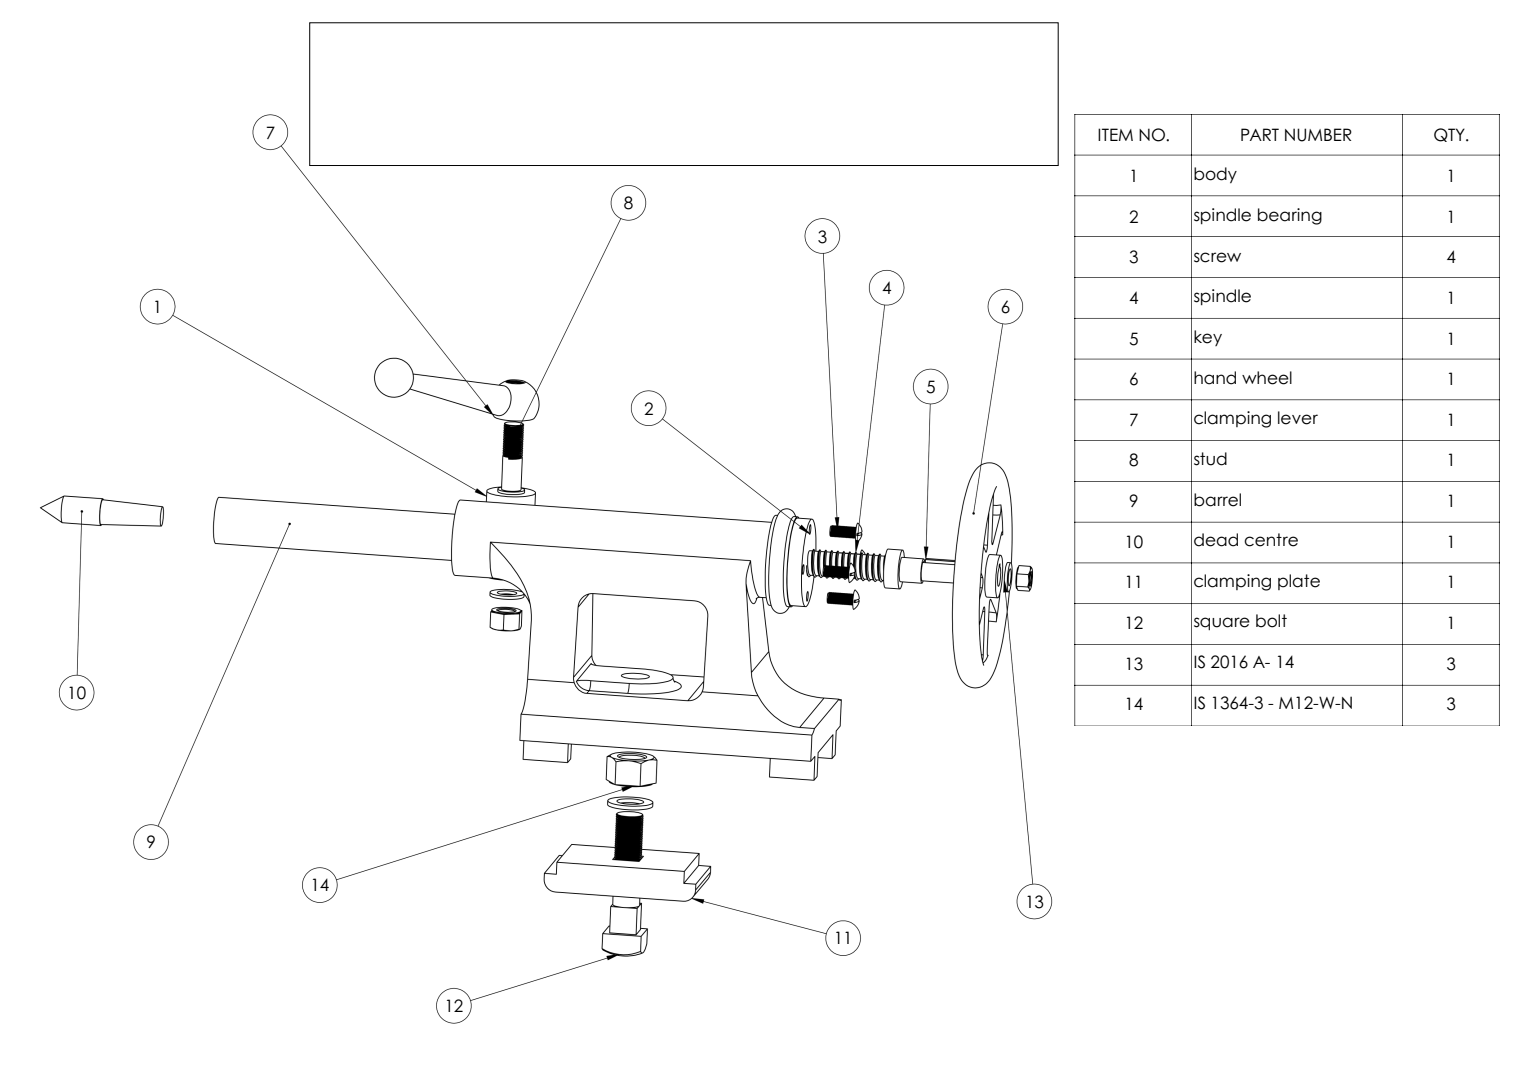
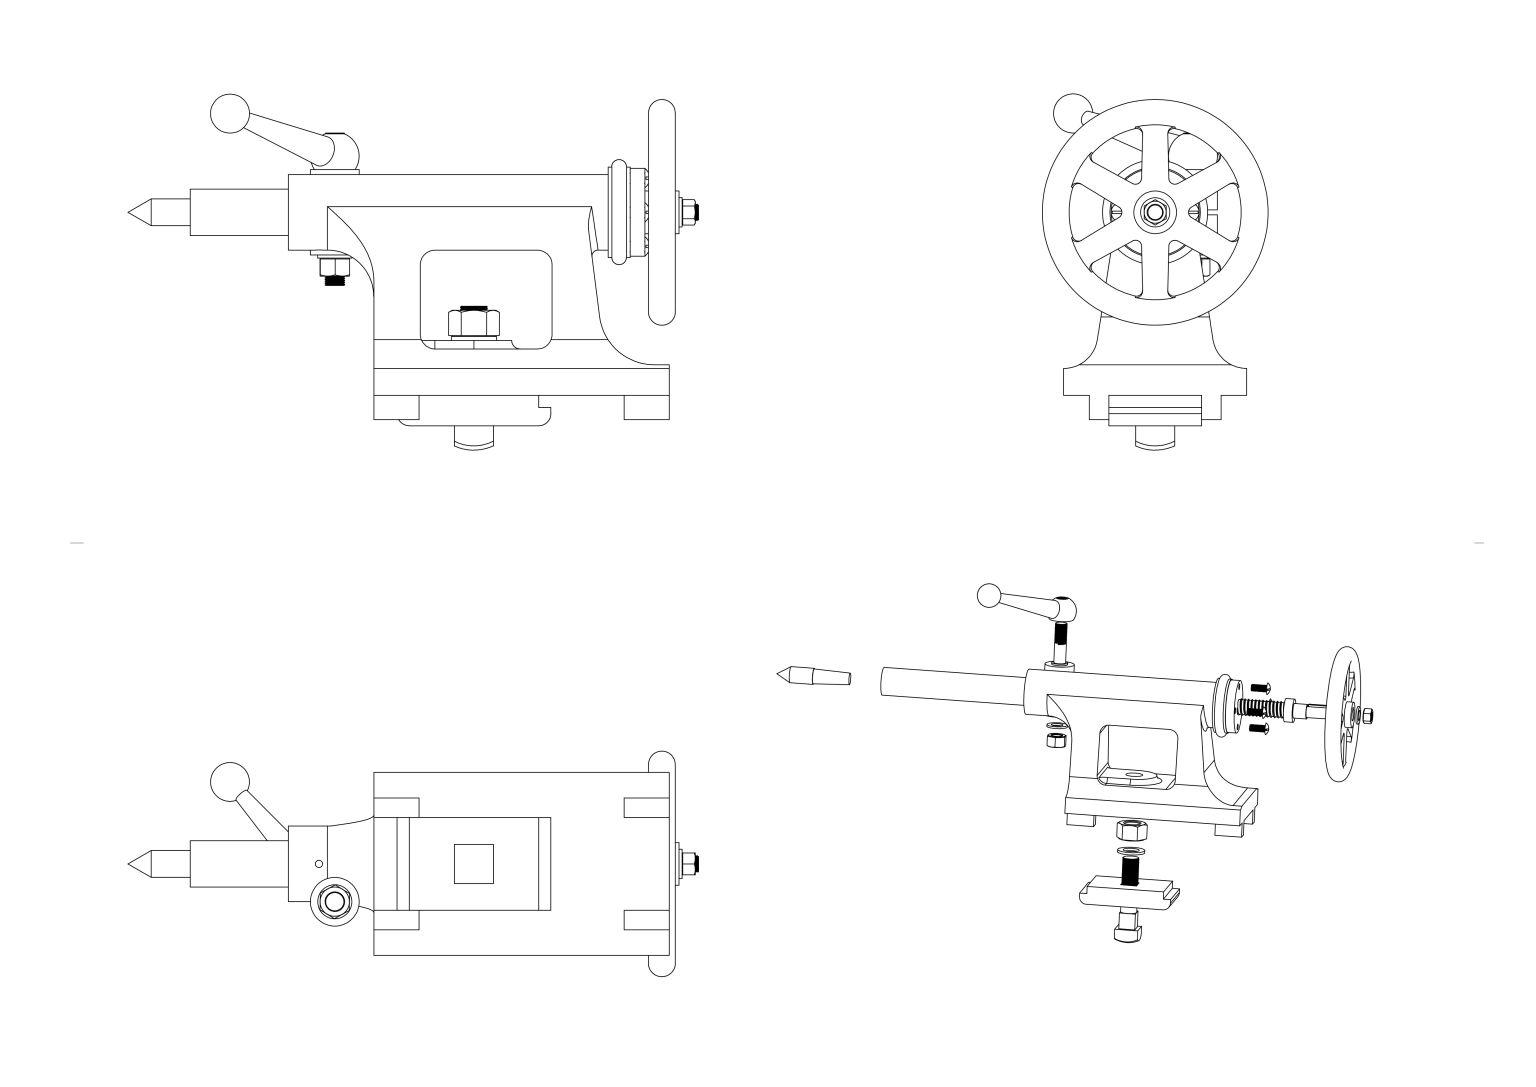
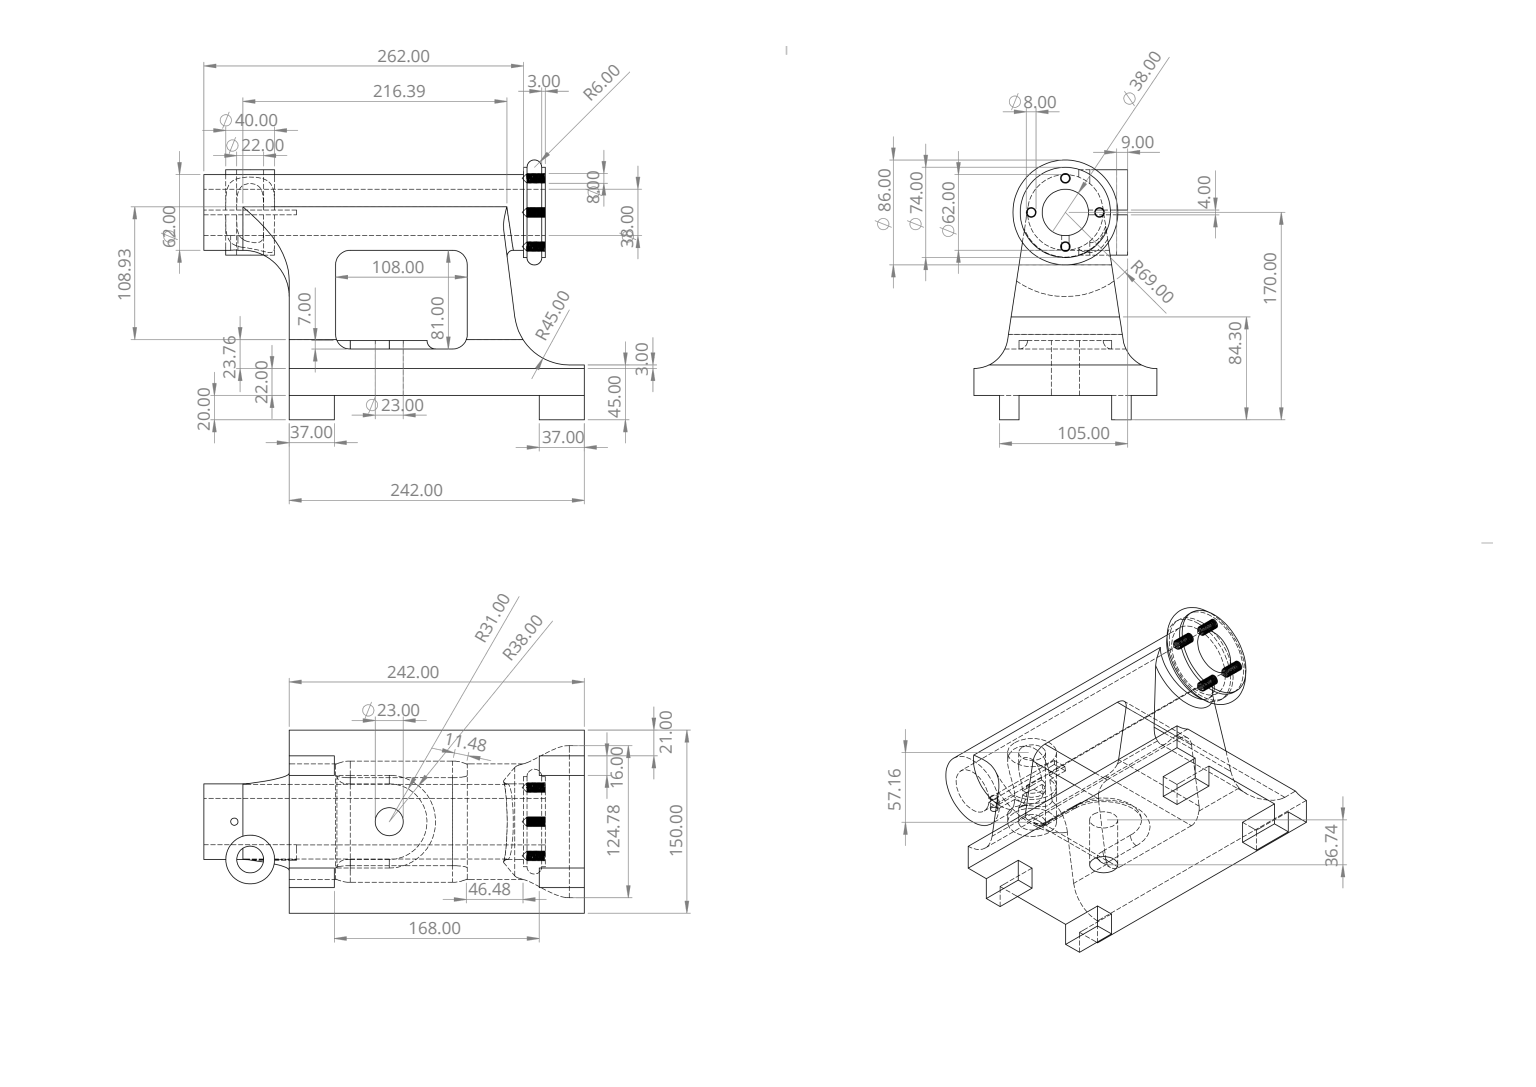
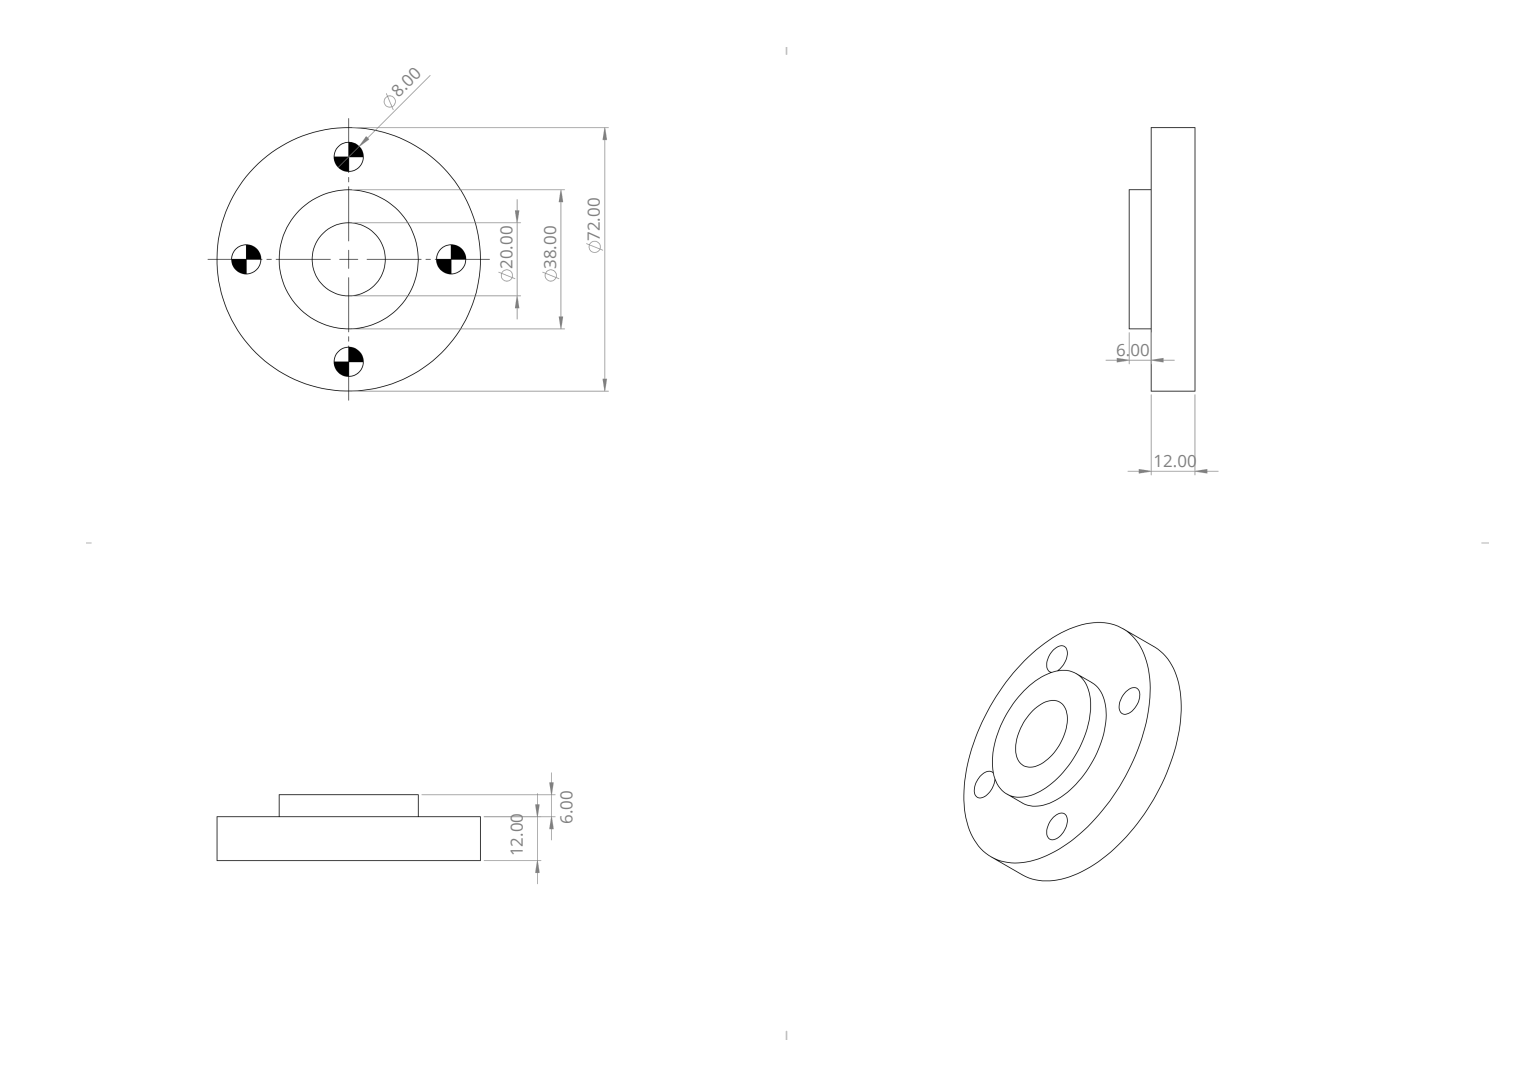
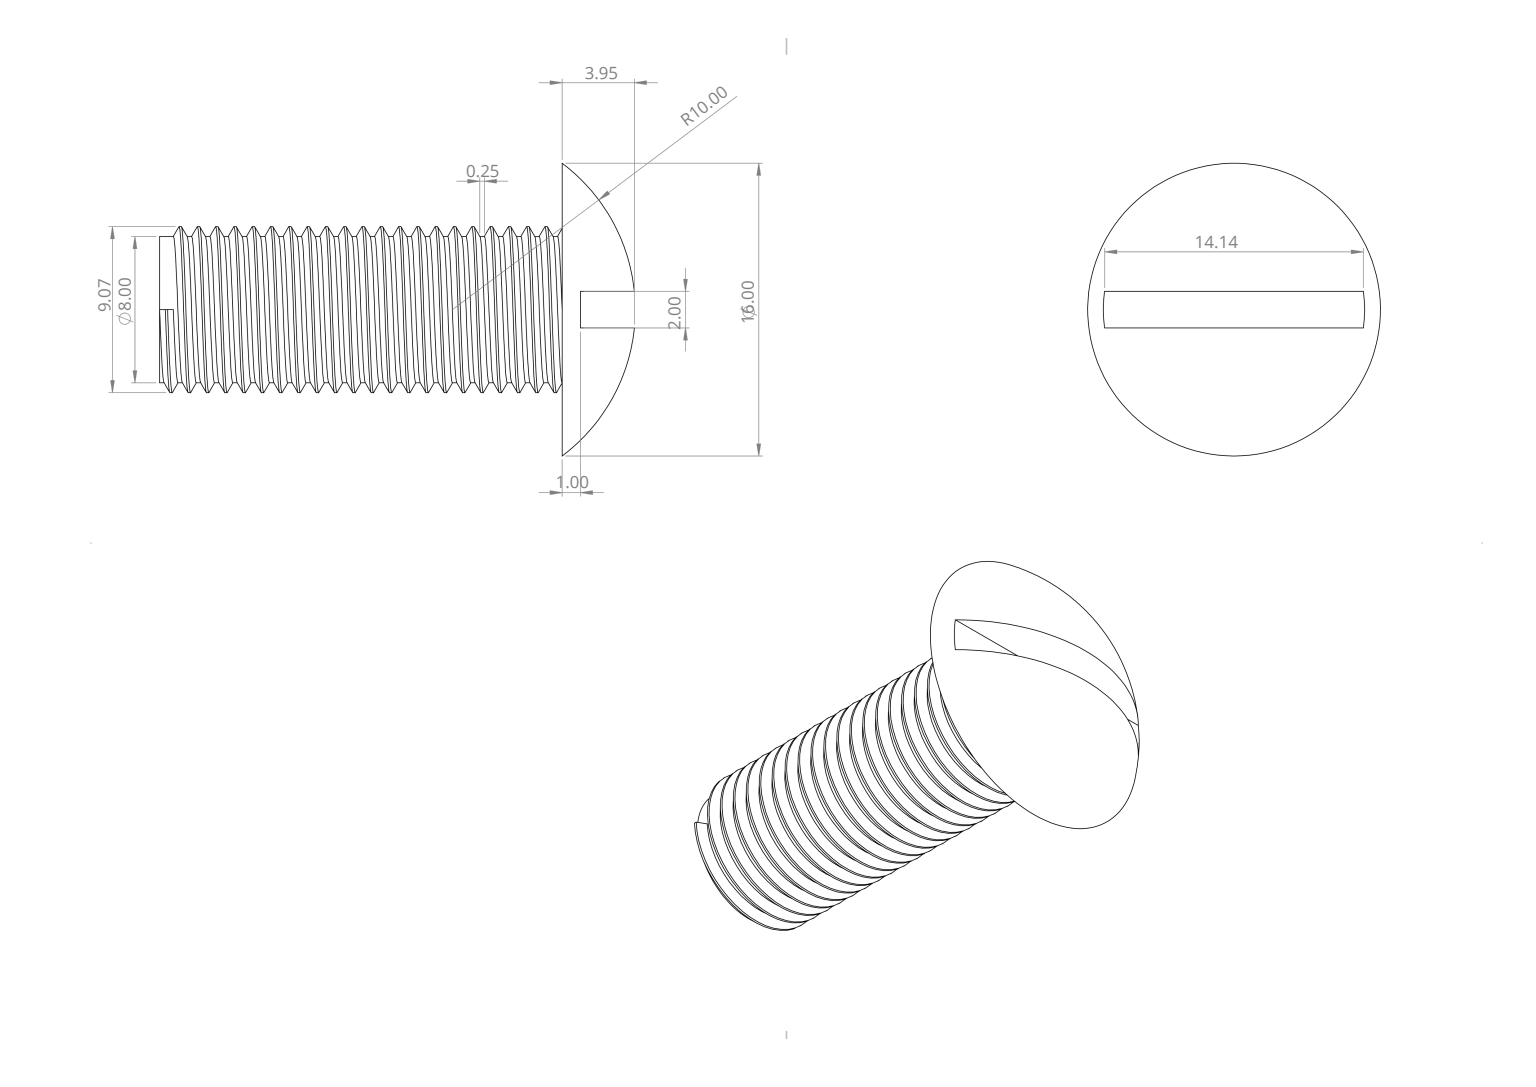
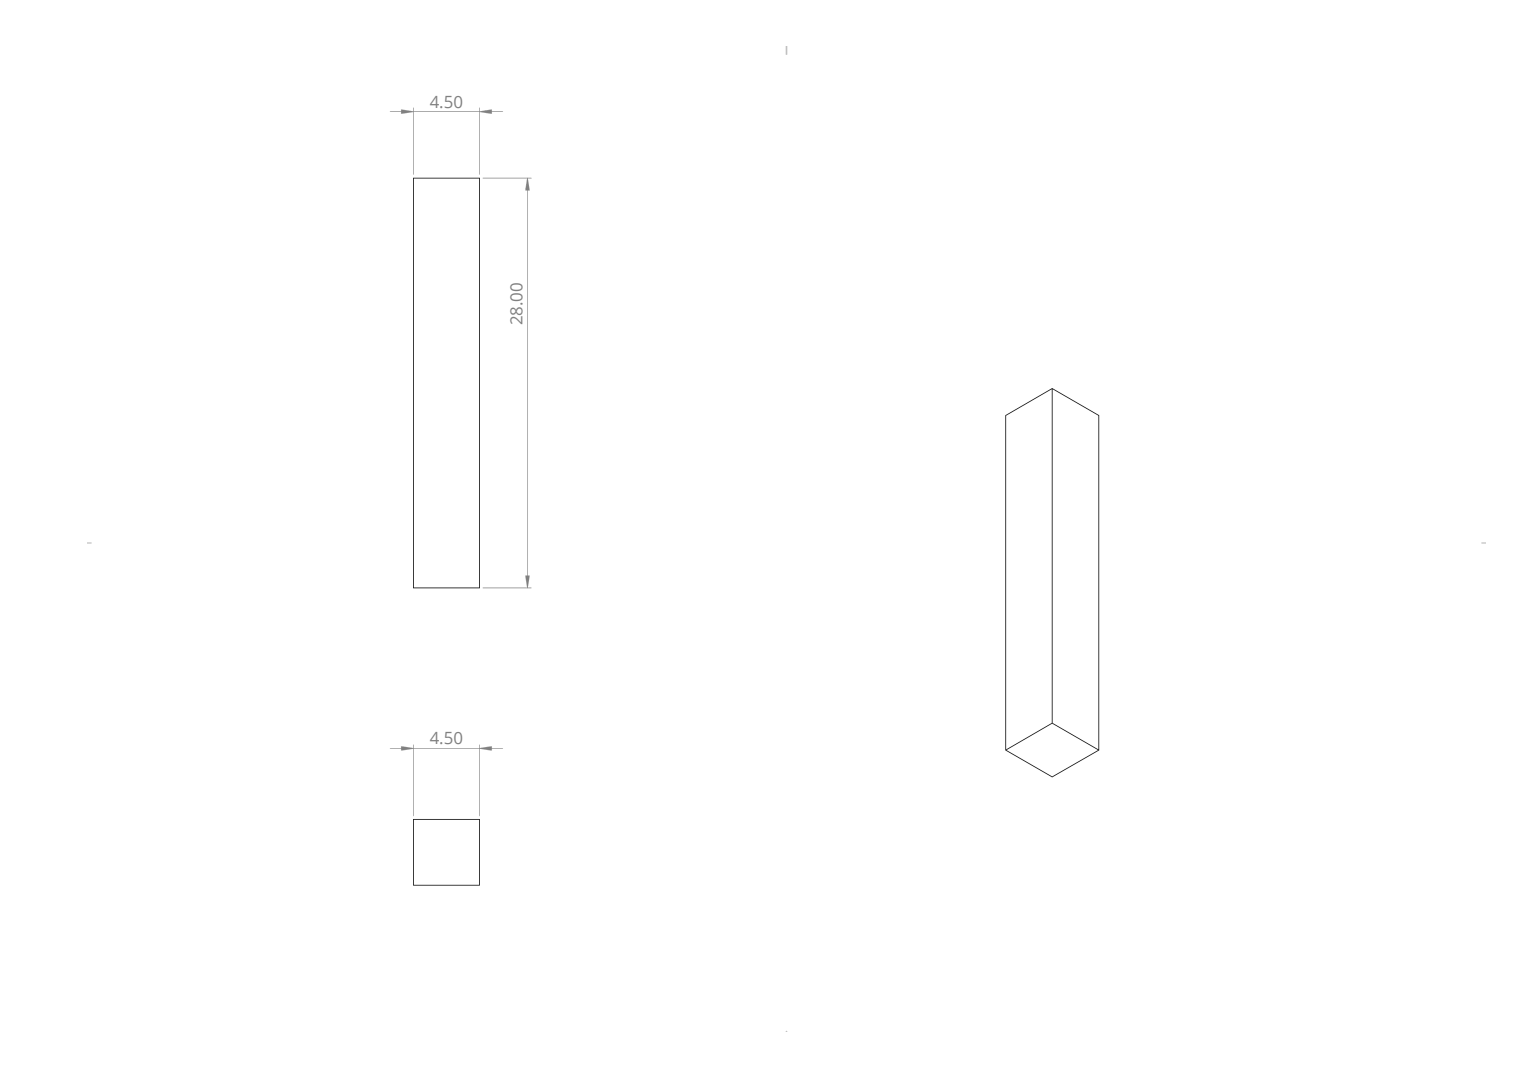
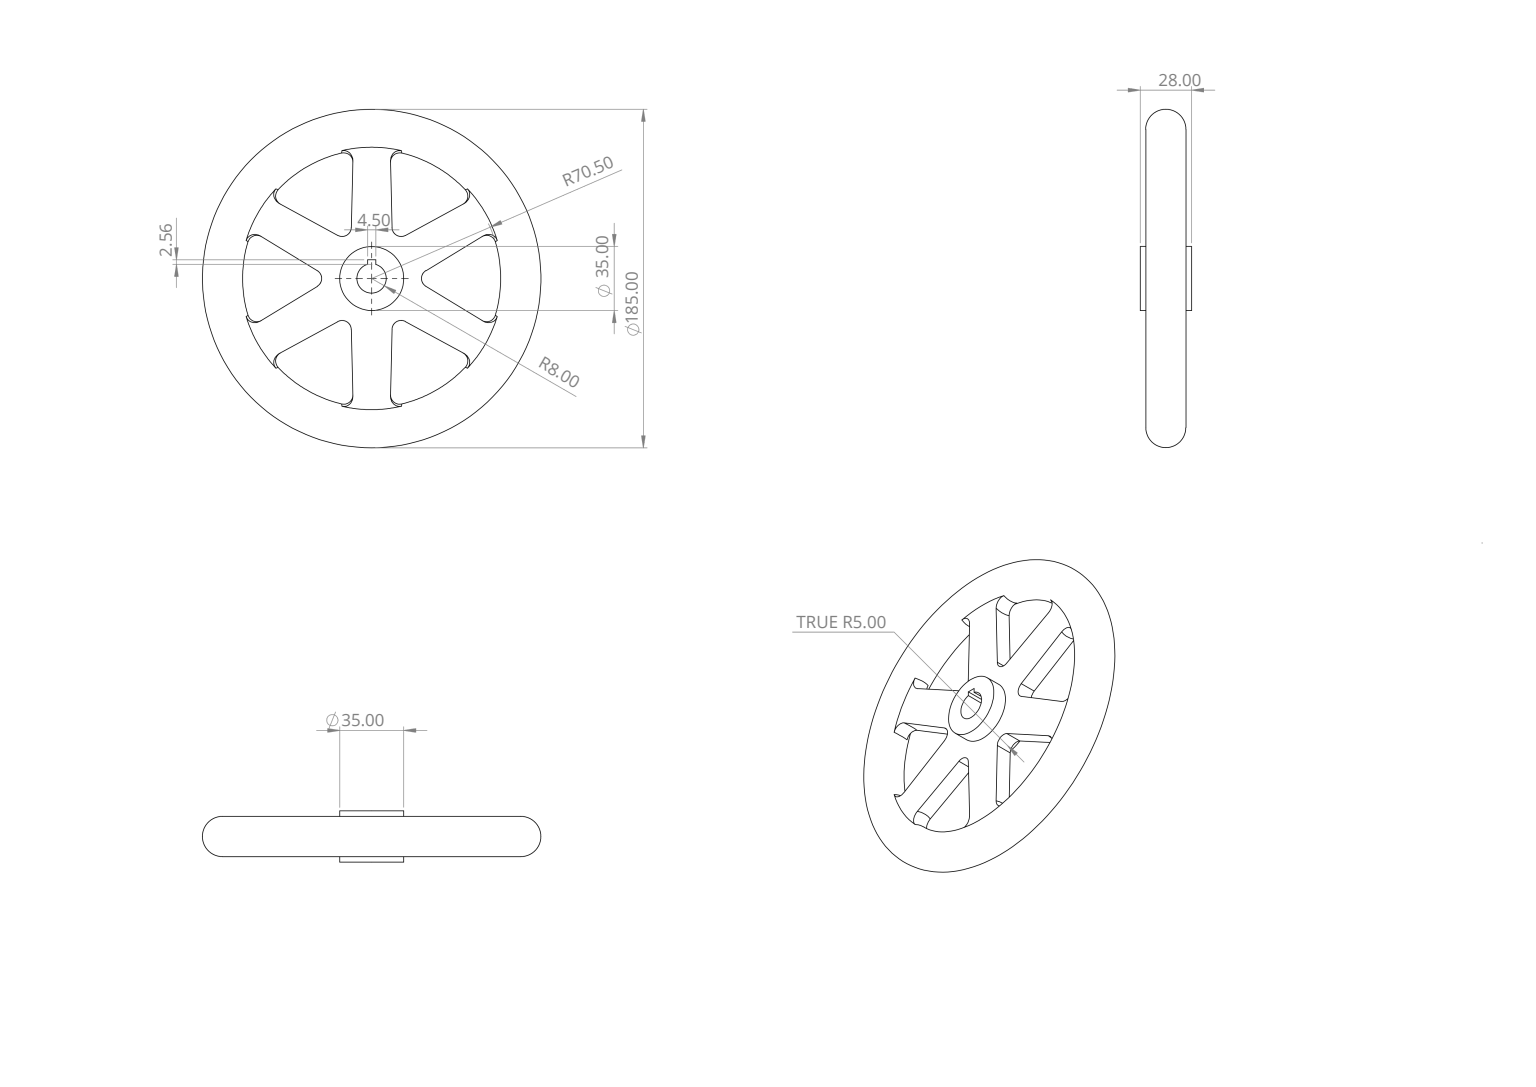
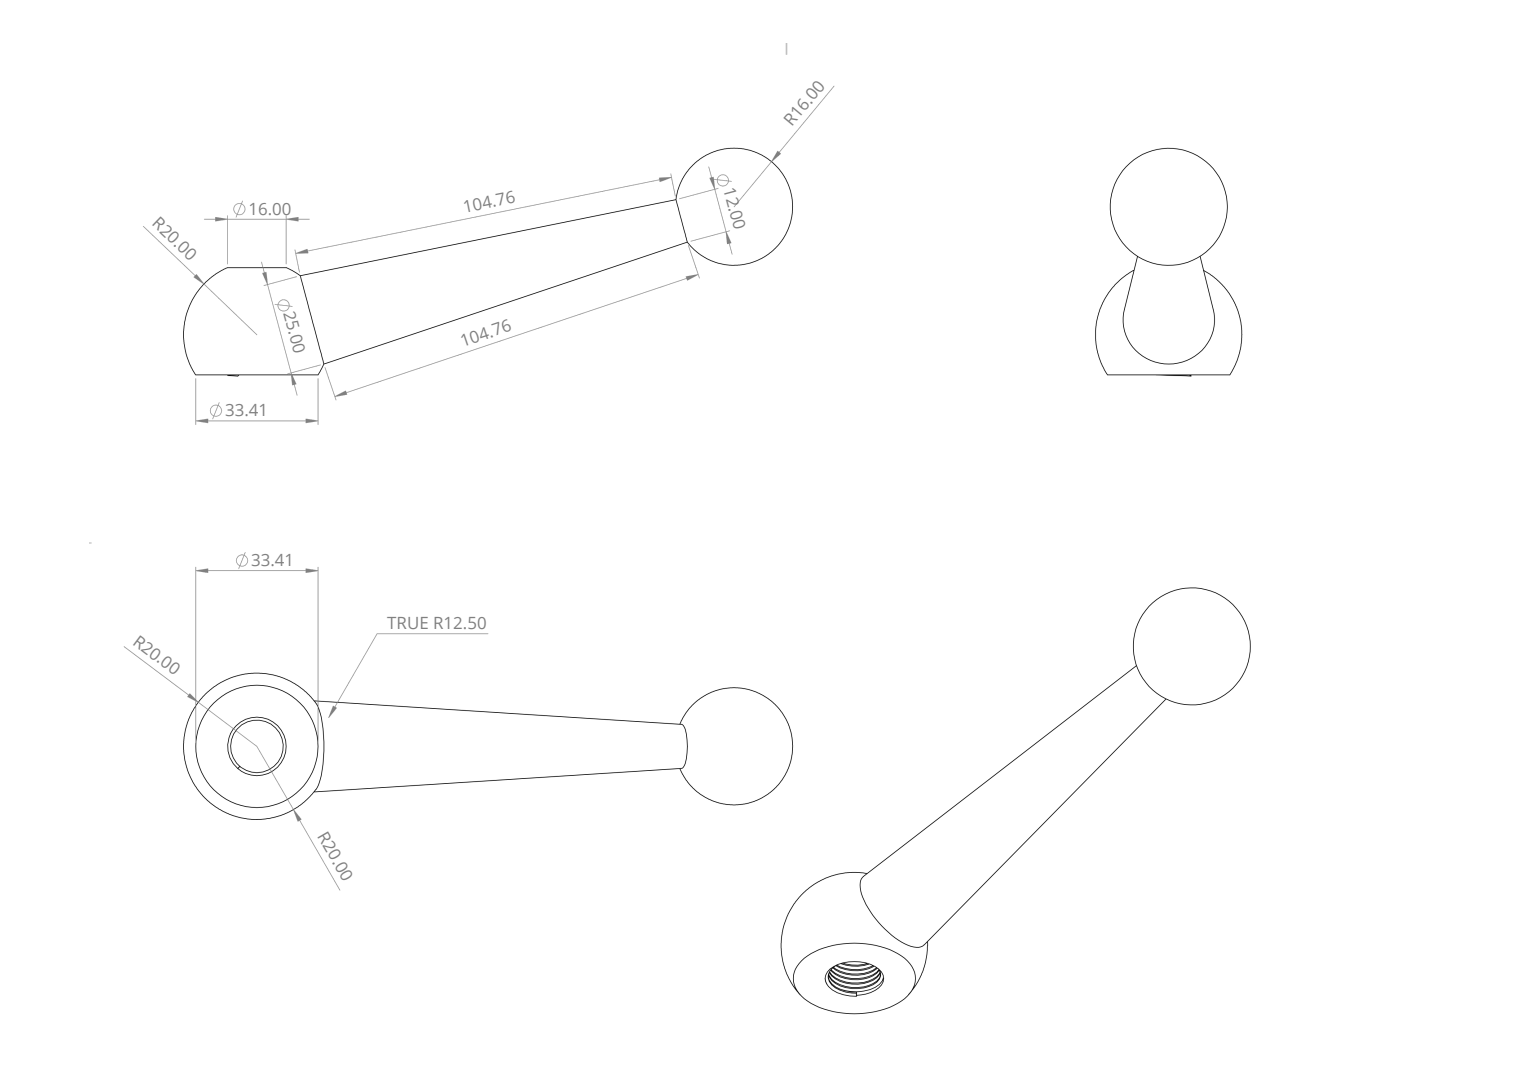
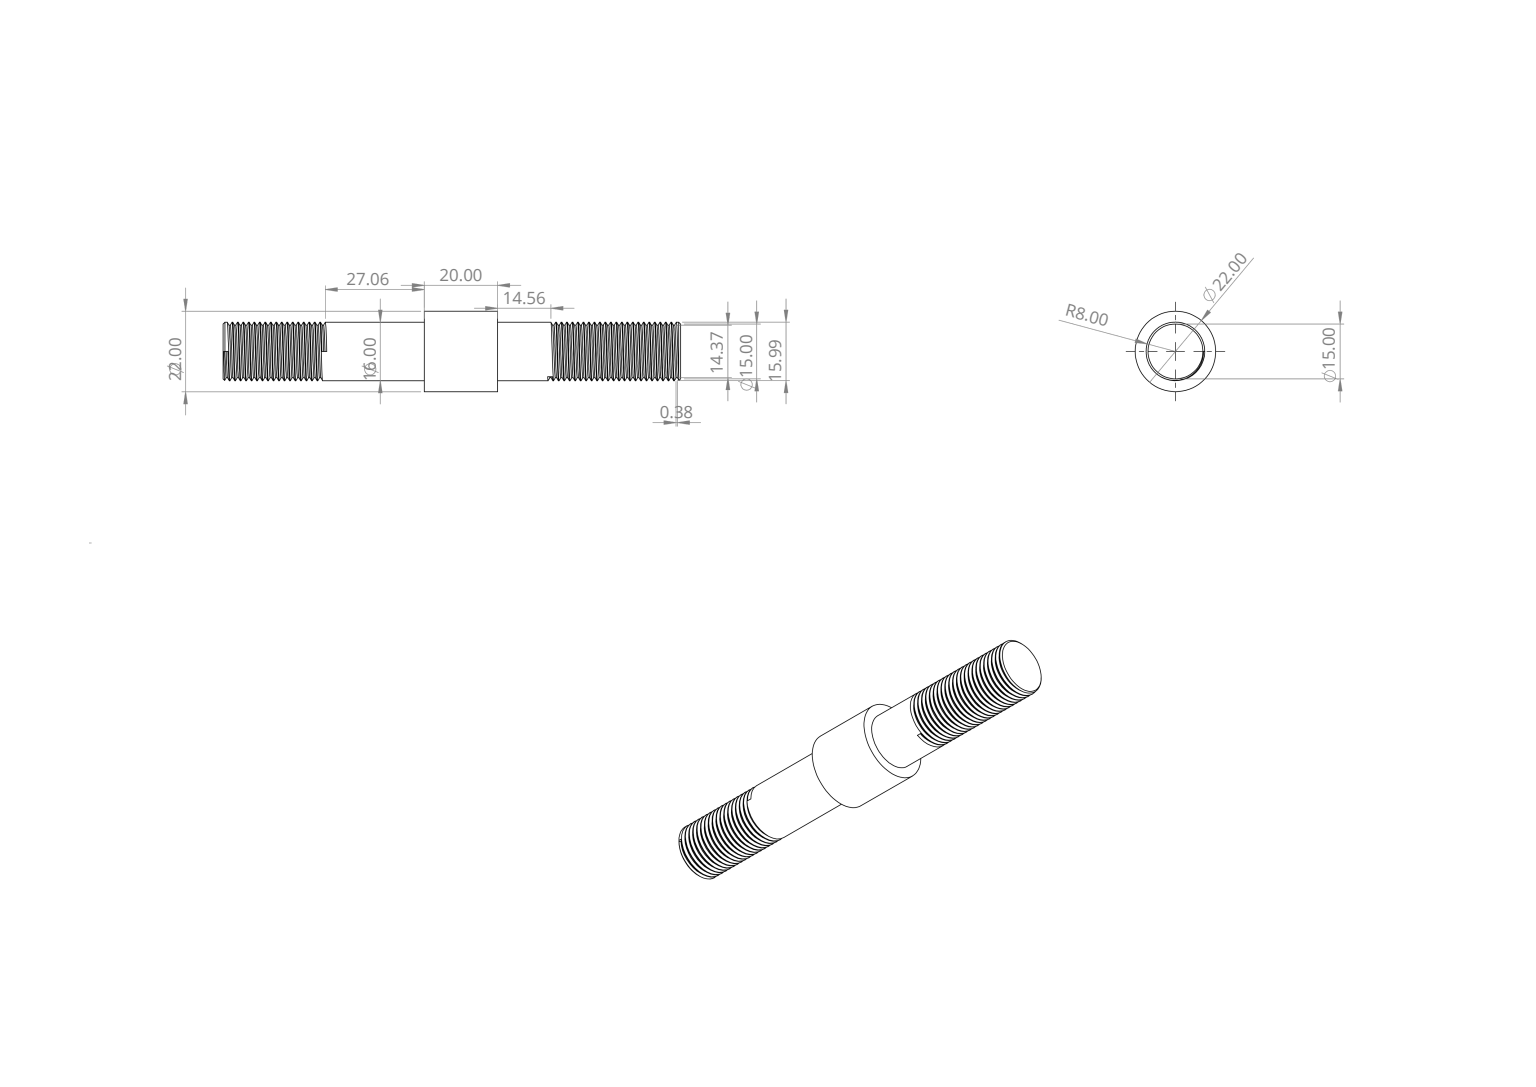
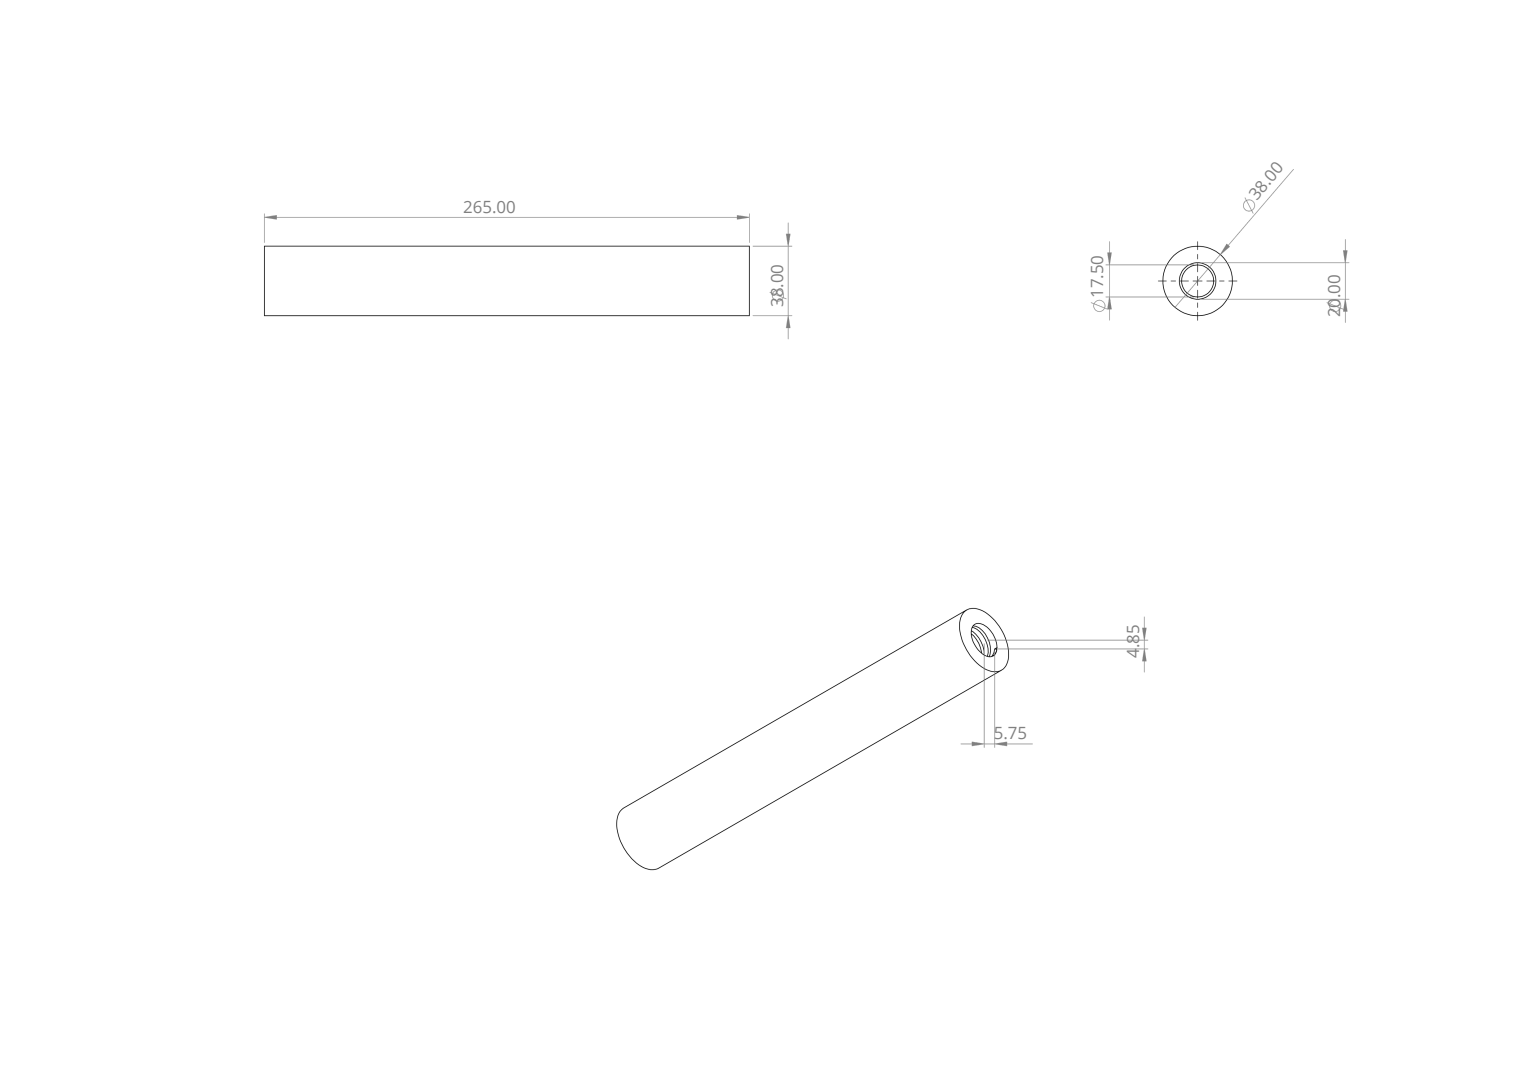
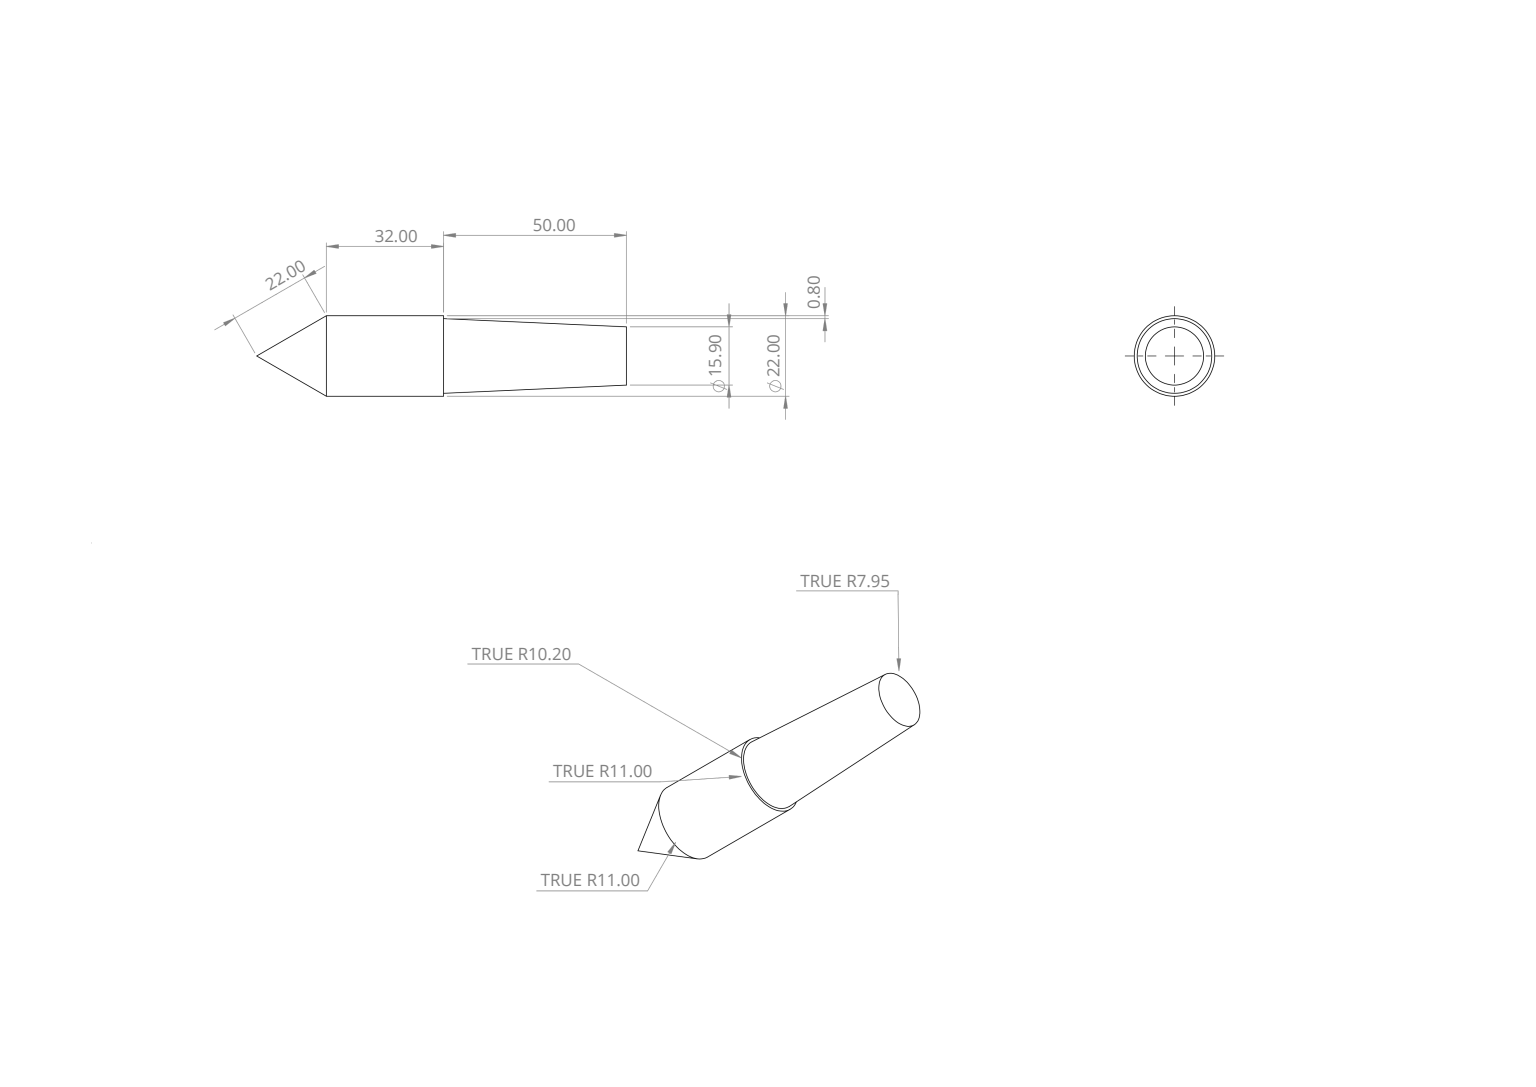
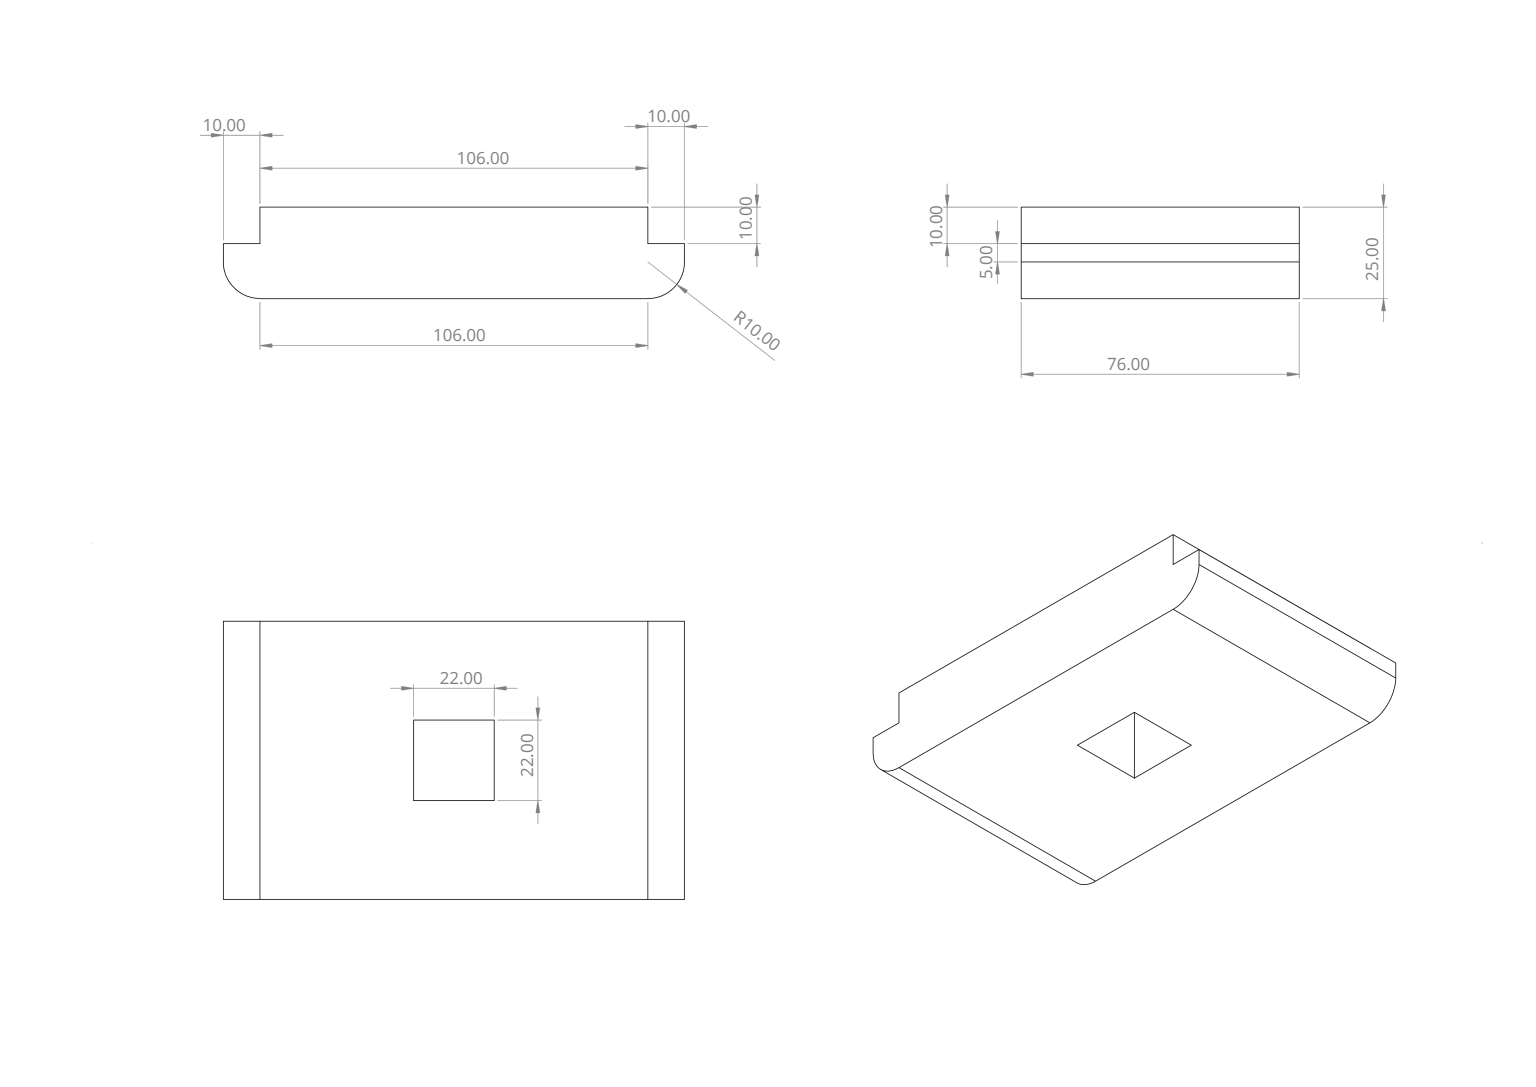
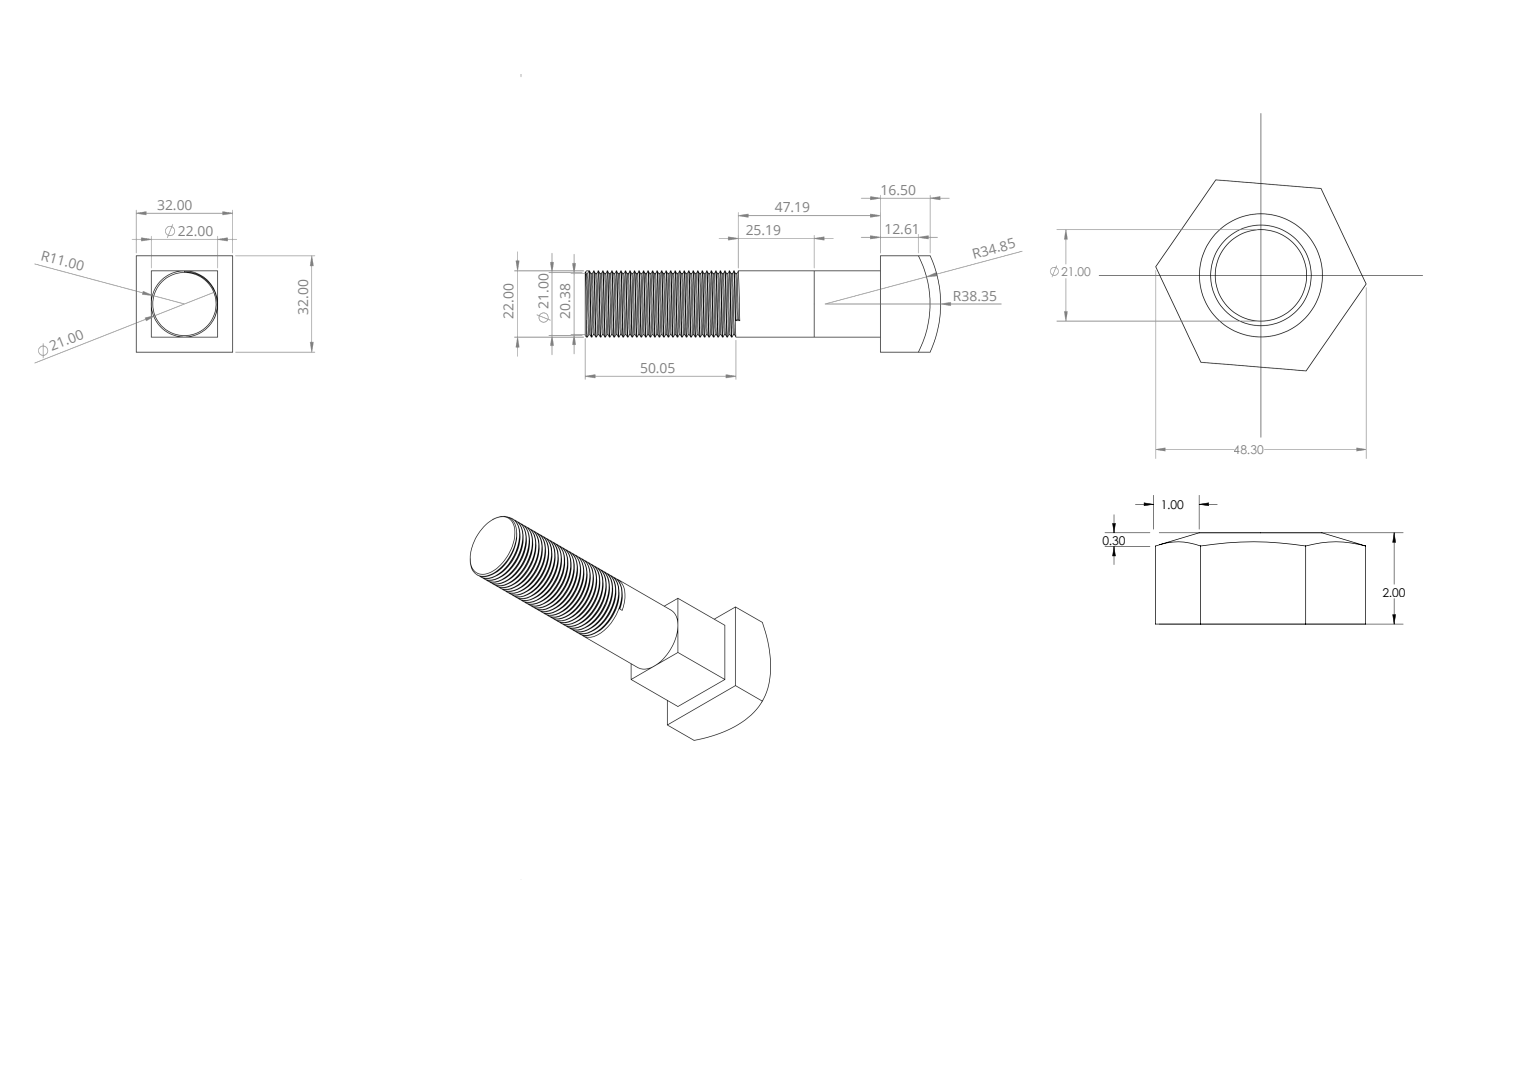
ISO-10303-21;
HEADER;
FILE_DESCRIPTION (('STEP AP214'),
    '1' );
FILE_NAME ('MAT-050',
    '2026-10-26T19:46:16',
    ( '' ),
    ( '' ),
    'SwSTEP 2.0',
    'SolidWorks 2025',
    '' );
FILE_SCHEMA (( 'AUTOMOTIVE_DESIGN' ));
ENDSEC;

DATA;
#1 = CARTESIAN_POINT ( 'NONE',  ( 7.204075437095966983, 7.204075437095967871, 116.9687500020483810 ) ) ;
#2 = CARTESIAN_POINT ( 'NONE',  ( 3.042071309553167069, 186.8229166632527267, -11.35316468749999785 ) ) ;
#3 = VERTEX_POINT ( 'NONE', #4394 ) ;
#4 = FACE_OUTER_BOUND ( 'NONE', #11968, .T. ) ;
#5 = CARTESIAN_POINT ( 'NONE',  ( -6.238412754330611322E-16, 10.18810118749999916, 71.78125000204838102 ) ) ;
#6 = CARTESIAN_POINT ( 'NONE',  ( 4.000000000000015987, 196.5000000000000000, 198.0000000000000284 ) ) ;
#8 = CARTESIAN_POINT ( 'NONE',  ( -9.832129032723418760, 182.8645833299193555, -5.676582343750004256 ) ) ;
#7 = LINE ( 'NONE', #69019, #15785 ) ;
#9 = CARTESIAN_POINT ( 'NONE',  ( -7.999999999999991118, 0.000000000000000000, 5.386552784329824206 ) ) ;
#10 = CARTESIAN_POINT ( 'NONE',  ( 3.313708498984756279, 7.999999999999991118, 4.861552779823363757 ) ) ;
#11 = CARTESIAN_POINT ( 'NONE',  ( -2.679491924311222295, 249.1666666734946887, 10.00000000000000178 ) ) ;
#12 = LINE ( 'NONE', #6025, #67368 ) ;
#13 = ORIENTED_EDGE ( 'NONE', *, *, #39325, .T. ) ;
#14 =( REPRESENTATION_RELATIONSHIP ('NONE','NONE', #46008, #61424 ) REPRESENTATION_RELATIONSHIP_WITH_TRANSFORMATION ( #30454 )SHAPE_REPRESENTATION_RELATIONSHIP( ) );
#15 = CIRCLE ( 'NONE', #38546, 16.70329308849007077 ) ;
#16 = CARTESIAN_POINT ( 'NONE',  ( 2.977408999572646486, 7.188101187499992051, 28.01780278187175455 ) ) ;
#17 = CARTESIAN_POINT ( 'NONE',  ( -8.311093377946836114, 122.9687499965860127, -8.311093377946837890 ) ) ;
#18 = CARTESIAN_POINT ( 'NONE',  ( -0.4500000000000013989, 255.9999999999997726, 5.815332135061025198 ) ) ;
#19 = VERTEX_POINT ( 'NONE', #73420 ) ;
#20 = CARTESIAN_POINT ( 'NONE',  ( -8.342170076843785083E-16, 9.187499998634407916, 4.541265875000002339 ) ) ;
#21 = AXIS2_PLACEMENT_3D ( 'NONE', #49195, #67684, #9968 ) ;
#22 = CARTESIAN_POINT ( 'NONE',  ( 7.188101187500001821, 14.06249999795161365, -2.977408999572650483 ) ) ;
#23 = CARTESIAN_POINT ( 'NONE',  ( 5.656854249492381470, 104.7500000040967905, 5.656854249492379694 ) ) ;
#24 = CARTESIAN_POINT ( 'NONE',  ( -25.55430564589119058, 197.5625000013656063, 167.5543056458915316 ) ) ;
#25 = CARTESIAN_POINT ( 'NONE',  ( -2.828427124746190735, 8.375000000000000000, -2.828427124746191623 ) ) ;
#26 = CARTESIAN_POINT ( 'NONE',  ( -4.000000000000001776, 21.24999999726881583, -4.898587196589415787E-16 ) ) ;
#27 = CARTESIAN_POINT ( 'NONE',  ( -4.541265875000003227, 9.874999998634404363, 1.881053915767121110 ) ) ;
#28 = CARTESIAN_POINT ( 'NONE',  ( 1.469576158976822172E-15, -7.999999999999991118, 20.89280278392014623 ) ) ;
#29 = CARTESIAN_POINT ( 'NONE',  ( -2.751064625579944321E-14, 198.7500000000000000, 146.0000000000000284 ) ) ;
#30 = ORIENTED_EDGE ( 'NONE', *, *, #66787, .T. ) ;
#31 = LINE ( 'NONE', #63370, #20979 ) ;
#32 = CARTESIAN_POINT ( 'NONE',  ( -4.401442555609581635E-16, 107.2812500020483810, -7.188101187500000044 ) ) ;
#34 = CARTESIAN_POINT ( 'NONE',  ( 6.000000000000003553, 293.5625000000001137, -2.485281374238571761 ) ) ;
#33 = DIRECTION ( 'NONE',  ( 0.000000000000000000, 0.000000000000000000, 1.000000000000000000 ) ) ;
#35 =( NAMED_UNIT ( * ) PLANE_ANGLE_UNIT ( ) SI_UNIT ( $, .RADIAN. ) );
#36 = EDGE_CURVE ( 'NONE', #35937, #61038, #73180, .T. ) ;
#37 = EDGE_CURVE ( 'NONE', #72225, #25230, #72296, .T. ) ;
#38 = CARTESIAN_POINT ( 'NONE',  ( 1.881053915767122664, 22.12499999863441502, 4.541265875000001451 ) ) ;
#39 = CARTESIAN_POINT ( 'NONE',  ( 9.797174393178825657E-16, 125.0000000000000000, -8.000000000000000000 ) ) ;
#40 = ORIENTED_EDGE ( 'NONE', *, *, #24458, .F. ) ;
#41 = ORIENTED_EDGE ( 'NONE', *, *, #6114, .F. ) ;
#42 = CARTESIAN_POINT ( 'NONE',  ( -7.204075437095967871, 7.204075437095967871, 89.96875000204838102 ) ) ;
#43 = CARTESIAN_POINT ( 'NONE',  ( -10.99999999999989342, 4.556349186104152515, 92.40625000000000000 ) ) ;
#44 = CARTESIAN_POINT ( 'NONE',  ( -29.43265458321766914, 197.7500000013656063, 166.5412658750003629 ) ) ;
#45 = CARTESIAN_POINT ( 'NONE',  ( 11.00000000000000000, 4.556349186104045934, 99.34375000000000000 ) ) ;
#46 = CARTESIAN_POINT ( 'NONE',  ( -1.432654583217608080, 202.8750000013656347, 201.4587341250000350 ) ) ;
#48 = CARTESIAN_POINT ( 'NONE',  ( -4.088227598258586603E-16, 298.3593750017070079, -6.676582343750001591 ) ) ;
#47 = CARTESIAN_POINT ( 'NONE',  ( 0.000000000000000000, 210.0000000000000284, 207.0000000000000568 ) ) ;
#49 = CARTESIAN_POINT ( 'NONE',  ( -10.00000000000000355, 117.7083333333333286, 2.679491924311223183 ) ) ;
#50 = ADVANCED_FACE ( 'NONE', ( #38735 ), #56452, .F. ) ;
#51 = CARTESIAN_POINT ( 'NONE',  ( -5.656854249492380582, 97.81250000000000000, -5.656854249492380582 ) ) ;
#52 = CARTESIAN_POINT ( 'NONE',  ( -4.088227598258586603E-16, 288.3593750017070079, -6.676582343750001591 ) ) ;
#53 = CARTESIAN_POINT ( 'NONE',  ( 7.188101187499991163, 2.977408999572648707, 4.205302781871751883 ) ) ;
#54 = FACE_OUTER_BOUND ( 'NONE', #64584, .T. ) ;
#55 = AXIS2_PLACEMENT_3D ( 'NONE', #16883, #63657, #58395 ) ;
#56 = CARTESIAN_POINT ( 'NONE',  ( 25.55430564589115150, 201.3125000013656063, 172.4456943541086957 ) ) ;
#57 = CARTESIAN_POINT ( 'NONE',  ( 7.188101187500000044, 0.8437499979516100979, 0.000000000000000000 ) ) ;
#58 = CARTESIAN_POINT ( 'NONE',  ( 12.00000000000000178, -4.647306338817273286, -0.4736860157878156619 ) ) ;
#59 = CARTESIAN_POINT ( 'NONE',  ( -5.082755093536325930, 121.3437500020483952, -5.082755093536325930 ) ) ;
#61 = CARTESIAN_POINT ( 'NONE',  ( 2.823223908292128659, 194.8377262638588832, 195.3889393478124532 ) ) ;
#60 = PRESENTATION_STYLE_ASSIGNMENT (( #57392 ) ) ;
#62 = CARTESIAN_POINT ( 'NONE',  ( 3.042071309553163960, 237.7604166700806161, -11.35316468749999785 ) ) ;
#63 = CARTESIAN_POINT ( 'NONE',  ( 10.00000000000000178, 52.08333332650536818, -2.679491924311226736 ) ) ;
#64 = CARTESIAN_POINT ( 'NONE',  ( 27.99999999999996447, 197.0000000000000000, 173.9999999999999147 ) ) ;
#65 = CARTESIAN_POINT ( 'NONE',  ( -3.042071309553173730, 19.32291666325268409, 11.35316468749999785 ) ) ;
#66 =( BOUNDED_CURVE ( )  B_SPLINE_CURVE ( 2, ( #62124, #31597, #54994, #3301, #26287, #72324, #20638, #17588, #51930, #27790, #56850, #34966, #23250 ),
 .UNSPECIFIED., .F., .F. ) 
 B_SPLINE_CURVE_WITH_KNOTS ( ( 3, 2, 2, 2, 2, 2, 3 ),
 ( 0.4866946232415507168, 0.4919272298211807559, 0.4971598364008106841, 0.5023924429804407232, 0.5076250495600707069, 0.5128576561397006905, 0.5180902627193306742 ),
 .UNSPECIFIED. ) 
 CURVE ( )  GEOMETRIC_REPRESENTATION_ITEM ( )  RATIONAL_B_SPLINE_CURVE ( ( 0.9999999999999911182, 0.9659258262890771940, 1.000000000000000000, 0.9659258262890683122, 1.000000000000000000, 0.9659258262890683122, 1.000000000000000000, 0.9659258262890683122, 1.000000000000000000, 0.9659258262890683122, 1.000000000000000000, 0.9659258262893768432, 0.9999999999996914690 ) ) 
 REPRESENTATION_ITEM ( '' )  );
#67 = CARTESIAN_POINT ( 'NONE',  ( 2.977408999572650927, -7.188101187499990274, 0.8303027818717529929 ) ) ;
#69 = CARTESIAN_POINT ( 'NONE',  ( 3.042071309553167069, 217.1354166632526983, -11.35316468749999785 ) ) ;
#68 =( BOUNDED_CURVE ( )  B_SPLINE_CURVE ( 2, ( #33279, #10252, #21187, #32531, #61186, #72505, #55916, #72881, #38182 ),
 .UNSPECIFIED., .F., .F. ) 
 B_SPLINE_CURVE_WITH_KNOTS ( ( 3, 2, 2, 2, 3 ),
 ( 0.7708333333333317050, 0.7812499999999983347, 0.7916666666666649643, 0.8020833333333317050, 0.8124999999999983347 ),
 .UNSPECIFIED. ) 
 CURVE ( )  GEOMETRIC_REPRESENTATION_ITEM ( )  RATIONAL_B_SPLINE_CURVE ( ( 1.000000000000012212, 0.9238795325112745260, 1.000000000000000000, 0.9238795325112867385, 1.000000000000000000, 0.9238795325112867385, 1.000000000000000000, 0.9238795325112989509, 0.9999999999999877875 ) ) 
 REPRESENTATION_ITEM ( '' )  );
#70 = CARTESIAN_POINT ( 'NONE',  ( -30.82842712474615610, 198.3750000000000284, 172.8284271247465824 ) ) ;
#71 = CARTESIAN_POINT ( 'NONE',  ( -7.320508075688770155, 240.6249999999999716, 7.320508075688774596 ) ) ;
#73 = CARTESIAN_POINT ( 'NONE',  ( 2.449293598294707893E-16, 11.99999999726881406, -4.000000000000001776 ) ) ;
#72 = CARTESIAN_POINT ( 'NONE',  ( 4.000000000000016875, 208.4375000000000853, 199.6568542494924259 ) ) ;
#74 = AXIS2_PLACEMENT_3D ( 'NONE', #50594, #44950, #67957 ) ;
#75 = EDGE_LOOP ( 'NONE', ( #23247, #62636, #23741 ) ) ;
#76 = VECTOR ( 'NONE', #5091, 999.9999999999998863 ) ;
#77 = CARTESIAN_POINT ( 'NONE',  ( 3.458734124999960358, 199.6250000013656063, 143.4326545832176976 ) ) ;
#78 = CARTESIAN_POINT ( 'NONE',  ( 11.35316468749999785, 25.57291666325268409, 3.042071309553174174 ) ) ;
#79 = CARTESIAN_POINT ( 'NONE',  ( 7.778174593052023411, -7.778174593052021635, 93.25000000409677625 ) ) ;
#80 = CARTESIAN_POINT ( 'NONE',  ( 2.679491924311234730, 226.4583333333333144, 9.999999999999998224 ) ) ;
#81 = EDGE_CURVE ( 'NONE', #73625, #45401, #67113, .T. ) ;
#82 = CARTESIAN_POINT ( 'NONE',  ( -30.44569435410875968, 197.8125000013656063, 172.4456943541092642 ) ) ;
#83 = CARTESIAN_POINT ( 'NONE',  ( 5.656854249492378806, 7.124999995903221084, 5.656854249492381470 ) ) ;
#85 = CARTESIAN_POINT ( 'NONE',  ( 11.35316468750000141, 25.78124999658601624, 0.000000000000000000 ) ) ;
#84 = CARTESIAN_POINT ( 'NONE',  ( 2.977408999572654480, 112.6250000020483810, 7.188101187499999156 ) ) ;
#86 = CARTESIAN_POINT ( 'NONE',  ( -3.313708498984757167, 7.999999999999991118, 23.04905277982336642 ) ) ;
#87 = CARTESIAN_POINT ( 'NONE',  ( 5.676582343749993598, 129.9479166632526983, 9.832129032723422313 ) ) ;
#88 = CARTESIAN_POINT ( 'NONE',  ( 7.320508075688771044, 101.2499999931720112, 7.320508075688775484 ) ) ;
#89 = CARTESIAN_POINT ( 'NONE',  ( -7.188101187500000044, 114.0312500020483952, 0.000000000000000000 ) ) ;
#90 = DIRECTION ( 'NONE',  ( 0.000000000000000000, 0.000000000000000000, 1.000000000000000000 ) ) ;
#91 = CARTESIAN_POINT ( 'NONE',  ( -31.45873412499999944, 208.9375000013656063, 170.0000000000003979 ) ) ;
#92 = CARTESIAN_POINT ( 'NONE',  ( -5.000000000000000888, 53.34243969459547685, -47.33397984627131905 ) ) ;
#93 = ORIENTED_EDGE ( 'NONE', *, *, #56073, .F. ) ;
#94 = CARTESIAN_POINT ( 'NONE',  ( 5.676582343750001591, 11.92708332991935016, -9.832129032723420536 ) ) ;
#95 = CARTESIAN_POINT ( 'NONE',  ( -5.000000000000005329, 155.2083333265053682, 8.660254037844387298 ) ) ;
#96 = CARTESIAN_POINT ( 'NONE',  ( 1.226468279477575784E-15, 298.7031250017070079, 6.676582343750001591 ) ) ;
#97 = CARTESIAN_POINT ( 'NONE',  ( 11.35316468750000141, 140.7812499965860411, 0.000000000000000000 ) ) ;
#98 = CARTESIAN_POINT ( 'NONE',  ( -7.999999999999991118, 0.000000000000000000, 21.88655278432982243 ) ) ;
#99 = CARTESIAN_POINT ( 'NONE',  ( 13.99999999999999822, 2.249999999994893862, 7.677076266393539683 ) ) ;
#100 = CARTESIAN_POINT ( 'NONE',  ( 8.311093377946834337, 262.0312500034139589, -8.311093377946836114 ) ) ;
#101 = CARTESIAN_POINT ( 'NONE',  ( -4.220049686691937474, -10.18810118749999738, 95.31250000204838102 ) ) ;
#102 = EDGE_LOOP ( 'NONE', ( #72383, #48157, #74168, #29001 ) ) ;
#103 = VECTOR ( 'NONE', #43518, 1000.000000000000000 ) ;
#104 = CARTESIAN_POINT ( 'NONE',  ( 5.000000000000000000, 10.43216530810821219, 65.93415491242824089 ) ) ;
#105 = CARTESIAN_POINT ( 'NONE',  ( 5.000000000000000888, 66.79063484153816432, -23.29724706625311370 ) ) ;
#106 = CARTESIAN_POINT ( 'NONE',  ( 2.445694354108840063, 203.0625000013656063, 200.4456943541088663 ) ) ;
#107 = CARTESIAN_POINT ( 'NONE',  ( -2.085542519210945728E-15, 79.84374999658601268, 11.35316468750000141 ) ) ;
#108 = ORIENTED_EDGE ( 'NONE', *, *, #11114, .F. ) ;
#109 = CARTESIAN_POINT ( 'NONE',  ( 10.18810118749999916, 1.247682550866122264E-15, 105.9062500020483810 ) ) ;
#110 = CARTESIAN_POINT ( 'NONE',  ( 4.541265875000001451, 14.37499999863440969, 1.881053915767124440 ) ) ;
#111 = VERTEX_POINT ( 'NONE', #39096 ) ;
#112 = VERTEX_POINT ( 'NONE', #66264 ) ;
#113 = CARTESIAN_POINT ( 'NONE',  ( -5.656854249492381470, 0.9375000000000001110, 5.656854249492379694 ) ) ;
#114 = CARTESIAN_POINT ( 'NONE',  ( -8.660254037844390851, 109.7916666598387110, 4.999999999999998224 ) ) ;
#115 = CARTESIAN_POINT ( 'NONE',  ( -4.999999999999999112, -67.53158052529141742, -22.66975313813551907 ) ) ;
#116 = CARTESIAN_POINT ( 'NONE',  ( -1.320432766682874540E-15, 25.96874999795161543, 7.188101187500000044 ) ) ;
#117 = CARTESIAN_POINT ( 'NONE',  ( -38.00000000000000000, 272.0000000000000000, 20.00000000000003553 ) ) ;
#118 = CARTESIAN_POINT ( 'NONE',  ( 7.204075437095968759, -7.204075437095966983, 106.0937500020483810 ) ) ;
#119 = AXIS2_PLACEMENT_3D ( 'NONE', #48713, #60410, #49084 ) ;
#120 = CARTESIAN_POINT ( 'NONE',  ( 2.449293598294707893E-16, 10.99999999726881406, -4.000000000000001776 ) ) ;
#121 = CARTESIAN_POINT ( 'NONE',  ( 4.541265875000002339, 0.3749999986344066949, -1.881053915767121776 ) ) ;
#122 = EDGE_LOOP ( 'NONE', ( #35073, #51251, #40742, #51400, #60040, #5045 ) ) ;
#123 = EDGE_CURVE ( 'NONE', #13669, #16043, #62099, .T. ) ;
#124 = EDGE_CURVE ( 'NONE', #54105, #45186, #50774, .T. ) ;
#125 = DIRECTION ( 'NONE',  ( 0.000000000000000000, 0.000000000000000000, -1.000000000000000000 ) ) ;
#126 = CARTESIAN_POINT ( 'NONE',  ( 1.432654583217664479, 201.7500000013655779, 201.4587341250000065 ) ) ;
#127 = CONICAL_SURFACE ( 'NONE', #43492, 10.99999999999998934, 0.5235987755982931535 ) ;
#128 = CARTESIAN_POINT ( 'NONE',  ( -26.56734541678243033, 206.3750000013656063, 166.5412658750003345 ) ) ;
#129 = CARTESIAN_POINT ( 'NONE',  ( 30.82842712474616675, 199.5000000027312126, 167.1715728752537018 ) ) ;
#130 = CARTESIAN_POINT ( 'NONE',  ( -3.211159895383562723, 11.93749999863440614, 3.211159895383561391 ) ) ;
#131 = CARTESIAN_POINT ( 'NONE',  ( -4.000000000000001776, 10.18749999726881406, -1.656854249492381470 ) ) ;
#132 = CARTESIAN_POINT ( 'NONE',  ( -5.082755093536319713, 5.082755093536319713, 16.29905278187175455 ) ) ;
#133 = EDGE_LOOP ( 'NONE', ( #61900, #64409, #43973, #55022 ) ) ;
#134 = EDGE_LOOP ( 'NONE', ( #71997, #44977, #22170 ) ) ;
#135 = CARTESIAN_POINT ( 'NONE',  ( -6.238412754330611322E-16, 10.18810118749999916, 112.2812500020483810 ) ) ;
#136 = CARTESIAN_POINT ( 'NONE',  ( -8.660254037844385522, 220.4166666666666856, 5.000000000000004441 ) ) ;
#137 = CARTESIAN_POINT ( 'NONE',  ( -27.99999999999995737, 205.5000000000000284, 174.0000000000003695 ) ) ;
#138 = CARTESIAN_POINT ( 'NONE',  ( 2.754378923186476579E-14, 201.1875000013656063, 194.5412658750000219 ) ) ;
#139 = FACE_OUTER_BOUND ( 'NONE', #14459, .T. ) ;
#140 = CARTESIAN_POINT ( 'NONE',  ( 6.123233995736767268E-16, 81.25000000000000000, -10.00000000000000178 ) ) ;
#141 = EDGE_CURVE ( 'NONE', #28745, #3534, #4029, .T. ) ;
#142 = CARTESIAN_POINT ( 'NONE',  ( 8.000000000000000000, 121.2500000000000000, -9.797174393178825657E-16 ) ) ;
#143 = CARTESIAN_POINT ( 'NONE',  ( -2.085542519210945728E-15, 54.84374999658601979, 11.35316468750000141 ) ) ;
#144 = CARTESIAN_POINT ( 'NONE',  ( -6.000000000000003553, 289.9375000000000000, -2.485281374238571317 ) ) ;
#145 = EDGE_LOOP ( 'NONE', ( #69571, #68618, #12629, #39333 ) ) ;
#146 = ADVANCED_FACE ( 'NONE', ( #37606 ), #60606, .T. ) ;
#147 = CARTESIAN_POINT ( 'NONE',  ( 5.000000000000004441, 251.6666666666667140, 8.660254037844385522 ) ) ;
#148 = CARTESIAN_POINT ( 'NONE',  ( 0.3752463838878496993, -10.12385607954436928, 70.07152133708838448 ) ) ;
#149 = CARTESIAN_POINT ( 'NONE',  ( 1.656854249492348607, 196.3125000027312126, 138.0000000000000568 ) ) ;
#150 = CARTESIAN_POINT ( 'NONE',  ( -11.00000000000000000, 0.000000000000000000, 77.49999999999998579 ) ) ;
#151 = CARTESIAN_POINT ( 'NONE',  ( 8.000000000000000000, 5.812499995903220196, 0.000000000000000000 ) ) ;
#152 = CARTESIAN_POINT ( 'NONE',  ( -7.320508075688771932, 234.3750000000000000, -7.320508075688771932 ) ) ;
#153 = DIRECTION ( 'NONE',  ( -0.000000000000000000, -1.000000000000000000, -0.000000000000000000 ) ) ;
#154 = CARTESIAN_POINT ( 'NONE',  ( -10.18810118749999916, 4.220049686691934809, 67.93750000204838102 ) ) ;
#155 = CARTESIAN_POINT ( 'NONE',  ( 8.660254037844385522, 199.5833333333333428, 5.000000000000005329 ) ) ;
#156 = CARTESIAN_POINT ( 'NONE',  ( -7.188101187499992051, 2.977408999572646930, 18.26780278187175455 ) ) ;
#157 = CARTESIAN_POINT ( 'NONE',  ( 11.35316468749999785, 170.8854166632526983, 3.042071309553174174 ) ) ;
#158 = CARTESIAN_POINT ( 'NONE',  ( 4.000000000000001776, 1.749999997268813168, 0.000000000000000000 ) ) ;
#159 = CARTESIAN_POINT ( 'NONE',  ( -30.64284399271078740, 271.9999999999999432, 174.6921329945331536 ) ) ;
#160 = ORIENTED_EDGE ( 'NONE', *, *, #64767, .F. ) ;
#161 = CARTESIAN_POINT ( 'NONE',  ( -1.432654583217664479, 195.7500000013656063, 138.5412658750000787 ) ) ;
#162 = CARTESIAN_POINT ( 'NONE',  ( 11.35316468749999785, 40.88541666325268409, 3.042071309553174174 ) ) ;
#163 = CARTESIAN_POINT ( 'NONE',  ( -7.778174593052023411, 7.778174593052023411, 109.0000000040967763 ) ) ;
#164 = ADVANCED_FACE ( 'NONE', ( #60981 ), #9302, .F. ) ;
#165 = CARTESIAN_POINT ( 'NONE',  ( -3.426202465283580523, 194.4587341250000350, 198.4732635780662235 ) ) ;
#166 = CARTESIAN_POINT ( 'NONE',  ( 23.99999999999999289, 207.8750000027312126, 169.9999999999999432 ) ) ;
#168 = CARTESIAN_POINT ( 'NONE',  ( 3.000000000000001332, -45.00000000000001421, 151.2383369607063344 ) ) ;
#167 = DIRECTION ( 'NONE',  ( 0.000000000000000000, 0.000000000000000000, 1.000000000000000000 ) ) ;
#169 = CARTESIAN_POINT ( 'NONE',  ( -24.96426921882697059, -51.06966541334224985, 188.3850155782641025 ) ) ;
#170 = CARTESIAN_POINT ( 'NONE',  ( -3.458734125000015425, 197.9375000013655779, 142.0000000000000568 ) ) ;
#171 =( BOUNDED_CURVE ( )  B_SPLINE_CURVE ( 2, ( #47416, #64413, #24036, #1427, #24411, #35019, #22928, #63283, #6340 ),
 .UNSPECIFIED., .F., .F. ) 
 B_SPLINE_CURVE_WITH_KNOTS ( ( 3, 2, 2, 2, 3 ),
 ( 0.4558823529411764608, 0.4595588235294117418, 0.4632352941176470784, 0.4669117647058824150, 0.4705882352941176960 ),
 .UNSPECIFIED. ) 
 CURVE ( )  GEOMETRIC_REPRESENTATION_ITEM ( )  RATIONAL_B_SPLINE_CURVE ( ( 1.000000000000000000, 0.9238795325112867385, 1.000000000000000000, 0.9238795325112867385, 1.000000000000000000, 0.9238795325112867385, 1.000000000000000000, 0.9238795325112856283, 1.000000000000001110 ) ) 
 REPRESENTATION_ITEM ( '' )  );
#172 = CARTESIAN_POINT ( 'NONE',  ( 2.679491924311228956, 57.91666665983870388, -10.00000000000000000 ) ) ;
#173 = CARTESIAN_POINT ( 'NONE',  ( -7.188101187500000044, 98.65625000204838102, 0.000000000000000000 ) ) ;
#174 = CARTESIAN_POINT ( 'NONE',  ( 3.211159895383560947, 12.31249999863440792, 3.211159895383562723 ) ) ;
#175 = CARTESIAN_POINT ( 'NONE',  ( -30.82842712474624847, 206.2500000027312126, 167.1715728752542418 ) ) ;
#176 = CARTESIAN_POINT ( 'NONE',  ( -5.656854249492373476, -5.656854249492376141, 5.517802779823364645 ) ) ;
#177 = CARTESIAN_POINT ( 'NONE',  ( 8.660254037844385522, 101.4583333265053824, 5.000000000000005329 ) ) ;
#178 = ORIENTED_EDGE ( 'NONE', *, *, #23200, .T. ) ;
#179 = EDGE_LOOP ( 'NONE', ( #4857, #25944, #64866, #27879 ) ) ;
#180 = CARTESIAN_POINT ( 'NONE',  ( 2.751064625579944321E-14, 204.8750000027312126, 194.0000000000000568 ) ) ;
#181 = CARTESIAN_POINT ( 'NONE',  ( 1.226468279477575784E-15, 298.8593750017070079, 6.676582343750001591 ) ) ;
#182 = CARTESIAN_POINT ( 'NONE',  ( -4.556349186104045934, 11.00000000000000000, 104.2187500000000000 ) ) ;
#183 = CARTESIAN_POINT ( 'NONE',  ( -0.4368895104449371236, 51.14729664189285785, -48.52014062454940557 ) ) ;
#184 = CARTESIAN_POINT ( 'NONE',  ( 8.311093377946834337, 155.1562499965860127, 8.311093377946839666 ) ) ;
#185 = CARTESIAN_POINT ( 'NONE',  ( 2.828427124746190291, 6.875000000000000000, 2.828427124746192067 ) ) ;
#186 = CARTESIAN_POINT ( 'NONE',  ( 7.204075437095968759, -7.204075437095966983, 81.71875000204836681 ) ) ;
#187 = DIRECTION ( 'NONE',  ( -1.000000000000000000, -0.000000000000000000, -0.000000000000000000 ) ) ;
#188 = CARTESIAN_POINT ( 'NONE',  ( 2.751064625579944321E-14, 205.7500000000000284, 194.0000000000000568 ) ) ;
#189 = CARTESIAN_POINT ( 'NONE',  ( 7.458676001334752392, -2.916525548322098427, -0.000000000000000000 ) ) ;
#190 = CARTESIAN_POINT ( 'NONE',  ( 1.871523826299183495E-15, -10.18810118749999916, 116.4062500020483810 ) ) ;
#191 = EDGE_LOOP ( 'NONE', ( #73079, #34833, #18935, #37812 ) ) ;
#192 =( BOUNDED_CURVE ( )  B_SPLINE_CURVE ( 2, ( #22202, #22962, #68610, #56933, #28993, #11272, #73520, #10154, #349 ),
 .UNSPECIFIED., .F., .F. ) 
 B_SPLINE_CURVE_WITH_KNOTS ( ( 3, 2, 2, 2, 3 ),
 ( 0.7159090909090909394, 0.7215909090909090606, 0.7272727272727272929, 0.7329545454545454142, 0.7386363636363636465 ),
 .UNSPECIFIED. ) 
 CURVE ( )  GEOMETRIC_REPRESENTATION_ITEM ( )  RATIONAL_B_SPLINE_CURVE ( ( 1.000000000000000000, 0.9238795325112867385, 1.000000000000000000, 0.9238795325112867385, 1.000000000000000000, 0.9238795325112867385, 1.000000000000000000, 0.9238795325112867385, 1.000000000000000000 ) ) 
 REPRESENTATION_ITEM ( '' )  );
#193 = CARTESIAN_POINT ( 'NONE',  ( 31.43535510153570911, -32.23507837658848985, 169.5164923427215342 ) ) ;
#194 = CARTESIAN_POINT ( 'NONE',  ( 19.81901786545334332, 177.9744831197517954, 139.1998822286107895 ) ) ;
#195 = CARTESIAN_POINT ( 'NONE',  ( -3.042071309553163960, 132.5520833299193555, -11.35316468749999963 ) ) ;
#196 = CARTESIAN_POINT ( 'NONE',  ( 2.445694354108838731, 198.0625000013656063, 195.5543056458912190 ) ) ;
#197 = CARTESIAN_POINT ( 'NONE',  ( 5.082755093536324154, 26.15624999795161543, 5.082755093536326818 ) ) ;
#198 = CARTESIAN_POINT ( 'NONE',  ( -7.204075437095967871, 7.204075437095967871, 75.34375000204838102 ) ) ;
#199 = CARTESIAN_POINT ( 'NONE',  ( 3.042071309553159519, 30.05208332991934839, 11.35316468750000141 ) ) ;
#200 = ORIENTED_EDGE ( 'NONE', *, *, #53117, .T. ) ;
#201 = CARTESIAN_POINT ( 'NONE',  ( 4.999999999999993783, 36.04166665983870388, 8.660254037844390851 ) ) ;
#202 = CARTESIAN_POINT ( 'NONE',  ( 4.541265875000002339, 2.499999998634407028, -1.881053915767121776 ) ) ;
#203 = CARTESIAN_POINT ( 'NONE',  ( -4.903558642999205574E-16, 8.008118988124991233, 12.63811528394063011 ) ) ;
#204 = CARTESIAN_POINT ( 'NONE',  ( -3.458734125000016757, 208.1250000013656063, 140.5673454167824161 ) ) ;
#205 = CONICAL_SURFACE ( 'NONE', #29092, 10.49999999999998224, 0.7853981633974378429 ) ;
#206 = CARTESIAN_POINT ( 'NONE',  ( 5.082755093536324154, 9.281249997951610098, 5.082755093536326818 ) ) ;
#207 = CARTESIAN_POINT ( 'NONE',  ( 2.485281374238575314, 296.3750000034140157, 6.000000000000000888 ) ) ;
#208 = CARTESIAN_POINT ( 'NONE',  ( -33.01026376120496053, -12.09627671384102676, 145.3380100151787815 ) ) ;
#209 = CARTESIAN_POINT ( 'NONE',  ( 5.082755093536325930, 5.531249997951610098, -5.082755093536325930 ) ) ;
#210 = CARTESIAN_POINT ( 'NONE',  ( 5.082755093536320601, -5.082755093536318824, 14.04905278187175455 ) ) ;
#211 = CARTESIAN_POINT ( 'NONE',  ( 5.676582343749993598, 150.2604166632526699, 9.832129032723422313 ) ) ;
#212 = CARTESIAN_POINT ( 'NONE',  ( -6.238412754330611322E-16, 10.18810118749999916, 71.78125000204838102 ) ) ;
#213 = CARTESIAN_POINT ( 'NONE',  ( -26.56734541678232731, 207.2500000013655779, 173.4587341250003760 ) ) ;
#214 = DIRECTION ( 'NONE',  ( 0.000000000000000000, 0.000000000000000000, 1.000000000000000000 ) ) ;
#215 = CARTESIAN_POINT ( 'NONE',  ( -1.881053915767124440, 20.12499999863441147, 4.541265875000001451 ) ) ;
#216 = ORIENTED_EDGE ( 'NONE', *, *, #37600, .T. ) ;
#217 = ADVANCED_FACE ( 'NONE', ( #26642 ), #49664, .T. ) ;
#218 = CARTESIAN_POINT ( 'NONE',  ( -3.999999999999960032, 199.0625000027312126, 196.3431457505076594 ) ) ;
#219 = CARTESIAN_POINT ( 'NONE',  ( 1.656854249492347719, 206.8125000000000000, 146.0000000000000284 ) ) ;
#220 = CARTESIAN_POINT ( 'NONE',  ( -23.99999999999995737, 200.8125000027311842, 171.6568542494926817 ) ) ;
#221 = DIRECTION ( 'NONE',  ( 0.000000000000000000, -1.000000000000000000, -0.000000000000000000 ) ) ;
#222 = CARTESIAN_POINT ( 'NONE',  ( 7.999999999999992895, -3.313708498984756279, 9.174052783920144449 ) ) ;
#223 = ORIENTED_EDGE ( 'NONE', *, *, #26791, .F. ) ;
#224 = CARTESIAN_POINT ( 'NONE',  ( -2.977408999572654480, 16.49999999795161543, 7.188101187499999156 ) ) ;
#225 = PLANE ( 'NONE',  #9909 ) ;
#226 = CARTESIAN_POINT ( 'NONE',  ( 3.373128826976368178, -10.27267468567300668, -63.92035228378879452 ) ) ;
#227 = CARTESIAN_POINT ( 'NONE',  ( -1.836970198721029983E-15, 43.75000000000000711, 10.00000000000000178 ) ) ;
#228 = CARTESIAN_POINT ( 'NONE',  ( 1.320432766682874540E-15, 108.4062500020483810, 7.188101187500000044 ) ) ;
#229 = CARTESIAN_POINT ( 'NONE',  ( -28.00000000000002487, 207.6875000013656063, 166.5412658750003629 ) ) ;
#230 = CARTESIAN_POINT ( 'NONE',  ( -25.17157287525381903, 196.8750000000000284, 167.1715728752541565 ) ) ;
#232 = CARTESIAN_POINT ( 'NONE',  ( 28.00000000000002132, 201.1250000027312126, 173.9999999999999147 ) ) ;
#231 = CARTESIAN_POINT ( 'NONE',  ( -9.000000000000000000, 0.000000000000000000, -10.20000000000000462 ) ) ;
#233 = ORIENTED_EDGE ( 'NONE', *, *, #22637, .F. ) ;
#234 = ADVANCED_FACE ( 'NONE', ( #9685 ), #32705, .T. ) ;
#235 = CARTESIAN_POINT ( 'NONE',  ( 9.832129032723420536, 250.9895833367473017, 5.676582343749996262 ) ) ;
#236 = CARTESIAN_POINT ( 'NONE',  ( -7.188101187499992051, 0.000000000000000000, 15.36155278187175455 ) ) ;
#237 = AXIS2_PLACEMENT_3D ( 'NONE', #10666, #63087, #11411 ) ;
#238 = CARTESIAN_POINT ( 'NONE',  ( -4.999999999999998224, 8.541666659838698550, -8.660254037844389075 ) ) ;
#239 = CARTESIAN_POINT ( 'NONE',  ( -9.950350709847000985, 219.9999999999999432, 3.187220239308521386 ) ) ;
#240 = CARTESIAN_POINT ( 'NONE',  ( 2.828427124746208943, 198.7500000027312126, 195.1715728752538439 ) ) ;
#241 = CARTESIAN_POINT ( 'NONE',  ( 0.000000000000000000, 125.0000000000000000, 0.000000000000000000 ) ) ;
#242 = CARTESIAN_POINT ( 'NONE',  ( -2.679491924311235618, 158.5416666666666003, 10.00000000000000000 ) ) ;
#243 = CARTESIAN_POINT ( 'NONE',  ( 0.000000000000000000, 19.05255888325788050, 10.99999999999998934 ) ) ;
#244 = DIRECTION ( 'NONE',  ( -0.000000000000000000, 1.000000000000000000, -1.563033456626094573E-30 ) ) ;
#245 = CARTESIAN_POINT ( 'NONE',  ( 11.35316468750000141, 131.0937499965860127, 0.000000000000000000 ) ) ;
#246 = CARTESIAN_POINT ( 'NONE',  ( -6.000000000000003553, 294.0000000034140157, -2.485281374238571317 ) ) ;
#247 = CARTESIAN_POINT ( 'NONE',  ( -8.000000000000000000, 5.156250000000000888, -3.313708498984762496 ) ) ;
#250 = CARTESIAN_POINT ( 'NONE',  ( -4.556349186104045934, 11.00000000000000000, 84.90625000409676204 ) ) ;
#249 = CARTESIAN_POINT ( 'NONE',  ( 24.54126587499998990, 196.1875000013655779, 169.9999999999999432 ) ) ;
#248 = CARTESIAN_POINT ( 'NONE',  ( 25.17157287525378706, 209.8750000000000284, 172.8284271247460424 ) ) ;
#251 = ORIENTED_EDGE ( 'NONE', *, *, #53078, .F. ) ;
#252 = CARTESIAN_POINT ( 'NONE',  ( -2.828427124746152987, 206.1250000000000284, 200.8284271247462129 ) ) ;
#253 = DIRECTION ( 'NONE',  ( 1.000000000000000000, -0.000000000000000000, 0.000000000000000000 ) ) ;
#254 = CARTESIAN_POINT ( 'NONE',  ( -3.190679070438028606E-13, 193.7500000000000000, 10.00000000000000533 ) ) ;
#255 = EDGE_CURVE ( 'NONE', #7966, #8230, #16802, .T. ) ;
#256 = CARTESIAN_POINT ( 'NONE',  ( -10.00000000000000355, 19.58333332650536818, 2.679491924311223183 ) ) ;
#257 = CARTESIAN_POINT ( 'NONE',  ( -2.977408999572651815, 119.9375000020483952, 7.188101187500000933 ) ) ;
#258 = CARTESIAN_POINT ( 'NONE',  ( 4.541265875000002339, 21.37499999863441147, -1.881053915767121554 ) ) ;
#259 = CARTESIAN_POINT ( 'NONE',  ( -3.511653767260603853, -51.69076377080480711, 48.72852442694462383 ) ) ;
#260 = CARTESIAN_POINT ( 'NONE',  ( -5.656854249492373476, -5.656854249492376141, 22.01780277982336997 ) ) ;
#262 = CARTESIAN_POINT ( 'NONE',  ( -32.00000000000001421, 207.1875000000000284, 168.3431457505080289 ) ) ;
#261 = PLANE ( 'NONE',  #994 ) ;
#263 = CARTESIAN_POINT ( 'NONE',  ( 9.832129032723416984, 105.3645833299193555, 5.676582343750006032 ) ) ;
#264 = ORIENTED_EDGE ( 'NONE', *, *, #10411, .T. ) ;
#265 = CARTESIAN_POINT ( 'NONE',  ( -2.828427124746209831, 205.5000000027312126, 139.1715728752538723 ) ) ;
#266 = CARTESIAN_POINT ( 'NONE',  ( -5.082755093536326818, 23.90624999795161543, 5.082755093536325042 ) ) ;
#267 = DIRECTION ( 'NONE',  ( -0.000000000000000000, 0.000000000000000000, 1.000000000000000000 ) ) ;
#268 = CARTESIAN_POINT ( 'NONE',  ( -11.35316468749999785, 244.0104166700806729, -3.042071309553164848 ) ) ;
#269 = AXIS2_PLACEMENT_3D ( 'NONE', #63986, #56848, #58346 ) ;
#270 = CARTESIAN_POINT ( 'NONE',  ( -11.35316468749999785, 108.0729166632526699, -3.042071309553167513 ) ) ;
#271 = VERTEX_POINT ( 'NONE', #62834 ) ;
#272 = CARTESIAN_POINT ( 'NONE',  ( 3.313708498984802020, 25.78125000000000355, -7.999999999999958256 ) ) ;
#273 = CARTESIAN_POINT ( 'NONE',  ( -6.238412754330611322E-16, 10.18810118749999916, 103.2812500020483810 ) ) ;
#274 = CARTESIAN_POINT ( 'NONE',  ( 10.00000000000000000, 226.6666666598386541, 2.679491924311236062 ) ) ;
#275 = CARTESIAN_POINT ( 'NONE',  ( 3.458734125000015869, 202.1875000013656063, 198.0000000000000284 ) ) ;
#276 = CARTESIAN_POINT ( 'NONE',  ( 4.556349186104052151, -10.99999999999999822, 68.96875000000000000 ) ) ;
#278 = CARTESIAN_POINT ( 'NONE',  ( -2.085542519210945728E-15, 99.53124999658602690, 11.35316468750000141 ) ) ;
#277 = CARTESIAN_POINT ( 'NONE',  ( -2.828427124746153876, 206.0000000027312126, 195.1715728752538439 ) ) ;
#279 = CARTESIAN_POINT ( 'NONE',  ( 5.656854249492376141, -5.656854249492374365, 13.58030278392014623 ) ) ;
#280 = CARTESIAN_POINT ( 'NONE',  ( -24.54126587499999346, 198.4375000013655779, 170.0000000000003411 ) ) ;
#281 = CARTESIAN_POINT ( 'NONE',  ( -5.656854249492381470, 27.74999999590322020, 5.656854249492379694 ) ) ;
#282 = VERTEX_POINT ( 'NONE', #23223 ) ;
#283 = CARTESIAN_POINT ( 'NONE',  ( -2.679491924311235618, 190.4166666598387394, 10.00000000000000000 ) ) ;
#284 = CARTESIAN_POINT ( 'NONE',  ( 3.313708498984652362, 115.5312500000000000, -8.000000000000108358 ) ) ;
#285 = EDGE_CURVE ( 'NONE', #59945, #25965, #51151, .T. ) ;
#286 = CARTESIAN_POINT ( 'NONE',  ( 2.775557561562891351E-14, 271.9999999999999432, 170.0000000000000284 ) ) ;
#287 = CARTESIAN_POINT ( 'NONE',  ( -8.311093377946841443, 89.21874999658602690, 8.311093377946834337 ) ) ;
#288 = CARTESIAN_POINT ( 'NONE',  ( -2.765530957081996810, 290.2656250017068942, -6.676582343750003368 ) ) ;
#289 = CARTESIAN_POINT ( 'NONE',  ( -2.977408999572650039, 5.812499997951610986, -7.188101187500000933 ) ) ;
#290 =( BOUNDED_CURVE ( )  B_SPLINE_CURVE ( 2, ( #68375, #16672, #62703, #11041, #5381, #30972, #35180, #7969, #58556 ),
 .UNSPECIFIED., .F., .F. ) 
 B_SPLINE_CURVE_WITH_KNOTS ( ( 3, 2, 2, 2, 3 ),
 ( 0.4895833333333333148, 0.4947916666666666852, 0.5000000000000000000, 0.5052083333333333703, 0.5104166666666666297 ),
 .UNSPECIFIED. ) 
 CURVE ( )  GEOMETRIC_REPRESENTATION_ITEM ( )  RATIONAL_B_SPLINE_CURVE ( ( 1.000000000000000000, 0.9238795325112867385, 1.000000000000000000, 0.9238795325112867385, 1.000000000000000000, 0.9238795325112867385, 1.000000000000000000, 0.9238795325112867385, 1.000000000000000000 ) ) 
 REPRESENTATION_ITEM ( '' )  );
#291 = CARTESIAN_POINT ( 'NONE',  ( 10.18810118750000093, -4.220049686691933033, 95.68750000204838102 ) ) ;
#292 = CARTESIAN_POINT ( 'NONE',  ( 11.35316468750000141, 215.7812499965860411, 0.000000000000000000 ) ) ;
#293 = ORIENTED_EDGE ( 'NONE', *, *, #58065, .F. ) ;
#294 = CARTESIAN_POINT ( 'NONE',  ( -7.347880794884122694E-16, 20.49999999726881583, 4.000000000000001776 ) ) ;
#295 = CARTESIAN_POINT ( 'NONE',  ( 1.656854249492521136, 196.8125000027311557, 194.0000000000001990 ) ) ;
#296 = CARTESIAN_POINT ( 'NONE',  ( 11.35316468750000141, 220.7812499965860127, 0.000000000000000000 ) ) ;
#297 = CARTESIAN_POINT ( 'NONE',  ( -7.320508075688770155, 218.7500000068280031, 7.320508075688774596 ) ) ;
#298 = CARTESIAN_POINT ( 'NONE',  ( -0.8721677472748831095, -16.44158143986581422, -68.58266913489941885 ) ) ;
#299 = CARTESIAN_POINT ( 'NONE',  ( 4.721056650415999201, 295.0781250017069510, -4.721056650415999201 ) ) ;
#300 = VERTEX_POINT ( 'NONE', #243 ) ;
#301 = CARTESIAN_POINT ( 'NONE',  ( -1.736494649845399918, -51.27805538754612513, -48.57014059985662868 ) ) ;
#302 = CARTESIAN_POINT ( 'NONE',  ( -11.35316468750000141, 203.5937499965860127, -1.390361679473963753E-15 ) ) ;
#303 = CARTESIAN_POINT ( 'NONE',  ( -6.238412754330611322E-16, 10.18810118749999916, 86.78125000204836681 ) ) ;
#304 = AXIS2_PLACEMENT_3D ( 'NONE', #33197, #73902, #51638 ) ;
#305 = CARTESIAN_POINT ( 'NONE',  ( -25.55430564589119413, 204.3125000013656063, 167.5543056458915316 ) ) ;
#306 = CARTESIAN_POINT ( 'NONE',  ( -3.313708498984760720, 18.46875000000000000, -8.000000000000000000 ) ) ;
#307 = EDGE_LOOP ( 'NONE', ( #31448, #30350, #12542, #61216 ) ) ;
#308 = ADVANCED_FACE ( 'NONE', ( #40955 ), #58321, .T. ) ;
#309 = CARTESIAN_POINT ( 'NONE',  ( 1.320432766682874540E-15, 121.5312500020483810, 7.188101187500000044 ) ) ;
#310 = CARTESIAN_POINT ( 'NONE',  ( -3.313708498984759387, -7.999999999999989342, 19.11155277982337353 ) ) ;
#311 = EDGE_CURVE ( 'NONE', #38095, #9013, #57196, .T. ) ;
#312 = CARTESIAN_POINT ( 'NONE',  ( -2.679491924311235618, 28.54166666666667140, 10.00000000000000000 ) ) ;
#313 = VECTOR ( 'NONE', #22146, 1000.000000000000000 ) ;
#314 = CARTESIAN_POINT ( 'NONE',  ( -5.000000000000000000, -50.64189880742115690, 41.08656465431877791 ) ) ;
#315 = CARTESIAN_POINT ( 'NONE',  ( 1.871523826299183495E-15, -10.18810118749999916, 77.40625000204836681 ) ) ;
#316 = ORIENTED_EDGE ( 'NONE', *, *, #39996, .F. ) ;
#317 = ADVANCED_FACE ( 'NONE', ( #63964 ), #68502, .F. ) ;
#318 = CARTESIAN_POINT ( 'NONE',  ( -1.737867177246331662, 21.99999999999999645, 4.195582608135537406 ) ) ;
#319 = DIRECTION ( 'NONE',  ( -1.000000000000000000, 0.000000000000000000, -0.000000000000000000 ) ) ;
#320 = PRESENTATION_STYLE_ASSIGNMENT (( #23298 ) ) ;
#321 = CARTESIAN_POINT ( 'NONE',  ( -5.000000000000000000, -10.28295106684163684, 65.17663434001590872 ) ) ;
#322 = CARTESIAN_POINT ( 'NONE',  ( 27.99999999999996803, 199.0000000000000000, 173.9999999999999147 ) ) ;
#323 = CARTESIAN_POINT ( 'NONE',  ( 4.721056650416000089, 294.8281250017069510, 4.721056650415999201 ) ) ;
#325 = CARTESIAN_POINT ( 'NONE',  ( -47.32259252271279593, 145.2267040872997939, 65.76194439203463560 ) ) ;
#324 = CARTESIAN_POINT ( 'NONE',  ( -5.676582343749992710, 239.7395833367473301, 9.832129032723422313 ) ) ;
#326 = CONTEXT_DEPENDENT_SHAPE_REPRESENTATION ( #26968, #29511 ) ;
#327 = VERTEX_POINT ( 'NONE', #22463 ) ;
#328 = CARTESIAN_POINT ( 'NONE',  ( -9.832129032723418760, 243.8020833367473301, -5.676582343749998927 ) ) ;
#329 = CARTESIAN_POINT ( 'NONE',  ( -2.977408999572648707, -7.188101187499990274, 4.767802781871753659 ) ) ;
#330 = EDGE_LOOP ( 'NONE', ( #38792, #67335, #71147 ) ) ;
#331 = CARTESIAN_POINT ( 'NONE',  ( 1.871523826299183495E-15, -10.18810118749999916, 69.53125000204838102 ) ) ;
#332 = CARTESIAN_POINT ( 'NONE',  ( -5.676582343750006032, 89.42708332991934128, 9.832129032723418760 ) ) ;
#333 = CARTESIAN_POINT ( 'NONE',  ( 1.656854249492381914, 20.81250000000000000, 4.000000000000000888 ) ) ;
#334 = CARTESIAN_POINT ( 'NONE',  ( -7.778174593052023411, 7.778174593052023411, 84.81249999999998579 ) ) ;
#337 = DIRECTION ( 'NONE',  ( 0.000000000000000000, 0.000000000000000000, -1.000000000000000000 ) ) ;
#336 = CARTESIAN_POINT ( 'NONE',  ( 26.56734541678238060, 207.3750000013656063, 173.4587341249998929 ) ) ;
#335 = CARTESIAN_POINT ( 'NONE',  ( 24.54126587499999701, 206.4375000013656063, 169.9999999999998863 ) ) ;
#338 = VERTEX_POINT ( 'NONE', #45122 ) ;
#339 = FACE_OUTER_BOUND ( 'NONE', #9097, .T. ) ;
#340 = CARTESIAN_POINT ( 'NONE',  ( 2.751064625579944321E-14, 202.8750000027312126, 194.0000000000000568 ) ) ;
#341 = CARTESIAN_POINT ( 'NONE',  ( 5.676582343750001591, 201.6145833299193555, -9.832129032723420536 ) ) ;
#342 = CARTESIAN_POINT ( 'NONE',  ( 2.445694354108783664, 205.3125000013656063, 144.4456943541088663 ) ) ;
#343 = CARTESIAN_POINT ( 'NONE',  ( 24.54126587500000056, 204.3750000013656063, 168.5673454167822172 ) ) ;
#344 = ADVANCED_FACE ( 'NONE', ( #11537 ), #51902, .T. ) ;
#345 = CARTESIAN_POINT ( 'NONE',  ( -7.188101187500000044, 22.59374999795161187, -8.802885111219163269E-16 ) ) ;
#346 = CARTESIAN_POINT ( 'NONE',  ( 11.35316468750000141, 186.0937499965860411, 0.000000000000000000 ) ) ;
#347 = CYLINDRICAL_SURFACE ( 'NONE', #9469, 10.50000000000000000 ) ;
#348 = CARTESIAN_POINT ( 'NONE',  ( -2.977408999572652260, 96.31250000204838102, 7.188101187500000044 ) ) ;
#350 = CARTESIAN_POINT ( 'NONE',  ( -10.00000000000000000, 107.7083333333333428, 2.679491924311222295 ) ) ;
#349 = CARTESIAN_POINT ( 'NONE',  ( 2.449293598294707893E-16, 16.99999999726881583, -4.000000000000001776 ) ) ;
#351 = CARTESIAN_POINT ( 'NONE',  ( -4.541265875000003227, 10.87499999863440792, 1.881053915767121110 ) ) ;
#352 = CARTESIAN_POINT ( 'NONE',  ( 24.54126587499998280, 203.5000000013655779, 171.4326545832175555 ) ) ;
#353 = CARTESIAN_POINT ( 'NONE',  ( -4.401442555609577197E-16, 7.188101187499992051, 8.986552781871752771 ) ) ;
#354 = CARTESIAN_POINT ( 'NONE',  ( 5.676582343749993598, 69.94791666325268409, 9.832129032723422313 ) ) ;
#355 = CARTESIAN_POINT ( 'NONE',  ( -5.000000000000000000, -53.20585484986825975, 47.69738026034712419 ) ) ;
#356 = CARTESIAN_POINT ( 'NONE',  ( 7.999999999999991118, 3.313708498984757611, 1.730302784329821320 ) ) ;
#357 = ORIENTED_EDGE ( 'NONE', *, *, #65945, .F. ) ;
#358 = LINE ( 'NONE', #74275, #65132 ) ;
#359 = CARTESIAN_POINT ( 'NONE',  ( -4.556349186104048599, -10.99999999999999822, 116.7812499999999858 ) ) ;
#360 = CARTESIAN_POINT ( 'NONE',  ( -9.832129032723418760, 67.86458332991935549, -5.676582343750004256 ) ) ;
#361 = CARTESIAN_POINT ( 'NONE',  ( 4.556349186104045934, 11.00000000000000000, 71.21875000409677625 ) ) ;
#362 = CARTESIAN_POINT ( 'NONE',  ( -2.445694354108840063, 196.0625000013656063, 139.5543056458912190 ) ) ;
#363 = CARTESIAN_POINT ( 'NONE',  ( -30.93541659651594955, -37.37294455265293180, 167.9999999999997442 ) ) ;
#365 = CARTESIAN_POINT ( 'NONE',  ( -3.042071309553173730, 59.32291666325267698, 11.35316468749999785 ) ) ;
#364 = CARTESIAN_POINT ( 'NONE',  ( 1.320432766682874540E-15, 91.53125000204836681, 7.188101187500000044 ) ) ;
#366 = CARTESIAN_POINT ( 'NONE',  ( 5.656854249492374365, 5.656854249492375253, 1.767802779823364423 ) ) ;
#367 = CARTESIAN_POINT ( 'NONE',  ( -0.4888677760596382704, 194.9085675716885078, 145.8857357277319693 ) ) ;
#368 = CARTESIAN_POINT ( 'NONE',  ( 6.123233995736767268E-16, 153.1249999931720538, -10.00000000000000178 ) ) ;
#369 = VECTOR ( 'NONE', #48280, 1000.000000000000000 ) ;
#370 = CARTESIAN_POINT ( 'NONE',  ( 5.082755093536326818, 95.09375000204838102, 5.082755093536325042 ) ) ;
#371 = CARTESIAN_POINT ( 'NONE',  ( -4.556349186104045934, 11.00000000000000000, 108.7187499999999858 ) ) ;
#372 = CARTESIAN_POINT ( 'NONE',  ( -9.832129032723418760, 43.17708332991934839, -5.676582343750004256 ) ) ;
#373 = CARTESIAN_POINT ( 'NONE',  ( 1.871523826299183495E-15, -10.18810118749999916, 110.4062500020483668 ) ) ;
#374 = CARTESIAN_POINT ( 'NONE',  ( -5.676582343750006032, 179.1145833299193555, 9.832129032723418760 ) ) ;
#375 = ORIENTED_EDGE ( 'NONE', *, *, #72099, .F. ) ;
#376 = CARTESIAN_POINT ( 'NONE',  ( -2.266287154879899290, 60.33498852648347821, 22.96738997677451977 ) ) ;
#377 = CARTESIAN_POINT ( 'NONE',  ( -10.18810118749999738, -4.220049686691941915, 73.75000000204836681 ) ) ;
#378 = CARTESIAN_POINT ( 'NONE',  ( 27.99999999999996447, 203.6250000027312126, 165.9999999999998863 ) ) ;
#380 = CARTESIAN_POINT ( 'NONE',  ( 11.35316468749999785, 185.5729166632526983, 3.042071309553174174 ) ) ;
#379 = CARTESIAN_POINT ( 'NONE',  ( 2.449293598294707893E-16, 18.99999999726881228, -4.000000000000001776 ) ) ;
#381 = CARTESIAN_POINT ( 'NONE',  ( 3.313708498984762496, -7.999999999999989342, 7.355302784329823318 ) ) ;
#382 = CONICAL_SURFACE ( 'NONE', #64214, 18.00000000000000355, 1.047197551196596965 ) ;
#383 = DIRECTION ( 'NONE',  ( 0.000000000000000000, -0.5207998305029613029, -0.8536788251726096233 ) ) ;
#384 = CARTESIAN_POINT ( 'NONE',  ( -10.00000000000000000, 253.1250000068279746, 0.000000000000000000 ) ) ;
#385 = CARTESIAN_POINT ( 'NONE',  ( 5.000000000000000000, 16.14408868864073554, 27.96238185062412640 ) ) ;
#386 = ORIENTED_EDGE ( 'NONE', *, *, #24022, .T. ) ;
#387 = CARTESIAN_POINT ( 'NONE',  ( 8.311093377946837890, 166.7187499965860127, -8.311093377946837890 ) ) ;
#388 = CARTESIAN_POINT ( 'NONE',  ( 1.320432766682872962E-15, -7.188101187499992051, 24.36155278187175810 ) ) ;
#389 = CARTESIAN_POINT ( 'NONE',  ( 11.35316468749999963, 126.3020833299193555, -3.042071309553165293 ) ) ;
#390 = CARTESIAN_POINT ( 'NONE',  ( 30.82842712474616675, 195.1250000000000284, 172.8284271247460993 ) ) ;
#391 = ORIENTED_EDGE ( 'NONE', *, *, #6730, .T. ) ;
#392 = CARTESIAN_POINT ( 'NONE',  ( -3.211159895383562723, 13.06249999863440792, 3.211159895383561391 ) ) ;
#393 = CARTESIAN_POINT ( 'NONE',  ( 5.082755093536324154, 12.28124999795161187, 5.082755093536326818 ) ) ;
#394 = CARTESIAN_POINT ( 'NONE',  ( -5.656854249492378806, 104.3750000040967763, 5.656854249492381470 ) ) ;
#395 = EDGE_CURVE ( 'NONE', #73730, #54851, #613, .T. ) ;
#396 =( BOUNDED_CURVE ( )  B_SPLINE_CURVE ( 2, ( #48168, #19867, #36494, #24780, #47795, #35759, #30090, #2902, #53479, #70818, #36125, #65892, #2158 ),
 .UNSPECIFIED., .F., .F. ) 
 B_SPLINE_CURVE_WITH_KNOTS ( ( 3, 2, 2, 2, 2, 2, 3 ),
 ( 1.522886666904841757, 1.528120630700553040, 1.533354594496264545, 1.538588558291975827, 1.543822522087687332, 1.549056485883398615, 1.554290449679109676 ),
 .UNSPECIFIED. ) 
 CURVE ( )  GEOMETRIC_REPRESENTATION_ITEM ( )  RATIONAL_B_SPLINE_CURVE ( ( 0.9999999999999790168, 0.9659258262890890734, 0.9999999999999998890, 0.9659258262890682012, 0.9999999999999998890, 0.9659258262890682012, 0.9999999999999998890, 0.9659258262890682012, 0.9999999999999998890, 0.9659258262890682012, 0.9999999999999998890, 0.9659258262890682012, 0.9999999999999998890 ) ) 
 REPRESENTATION_ITEM ( '' )  );
#397 = CARTESIAN_POINT ( 'NONE',  ( -27.99999999999996447, 198.1875000013655779, 173.4587341250003760 ) ) ;
#398 = ADVANCED_FACE ( 'NONE', ( #69251 ), #45859, .F. ) ;
#399 = CARTESIAN_POINT ( 'NONE',  ( 1.656854249492381914, 11.81249999999999822, 4.000000000000000888 ) ) ;
#400 = CARTESIAN_POINT ( 'NONE',  ( 4.000000000000001776, 21.81249999726881583, -1.656854249492381248 ) ) ;
#401 = CARTESIAN_POINT ( 'NONE',  ( 3.211159895383560947, 13.18749999863440792, 3.211159895383562723 ) ) ;
#402 = CARTESIAN_POINT ( 'NONE',  ( 5.656854249492374365, 5.656854249492375253, 19.95530278392014623 ) ) ;
#403 = CARTESIAN_POINT ( 'NONE',  ( -8.660254037844389075, 187.0833333333333428, -5.000000000000006217 ) ) ;
#404 = ORIENTED_EDGE ( 'NONE', *, *, #58829, .T. ) ;
#405 = CARTESIAN_POINT ( 'NONE',  ( 2.828427124746152987, 205.1250000000000284, 139.1715728752538723 ) ) ;
#406 = CARTESIAN_POINT ( 'NONE',  ( -7.188101187500000044, 103.1562500020483810, 0.000000000000000000 ) ) ;
#408 = CARTESIAN_POINT ( 'NONE',  ( -8.000000000000001776, 15.65624999590322197, 3.313708498984759387 ) ) ;
#407 = DIRECTION ( 'NONE',  ( -1.000000000000000000, -0.000000000000000000, -0.000000000000000000 ) ) ;
#409 = ORIENTED_EDGE ( 'NONE', *, *, #69841, .T. ) ;
#410 = CARTESIAN_POINT ( 'NONE',  ( -4.330454160168800470, 16.29811171461321706, -69.49285720719208825 ) ) ;
#411 = CARTESIAN_POINT ( 'NONE',  ( 7.188101187499993827, -2.977408999572645598, 24.64280278187176165 ) ) ;
#412 = ORIENTED_EDGE ( 'NONE', *, *, #14077, .T. ) ;
#413 = VERTEX_POINT ( 'NONE', #63581 ) ;
#414 = CARTESIAN_POINT ( 'NONE',  ( -10.18810118749999738, -4.220049686691941915, 84.25000000204838102 ) ) ;
#415 = CARTESIAN_POINT ( 'NONE',  ( -4.000000000000001776, 9.187499997268814056, -1.656854249492381470 ) ) ;
#416 = CARTESIAN_POINT ( 'NONE',  ( -25.55430564589114795, 196.3125000013656063, 172.4456943541091789 ) ) ;
#417 = CARTESIAN_POINT ( 'NONE',  ( -10.99999999999999822, -4.556349186104052151, 100.0937500000000142 ) ) ;
#420 = CARTESIAN_POINT ( 'NONE',  ( -4.721056650415999201, 297.4843750017070079, -4.721056650415999201 ) ) ;
#419 = CARTESIAN_POINT ( 'NONE',  ( 29.65685424949235482, 206.5625000027312126, 165.9999999999998863 ) ) ;
#418 = CARTESIAN_POINT ( 'NONE',  ( -6.000000000000001776, 290.0625000034140157, 0.000000000000000000 ) ) ;
#421 = CARTESIAN_POINT ( 'NONE',  ( -8.660254037844390851, 137.9166666666666856, 4.999999999999998224 ) ) ;
#422 = AXIS2_PLACEMENT_3D ( 'NONE', #37971, #67004, #72668 ) ;
#423 = CARTESIAN_POINT ( 'NONE',  ( 5.656854249492379694, 100.4375000000000000, -5.656854249492380582 ) ) ;
#424 = CARTESIAN_POINT ( 'NONE',  ( 6.123233995736767268E-16, 138.1249999931720538, -10.00000000000000178 ) ) ;
#425 = CARTESIAN_POINT ( 'NONE',  ( 2.977408999572650927, -7.188101187499990274, 0.8303027818717529929 ) ) ;
#426 = CARTESIAN_POINT ( 'NONE',  ( 8.000000000000000000, 1.593750000000000222, -3.313708498984761164 ) ) ;
#427 = CARTESIAN_POINT ( 'NONE',  ( 31.45873412500001010, 202.7500000013655779, 168.5673454167822740 ) ) ;
#428 = CARTESIAN_POINT ( 'NONE',  ( -7.188101187500002709, 6.187499997951610986, 2.977408999572649151 ) ) ;
#429 = CARTESIAN_POINT ( 'NONE',  ( -3.317071493978880348, -8.008118988124989457, 5.794365283940630995 ) ) ;
#430 = CARTESIAN_POINT ( 'NONE',  ( -2.754378923186476579E-14, 196.1875000013655779, 145.4587341250000350 ) ) ;
#431 = CARTESIAN_POINT ( 'NONE',  ( -2.977408999572652260, 114.3125000020483668, 7.188101187500000044 ) ) ;
#433 = CARTESIAN_POINT ( 'NONE',  ( -5.656854249492373476, -5.656854249492376141, 7.017802779823365533 ) ) ;
#432 = LINE ( 'NONE', #45678, #46783 ) ;
#434 = CARTESIAN_POINT ( 'NONE',  ( 11.35316468749999963, 236.7187500034139873, -1.390361679473963556E-15 ) ) ;
#435 = CARTESIAN_POINT ( 'NONE',  ( -8.000000000000000000, 3.656250000000000444, -3.313708498984762496 ) ) ;
#436 = CARTESIAN_POINT ( 'NONE',  ( 5.082755093536318824, 5.082755093536319713, 25.29905278187175810 ) ) ;
#437 = CARTESIAN_POINT ( 'NONE',  ( 25.17157287525378351, 199.8750000000000284, 172.8284271247460424 ) ) ;
#438 = AXIS2_PLACEMENT_3D ( 'NONE', #32326, #55339, #3643 ) ;
#439 = CARTESIAN_POINT ( 'NONE',  ( -8.311093377946836114, 32.65624999658601268, -8.311093377946837890 ) ) ;
#440 = CARTESIAN_POINT ( 'NONE',  ( 10.00000000000033040, 25.00000000000018829, 0.000000000000000000 ) ) ;
#441 = CARTESIAN_POINT ( 'NONE',  ( 11.35316468749999963, 226.3020833299193555, -3.042071309553165293 ) ) ;
#442 = CARTESIAN_POINT ( 'NONE',  ( -7.320508075688773708, 218.7499999931720538, -7.320508075688774596 ) ) ;
#444 = CARTESIAN_POINT ( 'NONE',  ( -3.458734124999959914, 194.4587341250000065, 198.0000000000000284 ) ) ;
#443 = CARTESIAN_POINT ( 'NONE',  ( -4.556349186104045934, 11.00000000000000000, 99.71875000000000000 ) ) ;
#445 = VERTEX_POINT ( 'NONE', #68875 ) ;
#446 = CARTESIAN_POINT ( 'NONE',  ( -3.458734125000015425, 198.2500000013656347, 143.4326545832176976 ) ) ;
#447 = CARTESIAN_POINT ( 'NONE',  ( -11.35316468750000141, 18.28124999658601624, -1.390361679473963753E-15 ) ) ;
#448 = CARTESIAN_POINT ( 'NONE',  ( 7.778174593052021635, 7.778174593052023411, 92.12500000409677625 ) ) ;
#449 = CARTESIAN_POINT ( 'NONE',  ( -2.839093476692135984E-14, 208.9375000013656063, 138.5412658750000503 ) ) ;
#450 = CARTESIAN_POINT ( 'NONE',  ( -31.45873412499999233, 194.6875000013655779, 170.0000000000004547 ) ) ;
#451 = CARTESIAN_POINT ( 'NONE',  ( 0.000000000000000000, 0.000000000000000000, 0.000000000000000000 ) ) ;
#453 = CARTESIAN_POINT ( 'NONE',  ( -8.311093377946836114, 22.65624999658601979, -8.311093377946837890 ) ) ;
#452 = CARTESIAN_POINT ( 'NONE',  ( -7.188101187499999156, 109.2500000020483952, 2.977408999572654924 ) ) ;
#454 = CARTESIAN_POINT ( 'NONE',  ( 7.999999999999991118, 9.797174393178815797E-16, 22.58030277982336997 ) ) ;
#455 = CARTESIAN_POINT ( 'NONE',  ( 8.311093377946834337, 140.1562499965860127, 8.311093377946839666 ) ) ;
#456 = CARTESIAN_POINT ( 'NONE',  ( 10.00000000000000000, 111.6666666598387110, 2.679491924311236062 ) ) ;
#457 = CARTESIAN_POINT ( 'NONE',  ( 7.188101187500001821, 116.3750000020483810, -2.977408999572651371 ) ) ;
#458 = DIRECTION ( 'NONE',  ( 0.000000000000000000, 0.000000000000000000, -1.000000000000000000 ) ) ;
#459 = CARTESIAN_POINT ( 'NONE',  ( -28.00000000000002487, 209.6875000013656063, 166.5412658750003629 ) ) ;
#460 = AXIS2_PLACEMENT_3D ( 'NONE', #38862, #22233, #61866 ) ;
#461 = CARTESIAN_POINT ( 'NONE',  ( -4.999999999999998224, 53.32026166094924235, -44.27875806161890182 ) ) ;
#462 = ORIENTED_EDGE ( 'NONE', *, *, #68450, .F. ) ;
#463 = CARTESIAN_POINT ( 'NONE',  ( -2.085542519210945728E-15, 4.843749996586016238, 11.35316468750000141 ) ) ;
#464 = CARTESIAN_POINT ( 'NONE',  ( 11.00000000000000000, 1.347111479062088405E-15, 100.7499999999999858 ) ) ;
#465 = CARTESIAN_POINT ( 'NONE',  ( -4.721056650415999201, 297.3281250017069510, -4.721056650415999201 ) ) ;
#466 = CARTESIAN_POINT ( 'NONE',  ( 3.042071309553159519, 134.7395833299193555, 11.35316468750000141 ) ) ;
#467 = CARTESIAN_POINT ( 'NONE',  ( 7.999999999999992895, -3.313708498984756279, 24.04280278432983309 ) ) ;
#468 = CARTESIAN_POINT ( 'NONE',  ( -26.34314575050754570, 198.9375000000000568, 166.0000000000004263 ) ) ;
#469 = CARTESIAN_POINT ( 'NONE',  ( 3.042071309553163960, 252.4479166700806729, -11.35316468749999785 ) ) ;
#470 = CARTESIAN_POINT ( 'NONE',  ( -7.204075437095965206, -7.204075437095968759, 99.71875000204838102 ) ) ;
#471 = VERTEX_POINT ( 'NONE', #17185 ) ;
#472 = EDGE_CURVE ( 'NONE', #10738, #68741, #23593, .T. ) ;
#473 = EDGE_CURVE ( 'NONE', #34245, #9171, #2555, .T. ) ;
#474 = DIRECTION ( 'NONE',  ( -1.000000000000000000, 0.000000000000000000, 0.000000000000000000 ) ) ;
#475 = CARTESIAN_POINT ( 'NONE',  ( 5.000000000000000888, 62.69792629052230382, -24.03557775816830500 ) ) ;
#476 = CARTESIAN_POINT ( 'NONE',  ( -3.042071309553173730, 84.63541666325265567, 11.35316468749999785 ) ) ;
#477 = ORIENTED_EDGE ( 'NONE', *, *, #61037, .F. ) ;
#478 = CARTESIAN_POINT ( 'NONE',  ( -10.18810118749999916, 4.220049686691934809, 109.5625000020483810 ) ) ;
#479 = CARTESIAN_POINT ( 'NONE',  ( -1.881053915767121776, 14.74999999863440969, -4.541265875000002339 ) ) ;
#480 = ORIENTED_EDGE ( 'NONE', *, *, #52569, .F. ) ;
#481 = ORIENTED_EDGE ( 'NONE', *, *, #22346, .T. ) ;
#482 = AXIS2_PLACEMENT_3D ( 'NONE', #15243, #60904, #55265 ) ;
#483 = CARTESIAN_POINT ( 'NONE',  ( -8.000000000000000000, 3.750000000000000888, -9.797174393178825657E-16 ) ) ;
#484 = LINE ( 'NONE', #23464, #58928 ) ;
#485 = CARTESIAN_POINT ( 'NONE',  ( 11.00000000000010836, -4.556349186103939353, 76.84375000409676204 ) ) ;
#486 = CARTESIAN_POINT ( 'NONE',  ( 5.082755093536325930, 26.53124999795161543, -5.082755093536325930 ) ) ;
#487 = CARTESIAN_POINT ( 'NONE',  ( -7.999999999999998224, 120.7812500040967905, 3.313708498984766493 ) ) ;
#488 = CARTESIAN_POINT ( 'NONE',  ( -10.18810118749999916, 0.000000000000000000, 102.5312500020483810 ) ) ;
#489 =( BOUNDED_CURVE ( )  B_SPLINE_CURVE ( 2, ( #5942, #35723, #28941, #1035, #12332, #51960, #24015, #40634, #63634 ),
 .UNSPECIFIED., .F., .F. ) 
 B_SPLINE_CURVE_WITH_KNOTS ( ( 3, 2, 2, 2, 3 ),
 ( 0.5824082574719842142, 0.5890265270166560319, 0.5956448026011128549, 0.6022630781855697890, 0.6088813560782819767 ),
 .UNSPECIFIED. ) 
 CURVE ( )  GEOMETRIC_REPRESENTATION_ITEM ( )  RATIONAL_B_SPLINE_CURVE ( ( 1.000000000000000000, 0.9238795325112867385, 1.000000000000000000, 0.9238795325112867385, 1.000000000000000000, 0.9238795325112867385, 1.000000000000000000, 0.9238795325112867385, 1.000000000000000000 ) ) 
 REPRESENTATION_ITEM ( '' )  );
#490 = CARTESIAN_POINT ( 'NONE',  ( 4.000000000000016875, 204.4375000000000568, 199.6568542494924259 ) ) ;
#491 = CARTESIAN_POINT ( 'NONE',  ( 2.449293598294707893E-16, 11.99999999726881406, -4.000000000000001776 ) ) ;
#492 = CARTESIAN_POINT ( 'NONE',  ( -3.211159895383561391, 1.687499998634406584, -3.211159895383561835 ) ) ;
#493 = VERTEX_POINT ( 'NONE', #52645 ) ;
#494 = CARTESIAN_POINT ( 'NONE',  ( -7.320508075688771932, 262.5000000068279746, -7.320508075688771932 ) ) ;
#495 = CARTESIAN_POINT ( 'NONE',  ( 3.458734125000015425, 199.0000000013656063, 196.5673454167823877 ) ) ;
#496 = CARTESIAN_POINT ( 'NONE',  ( -27.99999999999991829, 203.9375000013656063, 173.4587341250003760 ) ) ;
#497 = CARTESIAN_POINT ( 'NONE',  ( 1.881053915767122664, 12.12499999863440969, 4.541265875000001451 ) ) ;
#498 = AXIS2_PLACEMENT_3D ( 'NONE', #69594, #73760, #22068 ) ;
#499 = CARTESIAN_POINT ( 'NONE',  ( 7.188101187499993827, -2.977408999572645598, 11.14280278187175810 ) ) ;
#500 = ORIENTED_EDGE ( 'NONE', *, *, #41762, .F. ) ;
#501 =( BOUNDED_SURFACE ( )  B_SPLINE_SURFACE ( 3, 2, ( 
 ( #20909, #43929, #9609 ),
 ( #55637, #25068, #36784 ),
 ( #59794, #25441, #71462 ),
 ( #14117, #71837, #20153 ),
 ( #60529, #31864, #51074 ),
 ( #74087, #61658, #15989 ),
 ( #9976, #57120, #62023 ),
 ( #11464, #4321, #45050 ),
 ( #21280, #34498, #27310 ),
 ( #39020, #22386, #50326 ),
 ( #73713, #34119, #16726 ),
 ( #33745, #39752, #3953 ),
 ( #63136, #10347, #68060 ),
 ( #21651, #45407, #17106 ),
 ( #28063, #22764, #33372 ),
 ( #33007, #62387, #56373 ),
 ( #68423, #4693, #56008 ),
 ( #39388, #73347, #26941 ) ),
 .UNSPECIFIED., .F., .F., .T. ) 
 B_SPLINE_SURFACE_WITH_KNOTS ( ( 4, 2, 2, 2, 2, 2, 2, 2, 4 ),
 ( 3, 3 ),
 ( 0.04202945594034800114, 0.04396162471218434398, 0.04589379348402068681, 0.04782596225585702965, 0.04975813102769336554, 0.05169029979952970144, 0.05265638418544787286, 0.05362246857136604428, 0.05748680611503872995 ),
 ( 0.000000000000000000, 1.000000000000000000 ),
 .UNSPECIFIED. ) 
 GEOMETRIC_REPRESENTATION_ITEM ( )  RATIONAL_B_SPLINE_SURFACE ( (
 ( 1.000000000000000000, 0.6241276099607504513, 1.000000000000000000),
 ( 1.000000000000000000, 0.6218761496800027100, 1.000000000000000000),
 ( 1.000000000000000000, 0.6198047272363174098, 1.000000000000000000),
 ( 1.000000000000000000, 0.6161935119824322182, 1.000000000000000000),
 ( 1.000000000000000000, 0.6146642324080623387, 1.000000000000000000),
 ( 1.000000000000000000, 0.6121850116870836134, 1.000000000000000000),
 ( 1.000000000000000000, 0.6112350889398197040, 1.000000000000000000),
 ( 1.000000000000000000, 0.6099522725974151349, 1.000000000000000000),
 ( 1.000000000000000000, 0.6096208180308361202, 1.000000000000000000),
 ( 1.000000000000000000, 0.6096183796348998429, 1.000000000000000000),
 ( 1.000000000000000000, 0.6099422200100823588, 1.000000000000000000),
 ( 1.000000000000000000, 0.6109087447823940975, 1.000000000000000000),
 ( 1.000000000000000000, 0.6113123981688524111, 1.000000000000000000),
 ( 1.000000000000000000, 0.6122677719809250796, 1.000000000000000000),
 ( 1.000000000000000000, 0.6128199619021360567, 1.000000000000000000),
 ( 1.000000000000000000, 0.6159350830264649357, 1.000000000000000000),
 ( 1.000000000000000000, 0.6195556778516543295, 1.000000000000000000),
 ( 1.000000000000000000, 0.6241278272307883013, 1.000000000000000000) ) ) 
 REPRESENTATION_ITEM ( '' )  SURFACE ( )  );
#502 = VERTEX_POINT ( 'NONE', #16429 ) ;
#503 = CARTESIAN_POINT ( 'NONE',  ( -10.18810118749999738, -4.220049686691941915, 111.2500000020483952 ) ) ;
#504 = CARTESIAN_POINT ( 'NONE',  ( -18.00000000000000000, -10.39230484541329247, -1.607695154586745501 ) ) ;
#505 = CARTESIAN_POINT ( 'NONE',  ( -26.34314575050764518, 203.9375000000000000, 166.0000000000003695 ) ) ;
#506 = CARTESIAN_POINT ( 'NONE',  ( -1.432654583217607192, 201.2500000013656063, 194.5412658750000219 ) ) ;
#507 = CARTESIAN_POINT ( 'NONE',  ( 25.55430564589118703, 197.3125000013656063, 172.4456943541087526 ) ) ;
#508 = CARTESIAN_POINT ( 'NONE',  ( 4.999999999999993783, 94.16666666666667140, 8.660254037844390851 ) ) ;
#509 = CARTESIAN_POINT ( 'NONE',  ( -5.656854249492380582, 117.3125000000000000, -5.656854249492380582 ) ) ;
#510 = CARTESIAN_POINT ( 'NONE',  ( 11.35316468750000141, 61.09374999658602690, 0.000000000000000000 ) ) ;
#511 = CARTESIAN_POINT ( 'NONE',  ( 2.765530957081996366, 299.2968750017070079, -6.676582343750003368 ) ) ;
#512 = VERTEX_POINT ( 'NONE', #39465 ) ;
#513 = FACE_OUTER_BOUND ( 'NONE', #13877, .T. ) ;
#514 = CARTESIAN_POINT ( 'NONE',  ( -0.3794862803136856422, -10.12385276104027376, 70.07165850195889334 ) ) ;
#515 = CARTESIAN_POINT ( 'NONE',  ( 3.458734124999959914, 207.3750000013656063, 143.4326545832176976 ) ) ;
#516 = CARTESIAN_POINT ( 'NONE',  ( -8.660254037844390851, 104.7916666598386968, 4.999999999999998224 ) ) ;
#517 = CARTESIAN_POINT ( 'NONE',  ( 27.99999999999996092, 194.4587341250000350, 173.4587341249998929 ) ) ;
#518 = CARTESIAN_POINT ( 'NONE',  ( 7.320508075688771044, 233.1250000000000284, -7.320508075688771932 ) ) ;
#519 = FACE_OUTER_BOUND ( 'NONE', #6926, .T. ) ;
#520 = CARTESIAN_POINT ( 'NONE',  ( 4.556349186104045934, 11.00000000000000000, 117.5312500000000142 ) ) ;
#521 = CARTESIAN_POINT ( 'NONE',  ( -10.00000000000000178, 202.5000000000000000, -1.224646799147353454E-15 ) ) ;
#522 = CARTESIAN_POINT ( 'NONE',  ( 2.977408999572650927, -7.188101187499990274, 12.83030278187175277 ) ) ;
#523 = CARTESIAN_POINT ( 'NONE',  ( -8.311093377946836114, 182.9687499965859843, -8.311093377946837890 ) ) ;
#524 = DIRECTION ( 'NONE',  ( 0.000000000000000000, 0.000000000000000000, -1.000000000000000000 ) ) ;
#526 = CARTESIAN_POINT ( 'NONE',  ( -7.999999999999991118, 0.000000000000000000, 24.83030277982336642 ) ) ;
#525 = CARTESIAN_POINT ( 'NONE',  ( 1.836970198721029589E-15, 229.3750000068279746, 10.00000000000000000 ) ) ;
#527 = ORIENTED_EDGE ( 'NONE', *, *, #13294, .T. ) ;
#528 = VECTOR ( 'NONE', #35232, 1000.000000000000000 ) ;
#529 = CARTESIAN_POINT ( 'NONE',  ( 2.445694354108784108, 209.5625000013656063, 144.4456943541088663 ) ) ;
#530 = CARTESIAN_POINT ( 'NONE',  ( 6.951808397369818766E-16, 37.34374999658601979, -11.35316468750000141 ) ) ;
#531 = CARTESIAN_POINT ( 'NONE',  ( -4.556349186104047710, -10.99999999999999822, 107.9687500040967905 ) ) ;
#532 = CARTESIAN_POINT ( 'NONE',  ( -29.43265458321755546, 204.8750000013656063, 173.4587341250004044 ) ) ;
#533 = CARTESIAN_POINT ( 'NONE',  ( -2.679491924311226292, 123.3333333265053540, -10.00000000000000178 ) ) ;
#535 = CARTESIAN_POINT ( 'NONE',  ( -7.778174593052020747, -7.778174593052023411, 107.8750000040967763 ) ) ;
#534 = FACE_OUTER_BOUND ( 'NONE', #63677, .T. ) ;
#536 = CARTESIAN_POINT ( 'NONE',  ( 2.445694354108782775, 200.5625000013656063, 139.5543056458912190 ) ) ;
#537 = EDGE_CURVE ( 'NONE', #26622, #55859, #33424, .T. ) ;
#538 = CARTESIAN_POINT ( 'NONE',  ( 4.999999999999993783, 81.04166665983871098, 8.660254037844390851 ) ) ;
#539 = CARTESIAN_POINT ( 'NONE',  ( -4.401442555609581635E-16, 96.78125000204838102, -7.188101187500000044 ) ) ;
#540 = CARTESIAN_POINT ( 'NONE',  ( -1.881053915767121554, 13.74999999863440969, -4.541265875000002339 ) ) ;
#541 = CARTESIAN_POINT ( 'NONE',  ( 2.679491924311583784, 216.0416666666667709, -10.00000000000005151 ) ) ;
#542 = CARTESIAN_POINT ( 'NONE',  ( 7.999999999999991118, 9.797174393178815797E-16, 1.580302779823364201 ) ) ;
#543 = CARTESIAN_POINT ( 'NONE',  ( -4.000000000000001776, 4.249999997268813168, -4.898587196589415787E-16 ) ) ;
#544 = ORIENTED_EDGE ( 'NONE', *, *, #25083, .T. ) ;
#545 = VERTEX_POINT ( 'NONE', #46971 ) ;
#546 = CARTESIAN_POINT ( 'NONE',  ( -7.999999999999948486, 3.313708498984799355, 11.23655277982336642 ) ) ;
#547 = CARTESIAN_POINT ( 'NONE',  ( -2.765530957081998586, 297.7968750017069510, 6.676582343750001591 ) ) ;
#548 = CARTESIAN_POINT ( 'NONE',  ( -15.99999999999999645, 15.99999999999999645, 20.00000000000000000 ) ) ;
#549 = CARTESIAN_POINT ( 'NONE',  ( 10.00000000000000178, 42.08333332650537528, -2.679491924311226736 ) ) ;
#550 = CARTESIAN_POINT ( 'NONE',  ( -8.311093377946841443, 158.9062499965860411, 8.311093377946830785 ) ) ;
#551 = CARTESIAN_POINT ( 'NONE',  ( -8.000000000000000000, 6.468749995903221084, -3.313708498984762496 ) ) ;
#552 = CARTESIAN_POINT ( 'NONE',  ( 7.204075437095968759, -7.204075437095966983, 83.21875000204836681 ) ) ;
#553 = CARTESIAN_POINT ( 'NONE',  ( -31.06932850344458785, 194.5499615265469799, 168.2019267050766018 ) ) ;
#554 = CARTESIAN_POINT ( 'NONE',  ( -1.656854249492348607, 202.1875000000000568, 202.0000000000000284 ) ) ;
#555 = DIRECTION ( 'NONE',  ( 0.000000000000000000, 0.000000000000000000, 1.000000000000000000 ) ) ;
#556 = CARTESIAN_POINT ( 'NONE',  ( 4.220049686691941027, -10.18810118749999738, 113.5000000020483810 ) ) ;
#557 = ORIENTED_EDGE ( 'NONE', *, *, #10968, .F. ) ;
#558 = CARTESIAN_POINT ( 'NONE',  ( -1.469576158976823947E-15, 17.43749999590322375, 8.000000000000000000 ) ) ;
#559 = CARTESIAN_POINT ( 'NONE',  ( 23.97073152254042938, 177.5684002068729512, 142.3808650461618868 ) ) ;
#560 = CARTESIAN_POINT ( 'NONE',  ( -3.042071309553163960, 122.5520833299193271, -11.35316468749999963 ) ) ;
#561 = CARTESIAN_POINT ( 'NONE',  ( 3.458734125000015425, 200.0000000013656063, 196.5673454167823877 ) ) ;
#562 = CARTESIAN_POINT ( 'NONE',  ( -1.320432766682874540E-15, 24.46874999795161543, 7.188101187500000044 ) ) ;
#563 = CARTESIAN_POINT ( 'NONE',  ( 1.871523826299183495E-15, -10.18810118749999916, 78.90625000204836681 ) ) ;
#564 = CARTESIAN_POINT ( 'NONE',  ( 11.35316468750000141, 51.09374999658601268, 0.000000000000000000 ) ) ;
#565 = ORIENTED_EDGE ( 'NONE', *, *, #46470, .T. ) ;
#566 = CARTESIAN_POINT ( 'NONE',  ( 10.00000000000000178, 36.87499999317203958, 0.000000000000000000 ) ) ;
#567 = CARTESIAN_POINT ( 'NONE',  ( 1.881053915767122664, 1.249999998634407028, 4.541265875000001451 ) ) ;
#568 = CARTESIAN_POINT ( 'NONE',  ( -3.317071493978878571, 8.008118988124991233, 17.23186528394063188 ) ) ;
#569 = CARTESIAN_POINT ( 'NONE',  ( 3.458734124999959469, 205.7500000013656063, 140.5673454167824161 ) ) ;
#570 = EDGE_CURVE ( 'NONE', #31223, #17827, #41112, .T. ) ;
#571 = ADVANCED_FACE ( 'NONE', ( #36403 ), #25054, .F. ) ;
#572 = CARTESIAN_POINT ( 'NONE',  ( -2.977408999572650039, 17.43749999795161187, -7.188101187500001821 ) ) ;
#573 = CARTESIAN_POINT ( 'NONE',  ( -2.485281374238571761, 295.8750000034140157, -6.000000000000003553 ) ) ;
#574 = CARTESIAN_POINT ( 'NONE',  ( 0.000000000000000000, 0.000000000000000000, 0.000000000000000000 ) ) ;
#575 = CARTESIAN_POINT ( 'NONE',  ( -2.977408999572654480, 4.874999997951610098, 7.188101187499999156 ) ) ;
#576 = CARTESIAN_POINT ( 'NONE',  ( 5.082755093536320601, -5.082755093536318824, 11.04905278187175455 ) ) ;
#577 = CARTESIAN_POINT ( 'NONE',  ( 1.871523826299183495E-15, -10.18810118749999916, 71.03125000204838102 ) ) ;
#578 = CARTESIAN_POINT ( 'NONE',  ( -30.44569435410883429, 205.8125000013656063, 167.5543056458915885 ) ) ;
#579 = CARTESIAN_POINT ( 'NONE',  ( -7.347880794884122694E-16, 15.75000000000000000, 4.000000000000001776 ) ) ;
#580 = CARTESIAN_POINT ( 'NONE',  ( 2.780723358947928197E-16, 18.68749999863440436, -4.541265875000002339 ) ) ;
#581 = UNCERTAINTY_MEASURE_WITH_UNIT (LENGTH_MEASURE( 1.000000000000000082E-05 ), #26051, 'distance_accuracy_value', 'NONE');
#582 = ORIENTED_EDGE ( 'NONE', *, *, #25162, .F. ) ;
#583 = AXIS2_PLACEMENT_3D ( 'NONE', #68483, #27005, #16786 ) ;
#584 = CARTESIAN_POINT ( 'NONE',  ( 1.656854249492405451, 194.4375000027312126, 202.0000000000000284 ) ) ;
#585 = EDGE_CURVE ( 'NONE', #64535, #11426, #41555, .T. ) ;
#586 = CARTESIAN_POINT ( 'NONE',  ( -2.751064625579944321E-14, 207.7500000000000284, 146.0000000000000284 ) ) ;
#587 = CARTESIAN_POINT ( 'NONE',  ( -29.65685424949245785, 201.1875000027312694, 166.0000000000004263 ) ) ;
#588 = CARTESIAN_POINT ( 'NONE',  ( -5.082755093536325930, 116.4687500020483810, -5.082755093536325930 ) ) ;
#589 = CARTESIAN_POINT ( 'NONE',  ( 3.313708498984762496, -7.999999999999989342, 8.986552783920146226 ) ) ;
#590 = ORIENTED_EDGE ( 'NONE', *, *, #3458, .F. ) ;
#591 = CARTESIAN_POINT ( 'NONE',  ( 4.401442555609581635E-16, 15.84374999795161365, -7.188101187500000044 ) ) ;
#592 = ORIENTED_EDGE ( 'NONE', *, *, #73366, .T. ) ;
#593 = CARTESIAN_POINT ( 'NONE',  ( 0.000000000000000000, 0.000000000000000000, 0.000000000000000000 ) ) ;
#594 = CARTESIAN_POINT ( 'NONE',  ( 5.000000000000000000, -10.26105934116143281, -64.40045319026697257 ) ) ;
#595 = CARTESIAN_POINT ( 'NONE',  ( -10.00000000000000000, 47.29166666666667140, -2.679491924311229845 ) ) ;
#596 = CARTESIAN_POINT ( 'NONE',  ( 2.977408999572650039, 98.56250000204838102, -7.188101187500001821 ) ) ;
#597 = CARTESIAN_POINT ( 'NONE',  ( -31.45873412499999944, 208.9375000013656063, 170.0000000000003979 ) ) ;
#598 = CARTESIAN_POINT ( 'NONE',  ( -2.485281374238571761, 299.8125000000000000, -6.000000000000003553 ) ) ;
#599 = VECTOR ( 'NONE', #15894, 1000.000000000000000 ) ;
#601 = CARTESIAN_POINT ( 'NONE',  ( -1.836970198721029983E-15, 195.6249999931720254, 10.00000000000000178 ) ) ;
#600 = CARTESIAN_POINT ( 'NONE',  ( -2.485281374238288432, 288.2500000034140726, 6.000000000000285105 ) ) ;
#602 =( BOUNDED_CURVE ( )  B_SPLINE_CURVE ( 2, ( #25679, #36654, #49451, #55504, #3816, #48698, #59664, #30983, #20021 ),
 .UNSPECIFIED., .F., .F. ) 
 B_SPLINE_CURVE_WITH_KNOTS ( ( 3, 2, 2, 2, 3 ),
 ( 0.1333333333333334425, 0.1416666666666667740, 0.1500000000000001332, 0.1583333333333334925, 0.1666666666666668239 ),
 .UNSPECIFIED. ) 
 CURVE ( )  GEOMETRIC_REPRESENTATION_ITEM ( )  RATIONAL_B_SPLINE_CURVE ( ( 0.9999999999999990008, 0.9238795325112877377, 1.000000000000000000, 0.9238795325112867385, 1.000000000000000000, 0.9238795325112867385, 1.000000000000000000, 0.9238795325112851842, 1.000000000000001554 ) ) 
 REPRESENTATION_ITEM ( '' )  );
#603 = ORIENTED_EDGE ( 'NONE', *, *, #5179, .F. ) ;
#604 = CARTESIAN_POINT ( 'NONE',  ( -9.832129032723415207, 244.3229166700806445, 5.676582343750005144 ) ) ;
#605 = PRODUCT_DEFINITION_SHAPE ( 'NONE', 'NONE',  #74669 ) ;
#606 = CARTESIAN_POINT ( 'NONE',  ( -7.188101187499990274, -2.977408999572651371, 19.95530278187175810 ) ) ;
#607 = AXIS2_PLACEMENT_3D ( 'NONE', #26720, #11985, #40282 ) ;
#608 = CARTESIAN_POINT ( 'NONE',  ( 4.999999999999993783, 90.83333333333332860, -8.660254037844374864 ) ) ;
#609 = CARTESIAN_POINT ( 'NONE',  ( 30.82842712474617031, 206.1250000000000284, 172.8284271247460993 ) ) ;
#610 = CARTESIAN_POINT ( 'NONE',  ( 2.849036369511732440E-14, 198.3750000027312126, 202.0000000000000000 ) ) ;
#611 = LINE ( 'NONE', #23591, #74060 ) ;
#612 = CARTESIAN_POINT ( 'NONE',  ( -2.679491924311225848, 161.4583333333333144, -10.00000000000000178 ) ) ;
#613 = LINE ( 'NONE', #28883, #48986 ) ;
#614 = CARTESIAN_POINT ( 'NONE',  ( -10.99999999999999822, 218.7023502760175973, 0.000000000000000000 ) ) ;
#615 = CARTESIAN_POINT ( 'NONE',  ( 2.775557561562891351E-14, 210.0000000000000284, 198.0000000000000284 ) ) ;
#616 = CARTESIAN_POINT ( 'NONE',  ( 3.042071309553167069, 142.1354166632526415, -11.35316468749999785 ) ) ;
#617 = DIRECTION ( 'NONE',  ( 1.000000000000000000, -0.000000000000000000, -0.000000000000000000 ) ) ;
#618 = DIRECTION ( 'NONE',  ( -0.000000000000000000, -1.000000000000000000, -0.000000000000000000 ) ) ;
#621 = CARTESIAN_POINT ( 'NONE',  ( 2.775557561562891351E-14, 195.0000000000000000, 198.0000000000000284 ) ) ;
#620 = CARTESIAN_POINT ( 'NONE',  ( 1.469576158976823947E-15, 110.3750000000000000, 8.000000000000000000 ) ) ;
#619 = CARTESIAN_POINT ( 'NONE',  ( 29.65685424949240101, 204.4375000000000853, 165.9999999999998863 ) ) ;
#622 = ORIENTED_EDGE ( 'NONE', *, *, #15879, .T. ) ;
#623 = CARTESIAN_POINT ( 'NONE',  ( 5.656854249492378806, 10.31250000000000178, 5.656854249492381470 ) ) ;
#624 = LINE ( 'NONE', #36416, #49421 ) ;
#625 = CARTESIAN_POINT ( 'NONE',  ( 2.445694354108783664, 209.3125000013656063, 144.4456943541088663 ) ) ;
#626 =( BOUNDED_SURFACE ( )  B_SPLINE_SURFACE ( 1, 2, ( 
 ( #14631, #37671, #32007, #26708, #55026, #72743, #65580, #11596, #16491, #33150, #68566, #27829, #33513, #10111, #27083, #33887, #73111, #44442, #56517, #56144, #67454, #4454, #5575, #16117, #45548, #62898, #67824, #21418, #39893, #39155, #40269, #11230, #4832, #74223, #5203, #15749, #34258, #50461, #73476, #63270, #62158, #28575, #61793, #27446, #21784, #38790, #57262, #74599, #16867, #44813, #50839, #57638, #28201, #10481, #73850, #22156, #50095, #34631, #51214, #45184, #22527, #68195, #39529, #62525, #10853, #51581, #56889, #22912, #45924, #68937, #17247, #51968, #23284, #35373, #63645, #46294, #58021, #59115, #69689, #24397, #41752, #46667, #305, #18744, #18002, #19101, #64760, #58384, #53079, #58747, #69315, #13061, #29329, #52338, #42106, #41019, #7425, #40642, #11974, #676, #17624, #36099, #53451, #47404, #35005, #29694, #36464, #7057, #6327, #23662, #64027, #5949, #65117, #12340, #24755, #18374, #30432, #6690, #1771, #1043, #24023, #30065, #52710, #47032, #47765, #28948, #13427, #1413, #70427, #70066, #70786, #41388, #64400, #12699, #35730, #48878, #71512, #14169, #37578, #2869, #31915, #54937, #66237, #20955, #37203, #48506, #49251, #36835, #14914, #8526, #19466, #13790, #71888, #7792, #59480, #60578, #31541, #60955, #43220, #54562, #14540, #59842, #60202, #72268, #54191, #8902, #8156, #66608, #53817, #65860, #32294, #25492, #31164, #25856, #42479, #25118, #20200, #3245, #26233, #2498, #20581, #66988, #43594, #37954, #65495, #9273, #55310, #19835, #3617, #26614, #30796, #72653, #42842, #2126, #49637, #43976, #15288, #48136, #71144, #74502, #62433, #62070, #26991, #4365, #73021, #57163, #10025, #33058, #10396, #10759, #45830, #62802, #27357, #5115, #28482, #5480, #51491, #39434, #50745, #68106, #16398, #22066, #56795, #38324, #55687, #68843, #28106, #45092, #33797, #61329, #39797, #9657, #32677, #73392, #22434, #51120, #56419, #22813, #74132, #50004, #4002 ),
 ( #21332, #44353, #11142, #68471, #45454, #16771, #73759, #56057, #33420, #34164, #61704, #67364, #38703, #15662, #21697, #50374, #44723, #67740, #16035, #39067, #4741, #27734, #58290, #40921, #12240, #29599, #46205, #23930, #40177, #63180, #69593, #11507, #28851, #51873, #24298, #23192, #40546, #34540, #52613, #213, #11876, #35278, #52245, #46571, #6592, #47310, #18277, #69219, #17529, #63551, #18649, #34912, #35635, #69968, #63931, #949, #57921, #6229, #12967, #64303, #29232, #17905, #578, #59021, #46939, #41292, #12607, #58650, #6957, #17156, #57547, #25673, #29967, #52982, #1314, #5855, #41656, #23560, #70335, #64666, #36004, #8334, #31347, #54376, #2685, #48691, #71697, #56239, #37769, #54749, #72839, #66803, #44539, #9468, #15477, #33239, #4553, #67552, #27175, #38515, #26807, #32486, #43405, #15106, #55497, #20391, #3809, #72072, #14356, #55123, #3058, #27547, #49820, #10210, #61517, #38138, #43789, #61138, #20769, #21144, #44168, #26042, #67181, #20016, #43026, #49444, #66049, #8713, #31727, #4187, #49062, #66419, #37386, #9840, #14730, #60767, #32866, #32105, #26418, #55871, #50192, #73212, #9090, #3427, #72462, #21518, #15848, #38883, #61887, #60388, #28299, #50936, #33608, #63362, #11323, #4931, #62623, #56616, #34727, #33988, #45644, #45279, #56983, #74319, #73575, #6037, #68289, #21885, #27927, #10578, #52061, #73948, #51678, #29042, #62999, #5297, #16214, #22251, #62251, #11688, #16586, #39623, #51307, #34356, #397, #40362, #10954, #5668, #57731, #50561, #44914, #28664, #39995, #67921, #24, #22625, #68660, #16970, #39252, #23011, #57356, #46017, #69037, #17340, #14978, #72330, #39126, #15724, #43660, #72714, #20645, #10453, #67051, #27056, #32358, #15351, #32737, #14605, #56486, #55372, #66298, #66672, #26293, #50810, #61013, #56116, #4804, #67426, #38386, #31976, #9338, #3307, #62130, #38014, #3678, #61390, #38767, #73821, #67800, #26677, #10084 ) ),
 .UNSPECIFIED., .F., .F., .F. ) 
 B_SPLINE_SURFACE_WITH_KNOTS ( ( 2, 2 ),
 ( 3, 2, 2, 2, 2, 2, 2, 2, 2, 2, 2, 2, 2, 2, 2, 2, 2, 2, 2, 2, 2, 2, 2, 2, 2, 2, 2, 2, 2, 2, 2, 2, 2, 2, 2, 2, 2, 2, 2, 2, 2, 2, 2, 2, 2, 2, 2, 2, 2, 2, 2, 2, 2, 2, 2, 2, 2, 2, 2, 2, 2, 2, 2, 2, 2, 2, 2, 2, 2, 2, 2, 2, 2, 2, 2, 2, 2, 2, 2, 2, 2, 2, 2, 2, 2, 2, 2, 2, 2, 2, 2, 2, 2, 2, 2, 2, 2, 2, 2, 2, 2, 2, 2, 2, 2, 2, 2, 2, 2, 2, 2, 2, 2, 2, 2, 2, 2, 2, 2, 2, 3 ),
 ( 0.000000000000000000, 1.000000000000000000 ),
 ( 0.000000000000000000, 0.008333333333333333218, 0.01666666666666666644, 0.02500000000000000139, 0.03333333333333333287, 0.04166666666666666435, 0.05000000000000000278, 0.05833333333333333426, 0.06666666666666666574, 0.07499999999999999722, 0.08333333333333332871, 0.09166666666666666019, 0.1000000000000000056, 0.1083333333333333370, 0.1166666666666666685, 0.1250000000000000000, 0.1333333333333333315, 0.1416666666666666630, 0.1499999999999999944, 0.1583333333333333259, 0.1666666666666666574, 0.1749999999999999889, 0.1833333333333333204, 0.1916666666666666796, 0.2000000000000000111, 0.2083333333333333426, 0.2166666666666666741, 0.2250000000000000056, 0.2333333333333333370, 0.2416666666666666685, 0.2500000000000000000, 0.2583333333333333592, 0.2666666666666666630, 0.2750000000000000222, 0.2833333333333333259, 0.2916666666666666852, 0.2999999999999999889, 0.3083333333333333481, 0.3166666666666666519, 0.3250000000000000111, 0.3333333333333333148, 0.3416666666666666741, 0.3499999999999999778, 0.3583333333333333370, 0.3666666666666666408, 0.3750000000000000000, 0.3833333333333333592, 0.3916666666666666630, 0.4000000000000000222, 0.4083333333333333259, 0.4166666666666666852, 0.4249999999999999889, 0.4333333333333333481, 0.4416666666666666519, 0.4500000000000000111, 0.4583333333333333148, 0.4666666666666666741, 0.4749999999999999778, 0.4833333333333333370, 0.4916666666666666408, 0.5000000000000000000, 0.5083333333333333037, 0.5166666666666667185, 0.5250000000000000222, 0.5333333333333333259, 0.5416666666666666297, 0.5500000000000000444, 0.5583333333333333481, 0.5666666666666666519, 0.5749999999999999556, 0.5833333333333333703, 0.5916666666666666741, 0.5999999999999999778, 0.6083333333333332815, 0.6166666666666666963, 0.6250000000000000000, 0.6333333333333333037, 0.6416666666666667185, 0.6500000000000000222, 0.6583333333333333259, 0.6666666666666666297, 0.6750000000000000444, 0.6833333333333333481, 0.6916666666666666519, 0.6999999999999999556, 0.7083333333333333703, 0.7166666666666666741, 0.7249999999999999778, 0.7333333333333332815, 0.7416666666666666963, 0.7500000000000000000, 0.7583333333333333037, 0.7666666666666667185, 0.7750000000000000222, 0.7833333333333333259, 0.7916666666666666297, 0.8000000000000000444, 0.8083333333333333481, 0.8166666666666666519, 0.8249999999999999556, 0.8333333333333333703, 0.8416666666666666741, 0.8499999999999999778, 0.8583333333333332815, 0.8666666666666666963, 0.8750000000000000000, 0.8833333333333333037, 0.8916666666666667185, 0.9000000000000000222, 0.9083333333333333259, 0.9166666666666666297, 0.9250000000000000444, 0.9333333333333333481, 0.9416666666666666519, 0.9499999999999999556, 0.9583333333333333703, 0.9666666666666666741, 0.9749999999999999778, 0.9833333333333332815, 0.9916666666666666963, 1.000000000000000000 ),
 .UNSPECIFIED. ) 
 GEOMETRIC_REPRESENTATION_ITEM ( )  RATIONAL_B_SPLINE_SURFACE ( (
 ( 1.000000000000000000, 0.9238795325112867385, 1.000000000000000000, 0.9238795325112867385, 1.000000000000000000, 0.9238795325112867385, 1.000000000000000000, 0.9238795325112867385, 1.000000000000000000, 0.9238795325112867385, 1.000000000000000000, 0.9238795325112867385, 1.000000000000000000, 0.9238795325112867385, 1.000000000000000000, 0.9238795325112867385, 1.000000000000000000, 0.9238795325112867385, 1.000000000000000000, 0.9238795325112867385, 1.000000000000000000, 0.9238795325112867385, 1.000000000000000000, 0.9238795325112867385, 1.000000000000000000, 0.9238795325112867385, 1.000000000000000000, 0.9238795325112867385, 1.000000000000000000, 0.9238795325112867385, 1.000000000000000000, 0.9238795325112867385, 1.000000000000000000, 0.9238795325112867385, 1.000000000000000000, 0.9238795325112867385, 1.000000000000000000, 0.9238795325112867385, 1.000000000000000000, 0.9238795325112867385, 1.000000000000000000, 0.9238795325112867385, 1.000000000000000000, 0.9238795325112867385, 1.000000000000000000, 0.9238795325112867385, 1.000000000000000000, 0.9238795325112867385, 1.000000000000000000, 0.9238795325112867385, 1.000000000000000000, 0.9238795325112867385, 1.000000000000000000, 0.9238795325112867385, 1.000000000000000000, 0.9238795325112867385, 1.000000000000000000, 0.9238795325112867385, 1.000000000000000000, 0.9238795325112867385, 1.000000000000000000, 0.9238795325112867385, 1.000000000000000000, 0.9238795325112867385, 1.000000000000000000, 0.9238795325112867385, 1.000000000000000000, 0.9238795325112867385, 1.000000000000000000, 0.9238795325112867385, 1.000000000000000000, 0.9238795325112867385, 1.000000000000000000, 0.9238795325112867385, 1.000000000000000000, 0.9238795325112867385, 1.000000000000000000, 0.9238795325112867385, 1.000000000000000000, 0.9238795325112867385, 1.000000000000000000, 0.9238795325112867385, 1.000000000000000000, 0.9238795325112867385, 1.000000000000000000, 0.9238795325112867385, 1.000000000000000000, 0.9238795325112867385, 1.000000000000000000, 0.9238795325112867385, 1.000000000000000000, 0.9238795325112867385, 1.000000000000000000, 0.9238795325112867385, 1.000000000000000000, 0.9238795325112867385, 1.000000000000000000, 0.9238795325112867385, 1.000000000000000000, 0.9238795325112867385, 1.000000000000000000, 0.9238795325112867385, 1.000000000000000000, 0.9238795325112867385, 1.000000000000000000, 0.9238795325112867385, 1.000000000000000000, 0.9238795325112867385, 1.000000000000000000, 0.9238795325112867385, 1.000000000000000000, 0.9238795325112867385, 1.000000000000000000, 0.9238795325112867385, 1.000000000000000000, 0.9238795325112867385, 1.000000000000000000, 0.9238795325112867385, 1.000000000000000000, 0.9238795325112867385, 1.000000000000000000, 0.9238795325112867385, 1.000000000000000000, 0.9238795325112867385, 1.000000000000000000, 0.9238795325112867385, 1.000000000000000000, 0.9238795325112867385, 1.000000000000000000, 0.9238795325112867385, 1.000000000000000000, 0.9238795325112867385, 1.000000000000000000, 0.9238795325112867385, 1.000000000000000000, 0.9238795325112867385, 1.000000000000000000, 0.9238795325112867385, 1.000000000000000000, 0.9238795325112867385, 1.000000000000000000, 0.9238795325112867385, 1.000000000000000000, 0.9238795325112867385, 1.000000000000000000, 0.9238795325112867385, 1.000000000000000000, 0.9238795325112867385, 1.000000000000000000, 0.9238795325112867385, 1.000000000000000000, 0.9238795325112867385, 1.000000000000000000, 0.9238795325112867385, 1.000000000000000000, 0.9238795325112867385, 1.000000000000000000, 0.9238795325112867385, 1.000000000000000000, 0.9238795325112867385, 1.000000000000000000, 0.9238795325112867385, 1.000000000000000000, 0.9238795325112867385, 1.000000000000000000, 0.9238795325112867385, 1.000000000000000000, 0.9238795325112867385, 1.000000000000000000, 0.9238795325112867385, 1.000000000000000000, 0.9238795325112867385, 1.000000000000000000, 0.9238795325112867385, 1.000000000000000000, 0.9238795325112867385, 1.000000000000000000, 0.9238795325112867385, 1.000000000000000000, 0.9238795325112867385, 1.000000000000000000, 0.9238795325112867385, 1.000000000000000000, 0.9238795325112867385, 1.000000000000000000, 0.9238795325112867385, 1.000000000000000000, 0.9238795325112867385, 1.000000000000000000, 0.9238795325112867385, 1.000000000000000000, 0.9238795325112867385, 1.000000000000000000, 0.9238795325112867385, 1.000000000000000000, 0.9238795325112867385, 1.000000000000000000, 0.9238795325112867385, 1.000000000000000000, 0.9238795325112867385, 1.000000000000000000, 0.9238795325112867385, 1.000000000000000000, 0.9238795325112867385, 1.000000000000000000, 0.9238795325112867385, 1.000000000000000000, 0.9238795325112867385, 1.000000000000000000, 0.9238795325112867385, 1.000000000000000000, 0.9238795325112867385, 1.000000000000000000, 0.9238795325112867385, 1.000000000000000000, 0.9238795325112867385, 1.000000000000000000, 0.9238795325112867385, 1.000000000000000000, 0.9238795325112867385, 1.000000000000000000, 0.9238795325112867385, 1.000000000000000000, 0.9238795325112867385, 1.000000000000000000, 0.9238795325112867385, 1.000000000000000000, 0.9238795325112867385, 1.000000000000000000, 0.9238795325112867385, 1.000000000000000000, 0.9238795325112867385, 1.000000000000000000, 0.9238795325112867385, 1.000000000000000000, 0.9238795325112867385, 1.000000000000000000, 0.9238795325112867385, 1.000000000000000000, 0.9238795325112867385, 1.000000000000000000),
 ( 1.000000000000000000, 0.9238795325112867385, 1.000000000000000000, 0.9238795325112867385, 1.000000000000000000, 0.9238795325112867385, 1.000000000000000000, 0.9238795325112867385, 1.000000000000000000, 0.9238795325112867385, 1.000000000000000000, 0.9238795325112867385, 1.000000000000000000, 0.9238795325112867385, 1.000000000000000000, 0.9238795325112867385, 1.000000000000000000, 0.9238795325112867385, 1.000000000000000000, 0.9238795325112867385, 1.000000000000000000, 0.9238795325112867385, 1.000000000000000000, 0.9238795325112867385, 1.000000000000000000, 0.9238795325112867385, 1.000000000000000000, 0.9238795325112867385, 1.000000000000000000, 0.9238795325112867385, 1.000000000000000000, 0.9238795325112867385, 1.000000000000000000, 0.9238795325112867385, 1.000000000000000000, 0.9238795325112867385, 1.000000000000000000, 0.9238795325112867385, 1.000000000000000000, 0.9238795325112867385, 1.000000000000000000, 0.9238795325112867385, 1.000000000000000000, 0.9238795325112867385, 1.000000000000000000, 0.9238795325112867385, 1.000000000000000000, 0.9238795325112867385, 1.000000000000000000, 0.9238795325112867385, 1.000000000000000000, 0.9238795325112867385, 1.000000000000000000, 0.9238795325112867385, 1.000000000000000000, 0.9238795325112867385, 1.000000000000000000, 0.9238795325112867385, 1.000000000000000000, 0.9238795325112867385, 1.000000000000000000, 0.9238795325112867385, 1.000000000000000000, 0.9238795325112867385, 1.000000000000000000, 0.9238795325112867385, 1.000000000000000000, 0.9238795325112867385, 1.000000000000000000, 0.9238795325112867385, 1.000000000000000000, 0.9238795325112867385, 1.000000000000000000, 0.9238795325112867385, 1.000000000000000000, 0.9238795325112867385, 1.000000000000000000, 0.9238795325112867385, 1.000000000000000000, 0.9238795325112867385, 1.000000000000000000, 0.9238795325112867385, 1.000000000000000000, 0.9238795325112867385, 1.000000000000000000, 0.9238795325112867385, 1.000000000000000000, 0.9238795325112867385, 1.000000000000000000, 0.9238795325112867385, 1.000000000000000000, 0.9238795325112867385, 1.000000000000000000, 0.9238795325112867385, 1.000000000000000000, 0.9238795325112867385, 1.000000000000000000, 0.9238795325112867385, 1.000000000000000000, 0.9238795325112867385, 1.000000000000000000, 0.9238795325112867385, 1.000000000000000000, 0.9238795325112867385, 1.000000000000000000, 0.9238795325112867385, 1.000000000000000000, 0.9238795325112867385, 1.000000000000000000, 0.9238795325112867385, 1.000000000000000000, 0.9238795325112867385, 1.000000000000000000, 0.9238795325112867385, 1.000000000000000000, 0.9238795325112867385, 1.000000000000000000, 0.9238795325112867385, 1.000000000000000000, 0.9238795325112867385, 1.000000000000000000, 0.9238795325112867385, 1.000000000000000000, 0.9238795325112867385, 1.000000000000000000, 0.9238795325112867385, 1.000000000000000000, 0.9238795325112867385, 1.000000000000000000, 0.9238795325112867385, 1.000000000000000000, 0.9238795325112867385, 1.000000000000000000, 0.9238795325112867385, 1.000000000000000000, 0.9238795325112867385, 1.000000000000000000, 0.9238795325112867385, 1.000000000000000000, 0.9238795325112867385, 1.000000000000000000, 0.9238795325112867385, 1.000000000000000000, 0.9238795325112867385, 1.000000000000000000, 0.9238795325112867385, 1.000000000000000000, 0.9238795325112867385, 1.000000000000000000, 0.9238795325112867385, 1.000000000000000000, 0.9238795325112867385, 1.000000000000000000, 0.9238795325112867385, 1.000000000000000000, 0.9238795325112867385, 1.000000000000000000, 0.9238795325112867385, 1.000000000000000000, 0.9238795325112867385, 1.000000000000000000, 0.9238795325112867385, 1.000000000000000000, 0.9238795325112867385, 1.000000000000000000, 0.9238795325112867385, 1.000000000000000000, 0.9238795325112867385, 1.000000000000000000, 0.9238795325112867385, 1.000000000000000000, 0.9238795325112867385, 1.000000000000000000, 0.9238795325112867385, 1.000000000000000000, 0.9238795325112867385, 1.000000000000000000, 0.9238795325112867385, 1.000000000000000000, 0.9238795325112867385, 1.000000000000000000, 0.9238795325112867385, 1.000000000000000000, 0.9238795325112867385, 1.000000000000000000, 0.9238795325112867385, 1.000000000000000000, 0.9238795325112867385, 1.000000000000000000, 0.9238795325112867385, 1.000000000000000000, 0.9238795325112867385, 1.000000000000000000, 0.9238795325112867385, 1.000000000000000000, 0.9238795325112867385, 1.000000000000000000, 0.9238795325112867385, 1.000000000000000000, 0.9238795325112867385, 1.000000000000000000, 0.9238795325112867385, 1.000000000000000000, 0.9238795325112867385, 1.000000000000000000, 0.9238795325112867385, 1.000000000000000000, 0.9238795325112867385, 1.000000000000000000, 0.9238795325112867385, 1.000000000000000000, 0.9238795325112867385, 1.000000000000000000, 0.9238795325112867385, 1.000000000000000000, 0.9238795325112867385, 1.000000000000000000, 0.9238795325112867385, 1.000000000000000000, 0.9238795325112867385, 1.000000000000000000, 0.9238795325112867385, 1.000000000000000000, 0.9238795325112867385, 1.000000000000000000, 0.9238795325112867385, 1.000000000000000000, 0.9238795325112867385, 1.000000000000000000, 0.9238795325112867385, 1.000000000000000000, 0.9238795325112867385, 1.000000000000000000, 0.9238795325112867385, 1.000000000000000000, 0.9238795325112867385, 1.000000000000000000, 0.9238795325112867385, 1.000000000000000000, 0.9238795325112867385, 1.000000000000000000) ) ) 
 REPRESENTATION_ITEM ( '' )  SURFACE ( )  );
#627 = CARTESIAN_POINT ( 'NONE',  ( 29.43265458321766204, 195.1250000013656063, 166.5412658749999650 ) ) ;
#628 = CARTESIAN_POINT ( 'NONE',  ( 6.123233995736767268E-16, 18.12499999317203248, -10.00000000000000178 ) ) ;
#629 = CARTESIAN_POINT ( 'NONE',  ( -7.188101187500001821, 118.0625000020483952, -2.977408999572650483 ) ) ;
#630 = CARTESIAN_POINT ( 'NONE',  ( 4.541265875000001451, 1.374999998634407250, 1.881053915767124440 ) ) ;
#631 = CARTESIAN_POINT ( 'NONE',  ( -4.336811714532579742, -52.00708776949259260, 48.85034107299725292 ) ) ;
#632 = CARTESIAN_POINT ( 'NONE',  ( -4.898587196589407898E-16, 7.999999999999991118, 19.95530277982336642 ) ) ;
#634 = CARTESIAN_POINT ( 'NONE',  ( 0.000000000000000000, 0.000000000000000000, 0.000000000000000000 ) ) ;
#633 = CARTESIAN_POINT ( 'NONE',  ( -2.250000000000000888, -2.250000000000000000, 28.00000000000000000 ) ) ;
#635 = CARTESIAN_POINT ( 'NONE',  ( -8.311093377946841443, 108.9062499965860127, 8.311093377946830785 ) ) ;
#636 = ORIENTED_EDGE ( 'NONE', *, *, #73110, .F. ) ;
#637 = FACE_OUTER_BOUND ( 'NONE', #19104, .T. ) ;
#638 = CARTESIAN_POINT ( 'NONE',  ( -5.000000000000000000, 16.24494643555759410, 69.83755725260752456 ) ) ;
#639 = DIRECTION ( 'NONE',  ( -1.000000000000000000, -0.000000000000000000, -0.000000000000000000 ) ) ;
#640 = CARTESIAN_POINT ( 'NONE',  ( -5.676582343749992710, 245.0520833367473301, 9.832129032723422313 ) ) ;
#641 = CARTESIAN_POINT ( 'NONE',  ( -5.676582343750006032, 109.1145833299193555, 9.832129032723418760 ) ) ;
#642 = ORIENTED_EDGE ( 'NONE', *, *, #30933, .T. ) ;
#643 = EDGE_CURVE ( 'NONE', #25993, #13507, #1348, .T. ) ;
#644 = CARTESIAN_POINT ( 'NONE',  ( 10.18810118749999916, 1.247682550866122264E-15, 101.4062500020483810 ) ) ;
#645 = CARTESIAN_POINT ( 'NONE',  ( -2.679491924311225848, 223.3333333265053398, -10.00000000000000178 ) ) ;
#646 = CARTESIAN_POINT ( 'NONE',  ( 2.445694354108839175, 200.3125000013656063, 195.5543056458912190 ) ) ;
#647 = LINE ( 'NONE', #58717, #5863 ) ;
#649 = CARTESIAN_POINT ( 'NONE',  ( 9.832129032723416984, 105.3645833299193555, 5.676582343750006032 ) ) ;
#648 = CARTESIAN_POINT ( 'NONE',  ( -2.679491924310645423, 183.5416666666667425, 10.00000000000033573 ) ) ;
#650 = CARTESIAN_POINT ( 'NONE',  ( -3.313708498984757167, 7.999999999999991118, 5.236552783920145338 ) ) ;
#651 = CARTESIAN_POINT ( 'NONE',  ( -26.56734541678237704, 195.6250000013656063, 166.5412658750003629 ) ) ;
#652 = CARTESIAN_POINT ( 'NONE',  ( -3.166186134455097228E-13, 171.2500000000000284, -9.999999999999998224 ) ) ;
#653 = VERTEX_POINT ( 'NONE', #71083 ) ;
#654 = CARTESIAN_POINT ( 'NONE',  ( -4.999999999999998224, 198.5416666598387110, -8.660254037844389075 ) ) ;
#655 = CARTESIAN_POINT ( 'NONE',  ( 28.00000000000002132, 201.1250000027312126, 173.9999999999999147 ) ) ;
#656 = CARTESIAN_POINT ( 'NONE',  ( 10.99999999999989342, 4.556349186104152515, 99.53125000409680467 ) ) ;
#657 = CARTESIAN_POINT ( 'NONE',  ( -5.676582343750006032, 94.42708332991935549, 9.832129032723418760 ) ) ;
#658 = CARTESIAN_POINT ( 'NONE',  ( 4.898587196589415787E-16, 0.000000000000000000, 4.000000000000001776 ) ) ;
#659 = CARTESIAN_POINT ( 'NONE',  ( 5.082755093536325930, 8.531249997951611874, -5.082755093536325930 ) ) ;
#661 = CARTESIAN_POINT ( 'NONE',  ( -4.220049686691935698, 10.18810118749999916, 93.25000000204838102 ) ) ;
#660 = B_SPLINE_CURVE_WITH_KNOTS ( 'NONE', 3,
 ( #33434, #4754, #74144, #61716, #22080, #21344, #10036, #57179, #33072, #68119, #44364, #4014, #26626, #62818, #16413, #27370, #67377, #56068, #50389, #72664, #62445, #73405 ),
 .UNSPECIFIED., .F., .F.,
 ( 4, 2, 2, 2, 2, 2, 2, 2, 2, 2, 4 ),
 ( 0.000000000000000000, 0.001156727053362476953, 0.001735090580043700901, 0.002313454106724924849, 0.003470181160087385322, 0.004048544686768620546, 0.004626908213449854902, 0.005783635266812324482, 0.006940362320174794063, 0.008097089373537263643, 0.009253816426899734091 ),
 .UNSPECIFIED. ) ;
#662 = CARTESIAN_POINT ( 'NONE',  ( 6.951808397369818766E-16, 222.0312499965860127, -11.35316468750000141 ) ) ;
#663 = VERTEX_POINT ( 'NONE', #70001 ) ;
#664 = DIRECTION ( 'NONE',  ( -1.000000000000000000, 0.000000000000000000, 0.000000000000000000 ) ) ;
#665 = DIRECTION ( 'NONE',  ( 1.000000000000000000, -0.000000000000000000, 0.000000000000000000 ) ) ;
#666 = CARTESIAN_POINT ( 'NONE',  ( 3.042071309553159519, 214.7395833299193555, 11.35316468750000141 ) ) ;
#667 = CARTESIAN_POINT ( 'NONE',  ( -4.220049686691937474, -10.18810118749999738, 77.31250000204836681 ) ) ;
#668 = EDGE_CURVE ( 'NONE', #30116, #59754, #15135, .T. ) ;
#669 = CARTESIAN_POINT ( 'NONE',  ( 7.320508075688774596, 47.49999999317203958, -7.320508075688774596 ) ) ;
#670 = CARTESIAN_POINT ( 'NONE',  ( 1.836970198721029589E-15, 241.2500000000000284, 10.00000000000000000 ) ) ;
#671 = CARTESIAN_POINT ( 'NONE',  ( -6.676582343750001591, 296.4531250017069510, 0.000000000000000000 ) ) ;
#672 = EDGE_LOOP ( 'NONE', ( #69972, #67314, #71784, #73672 ) ) ;
#673 = CARTESIAN_POINT ( 'NONE',  ( -2.160335347077957380, -51.35526406371566566, -48.59969451235782856 ) ) ;
#674 = CARTESIAN_POINT ( 'NONE',  ( -11.35316468749999785, 203.3854166632526983, -3.042071309553167957 ) ) ;
#675 = CARTESIAN_POINT ( 'NONE',  ( 7.204075437095966983, 7.204075437095967871, 89.59375000204838102 ) ) ;
#676 = CARTESIAN_POINT ( 'NONE',  ( -24.54126587500000056, 203.2500000013656063, 168.5673454167827003 ) ) ;
#677 = CARTESIAN_POINT ( 'NONE',  ( -3.313708498984765161, 16.03125000000000355, 7.999999999999998224 ) ) ;
#678 = ORIENTED_EDGE ( 'NONE', *, *, #60948, .F. ) ;
#679 = CARTESIAN_POINT ( 'NONE',  ( -2.977408999572651815, 121.4375000020483668, 7.188101187500000933 ) ) ;
#680 = LINE ( 'NONE', #62903, #65729 ) ;
#681 = ADVANCED_FACE ( 'NONE', ( #981 ), #70368, .T. ) ;
#682 = CARTESIAN_POINT ( 'NONE',  ( -7.320508075688778149, 33.12500000000000000, 7.320508075688769267 ) ) ;
#683 = EDGE_CURVE ( 'NONE', #64551, #25226, #40143, .T. ) ;
#684 = FACE_OUTER_BOUND ( 'NONE', #68235, .T. ) ;
#685 = CARTESIAN_POINT ( 'NONE',  ( -7.204075437095965206, -7.204075437095968759, 75.71875000204836681 ) ) ;
#686 = ORIENTED_EDGE ( 'NONE', *, *, #62121, .F. ) ;
#687 = CARTESIAN_POINT ( 'NONE',  ( -1.320432766682874540E-15, 1.593749997951610098, 7.188101187500000044 ) ) ;
#688 = ADVANCED_FACE ( 'NONE', ( #24331 ), #48445, .F. ) ;
#689 = CARTESIAN_POINT ( 'NONE',  ( -4.556349186104048599, -10.99999999999999822, 112.2812500000000000 ) ) ;
#690 = ADVANCED_FACE ( 'NONE', ( #59416 ), #70723, .F. ) ;
#691 = CARTESIAN_POINT ( 'NONE',  ( 2.977408999572650039, 124.0625000020483810, -7.188101187500001821 ) ) ;
#692 = CARTESIAN_POINT ( 'NONE',  ( 1.469576158976823947E-15, 101.5625000040967763, 8.000000000000000000 ) ) ;
#693 = CARTESIAN_POINT ( 'NONE',  ( -6.676582343750001591, 297.4531250017069510, 0.000000000000000000 ) ) ;
#695 = CARTESIAN_POINT ( 'NONE',  ( -27.99999999999999645, 195.0000000000000000, 170.0000000000003695 ) ) ;
#694 = CARTESIAN_POINT ( 'NONE',  ( -6.951808397369817780E-16, 232.6562500034139873, -11.35316468749999963 ) ) ;
#696 = ORIENTED_EDGE ( 'NONE', *, *, #25087, .F. ) ;
#697 = CARTESIAN_POINT ( 'NONE',  ( -9.832129032723418760, 238.8020833367473301, -5.676582343749998927 ) ) ;
#698 = ADVANCED_FACE ( 'NONE', ( #64702 ), #56549, .F. ) ;
#699 = CARTESIAN_POINT ( 'NONE',  ( -2.977408999572647819, 7.188101187499991163, 5.705302781871753659 ) ) ;
#700 = EDGE_LOOP ( 'NONE', ( #13343, #47684, #31600, #1250 ) ) ;
#701 = CARTESIAN_POINT ( 'NONE',  ( 7.204075437095968759, -7.204075437095966983, 68.21875000204836681 ) ) ;
#702 = CARTESIAN_POINT ( 'NONE',  ( -9.832129032723418760, 88.17708332991934128, -5.676582343750004256 ) ) ;
#703 = DIRECTION ( 'NONE',  ( 1.000000000000000000, 0.000000000000000000, 0.000000000000000000 ) ) ;
#704 = CARTESIAN_POINT ( 'NONE',  ( -6.735557395310442023E-16, 11.00000000000000000, 84.62499999999997158 ) ) ;
#707 = CARTESIAN_POINT ( 'NONE',  ( -6.676582343750001591, 287.6093750017069510, 0.000000000000000000 ) ) ;
#706 = CARTESIAN_POINT ( 'NONE',  ( 24.54126587499999701, 209.1875000013656063, 169.9999999999999432 ) ) ;
#705 = CARTESIAN_POINT ( 'NONE',  ( 25.55430564589119768, 207.3125000013656063, 167.5543056458910485 ) ) ;
#708 = ORIENTED_EDGE ( 'NONE', *, *, #37558, .F. ) ;
#709 = CARTESIAN_POINT ( 'NONE',  ( -25.17157287525373732, 195.7500000027312126, 172.8284271247464972 ) ) ;
#710 = CARTESIAN_POINT ( 'NONE',  ( -37.94562015984925551, 146.0000000000000000, 127.0000000000000000 ) ) ;
#711 = CONICAL_SURFACE ( 'NONE', #72949, 8.999999999999998224, 1.047197551196595855 ) ;
#712 = CARTESIAN_POINT ( 'NONE',  ( 11.35316468749999963, 200.9895833299193839, -3.042071309553165293 ) ) ;
#713 = CARTESIAN_POINT ( 'NONE',  ( 3.458734124999959025, 205.5000000013655779, 140.5673454167824161 ) ) ;
#714 = CARTESIAN_POINT ( 'NONE',  ( 24.54126587499998280, 205.5000000013655779, 171.4326545832175555 ) ) ;
#715 = CARTESIAN_POINT ( 'NONE',  ( -7.188101187500002709, 21.18749999795161187, 2.977408999572649151 ) ) ;
#716 = CARTESIAN_POINT ( 'NONE',  ( -11.35316468749999785, 183.3854166632526699, -3.042071309553167513 ) ) ;
#717 = CARTESIAN_POINT ( 'NONE',  ( 7.188101187500002709, 99.68750000204838102, 2.977408999572649151 ) ) ;
#719 = CARTESIAN_POINT ( 'NONE',  ( 1.656854249492381914, 9.812500000000000000, 4.000000000000000888 ) ) ;
#718 = DIRECTION ( 'NONE',  ( 1.000000000000000000, 0.000000000000000000, 0.000000000000000000 ) ) ;
#720 = CARTESIAN_POINT ( 'NONE',  ( -1.881053915767121554, 10.62499999863440792, -4.541265875000002339 ) ) ;
#721 = CARTESIAN_POINT ( 'NONE',  ( 24.54126587500000412, 203.3750000013656063, 168.5673454167822172 ) ) ;
#722 = AXIS2_PLACEMENT_3D ( 'NONE', #11419, #28762, #52161 ) ;
#723 = CARTESIAN_POINT ( 'NONE',  ( 7.188101187499993827, -2.977408999572645598, 10.01780278187175632 ) ) ;
#724 = CARTESIAN_POINT ( 'NONE',  ( -11.35316468749999785, 68.07291666325266988, -3.042071309553167513 ) ) ;
#725 =( BOUNDED_CURVE ( )  B_SPLINE_CURVE ( 2, ( #40249, #284, #10464, #63251, #46275, #74203, #63623, #11953, #68176 ),
 .UNSPECIFIED., .F., .F. ) 
 B_SPLINE_CURVE_WITH_KNOTS ( ( 3, 2, 2, 2, 3 ),
 ( 0.2604166666666664631, 0.2656249999999997780, 0.2708333333333330928, 0.2760416666666664631, 0.2812499999999997780 ),
 .UNSPECIFIED. ) 
 CURVE ( )  GEOMETRIC_REPRESENTATION_ITEM ( )  RATIONAL_B_SPLINE_CURVE ( ( 1.000000000000003331, 0.9238795325112835188, 1.000000000000000000, 0.9238795325112867385, 1.000000000000000000, 0.9238795325112867385, 1.000000000000000000, 0.9238795325112899581, 0.9999999999999967804 ) ) 
 REPRESENTATION_ITEM ( '' )  );
#726 = CARTESIAN_POINT ( 'NONE',  ( 26.34314575050762031, 205.6875000027312126, 165.9999999999998579 ) ) ;
#727 = CARTESIAN_POINT ( 'NONE',  ( -5.656854249492373476, -5.656854249492376141, 1.074052784329823984 ) ) ;
#728 = VERTEX_POINT ( 'NONE', #11183 ) ;
#729 = CARTESIAN_POINT ( 'NONE',  ( 6.000000000000023093, 10.39230484541324984, 0.000000000000000000 ) ) ;
#730 = CARTESIAN_POINT ( 'NONE',  ( 7.778174593052023411, -7.778174593052021635, 117.0625000000000000 ) ) ;
#731 = CARTESIAN_POINT ( 'NONE',  ( 9.832129032723416984, 75.36458332991935549, 5.676582343750006032 ) ) ;
#732 = CARTESIAN_POINT ( 'NONE',  ( 4.556349186104045934, 11.00000000000000000, 68.21875000409676204 ) ) ;
#733 = CARTESIAN_POINT ( 'NONE',  ( -1.432654583217664701, 198.0000000013656063, 138.5412658750000787 ) ) ;
#734 = CARTESIAN_POINT ( 'NONE',  ( 4.898587196589412829E-16, 25.68749999590322375, -8.000000000000000000 ) ) ;
#736 = CARTESIAN_POINT ( 'NONE',  ( 5.676582343750001591, 56.61458332991934839, -9.832129032723420536 ) ) ;
#735 = CARTESIAN_POINT ( 'NONE',  ( -5.082755093536324154, 89.84375000204839523, 5.082755093536326818 ) ) ;
#737 = CARTESIAN_POINT ( 'NONE',  ( 3.313708498984762496, -7.999999999999989342, 22.48655278392014623 ) ) ;
#738 = DIRECTION ( 'NONE',  ( 0.000000000000000000, 0.2588190451025140781, -0.9659258262890700886 ) ) ;
#739 = CARTESIAN_POINT ( 'NONE',  ( -1.836970198721029983E-15, 150.6249999931720538, 10.00000000000000178 ) ) ;
#740 = CARTESIAN_POINT ( 'NONE',  ( -7.188101187500001821, 98.93750000204838102, -2.977408999572650483 ) ) ;
#741 = LINE ( 'NONE', #18067, #38801 ) ;
#742 = CARTESIAN_POINT ( 'NONE',  ( -5.676582343750006032, 54.42708332991935549, 9.832129032723418760 ) ) ;
#743 = EDGE_CURVE ( 'NONE', #22266, #8905, #71825, .T. ) ;
#744 = CARTESIAN_POINT ( 'NONE',  ( -4.220049686691937474, -10.18810118749999738, 111.8125000020483952 ) ) ;
#745 = CARTESIAN_POINT ( 'NONE',  ( -5.676582343749998039, 177.4479166632526983, -9.832129032723420536 ) ) ;
#746 = VERTEX_POINT ( 'NONE', #28151 ) ;
#747 = CARTESIAN_POINT ( 'NONE',  ( 3.223881452106005518, 60.47365957010377002, 23.05198836891398528 ) ) ;
#748 = CARTESIAN_POINT ( 'NONE',  ( 1.871523826299183495E-15, -10.18810118749999916, 68.03125000204838102 ) ) ;
#749 = DIRECTION ( 'NONE',  ( -0.000000000000000000, 1.000000000000000000, 4.476705744456276341E-16 ) ) ;
#751 = CARTESIAN_POINT ( 'NONE',  ( -3.042071309553173730, 179.3229166632526699, 11.35316468749999785 ) ) ;
#750 = CARTESIAN_POINT ( 'NONE',  ( -14.00000000000000178, 0.000000000000000000, 0.000000000000000000 ) ) ;
#752 = CARTESIAN_POINT ( 'NONE',  ( -5.656854249492381470, 11.24999999590322197, 5.656854249492379694 ) ) ;
#753 = CARTESIAN_POINT ( 'NONE',  ( 10.00000000000000178, 250.4166666734946887, 2.679491924311222739 ) ) ;
#754 = FACE_OUTER_BOUND ( 'NONE', #36560, .T. ) ;
#755 = ORIENTED_EDGE ( 'NONE', *, *, #38449, .F. ) ;
#756 = CARTESIAN_POINT ( 'NONE',  ( 11.35316468749999785, 170.8854166632526983, 3.042071309553174174 ) ) ;
#757 = EDGE_CURVE ( 'NONE', #39246, #4559, #64250, .T. ) ;
#758 = CARTESIAN_POINT ( 'NONE',  ( -7.188101187499990274, -2.977408999572651815, 25.58030278187175455 ) ) ;
#759 = CARTESIAN_POINT ( 'NONE',  ( 11.35316468750000141, 126.0937499965860127, 0.000000000000000000 ) ) ;
#760 = DIRECTION ( 'NONE',  ( 1.000000000000000000, 0.000000000000000000, 0.000000000000000000 ) ) ;
#761 = EDGE_LOOP ( 'NONE', ( #29482, #20834, #25330, #23440, #49814, #57819 ) ) ;
#762 = VECTOR ( 'NONE', #41647, 1000.000000000000000 ) ;
#763 = CARTESIAN_POINT ( 'NONE',  ( -5.656854249492378806, 105.8750000040967763, 5.656854249492381470 ) ) ;
#764 = EDGE_CURVE ( 'NONE', #68433, #34625, #61728, .T. ) ;
#765 = EDGE_CURVE ( 'NONE', #10294, #72478, #11549, .T. ) ;
#766 = CARTESIAN_POINT ( 'NONE',  ( -4.000000000000002665, 12.56250000000000000, 1.656854249492380804 ) ) ;
#767 = LINE ( 'NONE', #12059, #60085 ) ;
#768 = CARTESIAN_POINT ( 'NONE',  ( 3.211159895383560947, 12.18749999863440614, 3.211159895383562723 ) ) ;
#769 = CARTESIAN_POINT ( 'NONE',  ( -7.999999999999991118, 3.313708498984756723, 18.92405278392014978 ) ) ;
#770 = DIRECTION ( 'NONE',  ( -0.000000000000000000, -0.000000000000000000, 1.000000000000000000 ) ) ;
#771 = ORIENTED_EDGE ( 'NONE', *, *, #45418, .F. ) ;
#772 = DIRECTION ( 'NONE',  ( 0.000000000000000000, 0.000000000000000000, 1.000000000000000000 ) ) ;
#773 = CARTESIAN_POINT ( 'NONE',  ( 5.082755093536325042, 107.0937500020483810, -5.082755093536325930 ) ) ;
#775 = CARTESIAN_POINT ( 'NONE',  ( -1.656854249492418107, 209.3125000000000000, 138.0000000000000568 ) ) ;
#774 = CARTESIAN_POINT ( 'NONE',  ( -29.43265458321755546, 194.8750000013656063, 173.4587341250004044 ) ) ;
#776 = CARTESIAN_POINT ( 'NONE',  ( 1393.688200795887042, 596.9677537767821605, 1032.842160456058991 ) ) ;
#777 = ORIENTED_EDGE ( 'NONE', *, *, #6709, .F. ) ;
#779 = AXIS2_PLACEMENT_3D ( 'NONE', #50257, #71768, #60455 ) ;
#778 = CARTESIAN_POINT ( 'NONE',  ( 4.336811714531698669, 16.30209246799961065, -69.46462972172668060 ) ) ;
#780 = CARTESIAN_POINT ( 'NONE',  ( 7.188101187499992051, 8.802885111219154394E-16, 21.73655278187175455 ) ) ;
#781 = ORIENTED_EDGE ( 'NONE', *, *, #3044, .F. ) ;
#782 = EDGE_CURVE ( 'NONE', #49563, #64433, #74386, .T. ) ;
#783 = VERTEX_POINT ( 'NONE', #47718 ) ;
#784 = CARTESIAN_POINT ( 'NONE',  ( 4.220049686691934809, 10.18810118749999916, 86.68750000204838102 ) ) ;
#785 = CARTESIAN_POINT ( 'NONE',  ( -1.469576158976823947E-15, 2.625000000000000444, 8.000000000000000000 ) ) ;
#786 = CARTESIAN_POINT ( 'NONE',  ( -31.45873412499999944, 195.8750000013655779, 168.5673454167827572 ) ) ;
#787 = CARTESIAN_POINT ( 'NONE',  ( -7.778174593052023411, 7.778174593052023411, 102.8124999999999858 ) ) ;
#790 = CARTESIAN_POINT ( 'NONE',  ( -4.721056650415999201, 298.4843750017070079, -4.721056650415999201 ) ) ;
#789 = CARTESIAN_POINT ( 'NONE',  ( 28.00000000000002132, 205.1250000027312126, 173.9999999999999147 ) ) ;
#788 = DIRECTION ( 'NONE',  ( -0.000000000000000000, 1.000000000000000000, -0.000000000000000000 ) ) ;
#791 = CARTESIAN_POINT ( 'NONE',  ( 10.00000000000000178, 135.0000000000000000, 0.000000000000000000 ) ) ;
#792 = CARTESIAN_POINT ( 'NONE',  ( 8.000000000000001776, 98.65625000000001421, 3.313708498984759387 ) ) ;
#793 = CARTESIAN_POINT ( 'NONE',  ( -4.088227598258586603E-16, 289.3593750017070079, -6.676582343750001591 ) ) ;
#794 = CARTESIAN_POINT ( 'NONE',  ( -4.556349186104045934, 11.00000000000000000, 78.71874999999998579 ) ) ;
#795 = DIRECTION ( 'NONE',  ( 0.000000000000000000, 0.000000000000000000, 1.000000000000000000 ) ) ;
#796 = CARTESIAN_POINT ( 'NONE',  ( 26.56734541678238060, 202.0000000013656063, 166.5412658749999650 ) ) ;
#797 = CARTESIAN_POINT ( 'NONE',  ( 4.401442555609581635E-16, 4.218749997951610098, -7.188101187500000044 ) ) ;
#798 = CARTESIAN_POINT ( 'NONE',  ( -8.008118988124989457, -3.317071493978883900, 2.606865283940627886 ) ) ;
#799 = CARTESIAN_POINT ( 'NONE',  ( -1.432654583217664479, 195.7500000013656063, 138.5412658750000787 ) ) ;
#800 = CARTESIAN_POINT ( 'NONE',  ( 7.188101187500000933, 113.3750000020483810, -2.977408999572651371 ) ) ;
#802 = CARTESIAN_POINT ( 'NONE',  ( 2.845451689122903360, 194.6919015541251099, 200.3652389120658484 ) ) ;
#801 = LINE ( 'NONE', #7551, #68493 ) ;
#803 = CARTESIAN_POINT ( 'NONE',  ( -3.042071309553159075, 230.2604166700806445, 11.35316468749999963 ) ) ;
#804 = CARTESIAN_POINT ( 'NONE',  ( -5.082755093536319713, 5.082755093536319713, 27.17405278187175455 ) ) ;
#805 = CARTESIAN_POINT ( 'NONE',  ( 31.99999999999999289, 197.2500000000000000, 169.9999999999999432 ) ) ;
#806 = CARTESIAN_POINT ( 'NONE',  ( -2.085542519210945728E-15, 29.53124999658601624, 11.35316468750000141 ) ) ;
#807 = CARTESIAN_POINT ( 'NONE',  ( -3.999999999999960032, 202.9375000000000284, 196.3431457505076594 ) ) ;
#808 = CARTESIAN_POINT ( 'NONE',  ( -9.832129032723418760, 218.1770833299193555, -5.676582343750004256 ) ) ;
#809 = CARTESIAN_POINT ( 'NONE',  ( 0.000000000000000000, 300.0000000000000000, 0.000000000000000000 ) ) ;
#811 = FACE_OUTER_BOUND ( 'NONE', #21335, .T. ) ;
#810 = LINE ( 'NONE', #23798, #70809 ) ;
#812 = EDGE_LOOP ( 'NONE', ( #5205, #42655, #24587, #50982, #58213 ) ) ;
#813 = CARTESIAN_POINT ( 'NONE',  ( 2.445694354108784108, 195.5625000013656063, 144.4456943541088663 ) ) ;
#814 = CARTESIAN_POINT ( 'NONE',  ( -3.042071309553164404, 17.23958332991935194, -11.35316468749999963 ) ) ;
#815 = CARTESIAN_POINT ( 'NONE',  ( 11.00000000000000355, -4.556349186104045046, 84.34375000409677625 ) ) ;
#816 = AXIS2_PLACEMENT_3D ( 'NONE', #7526, #69789, #63751 ) ;
#817 = CARTESIAN_POINT ( 'NONE',  ( -1.432654583217662481, 207.3750000013656063, 145.4587341250000350 ) ) ;
#818 = CARTESIAN_POINT ( 'NONE',  ( -24.54126587499995793, 195.1250000013656063, 171.4326545832179534 ) ) ;
#819 = DIRECTION ( 'NONE',  ( -0.000000000000000000, 1.000000000000000000, -1.563033456626094573E-30 ) ) ;
#821 = CARTESIAN_POINT ( 'NONE',  ( -5.676582343749998039, 22.44791666325268409, -9.832129032723420536 ) ) ;
#820 = CARTESIAN_POINT ( 'NONE',  ( 5.082755093536326818, 114.2187500020483810, 5.082755093536325042 ) ) ;
#823 = EDGE_CURVE ( 'NONE', #12576, #61133, #52080, .T. ) ;
#822 = CARTESIAN_POINT ( 'NONE',  ( -4.898587196589407898E-16, 7.999999999999991118, 21.45530277982336642 ) ) ;
#824 = CARTESIAN_POINT ( 'NONE',  ( -11.35316468749999785, 143.0729166632526983, -3.042071309553167513 ) ) ;
#825 = CARTESIAN_POINT ( 'NONE',  ( -10.00000000000000000, 109.1666666598386968, -2.679491924311229845 ) ) ;
#826 = CARTESIAN_POINT ( 'NONE',  ( 7.188101187500000044, 116.2812500020483810, -8.802885111219163269E-16 ) ) ;
#827 = CYLINDRICAL_SURFACE ( 'NONE', #62611, 10.00000000000000000 ) ;
#828 = CARTESIAN_POINT ( 'NONE',  ( -31.45873412499999944, 204.9375000013656063, 170.0000000000003979 ) ) ;
#829 = EDGE_LOOP ( 'NONE', ( #61003, #27181, #44033, #34713 ) ) ;
#830 = CARTESIAN_POINT ( 'NONE',  ( -2.085542519210945728E-15, 14.84374999658601624, 11.35316468750000141 ) ) ;
#831 = EDGE_CURVE ( 'NONE', #72883, #74244, #48089, .T. ) ;
#832 = VERTEX_POINT ( 'NONE', #13014 ) ;
#833 = CARTESIAN_POINT ( 'NONE',  ( -0.8761883848948450737, 16.44150283900180654, -68.58316157021027948 ) ) ;
#834 = CARTESIAN_POINT ( 'NONE',  ( -2.765530957081998586, 296.6406250017069510, 6.676582343750001591 ) ) ;
#835 = CARTESIAN_POINT ( 'NONE',  ( 5.676582343749993598, 144.9479166632526983, 9.832129032723422313 ) ) ;
#836 =( NAMED_UNIT ( * ) SI_UNIT ( $, .STERADIAN. ) SOLID_ANGLE_UNIT ( ) );
#837 = CARTESIAN_POINT ( 'NONE',  ( 7.999999999999991118, 3.313708498984757611, 22.73030278432982598 ) ) ;
#838 = CARTESIAN_POINT ( 'NONE',  ( 48.00617930786962972, 193.9745438402055413, 62.51665008897824549 ) ) ;
#839 = CARTESIAN_POINT ( 'NONE',  ( -6.951808397369817780E-16, 247.6562500034140157, -11.35316468749999963 ) ) ;
#840 = CARTESIAN_POINT ( 'NONE',  ( 7.204075437095968759, -7.204075437095966983, 94.09375000204838102 ) ) ;
#841 = ORIENTED_EDGE ( 'NONE', *, *, #24658, .F. ) ;
#842 =( BOUNDED_CURVE ( )  B_SPLINE_CURVE ( 2, ( #34612, #69667, #17981, #12322, #41000, #6670, #31141, #14148, #65098 ),
 .UNSPECIFIED., .F., .F. ) 
 B_SPLINE_CURVE_WITH_KNOTS ( ( 3, 2, 2, 2, 3 ),
 ( 0.5000000000000004441, 0.5083333333333337478, 0.5166666666666671626, 0.5250000000000004663, 0.5333333333333337700 ),
 .UNSPECIFIED. ) 
 CURVE ( )  GEOMETRIC_REPRESENTATION_ITEM ( )  RATIONAL_B_SPLINE_CURVE ( ( 0.9999999999999958922, 0.9238795325112908463, 1.000000000000000000, 0.9238795325112867385, 1.000000000000000000, 0.9238795325112867385, 1.000000000000000000, 0.9238795325112826307, 1.000000000000003997 ) ) 
 REPRESENTATION_ITEM ( '' )  );
#843 = CARTESIAN_POINT ( 'NONE',  ( -10.00000000000000000, 204.1666666598387110, -2.679491924311229845 ) ) ;
#844 = CARTESIAN_POINT ( 'NONE',  ( 5.000000000000000888, 63.85408791058100064, -24.15552328276435290 ) ) ;
#845 = UNCERTAINTY_MEASURE_WITH_UNIT (LENGTH_MEASURE( 1.000000000000000082E-05 ), #3126, 'distance_accuracy_value', 'NONE');
#846 = CARTESIAN_POINT ( 'NONE',  ( 5.676582343750001591, 91.92708332991935549, -9.832129032723420536 ) ) ;
#848 = ADVANCED_FACE ( 'NONE', ( #30384 ), #19058, .F. ) ;
#847 = ORIENTED_EDGE ( 'NONE', *, *, #10496, .T. ) ;
#849 = CARTESIAN_POINT ( 'NONE',  ( -10.18810118749999738, -4.220049686691941915, 108.2500000020483810 ) ) ;
#850 = CARTESIAN_POINT ( 'NONE',  ( 4.541265875000002339, 17.49999999863440436, -1.881053915767121776 ) ) ;
#851 = VERTEX_POINT ( 'NONE', #13380 ) ;
#852 = VERTEX_POINT ( 'NONE', #71097 ) ;
#853 = CARTESIAN_POINT ( 'NONE',  ( -3.313708498984760720, 7.968750000000000888, -8.000000000000000000 ) ) ;
#854 = CARTESIAN_POINT ( 'NONE',  ( -3.211159895383561391, 1.812499998634406584, -3.211159895383561835 ) ) ;
#855 = CARTESIAN_POINT ( 'NONE',  ( -1.320432766682874540E-15, 21.46874999795161543, 7.188101187500000044 ) ) ;
#856 = CARTESIAN_POINT ( 'NONE',  ( 8.000000000000001776, 121.3437500040967763, 3.313708498984759387 ) ) ;
#857 = CARTESIAN_POINT ( 'NONE',  ( 7.204075437095968759, -7.204075437095966983, 104.5937500020483810 ) ) ;
#858 = CARTESIAN_POINT ( 'NONE',  ( -3.313708498984765161, 7.031250000000000888, 7.999999999999998224 ) ) ;
#859 = CARTESIAN_POINT ( 'NONE',  ( 4.000000000000000888, 14.68749999726881406, 1.656854249492384135 ) ) ;
#860 = CARTESIAN_POINT ( 'NONE',  ( -4.898587196589407898E-16, 7.999999999999991118, 12.64280278392014623 ) ) ;
#861 = EDGE_LOOP ( 'NONE', ( #74104, #6053, #73709, #24682 ) ) ;
#862 = CARTESIAN_POINT ( 'NONE',  ( -6.123233995736766282E-16, 261.8750000068280315, -10.00000000000000178 ) ) ;
#863 = CARTESIAN_POINT ( 'NONE',  ( 3.458734125000016313, 196.8750000013656063, 199.4326545832176691 ) ) ;
#864 = AXIS2_PLACEMENT_3D ( 'NONE', #54667, #60688, #2976 ) ;
#865 = CARTESIAN_POINT ( 'NONE',  ( -28.00000000000007105, 203.4375000013656063, 166.5412658750003629 ) ) ;
#866 = B_SPLINE_CURVE_WITH_KNOTS ( 'NONE', 3,
 ( #46307, #1054, #11983, #45563, #68576, #58029 ),
 .UNSPECIFIED., .F., .F.,
 ( 4, 2, 4 ),
 ( 0.009270618776430220032, 0.01189894710419331543, 0.01452727543195641083 ),
 .UNSPECIFIED. ) ;
#867 = CARTESIAN_POINT ( 'NONE',  ( 4.541265875000002339, 13.31249999863440792, 0.000000000000000000 ) ) ;
#868 = CARTESIAN_POINT ( 'NONE',  ( -2.828427124746152987, 200.2500000027312126, 200.8284271247462129 ) ) ;
#869 = CARTESIAN_POINT ( 'NONE',  ( -7.188101187499992051, 0.000000000000000000, 11.98655278187175277 ) ) ;
#870 = VERTEX_POINT ( 'NONE', #53404 ) ;
#871 = EDGE_LOOP ( 'NONE', ( #7452, #65352, #2298, #33672 ) ) ;
#872 = CARTESIAN_POINT ( 'NONE',  ( 4.220049686691941027, -10.18810118749999738, 105.6250000020483668 ) ) ;
#873 = CARTESIAN_POINT ( 'NONE',  ( -7.778174593052020747, -7.778174593052023411, 103.1874999999999858 ) ) ;
#874 = CARTESIAN_POINT ( 'NONE',  ( -25.17157287525382259, 203.8750000000000284, 167.1715728752541565 ) ) ;
#875 = CARTESIAN_POINT ( 'NONE',  ( -3.458734124999959914, 201.4375000013656063, 198.0000000000000284 ) ) ;
#876 = PLANE ( 'NONE',  #50648 ) ;
#877 = CARTESIAN_POINT ( 'NONE',  ( -7.320508075688773708, 91.87500000000001421, -7.320508075688774596 ) ) ;
#878 = CARTESIAN_POINT ( 'NONE',  ( -3.313708498984762496, 116.2812500000000000, 7.999999999999998224 ) ) ;
#879 = CARTESIAN_POINT ( 'NONE',  ( 5.676582343750001591, 66.92708332991935549, -9.832129032723420536 ) ) ;
#880 = CARTESIAN_POINT ( 'NONE',  ( 2.765530957081996366, 298.2968750017069510, -6.676582343750003368 ) ) ;
#881 = ORIENTED_EDGE ( 'NONE', *, *, #18697, .T. ) ;
#882 = EDGE_CURVE ( 'NONE', #48510, #70312, #66666, .T. ) ;
#883 = VECTOR ( 'NONE', #74149, 1000.000000000000000 ) ;
#884 = CARTESIAN_POINT ( 'NONE',  ( 2.828427124746209831, 203.3750000000000284, 200.8284271247462129 ) ) ;
#885 = CARTESIAN_POINT ( 'NONE',  ( 5.656854249492380582, 14.99999999590322020, -5.656854249492380582 ) ) ;
#886 = CARTESIAN_POINT ( 'NONE',  ( 1.432654583217607192, 208.2500000013656063, 145.4587341250000634 ) ) ;
#887 = CARTESIAN_POINT ( 'NONE',  ( 7.320508075688781702, 85.62500000000000000, -7.320508075688781702 ) ) ;
#888 = CARTESIAN_POINT ( 'NONE',  ( -1.469576158976823947E-15, 12.93749999590322197, 8.000000000000000000 ) ) ;
#889 = CARTESIAN_POINT ( 'NONE',  ( 2.679491924311225848, 223.5416666666666856, -10.00000000000000000 ) ) ;
#890 = CARTESIAN_POINT ( 'NONE',  ( -29.65685424949240456, 202.1875000027311842, 166.0000000000003695 ) ) ;
#891 = CARTESIAN_POINT ( 'NONE',  ( 4.220049686691934809, 10.18810118749999916, 70.56250000204836681 ) ) ;
#892 = CARTESIAN_POINT ( 'NONE',  ( 10.00000000000000178, 220.2083333333333428, -2.679491924311226736 ) ) ;
#893 = CARTESIAN_POINT ( 'NONE',  ( -2.977408999572647819, 7.188101187499992051, 10.58030278187175455 ) ) ;
#894 = CARTESIAN_POINT ( 'NONE',  ( 11.35316468749999785, 185.8854166632526983, 3.042071309553174174 ) ) ;
#895 = CARTESIAN_POINT ( 'NONE',  ( -1.881053915767121554, 3.624999998634406584, -4.541265875000002339 ) ) ;
#897 = CARTESIAN_POINT ( 'NONE',  ( 8.660254037844385522, 86.45833332650538239, 5.000000000000005329 ) ) ;
#896 = CARTESIAN_POINT ( 'NONE',  ( -6.123233995736766282E-16, 226.8750000068279746, -10.00000000000000000 ) ) ;
#898 = ORIENTED_EDGE ( 'NONE', *, *, #73539, .T. ) ;
#899 = CARTESIAN_POINT ( 'NONE',  ( 3.458734124999960358, 209.6875000013656063, 142.0000000000000568 ) ) ;
#900 = CARTESIAN_POINT ( 'NONE',  ( -11.35316468750000141, 38.59374999658601979, -1.390361679473963753E-15 ) ) ;
#901 = CARTESIAN_POINT ( 'NONE',  ( -11.00000000000000000, 4.556349186104045934, 106.0937500040968047 ) ) ;
#902 = CARTESIAN_POINT ( 'NONE',  ( -31.45873412499996391, 203.7500000013656063, 171.4326545832181239 ) ) ;
#903 = CARTESIAN_POINT ( 'NONE',  ( -11.00000000000000000, 0.000000000000000000, 71.49999999999998579 ) ) ;
#905 = DIRECTION ( 'NONE',  ( 1.000000000000000000, 0.000000000000000000, 0.000000000000000000 ) ) ;
#904 = LINE ( 'NONE', #74455, #27987 ) ;
#907 = ADVANCED_FACE ( 'NONE', ( #34825 ), #6872, .F. ) ;
#906 = CARTESIAN_POINT ( 'NONE',  ( -2.839093476692135984E-14, 199.6875000013656063, 138.5412658750000503 ) ) ;
#908 = CARTESIAN_POINT ( 'NONE',  ( 10.00000000000000178, 72.08333332650536818, -2.679491924311226736 ) ) ;
#909 = CARTESIAN_POINT ( 'NONE',  ( 1.320432766682874540E-15, 96.03125000204838102, 7.188101187500000044 ) ) ;
#910 = CARTESIAN_POINT ( 'NONE',  ( -1.881053915767121554, 11.74999999863440792, -4.541265875000002339 ) ) ;
#911 = CARTESIAN_POINT ( 'NONE',  ( 7.320508075688808347, 64.37500000000002842, 7.320508075688812788 ) ) ;
#912 = CARTESIAN_POINT ( 'NONE',  ( -4.999999999999998224, 48.54166665983870388, -8.660254037844389075 ) ) ;
#913 = CARTESIAN_POINT ( 'NONE',  ( 8.660254037844389075, 102.2916666598386968, -5.000000000000000000 ) ) ;
#914 = EDGE_LOOP ( 'NONE', ( #12849, #200, #42003, #17496 ) ) ;
#915 = ORIENTED_EDGE ( 'NONE', *, *, #33524, .F. ) ;
#916 = EDGE_CURVE ( 'NONE', #51725, #18289, #18190, .T. ) ;
#917 = CARTESIAN_POINT ( 'NONE',  ( -3.673940397442060854E-16, 288.7500000000000000, -6.000000000000001776 ) ) ;
#918 = CARTESIAN_POINT ( 'NONE',  ( -2.765530957081996810, 296.4218750017070079, -6.676582343750003368 ) ) ;
#919 = DIRECTION ( 'NONE',  ( 1.000000000000000000, 0.000000000000000000, 0.000000000000000000 ) ) ;
#920 = AXIS2_PLACEMENT_3D ( 'NONE', #37998, #55729, #39750 ) ;
#921 = CARTESIAN_POINT ( 'NONE',  ( -1.739508062057944393, 51.27839935804234983, -48.57027215863329417 ) ) ;
#922 = CARTESIAN_POINT ( 'NONE',  ( -9.832129032723420536, 153.6979166632526983, 5.676582343749997150 ) ) ;
#923 = CARTESIAN_POINT ( 'NONE',  ( -7.204075437095965206, -7.204075437095968759, 84.34375000204836681 ) ) ;
#924 = CARTESIAN_POINT ( 'NONE',  ( -1.836970198721029983E-15, 3.750000000000000444, 10.00000000000000178 ) ) ;
#925 = CARTESIAN_POINT ( 'NONE',  ( -3.999999999999959144, 205.0625000000000568, 199.6568542494924259 ) ) ;
#926 = DIRECTION ( 'NONE',  ( -1.000000000000000000, -0.000000000000000000, -0.000000000000000000 ) ) ;
#927 = CARTESIAN_POINT ( 'NONE',  ( -7.204075437095967871, 7.204075437095967871, 109.8437500020483810 ) ) ;
#928 = ORIENTED_EDGE ( 'NONE', *, *, #14905, .T. ) ;
#929 = CARTESIAN_POINT ( 'NONE',  ( 3.313708498984802020, 18.09374999590322020, -7.999999999999958256 ) ) ;
#930 = CLOSED_SHELL ( 'NONE', ( #53514, #18000, #60311, #31115, #43787, #19093, #37149, #47317, #49746, #67519, #37721, #31449, #51316, #39633, #44816, #10281, #12434, #56331, #30520, #59091, #14525, #47783, #43704, #55496, #6376, #308, #70391, #29353, #51728, #23744, #10579, #38890, #50434, #64293, #60151, #36189, #64670, #63661, #60820, #61884, #46953, #47094, #2677, #62513, #3095, #53816, #65760, #63914, #61256, #62071, #47220, #43361, #60220, #5353, #10859, #45491, #46407, #69702, #64376, #15469, #30860, #59977, #40736, #18077, #65645, #26081, #54283, #59683, #24802, #16598, #50305, #48307, #217, #18722, #66993, #74304, #49636, #64399, #31436, #28895, #4640, #3079, #36392, #47949, #42933, #9569, #67487, #58394, #12651, #51210, #44023, #62069, #53673, #53231, #36000, #63563, #3965, #2864, #5983, #15096, #64347, #18944, #31178, #18920, #74500 ) ) ;
#931 = CARTESIAN_POINT ( 'NONE',  ( -10.33666931816624945, 178.5382482961798019, 134.7837216799249518 ) ) ;
#932 = CARTESIAN_POINT ( 'NONE',  ( -11.35316468750000141, 123.8020833299193413, 3.042071309553159963 ) ) ;
#933 = CARTESIAN_POINT ( 'NONE',  ( 3.458734125000016313, 197.8750000013656063, 199.4326545832176976 ) ) ;
#934 = CARTESIAN_POINT ( 'NONE',  ( 3.458734125000015869, 209.1875000013656063, 198.0000000000000284 ) ) ;
#935 =( BOUNDED_CURVE ( )  B_SPLINE_CURVE ( 2, ( #68885, #57964, #252, #13010, #36048, #69262, #7372, #23234, #64343 ),
 .UNSPECIFIED., .F., .F. ) 
 B_SPLINE_CURVE_WITH_KNOTS ( ( 3, 2, 2, 2, 3 ),
 ( 0.2500000000000001110, 0.2583333333333335258, 0.2666666666666668850, 0.2750000000000002998, 0.2833333333333336590 ),
 .UNSPECIFIED. ) 
 CURVE ( )  GEOMETRIC_REPRESENTATION_ITEM ( )  RATIONAL_B_SPLINE_CURVE ( ( 0.9999999999999990008, 0.9238795325112877377, 1.000000000000000000, 0.9238795325112867385, 1.000000000000000000, 0.9238795325112867385, 1.000000000000000000, 0.9238795325112837409, 1.000000000000003109 ) ) 
 REPRESENTATION_ITEM ( '' )  );
#936 = CARTESIAN_POINT ( 'NONE',  ( 7.204075437095966983, 7.204075437095967871, 79.46875000204836681 ) ) ;
#937 = CARTESIAN_POINT ( 'NONE',  ( 9.832129032723420536, 46.51041666325269119, -5.676582343749999815 ) ) ;
#938 = EDGE_LOOP ( 'NONE', ( #71940, #18013, #14935, #7021 ) ) ;
#939 = CYLINDRICAL_SURFACE ( 'NONE', #47674, 8.000000000000000000 ) ;
#940 = CARTESIAN_POINT ( 'NONE',  ( 4.541265875000001451, 2.374999998634407028, 1.881053915767124440 ) ) ;
#941 = CARTESIAN_POINT ( 'NONE',  ( 3.317071493978877683, 8.008118988124991233, 17.04436528394063188 ) ) ;
#942 = CARTESIAN_POINT ( 'NONE',  ( -5.082755093536325042, 16.03124999795161543, -5.082755093536325930 ) ) ;
#943 = CARTESIAN_POINT ( 'NONE',  ( 1.102182119232618108E-15, 292.3125000034140157, 6.000000000000001776 ) ) ;
#944 = CARTESIAN_POINT ( 'NONE',  ( -48.52588466223724595, 141.8056711710915181, 60.88070576291119096 ) ) ;
#945 = CARTESIAN_POINT ( 'NONE',  ( 7.188101187500001821, 5.437499997951610098, -2.977408999572650483 ) ) ;
#946 = CARTESIAN_POINT ( 'NONE',  ( -5.082755093536317936, -5.082755093536320601, 10.67405278187175455 ) ) ;
#947 = VECTOR ( 'NONE', #19692, 1000.000000000000000 ) ;
#948 = CARTESIAN_POINT ( 'NONE',  ( -10.18810118749999916, 4.220049686691934809, 73.56250000204835260 ) ) ;
#949 = CARTESIAN_POINT ( 'NONE',  ( -26.56734541678232731, 206.2500000013656063, 173.4587341250003760 ) ) ;
#950 =( BOUNDED_CURVE ( )  B_SPLINE_CURVE ( 2, ( #55035, #25590, #9002, #49353, #9376, #32395, #72371, #19562, #36927, #14266, #65590, #13888, #20681 ),
 .UNSPECIFIED., .F., .F. ) 
 B_SPLINE_CURVE_WITH_KNOTS ( ( 3, 2, 2, 2, 2, 2, 3 ),
 ( 0.3176771498271482308, 0.3176772280539318372, 0.3242955036383868839, 0.3309137792228418751, 0.3375320548072968108, 0.3441503303917518020, 0.3441504249343935173 ),
 .UNSPECIFIED. ) 
 CURVE ( )  GEOMETRIC_REPRESENTATION_ITEM ( )  RATIONAL_B_SPLINE_CURVE ( ( 0.9999982005617984449, 0.9999991002702646181, 1.000000000000000000, 0.9238795325112867385, 1.000000000000000000, 0.9238795325112867385, 1.000000000000000000, 0.9238795325112867385, 1.000000000000000000, 0.9238795325112867385, 1.000000000000000000, 0.9999989126125087280, 0.9999978252560842718 ) ) 
 REPRESENTATION_ITEM ( '' )  );
#951 = CARTESIAN_POINT ( 'NONE',  ( -47.11462393093396628, 145.7394130188241661, 67.12012181809814138 ) ) ;
#952 = CARTESIAN_POINT ( 'NONE',  ( -3.211159895383562723, 18.06249999863440792, 3.211159895383561391 ) ) ;
#953 = ORIENTED_EDGE ( 'NONE', *, *, #8192, .T. ) ;
#954 = ADVANCED_FACE ( 'NONE', ( #64215 ), #22724, .T. ) ;
#955 = CARTESIAN_POINT ( 'NONE',  ( -3.999999999999960032, 197.1250000027312126, 198.0000000000000284 ) ) ;
#956 = CARTESIAN_POINT ( 'NONE',  ( -2.828427124746208943, 205.6250000000000284, 144.8284271247462129 ) ) ;
#957 = CARTESIAN_POINT ( 'NONE',  ( -31.99999999999996447, 203.4375000027312126, 171.6568542494928522 ) ) ;
#958 = CARTESIAN_POINT ( 'NONE',  ( -5.082755093536324154, 113.8437500020483810, 5.082755093536326818 ) ) ;
#959 = CARTESIAN_POINT ( 'NONE',  ( 8.660254037844389075, 250.2083333401612890, 4.999999999999997335 ) ) ;
#960 = CARTESIAN_POINT ( 'NONE',  ( 1.469576158976822172E-15, -7.999999999999991118, 2.892802783920144005 ) ) ;
#961 = ORIENTED_EDGE ( 'NONE', *, *, #44827, .T. ) ;
#962 = CARTESIAN_POINT ( 'NONE',  ( -5.082755093536326818, 14.90624999795161187, 5.082755093536325042 ) ) ;
#963 = ORIENTED_EDGE ( 'NONE', *, *, #56687, .F. ) ;
#964 = CARTESIAN_POINT ( 'NONE',  ( -6.123233995736766282E-16, 256.8750000068279746, -10.00000000000000000 ) ) ;
#965 = CARTESIAN_POINT ( 'NONE',  ( -0.7785336552199920712, -47.90394811185176849, 151.0149672810441075 ) ) ;
#966 = CARTESIAN_POINT ( 'NONE',  ( 7.320508075688771044, 59.37500000000000711, 7.320508075688775484 ) ) ;
#967 = CARTESIAN_POINT ( 'NONE',  ( 7.188101187500001821, 102.8750000020483810, -2.977408999572651371 ) ) ;
#968 = CARTESIAN_POINT ( 'NONE',  ( -27.99999999999996447, 205.1875000013656063, 173.4587341250003760 ) ) ;
#969 = CARTESIAN_POINT ( 'NONE',  ( 3.729367062499960195, 194.8437500006828031, 142.0000000000000568 ) ) ;
#970 = VECTOR ( 'NONE', #14893, 1000.000000000000000 ) ;
#972 = CARTESIAN_POINT ( 'NONE',  ( -24.54323509149329752, -40.90842742948011335, 188.9397108500383524 ) ) ;
#971 = CARTESIAN_POINT ( 'NONE',  ( -2.679491924311226292, 33.33333332650536107, -10.00000000000000178 ) ) ;
#973 = ORIENTED_EDGE ( 'NONE', *, *, #50785, .F. ) ;
#974 = CARTESIAN_POINT ( 'NONE',  ( 11.35316468749999963, 251.4062500034139873, -1.390361679473963556E-15 ) ) ;
#975 = CARTESIAN_POINT ( 'NONE',  ( 5.082755093536318824, 5.082755093536319713, 19.29905278187175455 ) ) ;
#976 = CARTESIAN_POINT ( 'NONE',  ( 3.511653767258654302, 51.69076377080344997, 48.72852442694496489 ) ) ;
#977 = DIRECTION ( 'NONE',  ( 0.000000000000000000, 0.000000000000000000, 1.000000000000000000 ) ) ;
#978 = CARTESIAN_POINT ( 'NONE',  ( -10.00000000000000355, 147.7083333333333144, 2.679491924311223183 ) ) ;
#979 = DIRECTION ( 'NONE',  ( -0.000000000000000000, 1.000000000000000000, -0.000000000000000000 ) ) ;
#980 = CARTESIAN_POINT ( 'NONE',  ( 8.660254037844385522, 169.5833333333333428, 5.000000000000005329 ) ) ;
#981 = FACE_OUTER_BOUND ( 'NONE', #9439, .T. ) ;
#982 = CARTESIAN_POINT ( 'NONE',  ( -7.999999999999998224, 119.0937500000000000, 3.313708498984766049 ) ) ;
#983 = CARTESIAN_POINT ( 'NONE',  ( -2.085542519210945728E-15, 144.8437499965860411, 11.35316468750000141 ) ) ;
#984 = DIRECTION ( 'NONE',  ( -0.000000000000000000, 1.000000000000000000, -0.000000000000000000 ) ) ;
#987 = CARTESIAN_POINT ( 'NONE',  ( -10.99999999999999822, 219.4226497308103774, 0.000000000000000000 ) ) ;
#986 = CARTESIAN_POINT ( 'NONE',  ( 5.656854249492381470, 110.5625000000000000, 5.656854249492379694 ) ) ;
#985 = CARTESIAN_POINT ( 'NONE',  ( 29.65685424949235482, 208.0625000000000000, 173.9999999999999147 ) ) ;
#988 = ORIENTED_EDGE ( 'NONE', *, *, #71663, .F. ) ;
#989 = EDGE_CURVE ( 'NONE', #43256, #54025, #57831, .T. ) ;
#990 = CONICAL_SURFACE ( 'NONE', #45552, 12.00000000000000178, 0.9599310885968795892 ) ;
#991 = CARTESIAN_POINT ( 'NONE',  ( -4.898587196589412829E-16, 111.3125000040967905, -8.000000000000000000 ) ) ;
#992 = CARTESIAN_POINT ( 'NONE',  ( -27.99999999999996092, 209.5000000000000284, 174.0000000000003695 ) ) ;
#993 = CARTESIAN_POINT ( 'NONE',  ( 0.000000000000000000, 125.0000000000000000, 0.000000000000000000 ) ) ;
#994 = AXIS2_PLACEMENT_3D ( 'NONE', #5165, #33472, #5905 ) ;
#995 = CARTESIAN_POINT ( 'NONE',  ( 5.000000000000000000, -65.19475225706619881, -23.98307544244962841 ) ) ;
#996 = CARTESIAN_POINT ( 'NONE',  ( 8.660254037844389075, 42.29166665983870388, -5.000000000000000000 ) ) ;
#997 = CARTESIAN_POINT ( 'NONE',  ( 5.082755093536326818, 115.7187500020483810, 5.082755093536325042 ) ) ;
#998 = CARTESIAN_POINT ( 'NONE',  ( 3.211159895383561835, 0.5624999986344069169, -3.211159895383561835 ) ) ;
#999 = CARTESIAN_POINT ( 'NONE',  ( -3.223881452105248790, 60.47365957010899962, -23.05198836891563730 ) ) ;
#1000 = CARTESIAN_POINT ( 'NONE',  ( 7.999999999999991118, 9.797174393178815797E-16, 15.08030277982336642 ) ) ;
#1002 = CARTESIAN_POINT ( 'NONE',  ( 2.449293598294707893E-16, 19.99999999726881228, -4.000000000000001776 ) ) ;
#1001 = CARTESIAN_POINT ( 'NONE',  ( -8.660254037844385522, 238.5416666734946318, 5.000000000000004441 ) ) ;
#1003 = ORIENTED_EDGE ( 'NONE', *, *, #50615, .F. ) ;
#1004 = CARTESIAN_POINT ( 'NONE',  ( 27.99999999999996092, 194.7622595281506790, 166.2377404718492357 ) ) ;
#1005 = CARTESIAN_POINT ( 'NONE',  ( -0.6562093533523021271, 225.9999999999999716, -10.00003937256114028 ) ) ;
#1006 = CARTESIAN_POINT ( 'NONE',  ( 3.313708498984733186, 109.5312500000000000, -8.000000000000026645 ) ) ;
#1007 = CARTESIAN_POINT ( 'NONE',  ( 3.042071309553173286, 240.6770833367473017, 11.35316468749999608 ) ) ;
#1008 = CARTESIAN_POINT ( 'NONE',  ( 11.35316468749999963, 110.9895833299193697, -3.042071309553165293 ) ) ;
#1009 = VERTEX_POINT ( 'NONE', #29882 ) ;
#1010 = CARTESIAN_POINT ( 'NONE',  ( -9.761837184982935511, 4.601249817483572535, 117.7500899827576859 ) ) ;
#1011 = CARTESIAN_POINT ( 'NONE',  ( -4.220049686691935698, 10.18810118749999916, 98.87500000204836681 ) ) ;
#1012 = DIRECTION ( 'NONE',  ( -0.000000000000000000, -0.000000000000000000, 1.000000000000000000 ) ) ;
#1013 = CARTESIAN_POINT ( 'NONE',  ( 2.445694354108839175, 202.3125000013656063, 195.5543056458912190 ) ) ;
#1014 = CARTESIAN_POINT ( 'NONE',  ( 2.449293598294707893E-16, 5.999999997268813168, -4.000000000000001776 ) ) ;
#1016 = CARTESIAN_POINT ( 'NONE',  ( 3.042071309553167513, 96.82291666325269830, -11.35316468749999785 ) ) ;
#1015 = DIRECTION ( 'NONE',  ( 0.000000000000000000, 0.000000000000000000, -1.000000000000000000 ) ) ;
#1017 = EDGE_CURVE ( 'NONE', #43392, #29523, #38248, .T. ) ;
#1018 = CARTESIAN_POINT ( 'NONE',  ( -3.313708498984758943, -7.999999999999989342, 7.299052783920144449 ) ) ;
#1019 = CARTESIAN_POINT ( 'NONE',  ( -24.54126587499998280, 198.3750000013655779, 171.4326545832179818 ) ) ;
#1020 = CARTESIAN_POINT ( 'NONE',  ( 10.00000000000008882, 174.7916666666666856, 2.679491924311259154 ) ) ;
#1021 = ORIENTED_EDGE ( 'NONE', *, *, #61089, .F. ) ;
#1022 = CARTESIAN_POINT ( 'NONE',  ( -8.660254037844390851, 194.7916666598387110, 4.999999999999998224 ) ) ;
#1023 = CARTESIAN_POINT ( 'NONE',  ( -2.849036369511732440E-14, 206.2500000000000284, 138.0000000000000568 ) ) ;
#1024 = CARTESIAN_POINT ( 'NONE',  ( 1.329584132941740160, -47.69645429178699914, 139.0279924659086532 ) ) ;
#1025 = CARTESIAN_POINT ( 'NONE',  ( 9.832129032723420536, 91.51041666325268409, -5.676582343749999815 ) ) ;
#1026 = DIRECTION ( 'NONE',  ( 0.000000000000000000, -1.000000000000000000, 0.000000000000000000 ) ) ;
#1027 = CARTESIAN_POINT ( 'NONE',  ( -5.082755093536326818, 6.281249997951610098, 5.082755093536325042 ) ) ;
#1028 = CARTESIAN_POINT ( 'NONE',  ( -7.204075437095965206, -7.204075437095968759, 95.21875000204838102 ) ) ;
#1029 = CARTESIAN_POINT ( 'NONE',  ( 8.311093377946837890, 6.718749996586016238, -8.311093377946837890 ) ) ;
#1030 = EDGE_LOOP ( 'NONE', ( #70979, #11087, #73660, #67600, #68806, #29781 ) ) ;
#1031 = CARTESIAN_POINT ( 'NONE',  ( -8.660254037844394404, 137.0833333333333428, -5.000000000000008882 ) ) ;
#1032 = CARTESIAN_POINT ( 'NONE',  ( 1.656854249492321074, 196.4375000027312126, 202.0000000000001137 ) ) ;
#1033 = CARTESIAN_POINT ( 'NONE',  ( -9.832129032723418760, 222.8645833299193839, -5.676582343750004256 ) ) ;
#1034 = CARTESIAN_POINT ( 'NONE',  ( -6.238412754330611322E-16, 10.18810118749999916, 78.15625000204836681 ) ) ;
#1035 = CARTESIAN_POINT ( 'NONE',  ( -3.313708498984757611, 7.999999999999991118, 11.23655278392014445 ) ) ;
#1036 = CARTESIAN_POINT ( 'NONE',  ( -5.656854249492380582, 93.50000000409677625, -5.656854249492380582 ) ) ;
#1037 = CARTESIAN_POINT ( 'NONE',  ( 4.721056650415999201, 292.0781250017069510, -4.721056650415999201 ) ) ;
#1038 = ORIENTED_EDGE ( 'NONE', *, *, #48501, .F. ) ;
#1039 = CARTESIAN_POINT ( 'NONE',  ( 4.000000000000015987, 199.5000000000000000, 198.0000000000000284 ) ) ;
#1040 = CARTESIAN_POINT ( 'NONE',  ( -5.676582343749998039, 202.7604166632526983, -9.832129032723420536 ) ) ;
#1041 = CARTESIAN_POINT ( 'NONE',  ( -7.204075437095965206, -7.204075437095968759, 88.84375000204838102 ) ) ;
#1042 = AXIS2_PLACEMENT_3D ( 'NONE', #73505, #72388, #67110 ) ;
#1043 = CARTESIAN_POINT ( 'NONE',  ( -26.56734541678232375, 202.0000000013656063, 173.4587341250003760 ) ) ;
#1044 = CARTESIAN_POINT ( 'NONE',  ( 5.656854249492380582, 18.18750000000000355, -5.656854249492380582 ) ) ;
#1045 = ORIENTED_EDGE ( 'NONE', *, *, #35833, .T. ) ;
#1046 = CIRCLE ( 'NONE', #5871, 18.99999999999998934 ) ;
#1047 = CARTESIAN_POINT ( 'NONE',  ( 2.977408999572650039, 122.1875000020483668, -7.188101187500001821 ) ) ;
#1048 = CARTESIAN_POINT ( 'NONE',  ( 2.751064625579944321E-14, 205.8750000027312126, 194.0000000000000568 ) ) ;
#1049 =( BOUNDED_CURVE ( )  B_SPLINE_CURVE ( 2, ( #3000, #66743, #54319, #2630, #26360, #25981, #48632, #1887, #72016 ),
 .UNSPECIFIED., .F., .F. ) 
 B_SPLINE_CURVE_WITH_KNOTS ( ( 3, 2, 2, 2, 3 ),
 ( 0.2159090909090909116, 0.2215909090909090884, 0.2272727272727272652, 0.2329545454545454419, 0.2386363636363636465 ),
 .UNSPECIFIED. ) 
 CURVE ( )  GEOMETRIC_REPRESENTATION_ITEM ( )  RATIONAL_B_SPLINE_CURVE ( ( 1.000000000000000000, 0.9238795325112867385, 1.000000000000000000, 0.9238795325112867385, 1.000000000000000000, 0.9238795325112867385, 1.000000000000000000, 0.9238795325112867385, 1.000000000000000000 ) ) 
 REPRESENTATION_ITEM ( '' )  );
#1050 = CARTESIAN_POINT ( 'NONE',  ( 4.999999999999993783, 29.16666666666666785, 8.660254037844390851 ) ) ;
#1051 = VECTOR ( 'NONE', #57308, 1000.000000000000000 ) ;
#1052 = CARTESIAN_POINT ( 'NONE',  ( 1.871523826299183495E-15, -10.18810118749999916, 74.40625000204836681 ) ) ;
#1053 = ORIENTED_EDGE ( 'NONE', *, *, #26829, .F. ) ;
#1054 = CARTESIAN_POINT ( 'NONE',  ( 9.000000000000001776, -4.351040328464082840, -0.5598847297401613465 ) ) ;
#1055 = CARTESIAN_POINT ( 'NONE',  ( 11.00000000000000000, 1.347111479062088405E-15, 118.0000000000000000 ) ) ;
#1056 = ADVANCED_FACE ( 'NONE', ( #6137 ), #29515, .T. ) ;
#1057 = CARTESIAN_POINT ( 'NONE',  ( -2.775557561562891351E-14, 210.0000000000000284, 142.0000000000000568 ) ) ;
#1058 = CARTESIAN_POINT ( 'NONE',  ( 7.188101187500001821, 119.3750000020483810, -2.977408999572651371 ) ) ;
#1059 = CARTESIAN_POINT ( 'NONE',  ( 9.000000000000023093, -15.58845726811988541, 0.000000000000000000 ) ) ;
#1060 = CARTESIAN_POINT ( 'NONE',  ( 2.765530957082001251, 295.7656250017069510, 6.676582343749999815 ) ) ;
#1062 = DIRECTION ( 'NONE',  ( -0.000000000000000000, -1.000000000000000000, -0.000000000000000000 ) ) ;
#1061 = CARTESIAN_POINT ( 'NONE',  ( 9.832129032723420536, 235.9895833367473301, 5.676582343749996262 ) ) ;
#1063 = ITEM_DEFINED_TRANSFORMATION ( 'NONE', 'NONE', #71862,  #57354 ) ;
#1064 = ORIENTED_EDGE ( 'NONE', *, *, #62606, .T. ) ;
#1065 =( BOUNDED_CURVE ( )  B_SPLINE_CURVE ( 2, ( #44550, #73586, #15856, #38892, #20399, #61896, #10219, #32114, #56247 ),
 .UNSPECIFIED., .F., .F. ) 
 B_SPLINE_CURVE_WITH_KNOTS ( ( 3, 2, 2, 2, 3 ),
 ( 0.6666666666666672958, 0.6750000000000007105, 0.6833333333333340143, 0.6916666666666673180, 0.7000000000000006217 ),
 .UNSPECIFIED. ) 
 CURVE ( )  GEOMETRIC_REPRESENTATION_ITEM ( )  RATIONAL_B_SPLINE_CURVE ( ( 0.9999999999999938938, 0.9238795325112928447, 1.000000000000000000, 0.9238795325112867385, 1.000000000000000000, 0.9238795325112867385, 1.000000000000000000, 0.9238795325112806323, 1.000000000000005995 ) ) 
 REPRESENTATION_ITEM ( '' )  );
#1066 = CARTESIAN_POINT ( 'NONE',  ( -11.35316468749999785, 244.0104166700806729, -3.042071309553164848 ) ) ;
#1067 = CARTESIAN_POINT ( 'NONE',  ( -7.188101187499992051, 0.000000000000000000, 5.986552781871753659 ) ) ;
#1068 = ORIENTED_EDGE ( 'NONE', *, *, #43318, .T. ) ;
#1069 = CARTESIAN_POINT ( 'NONE',  ( -28.00000000000001776, 194.6875000013655779, 166.5412658750003629 ) ) ;
#1070 = CARTESIAN_POINT ( 'NONE',  ( 11.35316468749999785, 95.88541666325269830, 3.042071309553174174 ) ) ;
#1071 = PLANE ( 'NONE',  #13150 ) ;
#1072 = CARTESIAN_POINT ( 'NONE',  ( -4.556349186104045934, 11.00000000000000000, 81.71874999999998579 ) ) ;
#1075 = CARTESIAN_POINT ( 'NONE',  ( -1.328591152368359007E-11, 1.250000000001033174, -10.00000000000000533 ) ) ;
#1074 = CARTESIAN_POINT ( 'NONE',  ( 27.99999999999996803, 203.9375000013656063, 166.5412658749999082 ) ) ;
#1073 = CARTESIAN_POINT ( 'NONE',  ( 25.55430564589119413, 204.3125000013656063, 167.5543056458910485 ) ) ;
#1076 = VERTEX_POINT ( 'NONE', #17440 ) ;
#1077 = EDGE_CURVE ( 'NONE', #51670, #43329, #64586, .T. ) ;
#1078 = CARTESIAN_POINT ( 'NONE',  ( -2.775557561562891351E-14, 210.0000000000000284, 142.0000000000000568 ) ) ;
#1079 = DIRECTION ( 'NONE',  ( -0.000000000000000000, 1.000000000000000000, -1.563033456626094573E-30 ) ) ;
#1080 = CARTESIAN_POINT ( 'NONE',  ( 3.042071309553159519, 209.7395833299193839, 11.35316468750000141 ) ) ;
#1082 = ADVANCED_FACE ( 'NONE', ( #52525 ), #41571, .T. ) ;
#1081 = CARTESIAN_POINT ( 'NONE',  ( 3.458734124999959914, 205.3750000013656063, 143.4326545832176976 ) ) ;
#1083 = CARTESIAN_POINT ( 'NONE',  ( 26.56734541678232731, 206.6250000013656063, 173.4587341249998929 ) ) ;
#1084 = AXIS2_PLACEMENT_3D ( 'NONE', #45896, #29301, #57991 ) ;
#1085 = CARTESIAN_POINT ( 'NONE',  ( 5.082755093536325930, 23.53124999795161543, -5.082755093536325930 ) ) ;
#1086 = CARTESIAN_POINT ( 'NONE',  ( -5.676582343750006032, 174.4270833299193555, 9.832129032723418760 ) ) ;
#1087 = CARTESIAN_POINT ( 'NONE',  ( 5.082755093536326818, 99.59375000204838102, 5.082755093536325042 ) ) ;
#1088 = CARTESIAN_POINT ( 'NONE',  ( -11.00000000000000000, 0.000000000000000000, 107.4999999999999858 ) ) ;
#1089 = CARTESIAN_POINT ( 'NONE',  ( -3.211159895383562723, 8.937499998634407916, 3.211159895383561391 ) ) ;
#1090 = CARTESIAN_POINT ( 'NONE',  ( 25.55430564589115150, 203.5625000013656063, 172.4456943541086957 ) ) ;
#1091 = CARTESIAN_POINT ( 'NONE',  ( -4.401442555609577197E-16, 7.188101187499992051, 11.98655278187175632 ) ) ;
#1092 = CARTESIAN_POINT ( 'NONE',  ( 9.832129032723416984, 70.36458332991936970, 5.676582343750006032 ) ) ;
#1093 = CARTESIAN_POINT ( 'NONE',  ( 9.491012693391981871E-16, 0.000000000000000000, -7.499999999999992895 ) ) ;
#1094 = CARTESIAN_POINT ( 'NONE',  ( -5.867873826482948196, -5.445834672501801421, -0.4343901754555773431 ) ) ;
#1095 = ORIENTED_EDGE ( 'NONE', *, *, #30229, .F. ) ;
#1096 = DIRECTION ( 'NONE',  ( -0.000000000000000000, 1.000000000000000000, -0.000000000000000000 ) ) ;
#1097 = CARTESIAN_POINT ( 'NONE',  ( -4.000000000000015987, 203.6875000027311842, 143.6568542494924259 ) ) ;
#1098 = CARTESIAN_POINT ( 'NONE',  ( 11.35316468749999963, 80.98958332991934128, -3.042071309553165293 ) ) ;
#1099 = AXIS2_PLACEMENT_3D ( 'NONE', #65004, #59365, #21871 ) ;
#1100 = CARTESIAN_POINT ( 'NONE',  ( -7.778174593052023411, 7.778174593052023411, 70.00000000409677625 ) ) ;
#1101 = CARTESIAN_POINT ( 'NONE',  ( 3.458734124999960358, 197.6250000013656063, 143.4326545832176976 ) ) ;
#1102 = CARTESIAN_POINT ( 'NONE',  ( 4.000000000000001776, 8.812499997268814056, -1.656854249492381248 ) ) ;
#1103 = CARTESIAN_POINT ( 'NONE',  ( -9.832129032723418760, 62.86458332991935549, -5.676582343750004256 ) ) ;
#1104 = EDGE_CURVE ( 'NONE', #72546, #34245, #53672, .T. ) ;
#1105 = CARTESIAN_POINT ( 'NONE',  ( 3.313708498984762496, -7.999999999999989342, 25.48655278392014623 ) ) ;
#1106 = CARTESIAN_POINT ( 'NONE',  ( -3.563081508477248249, 194.7984481092556166, 143.3390198074419004 ) ) ;
#1107 = AXIS2_PLACEMENT_3D ( 'NONE', #26560, #67318, #10346 ) ;
#1108 = CARTESIAN_POINT ( 'NONE',  ( -10.00000000000000355, 149.5833333265053398, 2.679491924311223183 ) ) ;
#1109 = CARTESIAN_POINT ( 'NONE',  ( 7.188101187500001821, 95.37500000204839523, -2.977408999572651371 ) ) ;
#1110 = CARTESIAN_POINT ( 'NONE',  ( -7.320508075688778149, 54.99999999317203958, 7.320508075688769267 ) ) ;
#1111 = CARTESIAN_POINT ( 'NONE',  ( -11.35316468750000141, 48.59374999658601268, -1.390361679473963753E-15 ) ) ;
#1112 = CARTESIAN_POINT ( 'NONE',  ( 1.871523826299183495E-15, -10.18810118749999916, 114.9062500020483810 ) ) ;
#1113 = CARTESIAN_POINT ( 'NONE',  ( -2.085542519210945728E-15, 189.5312499965860127, 11.35316468750000141 ) ) ;
#1114 = ORIENTED_EDGE ( 'NONE', *, *, #36215, .T. ) ;
#1115 = CARTESIAN_POINT ( 'NONE',  ( 3.074111742570772243, 67.95395293240336798, 20.32712440775923568 ) ) ;
#1116 = CARTESIAN_POINT ( 'NONE',  ( 5.000000000000000000, -68.60357193678713372, 20.85024232999320404 ) ) ;
#1117 = CARTESIAN_POINT ( 'NONE',  ( -1.836970198721029983E-15, 160.6249999931720254, 10.00000000000000178 ) ) ;
#1119 = CARTESIAN_POINT ( 'NONE',  ( -11.35316468749999785, 178.0729166632526983, -3.042071309553167957 ) ) ;
#1118 = CARTESIAN_POINT ( 'NONE',  ( 4.999999999999997335, 263.3333333333333712, -8.660254037844387298 ) ) ;
#1120 = CARTESIAN_POINT ( 'NONE',  ( 4.898587196589412829E-16, 10.68749999590322020, -8.000000000000000000 ) ) ;
#1121 = CARTESIAN_POINT ( 'NONE',  ( 4.999999999999997335, 246.4583333401613174, -8.660254037844387298 ) ) ;
#1122 = CARTESIAN_POINT ( 'NONE',  ( 8.000000000000003553, 0.000000000000000000, -14.80000000000000071 ) ) ;
#1123 = VERTEX_POINT ( 'NONE', #28393 ) ;
#1124 = CARTESIAN_POINT ( 'NONE',  ( -8.311093377946836114, 167.9687499965860127, -8.311093377946837890 ) ) ;
#1125 = EDGE_CURVE ( 'NONE', #17893, #13268, #49731, .T. ) ;
#1126 = CARTESIAN_POINT ( 'NONE',  ( 2.977408999572646486, 7.188101187499992051, 26.51780278187175455 ) ) ;
#1127 = CARTESIAN_POINT ( 'NONE',  ( -3.042071309553173730, 134.6354166632526983, 11.35316468749999785 ) ) ;
#1128 = DIRECTION ( 'NONE',  ( 0.000000000000000000, 0.000000000000000000, 1.000000000000000000 ) ) ;
#1129 = VERTEX_POINT ( 'NONE', #51401 ) ;
#1130 = CARTESIAN_POINT ( 'NONE',  ( -8.000000000000000000, 102.6875000040967763, 0.000000000000000000 ) ) ;
#1131 = CARTESIAN_POINT ( 'NONE',  ( -1.656854249492383691, 10.68750000000000000, 4.000000000000000888 ) ) ;
#1132 = LINE ( 'NONE', #24110, #55314 ) ;
#1133 = CARTESIAN_POINT ( 'NONE',  ( 1.881053915767121998, 13.49999999863440792, -4.541265875000002339 ) ) ;
#1134 = CARTESIAN_POINT ( 'NONE',  ( -5.656854249492373476, -5.656854249492376141, 22.20530278392014623 ) ) ;
#1135 = CARTESIAN_POINT ( 'NONE',  ( -8.660254037844390851, 187.9166666666666856, 5.000000000000000000 ) ) ;
#1136 = AXIS2_PLACEMENT_3D ( 'NONE', #60648, #56493, #21766 ) ;
#1137 = ORIENTED_EDGE ( 'NONE', *, *, #6203, .F. ) ;
#1138 = LINE ( 'NONE', #36196, #1728 ) ;
#1139 = CARTESIAN_POINT ( 'NONE',  ( 2.977408999572654480, 97.62500000204836681, 7.188101187499999156 ) ) ;
#1141 = CARTESIAN_POINT ( 'NONE',  ( 3.313708498984731410, 119.6562500040967905, 8.000000000000031974 ) ) ;
#1140 = CARTESIAN_POINT ( 'NONE',  ( 3.999999999999959144, 204.1875000027311557, 140.3431457505076594 ) ) ;
#1142 = VERTEX_POINT ( 'NONE', #74415 ) ;
#1143 = CARTESIAN_POINT ( 'NONE',  ( -0.3794862803194745116, 10.12385276104027376, -70.07165850195889334 ) ) ;
#1144 = CARTESIAN_POINT ( 'NONE',  ( 2.449293598294707893E-16, 2.250000000000000444, -4.000000000000001776 ) ) ;
#1145 = CARTESIAN_POINT ( 'NONE',  ( -4.401442555609577197E-16, 7.188101187499992051, 26.61155278187175455 ) ) ;
#1146 = ORIENTED_EDGE ( 'NONE', *, *, #23656, .F. ) ;
#1147 =( BOUNDED_CURVE ( )  B_SPLINE_CURVE ( 2, ( #9682, #37979, #32702, #55711, #4025, #20605, #60603, #8927, #49277 ),
 .UNSPECIFIED., .F., .F. ) 
 B_SPLINE_CURVE_WITH_KNOTS ( ( 3, 2, 2, 2, 3 ),
 ( 0.6527777777777777901, 0.6597222222222222099, 0.6666666666666665186, 0.6736111111111110494, 0.6805555555555554692 ),
 .UNSPECIFIED. ) 
 CURVE ( )  GEOMETRIC_REPRESENTATION_ITEM ( )  RATIONAL_B_SPLINE_CURVE ( ( 1.000000000000000000, 0.9238795325112867385, 1.000000000000000000, 0.9238795325112867385, 1.000000000000000000, 0.9238795325112867385, 1.000000000000000000, 0.9238795325112879597, 0.9999999999999987788 ) ) 
 REPRESENTATION_ITEM ( '' )  );
#1148 = ORIENTED_EDGE ( 'NONE', *, *, #4407, .T. ) ;
#1149 = CARTESIAN_POINT ( 'NONE',  ( -10.18810118749999916, 4.220049686691934809, 87.06250000204838102 ) ) ;
#1150 = UNCERTAINTY_MEASURE_WITH_UNIT (LENGTH_MEASURE( 1.000000000000000082E-05 ), #27939, 'distance_accuracy_value', 'NONE');
#1151 = CARTESIAN_POINT ( 'NONE',  ( -31.45873412499999944, 194.8750000013656347, 168.5673454167827572 ) ) ;
#1152 = CARTESIAN_POINT ( 'NONE',  ( -7.778174593052020747, -7.778174593052023411, 100.1874999999999858 ) ) ;
#1155 = CARTESIAN_POINT ( 'NONE',  ( 2.765530957081996366, 296.2968750017070079, -6.676582343750002480 ) ) ;
#1154 = CARTESIAN_POINT ( 'NONE',  ( 26.34314575050758833, 202.6875000027311842, 165.9999999999998863 ) ) ;
#1153 = LINE ( 'NONE', #19215, #71153 ) ;
#1156 = CARTESIAN_POINT ( 'NONE',  ( -8.660254037844390851, 132.9166666666666856, 4.999999999999998224 ) ) ;
#1157 = CARTESIAN_POINT ( 'NONE',  ( -3.313708498984762496, 98.28125000000000000, 7.999999999999998224 ) ) ;
#1158 = CARTESIAN_POINT ( 'NONE',  ( 2.449293598294707893E-16, 0.2500000000000001665, -4.000000000000001776 ) ) ;
#1159 = CARTESIAN_POINT ( 'NONE',  ( 11.00000000000000000, 1.347111479062088405E-15, 78.24999999999998579 ) ) ;
#1160 = CARTESIAN_POINT ( 'NONE',  ( 4.242640687119285658, 290.6875000034139589, -4.242640687119286547 ) ) ;
#1161 = ADVANCED_FACE ( 'NONE', ( #45741 ), #17816, .F. ) ;
#1162 = CARTESIAN_POINT ( 'NONE',  ( 24.54126587500000056, 201.1250000013656347, 168.5673454167822172 ) ) ;
#1163 = CARTESIAN_POINT ( 'NONE',  ( -2.977408999572654480, 6.374999997951610098, 7.188101187499999156 ) ) ;
#1164 = CARTESIAN_POINT ( 'NONE',  ( -5.662595241051933570, -5.662595241051936235, 4.200615283940629219 ) ) ;
#1165 = CARTESIAN_POINT ( 'NONE',  ( -2.977408999572650927, 116.7500000020483810, -7.188101187500000933 ) ) ;
#1167 = CARTESIAN_POINT ( 'NONE',  ( 0.4917886453872676866, 194.6170594543941093, 201.5920499129032351 ) ) ;
#1166 = DIRECTION ( 'NONE',  ( 0.000000000000000000, 0.000000000000000000, -1.000000000000000000 ) ) ;
#1168 = CARTESIAN_POINT ( 'NONE',  ( -3.042071309553159075, 225.2604166700806161, 11.35316468749999963 ) ) ;
#1169 = CARTESIAN_POINT ( 'NONE',  ( 4.898587196589415787E-16, 0.000000000000000000, 4.000000000000001776 ) ) ;
#1170 = CARTESIAN_POINT ( 'NONE',  ( -6.735557395310442023E-16, 11.00000000000000000, 86.12499999999998579 ) ) ;
#1171 = CARTESIAN_POINT ( 'NONE',  ( 24.00000000000000355, 199.6875000000000000, 168.3431457505075173 ) ) ;
#1172 = CARTESIAN_POINT ( 'NONE',  ( 8.311093377946837890, 31.40624999658601624, -8.311093377946837890 ) ) ;
#1173 = CARTESIAN_POINT ( 'NONE',  ( 4.979315568031101868, -10.98159727696820731, -0.02533325329317183752 ) ) ;
#1174 = CARTESIAN_POINT ( 'NONE',  ( 6.951808397369818766E-16, 222.3437499965860127, -11.35316468750000141 ) ) ;
#1175 = DIRECTION ( 'NONE',  ( 1.000000000000000000, 0.000000000000000000, 0.000000000000000000 ) ) ;
#1177 = CARTESIAN_POINT ( 'NONE',  ( -15.99999999999999645, -16.00000000000000355, 20.00000000000000000 ) ) ;
#1176 = CARTESIAN_POINT ( 'NONE',  ( 5.000000000000000000, -16.24494643555759410, 69.83755725260752456 ) ) ;
#1178 = VERTEX_POINT ( 'NONE', #69878 ) ;
#1179 = CARTESIAN_POINT ( 'NONE',  ( -3.458734125000015869, 198.1875000013655779, 142.0000000000000568 ) ) ;
#1180 = CARTESIAN_POINT ( 'NONE',  ( -11.35316468750000141, 38.28124999658601979, -1.390361679473963753E-15 ) ) ;
#1181 = CARTESIAN_POINT ( 'NONE',  ( 7.778174593052021635, 7.778174593052023411, 87.62500000409677625 ) ) ;
#1182 = CARTESIAN_POINT ( 'NONE',  ( 3.458734124999960358, 208.6250000013656063, 143.4326545832176976 ) ) ;
#1183 = CYLINDRICAL_SURFACE ( 'NONE', #3487, 8.000000000000000000 ) ;
#1184 = CARTESIAN_POINT ( 'NONE',  ( 11.00000000000000000, 1.347111479062088405E-15, 103.9375000040967763 ) ) ;
#1186 = CARTESIAN_POINT ( 'NONE',  ( 3.042071309553167513, 16.82291666325268054, -11.35316468749999785 ) ) ;
#1185 = CARTESIAN_POINT ( 'NONE',  ( -4.401442555609581635E-16, 107.2812500020483810, -7.188101187500000044 ) ) ;
#1187 = CARTESIAN_POINT ( 'NONE',  ( -7.999999999999991118, 0.000000000000000000, 15.83030277982336642 ) ) ;
#1188 = CARTESIAN_POINT ( 'NONE',  ( -5.676582343750006032, 149.1145833299193555, 9.832129032723418760 ) ) ;
#1189 = EDGE_CURVE ( 'NONE', #59197, #7770, #19801, .T. ) ;
#1190 = CARTESIAN_POINT ( 'NONE',  ( -1.836970198721029983E-15, 115.6249999931720396, 10.00000000000000178 ) ) ;
#1191 = CARTESIAN_POINT ( 'NONE',  ( 2.977408999572654480, 117.5000000020483810, 7.188101187499999156 ) ) ;
#1192 = CARTESIAN_POINT ( 'NONE',  ( 10.00000000000000178, 171.8749999931720538, 0.000000000000000000 ) ) ;
#1193 = CARTESIAN_POINT ( 'NONE',  ( -31.45873412499999944, 205.9375000013656063, 170.0000000000003979 ) ) ;
#1194 = ORIENTED_EDGE ( 'NONE', *, *, #15500, .T. ) ;
#1195 = CARTESIAN_POINT ( 'NONE',  ( 11.35316468749999785, 10.88541666325268409, 3.042071309553174174 ) ) ;
#1196 = EDGE_CURVE ( 'NONE', #36272, #64551, #47957, .T. ) ;
#1197 = ORIENTED_EDGE ( 'NONE', *, *, #65708, .F. ) ;
#1198 = FACE_OUTER_BOUND ( 'NONE', #54810, .T. ) ;
#1199 = CARTESIAN_POINT ( 'NONE',  ( 6.676582343750003368, 297.0156250017070079, -2.765530957081997254 ) ) ;
#1201 = CARTESIAN_POINT ( 'NONE',  ( 11.35316468749999963, 140.9895833299193555, -3.042071309553165293 ) ) ;
#1200 = CARTESIAN_POINT ( 'NONE',  ( -5.656854249492378806, 108.6874999999999858, 5.656854249492381470 ) ) ;
#1202 = CARTESIAN_POINT ( 'NONE',  ( -5.656854249492373476, -5.656854249492376141, 16.07405278432982954 ) ) ;
#1203 = CARTESIAN_POINT ( 'NONE',  ( -6.735557395310442023E-16, 11.00000000000000000, 90.81250000409676204 ) ) ;
#1204 = AXIS2_PLACEMENT_3D ( 'NONE', #1366, #71469, #60161 ) ;
#1205 = CARTESIAN_POINT ( 'NONE',  ( 8.311093377946834337, 247.0312500034139873, -8.311093377946836114 ) ) ;
#1206 = CARTESIAN_POINT ( 'NONE',  ( -7.204075437095967871, 7.204075437095967871, 91.84375000204838102 ) ) ;
#1207 = EDGE_LOOP ( 'NONE', ( #17720, #16811, #4703, #17131 ) ) ;
#1208 = ADVANCED_FACE ( 'NONE', ( #71333, #13616 ), #54382, .F. ) ;
#1209 = CARTESIAN_POINT ( 'NONE',  ( -7.320508075688778149, 204.9999999931720254, 7.320508075688769267 ) ) ;
#1210 = PLANE ( 'NONE',  #5022 ) ;
#1211 = EDGE_CURVE ( 'NONE', #55047, #16735, #36653, .T. ) ;
#1212 = CARTESIAN_POINT ( 'NONE',  ( -9.832129032723420536, 84.01041666325268409, 5.676582343749997150 ) ) ;
#1213 = B_SPLINE_CURVE_WITH_KNOTS ( 'NONE', 3,
 ( #46197, #28844, #58645, #208, #69213, #18271, #40914, #40541, #68466, #63925, #69963, #40173, #41286, #63546, #12235, #28100, #34159, #64296, #11871, #22805, #34536, #57542, #51867, #34907, #57159, #12603, #39793, #28477, #57915, #5851, #35272, #6224, #29227, #23556, #35630, #46567, #58285, #51115, #16766, #62797, #51485, #74496 ),
 .UNSPECIFIED., .F., .F.,
 ( 4, 2, 2, 2, 2, 2, 2, 2, 2, 2, 2, 2, 2, 2, 2, 2, 2, 2, 2, 2, 4 ),
 ( 0.02713212987092798040, 0.02960632640565482795, 0.03208052294038167551, 0.03455471947510850572, 0.03702891600983534287, 0.03826601427719878573, 0.03950311254456222859, 0.04197730907928907268, 0.04321440734665251554, 0.04445150561401595146, 0.04692570214874285106, 0.04816280041610629392, 0.04939989868346973678, 0.05187409521819663638, 0.05434829175292353598, 0.05682248828765043558, 0.05805958655501387844, 0.05929668482237732130, 0.06177088135710420702, 0.06424507789183110662, 0.06671927442655799234 ),
 .UNSPECIFIED. ) ;
#1214 = CARTESIAN_POINT ( 'NONE',  ( -10.18810118749999916, 0.000000000000000000, 102.1562500020483810 ) ) ;
#1215 = CARTESIAN_POINT ( 'NONE',  ( 4.541265875000002339, 17.43749999863440792, 0.000000000000000000 ) ) ;
#1216 = VERTEX_POINT ( 'NONE', #2315 ) ;
#1217 = VERTEX_POINT ( 'NONE', #71703 ) ;
#1218 = CARTESIAN_POINT ( 'NONE',  ( 7.999999999999998224, 4.406250000000000000, 3.313708498984766493 ) ) ;
#1219 = CARTESIAN_POINT ( 'NONE',  ( 4.541265875000002339, 0.4374999986344068059, 0.000000000000000000 ) ) ;
#1220 = CARTESIAN_POINT ( 'NONE',  ( 7.188101187500001821, 3.562499997951610542, -2.977408999572650483 ) ) ;
#1221 = CARTESIAN_POINT ( 'NONE',  ( 1.469576158976823947E-15, 119.5625000040967763, 8.000000000000000000 ) ) ;
#1222 = CARTESIAN_POINT ( 'NONE',  ( -7.204075437095965206, -7.204075437095968759, 101.2187500020483668 ) ) ;
#1223 = PRODUCT ( 'screw', 'screw', '', ( #51605 ) ) ;
#1224 = CARTESIAN_POINT ( 'NONE',  ( -4.000000000000002665, 0.5625000000000002220, 1.656854249492380804 ) ) ;
#1225 = CARTESIAN_POINT ( 'NONE',  ( 2.449293598294707893E-16, 12.99999999726881406, -4.000000000000001776 ) ) ;
#1226 = LINE ( 'NONE', #29880, #67407 ) ;
#1227 = ORIENTED_EDGE ( 'NONE', *, *, #62624, .F. ) ;
#1228 = EDGE_CURVE ( 'NONE', #23857, #38745, #61384, .T. ) ;
#1229 = DIRECTION ( 'NONE',  ( -0.000000000000000000, 1.000000000000000000, 4.476705744456276341E-16 ) ) ;
#1230 = CARTESIAN_POINT ( 'NONE',  ( 1.432654583217664479, 198.7500000013656063, 201.4587341250000065 ) ) ;
#1231 = ADVANCED_FACE ( 'NONE', ( #8720 ), #20514, .F. ) ;
#1233 = CYLINDRICAL_SURFACE ( 'NONE', #14076, 10.00000000000000178 ) ;
#1232 = CARTESIAN_POINT ( 'NONE',  ( -25.55430564589122966, 199.3125000013656063, 167.5543056458915032 ) ) ;
#1234 = CARTESIAN_POINT ( 'NONE',  ( -3.211159895383562723, 14.93749999863440792, 3.211159895383561391 ) ) ;
#1235 = CARTESIAN_POINT ( 'NONE',  ( 1.714505518806294638E-15, 0.000000000000000000, -14.00000000000000000 ) ) ;
#1236 = CARTESIAN_POINT ( 'NONE',  ( 2.977408999572650927, -7.188101187499990274, 12.45530278187175277 ) ) ;
#1237 = ORIENTED_EDGE ( 'NONE', *, *, #15505, .F. ) ;
#1238 = EDGE_CURVE ( 'NONE', #27473, #33233, #43075, .T. ) ;
#1239 = VERTEX_POINT ( 'NONE', #43744 ) ;
#1240 = CARTESIAN_POINT ( 'NONE',  ( -10.18810118749999738, -4.220049686691941915, 102.2500000020483810 ) ) ;
#1241 = DIRECTION ( 'NONE',  ( 0.000000000000000000, 0.000000000000000000, 1.000000000000000000 ) ) ;
#1242 = CARTESIAN_POINT ( 'NONE',  ( -31.99999999999998579, 206.3125000000000284, 171.6568542494928238 ) ) ;
#1243 = CARTESIAN_POINT ( 'NONE',  ( 2.445694354108839619, 199.8125000013656063, 200.4456943541088663 ) ) ;
#1244 = CARTESIAN_POINT ( 'NONE',  ( 31.45873412499999233, 196.6875000013655779, 169.9999999999998863 ) ) ;
#1245 = CARTESIAN_POINT ( 'NONE',  ( 7.320508075688771044, 99.37500000000000000, 7.320508075688775484 ) ) ;
#1246 = AXIS2_PLACEMENT_3D ( 'NONE', #47272, #48380, #71383 ) ;
#1247 = CARTESIAN_POINT ( 'NONE',  ( 5.656854249492379694, 116.9375000000000000, -5.656854249492380582 ) ) ;
#1248 = CARTESIAN_POINT ( 'NONE',  ( -8.311093377946836114, 67.96874999658602690, -8.311093377946837890 ) ) ;
#1249 = CARTESIAN_POINT ( 'NONE',  ( -2.765530957081996810, 295.4218750017069510, -6.676582343750003368 ) ) ;
#1250 = ORIENTED_EDGE ( 'NONE', *, *, #4932, .T. ) ;
#1251 = CARTESIAN_POINT ( 'NONE',  ( -11.00000000000010303, -4.556349186103947346, 109.0937499999999858 ) ) ;
#1252 = CARTESIAN_POINT ( 'NONE',  ( -8.000000000000001776, 14.15624999590322730, 3.313708498984759387 ) ) ;
#1253 = CARTESIAN_POINT ( 'NONE',  ( -1.432654583217664479, 206.7500000013655779, 138.5412658750000787 ) ) ;
#1254 = CARTESIAN_POINT ( 'NONE',  ( 8.660254037844392627, 84.58333333333334281, 5.000000000000010658 ) ) ;
#1255 =( LENGTH_UNIT ( ) NAMED_UNIT ( * ) SI_UNIT ( .MILLI., .METRE. ) );
#1256 = CARTESIAN_POINT ( 'NONE',  ( -10.00000000000000000, 229.7916666666666572, -2.679491924311226292 ) ) ;
#1257 = CARTESIAN_POINT ( 'NONE',  ( -4.556349186104045934, 11.00000000000000000, 72.90625000409677625 ) ) ;
#1258 = CARTESIAN_POINT ( 'NONE',  ( -7.204075437095967871, 7.204075437095967871, 69.34375000204836681 ) ) ;
#1259 = CARTESIAN_POINT ( 'NONE',  ( 4.999999999999993783, 214.1666666666666856, 8.660254037844390851 ) ) ;
#1260 = CARTESIAN_POINT ( 'NONE',  ( -2.977408999572647819, 7.188101187499992051, 12.08030278187175277 ) ) ;
#1261 = CARTESIAN_POINT ( 'NONE',  ( -5.676582343750006032, 179.4270833299193555, 9.832129032723418760 ) ) ;
#1262 = CARTESIAN_POINT ( 'NONE',  ( 4.541265875000001451, 3.249999998634406584, 1.881053915767124440 ) ) ;
#1263 = CARTESIAN_POINT ( 'NONE',  ( -2.980505758208118028, -44.60553437943509891, 151.2351892632412103 ) ) ;
#1265 = DIRECTION ( 'NONE',  ( -1.000000000000000000, 0.000000000000000000, 0.000000000000000000 ) ) ;
#1264 = DIRECTION ( 'NONE',  ( -0.000000000000000000, 1.000000000000000000, 4.476705744456276341E-16 ) ) ;
#1266 = EDGE_LOOP ( 'NONE', ( #5013, #66794 ) ) ;
#1267 = CARTESIAN_POINT ( 'NONE',  ( 2.445694354108784108, 208.5625000013656063, 144.4456943541088663 ) ) ;
#1268 = CARTESIAN_POINT ( 'NONE',  ( 6.951808397369818766E-16, 32.34374999658601268, -11.35316468750000141 ) ) ;
#1269 = CARTESIAN_POINT ( 'NONE',  ( -6.735557395310442023E-16, 11.00000000000000000, 107.3125000040967905 ) ) ;
#1270 = CARTESIAN_POINT ( 'NONE',  ( 8.311093377946837890, 221.7187499965860127, -8.311093377946837890 ) ) ;
#1271 = CARTESIAN_POINT ( 'NONE',  ( -30.44569435410887337, 206.5625000013656063, 167.5543056458916169 ) ) ;
#1272 = CARTESIAN_POINT ( 'NONE',  ( -10.00000000000000178, 124.3749999931720396, -1.224646799147353454E-15 ) ) ;
#1274 = DIRECTION ( 'NONE',  ( -0.000000000000000000, 1.000000000000000000, -4.476705744456276341E-16 ) ) ;
#1273 = CARTESIAN_POINT ( 'NONE',  ( 1.320432766682874540E-15, 121.5312500020483810, 7.188101187500000044 ) ) ;
#1275 = CARTESIAN_POINT ( 'NONE',  ( 13.99999999999999822, 2.249999999994893862, 10.23492587299426404 ) ) ;
#1276 = AXIS2_PLACEMENT_3D ( 'NONE', #34561, #11159, #68491 ) ;
#1277 =( BOUNDED_CURVE ( )  B_SPLINE_CURVE ( 2, ( #39492, #45145, #46256, #68156, #74183, #51927, #265, #39856, #16455 ),
 .UNSPECIFIED., .F., .F. ) 
 B_SPLINE_CURVE_WITH_KNOTS ( ( 3, 2, 2, 2, 3 ),
 ( 0.2166666666666669516, 0.2250000000000002554, 0.2333333333333335313, 0.2416666666666668073, 0.2500000000000001110 ),
 .UNSPECIFIED. ) 
 CURVE ( )  GEOMETRIC_REPRESENTATION_ITEM ( )  RATIONAL_B_SPLINE_CURVE ( ( 0.9999999999999974465, 0.9238795325112892920, 1.000000000000000000, 0.9238795325112867385, 1.000000000000000000, 0.9238795325112867385, 1.000000000000000000, 0.9238795325112857393, 1.000000000000001110 ) ) 
 REPRESENTATION_ITEM ( '' )  );
#1278 = EDGE_CURVE ( 'NONE', #39383, #68267, #50313, .T. ) ;
#1279 = CARTESIAN_POINT ( 'NONE',  ( -1.836970198721029983E-15, 70.62499999317203958, 10.00000000000000178 ) ) ;
#1280 = CARTESIAN_POINT ( 'NONE',  ( 5.082755093536325042, 98.09375000204838102, -5.082755093536325930 ) ) ;
#1281 = CARTESIAN_POINT ( 'NONE',  ( 4.541265875000001451, 18.37499999863441147, 1.881053915767124440 ) ) ;
#1282 = CARTESIAN_POINT ( 'NONE',  ( -7.347880794884122694E-16, 10.75000000000000000, 4.000000000000001776 ) ) ;
#1283 = CYLINDRICAL_SURFACE ( 'NONE', #13157, 10.00000000000000178 ) ;
#1284 = DIRECTION ( 'NONE',  ( 1.000000000000000000, 0.000000000000000000, 0.000000000000000000 ) ) ;
#1285 = ORIENTED_EDGE ( 'NONE', *, *, #28712, .F. ) ;
#1286 = ORIENTED_EDGE ( 'NONE', *, *, #51863, .T. ) ;
#1287 = CARTESIAN_POINT ( 'NONE',  ( -4.088227598258586603E-16, 297.3593750017070079, -6.676582343750001591 ) ) ;
#1288 = DIRECTION ( 'NONE',  ( -0.000000000000000000, -0.000000000000000000, 1.000000000000000000 ) ) ;
#1289 = DIRECTION ( 'NONE',  ( 0.000000000000000000, 0.000000000000000000, 1.000000000000000000 ) ) ;
#1290 = CARTESIAN_POINT ( 'NONE',  ( -5.676582343749998039, 157.4479166632526983, -9.832129032723420536 ) ) ;
#1291 = CARTESIAN_POINT ( 'NONE',  ( 10.18810118749999916, 4.220049686691935698, 85.00000000204838102 ) ) ;
#1292 = CARTESIAN_POINT ( 'NONE',  ( 3.313708498984756279, 7.999999999999991118, 9.361552779823366421 ) ) ;
#1293 = CARTESIAN_POINT ( 'NONE',  ( -3.999999999999960032, 204.0000000000000284, 198.0000000000000284 ) ) ;
#1294 = DIRECTION ( 'NONE',  ( -0.000000000000000000, 1.000000000000000000, 4.689100369878284071E-30 ) ) ;
#1295 = CARTESIAN_POINT ( 'NONE',  ( -6.238412754330611322E-16, 10.18810118749999916, 109.6562500020483668 ) ) ;
#1296 = ORIENTED_EDGE ( 'NONE', *, *, #23196, .T. ) ;
#1297 = AXIS2_PLACEMENT_3D ( 'NONE', #53284, #8736, #42682 ) ;
#1298 = CARTESIAN_POINT ( 'NONE',  ( 5.676582343749993598, 135.2604166632526983, 9.832129032723422313 ) ) ;
#1299 = CARTESIAN_POINT ( 'NONE',  ( 1.432654583217662259, 199.1250000013656347, 194.5412658750000219 ) ) ;
#1300 = CARTESIAN_POINT ( 'NONE',  ( 1.432654583217664701, 209.0000000013656063, 201.4587341250000065 ) ) ;
#1301 = CARTESIAN_POINT ( 'NONE',  ( -7.204075437095967871, 7.204075437095967871, 76.84375000204838102 ) ) ;
#1302 = CARTESIAN_POINT ( 'NONE',  ( 5.676582343750001591, 46.92708332991934839, -9.832129032723420536 ) ) ;
#1303 = ORIENTED_EDGE ( 'NONE', *, *, #27274, .T. ) ;
#1304 = CARTESIAN_POINT ( 'NONE',  ( 7.778174593052023411, -7.778174593052021635, 94.75000000409677625 ) ) ;
#1305 = CARTESIAN_POINT ( 'NONE',  ( 4.541265875000002339, 5.437499998634407028, 0.000000000000000000 ) ) ;
#1306 = CARTESIAN_POINT ( 'NONE',  ( 3.317071493978877683, 8.008118988124991233, 12.54436528394063011 ) ) ;
#1307 = CARTESIAN_POINT ( 'NONE',  ( 2.977408999572651815, 18.18749999795161187, 7.188101187500000933 ) ) ;
#1308 = EDGE_CURVE ( 'NONE', #2093, #60340, #7533, .T. ) ;
#1309 = CARTESIAN_POINT ( 'NONE',  ( -6.000000000000000888, 291.1250000034140157, 2.485281374238575758 ) ) ;
#1310 = DIRECTION ( 'NONE',  ( 0.000000000000000000, 1.000000000000000000, 4.283267841918042741E-17 ) ) ;
#1311 = CARTESIAN_POINT ( 'NONE',  ( 4.401442555609581635E-16, 11.71874999795161010, -7.188101187500000044 ) ) ;
#1312 = CARTESIAN_POINT ( 'NONE',  ( 7.188101187499993827, -2.977408999572645598, 11.14280278187175455 ) ) ;
#1313 = CARTESIAN_POINT ( 'NONE',  ( -10.18810118749999916, 4.220049686691934809, 70.56250000204836681 ) ) ;
#1314 = CARTESIAN_POINT ( 'NONE',  ( -30.44569435410879166, 205.0625000013656063, 172.4456943541092357 ) ) ;
#1315 = CARTESIAN_POINT ( 'NONE',  ( -46.67364751762349329, 146.0000000000000000, 69.99999999999997158 ) ) ;
#1316 = CARTESIAN_POINT ( 'NONE',  ( -2.828427124746190735, 2.124999997268813168, -2.828427124746191623 ) ) ;
#1317 = ORIENTED_EDGE ( 'NONE', *, *, #21072, .T. ) ;
#1318 = CARTESIAN_POINT ( 'NONE',  ( 2.828427124746208943, 194.7500000027312126, 195.1715728752538439 ) ) ;
#1319 = EDGE_CURVE ( 'NONE', #39861, #70940, #23217, .T. ) ;
#1320 = AXIS2_PLACEMENT_3D ( 'NONE', #19498, #54600, #37239 ) ;
#1321 = CARTESIAN_POINT ( 'NONE',  ( 3.999999999999960032, 207.9375000000000000, 143.6568542494924543 ) ) ;
#1322 = CARTESIAN_POINT ( 'NONE',  ( -25.17157287525385811, 203.0000000027312126, 167.1715728752541281 ) ) ;
#1323 = CARTESIAN_POINT ( 'NONE',  ( -4.541265875000002339, 0.7499999986344069169, -1.881053915767121998 ) ) ;
#1324 = CARTESIAN_POINT ( 'NONE',  ( 5.082755093536325042, 116.0937500020483810, -5.082755093536325930 ) ) ;
#1325 = CARTESIAN_POINT ( 'NONE',  ( 38.00000000000000000, 63.00000000000000000, 15.00000000000000178 ) ) ;
#1326 = CARTESIAN_POINT ( 'NONE',  ( -3.313708498984757167, 7.999999999999991118, 0.7365527839201455595 ) ) ;
#1327 = EDGE_LOOP ( 'NONE', ( #36800, #14255 ) ) ;
#1328 = B_SPLINE_CURVE_WITH_KNOTS ( 'NONE', 3,
 ( #68820, #10374, #62049, #23168, #4719, #193, #68451, #46181, #50724, #22046, #45073, #63532, #69198, #40526, #11857, #34892, #57899, #10740, #68088, #50353, #73372, #16377, #7677, #2014, #35987, #7309, #48022 ),
 .UNSPECIFIED., .F., .F.,
 ( 4, 2, 1, 2, 2, 2, 2, 2, 2, 2, 2, 2, 2, 4 ),
 ( -3.898717738006102928E-05, 0.002293416704473783072, 0.004625820586327627180, 0.009290628350035384786, 0.01862024387745089826, 0.02794985940486641174, 0.03261466716857416154, 0.03727947493228192521, 0.04660909045969743175, 0.05593870598711293829, 0.05827110986896676115, 0.06060351375082057707, 0.06526832151452821584, 0.07459793704194357666 ),
 .UNSPECIFIED. ) ;
#1329 = EDGE_CURVE ( 'NONE', #9311, #18027, #60342, .T. ) ;
#1330 = CARTESIAN_POINT ( 'NONE',  ( -2.977408999572654480, 20.99999999795161898, 7.188101187499999156 ) ) ;
#1331 = ORIENTED_EDGE ( 'NONE', *, *, #45834, .T. ) ;
#1332 = CARTESIAN_POINT ( 'NONE',  ( 31.99999999999997868, 200.1875000000000853, 171.6568542494923122 ) ) ;
#1333 = CARTESIAN_POINT ( 'NONE',  ( 8.000000000000000000, 13.50000000000000178, 0.000000000000000000 ) ) ;
#1334 = CARTESIAN_POINT ( 'NONE',  ( 25.55430564589119413, 208.3125000013656063, 172.4456943541087526 ) ) ;
#1335 = CARTESIAN_POINT ( 'NONE',  ( 8.660254037844385522, 59.58333333333333570, 5.000000000000005329 ) ) ;
#1336 = CARTESIAN_POINT ( 'NONE',  ( 5.082755093536326818, 99.59375000204838102, 5.082755093536325042 ) ) ;
#1337 = CARTESIAN_POINT ( 'NONE',  ( -26.34314575050768781, 196.5625000000000000, 174.0000000000004547 ) ) ;
#1339 = CARTESIAN_POINT ( 'NONE',  ( -30.34616037616659057, -42.98117801685430095, 176.3648267577018771 ) ) ;
#1338 = CARTESIAN_POINT ( 'NONE',  ( 11.00000000000000000, 8.673617379884037444E-16, 41.99999999999999289 ) ) ;
#1340 = ORIENTED_EDGE ( 'NONE', *, *, #49128, .F. ) ;
#1341 = CARTESIAN_POINT ( 'NONE',  ( 5.676582343749997150, 232.2395833367473301, -9.832129032723418760 ) ) ;
#1342 = CARTESIAN_POINT ( 'NONE',  ( -4.401442555609577197E-16, 7.188101187499992051, 14.98655278187175455 ) ) ;
#1343 = CARTESIAN_POINT ( 'NONE',  ( 4.336811714528937323, 52.00708776950180123, 48.85034107298458395 ) ) ;
#1344 = CARTESIAN_POINT ( 'NONE',  ( -28.00000000000007816, 204.1250000027312126, 166.0000000000003695 ) ) ;
#1345 = CARTESIAN_POINT ( 'NONE',  ( 26.15334609510014019, 194.8133403918676834, 166.6418648200710209 ) ) ;
#1346 = CARTESIAN_POINT ( 'NONE',  ( -5.000000000000005329, 140.2083333265053682, 8.660254037844387298 ) ) ;
#1347 = CARTESIAN_POINT ( 'NONE',  ( 10.00000000000000178, 180.0000000000000284, 0.000000000000000000 ) ) ;
#1348 = LINE ( 'NONE', #19401, #58660 ) ;
#1349 = CARTESIAN_POINT ( 'NONE',  ( 3.313708498984869077, 91.53125000000000000, -7.999999999999892530 ) ) ;
#1350 = CARTESIAN_POINT ( 'NONE',  ( 1.320432766682872962E-15, -7.188101187499992051, 27.73655278187175455 ) ) ;
#1351 = CARTESIAN_POINT ( 'NONE',  ( 9.832129032723420536, 141.5104166632526699, -5.676582343749999815 ) ) ;
#1352 = CARTESIAN_POINT ( 'NONE',  ( -27.99999999999991118, 199.6250000027312126, 174.0000000000003695 ) ) ;
#1355 = CARTESIAN_POINT ( 'NONE',  ( 2.849036369511732440E-14, 208.2500000000000284, 202.0000000000000000 ) ) ;
#1354 = CARTESIAN_POINT ( 'NONE',  ( 3.313708498984706985, 111.0312500000000284, -8.000000000000055067 ) ) ;
#1353 = CARTESIAN_POINT ( 'NONE',  ( 29.65685424949240101, 206.4375000000000568, 165.9999999999998863 ) ) ;
#1356 = ORIENTED_EDGE ( 'NONE', *, *, #4299, .T. ) ;
#1357 = CARTESIAN_POINT ( 'NONE',  ( 3.369429374625368734, -60.49191766694071504, 23.06312700027830687 ) ) ;
#1358 = VECTOR ( 'NONE', #57601, 1000.000000000000000 ) ;
#1359 = CARTESIAN_POINT ( 'NONE',  ( 5.656854249492376141, -5.656854249492374365, 25.39280277982336642 ) ) ;
#1360 = CARTESIAN_POINT ( 'NONE',  ( 1.432654583217607858, 206.6250000013656063, 138.5412658750000787 ) ) ;
#1361 = CARTESIAN_POINT ( 'NONE',  ( -2.751064625579944321E-14, 202.7500000000000000, 146.0000000000000284 ) ) ;
#1362 = CARTESIAN_POINT ( 'NONE',  ( 7.320508075688771044, 41.24999999317203248, 7.320508075688775484 ) ) ;
#1363 = VECTOR ( 'NONE', #45798, 1000.000000000000000 ) ;
#1364 = CARTESIAN_POINT ( 'NONE',  ( -7.188101187500000044, 116.6562500020483810, 0.000000000000000000 ) ) ;
#1365 = CARTESIAN_POINT ( 'NONE',  ( 3.211159895383561835, 2.562499998634407028, -3.211159895383561835 ) ) ;
#1366 = CARTESIAN_POINT ( 'NONE',  ( 0.000000000000000000, 0.000000000000000000, 118.0000000000000000 ) ) ;
#1367 = CARTESIAN_POINT ( 'NONE',  ( -5.656854249492375253, 5.656854249492375253, 14.14280277982336465 ) ) ;
#1369 = CARTESIAN_POINT ( 'NONE',  ( 26.34314575050748530, 196.9375000000000284, 173.9999999999997726 ) ) ;
#1368 = CARTESIAN_POINT ( 'NONE',  ( -11.00000000000010658, 4.556349186103942017, 101.5937500040967763 ) ) ;
#1370 = ORIENTED_EDGE ( 'NONE', *, *, #537, .T. ) ;
#1371 =( BOUNDED_CURVE ( )  B_SPLINE_CURVE ( 2, ( #6092, #44592, #11373, #57410, #4603, #27981, #45694, #45326, #57035, #22301, #74366, #51356, #5347 ),
 .UNSPECIFIED., .F., .F. ) 
 B_SPLINE_CURVE_WITH_KNOTS ( ( 3, 2, 2, 2, 2, 2, 3 ),
 ( 2.621882283550707182, 2.627116002474152889, 2.632349721397599041, 2.637583440321044304, 2.642817159244490011, 2.648050878167936162, 2.653284597091381869 ),
 .UNSPECIFIED. ) 
 CURVE ( )  GEOMETRIC_REPRESENTATION_ITEM ( )  RATIONAL_B_SPLINE_CURVE ( ( 1.000000000000350830, 0.9659258262887174817, 1.000000000000000000, 0.9659258262890683122, 1.000000000000000000, 0.9659258262890683122, 1.000000000000000000, 0.9659258262890683122, 1.000000000000000000, 0.9659258262890683122, 1.000000000000000000, 0.9659258262890662028, 1.000000000000001998 ) ) 
 REPRESENTATION_ITEM ( '' )  );
#1372 = DIRECTION ( 'NONE',  ( -1.000000000000000000, -0.000000000000000000, -0.000000000000000000 ) ) ;
#1373 = DIRECTION ( 'NONE',  ( 0.000000000000000000, 0.000000000000000000, 1.000000000000000000 ) ) ;
#1374 = AXIS2_PLACEMENT_3D ( 'NONE', #28797, #5061, #28057 ) ;
#1375 = CARTESIAN_POINT ( 'NONE',  ( 8.000000000000000000, 109.2500000000000000, -9.797174393178825657E-16 ) ) ;
#1376 = CARTESIAN_POINT ( 'NONE',  ( -11.35316468749999608, 244.4270833367473017, 3.042071309553173730 ) ) ;
#1377 = CARTESIAN_POINT ( 'NONE',  ( 9.832129032723416984, 120.3645833299193697, 5.676582343750006032 ) ) ;
#1378 = VERTEX_POINT ( 'NONE', #55451 ) ;
#1379 = CARTESIAN_POINT ( 'NONE',  ( -3.652275167153403945, 10.24818182827785229, 117.6308536796923363 ) ) ;
#1380 = CARTESIAN_POINT ( 'NONE',  ( -6.238412754330611322E-16, 10.18810118749999916, 100.2812500020483810 ) ) ;
#1381 = DIRECTION ( 'NONE',  ( -0.000000000000000000, -1.000000000000000000, -0.000000000000000000 ) ) ;
#1382 = CARTESIAN_POINT ( 'NONE',  ( -1.432654583217608080, 198.8750000013656347, 201.4587341250000350 ) ) ;
#1383 = LINE ( 'NONE', #63997, #11885 ) ;
#1385 = CARTESIAN_POINT ( 'NONE',  ( -9.832129032723420536, 113.6979166632526983, 5.676582343749997150 ) ) ;
#1384 = CARTESIAN_POINT ( 'NONE',  ( 0.000000000000000000, 125.0000000000000000, 0.000000000000000000 ) ) ;
#1386 = CARTESIAN_POINT ( 'NONE',  ( -7.999999999999991118, 3.313708498984756723, 6.924052783920144449 ) ) ;
#1387 = CARTESIAN_POINT ( 'NONE',  ( -31.45873412499999944, 196.8750000013656063, 168.5673454167827572 ) ) ;
#1388 = CARTESIAN_POINT ( 'NONE',  ( -1.469576158976823947E-15, 26.43749999590322375, 8.000000000000000000 ) ) ;
#1389 = VERTEX_POINT ( 'NONE', #37725 ) ;
#1390 = CARTESIAN_POINT ( 'NONE',  ( -10.00000000000000355, 199.5833333265053398, 2.679491924311223183 ) ) ;
#1391 = CARTESIAN_POINT ( 'NONE',  ( 27.99999999999999645, 210.0000000000000284, 169.9999999999999147 ) ) ;
#1392 = CARTESIAN_POINT ( 'NONE',  ( 46.46053351546693477, 188.1068786666309336, 71.39178048200128046 ) ) ;
#1393 = CARTESIAN_POINT ( 'NONE',  ( -8.311093377946836114, 107.9687499965860269, -8.311093377946837890 ) ) ;
#1394 = CARTESIAN_POINT ( 'NONE',  ( 0.000000000000000000, 0.000000000000000000, 0.000000000000000000 ) ) ;
#1395 = CARTESIAN_POINT ( 'NONE',  ( 7.188101187499999156, 9.749999997951610098, 2.977408999572654924 ) ) ;
#1396 = CARTESIAN_POINT ( 'NONE',  ( -10.18810118749999738, -4.220049686691941915, 98.12500000204838102 ) ) ;
#1397 = CARTESIAN_POINT ( 'NONE',  ( -11.35316468750000141, 3.593749996586016682, -1.390361679473963753E-15 ) ) ;
#1399 = ORIENTED_EDGE ( 'NONE', *, *, #29993, .F. ) ;
#1398 =( BOUNDED_CURVE ( )  B_SPLINE_CURVE ( 2, ( #23400, #57756, #70539, #47513, #6798, #57380, #5690, #41497, #6439, #41131, #12446, #28688, #17365, #17738, #51702, #23032, #30176, #52088, #790, #18117, #48, #35478, #40388, #35845, #63762, #6061, #41861, #63387, #58859, #34751, #64138, #46041, #29067, #69060, #420, #69429, #11711, #53193, #24133, #29441, #46415, #52820, #12080, #35116, #58130, #52452, #1529, #23774, #58492, #46777, #69801, #18854, #29810, #1155, #70178, #71630, #48253, #3362, #60319, #20703, #60701, #36577, #9021, #25972, #43721, #43336, #26352, #19579, #7903, #13908, #66356, #2242, #42594, #72005, #13175, #13538, #48995, #37701, #42222, #49373, #54309, #36211, #59228, #20320, #59952, #19952, #65980, #7540, #70902, #71260, #30546, #1878, #32035, #30909, #2620, #42961, #53562, #14284, #65234, #37322, #14660, #59590, #24864, #19217, #55055, #53929, #8647, #47883, #25236, #65609, #36947, #8267, #31281, #72390, #2988, #25610, #48623, #31661, #54682, #21450, #50128, #66734, #73886, #10140, #44847, #73144, #67486, #5235, #15039, #51244, #44473, #32796, #38075, #10515, #3738, #74255, #15784, #55429, #38821, #28236, #72774, #62557, #22190, #22563, #67112, #10888, #4120, #61074, #61822, #26737, #39563, #67854, #33178, #4865, #45215, #56922, #27861, #39184, #9396, #33922, #68226, #32416, #56176, #9777, #49757, #38447, #16523, #4489, #21080, #44104, #27480, #15407, #50494, #27113, #61450, #55804, #73507, #21814, #16145, #62188, #33547, #56548, #50870, #68974, #23318, #46330, #35035, #6720, #64058, #34291, #35404, #40300, #707 ),
 .UNSPECIFIED., .F., .F. ) 
 B_SPLINE_CURVE_WITH_KNOTS ( ( 3, 2, 2, 2, 2, 2, 2, 2, 2, 2, 2, 2, 2, 2, 2, 2, 2, 2, 2, 2, 2, 2, 2, 2, 2, 2, 2, 2, 2, 2, 2, 2, 2, 2, 2, 2, 2, 2, 2, 2, 2, 2, 2, 2, 2, 2, 2, 2, 2, 2, 2, 2, 2, 2, 2, 2, 2, 2, 2, 2, 2, 2, 2, 2, 2, 2, 2, 2, 2, 2, 2, 2, 2, 2, 2, 2, 2, 2, 2, 2, 2, 2, 2, 2, 2, 2, 2, 2, 2, 2, 2, 2, 2, 2, 2, 2, 3 ),
 ( 0.000000000000000000, 0.01041666666666666609, 0.02083333333333333218, 0.03125000000000000000, 0.04166666666666666435, 0.05208333333333333565, 0.06250000000000000000, 0.07291666666666667129, 0.08333333333333332871, 0.09375000000000000000, 0.1041666666666666713, 0.1145833333333333287, 0.1250000000000000000, 0.1354166666666666574, 0.1458333333333333426, 0.1562500000000000000, 0.1666666666666666574, 0.1770833333333333426, 0.1875000000000000000, 0.1979166666666666574, 0.2083333333333333426, 0.2187500000000000000, 0.2291666666666666574, 0.2395833333333333426, 0.2500000000000000000, 0.2604166666666666852, 0.2708333333333333148, 0.2812500000000000000, 0.2916666666666666852, 0.3020833333333333148, 0.3125000000000000000, 0.3229166666666666852, 0.3333333333333333148, 0.3437500000000000000, 0.3541666666666666852, 0.3645833333333333148, 0.3750000000000000000, 0.3854166666666666852, 0.3958333333333333148, 0.4062500000000000000, 0.4166666666666666852, 0.4270833333333333148, 0.4375000000000000000, 0.4479166666666666852, 0.4583333333333333148, 0.4687500000000000000, 0.4791666666666666852, 0.4895833333333333148, 0.5000000000000000000, 0.5104166666666666297, 0.5208333333333333703, 0.5312500000000000000, 0.5416666666666666297, 0.5520833333333333703, 0.5625000000000000000, 0.5729166666666666297, 0.5833333333333333703, 0.5937500000000000000, 0.6041666666666666297, 0.6145833333333333703, 0.6250000000000000000, 0.6354166666666666297, 0.6458333333333333703, 0.6562500000000000000, 0.6666666666666666297, 0.6770833333333333703, 0.6875000000000000000, 0.6979166666666666297, 0.7083333333333333703, 0.7187500000000000000, 0.7291666666666666297, 0.7395833333333333703, 0.7500000000000000000, 0.7604166666666666297, 0.7708333333333333703, 0.7812500000000000000, 0.7916666666666666297, 0.8020833333333333703, 0.8125000000000000000, 0.8229166666666666297, 0.8333333333333333703, 0.8437500000000000000, 0.8541666666666666297, 0.8645833333333333703, 0.8750000000000000000, 0.8854166666666666297, 0.8958333333333333703, 0.9062500000000000000, 0.9166666666666666297, 0.9270833333333333703, 0.9375000000000000000, 0.9479166666666666297, 0.9583333333333333703, 0.9687500000000000000, 0.9791666666666666297, 0.9895833333333333703, 1.000000000000000000 ),
 .UNSPECIFIED. ) 
 CURVE ( )  GEOMETRIC_REPRESENTATION_ITEM ( )  RATIONAL_B_SPLINE_CURVE ( ( 1.000000000000000000, 0.9238795325112867385, 1.000000000000000000, 0.9238795325112867385, 1.000000000000000000, 0.9238795325112867385, 1.000000000000000000, 0.9238795325112867385, 1.000000000000000000, 0.9238795325112867385, 1.000000000000000000, 0.9238795325112867385, 1.000000000000000000, 0.9238795325112867385, 1.000000000000000000, 0.9238795325112867385, 1.000000000000000000, 0.9238795325112867385, 1.000000000000000000, 0.9238795325112867385, 1.000000000000000000, 0.9238795325112867385, 1.000000000000000000, 0.9238795325112867385, 1.000000000000000000, 0.9238795325112867385, 1.000000000000000000, 0.9238795325112867385, 1.000000000000000000, 0.9238795325112867385, 1.000000000000000000, 0.9238795325112867385, 1.000000000000000000, 0.9238795325112867385, 1.000000000000000000, 0.9238795325112867385, 1.000000000000000000, 0.9238795325112867385, 1.000000000000000000, 0.9238795325112867385, 1.000000000000000000, 0.9238795325112867385, 1.000000000000000000, 0.9238795325112867385, 1.000000000000000000, 0.9238795325112867385, 1.000000000000000000, 0.9238795325112867385, 1.000000000000000000, 0.9238795325112867385, 1.000000000000000000, 0.9238795325112867385, 1.000000000000000000, 0.9238795325112867385, 1.000000000000000000, 0.9238795325112867385, 1.000000000000000000, 0.9238795325112867385, 1.000000000000000000, 0.9238795325112867385, 1.000000000000000000, 0.9238795325112867385, 1.000000000000000000, 0.9238795325112867385, 1.000000000000000000, 0.9238795325112867385, 1.000000000000000000, 0.9238795325112867385, 1.000000000000000000, 0.9238795325112867385, 1.000000000000000000, 0.9238795325112867385, 1.000000000000000000, 0.9238795325112867385, 1.000000000000000000, 0.9238795325112867385, 1.000000000000000000, 0.9238795325112867385, 1.000000000000000000, 0.9238795325112867385, 1.000000000000000000, 0.9238795325112867385, 1.000000000000000000, 0.9238795325112867385, 1.000000000000000000, 0.9238795325112867385, 1.000000000000000000, 0.9238795325112867385, 1.000000000000000000, 0.9238795325112867385, 1.000000000000000000, 0.9238795325112867385, 1.000000000000000000, 0.9238795325112867385, 1.000000000000000000, 0.9238795325112867385, 1.000000000000000000, 0.9238795325112867385, 1.000000000000000000, 0.9238795325112867385, 1.000000000000000000, 0.9238795325112867385, 1.000000000000000000, 0.9238795325112867385, 1.000000000000000000, 0.9238795325112867385, 1.000000000000000000, 0.9238795325112867385, 1.000000000000000000, 0.9238795325112867385, 1.000000000000000000, 0.9238795325112867385, 1.000000000000000000, 0.9238795325112867385, 1.000000000000000000, 0.9238795325112867385, 1.000000000000000000, 0.9238795325112867385, 1.000000000000000000, 0.9238795325112867385, 1.000000000000000000, 0.9238795325112867385, 1.000000000000000000, 0.9238795325112867385, 1.000000000000000000, 0.9238795325112867385, 1.000000000000000000, 0.9238795325112867385, 1.000000000000000000, 0.9238795325112867385, 1.000000000000000000, 0.9238795325112867385, 1.000000000000000000, 0.9238795325112867385, 1.000000000000000000, 0.9238795325112867385, 1.000000000000000000, 0.9238795325112867385, 1.000000000000000000, 0.9238795325112867385, 1.000000000000000000, 0.9238795325112867385, 1.000000000000000000, 0.9238795325112867385, 1.000000000000000000, 0.9238795325112867385, 1.000000000000000000, 0.9238795325112867385, 1.000000000000000000, 0.9238795325112867385, 1.000000000000000000, 0.9238795325112867385, 1.000000000000000000, 0.9238795325112867385, 1.000000000000000000, 0.9238795325112867385, 1.000000000000000000, 0.9238795325112867385, 1.000000000000000000, 0.9238795325112867385, 1.000000000000000000, 0.9238795325112867385, 1.000000000000000000, 0.9238795325112867385, 1.000000000000000000, 0.9238795325112867385, 1.000000000000000000, 0.9238795325112867385, 1.000000000000000000, 0.9238795325112867385, 1.000000000000000000, 0.9238795325112867385, 1.000000000000000000, 0.9238795325112867385, 1.000000000000000000, 0.9238795325112867385, 1.000000000000000000, 0.9238795325112867385, 1.000000000000000000, 0.9238795325112867385, 1.000000000000000000, 0.9238795325112867385, 1.000000000000000000, 0.9238795325112867385, 1.000000000000000000, 0.9238795325112867385, 1.000000000000000000, 0.9238795325112867385, 1.000000000000000000, 0.9238795325112867385, 1.000000000000000000, 0.9238795325112867385, 1.000000000000000000 ) ) 
 REPRESENTATION_ITEM ( '' )  );
#1400 = DIRECTION ( 'NONE',  ( -0.000000000000000000, 1.000000000000000000, -0.000000000000000000 ) ) ;
#1401 = CARTESIAN_POINT ( 'NONE',  ( 8.000000000000000000, 98.93750000409677625, -9.797174393178825657E-16 ) ) ;
#1402 = CARTESIAN_POINT ( 'NONE',  ( -6.735557395310442023E-16, 11.00000000000000000, 102.6250000000000000 ) ) ;
#1403 = CARTESIAN_POINT ( 'NONE',  ( -4.220049686691935698, 10.18810118749999916, 73.75000000204836681 ) ) ;
#1404 = CIRCLE ( 'NONE', #31466, 11.00000000000000355 ) ;
#1405 = CYLINDRICAL_SURFACE ( 'NONE', #24159, 3.999999999999976019 ) ;
#1406 = DIRECTION ( 'NONE',  ( 0.000000000000000000, 0.000000000000000000, 1.000000000000000000 ) ) ;
#1407 = CARTESIAN_POINT ( 'NONE',  ( -6.676582343750000703, 291.5156250017069510, 2.765530957082001251 ) ) ;
#1408 = CARTESIAN_POINT ( 'NONE',  ( -4.217983994790169611, -51.98644305214799743, -48.84278562423040171 ) ) ;
#1409 = CARTESIAN_POINT ( 'NONE',  ( -11.35316468749999785, 208.3854166632526699, -3.042071309553167957 ) ) ;
#1410 = EDGE_CURVE ( 'NONE', #3350, #5379, #66560, .T. ) ;
#1411 = EDGE_CURVE ( 'NONE', #11029, #15561, #48507, .T. ) ;
#1412 = CARTESIAN_POINT ( 'NONE',  ( -4.220049686691935698, 10.18810118749999916, 86.87500000204836681 ) ) ;
#1413 = CARTESIAN_POINT ( 'NONE',  ( -29.43265458321766559, 201.5000000013655779, 166.5412658750003629 ) ) ;
#1414 = CARTESIAN_POINT ( 'NONE',  ( 5.656854249492380582, 24.18750000000000355, -5.656854249492380582 ) ) ;
#1415 = EDGE_LOOP ( 'NONE', ( #48797, #70452, #31649, #37057 ) ) ;
#1416 = CARTESIAN_POINT ( 'NONE',  ( -22.50157160325127847, -50.11546549537403905, 148.6621012010367053 ) ) ;
#1417 = AXIS2_PLACEMENT_3D ( 'NONE', #68435, #17500, #63522 ) ;
#1418 = CARTESIAN_POINT ( 'NONE',  ( 2.828427124746208943, 206.7500000027312126, 195.1715728752538439 ) ) ;
#1419 = CARTESIAN_POINT ( 'NONE',  ( -4.999999999999998224, 31.66666666666666785, -8.660254037844389075 ) ) ;
#1420 = AXIS2_PLACEMENT_3D ( 'NONE', #39706, #32957, #55962 ) ;
#1421 = CARTESIAN_POINT ( 'NONE',  ( -1.300830538084598961E-11, 173.7499999999989768, 10.00000000000000178 ) ) ;
#1422 = CARTESIAN_POINT ( 'NONE',  ( 7.204075437095966983, 7.204075437095967871, 76.46875000204836681 ) ) ;
#1423 = VERTEX_POINT ( 'NONE', #20726 ) ;
#1424 = CARTESIAN_POINT ( 'NONE',  ( 2.977408999572652260, 6.187499997951610986, 7.188101187500000044 ) ) ;
#1425 = VECTOR ( 'NONE', #22117, 1000.000000000000000 ) ;
#1426 = CARTESIAN_POINT ( 'NONE',  ( 6.123233995736767268E-16, 223.1249999931720254, -10.00000000000000178 ) ) ;
#1427 = CARTESIAN_POINT ( 'NONE',  ( 4.556349186104052151, -10.99999999999999822, 93.15625000409677625 ) ) ;
#1428 = CARTESIAN_POINT ( 'NONE',  ( -2.977408999572651815, 120.3125000020483668, 7.188101187500000933 ) ) ;
#1429 = EDGE_CURVE ( 'NONE', #22621, #11774, #13546, .T. ) ;
#1430 = CARTESIAN_POINT ( 'NONE',  ( 0.4589999999999999636, 267.1439999999997212, 5.793779103867645830 ) ) ;
#1431 = CARTESIAN_POINT ( 'NONE',  ( 6.676582343750001591, 296.9531250017069510, -8.176455196517173205E-16 ) ) ;
#1433 = CARTESIAN_POINT ( 'NONE',  ( 0.000000000000000000, -2.500000000000000444, 0.000000000000000000 ) ) ;
#1432 = CARTESIAN_POINT ( 'NONE',  ( 3.042071309553163516, 237.4479166700806729, -11.35316468749999785 ) ) ;
#1434 = ITEM_DEFINED_TRANSFORMATION ( 'NONE', 'NONE', #39347,  #57354 ) ;
#1435 = APPLICATION_CONTEXT ( 'automotive_design' ) ;
#1436 = ORIENTED_EDGE ( 'NONE', *, *, #60922, .F. ) ;
#1437 = CARTESIAN_POINT ( 'NONE',  ( -9.832129032723415207, 239.6354166700806445, 5.676582343750005144 ) ) ;
#1438 = CARTESIAN_POINT ( 'NONE',  ( -5.082755093536317936, -5.082755093536320601, 9.174052781871752771 ) ) ;
#1439 = CARTESIAN_POINT ( 'NONE',  ( -1.432654583217607414, 204.5000000013656063, 194.5412658750000219 ) ) ;
#1440 = ORIENTED_EDGE ( 'NONE', *, *, #10946, .F. ) ;
#1441 = CARTESIAN_POINT ( 'NONE',  ( 3.313708498984765161, 104.6562500040968047, 7.999999999999998224 ) ) ;
#1442 = CARTESIAN_POINT ( 'NONE',  ( -8.311093377946836114, 107.9687499965860269, -8.311093377946837890 ) ) ;
#1443 = CARTESIAN_POINT ( 'NONE',  ( 1.102182119232618108E-15, 295.3125000034140157, 6.000000000000001776 ) ) ;
#1444 = CARTESIAN_POINT ( 'NONE',  ( -4.556349186104047710, -10.99999999999999822, 77.78125000000001421 ) ) ;
#1447 = CARTESIAN_POINT ( 'NONE',  ( -3.313708498984760276, 1.968750000000000444, -8.000000000000000000 ) ) ;
#1446 = CARTESIAN_POINT ( 'NONE',  ( 31.45873412500001010, 205.6250000013656063, 171.4326545832175555 ) ) ;
#1445 = CARTESIAN_POINT ( 'NONE',  ( 25.55430564589115150, 201.5625000013656063, 172.4456943541086957 ) ) ;
#1448 = ORIENTED_EDGE ( 'NONE', *, *, #12284, .F. ) ;
#1449 = VECTOR ( 'NONE', #45886, 1000.000000000000000 ) ;
#1450 = CARTESIAN_POINT ( 'NONE',  ( -24.00000000000002132, 195.9375000027312126, 168.3431457505079152 ) ) ;
#1451 = CARTESIAN_POINT ( 'NONE',  ( -2.679491924311226292, 178.3333333265053966, -10.00000000000000178 ) ) ;
#1452 = CARTESIAN_POINT ( 'NONE',  ( -3.042071309553173730, 209.3229166632526983, 11.35316468749999785 ) ) ;
#1453 = CARTESIAN_POINT ( 'NONE',  ( -1.432654583217662481, 207.1250000013656347, 145.4587341250000634 ) ) ;
#1454 = CARTESIAN_POINT ( 'NONE',  ( 31.45873412499999944, 205.9375000013656063, 169.9999999999999432 ) ) ;
#1455 = CARTESIAN_POINT ( 'NONE',  ( -5.082755093536325042, 20.90624999795161543, -5.082755093536325930 ) ) ;
#1456 = CARTESIAN_POINT ( 'NONE',  ( 3.042071309553159519, 185.0520833299193555, 11.35316468750000141 ) ) ;
#1457 = CARTESIAN_POINT ( 'NONE',  ( -7.188101187500000044, 100.5312500020483810, 0.000000000000000000 ) ) ;
#1458 = CARTESIAN_POINT ( 'NONE',  ( -5.000000000000000000, 61.58609660504401973, -23.68302032025023252 ) ) ;
#1459 = CARTESIAN_POINT ( 'NONE',  ( -32.00000000000000711, 195.1875000000000000, 168.3431457505080004 ) ) ;
#1460 = CARTESIAN_POINT ( 'NONE',  ( 4.541265875000002339, 9.374999998634404363, -1.881053915767121554 ) ) ;
#1461 = CARTESIAN_POINT ( 'NONE',  ( 29.43265458321766914, 201.1250000013656347, 166.5412658749999650 ) ) ;
#1462 = CARTESIAN_POINT ( 'NONE',  ( -4.401442555609577197E-16, 7.188101187499992051, 5.986552781871753659 ) ) ;
#1463 = CARTESIAN_POINT ( 'NONE',  ( -9.832129032723420536, 68.69791666325268409, 5.676582343749997150 ) ) ;
#1464 = CARTESIAN_POINT ( 'NONE',  ( 0.000000000000000000, 28.00000000000000000, 0.000000000000000000 ) ) ;
#1465 = CARTESIAN_POINT ( 'NONE',  ( 2.849036369511732440E-14, 209.2500000000000284, 202.0000000000000000 ) ) ;
#1466 = VERTEX_POINT ( 'NONE', #42984 ) ;
#1467 = DIRECTION ( 'NONE',  ( 0.000000000000000000, 4.476705744456276341E-16, -1.000000000000000000 ) ) ;
#1468 = CARTESIAN_POINT ( 'NONE',  ( 30.82842712474621294, 206.2500000027312126, 172.8284271247460424 ) ) ;
#1469 = CARTESIAN_POINT ( 'NONE',  ( -8.311093377946841443, 73.90624999658601268, 8.311093377946830785 ) ) ;
#1470 = CARTESIAN_POINT ( 'NONE',  ( -4.556349186104045934, 11.00000000000000000, 66.90625000409677625 ) ) ;
#1471 = CARTESIAN_POINT ( 'NONE',  ( -3.458734125000015869, 196.1875000013655779, 142.0000000000000568 ) ) ;
#1472 = CYLINDRICAL_SURFACE ( 'NONE', #62506, 8.000000000000000000 ) ;
#1474 = CARTESIAN_POINT ( 'NONE',  ( -11.35316468750000141, 78.48958332991935549, 3.042071309553159963 ) ) ;
#1473 = CARTESIAN_POINT ( 'NONE',  ( 7.188101187500000044, 90.40625000204838102, -8.802885111219163269E-16 ) ) ;
#1475 = CARTESIAN_POINT ( 'NONE',  ( -7.999999999999989342, -3.313708498984762496, 26.61155278392014978 ) ) ;
#1476 = CARTESIAN_POINT ( 'NONE',  ( -3.275807840863746989, 194.7121737025869095, 140.2366324401471047 ) ) ;
#1477 = CARTESIAN_POINT ( 'NONE',  ( -7.320508075688773708, 158.7499999931720254, -7.320508075688774596 ) ) ;
#1478 = CARTESIAN_POINT ( 'NONE',  ( -7.188101187500000044, 93.03125000204836681, 0.000000000000000000 ) ) ;
#1479 = EDGE_CURVE ( 'NONE', #27743, #58925, #3013, .T. ) ;
#1480 = VECTOR ( 'NONE', #55823, 1000.000000000000000 ) ;
#1481 = CARTESIAN_POINT ( 'NONE',  ( -7.320508075688773708, 53.74999999317203248, -7.320508075688774596 ) ) ;
#1482 = CARTESIAN_POINT ( 'NONE',  ( -5.676582343749998039, 47.76041666325269119, -9.832129032723420536 ) ) ;
#1483 = CARTESIAN_POINT ( 'NONE',  ( 4.220049686691934809, 10.18810118749999916, 114.0625000020483668 ) ) ;
#1484 = CARTESIAN_POINT ( 'NONE',  ( -9.832129032723418760, 192.8645833299193839, -5.676582343750004256 ) ) ;
#1485 = ORIENTED_EDGE ( 'NONE', *, *, #72310, .F. ) ;
#1486 = CARTESIAN_POINT ( 'NONE',  ( 0.7581620860322625388, 65.76154746682546204, 26.27794529688427971 ) ) ;
#1487 = CARTESIAN_POINT ( 'NONE',  ( -26.34314575050763452, 198.6875000027312126, 174.0000000000004547 ) ) ;
#1488 = CARTESIAN_POINT ( 'NONE',  ( 5.000000000000001776, 162.7083333265053966, -8.660254037844389075 ) ) ;
#1490 = CARTESIAN_POINT ( 'NONE',  ( -9.832129032723418760, 177.8645833299193555, -5.676582343750004256 ) ) ;
#1489 = CARTESIAN_POINT ( 'NONE',  ( 9.999999999999998224, 262.7083333333333144, -2.679491924311229401 ) ) ;
#1491 = CARTESIAN_POINT ( 'NONE',  ( 0.000000000000000000, 0.000000000000000000, 0.000000000000000000 ) ) ;
#1492 = CARTESIAN_POINT ( 'NONE',  ( 8.660254037844385522, 246.0416666734946318, -5.000000000000003553 ) ) ;
#1493 = CARTESIAN_POINT ( 'NONE',  ( -2.679491924311235174, 190.4166666598387110, 10.00000000000000000 ) ) ;
#1494 = ORIENTED_EDGE ( 'NONE', *, *, #21867, .T. ) ;
#1495 = CARTESIAN_POINT ( 'NONE',  ( -3.042071309553173730, 174.6354166632526983, 11.35316468749999785 ) ) ;
#1496 =( BOUNDED_CURVE ( )  B_SPLINE_CURVE ( 2, ( #59318, #54769, #64600, #2705, #7624, #70986, #20035, #19670, #19302 ),
 .UNSPECIFIED., .F., .F. ) 
 B_SPLINE_CURVE_WITH_KNOTS ( ( 3, 2, 2, 2, 3 ),
 ( 0.4666666666666670626, 0.4750000000000003664, 0.4833333333333337256, 0.4916666666666670849, 0.5000000000000004441 ),
 .UNSPECIFIED. ) 
 CURVE ( )  GEOMETRIC_REPRESENTATION_ITEM ( )  RATIONAL_B_SPLINE_CURVE ( ( 0.9999999999999964473, 0.9238795325112902912, 1.000000000000000000, 0.9238795325112867385, 1.000000000000000000, 0.9238795325112867385, 1.000000000000000000, 0.9238795325112826307, 1.000000000000003997 ) ) 
 REPRESENTATION_ITEM ( '' )  );
#1497 = VECTOR ( 'NONE', #16945, 1000.000000000000000 ) ;
#1498 = CARTESIAN_POINT ( 'NONE',  ( 7.188101187499992051, 2.977408999572647819, 23.33030278187175455 ) ) ;
#1499 = CARTESIAN_POINT ( 'NONE',  ( 8.162799457232734923, 225.9999999999999716, -7.016166167730306213 ) ) ;
#1500 = ORIENTED_EDGE ( 'NONE', *, *, #22513, .T. ) ;
#1501 = AXIS2_PLACEMENT_3D ( 'NONE', #19533, #13859, #42913 ) ;
#1502 = EDGE_CURVE ( 'NONE', #61146, #45464, #50803, .T. ) ;
#1503 = EDGE_CURVE ( 'NONE', #10820, #23833, #40674, .T. ) ;
#1504 = CARTESIAN_POINT ( 'NONE',  ( 8.000000000000000000, 102.0312500040967905, -3.313708498984762496 ) ) ;
#1505 = VECTOR ( 'NONE', #30123, 1000.000000000000000 ) ;
#1506 = EDGE_CURVE ( 'NONE', #74050, #11179, #62211, .T. ) ;
#1507 = CARTESIAN_POINT ( 'NONE',  ( -2.828427124746192067, 10.62500000000000000, 2.828427124746190735 ) ) ;
#1508 = DIRECTION ( 'NONE',  ( -0.000000000000000000, 1.000000000000000000, -0.000000000000000000 ) ) ;
#1509 = CARTESIAN_POINT ( 'NONE',  ( -1.881053915767121776, 12.62499999863441147, -4.541265875000002339 ) ) ;
#1510 = CARTESIAN_POINT ( 'NONE',  ( -7.999999999999989342, -3.313708498984762496, 17.61155278392014623 ) ) ;
#1511 = CARTESIAN_POINT ( 'NONE',  ( -2.849036369511732440E-14, 196.2500000000000000, 138.0000000000000568 ) ) ;
#1512 = VERTEX_POINT ( 'NONE', #27881 ) ;
#1513 = CARTESIAN_POINT ( 'NONE',  ( 1.656854249492280440, 204.8125000000000284, 146.0000000000001421 ) ) ;
#1514 = CARTESIAN_POINT ( 'NONE',  ( 7.188101187500001821, 101.0000000020483810, -2.977408999572651371 ) ) ;
#1515 = ADVANCED_FACE ( 'NONE', ( #56942 ), #56198, .F. ) ;
#1517 = CARTESIAN_POINT ( 'NONE',  ( 2.449293598294707893E-16, 13.99999999726881406, -4.000000000000001776 ) ) ;
#1516 = CARTESIAN_POINT ( 'NONE',  ( 3.999999999999960032, 204.1250000027312126, 142.0000000000000568 ) ) ;
#1518 =( LENGTH_UNIT ( ) NAMED_UNIT ( * ) SI_UNIT ( .MILLI., .METRE. ) );
#1519 = ORIENTED_EDGE ( 'NONE', *, *, #22892, .T. ) ;
#1520 = CARTESIAN_POINT ( 'NONE',  ( -1.308779242311570501, 10.28008949575769293, -63.61387346695496348 ) ) ;
#1521 = CARTESIAN_POINT ( 'NONE',  ( -18.00000000000000000, -10.39230484541329425, -20.69999999999999929 ) ) ;
#1522 = CARTESIAN_POINT ( 'NONE',  ( 7.188101187499991163, 2.977408999572648707, 24.83030278187175455 ) ) ;
#1523 = ORIENTED_EDGE ( 'NONE', *, *, #9043, .T. ) ;
#1524 = VERTEX_POINT ( 'NONE', #56572 ) ;
#1525 = CARTESIAN_POINT ( 'NONE',  ( 4.220049686691934809, 10.18810118749999916, 88.18750000204838102 ) ) ;
#1526 = CARTESIAN_POINT ( 'NONE',  ( -7.778174593052020747, -7.778174593052023411, 97.18749999999998579 ) ) ;
#1529 = CARTESIAN_POINT ( 'NONE',  ( -4.721056650415998313, 296.7343750017069510, 4.721056650416000089 ) ) ;
#1528 = CARTESIAN_POINT ( 'NONE',  ( 25.17157287525381903, 201.0000000027312126, 172.8284271247460993 ) ) ;
#1527 = CARTESIAN_POINT ( 'NONE',  ( -30.82842712474612412, 198.5000000027312126, 172.8284271247466108 ) ) ;
#1530 = CARTESIAN_POINT ( 'NONE',  ( 4.999999999999993783, 134.1666666666666856, 8.660254037844390851 ) ) ;
#1531 = CARTESIAN_POINT ( 'NONE',  ( -25.17157287525382259, 203.8750000000000284, 167.1715728752541565 ) ) ;
#1532 = CARTESIAN_POINT ( 'NONE',  ( 4.556349186104045934, 11.00000000000000000, 78.53125000000000000 ) ) ;
#1534 = CARTESIAN_POINT ( 'NONE',  ( 31.45873412500001010, 201.7500000013655779, 168.5673454167822740 ) ) ;
#1533 = AXIS2_PLACEMENT_3D ( 'NONE', #55079, #71286, #32442 ) ;
#1535 = CARTESIAN_POINT ( 'NONE',  ( -7.188101187500000044, 7.593749997951610986, -8.802885111219163269E-16 ) ) ;
#1536 = CARTESIAN_POINT ( 'NONE',  ( -8.008118988124989457, -3.317071493978883900, 1.106865283940629885 ) ) ;
#1537 = CARTESIAN_POINT ( 'NONE',  ( -1.432654583217664479, 196.7500000013656063, 138.5412658750000787 ) ) ;
#1538 = CARTESIAN_POINT ( 'NONE',  ( -7.188101187499999156, 118.6250000020483810, 2.977408999572654924 ) ) ;
#1540 = CARTESIAN_POINT ( 'NONE',  ( -4.737866951563398210, -52.21905653845826834, -48.93292554254780669 ) ) ;
#1539 = CARTESIAN_POINT ( 'NONE',  ( 1.836970198721029589E-15, 251.2500000000000284, 10.00000000000000000 ) ) ;
#1541 = CARTESIAN_POINT ( 'NONE',  ( 3.042071309553173286, 225.6770833367473017, 11.35316468749999608 ) ) ;
#1542 = CARTESIAN_POINT ( 'NONE',  ( -1.469576158976823947E-15, 4.125000000000000888, 8.000000000000000000 ) ) ;
#1543 = CARTESIAN_POINT ( 'NONE',  ( -2.977408999572647819, 7.188101187499991163, 19.58030278187175455 ) ) ;
#1544 = DIRECTION ( 'NONE',  ( 1.734723475976805517E-15, 1.000000000000000000, 0.000000000000000000 ) ) ;
#1545 = CARTESIAN_POINT ( 'NONE',  ( -8.311093377946836114, 22.65624999658601979, -8.311093377946837890 ) ) ;
#1546 = CARTESIAN_POINT ( 'NONE',  ( 5.676582343750001591, 221.9270833299193555, -9.832129032723420536 ) ) ;
#1547 = CARTESIAN_POINT ( 'NONE',  ( -2.679491924311287132, 238.9583333333333997, -9.999999999999968026 ) ) ;
#1548 = CARTESIAN_POINT ( 'NONE',  ( 2.666560895877943341E-14, -16.44602605510714355, 68.55492853905353456 ) ) ;
#1549 = VERTEX_POINT ( 'NONE', #4885 ) ;
#1550 = CARTESIAN_POINT ( 'NONE',  ( -11.00000000000013145, 4.556349186103913596, 104.5937500040967905 ) ) ;
#1551 = AXIS2_PLACEMENT_3D ( 'NONE', #8041, #30317, #12948 ) ;
#1552 = CARTESIAN_POINT ( 'NONE',  ( -2.754378923186476579E-14, 196.4375000013655779, 145.4587341250000350 ) ) ;
#1553 = CARTESIAN_POINT ( 'NONE',  ( -3.042071309553164404, 32.23958332991935549, -11.35316468749999963 ) ) ;
#1554 = CARTESIAN_POINT ( 'NONE',  ( -11.00000000000000000, 0.000000000000000000, 83.68750000409677625 ) ) ;
#1555 = CARTESIAN_POINT ( 'NONE',  ( -2.445694354108839175, 206.3125000013656063, 144.4456943541088663 ) ) ;
#1556 = CARTESIAN_POINT ( 'NONE',  ( -25.55430564589122611, 195.3125000013656063, 167.5543056458915032 ) ) ;
#1557 = CARTESIAN_POINT ( 'NONE',  ( 9.797174393178825657E-16, 125.0000000000000000, -8.000000000000000000 ) ) ;
#1559 = CARTESIAN_POINT ( 'NONE',  ( -9.832129032723418760, 17.86458332991935194, -5.676582343750004256 ) ) ;
#1558 = CARTESIAN_POINT ( 'NONE',  ( -2.977408999572650927, 105.8750000020483668, -7.188101187500000933 ) ) ;
#1560 = CARTESIAN_POINT ( 'NONE',  ( -7.999999999999991118, 0.000000000000000000, 14.33030277982336465 ) ) ;
#1561 = CARTESIAN_POINT ( 'NONE',  ( -9.832129032723418760, 152.8645833299193555, -5.676582343750004256 ) ) ;
#1562 = CARTESIAN_POINT ( 'NONE',  ( -7.320508075688778149, 114.9999999931720112, 7.320508075688769267 ) ) ;
#1563 = CARTESIAN_POINT ( 'NONE',  ( -4.401442555609581635E-16, 113.6562500020483952, -7.188101187500000044 ) ) ;
#1564 = DIRECTION ( 'NONE',  ( 0.000000000000000000, 0.000000000000000000, 1.000000000000000000 ) ) ;
#1565 = CARTESIAN_POINT ( 'NONE',  ( -25.55430564589119413, 203.5625000013656063, 167.5543056458915316 ) ) ;
#1566 = ORIENTED_EDGE ( 'NONE', *, *, #44525, .F. ) ;
#1567 = CARTESIAN_POINT ( 'NONE',  ( 8.311093377946834337, 5.468749996586018014, 8.311093377946839666 ) ) ;
#1568 = ORIENTED_EDGE ( 'NONE', *, *, #7512, .T. ) ;
#1569 = CARTESIAN_POINT ( 'NONE',  ( -12.00000000000000000, 6.928203230275504332, -14.00000000000000178 ) ) ;
#1571 = CARTESIAN_POINT ( 'NONE',  ( 5.676582343750001591, 141.6145833299193555, -9.832129032723420536 ) ) ;
#1570 = CARTESIAN_POINT ( 'NONE',  ( -28.99136014929241867, -21.17931434262681378, 150.5169643591154056 ) ) ;
#1572 = DIRECTION ( 'NONE',  ( 0.000000000000000000, 0.2588190451025140781, -0.9659258262890700886 ) ) ;
#1573 = CARTESIAN_POINT ( 'NONE',  ( -3.313708498984758943, -7.999999999999989342, 16.16780278432982598 ) ) ;
#1574 = EDGE_CURVE ( 'NONE', #43604, #47208, #5258, .T. ) ;
#1575 = DIRECTION ( 'NONE',  ( -0.000000000000000000, -0.000000000000000000, -1.000000000000000000 ) ) ;
#1576 = CARTESIAN_POINT ( 'NONE',  ( 11.35316468749999963, 246.4062500034139873, -1.390361679473963556E-15 ) ) ;
#1577 = CARTESIAN_POINT ( 'NONE',  ( -4.220049686691937474, -10.18810118749999738, 93.81250000204839523 ) ) ;
#1578 = ORIENTED_EDGE ( 'NONE', *, *, #56098, .T. ) ;
#1579 = CARTESIAN_POINT ( 'NONE',  ( 5.676582343749993598, 85.26041666325268409, 9.832129032723422313 ) ) ;
#1580 = CARTESIAN_POINT ( 'NONE',  ( -10.18810118749999916, 0.000000000000000000, 100.6562500020483810 ) ) ;
#1581 = CARTESIAN_POINT ( 'NONE',  ( 3.211159895383560947, 18.31249999863440792, 3.211159895383562723 ) ) ;
#1582 = EDGE_LOOP ( 'NONE', ( #37871, #41850, #68765, #14821, #16320, #25666 ) ) ;
#1583 = ORIENTED_EDGE ( 'NONE', *, *, #71237, .T. ) ;
#1584 = CARTESIAN_POINT ( 'NONE',  ( -5.656854249492381470, 6.937500000000000888, 5.656854249492379694 ) ) ;
#1585 = CARTESIAN_POINT ( 'NONE',  ( -1.469576158976823947E-15, 11.62500000000000178, 8.000000000000000000 ) ) ;
#1586 = EDGE_CURVE ( 'NONE', #36674, #9475, #9375, .T. ) ;
#1587 = CARTESIAN_POINT ( 'NONE',  ( -7.188101187500000044, 27.09374999795161898, -8.802885111219163269E-16 ) ) ;
#1588 = CARTESIAN_POINT ( 'NONE',  ( 10.18810118750000093, -4.220049686691933921, 95.68750000204838102 ) ) ;
#1589 =( BOUNDED_CURVE ( )  B_SPLINE_CURVE ( 2, ( #58125, #6056, #71537, #51697, #13451, #40384, #31189, #36489, #52447 ),
 .UNSPECIFIED., .F., .F. ) 
 B_SPLINE_CURVE_WITH_KNOTS ( ( 3, 2, 2, 2, 3 ),
 ( 0.9000000000000007994, 0.9083333333333341031, 0.9166666666666674068, 0.9250000000000008216, 0.9333333333333341253 ),
 .UNSPECIFIED. ) 
 CURVE ( )  GEOMETRIC_REPRESENTATION_ITEM ( )  RATIONAL_B_SPLINE_CURVE ( ( 0.9999999999999928946, 0.9238795325112938439, 1.000000000000000000, 0.9238795325112867385, 1.000000000000000000, 0.9238795325112867385, 1.000000000000000000, 0.9238795325112796331, 1.000000000000007105 ) ) 
 REPRESENTATION_ITEM ( '' )  );
#1590 = CARTESIAN_POINT ( 'NONE',  ( 4.000000000000001776, 1.806524977843537691E-16, 0.000000000000000000 ) ) ;
#1591 = CARTESIAN_POINT ( 'NONE',  ( -1.656854249492383691, 13.43749999726881406, 4.000000000000000888 ) ) ;
#1592 = CARTESIAN_POINT ( 'NONE',  ( 1.881053915767122664, 1.124999998634406584, 4.541265875000001451 ) ) ;
#1593 = VERTEX_POINT ( 'NONE', #38843 ) ;
#1594 = DIRECTION ( 'NONE',  ( -1.652117596168387509E-16, -4.283267841918042125E-17, 1.000000000000000000 ) ) ;
#1595 = CARTESIAN_POINT ( 'NONE',  ( -1.432654583217607192, 200.2500000013656631, 194.5412658750000219 ) ) ;
#1596 = EDGE_CURVE ( 'NONE', #38779, #65598, #30095, .T. ) ;
#1598 = CARTESIAN_POINT ( 'NONE',  ( -5.656854249492381470, 15.93750000000000355, 5.656854249492379694 ) ) ;
#1597 = CARTESIAN_POINT ( 'NONE',  ( -25.55430564589111953, 200.0625000013656063, 172.4456943541091505 ) ) ;
#1599 = EDGE_CURVE ( 'NONE', #73206, #64471, #35405, .T. ) ;
#1600 = CARTESIAN_POINT ( 'NONE',  ( 2.780723358947928197E-16, 12.56249999863440792, -4.541265875000002339 ) ) ;
#1601 = CARTESIAN_POINT ( 'NONE',  ( 2.751064625579944321E-14, 199.8750000027312126, 194.0000000000000568 ) ) ;
#1602 = CARTESIAN_POINT ( 'NONE',  ( 5.082755093536318824, 5.082755093536319713, 15.92405278187175632 ) ) ;
#1603 = VERTEX_POINT ( 'NONE', #16545 ) ;
#1604 = ORIENTED_EDGE ( 'NONE', *, *, #55621, .T. ) ;
#1605 = CARTESIAN_POINT ( 'NONE',  ( 10.18810118750000093, -4.220049686691933033, 102.8125000020483952 ) ) ;
#1606 = DIRECTION ( 'NONE',  ( -0.000000000000000000, 1.000000000000000000, 4.476705744456276341E-16 ) ) ;
#1607 = CARTESIAN_POINT ( 'NONE',  ( -29.65685424949234061, 204.4375000000000853, 174.0000000000004547 ) ) ;
#1608 = CARTESIAN_POINT ( 'NONE',  ( -3.458734124999959025, 194.5000000013656063, 199.4326545832176691 ) ) ;
#1609 = CARTESIAN_POINT ( 'NONE',  ( 8.000000000000000000, 104.7500000000000000, -9.797174393178825657E-16 ) ) ;
#1610 = CARTESIAN_POINT ( 'NONE',  ( -1.836970198721029983E-15, 88.75000000000001421, 10.00000000000000178 ) ) ;
#1611 = EDGE_CURVE ( 'NONE', #29602, #10820, #37813, .T. ) ;
#1612 = CARTESIAN_POINT ( 'NONE',  ( 3.313708498984765161, 120.9687500000000284, 7.999999999999998224 ) ) ;
#1613 = CARTESIAN_POINT ( 'NONE',  ( 1.226468279477575784E-15, 296.8593750017070079, 6.676582343750001591 ) ) ;
#1614 = ORIENTED_EDGE ( 'NONE', *, *, #10507, .F. ) ;
#1615 = CARTESIAN_POINT ( 'NONE',  ( -7.320508075688773708, 173.7499999931719969, -7.320508075688774596 ) ) ;
#1616 = EDGE_CURVE ( 'NONE', #13736, #6741, #35786, .T. ) ;
#1617 = CARTESIAN_POINT ( 'NONE',  ( -3.313708498984760720, 12.28124999590322375, -8.000000000000000000 ) ) ;
#1618 = VECTOR ( 'NONE', #42640, 1000.000000000000000 ) ;
#1619 = CARTESIAN_POINT ( 'NONE',  ( -3.458734125000016313, 206.8750000013656347, 140.5673454167824161 ) ) ;
#1620 = CARTESIAN_POINT ( 'NONE',  ( -2.679491924299816752, 51.45833333333229831, -10.00000000000659206 ) ) ;
#1621 = CARTESIAN_POINT ( 'NONE',  ( -2.062184786512628451E-11, 138.7499999999984084, 10.00000000000000178 ) ) ;
#1622 = CARTESIAN_POINT ( 'NONE',  ( 9.999999999999998224, 227.7083333333333144, -2.679491924311229401 ) ) ;
#1623 = CYLINDRICAL_SURFACE ( 'NONE', #28294, 3.999999999999976019 ) ;
#1624 = CARTESIAN_POINT ( 'NONE',  ( 10.18810118749999916, 4.220049686691935698, 70.37500000204838102 ) ) ;
#1625 = CARTESIAN_POINT ( 'NONE',  ( 2.679491924311228956, 216.0416666666666572, -10.00000000000000000 ) ) ;
#1626 = CARTESIAN_POINT ( 'NONE',  ( -7.188101187499992051, 0.000000000000000000, 12.36155278187175277 ) ) ;
#1627 = CARTESIAN_POINT ( 'NONE',  ( 9.832129032723416984, 180.6770833299193555, 5.676582343750006032 ) ) ;
#1628 = CARTESIAN_POINT ( 'NONE',  ( -8.342170076843785083E-16, 1.062499998634406584, 4.541265875000002339 ) ) ;
#1629 = DIRECTION ( 'NONE',  ( -0.000000000000000000, 1.000000000000000000, -0.000000000000000000 ) ) ;
#1631 = CARTESIAN_POINT ( 'NONE',  ( -3.313708498984757611, 7.999999999999991118, 3.736552783920145338 ) ) ;
#1630 = CARTESIAN_POINT ( 'NONE',  ( -1.656854249492382358, 203.3125000027312126, 202.0000000000000000 ) ) ;
#1632 = ORIENTED_EDGE ( 'NONE', *, *, #26944, .F. ) ;
#1633 = CARTESIAN_POINT ( 'NONE',  ( 3.458734124999960358, 206.6875000013656063, 142.0000000000000568 ) ) ;
#1634 = CARTESIAN_POINT ( 'NONE',  ( 9.832129032723416984, 50.67708332991935549, 5.676582343750006032 ) ) ;
#1635 = CARTESIAN_POINT ( 'NONE',  ( 7.778174593052023411, -7.778174593052021635, 106.7500000040967763 ) ) ;
#1636 = CARTESIAN_POINT ( 'NONE',  ( 9.832129032723420536, 216.5104166632526983, -5.676582343749999815 ) ) ;
#1637 = CARTESIAN_POINT ( 'NONE',  ( -28.00000000000007105, 205.4375000013656063, 166.5412658750003629 ) ) ;
#1638 = CARTESIAN_POINT ( 'NONE',  ( -7.778174593052023411, 7.778174593052023411, 71.31249999999998579 ) ) ;
#1640 = CARTESIAN_POINT ( 'NONE',  ( -7.999999999999991118, 9.797174393178815797E-16, 30.00000000000000000 ) ) ;
#1639 = CARTESIAN_POINT ( 'NONE',  ( 5.082755093536325042, 123.5937500020483952, -5.082755093536325930 ) ) ;
#1641 = CARTESIAN_POINT ( 'NONE',  ( 3.267228342394235430, 194.5118150472866319, 140.3758396341766854 ) ) ;
#1642 = CARTESIAN_POINT ( 'NONE',  ( -5.000000000000005329, 70.20833332650538239, 8.660254037844387298 ) ) ;
#1643 = CARTESIAN_POINT ( 'NONE',  ( -2.977408999572651815, 97.43750000204839523, 7.188101187500000933 ) ) ;
#1644 = CARTESIAN_POINT ( 'NONE',  ( -1.881053915767124440, 15.12499999863441147, 4.541265875000001451 ) ) ;
#1645 = PLANE ( 'NONE',  #16886 ) ;
#1646 = DIRECTION ( 'NONE',  ( 0.000000000000000000, 0.000000000000000000, 1.000000000000000000 ) ) ;
#1647 = CARTESIAN_POINT ( 'NONE',  ( 0.000000000000000000, 0.000000000000000000, 0.000000000000000000 ) ) ;
#1648 = EDGE_LOOP ( 'NONE', ( #33481, #15153, #66287, #39551 ) ) ;
#1649 = ORIENTED_EDGE ( 'NONE', *, *, #19501, .T. ) ;
#1650 = CARTESIAN_POINT ( 'NONE',  ( 4.721056650416000089, 296.9843750017070079, 4.721056650415999201 ) ) ;
#1651 = CARTESIAN_POINT ( 'NONE',  ( -1.836970198721029983E-15, 185.6249999931720538, 10.00000000000000178 ) ) ;
#1652 = CARTESIAN_POINT ( 'NONE',  ( -8.660254037844396180, 17.91666666666667140, 5.000000000000002665 ) ) ;
#1653 = CARTESIAN_POINT ( 'NONE',  ( 5.676582343750001591, 161.6145833299193839, -9.832129032723420536 ) ) ;
#1654 = CARTESIAN_POINT ( 'NONE',  ( 0.000000000000000000, 300.0000000000000000, 0.000000000000000000 ) ) ;
#1655 = CARTESIAN_POINT ( 'NONE',  ( -2.828427124746153876, 198.8750000000000284, 195.1715728752538439 ) ) ;
#1656 = FACE_OUTER_BOUND ( 'NONE', #38500, .T. ) ;
#1657 = EDGE_CURVE ( 'NONE', #13532, #49077, #53135, .T. ) ;
#1658 = CARTESIAN_POINT ( 'NONE',  ( -10.18810118749999916, 0.000000000000000000, 107.0312500020483810 ) ) ;
#1659 = ORIENTED_EDGE ( 'NONE', *, *, #40654, .T. ) ;
#1660 = CARTESIAN_POINT ( 'NONE',  ( 8.000000000000000000, 17.90624999590322375, -3.313708498984761164 ) ) ;
#1661 = CYLINDRICAL_SURFACE ( 'NONE', #24410, 3.999999999999976019 ) ;
#1662 = CARTESIAN_POINT ( 'NONE',  ( -3.042071309553163960, 137.5520833299193555, -11.35316468749999963 ) ) ;
#1663 = CARTESIAN_POINT ( 'NONE',  ( -3.458734124999958581, 198.5000000013656063, 199.4326545832176976 ) ) ;
#1664 = CARTESIAN_POINT ( 'NONE',  ( 7.188101187499999156, 27.74999999795161543, 2.977408999572654924 ) ) ;
#1666 = EDGE_CURVE ( 'NONE', #64786, #22710, #45980, .T. ) ;
#1665 = CARTESIAN_POINT ( 'NONE',  ( 4.220049686691934809, 10.18810118749999916, 69.06250000204838102 ) ) ;
#1667 = CARTESIAN_POINT ( 'NONE',  ( -3.042071309553173730, 44.63541666325269119, 11.35316468749999785 ) ) ;
#1668 = EDGE_LOOP ( 'NONE', ( #11795, #58115, #44784, #2229, #47593 ) ) ;
#1669 = CARTESIAN_POINT ( 'NONE',  ( -23.99999999999999289, 208.8750000027312126, 170.0000000000002842 ) ) ;
#1670 = CARTESIAN_POINT ( 'NONE',  ( -3.211159895383562723, 4.062499998634407028, 3.211159895383561391 ) ) ;
#1671 = CARTESIAN_POINT ( 'NONE',  ( 3.317071493978877683, 8.008118988124991233, 11.04436528394063366 ) ) ;
#1672 = CARTESIAN_POINT ( 'NONE',  ( -7.188101187500001821, 13.12499999795161187, -2.977408999572651371 ) ) ;
#1673 = CARTESIAN_POINT ( 'NONE',  ( 4.242640687119287435, 294.4375000034140157, 4.242640687119285658 ) ) ;
#1674 = CARTESIAN_POINT ( 'NONE',  ( 0.6939194017716557861, 124.5665190883579783, -7.910544316330307524 ) ) ;
#1675 = CARTESIAN_POINT ( 'NONE',  ( -5.082755093536326818, 9.281249997951610098, 5.082755093536325042 ) ) ;
#1676 = CARTESIAN_POINT ( 'NONE',  ( -2.977408999572647819, -7.188101187499990274, 7.767802781871751883 ) ) ;
#1677 = CARTESIAN_POINT ( 'NONE',  ( 4.220049686691941027, -10.18810118749999738, 69.62500000204838102 ) ) ;
#1678 = EDGE_CURVE ( 'NONE', #38403, #28928, #36151, .T. ) ;
#1679 = AXIS2_PLACEMENT_3D ( 'NONE', #15570, #31445, #66895 ) ;
#1680 = CARTESIAN_POINT ( 'NONE',  ( -11.00000000000000533, -11.00000000000000355, 41.99999999999999289 ) ) ;
#1681 = CARTESIAN_POINT ( 'NONE',  ( -1.656854249492383691, 3.437499997268814500, 4.000000000000000888 ) ) ;
#1682 = ORIENTED_EDGE ( 'NONE', *, *, #21963, .T. ) ;
#1683 =( BOUNDED_CURVE ( )  B_SPLINE_CURVE ( 2, ( #34653, #51987, #18393, #28221, #40288, #34278, #58402, #46684, #41405 ),
 .UNSPECIFIED., .F., .F. ) 
 B_SPLINE_CURVE_WITH_KNOTS ( ( 3, 2, 2, 2, 3 ),
 ( 0.2166666666666669516, 0.2250000000000002554, 0.2333333333333335313, 0.2416666666666668073, 0.2500000000000001110 ),
 .UNSPECIFIED. ) 
 CURVE ( )  GEOMETRIC_REPRESENTATION_ITEM ( )  RATIONAL_B_SPLINE_CURVE ( ( 0.9999999999999974465, 0.9238795325112892920, 1.000000000000000000, 0.9238795325112867385, 1.000000000000000000, 0.9238795325112867385, 1.000000000000000000, 0.9238795325112857393, 1.000000000000001110 ) ) 
 REPRESENTATION_ITEM ( '' )  );
#1684 = CARTESIAN_POINT ( 'NONE',  ( -3.999999999999960032, 196.0625000027312694, 196.3431457505076594 ) ) ;
#1685 = CARTESIAN_POINT ( 'NONE',  ( -4.000000000000015099, 201.5625000000000853, 143.6568542494924543 ) ) ;
#1686 = CARTESIAN_POINT ( 'NONE',  ( -27.99999999999991118, 197.6250000027312126, 174.0000000000003695 ) ) ;
#1687 = EDGE_CURVE ( 'NONE', #68939, #6054, #28255, .T. ) ;
#1688 = CARTESIAN_POINT ( 'NONE',  ( 4.541265875000002339, 4.312499998634407028, 0.000000000000000000 ) ) ;
#1689 = CARTESIAN_POINT ( 'NONE',  ( -7.188101187499999156, 116.7500000020483810, 2.977408999572654924 ) ) ;
#1690 = DIRECTION ( 'NONE',  ( -0.000000000000000000, 1.000000000000000000, -0.000000000000000000 ) ) ;
#1691 = CARTESIAN_POINT ( 'NONE',  ( -4.898587196589407898E-16, 7.999999999999991118, 2.142802783920143117 ) ) ;
#1692 = EDGE_LOOP ( 'NONE', ( #54864, #32986, #56743, #35264 ) ) ;
#1693 = CARTESIAN_POINT ( 'NONE',  ( 4.401442555609581635E-16, 20.34374999795161543, -7.188101187500000044 ) ) ;
#1694 = VERTEX_POINT ( 'NONE', #64454 ) ;
#1695 = CARTESIAN_POINT ( 'NONE',  ( 2.679491924311350193, 254.5833333401612606, 9.999999999999930722 ) ) ;
#1696 = CARTESIAN_POINT ( 'NONE',  ( 2.839093476692135984E-14, 208.6875000013656063, 201.4587341250000350 ) ) ;
#1697 = CARTESIAN_POINT ( 'NONE',  ( 24.54126587500000412, 205.2500000013655779, 171.4326545832176123 ) ) ;
#1698 = CARTESIAN_POINT ( 'NONE',  ( -2.679491924311235618, 58.54166666666666430, 10.00000000000000000 ) ) ;
#1699 = CIRCLE ( 'NONE', #69167, 4.000000000000003553 ) ;
#1700 = CARTESIAN_POINT ( 'NONE',  ( -5.082755093536324154, 99.21875000204838102, 5.082755093536326818 ) ) ;
#1701 = CARTESIAN_POINT ( 'NONE',  ( -4.242640687119286547, 294.8750000000000000, -4.242640687119286547 ) ) ;
#1703 = CARTESIAN_POINT ( 'NONE',  ( 2.828427124746209831, 197.5000000027312126, 200.8284271247462129 ) ) ;
#1702 = CARTESIAN_POINT ( 'NONE',  ( 33.36290227352207438, 175.7112823378519124, 156.9282883534935706 ) ) ;
#1704 = ORIENTED_EDGE ( 'NONE', *, *, #52857, .F. ) ;
#1705 =( BOUNDED_CURVE ( )  B_SPLINE_CURVE ( 2, ( #43005, #1922, #36259, #37365, #47557, #2661, #25281, #48299, #70944 ),
 .UNSPECIFIED., .F., .F. ) 
 B_SPLINE_CURVE_WITH_KNOTS ( ( 3, 2, 2, 2, 3 ),
 ( 0.4705882352941176960, 0.4742647058823529771, 0.4779411764705883137, 0.4816176470588235947, 0.4852941176470588758 ),
 .UNSPECIFIED. ) 
 CURVE ( )  GEOMETRIC_REPRESENTATION_ITEM ( )  RATIONAL_B_SPLINE_CURVE ( ( 0.9999999999999988898, 0.9238795325112878487, 1.000000000000000000, 0.9238795325112867385, 1.000000000000000000, 0.9238795325112867385, 1.000000000000000000, 0.9238795325112856283, 1.000000000000001110 ) ) 
 REPRESENTATION_ITEM ( '' )  );
#1706 = CARTESIAN_POINT ( 'NONE',  ( 5.676582343749997150, 237.2395833367473301, -9.832129032723418760 ) ) ;
#1707 = CARTESIAN_POINT ( 'NONE',  ( 2.977408999572646486, 7.188101187499991163, 10.39280278187175810 ) ) ;
#1708 = DIRECTION ( 'NONE',  ( -0.000000000000000000, 1.000000000000000000, -0.000000000000000000 ) ) ;
#1709 = CARTESIAN_POINT ( 'NONE',  ( -5.656854249492375253, 5.656854249492375253, 3.642802779823362869 ) ) ;
#1710 = CARTESIAN_POINT ( 'NONE',  ( -1.656854249492381248, 17.06249999726881938, -4.000000000000001776 ) ) ;
#1711 = CARTESIAN_POINT ( 'NONE',  ( -8.660254037844385522, 260.4166666666666856, 5.000000000000004441 ) ) ;
#1712 = CARTESIAN_POINT ( 'NONE',  ( 1.469576158976822172E-15, -7.999999999999991118, 19.39280278392014978 ) ) ;
#1713 = CARTESIAN_POINT ( 'NONE',  ( -10.00000000000000355, 172.7083333333333144, 2.679491924311223183 ) ) ;
#1714 = CARTESIAN_POINT ( 'NONE',  ( 6.000000000000003553, 297.6250000034140157, -2.485281374238571761 ) ) ;
#1715 = CARTESIAN_POINT ( 'NONE',  ( 8.660254037844389075, 240.2083333401613174, 4.999999999999997335 ) ) ;
#1716 = CARTESIAN_POINT ( 'NONE',  ( 2.977408999572646486, 7.188101187499992051, 26.89280278187175455 ) ) ;
#1717 = CARTESIAN_POINT ( 'NONE',  ( 3.042071309553167069, 147.1354166632526983, -11.35316468749999785 ) ) ;
#1718 = CARTESIAN_POINT ( 'NONE',  ( 10.00000000000000000, 26.66666665983870033, 2.679491924311235618 ) ) ;
#1721 = FACE_OUTER_BOUND ( 'NONE', #24090, .T. ) ;
#1720 = CARTESIAN_POINT ( 'NONE',  ( 5.656854249492379694, 110.9375000000000000, -5.656854249492380582 ) ) ;
#1719 = CARTESIAN_POINT ( 'NONE',  ( 27.99999999999996803, 206.0000000000000284, 173.9999999999999147 ) ) ;
#1722 = ORIENTED_EDGE ( 'NONE', *, *, #33764, .F. ) ;
#1723 = CARTESIAN_POINT ( 'NONE',  ( 5.676582343749993598, 5.260416663252683200, 9.832129032723422313 ) ) ;
#1724 = DIRECTION ( 'NONE',  ( -0.000000000000000000, 1.000000000000000000, -0.000000000000000000 ) ) ;
#1725 = DIRECTION ( 'NONE',  ( -0.000000000000000000, 0.000000000000000000, -1.000000000000000000 ) ) ;
#1726 = CARTESIAN_POINT ( 'NONE',  ( 3.458734124999959914, 205.4375000013656063, 142.0000000000000568 ) ) ;
#1727 = CARTESIAN_POINT ( 'NONE',  ( 8.660254037844385522, 31.45833332650536818, 5.000000000000005329 ) ) ;
#1728 = VECTOR ( 'NONE', #41845, 1000.000000000000000 ) ;
#1729 = CARTESIAN_POINT ( 'NONE',  ( -2.977408999572650927, 117.8750000020483810, -7.188101187500001821 ) ) ;
#1730 = CARTESIAN_POINT ( 'NONE',  ( -8.342170076843785083E-16, 4.187499998634407028, 4.541265875000002339 ) ) ;
#1731 = CARTESIAN_POINT ( 'NONE',  ( 7.999999999999992895, -3.313708498984756279, 13.67405278392014800 ) ) ;
#1732 = CARTESIAN_POINT ( 'NONE',  ( -7.999999999999991118, 3.313708498984756723, 12.73655277982336287 ) ) ;
#1734 = CARTESIAN_POINT ( 'NONE',  ( -10.99999999999986677, -4.556349186104185378, 104.7812500040967905 ) ) ;
#1733 = CARTESIAN_POINT ( 'NONE',  ( 27.99999999999999645, 210.0000000000000284, 165.9999999999999147 ) ) ;
#1735 = VERTEX_POINT ( 'NONE', #24449 ) ;
#1736 = CARTESIAN_POINT ( 'NONE',  ( 1.469576158976823947E-15, 92.56250000409677625, 8.000000000000000000 ) ) ;
#1737 = CARTESIAN_POINT ( 'NONE',  ( 1.469576158976823947E-15, 108.8750000000000000, 8.000000000000000000 ) ) ;
#1738 = CARTESIAN_POINT ( 'NONE',  ( -8.311093377946834337, 229.8437500034140157, 8.311093377946837890 ) ) ;
#1739 = CARTESIAN_POINT ( 'NONE',  ( -2.085542519210945728E-15, 109.5312499965860269, 11.35316468750000141 ) ) ;
#1740 = ORIENTED_EDGE ( 'NONE', *, *, #19433, .T. ) ;
#1741 = CARTESIAN_POINT ( 'NONE',  ( 4.000000000000016875, 198.4375000000000568, 199.6568542494924259 ) ) ;
#1742 = CARTESIAN_POINT ( 'NONE',  ( -4.220049686691937474, -10.18810118749999738, 99.43750000204836681 ) ) ;
#1743 = DIRECTION ( 'NONE',  ( 1.224646799147353207E-16, 0.000000000000000000, 1.000000000000000000 ) ) ;
#1744 = CARTESIAN_POINT ( 'NONE',  ( -3.458734124999960358, 197.6875000013655779, 198.0000000000000284 ) ) ;
#1745 = CARTESIAN_POINT ( 'NONE',  ( 29.65685424949250404, 197.4375000000000284, 165.9999999999999716 ) ) ;
#1747 = CARTESIAN_POINT ( 'NONE',  ( 11.35316468749999785, 110.5729166632526983, 3.042071309553174174 ) ) ;
#1746 = CYLINDRICAL_SURFACE ( 'NONE', #73756, 11.00000000000000000 ) ;
#1748 = CARTESIAN_POINT ( 'NONE',  ( -24.00000000000001421, 209.8125000000000000, 168.3431457505080004 ) ) ;
#1749 = EDGE_CURVE ( 'NONE', #58573, #2613, #66226, .T. ) ;
#1750 = CARTESIAN_POINT ( 'NONE',  ( 10.00000000000000711, 50.20833333333334281, -2.679491924311227624 ) ) ;
#1751 = ORIENTED_EDGE ( 'NONE', *, *, #12564, .F. ) ;
#1752 = CARTESIAN_POINT ( 'NONE',  ( 5.000000000000001776, 207.7083333265053682, -8.660254037844389075 ) ) ;
#1753 = DIRECTION ( 'NONE',  ( 0.000000000000000000, 0.000000000000000000, 1.000000000000000000 ) ) ;
#1754 = CARTESIAN_POINT ( 'NONE',  ( -4.000000000000001776, 9.437500000000000000, -1.656854249492381470 ) ) ;
#1755 = CARTESIAN_POINT ( 'NONE',  ( 5.676582343750001591, 101.9270833299193555, -9.832129032723420536 ) ) ;
#1756 = CARTESIAN_POINT ( 'NONE',  ( -6.676582343750000703, 287.5156250017069510, 2.765530957082001251 ) ) ;
#1757 = CARTESIAN_POINT ( 'NONE',  ( -5.082755093536326818, 15.28124999795161187, 5.082755093536325042 ) ) ;
#1759 = EDGE_CURVE ( 'NONE', #33217, #31137, #14639, .T. ) ;
#1758 = CARTESIAN_POINT ( 'NONE',  ( -7.204075437095965206, -7.204075437095968759, 86.21875000204836681 ) ) ;
#1760 = CARTESIAN_POINT ( 'NONE',  ( -9.832129032723420536, 9.010416663252684089, 5.676582343749997150 ) ) ;
#1761 = VERTEX_POINT ( 'NONE', #41804 ) ;
#1762 = CARTESIAN_POINT ( 'NONE',  ( 12.00000000000000000, 6.928203230275542523, -1.071796769724504550 ) ) ;
#1763 = CARTESIAN_POINT ( 'NONE',  ( 0.7771339217342709826, -42.09580902349574671, 139.0091484142746481 ) ) ;
#1764 = CARTESIAN_POINT ( 'NONE',  ( 4.220049686691934809, 10.18810118749999916, 72.06250000204836681 ) ) ;
#1765 = CARTESIAN_POINT ( 'NONE',  ( -8.000000000000000000, 98.18750000409677625, 0.000000000000000000 ) ) ;
#1766 = CARTESIAN_POINT ( 'NONE',  ( 4.898587196589415787E-16, 0.000000000000000000, 4.000000000000001776 ) ) ;
#1767 = CARTESIAN_POINT ( 'NONE',  ( -4.088227598258586603E-16, 291.2031250017069510, -6.676582343750001591 ) ) ;
#1768 = CARTESIAN_POINT ( 'NONE',  ( 12.00000000000000355, 0.000000000000000000, -21.50000000000000000 ) ) ;
#1769 = CARTESIAN_POINT ( 'NONE',  ( -11.35316468750000141, 223.8020833299193271, 3.042071309553159963 ) ) ;
#1770 = CARTESIAN_POINT ( 'NONE',  ( 10.18810118750000093, -4.220049686691933921, 87.81250000204838102 ) ) ;
#1771 = CARTESIAN_POINT ( 'NONE',  ( -25.55430564589115150, 202.0625000013656063, 172.4456943541091789 ) ) ;
#1772 = CARTESIAN_POINT ( 'NONE',  ( -1.469576158976823947E-15, 26.62500000000000355, 8.000000000000000000 ) ) ;
#1773 = CARTESIAN_POINT ( 'NONE',  ( 3.211159895383561835, 10.56249999863440792, -3.211159895383561835 ) ) ;
#1774 = VERTEX_POINT ( 'NONE', #38164 ) ;
#1775 = CARTESIAN_POINT ( 'NONE',  ( -29.30142354842655905, -51.92935866475845330, 159.8446510199293868 ) ) ;
#1776 = CARTESIAN_POINT ( 'NONE',  ( 1.432654583217607414, 197.5000000013656063, 145.4587341250000634 ) ) ;
#1777 = CARTESIAN_POINT ( 'NONE',  ( 3.999999999999959144, 205.1875000027311842, 140.3431457505076594 ) ) ;
#1778 = CARTESIAN_POINT ( 'NONE',  ( 5.000000000000000000, 14.89980876190738002, -69.94558486267359854 ) ) ;
#1779 = CARTESIAN_POINT ( 'NONE',  ( -6.238412754330611322E-16, 10.18810118749999916, 76.65625000204836681 ) ) ;
#1780 = ORIENTED_EDGE ( 'NONE', *, *, #69966, .F. ) ;
#1781 = CARTESIAN_POINT ( 'NONE',  ( 5.082755093536324154, 3.281249997951610098, 5.082755093536326818 ) ) ;
#1782 = CARTESIAN_POINT ( 'NONE',  ( -3.313708498984757611, 7.999999999999991118, 6.549052779823365533 ) ) ;
#1783 = CARTESIAN_POINT ( 'NONE',  ( -2.977408999572651815, 118.8125000020484094, 7.188101187500000933 ) ) ;
#1784 = CARTESIAN_POINT ( 'NONE',  ( -2.295000000000000373, 278.5679999999998699, 5.413231402903075029 ) ) ;
#1785 = CARTESIAN_POINT ( 'NONE',  ( 6.676582343750003368, 291.8906250017069510, 2.765530957081995478 ) ) ;
#1787 = CARTESIAN_POINT ( 'NONE',  ( 2.449293598294707893E-16, 14.99999999726881406, -4.000000000000001776 ) ) ;
#1786 = CARTESIAN_POINT ( 'NONE',  ( -3.042071309553166625, 232.8645833367473017, -11.35316468749999608 ) ) ;
#1788 = ORIENTED_EDGE ( 'NONE', *, *, #39922, .F. ) ;
#1789 = CARTESIAN_POINT ( 'NONE',  ( -6.951808397369817780E-16, 222.9687500034139873, -11.35316468749999963 ) ) ;
#1790 = CARTESIAN_POINT ( 'NONE',  ( 2.977408999572650927, -7.188101187499990274, 1.955302781871753881 ) ) ;
#1791 =( BOUNDED_CURVE ( )  B_SPLINE_CURVE ( 2, ( #71488, #2476, #18350, #30408, #53426, #42819, #19442, #1750, #41363, #24372, #30772, #37178, #70763 ),
 .UNSPECIFIED., .F., .F. ) 
 B_SPLINE_CURVE_WITH_KNOTS ( ( 3, 2, 2, 2, 2, 2, 3 ),
 ( 0.6122908167314494721, 0.6175241636365315090, 0.6227575105416134349, 0.6279908574466953608, 0.6332242043517773977, 0.6384575512568593236, 0.6436908981619412495 ),
 .UNSPECIFIED. ) 
 CURVE ( )  GEOMETRIC_REPRESENTATION_ITEM ( )  RATIONAL_B_SPLINE_CURVE ( ( 0.9999999999999901190, 0.9659258262890781932, 1.000000000000000000, 0.9659258262890683122, 1.000000000000000000, 0.9659258262890683122, 1.000000000000000000, 0.9659258262890683122, 1.000000000000000000, 0.9659258262890683122, 1.000000000000000000, 0.9659258262892301827, 0.9999999999998381295 ) ) 
 REPRESENTATION_ITEM ( '' )  );
#1792 = CARTESIAN_POINT ( 'NONE',  ( 3.458734125000016757, 205.1250000013656347, 199.4326545832176691 ) ) ;
#1793 = EDGE_LOOP ( 'NONE', ( #56973, #6881, #4793, #66703 ) ) ;
#1794 = CARTESIAN_POINT ( 'NONE',  ( 8.000000000000001776, 104.8437500040967763, 3.313708498984759387 ) ) ;
#1795 = CARTESIAN_POINT ( 'NONE',  ( 3.042071309553167069, 102.1354166632526983, -11.35316468749999785 ) ) ;
#1796 = CARTESIAN_POINT ( 'NONE',  ( -1.656854249492318409, 208.8125000000000000, 194.0000000000000284 ) ) ;
#1797 = CARTESIAN_POINT ( 'NONE',  ( 11.00000000000000355, -4.556349186104045046, 79.65625000000000000 ) ) ;
#1800 = CARTESIAN_POINT ( 'NONE',  ( -11.00000000000000000, 0.000000000000000000, 83.49999999999998579 ) ) ;
#1799 = CARTESIAN_POINT ( 'NONE',  ( 24.54126587499999701, 206.1875000013656063, 169.9999999999999432 ) ) ;
#1798 = CARTESIAN_POINT ( 'NONE',  ( 25.55430564589119413, 203.3125000013656063, 167.5543056458910485 ) ) ;
#1801 = ORIENTED_EDGE ( 'NONE', *, *, #26764, .F. ) ;
#1802 = CARTESIAN_POINT ( 'NONE',  ( -38.00000000000000000, 37.00000000000000711, 20.00000000000003553 ) ) ;
#1803 = CARTESIAN_POINT ( 'NONE',  ( -11.35316468750000141, 218.4895833299193271, 3.042071309553159963 ) ) ;
#1804 = CARTESIAN_POINT ( 'NONE',  ( 3.458734124999959025, 201.5000000013655779, 140.5673454167824161 ) ) ;
#1805 = ADVANCED_FACE ( 'NONE', ( #64814 ), #64081, .F. ) ;
#1806 = CARTESIAN_POINT ( 'NONE',  ( 24.54126587500000056, 203.3750000013656063, 168.5673454167822172 ) ) ;
#1807 = CARTESIAN_POINT ( 'NONE',  ( 2.977408999572650927, 22.12499999795161543, -7.188101187500001821 ) ) ;
#1808 = CARTESIAN_POINT ( 'NONE',  ( -11.35316468750000141, 193.8020833299193271, 3.042071309553159963 ) ) ;
#1809 = CARTESIAN_POINT ( 'NONE',  ( 7.188101187500000933, 93.87500000204838102, -2.977408999572651371 ) ) ;
#1810 = CARTESIAN_POINT ( 'NONE',  ( 27.99999999999996803, 203.0000000000000000, 173.9999999999999147 ) ) ;
#1811 = CARTESIAN_POINT ( 'NONE',  ( -28.00000000000002487, 197.0000000000000000, 166.0000000000003695 ) ) ;
#1812 = CARTESIAN_POINT ( 'NONE',  ( -1.881053915767124440, 15.99999999863440614, 4.541265875000001451 ) ) ;
#1813 = CARTESIAN_POINT ( 'NONE',  ( 25.55430564589115150, 199.5625000013656063, 172.4456943541086957 ) ) ;
#1814 = CARTESIAN_POINT ( 'NONE',  ( 2.977408999572646486, 7.188101187499991163, 2.892802781871751439 ) ) ;
#1815 = CARTESIAN_POINT ( 'NONE',  ( 11.35316468749999963, 70.98958332991934128, -3.042071309553165293 ) ) ;
#1817 =( BOUNDED_CURVE ( )  B_SPLINE_CURVE ( 2, ( #60506, #33631, #16991, #40018, #8832, #54863, #31843, #72580, #4952, #57005, #54494, #39646, #27951 ),
 .UNSPECIFIED., .F., .F. ) 
 B_SPLINE_CURVE_WITH_KNOTS ( ( 3, 2, 2, 2, 2, 2, 3 ),
 ( 0.1944444444444440034, 0.2037037037037032483, 0.2129629629629625209, 0.2222222222222217658, 0.2314814814814810662, 0.2407407407407403110, 0.2499999999999995837 ),
 .UNSPECIFIED. ) 
 CURVE ( )  GEOMETRIC_REPRESENTATION_ITEM ( )  RATIONAL_B_SPLINE_CURVE ( ( 1.000000000000001554, 0.9659258262890666469, 1.000000000000000000, 0.9659258262890683122, 1.000000000000000000, 0.9659258262890683122, 1.000000000000000000, 0.9659258262890683122, 1.000000000000000000, 0.9659258262890683122, 1.000000000000000000, 0.9659258262890698665, 0.9999999999999984457 ) ) 
 REPRESENTATION_ITEM ( '' )  );
#1816 = CARTESIAN_POINT ( 'NONE',  ( -4.999999999999998224, -52.16438407847157777, 42.28020805311177810 ) ) ;
#1818 = CYLINDRICAL_SURFACE ( 'NONE', #45959, 8.000000000000000000 ) ;
#1819 = VERTEX_POINT ( 'NONE', #69368 ) ;
#1820 = FACE_BOUND ( 'NONE', #43020, .T. ) ;
#1821 = CARTESIAN_POINT ( 'NONE',  ( 8.660254037844389075, 232.0833333333333428, 4.999999999999997335 ) ) ;
#1822 = CARTESIAN_POINT ( 'NONE',  ( 6.951808397369818766E-16, 77.03124999658601268, -11.35316468750000141 ) ) ;
#1823 = CARTESIAN_POINT ( 'NONE',  ( -7.204075437095967871, 7.204075437095967871, 84.34375000204836681 ) ) ;
#1824 = CARTESIAN_POINT ( 'NONE',  ( -4.556349186104045934, 11.00000000000000000, 69.90625000409677625 ) ) ;
#1825 = LINE ( 'NONE', #18059, #20216 ) ;
#1826 = CARTESIAN_POINT ( 'NONE',  ( 5.000000000000000000, 16.14408868864073554, -27.96238185062347981 ) ) ;
#1828 = CARTESIAN_POINT ( 'NONE',  ( 11.35316468749999963, 70.98958332991935549, -3.042071309553165293 ) ) ;
#1827 = CARTESIAN_POINT ( 'NONE',  ( -4.000000000000002665, 13.31249999726881406, 1.656854249492380582 ) ) ;
#1829 = CARTESIAN_POINT ( 'NONE',  ( -5.656854249492375253, 5.656854249492375253, 27.83030278392014978 ) ) ;
#1830 = EDGE_CURVE ( 'NONE', #61757, #61247, #71503, .T. ) ;
#1831 = CARTESIAN_POINT ( 'NONE',  ( 2.828427124746191623, 13.12500000000000000, -2.828427124746191623 ) ) ;
#1832 = CARTESIAN_POINT ( 'NONE',  ( -10.00000000000000000, 174.1666666598386826, -2.679491924311229845 ) ) ;
#1833 = CARTESIAN_POINT ( 'NONE',  ( 5.082755093536326818, 92.09375000204838102, 5.082755093536325042 ) ) ;
#1834 = AXIS2_PLACEMENT_3D ( 'NONE', #17940, #17186, #64703 ) ;
#1835 = CARTESIAN_POINT ( 'NONE',  ( -24.07362206087098144, 194.9222032098518866, 169.9390543940447174 ) ) ;
#1836 = CARTESIAN_POINT ( 'NONE',  ( -3.042071309553163960, 62.55208332991934839, -11.35316468749999963 ) ) ;
#1837 = EDGE_CURVE ( 'NONE', #68369, #7437, #45512, .T. ) ;
#1838 = CARTESIAN_POINT ( 'NONE',  ( -7.204075437095967871, 7.204075437095967871, 115.8437500020483810 ) ) ;
#1839 = CARTESIAN_POINT ( 'NONE',  ( 9.832129032723416984, 195.3645833299193839, 5.676582343750006032 ) ) ;
#1840 = ORIENTED_EDGE ( 'NONE', *, *, #7857, .F. ) ;
#1841 = CARTESIAN_POINT ( 'NONE',  ( -0.7509181236786398594, 65.76106071587237523, 26.27764834701797980 ) ) ;
#1842 = CARTESIAN_POINT ( 'NONE',  ( -2.775557561562891351E-14, 210.0000000000000284, 142.0000000000000568 ) ) ;
#1844 = CARTESIAN_POINT ( 'NONE',  ( 11.35316468749999963, 195.9895833299193555, -3.042071309553165293 ) ) ;
#1843 = CARTESIAN_POINT ( 'NONE',  ( 2.679491924311375506, 261.4583333333334281, 9.999999999999916511 ) ) ;
#1845 = CARTESIAN_POINT ( 'NONE',  ( 12.00000000000000000, 0.000000000000000000, 0.000000000000000000 ) ) ;
#1846 = CARTESIAN_POINT ( 'NONE',  ( 1.836970198721029589E-15, 244.3750000068280031, 10.00000000000000000 ) ) ;
#1847 = LINE ( 'NONE', #36175, #38448 ) ;
#1848 = ORIENTED_EDGE ( 'NONE', *, *, #40554, .F. ) ;
#1849 = CARTESIAN_POINT ( 'NONE',  ( -5.676582343750006032, 184.4270833299193555, 9.832129032723418760 ) ) ;
#1850 = CARTESIAN_POINT ( 'NONE',  ( -7.188101187499992051, 0.000000000000000000, 20.98655278187175455 ) ) ;
#1851 = LINE ( 'NONE', #59561, #1997 ) ;
#1852 = ORIENTED_EDGE ( 'NONE', *, *, #9486, .F. ) ;
#1853 = CARTESIAN_POINT ( 'NONE',  ( 8.000000000000001776, 100.3437500040967905, 3.313708498984759387 ) ) ;
#1854 = CARTESIAN_POINT ( 'NONE',  ( -8.660254037844390851, 2.916666666666666963, 4.999999999999998224 ) ) ;
#1855 = CARTESIAN_POINT ( 'NONE',  ( 1.656854249492381914, 10.81250000000000178, 4.000000000000000888 ) ) ;
#1856 = LINE ( 'NONE', #47860, #69782 ) ;
#1857 = CARTESIAN_POINT ( 'NONE',  ( -3.211159895383561391, 16.68749999863440436, -3.211159895383561835 ) ) ;
#1858 = CARTESIAN_POINT ( 'NONE',  ( -7.999999999999991118, 3.313708498984756723, 12.92405278392014800 ) ) ;
#1859 = CARTESIAN_POINT ( 'NONE',  ( -10.00000000000000533, 187.5000000000000000, -1.224646799147353848E-15 ) ) ;
#1860 = ORIENTED_EDGE ( 'NONE', *, *, #28662, .T. ) ;
#1861 = CARTESIAN_POINT ( 'NONE',  ( -11.00000000000000000, 0.000000000000000000, 72.99999999999998579 ) ) ;
#1862 = CARTESIAN_POINT ( 'NONE',  ( -5.082755093536325930, 99.96875000204838102, -5.082755093536325930 ) ) ;
#1863 = VECTOR ( 'NONE', #60276, 1000.000000000000000 ) ;
#1864 = CARTESIAN_POINT ( 'NONE',  ( 2.828427124746190291, 13.62499999726881406, 2.828427124746192067 ) ) ;
#1865 = DIRECTION ( 'NONE',  ( 0.000000000000000000, 0.000000000000000000, 1.000000000000000000 ) ) ;
#1866 = ORIENTED_EDGE ( 'NONE', *, *, #48044, .T. ) ;
#1867 = CARTESIAN_POINT ( 'NONE',  ( -1.877992804784532677, 10.12031740952137859, -70.21778636471140089 ) ) ;
#1868 = CARTESIAN_POINT ( 'NONE',  ( -5.656854249492378806, 101.3750000040967905, 5.656854249492381470 ) ) ;
#1869 = VECTOR ( 'NONE', #26738, 1000.000000000000000 ) ;
#1870 = CARTESIAN_POINT ( 'NONE',  ( -7.188101187499990274, -2.977408999572651371, 27.08030278187175810 ) ) ;
#1871 = VERTEX_POINT ( 'NONE', #71944 ) ;
#1872 = VERTEX_POINT ( 'NONE', #7481 ) ;
#1873 = CARTESIAN_POINT ( 'NONE',  ( 4.220049686691941027, -10.18810118749999738, 86.12500000204836681 ) ) ;
#1874 = CARTESIAN_POINT ( 'NONE',  ( 7.320508075688771044, 91.24999999317203958, 7.320508075688775484 ) ) ;
#1875 = CARTESIAN_POINT ( 'NONE',  ( -7.778174593052023411, 7.778174593052023411, 96.81250000000000000 ) ) ;
#1878 = CARTESIAN_POINT ( 'NONE',  ( 2.765530957082001251, 293.9218750017069510, 6.676582343749999815 ) ) ;
#1877 = CARTESIAN_POINT ( 'NONE',  ( 30.82842712474620939, 202.2500000027312126, 172.8284271247460424 ) ) ;
#1876 = LINE ( 'NONE', #48251, #31423 ) ;
#1879 = CARTESIAN_POINT ( 'NONE',  ( 7.320508075688771044, 134.3749999999999716, 7.320508075688775484 ) ) ;
#1880 = DIRECTION ( 'NONE',  ( 0.000000000000000000, -0.8536788251726096233, 0.5207998305029611918 ) ) ;
#1881 = LINE ( 'NONE', #30550, #16673 ) ;
#1882 = CARTESIAN_POINT ( 'NONE',  ( -2.679491924311193429, 234.1666666734946034, 10.00000000000001954 ) ) ;
#1883 = CARTESIAN_POINT ( 'NONE',  ( -1.469576158976823947E-15, 3.937499995903220640, 8.000000000000000000 ) ) ;
#1884 = CARTESIAN_POINT ( 'NONE',  ( 31.45873412499999233, 197.6875000013655779, 169.9999999999999432 ) ) ;
#1885 = CARTESIAN_POINT ( 'NONE',  ( 2.977408999572650927, 7.124999997951610098, -7.188101187500001821 ) ) ;
#1886 = CARTESIAN_POINT ( 'NONE',  ( 3.317071493978883456, -8.008118988124989457, 5.981865283940630995 ) ) ;
#1887 = CARTESIAN_POINT ( 'NONE',  ( 1.656854249492381248, 5.937499997268813168, -4.000000000000001776 ) ) ;
#1888 = CARTESIAN_POINT ( 'NONE',  ( 2.977408999572650039, 116.5625000020483810, -7.188101187500000933 ) ) ;
#1889 = CARTESIAN_POINT ( 'NONE',  ( -6.298842414731647743, -51.07418104651127777, -41.32239042995288969 ) ) ;
#1890 = CARTESIAN_POINT ( 'NONE',  ( -11.35316468749999785, 224.0104166700806161, -3.042071309553164848 ) ) ;
#1891 = CARTESIAN_POINT ( 'NONE',  ( -3.673940397442060854E-16, 288.8125000034140157, -6.000000000000001776 ) ) ;
#1892 = CARTESIAN_POINT ( 'NONE',  ( -7.188101187499992051, 0.000000000000000000, 24.36155278187175810 ) ) ;
#1893 = CARTESIAN_POINT ( 'NONE',  ( 25.17157287525381193, 195.6250000000000284, 167.1715728752537018 ) ) ;
#1894 = CARTESIAN_POINT ( 'NONE',  ( 5.676582343749993598, 24.94791666325268764, 9.832129032723422313 ) ) ;
#1895 = CARTESIAN_POINT ( 'NONE',  ( 6.000000000000011546, -10.39230484541325694, 0.000000000000000000 ) ) ;
#1896 = CARTESIAN_POINT ( 'NONE',  ( 5.000000000000001776, 7.708333326505366401, -8.660254037844389075 ) ) ;
#1897 = CARTESIAN_POINT ( 'NONE',  ( 3.313708498984846429, 111.9687500000000000, 7.999999999999918288 ) ) ;
#1898 = CARTESIAN_POINT ( 'NONE',  ( 0.000000000000000000, 300.0000000000000000, 10.00000000000000178 ) ) ;
#1899 = ORIENTED_EDGE ( 'NONE', *, *, #64384, .F. ) ;
#1900 = CYLINDRICAL_SURFACE ( 'NONE', #47044, 10.00000000000000000 ) ;
#1901 = CARTESIAN_POINT ( 'NONE',  ( 3.458734124999960358, 196.6250000013656063, 143.4326545832176976 ) ) ;
#1902 = EDGE_CURVE ( 'NONE', #53551, #15239, #48559, .T. ) ;
#1903 = CARTESIAN_POINT ( 'NONE',  ( 9.832129032723416984, 40.36458332991934839, 5.676582343750006032 ) ) ;
#1904 = CARTESIAN_POINT ( 'NONE',  ( -10.99999999999999822, -4.556349186104052151, 85.28125000409677625 ) ) ;
#1905 = CARTESIAN_POINT ( 'NONE',  ( -1.432654583217664701, 208.0000000013656063, 138.5412658750000787 ) ) ;
#1906 = CARTESIAN_POINT ( 'NONE',  ( 3.490152628695403868E-12, 151.2499999999997442, -10.00000000000000178 ) ) ;
#1907 = LINE ( 'NONE', #52482, #63571 ) ;
#1909 = CARTESIAN_POINT ( 'NONE',  ( 8.311093377946837890, 26.40624999658601624, -8.311093377946837890 ) ) ;
#1908 = CARTESIAN_POINT ( 'NONE',  ( -2.977408999572652260, 104.9375000020483810, 7.188101187500000044 ) ) ;
#1910 = CARTESIAN_POINT ( 'NONE',  ( -3.313708498984758943, -7.999999999999989342, 14.61155277982336465 ) ) ;
#1911 =( BOUNDED_CURVE ( )  B_SPLINE_CURVE ( 2, ( #62281, #57761, #17744, #34016, #35122, #46046, #58137, #29447, #52457 ),
 .UNSPECIFIED., .F., .F. ) 
 B_SPLINE_CURVE_WITH_KNOTS ( ( 3, 2, 2, 2, 3 ),
 ( 0.06666666666666672125, 0.07500000000000006661, 0.08333333333333339810, 0.09166666666666672958, 0.1000000000000000888 ),
 .UNSPECIFIED. ) 
 CURVE ( )  GEOMETRIC_REPRESENTATION_ITEM ( )  RATIONAL_B_SPLINE_CURVE ( ( 0.9999999999999994449, 0.9238795325112872936, 1.000000000000000000, 0.9238795325112867385, 1.000000000000000000, 0.9238795325112867385, 1.000000000000000000, 0.9238795325112859613, 1.000000000000000666 ) ) 
 REPRESENTATION_ITEM ( '' )  );
#1912 = CARTESIAN_POINT ( 'NONE',  ( 11.35316468749999963, 145.9895833299193839, -3.042071309553165293 ) ) ;
#1913 = CARTESIAN_POINT ( 'NONE',  ( -8.660254037844390851, 119.7916666598386968, 4.999999999999998224 ) ) ;
#1914 = CARTESIAN_POINT ( 'NONE',  ( -2.977408999572651815, 108.3125000020483810, 7.188101187500000933 ) ) ;
#1915 = CARTESIAN_POINT ( 'NONE',  ( 11.00000000000000000, 11.00000000000000000, -6.938893903907228378E-15 ) ) ;
#1916 = CARTESIAN_POINT ( 'NONE',  ( -24.54126587500000056, 204.5000000013656063, 168.5673454167827003 ) ) ;
#1917 = ORIENTED_EDGE ( 'NONE', *, *, #61226, .F. ) ;
#1918 = CARTESIAN_POINT ( 'NONE',  ( -3.042071309553173730, 24.63541666325267698, 11.35316468749999785 ) ) ;
#1919 = ORIENTED_EDGE ( 'NONE', *, *, #66888, .F. ) ;
#1920 = CARTESIAN_POINT ( 'NONE',  ( 2.828427124746191623, 7.125000000000000000, -2.828427124746191623 ) ) ;
#1921 = CARTESIAN_POINT ( 'NONE',  ( -2.967813307894019431E-11, 16.44602605510714355, -68.55492853905352035 ) ) ;
#1923 = CARTESIAN_POINT ( 'NONE',  ( 11.35316468749999785, 155.5729166632526983, 3.042071309553174174 ) ) ;
#1922 = CARTESIAN_POINT ( 'NONE',  ( -10.99999999999994849, 4.556349186104097448, 92.59375000409679046 ) ) ;
#1924 = CARTESIAN_POINT ( 'NONE',  ( -30.82842712474612767, 207.5000000027312126, 172.8284271247466108 ) ) ;
#1925 = CARTESIAN_POINT ( 'NONE',  ( -7.999999999999991118, 0.000000000000000000, 15.88655278432982776 ) ) ;
#1926 = CARTESIAN_POINT ( 'NONE',  ( 50.92897276528687200, 200.5194468074884071, 55.62571810886593227 ) ) ;
#1927 = CARTESIAN_POINT ( 'NONE',  ( -3.042071309553166181, 242.8645833367473017, -11.35316468749999608 ) ) ;
#1928 = ADVANCED_FACE ( 'NONE', ( #2182 ), #25546, .F. ) ;
#1929 = CARTESIAN_POINT ( 'NONE',  ( -4.220049686691935698, 10.18810118749999916, 91.75000000204836681 ) ) ;
#1930 = ORIENTED_EDGE ( 'NONE', *, *, #71883, .T. ) ;
#1931 = LINE ( 'NONE', #47934, #52159 ) ;
#1932 = CARTESIAN_POINT ( 'NONE',  ( -8.000000000000000000, 122.0937500040967905, -3.313708498984761164 ) ) ;
#1933 = CARTESIAN_POINT ( 'NONE',  ( -9.832129032723418760, 88.17708332991934128, -5.676582343750004256 ) ) ;
#1934 = CARTESIAN_POINT ( 'NONE',  ( -6.238412754330611322E-16, 10.18810118749999916, 103.2812500020483810 ) ) ;
#1935 = CARTESIAN_POINT ( 'NONE',  ( -3.211159895383562723, 18.06249999863440792, 3.211159895383561391 ) ) ;
#1936 = EDGE_LOOP ( 'NONE', ( #7898, #15824, #66533, #4482, #55209 ) ) ;
#1937 = VERTEX_POINT ( 'NONE', #59531 ) ;
#1938 = CARTESIAN_POINT ( 'NONE',  ( -3.313708498984760720, 3.468750000000000444, -8.000000000000000000 ) ) ;
#1939 = CARTESIAN_POINT ( 'NONE',  ( -1.881053915767121554, 1.749999998634407250, -4.541265875000002339 ) ) ;
#1940 = CARTESIAN_POINT ( 'NONE',  ( -1.320432766682874540E-15, 4.593749997951610986, 7.188101187500000044 ) ) ;
#1941 = CARTESIAN_POINT ( 'NONE',  ( -5.656854249492380582, 120.5000000040967905, -5.656854249492380582 ) ) ;
#1942 = CARTESIAN_POINT ( 'NONE',  ( -7.204075437095965206, -7.204075437095968759, 98.21875000204838102 ) ) ;
#1943 = AXIS2_PLACEMENT_3D ( 'NONE', #1654, #64275, #71027 ) ;
#1944 = DIRECTION ( 'NONE',  ( 0.000000000000000000, 0.000000000000000000, 1.000000000000000000 ) ) ;
#1945 = CARTESIAN_POINT ( 'NONE',  ( 4.000000000000001776, 0.06250000000000018041, -1.656854249492381248 ) ) ;
#1946 = CARTESIAN_POINT ( 'NONE',  ( -4.000000000000002665, 15.31249999726881406, 1.656854249492380804 ) ) ;
#1947 = CARTESIAN_POINT ( 'NONE',  ( -1.881053915767121776, 4.624999998634407028, -4.541265875000002339 ) ) ;
#1948 = EDGE_LOOP ( 'NONE', ( #65152, #64749, #21103, #7580, #48981, #52895, #23273, #15632, #6768, #23054, #10594, #55276, #74576, #29728, #47741, #59446, #66811, #18384, #2114, #41930, #66850, #47110, #57660, #37417, #41912, #30625, #21531, #43796, #16201, #22550, #33624, #68574, #58484, #50377, #39556, #3342, #36108, #62978, #39030, #73499, #59739, #15430, #24758 ) ) ;
#1949 = CARTESIAN_POINT ( 'NONE',  ( 3.458734124999959914, 207.4375000013656063, 142.0000000000000568 ) ) ;
#1950 = CARTESIAN_POINT ( 'NONE',  ( -2.445694354108782775, 197.5625000013656063, 200.4456943541088663 ) ) ;
#1952 = DIRECTION ( 'NONE',  ( -0.000000000000000000, -1.000000000000000000, -4.283267841918042741E-17 ) ) ;
#1951 = CARTESIAN_POINT ( 'NONE',  ( -31.45873412499996746, 201.7500000013655779, 171.4326545832181239 ) ) ;
#1953 =( NAMED_UNIT ( * ) SI_UNIT ( $, .STERADIAN. ) SOLID_ANGLE_UNIT ( ) );
#1954 = CARTESIAN_POINT ( 'NONE',  ( 4.541265875000001451, 14.24999999863440969, 1.881053915767124440 ) ) ;
#1955 = CARTESIAN_POINT ( 'NONE',  ( 2.849036369511732440E-14, 200.3750000027312126, 202.0000000000000000 ) ) ;
#1956 = CARTESIAN_POINT ( 'NONE',  ( -7.188101187499990274, -2.977408999572651371, 12.08030278187175099 ) ) ;
#1957 = ORIENTED_EDGE ( 'NONE', *, *, #36684, .F. ) ;
#1958 = ORIENTED_EDGE ( 'NONE', *, *, #28415, .T. ) ;
#1959 = CARTESIAN_POINT ( 'NONE',  ( -10.18810118749999738, -4.220049686691941915, 106.7500000020483668 ) ) ;
#1960 = CARTESIAN_POINT ( 'NONE',  ( -6.735557395310442023E-16, 11.00000000000000000, 114.8125000040967763 ) ) ;
#1961 = CARTESIAN_POINT ( 'NONE',  ( -23.99999999999997513, 201.6875000000000000, 171.6568542494927385 ) ) ;
#1962 = CARTESIAN_POINT ( 'NONE',  ( 2.839093476692135984E-14, 197.6875000013655779, 201.4587341250000350 ) ) ;
#1963 = CARTESIAN_POINT ( 'NONE',  ( -4.898587196589412829E-16, 105.1250000000000000, -8.000000000000000000 ) ) ;
#1964 = CARTESIAN_POINT ( 'NONE',  ( 8.660254037844385522, 94.58333333333334281, 5.000000000000005329 ) ) ;
#1965 = EDGE_CURVE ( 'NONE', #29935, #21159, #53818, .T. ) ;
#1966 = CARTESIAN_POINT ( 'NONE',  ( 5.656854249492379694, 119.9375000000000000, -5.656854249492380582 ) ) ;
#1967 = CARTESIAN_POINT ( 'NONE',  ( -4.721056650415999201, 297.4843750017070079, -4.721056650415999201 ) ) ;
#1968 =( GEOMETRIC_REPRESENTATION_CONTEXT ( 3 ) GLOBAL_UNCERTAINTY_ASSIGNED_CONTEXT ( ( #64509 ) ) GLOBAL_UNIT_ASSIGNED_CONTEXT ( ( #4941, #10591, #68299 ) ) REPRESENTATION_CONTEXT ( 'NONE', 'WORKASPACE' ) );
#1969 = ORIENTED_EDGE ( 'NONE', *, *, #25390, .F. ) ;
#1970 = CARTESIAN_POINT ( 'NONE',  ( 8.660254037844419273, 189.5833333333333712, 5.000000000000024869 ) ) ;
#1971 = CARTESIAN_POINT ( 'NONE',  ( -8.000000000000001776, 12.65624999590322375, 3.313708498984759387 ) ) ;
#1972 = CARTESIAN_POINT ( 'NONE',  ( 3.458734124999959914, 209.4375000013656063, 142.0000000000000568 ) ) ;
#1973 = CARTESIAN_POINT ( 'NONE',  ( 6.123233995736767268E-16, 103.1249999931720396, -10.00000000000000178 ) ) ;
#1974 = CARTESIAN_POINT ( 'NONE',  ( 9.999999999999998224, 222.7083333333333428, -2.679491924311229401 ) ) ;
#1975 = DIRECTION ( 'NONE',  ( 0.000000000000000000, 0.000000000000000000, -1.000000000000000000 ) ) ;
#1976 = CARTESIAN_POINT ( 'NONE',  ( 11.00000000000000355, -4.556349186104045046, 112.6562499999999858 ) ) ;
#1977 = CARTESIAN_POINT ( 'NONE',  ( 8.660254037844385522, 209.5833333333333428, 5.000000000000005329 ) ) ;
#1978 = CARTESIAN_POINT ( 'NONE',  ( 5.082755093536320601, -5.082755093536318824, 8.424052781871752771 ) ) ;
#1979 = CARTESIAN_POINT ( 'NONE',  ( -5.676582343749998039, 177.7604166632526699, -9.832129032723420536 ) ) ;
#1980 = CARTESIAN_POINT ( 'NONE',  ( 7.778174593052023411, -7.778174593052021635, 102.0624999999999858 ) ) ;
#1981 = CARTESIAN_POINT ( 'NONE',  ( -3.211159895383561391, 3.687499998634407028, -3.211159895383561835 ) ) ;
#1982 = CARTESIAN_POINT ( 'NONE',  ( 3.999999999999960032, 210.0000000000000284, 142.0000000000000568 ) ) ;
#1984 = CARTESIAN_POINT ( 'NONE',  ( -7.347880794884122694E-16, 12.75000000000000178, 4.000000000000001776 ) ) ;
#1983 = CARTESIAN_POINT ( 'NONE',  ( -10.00000000000000000, 228.1250000068279746, 0.000000000000000000 ) ) ;
#1985 = ORIENTED_EDGE ( 'NONE', *, *, #25955, .F. ) ;
#1987 = ADVANCED_FACE ( 'NONE', ( #65917 ), #70843, .T. ) ;
#1986 = CARTESIAN_POINT ( 'NONE',  ( 3.458734124999960358, 209.6250000013656063, 143.4326545832176976 ) ) ;
#1988 = CARTESIAN_POINT ( 'NONE',  ( -11.35316468749999785, 53.38541666325267698, -3.042071309553167513 ) ) ;
#1989 = CARTESIAN_POINT ( 'NONE',  ( 2.020667218593132706E-15, -11.00000000000000000, 106.5625000040967763 ) ) ;
#1990 = CARTESIAN_POINT ( 'NONE',  ( -8.311093377946836114, 217.9687499965860127, -8.311093377946837890 ) ) ;
#1991 = CARTESIAN_POINT ( 'NONE',  ( -29.43265458321770822, 203.5000000013655779, 166.5412658750003914 ) ) ;
#1992 = CARTESIAN_POINT ( 'NONE',  ( 11.00000000000000000, 4.556349186104045934, 70.84374999999998579 ) ) ;
#1993 = CARTESIAN_POINT ( 'NONE',  ( -2.679491924311308448, 60.41666665983868967, 9.999999999999957367 ) ) ;
#1994 = CARTESIAN_POINT ( 'NONE',  ( 2.445694354108782775, 196.5625000013656063, 139.5543056458912190 ) ) ;
#1995 = CARTESIAN_POINT ( 'NONE',  ( -11.35316468749999785, 103.0729166632526841, -3.042071309553167513 ) ) ;
#1996 = EDGE_CURVE ( 'NONE', #58040, #48595, #31598, .T. ) ;
#1997 = VECTOR ( 'NONE', #40725, 1000.000000000000000 ) ;
#1998 = CARTESIAN_POINT ( 'NONE',  ( -2.679491924311235618, 80.41666665983871098, 10.00000000000000000 ) ) ;
#1999 = CARTESIAN_POINT ( 'NONE',  ( -2.977408999572651815, 92.93750000204839523, 7.188101187500000933 ) ) ;
#2000 = CARTESIAN_POINT ( 'NONE',  ( 2.780723358947928197E-16, 15.68749999863440436, -4.541265875000002339 ) ) ;
#2001 = CARTESIAN_POINT ( 'NONE',  ( 1.656854249492381248, 11.18750000000000000, -4.000000000000001776 ) ) ;
#2002 = FACE_OUTER_BOUND ( 'NONE', #20229, .T. ) ;
#2003 = ORIENTED_EDGE ( 'NONE', *, *, #72909, .T. ) ;
#2004 = ORIENTED_EDGE ( 'NONE', *, *, #57482, .F. ) ;
#2005 = CARTESIAN_POINT ( 'NONE',  ( -4.721056650415998313, 295.7343750017069510, 4.721056650416000089 ) ) ;
#2006 = DIRECTION ( 'NONE',  ( 0.000000000000000000, -0.02418647091589873691, -0.9997074645238147594 ) ) ;
#2007 = CARTESIAN_POINT ( 'NONE',  ( -5.676582343749998039, 167.4479166632526983, -9.832129032723420536 ) ) ;
#2008 = PLANE ( 'NONE',  #70655 ) ;
#2009 = CARTESIAN_POINT ( 'NONE',  ( 4.000000000000015987, 198.5000000000000000, 198.0000000000000284 ) ) ;
#2010 = CARTESIAN_POINT ( 'NONE',  ( -31.99999999999999289, 201.2500000000000000, 170.0000000000003979 ) ) ;
#2011 = EDGE_CURVE ( 'NONE', #37658, #51670, #19930, .T. ) ;
#2012 = CARTESIAN_POINT ( 'NONE',  ( 7.204075437095966983, 7.204075437095967871, 109.4687500020483810 ) ) ;
#2013 = VERTEX_POINT ( 'NONE', #36521 ) ;
#2014 = CARTESIAN_POINT ( 'NONE',  ( 38.33487889105908408, -1.176080951904068028, 124.4578737245594482 ) ) ;
#2015 = CARTESIAN_POINT ( 'NONE',  ( 54.00000000000000000, 242.0000000000000284, 4.085831468968142743E-14 ) ) ;
#2016 = CARTESIAN_POINT ( 'NONE',  ( 8.311093377946834337, 145.4687499965860127, 8.311093377946839666 ) ) ;
#2017 = CARTESIAN_POINT ( 'NONE',  ( 1.901548650871797615E-12, 218.7500000000001990, 10.00000000000000533 ) ) ;
#2018 = CARTESIAN_POINT ( 'NONE',  ( -2.445694354108783219, 208.8125000013656063, 200.4456943541088663 ) ) ;
#2019 = CARTESIAN_POINT ( 'NONE',  ( 7.204075437095968759, -7.204075437095966983, 68.59375000204836681 ) ) ;
#2020 = CARTESIAN_POINT ( 'NONE',  ( 6.951808397369818766E-16, 52.34374999658601979, -11.35316468750000141 ) ) ;
#2022 = VERTEX_POINT ( 'NONE', #31221 ) ;
#2021 =( BOUNDED_CURVE ( )  B_SPLINE_CURVE ( 3, ( #45721, #21590, #73287, #28374 ),
 .UNSPECIFIED., .F., .F. ) 
 B_SPLINE_CURVE_WITH_KNOTS ( ( 4, 4 ),
 ( 4.679914544886747407, 4.717395569102015962 ),
 .UNSPECIFIED. ) 
 CURVE ( )  GEOMETRIC_REPRESENTATION_ITEM ( )  RATIONAL_B_SPLINE_CURVE ( ( 1.000000000000000000, 0.9998829344948912956, 0.9998829344948912956, 1.000000000000000000 ) ) 
 REPRESENTATION_ITEM ( '' )  );
#2023 = DIRECTION ( 'NONE',  ( -1.000000000000000000, 0.000000000000000000, 0.000000000000000000 ) ) ;
#2025 = CARTESIAN_POINT ( 'NONE',  ( 4.541265875000001451, 5.374999998634407028, 1.881053915767124440 ) ) ;
#2024 =( BOUNDED_CURVE ( )  B_SPLINE_CURVE ( 2, ( #69722, #6722, #13463, #23693, #12733, #53485, #24786, #47801, #70824 ),
 .UNSPECIFIED., .F., .F. ) 
 B_SPLINE_CURVE_WITH_KNOTS ( ( 3, 2, 2, 2, 3 ),
 ( 0.8522727272727272929, 0.8579545454545454142, 0.8636363636363636465, 0.8693181818181817677, 0.8750000000000000000 ),
 .UNSPECIFIED. ) 
 CURVE ( )  GEOMETRIC_REPRESENTATION_ITEM ( )  RATIONAL_B_SPLINE_CURVE ( ( 1.000000000000000000, 0.9238795325112867385, 1.000000000000000000, 0.9238795325112867385, 1.000000000000000000, 0.9238795325112867385, 1.000000000000000000, 0.9238795325112867385, 1.000000000000000000 ) ) 
 REPRESENTATION_ITEM ( '' )  );
#2026 = CARTESIAN_POINT ( 'NONE',  ( 3.317071493978877683, 8.008118988124991233, 6.544365283940627442 ) ) ;
#2027 = VECTOR ( 'NONE', #1606, 1000.000000000000000 ) ;
#2028 = CARTESIAN_POINT ( 'NONE',  ( 7.188101187499999156, 15.37499999795161187, 2.977408999572654924 ) ) ;
#2029 = CARTESIAN_POINT ( 'NONE',  ( 2.485281374238571317, 293.7500000034140157, -6.000000000000003553 ) ) ;
#2030 = LINE ( 'NONE', #14441, #63022 ) ;
#2031 = CARTESIAN_POINT ( 'NONE',  ( 7.188101187500001821, 12.93749999795161365, -2.977408999572650483 ) ) ;
#2032 = CARTESIAN_POINT ( 'NONE',  ( 7.188101187499992051, 8.802885111219154394E-16, 9.736552781871754547 ) ) ;
#2033 = CARTESIAN_POINT ( 'NONE',  ( -4.220049686691935698, 10.18810118749999916, 115.7500000020483668 ) ) ;
#2034 = EDGE_CURVE ( 'NONE', #35739, #24196, #65549, .T. ) ;
#2035 = FACE_OUTER_BOUND ( 'NONE', #20177, .T. ) ;
#2036 = CARTESIAN_POINT ( 'NONE',  ( -2.828427124746192067, 2.374999997268813612, 2.828427124746190735 ) ) ;
#2037 = ORIENTED_EDGE ( 'NONE', *, *, #24852, .T. ) ;
#2038 = CARTESIAN_POINT ( 'NONE',  ( 2.849036369511732440E-14, 195.3750000027311842, 202.0000000000000000 ) ) ;
#2039 = CARTESIAN_POINT ( 'NONE',  ( 2.828427124746153876, 202.8750000000000284, 144.8284271247462129 ) ) ;
#2040 = CARTESIAN_POINT ( 'NONE',  ( -26.34314575050769491, 199.0625000027312126, 166.0000000000003695 ) ) ;
#2041 = VECTOR ( 'NONE', #54132, 1000.000000000000000 ) ;
#2042 = CARTESIAN_POINT ( 'NONE',  ( 1.881053915767121776, 1.499999998634406806, -4.541265875000002339 ) ) ;
#2043 = CARTESIAN_POINT ( 'NONE',  ( 2.977408999572650039, 116.1875000020483952, -7.188101187500001821 ) ) ;
#2044 = CARTESIAN_POINT ( 'NONE',  ( 6.023803224821318913, -6.914460432017358826, -0.07661102881318833380 ) ) ;
#2045 = CARTESIAN_POINT ( 'NONE',  ( -7.999999999999989342, -3.313708498984762496, 4.111552783920145338 ) ) ;
#2046 = ORIENTED_EDGE ( 'NONE', *, *, #44541, .F. ) ;
#2047 = CARTESIAN_POINT ( 'NONE',  ( -5.082755093536326818, 22.40624999795161187, 5.082755093536325042 ) ) ;
#2048 = ORIENTED_EDGE ( 'NONE', *, *, #6228, .T. ) ;
#2049 = CARTESIAN_POINT ( 'NONE',  ( 0.000000000000000000, 4.898587196589400010E-16, -24.00000000000001421 ) ) ;
#2050 = CARTESIAN_POINT ( 'NONE',  ( 3.458734125000015425, 209.0000000013655779, 196.5673454167823877 ) ) ;
#2051 = CARTESIAN_POINT ( 'NONE',  ( 31.45873412499999944, 202.6875000013656063, 169.9999999999998863 ) ) ;
#2052 = CARTESIAN_POINT ( 'NONE',  ( -7.320508075688778149, 48.12499999999999289, 7.320508075688769267 ) ) ;
#2053 = CARTESIAN_POINT ( 'NONE',  ( -7.188101187499999156, 97.62500000204836681, 2.977408999572654924 ) ) ;
#2054 = CARTESIAN_POINT ( 'NONE',  ( 2.485281374238575314, 296.3124999999999432, 6.000000000000000888 ) ) ;
#2056 = LINE ( 'NONE', #71072, #6048 ) ;
#2055 = CARTESIAN_POINT ( 'NONE',  ( -12.00000000000000000, 0.000000000000000000, -14.00000000000000178 ) ) ;
#2057 = VERTEX_POINT ( 'NONE', #25914 ) ;
#2058 = CARTESIAN_POINT ( 'NONE',  ( -9.832129032723415207, 229.3229166700806729, 5.676582343750005144 ) ) ;
#2059 = CARTESIAN_POINT ( 'NONE',  ( 27.99999999999999645, 210.0000000000000284, 165.9999999999999147 ) ) ;
#2060 = DIRECTION ( 'NONE',  ( 0.000000000000000000, 0.000000000000000000, 1.000000000000000000 ) ) ;
#2061 = CARTESIAN_POINT ( 'NONE',  ( 2.449293598294707893E-16, 16.99999999726881583, -4.000000000000001776 ) ) ;
#2062 = CARTESIAN_POINT ( 'NONE',  ( 8.660254037844389075, 262.0833333333333144, 4.999999999999997335 ) ) ;
#2064 = ADVANCED_FACE ( 'NONE', ( #31970 ), #66293, .T. ) ;
#2063 = DIRECTION ( 'NONE',  ( -0.000000000000000000, -0.000000000000000000, -1.000000000000000000 ) ) ;
#2065 = CARTESIAN_POINT ( 'NONE',  ( 4.999999999999993783, 169.1666666666666856, 8.660254037844390851 ) ) ;
#2066 = CARTESIAN_POINT ( 'NONE',  ( -7.999999999999991118, 0.000000000000000000, 5.330302779823363757 ) ) ;
#2067 = CARTESIAN_POINT ( 'NONE',  ( 7.188101187499992051, 2.977408999572647819, 28.20530278187175810 ) ) ;
#2068 = CARTESIAN_POINT ( 'NONE',  ( -5.676582343749998039, 137.7604166632526983, -9.832129032723420536 ) ) ;
#2069 = CYLINDRICAL_SURFACE ( 'NONE', #18024, 7.999999999999991118 ) ;
#2070 = FACE_OUTER_BOUND ( 'NONE', #35726, .T. ) ;
#2073 = CARTESIAN_POINT ( 'NONE',  ( -5.000000000000007105, 168.3333333333333428, 8.660254037844389075 ) ) ;
#2072 = CARTESIAN_POINT ( 'NONE',  ( -5.000000000000000000, -52.35862550122958936, 48.98731492261398301 ) ) ;
#2071 = CARTESIAN_POINT ( 'NONE',  ( 30.82842712474620228, 205.3750000000000284, 167.1715728752537586 ) ) ;
#2074 = AXIS2_PLACEMENT_3D ( 'NONE', #43154, #60512, #9957 ) ;
#2075 = ORIENTED_EDGE ( 'NONE', *, *, #4466, .F. ) ;
#2076 = CARTESIAN_POINT ( 'NONE',  ( -9.832129032723420536, 14.01041666325268409, 5.676582343749997150 ) ) ;
#2077 = CARTESIAN_POINT ( 'NONE',  ( -8.660254037844385522, 112.9166666666666714, 4.999999999999994671 ) ) ;
#2078 = CARTESIAN_POINT ( 'NONE',  ( 11.00000000000000000, 1.347111479062088405E-15, 67.93750000409676204 ) ) ;
#2079 = CARTESIAN_POINT ( 'NONE',  ( -2.754378923186476579E-14, 208.1875000013656063, 145.4587341250000350 ) ) ;
#2080 = EDGE_CURVE ( 'NONE', #41819, #4091, #11163, .T. ) ;
#2081 = CARTESIAN_POINT ( 'NONE',  ( -2.679491924311225848, 38.33333332650536818, -10.00000000000000178 ) ) ;
#2082 = CARTESIAN_POINT ( 'NONE',  ( -5.082755093536325930, 113.4687500020483810, -5.082755093536325930 ) ) ;
#2083 = CARTESIAN_POINT ( 'NONE',  ( 3.211159895383561835, 3.562499998634407028, -3.211159895383561835 ) ) ;
#2084 = CARTESIAN_POINT ( 'NONE',  ( -10.99999999999989164, -4.556349186104158733, 85.09375000000001421 ) ) ;
#2085 = CARTESIAN_POINT ( 'NONE',  ( 7.999999999999991118, 9.797174393178815797E-16, 16.58030277982336287 ) ) ;
#2087 = CARTESIAN_POINT ( 'NONE',  ( 11.00000000000000000, 1.347111479062088405E-15, 108.2499999999999858 ) ) ;
#2086 = CARTESIAN_POINT ( 'NONE',  ( 2.485281374238247132, 291.7500000034140157, -6.000000000000325961 ) ) ;
#2088 = ORIENTED_EDGE ( 'NONE', *, *, #34628, .T. ) ;
#2089 = CARTESIAN_POINT ( 'NONE',  ( 8.660254037844389075, 29.58333333333334281, 5.000000000000007994 ) ) ;
#2090 = LINE ( 'NONE', #42070, #38721 ) ;
#2091 = CARTESIAN_POINT ( 'NONE',  ( -11.35316468749999963, 234.2187500034139873, 0.000000000000000000 ) ) ;
#2092 = CARTESIAN_POINT ( 'NONE',  ( -11.35316468750000141, 118.4895833299193697, 3.042071309553159963 ) ) ;
#2093 = VERTEX_POINT ( 'NONE', #8210 ) ;
#2094 = DIRECTION ( 'NONE',  ( -0.000000000000000000, -0.000000000000000000, -1.000000000000000000 ) ) ;
#2095 = CARTESIAN_POINT ( 'NONE',  ( -7.204075437095965206, -7.204075437095968759, 97.84375000204836681 ) ) ;
#2096 = CARTESIAN_POINT ( 'NONE',  ( 27.99999999999996092, 195.6250000027311842, 165.9999999999998863 ) ) ;
#2097 = CARTESIAN_POINT ( 'NONE',  ( 3.458734125000015425, 195.2500000013656063, 196.5673454167823877 ) ) ;
#2098 = FACE_OUTER_BOUND ( 'NONE', #51963, .T. ) ;
#2100 = CARTESIAN_POINT ( 'NONE',  ( -8.311093377946841443, 118.9062499965860411, 8.311093377946834337 ) ) ;
#2099 = CARTESIAN_POINT ( 'NONE',  ( 1.102182119232618108E-15, 292.3125000034140157, 6.000000000000001776 ) ) ;
#2101 = CARTESIAN_POINT ( 'NONE',  ( -32.00000000000000000, 209.2500000000000284, 170.0000000000003979 ) ) ;
#2102 = CARTESIAN_POINT ( 'NONE',  ( 7.999999999999991118, 3.313708498984758055, 6.361552783920146226 ) ) ;
#2103 = ORIENTED_EDGE ( 'NONE', *, *, #23555, .F. ) ;
#2104 = CARTESIAN_POINT ( 'NONE',  ( 2.679491924311228956, 207.9166666598387110, -10.00000000000000000 ) ) ;
#2105 = EDGE_CURVE ( 'NONE', #58601, #16650, #4546, .T. ) ;
#2106 = DIRECTION ( 'NONE',  ( 0.000000000000000000, 0.000000000000000000, 1.000000000000000000 ) ) ;
#2107 = CYLINDRICAL_SURFACE ( 'NONE', #21982, 3.999999999999986233 ) ;
#2108 = CARTESIAN_POINT ( 'NONE',  ( 5.676582343750001591, 96.92708332991935549, -9.832129032723420536 ) ) ;
#2109 = CARTESIAN_POINT ( 'NONE',  ( 4.000000000000015987, 205.5625000000000284, 196.3431457505076594 ) ) ;
#2110 = CARTESIAN_POINT ( 'NONE',  ( -1.320432766682874540E-15, 9.468749997951610098, 7.188101187500000044 ) ) ;
#2111 = CARTESIAN_POINT ( 'NONE',  ( 10.18810118749999916, 4.220049686691935698, 89.87500000204836681 ) ) ;
#2112 = EDGE_CURVE ( 'NONE', #26793, #2485, #22970, .T. ) ;
#2113 = CARTESIAN_POINT ( 'NONE',  ( 3.042071309553167069, 12.13541666325268054, -11.35316468749999785 ) ) ;
#2114 = ORIENTED_EDGE ( 'NONE', *, *, #17459, .T. ) ;
#2115 = CARTESIAN_POINT ( 'NONE',  ( 4.000000000000001776, 20.81249999726881583, -1.656854249492381248 ) ) ;
#2116 = CARTESIAN_POINT ( 'NONE',  ( 1.471067592899761672E-15, -8.008118988124991233, 23.88811528394063188 ) ) ;
#2117 = CARTESIAN_POINT ( 'NONE',  ( -11.00000000000005151, 4.556349186103993532, 102.9062499999999858 ) ) ;
#2118 = CARTESIAN_POINT ( 'NONE',  ( 10.18810118749999916, 1.247682550866122264E-15, 74.78125000204836681 ) ) ;
#2119 = LINE ( 'NONE', #54555, #72362 ) ;
#2120 = CARTESIAN_POINT ( 'NONE',  ( 6.676582343750001591, 292.9531250017069510, -8.176455196517173205E-16 ) ) ;
#2121 = CARTESIAN_POINT ( 'NONE',  ( -4.000000000000016875, 199.4375000000000284, 140.3431457505076594 ) ) ;
#2122 = CARTESIAN_POINT ( 'NONE',  ( -5.676582343750006032, 219.4270833299193555, 9.832129032723418760 ) ) ;
#2123 = CARTESIAN_POINT ( 'NONE',  ( -4.220049686691935698, 10.18810118749999916, 83.87500000204835260 ) ) ;
#2124 = EDGE_CURVE ( 'NONE', #48333, #2977, #20922, .T. ) ;
#2125 = VECTOR ( 'NONE', #40089, 1000.000000000000000 ) ;
#2126 = CARTESIAN_POINT ( 'NONE',  ( -26.56734541678237704, 197.3750000013656063, 166.5412658750003629 ) ) ;
#2127 = CARTESIAN_POINT ( 'NONE',  ( -5.656854249492379694, 24.56250000000000355, -5.656854249492380582 ) ) ;
#2128 = CARTESIAN_POINT ( 'NONE',  ( 1.881053915767121776, 10.62499999863440792, -4.541265875000002339 ) ) ;
#2129 = EDGE_LOOP ( 'NONE', ( #23480, #45274, #13668, #9620 ) ) ;
#2130 = CARTESIAN_POINT ( 'NONE',  ( -26.03349122889995471, -51.37860266882407245, 153.1493458656407540 ) ) ;
#2131 = CARTESIAN_POINT ( 'NONE',  ( -2.828427124746153876, 209.0000000027312126, 195.1715728752538439 ) ) ;
#2132 = VECTOR ( 'NONE', #74281, 1000.000000000000000 ) ;
#2133 = CARTESIAN_POINT ( 'NONE',  ( 3.458734124999959469, 200.7500000013656347, 140.5673454167824161 ) ) ;
#2135 =( BOUNDED_CURVE ( )  B_SPLINE_CURVE ( 2, ( #65724, #13291, #7287, #24253, #64983, #12926, #36699, #58980, #24984 ),
 .UNSPECIFIED., .F., .F. ) 
 B_SPLINE_CURVE_WITH_KNOTS ( ( 3, 2, 2, 2, 3 ),
 ( 0.8823529411764705621, 0.8860294117647058432, 0.8897058823529411242, 0.8933823529411765163, 0.8970588235294117974 ),
 .UNSPECIFIED. ) 
 CURVE ( )  GEOMETRIC_REPRESENTATION_ITEM ( )  RATIONAL_B_SPLINE_CURVE ( ( 1.000000000000000000, 0.9238795325112867385, 1.000000000000000000, 0.9238795325112867385, 1.000000000000000000, 0.9238795325112867385, 1.000000000000000000, 0.9238795325112867385, 1.000000000000000000 ) ) 
 REPRESENTATION_ITEM ( '' )  );
#2134 = CARTESIAN_POINT ( 'NONE',  ( -2.849036369511732440E-14, 203.3750000027312126, 138.0000000000000568 ) ) ;
#2136 = CARTESIAN_POINT ( 'NONE',  ( 5.000000000000000000, 11.00774715070946108, -67.37702390743022818 ) ) ;
#2137 = CARTESIAN_POINT ( 'NONE',  ( 10.18810118749999916, 1.247682550866122264E-15, 68.78125000204838102 ) ) ;
#2138 = EDGE_LOOP ( 'NONE', ( #9116, #36634, #7967 ) ) ;
#2139 = CARTESIAN_POINT ( 'NONE',  ( -2.977408999572650039, 2.437499997951610542, -7.188101187500000933 ) ) ;
#2140 = EDGE_CURVE ( 'NONE', #59499, #25519, #30674, .T. ) ;
#2141 = CARTESIAN_POINT ( 'NONE',  ( 7.188101187500002709, 117.6875000020484094, 2.977408999572649151 ) ) ;
#2142 = CARTESIAN_POINT ( 'NONE',  ( 1.377000000000000002, 272.8559999999997672, 5.668132533241393212 ) ) ;
#2143 = CARTESIAN_POINT ( 'NONE',  ( -4.721056650415999201, 292.3281250017069510, -4.721056650415999201 ) ) ;
#2144 = EDGE_CURVE ( 'NONE', #52626, #18054, #51956, .T. ) ;
#2146 = CARTESIAN_POINT ( 'NONE',  ( 8.660254037844385522, 136.4583333265053682, 5.000000000000005329 ) ) ;
#2145 = CARTESIAN_POINT ( 'NONE',  ( 5.676582343750005144, 230.5729166700806729, 9.832129032723416984 ) ) ;
#2147 = ORIENTED_EDGE ( 'NONE', *, *, #5446, .T. ) ;
#2148 = CIRCLE ( 'NONE', #44331, 6.000000000000001776 ) ;
#2149 = CARTESIAN_POINT ( 'NONE',  ( 8.311093377946834337, 222.3437500034139589, -8.311093377946836114 ) ) ;
#2151 = CARTESIAN_POINT ( 'NONE',  ( -5.082755093536319713, 5.082755093536319713, 27.17405278187175455 ) ) ;
#2150 = SHAPE_REPRESENTATION ( 'dead centre', ( #57354 ), #21241 ) ;
#2152 = CARTESIAN_POINT ( 'NONE',  ( 5.656854249492378806, 2.812500000000000444, 5.656854249492381470 ) ) ;
#2154 = EDGE_CURVE ( 'NONE', #39667, #41903, #29258, .T. ) ;
#2153 = CARTESIAN_POINT ( 'NONE',  ( -3.458734124999960358, 198.6875000013655779, 198.0000000000000284 ) ) ;
#2155 = EDGE_LOOP ( 'NONE', ( #70942, #23548, #36486, #17977 ) ) ;
#2156 = DIRECTION ( 'NONE',  ( 1.000000000000000000, 0.000000000000000000, -0.000000000000000000 ) ) ;
#2157 = CARTESIAN_POINT ( 'NONE',  ( 9.832129032723416984, 95.67708332991935549, 5.676582343750006032 ) ) ;
#2158 = CARTESIAN_POINT ( 'NONE',  ( -1.836970198721029983E-15, 123.7500000000000142, 10.00000000000000178 ) ) ;
#2159 = CARTESIAN_POINT ( 'NONE',  ( -4.556349186104045934, 11.00000000000000000, 75.71874999999998579 ) ) ;
#2162 = CARTESIAN_POINT ( 'NONE',  ( -7.778174593052020747, -7.778174593052023411, 113.6875000000000000 ) ) ;
#2161 = CARTESIAN_POINT ( 'NONE',  ( 31.45873412499999944, 203.6875000013656063, 169.9999999999998863 ) ) ;
#2160 = CARTESIAN_POINT ( 'NONE',  ( 30.44569435410879166, 204.8125000013656063, 172.4456943541087526 ) ) ;
#2163 = ORIENTED_EDGE ( 'NONE', *, *, #45223, .T. ) ;
#2164 = DIRECTION ( 'NONE',  ( -0.000000000000000000, 1.000000000000000000, -0.000000000000000000 ) ) ;
#2165 = CARTESIAN_POINT ( 'NONE',  ( 11.35316468750000141, 210.7812499965860411, 0.000000000000000000 ) ) ;
#2166 = CARTESIAN_POINT ( 'NONE',  ( -3.458734125000015425, 201.0000000013655779, 143.4326545832176976 ) ) ;
#2167 = CARTESIAN_POINT ( 'NONE',  ( 31.45873412500001010, 203.0000000013655779, 168.5673454167822740 ) ) ;
#2168 = CARTESIAN_POINT ( 'NONE',  ( -7.188101187500001821, 26.99999999795161543, -2.977408999572651371 ) ) ;
#2169 = CARTESIAN_POINT ( 'NONE',  ( 5.676582343750001591, 196.9270833299193839, -9.832129032723420536 ) ) ;
#2170 = CARTESIAN_POINT ( 'NONE',  ( 7.188101187500002709, 92.18750000204838102, 2.977408999572649151 ) ) ;
#2171 = CARTESIAN_POINT ( 'NONE',  ( -4.242640687119286547, 295.9375000034140157, -4.242640687119286547 ) ) ;
#2172 = CARTESIAN_POINT ( 'NONE',  ( -26.34314575050757412, 197.5625000000000853, 174.0000000000003411 ) ) ;
#2173 = CARTESIAN_POINT ( 'NONE',  ( 4.541265875000002339, 15.37499999863440614, -1.881053915767121554 ) ) ;
#2174 = CARTESIAN_POINT ( 'NONE',  ( 29.43265458321766914, 199.1250000013656347, 166.5412658749999650 ) ) ;
#2175 = CARTESIAN_POINT ( 'NONE',  ( -2.977408999572647819, 7.188101187499991163, 1.580302781871753437 ) ) ;
#2176 = CARTESIAN_POINT ( 'NONE',  ( 5.676582343750001591, 86.61458332991936970, -9.832129032723420536 ) ) ;
#2177 = ORIENTED_EDGE ( 'NONE', *, *, #6585, .F. ) ;
#2178 = CARTESIAN_POINT ( 'NONE',  ( -5.000000000000000000, -52.63770595436704269, 42.88862352055295446 ) ) ;
#2179 = CARTESIAN_POINT ( 'NONE',  ( -2.828427124746209831, 201.3750000000000284, 139.1715728752538723 ) ) ;
#2180 = ORIENTED_EDGE ( 'NONE', *, *, #32956, .F. ) ;
#2181 = PLANE ( 'NONE',  #25393 ) ;
#2182 = FACE_OUTER_BOUND ( 'NONE', #30962, .T. ) ;
#2183 = CARTESIAN_POINT ( 'NONE',  ( 11.35316468749999963, 70.98958332991934128, -3.042071309553165293 ) ) ;
#2184 = EDGE_LOOP ( 'NONE', ( #39855, #1852 ) ) ;
#2185 = CARTESIAN_POINT ( 'NONE',  ( -7.204075437095967871, 7.204075437095967871, 88.84375000204838102 ) ) ;
#2186 = CARTESIAN_POINT ( 'NONE',  ( -10.18810118749999738, -4.220049686691941915, 115.7500000020483668 ) ) ;
#2187 = CARTESIAN_POINT ( 'NONE',  ( -5.000000000000000000, 16.24494643555759410, 69.83755725260752456 ) ) ;
#2189 = CARTESIAN_POINT ( 'NONE',  ( 5.676582343750001591, 76.61458332991935549, -9.832129032723420536 ) ) ;
#2188 = CARTESIAN_POINT ( 'NONE',  ( -5.082755093536325930, 89.46875000204838102, -5.082755093536325930 ) ) ;
#2191 = AXIS2_PLACEMENT_3D ( 'NONE', #17510, #45436, #34523 ) ;
#2190 = CARTESIAN_POINT ( 'NONE',  ( -7.999999999999991118, 0.000000000000000000, 25.01780278392014978 ) ) ;
#2192 = CARTESIAN_POINT ( 'NONE',  ( -7.999999999999991118, 0.000000000000000000, 29.09592778084756048 ) ) ;
#2193 = CARTESIAN_POINT ( 'NONE',  ( -1.836970198721029983E-15, 170.6249999931720538, 10.00000000000000178 ) ) ;
#2194 = CARTESIAN_POINT ( 'NONE',  ( -5.082755093536324154, 93.21875000204838102, 5.082755093536326818 ) ) ;
#2195 = AXIS2_PLACEMENT_3D ( 'NONE', #45969, #54137, #64714 ) ;
#2196 = CARTESIAN_POINT ( 'NONE',  ( 28.47326357806521813, 194.4587341250000350, 173.4262024652836658 ) ) ;
#2197 = CARTESIAN_POINT ( 'NONE',  ( -2.085542519210945728E-15, 59.84374999658602690, 11.35316468750000141 ) ) ;
#2198 = CARTESIAN_POINT ( 'NONE',  ( -4.220049686691935698, 10.18810118749999916, 106.7500000020483668 ) ) ;
#2199 = CARTESIAN_POINT ( 'NONE',  ( -3.042071309553173730, 199.3229166632526983, 11.35316468749999785 ) ) ;
#2200 = ORIENTED_EDGE ( 'NONE', *, *, #59270, .T. ) ;
#2201 = CARTESIAN_POINT ( 'NONE',  ( -1.882291019709217084, 65.87523470714100426, 26.34730193751279614 ) ) ;
#2202 = DIRECTION ( 'NONE',  ( -0.000000000000000000, 1.000000000000000000, -4.476705744456276341E-16 ) ) ;
#2203 = CYLINDRICAL_SURFACE ( 'NONE', #26248, 3.999999999999976019 ) ;
#2205 = CARTESIAN_POINT ( 'NONE',  ( 11.35316468749999785, 190.5729166632526699, 3.042071309553174174 ) ) ;
#2204 = DIRECTION ( 'NONE',  ( 0.000000000000000000, 0.000000000000000000, 1.000000000000000000 ) ) ;
#2206 = DIRECTION ( 'NONE',  ( -1.000000000000000000, 0.000000000000000000, 0.000000000000000000 ) ) ;
#2207 = VECTOR ( 'NONE', #51731, 1000.000000000000000 ) ;
#2208 = CARTESIAN_POINT ( 'NONE',  ( 10.00000000000000000, 235.6250000068279746, -1.224646799147353256E-15 ) ) ;
#2209 = CYLINDRICAL_SURFACE ( 'NONE', #69743, 10.00000000000000178 ) ;
#2210 = VERTEX_POINT ( 'NONE', #69563 ) ;
#2211 = CARTESIAN_POINT ( 'NONE',  ( 9.832129032723420536, 176.5104166632526699, -5.676582343749999815 ) ) ;
#2212 = VECTOR ( 'NONE', #37712, 1000.000000000000000 ) ;
#2213 = CARTESIAN_POINT ( 'NONE',  ( 1.320432766682872962E-15, -7.188101187499992051, 21.36155278187175455 ) ) ;
#2214 = CARTESIAN_POINT ( 'NONE',  ( -3.313708498984770934, 3.843749995903220196, 7.999999999999992895 ) ) ;
#2215 = VERTEX_POINT ( 'NONE', #11479 ) ;
#2216 = CARTESIAN_POINT ( 'NONE',  ( -4.898587196589412829E-16, 100.8125000040967763, -8.000000000000000000 ) ) ;
#2217 = CARTESIAN_POINT ( 'NONE',  ( 2.679491924311228956, 1.041666666666666519, -10.00000000000000000 ) ) ;
#2218 =( BOUNDED_CURVE ( )  B_SPLINE_CURVE ( 2, ( #58326, #45865, #39470, #5516, #68507, #28516, #29637, #69630, #23598 ),
 .UNSPECIFIED., .F., .F. ) 
 B_SPLINE_CURVE_WITH_KNOTS ( ( 3, 2, 2, 2, 3 ),
 ( 0.2058823529411766273, 0.2095588235294118529, 0.2132352941176470784, 0.2169117647058823040, 0.2205882352941175295 ),
 .UNSPECIFIED. ) 
 CURVE ( )  GEOMETRIC_REPRESENTATION_ITEM ( )  RATIONAL_B_SPLINE_CURVE ( ( 0.9999999999999965583, 0.9238795325112901802, 1.000000000000000000, 0.9238795325112867385, 1.000000000000000000, 0.9238795325112867385, 1.000000000000000000, 0.9238795325112890700, 0.9999999999999976685 ) ) 
 REPRESENTATION_ITEM ( '' )  );
#2219 = CARTESIAN_POINT ( 'NONE',  ( 2.449293598294707893E-16, 14.25000000000000000, -4.000000000000001776 ) ) ;
#2220 = CARTESIAN_POINT ( 'NONE',  ( -8.342170076843785083E-16, 16.06249999863440436, 4.541265875000002339 ) ) ;
#2221 = CARTESIAN_POINT ( 'NONE',  ( 5.656854249492374365, 5.656854249492375253, 13.95530278392014623 ) ) ;
#2222 = CARTESIAN_POINT ( 'NONE',  ( 2.020667218593132706E-15, -11.00000000000000000, 78.06250000409677625 ) ) ;
#2223 = ORIENTED_EDGE ( 'NONE', *, *, #31265, .T. ) ;
#2224 = CARTESIAN_POINT ( 'NONE',  ( 5.000000000000001776, -10.38759426015435317, -65.74583990312707726 ) ) ;
#2225 = CARTESIAN_POINT ( 'NONE',  ( 1.320432766682874540E-15, 97.53125000204838102, 7.188101187500000044 ) ) ;
#2226 = EDGE_CURVE ( 'NONE', #69045, #31632, #19585, .T. ) ;
#2228 = CARTESIAN_POINT ( 'NONE',  ( -30.64284399271074832, -37.99999999999991473, 174.6921329945331536 ) ) ;
#2227 = CARTESIAN_POINT ( 'NONE',  ( 4.000000000000015987, 196.5000000000000000, 198.0000000000000284 ) ) ;
#2229 = ORIENTED_EDGE ( 'NONE', *, *, #33019, .F. ) ;
#2231 = CARTESIAN_POINT ( 'NONE',  ( -3.313708498984762496, 101.4687500040967763, 7.999999999999998224 ) ) ;
#2230 = VECTOR ( 'NONE', #52311, 1000.000000000000000 ) ;
#2232 = CARTESIAN_POINT ( 'NONE',  ( 7.188101187499992051, 8.802885111219154394E-16, 17.23655278187175810 ) ) ;
#2233 = ORIENTED_EDGE ( 'NONE', *, *, #30702, .F. ) ;
#2234 = EDGE_CURVE ( 'NONE', #12265, #20466, #15232, .T. ) ;
#2235 =( BOUNDED_SURFACE ( )  B_SPLINE_SURFACE ( 1, 2, ( 
 ( #13912, #65240, #3369, #59957, #19959, #8653, #8275, #65616, #43725, #66361, #53567, #53935, #71265, #25977, #55060, #49002, #31668, #26356, #19584, #36951, #37706, #25614, #59235, #20326, #65986, #2625, #43342, #60707, #1883, #9027, #7908, #14291, #32040, #24869, #47888, #49377, #72396, #25242, #70908, #31285, #19222, #20708, #54314, #42227, #13544, #36584, #59595, #2249, #48258, #48628, #71636, #22195, #4493, #50499, #10146, #67492, #44108, #33551, #27485, #38825, #72779, #32800, #27865, #3742, #21820, #15044, #44852, #21085, #73148, #56555, #33927, #56180, #21455, #15790, #33184, #74259, #9403, #50875, #28242, #32422, #51250, #10519, #67118, #15412, #4127, #61455, #27118, #38453, #67858, #44478, #73891, #66739, #9781, #4870, #16527, #55809, #56926, #26742, #38079, #50132, #16150, #49762, #61827, #73513, #39190, #45220, #62193, #68232, #39566, #62562, #22568, #61077, #10893, #5241, #55433, #54028, #69527, #1617, #58958, #36677, #46880, #1971, #12905, #41228, #7265, #2338, #70270, #46508, #31003, #18583, #19308, #29905, #24963, #58230, #17839, #41595, #35213, #1252, #7997, #52546, #23870, #41952, #52919, #64235, #7634, #24230, #885, #12545, #69903, #53293, #40855, #6529, #58587, #24599, #63862, #47978, #29535, #70991, #12175, #30640, #70629, #18215, #47244, #35573, #6893, #64609, #42318, #35939, #30274, #47605, #18948, #64960, #13269, #36308, #59325, #65336, #53659, #13638, #59689, #49473, #9118, #60419, #15508, #72492, #32898, #31379, #54405, #3087, #55902, #54776, #26072, #31755, #21173, #43819, #66451, #66075, #8746, #61549, #20801, #60042, #3840, #14758, #14385, #48720, #9870, #25332, #49093, #48347, #71354, #32517, #72106, #32135, #3459, #2712, #15136, #20418, #19677, #66834, #38169, #49850, #55153, #9502, #26448, #38548, #42689, #65701, #61172, #37797, #14005, #25699, #55530, #60793, #20041, #26836, #37042, #43435, #8363, #71727, #72869, #44198, #43059, #67211, #37419, #11353, #50220, #11721, #5327, #34388, #33638, #57389, #22283, #57015, #10612, #4959, #17372, #34018, #56645, #63028, #4214, #4584, #16999, #28696, #33267, #69068, #15881, #27203, #44944, #28330, #61914, #27579, #27961, #10240, #5697, #39653, #10984, #68690, #50588, #63395, #34761, #74346, #73606, #38913, #73241, #51338, #62651, #21546, #22656, #51710, #45675 ),
 ( #57, #40397, #40026, #23038, #46049, #44572, #67585, #56266, #21913, #50966, #67951, #45306, #16244, #73979, #68320, #39282, #62284, #16618, #29817, #30555, #41140, #13182, #69437, #65242, #6804, #46423, #12456, #19224, #63770, #35124, #53201, #64146, #52459, #18861, #35485, #12087, #797, #58140, #64519, #57763, #17748, #69809, #12817, #42230, #59238, #40763, #7547, #6069, #41867, #7178, #52096, #58498, #23783, #23407, #29449, #53569, #52830, #428, #6447, #1163, #29076, #24141, #46787, #13548, #36220, #18125, #64880, #1885, #30184, #41502, #47152, #47890, #1535, #70185, #18494, #35852, #58867, #24515, #47519, #70545, #24871, #70910, #55062, #2998, #2627, #71639, #44112, #60327, #25244, #65988, #72782, #42603, #13914, #32042, #42967, #31287, #72399, #14293, #65618, #54317, #36953, #43345, #36586, #48261, #48630, #66363, #21088, #38082, #71267, #61079, #59597, #20710, #60709, #30916, #37330, #25616, #2251, #8277, #9407, #8655, #53937, #19587, #31670, #7910, #54689, #59959, #67121, #15046, #19961, #43727, #66741, #9029, #20329, #25979, #26746, #3371, #49004, #72014, #14668, #37708, #26358, #49380, #32425, #55436, #3746, #49765, #56558, #56184, #50502, #51628, #62566, #50136, #68606, #4873, #4496, #38828, #74643, #22958, #73516, #15416, #45967, #22572, #62197, #22198, #68237, #67495, #5245, #21823, #61458, #10896, #33930, #39938, #73894, #74264, #16530, #5615, #38456, #9784, #45224, #27868, #28615, #15793, #45592, #50878, #10150, #39570, #32804, #39194, #55813, #4130, #16915, #62944, #27121, #56929, #11268, #34300, #73151, #21459, #28245, #57303, #44855, #44481, #33554, #51253, #67861, #16154, #61831, #33187, #27489, #10522, #41791, #52379, #24436, #5987, #1455, #12376, #47071, #715, #69728, #7468, #68981, #53490, #41058, #64799, #23699, #47444, #28989, #1807, #18043, #57679, #46704, #30473, #345, #46337, #64440, #64068, #63684, #30105, #35412, #23325, #12011, #69353, #1085, #17290, #52007, #6367, #24061, #24793, #70468, #17664, #18785, #40309, #53122, #18414, #63311, #58422, #35044, #34674, #40682, #13102, #6728, #11638, #58056, #29734, #29373, #52749, #70108, #41428, #36138, #12740, #59159, #35771, #58787, #7097, #8196, #37996, #20243, #55353, #53856, #2168, #25533, #3658, #2541, #48546, #54233, #43641, #66278, #14209, #13829 ) ),
 .UNSPECIFIED., .F., .F., .F. ) 
 B_SPLINE_SURFACE_WITH_KNOTS ( ( 2, 2 ),
 ( 3, 2, 2, 2, 2, 2, 2, 2, 2, 2, 2, 2, 2, 2, 2, 2, 2, 2, 2, 2, 2, 2, 2, 2, 2, 2, 2, 2, 2, 2, 2, 2, 2, 2, 2, 2, 2, 2, 2, 2, 2, 2, 2, 2, 2, 2, 2, 2, 2, 2, 2, 2, 2, 2, 2, 2, 2, 2, 2, 2, 2, 2, 2, 2, 2, 2, 2, 2, 2, 2, 2, 2, 2, 2, 2, 2, 2, 2, 2, 2, 2, 2, 2, 2, 2, 2, 2, 2, 2, 2, 2, 2, 2, 2, 2, 2, 2, 2, 2, 2, 2, 2, 2, 2, 2, 2, 2, 2, 2, 2, 2, 2, 2, 2, 2, 2, 2, 2, 2, 2, 2, 2, 2, 2, 2, 2, 2, 2, 2, 2, 2, 2, 2, 2, 2, 2, 2, 2, 2, 2, 2, 2, 2, 2, 3 ),
 ( 0.000000000000000000, 1.000000000000000000 ),
 ( 0.000000000000000000, 0.006944444444444444059, 0.01388888888888888812, 0.02083333333333333218, 0.02777777777777777624, 0.03472222222222222376, 0.04166666666666666435, 0.04861111111111111188, 0.05555555555555555247, 0.06250000000000000000, 0.06944444444444444753, 0.07638888888888889506, 0.08333333333333332871, 0.09027777777777777624, 0.09722222222222222376, 0.1041666666666666713, 0.1111111111111111049, 0.1180555555555555525, 0.1250000000000000000, 0.1319444444444444475, 0.1388888888888888951, 0.1458333333333333426, 0.1527777777777777901, 0.1597222222222222099, 0.1666666666666666574, 0.1736111111111111049, 0.1805555555555555525, 0.1875000000000000000, 0.1944444444444444475, 0.2013888888888888951, 0.2083333333333333426, 0.2152777777777777901, 0.2222222222222222099, 0.2291666666666666574, 0.2361111111111111049, 0.2430555555555555525, 0.2500000000000000000, 0.2569444444444444198, 0.2638888888888888951, 0.2708333333333333148, 0.2777777777777777901, 0.2847222222222222099, 0.2916666666666666852, 0.2986111111111111049, 0.3055555555555555802, 0.3125000000000000000, 0.3194444444444444198, 0.3263888888888888951, 0.3333333333333333148, 0.3402777777777777901, 0.3472222222222222099, 0.3541666666666666852, 0.3611111111111111049, 0.3680555555555555802, 0.3750000000000000000, 0.3819444444444444198, 0.3888888888888888951, 0.3958333333333333148, 0.4027777777777777901, 0.4097222222222222099, 0.4166666666666666852, 0.4236111111111111049, 0.4305555555555555802, 0.4375000000000000000, 0.4444444444444444198, 0.4513888888888888951, 0.4583333333333333148, 0.4652777777777777901, 0.4722222222222222099, 0.4791666666666666852, 0.4861111111111111049, 0.4930555555555555802, 0.5000000000000000000, 0.5069444444444444198, 0.5138888888888888395, 0.5208333333333333703, 0.5277777777777777901, 0.5347222222222222099, 0.5416666666666666297, 0.5486111111111111605, 0.5555555555555555802, 0.5625000000000000000, 0.5694444444444444198, 0.5763888888888888395, 0.5833333333333333703, 0.5902777777777777901, 0.5972222222222222099, 0.6041666666666666297, 0.6111111111111111605, 0.6180555555555555802, 0.6250000000000000000, 0.6319444444444444198, 0.6388888888888888395, 0.6458333333333333703, 0.6527777777777777901, 0.6597222222222222099, 0.6666666666666666297, 0.6736111111111111605, 0.6805555555555555802, 0.6875000000000000000, 0.6944444444444444198, 0.7013888888888888395, 0.7083333333333333703, 0.7152777777777777901, 0.7222222222222222099, 0.7291666666666666297, 0.7361111111111111605, 0.7430555555555555802, 0.7500000000000000000, 0.7569444444444444198, 0.7638888888888888395, 0.7708333333333333703, 0.7777777777777777901, 0.7847222222222222099, 0.7916666666666666297, 0.7986111111111111605, 0.8055555555555555802, 0.8125000000000000000, 0.8194444444444444198, 0.8263888888888888395, 0.8333333333333333703, 0.8402777777777777901, 0.8472222222222222099, 0.8541666666666666297, 0.8611111111111111605, 0.8680555555555555802, 0.8750000000000000000, 0.8819444444444444198, 0.8888888888888888395, 0.8958333333333333703, 0.9027777777777777901, 0.9097222222222222099, 0.9166666666666666297, 0.9236111111111111605, 0.9305555555555555802, 0.9375000000000000000, 0.9444444444444444198, 0.9513888888888888395, 0.9583333333333333703, 0.9652777777777777901, 0.9722222222222222099, 0.9791666666666666297, 0.9861111111111111605, 0.9930555555555555802, 1.000000000000000000 ),
 .UNSPECIFIED. ) 
 GEOMETRIC_REPRESENTATION_ITEM ( )  RATIONAL_B_SPLINE_SURFACE ( (
 ( 1.000000000000000000, 0.9238795325112867385, 1.000000000000000000, 0.9238795325112867385, 1.000000000000000000, 0.9238795325112867385, 1.000000000000000000, 0.9238795325112867385, 1.000000000000000000, 0.9238795325112867385, 1.000000000000000000, 0.9238795325112867385, 1.000000000000000000, 0.9238795325112867385, 1.000000000000000000, 0.9238795325112867385, 1.000000000000000000, 0.9238795325112867385, 1.000000000000000000, 0.9238795325112867385, 1.000000000000000000, 0.9238795325112867385, 1.000000000000000000, 0.9238795325112867385, 1.000000000000000000, 0.9238795325112867385, 1.000000000000000000, 0.9238795325112867385, 1.000000000000000000, 0.9238795325112867385, 1.000000000000000000, 0.9238795325112867385, 1.000000000000000000, 0.9238795325112867385, 1.000000000000000000, 0.9238795325112867385, 1.000000000000000000, 0.9238795325112867385, 1.000000000000000000, 0.9238795325112867385, 1.000000000000000000, 0.9238795325112867385, 1.000000000000000000, 0.9238795325112867385, 1.000000000000000000, 0.9238795325112867385, 1.000000000000000000, 0.9238795325112867385, 1.000000000000000000, 0.9238795325112867385, 1.000000000000000000, 0.9238795325112867385, 1.000000000000000000, 0.9238795325112867385, 1.000000000000000000, 0.9238795325112867385, 1.000000000000000000, 0.9238795325112867385, 1.000000000000000000, 0.9238795325112867385, 1.000000000000000000, 0.9238795325112867385, 1.000000000000000000, 0.9238795325112867385, 1.000000000000000000, 0.9238795325112867385, 1.000000000000000000, 0.9238795325112867385, 1.000000000000000000, 0.9238795325112867385, 1.000000000000000000, 0.9238795325112867385, 1.000000000000000000, 0.9238795325112867385, 1.000000000000000000, 0.9238795325112867385, 1.000000000000000000, 0.9238795325112867385, 1.000000000000000000, 0.9238795325112867385, 1.000000000000000000, 0.9238795325112867385, 1.000000000000000000, 0.9238795325112867385, 1.000000000000000000, 0.9238795325112867385, 1.000000000000000000, 0.9238795325112867385, 1.000000000000000000, 0.9238795325112867385, 1.000000000000000000, 0.9238795325112867385, 1.000000000000000000, 0.9238795325112867385, 1.000000000000000000, 0.9238795325112867385, 1.000000000000000000, 0.9238795325112867385, 1.000000000000000000, 0.9238795325112867385, 1.000000000000000000, 0.9238795325112867385, 1.000000000000000000, 0.9238795325112867385, 1.000000000000000000, 0.9238795325112867385, 1.000000000000000000, 0.9238795325112867385, 1.000000000000000000, 0.9238795325112867385, 1.000000000000000000, 0.9238795325112867385, 1.000000000000000000, 0.9238795325112867385, 1.000000000000000000, 0.9238795325112867385, 1.000000000000000000, 0.9238795325112867385, 1.000000000000000000, 0.9238795325112867385, 1.000000000000000000, 0.9238795325112867385, 1.000000000000000000, 0.9238795325112867385, 1.000000000000000000, 0.9238795325112867385, 1.000000000000000000, 0.9238795325112867385, 1.000000000000000000, 0.9238795325112867385, 1.000000000000000000, 0.9238795325112867385, 1.000000000000000000, 0.9238795325112867385, 1.000000000000000000, 0.9238795325112867385, 1.000000000000000000, 0.9238795325112867385, 1.000000000000000000, 0.9238795325112867385, 1.000000000000000000, 0.9238795325112867385, 1.000000000000000000, 0.9238795325112867385, 1.000000000000000000, 0.9238795325112867385, 1.000000000000000000, 0.9238795325112867385, 1.000000000000000000, 0.9238795325112867385, 1.000000000000000000, 0.9238795325112867385, 1.000000000000000000, 0.9238795325112867385, 1.000000000000000000, 0.9238795325112867385, 1.000000000000000000, 0.9238795325112867385, 1.000000000000000000, 0.9238795325112867385, 1.000000000000000000, 0.9238795325112867385, 1.000000000000000000, 0.9238795325112867385, 1.000000000000000000, 0.9238795325112867385, 1.000000000000000000, 0.9238795325112867385, 1.000000000000000000, 0.9238795325112867385, 1.000000000000000000, 0.9238795325112867385, 1.000000000000000000, 0.9238795325112867385, 1.000000000000000000, 0.9238795325112867385, 1.000000000000000000, 0.9238795325112867385, 1.000000000000000000, 0.9238795325112867385, 1.000000000000000000, 0.9238795325112867385, 1.000000000000000000, 0.9238795325112867385, 1.000000000000000000, 0.9238795325112867385, 1.000000000000000000, 0.9238795325112867385, 1.000000000000000000, 0.9238795325112867385, 1.000000000000000000, 0.9238795325112867385, 1.000000000000000000, 0.9238795325112867385, 1.000000000000000000, 0.9238795325112867385, 1.000000000000000000, 0.9238795325112867385, 1.000000000000000000, 0.9238795325112867385, 1.000000000000000000, 0.9238795325112867385, 1.000000000000000000, 0.9238795325112867385, 1.000000000000000000, 0.9238795325112867385, 1.000000000000000000, 0.9238795325112867385, 1.000000000000000000, 0.9238795325112867385, 1.000000000000000000, 0.9238795325112867385, 1.000000000000000000, 0.9238795325112867385, 1.000000000000000000, 0.9238795325112867385, 1.000000000000000000, 0.9238795325112867385, 1.000000000000000000, 0.9238795325112867385, 1.000000000000000000, 0.9238795325112867385, 1.000000000000000000, 0.9238795325112867385, 1.000000000000000000, 0.9238795325112867385, 1.000000000000000000, 0.9238795325112867385, 1.000000000000000000, 0.9238795325112867385, 1.000000000000000000, 0.9238795325112867385, 1.000000000000000000, 0.9238795325112867385, 1.000000000000000000, 0.9238795325112867385, 1.000000000000000000, 0.9238795325112867385, 1.000000000000000000, 0.9238795325112867385, 1.000000000000000000, 0.9238795325112867385, 1.000000000000000000, 0.9238795325112867385, 1.000000000000000000, 0.9238795325112867385, 1.000000000000000000, 0.9238795325112867385, 1.000000000000000000, 0.9238795325112867385, 1.000000000000000000, 0.9238795325112867385, 1.000000000000000000, 0.9238795325112867385, 1.000000000000000000, 0.9238795325112867385, 1.000000000000000000, 0.9238795325112867385, 1.000000000000000000, 0.9238795325112867385, 1.000000000000000000, 0.9238795325112867385, 1.000000000000000000, 0.9238795325112867385, 1.000000000000000000, 0.9238795325112867385, 1.000000000000000000, 0.9238795325112867385, 1.000000000000000000, 0.9238795325112867385, 1.000000000000000000, 0.9238795325112867385, 1.000000000000000000, 0.9238795325112867385, 1.000000000000000000, 0.9238795325112867385, 1.000000000000000000, 0.9238795325112867385, 1.000000000000000000, 0.9238795325112867385, 1.000000000000000000, 0.9238795325112867385, 1.000000000000000000, 0.9238795325112867385, 1.000000000000000000, 0.9238795325112867385, 1.000000000000000000, 0.9238795325112867385, 1.000000000000000000),
 ( 1.000000000000000000, 0.9238795325112867385, 1.000000000000000000, 0.9238795325112867385, 1.000000000000000000, 0.9238795325112867385, 1.000000000000000000, 0.9238795325112867385, 1.000000000000000000, 0.9238795325112867385, 1.000000000000000000, 0.9238795325112867385, 1.000000000000000000, 0.9238795325112867385, 1.000000000000000000, 0.9238795325112867385, 1.000000000000000000, 0.9238795325112867385, 1.000000000000000000, 0.9238795325112867385, 1.000000000000000000, 0.9238795325112867385, 1.000000000000000000, 0.9238795325112867385, 1.000000000000000000, 0.9238795325112867385, 1.000000000000000000, 0.9238795325112867385, 1.000000000000000000, 0.9238795325112867385, 1.000000000000000000, 0.9238795325112867385, 1.000000000000000000, 0.9238795325112867385, 1.000000000000000000, 0.9238795325112867385, 1.000000000000000000, 0.9238795325112867385, 1.000000000000000000, 0.9238795325112867385, 1.000000000000000000, 0.9238795325112867385, 1.000000000000000000, 0.9238795325112867385, 1.000000000000000000, 0.9238795325112867385, 1.000000000000000000, 0.9238795325112867385, 1.000000000000000000, 0.9238795325112867385, 1.000000000000000000, 0.9238795325112867385, 1.000000000000000000, 0.9238795325112867385, 1.000000000000000000, 0.9238795325112867385, 1.000000000000000000, 0.9238795325112867385, 1.000000000000000000, 0.9238795325112867385, 1.000000000000000000, 0.9238795325112867385, 1.000000000000000000, 0.9238795325112867385, 1.000000000000000000, 0.9238795325112867385, 1.000000000000000000, 0.9238795325112867385, 1.000000000000000000, 0.9238795325112867385, 1.000000000000000000, 0.9238795325112867385, 1.000000000000000000, 0.9238795325112867385, 1.000000000000000000, 0.9238795325112867385, 1.000000000000000000, 0.9238795325112867385, 1.000000000000000000, 0.9238795325112867385, 1.000000000000000000, 0.9238795325112867385, 1.000000000000000000, 0.9238795325112867385, 1.000000000000000000, 0.9238795325112867385, 1.000000000000000000, 0.9238795325112867385, 1.000000000000000000, 0.9238795325112867385, 1.000000000000000000, 0.9238795325112867385, 1.000000000000000000, 0.9238795325112867385, 1.000000000000000000, 0.9238795325112867385, 1.000000000000000000, 0.9238795325112867385, 1.000000000000000000, 0.9238795325112867385, 1.000000000000000000, 0.9238795325112867385, 1.000000000000000000, 0.9238795325112867385, 1.000000000000000000, 0.9238795325112867385, 1.000000000000000000, 0.9238795325112867385, 1.000000000000000000, 0.9238795325112867385, 1.000000000000000000, 0.9238795325112867385, 1.000000000000000000, 0.9238795325112867385, 1.000000000000000000, 0.9238795325112867385, 1.000000000000000000, 0.9238795325112867385, 1.000000000000000000, 0.9238795325112867385, 1.000000000000000000, 0.9238795325112867385, 1.000000000000000000, 0.9238795325112867385, 1.000000000000000000, 0.9238795325112867385, 1.000000000000000000, 0.9238795325112867385, 1.000000000000000000, 0.9238795325112867385, 1.000000000000000000, 0.9238795325112867385, 1.000000000000000000, 0.9238795325112867385, 1.000000000000000000, 0.9238795325112867385, 1.000000000000000000, 0.9238795325112867385, 1.000000000000000000, 0.9238795325112867385, 1.000000000000000000, 0.9238795325112867385, 1.000000000000000000, 0.9238795325112867385, 1.000000000000000000, 0.9238795325112867385, 1.000000000000000000, 0.9238795325112867385, 1.000000000000000000, 0.9238795325112867385, 1.000000000000000000, 0.9238795325112867385, 1.000000000000000000, 0.9238795325112867385, 1.000000000000000000, 0.9238795325112867385, 1.000000000000000000, 0.9238795325112867385, 1.000000000000000000, 0.9238795325112867385, 1.000000000000000000, 0.9238795325112867385, 1.000000000000000000, 0.9238795325112867385, 1.000000000000000000, 0.9238795325112867385, 1.000000000000000000, 0.9238795325112867385, 1.000000000000000000, 0.9238795325112867385, 1.000000000000000000, 0.9238795325112867385, 1.000000000000000000, 0.9238795325112867385, 1.000000000000000000, 0.9238795325112867385, 1.000000000000000000, 0.9238795325112867385, 1.000000000000000000, 0.9238795325112867385, 1.000000000000000000, 0.9238795325112867385, 1.000000000000000000, 0.9238795325112867385, 1.000000000000000000, 0.9238795325112867385, 1.000000000000000000, 0.9238795325112867385, 1.000000000000000000, 0.9238795325112867385, 1.000000000000000000, 0.9238795325112867385, 1.000000000000000000, 0.9238795325112867385, 1.000000000000000000, 0.9238795325112867385, 1.000000000000000000, 0.9238795325112867385, 1.000000000000000000, 0.9238795325112867385, 1.000000000000000000, 0.9238795325112867385, 1.000000000000000000, 0.9238795325112867385, 1.000000000000000000, 0.9238795325112867385, 1.000000000000000000, 0.9238795325112867385, 1.000000000000000000, 0.9238795325112867385, 1.000000000000000000, 0.9238795325112867385, 1.000000000000000000, 0.9238795325112867385, 1.000000000000000000, 0.9238795325112867385, 1.000000000000000000, 0.9238795325112867385, 1.000000000000000000, 0.9238795325112867385, 1.000000000000000000, 0.9238795325112867385, 1.000000000000000000, 0.9238795325112867385, 1.000000000000000000, 0.9238795325112867385, 1.000000000000000000, 0.9238795325112867385, 1.000000000000000000, 0.9238795325112867385, 1.000000000000000000, 0.9238795325112867385, 1.000000000000000000, 0.9238795325112867385, 1.000000000000000000, 0.9238795325112867385, 1.000000000000000000, 0.9238795325112867385, 1.000000000000000000, 0.9238795325112867385, 1.000000000000000000, 0.9238795325112867385, 1.000000000000000000, 0.9238795325112867385, 1.000000000000000000, 0.9238795325112867385, 1.000000000000000000, 0.9238795325112867385, 1.000000000000000000, 0.9238795325112867385, 1.000000000000000000, 0.9238795325112867385, 1.000000000000000000, 0.9238795325112867385, 1.000000000000000000, 0.9238795325112867385, 1.000000000000000000, 0.9238795325112867385, 1.000000000000000000, 0.9238795325112867385, 1.000000000000000000, 0.9238795325112867385, 1.000000000000000000, 0.9238795325112867385, 1.000000000000000000, 0.9238795325112867385, 1.000000000000000000, 0.9238795325112867385, 1.000000000000000000, 0.9238795325112867385, 1.000000000000000000, 0.9238795325112867385, 1.000000000000000000, 0.9238795325112867385, 1.000000000000000000, 0.9238795325112867385, 1.000000000000000000, 0.9238795325112867385, 1.000000000000000000, 0.9238795325112867385, 1.000000000000000000, 0.9238795325112867385, 1.000000000000000000, 0.9238795325112867385, 1.000000000000000000, 0.9238795325112867385, 1.000000000000000000, 0.9238795325112867385, 1.000000000000000000) ) ) 
 REPRESENTATION_ITEM ( '' )  SURFACE ( )  );
#2236 = ORIENTED_EDGE ( 'NONE', *, *, #7464, .T. ) ;
#2237 = CARTESIAN_POINT ( 'NONE',  ( -7.204075437095967871, 7.204075437095967871, 82.46875000204836681 ) ) ;
#2238 = FACE_OUTER_BOUND ( 'NONE', #27645, .T. ) ;
#2239 = CARTESIAN_POINT ( 'NONE',  ( 11.00000000000000000, 1.347111479062088405E-15, 97.74999999999998579 ) ) ;
#2242 = CARTESIAN_POINT ( 'NONE',  ( 6.676582343750002480, 295.1718750017070079, -2.765530957081997254 ) ) ;
#2241 = CARTESIAN_POINT ( 'NONE',  ( 29.65685424949240456, 200.1875000027312126, 173.9999999999999147 ) ) ;
#2240 = CARTESIAN_POINT ( 'NONE',  ( -30.82842712474624491, 198.2500000027312126, 167.1715728752542418 ) ) ;
#2243 = CARTESIAN_POINT ( 'NONE',  ( -1.836970198721029983E-15, 153.7500000000000000, 10.00000000000000178 ) ) ;
#2244 = CIRCLE ( 'NONE', #57695, 8.000000000000003553 ) ;
#2245 = CARTESIAN_POINT ( 'NONE',  ( -10.99999999999986855, 4.556349186104178273, 106.0937500040967763 ) ) ;
#2246 = CARTESIAN_POINT ( 'NONE',  ( 7.999999999999991118, 9.797174393178815797E-16, 25.58030277982336997 ) ) ;
#2247 = VECTOR ( 'NONE', #10615, 1000.000000000000000 ) ;
#2248 = FACE_OUTER_BOUND ( 'NONE', #60683, .T. ) ;
#2249 = CARTESIAN_POINT ( 'NONE',  ( 7.999999999999998224, 5.718749995903220196, 3.313708498984766493 ) ) ;
#2250 = CARTESIAN_POINT ( 'NONE',  ( 24.54126587499998990, 197.1875000013655779, 169.9999999999998863 ) ) ;
#2251 = CARTESIAN_POINT ( 'NONE',  ( 4.401442555609581635E-16, 11.71874999795161010, -7.188101187500000044 ) ) ;
#2252 = CARTESIAN_POINT ( 'NONE',  ( 1.469576158976822172E-15, -7.999999999999991118, 25.39280278392014978 ) ) ;
#2253 = DIRECTION ( 'NONE',  ( -0.000000000000000000, 1.000000000000000000, 4.476705744456276341E-16 ) ) ;
#2254 = CARTESIAN_POINT ( 'NONE',  ( 7.188101187500000933, 111.8750000020483810, -2.977408999572651371 ) ) ;
#2256 = DIRECTION ( 'NONE',  ( -0.000000000000000000, -0.000000000000000000, -1.000000000000000000 ) ) ;
#2255 = PLANE ( 'NONE',  #32383 ) ;
#2257 = CARTESIAN_POINT ( 'NONE',  ( -11.35316468749999608, 224.4270833367473017, 3.042071309553173730 ) ) ;
#2258 = CARTESIAN_POINT ( 'NONE',  ( 7.188101187499992051, 8.802885111219154394E-16, 23.61155278187175455 ) ) ;
#2259 = CYLINDRICAL_SURFACE ( 'NONE', #29929, 8.000000000000000000 ) ;
#2260 = CARTESIAN_POINT ( 'NONE',  ( 6.951808397369818766E-16, 37.03124999658602690, -11.35316468750000141 ) ) ;
#2261 = LINE ( 'NONE', #3382, #60461 ) ;
#2262 = CARTESIAN_POINT ( 'NONE',  ( 4.999999999999993783, 11.04166665983870033, 8.660254037844390851 ) ) ;
#2263 = CARTESIAN_POINT ( 'NONE',  ( 12.00000000000000000, 6.928203230275491009, -14.80000000000000071 ) ) ;
#2264 = LINE ( 'NONE', #36601, #53965 ) ;
#2265 = ORIENTED_EDGE ( 'NONE', *, *, #27826, .F. ) ;
#2266 = CARTESIAN_POINT ( 'NONE',  ( -8.660254037844390851, 129.7916666598387110, 4.999999999999998224 ) ) ;
#2267 = CARTESIAN_POINT ( 'NONE',  ( -4.000000000000001776, 14.43750000000000000, -1.656854249492381470 ) ) ;
#2268 = CARTESIAN_POINT ( 'NONE',  ( 3.042071309553167069, 36.82291666325267698, -11.35316468749999785 ) ) ;
#2269 = CARTESIAN_POINT ( 'NONE',  ( 7.778174593052021635, 7.778174593052023411, 89.12500000409677625 ) ) ;
#2270 = CARTESIAN_POINT ( 'NONE',  ( 3.458734124999959469, 205.7500000013656063, 140.5673454167823593 ) ) ;
#2271 = CARTESIAN_POINT ( 'NONE',  ( 25.17157287525378351, 202.8750000000000284, 172.8284271247460424 ) ) ;
#2272 = DIRECTION ( 'NONE',  ( 0.000000000000000000, 0.000000000000000000, -1.000000000000000000 ) ) ;
#2274 = CARTESIAN_POINT ( 'NONE',  ( 3.042071309553159519, 29.73958332991934839, 11.35316468750000141 ) ) ;
#2273 = CARTESIAN_POINT ( 'NONE',  ( -7.188101187499999156, 106.2500000020484094, 2.977408999572654924 ) ) ;
#2275 = CARTESIAN_POINT ( 'NONE',  ( 7.999999999999992895, -3.313708498984756279, 16.48655277982336642 ) ) ;
#2276 = CARTESIAN_POINT ( 'NONE',  ( -5.676582343750006032, 154.1145833299193555, 9.832129032723418760 ) ) ;
#2277 = CARTESIAN_POINT ( 'NONE',  ( -2.679491924311235618, 130.4166666598386541, 10.00000000000000000 ) ) ;
#2278 = CARTESIAN_POINT ( 'NONE',  ( 1.320432766682874540E-15, 106.9062500020483810, 7.188101187500000044 ) ) ;
#2279 = CARTESIAN_POINT ( 'NONE',  ( -31.45873412499999944, 202.9375000013656063, 170.0000000000003979 ) ) ;
#2280 = VERTEX_POINT ( 'NONE', #28820 ) ;
#2281 = DIRECTION ( 'NONE',  ( 0.000000000000000000, -0.000000000000000000, 1.000000000000000000 ) ) ;
#2282 = CARTESIAN_POINT ( 'NONE',  ( 8.311093377946837890, 21.71874999658601268, -8.311093377946837890 ) ) ;
#2283 = VERTEX_POINT ( 'NONE', #29572 ) ;
#2284 = LINE ( 'NONE', #42639, #54821 ) ;
#2285 = CYLINDRICAL_SURFACE ( 'NONE', #29356, 3.999999999999976019 ) ;
#2286 = CARTESIAN_POINT ( 'NONE',  ( -11.35316468749999785, 148.0729166632526983, -3.042071309553167957 ) ) ;
#2287 = FACE_OUTER_BOUND ( 'NONE', #35517, .T. ) ;
#2288 = CARTESIAN_POINT ( 'NONE',  ( 7.999999999999991118, 9.797174393178815797E-16, 15.13655278432982421 ) ) ;
#2289 = CARTESIAN_POINT ( 'NONE',  ( -20.35922444301700551, -29.15679641955479440, 193.3784919597981400 ) ) ;
#2290 = CARTESIAN_POINT ( 'NONE',  ( 5.676582343750005144, 240.5729166700806445, 9.832129032723416984 ) ) ;
#2291 = CARTESIAN_POINT ( 'NONE',  ( -10.18810118749999916, 0.000000000000000000, 89.03125000204836681 ) ) ;
#2292 = ORIENTED_EDGE ( 'NONE', *, *, #27287, .T. ) ;
#2293 = AXIS2_PLACEMENT_3D ( 'NONE', #6357, #29361, #22559 ) ;
#2294 = CARTESIAN_POINT ( 'NONE',  ( -5.000000000000005329, 205.2083333265053682, 8.660254037844387298 ) ) ;
#2295 = CARTESIAN_POINT ( 'NONE',  ( -5.676582343749998039, 97.76041666325269830, -9.832129032723420536 ) ) ;
#2296 = CARTESIAN_POINT ( 'NONE',  ( -10.18810118749999916, 4.220049686691934809, 102.0625000020483810 ) ) ;
#2297 = CARTESIAN_POINT ( 'NONE',  ( 3.211159895383560947, 15.31249999863440792, 3.211159895383562723 ) ) ;
#2298 = ORIENTED_EDGE ( 'NONE', *, *, #34648, .T. ) ;
#2299 = ORIENTED_EDGE ( 'NONE', *, *, #23828, .T. ) ;
#2300 = CARTESIAN_POINT ( 'NONE',  ( 4.898587196589412829E-16, 13.87500000000000178, -8.000000000000000000 ) ) ;
#2301 = CARTESIAN_POINT ( 'NONE',  ( -4.541265875000003227, 4.999999998634406140, 1.881053915767121110 ) ) ;
#2302 = VECTOR ( 'NONE', #71596, 1000.000000000000000 ) ;
#2303 = CARTESIAN_POINT ( 'NONE',  ( -7.188101187500001821, 2.624999997951610542, -2.977408999572651371 ) ) ;
#2304 = CARTESIAN_POINT ( 'NONE',  ( -5.656854249492378806, 117.8750000040967905, 5.656854249492381470 ) ) ;
#2306 = EDGE_CURVE ( 'NONE', #71882, #46242, #46171, .T. ) ;
#2305 = CARTESIAN_POINT ( 'NONE',  ( 7.204075437095966983, 7.204075437095967871, 100.4687500020483810 ) ) ;
#2307 = EDGE_CURVE ( 'NONE', #34668, #56998, #42953, .T. ) ;
#2308 = CARTESIAN_POINT ( 'NONE',  ( -8.032507269244980819, -9.218836226384828691, -0.1233701403699506427 ) ) ;
#2309 = CARTESIAN_POINT ( 'NONE',  ( -2.828427124746190735, 1.375000000000000222, -2.828427124746191623 ) ) ;
#2310 = CARTESIAN_POINT ( 'NONE',  ( 2.828427124746190291, 13.62499999726881406, 2.828427124746192067 ) ) ;
#2311 = CARTESIAN_POINT ( 'NONE',  ( 2.780723358947928197E-16, 5.562499998634407028, -4.541265875000002339 ) ) ;
#2312 = VERTEX_POINT ( 'NONE', #23159 ) ;
#2313 = B_SPLINE_CURVE_WITH_KNOTS ( 'NONE', 3,
 ( #15173, #1005, #61206, #8397, #42723, #46994, #20451, #12661, #9537, #25732, #64359, #31411, #38203, #7017, #53041, #49127, #58707, #30026, #65736, #32552, #43852, #26107, #70025, #54438, #19710, #41349, #48383, #26483, #48753, #18334, #35692, #2746, #23985, #71762 ),
 .UNSPECIFIED., .F., .F.,
 ( 4, 2, 2, 2, 2, 2, 2, 2, 2, 2, 2, 2, 2, 2, 2, 2, 4 ),
 ( 0.5000000000000000000, 0.5312500000000000000, 0.5625000000000000000, 0.5937500000000000000, 0.6250000000000000000, 0.6562500000000000000, 0.6875000000000000000, 0.7187500000000000000, 0.7500000000000000000, 0.7812500000000000000, 0.8125000000000000000, 0.8437500000000000000, 0.8750000000000000000, 0.9062500000000000000, 0.9375000000000000000, 0.9687500000000000000, 1.000000000000000000 ),
 .UNSPECIFIED. ) ;
#2314 = EDGE_CURVE ( 'NONE', #23507, #53794, #9963, .T. ) ;
#2315 = CARTESIAN_POINT ( 'NONE',  ( -11.00000000000000000, 0.000000000000000000, 86.68750000409677625 ) ) ;
#2316 = CARTESIAN_POINT ( 'NONE',  ( 1.224646799147353454E-15, 300.0000000000000000, -10.00000000000000178 ) ) ;
#2318 = CARTESIAN_POINT ( 'NONE',  ( 38.00000000000000000, 272.0000000000000000, 20.00000000000002132 ) ) ;
#2317 = CARTESIAN_POINT ( 'NONE',  ( -29.43265458321755901, 199.8750000013655779, 173.4587341250004044 ) ) ;
#2319 = CARTESIAN_POINT ( 'NONE',  ( -1.881053915767121554, 15.62499999863440614, -4.541265875000002339 ) ) ;
#2320 = CARTESIAN_POINT ( 'NONE',  ( 2.849036369511732440E-14, 201.3750000027312126, 202.0000000000000000 ) ) ;
#2321 = CARTESIAN_POINT ( 'NONE',  ( 2.977408999572646486, 7.188101187499991163, 5.517802781871753659 ) ) ;
#2322 = ORIENTED_EDGE ( 'NONE', *, *, #23335, .T. ) ;
#2323 = ORIENTED_EDGE ( 'NONE', *, *, #9869, .F. ) ;
#2324 = CARTESIAN_POINT ( 'NONE',  ( -10.18810118749999916, 0.000000000000000000, 97.65625000204838102 ) ) ;
#2325 = FACE_OUTER_BOUND ( 'NONE', #28873, .T. ) ;
#2326 = CARTESIAN_POINT ( 'NONE',  ( -30.44569435410883429, 202.8125000013656063, 167.5543056458915885 ) ) ;
#2327 = CARTESIAN_POINT ( 'NONE',  ( -30.82842712474615965, 199.3750000000000284, 172.8284271247465824 ) ) ;
#2328 = CARTESIAN_POINT ( 'NONE',  ( 1.432654583217662481, 198.1250000013656063, 194.5412658750000219 ) ) ;
#2329 = CARTESIAN_POINT ( 'NONE',  ( 8.000000000000001776, 104.6562499999999858, 3.313708498984759387 ) ) ;
#2330 = CARTESIAN_POINT ( 'NONE',  ( -10.00000000000000178, 102.5000000000000142, -1.224646799147353454E-15 ) ) ;
#2331 = CARTESIAN_POINT ( 'NONE',  ( 5.656854249492379694, 109.4375000000000000, -5.656854249492380582 ) ) ;
#2332 = CARTESIAN_POINT ( 'NONE',  ( 2.765530957082001251, 295.9218750017070079, 6.676582343750000703 ) ) ;
#2333 = EDGE_CURVE ( 'NONE', #29624, #37372, #6961, .T. ) ;
#2334 = ORIENTED_EDGE ( 'NONE', *, *, #30771, .T. ) ;
#2335 =( BOUNDED_CURVE ( )  B_SPLINE_CURVE ( 2, ( #19307, #7632, #58956, #71353, #65335, #52917, #30638, #71725, #53291 ),
 .UNSPECIFIED., .F., .F. ) 
 B_SPLINE_CURVE_WITH_KNOTS ( ( 3, 2, 2, 2, 3 ),
 ( 0.8529411764705883137, 0.8566176470588235947, 0.8602941176470589868, 0.8639705882352942679, 0.8676470588235295489 ),
 .UNSPECIFIED. ) 
 CURVE ( )  GEOMETRIC_REPRESENTATION_ITEM ( )  RATIONAL_B_SPLINE_CURVE ( ( 0.9999999999999976685, 0.9238795325112890700, 1.000000000000000000, 0.9238795325112867385, 1.000000000000000000, 0.9238795325112867385, 1.000000000000000000, 0.9238795325112844070, 1.000000000000002220 ) ) 
 REPRESENTATION_ITEM ( '' )  );
#2336 = CARTESIAN_POINT ( 'NONE',  ( -5.000000000000005329, 145.2083333265053682, 8.660254037844387298 ) ) ;
#2337 = AXIS2_PLACEMENT_3D ( 'NONE', #58900, #36251, #1564 ) ;
#2338 = CARTESIAN_POINT ( 'NONE',  ( 3.313708498984762496, 13.03124999590322197, 7.999999999999998224 ) ) ;
#2339 = CARTESIAN_POINT ( 'NONE',  ( -2.445694354108839619, 204.8125000013656063, 139.5543056458912190 ) ) ;
#2340 = CARTESIAN_POINT ( 'NONE',  ( 6.123233995736767268E-16, 183.1249999931720538, -10.00000000000000178 ) ) ;
#2341 = CARTESIAN_POINT ( 'NONE',  ( 8.000000000000000000, 114.0312500040967763, -3.313708498984762496 ) ) ;
#2342 = CARTESIAN_POINT ( 'NONE',  ( -10.00000000000000000, 224.7916666666666288, -2.679491924311226292 ) ) ;
#2343 = CARTESIAN_POINT ( 'NONE',  ( -4.000000000000015987, 207.5000000000000284, 142.0000000000000568 ) ) ;
#2344 = CARTESIAN_POINT ( 'NONE',  ( -11.00000000000000000, 0.000000000000000000, 114.9999999999999858 ) ) ;
#2345 = CARTESIAN_POINT ( 'NONE',  ( 10.00000000000000178, 215.2083333333333144, -2.679491924311226736 ) ) ;
#2346 = VECTOR ( 'NONE', #19963, 1000.000000000000000 ) ;
#2347 = CARTESIAN_POINT ( 'NONE',  ( 7.188101187499992051, 2.977408999572647819, 2.705302781871750994 ) ) ;
#2348 = CARTESIAN_POINT ( 'NONE',  ( -9.832129032723418760, 193.1770833299193555, -5.676582343750004256 ) ) ;
#2349 = CARTESIAN_POINT ( 'NONE',  ( 4.541265875000002339, 1.374999998634407250, -1.881053915767121554 ) ) ;
#2350 = DIRECTION ( 'NONE',  ( 0.000000000000000000, 0.000000000000000000, 1.000000000000000000 ) ) ;
#2352 = CARTESIAN_POINT ( 'NONE',  ( -7.999999999999991118, 0.000000000000000000, 4.017802783920145338 ) ) ;
#2351 = CARTESIAN_POINT ( 'NONE',  ( -7.999999999999998224, 107.2812500040967763, 3.313708498984766049 ) ) ;
#2353 = EDGE_LOOP ( 'NONE', ( #21587, #66906, #37007, #17066 ) ) ;
#2354 = CIRCLE ( 'NONE', #28856, 3.999999999999988010 ) ;
#2355 = CARTESIAN_POINT ( 'NONE',  ( -3.458734125000015425, 203.2500000013656063, 143.4326545832176976 ) ) ;
#2356 = CARTESIAN_POINT ( 'NONE',  ( 11.35316468749999963, 46.30208332991934128, -3.042071309553165293 ) ) ;
#2357 = CARTESIAN_POINT ( 'NONE',  ( 2.020667218593132706E-15, -11.00000000000000000, 103.5625000040967763 ) ) ;
#2358 = CARTESIAN_POINT ( 'NONE',  ( 9.832129032723416984, 225.6770833299193839, 5.676582343750006032 ) ) ;
#2359 = CARTESIAN_POINT ( 'NONE',  ( -24.54126587499999346, 202.1875000013656063, 170.0000000000002842 ) ) ;
#2360 = CYLINDRICAL_SURFACE ( 'NONE', #29807, 19.00000000000001776 ) ;
#2362 = CARTESIAN_POINT ( 'NONE',  ( 3.999999999999960032, 203.9375000000000000, 143.6568542494924259 ) ) ;
#2361 = CARTESIAN_POINT ( 'NONE',  ( -7.188101187500000933, 124.0625000020483810, -2.977408999572650483 ) ) ;
#2363 = EDGE_CURVE ( 'NONE', #10358, #56251, #17675, .T. ) ;
#2364 = CARTESIAN_POINT ( 'NONE',  ( 11.35316468749999963, 105.9895833299193555, -3.042071309553165293 ) ) ;
#2365 = CARTESIAN_POINT ( 'NONE',  ( 2.679491924311228956, 82.91666665983869677, -10.00000000000000000 ) ) ;
#2366 = CARTESIAN_POINT ( 'NONE',  ( 1.320432766682874540E-15, 93.03125000204836681, 7.188101187500000044 ) ) ;
#2367 = CARTESIAN_POINT ( 'NONE',  ( 3.211159895383560947, 17.31249999863440792, 3.211159895383562723 ) ) ;
#2368 = CARTESIAN_POINT ( 'NONE',  ( -7.320508075688782590, 73.12500000000001421, 7.320508075688774596 ) ) ;
#2369 = CARTESIAN_POINT ( 'NONE',  ( -3.313708498984759387, -7.999999999999989342, 23.61155277982336997 ) ) ;
#2370 = VERTEX_POINT ( 'NONE', #38486 ) ;
#2371 = ORIENTED_EDGE ( 'NONE', *, *, #65856, .T. ) ;
#2372 = CARTESIAN_POINT ( 'NONE',  ( 1.226468279477575784E-15, 293.8593750017070079, 6.676582343750001591 ) ) ;
#2373 = CARTESIAN_POINT ( 'NONE',  ( 6.123233995736767268E-16, 188.1249999931720254, -10.00000000000000178 ) ) ;
#2374 = CARTESIAN_POINT ( 'NONE',  ( 11.35316468750000141, 170.7812499965860411, 0.000000000000000000 ) ) ;
#2375 = CYLINDRICAL_SURFACE ( 'NONE', #1943, 10.00000000000000178 ) ;
#2376 = CARTESIAN_POINT ( 'NONE',  ( -3.999999999999960032, 199.9375000000000000, 196.3431457505076594 ) ) ;
#2377 = CARTESIAN_POINT ( 'NONE',  ( -7.778174593052023411, 7.778174593052023411, 69.81249999999998579 ) ) ;
#2378 = CARTESIAN_POINT ( 'NONE',  ( -10.18810118749999916, 4.220049686691934809, 108.4375000020483668 ) ) ;
#2379 = EDGE_LOOP ( 'NONE', ( #73484, #36967, #4096, #32335, #14649, #52420, #58215, #29514, #59829, #62244, #52359, #26218, #58884, #72306, #58361, #42863, #55656, #64132, #60913, #2501, #11329, #69260, #67821, #16128, #16489, #3594, #30902, #22940, #13439, #22835, #9282, #49216, #34373, #31052, #9443, #54495, #357, #58991, #4403, #51856, #5674, #38068, #29978, #64131, #20541, #68866 ) ) ;
#2380 = CARTESIAN_POINT ( 'NONE',  ( 1.781595147087400743, 51.28498669164871870, -48.57279346520080310 ) ) ;
#2381 = CARTESIAN_POINT ( 'NONE',  ( -1.656854249492381248, 17.31250000000000000, -4.000000000000001776 ) ) ;
#2382 = CARTESIAN_POINT ( 'NONE',  ( -11.35316468750000141, 138.5937499965860127, -1.390361679473963753E-15 ) ) ;
#2383 = CARTESIAN_POINT ( 'NONE',  ( 2.754378923186476579E-14, 195.1875000013655779, 194.5412658750000219 ) ) ;
#2384 = CARTESIAN_POINT ( 'NONE',  ( 2.445694354108839175, 208.3125000013656063, 195.5543056458912190 ) ) ;
#2385 = CARTESIAN_POINT ( 'NONE',  ( 4.220049686691934809, 10.18810118749999916, 73.56250000204836681 ) ) ;
#2386 = CARTESIAN_POINT ( 'NONE',  ( -9.832129032723418760, 68.17708332991935549, -5.676582343750004256 ) ) ;
#2387 = EDGE_LOOP ( 'NONE', ( #69674, #2608, #58028, #62616 ) ) ;
#2388 = CARTESIAN_POINT ( 'NONE',  ( 7.999999999999991118, 9.797174393178815797E-16, 13.58030277982336465 ) ) ;
#2389 = CARTESIAN_POINT ( 'NONE',  ( -1.881053915767124440, 5.124999998634407028, 4.541265875000001451 ) ) ;
#2390 = CARTESIAN_POINT ( 'NONE',  ( 8.008118988124991233, 3.317071493978879015, 9.356865283940631883 ) ) ;
#2391 = ORIENTED_EDGE ( 'NONE', *, *, #52425, .T. ) ;
#2392 = EDGE_CURVE ( 'NONE', #60974, #61189, #74516, .T. ) ;
#2393 = EDGE_CURVE ( 'NONE', #41819, #50322, #11449, .T. ) ;
#2394 = CARTESIAN_POINT ( 'NONE',  ( -7.188101187500002709, 20.81249999795161543, 2.977408999572649151 ) ) ;
#2395 = CARTESIAN_POINT ( 'NONE',  ( -6.000000000000001776, 294.0625000034140157, 0.000000000000000000 ) ) ;
#2396 = CARTESIAN_POINT ( 'NONE',  ( 2.381929342089941226, 124.5336769686386589, -7.609644401984009932 ) ) ;
#2397 = CARTESIAN_POINT ( 'NONE',  ( 7.188101187499999156, 12.74999999795161187, 2.977408999572654924 ) ) ;
#2398 = CARTESIAN_POINT ( 'NONE',  ( 7.188101187499992051, 8.802885111219154394E-16, 0.7365527818717527708 ) ) ;
#2399 = CARTESIAN_POINT ( 'NONE',  ( -10.18810118749999916, 0.000000000000000000, 116.0312500020483810 ) ) ;
#2400 = AXIS2_PLACEMENT_3D ( 'NONE', #62351, #7161, #11427 ) ;
#2401 = EDGE_CURVE ( 'NONE', #15401, #34004, #37360, .T. ) ;
#2402 = CARTESIAN_POINT ( 'NONE',  ( 1.656854249492394349, 8.812500000000000000, 3.999999999999988898 ) ) ;
#2403 = CARTESIAN_POINT ( 'NONE',  ( 2.828427124746191623, 3.874999997268813168, -2.828427124746191623 ) ) ;
#2404 = ORIENTED_EDGE ( 'NONE', *, *, #58904, .F. ) ;
#2405 = EDGE_CURVE ( 'NONE', #39639, #38422, #55771, .T. ) ;
#2406 = EDGE_CURVE ( 'NONE', #54226, #6848, #23205, .T. ) ;
#2407 = CARTESIAN_POINT ( 'NONE',  ( 3.458734125000015425, 204.9375000013656063, 198.0000000000000284 ) ) ;
#2408 = CARTESIAN_POINT ( 'NONE',  ( -1.656854249492403008, 200.6875000000000284, 146.0000000000000284 ) ) ;
#2409 = CARTESIAN_POINT ( 'NONE',  ( -26.34314575050769136, 197.0625000027311842, 166.0000000000003695 ) ) ;
#2410 = EDGE_CURVE ( 'NONE', #28168, #3547, #54517, .T. ) ;
#2411 = CARTESIAN_POINT ( 'NONE',  ( 3.211159895383561835, 2.437499998634407028, -3.211159895383561835 ) ) ;
#2412 = CARTESIAN_POINT ( 'NONE',  ( 7.188101187500001821, 111.5000000020483810, -2.977408999572651371 ) ) ;
#2413 = CARTESIAN_POINT ( 'NONE',  ( -4.242640687119286547, 294.8750000000000000, -4.242640687119286547 ) ) ;
#2414 = CARTESIAN_POINT ( 'NONE',  ( -5.082755093536319713, 5.082755093536319713, 28.29905278187175810 ) ) ;
#2415 = VERTEX_POINT ( 'NONE', #31701 ) ;
#2416 = CARTESIAN_POINT ( 'NONE',  ( -2.977408999572650039, 20.43749999795161543, -7.188101187500000933 ) ) ;
#2417 = ORIENTED_EDGE ( 'NONE', *, *, #55230, .T. ) ;
#2418 = CARTESIAN_POINT ( 'NONE',  ( 12.00000000000000355, 0.000000000000000000, -14.80000000000000071 ) ) ;
#2419 = CARTESIAN_POINT ( 'NONE',  ( 3.458734125000015425, 207.9375000013656063, 198.0000000000000284 ) ) ;
#2420 = CARTESIAN_POINT ( 'NONE',  ( 26.56734541678233086, 204.0000000013656063, 166.5412658749999650 ) ) ;
#2421 = CARTESIAN_POINT ( 'NONE',  ( -7.320508075688778149, 53.12500000000000711, 7.320508075688769267 ) ) ;
#2422 = CARTESIAN_POINT ( 'NONE',  ( -5.082755093536324154, 94.71875000204838102, 5.082755093536326818 ) ) ;
#2423 = CARTESIAN_POINT ( 'NONE',  ( 6.000000000000003553, 296.4375000000000000, 2.485281374238571317 ) ) ;
#2424 = EDGE_CURVE ( 'NONE', #31802, #12427, #38402, .T. ) ;
#2426 = CARTESIAN_POINT ( 'NONE',  ( -19.99999999999992895, -32.31627791185601239, 193.6854385646540209 ) ) ;
#2425 = CARTESIAN_POINT ( 'NONE',  ( 23.99999999999998224, 208.8125000027312126, 168.3431457505075741 ) ) ;
#2427 = CIRCLE ( 'NONE', #22954, 7.000000000000000000 ) ;
#2428 = ORIENTED_EDGE ( 'NONE', *, *, #72520, .T. ) ;
#2429 = CARTESIAN_POINT ( 'NONE',  ( 8.311093377946834337, 227.0312500034140157, -8.311093377946836114 ) ) ;
#2430 = CARTESIAN_POINT ( 'NONE',  ( -1.656854249492405451, 199.4375000027312410, 138.0000000000000568 ) ) ;
#2431 = FACE_OUTER_BOUND ( 'NONE', #42648, .T. ) ;
#2432 = CARTESIAN_POINT ( 'NONE',  ( 26.34314575050766649, 206.5624999999999432, 165.9999999999998579 ) ) ;
#2433 = CARTESIAN_POINT ( 'NONE',  ( 0.000000000000000000, 300.0000000000000000, 0.000000000000000000 ) ) ;
#2434 = CARTESIAN_POINT ( 'NONE',  ( 0.000000000000000000, 0.000000000000000000, 0.000000000000000000 ) ) ;
#2435 = CARTESIAN_POINT ( 'NONE',  ( 8.660254037844385522, 174.5833333333333428, 5.000000000000005329 ) ) ;
#2436 = DIRECTION ( 'NONE',  ( 0.000000000000000000, 0.000000000000000000, 1.000000000000000000 ) ) ;
#2437 = LINE ( 'NONE', #42414, #17489 ) ;
#2438 = CARTESIAN_POINT ( 'NONE',  ( -11.00000000000010303, -4.556349186103947346, 68.78125000409676204 ) ) ;
#2439 = CARTESIAN_POINT ( 'NONE',  ( 5.676582343750001591, 151.9270833299193555, -9.832129032723420536 ) ) ;
#2440 = CARTESIAN_POINT ( 'NONE',  ( 4.556349186104045934, 11.00000000000000000, 75.71875000409677625 ) ) ;
#2441 = CARTESIAN_POINT ( 'NONE',  ( -9.000000000000000000, 5.196152422706624918, -10.80000000000000071 ) ) ;
#2444 = CARTESIAN_POINT ( 'NONE',  ( 18.00000000000000000, 10.39230484541329247, -1.607695154586745501 ) ) ;
#2443 = DIRECTION ( 'NONE',  ( 1.000000000000000000, 3.154042683594195121E-16, 0.000000000000000000 ) ) ;
#2442 = CARTESIAN_POINT ( 'NONE',  ( 23.99999999999997868, 202.8125000000000000, 171.6568542494922553 ) ) ;
#2445 = ORIENTED_EDGE ( 'NONE', *, *, #25403, .F. ) ;
#2446 = CARTESIAN_POINT ( 'NONE',  ( 8.311093377946834337, 15.46874999658601624, 8.311093377946839666 ) ) ;
#2447 = DIRECTION ( 'NONE',  ( 0.000000000000000000, 0.000000000000000000, 1.000000000000000000 ) ) ;
#2448 = DIRECTION ( 'NONE',  ( -0.000000000000000000, -1.000000000000000000, -0.000000000000000000 ) ) ;
#2449 = DIRECTION ( 'NONE',  ( 1.000000000000000000, 0.000000000000000000, 0.000000000000000000 ) ) ;
#2450 = CARTESIAN_POINT ( 'NONE',  ( -1.432654583217662259, 206.1250000013656063, 145.4587341250000350 ) ) ;
#2451 = CARTESIAN_POINT ( 'NONE',  ( -0.5119134307784274363, 124.5885204352452718, -7.911479564754728244 ) ) ;
#2452 = AXIS2_PLACEMENT_3D ( 'NONE', #68297, #23021, #46027 ) ;
#2453 = CARTESIAN_POINT ( 'NONE',  ( -7.320508075688773708, 33.74999999317202537, -7.320508075688774596 ) ) ;
#2454 = CARTESIAN_POINT ( 'NONE',  ( 2.977408999572650039, 107.1875000020483810, -7.188101187500001821 ) ) ;
#2455 = CARTESIAN_POINT ( 'NONE',  ( -1.881053915767124440, 3.124999998634407472, 4.541265875000001451 ) ) ;
#2456 = CARTESIAN_POINT ( 'NONE',  ( -11.07651521577767006, -34.01980787861290878, 140.8363281663140754 ) ) ;
#2457 = CARTESIAN_POINT ( 'NONE',  ( 7.999999999999991118, 3.313708498984757611, 12.17405277982336642 ) ) ;
#2459 = CARTESIAN_POINT ( 'NONE',  ( -3.313708498984765161, 24.84374999590322375, 7.999999999999998224 ) ) ;
#2458 = CARTESIAN_POINT ( 'NONE',  ( -29.65685424949239035, 203.4375000000000284, 174.0000000000003979 ) ) ;
#2460 = ORIENTED_EDGE ( 'NONE', *, *, #49917, .T. ) ;
#2461 =( BOUNDED_CURVE ( )  B_SPLINE_CURVE ( 2, ( #25812, #32249, #48831, #20154, #15244, #61282, #9610, #32629, #55638 ),
 .UNSPECIFIED., .F., .F. ) 
 B_SPLINE_CURVE_WITH_KNOTS ( ( 3, 2, 2, 2, 3 ),
 ( 0.8500000000000005329, 0.8583333333333339477, 0.8666666666666673624, 0.8750000000000007772, 0.8833333333333341919 ),
 .UNSPECIFIED. ) 
 CURVE ( )  GEOMETRIC_REPRESENTATION_ITEM ( )  RATIONAL_B_SPLINE_CURVE ( ( 0.9999999999999948930, 0.9238795325112918455, 1.000000000000000000, 0.9238795325112867385, 1.000000000000000000, 0.9238795325112867385, 1.000000000000000000, 0.9238795325112786339, 1.000000000000008216 ) ) 
 REPRESENTATION_ITEM ( '' )  );
#2462 =( BOUNDED_CURVE ( )  B_SPLINE_CURVE ( 2, ( #34014, #45671, #40392, #39278, #11714, #6064, #68685, #27955, #40757 ),
 .UNSPECIFIED., .F., .F. ) 
 B_SPLINE_CURVE_WITH_KNOTS ( ( 3, 2, 2, 2, 3 ),
 ( 0.5735294117647057321, 0.5772058823529410132, 0.5808823529411764053, 0.5845588235294115753, 0.5882352941176468564 ),
 .UNSPECIFIED. ) 
 CURVE ( )  GEOMETRIC_REPRESENTATION_ITEM ( )  RATIONAL_B_SPLINE_CURVE ( ( 1.000000000000002220, 0.9238795325112844070, 1.000000000000000000, 0.9238795325112867385, 1.000000000000000000, 0.9238795325112867385, 1.000000000000000000, 0.9238795325112912904, 0.9999999999999954481 ) ) 
 REPRESENTATION_ITEM ( '' )  );
#2463 = CARTESIAN_POINT ( 'NONE',  ( 8.660254037844385522, 221.0416666734946602, -5.000000000000003553 ) ) ;
#2464 = VECTOR ( 'NONE', #27311, 1000.000000000000000 ) ;
#2465 = CARTESIAN_POINT ( 'NONE',  ( -11.00000000000000000, 0.000000000000000000, 82.18750000409677625 ) ) ;
#2466 = CARTESIAN_POINT ( 'NONE',  ( -6.951808397369817780E-16, 232.9687500034139873, -11.35316468749999963 ) ) ;
#2467 = CARTESIAN_POINT ( 'NONE',  ( 5.676582343750001591, 131.6145833299193555, -9.832129032723420536 ) ) ;
#2468 = ORIENTED_EDGE ( 'NONE', *, *, #32581, .T. ) ;
#2469 = CARTESIAN_POINT ( 'NONE',  ( 2.751064625579944321E-14, 198.7500000000000000, 194.0000000000000568 ) ) ;
#2470 = AXIS2_PLACEMENT_3D ( 'NONE', #61580, #32929, #50250 ) ;
#2471 = CARTESIAN_POINT ( 'NONE',  ( -10.18810118749999738, -4.220049686691941915, 97.75000000204838102 ) ) ;
#2472 = CARTESIAN_POINT ( 'NONE',  ( 11.00000000000000000, 1.347111479062088405E-15, 85.93750000409677625 ) ) ;
#2473 = CARTESIAN_POINT ( 'NONE',  ( 3.458734125000016757, 196.1250000013655779, 199.4326545832176691 ) ) ;
#2474 = CARTESIAN_POINT ( 'NONE',  ( -9.832129032723420536, 118.6979166632526841, 5.676582343749997150 ) ) ;
#2475 = CARTESIAN_POINT ( 'NONE',  ( -32.00000000000001421, 209.1875000000000000, 168.3431457505080004 ) ) ;
#2476 = CARTESIAN_POINT ( 'NONE',  ( 2.679491924311923512, 48.95833333333340676, 9.999999999999605649 ) ) ;
#2477 = ORIENTED_EDGE ( 'NONE', *, *, #61577, .F. ) ;
#2478 = CARTESIAN_POINT ( 'NONE',  ( 3.999999999999960032, 206.0000000000000284, 142.0000000000000568 ) ) ;
#2479 = FACE_OUTER_BOUND ( 'NONE', #62825, .T. ) ;
#2480 = CARTESIAN_POINT ( 'NONE',  ( -8.311093377946836114, 97.96874999658599847, -8.311093377946837890 ) ) ;
#2481 = CARTESIAN_POINT ( 'NONE',  ( 1.432654583217664479, 205.7500000013656063, 201.4587341250000065 ) ) ;
#2482 = CARTESIAN_POINT ( 'NONE',  ( -7.188101187500000933, 13.49999999795161187, -2.977408999572651371 ) ) ;
#2483 = CARTESIAN_POINT ( 'NONE',  ( -6.238412754330611322E-16, 10.18810118749999916, 88.65625000204838102 ) ) ;
#2484 = CARTESIAN_POINT ( 'NONE',  ( 8.311093377946837890, 26.71874999658601624, -8.311093377946837890 ) ) ;
#2485 = VERTEX_POINT ( 'NONE', #26014 ) ;
#2486 = CARTESIAN_POINT ( 'NONE',  ( -1.836970198721029983E-15, 110.6249999931720396, 10.00000000000000178 ) ) ;
#2487 = CARTESIAN_POINT ( 'NONE',  ( 3.317071493978877683, 8.008118988124991233, 27.54436528394063188 ) ) ;
#2488 = DIRECTION ( 'NONE',  ( 1.000000000000000000, -1.486057055854349470E-32, 3.469446951953617147E-16 ) ) ;
#2489 = CARTESIAN_POINT ( 'NONE',  ( 7.204075437095968759, -7.204075437095966983, 74.59375000204838102 ) ) ;
#2490 = EDGE_CURVE ( 'NONE', #14543, #64059, #49037, .T. ) ;
#2491 = LINE ( 'NONE', #25484, #22998 ) ;
#2492 = CARTESIAN_POINT ( 'NONE',  ( -10.00000000000000178, 149.3749999931720538, -1.224646799147353454E-15 ) ) ;
#2493 = CARTESIAN_POINT ( 'NONE',  ( 1.226468279477575784E-15, 291.7031250017069510, 6.676582343750001591 ) ) ;
#2494 = CARTESIAN_POINT ( 'NONE',  ( 2.751064625579944321E-14, 206.7500000000000284, 194.0000000000000568 ) ) ;
#2495 = CARTESIAN_POINT ( 'NONE',  ( 8.311093377946837890, 216.7187499965860127, -8.311093377946837890 ) ) ;
#2496 = CARTESIAN_POINT ( 'NONE',  ( -8.311093377946841443, 124.2187499965860127, 8.311093377946830785 ) ) ;
#2497 = CARTESIAN_POINT ( 'NONE',  ( -10.18810118749999916, 0.000000000000000000, 84.15625000204838102 ) ) ;
#2498 = CARTESIAN_POINT ( 'NONE',  ( -24.54126587500000056, 198.2500000013656347, 168.5673454167827003 ) ) ;
#2499 = CARTESIAN_POINT ( 'NONE',  ( -8.000000000000001776, 23.34375000000000355, 3.313708498984759387 ) ) ;
#2500 = CARTESIAN_POINT ( 'NONE',  ( 1.881053915767121776, 12.62499999863441147, -4.541265875000002339 ) ) ;
#2501 = ORIENTED_EDGE ( 'NONE', *, *, #44244, .F. ) ;
#2502 = CARTESIAN_POINT ( 'NONE',  ( 4.000000000000015987, 208.6250000027312126, 198.0000000000000284 ) ) ;
#2503 = CARTESIAN_POINT ( 'NONE',  ( -3.458734125000016757, 197.1250000013656347, 140.5673454167824161 ) ) ;
#2504 = CARTESIAN_POINT ( 'NONE',  ( 1.656854249492348607, 205.3125000027312126, 138.0000000000000568 ) ) ;
#2505 = EDGE_CURVE ( 'NONE', #25744, #54290, #38858, .T. ) ;
#2506 = VECTOR ( 'NONE', #17364, 1000.000000000000000 ) ;
#2507 = FACE_OUTER_BOUND ( 'NONE', #40414, .T. ) ;
#2508 = CARTESIAN_POINT ( 'NONE',  ( -7.204075437095967871, 7.204075437095967871, 67.84375000204836681 ) ) ;
#2509 = ORIENTED_EDGE ( 'NONE', *, *, #53355, .T. ) ;
#2510 = CARTESIAN_POINT ( 'NONE',  ( -7.188101187500000044, 4.218749997951610986, -8.802885111219163269E-16 ) ) ;
#2511 = CARTESIAN_POINT ( 'NONE',  ( 7.999999999996472155, 7.505344305739403062E-06, 9.267802996260090964 ) ) ;
#2512 = CARTESIAN_POINT ( 'NONE',  ( 4.000000000000001776, 20.00000000000000000, 0.000000000000000000 ) ) ;
#2513 = CARTESIAN_POINT ( 'NONE',  ( -7.188101187500001821, 119.9375000020483952, -2.977408999572650483 ) ) ;
#2514 = AXIS2_PLACEMENT_3D ( 'NONE', #45979, #16928, #68995 ) ;
#2515 = CARTESIAN_POINT ( 'NONE',  ( -4.443259691721288540, 21.99999999999999645, 0.3623607534594540658 ) ) ;
#2516 = CARTESIAN_POINT ( 'NONE',  ( 1.226468279477575784E-15, 291.7031250017069510, 6.676582343750001591 ) ) ;
#2517 = EDGE_CURVE ( 'NONE', #12256, #23017, #46099, .T. ) ;
#2519 = DIRECTION ( 'NONE',  ( 0.000000000000000000, 0.000000000000000000, -1.000000000000000000 ) ) ;
#2518 = CARTESIAN_POINT ( 'NONE',  ( 10.00000000000000000, 131.6666666598386826, 2.679491924311235618 ) ) ;
#2520 = ORIENTED_EDGE ( 'NONE', *, *, #40133, .F. ) ;
#2521 = ADVANCED_FACE ( 'NONE', ( #45253 ), #73185, .F. ) ;
#2522 = CARTESIAN_POINT ( 'NONE',  ( -5.676582343750000703, 228.3854166700806729, -9.832129032723418760 ) ) ;
#2523 = CARTESIAN_POINT ( 'NONE',  ( 5.082755093536320601, -5.082755093536318824, 27.92405278187175455 ) ) ;
#2524 = CARTESIAN_POINT ( 'NONE',  ( -1.836970198721029983E-15, 165.6249999931720254, 10.00000000000000178 ) ) ;
#2525 = LINE ( 'NONE', #25517, #63460 ) ;
#2526 = CARTESIAN_POINT ( 'NONE',  ( 2.839093476692135984E-14, 198.9375000013655779, 201.4587341250000350 ) ) ;
#2527 = EDGE_LOOP ( 'NONE', ( #71396, #50876, #73650, #74434 ) ) ;
#2528 = CARTESIAN_POINT ( 'NONE',  ( -10.99999999999999822, 218.7023502760175973, 0.000000000000000000 ) ) ;
#2529 = CARTESIAN_POINT ( 'NONE',  ( -4.898587196589412829E-16, 102.1250000000000000, -8.000000000000000000 ) ) ;
#2530 = CARTESIAN_POINT ( 'NONE',  ( 5.676582343749993598, 95.26041666325268409, 9.832129032723422313 ) ) ;
#2531 = CARTESIAN_POINT ( 'NONE',  ( -3.999999999999959144, 209.0625000000000568, 199.6568542494924259 ) ) ;
#2532 = CARTESIAN_POINT ( 'NONE',  ( -10.99999999999999822, -4.556349186104052151, 76.09375000000000000 ) ) ;
#2535 = CARTESIAN_POINT ( 'NONE',  ( -3.999999999999959144, 202.0625000000000284, 199.6568542494924259 ) ) ;
#2534 = CARTESIAN_POINT ( 'NONE',  ( 30.44569435410879876, 205.8125000013656063, 167.5543056458910485 ) ) ;
#2533 = CARTESIAN_POINT ( 'NONE',  ( 31.45873412500001010, 204.0000000013656347, 168.5673454167822740 ) ) ;
#2536 = ORIENTED_EDGE ( 'NONE', *, *, #58834, .T. ) ;
#2537 = FACE_OUTER_BOUND ( 'NONE', #44215, .T. ) ;
#2538 = CARTESIAN_POINT ( 'NONE',  ( -2.085542519210945728E-15, 214.5312499965860411, 11.35316468750000141 ) ) ;
#2539 = CARTESIAN_POINT ( 'NONE',  ( -3.458734125000015425, 202.0000000013656063, 143.4326545832176976 ) ) ;
#2540 = CARTESIAN_POINT ( 'NONE',  ( 25.55430564589115150, 203.5625000013656063, 172.4456943541086957 ) ) ;
#2541 = CARTESIAN_POINT ( 'NONE',  ( -5.082755093536326818, 27.28124999795161543, 5.082755093536325042 ) ) ;
#2542 = EDGE_CURVE ( 'NONE', #51437, #53888, #32981, .T. ) ;
#2543 = CARTESIAN_POINT ( 'NONE',  ( -8.311093377946836114, 197.9687499965860411, -8.311093377946837890 ) ) ;
#2544 = CARTESIAN_POINT ( 'NONE',  ( 7.188101187500000044, 92.28125000204836681, -8.802885111219163269E-16 ) ) ;
#2545 = CYLINDRICAL_SURFACE ( 'NONE', #24107, 4.000000000000001776 ) ;
#2546 = CARTESIAN_POINT ( 'NONE',  ( 1.881053915767121776, 12.49999999863440969, -4.541265875000002339 ) ) ;
#2547 = CARTESIAN_POINT ( 'NONE',  ( 30.44569435410878810, 196.8125000013656063, 172.4456943541087526 ) ) ;
#2548 = CARTESIAN_POINT ( 'NONE',  ( -2.977408999572648707, -7.188101187499990274, 2.142802781871754103 ) ) ;
#2549 = DIRECTION ( 'NONE',  ( 0.000000000000000000, 0.000000000000000000, -1.000000000000000000 ) ) ;
#2550 = CARTESIAN_POINT ( 'NONE',  ( 3.042071309553167069, 76.82291666325269830, -11.35316468749999785 ) ) ;
#2551 = ORIENTED_EDGE ( 'NONE', *, *, #14339, .F. ) ;
#2552 = CARTESIAN_POINT ( 'NONE',  ( -4.999999999999999112, -53.55923425356129286, 45.42020841079056481 ) ) ;
#2553 = DIRECTION ( 'NONE',  ( 0.000000000000000000, 0.000000000000000000, 1.000000000000000000 ) ) ;
#2554 = CARTESIAN_POINT ( 'NONE',  ( 4.898587196589412829E-16, 9.187499995903221972, -8.000000000000000000 ) ) ;
#2555 =( BOUNDED_CURVE ( )  B_SPLINE_CURVE ( 2, ( #63208, #34569, #34942, #69625, #35309, #5885, #6628, #68134, #29632 ),
 .UNSPECIFIED., .F., .F. ) 
 B_SPLINE_CURVE_WITH_KNOTS ( ( 3, 2, 2, 2, 3 ),
 ( 0.7352941176470587648, 0.7389705882352940458, 0.7426470588235294379, 0.7463235294117647189, 0.7500000000000000000 ),
 .UNSPECIFIED. ) 
 CURVE ( )  GEOMETRIC_REPRESENTATION_ITEM ( )  RATIONAL_B_SPLINE_CURVE ( ( 1.000000000000002220, 0.9238795325112844070, 1.000000000000000000, 0.9238795325112867385, 1.000000000000000000, 0.9238795325112867385, 1.000000000000000000, 0.9238795325112867385, 1.000000000000000000 ) ) 
 REPRESENTATION_ITEM ( '' )  );
#2556 = CARTESIAN_POINT ( 'NONE',  ( 0.000000000000000000, 300.0000000000000000, 0.000000000000000000 ) ) ;
#2557 = VECTOR ( 'NONE', #57714, 1000.000000000000000 ) ;
#2558 = CARTESIAN_POINT ( 'NONE',  ( -9.832129032723420536, 83.69791666325268409, 5.676582343749997150 ) ) ;
#2559 = VERTEX_POINT ( 'NONE', #45622 ) ;
#2560 = CARTESIAN_POINT ( 'NONE',  ( -10.18810118749999738, -4.220049686691941915, 87.62500000204836681 ) ) ;
#2561 = CARTESIAN_POINT ( 'NONE',  ( -7.204075437095967871, 7.204075437095967871, 113.9687500020483810 ) ) ;
#2562 = CARTESIAN_POINT ( 'NONE',  ( -3.313708498984707429, 102.2187500000000284, -8.000000000000055067 ) ) ;
#2563 = CARTESIAN_POINT ( 'NONE',  ( 10.00000000000003553, 75.00000000000002842, 0.000000000000000000 ) ) ;
#2565 = CARTESIAN_POINT ( 'NONE',  ( -11.35316468750000141, 78.28124999658601268, -1.390361679473963753E-15 ) ) ;
#2564 = CARTESIAN_POINT ( 'NONE',  ( -27.99999999999991473, 206.6250000027312126, 174.0000000000003695 ) ) ;
#2566 = CARTESIAN_POINT ( 'NONE',  ( -3.313708498984758943, -7.999999999999989342, 20.79905278392014978 ) ) ;
#2567 = CARTESIAN_POINT ( 'NONE',  ( -7.347880794884122694E-16, 12.75000000000000178, 4.000000000000001776 ) ) ;
#2568 =( BOUNDED_CURVE ( )  B_SPLINE_CURVE ( 2, ( #7082, #53477, #47056, #70093, #18399, #1794, #30088, #1441, #18771 ),
 .UNSPECIFIED., .F., .F. ) 
 B_SPLINE_CURVE_WITH_KNOTS ( ( 3, 2, 2, 2, 3 ),
 ( 0.5104166666666666297, 0.5156250000000000000, 0.5208333333333333703, 0.5260416666666666297, 0.5312500000000000000 ),
 .UNSPECIFIED. ) 
 CURVE ( )  GEOMETRIC_REPRESENTATION_ITEM ( )  RATIONAL_B_SPLINE_CURVE ( ( 1.000000000000000000, 0.9238795325112867385, 1.000000000000000000, 0.9238795325112867385, 1.000000000000000000, 0.9238795325112867385, 1.000000000000000000, 0.9238795325112867385, 1.000000000000000000 ) ) 
 REPRESENTATION_ITEM ( '' )  );
#2569 = CARTESIAN_POINT ( 'NONE',  ( -8.660254037844387298, 163.9583333265053966, -5.000000000000004441 ) ) ;
#2570 = CARTESIAN_POINT ( 'NONE',  ( -7.999999999999998224, 113.2812500040967763, 3.313708498984766049 ) ) ;
#2571 = CARTESIAN_POINT ( 'NONE',  ( -24.08860760445115190, 194.9317364962658132, 169.5572342916353819 ) ) ;
#2572 = CARTESIAN_POINT ( 'NONE',  ( -3.042071309553163960, 57.55208332991936260, -11.35316468749999963 ) ) ;
#2573 = CARTESIAN_POINT ( 'NONE',  ( 4.721056650416000089, 291.8281250017069510, 4.721056650415999201 ) ) ;
#2574 = CARTESIAN_POINT ( 'NONE',  ( -7.204075437095967871, 7.204075437095967871, 108.3437500020483810 ) ) ;
#2575 = CARTESIAN_POINT ( 'NONE',  ( -8.311093377946836114, 192.6562499965860127, -8.311093377946837890 ) ) ;
#2576 = EDGE_LOOP ( 'NONE', ( #18842, #21994, #21980 ) ) ;
#2577 = LINE ( 'NONE', #25566, #1863 ) ;
#2578 = CARTESIAN_POINT ( 'NONE',  ( 1.102182119232618108E-15, 290.2500000000000000, 6.000000000000001776 ) ) ;
#2579 = CARTESIAN_POINT ( 'NONE',  ( 5.000000000000000000, 68.48952624890506513, 21.22548696402972013 ) ) ;
#2581 = CARTESIAN_POINT ( 'NONE',  ( -3.042071309553173730, 194.3229166632526983, 11.35316468749999785 ) ) ;
#2580 = CARTESIAN_POINT ( 'NONE',  ( 2.751064625579944321E-14, 195.7500000000000000, 194.0000000000000568 ) ) ;
#2582 = CARTESIAN_POINT ( 'NONE',  ( 23.99999999999999645, 195.6875000000000000, 168.3431457505074889 ) ) ;
#2583 = CARTESIAN_POINT ( 'NONE',  ( -9.999999999999998224, 243.3333333401612606, 2.679491924311235618 ) ) ;
#2584 = ORIENTED_EDGE ( 'NONE', *, *, #41976, .T. ) ;
#2585 = EDGE_CURVE ( 'NONE', #5256, #38870, #61519, .T. ) ;
#2586 = CARTESIAN_POINT ( 'NONE',  ( 11.35316468749999963, 186.3020833299193555, -3.042071309553165293 ) ) ;
#2587 =( BOUNDED_CURVE ( )  B_SPLINE_CURVE ( 3, ( #59089, #53790, #7398, #30405 ),
 .UNSPECIFIED., .F., .F. ) 
 B_SPLINE_CURVE_WITH_KNOTS ( ( 4, 4 ),
 ( 1.946939031484073990, 4.336246275695508245 ),
 .UNSPECIFIED. ) 
 CURVE ( )  GEOMETRIC_REPRESENTATION_ITEM ( )  RATIONAL_B_SPLINE_CURVE ( ( 1.000000000000000000, 0.5782237234286481398, 0.5782237234286481398, 1.000000000000000000 ) ) 
 REPRESENTATION_ITEM ( '' )  );
#2588 = AXIS2_PLACEMENT_3D ( 'NONE', #48301, #65655, #66027 ) ;
#2589 = CARTESIAN_POINT ( 'NONE',  ( 1.320432766682872962E-15, -7.188101187499992051, 18.36155278187175455 ) ) ;
#2590 = EDGE_CURVE ( 'NONE', #44362, #32606, #68636, .T. ) ;
#2591 = CARTESIAN_POINT ( 'NONE',  ( -2.679491924311224516, 91.45833333333332860, -9.999999999999994671 ) ) ;
#2592 = AXIS2_PLACEMENT_3D ( 'NONE', #46437, #48925, #54240 ) ;
#2593 = VERTEX_POINT ( 'NONE', #73922 ) ;
#2594 = CARTESIAN_POINT ( 'NONE',  ( 8.000000000000000000, 98.93750000409677625, -9.797174393178825657E-16 ) ) ;
#2595 = CARTESIAN_POINT ( 'NONE',  ( 5.000000000000001776, 0.8333333333333333703, -8.660254037844389075 ) ) ;
#2596 = EDGE_CURVE ( 'NONE', #13320, #25175, #35974, .T. ) ;
#2597 = CARTESIAN_POINT ( 'NONE',  ( 4.000000000000000888, 16.93750000000000000, 1.656854249492384135 ) ) ;
#2598 = CARTESIAN_POINT ( 'NONE',  ( 1.881053915767121998, 15.49999999863440614, -4.541265875000002339 ) ) ;
#2599 = CARTESIAN_POINT ( 'NONE',  ( 1.469576158976822172E-15, -7.999999999999991118, 14.89280278392014623 ) ) ;
#2600 = CARTESIAN_POINT ( 'NONE',  ( 2.775557561562891351E-14, 210.0000000000000284, 202.0000000000000000 ) ) ;
#2601 = AXIS2_PLACEMENT_3D ( 'NONE', #6625, #11534, #40202 ) ;
#2602 = VERTEX_POINT ( 'NONE', #3890 ) ;
#2603 = CARTESIAN_POINT ( 'NONE',  ( -7.240284387734133737E-08, 22.00000000000001066, -4.000000000000000888 ) ) ;
#2604 = CARTESIAN_POINT ( 'NONE',  ( -4.401442555609581635E-16, 98.28125000204838102, -7.188101187500000044 ) ) ;
#2606 = CARTESIAN_POINT ( 'NONE',  ( -25.17157287525374088, 204.7500000027312126, 172.8284271247464972 ) ) ;
#2605 = CARTESIAN_POINT ( 'NONE',  ( 5.656854249492380582, 16.49999999590322375, -5.656854249492380582 ) ) ;
#2607 = APPLICATION_PROTOCOL_DEFINITION ( 'draft international standard', 'automotive_design', 1998, #50548 ) ;
#2608 = ORIENTED_EDGE ( 'NONE', *, *, #6508, .F. ) ;
#2609 = EDGE_CURVE ( 'NONE', #54540, #5560, #5095, .T. ) ;
#2610 = CARTESIAN_POINT ( 'NONE',  ( -4.556349186104045934, 11.00000000000000000, 83.21874999999998579 ) ) ;
#2611 = CARTESIAN_POINT ( 'NONE',  ( -5.082755093536317936, -5.082755093536320601, 19.67405278187175455 ) ) ;
#2612 = VERTEX_POINT ( 'NONE', #72914 ) ;
#2613 = VERTEX_POINT ( 'NONE', #38595 ) ;
#2614 = CARTESIAN_POINT ( 'NONE',  ( 10.18810118750000093, -4.220049686691933033, 83.31250000204836681 ) ) ;
#2615 = CARTESIAN_POINT ( 'NONE',  ( -8.311093377946836114, 62.96874999658601979, -8.311093377946837890 ) ) ;
#2616 = CARTESIAN_POINT ( 'NONE',  ( 10.00000000000000178, 91.87499999317203958, 0.000000000000000000 ) ) ;
#2617 = CARTESIAN_POINT ( 'NONE',  ( -4.556349186104047710, -10.99999999999999822, 92.78124999999998579 ) ) ;
#2620 = CARTESIAN_POINT ( 'NONE',  ( -4.721056650415998313, 293.7343750017069510, 4.721056650416000089 ) ) ;
#2619 = CARTESIAN_POINT ( 'NONE',  ( 31.99999999999997868, 199.4375000027312410, 168.3431457505075173 ) ) ;
#2618 = CARTESIAN_POINT ( 'NONE',  ( 2.449293598294707893E-16, 2.999999997268813168, -4.000000000000001776 ) ) ;
#2621 = CARTESIAN_POINT ( 'NONE',  ( 5.000000000000001776, 150.8333333333333428, -8.660254037844389075 ) ) ;
#2622 = LINE ( 'NONE', #53564, #60954 ) ;
#2623 = CARTESIAN_POINT ( 'NONE',  ( 30.82842712474617386, 209.1250000000000284, 172.8284271247460993 ) ) ;
#2624 = CARTESIAN_POINT ( 'NONE',  ( -7.320508075688771932, 232.5000000068279746, -7.320508075688771932 ) ) ;
#2625 = CARTESIAN_POINT ( 'NONE',  ( -8.000000000000001776, 3.656249995903220196, 3.313708498984759387 ) ) ;
#2626 = CARTESIAN_POINT ( 'NONE',  ( 31.45873412499999233, 200.6875000013656063, 169.9999999999999432 ) ) ;
#2627 = CARTESIAN_POINT ( 'NONE',  ( 4.401442555609581635E-16, 8.718749997951611874, -7.188101187500000044 ) ) ;
#2628 = CIRCLE ( 'NONE', #18303, 11.00000000000000000 ) ;
#2629 = CARTESIAN_POINT ( 'NONE',  ( 8.008118988124991233, 9.807117285998411148E-16, 0.2631152839406289967 ) ) ;
#2630 = CARTESIAN_POINT ( 'NONE',  ( 4.000000000000000888, 5.687499997268812280, 1.656854249492384135 ) ) ;
#2631 = CARTESIAN_POINT ( 'NONE',  ( -2.977408999572652260, 111.3125000020483810, 7.188101187500000044 ) ) ;
#2633 = CARTESIAN_POINT ( 'NONE',  ( 0.000000000000000000, 0.000000000000000000, 118.0000000000000000 ) ) ;
#2632 = CARTESIAN_POINT ( 'NONE',  ( -5.000000000000005329, 20.20833332650536462, 8.660254037844387298 ) ) ;
#2634 = CARTESIAN_POINT ( 'NONE',  ( -7.778174593052020747, -7.778174593052023411, 112.3750000040967763 ) ) ;
#2635 = DIRECTION ( 'NONE',  ( -0.000000000000000000, 1.000000000000000000, -4.476705744456276341E-16 ) ) ;
#2636 = CARTESIAN_POINT ( 'NONE',  ( 5.082755093536320601, -5.082755093536318824, 20.42405278187175810 ) ) ;
#2637 = CARTESIAN_POINT ( 'NONE',  ( 30.82842712474620939, 200.2500000027312126, 172.8284271247460424 ) ) ;
#2638 = CARTESIAN_POINT ( 'NONE',  ( -5.676582343750006032, 44.11458332991935549, 9.832129032723418760 ) ) ;
#2639 = CARTESIAN_POINT ( 'NONE',  ( 7.320508075688773708, 149.3750000000000000, 7.320508075688777261 ) ) ;
#2640 = CARTESIAN_POINT ( 'NONE',  ( -10.00000000000000178, 14.37499999317203425, -1.224646799147353454E-15 ) ) ;
#2641 = EDGE_LOOP ( 'NONE', ( #4450, #8629, #2872, #51592 ) ) ;
#2642 = CARTESIAN_POINT ( 'NONE',  ( -10.00000000000000000, 129.1666666598387110, -2.679491924311229845 ) ) ;
#2643 = CARTESIAN_POINT ( 'NONE',  ( -2.828427124746190735, 14.37500000000000000, -2.828427124746191623 ) ) ;
#2644 = CARTESIAN_POINT ( 'NONE',  ( 8.311093377946834337, 30.15624999658601624, 8.311093377946839666 ) ) ;
#2645 = CARTESIAN_POINT ( 'NONE',  ( -6.735557395310442023E-16, 11.00000000000000000, 81.81250000409677625 ) ) ;
#2646 = CARTESIAN_POINT ( 'NONE',  ( 3.458734124999960358, 203.6875000013656063, 142.0000000000000568 ) ) ;
#2647 = DIRECTION ( 'NONE',  ( -1.000000000000000000, 0.000000000000000000, 6.409875649288994867E-15 ) ) ;
#2648 = CARTESIAN_POINT ( 'NONE',  ( 0.000000000000000000, 125.0000000000000000, 0.000000000000000000 ) ) ;
#2650 = CARTESIAN_POINT ( 'NONE',  ( 5.676582343749993598, 29.94791666325268409, 9.832129032723422313 ) ) ;
#2649 = CARTESIAN_POINT ( 'NONE',  ( 2.977408999572650039, 107.1875000020483810, -7.188101187500000933 ) ) ;
#2651 = CARTESIAN_POINT ( 'NONE',  ( -7.999999999999989342, -3.313708498984762496, 6.924052779823366421 ) ) ;
#2652 = CARTESIAN_POINT ( 'NONE',  ( -11.35316468749999785, 163.0729166632526415, -3.042071309553167513 ) ) ;
#2653 = CARTESIAN_POINT ( 'NONE',  ( -1.836970198721029983E-15, 130.6249999931720254, 10.00000000000000178 ) ) ;
#2654 = CARTESIAN_POINT ( 'NONE',  ( -7.188101187500001821, 110.9375000020483810, -2.977408999572650483 ) ) ;
#2655 = EDGE_LOOP ( 'NONE', ( #19563, #63147, #63944, #69223 ) ) ;
#2656 = CARTESIAN_POINT ( 'NONE',  ( 3.042071309553167513, 17.13541666325268764, -11.35316468749999785 ) ) ;
#2657 = ORIENTED_EDGE ( 'NONE', *, *, #50459, .F. ) ;
#2658 = DIRECTION ( 'NONE',  ( -0.000000000000000000, 1.000000000000000000, -0.000000000000000000 ) ) ;
#2659 = CARTESIAN_POINT ( 'NONE',  ( -7.204075437095967871, 7.204075437095967871, 76.46875000204836681 ) ) ;
#2660 = CARTESIAN_POINT ( 'NONE',  ( -32.00000000000000711, 197.1875000000000284, 168.3431457505080289 ) ) ;
#2662 = CARTESIAN_POINT ( 'NONE',  ( 11.35316468750000141, 150.7812499965860411, 0.000000000000000000 ) ) ;
#2661 = CARTESIAN_POINT ( 'NONE',  ( 4.556349186104045934, 11.00000000000000000, 92.21875000409677625 ) ) ;
#2663 = CARTESIAN_POINT ( 'NONE',  ( 5.082755093536325930, 1.031249997951610098, -5.082755093536325930 ) ) ;
#2664 = CARTESIAN_POINT ( 'NONE',  ( -3.313708498984757167, 7.999999999999991118, 18.60530278432982598 ) ) ;
#2665 = AXIS2_PLACEMENT_3D ( 'NONE', #14325, #6562, #8684 ) ;
#2666 = CARTESIAN_POINT ( 'NONE',  ( -21.03064981308606818, -27.34344282692152461, 192.7758261021089936 ) ) ;
#2667 = CARTESIAN_POINT ( 'NONE',  ( -8.311093377946836114, 238.2812500034140157, -8.311093377946836114 ) ) ;
#2668 = CARTESIAN_POINT ( 'NONE',  ( -6.238412754330611322E-16, 10.18810118749999916, 88.65625000204838102 ) ) ;
#2669 = ORIENTED_EDGE ( 'NONE', *, *, #67432, .T. ) ;
#2670 = EDGE_CURVE ( 'NONE', #52445, #16856, #18110, .T. ) ;
#2671 = AXIS2_PLACEMENT_3D ( 'NONE', #56861, #39129, #61769 ) ;
#2672 = CARTESIAN_POINT ( 'NONE',  ( 2.020667218593132706E-15, -11.00000000000000000, 90.06250000409676204 ) ) ;
#2673 = CARTESIAN_POINT ( 'NONE',  ( -3.999999999999960032, 199.0625000027312126, 196.3431457505076594 ) ) ;
#2674 = CARTESIAN_POINT ( 'NONE',  ( 3.042071309553167069, 97.13541666325266988, -11.35316468749999785 ) ) ;
#2675 =( BOUNDED_CURVE ( )  B_SPLINE_CURVE ( 2, ( #46743, #23000, #51669, #74307, #23365, #47108, #63351, #11676, #34712 ),
 .UNSPECIFIED., .F., .F. ) 
 B_SPLINE_CURVE_WITH_KNOTS ( ( 3, 2, 2, 2, 3 ),
 ( 0.2333333333333335313, 0.2416666666666668628, 0.2500000000000002220, 0.2583333333333335813, 0.2666666666666668850 ),
 .UNSPECIFIED. ) 
 CURVE ( )  GEOMETRIC_REPRESENTATION_ITEM ( )  RATIONAL_B_SPLINE_CURVE ( ( 0.9999999999999982236, 0.9238795325112885148, 1.000000000000000000, 0.9238795325112867385, 1.000000000000000000, 0.9238795325112867385, 1.000000000000000000, 0.9238795325112847401, 1.000000000000001998 ) ) 
 REPRESENTATION_ITEM ( '' )  );
#2676 = CARTESIAN_POINT ( 'NONE',  ( -10.18810118749999916, 0.000000000000000000, 99.15625000204838102 ) ) ;
#2677 = ADVANCED_FACE ( 'NONE', ( #26883 ), #33315, .T. ) ;
#2678 = CARTESIAN_POINT ( 'NONE',  ( 2.780723358947928197E-16, 20.68749999863440436, -4.541265875000002339 ) ) ;
#2679 = ORIENTED_EDGE ( 'NONE', *, *, #42258, .F. ) ;
#2680 = ORIENTED_EDGE ( 'NONE', *, *, #9152, .F. ) ;
#2681 = CARTESIAN_POINT ( 'NONE',  ( -3.211159895383561391, 4.812499998634407028, -3.211159895383561835 ) ) ;
#2682 = CARTESIAN_POINT ( 'NONE',  ( -7.188101187500000044, 1.218749997951610098, -8.802885111219163269E-16 ) ) ;
#2683 = CARTESIAN_POINT ( 'NONE',  ( -7.999999999999998224, 113.2812500040967763, 3.313708498984766493 ) ) ;
#2684 = CARTESIAN_POINT ( 'NONE',  ( -10.18810118749999738, -4.220049686691941915, 96.62500000204838102 ) ) ;
#2685 = CARTESIAN_POINT ( 'NONE',  ( -24.54126587499999346, 204.4375000013656063, 170.0000000000003411 ) ) ;
#2686 = DIRECTION ( 'NONE',  ( 0.000000000000000000, 0.000000000000000000, 1.000000000000000000 ) ) ;
#2687 = AXIS2_PLACEMENT_3D ( 'NONE', #33432, #56432, #27745 ) ;
#2688 = CARTESIAN_POINT ( 'NONE',  ( -2.828427124746190735, 2.375000000000000000, -2.828427124746191623 ) ) ;
#2689 = CARTESIAN_POINT ( 'NONE',  ( -2.828427124746190735, 18.12499999726881583, -2.828427124746191623 ) ) ;
#2690 = CARTESIAN_POINT ( 'NONE',  ( 4.541265875000002339, 3.312499998634407028, 0.000000000000000000 ) ) ;
#2691 = CARTESIAN_POINT ( 'NONE',  ( -3.458734125000016313, 208.8750000013656347, 140.5673454167824161 ) ) ;
#2692 = DIRECTION ( 'NONE',  ( 1.000000000000000000, 0.000000000000000000, 0.000000000000000000 ) ) ;
#2694 = CARTESIAN_POINT ( 'NONE',  ( -1.469576158976823947E-15, 16.12500000000000355, 8.000000000000000000 ) ) ;
#2693 = CARTESIAN_POINT ( 'NONE',  ( -29.43265458321771177, 202.5000000013656063, 166.5412658750003914 ) ) ;
#2695 = CARTESIAN_POINT ( 'NONE',  ( 4.541265875000001451, 17.24999999863440792, 1.881053915767124440 ) ) ;
#2696 = CARTESIAN_POINT ( 'NONE',  ( 2.903480932863696129, -45.77996154868380074, 151.2231176023142893 ) ) ;
#2697 = CARTESIAN_POINT ( 'NONE',  ( 2.977408999572650927, -7.188101187499990274, 7.955302781871752771 ) ) ;
#2698 = VERTEX_POINT ( 'NONE', #9552 ) ;
#2699 = VERTEX_POINT ( 'NONE', #67261 ) ;
#2700 = CARTESIAN_POINT ( 'NONE',  ( -10.18810118749999738, -4.220049686691941915, 96.25000000204838102 ) ) ;
#2701 = CARTESIAN_POINT ( 'NONE',  ( 11.00000000000000000, 1.347111479062088405E-15, 114.4375000040967763 ) ) ;
#2702 = CARTESIAN_POINT ( 'NONE',  ( -24.54126587500000412, 204.5000000013655779, 168.5673454167827003 ) ) ;
#2703 = CARTESIAN_POINT ( 'NONE',  ( -31.99999999999997868, 200.3125000000000284, 171.6568542494928238 ) ) ;
#2704 = CARTESIAN_POINT ( 'NONE',  ( 2.754378923186476579E-14, 196.1875000013655779, 194.5412658750000219 ) ) ;
#2705 = CARTESIAN_POINT ( 'NONE',  ( -24.00000000000002487, 201.9375000027311842, 168.3431457505079152 ) ) ;
#2706 = CARTESIAN_POINT ( 'NONE',  ( -2.679491924311235618, 103.5416666666666572, 10.00000000000000000 ) ) ;
#2707 = CARTESIAN_POINT ( 'NONE',  ( -5.656854249492380582, 111.3125000000000000, -5.656854249492380582 ) ) ;
#2708 = CARTESIAN_POINT ( 'NONE',  ( 4.721056650416000089, 296.9843750017070079, 4.721056650415999201 ) ) ;
#2709 = ORIENTED_EDGE ( 'NONE', *, *, #4830, .T. ) ;
#2710 = AXIS2_PLACEMENT_3D ( 'NONE', #8838, #54872, #72586 ) ;
#2711 = CARTESIAN_POINT ( 'NONE',  ( -4.556349186104048599, -10.99999999999999822, 109.2812500000000000 ) ) ;
#2712 = CARTESIAN_POINT ( 'NONE',  ( -3.313708498984760720, 21.28124999590322375, -8.000000000000000000 ) ) ;
#2713 = CARTESIAN_POINT ( 'NONE',  ( -3.458734125000016313, 201.8750000013656063, 140.5673454167824161 ) ) ;
#2714 = CARTESIAN_POINT ( 'NONE',  ( -21.64495410811206710, -37.79178974995390661, 147.8069330257710874 ) ) ;
#2715 = CARTESIAN_POINT ( 'NONE',  ( 6.123233995736767268E-16, 198.1249999931720538, -10.00000000000000178 ) ) ;
#2716 = CARTESIAN_POINT ( 'NONE',  ( 9.832129032723416984, 252.1354166700806445, -5.676582343750003368 ) ) ;
#2717 = CARTESIAN_POINT ( 'NONE',  ( 2.849036369511732440E-14, 198.2500000000000000, 202.0000000000000000 ) ) ;
#2718 = CARTESIAN_POINT ( 'NONE',  ( 4.556349186104051263, -10.99999999999999822, 112.4687499999999858 ) ) ;
#2719 = CARTESIAN_POINT ( 'NONE',  ( 8.311093377946834337, 5.156249996586015349, 8.311093377946839666 ) ) ;
#2720 = CARTESIAN_POINT ( 'NONE',  ( 1.320432766682872962E-15, -7.188101187499992051, 3.736552781871751883 ) ) ;
#2721 = CARTESIAN_POINT ( 'NONE',  ( 3.042071309553159519, 190.0520833299193839, 11.35316468750000141 ) ) ;
#2722 = DIRECTION ( 'NONE',  ( 1.000000000000000000, 0.000000000000000000, 0.000000000000000000 ) ) ;
#2723 = CARTESIAN_POINT ( 'NONE',  ( -8.342170076843785083E-16, 8.062499998634406140, 4.541265875000002339 ) ) ;
#2724 = DIRECTION ( 'NONE',  ( -0.000000000000000000, 1.000000000000000000, -0.000000000000000000 ) ) ;
#2726 = DIRECTION ( 'NONE',  ( 1.000000000000000000, 0.000000000000000000, 0.000000000000000000 ) ) ;
#2725 = CARTESIAN_POINT ( 'NONE',  ( 2.449293598294707893E-16, 13.99999999726881406, -4.000000000000001776 ) ) ;
#2727 = VERTEX_POINT ( 'NONE', #27628 ) ;
#2728 = CARTESIAN_POINT ( 'NONE',  ( -2.839093476692135984E-14, 204.9375000013656063, 138.5412658750000503 ) ) ;
#2729 = CARTESIAN_POINT ( 'NONE',  ( 11.35316468749999785, 50.88541666325269119, 3.042071309553174174 ) ) ;
#2730 = CARTESIAN_POINT ( 'NONE',  ( 2.020667218593132706E-15, -11.00000000000000000, 100.5625000040967763 ) ) ;
#2731 = DIRECTION ( 'NONE',  ( -0.000000000000000000, 1.000000000000000000, 4.689100369878284071E-30 ) ) ;
#2732 = CARTESIAN_POINT ( 'NONE',  ( -28.00000000000007105, 200.4375000013656063, 166.5412658750003629 ) ) ;
#2733 = DIRECTION ( 'NONE',  ( -0.000000000000000000, 1.000000000000000000, -0.000000000000000000 ) ) ;
#2735 = CYLINDRICAL_SURFACE ( 'NONE', #51068, 8.000000000000000000 ) ;
#2734 = CARTESIAN_POINT ( 'NONE',  ( 7.778174593052023411, -7.778174593052021635, 108.0624999999999858 ) ) ;
#2736 = CARTESIAN_POINT ( 'NONE',  ( -2.754378923186476579E-14, 196.1875000013655779, 145.4587341250000350 ) ) ;
#2737 = CARTESIAN_POINT ( 'NONE',  ( 11.35316468750000141, 115.7812499965860269, 0.000000000000000000 ) ) ;
#2738 = EDGE_CURVE ( 'NONE', #50120, #12576, #63694, .T. ) ;
#2739 = EDGE_CURVE ( 'NONE', #69617, #51761, #46584, .T. ) ;
#2740 = CARTESIAN_POINT ( 'NONE',  ( -10.00000000000000000, 94.16666665983868256, -2.679491924311229845 ) ) ;
#2741 = CARTESIAN_POINT ( 'NONE',  ( 5.082755093536326818, 90.21875000204838102, 5.082755093536325042 ) ) ;
#2742 = CARTESIAN_POINT ( 'NONE',  ( -1.881053915767124440, 16.12499999863440792, 4.541265875000001451 ) ) ;
#2743 = DIRECTION ( 'NONE',  ( 1.000000000000000000, 0.000000000000000000, 0.000000000000000000 ) ) ;
#2744 = CARTESIAN_POINT ( 'NONE',  ( 11.00000000000000000, 1.347111479062088405E-15, 70.74999999999998579 ) ) ;
#2745 = ORIENTED_EDGE ( 'NONE', *, *, #55005, .F. ) ;
#2746 = CARTESIAN_POINT ( 'NONE',  ( -1.307112308314578586, 225.9999999999999432, 9.935950934677435953 ) ) ;
#2747 = ORIENTED_EDGE ( 'NONE', *, *, #2739, .F. ) ;
#2748 = CARTESIAN_POINT ( 'NONE',  ( 6.676582343750004256, 295.0468750017069510, 2.765530957081995478 ) ) ;
#2749 = CARTESIAN_POINT ( 'NONE',  ( 0.000000000000000000, 284.0000000000000000, 0.000000000000000000 ) ) ;
#2750 = CARTESIAN_POINT ( 'NONE',  ( 7.999999999999991118, 9.797174393178815797E-16, 4.767802783920145338 ) ) ;
#2751 = CARTESIAN_POINT ( 'NONE',  ( -2.085542519210945728E-15, 174.5312499965860411, 11.35316468750000141 ) ) ;
#2752 = DIRECTION ( 'NONE',  ( 0.000000000000000000, 0.9659258262890700886, 0.2588190451025146888 ) ) ;
#2753 = CARTESIAN_POINT ( 'NONE',  ( -3.999999999999960032, 199.0000000000000000, 198.0000000000000284 ) ) ;
#2754 = CARTESIAN_POINT ( 'NONE',  ( -3.190679070438028606E-13, 193.7500000000000000, 10.00000000000000533 ) ) ;
#2755 = CARTESIAN_POINT ( 'NONE',  ( 7.204075437095968759, -7.204075437095966983, 103.0937500020483668 ) ) ;
#2756 = ORIENTED_EDGE ( 'NONE', *, *, #65112, .F. ) ;
#2757 = EDGE_CURVE ( 'NONE', #64164, #35360, #7508, .T. ) ;
#2758 = CARTESIAN_POINT ( 'NONE',  ( 4.465349678513709009, 56.41423509509570522, -44.23558526900735899 ) ) ;
#2759 = LINE ( 'NONE', #25004, #13513 ) ;
#2760 = CARTESIAN_POINT ( 'NONE',  ( -11.35316468749999785, 138.3854166632526983, -3.042071309553167957 ) ) ;
#2761 = CARTESIAN_POINT ( 'NONE',  ( -2.679491924310933193, 216.4583333333333144, -10.00000000000017586 ) ) ;
#2762 = CARTESIAN_POINT ( 'NONE',  ( 2.445694354108839175, 207.3125000013656063, 195.5543056458912190 ) ) ;
#2763 = CARTESIAN_POINT ( 'NONE',  ( -7.204075437095965206, -7.204075437095968759, 72.71875000204838102 ) ) ;
#2764 = CARTESIAN_POINT ( 'NONE',  ( 3.042071309553167069, 62.13541666325267698, -11.35316468749999785 ) ) ;
#2765 = ORIENTED_EDGE ( 'NONE', *, *, #72935, .F. ) ;
#2766 = FACE_OUTER_BOUND ( 'NONE', #23101, .T. ) ;
#2767 = CARTESIAN_POINT ( 'NONE',  ( -4.541265875000002339, 6.874999998634407916, -1.881053915767121998 ) ) ;
#2768 = CARTESIAN_POINT ( 'NONE',  ( 8.008118988124991233, 9.807117285998411148E-16, 9.263115283940630107 ) ) ;
#2769 = VERTEX_POINT ( 'NONE', #21964 ) ;
#2770 = VECTOR ( 'NONE', #32091, 1000.000000000000000 ) ;
#2771 = CARTESIAN_POINT ( 'NONE',  ( -7.188101187500001821, 19.12499999795161187, -2.977408999572651371 ) ) ;
#2772 = CARTESIAN_POINT ( 'NONE',  ( 2.485281374238575314, 288.3750000034140157, 6.000000000000000888 ) ) ;
#2773 = CARTESIAN_POINT ( 'NONE',  ( -8.000000000000000000, 117.6875000040967763, 0.000000000000000000 ) ) ;
#2774 = CARTESIAN_POINT ( 'NONE',  ( 5.082755093536324154, 14.15624999795161187, 5.082755093536326818 ) ) ;
#2775 = CARTESIAN_POINT ( 'NONE',  ( 2.977408999572650927, -7.188101187499990274, 3.455302781871751883 ) ) ;
#2776 = CARTESIAN_POINT ( 'NONE',  ( 1.871523826299183495E-15, -10.18810118749999916, 114.9062500020483810 ) ) ;
#2777 = B_SPLINE_CURVE_WITH_KNOTS ( 'NONE', 3,
 ( #41680, #1702, #24680, #69241, #47690, #70712, #26161, #37506, #54862, #3172, #8831, #43517, #25044, #42402, #32604, #66531, #31842, #20502 ),
 .UNSPECIFIED., .F., .F.,
 ( 4, 2, 2, 2, 2, 2, 2, 2, 4 ),
 ( 0.000000000000000000, 0.002371138676862861398, 0.004742277353725722795, 0.007113416030588583759, 0.009484554707451445590, 0.01422683206117716752, 0.01659797073804000073, 0.01778354007647141646, 0.01896910941490283220 ),
 .UNSPECIFIED. ) ;
#2778 = FACE_OUTER_BOUND ( 'NONE', #69494, .T. ) ;
#2779 = CARTESIAN_POINT ( 'NONE',  ( -2.828427124746190735, 8.124999997268814056, -2.828427124746191623 ) ) ;
#2780 = ORIENTED_EDGE ( 'NONE', *, *, #5070, .F. ) ;
#2781 = CARTESIAN_POINT ( 'NONE',  ( 2.839093476692135984E-14, 206.6875000013656063, 201.4587341250000350 ) ) ;
#2783 =( BOUNDED_CURVE ( )  B_SPLINE_CURVE ( 2, ( #30964, #53983, #48308, #71316, #69859, #18172, #9826, #26795, #61503 ),
 .UNSPECIFIED., .F., .F. ) 
 B_SPLINE_CURVE_WITH_KNOTS ( ( 3, 2, 2, 2, 3 ),
 ( 0.7083333333333332593, 0.7152777777777776791, 0.7222222222222220989, 0.7291666666666665186, 0.7361111111111110494 ),
 .UNSPECIFIED. ) 
 CURVE ( )  GEOMETRIC_REPRESENTATION_ITEM ( )  RATIONAL_B_SPLINE_CURVE ( ( 1.000000000000001110, 0.9238795325112855172, 1.000000000000000000, 0.9238795325112867385, 1.000000000000000000, 0.9238795325112867385, 1.000000000000000000, 0.9238795325112879597, 0.9999999999999987788 ) ) 
 REPRESENTATION_ITEM ( '' )  );
#2782 = CARTESIAN_POINT ( 'NONE',  ( -31.99999999999995737, 197.4375000027312126, 171.6568542494928522 ) ) ;
#2784 = CARTESIAN_POINT ( 'NONE',  ( 1.881053915767122664, 4.124999998634407028, 4.541265875000001451 ) ) ;
#2785 = CARTESIAN_POINT ( 'NONE',  ( 2.977408999572654480, 112.6250000020483668, 7.188101187499999156 ) ) ;
#2786 = CARTESIAN_POINT ( 'NONE',  ( -6.000000000000003553, 294.9374999999998863, -2.485281374238571317 ) ) ;
#2787 = CARTESIAN_POINT ( 'NONE',  ( 2.977408999572650927, -7.188101187499990274, 27.45530278187175810 ) ) ;
#2788 = EDGE_LOOP ( 'NONE', ( #7874, #14744, #52742, #6406 ) ) ;
#2789 = CARTESIAN_POINT ( 'NONE',  ( 5.082755093536325930, 24.65624999795161543, -5.082755093536325930 ) ) ;
#2790 = ORIENTED_EDGE ( 'NONE', *, *, #11874, .F. ) ;
#2791 = CARTESIAN_POINT ( 'NONE',  ( -9.999999999999996447, 2.291666666666665186, -2.679491924311228956 ) ) ;
#2792 = CARTESIAN_POINT ( 'NONE',  ( 4.041179811480690276, 6.985140028428005188, 0.000000000000000000 ) ) ;
#2793 = CARTESIAN_POINT ( 'NONE',  ( 1.432654583217662481, 208.1250000013656063, 194.5412658750000219 ) ) ;
#2794 = CARTESIAN_POINT ( 'NONE',  ( 31.45873412500001010, 204.6250000013656063, 171.4326545832175555 ) ) ;
#2795 = CARTESIAN_POINT ( 'NONE',  ( 2.679491924311222739, 73.95833333333334281, 10.00000000000000355 ) ) ;
#2796 = CARTESIAN_POINT ( 'NONE',  ( 5.082755093536326818, 93.59375000204838102, 5.082755093536325042 ) ) ;
#2797 = CARTESIAN_POINT ( 'NONE',  ( -6.000000000000000888, 296.0625000000000000, 2.485281374238575758 ) ) ;
#2799 = DIRECTION ( 'NONE',  ( -1.000000000000000000, 0.000000000000000000, 0.000000000000000000 ) ) ;
#2798 = CARTESIAN_POINT ( 'NONE',  ( 28.00000000000002487, 208.1250000027312126, 173.9999999999999147 ) ) ;
#2800 = ORIENTED_EDGE ( 'NONE', *, *, #24668, .F. ) ;
#2801 = CARTESIAN_POINT ( 'NONE',  ( 5.676582343750005144, 230.5729166700806729, 9.832129032723416984 ) ) ;
#2802 = EDGE_CURVE ( 'NONE', #8416, #44642, #17133, .T. ) ;
#2803 = LINE ( 'NONE', #66920, #35256 ) ;
#2804 = CARTESIAN_POINT ( 'NONE',  ( 3.999999999999960032, 198.1250000027312126, 142.0000000000000568 ) ) ;
#2805 = CARTESIAN_POINT ( 'NONE',  ( 11.00000000000000000, 1.347111479062088405E-15, 118.0000000000000000 ) ) ;
#2806 = LINE ( 'NONE', #47698, #30288 ) ;
#2807 = DIRECTION ( 'NONE',  ( -0.000000000000000000, 1.000000000000000000, 4.689100369878284071E-30 ) ) ;
#2808 = CARTESIAN_POINT ( 'NONE',  ( 3.313708498984819339, 107.6562500040967905, 7.999999999999943157 ) ) ;
#2809 = CARTESIAN_POINT ( 'NONE',  ( -10.00000000000000000, 192.2916666666666856, -2.679491924311229845 ) ) ;
#2810 = LINE ( 'NONE', #30737, #19905 ) ;
#2811 = CARTESIAN_POINT ( 'NONE',  ( -2.977408999572647819, 7.188101187499992051, 25.58030278187175455 ) ) ;
#2812 = CARTESIAN_POINT ( 'NONE',  ( 3.042071309553159519, 155.0520833299192986, 11.35316468750000141 ) ) ;
#2813 = CARTESIAN_POINT ( 'NONE',  ( -5.000000000000000000, 51.88457047716679682, 42.00159762951515319 ) ) ;
#2816 = DIRECTION ( 'NONE',  ( 1.000000000000000000, 0.000000000000000000, 3.016910393003145324E-16 ) ) ;
#2815 = CARTESIAN_POINT ( 'NONE',  ( 0.000000000000000000, 0.000000000000000000, 0.000000000000000000 ) ) ;
#2814 = CARTESIAN_POINT ( 'NONE',  ( 23.99999999999997868, 203.8125000000000284, 171.6568542494922553 ) ) ;
#2817 = ORIENTED_EDGE ( 'NONE', *, *, #13618, .F. ) ;
#2818 = VECTOR ( 'NONE', #31930, 1000.000000000000000 ) ;
#2819 = CARTESIAN_POINT ( 'NONE',  ( -8.311093377946836114, 7.968749996586014461, -8.311093377946837890 ) ) ;
#2820 = CARTESIAN_POINT ( 'NONE',  ( 2.849036369511732440E-14, 200.3750000027312126, 202.0000000000000000 ) ) ;
#2821 = DIRECTION ( 'NONE',  ( -0.000000000000000000, 1.000000000000000000, -0.000000000000000000 ) ) ;
#2822 = CARTESIAN_POINT ( 'NONE',  ( -28.00000000000002487, 196.0000000000000000, 166.0000000000003695 ) ) ;
#2823 = CARTESIAN_POINT ( 'NONE',  ( 2.445694354108783664, 207.3125000013656063, 144.4456943541088663 ) ) ;
#2824 = CARTESIAN_POINT ( 'NONE',  ( -2.679491924311225848, 48.33333332650537528, -10.00000000000000178 ) ) ;
#2825 = CARTESIAN_POINT ( 'NONE',  ( 5.082755093536326818, 106.7187500020483952, 5.082755093536325042 ) ) ;
#2826 = CARTESIAN_POINT ( 'NONE',  ( 2.780723358947928197E-16, 2.687499998634407028, -4.541265875000002339 ) ) ;
#2827 = CARTESIAN_POINT ( 'NONE',  ( 7.999999999999992895, -3.313708498984756279, 11.98655277982336997 ) ) ;
#2829 = CARTESIAN_POINT ( 'NONE',  ( -5.908781966428503729, -5.087229025050659104, 0.8834915628530353171 ) ) ;
#2828 = CARTESIAN_POINT ( 'NONE',  ( 6.123233995736767268E-16, 21.25000000000000000, -10.00000000000000178 ) ) ;
#2830 = ORIENTED_EDGE ( 'NONE', *, *, #21704, .T. ) ;
#2831 = CARTESIAN_POINT ( 'NONE',  ( -1.469576158976823947E-15, 27.93749999590322375, 8.000000000000000000 ) ) ;
#2832 = CARTESIAN_POINT ( 'NONE',  ( 4.556349186104052151, -10.99999999999999822, 82.46874999999998579 ) ) ;
#2833 = CARTESIAN_POINT ( 'NONE',  ( 11.35316468749999963, 236.5104166700806445, 3.042071309553159519 ) ) ;
#2834 = CARTESIAN_POINT ( 'NONE',  ( -5.676582343750006032, 129.1145833299193839, 9.832129032723418760 ) ) ;
#2835 = ORIENTED_EDGE ( 'NONE', *, *, #7521, .T. ) ;
#2836 = EDGE_CURVE ( 'NONE', #73226, #26236, #69233, .T. ) ;
#2837 = ADVANCED_FACE ( 'NONE', ( #2996 ), #60325, .T. ) ;
#2838 = CARTESIAN_POINT ( 'NONE',  ( -6.238412754330611322E-16, 10.18810118749999916, 97.28125000204838102 ) ) ;
#2839 = DIRECTION ( 'NONE',  ( -1.000000000000000000, 0.000000000000000000, 0.000000000000000000 ) ) ;
#2840 = CARTESIAN_POINT ( 'NONE',  ( -2.445694354108783219, 197.8125000013656063, 200.4456943541088663 ) ) ;
#2841 = CARTESIAN_POINT ( 'NONE',  ( 32.00000000000000000, 197.3125000000000568, 168.3431457505075457 ) ) ;
#2843 = CARTESIAN_POINT ( 'NONE',  ( 6.951808397369818766E-16, 107.0312499965860269, -11.35316468750000141 ) ) ;
#2842 = CARTESIAN_POINT ( 'NONE',  ( 1.298305728747444210, 220.0000000000000853, 10.86222807232588394 ) ) ;
#2844 = CARTESIAN_POINT ( 'NONE',  ( -30.82842712474621649, 209.1250000000000284, 167.1715728752542134 ) ) ;
#2845 = CARTESIAN_POINT ( 'NONE',  ( 8.660254037844389075, 82.29166665983871098, -5.000000000000000000 ) ) ;
#2846 = VERTEX_POINT ( 'NONE', #36217 ) ;
#2847 = APPLICATION_CONTEXT ( 'automotive_design' ) ;
#2848 = CARTESIAN_POINT ( 'NONE',  ( -11.00000000000000000, 0.000000000000000000, 77.49999999999998579 ) ) ;
#2849 = VECTOR ( 'NONE', #65467, 1000.000000000000000 ) ;
#2850 = CARTESIAN_POINT ( 'NONE',  ( -4.000000000000002665, 9.562500000000000000, 1.656854249492380582 ) ) ;
#2851 = CARTESIAN_POINT ( 'NONE',  ( -3.042071309553163960, 107.5520833299193555, -11.35316468749999963 ) ) ;
#2852 = CARTESIAN_POINT ( 'NONE',  ( -1.432654583217607192, 207.2500000013655779, 194.5412658750000219 ) ) ;
#2853 = CARTESIAN_POINT ( 'NONE',  ( 2.977408999572652260, 20.06249999795161543, 7.188101187500000044 ) ) ;
#2854 = CARTESIAN_POINT ( 'NONE',  ( -4.220049686691935698, 10.18810118749999916, 88.75000000204836681 ) ) ;
#2855 = CARTESIAN_POINT ( 'NONE',  ( 9.832129032723416984, 20.67708332991935194, 5.676582343750006032 ) ) ;
#2856 = EDGE_LOOP ( 'NONE', ( #15865, #18406, #15269, #67416 ) ) ;
#2857 = CARTESIAN_POINT ( 'NONE',  ( -3.407298021519497233, 68.04056125361158536, -20.39715949456229183 ) ) ;
#2858 = CARTESIAN_POINT ( 'NONE',  ( -3.317071493978878571, 8.008118988124991233, 26.23186528394063188 ) ) ;
#2859 = FACE_OUTER_BOUND ( 'NONE', #37853, .T. ) ;
#2860 = CARTESIAN_POINT ( 'NONE',  ( 4.220049686691934809, 10.18810118749999916, 75.06250000204836681 ) ) ;
#2861 = CARTESIAN_POINT ( 'NONE',  ( -1.903569318090136080E-11, 13.74999999999851852, 10.00000000000000178 ) ) ;
#2862 = CARTESIAN_POINT ( 'NONE',  ( 2.977408999572651815, 6.187499997951610986, 7.188101187500000933 ) ) ;
#2863 = CARTESIAN_POINT ( 'NONE',  ( -2.765530957081998586, 289.6406250017070079, 6.676582343750001591 ) ) ;
#2864 = ADVANCED_FACE ( 'NONE', ( #42965 ), #2235, .T. ) ;
#2865 = CARTESIAN_POINT ( 'NONE',  ( -1.836970198721029983E-15, 125.6249999931720254, 10.00000000000000178 ) ) ;
#2866 = CARTESIAN_POINT ( 'NONE',  ( 11.27292232226671054, 225.9999999999999432, 1.347431162485829281 ) ) ;
#2867 = CARTESIAN_POINT ( 'NONE',  ( 8.311093377946837890, 136.7187499965860411, -8.311093377946837890 ) ) ;
#2868 = CARTESIAN_POINT ( 'NONE',  ( 7.204075437095966983, 7.204075437095967871, 82.09375000204838102 ) ) ;
#2869 = CARTESIAN_POINT ( 'NONE',  ( -31.45873412499997812, 200.7500000013656347, 171.4326545832180386 ) ) ;
#2870 = DIRECTION ( 'NONE',  ( -0.1513591288559071046, 0.000000000000000000, -0.9884788384745426537 ) ) ;
#2871 = CARTESIAN_POINT ( 'NONE',  ( -4.541265875000002339, 11.87499999863440969, -1.881053915767121998 ) ) ;
#2872 = ORIENTED_EDGE ( 'NONE', *, *, #56977, .F. ) ;
#2873 = AXIS2_PLACEMENT_3D ( 'NONE', #7665, #42351, #37073 ) ;
#2874 = CARTESIAN_POINT ( 'NONE',  ( -2.828427124746152987, 203.2500000027312126, 200.8284271247462129 ) ) ;
#2875 = CARTESIAN_POINT ( 'NONE',  ( -2.445694354108840063, 200.0625000013656063, 139.5543056458912190 ) ) ;
#2876 = CARTESIAN_POINT ( 'NONE',  ( -2.751064625579944321E-14, 204.8750000027312126, 146.0000000000000284 ) ) ;
#2877 = DIRECTION ( 'NONE',  ( 1.000000000000000000, -0.000000000000000000, 0.000000000000000000 ) ) ;
#2879 = VERTEX_POINT ( 'NONE', #9320 ) ;
#2878 =( BOUNDED_CURVE ( )  B_SPLINE_CURVE ( 2, ( #13138, #59193, #37288, #55019, #43304, #25941, #59921, #8607, #48958 ),
 .UNSPECIFIED., .F., .F. ) 
 B_SPLINE_CURVE_WITH_KNOTS ( ( 3, 2, 2, 2, 3 ),
 ( 0.04166666666666666435, 0.04861111111111111188, 0.05555555555555555247, 0.06250000000000000000, 0.06944444444444444753 ),
 .UNSPECIFIED. ) 
 CURVE ( )  GEOMETRIC_REPRESENTATION_ITEM ( )  RATIONAL_B_SPLINE_CURVE ( ( 1.000000000000000000, 0.9238795325112867385, 1.000000000000000000, 0.9238795325112867385, 1.000000000000000000, 0.9238795325112867385, 1.000000000000000000, 0.9238795325112867385, 1.000000000000000000 ) ) 
 REPRESENTATION_ITEM ( '' )  );
#2880 = CARTESIAN_POINT ( 'NONE',  ( 5.082755093536325930, 5.156249997951610986, -5.082755093536325930 ) ) ;
#2881 = CARTESIAN_POINT ( 'NONE',  ( -30.64284399271078740, -12.00318926462334801, 174.6921329945331536 ) ) ;
#2882 = CARTESIAN_POINT ( 'NONE',  ( 27.99999999999996447, 204.6250000027312126, 165.9999999999998863 ) ) ;
#2883 = CARTESIAN_POINT ( 'NONE',  ( -9.832129032723420536, 188.6979166632526983, 5.676582343749997150 ) ) ;
#2884 = CARTESIAN_POINT ( 'NONE',  ( -5.082755093536325930, 109.3437500020483810, -5.082755093536325930 ) ) ;
#2885 = FACE_OUTER_BOUND ( 'NONE', #17803, .T. ) ;
#2886 = CARTESIAN_POINT ( 'NONE',  ( 6.676582343750002480, 291.0156250017069510, -2.765530957081997254 ) ) ;
#2888 = CARTESIAN_POINT ( 'NONE',  ( 10.00000000000000178, 136.8749999931720538, 0.000000000000000000 ) ) ;
#2887 = CARTESIAN_POINT ( 'NONE',  ( -9.832129032723415207, 224.3229166700806729, 5.676582343750005144 ) ) ;
#2889 = ORIENTED_EDGE ( 'NONE', *, *, #15186, .F. ) ;
#2890 = CARTESIAN_POINT ( 'NONE',  ( -5.676582343749992710, 220.0520833367473301, 9.832129032723422313 ) ) ;
#2891 = PRODUCT_DEFINITION_SHAPE ( 'NONE', 'NONE',  #3035 ) ;
#2892 = CARTESIAN_POINT ( 'NONE',  ( 7.188101187499992051, 8.802885111219154394E-16, 0.7365527818717527708 ) ) ;
#2893 = CIRCLE ( 'NONE', #33037, 18.99999999999998934 ) ;
#2894 = CARTESIAN_POINT ( 'NONE',  ( 8.000000000000000000, 106.3437500000000000, -3.313708498984762496 ) ) ;
#2895 = DIRECTION ( 'NONE',  ( 1.000000000000000000, 0.000000000000000000, 0.000000000000000000 ) ) ;
#2896 = CARTESIAN_POINT ( 'NONE',  ( 2.754378923186476579E-14, 201.4375000013656063, 194.5412658750000219 ) ) ;
#2897 =( BOUNDED_CURVE ( )  B_SPLINE_CURVE ( 2, ( #49241, #72256, #26221, #32667, #9646, #27724, #26981, #56047, #20570, #4356, #14904, #73382, #49995 ),
 .UNSPECIFIED., .F., .F. ) 
 B_SPLINE_CURVE_WITH_KNOTS ( ( 3, 2, 2, 2, 2, 2, 3 ),
 ( 0.5833333333333331483, 0.5925925925925923377, 0.6018518518518516380, 0.6111111111111109384, 0.6203703703703702388, 0.6296296296296295392, 0.6388888888888887285 ),
 .UNSPECIFIED. ) 
 CURVE ( )  GEOMETRIC_REPRESENTATION_ITEM ( )  RATIONAL_B_SPLINE_CURVE ( ( 1.000000000000000888, 0.9659258262890675351, 1.000000000000000000, 0.9659258262890683122, 1.000000000000000000, 0.9659258262890683122, 1.000000000000000000, 0.9659258262890683122, 1.000000000000000000, 0.9659258262890683122, 1.000000000000000000, 0.9659258262890687563, 0.9999999999999995559 ) ) 
 REPRESENTATION_ITEM ( '' )  );
#2898 = ORIENTED_EDGE ( 'NONE', *, *, #64168, .F. ) ;
#2899 = CARTESIAN_POINT ( 'NONE',  ( 5.656854249492380582, 24.18750000000000355, -5.656854249492380582 ) ) ;
#2900 = CARTESIAN_POINT ( 'NONE',  ( 3.313708498984765161, 96.96875000000000000, 7.999999999999998224 ) ) ;
#2901 = CARTESIAN_POINT ( 'NONE',  ( -11.35316468749999785, 108.3854166632526841, -3.042071309553167513 ) ) ;
#2902 = CARTESIAN_POINT ( 'NONE',  ( -9.999999999999998224, 122.7083333333333428, 2.679491924311222295 ) ) ;
#2903 = CARTESIAN_POINT ( 'NONE',  ( 11.00000000000000355, -4.556349186104045046, 78.15624999999998579 ) ) ;
#2906 = DIRECTION ( 'NONE',  ( -0.000000000000000000, -1.000000000000000000, -0.000000000000000000 ) ) ;
#2905 = CARTESIAN_POINT ( 'NONE',  ( 29.43265458321766559, 201.5000000013655779, 173.4587341249998929 ) ) ;
#2904 = CARTESIAN_POINT ( 'NONE',  ( 31.45873412499997812, 200.8750000013656063, 171.4326545832175839 ) ) ;
#2907 = ORIENTED_EDGE ( 'NONE', *, *, #54094, .F. ) ;
#2908 = EDGE_CURVE ( 'NONE', #12358, #36743, #31208, .T. ) ;
#2909 = DIRECTION ( 'NONE',  ( -0.000000000000000000, -0.000000000000000000, -1.000000000000000000 ) ) ;
#2910 = CARTESIAN_POINT ( 'NONE',  ( -11.35316468750000141, 223.2812499965860127, -1.390361679473963753E-15 ) ) ;
#2911 = CARTESIAN_POINT ( 'NONE',  ( -2.839093476692135984E-14, 200.6875000013656063, 138.5412658750000503 ) ) ;
#2912 = CARTESIAN_POINT ( 'NONE',  ( 31.45873412499998523, 202.8750000013656347, 171.4326545832175839 ) ) ;
#2913 = CARTESIAN_POINT ( 'NONE',  ( 7.778174593052021635, 7.778174593052023411, 116.1250000040967905 ) ) ;
#2914 = CARTESIAN_POINT ( 'NONE',  ( 6.951808397369818766E-16, 197.3437499965860127, -11.35316468750000141 ) ) ;
#2915 = CARTESIAN_POINT ( 'NONE',  ( -7.188101187500000933, 94.43750000204838102, -2.977408999572650483 ) ) ;
#2916 = CARTESIAN_POINT ( 'NONE',  ( 8.571184731088893116, 225.9999999999998863, 6.322102520634380163 ) ) ;
#2917 = CARTESIAN_POINT ( 'NONE',  ( 3.211159895383561835, 13.43749999863440614, -3.211159895383561835 ) ) ;
#2918 = CARTESIAN_POINT ( 'NONE',  ( 29.43265458321761230, 198.7500000013656063, 173.4587341249998929 ) ) ;
#2919 = CARTESIAN_POINT ( 'NONE',  ( 2.977408999572650927, -7.188101187499990274, 6.830302781871755435 ) ) ;
#2920 = CARTESIAN_POINT ( 'NONE',  ( 0.000000000000000000, 300.0000000000000000, 0.000000000000000000 ) ) ;
#2921 = CARTESIAN_POINT ( 'NONE',  ( 8.311093377946837890, 81.40624999658601268, -8.311093377946837890 ) ) ;
#2922 = ORIENTED_EDGE ( 'NONE', *, *, #18195, .F. ) ;
#2923 = CARTESIAN_POINT ( 'NONE',  ( 4.999999999999998224, 139.1666666666666856, 8.660254037844399733 ) ) ;
#2924 = CARTESIAN_POINT ( 'NONE',  ( -4.898587196589412829E-16, 93.12499999999998579, -8.000000000000000000 ) ) ;
#2925 = DIRECTION ( 'NONE',  ( 0.000000000000000000, 0.000000000000000000, 1.000000000000000000 ) ) ;
#2927 = DIRECTION ( 'NONE',  ( -0.000000000000000000, -0.000000000000000000, -1.000000000000000000 ) ) ;
#2926 = VECTOR ( 'NONE', #52722, 1000.000000000000000 ) ;
#2928 = CARTESIAN_POINT ( 'NONE',  ( -9.832129032723418760, 82.86458332991935549, -5.676582343750004256 ) ) ;
#2929 = VERTEX_POINT ( 'NONE', #49295 ) ;
#2930 = CARTESIAN_POINT ( 'NONE',  ( 10.18810118750000093, -4.220049686691933921, 89.68750000204836681 ) ) ;
#2931 = EDGE_CURVE ( 'NONE', #29918, #68294, #42145, .T. ) ;
#2932 = CARTESIAN_POINT ( 'NONE',  ( 4.220049686691941027, -10.18810118749999738, 111.6250000020483810 ) ) ;
#2933 = DIRECTION ( 'NONE',  ( 0.000000000000000000, 0.000000000000000000, 1.000000000000000000 ) ) ;
#2934 = CARTESIAN_POINT ( 'NONE',  ( 8.660254037844412167, 74.58333333333334281, 5.000000000000022204 ) ) ;
#2936 = CARTESIAN_POINT ( 'NONE',  ( -3.042071309553163960, 77.23958332991935549, -11.35316468749999963 ) ) ;
#2935 = CARTESIAN_POINT ( 'NONE',  ( 8.000000000000000000, 121.5312500040968047, -3.313708498984762496 ) ) ;
#2937 = CARTESIAN_POINT ( 'NONE',  ( -7.999999999999991118, 0.000000000000000000, 17.51780278392014623 ) ) ;
#2938 = CARTESIAN_POINT ( 'NONE',  ( 1.656854249492381248, 13.18750000000000000, -4.000000000000001776 ) ) ;
#2939 = CARTESIAN_POINT ( 'NONE',  ( 10.00000000000000178, 167.0833333265053682, -2.679491924311226736 ) ) ;
#2940 = CARTESIAN_POINT ( 'NONE',  ( -8.000000000000000000, 113.0937500040968047, -3.313708498984761164 ) ) ;
#2941 = CARTESIAN_POINT ( 'NONE',  ( -24.23812689673045995, 194.8931109331405764, 171.0716827053657596 ) ) ;
#2942 = CARTESIAN_POINT ( 'NONE',  ( -9.832129032723418760, 63.17708332991934839, -5.676582343750004256 ) ) ;
#2943 = CARTESIAN_POINT ( 'NONE',  ( 4.721056650416000089, 292.8281250017069510, 4.721056650415999201 ) ) ;
#2944 = CARTESIAN_POINT ( 'NONE',  ( 1.871523826299183495E-15, -10.18810118749999916, 104.4062500020483810 ) ) ;
#2945 = CARTESIAN_POINT ( 'NONE',  ( 8.311093377946834337, 210.1562499965860411, 8.311093377946839666 ) ) ;
#2946 = EDGE_LOOP ( 'NONE', ( #66295, #26528, #4181 ) ) ;
#2947 = CARTESIAN_POINT ( 'NONE',  ( -2.219371606097053640, 67.78152867896183409, 20.18750705526327138 ) ) ;
#2948 = CARTESIAN_POINT ( 'NONE',  ( -30.82842712474624491, 203.2500000027312126, 167.1715728752542418 ) ) ;
#2950 = CARTESIAN_POINT ( 'NONE',  ( -5.676582343750006032, 199.1145833299193555, 9.832129032723418760 ) ) ;
#2949 = PLANE ( 'NONE',  #6174 ) ;
#2951 = DIRECTION ( 'NONE',  ( -0.000000000000000000, -0.000000000000000000, 1.000000000000000000 ) ) ;
#2952 = CARTESIAN_POINT ( 'NONE',  ( 7.320508075688776373, 235.0000000068279746, 7.320508075688767491 ) ) ;
#2953 = CARTESIAN_POINT ( 'NONE',  ( -5.656854249492373476, -5.656854249492376141, 11.70530278392014445 ) ) ;
#2954 = EDGE_CURVE ( 'NONE', #6656, #42139, #37669, .T. ) ;
#2955 = ORIENTED_EDGE ( 'NONE', *, *, #38427, .F. ) ;
#2956 = CARTESIAN_POINT ( 'NONE',  ( -3.042071309553163960, 187.5520833299193555, -11.35316468749999963 ) ) ;
#2957 = B_SPLINE_CURVE_WITH_KNOTS ( 'NONE', 3,
 ( #63274, #28579, #57266, #51219, #74604, #22534 ),
 .UNSPECIFIED., .F., .F.,
 ( 4, 2, 4 ),
 ( 2.380728323691399658E-07, 0.005257893135091114105, 0.01051554819734985997 ),
 .UNSPECIFIED. ) ;
#2958 = VECTOR ( 'NONE', #57365, 1000.000000000000000 ) ;
#2959 = CARTESIAN_POINT ( 'NONE',  ( -5.082755093536319713, 5.082755093536319713, 20.79905278187175455 ) ) ;
#2960 = DIRECTION ( 'NONE',  ( -0.8191520442889907994, 0.000000000000000000, -0.5735764363510474917 ) ) ;
#2961 = EDGE_LOOP ( 'NONE', ( #72814, #30144, #61276, #43520 ) ) ;
#2962 = EDGE_CURVE ( 'NONE', #21298, #21405, #43263, .T. ) ;
#2963 = CARTESIAN_POINT ( 'NONE',  ( 1.469576158976823947E-15, 95.56250000409677625, 8.000000000000000000 ) ) ;
#2964 = CARTESIAN_POINT ( 'NONE',  ( 23.99999999999999289, 208.7500000000000284, 169.9999999999998863 ) ) ;
#2965 = ADVANCED_FACE ( 'NONE', ( #60994 ), #25798, .T. ) ;
#2966 = CARTESIAN_POINT ( 'NONE',  ( 2.449293598294707893E-16, 15.25000000000000000, -4.000000000000001776 ) ) ;
#2967 = CARTESIAN_POINT ( 'NONE',  ( -1.881053915767121776, 15.62499999863440614, -4.541265875000002339 ) ) ;
#2968 = CARTESIAN_POINT ( 'NONE',  ( -5.656854249492375253, 5.656854249492375253, 14.33030278392014800 ) ) ;
#2970 = CARTESIAN_POINT ( 'NONE',  ( 28.22735846810412141, 194.7564787015572563, 166.2435212984425448 ) ) ;
#2969 = AXIS2_PLACEMENT_3D ( 'NONE', #241, #979, #63579 ) ;
#2971 = VERTEX_POINT ( 'NONE', #35803 ) ;
#2972 = CARTESIAN_POINT ( 'NONE',  ( 2.485281374238216490, 293.7500000034140157, -6.000000000000357048 ) ) ;
#2973 = CARTESIAN_POINT ( 'NONE',  ( -7.188101187499999156, 89.75000000204839523, 2.977408999572654924 ) ) ;
#2975 = CARTESIAN_POINT ( 'NONE',  ( 9.832129032723416984, 256.8229166700806445, -5.676582343750003368 ) ) ;
#2974 = CARTESIAN_POINT ( 'NONE',  ( -2.679491924304484574, 81.45833333333280279, -10.00000000000402700 ) ) ;
#2976 = DIRECTION ( 'NONE',  ( 1.000000000000000000, 0.000000000000000000, 0.000000000000000000 ) ) ;
#2977 = VERTEX_POINT ( 'NONE', #64831 ) ;
#2978 = CARTESIAN_POINT ( 'NONE',  ( -3.042071309553166181, 263.1770833367473301, -11.35316468749999608 ) ) ;
#2979 = CARTESIAN_POINT ( 'NONE',  ( -7.188101187499990274, -2.977408999572651371, 18.08030278187175455 ) ) ;
#2980 = ORIENTED_EDGE ( 'NONE', *, *, #7143, .F. ) ;
#2981 = ORIENTED_EDGE ( 'NONE', *, *, #1125, .F. ) ;
#2982 = CARTESIAN_POINT ( 'NONE',  ( -6.238412754330611322E-16, 10.18810118749999916, 80.78125000204838102 ) ) ;
#2983 = CARTESIAN_POINT ( 'NONE',  ( 8.311093377946837890, 76.71874999658599847, -8.311093377946837890 ) ) ;
#2984 = CARTESIAN_POINT ( 'NONE',  ( -5.656854249492373476, -5.656854249492376141, 5.705302783920146226 ) ) ;
#2985 = CARTESIAN_POINT ( 'NONE',  ( -7.778174593052023411, 7.778174593052023411, 93.81250000000000000 ) ) ;
#2988 = CARTESIAN_POINT ( 'NONE',  ( -4.721056650415999201, 292.4843750017070079, -4.721056650415999201 ) ) ;
#2987 = CARTESIAN_POINT ( 'NONE',  ( 26.34314575050763452, 197.0625000027311842, 173.9999999999999147 ) ) ;
#2986 = DIRECTION ( 'NONE',  ( 0.5000000000000008882, -0.8660254037844381525, 0.000000000000000000 ) ) ;
#2989 = CARTESIAN_POINT ( 'NONE',  ( 7.320508075688771044, 149.3750000000000000, 7.320508075688775484 ) ) ;
#2990 = CARTESIAN_POINT ( 'NONE',  ( 4.556349186104045934, 11.00000000000000000, 89.03124999999998579 ) ) ;
#2991 = CARTESIAN_POINT ( 'NONE',  ( 3.999999999999960032, 209.1250000027312126, 142.0000000000000568 ) ) ;
#2992 = AXIS2_PLACEMENT_3D ( 'NONE', #64532, #12830, #36233 ) ;
#2993 =( BOUNDED_CURVE ( )  B_SPLINE_CURVE ( 2, ( #37983, #48532, #8931, #9303, #60230, #65524, #54965, #20609, #3274 ),
 .UNSPECIFIED., .F., .F. ) 
 B_SPLINE_CURVE_WITH_KNOTS ( ( 3, 2, 2, 2, 3 ),
 ( 0.05882352941176474670, 0.06250000000000004163, 0.06617647058823533657, 0.06985294117647064538, 0.07352941176470594031 ),
 .UNSPECIFIED. ) 
 CURVE ( )  GEOMETRIC_REPRESENTATION_ITEM ( )  RATIONAL_B_SPLINE_CURVE ( ( 0.9999999999999991118, 0.9238795325112876267, 1.000000000000000000, 0.9238795325112867385, 1.000000000000000000, 0.9238795325112867385, 1.000000000000000000, 0.9238795325112856283, 1.000000000000001110 ) ) 
 REPRESENTATION_ITEM ( '' )  );
#2994 = CARTESIAN_POINT ( 'NONE',  ( 2.445694354108839175, 200.3125000013656063, 195.5543056458912190 ) ) ;
#2995 = CARTESIAN_POINT ( 'NONE',  ( -6.123233995736766282E-16, 231.8750000068279746, -10.00000000000000000 ) ) ;
#2996 = FACE_OUTER_BOUND ( 'NONE', #9605, .T. ) ;
#2997 = CARTESIAN_POINT ( 'NONE',  ( 31.45873412499999944, 198.7500000013656063, 168.5673454167822740 ) ) ;
#2998 = CARTESIAN_POINT ( 'NONE',  ( 2.977408999572650927, 8.624999997951611874, -7.188101187500001821 ) ) ;
#2999 = CARTESIAN_POINT ( 'NONE',  ( -7.999999999999991118, 3.313708498984756723, 27.92405278392015333 ) ) ;
#3000 = CARTESIAN_POINT ( 'NONE',  ( -7.347880794884122694E-16, 5.499999997268813168, 4.000000000000001776 ) ) ;
#3001 = CARTESIAN_POINT ( 'NONE',  ( 2.977408999572654480, 110.0000000020483810, 7.188101187499999156 ) ) ;
#3003 = DIRECTION ( 'NONE',  ( 0.000000000000000000, 0.000000000000000000, -1.000000000000000000 ) ) ;
#3002 = CARTESIAN_POINT ( 'NONE',  ( 1.102182119232618108E-15, 293.3125000034140157, 6.000000000000001776 ) ) ;
#3004 = CARTESIAN_POINT ( 'NONE',  ( 3.178432602446558121E-13, 136.2499999999999716, -10.00000000000000533 ) ) ;
#3005 = CARTESIAN_POINT ( 'NONE',  ( 24.54126587499998635, 209.5000000013656063, 171.4326545832175555 ) ) ;
#3006 = CARTESIAN_POINT ( 'NONE',  ( -4.401442555609577197E-16, 7.188101187499992051, 20.98655278187175455 ) ) ;
#3007 = CARTESIAN_POINT ( 'NONE',  ( 8.000000000000000000, 0.6562499979516100979, 0.000000000000000000 ) ) ;
#3008 = CARTESIAN_POINT ( 'NONE',  ( 11.35316468750000141, 45.78124999658601979, 0.000000000000000000 ) ) ;
#3009 = ADVANCED_FACE ( 'NONE', ( #64474 ), #41460, .T. ) ;
#3010 = CARTESIAN_POINT ( 'NONE',  ( -8.660254037844387298, 3.958333326505365957, -5.000000000000004441 ) ) ;
#3011 = VERTEX_POINT ( 'NONE', #58819 ) ;
#3012 = CARTESIAN_POINT ( 'NONE',  ( 0.000000000000000000, 300.0000000000000000, 0.000000000000000000 ) ) ;
#3013 = LINE ( 'NONE', #20344, #17178 ) ;
#3014 = CARTESIAN_POINT ( 'NONE',  ( 11.35316468750000141, 45.78124999658601979, 0.000000000000000000 ) ) ;
#3015 = CARTESIAN_POINT ( 'NONE',  ( 2.020667218593132706E-15, -11.00000000000000000, 81.06250000409677625 ) ) ;
#3016 = CARTESIAN_POINT ( 'NONE',  ( -1.432654583217662481, 205.3750000013656063, 145.4587341250000350 ) ) ;
#3017 = DIRECTION ( 'NONE',  ( 6.409875649288994867E-15, 0.000000000000000000, 1.000000000000000000 ) ) ;
#3019 = CARTESIAN_POINT ( 'NONE',  ( -2.085542519210945728E-15, 29.53124999658601624, 11.35316468750000141 ) ) ;
#3018 = CARTESIAN_POINT ( 'NONE',  ( 2.977408999572650039, 101.1875000020483810, -7.188101187500000933 ) ) ;
#3020 = CARTESIAN_POINT ( 'NONE',  ( 3.313708498984756279, 7.999999999999991118, 7.861552779823362869 ) ) ;
#3021 = CARTESIAN_POINT ( 'NONE',  ( -1.836970198721029983E-15, 50.62499999317203248, 10.00000000000000178 ) ) ;
#3022 = CARTESIAN_POINT ( 'NONE',  ( -3.042071309553173730, 159.3229166632526699, 11.35316468749999785 ) ) ;
#3023 =( BOUNDED_CURVE ( )  B_SPLINE_CURVE ( 2, ( #41955, #64612, #54408, #2341, #60045, #25335, #58961, #8749, #73244 ),
 .UNSPECIFIED., .F., .F. ) 
 B_SPLINE_CURVE_WITH_KNOTS ( ( 3, 2, 2, 2, 3 ),
 ( 0.2604166666666664631, 0.2656249999999997780, 0.2708333333333330928, 0.2760416666666664631, 0.2812499999999997780 ),
 .UNSPECIFIED. ) 
 CURVE ( )  GEOMETRIC_REPRESENTATION_ITEM ( )  RATIONAL_B_SPLINE_CURVE ( ( 1.000000000000003331, 0.9238795325112835188, 1.000000000000000000, 0.9238795325112867385, 1.000000000000000000, 0.9238795325112867385, 1.000000000000000000, 0.9238795325112899581, 0.9999999999999967804 ) ) 
 REPRESENTATION_ITEM ( '' )  );
#3024 = EDGE_CURVE ( 'NONE', #48333, #48764, #48363, .T. ) ;
#3025 = CARTESIAN_POINT ( 'NONE',  ( -8.660254037844387298, 133.9583333265053682, -5.000000000000004441 ) ) ;
#3026 = CARTESIAN_POINT ( 'NONE',  ( -2.977408999572651815, 109.8125000020483952, 7.188101187500000933 ) ) ;
#3027 = ORIENTED_EDGE ( 'NONE', *, *, #13953, .T. ) ;
#3028 = CARTESIAN_POINT ( 'NONE',  ( 8.660254037844385522, 21.45833332650536818, 5.000000000000005329 ) ) ;
#3029 = CARTESIAN_POINT ( 'NONE',  ( 8.311093377946837890, 16.71874999658601268, -8.311093377946837890 ) ) ;
#3030 = CARTESIAN_POINT ( 'NONE',  ( -2.828427124746209831, 195.5000000027312126, 139.1715728752538723 ) ) ;
#3031 = VERTEX_POINT ( 'NONE', #7129 ) ;
#3032 = CYLINDRICAL_SURFACE ( 'NONE', #16285, 6.000000000000001776 ) ;
#3033 = CARTESIAN_POINT ( 'NONE',  ( -7.204075437095965206, -7.204075437095968759, 76.84375000204838102 ) ) ;
#3034 = CYLINDRICAL_SURFACE ( 'NONE', #10067, 5.000000000000000888 ) ;
#3035 = PRODUCT_DEFINITION ( 'UNKNOWN', '', #55082, #51585 ) ;
#3037 = CARTESIAN_POINT ( 'NONE',  ( -8.311093377946836114, 152.6562499965860127, -8.311093377946837890 ) ) ;
#3036 = CARTESIAN_POINT ( 'NONE',  ( -7.347880794884122694E-16, 21.75000000000000355, 4.000000000000001776 ) ) ;
#3038 = CARTESIAN_POINT ( 'NONE',  ( 7.188101187500000933, 2.437499997951610542, -2.977408999572650483 ) ) ;
#3039 = CARTESIAN_POINT ( 'NONE',  ( 5.656854249492374365, 5.656854249492375253, 10.82405278432982598 ) ) ;
#3040 = CARTESIAN_POINT ( 'NONE',  ( -22.53198954135269361, -24.97489344904381880, 191.2921881415132361 ) ) ;
#3041 = CARTESIAN_POINT ( 'NONE',  ( -3.042071309553166181, 232.8645833367473017, -11.35316468749999608 ) ) ;
#3042 = CARTESIAN_POINT ( 'NONE',  ( 4.220049686691934809, 10.18810118749999916, 88.56250000204836681 ) ) ;
#3043 = ORIENTED_EDGE ( 'NONE', *, *, #15445, .T. ) ;
#3044 = EDGE_CURVE ( 'NONE', #59314, #9758, #53243, .T. ) ;
#3045 = CARTESIAN_POINT ( 'NONE',  ( -2.249999999999999112, 284.0000000000000000, 7.677076266392047543 ) ) ;
#3046 = CARTESIAN_POINT ( 'NONE',  ( -3.313708498984744732, 121.9062500040967905, -8.000000000000019540 ) ) ;
#3047 = CARTESIAN_POINT ( 'NONE',  ( 3.042071309553159519, 100.0520833299193555, 11.35316468750000141 ) ) ;
#3048 = CARTESIAN_POINT ( 'NONE',  ( -10.18810118749999916, 4.220049686691934809, 93.06250000204839523 ) ) ;
#3049 = EDGE_CURVE ( 'NONE', #55780, #14563, #13501, .T. ) ;
#3050 = CARTESIAN_POINT ( 'NONE',  ( 10.00000000000001066, 15.20833333333333748, -2.679491924311229401 ) ) ;
#3051 = ORIENTED_EDGE ( 'NONE', *, *, #35420, .F. ) ;
#3052 = ORIENTED_EDGE ( 'NONE', *, *, #19188, .T. ) ;
#3053 = CARTESIAN_POINT ( 'NONE',  ( -4.541265875000002339, 5.874999998634407028, -1.881053915767121998 ) ) ;
#3054 = CARTESIAN_POINT ( 'NONE',  ( 2.977408999572651815, 10.68749999795161187, 7.188101187500000933 ) ) ;
#3055 = AXIS2_PLACEMENT_3D ( 'NONE', #56877, #5561, #4821 ) ;
#3056 = CARTESIAN_POINT ( 'NONE',  ( -3.313708498984762052, 118.9062500040967905, -8.000000000000000000 ) ) ;
#3057 = CARTESIAN_POINT ( 'NONE',  ( 1.871523826299183495E-15, -10.18810118749999916, 95.40625000204836681 ) ) ;
#3058 = CARTESIAN_POINT ( 'NONE',  ( -30.44569435410883429, 202.8125000013656063, 167.5543056458915885 ) ) ;
#3059 = MECHANICAL_DESIGN_GEOMETRIC_PRESENTATION_REPRESENTATION (  '', ( #35598 ), #45225 ) ;
#3060 = ADVANCED_FACE ( 'NONE', ( #52412 ), #24468, .F. ) ;
#3061 = CARTESIAN_POINT ( 'NONE',  ( -1.656854249492381248, 4.312500000000000888, -4.000000000000001776 ) ) ;
#3062 = CARTESIAN_POINT ( 'NONE',  ( -1.656854249492383691, 17.43749999726881583, 4.000000000000000888 ) ) ;
#3063 = CARTESIAN_POINT ( 'NONE',  ( -1.881053915767124440, 4.999999998634407028, 4.541265875000001451 ) ) ;
#3064 = CARTESIAN_POINT ( 'NONE',  ( 1.432654583217607192, 209.2500000013655779, 145.4587341250000634 ) ) ;
#3065 = CARTESIAN_POINT ( 'NONE',  ( -2.445694354108783664, 195.3125000013656063, 195.5543056458912190 ) ) ;
#3067 = DIRECTION ( 'NONE',  ( -0.000000000000000000, 0.9997074645238147594, 0.02418647091589873691 ) ) ;
#3066 = CARTESIAN_POINT ( 'NONE',  ( -31.45873412500001720, 196.6250000013656063, 168.5673454167828140 ) ) ;
#3068 = CARTESIAN_POINT ( 'NONE',  ( 4.541265875000002339, 17.31249999863440792, 0.000000000000000000 ) ) ;
#3069 = CARTESIAN_POINT ( 'NONE',  ( 2.679491924311155682, 72.91666665983871098, -10.00000000000004441 ) ) ;
#3070 = CARTESIAN_POINT ( 'NONE',  ( 1.320432766682872962E-15, -7.188101187499992051, 6.361552781871754547 ) ) ;
#3071 = EDGE_LOOP ( 'NONE', ( #40009, #63604, #12298, #27396 ) ) ;
#3072 = ORIENTED_EDGE ( 'NONE', *, *, #38793, .T. ) ;
#3073 = CARTESIAN_POINT ( 'NONE',  ( 4.220049686691934809, 10.18810118749999916, 95.68750000204838102 ) ) ;
#3074 = CARTESIAN_POINT ( 'NONE',  ( 27.99999999999993960, 191.0000000000000284, 169.9999999999999147 ) ) ;
#3075 = CARTESIAN_POINT ( 'NONE',  ( -24.54126587500000412, 205.5000000013655779, 168.5673454167827003 ) ) ;
#3076 = CARTESIAN_POINT ( 'NONE',  ( -27.99999999999995737, 202.5000000000000000, 174.0000000000003695 ) ) ;
#3077 = CARTESIAN_POINT ( 'NONE',  ( 2.445694354108839619, 194.8125000013656063, 200.4456943541088663 ) ) ;
#3078 = CARTESIAN_POINT ( 'NONE',  ( -9.999999999999998224, 32.70833333333333570, 2.679491924311222295 ) ) ;
#3079 = ADVANCED_FACE ( 'NONE', ( #59551 ), #7866, .T. ) ;
#3080 = CARTESIAN_POINT ( 'NONE',  ( -4.999999999999998224, 106.6666666666666714, -8.660254037844389075 ) ) ;
#3081 = CARTESIAN_POINT ( 'NONE',  ( 8.000000000000001776, 110.6562500000000000, 3.313708498984759387 ) ) ;
#3082 = CARTESIAN_POINT ( 'NONE',  ( -4.721056650415998313, 291.7343750017069510, 4.721056650416000089 ) ) ;
#3083 = CARTESIAN_POINT ( 'NONE',  ( 7.188101187499993827, -2.977408999572645598, 10.01780278187175632 ) ) ;
#3084 = EDGE_CURVE ( 'NONE', #20382, #25230, #5137, .T. ) ;
#3085 = ORIENTED_EDGE ( 'NONE', *, *, #29237, .F. ) ;
#3086 = CARTESIAN_POINT ( 'NONE',  ( 0.000000000000000000, 300.0000000000000000, 0.000000000000000000 ) ) ;
#3087 = CARTESIAN_POINT ( 'NONE',  ( -3.313708498984765161, 18.84374999590322020, 7.999999999999998224 ) ) ;
#3088 = CARTESIAN_POINT ( 'NONE',  ( -3.458734125000015425, 203.0000000013655779, 143.4326545832176976 ) ) ;
#3089 = CYLINDRICAL_SURFACE ( 'NONE', #47847, 3.999999999999976019 ) ;
#3090 = FACE_OUTER_BOUND ( 'NONE', #25686, .T. ) ;
#3091 = CARTESIAN_POINT ( 'NONE',  ( 2.085542519210945334E-15, 260.4687500034140157, 11.35316468749999963 ) ) ;
#3092 = CARTESIAN_POINT ( 'NONE',  ( -3.999999999999960032, 207.1250000027312126, 198.0000000000000284 ) ) ;
#3093 = CARTESIAN_POINT ( 'NONE',  ( -7.778174593052023411, 7.778174593052023411, 111.8125000000000000 ) ) ;
#3094 = CARTESIAN_POINT ( 'NONE',  ( -7.320508075688773708, 221.8750000000000284, -7.320508075688774596 ) ) ;
#3095 = ADVANCED_FACE ( 'NONE', ( #41089 ), #35442, .T. ) ;
#3096 = CARTESIAN_POINT ( 'NONE',  ( -5.082755093536319713, 5.082755093536319713, 7.674052781871751883 ) ) ;
#3097 = CARTESIAN_POINT ( 'NONE',  ( 3.042071309553167069, 192.1354166632526130, -11.35316468749999785 ) ) ;
#3098 = DIRECTION ( 'NONE',  ( -1.000000000000000000, -0.000000000000000000, -0.000000000000000000 ) ) ;
#3099 = CARTESIAN_POINT ( 'NONE',  ( -1.881053915767121554, 4.624999998634407028, -4.541265875000002339 ) ) ;
#3100 = FACE_OUTER_BOUND ( 'NONE', #63630, .T. ) ;
#3102 = CARTESIAN_POINT ( 'NONE',  ( 2.849036369511732440E-14, 199.3750000027312126, 202.0000000000000000 ) ) ;
#3101 = CARTESIAN_POINT ( 'NONE',  ( -7.347880794884122694E-16, 14.49999999726881406, 4.000000000000001776 ) ) ;
#3103 = EDGE_LOOP ( 'NONE', ( #62471, #61789, #63324, #7428 ) ) ;
#3104 = CARTESIAN_POINT ( 'NONE',  ( -3.458734125000015869, 203.1875000013656063, 142.0000000000000568 ) ) ;
#3105 = CARTESIAN_POINT ( 'NONE',  ( 9.832129032723420536, 6.197916663252683200, -5.676582343749999815 ) ) ;
#3106 = CARTESIAN_POINT ( 'NONE',  ( 7.778174593052021635, 7.778174593052023411, 98.12500000409676204 ) ) ;
#3107 = AXIS2_PLACEMENT_3D ( 'NONE', #67726, #50733, #10748 ) ;
#3108 = CARTESIAN_POINT ( 'NONE',  ( 4.000000000000001776, 19.74999999726881228, 0.000000000000000000 ) ) ;
#3109 = CARTESIAN_POINT ( 'NONE',  ( -26.56734541678228112, 203.0000000013655779, 173.4587341250003476 ) ) ;
#3110 = LINE ( 'NONE', #26472, #6929 ) ;
#3112 = CARTESIAN_POINT ( 'NONE',  ( 1.347111479062088405E-15, 125.0000000000000000, -11.00000000000000000 ) ) ;
#3111 = CARTESIAN_POINT ( 'NONE',  ( -5.082755093536325930, 119.4687500020483810, -5.082755093536325930 ) ) ;
#3113 = CARTESIAN_POINT ( 'NONE',  ( 1.469576158976822172E-15, -7.999999999999991118, 26.70530277982336642 ) ) ;
#3114 = CARTESIAN_POINT ( 'NONE',  ( 11.35316468749999963, 125.9895833299193271, -3.042071309553165293 ) ) ;
#3115 = CARTESIAN_POINT ( 'NONE',  ( -8.660254037844387298, 83.95833332650536818, -5.000000000000004441 ) ) ;
#3116 = AXIS2_PLACEMENT_3D ( 'NONE', #32314, #67758, #16051 ) ;
#3117 = CARTESIAN_POINT ( 'NONE',  ( 5.082755093536326818, 93.21875000204838102, 5.082755093536325042 ) ) ;
#3118 = CARTESIAN_POINT ( 'NONE',  ( -3.211159895383562723, 20.06249999863440436, 3.211159895383561391 ) ) ;
#3119 = CARTESIAN_POINT ( 'NONE',  ( 5.656854249492376141, -5.656854249492374365, 25.58030278392014978 ) ) ;
#3120 = VERTEX_POINT ( 'NONE', #1116 ) ;
#3121 = CARTESIAN_POINT ( 'NONE',  ( -2.849036369511732440E-14, 200.3750000027312126, 138.0000000000000568 ) ) ;
#3122 = VERTEX_POINT ( 'NONE', #2578 ) ;
#3124 = EDGE_CURVE ( 'NONE', #17271, #6891, #66315, .T. ) ;
#3123 =( BOUNDED_CURVE ( )  B_SPLINE_CURVE ( 2, ( #47744, #70767, #36812, #58726, #65097, #59096, #48487, #64006, #64377 ),
 .UNSPECIFIED., .F., .F. ) 
 B_SPLINE_CURVE_WITH_KNOTS ( ( 3, 2, 2, 2, 3 ),
 ( 0.3020833333333331483, 0.3072916666666665186, 0.3124999999999998335, 0.3177083333333331483, 0.3229166666666665186 ),
 .UNSPECIFIED. ) 
 CURVE ( )  GEOMETRIC_REPRESENTATION_ITEM ( )  RATIONAL_B_SPLINE_CURVE ( ( 1.000000000000002442, 0.9238795325112842960, 1.000000000000000000, 0.9238795325112867385, 1.000000000000000000, 0.9238795325112867385, 1.000000000000000000, 0.9238795325112891810, 0.9999999999999975575 ) ) 
 REPRESENTATION_ITEM ( '' )  );
#3125 = CARTESIAN_POINT ( 'NONE',  ( 2.765530957082001251, 293.9218750017069510, 6.676582343750000703 ) ) ;
#3126 =( LENGTH_UNIT ( ) NAMED_UNIT ( * ) SI_UNIT ( .MILLI., .METRE. ) );
#3127 = CARTESIAN_POINT ( 'NONE',  ( 3.313708498984756279, 7.999999999999991118, 5.049052783920146226 ) ) ;
#3128 = CARTESIAN_POINT ( 'NONE',  ( -3.042071309553173730, 164.3229166632526415, 11.35316468749999785 ) ) ;
#3129 = CARTESIAN_POINT ( 'NONE',  ( -28.00000000000007816, 209.2812500020483810, 166.2706329375003804 ) ) ;
#3130 = CARTESIAN_POINT ( 'NONE',  ( 1.656854249492405451, 199.3125000000000853, 202.0000000000000284 ) ) ;
#3131 = CARTESIAN_POINT ( 'NONE',  ( 6.123233995736767268E-16, 8.124999993172032475, -10.00000000000000178 ) ) ;
#3132 = CARTESIAN_POINT ( 'NONE',  ( 10.18810118750000093, -4.220049686691933921, 103.1875000020483810 ) ) ;
#3133 = VERTEX_POINT ( 'NONE', #15368 ) ;
#3134 = CARTESIAN_POINT ( 'NONE',  ( 4.999999999999993783, 156.0416666598387110, 8.660254037844390851 ) ) ;
#3135 = CARTESIAN_POINT ( 'NONE',  ( -8.311093377946841443, 154.2187499965859843, 8.311093377946834337 ) ) ;
#3136 = CARTESIAN_POINT ( 'NONE',  ( -10.00000000000000711, 217.7083333333333428, 2.679491924311224516 ) ) ;
#3137 = CARTESIAN_POINT ( 'NONE',  ( 2.839093476692135984E-14, 205.9375000013656063, 201.4587341250000350 ) ) ;
#3138 = CARTESIAN_POINT ( 'NONE',  ( -7.204075437095965206, -7.204075437095968759, 71.21875000204836681 ) ) ;
#3139 = CARTESIAN_POINT ( 'NONE',  ( 5.676582343749993598, 65.26041666325268409, 9.832129032723422313 ) ) ;
#3140 = ORIENTED_EDGE ( 'NONE', *, *, #41186, .F. ) ;
#3141 = DIRECTION ( 'NONE',  ( 1.000000000000000000, 0.000000000000000000, 0.000000000000000000 ) ) ;
#3142 = EDGE_CURVE ( 'NONE', #53254, #22266, #27614, .T. ) ;
#3143 = CARTESIAN_POINT ( 'NONE',  ( -3.211159895383562723, 7.062499998634407028, 3.211159895383561391 ) ) ;
#3144 = CARTESIAN_POINT ( 'NONE',  ( -5.662595241051933570, -5.662595241051936235, 8.700615283940630107 ) ) ;
#3145 = EDGE_LOOP ( 'NONE', ( #71386, #7845, #41087, #24612 ) ) ;
#3146 = CARTESIAN_POINT ( 'NONE',  ( -7.188101187500001821, 22.12499999795161187, -2.977408999572651371 ) ) ;
#3147 = CARTESIAN_POINT ( 'NONE',  ( 6.000000000000003553, 288.5000000034140157, 2.485281374238571317 ) ) ;
#3148 = CARTESIAN_POINT ( 'NONE',  ( -5.082755093536325042, 17.90624999795161187, -5.082755093536325930 ) ) ;
#3149 = CARTESIAN_POINT ( 'NONE',  ( 2.977408999572646486, 7.188101187499992051, 5.517802781871753659 ) ) ;
#3150 = CARTESIAN_POINT ( 'NONE',  ( 7.204075437095968759, -7.204075437095966983, 113.5937500020483810 ) ) ;
#3151 = PLANE ( 'NONE',  #60677 ) ;
#3152 = CARTESIAN_POINT ( 'NONE',  ( -4.000000000000001776, 6.249999997268812280, -4.898587196589415787E-16 ) ) ;
#3153 = ORIENTED_EDGE ( 'NONE', *, *, #45763, .T. ) ;
#3154 = CARTESIAN_POINT ( 'NONE',  ( 2.445694354108838731, 208.0625000013656063, 195.5543056458912190 ) ) ;
#3155 = CARTESIAN_POINT ( 'NONE',  ( -25.17157287525385811, 199.0000000027312126, 167.1715728752541281 ) ) ;
#3156 = EDGE_CURVE ( 'NONE', #56591, #58773, #25367, .T. ) ;
#3157 = CARTESIAN_POINT ( 'NONE',  ( -1.881053915767124440, 6.999999998634407916, 4.541265875000001451 ) ) ;
#3158 = CARTESIAN_POINT ( 'NONE',  ( 2.977408999572654480, 108.1250000020483810, 7.188101187499999156 ) ) ;
#3159 = AXIS2_PLACEMENT_3D ( 'NONE', #73508, #35037, #28609 ) ;
#3160 = CARTESIAN_POINT ( 'NONE',  ( 5.656854249492376141, -5.656854249492374365, 10.39280277982336465 ) ) ;
#3161 = CARTESIAN_POINT ( 'NONE',  ( 5.082755093536320601, -5.082755093536318824, 26.04905278187175810 ) ) ;
#3162 = ORIENTED_EDGE ( 'NONE', *, *, #47669, .T. ) ;
#3163 = CARTESIAN_POINT ( 'NONE',  ( 4.556349186104045934, 11.00000000000000000, 90.53125000000000000 ) ) ;
#3164 = ORIENTED_EDGE ( 'NONE', *, *, #25724, .F. ) ;
#3165 = CARTESIAN_POINT ( 'NONE',  ( -4.220049686691935698, 10.18810118749999916, 113.8750000020483810 ) ) ;
#3166 = CARTESIAN_POINT ( 'NONE',  ( 1.469576158976823947E-15, 116.3750000000000000, 8.000000000000000000 ) ) ;
#3167 = CARTESIAN_POINT ( 'NONE',  ( -2.445694354108783664, 207.3125000013656063, 195.5543056458912190 ) ) ;
#3168 = CARTESIAN_POINT ( 'NONE',  ( 30.44569435410883074, 203.5625000013656063, 172.4456943541086957 ) ) ;
#3169 = CARTESIAN_POINT ( 'NONE',  ( 10.00000000000000000, 64.79166666666665719, 2.679491924311236062 ) ) ;
#3170 = CARTESIAN_POINT ( 'NONE',  ( 7.188101187500001821, 93.87500000204836681, -2.977408999572651371 ) ) ;
#3171 = CARTESIAN_POINT ( 'NONE',  ( 4.242640687119285658, 293.6249999999999432, -4.242640687119286547 ) ) ;
#3173 = CARTESIAN_POINT ( 'NONE',  ( -11.00000000000000533, 11.00000000000000000, 41.99999999999999289 ) ) ;
#3172 = CARTESIAN_POINT ( 'NONE',  ( 31.81199079273499564, 176.5295069804214450, 167.0568031691722979 ) ) ;
#3174 = EDGE_CURVE ( 'NONE', #9634, #57404, #20278, .T. ) ;
#3175 = VERTEX_POINT ( 'NONE', #61407 ) ;
#3176 = VECTOR ( 'NONE', #33098, 1000.000000000000000 ) ;
#3177 = CARTESIAN_POINT ( 'NONE',  ( 9.832129032723420536, 220.9895833367473301, 5.676582343749996262 ) ) ;
#3178 = CARTESIAN_POINT ( 'NONE',  ( 0.000000000000000000, 0.000000000000000000, 118.0000000000000000 ) ) ;
#3179 = CARTESIAN_POINT ( 'NONE',  ( -2.751064625579944321E-14, 199.8750000027312126, 146.0000000000000284 ) ) ;
#3180 = CARTESIAN_POINT ( 'NONE',  ( -7.999994399014834556, 3.313714099969915505, 24.92405255982296808 ) ) ;
#3181 = CARTESIAN_POINT ( 'NONE',  ( 7.999999999999991118, 9.797174393178815797E-16, 22.58030277982336997 ) ) ;
#3182 = CARTESIAN_POINT ( 'NONE',  ( 4.999999999999997335, 253.3333333333333428, -8.660254037844387298 ) ) ;
#3183 = CARTESIAN_POINT ( 'NONE',  ( 0.000000000000000000, 0.000000000000000000, 118.0000000000000000 ) ) ;
#3184 = CARTESIAN_POINT ( 'NONE',  ( -10.00000000000000355, 182.7083333333333428, 2.679491924311223183 ) ) ;
#3185 = ADVANCED_FACE ( 'NONE', ( #8232 ), #72349, .T. ) ;
#3186 = CARTESIAN_POINT ( 'NONE',  ( -10.99999999999989164, -4.556349186104158733, 89.59374999999998579 ) ) ;
#3187 = CARTESIAN_POINT ( 'NONE',  ( 5.082755093536320601, -5.082755093536318824, 20.42405278187175810 ) ) ;
#3188 = CARTESIAN_POINT ( 'NONE',  ( -11.35316468749999785, 158.3854166632526699, -3.042071309553167513 ) ) ;
#3189 = CARTESIAN_POINT ( 'NONE',  ( 5.656854249492376141, -5.656854249492374365, 22.58030278392014623 ) ) ;
#3190 = CARTESIAN_POINT ( 'NONE',  ( 8.660254037844385522, 261.0416666734946602, -5.000000000000003553 ) ) ;
#3191 = CARTESIAN_POINT ( 'NONE',  ( 5.094045771088254959, 8.823157229062946527, 67.15552375567561683 ) ) ;
#3194 = CARTESIAN_POINT ( 'NONE',  ( -27.99999999999991118, 197.6250000027312126, 174.0000000000003695 ) ) ;
#3193 = CARTESIAN_POINT ( 'NONE',  ( -11.00000000000000533, -11.00000000000000355, 41.99999999999999289 ) ) ;
#3192 = CARTESIAN_POINT ( 'NONE',  ( 29.65685424949240101, 202.4375000000000568, 165.9999999999998863 ) ) ;
#3195 = ORIENTED_EDGE ( 'NONE', *, *, #22637, .T. ) ;
#3196 = CARTESIAN_POINT ( 'NONE',  ( 9.832129032723420536, 16.51041666325268054, -5.676582343749999815 ) ) ;
#3197 = CARTESIAN_POINT ( 'NONE',  ( -3.999999999999960032, 199.0000000000000000, 198.0000000000000284 ) ) ;
#3198 = DIRECTION ( 'NONE',  ( 1.000000000000000000, 0.000000000000000000, 0.000000000000000000 ) ) ;
#3199 = CARTESIAN_POINT ( 'NONE',  ( 5.000000000000000000, 32.28817737728141424, 3.295974604355933479E-13 ) ) ;
#3200 = CARTESIAN_POINT ( 'NONE',  ( 3.458734124999959914, 202.3750000013656063, 143.4326545832176976 ) ) ;
#3201 = CARTESIAN_POINT ( 'NONE',  ( -10.00000000000000355, 54.58333332650536818, 2.679491924311223183 ) ) ;
#3202 = CARTESIAN_POINT ( 'NONE',  ( -7.188101187499999156, 106.2500000020484094, 2.977408999572654924 ) ) ;
#3203 = CARTESIAN_POINT ( 'NONE',  ( 2.780723358947928197E-16, 9.687499998634406140, -4.541265875000002339 ) ) ;
#3204 = CARTESIAN_POINT ( 'NONE',  ( 10.00000000000001243, 220.2083333333333428, -2.679491924311229845 ) ) ;
#3205 = CARTESIAN_POINT ( 'NONE',  ( -7.999999999999991118, 3.313708498984756723, 11.23655277982336820 ) ) ;
#3207 = CARTESIAN_POINT ( 'NONE',  ( 2.679491924311222739, 5.833333326505365513, 10.00000000000000355 ) ) ;
#3206 = CARTESIAN_POINT ( 'NONE',  ( 28.00000000000001776, 203.5000000000000000, 165.9999999999998863 ) ) ;
#3208 = VERTEX_POINT ( 'NONE', #8980 ) ;
#3209 = CARTESIAN_POINT ( 'NONE',  ( 0.000000000000000000, -28.00000000000000000, -3.999999999999988010 ) ) ;
#3210 = DIRECTION ( 'NONE',  ( -0.000000000000000000, -1.000000000000000000, -0.000000000000000000 ) ) ;
#3211 = CARTESIAN_POINT ( 'NONE',  ( 8.311093377946839666, 236.0937500034139589, 8.311093377946830785 ) ) ;
#3212 = CARTESIAN_POINT ( 'NONE',  ( 9.832129032723416984, 130.3645833299193555, 5.676582343750006032 ) ) ;
#3213 = ORIENTED_EDGE ( 'NONE', *, *, #69031, .F. ) ;
#3214 = CARTESIAN_POINT ( 'NONE',  ( -7.999999999961182162, -1.665870058181487338E-05, 5.518425684709454160 ) ) ;
#3215 = CARTESIAN_POINT ( 'NONE',  ( 4.220049686691934809, 10.18810118749999916, 97.18750000204836681 ) ) ;
#3216 = CYLINDRICAL_SURFACE ( 'NONE', #51380, 11.00000000000000000 ) ;
#3217 = CARTESIAN_POINT ( 'NONE',  ( 2.445694354108840063, 196.0625000013656063, 200.4456943541088663 ) ) ;
#3218 = CARTESIAN_POINT ( 'NONE',  ( 0.000000000000000000, 0.000000000000000000, 0.000000000000000000 ) ) ;
#3220 = CARTESIAN_POINT ( 'NONE',  ( 6.951808397369818766E-16, 122.0312499965860269, -11.35316468750000141 ) ) ;
#3219 = CARTESIAN_POINT ( 'NONE',  ( 31.99999999999999289, 196.2500000000000000, 169.9999999999999432 ) ) ;
#3221 = AXIS2_PLACEMENT_3D ( 'NONE', #13895, #37688, #60306 ) ;
#3222 = CARTESIAN_POINT ( 'NONE',  ( -27.99999999999999645, 210.0000000000000284, 174.0000000000003411 ) ) ;
#3223 = ORIENTED_EDGE ( 'NONE', *, *, #55760, .F. ) ;
#3224 = CARTESIAN_POINT ( 'NONE',  ( -3.313708498984708317, 110.2812500000000000, 8.000000000000053291 ) ) ;
#3225 = CARTESIAN_POINT ( 'NONE',  ( -35.84459951466005379, 174.6650488676598627, 165.1237838699977658 ) ) ;
#3226 = CARTESIAN_POINT ( 'NONE',  ( -9.832129032723420536, 114.0104166632526983, 5.676582343749997150 ) ) ;
#3227 = CARTESIAN_POINT ( 'NONE',  ( -1.432654583217607192, 205.2500000013655779, 194.5412658750000219 ) ) ;
#3228 = CARTESIAN_POINT ( 'NONE',  ( 5.082755093536324154, 18.65624999795161187, 5.082755093536326818 ) ) ;
#3229 = CARTESIAN_POINT ( 'NONE',  ( 10.18810118749999916, 1.247682550866122264E-15, 89.78125000204836681 ) ) ;
#3230 = CARTESIAN_POINT ( 'NONE',  ( 3.042071309553159519, 25.05208332991934483, 11.35316468750000141 ) ) ;
#3231 = ORIENTED_EDGE ( 'NONE', *, *, #27662, .F. ) ;
#3232 = CARTESIAN_POINT ( 'NONE',  ( 2.449293598294707893E-16, 20.99999999726881583, -4.000000000000001776 ) ) ;
#3233 = CARTESIAN_POINT ( 'NONE',  ( 7.320508075688771044, 246.2500000068279746, -7.320508075688771932 ) ) ;
#3234 = DIRECTION ( 'NONE',  ( 0.000000000000000000, 0.000000000000000000, 1.000000000000000000 ) ) ;
#3235 = ADVANCED_FACE ( 'NONE', ( #31995 ), #50087, .F. ) ;
#3236 = CARTESIAN_POINT ( 'NONE',  ( -1.403917192747188514, 21.99999999999999645, 4.310151135844173531 ) ) ;
#3237 = CARTESIAN_POINT ( 'NONE',  ( 2.977408999572650927, 5.249999997951610986, -7.188101187500001821 ) ) ;
#3238 = CARTESIAN_POINT ( 'NONE',  ( 2.765530957082001251, 287.7656250017069510, 6.676582343750000703 ) ) ;
#3239 = CARTESIAN_POINT ( 'NONE',  ( 5.000000000000001776, 127.7083333265053824, -8.660254037844389075 ) ) ;
#3240 = CARTESIAN_POINT ( 'NONE',  ( 5.676582343749993598, 215.2604166632526983, 9.832129032723422313 ) ) ;
#3241 = EDGE_LOOP ( 'NONE', ( #10022, #7804, #71438, #5627 ) ) ;
#3242 =( BOUNDED_CURVE ( )  B_SPLINE_CURVE ( 2, ( #43863, #43104, #55571, #61957, #37844, #67257, #20090, #3886, #25746 ),
 .UNSPECIFIED., .F., .F. ) 
 B_SPLINE_CURVE_WITH_KNOTS ( ( 3, 2, 2, 2, 3 ),
 ( 0.7638888888888888395, 0.7708333333333333703, 0.7777777777777779011, 0.7847222222222223209, 0.7916666666666667407 ),
 .UNSPECIFIED. ) 
 CURVE ( )  GEOMETRIC_REPRESENTATION_ITEM ( )  RATIONAL_B_SPLINE_CURVE ( ( 1.000000000000000000, 0.9238795325112867385, 1.000000000000000000, 0.9238795325112867385, 1.000000000000000000, 0.9238795325112867385, 1.000000000000000000, 0.9238795325112855172, 1.000000000000001110 ) ) 
 REPRESENTATION_ITEM ( '' )  );
#3243 = CARTESIAN_POINT ( 'NONE',  ( 11.35316468749999963, 141.3020833299193271, -3.042071309553165293 ) ) ;
#3244 = CARTESIAN_POINT ( 'NONE',  ( -7.204075437095967871, 7.204075437095967871, 85.46875000204836681 ) ) ;
#3245 = CARTESIAN_POINT ( 'NONE',  ( -26.56734541678238060, 198.3750000013655779, 166.5412658750003629 ) ) ;
#3246 = CARTESIAN_POINT ( 'NONE',  ( -1.656854249492504705, 198.6875000000000284, 145.9999999999999716 ) ) ;
#3247 = CARTESIAN_POINT ( 'NONE',  ( -1.881053915767121554, 16.74999999863440792, -4.541265875000002339 ) ) ;
#3248 = ORIENTED_EDGE ( 'NONE', *, *, #58752, .T. ) ;
#3249 = CARTESIAN_POINT ( 'NONE',  ( 2.849036369511732440E-14, 204.3750000027312126, 202.0000000000000000 ) ) ;
#3250 = CARTESIAN_POINT ( 'NONE',  ( 3.458734124999960358, 199.6875000013656063, 142.0000000000000568 ) ) ;
#3251 = CARTESIAN_POINT ( 'NONE',  ( 2.828427124746153876, 203.0000000027312126, 144.8284271247462129 ) ) ;
#3252 = EDGE_CURVE ( 'NONE', #61426, #12586, #43679, .T. ) ;
#3253 = EDGE_CURVE ( 'NONE', #6741, #26308, #43676, .T. ) ;
#3254 = LINE ( 'NONE', #15672, #21145 ) ;
#3255 = VERTEX_POINT ( 'NONE', #54639 ) ;
#3256 = CARTESIAN_POINT ( 'NONE',  ( -5.082755093536326818, 13.40624999795161187, 5.082755093536325042 ) ) ;
#3257 = CARTESIAN_POINT ( 'NONE',  ( 1.469576158976822172E-15, -7.999999999999991118, 8.892802783920146226 ) ) ;
#3258 = CARTESIAN_POINT ( 'NONE',  ( 1.656854249492356157, 20.18750000000000000, -4.000000000000026645 ) ) ;
#3259 = CARTESIAN_POINT ( 'NONE',  ( -3.042071309553173730, 184.3229166632526983, 11.35316468749999785 ) ) ;
#3260 = EDGE_CURVE ( 'NONE', #30970, #27817, #27660, .T. ) ;
#3261 = CARTESIAN_POINT ( 'NONE',  ( 5.082755093536325042, 113.4687500020483810, -5.082755093536325930 ) ) ;
#3262 = CARTESIAN_POINT ( 'NONE',  ( -6.000000000000001776, 291.0625000034140157, 0.000000000000000000 ) ) ;
#3263 = CARTESIAN_POINT ( 'NONE',  ( 4.721056650416000089, 293.8281250017069510, 4.721056650415999201 ) ) ;
#3265 = CARTESIAN_POINT ( 'NONE',  ( 9.999999999999996447, 95.20833333333334281, -2.679491924311225848 ) ) ;
#3264 = CARTESIAN_POINT ( 'NONE',  ( 6.326249034914468552E-13, 178.7500000000000853, 10.00000000000000533 ) ) ;
#3266 = VERTEX_POINT ( 'NONE', #45914 ) ;
#3267 = CARTESIAN_POINT ( 'NONE',  ( 3.042071309553163960, 227.7604166700806445, -11.35316468749999785 ) ) ;
#3268 = CARTESIAN_POINT ( 'NONE',  ( -4.401442555609577197E-16, 7.188101187499992051, 26.98655278187175455 ) ) ;
#3269 = CARTESIAN_POINT ( 'NONE',  ( 9.797174393178825657E-16, 125.0000000000000000, -8.000000000000000000 ) ) ;
#3270 = DIRECTION ( 'NONE',  ( 1.000000000000000000, 0.000000000000000000, 0.000000000000000000 ) ) ;
#3271 = CARTESIAN_POINT ( 'NONE',  ( -2.266287154879861987, -60.33498852648448008, -22.96738997677460858 ) ) ;
#3272 = CARTESIAN_POINT ( 'NONE',  ( 3.458734125000015425, 200.2500000013656631, 196.5673454167823877 ) ) ;
#3273 = CARTESIAN_POINT ( 'NONE',  ( -15.99999999999999645, 15.99999999999999645, 20.00000000000000000 ) ) ;
#3274 = CARTESIAN_POINT ( 'NONE',  ( 11.00000000000000000, 1.347111479062088405E-15, 114.2499999999999858 ) ) ;
#3275 = CARTESIAN_POINT ( 'NONE',  ( -8.000000000000000000, 93.50000000000000000, 0.000000000000000000 ) ) ;
#3276 = CARTESIAN_POINT ( 'NONE',  ( 9.832129032723416984, 115.6770833299193555, 5.676582343750006032 ) ) ;
#3277 = CARTESIAN_POINT ( 'NONE',  ( -5.999999999999999112, 296.0625000000000000, 2.485281374238575314 ) ) ;
#3278 = CARTESIAN_POINT ( 'NONE',  ( 4.556349186104045934, 11.00000000000000000, 72.53124999999998579 ) ) ;
#3280 = CARTESIAN_POINT ( 'NONE',  ( 26.56734541678237704, 202.3750000013655779, 173.4587341249998929 ) ) ;
#3279 = CARTESIAN_POINT ( 'NONE',  ( 27.99999999999996447, 199.6875000013656063, 173.4587341249998929 ) ) ;
#3281 = ORIENTED_EDGE ( 'NONE', *, *, #19126, .T. ) ;
#3282 = DIRECTION ( 'NONE',  ( -1.000000000000000000, -0.000000000000000000, -0.000000000000000000 ) ) ;
#3283 = EDGE_CURVE ( 'NONE', #38945, #71897, #33503, .T. ) ;
#3284 = CARTESIAN_POINT ( 'NONE',  ( 0.000000000000000000, 0.000000000000000000, -4.000000000000001776 ) ) ;
#3285 = CARTESIAN_POINT ( 'NONE',  ( -3.458734125000015425, 195.9375000013655779, 142.0000000000000568 ) ) ;
#3286 = AXIS2_PLACEMENT_3D ( 'NONE', #71247, #19567, #13526 ) ;
#3287 = CARTESIAN_POINT ( 'NONE',  ( 29.43265458321760519, 197.7500000013656063, 173.4587341249998929 ) ) ;
#3288 = CARTESIAN_POINT ( 'NONE',  ( 9.797174393178825657E-16, 125.0000000000000000, -8.000000000000000000 ) ) ;
#3289 = CARTESIAN_POINT ( 'NONE',  ( 3.042071309553159519, 200.0520833299193839, 11.35316468750000141 ) ) ;
#3290 = CARTESIAN_POINT ( 'NONE',  ( -2.977408999572650927, 91.25000000204838102, -7.188101187500000933 ) ) ;
#3291 = CARTESIAN_POINT ( 'NONE',  ( -11.00000000000000533, 11.00000000000000000, 41.99999999999999289 ) ) ;
#3292 = CARTESIAN_POINT ( 'NONE',  ( -1.881053915767121554, 14.62499999863440969, -4.541265875000002339 ) ) ;
#3293 = CARTESIAN_POINT ( 'NONE',  ( 31.45873412499999944, 198.0000000013656063, 168.5673454167822740 ) ) ;
#3294 = CARTESIAN_POINT ( 'NONE',  ( -7.999999999999991118, 3.313708498984756723, 27.73655277982336642 ) ) ;
#3295 = CARTESIAN_POINT ( 'NONE',  ( 2.249999999999996003, 255.9999999999999432, 7.677076266392048431 ) ) ;
#3296 = CARTESIAN_POINT ( 'NONE',  ( -9.832129032723418760, 82.86458332991935549, -5.676582343750004256 ) ) ;
#3297 = EDGE_LOOP ( 'NONE', ( #53821, #23972, #61065, #47082 ) ) ;
#3298 = LINE ( 'NONE', #71565, #14669 ) ;
#3299 = CARTESIAN_POINT ( 'NONE',  ( 2.824543433528785410E-14, 210.0000000000000284, 194.0000000000000568 ) ) ;
#3300 = CARTESIAN_POINT ( 'NONE',  ( -1.320432766682874540E-15, 19.59374999795161543, 7.188101187500000044 ) ) ;
#3301 = CARTESIAN_POINT ( 'NONE',  ( 7.320508075688886507, 39.37500000000009237, 7.320508075688890948 ) ) ;
#3302 = CARTESIAN_POINT ( 'NONE',  ( 10.00000000000000178, 232.2916666666666856, 2.679491924311222739 ) ) ;
#3303 = CARTESIAN_POINT ( 'NONE',  ( -9.832129032723418760, 87.86458332991935549, -5.676582343750004256 ) ) ;
#3304 = ORIENTED_EDGE ( 'NONE', *, *, #63738, .F. ) ;
#3305 = CARTESIAN_POINT ( 'NONE',  ( -4.220049686691937474, -10.18810118749999738, 84.81250000204838102 ) ) ;
#3306 = CARTESIAN_POINT ( 'NONE',  ( -4.220049686691935698, 10.18810118749999916, 115.3750000020483810 ) ) ;
#3307 = CARTESIAN_POINT ( 'NONE',  ( -26.56734541678232375, 195.2500000013656063, 173.4587341250003760 ) ) ;
#3308 = CARTESIAN_POINT ( 'NONE',  ( 2.445694354108839175, 208.3125000013656063, 195.5543056458912190 ) ) ;
#3310 = CARTESIAN_POINT ( 'NONE',  ( 8.311093377946834337, 85.15624999658602690, 8.311093377946839666 ) ) ;
#3309 = LINE ( 'NONE', #31979, #34045 ) ;
#3311 = CARTESIAN_POINT ( 'NONE',  ( 7.999999999999991118, 9.797174393178815797E-16, 19.76780278392014623 ) ) ;
#3312 = CARTESIAN_POINT ( 'NONE',  ( 1.656854249492381248, 15.18750000000000000, -4.000000000000001776 ) ) ;
#3313 = CARTESIAN_POINT ( 'NONE',  ( 7.320508075688771044, 166.2499999931720822, 7.320508075688775484 ) ) ;
#3314 = CARTESIAN_POINT ( 'NONE',  ( 7.999999999999992895, -9.797174393178815797E-16, 0.000000000000000000 ) ) ;
#3315 = CARTESIAN_POINT ( 'NONE',  ( 4.999999999999998224, -53.50647209750589894, 45.02947987234036020 ) ) ;
#3316 = CARTESIAN_POINT ( 'NONE',  ( -9.832129032723420536, 69.01041666325268409, 5.676582343749997150 ) ) ;
#3317 = CARTESIAN_POINT ( 'NONE',  ( -2.765530957081996810, 294.2656250017069510, -6.676582343750003368 ) ) ;
#3318 = CARTESIAN_POINT ( 'NONE',  ( -4.220049686691937474, -10.18810118749999738, 105.8125000020483952 ) ) ;
#3319 = CARTESIAN_POINT ( 'NONE',  ( -9.832129032723418760, 212.8645833299193555, -5.676582343750004256 ) ) ;
#3320 = ORIENTED_EDGE ( 'NONE', *, *, #40150, .T. ) ;
#3321 = CARTESIAN_POINT ( 'NONE',  ( 1.656854249492390574, 203.1875000000000284, 138.0000000000000853 ) ) ;
#3322 = CARTESIAN_POINT ( 'NONE',  ( -27.99999999999999645, 210.0000000000000284, 170.0000000000003695 ) ) ;
#3323 = CARTESIAN_POINT ( 'NONE',  ( 4.999999999999999112, 65.00653492603716188, 24.02639942437878773 ) ) ;
#3325 = CARTESIAN_POINT ( 'NONE',  ( 6.951808397369818766E-16, 197.0312499965860411, -11.35316468750000141 ) ) ;
#3324 = CARTESIAN_POINT ( 'NONE',  ( 27.99999999999997158, 207.0000000000000284, 173.9999999999999147 ) ) ;
#3326 = VECTOR ( 'NONE', #41230, 1000.000000000000114 ) ;
#3327 = FACE_OUTER_BOUND ( 'NONE', #191, .T. ) ;
#3328 = CARTESIAN_POINT ( 'NONE',  ( -9.999999999999998224, 233.3333333401613174, 2.679491924311235618 ) ) ;
#3329 = CARTESIAN_POINT ( 'NONE',  ( -4.000000000000001776, 20.43750000000000000, -1.656854249492381470 ) ) ;
#3330 = ORIENTED_EDGE ( 'NONE', *, *, #26684, .F. ) ;
#3331 = CARTESIAN_POINT ( 'NONE',  ( -9.832129032723418760, 188.1770833299193555, -5.676582343750004256 ) ) ;
#3332 = CARTESIAN_POINT ( 'NONE',  ( 7.188101187499993827, -2.977408999572645598, 12.64280278187175277 ) ) ;
#3333 =( BOUNDED_CURVE ( )  B_SPLINE_CURVE ( 2, ( #70420, #48130, #7417, #19459, #1765, #8893, #31906, #13780, #30424 ),
 .UNSPECIFIED., .F., .F. ) 
 B_SPLINE_CURVE_WITH_KNOTS ( ( 3, 2, 2, 2, 3 ),
 ( 0.6979166666666667407, 0.7031250000000001110, 0.7083333333333334814, 0.7135416666666667407, 0.7187500000000001110 ),
 .UNSPECIFIED. ) 
 CURVE ( )  GEOMETRIC_REPRESENTATION_ITEM ( )  RATIONAL_B_SPLINE_CURVE ( ( 0.9999999999999983347, 0.9238795325112884038, 1.000000000000000000, 0.9238795325112867385, 1.000000000000000000, 0.9238795325112867385, 1.000000000000000000, 0.9238795325112850731, 1.000000000000001554 ) ) 
 REPRESENTATION_ITEM ( '' )  );
#3334 = DIRECTION ( 'NONE',  ( -0.000000000000000000, -0.000000000000000000, -1.000000000000000000 ) ) ;
#3335 = ORIENTED_EDGE ( 'NONE', *, *, #39276, .T. ) ;
#3336 = CARTESIAN_POINT ( 'NONE',  ( 8.000000000000001776, 98.84375000409677625, 3.313708498984759387 ) ) ;
#3337 = CARTESIAN_POINT ( 'NONE',  ( 7.320508075688771044, 4.374999999999999112, 7.320508075688775484 ) ) ;
#3338 = CARTESIAN_POINT ( 'NONE',  ( 2.828427124746191623, 14.12500000000000000, -2.828427124746191623 ) ) ;
#3339 =( BOUNDED_CURVE ( )  B_SPLINE_CURVE ( 2, ( #17669, #7741, #40686, #51258, #57309, #69359, #74268, #23702, #51633, #16920, #53768, #45597, #34678 ),
 .UNSPECIFIED., .F., .F. ) 
 B_SPLINE_CURVE_WITH_KNOTS ( ( 3, 2, 2, 2, 2, 2, 3 ),
 ( 0.3750000000000000000, 0.3768115942028985588, 0.3786231884057971175, 0.3804347826086956763, 0.3822463768115941796, 0.3840579710144927383, 0.3858695652173912971 ),
 .UNSPECIFIED. ) 
 CURVE ( )  GEOMETRIC_REPRESENTATION_ITEM ( )  RATIONAL_B_SPLINE_CURVE ( ( 1.000000000000000000, 0.9659258262890683122, 1.000000000000000000, 0.9659258262890683122, 1.000000000000000000, 0.9659258262890683122, 1.000000000000000000, 0.9659258262890683122, 1.000000000000000000, 0.9659258262890683122, 1.000000000000000000, 0.9659258262890683122, 1.000000000000000000 ) ) 
 REPRESENTATION_ITEM ( '' )  );
#3340 = CARTESIAN_POINT ( 'NONE',  ( -1.881053915767124440, 16.99999999863440436, 4.541265875000001451 ) ) ;
#3341 = CARTESIAN_POINT ( 'NONE',  ( -7.999999999999991118, 0.000000000000000000, 11.51780278392014445 ) ) ;
#3343 = EDGE_CURVE ( 'NONE', #34934, #9708, #10102, .T. ) ;
#3342 = ORIENTED_EDGE ( 'NONE', *, *, #46210, .T. ) ;
#3344 = CARTESIAN_POINT ( 'NONE',  ( 4.999999999999999112, -11.44657803507905491, -68.01244171956638240 ) ) ;
#3345 = CARTESIAN_POINT ( 'NONE',  ( -5.082755093536324154, 91.34375000204838102, 5.082755093536326818 ) ) ;
#3348 = CARTESIAN_POINT ( 'NONE',  ( 4.000000000000016875, 197.4375000000000284, 199.6568542494924259 ) ) ;
#3347 = CARTESIAN_POINT ( 'NONE',  ( -5.676582343750000703, 253.0729166700807014, -9.832129032723418760 ) ) ;
#3346 = DIRECTION ( 'NONE',  ( -0.000000000000000000, 1.000000000000000000, -4.476705744456276341E-16 ) ) ;
#3349 = DIRECTION ( 'NONE',  ( 1.000000000000000000, 0.000000000000000000, 0.000000000000000000 ) ) ;
#3350 = VERTEX_POINT ( 'NONE', #16108 ) ;
#3351 = ADVANCED_FACE ( 'NONE', ( #62149 ), #22902, .T. ) ;
#3352 = DIRECTION ( 'NONE',  ( 0.000000000000000000, 0.000000000000000000, 1.000000000000000000 ) ) ;
#3353 = CARTESIAN_POINT ( 'NONE',  ( 2.977408999572646486, 7.188101187499991163, 19.01780278187175810 ) ) ;
#3354 = ORIENTED_EDGE ( 'NONE', *, *, #12254, .F. ) ;
#3355 = ORIENTED_EDGE ( 'NONE', *, *, #72758, .F. ) ;
#3356 = CARTESIAN_POINT ( 'NONE',  ( 7.204075437095966983, 7.204075437095967871, 79.09375000204838102 ) ) ;
#3357 = CARTESIAN_POINT ( 'NONE',  ( 3.042071309553159519, 70.05208332991934128, 11.35316468750000141 ) ) ;
#3358 = CARTESIAN_POINT ( 'NONE',  ( -7.999999999999998224, 105.7812500040967905, 3.313708498984766049 ) ) ;
#3359 = CARTESIAN_POINT ( 'NONE',  ( -11.00000000000000000, 4.556349186104045934, 89.40625000000000000 ) ) ;
#3362 = CARTESIAN_POINT ( 'NONE',  ( 6.676582343750003368, 296.0468750017069510, 2.765530957081995478 ) ) ;
#3361 = CARTESIAN_POINT ( 'NONE',  ( 31.99999999999999289, 198.3750000027312126, 169.9999999999998863 ) ) ;
#3360 = CARTESIAN_POINT ( 'NONE',  ( 2.849036369511732440E-14, 206.2500000000000284, 202.0000000000000000 ) ) ;
#3363 = DIRECTION ( 'NONE',  ( 0.000000000000000000, 0.000000000000000000, 1.000000000000000000 ) ) ;
#3364 = DIRECTION ( 'NONE',  ( 0.000000000000000000, -6.938893903907228378E-16, -1.000000000000000000 ) ) ;
#3365 = ADVANCED_FACE ( 'NONE', ( #74588, #73840 ), #73467, .T. ) ;
#3366 = AXIS2_PLACEMENT_3D ( 'NONE', #61936, #27600, #50611 ) ;
#3367 = CARTESIAN_POINT ( 'NONE',  ( -3.458734124999960358, 197.6875000013655779, 198.0000000000000284 ) ) ;
#3368 = CARTESIAN_POINT ( 'NONE',  ( 1.656854249492416109, 199.1875000000000000, 138.0000000000000853 ) ) ;
#3369 = CARTESIAN_POINT ( 'NONE',  ( 5.656854249492380582, 1.499999995903219974, -5.656854249492380582 ) ) ;
#3370 = CARTESIAN_POINT ( 'NONE',  ( 24.54126587499999346, 200.1875000013656063, 169.9999999999998863 ) ) ;
#3371 = CARTESIAN_POINT ( 'NONE',  ( -7.188101187500001821, 13.49999999795161187, -2.977408999572651371 ) ) ;
#3372 = CARTESIAN_POINT ( 'NONE',  ( -3.313708498984758943, -7.999999999999989342, 26.79905278392014623 ) ) ;
#3373 = CARTESIAN_POINT ( 'NONE',  ( 2.775557561562891351E-14, 195.0000000000000000, 198.0000000000000284 ) ) ;
#3374 = CARTESIAN_POINT ( 'NONE',  ( 2.977408999572654480, 108.5000000020483810, 7.188101187499999156 ) ) ;
#3376 = CARTESIAN_POINT ( 'NONE',  ( 3.728321214240318149, -56.13798660958080688, -44.08488161416449458 ) ) ;
#3375 = CARTESIAN_POINT ( 'NONE',  ( 6.000000000000003553, 289.6250000034140157, -2.485281374238571761 ) ) ;
#3377 = CARTESIAN_POINT ( 'NONE',  ( -11.00000000000000000, 0.000000000000000000, 118.0000000000000000 ) ) ;
#3378 = DIRECTION ( 'NONE',  ( 0.000000000000000000, 0.000000000000000000, -1.000000000000000000 ) ) ;
#3379 = CARTESIAN_POINT ( 'NONE',  ( -5.082755093536319713, 5.082755093536319713, 13.67405278187175455 ) ) ;
#3380 = CARTESIAN_POINT ( 'NONE',  ( -4.000000000000015987, 206.5625000027312126, 140.3431457505076594 ) ) ;
#3381 = CARTESIAN_POINT ( 'NONE',  ( -3.042071309553164404, 42.23958332991934128, -11.35316468749999963 ) ) ;
#3382 = CARTESIAN_POINT ( 'NONE',  ( 0.000000000000000000, 300.0000000000000000, 10.00000000000000178 ) ) ;
#3383 = CARTESIAN_POINT ( 'NONE',  ( 10.00000000000000178, 12.08333332650536462, -2.679491924311226736 ) ) ;
#3384 = CARTESIAN_POINT ( 'NONE',  ( -32.00000000000002842, 200.3125000027312126, 168.3431457505080857 ) ) ;
#3385 = ORIENTED_EDGE ( 'NONE', *, *, #49128, .T. ) ;
#3386 = DIRECTION ( 'NONE',  ( 0.000000000000000000, 0.000000000000000000, 1.000000000000000000 ) ) ;
#3387 = CARTESIAN_POINT ( 'NONE',  ( 8.000000000000012434, 3.313708498984737183, 18.17405277982336997 ) ) ;
#3388 = CARTESIAN_POINT ( 'NONE',  ( 11.35316468749999963, 45.98958332991934128, -3.042071309553165293 ) ) ;
#3389 = VECTOR ( 'NONE', #27820, 1000.000000000000227 ) ;
#3390 = CARTESIAN_POINT ( 'NONE',  ( 7.778174593052021635, 7.778174593052023411, 80.12500000409677625 ) ) ;
#3391 = CARTESIAN_POINT ( 'NONE',  ( -2.754378923186476579E-14, 205.4375000013656063, 145.4587341250000350 ) ) ;
#3392 = LINE ( 'NONE', #61099, #66102 ) ;
#3393 = LINE ( 'NONE', #54337, #61214 ) ;
#3395 = CARTESIAN_POINT ( 'NONE',  ( 9.832129032723420536, 36.19791666325267698, -5.676582343749999815 ) ) ;
#3394 = CARTESIAN_POINT ( 'NONE',  ( -7.188101187500000044, 101.6562500020483810, 0.000000000000000000 ) ) ;
#3396 = CARTESIAN_POINT ( 'NONE',  ( 7.999999999999991118, 3.313708498984757611, 12.17405277982336642 ) ) ;
#3397 = DIRECTION ( 'NONE',  ( 0.000000000000000000, 0.000000000000000000, 1.000000000000000000 ) ) ;
#3398 = CARTESIAN_POINT ( 'NONE',  ( 5.676582343750001591, 166.6145833299193555, -9.832129032723420536 ) ) ;
#3399 = CARTESIAN_POINT ( 'NONE',  ( 7.320508075688774596, 127.4999999931720396, -7.320508075688774596 ) ) ;
#3400 = CARTESIAN_POINT ( 'NONE',  ( -5.082755093536324154, 108.2187500020483810, 5.082755093536326818 ) ) ;
#3401 = EDGE_LOOP ( 'NONE', ( #24639, #63539, #3626 ) ) ;
#3402 = FACE_OUTER_BOUND ( 'NONE', #12420, .T. ) ;
#3403 = CARTESIAN_POINT ( 'NONE',  ( 11.35316468749999785, 25.88541666325268764, 3.042071309553174174 ) ) ;
#3404 = CARTESIAN_POINT ( 'NONE',  ( 0.000000000000000000, 300.0000000000000000, 10.00000000000000178 ) ) ;
#3405 = ORIENTED_EDGE ( 'NONE', *, *, #68581, .T. ) ;
#3406 = CARTESIAN_POINT ( 'NONE',  ( 10.99999999999999645, -10.99999999999999645, 41.99999999999999289 ) ) ;
#3407 = CARTESIAN_POINT ( 'NONE',  ( -10.18810118749999916, 0.000000000000000000, 78.15625000204836681 ) ) ;
#3408 = CARTESIAN_POINT ( 'NONE',  ( -11.00000000000000000, 0.000000000000000000, 118.0000000000000000 ) ) ;
#3410 = CARTESIAN_POINT ( 'NONE',  ( 3.042071309553167513, 146.8229166632526983, -11.35316468749999785 ) ) ;
#3409 = CARTESIAN_POINT ( 'NONE',  ( -7.999985422794280154, -3.313723076190473016, 2.611553367158739647 ) ) ;
#3411 = CARTESIAN_POINT ( 'NONE',  ( 13.99999999999999822, -2.250000000005106138, 10.23492587299426404 ) ) ;
#3412 = CARTESIAN_POINT ( 'NONE',  ( -3.313708498984757167, 7.999999999999991118, 9.605302784329824206 ) ) ;
#3413 = CARTESIAN_POINT ( 'NONE',  ( -2.751064625579944321E-14, 200.7500000000000000, 146.0000000000000284 ) ) ;
#3414 = CARTESIAN_POINT ( 'NONE',  ( 3.042071309553173286, 230.3645833367472733, 11.35316468749999608 ) ) ;
#3415 = CARTESIAN_POINT ( 'NONE',  ( 7.204075437095968759, -7.204075437095966983, 88.09375000204836681 ) ) ;
#3416 = ORIENTED_EDGE ( 'NONE', *, *, #52675, .T. ) ;
#3417 = LINE ( 'NONE', #4176, #4015 ) ;
#3418 = CARTESIAN_POINT ( 'NONE',  ( -9.832129032723418760, 98.17708332991935549, -5.676582343750004256 ) ) ;
#3419 = CARTESIAN_POINT ( 'NONE',  ( 4.220049686691934809, 10.18810118749999916, 95.68750000204838102 ) ) ;
#3420 = CARTESIAN_POINT ( 'NONE',  ( 1.881053915767122664, 20.24999999863440436, 4.541265875000001451 ) ) ;
#3421 = ORIENTED_EDGE ( 'NONE', *, *, #50964, .F. ) ;
#3422 = VERTEX_POINT ( 'NONE', #57249 ) ;
#3423 = CARTESIAN_POINT ( 'NONE',  ( -3.211159895383562723, 3.062499998634407028, 3.211159895383561391 ) ) ;
#3424 = CARTESIAN_POINT ( 'NONE',  ( 2.977408999572650927, 8.249999997951611874, -7.188101187500001821 ) ) ;
#3425 = CARTESIAN_POINT ( 'NONE',  ( 5.656854249492379694, 118.6250000040967905, -5.656854249492380582 ) ) ;
#3426 = CARTESIAN_POINT ( 'NONE',  ( -10.18810118749999916, 4.220049686691934809, 91.93750000204836681 ) ) ;
#3427 = CARTESIAN_POINT ( 'NONE',  ( -29.43265458321766559, 200.7500000013656347, 166.5412658750003629 ) ) ;
#3428 = DIRECTION ( 'NONE',  ( -0.000000000000000000, -0.000000000000000000, -1.000000000000000000 ) ) ;
#3429 = CARTESIAN_POINT ( 'NONE',  ( 1.656854249492381914, 4.812500000000000888, 4.000000000000000888 ) ) ;
#3430 = CARTESIAN_POINT ( 'NONE',  ( -4.000000000000001776, 17.18749999726881228, -1.656854249492381470 ) ) ;
#3431 = CARTESIAN_POINT ( 'NONE',  ( 4.541265875000001451, 5.249999998634407028, 1.881053915767124440 ) ) ;
#3432 = CIRCLE ( 'NONE', #38409, 20.00000000000001066 ) ;
#3433 = VERTEX_POINT ( 'NONE', #10472 ) ;
#3434 = CARTESIAN_POINT ( 'NONE',  ( 3.458734125000015425, 194.9375000013655779, 198.0000000000000284 ) ) ;
#3437 = FACE_OUTER_BOUND ( 'NONE', #32097, .T. ) ;
#3436 = CARTESIAN_POINT ( 'NONE',  ( -24.54126587500002188, 198.2500000013656347, 168.5673454167826435 ) ) ;
#3435 =( BOUNDED_CURVE ( )  B_SPLINE_CURVE ( 2, ( #18804, #11656, #40326, #6747, #52764, #1102, #41446, #64458, #12758 ),
 .UNSPECIFIED., .F., .F. ) 
 B_SPLINE_CURVE_WITH_KNOTS ( ( 3, 2, 2, 2, 3 ),
 ( 0.3522727272727273484, 0.3579545454545455252, 0.3636363636363636465, 0.3693181818181818232, 0.3750000000000000000 ),
 .UNSPECIFIED. ) 
 CURVE ( )  GEOMETRIC_REPRESENTATION_ITEM ( )  RATIONAL_B_SPLINE_CURVE ( ( 0.9999999999999992228, 0.9238795325112875156, 1.000000000000000000, 0.9238795325112867385, 1.000000000000000000, 0.9238795325112867385, 1.000000000000000000, 0.9238795325112867385, 1.000000000000000000 ) ) 
 REPRESENTATION_ITEM ( '' )  );
#3438 =( LENGTH_UNIT ( ) NAMED_UNIT ( * ) SI_UNIT ( .MILLI., .METRE. ) );
#3439 = EDGE_CURVE ( 'NONE', #16735, #46685, #67444, .T. ) ;
#3440 = CARTESIAN_POINT ( 'NONE',  ( 4.541265875000002339, 17.37499999863440436, -1.881053915767121554 ) ) ;
#3441 = CARTESIAN_POINT ( 'NONE',  ( 4.999999999999993783, 71.04166665983869677, 8.660254037844390851 ) ) ;
#3442 = CARTESIAN_POINT ( 'NONE',  ( -5.082755093536319713, 5.082755093536319713, 8.799052781871752771 ) ) ;
#3443 = EDGE_LOOP ( 'NONE', ( #34992, #24925 ) ) ;
#3444 = VERTEX_POINT ( 'NONE', #4445 ) ;
#3445 = CARTESIAN_POINT ( 'NONE',  ( 4.220049686691934809, 10.18810118749999916, 100.1875000020483952 ) ) ;
#3446 = CARTESIAN_POINT ( 'NONE',  ( 4.898587196589412829E-16, 27.18749999590322375, -8.000000000000000000 ) ) ;
#3447 = CARTESIAN_POINT ( 'NONE',  ( -31.45873412500001010, 203.8750000013656063, 168.5673454167827572 ) ) ;
#3448 = CARTESIAN_POINT ( 'NONE',  ( -24.00000000000001066, 202.8125000000000000, 168.3431457505080004 ) ) ;
#3449 = CARTESIAN_POINT ( 'NONE',  ( -3.458734124999959469, 207.7500000013656063, 199.4326545832176691 ) ) ;
#3450 = CARTESIAN_POINT ( 'NONE',  ( -4.898587196589412829E-16, 111.1250000000000000, -8.000000000000000000 ) ) ;
#3451 = CARTESIAN_POINT ( 'NONE',  ( 4.999999999999993783, 104.1666666666666714, 8.660254037844390851 ) ) ;
#3452 = CARTESIAN_POINT ( 'NONE',  ( 3.313708498984760720, 112.5312500000000284, -8.000000000000000000 ) ) ;
#3453 = CARTESIAN_POINT ( 'NONE',  ( -2.765530957081996810, 291.4218750017070079, -6.676582343750003368 ) ) ;
#3454 = CARTESIAN_POINT ( 'NONE',  ( 5.082755093536320601, -5.082755093536318824, 11.42405278187175455 ) ) ;
#3455 = VERTEX_POINT ( 'NONE', #28191 ) ;
#3457 =( BOUNDED_CURVE ( )  B_SPLINE_CURVE ( 2, ( #64499, #52806, #59579, #18841, #54294, #30897, #53914, #1141, #24119 ),
 .UNSPECIFIED., .F., .F. ) 
 B_SPLINE_CURVE_WITH_KNOTS ( ( 3, 2, 2, 2, 3 ),
 ( 0.09375000000000006939, 0.09895833333333339810, 0.1041666666666667407, 0.1093750000000000694, 0.1145833333333333981 ),
 .UNSPECIFIED. ) 
 CURVE ( )  GEOMETRIC_REPRESENTATION_ITEM ( )  RATIONAL_B_SPLINE_CURVE ( ( 0.9999999999999990008, 0.9238795325112877377, 1.000000000000000000, 0.9238795325112867385, 1.000000000000000000, 0.9238795325112867385, 1.000000000000000000, 0.9238795325112857393, 1.000000000000001110 ) ) 
 REPRESENTATION_ITEM ( '' )  );
#3456 = FACE_OUTER_BOUND ( 'NONE', #7297, .T. ) ;
#3458 = EDGE_CURVE ( 'NONE', #19919, #30602, #28564, .T. ) ;
#3459 = CARTESIAN_POINT ( 'NONE',  ( 4.898587196589412829E-16, 21.18749999590322375, -8.000000000000000000 ) ) ;
#3460 = CARTESIAN_POINT ( 'NONE',  ( 1.432654583217607858, 203.6250000013656063, 138.5412658750000787 ) ) ;
#3461 = CARTESIAN_POINT ( 'NONE',  ( 0.000000000000000000, 0.000000000000000000, -19.00000000000000000 ) ) ;
#3463 = CARTESIAN_POINT ( 'NONE',  ( 3.458734124999959469, 202.7500000013655779, 140.5673454167824161 ) ) ;
#3462 = CARTESIAN_POINT ( 'NONE',  ( 0.5213318599189683544, 194.9337052864029545, 145.9075847876785303 ) ) ;
#3464 = CARTESIAN_POINT ( 'NONE',  ( 3.042071309553163960, 257.7604166700806445, -11.35316468749999785 ) ) ;
#3465 = PLANE ( 'NONE',  #74 ) ;
#3466 = CARTESIAN_POINT ( 'NONE',  ( 0.000000000000000000, 0.000000000000000000, 0.000000000000000000 ) ) ;
#3467 = CARTESIAN_POINT ( 'NONE',  ( -8.311093377946836114, 2.656249996586016238, -8.311093377946837890 ) ) ;
#3468 = EDGE_CURVE ( 'NONE', #8618, #74545, #56135, .T. ) ;
#3469 = CARTESIAN_POINT ( 'NONE',  ( -2.977408999572647819, 7.188101187499992051, 3.080302781871751439 ) ) ;
#3470 = CARTESIAN_POINT ( 'NONE',  ( -3.042071309553173730, 194.6354166632526415, 11.35316468749999785 ) ) ;
#3471 = CARTESIAN_POINT ( 'NONE',  ( 11.00000000000000000, 1.347111479062088405E-15, 102.2500000000000000 ) ) ;
#3472 = CARTESIAN_POINT ( 'NONE',  ( 4.541265875000002339, 6.374999998634407028, -1.881053915767121554 ) ) ;
#3473 = DIRECTION ( 'NONE',  ( 1.000000000000000000, 0.000000000000000000, 0.000000000000000000 ) ) ;
#3475 = CARTESIAN_POINT ( 'NONE',  ( 4.242640687119285658, 297.6250000000000000, -4.242640687119286547 ) ) ;
#3474 = FACE_OUTER_BOUND ( 'NONE', #4624, .T. ) ;
#3476 = ORIENTED_EDGE ( 'NONE', *, *, #20343, .F. ) ;
#3477 = CARTESIAN_POINT ( 'NONE',  ( 2.445694354108783219, 204.8125000013656063, 139.5543056458912190 ) ) ;
#3478 = CARTESIAN_POINT ( 'NONE',  ( 8.311093377946837890, 6.406249996586016238, -8.311093377946837890 ) ) ;
#3479 = CARTESIAN_POINT ( 'NONE',  ( 7.778174593052023411, -7.778174593052021635, 100.7500000040967763 ) ) ;
#3480 = CARTESIAN_POINT ( 'NONE',  ( -4.000000000000015987, 205.5000000000000284, 142.0000000000000568 ) ) ;
#3481 = CARTESIAN_POINT ( 'NONE',  ( -28.00000000000007105, 202.4375000013656063, 166.5412658750003629 ) ) ;
#3482 = CARTESIAN_POINT ( 'NONE',  ( -75.00000000000001421, 242.0000000000000284, 20.00000000000003553 ) ) ;
#3484 = CARTESIAN_POINT ( 'NONE',  ( 8.000000000000000000, 119.8437499999999858, -3.313708498984762496 ) ) ;
#3483 = CARTESIAN_POINT ( 'NONE',  ( 2.977408999572650039, 116.1875000020483952, -7.188101187500000933 ) ) ;
#3485 = FACE_OUTER_BOUND ( 'NONE', #69403, .T. ) ;
#3486 = CARTESIAN_POINT ( 'NONE',  ( 3.042071309553167069, 126.8229166632526841, -11.35316468749999785 ) ) ;
#3487 = AXIS2_PLACEMENT_3D ( 'NONE', #41889, #11744, #24164 ) ;
#3488 = CARTESIAN_POINT ( 'NONE',  ( -10.00000000000000355, 94.58333332650535397, 2.679491924311223183 ) ) ;
#3489 = EDGE_CURVE ( 'NONE', #31186, #34923, #56110, .T. ) ;
#3490 = CARTESIAN_POINT ( 'NONE',  ( 7.188101187500001821, 123.8750000020483810, -2.977408999572651371 ) ) ;
#3491 = CARTESIAN_POINT ( 'NONE',  ( 1.881053915767122664, 20.24999999863440436, 4.541265875000001451 ) ) ;
#3492 = CARTESIAN_POINT ( 'NONE',  ( -25.17157287525377640, 204.6250000000000284, 172.8284271247465256 ) ) ;
#3493 = DIRECTION ( 'NONE',  ( -0.000000000000000000, -1.000000000000000000, -4.283267841918042741E-17 ) ) ;
#3494 = ORIENTED_EDGE ( 'NONE', *, *, #22892, .F. ) ;
#3495 = CARTESIAN_POINT ( 'NONE',  ( 27.99999999999999645, 210.0000000000000284, 169.9999999999999147 ) ) ;
#3496 = CARTESIAN_POINT ( 'NONE',  ( -2.765530957081996810, 295.4218750017069510, -6.676582343750003368 ) ) ;
#3497 = CARTESIAN_POINT ( 'NONE',  ( 1.836970198721029589E-15, 229.3750000068279746, 10.00000000000000000 ) ) ;
#3498 = CARTESIAN_POINT ( 'NONE',  ( 3.313708498984756279, 7.999999999999991118, 2.049052783920143117 ) ) ;
#3499 = CARTESIAN_POINT ( 'NONE',  ( 3.042071309553167069, 166.8229166632526699, -11.35316468749999785 ) ) ;
#3500 = CARTESIAN_POINT ( 'NONE',  ( 2.828427124746152987, 198.1250000000000284, 139.1715728752538723 ) ) ;
#3501 = CARTESIAN_POINT ( 'NONE',  ( 6.123233995736767268E-16, 203.1249999931720538, -10.00000000000000178 ) ) ;
#3502 = DIRECTION ( 'NONE',  ( -1.000000000000000000, 0.000000000000000000, 0.000000000000000000 ) ) ;
#3503 = CARTESIAN_POINT ( 'NONE',  ( 7.204075437095968759, -7.204075437095966983, 101.5937500020483668 ) ) ;
#3504 = VERTEX_POINT ( 'NONE', #68555 ) ;
#3505 = CARTESIAN_POINT ( 'NONE',  ( -11.35316468749999963, 219.0625000034139873, 0.000000000000000000 ) ) ;
#3506 = CARTESIAN_POINT ( 'NONE',  ( -11.35316468750000141, 153.5937499965860127, -1.390361679473963753E-15 ) ) ;
#3507 = CARTESIAN_POINT ( 'NONE',  ( -3.458734124999959914, 196.3750000013656063, 196.5673454167823877 ) ) ;
#3508 = CARTESIAN_POINT ( 'NONE',  ( 3.458734125000015425, 205.2500000013655779, 196.5673454167823877 ) ) ;
#3509 = CARTESIAN_POINT ( 'NONE',  ( -10.18810118749999738, -4.220049686691941915, 68.12500000204838102 ) ) ;
#3510 = CARTESIAN_POINT ( 'NONE',  ( -11.35316468749999785, 63.38541666325269119, -3.042071309553167513 ) ) ;
#3511 = ORIENTED_EDGE ( 'NONE', *, *, #49252, .T. ) ;
#3512 = CARTESIAN_POINT ( 'NONE',  ( -4.220049686691935698, 10.18810118749999916, 110.8750000020483810 ) ) ;
#3513 = CARTESIAN_POINT ( 'NONE',  ( -3.211159895383561391, 7.812499998634407028, -3.211159895383561835 ) ) ;
#3514 = EDGE_LOOP ( 'NONE', ( #9765, #9260, #46273, #7213 ) ) ;
#3515 = EDGE_CURVE ( 'NONE', #67659, #32201, #60943, .T. ) ;
#3516 = CARTESIAN_POINT ( 'NONE',  ( -5.082755093536326818, 23.90624999795161543, 5.082755093536325042 ) ) ;
#3517 = CARTESIAN_POINT ( 'NONE',  ( 6.123233995736767268E-16, 108.1249999931720396, -10.00000000000000178 ) ) ;
#3518 = DIRECTION ( 'NONE',  ( -0.000000000000000000, 1.000000000000000000, -4.476705744456276341E-16 ) ) ;
#3519 = CARTESIAN_POINT ( 'NONE',  ( -7.188101187500001821, 16.49999999795161543, -2.977408999572651371 ) ) ;
#3520 = CARTESIAN_POINT ( 'NONE',  ( 7.188101187499993827, -2.977408999572645598, 2.142802781871750550 ) ) ;
#3521 = EDGE_CURVE ( 'NONE', #60057, #64023, #33564, .T. ) ;
#3522 = CARTESIAN_POINT ( 'NONE',  ( -10.18810118749999738, -4.220049686691941915, 111.6250000020483810 ) ) ;
#3523 = EDGE_CURVE ( 'NONE', #1216, #41579, #14846, .T. ) ;
#3524 = FACE_OUTER_BOUND ( 'NONE', #54933, .T. ) ;
#3525 = CARTESIAN_POINT ( 'NONE',  ( 2.449293598294707893E-16, 5.999999997268813168, -4.000000000000001776 ) ) ;
#3526 = CYLINDRICAL_SURFACE ( 'NONE', #26565, 3.999999999999976019 ) ;
#3527 = ORIENTED_EDGE ( 'NONE', *, *, #73874, .F. ) ;
#3528 = CARTESIAN_POINT ( 'NONE',  ( -1.432654583217607858, 208.6250000013655779, 201.4587341250000065 ) ) ;
#3529 = CARTESIAN_POINT ( 'NONE',  ( -31.99999999999999289, 194.3750000027311842, 170.0000000000004547 ) ) ;
#3530 = CARTESIAN_POINT ( 'NONE',  ( 4.541265875000001451, 8.249999998634406140, 1.881053915767124440 ) ) ;
#3531 = AXIS2_PLACEMENT_3D ( 'NONE', #34559, #22085, #27749 ) ;
#3532 = CARTESIAN_POINT ( 'NONE',  ( 7.999999999999991118, 9.797174393178815797E-16, 10.58030277982336465 ) ) ;
#3533 = CARTESIAN_POINT ( 'NONE',  ( 5.082755093536318824, 5.082755093536319713, 26.42405278187175455 ) ) ;
#3534 = VERTEX_POINT ( 'NONE', #9955 ) ;
#3535 = CARTESIAN_POINT ( 'NONE',  ( -3.673940397442060854E-16, 299.7500000000000000, -6.000000000000001776 ) ) ;
#3536 = ORIENTED_EDGE ( 'NONE', *, *, #16971, .F. ) ;
#3537 = CARTESIAN_POINT ( 'NONE',  ( 10.18810118750000093, -4.220049686691933033, 116.3125000020483810 ) ) ;
#3538 = CARTESIAN_POINT ( 'NONE',  ( 11.00000000000010836, -4.556349186103939353, 84.34375000409677625 ) ) ;
#3539 = CARTESIAN_POINT ( 'NONE',  ( 1.432654583217664479, 205.7500000013656063, 201.4587341250000065 ) ) ;
#3540 = CARTESIAN_POINT ( 'NONE',  ( 27.99999999999996803, 199.9375000013656063, 166.5412658749999082 ) ) ;
#3541 = CARTESIAN_POINT ( 'NONE',  ( -4.999999999999998224, 61.66666666666667140, -8.660254037844389075 ) ) ;
#3542 = AXIS2_PLACEMENT_3D ( 'NONE', #53540, #18464, #64490 ) ;
#3543 = CARTESIAN_POINT ( 'NONE',  ( -2.977408999572651815, 91.81250000204839523, 7.188101187500000933 ) ) ;
#3544 = CARTESIAN_POINT ( 'NONE',  ( 6.000000000000003553, 292.5624999999999432, -2.485281374238571761 ) ) ;
#3546 = CARTESIAN_POINT ( 'NONE',  ( -10.00000000000000533, 127.2916666666666572, -2.679491924311232065 ) ) ;
#3545 = CARTESIAN_POINT ( 'NONE',  ( 25.17157287525382259, 208.0000000027312126, 172.8284271247460993 ) ) ;
#3547 = VERTEX_POINT ( 'NONE', #50308 ) ;
#3548 = CARTESIAN_POINT ( 'NONE',  ( 3.313708498984782924, 8.531249995903223748, 7.999999999999979572 ) ) ;
#3549 = ADVANCED_FACE ( 'NONE', ( #55989 ), #60510, .T. ) ;
#3550 = CARTESIAN_POINT ( 'NONE',  ( -5.086519500874237210, -10.26068667857087213, 64.41585657734346171 ) ) ;
#3551 = CARTESIAN_POINT ( 'NONE',  ( 1.656854249492348607, 198.3125000027312126, 138.0000000000000568 ) ) ;
#3552 = CARTESIAN_POINT ( 'NONE',  ( -1.970469249063935269E-15, 20.78460969082654231, -20.69999999999999929 ) ) ;
#3553 = CARTESIAN_POINT ( 'NONE',  ( -4.556349186104048599, -10.99999999999999822, 94.28124999999998579 ) ) ;
#3554 = CARTESIAN_POINT ( 'NONE',  ( -8.660254037844385522, 255.4166666666666856, 5.000000000000004441 ) ) ;
#3555 = DIRECTION ( 'NONE',  ( 0.000000000000000000, 0.000000000000000000, 1.000000000000000000 ) ) ;
#3556 =( BOUNDED_CURVE ( )  B_SPLINE_CURVE ( 2, ( #67198, #10226, #33626, #44557, #22271, #33254, #15496, #57000, #27568 ),
 .UNSPECIFIED., .F., .F. ) 
 B_SPLINE_CURVE_WITH_KNOTS ( ( 3, 2, 2, 2, 3 ),
 ( 0.3000000000000002109, 0.3083333333333335702, 0.3166666666666669294, 0.3250000000000002887, 0.3333333333333336479 ),
 .UNSPECIFIED. ) 
 CURVE ( )  GEOMETRIC_REPRESENTATION_ITEM ( )  RATIONAL_B_SPLINE_CURVE ( ( 0.9999999999999980016, 0.9238795325112887369, 1.000000000000000000, 0.9238795325112867385, 1.000000000000000000, 0.9238795325112867385, 1.000000000000000000, 0.9238795325112837409, 1.000000000000003109 ) ) 
 REPRESENTATION_ITEM ( '' )  );
#3557 = CARTESIAN_POINT ( 'NONE',  ( -4.999999999999998224, 191.6666666666666856, -8.660254037844389075 ) ) ;
#3558 = CARTESIAN_POINT ( 'NONE',  ( -7.778174593052020747, -7.778174593052023411, 110.6875000000000000 ) ) ;
#3559 = CARTESIAN_POINT ( 'NONE',  ( 1.320432766682872962E-15, -7.188101187499992051, 21.73655278187175455 ) ) ;
#3560 = CARTESIAN_POINT ( 'NONE',  ( 11.35316468749999785, 155.8854166632526699, 3.042071309553174174 ) ) ;
#3561 = CARTESIAN_POINT ( 'NONE',  ( 0.000000000000000000, 0.000000000000000000, 118.0000000000000000 ) ) ;
#3562 = CARTESIAN_POINT ( 'NONE',  ( -5.000000000000000000, 53.35645474066748051, 47.33026262608808565 ) ) ;
#3563 = DIRECTION ( 'NONE',  ( -0.000000000000000000, -1.000000000000000000, -0.000000000000000000 ) ) ;
#3566 = DIRECTION ( 'NONE',  ( -1.000000000000000000, 0.000000000000000000, 0.000000000000000000 ) ) ;
#3565 = CARTESIAN_POINT ( 'NONE',  ( 1.224646799147353454E-15, 300.0000000000000000, -10.00000000000000178 ) ) ;
#3564 = CARTESIAN_POINT ( 'NONE',  ( 31.99999999999999289, 201.2500000000000000, 169.9999999999999432 ) ) ;
#3567 = VERTEX_POINT ( 'NONE', #8835 ) ;
#3568 = CARTESIAN_POINT ( 'NONE',  ( 9.832129032723416984, 20.67708332991935194, 5.676582343750006032 ) ) ;
#3569 = CARTESIAN_POINT ( 'NONE',  ( 10.00000000000000000, 96.66666665983871098, 2.679491924311235618 ) ) ;
#3571 = CARTESIAN_POINT ( 'NONE',  ( 10.00000000000000000, 31.66666665983870033, 2.679491924311235618 ) ) ;
#3570 = CARTESIAN_POINT ( 'NONE',  ( 3.313708498984756279, 7.999999999999991118, 17.04905278392014623 ) ) ;
#3572 = FACE_OUTER_BOUND ( 'NONE', #74054, .T. ) ;
#3573 = CARTESIAN_POINT ( 'NONE',  ( -1.432654583217664479, 204.7500000013655779, 138.5412658750000787 ) ) ;
#3574 = CARTESIAN_POINT ( 'NONE',  ( -1.836970198721029983E-15, 50.62499999317203248, 10.00000000000000178 ) ) ;
#3575 = CARTESIAN_POINT ( 'NONE',  ( -7.188101187500000044, 110.6562500020483810, 0.000000000000000000 ) ) ;
#3576 = CARTESIAN_POINT ( 'NONE',  ( -3.211159895383561391, 9.812499998634406140, -3.211159895383561835 ) ) ;
#3577 = CARTESIAN_POINT ( 'NONE',  ( 5.000000000000000000, 219.1666666666666856, 8.660254037844401509 ) ) ;
#3578 = CARTESIAN_POINT ( 'NONE',  ( 1.469576158976822172E-15, -7.999999999999991118, 11.70530277982336642 ) ) ;
#3579 = CARTESIAN_POINT ( 'NONE',  ( -2.841757666793576517E-14, 194.6037658790967271, 138.3962341209032445 ) ) ;
#3580 = ORIENTED_EDGE ( 'NONE', *, *, #67238, .F. ) ;
#3581 = EDGE_LOOP ( 'NONE', ( #293, #43508, #53671, #42316 ) ) ;
#3582 = CARTESIAN_POINT ( 'NONE',  ( -5.000000000000000000, -62.31673578527556145, 23.93255728291356021 ) ) ;
#3583 = CARTESIAN_POINT ( 'NONE',  ( 7.999986417242976877, 3.313722081741772296, 13.86155332737053314 ) ) ;
#3584 = CARTESIAN_POINT ( 'NONE',  ( -22.01899197589878909, -38.36653287508233490, 148.1762431665184465 ) ) ;
#3585 = CARTESIAN_POINT ( 'NONE',  ( 11.35316468749999785, 130.5729166632526983, 3.042071309553174174 ) ) ;
#3586 = EDGE_LOOP ( 'NONE', ( #23027, #55411, #28461, #49599 ) ) ;
#3587 = CARTESIAN_POINT ( 'NONE',  ( -4.999999999999999112, 13.57248045702108818, -69.64920683919132216 ) ) ;
#3588 = CARTESIAN_POINT ( 'NONE',  ( 10.18810118749999916, 1.247682550866122264E-15, 95.40625000204836681 ) ) ;
#3589 = CARTESIAN_POINT ( 'NONE',  ( -7.999999999999998224, 93.59375000000000000, 3.313708498984766049 ) ) ;
#3590 = CARTESIAN_POINT ( 'NONE',  ( 4.000000000000015987, 209.4375000000000284, 199.6568542494924259 ) ) ;
#3591 = CARTESIAN_POINT ( 'NONE',  ( 0.000000000000000000, 125.0000000000000000, 8.000000000000000000 ) ) ;
#3592 = CARTESIAN_POINT ( 'NONE',  ( 5.676582343750001591, 121.6145833299193555, -9.832129032723420536 ) ) ;
#3593 = CARTESIAN_POINT ( 'NONE',  ( 11.00000000000000000, 1.347111479062088405E-15, 96.24999999999998579 ) ) ;
#3594 = ORIENTED_EDGE ( 'NONE', *, *, #68852, .F. ) ;
#3595 = VECTOR ( 'NONE', #33703, 1000.000000000000000 ) ;
#3596 = CARTESIAN_POINT ( 'NONE',  ( 3.999982273345623174, 89.99927424231840689, -6.928213464733948612 ) ) ;
#3597 = CARTESIAN_POINT ( 'NONE',  ( 49.04219544972652045, 44.16163007259360285, 59.49880266147246033 ) ) ;
#3598 = CARTESIAN_POINT ( 'NONE',  ( -2.085542519210945728E-15, 119.8437499965860269, 11.35316468750000141 ) ) ;
#3599 = CARTESIAN_POINT ( 'NONE',  ( -2.445694354108782775, 206.5625000013656063, 200.4456943541088663 ) ) ;
#3600 = CARTESIAN_POINT ( 'NONE',  ( 5.082755093536325930, 17.53124999795161543, -5.082755093536325930 ) ) ;
#3601 = CARTESIAN_POINT ( 'NONE',  ( 4.220049686691941027, -10.18810118749999738, 82.00000000204838102 ) ) ;
#3602 = CARTESIAN_POINT ( 'NONE',  ( 3.042071309553167069, 22.13541666325268409, -11.35316468749999785 ) ) ;
#3603 = EDGE_LOOP ( 'NONE', ( #25086, #65949, #20405, #65687, #67874, #65968 ) ) ;
#3604 = CARTESIAN_POINT ( 'NONE',  ( -2.775557561562891351E-14, 210.0000000000000284, 146.0000000000000284 ) ) ;
#3605 = CARTESIAN_POINT ( 'NONE',  ( -8.008118988124991233, 0.000000000000000000, 28.01311528394063188 ) ) ;
#3606 = CARTESIAN_POINT ( 'NONE',  ( -3.458734125000016757, 209.1250000013656631, 140.5673454167824161 ) ) ;
#3607 = AXIS2_PLACEMENT_3D ( 'NONE', #4342, #27711, #71864 ) ;
#3608 = CARTESIAN_POINT ( 'NONE',  ( 0.000000000000000000, 0.000000000000000000, 118.0000000000000000 ) ) ;
#3609 = CARTESIAN_POINT ( 'NONE',  ( -7.188101187500001821, 2.624999997951610542, -2.977408999572651371 ) ) ;
#3610 = CARTESIAN_POINT ( 'NONE',  ( -4.721056650415999201, 290.3281250017069510, -4.721056650415999201 ) ) ;
#3611 = CARTESIAN_POINT ( 'NONE',  ( -2.485281374238947016, 296.8125000000000568, -5.999999999999626965 ) ) ;
#3612 = CARTESIAN_POINT ( 'NONE',  ( 0.000000000000000000, 300.0000000000000000, 0.000000000000000000 ) ) ;
#3613 = ADVANCED_FACE ( 'NONE', ( #54869 ), #60135, .T. ) ;
#3614 = VERTEX_POINT ( 'NONE', #72583 ) ;
#3615 = CARTESIAN_POINT ( 'NONE',  ( 8.311093377946837890, 141.7187499965859843, -8.311093377946837890 ) ) ;
#3616 = CARTESIAN_POINT ( 'NONE',  ( 4.220049686691941027, -10.18810118749999738, 81.62500000204836681 ) ) ;
#3617 = CARTESIAN_POINT ( 'NONE',  ( -31.45873412499999233, 197.6875000013655779, 170.0000000000003979 ) ) ;
#3618 = EDGE_CURVE ( 'NONE', #54736, #47864, #58539, .T. ) ;
#3619 = CARTESIAN_POINT ( 'NONE',  ( -7.778174593052023411, 7.778174593052023411, 110.3125000000000000 ) ) ;
#3620 = CARTESIAN_POINT ( 'NONE',  ( -4.541265875000002339, 15.87499999863440436, -1.881053915767121998 ) ) ;
#3621 = ORIENTED_EDGE ( 'NONE', *, *, #13197, .F. ) ;
#3622 = CARTESIAN_POINT ( 'NONE',  ( 1.656854249492405451, 204.4375000027311842, 202.0000000000000284 ) ) ;
#3623 = CARTESIAN_POINT ( 'NONE',  ( 2.828427124746153876, 208.8750000000000284, 144.8284271247462129 ) ) ;
#3624 = CARTESIAN_POINT ( 'NONE',  ( -24.00000000000002487, 203.9375000027311842, 168.3431457505079152 ) ) ;
#3625 = CARTESIAN_POINT ( 'NONE',  ( -7.999999999999991118, 0.000000000000000000, 14.33030277982336465 ) ) ;
#3626 = ORIENTED_EDGE ( 'NONE', *, *, #24136, .F. ) ;
#3627 = CARTESIAN_POINT ( 'NONE',  ( 2.977408999572652260, 9.187499997951610098, 7.188101187500000044 ) ) ;
#3628 = CARTESIAN_POINT ( 'NONE',  ( 11.00000000000000000, 1.347111479062088405E-15, 76.74999999999998579 ) ) ;
#3629 = DIRECTION ( 'NONE',  ( -6.409875649288994867E-15, 0.000000000000000000, -1.000000000000000000 ) ) ;
#3630 = CARTESIAN_POINT ( 'NONE',  ( -8.311093377946836114, 192.6562499965860127, -8.311093377946837890 ) ) ;
#3631 = CARTESIAN_POINT ( 'NONE',  ( 7.188101187500001821, 113.3750000020483810, -2.977408999572651371 ) ) ;
#3632 = CARTESIAN_POINT ( 'NONE',  ( -0.7010234751563706457, 22.00000000000001066, -4.000757560460977302 ) ) ;
#3633 = CARTESIAN_POINT ( 'NONE',  ( -6.676582343750001591, 289.4531250017069510, 0.000000000000000000 ) ) ;
#3635 = CARTESIAN_POINT ( 'NONE',  ( -10.00000000000000711, 67.70833333333334281, 2.679491924311224071 ) ) ;
#3634 = CARTESIAN_POINT ( 'NONE',  ( -11.35316468749999608, 224.1145833367473301, 3.042071309553173730 ) ) ;
#3636 = ORIENTED_EDGE ( 'NONE', *, *, #15752, .F. ) ;
#3637 = CARTESIAN_POINT ( 'NONE',  ( -11.35316468749999785, 258.6979166700807014, -3.042071309553164848 ) ) ;
#3638 = CARTESIAN_POINT ( 'NONE',  ( -2.977408999572648707, -7.188101187499990274, 23.14280278187176165 ) ) ;
#3639 = CYLINDRICAL_SURFACE ( 'NONE', #48602, 3.999999999999976019 ) ;
#3640 = CYLINDRICAL_SURFACE ( 'NONE', #40589, 37.00000000000000711 ) ;
#3641 = CARTESIAN_POINT ( 'NONE',  ( 1.877992804783702008, -65.87054549412334836, -26.34444121135540939 ) ) ;
#3642 = CARTESIAN_POINT ( 'NONE',  ( -2.445694354108783219, 197.8125000013656063, 200.4456943541088663 ) ) ;
#3643 = DIRECTION ( 'NONE',  ( 0.000000000000000000, 0.000000000000000000, -1.000000000000000000 ) ) ;
#3644 = CARTESIAN_POINT ( 'NONE',  ( -5.656854249492378806, 93.68750000000000000, 5.656854249492381470 ) ) ;
#3645 = CARTESIAN_POINT ( 'NONE',  ( 8.311093377946837890, 116.7187499965859985, -8.311093377946837890 ) ) ;
#3646 = CARTESIAN_POINT ( 'NONE',  ( 23.99999999999998934, 205.7500000000000284, 169.9999999999998863 ) ) ;
#3647 = CARTESIAN_POINT ( 'NONE',  ( 11.00000000000000000, 4.556349186104045934, 70.84374999999997158 ) ) ;
#3648 = AXIS2_PLACEMENT_3D ( 'NONE', #73612, #61178, #73247 ) ;
#3651 = CARTESIAN_POINT ( 'NONE',  ( 2.485281374238163199, 298.6875000000000000, -6.000000000000410338 ) ) ;
#3650 = CARTESIAN_POINT ( 'NONE',  ( 27.99999999999996803, 200.9375000013656063, 166.5412658749999082 ) ) ;
#3649 = CARTESIAN_POINT ( 'NONE',  ( 24.54126587499999346, 200.4375000013656063, 169.9999999999998863 ) ) ;
#3652 = ORIENTED_EDGE ( 'NONE', *, *, #7614, .F. ) ;
#3653 = CONICAL_SURFACE ( 'NONE', #14450, 5.009999999999998899, 0.9599310885968824758 ) ;
#3654 = CARTESIAN_POINT ( 'NONE',  ( -18.00000000000000000, -10.39230484541329425, -21.50000000000000000 ) ) ;
#3655 = CARTESIAN_POINT ( 'NONE',  ( 2.020667218593132706E-15, -11.00000000000000000, 114.0625000040967763 ) ) ;
#3656 = CARTESIAN_POINT ( 'NONE',  ( 3.458734124999959914, 196.4375000013655779, 142.0000000000000568 ) ) ;
#3657 = CARTESIAN_POINT ( 'NONE',  ( 26.56734541678238060, 198.2500000013656347, 166.5412658749999650 ) ) ;
#3658 = CARTESIAN_POINT ( 'NONE',  ( -7.188101187500002709, 27.18749999795162609, 2.977408999572649151 ) ) ;
#3659 = CARTESIAN_POINT ( 'NONE',  ( -3.042071309553164404, 212.5520833299193839, -11.35316468749999963 ) ) ;
#3660 = LINE ( 'NONE', #38368, #67135 ) ;
#3661 = CARTESIAN_POINT ( 'NONE',  ( 11.27292232226671054, 225.9999999999999432, 1.347431162485829281 ) ) ;
#3662 = CARTESIAN_POINT ( 'NONE',  ( 4.541265875000002339, 17.37499999863440436, -1.881053915767121554 ) ) ;
#3663 = CARTESIAN_POINT ( 'NONE',  ( 28.00000000000001776, 195.1875000013655779, 166.5412658749999082 ) ) ;
#3664 = CARTESIAN_POINT ( 'NONE',  ( 7.188101187499993827, -2.977408999572645598, 1.017802781871753215 ) ) ;
#3666 = CARTESIAN_POINT ( 'NONE',  ( 27.99999999999996447, 198.0000000000000000, 173.9999999999999147 ) ) ;
#3665 = CARTESIAN_POINT ( 'NONE',  ( 2.679491924311810269, 183.9583333333334281, 9.999999999999657163 ) ) ;
#3667 = CARTESIAN_POINT ( 'NONE',  ( 5.676582343749993598, 79.94791666325269830, 9.832129032723422313 ) ) ;
#3668 = ORIENTED_EDGE ( 'NONE', *, *, #23453, .F. ) ;
#3669 = EDGE_CURVE ( 'NONE', #49734, #28033, #2803, .T. ) ;
#3670 = DIRECTION ( 'NONE',  ( 0.000000000000000000, 0.000000000000000000, -1.000000000000000000 ) ) ;
#3671 = CARTESIAN_POINT ( 'NONE',  ( 5.082755093536325930, 20.15624999795161543, -5.082755093536325930 ) ) ;
#3672 = CARTESIAN_POINT ( 'NONE',  ( -8.660254037844385522, 223.5416666734946602, 5.000000000000004441 ) ) ;
#3673 = CARTESIAN_POINT ( 'NONE',  ( 8.311093377946834337, 262.3437500034139589, -8.311093377946836114 ) ) ;
#3674 = CARTESIAN_POINT ( 'NONE',  ( -3.042071309553173730, 89.32291666325268409, 11.35316468749999785 ) ) ;
#3675 = ORIENTED_EDGE ( 'NONE', *, *, #42128, .T. ) ;
#3676 = CARTESIAN_POINT ( 'NONE',  ( 6.123233995736767268E-16, 58.12499999317203248, -10.00000000000000178 ) ) ;
#3677 = CARTESIAN_POINT ( 'NONE',  ( -4.220049686691937474, -10.18810118749999738, 112.9375000020483810 ) ) ;
#3678 = CARTESIAN_POINT ( 'NONE',  ( -30.44569435410878810, 195.0625000013656063, 172.4456943541092357 ) ) ;
#3679 = CARTESIAN_POINT ( 'NONE',  ( 2.754378923186476579E-14, 208.4375000013656063, 194.5412658750000219 ) ) ;
#3680 = CARTESIAN_POINT ( 'NONE',  ( 5.656854249492381470, 118.0625000000000000, 5.656854249492379694 ) ) ;
#3682 = CARTESIAN_POINT ( 'NONE',  ( 11.35316468749999963, 90.98958332991935549, -3.042071309553165293 ) ) ;
#3681 = CARTESIAN_POINT ( 'NONE',  ( 2.020667218593132706E-15, -11.00000000000000000, 106.3750000000000000 ) ) ;
#3683 = CARTESIAN_POINT ( 'NONE',  ( -5.656854249492373476, -5.656854249492376141, 16.20530278392014978 ) ) ;
#3684 = CARTESIAN_POINT ( 'NONE',  ( -29.43265458321760519, 202.1250000013656063, 173.4587341250003760 ) ) ;
#3685 = CARTESIAN_POINT ( 'NONE',  ( -30.82842712474624136, 196.2500000027312126, 167.1715728752542418 ) ) ;
#3686 = AXIS2_PLACEMENT_3D ( 'NONE', #69242, #46593, #22088 ) ;
#3687 =( BOUNDED_CURVE ( )  B_SPLINE_CURVE ( 2, ( #54188, #24750, #13783, #47760, #54557, #48502, #70783, #41747, #25115 ),
 .UNSPECIFIED., .F., .F. ) 
 B_SPLINE_CURVE_WITH_KNOTS ( ( 3, 2, 2, 2, 3 ),
 ( 0.2833333333333336590, 0.2916666666666669627, 0.3000000000000002665, 0.3083333333333335702, 0.3166666666666668184 ),
 .UNSPECIFIED. ) 
 CURVE ( )  GEOMETRIC_REPRESENTATION_ITEM ( )  RATIONAL_B_SPLINE_CURVE ( ( 0.9999999999999970024, 0.9238795325112897361, 1.000000000000000000, 0.9238795325112867385, 1.000000000000000000, 0.9238795325112867385, 1.000000000000000000, 0.9238795325112851842, 1.000000000000001554 ) ) 
 REPRESENTATION_ITEM ( '' )  );
#3688 = ADVANCED_FACE ( 'NONE', ( #49184 ), #12805, .F. ) ;
#3689 = EDGE_CURVE ( 'NONE', #58023, #12693, #33137, .T. ) ;
#3690 = CARTESIAN_POINT ( 'NONE',  ( 6.123233995736767268E-16, 178.1249999931720538, -10.00000000000000178 ) ) ;
#3691 = CARTESIAN_POINT ( 'NONE',  ( 3.000000000000001776, -45.19575662317867426, 139.1455027589171038 ) ) ;
#3692 = CARTESIAN_POINT ( 'NONE',  ( 5.676582343749993598, 75.26041666325268409, 9.832129032723422313 ) ) ;
#3693 = CARTESIAN_POINT ( 'NONE',  ( 6.676582343750003368, 292.0156250017069510, -2.765530957081997254 ) ) ;
#3694 = CARTESIAN_POINT ( 'NONE',  ( -10.18810118749999738, -4.220049686691941915, 108.6250000020483668 ) ) ;
#3695 = CARTESIAN_POINT ( 'NONE',  ( -3.042071309553173730, 204.3229166632526699, 11.35316468749999785 ) ) ;
#3696 = ORIENTED_EDGE ( 'NONE', *, *, #73767, .T. ) ;
#3697 = CARTESIAN_POINT ( 'NONE',  ( 5.656854249492376141, -5.656854249492374365, 27.08030278392014978 ) ) ;
#3698 = DIRECTION ( 'NONE',  ( -0.000000000000000000, 1.000000000000000000, -0.000000000000000000 ) ) ;
#3699 = CARTESIAN_POINT ( 'NONE',  ( 5.000000000000000888, 68.32828612846134320, 21.58087353894222105 ) ) ;
#3701 = CARTESIAN_POINT ( 'NONE',  ( -8.311093377946836114, 212.6562499965860411, -8.311093377946837890 ) ) ;
#3700 = DIRECTION ( 'NONE',  ( -1.000000000000000000, 0.000000000000000000, 0.000000000000000000 ) ) ;
#3702 = DIRECTION ( 'NONE',  ( -0.000000000000000000, -0.000000000000000000, -1.000000000000000000 ) ) ;
#3703 = CARTESIAN_POINT ( 'NONE',  ( 1.836970198721029589E-15, 224.3750000068279746, 10.00000000000000000 ) ) ;
#3704 = CARTESIAN_POINT ( 'NONE',  ( 0.000000000000000000, 300.0000000000000000, 0.000000000000000000 ) ) ;
#3705 = EDGE_LOOP ( 'NONE', ( #52686, #44554, #12659, #20785, #50092, #58016 ) ) ;
#3706 = CARTESIAN_POINT ( 'NONE',  ( 9.832129032723420536, 201.5104166632526983, -5.676582343749999815 ) ) ;
#3707 = AXIS2_PLACEMENT_3D ( 'NONE', #58865, #47517, #59594 ) ;
#3708 = CARTESIAN_POINT ( 'NONE',  ( -7.188101187499992051, 0.000000000000000000, 13.48655278187175455 ) ) ;
#3709 = CARTESIAN_POINT ( 'NONE',  ( -11.92121597166104863, -37.99999999999992184, 141.3838400592076709 ) ) ;
#3710 = CARTESIAN_POINT ( 'NONE',  ( -3.313708498984765161, 10.03125000000000355, 7.999999999999998224 ) ) ;
#3711 = ORIENTED_EDGE ( 'NONE', *, *, #74583, .F. ) ;
#3712 = AXIS2_PLACEMENT_3D ( 'NONE', #21323, #20946, #9648 ) ;
#3713 = CARTESIAN_POINT ( 'NONE',  ( 8.000000000000000000, 90.03125000409677625, -3.313708498984762496 ) ) ;
#3714 = CARTESIAN_POINT ( 'NONE',  ( 10.00000000000000000, 9.791666666666667851, 2.679491924311236062 ) ) ;
#3715 = ORIENTED_EDGE ( 'NONE', *, *, #61577, .T. ) ;
#3716 = CARTESIAN_POINT ( 'NONE',  ( -4.000000000000001776, 17.50000000000000000, -4.898587196589415787E-16 ) ) ;
#3717 = CARTESIAN_POINT ( 'NONE',  ( 1.881053915767122664, 20.12499999863441147, 4.541265875000001451 ) ) ;
#3718 = CARTESIAN_POINT ( 'NONE',  ( -7.999999999999989342, -3.313708498984762496, 8.611552783920146226 ) ) ;
#3719 = CARTESIAN_POINT ( 'NONE',  ( -23.99999999999997158, 195.6875000000000000, 171.6568542494927385 ) ) ;
#3720 = VERTEX_POINT ( 'NONE', #28417 ) ;
#3721 = DIRECTION ( 'NONE',  ( -0.000000000000000000, -0.000000000000000000, -1.000000000000000000 ) ) ;
#3722 = CARTESIAN_POINT ( 'NONE',  ( 2.977408999572654480, 93.12500000204836681, 7.188101187499999156 ) ) ;
#3725 = CARTESIAN_POINT ( 'NONE',  ( 2.828427124746208943, 197.6250000000000284, 195.1715728752538439 ) ) ;
#3724 = CARTESIAN_POINT ( 'NONE',  ( 3.042071309553173286, 260.3645833367473301, 11.35316468749999608 ) ) ;
#3723 = CARTESIAN_POINT ( 'NONE',  ( -2.775557561562891351E-14, 210.0000000000000284, 142.0000000000000568 ) ) ;
#3726 = CARTESIAN_POINT ( 'NONE',  ( 0.000000000000000000, 0.000000000000000000, 0.000000000000000000 ) ) ;
#3727 = VERTEX_POINT ( 'NONE', #40108 ) ;
#3728 = CARTESIAN_POINT ( 'NONE',  ( -3.042071309553166181, 253.1770833367473017, -11.35316468749999608 ) ) ;
#3729 = CARTESIAN_POINT ( 'NONE',  ( 7.188101187499991163, 2.977408999572648707, 15.83030278187175277 ) ) ;
#3730 = ORIENTED_EDGE ( 'NONE', *, *, #64012, .T. ) ;
#3731 = ORIENTED_EDGE ( 'NONE', *, *, #20294, .F. ) ;
#3732 = CARTESIAN_POINT ( 'NONE',  ( -10.18810118749999738, -4.220049686691941915, 82.75000000204838102 ) ) ;
#3733 = CARTESIAN_POINT ( 'NONE',  ( 11.35316468750000141, 81.09374999658601268, 0.000000000000000000 ) ) ;
#3734 = CARTESIAN_POINT ( 'NONE',  ( -3.313708498984761608, 105.4062500040967905, -8.000000000000000000 ) ) ;
#3735 = CARTESIAN_POINT ( 'NONE',  ( -7.778174593052020747, -7.778174593052023411, 91.18749999999998579 ) ) ;
#3738 = CARTESIAN_POINT ( 'NONE',  ( 4.721056650415999201, 291.2343750017069510, -4.721056650415999201 ) ) ;
#3737 = CARTESIAN_POINT ( 'NONE',  ( 23.99999999999997868, 198.8125000027312126, 168.3431457505075741 ) ) ;
#3736 = FACE_OUTER_BOUND ( 'NONE', #66688, .T. ) ;
#3739 = CARTESIAN_POINT ( 'NONE',  ( 0.000000000000000000, -45.00000000000001421, 201.0010000000000048 ) ) ;
#3740 = CARTESIAN_POINT ( 'NONE',  ( -10.00000000000000000, 164.1666666598387110, -2.679491924311229845 ) ) ;
#3741 = CARTESIAN_POINT ( 'NONE',  ( 2.445694354108840063, 198.0625000013656063, 200.4456943541088663 ) ) ;
#3742 = CARTESIAN_POINT ( 'NONE',  ( 7.999999999999998224, 7.218749995903221084, 3.313708498984766493 ) ) ;
#3743 = ORIENTED_EDGE ( 'NONE', *, *, #36067, .F. ) ;
#3744 = CARTESIAN_POINT ( 'NONE',  ( 31.45873412499997812, 196.6250000013656063, 171.4326545832175839 ) ) ;
#3745 = ADVANCED_FACE ( 'NONE', ( #11440 ), #51387, .F. ) ;
#3746 = CARTESIAN_POINT ( 'NONE',  ( 7.188101187500000044, 14.34374999795161187, 0.000000000000000000 ) ) ;
#3747 = CARTESIAN_POINT ( 'NONE',  ( -3.313708498984758943, -7.999999999999989342, 23.79905278392014978 ) ) ;
#3748 = DIRECTION ( 'NONE',  ( 0.000000000000000000, 0.000000000000000000, 1.000000000000000000 ) ) ;
#3749 = CARTESIAN_POINT ( 'NONE',  ( 2.977408999572654480, 105.5000000020483810, 7.188101187499999156 ) ) ;
#3751 = CARTESIAN_POINT ( 'NONE',  ( 2.997005883572143592, -55.94527535362117732, -43.97975057404410393 ) ) ;
#3750 = CARTESIAN_POINT ( 'NONE',  ( 4.000000000000016875, 201.4375000000000284, 199.6568542494924259 ) ) ;
#3752 = CARTESIAN_POINT ( 'NONE',  ( 5.676582343750005144, 220.8854166700806445, 9.832129032723416984 ) ) ;
#3753 = CARTESIAN_POINT ( 'NONE',  ( 28.00000000000002487, 206.1875000013656063, 166.5412658749999082 ) ) ;
#3754 = CARTESIAN_POINT ( 'NONE',  ( -5.082755093536317936, -5.082755093536320601, 18.54905278187175455 ) ) ;
#3755 = CARTESIAN_POINT ( 'NONE',  ( 3.999999999999960032, 208.1250000027312126, 142.0000000000000568 ) ) ;
#3756 = CARTESIAN_POINT ( 'NONE',  ( 11.35316468749999963, 35.98958332991933418, -3.042071309553165293 ) ) ;
#3757 = DIRECTION ( 'NONE',  ( -0.000000000000000000, 1.000000000000000000, -0.000000000000000000 ) ) ;
#3758 = CARTESIAN_POINT ( 'NONE',  ( -1.836970198721029983E-15, 20.62499999317203603, 10.00000000000000178 ) ) ;
#3759 = CARTESIAN_POINT ( 'NONE',  ( -31.99999999999995737, 200.4375000027311842, 171.6568542494928522 ) ) ;
#3760 = ORIENTED_EDGE ( 'NONE', *, *, #2802, .F. ) ;
#3761 = CARTESIAN_POINT ( 'NONE',  ( 2.775557561562891351E-14, 210.0000000000000284, 198.0000000000000284 ) ) ;
#3762 = CARTESIAN_POINT ( 'NONE',  ( 5.656854249492374365, 5.656854249492375253, 18.26780277982336642 ) ) ;
#3763 = CARTESIAN_POINT ( 'NONE',  ( 11.35316468750000141, 50.78124999658601268, 0.000000000000000000 ) ) ;
#3764 = CARTESIAN_POINT ( 'NONE',  ( 2.020667218593132706E-15, -11.00000000000000000, 78.06250000409677625 ) ) ;
#3765 = CARTESIAN_POINT ( 'NONE',  ( -3.458734125000015425, 202.2500000013655779, 143.4326545832176976 ) ) ;
#3767 = AXIS2_PLACEMENT_3D ( 'NONE', #14042, #8401, #60452 ) ;
#3766 = CARTESIAN_POINT ( 'NONE',  ( 7.594050593750000466, 27.23437499897580949, 0.000000000000000000 ) ) ;
#3768 = CARTESIAN_POINT ( 'NONE',  ( -4.000000000000015987, 195.5625000000000568, 143.6568542494924259 ) ) ;
#3770 = CARTESIAN_POINT ( 'NONE',  ( 11.35316468749999785, 40.57291666325268409, 3.042071309553174174 ) ) ;
#3769 = CARTESIAN_POINT ( 'NONE',  ( -5.082755093536324154, 97.34375000204838102, 5.082755093536326818 ) ) ;
#3771 = CARTESIAN_POINT ( 'NONE',  ( 7.999999999999991118, 9.797174393178815797E-16, 12.08030277982336642 ) ) ;
#3772 = CARTESIAN_POINT ( 'NONE',  ( -8.311093377946836114, 157.6562499965860411, -8.311093377946837890 ) ) ;
#3773 = CARTESIAN_POINT ( 'NONE',  ( -10.00000000000000178, 129.3749999931720254, -1.224646799147353454E-15 ) ) ;
#3774 = CARTESIAN_POINT ( 'NONE',  ( 7.188101187500002709, 101.1875000020483810, 2.977408999572649151 ) ) ;
#3775 = COLOUR_RGB ( '',0.7921568627450980005, 0.8196078431372548767, 0.9333333333333333481 ) ;
#3776 = CARTESIAN_POINT ( 'NONE',  ( -2.695772498912065718, -46.33096692831604457, 139.1173425518593376 ) ) ;
#3777 = CARTESIAN_POINT ( 'NONE',  ( 5.676582343749993598, 35.26041666325269119, 9.832129032723422313 ) ) ;
#3778 =( BOUNDED_CURVE ( )  B_SPLINE_CURVE ( 2, ( #55678, #4357, #15653, #73013, #49628, #27726, #66977, #38316, #49242 ),
 .UNSPECIFIED., .F., .F. ) 
 B_SPLINE_CURVE_WITH_KNOTS ( ( 3, 2, 2, 2, 3 ),
 ( 0.5833333333333337034, 0.5916666666666670071, 0.6000000000000004219, 0.6083333333333338366, 0.6166666666666672514 ),
 .UNSPECIFIED. ) 
 CURVE ( )  GEOMETRIC_REPRESENTATION_ITEM ( )  RATIONAL_B_SPLINE_CURVE ( ( 0.9999999999999970024, 0.9238795325112897361, 1.000000000000000000, 0.9238795325112867385, 1.000000000000000000, 0.9238795325112867385, 1.000000000000000000, 0.9238795325112816315, 1.000000000000005107 ) ) 
 REPRESENTATION_ITEM ( '' )  );
#3779 = CARTESIAN_POINT ( 'NONE',  ( -28.15849992381814104, 194.4587341250001487, 166.5412658750004482 ) ) ;
#3780 = EDGE_LOOP ( 'NONE', ( #40358, #11191, #18710, #29366 ) ) ;
#3781 = CARTESIAN_POINT ( 'NONE',  ( -27.99999999999991473, 205.6250000027312126, 174.0000000000003695 ) ) ;
#3782 = CARTESIAN_POINT ( 'NONE',  ( 7.204075437095968759, -7.204075437095966983, 78.71875000204836681 ) ) ;
#3783 = CARTESIAN_POINT ( 'NONE',  ( -30.71123746002426458, -37.49971568839507796, 174.2454767826460511 ) ) ;
#3785 = CARTESIAN_POINT ( 'NONE',  ( 3.042071309553159519, 169.7395833299193555, 11.35316468750000141 ) ) ;
#3784 = CARTESIAN_POINT ( 'NONE',  ( -7.999999999961178609, -1.665943300379353739E-05, 2.518425711869641592 ) ) ;
#3786 = CIRCLE ( 'NONE', #39907, 34.85072926314708752 ) ;
#3787 = CARTESIAN_POINT ( 'NONE',  ( -3.313708498984758943, -7.999999999999989342, 11.66780278432982421 ) ) ;
#3788 = CARTESIAN_POINT ( 'NONE',  ( -30.22934957671015255, -21.02292819077957020, 176.9643053031147701 ) ) ;
#3789 = EDGE_CURVE ( 'NONE', #40886, #51512, #73942, .T. ) ;
#3790 = EDGE_CURVE ( 'NONE', #61682, #16277, #49885, .T. ) ;
#3791 = CARTESIAN_POINT ( 'NONE',  ( 9.832129032723420536, 220.9895833367473301, 5.676582343749996262 ) ) ;
#3792 = CARTESIAN_POINT ( 'NONE',  ( 10.18810118749999916, 4.220049686691935698, 86.87500000204836681 ) ) ;
#3793 = VERTEX_POINT ( 'NONE', #33302 ) ;
#3794 = EDGE_CURVE ( 'NONE', #47241, #6116, #20738, .T. ) ;
#3795 = CARTESIAN_POINT ( 'NONE',  ( 7.778174593052023411, -7.778174593052021635, 90.25000000409677625 ) ) ;
#3796 = CARTESIAN_POINT ( 'NONE',  ( -2.828427124746153876, 204.0000000027312126, 195.1715728752538439 ) ) ;
#3797 = CARTESIAN_POINT ( 'NONE',  ( -11.35316468750000141, 118.5937499965860269, -1.390361679473963753E-15 ) ) ;
#3798 = CARTESIAN_POINT ( 'NONE',  ( -10.18810118749999916, 4.220049686691934809, 97.56250000204836681 ) ) ;
#3799 =( BOUNDED_CURVE ( )  B_SPLINE_CURVE ( 2, ( #37901, #56002, #72970, #55631, #60899, #26556, #21646, #49199, #38650 ),
 .UNSPECIFIED., .F., .F. ) 
 B_SPLINE_CURVE_WITH_KNOTS ( ( 3, 2, 2, 2, 3 ),
 ( 0.6249999999999998890, 0.6319444444444443088, 0.6388888888888888395, 0.6458333333333333703, 0.6527777777777777901 ),
 .UNSPECIFIED. ) 
 CURVE ( )  GEOMETRIC_REPRESENTATION_ITEM ( )  RATIONAL_B_SPLINE_CURVE ( ( 1.000000000000001110, 0.9238795325112855172, 1.000000000000000000, 0.9238795325112867385, 1.000000000000000000, 0.9238795325112867385, 1.000000000000000000, 0.9238795325112867385, 1.000000000000000000 ) ) 
 REPRESENTATION_ITEM ( '' )  );
#3800 = CARTESIAN_POINT ( 'NONE',  ( 3.211159895383560947, 20.31249999863440436, 3.211159895383562723 ) ) ;
#3801 = ORIENTED_EDGE ( 'NONE', *, *, #44665, .T. ) ;
#3802 = VERTEX_POINT ( 'NONE', #67246 ) ;
#3803 = AXIS2_PLACEMENT_3D ( 'NONE', #16083, #44778, #49693 ) ;
#3804 = CARTESIAN_POINT ( 'NONE',  ( -8.342170076843785083E-16, 5.187499998634407028, 4.541265875000002339 ) ) ;
#3805 = CARTESIAN_POINT ( 'NONE',  ( 4.401442555609581635E-16, 11.34374999795161010, -7.188101187500000044 ) ) ;
#3806 = EDGE_CURVE ( 'NONE', #19205, #6677, #40816, .T. ) ;
#3807 = CARTESIAN_POINT ( 'NONE',  ( -5.656854249492378806, 111.8750000040967763, 5.656854249492381470 ) ) ;
#3808 = CARTESIAN_POINT ( 'NONE',  ( -10.18810118749999738, -4.220049686691941915, 92.12500000204836681 ) ) ;
#3809 = CARTESIAN_POINT ( 'NONE',  ( -30.44569435410879166, 203.0625000013656063, 172.4456943541092357 ) ) ;
#3810 = CARTESIAN_POINT ( 'NONE',  ( -26.34314575050763452, 199.6875000027312126, 174.0000000000004547 ) ) ;
#3811 = CARTESIAN_POINT ( 'NONE',  ( 2.828427124746190291, 3.875000000000000000, 2.828427124746192067 ) ) ;
#3812 = CARTESIAN_POINT ( 'NONE',  ( -7.347880794884122694E-16, 17.49999999726881583, 4.000000000000001776 ) ) ;
#3813 = CARTESIAN_POINT ( 'NONE',  ( -1.881053915767124440, 7.999999998634407028, 4.541265875000001451 ) ) ;
#3814 = CARTESIAN_POINT ( 'NONE',  ( 2.828427124746152987, 203.1250000000000284, 139.1715728752538723 ) ) ;
#3815 = VERTEX_POINT ( 'NONE', #66232 ) ;
#3816 = CARTESIAN_POINT ( 'NONE',  ( 23.99999999999999289, 207.7500000000000284, 169.9999999999998863 ) ) ;
#3817 = AXIS2_PLACEMENT_3D ( 'NONE', #24344, #36050, #7375 ) ;
#3819 = CARTESIAN_POINT ( 'NONE',  ( -4.898587196589407898E-16, 7.999999999999991118, 16.95530277982336287 ) ) ;
#3818 = CARTESIAN_POINT ( 'NONE',  ( -28.00000000000007105, 198.4375000013655779, 166.5412658750003629 ) ) ;
#3820 = CARTESIAN_POINT ( 'NONE',  ( -1.881053915767124440, 18.99999999863440436, 4.541265875000001451 ) ) ;
#3821 = CARTESIAN_POINT ( 'NONE',  ( 0.000000000000000000, 75.00000000000000000, 0.000000000000000000 ) ) ;
#3822 = AXIS2_PLACEMENT_3D ( 'NONE', #35172, #58186, #42651 ) ;
#3823 = CARTESIAN_POINT ( 'NONE',  ( 7.188101187499991163, 2.977408999572648707, 5.330302781871753659 ) ) ;
#3824 = VERTEX_POINT ( 'NONE', #48134 ) ;
#3825 = ORIENTED_EDGE ( 'NONE', *, *, #27919, .F. ) ;
#3826 = CARTESIAN_POINT ( 'NONE',  ( -10.18810118749999738, -4.220049686691941915, 100.7500000020483810 ) ) ;
#3827 = CARTESIAN_POINT ( 'NONE',  ( 1.224646799147353454E-15, 300.0000000000000000, -10.00000000000000178 ) ) ;
#3828 = CARTESIAN_POINT ( 'NONE',  ( -24.54126587499998280, 198.3750000013656063, 171.4326545832179818 ) ) ;
#3829 = CARTESIAN_POINT ( 'NONE',  ( 7.778174593052021635, 7.778174593052023411, 109.9375000000000000 ) ) ;
#3830 = CARTESIAN_POINT ( 'NONE',  ( -1.432654583217608080, 206.8750000013656347, 201.4587341250000350 ) ) ;
#3831 = CARTESIAN_POINT ( 'NONE',  ( -3.313708498984681672, 111.7812500000000142, 8.000000000000078160 ) ) ;
#3832 = CARTESIAN_POINT ( 'NONE',  ( 10.00000000000000178, 110.0000000000000000, 0.000000000000000000 ) ) ;
#3833 = B_SPLINE_CURVE_WITH_KNOTS ( 'NONE', 3,
 ( #34560, #28870, #57565, #69240, #52634, #39817, #6614, #68862, #17173, #57943, #17549, #40568 ),
 .UNSPECIFIED., .F., .F.,
 ( 4, 2, 2, 2, 2, 4 ),
 ( 0.000000000000000000, 0.002547658444427992625, 0.005095316888855985250, 0.006369146111069981346, 0.007642975333283978309, 0.01019063377771197050 ),
 .UNSPECIFIED. ) ;
#3834 = CARTESIAN_POINT ( 'NONE',  ( 8.000000000000000000, 109.2500000000000000, -9.797174393178825657E-16 ) ) ;
#3835 = CARTESIAN_POINT ( 'NONE',  ( 2.765530957082001251, 291.9218750017069510, 6.676582343750000703 ) ) ;
#3836 = CARTESIAN_POINT ( 'NONE',  ( -7.188101187499991163, 2.977408999572646930, 10.76780278187175632 ) ) ;
#3837 = EDGE_LOOP ( 'NONE', ( #22455, #67088, #9242, #64730 ) ) ;
#3838 = LINE ( 'NONE', #26834, #72288 ) ;
#3839 = CARTESIAN_POINT ( 'NONE',  ( 27.99999999999996447, 205.4375000013656063, 173.4587341249998929 ) ) ;
#3840 = CARTESIAN_POINT ( 'NONE',  ( -8.000000000000000000, 20.06249999590322375, -9.797174393178825657E-16 ) ) ;
#3841 = CARTESIAN_POINT ( 'NONE',  ( 2.445694354108783664, 200.3125000013656063, 144.4456943541088663 ) ) ;
#3842 = CARTESIAN_POINT ( 'NONE',  ( -21.51387463477770723, -37.57477141138681276, 147.6775694455229768 ) ) ;
#3844 = CARTESIAN_POINT ( 'NONE',  ( -2.445694354108839175, 201.3125000013656063, 144.4456943541088663 ) ) ;
#3843 = CARTESIAN_POINT ( 'NONE',  ( 7.999999999999991118, 0.000000000000000000, 30.00000000000000000 ) ) ;
#3845 = CARTESIAN_POINT ( 'NONE',  ( -5.676582343749992710, 260.0520833367473301, 9.832129032723422313 ) ) ;
#3846 = CARTESIAN_POINT ( 'NONE',  ( -5.447321192899549303, -4.689935021205116961, 0.1569292013794422458 ) ) ;
#3847 = CYLINDRICAL_SURFACE ( 'NONE', #26411, 3.999999999999976019 ) ;
#3848 = CARTESIAN_POINT ( 'NONE',  ( -2.085542519210945728E-15, 4.531249996586016238, 11.35316468750000141 ) ) ;
#3849 = CARTESIAN_POINT ( 'NONE',  ( 5.082755093536318824, 5.082755093536319713, 5.799052781871753659 ) ) ;
#3850 = CARTESIAN_POINT ( 'NONE',  ( 6.951808397369818766E-16, 192.3437499965860127, -11.35316468750000141 ) ) ;
#3851 = CARTESIAN_POINT ( 'NONE',  ( 1.224646799147353454E-15, 300.0000000000000000, -10.00000000000000178 ) ) ;
#3852 = CARTESIAN_POINT ( 'NONE',  ( -1.881053915767121554, 6.624999998634407916, -4.541265875000002339 ) ) ;
#3853 = CARTESIAN_POINT ( 'NONE',  ( -31.99999999999999289, 198.2500000000000000, 170.0000000000003979 ) ) ;
#3855 = CARTESIAN_POINT ( 'NONE',  ( -4.000000000000016875, 206.4375000000000568, 140.3431457505076594 ) ) ;
#3854 = CARTESIAN_POINT ( 'NONE',  ( -2.828427124746192067, 14.37499999726881406, 2.828427124746190735 ) ) ;
#3856 = VERTEX_POINT ( 'NONE', #14533 ) ;
#3857 = VECTOR ( 'NONE', #49035, 1000.000000000000000 ) ;
#3858 = EDGE_CURVE ( 'NONE', #34067, #29307, #30385, .T. ) ;
#3859 = CARTESIAN_POINT ( 'NONE',  ( 3.458734124999959469, 204.7500000013656063, 140.5673454167824161 ) ) ;
#3860 = CARTESIAN_POINT ( 'NONE',  ( 3.042071309553159519, 9.739583329919350163, 11.35316468750000141 ) ) ;
#3861 = CARTESIAN_POINT ( 'NONE',  ( -11.00000000000000000, 4.556349186104045934, 100.0937500040967905 ) ) ;
#3862 = DIRECTION ( 'NONE',  ( 1.000000000000000000, 0.000000000000000000, 0.000000000000000000 ) ) ;
#3863 = CARTESIAN_POINT ( 'NONE',  ( -25.55430564589122966, 203.3125000013656063, 167.5543056458915032 ) ) ;
#3864 = DIRECTION ( 'NONE',  ( -0.000000000000000000, 1.000000000000000000, -0.000000000000000000 ) ) ;
#3866 = CARTESIAN_POINT ( 'NONE',  ( -5.676582343750006032, 4.114583329919349275, 9.832129032723418760 ) ) ;
#3865 = CARTESIAN_POINT ( 'NONE',  ( 1.320432766682874540E-15, 118.5312500020483810, 7.188101187500000044 ) ) ;
#3867 = CARTESIAN_POINT ( 'NONE',  ( -7.999999999999991118, 3.313708498984756723, 26.23655277982336642 ) ) ;
#3868 = CARTESIAN_POINT ( 'NONE',  ( 8.311093377946834337, 120.1562499965860127, 8.311093377946839666 ) ) ;
#3869 = CARTESIAN_POINT ( 'NONE',  ( -10.00000000000000000, 89.16666665983868256, -2.679491924311229845 ) ) ;
#3870 = CARTESIAN_POINT ( 'NONE',  ( -7.188101187500001821, 118.4375000020483810, -2.977408999572650483 ) ) ;
#3871 = CARTESIAN_POINT ( 'NONE',  ( 3.211159895383561835, 20.56249999863440436, -3.211159895383561835 ) ) ;
#3872 = CARTESIAN_POINT ( 'NONE',  ( -5.000000000000005329, 200.2083333265053682, 8.660254037844387298 ) ) ;
#3873 = CARTESIAN_POINT ( 'NONE',  ( 8.660254037844392627, 145.4166666666666572, -5.000000000000003553 ) ) ;
#3874 = ORIENTED_EDGE ( 'NONE', *, *, #17034, .F. ) ;
#3875 = CARTESIAN_POINT ( 'NONE',  ( 3.228176881614474247, -60.48309044411903557, 23.05774181791956678 ) ) ;
#3876 = CARTESIAN_POINT ( 'NONE',  ( 6.676582343750003368, 290.1718750017070079, -2.765530957081997254 ) ) ;
#3877 = CARTESIAN_POINT ( 'NONE',  ( -2.828427124746190735, 12.12499999726881406, -2.828427124746191623 ) ) ;
#3878 = CARTESIAN_POINT ( 'NONE',  ( 7.999999999999991118, 9.797174393178815797E-16, 1.767802783920142895 ) ) ;
#3879 = CARTESIAN_POINT ( 'NONE',  ( 9.000000000000001776, 0.8785859941773073167, -9.452887691357987840E-16 ) ) ;
#3880 = EDGE_CURVE ( 'NONE', #39861, #29704, #65492, .T. ) ;
#3881 = CARTESIAN_POINT ( 'NONE',  ( -10.00000000000000178, 209.3749999931720538, -1.224646799147353454E-15 ) ) ;
#3882 = CARTESIAN_POINT ( 'NONE',  ( -11.00000000000000000, 0.000000000000000000, 69.99999999999998579 ) ) ;
#3883 = CARTESIAN_POINT ( 'NONE',  ( -10.18810118749999738, -4.220049686691941915, 102.6250000020483810 ) ) ;
#3884 = ORIENTED_EDGE ( 'NONE', *, *, #34203, .T. ) ;
#3885 = VECTOR ( 'NONE', #66248, 1000.000000000000000 ) ;
#3886 = CARTESIAN_POINT ( 'NONE',  ( 3.313708498984720308, 22.59374999590322020, -8.000000000000040856 ) ) ;
#3887 = CARTESIAN_POINT ( 'NONE',  ( 11.35316468749999963, 156.3020833299192986, -3.042071309553165293 ) ) ;
#3888 =( LENGTH_UNIT ( ) NAMED_UNIT ( * ) SI_UNIT ( .MILLI., .METRE. ) );
#3889 = CARTESIAN_POINT ( 'NONE',  ( 1.432654583217662481, 204.3750000013656063, 194.5412658750000219 ) ) ;
#3890 = CARTESIAN_POINT ( 'NONE',  ( -31.66756539373085388, -30.58405805906214781, 167.9999999999997726 ) ) ;
#3891 = CARTESIAN_POINT ( 'NONE',  ( -8.311093377946836114, 67.96874999658602690, -8.311093377946837890 ) ) ;
#3892 = ORIENTED_EDGE ( 'NONE', *, *, #61089, .T. ) ;
#3893 = CARTESIAN_POINT ( 'NONE',  ( 1.871523826299183495E-15, -10.18810118749999916, 114.5312500020483810 ) ) ;
#3894 = CARTESIAN_POINT ( 'NONE',  ( -4.541265875000003227, 6.999999998634407916, 1.881053915767121110 ) ) ;
#3895 = ORIENTED_EDGE ( 'NONE', *, *, #22159, .T. ) ;
#3896 = CARTESIAN_POINT ( 'NONE',  ( -2.977408999572654480, 20.99999999795161898, 7.188101187499999156 ) ) ;
#3897 = CARTESIAN_POINT ( 'NONE',  ( -6.000000000000003553, 289.0000000034140157, -2.485281374238571317 ) ) ;
#3898 = CARTESIAN_POINT ( 'NONE',  ( -24.00000000000002487, 197.9375000027312126, 168.3431457505079152 ) ) ;
#3899 = CARTESIAN_POINT ( 'NONE',  ( -5.082755093536325042, 19.40624999795161543, -5.082755093536325930 ) ) ;
#3900 = ADVANCED_FACE ( 'NONE', ( #31157 ), #61725, .T. ) ;
#3901 = CARTESIAN_POINT ( 'NONE',  ( -2.977408999572647819, -7.188101187499990274, 3.267802781871751439 ) ) ;
#3902 =( BOUNDED_CURVE ( )  B_SPLINE_CURVE ( 2, ( #46083, #33675, #23073, #68358, #28730, #34795, #51746, #45340, #16652 ),
 .UNSPECIFIED., .F., .F. ) 
 B_SPLINE_CURVE_WITH_KNOTS ( ( 3, 2, 2, 2, 3 ),
 ( 0.8750000000000000000, 0.8806818181818182323, 0.8863636363636363535, 0.8920454545454545858, 0.8977272727272727071 ),
 .UNSPECIFIED. ) 
 CURVE ( )  GEOMETRIC_REPRESENTATION_ITEM ( )  RATIONAL_B_SPLINE_CURVE ( ( 1.000000000000000000, 0.9238795325112867385, 1.000000000000000000, 0.9238795325112867385, 1.000000000000000000, 0.9238795325112867385, 1.000000000000000000, 0.9238795325112867385, 1.000000000000000000 ) ) 
 REPRESENTATION_ITEM ( '' )  );
#3903 = CARTESIAN_POINT ( 'NONE',  ( -4.220049686691935698, 10.18810118749999916, 109.7500000020483810 ) ) ;
#3904 = EDGE_CURVE ( 'NONE', #20204, #34236, #22358, .T. ) ;
#3905 = AXIS2_PLACEMENT_3D ( 'NONE', #29404, #46736, #18073 ) ;
#3906 = CARTESIAN_POINT ( 'NONE',  ( 2.696570579032583126, -43.67081821164629929, 151.1921763386567932 ) ) ;
#3907 = CARTESIAN_POINT ( 'NONE',  ( -1.656854249492383691, 5.437499997268813168, 4.000000000000000888 ) ) ;
#3908 = CARTESIAN_POINT ( 'NONE',  ( -29.80802767412484400, -51.96606372635251603, 161.4451171223731194 ) ) ;
#3909 = ORIENTED_EDGE ( 'NONE', *, *, #55662, .F. ) ;
#3910 = ADVANCED_FACE ( 'NONE', ( #5111 ), #55304, .T. ) ;
#3911 = CIRCLE ( 'NONE', #54527, 38.00000000000000711 ) ;
#3912 = ADVANCED_FACE ( 'NONE', ( #49246 ), #27731, .F. ) ;
#3913 = CARTESIAN_POINT ( 'NONE',  ( -1.432654583217607858, 207.6250000013656347, 201.4587341250000065 ) ) ;
#3914 = CARTESIAN_POINT ( 'NONE',  ( -30.44569435410887337, 207.5625000013656063, 167.5543056458916169 ) ) ;
#3915 = CARTESIAN_POINT ( 'NONE',  ( -11.00000000000000000, 0.000000000000000000, 98.49999999999998579 ) ) ;
#3916 = CARTESIAN_POINT ( 'NONE',  ( 4.541265875000002339, 7.312499998634407028, 0.000000000000000000 ) ) ;
#3917 = EDGE_CURVE ( 'NONE', #38634, #663, #66807, .T. ) ;
#3918 = CARTESIAN_POINT ( 'NONE',  ( -4.000000000000001776, 13.43750000000000000, -1.656854249492381470 ) ) ;
#3919 = CARTESIAN_POINT ( 'NONE',  ( 5.082755093536318824, 5.082755093536319713, 24.92405278187175810 ) ) ;
#3920 = ORIENTED_EDGE ( 'NONE', *, *, #2590, .F. ) ;
#3921 = CARTESIAN_POINT ( 'NONE',  ( 4.242640687119287435, 299.3750000000000000, 4.242640687119285658 ) ) ;
#3922 = ORIENTED_EDGE ( 'NONE', *, *, #42215, .T. ) ;
#3923 = CARTESIAN_POINT ( 'NONE',  ( 10.18810118749999916, 4.220049686691935698, 116.5000000020483810 ) ) ;
#3924 = CARTESIAN_POINT ( 'NONE',  ( -11.00000000000000000, 0.000000000000000000, 83.68750000409677625 ) ) ;
#3925 = CARTESIAN_POINT ( 'NONE',  ( 3.458734125000016313, 204.8750000013656063, 199.4326545832176691 ) ) ;
#3926 = CARTESIAN_POINT ( 'NONE',  ( 28.00000000000001421, 197.4375000013655779, 173.4587341249998929 ) ) ;
#3927 = CARTESIAN_POINT ( 'NONE',  ( -8.660254037844390851, 67.91666666666667140, 4.999999999999998224 ) ) ;
#3928 = CARTESIAN_POINT ( 'NONE',  ( 5.082755093536326818, 95.09375000204838102, 5.082755093536325042 ) ) ;
#3929 = CARTESIAN_POINT ( 'NONE',  ( 1.102182119232618108E-15, 292.2500000000000000, 6.000000000000001776 ) ) ;
#3930 = CARTESIAN_POINT ( 'NONE',  ( 23.99999999999999289, 206.8750000027312126, 169.9999999999999432 ) ) ;
#3931 = ORIENTED_EDGE ( 'NONE', *, *, #71142, .T. ) ;
#3932 = CARTESIAN_POINT ( 'NONE',  ( 3.313708498984869077, 94.53125000000001421, -7.999999999999892530 ) ) ;
#3933 = CARTESIAN_POINT ( 'NONE',  ( -3.734423912253595379, -10.10901040137823159, 70.68514270129077204 ) ) ;
#3934 = CARTESIAN_POINT ( 'NONE',  ( -2.828427124746208943, 198.7500000027312126, 144.8284271247462129 ) ) ;
#3935 = CARTESIAN_POINT ( 'NONE',  ( 11.00000000000000355, -4.556349186104044158, 78.15624999999998579 ) ) ;
#3936 = CARTESIAN_POINT ( 'NONE',  ( 4.000000000000001776, 0.3749999986344067504, 0.000000000000000000 ) ) ;
#3937 = CARTESIAN_POINT ( 'NONE',  ( -5.000000000000000888, 249.1666666666666856, -8.660254037844387298 ) ) ;
#3938 = CARTESIAN_POINT ( 'NONE',  ( 1.268984979720182487E-11, 76.24999999999903366, -10.00000000000000178 ) ) ;
#3939 = CARTESIAN_POINT ( 'NONE',  ( -7.320508075688773708, 181.8750000000000284, -7.320508075688774596 ) ) ;
#3940 = CARTESIAN_POINT ( 'NONE',  ( 31.99999999999999289, 198.3750000027312126, 169.9999999999998863 ) ) ;
#3941 = CARTESIAN_POINT ( 'NONE',  ( -5.082755093536317936, -5.082755093536320601, 23.04905278187175455 ) ) ;
#3942 = CARTESIAN_POINT ( 'NONE',  ( 11.35316468749999785, 160.8854166632526983, 3.042071309553174174 ) ) ;
#3943 = CARTESIAN_POINT ( 'NONE',  ( -4.000000000000015987, 204.6250000027312126, 142.0000000000000568 ) ) ;
#3944 = CARTESIAN_POINT ( 'NONE',  ( 5.000000000000000000, 0.000000000000000000, 0.000000000000000000 ) ) ;
#3945 = CARTESIAN_POINT ( 'NONE',  ( 2.696524195522682164E-11, 156.2499999999978968, -10.00000000000000178 ) ) ;
#3947 = FACE_OUTER_BOUND ( 'NONE', #14700, .T. ) ;
#3946 = CARTESIAN_POINT ( 'NONE',  ( -10.00000000000000355, 84.58333332650538239, 2.679491924311223183 ) ) ;
#3948 = EDGE_LOOP ( 'NONE', ( #17612, #33910, #70776, #26423 ) ) ;
#3949 = CARTESIAN_POINT ( 'NONE',  ( 11.35316468749999785, 25.88541666325268764, 3.042071309553174174 ) ) ;
#3950 = CARTESIAN_POINT ( 'NONE',  ( 0.000000000000000000, 0.000000000000000000, 0.000000000000000000 ) ) ;
#3951 = EDGE_CURVE ( 'NONE', #22045, #37361, #31343, .T. ) ;
#3953 = CARTESIAN_POINT ( 'NONE',  ( -2.266287154886498456, -10.27715108473166694, -63.73532778936405663 ) ) ;
#3952 = CARTESIAN_POINT ( 'NONE',  ( -11.00000000000000000, 0.000000000000000000, 116.6875000040967763 ) ) ;
#3954 = CARTESIAN_POINT ( 'NONE',  ( 3.458734124999958581, 201.5000000013655779, 140.5673454167823593 ) ) ;
#3955 = AXIS2_PLACEMENT_3D ( 'NONE', #52582, #57134, #18247 ) ;
#3956 = CARTESIAN_POINT ( 'NONE',  ( -5.000000000000005329, 50.20833332650537528, 8.660254037844387298 ) ) ;
#3957 = CARTESIAN_POINT ( 'NONE',  ( -7.188101187500001821, 109.0625000020483810, -2.977408999572650483 ) ) ;
#3958 = CARTESIAN_POINT ( 'NONE',  ( 1.881053915767121776, 7.624999998634408804, -4.541265875000002339 ) ) ;
#3959 = CARTESIAN_POINT ( 'NONE',  ( 2.679491924316444784, 98.95833333333378334, 9.999999999996969535 ) ) ;
#3960 = CARTESIAN_POINT ( 'NONE',  ( -7.999999999999991118, 0.000000000000000000, 11.33030277982336642 ) ) ;
#3962 = CARTESIAN_POINT ( 'NONE',  ( 8.660254037844399733, 159.5833333333333712, 5.000000000000014211 ) ) ;
#3961 = CYLINDRICAL_SURFACE ( 'NONE', #45557, 10.00000000000000000 ) ;
#3963 = VERTEX_POINT ( 'NONE', #44349 ) ;
#3964 = VERTEX_POINT ( 'NONE', #33415 ) ;
#3965 = ADVANCED_FACE ( 'NONE', ( #60950 ), #56241, .T. ) ;
#3966 = CARTESIAN_POINT ( 'NONE',  ( 8.000000000000000000, 28.31249999590322375, 0.000000000000000000 ) ) ;
#3967 = DIRECTION ( 'NONE',  ( 1.000000000000000000, 0.000000000000000000, 0.000000000000000000 ) ) ;
#3968 = CARTESIAN_POINT ( 'NONE',  ( -4.556349186104048599, -10.99999999999999822, 82.28124999999998579 ) ) ;
#3969 = CARTESIAN_POINT ( 'NONE',  ( -21.78045554270713424, -37.99999999999992184, 147.9407217626652198 ) ) ;
#3970 = CIRCLE ( 'NONE', #62986, 3.999999999999986233 ) ;
#3971 = CARTESIAN_POINT ( 'NONE',  ( -8.311093377946836114, 122.6562499965860269, -8.311093377946837890 ) ) ;
#3972 = VERTEX_POINT ( 'NONE', #23620 ) ;
#3973 = CARTESIAN_POINT ( 'NONE',  ( -8.000000000000003553, 284.0000000000000000, 0.000000000000000000 ) ) ;
#3974 = CARTESIAN_POINT ( 'NONE',  ( -10.18810118749999916, 0.000000000000000000, 91.65625000204836681 ) ) ;
#3975 = DIRECTION ( 'NONE',  ( 0.000000000000000000, 0.000000000000000000, -1.000000000000000000 ) ) ;
#3976 = CARTESIAN_POINT ( 'NONE',  ( -2.828427124746153876, 209.8750000000000284, 195.1715728752538439 ) ) ;
#3978 = CARTESIAN_POINT ( 'NONE',  ( -2.085542519210945728E-15, 124.5312499965860269, 11.35316468750000141 ) ) ;
#3977 = CARTESIAN_POINT ( 'NONE',  ( 8.660254037844408614, 45.41666666666667851, -5.000000000000012434 ) ) ;
#3979 = CARTESIAN_POINT ( 'NONE',  ( 10.02978802437157135, -8.065705644765241544, -0.4750804646944294385 ) ) ;
#3980 = VERTEX_POINT ( 'NONE', #17587 ) ;
#3981 = ADVANCED_FACE ( 'NONE', ( #63607 ), #34965, .T. ) ;
#3982 = CARTESIAN_POINT ( 'NONE',  ( -6.735557395310442023E-16, 11.00000000000000000, 77.12499999999998579 ) ) ;
#3983 = CARTESIAN_POINT ( 'NONE',  ( -31.07018350459614098, 178.9577932314737438, 170.8454493557645435 ) ) ;
#3984 = CARTESIAN_POINT ( 'NONE',  ( -11.35316468750000141, 113.5937499965860127, -1.390361679473963753E-15 ) ) ;
#3985 = CARTESIAN_POINT ( 'NONE',  ( 2.839093476692135984E-14, 206.6875000013656063, 201.4587341250000350 ) ) ;
#3986 = CARTESIAN_POINT ( 'NONE',  ( 2.977408999572650927, 20.62499999795161543, -7.188101187500000933 ) ) ;
#3987 = CARTESIAN_POINT ( 'NONE',  ( -7.204075437095965206, -7.204075437095968759, 84.71875000204836681 ) ) ;
#3988 = CARTESIAN_POINT ( 'NONE',  ( 11.35316468749999785, 25.88541666325268764, 3.042071309553174174 ) ) ;
#3989 = VERTEX_POINT ( 'NONE', #638 ) ;
#3990 = CARTESIAN_POINT ( 'NONE',  ( -3.313708498984707429, 96.40625000409680467, -8.000000000000055067 ) ) ;
#3991 = CARTESIAN_POINT ( 'NONE',  ( 3.317071493978883456, -8.008118988124989457, 22.48186528394063544 ) ) ;
#3992 = CARTESIAN_POINT ( 'NONE',  ( 3.313708498984756279, 7.999999999999991118, 23.04905278392014623 ) ) ;
#3993 = DIRECTION ( 'NONE',  ( -0.000000000000000000, -0.000000000000000000, -1.000000000000000000 ) ) ;
#3994 = CARTESIAN_POINT ( 'NONE',  ( 2.977408999572650927, 2.249999997951610098, -7.188101187500001821 ) ) ;
#3995 = CARTESIAN_POINT ( 'NONE',  ( 6.676582343750004256, 289.8906250017069510, 2.765530957081995478 ) ) ;
#3996 = CARTESIAN_POINT ( 'NONE',  ( -49.26344083597083312, 138.7591410929514097, 58.96767091637842384 ) ) ;
#3997 = CARTESIAN_POINT ( 'NONE',  ( 4.898587196589412829E-16, 16.68749999590322375, -8.000000000000000000 ) ) ;
#3998 = ORIENTED_EDGE ( 'NONE', *, *, #33498, .T. ) ;
#3999 = CARTESIAN_POINT ( 'NONE',  ( -5.676582343750006032, 139.4270833299193555, 9.832129032723418760 ) ) ;
#4000 = CARTESIAN_POINT ( 'NONE',  ( -7.204075437095967871, 7.204075437095967871, 77.96875000204836681 ) ) ;
#4001 = EDGE_CURVE ( 'NONE', #64740, #71548, #69649, .T. ) ;
#4002 = CARTESIAN_POINT ( 'NONE',  ( -28.00000000000001776, 194.4375000013656063, 166.5412658750003629 ) ) ;
#4003 = CARTESIAN_POINT ( 'NONE',  ( -1.881053915767121554, 17.74999999863440792, -4.541265875000002339 ) ) ;
#4004 = VERTEX_POINT ( 'NONE', #63987 ) ;
#4005 = CARTESIAN_POINT ( 'NONE',  ( 4.000000000000015987, 201.5625000027311842, 199.6568542494924259 ) ) ;
#4006 = CARTESIAN_POINT ( 'NONE',  ( 1.656854249492348607, 209.1875000000000000, 138.0000000000000568 ) ) ;
#4007 = CARTESIAN_POINT ( 'NONE',  ( -25.17157287525374088, 204.7500000027312126, 172.8284271247464972 ) ) ;
#4008 = CARTESIAN_POINT ( 'NONE',  ( -4.898587196589407898E-16, 7.999999999999991118, 13.95530277982336465 ) ) ;
#4009 = ORIENTED_EDGE ( 'NONE', *, *, #48376, .T. ) ;
#4010 = EDGE_CURVE ( 'NONE', #17570, #512, #2313, .T. ) ;
#4011 =( BOUNDED_CURVE ( )  B_SPLINE_CURVE ( 2, ( #7731, #47705, #30372, #13002, #12639, #35670, #58685, #2438, #59785 ),
 .UNSPECIFIED., .F., .F. ) 
 B_SPLINE_CURVE_WITH_KNOTS ( ( 3, 2, 2, 2, 3 ),
 ( 0.9264705882352940458, 0.9301470588235294379, 0.9338235294117647189, 0.9375000000000000000, 0.9411764705882353921 ),
 .UNSPECIFIED. ) 
 CURVE ( )  GEOMETRIC_REPRESENTATION_ITEM ( )  RATIONAL_B_SPLINE_CURVE ( ( 1.000000000000002220, 0.9238795325112844070, 1.000000000000000000, 0.9238795325112867385, 1.000000000000000000, 0.9238795325112867385, 1.000000000000000000, 0.9238795325112844070, 1.000000000000002220 ) ) 
 REPRESENTATION_ITEM ( '' )  );
#4012 = CARTESIAN_POINT ( 'NONE',  ( 5.082755093536324154, 10.78124999795161187, 5.082755093536326818 ) ) ;
#4013 = CARTESIAN_POINT ( 'NONE',  ( -2.828427124746209831, 208.3750000000000284, 139.1715728752538723 ) ) ;
#4014 = CARTESIAN_POINT ( 'NONE',  ( 5.000000000000000888, 53.31073972600231770, -44.28411094575927365 ) ) ;
#4015 = VECTOR ( 'NONE', #66788, 1000.000000000000000 ) ;
#4016 = CARTESIAN_POINT ( 'NONE',  ( -5.676582343749998039, 187.4479166632526983, -9.832129032723420536 ) ) ;
#4017 = CARTESIAN_POINT ( 'NONE',  ( 2.977408999572650039, 110.5625000020483810, -7.188101187500001821 ) ) ;
#4018 = CARTESIAN_POINT ( 'NONE',  ( -4.242640687119286547, 290.9375000034140157, -4.242640687119286547 ) ) ;
#4019 = CARTESIAN_POINT ( 'NONE',  ( 6.676582343750001591, 287.9531250017069510, -8.176455196517173205E-16 ) ) ;
#4020 = FACE_OUTER_BOUND ( 'NONE', #58733, .T. ) ;
#4021 = ORIENTED_EDGE ( 'NONE', *, *, #57781, .F. ) ;
#4022 = CARTESIAN_POINT ( 'NONE',  ( -3.042071309553166181, 262.8645833367473301, -11.35316468749999608 ) ) ;
#4023 = CARTESIAN_POINT ( 'NONE',  ( -5.082755093536319713, 5.082755093536319713, 21.17405278187175455 ) ) ;
#4024 = CARTESIAN_POINT ( 'NONE',  ( -4.000000000000001776, 2.249999997268813612, -4.898587196589415787E-16 ) ) ;
#4025 = CARTESIAN_POINT ( 'NONE',  ( 8.000000000000000000, 19.31249999590322020, 0.000000000000000000 ) ) ;
#4026 = CARTESIAN_POINT ( 'NONE',  ( 2.216418498321875319, -67.77535163244932903, -20.18253627485106705 ) ) ;
#4027 = VECTOR ( 'NONE', #14571, 1000.000000000000000 ) ;
#4028 = CARTESIAN_POINT ( 'NONE',  ( -1.432654583217607414, 196.5000000013656063, 194.5412658750000219 ) ) ;
#4029 = LINE ( 'NONE', #73788, #4027 ) ;
#4030 = LINE ( 'NONE', #67769, #27081 ) ;
#4031 = CARTESIAN_POINT ( 'NONE',  ( -3.313708498984762052, 93.21874999999998579, -8.000000000000000000 ) ) ;
#4032 = CARTESIAN_POINT ( 'NONE',  ( -9.832129032723420536, 109.0104166632526841, 5.676582343749997150 ) ) ;
#4033 = CARTESIAN_POINT ( 'NONE',  ( -5.000000000000000000, -12.24744670179871164, -68.85644987591972210 ) ) ;
#4034 = CARTESIAN_POINT ( 'NONE',  ( 7.778174593052021635, 7.778174593052023411, 70.93749999999998579 ) ) ;
#4037 = CARTESIAN_POINT ( 'NONE',  ( -4.556349186104045934, 11.00000000000000000, 110.4062500040967620 ) ) ;
#4036 = CARTESIAN_POINT ( 'NONE',  ( 31.45873412499999944, 201.6875000013656063, 169.9999999999998863 ) ) ;
#4035 = CARTESIAN_POINT ( 'NONE',  ( 27.99999999999996447, 200.6875000013656063, 173.4587341249998929 ) ) ;
#4038 = EDGE_LOOP ( 'NONE', ( #32213, #36167, #62701, #46097 ) ) ;
#4039 = CARTESIAN_POINT ( 'NONE',  ( 9.973997309829867319, 225.0610850109414969, -0.7786812090345707205 ) ) ;
#4040 = EDGE_CURVE ( 'NONE', #66273, #44869, #63885, .T. ) ;
#4041 = CARTESIAN_POINT ( 'NONE',  ( -3.673940397442060854E-16, 287.8125000034140157, -6.000000000000001776 ) ) ;
#4042 = CARTESIAN_POINT ( 'NONE',  ( 3.458734124999959914, 195.4375000013655779, 142.0000000000000568 ) ) ;
#4043 = CARTESIAN_POINT ( 'NONE',  ( 31.45873412499999944, 197.0000000013656347, 168.5673454167822740 ) ) ;
#4044 = CARTESIAN_POINT ( 'NONE',  ( -9.832129032723420536, 214.0104166632526699, 5.676582343749997150 ) ) ;
#4045 = DIRECTION ( 'NONE',  ( 0.000000000000000000, 0.000000000000000000, 1.000000000000000000 ) ) ;
#4046 = AXIS2_PLACEMENT_3D ( 'NONE', #53789, #41723, #13034 ) ;
#4047 = CARTESIAN_POINT ( 'NONE',  ( 10.72662151423591226, 225.9999999999999432, 3.025688605616037030 ) ) ;
#4048 = CARTESIAN_POINT ( 'NONE',  ( -8.342170076843785083E-16, 19.06249999863440436, 4.541265875000002339 ) ) ;
#4049 = CARTESIAN_POINT ( 'NONE',  ( 2.591411123053486421, -50.09422832877199738, 40.78779037275008790 ) ) ;
#4050 = CARTESIAN_POINT ( 'NONE',  ( 3.313708498984756279, 7.999999999999991118, 25.86155277982337353 ) ) ;
#4051 = CARTESIAN_POINT ( 'NONE',  ( -29.65685424949246141, 208.1875000027312126, 166.0000000000004263 ) ) ;
#4052 = CARTESIAN_POINT ( 'NONE',  ( -2.085542519210945728E-15, 99.53124999658602690, 11.35316468750000141 ) ) ;
#4053 = EDGE_LOOP ( 'NONE', ( #42676, #3231, #49429 ) ) ;
#4054 = EDGE_CURVE ( 'NONE', #18829, #22730, #41260, .T. ) ;
#4055 = CARTESIAN_POINT ( 'NONE',  ( 23.99999999999998934, 204.8750000027312126, 169.9999999999999432 ) ) ;
#4056 = CARTESIAN_POINT ( 'NONE',  ( -2.977408999572650039, 18.93749999795161187, -7.188101187500001821 ) ) ;
#4057 = CARTESIAN_POINT ( 'NONE',  ( 2.775557561562891351E-14, 210.0000000000000284, 198.0000000000000284 ) ) ;
#4058 = CARTESIAN_POINT ( 'NONE',  ( 11.35316468749999963, 261.7187500034140157, -1.390361679473963556E-15 ) ) ;
#4059 = CARTESIAN_POINT ( 'NONE',  ( -8.311093377946841443, 93.90624999658599847, 8.311093377946830785 ) ) ;
#4060 = ORIENTED_EDGE ( 'NONE', *, *, #33788, .F. ) ;
#4061 = CARTESIAN_POINT ( 'NONE',  ( 37.99999999999999289, 37.00000000000000000, 0.000000000000000000 ) ) ;
#4062 = CARTESIAN_POINT ( 'NONE',  ( -4.220049686691937474, -10.18810118749999738, 106.9375000020483810 ) ) ;
#4063 = DIRECTION ( 'NONE',  ( -0.000000000000000000, 1.000000000000000000, -0.000000000000000000 ) ) ;
#4064 = CARTESIAN_POINT ( 'NONE',  ( 1.432654583217662481, 204.3750000013656063, 194.5412658750000219 ) ) ;
#4065 = CARTESIAN_POINT ( 'NONE',  ( -1.836970198721029983E-15, 75.62499999317203958, 10.00000000000000178 ) ) ;
#4067 = CARTESIAN_POINT ( 'NONE',  ( 8.311093377946834337, 80.15624999658601268, 8.311093377946839666 ) ) ;
#4066 = CARTESIAN_POINT ( 'NONE',  ( -2.751064625579944321E-14, 201.7500000000000000, 146.0000000000000284 ) ) ;
#4068 = CARTESIAN_POINT ( 'NONE',  ( 5.656854249492374365, 5.656854249492375253, 19.95530278392014623 ) ) ;
#4069 = CARTESIAN_POINT ( 'NONE',  ( -29.43265458321760519, 200.1250000013656063, 173.4587341250003760 ) ) ;
#4070 = CARTESIAN_POINT ( 'NONE',  ( -1.347111479062088207E-15, 0.000000000000000000, 0.000000000000000000 ) ) ;
#4071 = CARTESIAN_POINT ( 'NONE',  ( 8.660254037844389075, 187.2916666598387110, -5.000000000000000000 ) ) ;
#4072 = CYLINDRICAL_SURFACE ( 'NONE', #46114, 4.000000000000001776 ) ;
#4073 = CARTESIAN_POINT ( 'NONE',  ( 3.042071309553159519, 75.05208332991934128, 11.35316468750000141 ) ) ;
#4074 = CARTESIAN_POINT ( 'NONE',  ( -6.676582343750003368, 294.3906250017070079, -2.765530957081996810 ) ) ;
#4075 = CARTESIAN_POINT ( 'NONE',  ( -7.204075437095965206, -7.204075437095968759, 101.2187500020483668 ) ) ;
#4076 = CARTESIAN_POINT ( 'NONE',  ( -5.676582343749998039, 207.4479166632527267, -9.832129032723420536 ) ) ;
#4077 = ORIENTED_EDGE ( 'NONE', *, *, #72067, .T. ) ;
#4078 = CARTESIAN_POINT ( 'NONE',  ( -1.656854249492383468, 1.437499997268813390, 4.000000000000000888 ) ) ;
#4079 = CARTESIAN_POINT ( 'NONE',  ( -27.99999999999991118, 203.6250000027312126, 174.0000000000003695 ) ) ;
#4080 = CARTESIAN_POINT ( 'NONE',  ( -3.407298021510799302, -16.35582233947175013, 69.12343428065700834 ) ) ;
#4082 = CARTESIAN_POINT ( 'NONE',  ( -8.311093377946836114, 202.6562499965860127, -8.311093377946837890 ) ) ;
#4081 = CARTESIAN_POINT ( 'NONE',  ( 26.34314575050756702, 206.9375000000000284, 173.9999999999998863 ) ) ;
#4083 = AXIS2_PLACEMENT_3D ( 'NONE', #26186, #25811, #3198 ) ;
#4084 = CARTESIAN_POINT ( 'NONE',  ( 8.660254037844389075, 225.2083333401613174, 4.999999999999997335 ) ) ;
#4085 = CARTESIAN_POINT ( 'NONE',  ( -4.000000000000001776, 20.50000000000000000, -4.898587196589415787E-16 ) ) ;
#4086 = EDGE_LOOP ( 'NONE', ( #49552, #55957, #57063 ) ) ;
#4087 = CARTESIAN_POINT ( 'NONE',  ( -11.35316468750000141, 198.5937499965860127, -1.390361679473963753E-15 ) ) ;
#4088 = CARTESIAN_POINT ( 'NONE',  ( 7.188101187499993827, -2.977408999572645598, 14.14280278187175455 ) ) ;
#4089 = CARTESIAN_POINT ( 'NONE',  ( 1.688721909672333155, 60.25432409644750464, -22.91817940688229527 ) ) ;
#4090 = CARTESIAN_POINT ( 'NONE',  ( -8.000000000000000000, 9.656250000000001776, -3.313708498984762496 ) ) ;
#4091 = VERTEX_POINT ( 'NONE', #43092 ) ;
#4092 = CARTESIAN_POINT ( 'NONE',  ( 3.313708498984760720, 93.21875000409680467, -8.000000000000000000 ) ) ;
#4093 = CARTESIAN_POINT ( 'NONE',  ( -2.679491924311235618, 18.54166666666666785, 10.00000000000000000 ) ) ;
#4094 = VECTOR ( 'NONE', #26234, 1000.000000000000000 ) ;
#4095 = CARTESIAN_POINT ( 'NONE',  ( -7.204075437095965206, -7.204075437095968759, 81.71875000204836681 ) ) ;
#4096 = ORIENTED_EDGE ( 'NONE', *, *, #37547, .F. ) ;
#4097 = CARTESIAN_POINT ( 'NONE',  ( 2.449293598294707893E-16, 18.25000000000000000, -4.000000000000001776 ) ) ;
#4098 = CARTESIAN_POINT ( 'NONE',  ( -3.211159895383562723, 19.93749999863440436, 3.211159895383561391 ) ) ;
#4099 = CARTESIAN_POINT ( 'NONE',  ( -7.999999999999989342, -3.313708498984762496, 10.11155278392014623 ) ) ;
#4100 = CARTESIAN_POINT ( 'NONE',  ( 31.60757109211641236, 194.6015308780792168, 170.0870517240356037 ) ) ;
#4101 = ORIENTED_EDGE ( 'NONE', *, *, #64449, .F. ) ;
#4102 = DIRECTION ( 'NONE',  ( -0.000000000000000000, -1.000000000000000000, -4.283267841918042741E-17 ) ) ;
#4103 = CARTESIAN_POINT ( 'NONE',  ( 7.188101187500001821, 90.50000000204840944, -2.977408999572651371 ) ) ;
#4106 = CARTESIAN_POINT ( 'NONE',  ( 2.160335347077974699, -51.35526406371597830, 48.59969451235745197 ) ) ;
#4105 = CARTESIAN_POINT ( 'NONE',  ( -11.35316468749999963, 258.9062500034140157, 0.000000000000000000 ) ) ;
#4104 = CARTESIAN_POINT ( 'NONE',  ( -8.660254037844387298, 257.7083333401612890, -4.999999999999999112 ) ) ;
#4107 = SHAPE_DEFINITION_REPRESENTATION ( #25143, #46008 ) ;
#4108 = VERTEX_POINT ( 'NONE', #66109 ) ;
#4109 = EDGE_CURVE ( 'NONE', #34420, #10274, #17533, .T. ) ;
#4110 = CARTESIAN_POINT ( 'NONE',  ( 11.35316468749999963, 256.5104166700807014, 3.042071309553159519 ) ) ;
#4111 = CARTESIAN_POINT ( 'NONE',  ( 5.082755093536320601, -5.082755093536318824, 14.04905278187175455 ) ) ;
#4112 = EDGE_LOOP ( 'NONE', ( #9168, #48486, #34745, #31175 ) ) ;
#4113 = ORIENTED_EDGE ( 'NONE', *, *, #63748, .F. ) ;
#4114 = CARTESIAN_POINT ( 'NONE',  ( -6.238412754330611322E-16, 10.18810118749999916, 71.78125000204838102 ) ) ;
#4115 = CARTESIAN_POINT ( 'NONE',  ( -9.832129032723418760, 68.17708332991935549, -5.676582343750004256 ) ) ;
#4116 = CARTESIAN_POINT ( 'NONE',  ( -7.999994587436531468, -3.313713911548220814, 23.61155300047851568 ) ) ;
#4117 = CARTESIAN_POINT ( 'NONE',  ( 11.00000000000000000, 4.556349186104045934, 88.84374999999997158 ) ) ;
#4120 = CARTESIAN_POINT ( 'NONE',  ( -4.721056650415999201, 290.4843750017070079, -4.721056650415999201 ) ) ;
#4119 = CARTESIAN_POINT ( 'NONE',  ( 25.17157287525377996, 197.7500000027312126, 167.1715728752537586 ) ) ;
#4118 = CARTESIAN_POINT ( 'NONE',  ( -23.99999999999999289, 205.8750000027312126, 170.0000000000002842 ) ) ;
#4121 = AXIS2_PLACEMENT_3D ( 'NONE', #63883, #6551, #905 ) ;
#4122 = CYLINDRICAL_SURFACE ( 'NONE', #20004, 18.00000000000000355 ) ;
#4123 = PLANE ( 'NONE',  #35981 ) ;
#4124 = ADVANCED_FACE ( 'NONE', ( #9151 ), #55189, .F. ) ;
#4125 = CARTESIAN_POINT ( 'NONE',  ( -1.432654583217608080, 199.8750000013656063, 201.4587341250000350 ) ) ;
#4126 =( BOUNDED_CURVE ( )  B_SPLINE_CURVE ( 2, ( #35962, #47631, #18972, #25357, #25723, #71377, #71752, #20066, #6916 ),
 .UNSPECIFIED., .F., .F. ) 
 B_SPLINE_CURVE_WITH_KNOTS ( ( 3, 2, 2, 2, 3 ),
 ( 0.5882352941176469674, 0.5919117647058822484, 0.5955882352941175295, 0.5992647058823528106, 0.6029411764705880916 ),
 .UNSPECIFIED. ) 
 CURVE ( )  GEOMETRIC_REPRESENTATION_ITEM ( )  RATIONAL_B_SPLINE_CURVE ( ( 1.000000000000002220, 0.9238795325112844070, 1.000000000000000000, 0.9238795325112867385, 1.000000000000000000, 0.9238795325112867385, 1.000000000000000000, 0.9238795325112890700, 0.9999999999999976685 ) ) 
 REPRESENTATION_ITEM ( '' )  );
#4127 = CARTESIAN_POINT ( 'NONE',  ( 4.898587196589412829E-16, 9.187499995903221972, -8.000000000000000000 ) ) ;
#4128 = ORIENTED_EDGE ( 'NONE', *, *, #124, .T. ) ;
#4129 = CARTESIAN_POINT ( 'NONE',  ( 28.00000000000001776, 195.9375000013655779, 166.5412658749999082 ) ) ;
#4130 = CARTESIAN_POINT ( 'NONE',  ( 2.977408999572651815, 18.56249999795161187, 7.188101187500000933 ) ) ;
#4131 = CARTESIAN_POINT ( 'NONE',  ( -11.35316468750000141, 163.8020833299193555, 3.042071309553159963 ) ) ;
#4132 = FACE_OUTER_BOUND ( 'NONE', #32860, .T. ) ;
#4133 = CARTESIAN_POINT ( 'NONE',  ( -7.188101187500000933, 101.9375000020483810, -2.977408999572650483 ) ) ;
#4135 = CARTESIAN_POINT ( 'NONE',  ( -4.999999999999992895, 235.8333333333333428, 8.660254037844390851 ) ) ;
#4134 = PLANE ( 'NONE',  #44373 ) ;
#4136 = CARTESIAN_POINT ( 'NONE',  ( 24.54126587499999701, 207.4375000013656063, 169.9999999999998863 ) ) ;
#4137 = EDGE_CURVE ( 'NONE', #59151, #22196, #2427, .T. ) ;
#4138 = CARTESIAN_POINT ( 'NONE',  ( 5.082755093536320601, -5.082755093536318824, 18.92405278187175455 ) ) ;
#4139 = CARTESIAN_POINT ( 'NONE',  ( -4.000000000000015099, 206.6875000027312126, 143.6568542494924543 ) ) ;
#4140 = CARTESIAN_POINT ( 'NONE',  ( 11.35316468749999785, 60.57291666325269830, 3.042071309553174174 ) ) ;
#4141 = CARTESIAN_POINT ( 'NONE',  ( 5.656854249492380582, 21.18750000000000355, -5.656854249492380582 ) ) ;
#4142 = CARTESIAN_POINT ( 'NONE',  ( -10.00000000000000178, 19.37499999317203603, -1.224646799147353454E-15 ) ) ;
#4143 = CARTESIAN_POINT ( 'NONE',  ( 29.65685424949250404, 199.4375000000000000, 165.9999999999999716 ) ) ;
#4144 = ORIENTED_EDGE ( 'NONE', *, *, #51043, .T. ) ;
#4145 = CARTESIAN_POINT ( 'NONE',  ( 2.679491924311222739, 140.8333333265053966, 10.00000000000000355 ) ) ;
#4146 = CARTESIAN_POINT ( 'NONE',  ( 11.00000000000010836, -4.556349186103939353, 81.34375000409679046 ) ) ;
#4147 = CARTESIAN_POINT ( 'NONE',  ( 3.042071309553159519, 49.73958332991934839, 11.35316468750000141 ) ) ;
#4148 = CARTESIAN_POINT ( 'NONE',  ( -4.556349186104045934, 11.00000000000000000, 80.40625000409676204 ) ) ;
#4149 = CARTESIAN_POINT ( 'NONE',  ( -1.432654583217664701, 199.0000000013656063, 138.5412658750000787 ) ) ;
#4150 = CARTESIAN_POINT ( 'NONE',  ( 1.781595147095969001, 16.42277972781688433, 68.70049804031583562 ) ) ;
#4151 = CARTESIAN_POINT ( 'NONE',  ( 4.000000000000016875, 207.4375000000000284, 199.6568542494924259 ) ) ;
#4153 = CARTESIAN_POINT ( 'NONE',  ( -2.085542519210945728E-15, 44.53124999658601979, 11.35316468750000141 ) ) ;
#4152 = CARTESIAN_POINT ( 'NONE',  ( -4.401442555609581635E-16, 98.28125000204838102, -7.188101187500000044 ) ) ;
#4154 = CARTESIAN_POINT ( 'NONE',  ( 3.313708498984762496, -7.999999999999989342, 10.29905277982336465 ) ) ;
#4155 = CARTESIAN_POINT ( 'NONE',  ( 7.320508075688771932, 205.6250000000000284, -7.320508075688771932 ) ) ;
#4156 = CARTESIAN_POINT ( 'NONE',  ( 11.35316468750000141, 155.7812499965860127, 0.000000000000000000 ) ) ;
#4158 = CARTESIAN_POINT ( 'NONE',  ( -7.320508075688778149, 139.9999999931720538, 7.320508075688769267 ) ) ;
#4157 = PRODUCT ( 'key', 'key', '', ( #45946 ) ) ;
#4159 = CARTESIAN_POINT ( 'NONE',  ( -2.977408999572650927, 101.7500000020483810, -7.188101187500001821 ) ) ;
#4160 = PRESENTATION_LAYER_ASSIGNMENT (  '', '', ( #72810 ) ) ;
#4161 = DIRECTION ( 'NONE',  ( 0.000000000000000000, 0.000000000000000000, -1.000000000000000000 ) ) ;
#4162 = CARTESIAN_POINT ( 'NONE',  ( 6.951808397369818766E-16, 37.34374999658601979, -11.35316468750000141 ) ) ;
#4163 = DIRECTION ( 'NONE',  ( -0.000000000000000000, -1.000000000000000000, -4.283267841918042741E-17 ) ) ;
#4164 = VERTEX_POINT ( 'NONE', #4475 ) ;
#4165 = CARTESIAN_POINT ( 'NONE',  ( 49.61244609327837196, 136.1494882842762308, 58.19005307411759276 ) ) ;
#4166 = CARTESIAN_POINT ( 'NONE',  ( 1.871523826299183495E-15, -10.18810118749999916, 78.53125000204836681 ) ) ;
#4167 = CARTESIAN_POINT ( 'NONE',  ( -5.204170427930421283E-15, 20.78460969082654231, -1.607695154586745501 ) ) ;
#4169 = CARTESIAN_POINT ( 'NONE',  ( 8.311093377946837890, 171.4062499965860127, -8.311093377946837890 ) ) ;
#4168 = CARTESIAN_POINT ( 'NONE',  ( 0.000000000000000000, 0.000000000000000000, 118.0000000000000000 ) ) ;
#4170 = CARTESIAN_POINT ( 'NONE',  ( 7.999999999999992895, -3.313708498984756279, 12.04280278432982243 ) ) ;
#4171 = CARTESIAN_POINT ( 'NONE',  ( 2.828427124746153876, 208.0000000027312126, 144.8284271247462129 ) ) ;
#4172 = CARTESIAN_POINT ( 'NONE',  ( 3.042071309553173286, 220.3645833367472733, 11.35316468749999608 ) ) ;
#4173 = CARTESIAN_POINT ( 'NONE',  ( -4.465384415997284862, 56.41424811512398207, -44.23559237190911375 ) ) ;
#4174 = CARTESIAN_POINT ( 'NONE',  ( -4.220049686691935698, 10.18810118749999916, 84.25000000204838102 ) ) ;
#4175 = ORIENTED_EDGE ( 'NONE', *, *, #68445, .F. ) ;
#4176 = CARTESIAN_POINT ( 'NONE',  ( -18.00000000000000000, 10.39230484541324628, -21.50000000000000000 ) ) ;
#4177 = CARTESIAN_POINT ( 'NONE',  ( -11.00000000000000000, 0.000000000000000000, 106.0000000000000000 ) ) ;
#4178 = CARTESIAN_POINT ( 'NONE',  ( 3.042071309553167069, 112.1354166632526699, -11.35316468749999785 ) ) ;
#4179 = CARTESIAN_POINT ( 'NONE',  ( -8.342170076843785083E-16, 19.18749999863440436, 4.541265875000002339 ) ) ;
#4180 = ORIENTED_EDGE ( 'NONE', *, *, #50871, .T. ) ;
#4181 = ORIENTED_EDGE ( 'NONE', *, *, #74544, .F. ) ;
#4182 = VECTOR ( 'NONE', #33358, 1000.000000000000000 ) ;
#4183 = CARTESIAN_POINT ( 'NONE',  ( 3.211159895383561835, 6.562499998634407028, -3.211159895383561835 ) ) ;
#4184 = CARTESIAN_POINT ( 'NONE',  ( -7.188101187500002709, 7.312499997951610986, 2.977408999572649151 ) ) ;
#4185 = CARTESIAN_POINT ( 'NONE',  ( 8.000000000000000000, 109.5312500040968047, -3.313708498984762496 ) ) ;
#4186 = CARTESIAN_POINT ( 'NONE',  ( 1.871523826299183495E-15, -10.18810118749999916, 90.90625000204838102 ) ) ;
#4187 = CARTESIAN_POINT ( 'NONE',  ( -26.56734541678238060, 201.6250000013656063, 166.5412658750003629 ) ) ;
#4188 = CARTESIAN_POINT ( 'NONE',  ( -4.000000000000001776, 7.437500000000000888, -1.656854249492381470 ) ) ;
#4189 = CARTESIAN_POINT ( 'NONE',  ( 2.828427124746191623, 18.87499999726881228, -2.828427124746191623 ) ) ;
#4190 = CARTESIAN_POINT ( 'NONE',  ( -4.541265875000003227, 8.874999998634407916, 1.881053915767121110 ) ) ;
#4191 = CARTESIAN_POINT ( 'NONE',  ( -4.000000000000015099, 196.5625000000000284, 143.6568542494924543 ) ) ;
#4192 = VERTEX_POINT ( 'NONE', #49743 ) ;
#4193 = SURFACE_STYLE_FILL_AREA ( #4938 ) ;
#4195 = CARTESIAN_POINT ( 'NONE',  ( 11.00000000000000000, 1.347111479062088405E-15, 96.43750000409677625 ) ) ;
#4194 = CARTESIAN_POINT ( 'NONE',  ( -31.45873412499995680, 196.7500000013656063, 171.4326545832181239 ) ) ;
#4196 = CARTESIAN_POINT ( 'NONE',  ( 3.211159895383560947, 20.18749999863440436, 3.211159895383562723 ) ) ;
#4197 = CARTESIAN_POINT ( 'NONE',  ( 0.000000000000000000, 125.0000000000000000, 0.000000000000000000 ) ) ;
#4198 = CARTESIAN_POINT ( 'NONE',  ( 2.775557561562891351E-14, -70.00000000000000000, 170.0000000000000000 ) ) ;
#4199 = VERTEX_POINT ( 'NONE', #66721 ) ;
#4200 = VERTEX_POINT ( 'NONE', #56533 ) ;
#4201 = CARTESIAN_POINT ( 'NONE',  ( 10.18810118750000093, -4.220049686691933033, 95.31250000204838102 ) ) ;
#4202 = CARTESIAN_POINT ( 'NONE',  ( -25.55430564589115150, 200.3125000013656063, 172.4456943541091789 ) ) ;
#4203 = CARTESIAN_POINT ( 'NONE',  ( -4.556349186104045934, 11.00000000000000000, 105.7187499999999716 ) ) ;
#4204 = CARTESIAN_POINT ( 'NONE',  ( 1.432654583217662481, 207.3750000013656063, 194.5412658750000219 ) ) ;
#4205 = CARTESIAN_POINT ( 'NONE',  ( 0.000000000000000000, 300.0000000000000000, 6.000000000000001776 ) ) ;
#4206 = CARTESIAN_POINT ( 'NONE',  ( 10.00000000000000178, 125.0000000000000000, 0.000000000000000000 ) ) ;
#4207 = ADVANCED_FACE ( 'NONE', ( #61059 ), #61809, .T. ) ;
#4208 = CARTESIAN_POINT ( 'NONE',  ( -5.656854249492380582, 108.3124999999999858, -5.656854249492380582 ) ) ;
#4209 = CARTESIAN_POINT ( 'NONE',  ( 2.765530957081996366, 290.2968750017069510, -6.676582343750003368 ) ) ;
#4210 = CARTESIAN_POINT ( 'NONE',  ( 7.188101187499992051, 8.802885111219154394E-16, 13.11155278187175277 ) ) ;
#4211 = ORIENTED_EDGE ( 'NONE', *, *, #48966, .F. ) ;
#4212 = CARTESIAN_POINT ( 'NONE',  ( -7.999999999999998224, 102.7812500040967763, 3.313708498984766049 ) ) ;
#4213 = CARTESIAN_POINT ( 'NONE',  ( 29.43265458321761230, 205.5000000013655779, 173.4587341249998929 ) ) ;
#4214 = CARTESIAN_POINT ( 'NONE',  ( 5.656854249492380582, 25.49999999590322375, -5.656854249492380582 ) ) ;
#4215 = CARTESIAN_POINT ( 'NONE',  ( -3.458734125000015425, 199.0000000013656063, 143.4326545832176976 ) ) ;
#4216 = CARTESIAN_POINT ( 'NONE',  ( 1.320432766682874540E-15, 121.9062500020483810, 7.188101187500000044 ) ) ;
#4218 = CARTESIAN_POINT ( 'NONE',  ( 1.432654583217608080, 201.8750000013656063, 138.5412658750000503 ) ) ;
#4217 = CARTESIAN_POINT ( 'NONE',  ( 0.2583006032756246517, 194.9270552508774017, 145.9270552508773733 ) ) ;
#4219 = CARTESIAN_POINT ( 'NONE',  ( 11.35316468749999963, 256.7187500034139589, -1.390361679473963556E-15 ) ) ;
#4220 = DIRECTION ( 'NONE',  ( 0.000000000000000000, 0.000000000000000000, 1.000000000000000000 ) ) ;
#4221 = DIRECTION ( 'NONE',  ( 0.000000000000000000, -0.8778652960885044987, 0.4789076340208435756 ) ) ;
#4222 =( BOUNDED_CURVE ( )  B_SPLINE_CURVE ( 2, ( #40960, #6632, #12280, #35315, #13732, #1718, #6997, #48450, #19047, #30375, #30008, #8465, #7734 ),
 .UNSPECIFIED., .F., .F. ) 
 B_SPLINE_CURVE_WITH_KNOTS ( ( 3, 2, 2, 2, 2, 2, 3 ),
 ( 0.1032608695652173919, 0.1050724637681159368, 0.1068840579710144956, 0.1086956521739130405, 0.1105072463768115992, 0.1123188405797101441, 0.1141304347826086890 ),
 .UNSPECIFIED. ) 
 CURVE ( )  GEOMETRIC_REPRESENTATION_ITEM ( )  RATIONAL_B_SPLINE_CURVE ( ( 1.000000000000000000, 0.9659258262890683122, 1.000000000000000000, 0.9659258262890683122, 1.000000000000000000, 0.9659258262890683122, 1.000000000000000000, 0.9659258262890683122, 1.000000000000000000, 0.9659258262890683122, 1.000000000000000000, 0.9659258262890683122, 1.000000000000000000 ) ) 
 REPRESENTATION_ITEM ( '' )  );
#4223 = CARTESIAN_POINT ( 'NONE',  ( -8.311093377946841443, 3.906249996586016682, 8.311093377946830785 ) ) ;
#4224 = CARTESIAN_POINT ( 'NONE',  ( 1.320432766682872962E-15, -7.188101187499992051, 0.7365527818717527708 ) ) ;
#4225 = CARTESIAN_POINT ( 'NONE',  ( -2.085542519210945728E-15, 204.8437499965860411, 11.35316468750000141 ) ) ;
#4226 = CARTESIAN_POINT ( 'NONE',  ( 1.224646799147353454E-15, 300.0000000000000000, -10.00000000000000178 ) ) ;
#4227 = CARTESIAN_POINT ( 'NONE',  ( -1.881053915767121554, 5.624999998634407028, -4.541265875000002339 ) ) ;
#4228 = CARTESIAN_POINT ( 'NONE',  ( -30.82842712474620939, 198.1250000000000284, 167.1715728752542134 ) ) ;
#4230 = DIRECTION ( 'NONE',  ( -1.000000000000000000, -9.955163135201253416E-17, 0.000000000000000000 ) ) ;
#4229 = CARTESIAN_POINT ( 'NONE',  ( 1.656854249492280440, 202.9375000027312410, 146.0000000000001421 ) ) ;
#4231 = ORIENTED_EDGE ( 'NONE', *, *, #17110, .F. ) ;
#4232 = CARTESIAN_POINT ( 'NONE',  ( -2.839093476692135984E-14, 201.9375000013656063, 138.5412658750000503 ) ) ;
#4233 = CARTESIAN_POINT ( 'NONE',  ( -3.042071309553164404, 12.23958332991935194, -11.35316468749999963 ) ) ;
#4234 = CARTESIAN_POINT ( 'NONE',  ( -10.99999999999999822, -4.556349186104052151, 95.78125000409680467 ) ) ;
#4235 = CARTESIAN_POINT ( 'NONE',  ( 6.123233995736767268E-16, 158.1249999931720254, -10.00000000000000178 ) ) ;
#4236 = ADVANCED_FACE ( 'NONE', ( #50114 ), #62544, .T. ) ;
#4237 = CARTESIAN_POINT ( 'NONE',  ( -24.54126587499999346, 198.1875000013655779, 170.0000000000002842 ) ) ;
#4238 = PLANE ( 'NONE',  #61144 ) ;
#4240 = CARTESIAN_POINT ( 'NONE',  ( -8.311093377946836114, 2.656249996586016238, -8.311093377946837890 ) ) ;
#4239 = CARTESIAN_POINT ( 'NONE',  ( -7.188101187499999156, 116.7500000020483810, 2.977408999572654924 ) ) ;
#4241 = CARTESIAN_POINT ( 'NONE',  ( -7.999999999999991118, 3.313708498984756723, 29.23655277982336642 ) ) ;
#4242 = CARTESIAN_POINT ( 'NONE',  ( -3.042071309553173730, 119.3229166632526699, 11.35316468749999785 ) ) ;
#4243 = CARTESIAN_POINT ( 'NONE',  ( 7.320508075688774596, 97.49999999317203958, -7.320508075688774596 ) ) ;
#4244 = CARTESIAN_POINT ( 'NONE',  ( -2.977408999572651815, 118.8125000020484094, 7.188101187500000933 ) ) ;
#4245 = CARTESIAN_POINT ( 'NONE',  ( -1.881053915767124440, 22.12499999863441502, 4.541265875000001451 ) ) ;
#4246 = CARTESIAN_POINT ( 'NONE',  ( -3.313708498984759387, -7.999999999999989342, 25.29905278392014978 ) ) ;
#4247 = CARTESIAN_POINT ( 'NONE',  ( 7.320508075688776373, 144.3750000000000000, 7.320508075688779925 ) ) ;
#4248 = ORIENTED_EDGE ( 'NONE', *, *, #74483, .T. ) ;
#4249 = CARTESIAN_POINT ( 'NONE',  ( 5.126144196591281066, -68.65853088339385124, 20.89430926783037634 ) ) ;
#4250 =( BOUNDED_CURVE ( )  B_SPLINE_CURVE ( 2, ( #72191, #20503, #16609, #28321, #20133, #66165, #74339, #22647, #45667 ),
 .UNSPECIFIED., .F., .F. ) 
 B_SPLINE_CURVE_WITH_KNOTS ( ( 3, 2, 2, 2, 3 ),
 ( 0.05882352941176473976, 0.06250000000000004163, 0.06617647058823533657, 0.06985294117647063150, 0.07352941176470592644 ),
 .UNSPECIFIED. ) 
 CURVE ( )  GEOMETRIC_REPRESENTATION_ITEM ( )  RATIONAL_B_SPLINE_CURVE ( ( 0.9999999999999993339, 0.9238795325112874046, 1.000000000000000000, 0.9238795325112867385, 1.000000000000000000, 0.9238795325112867385, 1.000000000000000000, 0.9238795325112858503, 1.000000000000000888 ) ) 
 REPRESENTATION_ITEM ( '' )  );
#4251 = CARTESIAN_POINT ( 'NONE',  ( -6.676582343750003368, 288.5468750017070079, -2.765530957081996810 ) ) ;
#4252 = CARTESIAN_POINT ( 'NONE',  ( -3.313708498984757167, 7.999999999999991118, 27.60530278432982954 ) ) ;
#4253 = CARTESIAN_POINT ( 'NONE',  ( 2.751064625579944321E-14, 200.8750000027312126, 194.0000000000000568 ) ) ;
#4254 = CARTESIAN_POINT ( 'NONE',  ( 3.042071309553173286, 260.3645833367473301, 11.35316468749999608 ) ) ;
#4255 = CARTESIAN_POINT ( 'NONE',  ( -4.220049686691935698, 10.18810118749999916, 100.7500000020483526 ) ) ;
#4256 = EDGE_LOOP ( 'NONE', ( #29127, #59898, #40141, #63474 ) ) ;
#4257 = AXIS2_PLACEMENT_3D ( 'NONE', #53997, #24933, #20017 ) ;
#4258 = CARTESIAN_POINT ( 'NONE',  ( 10.00000000000000178, 157.0833333265053398, -2.679491924311226736 ) ) ;
#4259 = CARTESIAN_POINT ( 'NONE',  ( -9.832129032723418760, 158.1770833299193555, -5.676582343750004256 ) ) ;
#4260 = CARTESIAN_POINT ( 'NONE',  ( -4.556349186104045934, 11.00000000000000000, 98.21875000000000000 ) ) ;
#4261 = CARTESIAN_POINT ( 'NONE',  ( -3.458734124999960358, 204.6250000013656063, 196.5673454167823877 ) ) ;
#4262 = CARTESIAN_POINT ( 'NONE',  ( 9.999999999999998224, 230.8333333401612890, -2.679491924311229401 ) ) ;
#4263 = CARTESIAN_POINT ( 'NONE',  ( 3.042071309553167069, 72.13541666325268409, -11.35316468749999785 ) ) ;
#4264 = EDGE_LOOP ( 'NONE', ( #42185, #33044 ) ) ;
#4265 = CARTESIAN_POINT ( 'NONE',  ( 10.18810118749999916, 4.220049686691935698, 115.0000000020483668 ) ) ;
#4266 = CARTESIAN_POINT ( 'NONE',  ( -4.541265875000002339, 9.937499998634406140, -5.561446717895856393E-16 ) ) ;
#4267 = VERTEX_POINT ( 'NONE', #10499 ) ;
#4268 = CARTESIAN_POINT ( 'NONE',  ( 8.000000000000000000, 1.593750000000000000, -3.313708498984761608 ) ) ;
#4269 = CARTESIAN_POINT ( 'NONE',  ( -6.000000000000000888, 290.1250000034140157, 2.485281374238575758 ) ) ;
#4270 = CARTESIAN_POINT ( 'NONE',  ( 6.123233995736767268E-16, 68.12499999317203958, -10.00000000000000178 ) ) ;
#4271 = CARTESIAN_POINT ( 'NONE',  ( 5.082755093536324154, 18.65624999795161187, 5.082755093536326818 ) ) ;
#4272 = DIRECTION ( 'NONE',  ( -0.000000000000000000, -0.000000000000000000, 1.000000000000000000 ) ) ;
#4273 = CARTESIAN_POINT ( 'NONE',  ( 7.204075437095968759, -7.204075437095966983, 109.0937500020483810 ) ) ;
#4274 = CARTESIAN_POINT ( 'NONE',  ( 11.00000000000000000, 1.347111479062088405E-15, 118.0000000000000000 ) ) ;
#4275 = CARTESIAN_POINT ( 'NONE',  ( -4.000000000000002665, 7.312499997268812280, 1.656854249492380804 ) ) ;
#4276 = CARTESIAN_POINT ( 'NONE',  ( -3.209238430557093125E-14, 191.0000000000000284, 142.0000000000000568 ) ) ;
#4277 = ORIENTED_EDGE ( 'NONE', *, *, #45362, .F. ) ;
#4278 = EDGE_CURVE ( 'NONE', #58637, #20164, #37472, .T. ) ;
#4279 = CARTESIAN_POINT ( 'NONE',  ( -3.458734124999959025, 203.5000000013655779, 199.4326545832176691 ) ) ;
#4280 = CARTESIAN_POINT ( 'NONE',  ( -29.43265458321756256, 208.8750000013656347, 173.4587341250004044 ) ) ;
#4281 = CARTESIAN_POINT ( 'NONE',  ( -7.347880794884122694E-16, 12.49999999726881406, 4.000000000000001776 ) ) ;
#4282 = CARTESIAN_POINT ( 'NONE',  ( 1.881053915767121776, 5.499999998634407028, -4.541265875000002339 ) ) ;
#4283 = CARTESIAN_POINT ( 'NONE',  ( -2.828427124746190735, 13.37500000000000000, -2.828427124746191623 ) ) ;
#4284 = CARTESIAN_POINT ( 'NONE',  ( -2.977408999572647819, 7.188101187499991163, 20.70530278187175455 ) ) ;
#4285 = ORIENTED_EDGE ( 'NONE', *, *, #28200, .T. ) ;
#4286 = CARTESIAN_POINT ( 'NONE',  ( -11.00000000000021139, 4.556349186103834548, 90.90625000000001421 ) ) ;
#4287 = ORIENTED_EDGE ( 'NONE', *, *, #4737, .F. ) ;
#4288 = CARTESIAN_POINT ( 'NONE',  ( -7.204075437095965206, -7.204075437095968759, 115.8437500020483810 ) ) ;
#4289 = CARTESIAN_POINT ( 'NONE',  ( -2.828427124746192067, 18.62500000000000000, 2.828427124746190735 ) ) ;
#4290 = CARTESIAN_POINT ( 'NONE',  ( -2.445694354108782775, 203.5625000013656063, 200.4456943541088663 ) ) ;
#4291 = CARTESIAN_POINT ( 'NONE',  ( 26.56734541678233086, 201.0000000013655779, 166.5412658749999650 ) ) ;
#4292 = CARTESIAN_POINT ( 'NONE',  ( 2.679491924311222739, 63.95833333333334281, 10.00000000000000355 ) ) ;
#4293 = ADVANCED_FACE ( 'NONE', ( #20688 ), #72761, .F. ) ;
#4294 = CARTESIAN_POINT ( 'NONE',  ( -7.188101187500000044, 90.03125000204838102, 0.000000000000000000 ) ) ;
#4295 = CARTESIAN_POINT ( 'NONE',  ( 6.000000000000003553, 292.4375000000000000, 2.485281374238571317 ) ) ;
#4296 = VECTOR ( 'NONE', #37566, 1000.000000000000000 ) ;
#4297 = CARTESIAN_POINT ( 'NONE',  ( 23.99999999999998934, 203.8750000027312126, 169.9999999999999432 ) ) ;
#4298 = VERTEX_POINT ( 'NONE', #27465 ) ;
#4299 = EDGE_CURVE ( 'NONE', #1142, #60974, #25218, .T. ) ;
#4300 = DIRECTION ( 'NONE',  ( -0.000000000000000000, 1.000000000000000000, -0.000000000000000000 ) ) ;
#4301 = VECTOR ( 'NONE', #63942, 1000.000000000000000 ) ;
#4302 = CARTESIAN_POINT ( 'NONE',  ( -11.00000000000000000, 0.000000000000000000, 118.0000000000000000 ) ) ;
#4303 = CARTESIAN_POINT ( 'NONE',  ( -2.751064625579944321E-14, 195.8750000027311842, 146.0000000000000284 ) ) ;
#4304 = DIRECTION ( 'NONE',  ( -0.000000000000000000, 1.000000000000000000, -0.000000000000000000 ) ) ;
#4305 = DIRECTION ( 'NONE',  ( 0.000000000000000000, -1.000000000000000000, 0.000000000000000000 ) ) ;
#4306 = CARTESIAN_POINT ( 'NONE',  ( 5.000000000000004441, 246.6666666666666856, 8.660254037844385522 ) ) ;
#4307 = CARTESIAN_POINT ( 'NONE',  ( 32.00000000000000711, 203.3125000027312126, 171.6568542494922553 ) ) ;
#4308 = CARTESIAN_POINT ( 'NONE',  ( 7.320508075688771044, 184.3750000000000000, 7.320508075688775484 ) ) ;
#4309 = DIRECTION ( 'NONE',  ( -0.000000000000000000, 1.000000000000000000, -0.000000000000000000 ) ) ;
#4310 = CARTESIAN_POINT ( 'NONE',  ( -5.082755093536317936, -5.082755093536320601, 24.54905278187175810 ) ) ;
#4311 = CARTESIAN_POINT ( 'NONE',  ( 11.35316468750000141, 171.0937499965860127, 0.000000000000000000 ) ) ;
#4312 = CARTESIAN_POINT ( 'NONE',  ( 0.000000000000000000, 0.000000000000000000, 0.000000000000000000 ) ) ;
#4313 = CARTESIAN_POINT ( 'NONE',  ( -5.000000000000001776, 53.53174224766548406, 46.57871628774437056 ) ) ;
#4314 = LINE ( 'NONE', #62377, #30835 ) ;
#4316 = CARTESIAN_POINT ( 'NONE',  ( -3.469446951953614189E-15, 16.00000000000000000, 38.34805510287551300 ) ) ;
#4315 = FACE_OUTER_BOUND ( 'NONE', #62516, .T. ) ;
#4317 = ORIENTED_EDGE ( 'NONE', *, *, #8619, .F. ) ;
#4318 = CARTESIAN_POINT ( 'NONE',  ( 3.042071309553159519, 20.05208332991934839, 11.35316468750000141 ) ) ;
#4319 = ADVANCED_FACE ( 'NONE', ( #26724 ), #38808, .F. ) ;
#4321 = CARTESIAN_POINT ( 'NONE',  ( 0.7581620860255156025, -10.12340554704895901, -70.09014334688596648 ) ) ;
#4320 = CARTESIAN_POINT ( 'NONE',  ( -7.999999999999991118, 9.797174393178815797E-16, 30.00000000000000000 ) ) ;
#4322 = CARTESIAN_POINT ( 'NONE',  ( -10.99999999999992184, -31.99999999999978684, 198.9827534923788619 ) ) ;
#4323 = CARTESIAN_POINT ( 'NONE',  ( -3.458734125000015425, 201.0000000013655779, 143.4326545832176976 ) ) ;
#4324 = CARTESIAN_POINT ( 'NONE',  ( -8.660254037844387298, 48.95833332650536818, -5.000000000000004441 ) ) ;
#4325 = CARTESIAN_POINT ( 'NONE',  ( -5.082755093536324154, 100.3437500020483810, 5.082755093536326818 ) ) ;
#4326 = CARTESIAN_POINT ( 'NONE',  ( -3.211159895383561391, 6.812499998634407028, -3.211159895383561835 ) ) ;
#4327 = CARTESIAN_POINT ( 'NONE',  ( 9.999999999999985789, 100.0000000000000142, 0.000000000000000000 ) ) ;
#4328 = CARTESIAN_POINT ( 'NONE',  ( -7.999999999999991118, 3.313708498984756723, 6.736552779823365533 ) ) ;
#4329 = ORIENTED_EDGE ( 'NONE', *, *, #26977, .F. ) ;
#4330 = VERTEX_POINT ( 'NONE', #21801 ) ;
#4331 = CARTESIAN_POINT ( 'NONE',  ( 5.656854249492378806, 28.12499999590322375, 5.656854249492381470 ) ) ;
#4332 = CARTESIAN_POINT ( 'NONE',  ( 1.432654583217664701, 196.0000000013656063, 201.4587341250000065 ) ) ;
#4333 = CARTESIAN_POINT ( 'NONE',  ( 3.313708498984756279, 7.999999999999991118, 1.861552779823364867 ) ) ;
#4334 = CARTESIAN_POINT ( 'NONE',  ( -23.07465293256997541, -39.63775957370906156, 149.2940779566946219 ) ) ;
#4335 = CARTESIAN_POINT ( 'NONE',  ( 8.311093377946834337, 145.1562499965860127, 8.311093377946839666 ) ) ;
#4336 = VERTEX_POINT ( 'NONE', #15025 ) ;
#4337 = CARTESIAN_POINT ( 'NONE',  ( -5.000000000000000888, 10.54112798502250214, -66.30787999718575065 ) ) ;
#4338 = CARTESIAN_POINT ( 'NONE',  ( 7.204075437095968759, -7.204075437095966983, 92.21875000204838102 ) ) ;
#4339 = CARTESIAN_POINT ( 'NONE',  ( -7.999999999999991118, -6.056862366737761932E-06, 20.51780295527825970 ) ) ;
#4340 = CARTESIAN_POINT ( 'NONE',  ( -3.999999999999959144, 209.0625000000000568, 199.6568542494924259 ) ) ;
#4341 = CARTESIAN_POINT ( 'NONE',  ( -8.000000000000000000, 18.46874999590322020, -3.313708498984762496 ) ) ;
#4342 = CARTESIAN_POINT ( 'NONE',  ( 0.000000000000000000, 0.000000000000000000, 0.000000000000000000 ) ) ;
#4343 = VERTEX_POINT ( 'NONE', #44088 ) ;
#4344 =( BOUNDED_CURVE ( )  B_SPLINE_CURVE ( 2, ( #36931, #8251, #53178, #1140, #1516, #31266, #24118, #47132, #70164 ),
 .UNSPECIFIED., .F., .F. ) 
 B_SPLINE_CURVE_WITH_KNOTS ( ( 3, 2, 2, 2, 3 ),
 ( 0.3166666666666668184, 0.3250000000000002331, 0.3333333333333335924, 0.3416666666666670626, 0.3500000000000004219 ),
 .UNSPECIFIED. ) 
 CURVE ( )  GEOMETRIC_REPRESENTATION_ITEM ( )  RATIONAL_B_SPLINE_CURVE ( ( 0.9999999999999984457, 0.9238795325112882928, 1.000000000000000000, 0.9238795325112867385, 1.000000000000000000, 0.9238795325112867385, 1.000000000000000000, 0.9238795325112826307, 1.000000000000003997 ) ) 
 REPRESENTATION_ITEM ( '' )  );
#4345 = CARTESIAN_POINT ( 'NONE',  ( 2.679491924311350193, 256.4583333333333712, 9.999999999999930722 ) ) ;
#4346 = EDGE_CURVE ( 'NONE', #23901, #16471, #63811, .T. ) ;
#4347 = CARTESIAN_POINT ( 'NONE',  ( -35.91417783104116523, 173.6629059085571782, 172.9739037163024307 ) ) ;
#4348 = CARTESIAN_POINT ( 'NONE',  ( -9.832129032723418760, 113.1770833299193555, -5.676582343750004256 ) ) ;
#4349 = CARTESIAN_POINT ( 'NONE',  ( -1.432654583217607858, 203.6250000013656063, 201.4587341250000065 ) ) ;
#4350 = CARTESIAN_POINT ( 'NONE',  ( -2.977408999572654480, 15.37499999795161187, 7.188101187499999156 ) ) ;
#4351 = CARTESIAN_POINT ( 'NONE',  ( -4.220049686691935698, 10.18810118749999916, 81.25000000204838102 ) ) ;
#4352 = CARTESIAN_POINT ( 'NONE',  ( 11.35316468750000141, 36.09374999658601979, 0.000000000000000000 ) ) ;
#4353 = VERTEX_POINT ( 'NONE', #44459 ) ;
#4354 = CARTESIAN_POINT ( 'NONE',  ( 3.313708498984819339, 89.65625000409679046, 7.999999999999943157 ) ) ;
#4355 = CARTESIAN_POINT ( 'NONE',  ( 3.317071493978877683, 8.008118988124991233, 21.54436528394063188 ) ) ;
#4356 = CARTESIAN_POINT ( 'NONE',  ( 7.320508075688776373, 236.8749999999999716, 7.320508075688767491 ) ) ;
#4357 = CARTESIAN_POINT ( 'NONE',  ( 1.656854249492399234, 201.1875000000000284, 138.0000000000000853 ) ) ;
#4358 = CARTESIAN_POINT ( 'NONE',  ( 4.401442555609581635E-16, 5.343749997951610986, -7.188101187500000044 ) ) ;
#4359 = CARTESIAN_POINT ( 'NONE',  ( -6.000000000000001776, 299.0625000034140157, 0.000000000000000000 ) ) ;
#4360 = CARTESIAN_POINT ( 'NONE',  ( -6.000000000000003553, 296.9374999999999432, -2.485281374238571317 ) ) ;
#4361 = CARTESIAN_POINT ( 'NONE',  ( -1.320432766682874540E-15, 1.968749997951609876, 7.188101187500000044 ) ) ;
#4362 = EDGE_LOOP ( 'NONE', ( #48334, #61367 ) ) ;
#4363 = CARTESIAN_POINT ( 'NONE',  ( 3.042071309553167069, 147.1354166632526983, -11.35316468749999785 ) ) ;
#4364 = CARTESIAN_POINT ( 'NONE',  ( 7.204075437095966983, 7.204075437095967871, 77.59375000204838102 ) ) ;
#4365 = CARTESIAN_POINT ( 'NONE',  ( -31.45873412499997812, 196.7500000013656063, 171.4326545832180386 ) ) ;
#4366 = CARTESIAN_POINT ( 'NONE',  ( -4.000000000000015987, 198.5625000000000568, 143.6568542494924259 ) ) ;
#4367 = CARTESIAN_POINT ( 'NONE',  ( 2.780723358947928197E-16, 16.68749999863440436, -4.541265875000002339 ) ) ;
#4368 = EDGE_LOOP ( 'NONE', ( #6527, #66153, #41185, #6497, #35973 ) ) ;
#4369 = CARTESIAN_POINT ( 'NONE',  ( -1.656854249492348607, 204.3125000027312126, 202.0000000000000284 ) ) ;
#4370 = CARTESIAN_POINT ( 'NONE',  ( -1.656854249492403008, 208.6875000000000284, 146.0000000000000284 ) ) ;
#4371 = CARTESIAN_POINT ( 'NONE',  ( -25.17157287525386167, 206.0000000027312126, 167.1715728752541281 ) ) ;
#4372 = AXIS2_PLACEMENT_3D ( 'NONE', #43857, #2752, #25740 ) ;
#4373 = CARTESIAN_POINT ( 'NONE',  ( 1.469576158976823947E-15, 104.3750000000000000, 8.000000000000000000 ) ) ;
#4374 = ORIENTED_EDGE ( 'NONE', *, *, #19554, .T. ) ;
#4375 = CARTESIAN_POINT ( 'NONE',  ( -2.977408999572650039, 12.93749999795161187, -7.188101187500000933 ) ) ;
#4376 = CARTESIAN_POINT ( 'NONE',  ( 2.849036369511732440E-14, 195.3750000027311842, 202.0000000000000000 ) ) ;
#4377 = CARTESIAN_POINT ( 'NONE',  ( 4.556349186104052151, -10.99999999999999822, 73.65625000409676204 ) ) ;
#4378 = CARTESIAN_POINT ( 'NONE',  ( 11.35316468750000141, 190.7812499965860127, 0.000000000000000000 ) ) ;
#4379 = CARTESIAN_POINT ( 'NONE',  ( 7.188101187500000044, 114.7812500020483952, -8.802885111219163269E-16 ) ) ;
#4380 = CYLINDRICAL_SURFACE ( 'NONE', #422, 3.999999999999976019 ) ;
#4382 = EDGE_CURVE ( 'NONE', #27684, #15778, #15770, .T. ) ;
#4381 = CARTESIAN_POINT ( 'NONE',  ( -4.721056650415999201, 289.3281250017069510, -4.721056650415999201 ) ) ;
#4384 = CARTESIAN_POINT ( 'NONE',  ( 54.00000000000000000, 205.0000000000000284, 4.085831468968142743E-14 ) ) ;
#4383 = CARTESIAN_POINT ( 'NONE',  ( 10.00000000000011546, 80.00000000000007105, 0.000000000000000000 ) ) ;
#4385 = ORIENTED_EDGE ( 'NONE', *, *, #16196, .F. ) ;
#4386 = EDGE_CURVE ( 'NONE', #13669, #54736, #68654, .T. ) ;
#4387 = CARTESIAN_POINT ( 'NONE',  ( -8.311093377946836114, 258.2812500034140157, -8.311093377946836114 ) ) ;
#4388 = CARTESIAN_POINT ( 'NONE',  ( 5.082755093536318824, 5.082755093536319713, 20.79905278187175455 ) ) ;
#4389 = CARTESIAN_POINT ( 'NONE',  ( -8.660254037844390851, 9.791666659838700326, 4.999999999999998224 ) ) ;
#4390 = DIRECTION ( 'NONE',  ( -0.000000000000000000, 1.000000000000000000, -0.000000000000000000 ) ) ;
#4391 = CARTESIAN_POINT ( 'NONE',  ( -0.7509181236779562951, -65.76106071587255997, -26.27764834702091434 ) ) ;
#4392 = CARTESIAN_POINT ( 'NONE',  ( -2.793570158735337650, 21.99999999999999645, 3.629683044105539214 ) ) ;
#4393 = CARTESIAN_POINT ( 'NONE',  ( -8.660254037844387298, 147.0833333333333428, -5.000000000000004441 ) ) ;
#4394 = CARTESIAN_POINT ( 'NONE',  ( 5.000000000000000000, -29.68417822476656553, 4.268394125862918997 ) ) ;
#4395 = CARTESIAN_POINT ( 'NONE',  ( 0.000000000000000000, 15.08051212944140218, 15.04081104653146994 ) ) ;
#4396 = CARTESIAN_POINT ( 'NONE',  ( 8.000000000000000000, 94.34374999999998579, -3.313708498984762496 ) ) ;
#4397 = CARTESIAN_POINT ( 'NONE',  ( 5.676582343750001591, 111.9270833299193555, -9.832129032723420536 ) ) ;
#4398 = CARTESIAN_POINT ( 'NONE',  ( 5.000000000000001776, 212.7083333265053682, -8.660254037844389075 ) ) ;
#4399 = CARTESIAN_POINT ( 'NONE',  ( 2.020667218593132706E-15, -11.00000000000000000, 68.87499999999998579 ) ) ;
#4402 = DIRECTION ( 'NONE',  ( 0.000000000000000000, 0.000000000000000000, 1.000000000000000000 ) ) ;
#4401 = CARTESIAN_POINT ( 'NONE',  ( 31.45873412499999944, 199.6250000013656063, 171.4326545832175555 ) ) ;
#4400 = CARTESIAN_POINT ( 'NONE',  ( 29.43265458321766559, 198.1250000013656063, 166.5412658749999650 ) ) ;
#4403 = ORIENTED_EDGE ( 'NONE', *, *, #3156, .F. ) ;
#4404 = CARTESIAN_POINT ( 'NONE',  ( 7.869550824153699331, 225.5298564079165544, -6.197952182080146422 ) ) ;
#4405 = CARTESIAN_POINT ( 'NONE',  ( 5.676582343749993598, 224.9479166632526983, 9.832129032723422313 ) ) ;
#4406 = CARTESIAN_POINT ( 'NONE',  ( 28.00000000000002132, 199.1875000013655779, 166.5412658749999082 ) ) ;
#4407 = EDGE_CURVE ( 'NONE', #38634, #30969, #56908, .T. ) ;
#4408 = CARTESIAN_POINT ( 'NONE',  ( 9.832129032723416984, 210.6770833299193555, 5.676582343750006032 ) ) ;
#4409 = CARTESIAN_POINT ( 'NONE',  ( -7.188101187500000044, 119.6562500020483810, 0.000000000000000000 ) ) ;
#4410 = CARTESIAN_POINT ( 'NONE',  ( -4.541265875000003227, 18.87499999863441147, 1.881053915767121110 ) ) ;
#4411 = CARTESIAN_POINT ( 'NONE',  ( 25.55430564589114795, 196.5625000013656063, 172.4456943541086957 ) ) ;
#4412 = CARTESIAN_POINT ( 'NONE',  ( 3.313708498984756279, 7.999999999999991118, 24.36155277982336997 ) ) ;
#4413 = CARTESIAN_POINT ( 'NONE',  ( -48.05475929102906463, 40.72228170591533569, 62.38327136324792122 ) ) ;
#4414 = CARTESIAN_POINT ( 'NONE',  ( 8.311093377946837890, 101.4062499965859985, -8.311093377946837890 ) ) ;
#4415 = ORIENTED_EDGE ( 'NONE', *, *, #50379, .T. ) ;
#4416 = EDGE_CURVE ( 'NONE', #51670, #59533, #1683, .T. ) ;
#4417 = CARTESIAN_POINT ( 'NONE',  ( -7.999999999999991118, 9.797174393178815797E-16, 30.00000000000000000 ) ) ;
#4418 = CARTESIAN_POINT ( 'NONE',  ( -7.188101187500002709, 19.31249999795161543, 2.977408999572649151 ) ) ;
#4419 = CARTESIAN_POINT ( 'NONE',  ( -4.898587196589412829E-16, 108.3125000040967905, -8.000000000000000000 ) ) ;
#4420 = CARTESIAN_POINT ( 'NONE',  ( 11.35316468749999963, 256.7187500034139589, -1.390361679473963556E-15 ) ) ;
#4421 = CARTESIAN_POINT ( 'NONE',  ( 9.832129032723420536, 96.19791666325269830, -5.676582343749999815 ) ) ;
#4422 = VERTEX_POINT ( 'NONE', #28593 ) ;
#4423 = LINE ( 'NONE', #44410, #56062 ) ;
#4424 = CARTESIAN_POINT ( 'NONE',  ( -4.220049686691937474, -10.18810118749999738, 108.4375000020483668 ) ) ;
#4425 = DIRECTION ( 'NONE',  ( 0.8191520442889924647, 0.000000000000000000, 0.5735764363510451602 ) ) ;
#4426 = CARTESIAN_POINT ( 'NONE',  ( 2.445694354108839175, 205.3125000013656063, 195.5543056458912190 ) ) ;
#4427 = CARTESIAN_POINT ( 'NONE',  ( -32.00000000000000000, 201.3750000027312126, 170.0000000000004547 ) ) ;
#4429 = CARTESIAN_POINT ( 'NONE',  ( 5.676582343749993598, 84.94791666325268409, 9.832129032723422313 ) ) ;
#4428 = CARTESIAN_POINT ( 'NONE',  ( 11.00000000000000000, 1.347111479062088405E-15, 97.74999999999998579 ) ) ;
#4430 = CARTESIAN_POINT ( 'NONE',  ( 5.656854249492374365, 5.656854249492375253, 10.95530278392014800 ) ) ;
#4431 = CARTESIAN_POINT ( 'NONE',  ( -26.56734541678238060, 200.6250000013655779, 166.5412658750003629 ) ) ;
#4432 = DIRECTION ( 'NONE',  ( 1.000000000000000000, -0.000000000000000000, -0.000000000000000000 ) ) ;
#4433 = VECTOR ( 'NONE', #28367, 1000.000000000000000 ) ;
#4434 = CARTESIAN_POINT ( 'NONE',  ( -10.00000000000000000, 179.1666666598387394, -2.679491924311229845 ) ) ;
#4435 = EDGE_CURVE ( 'NONE', #10198, #28197, #22935, .T. ) ;
#4436 = AXIS2_PLACEMENT_3D ( 'NONE', #53754, #42413, #42784 ) ;
#4437 = CARTESIAN_POINT ( 'NONE',  ( 1.459323541827198180E-11, 81.24999999999886313, -10.00000000000000533 ) ) ;
#4438 = CARTESIAN_POINT ( 'NONE',  ( 11.35316468749999785, 75.88541666325268409, 3.042071309553174174 ) ) ;
#4439 = CARTESIAN_POINT ( 'NONE',  ( 1.226468279477575784E-15, 287.7031250017069510, 6.676582343750001591 ) ) ;
#4440 = EDGE_CURVE ( 'NONE', #71803, #18289, #12245, .T. ) ;
#4441 = CARTESIAN_POINT ( 'NONE',  ( -7.204075437095967871, 7.204075437095967871, 103.8437500020483810 ) ) ;
#4442 = CARTESIAN_POINT ( 'NONE',  ( -5.676582343749998039, 202.4479166632526983, -9.832129032723420536 ) ) ;
#4443 = VERTEX_POINT ( 'NONE', #74242 ) ;
#4444 = CARTESIAN_POINT ( 'NONE',  ( 2.449293598294707893E-16, 2.250000000000000444, -4.000000000000001776 ) ) ;
#4445 = CARTESIAN_POINT ( 'NONE',  ( -6.676582343750001591, 287.6093750017069510, 0.000000000000000000 ) ) ;
#4446 = CARTESIAN_POINT ( 'NONE',  ( -5.656854249492378806, 120.6875000000000000, 5.656854249492381470 ) ) ;
#4447 = CARTESIAN_POINT ( 'NONE',  ( -9.832129032723418760, 212.8645833299193555, -5.676582343750004256 ) ) ;
#4448 = CARTESIAN_POINT ( 'NONE',  ( 7.320508075688776373, 225.0000000068279746, 7.320508075688767491 ) ) ;
#4449 = CARTESIAN_POINT ( 'NONE',  ( 6.123233995736767268E-16, 18.12499999317203248, -10.00000000000000178 ) ) ;
#4450 = ORIENTED_EDGE ( 'NONE', *, *, #5122, .T. ) ;
#4451 = CARTESIAN_POINT ( 'NONE',  ( -8.311093377946841443, 194.2187499965860127, 8.311093377946834337 ) ) ;
#4452 = CARTESIAN_POINT ( 'NONE',  ( 2.977408999572646486, 7.188101187499992051, 14.51780278187175455 ) ) ;
#4453 =( BOUNDED_CURVE ( )  B_SPLINE_CURVE ( 2, ( #36629, #19999, #2663, #13591, #49044, #49420, #59635, #53977, #48671, #61119, #25655, #71678, #14335, #60367, #54731, #72442, #14710, #3038, #26021, #20368, #66402, #37748, #20751, #43767, #66781, #15085, #32466, #58004, #58368, #39515, #28559, #17984, #28185, #45532, #22897, #51197, #74208, #6309, #69298, #10838, #5189, #17232, #28934, #51952, #68181, #46279, #22511, #23645, #45909, #12325, #64010, #6673, #56873, #289, #29314, #40627, #68550, #51565, #1027, #40253, #16853, #62512, #11580, #52323, #34242, #33873, #41003, #45170, #23270, #39879, #34615, #16477, #17609, #62881, #11214, #57244, #63627, #29677, #63255, #57621, #11957, #68922, #659, #34988, #5933, #46652, #69670, #35356, #52693, #5556, #74581, #48491, #2110, #41736, #58730, #1395, #35715, #65101, #30415, #30780, #42089, #13772, #7408, #25104, #64381, #19450, #59825, #36816, #65479, #71127, #7776, #13412, #24738, #24381, #47388, #53062, #37186, #19819, #19086, #54546, #36450, #47748, #64746, #70772, #8141, #42462, #31144, #71495, #54176, #59463, #41372, #30049, #70411, #36082, #48121, #2482, #25474, #42825, #12681, #65843, #53436, #14151, #60185, #18727, #8508, #31524, #7041, #70048, #13044, #24007, #53800, #47016, #18357, #59100, #1757, #4350, #43201, #73005, #21314, #55294, #10009, #49619, #32660, #56041, #61688, #67722, #66593, #20563, #27340, #55669, #43577, #37562, #54919, #14523, #43960, #9257, #9640, #20939, #3600, #66218, #49989, #60561, #44336, #38686, #15645, #67347, #33041, #61315, #66969, #26597, #3228, #26215, #31898, #16020, #73376, #72635, #33404, #15273, #50357, #8885, #21681, #44707, #39050, #62053, #10378, #2853, #38309, #20184, #49235, #72249, #14898, #3986, #25841, #48861, #71870, #37935, #60935, #32280, #26975, #50729, #34527, #69203, #46557, #73744, #27718, #11126, #68455, #69578, #40161, #17514, #17889, #22050, #39781, #29217, #39420, #56778, #34149, #62419, #10744, #40530, #5840, #22418, #5465, #28466, #63167, #11492, #4723, #57532, #33778, #34896, #57149, #23545, #562, #40904, #68092, #28834, #63536, #51853, #5099, #62784, #12224, #57903, #28090, #45078, #22794, #11861, #45440, #16381, #52230, #56404, #197, #51105, #16755, #51474, #74487, #23173, #46185, #74117, #6210, #45814, #63912, #68825, #17137, #36355, #64286, #54076, #59370, #1664, #30320 ),
 .UNSPECIFIED., .F., .F. ) 
 B_SPLINE_CURVE_WITH_KNOTS ( ( 3, 2, 2, 2, 2, 2, 2, 2, 2, 2, 2, 2, 2, 2, 2, 2, 2, 2, 2, 2, 2, 2, 2, 2, 2, 2, 2, 2, 2, 2, 2, 2, 2, 2, 2, 2, 2, 2, 2, 2, 2, 2, 2, 2, 2, 2, 2, 2, 2, 2, 2, 2, 2, 2, 2, 2, 2, 2, 2, 2, 2, 2, 2, 2, 2, 2, 2, 2, 2, 2, 2, 2, 2, 2, 2, 2, 2, 2, 2, 2, 2, 2, 2, 2, 2, 2, 2, 2, 2, 2, 2, 2, 2, 2, 2, 2, 2, 2, 2, 2, 2, 2, 2, 2, 2, 2, 2, 2, 2, 2, 2, 2, 2, 2, 2, 2, 2, 2, 2, 2, 2, 2, 2, 2, 2, 2, 2, 2, 2, 2, 2, 2, 2, 2, 2, 2, 2, 2, 2, 2, 2, 2, 2, 2, 3 ),
 ( 0.000000000000000000, 0.006944444444444444059, 0.01388888888888888812, 0.02083333333333333218, 0.02777777777777777624, 0.03472222222222222376, 0.04166666666666666435, 0.04861111111111111188, 0.05555555555555555247, 0.06250000000000000000, 0.06944444444444444753, 0.07638888888888889506, 0.08333333333333332871, 0.09027777777777777624, 0.09722222222222222376, 0.1041666666666666713, 0.1111111111111111049, 0.1180555555555555525, 0.1250000000000000000, 0.1319444444444444475, 0.1388888888888888951, 0.1458333333333333426, 0.1527777777777777901, 0.1597222222222222099, 0.1666666666666666574, 0.1736111111111111049, 0.1805555555555555525, 0.1875000000000000000, 0.1944444444444444475, 0.2013888888888888951, 0.2083333333333333426, 0.2152777777777777901, 0.2222222222222222099, 0.2291666666666666574, 0.2361111111111111049, 0.2430555555555555525, 0.2500000000000000000, 0.2569444444444444198, 0.2638888888888888951, 0.2708333333333333148, 0.2777777777777777901, 0.2847222222222222099, 0.2916666666666666852, 0.2986111111111111049, 0.3055555555555555802, 0.3125000000000000000, 0.3194444444444444198, 0.3263888888888888951, 0.3333333333333333148, 0.3402777777777777901, 0.3472222222222222099, 0.3541666666666666852, 0.3611111111111111049, 0.3680555555555555802, 0.3750000000000000000, 0.3819444444444444198, 0.3888888888888888951, 0.3958333333333333148, 0.4027777777777777901, 0.4097222222222222099, 0.4166666666666666852, 0.4236111111111111049, 0.4305555555555555802, 0.4375000000000000000, 0.4444444444444444198, 0.4513888888888888951, 0.4583333333333333148, 0.4652777777777777901, 0.4722222222222222099, 0.4791666666666666852, 0.4861111111111111049, 0.4930555555555555802, 0.5000000000000000000, 0.5069444444444444198, 0.5138888888888888395, 0.5208333333333333703, 0.5277777777777777901, 0.5347222222222222099, 0.5416666666666666297, 0.5486111111111111605, 0.5555555555555555802, 0.5625000000000000000, 0.5694444444444444198, 0.5763888888888888395, 0.5833333333333333703, 0.5902777777777777901, 0.5972222222222222099, 0.6041666666666666297, 0.6111111111111111605, 0.6180555555555555802, 0.6250000000000000000, 0.6319444444444444198, 0.6388888888888888395, 0.6458333333333333703, 0.6527777777777777901, 0.6597222222222222099, 0.6666666666666666297, 0.6736111111111111605, 0.6805555555555555802, 0.6875000000000000000, 0.6944444444444444198, 0.7013888888888888395, 0.7083333333333333703, 0.7152777777777777901, 0.7222222222222222099, 0.7291666666666666297, 0.7361111111111111605, 0.7430555555555555802, 0.7500000000000000000, 0.7569444444444444198, 0.7638888888888888395, 0.7708333333333333703, 0.7777777777777777901, 0.7847222222222222099, 0.7916666666666666297, 0.7986111111111111605, 0.8055555555555555802, 0.8125000000000000000, 0.8194444444444444198, 0.8263888888888888395, 0.8333333333333333703, 0.8402777777777777901, 0.8472222222222222099, 0.8541666666666666297, 0.8611111111111111605, 0.8680555555555555802, 0.8750000000000000000, 0.8819444444444444198, 0.8888888888888888395, 0.8958333333333333703, 0.9027777777777777901, 0.9097222222222222099, 0.9166666666666666297, 0.9236111111111111605, 0.9305555555555555802, 0.9375000000000000000, 0.9444444444444444198, 0.9513888888888888395, 0.9583333333333333703, 0.9652777777777777901, 0.9722222222222222099, 0.9791666666666666297, 0.9861111111111111605, 0.9930555555555555802, 1.000000000000000000 ),
 .UNSPECIFIED. ) 
 CURVE ( )  GEOMETRIC_REPRESENTATION_ITEM ( )  RATIONAL_B_SPLINE_CURVE ( ( 1.000000000000000000, 0.9238795325112867385, 1.000000000000000000, 0.9238795325112867385, 1.000000000000000000, 0.9238795325112867385, 1.000000000000000000, 0.9238795325112867385, 1.000000000000000000, 0.9238795325112867385, 1.000000000000000000, 0.9238795325112867385, 1.000000000000000000, 0.9238795325112867385, 1.000000000000000000, 0.9238795325112867385, 1.000000000000000000, 0.9238795325112867385, 1.000000000000000000, 0.9238795325112867385, 1.000000000000000000, 0.9238795325112867385, 1.000000000000000000, 0.9238795325112867385, 1.000000000000000000, 0.9238795325112867385, 1.000000000000000000, 0.9238795325112867385, 1.000000000000000000, 0.9238795325112867385, 1.000000000000000000, 0.9238795325112867385, 1.000000000000000000, 0.9238795325112867385, 1.000000000000000000, 0.9238795325112867385, 1.000000000000000000, 0.9238795325112867385, 1.000000000000000000, 0.9238795325112867385, 1.000000000000000000, 0.9238795325112867385, 1.000000000000000000, 0.9238795325112867385, 1.000000000000000000, 0.9238795325112867385, 1.000000000000000000, 0.9238795325112867385, 1.000000000000000000, 0.9238795325112867385, 1.000000000000000000, 0.9238795325112867385, 1.000000000000000000, 0.9238795325112867385, 1.000000000000000000, 0.9238795325112867385, 1.000000000000000000, 0.9238795325112867385, 1.000000000000000000, 0.9238795325112867385, 1.000000000000000000, 0.9238795325112867385, 1.000000000000000000, 0.9238795325112867385, 1.000000000000000000, 0.9238795325112867385, 1.000000000000000000, 0.9238795325112867385, 1.000000000000000000, 0.9238795325112867385, 1.000000000000000000, 0.9238795325112867385, 1.000000000000000000, 0.9238795325112867385, 1.000000000000000000, 0.9238795325112867385, 1.000000000000000000, 0.9238795325112867385, 1.000000000000000000, 0.9238795325112867385, 1.000000000000000000, 0.9238795325112867385, 1.000000000000000000, 0.9238795325112867385, 1.000000000000000000, 0.9238795325112867385, 1.000000000000000000, 0.9238795325112867385, 1.000000000000000000, 0.9238795325112867385, 1.000000000000000000, 0.9238795325112867385, 1.000000000000000000, 0.9238795325112867385, 1.000000000000000000, 0.9238795325112867385, 1.000000000000000000, 0.9238795325112867385, 1.000000000000000000, 0.9238795325112867385, 1.000000000000000000, 0.9238795325112867385, 1.000000000000000000, 0.9238795325112867385, 1.000000000000000000, 0.9238795325112867385, 1.000000000000000000, 0.9238795325112867385, 1.000000000000000000, 0.9238795325112867385, 1.000000000000000000, 0.9238795325112867385, 1.000000000000000000, 0.9238795325112867385, 1.000000000000000000, 0.9238795325112867385, 1.000000000000000000, 0.9238795325112867385, 1.000000000000000000, 0.9238795325112867385, 1.000000000000000000, 0.9238795325112867385, 1.000000000000000000, 0.9238795325112867385, 1.000000000000000000, 0.9238795325112867385, 1.000000000000000000, 0.9238795325112867385, 1.000000000000000000, 0.9238795325112867385, 1.000000000000000000, 0.9238795325112867385, 1.000000000000000000, 0.9238795325112867385, 1.000000000000000000, 0.9238795325112867385, 1.000000000000000000, 0.9238795325112867385, 1.000000000000000000, 0.9238795325112867385, 1.000000000000000000, 0.9238795325112867385, 1.000000000000000000, 0.9238795325112867385, 1.000000000000000000, 0.9238795325112867385, 1.000000000000000000, 0.9238795325112867385, 1.000000000000000000, 0.9238795325112867385, 1.000000000000000000, 0.9238795325112867385, 1.000000000000000000, 0.9238795325112867385, 1.000000000000000000, 0.9238795325112867385, 1.000000000000000000, 0.9238795325112867385, 1.000000000000000000, 0.9238795325112867385, 1.000000000000000000, 0.9238795325112867385, 1.000000000000000000, 0.9238795325112867385, 1.000000000000000000, 0.9238795325112867385, 1.000000000000000000, 0.9238795325112867385, 1.000000000000000000, 0.9238795325112867385, 1.000000000000000000, 0.9238795325112867385, 1.000000000000000000, 0.9238795325112867385, 1.000000000000000000, 0.9238795325112867385, 1.000000000000000000, 0.9238795325112867385, 1.000000000000000000, 0.9238795325112867385, 1.000000000000000000, 0.9238795325112867385, 1.000000000000000000, 0.9238795325112867385, 1.000000000000000000, 0.9238795325112867385, 1.000000000000000000, 0.9238795325112867385, 1.000000000000000000, 0.9238795325112867385, 1.000000000000000000, 0.9238795325112867385, 1.000000000000000000, 0.9238795325112867385, 1.000000000000000000, 0.9238795325112867385, 1.000000000000000000, 0.9238795325112867385, 1.000000000000000000, 0.9238795325112867385, 1.000000000000000000, 0.9238795325112867385, 1.000000000000000000, 0.9238795325112867385, 1.000000000000000000, 0.9238795325112867385, 1.000000000000000000, 0.9238795325112867385, 1.000000000000000000, 0.9238795325112867385, 1.000000000000000000, 0.9238795325112867385, 1.000000000000000000, 0.9238795325112867385, 1.000000000000000000, 0.9238795325112867385, 1.000000000000000000, 0.9238795325112867385, 1.000000000000000000, 0.9238795325112867385, 1.000000000000000000, 0.9238795325112867385, 1.000000000000000000, 0.9238795325112867385, 1.000000000000000000, 0.9238795325112867385, 1.000000000000000000, 0.9238795325112867385, 1.000000000000000000, 0.9238795325112867385, 1.000000000000000000, 0.9238795325112867385, 1.000000000000000000, 0.9238795325112867385, 1.000000000000000000, 0.9238795325112867385, 1.000000000000000000, 0.9238795325112867385, 1.000000000000000000, 0.9238795325112867385, 1.000000000000000000, 0.9238795325112867385, 1.000000000000000000, 0.9238795325112867385, 1.000000000000000000, 0.9238795325112867385, 1.000000000000000000, 0.9238795325112867385, 1.000000000000000000, 0.9238795325112867385, 1.000000000000000000, 0.9238795325112867385, 1.000000000000000000, 0.9238795325112867385, 1.000000000000000000, 0.9238795325112867385, 1.000000000000000000, 0.9238795325112867385, 1.000000000000000000, 0.9238795325112867385, 1.000000000000000000, 0.9238795325112867385, 1.000000000000000000, 0.9238795325112867385, 1.000000000000000000, 0.9238795325112867385, 1.000000000000000000, 0.9238795325112867385, 1.000000000000000000, 0.9238795325112867385, 1.000000000000000000, 0.9238795325112867385, 1.000000000000000000, 0.9238795325112867385, 1.000000000000000000, 0.9238795325112867385, 1.000000000000000000, 0.9238795325112867385, 1.000000000000000000, 0.9238795325112867385, 1.000000000000000000, 0.9238795325112867385, 1.000000000000000000, 0.9238795325112867385, 1.000000000000000000, 0.9238795325112867385, 1.000000000000000000, 0.9238795325112867385, 1.000000000000000000 ) ) 
 REPRESENTATION_ITEM ( '' )  );
#4454 = CARTESIAN_POINT ( 'NONE',  ( -24.54126587499998635, 208.1250000013656063, 171.4326545832179818 ) ) ;
#4455 =( BOUNDED_CURVE ( )  B_SPLINE_CURVE ( 2, ( #27328, #33390, #43947, #27704, #43562, #26960, #56390, #50715, #67336, #38673, #61675 ),
 .UNSPECIFIED., .F., .F. ) 
 B_SPLINE_CURVE_WITH_KNOTS ( ( 3, 2, 2, 2, 2, 3 ),
 ( 0.6088813560782819767, 0.6154996293544834352, 0.6221179049389403692, 0.6287361805233971923, 0.6353544561078539044, 0.6353544975714136012 ),
 .UNSPECIFIED. ) 
 CURVE ( )  GEOMETRIC_REPRESENTATION_ITEM ( )  RATIONAL_B_SPLINE_CURVE ( ( 1.000000000000000000, 0.9238795325112867385, 1.000000000000000000, 0.9238795325112867385, 1.000000000000000000, 0.9238795325112867385, 1.000000000000000000, 0.9238795325112867385, 1.000000000000000000, 0.9999995231045452071, 0.9999990462150658566 ) ) 
 REPRESENTATION_ITEM ( '' )  );
#4456 = CARTESIAN_POINT ( 'NONE',  ( -5.656854249492379694, 9.562500000000001776, -5.656854249492380582 ) ) ;
#4457 = VECTOR ( 'NONE', #50770, 1000.000000000000000 ) ;
#4458 = VERTEX_POINT ( 'NONE', #68959 ) ;
#4459 = ADVANCED_FACE ( 'NONE', ( #22548 ), #18021, .F. ) ;
#4460 = CARTESIAN_POINT ( 'NONE',  ( -5.082755093536325930, 95.84375000204838102, -5.082755093536325930 ) ) ;
#4461 = CARTESIAN_POINT ( 'NONE',  ( -5.656854249492378806, 89.37500000409679046, 5.656854249492381470 ) ) ;
#4462 = EDGE_CURVE ( 'NONE', #72985, #60077, #58203, .T. ) ;
#4463 = CARTESIAN_POINT ( 'NONE',  ( -1.836970198721029983E-15, 18.75000000000000355, 10.00000000000000178 ) ) ;
#4464 = CARTESIAN_POINT ( 'NONE',  ( 10.18810118749999916, 1.247682550866122264E-15, 80.78125000204838102 ) ) ;
#4465 = ORIENTED_EDGE ( 'NONE', *, *, #19462, .T. ) ;
#4466 = EDGE_CURVE ( 'NONE', #73371, #271, #48951, .T. ) ;
#4467 = CARTESIAN_POINT ( 'NONE',  ( -4.000000000000002665, 21.56250000000000000, 1.656854249492380804 ) ) ;
#4468 = CARTESIAN_POINT ( 'NONE',  ( -4.541265875000002339, 18.74999999863440436, -1.881053915767121998 ) ) ;
#4469 = CARTESIAN_POINT ( 'NONE',  ( 30.14770426596588848, 194.5119512990349051, 172.7880003522331265 ) ) ;
#4470 = VERTEX_POINT ( 'NONE', #325 ) ;
#4471 = CARTESIAN_POINT ( 'NONE',  ( -38.00000000000000000, 0.000000000000000000, 20.00000000000003553 ) ) ;
#4472 = CARTESIAN_POINT ( 'NONE',  ( -7.188101187500001821, 89.56250000204838102, -2.977408999572650483 ) ) ;
#4475 = CARTESIAN_POINT ( 'NONE',  ( 2.849036369511732440E-14, 196.2500000000000000, 202.0000000000000000 ) ) ;
#4474 = CARTESIAN_POINT ( 'NONE',  ( 11.35316468749999963, 251.1979166700806729, 3.042071309553159519 ) ) ;
#4473 = DIRECTION ( 'NONE',  ( -0.000000000000000000, 1.000000000000000000, -0.000000000000000000 ) ) ;
#4476 = APPLICATION_PROTOCOL_DEFINITION ( 'draft international standard', 'automotive_design', 1998, #41407 ) ;
#4477 = ORIENTED_EDGE ( 'NONE', *, *, #67248, .F. ) ;
#4478 = AXIS2_PLACEMENT_3D ( 'NONE', #36390, #6978, #29988 ) ;
#4479 = CARTESIAN_POINT ( 'NONE',  ( 8.311093377946839666, 256.0937500034140157, 8.311093377946829008 ) ) ;
#4480 = CARTESIAN_POINT ( 'NONE',  ( 2.977408999572650927, -7.188101187499990274, 15.45530278187175455 ) ) ;
#4481 = ORIENTED_EDGE ( 'NONE', *, *, #56056, .F. ) ;
#4482 = ORIENTED_EDGE ( 'NONE', *, *, #37486, .F. ) ;
#4483 = CARTESIAN_POINT ( 'NONE',  ( 7.204075437095968759, -7.204075437095966983, 77.21875000204836681 ) ) ;
#4484 = CARTESIAN_POINT ( 'NONE',  ( 11.35316468749999785, 75.88541666325268409, 3.042071309553174174 ) ) ;
#4485 = CARTESIAN_POINT ( 'NONE',  ( -3.313708498984759387, -7.999999999999989342, 17.61155277982336997 ) ) ;
#4486 = CARTESIAN_POINT ( 'NONE',  ( 7.778174593052023411, -7.778174593052021635, 91.56249999999998579 ) ) ;
#4489 = CARTESIAN_POINT ( 'NONE',  ( 6.676582343750002480, 289.1718750017071216, -2.765530957081997254 ) ) ;
#4488 = CARTESIAN_POINT ( 'NONE',  ( 27.99999999999996447, 197.6250000027312126, 165.9999999999998863 ) ) ;
#4487 = CARTESIAN_POINT ( 'NONE',  ( 24.54126587499998635, 209.5000000013656063, 171.4326545832175555 ) ) ;
#4490 = CARTESIAN_POINT ( 'NONE',  ( -62.39047978708157416, 229.6205190061017447, 45.00000000000000000 ) ) ;
#4491 = LINE ( 'NONE', #22953, #26315 ) ;
#4492 = CARTESIAN_POINT ( 'NONE',  ( -3.458734124999960358, 198.6875000013655779, 198.0000000000000284 ) ) ;
#4493 = CARTESIAN_POINT ( 'NONE',  ( 4.898587196589412829E-16, 6.187499995903221084, -8.000000000000000000 ) ) ;
#4494 = ORIENTED_EDGE ( 'NONE', *, *, #11398, .T. ) ;
#4495 = CARTESIAN_POINT ( 'NONE',  ( 30.44569435410883074, 194.8125000013656063, 167.5543056458911053 ) ) ;
#4496 = CARTESIAN_POINT ( 'NONE',  ( -5.082755093536326818, 15.28124999795161187, 5.082755093536325042 ) ) ;
#4497 = CARTESIAN_POINT ( 'NONE',  ( 11.35316468750000141, 166.0937499965860127, 0.000000000000000000 ) ) ;
#4498 = CARTESIAN_POINT ( 'NONE',  ( 4.556349186104052151, -10.99999999999999822, 99.15625000409677625 ) ) ;
#4499 = CARTESIAN_POINT ( 'NONE',  ( -5.082755093536324154, 102.2187500020483810, 5.082755093536326818 ) ) ;
#4501 = CARTESIAN_POINT ( 'NONE',  ( 1.882291019708790536, -55.75505015263587438, -43.87597576789006126 ) ) ;
#4500 = FACE_OUTER_BOUND ( 'NONE', #32423, .T. ) ;
#4502 = CARTESIAN_POINT ( 'NONE',  ( 31.45873412499999944, 206.9375000013656063, 169.9999999999999432 ) ) ;
#4503 = CARTESIAN_POINT ( 'NONE',  ( -7.188101187499990274, -2.977408999572651371, 18.45530278187175455 ) ) ;
#4504 = CARTESIAN_POINT ( 'NONE',  ( -4.000000000000015099, 207.6875000027311842, 143.6568542494924543 ) ) ;
#4505 = CARTESIAN_POINT ( 'NONE',  ( -5.676582343749998039, 52.44791666325268409, -9.832129032723420536 ) ) ;
#4506 = CARTESIAN_POINT ( 'NONE',  ( -1.836970198721029983E-15, 55.62499999317203958, 10.00000000000000178 ) ) ;
#4507 = CARTESIAN_POINT ( 'NONE',  ( -5.000000000000005329, 25.20833332650536818, 8.660254037844387298 ) ) ;
#4508 = CARTESIAN_POINT ( 'NONE',  ( 31.99999999999999289, 199.2500000000000000, 169.9999999999999432 ) ) ;
#4509 = ORIENTED_EDGE ( 'NONE', *, *, #29684, .T. ) ;
#4510 = CARTESIAN_POINT ( 'NONE',  ( 27.99999999999996092, 194.6875000013655779, 173.4587341249998929 ) ) ;
#4511 = CARTESIAN_POINT ( 'NONE',  ( 0.000000000000000000, 0.000000000000000000, -25.03750572909317285 ) ) ;
#4512 = CARTESIAN_POINT ( 'NONE',  ( -8.311093377946836114, 47.65624999658601268, -8.311093377946837890 ) ) ;
#4513 = CARTESIAN_POINT ( 'NONE',  ( 4.556349186104051263, -10.99999999999999822, 76.65625000409676204 ) ) ;
#4514 = CARTESIAN_POINT ( 'NONE',  ( -2.839093476692135984E-14, 198.9375000013655779, 138.5412658750000503 ) ) ;
#4515 = CARTESIAN_POINT ( 'NONE',  ( -27.99999999999999645, 210.0000000000000284, 170.0000000000003695 ) ) ;
#4516 = CARTESIAN_POINT ( 'NONE',  ( -2.679491924311150353, 246.0416666666666856, 10.00000000000004441 ) ) ;
#4518 = CARTESIAN_POINT ( 'NONE',  ( -3.042071309553163960, 52.23958332991934128, -11.35316468749999963 ) ) ;
#4517 = CARTESIAN_POINT ( 'NONE',  ( -2.977408999572652260, 97.43750000204839523, 7.188101187500000044 ) ) ;
#4519 = CARTESIAN_POINT ( 'NONE',  ( -5.656854249492373476, -5.656854249492376141, 1.017802779823363757 ) ) ;
#4520 = CARTESIAN_POINT ( 'NONE',  ( -30.97515058655512377, -35.99359531161695003, 171.9999999999997726 ) ) ;
#4521 = CARTESIAN_POINT ( 'NONE',  ( -8.311093377946841443, 178.9062499965859843, 8.311093377946830785 ) ) ;
#4522 = CARTESIAN_POINT ( 'NONE',  ( -5.000000000000005329, 140.2083333265053682, 8.660254037844387298 ) ) ;
#4523 = CLOSED_SHELL ( 'NONE', ( #71611, #47029, #11209, #22063, #61453, #46945, #73459, #68338, #22077, #31450, #31803, #63904, #26056, #46855, #59388, #5652, #28398, #53352, #7024, #13467, #40132, #30038, #38139, #50262, #848, #17255, #65211, #37387, #10011, #1161, #63333, #7871, #54554, #32526, #57451, #69911, #28215, #571, #57405, #65582, #27835, #66650, #24853, #18743, #18795, #71637, #66629, #15426, #8446, #27623, #34422, #34348, #47600 ) ) ;
#4524 = CARTESIAN_POINT ( 'NONE',  ( -5.082755093536325930, 100.3437500020483810, -5.082755093536325930 ) ) ;
#4525 = CARTESIAN_POINT ( 'NONE',  ( 2.775557561562891351E-14, 183.6788756342477029, 139.0000000000000568 ) ) ;
#4526 = CARTESIAN_POINT ( 'NONE',  ( -5.676582343749998039, 37.76041666325267698, -9.832129032723420536 ) ) ;
#4527 = CARTESIAN_POINT ( 'NONE',  ( -7.320508075688773708, 78.74999999317202537, -7.320508075688774596 ) ) ;
#4528 = ORIENTED_EDGE ( 'NONE', *, *, #51032, .T. ) ;
#4529 = CYLINDRICAL_SURFACE ( 'NONE', #50073, 6.000000000000001776 ) ;
#4530 = CARTESIAN_POINT ( 'NONE',  ( -4.220049686691935698, 10.18810118749999916, 71.87500000204836681 ) ) ;
#4531 = CARTESIAN_POINT ( 'NONE',  ( 1.656854249492403008, 195.6875000000000284, 194.0000000000000853 ) ) ;
#4532 = CARTESIAN_POINT ( 'NONE',  ( 35.04702474127692824, 39.80630860980398467, 65.00000000000002842 ) ) ;
#4534 = CARTESIAN_POINT ( 'NONE',  ( 9.832129032723420536, 161.1979166632526983, -5.676582343749999815 ) ) ;
#4533 = DIRECTION ( 'NONE',  ( -0.000000000000000000, -0.000000000000000000, -1.000000000000000000 ) ) ;
#4535 = CARTESIAN_POINT ( 'NONE',  ( 3.313708498984762496, -7.999999999999989342, 8.855302784329824206 ) ) ;
#4536 = CARTESIAN_POINT ( 'NONE',  ( -31.00000000000001421, 50.00000000000000711, 65.00000000000000000 ) ) ;
#4537 = CARTESIAN_POINT ( 'NONE',  ( 1.836970198721029589E-15, 259.3750000068280315, 10.00000000000000000 ) ) ;
#4538 = CARTESIAN_POINT ( 'NONE',  ( 5.086519500873676769, 50.65542486323139570, -41.09394361258735984 ) ) ;
#4539 = CARTESIAN_POINT ( 'NONE',  ( 10.18810118750000093, -4.220049686691933921, 82.18750000204836681 ) ) ;
#4540 = ORIENTED_EDGE ( 'NONE', *, *, #37, .T. ) ;
#4541 = VECTOR ( 'NONE', #55169, 999.9999999999998863 ) ;
#4542 = DIRECTION ( 'NONE',  ( -0.000000000000000000, -1.000000000000000000, -0.000000000000000000 ) ) ;
#4543 = CARTESIAN_POINT ( 'NONE',  ( -3.042071309553173730, 119.6354166632526841, 11.35316468749999785 ) ) ;
#4544 = DIRECTION ( 'NONE',  ( 0.000000000000000000, 0.8778652960885079404, -0.4789076340208374138 ) ) ;
#4545 = ORIENTED_EDGE ( 'NONE', *, *, #43452, .F. ) ;
#4547 = ORIENTED_EDGE ( 'NONE', *, *, #63139, .F. ) ;
#4546 =( BOUNDED_CURVE ( )  B_SPLINE_CURVE ( 2, ( #74186, #5170, #68159, #50431, #21753, #56111, #38761, #15345, #51178, #3673, #26671, #55741, #4058, #73816, #49696, #67795, #16458, #27051, #27415, #9711, #4797, #62125, #44781, #73077, #28166, #10449, #45513, #61385, #72709, #32733, #21013, #67420, #15719, #44407, #33853, #56481, #4420, #50063, #21384, #22491, #33479, #38009, #38381, #50804, #62490, #67045, #68529, #44037, #61007, #61761, #16086, #10079, #33117, #73446, #39121, #27791, #22124, #45149, #9333, #39495, #10818, #56851, #32353, #55367, #46631, #70028, #57602, #6287, #63235, #58349, #58709, #29294, #23251, #40607, #34967, #24359, #34222, #52304, #11562, #17964, #7019, #69278, #46259, #12663, #35337, #57984, #5912, #51931, #53043, #63990, #51546, #18336, #640, #28914, #40232, #1376, #47367, #268, #16832, #39859, #23987, #17213, #17589, #22876, #46996, #23622, #69651, #6654, #34595, #62860, #11194, #12304, #63609, #1007, #52671, #40982, #29656, #57224, #41351, #64361, #35694, #30028, #11936, #5536, #28538, #74564, #45889, #68902, #25824, #20167, #31879, #71476, #48843, #2833, #41716, #3211, #19802, #71852, #25084, #43185, #13754, #8488, #42808, #60543, #2091, #19430, #66201, #8122, #64728, #60169, #2466, #59808, #31507, #14132, #59080, #54526, #65080, #25457, #14505, #37544, #48100, #71109, #42441, #24719, #13393, #1738, #48471, #70393, #7390, #7758, #65825, #54902, #8868, #30396, #26199, #18708, #13026, #37167, #36063, #65460, #53415, #47728, #36430, #70752, #19068, #42071, #36798, #59444, #30761, #31125, #53782, #54155, #49603, #33761, #56762, #44690, #43944, #33387, #10362, #33023, #9992, #61672, #39402, #72617, #4707, #15630, #66953, #68076, #66574, #56387, #32262, #5083, #27701, #73728, #10728, #50339, #50712 ),
 .UNSPECIFIED., .F., .F. ) 
 B_SPLINE_CURVE_WITH_KNOTS ( ( 3, 2, 2, 2, 2, 2, 2, 2, 2, 2, 2, 2, 2, 2, 2, 2, 2, 2, 2, 2, 2, 2, 2, 2, 2, 2, 2, 2, 2, 2, 2, 2, 2, 2, 2, 2, 2, 2, 2, 2, 2, 2, 2, 2, 2, 2, 2, 2, 2, 2, 2, 2, 2, 2, 2, 2, 2, 2, 2, 2, 2, 2, 2, 2, 2, 2, 2, 2, 2, 2, 2, 2, 2, 2, 2, 2, 2, 2, 2, 2, 2, 2, 2, 2, 2, 2, 2, 2, 2, 2, 2, 2, 2, 2, 2, 2, 2, 2, 2, 2, 2, 2, 2, 2, 2, 2, 2, 2, 3 ),
 ( 0.000000000000000000, 0.009259259259259258745, 0.01851851851851851749, 0.02777777777777777624, 0.03703703703703703498, 0.04629629629629629373, 0.05555555555555555247, 0.06481481481481481122, 0.07407407407407406996, 0.08333333333333332871, 0.09259259259259258745, 0.1018518518518518462, 0.1111111111111111049, 0.1203703703703703637, 0.1296296296296296224, 0.1388888888888888951, 0.1481481481481481399, 0.1574074074074074125, 0.1666666666666666574, 0.1759259259259259300, 0.1851851851851851749, 0.1944444444444444475, 0.2037037037037036924, 0.2129629629629629650, 0.2222222222222222099, 0.2314814814814814825, 0.2407407407407407274, 0.2500000000000000000, 0.2592592592592592449, 0.2685185185185185452, 0.2777777777777777901, 0.2870370370370370350, 0.2962962962962962798, 0.3055555555555555802, 0.3148148148148148251, 0.3240740740740740700, 0.3333333333333333148, 0.3425925925925926152, 0.3518518518518518601, 0.3611111111111111049, 0.3703703703703703498, 0.3796296296296296502, 0.3888888888888888951, 0.3981481481481481399, 0.4074074074074073848, 0.4166666666666666852, 0.4259259259259259300, 0.4351851851851851749, 0.4444444444444444198, 0.4537037037037037202, 0.4629629629629629650, 0.4722222222222222099, 0.4814814814814814548, 0.4907407407407407551, 0.5000000000000000000, 0.5092592592592593004, 0.5185185185185184897, 0.5277777777777777901, 0.5370370370370370905, 0.5462962962962962798, 0.5555555555555555802, 0.5648148148148147696, 0.5740740740740740700, 0.5833333333333333703, 0.5925925925925925597, 0.6018518518518518601, 0.6111111111111111605, 0.6203703703703703498, 0.6296296296296296502, 0.6388888888888888395, 0.6481481481481481399, 0.6574074074074074403, 0.6666666666666666297, 0.6759259259259259300, 0.6851851851851852304, 0.6944444444444444198, 0.7037037037037037202, 0.7129629629629629095, 0.7222222222222222099, 0.7314814814814815103, 0.7407407407407406996, 0.7500000000000000000, 0.7592592592592593004, 0.7685185185185184897, 0.7777777777777777901, 0.7870370370370370905, 0.7962962962962962798, 0.8055555555555555802, 0.8148148148148147696, 0.8240740740740740700, 0.8333333333333333703, 0.8425925925925925597, 0.8518518518518518601, 0.8611111111111111605, 0.8703703703703703498, 0.8796296296296296502, 0.8888888888888888395, 0.8981481481481481399, 0.9074074074074074403, 0.9166666666666666297, 0.9259259259259259300, 0.9351851851851852304, 0.9444444444444444198, 0.9537037037037037202, 0.9629629629629629095, 0.9722222222222222099, 0.9814814814814815103, 0.9907407407407406996, 1.000000000000000000 ),
 .UNSPECIFIED. ) 
 CURVE ( )  GEOMETRIC_REPRESENTATION_ITEM ( )  RATIONAL_B_SPLINE_CURVE ( ( 1.000000000000000000, 0.9659258262890683122, 1.000000000000000000, 0.9659258262890683122, 1.000000000000000000, 0.9659258262890683122, 1.000000000000000000, 0.9659258262890683122, 1.000000000000000000, 0.9659258262890683122, 1.000000000000000000, 0.9659258262890683122, 1.000000000000000000, 0.9659258262890683122, 1.000000000000000000, 0.9659258262890683122, 1.000000000000000000, 0.9659258262890683122, 1.000000000000000000, 0.9659258262890683122, 1.000000000000000000, 0.9659258262890683122, 1.000000000000000000, 0.9659258262890683122, 1.000000000000000000, 0.9659258262890683122, 1.000000000000000000, 0.9659258262890683122, 1.000000000000000000, 0.9659258262890683122, 1.000000000000000000, 0.9659258262890683122, 1.000000000000000000, 0.9659258262890683122, 1.000000000000000000, 0.9659258262890683122, 1.000000000000000000, 0.9659258262890683122, 1.000000000000000000, 0.9659258262890683122, 1.000000000000000000, 0.9659258262890683122, 1.000000000000000000, 0.9659258262890683122, 1.000000000000000000, 0.9659258262890683122, 1.000000000000000000, 0.9659258262890683122, 1.000000000000000000, 0.9659258262890683122, 1.000000000000000000, 0.9659258262890683122, 1.000000000000000000, 0.9659258262890683122, 1.000000000000000000, 0.9659258262890683122, 1.000000000000000000, 0.9659258262890683122, 1.000000000000000000, 0.9659258262890683122, 1.000000000000000000, 0.9659258262890683122, 1.000000000000000000, 0.9659258262890683122, 1.000000000000000000, 0.9659258262890683122, 1.000000000000000000, 0.9659258262890683122, 1.000000000000000000, 0.9659258262890683122, 1.000000000000000000, 0.9659258262890683122, 1.000000000000000000, 0.9659258262890683122, 1.000000000000000000, 0.9659258262890683122, 1.000000000000000000, 0.9659258262890683122, 1.000000000000000000, 0.9659258262890683122, 1.000000000000000000, 0.9659258262890683122, 1.000000000000000000, 0.9659258262890683122, 1.000000000000000000, 0.9659258262890683122, 1.000000000000000000, 0.9659258262890683122, 1.000000000000000000, 0.9659258262890683122, 1.000000000000000000, 0.9659258262890683122, 1.000000000000000000, 0.9659258262890683122, 1.000000000000000000, 0.9659258262890683122, 1.000000000000000000, 0.9659258262890683122, 1.000000000000000000, 0.9659258262890683122, 1.000000000000000000, 0.9659258262890683122, 1.000000000000000000, 0.9659258262890683122, 1.000000000000000000, 0.9659258262890683122, 1.000000000000000000, 0.9659258262890683122, 1.000000000000000000, 0.9659258262890683122, 1.000000000000000000, 0.9659258262890683122, 1.000000000000000000, 0.9659258262890683122, 1.000000000000000000, 0.9659258262890683122, 1.000000000000000000, 0.9659258262890683122, 1.000000000000000000, 0.9659258262890683122, 1.000000000000000000, 0.9659258262890683122, 1.000000000000000000, 0.9659258262890683122, 1.000000000000000000, 0.9659258262890683122, 1.000000000000000000, 0.9659258262890683122, 1.000000000000000000, 0.9659258262890683122, 1.000000000000000000, 0.9659258262890683122, 1.000000000000000000, 0.9659258262890683122, 1.000000000000000000, 0.9659258262890683122, 1.000000000000000000, 0.9659258262890683122, 1.000000000000000000, 0.9659258262890683122, 1.000000000000000000, 0.9659258262890683122, 1.000000000000000000, 0.9659258262890683122, 1.000000000000000000, 0.9659258262890683122, 1.000000000000000000, 0.9659258262890683122, 1.000000000000000000, 0.9659258262890683122, 1.000000000000000000, 0.9659258262890683122, 1.000000000000000000, 0.9659258262890683122, 1.000000000000000000, 0.9659258262890683122, 1.000000000000000000, 0.9659258262890683122, 1.000000000000000000, 0.9659258262890683122, 1.000000000000000000, 0.9659258262890683122, 1.000000000000000000, 0.9659258262890683122, 1.000000000000000000, 0.9659258262890683122, 1.000000000000000000, 0.9659258262890683122, 1.000000000000000000, 0.9659258262890683122, 1.000000000000000000, 0.9659258262890683122, 1.000000000000000000, 0.9659258262890683122, 1.000000000000000000, 0.9659258262890683122, 1.000000000000000000, 0.9659258262890683122, 1.000000000000000000, 0.9659258262890683122, 1.000000000000000000, 0.9659258262890683122, 1.000000000000000000, 0.9659258262890683122, 1.000000000000000000, 0.9659258262890683122, 1.000000000000000000, 0.9659258262890683122, 1.000000000000000000, 0.9659258262890683122, 1.000000000000000000, 0.9659258262890683122, 1.000000000000000000, 0.9659258262890683122, 1.000000000000000000, 0.9659258262890683122, 1.000000000000000000, 0.9659258262890683122, 1.000000000000000000, 0.9659258262890683122, 1.000000000000000000, 0.9659258262890683122, 1.000000000000000000, 0.9659258262890683122, 1.000000000000000000, 0.9659258262890683122, 1.000000000000000000, 0.9659258262890683122, 1.000000000000000000, 0.9659258262890683122, 1.000000000000000000, 0.9659258262890683122, 1.000000000000000000, 0.9659258262890683122, 1.000000000000000000, 0.9659258262890683122, 1.000000000000000000 ) ) 
 REPRESENTATION_ITEM ( '' )  );
#4548 = CARTESIAN_POINT ( 'NONE',  ( -3.211159895383562723, 6.062499998634407028, 3.211159895383561391 ) ) ;
#4549 = CARTESIAN_POINT ( 'NONE',  ( -5.082755093536325042, 8.531249997951611874, -5.082755093536325930 ) ) ;
#4550 = CARTESIAN_POINT ( 'NONE',  ( 5.656854249492379694, 111.1250000040967763, -5.656854249492380582 ) ) ;
#4551 = EDGE_CURVE ( 'NONE', #47128, #66240, #35390, .T. ) ;
#4552 = CARTESIAN_POINT ( 'NONE',  ( -10.18810118749999738, -4.220049686691941915, 90.62500000204836681 ) ) ;
#4553 = CARTESIAN_POINT ( 'NONE',  ( -28.00000000000002132, 203.6875000013656063, 166.5412658750003629 ) ) ;
#4554 = ADVANCED_FACE ( 'NONE', ( #29350 ), #38633, .F. ) ;
#4555 = CARTESIAN_POINT ( 'NONE',  ( 2.828427124746191623, 6.125000000000000000, -2.828427124746191623 ) ) ;
#4556 = CARTESIAN_POINT ( 'NONE',  ( 4.000000000000000888, 20.68749999726881228, 1.656854249492384135 ) ) ;
#4557 = CARTESIAN_POINT ( 'NONE',  ( -8.342170076843785083E-16, 8.062499998634406140, 4.541265875000002339 ) ) ;
#4558 = CARTESIAN_POINT ( 'NONE',  ( 3.999999999999960032, 198.9375000000000000, 143.6568542494924543 ) ) ;
#4559 = VERTEX_POINT ( 'NONE', #19484 ) ;
#4560 = CARTESIAN_POINT ( 'NONE',  ( -7.188101187500000044, 112.1562500020483952, 0.000000000000000000 ) ) ;
#4561 = VECTOR ( 'NONE', #70931, 1000.000000000000000 ) ;
#4562 = CARTESIAN_POINT ( 'NONE',  ( -26.56734541678242323, 196.3750000013656063, 166.5412658750003345 ) ) ;
#4563 =( NAMED_UNIT ( * ) SI_UNIT ( $, .STERADIAN. ) SOLID_ANGLE_UNIT ( ) );
#4564 =( BOUNDED_CURVE ( )  B_SPLINE_CURVE ( 2, ( #30025, #19799, #24717, #53413, #2463, #64357, #58706, #7016, #42806, #37165, #19066 ),
 .UNSPECIFIED., .F., .F. ) 
 B_SPLINE_CURVE_WITH_KNOTS ( ( 3, 2, 2, 2, 2, 3 ),
 ( 0.9166666666666668517, 0.9259259259259261521, 0.9351851851851853414, 0.9444444444444445308, 0.9537037037037037202, 0.9583333334824809535 ),
 .UNSPECIFIED. ) 
 CURVE ( )  GEOMETRIC_REPRESENTATION_ITEM ( )  RATIONAL_B_SPLINE_CURVE ( ( 0.9999999999999992228, 0.9659258262890690894, 1.000000000000000000, 0.9659258262890683122, 1.000000000000000000, 0.9659258262890683122, 1.000000000000000000, 0.9659258262890683122, 1.000000000000000000, 0.9829629125956692581, 0.9829629131445342116 ) ) 
 REPRESENTATION_ITEM ( '' )  );
#4565 = LINE ( 'NONE', #27561, #28208 ) ;
#4566 = CARTESIAN_POINT ( 'NONE',  ( 7.188101187499992051, 8.802885111219154394E-16, 3.736552781871751883 ) ) ;
#4567 = ORIENTED_EDGE ( 'NONE', *, *, #26684, .T. ) ;
#4568 = EDGE_LOOP ( 'NONE', ( #18836, #10683, #54483, #26196, #69493, #24018, #2236, #27772, #52286 ) ) ;
#4569 = CARTESIAN_POINT ( 'NONE',  ( -7.204075437095965206, -7.204075437095968759, 94.84375000204838102 ) ) ;
#4570 = CARTESIAN_POINT ( 'NONE',  ( 4.242640687119287435, 288.3750000000000000, 4.242640687119285658 ) ) ;
#4571 = CARTESIAN_POINT ( 'NONE',  ( -27.99999999999996447, 202.1875000013656063, 173.4587341250003760 ) ) ;
#4572 = CARTESIAN_POINT ( 'NONE',  ( 11.00000000000000355, -4.556349186104045046, 106.6562500000000000 ) ) ;
#4573 = CARTESIAN_POINT ( 'NONE',  ( 1.432654583217664701, 206.0000000013656347, 201.4587341250000065 ) ) ;
#4574 = DIRECTION ( 'NONE',  ( -0.000000000000000000, -0.000000000000000000, 1.000000000000000000 ) ) ;
#4575 = CARTESIAN_POINT ( 'NONE',  ( 4.999999999999993783, 119.1666666666666714, 8.660254037844390851 ) ) ;
#4576 = CARTESIAN_POINT ( 'NONE',  ( 8.000000000000000000, 104.8437500000000000, -3.313708498984762496 ) ) ;
#4577 = AXIS2_PLACEMENT_3D ( 'NONE', #56879, #5563, #50452 ) ;
#4578 = CARTESIAN_POINT ( 'NONE',  ( -4.721056650415998313, 293.7343750017069510, 4.721056650416000089 ) ) ;
#4579 = CARTESIAN_POINT ( 'NONE',  ( 7.188101187499993827, -2.977408999572645598, 7.017802781871755435 ) ) ;
#4580 = EDGE_LOOP ( 'NONE', ( #55421, #61054 ) ) ;
#4581 = AXIS2_PLACEMENT_3D ( 'NONE', #14875, #8482, #43179 ) ;
#4582 = DIRECTION ( 'NONE',  ( -1.000000000000000000, -0.000000000000000000, -0.000000000000000000 ) ) ;
#4583 = CARTESIAN_POINT ( 'NONE',  ( 24.54126587499999346, 205.1875000013656063, 169.9999999999998863 ) ) ;
#4584 = CARTESIAN_POINT ( 'NONE',  ( 3.313708498984762052, 25.59374999590322375, -8.000000000000000000 ) ) ;
#4585 = SHAPE_REPRESENTATION ( 'barrel', ( #57354 ), #47738 ) ;
#4586 = CARTESIAN_POINT ( 'NONE',  ( 3.458734124999959914, 199.3750000013656063, 143.4326545832176976 ) ) ;
#4587 = CARTESIAN_POINT ( 'NONE',  ( 0.000000000000000000, 0.000000000000000000, 0.000000000000000000 ) ) ;
#4589 = CARTESIAN_POINT ( 'NONE',  ( -3.458734125000015425, 202.2500000013656063, 143.4326545832176976 ) ) ;
#4588 = CARTESIAN_POINT ( 'NONE',  ( 11.00000000000010658, 4.556349186103942017, 111.3437499999999858 ) ) ;
#4590 = CARTESIAN_POINT ( 'NONE',  ( 11.35316468749999608, 236.9270833367473017, -3.042071309553167069 ) ) ;
#4591 = FACE_BOUND ( 'NONE', #5914, .T. ) ;
#4592 = CARTESIAN_POINT ( 'NONE',  ( -2.679491924311226292, 213.3333333265053682, -10.00000000000000178 ) ) ;
#4593 = CARTESIAN_POINT ( 'NONE',  ( -11.35316468750000141, 13.28124999658601624, -1.390361679473963753E-15 ) ) ;
#4594 = CARTESIAN_POINT ( 'NONE',  ( 8.000000000000000000, 100.4375000040967763, -9.797174393178825657E-16 ) ) ;
#4595 = CARTESIAN_POINT ( 'NONE',  ( 3.042071309553167069, 212.1354166632526983, -11.35316468749999785 ) ) ;
#4596 = CARTESIAN_POINT ( 'NONE',  ( -29.65685424949244364, 198.4375000000000568, 174.0000000000003126 ) ) ;
#4598 = CARTESIAN_POINT ( 'NONE',  ( 0.000000000000000000, 125.0000000000000000, 8.000000000000000000 ) ) ;
#4597 = CARTESIAN_POINT ( 'NONE',  ( 4.000000000000015987, 208.5625000000000000, 196.3431457505076594 ) ) ;
#4599 = ORIENTED_EDGE ( 'NONE', *, *, #11136, .T. ) ;
#4600 = CARTESIAN_POINT ( 'NONE',  ( 1.432654583217607414, 201.5000000013655779, 145.4587341250000634 ) ) ;
#4601 = CARTESIAN_POINT ( 'NONE',  ( -9.832129032723420536, 8.697916663252684089, 5.676582343749997150 ) ) ;
#4602 = CARTESIAN_POINT ( 'NONE',  ( -11.00000000000000000, 4.556349186104045934, 92.59375000409677625 ) ) ;
#4603 = CARTESIAN_POINT ( 'NONE',  ( 8.660254037844385522, 209.5833333333333428, 5.000000000000006217 ) ) ;
#4604 = CARTESIAN_POINT ( 'NONE',  ( -26.56734541678243033, 199.3750000013656063, 166.5412658750003345 ) ) ;
#4605 = DIRECTION ( 'NONE',  ( 0.000000000000000000, 0.000000000000000000, 1.000000000000000000 ) ) ;
#4607 = CARTESIAN_POINT ( 'NONE',  ( -8.311093377946836114, 12.65624999658601624, -8.311093377946837890 ) ) ;
#4606 = CARTESIAN_POINT ( 'NONE',  ( -5.082755093536325930, 114.9687500020483810, -5.082755093536325930 ) ) ;
#4608 = CARTESIAN_POINT ( 'NONE',  ( -3.313708498984757167, 7.999999999999991118, 27.54905277982337353 ) ) ;
#4609 = CARTESIAN_POINT ( 'NONE',  ( -11.35316468750000141, 138.2812499965860411, -1.390361679473963753E-15 ) ) ;
#4610 = CARTESIAN_POINT ( 'NONE',  ( -10.00000000000000000, 104.1666666598386968, -2.679491924311229845 ) ) ;
#4611 = CARTESIAN_POINT ( 'NONE',  ( 1.320432766682874540E-15, 121.9062500020483810, 7.188101187500000044 ) ) ;
#4612 = CARTESIAN_POINT ( 'NONE',  ( -8.342170076843785083E-16, 22.18749999863440792, 4.541265875000002339 ) ) ;
#4613 = CARTESIAN_POINT ( 'NONE',  ( -7.999999999999991118, 0.000000000000000000, 6.830302779823365533 ) ) ;
#4614 = PLANE ( 'NONE',  #40191 ) ;
#4615 = ORIENTED_EDGE ( 'NONE', *, *, #61226, .T. ) ;
#4616 = CARTESIAN_POINT ( 'NONE',  ( -0.4501631047672374208, -67.59340899456745433, 20.03485802339921307 ) ) ;
#4617 = CARTESIAN_POINT ( 'NONE',  ( -4.721056650415998313, 290.7343750017069510, 4.721056650416000089 ) ) ;
#4618 = CARTESIAN_POINT ( 'NONE',  ( 4.999999999999999112, 51.89737250574476235, 42.00009673807167587 ) ) ;
#4619 = CARTESIAN_POINT ( 'NONE',  ( 7.999999999999991118, 9.797174393178815797E-16, 3.267802783920144449 ) ) ;
#4620 = CARTESIAN_POINT ( 'NONE',  ( 0.8761883848702602950, 67.61551161115370689, 20.05282165013497320 ) ) ;
#4621 = CARTESIAN_POINT ( 'NONE',  ( 0.000000000000000000, 265.0000000000000000, 10.00000000000000000 ) ) ;
#4622 = AXIS2_PLACEMENT_3D ( 'NONE', #22841, #57572, #22459 ) ;
#4623 = CARTESIAN_POINT ( 'NONE',  ( 7.204075437095966983, 7.204075437095967871, 97.46875000204838102 ) ) ;
#4624 = EDGE_LOOP ( 'NONE', ( #44465, #12342, #67187, #23154 ) ) ;
#4625 = EDGE_CURVE ( 'NONE', #12103, #47682, #44691, .T. ) ;
#4626 = EDGE_CURVE ( 'NONE', #31876, #54025, #56696, .T. ) ;
#4627 = VECTOR ( 'NONE', #71642, 1000.000000000000000 ) ;
#4628 = DIRECTION ( 'NONE',  ( 0.000000000000000000, 0.02418647091589873691, 0.9997074645238147594 ) ) ;
#4629 = CARTESIAN_POINT ( 'NONE',  ( -3.042071309553163960, 167.5520833299193271, -11.35316468749999963 ) ) ;
#4630 = FACE_BOUND ( 'NONE', #52260, .T. ) ;
#4631 = CARTESIAN_POINT ( 'NONE',  ( -1.432654583217608080, 202.8750000013656063, 201.4587341250000350 ) ) ;
#4632 = CARTESIAN_POINT ( 'NONE',  ( -7.683012701892240059, 124.8169872981077901, 0.000000000000000000 ) ) ;
#4633 = CARTESIAN_POINT ( 'NONE',  ( -9.832129032723420536, 74.01041666325268409, 5.676582343749997150 ) ) ;
#4634 = ORIENTED_EDGE ( 'NONE', *, *, #50926, .F. ) ;
#4635 = CARTESIAN_POINT ( 'NONE',  ( 10.18810118750000093, -4.220049686691933921, 111.8125000020483952 ) ) ;
#4636 = CARTESIAN_POINT ( 'NONE',  ( 4.541265875000002339, 13.43749999863440792, 0.000000000000000000 ) ) ;
#4637 = ORIENTED_EDGE ( 'NONE', *, *, #62476, .T. ) ;
#4638 = EDGE_CURVE ( 'NONE', #15222, #39861, #24772, .T. ) ;
#4639 = CARTESIAN_POINT ( 'NONE',  ( 8.000000000000000000, 0.09374999999999990286, -3.313708498984761608 ) ) ;
#4640 = ADVANCED_FACE ( 'NONE', ( #13080 ), #47785, .T. ) ;
#4641 = CARTESIAN_POINT ( 'NONE',  ( -2.679491924311161455, 110.4166666598387110, 10.00000000000004441 ) ) ;
#4642 = VECTOR ( 'NONE', #2909, 1000.000000000000000 ) ;
#4643 = CARTESIAN_POINT ( 'NONE',  ( 2.679491924311222739, 65.83333332650536818, 10.00000000000000355 ) ) ;
#4644 = CARTESIAN_POINT ( 'NONE',  ( -5.082755093536325042, 20.90624999795161543, -5.082755093536325930 ) ) ;
#4645 = CARTESIAN_POINT ( 'NONE',  ( 3.999999999999959144, 200.0625000000000284, 140.3431457505076594 ) ) ;
#4646 = AXIS2_PLACEMENT_3D ( 'NONE', #65247, #6808, #1166 ) ;
#4647 = CARTESIAN_POINT ( 'NONE',  ( -10.18810118749999916, 4.220049686691934809, 108.4375000020483668 ) ) ;
#4648 = CARTESIAN_POINT ( 'NONE',  ( -1.469576158976823947E-15, 20.43749999590322375, 8.000000000000000000 ) ) ;
#4649 = CARTESIAN_POINT ( 'NONE',  ( -4.000000000000001776, 12.18749999726881406, -1.656854249492381470 ) ) ;
#4650 = CARTESIAN_POINT ( 'NONE',  ( 23.99999999999998224, 206.8125000027312126, 168.3431457505075457 ) ) ;
#4651 = ORIENTED_EDGE ( 'NONE', *, *, #53367, .T. ) ;
#4652 = CARTESIAN_POINT ( 'NONE',  ( 2.839093476692135984E-14, 201.6875000013656063, 201.4587341250000350 ) ) ;
#4653 = ADVANCED_FACE ( 'NONE', ( #42124 ), #66305, .T. ) ;
#4654 = CARTESIAN_POINT ( 'NONE',  ( -26.34314575050769136, 195.0625000027312126, 166.0000000000003695 ) ) ;
#4655 = CARTESIAN_POINT ( 'NONE',  ( 1.656854249492356157, 12.93749999726881406, -4.000000000000026645 ) ) ;
#4656 = CARTESIAN_POINT ( 'NONE',  ( -3.211159895383562723, 6.937499998634407028, 3.211159895383561391 ) ) ;
#4657 = CARTESIAN_POINT ( 'NONE',  ( -2.977408999572648707, -7.188101187499990274, 19.76780278187175455 ) ) ;
#4658 = ORIENTED_EDGE ( 'NONE', *, *, #50525, .F. ) ;
#4659 =( BOUNDED_CURVE ( )  B_SPLINE_CURVE ( 2, ( #3593, #43569, #37554, #9251, #60929, #44701, #32272, #4717, #27334 ),
 .UNSPECIFIED., .F., .F. ) 
 B_SPLINE_CURVE_WITH_KNOTS ( ( 3, 2, 2, 2, 3 ),
 ( 0.4264705882352941568, 0.4301470588235294934, 0.4338235294117647745, 0.4375000000000000555, 0.4411764705882353366 ),
 .UNSPECIFIED. ) 
 CURVE ( )  GEOMETRIC_REPRESENTATION_ITEM ( )  RATIONAL_B_SPLINE_CURVE ( ( 0.9999999999999988898, 0.9238795325112878487, 1.000000000000000000, 0.9238795325112867385, 1.000000000000000000, 0.9238795325112867385, 1.000000000000000000, 0.9238795325112856283, 1.000000000000001110 ) ) 
 REPRESENTATION_ITEM ( '' )  );
#4660 = CARTESIAN_POINT ( 'NONE',  ( -1.320432766682874540E-15, 27.09374999795161543, 7.188101187500000044 ) ) ;
#4661 = VERTEX_POINT ( 'NONE', #7445 ) ;
#4662 = CARTESIAN_POINT ( 'NONE',  ( -4.220049686691935698, 10.18810118749999916, 107.8750000020483810 ) ) ;
#4663 = DIRECTION ( 'NONE',  ( -0.000000000000000000, 1.000000000000000000, -0.000000000000000000 ) ) ;
#4664 = CARTESIAN_POINT ( 'NONE',  ( -3.458734124999959914, 204.4375000013656063, 198.0000000000000284 ) ) ;
#4665 = CARTESIAN_POINT ( 'NONE',  ( 24.54126587499999346, 198.1875000013655779, 169.9999999999999432 ) ) ;
#4666 = CARTESIAN_POINT ( 'NONE',  ( -2.679491924311235618, 78.54166666666667140, 10.00000000000000000 ) ) ;
#4667 = CARTESIAN_POINT ( 'NONE',  ( -4.401442555609581635E-16, 91.15625000204838102, -7.188101187500000044 ) ) ;
#4668 = CARTESIAN_POINT ( 'NONE',  ( -3.673940397442060854E-16, 290.7500000000000000, -6.000000000000001776 ) ) ;
#4669 = CARTESIAN_POINT ( 'NONE',  ( 32.00000000000000711, 203.3125000027311842, 171.6568542494922553 ) ) ;
#4670 = ORIENTED_EDGE ( 'NONE', *, *, #54154, .T. ) ;
#4671 = CARTESIAN_POINT ( 'NONE',  ( -5.676582343750000703, 223.0729166700806729, -9.832129032723418760 ) ) ;
#4672 = AXIS2_PLACEMENT_3D ( 'NONE', #62962, #67881, #38474 ) ;
#4673 = CARTESIAN_POINT ( 'NONE',  ( 3.544144923088449861, -10.27124247550364977, 63.97955030412197175 ) ) ;
#4674 = CARTESIAN_POINT ( 'NONE',  ( -1.656854249492403008, 194.8125000027312126, 146.0000000000000284 ) ) ;
#4675 = LINE ( 'NONE', #63116, #53894 ) ;
#4676 = DIRECTION ( 'NONE',  ( -0.000000000000000000, 1.000000000000000000, -1.563033456626094573E-30 ) ) ;
#4677 = CARTESIAN_POINT ( 'NONE',  ( -9.999999999999998224, 255.2083333333333712, 2.679491924311235618 ) ) ;
#4678 = CARTESIAN_POINT ( 'NONE',  ( 11.00000000000010658, 4.556349186103942017, 107.0312500040967763 ) ) ;
#4679 = CARTESIAN_POINT ( 'NONE',  ( -2.679491924311235618, 198.5416666666666288, 10.00000000000000000 ) ) ;
#4680 =( BOUNDED_CURVE ( )  B_SPLINE_CURVE ( 2, ( #31860, #54884, #16345, #56742, #40869, #11086, #34490, #51814, #39382 ),
 .UNSPECIFIED., .F., .F. ) 
 B_SPLINE_CURVE_WITH_KNOTS ( ( 3, 2, 2, 2, 3 ),
 ( 0.1458333333333311499, 0.1562499999999978073, 0.1666666666666644647, 0.1770833333333311777, 0.1874999999999978351 ),
 .UNSPECIFIED. ) 
 CURVE ( )  GEOMETRIC_REPRESENTATION_ITEM ( )  RATIONAL_B_SPLINE_CURVE ( ( 1.000000000000015987, 0.9238795325112707513, 1.000000000000000000, 0.9238795325112867385, 1.000000000000000000, 0.9238795325112867385, 1.000000000000000000, 0.9238795325113025037, 0.9999999999999842348 ) ) 
 REPRESENTATION_ITEM ( '' )  );
#4681 = LINE ( 'NONE', #68048, #54868 ) ;
#4682 = CARTESIAN_POINT ( 'NONE',  ( -7.188101187499992051, 0.000000000000000000, 16.86155278187175810 ) ) ;
#4683 = CARTESIAN_POINT ( 'NONE',  ( 9.832129032723416984, 165.6770833299193555, 5.676582343750006032 ) ) ;
#4684 = CARTESIAN_POINT ( 'NONE',  ( 0.000000000000000000, 0.000000000000000000, 118.0000000000000000 ) ) ;
#4685 = CARTESIAN_POINT ( 'NONE',  ( 1.469576158976823947E-15, 90.87500000000000000, 8.000000000000000000 ) ) ;
#4686 = CARTESIAN_POINT ( 'NONE',  ( -7.999999999974042098, 1.357258486152048259E-05, 14.51729352187485311 ) ) ;
#4688 = CARTESIAN_POINT ( 'NONE',  ( -1.656854249492383468, 7.437499997268813168, 4.000000000000000888 ) ) ;
#4687 = CARTESIAN_POINT ( 'NONE',  ( -30.64284399271078740, 146.0000000000000000, 174.6921329945331536 ) ) ;
#4689 = ORIENTED_EDGE ( 'NONE', *, *, #18600, .T. ) ;
#4690 = CARTESIAN_POINT ( 'NONE',  ( 9.832129032723420536, 26.51041666325268409, -5.676582343749999815 ) ) ;
#4691 = CARTESIAN_POINT ( 'NONE',  ( -24.00000000000000711, 200.8125000000000284, 168.3431457505080289 ) ) ;
#4693 = CARTESIAN_POINT ( 'NONE',  ( -3.728321214207148238, -10.10963409588650919, -70.65936332836869838 ) ) ;
#4692 = DIRECTION ( 'NONE',  ( 0.000000000000000000, 0.000000000000000000, 1.000000000000000000 ) ) ;
#4694 = CARTESIAN_POINT ( 'NONE',  ( -14.44998917039853481, -43.23887967932489573, 197.4276862866674094 ) ) ;
#4695 = CARTESIAN_POINT ( 'NONE',  ( -3.458734125000015425, 204.0000000013656063, 143.4326545832176976 ) ) ;
#4696 = VECTOR ( 'NONE', #32247, 1000.000000000000000 ) ;
#4697 = CARTESIAN_POINT ( 'NONE',  ( 10.00000000000000000, 56.66666665983868967, 2.679491924311236062 ) ) ;
#4698 = CARTESIAN_POINT ( 'NONE',  ( 7.188101187500000044, 102.4062500020483810, -8.802885111219163269E-16 ) ) ;
#4699 = CARTESIAN_POINT ( 'NONE',  ( -4.541265875000002339, 7.937499998634407028, -5.561446717895856393E-16 ) ) ;
#4700 = CARTESIAN_POINT ( 'NONE',  ( 6.123233995736767268E-16, 101.2500000000000000, -10.00000000000000178 ) ) ;
#4701 = CARTESIAN_POINT ( 'NONE',  ( 5.656854249492376141, -5.656854249492374365, 2.892802779823365533 ) ) ;
#4702 = ORIENTED_EDGE ( 'NONE', *, *, #62535, .F. ) ;
#4703 = ORIENTED_EDGE ( 'NONE', *, *, #16914, .F. ) ;
#4704 = DIRECTION ( 'NONE',  ( 0.000000000000000000, 0.000000000000000000, 1.000000000000000000 ) ) ;
#4705 = CARTESIAN_POINT ( 'NONE',  ( -1.432654583217608080, 194.8750000013656347, 201.4587341250000350 ) ) ;
#4706 = CARTESIAN_POINT ( 'NONE',  ( -6.735557395310442023E-16, 11.00000000000000000, 104.1250000000000000 ) ) ;
#4707 = CARTESIAN_POINT ( 'NONE',  ( 11.35316468749999963, 221.7187500034139873, -1.390361679473963556E-15 ) ) ;
#4708 = CARTESIAN_POINT ( 'NONE',  ( 6.951808397369818766E-16, 147.0312499965860411, -11.35316468750000141 ) ) ;
#4709 = VERTEX_POINT ( 'NONE', #13447 ) ;
#4710 = EDGE_CURVE ( 'NONE', #60564, #73315, #70805, .T. ) ;
#4711 = CARTESIAN_POINT ( 'NONE',  ( -5.000000000000000000, 15.86295220590816513, -69.92641310672760824 ) ) ;
#4712 = CARTESIAN_POINT ( 'NONE',  ( -10.18810118749999916, 4.220049686691934809, 91.56250000204836681 ) ) ;
#4713 = CARTESIAN_POINT ( 'NONE',  ( -3.313708498984599515, 93.21875000000000000, -8.000000000000163425 ) ) ;
#4714 = CARTESIAN_POINT ( 'NONE',  ( -2.828427124746152987, 209.1250000000000284, 200.8284271247462129 ) ) ;
#4715 = CARTESIAN_POINT ( 'NONE',  ( 7.320508075688776373, 246.8750000000000000, 7.320508075688767491 ) ) ;
#4716 = CARTESIAN_POINT ( 'NONE',  ( -29.65685424949235838, 197.1875000027312410, 166.0000000000003411 ) ) ;
#4717 = CARTESIAN_POINT ( 'NONE',  ( -11.00000000000004796, -4.556349186104000637, 95.59375000000000000 ) ) ;
#4718 = EDGE_LOOP ( 'NONE', ( #27806, #8190, #59139, #37546 ) ) ;
#4719 = CARTESIAN_POINT ( 'NONE',  ( 31.19657079693917012, -33.95763485826271477, 171.0759174916215670 ) ) ;
#4720 = CARTESIAN_POINT ( 'NONE',  ( -29.13614168219697831, 175.4267435998100382, 159.1571751346558585 ) ) ;
#4721 = CARTESIAN_POINT ( 'NONE',  ( 5.676582343750001591, 111.9270833299193555, -9.832129032723420536 ) ) ;
#4722 = CARTESIAN_POINT ( 'NONE',  ( 3.458734125000016313, 201.8750000013656063, 199.4326545832176976 ) ) ;
#4723 = CARTESIAN_POINT ( 'NONE',  ( -5.082755093536325042, 23.90624999795161543, -5.082755093536325930 ) ) ;
#4724 = CARTESIAN_POINT ( 'NONE',  ( 4.220049686691934809, 10.18810118749999916, 82.56250000204836681 ) ) ;
#4725 = CARTESIAN_POINT ( 'NONE',  ( 8.311093377946834337, 40.46874999658601979, 8.311093377946839666 ) ) ;
#4726 = ORIENTED_EDGE ( 'NONE', *, *, #65207, .T. ) ;
#4727 = CARTESIAN_POINT ( 'NONE',  ( 0.000000000000000000, 284.0000000000000000, 0.000000000000000000 ) ) ;
#4728 = CARTESIAN_POINT ( 'NONE',  ( 3.317071493978883456, -8.008118988124989457, 20.98186528394063899 ) ) ;
#4729 = LINE ( 'NONE', #50735, #30604 ) ;
#4730 = EDGE_CURVE ( 'NONE', #17458, #33763, #57876, .T. ) ;
#4731 = EDGE_CURVE ( 'NONE', #72830, #47939, #30813, .T. ) ;
#4732 = CARTESIAN_POINT ( 'NONE',  ( -1.656854249492383468, 7.687500000000000000, 4.000000000000000888 ) ) ;
#4733 = CARTESIAN_POINT ( 'NONE',  ( 2.977408999572650927, 9.749999997951611874, -7.188101187500001821 ) ) ;
#4734 = CARTESIAN_POINT ( 'NONE',  ( -6.000000000000000888, 297.1250000034141294, 2.485281374238575758 ) ) ;
#4735 = CARTESIAN_POINT ( 'NONE',  ( -6.000000000000001776, 297.0000000000000000, 0.000000000000000000 ) ) ;
#4736 = CARTESIAN_POINT ( 'NONE',  ( 7.188101187500001821, 2.437499997951610542, -2.977408999572650483 ) ) ;
#4737 = EDGE_CURVE ( 'NONE', #13964, #69323, #64401, .T. ) ;
#4738 = CARTESIAN_POINT ( 'NONE',  ( 9.832129032723420536, 156.5104166632526983, -5.676582343749999815 ) ) ;
#4739 = CARTESIAN_POINT ( 'NONE',  ( -4.220049686691935698, 10.18810118749999916, 79.37500000204838102 ) ) ;
#4740 = VECTOR ( 'NONE', #35314, 1000.000000000000000 ) ;
#4741 = CARTESIAN_POINT ( 'NONE',  ( -24.54126587499999701, 208.4375000013656063, 170.0000000000003411 ) ) ;
#4742 = CARTESIAN_POINT ( 'NONE',  ( 4.000000000000001776, 3.062500000000000000, -1.656854249492381248 ) ) ;
#4743 = CARTESIAN_POINT ( 'NONE',  ( -1.881053915767124440, 15.12499999863441147, 4.541265875000001451 ) ) ;
#4744 = VERTEX_POINT ( 'NONE', #47421 ) ;
#4745 = CIRCLE ( 'NONE', #52936, 10.00000000000000178 ) ;
#4746 = CARTESIAN_POINT ( 'NONE',  ( 2.849036369511732440E-14, 199.3750000027312126, 202.0000000000000000 ) ) ;
#4747 = EDGE_CURVE ( 'NONE', #64535, #4422, #24416, .T. ) ;
#4748 = CARTESIAN_POINT ( 'NONE',  ( -3.458734125000015869, 196.1875000013655779, 142.0000000000000568 ) ) ;
#4749 = CARTESIAN_POINT ( 'NONE',  ( -25.17157287525374443, 205.7500000027312126, 172.8284271247464972 ) ) ;
#4750 = LINE ( 'NONE', #50753, #27176 ) ;
#4751 = ORIENTED_EDGE ( 'NONE', *, *, #823, .T. ) ;
#4752 = CARTESIAN_POINT ( 'NONE',  ( -5.082755093536325042, 8.531249997951611874, -5.082755093536325930 ) ) ;
#4753 = CARTESIAN_POINT ( 'NONE',  ( 6.123233995736767268E-16, 208.1249999931720538, -10.00000000000000178 ) ) ;
#4754 = CARTESIAN_POINT ( 'NONE',  ( 4.999999999999995559, 50.98531617258545623, -41.27391139027573530 ) ) ;
#4755 = CARTESIAN_POINT ( 'NONE',  ( 10.00000000000000178, 40.20833333333334281, -2.679491924311226736 ) ) ;
#4756 = CARTESIAN_POINT ( 'NONE',  ( 7.188101187500002709, 107.1875000020483810, 2.977408999572649151 ) ) ;
#4757 = CARTESIAN_POINT ( 'NONE',  ( -31.45873412499998523, 209.0000000013656063, 171.4326545832180386 ) ) ;
#4758 = CARTESIAN_POINT ( 'NONE',  ( -6.676582343750001591, 288.4531250017069510, 0.000000000000000000 ) ) ;
#4760 = CARTESIAN_POINT ( 'NONE',  ( -18.00000000000000000, -8.694318397447188929, -1.139757812215645094 ) ) ;
#4759 = CARTESIAN_POINT ( 'NONE',  ( 0.000000000000000000, 125.0000000000000000, 0.000000000000000000 ) ) ;
#4761 = VERTEX_POINT ( 'NONE', #8546 ) ;
#4762 = CARTESIAN_POINT ( 'NONE',  ( -9.832129032723415207, 254.3229166700806729, 5.676582343750005144 ) ) ;
#4763 = PRODUCT ( 'clamping plate', 'clamping plate', '', ( #67842 ) ) ;
#4764 = CARTESIAN_POINT ( 'NONE',  ( -7.188101187499992051, 0.000000000000000000, 24.36155278187175810 ) ) ;
#4765 = CARTESIAN_POINT ( 'NONE',  ( -7.456155213548121274, 51.58724325107812803, 41.60228463193340787 ) ) ;
#4766 = FACE_OUTER_BOUND ( 'NONE', #69946, .T. ) ;
#4767 = FACE_OUTER_BOUND ( 'NONE', #41761, .T. ) ;
#4768 = CARTESIAN_POINT ( 'NONE',  ( -3.458734124999960358, 196.6250000013656063, 196.5673454167823877 ) ) ;
#4769 = CARTESIAN_POINT ( 'NONE',  ( -10.00000000000000178, 152.5000000000000000, -1.224646799147353454E-15 ) ) ;
#4770 = DIRECTION ( 'NONE',  ( -0.000000000000000000, -0.000000000000000000, -1.000000000000000000 ) ) ;
#4771 = CARTESIAN_POINT ( 'NONE',  ( 10.91045974869143542, 14.48545281793694883, -0.07476367467994476934 ) ) ;
#4772 = CARTESIAN_POINT ( 'NONE',  ( 3.313708498984765161, 90.96875000000000000, 7.999999999999998224 ) ) ;
#4773 = CARTESIAN_POINT ( 'NONE',  ( 5.676582343750001591, 121.9270833299193413, -9.832129032723420536 ) ) ;
#4774 = CARTESIAN_POINT ( 'NONE',  ( -3.673940397442060854E-16, 295.7500000000000000, -6.000000000000001776 ) ) ;
#4775 = CARTESIAN_POINT ( 'NONE',  ( -4.556349186104047710, -10.99999999999999822, 73.28125000000000000 ) ) ;
#4778 = CARTESIAN_POINT ( 'NONE',  ( 10.53333261448113944, -14.70318727039201967, -1.996964876446738479E-14 ) ) ;
#4777 = CARTESIAN_POINT ( 'NONE',  ( 24.54126587499999346, 198.1875000013655779, 169.9999999999999432 ) ) ;
#4776 = CARTESIAN_POINT ( 'NONE',  ( 28.00000000000002132, 208.5000000000000284, 165.9999999999998863 ) ) ;
#4779 = ORIENTED_EDGE ( 'NONE', *, *, #22420, .F. ) ;
#4780 = CARTESIAN_POINT ( 'NONE',  ( 9.088647732546041524, 225.3440916664238785, -4.181359934662540745 ) ) ;
#4781 = FACE_OUTER_BOUND ( 'NONE', #63589, .T. ) ;
#4782 =( BOUNDED_CURVE ( )  B_SPLINE_CURVE ( 2, ( #35155, #68352, #16647, #23068, #34049, #46077, #69096, #67979, #17403 ),
 .UNSPECIFIED., .F., .F. ) 
 B_SPLINE_CURVE_WITH_KNOTS ( ( 3, 2, 2, 2, 3 ),
 ( 0.07291666666666671293, 0.07812500000000005551, 0.08333333333333338422, 0.08854166666666674068, 0.09375000000000006939 ),
 .UNSPECIFIED. ) 
 CURVE ( )  GEOMETRIC_REPRESENTATION_ITEM ( )  RATIONAL_B_SPLINE_CURVE ( ( 0.9999999999999994449, 0.9238795325112872936, 1.000000000000000000, 0.9238795325112867385, 1.000000000000000000, 0.9238795325112867385, 1.000000000000000000, 0.9238795325112857393, 1.000000000000001110 ) ) 
 REPRESENTATION_ITEM ( '' )  );
#4783 = CARTESIAN_POINT ( 'NONE',  ( 26.56734541678232375, 197.6250000013656063, 173.4587341249998929 ) ) ;
#4784 = AXIS2_PLACEMENT_3D ( 'NONE', #58687, #41693, #64706 ) ;
#4785 = CARTESIAN_POINT ( 'NONE',  ( 8.311093377946837890, 206.7187499965859843, -8.311093377946837890 ) ) ;
#4786 = CARTESIAN_POINT ( 'NONE',  ( -7.188101187500001821, 124.0625000020483810, -2.977408999572650483 ) ) ;
#4787 = CARTESIAN_POINT ( 'NONE',  ( -4.541265875000002339, 18.81249999863440436, -5.561446717895856393E-16 ) ) ;
#4788 = CARTESIAN_POINT ( 'NONE',  ( 3.734423912251746636, -56.16062404875972902, 44.09723116536054732 ) ) ;
#4789 = CARTESIAN_POINT ( 'NONE',  ( -7.999999999999991118, 0.000000000000000000, 18.83030277982336642 ) ) ;
#4791 = CARTESIAN_POINT ( 'NONE',  ( -28.00000000000008171, 208.1250000027312126, 166.0000000000003695 ) ) ;
#4790 = CARTESIAN_POINT ( 'NONE',  ( -49.61244609327839328, 47.85051171572388995, 58.19005307411759276 ) ) ;
#4792 = CARTESIAN_POINT ( 'NONE',  ( 3.042071309553159519, 99.73958332991934128, 11.35316468750000141 ) ) ;
#4793 = ORIENTED_EDGE ( 'NONE', *, *, #24640, .T. ) ;
#4794 = CARTESIAN_POINT ( 'NONE',  ( 3.313708498984657247, 92.46874999999998579, 8.000000000000106581 ) ) ;
#4795 = CARTESIAN_POINT ( 'NONE',  ( 2.977408999572651815, 16.68749999795161543, 7.188101187500000933 ) ) ;
#4796 = DIRECTION ( 'NONE',  ( -0.000000000000000000, 1.000000000000000000, -4.476705744456276341E-16 ) ) ;
#4797 = CARTESIAN_POINT ( 'NONE',  ( -5.676582343749992710, 260.0520833367473301, 9.832129032723422313 ) ) ;
#4798 = CARTESIAN_POINT ( 'NONE',  ( -3.042071309553164404, 97.23958332991936970, -11.35316468749999963 ) ) ;
#4799 = EDGE_LOOP ( 'NONE', ( #52628, #25401, #16898, #30672 ) ) ;
#4800 = EDGE_CURVE ( 'NONE', #50149, #18829, #72076, .T. ) ;
#4801 = CARTESIAN_POINT ( 'NONE',  ( 6.123233995736767268E-16, 208.1249999931720538, -10.00000000000000178 ) ) ;
#4802 = VECTOR ( 'NONE', #33378, 1000.000000000000000 ) ;
#4803 = CARTESIAN_POINT ( 'NONE',  ( -7.204075437095967871, 7.204075437095967871, 106.4687500020483810 ) ) ;
#4804 = CARTESIAN_POINT ( 'NONE',  ( -25.55430564589119058, 195.5625000013656063, 167.5543056458915316 ) ) ;
#4805 = CARTESIAN_POINT ( 'NONE',  ( 1.432654583217662481, 206.3750000013656063, 194.5412658750000219 ) ) ;
#4807 = CARTESIAN_POINT ( 'NONE',  ( 3.042071309553167513, 91.82291666325269830, -11.35316468749999785 ) ) ;
#4806 = CARTESIAN_POINT ( 'NONE',  ( -4.898587196589407898E-16, 7.999999999999991118, 22.95530277982336642 ) ) ;
#4808 = CARTESIAN_POINT ( 'NONE',  ( -7.999999999999991118, 3.313708498984756723, 15.92405278392014623 ) ) ;
#4809 = CARTESIAN_POINT ( 'NONE',  ( -31.45873412499999233, 198.9375000013655779, 170.0000000000003979 ) ) ;
#4810 = DIRECTION ( 'NONE',  ( -0.000000000000000000, 1.000000000000000000, 4.689100369878284071E-30 ) ) ;
#4811 = EDGE_LOOP ( 'NONE', ( #61471, #8291, #8866, #66434, #24547, #62910 ) ) ;
#4812 = CARTESIAN_POINT ( 'NONE',  ( -2.679491924311225848, 183.3333333265053113, -10.00000000000000178 ) ) ;
#4813 = CARTESIAN_POINT ( 'NONE',  ( -7.347880794884122694E-16, 5.750000000000000000, 4.000000000000001776 ) ) ;
#4814 = FACE_OUTER_BOUND ( 'NONE', #29957, .T. ) ;
#4815 = CARTESIAN_POINT ( 'NONE',  ( 11.35316468749999963, 81.30208332991935549, -3.042071309553165293 ) ) ;
#4816 = CARTESIAN_POINT ( 'NONE',  ( -2.765530957081996810, 289.2656250017069510, -6.676582343750003368 ) ) ;
#4817 = DIRECTION ( 'NONE',  ( 1.000000000000000000, 0.000000000000000000, 0.000000000000000000 ) ) ;
#4818 = CARTESIAN_POINT ( 'NONE',  ( -4.220049686691935698, 10.18810118749999916, 99.25000000204838102 ) ) ;
#4819 = CARTESIAN_POINT ( 'NONE',  ( 9.832129032723416984, 225.3645833299193839, 5.676582343750006032 ) ) ;
#4820 = ORIENTED_EDGE ( 'NONE', *, *, #15359, .T. ) ;
#4821 = DIRECTION ( 'NONE',  ( 1.000000000000000000, 0.000000000000000000, 0.000000000000000000 ) ) ;
#4822 = CARTESIAN_POINT ( 'NONE',  ( 9.184850993605175555E-16, 125.0000000000000000, 7.500000000000020428 ) ) ;
#4823 = CARTESIAN_POINT ( 'NONE',  ( -11.00000000000000000, 0.000000000000000000, 106.1875000040967620 ) ) ;
#4824 = CARTESIAN_POINT ( 'NONE',  ( 6.951808397369818766E-16, 207.0312499965860411, -11.35316468750000141 ) ) ;
#4825 = CARTESIAN_POINT ( 'NONE',  ( -8.660254037844387298, 227.7083333401613174, -4.999999999999999112 ) ) ;
#4826 = CARTESIAN_POINT ( 'NONE',  ( 0.000000000000000000, 300.0000000000000000, 0.000000000000000000 ) ) ;
#4827 = CARTESIAN_POINT ( 'NONE',  ( -4.088227598258586603E-16, 299.2031250017070079, -6.676582343750001591 ) ) ;
#4828 = EDGE_LOOP ( 'NONE', ( #67927, #32387, #20374, #52905 ) ) ;
#4829 = CARTESIAN_POINT ( 'NONE',  ( 9.832129032723420536, 191.5104166632526983, -5.676582343749999815 ) ) ;
#4830 = EDGE_CURVE ( 'NONE', #30304, #30024, #35002, .T. ) ;
#4831 = CARTESIAN_POINT ( 'NONE',  ( 2.977408999572646486, 7.188101187499992051, 17.51780278187175455 ) ) ;
#4832 = CARTESIAN_POINT ( 'NONE',  ( -28.00000000000002487, 207.4375000013656063, 166.5412658750003629 ) ) ;
#4833 = CARTESIAN_POINT ( 'NONE',  ( 5.656854249492380582, 13.68750000000000178, -5.656854249492380582 ) ) ;
#4834 = EDGE_LOOP ( 'NONE', ( #63727, #47482, #30784, #4385 ) ) ;
#4835 = CARTESIAN_POINT ( 'NONE',  ( -8.000000000000000000, 92.09375000409679046, -3.313708498984761608 ) ) ;
#4836 = EDGE_CURVE ( 'NONE', #46242, #70220, #5127, .T. ) ;
#4837 = CARTESIAN_POINT ( 'NONE',  ( 8.660254037844385522, 9.583333333333333925, 5.000000000000005329 ) ) ;
#4838 = EDGE_CURVE ( 'NONE', #1378, #43896, #30248, .T. ) ;
#4839 = CIRCLE ( 'NONE', #26512, 7.000000000000000000 ) ;
#4840 = CARTESIAN_POINT ( 'NONE',  ( 10.18810118749999916, 1.247682550866122264E-15, 79.28125000204836681 ) ) ;
#4841 = EDGE_LOOP ( 'NONE', ( #56407, #35025, #72090 ) ) ;
#4842 = CARTESIAN_POINT ( 'NONE',  ( 1.656854249492381248, 19.18749999999999645, -4.000000000000001776 ) ) ;
#4843 = CARTESIAN_POINT ( 'NONE',  ( -4.541265875000003227, 17.87499999863441147, 1.881053915767121110 ) ) ;
#4844 = SPHERICAL_SURFACE ( 'NONE', #19763, 20.00000000000000355 ) ;
#4845 = VECTOR ( 'NONE', #30191, 1000.000000000000000 ) ;
#4846 = VERTEX_POINT ( 'NONE', #10042 ) ;
#4847 = DIRECTION ( 'NONE',  ( -0.000000000000000000, -0.000000000000000000, -1.000000000000000000 ) ) ;
#4848 = CARTESIAN_POINT ( 'NONE',  ( 1.926037949307475294, 89.22060463630471361, -7.188101187500001821 ) ) ;
#4851 = CARTESIAN_POINT ( 'NONE',  ( -3.107148544787702027E-14, -51.14729664189371761, 48.52014062455021559 ) ) ;
#4850 = CARTESIAN_POINT ( 'NONE',  ( 3.042071309553173286, 245.3645833367473017, 11.35316468749999608 ) ) ;
#4849 = CARTESIAN_POINT ( 'NONE',  ( 24.54126587500000767, 209.2500000013656063, 171.4326545832176123 ) ) ;
#4852 = SHAPE_DEFINITION_REPRESENTATION ( #21604, #43124 ) ;
#4853 = VERTEX_POINT ( 'NONE', #31933 ) ;
#4854 = CARTESIAN_POINT ( 'NONE',  ( -6.951808397369817780E-16, 247.9687500034140157, -11.35316468749999963 ) ) ;
#4855 = EDGE_CURVE ( 'NONE', #300, #27460, #9676, .T. ) ;
#4856 = CARTESIAN_POINT ( 'NONE',  ( 7.188101187499993827, -2.977408999572645598, 12.64280278187175277 ) ) ;
#4857 = ORIENTED_EDGE ( 'NONE', *, *, #72099, .T. ) ;
#4858 = ORIENTED_EDGE ( 'NONE', *, *, #9991, .T. ) ;
#4859 = CARTESIAN_POINT ( 'NONE',  ( -10.18810118749999738, -4.220049686691941915, 76.75000000204838102 ) ) ;
#4860 = CARTESIAN_POINT ( 'NONE',  ( 5.676582343749993598, 85.26041666325268409, 9.832129032723422313 ) ) ;
#4861 = CARTESIAN_POINT ( 'NONE',  ( 0.000000000000000000, 0.000000000000000000, 0.000000000000000000 ) ) ;
#4862 = CARTESIAN_POINT ( 'NONE',  ( -10.99999999999999822, -4.556349186104052151, 86.59375000000000000 ) ) ;
#4865 = CARTESIAN_POINT ( 'NONE',  ( 6.676582343750003368, 290.0468750017070079, 2.765530957081995478 ) ) ;
#4864 = CARTESIAN_POINT ( 'NONE',  ( 23.99999999999999645, 194.9375000027312126, 171.6568542494923122 ) ) ;
#4863 = CARTESIAN_POINT ( 'NONE',  ( 27.99999999999996803, 208.6875000013656063, 173.4587341249998929 ) ) ;
#4866 = CARTESIAN_POINT ( 'NONE',  ( 27.99999999999999645, 210.0000000000000284, 169.9999999999999147 ) ) ;
#4867 = DIRECTION ( 'NONE',  ( 0.000000000000000000, 0.000000000000000000, 1.000000000000000000 ) ) ;
#4868 = VECTOR ( 'NONE', #17642, 1000.000000000000000 ) ;
#4869 = CARTESIAN_POINT ( 'NONE',  ( 3.042071309553167069, 196.8229166632526983, -11.35316468749999785 ) ) ;
#4870 = CARTESIAN_POINT ( 'NONE',  ( 3.313708498984762496, 10.03124999590321842, 7.999999999999998224 ) ) ;
#4871 = ORIENTED_EDGE ( 'NONE', *, *, #5667, .F. ) ;
#4872 = CARTESIAN_POINT ( 'NONE',  ( 30.44569435410883784, 209.0625000013656063, 167.5543056458911053 ) ) ;
#4873 = CARTESIAN_POINT ( 'NONE',  ( -7.188101187500002709, 15.18749999795161365, 2.977408999572649151 ) ) ;
#4874 = CARTESIAN_POINT ( 'NONE',  ( -8.311093377946836114, 162.9687499965860411, -8.311093377946837890 ) ) ;
#4875 = CARTESIAN_POINT ( 'NONE',  ( -5.656854249492380582, 105.3125000000000000, -5.656854249492380582 ) ) ;
#4876 = CARTESIAN_POINT ( 'NONE',  ( -2.977408999572652260, 105.3125000020483810, 7.188101187500000044 ) ) ;
#4878 = DIRECTION ( 'NONE',  ( -0.000000000000000000, 1.000000000000000000, -0.000000000000000000 ) ) ;
#4877 = CARTESIAN_POINT ( 'NONE',  ( -8.660254037844387298, 207.9166666666667140, 4.999999999999995559 ) ) ;
#4879 = CARTESIAN_POINT ( 'NONE',  ( 29.43265458321761230, 205.7500000013656063, 173.4587341249998929 ) ) ;
#4880 = CARTESIAN_POINT ( 'NONE',  ( 2.977408999572646486, 7.188101187499991163, 16.39280278187175455 ) ) ;
#4881 = CARTESIAN_POINT ( 'NONE',  ( -3.042071309553173730, 59.32291666325268409, 11.35316468749999785 ) ) ;
#4882 = CARTESIAN_POINT ( 'NONE',  ( -3.313708498984759387, -7.999999999999989342, 1.299052783920146226 ) ) ;
#4883 = CARTESIAN_POINT ( 'NONE',  ( 1.656854249492381914, 16.81250000000000000, 4.000000000000000888 ) ) ;
#4884 = EDGE_LOOP ( 'NONE', ( #17140, #32947, #3621, #557 ) ) ;
#4885 = CARTESIAN_POINT ( 'NONE',  ( 27.99999999999996447, 195.0000000000000000, 173.9999999999999147 ) ) ;
#4886 = CARTESIAN_POINT ( 'NONE',  ( -9.832129032723420536, 63.69791666325269830, 5.676582343749997150 ) ) ;
#4887 = CARTESIAN_POINT ( 'NONE',  ( -7.778174593052020747, -7.778174593052023411, 76.37500000409677625 ) ) ;
#4888 = CARTESIAN_POINT ( 'NONE',  ( -3.458734125000016757, 202.1250000013656063, 140.5673454167823593 ) ) ;
#4889 = CARTESIAN_POINT ( 'NONE',  ( 4.104248244565246395, 10.10575198620100856, 70.81982386211579694 ) ) ;
#4890 = CARTESIAN_POINT ( 'NONE',  ( -2.751064625579944321E-14, 196.8750000027312126, 146.0000000000000284 ) ) ;
#4892 = CARTESIAN_POINT ( 'NONE',  ( -9.832129032723420536, 43.69791666325268409, 5.676582343749997150 ) ) ;
#4891 = CARTESIAN_POINT ( 'NONE',  ( -5.082755093536325930, 90.96875000204838102, -5.082755093536325930 ) ) ;
#4894 = EDGE_CURVE ( 'NONE', #19485, #38928, #59116, .T. ) ;
#4893 = CARTESIAN_POINT ( 'NONE',  ( -4.898587196589407898E-16, 7.999999999999991118, 4.955302779823363757 ) ) ;
#4895 = CARTESIAN_POINT ( 'NONE',  ( -31.05507224581699077, -34.98990058138039672, 171.9999999999997726 ) ) ;
#4896 = CARTESIAN_POINT ( 'NONE',  ( -3.042071309553164404, 172.2395833299193839, -11.35316468749999963 ) ) ;
#4897 = VECTOR ( 'NONE', #24138, 1000.000000000000000 ) ;
#4898 = CARTESIAN_POINT ( 'NONE',  ( -7.320508075688773708, 148.7499999931720538, -7.320508075688774596 ) ) ;
#4899 = CARTESIAN_POINT ( 'NONE',  ( -5.082755093536324154, 100.7187500020483810, 5.082755093536326818 ) ) ;
#4900 = CARTESIAN_POINT ( 'NONE',  ( 20.42802198618029763, 183.6788756342476745, 139.0000000000000284 ) ) ;
#4901 = CARTESIAN_POINT ( 'NONE',  ( -11.35316468749999785, 33.38541666325269119, -3.042071309553167957 ) ) ;
#4902 = EDGE_CURVE ( 'NONE', #29797, #65791, #20599, .T. ) ;
#4903 =( BOUNDED_CURVE ( )  B_SPLINE_CURVE ( 2, ( #70583, #23445, #47194, #18535, #18900, #41542, #35893, #58910, #29115 ),
 .UNSPECIFIED., .F., .F. ) 
 B_SPLINE_CURVE_WITH_KNOTS ( ( 3, 2, 2, 2, 3 ),
 ( 0.6931818181818182323, 0.6988636363636363535, 0.7045454545454545858, 0.7102272727272727071, 0.7159090909090909394 ),
 .UNSPECIFIED. ) 
 CURVE ( )  GEOMETRIC_REPRESENTATION_ITEM ( )  RATIONAL_B_SPLINE_CURVE ( ( 1.000000000000000000, 0.9238795325112867385, 1.000000000000000000, 0.9238795325112867385, 1.000000000000000000, 0.9238795325112867385, 1.000000000000000000, 0.9238795325112867385, 1.000000000000000000 ) ) 
 REPRESENTATION_ITEM ( '' )  );
#4904 = CARTESIAN_POINT ( 'NONE',  ( -1.836970198721029983E-15, 80.62499999317203958, 10.00000000000000178 ) ) ;
#4905 = CARTESIAN_POINT ( 'NONE',  ( -9.832129032723418760, 182.8645833299193555, -5.676582343750004256 ) ) ;
#4906 = ORIENTED_EDGE ( 'NONE', *, *, #42074, .T. ) ;
#4908 =( BOUNDED_CURVE ( )  B_SPLINE_CURVE ( 2, ( #8375, #18594, #48733, #12916, #71739, #20054, #43071, #35951, #66087 ),
 .UNSPECIFIED., .F., .F. ) 
 B_SPLINE_CURVE_WITH_KNOTS ( ( 3, 2, 2, 2, 3 ),
 ( 0.6562500000000000000, 0.6614583333333333703, 0.6666666666666667407, 0.6718750000000001110, 0.6770833333333334814 ),
 .UNSPECIFIED. ) 
 CURVE ( )  GEOMETRIC_REPRESENTATION_ITEM ( )  RATIONAL_B_SPLINE_CURVE ( ( 1.000000000000000000, 0.9238795325112867385, 1.000000000000000000, 0.9238795325112867385, 1.000000000000000000, 0.9238795325112867385, 1.000000000000000000, 0.9238795325112850731, 1.000000000000001554 ) ) 
 REPRESENTATION_ITEM ( '' )  );
#4907 = DIRECTION ( 'NONE',  ( 0.000000000000000000, 0.000000000000000000, -1.000000000000000000 ) ) ;
#4909 = CARTESIAN_POINT ( 'NONE',  ( 4.220049686691941027, -10.18810118749999738, 74.12500000204836681 ) ) ;
#4910 = CARTESIAN_POINT ( 'NONE',  ( -3.999999999999960032, 195.9375000000000000, 196.3431457505076594 ) ) ;
#4911 = CARTESIAN_POINT ( 'NONE',  ( 37.99999999999999289, 39.09128788536428800, 65.00000000000000000 ) ) ;
#4913 = CARTESIAN_POINT ( 'NONE',  ( -2.085542519210945728E-15, 164.5312499965860127, 11.35316468750000141 ) ) ;
#4912 = CARTESIAN_POINT ( 'NONE',  ( 0.4368895104442291899, -67.59332269699979179, 20.03478791450223895 ) ) ;
#4914 = AXIS2_PLACEMENT_3D ( 'NONE', #14307, #59975, #65633 ) ;
#4915 = CARTESIAN_POINT ( 'NONE',  ( -3.313708498984758943, -7.999999999999989342, 4.167802784329823318 ) ) ;
#4916 = CARTESIAN_POINT ( 'NONE',  ( -4.898587196589407898E-16, 7.999999999999991118, 4.955302779823363757 ) ) ;
#4917 = CARTESIAN_POINT ( 'NONE',  ( -11.35316468749999963, 223.9062500034139873, 0.000000000000000000 ) ) ;
#4918 = CARTESIAN_POINT ( 'NONE',  ( -4.336811714531673800, 52.00708776950106227, -48.85034107298749007 ) ) ;
#4919 = CARTESIAN_POINT ( 'NONE',  ( -7.204075437095967871, 7.204075437095967871, 78.34375000204838102 ) ) ;
#4920 = EDGE_LOOP ( 'NONE', ( #38222, #1317, #5801, #53371, #70239, #44993, #9084, #58954, #56182, #47620 ) ) ;
#4921 = ADVANCED_FACE ( 'NONE', ( #4020 ), #9293, .F. ) ;
#4922 = CARTESIAN_POINT ( 'NONE',  ( -3.999999999999959144, 204.0625000000000000, 199.6568542494924259 ) ) ;
#4923 = CARTESIAN_POINT ( 'NONE',  ( 5.676582343749993598, 120.2604166632526841, 9.832129032723422313 ) ) ;
#4924 = PRODUCT_RELATED_PRODUCT_CATEGORY ( 'part', '', ( #39708 ) ) ;
#4925 = ORIENTED_EDGE ( 'NONE', *, *, #12739, .T. ) ;
#4926 = EDGE_LOOP ( 'NONE', ( #26254, #16119, #23664, #53536 ) ) ;
#4927 = CARTESIAN_POINT ( 'NONE',  ( 4.541265875000002339, 9.437499998634407916, 0.000000000000000000 ) ) ;
#4928 = CARTESIAN_POINT ( 'NONE',  ( -1.320432766682874540E-15, 12.09374999795161187, 7.188101187500000044 ) ) ;
#4929 = CARTESIAN_POINT ( 'NONE',  ( -3.313708498984762052, 111.4062500040967763, -8.000000000000000000 ) ) ;
#4930 = VECTOR ( 'NONE', #45868, 1000.000000000000000 ) ;
#4931 = CARTESIAN_POINT ( 'NONE',  ( -31.45873412499997812, 200.0000000013656347, 171.4326545832180386 ) ) ;
#4932 = EDGE_CURVE ( 'NONE', #56053, #34167, #30234, .T. ) ;
#4933 = CARTESIAN_POINT ( 'NONE',  ( 4.000000000000001776, 10.06250000000000000, -1.656854249492381248 ) ) ;
#4934 = CARTESIAN_POINT ( 'NONE',  ( 1.656854249492381914, 20.56249999726881583, 4.000000000000000888 ) ) ;
#4935 = CARTESIAN_POINT ( 'NONE',  ( 1.881053915767121998, 8.499999998634407916, -4.541265875000002339 ) ) ;
#4936 = CARTESIAN_POINT ( 'NONE',  ( -1.656854249492405451, 199.3125000000000853, 138.0000000000000568 ) ) ;
#4937 = ORIENTED_EDGE ( 'NONE', *, *, #12145, .T. ) ;
#4938 = FILL_AREA_STYLE ('',( #45652 ) ) ;
#4939 = CARTESIAN_POINT ( 'NONE',  ( -7.188101187499999156, 112.2500000020483952, 2.977408999572654924 ) ) ;
#4940 = LINE ( 'NONE', #27937, #16940 ) ;
#4941 =( LENGTH_UNIT ( ) NAMED_UNIT ( * ) SI_UNIT ( .MILLI., .METRE. ) );
#4942 = CARTESIAN_POINT ( 'NONE',  ( -2.828427124746192067, 10.62500000000000000, 2.828427124746190735 ) ) ;
#4943 = CARTESIAN_POINT ( 'NONE',  ( -7.188101187499991163, 2.977408999572646930, 1.392802781871753437 ) ) ;
#4944 = ORIENTED_EDGE ( 'NONE', *, *, #47539, .F. ) ;
#4945 = ORIENTED_EDGE ( 'NONE', *, *, #3156, .T. ) ;
#4946 = CARTESIAN_POINT ( 'NONE',  ( -4.220049686691937474, -10.18810118749999738, 94.93750000204836681 ) ) ;
#4947 = CARTESIAN_POINT ( 'NONE',  ( 2.485281374238838215, 288.3125000000000000, 5.999999999999736211 ) ) ;
#4948 = CARTESIAN_POINT ( 'NONE',  ( -25.55430564589119413, 201.5625000013656063, 167.5543056458915316 ) ) ;
#4949 = CARTESIAN_POINT ( 'NONE',  ( -11.00000000000000000, 4.556349186104045934, 104.4062500000000000 ) ) ;
#4950 = CARTESIAN_POINT ( 'NONE',  ( -3.458734124999960358, 206.6875000013656063, 198.0000000000000284 ) ) ;
#4952 = CARTESIAN_POINT ( 'NONE',  ( -8.660254037844387298, 254.5833333333333144, -4.999999999999999112 ) ) ;
#4951 = CARTESIAN_POINT ( 'NONE',  ( 7.320508075688828775, 59.37500000000004263, 7.320508075688831440 ) ) ;
#4953 = CARTESIAN_POINT ( 'NONE',  ( 10.00000000000000000, 124.7916666666666572, 2.679491924311236062 ) ) ;
#4954 = CARTESIAN_POINT ( 'NONE',  ( -5.656854249492380582, 106.8125000000000000, -5.656854249492380582 ) ) ;
#4955 = CARTESIAN_POINT ( 'NONE',  ( -6.676582343750001591, 288.6093750017069510, 0.000000000000000000 ) ) ;
#4956 = CARTESIAN_POINT ( 'NONE',  ( -7.188101187499992051, 0.000000000000000000, 4.861552781871752771 ) ) ;
#4957 = CARTESIAN_POINT ( 'NONE',  ( -3.313708498984816231, 98.28125000000000000, 7.999999999999943157 ) ) ;
#4958 = CARTESIAN_POINT ( 'NONE',  ( 31.45873412500001010, 205.7500000013656063, 168.5673454167822740 ) ) ;
#4959 = CARTESIAN_POINT ( 'NONE',  ( 3.313708498984762496, 25.03124999590322020, 7.999999999999998224 ) ) ;
#4960 = MECHANICAL_DESIGN_GEOMETRIC_PRESENTATION_REPRESENTATION (  '', ( #72431 ), #25446 ) ;
#4961 = CARTESIAN_POINT ( 'NONE',  ( 2.445694354108783664, 199.3125000013656063, 144.4456943541088663 ) ) ;
#4962 = CARTESIAN_POINT ( 'NONE',  ( -2.977408999572652260, 121.8125000020483810, 7.188101187500000044 ) ) ;
#4964 = CARTESIAN_POINT ( 'NONE',  ( -2.445694354108840063, 203.0625000013656063, 139.5543056458912190 ) ) ;
#4963 = CARTESIAN_POINT ( 'NONE',  ( 27.99999999999999645, 210.0000000000000284, 173.9999999999998863 ) ) ;
#4965 = CARTESIAN_POINT ( 'NONE',  ( 3.042071309553173286, 235.6770833367473017, 11.35316468749999608 ) ) ;
#4966 = CARTESIAN_POINT ( 'NONE',  ( -7.320508075688773708, 93.74999999317202537, -7.320508075688774596 ) ) ;
#4967 = CARTESIAN_POINT ( 'NONE',  ( 25.17157287525381548, 202.6250000000000284, 167.1715728752537018 ) ) ;
#4968 = CARTESIAN_POINT ( 'NONE',  ( 11.35316468749999963, 10.98958332991935016, -3.042071309553165293 ) ) ;
#4969 = CARTESIAN_POINT ( 'NONE',  ( 5.000000000000001776, 0.8333333333333323711, -8.660254037844389075 ) ) ;
#4970 = CARTESIAN_POINT ( 'NONE',  ( -8.311093377946841443, 204.2187499965860411, 8.311093377946830785 ) ) ;
#4971 = DIRECTION ( 'NONE',  ( -0.000000000000000000, -1.000000000000000000, -0.000000000000000000 ) ) ;
#4972 = DIRECTION ( 'NONE',  ( 1.000000000000000000, 0.000000000000000000, 0.000000000000000000 ) ) ;
#4974 = DIRECTION ( 'NONE',  ( 0.000000000000000000, 0.000000000000000000, 1.000000000000000000 ) ) ;
#4973 = LINE ( 'NONE', #34031, #32275 ) ;
#4975 = VECTOR ( 'NONE', #58243, 1000.000000000000000 ) ;
#4976 = ORIENTED_EDGE ( 'NONE', *, *, #33794, .T. ) ;
#4977 = CARTESIAN_POINT ( 'NONE',  ( -2.754378923186476579E-14, 201.4375000013656063, 145.4587341250000350 ) ) ;
#4978 = CARTESIAN_POINT ( 'NONE',  ( 5.676582343750001591, 16.61458332991935194, -9.832129032723420536 ) ) ;
#4979 = CARTESIAN_POINT ( 'NONE',  ( 4.556349186104051263, -10.99999999999999822, 94.65625000409680467 ) ) ;
#4980 = DIRECTION ( 'NONE',  ( 1.000000000000000000, 9.637352644315595243E-17, 0.000000000000000000 ) ) ;
#4981 = CARTESIAN_POINT ( 'NONE',  ( -31.45873412499999233, 197.6875000013655779, 170.0000000000004547 ) ) ;
#4982 = DIRECTION ( 'NONE',  ( 0.000000000000000000, 0.000000000000000000, 1.000000000000000000 ) ) ;
#4984 = CARTESIAN_POINT ( 'NONE',  ( 11.35316468749999785, 5.572916663252682312, 3.042071309553174174 ) ) ;
#4983 = CARTESIAN_POINT ( 'NONE',  ( 5.082755093536325042, 114.5937500020483810, -5.082755093536325930 ) ) ;
#4986 = EDGE_CURVE ( 'NONE', #5468, #42176, #29787, .T. ) ;
#4985 = CARTESIAN_POINT ( 'NONE',  ( 5.656854249492376141, -5.656854249492374365, 19.39280277982336642 ) ) ;
#4987 = CARTESIAN_POINT ( 'NONE',  ( 3.042071309553167069, 141.8229166632526983, -11.35316468749999785 ) ) ;
#4988 = CARTESIAN_POINT ( 'NONE',  ( 10.00000000000000178, 96.87499999317203958, 0.000000000000000000 ) ) ;
#4989 = CARTESIAN_POINT ( 'NONE',  ( -7.188101187500000044, 120.0312500020483810, 0.000000000000000000 ) ) ;
#4990 = CARTESIAN_POINT ( 'NONE',  ( 1.739508062058950699, 67.70228923712218716, -20.12326043015055177 ) ) ;
#4991 = CARTESIAN_POINT ( 'NONE',  ( -29.43265458321766559, 208.7500000013656063, 166.5412658750003629 ) ) ;
#4992 = CARTESIAN_POINT ( 'NONE',  ( -5.000000000000000888, 53.53067326687928329, -46.58593137613046764 ) ) ;
#4993 = VERTEX_POINT ( 'NONE', #232 ) ;
#4994 = CARTESIAN_POINT ( 'NONE',  ( 7.456209740496413829, -61.82228229130296882, 23.87473629694196831 ) ) ;
#4995 = ADVANCED_FACE ( 'NONE', ( #17175 ), #52268, .F. ) ;
#4996 = CARTESIAN_POINT ( 'NONE',  ( -4.898587196589412829E-16, 108.1250000000000000, -8.000000000000000000 ) ) ;
#4997 = CARTESIAN_POINT ( 'NONE',  ( -2.765530957081996810, 290.4218750017068942, -6.676582343750003368 ) ) ;
#4998 = PRESENTATION_STYLE_ASSIGNMENT (( #17038 ) ) ;
#4999 = CARTESIAN_POINT ( 'NONE',  ( 3.313708498984762496, -7.999999999999989342, 23.85530278432982954 ) ) ;
#5000 = AXIS2_PLACEMENT_3D ( 'NONE', #9447, #56219, #21125 ) ;
#5001 = DIRECTION ( 'NONE',  ( -0.000000000000000000, -0.000000000000000000, -1.000000000000000000 ) ) ;
#5002 = CARTESIAN_POINT ( 'NONE',  ( 2.085542519210945334E-15, 260.1562500034140157, 11.35316468749999963 ) ) ;
#5003 = CARTESIAN_POINT ( 'NONE',  ( -6.238412754330611322E-16, 10.18810118749999916, 96.15625000204838102 ) ) ;
#5004 = ORIENTED_EDGE ( 'NONE', *, *, #67751, .F. ) ;
#5005 =( BOUNDED_CURVE ( )  B_SPLINE_CURVE ( 2, ( #46404, #67933, #38893, #63010, #68672, #52074, #4942, #27940, #74329 ),
 .UNSPECIFIED., .F., .F. ) 
 B_SPLINE_CURVE_WITH_KNOTS ( ( 3, 2, 2, 2, 3 ),
 ( 0.4659090909090909394, 0.4715909090909091717, 0.4772727272727272929, 0.4829545454545454697, 0.4886363636363636465 ),
 .UNSPECIFIED. ) 
 CURVE ( )  GEOMETRIC_REPRESENTATION_ITEM ( )  RATIONAL_B_SPLINE_CURVE ( ( 0.9999999999999992228, 0.9238795325112875156, 1.000000000000000000, 0.9238795325112867385, 1.000000000000000000, 0.9238795325112867385, 1.000000000000000000, 0.9238795325112867385, 1.000000000000000000 ) ) 
 REPRESENTATION_ITEM ( '' )  );
#5006 = LINE ( 'NONE', #56689, #48472 ) ;
#5007 = CARTESIAN_POINT ( 'NONE',  ( 0.000000000000000000, 0.000000000000000000, 0.000000000000000000 ) ) ;
#5008 = CARTESIAN_POINT ( 'NONE',  ( -2.445694354108783219, 200.8125000013656063, 200.4456943541088663 ) ) ;
#5009 = CARTESIAN_POINT ( 'NONE',  ( -3.042071309553164404, 82.55208332991936970, -11.35316468749999963 ) ) ;
#5010 = ORIENTED_EDGE ( 'NONE', *, *, #19179, .F. ) ;
#5011 = CARTESIAN_POINT ( 'NONE',  ( 1.871523826299183495E-15, -10.18810118749999916, 113.0312500020483810 ) ) ;
#5012 = CARTESIAN_POINT ( 'NONE',  ( 2.780723358947928197E-16, 12.68749999863440792, -4.541265875000002339 ) ) ;
#5013 = ORIENTED_EDGE ( 'NONE', *, *, #54714, .T. ) ;
#5014 = CARTESIAN_POINT ( 'NONE',  ( 2.977408999572650927, 24.74999999795161543, -7.188101187500001821 ) ) ;
#5015 = CARTESIAN_POINT ( 'NONE',  ( -8.000000000000000000, 110.0937500040967905, -3.313708498984761164 ) ) ;
#5016 = COLOUR_RGB ( '',0.7921568627450980005, 0.8196078431372548767, 0.9333333333333333481 ) ;
#5017 = CARTESIAN_POINT ( 'NONE',  ( -3.999999999999960032, 197.0625000027312126, 196.3431457505076594 ) ) ;
#5018 = CARTESIAN_POINT ( 'NONE',  ( 7.188101187500000044, 23.34374999795161543, 0.000000000000000000 ) ) ;
#5019 = CARTESIAN_POINT ( 'NONE',  ( 3.999999999999960032, 200.0000000000000000, 142.0000000000000568 ) ) ;
#5020 =( BOUNDED_CURVE ( )  B_SPLINE_CURVE ( 2, ( #23041, #73983, #74349, #63774, #39656, #22286, #11725, #62654, #12091 ),
 .UNSPECIFIED., .F., .F. ) 
 B_SPLINE_CURVE_WITH_KNOTS ( ( 3, 2, 2, 2, 3 ),
 ( 0.3500000000000004219, 0.3583333333333337256, 0.3666666666666669738, 0.3750000000000002776, 0.3833333333333335813 ),
 .UNSPECIFIED. ) 
 CURVE ( )  GEOMETRIC_REPRESENTATION_ITEM ( )  RATIONAL_B_SPLINE_CURVE ( ( 0.9999999999999958922, 0.9238795325112908463, 1.000000000000000000, 0.9238795325112867385, 1.000000000000000000, 0.9238795325112867385, 1.000000000000000000, 0.9238795325112847401, 1.000000000000001998 ) ) 
 REPRESENTATION_ITEM ( '' )  );
#5021 = CARTESIAN_POINT ( 'NONE',  ( 4.220049686691934809, 10.18810118749999916, 108.0625000020483810 ) ) ;
#5022 = AXIS2_PLACEMENT_3D ( 'NONE', #69487, #12502, #51758 ) ;
#5023 = CARTESIAN_POINT ( 'NONE',  ( -6.735557395310442023E-16, 11.00000000000000000, 75.62499999999998579 ) ) ;
#5024 = CARTESIAN_POINT ( 'NONE',  ( -1.656854249492381248, 10.06249999726881406, -4.000000000000001776 ) ) ;
#5025 = CARTESIAN_POINT ( 'NONE',  ( -41.99999999999992895, -31.99999999999978684, 167.9999999999997726 ) ) ;
#5026 = ORIENTED_EDGE ( 'NONE', *, *, #67136, .F. ) ;
#5027 = CARTESIAN_POINT ( 'NONE',  ( 1.432654583217664479, 203.7500000013656063, 201.4587341250000065 ) ) ;
#5028 = CARTESIAN_POINT ( 'NONE',  ( -31.45873412499999944, 206.6875000013656063, 170.0000000000004547 ) ) ;
#5029 = CARTESIAN_POINT ( 'NONE',  ( -34.69679471024809203, -12.34462646322155699, 148.2170566195945298 ) ) ;
#5030 = CARTESIAN_POINT ( 'NONE',  ( -4.541265875000003227, 10.87499999863440792, 1.881053915767121110 ) ) ;
#5032 = CARTESIAN_POINT ( 'NONE',  ( 1.656854249492381914, 15.81250000000000000, 4.000000000000000888 ) ) ;
#5031 = SHAPE_REPRESENTATION ( 'hand wheel', ( #57354 ), #64563 ) ;
#5033 = CARTESIAN_POINT ( 'NONE',  ( -7.188101187499991163, 2.977408999572646930, 20.89280278187176521 ) ) ;
#5034 = ORIENTED_EDGE ( 'NONE', *, *, #6641, .F. ) ;
#5035 = CARTESIAN_POINT ( 'NONE',  ( -4.898587196589412829E-16, 103.8125000040967763, -8.000000000000000000 ) ) ;
#5036 = VERTEX_POINT ( 'NONE', #39820 ) ;
#5037 = CARTESIAN_POINT ( 'NONE',  ( -10.18810118749999916, 4.220049686691934809, 111.0625000020483810 ) ) ;
#5038 = CARTESIAN_POINT ( 'NONE',  ( 23.99999999999998224, 208.8125000027312126, 168.3431457505075457 ) ) ;
#5039 = CARTESIAN_POINT ( 'NONE',  ( -2.445694354108783664, 204.3125000013656063, 195.5543056458912190 ) ) ;
#5040 = CARTESIAN_POINT ( 'NONE',  ( 25.55430564589119058, 199.3125000013656063, 172.4456943541087526 ) ) ;
#5041 = CARTESIAN_POINT ( 'NONE',  ( -8.660254037844387298, 87.08333333333332860, -5.000000000000004441 ) ) ;
#5042 = AXIS2_PLACEMENT_3D ( 'NONE', #39118, #27412, #67792 ) ;
#5043 = CARTESIAN_POINT ( 'NONE',  ( -2.977408999572651815, 90.31250000204838102, 7.188101187500000933 ) ) ;
#5044 = CARTESIAN_POINT ( 'NONE',  ( -2.765530957081998586, 298.7968750017069510, 6.676582343750001591 ) ) ;
#5045 = ORIENTED_EDGE ( 'NONE', *, *, #20935, .F. ) ;
#5046 = ADVANCED_FACE ( 'NONE', ( #45847 ), #23583, .F. ) ;
#5047 = CARTESIAN_POINT ( 'NONE',  ( 0.000000000000000000, 300.0000000000000000, 10.00000000000000178 ) ) ;
#5048 = ADVANCED_FACE ( 'NONE', ( #23214 ), #43403, .T. ) ;
#5049 = CARTESIAN_POINT ( 'NONE',  ( 2.997005883567212869, -10.11494357241825526, 70.43990496500141774 ) ) ;
#5050 = CARTESIAN_POINT ( 'NONE',  ( -2.849036369511732440E-14, 196.3750000027311842, 138.0000000000000568 ) ) ;
#5051 = LINE ( 'NONE', #10697, #63523 ) ;
#5052 = DIRECTION ( 'NONE',  ( 1.000000000000000000, 0.000000000000000000, 1.224646799147353207E-16 ) ) ;
#5053 = CARTESIAN_POINT ( 'NONE',  ( 9.999999999999998224, 232.7083333333333712, -2.679491924311229401 ) ) ;
#5054 = DIRECTION ( 'NONE',  ( -0.000000000000000000, -0.000000000000000000, -1.000000000000000000 ) ) ;
#5055 = CARTESIAN_POINT ( 'NONE',  ( 2.679491924311222739, 198.9583333333333144, 10.00000000000000355 ) ) ;
#5056 = CARTESIAN_POINT ( 'NONE',  ( -7.188101187499992051, 2.977408999572646930, 16.76780278187175455 ) ) ;
#5057 = CARTESIAN_POINT ( 'NONE',  ( -8.311093377946841443, 169.2187499965859843, 8.311093377946830785 ) ) ;
#5058 = CARTESIAN_POINT ( 'NONE',  ( -7.320508075688771932, 36.87500000000001421, -7.320508075688772820 ) ) ;
#5059 = CARTESIAN_POINT ( 'NONE',  ( 5.000000000000094147, 155.8333333333334565, -8.660254037844545394 ) ) ;
#5061 = DIRECTION ( 'NONE',  ( -0.000000000000000000, 1.000000000000000000, 4.476705744456276341E-16 ) ) ;
#5060 = LINE ( 'NONE', #73707, #34656 ) ;
#5062 = ORIENTED_EDGE ( 'NONE', *, *, #40069, .T. ) ;
#5063 = CARTESIAN_POINT ( 'NONE',  ( 8.311093377946837890, 26.71874999658601624, -8.311093377946837890 ) ) ;
#5064 = CARTESIAN_POINT ( 'NONE',  ( 11.00000000000000355, -4.556349186104045046, 111.3437500040967763 ) ) ;
#5065 = CARTESIAN_POINT ( 'NONE',  ( -27.99999999999992184, 207.9375000013656063, 173.4587341250003760 ) ) ;
#5067 = CARTESIAN_POINT ( 'NONE',  ( 25.17157287525378351, 199.8750000000000284, 172.8284271247460424 ) ) ;
#5066 = DIRECTION ( 'NONE',  ( -1.000000000000000000, 0.000000000000000000, 0.000000000000000000 ) ) ;
#5068 = CARTESIAN_POINT ( 'NONE',  ( -12.44724857414599306, -39.52949414383339644, 198.3946604793865447 ) ) ;
#5070 = EDGE_CURVE ( 'NONE', #45401, #15013, #17551, .T. ) ;
#5069 = CARTESIAN_POINT ( 'NONE',  ( -2.754378923186476579E-14, 197.1875000013655779, 145.4587341250000350 ) ) ;
#5071 = CARTESIAN_POINT ( 'NONE',  ( 8.660254037844385522, 66.45833332650536818, 5.000000000000005329 ) ) ;
#5072 = VECTOR ( 'NONE', #39949, 999.9999999999998863 ) ;
#5073 = CARTESIAN_POINT ( 'NONE',  ( 1.320432766682874540E-15, 100.5312500020483810, 7.188101187500000044 ) ) ;
#5074 = CARTESIAN_POINT ( 'NONE',  ( 4.541265875000002339, 11.49999999863440792, -1.881053915767121554 ) ) ;
#5075 = CYLINDRICAL_SURFACE ( 'NONE', #6086, 8.000000000000000000 ) ;
#5076 = CARTESIAN_POINT ( 'NONE',  ( -5.656854249492375253, 5.656854249492375253, 2.142802779823364645 ) ) ;
#5077 = CARTESIAN_POINT ( 'NONE',  ( 7.999999999999991118, 9.797174393178815797E-16, 21.26780278392014623 ) ) ;
#5078 = EDGE_LOOP ( 'NONE', ( #61814, #67294, #13238, #74063 ) ) ;
#5079 = ORIENTED_EDGE ( 'NONE', *, *, #47791, .F. ) ;
#5080 = CARTESIAN_POINT ( 'NONE',  ( 7.778174593052021635, 7.778174593052023411, 115.9375000000000000 ) ) ;
#5081 = CARTESIAN_POINT ( 'NONE',  ( 2.839093476692135984E-14, 195.9375000013655779, 201.4587341250000350 ) ) ;
#5082 =( NAMED_UNIT ( * ) PLANE_ANGLE_UNIT ( ) SI_UNIT ( $, .RADIAN. ) );
#5083 = CARTESIAN_POINT ( 'NONE',  ( -3.042071309553159075, 220.2604166700806445, 11.35316468749999963 ) ) ;
#5084 = CARTESIAN_POINT ( 'NONE',  ( -11.35316468750000141, 143.2812499965860411, -1.390361679473963753E-15 ) ) ;
#5085 = ORIENTED_EDGE ( 'NONE', *, *, #46723, .F. ) ;
#5086 = CARTESIAN_POINT ( 'NONE',  ( 31.99999999999999289, 201.2500000000000000, 169.9999999999999432 ) ) ;
#5087 = CARTESIAN_POINT ( 'NONE',  ( -4.220049686691937474, -10.18810118749999738, 88.93750000204839523 ) ) ;
#5088 = CARTESIAN_POINT ( 'NONE',  ( -31.28528697797168689, 194.5631545839482044, 168.6019376775367959 ) ) ;
#5089 = CARTESIAN_POINT ( 'NONE',  ( 2.849036369511732440E-14, 206.2500000000000284, 202.0000000000000000 ) ) ;
#5090 = CARTESIAN_POINT ( 'NONE',  ( 1.469576158976823947E-15, 104.5625000040967763, 8.000000000000000000 ) ) ;
#5091 = DIRECTION ( 'NONE',  ( 8.659560562354941486E-17, 0.7071067811865472397, -0.7071067811865479058 ) ) ;
#5092 = CARTESIAN_POINT ( 'NONE',  ( 7.204075437095966983, 7.204075437095967871, 116.9687500020483810 ) ) ;
#5093 = ORIENTED_EDGE ( 'NONE', *, *, #33466, .F. ) ;
#5094 = CARTESIAN_POINT ( 'NONE',  ( 7.778174593052021635, 7.778174593052023411, 108.6250000040967763 ) ) ;
#5095 = CIRCLE ( 'NONE', #47226, 20.00000000000001066 ) ;
#5096 = CARTESIAN_POINT ( 'NONE',  ( -11.04632294300149553, 183.3901644024232382, 140.9474641887929920 ) ) ;
#5097 = CARTESIAN_POINT ( 'NONE',  ( 3.042071309553167513, 132.1354166632526699, -11.35316468749999785 ) ) ;
#5098 = CARTESIAN_POINT ( 'NONE',  ( 2.445694354108838731, 203.0625000013656063, 195.5543056458912190 ) ) ;
#5099 = CARTESIAN_POINT ( 'NONE',  ( 5.082755093536325930, 25.03124999795161543, -5.082755093536325930 ) ) ;
#5100 = CARTESIAN_POINT ( 'NONE',  ( -10.18810118749999916, 0.000000000000000000, 81.53125000204838102 ) ) ;
#5101 = CARTESIAN_POINT ( 'NONE',  ( 3.042071309553167069, 42.13541666325267698, -11.35316468749999785 ) ) ;
#5102 = ORIENTED_EDGE ( 'NONE', *, *, #57275, .F. ) ;
#5103 = CARTESIAN_POINT ( 'NONE',  ( 0.000000000000000000, 22.99999999999999645, 0.000000000000000000 ) ) ;
#5104 = DIRECTION ( 'NONE',  ( 1.000000000000000000, 0.000000000000000000, 0.000000000000000000 ) ) ;
#5105 = CARTESIAN_POINT ( 'NONE',  ( 5.662595241051936235, -5.662595241051934458, 22.57561528394063188 ) ) ;
#5106 = CARTESIAN_POINT ( 'NONE',  ( 1.432654583217608080, 207.8750000013656063, 138.5412658750000503 ) ) ;
#5107 = AXIS2_PLACEMENT_3D ( 'NONE', #36163, #31987, #37652 ) ;
#5108 = CARTESIAN_POINT ( 'NONE',  ( -5.082755093536325042, 11.53124999795161010, -5.082755093536325930 ) ) ;
#5109 = CARTESIAN_POINT ( 'NONE',  ( -6.000000000000003553, 296.0000000034139589, -2.485281374238571317 ) ) ;
#5110 = DIRECTION ( 'NONE',  ( -0.000000000000000000, 1.000000000000000000, -0.000000000000000000 ) ) ;
#5111 = FACE_OUTER_BOUND ( 'NONE', #28828, .T. ) ;
#5112 = CARTESIAN_POINT ( 'NONE',  ( 11.35316468750000141, 156.0937499965860127, 0.000000000000000000 ) ) ;
#5113 = CARTESIAN_POINT ( 'NONE',  ( -10.18810118749999916, 4.220049686691934809, 75.06250000204836681 ) ) ;
#5114 =( BOUNDED_CURVE ( )  B_SPLINE_CURVE ( 2, ( #50227, #4592, #27586, #26455, #16251, #44579, #56651, #55910, #45312, #22289, #39659, #15144, #50595 ),
 .UNSPECIFIED., .F., .F. ) 
 B_SPLINE_CURVE_WITH_KNOTS ( ( 3, 2, 2, 2, 2, 2, 3 ),
 ( 0.9184782608695651884, 0.9202898550724637472, 0.9221014492753623060, 0.9239130434782609758, 0.9257246376811595345, 0.9275362318840580933, 0.9293478260869566521 ),
 .UNSPECIFIED. ) 
 CURVE ( )  GEOMETRIC_REPRESENTATION_ITEM ( )  RATIONAL_B_SPLINE_CURVE ( ( 1.000000000000000000, 0.9659258262890683122, 1.000000000000000000, 0.9659258262890683122, 1.000000000000000000, 0.9659258262890683122, 1.000000000000000000, 0.9659258262890683122, 1.000000000000000000, 0.9659258262890683122, 1.000000000000000000, 0.9659258262890662028, 1.000000000000001998 ) ) 
 REPRESENTATION_ITEM ( '' )  );
#5115 = CARTESIAN_POINT ( 'NONE',  ( -24.54126587499997925, 196.1250000013655779, 171.4326545832179818 ) ) ;
#5116 = CARTESIAN_POINT ( 'NONE',  ( 4.556349186104045934, 11.00000000000000000, 110.0312500000000000 ) ) ;
#5117 = CARTESIAN_POINT ( 'NONE',  ( 1.881053915767122664, 21.24999999863440436, 4.541265875000001451 ) ) ;
#5118 = ORIENTED_EDGE ( 'NONE', *, *, #65592, .F. ) ;
#5119 = CARTESIAN_POINT ( 'NONE',  ( 4.000000000000015987, 197.6250000027312126, 198.0000000000000284 ) ) ;
#5120 = CARTESIAN_POINT ( 'NONE',  ( -2.445694354108840063, 195.0625000013656063, 139.5543056458912190 ) ) ;
#5121 = CARTESIAN_POINT ( 'NONE',  ( -25.17157287525374443, 206.7500000027312126, 172.8284271247464972 ) ) ;
#5122 = EDGE_CURVE ( 'NONE', #22824, #12782, #65914, .T. ) ;
#5123 = AXIS2_PLACEMENT_3D ( 'NONE', #10685, #57088, #33718 ) ;
#5124 = CARTESIAN_POINT ( 'NONE',  ( -5.000000000000038192, 56.66666666666672114, -8.660254037844456576 ) ) ;
#5125 = ORIENTED_EDGE ( 'NONE', *, *, #29937, .F. ) ;
#5127 =( BOUNDED_CURVE ( )  B_SPLINE_CURVE ( 2, ( #37597, #43998, #14562, #20973, #55330, #56441, #72286, #3635, #27376, #50396, #15683, #27012, #26632 ),
 .UNSPECIFIED., .F., .F. ) 
 B_SPLINE_CURVE_WITH_KNOTS ( ( 3, 2, 2, 2, 2, 2, 3 ),
 ( 0.8320903676337926269, 0.8373236054718522503, 0.8425568433099117627, 0.8477900811479713861, 0.8530233189860307874, 0.8582565568240904108, 0.8634897946621500342 ),
 .UNSPECIFIED. ) 
 CURVE ( )  GEOMETRIC_REPRESENTATION_ITEM ( )  RATIONAL_B_SPLINE_CURVE ( ( 1.000000000000390576, 0.9659258262886779578, 1.000000000000000000, 0.9659258262890684232, 1.000000000000000000, 0.9659258262890684232, 1.000000000000000000, 0.9659258262890684232, 1.000000000000000000, 0.9659258262890684232, 1.000000000000000000, 0.9659258262890632052, 1.000000000000005329 ) ) 
 REPRESENTATION_ITEM ( '' )  );
#5126 = CARTESIAN_POINT ( 'NONE',  ( 7.188101187500000044, 18.46874999795161187, 0.000000000000000000 ) ) ;
#5128 = DIRECTION ( 'NONE',  ( 0.000000000000000000, -0.000000000000000000, 1.000000000000000000 ) ) ;
#5129 = CARTESIAN_POINT ( 'NONE',  ( -10.00000000000000178, 42.50000000000000000, -1.224646799147353454E-15 ) ) ;
#5130 = CARTESIAN_POINT ( 'NONE',  ( 7.188101187500000044, 107.2812500020483810, -8.802885111219163269E-16 ) ) ;
#5131 = CARTESIAN_POINT ( 'NONE',  ( -31.45873412500001010, 207.8750000013656063, 168.5673454167827572 ) ) ;
#5132 = CARTESIAN_POINT ( 'NONE',  ( -4.721056650415998313, 287.5781250017069510, 4.721056650416000089 ) ) ;
#5134 = CARTESIAN_POINT ( 'NONE',  ( -7.323353171866783917, -3.228862220574169939, 0.000000000000000000 ) ) ;
#5133 = CARTESIAN_POINT ( 'NONE',  ( -24.00000000000000711, 201.8125000000000000, 168.3431457505080289 ) ) ;
#5135 = EDGE_LOOP ( 'NONE', ( #23817, #12140, #70643 ) ) ;
#5136 = CARTESIAN_POINT ( 'NONE',  ( -6.951808397369817780E-16, 262.6562500034140157, -11.35316468749999963 ) ) ;
#5137 = CIRCLE ( 'NONE', #3905, 34.85072926314708752 ) ;
#5138 = CARTESIAN_POINT ( 'NONE',  ( 5.082755093536320601, -5.082755093536318824, 24.92405278187175810 ) ) ;
#5139 = FACE_OUTER_BOUND ( 'NONE', #37402, .T. ) ;
#5140 = CARTESIAN_POINT ( 'NONE',  ( -7.347880794884122694E-16, 17.75000000000000355, 4.000000000000001776 ) ) ;
#5141 = CARTESIAN_POINT ( 'NONE',  ( -8.660254037844390851, 147.9166666666666572, 4.999999999999998224 ) ) ;
#5142 = CARTESIAN_POINT ( 'NONE',  ( -3.458734124999960358, 194.6875000013655779, 198.0000000000000284 ) ) ;
#5143 = CARTESIAN_POINT ( 'NONE',  ( -10.00000000000000000, 167.2916666666666856, -2.679491924311229845 ) ) ;
#5144 = CARTESIAN_POINT ( 'NONE',  ( -4.242640687119286547, 299.8750000000000000, -4.242640687119286547 ) ) ;
#5145 = CARTESIAN_POINT ( 'NONE',  ( 105.0000000000000000, 133.9999999999999716, 69.99999999999998579 ) ) ;
#5146 = FACE_OUTER_BOUND ( 'NONE', #5503, .T. ) ;
#5147 = CARTESIAN_POINT ( 'NONE',  ( -9.832129032723420536, 129.0104166632526983, 5.676582343749997150 ) ) ;
#5148 = CARTESIAN_POINT ( 'NONE',  ( 36.10814071610729314, 38.00000000000000000, 127.0000000000000000 ) ) ;
#5149 = CARTESIAN_POINT ( 'NONE',  ( 8.000000000000049738, 3.313708498984697215, 27.36155278392014623 ) ) ;
#5152 = CARTESIAN_POINT ( 'NONE',  ( 11.00000000000000000, 1.347111479062088405E-15, 84.43750000409677625 ) ) ;
#5151 = CARTESIAN_POINT ( 'NONE',  ( 29.43265458321766204, 197.5000000013656063, 173.4587341249998929 ) ) ;
#5150 = CARTESIAN_POINT ( 'NONE',  ( 29.43265458321760519, 195.7500000013656063, 173.4587341249998929 ) ) ;
#5153 = ORIENTED_EDGE ( 'NONE', *, *, #19522, .T. ) ;
#5154 = ADVANCED_FACE ( 'NONE', ( #68865 ), #40945, .F. ) ;
#5155 = EDGE_CURVE ( 'NONE', #73412, #60564, #50018, .T. ) ;
#5156 = CARTESIAN_POINT ( 'NONE',  ( -3.313708498984765161, 20.53125000000000711, 7.999999999999998224 ) ) ;
#5157 = DIRECTION ( 'NONE',  ( -0.000000000000000000, 1.000000000000000000, -0.000000000000000000 ) ) ;
#5158 = CARTESIAN_POINT ( 'NONE',  ( 9.000000000000000000, 5.196152422706622254, -10.80000000000000071 ) ) ;
#5159 = CARTESIAN_POINT ( 'NONE',  ( 5.000000000000000000, -62.13136467932972806, -23.87699943806472547 ) ) ;
#5160 = CARTESIAN_POINT ( 'NONE',  ( 8.311093377946834337, 205.4687499965859843, 8.311093377946839666 ) ) ;
#5161 = CARTESIAN_POINT ( 'NONE',  ( 7.188101187500001821, 123.5000000020483952, -2.977408999572651371 ) ) ;
#5162 = CARTESIAN_POINT ( 'NONE',  ( -4.541265875000002339, 0.9374999986344068059, -5.561446717895856393E-16 ) ) ;
#5163 = CARTESIAN_POINT ( 'NONE',  ( -4.737866951563012741, 68.48668487056758636, -20.75656675268732698 ) ) ;
#5164 = CARTESIAN_POINT ( 'NONE',  ( -7.999999999999991118, 3.313708498984756723, 20.23655277982336642 ) ) ;
#5165 = CARTESIAN_POINT ( 'NONE',  ( 5.000000000000000000, 0.000000000000000000, 0.000000000000000000 ) ) ;
#5166 = CARTESIAN_POINT ( 'NONE',  ( 11.35316468750000141, 95.78124999658602690, 0.000000000000000000 ) ) ;
#5167 = ORIENTED_EDGE ( 'NONE', *, *, #74467, .F. ) ;
#5168 = CARTESIAN_POINT ( 'NONE',  ( 5.082755093536324154, 27.28124999795161543, 5.082755093536326818 ) ) ;
#5169 = CARTESIAN_POINT ( 'NONE',  ( 3.155198069298570310E-14, -70.00000000000000000, 200.9999999999999432 ) ) ;
#5170 = CARTESIAN_POINT ( 'NONE',  ( -11.35316468749999785, 264.0104166700807014, -3.042071309553164848 ) ) ;
#5171 = CARTESIAN_POINT ( 'NONE',  ( 5.676582343749993598, 99.94791666325268409, 9.832129032723422313 ) ) ;
#5172 = VERTEX_POINT ( 'NONE', #30358 ) ;
#5173 = LINE ( 'NONE', #28169, #6685 ) ;
#5174 = CARTESIAN_POINT ( 'NONE',  ( 7.204075437095966983, 7.204075437095967871, 104.5937500020483810 ) ) ;
#5175 = CARTESIAN_POINT ( 'NONE',  ( 10.00000000000000178, 222.0833333265053682, -2.679491924311226736 ) ) ;
#5176 = CARTESIAN_POINT ( 'NONE',  ( 2.839093476692135984E-14, 203.9375000013656063, 201.4587341250000350 ) ) ;
#5178 = CARTESIAN_POINT ( 'NONE',  ( 11.35316468750000141, 95.78124999658602690, 0.000000000000000000 ) ) ;
#5177 = CARTESIAN_POINT ( 'NONE',  ( -10.99999999999989164, -4.556349186104158733, 106.0937500000000142 ) ) ;
#5179 = EDGE_CURVE ( 'NONE', #46323, #2013, #50486, .T. ) ;
#5180 = CARTESIAN_POINT ( 'NONE',  ( 3.313708498984762496, -7.999999999999989342, 11.98655278392014445 ) ) ;
#5181 = CARTESIAN_POINT ( 'NONE',  ( -24.54126587499998280, 199.3750000013656063, 171.4326545832179818 ) ) ;
#5182 = CARTESIAN_POINT ( 'NONE',  ( -27.99999999999999645, 210.0000000000000284, 174.0000000000003411 ) ) ;
#5183 = ORIENTED_EDGE ( 'NONE', *, *, #58993, .T. ) ;
#5184 = CARTESIAN_POINT ( 'NONE',  ( 2.679491924311228956, 182.9166666598386826, -10.00000000000000000 ) ) ;
#5185 = CARTESIAN_POINT ( 'NONE',  ( 27.99999999999996092, 194.8437500006828031, 173.7293670624999038 ) ) ;
#5186 = CARTESIAN_POINT ( 'NONE',  ( 2.602491298663630381, -46.50506164849257829, 139.1092423425233449 ) ) ;
#5187 = CARTESIAN_POINT ( 'NONE',  ( 5.676582343750001591, 86.92708332991935549, -9.832129032723420536 ) ) ;
#5188 = CARTESIAN_POINT ( 'NONE',  ( 6.676582343750003368, 288.0156250017069510, -2.765530957081997254 ) ) ;
#5189 = CARTESIAN_POINT ( 'NONE',  ( -7.188101187500000044, 4.593749997951610098, -8.802885111219163269E-16 ) ) ;
#5190 = CARTESIAN_POINT ( 'NONE',  ( 7.204075437095966983, 7.204075437095967871, 100.4687500020483810 ) ) ;
#5191 = CARTESIAN_POINT ( 'NONE',  ( 8.311093377946837890, 221.4062499965860411, -8.311093377946837890 ) ) ;
#5192 = ORIENTED_EDGE ( 'NONE', *, *, #10905, .F. ) ;
#5193 = CARTESIAN_POINT ( 'NONE',  ( -2.679491924311226292, 68.33333332650535397, -10.00000000000000178 ) ) ;
#5194 = CARTESIAN_POINT ( 'NONE',  ( -18.00000000000000000, 10.39230484541324628, -20.69999999999999929 ) ) ;
#5195 = CARTESIAN_POINT ( 'NONE',  ( -8.000000000000000000, 120.5000000000000000, 0.000000000000000000 ) ) ;
#5196 = CARTESIAN_POINT ( 'NONE',  ( 5.676582343749993598, 199.9479166632526983, 9.832129032723422313 ) ) ;
#5197 = CARTESIAN_POINT ( 'NONE',  ( 10.00000000000000000, 220.6250000068279746, -1.224646799147353256E-15 ) ) ;
#5198 = CARTESIAN_POINT ( 'NONE',  ( -28.00000000000008171, 208.1250000027312126, 166.0000000000003695 ) ) ;
#5199 = CARTESIAN_POINT ( 'NONE',  ( 4.721056650415999201, 296.0781250017069510, -4.721056650415999201 ) ) ;
#5200 = ORIENTED_EDGE ( 'NONE', *, *, #30328, .T. ) ;
#5201 = CARTESIAN_POINT ( 'NONE',  ( 8.311093377946837890, 191.7187499965860411, -8.311093377946837890 ) ) ;
#5202 = CARTESIAN_POINT ( 'NONE',  ( -4.220049686691935698, 10.18810118749999916, 95.87500000204838102 ) ) ;
#5203 = CARTESIAN_POINT ( 'NONE',  ( -25.55430564589119768, 207.3125000013656063, 167.5543056458915316 ) ) ;
#5204 = CARTESIAN_POINT ( 'NONE',  ( 5.656854249492378806, 19.31250000000000355, 5.656854249492381470 ) ) ;
#5205 = ORIENTED_EDGE ( 'NONE', *, *, #39900, .F. ) ;
#5206 = AXIS2_PLACEMENT_3D ( 'NONE', #72646, #20949, #43971 ) ;
#5207 = CARTESIAN_POINT ( 'NONE',  ( 3.313708498984760720, 91.71875000409679046, -8.000000000000000000 ) ) ;
#5208 = CARTESIAN_POINT ( 'NONE',  ( -10.00000000000000355, 17.70833333333332860, 2.679491924311223183 ) ) ;
#5209 = CARTESIAN_POINT ( 'NONE',  ( 4.220049686691934809, 10.18810118749999916, 78.06250000204838102 ) ) ;
#5210 = ORIENTED_EDGE ( 'NONE', *, *, #20527, .T. ) ;
#5211 = CARTESIAN_POINT ( 'NONE',  ( -1.656854249492381248, 21.31250000000000355, -4.000000000000001776 ) ) ;
#5212 = CARTESIAN_POINT ( 'NONE',  ( -1.881053915767121776, 18.62499999863441147, -4.541265875000002339 ) ) ;
#5213 = CARTESIAN_POINT ( 'NONE',  ( 30.49788809810168644, 194.5246287112379093, 172.4970663292654933 ) ) ;
#5214 = EDGE_CURVE ( 'NONE', #68280, #52559, #36027, .T. ) ;
#5215 = CARTESIAN_POINT ( 'NONE',  ( 4.000000000000001776, 4.749999997268813168, 0.000000000000000000 ) ) ;
#5216 = CARTESIAN_POINT ( 'NONE',  ( -4.401442555609581635E-16, 124.1562500020483810, -7.188101187500000044 ) ) ;
#5217 = CARTESIAN_POINT ( 'NONE',  ( 5.000000000000001776, 152.7083333265053682, -8.660254037844389075 ) ) ;
#5220 = CARTESIAN_POINT ( 'NONE',  ( -1.656854249492487607, 199.8125000027312126, 145.9999999999999716 ) ) ;
#5219 = CARTESIAN_POINT ( 'NONE',  ( 9.832129032723416984, 251.8229166700806729, -5.676582343750003368 ) ) ;
#5218 = CARTESIAN_POINT ( 'NONE',  ( 31.45873412500001010, 206.6250000013656063, 171.4326545832175555 ) ) ;
#5221 = APPLICATION_PROTOCOL_DEFINITION ( 'draft international standard', 'automotive_design', 1998, #65515 ) ;
#5222 =( BOUNDED_CURVE ( )  B_SPLINE_CURVE ( 2, ( #33162, #71992, #55415, #21434, #26722, #14270, #60303, #37686, #4104, #32020, #49742, #56159, #26337 ),
 .UNSPECIFIED., .F., .F. ) 
 B_SPLINE_CURVE_WITH_KNOTS ( ( 3, 2, 2, 2, 2, 2, 3 ),
 ( 0.08333333333333278747, 0.09259259259259206010, 0.1018518518518513188, 0.1111111111111105776, 0.1203703703703698502, 0.1296296296296291228, 0.1388888888888883955 ),
 .UNSPECIFIED. ) 
 CURVE ( )  GEOMETRIC_REPRESENTATION_ITEM ( )  RATIONAL_B_SPLINE_CURVE ( ( 1.000000000000001998, 0.9659258262890662028, 1.000000000000000000, 0.9659258262890683122, 1.000000000000000000, 0.9659258262890683122, 1.000000000000000000, 0.9659258262890683122, 1.000000000000000000, 0.9659258262890683122, 1.000000000000000000, 0.9659258262890701996, 0.9999999999999981126 ) ) 
 REPRESENTATION_ITEM ( '' )  );
#5223 = ORIENTED_EDGE ( 'NONE', *, *, #67248, .T. ) ;
#5224 = CARTESIAN_POINT ( 'NONE',  ( 8.311093377946834337, 247.3437500034139589, -8.311093377946836114 ) ) ;
#5225 = CARTESIAN_POINT ( 'NONE',  ( 5.082755093536320601, -5.082755093536318824, 11.04905278187175455 ) ) ;
#5226 = VECTOR ( 'NONE', #41904, 1000.000000000000000 ) ;
#5227 = VERTEX_POINT ( 'NONE', #14094 ) ;
#5228 = ORIENTED_EDGE ( 'NONE', *, *, #64835, .T. ) ;
#5229 = CARTESIAN_POINT ( 'NONE',  ( -10.18810118749999916, 0.000000000000000000, 72.15625000204836681 ) ) ;
#5230 = CARTESIAN_POINT ( 'NONE',  ( 8.311093377946837890, 91.71874999658599847, -8.311093377946837890 ) ) ;
#5231 = CYLINDRICAL_SURFACE ( 'NONE', #11952, 30.99999999999997158 ) ;
#5232 = CARTESIAN_POINT ( 'NONE',  ( 4.556349186104051263, -10.99999999999999822, 80.96874999999997158 ) ) ;
#5235 = CARTESIAN_POINT ( 'NONE',  ( -6.676582343749999815, 291.6718750017070079, 2.765530957082001251 ) ) ;
#5234 = CARTESIAN_POINT ( 'NONE',  ( 32.00000000000000000, 194.3125000027312126, 171.6568542494922553 ) ) ;
#5233 = CARTESIAN_POINT ( 'NONE',  ( 26.56734541678232731, 206.6250000013656063, 173.4587341249998929 ) ) ;
#5236 = B_SPLINE_CURVE_WITH_KNOTS ( 'NONE', 3,
 ( #29765, #47102, #70500, #69388 ),
 .UNSPECIFIED., .F., .F.,
 ( 4, 4 ),
 ( 0.000000000000000000, 0.2375773127046199029 ),
 .UNSPECIFIED. ) ;
#5237 = EDGE_CURVE ( 'NONE', #8780, #71806, #20205, .T. ) ;
#5238 = CARTESIAN_POINT ( 'NONE',  ( -51.10910287431129717, 200.8521862711060066, 55.39363855836536743 ) ) ;
#5239 = DIRECTION ( 'NONE',  ( 0.1513591288559072157, 8.467839242509012188E-17, -0.9884788384745425427 ) ) ;
#5240 = CARTESIAN_POINT ( 'NONE',  ( 8.311093377946837890, 201.4062499965860127, -8.311093377946837890 ) ) ;
#5242 = EDGE_CURVE ( 'NONE', #7343, #2312, #2056, .T. ) ;
#5241 = CARTESIAN_POINT ( 'NONE',  ( 8.000000000000000000, 11.90624999590322197, -3.313708498984761608 ) ) ;
#5243 = VERTEX_POINT ( 'NONE', #53006 ) ;
#5244 = CARTESIAN_POINT ( 'NONE',  ( 24.54126587499999701, 209.4375000013656063, 169.9999999999998863 ) ) ;
#5245 = CARTESIAN_POINT ( 'NONE',  ( -5.082755093536325042, 16.40624999795161543, -5.082755093536325930 ) ) ;
#5246 = CARTESIAN_POINT ( 'NONE',  ( 11.35316468750000141, 161.0937499965860127, 0.000000000000000000 ) ) ;
#5247 = CYLINDRICAL_SURFACE ( 'NONE', #50384, 10.00000000000000178 ) ;
#5248 = CARTESIAN_POINT ( 'NONE',  ( 7.188101187500000044, 101.2812500020483810, -8.802885111219163269E-16 ) ) ;
#5250 = CARTESIAN_POINT ( 'NONE',  ( -9.999999999999998224, 235.2083333333333428, 2.679491924311235174 ) ) ;
#5249 = CARTESIAN_POINT ( 'NONE',  ( -5.000000000000002665, 208.3333333333333712, 8.660254037844383745 ) ) ;
#5251 = CARTESIAN_POINT ( 'NONE',  ( 24.54126587499998635, 207.5000000013656063, 171.4326545832175555 ) ) ;
#5252 = CARTESIAN_POINT ( 'NONE',  ( -5.082755093536317936, -5.082755093536320601, 9.549052781871754547 ) ) ;
#5253 = CARTESIAN_POINT ( 'NONE',  ( -8.311093377946841443, 53.90624999658602690, 8.311093377946830785 ) ) ;
#5254 = CARTESIAN_POINT ( 'NONE',  ( -2.849036369511732440E-14, 208.2500000000000284, 138.0000000000000568 ) ) ;
#5255 = CARTESIAN_POINT ( 'NONE',  ( -4.898587196589407898E-16, 7.999999999999991118, 3.511552784329822874 ) ) ;
#5256 = VERTEX_POINT ( 'NONE', #25045 ) ;
#5257 = CARTESIAN_POINT ( 'NONE',  ( 6.509199954993393433, 10.09831811432648685, 6.904800827780242789E-15 ) ) ;
#5258 = LINE ( 'NONE', #74276, #59366 ) ;
#5259 = CARTESIAN_POINT ( 'NONE',  ( -3.042071309553173730, 64.32291666325269830, 11.35316468749999785 ) ) ;
#5260 = CARTESIAN_POINT ( 'NONE',  ( -4.556349186104047710, -10.99999999999999822, 73.46875000409677625 ) ) ;
#5261 = CARTESIAN_POINT ( 'NONE',  ( -2.839093476692135984E-14, 200.9375000013656063, 138.5412658750000503 ) ) ;
#5262 = CARTESIAN_POINT ( 'NONE',  ( 0.6547826978431545708, 10.28110016890869716, 63.57209897671332754 ) ) ;
#5263 = CARTESIAN_POINT ( 'NONE',  ( 4.000000000000015987, 207.5625000000000000, 196.3431457505076594 ) ) ;
#5265 = CARTESIAN_POINT ( 'NONE',  ( 11.35316468750000141, 60.78124999658601979, 0.000000000000000000 ) ) ;
#5264 = CARTESIAN_POINT ( 'NONE',  ( 2.977408999572650039, 92.18750000204838102, -7.188101187500000933 ) ) ;
#5266 = EDGE_CURVE ( 'NONE', #73730, #6581, #41681, .T. ) ;
#5267 = CARTESIAN_POINT ( 'NONE',  ( -7.999999999999989342, -3.313708498984762496, 3.924052779823362425 ) ) ;
#5268 = CARTESIAN_POINT ( 'NONE',  ( 1.469576158976822172E-15, -7.999999999999991118, 4.392802783920145338 ) ) ;
#5269 = CARTESIAN_POINT ( 'NONE',  ( -11.35316468749999785, 173.0729166632526983, -3.042071309553167513 ) ) ;
#5270 = CARTESIAN_POINT ( 'NONE',  ( -2.679491924311225848, 148.3333333265053398, -10.00000000000000178 ) ) ;
#5271 = CARTESIAN_POINT ( 'NONE',  ( 5.082755093536325042, 102.9687500020483810, -5.082755093536325930 ) ) ;
#5272 = CARTESIAN_POINT ( 'NONE',  ( 33.73481160478831953, 181.3810825260465549, 154.4994655493011351 ) ) ;
#5273 = CARTESIAN_POINT ( 'NONE',  ( 5.676582343749993598, 30.26041666325268409, 9.832129032723422313 ) ) ;
#5274 = CARTESIAN_POINT ( 'NONE',  ( 6.123233995736767268E-16, 78.12499999317202537, -10.00000000000000178 ) ) ;
#5275 = CARTESIAN_POINT ( 'NONE',  ( -11.35316468750000141, 188.2812499965860127, -1.390361679473963753E-15 ) ) ;
#5276 = ORIENTED_EDGE ( 'NONE', *, *, #61338, .T. ) ;
#5277 = CARTESIAN_POINT ( 'NONE',  ( 2.775557561562891351E-14, 210.0000000000000284, 202.0000000000000000 ) ) ;
#5278 = CARTESIAN_POINT ( 'NONE',  ( -6.238412754330611322E-16, 10.18810118749999916, 70.28125000204838102 ) ) ;
#5279 = CARTESIAN_POINT ( 'NONE',  ( 2.751064625579944321E-14, 196.7500000000000000, 194.0000000000000568 ) ) ;
#5280 = CARTESIAN_POINT ( 'NONE',  ( 33.54872378484518691, 40.86850235519607111, 64.99999999999998579 ) ) ;
#5282 = CARTESIAN_POINT ( 'NONE',  ( -11.35316468749999785, 168.0729166632526983, -3.042071309553167957 ) ) ;
#5281 = CARTESIAN_POINT ( 'NONE',  ( 0.000000000000000000, 23.85640646055104241, -14.00000000000000178 ) ) ;
#5283 = CARTESIAN_POINT ( 'NONE',  ( -7.999999999999989342, -3.313708498984762496, 6.980302784329822430 ) ) ;
#5284 = EDGE_CURVE ( 'NONE', #15595, #18027, #1817, .T. ) ;
#5285 = CARTESIAN_POINT ( 'NONE',  ( 2.250000000000001332, 267.1999999999996476, 5.427798388956546205 ) ) ;
#5286 = CARTESIAN_POINT ( 'NONE',  ( -10.00000000000000000, 263.1250000068279746, 0.000000000000000000 ) ) ;
#5287 = FACE_BOUND ( 'NONE', #32571, .T. ) ;
#5288 = ORIENTED_EDGE ( 'NONE', *, *, #67533, .T. ) ;
#5289 = ADVANCED_FACE ( 'NONE', ( #63020 ), #62643, .F. ) ;
#5290 = CARTESIAN_POINT ( 'NONE',  ( -4.000000000000016875, 198.5625000027312126, 140.3431457505076594 ) ) ;
#5291 = CARTESIAN_POINT ( 'NONE',  ( -9.832129032723420536, 119.0104166632526841, 5.676582343749997150 ) ) ;
#5292 = DIRECTION ( 'NONE',  ( -1.000000000000000000, 0.000000000000000000, -0.000000000000000000 ) ) ;
#5293 = ORIENTED_EDGE ( 'NONE', *, *, #38478, .F. ) ;
#5294 = CARTESIAN_POINT ( 'NONE',  ( -1.881053915767124440, 8.124999998634407916, 4.541265875000001451 ) ) ;
#5295 = CARTESIAN_POINT ( 'NONE',  ( 2.977408999572651815, 15.18749999795161365, 7.188101187500000933 ) ) ;
#5296 = CARTESIAN_POINT ( 'NONE',  ( -4.898587196589412829E-16, 109.8125000040967905, -8.000000000000000000 ) ) ;
#5297 = CARTESIAN_POINT ( 'NONE',  ( -29.43265458321766559, 198.7500000013656063, 166.5412658750003629 ) ) ;
#5298 = CARTESIAN_POINT ( 'NONE',  ( -1.656854249492381248, 7.312500000000000888, -4.000000000000001776 ) ) ;
#5299 = CARTESIAN_POINT ( 'NONE',  ( 2.849036369511732440E-14, 198.2500000000000000, 202.0000000000000000 ) ) ;
#5300 = CARTESIAN_POINT ( 'NONE',  ( 3.211159895383561835, 6.437499998634407028, -3.211159895383561835 ) ) ;
#5302 = AXIS2_PLACEMENT_3D ( 'NONE', #29190, #12927, #7288 ) ;
#5301 = CARTESIAN_POINT ( 'NONE',  ( -2.828427124746208943, 199.6250000000000284, 144.8284271247462129 ) ) ;
#5303 = EDGE_LOOP ( 'NONE', ( #19051, #14722, #55313, #64595 ) ) ;
#5304 = CARTESIAN_POINT ( 'NONE',  ( 5.656854249492379694, 116.9375000000000000, -5.656854249492380582 ) ) ;
#5305 = CARTESIAN_POINT ( 'NONE',  ( 2.977408999572654480, 103.6250000020483810, 7.188101187499999156 ) ) ;
#5307 = CARTESIAN_POINT ( 'NONE',  ( 2.485281374238919927, 293.3125000000000568, 5.999999999999654499 ) ) ;
#5306 = CYLINDRICAL_SURFACE ( 'NONE', #19291, 11.00000000000000000 ) ;
#5308 = CARTESIAN_POINT ( 'NONE',  ( -4.465349678524273003, 10.10202304668574591, -70.97395336192860782 ) ) ;
#5309 = CARTESIAN_POINT ( 'NONE',  ( -5.082755093536317936, -5.082755093536320601, 3.174052781871751439 ) ) ;
#5310 = ORIENTED_EDGE ( 'NONE', *, *, #29310, .F. ) ;
#5311 = ADVANCED_FACE ( 'NONE', ( #48807 ), #49562, .F. ) ;
#5312 = ORIENTED_EDGE ( 'NONE', *, *, #72670, .T. ) ;
#5313 = CARTESIAN_POINT ( 'NONE',  ( -7.204075437095967871, 7.204075437095967871, 91.46875000204838102 ) ) ;
#5314 = DIRECTION ( 'NONE',  ( 1.000000000000000000, 0.000000000000000000, 0.000000000000000000 ) ) ;
#5315 = CARTESIAN_POINT ( 'NONE',  ( -24.54126587499999346, 198.4375000013655779, 170.0000000000003411 ) ) ;
#5316 = CARTESIAN_POINT ( 'NONE',  ( -11.00000000000000000, 0.000000000000000000, 107.4999999999999858 ) ) ;
#5317 = CARTESIAN_POINT ( 'NONE',  ( 2.445694354108839175, 204.3125000013656063, 195.5543056458912190 ) ) ;
#5319 = DIRECTION ( 'NONE',  ( -0.000000000000000000, 1.000000000000000000, 2.238352872228138170E-16 ) ) ;
#5318 = CARTESIAN_POINT ( 'NONE',  ( 28.00000000000002132, 203.1250000027312126, 173.9999999999999147 ) ) ;
#5320 = CARTESIAN_POINT ( 'NONE',  ( -10.00000000000000000, 122.2916666666666430, -2.679491924311229845 ) ) ;
#5321 = CARTESIAN_POINT ( 'NONE',  ( -7.999999999999998224, 105.5937500000000000, 3.313708498984766493 ) ) ;
#5322 = CARTESIAN_POINT ( 'NONE',  ( 6.676582343750003368, 288.1718750017069510, -2.765530957081997254 ) ) ;
#5323 = CARTESIAN_POINT ( 'NONE',  ( -5.082755093536317936, -5.082755093536320601, 3.549052781871751883 ) ) ;
#5324 = CARTESIAN_POINT ( 'NONE',  ( 5.656854249492380582, 1.687500000000000222, -5.656854249492380582 ) ) ;
#5325 = EDGE_CURVE ( 'NONE', #6581, #34878, #72338, .T. ) ;
#5326 = CARTESIAN_POINT ( 'NONE',  ( 27.99999999999996803, 206.4375000013656063, 173.4587341249998929 ) ) ;
#5327 = CARTESIAN_POINT ( 'NONE',  ( -5.656854249492379694, 24.37499999590322375, -5.656854249492380582 ) ) ;
#5328 = VECTOR ( 'NONE', #43033, 1000.000000000000000 ) ;
#5329 = CARTESIAN_POINT ( 'NONE',  ( -3.458734125000016313, 200.8750000013656063, 140.5673454167824161 ) ) ;
#5330 = CARTESIAN_POINT ( 'NONE',  ( -7.188101187500000933, 122.9375000020483810, -2.977408999572650483 ) ) ;
#5332 = CARTESIAN_POINT ( 'NONE',  ( 7.999999999999991118, 9.797174393178815797E-16, 7.580302779823366421 ) ) ;
#5331 = CARTESIAN_POINT ( 'NONE',  ( -27.99999999999999645, 210.0000000000000284, 166.0000000000003979 ) ) ;
#5333 = CARTESIAN_POINT ( 'NONE',  ( 11.35316468749999963, 246.5104166700806161, 3.042071309553159519 ) ) ;
#5334 = CARTESIAN_POINT ( 'NONE',  ( -7.188101187499991163, 2.977408999572646930, 25.76780278187175810 ) ) ;
#5335 = CARTESIAN_POINT ( 'NONE',  ( 25.17157287525378351, 198.8750000000000284, 172.8284271247460424 ) ) ;
#5336 = CARTESIAN_POINT ( 'NONE',  ( 8.311093377946837890, 21.40624999658601268, -8.311093377946837890 ) ) ;
#5337 =( BOUNDED_CURVE ( )  B_SPLINE_CURVE ( 2, ( #8867, #49218, #9623, #65824, #60916, #55279, #32643, #3583, #14131 ),
 .UNSPECIFIED., .F., .F. ) 
 B_SPLINE_CURVE_WITH_KNOTS ( ( 3, 2, 2, 2, 3 ),
 ( 0.4765158731794318925, 0.4831341176653472513, 0.4897523932498040744, 0.4963706688342608420, 0.5029889089742047847 ),
 .UNSPECIFIED. ) 
 CURVE ( )  GEOMETRIC_REPRESENTATION_ITEM ( )  RATIONAL_B_SPLINE_CURVE ( ( 0.9999992846401264401, 0.9238798901929041740, 1.000000000000000000, 0.9238795325112867385, 1.000000000000000000, 0.9238795325112867385, 1.000000000000000000, 0.9238799401783380771, 0.9999991846702638298 ) ) 
 REPRESENTATION_ITEM ( '' )  );
#5338 = DIRECTION ( 'NONE',  ( 0.000000000000000000, 0.000000000000000000, 1.000000000000000000 ) ) ;
#5339 = CARTESIAN_POINT ( 'NONE',  ( 8.311093377946834337, 205.4687499965859843, 8.311093377946839666 ) ) ;
#5340 = CARTESIAN_POINT ( 'NONE',  ( -1.656854249492504705, 197.8125000027312694, 145.9999999999999716 ) ) ;
#5342 = CARTESIAN_POINT ( 'NONE',  ( 4.000000000000000888, 11.68749999726881406, 1.656854249492384135 ) ) ;
#5341 = CARTESIAN_POINT ( 'NONE',  ( -28.00000000000002487, 196.0000000000000000, 166.0000000000003695 ) ) ;
#5343 = ORIENTED_EDGE ( 'NONE', *, *, #11362, .T. ) ;
#5344 = CARTESIAN_POINT ( 'NONE',  ( 1.432654583217608080, 200.8750000013656063, 138.5412658750000503 ) ) ;
#5345 = CARTESIAN_POINT ( 'NONE',  ( -8.311093377946836114, 17.65624999658601979, -8.311093377946837890 ) ) ;
#5346 = CARTESIAN_POINT ( 'NONE',  ( -7.778174593052020747, -7.778174593052023411, 89.87500000409677625 ) ) ;
#5347 = CARTESIAN_POINT ( 'NONE',  ( -3.166186134455097228E-13, 211.2500000000000568, -9.999999999999998224 ) ) ;
#5348 = CARTESIAN_POINT ( 'NONE',  ( -31.45873412499999233, 198.6875000013655779, 170.0000000000004547 ) ) ;
#5350 = CARTESIAN_POINT ( 'NONE',  ( 11.35316468749999963, 5.989583329919350163, -3.042071309553165293 ) ) ;
#5349 = CARTESIAN_POINT ( 'NONE',  ( 5.082755093536326818, 111.2187500020483810, 5.082755093536325042 ) ) ;
#5351 = CARTESIAN_POINT ( 'NONE',  ( 7.999999999999992895, -3.313708498984756279, 19.48655277982336642 ) ) ;
#5352 = CARTESIAN_POINT ( 'NONE',  ( 5.676582343750001591, 131.6145833299193555, -9.832129032723420536 ) ) ;
#5353 = ADVANCED_FACE ( 'NONE', ( #26162 ), #22276, .T. ) ;
#5354 = CARTESIAN_POINT ( 'NONE',  ( -2.679491924311225848, 103.3333333265053824, -10.00000000000000178 ) ) ;
#5355 = CARTESIAN_POINT ( 'NONE',  ( 2.977408999572650039, 119.5625000020483810, -7.188101187500001821 ) ) ;
#5356 = CARTESIAN_POINT ( 'NONE',  ( 4.541265875000002339, 22.43749999863440436, 0.000000000000000000 ) ) ;
#5357 = CARTESIAN_POINT ( 'NONE',  ( -4.556349186104045934, 11.00000000000000000, 102.9062500040967763 ) ) ;
#5358 = CARTESIAN_POINT ( 'NONE',  ( -4.999999999999998224, 52.16438407847190462, -42.28020805311142993 ) ) ;
#5359 = VERTEX_POINT ( 'NONE', #32222 ) ;
#5360 = CARTESIAN_POINT ( 'NONE',  ( 2.436599634630554068, -67.82108862182708720, 20.21956363438967941 ) ) ;
#5361 = EDGE_CURVE ( 'NONE', #26153, #68525, #32605, .T. ) ;
#5362 = LINE ( 'NONE', #63431, #34163 ) ;
#5363 = CARTESIAN_POINT ( 'NONE',  ( -4.721056650415998313, 288.7343750017069510, 4.721056650416000089 ) ) ;
#5364 = CARTESIAN_POINT ( 'NONE',  ( 8.311093377946834337, 120.1562499965860127, 8.311093377946839666 ) ) ;
#5365 = CARTESIAN_POINT ( 'NONE',  ( -2.849036369511732440E-14, 207.3750000027312126, 138.0000000000000568 ) ) ;
#5366 = CARTESIAN_POINT ( 'NONE',  ( 3.313708498984762496, -7.999999999999989342, 20.85530278432983309 ) ) ;
#5367 = VECTOR ( 'NONE', #74518, 1000.000000000000000 ) ;
#5368 = CARTESIAN_POINT ( 'NONE',  ( -1.469576158976823947E-15, 19.12500000000000355, 8.000000000000000000 ) ) ;
#5369 = CARTESIAN_POINT ( 'NONE',  ( -5.676582343750000703, 263.0729166700806445, -9.832129032723418760 ) ) ;
#5370 = CARTESIAN_POINT ( 'NONE',  ( 4.220049686691934809, 10.18810118749999916, 99.06250000204836681 ) ) ;
#5371 = ORIENTED_EDGE ( 'NONE', *, *, #8579, .T. ) ;
#5372 = CARTESIAN_POINT ( 'NONE',  ( 5.656854249492374365, 5.656854249492375253, 24.26780277982336642 ) ) ;
#5373 = CARTESIAN_POINT ( 'NONE',  ( 3.458734125000015425, 203.2500000013655495, 196.5673454167823877 ) ) ;
#5374 = EDGE_CURVE ( 'NONE', #2057, #47752, #56637, .T. ) ;
#5375 = CARTESIAN_POINT ( 'NONE',  ( 8.311093377946834337, 70.46874999658599847, 8.311093377946839666 ) ) ;
#5376 = ORIENTED_EDGE ( 'NONE', *, *, #34898, .F. ) ;
#5377 = CARTESIAN_POINT ( 'NONE',  ( 10.18810118749999916, 4.220049686691935698, 104.5000000020483668 ) ) ;
#5378 = CARTESIAN_POINT ( 'NONE',  ( 3.211159895383560947, 11.31249999863440792, 3.211159895383562723 ) ) ;
#5379 = VERTEX_POINT ( 'NONE', #45298 ) ;
#5380 = CARTESIAN_POINT ( 'NONE',  ( -7.188101187500001821, 26.62499999795161543, -2.977408999572651371 ) ) ;
#5381 = CARTESIAN_POINT ( 'NONE',  ( -8.000000000000000000, 107.0000000000000000, 0.000000000000000000 ) ) ;
#5382 = CARTESIAN_POINT ( 'NONE',  ( -4.999999999999999112, -64.62627855237427354, -24.10294814404728569 ) ) ;
#5383 = CARTESIAN_POINT ( 'NONE',  ( 7.188101187500001821, 23.43749999795161898, -2.977408999572650483 ) ) ;
#5384 = CARTESIAN_POINT ( 'NONE',  ( 0.000000000000000000, 0.000000000000000000, 11.00000000000000000 ) ) ;
#5385 = CARTESIAN_POINT ( 'NONE',  ( 10.18810118750000093, -4.220049686691933921, 104.6875000020483810 ) ) ;
#5386 = PRODUCT_DEFINITION_SHAPE ( 'NONE', 'NONE',  #74663 ) ;
#5387 = PRESENTATION_LAYER_ASSIGNMENT (  '', '', ( #28273 ) ) ;
#5388 = CARTESIAN_POINT ( 'NONE',  ( -11.00000000000000000, 0.000000000000000000, 75.99999999999998579 ) ) ;
#5389 = CARTESIAN_POINT ( 'NONE',  ( 4.000000000000001776, 11.74999999726881406, 0.000000000000000000 ) ) ;
#5390 = FACE_OUTER_BOUND ( 'NONE', #7700, .T. ) ;
#5391 = ORIENTED_EDGE ( 'NONE', *, *, #45373, .T. ) ;
#5392 = EDGE_CURVE ( 'NONE', #62397, #32492, #4250, .T. ) ;
#5393 = CARTESIAN_POINT ( 'NONE',  ( 3.458734125000016313, 202.8750000013656347, 199.4326545832176691 ) ) ;
#5394 = EDGE_CURVE ( 'NONE', #16317, #23374, #68682, .T. ) ;
#5395 = CARTESIAN_POINT ( 'NONE',  ( -25.55430564589111953, 204.0625000013656063, 172.4456943541091505 ) ) ;
#5396 = CARTESIAN_POINT ( 'NONE',  ( 3.211159895383560947, 10.18749999863440614, 3.211159895383562723 ) ) ;
#5397 = CARTESIAN_POINT ( 'NONE',  ( -7.347880794884122694E-16, 15.75000000000000000, 4.000000000000001776 ) ) ;
#5398 = CARTESIAN_POINT ( 'NONE',  ( 1.320432766682872962E-15, -7.188101187499992051, 21.36155278187175455 ) ) ;
#5399 = ORIENTED_EDGE ( 'NONE', *, *, #20267, .F. ) ;
#5400 = EDGE_CURVE ( 'NONE', #28551, #23989, #9538, .T. ) ;
#5401 = CARTESIAN_POINT ( 'NONE',  ( -5.999999999999999112, 292.0625000000000000, 2.485281374238575314 ) ) ;
#5402 = ORIENTED_EDGE ( 'NONE', *, *, #60670, .F. ) ;
#5403 = CARTESIAN_POINT ( 'NONE',  ( -4.220049686691935698, 10.18810118749999916, 110.8750000020483810 ) ) ;
#5404 = CARTESIAN_POINT ( 'NONE',  ( 25.17157287525378351, 208.7500000027312126, 167.1715728752537586 ) ) ;
#5405 = CARTESIAN_POINT ( 'NONE',  ( -1.432654583217607858, 199.6250000013656063, 201.4587341250000065 ) ) ;
#5406 = CARTESIAN_POINT ( 'NONE',  ( 25.55430564589115150, 196.0625000013656063, 167.5543056458911053 ) ) ;
#5407 = CARTESIAN_POINT ( 'NONE',  ( -8.660254037844387298, 77.08333333333334281, -5.000000000000004441 ) ) ;
#5408 = CARTESIAN_POINT ( 'NONE',  ( -5.082755093536324154, 90.21875000204838102, 5.082755093536326818 ) ) ;
#5409 = CARTESIAN_POINT ( 'NONE',  ( -6.000000000000001776, 290.0000000000000000, 0.000000000000000000 ) ) ;
#5410 = VERTEX_POINT ( 'NONE', #34380 ) ;
#5411 = CARTESIAN_POINT ( 'NONE',  ( 9.999999999999998224, 252.7083333333333712, -2.679491924311229401 ) ) ;
#5412 = CARTESIAN_POINT ( 'NONE',  ( 1.317228840348607655, -10.12208498181994543, 70.14472670972676838 ) ) ;
#5413 = CARTESIAN_POINT ( 'NONE',  ( -2.828427124746208943, 194.7500000027312126, 144.8284271247462129 ) ) ;
#5414 = CARTESIAN_POINT ( 'NONE',  ( -10.99999999999978684, -4.556349186104264426, 91.09375000000001421 ) ) ;
#5415 = CARTESIAN_POINT ( 'NONE',  ( 1.836970198721029589E-15, 231.2500000000000000, 10.00000000000000000 ) ) ;
#5416 = CARTESIAN_POINT ( 'NONE',  ( -38.00000000000000000, -63.00000000000000000, 15.00000000000000178 ) ) ;
#5417 = ADVANCED_FACE ( 'NONE', ( #18487 ), #7171, .F. ) ;
#5418 = CARTESIAN_POINT ( 'NONE',  ( -10.00000000000000355, 202.7083333333333144, 2.679491924311223183 ) ) ;
#5419 = CARTESIAN_POINT ( 'NONE',  ( -5.082755093536317936, -5.082755093536320601, 17.04905278187175810 ) ) ;
#5420 = CARTESIAN_POINT ( 'NONE',  ( -11.35316468750000141, 163.8020833299193555, 3.042071309553159963 ) ) ;
#5421 = CARTESIAN_POINT ( 'NONE',  ( 4.541265875000002339, 0.3124999986344066949, 0.000000000000000000 ) ) ;
#5422 = DIRECTION ( 'NONE',  ( -0.000000000000000000, -1.000000000000000000, -0.000000000000000000 ) ) ;
#5424 = CARTESIAN_POINT ( 'NONE',  ( 7.999999999999991118, 0.000000000000000000, 29.33030277982336642 ) ) ;
#5423 =( LENGTH_UNIT ( ) NAMED_UNIT ( * ) SI_UNIT ( .MILLI., .METRE. ) );
#5425 = EDGE_LOOP ( 'NONE', ( #58485, #50639, #6699, #59584 ) ) ;
#5426 = CARTESIAN_POINT ( 'NONE',  ( -2.839093476692135984E-14, 196.6875000013655779, 138.5412658750000503 ) ) ;
#5427 = CARTESIAN_POINT ( 'NONE',  ( 11.35316468749999785, 30.88541666325268409, 3.042071309553174174 ) ) ;
#5428 = CARTESIAN_POINT ( 'NONE',  ( -11.00000000000000000, 0.000000000000000000, 110.6875000040967763 ) ) ;
#5429 = AXIS2_PLACEMENT_3D ( 'NONE', #58882, #65257, #13927 ) ;
#5430 = CARTESIAN_POINT ( 'NONE',  ( -31.45873412499996391, 207.7500000013656063, 171.4326545832181239 ) ) ;
#5431 = CARTESIAN_POINT ( 'NONE',  ( 6.938893903907228378E-15, 10.39230484541326938, -10.80000000000000071 ) ) ;
#5433 = CARTESIAN_POINT ( 'NONE',  ( 5.000000000000000000, 10.26105934116143459, -64.40045319026695836 ) ) ;
#5432 = CARTESIAN_POINT ( 'NONE',  ( 2.679491924311376394, 222.9166666598387110, -9.999999999999914735 ) ) ;
#5434 = CARTESIAN_POINT ( 'NONE',  ( -22.25025445354526710, -49.99926196677280643, 191.6039757372747090 ) ) ;
#5435 = CARTESIAN_POINT ( 'NONE',  ( 1.432654583217607858, 199.6250000013656063, 138.5412658750000787 ) ) ;
#5436 =( BOUNDED_CURVE ( )  B_SPLINE_CURVE ( 2, ( #17539, #34550, #74511, #22443, #18287, #46949, #40932, #52255, #959, #23942, #57555, #74140, #16781 ),
 .UNSPECIFIED., .F., .F. ) 
 B_SPLINE_CURVE_WITH_KNOTS ( ( 3, 2, 2, 2, 2, 2, 3 ),
 ( 0.2499999999999995837, 0.2592592592592589118, 0.2685185185185183232, 0.2777777777777776791, 0.2870370370370370350, 0.2962962962962963909, 0.3055555555555558023 ),
 .UNSPECIFIED. ) 
 CURVE ( )  GEOMETRIC_REPRESENTATION_ITEM ( )  RATIONAL_B_SPLINE_CURVE ( ( 1.000000000000001554, 0.9659258262890668689, 1.000000000000000000, 0.9659258262890683122, 1.000000000000000000, 0.9659258262890683122, 1.000000000000000000, 0.9659258262890683122, 1.000000000000000000, 0.9659258262890683122, 1.000000000000000000, 0.9659258262890675351, 1.000000000000000888 ) ) 
 REPRESENTATION_ITEM ( '' )  );
#5437 = CARTESIAN_POINT ( 'NONE',  ( 7.320508075688774596, 67.49999999317201116, -7.320508075688774596 ) ) ;
#5438 = VECTOR ( 'NONE', #61645, 1000.000000000000000 ) ;
#5439 = CARTESIAN_POINT ( 'NONE',  ( 5.082755093536325042, 105.5937500020483810, -5.082755093536325930 ) ) ;
#5440 = CARTESIAN_POINT ( 'NONE',  ( -8.342170076843785083E-16, 14.18749999863440792, 4.541265875000002339 ) ) ;
#5441 = CARTESIAN_POINT ( 'NONE',  ( 8.660254037844429931, 64.58333333333337123, 5.000000000000031086 ) ) ;
#5442 = CARTESIAN_POINT ( 'NONE',  ( -5.656854249492373476, -5.656854249492376141, 2.517802779823365089 ) ) ;
#5443 = PLANE ( 'NONE',  #28122 ) ;
#5444 = ORIENTED_EDGE ( 'NONE', *, *, #48808, .F. ) ;
#5445 = ORIENTED_EDGE ( 'NONE', *, *, #15858, .T. ) ;
#5446 = EDGE_CURVE ( 'NONE', #30484, #3444, #1398, .T. ) ;
#5447 = CARTESIAN_POINT ( 'NONE',  ( -7.320508075688851868, 196.8750000000001421, -7.320508075688852756 ) ) ;
#5448 = CARTESIAN_POINT ( 'NONE',  ( 0.000000000000000000, 28.00000000000000000, -3.999999999999986233 ) ) ;
#5449 = FACE_OUTER_BOUND ( 'NONE', #32568, .T. ) ;
#5450 = CARTESIAN_POINT ( 'NONE',  ( -10.00000000000000355, 87.70833333333332860, 2.679491924311222739 ) ) ;
#5451 = CARTESIAN_POINT ( 'NONE',  ( -3.042071309553164404, 147.2395833299193555, -11.35316468749999963 ) ) ;
#5452 = CARTESIAN_POINT ( 'NONE',  ( 9.999999999999987566, 105.0000000000000000, 0.000000000000000000 ) ) ;
#5453 = CARTESIAN_POINT ( 'NONE',  ( 7.204075437095968759, -7.204075437095966983, 89.21875000204838102 ) ) ;
#5454 = CARTESIAN_POINT ( 'NONE',  ( 3.313708498984762496, 4.218750000000000000, 7.999999999999998224 ) ) ;
#5455 = CARTESIAN_POINT ( 'NONE',  ( -1.656854249492348607, 205.1875000000000000, 202.0000000000000284 ) ) ;
#5456 = CARTESIAN_POINT ( 'NONE',  ( 7.320508075688771044, 248.1250000000000000, -7.320508075688771932 ) ) ;
#5457 = CARTESIAN_POINT ( 'NONE',  ( 6.803355351215364166, -4.261158589325806823, -0.000000000000000000 ) ) ;
#5458 = CARTESIAN_POINT ( 'NONE',  ( 7.204075437095966983, 7.204075437095967871, 115.4687500020483810 ) ) ;
#5459 = ORIENTED_EDGE ( 'NONE', *, *, #38709, .T. ) ;
#5460 =( BOUNDED_CURVE ( )  B_SPLINE_CURVE ( 2, ( #44116, #72018, #67125, #3375, #43349, #72403, #32046, #15420, #32809 ),
 .UNSPECIFIED., .F., .F. ) 
 B_SPLINE_CURVE_WITH_KNOTS ( ( 3, 2, 2, 2, 3 ),
 ( 0.7708333333333317050, 0.7812499999999983347, 0.7916666666666649643, 0.8020833333333317050, 0.8124999999999983347 ),
 .UNSPECIFIED. ) 
 CURVE ( )  GEOMETRIC_REPRESENTATION_ITEM ( )  RATIONAL_B_SPLINE_CURVE ( ( 1.000000000000012212, 0.9238795325112745260, 1.000000000000000000, 0.9238795325112867385, 1.000000000000000000, 0.9238795325112867385, 1.000000000000000000, 0.9238795325112989509, 0.9999999999999877875 ) ) 
 REPRESENTATION_ITEM ( '' )  );
#5461 = LINE ( 'NONE', #40157, #20207 ) ;
#5462 = CARTESIAN_POINT ( 'NONE',  ( -8.698841371901522734, 177.8514410235502794, 140.1637119819116037 ) ) ;
#5463 = CARTESIAN_POINT ( 'NONE',  ( -11.35316468749999785, 133.3854166632526699, -3.042071309553167957 ) ) ;
#5464 = CARTESIAN_POINT ( 'NONE',  ( 2.445694354108839619, 202.8125000013656063, 200.4456943541088663 ) ) ;
#5465 = CARTESIAN_POINT ( 'NONE',  ( 5.082755093536325930, 23.53124999795161543, -5.082755093536325930 ) ) ;
#5466 = CARTESIAN_POINT ( 'NONE',  ( -4.220049686691937474, -10.18810118749999738, 78.81250000204838102 ) ) ;
#5467 = CARTESIAN_POINT ( 'NONE',  ( -8.311093377946841443, 39.21874999658600558, 8.311093377946830785 ) ) ;
#5468 = VERTEX_POINT ( 'NONE', #12731 ) ;
#5469 = CARTESIAN_POINT ( 'NONE',  ( 7.320508075688771044, 36.24999999317202537, 7.320508075688775484 ) ) ;
#5470 = CARTESIAN_POINT ( 'NONE',  ( 1.881053915767121998, 0.6249999986344068059, -4.541265875000002339 ) ) ;
#5471 = CARTESIAN_POINT ( 'NONE',  ( -3.317071493978878571, 8.008118988124991233, 18.73186528394063188 ) ) ;
#5472 = CARTESIAN_POINT ( 'NONE',  ( 1.432654583217607414, 207.5000000013655779, 145.4587341250000634 ) ) ;
#5473 = CARTESIAN_POINT ( 'NONE',  ( -7.188101187500000044, 8.718749997951611874, -8.802885111219163269E-16 ) ) ;
#5474 = CARTESIAN_POINT ( 'NONE',  ( 1.102182119232618108E-15, 298.3125000034140157, 6.000000000000001776 ) ) ;
#5475 = DIRECTION ( 'NONE',  ( -1.000000000000000000, 0.000000000000000000, 0.000000000000000000 ) ) ;
#5476 = CARTESIAN_POINT ( 'NONE',  ( 2.977408999572651815, 8.062499997951611874, 7.188101187500000933 ) ) ;
#5477 = ADVANCED_FACE ( 'NONE', ( #58047 ), #51618, .T. ) ;
#5478 = CARTESIAN_POINT ( 'NONE',  ( -3.042071309553164404, 152.5520833299193271, -11.35316468749999963 ) ) ;
#5479 = CARTESIAN_POINT ( 'NONE',  ( -4.220049686691935698, 10.18810118749999916, 76.37500000204838102 ) ) ;
#5480 = CARTESIAN_POINT ( 'NONE',  ( -26.56734541678232375, 196.0000000013656347, 173.4587341250003760 ) ) ;
#5481 = CYLINDRICAL_SURFACE ( 'NONE', #41411, 8.000000000000000000 ) ;
#5482 = CARTESIAN_POINT ( 'NONE',  ( 4.541265875000002339, 21.43749999863440792, 0.000000000000000000 ) ) ;
#5483 = VERTEX_POINT ( 'NONE', #24053 ) ;
#5484 = CARTESIAN_POINT ( 'NONE',  ( -3.999999999999960032, 201.0625000027312126, 196.3431457505076594 ) ) ;
#5485 = VECTOR ( 'NONE', #7412, 1000.000000000000000 ) ;
#5486 = EDGE_CURVE ( 'NONE', #71847, #71972, #48240, .T. ) ;
#5487 = CARTESIAN_POINT ( 'NONE',  ( -4.000000000000015987, 207.4375000000000284, 140.3431457505076594 ) ) ;
#5488 = CARTESIAN_POINT ( 'NONE',  ( -26.34314575050769491, 203.0625000027311842, 166.0000000000003695 ) ) ;
#5489 = AXIS2_PLACEMENT_3D ( 'NONE', #71262, #29813, #30178 ) ;
#5490 = CARTESIAN_POINT ( 'NONE',  ( -8.660254037844458352, 57.91666666666671404, 5.000000000000038192 ) ) ;
#5491 = CARTESIAN_POINT ( 'NONE',  ( 5.656854249492374365, 5.656854249492375253, 7.955302783920145338 ) ) ;
#5492 = ORIENTED_EDGE ( 'NONE', *, *, #18349, .T. ) ;
#5493 = EDGE_CURVE ( 'NONE', #70220, #64059, #73643, .T. ) ;
#5494 = CARTESIAN_POINT ( 'NONE',  ( 5.082755093536324154, 19.78124999795161543, 5.082755093536326818 ) ) ;
#5495 = CARTESIAN_POINT ( 'NONE',  ( 0.000000000000000000, 300.0000000000000000, 0.000000000000000000 ) ) ;
#5496 = DIRECTION ( 'NONE',  ( 0.000000000000000000, 0.000000000000000000, 1.000000000000000000 ) ) ;
#5497 = CARTESIAN_POINT ( 'NONE',  ( 8.660254037844385522, 44.58333333333333570, 5.000000000000005329 ) ) ;
#5498 = CARTESIAN_POINT ( 'NONE',  ( 2.977408999572654480, 105.5000000020483810, 7.188101187499999156 ) ) ;
#5499 = CARTESIAN_POINT ( 'NONE',  ( -26.56734541678238415, 207.6250000013656063, 166.5412658750003629 ) ) ;
#5500 = CARTESIAN_POINT ( 'NONE',  ( 4.242640687119285658, 298.6250000000000000, -4.242640687119286547 ) ) ;
#5502 = CARTESIAN_POINT ( 'NONE',  ( -11.00000000000000000, 0.000000000000000000, 74.68750000409676204 ) ) ;
#5501 = CARTESIAN_POINT ( 'NONE',  ( 4.999999999999992006, 34.16666666666667140, 8.660254037844389075 ) ) ;
#5503 = EDGE_LOOP ( 'NONE', ( #59876, #74120, #25877, #23264 ) ) ;
#5504 = CARTESIAN_POINT ( 'NONE',  ( -9.832129032723418760, 238.4895833367473301, -5.676582343749998927 ) ) ;
#5505 = CARTESIAN_POINT ( 'NONE',  ( -4.401442555609577197E-16, 7.188101187499992051, 19.48655278187175455 ) ) ;
#5506 = DIRECTION ( 'NONE',  ( 1.000000000000000000, 0.000000000000000000, 0.000000000000000000 ) ) ;
#5507 = CARTESIAN_POINT ( 'NONE',  ( -3.171697045051319909E-12, 121.2500000000002558, -10.00000000000000178 ) ) ;
#5508 = CARTESIAN_POINT ( 'NONE',  ( 24.42570115618327264, 194.9664015783984041, 171.7300857826774347 ) ) ;
#5509 = CARTESIAN_POINT ( 'NONE',  ( 2.839093476692135984E-14, 194.9375000013655779, 201.4587341250000350 ) ) ;
#5510 = CARTESIAN_POINT ( 'NONE',  ( 2.679491924311228956, 156.0416666666666856, -10.00000000000000000 ) ) ;
#5511 = CARTESIAN_POINT ( 'NONE',  ( 0.000000000000000000, 0.000000000000000000, 0.000000000000000000 ) ) ;
#5512 = CARTESIAN_POINT ( 'NONE',  ( -5.656854249492380582, 118.8125000000000000, -5.656854249492380582 ) ) ;
#5513 = CYLINDRICAL_SURFACE ( 'NONE', #43547, 3.999999999999976019 ) ;
#5514 = CARTESIAN_POINT ( 'NONE',  ( -11.35316468750000141, 123.5937499965860269, -1.390361679473963753E-15 ) ) ;
#5515 = CARTESIAN_POINT ( 'NONE',  ( -2.485281374238927032, 293.8750000034140157, -5.999999999999647393 ) ) ;
#5516 = CARTESIAN_POINT ( 'NONE',  ( -4.556349186104045934, 11.00000000000000000, 107.2187499999999858 ) ) ;
#5519 = CARTESIAN_POINT ( 'NONE',  ( 3.999999999999960032, 197.0000000000000000, 142.0000000000000568 ) ) ;
#5518 = CARTESIAN_POINT ( 'NONE',  ( 26.56734541678237349, 197.3750000013656063, 173.4587341249998929 ) ) ;
#5517 = CARTESIAN_POINT ( 'NONE',  ( 24.54126587499999701, 195.3750000013656063, 168.5673454167822172 ) ) ;
#5520 = VERTEX_POINT ( 'NONE', #1075 ) ;
#5521 = CARTESIAN_POINT ( 'NONE',  ( 1.181652764918876164, 223.8432429321183292, 9.934327413902742876 ) ) ;
#5522 = CYLINDRICAL_SURFACE ( 'NONE', #7254, 10.00000000000000178 ) ;
#5523 = DIRECTION ( 'NONE',  ( -0.8191520442889907994, 0.000000000000000000, -0.5735764363510476027 ) ) ;
#5524 = CARTESIAN_POINT ( 'NONE',  ( 29.43265458321760519, 195.7500000013656063, 173.4587341249998929 ) ) ;
#5525 = CARTESIAN_POINT ( 'NONE',  ( -3.042071309553164404, 217.5520833299193555, -11.35316468749999963 ) ) ;
#5526 = CARTESIAN_POINT ( 'NONE',  ( 7.188101187500002709, 121.8125000020483810, 2.977408999572649151 ) ) ;
#5527 = CARTESIAN_POINT ( 'NONE',  ( 4.541265875000002339, 22.31249999863440436, 0.000000000000000000 ) ) ;
#5528 = CARTESIAN_POINT ( 'NONE',  ( -5.126144196591224222, -52.42426806216685264, 49.01287729762206880 ) ) ;
#5529 = CARTESIAN_POINT ( 'NONE',  ( -7.999999999999989342, -3.313708498984762496, 20.42405277982336642 ) ) ;
#5531 = CARTESIAN_POINT ( 'NONE',  ( 23.99999999999998579, 196.7500000000000000, 169.9999999999998863 ) ) ;
#5530 = CARTESIAN_POINT ( 'NONE',  ( -49.48363024973253488, 46.65835847153574889, 58.47069285135006567 ) ) ;
#5532 = CARTESIAN_POINT ( 'NONE',  ( -3.042071309553173730, 99.32291666325268409, 11.35316468749999785 ) ) ;
#5533 = ORIENTED_EDGE ( 'NONE', *, *, #66685, .T. ) ;
#5534 = CARTESIAN_POINT ( 'NONE',  ( -1.836970198721029983E-15, 145.6249999931720538, 10.00000000000000178 ) ) ;
#5535 = CARTESIAN_POINT ( 'NONE',  ( -2.977408999572650039, 26.43749999795162253, -7.188101187500001821 ) ) ;
#5536 = CARTESIAN_POINT ( 'NONE',  ( -8.311093377946836114, 238.5937500034139589, -8.311093377946836114 ) ) ;
#5537 = CARTESIAN_POINT ( 'NONE',  ( 3.042071309553159519, 99.73958332991934128, 11.35316468750000141 ) ) ;
#5538 = VERTEX_POINT ( 'NONE', #18034 ) ;
#5539 = CARTESIAN_POINT ( 'NONE',  ( -1.840719112916308964, 10.74941063447380785, 117.6042820761836794 ) ) ;
#5540 = CARTESIAN_POINT ( 'NONE',  ( -10.18810118749999738, -4.220049686691941915, 106.7500000020483668 ) ) ;
#5541 = CARTESIAN_POINT ( 'NONE',  ( 10.00000000000000178, 221.8749999931720254, 0.000000000000000000 ) ) ;
#5542 = CARTESIAN_POINT ( 'NONE',  ( -3.458734124999960358, 204.6875000013656063, 198.0000000000000284 ) ) ;
#5543 = CARTESIAN_POINT ( 'NONE',  ( 2.775557561562891351E-14, 210.0000000000000284, 198.0000000000000284 ) ) ;
#5545 = CARTESIAN_POINT ( 'NONE',  ( 11.35316468749999785, 95.57291666325269830, 3.042071309553174174 ) ) ;
#5544 = DIRECTION ( 'NONE',  ( 0.9884788384745426537, 6.483116892092363099E-18, -0.1513591288559071046 ) ) ;
#5546 = CARTESIAN_POINT ( 'NONE',  ( -4.898587196589407898E-16, 7.999999999999991118, 12.64280278392014623 ) ) ;
#5547 = CARTESIAN_POINT ( 'NONE',  ( -24.54126587499997925, 195.3750000013656063, 171.4326545832179818 ) ) ;
#5548 = CARTESIAN_POINT ( 'NONE',  ( 1.469576158976823947E-15, 92.37499999999998579, 8.000000000000000000 ) ) ;
#5549 = VERTEX_POINT ( 'NONE', #63676 ) ;
#5550 = CARTESIAN_POINT ( 'NONE',  ( -8.660254037844387298, 198.9583333265053682, -5.000000000000004441 ) ) ;
#5551 = CARTESIAN_POINT ( 'NONE',  ( 0.000000000000000000, 75.00000000000000000, 0.000000000000000000 ) ) ;
#5552 = AXIS2_PLACEMENT_3D ( 'NONE', #52530, #34086, #40094 ) ;
#5553 = CARTESIAN_POINT ( 'NONE',  ( 1.504986176529075959, -47.60253276711755177, 139.0361264474854863 ) ) ;
#5554 = CARTESIAN_POINT ( 'NONE',  ( 3.042071309553159519, 90.05208332991932707, 11.35316468750000141 ) ) ;
#5555 = CARTESIAN_POINT ( 'NONE',  ( -2.765530957081998586, 288.6406250017069510, 6.676582343750001591 ) ) ;
#5556 = CARTESIAN_POINT ( 'NONE',  ( -7.188101187500002709, 9.187499997951611874, 2.977408999572649151 ) ) ;
#5557 =( BOUNDED_CURVE ( )  B_SPLINE_CURVE ( 2, ( #60665, #21412, #32760, #20667, #9361, #10107, #72355, #50456, #73471, #39149, #55768, #20285, #14626 ),
 .UNSPECIFIED., .F., .F. ) 
 B_SPLINE_CURVE_WITH_KNOTS ( ( 3, 2, 2, 2, 2, 2, 3 ),
 ( 0.1944444444444440034, 0.2037037037037032483, 0.2129629629629625209, 0.2222222222222217658, 0.2314814814814810662, 0.2407407407407403110, 0.2499999999999995837 ),
 .UNSPECIFIED. ) 
 CURVE ( )  GEOMETRIC_REPRESENTATION_ITEM ( )  RATIONAL_B_SPLINE_CURVE ( ( 1.000000000000001554, 0.9659258262890666469, 1.000000000000000000, 0.9659258262890683122, 1.000000000000000000, 0.9659258262890683122, 1.000000000000000000, 0.9659258262890683122, 1.000000000000000000, 0.9659258262890683122, 1.000000000000000000, 0.9659258262890698665, 0.9999999999999984457 ) ) 
 REPRESENTATION_ITEM ( '' )  );
#5558 = CARTESIAN_POINT ( 'NONE',  ( 4.220049686691934809, 10.18810118749999916, 103.5625000020483810 ) ) ;
#5559 = CARTESIAN_POINT ( 'NONE',  ( 6.951808397369818766E-16, 2.343749996586016682, -11.35316468750000141 ) ) ;
#5560 = VERTEX_POINT ( 'NONE', #12003 ) ;
#5561 = DIRECTION ( 'NONE',  ( -0.000000000000000000, -0.000000000000000000, 1.000000000000000000 ) ) ;
#5562 = CARTESIAN_POINT ( 'NONE',  ( 3.313708498984887285, 115.1562500040967763, 7.999999999999878320 ) ) ;
#5563 = DIRECTION ( 'NONE',  ( -0.000000000000000000, 0.000000000000000000, 1.000000000000000000 ) ) ;
#5564 = CARTESIAN_POINT ( 'NONE',  ( -3.042071309553173730, 214.3229166632526699, 11.35316468749999785 ) ) ;
#5565 = PLANE ( 'NONE',  #36237 ) ;
#5566 = CARTESIAN_POINT ( 'NONE',  ( -5.000000000000000000, -16.24494643555759410, -69.83755725260751035 ) ) ;
#5567 = CARTESIAN_POINT ( 'NONE',  ( 6.676582343750001591, 296.9531250017069510, -8.176455196517173205E-16 ) ) ;
#5568 = EDGE_LOOP ( 'NONE', ( #3536, #5744, #14073 ) ) ;
#5569 = CARTESIAN_POINT ( 'NONE',  ( 2.828427124746209831, 199.3750000000000284, 200.8284271247462129 ) ) ;
#5570 = CARTESIAN_POINT ( 'NONE',  ( 9.832129032723416984, 210.6770833299193555, 5.676582343750006032 ) ) ;
#5571 = ADVANCED_FACE ( 'NONE', ( #57295 ), #29365, .T. ) ;
#5572 = ADVANCED_FACE ( 'NONE', ( #23690 ), #45957, .T. ) ;
#5573 = AXIS2_PLACEMENT_3D ( 'NONE', #19807, #19436, #41721 ) ;
#5574 = CARTESIAN_POINT ( 'NONE',  ( 7.204075437095968759, -7.204075437095966983, 98.21875000204838102 ) ) ;
#5575 = CARTESIAN_POINT ( 'NONE',  ( -25.55430564589115505, 208.0625000013656063, 172.4456943541091789 ) ) ;
#5576 = CARTESIAN_POINT ( 'NONE',  ( 5.656854249492380582, 19.68750000000000355, -5.656854249492380582 ) ) ;
#5577 = ORIENTED_EDGE ( 'NONE', *, *, #12046, .F. ) ;
#5578 = EDGE_CURVE ( 'NONE', #42278, #24630, #66348, .T. ) ;
#5579 = PRODUCT_DEFINITION_CONTEXT ( 'detailed design', #51531, 'design' ) ;
#5580 = CARTESIAN_POINT ( 'NONE',  ( -2.977408999572651815, 119.9375000020483952, 7.188101187500000933 ) ) ;
#5581 = DIRECTION ( 'NONE',  ( -0.000000000000000000, 1.000000000000000000, -4.476705744456276341E-16 ) ) ;
#5582 = CARTESIAN_POINT ( 'NONE',  ( -8.660254037844390851, 22.91666666666666785, 4.999999999999998224 ) ) ;
#5583 = CARTESIAN_POINT ( 'NONE',  ( -36.10814071610732867, 42.97056274847712132, 139.0000000000000000 ) ) ;
#5584 = CARTESIAN_POINT ( 'NONE',  ( -10.18810118749999916, 0.000000000000000000, 83.03125000204838102 ) ) ;
#5585 = ORIENTED_EDGE ( 'NONE', *, *, #8619, .T. ) ;
#5586 = CARTESIAN_POINT ( 'NONE',  ( 2.828427124746191623, 18.12500000000000000, -2.828427124746191623 ) ) ;
#5587 = DIRECTION ( 'NONE',  ( 0.000000000000000000, 0.000000000000000000, 1.000000000000000000 ) ) ;
#5588 = CARTESIAN_POINT ( 'NONE',  ( 29.56585189577826256, 194.4922901696101576, 173.1296674814865071 ) ) ;
#5589 = FILL_AREA_STYLE ('',( #7070 ) ) ;
#5590 = CARTESIAN_POINT ( 'NONE',  ( -5.000000000000000000, -12.55023575007693104, 69.09043692422063998 ) ) ;
#5591 = EDGE_CURVE ( 'NONE', #68586, #56611, #60633, .T. ) ;
#5592 = CARTESIAN_POINT ( 'NONE',  ( 4.999999999999999112, -67.91007042436125118, 22.22893179987950774 ) ) ;
#5593 = CARTESIAN_POINT ( 'NONE',  ( -6.676582343750001591, 295.4531250017069510, 0.000000000000000000 ) ) ;
#5596 = CARTESIAN_POINT ( 'NONE',  ( 1.102182119232618108E-15, 289.3125000034140157, 6.000000000000001776 ) ) ;
#5595 = CARTESIAN_POINT ( 'NONE',  ( -8.311093377946836114, 243.2812500034139589, -8.311093377946836114 ) ) ;
#5594 = CARTESIAN_POINT ( 'NONE',  ( 24.54126587499999701, 207.1875000013656063, 169.9999999999999432 ) ) ;
#5597 = SHAPE_DEFINITION_REPRESENTATION ( #24083, #66259 ) ;
#5598 = VERTEX_POINT ( 'NONE', #1800 ) ;
#5599 = CARTESIAN_POINT ( 'NONE',  ( -3.042071309553159075, 235.2604166700806161, 11.35316468749999963 ) ) ;
#5600 = CARTESIAN_POINT ( 'NONE',  ( 7.188101187499993827, -2.977408999572645598, 8.142802781871750994 ) ) ;
#5601 = ORIENTED_EDGE ( 'NONE', *, *, #29419, .T. ) ;
#5602 = ORIENTED_EDGE ( 'NONE', *, *, #62383, .T. ) ;
#5603 = CARTESIAN_POINT ( 'NONE',  ( -7.204075437095967871, 7.204075437095967871, 71.96875000204836681 ) ) ;
#5604 = CARTESIAN_POINT ( 'NONE',  ( 3.042071309553167069, 92.13541666325266988, -11.35316468749999785 ) ) ;
#5605 = CARTESIAN_POINT ( 'NONE',  ( -1.688721909672325161, 60.25432409644700726, 22.91817940688352451 ) ) ;
#5606 = CARTESIAN_POINT ( 'NONE',  ( 4.556349186104045934, 11.00000000000000000, 83.03124999999998579 ) ) ;
#5609 = CARTESIAN_POINT ( 'NONE',  ( 10.99999999999995026, -4.556349186104096560, 114.1562499999999716 ) ) ;
#5608 = CARTESIAN_POINT ( 'NONE',  ( 29.43265458321761585, 206.8750000013656347, 166.5412658749999650 ) ) ;
#5607 = CARTESIAN_POINT ( 'NONE',  ( 28.00000000000002487, 208.1875000013656063, 166.5412658749999082 ) ) ;
#5610 = CARTESIAN_POINT ( 'NONE',  ( -59.02658084577326747, 216.3289279680267043, 46.99796656044565424 ) ) ;
#5611 = CARTESIAN_POINT ( 'NONE',  ( 8.000000000000001776, 101.6562500000000142, 3.313708498984759387 ) ) ;
#5612 = CARTESIAN_POINT ( 'NONE',  ( -11.35316468750000141, 193.4895833299193271, 3.042071309553159963 ) ) ;
#5613 = CARTESIAN_POINT ( 'NONE',  ( -3.458734125000015425, 204.9375000013656063, 142.0000000000000568 ) ) ;
#5614 = CARTESIAN_POINT ( 'NONE',  ( 24.54126587499999346, 204.4375000013656063, 169.9999999999998863 ) ) ;
#5615 = CARTESIAN_POINT ( 'NONE',  ( 7.188101187499999156, 17.24999999795162253, 2.977408999572654924 ) ) ;
#5616 = CARTESIAN_POINT ( 'NONE',  ( 11.35316468749999963, 176.3020833299193839, -3.042071309553165293 ) ) ;
#5617 = DIRECTION ( 'NONE',  ( -1.000000000000000000, 0.000000000000000000, 0.000000000000000000 ) ) ;
#5618 = CARTESIAN_POINT ( 'NONE',  ( -4.401442555609581635E-16, 95.65625000204838102, -7.188101187500000044 ) ) ;
#5620 = CARTESIAN_POINT ( 'NONE',  ( -7.320508075688774596, 108.1250000000000142, 7.320508075688765715 ) ) ;
#5619 = CARTESIAN_POINT ( 'NONE',  ( -8.660254037844383745, 207.0833333333333997, -5.000000000000001776 ) ) ;
#5621 = CARTESIAN_POINT ( 'NONE',  ( 4.541265875000002339, 9.312499998634407916, 0.000000000000000000 ) ) ;
#5622 = CARTESIAN_POINT ( 'NONE',  ( 24.54126587499998280, 204.5000000013655779, 171.4326545832175555 ) ) ;
#5623 = CARTESIAN_POINT ( 'NONE',  ( 7.188101187499991163, 2.977408999572648707, 8.705302781871752771 ) ) ;
#5624 = CARTESIAN_POINT ( 'NONE',  ( -3.042071309553164404, 57.23958332991934839, -11.35316468749999963 ) ) ;
#5625 = LINE ( 'NONE', #39579, #1480 ) ;
#5626 = CARTESIAN_POINT ( 'NONE',  ( 5.656854249492376141, -5.656854249492374365, 2.949052784329821986 ) ) ;
#5627 = ORIENTED_EDGE ( 'NONE', *, *, #58770, .F. ) ;
#5628 = DIRECTION ( 'NONE',  ( -1.000000000000000000, 0.000000000000000000, 0.000000000000000000 ) ) ;
#5629 = CARTESIAN_POINT ( 'NONE',  ( 5.499989586027935751, 9.526285454130809072, 66.68677389048282578 ) ) ;
#5630 = CARTESIAN_POINT ( 'NONE',  ( -9.832129032723420536, 68.69791666325268409, 5.676582343749997150 ) ) ;
#5631 = CARTESIAN_POINT ( 'NONE',  ( -7.778174593052023411, 7.778174593052023411, 74.50000000409676204 ) ) ;
#5632 = CARTESIAN_POINT ( 'NONE',  ( 1.432654583217607414, 201.5000000013655779, 145.4587341250000350 ) ) ;
#5633 = CARTESIAN_POINT ( 'NONE',  ( 7.456155213548131044, 10.23501372118544595, 65.47700548260780806 ) ) ;
#5635 = CARTESIAN_POINT ( 'NONE',  ( 11.35316468749999785, 60.57291666325268409, 3.042071309553174174 ) ) ;
#5634 = CARTESIAN_POINT ( 'NONE',  ( -7.188101187499999156, 95.75000000204838102, 2.977408999572654924 ) ) ;
#5636 = CARTESIAN_POINT ( 'NONE',  ( 5.656854249492374365, 5.656854249492375253, 6.267802779823364645 ) ) ;
#5637 = CARTESIAN_POINT ( 'NONE',  ( -4.999999999999998224, 13.54166665983870033, -8.660254037844389075 ) ) ;
#5638 = CARTESIAN_POINT ( 'NONE',  ( 5.676582343749993598, 174.9479166632526699, 9.832129032723422313 ) ) ;
#5639 = CARTESIAN_POINT ( 'NONE',  ( -4.999999999999998224, 148.5416666598387110, -8.660254037844389075 ) ) ;
#5640 = CARTESIAN_POINT ( 'NONE',  ( 7.188101187500000044, 98.28125000204838102, -8.802885111219163269E-16 ) ) ;
#5641 = CARTESIAN_POINT ( 'NONE',  ( 0.000000000000000000, 210.0000000000000284, 170.0000000000000284 ) ) ;
#5642 = CARTESIAN_POINT ( 'NONE',  ( 6.951808397369818766E-16, 52.34374999658601979, -11.35316468750000141 ) ) ;
#5643 = CARTESIAN_POINT ( 'NONE',  ( 6.000000000000003553, 295.6250000034140157, -2.485281374238571761 ) ) ;
#5644 = CARTESIAN_POINT ( 'NONE',  ( 9.832129032723420536, 176.1979166632526983, -5.676582343749999815 ) ) ;
#5645 = ORIENTED_EDGE ( 'NONE', *, *, #43204, .F. ) ;
#5646 = DIRECTION ( 'NONE',  ( -0.000000000000000000, 1.000000000000000000, -1.563033456626094573E-30 ) ) ;
#5647 = CARTESIAN_POINT ( 'NONE',  ( 7.204075437095968759, -7.204075437095966983, 69.71875000204836681 ) ) ;
#5648 = CARTESIAN_POINT ( 'NONE',  ( 2.849036369511732440E-14, 195.2500000000000000, 202.0000000000000000 ) ) ;
#5649 = CARTESIAN_POINT ( 'NONE',  ( -5.676582343749998039, 182.4479166632526983, -9.832129032723420536 ) ) ;
#5650 = CARTESIAN_POINT ( 'NONE',  ( 5.656854249492376141, -5.656854249492374365, 4.449052784329823318 ) ) ;
#5651 = EDGE_CURVE ( 'NONE', #73379, #22362, #63495, .T. ) ;
#5652 = ADVANCED_FACE ( 'NONE', ( #65531 ), #60237, .F. ) ;
#5653 = CARTESIAN_POINT ( 'NONE',  ( 8.000000000000005329, 9.797174393178833546E-16, -14.77459999999999951 ) ) ;
#5654 = CARTESIAN_POINT ( 'NONE',  ( -6.123233995736766282E-16, 251.8750000068280031, -10.00000000000000000 ) ) ;
#5655 = FACE_OUTER_BOUND ( 'NONE', #66520, .T. ) ;
#5656 = PRODUCT_DEFINITION_FORMATION_WITH_SPECIFIED_SOURCE ( 'ANY', '', #54717, .NOT_KNOWN. ) ;
#5657 = ORIENTED_EDGE ( 'NONE', *, *, #23020, .T. ) ;
#5658 = CARTESIAN_POINT ( 'NONE',  ( 1.320432766682872962E-15, -7.188101187499992051, 27.36155278187175455 ) ) ;
#5659 = CARTESIAN_POINT ( 'NONE',  ( -9.832129032723420536, 129.0104166632526983, 5.676582343749997150 ) ) ;
#5660 = CARTESIAN_POINT ( 'NONE',  ( 12.00000000000000000, 4.898587196589398038E-16, 31.99999999999998579 ) ) ;
#5661 = ORIENTED_EDGE ( 'NONE', *, *, #3951, .T. ) ;
#5662 = CARTESIAN_POINT ( 'NONE',  ( 3.211159895383560947, 6.312499998634407028, 3.211159895383562723 ) ) ;
#5663 = ADVANCED_FACE ( 'NONE', ( #60614 ), #71547, .T. ) ;
#5664 = CARTESIAN_POINT ( 'NONE',  ( 7.188101187500000044, 12.46874999795161187, 0.000000000000000000 ) ) ;
#5665 = CARTESIAN_POINT ( 'NONE',  ( 3.313708498984765161, 103.1562500040967763, 7.999999999999998224 ) ) ;
#5666 =( BOUNDED_CURVE ( )  B_SPLINE_CURVE ( 2, ( #8806, #27637, #49908, #3898, #66504, #44626, #61603, #49152, #31817 ),
 .UNSPECIFIED., .F., .F. ) 
 B_SPLINE_CURVE_WITH_KNOTS ( ( 3, 2, 2, 2, 3 ),
 ( 0.7333333333333339477, 0.7416666666666673624, 0.7500000000000006661, 0.7583333333333339699, 0.7666666666666673846 ),
 .UNSPECIFIED. ) 
 CURVE ( )  GEOMETRIC_REPRESENTATION_ITEM ( )  RATIONAL_B_SPLINE_CURVE ( ( 0.9999999999999938938, 0.9238795325112928447, 1.000000000000000000, 0.9238795325112867385, 1.000000000000000000, 0.9238795325112867385, 1.000000000000000000, 0.9238795325112806323, 1.000000000000005995 ) ) 
 REPRESENTATION_ITEM ( '' )  );
#5667 = EDGE_CURVE ( 'NONE', #60631, #26236, #8562, .T. ) ;
#5668 = CARTESIAN_POINT ( 'NONE',  ( -31.45873412499997812, 198.0000000013656063, 171.4326545832180386 ) ) ;
#5669 = CARTESIAN_POINT ( 'NONE',  ( 4.000000000000001776, 8.000000000000000000, 0.000000000000000000 ) ) ;
#5670 = CARTESIAN_POINT ( 'NONE',  ( -2.828427124746152987, 198.1250000000000284, 200.8284271247462129 ) ) ;
#5671 = CARTESIAN_POINT ( 'NONE',  ( 4.541265875000002339, 13.37499999863440792, -1.881053915767121776 ) ) ;
#5672 = CARTESIAN_POINT ( 'NONE',  ( 5.656854249492376141, -5.656854249492374365, 21.08030278392014623 ) ) ;
#5673 = CARTESIAN_POINT ( 'NONE',  ( 3.999999999999960032, 197.0000000000000000, 142.0000000000000568 ) ) ;
#5674 = ORIENTED_EDGE ( 'NONE', *, *, #55869, .F. ) ;
#5675 = CARTESIAN_POINT ( 'NONE',  ( 7.188101187500001821, 107.0000000020483810, -2.977408999572651371 ) ) ;
#5676 = EDGE_CURVE ( 'NONE', #60122, #35339, #18777, .T. ) ;
#5678 = CARTESIAN_POINT ( 'NONE',  ( 2.485281374238225816, 293.6875000000000000, -6.000000000000346390 ) ) ;
#5677 = DIRECTION ( 'NONE',  ( 1.000000000000000000, 0.000000000000000000, -0.000000000000000000 ) ) ;
#5679 = CARTESIAN_POINT ( 'NONE',  ( -4.541265875000002339, 21.74999999863440436, -1.881053915767121998 ) ) ;
#5680 = CARTESIAN_POINT ( 'NONE',  ( -5.272365137108047328, -4.893145049964592097, 0.1656095422372733106 ) ) ;
#5681 = ORIENTED_EDGE ( 'NONE', *, *, #51557, .T. ) ;
#5682 = EDGE_LOOP ( 'NONE', ( #48736, #15210, #70349, #71217, #9181 ) ) ;
#5683 = CARTESIAN_POINT ( 'NONE',  ( -4.220049686691937474, -10.18810118749999738, 93.43750000204836681 ) ) ;
#5684 = CARTESIAN_POINT ( 'NONE',  ( 7.778174593052021635, 7.778174593052023411, 91.93749999999998579 ) ) ;
#5685 = CARTESIAN_POINT ( 'NONE',  ( -24.54126587499998990, 195.4375000013655779, 170.0000000000003411 ) ) ;
#5686 = CARTESIAN_POINT ( 'NONE',  ( -7.778174593052023411, 7.778174593052023411, 99.81250000000000000 ) ) ;
#5688 = CARTESIAN_POINT ( 'NONE',  ( 2.839093476692135984E-14, 204.9375000013656063, 201.4587341250000350 ) ) ;
#5687 = AXIS2_PLACEMENT_3D ( 'NONE', #19771, #72585, #66539 ) ;
#5690 = CARTESIAN_POINT ( 'NONE',  ( 4.721056650415999201, 299.2343750017069510, -4.721056650415999201 ) ) ;
#5689 = CARTESIAN_POINT ( 'NONE',  ( 25.17157287525377996, 202.7500000027312126, 167.1715728752537586 ) ) ;
#5691 = CARTESIAN_POINT ( 'NONE',  ( 8.660254037844389075, 125.4166666666666714, -5.000000000000000000 ) ) ;
#5692 = CARTESIAN_POINT ( 'NONE',  ( -4.898587196589412829E-16, 103.6250000000000000, -8.000000000000000000 ) ) ;
#5693 = CARTESIAN_POINT ( 'NONE',  ( 1.226468279477575784E-15, 288.8593750017070079, 6.676582343750001591 ) ) ;
#5694 = CARTESIAN_POINT ( 'NONE',  ( 1.320432766682872962E-15, -7.188101187499992051, 8.236552781871752771 ) ) ;
#5695 = CARTESIAN_POINT ( 'NONE',  ( 2.751064625579944321E-14, 200.7500000000000000, 194.0000000000000568 ) ) ;
#5696 = CARTESIAN_POINT ( 'NONE',  ( 28.00000000000002132, 202.9375000013656063, 166.5412658749999082 ) ) ;
#5697 = CARTESIAN_POINT ( 'NONE',  ( 8.000000000000000000, 26.81249999590322375, 0.000000000000000000 ) ) ;
#5698 = CARTESIAN_POINT ( 'NONE',  ( 12.00000000000000355, -6.928203230275539859, -1.071796769724504550 ) ) ;
#5699 = CARTESIAN_POINT ( 'NONE',  ( 7.188101187500000044, 123.7812500020483810, -8.802885111219163269E-16 ) ) ;
#5701 = PLANE ( 'NONE',  #26937 ) ;
#5700 = LINE ( 'NONE', #17377, #2247 ) ;
#5702 = CARTESIAN_POINT ( 'NONE',  ( 9.832129032723420536, 236.3020833367473301, 5.676582343749996262 ) ) ;
#5703 = CARTESIAN_POINT ( 'NONE',  ( -4.401442555609577197E-16, 7.188101187499992051, 26.98655278187175455 ) ) ;
#5704 = CARTESIAN_POINT ( 'NONE',  ( 23.99999999999997868, 198.8125000000000284, 171.6568542494922553 ) ) ;
#5705 = CARTESIAN_POINT ( 'NONE',  ( 3.042071309553167069, 16.82291666325268054, -11.35316468749999785 ) ) ;
#5706 = CARTESIAN_POINT ( 'NONE',  ( 1.469576158976823947E-15, 122.3750000000000000, 8.000000000000000000 ) ) ;
#5707 = CARTESIAN_POINT ( 'NONE',  ( -11.35316468749999785, 208.3854166632526415, -3.042071309553167513 ) ) ;
#5708 = CARTESIAN_POINT ( 'NONE',  ( -24.00000000000000355, 197.8125000000000284, 168.3431457505080004 ) ) ;
#5709 = CARTESIAN_POINT ( 'NONE',  ( -2.679491924311521167, 218.3333333265053966, -9.999999999999833022 ) ) ;
#5711 = CARTESIAN_POINT ( 'NONE',  ( -7.320508075688897165, 43.12500000000009237, 7.320508075688889171 ) ) ;
#5710 = CARTESIAN_POINT ( 'NONE',  ( -10.99999999999989164, -4.556349186104158733, 88.09375000000000000 ) ) ;
#5712 = ORIENTED_EDGE ( 'NONE', *, *, #10955, .F. ) ;
#5713 = CARTESIAN_POINT ( 'NONE',  ( -3.458734125000015425, 201.2500000013656063, 143.4326545832176976 ) ) ;
#5714 = CARTESIAN_POINT ( 'NONE',  ( -11.35316468750000141, 23.48958332991934483, 3.042071309553159963 ) ) ;
#5715 = CARTESIAN_POINT ( 'NONE',  ( -4.556349186104047710, -10.99999999999999822, 94.46875000409677625 ) ) ;
#5716 = CARTESIAN_POINT ( 'NONE',  ( 5.000000000000004441, 226.6666666666666856, 8.660254037844385522 ) ) ;
#5717 = CARTESIAN_POINT ( 'NONE',  ( -30.44569435410875613, 195.8125000013656063, 172.4456943541092642 ) ) ;
#5718 = DIRECTION ( 'NONE',  ( 0.000000000000000000, 0.8660254037844414832, 0.4999999999999950595 ) ) ;
#5720 = CARTESIAN_POINT ( 'NONE',  ( 3.042071309553159519, 19.73958332991934483, 11.35316468750000141 ) ) ;
#5719 = CARTESIAN_POINT ( 'NONE',  ( -4.401442555609581635E-16, 110.2812500020483810, -7.188101187500000044 ) ) ;
#5721 = CARTESIAN_POINT ( 'NONE',  ( 3.313708498984762496, -7.999999999999989342, 20.79905277982336642 ) ) ;
#5722 = CARTESIAN_POINT ( 'NONE',  ( 3.042071309553159519, 134.7395833299193839, 11.35316468750000141 ) ) ;
#5723 = VECTOR ( 'NONE', #11527, 1000.000000000000000 ) ;
#5724 = CARTESIAN_POINT ( 'NONE',  ( -7.320508075688778149, 104.9999999931720396, 7.320508075688769267 ) ) ;
#5725 = CARTESIAN_POINT ( 'NONE',  ( -4.401442555609581635E-16, 115.1562500020483810, -7.188101187500000044 ) ) ;
#5726 = CARTESIAN_POINT ( 'NONE',  ( -5.656854249492379694, 13.87499999590322375, -5.656854249492380582 ) ) ;
#5727 = CARTESIAN_POINT ( 'NONE',  ( -24.54126587499998635, 207.3750000013656063, 171.4326545832179818 ) ) ;
#5728 = CARTESIAN_POINT ( 'NONE',  ( -5.000000000000000000, -51.30314553820197432, -41.49361401976533870 ) ) ;
#5729 = ADVANCED_BREP_SHAPE_REPRESENTATION ( '', ( #16403, #57354 ), #14000 ) ;
#5730 = EDGE_LOOP ( 'NONE', ( #52300, #73041, #53784, #57237 ) ) ;
#5731 = CARTESIAN_POINT ( 'NONE',  ( 3.042071309553167513, 7.135416663252683200, -11.35316468749999785 ) ) ;
#5732 = CARTESIAN_POINT ( 'NONE',  ( 5.656854249492381470, 107.5625000000000000, 5.656854249492379694 ) ) ;
#5733 = CARTESIAN_POINT ( 'NONE',  ( -4.721056650415998313, 298.5781250017069510, 4.721056650416000089 ) ) ;
#5734 = CARTESIAN_POINT ( 'NONE',  ( -8.311093377946836114, 132.6562499965860411, -8.311093377946837890 ) ) ;
#5735 = CARTESIAN_POINT ( 'NONE',  ( 1.469576158976822172E-15, -7.999999999999991118, 22.26155278432982243 ) ) ;
#5736 = EDGE_CURVE ( 'NONE', #12947, #3793, #64793, .T. ) ;
#5737 = CARTESIAN_POINT ( 'NONE',  ( -10.99999999999992006, -31.99999999999978684, 205.0000000000000284 ) ) ;
#5738 = DIRECTION ( 'NONE',  ( -1.000000000000000000, 0.000000000000000000, -1.836970198721037823E-16 ) ) ;
#5739 = CARTESIAN_POINT ( 'NONE',  ( -6.238412754330611322E-16, 10.18810118749999916, 97.65625000204838102 ) ) ;
#5740 = ORIENTED_EDGE ( 'NONE', *, *, #15182, .T. ) ;
#5741 = CYLINDRICAL_SURFACE ( 'NONE', #6339, 6.000000000000001776 ) ;
#5742 = CARTESIAN_POINT ( 'NONE',  ( -3.458734124999960358, 201.6250000013656063, 196.5673454167823877 ) ) ;
#5743 = CARTESIAN_POINT ( 'NONE',  ( -3.042071309553173730, 79.63541666325268409, 11.35316468749999785 ) ) ;
#5744 = ORIENTED_EDGE ( 'NONE', *, *, #40247, .T. ) ;
#5745 = B_SPLINE_CURVE_WITH_KNOTS ( 'NONE', 3,
 ( #53834, #53466, #24038, #24413, #2515, #48151, #71161, #59858, #70083, #8171, #64415, #54206, #71527, #12713, #19854, #35745, #65877, #70443, #18758, #41766, #3632, #73036, #26630 ),
 .UNSPECIFIED., .F., .F.,
 ( 4, 2, 2, 2, 2, 2, 2, 2, 1, 2, 2, 4 ),
 ( 0.000000000000000000, 0.001047525702552857358, 0.001571288553829286146, 0.002095051405105714717, 0.003142577107658572292, 0.004190102810211429434, 0.005237628512764286141, 0.005761391364040716230, 0.006285154215317145451, 0.006808917066593575540, 0.007332679917870004761, 0.008380205620422864071 ),
 .UNSPECIFIED. ) ;
#5746 = CARTESIAN_POINT ( 'NONE',  ( -4.220049686691935698, 10.18810118749999916, 107.8750000020483668 ) ) ;
#5747 = CARTESIAN_POINT ( 'NONE',  ( -4.541265875000002339, 10.93749999863440792, -5.561446717895856393E-16 ) ) ;
#5748 = EDGE_LOOP ( 'NONE', ( #17016, #60402, #16082, #67832 ) ) ;
#5749 = VECTOR ( 'NONE', #46069, 1000.000000000000000 ) ;
#5750 = ORIENTED_EDGE ( 'NONE', *, *, #6051, .T. ) ;
#5751 = CARTESIAN_POINT ( 'NONE',  ( 4.898587196589412829E-16, 0.3749999999999999445, -8.000000000000000000 ) ) ;
#5752 = CARTESIAN_POINT ( 'NONE',  ( 5.000000000000001776, 115.8333333333333712, -8.660254037844389075 ) ) ;
#5753 = CARTESIAN_POINT ( 'NONE',  ( 1.224646799147353256E-15, 0.000000000000000000, 10.00000000000000000 ) ) ;
#5754 = CARTESIAN_POINT ( 'NONE',  ( -7.188101187500000044, 25.59374999795161543, -8.802885111219163269E-16 ) ) ;
#5755 = DIRECTION ( 'NONE',  ( -0.000000000000000000, 1.000000000000000000, -0.000000000000000000 ) ) ;
#5756 = CARTESIAN_POINT ( 'NONE',  ( -4.220049686691935698, 10.18810118749999916, 102.2500000020483952 ) ) ;
#5757 = EDGE_CURVE ( 'NONE', #29151, #31018, #13824, .T. ) ;
#5758 =( BOUNDED_SURFACE ( )  B_SPLINE_SURFACE ( 1, 2, ( 
 ( #40965, #40216, #24343, #46243, #35678, #63590, #46614, #11919, #6271, #69635, #17949, #58694, #71460, #24703, #19411, #30745, #25809, #43539, #25065, #37147, #1723, #59427, #42424, #53400, #60901, #47713, #66184, #37526, #7739, #8104, #70733, #66553, #48828, #2819, #42056, #31862, #8470, #65063, #71835, #72212, #19785, #65442, #59792, #31490, #48455, #20152, #43168, #60150, #14864, #31107, #13737, #14487, #53765, #60527, #8854, #49202, #65809, #30380, #19053, #13375, #36782, #36413, #2076, #54513, #54135, #48084, #71093, #54886, #37903, #2446, #42793, #25438, #14115, #26183, #3196, #20525, #74082, #10344, #68056, #15240, #62019, #50691, #32625, #33004, #9223, #55633, #16347, #32245, #33368, #38652, #73710, #4318, #67689, #26558, #3568, #22021, #39384, #72599, #27307, #62381, #21277, #61278, #55262, #15986, #49581, #20905, #39017, #43926, #56369, #44674, #10709, #33741, #22382, #72972, #49957, #66936, #45047, #44300, #26938, #3949, #51070, #56744, #4690, #5063, #67316, #28059, #45403, #27685, #68419, #16720, #38274, #39747, #9606, #15613, #61654, #9973, #56004, #50323, #73345, #21648, #64253, #17478, #18230, #5427, #12190, #28431, #11458, #11089, #40124, #17101, #1268, #58603, #11826, #52938, #63131, #70287, #40498, #68792, #29552, #34115, #18601, #62748, #52561, #63504, #69544, #40873, #6909, #28800, #47260, #51818, #45781, #63878, #57869, #35589, #530, #6546, #34864, #35228, #57115, #6177, #900, #17854, #23509, #34493, #29184, #46525, #57500, #58246, #5803, #51439, #46152, #162, #24248, #74450, #23140, #29920, #69169, #23887, #46896, #22759, #69920, #52199, #41245, #12562, #8014, #43077, #31021, #35955, #64625, #64978, #48366, #7282, #24615, #42706, #30290, #8381, #54045, #2356, #12921, #71744, #66093, #7652, #65718, #36694, #30658, #20059, #31396, #37060, #54423, #41610, #25350, #60060, #71370, #19695, #13286, #14022, #58975, #48738, #1634, #2729, #59705, #25717, #47995, #53310, #47623, #70645, #18965, #41968, #36326, #59340, #53675, #1988, #24978, #71009, #19324, #42337, #65354, #13654, #143, #47239, #17835, #42956, #8262, #13903, #59947, #57477, #18209, #70266, #69898, #41223, #34842, #12540, #65975, #36942, #28779, #18579, #6524, #64231, #46501, #29531, #46875, #51796, #71625, #69521, #41590, #35208, #40477, #31276, #510, #64603, #19947, #6889, #54304, #35568, #23119, #14279, #24225, #2615, #63482, #29900, #40849, #52541, #69149, #58581, #25605, #12172, #48618, #46131, #52913, #17456, #6155, #5783, #57849, #11804, #29163, #52178, #879, #23489, #63857, #58225, #23865, #1248, #4115, #8642, #44842, #67849, #27108, #15034, #44099, #15403, #56171, #3357, #21809, #26347, #20315, #38442, #32411, #10135, #49752, #55799, #38070, #61445, #37317, #61069, #50123, #67107, #72769, #9016, #55424, #21075, #60696, #9772, #37696, #54677, #20698, #43332, #50489, #73502, #55050, #4484, #66351, #73139, #32791, #2983, #21445, #9391, #32030, #27475, #44468, #60314, #67481, #25968, #31656, #49368, #15780, #48990, #14655, #38818, #61817, #72385, #33173, #43716, #72000, #66730, #3733, #26732, #29360, #33917, #58042, #45210, #28975, #40295, #56543, #11624, #16900, #39558, #6356, #45952, #23685, #68969, #33542, #62183, #56917, #34662, #4860, #68221, #51995, #50865, #17649, #17278, #22945, #10510, #52366, #27856, #45579, #73881, #5972, #51239, #702, #40668, #46325, #63671, #16140, #51613, #332, #28602, #74629, #16518, #63296, #46691, #69339, #22185, #23313, #39926, #57665, #5230, #62932, #5604, #62552, #39179, #28231, #11998, #68594, #10883, #35030, #74250, #22558, #11257, #34286, #57290, #53478, #64053, #2530, #36493, #2157, #1070, #42134, #30089, #64788, #6715, #59145, #71175, #24423, #25150, #12364, #19129, #35399, #18400, #18029, #47057, #24048, #8184, #65526, #18772, #59871, #70094, #25522, #47430, #41415, #59506, #41045, #69715, #58409, #7819, #70454, #1795, #47794, #13819, #35758, #54219, #58775, #52736, #70817, #13089, #42509, #7454, #13456, #41777, #65146, #29722, #36124, #30822, #24779, #30461, #64427, #53844, #12725, #48167, #19493, #7083, #36863, #53108, #31195, #1442, #26263, #2901, #38738, #20611, #4032, #73051, #14946, #42872, #37609, #48905, #44010, #61737, #43251, #55342, #19866, #25886, #60609, #71542, #4397, #65891, #9688, #55717, #71919, #49283, #14197, #10054, #67020, #20986, #60232, #50037, #26645, #8557, #15317, #15696, #37985, #8933, #3276, #49667, #66639, #38353, #61361, #3645, #33091, #72299, #31944, #32708, #20232, #27026, #21359, #67394, #9305, #48534, #37234, #31571, #54967, #54595, #66267, #72684, #43629, #14574, #60984, #44383, #56088, #32329, #16805, #16432, #4773, #23226, #34195, #34945, #17564, #28514, #11540, #33455, #5514, #68878, #56456, #62465, #74162, #63211, #34572, #27390, #51523, #56826, #17188, #22466, #11173, #44758, #21728, #40207, #57578, #16065, #45486, #5888, #39468, #27765, #50409, #57199, #73423, #67771, #5147, #10425, #39099, #50777, #28886, #51905, #40583, #10793, #68137, #62102, #245, #33829, #45125, #73791, #69254, #46236, #22849, #22100, #63584, #68505, #11912, #28140, #57957, #51155, #39833, #62837, #74538, #45863, #63966, #64336, #29268, #17942, #59057, #12640, #6264, #35313, #19045, #65434, #70004, #70370, #18313, #58324, #2068, #13003, #13730, #71086, #7365, #65056, #12278, #30373, #47706, #6630, #41326, #53020, #42049, #13367, #52280, #53392, #35671, #70726, #1351, #64705, #23596, #616, #36406, #59419, #69628, #24335, #7732, #58686, #29635, #46605, #36041, #40958, #52648, #6995, #983, #23966, #46974, #30739, #53757, #19404, #30006, #47345, #18686, #25057, #41692, #1717, #24695, #48078, #42416, #36775, #37140, #49950, #26174, #60143, #20897, #49193, #67308, #32618, #54128, #14855, #71450, #37520, #14108, #72965, #31855, #15235, #9599, #72204, #2439, #48821, #8463, #55253, #21270, #54506, #66546, #31099, #31483, #71828, #8096, #15606, #25432, #43919, #66930, #2812, #60519, #48448, #44294, #3560, #32236, #19778, #61270, #37895, #42786, #26550, #26931, #20517, #20145, #14481, #60893, #3188, #49574, #72592, #9215, #59786, #8845, #43161, #43531, #55626, #54878, #38266, #65802, #3942, #25801, #66177, #61647, #15979, #67682, #51810, #34486, #62375, #28794, #39009, #46145, #16341, #44668, #5420, #9966, #69162, #38645, #28425, #39378, #45396, #16712, #57492, #4683, #23133, #27678, #21642, #39742, #33736, #11451, #51062, #57107, #10702, #62742, #32997, #56738, #51432, #68412, #74075, #10337, #5057, #22375, #62012, #11082, #33362, #55997, #22015, #56363, #157, #4311, #50684, #5797, #73703, #74444, #34109, #27301, #22751, #28053, #45041, #50317, #45774, #73338, #68786, #68050, #17095, #40117, #63123, #6168, #46518, #53303, #52192, #18957, #70280, #24240, #63497, #30649, #11819, #46889, #34856, #7275, #52555, #1979, #41961, #47615, #64969, #17471, #52930, #30282, #29913, #1261, #69537, #47253, #24971, #70638, #57862, #1627, #41238, #18592, #6538, #64244, #6902, #29177, #53667, #29544, #24607, #69913, #523, #13278, #35220, #36318, #47987, #41603, #59333, #64618, #23503, #40492, #58967, #7644, #17848, #12914, #894, #12554, #40865, #35949, #63871, #18223, #23880, #12183, #58240, #35582, #58596, #15147, #31766, #71000, #65346, #54037, #54414, #19316, #8005, #49103, #2721, #42328, #25342, #9127, #55540, #60051, #60428, #8372, #48356, #66844, #3097, #3850, #61183, #72115, #55164, #2348, #20428, #37806, #71362, #31388, #43068, #32144, #3470, #13647, #43444, #25709, #60802, #66084, #54785, #36686, #59697, #26459, #49483, #31012, #14394, #72502, #48730, #19688, #42697, #26082, #65710, #14014, #71736, #37051, #20052, #37428, #20811, #43829, #9513, #8755, #66459, #14768, #38179, #32528, #26846, #21556, #17010, #74356, #45316, #27213, #40036, #16255, #50230, #10995, #39294, #57399, #22666, #44209, #4970, #61559, #27589, #4225, #63039, #21924, #5339, #45685, #62294, #67222, #38923, #73251, #68331, #11364, #44583, #56655, #21184, #67595, #61924, #72879, #5707, #15518, #34028, #57026, #15892, #50599, #38558, #34398, #16628, #22292, #9880, #51346, #27972, #32908, #39663, #49861, #10623, #10250, #4595, #50976, #67962, #62661, #28338, #55913, #33277, #73619, #56276, #68700, #44955, #33649, #73990, #58881, #30196, #28706, #64160, #41515, #41153, #12467, #6080, #58511, #36232, #7191, #69, #64531, #52472, #35498, #17760, #808, #18137, #23049, #41880, #40774, #18506, #6459, #11733, #53213, #46435, #12829, #64892, #52842, #35864, #6817, #46060, #59248, #70198, #1546, #34773, #1174, #63782, #23796, #40410, #29829, #24526, #58151, #47532, #69079, #24153, #17385, #52108, #51720, #29088, #57776, #13193, #70557, #46799, #18873, #441, #63407, #29462, #23420, #69452, #12099 ),
 ( #35135, #69821, #47166, #20722, #25256, #49392, #36599, #20340, #31682, #47902, #3010, #8289, #30927, #72411, #37341, #15058, #60339, #24883, #53584, #48275, #25992, #70921, #59609, #43357, #42242, #9041, #8667, #14305, #1896, #66374, #54701, #19235, #49016, #31299, #53949, #43739, #72026, #38093, #14681, #65256, #13560, #71280, #37722, #7922, #2262, #60720, #19600, #32055, #55074, #3383, #42615, #66754, #65629, #36965, #13926, #26370, #59971, #7559, #30565, #54329, #2640, #25628, #42981, #48643, #19973, #66000, #71652, #16164, #69639, #17577, #32438, #23239, #10161, #44867, #50147, #33198, #50513, #55448, #628, #73163, #51918, #38839, #44124, #11923, #4142, #256, #23609, #10532, #69266, #67872, #3758, #17953, #28900, #40595, #67132, #34584, #21471, #56194, #72793, #73527, #63596, #15804, #34955, #26759, #57590, #49777, #9794, #9419, #38466, #15428, #46619, #57970, #4507, #52291, #61469, #61091, #61842, #32816, #46246, #21101, #55824, #27133, #6276, #27501, #39205, #62208, #29282, #44492, #67505, #21835, #5900, #42061, #36053, #13744, #53405, #59434, #41705, #65069, #40971, #64719, #7745, #70741, #1727, #12652, #59070, #24708, #64348, #47720, #41339, #58338, #24348, #46985, #54144, #2453, #58698, #8111, #70017, #18698, #18324, #30751, #12291, #48461, #71466, #53772, #13015, #19059, #13381, #59798, #7009, #25445, #30018, #23977, #36420, #7378, #36788, #2081, #25073, #30386, #48090, #63978, #71099, #19418, #42432, #65448, #35683, #31116, #35326, #53032, #6642, #1362, #29645, #47357, #70382, #52660, #996, #37532, #61661, #48834, #32632, #43932, #60158, #15246, #20533, #43174, #9980, #49589, #27313, #72606, #37156, #65815, #60533, #38280, #8477, #71840, #55640, #54518, #21284, #20912, #26566, #14122, #33011, #31496, #49209, #2824, #9612, #54890, #4324, #44307, #49963, #67322, #19791, #55269, #3956, #32251, #3574, #20157, #66942, #50329, #72978, #25814, #26945, #43546, #61285, #8859, #66561, #9229, #66190, #56012, #31868, #15619, #72218, #14494, #38659, #3201, #42799, #26189, #14870, #37909, #60906, #67695, #6184, #40134, #5813, #4697, #45790, #33749, #68426, #10351, #62757, #172, #28066, #28808, #15993, #22767, #39023, #22027, #21655, #50699, #27690, #11836, #69178, #22390, #63512, #73716, #29192, #45053, #68800, #56752, #16729, #33375, #11099, #23148, #51077, #51826, #62026, #17111, #56376, #68063, #44680, #16353, #39391, #34871, #17488, #45410, #57877, #62390, #73351, #74090, #10717, #63140, #5071, #39755, #34123, #11467, #57123, #5437, #51446, #40508, #28440, #74459, #34502, #57507, #46161, #47268, #24988, #64633, #70656, #52946, #1642, #52205, #1279, #18973, #7291, #12930, #23894, #70295, #35966, #908, #58986, #52571, #69552, #35597, #58253, #65364, #13663, #69927, #19335, #6554, #64988, #24623, #17863, #47633, #24256, #46903, #42347, #30299, #59714, #53318, #40880, #23519, #18237, #41977, #63886, #29560, #13297, #12197, #53686, #36335, #59350, #46534, #36703, #35234, #6919, #41252, #7661, #12569, #8023, #1998, #30667, #48005, #538, #71018, #64261, #58613, #29930, #18610, #41620, #38577, #61200, #2365, #66859, #54805, #14785, #20069, #3115, #20446, #25360, #44229, #43086, #20829, #8773, #14032, #55556, #48747, #43846, #67240, #55183, #38197, #37825, #48377, #61576, #72521, #9531, #15536, #31785, #66103, #15166, #8391, #32545, #3869, #49879, #66477, #31031, #71380, #37069, #14413, #54056, #42717, #9144, #37445, #19704, #60072, #26865, #65728, #60443, #43463, #26101, #31405, #72894, #60822, #54432, #21201, #32162, #2740, #25726, #3488, #71755, #49120, #72133, #26477, #49502, #17027, #9896, #11014, #39314, #51363, #4988, #68350, #27230, #4243, #22685, #40053, #73269, #27989, #68716, #21943, #61941, #32926, #16645, #55932, #50247, #62312, #67612, #21573, #10269, #63056, #11380, #88, #73636, #50617, #44599, #45703, #44971, #27607, #56294, #51739, #34415, #5354, #33295, #23066, #50994, #4610, #57417, #74005, #17401, #5724, #15908, #39678, #38940, #10638, #67977, #46075, #56672, #28723, #69094, #22308, #16272, #33667, #45333, #28355, #40424, #62677, #34047, #57042, #74374, #825, #11750, #19249, #34788, #24541, #70573, #17778, #41168, #57792, #24900, #58898, #35881, #456, #64905, #41531, #23435, #7209, #30579, #52858, #23813, #18153, #64547, #6833, #30211, #53230, #70214, #63423, #40790, #1562, #47917, #52487, #1190, #46815, #63797, #59264, #18523, #70936, #53601, #12843, #47549, #69468, #18890, #41896, #12115, #69840, #35513, #13211, #36249, #6100, #7575, #64179, #1913, #58526, #47182, #29105, #52124, #46450, #35153, #58169, #29847, #6474, #12483, #29478, #24171, #49031, #13578, #59624, #71667, #25272, #7939, #19617, #20737, #26383, #32454, #31315, #8305, #36614, #55093, #54342, #59988, #13941, #9437, #66769, #37736, #42632, #55464, #8681, #65644, #3399, #31696, #49793, #15073, #30944, #72039, #53966, #19986, #71297, #3773, #14322, #72429, #38107, #54718, #2277, #2653, #36983, #60735, #26775, #25643, #20356, #48290, #48658, #42995, #65272, #72808, #66015, #49408, #43755, #37355, #60354, #3025, #42260, #9057, #14696, #26008, #61107, #43373, #66389, #32071, #62970, #10548, #33212, #50529, #73918, #39222, #68261, #16556, #27894, #57328, #73545, #10178, #10921, #73179, #51278, #74287, #39965, #56585, #21116, #15446, #4158, #4522, #44139, #32831, #22222, #27518, #28639, #62590, #28271, #27146, #39594, #56209, #16180, #55841, #33581, #22597, #21852, #45618, #38482, #45249, #61485, #44509, #67151, #21488, #50163, #34327, #16941, #44883, #11295, #67520, #51654, #67888, #15818, #33956, #9809, #38853, #61858, #56954, #62222, #50904, #5270, #5639, #4898, #68632, #40705, #57704, #1108, #69752, #47468, #12400, #18438, #739, #24084, #6874, #23723, #41451, #29755, #35434, #46362, #18065, #58443, #23350, #6752, #368, #17313, #58079, #6011, #13126, #36161, #17688, #41813, #29014, #12763, #47092, #40333, #70131, #46727, #69378, #64824, #52770, #7491, #64464, #63336, #45991, #63709, #35795, #11661, #52031, #58810, #34696, #1477, #7121, #30129, #69006, #59182, #12033, #29396, #35067, #53144, #6390, #30495, #24460, #70491, #18809, #22985, #52404, #41081, #64091, #65930, #30863, #8594, #61022, #8971, #24820, #14612, #2569, #37274, #42548, #25557, #42910, #47833, #66681, #65560, #43291, #31233, #36532, #3313, #71211, #66306, #14985, #2939, #60649, #60268, #70855, #19167, #36900, #59542, #38022, #9347, #19530, #20652, #7858, #37650, #25927, #42169, #48944, #54258, #2193, #43668, #31608, #53515, #54630, #65182, #13493, #13855, #71954, #53882, #25189, #31984, #48203, #55008, #20268, #26300, #59908, #1832, #8222, #48571, #71581, #49324, #19903, #14235, #72339, #62505, #33868, #32366, #67808, #45164, #44795, #16100, #9725, #62139, #39874, #10833, #3690, #68175, #56125, #39135, #21398, #4434, #21768, #26686, #45527, #44421, #22137, #10093, #15360, #56868, #50077, #16472, #68543, #56495, #39509, #10462, #49709, #62876, #73830, #5184, #38395, #4812, #67436, #27428, #44051, #33492, #28180, #61776, #51192, #72722, #27808, #21026, #55755, #55380, #32747, #61399, #16847, #74201, #50443, #22506, #4071, #67061, #33130, #27064, #73092, #15734, #38773, #73460, #50819, #63622, #17978, #64005, #30043, #51946, #70406, #283, #68917, #12320, #6303, #58725, #23640, #29671, #11951, #35351, #11210, #34983, #52688, #40998, #46647, #57617, #29309, #69665, #34610, #58362, #11576, #17227, #1022, #57239, #18721, #41730, #24001, #57998, #6668, #47011, #53058, #23265, #34237, #46274, #40248, #70043, #52318, #7036, #18353, #41366, #654, #64375, #5550, #12676, #35709, #1390, #24376, #5927, #47382, #28554, #28929, #51560, #69294, #74577, #17604, #63250, #22891, #45903, #40622, #49891, #47742, #43858, #3501, #7403, #49515, #48115, #42084, #72905, #31138, #67253, #55195, #59095, #13040, #13407, #72533, #30410, #70766, #66870, #53429, #32557, #26489, #20840, #36077, #21213, #1752, #2104, #24733, #15178, #30775, #44240, #55567, #61212, #3881, #64741, #38209, #15548, #9544, #26876, #25098, #19081, #65096, #36445, #7771, #59457, #53795, #71123, #19445, #42457, #65473, #36811, #13767, #59821, #8135, #40612, #57989, #62867, #68164, #34973, #34227, #39865, #68534, #63995, #46636, #17594, #74191, #12310, #63240, #22496, #6293, #11566, #29662, #69656, #16463, #51936, #33859, #74569, #51183, #35342, #68908, #52309, #17969, #34600, #39500, #11200, #45518, #63614, #58354, #16838, #28920, #6659, #57229, #45154, #5541, #5175, #52678, #28543, #29299, #22129, #46265, #645, #5917, #62495, #10824, #11941, #23629, #28171, #69285, #51551, #17219, #56858, #57607, #40988, #22882, #45894, #40238, #274, #23256, #24365, #23992, #53049, #30033, #14137, #71481 ) ),
 .UNSPECIFIED., .F., .F., .F. ) 
 B_SPLINE_SURFACE_WITH_KNOTS ( ( 2, 2 ),
 ( 3, 2, 2, 2, 2, 2, 2, 2, 2, 2, 2, 2, 2, 2, 2, 2, 2, 2, 2, 2, 2, 2, 2, 2, 2, 2, 2, 2, 2, 2, 2, 2, 2, 2, 2, 2, 2, 2, 2, 2, 2, 2, 2, 2, 2, 2, 2, 2, 2, 2, 2, 2, 2, 2, 2, 2, 2, 2, 2, 2, 2, 2, 2, 2, 2, 2, 2, 2, 2, 2, 2, 2, 2, 2, 2, 2, 2, 2, 2, 2, 2, 2, 2, 2, 2, 2, 2, 2, 2, 2, 2, 2, 2, 2, 2, 2, 2, 2, 2, 2, 2, 2, 2, 2, 2, 2, 2, 2, 2, 2, 2, 2, 2, 2, 2, 2, 2, 2, 2, 2, 2, 2, 2, 2, 2, 2, 2, 2, 2, 2, 2, 2, 2, 2, 2, 2, 2, 2, 2, 2, 2, 2, 2, 2, 2, 2, 2, 2, 2, 2, 2, 2, 2, 2, 2, 2, 2, 2, 2, 2, 2, 2, 2, 2, 2, 2, 2, 2, 2, 2, 2, 2, 2, 2, 2, 2, 2, 2, 2, 2, 2, 2, 2, 2, 2, 2, 2, 2, 2, 2, 2, 2, 2, 2, 2, 2, 2, 2, 2, 2, 2, 2, 2, 2, 2, 2, 2, 2, 2, 2, 2, 2, 2, 2, 2, 2, 2, 2, 2, 2, 2, 2, 2, 2, 2, 2, 2, 2, 2, 2, 2, 2, 2, 2, 2, 2, 2, 2, 2, 2, 2, 2, 2, 2, 2, 2, 2, 2, 2, 2, 2, 2, 2, 2, 2, 2, 2, 2, 2, 2, 2, 2, 2, 2, 2, 2, 2, 2, 2, 2, 2, 2, 2, 2, 2, 2, 2, 2, 2, 2, 2, 2, 2, 2, 2, 2, 2, 2, 2, 2, 2, 2, 2, 2, 2, 2, 2, 2, 2, 2, 2, 2, 2, 2, 2, 2, 2, 2, 2, 2, 2, 2, 2, 2, 2, 2, 2, 2, 2, 2, 2, 2, 2, 2, 2, 2, 2, 2, 2, 2, 2, 2, 2, 2, 2, 2, 2, 2, 2, 2, 2, 2, 2, 2, 2, 2, 2, 2, 2, 2, 2, 2, 2, 2, 2, 2, 2, 2, 2, 2, 2, 2, 2, 2, 2, 2, 2, 2, 2, 2, 2, 2, 2, 2, 2, 2, 2, 2, 2, 2, 2, 2, 2, 2, 2, 2, 2, 2, 2, 2, 2, 2, 2, 2, 2, 2, 2, 2, 2, 2, 2, 2, 2, 2, 2, 2, 2, 2, 2, 2, 2, 2, 2, 2, 2, 2, 2, 2, 2, 2, 2, 2, 2, 2, 2, 2, 2, 2, 2, 2, 2, 2, 2, 2, 2, 2, 2, 2, 2, 2, 2, 2, 2, 2, 2, 2, 2, 2, 2, 2, 2, 2, 2, 2, 2, 2, 2, 2, 2, 2, 2, 2, 2, 2, 2, 2, 2, 2, 2, 2, 2, 2, 2, 2, 2, 2, 2, 2, 2, 2, 2, 2, 2, 2, 2, 2, 2, 2, 2, 2, 2, 2, 2, 2, 2, 2, 2, 2, 2, 2, 2, 2, 2, 2, 2, 2, 2, 2, 2, 2, 2, 2, 2, 2, 2, 2, 2, 2, 2, 2, 2, 2, 2, 2, 2, 2, 2, 2, 2, 2, 2, 2, 2, 2, 2, 2, 2, 2, 2, 2, 2, 2, 2, 3 ),
 ( 0.000000000000000000, 1.000000000000000000 ),
 ( 0.000000000000000000, 0.001811594202898550747, 0.003623188405797101493, 0.005434782608695652023, 0.007246376811594202987, 0.009057971014492753950, 0.01086956521739130405, 0.01268115942028985588, 0.01449275362318840597, 0.01630434782608695607, 0.01811594202898550790, 0.01992753623188405626, 0.02173913043478260809, 0.02355072463768115992, 0.02536231884057971175, 0.02717391304347826012, 0.02898550724637681195, 0.03079710144927536378, 0.03260869565217391214, 0.03442028985507246397, 0.03623188405797101580, 0.03804347826086956763, 0.03985507246376811252, 0.04166666666666666435, 0.04347826086956521618, 0.04528985507246376802, 0.04710144927536231985, 0.04891304347826087168, 0.05072463768115942351, 0.05253623188405796840, 0.05434782608695652023, 0.05615942028985507206, 0.05797101449275362389, 0.05978260869565217572, 0.06159420289855072755, 0.06340579710144927938, 0.06521739130434782428, 0.06702898550724638305, 0.06884057971014492794, 0.07065217391304347283, 0.07246376811594203160, 0.07427536231884057649, 0.07608695652173913526, 0.07789855072463768015, 0.07971014492753622505, 0.08152173913043478382, 0.08333333333333332871, 0.08514492753623188748, 0.08695652173913043237, 0.08876811594202899114, 0.09057971014492753603, 0.09239130434782608092, 0.09420289855072463969, 0.09601449275362318458, 0.09782608695652174335, 0.09963768115942028825, 0.1014492753623188470, 0.1032608695652173919, 0.1050724637681159368, 0.1068840579710144956, 0.1086956521739130405, 0.1105072463768115992, 0.1123188405797101441, 0.1141304347826086890, 0.1159420289855072478, 0.1177536231884057927, 0.1195652173913043514, 0.1213768115942028963, 0.1231884057971014551, 0.1250000000000000000, 0.1268115942028985588, 0.1286231884057970898, 0.1304347826086956486, 0.1322463768115942073, 0.1340579710144927661, 0.1358695652173912971, 0.1376811594202898559, 0.1394927536231884146, 0.1413043478260869457, 0.1431159420289855044, 0.1449275362318840632, 0.1467391304347826220, 0.1485507246376811530, 0.1503623188405797118, 0.1521739130434782705, 0.1539855072463768015, 0.1557971014492753603, 0.1576086956521739191, 0.1594202898550724501, 0.1612318840579710089, 0.1630434782608695676, 0.1648550724637681264, 0.1666666666666666574, 0.1684782608695652162, 0.1702898550724637750, 0.1721014492753623060, 0.1739130434782608647, 0.1757246376811594235, 0.1775362318840579823, 0.1793478260869565133, 0.1811594202898550721, 0.1829710144927536308, 0.1847826086956521618, 0.1865942028985507206, 0.1884057971014492794, 0.1902173913043478382, 0.1920289855072463692, 0.1938405797101449279, 0.1956521739130434867, 0.1974637681159420177, 0.1992753623188405765, 0.2010869565217391353, 0.2028985507246376940, 0.2047101449275362250, 0.2065217391304347838, 0.2083333333333333426, 0.2101449275362318736, 0.2119565217391304324, 0.2137681159420289911, 0.2155797101449275499, 0.2173913043478260809, 0.2192028985507246397, 0.2210144927536231985, 0.2228260869565217295, 0.2246376811594202882, 0.2264492753623188470, 0.2282608695652173780, 0.2300724637681159368, 0.2318840579710144956, 0.2336956521739130543, 0.2355072463768115854, 0.2373188405797101441, 0.2391304347826087029, 0.2409420289855072339, 0.2427536231884057927, 0.2445652173913043514, 0.2463768115942029102, 0.2481884057971014412, 0.2500000000000000000, 0.2518115942028985588, 0.2536231884057971175, 0.2554347826086956763, 0.2572463768115941796, 0.2590579710144927383, 0.2608695652173912971, 0.2626811594202898559, 0.2644927536231884146, 0.2663043478260869734, 0.2681159420289855322, 0.2699275362318840354, 0.2717391304347825942, 0.2735507246376811530, 0.2753623188405797118, 0.2771739130434782705, 0.2789855072463768293, 0.2807971014492753881, 0.2826086956521738913, 0.2844202898550724501, 0.2862318840579710089, 0.2880434782608695676, 0.2898550724637681264, 0.2916666666666666852, 0.2934782608695652439, 0.2952898550724637472, 0.2971014492753623060, 0.2989130434782608647, 0.3007246376811594235, 0.3025362318840579823, 0.3043478260869565410, 0.3061594202898550998, 0.3079710144927536031, 0.3097826086956521618, 0.3115942028985507206, 0.3134057971014492794, 0.3152173913043478382, 0.3170289855072463969, 0.3188405797101449002, 0.3206521739130434590, 0.3224637681159420177, 0.3242753623188405765, 0.3260869565217391353, 0.3278985507246376940, 0.3297101449275362528, 0.3315217391304347561, 0.3333333333333333148, 0.3351449275362318736, 0.3369565217391304324, 0.3387681159420289911, 0.3405797101449275499, 0.3423913043478261087, 0.3442028985507246119, 0.3460144927536231707, 0.3478260869565217295, 0.3496376811594202882, 0.3514492753623188470, 0.3532608695652174058, 0.3550724637681159646, 0.3568840579710144678, 0.3586956521739130266, 0.3605072463768115854, 0.3623188405797101441, 0.3641304347826087029, 0.3659420289855072617, 0.3677536231884058204, 0.3695652173913043237, 0.3713768115942028825, 0.3731884057971014412, 0.3750000000000000000, 0.3768115942028985588, 0.3786231884057971175, 0.3804347826086956763, 0.3822463768115941796, 0.3840579710144927383, 0.3858695652173912971, 0.3876811594202898559, 0.3894927536231884146, 0.3913043478260869734, 0.3931159420289855322, 0.3949275362318840354, 0.3967391304347825942, 0.3985507246376811530, 0.4003623188405797118, 0.4021739130434782705, 0.4039855072463768293, 0.4057971014492753881, 0.4076086956521738913, 0.4094202898550724501, 0.4112318840579710089, 0.4130434782608695676, 0.4148550724637681264, 0.4166666666666666852, 0.4184782608695652439, 0.4202898550724637472, 0.4221014492753623060, 0.4239130434782608647, 0.4257246376811594235, 0.4275362318840579823, 0.4293478260869565410, 0.4311594202898550998, 0.4329710144927536031, 0.4347826086956521618, 0.4365942028985507206, 0.4384057971014492794, 0.4402173913043478382, 0.4420289855072463969, 0.4438405797101449002, 0.4456521739130434590, 0.4474637681159420177, 0.4492753623188405765, 0.4510869565217391353, 0.4528985507246376940, 0.4547101449275362528, 0.4565217391304347561, 0.4583333333333333148, 0.4601449275362318736, 0.4619565217391304324, 0.4637681159420289911, 0.4655797101449275499, 0.4673913043478261087, 0.4692028985507246119, 0.4710144927536231707, 0.4728260869565217295, 0.4746376811594202882, 0.4764492753623188470, 0.4782608695652174058, 0.4800724637681159646, 0.4818840579710144678, 0.4836956521739130266, 0.4855072463768115854, 0.4873188405797101441, 0.4891304347826087029, 0.4909420289855072617, 0.4927536231884058204, 0.4945652173913043237, 0.4963768115942028825, 0.4981884057971014412, 0.5000000000000000000, 0.5018115942028985588, 0.5036231884057971175, 0.5054347826086956763, 0.5072463768115942351, 0.5090579710144927938, 0.5108695652173913526, 0.5126811594202898004, 0.5144927536231883591, 0.5163043478260869179, 0.5181159420289854767, 0.5199275362318840354, 0.5217391304347825942, 0.5235507246376811530, 0.5253623188405797118, 0.5271739130434782705, 0.5289855072463768293, 0.5307971014492753881, 0.5326086956521739468, 0.5344202898550725056, 0.5362318840579710644, 0.5380434782608695121, 0.5398550724637680709, 0.5416666666666666297, 0.5434782608695651884, 0.5452898550724637472, 0.5471014492753623060, 0.5489130434782608647, 0.5507246376811594235, 0.5525362318840579823, 0.5543478260869565410, 0.5561594202898550998, 0.5579710144927536586, 0.5597826086956522174, 0.5615942028985507761, 0.5634057971014492239, 0.5652173913043477826, 0.5670289855072463414, 0.5688405797101449002, 0.5706521739130434590, 0.5724637681159420177, 0.5742753623188405765, 0.5760869565217391353, 0.5778985507246376940, 0.5797101449275362528, 0.5815217391304348116, 0.5833333333333333703, 0.5851449275362319291, 0.5869565217391304879, 0.5887681159420289356, 0.5905797101449274944, 0.5923913043478260532, 0.5942028985507246119, 0.5960144927536231707, 0.5978260869565217295, 0.5996376811594202882, 0.6014492753623188470, 0.6032608695652174058, 0.6050724637681159646, 0.6068840579710145233, 0.6086956521739130821, 0.6105072463768116409, 0.6123188405797101996, 0.6141304347826086474, 0.6159420289855072062, 0.6177536231884057649, 0.6195652173913043237, 0.6213768115942028825, 0.6231884057971014412, 0.6250000000000000000, 0.6268115942028985588, 0.6286231884057971175, 0.6304347826086956763, 0.6322463768115942351, 0.6340579710144927938, 0.6358695652173913526, 0.6376811594202898004, 0.6394927536231883591, 0.6413043478260869179, 0.6431159420289854767, 0.6449275362318840354, 0.6467391304347825942, 0.6485507246376811530, 0.6503623188405797118, 0.6521739130434782705, 0.6539855072463768293, 0.6557971014492753881, 0.6576086956521739468, 0.6594202898550725056, 0.6612318840579710644, 0.6630434782608695121, 0.6648550724637680709, 0.6666666666666666297, 0.6684782608695651884, 0.6702898550724637472, 0.6721014492753623060, 0.6739130434782608647, 0.6757246376811594235, 0.6775362318840579823, 0.6793478260869565410, 0.6811594202898550998, 0.6829710144927536586, 0.6847826086956522174, 0.6865942028985507761, 0.6884057971014492239, 0.6902173913043477826, 0.6920289855072463414, 0.6938405797101449002, 0.6956521739130434590, 0.6974637681159420177, 0.6992753623188405765, 0.7010869565217391353, 0.7028985507246376940, 0.7047101449275362528, 0.7065217391304348116, 0.7083333333333333703, 0.7101449275362319291, 0.7119565217391304879, 0.7137681159420289356, 0.7155797101449274944, 0.7173913043478260532, 0.7192028985507246119, 0.7210144927536231707, 0.7228260869565217295, 0.7246376811594202882, 0.7264492753623188470, 0.7282608695652174058, 0.7300724637681159646, 0.7318840579710145233, 0.7336956521739130821, 0.7355072463768116409, 0.7373188405797101996, 0.7391304347826086474, 0.7409420289855072062, 0.7427536231884057649, 0.7445652173913043237, 0.7463768115942028825, 0.7481884057971014412, 0.7500000000000000000, 0.7518115942028985588, 0.7536231884057971175, 0.7554347826086956763, 0.7572463768115942351, 0.7590579710144927938, 0.7608695652173913526, 0.7626811594202898004, 0.7644927536231883591, 0.7663043478260869179, 0.7681159420289854767, 0.7699275362318840354, 0.7717391304347825942, 0.7735507246376811530, 0.7753623188405797118, 0.7771739130434782705, 0.7789855072463768293, 0.7807971014492753881, 0.7826086956521739468, 0.7844202898550725056, 0.7862318840579710644, 0.7880434782608695121, 0.7898550724637680709, 0.7916666666666666297, 0.7934782608695651884, 0.7952898550724637472, 0.7971014492753623060, 0.7989130434782608647, 0.8007246376811594235, 0.8025362318840579823, 0.8043478260869565410, 0.8061594202898550998, 0.8079710144927536586, 0.8097826086956522174, 0.8115942028985507761, 0.8134057971014492239, 0.8152173913043477826, 0.8170289855072463414, 0.8188405797101449002, 0.8206521739130434590, 0.8224637681159420177, 0.8242753623188405765, 0.8260869565217391353, 0.8278985507246376940, 0.8297101449275362528, 0.8315217391304348116, 0.8333333333333333703, 0.8351449275362319291, 0.8369565217391304879, 0.8387681159420289356, 0.8405797101449274944, 0.8423913043478260532, 0.8442028985507246119, 0.8460144927536231707, 0.8478260869565217295, 0.8496376811594202882, 0.8514492753623188470, 0.8532608695652174058, 0.8550724637681159646, 0.8568840579710145233, 0.8586956521739130821, 0.8605072463768116409, 0.8623188405797101996, 0.8641304347826086474, 0.8659420289855072062, 0.8677536231884057649, 0.8695652173913043237, 0.8713768115942028825, 0.8731884057971014412, 0.8750000000000000000, 0.8768115942028985588, 0.8786231884057971175, 0.8804347826086956763, 0.8822463768115942351, 0.8840579710144927938, 0.8858695652173913526, 0.8876811594202898004, 0.8894927536231883591, 0.8913043478260869179, 0.8931159420289854767, 0.8949275362318840354, 0.8967391304347825942, 0.8985507246376811530, 0.9003623188405797118, 0.9021739130434782705, 0.9039855072463768293, 0.9057971014492753881, 0.9076086956521739468, 0.9094202898550725056, 0.9112318840579710644, 0.9130434782608695121, 0.9148550724637680709, 0.9166666666666666297, 0.9184782608695651884, 0.9202898550724637472, 0.9221014492753623060, 0.9239130434782608647, 0.9257246376811594235, 0.9275362318840579823, 0.9293478260869565410, 0.9311594202898550998, 0.9329710144927536586, 0.9347826086956522174, 0.9365942028985507761, 0.9384057971014492239, 0.9402173913043477826, 0.9420289855072463414, 0.9438405797101449002, 0.9456521739130434590, 0.9474637681159420177, 0.9492753623188405765, 0.9510869565217391353, 0.9528985507246376940, 0.9547101449275362528, 0.9565217391304348116, 0.9583333333333333703, 0.9601449275362319291, 0.9619565217391304879, 0.9637681159420289356, 0.9655797101449274944, 0.9673913043478260532, 0.9692028985507246119, 0.9710144927536231707, 0.9728260869565217295, 0.9746376811594202882, 0.9764492753623188470, 0.9782608695652174058, 0.9800724637681159646, 0.9818840579710145233, 0.9826096977668656862 ),
 .UNSPECIFIED. ) 
 GEOMETRIC_REPRESENTATION_ITEM ( )  RATIONAL_B_SPLINE_SURFACE ( (
 ( 1.000000000000000000, 0.9659258262890683122, 1.000000000000000000, 0.9659258262890683122, 1.000000000000000000, 0.9659258262890683122, 1.000000000000000000, 0.9659258262890683122, 1.000000000000000000, 0.9659258262890683122, 1.000000000000000000, 0.9659258262890683122, 1.000000000000000000, 0.9659258262890683122, 1.000000000000000000, 0.9659258262890683122, 1.000000000000000000, 0.9659258262890683122, 1.000000000000000000, 0.9659258262890683122, 1.000000000000000000, 0.9659258262890683122, 1.000000000000000000, 0.9659258262890683122, 1.000000000000000000, 0.9659258262890683122, 1.000000000000000000, 0.9659258262890683122, 1.000000000000000000, 0.9659258262890683122, 1.000000000000000000, 0.9659258262890683122, 1.000000000000000000, 0.9659258262890683122, 1.000000000000000000, 0.9659258262890683122, 1.000000000000000000, 0.9659258262890683122, 1.000000000000000000, 0.9659258262890683122, 1.000000000000000000, 0.9659258262890683122, 1.000000000000000000, 0.9659258262890683122, 1.000000000000000000, 0.9659258262890683122, 1.000000000000000000, 0.9659258262890683122, 1.000000000000000000, 0.9659258262890683122, 1.000000000000000000, 0.9659258262890683122, 1.000000000000000000, 0.9659258262890683122, 1.000000000000000000, 0.9659258262890683122, 1.000000000000000000, 0.9659258262890683122, 1.000000000000000000, 0.9659258262890683122, 1.000000000000000000, 0.9659258262890683122, 1.000000000000000000, 0.9659258262890683122, 1.000000000000000000, 0.9659258262890683122, 1.000000000000000000, 0.9659258262890683122, 1.000000000000000000, 0.9659258262890683122, 1.000000000000000000, 0.9659258262890683122, 1.000000000000000000, 0.9659258262890683122, 1.000000000000000000, 0.9659258262890683122, 1.000000000000000000, 0.9659258262890683122, 1.000000000000000000, 0.9659258262890683122, 1.000000000000000000, 0.9659258262890683122, 1.000000000000000000, 0.9659258262890683122, 1.000000000000000000, 0.9659258262890683122, 1.000000000000000000, 0.9659258262890683122, 1.000000000000000000, 0.9659258262890683122, 1.000000000000000000, 0.9659258262890683122, 1.000000000000000000, 0.9659258262890683122, 1.000000000000000000, 0.9659258262890683122, 1.000000000000000000, 0.9659258262890683122, 1.000000000000000000, 0.9659258262890683122, 1.000000000000000000, 0.9659258262890683122, 1.000000000000000000, 0.9659258262890683122, 1.000000000000000000, 0.9659258262890683122, 1.000000000000000000, 0.9659258262890683122, 1.000000000000000000, 0.9659258262890683122, 1.000000000000000000, 0.9659258262890683122, 1.000000000000000000, 0.9659258262890683122, 1.000000000000000000, 0.9659258262890683122, 1.000000000000000000, 0.9659258262890683122, 1.000000000000000000, 0.9659258262890683122, 1.000000000000000000, 0.9659258262890683122, 1.000000000000000000, 0.9659258262890683122, 1.000000000000000000, 0.9659258262890683122, 1.000000000000000000, 0.9659258262890683122, 1.000000000000000000, 0.9659258262890683122, 1.000000000000000000, 0.9659258262890683122, 1.000000000000000000, 0.9659258262890683122, 1.000000000000000000, 0.9659258262890683122, 1.000000000000000000, 0.9659258262890683122, 1.000000000000000000, 0.9659258262890683122, 1.000000000000000000, 0.9659258262890683122, 1.000000000000000000, 0.9659258262890683122, 1.000000000000000000, 0.9659258262890683122, 1.000000000000000000, 0.9659258262890683122, 1.000000000000000000, 0.9659258262890683122, 1.000000000000000000, 0.9659258262890683122, 1.000000000000000000, 0.9659258262890683122, 1.000000000000000000, 0.9659258262890683122, 1.000000000000000000, 0.9659258262890683122, 1.000000000000000000, 0.9659258262890683122, 1.000000000000000000, 0.9659258262890683122, 1.000000000000000000, 0.9659258262890683122, 1.000000000000000000, 0.9659258262890683122, 1.000000000000000000, 0.9659258262890683122, 1.000000000000000000, 0.9659258262890683122, 1.000000000000000000, 0.9659258262890683122, 1.000000000000000000, 0.9659258262890683122, 1.000000000000000000, 0.9659258262890683122, 1.000000000000000000, 0.9659258262890683122, 1.000000000000000000, 0.9659258262890683122, 1.000000000000000000, 0.9659258262890683122, 1.000000000000000000, 0.9659258262890683122, 1.000000000000000000, 0.9659258262890683122, 1.000000000000000000, 0.9659258262890683122, 1.000000000000000000, 0.9659258262890683122, 1.000000000000000000, 0.9659258262890683122, 1.000000000000000000, 0.9659258262890683122, 1.000000000000000000, 0.9659258262890683122, 1.000000000000000000, 0.9659258262890683122, 1.000000000000000000, 0.9659258262890683122, 1.000000000000000000, 0.9659258262890683122, 1.000000000000000000, 0.9659258262890683122, 1.000000000000000000, 0.9659258262890683122, 1.000000000000000000, 0.9659258262890683122, 1.000000000000000000, 0.9659258262890683122, 1.000000000000000000, 0.9659258262890683122, 1.000000000000000000, 0.9659258262890683122, 1.000000000000000000, 0.9659258262890683122, 1.000000000000000000, 0.9659258262890683122, 1.000000000000000000, 0.9659258262890683122, 1.000000000000000000, 0.9659258262890683122, 1.000000000000000000, 0.9659258262890683122, 1.000000000000000000, 0.9659258262890683122, 1.000000000000000000, 0.9659258262890683122, 1.000000000000000000, 0.9659258262890683122, 1.000000000000000000, 0.9659258262890683122, 1.000000000000000000, 0.9659258262890683122, 1.000000000000000000, 0.9659258262890683122, 1.000000000000000000, 0.9659258262890683122, 1.000000000000000000, 0.9659258262890683122, 1.000000000000000000, 0.9659258262890683122, 1.000000000000000000, 0.9659258262890683122, 1.000000000000000000, 0.9659258262890683122, 1.000000000000000000, 0.9659258262890683122, 1.000000000000000000, 0.9659258262890683122, 1.000000000000000000, 0.9659258262890683122, 1.000000000000000000, 0.9659258262890683122, 1.000000000000000000, 0.9659258262890683122, 1.000000000000000000, 0.9659258262890683122, 1.000000000000000000, 0.9659258262890683122, 1.000000000000000000, 0.9659258262890683122, 1.000000000000000000, 0.9659258262890683122, 1.000000000000000000, 0.9659258262890683122, 1.000000000000000000, 0.9659258262890683122, 1.000000000000000000, 0.9659258262890683122, 1.000000000000000000, 0.9659258262890683122, 1.000000000000000000, 0.9659258262890683122, 1.000000000000000000, 0.9659258262890683122, 1.000000000000000000, 0.9659258262890683122, 1.000000000000000000, 0.9659258262890683122, 1.000000000000000000, 0.9659258262890683122, 1.000000000000000000, 0.9659258262890683122, 1.000000000000000000, 0.9659258262890683122, 1.000000000000000000, 0.9659258262890683122, 1.000000000000000000, 0.9659258262890683122, 1.000000000000000000, 0.9659258262890683122, 1.000000000000000000, 0.9659258262890683122, 1.000000000000000000, 0.9659258262890683122, 1.000000000000000000, 0.9659258262890683122, 1.000000000000000000, 0.9659258262890683122, 1.000000000000000000, 0.9659258262890683122, 1.000000000000000000, 0.9659258262890683122, 1.000000000000000000, 0.9659258262890683122, 1.000000000000000000, 0.9659258262890683122, 1.000000000000000000, 0.9659258262890683122, 1.000000000000000000, 0.9659258262890683122, 1.000000000000000000, 0.9659258262890683122, 1.000000000000000000, 0.9659258262890683122, 1.000000000000000000, 0.9659258262890683122, 1.000000000000000000, 0.9659258262890683122, 1.000000000000000000, 0.9659258262890683122, 1.000000000000000000, 0.9659258262890683122, 1.000000000000000000, 0.9659258262890683122, 1.000000000000000000, 0.9659258262890683122, 1.000000000000000000, 0.9659258262890683122, 1.000000000000000000, 0.9659258262890683122, 1.000000000000000000, 0.9659258262890683122, 1.000000000000000000, 0.9659258262890683122, 1.000000000000000000, 0.9659258262890683122, 1.000000000000000000, 0.9659258262890683122, 1.000000000000000000, 0.9659258262890683122, 1.000000000000000000, 0.9659258262890683122, 1.000000000000000000, 0.9659258262890683122, 1.000000000000000000, 0.9659258262890683122, 1.000000000000000000, 0.9659258262890683122, 1.000000000000000000, 0.9659258262890683122, 1.000000000000000000, 0.9659258262890683122, 1.000000000000000000, 0.9659258262890683122, 1.000000000000000000, 0.9659258262890683122, 1.000000000000000000, 0.9659258262890683122, 1.000000000000000000, 0.9659258262890683122, 1.000000000000000000, 0.9659258262890683122, 1.000000000000000000, 0.9659258262890683122, 1.000000000000000000, 0.9659258262890683122, 1.000000000000000000, 0.9659258262890683122, 1.000000000000000000, 0.9659258262890683122, 1.000000000000000000, 0.9659258262890683122, 1.000000000000000000, 0.9659258262890683122, 1.000000000000000000, 0.9659258262890683122, 1.000000000000000000, 0.9659258262890683122, 1.000000000000000000, 0.9659258262890683122, 1.000000000000000000, 0.9659258262890683122, 1.000000000000000000, 0.9659258262890683122, 1.000000000000000000, 0.9659258262890683122, 1.000000000000000000, 0.9659258262890683122, 1.000000000000000000, 0.9659258262890683122, 1.000000000000000000, 0.9659258262890683122, 1.000000000000000000, 0.9659258262890683122, 1.000000000000000000, 0.9659258262890683122, 1.000000000000000000, 0.9659258262890683122, 1.000000000000000000, 0.9659258262890683122, 1.000000000000000000, 0.9659258262890683122, 1.000000000000000000, 0.9659258262890683122, 1.000000000000000000, 0.9659258262890683122, 1.000000000000000000, 0.9659258262890683122, 1.000000000000000000, 0.9659258262890683122, 1.000000000000000000, 0.9659258262890683122, 1.000000000000000000, 0.9659258262890683122, 1.000000000000000000, 0.9659258262890683122, 1.000000000000000000, 0.9659258262890683122, 1.000000000000000000, 0.9659258262890683122, 1.000000000000000000, 0.9659258262890683122, 1.000000000000000000, 0.9659258262890683122, 1.000000000000000000, 0.9659258262890683122, 1.000000000000000000, 0.9659258262890683122, 1.000000000000000000, 0.9659258262890683122, 1.000000000000000000, 0.9659258262890683122, 1.000000000000000000, 0.9659258262890683122, 1.000000000000000000, 0.9659258262890683122, 1.000000000000000000, 0.9659258262890683122, 1.000000000000000000, 0.9659258262890683122, 1.000000000000000000, 0.9659258262890683122, 1.000000000000000000, 0.9659258262890683122, 1.000000000000000000, 0.9659258262890683122, 1.000000000000000000, 0.9659258262890683122, 1.000000000000000000, 0.9659258262890683122, 1.000000000000000000, 0.9659258262890683122, 1.000000000000000000, 0.9659258262890683122, 1.000000000000000000, 0.9659258262890683122, 1.000000000000000000, 0.9659258262890683122, 1.000000000000000000, 0.9659258262890683122, 1.000000000000000000, 0.9659258262890683122, 1.000000000000000000, 0.9659258262890683122, 1.000000000000000000, 0.9659258262890683122, 1.000000000000000000, 0.9659258262890683122, 1.000000000000000000, 0.9659258262890683122, 1.000000000000000000, 0.9659258262890683122, 1.000000000000000000, 0.9659258262890683122, 1.000000000000000000, 0.9659258262890683122, 1.000000000000000000, 0.9659258262890683122, 1.000000000000000000, 0.9659258262890683122, 1.000000000000000000, 0.9659258262890683122, 1.000000000000000000, 0.9659258262890683122, 1.000000000000000000, 0.9659258262890683122, 1.000000000000000000, 0.9659258262890683122, 1.000000000000000000, 0.9659258262890683122, 1.000000000000000000, 0.9659258262890683122, 1.000000000000000000, 0.9659258262890683122, 1.000000000000000000, 0.9659258262890683122, 1.000000000000000000, 0.9659258262890683122, 1.000000000000000000, 0.9659258262890683122, 1.000000000000000000, 0.9659258262890683122, 1.000000000000000000, 0.9659258262890683122, 1.000000000000000000, 0.9659258262890683122, 1.000000000000000000, 0.9659258262890683122, 1.000000000000000000, 0.9659258262890683122, 1.000000000000000000, 0.9659258262890683122, 1.000000000000000000, 0.9659258262890683122, 1.000000000000000000, 0.9659258262890683122, 1.000000000000000000, 0.9659258262890683122, 1.000000000000000000, 0.9659258262890683122, 1.000000000000000000, 0.9659258262890683122, 1.000000000000000000, 0.9659258262890683122, 1.000000000000000000, 0.9659258262890683122, 1.000000000000000000, 0.9659258262890683122, 1.000000000000000000, 0.9659258262890683122, 1.000000000000000000, 0.9659258262890683122, 1.000000000000000000, 0.9659258262890683122, 1.000000000000000000, 0.9659258262890683122, 1.000000000000000000, 0.9659258262890683122, 1.000000000000000000, 0.9659258262890683122, 1.000000000000000000, 0.9659258262890683122, 1.000000000000000000, 0.9659258262890683122, 1.000000000000000000, 0.9659258262890683122, 1.000000000000000000, 0.9659258262890683122, 1.000000000000000000, 0.9659258262890683122, 1.000000000000000000, 0.9659258262890683122, 1.000000000000000000, 0.9659258262890683122, 1.000000000000000000, 0.9659258262890683122, 1.000000000000000000, 0.9659258262890683122, 1.000000000000000000, 0.9659258262890683122, 1.000000000000000000, 0.9659258262890683122, 1.000000000000000000, 0.9659258262890683122, 1.000000000000000000, 0.9659258262890683122, 1.000000000000000000, 0.9659258262890683122, 1.000000000000000000, 0.9659258262890683122, 1.000000000000000000, 0.9659258262890683122, 1.000000000000000000, 0.9659258262890683122, 1.000000000000000000, 0.9659258262890683122, 1.000000000000000000, 0.9659258262890683122, 1.000000000000000000, 0.9659258262890683122, 1.000000000000000000, 0.9659258262890683122, 1.000000000000000000, 0.9659258262890683122, 1.000000000000000000, 0.9659258262890683122, 1.000000000000000000, 0.9659258262890683122, 1.000000000000000000, 0.9659258262890683122, 1.000000000000000000, 0.9659258262890683122, 1.000000000000000000, 0.9659258262890683122, 1.000000000000000000, 0.9659258262890683122, 1.000000000000000000, 0.9659258262890683122, 1.000000000000000000, 0.9659258262890683122, 1.000000000000000000, 0.9659258262890683122, 1.000000000000000000, 0.9659258262890683122, 1.000000000000000000, 0.9659258262890683122, 1.000000000000000000, 0.9659258262890683122, 1.000000000000000000, 0.9659258262890683122, 1.000000000000000000, 0.9659258262890683122, 1.000000000000000000, 0.9659258262890683122, 1.000000000000000000, 0.9659258262890683122, 1.000000000000000000, 0.9659258262890683122, 1.000000000000000000, 0.9659258262890683122, 1.000000000000000000, 0.9659258262890683122, 1.000000000000000000, 0.9659258262890683122, 1.000000000000000000, 0.9659258262890683122, 1.000000000000000000, 0.9659258262890683122, 1.000000000000000000, 0.9659258262890683122, 1.000000000000000000, 0.9659258262890683122, 1.000000000000000000, 0.9659258262890683122, 1.000000000000000000, 0.9659258262890683122, 1.000000000000000000, 0.9659258262890683122, 1.000000000000000000, 0.9659258262890683122, 1.000000000000000000, 0.9659258262890683122, 1.000000000000000000, 0.9659258262890683122, 1.000000000000000000, 0.9659258262890683122, 1.000000000000000000, 0.9659258262890683122, 1.000000000000000000, 0.9659258262890683122, 1.000000000000000000, 0.9659258262890683122, 1.000000000000000000, 0.9659258262890683122, 1.000000000000000000, 0.9659258262890683122, 1.000000000000000000, 0.9659258262890683122, 1.000000000000000000, 0.9659258262890683122, 1.000000000000000000, 0.9659258262890683122, 1.000000000000000000, 0.9659258262890683122, 1.000000000000000000, 0.9659258262890683122, 1.000000000000000000, 0.9659258262890683122, 1.000000000000000000, 0.9659258262890683122, 1.000000000000000000, 0.9659258262890683122, 1.000000000000000000, 0.9659258262890683122, 1.000000000000000000, 0.9659258262890683122, 1.000000000000000000, 0.9659258262890683122, 1.000000000000000000, 0.9659258262890683122, 1.000000000000000000, 0.9659258262890683122, 1.000000000000000000, 0.9659258262890683122, 1.000000000000000000, 0.9659258262890683122, 1.000000000000000000, 0.9659258262890683122, 1.000000000000000000, 0.9659258262890683122, 1.000000000000000000, 0.9659258262890683122, 1.000000000000000000, 0.9659258262890683122, 1.000000000000000000, 0.9659258262890683122, 1.000000000000000000, 0.9659258262890683122, 1.000000000000000000, 0.9659258262890683122, 1.000000000000000000, 0.9659258262890683122, 1.000000000000000000, 0.9659258262890683122, 1.000000000000000000, 0.9659258262890683122, 1.000000000000000000, 0.9659258262890683122, 1.000000000000000000, 0.9659258262890683122, 1.000000000000000000, 0.9659258262890683122, 1.000000000000000000, 0.9659258262890683122, 1.000000000000000000, 0.9659258262890683122, 1.000000000000000000, 0.9659258262890683122, 1.000000000000000000, 0.9659258262890683122, 1.000000000000000000, 0.9659258262890683122, 1.000000000000000000, 0.9659258262890683122, 1.000000000000000000, 0.9659258262890683122, 1.000000000000000000, 0.9659258262890683122, 1.000000000000000000, 0.9659258262890683122, 1.000000000000000000, 0.9659258262890683122, 1.000000000000000000, 0.9659258262890683122, 1.000000000000000000, 0.9659258262890683122, 1.000000000000000000, 0.9659258262890683122, 1.000000000000000000, 0.9659258262890683122, 1.000000000000000000, 0.9659258262890683122, 1.000000000000000000, 0.9659258262890683122, 1.000000000000000000, 0.9659258262890683122, 1.000000000000000000, 0.9659258262890683122, 1.000000000000000000, 0.9659258262890683122, 1.000000000000000000, 0.9659258262890683122, 1.000000000000000000, 0.9659258262890683122, 1.000000000000000000, 0.9659258262890683122, 1.000000000000000000, 0.9659258262890683122, 1.000000000000000000, 0.9659258262890683122, 1.000000000000000000, 0.9659258262890683122, 1.000000000000000000, 0.9659258262890683122, 1.000000000000000000, 0.9659258262890683122, 1.000000000000000000, 0.9659258262890683122, 1.000000000000000000, 0.9659258262890683122, 1.000000000000000000, 0.9659258262890683122, 1.000000000000000000, 0.9659258262890683122, 1.000000000000000000, 0.9659258262890683122, 1.000000000000000000, 0.9659258262890683122, 1.000000000000000000, 0.9659258262890683122, 1.000000000000000000, 0.9659258262890683122, 1.000000000000000000, 0.9659258262890683122, 1.000000000000000000, 0.9659258262890683122, 1.000000000000000000, 0.9659258262890683122, 1.000000000000000000, 0.9659258262890683122, 1.000000000000000000, 0.9659258262890683122, 1.000000000000000000, 0.9659258262890683122, 1.000000000000000000, 0.9659258262890683122, 1.000000000000000000, 0.9659258262890683122, 1.000000000000000000, 0.9659258262890683122, 1.000000000000000000, 0.9659258262890683122, 1.000000000000000000, 0.9659258262890683122, 1.000000000000000000, 0.9659258262890683122, 1.000000000000000000, 0.9659258262890683122, 1.000000000000000000, 0.9659258262890683122, 1.000000000000000000, 0.9659258262890683122, 1.000000000000000000, 0.9659258262890683122, 1.000000000000000000, 0.9659258262890683122, 1.000000000000000000, 0.9659258262890683122, 1.000000000000000000, 0.9659258262890683122, 1.000000000000000000, 0.9659258262890683122, 1.000000000000000000, 0.9659258262890683122, 1.000000000000000000, 0.9659258262890683122, 1.000000000000000000, 0.9659258262890683122, 1.000000000000000000, 0.9659258262890683122, 1.000000000000000000, 0.9659258262890683122, 1.000000000000000000, 0.9659258262890683122, 1.000000000000000000, 0.9659258262890683122, 1.000000000000000000, 0.9659258262890683122, 1.000000000000000000, 0.9659258262890683122, 1.000000000000000000, 0.9659258262890683122, 1.000000000000000000, 0.9659258262890683122, 1.000000000000000000, 0.9659258262890683122, 1.000000000000000000, 0.9659258262890683122, 1.000000000000000000, 0.9659258262890683122, 1.000000000000000000, 0.9659258262890683122, 1.000000000000000000, 0.9659258262890683122, 1.000000000000000000, 0.9659258262890683122, 1.000000000000000000, 0.9659258262890683122, 1.000000000000000000, 0.9659258262890683122, 1.000000000000000000, 0.9659258262890683122, 1.000000000000000000, 0.9659258262890683122, 1.000000000000000000, 0.9659258262890683122, 1.000000000000000000, 0.9659258262890683122, 1.000000000000000000, 0.9659258262890683122, 1.000000000000000000, 0.9659258262890683122, 1.000000000000000000, 0.9659258262890683122, 1.000000000000000000, 0.9659258262890683122, 1.000000000000000000, 0.9659258262890683122, 1.000000000000000000, 0.9659258262890683122, 1.000000000000000000, 0.9659258262890683122, 1.000000000000000000, 0.9659258262890683122, 1.000000000000000000, 0.9659258262890683122, 1.000000000000000000, 0.9659258262890683122, 1.000000000000000000, 0.9659258262890683122, 1.000000000000000000, 0.9659258262890683122, 1.000000000000000000, 0.9659258262890683122, 1.000000000000000000, 0.9659258262890683122, 1.000000000000000000, 0.9659258262890683122, 1.000000000000000000, 0.9659258262890683122, 1.000000000000000000, 0.9659258262890683122, 1.000000000000000000, 0.9659258262890683122, 1.000000000000000000, 0.9659258262890683122, 1.000000000000000000, 0.9659258262890683122, 1.000000000000000000, 0.9659258262890683122, 1.000000000000000000, 0.9659258262890683122, 1.000000000000000000, 0.9659258262890683122, 1.000000000000000000, 0.9659258262890683122, 1.000000000000000000, 0.9659258262890683122, 1.000000000000000000, 0.9659258262890683122, 1.000000000000000000, 0.9659258262890683122, 1.000000000000000000, 0.9659258262890683122, 1.000000000000000000, 0.9659258262890683122, 1.000000000000000000, 0.9659258262890683122, 1.000000000000000000, 0.9659258262890683122, 1.000000000000000000, 0.9659258262890683122, 1.000000000000000000, 0.9659258262890683122, 1.000000000000000000, 0.9659258262890683122, 1.000000000000000000, 0.9659258262890683122, 1.000000000000000000, 0.9659258262890683122, 1.000000000000000000, 0.9659258262890683122, 1.000000000000000000, 0.9659258262890683122, 1.000000000000000000, 0.9659258262890683122, 1.000000000000000000, 0.9659258262890683122, 1.000000000000000000, 0.9659258262890683122, 1.000000000000000000, 0.9659258262890683122, 1.000000000000000000, 0.9659258262890683122, 1.000000000000000000, 0.9659258262890683122, 1.000000000000000000, 0.9659258262890683122, 1.000000000000000000, 0.9659258262890683122, 1.000000000000000000, 0.9659258262890683122, 1.000000000000000000, 0.9659258262890683122, 1.000000000000000000, 0.9659258262890683122, 1.000000000000000000, 0.9659258262890683122, 1.000000000000000000, 0.9659258262890683122, 1.000000000000000000, 0.9659258262890683122, 1.000000000000000000, 0.9659258262890683122, 1.000000000000000000, 0.9659258262890683122, 1.000000000000000000, 0.9659258262890683122, 1.000000000000000000, 0.9659258262890683122, 1.000000000000000000, 0.9659258262890683122, 1.000000000000000000, 0.9659258262890683122, 1.000000000000000000, 0.9659258262890683122, 1.000000000000000000, 0.9659258262890683122, 1.000000000000000000, 0.9659258262890683122, 1.000000000000000000, 0.9659258262890683122, 1.000000000000000000, 0.9659258262890683122, 1.000000000000000000, 0.9659258262890683122, 1.000000000000000000, 0.9659258262890683122, 1.000000000000000000, 0.9659258262890683122, 1.000000000000000000, 0.9659258262890683122, 1.000000000000000000, 0.9659258262890683122, 1.000000000000000000, 0.9659258262890683122, 1.000000000000000000, 0.9659258262890683122, 1.000000000000000000, 0.9659258262890683122, 1.000000000000000000, 0.9659258262890683122, 1.000000000000000000, 0.9659258262890683122, 1.000000000000000000, 0.9659258262890683122, 1.000000000000000000, 0.9659258262890683122, 1.000000000000000000, 0.9659258262890683122, 1.000000000000000000, 0.9659258262890683122, 1.000000000000000000, 0.9659258262890683122, 1.000000000000000000, 0.9659258262890683122, 1.000000000000000000, 0.9659258262890683122, 1.000000000000000000, 0.9659258262890683122, 1.000000000000000000, 0.9659258262890683122, 1.000000000000000000, 0.9659258262890683122, 1.000000000000000000, 0.9659258262890683122, 1.000000000000000000, 0.9659258262890683122, 1.000000000000000000, 0.9659258262890683122, 1.000000000000000000, 0.9659258262890683122, 1.000000000000000000, 0.9659258262890683122, 1.000000000000000000, 0.9659258262890683122, 1.000000000000000000, 0.9659258262890683122, 1.000000000000000000, 0.9659258262890683122, 1.000000000000000000, 0.9659258262890683122, 1.000000000000000000, 0.9659258262890683122, 1.000000000000000000, 0.9659258262890683122, 1.000000000000000000, 0.9659258262890683122, 1.000000000000000000, 0.9659258262890683122, 1.000000000000000000, 0.9659258262890683122, 1.000000000000000000, 0.9659258262890683122, 1.000000000000000000, 0.9659258262890683122, 1.000000000000000000, 0.9659258262890683122, 1.000000000000000000, 0.9659258262890683122, 1.000000000000000000, 0.9659258262890683122, 1.000000000000000000, 0.9659258262890683122, 1.000000000000000000, 0.9659258262890683122, 1.000000000000000000, 0.9659258262890683122, 1.000000000000000000, 0.9659258262890683122, 1.000000000000000000, 0.9659258262890683122, 1.000000000000000000, 0.9863514817966205772, 0.9836368779841404564),
 ( 1.000000000000000000, 0.9659258262890683122, 1.000000000000000000, 0.9659258262890683122, 1.000000000000000000, 0.9659258262890683122, 1.000000000000000000, 0.9659258262890683122, 1.000000000000000000, 0.9659258262890683122, 1.000000000000000000, 0.9659258262890683122, 1.000000000000000000, 0.9659258262890683122, 1.000000000000000000, 0.9659258262890683122, 1.000000000000000000, 0.9659258262890683122, 1.000000000000000000, 0.9659258262890683122, 1.000000000000000000, 0.9659258262890683122, 1.000000000000000000, 0.9659258262890683122, 1.000000000000000000, 0.9659258262890683122, 1.000000000000000000, 0.9659258262890683122, 1.000000000000000000, 0.9659258262890683122, 1.000000000000000000, 0.9659258262890683122, 1.000000000000000000, 0.9659258262890683122, 1.000000000000000000, 0.9659258262890683122, 1.000000000000000000, 0.9659258262890683122, 1.000000000000000000, 0.9659258262890683122, 1.000000000000000000, 0.9659258262890683122, 1.000000000000000000, 0.9659258262890683122, 1.000000000000000000, 0.9659258262890683122, 1.000000000000000000, 0.9659258262890683122, 1.000000000000000000, 0.9659258262890683122, 1.000000000000000000, 0.9659258262890683122, 1.000000000000000000, 0.9659258262890683122, 1.000000000000000000, 0.9659258262890683122, 1.000000000000000000, 0.9659258262890683122, 1.000000000000000000, 0.9659258262890683122, 1.000000000000000000, 0.9659258262890683122, 1.000000000000000000, 0.9659258262890683122, 1.000000000000000000, 0.9659258262890683122, 1.000000000000000000, 0.9659258262890683122, 1.000000000000000000, 0.9659258262890683122, 1.000000000000000000, 0.9659258262890683122, 1.000000000000000000, 0.9659258262890683122, 1.000000000000000000, 0.9659258262890683122, 1.000000000000000000, 0.9659258262890683122, 1.000000000000000000, 0.9659258262890683122, 1.000000000000000000, 0.9659258262890683122, 1.000000000000000000, 0.9659258262890683122, 1.000000000000000000, 0.9659258262890683122, 1.000000000000000000, 0.9659258262890683122, 1.000000000000000000, 0.9659258262890683122, 1.000000000000000000, 0.9659258262890683122, 1.000000000000000000, 0.9659258262890683122, 1.000000000000000000, 0.9659258262890683122, 1.000000000000000000, 0.9659258262890683122, 1.000000000000000000, 0.9659258262890683122, 1.000000000000000000, 0.9659258262890683122, 1.000000000000000000, 0.9659258262890683122, 1.000000000000000000, 0.9659258262890683122, 1.000000000000000000, 0.9659258262890683122, 1.000000000000000000, 0.9659258262890683122, 1.000000000000000000, 0.9659258262890683122, 1.000000000000000000, 0.9659258262890683122, 1.000000000000000000, 0.9659258262890683122, 1.000000000000000000, 0.9659258262890683122, 1.000000000000000000, 0.9659258262890683122, 1.000000000000000000, 0.9659258262890683122, 1.000000000000000000, 0.9659258262890683122, 1.000000000000000000, 0.9659258262890683122, 1.000000000000000000, 0.9659258262890683122, 1.000000000000000000, 0.9659258262890683122, 1.000000000000000000, 0.9659258262890683122, 1.000000000000000000, 0.9659258262890683122, 1.000000000000000000, 0.9659258262890683122, 1.000000000000000000, 0.9659258262890683122, 1.000000000000000000, 0.9659258262890683122, 1.000000000000000000, 0.9659258262890683122, 1.000000000000000000, 0.9659258262890683122, 1.000000000000000000, 0.9659258262890683122, 1.000000000000000000, 0.9659258262890683122, 1.000000000000000000, 0.9659258262890683122, 1.000000000000000000, 0.9659258262890683122, 1.000000000000000000, 0.9659258262890683122, 1.000000000000000000, 0.9659258262890683122, 1.000000000000000000, 0.9659258262890683122, 1.000000000000000000, 0.9659258262890683122, 1.000000000000000000, 0.9659258262890683122, 1.000000000000000000, 0.9659258262890683122, 1.000000000000000000, 0.9659258262890683122, 1.000000000000000000, 0.9659258262890683122, 1.000000000000000000, 0.9659258262890683122, 1.000000000000000000, 0.9659258262890683122, 1.000000000000000000, 0.9659258262890683122, 1.000000000000000000, 0.9659258262890683122, 1.000000000000000000, 0.9659258262890683122, 1.000000000000000000, 0.9659258262890683122, 1.000000000000000000, 0.9659258262890683122, 1.000000000000000000, 0.9659258262890683122, 1.000000000000000000, 0.9659258262890683122, 1.000000000000000000, 0.9659258262890683122, 1.000000000000000000, 0.9659258262890683122, 1.000000000000000000, 0.9659258262890683122, 1.000000000000000000, 0.9659258262890683122, 1.000000000000000000, 0.9659258262890683122, 1.000000000000000000, 0.9659258262890683122, 1.000000000000000000, 0.9659258262890683122, 1.000000000000000000, 0.9659258262890683122, 1.000000000000000000, 0.9659258262890683122, 1.000000000000000000, 0.9659258262890683122, 1.000000000000000000, 0.9659258262890683122, 1.000000000000000000, 0.9659258262890683122, 1.000000000000000000, 0.9659258262890683122, 1.000000000000000000, 0.9659258262890683122, 1.000000000000000000, 0.9659258262890683122, 1.000000000000000000, 0.9659258262890683122, 1.000000000000000000, 0.9659258262890683122, 1.000000000000000000, 0.9659258262890683122, 1.000000000000000000, 0.9659258262890683122, 1.000000000000000000, 0.9659258262890683122, 1.000000000000000000, 0.9659258262890683122, 1.000000000000000000, 0.9659258262890683122, 1.000000000000000000, 0.9659258262890683122, 1.000000000000000000, 0.9659258262890683122, 1.000000000000000000, 0.9659258262890683122, 1.000000000000000000, 0.9659258262890683122, 1.000000000000000000, 0.9659258262890683122, 1.000000000000000000, 0.9659258262890683122, 1.000000000000000000, 0.9659258262890683122, 1.000000000000000000, 0.9659258262890683122, 1.000000000000000000, 0.9659258262890683122, 1.000000000000000000, 0.9659258262890683122, 1.000000000000000000, 0.9659258262890683122, 1.000000000000000000, 0.9659258262890683122, 1.000000000000000000, 0.9659258262890683122, 1.000000000000000000, 0.9659258262890683122, 1.000000000000000000, 0.9659258262890683122, 1.000000000000000000, 0.9659258262890683122, 1.000000000000000000, 0.9659258262890683122, 1.000000000000000000, 0.9659258262890683122, 1.000000000000000000, 0.9659258262890683122, 1.000000000000000000, 0.9659258262890683122, 1.000000000000000000, 0.9659258262890683122, 1.000000000000000000, 0.9659258262890683122, 1.000000000000000000, 0.9659258262890683122, 1.000000000000000000, 0.9659258262890683122, 1.000000000000000000, 0.9659258262890683122, 1.000000000000000000, 0.9659258262890683122, 1.000000000000000000, 0.9659258262890683122, 1.000000000000000000, 0.9659258262890683122, 1.000000000000000000, 0.9659258262890683122, 1.000000000000000000, 0.9659258262890683122, 1.000000000000000000, 0.9659258262890683122, 1.000000000000000000, 0.9659258262890683122, 1.000000000000000000, 0.9659258262890683122, 1.000000000000000000, 0.9659258262890683122, 1.000000000000000000, 0.9659258262890683122, 1.000000000000000000, 0.9659258262890683122, 1.000000000000000000, 0.9659258262890683122, 1.000000000000000000, 0.9659258262890683122, 1.000000000000000000, 0.9659258262890683122, 1.000000000000000000, 0.9659258262890683122, 1.000000000000000000, 0.9659258262890683122, 1.000000000000000000, 0.9659258262890683122, 1.000000000000000000, 0.9659258262890683122, 1.000000000000000000, 0.9659258262890683122, 1.000000000000000000, 0.9659258262890683122, 1.000000000000000000, 0.9659258262890683122, 1.000000000000000000, 0.9659258262890683122, 1.000000000000000000, 0.9659258262890683122, 1.000000000000000000, 0.9659258262890683122, 1.000000000000000000, 0.9659258262890683122, 1.000000000000000000, 0.9659258262890683122, 1.000000000000000000, 0.9659258262890683122, 1.000000000000000000, 0.9659258262890683122, 1.000000000000000000, 0.9659258262890683122, 1.000000000000000000, 0.9659258262890683122, 1.000000000000000000, 0.9659258262890683122, 1.000000000000000000, 0.9659258262890683122, 1.000000000000000000, 0.9659258262890683122, 1.000000000000000000, 0.9659258262890683122, 1.000000000000000000, 0.9659258262890683122, 1.000000000000000000, 0.9659258262890683122, 1.000000000000000000, 0.9659258262890683122, 1.000000000000000000, 0.9659258262890683122, 1.000000000000000000, 0.9659258262890683122, 1.000000000000000000, 0.9659258262890683122, 1.000000000000000000, 0.9659258262890683122, 1.000000000000000000, 0.9659258262890683122, 1.000000000000000000, 0.9659258262890683122, 1.000000000000000000, 0.9659258262890683122, 1.000000000000000000, 0.9659258262890683122, 1.000000000000000000, 0.9659258262890683122, 1.000000000000000000, 0.9659258262890683122, 1.000000000000000000, 0.9659258262890683122, 1.000000000000000000, 0.9659258262890683122, 1.000000000000000000, 0.9659258262890683122, 1.000000000000000000, 0.9659258262890683122, 1.000000000000000000, 0.9659258262890683122, 1.000000000000000000, 0.9659258262890683122, 1.000000000000000000, 0.9659258262890683122, 1.000000000000000000, 0.9659258262890683122, 1.000000000000000000, 0.9659258262890683122, 1.000000000000000000, 0.9659258262890683122, 1.000000000000000000, 0.9659258262890683122, 1.000000000000000000, 0.9659258262890683122, 1.000000000000000000, 0.9659258262890683122, 1.000000000000000000, 0.9659258262890683122, 1.000000000000000000, 0.9659258262890683122, 1.000000000000000000, 0.9659258262890683122, 1.000000000000000000, 0.9659258262890683122, 1.000000000000000000, 0.9659258262890683122, 1.000000000000000000, 0.9659258262890683122, 1.000000000000000000, 0.9659258262890683122, 1.000000000000000000, 0.9659258262890683122, 1.000000000000000000, 0.9659258262890683122, 1.000000000000000000, 0.9659258262890683122, 1.000000000000000000, 0.9659258262890683122, 1.000000000000000000, 0.9659258262890683122, 1.000000000000000000, 0.9659258262890683122, 1.000000000000000000, 0.9659258262890683122, 1.000000000000000000, 0.9659258262890683122, 1.000000000000000000, 0.9659258262890683122, 1.000000000000000000, 0.9659258262890683122, 1.000000000000000000, 0.9659258262890683122, 1.000000000000000000, 0.9659258262890683122, 1.000000000000000000, 0.9659258262890683122, 1.000000000000000000, 0.9659258262890683122, 1.000000000000000000, 0.9659258262890683122, 1.000000000000000000, 0.9659258262890683122, 1.000000000000000000, 0.9659258262890683122, 1.000000000000000000, 0.9659258262890683122, 1.000000000000000000, 0.9659258262890683122, 1.000000000000000000, 0.9659258262890683122, 1.000000000000000000, 0.9659258262890683122, 1.000000000000000000, 0.9659258262890683122, 1.000000000000000000, 0.9659258262890683122, 1.000000000000000000, 0.9659258262890683122, 1.000000000000000000, 0.9659258262890683122, 1.000000000000000000, 0.9659258262890683122, 1.000000000000000000, 0.9659258262890683122, 1.000000000000000000, 0.9659258262890683122, 1.000000000000000000, 0.9659258262890683122, 1.000000000000000000, 0.9659258262890683122, 1.000000000000000000, 0.9659258262890683122, 1.000000000000000000, 0.9659258262890683122, 1.000000000000000000, 0.9659258262890683122, 1.000000000000000000, 0.9659258262890683122, 1.000000000000000000, 0.9659258262890683122, 1.000000000000000000, 0.9659258262890683122, 1.000000000000000000, 0.9659258262890683122, 1.000000000000000000, 0.9659258262890683122, 1.000000000000000000, 0.9659258262890683122, 1.000000000000000000, 0.9659258262890683122, 1.000000000000000000, 0.9659258262890683122, 1.000000000000000000, 0.9659258262890683122, 1.000000000000000000, 0.9659258262890683122, 1.000000000000000000, 0.9659258262890683122, 1.000000000000000000, 0.9659258262890683122, 1.000000000000000000, 0.9659258262890683122, 1.000000000000000000, 0.9659258262890683122, 1.000000000000000000, 0.9659258262890683122, 1.000000000000000000, 0.9659258262890683122, 1.000000000000000000, 0.9659258262890683122, 1.000000000000000000, 0.9659258262890683122, 1.000000000000000000, 0.9659258262890683122, 1.000000000000000000, 0.9659258262890683122, 1.000000000000000000, 0.9659258262890683122, 1.000000000000000000, 0.9659258262890683122, 1.000000000000000000, 0.9659258262890683122, 1.000000000000000000, 0.9659258262890683122, 1.000000000000000000, 0.9659258262890683122, 1.000000000000000000, 0.9659258262890683122, 1.000000000000000000, 0.9659258262890683122, 1.000000000000000000, 0.9659258262890683122, 1.000000000000000000, 0.9659258262890683122, 1.000000000000000000, 0.9659258262890683122, 1.000000000000000000, 0.9659258262890683122, 1.000000000000000000, 0.9659258262890683122, 1.000000000000000000, 0.9659258262890683122, 1.000000000000000000, 0.9659258262890683122, 1.000000000000000000, 0.9659258262890683122, 1.000000000000000000, 0.9659258262890683122, 1.000000000000000000, 0.9659258262890683122, 1.000000000000000000, 0.9659258262890683122, 1.000000000000000000, 0.9659258262890683122, 1.000000000000000000, 0.9659258262890683122, 1.000000000000000000, 0.9659258262890683122, 1.000000000000000000, 0.9659258262890683122, 1.000000000000000000, 0.9659258262890683122, 1.000000000000000000, 0.9659258262890683122, 1.000000000000000000, 0.9659258262890683122, 1.000000000000000000, 0.9659258262890683122, 1.000000000000000000, 0.9659258262890683122, 1.000000000000000000, 0.9659258262890683122, 1.000000000000000000, 0.9659258262890683122, 1.000000000000000000, 0.9659258262890683122, 1.000000000000000000, 0.9659258262890683122, 1.000000000000000000, 0.9659258262890683122, 1.000000000000000000, 0.9659258262890683122, 1.000000000000000000, 0.9659258262890683122, 1.000000000000000000, 0.9659258262890683122, 1.000000000000000000, 0.9659258262890683122, 1.000000000000000000, 0.9659258262890683122, 1.000000000000000000, 0.9659258262890683122, 1.000000000000000000, 0.9659258262890683122, 1.000000000000000000, 0.9659258262890683122, 1.000000000000000000, 0.9659258262890683122, 1.000000000000000000, 0.9659258262890683122, 1.000000000000000000, 0.9659258262890683122, 1.000000000000000000, 0.9659258262890683122, 1.000000000000000000, 0.9659258262890683122, 1.000000000000000000, 0.9659258262890683122, 1.000000000000000000, 0.9659258262890683122, 1.000000000000000000, 0.9659258262890683122, 1.000000000000000000, 0.9659258262890683122, 1.000000000000000000, 0.9659258262890683122, 1.000000000000000000, 0.9659258262890683122, 1.000000000000000000, 0.9659258262890683122, 1.000000000000000000, 0.9659258262890683122, 1.000000000000000000, 0.9659258262890683122, 1.000000000000000000, 0.9659258262890683122, 1.000000000000000000, 0.9659258262890683122, 1.000000000000000000, 0.9659258262890683122, 1.000000000000000000, 0.9659258262890683122, 1.000000000000000000, 0.9659258262890683122, 1.000000000000000000, 0.9659258262890683122, 1.000000000000000000, 0.9659258262890683122, 1.000000000000000000, 0.9659258262890683122, 1.000000000000000000, 0.9659258262890683122, 1.000000000000000000, 0.9659258262890683122, 1.000000000000000000, 0.9659258262890683122, 1.000000000000000000, 0.9659258262890683122, 1.000000000000000000, 0.9659258262890683122, 1.000000000000000000, 0.9659258262890683122, 1.000000000000000000, 0.9659258262890683122, 1.000000000000000000, 0.9659258262890683122, 1.000000000000000000, 0.9659258262890683122, 1.000000000000000000, 0.9659258262890683122, 1.000000000000000000, 0.9659258262890683122, 1.000000000000000000, 0.9659258262890683122, 1.000000000000000000, 0.9659258262890683122, 1.000000000000000000, 0.9659258262890683122, 1.000000000000000000, 0.9659258262890683122, 1.000000000000000000, 0.9659258262890683122, 1.000000000000000000, 0.9659258262890683122, 1.000000000000000000, 0.9659258262890683122, 1.000000000000000000, 0.9659258262890683122, 1.000000000000000000, 0.9659258262890683122, 1.000000000000000000, 0.9659258262890683122, 1.000000000000000000, 0.9659258262890683122, 1.000000000000000000, 0.9659258262890683122, 1.000000000000000000, 0.9659258262890683122, 1.000000000000000000, 0.9659258262890683122, 1.000000000000000000, 0.9659258262890683122, 1.000000000000000000, 0.9659258262890683122, 1.000000000000000000, 0.9659258262890683122, 1.000000000000000000, 0.9659258262890683122, 1.000000000000000000, 0.9659258262890683122, 1.000000000000000000, 0.9659258262890683122, 1.000000000000000000, 0.9659258262890683122, 1.000000000000000000, 0.9659258262890683122, 1.000000000000000000, 0.9659258262890683122, 1.000000000000000000, 0.9659258262890683122, 1.000000000000000000, 0.9659258262890683122, 1.000000000000000000, 0.9659258262890683122, 1.000000000000000000, 0.9659258262890683122, 1.000000000000000000, 0.9659258262890683122, 1.000000000000000000, 0.9659258262890683122, 1.000000000000000000, 0.9659258262890683122, 1.000000000000000000, 0.9659258262890683122, 1.000000000000000000, 0.9659258262890683122, 1.000000000000000000, 0.9659258262890683122, 1.000000000000000000, 0.9659258262890683122, 1.000000000000000000, 0.9659258262890683122, 1.000000000000000000, 0.9659258262890683122, 1.000000000000000000, 0.9659258262890683122, 1.000000000000000000, 0.9659258262890683122, 1.000000000000000000, 0.9659258262890683122, 1.000000000000000000, 0.9659258262890683122, 1.000000000000000000, 0.9659258262890683122, 1.000000000000000000, 0.9659258262890683122, 1.000000000000000000, 0.9659258262890683122, 1.000000000000000000, 0.9659258262890683122, 1.000000000000000000, 0.9659258262890683122, 1.000000000000000000, 0.9659258262890683122, 1.000000000000000000, 0.9659258262890683122, 1.000000000000000000, 0.9659258262890683122, 1.000000000000000000, 0.9659258262890683122, 1.000000000000000000, 0.9659258262890683122, 1.000000000000000000, 0.9659258262890683122, 1.000000000000000000, 0.9659258262890683122, 1.000000000000000000, 0.9659258262890683122, 1.000000000000000000, 0.9659258262890683122, 1.000000000000000000, 0.9659258262890683122, 1.000000000000000000, 0.9659258262890683122, 1.000000000000000000, 0.9659258262890683122, 1.000000000000000000, 0.9659258262890683122, 1.000000000000000000, 0.9659258262890683122, 1.000000000000000000, 0.9659258262890683122, 1.000000000000000000, 0.9659258262890683122, 1.000000000000000000, 0.9659258262890683122, 1.000000000000000000, 0.9659258262890683122, 1.000000000000000000, 0.9659258262890683122, 1.000000000000000000, 0.9659258262890683122, 1.000000000000000000, 0.9659258262890683122, 1.000000000000000000, 0.9659258262890683122, 1.000000000000000000, 0.9659258262890683122, 1.000000000000000000, 0.9659258262890683122, 1.000000000000000000, 0.9659258262890683122, 1.000000000000000000, 0.9659258262890683122, 1.000000000000000000, 0.9659258262890683122, 1.000000000000000000, 0.9659258262890683122, 1.000000000000000000, 0.9659258262890683122, 1.000000000000000000, 0.9659258262890683122, 1.000000000000000000, 0.9659258262890683122, 1.000000000000000000, 0.9659258262890683122, 1.000000000000000000, 0.9659258262890683122, 1.000000000000000000, 0.9659258262890683122, 1.000000000000000000, 0.9659258262890683122, 1.000000000000000000, 0.9659258262890683122, 1.000000000000000000, 0.9659258262890683122, 1.000000000000000000, 0.9659258262890683122, 1.000000000000000000, 0.9659258262890683122, 1.000000000000000000, 0.9659258262890683122, 1.000000000000000000, 0.9659258262890683122, 1.000000000000000000, 0.9659258262890683122, 1.000000000000000000, 0.9659258262890683122, 1.000000000000000000, 0.9659258262890683122, 1.000000000000000000, 0.9659258262890683122, 1.000000000000000000, 0.9659258262890683122, 1.000000000000000000, 0.9659258262890683122, 1.000000000000000000, 0.9659258262890683122, 1.000000000000000000, 0.9659258262890683122, 1.000000000000000000, 0.9659258262890683122, 1.000000000000000000, 0.9659258262890683122, 1.000000000000000000, 0.9659258262890683122, 1.000000000000000000, 0.9659258262890683122, 1.000000000000000000, 0.9659258262890683122, 1.000000000000000000, 0.9659258262890683122, 1.000000000000000000, 0.9659258262890683122, 1.000000000000000000, 0.9659258262890683122, 1.000000000000000000, 0.9659258262890683122, 1.000000000000000000, 0.9659258262890683122, 1.000000000000000000, 0.9659258262890683122, 1.000000000000000000, 0.9659258262890683122, 1.000000000000000000, 0.9659258262890683122, 1.000000000000000000, 0.9659258262890683122, 1.000000000000000000, 0.9659258262890683122, 1.000000000000000000, 0.9659258262890683122, 1.000000000000000000, 0.9659258262890683122, 1.000000000000000000, 0.9659258262890683122, 1.000000000000000000, 0.9659258262890683122, 1.000000000000000000, 0.9659258262890683122, 1.000000000000000000, 0.9659258262890683122, 1.000000000000000000, 0.9659258262890683122, 1.000000000000000000, 0.9659258262890683122, 1.000000000000000000, 0.9659258262890683122, 1.000000000000000000, 0.9659258262890683122, 1.000000000000000000, 0.9659258262890683122, 1.000000000000000000, 0.9659258262890683122, 1.000000000000000000, 0.9659258262890683122, 1.000000000000000000, 0.9659258262890683122, 1.000000000000000000, 0.9659258262890683122, 1.000000000000000000, 0.9659258262890683122, 1.000000000000000000, 0.9659258262890683122, 1.000000000000000000, 0.9659258262890683122, 1.000000000000000000, 0.9659258262890683122, 1.000000000000000000, 0.9659258262890683122, 1.000000000000000000, 0.9659258262890683122, 1.000000000000000000, 0.9659258262890683122, 1.000000000000000000, 0.9659258262890683122, 1.000000000000000000, 0.9659258262890683122, 1.000000000000000000, 0.9659258262890683122, 1.000000000000000000, 0.9659258262890683122, 1.000000000000000000, 0.9659258262890683122, 1.000000000000000000, 0.9659258262890683122, 1.000000000000000000, 0.9659258262890683122, 1.000000000000000000, 0.9659258262890683122, 1.000000000000000000, 0.9659258262890683122, 1.000000000000000000, 0.9659258262890683122, 1.000000000000000000, 0.9659258262890683122, 1.000000000000000000, 0.9659258262890683122, 1.000000000000000000, 0.9659258262890683122, 1.000000000000000000, 0.9659258262890683122, 1.000000000000000000, 0.9659258262890683122, 1.000000000000000000, 0.9659258262890683122, 1.000000000000000000, 0.9659258262890683122, 1.000000000000000000, 0.9659258262890683122, 1.000000000000000000, 0.9659258262890683122, 1.000000000000000000, 0.9659258262890683122, 1.000000000000000000, 0.9659258262890683122, 1.000000000000000000, 0.9659258262890683122, 1.000000000000000000, 0.9659258262890683122, 1.000000000000000000, 0.9659258262890683122, 1.000000000000000000, 0.9659258262890683122, 1.000000000000000000, 0.9659258262890683122, 1.000000000000000000, 0.9659258262890683122, 1.000000000000000000, 0.9659258262890683122, 1.000000000000000000, 0.9659258262890683122, 1.000000000000000000, 0.9659258262890683122, 1.000000000000000000, 0.9659258262890683122, 1.000000000000000000, 0.9659258262890683122, 1.000000000000000000, 0.9659258262890683122, 1.000000000000000000, 0.9659258262890683122, 1.000000000000000000, 0.9659258262890683122, 1.000000000000000000, 0.9659258262890683122, 1.000000000000000000, 0.9659258262890683122, 1.000000000000000000, 0.9659258262890683122, 1.000000000000000000, 0.9659258262890683122, 1.000000000000000000, 0.9659258262890683122, 1.000000000000000000, 0.9659258262890683122, 1.000000000000000000, 0.9659258262890683122, 1.000000000000000000, 0.9659258262890683122, 1.000000000000000000, 0.9659258262890683122, 1.000000000000000000, 0.9659258262890683122, 1.000000000000000000, 0.9659258262890683122, 1.000000000000000000, 0.9659258262890683122, 1.000000000000000000, 0.9659258262890683122, 1.000000000000000000, 0.9659258262890683122, 1.000000000000000000, 0.9659258262890683122, 1.000000000000000000, 0.9659258262890683122, 1.000000000000000000, 0.9659258262890683122, 1.000000000000000000, 0.9659258262890683122, 1.000000000000000000, 0.9659258262890683122, 1.000000000000000000, 0.9659258262890683122, 1.000000000000000000, 0.9659258262890683122, 1.000000000000000000, 0.9659258262890683122, 1.000000000000000000, 0.9659258262890683122, 1.000000000000000000, 0.9659258262890683122, 1.000000000000000000, 0.9659258262890683122, 1.000000000000000000, 0.9659258262890683122, 1.000000000000000000, 0.9659258262890683122, 1.000000000000000000, 0.9659258262890683122, 1.000000000000000000, 0.9659258262890683122, 1.000000000000000000, 0.9659258262890683122, 1.000000000000000000, 0.9659258262890683122, 1.000000000000000000, 0.9659258262890683122, 1.000000000000000000, 0.9659258262890683122, 1.000000000000000000, 0.9659258262890683122, 1.000000000000000000, 0.9659258262890683122, 1.000000000000000000, 0.9659258262890683122, 1.000000000000000000, 0.9659258262890683122, 1.000000000000000000, 0.9659258262890683122, 1.000000000000000000, 0.9659258262890683122, 1.000000000000000000, 0.9659258262890683122, 1.000000000000000000, 0.9659258262890683122, 1.000000000000000000, 0.9659258262890683122, 1.000000000000000000, 0.9659258262890683122, 1.000000000000000000, 0.9863514817966205772, 0.9836368779841404564) ) ) 
 REPRESENTATION_ITEM ( '' )  SURFACE ( )  );
#5759 = CARTESIAN_POINT ( 'NONE',  ( 32.00000000000000711, 208.3125000000000000, 168.3431457505075457 ) ) ;
#5760 = CARTESIAN_POINT ( 'NONE',  ( 1.656854249492381914, 10.56249999726881406, 4.000000000000000888 ) ) ;
#5761 = DIRECTION ( 'NONE',  ( -0.000000000000000000, -0.000000000000000000, -1.000000000000000000 ) ) ;
#5762 = ORIENTED_EDGE ( 'NONE', *, *, #46785, .F. ) ;
#5763 = DIRECTION ( 'NONE',  ( 1.000000000000000000, 0.000000000000000000, 0.000000000000000000 ) ) ;
#5764 = CARTESIAN_POINT ( 'NONE',  ( 2.445694354108839619, 200.8125000013656063, 200.4456943541088663 ) ) ;
#5765 = CARTESIAN_POINT ( 'NONE',  ( -24.54126587499996148, 205.1250000013656347, 171.4326545832179534 ) ) ;
#5766 = VECTOR ( 'NONE', #47168, 1000.000000000000000 ) ;
#5767 = ADVANCED_FACE ( 'NONE', ( #59150 ), #10952, .T. ) ;
#5768 = CARTESIAN_POINT ( 'NONE',  ( -4.541265875000002339, 11.81249999863440614, -5.561446717895856393E-16 ) ) ;
#5769 = DIRECTION ( 'NONE',  ( 0.000000000000000000, 0.000000000000000000, -1.000000000000000000 ) ) ;
#5770 = CARTESIAN_POINT ( 'NONE',  ( 7.188101187499992051, 8.802885111219154394E-16, 17.23655278187175810 ) ) ;
#5771 = ORIENTED_EDGE ( 'NONE', *, *, #7856, .T. ) ;
#5772 = EDGE_CURVE ( 'NONE', #56539, #60122, #6676, .T. ) ;
#5774 =( BOUNDED_CURVE ( )  B_SPLINE_CURVE ( 2, ( #5332, #35491, #12092, #41508, #40768, #63775, #433, #17378, #34392 ),
 .UNSPECIFIED., .F., .F. ) 
 B_SPLINE_CURVE_WITH_KNOTS ( ( 3, 2, 2, 2, 3 ),
 ( 0.7631578947368420351, 0.7697368421052630527, 0.7763157894736840703, 0.7828947368421053099, 0.7894736842105263275 ),
 .UNSPECIFIED. ) 
 CURVE ( )  GEOMETRIC_REPRESENTATION_ITEM ( )  RATIONAL_B_SPLINE_CURVE ( ( 1.000000000000001332, 0.9238795325112854062, 1.000000000000000000, 0.9238795325112867385, 1.000000000000000000, 0.9238795325112867385, 1.000000000000000000, 0.9238795325112867385, 1.000000000000000000 ) ) 
 REPRESENTATION_ITEM ( '' )  );
#5773 = CARTESIAN_POINT ( 'NONE',  ( 4.898587196589415787E-16, 0.000000000000000000, 4.000000000000001776 ) ) ;
#5775 = VERTEX_POINT ( 'NONE', #14202 ) ;
#5776 = CARTESIAN_POINT ( 'NONE',  ( -10.18810118749999738, -4.220049686691941915, 112.7500000020483810 ) ) ;
#5777 = DIRECTION ( 'NONE',  ( 1.000000000000000000, 0.000000000000000000, 0.000000000000000000 ) ) ;
#5778 = CARTESIAN_POINT ( 'NONE',  ( -32.00000000000000000, 206.2500000000000284, 170.0000000000003979 ) ) ;
#5779 = CARTESIAN_POINT ( 'NONE',  ( 3.458734125000015425, 199.9375000013656063, 198.0000000000000284 ) ) ;
#5780 = DIRECTION ( 'NONE',  ( 0.000000000000000000, -0.02418647091589873691, -0.9997074645238147594 ) ) ;
#5781 = CARTESIAN_POINT ( 'NONE',  ( -7.320508075688778149, 78.12499999999998579, 7.320508075688769267 ) ) ;
#5782 = CARTESIAN_POINT ( 'NONE',  ( 12.79996984384835912, 89.17133544502674170, -0.9100696820822021804 ) ) ;
#5783 = CARTESIAN_POINT ( 'NONE',  ( 11.35316468749999785, 65.88541666325268409, 3.042071309553174174 ) ) ;
#5784 = CARTESIAN_POINT ( 'NONE',  ( 1.102182119232618108E-15, 289.2500000000000000, 6.000000000000001776 ) ) ;
#5785 = ORIENTED_EDGE ( 'NONE', *, *, #31346, .T. ) ;
#5786 = CARTESIAN_POINT ( 'NONE',  ( -27.99999999999999645, 210.0000000000000284, 170.0000000000003695 ) ) ;
#5787 = EDGE_CURVE ( 'NONE', #65581, #8182, #54295, .T. ) ;
#5788 = CARTESIAN_POINT ( 'NONE',  ( -2.620431783929382252, -65.99617417813543341, 26.42108291244370122 ) ) ;
#5789 = CARTESIAN_POINT ( 'NONE',  ( 2.828427124746152987, 195.2500000027312126, 139.1715728752538723 ) ) ;
#5790 = CARTESIAN_POINT ( 'NONE',  ( 2.679491924311260043, 55.83333332650537528, 9.999999999999982236 ) ) ;
#5791 = CARTESIAN_POINT ( 'NONE',  ( -8.000000000000000000, 23.15625000000000355, -3.313708498984762496 ) ) ;
#5792 = CARTESIAN_POINT ( 'NONE',  ( 7.320508075688771044, 243.1249999999999716, -7.320508075688771932 ) ) ;
#5793 = CARTESIAN_POINT ( 'NONE',  ( -32.00000000000003553, 202.3125000027312410, 168.3431457505080857 ) ) ;
#5794 = CARTESIAN_POINT ( 'NONE',  ( 2.729886528703372228, 10.18810118749999916, 67.59560454024895648 ) ) ;
#5795 = CARTESIAN_POINT ( 'NONE',  ( -2.679491924311225848, 201.4583333333333144, -10.00000000000000178 ) ) ;
#5796 = CARTESIAN_POINT ( 'NONE',  ( -7.188101187499992051, 2.977408999572646930, 19.76780278187175455 ) ) ;
#5797 = CARTESIAN_POINT ( 'NONE',  ( 9.832129032723420536, 171.5104166632526983, -5.676582343749999815 ) ) ;
#5798 = PLANE ( 'NONE',  #27650 ) ;
#5799 = CARTESIAN_POINT ( 'NONE',  ( 30.82842712474620583, 197.2500000027312126, 172.8284271247460424 ) ) ;
#5800 = CARTESIAN_POINT ( 'NONE',  ( 5.000000000000001776, 87.70833332650538239, -8.660254037844389075 ) ) ;
#5801 = ORIENTED_EDGE ( 'NONE', *, *, #56126, .T. ) ;
#5802 = CARTESIAN_POINT ( 'NONE',  ( 2.445694354108782775, 197.5625000013656063, 139.5543056458912190 ) ) ;
#5803 = CARTESIAN_POINT ( 'NONE',  ( 5.676582343749993598, 40.26041666325268409, 9.832129032723422313 ) ) ;
#5804 = CARTESIAN_POINT ( 'NONE',  ( 11.00000000000000355, -4.556349186104045046, 112.8437500040967620 ) ) ;
#5805 = CARTESIAN_POINT ( 'NONE',  ( -26.56734541678228112, 209.0000000013656063, 173.4587341250003476 ) ) ;
#5806 = AXIS2_PLACEMENT_3D ( 'NONE', #15438, #48652, #7934 ) ;
#5807 = CARTESIAN_POINT ( 'NONE',  ( -6.123233995736766282E-16, 226.8750000068279746, -10.00000000000000000 ) ) ;
#5809 = CARTESIAN_POINT ( 'NONE',  ( 10.99999999999992006, -4.556349186104122317, 108.3437500040967763 ) ) ;
#5808 = FACE_OUTER_BOUND ( 'NONE', #61490, .T. ) ;
#5810 = CARTESIAN_POINT ( 'NONE',  ( 26.34314575050757412, 202.0625000027312126, 173.9999999999998295 ) ) ;
#5811 = CARTESIAN_POINT ( 'NONE',  ( 3.458734124999959914, 200.3750000013656063, 143.4326545832176976 ) ) ;
#5812 = AXIS2_PLACEMENT_3D ( 'NONE', #19589, #42605, #65620 ) ;
#5813 = CARTESIAN_POINT ( 'NONE',  ( 8.660254037844385522, 56.45833332650536818, 5.000000000000005329 ) ) ;
#5814 = CARTESIAN_POINT ( 'NONE',  ( -2.977408999572651815, 100.4375000020483668, 7.188101187500000933 ) ) ;
#5815 = CARTESIAN_POINT ( 'NONE',  ( -3.211159895383562723, 11.06249999863440792, 3.211159895383561391 ) ) ;
#5816 = CARTESIAN_POINT ( 'NONE',  ( -31.99999999999996447, 206.4375000027312126, 171.6568542494928522 ) ) ;
#5817 = CARTESIAN_POINT ( 'NONE',  ( -4.898587196589407898E-16, 7.999999999999991118, 4.955302779823363757 ) ) ;
#5818 = CARTESIAN_POINT ( 'NONE',  ( 4.000000000000001776, 7.749999997268813168, 0.000000000000000000 ) ) ;
#5819 = VERTEX_POINT ( 'NONE', #54225 ) ;
#5820 = ORIENTED_EDGE ( 'NONE', *, *, #9926, .T. ) ;
#5821 = CARTESIAN_POINT ( 'NONE',  ( -1.967015505459129087E-11, 198.7499999999984936, 10.00000000000000533 ) ) ;
#5822 = CARTESIAN_POINT ( 'NONE',  ( 2.765530957082001251, 298.9218750017070647, 6.676582343750000703 ) ) ;
#5823 = ADVANCED_FACE ( 'NONE', ( #48539 ), #42877, .F. ) ;
#5824 = CARTESIAN_POINT ( 'NONE',  ( -10.00000000000000178, 87.50000000000001421, -1.224646799147353256E-15 ) ) ;
#5825 = CARTESIAN_POINT ( 'NONE',  ( -2.085542519210945728E-15, 144.5312499965860411, 11.35316468750000141 ) ) ;
#5826 = CARTESIAN_POINT ( 'NONE',  ( -3.313708498984760276, 6.281249995903221084, -8.000000000000000000 ) ) ;
#5827 = CARTESIAN_POINT ( 'NONE',  ( 4.220049686691934809, 10.18810118749999916, 82.18750000204836681 ) ) ;
#5828 = DIRECTION ( 'NONE',  ( -0.000000000000000000, 1.000000000000000000, -0.000000000000000000 ) ) ;
#5829 = AXIS2_PLACEMENT_3D ( 'NONE', #65721, #9523, #3862 ) ;
#5830 = CARTESIAN_POINT ( 'NONE',  ( 4.000000000000015099, 203.5625000000000000, 196.3431457505076594 ) ) ;
#5831 = CARTESIAN_POINT ( 'NONE',  ( 3.999985685286083115, 88.68677412680156635, -6.928211494859723985 ) ) ;
#5832 = EDGE_CURVE ( 'NONE', #64356, #3031, #14792, .T. ) ;
#5833 = CARTESIAN_POINT ( 'NONE',  ( -7.204075437095965206, -7.204075437095968759, 116.2187500020483810 ) ) ;
#5834 = VERTEX_POINT ( 'NONE', #62470 ) ;
#5835 = VECTOR ( 'NONE', #54523, 1000.000000000000000 ) ;
#5836 = CARTESIAN_POINT ( 'NONE',  ( -4.556349186104045934, 11.00000000000000000, 108.9062500040967763 ) ) ;
#5837 = CARTESIAN_POINT ( 'NONE',  ( 12.82798793381997449, 178.4304155043948299, 135.6284118822403286 ) ) ;
#5838 = CARTESIAN_POINT ( 'NONE',  ( -8.311093377946841443, 134.2187499965860411, 8.311093377946834337 ) ) ;
#5839 = CARTESIAN_POINT ( 'NONE',  ( 3.458734125000015425, 200.9375000013656063, 198.0000000000000284 ) ) ;
#5840 = CARTESIAN_POINT ( 'NONE',  ( 7.188101187500000044, 23.34374999795161543, 0.000000000000000000 ) ) ;
#5842 = EDGE_CURVE ( 'NONE', #64770, #1466, #14534, .T. ) ;
#5841 = CARTESIAN_POINT ( 'NONE',  ( -7.204075437095965206, -7.204075437095968759, 74.21875000204838102 ) ) ;
#5843 = CARTESIAN_POINT ( 'NONE',  ( -3.042071309553164404, 37.55208332991935549, -11.35316468749999963 ) ) ;
#5844 = VERTEX_POINT ( 'NONE', #9693 ) ;
#5845 = CARTESIAN_POINT ( 'NONE',  ( -10.99999999999999822, -4.556349186104053040, 94.28125000409676204 ) ) ;
#5846 = CARTESIAN_POINT ( 'NONE',  ( -3.211159895383562723, 2.062499998634407028, 3.211159895383561391 ) ) ;
#5847 = CARTESIAN_POINT ( 'NONE',  ( 5.662595241051936235, -5.662595241051934458, 16.57561528394063188 ) ) ;
#5848 = CARTESIAN_POINT ( 'NONE',  ( -3.458734125000015869, 205.1875000013656063, 142.0000000000000568 ) ) ;
#5849 = CARTESIAN_POINT ( 'NONE',  ( 2.977408999572650927, 8.249999997951611874, -7.188101187500001821 ) ) ;
#5850 = CARTESIAN_POINT ( 'NONE',  ( -6.000000000000003553, 298.0000000034140726, -2.485281374238571317 ) ) ;
#5851 = CARTESIAN_POINT ( 'NONE',  ( -14.16110650781452840, -21.17774416547165472, 138.0804099437337698 ) ) ;
#5852 = CARTESIAN_POINT ( 'NONE',  ( 4.401442555609581635E-16, 4.218749997951610098, -7.188101187500000044 ) ) ;
#5853 = CARTESIAN_POINT ( 'NONE',  ( 9.832129032723416984, 160.6770833299193555, 5.676582343750006032 ) ) ;
#5854 = CARTESIAN_POINT ( 'NONE',  ( 7.204075437095968759, -7.204075437095966983, 72.71875000204838102 ) ) ;
#5855 = CARTESIAN_POINT ( 'NONE',  ( -31.45873412499998523, 205.0000000013655779, 171.4326545832180386 ) ) ;
#5856 = CARTESIAN_POINT ( 'NONE',  ( 1.656854249492381248, 3.187500000000000444, -4.000000000000001776 ) ) ;
#5857 = CARTESIAN_POINT ( 'NONE',  ( -4.541265875000002339, 18.87499999863441147, -1.881053915767121998 ) ) ;
#5858 = ORIENTED_EDGE ( 'NONE', *, *, #18276, .F. ) ;
#5859 = CARTESIAN_POINT ( 'NONE',  ( -3.999999999999960032, 200.1250000027312126, 198.0000000000000284 ) ) ;
#5860 = CARTESIAN_POINT ( 'NONE',  ( -1.656854249492403008, 207.6875000000000000, 146.0000000000000284 ) ) ;
#5861 = CARTESIAN_POINT ( 'NONE',  ( -25.17157287525374088, 202.7500000027312126, 172.8284271247464972 ) ) ;
#5862 = EDGE_CURVE ( 'NONE', #10364, #2929, #63946, .T. ) ;
#5863 = VECTOR ( 'NONE', #63616, 1000.000000000000000 ) ;
#5864 = CARTESIAN_POINT ( 'NONE',  ( -7.320508075688831440, 56.87500000000004974, -7.320508075688833216 ) ) ;
#5865 = CARTESIAN_POINT ( 'NONE',  ( -5.656854249492373476, -5.656854249492376141, 10.20530278392014623 ) ) ;
#5866 = VERTEX_POINT ( 'NONE', #33460 ) ;
#5867 = CARTESIAN_POINT ( 'NONE',  ( -7.188101187500002709, 16.31249999795161543, 2.977408999572649151 ) ) ;
#5868 = CARTESIAN_POINT ( 'NONE',  ( -10.00000000000000000, 209.1666666598386541, -2.679491924311229845 ) ) ;
#5869 = CARTESIAN_POINT ( 'NONE',  ( -28.00000000000003197, 208.0000000000000284, 166.0000000000003695 ) ) ;
#5870 = CARTESIAN_POINT ( 'NONE',  ( 6.123233995736767268E-16, 36.25000000000000711, -10.00000000000000178 ) ) ;
#5871 = AXIS2_PLACEMENT_3D ( 'NONE', #4198, #16228, #61898 ) ;
#5872 = CARTESIAN_POINT ( 'NONE',  ( -7.188101187500001821, 107.9375000020483810, -2.977408999572650483 ) ) ;
#5873 = CARTESIAN_POINT ( 'NONE',  ( -31.45873412499999944, 206.9375000013656063, 170.0000000000003979 ) ) ;
#5874 = CARTESIAN_POINT ( 'NONE',  ( -27.99999999999995381, 196.5000000000000000, 174.0000000000003695 ) ) ;
#5876 = CARTESIAN_POINT ( 'NONE',  ( -4.898587196589412829E-16, 94.81250000409677625, -8.000000000000000000 ) ) ;
#5875 = CARTESIAN_POINT ( 'NONE',  ( -5.656854249492378806, 111.8750000040967763, 5.656854249492381470 ) ) ;
#5877 =( BOUNDED_CURVE ( )  B_SPLINE_CURVE ( 2, ( #59218, #7529, #24854, #47872, #18107, #41121, #34623, #69306, #22906, #51961, #51206, #16862, #29323 ),
 .UNSPECIFIED., .F., .F. ) 
 B_SPLINE_CURVE_WITH_KNOTS ( ( 3, 2, 2, 2, 2, 2, 3 ),
 ( 1.962484770107478571, 1.967718660707278744, 1.972952551307078695, 1.978186441906878867, 1.983420332506679040, 1.988654223106478769, 1.993888113706278942 ),
 .UNSPECIFIED. ) 
 CURVE ( )  GEOMETRIC_REPRESENTATION_ITEM ( )  RATIONAL_B_SPLINE_CURVE ( ( 1.000000000000355049, 0.9659258262887133739, 1.000000000000000000, 0.9659258262890684232, 1.000000000000000000, 0.9659258262890684232, 1.000000000000000000, 0.9659258262890684232, 1.000000000000000000, 0.9659258262890684232, 1.000000000000000000, 0.9659258262890663138, 1.000000000000001998 ) ) 
 REPRESENTATION_ITEM ( '' )  );
#5878 = ORIENTED_EDGE ( 'NONE', *, *, #54143, .F. ) ;
#5879 = CARTESIAN_POINT ( 'NONE',  ( 8.311093377946834337, 247.0312500034139873, -8.311093377946836114 ) ) ;
#5880 = CARTESIAN_POINT ( 'NONE',  ( -4.401442555609577197E-16, 7.188101187499992051, 17.98655278187175810 ) ) ;
#5881 = CARTESIAN_POINT ( 'NONE',  ( 2.219371606097276572, 51.37365828841448234, 48.60677221569496709 ) ) ;
#5882 = CARTESIAN_POINT ( 'NONE',  ( 8.000000000000000000, 27.65624999795161187, 0.000000000000000000 ) ) ;
#5883 = CARTESIAN_POINT ( 'NONE',  ( 5.000000000000001776, 202.7083333265053682, -8.660254037844389075 ) ) ;
#5884 = CARTESIAN_POINT ( 'NONE',  ( -8.660254037844390851, 157.9166666666666856, 4.999999999999998224 ) ) ;
#5885 = CARTESIAN_POINT ( 'NONE',  ( 4.556349186104045934, 11.00000000000000000, 80.03124999999998579 ) ) ;
#5886 = CARTESIAN_POINT ( 'NONE',  ( -33.36290341065817699, 175.7112832858873617, 156.9282809272156669 ) ) ;
#5887 = CARTESIAN_POINT ( 'NONE',  ( 4.999999999999998224, -52.84634075987109014, -43.22150062466552356 ) ) ;
#5888 = CARTESIAN_POINT ( 'NONE',  ( -3.042071309553164404, 127.5520833299193555, -11.35316468749999963 ) ) ;
#5889 = CARTESIAN_POINT ( 'NONE',  ( 11.00000000000000000, 1.347111479062088405E-15, 118.0000000000000000 ) ) ;
#5890 = CARTESIAN_POINT ( 'NONE',  ( -3.313708498984760276, 4.968750000000000888, -8.000000000000000000 ) ) ;
#5893 = DIRECTION ( 'NONE',  ( 0.000000000000000000, 0.000000000000000000, 1.000000000000000000 ) ) ;
#5892 = CARTESIAN_POINT ( 'NONE',  ( 27.99999999999996447, 196.9375000013655779, 166.5412658749999082 ) ) ;
#5891 = CARTESIAN_POINT ( 'NONE',  ( 27.99999999999997158, 210.0000000000000284, 173.9999999999999147 ) ) ;
#5894 = VERTEX_POINT ( 'NONE', #27771 ) ;
#5895 = CARTESIAN_POINT ( 'NONE',  ( 8.000000000000000000, 10.50000000000000178, 0.000000000000000000 ) ) ;
#5896 = LINE ( 'NONE', #45133, #55474 ) ;
#5897 = CYLINDRICAL_SURFACE ( 'NONE', #6234, 8.000000000000000000 ) ;
#5898 =( BOUNDED_CURVE ( )  B_SPLINE_CURVE ( 2, ( #36026, #600, #64321, #65043, #29622, #57944, #7350, #52635, #53744 ),
 .UNSPECIFIED., .F., .F. ) 
 B_SPLINE_CURVE_WITH_KNOTS ( ( 3, 2, 2, 2, 3 ),
 ( 0.8958333333333318160, 0.9062499999999984457, 0.9166666666666650753, 0.9270833333333318160, 0.9374999999999984457 ),
 .UNSPECIFIED. ) 
 CURVE ( )  GEOMETRIC_REPRESENTATION_ITEM ( )  RATIONAL_B_SPLINE_CURVE ( ( 1.000000000000011324, 0.9238795325112754142, 1.000000000000000000, 0.9238795325112867385, 1.000000000000000000, 0.9238795325112867385, 1.000000000000000000, 0.9238795325112980628, 0.9999999999999886757 ) ) 
 REPRESENTATION_ITEM ( '' )  );
#5899 = CARTESIAN_POINT ( 'NONE',  ( 9.797174393178825657E-16, 125.0000000000000000, -8.000000000000000000 ) ) ;
#5900 = CARTESIAN_POINT ( 'NONE',  ( -8.660254037844387298, 28.95833332650536818, -5.000000000000004441 ) ) ;
#5901 = CARTESIAN_POINT ( 'NONE',  ( 2.977408999572650039, 122.1875000020483668, -7.188101187500001821 ) ) ;
#5902 = CARTESIAN_POINT ( 'NONE',  ( -1.881053915767121554, 20.62499999863441147, -4.541265875000002339 ) ) ;
#5903 = CARTESIAN_POINT ( 'NONE',  ( -0.6547826978430097977, 60.19560277018368311, -22.88235556322664976 ) ) ;
#5904 = CARTESIAN_POINT ( 'NONE',  ( 5.656854249492374365, 5.656854249492375253, 21.26780277982336642 ) ) ;
#5906 = LINE ( 'NONE', #46253, #60663 ) ;
#5905 = DIRECTION ( 'NONE',  ( -0.000000000000000000, 0.000000000000000000, 1.000000000000000000 ) ) ;
#5907 = CARTESIAN_POINT ( 'NONE',  ( -8.311093377946841443, 113.9062499965859985, 8.311093377946830785 ) ) ;
#5908 = ORIENTED_EDGE ( 'NONE', *, *, #28712, .T. ) ;
#5909 = CARTESIAN_POINT ( 'NONE',  ( 0.000000000000000000, 300.0000000000000000, 10.00000000000000178 ) ) ;
#5910 = CARTESIAN_POINT ( 'NONE',  ( 7.188101187500000044, 27.46874999795161543, 0.000000000000000000 ) ) ;
#5911 = CARTESIAN_POINT ( 'NONE',  ( -8.000000000000033751, -3.313708498984719864, 8.424052779823361092 ) ) ;
#5912 = CARTESIAN_POINT ( 'NONE',  ( 9.832129032723420536, 246.3020833367473301, 5.676582343749996262 ) ) ;
#5913 = CARTESIAN_POINT ( 'NONE',  ( -5.676582343749998039, 107.4479166632526983, -9.832129032723420536 ) ) ;
#5914 = EDGE_LOOP ( 'NONE', ( #18227, #52514 ) ) ;
#5915 = CARTESIAN_POINT ( 'NONE',  ( 7.999999999999998224, 25.40625000000000355, 3.313708498984766049 ) ) ;
#5916 = CARTESIAN_POINT ( 'NONE',  ( 1.871523826299183495E-15, -10.18810118749999916, 102.5312500020483810 ) ) ;
#5917 = CARTESIAN_POINT ( 'NONE',  ( -4.999999999999998224, 223.5416666598387110, -8.660254037844389075 ) ) ;
#5918 = CARTESIAN_POINT ( 'NONE',  ( 1.432654583217664701, 202.0000000013656063, 201.4587341250000065 ) ) ;
#5919 = CARTESIAN_POINT ( 'NONE',  ( 7.778174593052023411, -7.778174593052021635, 69.06249999999998579 ) ) ;
#5921 = CARTESIAN_POINT ( 'NONE',  ( -3.042071309553163960, 97.23958332991935549, -11.35316468749999963 ) ) ;
#5920 = CARTESIAN_POINT ( 'NONE',  ( -3.999999999999960032, 206.1250000027312126, 198.0000000000000284 ) ) ;
#5922 = CARTESIAN_POINT ( 'NONE',  ( 7.999999999999991118, 9.797174393178815797E-16, 10.76780278392014800 ) ) ;
#5923 = CARTESIAN_POINT ( 'NONE',  ( -31.45873412499997812, 195.0000000013656063, 171.4326545832180386 ) ) ;
#5924 = EDGE_CURVE ( 'NONE', #55396, #50470, #38358, .T. ) ;
#5925 = CARTESIAN_POINT ( 'NONE',  ( 5.000000000000001776, 170.8333333333333428, -8.660254037844389075 ) ) ;
#5926 = ORIENTED_EDGE ( 'NONE', *, *, #44001, .T. ) ;
#5927 = CARTESIAN_POINT ( 'NONE',  ( -7.320508075688778149, 199.9999999931720254, 7.320508075688769267 ) ) ;
#5928 = AXIS2_PLACEMENT_3D ( 'NONE', #70455, #59507, #43252 ) ;
#5929 = CARTESIAN_POINT ( 'NONE',  ( 2.824543433528785410E-14, 210.0000000000000284, 194.0000000000000568 ) ) ;
#5930 = CARTESIAN_POINT ( 'NONE',  ( 28.00000000000001776, 195.1250000027311842, 173.9999999999999147 ) ) ;
#5931 = CARTESIAN_POINT ( 'NONE',  ( 11.35316468750000141, 86.09374999658601268, 0.000000000000000000 ) ) ;
#5932 = CARTESIAN_POINT ( 'NONE',  ( 2.765530957082001251, 287.7656250017069510, 6.676582343750000703 ) ) ;
#5933 = CARTESIAN_POINT ( 'NONE',  ( 4.401442555609581635E-16, 8.718749997951611874, -7.188101187500000044 ) ) ;
#5935 = ADVANCED_FACE ( 'NONE', ( #68142 ), #73056, .F. ) ;
#5934 = CARTESIAN_POINT ( 'NONE',  ( -10.18810118749999916, 0.000000000000000000, 98.03125000204838102 ) ) ;
#5936 = CARTESIAN_POINT ( 'NONE',  ( 9.832129032723420536, 216.1979166632526983, -5.676582343749999815 ) ) ;
#5937 = ORIENTED_EDGE ( 'NONE', *, *, #73198, .T. ) ;
#5938 = CARTESIAN_POINT ( 'NONE',  ( -5.656854249492373476, -5.656854249492376141, 26.51780277982336997 ) ) ;
#5939 = CARTESIAN_POINT ( 'NONE',  ( 1.983827303899642569, -42.74108338342507096, 139.0632315445211873 ) ) ;
#5940 = CARTESIAN_POINT ( 'NONE',  ( -5.676582343750006032, 219.1145833299193839, 9.832129032723418760 ) ) ;
#5941 = VECTOR ( 'NONE', #57821, 1000.000000000000000 ) ;
#5942 = CARTESIAN_POINT ( 'NONE',  ( -7.999999999999015010, 2.678670460604446806E-06, 11.51770387648012317 ) ) ;
#5943 = CARTESIAN_POINT ( 'NONE',  ( -2.170320029210515145, -16.41060967376241564, -68.77687409974784316 ) ) ;
#5944 = CARTESIAN_POINT ( 'NONE',  ( -2.765530957081996810, 295.2656250017070079, -6.676582343750003368 ) ) ;
#5945 = VERTEX_POINT ( 'NONE', #44388 ) ;
#5946 = CARTESIAN_POINT ( 'NONE',  ( -7.320508075688778149, 119.9999999931720396, 7.320508075688769267 ) ) ;
#5947 = CARTESIAN_POINT ( 'NONE',  ( -5.676582343749998039, 212.7604166632526699, -9.832129032723420536 ) ) ;
#5948 = CARTESIAN_POINT ( 'NONE',  ( -10.18810118749999738, -4.220049686691941915, 87.25000000204838102 ) ) ;
#5949 = CARTESIAN_POINT ( 'NONE',  ( -29.43265458321766559, 202.5000000013656063, 166.5412658750003629 ) ) ;
#5950 = CARTESIAN_POINT ( 'NONE',  ( -5.656854249492381470, 17.43750000000000000, 5.656854249492379694 ) ) ;
#5951 = VERTEX_POINT ( 'NONE', #67399 ) ;
#5952 = CARTESIAN_POINT ( 'NONE',  ( 7.188101187500001821, 122.0000000020483668, -2.977408999572651371 ) ) ;
#5953 = CARTESIAN_POINT ( 'NONE',  ( -1.836970198721029983E-15, 33.75000000000000000, 10.00000000000000178 ) ) ;
#5954 = CARTESIAN_POINT ( 'NONE',  ( -1.469576158976823947E-15, 8.625000000000000000, 8.000000000000000000 ) ) ;
#5955 = CARTESIAN_POINT ( 'NONE',  ( -4.220049686691937474, -10.18810118749999738, 75.81250000204838102 ) ) ;
#5956 = VERTEX_POINT ( 'NONE', #39473 ) ;
#5957 = DIRECTION ( 'NONE',  ( -0.000000000000000000, -0.000000000000000000, 1.000000000000000000 ) ) ;
#5958 = DIRECTION ( 'NONE',  ( -1.000000000000000000, -9.637352644315595243E-17, 0.000000000000000000 ) ) ;
#5959 = CARTESIAN_POINT ( 'NONE',  ( -5.000000000000000000, -10.43216530810821219, 65.93415491242824089 ) ) ;
#5960 = DIRECTION ( 'NONE',  ( 0.000000000000000000, -1.000000000000000000, 0.000000000000000000 ) ) ;
#5961 = CARTESIAN_POINT ( 'NONE',  ( 2.765530957081996366, 296.1406250017070647, -6.676582343750002480 ) ) ;
#5964 = CARTESIAN_POINT ( 'NONE',  ( -3.673940397442060854E-16, 288.8125000034140157, -6.000000000000001776 ) ) ;
#5963 = CARTESIAN_POINT ( 'NONE',  ( -3.042071309553166625, 247.8645833367473017, -11.35316468749999608 ) ) ;
#5962 = CARTESIAN_POINT ( 'NONE',  ( 24.54126587500000767, 208.2500000013656063, 171.4326545832176123 ) ) ;
#5965 = APPLICATION_PROTOCOL_DEFINITION ( 'draft international standard', 'automotive_design', 1998, #69837 ) ;
#5966 = VERTEX_POINT ( 'NONE', #20617 ) ;
#5968 = VECTOR ( 'NONE', #51775, 1000.000000000000000 ) ;
#5967 = CARTESIAN_POINT ( 'NONE',  ( -11.35316468749999785, 234.0104166700806161, -3.042071309553164848 ) ) ;
#5969 = CARTESIAN_POINT ( 'NONE',  ( -7.188101187499992051, 0.000000000000000000, 7.486552781871751883 ) ) ;
#5970 = ORIENTED_EDGE ( 'NONE', *, *, #73012, .F. ) ;
#5971 = LINE ( 'NONE', #70453, #35546 ) ;
#5972 = CARTESIAN_POINT ( 'NONE',  ( -5.676582343749998039, 87.76041666325268409, -9.832129032723420536 ) ) ;
#5973 = CARTESIAN_POINT ( 'NONE',  ( 4.000000000000001776, 21.00000000000000000, 0.000000000000000000 ) ) ;
#5974 = CARTESIAN_POINT ( 'NONE',  ( 7.778174593052021635, 7.778174593052023411, 85.93749999999998579 ) ) ;
#5977 = CARTESIAN_POINT ( 'NONE',  ( 0.000000000000000000, 0.000000000000000000, 0.000000000000000000 ) ) ;
#5976 = CARTESIAN_POINT ( 'NONE',  ( 31.45873412499998523, 207.7500000013656063, 168.5673454167822172 ) ) ;
#5975 = CARTESIAN_POINT ( 'NONE',  ( 25.55430564589115505, 206.5625000013656063, 172.4456943541086957 ) ) ;
#5978 = ORIENTED_EDGE ( 'NONE', *, *, #9397, .T. ) ;
#5979 = AXIS2_PLACEMENT_3D ( 'NONE', #6558, #14318, #23898 ) ;
#5980 = CYLINDRICAL_SURFACE ( 'NONE', #13959, 3.999999999999976019 ) ;
#5981 = DIRECTION ( 'NONE',  ( -0.000000000000000000, -0.000000000000000000, -1.000000000000000000 ) ) ;
#5982 = CARTESIAN_POINT ( 'NONE',  ( -5.676582343749998039, 202.4479166632526983, -9.832129032723420536 ) ) ;
#5983 = ADVANCED_FACE ( 'NONE', ( #15701 ), #8521, .T. ) ;
#5984 = CARTESIAN_POINT ( 'NONE',  ( 1.432654583217607858, 203.6250000013656063, 138.5412658750000787 ) ) ;
#5985 = ADVANCED_FACE ( 'NONE', ( #43634 ), #37443, .T. ) ;
#5986 = CARTESIAN_POINT ( 'NONE',  ( 30.44569435410879166, 204.8125000013656063, 172.4456943541087526 ) ) ;
#5987 = CARTESIAN_POINT ( 'NONE',  ( -2.977408999572650039, 20.81249999795161543, -7.188101187500001821 ) ) ;
#5988 = CARTESIAN_POINT ( 'NONE',  ( -3.042071309553173730, 184.6354166632526983, 11.35316468749999785 ) ) ;
#5989 = CARTESIAN_POINT ( 'NONE',  ( -1.469576158976823947E-15, 8.437499995903221972, 8.000000000000000000 ) ) ;
#5990 = CARTESIAN_POINT ( 'NONE',  ( -7.188101187499999156, 97.62500000204836681, 2.977408999572654924 ) ) ;
#5992 = CARTESIAN_POINT ( 'NONE',  ( -27.99999999999991118, 198.6250000027312126, 174.0000000000003695 ) ) ;
#5991 = CARTESIAN_POINT ( 'NONE',  ( 4.000000000000001776, 17.81249999726881938, -1.656854249492381248 ) ) ;
#5993 = CARTESIAN_POINT ( 'NONE',  ( 4.541265875000002339, 12.31249999863440792, 0.000000000000000000 ) ) ;
#5994 = CARTESIAN_POINT ( 'NONE',  ( 29.43265458321761230, 200.7500000013656063, 173.4587341249998929 ) ) ;
#5995 = CARTESIAN_POINT ( 'NONE',  ( 7.188101187499993827, -2.977408999572645598, 8.517802781871754547 ) ) ;
#5996 = CARTESIAN_POINT ( 'NONE',  ( -2.085542519210945728E-15, 64.53124999658602690, 11.35316468750000141 ) ) ;
#5997 =( BOUNDED_CURVE ( )  B_SPLINE_CURVE ( 2, ( #17922, #11892, #59399, #52999, #24674, #1332, #6244, #46956, #58304 ),
 .UNSPECIFIED., .F., .F. ) 
 B_SPLINE_CURVE_WITH_KNOTS ( ( 3, 2, 2, 2, 3 ),
 ( 0.6333333333333339699, 0.6416666666666673846, 0.6500000000000006883, 0.6583333333333339921, 0.6666666666666672958 ),
 .UNSPECIFIED. ) 
 CURVE ( )  GEOMETRIC_REPRESENTATION_ITEM ( )  RATIONAL_B_SPLINE_CURVE ( ( 0.9999999999999938938, 0.9238795325112928447, 1.000000000000000000, 0.9238795325112867385, 1.000000000000000000, 0.9238795325112867385, 1.000000000000000000, 0.9238795325112806323, 1.000000000000005995 ) ) 
 REPRESENTATION_ITEM ( '' )  );
#5998 = CARTESIAN_POINT ( 'NONE',  ( 25.17157287525378351, 205.7500000027312126, 167.1715728752537586 ) ) ;
#5999 = CARTESIAN_POINT ( 'NONE',  ( 1.469576158976822172E-15, -7.999999999999991118, 1.261552784329824206 ) ) ;
#6000 = EDGE_LOOP ( 'NONE', ( #3874, #24673, #39924, #17167, #61293 ) ) ;
#6001 = CARTESIAN_POINT ( 'NONE',  ( 4.556349186104052151, -10.99999999999999822, 74.96874999999998579 ) ) ;
#6002 = CARTESIAN_POINT ( 'NONE',  ( -11.00000000000000000, 0.000000000000000000, 67.18750000409676204 ) ) ;
#6003 = CARTESIAN_POINT ( 'NONE',  ( 5.676582343749993598, 64.94791666325269830, 9.832129032723422313 ) ) ;
#6004 = CARTESIAN_POINT ( 'NONE',  ( -4.556349186104047710, -10.99999999999999822, 76.46875000409677625 ) ) ;
#6005 = CARTESIAN_POINT ( 'NONE',  ( -3.458734125000016757, 195.1250000013656063, 140.5673454167823593 ) ) ;
#6006 = FACE_OUTER_BOUND ( 'NONE', #64268, .T. ) ;
#6008 = CARTESIAN_POINT ( 'NONE',  ( 8.311093377946837890, 61.40624999658601979, -8.311093377946837890 ) ) ;
#6007 = CARTESIAN_POINT ( 'NONE',  ( -7.188101187500000044, 91.15625000204838102, 0.000000000000000000 ) ) ;
#6009 = CARTESIAN_POINT ( 'NONE',  ( 7.999999999999992895, -3.313708498984756279, 5.986552779823365533 ) ) ;
#6010 = CARTESIAN_POINT ( 'NONE',  ( -3.673940397442060854E-16, 287.8125000034140157, -6.000000000000001776 ) ) ;
#6011 = CARTESIAN_POINT ( 'NONE',  ( -7.320508075688773708, 153.7499999931720538, -7.320508075688774596 ) ) ;
#6012 = CARTESIAN_POINT ( 'NONE',  ( 5.082755093536325042, 96.96875000204838102, -5.082755093536325930 ) ) ;
#6013 = CARTESIAN_POINT ( 'NONE',  ( -9.832129032723420536, 44.01041666325268409, 5.676582343749997150 ) ) ;
#6014 = CARTESIAN_POINT ( 'NONE',  ( 4.220049686691934809, 10.18810118749999916, 111.0625000020483810 ) ) ;
#6015 = CARTESIAN_POINT ( 'NONE',  ( -3.042071309553164404, 177.2395833299193555, -11.35316468749999963 ) ) ;
#6016 = ORIENTED_EDGE ( 'NONE', *, *, #4416, .F. ) ;
#6017 = CARTESIAN_POINT ( 'NONE',  ( 6.298842414732967576, 61.32333038069117492, 23.57034304878763464 ) ) ;
#6018 = CARTESIAN_POINT ( 'NONE',  ( -10.18810118749999916, 4.220049686691934809, 72.06250000204836681 ) ) ;
#6019 = CARTESIAN_POINT ( 'NONE',  ( 2.849036369511732440E-14, 197.2500000000000000, 202.0000000000000000 ) ) ;
#6021 = CARTESIAN_POINT ( 'NONE',  ( 6.951808397369818766E-16, 182.0312499965860411, -11.35316468750000141 ) ) ;
#6020 = CARTESIAN_POINT ( 'NONE',  ( 0.8721677472496979222, -67.61512445009702788, 20.05250736213360341 ) ) ;
#6022 = CARTESIAN_POINT ( 'NONE',  ( -5.656854249492375253, 5.656854249492375253, 8.199052784329824206 ) ) ;
#6023 = DIRECTION ( 'NONE',  ( 0.000000000000000000, 0.7071067811865426878, 0.7071067811865524577 ) ) ;
#6024 = CARTESIAN_POINT ( 'NONE',  ( -10.00000000000000000, 247.9166666734946887, -2.679491924311226292 ) ) ;
#6025 = CARTESIAN_POINT ( 'NONE',  ( -75.00000000000000000, 272.0000000000000000, 42.00000000000004974 ) ) ;
#6026 = EDGE_LOOP ( 'NONE', ( #49623, #8922, #53427, #66587 ) ) ;
#6027 = CARTESIAN_POINT ( 'NONE',  ( 5.676582343750001591, 166.9270833299193555, -9.832129032723420536 ) ) ;
#6028 = VECTOR ( 'NONE', #15224, 1000.000000000000000 ) ;
#6029 = CARTESIAN_POINT ( 'NONE',  ( -2.977408999572647819, -7.188101187499990274, 27.26780278187175455 ) ) ;
#6030 = CARTESIAN_POINT ( 'NONE',  ( 5.676582343749993598, 135.2604166632526983, 9.832129032723422313 ) ) ;
#6031 = CARTESIAN_POINT ( 'NONE',  ( -9.000000000000019540, 15.58845726811987831, -20.69999999999999929 ) ) ;
#6032 = ORIENTED_EDGE ( 'NONE', *, *, #1611, .F. ) ;
#6033 = CARTESIAN_POINT ( 'NONE',  ( 2.780723358947928197E-16, 12.68749999863440792, -4.541265875000002339 ) ) ;
#6034 = AXIS2_PLACEMENT_3D ( 'NONE', #40585, #17944, #40209 ) ;
#6035 = CARTESIAN_POINT ( 'NONE',  ( -5.082755093536325042, 13.03124999795161187, -5.082755093536325930 ) ) ;
#6036 = CARTESIAN_POINT ( 'NONE',  ( -3.313708498984762496, 104.4687500040967763, 7.999999999999998224 ) ) ;
#6037 = CARTESIAN_POINT ( 'NONE',  ( -24.54126587499998280, 199.3750000013656063, 171.4326545832179818 ) ) ;
#6038 = CARTESIAN_POINT ( 'NONE',  ( -4.000000000000001776, 11.43750000000000000, -1.656854249492381470 ) ) ;
#6039 = CARTESIAN_POINT ( 'NONE',  ( 4.000000000000001776, 20.81249999726881583, -1.656854249492381248 ) ) ;
#6040 = CARTESIAN_POINT ( 'NONE',  ( -4.541265875000002339, 11.74999999863440792, -1.881053915767121998 ) ) ;
#6041 = CARTESIAN_POINT ( 'NONE',  ( 7.999999999999992895, -3.313708498984756279, 22.67405278392015333 ) ) ;
#6042 = CARTESIAN_POINT ( 'NONE',  ( 1.656854249492466735, 196.1875000000000284, 138.0000000000001705 ) ) ;
#6043 = EDGE_LOOP ( 'NONE', ( #65120, #32017, #50748, #20469 ) ) ;
#6044 = CARTESIAN_POINT ( 'NONE',  ( -2.679491924326700136, 176.4583333333347639, -9.999999999991132427 ) ) ;
#6045 = CARTESIAN_POINT ( 'NONE',  ( 7.188101187500002709, 105.3125000020483668, 2.977408999572649151 ) ) ;
#6048 = VECTOR ( 'NONE', #6979, 1000.000000000000000 ) ;
#6047 = CARTESIAN_POINT ( 'NONE',  ( 1.469576158976823947E-15, 123.8750000000000000, 8.000000000000000000 ) ) ;
#6046 = CARTESIAN_POINT ( 'NONE',  ( -7.999999999999991118, 0.000000000000000000, 8.330302779823362869 ) ) ;
#6049 = ORIENTED_EDGE ( 'NONE', *, *, #57387, .F. ) ;
#6050 = CARTESIAN_POINT ( 'NONE',  ( -3.211159895383561391, 20.68749999863440436, -3.211159895383561835 ) ) ;
#6051 = EDGE_CURVE ( 'NONE', #25548, #45848, #32334, .T. ) ;
#6052 = CARTESIAN_POINT ( 'NONE',  ( -2.977408999572648707, -7.188101187499990274, 24.26780278187175455 ) ) ;
#6053 = ORIENTED_EDGE ( 'NONE', *, *, #74560, .T. ) ;
#6054 = VERTEX_POINT ( 'NONE', #10059 ) ;
#6055 = CARTESIAN_POINT ( 'NONE',  ( 4.220049686691941027, -10.18810118749999738, 89.12500000204836681 ) ) ;
#6056 = CARTESIAN_POINT ( 'NONE',  ( -29.65685424949240456, 195.5625000027311842, 174.0000000000002842 ) ) ;
#6057 = CARTESIAN_POINT ( 'NONE',  ( -26.56734541678232731, 197.2500000013656063, 173.4587341250003760 ) ) ;
#6058 = CARTESIAN_POINT ( 'NONE',  ( -10.99999999999999822, -4.556349186104052151, 101.5937499999999858 ) ) ;
#6061 = CARTESIAN_POINT ( 'NONE',  ( 6.676582343750003368, 298.0468750017070079, 2.765530957081995478 ) ) ;
#6060 = CARTESIAN_POINT ( 'NONE',  ( 29.65685424949235482, 205.5625000027311842, 165.9999999999998863 ) ) ;
#6059 = FACE_OUTER_BOUND ( 'NONE', #48415, .T. ) ;
#6062 = CARTESIAN_POINT ( 'NONE',  ( -10.00000000000000000, 137.2916666666666572, -2.679491924311229845 ) ) ;
#6063 = CARTESIAN_POINT ( 'NONE',  ( -8.000000000000000000, 100.9062500000000000, -3.313708498984761608 ) ) ;
#6064 = CARTESIAN_POINT ( 'NONE',  ( -4.556349186104048599, -10.99999999999999822, 86.96875000409677625 ) ) ;
#6065 = CARTESIAN_POINT ( 'NONE',  ( 7.188101187499991163, 2.977408999572648707, 2.705302781871750994 ) ) ;
#6066 = CARTESIAN_POINT ( 'NONE',  ( -4.898587196589412829E-16, 97.62499999999998579, -8.000000000000000000 ) ) ;
#6067 = VECTOR ( 'NONE', #50580, 1000.000000000000000 ) ;
#6068 = CARTESIAN_POINT ( 'NONE',  ( 25.55430564589115150, 202.3125000013656063, 172.4456943541086957 ) ) ;
#6069 = CARTESIAN_POINT ( 'NONE',  ( 7.188101187499999156, 5.249999997951610098, 2.977408999572654924 ) ) ;
#6070 = CARTESIAN_POINT ( 'NONE',  ( -3.317071493978880348, -8.008118988124989457, 2.794365283940627886 ) ) ;
#6071 = CARTESIAN_POINT ( 'NONE',  ( 2.445694354108782775, 194.5625000013656063, 139.5543056458912190 ) ) ;
#6072 = CARTESIAN_POINT ( 'NONE',  ( 2.977408999572654480, 114.5000000020483810, 7.188101187499999156 ) ) ;
#6073 = DIRECTION ( 'NONE',  ( -0.000000000000000000, 1.000000000000000000, -0.000000000000000000 ) ) ;
#6074 = CARTESIAN_POINT ( 'NONE',  ( -3.042071309553166181, 248.1770833367472733, -11.35316468749999608 ) ) ;
#6075 = CARTESIAN_POINT ( 'NONE',  ( -4.898587196589412829E-16, 96.31250000409677625, -8.000000000000000000 ) ) ;
#6076 = CARTESIAN_POINT ( 'NONE',  ( -7.188101187499992051, 0.000000000000000000, 25.86155278187175810 ) ) ;
#6077 = CARTESIAN_POINT ( 'NONE',  ( 30.82842712474620228, 200.3750000000000284, 167.1715728752537586 ) ) ;
#6078 = CARTESIAN_POINT ( 'NONE',  ( 5.676582343750001591, 16.61458332991935194, -9.832129032723420536 ) ) ;
#6079 = CARTESIAN_POINT ( 'NONE',  ( -2.319934922699201535E-11, 23.74999999999819522, 10.00000000000000178 ) ) ;
#6080 = CARTESIAN_POINT ( 'NONE',  ( 11.35316468749999963, 216.3020833299193555, -3.042071309553165293 ) ) ;
#6081 = DIRECTION ( 'NONE',  ( 0.000000000000000000, 0.000000000000000000, 1.000000000000000000 ) ) ;
#6083 = CARTESIAN_POINT ( 'NONE',  ( 2.752039609470550924E-11, 41.24999999999786127, -9.999999999999998224 ) ) ;
#6082 = CARTESIAN_POINT ( 'NONE',  ( -4.217983994794604286, 51.98644305214961747, 48.84278562423152437 ) ) ;
#6084 = VECTOR ( 'NONE', #30382, 1000.000000000000000 ) ;
#6085 = ORIENTED_EDGE ( 'NONE', *, *, #39491, .T. ) ;
#6086 = AXIS2_PLACEMENT_3D ( 'NONE', #34505, #46537, #45793 ) ;
#6088 = EDGE_CURVE ( 'NONE', #70161, #20252, #31999, .T. ) ;
#6087 = CARTESIAN_POINT ( 'NONE',  ( -2.445694354108840063, 198.0625000013656063, 139.5543056458912190 ) ) ;
#6089 = EDGE_CURVE ( 'NONE', #18394, #35448, #21732, .T. ) ;
#6090 = CARTESIAN_POINT ( 'NONE',  ( -3.042071309553164404, 22.23958332991935549, -11.35316468749999963 ) ) ;
#6091 = CARTESIAN_POINT ( 'NONE',  ( -7.778174593052020747, -7.778174593052023411, 94.37500000409677625 ) ) ;
#6092 = CARTESIAN_POINT ( 'NONE',  ( -2.664923566518097392E-11, 208.7499999999979252, 10.00000000000000178 ) ) ;
#6093 = CARTESIAN_POINT ( 'NONE',  ( 11.00000000000000000, 1.347111479062088405E-15, 111.4375000040967763 ) ) ;
#6094 = CARTESIAN_POINT ( 'NONE',  ( -7.778174593052023411, 7.778174593052023411, 101.3124999999999858 ) ) ;
#6096 = CARTESIAN_POINT ( 'NONE',  ( 11.35316468750000141, 15.78124999658601624, 0.000000000000000000 ) ) ;
#6095 = CARTESIAN_POINT ( 'NONE',  ( -4.401442555609581635E-16, 108.7812500020483810, -7.188101187500000044 ) ) ;
#6097 = CARTESIAN_POINT ( 'NONE',  ( 1.469576158976822172E-15, -7.999999999999991118, 23.70530277982336642 ) ) ;
#6098 = CARTESIAN_POINT ( 'NONE',  ( -3.042071309553164404, 137.2395833299193271, -11.35316468749999963 ) ) ;
#6099 = EDGE_CURVE ( 'NONE', #20100, #17783, #9081, .T. ) ;
#6100 = CARTESIAN_POINT ( 'NONE',  ( -10.00000000000000000, 119.1666666598387110, -2.679491924311229845 ) ) ;
#6101 = CARTESIAN_POINT ( 'NONE',  ( -7.188101187500000044, 115.5312500020483952, 0.000000000000000000 ) ) ;
#6102 = CARTESIAN_POINT ( 'NONE',  ( -7.320508075688778149, 4.999999993172033363, 7.320508075688769267 ) ) ;
#6103 = CARTESIAN_POINT ( 'NONE',  ( -24.54126587499998635, 209.3750000013656063, 171.4326545832179818 ) ) ;
#6104 = CARTESIAN_POINT ( 'NONE',  ( -5.000000000000000000, -52.85372778481321632, -48.38359481482913083 ) ) ;
#6105 = ORIENTED_EDGE ( 'NONE', *, *, #24701, .T. ) ;
#6106 = CARTESIAN_POINT ( 'NONE',  ( -9.832129032723418760, 13.17708332991935194, -5.676582343750004256 ) ) ;
#6107 = CARTESIAN_POINT ( 'NONE',  ( -2.679491924311226292, 153.3333333265053682, -10.00000000000000178 ) ) ;
#6108 = CARTESIAN_POINT ( 'NONE',  ( 6.676582343750004256, 295.8906250017069510, 2.765530957081995478 ) ) ;
#6109 = CARTESIAN_POINT ( 'NONE',  ( 9.832129032723420536, 141.1979166632526699, -5.676582343749999815 ) ) ;
#6110 = CARTESIAN_POINT ( 'NONE',  ( -31.99999999999996447, 207.4375000027312410, 171.6568542494928522 ) ) ;
#6111 = CARTESIAN_POINT ( 'NONE',  ( 5.656854249492374365, 5.656854249492375253, 22.82405278432982598 ) ) ;
#6112 = CARTESIAN_POINT ( 'NONE',  ( 5.000000000000001776, 68.60357193678683529, 20.85024232999420946 ) ) ;
#6113 = CARTESIAN_POINT ( 'NONE',  ( 5.676582343750005144, 250.5729166700807014, 9.832129032723416984 ) ) ;
#6114 = EDGE_CURVE ( 'NONE', #1217, #51619, #23231, .T. ) ;
#6115 = CARTESIAN_POINT ( 'NONE',  ( -4.220049686691935698, 10.18810118749999916, 94.75000000204838102 ) ) ;
#6116 = VERTEX_POINT ( 'NONE', #64341 ) ;
#6117 = VECTOR ( 'NONE', #54972, 1000.000000000000000 ) ;
#6118 =( BOUNDED_CURVE ( )  B_SPLINE_CURVE ( 2, ( #65005, #47653, #46923, #41997, #13314, #37089, #59731, #7678, #12589 ),
 .UNSPECIFIED., .F., .F. ) 
 B_SPLINE_CURVE_WITH_KNOTS ( ( 3, 2, 2, 2, 3 ),
 ( 0.1323529411764706731, 0.1360294117647059542, 0.1397058823529412630, 0.1433823529411765441, 0.1470588235294118529 ),
 .UNSPECIFIED. ) 
 CURVE ( )  GEOMETRIC_REPRESENTATION_ITEM ( )  RATIONAL_B_SPLINE_CURVE ( ( 0.9999999999999982236, 0.9238795325112885148, 1.000000000000000000, 0.9238795325112867385, 1.000000000000000000, 0.9238795325112867385, 1.000000000000000000, 0.9238795325112849621, 1.000000000000001776 ) ) 
 REPRESENTATION_ITEM ( '' )  );
#6119 = DIRECTION ( 'NONE',  ( -0.000000000000000000, -0.000000000000000000, 1.000000000000000000 ) ) ;
#6120 = CARTESIAN_POINT ( 'NONE',  ( 4.999999999999999112, 67.53158052529175848, -22.66975313813455273 ) ) ;
#6121 = CARTESIAN_POINT ( 'NONE',  ( 3.042071309553159519, 95.05208332991935549, 11.35316468750000141 ) ) ;
#6122 = ORIENTED_EDGE ( 'NONE', *, *, #10852, .T. ) ;
#6123 = CARTESIAN_POINT ( 'NONE',  ( 1.871523826299183495E-15, -10.18810118749999916, 107.0312500020483810 ) ) ;
#6124 = CARTESIAN_POINT ( 'NONE',  ( -4.541265875000003227, 10.99999999863440969, 1.881053915767121110 ) ) ;
#6125 = ORIENTED_EDGE ( 'NONE', *, *, #20691, .F. ) ;
#6126 = VERTEX_POINT ( 'NONE', #63588 ) ;
#6127 = CARTESIAN_POINT ( 'NONE',  ( 5.656854249492378806, 4.312500000000000000, 5.656854249492381470 ) ) ;
#6128 = CARTESIAN_POINT ( 'NONE',  ( -4.999999999999998224, -62.69792629052194144, -24.03557775816916120 ) ) ;
#6129 = CARTESIAN_POINT ( 'NONE',  ( 2.977408999572650927, 25.12499999795161187, -7.188101187500001821 ) ) ;
#6130 = CARTESIAN_POINT ( 'NONE',  ( 3.313708498984760720, 121.7187500040967763, -8.000000000000000000 ) ) ;
#6131 = CARTESIAN_POINT ( 'NONE',  ( 4.220049686691934809, 10.18810118749999916, 106.5625000020483668 ) ) ;
#6132 = CIRCLE ( 'NONE', #67563, 10.00000000000000178 ) ;
#6133 = CYLINDRICAL_SURFACE ( 'NONE', #52292, 4.000000000000001776 ) ;
#6134 = CARTESIAN_POINT ( 'NONE',  ( -4.000000000000002665, 8.312499997268814056, 1.656854249492380804 ) ) ;
#6135 = CARTESIAN_POINT ( 'NONE',  ( 1.881053915767121998, 1.499999998634406806, -4.541265875000002339 ) ) ;
#6136 = EDGE_LOOP ( 'NONE', ( #20286, #74199, #55826, #33232 ) ) ;
#6137 = FACE_OUTER_BOUND ( 'NONE', #27094, .T. ) ;
#6138 = CARTESIAN_POINT ( 'NONE',  ( 2.839093476692135984E-14, 199.6875000013656063, 201.4587341250000350 ) ) ;
#6139 = CIRCLE ( 'NONE', #51913, 37.00000000000000711 ) ;
#6140 = CARTESIAN_POINT ( 'NONE',  ( -25.55430564589111953, 205.0625000013656063, 172.4456943541091505 ) ) ;
#6141 = CARTESIAN_POINT ( 'NONE',  ( 3.211159895383560947, 9.187499998634407916, 3.211159895383562723 ) ) ;
#6142 = CARTESIAN_POINT ( 'NONE',  ( -27.99999999999991473, 207.6250000027312126, 174.0000000000003695 ) ) ;
#6143 = CARTESIAN_POINT ( 'NONE',  ( 7.188101187499992051, 8.802885111219154394E-16, 11.23655278187175455 ) ) ;
#6144 = ORIENTED_EDGE ( 'NONE', *, *, #62206, .F. ) ;
#6145 = ORIENTED_EDGE ( 'NONE', *, *, #31714, .T. ) ;
#6146 = CARTESIAN_POINT ( 'NONE',  ( 4.220049686691934809, 10.18810118749999916, 112.1875000020483810 ) ) ;
#6147 = CARTESIAN_POINT ( 'NONE',  ( 3.313708498984815343, 96.21875000409679046, -7.999999999999944933 ) ) ;
#6148 = CIRCLE ( 'NONE', #50736, 3.999999999999976019 ) ;
#6149 = CARTESIAN_POINT ( 'NONE',  ( -23.99999999999998934, 204.7500000000000284, 170.0000000000003411 ) ) ;
#6150 = CARTESIAN_POINT ( 'NONE',  ( -3.458734124999959025, 199.5000000013656063, 199.4326545832176691 ) ) ;
#6151 = CARTESIAN_POINT ( 'NONE',  ( 30.44569435410882718, 196.5625000013656063, 172.4456943541086957 ) ) ;
#6152 = CARTESIAN_POINT ( 'NONE',  ( 8.660254037844389075, 100.4166666666666714, -5.000000000000000000 ) ) ;
#6153 = EDGE_CURVE ( 'NONE', #64433, #44389, #22067, .T. ) ;
#6154 = CARTESIAN_POINT ( 'NONE',  ( 8.000000000000000000, 118.3437499999999858, -3.313708498984762496 ) ) ;
#6155 = CARTESIAN_POINT ( 'NONE',  ( 9.832129032723416984, 65.67708332991935549, 5.676582343750006032 ) ) ;
#6156 = CARTESIAN_POINT ( 'NONE',  ( -6.000000000000000888, 288.0625000000000000, 2.485281374238575758 ) ) ;
#6157 = VERTEX_POINT ( 'NONE', #23601 ) ;
#6158 = CARTESIAN_POINT ( 'NONE',  ( -1.737867177246331662, 21.99999999999999645, 4.195582608135537406 ) ) ;
#6159 = CARTESIAN_POINT ( 'NONE',  ( 1.296342370391023291, -10.28012030475504091, 63.61260002839785699 ) ) ;
#6160 = CARTESIAN_POINT ( 'NONE',  ( 3.458734124999959025, 206.5000000013655779, 140.5673454167824161 ) ) ;
#6161 = CARTESIAN_POINT ( 'NONE',  ( -10.00000000000000000, 104.1666666598386968, -2.679491924311229845 ) ) ;
#6162 = CARTESIAN_POINT ( 'NONE',  ( -14.00000000000000178, -2.250000000005106138, 7.677076266390546522 ) ) ;
#6163 = CARTESIAN_POINT ( 'NONE',  ( -8.660254037844385522, 240.4166666666666572, 5.000000000000004441 ) ) ;
#6164 = CARTESIAN_POINT ( 'NONE',  ( 1.224646799147353256E-15, 0.000000000000000000, 10.00000000000000000 ) ) ;
#6165 = CARTESIAN_POINT ( 'NONE',  ( 7.204075437095966983, 7.204075437095967871, 68.96875000204836681 ) ) ;
#6166 = CARTESIAN_POINT ( 'NONE',  ( -7.320508075688778149, 203.1249999999999432, 7.320508075688769267 ) ) ;
#6167 = CARTESIAN_POINT ( 'NONE',  ( 5.082755093536318824, 5.082755093536319713, 14.79905278187175455 ) ) ;
#6168 = CARTESIAN_POINT ( 'NONE',  ( -2.085542519210945728E-15, 174.8437499965860411, 11.35316468750000141 ) ) ;
#6169 = CARTESIAN_POINT ( 'NONE',  ( -10.00000000000022560, 212.7083333333334565, 2.679491924311282691 ) ) ;
#6170 = DIRECTION ( 'NONE',  ( -0.000000000000000000, 1.000000000000000000, -0.000000000000000000 ) ) ;
#6172 = DIRECTION ( 'NONE',  ( -1.000000000000000000, 0.000000000000000000, 0.000000000000000000 ) ) ;
#6171 = CARTESIAN_POINT ( 'NONE',  ( -5.000000000000000888, 227.2916666734946602, -8.660254037844387298 ) ) ;
#6173 = VERTEX_POINT ( 'NONE', #40588 ) ;
#6174 = AXIS2_PLACEMENT_3D ( 'NONE', #67446, #49335, #3700 ) ;
#6176 = EDGE_CURVE ( 'NONE', #22089, #4336, #71622, .T. ) ;
#6175 = CARTESIAN_POINT ( 'NONE',  ( -3.458734125000015425, 208.2500000013656063, 143.4326545832176976 ) ) ;
#6177 = CARTESIAN_POINT ( 'NONE',  ( -11.35316468749999785, 38.38541666325268409, -3.042071309553167513 ) ) ;
#6178 = CARTESIAN_POINT ( 'NONE',  ( 4.556349186104051263, -10.99999999999999822, 108.1562500040967620 ) ) ;
#6179 = CARTESIAN_POINT ( 'NONE',  ( -29.43265458321755901, 205.8750000013656063, 173.4587341250004044 ) ) ;
#6180 = PLANE ( 'NONE',  #44255 ) ;
#6182 = FACE_OUTER_BOUND ( 'NONE', #42941, .T. ) ;
#6181 = CARTESIAN_POINT ( 'NONE',  ( 10.00000000000000000, 221.6666666598386826, 2.679491924311235618 ) ) ;
#6183 = CARTESIAN_POINT ( 'NONE',  ( -1.432654583217664479, 197.7500000013656063, 138.5412658750000787 ) ) ;
#6184 = CARTESIAN_POINT ( 'NONE',  ( 4.999999999999993783, 56.04166665983870388, 8.660254037844390851 ) ) ;
#6185 = CARTESIAN_POINT ( 'NONE',  ( -5.082755093536324154, 95.84375000204838102, 5.082755093536326818 ) ) ;
#6186 = CARTESIAN_POINT ( 'NONE',  ( 4.541265875000002339, 12.43749999863440792, 0.000000000000000000 ) ) ;
#6187 = CARTESIAN_POINT ( 'NONE',  ( 7.320508075688770155, 55.62499999999998579, -7.320508075688770155 ) ) ;
#6188 = CARTESIAN_POINT ( 'NONE',  ( 5.656854249492374365, 5.656854249492375253, 1.767802779823364423 ) ) ;
#6189 = CARTESIAN_POINT ( 'NONE',  ( 38.00000000000000000, 272.0000000000000000, 20.00000000000002132 ) ) ;
#6190 = EDGE_LOOP ( 'NONE', ( #2004, #26027, #51420, #5371 ) ) ;
#6191 = VERTEX_POINT ( 'NONE', #52285 ) ;
#6192 = CARTESIAN_POINT ( 'NONE',  ( -11.00000000000000000, 0.000000000000000000, 116.4999999999999858 ) ) ;
#6193 = CARTESIAN_POINT ( 'NONE',  ( 4.721056650415999201, 297.2343750017069510, -4.721056650415999201 ) ) ;
#6194 = CARTESIAN_POINT ( 'NONE',  ( -2.978189300774432354E-14, -67.59332269700065865, -20.03478791450352858 ) ) ;
#6195 = CARTESIAN_POINT ( 'NONE',  ( -3.428378827818324037, 51.66489094707790031, -48.71857030467307936 ) ) ;
#6196 = CARTESIAN_POINT ( 'NONE',  ( -5.676582343749998039, 152.4479166632526983, -9.832129032723420536 ) ) ;
#6197 = FACE_OUTER_BOUND ( 'NONE', #49262, .T. ) ;
#6198 = CARTESIAN_POINT ( 'NONE',  ( -10.18810118749999738, -4.220049686691941915, 84.25000000204838102 ) ) ;
#6199 = CARTESIAN_POINT ( 'NONE',  ( -30.28816258356541269, 194.6946065536776587, 172.9096376744251984 ) ) ;
#6200 = CARTESIAN_POINT ( 'NONE',  ( -2.828427124746153876, 204.8750000000000284, 195.1715728752538439 ) ) ;
#6201 = CARTESIAN_POINT ( 'NONE',  ( -7.999999999999991118, 9.797174393178815797E-16, 30.00000000000000000 ) ) ;
#6202 = AXIS2_PLACEMENT_3D ( 'NONE', #26956, #3210, #15629 ) ;
#6203 = EDGE_CURVE ( 'NONE', #68267, #8780, #46241, .T. ) ;
#6204 = CARTESIAN_POINT ( 'NONE',  ( 7.204075437095968759, -7.204075437095966983, 115.0937500020483810 ) ) ;
#6205 = VERTEX_POINT ( 'NONE', #11917 ) ;
#6206 = EDGE_CURVE ( 'NONE', #65581, #59754, #34950, .T. ) ;
#6207 = CARTESIAN_POINT ( 'NONE',  ( 5.230138811819043276, 178.6826066192556084, 133.6529148158310250 ) ) ;
#6208 = CARTESIAN_POINT ( 'NONE',  ( 11.35316468749999785, 125.8854166632526983, 3.042071309553174174 ) ) ;
#6209 = CARTESIAN_POINT ( 'NONE',  ( 2.445694354108838731, 200.0625000013656063, 195.5543056458912190 ) ) ;
#6210 = CARTESIAN_POINT ( 'NONE',  ( -5.082755093536325042, 26.90624999795161898, -5.082755093536325930 ) ) ;
#6211 =( BOUNDED_CURVE ( )  B_SPLINE_CURVE ( 2, ( #71263, #25974, #54312, #26739, #42598, #65612, #2623, #49759, #20324 ),
 .UNSPECIFIED., .F., .F. ) 
 B_SPLINE_CURVE_WITH_KNOTS ( ( 3, 2, 2, 2, 3 ),
 ( 0.03333333333333336063, 0.04166666666666669905, 0.05000000000000004441, 0.05833333333333338283, 0.06666666666666672125 ),
 .UNSPECIFIED. ) 
 CURVE ( )  GEOMETRIC_REPRESENTATION_ITEM ( )  RATIONAL_B_SPLINE_CURVE ( ( 0.9999999999999997780, 0.9238795325112869605, 1.000000000000000000, 0.9238795325112867385, 1.000000000000000000, 0.9238795325112867385, 1.000000000000000000, 0.9238795325112861834, 1.000000000000000444 ) ) 
 REPRESENTATION_ITEM ( '' )  );
#6212 = CARTESIAN_POINT ( 'NONE',  ( 7.204075437095966983, 7.204075437095967871, 76.46875000204836681 ) ) ;
#6213 = CARTESIAN_POINT ( 'NONE',  ( -2.085542519210945728E-15, 44.84374999658602690, 11.35316468750000141 ) ) ;
#6214 = ORIENTED_EDGE ( 'NONE', *, *, #5736, .T. ) ;
#6215 = CARTESIAN_POINT ( 'NONE',  ( 2.679491924311228956, 37.91666665983869677, -10.00000000000000000 ) ) ;
#6216 = CARTESIAN_POINT ( 'NONE',  ( -1.881053915767121776, 0.7499999986344069169, -4.541265875000002339 ) ) ;
#6217 = CARTESIAN_POINT ( 'NONE',  ( -5.662595241051933570, -5.662595241051936235, 14.70061528394063188 ) ) ;
#6218 = CARTESIAN_POINT ( 'NONE',  ( -2.445694354108839175, 207.3125000013656063, 144.4456943541088663 ) ) ;
#6219 = CIRCLE ( 'NONE', #2592, 7.500000000000020428 ) ;
#6220 = EDGE_CURVE ( 'NONE', #25826, #26283, #73624, .T. ) ;
#6221 = EDGE_CURVE ( 'NONE', #9770, #36810, #37495, .T. ) ;
#6222 = CARTESIAN_POINT ( 'NONE',  ( -5.082755093536326818, 7.406249997951610986, 5.082755093536325042 ) ) ;
#6223 = CARTESIAN_POINT ( 'NONE',  ( 6.000000000000003553, 296.6250000034139589, -2.485281374238571761 ) ) ;
#6224 = CARTESIAN_POINT ( 'NONE',  ( -13.16080087645149632, -22.94855820181512485, 138.5354884549738301 ) ) ;
#6225 = CARTESIAN_POINT ( 'NONE',  ( -1.320432766682874540E-15, 7.968749997951610986, 7.188101187500000044 ) ) ;
#6226 = CARTESIAN_POINT ( 'NONE',  ( -7.188101187499992051, 0.000000000000000000, 8.986552781871752771 ) ) ;
#6227 = CARTESIAN_POINT ( 'NONE',  ( 4.220049686691941027, -10.18810118749999738, 71.12500000204836681 ) ) ;
#6228 = EDGE_CURVE ( 'NONE', #33407, #7437, #31447, .T. ) ;
#6229 = CARTESIAN_POINT ( 'NONE',  ( -29.43265458321761230, 206.1250000013655779, 173.4587341250003760 ) ) ;
#6230 =( BOUNDED_CURVE ( )  B_SPLINE_CURVE ( 2, ( #18467, #17719, #35825, #37682, #2222, #32016, #42576, #26332, #37302 ),
 .UNSPECIFIED., .F., .F. ) 
 B_SPLINE_CURVE_WITH_KNOTS ( ( 3, 2, 2, 2, 3 ),
 ( 0.7499999999999998890, 0.7536764705882351700, 0.7573529411764705621, 0.7610294117647058432, 0.7647058823529411242 ),
 .UNSPECIFIED. ) 
 CURVE ( )  GEOMETRIC_REPRESENTATION_ITEM ( )  RATIONAL_B_SPLINE_CURVE ( ( 1.000000000000002220, 0.9238795325112844070, 1.000000000000000000, 0.9238795325112867385, 1.000000000000000000, 0.9238795325112867385, 1.000000000000000000, 0.9238795325112867385, 1.000000000000000000 ) ) 
 REPRESENTATION_ITEM ( '' )  );
#6231 = FACE_OUTER_BOUND ( 'NONE', #3071, .T. ) ;
#6232 = CARTESIAN_POINT ( 'NONE',  ( -8.342170076843785083E-16, 20.18749999863440436, 4.541265875000002339 ) ) ;
#6233 = EDGE_LOOP ( 'NONE', ( #19872, #60171, #53952, #5183 ) ) ;
#6234 = AXIS2_PLACEMENT_3D ( 'NONE', #993, #68514, #40218 ) ;
#6235 = CARTESIAN_POINT ( 'NONE',  ( 2.751064625579944321E-14, 197.8750000027312126, 194.0000000000000568 ) ) ;
#6236 = CARTESIAN_POINT ( 'NONE',  ( -4.000000000000015987, 204.4375000000000853, 140.3431457505076594 ) ) ;
#6237 = CARTESIAN_POINT ( 'NONE',  ( -23.99999999999995737, 201.8125000027312126, 171.6568542494926817 ) ) ;
#6238 = CARTESIAN_POINT ( 'NONE',  ( 2.977408999572650039, 114.6875000020484094, -7.188101187500001821 ) ) ;
#6239 = CARTESIAN_POINT ( 'NONE',  ( -27.99999999999991118, 202.6250000027312126, 174.0000000000003695 ) ) ;
#6240 = CARTESIAN_POINT ( 'NONE',  ( 5.656854249492374365, 5.656854249492375253, 9.455302783920146226 ) ) ;
#6241 = ORIENTED_EDGE ( 'NONE', *, *, #38040, .F. ) ;
#6242 = CARTESIAN_POINT ( 'NONE',  ( 2.977408999572652260, 15.18749999795161365, 7.188101187500000044 ) ) ;
#6243 = EDGE_LOOP ( 'NONE', ( #58554, #19382, #56979, #64425 ) ) ;
#6244 = CARTESIAN_POINT ( 'NONE',  ( 30.82842712474617031, 200.1250000000000284, 172.8284271247460993 ) ) ;
#6245 = CARTESIAN_POINT ( 'NONE',  ( -0.3909958203064078375, -47.98096487016210432, 151.0030343406995428 ) ) ;
#6246 = CARTESIAN_POINT ( 'NONE',  ( 7.320508075688771044, 44.37500000000000000, 7.320508075688775484 ) ) ;
#6247 = CARTESIAN_POINT ( 'NONE',  ( 7.188101187500001821, 108.8750000020483810, -2.977408999572651371 ) ) ;
#6248 = CARTESIAN_POINT ( 'NONE',  ( -30.44569435410879521, 207.0625000013656063, 172.4456943541092357 ) ) ;
#6249 = DIRECTION ( 'NONE',  ( -0.8660254037844312691, -0.5000000000000128786, -0.000000000000000000 ) ) ;
#6251 = CARTESIAN_POINT ( 'NONE',  ( -8.000000000000000000, 95.09375000409679046, -3.313708498984761164 ) ) ;
#6250 = CARTESIAN_POINT ( 'NONE',  ( -10.00000000000000178, 34.37499999317203248, -1.224646799147353454E-15 ) ) ;
#6252 = ORIENTED_EDGE ( 'NONE', *, *, #13058, .T. ) ;
#6253 = CARTESIAN_POINT ( 'NONE',  ( 8.311093377946839666, 245.7812500034139873, 8.311093377946829008 ) ) ;
#6254 = CARTESIAN_POINT ( 'NONE',  ( -2.977408999572647819, 7.188101187499991163, 16.58030278187175455 ) ) ;
#6255 = VECTOR ( 'NONE', #69253, 1000.000000000000000 ) ;
#6256 = LINE ( 'NONE', #2059, #25700 ) ;
#6257 = CARTESIAN_POINT ( 'NONE',  ( 30.82842712474620583, 206.3750000000000284, 167.1715728752537586 ) ) ;
#6258 = CARTESIAN_POINT ( 'NONE',  ( -9.000000000000000000, -5.196152422706644458, -10.20000000000000284 ) ) ;
#6260 = ADVANCED_FACE ( 'NONE', ( #16810 ), #62792, .F. ) ;
#6259 = CARTESIAN_POINT ( 'NONE',  ( -4.556349186104045934, 11.00000000000000000, 116.4062500040967905 ) ) ;
#6261 = CARTESIAN_POINT ( 'NONE',  ( 6.123233995736767268E-16, 156.2500000000000000, -10.00000000000000178 ) ) ;
#6262 = DIRECTION ( 'NONE',  ( -0.000000000000000000, 1.000000000000000000, -0.000000000000000000 ) ) ;
#6263 = CARTESIAN_POINT ( 'NONE',  ( 4.999999999999999112, -53.34243969459480894, -47.33397984627203670 ) ) ;
#6264 = CARTESIAN_POINT ( 'NONE',  ( 11.35316468750000141, 136.0937499965860127, 0.000000000000000000 ) ) ;
#6265 = CARTESIAN_POINT ( 'NONE',  ( 0.000000000000000000, 125.0000000000000000, 0.000000000000000000 ) ) ;
#6266 = CARTESIAN_POINT ( 'NONE',  ( -3.313708498984775375, 5.531249999999999112, 7.999999999999988454 ) ) ;
#6269 = CARTESIAN_POINT ( 'NONE',  ( 7.778174593052021635, 7.778174593052023411, 84.62500000409677625 ) ) ;
#6268 = FACE_OUTER_BOUND ( 'NONE', #63291, .T. ) ;
#6267 = CARTESIAN_POINT ( 'NONE',  ( 29.43265458321760519, 194.7500000013656063, 173.4587341249998929 ) ) ;
#6270 = ORIENTED_EDGE ( 'NONE', *, *, #8996, .F. ) ;
#6271 = CARTESIAN_POINT ( 'NONE',  ( -5.676582343749998039, 2.760416663252683644, -9.832129032723420536 ) ) ;
#6272 = DIRECTION ( 'NONE',  ( -1.000000000000000000, 0.000000000000000000, 0.000000000000000000 ) ) ;
#6273 =( REPRESENTATION_RELATIONSHIP ('NONE','NONE', #46008, #48857 ) REPRESENTATION_RELATIONSHIP_WITH_TRANSFORMATION ( #1434 )SHAPE_REPRESENTATION_RELATIONSHIP( ) );
#6274 = CARTESIAN_POINT ( 'NONE',  ( 2.449293598294707893E-16, 11.25000000000000000, -4.000000000000001776 ) ) ;
#6275 = EDGE_CURVE ( 'NONE', #50334, #66510, #58329, .T. ) ;
#6276 = CARTESIAN_POINT ( 'NONE',  ( 8.660254037844389075, 27.29166665983870033, -5.000000000000000000 ) ) ;
#6277 = CARTESIAN_POINT ( 'NONE',  ( -4.401442555609581635E-16, 116.2812500020483810, -7.188101187500000044 ) ) ;
#6278 = CARTESIAN_POINT ( 'NONE',  ( -8.342170076843785083E-16, 1.187499998634406806, 4.541265875000002339 ) ) ;
#6279 = CARTESIAN_POINT ( 'NONE',  ( 5.656854249492376141, -5.656854249492374365, 19.39280277982336642 ) ) ;
#6281 = CARTESIAN_POINT ( 'NONE',  ( -32.00000000000000000, 207.2500000000000284, 170.0000000000003979 ) ) ;
#6280 = CARTESIAN_POINT ( 'NONE',  ( -48.52446885514075348, 42.18184438052347929, 60.87679713484597244 ) ) ;
#6282 = CARTESIAN_POINT ( 'NONE',  ( 5.676582343749993598, 104.9479166632526841, 9.832129032723422313 ) ) ;
#6283 = VERTEX_POINT ( 'NONE', #987 ) ;
#6284 = CARTESIAN_POINT ( 'NONE',  ( -2.828427124746192067, 19.37499999726881228, 2.828427124746190735 ) ) ;
#6286 = DIRECTION ( 'NONE',  ( 0.000000000000000000, 0.000000000000000000, 1.000000000000000000 ) ) ;
#6285 = PRODUCT_DEFINITION ( 'UNKNOWN', '', #67084, #22915 ) ;
#6287 = CARTESIAN_POINT ( 'NONE',  ( -3.042071309553159075, 250.2604166700806445, 11.35316468749999963 ) ) ;
#6288 = AXIS2_PLACEMENT_3D ( 'NONE', #17315, #34330, #69754 ) ;
#6289 = CARTESIAN_POINT ( 'NONE',  ( -9.832129032723418760, 112.8645833299193555, -5.676582343750004256 ) ) ;
#6290 = VERTEX_POINT ( 'NONE', #23971 ) ;
#6291 = CARTESIAN_POINT ( 'NONE',  ( -18.00000000000000000, -10.39230484541329425, -20.69999999999999929 ) ) ;
#6292 = CARTESIAN_POINT ( 'NONE',  ( 4.220049686691941027, -10.18810118749999738, 99.62500000204838102 ) ) ;
#6293 = CARTESIAN_POINT ( 'NONE',  ( 10.00000000000000178, 216.8749999931720538, 0.000000000000000000 ) ) ;
#6294 = CARTESIAN_POINT ( 'NONE',  ( -1.432654583217607414, 202.5000000013656063, 194.5412658750000219 ) ) ;
#6295 = CARTESIAN_POINT ( 'NONE',  ( -7.778174593052020747, -7.778174593052023411, 68.68749999999998579 ) ) ;
#6297 = CARTESIAN_POINT ( 'NONE',  ( 5.676582343749993598, 104.9479166632526841, 9.832129032723422313 ) ) ;
#6296 = CARTESIAN_POINT ( 'NONE',  ( -10.00000000000000000, 182.5000000000000568, -1.224646799147353059E-15 ) ) ;
#6298 = CARTESIAN_POINT ( 'NONE',  ( 7.999999999999992895, -3.313708498984756279, 6.174052783920146226 ) ) ;
#6299 = CARTESIAN_POINT ( 'NONE',  ( -31.45873412499999233, 196.9375000013655779, 170.0000000000003979 ) ) ;
#6300 = CARTESIAN_POINT ( 'NONE',  ( 2.849036369511732440E-14, 208.3750000027312126, 202.0000000000000000 ) ) ;
#6301 = EDGE_LOOP ( 'NONE', ( #34744, #61674, #53412, #67936 ) ) ;
#6302 = AXIS2_PLACEMENT_3D ( 'NONE', #69173, #167, #11830 ) ;
#6303 = CARTESIAN_POINT ( 'NONE',  ( 4.999999999999993783, 191.0416666598387110, 8.660254037844390851 ) ) ;
#6304 = EDGE_CURVE ( 'NONE', #29704, #56610, #46978, .T. ) ;
#6305 = CARTESIAN_POINT ( 'NONE',  ( 2.828427124746191623, 6.125000000000000000, -2.828427124746191623 ) ) ;
#6306 = DIRECTION ( 'NONE',  ( -0.000000000000000000, -0.000000000000000000, -1.000000000000000000 ) ) ;
#6307 = CARTESIAN_POINT ( 'NONE',  ( -3.042071309553173730, 84.63541666325266988, 11.35316468749999785 ) ) ;
#6308 = CARTESIAN_POINT ( 'NONE',  ( -2.765530957081998586, 287.6406250017069510, 6.676582343750001591 ) ) ;
#6309 = CARTESIAN_POINT ( 'NONE',  ( -2.977408999572650039, 4.312499997951610098, -7.188101187500000933 ) ) ;
#6310 = CARTESIAN_POINT ( 'NONE',  ( -7.204075437095967871, 7.204075437095967871, 93.34375000204838102 ) ) ;
#6311 = EDGE_CURVE ( 'NONE', #38945, #70823, #55592, .T. ) ;
#6312 = CARTESIAN_POINT ( 'NONE',  ( -9.832129032723418760, 217.8645833299193839, -5.676582343750004256 ) ) ;
#6313 = ORIENTED_EDGE ( 'NONE', *, *, #63443, .F. ) ;
#6314 = CARTESIAN_POINT ( 'NONE',  ( 1.656854249492381914, 20.56249999726881583, 4.000000000000000888 ) ) ;
#6315 = CARTESIAN_POINT ( 'NONE',  ( 2.846472598640537921, -44.03263910056732300, 139.1308692895143224 ) ) ;
#6316 = CARTESIAN_POINT ( 'NONE',  ( -5.676582343750006032, 224.1145833299193839, 9.832129032723418760 ) ) ;
#6317 = CARTESIAN_POINT ( 'NONE',  ( -10.18810118749999916, 4.220049686691934809, 81.43750000204836681 ) ) ;
#6318 = CARTESIAN_POINT ( 'NONE',  ( 11.00000000000000000, 1.347111479062088405E-15, 73.74999999999998579 ) ) ;
#6319 = DIRECTION ( 'NONE',  ( -1.000000000000000000, 0.000000000000000000, -0.000000000000000000 ) ) ;
#6320 = CARTESIAN_POINT ( 'NONE',  ( 2.765530957082001251, 295.7656250017069510, 6.676582343750000703 ) ) ;
#6321 = ORIENTED_EDGE ( 'NONE', *, *, #17785, .F. ) ;
#6322 = CARTESIAN_POINT ( 'NONE',  ( -10.00000000000000355, 119.5833333265053824, 2.679491924311223183 ) ) ;
#6323 = CARTESIAN_POINT ( 'NONE',  ( -8.311093377946841443, 214.2187499965860127, 8.311093377946834337 ) ) ;
#6324 = CARTESIAN_POINT ( 'NONE',  ( -4.220049686691937474, -10.18810118749999738, 90.43750000204836681 ) ) ;
#6325 = AXIS2_PLACEMENT_3D ( 'NONE', #24070, #22969, #35782 ) ;
#6326 = EDGE_CURVE ( 'NONE', #11982, #41993, #53370, .T. ) ;
#6327 = CARTESIAN_POINT ( 'NONE',  ( -31.45873412499999944, 202.6875000013656063, 170.0000000000003979 ) ) ;
#6328 = CARTESIAN_POINT ( 'NONE',  ( -5.656854249492379694, 15.56250000000000355, -5.656854249492380582 ) ) ;
#6329 = ORIENTED_EDGE ( 'NONE', *, *, #11517, .T. ) ;
#6330 = CARTESIAN_POINT ( 'NONE',  ( -7.188101187500000044, 124.1562500020483810, 0.000000000000000000 ) ) ;
#6331 =( BOUNDED_CURVE ( )  B_SPLINE_CURVE ( 2, ( #28132, #17180, #238, #21720, #27382, #63204, #40573, #22458, #4389, #51897, #23219, #16057, #50401 ),
 .UNSPECIFIED., .F., .F. ) 
 B_SPLINE_CURVE_WITH_KNOTS ( ( 3, 2, 2, 2, 2, 2, 3 ),
 ( 0.02717391304347826012, 0.02898550724637681195, 0.03079710144927536378, 0.03260869565217391214, 0.03442028985507246397, 0.03623188405797101580, 0.03804347826086956763 ),
 .UNSPECIFIED. ) 
 CURVE ( )  GEOMETRIC_REPRESENTATION_ITEM ( )  RATIONAL_B_SPLINE_CURVE ( ( 1.000000000000000000, 0.9659258262890683122, 1.000000000000000000, 0.9659258262890683122, 1.000000000000000000, 0.9659258262890683122, 1.000000000000000000, 0.9659258262890683122, 1.000000000000000000, 0.9659258262890683122, 1.000000000000000000, 0.9659258262890683122, 1.000000000000000000 ) ) 
 REPRESENTATION_ITEM ( '' )  );
#6332 = CARTESIAN_POINT ( 'NONE',  ( -10.00000000000000178, 27.50000000000000000, -1.224646799147353454E-15 ) ) ;
#6333 = VECTOR ( 'NONE', #36829, 1000.000000000000000 ) ;
#6334 = CARTESIAN_POINT ( 'NONE',  ( -25.17157287525381903, 197.8750000000000284, 167.1715728752541565 ) ) ;
#6335 = CARTESIAN_POINT ( 'NONE',  ( 10.18810118749999916, 1.247682550866122264E-15, 74.78125000204836681 ) ) ;
#6336 = ORIENTED_EDGE ( 'NONE', *, *, #67567, .T. ) ;
#6337 = CARTESIAN_POINT ( 'NONE',  ( -5.082755093536325042, 1.031249997951609876, -5.082755093536325930 ) ) ;
#6338 = CARTESIAN_POINT ( 'NONE',  ( 0.000000000000000000, 0.000000000000000000, -17.50000000000000000 ) ) ;
#6339 = AXIS2_PLACEMENT_3D ( 'NONE', #40070, #34434, #34063 ) ;
#6340 = CARTESIAN_POINT ( 'NONE',  ( -11.00000000000000000, 0.000000000000000000, 92.68750000409677625 ) ) ;
#6341 = CARTESIAN_POINT ( 'NONE',  ( -5.082755093536324154, 123.2187500020483952, 5.082755093536326818 ) ) ;
#6342 = CARTESIAN_POINT ( 'NONE',  ( 5.000000000000001776, -67.10993666412744574, 23.06595724273596204 ) ) ;
#6343 = CARTESIAN_POINT ( 'NONE',  ( -4.088227598258586603E-16, 298.2031250017070079, -6.676582343750001591 ) ) ;
#6344 = EDGE_CURVE ( 'NONE', #9485, #52532, #14347, .T. ) ;
#6346 = CARTESIAN_POINT ( 'NONE',  ( -7.188101187500000044, 124.1562500020483810, 0.000000000000000000 ) ) ;
#6345 = CARTESIAN_POINT ( 'NONE',  ( -11.35316468749999785, 238.6979166700806729, -3.042071309553164848 ) ) ;
#6347 = ITEM_DEFINED_TRANSFORMATION ( 'NONE', 'NONE', #3221,  #57354 ) ;
#6348 = AXIS2_PLACEMENT_3D ( 'NONE', #58718, #40991, #63998 ) ;
#6349 = ORIENTED_EDGE ( 'NONE', *, *, #27893, .F. ) ;
#6350 =( BOUNDED_CURVE ( )  B_SPLINE_CURVE ( 2, ( #62322, #51008, #45344, #11026, #51376, #74387, #47562, #30594, #7222, #17791, #30958, #64917, #53612 ),
 .UNSPECIFIED., .F., .F. ) 
 B_SPLINE_CURVE_WITH_KNOTS ( ( 3, 2, 2, 2, 2, 2, 3 ),
 ( 0.8055555555555555802, 0.8148148148148147696, 0.8240740740740740700, 0.8333333333333333703, 0.8425925925925925597, 0.8518518518518518601, 0.8611111111111111605 ),
 .UNSPECIFIED. ) 
 CURVE ( )  GEOMETRIC_REPRESENTATION_ITEM ( )  RATIONAL_B_SPLINE_CURVE ( ( 1.000000000000000000, 0.9659258262890683122, 1.000000000000000000, 0.9659258262890683122, 1.000000000000000000, 0.9659258262890683122, 1.000000000000000000, 0.9659258262890683122, 1.000000000000000000, 0.9659258262890683122, 1.000000000000000000, 0.9659258262890683122, 1.000000000000000000 ) ) 
 REPRESENTATION_ITEM ( '' )  );
#6351 = CARTESIAN_POINT ( 'NONE',  ( 3.042071309553173286, 240.6770833367473301, 11.35316468749999608 ) ) ;
#6352 = CARTESIAN_POINT ( 'NONE',  ( 1.320432766682872962E-15, -7.188101187499992051, 4.861552781871752771 ) ) ;
#6353 = EDGE_CURVE ( 'NONE', #653, #25916, #59202, .T. ) ;
#6354 = ORIENTED_EDGE ( 'NONE', *, *, #1228, .T. ) ;
#6355 = CARTESIAN_POINT ( 'NONE',  ( 4.220049686691941027, -10.18810118749999738, 71.12500000204836681 ) ) ;
#6356 = CARTESIAN_POINT ( 'NONE',  ( -11.35316468750000141, 83.59374999658601268, -1.390361679473963753E-15 ) ) ;
#6357 = CARTESIAN_POINT ( 'NONE',  ( 12.00000000000000000, 6.928203230275491009, -14.80000000000000071 ) ) ;
#6358 = CARTESIAN_POINT ( 'NONE',  ( 11.00000000000000000, 4.556349186104045934, 84.34375000000000000 ) ) ;
#6360 = CARTESIAN_POINT ( 'NONE',  ( 29.65685424949240101, 194.1875000027312126, 173.9999999999999147 ) ) ;
#6359 = CARTESIAN_POINT ( 'NONE',  ( 31.45873412500001010, 209.0000000013655779, 168.5673454167822740 ) ) ;
#6361 = ORIENTED_EDGE ( 'NONE', *, *, #53078, .T. ) ;
#6362 = CARTESIAN_POINT ( 'NONE',  ( -27.99999999999999645, 210.0000000000000284, 174.0000000000003411 ) ) ;
#6363 = DIRECTION ( 'NONE',  ( -1.000000000000000000, 0.000000000000000000, -0.000000000000000000 ) ) ;
#6364 = CARTESIAN_POINT ( 'NONE',  ( 9.832129032723416984, 205.3645833299193555, 5.676582343750006032 ) ) ;
#6365 = CARTESIAN_POINT ( 'NONE',  ( -2.754378923186476579E-14, 207.1875000013656063, 145.4587341250000350 ) ) ;
#6366 = CARTESIAN_POINT ( 'NONE',  ( 29.43265458321761230, 204.7500000013656063, 173.4587341249998929 ) ) ;
#6367 = CARTESIAN_POINT ( 'NONE',  ( -2.977408999572650039, 23.81249999795161543, -7.188101187500001821 ) ) ;
#6368 = CARTESIAN_POINT ( 'NONE',  ( -8.311093377946841443, 179.2187499965859843, 8.311093377946830785 ) ) ;
#6369 = CARTESIAN_POINT ( 'NONE',  ( 5.082755093536326818, 95.09375000204838102, 5.082755093536325042 ) ) ;
#6371 = CARTESIAN_POINT ( 'NONE',  ( 0.000000000000000000, 124.5000000000000284, 8.000000000000000000 ) ) ;
#6370 = CARTESIAN_POINT ( 'NONE',  ( -5.000000000000000000, 67.91996363552695470, -22.23680535815822168 ) ) ;
#6372 = CARTESIAN_POINT ( 'NONE',  ( 4.541265875000001451, 10.24999999863440792, 1.881053915767124440 ) ) ;
#6373 = CARTESIAN_POINT ( 'NONE',  ( 25.55430564589115150, 201.5625000013656063, 172.4456943541086957 ) ) ;
#6374 = CARTESIAN_POINT ( 'NONE',  ( 7.188101187499991163, 2.977408999572648707, 7.205302781871754547 ) ) ;
#6375 = CARTESIAN_POINT ( 'NONE',  ( -11.35316468750000141, 63.48958332991935549, 3.042071309553159963 ) ) ;
#6376 = ADVANCED_FACE ( 'NONE', ( #1721 ), #71091, .T. ) ;
#6377 = CARTESIAN_POINT ( 'NONE',  ( -30.93541659651595310, 271.9999999999999432, 167.9999999999998295 ) ) ;
#6378 = CARTESIAN_POINT ( 'NONE',  ( -5.656854249492373476, -5.656854249492376141, 2.574052784329821986 ) ) ;
#6379 = EDGE_LOOP ( 'NONE', ( #67725, #35718, #41421, #44547 ) ) ;
#6380 = DIRECTION ( 'NONE',  ( 0.000000000000000000, 0.000000000000000000, -1.000000000000000000 ) ) ;
#6381 = DIRECTION ( 'NONE',  ( -0.8660254037844381525, 0.5000000000000008882, 0.000000000000000000 ) ) ;
#6382 = CARTESIAN_POINT ( 'NONE',  ( 9.832129032723416984, 60.36458332991934839, 5.676582343750006032 ) ) ;
#6383 = CARTESIAN_POINT ( 'NONE',  ( -4.556349186104047710, -10.99999999999999822, 68.96875000409676204 ) ) ;
#6384 = CARTESIAN_POINT ( 'NONE',  ( -2.445694354108839175, 196.3125000013656063, 144.4456943541088663 ) ) ;
#6385 = CARTESIAN_POINT ( 'NONE',  ( 7.999999999999991118, 0.000000000000000000, 30.00000000000000000 ) ) ;
#6387 = CARTESIAN_POINT ( 'NONE',  ( -3.042071309553163960, 57.23958332991935549, -11.35316468749999963 ) ) ;
#6386 = CARTESIAN_POINT ( 'NONE',  ( -2.977408999572650927, 95.37500000204839523, -7.188101187500000933 ) ) ;
#6388 = CARTESIAN_POINT ( 'NONE',  ( 7.999999999999992895, -3.313708498984756279, 24.17405278392015333 ) ) ;
#6389 = DIRECTION ( 'NONE',  ( -1.000000000000000000, -0.000000000000000000, -0.000000000000000000 ) ) ;
#6390 = CARTESIAN_POINT ( 'NONE',  ( -1.836970198721029983E-15, 160.6249999931720254, 10.00000000000000178 ) ) ;
#6391 = CARTESIAN_POINT ( 'NONE',  ( 7.188101187500000044, 93.78125000204836681, -8.802885111219163269E-16 ) ) ;
#6392 = CARTESIAN_POINT ( 'NONE',  ( -11.00000000000000000, 0.000000000000000000, 108.9999999999999858 ) ) ;
#6393 = CARTESIAN_POINT ( 'NONE',  ( 3.042071309553167513, 42.13541666325267698, -11.35316468749999785 ) ) ;
#6394 = CARTESIAN_POINT ( 'NONE',  ( 4.220049686691934809, 10.18810118749999916, 115.5625000020483810 ) ) ;
#6395 = CARTESIAN_POINT ( 'NONE',  ( 11.35316468749999963, 185.9895833299193839, -3.042071309553165293 ) ) ;
#6396 = ORIENTED_EDGE ( 'NONE', *, *, #73603, .T. ) ;
#6397 = CARTESIAN_POINT ( 'NONE',  ( 2.449293598294707893E-16, 4.250000000000000000, -4.000000000000001776 ) ) ;
#6398 = DIRECTION ( 'NONE',  ( 0.000000000000000000, 0.000000000000000000, 1.000000000000000000 ) ) ;
#6399 = CARTESIAN_POINT ( 'NONE',  ( 10.00000000000000178, 61.87499999317203958, 0.000000000000000000 ) ) ;
#6401 = CARTESIAN_POINT ( 'NONE',  ( 5.676582343749993598, 179.9479166632526983, 9.832129032723422313 ) ) ;
#6400 = CARTESIAN_POINT ( 'NONE',  ( 3.428378827818083785, -68.02396499344416725, 20.38382289158473171 ) ) ;
#6402 = VECTOR ( 'NONE', #74127, 1000.000000000000000 ) ;
#6403 = CARTESIAN_POINT ( 'NONE',  ( 0.000000000000000000, 0.5000000000000004441, 8.000000000000000000 ) ) ;
#6404 = CARTESIAN_POINT ( 'NONE',  ( 10.00000000000000000, 255.6250000068279746, -1.224646799147353256E-15 ) ) ;
#6405 = DIRECTION ( 'NONE',  ( 0.000000000000000000, 0.000000000000000000, 1.000000000000000000 ) ) ;
#6406 = ORIENTED_EDGE ( 'NONE', *, *, #35396, .F. ) ;
#6407 = CARTESIAN_POINT ( 'NONE',  ( 3.042071309553159519, 170.0520833299193271, 11.35316468750000141 ) ) ;
#6408 = CARTESIAN_POINT ( 'NONE',  ( 4.541265875000002339, 0.3749999986344067504, 0.000000000000000000 ) ) ;
#6409 = CARTESIAN_POINT ( 'NONE',  ( -2.085542519210945728E-15, 129.8437499965860127, 11.35316468750000141 ) ) ;
#6410 = DIRECTION ( 'NONE',  ( 0.000000000000000000, 0.000000000000000000, 1.000000000000000000 ) ) ;
#6411 = VERTEX_POINT ( 'NONE', #36411 ) ;
#6412 = CARTESIAN_POINT ( 'NONE',  ( -3.313708498984762496, 102.9687500040967763, 7.999999999999998224 ) ) ;
#6413 = EDGE_CURVE ( 'NONE', #70940, #64507, #54133, .T. ) ;
#6414 = CARTESIAN_POINT ( 'NONE',  ( -4.000000000000001776, 10.50000000000000000, -4.898587196589415787E-16 ) ) ;
#6415 = CARTESIAN_POINT ( 'NONE',  ( 5.000000000000000000, 18.53862685874493010, -23.57305537018094554 ) ) ;
#6416 = CARTESIAN_POINT ( 'NONE',  ( -1.881053915767124440, 11.99999999863440792, 4.541265875000001451 ) ) ;
#6417 = CARTESIAN_POINT ( 'NONE',  ( -3.313708498984758943, -7.999999999999989342, 17.79905278392014623 ) ) ;
#6418 = CARTESIAN_POINT ( 'NONE',  ( -2.849036369511732440E-14, 195.2500000000000000, 138.0000000000000568 ) ) ;
#6419 = EDGE_LOOP ( 'NONE', ( #19798, #49970, #20312, #11281 ) ) ;
#6420 = CARTESIAN_POINT ( 'NONE',  ( 9.000000000000001776, 0.000000000000000000, -10.80000000000000071 ) ) ;
#6421 = CARTESIAN_POINT ( 'NONE',  ( 7.188101187500000044, 105.4062500020483810, -8.802885111219163269E-16 ) ) ;
#6422 = EDGE_CURVE ( 'NONE', #45912, #53417, #60148, .T. ) ;
#6424 = CARTESIAN_POINT ( 'NONE',  ( 47.11462393093395917, 38.26058698117582679, 67.12012181809807032 ) ) ;
#6423 = CARTESIAN_POINT ( 'NONE',  ( 5.000000000000000000, 16.14408868864073554, 27.96238185062412640 ) ) ;
#6425 = DIRECTION ( 'NONE',  ( 0.000000000000000000, 0.000000000000000000, 1.000000000000000000 ) ) ;
#6426 = ORIENTED_EDGE ( 'NONE', *, *, #44525, .T. ) ;
#6427 = CARTESIAN_POINT ( 'NONE',  ( 1.317228840344592422, 10.12208498181939120, -70.14472670972864421 ) ) ;
#6428 = CARTESIAN_POINT ( 'NONE',  ( 5.082755093536318824, 5.082755093536319713, 24.92405278187175810 ) ) ;
#6429 = ORIENTED_EDGE ( 'NONE', *, *, #17818, .F. ) ;
#6430 =( BOUNDED_CURVE ( )  B_SPLINE_CURVE ( 2, ( #4753, #34555, #50388, #50756, #57560, #5868, #23206, #69235, #16412, #73772, #17544, #39444, #40563 ),
 .UNSPECIFIED., .F., .F. ) 
 B_SPLINE_CURVE_WITH_KNOTS ( ( 3, 2, 2, 2, 2, 2, 3 ),
 ( 0.8967391304347825942, 0.8985507246376811530, 0.9003623188405797118, 0.9021739130434782705, 0.9039855072463767183, 0.9057971014492752770, 0.9076086956521738358 ),
 .UNSPECIFIED. ) 
 CURVE ( )  GEOMETRIC_REPRESENTATION_ITEM ( )  RATIONAL_B_SPLINE_CURVE ( ( 1.000000000000000000, 0.9659258262890683122, 1.000000000000000000, 0.9659258262890683122, 1.000000000000000000, 0.9659258262890683122, 1.000000000000000000, 0.9659258262890683122, 1.000000000000000000, 0.9659258262890683122, 1.000000000000000000, 0.9659258262890704216, 0.9999999999999978906 ) ) 
 REPRESENTATION_ITEM ( '' )  );
#6431 = EDGE_CURVE ( 'NONE', #72356, #34530, #60702, .T. ) ;
#6432 = ORIENTED_EDGE ( 'NONE', *, *, #48728, .F. ) ;
#6433 = CARTESIAN_POINT ( 'NONE',  ( 7.204075437095966983, 7.204075437095967871, 85.09375000204836681 ) ) ;
#6434 = CARTESIAN_POINT ( 'NONE',  ( 4.556349186104045934, 11.00000000000000000, 92.03124999999998579 ) ) ;
#6435 = CARTESIAN_POINT ( 'NONE',  ( -29.43265458321760164, 196.1250000013656063, 173.4587341250003760 ) ) ;
#6436 = CARTESIAN_POINT ( 'NONE',  ( 11.00000000000000355, -4.556349186104045046, 100.6562500000000000 ) ) ;
#6439 = CARTESIAN_POINT ( 'NONE',  ( 6.676582343750001591, 299.1093750017069510, -8.176455196517173205E-16 ) ) ;
#6438 = CARTESIAN_POINT ( 'NONE',  ( 31.99999999999998579, 206.4375000027311842, 168.3431457505075173 ) ) ;
#6437 = LINE ( 'NONE', #17736, #2506 ) ;
#6440 = CARTESIAN_POINT ( 'NONE',  ( 8.660254037844385522, 134.5833333333333428, 5.000000000000005329 ) ) ;
#6441 = VECTOR ( 'NONE', #18018, 1000.000000000000000 ) ;
#6442 = CARTESIAN_POINT ( 'NONE',  ( 8.000000000000000000, 100.2499999999999858, -9.797174393178825657E-16 ) ) ;
#6443 = CARTESIAN_POINT ( 'NONE',  ( 4.180849123998743089, 225.9999999999999716, 9.092589271092984760 ) ) ;
#6444 = CARTESIAN_POINT ( 'NONE',  ( -7.188101187499992051, 0.000000000000000000, 1.861552781871753881 ) ) ;
#6445 = CYLINDRICAL_SURFACE ( 'NONE', #19248, 4.000000000000001776 ) ;
#6446 = CARTESIAN_POINT ( 'NONE',  ( 31.45873412500001010, 204.7500000013656063, 168.5673454167822740 ) ) ;
#6447 = CARTESIAN_POINT ( 'NONE',  ( -5.082755093536326818, 6.281249997951610098, 5.082755093536325042 ) ) ;
#6448 = CARTESIAN_POINT ( 'NONE',  ( 8.008118988124991233, 9.807117285998411148E-16, 4.763115283940630107 ) ) ;
#6449 = FACE_OUTER_BOUND ( 'NONE', #46552, .T. ) ;
#6450 = CARTESIAN_POINT ( 'NONE',  ( 7.188101187500002709, 116.1875000020483952, 2.977408999572649151 ) ) ;
#6452 = CARTESIAN_POINT ( 'NONE',  ( 3.275807840863760312, 194.7121737025869379, 199.7633675598530374 ) ) ;
#6451 = DIRECTION ( 'NONE',  ( -0.000000000000000000, -1.000000000000000000, -4.283267841918042741E-17 ) ) ;
#6453 = CARTESIAN_POINT ( 'NONE',  ( 3.042071309553163960, 222.7604166700806161, -11.35316468749999785 ) ) ;
#6454 = CARTESIAN_POINT ( 'NONE',  ( 0.000000000000000000, 0.000000000000000000, 0.000000000000000000 ) ) ;
#6455 = CARTESIAN_POINT ( 'NONE',  ( 2.679491924311222739, 50.83333332650537528, 10.00000000000000355 ) ) ;
#6456 = CARTESIAN_POINT ( 'NONE',  ( 25.17157287525381548, 198.6250000000000284, 167.1715728752537018 ) ) ;
#6457 = CARTESIAN_POINT ( 'NONE',  ( -9.832129032723420536, 28.69791666325268409, 5.676582343749997150 ) ) ;
#6458 = CARTESIAN_POINT ( 'NONE',  ( 5.000000000000158096, 24.16666666666685614, 8.660254037844676844 ) ) ;
#6459 = CARTESIAN_POINT ( 'NONE',  ( -5.676582343750006032, 219.4270833299193555, 9.832129032723418760 ) ) ;
#6460 = CARTESIAN_POINT ( 'NONE',  ( -10.00000000000000000, 239.7916666666666572, -2.679491924311226292 ) ) ;
#6462 = CARTESIAN_POINT ( 'NONE',  ( 7.999999999999991118, 0.000000000000000000, 30.00000000000000000 ) ) ;
#6461 = CARTESIAN_POINT ( 'NONE',  ( 2.828427124746209831, 208.3750000000000284, 200.8284271247462129 ) ) ;
#6463 = EDGE_LOOP ( 'NONE', ( #40, #71283, #7511, #51091 ) ) ;
#6464 = CARTESIAN_POINT ( 'NONE',  ( -1.432654583217664701, 198.0000000013656063, 138.5412658750000787 ) ) ;
#6465 = CARTESIAN_POINT ( 'NONE',  ( 5.676582343750001591, 21.61458332991935194, -9.832129032723420536 ) ) ;
#6466 = CARTESIAN_POINT ( 'NONE',  ( -6.735557395310442023E-16, 11.00000000000000000, 84.81250000409676204 ) ) ;
#6467 = CARTESIAN_POINT ( 'NONE',  ( 3.458734124999960358, 209.6250000013656063, 143.4326545832176976 ) ) ;
#6468 = CARTESIAN_POINT ( 'NONE',  ( -2.485281374238197394, 295.2500000034139589, 6.000000000000376588 ) ) ;
#6469 = LINE ( 'NONE', #12477, #45544 ) ;
#6471 = CARTESIAN_POINT ( 'NONE',  ( 9.832129032723416984, 20.36458332991935194, 5.676582343750006032 ) ) ;
#6470 = CARTESIAN_POINT ( 'NONE',  ( 2.977408999572650039, 111.6875000020483810, -7.188101187500000933 ) ) ;
#6472 = CARTESIAN_POINT ( 'NONE',  ( 3.313708498984756279, 7.999999999999991118, 19.86155277982336997 ) ) ;
#6473 = CARTESIAN_POINT ( 'NONE',  ( 8.311093377946834337, 155.1562499965860127, 8.311093377946839666 ) ) ;
#6474 = CARTESIAN_POINT ( 'NONE',  ( 10.00000000000000000, 121.6666666598386968, 2.679491924311236062 ) ) ;
#6475 = CARTESIAN_POINT ( 'NONE',  ( -2.977408999572650927, 112.2500000020483952, -7.188101187500001821 ) ) ;
#6476 = DIRECTION ( 'NONE',  ( 0.000000000000000000, 0.000000000000000000, 1.000000000000000000 ) ) ;
#6477 = CARTESIAN_POINT ( 'NONE',  ( -26.56734541678232731, 206.2500000013656063, 173.4587341250003760 ) ) ;
#6478 = AXIS2_PLACEMENT_3D ( 'NONE', #44004, #72291, #20604 ) ;
#6479 = ORIENTED_EDGE ( 'NONE', *, *, #48677, .F. ) ;
#6480 = CARTESIAN_POINT ( 'NONE',  ( 9.832129032723420536, 6.510416663252683200, -5.676582343749999815 ) ) ;
#6481 = VERTEX_POINT ( 'NONE', #8468 ) ;
#6482 = CARTESIAN_POINT ( 'NONE',  ( 6.000000000000003553, 289.4375000000000000, 2.485281374238571317 ) ) ;
#6483 = CARTESIAN_POINT ( 'NONE',  ( 6.676582343750004256, 297.8906250017069510, 2.765530957081995478 ) ) ;
#6484 = CARTESIAN_POINT ( 'NONE',  ( 11.35316468749999963, 135.9895833299192986, -3.042071309553165293 ) ) ;
#6485 = CARTESIAN_POINT ( 'NONE',  ( -7.999999999999989342, -3.313708498984762496, 23.48030278432982954 ) ) ;
#6486 = CARTESIAN_POINT ( 'NONE',  ( 55.74052621678719532, 209.6370283557842527, 49.63976298940631438 ) ) ;
#6487 = CARTESIAN_POINT ( 'NONE',  ( 3.042071309553173286, 245.3645833367472733, 11.35316468749999608 ) ) ;
#6488 = CARTESIAN_POINT ( 'NONE',  ( -7.204075437095967871, 7.204075437095967871, 93.34375000204838102 ) ) ;
#6489 = EDGE_LOOP ( 'NONE', ( #30157, #953, #58750, #60205 ) ) ;
#6490 = CARTESIAN_POINT ( 'NONE',  ( -8.660254037844387298, 203.9583333265053682, -5.000000000000004441 ) ) ;
#6491 = CARTESIAN_POINT ( 'NONE',  ( -11.00000000000000000, 0.000000000000000000, 100.1875000040967763 ) ) ;
#6492 = CARTESIAN_POINT ( 'NONE',  ( 8.311093377946837890, 91.71874999658599847, -8.311093377946837890 ) ) ;
#6493 = ORIENTED_EDGE ( 'NONE', *, *, #51872, .T. ) ;
#6494 = CARTESIAN_POINT ( 'NONE',  ( -10.18810118749999916, 0.000000000000000000, 108.1562500020483668 ) ) ;
#6495 = CARTESIAN_POINT ( 'NONE',  ( 4.541265875000002339, 16.49999999863440436, -1.881053915767121776 ) ) ;
#6496 = VERTEX_POINT ( 'NONE', #1355 ) ;
#6497 = ORIENTED_EDGE ( 'NONE', *, *, #53292, .F. ) ;
#6498 = AXIS2_PLACEMENT_3D ( 'NONE', #18866, #71273, #24876 ) ;
#6499 = CARTESIAN_POINT ( 'NONE',  ( -8.000000000000000000, 8.250000000000001776, -9.797174393178825657E-16 ) ) ;
#6500 = CARTESIAN_POINT ( 'NONE',  ( -3.313708498984786033, 11.53125000000000533, 7.999999999999979572 ) ) ;
#6501 = CARTESIAN_POINT ( 'NONE',  ( -2.977408999572650039, 26.81249999795161543, -7.188101187500001821 ) ) ;
#6502 = CARTESIAN_POINT ( 'NONE',  ( 7.778174593052021635, 7.778174593052023411, 96.43749999999998579 ) ) ;
#6503 = CARTESIAN_POINT ( 'NONE',  ( 4.220049686691934809, 10.18810118749999916, 102.0625000020483810 ) ) ;
#6504 = CARTESIAN_POINT ( 'NONE',  ( 1.656854249492381914, 1.812500000000000444, 4.000000000000000888 ) ) ;
#6505 = CARTESIAN_POINT ( 'NONE',  ( -4.000000000000002665, 13.31249999726881406, 1.656854249492380804 ) ) ;
#6506 = CARTESIAN_POINT ( 'NONE',  ( 26.34314575050761675, 206.6875000027312126, 165.9999999999998579 ) ) ;
#6507 = ORIENTED_EDGE ( 'NONE', *, *, #30210, .T. ) ;
#6508 = EDGE_CURVE ( 'NONE', #29716, #7760, #7107, .T. ) ;
#6509 = DIRECTION ( 'NONE',  ( -0.000000000000000000, 1.000000000000000000, 4.476705744456276341E-16 ) ) ;
#6510 = CARTESIAN_POINT ( 'NONE',  ( -2.445694354108783664, 197.3125000013656063, 195.5543056458912190 ) ) ;
#6511 = CARTESIAN_POINT ( 'NONE',  ( -24.54126587500002188, 204.2500000013655779, 168.5673454167826435 ) ) ;
#6512 = CARTESIAN_POINT ( 'NONE',  ( -8.342170076843785083E-16, 13.06249999863440792, 4.541265875000002339 ) ) ;
#6513 = CARTESIAN_POINT ( 'NONE',  ( 26.34314575050768426, 204.5624999999999716, 165.9999999999998295 ) ) ;
#6514 = CARTESIAN_POINT ( 'NONE',  ( -5.082755093536319713, 5.082755093536319713, 10.29905278187175455 ) ) ;
#6515 = ORIENTED_EDGE ( 'NONE', *, *, #26864, .T. ) ;
#6516 = VERTEX_POINT ( 'NONE', #27305 ) ;
#6517 = CARTESIAN_POINT ( 'NONE',  ( -10.18810118749999916, 4.220049686691934809, 103.5625000020483810 ) ) ;
#6518 = CARTESIAN_POINT ( 'NONE',  ( 5.656854249492381470, 95.75000000409677625, 5.656854249492379694 ) ) ;
#6519 = CARTESIAN_POINT ( 'NONE',  ( -29.65685424949234061, 205.4375000000000000, 174.0000000000004547 ) ) ;
#6520 = CARTESIAN_POINT ( 'NONE',  ( 2.445694354108839619, 200.8125000013656063, 200.4456943541088663 ) ) ;
#6521 = CARTESIAN_POINT ( 'NONE',  ( 31.45873412499997812, 196.7500000013656063, 168.5673454167822172 ) ) ;
#6522 = CARTESIAN_POINT ( 'NONE',  ( 8.660254037844389075, 90.41666666666667140, -5.000000000000000000 ) ) ;
#6523 = CARTESIAN_POINT ( 'NONE',  ( -5.656854249492380582, 118.8125000000000000, -5.656854249492380582 ) ) ;
#6524 = CARTESIAN_POINT ( 'NONE',  ( -11.35316468750000141, 58.59374999658601979, -1.390361679473963753E-15 ) ) ;
#6525 = CARTESIAN_POINT ( 'NONE',  ( -4.721056650415999201, 298.4843750017070079, -4.721056650415999201 ) ) ;
#6526 = EDGE_CURVE ( 'NONE', #53341, #4192, #45207, .T. ) ;
#6527 = ORIENTED_EDGE ( 'NONE', *, *, #60754, .T. ) ;
#6528 = CARTESIAN_POINT ( 'NONE',  ( 2.679491924311335982, 251.4583333333333428, 9.999999999999939604 ) ) ;
#6529 = CARTESIAN_POINT ( 'NONE',  ( -8.000000000000000000, 15.46874999590322197, -3.313708498984762496 ) ) ;
#6530 = CARTESIAN_POINT ( 'NONE',  ( -1.432654583217662481, 209.1250000013656631, 145.4587341250000634 ) ) ;
#6531 = CARTESIAN_POINT ( 'NONE',  ( -2.679491924311235174, 105.4166666598386968, 10.00000000000000000 ) ) ;
#6532 = CARTESIAN_POINT ( 'NONE',  ( 3.313708498984756279, 7.999999999999991118, 26.04905278392014623 ) ) ;
#6533 = CARTESIAN_POINT ( 'NONE',  ( 1.836970198721029589E-15, 241.2500000000000284, 10.00000000000000000 ) ) ;
#6534 = FACE_OUTER_BOUND ( 'NONE', #6618, .T. ) ;
#6535 = CARTESIAN_POINT ( 'NONE',  ( -7.204075437095965206, -7.204075437095968759, 69.71875000204836681 ) ) ;
#6536 = CARTESIAN_POINT ( 'NONE',  ( 5.000000000000001776, 215.8333333333333428, -8.660254037844389075 ) ) ;
#6537 = CARTESIAN_POINT ( 'NONE',  ( -2.977408999572647819, -7.188101187499990274, 12.64280278187175277 ) ) ;
#6538 = CARTESIAN_POINT ( 'NONE',  ( 11.35316468749999963, 181.3020833299192986, -3.042071309553165293 ) ) ;
#6539 = CARTESIAN_POINT ( 'NONE',  ( 2.780723358947928197E-16, 2.562499998634407028, -4.541265875000002339 ) ) ;
#6540 = CARTESIAN_POINT ( 'NONE',  ( 4.000000000000001776, 1.812499997268813390, -1.656854249492381248 ) ) ;
#6542 = CARTESIAN_POINT ( 'NONE',  ( 5.000000000000000000, -16.14408868864072844, 22.96238185062368586 ) ) ;
#6541 = FACE_OUTER_BOUND ( 'NONE', #61224, .T. ) ;
#6543 = ORIENTED_EDGE ( 'NONE', *, *, #48064, .T. ) ;
#6544 = VECTOR ( 'NONE', #43700, 1000.000000000000000 ) ;
#6545 = CARTESIAN_POINT ( 'NONE',  ( -2.754378923186476579E-14, 207.4375000013656063, 145.4587341250000350 ) ) ;
#6546 = CARTESIAN_POINT ( 'NONE',  ( -3.042071309553164404, 37.55208332991935549, -11.35316468749999963 ) ) ;
#6547 = CARTESIAN_POINT ( 'NONE',  ( 4.556349186104051263, -10.99999999999999822, 102.1562500040967763 ) ) ;
#6548 = CARTESIAN_POINT ( 'NONE',  ( -24.54126587499999346, 205.1875000013656063, 170.0000000000002842 ) ) ;
#6549 = CARTESIAN_POINT ( 'NONE',  ( 7.778174593052021635, 7.778174593052023411, 95.12500000409676204 ) ) ;
#6551 = DIRECTION ( 'NONE',  ( -0.000000000000000000, -0.000000000000000000, 1.000000000000000000 ) ) ;
#6550 = CARTESIAN_POINT ( 'NONE',  ( -5.656854249492380582, 116.0000000040967905, -5.656854249492380582 ) ) ;
#6552 = CARTESIAN_POINT ( 'NONE',  ( -3.458734125000015425, 199.0000000013656063, 143.4326545832176976 ) ) ;
#6553 =( BOUNDED_CURVE ( )  B_SPLINE_CURVE ( 2, ( #67340, #57140, #39409, #5456, #15636, #50348, #74478, #62409, #67714, #4715, #22784, #58535, #21673 ),
 .UNSPECIFIED., .F., .F. ) 
 B_SPLINE_CURVE_WITH_KNOTS ( ( 3, 2, 2, 2, 2, 2, 3 ),
 ( 0.3611111111111107719, 0.3703703703703700167, 0.3796296296296293171, 0.3888888888888886175, 0.3981481481481478624, 0.4074074074074071072, 0.4166666666666664076 ),
 .UNSPECIFIED. ) 
 CURVE ( )  GEOMETRIC_REPRESENTATION_ITEM ( )  RATIONAL_B_SPLINE_CURVE ( ( 1.000000000000001332, 0.9659258262890670910, 1.000000000000000000, 0.9659258262890683122, 1.000000000000000000, 0.9659258262890683122, 1.000000000000000000, 0.9659258262890683122, 1.000000000000000000, 0.9659258262890683122, 1.000000000000000000, 0.9659258262890693114, 0.9999999999999990008 ) ) 
 REPRESENTATION_ITEM ( '' )  );
#6554 = CARTESIAN_POINT ( 'NONE',  ( -10.00000000000000000, 74.16666665983868256, -2.679491924311229845 ) ) ;
#6555 = CARTESIAN_POINT ( 'NONE',  ( 7.188101187500001821, 98.00000000204838102, -2.977408999572651371 ) ) ;
#6556 = CARTESIAN_POINT ( 'NONE',  ( 1.881053915767122664, 13.24999999863441147, 4.541265875000001451 ) ) ;
#6557 = CARTESIAN_POINT ( 'NONE',  ( 6.350741970897364085E-13, 216.2499999999999432, -9.999999999999998224 ) ) ;
#6558 = CARTESIAN_POINT ( 'NONE',  ( 5.000000000000000000, 0.000000000000000000, 0.000000000000000000 ) ) ;
#6559 = LINE ( 'NONE', #29565, #29386 ) ;
#6560 = ORIENTED_EDGE ( 'NONE', *, *, #63748, .T. ) ;
#6561 = ORIENTED_EDGE ( 'NONE', *, *, #7175, .F. ) ;
#6562 = DIRECTION ( 'NONE',  ( 1.000000000000000000, -0.000000000000000000, -0.000000000000000000 ) ) ;
#6563 = CARTESIAN_POINT ( 'NONE',  ( -4.721056650415999201, 299.4843750017070079, -4.721056650415999201 ) ) ;
#6564 = DIRECTION ( 'NONE',  ( 0.000000000000000000, -0.9997074645238147594, 0.02418647091589873691 ) ) ;
#6565 = CARTESIAN_POINT ( 'NONE',  ( -8.660254037844389075, 87.91666666666667140, 4.999999999999998224 ) ) ;
#6566 = CARTESIAN_POINT ( 'NONE',  ( 3.042071309553167069, 151.8229166632526699, -11.35316468749999785 ) ) ;
#6567 = CARTESIAN_POINT ( 'NONE',  ( 10.18810118749999916, 1.247682550866122264E-15, 81.90625000204838102 ) ) ;
#6568 = CARTESIAN_POINT ( 'NONE',  ( -4.898587196589407898E-16, 7.999999999999991118, 9.455302779823364645 ) ) ;
#6569 = CARTESIAN_POINT ( 'NONE',  ( 2.849036369511732440E-14, 203.2500000000000000, 202.0000000000000000 ) ) ;
#6570 = DIRECTION ( 'NONE',  ( -0.000000000000000000, 1.000000000000000000, -0.000000000000000000 ) ) ;
#6571 = CARTESIAN_POINT ( 'NONE',  ( 4.220049686691934809, 10.18810118749999916, 115.5625000020483810 ) ) ;
#6572 = VERTEX_POINT ( 'NONE', #3194 ) ;
#6573 = CARTESIAN_POINT ( 'NONE',  ( 10.49999999999998224, 1.285879139104718661E-15, 118.0000000000000000 ) ) ;
#6574 = CIRCLE ( 'NONE', #17373, 8.749999999999998224 ) ;
#6575 = CARTESIAN_POINT ( 'NONE',  ( 30.79034348655367381, 174.5916665501465275, 165.6986120235950182 ) ) ;
#6576 = CARTESIAN_POINT ( 'NONE',  ( -8.311093377946836114, 127.9687499965860269, -8.311093377946837890 ) ) ;
#6577 = CARTESIAN_POINT ( 'NONE',  ( -3.458734124999958581, 199.5000000013656063, 199.4326545832176976 ) ) ;
#6578 = CARTESIAN_POINT ( 'NONE',  ( 2.754378923186476579E-14, 209.4375000013656063, 194.5412658750000219 ) ) ;
#6579 = CARTESIAN_POINT ( 'NONE',  ( -7.204075437095967871, 7.204075437095967871, 78.34375000204838102 ) ) ;
#6580 = CARTESIAN_POINT ( 'NONE',  ( -9.832129032723420536, 44.01041666325268409, 5.676582343749997150 ) ) ;
#6581 = VERTEX_POINT ( 'NONE', #15984 ) ;
#6582 = CARTESIAN_POINT ( 'NONE',  ( 10.00000000000000178, 37.08333332650536107, -2.679491924311226736 ) ) ;
#6583 = CARTESIAN_POINT ( 'NONE',  ( -4.541265875000002339, 0.8749999986344069169, -1.881053915767121998 ) ) ;
#6584 = CARTESIAN_POINT ( 'NONE',  ( 8.008118988124993010, -3.317071493978877239, 15.16936528394063011 ) ) ;
#6585 = EDGE_CURVE ( 'NONE', #46843, #72690, #3786, .T. ) ;
#6586 = CARTESIAN_POINT ( 'NONE',  ( 2.977408999572650927, 12.74999999795161187, -7.188101187500001821 ) ) ;
#6587 = CARTESIAN_POINT ( 'NONE',  ( -2.485281374238572649, 294.2500000034140157, 6.000000000000002665 ) ) ;
#6588 = CARTESIAN_POINT ( 'NONE',  ( -48.45866277005243461, 142.0302559771922972, 61.07789613012157304 ) ) ;
#6589 = CARTESIAN_POINT ( 'NONE',  ( 7.188101187500000044, 6.843749997951610986, 0.000000000000000000 ) ) ;
#6590 = CARTESIAN_POINT ( 'NONE',  ( 1.320432766682872962E-15, -7.188101187499992051, 7.861552781871751883 ) ) ;
#6591 = CARTESIAN_POINT ( 'NONE',  ( -7.204075437095967871, 7.204075437095967871, 70.46875000204836681 ) ) ;
#6592 = CARTESIAN_POINT ( 'NONE',  ( -31.45873412499999944, 206.9375000013656063, 170.0000000000003979 ) ) ;
#6593 = CARTESIAN_POINT ( 'NONE',  ( 1.469576158976823947E-15, 98.56250000409677625, 8.000000000000000000 ) ) ;
#6594 = CARTESIAN_POINT ( 'NONE',  ( -4.541265875000003227, 19.99999999863440436, 1.881053915767121110 ) ) ;
#6595 = UNCERTAINTY_MEASURE_WITH_UNIT (LENGTH_MEASURE( 1.000000000000000082E-05 ), #32875, 'distance_accuracy_value', 'NONE');
#6596 = VERTEX_POINT ( 'NONE', #66934 ) ;
#6597 = CIRCLE ( 'NONE', #40302, 19.00000000000000000 ) ;
#6598 = ADVANCED_FACE ( 'NONE', ( #3947 ), #49955, .T. ) ;
#6599 = CARTESIAN_POINT ( 'NONE',  ( 4.000000000000015987, 196.6250000027312126, 198.0000000000000284 ) ) ;
#6600 = CARTESIAN_POINT ( 'NONE',  ( 2.828427124746152987, 207.1250000000000284, 139.1715728752538723 ) ) ;
#6601 = CARTESIAN_POINT ( 'NONE',  ( -31.99999999999995737, 200.4375000027311842, 171.6568542494928522 ) ) ;
#6602 = EDGE_CURVE ( 'NONE', #30597, #29307, #73342, .T. ) ;
#6603 = CARTESIAN_POINT ( 'NONE',  ( -7.188101187500001821, 116.5625000020483810, -2.977408999572650483 ) ) ;
#6604 = DIRECTION ( 'NONE',  ( 0.000000000000000000, 0.000000000000000000, -1.000000000000000000 ) ) ;
#6605 = CARTESIAN_POINT ( 'NONE',  ( 7.999999999999991118, 9.797174393178815797E-16, 0.2678027839201451155 ) ) ;
#6606 = ORIENTED_EDGE ( 'NONE', *, *, #21051, .T. ) ;
#6607 = CARTESIAN_POINT ( 'NONE',  ( -7.188101187500002709, 19.31249999795161543, 2.977408999572649151 ) ) ;
#6608 = ORIENTED_EDGE ( 'NONE', *, *, #50752, .T. ) ;
#6609 = DIRECTION ( 'NONE',  ( 0.000000000000000000, 0.000000000000000000, -1.000000000000000000 ) ) ;
#6610 = CARTESIAN_POINT ( 'NONE',  ( -4.193030820683907756, -10.26769724739506984, -64.12608639927678666 ) ) ;
#6611 = CARTESIAN_POINT ( 'NONE',  ( 10.00000000000000178, 55.20833333333332860, -2.679491924311226736 ) ) ;
#6612 = CARTESIAN_POINT ( 'NONE',  ( -7.188101187499999156, 99.12500000204838102, 2.977408999572654924 ) ) ;
#6613 = CARTESIAN_POINT ( 'NONE',  ( -29.43265458321760519, 205.1250000013656347, 173.4587341250003760 ) ) ;
#6614 = CARTESIAN_POINT ( 'NONE',  ( -0.8588954341814950544, -10.28066745654381542, 63.58998442112849858 ) ) ;
#6615 = AXIS2_PLACEMENT_3D ( 'NONE', #55167, #61562, #50233 ) ;
#6616 = EDGE_CURVE ( 'NONE', #37264, #55885, #67687, .T. ) ;
#6617 = CARTESIAN_POINT ( 'NONE',  ( -1.836970198721029983E-15, 35.62499999317203248, 10.00000000000000178 ) ) ;
#6618 = EDGE_LOOP ( 'NONE', ( #22908, #2657, #26124, #14038 ) ) ;
#6619 = CARTESIAN_POINT ( 'NONE',  ( 2.085542519210945334E-15, 240.1562500034140157, 11.35316468749999963 ) ) ;
#6620 = PRODUCT_DEFINITION_SHAPE ( 'NONE', 'NONE',  #74667 ) ;
#6621 = CARTESIAN_POINT ( 'NONE',  ( 5.082755093536320601, -5.082755093536318824, 17.42405278187175810 ) ) ;
#6622 = AXIS2_PLACEMENT_3D ( 'NONE', #28962, #32214, #20495 ) ;
#6623 = CARTESIAN_POINT ( 'NONE',  ( 3.728321214229567637, 56.13798660961509057, 44.08488161414512518 ) ) ;
#6624 = DIRECTION ( 'NONE',  ( -0.000000000000000000, -0.000000000000000000, 1.000000000000000000 ) ) ;
#6625 = CARTESIAN_POINT ( 'NONE',  ( 0.000000000000000000, 130.3999865490244190, 45.94057108883949070 ) ) ;
#6626 = CARTESIAN_POINT ( 'NONE',  ( 10.00000000000000178, 201.8749999931720538, 0.000000000000000000 ) ) ;
#6627 = CARTESIAN_POINT ( 'NONE',  ( 5.000000000000001776, 165.8333333333333428, -8.660254037844389075 ) ) ;
#6628 = CARTESIAN_POINT ( 'NONE',  ( 7.778174593052021635, 7.778174593052023411, 79.93750000000000000 ) ) ;
#6629 = CYLINDRICAL_SURFACE ( 'NONE', #1834, 3.999999999999976019 ) ;
#6630 = CARTESIAN_POINT ( 'NONE',  ( -3.042071309553173730, 139.6354166632526415, 11.35316468749999785 ) ) ;
#6631 = CARTESIAN_POINT ( 'NONE',  ( -4.242640687119286547, 293.9375000034140157, -4.242640687119286547 ) ) ;
#6632 = CARTESIAN_POINT ( 'NONE',  ( 2.679491924311222739, 25.83333332650536462, 10.00000000000000355 ) ) ;
#6635 = CARTESIAN_POINT ( 'NONE',  ( 2.249999999999999112, -2.249999999999999556, 0.000000000000000000 ) ) ;
#6634 = CARTESIAN_POINT ( 'NONE',  ( -1.739508062077480766, -51.27839935804527016, 48.57027215863489999 ) ) ;
#6633 = CARTESIAN_POINT ( 'NONE',  ( 28.00000000000002132, 206.5000000000000284, 165.9999999999998863 ) ) ;
#6636 = ORIENTED_EDGE ( 'NONE', *, *, #29310, .T. ) ;
#6637 = DIRECTION ( 'NONE',  ( -1.000000000000000000, 0.000000000000000000, 0.000000000000000000 ) ) ;
#6638 = CARTESIAN_POINT ( 'NONE',  ( -3.313708498984759387, -7.999999999999989342, 25.11155277982336997 ) ) ;
#6639 = CARTESIAN_POINT ( 'NONE',  ( -2.445694354108838731, 209.0625000013656063, 144.4456943541088663 ) ) ;
#6640 = CARTESIAN_POINT ( 'NONE',  ( 5.000000000000000000, -67.66743717231483402, -22.54291394824973338 ) ) ;
#6641 = EDGE_CURVE ( 'NONE', #54851, #72225, #49579, .T. ) ;
#6642 = CARTESIAN_POINT ( 'NONE',  ( 4.999999999999993783, 41.04166665983870388, 8.660254037844390851 ) ) ;
#6643 = CARTESIAN_POINT ( 'NONE',  ( -4.401442555609581635E-16, 113.2812500020483952, -7.188101187500000044 ) ) ;
#6644 = CARTESIAN_POINT ( 'NONE',  ( 1.881053915767121776, 20.49999999863440436, -4.541265875000002339 ) ) ;
#6645 = CARTESIAN_POINT ( 'NONE',  ( -2.219371606100991823, -51.37365828841591053, 48.60677221569458339 ) ) ;
#6646 = CARTESIAN_POINT ( 'NONE',  ( -7.999999999999991118, 0.000000000000000000, 17.33030277982336287 ) ) ;
#6648 = DIRECTION ( 'NONE',  ( 0.000000000000000000, 0.000000000000000000, 1.000000000000000000 ) ) ;
#6647 = CARTESIAN_POINT ( 'NONE',  ( -1.656854249492383468, 1.687500000000000222, 4.000000000000000888 ) ) ;
#6649 = ORIENTED_EDGE ( 'NONE', *, *, #13997, .T. ) ;
#6650 =( BOUNDED_CURVE ( )  B_SPLINE_CURVE ( 2, ( #7382, #20160, #43177, #1731, #25818, #30389, #8480, #8114, #24351, #54147, #59437 ),
 .UNSPECIFIED., .F., .F. ) 
 B_SPLINE_CURVE_WITH_KNOTS ( ( 3, 2, 2, 2, 2, 3 ),
 ( 0.5029889089742047847, 0.5029889444187176650, 0.5096072200031744881, 0.5162254955876313112, 0.5228437711720881342, 0.5294620445568896105 ),
 .UNSPECIFIED. ) 
 CURVE ( )  GEOMETRIC_REPRESENTATION_ITEM ( )  RATIONAL_B_SPLINE_CURVE ( ( 0.9999991846702638298, 0.9999995923329486613, 1.000000000000000000, 0.9238795325112867385, 1.000000000000000000, 0.9238795325112867385, 1.000000000000000000, 0.9238795325112867385, 1.000000000000000000, 0.9238795325112867385, 1.000000000000000000 ) ) 
 REPRESENTATION_ITEM ( '' )  );
#6651 = LINE ( 'NONE', #5909, #31578 ) ;
#6652 = CARTESIAN_POINT ( 'NONE',  ( -5.082755093536325042, 25.03124999795161543, -5.082755093536325930 ) ) ;
#6653 = CARTESIAN_POINT ( 'NONE',  ( -1.836970198721029983E-15, 63.75000000000000000, 10.00000000000000178 ) ) ;
#6654 = CARTESIAN_POINT ( 'NONE',  ( 11.35316468749999608, 241.9270833367473301, -3.042071309553167513 ) ) ;
#6655 = CARTESIAN_POINT ( 'NONE',  ( 3.042071309553167069, 121.8229166632526841, -11.35316468749999785 ) ) ;
#6656 = VERTEX_POINT ( 'NONE', #50689 ) ;
#6657 = CARTESIAN_POINT ( 'NONE',  ( 5.000000000000000000, -10.42446448370085577, 65.94449134867498685 ) ) ;
#6658 = CARTESIAN_POINT ( 'NONE',  ( 7.204075437095968759, -7.204075437095966983, 99.71875000204838102 ) ) ;
#6659 = CARTESIAN_POINT ( 'NONE',  ( 7.320508075688771044, 221.2499999931720538, 7.320508075688775484 ) ) ;
#6660 = CARTESIAN_POINT ( 'NONE',  ( -2.445694354108783219, 200.8125000013656063, 200.4456943541088663 ) ) ;
#6661 = CARTESIAN_POINT ( 'NONE',  ( -4.000000000000002665, 6.312499997268813168, 1.656854249492380582 ) ) ;
#6663 = CARTESIAN_POINT ( 'NONE',  ( -8.311093377946836114, 102.6562499965860269, -8.311093377946837890 ) ) ;
#6662 = CARTESIAN_POINT ( 'NONE',  ( 1.267086777181619559E-12, 183.7500000000001137, 10.00000000000000178 ) ) ;
#6664 = CARTESIAN_POINT ( 'NONE',  ( -7.999999999999989342, -3.313708498984762496, 4.111552783920145338 ) ) ;
#6665 = CARTESIAN_POINT ( 'NONE',  ( -24.54126587499997925, 196.3750000013656063, 171.4326545832179818 ) ) ;
#6666 = LINE ( 'NONE', #47009, #63814 ) ;
#6667 = ORIENTED_EDGE ( 'NONE', *, *, #57299, .T. ) ;
#6668 = CARTESIAN_POINT ( 'NONE',  ( 4.999999999999993783, 196.0416666598387110, 8.660254037844390851 ) ) ;
#6669 = FACE_OUTER_BOUND ( 'NONE', #2788, .T. ) ;
#6670 = CARTESIAN_POINT ( 'NONE',  ( 31.99999999999997868, 202.1875000000000568, 171.6568542494923122 ) ) ;
#6671 = CARTESIAN_POINT ( 'NONE',  ( -8.311093377946841443, 84.21874999658599847, 8.311093377946834337 ) ) ;
#6672 = DIRECTION ( 'NONE',  ( 1.000000000000000000, -0.000000000000000000, -0.000000000000000000 ) ) ;
#6673 = CARTESIAN_POINT ( 'NONE',  ( 2.977408999572650927, 5.624999997951610986, -7.188101187500000933 ) ) ;
#6674 = CARTESIAN_POINT ( 'NONE',  ( 4.220049686691934809, 10.18810118749999916, 97.56250000204836681 ) ) ;
#6675 = CARTESIAN_POINT ( 'NONE',  ( -3.042071309553173730, 14.63541666325268231, 11.35316468749999785 ) ) ;
#6677 = VERTEX_POINT ( 'NONE', #27683 ) ;
#6676 =( BOUNDED_CURVE ( )  B_SPLINE_CURVE ( 2, ( #36498, #25527, #47799, #25891, #7824, #70822, #19134, #42138, #8189 ),
 .UNSPECIFIED., .F., .F. ) 
 B_SPLINE_CURVE_WITH_KNOTS ( ( 3, 2, 2, 2, 3 ),
 ( 0.3000000000000002109, 0.3083333333333335702, 0.3166666666666669294, 0.3250000000000002887, 0.3333333333333336479 ),
 .UNSPECIFIED. ) 
 CURVE ( )  GEOMETRIC_REPRESENTATION_ITEM ( )  RATIONAL_B_SPLINE_CURVE ( ( 0.9999999999999980016, 0.9238795325112887369, 1.000000000000000000, 0.9238795325112867385, 1.000000000000000000, 0.9238795325112867385, 1.000000000000000000, 0.9238795325112837409, 1.000000000000003109 ) ) 
 REPRESENTATION_ITEM ( '' )  );
#6678 = CARTESIAN_POINT ( 'NONE',  ( -5.000000000000002665, 136.6666666666666856, -8.660254037844396180 ) ) ;
#6679 = CARTESIAN_POINT ( 'NONE',  ( 0.000000000000000000, 0.000000000000000000, 118.0000000000000000 ) ) ;
#6680 = CARTESIAN_POINT ( 'NONE',  ( -8.311093377946836114, 222.6562499965860411, -8.311093377946837890 ) ) ;
#6681 = CARTESIAN_POINT ( 'NONE',  ( 10.18810118750000093, -4.220049686691933921, 80.68750000204836681 ) ) ;
#6682 = CARTESIAN_POINT ( 'NONE',  ( -10.00000000000000000, 218.1250000068279746, 0.000000000000000000 ) ) ;
#6683 = LINE ( 'NONE', #48499, #57145 ) ;
#6684 = CARTESIAN_POINT ( 'NONE',  ( -4.088227598258586603E-16, 298.2031250017070079, -6.676582343750001591 ) ) ;
#6685 = VECTOR ( 'NONE', #45516, 1000.000000000000000 ) ;
#6686 = ORIENTED_EDGE ( 'NONE', *, *, #74129, .F. ) ;
#6687 = CARTESIAN_POINT ( 'NONE',  ( -5.000000000000000000, -70.11723469343094450, -28.93519894129240910 ) ) ;
#6688 = CARTESIAN_POINT ( 'NONE',  ( 9.832129032723420536, 211.5104166632526699, -5.676582343749999815 ) ) ;
#6689 = CARTESIAN_POINT ( 'NONE',  ( -7.204075437095967871, 7.204075437095967871, 91.46875000204838102 ) ) ;
#6690 = CARTESIAN_POINT ( 'NONE',  ( -24.54126587499998280, 202.1250000013656063, 171.4326545832179818 ) ) ;
#6691 = CARTESIAN_POINT ( 'NONE',  ( -1.469576158976823947E-15, 16.12500000000000355, 8.000000000000000000 ) ) ;
#6692 = ORIENTED_EDGE ( 'NONE', *, *, #11345, .F. ) ;
#6693 = CARTESIAN_POINT ( 'NONE',  ( -7.188101187500001821, 119.5625000020483810, -2.977408999572650483 ) ) ;
#6694 = CARTESIAN_POINT ( 'NONE',  ( -3.999999999999960032, 209.0625000027312126, 196.3431457505076594 ) ) ;
#6695 = CARTESIAN_POINT ( 'NONE',  ( -8.660254037844390851, 27.91666666666666785, 4.999999999999998224 ) ) ;
#6696 = EDGE_CURVE ( 'NONE', #13863, #15764, #20902, .T. ) ;
#6697 = CARTESIAN_POINT ( 'NONE',  ( -4.999999999999999112, 15.48016642534407694, 69.96422921944753170 ) ) ;
#6698 = CARTESIAN_POINT ( 'NONE',  ( 4.220049686691934809, 10.18810118749999916, 76.56250000204836681 ) ) ;
#6699 = ORIENTED_EDGE ( 'NONE', *, *, #42267, .T. ) ;
#6700 = CARTESIAN_POINT ( 'NONE',  ( 7.188101187500000044, 0.4687499979516099868, 0.000000000000000000 ) ) ;
#6701 = CARTESIAN_POINT ( 'NONE',  ( 9.797174393178825657E-16, 125.0000000000000000, -8.000000000000000000 ) ) ;
#6702 = FACE_OUTER_BOUND ( 'NONE', #58851, .T. ) ;
#6703 = CARTESIAN_POINT ( 'NONE',  ( 7.188101187500001821, 116.3750000020483810, -2.977408999572651371 ) ) ;
#6704 = CARTESIAN_POINT ( 'NONE',  ( -2.295000000000000373, 255.7199999999997715, 5.414445227810388950 ) ) ;
#6705 = CARTESIAN_POINT ( 'NONE',  ( -2.765530957081996810, 297.2656250017069510, -6.676582343750002480 ) ) ;
#6707 = CARTESIAN_POINT ( 'NONE',  ( -4.242640687119286547, 288.9375000034140157, -4.242640687119286547 ) ) ;
#6706 = CARTESIAN_POINT ( 'NONE',  ( -5.676582343750000703, 238.0729166700806445, -9.832129032723418760 ) ) ;
#6708 = ORIENTED_EDGE ( 'NONE', *, *, #1228, .F. ) ;
#6709 = EDGE_CURVE ( 'NONE', #30969, #38665, #3799, .T. ) ;
#6710 = CARTESIAN_POINT ( 'NONE',  ( 9.832129032723416984, 237.1354166700806445, -5.676582343750003368 ) ) ;
#6711 = CARTESIAN_POINT ( 'NONE',  ( -5.082755093536319713, 5.082755093536319713, 8.799052781871752771 ) ) ;
#6712 = EDGE_CURVE ( 'NONE', #49847, #18300, #26911, .T. ) ;
#6713 = ORIENTED_EDGE ( 'NONE', *, *, #51985, .F. ) ;
#6714 = CARTESIAN_POINT ( 'NONE',  ( -7.204075437095967871, 7.204075437095967871, 68.96875000204836681 ) ) ;
#6715 = CARTESIAN_POINT ( 'NONE',  ( 8.311093377946837890, 96.71874999658599847, -8.311093377946837890 ) ) ;
#6716 = CARTESIAN_POINT ( 'NONE',  ( -3.369429374625362517, 60.49191766694040240, 23.06312700027912399 ) ) ;
#6717 = CARTESIAN_POINT ( 'NONE',  ( -7.778174593052020747, -7.778174593052023411, 83.68750000000000000 ) ) ;
#6720 = CARTESIAN_POINT ( 'NONE',  ( 2.765530957082001251, 287.9218750017069510, 6.676582343749999815 ) ) ;
#6719 = CARTESIAN_POINT ( 'NONE',  ( 24.54126587499998280, 204.1250000013656063, 168.5673454167822740 ) ) ;
#6718 = CARTESIAN_POINT ( 'NONE',  ( 24.54126587500000056, 203.3750000013656063, 168.5673454167822172 ) ) ;
#6721 = VERTEX_POINT ( 'NONE', #62017 ) ;
#6722 = CARTESIAN_POINT ( 'NONE',  ( 1.656854249492381914, 18.81250000000000000, 4.000000000000000888 ) ) ;
#6723 = CARTESIAN_POINT ( 'NONE',  ( -10.00000000000000178, 179.3749999931720538, -1.224646799147353454E-15 ) ) ;
#6724 = AXIS2_PLACEMENT_3D ( 'NONE', #46656, #69675, #41007 ) ;
#6725 = CARTESIAN_POINT ( 'NONE',  ( -11.35316468749999785, 218.0729166632526699, -3.042071309553167513 ) ) ;
#6726 = CARTESIAN_POINT ( 'NONE',  ( -2.445694354108839619, 205.8125000013656063, 139.5543056458912190 ) ) ;
#6727 = CARTESIAN_POINT ( 'NONE',  ( 31.45873412499998523, 207.8750000013656063, 171.4326545832175839 ) ) ;
#6728 = CARTESIAN_POINT ( 'NONE',  ( 4.401442555609581635E-16, 25.21874999795161543, -7.188101187500000044 ) ) ;
#6730 = EDGE_CURVE ( 'NONE', #13507, #36205, #43221, .T. ) ;
#6729 = AXIS2_PLACEMENT_3D ( 'NONE', #11424, #62348, #5769 ) ;
#6731 = CARTESIAN_POINT ( 'NONE',  ( 11.35316468750000141, 181.0937499965860411, 0.000000000000000000 ) ) ;
#6732 = CARTESIAN_POINT ( 'NONE',  ( 2.977408999572650039, 100.0625000020483810, -7.188101187500000933 ) ) ;
#6733 = CARTESIAN_POINT ( 'NONE',  ( 1.656854249492433206, 196.3125000027312126, 138.0000000000001705 ) ) ;
#6734 = CARTESIAN_POINT ( 'NONE',  ( -1.881053915767124440, 10.99999999863440969, 4.541265875000001451 ) ) ;
#6735 = CARTESIAN_POINT ( 'NONE',  ( 29.43265458321766914, 202.1250000013656063, 166.5412658749999650 ) ) ;
#6736 = CARTESIAN_POINT ( 'NONE',  ( 7.188101187499992051, 8.802885111219154394E-16, 11.61155278187175632 ) ) ;
#6737 = CARTESIAN_POINT ( 'NONE',  ( -8.311093377946841443, 68.90624999658602690, 8.311093377946830785 ) ) ;
#6738 = EDGE_CURVE ( 'NONE', #17827, #31901, #4680, .T. ) ;
#6739 = DIRECTION ( 'NONE',  ( -0.000000000000000000, 1.000000000000000000, -0.000000000000000000 ) ) ;
#6740 = CARTESIAN_POINT ( 'NONE',  ( 5.656854249492374365, 5.656854249492375253, 1.824052784329821097 ) ) ;
#6741 = VERTEX_POINT ( 'NONE', #34860 ) ;
#6742 = CARTESIAN_POINT ( 'NONE',  ( -7.999999999999989342, -3.313708498984762496, 7.111552783920144449 ) ) ;
#6743 = CARTESIAN_POINT ( 'NONE',  ( -1.656854249492371256, 203.4375000027311557, 137.9999999999999716 ) ) ;
#6744 = CARTESIAN_POINT ( 'NONE',  ( 9.832129032723416984, 80.36458332991935549, 5.676582343750006032 ) ) ;
#6745 = CARTESIAN_POINT ( 'NONE',  ( 7.778174593052023411, -7.778174593052021635, 69.25000000409677625 ) ) ;
#6746 = CYLINDRICAL_SURFACE ( 'NONE', #36097, 3.999999999999976019 ) ;
#6747 = CARTESIAN_POINT ( 'NONE',  ( 4.000000000000000888, 8.687499997268814056, 1.656854249492384135 ) ) ;
#6749 = CARTESIAN_POINT ( 'NONE',  ( -11.35316468750000141, 53.48958332991934839, 3.042071309553159963 ) ) ;
#6748 = CARTESIAN_POINT ( 'NONE',  ( -4.898587196589412829E-16, 123.3125000040967905, -8.000000000000000000 ) ) ;
#6750 = CARTESIAN_POINT ( 'NONE',  ( -7.999999999999991118, 3.313708498984756723, 26.42405278392015333 ) ) ;
#6751 = CARTESIAN_POINT ( 'NONE',  ( -7.320508075688773708, 13.74999999317203070, -7.320508075688774596 ) ) ;
#6752 = CARTESIAN_POINT ( 'NONE',  ( 2.679491924311228956, 152.9166666598387394, -10.00000000000000000 ) ) ;
#6753 = CARTESIAN_POINT ( 'NONE',  ( -7.188101187500000044, 94.53125000204836681, 0.000000000000000000 ) ) ;
#6754 = CARTESIAN_POINT ( 'NONE',  ( 11.00000000000000000, 1.347111479062088405E-15, 108.2499999999999858 ) ) ;
#6755 = CARTESIAN_POINT ( 'NONE',  ( 9.832129032723420536, 46.51041666325269119, -5.676582343749999815 ) ) ;
#6756 = CARTESIAN_POINT ( 'NONE',  ( 1.871523826299183495E-15, -10.18810118749999916, 113.4062500020483810 ) ) ;
#6757 = CARTESIAN_POINT ( 'NONE',  ( -11.35316468750000141, 193.2812499965860127, -1.390361679473963753E-15 ) ) ;
#6758 = VERTEX_POINT ( 'NONE', #5424 ) ;
#6759 = CARTESIAN_POINT ( 'NONE',  ( 5.126106709314291798, 68.65851429197792299, 20.89429596904683706 ) ) ;
#6760 = DIRECTION ( 'NONE',  ( 0.000000000000000000, 0.000000000000000000, 1.000000000000000000 ) ) ;
#6761 = DIRECTION ( 'NONE',  ( 0.000000000000000000, 0.000000000000000000, -1.000000000000000000 ) ) ;
#6763 = CARTESIAN_POINT ( 'NONE',  ( -11.35316468750000141, 183.2812499965860411, -1.390361679473963753E-15 ) ) ;
#6762 = CARTESIAN_POINT ( 'NONE',  ( 0.000000000000000000, 0.000000000000000000, -1.050311307314560239 ) ) ;
#6764 = EDGE_CURVE ( 'NONE', #13268, #6848, #22754, .T. ) ;
#6765 = DIRECTION ( 'NONE',  ( -0.000000000000000000, 1.000000000000000000, -0.000000000000000000 ) ) ;
#6766 = CARTESIAN_POINT ( 'NONE',  ( -7.320508075688771932, 252.5000000068279178, -7.320508075688771932 ) ) ;
#6767 = CYLINDRICAL_SURFACE ( 'NONE', #9543, 4.000000000000001776 ) ;
#6768 = ORIENTED_EDGE ( 'NONE', *, *, #54813, .T. ) ;
#6769 = EDGE_CURVE ( 'NONE', #40870, #53439, #6148, .T. ) ;
#6770 = CARTESIAN_POINT ( 'NONE',  ( -3.042071309553163960, 172.5520833299193555, -11.35316468749999963 ) ) ;
#6771 =( BOUNDED_CURVE ( )  B_SPLINE_CURVE ( 2, ( #32246, #66185, #65810, #55263, #14488, #3569, #26559, #15614, #72600, #20907, #8855, #38653, #61656 ),
 .UNSPECIFIED., .F., .F. ) 
 B_SPLINE_CURVE_WITH_KNOTS ( ( 3, 2, 2, 2, 2, 2, 3 ),
 ( 0.4076086956521738913, 0.4094202898550724501, 0.4112318840579710089, 0.4130434782608695121, 0.4148550724637680709, 0.4166666666666666297, 0.4184782608695651884 ),
 .UNSPECIFIED. ) 
 CURVE ( )  GEOMETRIC_REPRESENTATION_ITEM ( )  RATIONAL_B_SPLINE_CURVE ( ( 1.000000000000000000, 0.9659258262890683122, 1.000000000000000000, 0.9659258262890683122, 1.000000000000000000, 0.9659258262890683122, 1.000000000000000000, 0.9659258262890683122, 1.000000000000000000, 0.9659258262890683122, 1.000000000000000000, 0.9659258262890693114, 0.9999999999999990008 ) ) 
 REPRESENTATION_ITEM ( '' )  );
#6772 = CARTESIAN_POINT ( 'NONE',  ( 0.000000000000000000, 0.000000000000000000, -14.80000000000000071 ) ) ;
#6773 = CARTESIAN_POINT ( 'NONE',  ( -5.676582343750006032, 124.4270833299193555, 9.832129032723418760 ) ) ;
#6774 = ADVANCED_FACE ( 'NONE', ( #57866 ), #205, .T. ) ;
#6775 = CARTESIAN_POINT ( 'NONE',  ( 23.99999999999997868, 203.8125000027312126, 168.3431457505075457 ) ) ;
#6776 = ORIENTED_EDGE ( 'NONE', *, *, #24459, .T. ) ;
#6777 = CARTESIAN_POINT ( 'NONE',  ( -3.313708498984762052, 103.9062500040967905, -8.000000000000000000 ) ) ;
#6778 = VECTOR ( 'NONE', #2724, 1000.000000000000000 ) ;
#6779 = CARTESIAN_POINT ( 'NONE',  ( 2.828427124746191623, 12.12500000000000000, -2.828427124746191623 ) ) ;
#6780 = CYLINDRICAL_SURFACE ( 'NONE', #25181, 10.00000000000000178 ) ;
#6781 = CARTESIAN_POINT ( 'NONE',  ( -3.211159895383562723, 12.93749999863440792, 3.211159895383561391 ) ) ;
#6782 = CARTESIAN_POINT ( 'NONE',  ( -3.313708498984757167, 7.999999999999991118, 17.23655278392014978 ) ) ;
#6783 = ORIENTED_EDGE ( 'NONE', *, *, #64417, .F. ) ;
#6784 = CARTESIAN_POINT ( 'NONE',  ( 7.188101187500001821, 96.50000000204838102, -2.977408999572651371 ) ) ;
#6786 = CARTESIAN_POINT ( 'NONE',  ( 2.449293598294707893E-16, 11.25000000000000000, -4.000000000000001776 ) ) ;
#6785 = CARTESIAN_POINT ( 'NONE',  ( 10.00000000000005507, 180.0000000000000568, 0.000000000000000000 ) ) ;
#6787 = CARTESIAN_POINT ( 'NONE',  ( 1424.688200795887951, 878.9677537767745434, 1005.827086329040412 ) ) ;
#6788 = VERTEX_POINT ( 'NONE', #62379 ) ;
#6790 = VECTOR ( 'NONE', #187, 1000.000000000000000 ) ;
#6789 = CARTESIAN_POINT ( 'NONE',  ( 0.8912353796322661781, 16.44139524822730891, -68.58382889509240954 ) ) ;
#6791 = CARTESIAN_POINT ( 'NONE',  ( 2.977408999572650927, -7.188101187499990274, 27.45530278187175810 ) ) ;
#6792 = ORIENTED_EDGE ( 'NONE', *, *, #56411, .F. ) ;
#6793 = VERTEX_POINT ( 'NONE', #526 ) ;
#6794 = CARTESIAN_POINT ( 'NONE',  ( -4.220049686691935698, 10.18810118749999916, 88.37500000204838102 ) ) ;
#6795 = CARTESIAN_POINT ( 'NONE',  ( -30.44569435410878810, 196.0625000013656063, 172.4456943541092357 ) ) ;
#6796 = CARTESIAN_POINT ( 'NONE',  ( 11.00000000000000000, 1.347111479062088405E-15, 103.7500000000000000 ) ) ;
#6798 = CARTESIAN_POINT ( 'NONE',  ( -4.088227598258586603E-16, 299.3593750017070079, -6.676582343750001591 ) ) ;
#6797 = CARTESIAN_POINT ( 'NONE',  ( 25.17157287525377996, 201.7500000027312126, 167.1715728752537586 ) ) ;
#6799 = CARTESIAN_POINT ( 'NONE',  ( 10.00000000000000178, 140.2083333333333712, -2.679491924311226736 ) ) ;
#6800 = CARTESIAN_POINT ( 'NONE',  ( 3.313708498984760720, 97.53125000000001421, -8.000000000000000000 ) ) ;
#6801 = CARTESIAN_POINT ( 'NONE',  ( 7.188101187499992051, 8.802885111219154394E-16, 1.111552781871753215 ) ) ;
#6802 = DIRECTION ( 'NONE',  ( 1.000000000000000000, 0.000000000000000000, 0.000000000000000000 ) ) ;
#6803 = CARTESIAN_POINT ( 'NONE',  ( 30.44569435410883429, 202.8125000013656063, 167.5543056458911053 ) ) ;
#6804 = CARTESIAN_POINT ( 'NONE',  ( -7.188101187500000044, 3.093749997951610542, -8.802885111219163269E-16 ) ) ;
#6805 = CARTESIAN_POINT ( 'NONE',  ( 3.317071493978877683, 8.008118988124991233, 2.044365283940627442 ) ) ;
#6806 = DIRECTION ( 'NONE',  ( 0.000000000000000000, 0.000000000000000000, -1.000000000000000000 ) ) ;
#6807 = CARTESIAN_POINT ( 'NONE',  ( 1.320432766682874540E-15, 115.9062500020483810, 7.188101187500000044 ) ) ;
#6809 = CARTESIAN_POINT ( 'NONE',  ( 1.672792093224622745, 194.6518978316834136, 201.2555130000236829 ) ) ;
#6808 = DIRECTION ( 'NONE',  ( -0.000000000000000000, -1.000000000000000000, -0.000000000000000000 ) ) ;
#6810 = CARTESIAN_POINT ( 'NONE',  ( 11.35316468749999608, 226.9270833367473301, -3.042071309553167069 ) ) ;
#6811 = CARTESIAN_POINT ( 'NONE',  ( -3.313708498984760276, 3.468750000000000444, -8.000000000000000000 ) ) ;
#6812 = CARTESIAN_POINT ( 'NONE',  ( 8.660254037844389075, 52.29166665983870388, -5.000000000000000000 ) ) ;
#6813 = CARTESIAN_POINT ( 'NONE',  ( 25.17157287525377996, 197.8750000000000284, 172.8284271247460424 ) ) ;
#6814 = CARTESIAN_POINT ( 'NONE',  ( -5.676582343750006032, 24.11458332991935194, 9.832129032723418760 ) ) ;
#6815 = B_SPLINE_CURVE_WITH_KNOTS ( 'NONE', 3,
 ( #70260, #34836, #17450, #47595, #40471, #58575, #18203, #23859, #52172, #504 ),
 .UNSPECIFIED., .F., .F.,
 ( 4, 2, 2, 2, 4 ),
 ( 0.01051554819734985997, 0.01182504667393350674, 0.01313454515051715524, 0.01575354210368444183, 0.02099153601001901848 ),
 .UNSPECIFIED. ) ;
#6816 = CARTESIAN_POINT ( 'NONE',  ( -30.82842712474621294, 199.1250000000000284, 167.1715728752542134 ) ) ;
#6817 = CARTESIAN_POINT ( 'NONE',  ( 11.35316468750000141, 221.0937499965860127, 0.000000000000000000 ) ) ;
#6818 = CARTESIAN_POINT ( 'NONE',  ( 30.82842712474616675, 201.5000000027312126, 167.1715728752537018 ) ) ;
#6820 = CARTESIAN_POINT ( 'NONE',  ( -5.656854249492378806, 96.68750000000000000, 5.656854249492381470 ) ) ;
#6819 = CARTESIAN_POINT ( 'NONE',  ( 3.428378827827394115, -16.35907404636618168, 69.10239319626211341 ) ) ;
#6821 = ORIENTED_EDGE ( 'NONE', *, *, #34919, .F. ) ;
#6822 = CARTESIAN_POINT ( 'NONE',  ( -1.432654583217662481, 195.3750000013656063, 145.4587341250000634 ) ) ;
#6823 = CARTESIAN_POINT ( 'NONE',  ( -5.676582343750006032, 34.11458332991934839, 9.832129032723418760 ) ) ;
#6824 = CARTESIAN_POINT ( 'NONE',  ( 2.020667218593132706E-15, -11.00000000000000000, 84.06250000409676204 ) ) ;
#6825 = AXIS2_PLACEMENT_3D ( 'NONE', #43325, #20306, #61437 ) ;
#6826 = CARTESIAN_POINT ( 'NONE',  ( 2.449293598294707893E-16, 21.25000000000000000, -4.000000000000001776 ) ) ;
#6827 = CARTESIAN_POINT ( 'NONE',  ( -7.320508075688779925, 151.8750000000000284, -7.320508075688779925 ) ) ;
#6828 = CARTESIAN_POINT ( 'NONE',  ( 11.99999999999999822, 0.5857239961182074683, -4.955142741437655135E-17 ) ) ;
#6830 = CARTESIAN_POINT ( 'NONE',  ( -11.35316468750000141, 13.28124999658601624, -1.390361679473963753E-15 ) ) ;
#6829 = CARTESIAN_POINT ( 'NONE',  ( 2.977408999572650039, 102.6875000020483810, -7.188101187500000933 ) ) ;
#6831 = CARTESIAN_POINT ( 'NONE',  ( -3.313708498984757167, 7.999999999999991118, 12.54905277982336287 ) ) ;
#6832 = CARTESIAN_POINT ( 'NONE',  ( -11.35316468750000141, 143.2812499965860411, -1.390361679473963753E-15 ) ) ;
#6833 = CARTESIAN_POINT ( 'NONE',  ( -7.320508075688773708, 113.7499999931720112, -7.320508075688774596 ) ) ;
#6834 = CARTESIAN_POINT ( 'NONE',  ( -7.188101187500001821, 113.9375000020483952, -2.977408999572650483 ) ) ;
#6835 = CARTESIAN_POINT ( 'NONE',  ( -1.836970198721029983E-15, 3.750000000000000444, 10.00000000000000178 ) ) ;
#6836 = CARTESIAN_POINT ( 'NONE',  ( -26.56734541678238060, 205.6250000013656063, 166.5412658750003629 ) ) ;
#6837 = VERTEX_POINT ( 'NONE', #17475 ) ;
#6838 = CARTESIAN_POINT ( 'NONE',  ( 11.35316468749999785, 5.885416663252683200, 3.042071309553174174 ) ) ;
#6839 = ORIENTED_EDGE ( 'NONE', *, *, #38495, .T. ) ;
#6840 = CARTESIAN_POINT ( 'NONE',  ( -2.995737153994535884, 16.37687539610356424, -68.98994273415323164 ) ) ;
#6841 = CARTESIAN_POINT ( 'NONE',  ( -2.765530957081998586, 297.6406250017070079, 6.676582343750001591 ) ) ;
#6843 = CARTESIAN_POINT ( 'NONE',  ( -11.35316468750000141, 133.4895833299193555, 3.042071309553159963 ) ) ;
#6842 = CYLINDRICAL_SURFACE ( 'NONE', #23189, 4.000000000000001776 ) ;
#6844 = CARTESIAN_POINT ( 'NONE',  ( -27.99999999999991473, 207.6250000027312126, 174.0000000000003695 ) ) ;
#6845 = CARTESIAN_POINT ( 'NONE',  ( -7.999999999999989342, -3.313708498984762496, 20.48030278432982598 ) ) ;
#6846 = CARTESIAN_POINT ( 'NONE',  ( -8.311093377946834337, 254.5312500034139873, 8.311093377946837890 ) ) ;
#6847 = CARTESIAN_POINT ( 'NONE',  ( 7.204075437095968759, -7.204075437095966983, 92.59375000204838102 ) ) ;
#6848 = VERTEX_POINT ( 'NONE', #57496 ) ;
#6849 = EDGE_CURVE ( 'NONE', #69504, #39383, #10706, .T. ) ;
#6850 = CONICAL_SURFACE ( 'NONE', #47762, 5.009999999999998899, 0.9599310885968824758 ) ;
#6851 = CARTESIAN_POINT ( 'NONE',  ( 5.000000000000000000, 15.86295220590816513, 69.92641310672760824 ) ) ;
#6852 = CARTESIAN_POINT ( 'NONE',  ( 2.020667218593132706E-15, -11.00000000000000000, 100.5625000040967763 ) ) ;
#6853 = UNCERTAINTY_MEASURE_WITH_UNIT (LENGTH_MEASURE( 1.000000000000000082E-05 ), #3888, 'distance_accuracy_value', 'NONE');
#6854 = CARTESIAN_POINT ( 'NONE',  ( 6.951808397369818766E-16, 92.34374999658602690, -11.35316468750000141 ) ) ;
#6855 = CARTESIAN_POINT ( 'NONE',  ( 7.204075437095968759, -7.204075437095966983, 108.7187500020483810 ) ) ;
#6856 = EDGE_CURVE ( 'NONE', #11129, #40340, #37484, .T. ) ;
#6857 = CARTESIAN_POINT ( 'NONE',  ( 3.211159895383561835, 16.56249999863440436, -3.211159895383561835 ) ) ;
#6858 = ORIENTED_EDGE ( 'NONE', *, *, #70064, .F. ) ;
#6859 = ORIENTED_EDGE ( 'NONE', *, *, #61037, .T. ) ;
#6860 = CARTESIAN_POINT ( 'NONE',  ( 7.999999999999998224, 2.906250000000000888, 3.313708498984766493 ) ) ;
#6861 = DIRECTION ( 'NONE',  ( -0.000000000000000000, -0.000000000000000000, 1.000000000000000000 ) ) ;
#6862 = CARTESIAN_POINT ( 'NONE',  ( 7.188101187500000044, 0.4687499979516099868, 0.000000000000000000 ) ) ;
#6863 = CARTESIAN_POINT ( 'NONE',  ( 3.313708498984765161, 121.1562500040967763, 7.999999999999998224 ) ) ;
#6864 = CARTESIAN_POINT ( 'NONE',  ( -4.220049686691935698, 10.18810118749999916, 105.2500000020483952 ) ) ;
#6865 =( BOUNDED_CURVE ( )  B_SPLINE_CURVE ( 2, ( #41943, #7621, #12165, #29525, #136, #23112, #48709 ),
 .UNSPECIFIED., .F., .F. ) 
 B_SPLINE_CURVE_WITH_KNOTS ( ( 3, 2, 2, 3 ),
 ( 0.9722222222222223209, 0.9814814814814816213, 0.9907407407407406996, 1.000000000000000000 ),
 .UNSPECIFIED. ) 
 CURVE ( )  GEOMETRIC_REPRESENTATION_ITEM ( )  RATIONAL_B_SPLINE_CURVE ( ( 0.9999999999999995559, 0.9659258262890687563, 1.000000000000000000, 0.9659258262890683122, 1.000000000000000000, 0.9659258262890683122, 1.000000000000000000 ) ) 
 REPRESENTATION_ITEM ( '' )  );
#6866 = CARTESIAN_POINT ( 'NONE',  ( 2.449293598294707893E-16, 0.2500000000000001665, -4.000000000000001776 ) ) ;
#6867 = CARTESIAN_POINT ( 'NONE',  ( 4.000000000000000888, 15.68749999726881406, 1.656854249492384135 ) ) ;
#6868 =( BOUNDED_CURVE ( )  B_SPLINE_CURVE ( 2, ( #52219, #69565, #74473, #17876, #19257, #34137, #5452, #40893, #11848, #51460, #59272, #68439, #57521 ),
 .UNSPECIFIED., .F., .F. ) 
 B_SPLINE_CURVE_WITH_KNOTS ( ( 3, 2, 2, 2, 2, 2, 3 ),
 ( 1.303087675546690472, 1.308321663417258307, 1.313555651287826143, 1.318789639158393756, 1.324023627028961592, 1.329257614899529427, 1.334491602770097263 ),
 .UNSPECIFIED. ) 
 CURVE ( )  GEOMETRIC_REPRESENTATION_ITEM ( )  RATIONAL_B_SPLINE_CURVE ( ( 1.000000000000101252, 0.9659258262889670599, 1.000000000000000000, 0.9659258262890683122, 1.000000000000000000, 0.9659258262890683122, 1.000000000000000000, 0.9659258262890683122, 1.000000000000000000, 0.9659258262890683122, 1.000000000000000000, 0.9659258262890704216, 0.9999999999999978906 ) ) 
 REPRESENTATION_ITEM ( '' )  );
#6869 = CARTESIAN_POINT ( 'NONE',  ( 5.656854249492374365, 5.656854249492375253, 12.45530278392014623 ) ) ;
#6870 = EDGE_LOOP ( 'NONE', ( #7392, #35333, #69699 ) ) ;
#6871 = AXIS2_PLACEMENT_3D ( 'NONE', #65426, #18677, #7724 ) ;
#6872 = CYLINDRICAL_SURFACE ( 'NONE', #16495, 3.999999999999976019 ) ;
#6873 = CARTESIAN_POINT ( 'NONE',  ( -3.458734124999959025, 200.5000000013655779, 199.4326545832176691 ) ) ;
#6874 = CARTESIAN_POINT ( 'NONE',  ( 4.999999999999993783, 151.0416666598387110, 8.660254037844390851 ) ) ;
#6876 = CARTESIAN_POINT ( 'NONE',  ( -10.00000000000000178, 224.3749999931720254, -1.224646799147353454E-15 ) ) ;
#6875 = CARTESIAN_POINT ( 'NONE',  ( -29.43265458321771177, 199.5000000013656063, 166.5412658750003914 ) ) ;
#6877 = CARTESIAN_POINT ( 'NONE',  ( -1.881053915767121554, 14.62499999863440969, -4.541265875000002339 ) ) ;
#6878 = CARTESIAN_POINT ( 'NONE',  ( 7.320508075688774596, 122.4999999931720254, -7.320508075688774596 ) ) ;
#6879 = CARTESIAN_POINT ( 'NONE',  ( -4.401442555609577197E-16, 7.188101187499992051, 13.11155278187175277 ) ) ;
#6880 = ORIENTED_EDGE ( 'NONE', *, *, #66984, .T. ) ;
#6881 = ORIENTED_EDGE ( 'NONE', *, *, #6856, .T. ) ;
#6882 = CARTESIAN_POINT ( 'NONE',  ( 1.871523826299183495E-15, -10.18810118749999916, 104.0312500020483810 ) ) ;
#6883 = CARTESIAN_POINT ( 'NONE',  ( 4.556349186104052151, -10.99999999999999822, 103.4687500000000000 ) ) ;
#6884 = CARTESIAN_POINT ( 'NONE',  ( -24.00000000000001066, 204.8124999999999716, 168.3431457505080004 ) ) ;
#6885 = CARTESIAN_POINT ( 'NONE',  ( 1.432654583217662481, 201.1250000013656347, 194.5412658750000219 ) ) ;
#6886 = CARTESIAN_POINT ( 'NONE',  ( 31.45873412499999233, 194.6875000013655779, 169.9999999999998863 ) ) ;
#6887 = CARTESIAN_POINT ( 'NONE',  ( 10.00000000000000178, 95.20833333333334281, -2.679491924311226736 ) ) ;
#6888 = CARTESIAN_POINT ( 'NONE',  ( -8.000000000000000000, 120.4062500000000142, -3.313708498984761608 ) ) ;
#6889 = CARTESIAN_POINT ( 'NONE',  ( 8.311093377946837890, 61.71874999658601979, -8.311093377946837890 ) ) ;
#6890 = CARTESIAN_POINT ( 'NONE',  ( -4.088227598258586603E-16, 296.3593750017070079, -6.676582343750001591 ) ) ;
#6891 = VERTEX_POINT ( 'NONE', #6542 ) ;
#6892 = CARTESIAN_POINT ( 'NONE',  ( -11.00000000000000000, 0.000000000000000000, 108.9999999999999858 ) ) ;
#6893 = CARTESIAN_POINT ( 'NONE',  ( 4.898587196589412829E-16, 16.68749999590322375, -8.000000000000000000 ) ) ;
#6894 = CARTESIAN_POINT ( 'NONE',  ( 3.458734124999959914, 209.3750000013656063, 143.4326545832176976 ) ) ;
#6895 = CARTESIAN_POINT ( 'NONE',  ( 2.679491924310495765, 86.04166666666674246, -10.00000000000043343 ) ) ;
#6896 = CARTESIAN_POINT ( 'NONE',  ( 47.32259252271278882, 272.0000000000000000, 65.76194439203457875 ) ) ;
#6897 = CARTESIAN_POINT ( 'NONE',  ( 10.00000000000000000, 227.5000000000000000, -1.224646799147353256E-15 ) ) ;
#6898 = CARTESIAN_POINT ( 'NONE',  ( -2.485281374238227592, 293.1874999999999432, 6.000000000000345501 ) ) ;
#6899 = CARTESIAN_POINT ( 'NONE',  ( -10.99999999999999822, -4.556349186104052151, 116.5937500000000000 ) ) ;
#6900 = CARTESIAN_POINT ( 'NONE',  ( 6.123233995736767268E-16, 221.2500000000000000, -10.00000000000000178 ) ) ;
#6901 = CARTESIAN_POINT ( 'NONE',  ( -2.977408999572647819, -7.188101187499990274, 11.14280278187175455 ) ) ;
#6902 = CARTESIAN_POINT ( 'NONE',  ( 8.311093377946837890, 181.7187499965859843, -8.311093377946837890 ) ) ;
#6903 = CARTESIAN_POINT ( 'NONE',  ( 4.541265875000002339, 3.374999998634406584, -1.881053915767121554 ) ) ;
#6904 = FACE_OUTER_BOUND ( 'NONE', #46594, .T. ) ;
#6906 = CARTESIAN_POINT ( 'NONE',  ( 1.656854249492381914, 4.812500000000000888, 4.000000000000000888 ) ) ;
#6905 = CARTESIAN_POINT ( 'NONE',  ( 1.469576158976822172E-15, -7.999999999999991118, 20.70530277982336642 ) ) ;
#6907 = ORIENTED_EDGE ( 'NONE', *, *, #43607, .F. ) ;
#6908 = CARTESIAN_POINT ( 'NONE',  ( -1.432654583217662481, 208.3750000013656063, 145.4587341250000634 ) ) ;
#6909 = CARTESIAN_POINT ( 'NONE',  ( 9.832129032723416984, 35.67708332991935549, 5.676582343750006032 ) ) ;
#6910 = CARTESIAN_POINT ( 'NONE',  ( 11.00000000000000000, 1.347111479062088405E-15, 102.4375000040967763 ) ) ;
#6911 = CARTESIAN_POINT ( 'NONE',  ( 11.35316468749999785, 220.8854166632526699, 3.042071309553174174 ) ) ;
#6912 = CARTESIAN_POINT ( 'NONE',  ( -26.56734541678243033, 207.3750000013656063, 166.5412658750003345 ) ) ;
#6913 = CARTESIAN_POINT ( 'NONE',  ( 27.99999999999996803, 207.6250000027312126, 165.9999999999998863 ) ) ;
#6915 = CARTESIAN_POINT ( 'NONE',  ( -9.999999999999978684, 102.2916666666666572, -2.679491924311224516 ) ) ;
#6914 = CARTESIAN_POINT ( 'NONE',  ( 3.410844894484189267E-12, 36.24999999999974420, -10.00000000000000178 ) ) ;
#6916 = CARTESIAN_POINT ( 'NONE',  ( 11.00000000000000000, 1.347111479062088405E-15, 87.25000000000000000 ) ) ;
#6917 = EDGE_CURVE ( 'NONE', #6191, #52335, #23884, .T. ) ;
#6918 = EDGE_CURVE ( 'NONE', #57818, #50631, #22515, .T. ) ;
#6919 = CARTESIAN_POINT ( 'NONE',  ( -10.00000000000000178, 79.37499999317202537, -1.224646799147353454E-15 ) ) ;
#6920 = CARTESIAN_POINT ( 'NONE',  ( -2.977408999572650927, 96.87500000204836681, -7.188101187500001821 ) ) ;
#6921 = CARTESIAN_POINT ( 'NONE',  ( -4.541265875000002339, 17.87499999863441147, -1.881053915767121998 ) ) ;
#6922 = CARTESIAN_POINT ( 'NONE',  ( -6.000000000000001776, 299.0625000034140157, 0.000000000000000000 ) ) ;
#6923 = CARTESIAN_POINT ( 'NONE',  ( 4.000000000000001776, 10.81249999726881406, -1.656854249492381248 ) ) ;
#6924 = CARTESIAN_POINT ( 'NONE',  ( -10.99999999999992006, -31.99999999999978684, 135.0000000000000000 ) ) ;
#6925 = ORIENTED_EDGE ( 'NONE', *, *, #32673, .T. ) ;
#6926 = EDGE_LOOP ( 'NONE', ( #56541, #14651, #26106, #22412 ) ) ;
#6927 = CARTESIAN_POINT ( 'NONE',  ( -6.676582343750000703, 298.6718750017070079, 2.765530957082001251 ) ) ;
#6928 = CARTESIAN_POINT ( 'NONE',  ( -5.000000000000004441, 141.6666666666666856, -8.660254037844399733 ) ) ;
#6929 = VECTOR ( 'NONE', #60064, 1000.000000000000000 ) ;
#6930 = CARTESIAN_POINT ( 'NONE',  ( -6.401276095387002485, -6.696526368584479805, -0.1469846612282594001 ) ) ;
#6931 = CARTESIAN_POINT ( 'NONE',  ( -8.311093377946841443, 153.9062499965860127, 8.311093377946830785 ) ) ;
#6932 = CARTESIAN_POINT ( 'NONE',  ( 10.18810118749999916, 4.220049686691935698, 83.50000000204840944 ) ) ;
#6933 = CARTESIAN_POINT ( 'NONE',  ( 7.320508075688771932, 4.374999999999999112, 7.320508075688776373 ) ) ;
#6934 = CARTESIAN_POINT ( 'NONE',  ( -1.656854249492348607, 203.1875000000000284, 202.0000000000000284 ) ) ;
#6935 = PLANE ( 'NONE',  #36187 ) ;
#6936 = CARTESIAN_POINT ( 'NONE',  ( -4.220049686691935698, 10.18810118749999916, 111.2500000020483952 ) ) ;
#6937 = ORIENTED_EDGE ( 'NONE', *, *, #30633, .F. ) ;
#6938 = CARTESIAN_POINT ( 'NONE',  ( -8.000000000000000000, 112.9062500000000000, -3.313708498984761164 ) ) ;
#6939 = CYLINDRICAL_SURFACE ( 'NONE', #14751, 8.000000000000000000 ) ;
#6940 = CARTESIAN_POINT ( 'NONE',  ( 5.676582343749993598, 140.2604166632526983, 9.832129032723422313 ) ) ;
#6941 = CARTESIAN_POINT ( 'NONE',  ( -1.432654583217607858, 198.6250000013656063, 201.4587341250000065 ) ) ;
#6942 = CARTESIAN_POINT ( 'NONE',  ( 3.458734125000015425, 209.2500000013656063, 196.5673454167823877 ) ) ;
#6943 = CARTESIAN_POINT ( 'NONE',  ( 10.18810118749999916, 4.220049686691935698, 74.87500000204836681 ) ) ;
#6944 = CARTESIAN_POINT ( 'NONE',  ( -9.832129032723420536, 49.01041666325269119, 5.676582343749997150 ) ) ;
#6945 = ORIENTED_EDGE ( 'NONE', *, *, #44508, .T. ) ;
#6946 = CARTESIAN_POINT ( 'NONE',  ( -10.00000000000000888, 27.50000000000000355, -1.224646799147354243E-15 ) ) ;
#6947 = CARTESIAN_POINT ( 'NONE',  ( 3.211159895383561835, 3.562499998634407028, -3.211159895383561835 ) ) ;
#6948 = CARTESIAN_POINT ( 'NONE',  ( 1.471067592899761672E-15, -8.008118988124991233, 13.38811528394063011 ) ) ;
#6949 = CARTESIAN_POINT ( 'NONE',  ( 2.977408999572650927, 15.74999999795161543, -7.188101187500001821 ) ) ;
#6950 = CARTESIAN_POINT ( 'NONE',  ( -4.242640687119286547, 293.9375000034140157, -4.242640687119286547 ) ) ;
#6951 = EDGE_CURVE ( 'NONE', #72883, #1423, #28428, .T. ) ;
#6952 = DIRECTION ( 'NONE',  ( -0.000000000000000000, 1.000000000000000000, 4.689100369878284071E-30 ) ) ;
#6953 = CARTESIAN_POINT ( 'NONE',  ( 5.082755093536325930, 10.03124999795161187, -5.082755093536325930 ) ) ;
#6954 = CARTESIAN_POINT ( 'NONE',  ( -7.188101187499992051, 0.000000000000000000, 10.48655278187175455 ) ) ;
#6955 = COLOUR_RGB ( '',0.7921568627450980005, 0.8196078431372548767, 0.9333333333333333481 ) ;
#6956 = CARTESIAN_POINT ( 'NONE',  ( -7.204075437095965206, -7.204075437095968759, 69.34375000204836681 ) ) ;
#6957 = CARTESIAN_POINT ( 'NONE',  ( -24.54126587499999346, 205.4375000013656063, 170.0000000000003411 ) ) ;
#6958 = DIRECTION ( 'NONE',  ( -3.154042683594195121E-16, 1.000000000000000000, 0.000000000000000000 ) ) ;
#6959 = CARTESIAN_POINT ( 'NONE',  ( 4.000000000000000888, 2.687499997268813612, 1.656854249492384135 ) ) ;
#6960 = ORIENTED_EDGE ( 'NONE', *, *, #71294, .T. ) ;
#6961 =( BOUNDED_CURVE ( )  B_SPLINE_CURVE ( 2, ( #46914, #12579, #74102, #45423, #16740, #72435, #14703, #72044, #43760 ),
 .UNSPECIFIED., .F., .F. ) 
 B_SPLINE_CURVE_WITH_KNOTS ( ( 3, 2, 2, 2, 3 ),
 ( 0.7166666666666671182, 0.7250000000000005329, 0.7333333333333338366, 0.7416666666666673624, 0.7500000000000006661 ),
 .UNSPECIFIED. ) 
 CURVE ( )  GEOMETRIC_REPRESENTATION_ITEM ( )  RATIONAL_B_SPLINE_CURVE ( ( 0.9999999999999958922, 0.9238795325112908463, 1.000000000000000000, 0.9238795325112867385, 1.000000000000000000, 0.9238795325112867385, 1.000000000000000000, 0.9238795325112806323, 1.000000000000005995 ) ) 
 REPRESENTATION_ITEM ( '' )  );
#6962 = CARTESIAN_POINT ( 'NONE',  ( 2.445694354108838731, 209.0625000013656063, 195.5543056458912190 ) ) ;
#6963 = CARTESIAN_POINT ( 'NONE',  ( -1.656854249492403008, 205.6875000000000284, 146.0000000000000284 ) ) ;
#6964 = CARTESIAN_POINT ( 'NONE',  ( -30.82842712474624491, 202.2500000027312126, 167.1715728752542418 ) ) ;
#6965 = CARTESIAN_POINT ( 'NONE',  ( 4.541265875000002339, 2.312499998634407028, 0.000000000000000000 ) ) ;
#6966 = CARTESIAN_POINT ( 'NONE',  ( 5.082755093536326818, 117.2187500020483810, 5.082755093536325042 ) ) ;
#6967 = FACE_OUTER_BOUND ( 'NONE', #16124, .T. ) ;
#6968 = CARTESIAN_POINT ( 'NONE',  ( -7.999999999999991118, 3.313708498984756723, 2.424052783920144005 ) ) ;
#6969 = VERTEX_POINT ( 'NONE', #63875 ) ;
#6970 = CARTESIAN_POINT ( 'NONE',  ( 5.082755093536324154, 25.78124999795161543, 5.082755093536326818 ) ) ;
#6971 = EDGE_LOOP ( 'NONE', ( #33423, #18979, #7666, #27320, #43925, #17243, #38963, #17425, #49181, #72226, #41225, #69337, #13685, #23944, #375, #14470, #30237, #44479, #8310, #39921, #48164, #46166, #21948, #52212, #66491, #70092, #17921, #37493, #39745, #582, #37076, #55797, #49528, #74080 ) ) ;
#6972 = CARTESIAN_POINT ( 'NONE',  ( -28.00000000000002842, 199.0000000000000000, 166.0000000000003695 ) ) ;
#6973 = CARTESIAN_POINT ( 'NONE',  ( 5.656854249492378806, 13.31250000000000178, 5.656854249492381470 ) ) ;
#6974 = CARTESIAN_POINT ( 'NONE',  ( -5.000000000000005329, 53.33333333333333570, 8.660254037844387298 ) ) ;
#6975 = CARTESIAN_POINT ( 'NONE',  ( -2.977408999572651815, 97.81250000204840944, 7.188101187500000933 ) ) ;
#6976 = CARTESIAN_POINT ( 'NONE',  ( -25.17157287525377285, 196.6250000000000284, 172.8284271247465256 ) ) ;
#6977 = VECTOR ( 'NONE', #18255, 1000.000000000000000 ) ;
#6979 = DIRECTION ( 'NONE',  ( -0.000000000000000000, 1.000000000000000000, -0.000000000000000000 ) ) ;
#6978 = DIRECTION ( 'NONE',  ( 0.000000000000000000, -0.9919497796038491133, -0.1266318867579376284 ) ) ;
#6980 = ORIENTED_EDGE ( 'NONE', *, *, #59303, .T. ) ;
#6981 = ORIENTED_EDGE ( 'NONE', *, *, #37201, .F. ) ;
#6982 =( BOUNDED_CURVE ( )  B_SPLINE_CURVE ( 2, ( #72733, #55765, #43302, #26312, #42922, #20280, #14995, #65941, #61032 ),
 .UNSPECIFIED., .F., .F. ) 
 B_SPLINE_CURVE_WITH_KNOTS ( ( 3, 2, 2, 2, 3 ),
 ( 0.8750000000000000000, 0.8806818181818182323, 0.8863636363636363535, 0.8920454545454545858, 0.8977272727272727071 ),
 .UNSPECIFIED. ) 
 CURVE ( )  GEOMETRIC_REPRESENTATION_ITEM ( )  RATIONAL_B_SPLINE_CURVE ( ( 1.000000000000000000, 0.9238795325112867385, 1.000000000000000000, 0.9238795325112867385, 1.000000000000000000, 0.9238795325112867385, 1.000000000000000000, 0.9238795325112867385, 1.000000000000000000 ) ) 
 REPRESENTATION_ITEM ( '' )  );
#6983 = CARTESIAN_POINT ( 'NONE',  ( -11.35316468749999785, 243.6979166700806445, -3.042071309553164848 ) ) ;
#6984 = ADVANCED_FACE ( 'NONE', ( #33739 ), #12187, .F. ) ;
#6985 = CARTESIAN_POINT ( 'NONE',  ( -2.977408999572647819, 7.188101187499991163, 18.08030278187175455 ) ) ;
#6986 = CARTESIAN_POINT ( 'NONE',  ( 7.347880794884121708E-16, 300.0000000000000000, -6.000000000000001776 ) ) ;
#6987 = DIRECTION ( 'NONE',  ( 1.000000000000000000, 0.000000000000000000, 0.000000000000000000 ) ) ;
#6988 = CARTESIAN_POINT ( 'NONE',  ( 3.999999999999960032, 197.0625000027312126, 143.6568542494924259 ) ) ;
#6989 = CARTESIAN_POINT ( 'NONE',  ( 4.999999999999997335, 258.3333333333333712, -8.660254037844387298 ) ) ;
#6990 = CARTESIAN_POINT ( 'NONE',  ( 3.313708498984762496, -7.999999999999989342, 19.48655278392014978 ) ) ;
#6991 = CARTESIAN_POINT ( 'NONE',  ( -7.320508075688773708, 171.8749999999999716, -7.320508075688774596 ) ) ;
#6992 = CARTESIAN_POINT ( 'NONE',  ( 26.56734541678232731, 209.3750000013656063, 173.4587341249998929 ) ) ;
#6993 = CARTESIAN_POINT ( 'NONE',  ( -8.000000000000000000, 119.0000000000000000, 0.000000000000000000 ) ) ;
#6994 = CARTESIAN_POINT ( 'NONE',  ( -4.401442555609577197E-16, 7.188101187499992051, 28.48655278187175810 ) ) ;
#6995 = CARTESIAN_POINT ( 'NONE',  ( -3.042071309553173730, 144.6354166632526983, 11.35316468749999785 ) ) ;
#6996 = CARTESIAN_POINT ( 'NONE',  ( 11.00000000000000000, 1.347111479062088405E-15, 75.43750000409676204 ) ) ;
#6997 = CARTESIAN_POINT ( 'NONE',  ( 10.00000000000000178, 26.87499999317203603, 0.000000000000000000 ) ) ;
#7000 = CARTESIAN_POINT ( 'NONE',  ( -2.679491924312266349, 168.5416666666666288, 9.999999999999408473 ) ) ;
#6999 = CARTESIAN_POINT ( 'NONE',  ( 7.320508075688771044, 106.2499999931720396, 7.320508075688775484 ) ) ;
#6998 = CARTESIAN_POINT ( 'NONE',  ( 25.17157287525381548, 205.6250000000000284, 167.1715728752537018 ) ) ;
#7001 = VERTEX_POINT ( 'NONE', #51066 ) ;
#7002 = EDGE_CURVE ( 'NONE', #31653, #1389, #68357, .T. ) ;
#7003 = VECTOR ( 'NONE', #21408, 1000.000000000000000 ) ;
#7004 = CARTESIAN_POINT ( 'NONE',  ( -23.99999999999997868, 209.6875000000000284, 171.6568542494927385 ) ) ;
#7005 = CARTESIAN_POINT ( 'NONE',  ( 7.320508075688850091, 194.3750000000000853, 7.320508075688853644 ) ) ;
#7006 = VECTOR ( 'NONE', #18951, 1000.000000000000000 ) ;
#7007 = CARTESIAN_POINT ( 'NONE',  ( -5.841315287305287818, 124.7066856464806364, -5.183856896381568546 ) ) ;
#7009 = CARTESIAN_POINT ( 'NONE',  ( 10.00000000000000178, 36.87499999317203958, 0.000000000000000000 ) ) ;
#7008 =( BOUNDED_CURVE ( )  B_SPLINE_CURVE ( 2, ( #57153, #17518, #201, #5469, #63540, #34901, #566, #6582, #46561, #70323, #23178, #6215, #11865 ),
 .UNSPECIFIED., .F., .F. ) 
 B_SPLINE_CURVE_WITH_KNOTS ( ( 3, 2, 2, 2, 2, 2, 3 ),
 ( 0.1467391304347825942, 0.1485507246376811252, 0.1503623188405796840, 0.1521739130434782705, 0.1539855072463768015, 0.1557971014492753603, 0.1576086956521739191 ),
 .UNSPECIFIED. ) 
 CURVE ( )  GEOMETRIC_REPRESENTATION_ITEM ( )  RATIONAL_B_SPLINE_CURVE ( ( 1.000000000000000444, 0.9659258262890677571, 1.000000000000000000, 0.9659258262890683122, 1.000000000000000000, 0.9659258262890683122, 1.000000000000000000, 0.9659258262890683122, 1.000000000000000000, 0.9659258262890683122, 1.000000000000000000, 0.9659258262890683122, 1.000000000000000000 ) ) 
 REPRESENTATION_ITEM ( '' )  );
#7010 = CARTESIAN_POINT ( 'NONE',  ( -5.082755093536324154, 112.3437500020483810, 5.082755093536326818 ) ) ;
#7011 = CARTESIAN_POINT ( 'NONE',  ( -4.541265875000002339, 5.937499998634407028, -5.561446717895856393E-16 ) ) ;
#7012 = CARTESIAN_POINT ( 'NONE',  ( 4.556349186104052151, -10.99999999999999822, 85.46874999999998579 ) ) ;
#7013 = CARTESIAN_POINT ( 'NONE',  ( 3.313708498984762496, -7.999999999999989342, 14.79905277982336465 ) ) ;
#7014 = CARTESIAN_POINT ( 'NONE',  ( -6.123233995736766282E-16, 236.8750000068279746, -10.00000000000000000 ) ) ;
#7015 = ORIENTED_EDGE ( 'NONE', *, *, #58745, .F. ) ;
#7016 = CARTESIAN_POINT ( 'NONE',  ( 10.00000000000000178, 220.4166666734946318, 2.679491924311222739 ) ) ;
#7017 = CARTESIAN_POINT ( 'NONE',  ( -9.489952148308621105, 225.9999999999999716, -3.220591000268780313 ) ) ;
#7018 = CARTESIAN_POINT ( 'NONE',  ( -10.00000000000005684, 62.70833333333337833, 2.679491924311237394 ) ) ;
#7019 = CARTESIAN_POINT ( 'NONE',  ( 5.676582343749997150, 247.5520833367473301, -9.832129032723418760 ) ) ;
#7020 = CARTESIAN_POINT ( 'NONE',  ( -8.311093377946841443, 113.9062499965859985, 8.311093377946830785 ) ) ;
#7021 = ORIENTED_EDGE ( 'NONE', *, *, #15763, .F. ) ;
#7022 = CARTESIAN_POINT ( 'NONE',  ( -5.771752292166722142, 9.182361355190234775, 117.6647434345326104 ) ) ;
#7023 = ADVANCED_FACE ( 'NONE', ( #13651 ), #8377, .F. ) ;
#7024 = ADVANCED_FACE ( 'NONE', ( #41242 ), #54419, .F. ) ;
#7025 = CARTESIAN_POINT ( 'NONE',  ( -7.204075437095965206, -7.204075437095968759, 99.34375000204836681 ) ) ;
#7026 = FACE_OUTER_BOUND ( 'NONE', #12794, .T. ) ;
#7027 = CARTESIAN_POINT ( 'NONE',  ( 2.754378923186476579E-14, 202.4375000013656063, 194.5412658750000219 ) ) ;
#7028 = CARTESIAN_POINT ( 'NONE',  ( 10.99999999999989697, -4.556349186104149851, 69.15624999999998579 ) ) ;
#7030 = CARTESIAN_POINT ( 'NONE',  ( 11.35316468749999963, 115.9895833299193697, -3.042071309553165293 ) ) ;
#7029 = CYLINDRICAL_SURFACE ( 'NONE', #62924, 8.000000000000000000 ) ;
#7031 = CARTESIAN_POINT ( 'NONE',  ( 7.999999999999991118, 9.797174393178815797E-16, 9.267802783920146226 ) ) ;
#7032 = CARTESIAN_POINT ( 'NONE',  ( -25.55430564589119058, 197.5625000013656063, 167.5543056458915316 ) ) ;
#7033 = CARTESIAN_POINT ( 'NONE',  ( 7.320508075688771044, 146.2499999931719969, 7.320508075688775484 ) ) ;
#7034 = VERTEX_POINT ( 'NONE', #18226 ) ;
#7035 = EDGE_CURVE ( 'NONE', #9105, #35502, #51979, .T. ) ;
#7036 = CARTESIAN_POINT ( 'NONE',  ( 2.679491924311228956, 197.9166666598386826, -10.00000000000000000 ) ) ;
#7037 = CARTESIAN_POINT ( 'NONE',  ( 3.999999999999960032, 205.9374999999999716, 143.6568542494924259 ) ) ;
#7038 = CARTESIAN_POINT ( 'NONE',  ( 2.449293598294707893E-16, 9.250000000000000000, -4.000000000000001776 ) ) ;
#7039 = CARTESIAN_POINT ( 'NONE',  ( -9.832129032723420536, 104.0104166632526841, 5.676582343749997150 ) ) ;
#7040 = CARTESIAN_POINT ( 'NONE',  ( 1.656854249492379916, 205.3125000000000284, 202.0000000000000284 ) ) ;
#7041 = CARTESIAN_POINT ( 'NONE',  ( 5.082755093536325930, 14.53124999795161187, -5.082755093536325930 ) ) ;
#7042 = CARTESIAN_POINT ( 'NONE',  ( 7.204075437095968759, -7.204075437095966983, 97.09375000204836681 ) ) ;
#7043 = CARTESIAN_POINT ( 'NONE',  ( -5.676582343749998039, 12.76041666325268409, -9.832129032723420536 ) ) ;
#7044 = ORIENTED_EDGE ( 'NONE', *, *, #25924, .F. ) ;
#7045 = LINE ( 'NONE', #45913, #69349 ) ;
#7046 = CARTESIAN_POINT ( 'NONE',  ( -11.00000000000000000, 0.000000000000000000, 80.49999999999998579 ) ) ;
#7047 = CARTESIAN_POINT ( 'NONE',  ( 5.676582343749993598, 224.9479166632526983, 9.832129032723422313 ) ) ;
#7048 = CARTESIAN_POINT ( 'NONE',  ( -7.204075437095967871, 7.204075437095967871, 79.84375000204838102 ) ) ;
#7049 = DIRECTION ( 'NONE',  ( -0.000000000000000000, 1.000000000000000000, -0.000000000000000000 ) ) ;
#7050 = CARTESIAN_POINT ( 'NONE',  ( -10.00000000000000000, 264.7916666666666856, -2.679491924311226292 ) ) ;
#7051 = CARTESIAN_POINT ( 'NONE',  ( 6.676582343750001591, 293.9531250017069510, -8.176455196517173205E-16 ) ) ;
#7052 = ADVANCED_FACE ( 'NONE', ( #25347 ), #60056, .F. ) ;
#7053 = VERTEX_POINT ( 'NONE', #1984 ) ;
#7054 = CARTESIAN_POINT ( 'NONE',  ( -11.35316468750000141, 203.8020833299193555, 3.042071309553159963 ) ) ;
#7055 = CARTESIAN_POINT ( 'NONE',  ( 4.220049686691934809, 10.18810118749999916, 88.18750000204838102 ) ) ;
#7056 = AXIS2_PLACEMENT_3D ( 'NONE', #3373, #2253, #71270 ) ;
#7057 = CARTESIAN_POINT ( 'NONE',  ( -31.45873412499998523, 202.7500000013655779, 171.4326545832180386 ) ) ;
#7058 = CARTESIAN_POINT ( 'NONE',  ( 8.000000000000000000, 24.00000000000000355, 0.000000000000000000 ) ) ;
#7059 = ORIENTED_EDGE ( 'NONE', *, *, #6526, .T. ) ;
#7060 = CARTESIAN_POINT ( 'NONE',  ( -26.34314575050770202, 208.0625000027312410, 166.0000000000003695 ) ) ;
#7061 = AXIS2_PLACEMENT_3D ( 'NONE', #47021, #64751, #70416 ) ;
#7062 = CARTESIAN_POINT ( 'NONE',  ( 2.849036369511732440E-14, 206.3750000027312126, 202.0000000000000000 ) ) ;
#7063 = CARTESIAN_POINT ( 'NONE',  ( 10.00000000000000000, 24.79166666666666785, 2.679491924311236062 ) ) ;
#7064 = AXIS2_PLACEMENT_3D ( 'NONE', #30188, #7914, #41871 ) ;
#7065 = CARTESIAN_POINT ( 'NONE',  ( -5.000000000000002665, 14.32120916179462711, 69.86289779849467152 ) ) ;
#7066 = CARTESIAN_POINT ( 'NONE',  ( 4.220049686691934809, 10.18810118749999916, 72.06250000204836681 ) ) ;
#7067 = ORIENTED_EDGE ( 'NONE', *, *, #55138, .T. ) ;
#7068 = CARTESIAN_POINT ( 'NONE',  ( -1.320432766682874540E-15, 4.593749997951610986, 7.188101187500000044 ) ) ;
#7069 = DIRECTION ( 'NONE',  ( 1.000000000000000000, 0.000000000000000000, 0.000000000000000000 ) ) ;
#7070 = FILL_AREA_STYLE_COLOUR ( '', #7801 ) ;
#7071 = CARTESIAN_POINT ( 'NONE',  ( -5.082755093536325930, 116.8437500020483810, -5.082755093536325930 ) ) ;
#7072 = CARTESIAN_POINT ( 'NONE',  ( 2.295000000000000373, 267.1439999999997212, 5.415577408903852863 ) ) ;
#7073 = CARTESIAN_POINT ( 'NONE',  ( -4.721056650415999201, 295.3281250017069510, -4.721056650415999201 ) ) ;
#7075 = CARTESIAN_POINT ( 'NONE',  ( -1.836970198721029983E-15, 135.6249999931720538, 10.00000000000000178 ) ) ;
#7074 = CARTESIAN_POINT ( 'NONE',  ( -3.042071309553166625, 237.8645833367473301, -11.35316468749999608 ) ) ;
#7076 = ORIENTED_EDGE ( 'NONE', *, *, #10320, .T. ) ;
#7077 = CARTESIAN_POINT ( 'NONE',  ( -3.042071309553166181, 243.1770833367473017, -11.35316468749999608 ) ) ;
#7078 = CARTESIAN_POINT ( 'NONE',  ( 2.977408999572650927, -7.188101187499990274, 4.955302781871753659 ) ) ;
#7079 =( BOUNDED_CURVE ( )  B_SPLINE_CURVE ( 2, ( #22135, #45161, #68173, #55754, #16470, #50076, #68541, #17602, #6300 ),
 .UNSPECIFIED., .F., .F. ) 
 B_SPLINE_CURVE_WITH_KNOTS ( ( 3, 2, 2, 2, 3 ),
 ( 0.01666666666666679827, 0.02500000000000007772, 0.03333333333333335369, 0.04166666666666662966, 0.04999999999999991951 ),
 .UNSPECIFIED. ) 
 CURVE ( )  GEOMETRIC_REPRESENTATION_ITEM ( )  RATIONAL_B_SPLINE_CURVE ( ( 0.9999999999999988898, 0.9238795325112879597, 1.000000000000000000, 0.9238795325112867385, 1.000000000000000000, 0.9238795325112867385, 1.000000000000000000, 0.9238795325112875156, 0.9999999999999992228 ) ) 
 REPRESENTATION_ITEM ( '' )  );
#7080 = CARTESIAN_POINT ( 'NONE',  ( -2.445694354108784108, 201.5625000013656063, 195.5543056458912190 ) ) ;
#7081 = ORIENTED_EDGE ( 'NONE', *, *, #41593, .T. ) ;
#7082 = CARTESIAN_POINT ( 'NONE',  ( -4.898587196589412829E-16, 105.3125000040967763, -8.000000000000000000 ) ) ;
#7083 = CARTESIAN_POINT ( 'NONE',  ( 3.042071309553167069, 107.1354166632526983, -11.35316468749999785 ) ) ;
#7084 = CARTESIAN_POINT ( 'NONE',  ( -2.751064625579944321E-14, 204.8750000027312126, 146.0000000000000284 ) ) ;
#7085 = CARTESIAN_POINT ( 'NONE',  ( -7.778174593052020747, -7.778174593052023411, 76.18749999999998579 ) ) ;
#7088 = DIRECTION ( 'NONE',  ( -1.000000000000000000, 0.000000000000000000, 0.000000000000000000 ) ) ;
#7087 = CARTESIAN_POINT ( 'NONE',  ( 24.54126587499998280, 203.1250000013656347, 168.5673454167822740 ) ) ;
#7086 = CARTESIAN_POINT ( 'NONE',  ( 31.45873412499999944, 201.9375000013656063, 169.9999999999999432 ) ) ;
#7089 = ORIENTED_EDGE ( 'NONE', *, *, #38047, .T. ) ;
#7090 = EDGE_CURVE ( 'NONE', #56231, #27106, #20614, .T. ) ;
#7091 = FACE_OUTER_BOUND ( 'NONE', #68805, .T. ) ;
#7092 = DIRECTION ( 'NONE',  ( -0.000000000000000000, 1.000000000000000000, -0.000000000000000000 ) ) ;
#7093 = CARTESIAN_POINT ( 'NONE',  ( -11.35316468750000141, 208.4895833299193555, 3.042071309553159963 ) ) ;
#7094 = CARTESIAN_POINT ( 'NONE',  ( 3.458734124999959914, 204.3750000013656063, 143.4326545832176976 ) ) ;
#7095 = CARTESIAN_POINT ( 'NONE',  ( 28.00000000000002132, 205.1875000013656063, 166.5412658749999082 ) ) ;
#7096 = AXIS2_PLACEMENT_3D ( 'NONE', #30856, #7486, #71206 ) ;
#7097 = CARTESIAN_POINT ( 'NONE',  ( 7.188101187500001821, 26.43749999795162253, -2.977408999572650483 ) ) ;
#7098 = CARTESIAN_POINT ( 'NONE',  ( -8.311093377946841443, 184.2187499965860127, 8.311093377946830785 ) ) ;
#7099 = CARTESIAN_POINT ( 'NONE',  ( -7.188101187500000933, 95.93750000204839523, -2.977408999572650483 ) ) ;
#7100 = CARTESIAN_POINT ( 'NONE',  ( -2.751064625579944321E-14, 195.8750000027311842, 146.0000000000000284 ) ) ;
#7101 = CARTESIAN_POINT ( 'NONE',  ( -30.82842712474620939, 196.1250000000000284, 167.1715728752542134 ) ) ;
#7102 = CARTESIAN_POINT ( 'NONE',  ( 3.211159895383561835, 9.437499998634406140, -3.211159895383561835 ) ) ;
#7103 = CARTESIAN_POINT ( 'NONE',  ( 29.43265458321761230, 203.7500000013656063, 173.4587341249998929 ) ) ;
#7104 = CARTESIAN_POINT ( 'NONE',  ( 7.188101187499992051, 8.802885111219154394E-16, 5.611552781871753659 ) ) ;
#7105 = CARTESIAN_POINT ( 'NONE',  ( 8.311093377946837890, 66.40624999658602690, -8.311093377946837890 ) ) ;
#7107 =( BOUNDED_CURVE ( )  B_SPLINE_CURVE ( 2, ( #42421, #47350, #65439, #31488, #25436, #48453, #54511, #25806, #48826 ),
 .UNSPECIFIED., .F., .F. ) 
 B_SPLINE_CURVE_WITH_KNOTS ( ( 3, 2, 2, 2, 3 ),
 ( 0.4791666666666647423, 0.4895833333333313719, 0.4999999999999981126, 0.5104166666666647423, 0.5208333333333314830 ),
 .UNSPECIFIED. ) 
 CURVE ( )  GEOMETRIC_REPRESENTATION_ITEM ( )  RATIONAL_B_SPLINE_CURVE ( ( 1.000000000000014211, 0.9238795325112725276, 1.000000000000000000, 0.9238795325112867385, 1.000000000000000000, 0.9238795325112867385, 1.000000000000000000, 0.9238795325113005052, 0.9999999999999862332 ) ) 
 REPRESENTATION_ITEM ( '' )  );
#7106 = CYLINDRICAL_SURFACE ( 'NONE', #20711, 10.00000000000000178 ) ;
#7108 = DIRECTION ( 'NONE',  ( -0.000000000000000000, 1.000000000000000000, -0.000000000000000000 ) ) ;
#7109 = ORIENTED_EDGE ( 'NONE', *, *, #37673, .F. ) ;
#7110 = CARTESIAN_POINT ( 'NONE',  ( -1.836970198721029983E-15, 140.6249999931720538, 10.00000000000000178 ) ) ;
#7111 = DIRECTION ( 'NONE',  ( -0.000000000000000000, -1.000000000000000000, -0.000000000000000000 ) ) ;
#7112 = CARTESIAN_POINT ( 'NONE',  ( 5.676582343749993598, 79.94791666325269830, 9.832129032723422313 ) ) ;
#7113 = AXIS2_PLACEMENT_3D ( 'NONE', #38965, #10296, #33322 ) ;
#7114 = CARTESIAN_POINT ( 'NONE',  ( 2.020667218593132706E-15, -11.00000000000000000, 70.56250000409677625 ) ) ;
#7115 = CARTESIAN_POINT ( 'NONE',  ( -1.432654583217664701, 196.0000000013656063, 138.5412658750000787 ) ) ;
#7116 = CARTESIAN_POINT ( 'NONE',  ( -4.336811714531968676, 16.30209246799915590, 69.46462972172692218 ) ) ;
#7118 = CARTESIAN_POINT ( 'NONE',  ( -11.35316468750000141, 68.28124999658602690, -1.390361679473963753E-15 ) ) ;
#7117 = CARTESIAN_POINT ( 'NONE',  ( -7.188101187499999156, 89.75000000204838102, 2.977408999572654924 ) ) ;
#7119 = CARTESIAN_POINT ( 'NONE',  ( -5.656854249492375253, 5.656854249492375253, 26.33030278392014623 ) ) ;
#7120 = CARTESIAN_POINT ( 'NONE',  ( -3.391401283215852214, 194.7190068104546583, 140.4536383052840733 ) ) ;
#7121 = CARTESIAN_POINT ( 'NONE',  ( -8.660254037844387298, 158.9583333265053966, -5.000000000000004441 ) ) ;
#7122 = CARTESIAN_POINT ( 'NONE',  ( 5.082755093536326818, 99.59375000204838102, 5.082755093536325042 ) ) ;
#7123 = CARTESIAN_POINT ( 'NONE',  ( 6.123233995736767268E-16, 21.25000000000000000, -10.00000000000000178 ) ) ;
#7124 = CARTESIAN_POINT ( 'NONE',  ( 3.042071309553167513, 47.13541666325269119, -11.35316468749999785 ) ) ;
#7125 = CARTESIAN_POINT ( 'NONE',  ( 7.204075437095968759, -7.204075437095966983, 112.0937500020483810 ) ) ;
#7126 = CARTESIAN_POINT ( 'NONE',  ( 3.042071309553167069, 196.8229166632526983, -11.35316468749999785 ) ) ;
#7127 = ORIENTED_EDGE ( 'NONE', *, *, #31183, .F. ) ;
#7128 = CARTESIAN_POINT ( 'NONE',  ( 3.734423912265594669, 66.26963445013785758, 26.58791153593135803 ) ) ;
#7129 = CARTESIAN_POINT ( 'NONE',  ( 1.469576158976823947E-15, 118.0625000040967763, 8.000000000000000000 ) ) ;
#7130 = CARTESIAN_POINT ( 'NONE',  ( 2.775557561562891351E-14, 210.0000000000000284, 202.0000000000000000 ) ) ;
#7132 = CARTESIAN_POINT ( 'NONE',  ( -11.35316468750000141, 183.4895833299193839, 3.042071309553159963 ) ) ;
#7131 = CARTESIAN_POINT ( 'NONE',  ( -35.99999999999995026, -2.949029909160572061E-14, 0.000000000000000000 ) ) ;
#7133 = CARTESIAN_POINT ( 'NONE',  ( 2.828427124746191623, 21.87499999726881583, -2.828427124746191623 ) ) ;
#7134 = CARTESIAN_POINT ( 'NONE',  ( -8.660254037844385522, 258.5416666734946602, 5.000000000000004441 ) ) ;
#7135 = CARTESIAN_POINT ( 'NONE',  ( 7.999999999999992895, -3.313708498984756279, 12.17405278392014623 ) ) ;
#7136 = EDGE_CURVE ( 'NONE', #23575, #48578, #52928, .T. ) ;
#7137 = VERTEX_POINT ( 'NONE', #35952 ) ;
#7138 = CARTESIAN_POINT ( 'NONE',  ( -11.35316468750000141, 173.5937499965860411, -1.390361679473963753E-15 ) ) ;
#7139 = EDGE_CURVE ( 'NONE', #26153, #37361, #41607, .T. ) ;
#7140 = CARTESIAN_POINT ( 'NONE',  ( 7.188101187499992051, 8.802885111219154394E-16, 26.23655278187175810 ) ) ;
#7141 = CARTESIAN_POINT ( 'NONE',  ( 9.086704206008372253, 225.9999999999998579, -6.074962670943044429 ) ) ;
#7142 = ORIENTED_EDGE ( 'NONE', *, *, #16874, .T. ) ;
#7143 = EDGE_CURVE ( 'NONE', #71548, #55503, #16772, .T. ) ;
#7144 = CARTESIAN_POINT ( 'NONE',  ( -4.898587196589412829E-16, 102.3125000040967763, -8.000000000000000000 ) ) ;
#7145 = VECTOR ( 'NONE', #60610, 1000.000000000000000 ) ;
#7146 = EDGE_CURVE ( 'NONE', #37240, #2210, #36298, .T. ) ;
#7147 = CARTESIAN_POINT ( 'NONE',  ( -1.656854249492381248, 12.31250000000000000, -4.000000000000001776 ) ) ;
#7148 = CARTESIAN_POINT ( 'NONE',  ( 6.401276095386993603, 6.696526368584462041, -0.1469846612282491305 ) ) ;
#7149 = CARTESIAN_POINT ( 'NONE',  ( 4.541265875000002339, 11.37499999863440969, -1.881053915767121776 ) ) ;
#7150 = CARTESIAN_POINT ( 'NONE',  ( -3.313708498984757167, 7.999999999999991118, 18.73655278392014623 ) ) ;
#7151 = CARTESIAN_POINT ( 'NONE',  ( 1.656854249492347719, 195.8125000000000284, 146.0000000000000284 ) ) ;
#7152 = AXIS2_PLACEMENT_3D ( 'NONE', #64992, #12934, #1646 ) ;
#7153 = EDGE_LOOP ( 'NONE', ( #71515, #51083, #48773, #42776 ) ) ;
#7154 = CARTESIAN_POINT ( 'NONE',  ( 0.000000000000000000, 0.000000000000000000, 30.00000000000000000 ) ) ;
#7155 = CARTESIAN_POINT ( 'NONE',  ( -2.977408999572650927, 99.87500000204838102, -7.188101187500001821 ) ) ;
#7157 = CARTESIAN_POINT ( 'NONE',  ( -28.00000000000007816, 205.1250000027312126, 166.0000000000003695 ) ) ;
#7156 = CARTESIAN_POINT ( 'NONE',  ( 2.828427124746209831, 196.3750000000000284, 200.8284271247462129 ) ) ;
#7158 = VERTEX_POINT ( 'NONE', #37056 ) ;
#7159 = AXIS2_PLACEMENT_3D ( 'NONE', #3608, #36319, #13279 ) ;
#7160 = CARTESIAN_POINT ( 'NONE',  ( 1.506524674528621377, 10.12152537343868808, -70.16785718945648398 ) ) ;
#7161 = DIRECTION ( 'NONE',  ( -0.000000000000000000, 1.000000000000000000, -0.000000000000000000 ) ) ;
#7162 = CARTESIAN_POINT ( 'NONE',  ( 5.082755093536320601, -5.082755093536318824, 27.54905278187175455 ) ) ;
#7163 = ORIENTED_EDGE ( 'NONE', *, *, #40853, .F. ) ;
#7164 = ORIENTED_EDGE ( 'NONE', *, *, #8790, .T. ) ;
#7165 = CARTESIAN_POINT ( 'NONE',  ( 4.220049686691934809, 10.18810118749999916, 83.68750000204836681 ) ) ;
#7166 = UNCERTAINTY_MEASURE_WITH_UNIT (LENGTH_MEASURE( 1.000000000000000082E-05 ), #1518, 'distance_accuracy_value', 'NONE');
#7167 = CARTESIAN_POINT ( 'NONE',  ( -30.44569435410879166, 198.0625000013656063, 172.4456943541092357 ) ) ;
#7168 = CARTESIAN_POINT ( 'NONE',  ( 4.556349186104051263, -10.99999999999999822, 103.4687500000000000 ) ) ;
#7171 = PLANE ( 'NONE',  #42207 ) ;
#7170 = CARTESIAN_POINT ( 'NONE',  ( 23.99999999999998934, 202.8750000027312126, 169.9999999999999432 ) ) ;
#7169 = CARTESIAN_POINT ( 'NONE',  ( -10.99999999999989164, -4.556349186104158733, 86.59375000000002842 ) ) ;
#7172 = CARTESIAN_POINT ( 'NONE',  ( -10.00000000000000178, 137.5000000000000000, -1.224646799147353454E-15 ) ) ;
#7173 = CARTESIAN_POINT ( 'NONE',  ( 28.00000000000002132, 200.1250000027312126, 173.9999999999999147 ) ) ;
#7174 = DIRECTION ( 'NONE',  ( -0.000000000000000000, -0.000000000000000000, -1.000000000000000000 ) ) ;
#7175 = EDGE_CURVE ( 'NONE', #60310, #15665, #53670, .T. ) ;
#7176 = DIRECTION ( 'NONE',  ( -1.000000000000000000, 0.000000000000000000, -0.000000000000000000 ) ) ;
#7177 = CARTESIAN_POINT ( 'NONE',  ( 31.45873412499999944, 204.6875000013656063, 169.9999999999999432 ) ) ;
#7178 = CARTESIAN_POINT ( 'NONE',  ( 7.188101187500001821, 5.437499997951610098, -2.977408999572650483 ) ) ;
#7179 = CARTESIAN_POINT ( 'NONE',  ( -5.662595241051935346, 5.662595241051935346, 2.325615283940627442 ) ) ;
#7180 = CARTESIAN_POINT ( 'NONE',  ( 2.445694354108782775, 196.5625000013656063, 139.5543056458912190 ) ) ;
#7181 = CARTESIAN_POINT ( 'NONE',  ( -7.188101187499999156, 117.1250000020483810, 2.977408999572654924 ) ) ;
#7183 = CARTESIAN_POINT ( 'NONE',  ( -4.000000000000001776, 16.43750000000000000, -1.656854249492381470 ) ) ;
#7182 = DIRECTION ( 'NONE',  ( -0.000000000000000000, 1.000000000000000000, -1.563033456626094573E-30 ) ) ;
#7184 = CARTESIAN_POINT ( 'NONE',  ( 11.35316468749999963, 226.7187500034139873, -1.390361679473963556E-15 ) ) ;
#7185 = CARTESIAN_POINT ( 'NONE',  ( 4.898587196589412829E-16, 3.375000000000000444, -8.000000000000000000 ) ) ;
#7186 = CARTESIAN_POINT ( 'NONE',  ( -5.082755093536319713, 5.082755093536319713, 21.17405278187175455 ) ) ;
#7187 = DIRECTION ( 'NONE',  ( 0.000000000000000000, -0.000000000000000000, -1.000000000000000000 ) ) ;
#7188 = CARTESIAN_POINT ( 'NONE',  ( -2.085542519210945728E-15, 34.53124999658601979, 11.35316468750000141 ) ) ;
#7189 = EDGE_CURVE ( 'NONE', #61945, #53587, #24487, .T. ) ;
#7190 = CARTESIAN_POINT ( 'NONE',  ( 8.660254037844669739, 24.58333333333352400, 5.000000000000169642 ) ) ;
#7191 = CARTESIAN_POINT ( 'NONE',  ( 5.676582343750001591, 216.9270833299193555, -9.832129032723420536 ) ) ;
#7192 = CARTESIAN_POINT ( 'NONE',  ( -4.898587196589412829E-16, 112.6250000000000000, -8.000000000000000000 ) ) ;
#7193 = CARTESIAN_POINT ( 'NONE',  ( -11.00000000000000000, 0.000000000000000000, 118.0000000000000000 ) ) ;
#7194 = EDGE_LOOP ( 'NONE', ( #24127, #5444, #62080 ) ) ;
#7195 = CARTESIAN_POINT ( 'NONE',  ( -10.00000000000000355, 129.5833333265053966, 2.679491924311223183 ) ) ;
#7196 = CARTESIAN_POINT ( 'NONE',  ( -3.458734125000015869, 196.1875000013655779, 142.0000000000000568 ) ) ;
#7197 = CARTESIAN_POINT ( 'NONE',  ( 9.832129032723420536, 31.19791666325268409, -5.676582343749999815 ) ) ;
#7198 = CARTESIAN_POINT ( 'NONE',  ( -11.00000000000000000, 4.556349186104045934, 85.09375000409676204 ) ) ;
#7199 = CARTESIAN_POINT ( 'NONE',  ( 1.432654583217607414, 208.5000000013656063, 145.4587341250000350 ) ) ;
#7200 = DIRECTION ( 'NONE',  ( -0.5000000000000012212, -0.8660254037844379305, 0.000000000000000000 ) ) ;
#7201 = CARTESIAN_POINT ( 'NONE',  ( -4.000000000000015987, 201.6250000027312126, 142.0000000000000568 ) ) ;
#7203 = CARTESIAN_POINT ( 'NONE',  ( 11.35316468749999963, 15.98958332991934661, -3.042071309553165293 ) ) ;
#7202 = CARTESIAN_POINT ( 'NONE',  ( 5.082755093536325042, 104.0937500020483810, -5.082755093536325930 ) ) ;
#7204 = CARTESIAN_POINT ( 'NONE',  ( -5.656854249492375253, 5.656854249492375253, 15.64280277982336642 ) ) ;
#7205 =( BOUNDED_CURVE ( )  B_SPLINE_CURVE ( 2, ( #17943, #40584, #11913, #28887, #62466, #246, #6631, #5515, #52281 ),
 .UNSPECIFIED., .F., .F. ) 
 B_SPLINE_CURVE_WITH_KNOTS ( ( 3, 2, 2, 2, 3 ),
 ( 0.3958333333333313164, 0.4062499999999980016, 0.4166666666666647423, 0.4270833333333313719, 0.4374999999999980571 ),
 .UNSPECIFIED. ) 
 CURVE ( )  GEOMETRIC_REPRESENTATION_ITEM ( )  RATIONAL_B_SPLINE_CURVE ( ( 1.000000000000014655, 0.9238795325112720835, 1.000000000000000000, 0.9238795325112867385, 1.000000000000000000, 0.9238795325112867385, 1.000000000000000000, 0.9238795325113009493, 0.9999999999999857891 ) ) 
 REPRESENTATION_ITEM ( '' )  );
#7206 = CARTESIAN_POINT ( 'NONE',  ( 6.951808397369818766E-16, 152.0312499965860411, -11.35316468750000141 ) ) ;
#7207 = EDGE_CURVE ( 'NONE', #65791, #69483, #48735, .T. ) ;
#7208 = CONICAL_SURFACE ( 'NONE', #4784, 6.000000000000000000, 0.9599310885968792562 ) ;
#7209 = CARTESIAN_POINT ( 'NONE',  ( 7.320508075688774596, 112.4999999931720396, -7.320508075688774596 ) ) ;
#7210 = CARTESIAN_POINT ( 'NONE',  ( 7.188101187500000044, 111.7812500020483810, -8.802885111219163269E-16 ) ) ;
#7211 = LINE ( 'NONE', #29849, #30084 ) ;
#7212 = CARTESIAN_POINT ( 'NONE',  ( -24.54126587499998635, 206.3750000013656063, 171.4326545832179818 ) ) ;
#7213 = ORIENTED_EDGE ( 'NONE', *, *, #53452, .F. ) ;
#7214 = CARTESIAN_POINT ( 'NONE',  ( 8.311093377946837890, 11.71874999658601801, -8.311093377946837890 ) ) ;
#7215 = ORIENTED_EDGE ( 'NONE', *, *, #33684, .T. ) ;
#7216 = EDGE_CURVE ( 'NONE', #43418, #30852, #43449, .T. ) ;
#7217 = CARTESIAN_POINT ( 'NONE',  ( 0.000000000000000000, 125.0000000000000000, 8.000000000000000000 ) ) ;
#7218 = PRODUCT_DEFINITION ( 'UNKNOWN', '', #5656, #11599 ) ;
#7220 = CARTESIAN_POINT ( 'NONE',  ( -8.311093377946836114, 137.6562499965859843, -8.311093377946837890 ) ) ;
#7219 = DIRECTION ( 'NONE',  ( 0.000000000000000000, 0.000000000000000000, 1.000000000000000000 ) ) ;
#7221 = CARTESIAN_POINT ( 'NONE',  ( -5.656854249492375253, 5.656854249492375253, 18.69905278432982243 ) ) ;
#7222 = CARTESIAN_POINT ( 'NONE',  ( 8.660254037844389075, 225.2083333401613174, 4.999999999999997335 ) ) ;
#7223 = CARTESIAN_POINT ( 'NONE',  ( 2.085542519210945334E-15, 250.1562500034140157, 11.35316468749999963 ) ) ;
#7224 = CARTESIAN_POINT ( 'NONE',  ( 7.204075437095966983, 7.204075437095967871, 94.46875000204838102 ) ) ;
#7225 = VERTEX_POINT ( 'NONE', #32532 ) ;
#7226 = ADVANCED_FACE ( 'NONE', ( #66849 ), #61564, .F. ) ;
#7227 = FACE_OUTER_BOUND ( 'NONE', #17870, .T. ) ;
#7228 = CARTESIAN_POINT ( 'NONE',  ( 5.000000000000000888, 61.23620218020190009, -23.51718915682011257 ) ) ;
#7229 = CARTESIAN_POINT ( 'NONE',  ( -8.311093377946836114, 82.96874999658601268, -8.311093377946837890 ) ) ;
#7230 = CARTESIAN_POINT ( 'NONE',  ( 7.204075437095966983, 7.204075437095967871, 103.0937500020483668 ) ) ;
#7231 = CARTESIAN_POINT ( 'NONE',  ( -4.541265875000003227, 15.99999999863440614, 1.881053915767121110 ) ) ;
#7232 = ORIENTED_EDGE ( 'NONE', *, *, #34800, .F. ) ;
#7233 = ORIENTED_EDGE ( 'NONE', *, *, #34980, .F. ) ;
#7234 = CARTESIAN_POINT ( 'NONE',  ( -8.000000000000001776, 6.843750000000000888, 3.313708498984759387 ) ) ;
#7235 = CARTESIAN_POINT ( 'NONE',  ( -8.000000000000000000, 11.25000000000000178, -9.797174393178825657E-16 ) ) ;
#7236 = CARTESIAN_POINT ( 'NONE',  ( 2.977408999572650927, 3.749999997951610542, -7.188101187500001821 ) ) ;
#7237 = CARTESIAN_POINT ( 'NONE',  ( -5.656854249492380582, 119.0000000040967905, -5.656854249492380582 ) ) ;
#7238 = CARTESIAN_POINT ( 'NONE',  ( 10.18810118750000093, -4.220049686691933921, 97.18750000204836681 ) ) ;
#7239 = CARTESIAN_POINT ( 'NONE',  ( -38.00000000000000000, 63.00000000000000000, 10.00000000000006217 ) ) ;
#7240 = CARTESIAN_POINT ( 'NONE',  ( -2.828427124746190735, 13.12499999726881406, -2.828427124746191623 ) ) ;
#7241 = ORIENTED_EDGE ( 'NONE', *, *, #36676, .T. ) ;
#7242 = CARTESIAN_POINT ( 'NONE',  ( 3.313708498984815343, 96.03124999999998579, -7.999999999999944933 ) ) ;
#7243 = CARTESIAN_POINT ( 'NONE',  ( -2.445694354108783664, 200.3125000013656063, 195.5543056458912190 ) ) ;
#7245 = CARTESIAN_POINT ( 'NONE',  ( -3.313708498984760276, 15.46875000000000711, -8.000000000000000000 ) ) ;
#7244 = CARTESIAN_POINT ( 'NONE',  ( -25.55430564589122966, 200.3125000013656063, 167.5543056458915032 ) ) ;
#7246 = CARTESIAN_POINT ( 'NONE',  ( -3.211159895383562723, 15.93749999863440436, 3.211159895383561391 ) ) ;
#7247 = CIRCLE ( 'NONE', #49407, 12.00000000000000000 ) ;
#7248 = DIRECTION ( 'NONE',  ( 0.000000000000000000, 0.000000000000000000, 1.000000000000000000 ) ) ;
#7249 = CARTESIAN_POINT ( 'NONE',  ( 2.977408999572646486, 7.188101187499991163, 13.01780278187175277 ) ) ;
#7250 = VERTEX_POINT ( 'NONE', #60431 ) ;
#7251 = VERTEX_POINT ( 'NONE', #3102 ) ;
#7252 = CARTESIAN_POINT ( 'NONE',  ( -10.18810118749999738, -4.220049686691941915, 105.2500000020483810 ) ) ;
#7253 = CARTESIAN_POINT ( 'NONE',  ( -4.898587196589412829E-16, 123.1250000000000000, -8.000000000000000000 ) ) ;
#7254 = AXIS2_PLACEMENT_3D ( 'NONE', #10434, #68886, #17198 ) ;
#7255 = CARTESIAN_POINT ( 'NONE',  ( -26.34314575050764518, 204.9375000000000284, 166.0000000000003695 ) ) ;
#7256 = CARTESIAN_POINT ( 'NONE',  ( 2.839093476692135984E-14, 194.6875000013655779, 201.4587341250000350 ) ) ;
#7257 = CARTESIAN_POINT ( 'NONE',  ( -2.679491924290171578, 31.45833333333144211, -10.00000000001215383 ) ) ;
#7258 = CARTESIAN_POINT ( 'NONE',  ( -1.836970198721029983E-15, 93.75000000000000000, 10.00000000000000178 ) ) ;
#7259 = AXIS2_PLACEMENT_3D ( 'NONE', #55935, #72897, #67243 ) ;
#7260 = CARTESIAN_POINT ( 'NONE',  ( -3.313708498984762496, 120.7812500000000142, 7.999999999999998224 ) ) ;
#7261 = CARTESIAN_POINT ( 'NONE',  ( -6.676582343750000703, 294.6718750017070079, 2.765530957082001251 ) ) ;
#7262 = ADVANCED_FACE ( 'NONE', ( #15896 ), #60807, .F. ) ;
#7263 = EDGE_LOOP ( 'NONE', ( #69109, #10312, #63484, #11699 ) ) ;
#7264 = CARTESIAN_POINT ( 'NONE',  ( -4.999999999999998224, 173.5416666598387110, -8.660254037844389075 ) ) ;
#7265 = CARTESIAN_POINT ( 'NONE',  ( -1.469576158976823947E-15, 12.93749999590322197, 8.000000000000000000 ) ) ;
#7266 = CARTESIAN_POINT ( 'NONE',  ( -1.432654583217662481, 207.1250000013656347, 145.4587341250000634 ) ) ;
#7267 = CARTESIAN_POINT ( 'NONE',  ( 0.000000000000000000, 300.0000000000000000, 6.000000000000001776 ) ) ;
#7268 = CARTESIAN_POINT ( 'NONE',  ( 4.000000000000001776, 8.062500000000000000, -1.656854249492381248 ) ) ;
#7269 = CARTESIAN_POINT ( 'NONE',  ( 7.320508075688771044, 228.1249999999999716, -7.320508075688771932 ) ) ;
#7270 = CARTESIAN_POINT ( 'NONE',  ( -32.00000000000000000, 202.3750000027312126, 170.0000000000004547 ) ) ;
#7271 = CARTESIAN_POINT ( 'NONE',  ( 4.220049686691934809, 10.18810118749999916, 69.06250000204839523 ) ) ;
#7272 = CARTESIAN_POINT ( 'NONE',  ( -1.836970198721029983E-15, 213.7500000000000284, 10.00000000000000178 ) ) ;
#7273 = EDGE_CURVE ( 'NONE', #32880, #13736, #11960, .T. ) ;
#7274 = CARTESIAN_POINT ( 'NONE',  ( -5.082755093536317936, -5.082755093536320601, 11.04905278187175455 ) ) ;
#7275 = CARTESIAN_POINT ( 'NONE',  ( 6.951808397369818766E-16, 177.3437499965860411, -11.35316468750000141 ) ) ;
#7276 = CARTESIAN_POINT ( 'NONE',  ( -4.541265875000002339, 1.812499998634406584, -5.561446717895856393E-16 ) ) ;
#7277 = CARTESIAN_POINT ( 'NONE',  ( -6.123233995736766282E-16, 243.7500000000000284, -10.00000000000000000 ) ) ;
#7279 = CARTESIAN_POINT ( 'NONE',  ( -7.999999999961189268, -1.665725685002260109E-05, 4.018425631117963803 ) ) ;
#7278 = CARTESIAN_POINT ( 'NONE',  ( 2.449293598294707893E-16, 4.250000000000000000, -4.000000000000001776 ) ) ;
#7280 = ORIENTED_EDGE ( 'NONE', *, *, #46723, .T. ) ;
#7281 = CARTESIAN_POINT ( 'NONE',  ( 2.445694354108783219, 208.8125000013656063, 139.5543056458912190 ) ) ;
#7282 = CARTESIAN_POINT ( 'NONE',  ( 3.042071309553159519, 45.05208332991935549, 11.35316468750000141 ) ) ;
#7283 = CARTESIAN_POINT ( 'NONE',  ( 11.00000000000000000, 4.556349186104045934, 107.0312500040967763 ) ) ;
#7284 = CARTESIAN_POINT ( 'NONE',  ( -9.832129032723420536, 224.0104166632526983, 5.676582343749997150 ) ) ;
#7285 = CARTESIAN_POINT ( 'NONE',  ( -30.44569435410886982, 205.5625000013656063, 167.5543056458916169 ) ) ;
#7286 = CARTESIAN_POINT ( 'NONE',  ( -3.673940397442060854E-16, 295.7500000000000000, -6.000000000000001776 ) ) ;
#7288 = DIRECTION ( 'NONE',  ( -1.000000000000000000, 0.000000000000000000, 0.000000000000000000 ) ) ;
#7287 = CARTESIAN_POINT ( 'NONE',  ( -7.778174593052023411, 7.778174593052023411, 71.50000000409677625 ) ) ;
#7289 = CARTESIAN_POINT ( 'NONE',  ( -2.839093476692135984E-14, 196.6875000013655779, 138.5412658750000503 ) ) ;
#7290 = AXIS2_PLACEMENT_3D ( 'NONE', #14843, #49180, #2799 ) ;
#7291 = CARTESIAN_POINT ( 'NONE',  ( 4.999999999999993783, 71.04166665983869677, 8.660254037844390851 ) ) ;
#7292 = CARTESIAN_POINT ( 'NONE',  ( -5.082755093536325930, 95.46875000204838102, -5.082755093536325930 ) ) ;
#7293 = CARTESIAN_POINT ( 'NONE',  ( 3.211159895383561835, 14.56249999863440792, -3.211159895383561835 ) ) ;
#7294 = CARTESIAN_POINT ( 'NONE',  ( -10.00000000000000711, 72.50000000000002842, -1.224646799147354243E-15 ) ) ;
#7295 = CARTESIAN_POINT ( 'NONE',  ( -28.00000000000007816, 203.1250000027312126, 166.0000000000003695 ) ) ;
#7296 = CARTESIAN_POINT ( 'NONE',  ( -5.867882488397293095, -5.445826010587458299, 1.009359473472040802 ) ) ;
#7297 = EDGE_LOOP ( 'NONE', ( #68432, #62746 ) ) ;
#7298 = ORIENTED_EDGE ( 'NONE', *, *, #35388, .T. ) ;
#7299 = CARTESIAN_POINT ( 'NONE',  ( 6.676582343750004256, 298.0468750017070647, 2.765530957081995478 ) ) ;
#7300 = PLANE ( 'NONE',  #56810 ) ;
#7301 = CARTESIAN_POINT ( 'NONE',  ( -10.00000000000001066, 17.50000000000000355, -1.224646799147354637E-15 ) ) ;
#7302 = CARTESIAN_POINT ( 'NONE',  ( 8.311093377946837890, 161.4062499965860411, -8.311093377946837890 ) ) ;
#7303 = CARTESIAN_POINT ( 'NONE',  ( 6.123233995736767268E-16, 3.124999993172032919, -10.00000000000000178 ) ) ;
#7304 = CARTESIAN_POINT ( 'NONE',  ( 4.000000000000015987, 199.5000000000000000, 198.0000000000000284 ) ) ;
#7305 = CARTESIAN_POINT ( 'NONE',  ( -62.39047978708157416, 229.6205190061017447, 45.00000000000000000 ) ) ;
#7306 = CARTESIAN_POINT ( 'NONE',  ( -7.204075437095965206, -7.204075437095968759, 107.2187500020483810 ) ) ;
#7307 = ORIENTED_EDGE ( 'NONE', *, *, #36996, .T. ) ;
#7308 = AXIS2_PLACEMENT_3D ( 'NONE', #70543, #18859, #6802 ) ;
#7309 = CARTESIAN_POINT ( 'NONE',  ( 39.49622823916701009, -8.402566836762649503E-16, 116.8734666038381533 ) ) ;
#7310 = LINE ( 'NONE', #65749, #60544 ) ;
#7311 = CARTESIAN_POINT ( 'NONE',  ( 9.832129032723420536, 146.5104166632526699, -5.676582343749999815 ) ) ;
#7312 = CARTESIAN_POINT ( 'NONE',  ( -1.432654583217607192, 199.2500000013656063, 194.5412658750000219 ) ) ;
#7313 = CARTESIAN_POINT ( 'NONE',  ( 2.445694354108840063, 209.0625000013656063, 200.4456943541088663 ) ) ;
#7314 = CARTESIAN_POINT ( 'NONE',  ( -10.18810118749999916, 4.220049686691934809, 69.43750000204838102 ) ) ;
#7315 = CARTESIAN_POINT ( 'NONE',  ( -8.311093377946836114, 52.96874999658601268, -8.311093377946837890 ) ) ;
#7317 = ORIENTED_EDGE ( 'NONE', *, *, #42630, .T. ) ;
#7316 =( BOUNDED_CURVE ( )  B_SPLINE_CURVE ( 2, ( #19415, #23605, #36785, #59795, #31111, #60530, #43171, #43930, #2822 ),
 .UNSPECIFIED., .F., .F. ) 
 B_SPLINE_CURVE_WITH_KNOTS ( ( 3, 2, 2, 2, 3 ),
 ( 0.9000000000000007994, 0.9083333333333341031, 0.9166666666666674068, 0.9250000000000008216, 0.9333333333333341253 ),
 .UNSPECIFIED. ) 
 CURVE ( )  GEOMETRIC_REPRESENTATION_ITEM ( )  RATIONAL_B_SPLINE_CURVE ( ( 0.9999999999999928946, 0.9238795325112938439, 1.000000000000000000, 0.9238795325112867385, 1.000000000000000000, 0.9238795325112867385, 1.000000000000000000, 0.9238795325112796331, 1.000000000000007105 ) ) 
 REPRESENTATION_ITEM ( '' )  );
#7318 = CARTESIAN_POINT ( 'NONE',  ( 5.656854249492376141, -5.656854249492374365, 13.39280277982336465 ) ) ;
#7320 = CARTESIAN_POINT ( 'NONE',  ( 4.541265875000001451, 6.374999998634408804, 1.881053915767124440 ) ) ;
#7319 =( BOUNDED_CURVE ( )  B_SPLINE_CURVE ( 2, ( #1982, #41605, #24974, #25712, #37054 ),
 .UNSPECIFIED., .F., .F. ) 
 B_SPLINE_CURVE_WITH_KNOTS ( ( 3, 2, 3 ),
 ( 0.000000000000000000, 0.008333333333333399137, 0.01666666666666679827 ),
 .UNSPECIFIED. ) 
 CURVE ( )  GEOMETRIC_REPRESENTATION_ITEM ( )  RATIONAL_B_SPLINE_CURVE ( ( 1.000000000000000000, 0.9238795325112867385, 1.000000000000000000, 0.9238795325112855172, 1.000000000000001110 ) ) 
 REPRESENTATION_ITEM ( '' )  );
#7321 = CARTESIAN_POINT ( 'NONE',  ( 8.008118988124991233, 9.807117285998411148E-16, 16.76311528394063188 ) ) ;
#7322 = VECTOR ( 'NONE', #25112, 1000.000000000000227 ) ;
#7323 = CARTESIAN_POINT ( 'NONE',  ( 5.082755093536324154, 13.78124999795161010, 5.082755093536326818 ) ) ;
#7324 = CARTESIAN_POINT ( 'NONE',  ( 4.242640687119287435, 293.4375000034140157, 4.242640687119285658 ) ) ;
#7325 = AXIS2_PLACEMENT_3D ( 'NONE', #68528, #39858, #62859 ) ;
#7326 = FACE_OUTER_BOUND ( 'NONE', #5078, .T. ) ;
#7327 = CARTESIAN_POINT ( 'NONE',  ( 7.188101187500001821, 14.43749999795161365, -2.977408999572650483 ) ) ;
#7328 = CARTESIAN_POINT ( 'NONE',  ( 1.320432766682872962E-15, -7.188101187499992051, 9.361552781871752771 ) ) ;
#7329 = CARTESIAN_POINT ( 'NONE',  ( 4.220049686691934809, 10.18810118749999916, 71.68750000204836681 ) ) ;
#7330 = PLANE ( 'NONE',  #66709 ) ;
#7331 = CARTESIAN_POINT ( 'NONE',  ( 4.000000000000001776, 0.7499999972688131678, 0.000000000000000000 ) ) ;
#7332 = ORIENTED_EDGE ( 'NONE', *, *, #21387, .F. ) ;
#7333 = CARTESIAN_POINT ( 'NONE',  ( 4.000000000000015987, 195.5625000027311842, 199.6568542494924259 ) ) ;
#7334 = CARTESIAN_POINT ( 'NONE',  ( -1.656854249492403008, 202.6875000000000284, 146.0000000000000284 ) ) ;
#7335 = CARTESIAN_POINT ( 'NONE',  ( -28.00000000000007461, 197.1250000027312126, 166.0000000000003695 ) ) ;
#7336 = EDGE_CURVE ( 'NONE', #29969, #28981, #26851, .T. ) ;
#7337 = CARTESIAN_POINT ( 'NONE',  ( -3.211159895383562723, 0.9374999986344068059, 3.211159895383561391 ) ) ;
#7338 = CARTESIAN_POINT ( 'NONE',  ( -7.188101187500000044, 118.1562500020483810, 0.000000000000000000 ) ) ;
#7339 = DIRECTION ( 'NONE',  ( -0.000000000000000000, -0.000000000000000000, 1.000000000000000000 ) ) ;
#7340 = CARTESIAN_POINT ( 'NONE',  ( -5.656854249492375253, 5.656854249492375253, 3.830302783920144893 ) ) ;
#7341 = ORIENTED_EDGE ( 'NONE', *, *, #36737, .T. ) ;
#7342 = CARTESIAN_POINT ( 'NONE',  ( 2.977408999572650927, 21.74999999795161898, -7.188101187500000933 ) ) ;
#7343 = VERTEX_POINT ( 'NONE', #38927 ) ;
#7344 = CARTESIAN_POINT ( 'NONE',  ( 5.000000000000004441, 254.7916666734946318, 8.660254037844385522 ) ) ;
#7345 = CARTESIAN_POINT ( 'NONE',  ( 4.242640687119287435, 296.3750000000000000, 4.242640687119285658 ) ) ;
#7346 = CARTESIAN_POINT ( 'NONE',  ( 29.43265458321761230, 202.8750000013656063, 166.5412658749999650 ) ) ;
#7347 = CARTESIAN_POINT ( 'NONE',  ( 5.000000000000001776, 55.83333333333333570, -8.660254037844389075 ) ) ;
#7348 = CARTESIAN_POINT ( 'NONE',  ( -7.188101187500001821, 101.9375000020483810, -2.977408999572650483 ) ) ;
#7349 = CARTESIAN_POINT ( 'NONE',  ( -3.673940397442060854E-16, 295.7500000000000000, -6.000000000000001776 ) ) ;
#7351 = CARTESIAN_POINT ( 'NONE',  ( -6.062687379811042554, -5.219768740853823807, 2.519839246067225784E-12 ) ) ;
#7350 = CARTESIAN_POINT ( 'NONE',  ( -4.242640687119286547, 287.9375000034140157, -4.242640687119286547 ) ) ;
#7352 = EDGE_CURVE ( 'NONE', #34878, #20382, #42308, .T. ) ;
#7353 = EDGE_LOOP ( 'NONE', ( #15276, #50205, #5657, #5210 ) ) ;
#7354 = CARTESIAN_POINT ( 'NONE',  ( -11.35316468749999963, 228.9062500034139873, 0.000000000000000000 ) ) ;
#7355 = CARTESIAN_POINT ( 'NONE',  ( 1.320432766682872962E-15, -7.188101187499992051, 12.73655278187175277 ) ) ;
#7356 = CARTESIAN_POINT ( 'NONE',  ( 1.656854249492466735, 195.3125000027312126, 138.0000000000001705 ) ) ;
#7357 = CARTESIAN_POINT ( 'NONE',  ( 6.123233995736767268E-16, 73.12499999317203958, -10.00000000000000178 ) ) ;
#7358 = CARTESIAN_POINT ( 'NONE',  ( 3.313708498984756279, 7.999999999999991118, 2.049052783920143117 ) ) ;
#7359 = CARTESIAN_POINT ( 'NONE',  ( 27.61630405986311843, 194.7720153983102875, 166.2279846016896556 ) ) ;
#7360 = CARTESIAN_POINT ( 'NONE',  ( 18.00000000000000000, 10.39230484541325161, -20.69999999999999929 ) ) ;
#7361 = CARTESIAN_POINT ( 'NONE',  ( 7.320508075688774596, 180.6250000000000284, -7.320508075688774596 ) ) ;
#7362 = CARTESIAN_POINT ( 'NONE',  ( 6.000000000000001776, 297.5625000034140157, -7.347880794884121708E-16 ) ) ;
#7363 = CARTESIAN_POINT ( 'NONE',  ( 8.660254037844385522, 241.0416666734946318, -5.000000000000003553 ) ) ;
#7364 = CYLINDRICAL_SURFACE ( 'NONE', #62828, 8.000000000000000000 ) ;
#7365 = CARTESIAN_POINT ( 'NONE',  ( -11.35316468750000141, 138.5937499965860127, -1.390361679473963753E-15 ) ) ;
#7366 = CARTESIAN_POINT ( 'NONE',  ( 23.99999999999998934, 201.7500000000000000, 169.9999999999998863 ) ) ;
#7367 = DIRECTION ( 'NONE',  ( -0.000000000000000000, -0.000000000000000000, 1.000000000000000000 ) ) ;
#7370 = DIRECTION ( 'NONE',  ( -0.000000000000000000, 1.000000000000000000, -0.000000000000000000 ) ) ;
#7369 = DIRECTION ( 'NONE',  ( -0.000000000000000000, 1.000000000000000000, -0.000000000000000000 ) ) ;
#7368 = CARTESIAN_POINT ( 'NONE',  ( 32.00000000000000000, 206.2500000000000284, 169.9999999999999432 ) ) ;
#7371 = ORIENTED_EDGE ( 'NONE', *, *, #48312, .T. ) ;
#7372 = CARTESIAN_POINT ( 'NONE',  ( -2.828427124746153876, 205.8750000000000284, 195.1715728752538439 ) ) ;
#7373 = VECTOR ( 'NONE', #63151, 1000.000000000000000 ) ;
#7374 = CARTESIAN_POINT ( 'NONE',  ( -7.347880794884122694E-16, 14.75000000000000178, 4.000000000000001776 ) ) ;
#7375 = DIRECTION ( 'NONE',  ( 0.000000000000000000, 0.000000000000000000, 1.000000000000000000 ) ) ;
#7376 = CARTESIAN_POINT ( 'NONE',  ( -1.432654583217662259, 207.1250000013656347, 145.4587341250000350 ) ) ;
#7377 = CARTESIAN_POINT ( 'NONE',  ( -4.000000000000016875, 202.4375000000000568, 140.3431457505076594 ) ) ;
#7378 = CARTESIAN_POINT ( 'NONE',  ( 2.679491924311228956, 37.91666665983870388, -10.00000000000000000 ) ) ;
#7379 = AXIS2_PLACEMENT_3D ( 'NONE', #5007, #51013, #55950 ) ;
#7380 = CARTESIAN_POINT ( 'NONE',  ( -7.188101187500000044, 113.6562500020483810, 0.000000000000000000 ) ) ;
#7381 = CARTESIAN_POINT ( 'NONE',  ( -4.541265875000002339, 2.937499998634407028, -5.561446717895856393E-16 ) ) ;
#7382 = CARTESIAN_POINT ( 'NONE',  ( 7.999999999932789763, 3.279097096261179525E-05, 13.76780373625499010 ) ) ;
#7383 = CARTESIAN_POINT ( 'NONE',  ( -5.656854249492373476, -5.656854249492376141, 13.01780277982336465 ) ) ;
#7385 = CARTESIAN_POINT ( 'NONE',  ( 5.656854249492376141, -5.656854249492374365, 18.08030278392014623 ) ) ;
#7384 = CARTESIAN_POINT ( 'NONE',  ( -29.65685424949235838, 203.0625000000000568, 166.0000000000003695 ) ) ;
#7386 = VERTEX_POINT ( 'NONE', #25714 ) ;
#7387 = CARTESIAN_POINT ( 'NONE',  ( 1.102182119232618108E-15, 292.3125000034140157, 6.000000000000001776 ) ) ;
#7388 = VECTOR ( 'NONE', #66182, 1000.000000000000000 ) ;
#7389 = CARTESIAN_POINT ( 'NONE',  ( -4.898587196589412829E-16, 109.6250000000000000, -8.000000000000000000 ) ) ;
#7390 = CARTESIAN_POINT ( 'NONE',  ( -11.35316468749999963, 229.2187500034139873, 0.000000000000000000 ) ) ;
#7391 = CARTESIAN_POINT ( 'NONE',  ( 8.311093377946834337, 120.1562499965860127, 8.311093377946839666 ) ) ;
#7392 = ORIENTED_EDGE ( 'NONE', *, *, #73865, .F. ) ;
#7393 = CARTESIAN_POINT ( 'NONE',  ( 11.99999999999999822, -6.928203230275538971, -14.00000000000000178 ) ) ;
#7394 = CARTESIAN_POINT ( 'NONE',  ( -10.18810118749999916, 0.000000000000000000, 99.15625000204838102 ) ) ;
#7395 = DIRECTION ( 'NONE',  ( -1.000000000000000000, 0.000000000000000000, 1.224646799147353207E-16 ) ) ;
#7396 = CARTESIAN_POINT ( 'NONE',  ( 3.458734125000015425, 201.2500000013656063, 196.5673454167823877 ) ) ;
#7397 = DIRECTION ( 'NONE',  ( -0.000000000000000000, -0.000000000000000000, -1.000000000000000000 ) ) ;
#7399 = CARTESIAN_POINT ( 'NONE',  ( -5.676582343750006032, 114.1145833299193555, 9.832129032723418760 ) ) ;
#7398 = CARTESIAN_POINT ( 'NONE',  ( 19.30232404098992305, 180.3952738753220615, 120.2370213099771377 ) ) ;
#7400 = CARTESIAN_POINT ( 'NONE',  ( -30.82842712474621649, 207.1250000000000284, 167.1715728752542134 ) ) ;
#7401 = FACE_OUTER_BOUND ( 'NONE', #60574, .T. ) ;
#7402 = EDGE_LOOP ( 'NONE', ( #52197, #49905, #23086, #40851 ) ) ;
#7403 = CARTESIAN_POINT ( 'NONE',  ( -2.679491924311225848, 203.3333333265053966, -10.00000000000000178 ) ) ;
#7404 = CARTESIAN_POINT ( 'NONE',  ( -6.123233995736766282E-16, 258.7500000000000568, -10.00000000000000000 ) ) ;
#7405 = DIRECTION ( 'NONE',  ( 0.000000000000000000, 0.000000000000000000, 1.000000000000000000 ) ) ;
#7406 = CARTESIAN_POINT ( 'NONE',  ( 8.311093377946834337, 100.4687499965860127, 8.311093377946839666 ) ) ;
#7407 = CARTESIAN_POINT ( 'NONE',  ( 2.839093476692135984E-14, 208.6875000013656063, 201.4587341250000350 ) ) ;
#7408 = CARTESIAN_POINT ( 'NONE',  ( -5.082755093536325042, 10.40624999795161187, -5.082755093536325930 ) ) ;
#7409 = CARTESIAN_POINT ( 'NONE',  ( -4.220049686691935698, 10.18810118749999916, 96.25000000204838102 ) ) ;
#7410 = CARTESIAN_POINT ( 'NONE',  ( -2.085542519210945728E-15, 14.84374999658601624, 11.35316468750000141 ) ) ;
#7411 = ORIENTED_EDGE ( 'NONE', *, *, #39979, .F. ) ;
#7412 = DIRECTION ( 'NONE',  ( -0.000000000000000000, -0.000000000000000000, 1.000000000000000000 ) ) ;
#7413 = CARTESIAN_POINT ( 'NONE',  ( 2.751064625579944321E-14, 196.8750000027312126, 194.0000000000000568 ) ) ;
#7414 = CARTESIAN_POINT ( 'NONE',  ( -4.556349186104045934, 11.00000000000000000, 102.7187500000000000 ) ) ;
#7415 = CARTESIAN_POINT ( 'NONE',  ( -7.204075437095965206, -7.204075437095968759, 74.21875000204838102 ) ) ;
#7416 = VECTOR ( 'NONE', #64833, 1000.000000000000000 ) ;
#7417 = CARTESIAN_POINT ( 'NONE',  ( -5.656854249492378806, 98.37500000409677625, 5.656854249492381470 ) ) ;
#7418 = LINE ( 'NONE', #65501, #68010 ) ;
#7419 = CARTESIAN_POINT ( 'NONE',  ( -6.676582343750003368, 291.3906250017070079, -2.765530957081996810 ) ) ;
#7420 = CARTESIAN_POINT ( 'NONE',  ( 1.736494649864627426, 51.27805538755001180, -48.57014059985714027 ) ) ;
#7421 = CARTESIAN_POINT ( 'NONE',  ( 3.042071309553159519, 225.0520833299193555, 11.35316468750000141 ) ) ;
#7422 =( BOUNDED_CURVE ( )  B_SPLINE_CURVE ( 2, ( #59308, #7616, #53645, #64591, #58942, #12889, #47589 ),
 .UNSPECIFIED., .F., .F. ) 
 B_SPLINE_CURVE_WITH_KNOTS ( ( 3, 2, 2, 3 ),
 ( 0.9705882352941178626, 0.9742647058823530326, 0.9779411764705883137, 0.9803851213646477269 ),
 .UNSPECIFIED. ) 
 CURVE ( )  GEOMETRIC_REPRESENTATION_ITEM ( )  RATIONAL_B_SPLINE_CURVE ( ( 0.9999999999999954481, 0.9238795325112912904, 1.000000000000000000, 0.9238795325112867385, 1.000000000000000000, 0.9493986900241293547, 0.9660721264009082265 ) ) 
 REPRESENTATION_ITEM ( '' )  );
#7423 = CARTESIAN_POINT ( 'NONE',  ( 4.220049686691941027, -10.18810118749999738, 92.12500000204836681 ) ) ;
#7424 = EDGE_CURVE ( 'NONE', #54851, #72690, #43073, .T. ) ;
#7425 = CARTESIAN_POINT ( 'NONE',  ( -28.00000000000002132, 203.4375000013656063, 166.5412658750003629 ) ) ;
#7426 = CARTESIAN_POINT ( 'NONE',  ( 8.000000000000000000, 24.09375000000000355, -3.313708498984761608 ) ) ;
#7427 = CARTESIAN_POINT ( 'NONE',  ( 3.211159895383560947, 13.31249999863440792, 3.211159895383562723 ) ) ;
#7428 = ORIENTED_EDGE ( 'NONE', *, *, #15952, .F. ) ;
#7429 = CARTESIAN_POINT ( 'NONE',  ( -20.81184046199496507, -49.21359884407514329, 147.0213769781566100 ) ) ;
#7430 = VECTOR ( 'NONE', #33273, 1000.000000000000227 ) ;
#7431 = CARTESIAN_POINT ( 'NONE',  ( -3.999999999999960032, 208.0625000027312410, 196.3431457505076594 ) ) ;
#7432 = CARTESIAN_POINT ( 'NONE',  ( 3.458734124999960358, 199.6250000013656063, 143.4326545832176976 ) ) ;
#7434 =( BOUNDED_CURVE ( )  B_SPLINE_CURVE ( 2, ( #44213, #34401, #68334, #16631, #55917, #51349, #50980, #4229, #68703 ),
 .UNSPECIFIED., .F., .F. ) 
 B_SPLINE_CURVE_WITH_KNOTS ( ( 3, 2, 2, 2, 3 ),
 ( 0.3833333333333335813, 0.3916666666666669405, 0.4000000000000003553, 0.4083333333333337145, 0.4166666666666671293 ),
 .UNSPECIFIED. ) 
 CURVE ( )  GEOMETRIC_REPRESENTATION_ITEM ( )  RATIONAL_B_SPLINE_CURVE ( ( 0.9999999999999980016, 0.9238795325112887369, 1.000000000000000000, 0.9238795325112867385, 1.000000000000000000, 0.9238795325112867385, 1.000000000000000000, 0.9238795325112826307, 1.000000000000003997 ) ) 
 REPRESENTATION_ITEM ( '' )  );
#7433 = CARTESIAN_POINT ( 'NONE',  ( 1.656854249492348607, 203.3125000027311842, 138.0000000000000568 ) ) ;
#7435 = CARTESIAN_POINT ( 'NONE',  ( 32.00000000000000000, 208.3750000027312126, 169.9999999999998863 ) ) ;
#7436 = CARTESIAN_POINT ( 'NONE',  ( -7.204075437095965206, -7.204075437095968759, 74.21875000204838102 ) ) ;
#7437 = VERTEX_POINT ( 'NONE', #21189 ) ;
#7438 = CARTESIAN_POINT ( 'NONE',  ( 5.082755093536325930, 6.656249997951611874, -5.082755093536325930 ) ) ;
#7439 = CARTESIAN_POINT ( 'NONE',  ( -4.898587196589407898E-16, 7.999999999999991118, 6.455302779823365533 ) ) ;
#7440 = ADVANCED_FACE ( 'NONE', ( #37811 ), #10254, .T. ) ;
#7441 = CARTESIAN_POINT ( 'NONE',  ( -7.188101187500001821, 118.4375000020483810, -2.977408999572650483 ) ) ;
#7442 = CARTESIAN_POINT ( 'NONE',  ( -7.285838599102589797E-14, -20.78460969082654231, -1.607695154586745501 ) ) ;
#7443 = CARTESIAN_POINT ( 'NONE',  ( -2.765530957081998142, 290.6406250017069510, 6.676582343750000703 ) ) ;
#7445 = CARTESIAN_POINT ( 'NONE',  ( -4.999999999999996447, 16.24494643555759410, -69.83755725260752456 ) ) ;
#7444 = CARTESIAN_POINT ( 'NONE',  ( -5.676582343749992710, 234.7395833367473301, 9.832129032723422313 ) ) ;
#7446 = ITEM_DEFINED_TRANSFORMATION ( 'NONE', 'NONE', #55028,  #57354 ) ;
#7447 = ORIENTED_EDGE ( 'NONE', *, *, #1599, .T. ) ;
#7448 = CARTESIAN_POINT ( 'NONE',  ( 8.311093377946839666, 231.0937500034139873, 8.311093377946829008 ) ) ;
#7450 = CARTESIAN_POINT ( 'NONE',  ( -5.272366635369878374, -4.893143551702760163, 0.1656094755204294555 ) ) ;
#7449 =( BOUNDED_CURVE ( )  B_SPLINE_CURVE ( 2, ( #10382, #73748, #55674, #22055, #74121, #9644, #32665, #45082, #39056 ),
 .UNSPECIFIED., .F., .F. ) 
 B_SPLINE_CURVE_WITH_KNOTS ( ( 3, 2, 2, 2, 3 ),
 ( 0.1931818181818181768, 0.1988636363636363535, 0.2045454545454545581, 0.2102272727272727348, 0.2159090909090909116 ),
 .UNSPECIFIED. ) 
 CURVE ( )  GEOMETRIC_REPRESENTATION_ITEM ( )  RATIONAL_B_SPLINE_CURVE ( ( 1.000000000000000000, 0.9238795325112867385, 1.000000000000000000, 0.9238795325112867385, 1.000000000000000000, 0.9238795325112867385, 1.000000000000000000, 0.9238795325112867385, 1.000000000000000000 ) ) 
 REPRESENTATION_ITEM ( '' )  );
#7451 = CARTESIAN_POINT ( 'NONE',  ( 2.445694354108840063, 204.0625000013656063, 200.4456943541088663 ) ) ;
#7452 = ORIENTED_EDGE ( 'NONE', *, *, #70622, .F. ) ;
#7453 = CARTESIAN_POINT ( 'NONE',  ( -4.220049686691937474, -10.18810118749999738, 69.43750000204838102 ) ) ;
#7454 = CARTESIAN_POINT ( 'NONE',  ( -8.311093377946841443, 104.2187499965859985, 8.311093377946830785 ) ) ;
#7455 = CARTESIAN_POINT ( 'NONE',  ( -3.999999999999960032, 208.9375000000000284, 196.3431457505076594 ) ) ;
#7456 = CARTESIAN_POINT ( 'NONE',  ( -11.00000000000000000, 0.000000000000000000, 77.49999999999998579 ) ) ;
#7459 = CARTESIAN_POINT ( 'NONE',  ( 0.000000000000000000, 101.0525588832578734, 0.000000000000000000 ) ) ;
#7458 = CARTESIAN_POINT ( 'NONE',  ( 26.56734541678237704, 204.3750000013656063, 173.4587341249998929 ) ) ;
#7457 = CARTESIAN_POINT ( 'NONE',  ( 24.54126587499998280, 203.5000000013655779, 171.4326545832175555 ) ) ;
#7460 = ORIENTED_EDGE ( 'NONE', *, *, #65683, .F. ) ;
#7461 = VECTOR ( 'NONE', #29279, 1000.000000000000000 ) ;
#7462 = DIRECTION ( 'NONE',  ( 0.000000000000000000, -0.000000000000000000, -1.000000000000000000 ) ) ;
#7463 = CARTESIAN_POINT ( 'NONE',  ( -11.35316468749999963, 219.0625000034139873, 0.000000000000000000 ) ) ;
#7464 = EDGE_CURVE ( 'NONE', #2613, #70285, #55170, .T. ) ;
#7465 = CARTESIAN_POINT ( 'NONE',  ( -5.676582343749998039, 217.4479166632526983, -9.832129032723420536 ) ) ;
#7466 = CARTESIAN_POINT ( 'NONE',  ( -1.432654583217662481, 201.1250000013656347, 145.4587341250000634 ) ) ;
#7467 = CARTESIAN_POINT ( 'NONE',  ( 31.45873412499999944, 203.9375000013656063, 169.9999999999999432 ) ) ;
#7468 = CARTESIAN_POINT ( 'NONE',  ( -2.977408999572654480, 21.37499999795161543, 7.188101187499999156 ) ) ;
#7469 = CARTESIAN_POINT ( 'NONE',  ( 11.35316468749999785, 195.8854166632526415, 3.042071309553174174 ) ) ;
#7470 = CARTESIAN_POINT ( 'NONE',  ( 1.320432766682874540E-15, 90.40625000204838102, 7.188101187500000044 ) ) ;
#7471 = CARTESIAN_POINT ( 'NONE',  ( -5.000000000000000000, 68.32828612846176952, -21.58087353894079641 ) ) ;
#7472 = CARTESIAN_POINT ( 'NONE',  ( -28.00000000000002487, 198.0000000000000000, 166.0000000000003695 ) ) ;
#7473 = CARTESIAN_POINT ( 'NONE',  ( -4.541265875000002339, 15.74999999863440614, -1.881053915767121998 ) ) ;
#7474 = CARTESIAN_POINT ( 'NONE',  ( 24.54126587499998280, 200.5000000013656063, 171.4326545832175555 ) ) ;
#7475 = CARTESIAN_POINT ( 'NONE',  ( 5.082755093536320601, -5.082755093536318824, 6.924052781871754547 ) ) ;
#7476 = CARTESIAN_POINT ( 'NONE',  ( 6.951808397369818766E-16, 72.03124999658602690, -11.35316468750000141 ) ) ;
#7477 = CARTESIAN_POINT ( 'NONE',  ( -5.000000000000000000, -52.35862550122958936, 48.98731492261398301 ) ) ;
#7478 = CARTESIAN_POINT ( 'NONE',  ( 4.000000000000002665, 22.00000000000000000, 0.000000000000000000 ) ) ;
#7479 = ORIENTED_EDGE ( 'NONE', *, *, #50026, .F. ) ;
#7480 = LINE ( 'NONE', #31220, #27832 ) ;
#7481 = CARTESIAN_POINT ( 'NONE',  ( -4.898587196589412829E-16, 94.62499999999998579, -8.000000000000000000 ) ) ;
#7482 = CARTESIAN_POINT ( 'NONE',  ( -9.832129032723418760, 72.86458332991935549, -5.676582343750004256 ) ) ;
#7483 = CARTESIAN_POINT ( 'NONE',  ( -10.18810118749999738, -4.220049686691941915, 86.12500000204836681 ) ) ;
#7484 = CARTESIAN_POINT ( 'NONE',  ( 11.00000000000000000, 1.347111479062088405E-15, 70.93750000409676204 ) ) ;
#7485 = CARTESIAN_POINT ( 'NONE',  ( -3.458734125000015869, 195.1875000013655779, 142.0000000000000568 ) ) ;
#7486 = DIRECTION ( 'NONE',  ( -0.000000000000000000, -0.000000000000000000, -1.000000000000000000 ) ) ;
#7488 = CARTESIAN_POINT ( 'NONE',  ( -11.35316468749999785, 68.07291666325266988, -3.042071309553167957 ) ) ;
#7487 = CARTESIAN_POINT ( 'NONE',  ( 7.188101187500000933, 90.50000000204839523, -2.977408999572651371 ) ) ;
#7489 = CARTESIAN_POINT ( 'NONE',  ( 3.313708498984756279, 7.999999999999991118, 24.54905278392014978 ) ) ;
#7490 = CARTESIAN_POINT ( 'NONE',  ( 1.656854249492381914, 12.81250000000000178, 4.000000000000000888 ) ) ;
#7491 = CARTESIAN_POINT ( 'NONE',  ( 10.00000000000000000, 156.6666666598386826, 2.679491924311236062 ) ) ;
#7492 = CARTESIAN_POINT ( 'NONE',  ( -2.977408999572651815, 91.81250000204839523, 7.188101187500000933 ) ) ;
#7493 = LINE ( 'NONE', #20271, #17145 ) ;
#7494 = CARTESIAN_POINT ( 'NONE',  ( -11.35316468749999785, 58.38541666325268409, -3.042071309553167957 ) ) ;
#7495 = CARTESIAN_POINT ( 'NONE',  ( -4.220049686691935698, 10.18810118749999916, 111.2500000020483952 ) ) ;
#7496 = CARTESIAN_POINT ( 'NONE',  ( 3.042071309553159519, 189.7395833299193271, 11.35316468750000141 ) ) ;
#7497 = VERTEX_POINT ( 'NONE', #61188 ) ;
#7498 = CARTESIAN_POINT ( 'NONE',  ( -0.8912353796320175991, 67.61603573606919326, 20.05324848891948619 ) ) ;
#7499 = DIRECTION ( 'NONE',  ( -1.000000000000000000, 0.000000000000000000, 0.000000000000000000 ) ) ;
#7500 = CARTESIAN_POINT ( 'NONE',  ( 8.660254037844389075, 62.29166665983869677, -5.000000000000000000 ) ) ;
#7502 = CARTESIAN_POINT ( 'NONE',  ( 8.311093377946834337, 190.1562499965860127, 8.311093377946839666 ) ) ;
#7501 = CARTESIAN_POINT ( 'NONE',  ( -2.775557561562891351E-14, 210.0000000000000284, 142.0000000000000568 ) ) ;
#7503 = CARTESIAN_POINT ( 'NONE',  ( 2.828427124746190291, 21.62499999726881583, 2.828427124746192067 ) ) ;
#7504 = CARTESIAN_POINT ( 'NONE',  ( -8.660254037844387298, 242.7083333401613174, -4.999999999999999112 ) ) ;
#7505 = CARTESIAN_POINT ( 'NONE',  ( -56.00000000000004974, 5.999999999999977796, 171.9999999999997726 ) ) ;
#7506 = ORIENTED_EDGE ( 'NONE', *, *, #48180, .T. ) ;
#7507 = CARTESIAN_POINT ( 'NONE',  ( 9.832129032723416984, 180.6770833299193555, 5.676582343750006032 ) ) ;
#7508 = CIRCLE ( 'NONE', #49658, 8.000000000000000000 ) ;
#7509 = CARTESIAN_POINT ( 'NONE',  ( 7.188101187499993827, -2.977408999572645598, 23.14280278187175810 ) ) ;
#7510 = CARTESIAN_POINT ( 'NONE',  ( 26.34314575050759188, 204.0625000027312410, 173.9999999999998863 ) ) ;
#7511 = ORIENTED_EDGE ( 'NONE', *, *, #68516, .T. ) ;
#7512 = EDGE_CURVE ( 'NONE', #44316, #52808, #50938, .T. ) ;
#7513 = CARTESIAN_POINT ( 'NONE',  ( -5.656854249492380582, 95.00000000409677625, -5.656854249492380582 ) ) ;
#7514 = AXIS2_PLACEMENT_3D ( 'NONE', #49317, #26296, #72333 ) ;
#7515 =( BOUNDED_CURVE ( )  B_SPLINE_CURVE ( 2, ( #19079, #18719, #60179, #13405, #47740, #41728, #12674, #2102, #13765, #53793, #25096 ),
 .UNSPECIFIED., .F., .F. ) 
 B_SPLINE_CURVE_WITH_KNOTS ( ( 3, 2, 2, 2, 2, 3 ),
 ( 0.7412468980011663877, 0.7478651410436197855, 0.7544834166280764975, 0.7611016922125333206, 0.7677199677969902547, 0.7677200384551818857 ),
 .UNSPECIFIED. ) 
 CURVE ( )  GEOMETRIC_REPRESENTATION_ITEM ( )  RATIONAL_B_SPLINE_CURVE ( ( 0.9999992514363272855, 0.9238799067949634569, 1.000000000000000000, 0.9238795325112867385, 1.000000000000000000, 0.9238795325112867385, 1.000000000000000000, 0.9238795325112867385, 1.000000000000000000, 0.9999991873208492477, 0.9999983746590511702 ) ) 
 REPRESENTATION_ITEM ( '' )  );
#7516 = CARTESIAN_POINT ( 'NONE',  ( 1.656854249492381248, 13.18749999999999822, -4.000000000000001776 ) ) ;
#7517 = CARTESIAN_POINT ( 'NONE',  ( 6.024380653971844524, 6.914127053141843504, -0.09252763182292059185 ) ) ;
#7518 = CARTESIAN_POINT ( 'NONE',  ( 1.881053915767122664, 14.12499999863440792, 4.541265875000001451 ) ) ;
#7519 = CARTESIAN_POINT ( 'NONE',  ( -3.313708498984758943, -7.999999999999989342, 16.29905278392014623 ) ) ;
#7520 = CARTESIAN_POINT ( 'NONE',  ( 3.999999999999960032, 195.9375000000000000, 143.6568542494924259 ) ) ;
#7522 = ORIENTED_EDGE ( 'NONE', *, *, #2105, .T. ) ;
#7521 = EDGE_CURVE ( 'NONE', #72263, #12103, #21793, .T. ) ;
#7523 = CARTESIAN_POINT ( 'NONE',  ( 7.347880794884121708E-16, 300.0000000000000000, -6.000000000000001776 ) ) ;
#7524 = CARTESIAN_POINT ( 'NONE',  ( -7.188101187500000044, 97.15625000204839523, 0.000000000000000000 ) ) ;
#7525 = CARTESIAN_POINT ( 'NONE',  ( 8.000000000000000000, 16.40624999590322375, -3.313708498984761164 ) ) ;
#7526 = CARTESIAN_POINT ( 'NONE',  ( 1396.688200795887496, 828.9677537767817057, 997.8421604560588776 ) ) ;
#7527 = VERTEX_POINT ( 'NONE', #62665 ) ;
#7528 = EDGE_CURVE ( 'NONE', #49656, #36985, #14632, .T. ) ;
#7529 = CARTESIAN_POINT ( 'NONE',  ( -2.679491924286246718, 156.4583333333312396, -10.00000000001463540 ) ) ;
#7530 = DIRECTION ( 'NONE',  ( 0.000000000000000000, 0.000000000000000000, 1.000000000000000000 ) ) ;
#7531 = CARTESIAN_POINT ( 'NONE',  ( 7.188101187499993827, -2.977408999572645598, 23.14280278187176165 ) ) ;
#7532 = ORIENTED_EDGE ( 'NONE', *, *, #24290, .T. ) ;
#7533 =( BOUNDED_CURVE ( )  B_SPLINE_CURVE ( 2, ( #54332, #25632, #2643, #2267, #13930, #53954, #54705, #47907, #59614 ),
 .UNSPECIFIED., .F., .F. ) 
 B_SPLINE_CURVE_WITH_KNOTS ( ( 3, 2, 2, 2, 3 ),
 ( 0.6477272727272727071, 0.6534090909090909394, 0.6590909090909091717, 0.6647727272727274039, 0.6704545454545455252 ),
 .UNSPECIFIED. ) 
 CURVE ( )  GEOMETRIC_REPRESENTATION_ITEM ( )  RATIONAL_B_SPLINE_CURVE ( ( 1.000000000000000000, 0.9238795325112867385, 1.000000000000000000, 0.9238795325112867385, 1.000000000000000000, 0.9238795325112867385, 1.000000000000000000, 0.9238795325112852952, 1.000000000000001554 ) ) 
 REPRESENTATION_ITEM ( '' )  );
#7534 = ORIENTED_EDGE ( 'NONE', *, *, #58134, .T. ) ;
#7535 = CARTESIAN_POINT ( 'NONE',  ( 10.18810118749999916, 1.247682550866122264E-15, 86.40625000204838102 ) ) ;
#7536 = CYLINDRICAL_SURFACE ( 'NONE', #28784, 7.999999999999991118 ) ;
#7537 = CARTESIAN_POINT ( 'NONE',  ( 11.00000000000000000, 4.556349186104045934, 97.84375000000000000 ) ) ;
#7540 = CARTESIAN_POINT ( 'NONE',  ( 6.676582343750002480, 294.1718750017070079, -2.765530957081997254 ) ) ;
#7539 = CARTESIAN_POINT ( 'NONE',  ( 26.34314575050763807, 202.0625000027312410, 173.9999999999999147 ) ) ;
#7538 = CARTESIAN_POINT ( 'NONE',  ( -2.775557561562891351E-14, 195.0000000000000000, 142.0000000000000568 ) ) ;
#7541 = CARTESIAN_POINT ( 'NONE',  ( -2.679491924311225848, 131.4583333333333428, -10.00000000000000178 ) ) ;
#7542 = CARTESIAN_POINT ( 'NONE',  ( -30.99999999999992895, -31.99999999999978684, 205.0000000000000284 ) ) ;
#7543 = ADVANCED_FACE ( 'NONE', ( #68335 ), #39298, .T. ) ;
#7544 = LINE ( 'NONE', #69807, #4897 ) ;
#7545 = CARTESIAN_POINT ( 'NONE',  ( 7.999999999714877852, 6.754118554053788561E-05, 0.2678047518895779744 ) ) ;
#7546 = CARTESIAN_POINT ( 'NONE',  ( 28.00000000000002132, 199.9375000013656063, 166.5412658749999082 ) ) ;
#7547 = CARTESIAN_POINT ( 'NONE',  ( 5.082755093536324154, 5.156249997951610098, 5.082755093536326818 ) ) ;
#7548 = CARTESIAN_POINT ( 'NONE',  ( 3.317071493978883456, -8.008118988124989457, 1.481865283940630329 ) ) ;
#7549 = CARTESIAN_POINT ( 'NONE',  ( -9.999999999999998224, 243.3333333401612606, 2.679491924311235174 ) ) ;
#7550 = CARTESIAN_POINT ( 'NONE',  ( -5.082755093536325930, 113.8437500020483810, -5.082755093536325930 ) ) ;
#7552 = DIRECTION ( 'NONE',  ( -0.000000000000000000, -0.000000000000000000, -1.000000000000000000 ) ) ;
#7551 = CARTESIAN_POINT ( 'NONE',  ( 5.000000000000000000, -60.11723469343085213, -46.25570701698114107 ) ) ;
#7553 = CARTESIAN_POINT ( 'NONE',  ( -3.042071309553166181, 223.1770833367473017, -11.35316468749999608 ) ) ;
#7554 = CARTESIAN_POINT ( 'NONE',  ( -4.000000000000001776, 12.43750000000000000, -1.656854249492381470 ) ) ;
#7555 = CARTESIAN_POINT ( 'NONE',  ( 7.188101187499992051, 8.802885111219154394E-16, 22.11155278187175455 ) ) ;
#7556 = DIRECTION ( 'NONE',  ( -0.000000000000000000, 1.000000000000000000, -1.563033456626094573E-30 ) ) ;
#7557 = CARTESIAN_POINT ( 'NONE',  ( -9.832129032723418760, 32.86458332991935549, -5.676582343750004256 ) ) ;
#7558 = CARTESIAN_POINT ( 'NONE',  ( -5.000000000000000000, 50.64189880742145533, -41.08656465431843685 ) ) ;
#7559 = CARTESIAN_POINT ( 'NONE',  ( -7.320508075688773708, 13.74999999317203070, -7.320508075688774596 ) ) ;
#7560 = CARTESIAN_POINT ( 'NONE',  ( 8.000000000000001776, 112.1562500000000000, 3.313708498984759387 ) ) ;
#7561 = CARTESIAN_POINT ( 'NONE',  ( -74.99999999999998579, 272.0000000000000000, 70.00000000000002842 ) ) ;
#7562 = ORIENTED_EDGE ( 'NONE', *, *, #70963, .F. ) ;
#7563 = CARTESIAN_POINT ( 'NONE',  ( -4.556349186104045934, 11.00000000000000000, 104.4062500040967620 ) ) ;
#7564 = AXIS2_PLACEMENT_3D ( 'NONE', #34239, #11954, #18355 ) ;
#7565 = CARTESIAN_POINT ( 'NONE',  ( -1.432654583217664701, 196.0000000013656347, 138.5412658750000787 ) ) ;
#7566 = CARTESIAN_POINT ( 'NONE',  ( 11.35316468749999963, 35.98958332991933418, -3.042071309553165293 ) ) ;
#7567 = CARTESIAN_POINT ( 'NONE',  ( 11.00000000000000000, 1.347111479062088405E-15, 85.93750000409677625 ) ) ;
#7568 = CARTESIAN_POINT ( 'NONE',  ( -1.432654583217662481, 208.3750000013656063, 145.4587341250000350 ) ) ;
#7569 = CARTESIAN_POINT ( 'NONE',  ( -31.45873412499995680, 194.7500000013656063, 171.4326545832181239 ) ) ;
#7570 = CARTESIAN_POINT ( 'NONE',  ( 4.556349186104045934, 11.00000000000000000, 101.0312499999999858 ) ) ;
#7572 = CARTESIAN_POINT ( 'NONE',  ( -2.085542519210945728E-15, 39.53124999658601268, 11.35316468750000141 ) ) ;
#7571 = CARTESIAN_POINT ( 'NONE',  ( -2.977408999572652260, 103.4375000020483810, 7.188101187500000044 ) ) ;
#7573 = CARTESIAN_POINT ( 'NONE',  ( 7.999999999999991118, 3.313708498984757611, 16.67405277982336642 ) ) ;
#7574 = CARTESIAN_POINT ( 'NONE',  ( 11.35316468749999785, 145.5729166632527267, 3.042071309553174174 ) ) ;
#7575 = CARTESIAN_POINT ( 'NONE',  ( -10.00000000000000178, 119.3749999931720396, -1.224646799147353454E-15 ) ) ;
#7576 = ADVANCED_FACE ( 'NONE', ( #56658 ), #28710, .T. ) ;
#7577 = CARTESIAN_POINT ( 'NONE',  ( 2.977408999572654480, 107.0000000020483810, 7.188101187499999156 ) ) ;
#7578 = CARTESIAN_POINT ( 'NONE',  ( 27.99999999999996803, 206.0000000000000284, 173.9999999999999147 ) ) ;
#7579 = CARTESIAN_POINT ( 'NONE',  ( -25.55430564589115150, 205.3125000013656063, 172.4456943541091789 ) ) ;
#7580 = ORIENTED_EDGE ( 'NONE', *, *, #46814, .T. ) ;
#7581 = CARTESIAN_POINT ( 'NONE',  ( -11.35316468750000141, 23.80208332991935194, 3.042071309553159963 ) ) ;
#7582 = ORIENTED_EDGE ( 'NONE', *, *, #38427, .T. ) ;
#7583 = CARTESIAN_POINT ( 'NONE',  ( -4.999999999999996447, 16.24494643555759410, -69.83755725260752456 ) ) ;
#7585 = CARTESIAN_POINT ( 'NONE',  ( 6.951808397369818766E-16, 152.0312499965860411, -11.35316468750000141 ) ) ;
#7584 = CARTESIAN_POINT ( 'NONE',  ( -32.75573181841404846, -21.13616108035461849, 157.7720380398369286 ) ) ;
#7586 = CARTESIAN_POINT ( 'NONE',  ( 5.656854249492376141, -5.656854249492374365, 19.44905278432982598 ) ) ;
#7587 = CARTESIAN_POINT ( 'NONE',  ( 4.556349186104045934, 11.00000000000000000, 90.71875000409676204 ) ) ;
#7588 = CARTESIAN_POINT ( 'NONE',  ( 8.311093377946839666, 250.7812500034139873, 8.311093377946829008 ) ) ;
#7589 = CARTESIAN_POINT ( 'NONE',  ( 10.18810118750000093, -4.220049686691933921, 92.68750000204838102 ) ) ;
#7590 = VERTEX_POINT ( 'NONE', #39666 ) ;
#7591 = CARTESIAN_POINT ( 'NONE',  ( -2.849036369511732440E-14, 197.2500000000000000, 138.0000000000000568 ) ) ;
#7592 = CARTESIAN_POINT ( 'NONE',  ( -2.828427124746152987, 199.2500000027312126, 200.8284271247462129 ) ) ;
#7593 = CARTESIAN_POINT ( 'NONE',  ( 11.35316468750000141, 86.09374999658601268, 0.000000000000000000 ) ) ;
#7594 = CARTESIAN_POINT ( 'NONE',  ( -4.220049686691935698, 10.18810118749999916, 100.3750000020484094 ) ) ;
#7595 = CARTESIAN_POINT ( 'NONE',  ( -4.541265875000002339, 14.93749999863440792, -5.561446717895856393E-16 ) ) ;
#7596 = VERTEX_POINT ( 'NONE', #57030 ) ;
#7597 = ORIENTED_EDGE ( 'NONE', *, *, #67828, .T. ) ;
#7598 = CARTESIAN_POINT ( 'NONE',  ( -1.469576158976823947E-15, 7.125000000000000888, 8.000000000000000000 ) ) ;
#7599 = LINE ( 'NONE', #53257, #31225 ) ;
#7600 = CARTESIAN_POINT ( 'NONE',  ( -7.188101187500000044, 4.218749997951610986, -8.802885111219163269E-16 ) ) ;
#7601 = CARTESIAN_POINT ( 'NONE',  ( 8.000000000000000000, 123.0312500040967763, -3.313708498984762496 ) ) ;
#7602 = CARTESIAN_POINT ( 'NONE',  ( -10.18810118749999738, -4.220049686691941915, 99.62500000204838102 ) ) ;
#7603 = CARTESIAN_POINT ( 'NONE',  ( -1.836970198721029983E-15, 160.6249999931720254, 10.00000000000000178 ) ) ;
#7604 = EDGE_CURVE ( 'NONE', #40293, #41608, #58238, .T. ) ;
#7605 = CARTESIAN_POINT ( 'NONE',  ( -2.828427124746192067, 1.625000000000000444, 2.828427124746190735 ) ) ;
#7606 = CARTESIAN_POINT ( 'NONE',  ( -4.000000000000001776, 14.24999999726881406, -4.898587196589415787E-16 ) ) ;
#7607 = CARTESIAN_POINT ( 'NONE',  ( -1.881053915767121776, 5.624999998634407028, -4.541265875000002339 ) ) ;
#7608 = ORIENTED_EDGE ( 'NONE', *, *, #1503, .T. ) ;
#7609 = VECTOR ( 'NONE', #60755, 1000.000000000000000 ) ;
#7610 = CARTESIAN_POINT ( 'NONE',  ( 3.458734124999959025, 207.5000000013655779, 140.5673454167824161 ) ) ;
#7611 = CARTESIAN_POINT ( 'NONE',  ( -3.458734124999959914, 199.3750000013656063, 196.5673454167823877 ) ) ;
#7613 = CARTESIAN_POINT ( 'NONE',  ( 1.469576158976823947E-15, 95.37499999999998579, 8.000000000000000000 ) ) ;
#7612 = CARTESIAN_POINT ( 'NONE',  ( -30.44569435410886982, 199.5625000013656063, 167.5543056458916169 ) ) ;
#7614 = EDGE_CURVE ( 'NONE', #51761, #852, #39923, .T. ) ;
#7615 = CARTESIAN_POINT ( 'NONE',  ( -3.211159895383561391, 12.68749999863440792, -3.211159895383561835 ) ) ;
#7616 = CARTESIAN_POINT ( 'NONE',  ( -10.99999999999978861, 4.556349186104256432, 68.40624999999997158 ) ) ;
#7617 = CARTESIAN_POINT ( 'NONE',  ( 5.082755093536318824, 5.082755093536319713, 14.42405278187175455 ) ) ;
#7618 = ORIENTED_EDGE ( 'NONE', *, *, #18831, .T. ) ;
#7619 = EDGE_LOOP ( 'NONE', ( #2747, #3052, #8823, #58480, #46101, #32976, #43074, #46080, #68285, #40839, #30535, #26912, #39345, #19603, #54763, #67083, #6432, #2477, #45947, #61132, #13811, #34969, #12832, #41712, #73812, #13095, #34591, #59082, #22493, #1848, #23392, #19822, #73853, #38875, #15341, #71602, #2520, #48704, #10381, #65206, #3652 ) ) ;
#7620 = CARTESIAN_POINT ( 'NONE',  ( 1.871523826299183495E-15, -10.18810118749999916, 102.5312500020483810 ) ) ;
#7621 = CARTESIAN_POINT ( 'NONE',  ( -2.679491924311250717, 221.0416666666666856, 9.999999999999984013 ) ) ;
#7622 = CARTESIAN_POINT ( 'NONE',  ( -26.34314575050764518, 199.9375000000000000, 166.0000000000003695 ) ) ;
#7623 = CARTESIAN_POINT ( 'NONE',  ( 2.445694354108838731, 195.0625000013656063, 195.5543056458912190 ) ) ;
#7624 = CARTESIAN_POINT ( 'NONE',  ( -23.99999999999998934, 201.8750000027312126, 170.0000000000002842 ) ) ;
#7625 = CARTESIAN_POINT ( 'NONE',  ( -8.660254037844387298, 97.08333333333334281, -5.000000000000004441 ) ) ;
#7626 = CARTESIAN_POINT ( 'NONE',  ( -4.898587196589412829E-16, 120.1250000000000000, -8.000000000000000000 ) ) ;
#7627 = CARTESIAN_POINT ( 'NONE',  ( -6.676582343750003368, 297.5468750017069510, -2.765530957081996810 ) ) ;
#7628 = ORIENTED_EDGE ( 'NONE', *, *, #10943, .T. ) ;
#7629 = B_SPLINE_CURVE_WITH_KNOTS ( 'NONE', 3,
 ( #7583, #47190, #64554, #46823, #6840, #64912, #36626, #833, #64186, #1921 ),
 .UNSPECIFIED., .F., .F.,
 ( 4, 2, 2, 2, 4 ),
 ( 0.000000000000000000, 0.001314083742615249203, 0.002628167485230497539, 0.003942251227845745658, 0.005256334970460992476 ),
 .UNSPECIFIED. ) ;
#7630 =( BOUNDED_CURVE ( )  B_SPLINE_CURVE ( 2, ( #49091, #32513, #9499, #9867, #15878, #27577, #72491, #67581, #20800 ),
 .UNSPECIFIED., .F., .F. ) 
 B_SPLINE_CURVE_WITH_KNOTS ( ( 3, 2, 2, 2, 3 ),
 ( 0.7083333333333332593, 0.7152777777777776791, 0.7222222222222220989, 0.7291666666666665186, 0.7361111111111110494 ),
 .UNSPECIFIED. ) 
 CURVE ( )  GEOMETRIC_REPRESENTATION_ITEM ( )  RATIONAL_B_SPLINE_CURVE ( ( 1.000000000000001110, 0.9238795325112855172, 1.000000000000000000, 0.9238795325112867385, 1.000000000000000000, 0.9238795325112867385, 1.000000000000000000, 0.9238795325112879597, 0.9999999999999987788 ) ) 
 REPRESENTATION_ITEM ( '' )  );
#7631 = B_SPLINE_CURVE_WITH_KNOTS ( 'NONE', 3,
 ( #35712, #26594, #55291, #20936, #33401, #3597, #21678, #37559, #43574, #66590, #14895, #15642, #73002, #67344, #43957, #16017, #32657, #15270 ),
 .UNSPECIFIED., .F., .F.,
 ( 4, 2, 2, 2, 2, 2, 2, 2, 4 ),
 ( 6.321633202427608947E-17, 0.003662049718959018308, 0.005493074578438499923, 0.007324099437917982840, 0.008239611867657722563, 0.009155124297397463154, 0.01098614915687694954, 0.01281717401635645327, 0.01464819887583595701 ),
 .UNSPECIFIED. ) ;
#7632 = CARTESIAN_POINT ( 'NONE',  ( -10.99999999999989342, 4.556349186104152515, 74.40625000000000000 ) ) ;
#7633 = EDGE_CURVE ( 'NONE', #21472, #37922, #20080, .T. ) ;
#7634 = CARTESIAN_POINT ( 'NONE',  ( 8.000000000000000000, 14.81249999590322020, 0.000000000000000000 ) ) ;
#7635 = CARTESIAN_POINT ( 'NONE',  ( -3.458734125000015425, 208.0000000013656347, 143.4326545832176976 ) ) ;
#7636 = CARTESIAN_POINT ( 'NONE',  ( -7.320508075688779925, 53.12500000000001421, 7.320508075688771044 ) ) ;
#7637 =( NAMED_UNIT ( * ) SI_UNIT ( $, .STERADIAN. ) SOLID_ANGLE_UNIT ( ) );
#7638 = CARTESIAN_POINT ( 'NONE',  ( -6.951808397369817780E-16, 262.9687500034140157, -11.35316468749999963 ) ) ;
#7639 = CARTESIAN_POINT ( 'NONE',  ( -1.656854249492401232, 207.3125000000000000, 138.0000000000000284 ) ) ;
#7640 = CARTESIAN_POINT ( 'NONE',  ( -11.00000000000000000, 4.556349186104045934, 114.9062499999999716 ) ) ;
#7641 = CARTESIAN_POINT ( 'NONE',  ( 10.00000000000000178, 210.0000000000000284, 0.000000000000000000 ) ) ;
#7642 = EDGE_CURVE ( 'NONE', #30705, #36538, #19732, .T. ) ;
#7643 = CARTESIAN_POINT ( 'NONE',  ( 7.188101187499992051, 2.977408999572647819, 8.705302781871752771 ) ) ;
#7644 = CARTESIAN_POINT ( 'NONE',  ( 5.676582343749993598, 185.2604166632526983, 9.832129032723422313 ) ) ;
#7645 = DIRECTION ( 'NONE',  ( -0.000000000000000000, 1.000000000000000000, -0.000000000000000000 ) ) ;
#7646 = CARTESIAN_POINT ( 'NONE',  ( 4.541265875000002339, 3.312499998634407028, 0.000000000000000000 ) ) ;
#7647 = CARTESIAN_POINT ( 'NONE',  ( 10.00000000000000178, 242.2916666666666572, 2.679491924311222739 ) ) ;
#7649 = CARTESIAN_POINT ( 'NONE',  ( 7.999999999999991118, 9.797174393178815797E-16, 3.267802783920144449 ) ) ;
#7648 = DIRECTION ( 'NONE',  ( 1.000000000000000000, -0.000000000000000000, -0.000000000000000000 ) ) ;
#7650 = ORIENTED_EDGE ( 'NONE', *, *, #18512, .T. ) ;
#7651 = CARTESIAN_POINT ( 'NONE',  ( -3.458734125000015425, 209.2500000013655779, 143.4326545832176976 ) ) ;
#7652 = CARTESIAN_POINT ( 'NONE',  ( 3.042071309553167069, 47.13541666325268409, -11.35316468749999785 ) ) ;
#7653 = CARTESIAN_POINT ( 'NONE',  ( 7.778174593052021635, 7.778174593052023411, 102.6250000040967763 ) ) ;
#7654 = CARTESIAN_POINT ( 'NONE',  ( 11.35316468750000141, 216.0937499965860411, 0.000000000000000000 ) ) ;
#7655 = CARTESIAN_POINT ( 'NONE',  ( -31.45873412499999944, 205.6875000013656063, 170.0000000000004547 ) ) ;
#7656 = CARTESIAN_POINT ( 'NONE',  ( -11.00000000000000000, 0.000000000000000000, 95.68750000409677625 ) ) ;
#7658 = CARTESIAN_POINT ( 'NONE',  ( -11.00000000000000000, 0.000000000000000000, 110.6875000040967763 ) ) ;
#7657 = CARTESIAN_POINT ( 'NONE',  ( -4.401442555609581635E-16, 120.7812500020483810, -7.188101187500000044 ) ) ;
#7659 = CARTESIAN_POINT ( 'NONE',  ( -2.839093476692135984E-14, 195.6875000013655779, 138.5412658750000503 ) ) ;
#7660 = CARTESIAN_POINT ( 'NONE',  ( -3.042071309553173730, 104.3229166632526983, 11.35316468749999785 ) ) ;
#7661 = CARTESIAN_POINT ( 'NONE',  ( -8.660254037844390851, 79.79166665983871098, 4.999999999999998224 ) ) ;
#7662 = CARTESIAN_POINT ( 'NONE',  ( 5.082755093536325042, 96.59375000204838102, -5.082755093536325930 ) ) ;
#7663 = CARTESIAN_POINT ( 'NONE',  ( -4.541265875000002339, 15.93749999863440436, -5.561446717895856393E-16 ) ) ;
#7664 = CARTESIAN_POINT ( 'NONE',  ( -31.99999999999996447, 204.4375000027312126, 171.6568542494928522 ) ) ;
#7665 = CARTESIAN_POINT ( 'NONE',  ( 27.99999999999999645, 210.0000000000000284, 169.9999999999999147 ) ) ;
#7666 = ORIENTED_EDGE ( 'NONE', *, *, #69283, .F. ) ;
#7668 = EDGE_CURVE ( 'NONE', #7386, #3972, #34776, .T. ) ;
#7667 = ORIENTED_EDGE ( 'NONE', *, *, #25072, .T. ) ;
#7669 = CARTESIAN_POINT ( 'NONE',  ( 6.676582343750003368, 294.1718750017070079, -2.765530957081997254 ) ) ;
#7670 = DIRECTION ( 'NONE',  ( -0.000000000000000000, 1.000000000000000000, -0.000000000000000000 ) ) ;
#7671 = CARTESIAN_POINT ( 'NONE',  ( -11.35316468749999785, 153.0729166632527267, -3.042071309553167513 ) ) ;
#7672 = CARTESIAN_POINT ( 'NONE',  ( 8.000000000000035527, 3.313708498984715423, 9.174052779823362869 ) ) ;
#7673 = CARTESIAN_POINT ( 'NONE',  ( -2.828427124746153876, 200.8750000000000284, 195.1715728752538439 ) ) ;
#7674 = CARTESIAN_POINT ( 'NONE',  ( 12.00000000000000178, 1.469576158976824144E-15, -21.47459999999999525 ) ) ;
#7675 = CARTESIAN_POINT ( 'NONE',  ( 7.204075437095968759, -7.204075437095966983, 112.0937500020483810 ) ) ;
#7676 = ORIENTED_EDGE ( 'NONE', *, *, #68773, .T. ) ;
#7677 = CARTESIAN_POINT ( 'NONE',  ( 38.10581460227392370, -1.532137509302638811, 125.9538205090439931 ) ) ;
#7678 = CARTESIAN_POINT ( 'NONE',  ( -11.00000000000007816, -4.556349186103974880, 109.2812500040967620 ) ) ;
#7679 = CARTESIAN_POINT ( 'NONE',  ( -8.311093377946836114, 147.9687499965860127, -8.311093377946837890 ) ) ;
#7680 = CARTESIAN_POINT ( 'NONE',  ( 1.432654583217664479, 197.7500000013656063, 201.4587341250000065 ) ) ;
#7681 = CARTESIAN_POINT ( 'NONE',  ( 6.000000000000001776, 298.5625000034140157, -7.347880794884121708E-16 ) ) ;
#7682 = CARTESIAN_POINT ( 'NONE',  ( 4.220049686691934809, 10.18810118749999916, 70.56250000204836681 ) ) ;
#7683 = CARTESIAN_POINT ( 'NONE',  ( 11.35316468750000141, 56.09374999658601979, 0.000000000000000000 ) ) ;
#7684 = ORIENTED_EDGE ( 'NONE', *, *, #19767, .T. ) ;
#7685 = CARTESIAN_POINT ( 'NONE',  ( -14.00000000000000178, 2.143131898507868248E-15, 17.50000000000000000 ) ) ;
#7686 = CARTESIAN_POINT ( 'NONE',  ( 4.541265875000001451, 4.374999998634407028, 1.881053915767124440 ) ) ;
#7687 = CARTESIAN_POINT ( 'NONE',  ( 5.662595241051934458, 5.662595241051935346, 7.950615283940629219 ) ) ;
#7688 = EDGE_CURVE ( 'NONE', #34934, #39259, #6219, .T. ) ;
#7689 = CARTESIAN_POINT ( 'NONE',  ( -2.977408999572654480, 13.49999999795161187, 7.188101187499999156 ) ) ;
#7690 = CARTESIAN_POINT ( 'NONE',  ( 2.485281374238575314, 293.3750000034140157, 6.000000000000000888 ) ) ;
#7691 = CARTESIAN_POINT ( 'NONE',  ( 3.674341569226420301, 124.5066941839809544, -7.107250865053953426 ) ) ;
#7692 = CARTESIAN_POINT ( 'NONE',  ( -5.082755093536325042, 11.90624999795161010, -5.082755093536325930 ) ) ;
#7693 = CARTESIAN_POINT ( 'NONE',  ( 7.188101187499993827, -2.977408999572645598, 6.642802781871754547 ) ) ;
#7694 = EDGE_CURVE ( 'NONE', #16846, #11938, #50780, .T. ) ;
#7695 =( REPRESENTATION_RELATIONSHIP ('NONE','NONE', #46008, #20419 ) REPRESENTATION_RELATIONSHIP_WITH_TRANSFORMATION ( #13081 )SHAPE_REPRESENTATION_RELATIONSHIP( ) );
#7696 = CARTESIAN_POINT ( 'NONE',  ( 10.18810118749999916, 1.247682550866122264E-15, 116.7812500020483810 ) ) ;
#7697 = ADVANCED_FACE ( 'NONE', ( #47169 ), #66285, .F. ) ;
#7698 = CARTESIAN_POINT ( 'NONE',  ( 0.000000000000000000, 0.000000000000000000, 118.0000000000000000 ) ) ;
#7699 = CARTESIAN_POINT ( 'NONE',  ( 4.541265875000002339, 22.43749999863440436, 0.000000000000000000 ) ) ;
#7700 = EDGE_LOOP ( 'NONE', ( #49144, #55321, #2669, #13454 ) ) ;
#7701 = CARTESIAN_POINT ( 'NONE',  ( 2.849036369511732440E-14, 197.3750000027312126, 202.0000000000000000 ) ) ;
#7702 = CARTESIAN_POINT ( 'NONE',  ( 1.656854249492347719, 201.8125000000000000, 146.0000000000000284 ) ) ;
#7703 = CARTESIAN_POINT ( 'NONE',  ( -26.34314575050753149, 198.6875000027312126, 174.0000000000003411 ) ) ;
#7704 = CARTESIAN_POINT ( 'NONE',  ( -4.541265875000002339, 1.749999998634406584, -1.881053915767121998 ) ) ;
#7705 = CARTESIAN_POINT ( 'NONE',  ( 2.977408999572650039, 117.6875000020484094, -7.188101187500001821 ) ) ;
#7706 = CARTESIAN_POINT ( 'NONE',  ( 0.000000000000000000, 300.0000000000000000, 0.000000000000000000 ) ) ;
#7707 = CARTESIAN_POINT ( 'NONE',  ( -4.898587196589407898E-16, 7.999999999999991118, 0.6428027839201454485 ) ) ;
#7708 = EDGE_LOOP ( 'NONE', ( #30168, #37672, #4545 ) ) ;
#7709 = ADVANCED_FACE ( 'NONE', ( #25540 ), #48337, .T. ) ;
#7710 = ADVANCED_FACE ( 'NONE', ( #20632 ), #49302, .T. ) ;
#7711 = CARTESIAN_POINT ( 'NONE',  ( 2.977408999572650927, 24.74999999795161543, -7.188101187500000933 ) ) ;
#7712 = ORIENTED_EDGE ( 'NONE', *, *, #36615, .T. ) ;
#7713 = CARTESIAN_POINT ( 'NONE',  ( -27.99999999999999645, 210.0000000000000284, 174.0000000000003411 ) ) ;
#7714 = CARTESIAN_POINT ( 'NONE',  ( -1.432654583217607192, 206.2500000013656063, 194.5412658750000219 ) ) ;
#7715 = CARTESIAN_POINT ( 'NONE',  ( 31.45873412499999944, 201.6250000013656063, 171.4326545832175555 ) ) ;
#7716 = CARTESIAN_POINT ( 'NONE',  ( 2.679491924311222739, 53.95833333333333570, 10.00000000000000355 ) ) ;
#7717 = VECTOR ( 'NONE', #8891, 1000.000000000000000 ) ;
#7718 = CARTESIAN_POINT ( 'NONE',  ( -7.188101187500000044, 102.0312500020483810, 0.000000000000000000 ) ) ;
#7719 = CARTESIAN_POINT ( 'NONE',  ( 6.000000000000001776, 297.5000000000000000, -7.347880794884121708E-16 ) ) ;
#7721 = CARTESIAN_POINT ( 'NONE',  ( -20.43041552119061421, -35.10693506728129165, 193.3167811493079284 ) ) ;
#7720 = CYLINDRICAL_SURFACE ( 'NONE', #30963, 10.00000000000000178 ) ;
#7722 = EDGE_LOOP ( 'NONE', ( #46689, #39045, #53972, #24072 ) ) ;
#7723 = CARTESIAN_POINT ( 'NONE',  ( -8.311093377946834337, 229.5312500034139873, 8.311093377946837890 ) ) ;
#7724 = DIRECTION ( 'NONE',  ( 0.000000000000000000, 0.000000000000000000, 1.000000000000000000 ) ) ;
#7725 = CARTESIAN_POINT ( 'NONE',  ( -11.00000000000000000, 0.000000000000000000, 83.68750000409677625 ) ) ;
#7726 = CARTESIAN_POINT ( 'NONE',  ( 25.51922947296858624, 194.8335204809880565, 167.0712042815414975 ) ) ;
#7727 = CARTESIAN_POINT ( 'NONE',  ( 0.000000000000000000, 192.0000000000000284, 207.0000000000000568 ) ) ;
#7728 = CARTESIAN_POINT ( 'NONE',  ( 8.660254037844389075, 170.4166666666666856, -5.000000000000000000 ) ) ;
#7729 = CARTESIAN_POINT ( 'NONE',  ( 26.56734541678238415, 209.0000000013655779, 166.5412658749999650 ) ) ;
#7730 = CARTESIAN_POINT ( 'NONE',  ( -1.469576158976823947E-15, 1.125000000000000222, 8.000000000000000000 ) ) ;
#7731 = CARTESIAN_POINT ( 'NONE',  ( 11.00000000000000000, 1.347111479062088405E-15, 69.43750000409676204 ) ) ;
#7732 = CARTESIAN_POINT ( 'NONE',  ( -9.832129032723418760, 143.1770833299193555, -5.676582343750004256 ) ) ;
#7733 = CARTESIAN_POINT ( 'NONE',  ( 0.000000000000000000, 0.000000000000000000, 38.34805510287551300 ) ) ;
#7734 = CARTESIAN_POINT ( 'NONE',  ( 6.123233995736767268E-16, 28.12499999317203603, -10.00000000000000178 ) ) ;
#7737 = CARTESIAN_POINT ( 'NONE',  ( 0.000000000000000000, 125.0000000000000000, 0.000000000000000000 ) ) ;
#7736 = CARTESIAN_POINT ( 'NONE',  ( 0.000000000000000000, 0.000000000000000000, 30.00000000000000000 ) ) ;
#7735 = CARTESIAN_POINT ( 'NONE',  ( 25.17157287525378706, 206.8750000000000284, 172.8284271247460424 ) ) ;
#7738 = VERTEX_POINT ( 'NONE', #65910 ) ;
#7739 = CARTESIAN_POINT ( 'NONE',  ( 5.676582343750001591, 6.927083329919350163, -9.832129032723420536 ) ) ;
#7740 = CARTESIAN_POINT ( 'NONE',  ( -3.313708498984760276, 7.781249995903221972, -8.000000000000000000 ) ) ;
#7741 = CARTESIAN_POINT ( 'NONE',  ( -2.679491924311226292, 88.33333332650536818, -10.00000000000000178 ) ) ;
#7742 = CARTESIAN_POINT ( 'NONE',  ( -25.17157287525377996, 209.6250000000000284, 172.8284271247465256 ) ) ;
#7743 = CARTESIAN_POINT ( 'NONE',  ( 3.458734124999959914, 206.3750000013656063, 143.4326545832176976 ) ) ;
#7744 = CARTESIAN_POINT ( 'NONE',  ( -8.000000000000001776, 5.156249995903221084, 3.313708498984759387 ) ) ;
#7745 = CARTESIAN_POINT ( 'NONE',  ( 4.999999999999993783, 31.04166665983870033, 8.660254037844390851 ) ) ;
#7746 = VECTOR ( 'NONE', #4102, 1000.000000000000000 ) ;
#7747 = CARTESIAN_POINT ( 'NONE',  ( -5.082755093536324154, 113.8437500020483810, 5.082755093536326818 ) ) ;
#7748 = CARTESIAN_POINT ( 'NONE',  ( 4.541265875000001451, 6.374999998634407028, 1.881053915767124440 ) ) ;
#7749 = CARTESIAN_POINT ( 'NONE',  ( -11.76730021030299156, -37.51057907174865846, 141.3197202389246456 ) ) ;
#7750 = CARTESIAN_POINT ( 'NONE',  ( 7.999999999999991118, 3.313708498984757611, 16.67405277982336642 ) ) ;
#7752 = CARTESIAN_POINT ( 'NONE',  ( 10.00000000000000178, 6.874999993172033363, 0.000000000000000000 ) ) ;
#7751 = CARTESIAN_POINT ( 'NONE',  ( -8.660254037844387298, 237.7083333401613174, -4.999999999999999112 ) ) ;
#7753 = ORIENTED_EDGE ( 'NONE', *, *, #255, .T. ) ;
#7754 =( BOUNDED_CURVE ( )  B_SPLINE_CURVE ( 2, ( #64344, #12648, #35679, #13740, #25069 ),
 .UNSPECIFIED., .F., .F. ) 
 B_SPLINE_CURVE_WITH_KNOTS ( ( 3, 2, 3 ),
 ( 0.000000000000000000, 0.008333333333333399137, 0.01666666666666679827 ),
 .UNSPECIFIED. ) 
 CURVE ( )  GEOMETRIC_REPRESENTATION_ITEM ( )  RATIONAL_B_SPLINE_CURVE ( ( 1.000000000000000000, 0.9238795325112867385, 1.000000000000000000, 0.9238795325112855172, 1.000000000000001110 ) ) 
 REPRESENTATION_ITEM ( '' )  );
#7755 =( BOUNDED_CURVE ( )  B_SPLINE_CURVE ( 3, ( #69759, #35441, #58086, #24091 ),
 .UNSPECIFIED., .F., .F. ) 
 B_SPLINE_CURVE_WITH_KNOTS ( ( 4, 4 ),
 ( 4.773114057545161160, 4.902148076229582152 ),
 .UNSPECIFIED. ) 
 CURVE ( )  GEOMETRIC_REPRESENTATION_ITEM ( )  RATIONAL_B_SPLINE_CURVE ( ( 1.000000000000000000, 0.9986129997113014634, 0.9986129997113014634, 1.000000000000000000 ) ) 
 REPRESENTATION_ITEM ( '' )  );
#7756 = DIRECTION ( 'NONE',  ( 0.000000000000000000, 0.000000000000000000, 1.000000000000000000 ) ) ;
#7757 = CARTESIAN_POINT ( 'NONE',  ( -4.556349186104048599, -10.99999999999999822, 115.2812500000000000 ) ) ;
#7758 = CARTESIAN_POINT ( 'NONE',  ( -11.35316468749999785, 229.0104166700806445, -3.042071309553164848 ) ) ;
#7759 = CARTESIAN_POINT ( 'NONE',  ( 6.951808397369818766E-16, 117.0312499965860269, -11.35316468750000141 ) ) ;
#7760 = VERTEX_POINT ( 'NONE', #59890 ) ;
#7761 = CARTESIAN_POINT ( 'NONE',  ( -2.828427124746209831, 200.3750000000000284, 139.1715728752538723 ) ) ;
#7762 = CARTESIAN_POINT ( 'NONE',  ( -10.18810118749999916, 4.220049686691934809, 94.56250000204838102 ) ) ;
#7763 = CARTESIAN_POINT ( 'NONE',  ( -11.00000000000021139, 4.556349186103834548, 86.59375000409681888 ) ) ;
#7764 = CARTESIAN_POINT ( 'NONE',  ( -3.458734124999960358, 196.6875000013655779, 198.0000000000000284 ) ) ;
#7765 = CARTESIAN_POINT ( 'NONE',  ( 0.000000000000000000, 0.000000000000000000, -10.00000000000000000 ) ) ;
#7767 = CARTESIAN_POINT ( 'NONE',  ( -11.35316468750000141, 118.2812499965860269, -1.390361679473963753E-15 ) ) ;
#7766 = CARTESIAN_POINT ( 'NONE',  ( -9.999999999999996447, 182.2916666666666856, -2.679491924311229401 ) ) ;
#7768 = CARTESIAN_POINT ( 'NONE',  ( -24.00000000000001421, 207.8125000000000284, 168.3431457505080004 ) ) ;
#7769 = CARTESIAN_POINT ( 'NONE',  ( 2.679491924311228956, 82.91666665983871098, -10.00000000000000000 ) ) ;
#7770 = VERTEX_POINT ( 'NONE', #37255 ) ;
#7771 = CARTESIAN_POINT ( 'NONE',  ( 8.660254037844385522, 211.4583333265053682, 5.000000000000005329 ) ) ;
#7772 = CARTESIAN_POINT ( 'NONE',  ( 4.556349186104052151, -10.99999999999999822, 73.46874999999998579 ) ) ;
#7773 = CARTESIAN_POINT ( 'NONE',  ( -2.849036369511732440E-14, 201.3750000027312126, 138.0000000000000568 ) ) ;
#7774 = CARTESIAN_POINT ( 'NONE',  ( 11.35316468749999785, 100.8854166632526841, 3.042071309553174174 ) ) ;
#7775 = CARTESIAN_POINT ( 'NONE',  ( 4.000000000000015987, 205.5000000000000284, 198.0000000000000284 ) ) ;
#7776 = CARTESIAN_POINT ( 'NONE',  ( 5.082755093536324154, 11.15624999795161187, 5.082755093536326818 ) ) ;
#7777 = CARTESIAN_POINT ( 'NONE',  ( -10.18810118749999738, -4.220049686691941915, 92.12500000204836681 ) ) ;
#7778 = CARTESIAN_POINT ( 'NONE',  ( -5.676582343749998039, 7.760416663252684089, -9.832129032723420536 ) ) ;
#7779 = ORIENTED_EDGE ( 'NONE', *, *, #24264, .T. ) ;
#7780 = CARTESIAN_POINT ( 'NONE',  ( 7.999999999999991118, 0.000000000000000000, 30.00000000000000000 ) ) ;
#7781 = CARTESIAN_POINT ( 'NONE',  ( 8.008118988124991233, 9.807117285998411148E-16, 27.26311528394063188 ) ) ;
#7782 = CARTESIAN_POINT ( 'NONE',  ( 7.320508075688771044, 116.2499999931720254, 7.320508075688775484 ) ) ;
#7783 = CARTESIAN_POINT ( 'NONE',  ( 10.18810118750000093, -4.220049686691933921, 76.18750000204839523 ) ) ;
#7784 = VECTOR ( 'NONE', #18308, 1000.000000000000227 ) ;
#7785 = CARTESIAN_POINT ( 'NONE',  ( -47.11462393093397338, 38.26058698117581258, 67.12012181809809874 ) ) ;
#7786 = CARTESIAN_POINT ( 'NONE',  ( 7.320508075688774596, 200.6250000000000000, -7.320508075688774596 ) ) ;
#7787 = CARTESIAN_POINT ( 'NONE',  ( 2.765530957082001251, 292.7656250017069510, 6.676582343750000703 ) ) ;
#7788 = CARTESIAN_POINT ( 'NONE',  ( -2.849036369511732440E-14, 199.2500000000000000, 138.0000000000000568 ) ) ;
#7789 = CARTESIAN_POINT ( 'NONE',  ( -5.676582343749998039, 217.7604166632526983, -9.832129032723420536 ) ) ;
#7790 = EDGE_CURVE ( 'NONE', #60459, #17960, #71938, .T. ) ;
#7791 = CARTESIAN_POINT ( 'NONE',  ( 10.18810118750000093, -4.220049686691933921, 84.81250000204838102 ) ) ;
#7792 = CARTESIAN_POINT ( 'NONE',  ( -29.43265458321760519, 199.8750000013655779, 173.4587341250003760 ) ) ;
#7793 = ADVANCED_FACE ( 'NONE', ( #48553 ), #20250, .T. ) ;
#7794 = CARTESIAN_POINT ( 'NONE',  ( -5.656854249492381470, 23.43750000000000355, 5.656854249492379694 ) ) ;
#7795 = CARTESIAN_POINT ( 'NONE',  ( 4.541265875000002339, 13.49999999863440969, -1.881053915767121554 ) ) ;
#7796 = ORIENTED_EDGE ( 'NONE', *, *, #10768, .T. ) ;
#7797 = CARTESIAN_POINT ( 'NONE',  ( -25.56993553944414188, -51.25543982005161325, 152.4540812346677683 ) ) ;
#7798 = CARTESIAN_POINT ( 'NONE',  ( -2.828427124746152987, 208.2500000027312126, 200.8284271247462129 ) ) ;
#7799 = CARTESIAN_POINT ( 'NONE',  ( -1.432654583217664701, 198.0000000013656063, 138.5412658750000787 ) ) ;
#7800 = CARTESIAN_POINT ( 'NONE',  ( -2.828427124746209831, 205.5000000027312126, 139.1715728752538723 ) ) ;
#7801 = COLOUR_RGB ( '',0.7921568627450980005, 0.8196078431372548767, 0.9333333333333333481 ) ;
#7802 = CARTESIAN_POINT ( 'NONE',  ( 4.999999999999996447, 15.86406185656353429, -69.92615499037644611 ) ) ;
#7803 = CARTESIAN_POINT ( 'NONE',  ( -7.999999999999991118, 9.797174393178815797E-16, 30.00000000000000000 ) ) ;
#7804 = ORIENTED_EDGE ( 'NONE', *, *, #56724, .T. ) ;
#7805 = CARTESIAN_POINT ( 'NONE',  ( 5.082755093536325930, 8.156249997951611874, -5.082755093536325930 ) ) ;
#7806 = CARTESIAN_POINT ( 'NONE',  ( -8.660254037844387298, 28.95833332650536818, -5.000000000000004441 ) ) ;
#7807 = CARTESIAN_POINT ( 'NONE',  ( -7.188101187500000044, 117.0312500020483810, 0.000000000000000000 ) ) ;
#7808 = CARTESIAN_POINT ( 'NONE',  ( 0.4589999999999999636, 278.5679999999998699, 5.805293472045523373 ) ) ;
#7809 = CARTESIAN_POINT ( 'NONE',  ( -2.765530957081996810, 294.2656250017069510, -6.676582343750002480 ) ) ;
#7811 = CARTESIAN_POINT ( 'NONE',  ( -6.000000000000012434, 10.39230484541325694, 0.000000000000000000 ) ) ;
#7810 = CARTESIAN_POINT ( 'NONE',  ( -5.676582343750000703, 233.0729166700806729, -9.832129032723418760 ) ) ;
#7812 = ORIENTED_EDGE ( 'NONE', *, *, #7512, .F. ) ;
#7813 = CARTESIAN_POINT ( 'NONE',  ( 5.676582343749997150, 227.5520833367473017, -9.832129032723418760 ) ) ;
#7814 = CARTESIAN_POINT ( 'NONE',  ( 7.188101187499991163, 2.977408999572648707, 0.8303027818717529929 ) ) ;
#7815 = CARTESIAN_POINT ( 'NONE',  ( -7.347880794884122694E-16, 9.499999997268814056, 4.000000000000001776 ) ) ;
#7816 = CARTESIAN_POINT ( 'NONE',  ( 3.458734125000015869, 199.1875000013655779, 198.0000000000000284 ) ) ;
#7817 = ORIENTED_EDGE ( 'NONE', *, *, #48596, .T. ) ;
#7818 = CARTESIAN_POINT ( 'NONE',  ( 5.656854249492378806, 23.81250000000000355, 5.656854249492381470 ) ) ;
#7819 = CARTESIAN_POINT ( 'NONE',  ( 8.311093377946837890, 101.7187499965860269, -8.311093377946837890 ) ) ;
#7820 = DIRECTION ( 'NONE',  ( -0.000000000000000000, 1.000000000000000000, -1.563033456626094573E-30 ) ) ;
#7821 = CARTESIAN_POINT ( 'NONE',  ( -4.556349186104047710, -10.99999999999999822, 76.28125000000000000 ) ) ;
#7824 = CARTESIAN_POINT ( 'NONE',  ( -32.00000000000000000, 205.2500000000000284, 170.0000000000003979 ) ) ;
#7823 = CARTESIAN_POINT ( 'NONE',  ( 27.99999999999996803, 204.9375000013656063, 166.5412658749999082 ) ) ;
#7822 = CARTESIAN_POINT ( 'NONE',  ( 30.44569435410883429, 204.0625000013656063, 167.5543056458911053 ) ) ;
#7825 = ORIENTED_EDGE ( 'NONE', *, *, #55490, .T. ) ;
#7826 = CARTESIAN_POINT ( 'NONE',  ( 32.00000000000000711, 205.3125000027312126, 171.6568542494922553 ) ) ;
#7827 = CARTESIAN_POINT ( 'NONE',  ( -8.311093377946841443, 213.9062499965860411, 8.311093377946830785 ) ) ;
#7828 = CARTESIAN_POINT ( 'NONE',  ( 3.458734124999959914, 200.3750000013656063, 143.4326545832176976 ) ) ;
#7829 = CARTESIAN_POINT ( 'NONE',  ( 27.99999999999996447, 202.6875000013656063, 173.4587341249998929 ) ) ;
#7830 = CARTESIAN_POINT ( 'NONE',  ( 11.00000000000000355, -4.556349186104045046, 115.8437500040967620 ) ) ;
#7831 = CARTESIAN_POINT ( 'NONE',  ( 9.832129032723416984, 190.6770833299193555, 5.676582343750006032 ) ) ;
#7832 = CARTESIAN_POINT ( 'NONE',  ( -5.082755093536324154, 91.71875000204838102, 5.082755093536326818 ) ) ;
#7833 = CARTESIAN_POINT ( 'NONE',  ( -4.242640687119285658, 296.1875000034139589, 4.242640687119287435 ) ) ;
#7834 = CARTESIAN_POINT ( 'NONE',  ( -25.17157287525377285, 197.6250000000000284, 172.8284271247465256 ) ) ;
#7835 = CARTESIAN_POINT ( 'NONE',  ( -1.881053915767121554, 12.62499999863441147, -4.541265875000002339 ) ) ;
#7836 = CARTESIAN_POINT ( 'NONE',  ( 26.56734541678237704, 197.2500000013656063, 166.5412658749999650 ) ) ;
#7837 = CARTESIAN_POINT ( 'NONE',  ( -5.082755093536319713, 5.082755093536319713, 1.674052781871753659 ) ) ;
#7838 = CARTESIAN_POINT ( 'NONE',  ( 11.35316468749999963, 80.98958332991934128, -3.042071309553165293 ) ) ;
#7839 = CARTESIAN_POINT ( 'NONE',  ( 5.000000000000006217, 140.8333333333333428, -8.660254037844396180 ) ) ;
#7840 = CARTESIAN_POINT ( 'NONE',  ( -4.000000000000016875, 201.4375000000000284, 140.3431457505076594 ) ) ;
#7841 = EDGE_LOOP ( 'NONE', ( #44322, #39638, #59251, #41828 ) ) ;
#7842 = CARTESIAN_POINT ( 'NONE',  ( 1.425702245604163669E-12, 48.75000000000012079, 10.00000000000000178 ) ) ;
#7843 = CARTESIAN_POINT ( 'NONE',  ( 2.849036369511732440E-14, 195.2500000000000000, 202.0000000000000284 ) ) ;
#7844 = CARTESIAN_POINT ( 'NONE',  ( 9.832129032723420536, 71.19791666325268409, -5.676582343749999815 ) ) ;
#7845 = ORIENTED_EDGE ( 'NONE', *, *, #39979, .T. ) ;
#7846 = CARTESIAN_POINT ( 'NONE',  ( -10.18810118749999738, -4.220049686691941915, 89.12500000204836681 ) ) ;
#7847 = CARTESIAN_POINT ( 'NONE',  ( 10.18810118749999916, 4.220049686691935698, 113.5000000020483810 ) ) ;
#7848 = CARTESIAN_POINT ( 'NONE',  ( 3.458734125000015425, 208.2500000013656063, 196.5673454167823877 ) ) ;
#7849 = CARTESIAN_POINT ( 'NONE',  ( 29.65685424949242588, 207.4375000000000284, 165.9999999999999147 ) ) ;
#7851 = CARTESIAN_POINT ( 'NONE',  ( 3.042071309553159519, 69.73958332991936970, 11.35316468750000141 ) ) ;
#7850 = CARTESIAN_POINT ( 'NONE',  ( -2.170320029210516921, 67.76782500014660116, 20.17643218080578293 ) ) ;
#7852 = AXIS2_PLACEMENT_3D ( 'NONE', #52348, #29702, #41026 ) ;
#7853 = CARTESIAN_POINT ( 'NONE',  ( 3.313708498984762496, -7.999999999999989342, 26.98655278392014623 ) ) ;
#7854 = CARTESIAN_POINT ( 'NONE',  ( -29.65685424949239035, 196.5625000027312126, 174.0000000000003126 ) ) ;
#7855 =( BOUNDED_CURVE ( )  B_SPLINE_CURVE ( 2, ( #36749, #37116, #54101, #31456, #25772, #2786, #2413, #25408, #48422 ),
 .UNSPECIFIED., .F., .F. ) 
 B_SPLINE_CURVE_WITH_KNOTS ( ( 3, 2, 2, 2, 3 ),
 ( 0.3958333333333313164, 0.4062499999999980016, 0.4166666666666647423, 0.4270833333333313719, 0.4374999999999980571 ),
 .UNSPECIFIED. ) 
 CURVE ( )  GEOMETRIC_REPRESENTATION_ITEM ( )  RATIONAL_B_SPLINE_CURVE ( ( 1.000000000000014655, 0.9238795325112720835, 1.000000000000000000, 0.9238795325112867385, 1.000000000000000000, 0.9238795325112867385, 1.000000000000000000, 0.9238795325113009493, 0.9999999999999857891 ) ) 
 REPRESENTATION_ITEM ( '' )  );
#7856 = EDGE_CURVE ( 'NONE', #25866, #23857, #63064, .T. ) ;
#7857 = EDGE_CURVE ( 'NONE', #2699, #4199, #14216, .T. ) ;
#7858 = CARTESIAN_POINT ( 'NONE',  ( -10.00000000000000178, 169.3749999931720538, -1.224646799147353454E-15 ) ) ;
#7859 = CARTESIAN_POINT ( 'NONE',  ( 1.656854249492399234, 200.3125000027312410, 138.0000000000000853 ) ) ;
#7860 = VECTOR ( 'NONE', #20895, 1000.000000000000000 ) ;
#7861 = CARTESIAN_POINT ( 'NONE',  ( -24.74639540312143993, 194.8627345059742026, 172.0907582697688269 ) ) ;
#7862 = CARTESIAN_POINT ( 'NONE',  ( 3.042071309553167513, 62.13541666325268409, -11.35316468749999785 ) ) ;
#7863 = CARTESIAN_POINT ( 'NONE',  ( 10.18810118749999916, 4.220049686691935698, 107.8750000020483810 ) ) ;
#7864 = CARTESIAN_POINT ( 'NONE',  ( 3.042071309553159519, 194.7395833299193555, 11.35316468750000141 ) ) ;
#7865 = ORIENTED_EDGE ( 'NONE', *, *, #30430, .F. ) ;
#7866 = CYLINDRICAL_SURFACE ( 'NONE', #14697, 8.000000000000000000 ) ;
#7867 = CARTESIAN_POINT ( 'NONE',  ( 8.660254037844385522, 161.4583333265053966, 5.000000000000005329 ) ) ;
#7869 = CARTESIAN_POINT ( 'NONE',  ( -5.676582343749998039, 192.4479166632526983, -9.832129032723420536 ) ) ;
#7868 = CARTESIAN_POINT ( 'NONE',  ( -25.17157287525374088, 200.7500000027312126, 172.8284271247464972 ) ) ;
#7870 = DIRECTION ( 'NONE',  ( 0.000000000000000000, 0.000000000000000000, 1.000000000000000000 ) ) ;
#7871 = ADVANCED_FACE ( 'NONE', ( #69824 ), #31592, .F. ) ;
#7872 = CARTESIAN_POINT ( 'NONE',  ( -8.660254037844385522, 233.5416666734946318, 5.000000000000004441 ) ) ;
#7873 = CARTESIAN_POINT ( 'NONE',  ( -27.99999999999995737, 200.5000000000000000, 174.0000000000003695 ) ) ;
#7874 = ORIENTED_EDGE ( 'NONE', *, *, #45669, .F. ) ;
#7875 = CARTESIAN_POINT ( 'NONE',  ( -3.042071309553173730, 179.6354166632526699, 11.35316468749999785 ) ) ;
#7876 =( BOUNDED_CURVE ( )  B_SPLINE_CURVE ( 2, ( #60552, #8876, #8498, #54536, #3219, #26207, #49611, #72626, #19439 ),
 .UNSPECIFIED., .F., .F. ) 
 B_SPLINE_CURVE_WITH_KNOTS ( ( 3, 2, 2, 2, 3 ),
 ( 0.9000000000000007994, 0.9083333333333341031, 0.9166666666666674068, 0.9250000000000008216, 0.9333333333333341253 ),
 .UNSPECIFIED. ) 
 CURVE ( )  GEOMETRIC_REPRESENTATION_ITEM ( )  RATIONAL_B_SPLINE_CURVE ( ( 0.9999999999999928946, 0.9238795325112938439, 1.000000000000000000, 0.9238795325112867385, 1.000000000000000000, 0.9238795325112867385, 1.000000000000000000, 0.9238795325112796331, 1.000000000000007105 ) ) 
 REPRESENTATION_ITEM ( '' )  );
#7877 = CARTESIAN_POINT ( 'NONE',  ( 7.188101187499993827, -2.977408999572645598, 21.64280278187176165 ) ) ;
#7878 = CARTESIAN_POINT ( 'NONE',  ( -19.99999999999993250, -31.99999999999978684, 205.0000000000000284 ) ) ;
#7879 = ORIENTED_EDGE ( 'NONE', *, *, #7688, .F. ) ;
#7880 = EDGE_CURVE ( 'NONE', #29199, #43392, #26281, .T. ) ;
#7881 = CARTESIAN_POINT ( 'NONE',  ( -3.313708498984762052, 96.40625000409677625, -8.000000000000000000 ) ) ;
#7882 = CARTESIAN_POINT ( 'NONE',  ( 8.660254037844389075, 5.416666666666666963, -5.000000000000000000 ) ) ;
#7883 = CARTESIAN_POINT ( 'NONE',  ( 2.828427124746190291, 17.87500000000000355, 2.828427124746192067 ) ) ;
#7884 = CARTESIAN_POINT ( 'NONE',  ( -4.541265875000002339, 17.81249999863440792, -5.561446717895856393E-16 ) ) ;
#7885 = CARTESIAN_POINT ( 'NONE',  ( 1.469576158976822172E-15, -7.999999999999991118, 11.89280278392014445 ) ) ;
#7886 = CARTESIAN_POINT ( 'NONE',  ( -23.99999999999999645, 195.8125000000000284, 168.3431457505080289 ) ) ;
#7887 = ORIENTED_EDGE ( 'NONE', *, *, #10091, .F. ) ;
#7888 = CARTESIAN_POINT ( 'NONE',  ( 5.000000000000000000, -11.69579520003551920, -68.31051037013783400 ) ) ;
#7889 = CARTESIAN_POINT ( 'NONE',  ( 7.188101187500001821, 99.50000000204838102, -2.977408999572651371 ) ) ;
#7890 = AXIS2_PLACEMENT_3D ( 'NONE', #27902, #22230, #22604 ) ;
#7892 = CARTESIAN_POINT ( 'NONE',  ( 4.556349186104052151, -10.99999999999999822, 98.96875000000000000 ) ) ;
#7891 = CARTESIAN_POINT ( 'NONE',  ( 6.123233995736767268E-16, 188.1249999931720254, -10.00000000000000178 ) ) ;
#7893 = ORIENTED_EDGE ( 'NONE', *, *, #39361, .F. ) ;
#7894 = CARTESIAN_POINT ( 'NONE',  ( -6.123233995736766282E-16, 221.8750000068279746, -10.00000000000000000 ) ) ;
#7895 = VECTOR ( 'NONE', #48051, 1000.000000000000000 ) ;
#7896 = CARTESIAN_POINT ( 'NONE',  ( -7.188101187499992051, 0.000000000000000000, 17.98655278187175455 ) ) ;
#7897 = ORIENTED_EDGE ( 'NONE', *, *, #10673, .F. ) ;
#7898 = ORIENTED_EDGE ( 'NONE', *, *, #39415, .T. ) ;
#7899 = CARTESIAN_POINT ( 'NONE',  ( 1.871523826299183495E-15, -10.18810118749999916, 78.53125000204836681 ) ) ;
#7900 = CARTESIAN_POINT ( 'NONE',  ( -10.00000000000000355, 114.5833333265053540, 2.679491924311223183 ) ) ;
#7901 = CARTESIAN_POINT ( 'NONE',  ( -11.00000000000000000, 0.000000000000000000, 93.99999999999998579 ) ) ;
#7903 = CARTESIAN_POINT ( 'NONE',  ( -4.088227598258586603E-16, 295.3593750017070079, -6.676582343750001591 ) ) ;
#7902 = CARTESIAN_POINT ( 'NONE',  ( 24.00000000000000355, 200.9375000027312410, 171.6568542494923122 ) ) ;
#7904 = CARTESIAN_POINT ( 'NONE',  ( -7.320508075688778149, 153.1250000000000284, 7.320508075688769267 ) ) ;
#7905 = CARTESIAN_POINT ( 'NONE',  ( 23.99999999999999645, 199.9375000027312126, 171.6568542494923122 ) ) ;
#7906 = CARTESIAN_POINT ( 'NONE',  ( 3.458734124999923942, 194.4587341250000918, 141.8415000761822569 ) ) ;
#7907 = DIRECTION ( 'NONE',  ( -0.000000000000000000, 1.000000000000000000, -4.476705744456276341E-16 ) ) ;
#7908 = CARTESIAN_POINT ( 'NONE',  ( 5.656854249492378806, 4.124999995903220196, 5.656854249492381470 ) ) ;
#7909 = CARTESIAN_POINT ( 'NONE',  ( 26.56734541678238060, 199.0000000013656063, 166.5412658749999650 ) ) ;
#7910 = CARTESIAN_POINT ( 'NONE',  ( -2.977408999572654480, 12.37499999795161010, 7.188101187499999156 ) ) ;
#7911 = CARTESIAN_POINT ( 'NONE',  ( 3.313708498984762496, -7.999999999999989342, 26.98655278392014623 ) ) ;
#7912 = CARTESIAN_POINT ( 'NONE',  ( -7.999999999999991118, 0.000000000000000000, 15.83030277982336642 ) ) ;
#7913 = CARTESIAN_POINT ( 'NONE',  ( -5.082755093536325930, 110.8437500020483810, -5.082755093536325930 ) ) ;
#7915 = CARTESIAN_POINT ( 'NONE',  ( 10.99999999999999467, 11.00000000000000355, 41.99999999999999289 ) ) ;
#7914 = DIRECTION ( 'NONE',  ( 0.000000000000000000, 0.000000000000000000, 1.000000000000000000 ) ) ;
#7916 = CARTESIAN_POINT ( 'NONE',  ( 3.042071309553163960, 232.7604166700806445, -11.35316468749999785 ) ) ;
#7917 = CARTESIAN_POINT ( 'NONE',  ( 6.000000000000003553, 288.6250000034139589, -2.485281374238571761 ) ) ;
#7918 = CARTESIAN_POINT ( 'NONE',  ( -2.977408999572648707, -7.188101187499990274, 20.14280278187176165 ) ) ;
#7919 = CARTESIAN_POINT ( 'NONE',  ( 32.00000000000000000, 196.3125000000000284, 168.3431457505075741 ) ) ;
#7920 = CARTESIAN_POINT ( 'NONE',  ( 11.35316468750000141, 30.78124999658601979, 0.000000000000000000 ) ) ;
#7921 = CARTESIAN_POINT ( 'NONE',  ( 10.00000000000000533, 150.2083333333333428, -2.679491924311227624 ) ) ;
#7922 = CARTESIAN_POINT ( 'NONE',  ( 2.679491924311222739, 10.83333332650536818, 10.00000000000000355 ) ) ;
#7923 = PLANE ( 'NONE',  #46399 ) ;
#7924 = CYLINDRICAL_SURFACE ( 'NONE', #28694, 27.99999999999999645 ) ;
#7925 = EDGE_LOOP ( 'NONE', ( #36273, #55488, #45018, #8602 ) ) ;
#7926 = CARTESIAN_POINT ( 'NONE',  ( -18.89444362769112473, 271.9999999999999432, 167.9999999999998295 ) ) ;
#7927 = EDGE_CURVE ( 'NONE', #42303, #29697, #54988, .T. ) ;
#7928 = EDGE_CURVE ( 'NONE', #28973, #59170, #14966, .T. ) ;
#7929 = DIRECTION ( 'NONE',  ( -0.000000000000000000, 1.000000000000000000, -0.000000000000000000 ) ) ;
#7930 = CARTESIAN_POINT ( 'NONE',  ( 8.311093377946837890, 31.40624999658601624, -8.311093377946837890 ) ) ;
#7931 = CARTESIAN_POINT ( 'NONE',  ( 7.778174593052023411, -7.778174593052021635, 87.25000000409677625 ) ) ;
#7932 = CARTESIAN_POINT ( 'NONE',  ( -2.445694354108839175, 203.3125000013656063, 144.4456943541088663 ) ) ;
#7933 = CARTESIAN_POINT ( 'NONE',  ( 0.000000000000000000, 0.000000000000000000, 18.50000000000000000 ) ) ;
#7934 = DIRECTION ( 'NONE',  ( 1.000000000000000000, 0.000000000000000000, 0.000000000000000000 ) ) ;
#7936 = CARTESIAN_POINT ( 'NONE',  ( 5.676582343750001591, 26.61458332991935194, -9.832129032723420536 ) ) ;
#7935 = CARTESIAN_POINT ( 'NONE',  ( 7.188101187500000044, 105.4062500020483810, -8.802885111219163269E-16 ) ) ;
#7937 = CARTESIAN_POINT ( 'NONE',  ( 7.999999999999991118, 3.313708498984757611, 13.67405277982336287 ) ) ;
#7938 = CARTESIAN_POINT ( 'NONE',  ( -11.35316468749999785, 148.0729166632527267, -3.042071309553167513 ) ) ;
#7939 = CARTESIAN_POINT ( 'NONE',  ( -4.999999999999998224, 123.5416666598387110, -8.660254037844389075 ) ) ;
#7940 = CARTESIAN_POINT ( 'NONE',  ( 2.977408999572650039, 107.5625000020483810, -7.188101187500001821 ) ) ;
#7941 = CARTESIAN_POINT ( 'NONE',  ( 8.660254037844389075, 172.2916666598387110, -5.000000000000000000 ) ) ;
#7942 = CARTESIAN_POINT ( 'NONE',  ( -26.56734541678238060, 203.6250000013656063, 166.5412658750003629 ) ) ;
#7943 = ORIENTED_EDGE ( 'NONE', *, *, #2112, .F. ) ;
#7944 = CARTESIAN_POINT ( 'NONE',  ( 2.976196775178699294, 8.673996836102547903, -0.07661102881317931323 ) ) ;
#7945 = CARTESIAN_POINT ( 'NONE',  ( 3.042071309553167513, 27.13541666325268409, -11.35316468749999785 ) ) ;
#7946 = EDGE_LOOP ( 'NONE', ( #21215, #12970, #10881, #2680, #10506 ) ) ;
#7947 = CARTESIAN_POINT ( 'NONE',  ( -8.000000000000000000, 0.6562500000000001110, -3.313708498984762496 ) ) ;
#7948 = CARTESIAN_POINT ( 'NONE',  ( 0.000000000000000000, 210.0000000000000284, 207.0000000000000568 ) ) ;
#7950 = CARTESIAN_POINT ( 'NONE',  ( -3.042071309553173730, 154.3229166632526983, 11.35316468749999785 ) ) ;
#7949 = CARTESIAN_POINT ( 'NONE',  ( -23.84257049579401055, -23.64316225706143371, 146.0187300984692911 ) ) ;
#7951 = LINE ( 'NONE', #54353, #41100 ) ;
#7952 = CARTESIAN_POINT ( 'NONE',  ( -3.313708498984757167, 7.999999999999991118, 20.10530278432982954 ) ) ;
#7953 = CARTESIAN_POINT ( 'NONE',  ( 8.000000000000000000, 15.00000000000000355, 0.000000000000000000 ) ) ;
#7954 = EDGE_CURVE ( 'NONE', #21431, #46180, #29465, .T. ) ;
#7955 = ADVANCED_FACE ( 'NONE', ( #811 ), #64163, .F. ) ;
#7956 = CARTESIAN_POINT ( 'NONE',  ( -9.832129032723418760, 228.4895833367473585, -5.676582343749998927 ) ) ;
#7957 = CARTESIAN_POINT ( 'NONE',  ( -10.18810118749999738, -4.220049686691941915, 89.12500000204836681 ) ) ;
#7958 = EDGE_LOOP ( 'NONE', ( #72899, #29182, #47186, #34098 ) ) ;
#7959 = EDGE_CURVE ( 'NONE', #54990, #3964, #32212, .T. ) ;
#7960 = VECTOR ( 'NONE', #39185, 1000.000000000000000 ) ;
#7961 = FACE_OUTER_BOUND ( 'NONE', #25687, .T. ) ;
#7962 = CARTESIAN_POINT ( 'NONE',  ( -8.311093377946841443, 99.21874999658601268, 8.311093377946830785 ) ) ;
#7963 =( BOUNDED_CURVE ( )  B_SPLINE_CURVE ( 2, ( #1023, #24377, #70044, #54171, #2478, #7037, #59822, #18354, #53796 ),
 .UNSPECIFIED., .F., .F. ) 
 B_SPLINE_CURVE_WITH_KNOTS ( ( 3, 2, 2, 2, 3 ),
 ( 0.2500000000000001110, 0.2583333333333335258, 0.2666666666666668850, 0.2750000000000002998, 0.2833333333333336590 ),
 .UNSPECIFIED. ) 
 CURVE ( )  GEOMETRIC_REPRESENTATION_ITEM ( )  RATIONAL_B_SPLINE_CURVE ( ( 0.9999999999999990008, 0.9238795325112877377, 1.000000000000000000, 0.9238795325112867385, 1.000000000000000000, 0.9238795325112867385, 1.000000000000000000, 0.9238795325112837409, 1.000000000000003109 ) ) 
 REPRESENTATION_ITEM ( '' )  );
#7964 = CARTESIAN_POINT ( 'NONE',  ( -4.220049686691937474, -10.18810118749999738, 103.9375000020483810 ) ) ;
#7965 = CARTESIAN_POINT ( 'NONE',  ( -3.211159895383562723, 15.06249999863440792, 3.211159895383561391 ) ) ;
#7966 = VERTEX_POINT ( 'NONE', #27784 ) ;
#7967 = ORIENTED_EDGE ( 'NONE', *, *, #831, .T. ) ;
#7968 = CARTESIAN_POINT ( 'NONE',  ( 8.000000000000000000, 12.00000000000000178, 0.000000000000000000 ) ) ;
#7969 = CARTESIAN_POINT ( 'NONE',  ( -3.313708498984761608, 106.7187500000000000, -8.000000000000000000 ) ) ;
#7970 = CARTESIAN_POINT ( 'NONE',  ( 2.977408999572650927, 5.249999997951610986, -7.188101187500001821 ) ) ;
#7971 = ADVANCED_FACE ( 'NONE', ( #50797 ), #67414, .F. ) ;
#7972 = CARTESIAN_POINT ( 'NONE',  ( -5.656854249492378806, 113.3750000040967763, 5.656854249492381470 ) ) ;
#7973 = CARTESIAN_POINT ( 'NONE',  ( 1.871523826299183495E-15, -10.18810118749999916, 98.40625000204838102 ) ) ;
#7974 = VECTOR ( 'NONE', #12668, 1000.000000000000114 ) ;
#7975 = DIRECTION ( 'NONE',  ( -0.000000000000000000, 1.000000000000000000, -0.000000000000000000 ) ) ;
#7976 = CARTESIAN_POINT ( 'NONE',  ( 1.656854249492381248, 14.93749999726881406, -4.000000000000001776 ) ) ;
#7977 = CARTESIAN_POINT ( 'NONE',  ( -4.541265875000002339, 2.812499998634407028, -5.561446717895856393E-16 ) ) ;
#7978 = ORIENTED_EDGE ( 'NONE', *, *, #65768, .T. ) ;
#7979 = CARTESIAN_POINT ( 'NONE',  ( 30.64284399271078385, 0.000000000000000000, 174.6921329945330399 ) ) ;
#7980 = CARTESIAN_POINT ( 'NONE',  ( -25.55430564589111953, 202.0625000013656063, 172.4456943541091505 ) ) ;
#7981 = CARTESIAN_POINT ( 'NONE',  ( 3.211159895383560947, 15.18749999863440792, 3.211159895383562723 ) ) ;
#7982 = CARTESIAN_POINT ( 'NONE',  ( -1.656854249492263564, 199.9375000027312126, 194.0000000000000000 ) ) ;
#7983 = CARTESIAN_POINT ( 'NONE',  ( -2.977408999572647819, 7.188101187499991163, 8.705302781871752771 ) ) ;
#7984 = ORIENTED_EDGE ( 'NONE', *, *, #14102, .F. ) ;
#7985 = ORIENTED_EDGE ( 'NONE', *, *, #27632, .F. ) ;
#7986 = CARTESIAN_POINT ( 'NONE',  ( -10.18810118749999916, 4.220049686691934809, 102.0625000020483810 ) ) ;
#7987 = CARTESIAN_POINT ( 'NONE',  ( 5.656854249492378806, 26.62499999590322375, 5.656854249492381470 ) ) ;
#7988 = CARTESIAN_POINT ( 'NONE',  ( -25.55430564589115150, 203.3125000013656063, 172.4456943541091789 ) ) ;
#7989 = CARTESIAN_POINT ( 'NONE',  ( -23.99999999999997513, 202.6875000000000284, 171.6568542494927385 ) ) ;
#7990 = CARTESIAN_POINT ( 'NONE',  ( -3.458734124999959914, 194.4375000013656063, 198.0000000000000284 ) ) ;
#7991 = DIRECTION ( 'NONE',  ( 0.000000000000000000, -1.000000000000000000, 0.000000000000000000 ) ) ;
#7992 = CARTESIAN_POINT ( 'NONE',  ( -8.660254037844390851, 102.9166666666666714, 4.999999999999998224 ) ) ;
#7993 = CARTESIAN_POINT ( 'NONE',  ( 5.656854249492381470, 115.0625000000000000, 5.656854249492379694 ) ) ;
#7994 = CARTESIAN_POINT ( 'NONE',  ( 2.765530957081996366, 297.2968750017070079, -6.676582343750003368 ) ) ;
#7995 = ORIENTED_EDGE ( 'NONE', *, *, #42838, .T. ) ;
#7996 = CARTESIAN_POINT ( 'NONE',  ( -10.00000000000000355, 144.5833333265053682, 2.679491924311223183 ) ) ;
#7997 = CARTESIAN_POINT ( 'NONE',  ( -5.656854249492381470, 14.24999999590322375, 5.656854249492379694 ) ) ;
#7998 = CARTESIAN_POINT ( 'NONE',  ( -2.445694354108839619, 202.8125000013656063, 139.5543056458912190 ) ) ;
#7999 = CARTESIAN_POINT ( 'NONE',  ( -8.660254037844387298, 183.9583333265053682, -5.000000000000004441 ) ) ;
#8000 = CARTESIAN_POINT ( 'NONE',  ( 2.824543433528785410E-14, 210.0000000000000284, 194.0000000000000568 ) ) ;
#8001 = CARTESIAN_POINT ( 'NONE',  ( 2.679491924311235174, 221.4583333333333428, 9.999999999999998224 ) ) ;
#8002 = CARTESIAN_POINT ( 'NONE',  ( -10.99999999999999822, -4.556349186104052151, 113.5937499999999858 ) ) ;
#8003 = CARTESIAN_POINT ( 'NONE',  ( -2.679491924311235618, 218.5416666666667140, 10.00000000000000000 ) ) ;
#8004 = CARTESIAN_POINT ( 'NONE',  ( -4.401442555609577197E-16, 7.188101187499992051, 13.48655278187175455 ) ) ;
#8005 = CARTESIAN_POINT ( 'NONE',  ( -3.042071309553173730, 189.6354166632526983, 11.35316468749999785 ) ) ;
#8006 = CARTESIAN_POINT ( 'NONE',  ( 5.000000000000001776, 192.7083333265053966, -8.660254037844389075 ) ) ;
#8007 = CARTESIAN_POINT ( 'NONE',  ( -4.541265875000002339, 0.8124999986344066949, -5.561446717895856393E-16 ) ) ;
#8008 = CARTESIAN_POINT ( 'NONE',  ( -7.999999999999861444, -9.580972845112835701E-07, 13.01783880491507261 ) ) ;
#8010 = CARTESIAN_POINT ( 'NONE',  ( 0.000000000000000000, 0.000000000000000000, 30.00000000000000000 ) ) ;
#8009 = LINE ( 'NONE', #25346, #947 ) ;
#8011 = ORIENTED_EDGE ( 'NONE', *, *, #4710, .F. ) ;
#8012 = ADVANCED_FACE ( 'NONE', ( #9327 ), #38003, .F. ) ;
#8013 = CARTESIAN_POINT ( 'NONE',  ( -3.458734125000015425, 204.2500000013655779, 143.4326545832176976 ) ) ;
#8014 = CARTESIAN_POINT ( 'NONE',  ( -11.35316468750000141, 43.59374999658601979, -1.390361679473963753E-15 ) ) ;
#8015 = CARTESIAN_POINT ( 'NONE',  ( 4.556349186104051263, -10.99999999999999822, 105.1562500040967763 ) ) ;
#8016 = CARTESIAN_POINT ( 'NONE',  ( 3.042071309553159519, 215.0520833299193555, 11.35316468750000141 ) ) ;
#8017 = CARTESIAN_POINT ( 'NONE',  ( -26.56734541678228112, 200.0000000013656063, 173.4587341250003476 ) ) ;
#8018 = CARTESIAN_POINT ( 'NONE',  ( -1.469576158976823947E-15, 3.937499995903220640, 8.000000000000000000 ) ) ;
#8019 = CARTESIAN_POINT ( 'NONE',  ( 2.849036369511732440E-14, 196.3750000027311842, 202.0000000000000000 ) ) ;
#8020 = CARTESIAN_POINT ( 'NONE',  ( 1.432654583217607858, 196.6250000013656063, 138.5412658750000787 ) ) ;
#8021 = CARTESIAN_POINT ( 'NONE',  ( -8.311093377946836114, 107.6562499965860127, -8.311093377946837890 ) ) ;
#8022 = VECTOR ( 'NONE', #62987, 999.9999999999998863 ) ;
#8023 = CARTESIAN_POINT ( 'NONE',  ( -5.000000000000005329, 80.20833332650536818, 8.660254037844387298 ) ) ;
#8024 = CARTESIAN_POINT ( 'NONE',  ( -7.188101187499999156, 92.75000000204839523, 2.977408999572654924 ) ) ;
#8025 = CARTESIAN_POINT ( 'NONE',  ( 1.881053915767121776, 17.62499999863440436, -4.541265875000002339 ) ) ;
#8026 = CARTESIAN_POINT ( 'NONE',  ( -32.00000000000003553, 204.3125000027312126, 168.3431457505080857 ) ) ;
#8027 = CARTESIAN_POINT ( 'NONE',  ( 7.999999999999991118, 9.797174393178815797E-16, 24.08030277982336642 ) ) ;
#8028 = VERTEX_POINT ( 'NONE', #32347 ) ;
#8029 = VERTEX_POINT ( 'NONE', #3666 ) ;
#8030 = CARTESIAN_POINT ( 'NONE',  ( -2.765530957081996810, 292.4218750017069510, -6.676582343750003368 ) ) ;
#8031 = CYLINDRICAL_SURFACE ( 'NONE', #41135, 11.00000000000000000 ) ;
#8032 = CARTESIAN_POINT ( 'NONE',  ( -8.311093377946841443, 163.9062499965859843, 8.311093377946830785 ) ) ;
#8033 = B_SPLINE_CURVE_WITH_KNOTS ( 'NONE', 3,
 ( #34407, #50609, #67604, #33658, #56285, #63415, #73261, #67970, #17393, #73629, #23058, #46067 ),
 .UNSPECIFIED., .F., .F.,
 ( 4, 2, 2, 2, 2, 4 ),
 ( 1.618164387277533384E-15, 0.002547658444429635408, 0.005095316888857652320, 0.006369146111071660558, 0.007642975333285669665, 0.01019063377771368614 ),
 .UNSPECIFIED. ) ;
#8034 = CARTESIAN_POINT ( 'NONE',  ( 2.679491924328703423, 6.041666666665100216, -9.999999999989912070 ) ) ;
#8035 = CARTESIAN_POINT ( 'NONE',  ( 2.751064625579944321E-14, 200.7500000000000000, 194.0000000000000568 ) ) ;
#8036 = CARTESIAN_POINT ( 'NONE',  ( -2.679491924305053896, 191.4583333333328312, -10.00000000000361489 ) ) ;
#8037 = CARTESIAN_POINT ( 'NONE',  ( 10.18810118749999916, 1.247682550866122264E-15, 109.2812500020483668 ) ) ;
#8038 = EDGE_LOOP ( 'NONE', ( #33889, #46854, #40984, #1788 ) ) ;
#8039 = EDGE_CURVE ( 'NONE', #49310, #44274, #15713, .T. ) ;
#8040 = CARTESIAN_POINT ( 'NONE',  ( -0.7509181236840809515, 55.63764137816388455, -43.81192498624520226 ) ) ;
#8041 = CARTESIAN_POINT ( 'NONE',  ( 0.000000000000000000, 0.000000000000000000, 0.000000000000000000 ) ) ;
#8042 = CARTESIAN_POINT ( 'NONE',  ( -8.311093377946841443, 139.2187499965859843, 8.311093377946834337 ) ) ;
#8043 = CARTESIAN_POINT ( 'NONE',  ( -3.458734124999958581, 195.5000000013656347, 199.4326545832176976 ) ) ;
#8044 = CARTESIAN_POINT ( 'NONE',  ( -6.000000000000003553, 290.9375000000000568, -2.485281374238571317 ) ) ;
#8045 = CARTESIAN_POINT ( 'NONE',  ( 4.220049686691934809, 10.18810118749999916, 72.06250000204836681 ) ) ;
#8046 = CARTESIAN_POINT ( 'NONE',  ( -5.676582343749998039, 57.76041666325268409, -9.832129032723420536 ) ) ;
#8047 = EDGE_LOOP ( 'NONE', ( #72276, #42422, #37965, #36149 ) ) ;
#8048 = CARTESIAN_POINT ( 'NONE',  ( 1.469576158976822172E-15, -7.999999999999991118, 13.20530277982336465 ) ) ;
#8049 = CARTESIAN_POINT ( 'NONE',  ( 3.211159895383560947, 6.312499998634407028, 3.211159895383562723 ) ) ;
#8050 = CARTESIAN_POINT ( 'NONE',  ( -8.008118988124991233, 0.000000000000000000, 10.01311528394063011 ) ) ;
#8051 = UNCERTAINTY_MEASURE_WITH_UNIT (LENGTH_MEASURE( 1.000000000000000082E-05 ), #27935, 'distance_accuracy_value', 'NONE');
#8052 = AXIS2_PLACEMENT_3D ( 'NONE', #45662, #28316, #5314 ) ;
#8053 = CARTESIAN_POINT ( 'NONE',  ( 5.082755093536324154, 16.78124999795161543, 5.082755093536326818 ) ) ;
#8054 = CARTESIAN_POINT ( 'NONE',  ( 1.102182119232618108E-15, 291.3125000034140157, 6.000000000000001776 ) ) ;
#8055 = PRODUCT_DEFINITION_SHAPE ( 'NONE', 'NONE',  #74659 ) ;
#8056 = DIRECTION ( 'NONE',  ( 1.000000000000000000, 0.000000000000000000, 0.000000000000000000 ) ) ;
#8057 = CARTESIAN_POINT ( 'NONE',  ( -5.082755093536326818, 10.78124999795161187, 5.082755093536325042 ) ) ;
#8058 = EDGE_CURVE ( 'NONE', #27085, #30970, #27044, .T. ) ;
#8059 = CARTESIAN_POINT ( 'NONE',  ( -4.401442555609577197E-16, 7.188101187499992051, 5.611552781871753659 ) ) ;
#8060 = CARTESIAN_POINT ( 'NONE',  ( 10.18810118750000093, -4.220049686691933921, 116.6875000020483952 ) ) ;
#8061 = ADVANCED_FACE ( 'NONE', ( #56104 ), #9706, .F. ) ;
#8062 = CARTESIAN_POINT ( 'NONE',  ( -7.320508075688773708, 63.74999999317203248, -7.320508075688774596 ) ) ;
#8063 = CARTESIAN_POINT ( 'NONE',  ( 4.000000000000001776, 1.749999997268813168, 0.000000000000000000 ) ) ;
#8064 = ORIENTED_EDGE ( 'NONE', *, *, #72278, .F. ) ;
#8065 = CARTESIAN_POINT ( 'NONE',  ( 4.000000000000015987, 194.6250000027311842, 198.0000000000000284 ) ) ;
#8066 = CARTESIAN_POINT ( 'NONE',  ( 3.999999999999960032, 203.0000000000000000, 142.0000000000000568 ) ) ;
#8068 =( BOUNDED_CURVE ( )  B_SPLINE_CURVE ( 2, ( #65147, #42873, #14198, #37235, #20987, #27027, #39100, #49284, #33456, #9306, #4398, #27766, #15697 ),
 .UNSPECIFIED., .F., .F. ) 
 B_SPLINE_CURVE_WITH_KNOTS ( ( 3, 2, 2, 2, 2, 2, 3 ),
 ( 0.9076086956521738358, 0.9094202898550723946, 0.9112318840579709534, 0.9130434782608694011, 0.9148550724637680709, 0.9166666666666666297, 0.9184782608695651884 ),
 .UNSPECIFIED. ) 
 CURVE ( )  GEOMETRIC_REPRESENTATION_ITEM ( )  RATIONAL_B_SPLINE_CURVE ( ( 1.000000000000001998, 0.9659258262890662028, 1.000000000000000000, 0.9659258262890683122, 1.000000000000000000, 0.9659258262890683122, 1.000000000000000000, 0.9659258262890683122, 1.000000000000000000, 0.9659258262890683122, 1.000000000000000000, 0.9659258262890683122, 1.000000000000000000 ) ) 
 REPRESENTATION_ITEM ( '' )  );
#8067 = CARTESIAN_POINT ( 'NONE',  ( -24.00000000000002487, 198.9375000027312126, 168.3431457505079152 ) ) ;
#8069 = CARTESIAN_POINT ( 'NONE',  ( -3.211159895383561391, 2.687499998634407028, -3.211159895383561835 ) ) ;
#8070 = CARTESIAN_POINT ( 'NONE',  ( -5.082755093536324154, 112.3437500020483810, 5.082755093536326818 ) ) ;
#8071 = EDGE_CURVE ( 'NONE', #5359, #49924, #61755, .T. ) ;
#8072 = FACE_OUTER_BOUND ( 'NONE', #33367, .T. ) ;
#8073 = CARTESIAN_POINT ( 'NONE',  ( 5.656854249492376141, -5.656854249492374365, 4.580302783920145338 ) ) ;
#8074 = ORIENTED_EDGE ( 'NONE', *, *, #39840, .F. ) ;
#8075 = CARTESIAN_POINT ( 'NONE',  ( -2.977408999572654480, 25.49999999795161187, 7.188101187499999156 ) ) ;
#8076 = ORIENTED_EDGE ( 'NONE', *, *, #15788, .F. ) ;
#8077 = CARTESIAN_POINT ( 'NONE',  ( -7.320508075688779037, 203.1249999999999716, 7.320508075688769267 ) ) ;
#8078 = CARTESIAN_POINT ( 'NONE',  ( 3.458734125000015425, 206.9375000013656063, 198.0000000000000284 ) ) ;
#8079 = CARTESIAN_POINT ( 'NONE',  ( 28.00000000000001776, 204.4375000013656063, 173.4587341249998929 ) ) ;
#8080 = CARTESIAN_POINT ( 'NONE',  ( 10.00000000000000178, 55.00000000000000000, 0.000000000000000000 ) ) ;
#8081 = CARTESIAN_POINT ( 'NONE',  ( 1.320432766682874540E-15, 96.40625000204838102, 7.188101187500000044 ) ) ;
#8082 = CARTESIAN_POINT ( 'NONE',  ( -6.000000000000001776, 297.0000000000000000, 0.000000000000000000 ) ) ;
#8084 = CARTESIAN_POINT ( 'NONE',  ( -30.85450503451334825, -42.99933534908173272, 173.2515164390132156 ) ) ;
#8083 = LINE ( 'NONE', #37882, #59881 ) ;
#8085 = ORIENTED_EDGE ( 'NONE', *, *, #62476, .F. ) ;
#8086 = CARTESIAN_POINT ( 'NONE',  ( -6.951808397369817780E-16, 227.6562500034139873, -11.35316468749999963 ) ) ;
#8087 = CARTESIAN_POINT ( 'NONE',  ( 3.999999999999960032, 201.1250000027312126, 142.0000000000000568 ) ) ;
#8088 = DIRECTION ( 'NONE',  ( -0.000000000000000000, 1.000000000000000000, -0.000000000000000000 ) ) ;
#8089 = CARTESIAN_POINT ( 'NONE',  ( 6.123233995736767268E-16, 131.2500000000000000, -10.00000000000000178 ) ) ;
#8090 = CARTESIAN_POINT ( 'NONE',  ( -2.679491924311228512, 258.9583333333332575, -9.999999999999998224 ) ) ;
#8091 = CYLINDRICAL_SURFACE ( 'NONE', #59571, 3.999999999999976019 ) ;
#8092 = CARTESIAN_POINT ( 'NONE',  ( -2.679491924311225848, 171.4583333333332860, -10.00000000000000178 ) ) ;
#8093 = DIRECTION ( 'NONE',  ( -1.000000000000000000, 0.000000000000000000, -0.000000000000000000 ) ) ;
#8094 = DIRECTION ( 'NONE',  ( 0.000000000000000000, 0.000000000000000000, 1.000000000000000000 ) ) ;
#8095 = CARTESIAN_POINT ( 'NONE',  ( -8.000000000000033751, -3.313708498984719864, 3.924052779823361092 ) ) ;
#8096 = CARTESIAN_POINT ( 'NONE',  ( -9.832129032723420536, 154.0104166632526983, 5.676582343749997150 ) ) ;
#8097 = FACE_OUTER_BOUND ( 'NONE', #7925, .T. ) ;
#8098 = CARTESIAN_POINT ( 'NONE',  ( 27.99999999999999645, 210.0000000000000284, 165.9999999999999147 ) ) ;
#8101 = CARTESIAN_POINT ( 'NONE',  ( -2.222453528114265639E-12, 168.7499999999998295, 10.00000000000000178 ) ) ;
#8100 = CARTESIAN_POINT ( 'NONE',  ( -7.347880794884122694E-16, 11.49999999726881406, 4.000000000000001776 ) ) ;
#8099 = CARTESIAN_POINT ( 'NONE',  ( 26.34314575050763452, 204.5625000000000000, 165.9999999999998863 ) ) ;
#8102 = AXIS2_PLACEMENT_3D ( 'NONE', #32990, #32611, #71443 ) ;
#8103 = VERTEX_POINT ( 'NONE', #50055 ) ;
#8104 = CARTESIAN_POINT ( 'NONE',  ( 3.042071309553167069, 7.135416663252682312, -11.35316468749999785 ) ) ;
#8105 = CARTESIAN_POINT ( 'NONE',  ( -3.313708498984744732, 8.343749995903223748, 8.000000000000019540 ) ) ;
#8106 = EDGE_CURVE ( 'NONE', #64023, #5844, #47613, .T. ) ;
#8107 = DIRECTION ( 'NONE',  ( 0.000000000000000000, 0.000000000000000000, 1.000000000000000000 ) ) ;
#8108 = CARTESIAN_POINT ( 'NONE',  ( -10.99999999999999822, -4.556349186104053040, 79.09375000000000000 ) ) ;
#8109 = CARTESIAN_POINT ( 'NONE',  ( 2.445694354108782775, 208.5625000013656063, 139.5543056458912190 ) ) ;
#8110 = CARTESIAN_POINT ( 'NONE',  ( -4.528114470331722430, 124.6731747980935836, -6.389158183658611101 ) ) ;
#8111 = CARTESIAN_POINT ( 'NONE',  ( -10.00000000000000000, 34.16666665983870388, -2.679491924311229845 ) ) ;
#8112 = CARTESIAN_POINT ( 'NONE',  ( 1.320432766682874540E-15, 108.0312500020483810, 7.188101187500000044 ) ) ;
#8113 = CARTESIAN_POINT ( 'NONE',  ( 4.541265875000002339, 2.437499998634407028, 0.000000000000000000 ) ) ;
#8114 = CARTESIAN_POINT ( 'NONE',  ( -3.313708498984759387, -7.999999999999989342, 13.29905278392014800 ) ) ;
#8115 = CARTESIAN_POINT ( 'NONE',  ( -3.313708498984757167, 7.999999999999991118, 14.04905277982336465 ) ) ;
#8117 = CARTESIAN_POINT ( 'NONE',  ( 2.679491924311228956, 7.916666659838700326, -10.00000000000000000 ) ) ;
#8116 = CARTESIAN_POINT ( 'NONE',  ( 4.556349186104045934, 11.00000000000000000, 101.2187500040967905 ) ) ;
#8118 = VERTEX_POINT ( 'NONE', #16451 ) ;
#8119 = EDGE_CURVE ( 'NONE', #24886, #49749, #12387, .T. ) ;
#8120 = B_SPLINE_CURVE_WITH_KNOTS ( 'NONE', 3,
 ( #12288, #58333, #70013, #47715, #42427, #47354 ),
 .UNSPECIFIED., .F., .F.,
 ( 4, 2, 4 ),
 ( 0.009270618776430214827, 0.01189894710419331370, 0.01452727543195641083 ),
 .UNSPECIFIED. ) ;
#8121 = CARTESIAN_POINT ( 'NONE',  ( -11.00000000000000000, 0.000000000000000000, 114.9999999999999858 ) ) ;
#8122 = CARTESIAN_POINT ( 'NONE',  ( -8.311093377946836114, 233.5937500034139589, -8.311093377946836114 ) ) ;
#8123 = CARTESIAN_POINT ( 'NONE',  ( -8.311093377946841443, 123.9062499965860411, 8.311093377946830785 ) ) ;
#8124 = ORIENTED_EDGE ( 'NONE', *, *, #52796, .T. ) ;
#8125 = CYLINDRICAL_SURFACE ( 'NONE', #66872, 11.00000000000000000 ) ;
#8126 = CARTESIAN_POINT ( 'NONE',  ( 10.18810118749999916, 4.220049686691935698, 92.50000000204838102 ) ) ;
#8127 = CARTESIAN_POINT ( 'NONE',  ( 0.000000000000000000, 15.99999999999998579, 0.000000000000000000 ) ) ;
#8128 = CARTESIAN_POINT ( 'NONE',  ( -3.458734124999959469, 195.7500000013656063, 199.4326545832176691 ) ) ;
#8129 = FACE_BOUND ( 'NONE', #34453, .T. ) ;
#8131 = CARTESIAN_POINT ( 'NONE',  ( 9.832129032723420536, 111.1979166632526983, -5.676582343749999815 ) ) ;
#8130 = CARTESIAN_POINT ( 'NONE',  ( 2.679491924311228956, 43.95833333333335702, 10.00000000000002842 ) ) ;
#8132 = CARTESIAN_POINT ( 'NONE',  ( -30.82842712474616320, 209.3750000000000284, 172.8284271247465824 ) ) ;
#8133 = CARTESIAN_POINT ( 'NONE',  ( -1.836970198721029983E-15, 145.6249999931720538, 10.00000000000000178 ) ) ;
#8134 = EDGE_LOOP ( 'NONE', ( #19210, #53607, #21070, #7371 ) ) ;
#8135 = CARTESIAN_POINT ( 'NONE',  ( -4.999999999999998224, 213.5416666598387110, -8.660254037844389075 ) ) ;
#8136 = EDGE_CURVE ( 'NONE', #59562, #18479, #56845, .T. ) ;
#8137 = CARTESIAN_POINT ( 'NONE',  ( 0.000000000000000000, 284.0000000000000000, 0.000000000000000000 ) ) ;
#8138 = DIRECTION ( 'NONE',  ( 1.000000000000000000, 0.000000000000000000, 0.000000000000000000 ) ) ;
#8139 = CARTESIAN_POINT ( 'NONE',  ( -9.832129032723418760, 103.1770833299193555, -5.676582343750004256 ) ) ;
#8140 = CARTESIAN_POINT ( 'NONE',  ( 2.445694354108839619, 205.8125000013656063, 200.4456943541088663 ) ) ;
#8141 = CARTESIAN_POINT ( 'NONE',  ( -1.320432766682874540E-15, 12.46874999795161187, 7.188101187500000044 ) ) ;
#8142 = CARTESIAN_POINT ( 'NONE',  ( -6.238412754330611322E-16, 10.18810118749999916, 90.15625000204838102 ) ) ;
#8143 = CARTESIAN_POINT ( 'NONE',  ( 6.951808397369818766E-16, 12.34374999658601801, -11.35316468750000141 ) ) ;
#8144 = ORIENTED_EDGE ( 'NONE', *, *, #58052, .F. ) ;
#8145 = CARTESIAN_POINT ( 'NONE',  ( 1.347111479062088405E-15, 75.00000000000000000, -11.00000000000000000 ) ) ;
#8146 = CARTESIAN_POINT ( 'NONE',  ( -8.008118988124989457, -3.317071493978883900, 25.10686528394063544 ) ) ;
#8147 = CARTESIAN_POINT ( 'NONE',  ( -7.204075437095967871, 7.204075437095967871, 73.84375000204838102 ) ) ;
#8148 = LINE ( 'NONE', #65109, #43429 ) ;
#8149 = CARTESIAN_POINT ( 'NONE',  ( 0.000000000000000000, 0.000000000000000000, 0.000000000000000000 ) ) ;
#8150 = CARTESIAN_POINT ( 'NONE',  ( 6.676582343750001591, 291.9531250017069510, -8.176455196517173205E-16 ) ) ;
#8151 = CARTESIAN_POINT ( 'NONE',  ( 8.660254037844385522, 126.4583333265053540, 5.000000000000005329 ) ) ;
#8152 = CARTESIAN_POINT ( 'NONE',  ( 3.042071309553159519, 220.0520833299193271, 11.35316468750000141 ) ) ;
#8153 = CARTESIAN_POINT ( 'NONE',  ( 5.676582343750001591, 126.9270833299193697, -9.832129032723420536 ) ) ;
#8154 = CARTESIAN_POINT ( 'NONE',  ( -10.18810118749999738, -4.220049686691941915, 82.75000000204838102 ) ) ;
#8155 = EDGE_CURVE ( 'NONE', #27563, #54242, #27816, .T. ) ;
#8156 = CARTESIAN_POINT ( 'NONE',  ( -25.55430564589115150, 199.0625000013656063, 172.4456943541091789 ) ) ;
#8157 = CARTESIAN_POINT ( 'NONE',  ( 3.313708498984762052, 22.78125000000000355, -8.000000000000000000 ) ) ;
#8158 = CARTESIAN_POINT ( 'NONE',  ( -8.342170076843785083E-16, 13.18749999863440792, 4.541265875000002339 ) ) ;
#8159 = VERTEX_POINT ( 'NONE', #68897 ) ;
#8160 = CARTESIAN_POINT ( 'NONE',  ( -24.00000000000002842, 208.9375000027312410, 168.3431457505079152 ) ) ;
#8161 = CARTESIAN_POINT ( 'NONE',  ( -3.999999999999960032, 206.0625000027312694, 196.3431457505076594 ) ) ;
#8162 = AXIS2_PLACEMENT_3D ( 'NONE', #35710, #17980, #52689 ) ;
#8163 = CARTESIAN_POINT ( 'NONE',  ( 3.458734124999960358, 198.6250000013655779, 143.4326545832176976 ) ) ;
#8164 = CARTESIAN_POINT ( 'NONE',  ( -2.751064625579944321E-14, 203.8750000027312126, 146.0000000000000284 ) ) ;
#8165 = CARTESIAN_POINT ( 'NONE',  ( 1.871523826299183495E-15, -10.18810118749999916, 68.40625000204836681 ) ) ;
#8167 = EDGE_LOOP ( 'NONE', ( #73114, #64949, #53039, #38841 ) ) ;
#8166 =( BOUNDED_CURVE ( )  B_SPLINE_CURVE ( 2, ( #40005, #5678, #10964, #34, #33999, #62263, #28309, #5307, #52438 ),
 .UNSPECIFIED., .F., .F. ) 
 B_SPLINE_CURVE_WITH_KNOTS ( ( 3, 2, 2, 2, 3 ),
 ( 0.5208333333333314830, 0.5312499999999981126, 0.5416666666666647423, 0.5520833333333314830, 0.5624999999999981126 ),
 .UNSPECIFIED. ) 
 CURVE ( )  GEOMETRIC_REPRESENTATION_ITEM ( )  RATIONAL_B_SPLINE_CURVE ( ( 1.000000000000013767, 0.9238795325112729717, 1.000000000000000000, 0.9238795325112867385, 1.000000000000000000, 0.9238795325112867385, 1.000000000000000000, 0.9238795325113005052, 0.9999999999999862332 ) ) 
 REPRESENTATION_ITEM ( '' )  );
#8168 = CARTESIAN_POINT ( 'NONE',  ( 4.401442555609581635E-16, 6.843749997951611874, -7.188101187500000044 ) ) ;
#8169 = CYLINDRICAL_SURFACE ( 'NONE', #49932, 6.000000000000001776 ) ;
#8170 = CARTESIAN_POINT ( 'NONE',  ( 2.977408999572654480, 116.0000000020483810, 7.188101187499999156 ) ) ;
#8171 = CARTESIAN_POINT ( 'NONE',  ( -4.002048012587626324, 22.00000000000000355, -1.673623243082883016 ) ) ;
#8172 = CARTESIAN_POINT ( 'NONE',  ( 4.721056650415999201, 293.0781250017069510, -4.721056650415999201 ) ) ;
#8174 = CARTESIAN_POINT ( 'NONE',  ( 7.999999999999991118, 0.000000000000000000, 30.00000000000000000 ) ) ;
#8173 = CARTESIAN_POINT ( 'NONE',  ( 8.660254037844389075, 132.2916666598387110, -5.000000000000000000 ) ) ;
#8175 = CONTEXT_DEPENDENT_SHAPE_REPRESENTATION ( #30814, #27641 ) ;
#8176 = ORIENTED_EDGE ( 'NONE', *, *, #70233, .T. ) ;
#8177 = CARTESIAN_POINT ( 'NONE',  ( -8.311093377946834337, 224.8437500034139589, 8.311093377946837890 ) ) ;
#8178 = CARTESIAN_POINT ( 'NONE',  ( -7.188101187499992051, 0.000000000000000000, 27.36155278187175455 ) ) ;
#8179 = CARTESIAN_POINT ( 'NONE',  ( 0.000000000000000000, 125.0000000000000000, 8.000000000000000000 ) ) ;
#8180 = CARTESIAN_POINT ( 'NONE',  ( 3.458734125000015869, 198.1875000013655779, 198.0000000000000284 ) ) ;
#8181 =( BOUNDED_CURVE ( )  B_SPLINE_CURVE ( 2, ( #38800, #44453, #28587, #11242, #56153, #51224, #50109, #16502, #62538 ),
 .UNSPECIFIED., .F., .F. ) 
 B_SPLINE_CURVE_WITH_KNOTS ( ( 3, 2, 2, 2, 3 ),
 ( 0.6666666666666672958, 0.6750000000000007105, 0.6833333333333340143, 0.6916666666666673180, 0.7000000000000006217 ),
 .UNSPECIFIED. ) 
 CURVE ( )  GEOMETRIC_REPRESENTATION_ITEM ( )  RATIONAL_B_SPLINE_CURVE ( ( 0.9999999999999938938, 0.9238795325112928447, 1.000000000000000000, 0.9238795325112867385, 1.000000000000000000, 0.9238795325112867385, 1.000000000000000000, 0.9238795325112806323, 1.000000000000005995 ) ) 
 REPRESENTATION_ITEM ( '' )  );
#8182 = VERTEX_POINT ( 'NONE', #39853 ) ;
#8183 = CARTESIAN_POINT ( 'NONE',  ( 3.313708498984765161, 99.96875000000000000, 7.999999999999998224 ) ) ;
#8184 = CARTESIAN_POINT ( 'NONE',  ( -8.311093377946841443, 99.21874999658601268, 8.311093377946830785 ) ) ;
#8185 = DIRECTION ( 'NONE',  ( 0.000000000000000000, 0.000000000000000000, 1.000000000000000000 ) ) ;
#8186 = CARTESIAN_POINT ( 'NONE',  ( 7.778174593052021635, 7.778174593052023411, 76.93749999999998579 ) ) ;
#8189 = CARTESIAN_POINT ( 'NONE',  ( -28.00000000000002842, 205.0000000000000284, 166.0000000000003695 ) ) ;
#8188 = CARTESIAN_POINT ( 'NONE',  ( 30.44569435410883074, 202.5625000013656063, 172.4456943541086957 ) ) ;
#8187 = CARTESIAN_POINT ( 'NONE',  ( 31.45873412499998523, 204.8750000013656063, 171.4326545832175839 ) ) ;
#8190 = ORIENTED_EDGE ( 'NONE', *, *, #9936, .T. ) ;
#8191 = DIRECTION ( 'NONE',  ( 0.000000000000000000, 0.000000000000000000, 1.000000000000000000 ) ) ;
#8192 = EDGE_CURVE ( 'NONE', #44095, #10770, #17206, .T. ) ;
#8193 = CARTESIAN_POINT ( 'NONE',  ( -3.042071309553164404, 207.2395833299193555, -11.35316468749999963 ) ) ;
#8194 = CARTESIAN_POINT ( 'NONE',  ( -2.754378923186476579E-14, 200.1875000013656063, 145.4587341250000350 ) ) ;
#8195 = CARTESIAN_POINT ( 'NONE',  ( 28.00000000000002132, 204.1875000013656063, 166.5412658749999082 ) ) ;
#8196 = CARTESIAN_POINT ( 'NONE',  ( 5.082755093536325930, 26.53124999795161543, -5.082755093536325930 ) ) ;
#8197 = CARTESIAN_POINT ( 'NONE',  ( -2.085542519210945728E-15, 199.8437499965860127, 11.35316468750000141 ) ) ;
#8198 = CARTESIAN_POINT ( 'NONE',  ( 7.188101187500000044, 90.78125000204838102, -8.802885111219163269E-16 ) ) ;
#8199 = CARTESIAN_POINT ( 'NONE',  ( -25.17157287525382259, 198.8750000000000284, 167.1715728752541565 ) ) ;
#8200 = CARTESIAN_POINT ( 'NONE',  ( -4.541265875000002339, 14.74999999863440969, -1.881053915767121998 ) ) ;
#8201 = CARTESIAN_POINT ( 'NONE',  ( 31.45873412499999233, 197.9375000013655779, 169.9999999999999432 ) ) ;
#8202 = CARTESIAN_POINT ( 'NONE',  ( -7.188101187499990274, -2.977408999572651371, 1.955302781871753881 ) ) ;
#8203 = DIRECTION ( 'NONE',  ( -0.000000000000000000, -1.000000000000000000, -0.000000000000000000 ) ) ;
#8204 = CARTESIAN_POINT ( 'NONE',  ( 3.042071309553167069, 81.82291666325268409, -11.35316468749999785 ) ) ;
#8205 = ORIENTED_EDGE ( 'NONE', *, *, #49985, .T. ) ;
#8206 = ADVANCED_FACE ( 'NONE', ( #11189 ), #29651, .T. ) ;
#8207 = CARTESIAN_POINT ( 'NONE',  ( 10.00000000000001243, 140.2083333333333428, -2.679491924311229401 ) ) ;
#8208 = CARTESIAN_POINT ( 'NONE',  ( 4.898587196589415787E-16, 0.000000000000000000, 4.000000000000001776 ) ) ;
#8209 = CARTESIAN_POINT ( 'NONE',  ( 0.000000000000000000, 125.0000000000000000, 0.000000000000000000 ) ) ;
#8210 = CARTESIAN_POINT ( 'NONE',  ( 2.449293598294707893E-16, 14.25000000000000000, -4.000000000000001776 ) ) ;
#8211 = CARTESIAN_POINT ( 'NONE',  ( -11.35316468749999785, 73.07291666325268409, -3.042071309553167513 ) ) ;
#8212 = ORIENTED_EDGE ( 'NONE', *, *, #51085, .T. ) ;
#8213 = CARTESIAN_POINT ( 'NONE',  ( 4.220049686691934809, 10.18810118749999916, 87.06250000204838102 ) ) ;
#8214 = CARTESIAN_POINT ( 'NONE',  ( -10.18810118749999738, -4.220049686691941915, 114.2500000020483952 ) ) ;
#8215 = CARTESIAN_POINT ( 'NONE',  ( 1.432654583217662481, 208.3750000013656063, 194.5412658750000219 ) ) ;
#8216 = CARTESIAN_POINT ( 'NONE',  ( 28.00000000000002132, 207.5000000000000284, 165.9999999999998863 ) ) ;
#8218 = CARTESIAN_POINT ( 'NONE',  ( 5.676582343749993598, 74.94791666325269830, 9.832129032723422313 ) ) ;
#8217 = CARTESIAN_POINT ( 'NONE',  ( -7.999999999970034636, -1.442163225726577833E-05, 17.51834960462420909 ) ) ;
#8220 = AXIS2_PLACEMENT_3D ( 'NONE', #48900, #14941, #26639 ) ;
#8219 = CARTESIAN_POINT ( 'NONE',  ( 3.313708498984756279, 7.999999999999991118, 18.54905278392014623 ) ) ;
#8221 = CARTESIAN_POINT ( 'NONE',  ( -0.9804963856519524068, 194.6309867350711329, 138.4951104068910581 ) ) ;
#8222 = CARTESIAN_POINT ( 'NONE',  ( -10.00000000000000178, 174.3749999931720538, -1.224646799147353454E-15 ) ) ;
#8223 = CARTESIAN_POINT ( 'NONE',  ( 1.320432766682874540E-15, 90.40625000204838102, 7.188101187500000044 ) ) ;
#8224 = AXIS2_PLACEMENT_3D ( 'NONE', #33556, #45227, #10524 ) ;
#8225 = DIRECTION ( 'NONE',  ( -0.000000000000000000, -0.000000000000000000, -1.000000000000000000 ) ) ;
#8226 = CARTESIAN_POINT ( 'NONE',  ( -11.35316468750000141, 63.59374999658601268, -1.390361679473963753E-15 ) ) ;
#8227 = CARTESIAN_POINT ( 'NONE',  ( 4.721056650416000089, 298.8281250017069510, 4.721056650415999201 ) ) ;
#8228 = CARTESIAN_POINT ( 'NONE',  ( 10.18810118750000093, -4.220049686691933033, 104.6875000020483810 ) ) ;
#8229 = CARTESIAN_POINT ( 'NONE',  ( -9.832129032723418760, 197.8645833299193555, -5.676582343750004256 ) ) ;
#8230 = VERTEX_POINT ( 'NONE', #1002 ) ;
#8231 = CARTESIAN_POINT ( 'NONE',  ( -5.126144196591286395, 68.65853088339355281, 20.89430926783131426 ) ) ;
#8232 = FACE_OUTER_BOUND ( 'NONE', #59011, .T. ) ;
#8233 = CARTESIAN_POINT ( 'NONE',  ( 4.999999999999992895, 61.23691386381934620, 23.51762333030286811 ) ) ;
#8234 = CARTESIAN_POINT ( 'NONE',  ( -8.311093377946841443, 188.9062499965860127, 8.311093377946834337 ) ) ;
#8235 = CARTESIAN_POINT ( 'NONE',  ( 27.99999999999996447, 196.0000000000000000, 173.9999999999999147 ) ) ;
#8236 = CARTESIAN_POINT ( 'NONE',  ( -7.320508075688771932, 237.5000000068279746, -7.320508075688771932 ) ) ;
#8237 = CARTESIAN_POINT ( 'NONE',  ( -27.99999999999999645, 210.0000000000000284, 174.0000000000003411 ) ) ;
#8238 = VERTEX_POINT ( 'NONE', #23245 ) ;
#8239 = CARTESIAN_POINT ( 'NONE',  ( -2.085542519210945728E-15, 184.8437499965860411, 11.35316468750000141 ) ) ;
#8240 = CARTESIAN_POINT ( 'NONE',  ( 5.082755093536320601, -5.082755093536318824, 21.54905278187175455 ) ) ;
#8241 = CARTESIAN_POINT ( 'NONE',  ( 4.193030820682222881, 60.66866849074683188, -23.17095654502590207 ) ) ;
#8242 = VERTEX_POINT ( 'NONE', #34215 ) ;
#8243 = CARTESIAN_POINT ( 'NONE',  ( 5.656854249492379694, 96.12500000409677625, -5.656854249492380582 ) ) ;
#8244 = CARTESIAN_POINT ( 'NONE',  ( 2.828427124746190291, 16.87500000000000000, 2.828427124746192067 ) ) ;
#8245 = CARTESIAN_POINT ( 'NONE',  ( -3.211159895383561391, 14.68749999863440792, -3.211159895383561835 ) ) ;
#8246 = CARTESIAN_POINT ( 'NONE',  ( -4.898587196589407898E-16, 7.999999999999991118, 11.14280278392014800 ) ) ;
#8247 = LINE ( 'NONE', #2600, #48686 ) ;
#8248 = ORIENTED_EDGE ( 'NONE', *, *, #22473, .T. ) ;
#8249 = CYLINDRICAL_SURFACE ( 'NONE', #46302, 8.000000000000000000 ) ;
#8250 = CARTESIAN_POINT ( 'NONE',  ( -4.401442555609581635E-16, 99.78125000204838102, -7.188101187500000044 ) ) ;
#8252 = CARTESIAN_POINT ( 'NONE',  ( 1.656854249492381248, 13.93749999726881406, -4.000000000000001776 ) ) ;
#8251 = CARTESIAN_POINT ( 'NONE',  ( 1.656854249492374143, 204.3125000027312126, 138.0000000000000568 ) ) ;
#8254 = EDGE_CURVE ( 'NONE', #52326, #17439, #70775, .T. ) ;
#8253 = ORIENTED_EDGE ( 'NONE', *, *, #57635, .F. ) ;
#8255 = EDGE_CURVE ( 'NONE', #10738, #20204, #45646, .T. ) ;
#8257 = CARTESIAN_POINT ( 'NONE',  ( -4.898587196589412829E-16, 100.8125000040967763, -8.000000000000000000 ) ) ;
#8256 = AXIS2_PLACEMENT_3D ( 'NONE', #3950, #72213, #60528 ) ;
#8258 = CARTESIAN_POINT ( 'NONE',  ( 5.082755093536318824, 5.082755093536319713, 17.42405278187175810 ) ) ;
#8259 = EDGE_LOOP ( 'NONE', ( #50198, #64403, #8833, #45434 ) ) ;
#8260 = ORIENTED_EDGE ( 'NONE', *, *, #24640, .F. ) ;
#8261 = CARTESIAN_POINT ( 'NONE',  ( 4.220049686691934809, 10.18810118749999916, 79.18750000204836681 ) ) ;
#8262 = CARTESIAN_POINT ( 'NONE',  ( 9.832129032723416984, 55.67708332991935549, 5.676582343750006032 ) ) ;
#8263 = CARTESIAN_POINT ( 'NONE',  ( 7.466667385518904076, 16.47372726584778846, 2.453007415248453782E-15 ) ) ;
#8264 = CARTESIAN_POINT ( 'NONE',  ( -10.99999999999999822, -4.556349186104052151, 97.09375000000001421 ) ) ;
#8267 = CARTESIAN_POINT ( 'NONE',  ( -6.676582343749999815, 292.6718750017069510, 2.765530957082001251 ) ) ;
#8266 = CARTESIAN_POINT ( 'NONE',  ( 30.82842712474616675, 199.5000000027312126, 167.1715728752537018 ) ) ;
#8265 = CYLINDRICAL_SURFACE ( 'NONE', #21782, 3.999999999999986233 ) ;
#8268 = CARTESIAN_POINT ( 'NONE',  ( 2.679491924311222739, 143.9583333333333712, 10.00000000000000355 ) ) ;
#8269 = CIRCLE ( 'NONE', #48016, 37.00000000000000711 ) ;
#8270 = CARTESIAN_POINT ( 'NONE',  ( -7.778174593052023411, 7.778174593052023411, 106.0000000040967763 ) ) ;
#8271 = CARTESIAN_POINT ( 'NONE',  ( -2.679491924311226292, 163.3333333265053682, -10.00000000000000178 ) ) ;
#8272 = EDGE_CURVE ( 'NONE', #20088, #55604, #5906, .T. ) ;
#8273 =( BOUNDED_CURVE ( )  B_SPLINE_CURVE ( 2, ( #23018, #11696, #405, #30158, #69046, #52435, #18469, #1513, #29793 ),
 .UNSPECIFIED., .F., .F. ) 
 B_SPLINE_CURVE_WITH_KNOTS ( ( 3, 2, 2, 2, 3 ),
 ( 0.3166666666666668184, 0.3250000000000002331, 0.3333333333333335924, 0.3416666666666670626, 0.3500000000000004219 ),
 .UNSPECIFIED. ) 
 CURVE ( )  GEOMETRIC_REPRESENTATION_ITEM ( )  RATIONAL_B_SPLINE_CURVE ( ( 0.9999999999999984457, 0.9238795325112882928, 1.000000000000000000, 0.9238795325112867385, 1.000000000000000000, 0.9238795325112867385, 1.000000000000000000, 0.9238795325112826307, 1.000000000000003997 ) ) 
 REPRESENTATION_ITEM ( '' )  );
#8274 = VECTOR ( 'NONE', #30838, 1000.000000000000000 ) ;
#8275 = CARTESIAN_POINT ( 'NONE',  ( -5.656854249492379694, 1.874999995903220196, -5.656854249492380582 ) ) ;
#8276 = CARTESIAN_POINT ( 'NONE',  ( 26.56734541678232375, 197.3750000013656063, 173.4587341249998929 ) ) ;
#8277 = CARTESIAN_POINT ( 'NONE',  ( -2.977408999572650039, 11.81249999795161187, -7.188101187500001821 ) ) ;
#8278 = CARTESIAN_POINT ( 'NONE',  ( -3.313708498984757167, 7.999999999999991118, 24.73655278392014978 ) ) ;
#8279 = CARTESIAN_POINT ( 'NONE',  ( 0.000000000000000000, 0.000000000000000000, 38.34805510287551300 ) ) ;
#8280 = CARTESIAN_POINT ( 'NONE',  ( -7.188101187499999156, 111.1250000020483810, 2.977408999572654924 ) ) ;
#8282 = CARTESIAN_POINT ( 'NONE',  ( 2.775557561562891351E-14, 0.000000000000000000, 170.0000000000000284 ) ) ;
#8281 = CARTESIAN_POINT ( 'NONE',  ( -10.00000000000000178, 19.37499999317203603, -1.224646799147353454E-15 ) ) ;
#8283 = CARTESIAN_POINT ( 'NONE',  ( 10.00000000000000355, 134.7916666666666288, 2.679491924311236506 ) ) ;
#8284 = CARTESIAN_POINT ( 'NONE',  ( 29.43265458321766914, 209.1250000013656347, 166.5412658749999650 ) ) ;
#8285 = CARTESIAN_POINT ( 'NONE',  ( 5.082755093536320601, -5.082755093536318824, 23.42405278187175455 ) ) ;
#8286 = CARTESIAN_POINT ( 'NONE',  ( 31.99999999999997868, 200.4375000027311842, 168.3431457505074889 ) ) ;
#8287 = CARTESIAN_POINT ( 'NONE',  ( -5.676582343749998039, 42.44791666325269119, -9.832129032723420536 ) ) ;
#8288 = CARTESIAN_POINT ( 'NONE',  ( 25.17157287525381548, 200.6250000000000284, 167.1715728752537018 ) ) ;
#8289 = CARTESIAN_POINT ( 'NONE',  ( -10.00000000000000000, 4.166666659838700326, -2.679491924311229845 ) ) ;
#8290 = DIRECTION ( 'NONE',  ( -0.000000000000000000, -0.000000000000000000, -1.000000000000000000 ) ) ;
#8291 = ORIENTED_EDGE ( 'NONE', *, *, #36898, .T. ) ;
#8292 = FACE_OUTER_BOUND ( 'NONE', #26987, .T. ) ;
#8293 = DIRECTION ( 'NONE',  ( 1.000000000000000000, 0.000000000000000000, 0.000000000000000000 ) ) ;
#8294 = CARTESIAN_POINT ( 'NONE',  ( 5.676582343750001591, 41.61458332991934839, -9.832129032723420536 ) ) ;
#8295 = CARTESIAN_POINT ( 'NONE',  ( 11.00000000000000000, 4.556349186104045934, 81.53125000409677625 ) ) ;
#8296 = CARTESIAN_POINT ( 'NONE',  ( -3.458734125000015869, 204.1875000013656063, 142.0000000000000568 ) ) ;
#8297 = DIRECTION ( 'NONE',  ( -0.000000000000000000, -0.000000000000000000, -1.000000000000000000 ) ) ;
#8298 = CARTESIAN_POINT ( 'NONE',  ( 5.000000000000000000, 11.14555136602166741, -27.84144949604398533 ) ) ;
#8300 = CARTESIAN_POINT ( 'NONE',  ( -8.311093377946841443, 38.90624999658600558, 8.311093377946834337 ) ) ;
#8299 = CARTESIAN_POINT ( 'NONE',  ( -5.082755093536325930, 102.9687500020483810, -5.082755093536325930 ) ) ;
#8301 = CARTESIAN_POINT ( 'NONE',  ( 5.656854249492374365, 5.656854249492375253, 18.26780277982336642 ) ) ;
#8302 = CARTESIAN_POINT ( 'NONE',  ( 11.35316468749999963, 165.9895833299193271, -3.042071309553165293 ) ) ;
#8303 =( BOUNDED_CURVE ( )  B_SPLINE_CURVE ( 2, ( #55000, #73452, #21758, #16091, #8343, #53271, #58568, #25312, #24583, #25681, #48329, #41935, #59667 ),
 .UNSPECIFIED., .F., .F. ) 
 B_SPLINE_CURVE_WITH_KNOTS ( ( 3, 2, 2, 2, 2, 2, 3 ),
 ( 0.2668949058765136551, 0.2721276204148235789, 0.2773603349531335027, 0.2825930494914434266, 0.2878257640297532949, 0.2930584785680632742, 0.2982911931063731426 ),
 .UNSPECIFIED. ) 
 CURVE ( )  GEOMETRIC_REPRESENTATION_ITEM ( )  RATIONAL_B_SPLINE_CURVE ( ( 1.000000000000000444, 0.9659258262890677571, 1.000000000000000000, 0.9659258262890683122, 1.000000000000000000, 0.9659258262890683122, 1.000000000000000000, 0.9659258262890683122, 1.000000000000000000, 0.9659258262890683122, 1.000000000000000000, 0.9659258262893742897, 0.9999999999996940225 ) ) 
 REPRESENTATION_ITEM ( '' )  );
#8305 = CARTESIAN_POINT ( 'NONE',  ( -8.660254037844390851, 124.7916666598387110, 4.999999999999998224 ) ) ;
#8304 = PRODUCT ( 'hexagon nut style 1_is_IS 1364-3 - M24-W-N', 'hexagon nut style 1_is_IS 1364-3 - M24-W-N', '', ( #11249 ) ) ;
#8306 = CARTESIAN_POINT ( 'NONE',  ( -5.082755093536325930, 106.3437500020483810, -5.082755093536325930 ) ) ;
#8307 = ORIENTED_EDGE ( 'NONE', *, *, #9063, .T. ) ;
#8308 = DIRECTION ( 'NONE',  ( -1.000000000000000000, 0.000000000000000000, -0.000000000000000000 ) ) ;
#8309 = CARTESIAN_POINT ( 'NONE',  ( -8.311093377946836114, 27.96874999658601624, -8.311093377946837890 ) ) ;
#8310 = ORIENTED_EDGE ( 'NONE', *, *, #782, .F. ) ;
#8311 = DIRECTION ( 'NONE',  ( 0.000000000000000000, 0.000000000000000000, 1.000000000000000000 ) ) ;
#8312 = CARTESIAN_POINT ( 'NONE',  ( 10.18810118750000093, -4.220049686691933921, 83.31250000204836681 ) ) ;
#8313 = CARTESIAN_POINT ( 'NONE',  ( -29.65685424949244009, 197.4375000000000284, 174.0000000000003126 ) ) ;
#8315 = CARTESIAN_POINT ( 'NONE',  ( 9.832129032723420536, 156.1979166632526983, -5.676582343749999815 ) ) ;
#8314 = CARTESIAN_POINT ( 'NONE',  ( -31.53109436301784640, -21.00444211406582795, 154.7404213206838222 ) ) ;
#8316 = CARTESIAN_POINT ( 'NONE',  ( 0.000000000000000000, 0.000000000000000000, 30.00000000000000000 ) ) ;
#8317 = CARTESIAN_POINT ( 'NONE',  ( -7.999999999999991118, 3.313708498984756723, 20.29280278432982954 ) ) ;
#8318 = CARTESIAN_POINT ( 'NONE',  ( 4.529167459315944555, 225.9997407208379911, 8.915528146188176351 ) ) ;
#8319 = CARTESIAN_POINT ( 'NONE',  ( -5.676582343749992710, 229.7395833367473301, 9.832129032723422313 ) ) ;
#8320 = CARTESIAN_POINT ( 'NONE',  ( -10.18810118749999738, -4.220049686691941915, 83.12500000204835260 ) ) ;
#8321 = ORIENTED_EDGE ( 'NONE', *, *, #54723, .F. ) ;
#8322 = AXIS2_PLACEMENT_3D ( 'NONE', #20233, #25887, #60233 ) ;
#8323 = LINE ( 'NONE', #20377, #7609 ) ;
#8324 = CARTESIAN_POINT ( 'NONE',  ( 29.65685424949230864, 205.0625000000000284, 173.9999999999999432 ) ) ;
#8325 = CARTESIAN_POINT ( 'NONE',  ( -5.676582343750006032, 99.42708332991935549, 9.832129032723418760 ) ) ;
#8326 = CARTESIAN_POINT ( 'NONE',  ( -10.18810118749999916, 4.220049686691934809, 100.5625000020483668 ) ) ;
#8327 = CARTESIAN_POINT ( 'NONE',  ( 1.881053915767121998, 21.62499999863441147, -4.541265875000002339 ) ) ;
#8328 = VERTEX_POINT ( 'NONE', #11929 ) ;
#8329 = ORIENTED_EDGE ( 'NONE', *, *, #73944, .F. ) ;
#8330 = CARTESIAN_POINT ( 'NONE',  ( -4.541265875000002339, 2.937499998634407028, -5.561446717895856393E-16 ) ) ;
#8331 = CARTESIAN_POINT ( 'NONE',  ( 7.188101187499999156, 27.74999999795161543, 2.977408999572654924 ) ) ;
#8332 = CARTESIAN_POINT ( 'NONE',  ( 3.313708498984760720, 117.2187500040968047, -8.000000000000000000 ) ) ;
#8333 = CARTESIAN_POINT ( 'NONE',  ( 7.204075437095968759, -7.204075437095966983, 98.59375000204836681 ) ) ;
#8334 = CARTESIAN_POINT ( 'NONE',  ( -26.56734541678238060, 204.6250000013655779, 166.5412658750003629 ) ) ;
#8335 = ADVANCED_FACE ( 'NONE', ( #29288 ), #52298, .T. ) ;
#8336 = CYLINDRICAL_SURFACE ( 'NONE', #25929, 11.00000000000000000 ) ;
#8337 = CARTESIAN_POINT ( 'NONE',  ( 4.000000000000001776, 3.062500000000000000, -1.656854249492381248 ) ) ;
#8338 = CARTESIAN_POINT ( 'NONE',  ( 1.656854249492381248, 16.93749999726881583, -4.000000000000001776 ) ) ;
#8339 = CARTESIAN_POINT ( 'NONE',  ( -3.211159895383562723, 1.937499998634406806, 3.211159895383561391 ) ) ;
#8340 = CARTESIAN_POINT ( 'NONE',  ( -1.432654583217662481, 208.1250000013656063, 145.4587341250000634 ) ) ;
#8341 = CARTESIAN_POINT ( 'NONE',  ( -3.458734124999959914, 194.4375000013656063, 198.0000000000000284 ) ) ;
#8343 = CARTESIAN_POINT ( 'NONE',  ( -8.660254037844671515, 22.08333333333352400, -5.000000000000169642 ) ) ;
#8342 = CARTESIAN_POINT ( 'NONE',  ( -25.55430564589122966, 202.3125000013656063, 167.5543056458915032 ) ) ;
#8344 = CARTESIAN_POINT ( 'NONE',  ( -1.881053915767121554, 19.62499999863441147, -4.541265875000002339 ) ) ;
#8345 = CARTESIAN_POINT ( 'NONE',  ( -7.347880794884122694E-16, 11.75000000000000000, 4.000000000000001776 ) ) ;
#8346 = CARTESIAN_POINT ( 'NONE',  ( 2.977408999572650927, -7.188101187499990274, 6.455302781871754547 ) ) ;
#8347 = VERTEX_POINT ( 'NONE', #46991 ) ;
#8348 = ORIENTED_EDGE ( 'NONE', *, *, #63443, .T. ) ;
#8349 = CARTESIAN_POINT ( 'NONE',  ( 10.18810118749999916, 1.247682550866122264E-15, 101.4062500020483810 ) ) ;
#8350 = CARTESIAN_POINT ( 'NONE',  ( -10.99999999999998579, 4.556349186104061921, 115.0937500040967620 ) ) ;
#8351 = CARTESIAN_POINT ( 'NONE',  ( -30.44569435410879521, 206.0625000013656063, 172.4456943541092357 ) ) ;
#8352 = CARTESIAN_POINT ( 'NONE',  ( -29.65685424949234061, 199.4375000000000284, 174.0000000000004547 ) ) ;
#8353 = CARTESIAN_POINT ( 'NONE',  ( 3.458734125000015425, 196.9375000013655779, 198.0000000000000284 ) ) ;
#8354 = CARTESIAN_POINT ( 'NONE',  ( -7.320508075688774596, 33.12500000000000000, 7.320508075688766603 ) ) ;
#8355 = CARTESIAN_POINT ( 'NONE',  ( 10.00000000000000178, 105.2083333333333286, -2.679491924311226736 ) ) ;
#8356 = EDGE_CURVE ( 'NONE', #12358, #41332, #55363, .T. ) ;
#8357 = EDGE_CURVE ( 'NONE', #9076, #31698, #35093, .T. ) ;
#8358 = CARTESIAN_POINT ( 'NONE',  ( -3.313708498984762052, 111.2187500000000142, -8.000000000000000000 ) ) ;
#8359 = CARTESIAN_POINT ( 'NONE',  ( -4.088227598258586603E-16, 294.3593750017070079, -6.676582343750001591 ) ) ;
#8360 = ORIENTED_EDGE ( 'NONE', *, *, #5757, .F. ) ;
#8361 = CARTESIAN_POINT ( 'NONE',  ( 2.679491924317424001, 191.0416666666661456, -9.999999999996470379 ) ) ;
#8362 = AXIS2_PLACEMENT_3D ( 'NONE', #16342, #51433, #29178 ) ;
#8363 = CARTESIAN_POINT ( 'NONE',  ( -1.469576158976823947E-15, 23.43749999590322020, 8.000000000000000000 ) ) ;
#8364 = CARTESIAN_POINT ( 'NONE',  ( 1.432654583217607192, 203.2500000013656063, 145.4587341250000634 ) ) ;
#8365 = CARTESIAN_POINT ( 'NONE',  ( -10.00000000000000000, 184.1666666598386826, -2.679491924311229845 ) ) ;
#8366 = PRESENTATION_STYLE_ASSIGNMENT (( #31382 ) ) ;
#8367 = CARTESIAN_POINT ( 'NONE',  ( -2.679491924311228512, 228.9583333333333144, -9.999999999999998224 ) ) ;
#8368 = CARTESIAN_POINT ( 'NONE',  ( 2.449293598294707893E-16, 2.999999997268813168, -4.000000000000001776 ) ) ;
#8369 = CARTESIAN_POINT ( 'NONE',  ( 11.00000000000000000, 1.347111479062088405E-15, 115.7499999999999858 ) ) ;
#8370 = CARTESIAN_POINT ( 'NONE',  ( 11.35316468749999963, 5.989583329919348387, -3.042071309553165293 ) ) ;
#8371 = CARTESIAN_POINT ( 'NONE',  ( -2.977408999572647819, 7.188101187499992051, 4.580302781871752771 ) ) ;
#8372 = CARTESIAN_POINT ( 'NONE',  ( 9.832129032723420536, 191.5104166632526983, -5.676582343749999815 ) ) ;
#8373 = CARTESIAN_POINT ( 'NONE',  ( 0.000000000000000000, 101.0525588832578734, 0.000000000000000000 ) ) ;
#8374 = CARTESIAN_POINT ( 'NONE',  ( -1.881053915767124440, 7.999999998634407028, 4.541265875000001451 ) ) ;
#8375 = CARTESIAN_POINT ( 'NONE',  ( 1.469576158976823947E-15, 100.0625000040967763, 8.000000000000000000 ) ) ;
#8377 = PLANE ( 'NONE',  #30265 ) ;
#8376 = CARTESIAN_POINT ( 'NONE',  ( -1.656854249492381248, 14.06249999726881406, -4.000000000000001776 ) ) ;
#8378 = EDGE_LOOP ( 'NONE', ( #13512, #58945, #4231, #9462 ) ) ;
#8379 = AXIS2_PLACEMENT_3D ( 'NONE', #8501, #36442, #36809 ) ;
#8380 = CARTESIAN_POINT ( 'NONE',  ( 2.445694354108783219, 202.8125000013656063, 139.5543056458912190 ) ) ;
#8381 = CARTESIAN_POINT ( 'NONE',  ( 11.35316468749999785, 45.88541666325268409, 3.042071309553174174 ) ) ;
#8382 = CARTESIAN_POINT ( 'NONE',  ( -11.00000000000000000, 4.556349186104045934, 101.5937500040967620 ) ) ;
#8383 = CYLINDRICAL_SURFACE ( 'NONE', #66005, 9.999999999999996447 ) ;
#8384 = EDGE_CURVE ( 'NONE', #67283, #46864, #55796, .T. ) ;
#8385 = CARTESIAN_POINT ( 'NONE',  ( -29.43265458321755546, 201.8750000013656063, 173.4587341250004044 ) ) ;
#8386 = CARTESIAN_POINT ( 'NONE',  ( 3.170472398252169882E-12, 128.7500000000002558, 10.00000000000000178 ) ) ;
#8388 = CARTESIAN_POINT ( 'NONE',  ( -10.00000000000000000, 230.0000000000000000, 0.000000000000000000 ) ) ;
#8387 = CARTESIAN_POINT ( 'NONE',  ( 7.188101187500002709, 121.8125000020483810, 2.977408999572649151 ) ) ;
#8389 = CARTESIAN_POINT ( 'NONE',  ( 1.432654583217607858, 194.6250000013656063, 138.5412658750000787 ) ) ;
#8390 = CARTESIAN_POINT ( 'NONE',  ( -2.085542519210945728E-15, 114.5312499965860269, 11.35316468750000141 ) ) ;
#8391 = CARTESIAN_POINT ( 'NONE',  ( -7.320508075688773708, 88.74999999317202537, -7.320508075688774596 ) ) ;
#8392 = CARTESIAN_POINT ( 'NONE',  ( 7.188101187500001821, 93.50000000204838102, -2.977408999572651371 ) ) ;
#8393 = CARTESIAN_POINT ( 'NONE',  ( -3.211159895383561391, 17.81249999863440792, -3.211159895383561835 ) ) ;
#8394 = CARTESIAN_POINT ( 'NONE',  ( 4.999999999999999112, 2.143131898507868248E-15, 17.50000000000000000 ) ) ;
#8395 = CARTESIAN_POINT ( 'NONE',  ( 1.469576158976822172E-15, -7.999999999999991118, 1.205302779823363979 ) ) ;
#8396 = ORIENTED_EDGE ( 'NONE', *, *, #6738, .F. ) ;
#8397 = CARTESIAN_POINT ( 'NONE',  ( -2.594511375997793134, 225.9999999999999716, -9.679871326005304866 ) ) ;
#8398 = VERTEX_POINT ( 'NONE', #59440 ) ;
#8399 =( BOUNDED_CURVE ( )  B_SPLINE_CURVE ( 2, ( #7404, #30411, #56038, #61311, #54915, #43198, #37182, #8880, #60557, #44332, #31894, #4345, #26970 ),
 .UNSPECIFIED., .F., .F. ) 
 B_SPLINE_CURVE_WITH_KNOTS ( ( 3, 2, 2, 2, 2, 2, 3 ),
 ( 0.1388888888888883955, 0.1481481481481476403, 0.1574074074074069407, 0.1666666666666661856, 0.1759259259259254859, 0.1851851851851847308, 0.1944444444444440034 ),
 .UNSPECIFIED. ) 
 CURVE ( )  GEOMETRIC_REPRESENTATION_ITEM ( )  RATIONAL_B_SPLINE_CURVE ( ( 1.000000000000001776, 0.9659258262890664248, 1.000000000000000000, 0.9659258262890683122, 1.000000000000000000, 0.9659258262890683122, 1.000000000000000000, 0.9659258262890683122, 1.000000000000000000, 0.9659258262890683122, 1.000000000000000000, 0.9659258262890699775, 0.9999999999999983347 ) ) 
 REPRESENTATION_ITEM ( '' )  );
#8400 = CARTESIAN_POINT ( 'NONE',  ( 2.765530957081996366, 293.2968750017069510, -6.676582343750003368 ) ) ;
#8401 = DIRECTION ( 'NONE',  ( -0.000000000000000000, -0.000000000000000000, -1.000000000000000000 ) ) ;
#8402 = CARTESIAN_POINT ( 'NONE',  ( -4.898587196589407898E-16, 7.999999999999991118, 5.142802783920146226 ) ) ;
#8403 = CARTESIAN_POINT ( 'NONE',  ( -5.676582343750006032, 174.1145833299193555, 9.832129032723418760 ) ) ;
#8404 = CARTESIAN_POINT ( 'NONE',  ( 8.999999999999998224, 0.000000000000000000, 0.000000000000000000 ) ) ;
#8405 = CARTESIAN_POINT ( 'NONE',  ( 4.000000000000015987, 201.4375000000000000, 199.6568542494924259 ) ) ;
#8406 = CARTESIAN_POINT ( 'NONE',  ( 11.00000000000000000, 1.347111479062088405E-15, 70.93750000409676204 ) ) ;
#8407 = CARTESIAN_POINT ( 'NONE',  ( -4.220049686691937474, -10.18810118749999738, 105.8125000020483952 ) ) ;
#8408 = VERTEX_POINT ( 'NONE', #2087 ) ;
#8409 = CARTESIAN_POINT ( 'NONE',  ( 0.3794862803134621543, 55.62190996748000771, -43.80334292620879211 ) ) ;
#8410 = CARTESIAN_POINT ( 'NONE',  ( 12.00000000000000178, -28.00000000000000000, 0.000000000000000000 ) ) ;
#8411 = CARTESIAN_POINT ( 'NONE',  ( -2.085542519210945728E-15, 139.8437499965860127, 11.35316468750000141 ) ) ;
#8412 = CARTESIAN_POINT ( 'NONE',  ( 2.445694354108838731, 195.0625000013656063, 195.5543056458912190 ) ) ;
#8413 = CARTESIAN_POINT ( 'NONE',  ( -2.445694354108784108, 206.5625000013656063, 195.5543056458912190 ) ) ;
#8414 = CARTESIAN_POINT ( 'NONE',  ( 10.18810118749999916, 4.220049686691935698, 70.37500000204838102 ) ) ;
#8415 = CARTESIAN_POINT ( 'NONE',  ( -9.832129032723418760, 58.17708332991936260, -5.676582343750004256 ) ) ;
#8416 = VERTEX_POINT ( 'NONE', #24714 ) ;
#8417 = CARTESIAN_POINT ( 'NONE',  ( -25.17157287525386167, 209.0000000027312126, 167.1715728752541281 ) ) ;
#8418 = CARTESIAN_POINT ( 'NONE',  ( 4.541265875000001451, 3.374999998634407028, 1.881053915767124440 ) ) ;
#8419 = CARTESIAN_POINT ( 'NONE',  ( 8.008118988124991233, 3.317071493978879015, 7.856865283940629219 ) ) ;
#8420 = VERTEX_POINT ( 'NONE', #60164 ) ;
#8421 = CARTESIAN_POINT ( 'NONE',  ( -7.188101187500002709, 19.31249999795161543, 2.977408999572649151 ) ) ;
#8422 = CARTESIAN_POINT ( 'NONE',  ( -6.000000000000001776, 289.0625000034140157, 0.000000000000000000 ) ) ;
#8423 = CARTESIAN_POINT ( 'NONE',  ( 1.656854249492478948, 202.6875000000000568, 194.0000000000001705 ) ) ;
#8424 = CARTESIAN_POINT ( 'NONE',  ( -1.320432766682874540E-15, 13.96874999795161187, 7.188101187500000044 ) ) ;
#8425 = CARTESIAN_POINT ( 'NONE',  ( 7.188101187499992051, 8.802885111219154394E-16, 5.236552781871753659 ) ) ;
#8426 = CARTESIAN_POINT ( 'NONE',  ( -4.220049686691935698, 10.18810118749999916, 117.2500000020484094 ) ) ;
#8427 = AXIS2_PLACEMENT_3D ( 'NONE', #32987, #4300, #72582 ) ;
#8428 = DIRECTION ( 'NONE',  ( -0.000000000000000000, -0.000000000000000000, -1.000000000000000000 ) ) ;
#8429 = CARTESIAN_POINT ( 'NONE',  ( 1.656854249492381248, 1.937499997268813168, -4.000000000000001776 ) ) ;
#8430 = EDGE_LOOP ( 'NONE', ( #49633, #6981, #31421, #73550, #70250, #63825, #63824, #71669, #46030, #38383, #13958, #43885, #14419, #21803, #33928, #70862, #19371, #74211, #38202, #29038, #57867, #26341, #26879, #35696, #21356, #4547, #68705, #27594, #71742, #66042, #34463, #26385, #16700, #51744, #14975, #29152, #9189, #4287, #50285, #56709, #49867, #24195, #41940, #33602, #48718, #65737, #70615, #64196, #1801, #16689, #54368, #55387, #47135, #5402, #71322, #28659, #42766, #72449, #14349, #21512, #18945, #45173, #47392, #10236, #56535, #47933, #30215, #4060, #33025, #72705, #55723, #66820, #2265, #61800, #5577, #52667, #42564, #50845, #12438, #25477, #38689, #5310, #28837, #20557, #11702, #9421, #27188, #67760, #72674, #62527, #55513, #63745, #65455, #31577 ) ) ;
#8431 = EDGE_CURVE ( 'NONE', #51609, #44274, #68784, .T. ) ;
#8432 = CARTESIAN_POINT ( 'NONE',  ( -2.445694354108782775, 208.5625000013656063, 200.4456943541088663 ) ) ;
#8433 = CARTESIAN_POINT ( 'NONE',  ( -24.00000000000002132, 195.9375000027312126, 168.3431457505079152 ) ) ;
#8434 = CARTESIAN_POINT ( 'NONE',  ( -3.211159895383562723, 3.937499998634406584, 3.211159895383561391 ) ) ;
#8435 = CARTESIAN_POINT ( 'NONE',  ( 7.188101187500001821, 108.5000000020483810, -2.977408999572651371 ) ) ;
#8436 = DIRECTION ( 'NONE',  ( -0.000000000000000000, 1.000000000000000000, -0.000000000000000000 ) ) ;
#8437 = CARTESIAN_POINT ( 'NONE',  ( 2.977408999572650927, -7.188101187499990274, 25.95530278187175455 ) ) ;
#8438 = ORIENTED_EDGE ( 'NONE', *, *, #36709, .T. ) ;
#8439 = CARTESIAN_POINT ( 'NONE',  ( -1.320432766682874540E-15, 21.09374999795161543, 7.188101187500000044 ) ) ;
#8440 = ORIENTED_EDGE ( 'NONE', *, *, #61987, .T. ) ;
#8441 = CARTESIAN_POINT ( 'NONE',  ( -7.204075437095967871, 7.204075437095967871, 116.9687500020483810 ) ) ;
#8442 = CARTESIAN_POINT ( 'NONE',  ( 7.999999999999991118, 9.797174393178815797E-16, 10.58030277982336465 ) ) ;
#8443 = DIRECTION ( 'NONE',  ( 0.000000000000000000, 0.000000000000000000, -1.000000000000000000 ) ) ;
#8444 = CARTESIAN_POINT ( 'NONE',  ( 30.44569435410883074, 202.5625000013656063, 172.4456943541086957 ) ) ;
#8445 = CARTESIAN_POINT ( 'NONE',  ( -4.999999999999998224, 71.66666666666667140, -8.660254037844389075 ) ) ;
#8446 = ADVANCED_FACE ( 'NONE', ( #26195 ), #48096, .F. ) ;
#8447 = CARTESIAN_POINT ( 'NONE',  ( 7.188101187500001821, 95.37500000204839523, -2.977408999572651371 ) ) ;
#8448 = CARTESIAN_POINT ( 'NONE',  ( 2.485281374238575314, 297.3125000000000000, 6.000000000000000888 ) ) ;
#8450 = CARTESIAN_POINT ( 'NONE',  ( 4.000000000000015987, 197.6250000027312126, 198.0000000000000284 ) ) ;
#8449 = CARTESIAN_POINT ( 'NONE',  ( 23.99999999999998224, 207.8125000027312410, 168.3431457505075741 ) ) ;
#8451 = AXIS2_PLACEMENT_3D ( 'NONE', #64419, #12716, #54209 ) ;
#8452 = EDGE_LOOP ( 'NONE', ( #50110, #11107, #72992, #70119, #26781, #28146 ) ) ;
#8453 = CARTESIAN_POINT ( 'NONE',  ( -8.311093377946836114, 228.2812500034140157, -8.311093377946836114 ) ) ;
#8454 = CARTESIAN_POINT ( 'NONE',  ( -11.00000000000021139, 4.556349186103834548, 88.09375000409677625 ) ) ;
#8455 = CARTESIAN_POINT ( 'NONE',  ( -4.000000000000015987, 198.5625000027312126, 140.3431457505076594 ) ) ;
#8456 = CARTESIAN_POINT ( 'NONE',  ( -7.999999999994261479, 6.398094505892175214E-06, 25.01756343669228499 ) ) ;
#8457 = CARTESIAN_POINT ( 'NONE',  ( 28.00000000000002132, 206.5000000000000284, 165.9999999999998863 ) ) ;
#8458 = CARTESIAN_POINT ( 'NONE',  ( -6.123233995736766282E-16, 263.7500000000000568, -10.00000000000000000 ) ) ;
#8459 = CARTESIAN_POINT ( 'NONE',  ( -7.683012701892240059, 124.8169872981077901, 0.000000000000000000 ) ) ;
#8460 = CARTESIAN_POINT ( 'NONE',  ( 7.320508075688771044, 194.3750000000000284, 7.320508075688775484 ) ) ;
#8461 = CARTESIAN_POINT ( 'NONE',  ( 10.00000000000000000, 240.6250000068279746, -1.224646799147353256E-15 ) ) ;
#8462 = CARTESIAN_POINT ( 'NONE',  ( -5.082755093536319713, 5.082755093536319713, 25.67405278187175810 ) ) ;
#8463 = CARTESIAN_POINT ( 'NONE',  ( 6.951808397369818766E-16, 152.3437499965860411, -11.35316468750000141 ) ) ;
#8464 = CARTESIAN_POINT ( 'NONE',  ( 26.34314575050752083, 201.9375000000000000, 173.9999999999998295 ) ) ;
#8465 = CARTESIAN_POINT ( 'NONE',  ( 2.679491924311228956, 27.91666665983870033, -10.00000000000000000 ) ) ;
#8468 = CARTESIAN_POINT ( 'NONE',  ( 1.102182119232618108E-15, 292.2500000000000000, 6.000000000000001776 ) ) ;
#8467 = CARTESIAN_POINT ( 'NONE',  ( -7.320508075688778149, 84.99999999317203958, 7.320508075688769267 ) ) ;
#8466 = CARTESIAN_POINT ( 'NONE',  ( 32.00000000000000000, 202.2500000000000000, 169.9999999999999432 ) ) ;
#8469 = ORIENTED_EDGE ( 'NONE', *, *, #40215, .F. ) ;
#8470 = CARTESIAN_POINT ( 'NONE',  ( -11.35316468750000141, 8.593749996586016238, -1.390361679473963753E-15 ) ) ;
#8471 = EDGE_CURVE ( 'NONE', #11312, #49646, #37955, .T. ) ;
#8472 = FACE_BOUND ( 'NONE', #36753, .T. ) ;
#8473 = CARTESIAN_POINT ( 'NONE',  ( 7.320508075688771044, 31.24999999317203603, 7.320508075688775484 ) ) ;
#8474 = DIRECTION ( 'NONE',  ( -0.000000000000000000, 1.000000000000000000, -0.000000000000000000 ) ) ;
#8475 = CARTESIAN_POINT ( 'NONE',  ( -2.445694354108838731, 206.0625000013656063, 144.4456943541088663 ) ) ;
#8476 = ADVANCED_FACE ( 'NONE', ( #31122 ), #20163, .T. ) ;
#8477 = CARTESIAN_POINT ( 'NONE',  ( 4.999999999999993783, 46.04166665983869677, 8.660254037844390851 ) ) ;
#8478 = CARTESIAN_POINT ( 'NONE',  ( 7.188101187500000044, 111.4062500020483810, -8.802885111219163269E-16 ) ) ;
#8479 = CARTESIAN_POINT ( 'NONE',  ( 2.780723358947928197E-16, 5.687499998634407028, -4.541265875000002339 ) ) ;
#8480 = CARTESIAN_POINT ( 'NONE',  ( 1.469576158976822172E-15, -7.999999999999991118, 13.39280278392014623 ) ) ;
#8481 = CARTESIAN_POINT ( 'NONE',  ( 5.656854249492374365, 5.656854249492375253, 10.76780277982336642 ) ) ;
#8483 = CARTESIAN_POINT ( 'NONE',  ( -3.313708498984759387, -7.999999999999989342, 17.79905278392014623 ) ) ;
#8482 = DIRECTION ( 'NONE',  ( -0.000000000000000000, -0.000000000000000000, -1.000000000000000000 ) ) ;
#8484 = ORIENTED_EDGE ( 'NONE', *, *, #63473, .T. ) ;
#8485 = CARTESIAN_POINT ( 'NONE',  ( 0.000000000000000000, 300.0000000000000000, 6.000000000000001776 ) ) ;
#8486 = CARTESIAN_POINT ( 'NONE',  ( -2.751064625579944321E-14, 196.7500000000000000, 146.0000000000000284 ) ) ;
#8487 = EDGE_CURVE ( 'NONE', #35448, #8939, #19640, .T. ) ;
#8488 = CARTESIAN_POINT ( 'NONE',  ( -8.311093377946834337, 234.8437500034139305, 8.311093377946837890 ) ) ;
#8489 = CARTESIAN_POINT ( 'NONE',  ( -8.311093377946841443, 128.9062499965860411, 8.311093377946830785 ) ) ;
#8490 = ORIENTED_EDGE ( 'NONE', *, *, #49092, .F. ) ;
#8491 = EDGE_CURVE ( 'NONE', #16032, #31550, #35536, .T. ) ;
#8492 = CARTESIAN_POINT ( 'NONE',  ( 5.055468900453003123, 9.773537533938954525, 117.5066621467264838 ) ) ;
#8493 = CONICAL_SURFACE ( 'NONE', #55478, 6.900000000000001243, 0.9599310885968755924 ) ;
#8494 = CARTESIAN_POINT ( 'NONE',  ( -4.220049686691935698, 10.18810118749999916, 92.87500000204838102 ) ) ;
#8495 = CARTESIAN_POINT ( 'NONE',  ( 4.898587196589415787E-16, 0.000000000000000000, 4.000000000000001776 ) ) ;
#8496 = CARTESIAN_POINT ( 'NONE',  ( 2.754378923186476579E-14, 198.4375000013655779, 194.5412658750000219 ) ) ;
#8497 = DIRECTION ( 'NONE',  ( -0.000000000000000000, -0.000000000000000000, 1.000000000000000000 ) ) ;
#8499 = CARTESIAN_POINT ( 'NONE',  ( 11.35316468749999785, 115.5729166632526841, 3.042071309553174174 ) ) ;
#8498 = CARTESIAN_POINT ( 'NONE',  ( 30.82842712474619873, 196.3750000000000284, 167.1715728752537586 ) ) ;
#8500 = CARTESIAN_POINT ( 'NONE',  ( -30.44569435410883074, 194.8125000013656063, 167.5543056458915885 ) ) ;
#8501 = CARTESIAN_POINT ( 'NONE',  ( 0.000000000000000000, 0.000000000000000000, 0.000000000000000000 ) ) ;
#8502 = ORIENTED_EDGE ( 'NONE', *, *, #56567, .T. ) ;
#8503 = CARTESIAN_POINT ( 'NONE',  ( -10.00000000000000355, 24.58333332650536818, 2.679491924311223183 ) ) ;
#8504 = EDGE_CURVE ( 'NONE', #12433, #9485, #17235, .T. ) ;
#8505 = DIRECTION ( 'NONE',  ( 1.000000000000000000, -0.000000000000000000, -0.000000000000000000 ) ) ;
#8506 = CARTESIAN_POINT ( 'NONE',  ( 9.832129032723420536, 96.51041666325268409, -5.676582343749999815 ) ) ;
#8507 = CARTESIAN_POINT ( 'NONE',  ( -2.445694354108782775, 204.5625000013656063, 200.4456943541088663 ) ) ;
#8508 = CARTESIAN_POINT ( 'NONE',  ( 7.188101187500000044, 14.34374999795161187, 0.000000000000000000 ) ) ;
#8509 = CARTESIAN_POINT ( 'NONE',  ( 4.220049686691934809, 10.18810118749999916, 87.06250000204838102 ) ) ;
#8510 = CARTESIAN_POINT ( 'NONE',  ( -11.35316468749999785, 28.38541666325268054, -3.042071309553167513 ) ) ;
#8511 = VERTEX_POINT ( 'NONE', #26572 ) ;
#8512 = CARTESIAN_POINT ( 'NONE',  ( -4.615726161709423181, 68.43878643976954379, -20.71807028113809679 ) ) ;
#8513 = CARTESIAN_POINT ( 'NONE',  ( -3.317071493978880348, -8.008118988124989457, 25.29436528394063544 ) ) ;
#8514 = CARTESIAN_POINT ( 'NONE',  ( 4.556349186104052151, -10.99999999999999822, 102.1562500040967763 ) ) ;
#8515 = CARTESIAN_POINT ( 'NONE',  ( -7.204075437095967871, 7.204075437095967871, 72.34375000204836681 ) ) ;
#8516 = CARTESIAN_POINT ( 'NONE',  ( -46.67364751762348618, 38.00000000000001421, 69.99999999999997158 ) ) ;
#8517 = CARTESIAN_POINT ( 'NONE',  ( -2.977408999572654480, 5.999999997951610098, 7.188101187499999156 ) ) ;
#8518 = CARTESIAN_POINT ( 'NONE',  ( -2.765530957081998586, 292.6406250017070079, 6.676582343750001591 ) ) ;
#8519 = FACE_OUTER_BOUND ( 'NONE', #6026, .T. ) ;
#8520 = CARTESIAN_POINT ( 'NONE',  ( -11.35316468750000141, 218.8020833299193271, 3.042071309553159963 ) ) ;
#8521 = CONICAL_SURFACE ( 'NONE', #18171, 8.000000000000000000, 0.7853981633974552734 ) ;
#8522 =( BOUNDED_CURVE ( )  B_SPLINE_CURVE ( 2, ( #32179, #33311, #60462, #20460, #26118, #43480, #49519, #66492, #14803 ),
 .UNSPECIFIED., .F., .F. ) 
 B_SPLINE_CURVE_WITH_KNOTS ( ( 3, 2, 2, 2, 3 ),
 ( 0.6333333333333339699, 0.6416666666666673846, 0.6500000000000006883, 0.6583333333333339921, 0.6666666666666672958 ),
 .UNSPECIFIED. ) 
 CURVE ( )  GEOMETRIC_REPRESENTATION_ITEM ( )  RATIONAL_B_SPLINE_CURVE ( ( 0.9999999999999938938, 0.9238795325112928447, 1.000000000000000000, 0.9238795325112867385, 1.000000000000000000, 0.9238795325112867385, 1.000000000000000000, 0.9238795325112806323, 1.000000000000005995 ) ) 
 REPRESENTATION_ITEM ( '' )  );
#8523 = CARTESIAN_POINT ( 'NONE',  ( -3.042071309553173730, 139.6354166632526415, 11.35316468749999785 ) ) ;
#8524 = CARTESIAN_POINT ( 'NONE',  ( -10.18810118749999916, 4.220049686691934809, 82.56250000204836681 ) ) ;
#8525 = ADVANCED_BREP_SHAPE_REPRESENTATION ( '', ( #42707, #57354 ), #33286 ) ;
#8526 = CARTESIAN_POINT ( 'NONE',  ( -24.54126587499998280, 200.1250000013656063, 171.4326545832179818 ) ) ;
#8527 = CARTESIAN_POINT ( 'NONE',  ( -5.656854249492381470, 21.93750000000000355, 5.656854249492379694 ) ) ;
#8528 = CARTESIAN_POINT ( 'NONE',  ( -4.541265875000003227, 13.99999999863440792, 1.881053915767121110 ) ) ;
#8529 = ORIENTED_EDGE ( 'NONE', *, *, #33794, .F. ) ;
#8530 = CARTESIAN_POINT ( 'NONE',  ( -3.999999999999960032, 205.0625000027312126, 196.3431457505076594 ) ) ;
#8531 = CARTESIAN_POINT ( 'NONE',  ( 2.445694354108783219, 200.8125000013656063, 139.5543056458912190 ) ) ;
#8532 = CARTESIAN_POINT ( 'NONE',  ( -2.828427124746208943, 202.7500000027312126, 144.8284271247462129 ) ) ;
#8533 = CIRCLE ( 'NONE', #51894, 27.99999999999999645 ) ;
#8534 = CARTESIAN_POINT ( 'NONE',  ( 5.000000000000000000, 10.25161785469019193, -64.79070129774501652 ) ) ;
#8535 = EDGE_LOOP ( 'NONE', ( #36016, #9353, #41484, #29131 ) ) ;
#8536 = EDGE_CURVE ( 'NONE', #47034, #50322, #37915, .T. ) ;
#8537 = CARTESIAN_POINT ( 'NONE',  ( -7.188101187500000933, 2.624999997951609654, -2.977408999572651371 ) ) ;
#8538 = CARTESIAN_POINT ( 'NONE',  ( -29.90045898025567794, -12.02908699469180931, 178.2331709717555839 ) ) ;
#8539 = CARTESIAN_POINT ( 'NONE',  ( -2.679491924311235174, 30.41666665983870033, 10.00000000000000000 ) ) ;
#8540 = CARTESIAN_POINT ( 'NONE',  ( 5.676582343749993598, 179.9479166632526983, 9.832129032723422313 ) ) ;
#8541 = CARTESIAN_POINT ( 'NONE',  ( -4.401442555609581635E-16, 113.6562500020483952, -7.188101187500000044 ) ) ;
#8542 = AXIS2_PLACEMENT_3D ( 'NONE', #34312, #22585, #6380 ) ;
#8543 = CARTESIAN_POINT ( 'NONE',  ( -0.4590000000000000746, 261.4319999999996753, 5.805293472044576575 ) ) ;
#8544 = CARTESIAN_POINT ( 'NONE',  ( -2.765530957081996810, 291.2656250017070079, -6.676582343750002480 ) ) ;
#8546 = CARTESIAN_POINT ( 'NONE',  ( 3.458734124999959914, 209.4375000013656063, 142.0000000000000568 ) ) ;
#8545 = CARTESIAN_POINT ( 'NONE',  ( -29.65685424949235482, 209.4375000000000568, 174.0000000000004547 ) ) ;
#8547 = ORIENTED_EDGE ( 'NONE', *, *, #70648, .T. ) ;
#8548 = EDGE_CURVE ( 'NONE', #54437, #27667, #11508, .T. ) ;
#8549 = CARTESIAN_POINT ( 'NONE',  ( 2.085542519210945334E-15, 220.4687500034139873, 11.35316468749999963 ) ) ;
#8550 = CARTESIAN_POINT ( 'NONE',  ( -2.977408999572648707, -7.188101187499990274, 27.64280278187175810 ) ) ;
#8551 = VECTOR ( 'NONE', #23644, 1000.000000000000000 ) ;
#8552 = CARTESIAN_POINT ( 'NONE',  ( -7.999999999998400391, 3.416934844025491914E-06, 16.01767659775488184 ) ) ;
#8553 = CARTESIAN_POINT ( 'NONE',  ( 1.432654583217662481, 199.3750000013656063, 194.5412658750000219 ) ) ;
#8554 = ORIENTED_EDGE ( 'NONE', *, *, #19016, .T. ) ;
#8555 = DIRECTION ( 'NONE',  ( -5.551115147383623936E-15, 0.4999999999999780731, -0.8660254037844513642 ) ) ;
#8556 = CARTESIAN_POINT ( 'NONE',  ( -4.898587196589412829E-16, 100.6249999999999858, -8.000000000000000000 ) ) ;
#8557 = CARTESIAN_POINT ( 'NONE',  ( -3.042071309553173730, 114.6354166632526983, 11.35316468749999785 ) ) ;
#8558 = CARTESIAN_POINT ( 'NONE',  ( -31.66756539373098533, 5.999999999999963585, 167.9999999999997726 ) ) ;
#8559 = CARTESIAN_POINT ( 'NONE',  ( -7.778174593052023411, 7.778174593052023411, 74.31249999999998579 ) ) ;
#8562 = LINE ( 'NONE', #71181, #57928 ) ;
#8561 = CARTESIAN_POINT ( 'NONE',  ( 30.44569435410883074, 201.5625000013656063, 172.4456943541086957 ) ) ;
#8560 = CARTESIAN_POINT ( 'NONE',  ( 31.45873412499999944, 198.0000000013656063, 168.5673454167822740 ) ) ;
#8563 = EDGE_LOOP ( 'NONE', ( #32698, #70702 ) ) ;
#8564 = CARTESIAN_POINT ( 'NONE',  ( 2.849036369511732440E-14, 202.3750000027312126, 202.0000000000000000 ) ) ;
#8565 = CARTESIAN_POINT ( 'NONE',  ( 9.832129032723420536, 221.1979166632526983, -5.676582343749999815 ) ) ;
#8566 = CARTESIAN_POINT ( 'NONE',  ( -2.445694354108839619, 201.8125000013656063, 139.5543056458912190 ) ) ;
#8567 = CARTESIAN_POINT ( 'NONE',  ( 26.56734541678232375, 201.6250000013656063, 173.4587341249998929 ) ) ;
#8568 = EDGE_CURVE ( 'NONE', #29918, #1512, #19195, .T. ) ;
#8569 = CARTESIAN_POINT ( 'NONE',  ( 11.00000000000000000, 1.347111479062088405E-15, 114.4375000040967763 ) ) ;
#8570 = CARTESIAN_POINT ( 'NONE',  ( -9.832129032723418760, 198.1770833299193555, -5.676582343750004256 ) ) ;
#8571 = CARTESIAN_POINT ( 'NONE',  ( -4.401442555609581635E-16, 94.15625000204838102, -7.188101187500000044 ) ) ;
#8572 = DIRECTION ( 'NONE',  ( 0.000000000000000000, 0.000000000000000000, -1.000000000000000000 ) ) ;
#8573 = CARTESIAN_POINT ( 'NONE',  ( 4.541265875000002339, 13.31249999863440792, 0.000000000000000000 ) ) ;
#8574 = CARTESIAN_POINT ( 'NONE',  ( 31.45873412499999233, 198.9375000013655779, 169.9999999999999432 ) ) ;
#8575 = CARTESIAN_POINT ( 'NONE',  ( -7.188101187499991163, 2.977408999572646930, 6.267802781871754547 ) ) ;
#8576 = CARTESIAN_POINT ( 'NONE',  ( 0.000000000000000000, 0.000000000000000000, 118.0000000000000000 ) ) ;
#8577 = CARTESIAN_POINT ( 'NONE',  ( -5.676582343749998039, 87.44791666325268409, -9.832129032723420536 ) ) ;
#8578 = ORIENTED_EDGE ( 'NONE', *, *, #42246, .T. ) ;
#8579 = EDGE_CURVE ( 'NONE', #58773, #52476, #58664, .T. ) ;
#8580 = CARTESIAN_POINT ( 'NONE',  ( -2.062184786512628451E-11, 138.7499999999984084, 10.00000000000000178 ) ) ;
#8581 = CARTESIAN_POINT ( 'NONE',  ( -2.249999999999998668, 255.9999999999999432, 7.677076266392047543 ) ) ;
#8582 = CARTESIAN_POINT ( 'NONE',  ( -2.828427124746153876, 206.8750000000000284, 195.1715728752538439 ) ) ;
#8583 = CIRCLE ( 'NONE', #66414, 17.50000000000000000 ) ;
#8584 = CARTESIAN_POINT ( 'NONE',  ( -5.676582343749998039, 92.44791666325269830, -9.832129032723420536 ) ) ;
#8585 = ORIENTED_EDGE ( 'NONE', *, *, #30348, .F. ) ;
#8586 = CARTESIAN_POINT ( 'NONE',  ( -4.220049686691937474, -10.18810118749999738, 86.31250000204838102 ) ) ;
#8587 = CARTESIAN_POINT ( 'NONE',  ( 10.18810118749999916, 4.220049686691935698, 112.0000000020483668 ) ) ;
#8588 = CARTESIAN_POINT ( 'NONE',  ( 2.445694354108839175, 209.3125000013656063, 195.5543056458912190 ) ) ;
#8589 = CARTESIAN_POINT ( 'NONE',  ( 5.000000000000010658, 74.16666666666669983, 8.660254037844419273 ) ) ;
#8591 = CARTESIAN_POINT ( 'NONE',  ( 8.311093377946837890, 66.40624999658604111, -8.311093377946837890 ) ) ;
#8590 = DIRECTION ( 'NONE',  ( -0.000000000000000000, -0.000000000000000000, -1.000000000000000000 ) ) ;
#8592 = CARTESIAN_POINT ( 'NONE',  ( -5.656854249492373476, -5.656854249492376141, 17.70530278392014623 ) ) ;
#8593 = CYLINDRICAL_SURFACE ( 'NONE', #43281, 7.999999999999991118 ) ;
#8594 = CARTESIAN_POINT ( 'NONE',  ( 2.679491924311228956, 162.9166666598387110, -10.00000000000000000 ) ) ;
#8595 = CARTESIAN_POINT ( 'NONE',  ( 5.082755093536326818, 90.59375000204839523, 5.082755093536325042 ) ) ;
#8596 = CARTESIAN_POINT ( 'NONE',  ( -28.00000000000002132, 194.8437500006828031, 166.2706329375003804 ) ) ;
#8597 = CARTESIAN_POINT ( 'NONE',  ( -8.311093377946836114, 62.96874999658602690, -8.311093377946837890 ) ) ;
#8598 = CARTESIAN_POINT ( 'NONE',  ( 2.765530957082001251, 291.7656250017069510, 6.676582343750000703 ) ) ;
#8599 = ADVANCED_FACE ( 'NONE', ( #57128 ), #5443, .F. ) ;
#8600 = CARTESIAN_POINT ( 'NONE',  ( 4.220049686691934809, 10.18810118749999916, 105.0625000020483810 ) ) ;
#8601 = CARTESIAN_POINT ( 'NONE',  ( 11.35316468750000141, 205.7812499965860411, 0.000000000000000000 ) ) ;
#8602 = ORIENTED_EDGE ( 'NONE', *, *, #22072, .F. ) ;
#8603 = CARTESIAN_POINT ( 'NONE',  ( -3.511653767258388736, 68.04552192806590938, 20.40125235306568996 ) ) ;
#8604 = CARTESIAN_POINT ( 'NONE',  ( 3.313708498984761608, 15.09374999590322020, -8.000000000000000000 ) ) ;
#8606 = CARTESIAN_POINT ( 'NONE',  ( 9.832129032723420536, 191.1979166632526983, -5.676582343749999815 ) ) ;
#8605 = FACE_OUTER_BOUND ( 'NONE', #25002, .T. ) ;
#8607 = CARTESIAN_POINT ( 'NONE',  ( 3.313708498984761608, 3.093749995903220196, -8.000000000000000000 ) ) ;
#8608 = CARTESIAN_POINT ( 'NONE',  ( -10.00000000000000000, 243.1250000068280031, 0.000000000000000000 ) ) ;
#8609 = DIRECTION ( 'NONE',  ( -0.000000000000000000, -0.000000000000000000, 1.000000000000000000 ) ) ;
#8610 = AXIS2_PLACEMENT_3D ( 'NONE', #23530, #30676, #53695 ) ;
#8611 = ORIENTED_EDGE ( 'NONE', *, *, #60690, .T. ) ;
#8612 = CARTESIAN_POINT ( 'NONE',  ( 11.35316468749999785, 185.8854166632526983, 3.042071309553174174 ) ) ;
#8613 = VECTOR ( 'NONE', #53799, 1000.000000000000000 ) ;
#8614 = CARTESIAN_POINT ( 'NONE',  ( -7.188101187499992051, 2.977408999572646930, 20.89280278187176521 ) ) ;
#8615 =( BOUNDED_CURVE ( )  B_SPLINE_CURVE ( 2, ( #22147, #74589, #4446, #51572, #5195, #27437, #28192, #45175, #68188 ),
 .UNSPECIFIED., .F., .F. ) 
 B_SPLINE_CURVE_WITH_KNOTS ( ( 3, 2, 2, 2, 3 ),
 ( 0.1145833333333333981, 0.1197916666666667407, 0.1250000000000000833, 0.1302083333333334259, 0.1354166666666667407 ),
 .UNSPECIFIED. ) 
 CURVE ( )  GEOMETRIC_REPRESENTATION_ITEM ( )  RATIONAL_B_SPLINE_CURVE ( ( 0.9999999999999990008, 0.9238795325112877377, 1.000000000000000000, 0.9238795325112867385, 1.000000000000000000, 0.9238795325112867385, 1.000000000000000000, 0.9238795325112855172, 1.000000000000001110 ) ) 
 REPRESENTATION_ITEM ( '' )  );
#8616 = CARTESIAN_POINT ( 'NONE',  ( 5.656854249492376141, -5.656854249492374365, 16.58030278392014978 ) ) ;
#8617 = VECTOR ( 'NONE', #13837, 1000.000000000000227 ) ;
#8618 = VERTEX_POINT ( 'NONE', #64266 ) ;
#8619 = EDGE_CURVE ( 'NONE', #23507, #37922, #6559, .T. ) ;
#8620 = CARTESIAN_POINT ( 'NONE',  ( -3.313708498984762496, 96.96875000409677625, 7.999999999999998224 ) ) ;
#8621 = ADVANCED_FACE ( 'NONE', ( #63146 ), #35603, .F. ) ;
#8622 = CARTESIAN_POINT ( 'NONE',  ( -10.00000000000000355, 7.708333333333332149, 2.679491924311223183 ) ) ;
#8623 = EDGE_CURVE ( 'NONE', #71522, #17647, #53016, .T. ) ;
#8624 = CARTESIAN_POINT ( 'NONE',  ( 1.656854249492381914, 14.81250000000000000, 4.000000000000000888 ) ) ;
#8625 =( BOUNDED_CURVE ( )  B_SPLINE_CURVE ( 2, ( #42469, #65486, #67353, #15651, #56410, #43966, #38692, #3992, #66975, #60942, #15278 ),
 .UNSPECIFIED., .F., .F. ) 
 B_SPLINE_CURVE_WITH_KNOTS ( ( 3, 2, 2, 2, 2, 3 ),
 ( 0.1588385999027599471, 0.1588386140269634761, 0.1654568896114202992, 0.1720751651958771222, 0.1786934407803339175, 0.1853116620478932886 ),
 .UNSPECIFIED. ) 
 CURVE ( )  GEOMETRIC_REPRESENTATION_ITEM ( )  RATIONAL_B_SPLINE_CURVE ( ( 0.9999996751000569395, 0.9999998375496818026, 1.000000000000000000, 0.9238795325112867385, 1.000000000000000000, 0.9238795325112867385, 1.000000000000000000, 0.9238795325112867385, 1.000000000000000000, 0.9238801572401263984, 0.9999987505525751441 ) ) 
 REPRESENTATION_ITEM ( '' )  );
#8626 = CARTESIAN_POINT ( 'NONE',  ( 2.780723358947928197E-16, 15.56249999863440614, -4.541265875000002339 ) ) ;
#8627 = CARTESIAN_POINT ( 'NONE',  ( -4.898587196589407898E-16, 7.999999999999991118, 15.64280278392014800 ) ) ;
#8628 = DIRECTION ( 'NONE',  ( 0.000000000000000000, 0.000000000000000000, -1.000000000000000000 ) ) ;
#8629 = ORIENTED_EDGE ( 'NONE', *, *, #74582, .T. ) ;
#8630 = CARTESIAN_POINT ( 'NONE',  ( 4.999999999999999112, -12.55023575007693104, -69.09043692422062577 ) ) ;
#8631 = CARTESIAN_POINT ( 'NONE',  ( 7.188101187500002709, 91.81250000204839523, 2.977408999572649151 ) ) ;
#8633 = CARTESIAN_POINT ( 'NONE',  ( 2.085542519210945334E-15, 260.1562500034140157, 11.35316468749999963 ) ) ;
#8632 = CARTESIAN_POINT ( 'NONE',  ( -7.999999999999991118, 0.000000000000000000, 12.83030277982336465 ) ) ;
#8634 = CARTESIAN_POINT ( 'NONE',  ( 1424.688200795887951, 881.4677537767814783, 997.8421604560580818 ) ) ;
#8635 = ORIENTED_EDGE ( 'NONE', *, *, #69981, .F. ) ;
#8636 = CARTESIAN_POINT ( 'NONE',  ( -9.832129032723418760, 263.8020833367473301, -5.676582343749998927 ) ) ;
#8637 = CARTESIAN_POINT ( 'NONE',  ( -5.082755093536319713, 5.082755093536319713, 17.79905278187175455 ) ) ;
#8638 = EDGE_LOOP ( 'NONE', ( #31683, #59580, #18189, #34371, #30626, #60689 ) ) ;
#8639 = EDGE_CURVE ( 'NONE', #74042, #9014, #74073, .T. ) ;
#8640 = ORIENTED_EDGE ( 'NONE', *, *, #22155, .F. ) ;
#8641 = CARTESIAN_POINT ( 'NONE',  ( -7.204075437095967871, 7.204075437095967871, 80.96875000204836681 ) ) ;
#8642 = CARTESIAN_POINT ( 'NONE',  ( -11.35316468749999785, 68.38541666325268409, -3.042071309553167513 ) ) ;
#8643 = CARTESIAN_POINT ( 'NONE',  ( -10.00000000000000000, 114.1666666598386968, -2.679491924311229845 ) ) ;
#8644 = CARTESIAN_POINT ( 'NONE',  ( 11.00000000000000000, 4.556349186104045934, 96.34374999999998579 ) ) ;
#8647 = CARTESIAN_POINT ( 'NONE',  ( 4.721056650416000089, 292.9843750017070079, 4.721056650415999201 ) ) ;
#8646 = CARTESIAN_POINT ( 'NONE',  ( 25.17157287525377640, 196.7500000027312126, 167.1715728752537586 ) ) ;
#8645 = CARTESIAN_POINT ( 'NONE',  ( 30.44569435410883784, 209.0625000013656063, 167.5543056458911053 ) ) ;
#8648 = CARTESIAN_POINT ( 'NONE',  ( 7.320508075688774596, 150.6250000000000000, -7.320508075688774596 ) ) ;
#8649 = CARTESIAN_POINT ( 'NONE',  ( 0.000000000000000000, 125.0000000000000000, 0.000000000000000000 ) ) ;
#8650 = CARTESIAN_POINT ( 'NONE',  ( 3.426202465283471721, 194.4587341250000350, 141.5267364219330943 ) ) ;
#8651 = CARTESIAN_POINT ( 'NONE',  ( -3.458734124999960358, 196.6875000013655779, 198.0000000000000284 ) ) ;
#8652 = CARTESIAN_POINT ( 'NONE',  ( 2.751064625579944321E-14, 202.7500000000000000, 194.0000000000000568 ) ) ;
#8653 = CARTESIAN_POINT ( 'NONE',  ( -3.313708498984760720, 1.781249995903220418, -8.000000000000000000 ) ) ;
#8654 = CARTESIAN_POINT ( 'NONE',  ( 24.54126587499998280, 199.2500000013656063, 171.4326545832175555 ) ) ;
#8655 = CARTESIAN_POINT ( 'NONE',  ( -7.188101187500001821, 11.99999999795161187, -2.977408999572651371 ) ) ;
#8656 = CARTESIAN_POINT ( 'NONE',  ( -5.656854249492375253, 5.656854249492375253, 27.83030278392014978 ) ) ;
#8657 = CARTESIAN_POINT ( 'NONE',  ( 1.836970198721029589E-15, 244.3750000068280031, 10.00000000000000000 ) ) ;
#8658 = CARTESIAN_POINT ( 'NONE',  ( -7.188101187499999156, 112.6250000020483810, 2.977408999572654924 ) ) ;
#8660 = CARTESIAN_POINT ( 'NONE',  ( -7.347880794884122694E-16, 16.75000000000000000, 4.000000000000001776 ) ) ;
#8659 = CARTESIAN_POINT ( 'NONE',  ( 1.656854249492354825, 201.3125000000000284, 202.0000000000000853 ) ) ;
#8661 = CARTESIAN_POINT ( 'NONE',  ( 5.000000000000003553, 135.8333333333333712, -8.660254037844390851 ) ) ;
#8662 = DIRECTION ( 'NONE',  ( 0.000000000000000000, 0.000000000000000000, 1.000000000000000000 ) ) ;
#8663 = CARTESIAN_POINT ( 'NONE',  ( -7.188101187499991163, 2.977408999572646930, 22.76780278187175455 ) ) ;
#8664 = FACE_OUTER_BOUND ( 'NONE', #67008, .T. ) ;
#8665 = CARTESIAN_POINT ( 'NONE',  ( 11.35316468749999785, 40.57291666325269119, 3.042071309553174174 ) ) ;
#8666 = CARTESIAN_POINT ( 'NONE',  ( -7.347880794884122694E-16, 6.750000000000000000, 4.000000000000001776 ) ) ;
#8667 = CARTESIAN_POINT ( 'NONE',  ( 8.660254037844389075, 7.291666659838699438, -5.000000000000000000 ) ) ;
#8668 = ORIENTED_EDGE ( 'NONE', *, *, #34898, .T. ) ;
#8669 = CARTESIAN_POINT ( 'NONE',  ( -11.00000000000000000, 0.000000000000000000, 104.6875000040967763 ) ) ;
#8670 = CARTESIAN_POINT ( 'NONE',  ( -6.735557395310442023E-16, 11.00000000000000000, 69.81250000409677625 ) ) ;
#8671 = CARTESIAN_POINT ( 'NONE',  ( -11.35316468749999785, 53.07291666325266988, -3.042071309553167513 ) ) ;
#8672 = CARTESIAN_POINT ( 'NONE',  ( 11.00000000000000355, -4.556349186104045046, 79.84375000409677625 ) ) ;
#8673 = CARTESIAN_POINT ( 'NONE',  ( 1.432654583217607414, 205.5000000013655779, 145.4587341250000350 ) ) ;
#8674 = CARTESIAN_POINT ( 'NONE',  ( 28.00000000000001776, 202.5000000000000000, 165.9999999999998863 ) ) ;
#8675 = CYLINDRICAL_SURFACE ( 'NONE', #57633, 11.49999999999999112 ) ;
#8677 = CARTESIAN_POINT ( 'NONE',  ( -11.35316468750000141, 33.28124999658601268, -1.390361679473963753E-15 ) ) ;
#8676 = CARTESIAN_POINT ( 'NONE',  ( 7.188101187500000933, 102.5000000020483810, -2.977408999572651371 ) ) ;
#8678 = CARTESIAN_POINT ( 'NONE',  ( -7.999999999999991118, 0.000000000000000000, 11.33030277982336642 ) ) ;
#8679 = CARTESIAN_POINT ( 'NONE',  ( 2.506878452759003562, 0.3721089088409397228, -7.479669363585287556 ) ) ;
#8680 = CARTESIAN_POINT ( 'NONE',  ( -9.832129032723418760, 162.8645833299193839, -5.676582343750004256 ) ) ;
#8681 = CARTESIAN_POINT ( 'NONE',  ( 10.00000000000000178, 127.0833333265053682, -2.679491924311226736 ) ) ;
#8682 = CARTESIAN_POINT ( 'NONE',  ( 7.188101187500000044, 105.7812500020483810, -8.802885111219163269E-16 ) ) ;
#8683 = ORIENTED_EDGE ( 'NONE', *, *, #7090, .T. ) ;
#8684 = DIRECTION ( 'NONE',  ( 0.000000000000000000, 0.000000000000000000, -1.000000000000000000 ) ) ;
#8685 = CARTESIAN_POINT ( 'NONE',  ( -9.832129032723420536, 19.01041666325268409, 5.676582343749997150 ) ) ;
#8686 = DIRECTION ( 'NONE',  ( 0.000000000000000000, 0.000000000000000000, 1.000000000000000000 ) ) ;
#8687 = ORIENTED_EDGE ( 'NONE', *, *, #17656, .F. ) ;
#8688 = CARTESIAN_POINT ( 'NONE',  ( 1.347111479062087024E-15, 101.0525588832578734, -10.99999999999998934 ) ) ;
#8689 = CARTESIAN_POINT ( 'NONE',  ( -6.238412754330611322E-16, 10.18810118749999916, 74.78125000204836681 ) ) ;
#8690 = CYLINDRICAL_SURFACE ( 'NONE', #53431, 19.00000000000001776 ) ;
#8692 = CARTESIAN_POINT ( 'NONE',  ( 9.832129032723416984, 150.3645833299193555, 5.676582343750006032 ) ) ;
#8691 = CARTESIAN_POINT ( 'NONE',  ( -29.31555159221728601, -21.12534714490642784, 150.9590529377151711 ) ) ;
#8693 = FACE_OUTER_BOUND ( 'NONE', #57978, .T. ) ;
#8694 = CARTESIAN_POINT ( 'NONE',  ( -5.656854249492375253, 5.656854249492375253, 11.19905278432982243 ) ) ;
#8695 = AXIS2_PLACEMENT_3D ( 'NONE', #63338, #34698, #57706 ) ;
#8696 = CARTESIAN_POINT ( 'NONE',  ( 1.469576158976822172E-15, -7.999999999999991118, 16.20530277982336287 ) ) ;
#8697 = CARTESIAN_POINT ( 'NONE',  ( -9.832129032723415207, 229.3229166700806729, 5.676582343750005144 ) ) ;
#8698 = CARTESIAN_POINT ( 'NONE',  ( -7.204075437095967871, 7.204075437095967871, 82.84375000204838102 ) ) ;
#8699 = VERTEX_POINT ( 'NONE', #23899 ) ;
#8700 = EDGE_CURVE ( 'NONE', #36205, #61146, #48055, .T. ) ;
#8701 = CARTESIAN_POINT ( 'NONE',  ( 6.123233995736767268E-16, 118.1249999931720396, -10.00000000000000178 ) ) ;
#8702 = CARTESIAN_POINT ( 'NONE',  ( -6.000000000000003553, 292.0000000034139589, -2.485281374238571317 ) ) ;
#8703 = CARTESIAN_POINT ( 'NONE',  ( -8.311093377946841443, 104.2187499965859985, 8.311093377946830785 ) ) ;
#8704 = CARTESIAN_POINT ( 'NONE',  ( 4.220049686691941027, -10.18810118749999738, 101.1250000020483810 ) ) ;
#8705 = CARTESIAN_POINT ( 'NONE',  ( 10.00000000000000888, 14.79166666666667140, 2.679491924311238282 ) ) ;
#8706 = VERTEX_POINT ( 'NONE', #29198 ) ;
#8707 = ORIENTED_EDGE ( 'NONE', *, *, #4800, .F. ) ;
#8708 = CARTESIAN_POINT ( 'NONE',  ( -1.881053915767121554, 5.749999998634407028, -4.541265875000002339 ) ) ;
#8709 = CARTESIAN_POINT ( 'NONE',  ( -1.320432766682874540E-15, 6.093749997951610986, 7.188101187500000044 ) ) ;
#8710 = CARTESIAN_POINT ( 'NONE',  ( 1.469576158976823947E-15, 116.5625000040967763, 8.000000000000000000 ) ) ;
#8711 = ADVANCED_FACE ( 'NONE', ( #18242, #52210 ), #41257, .F. ) ;
#8712 = CARTESIAN_POINT ( 'NONE',  ( 10.18810118749999916, 1.247682550866122264E-15, 95.78125000204836681 ) ) ;
#8713 = CARTESIAN_POINT ( 'NONE',  ( -29.43265458321766559, 201.7500000013655779, 166.5412658750003629 ) ) ;
#8714 = CARTESIAN_POINT ( 'NONE',  ( -8.535034553343571417, -8.928701963635374383, -0.1959795092987848819 ) ) ;
#8715 = CIRCLE ( 'NONE', #304, 30.99999999999997158 ) ;
#8716 = EDGE_CURVE ( 'NONE', #55422, #63985, #71760, .T. ) ;
#8717 = CARTESIAN_POINT ( 'NONE',  ( -1.656854249492383691, 3.687500000000000444, 4.000000000000000888 ) ) ;
#8718 = CARTESIAN_POINT ( 'NONE',  ( 2.449293598294707893E-16, 19.99999999726881228, -4.000000000000001776 ) ) ;
#8719 = CARTESIAN_POINT ( 'NONE',  ( 3.211159895383561835, 4.437499998634407028, -3.211159895383561835 ) ) ;
#8720 = FACE_OUTER_BOUND ( 'NONE', #65759, .T. ) ;
#8721 = CARTESIAN_POINT ( 'NONE',  ( 0.000000000000000000, 0.000000000000000000, 38.34805510287551300 ) ) ;
#8724 = CARTESIAN_POINT ( 'NONE',  ( 11.00000000000005329, -4.556349186103991755, 96.34375000409677625 ) ) ;
#8723 = CARTESIAN_POINT ( 'NONE',  ( -24.54126587499999346, 198.1875000013655779, 170.0000000000002842 ) ) ;
#8722 =( BOUNDED_CURVE ( )  B_SPLINE_CURVE ( 2, ( #21165, #61161, #9110, #4951, #32125, #20791, #66441, #9493, #38903, #33630, #49464, #67202, #72860 ),
 .UNSPECIFIED., .F., .F. ) 
 B_SPLINE_CURVE_WITH_KNOTS ( ( 3, 2, 2, 2, 2, 2, 3 ),
 ( 0.7378893796947577632, 0.7431232142107645489, 0.7483570487267714455, 0.7535908832427783421, 0.7588247177587852388, 0.7640585522747921354, 0.7692923867907990321 ),
 .UNSPECIFIED. ) 
 CURVE ( )  GEOMETRIC_REPRESENTATION_ITEM ( )  RATIONAL_B_SPLINE_CURVE ( ( 1.000000000000083489, 0.9659258262889848234, 1.000000000000000000, 0.9659258262890683122, 1.000000000000000000, 0.9659258262890683122, 1.000000000000000000, 0.9659258262890683122, 1.000000000000000000, 0.9659258262890683122, 1.000000000000000000, 0.9659258262888741342, 1.000000000000194289 ) ) 
 REPRESENTATION_ITEM ( '' )  );
#8725 = CARTESIAN_POINT ( 'NONE',  ( -3.211159895383561391, 16.68749999863440436, -3.211159895383561835 ) ) ;
#8726 = AXIS2_PLACEMENT_3D ( 'NONE', #44429, #51202, #21776 ) ;
#8727 = LINE ( 'NONE', #15860, #47679 ) ;
#8728 = CARTESIAN_POINT ( 'NONE',  ( -4.401442555609577197E-16, 7.188101187499992051, 7.111552781871751883 ) ) ;
#8729 = ORIENTED_EDGE ( 'NONE', *, *, #17798, .F. ) ;
#8730 = EDGE_LOOP ( 'NONE', ( #52170, #13624, #42210, #63101 ) ) ;
#8731 = CARTESIAN_POINT ( 'NONE',  ( -6.238412754330611322E-16, 10.18810118749999916, 98.78125000204838102 ) ) ;
#8732 = CARTESIAN_POINT ( 'NONE',  ( 2.775557561562891351E-14, 210.0000000000000284, 198.0000000000000284 ) ) ;
#8733 = CARTESIAN_POINT ( 'NONE',  ( -29.43265458321766914, 202.7500000013655779, 166.5412658750003629 ) ) ;
#8734 = CARTESIAN_POINT ( 'NONE',  ( -30.82842712474621294, 200.1250000000000284, 167.1715728752542134 ) ) ;
#8735 = CARTESIAN_POINT ( 'NONE',  ( 2.754378923186476579E-14, 195.1875000013655779, 194.5412658750000219 ) ) ;
#8736 = DIRECTION ( 'NONE',  ( -0.000000000000000000, -1.000000000000000000, -0.000000000000000000 ) ) ;
#8737 = CARTESIAN_POINT ( 'NONE',  ( -5.000000000000005329, 103.3333333333333428, 8.660254037844387298 ) ) ;
#8738 = AXIS2_PLACEMENT_3D ( 'NONE', #22508, #34985, #28182 ) ;
#8739 = CARTESIAN_POINT ( 'NONE',  ( -8.000000000000000000, 110.0000000000000000, 0.000000000000000000 ) ) ;
#8740 = CARTESIAN_POINT ( 'NONE',  ( 6.676582343750001591, 292.1093750017069510, -8.176455196517173205E-16 ) ) ;
#8741 = CARTESIAN_POINT ( 'NONE',  ( 7.188101187499993827, -2.977408999572645598, 14.51780278187175455 ) ) ;
#8742 = EDGE_LOOP ( 'NONE', ( #71420, #27434, #56718, #62176 ) ) ;
#8743 = AXIS2_PLACEMENT_3D ( 'NONE', #750, #28649, #68643 ) ;
#8745 =( BOUNDED_CURVE ( )  B_SPLINE_CURVE ( 2, ( #37006, #61508, #32858, #14348, #55863, #8705, #54741, #3050, #26034, #37760, #60760, #9082, #68653 ),
 .UNSPECIFIED., .F., .F. ) 
 B_SPLINE_CURVE_WITH_KNOTS ( ( 3, 2, 2, 2, 2, 2, 3 ),
 ( 0.1726919338016095207, 0.1779254737324397762, 0.1831590136632700316, 0.1883925535941002871, 0.1936260935249305426, 0.1988596334557607981, 0.2040931733865910258 ),
 .UNSPECIFIED. ) 
 CURVE ( )  GEOMETRIC_REPRESENTATION_ITEM ( )  RATIONAL_B_SPLINE_CURVE ( ( 1.000000000000187850, 0.9659258262888803515, 1.000000000000000000, 0.9659258262890683122, 1.000000000000000000, 0.9659258262890683122, 1.000000000000000000, 0.9659258262890683122, 1.000000000000000000, 0.9659258262890683122, 1.000000000000000000, 0.9659258262890675351, 1.000000000000000888 ) ) 
 REPRESENTATION_ITEM ( '' )  );
#8744 = CARTESIAN_POINT ( 'NONE',  ( 0.000000000000000000, 0.000000000000000000, 118.0000000000000000 ) ) ;
#8746 = CARTESIAN_POINT ( 'NONE',  ( 4.898587196589412829E-16, 19.68749999590322020, -8.000000000000000000 ) ) ;
#8747 = CARTESIAN_POINT ( 'NONE',  ( 1.432654583217607192, 202.2500000013656063, 145.4587341250000634 ) ) ;
#8748 = CARTESIAN_POINT ( 'NONE',  ( -19.99999999999993250, -31.99999999999978684, 145.6940130594346670 ) ) ;
#8749 = CARTESIAN_POINT ( 'NONE',  ( 3.313708498984873518, 113.6562500040967763, 7.999999999999890754 ) ) ;
#8750 = CARTESIAN_POINT ( 'NONE',  ( -11.35316468749999963, 249.2187500034139873, 0.000000000000000000 ) ) ;
#8751 = CARTESIAN_POINT ( 'NONE',  ( 0.000000000000000000, 0.000000000000000000, 0.000000000000000000 ) ) ;
#8752 = CARTESIAN_POINT ( 'NONE',  ( -4.556349186104045934, 11.00000000000000000, 111.7187499999999858 ) ) ;
#8753 = CARTESIAN_POINT ( 'NONE',  ( -3.042071309553173730, 4.322916663252682312, 11.35316468749999785 ) ) ;
#8754 = CARTESIAN_POINT ( 'NONE',  ( -7.188101187499992051, 0.000000000000000000, 1.861552781871753881 ) ) ;
#8755 = CARTESIAN_POINT ( 'NONE',  ( 5.676582343749993598, 200.2604166632526983, 9.832129032723422313 ) ) ;
#8756 = CARTESIAN_POINT ( 'NONE',  ( 10.00000000000000000, 191.6666666598387110, 2.679491924311235618 ) ) ;
#8757 = CARTESIAN_POINT ( 'NONE',  ( 1.881053915767121776, 6.499999998634407028, -4.541265875000002339 ) ) ;
#8758 = CARTESIAN_POINT ( 'NONE',  ( -7.999999999999991118, 9.797174393178815797E-16, 30.00000000000000000 ) ) ;
#8760 = CARTESIAN_POINT ( 'NONE',  ( -2.828427124746208943, 206.6250000000000284, 144.8284271247462129 ) ) ;
#8759 = CARTESIAN_POINT ( 'NONE',  ( -4.898587196589412829E-16, 106.8125000040967763, -8.000000000000000000 ) ) ;
#8761 = EDGE_LOOP ( 'NONE', ( #54885, #33884, #47659, #6937 ) ) ;
#8762 = ADVANCED_FACE ( 'NONE', ( #31409 ), #31732, .F. ) ;
#8763 = CARTESIAN_POINT ( 'NONE',  ( -2.839093476692135984E-14, 205.9375000013656063, 138.5412658750000503 ) ) ;
#8764 = CARTESIAN_POINT ( 'NONE',  ( 11.35316468749999963, 5.989583329919348387, -3.042071309553165293 ) ) ;
#8765 = CARTESIAN_POINT ( 'NONE',  ( 2.020667218593132706E-15, -11.00000000000000000, 99.06250000409677625 ) ) ;
#8766 = DIRECTION ( 'NONE',  ( -0.000000000000000000, 1.000000000000000000, -4.476705744456276341E-16 ) ) ;
#8767 = CARTESIAN_POINT ( 'NONE',  ( -29.43265458321770822, 199.5000000013656063, 166.5412658750003914 ) ) ;
#8768 = CARTESIAN_POINT ( 'NONE',  ( 12.00000000000000000, 0.000000000000000000, 6.938893903907228378E-15 ) ) ;
#8770 = CARTESIAN_POINT ( 'NONE',  ( -5.000000000000005329, 60.20833332650536818, 8.660254037844387298 ) ) ;
#8769 = CARTESIAN_POINT ( 'NONE',  ( 7.188101187500000933, 120.5000000020483810, -2.977408999572651371 ) ) ;
#8771 = CARTESIAN_POINT ( 'NONE',  ( 5.656854249492374365, 5.656854249492375253, 28.76780277982336642 ) ) ;
#8772 = CARTESIAN_POINT ( 'NONE',  ( -11.35316468749999785, 123.0729166632526983, -3.042071309553167513 ) ) ;
#8773 = CARTESIAN_POINT ( 'NONE',  ( -5.000000000000005329, 85.20833332650538239, 8.660254037844387298 ) ) ;
#8774 = CARTESIAN_POINT ( 'NONE',  ( -5.082755093536325930, 90.96875000204838102, -5.082755093536325930 ) ) ;
#8775 = CARTESIAN_POINT ( 'NONE',  ( 4.541265875000001451, 22.37499999863441147, 1.881053915767124440 ) ) ;
#8776 = CARTESIAN_POINT ( 'NONE',  ( -23.99999999999998934, 204.7500000000000284, 170.0000000000003411 ) ) ;
#8777 = CARTESIAN_POINT ( 'NONE',  ( -5.000000000000000000, 52.85071664756748788, -48.38833198888215037 ) ) ;
#8778 = ORIENTED_EDGE ( 'NONE', *, *, #47047, .T. ) ;
#8779 = CARTESIAN_POINT ( 'NONE',  ( -4.000000000000016875, 200.5625000027312126, 140.3431457505076594 ) ) ;
#8780 = VERTEX_POINT ( 'NONE', #65734 ) ;
#8781 = CARTESIAN_POINT ( 'NONE',  ( 1.226468279477575784E-15, 294.8593750017070079, 6.676582343750001591 ) ) ;
#8782 = DIRECTION ( 'NONE',  ( -0.000000000000000000, 1.000000000000000000, -0.000000000000000000 ) ) ;
#8783 = CARTESIAN_POINT ( 'NONE',  ( -4.898587196589407898E-16, 7.999999999999991118, 6.642802783920143561 ) ) ;
#8784 = CARTESIAN_POINT ( 'NONE',  ( -8.311093377946836114, 162.6562499965859843, -8.311093377946837890 ) ) ;
#8785 = PLANE ( 'NONE',  #13972 ) ;
#8786 = CARTESIAN_POINT ( 'NONE',  ( -3.999999999999960032, 200.9375000000000284, 196.3431457505076594 ) ) ;
#8787 = CARTESIAN_POINT ( 'NONE',  ( 7.778174593052021635, 7.778174593052023411, 69.43749999999998579 ) ) ;
#8788 = CARTESIAN_POINT ( 'NONE',  ( 4.220049686691934809, 10.18810118749999916, 105.0625000020483810 ) ) ;
#8789 = ORIENTED_EDGE ( 'NONE', *, *, #2424, .T. ) ;
#8790 = EDGE_CURVE ( 'NONE', #33251, #73315, #27358, .T. ) ;
#8791 = CARTESIAN_POINT ( 'NONE',  ( 6.123233995736767268E-16, 158.1249999931720254, -10.00000000000000178 ) ) ;
#8792 = CARTESIAN_POINT ( 'NONE',  ( 3.042071309553167513, 157.1354166632526983, -11.35316468749999785 ) ) ;
#8793 = CARTESIAN_POINT ( 'NONE',  ( -5.000000000000000000, 216.6666666666666856, -8.660254037844390851 ) ) ;
#8794 = CARTESIAN_POINT ( 'NONE',  ( -1.432654583217607414, 207.5000000013656063, 194.5412658750000219 ) ) ;
#8795 = CARTESIAN_POINT ( 'NONE',  ( 10.18810118749999916, 1.247682550866122264E-15, 70.28125000204838102 ) ) ;
#8796 = CARTESIAN_POINT ( 'NONE',  ( 5.676582343750001591, 66.92708332991935549, -9.832129032723420536 ) ) ;
#8797 = EDGE_LOOP ( 'NONE', ( #21511, #14259, #49835, #56911 ) ) ;
#8798 = CARTESIAN_POINT ( 'NONE',  ( 7.204075437095966983, 7.204075437095967871, 116.5937500020483810 ) ) ;
#8799 = CARTESIAN_POINT ( 'NONE',  ( 1.881053915767121998, 7.624999998634407916, -4.541265875000002339 ) ) ;
#8800 = CARTESIAN_POINT ( 'NONE',  ( -4.903558642999205574E-16, 8.008118988124991233, 8.138115283940630107 ) ) ;
#8801 = ORIENTED_EDGE ( 'NONE', *, *, #41305, .T. ) ;
#8802 = AXIS2_PLACEMENT_3D ( 'NONE', #72450, #44527, #21507 ) ;
#8803 = ADVANCED_FACE ( 'NONE', ( #2002 ), #54060, .T. ) ;
#8804 = CARTESIAN_POINT ( 'NONE',  ( -7.188101187500001821, 23.62499999795161543, -2.977408999572651371 ) ) ;
#8805 = CARTESIAN_POINT ( 'NONE',  ( -4.242640687119285658, 288.1875000034139589, 4.242640687119287435 ) ) ;
#8806 = CARTESIAN_POINT ( 'NONE',  ( -28.00000000000007816, 198.1250000027312126, 166.0000000000003695 ) ) ;
#8807 = CARTESIAN_POINT ( 'NONE',  ( -1.320432766682874540E-15, 15.46874999795161187, 7.188101187500000044 ) ) ;
#8808 = CARTESIAN_POINT ( 'NONE',  ( 2.977408999572646486, 7.188101187499992051, 1.017802781871752993 ) ) ;
#8809 = CARTESIAN_POINT ( 'NONE',  ( 10.18810118750000093, -4.220049686691933921, 113.6875000020483952 ) ) ;
#8810 = CARTESIAN_POINT ( 'NONE',  ( 0.3941532444159659976, -42.01957742515746475, 151.0031188547334864 ) ) ;
#8811 = CARTESIAN_POINT ( 'NONE',  ( 4.000000000000001776, 4.749999997268813168, 0.000000000000000000 ) ) ;
#8812 = ORIENTED_EDGE ( 'NONE', *, *, #6275, .T. ) ;
#8813 = CARTESIAN_POINT ( 'NONE',  ( 1.432654583217662481, 205.1250000013656347, 194.5412658750000219 ) ) ;
#8814 = ADVANCED_FACE ( 'NONE', ( #19708 ), #24628, .F. ) ;
#8815 = CARTESIAN_POINT ( 'NONE',  ( -29.65685424949229088, 197.5625000027312126, 174.0000000000004547 ) ) ;
#8816 = CARTESIAN_POINT ( 'NONE',  ( -4.541265875000003227, 7.874999998634407028, 1.881053915767121110 ) ) ;
#8817 = CARTESIAN_POINT ( 'NONE',  ( 2.977408999572650039, 111.6875000020483810, -7.188101187500001821 ) ) ;
#8818 = CARTESIAN_POINT ( 'NONE',  ( 25.17157287525378351, 204.8750000000000284, 172.8284271247460424 ) ) ;
#8819 = CIRCLE ( 'NONE', #50998, 6.000000000000000000 ) ;
#8820 = CARTESIAN_POINT ( 'NONE',  ( 7.188101187499991163, 2.977408999572648707, 26.33030278187175810 ) ) ;
#8821 = ORIENTED_EDGE ( 'NONE', *, *, #16361, .T. ) ;
#8822 = CARTESIAN_POINT ( 'NONE',  ( 7.188101187499999156, 27.37499999795161543, 2.977408999572654924 ) ) ;
#8823 = ORIENTED_EDGE ( 'NONE', *, *, #37181, .F. ) ;
#8824 = DIRECTION ( 'NONE',  ( -1.000000000000000000, 0.000000000000000000, 0.000000000000000000 ) ) ;
#8825 = CARTESIAN_POINT ( 'NONE',  ( -7.999999999999992895, 4.898587196589407898E-16, 0.000000000000000000 ) ) ;
#8826 = CARTESIAN_POINT ( 'NONE',  ( 3.458734125000016313, 206.8750000013656347, 199.4326545832176691 ) ) ;
#8827 = CARTESIAN_POINT ( 'NONE',  ( 30.44569435410879521, 204.8125000013656063, 167.5543056458910485 ) ) ;
#8828 = CARTESIAN_POINT ( 'NONE',  ( -8.660254037844387298, 62.08333333333333570, -5.000000000000004441 ) ) ;
#8829 = CARTESIAN_POINT ( 'NONE',  ( -4.401442555609581635E-16, 95.65625000204838102, -7.188101187500000044 ) ) ;
#8830 = CARTESIAN_POINT ( 'NONE',  ( -4.242640687119286547, 295.8750000000000000, -4.242640687119286547 ) ) ;
#8832 = CARTESIAN_POINT ( 'NONE',  ( -8.660254037844385522, 255.4166666666666856, 5.000000000000004441 ) ) ;
#8831 = CARTESIAN_POINT ( 'NONE',  ( 31.57687894400719486, 176.8634886272080564, 168.5922446645002708 ) ) ;
#8833 = ORIENTED_EDGE ( 'NONE', *, *, #70378, .T. ) ;
#8834 = CARTESIAN_POINT ( 'NONE',  ( 11.35316468749999963, 226.1979166700806729, 3.042071309553159519 ) ) ;
#8835 = CARTESIAN_POINT ( 'NONE',  ( 1.469576158976823947E-15, 92.56250000409677625, 8.000000000000000000 ) ) ;
#8836 = CARTESIAN_POINT ( 'NONE',  ( 1.656854249492347719, 199.9375000027312126, 146.0000000000000284 ) ) ;
#8837 = CYLINDRICAL_SURFACE ( 'NONE', #8102, 4.000000000000001776 ) ;
#8838 = CARTESIAN_POINT ( 'NONE',  ( 0.000000000000000000, -3.149999999999999911, 0.000000000000000000 ) ) ;
#8839 = CARTESIAN_POINT ( 'NONE',  ( 2.679491924311235174, 246.4583333333333428, 9.999999999999998224 ) ) ;
#8840 = FACE_OUTER_BOUND ( 'NONE', #64222, .T. ) ;
#8841 =( BOUNDED_CURVE ( )  B_SPLINE_CURVE ( 3, ( #17181, #63205, #17557, #40574 ),
 .UNSPECIFIED., .F., .F. ) 
 B_SPLINE_CURVE_WITH_KNOTS ( ( 4, 4 ),
 ( 3.141592653589793116, 4.864332078990434738 ),
 .UNSPECIFIED. ) 
 CURVE ( )  GEOMETRIC_REPRESENTATION_ITEM ( )  RATIONAL_B_SPLINE_CURVE ( ( 1.000000000000000000, 0.7675992199215417866, 0.7675992199215417866, 1.000000000000000000 ) ) 
 REPRESENTATION_ITEM ( '' )  );
#8842 = CARTESIAN_POINT ( 'NONE',  ( -1.836970198721029983E-15, 183.7500000000000284, 10.00000000000000178 ) ) ;
#8843 = CARTESIAN_POINT ( 'NONE',  ( 30.82842712474616675, 198.5000000027312126, 167.1715728752537018 ) ) ;
#8844 = CARTESIAN_POINT ( 'NONE',  ( 5.082755093536320601, -5.082755093536318824, 23.42405278187175455 ) ) ;
#8845 = CARTESIAN_POINT ( 'NONE',  ( -5.676582343750006032, 159.4270833299193555, 9.832129032723418760 ) ) ;
#8846 = DIRECTION ( 'NONE',  ( -1.000000000000000000, 0.000000000000000000, 0.000000000000000000 ) ) ;
#8847 = CARTESIAN_POINT ( 'NONE',  ( -4.999999999999999112, 52.28182290968012325, 42.43119126381112238 ) ) ;
#8848 = CARTESIAN_POINT ( 'NONE',  ( 47.32259252271278882, 145.2267040872997939, 65.76194439203457875 ) ) ;
#8851 = DIRECTION ( 'NONE',  ( 0.000000000000000000, 1.000000000000000000, 0.000000000000000000 ) ) ;
#8850 = CARTESIAN_POINT ( 'NONE',  ( 7.999999999999991118, 3.313708498984758055, 25.67405277982336997 ) ) ;
#8849 = CARTESIAN_POINT ( 'NONE',  ( 25.17157287525381548, 201.6250000000000284, 167.1715728752537018 ) ) ;
#8852 = EDGE_LOOP ( 'NONE', ( #74466, #4658 ) ) ;
#8853 = AXIS2_PLACEMENT_3D ( 'NONE', #70300, #18615, #41626 ) ;
#8854 = CARTESIAN_POINT ( 'NONE',  ( 6.951808397369818766E-16, 12.34374999658601801, -11.35316468750000141 ) ) ;
#8855 = CARTESIAN_POINT ( 'NONE',  ( 5.000000000000001776, 97.70833332650536818, -8.660254037844389075 ) ) ;
#8856 = CARTESIAN_POINT ( 'NONE',  ( 4.999999999999993783, 31.04166665983870033, 8.660254037844390851 ) ) ;
#8857 = CYLINDRICAL_SURFACE ( 'NONE', #26703, 7.000000000000000000 ) ;
#8858 = CARTESIAN_POINT ( 'NONE',  ( -2.839093476692135984E-14, 208.6875000013656063, 138.5412658750000503 ) ) ;
#8859 = CARTESIAN_POINT ( 'NONE',  ( 7.320508075688774596, 52.49999999317203248, -7.320508075688774596 ) ) ;
#8860 = CARTESIAN_POINT ( 'NONE',  ( -5.082755093536325930, 111.9687500020483810, -5.082755093536325930 ) ) ;
#8861 = CARTESIAN_POINT ( 'NONE',  ( -1.881053915767124440, 9.124999998634407916, 4.541265875000001451 ) ) ;
#8862 = CYLINDRICAL_SURFACE ( 'NONE', #69896, 10.00000000000000178 ) ;
#8863 = CARTESIAN_POINT ( 'NONE',  ( -5.656854249492375253, 5.656854249492375253, 11.14280277982336642 ) ) ;
#8865 = CARTESIAN_POINT ( 'NONE',  ( 4.999999999999993783, 6.041666659838699438, 8.660254037844390851 ) ) ;
#8864 = DIRECTION ( 'NONE',  ( 0.000000000000000000, 0.000000000000000000, -1.000000000000000000 ) ) ;
#8866 = ORIENTED_EDGE ( 'NONE', *, *, #65201, .T. ) ;
#8867 = CARTESIAN_POINT ( 'NONE',  ( -7.999999999974042098, 1.357258486152048259E-05, 14.51729352187485311 ) ) ;
#8868 = CARTESIAN_POINT ( 'NONE',  ( -5.676582343750000703, 228.3854166700806729, -9.832129032723418760 ) ) ;
#8869 = CARTESIAN_POINT ( 'NONE',  ( -3.042071309553164404, 127.2395833299193555, -11.35316468749999963 ) ) ;
#8870 = ORIENTED_EDGE ( 'NONE', *, *, #58546, .F. ) ;
#8871 = CARTESIAN_POINT ( 'NONE',  ( 5.656854249492374365, 5.656854249492375253, 4.955302783920146226 ) ) ;
#8872 = CARTESIAN_POINT ( 'NONE',  ( -7.204075437095967871, 7.204075437095967871, 94.46875000204838102 ) ) ;
#8873 = FACE_OUTER_BOUND ( 'NONE', #12901, .T. ) ;
#8874 = CARTESIAN_POINT ( 'NONE',  ( -1.432654583217607414, 196.5000000013656063, 194.5412658750000219 ) ) ;
#8875 = CARTESIAN_POINT ( 'NONE',  ( 29.65685424949224824, 197.0625000000000000, 174.0000000000000284 ) ) ;
#8877 = CARTESIAN_POINT ( 'NONE',  ( 11.35316468749999785, 125.5729166632526841, 3.042071309553174174 ) ) ;
#8876 = CARTESIAN_POINT ( 'NONE',  ( 29.65685424949251825, 196.4375000000000284, 166.0000000000000284 ) ) ;
#8878 = DIRECTION ( 'NONE',  ( -0.000000000000000000, 1.000000000000000000, -0.000000000000000000 ) ) ;
#8879 = VERTEX_POINT ( 'NONE', #12935 ) ;
#8880 = CARTESIAN_POINT ( 'NONE',  ( 10.00000000000000178, 257.2916666666666856, 2.679491924311222739 ) ) ;
#8881 = AXIS2_PLACEMENT_3D ( 'NONE', #65769, #35279, #18278 ) ;
#8882 = CARTESIAN_POINT ( 'NONE',  ( 2.249999999999999112, -2.249999999999999556, 0.000000000000000000 ) ) ;
#8883 = CARTESIAN_POINT ( 'NONE',  ( 5.676582343750001591, 116.9270833299193555, -9.832129032723420536 ) ) ;
#8884 = CARTESIAN_POINT ( 'NONE',  ( 2.754378923186476579E-14, 208.1875000013656063, 194.5412658750000219 ) ) ;
#8885 = CARTESIAN_POINT ( 'NONE',  ( -7.188101187500000933, 19.49999999795161898, -2.977408999572651371 ) ) ;
#8886 = CARTESIAN_POINT ( 'NONE',  ( 1.871523826299183495E-15, -10.18810118749999916, 86.40625000204838102 ) ) ;
#8887 = CARTESIAN_POINT ( 'NONE',  ( -3.042071309553164404, 22.55208332991935194, -11.35316468749999963 ) ) ;
#8888 = VERTEX_POINT ( 'NONE', #65368 ) ;
#8889 = CARTESIAN_POINT ( 'NONE',  ( -38.00000000000002132, 82.00000000000001421, 57.99999999999999289 ) ) ;
#8890 = FACE_OUTER_BOUND ( 'NONE', #1948, .T. ) ;
#8891 = DIRECTION ( 'NONE',  ( -1.000000000000000000, -1.577021341797097560E-16, -0.000000000000000000 ) ) ;
#8892 = EDGE_CURVE ( 'NONE', #8398, #13802, #19717, .T. ) ;
#8893 = CARTESIAN_POINT ( 'NONE',  ( -8.000000000000000000, 98.09375000409680467, -3.313708498984761164 ) ) ;
#8894 = CARTESIAN_POINT ( 'NONE',  ( 2.977408999572650927, 0.7499999979516099868, -7.188101187500001821 ) ) ;
#8895 = CARTESIAN_POINT ( 'NONE',  ( -4.721056650415999201, 288.3281250017069510, -4.721056650415999201 ) ) ;
#8896 = DIRECTION ( 'NONE',  ( -1.000000000000000000, 0.000000000000000000, -0.000000000000000000 ) ) ;
#8897 = CARTESIAN_POINT ( 'NONE',  ( 3.042071309553167513, 217.1354166632526983, -11.35316468749999785 ) ) ;
#8898 = ORIENTED_EDGE ( 'NONE', *, *, #35227, .F. ) ;
#8899 = EDGE_CURVE ( 'NONE', #26634, #58573, #42765, .T. ) ;
#8900 = CARTESIAN_POINT ( 'NONE',  ( -11.35316468750000141, 138.8020833299193271, 3.042071309553159963 ) ) ;
#8901 = CARTESIAN_POINT ( 'NONE',  ( -7.204075437095965206, -7.204075437095968759, 85.84375000204836681 ) ) ;
#8902 = CARTESIAN_POINT ( 'NONE',  ( -24.54126587499998280, 199.1250000013656347, 171.4326545832179818 ) ) ;
#8903 = LINE ( 'NONE', #60956, #25764 ) ;
#8904 = CARTESIAN_POINT ( 'NONE',  ( -8.342170076843785083E-16, 16.18749999863440436, 4.541265875000002339 ) ) ;
#8905 = VERTEX_POINT ( 'NONE', #54436 ) ;
#8906 = VECTOR ( 'NONE', #34645, 1000.000000000000000 ) ;
#8907 = CARTESIAN_POINT ( 'NONE',  ( 2.849036369511732440E-14, 203.3750000027312126, 202.0000000000000000 ) ) ;
#8908 = EDGE_CURVE ( 'NONE', #471, #59945, #61066, .T. ) ;
#8909 = CARTESIAN_POINT ( 'NONE',  ( 3.458734124999959469, 198.7500000013656063, 140.5673454167824161 ) ) ;
#8910 = CARTESIAN_POINT ( 'NONE',  ( -1.656854249492403008, 204.8125000027312126, 146.0000000000000284 ) ) ;
#8911 = DIRECTION ( 'NONE',  ( -0.000000000000000000, -0.9659258262890698665, -0.2588190451025146332 ) ) ;
#8912 = VERTEX_POINT ( 'NONE', #2744 ) ;
#8913 = CARTESIAN_POINT ( 'NONE',  ( -2.977408999572650039, 9.937499997951610098, -7.188101187500000933 ) ) ;
#8914 = CARTESIAN_POINT ( 'NONE',  ( -23.64921716555839737, -13.39059054445463914, 190.0622490757375829 ) ) ;
#8915 = CYLINDRICAL_SURFACE ( 'NONE', #22245, 3.999999999999976019 ) ;
#8916 = CARTESIAN_POINT ( 'NONE',  ( 3.042071309553167069, 191.8229166632526415, -11.35316468749999785 ) ) ;
#8917 = CARTESIAN_POINT ( 'NONE',  ( -7.188101187500001821, 113.9375000020483952, -2.977408999572650483 ) ) ;
#8918 = CARTESIAN_POINT ( 'NONE',  ( 2.828427124746209831, 207.5000000027312126, 200.8284271247462129 ) ) ;
#8919 = CARTESIAN_POINT ( 'NONE',  ( -6.676582343750002480, 293.3906250017069510, -2.765530957081996810 ) ) ;
#8921 = CARTESIAN_POINT ( 'NONE',  ( -17.99999999999999645, -1.756128610415477631, 1.992221491942114003E-15 ) ) ;
#8920 = CARTESIAN_POINT ( 'NONE',  ( 8.311093377946834337, 222.0312500034139873, -8.311093377946836114 ) ) ;
#8922 = ORIENTED_EDGE ( 'NONE', *, *, #60821, .T. ) ;
#8923 = CARTESIAN_POINT ( 'NONE',  ( -11.35316468749999785, 229.0104166700806445, -3.042071309553164848 ) ) ;
#8924 = CARTESIAN_POINT ( 'NONE',  ( -2.977408999572647819, 7.188101187499991163, 1.205302781871753215 ) ) ;
#8925 = VECTOR ( 'NONE', #2870, 1000.000000000000114 ) ;
#8926 = DIRECTION ( 'NONE',  ( 0.000000000000000000, 0.000000000000000000, -1.000000000000000000 ) ) ;
#8927 = CARTESIAN_POINT ( 'NONE',  ( 3.313708498984802020, 19.59374999590321664, -7.999999999999958256 ) ) ;
#8928 = CARTESIAN_POINT ( 'NONE',  ( 2.620431783929788150, -65.99617417813075804, -26.42108291243856399 ) ) ;
#8929 = CARTESIAN_POINT ( 'NONE',  ( 3.458734125000016757, 201.1250000013656347, 199.4326545832176691 ) ) ;
#8930 = CARTESIAN_POINT ( 'NONE',  ( 0.000000000000000000, 125.0000000000000000, 8.000000000000000000 ) ) ;
#8931 = CARTESIAN_POINT ( 'NONE',  ( -7.778174593052023411, 7.778174593052023411, 114.8125000000000000 ) ) ;
#8932 = CARTESIAN_POINT ( 'NONE',  ( -7.999999999999998224, 95.09375000000001421, 3.313708498984766493 ) ) ;
#8933 = CARTESIAN_POINT ( 'NONE',  ( 8.311093377946834337, 115.4687499965860269, 8.311093377946839666 ) ) ;
#8934 = CARTESIAN_POINT ( 'NONE',  ( -5.000000000000000000, -10.82378452496245735, -67.02990231369408036 ) ) ;
#8935 = CARTESIAN_POINT ( 'NONE',  ( -6.735557395310442023E-16, 11.00000000000000000, 74.12500000000000000 ) ) ;
#8938 = CARTESIAN_POINT ( 'NONE',  ( 2.751064625579944321E-14, 201.7500000000000000, 194.0000000000000568 ) ) ;
#8937 = CARTESIAN_POINT ( 'NONE',  ( 31.45873412499999233, 198.6875000013655779, 169.9999999999998863 ) ) ;
#8936 = CARTESIAN_POINT ( 'NONE',  ( 24.54126587499998990, 197.4375000013655779, 169.9999999999998863 ) ) ;
#8939 = VERTEX_POINT ( 'NONE', #25730 ) ;
#8940 = CARTESIAN_POINT ( 'NONE',  ( 27.99999999999996803, 205.6250000027312126, 165.9999999999998863 ) ) ;
#8941 = CARTESIAN_POINT ( 'NONE',  ( -9.832129032723420536, 223.6979166632526983, 5.676582343749997150 ) ) ;
#8942 = CARTESIAN_POINT ( 'NONE',  ( 2.445694354108782775, 200.5625000013656063, 139.5543056458912190 ) ) ;
#8943 = CARTESIAN_POINT ( 'NONE',  ( 27.99999999999996447, 200.6875000013656063, 173.4587341249998929 ) ) ;
#8944 = CARTESIAN_POINT ( 'NONE',  ( -11.00000000000000000, 0.000000000000000000, 115.1875000040967763 ) ) ;
#8945 = CARTESIAN_POINT ( 'NONE',  ( -11.35316468749999785, 193.3854166632526415, -3.042071309553167513 ) ) ;
#8946 = CARTESIAN_POINT ( 'NONE',  ( 2.977408999572654480, 93.50000000204838102, 7.188101187499999156 ) ) ;
#8947 = DIRECTION ( 'NONE',  ( 0.000000000000000000, 0.000000000000000000, 1.000000000000000000 ) ) ;
#8948 = CARTESIAN_POINT ( 'NONE',  ( 2.780723358947928197E-16, 12.56249999863440792, -4.541265875000002339 ) ) ;
#8949 = CARTESIAN_POINT ( 'NONE',  ( 31.45873412499999944, 200.0000000013656063, 168.5673454167822740 ) ) ;
#8950 = CARTESIAN_POINT ( 'NONE',  ( 5.082755093536320601, -5.082755093536318824, 0.9240527818717529929 ) ) ;
#8951 = CARTESIAN_POINT ( 'NONE',  ( -8.000000000000000000, 96.50000000000000000, 0.000000000000000000 ) ) ;
#8952 = CARTESIAN_POINT ( 'NONE',  ( -5.676582343749998039, 82.44791666325268409, -9.832129032723420536 ) ) ;
#8953 = ORIENTED_EDGE ( 'NONE', *, *, #66662, .T. ) ;
#8954 = CARTESIAN_POINT ( 'NONE',  ( -5.000000000000000000, -51.30401030464765455, 41.49390406302032375 ) ) ;
#8955 = DIRECTION ( 'NONE',  ( 1.000000000000000000, 0.000000000000000000, 0.000000000000000000 ) ) ;
#8956 = CARTESIAN_POINT ( 'NONE',  ( 7.188101187500000044, 21.46874999795161543, 0.000000000000000000 ) ) ;
#8958 = CARTESIAN_POINT ( 'NONE',  ( 10.35000000000000142, 0.000000000000000000, -1.155342438046016218 ) ) ;
#8957 = VECTOR ( 'NONE', #39813, 1000.000000000000000 ) ;
#8959 = CARTESIAN_POINT ( 'NONE',  ( -11.35316468749999785, 83.07291666325268409, -3.042071309553167513 ) ) ;
#8960 = EDGE_LOOP ( 'NONE', ( #15397, #72908, #73570, #57830 ) ) ;
#8961 = CARTESIAN_POINT ( 'NONE',  ( -10.18810118749999916, 4.220049686691934809, 87.43750000204838102 ) ) ;
#8962 = CARTESIAN_POINT ( 'NONE',  ( 10.18810118749999916, 1.247682550866122264E-15, 114.9062500020483810 ) ) ;
#8963 = DIRECTION ( 'NONE',  ( -0.000000000000000000, -0.000000000000000000, -1.000000000000000000 ) ) ;
#8964 = CARTESIAN_POINT ( 'NONE',  ( 2.445694354108840063, 207.0625000013656063, 200.4456943541088663 ) ) ;
#8965 = CARTESIAN_POINT ( 'NONE',  ( -2.170320029210519586, 16.41060967376241209, 68.77687409974782895 ) ) ;
#8967 = CARTESIAN_POINT ( 'NONE',  ( 8.311093377946834337, 90.15624999658602690, 8.311093377946839666 ) ) ;
#8966 = CARTESIAN_POINT ( 'NONE',  ( -11.00000000000000000, 0.000000000000000000, 68.49999999999997158 ) ) ;
#8968 = CARTESIAN_POINT ( 'NONE',  ( -5.656854249492373476, -5.656854249492376141, 19.20530278392014978 ) ) ;
#8969 = CYLINDRICAL_SURFACE ( 'NONE', #1136, 10.00000000000000000 ) ;
#8970 =( BOUNDED_CURVE ( )  B_SPLINE_CURVE ( 2, ( #23984, #41348, #46993, #53780, #2089, #25081, #13752, #60541, #9238, #16001, #49601, #20921, #72987 ),
 .UNSPECIFIED., .F., .F. ) 
 B_SPLINE_CURVE_WITH_KNOTS ( ( 3, 2, 2, 2, 2, 2, 3 ),
 ( 0.3610969255903727637, 0.3663293280448572387, 0.3715617304993417136, 0.3767941329538261885, 0.3820265354083106635, 0.3872589378627951939, 0.3924913403172796134 ),
 .UNSPECIFIED. ) 
 CURVE ( )  GEOMETRIC_REPRESENTATION_ITEM ( )  RATIONAL_B_SPLINE_CURVE ( ( 1.000000000000000000, 0.9659258262890683122, 1.000000000000000000, 0.9659258262890683122, 1.000000000000000000, 0.9659258262890683122, 1.000000000000000000, 0.9659258262890683122, 1.000000000000000000, 0.9659258262890683122, 1.000000000000000000, 0.9659258262893669622, 0.9999999999997013500 ) ) 
 REPRESENTATION_ITEM ( '' )  );
#8971 = CARTESIAN_POINT ( 'NONE',  ( -2.679491924311225848, 163.3333333265053682, -10.00000000000000178 ) ) ;
#8972 = CARTESIAN_POINT ( 'NONE',  ( -7.188101187499999156, 91.62500000204838102, 2.977408999572654924 ) ) ;
#8973 = DIRECTION ( 'NONE',  ( 0.000000000000000000, 0.000000000000000000, 1.000000000000000000 ) ) ;
#8974 = CARTESIAN_POINT ( 'NONE',  ( -9.832129032723420536, 59.01041666325268409, 5.676582343749997150 ) ) ;
#8975 = CARTESIAN_POINT ( 'NONE',  ( 6.676582343750004256, 292.8906250017068942, 2.765530957081995478 ) ) ;
#8976 = CARTESIAN_POINT ( 'NONE',  ( 10.18810118749999916, 1.247682550866122264E-15, 107.7812500020483810 ) ) ;
#8977 = CARTESIAN_POINT ( 'NONE',  ( 3.042071309553167069, 206.8229166632526699, -11.35316468749999785 ) ) ;
#8978 = ORIENTED_EDGE ( 'NONE', *, *, #37103, .F. ) ;
#8979 = CARTESIAN_POINT ( 'NONE',  ( -1.173938163346586453E-11, 213.7499999999991189, 10.00000000000000178 ) ) ;
#8980 = CARTESIAN_POINT ( 'NONE',  ( 7.347880794884121708E-16, 300.0000000000000000, -6.000000000000001776 ) ) ;
#8981 = CARTESIAN_POINT ( 'NONE',  ( -2.485281374238308860, 288.1875000000000568, 6.000000000000264677 ) ) ;
#8983 = CARTESIAN_POINT ( 'NONE',  ( -11.35316468749999785, 193.0729166632526699, -3.042071309553167957 ) ) ;
#8982 = LINE ( 'NONE', #60660, #38707 ) ;
#8984 = CARTESIAN_POINT ( 'NONE',  ( 25.17157287525381193, 195.6250000000000284, 167.1715728752537018 ) ) ;
#8985 = CARTESIAN_POINT ( 'NONE',  ( 9.999999999999998224, 235.8333333401613174, -2.679491924311229401 ) ) ;
#8986 = DIRECTION ( 'NONE',  ( 0.000000000000000000, 0.000000000000000000, 1.000000000000000000 ) ) ;
#8987 = EDGE_LOOP ( 'NONE', ( #8812, #59289, #54791, #30260 ) ) ;
#8988 = CARTESIAN_POINT ( 'NONE',  ( -8.311093377946836114, 177.9687499965860127, -8.311093377946837890 ) ) ;
#8989 = ADVANCED_FACE ( 'NONE', ( #29934 ), #48751, .T. ) ;
#8990 = AXIS2_PLACEMENT_3D ( 'NONE', #73587, #22636, #63376 ) ;
#8991 = CARTESIAN_POINT ( 'NONE',  ( -7.188101187499992051, 0.000000000000000000, 23.98655278187175455 ) ) ;
#8992 = CARTESIAN_POINT ( 'NONE',  ( -12.00000000000000178, 0.000000000000000000, -21.47459999999999525 ) ) ;
#8993 = VERTEX_POINT ( 'NONE', #6924 ) ;
#8994 = CARTESIAN_POINT ( 'NONE',  ( 8.000000000000001776, 95.84375000409677625, 3.313708498984759387 ) ) ;
#8995 = CARTESIAN_POINT ( 'NONE',  ( 26.34314575050765583, 208.5624999999999716, 165.9999999999998863 ) ) ;
#8996 = EDGE_CURVE ( 'NONE', #22395, #17893, #24923, .T. ) ;
#8997 = EDGE_CURVE ( 'NONE', #34004, #10894, #32679, .T. ) ;
#8998 = CARTESIAN_POINT ( 'NONE',  ( 4.000000000000001776, 17.06250000000000355, -1.656854249492381248 ) ) ;
#8999 = CARTESIAN_POINT ( 'NONE',  ( -4.541265875000002339, 16.81249999863440436, -5.561446717895856393E-16 ) ) ;
#9000 = CARTESIAN_POINT ( 'NONE',  ( -3.313708498984758943, -7.999999999999989342, 11.79905278392014800 ) ) ;
#9002 = CARTESIAN_POINT ( 'NONE',  ( -7.999999999999991118, 0.000000000000000000, 19.01780278392014623 ) ) ;
#9001 = AXIS2_PLACEMENT_3D ( 'NONE', #60798, #36313, #59329 ) ;
#9003 = EDGE_LOOP ( 'NONE', ( #43742, #64553, #17626, #9619 ) ) ;
#9004 = CARTESIAN_POINT ( 'NONE',  ( 5.000000000000000000, -10.60557809245594640, -66.49298242784793445 ) ) ;
#9005 = CARTESIAN_POINT ( 'NONE',  ( -2.977408999572650927, 90.87500000204838102, -7.188101187500001821 ) ) ;
#9007 = CARTESIAN_POINT ( 'NONE',  ( -9.832129032723418760, 253.4895833367473017, -5.676582343749998927 ) ) ;
#9006 = CARTESIAN_POINT ( 'NONE',  ( -10.18810118749999916, 0.000000000000000000, 117.5312500020483810 ) ) ;
#9008 = CARTESIAN_POINT ( 'NONE',  ( 1424.688200795887269, 710.9677537767815920, 895.9921604560587411 ) ) ;
#9009 = ORIENTED_EDGE ( 'NONE', *, *, #68991, .F. ) ;
#9010 = CARTESIAN_POINT ( 'NONE',  ( -11.35316468749999785, 264.0104166700807014, -3.042071309553164848 ) ) ;
#9011 = EDGE_CURVE ( 'NONE', #28769, #49646, #14789, .T. ) ;
#9012 = CARTESIAN_POINT ( 'NONE',  ( 7.188101187499993827, -2.977408999572645598, 17.14280278187175455 ) ) ;
#9013 = VERTEX_POINT ( 'NONE', #15171 ) ;
#9014 = VERTEX_POINT ( 'NONE', #54809 ) ;
#9015 = CARTESIAN_POINT ( 'NONE',  ( -7.204075437095967871, 7.204075437095967871, 79.46875000204836681 ) ) ;
#9016 = CARTESIAN_POINT ( 'NONE',  ( -11.35316468749999785, 73.38541666325268409, -3.042071309553167513 ) ) ;
#9017 = CARTESIAN_POINT ( 'NONE',  ( 2.955318825516778158, 19.07835557137325821, -0.7126204852947338741 ) ) ;
#9018 = CARTESIAN_POINT ( 'NONE',  ( -11.00000000000000000, 0.000000000000000000, 95.49999999999998579 ) ) ;
#9021 = CARTESIAN_POINT ( 'NONE',  ( -4.721056650415998313, 295.7343750017069510, 4.721056650416000089 ) ) ;
#9020 = CARTESIAN_POINT ( 'NONE',  ( 25.17157287525381903, 199.0000000027312126, 172.8284271247460993 ) ) ;
#9019 = DIRECTION ( 'NONE',  ( 0.000000000000000000, 0.000000000000000000, 1.000000000000000000 ) ) ;
#9022 = CARTESIAN_POINT ( 'NONE',  ( 1.656854249492381248, 14.18750000000000000, -4.000000000000001776 ) ) ;
#9023 = LINE ( 'NONE', #55431, #34815 ) ;
#9024 = AXIS2_PLACEMENT_3D ( 'NONE', #14547, #8911, #30804 ) ;
#9025 = CARTESIAN_POINT ( 'NONE',  ( -2.445694354108784108, 198.5625000013656063, 195.5543056458912190 ) ) ;
#9026 = LINE ( 'NONE', #55059, #20532 ) ;
#9027 = CARTESIAN_POINT ( 'NONE',  ( 3.313708498984762496, 4.031249995903220196, 7.999999999999998224 ) ) ;
#9028 = CARTESIAN_POINT ( 'NONE',  ( 30.44569435410883429, 200.8125000013656063, 167.5543056458911053 ) ) ;
#9029 = CARTESIAN_POINT ( 'NONE',  ( 2.977408999572650927, 13.12499999795161187, -7.188101187500001821 ) ) ;
#9030 = AXIS2_PLACEMENT_3D ( 'NONE', #72572, #55978, #8824 ) ;
#9031 = CARTESIAN_POINT ( 'NONE',  ( 7.999999999999992895, -3.313708498984756279, 27.17405278392014978 ) ) ;
#9032 = CARTESIAN_POINT ( 'NONE',  ( -4.999999999999992895, 243.9583333401613174, 8.660254037844390851 ) ) ;
#9033 = CARTESIAN_POINT ( 'NONE',  ( 2.977408999572650039, 112.0625000020483810, -7.188101187500000933 ) ) ;
#9034 = CARTESIAN_POINT ( 'NONE',  ( -3.496982156821605070, -51.71401992552402049, -48.73755072030548519 ) ) ;
#9035 = CARTESIAN_POINT ( 'NONE',  ( -5.711993833409989278E-12, 133.7499999999995737, 9.999999999999998224 ) ) ;
#9036 = CARTESIAN_POINT ( 'NONE',  ( -25.17157287525377996, 207.6250000000000284, 172.8284271247465256 ) ) ;
#9037 = CARTESIAN_POINT ( 'NONE',  ( 5.082755093536318824, 5.082755093536319713, 17.79905278187175810 ) ) ;
#9038 = CARTESIAN_POINT ( 'NONE',  ( 2.828427124746153876, 207.0000000027312126, 144.8284271247462129 ) ) ;
#9039 = CARTESIAN_POINT ( 'NONE',  ( -3.042071309553164404, 37.23958332991934839, -11.35316468749999963 ) ) ;
#9040 = CARTESIAN_POINT ( 'NONE',  ( -3.000000000000001332, -45.00000000000001421, 139.1455027589170470 ) ) ;
#9041 = CARTESIAN_POINT ( 'NONE',  ( 10.00000000000000178, 7.083333326505365513, -2.679491924311226736 ) ) ;
#9042 = ORIENTED_EDGE ( 'NONE', *, *, #2908, .F. ) ;
#9043 = EDGE_CURVE ( 'NONE', #23294, #23507, #40365, .T. ) ;
#9044 = DIRECTION ( 'NONE',  ( -0.000000000000000000, 1.000000000000000000, -0.000000000000000000 ) ) ;
#9045 = CARTESIAN_POINT ( 'NONE',  ( -7.778174593052023411, 7.778174593052023411, 70.00000000409677625 ) ) ;
#9046 = CARTESIAN_POINT ( 'NONE',  ( -8.311093377946841443, 43.90624999658601268, 8.311093377946830785 ) ) ;
#9047 = CARTESIAN_POINT ( 'NONE',  ( 2.020667218593132706E-15, -11.00000000000000000, 82.56250000409677625 ) ) ;
#9048 = CARTESIAN_POINT ( 'NONE',  ( 3.458734124999960358, 202.6250000013656063, 143.4326545832176976 ) ) ;
#9049 = CARTESIAN_POINT ( 'NONE',  ( -8.660254037844387298, 259.5833333333333144, -4.999999999999999112 ) ) ;
#9050 = DIRECTION ( 'NONE',  ( 0.000000000000000000, 0.000000000000000000, 1.000000000000000000 ) ) ;
#9052 = CARTESIAN_POINT ( 'NONE',  ( 9.832129032723416984, 35.36458332991934839, 5.676582343750006032 ) ) ;
#9051 = CARTESIAN_POINT ( 'NONE',  ( -5.082755093536325930, 99.96875000204838102, -5.082755093536325930 ) ) ;
#9054 = ADVANCED_FACE ( 'NONE', ( #9535 ), #72898, .F. ) ;
#9053 = CARTESIAN_POINT ( 'NONE',  ( -7.999999999999991118, 3.313708498984756723, 9.736552779823368198 ) ) ;
#9055 = DIRECTION ( 'NONE',  ( 0.000000000000000000, -1.000000000000000000, 0.000000000000000000 ) ) ;
#9056 = CARTESIAN_POINT ( 'NONE',  ( 9.832129032723420536, 166.1979166632526983, -5.676582343749999815 ) ) ;
#9057 = CARTESIAN_POINT ( 'NONE',  ( -10.00000000000000178, 134.3749999931720254, -1.224646799147353454E-15 ) ) ;
#9058 = CARTESIAN_POINT ( 'NONE',  ( -4.401442555609581635E-16, 107.6562500020483810, -7.188101187500000044 ) ) ;
#9059 = ORIENTED_EDGE ( 'NONE', *, *, #41020, .F. ) ;
#9060 = CARTESIAN_POINT ( 'NONE',  ( 5.000000000000001776, 22.70833332650536818, -8.660254037844389075 ) ) ;
#9061 = CARTESIAN_POINT ( 'NONE',  ( -2.085542519210945728E-15, 24.84374999658601624, 11.35316468750000141 ) ) ;
#9062 =( BOUNDED_CURVE ( )  B_SPLINE_CURVE ( 2, ( #64712, #47353, #623, #41699, #5895, #59064, #29276, #57585, #18320 ),
 .UNSPECIFIED., .F., .F. ) 
 B_SPLINE_CURVE_WITH_KNOTS ( ( 3, 2, 2, 2, 3 ),
 ( 0.3750000000000000000, 0.3819444444444444198, 0.3888888888888888395, 0.3958333333333332593, 0.4027777777777776791 ),
 .UNSPECIFIED. ) 
 CURVE ( )  GEOMETRIC_REPRESENTATION_ITEM ( )  RATIONAL_B_SPLINE_CURVE ( ( 1.000000000000000000, 0.9238795325112867385, 1.000000000000000000, 0.9238795325112867385, 1.000000000000000000, 0.9238795325112867385, 1.000000000000000000, 0.9238795325112879597, 0.9999999999999987788 ) ) 
 REPRESENTATION_ITEM ( '' )  );
#9063 = EDGE_CURVE ( 'NONE', #52340, #21543, #21469, .T. ) ;
#9064 = CARTESIAN_POINT ( 'NONE',  ( -4.881900264494508868, -7.573738413550474391, -6.853343576234544043E-15 ) ) ;
#9065 = ORIENTED_EDGE ( 'NONE', *, *, #2124, .F. ) ;
#9066 = CARTESIAN_POINT ( 'NONE',  ( -31.99999999999996447, 205.4375000027312126, 171.6568542494928522 ) ) ;
#9067 = CARTESIAN_POINT ( 'NONE',  ( -4.220049686691937474, -10.18810118749999738, 78.43750000204838102 ) ) ;
#9068 = CARTESIAN_POINT ( 'NONE',  ( -30.82842712474620939, 197.1250000000000284, 167.1715728752542134 ) ) ;
#9070 = CARTESIAN_POINT ( 'NONE',  ( -8.311093377946836114, 147.6562499965860127, -8.311093377946837890 ) ) ;
#9069 = CYLINDRICAL_SURFACE ( 'NONE', #24246, 8.000000000000000000 ) ;
#9071 = DIRECTION ( 'NONE',  ( 1.000000000000000000, -0.000000000000000000, -0.000000000000000000 ) ) ;
#9072 = CARTESIAN_POINT ( 'NONE',  ( -7.999999999999991118, 0.000000000000000000, 12.88655278432982421 ) ) ;
#9073 = CARTESIAN_POINT ( 'NONE',  ( -26.32261923518656488, -22.01951323694076734, 186.4110172268610199 ) ) ;
#9074 = CARTESIAN_POINT ( 'NONE',  ( -11.35316468749999608, 234.1145833367473017, 3.042071309553173730 ) ) ;
#9075 = CARTESIAN_POINT ( 'NONE',  ( -10.18810118749999738, -4.220049686691941915, 84.62500000204838102 ) ) ;
#9076 = VERTEX_POINT ( 'NONE', #15913 ) ;
#9077 = CARTESIAN_POINT ( 'NONE',  ( 0.000000000000000000, 125.0000000000000000, 0.000000000000000000 ) ) ;
#9078 = CARTESIAN_POINT ( 'NONE',  ( -7.999999999999998224, 122.2812500040967905, 3.313708498984766049 ) ) ;
#9079 = CARTESIAN_POINT ( 'NONE',  ( -9.832129032723418760, 103.1770833299193555, -5.676582343750004256 ) ) ;
#9080 = CARTESIAN_POINT ( 'NONE',  ( 10.18810118750000093, -4.220049686691933921, 96.81250000204839523 ) ) ;
#9081 =( BOUNDED_CURVE ( )  B_SPLINE_CURVE ( 2, ( #22105, #3651, #26651, #72689, #20991, #15322, #17569, #28891, #62843 ),
 .UNSPECIFIED., .F., .F. ) 
 B_SPLINE_CURVE_WITH_KNOTS ( ( 3, 2, 2, 2, 3 ),
 ( 0.1041666666666644370, 0.1145833333333311083, 0.1249999999999977796, 0.1354166666666644647, 0.1458333333333311499 ),
 .UNSPECIFIED. ) 
 CURVE ( )  GEOMETRIC_REPRESENTATION_ITEM ( )  RATIONAL_B_SPLINE_CURVE ( ( 1.000000000000016431, 0.9238795325112704182, 1.000000000000000000, 0.9238795325112867385, 1.000000000000000000, 0.9238795325112867385, 1.000000000000000000, 0.9238795325113027257, 0.9999999999999840128 ) ) 
 REPRESENTATION_ITEM ( '' )  );
#9082 = CARTESIAN_POINT ( 'NONE',  ( 2.679491924311176554, 16.04166666666667496, -10.00000000000004263 ) ) ;
#9083 = EDGE_LOOP ( 'NONE', ( #23389, #21966, #58924 ) ) ;
#9084 = ORIENTED_EDGE ( 'NONE', *, *, #32095, .F. ) ;
#9085 = CARTESIAN_POINT ( 'NONE',  ( -3.211159895383562723, 2.062499998634407028, 3.211159895383561391 ) ) ;
#9086 = CARTESIAN_POINT ( 'NONE',  ( 7.188101187499999156, 10.87499999795161187, 2.977408999572654924 ) ) ;
#9087 = VECTOR ( 'NONE', #44891, 1000.000000000000000 ) ;
#9088 = CARTESIAN_POINT ( 'NONE',  ( 8.000000000000000000, 118.4375000040967763, -9.797174393178825657E-16 ) ) ;
#9089 = CARTESIAN_POINT ( 'NONE',  ( 4.220049686691941027, -10.18810118749999738, 91.00000000204836681 ) ) ;
#9090 = CARTESIAN_POINT ( 'NONE',  ( -30.44569435410883429, 200.8125000013656063, 167.5543056458915885 ) ) ;
#9091 = ADVANCED_FACE ( 'NONE', ( #21206 ), #55560, .F. ) ;
#9092 = DIRECTION ( 'NONE',  ( -0.000000000000000000, 1.000000000000000000, -0.000000000000000000 ) ) ;
#9093 = AXIS2_PLACEMENT_3D ( 'NONE', #54377, #9092, #1944 ) ;
#9094 = CARTESIAN_POINT ( 'NONE',  ( 1.656854249492381248, 3.187500000000000000, -4.000000000000001776 ) ) ;
#9095 = CARTESIAN_POINT ( 'NONE',  ( -4.000000000000002665, 18.31249999726881938, 1.656854249492380804 ) ) ;
#9096 = CARTESIAN_POINT ( 'NONE',  ( 1.881053915767121998, 2.499999998634407028, -4.541265875000002339 ) ) ;
#9097 = EDGE_LOOP ( 'NONE', ( #42952, #21291, #66728, #7109 ) ) ;
#9098 = CARTESIAN_POINT ( 'NONE',  ( -1.432654583217607192, 195.2500000013656063, 194.5412658750000219 ) ) ;
#9100 = FACE_OUTER_BOUND ( 'NONE', #25221, .T. ) ;
#9099 = CARTESIAN_POINT ( 'NONE',  ( -29.43265458321771177, 197.5000000013656063, 166.5412658750003914 ) ) ;
#9101 = CARTESIAN_POINT ( 'NONE',  ( 3.211159895383561835, 17.43749999863440792, -3.211159895383561835 ) ) ;
#9102 = CARTESIAN_POINT ( 'NONE',  ( 2.765530957081996366, 299.1406250017068942, -6.676582343750002480 ) ) ;
#9103 = CARTESIAN_POINT ( 'NONE',  ( -7.188101187499990274, -2.977408999572651371, 6.080302781871753659 ) ) ;
#9104 = ORIENTED_EDGE ( 'NONE', *, *, #69176, .T. ) ;
#9105 = VERTEX_POINT ( 'NONE', #10273 ) ;
#9106 = CARTESIAN_POINT ( 'NONE',  ( -7.204075437095965206, -7.204075437095968759, 97.84375000204836681 ) ) ;
#9107 = CARTESIAN_POINT ( 'NONE',  ( -31.45873412499998523, 205.0000000013655779, 171.4326545832180386 ) ) ;
#9108 = CARTESIAN_POINT ( 'NONE',  ( -27.99999999999995737, 201.5000000000000000, 174.0000000000003695 ) ) ;
#9109 = CARTESIAN_POINT ( 'NONE',  ( 2.754378923186476579E-14, 208.4375000013656063, 194.5412658750000219 ) ) ;
#9110 = CARTESIAN_POINT ( 'NONE',  ( 5.000000000000032863, 59.16666666666672114, 8.660254037844458352 ) ) ;
#9111 = CARTESIAN_POINT ( 'NONE',  ( -8.660254037844390851, 107.9166666666666714, 4.999999999999998224 ) ) ;
#9112 = CARTESIAN_POINT ( 'NONE',  ( -7.999999999999998224, 110.0937499999999858, 3.313708498984766493 ) ) ;
#9113 = ADVANCED_FACE ( 'NONE', ( #33300, #56298 ), #4614, .F. ) ;
#9114 = CARTESIAN_POINT ( 'NONE',  ( -6.676582343750003368, 292.5468750017068942, -2.765530957081996810 ) ) ;
#9115 = CARTESIAN_POINT ( 'NONE',  ( -2.977408999572647819, 7.188101187499991163, 12.08030278187175099 ) ) ;
#9116 = ORIENTED_EDGE ( 'NONE', *, *, #65198, .F. ) ;
#9117 = CARTESIAN_POINT ( 'NONE',  ( -10.00000000000000355, 174.5833333265053966, 2.679491924311223183 ) ) ;
#9118 = CARTESIAN_POINT ( 'NONE',  ( 4.898587196589412829E-16, 18.18749999590322020, -8.000000000000000000 ) ) ;
#9119 = CARTESIAN_POINT ( 'NONE',  ( 3.458734124999959914, 203.4375000013656063, 142.0000000000000568 ) ) ;
#9120 = DIRECTION ( 'NONE',  ( 0.000000000000000000, -1.000000000000000000, 0.000000000000000000 ) ) ;
#9121 = CARTESIAN_POINT ( 'NONE',  ( -2.751549872419339698E-14, 194.9207531772045741, 145.9207531772046025 ) ) ;
#9122 = CARTESIAN_POINT ( 'NONE',  ( 5.676582343749997150, 257.5520833367473301, -9.832129032723418760 ) ) ;
#9123 = CARTESIAN_POINT ( 'NONE',  ( 38.00000000000000000, -63.00000000000000000, 15.00000000000000178 ) ) ;
#9124 = CARTESIAN_POINT ( 'NONE',  ( 7.778174593052021635, 7.778174593052023411, 114.4375000000000000 ) ) ;
#9125 = CARTESIAN_POINT ( 'NONE',  ( -11.35316468750000141, 8.281249996586016238, -1.390361679473963753E-15 ) ) ;
#9126 = CARTESIAN_POINT ( 'NONE',  ( -7.188101187499992051, 2.977408999572646930, 3.267802781871751439 ) ) ;
#9127 = CARTESIAN_POINT ( 'NONE',  ( 9.832129032723416984, 190.6770833299193555, 5.676582343750006032 ) ) ;
#9128 = LINE ( 'NONE', #27590, #55212 ) ;
#9129 = CARTESIAN_POINT ( 'NONE',  ( 1.881053915767122664, 6.124999998634407916, 4.541265875000001451 ) ) ;
#9130 = CYLINDRICAL_SURFACE ( 'NONE', #11577, 3.999999999999976019 ) ;
#9132 = DIRECTION ( 'NONE',  ( -1.084202172485504434E-16, 1.000000000000000000, 0.000000000000000000 ) ) ;
#9131 = CYLINDRICAL_SURFACE ( 'NONE', #19007, 11.00000000000000000 ) ;
#9133 = ORIENTED_EDGE ( 'NONE', *, *, #56617, .F. ) ;
#9134 = CARTESIAN_POINT ( 'NONE',  ( -2.445694354108840063, 206.0625000013656063, 139.5543056458912190 ) ) ;
#9135 = CARTESIAN_POINT ( 'NONE',  ( -3.042071309553173730, 14.32291666325268231, 11.35316468749999785 ) ) ;
#9136 = CARTESIAN_POINT ( 'NONE',  ( 11.00000000000000355, -4.556349186104045046, 100.8437500040967620 ) ) ;
#9137 = CARTESIAN_POINT ( 'NONE',  ( -11.00000000000000000, 0.000000000000000000, 106.1875000040967620 ) ) ;
#9138 = CARTESIAN_POINT ( 'NONE',  ( -27.99999999999991829, 201.9375000013656063, 173.4587341250003760 ) ) ;
#9139 = CARTESIAN_POINT ( 'NONE',  ( -2.775557561562891351E-14, 195.0000000000000000, 142.0000000000000568 ) ) ;
#9140 = CARTESIAN_POINT ( 'NONE',  ( 7.188101187500000933, 119.0000000020483810, -2.977408999572651371 ) ) ;
#9142 = EDGE_CURVE ( 'NONE', #56998, #19443, #35006, .T. ) ;
#9141 = CARTESIAN_POINT ( 'NONE',  ( 3.313708498984762496, -7.999999999999989342, 25.29905277982336642 ) ) ;
#9143 = CARTESIAN_POINT ( 'NONE',  ( -2.085542519210945728E-15, 124.5312499965860269, 11.35316468750000141 ) ) ;
#9144 = CARTESIAN_POINT ( 'NONE',  ( 4.999999999999993783, 91.04166665983871098, 8.660254037844390851 ) ) ;
#9145 = VECTOR ( 'NONE', #58659, 1000.000000000000000 ) ;
#9146 = CARTESIAN_POINT ( 'NONE',  ( 7.188101187500000044, 93.40625000204838102, -8.802885111219163269E-16 ) ) ;
#9147 = CARTESIAN_POINT ( 'NONE',  ( -8.342170076843785083E-16, 21.18749999863440792, 4.541265875000002339 ) ) ;
#9148 = CARTESIAN_POINT ( 'NONE',  ( -7.347880794884122694E-16, 7.750000000000000000, 4.000000000000001776 ) ) ;
#9149 = DIRECTION ( 'NONE',  ( 1.000000000000000000, 0.000000000000000000, 0.000000000000000000 ) ) ;
#9150 = ORIENTED_EDGE ( 'NONE', *, *, #27105, .F. ) ;
#9151 = FACE_OUTER_BOUND ( 'NONE', #26704, .T. ) ;
#9152 = EDGE_CURVE ( 'NONE', #7738, #13141, #69982, .T. ) ;
#9153 = CARTESIAN_POINT ( 'NONE',  ( -4.721056650415999201, 292.4843750017070079, -4.721056650415999201 ) ) ;
#9154 =( NAMED_UNIT ( * ) PLANE_ANGLE_UNIT ( ) SI_UNIT ( $, .RADIAN. ) );
#9155 = CARTESIAN_POINT ( 'NONE',  ( 1.469576158976822172E-15, -7.999999999999991118, 1.392802783920146004 ) ) ;
#9156 = CARTESIAN_POINT ( 'NONE',  ( 6.951808397369818766E-16, 167.0312499965860411, -11.35316468750000141 ) ) ;
#9157 = CARTESIAN_POINT ( 'NONE',  ( -2.849036369511732440E-14, 198.2500000000000000, 138.0000000000000568 ) ) ;
#9158 = CARTESIAN_POINT ( 'NONE',  ( 4.000000000000015987, 195.5000000000000000, 198.0000000000000284 ) ) ;
#9159 = CARTESIAN_POINT ( 'NONE',  ( -4.556349186104045934, 11.00000000000000000, 69.71875000000000000 ) ) ;
#9160 = CARTESIAN_POINT ( 'NONE',  ( 4.220049686691934809, 10.18810118749999916, 102.0625000020483810 ) ) ;
#9161 = ORIENTED_EDGE ( 'NONE', *, *, #14652, .T. ) ;
#9162 = CARTESIAN_POINT ( 'NONE',  ( 8.660254037844389075, 157.2916666598387110, -5.000000000000000000 ) ) ;
#9163 = CARTESIAN_POINT ( 'NONE',  ( -2.085542519210945728E-15, 149.8437499965860411, 11.35316468750000141 ) ) ;
#9164 = CARTESIAN_POINT ( 'NONE',  ( 3.458734125000016313, 194.8750000013656347, 199.4326545832176976 ) ) ;
#9165 = CARTESIAN_POINT ( 'NONE',  ( -3.458734124999959469, 207.7500000013656063, 199.4326545832176976 ) ) ;
#9166 = DIRECTION ( 'NONE',  ( 0.000000000000000000, 0.000000000000000000, 1.000000000000000000 ) ) ;
#9167 = CARTESIAN_POINT ( 'NONE',  ( 9.832129032723420536, 66.51041666325268409, -5.676582343749999815 ) ) ;
#9168 = ORIENTED_EDGE ( 'NONE', *, *, #27605, .T. ) ;
#9169 = CARTESIAN_POINT ( 'NONE',  ( 4.220049686691934809, 10.18810118749999916, 110.6875000020483952 ) ) ;
#9170 = CARTESIAN_POINT ( 'NONE',  ( -1.881053915767124440, 8.124999998634406140, 4.541265875000001451 ) ) ;
#9171 = VERTEX_POINT ( 'NONE', #45337 ) ;
#9172 = CARTESIAN_POINT ( 'NONE',  ( 2.977408999572650927, 20.24999999795161898, -7.188101187500001821 ) ) ;
#9173 = CARTESIAN_POINT ( 'NONE',  ( 4.242640687119287435, 290.4375000034140157, 4.242640687119285658 ) ) ;
#9174 = CARTESIAN_POINT ( 'NONE',  ( -4.999999999999992895, 248.9583333401613174, 8.660254037844390851 ) ) ;
#9175 = CARTESIAN_POINT ( 'NONE',  ( -1.320432766682874540E-15, 19.96874999795161543, 7.188101187500000044 ) ) ;
#9176 = CARTESIAN_POINT ( 'NONE',  ( 7.188101187499992051, 2.977408999572647819, 2.330302781871750550 ) ) ;
#9177 =( BOUNDED_CURVE ( )  B_SPLINE_CURVE ( 2, ( #40501, #51072, #15987, #4691, #28061, #28433, #50692, #63506, #21649 ),
 .UNSPECIFIED., .F., .F. ) 
 B_SPLINE_CURVE_WITH_KNOTS ( ( 3, 2, 2, 2, 3 ),
 ( 0.6000000000000004219, 0.6083333333333338366, 0.6166666666666672514, 0.6250000000000006661, 0.6333333333333339699 ),
 .UNSPECIFIED. ) 
 CURVE ( )  GEOMETRIC_REPRESENTATION_ITEM ( )  RATIONAL_B_SPLINE_CURVE ( ( 0.9999999999999958922, 0.9238795325112908463, 1.000000000000000000, 0.9238795325112867385, 1.000000000000000000, 0.9238795325112867385, 1.000000000000000000, 0.9238795325112806323, 1.000000000000005995 ) ) 
 REPRESENTATION_ITEM ( '' )  );
#9178 = CARTESIAN_POINT ( 'NONE',  ( -10.18810118749999916, 0.000000000000000000, 113.0312500020483810 ) ) ;
#9179 = DIRECTION ( 'NONE',  ( -0.000000000000000000, 1.000000000000000000, -0.000000000000000000 ) ) ;
#9180 = CARTESIAN_POINT ( 'NONE',  ( 4.000000000000000888, 4.687499997268812280, 1.656854249492384135 ) ) ;
#9181 = ORIENTED_EDGE ( 'NONE', *, *, #9991, .F. ) ;
#9182 = CARTESIAN_POINT ( 'NONE',  ( 1.432654583217662481, 206.1250000013655779, 194.5412658750000219 ) ) ;
#9183 = AXIS2_PLACEMENT_3D ( 'NONE', #8634, #19938, #3349 ) ;
#9184 = CARTESIAN_POINT ( 'NONE',  ( -24.54126587500002543, 209.2500000013655779, 168.5673454167826435 ) ) ;
#9185 = CARTESIAN_POINT ( 'NONE',  ( 3.211159895383560947, 8.187499998634406140, 3.211159895383562723 ) ) ;
#9186 = CARTESIAN_POINT ( 'NONE',  ( -5.082755093536325930, 111.9687500020483810, -5.082755093536325930 ) ) ;
#9187 = CARTESIAN_POINT ( 'NONE',  ( -4.000000000000002665, 13.56250000000000000, 1.656854249492380582 ) ) ;
#9188 = CARTESIAN_POINT ( 'NONE',  ( 5.082755093536320601, -5.082755093536318824, 27.54905278187175455 ) ) ;
#9189 = ORIENTED_EDGE ( 'NONE', *, *, #12241, .F. ) ;
#9190 = CARTESIAN_POINT ( 'NONE',  ( 4.898587196589412829E-16, 4.875000000000000888, -8.000000000000000000 ) ) ;
#9191 = ADVANCED_FACE ( 'NONE', ( #34419 ), #46453, .T. ) ;
#9192 = ORIENTED_EDGE ( 'NONE', *, *, #4010, .F. ) ;
#9193 = CARTESIAN_POINT ( 'NONE',  ( -7.204075437095967871, 7.204075437095967871, 115.4687500020483810 ) ) ;
#9194 = CARTESIAN_POINT ( 'NONE',  ( 9.797174393178825657E-16, 125.0000000000000000, -8.000000000000000000 ) ) ;
#9195 = CARTESIAN_POINT ( 'NONE',  ( -1.432654583217607858, 202.6250000013656063, 201.4587341250000065 ) ) ;
#9196 = CARTESIAN_POINT ( 'NONE',  ( 29.43265458321766914, 200.5000000013655779, 173.4587341249998929 ) ) ;
#9197 = CARTESIAN_POINT ( 'NONE',  ( 6.123233995736767268E-16, 66.25000000000000000, -10.00000000000000178 ) ) ;
#9198 = CARTESIAN_POINT ( 'NONE',  ( -7.188101187500001821, 95.93750000204839523, -2.977408999572650483 ) ) ;
#9199 = CARTESIAN_POINT ( 'NONE',  ( 1.102182119232618108E-15, 293.2500000000000000, 6.000000000000001776 ) ) ;
#9201 = CARTESIAN_POINT ( 'NONE',  ( -7.320508075688779037, 126.8750000000000142, -7.320508075688779925 ) ) ;
#9200 = CARTESIAN_POINT ( 'NONE',  ( 32.00000000000000000, 208.3750000027312126, 169.9999999999998863 ) ) ;
#9202 = ORIENTED_EDGE ( 'NONE', *, *, #64844, .T. ) ;
#9203 = EDGE_CURVE ( 'NONE', #43617, #5520, #51367, .T. ) ;
#9204 = EDGE_CURVE ( 'NONE', #26236, #3963, #71197, .T. ) ;
#9205 = CARTESIAN_POINT ( 'NONE',  ( -11.35316468749999963, 218.9062500034139873, 0.000000000000000000 ) ) ;
#9206 = CARTESIAN_POINT ( 'NONE',  ( -6.298842414715106308, -10.24914933418239471, 64.89273347873384523 ) ) ;
#9207 = CARTESIAN_POINT ( 'NONE',  ( -2.828427124746209831, 200.5000000027312126, 139.1715728752538723 ) ) ;
#9208 = LINE ( 'NONE', #55246, #43031 ) ;
#9209 = CARTESIAN_POINT ( 'NONE',  ( -12.00000000000000000, 6.928203230275504332, -14.80000000000000071 ) ) ;
#9210 = CARTESIAN_POINT ( 'NONE',  ( -2.679491924311222295, 246.0416666666666856, 10.00000000000000178 ) ) ;
#9211 = DIRECTION ( 'NONE',  ( -0.000000000000000000, 1.000000000000000000, -4.476705744456276341E-16 ) ) ;
#9212 = CARTESIAN_POINT ( 'NONE',  ( -10.00000000000000178, 182.5000000000000284, -1.224646799147353454E-15 ) ) ;
#9213 = CARTESIAN_POINT ( 'NONE',  ( 11.00000000000000000, 1.347111479062088405E-15, 111.2499999999999858 ) ) ;
#9214 = CARTESIAN_POINT ( 'NONE',  ( 7.188101187499993827, -2.977408999572645598, 25.01780278187175810 ) ) ;
#9215 = CARTESIAN_POINT ( 'NONE',  ( -9.832129032723420536, 159.0104166632526983, 5.676582343749997150 ) ) ;
#9216 = CARTESIAN_POINT ( 'NONE',  ( -7.999980374704816377, -3.313728124279936349, 22.11155356913438652 ) ) ;
#9217 = DIRECTION ( 'NONE',  ( 0.000000000000000000, 0.000000000000000000, -1.000000000000000000 ) ) ;
#9218 = DIRECTION ( 'NONE',  ( 0.000000000000000000, 0.000000000000000000, -1.000000000000000000 ) ) ;
#9221 = CARTESIAN_POINT ( 'NONE',  ( -4.000000000000001776, 7.187499997268813168, -1.656854249492381470 ) ) ;
#9220 = CARTESIAN_POINT ( 'NONE',  ( -2.751064625579944321E-14, 202.8750000027312126, 146.0000000000000284 ) ) ;
#9219 = CARTESIAN_POINT ( 'NONE',  ( 24.00000000000000355, 201.6875000000000000, 168.3431457505075173 ) ) ;
#9222 = ORIENTED_EDGE ( 'NONE', *, *, #8487, .T. ) ;
#9223 = CARTESIAN_POINT ( 'NONE',  ( -11.35316468750000141, 18.59374999658601979, -1.390361679473963753E-15 ) ) ;
#9224 = CARTESIAN_POINT ( 'NONE',  ( -4.556349186104045934, 11.00000000000000000, 77.40625000409679046 ) ) ;
#9226 = CARTESIAN_POINT ( 'NONE',  ( -1.836970198721029983E-15, 30.62499999317203248, 10.00000000000000178 ) ) ;
#9225 = DIRECTION ( 'NONE',  ( -0.000000000000000000, -0.000000000000000000, -1.000000000000000000 ) ) ;
#9227 = CYLINDRICAL_SURFACE ( 'NONE', #26516, 10.00000000000000178 ) ;
#9228 = CARTESIAN_POINT ( 'NONE',  ( 3.458734124999959914, 203.4375000013656063, 142.0000000000000568 ) ) ;
#9229 = CARTESIAN_POINT ( 'NONE',  ( 2.679491924311228956, 52.91666665983869677, -10.00000000000000000 ) ) ;
#9230 = CARTESIAN_POINT ( 'NONE',  ( 5.082755093536325042, 111.5937500020483810, -5.082755093536325930 ) ) ;
#9231 = CARTESIAN_POINT ( 'NONE',  ( 3.211159895383560947, 7.312499998634407028, 3.211159895383562723 ) ) ;
#9232 = CARTESIAN_POINT ( 'NONE',  ( 8.660254037844373087, 99.58333333333334281, 4.999999999999997335 ) ) ;
#9233 = CARTESIAN_POINT ( 'NONE',  ( -7.999999999999991118, 3.313708498984756723, 9.736552779823368198 ) ) ;
#9235 = CARTESIAN_POINT ( 'NONE',  ( 2.449293598294707893E-16, 1.250000000000000222, -4.000000000000001776 ) ) ;
#9234 = DIRECTION ( 'NONE',  ( -0.000000000000000000, 1.000000000000000000, -4.476705744456276341E-16 ) ) ;
#9236 = VERTEX_POINT ( 'NONE', #63032 ) ;
#9237 = ORIENTED_EDGE ( 'NONE', *, *, #38360, .T. ) ;
#9238 = CARTESIAN_POINT ( 'NONE',  ( 8.660254037844390851, 30.41666666666667140, -5.000000000000002665 ) ) ;
#9239 = CARTESIAN_POINT ( 'NONE',  ( 11.00000000000000000, 1.347111479062088405E-15, 81.43750000409677625 ) ) ;
#9240 = CARTESIAN_POINT ( 'NONE',  ( -4.898587196589412829E-16, 99.12499999999998579, -8.000000000000000000 ) ) ;
#9241 = CARTESIAN_POINT ( 'NONE',  ( 8.311093377946837890, 131.4062499965860411, -8.311093377946837890 ) ) ;
#9242 = ORIENTED_EDGE ( 'NONE', *, *, #34635, .F. ) ;
#9243 = CARTESIAN_POINT ( 'NONE',  ( -2.485281374238172081, 298.1875000000000568, 6.000000000000400568 ) ) ;
#9244 = CARTESIAN_POINT ( 'NONE',  ( 10.18810118749999916, 4.220049686691935698, 97.00000000204836681 ) ) ;
#9245 = CARTESIAN_POINT ( 'NONE',  ( 1.469576158976823947E-15, 93.87499999999998579, 8.000000000000000000 ) ) ;
#9246 = CARTESIAN_POINT ( 'NONE',  ( 4.000000000000015987, 207.4375000000000284, 199.6568542494924259 ) ) ;
#9247 = CARTESIAN_POINT ( 'NONE',  ( -5.000000000000000000, 60.11723469343052528, 46.25570701698154608 ) ) ;
#9249 = CARTESIAN_POINT ( 'NONE',  ( 3.042071309553159519, 124.7395833299193555, 11.35316468750000141 ) ) ;
#9248 = CARTESIAN_POINT ( 'NONE',  ( 10.00000000000002487, 44.79166666666667851, 2.679491924311242279 ) ) ;
#9250 = EDGE_CURVE ( 'NONE', #46585, #31802, #17004, .T. ) ;
#9251 = CARTESIAN_POINT ( 'NONE',  ( 4.556349186104052151, -10.99999999999999822, 95.96875000000000000 ) ) ;
#9252 = ORIENTED_EDGE ( 'NONE', *, *, #47632, .T. ) ;
#9253 = CARTESIAN_POINT ( 'NONE',  ( -6.000000000000001776, 288.0000000000000000, 0.000000000000000000 ) ) ;
#9254 = CARTESIAN_POINT ( 'NONE',  ( -26.43795870543543458, 181.5060313190927843, 153.6566396627847553 ) ) ;
#9255 = CARTESIAN_POINT ( 'NONE',  ( 11.35316468749999963, 116.3020833299193413, -3.042071309553165293 ) ) ;
#9256 = CARTESIAN_POINT ( 'NONE',  ( 3.458734125000016313, 207.8750000013656063, 199.4326545832176976 ) ) ;
#9257 = CARTESIAN_POINT ( 'NONE',  ( 7.188101187499999156, 17.24999999795162253, 2.977408999572654924 ) ) ;
#9258 = CARTESIAN_POINT ( 'NONE',  ( -6.238412754330611322E-16, 10.18810118749999916, 84.15625000204838102 ) ) ;
#9259 = CARTESIAN_POINT ( 'NONE',  ( -11.35316468750000141, 18.80208332991934839, 3.042071309553159963 ) ) ;
#9260 = ORIENTED_EDGE ( 'NONE', *, *, #141, .T. ) ;
#9261 = FACE_OUTER_BOUND ( 'NONE', #74481, .T. ) ;
#9262 = CARTESIAN_POINT ( 'NONE',  ( -8.008118988124991233, 3.317071493978878127, 23.41936528394063544 ) ) ;
#9263 = DIRECTION ( 'NONE',  ( -0.000000000000000000, 1.000000000000000000, -4.476705744456276341E-16 ) ) ;
#9264 = CARTESIAN_POINT ( 'NONE',  ( 0.000000000000000000, 0.000000000000000000, -21.47459999999999525 ) ) ;
#9265 = CARTESIAN_POINT ( 'NONE',  ( -2.977408999572650039, 3.937499997951610986, -7.188101187500001821 ) ) ;
#9266 = CARTESIAN_POINT ( 'NONE',  ( 6.676582343750003368, 289.0156250017070079, -2.765530957081997254 ) ) ;
#9267 = DIRECTION ( 'NONE',  ( 1.000000000000000000, 0.000000000000000000, 0.000000000000000000 ) ) ;
#9268 = CARTESIAN_POINT ( 'NONE',  ( 7.188101187500000044, 0.8437499979516099868, 0.000000000000000000 ) ) ;
#9269 = ORIENTED_EDGE ( 'NONE', *, *, #65422, .F. ) ;
#9270 = CARTESIAN_POINT ( 'NONE',  ( -11.35316468750000141, 143.8020833299193555, 3.042071309553159963 ) ) ;
#9271 = AXIS2_PLACEMENT_3D ( 'NONE', #12054, #1128, #760 ) ;
#9272 = CARTESIAN_POINT ( 'NONE',  ( -4.220049686691935698, 10.18810118749999916, 82.37500000204838102 ) ) ;
#9273 = CARTESIAN_POINT ( 'NONE',  ( -29.43265458321760519, 197.8750000013656063, 173.4587341250003760 ) ) ;
#9274 = FACE_OUTER_BOUND ( 'NONE', #28957, .T. ) ;
#9275 = CARTESIAN_POINT ( 'NONE',  ( 4.541265875000002339, 14.49999999863440969, -1.881053915767121554 ) ) ;
#9276 = VERTEX_POINT ( 'NONE', #51714 ) ;
#9277 = CARTESIAN_POINT ( 'NONE',  ( -3.999999999999959144, 204.1875000027312126, 199.6568542494924259 ) ) ;
#9278 = CARTESIAN_POINT ( 'NONE',  ( -4.000000000000015987, 208.5000000000000284, 142.0000000000000568 ) ) ;
#9279 = CARTESIAN_POINT ( 'NONE',  ( -26.34314575050769491, 204.0625000027312410, 166.0000000000003695 ) ) ;
#9280 = ADVANCED_FACE ( 'NONE', ( #29455 ), #18499, .T. ) ;
#9281 = DIRECTION ( 'NONE',  ( 1.000000000000000000, 0.000000000000000000, 0.000000000000000000 ) ) ;
#9282 = ORIENTED_EDGE ( 'NONE', *, *, #8700, .F. ) ;
#9283 =( BOUNDED_CURVE ( )  B_SPLINE_CURVE ( 2, ( #964, #35651, #47325, #18663, #12982, #36019, #19024, #59037, #65037, #53372, #7344, #1695, #36384 ),
 .UNSPECIFIED., .F., .F. ) 
 B_SPLINE_CURVE_WITH_KNOTS ( ( 3, 2, 2, 2, 2, 2, 3 ),
 ( 0.1388888888888883955, 0.1481481481481476403, 0.1574074074074069407, 0.1666666666666661856, 0.1759259259259254859, 0.1851851851851847308, 0.1944444444444440034 ),
 .UNSPECIFIED. ) 
 CURVE ( )  GEOMETRIC_REPRESENTATION_ITEM ( )  RATIONAL_B_SPLINE_CURVE ( ( 1.000000000000001776, 0.9659258262890664248, 1.000000000000000000, 0.9659258262890683122, 1.000000000000000000, 0.9659258262890683122, 1.000000000000000000, 0.9659258262890683122, 1.000000000000000000, 0.9659258262890683122, 1.000000000000000000, 0.9659258262890699775, 0.9999999999999983347 ) ) 
 REPRESENTATION_ITEM ( '' )  );
#9284 = CARTESIAN_POINT ( 'NONE',  ( -7.188101187500000044, 10.21874999795161187, -8.802885111219163269E-16 ) ) ;
#9285 = CARTESIAN_POINT ( 'NONE',  ( -30.33064993331720771, -12.01004434202216942, 176.4710297559720971 ) ) ;
#9286 = VECTOR ( 'NONE', #71729, 1000.000000000000000 ) ;
#9287 = CARTESIAN_POINT ( 'NONE',  ( 38.00000000000000000, 242.0000000000000284, 20.00000000000002132 ) ) ;
#9288 = CARTESIAN_POINT ( 'NONE',  ( -3.042071309553164404, 187.2395833299193839, -11.35316468749999963 ) ) ;
#9289 = CARTESIAN_POINT ( 'NONE',  ( 7.188101187500000044, 111.7812500020483810, -8.802885111219163269E-16 ) ) ;
#9290 = DIRECTION ( 'NONE',  ( 0.000000000000000000, 0.000000000000000000, -1.000000000000000000 ) ) ;
#9291 = FACE_OUTER_BOUND ( 'NONE', #17603, .T. ) ;
#9293 = CYLINDRICAL_SURFACE ( 'NONE', #9724, 8.000000000000000000 ) ;
#9292 = CARTESIAN_POINT ( 'NONE',  ( 2.085542519210945334E-15, 225.1562500034139873, 11.35316468749999963 ) ) ;
#9294 = ORIENTED_EDGE ( 'NONE', *, *, #40490, .T. ) ;
#9295 = CARTESIAN_POINT ( 'NONE',  ( 8.311093377946834337, 252.0312500034139589, -8.311093377946836114 ) ) ;
#9296 = CLOSED_SHELL ( 'NONE', ( #71303, #6774, #16683, #41926, #45494, #34171, #7710, #66035, #16539, #58955, #35570, #37087, #30103, #30681, #12538, #34829, #50483, #35251, #6598, #32496, #9477, #21874, #10098, #5477, #57979, #60302, #56834, #47504, #72071, #70426, #51217, #49872, #70751, #65614, #5571, #20040, #45508, #17358, #45435, #3009, #51727, #16849, #49534, #20201, #70829, #32863, #43613, #9191, #57078, #72105, #35964, #74362, #54975, #36076, #35042, #67532, #72652, #54655, #31784, #16597, #3613, #50951, #22860, #12537, #64229, #31626, #40759, #15282, #52363, #16582, #7955, #47719, #41715, #53618, #56974, #34054, #34827, #7052, #31162, #5311, #64065, #9820, #34202, #57164, #40356, #57448, #29160, #74514, #2965, #23639, #59827 ) ) ;
#9297 = CARTESIAN_POINT ( 'NONE',  ( 1.320432766682872962E-15, -7.188101187499992051, 26.23655278187175810 ) ) ;
#9298 = CARTESIAN_POINT ( 'NONE',  ( 8.660254037844385522, 166.4583333265053682, 5.000000000000005329 ) ) ;
#9299 = DIRECTION ( 'NONE',  ( 0.000000000000000000, 0.000000000000000000, -1.000000000000000000 ) ) ;
#9300 = CARTESIAN_POINT ( 'NONE',  ( 0.7581620860337424661, -65.76154746681217489, -26.27794529688043923 ) ) ;
#9301 = CARTESIAN_POINT ( 'NONE',  ( -1.432654583217608080, 197.8750000013656063, 201.4587341250000350 ) ) ;
#9302 = PLANE ( 'NONE',  #438 ) ;
#9303 = CARTESIAN_POINT ( 'NONE',  ( -4.556349186104045934, 11.00000000000000000, 114.7187500000000000 ) ) ;
#9304 = CARTESIAN_POINT ( 'NONE',  ( -8.000000000000000000, 94.90624999999998579, -3.313708498984761608 ) ) ;
#9305 = CARTESIAN_POINT ( 'NONE',  ( -11.35316468750000141, 118.5937499965860269, -1.390361679473963753E-15 ) ) ;
#9306 = CARTESIAN_POINT ( 'NONE',  ( 7.320508075688774596, 212.4999999931720254, -7.320508075688774596 ) ) ;
#9307 = CARTESIAN_POINT ( 'NONE',  ( 11.00000000000000000, 4.556349186104045934, 69.34374999999998579 ) ) ;
#9310 = CARTESIAN_POINT ( 'NONE',  ( 0.000000000000000000, 225.9999999999999432, 0.000000000000000000 ) ) ;
#9309 = CARTESIAN_POINT ( 'NONE',  ( 30.44569435410879521, 199.8125000013656063, 167.5543056458910485 ) ) ;
#9308 = CARTESIAN_POINT ( 'NONE',  ( 24.54126587499998280, 198.5000000013656347, 171.4326545832175555 ) ) ;
#9311 = VERTEX_POINT ( 'NONE', #69072 ) ;
#9312 = ADVANCED_FACE ( 'NONE', ( #47158 ), #5701, .F. ) ;
#9313 = EDGE_CURVE ( 'NONE', #33538, #5844, #41146, .T. ) ;
#9314 = DIRECTION ( 'NONE',  ( -0.000000000000000000, 1.000000000000000000, -0.000000000000000000 ) ) ;
#9315 = CARTESIAN_POINT ( 'NONE',  ( 4.556349186104052151, -10.99999999999999822, 114.1562500040967763 ) ) ;
#9317 = EDGE_CURVE ( 'NONE', #12693, #30893, #5774, .T. ) ;
#9316 = CARTESIAN_POINT ( 'NONE',  ( 2.445694354108783664, 195.3125000013656063, 144.4456943541088663 ) ) ;
#9318 = VECTOR ( 'NONE', #37644, 1000.000000000000000 ) ;
#9319 = CARTESIAN_POINT ( 'NONE',  ( 24.54126587499997925, 196.5000000013656063, 171.4326545832175555 ) ) ;
#9320 = CARTESIAN_POINT ( 'NONE',  ( -75.00000000000001421, 0.000000000000000000, 20.00000000000002132 ) ) ;
#9321 = CARTESIAN_POINT ( 'NONE',  ( -3.042071309553164404, 202.5520833299193839, -11.35316468749999963 ) ) ;
#9322 = CARTESIAN_POINT ( 'NONE',  ( -11.00000000000020783, -4.556349186103842541, 70.09375000000000000 ) ) ;
#9323 = FACE_OUTER_BOUND ( 'NONE', #7263, .T. ) ;
#9324 = CARTESIAN_POINT ( 'NONE',  ( 4.541265875000001451, 20.24999999863440436, 1.881053915767124440 ) ) ;
#9325 = FACE_OUTER_BOUND ( 'NONE', #70172, .T. ) ;
#9326 = CARTESIAN_POINT ( 'NONE',  ( 3.313708498984762496, -7.999999999999989342, 28.29905277982336997 ) ) ;
#9327 = FACE_OUTER_BOUND ( 'NONE', #12162, .T. ) ;
#9328 = CARTESIAN_POINT ( 'NONE',  ( 8.311093377946834337, 85.15624999658602690, 8.311093377946839666 ) ) ;
#9329 = EDGE_LOOP ( 'NONE', ( #12937, #63073, #28781, #27236 ) ) ;
#9330 = DIRECTION ( 'NONE',  ( -0.000000000000000000, -0.000000000000000000, 1.000000000000000000 ) ) ;
#9331 = CARTESIAN_POINT ( 'NONE',  ( -2.977408999572654480, 17.99999999795161898, 7.188101187499999156 ) ) ;
#9332 = CARTESIAN_POINT ( 'NONE',  ( 3.313708498984762496, -7.999999999999989342, 14.79905277982336642 ) ) ;
#9333 = CARTESIAN_POINT ( 'NONE',  ( 9.832129032723416984, 252.1354166700806445, -5.676582343750003368 ) ) ;
#9334 = CARTESIAN_POINT ( 'NONE',  ( 5.676582343749993598, 84.94791666325268409, 9.832129032723422313 ) ) ;
#9335 = ORIENTED_EDGE ( 'NONE', *, *, #33893, .F. ) ;
#9336 = CARTESIAN_POINT ( 'NONE',  ( -6.000000000000000000, 0.000000000000000000, -10.77459999999999951 ) ) ;
#9337 = CARTESIAN_POINT ( 'NONE',  ( 1.871523826299183495E-15, -10.18810118749999916, 113.0312500020483810 ) ) ;
#9338 = CARTESIAN_POINT ( 'NONE',  ( -25.55430564589114795, 195.3125000013656063, 172.4456943541091789 ) ) ;
#9339 = CARTESIAN_POINT ( 'NONE',  ( -2.445694354108784108, 209.5625000013656063, 195.5543056458912190 ) ) ;
#9340 = CARTESIAN_POINT ( 'NONE',  ( 1.469576158976822172E-15, -7.999999999999991118, 11.70530277982336642 ) ) ;
#9342 = CARTESIAN_POINT ( 'NONE',  ( 9.832129032723416984, 85.36458332991936970, 5.676582343750006032 ) ) ;
#9341 = CARTESIAN_POINT ( 'NONE',  ( 3.313708498984777595, 121.7187500040967620, -7.999999999999983125 ) ) ;
#9343 = EDGE_CURVE ( 'NONE', #70596, #4199, #14241, .T. ) ;
#9344 = CARTESIAN_POINT ( 'NONE',  ( -4.898587196589407898E-16, 7.999999999999991118, 17.14280278392014978 ) ) ;
#9345 = CARTESIAN_POINT ( 'NONE',  ( -26.56734541678238060, 201.6250000013656063, 166.5412658750003629 ) ) ;
#9346 = CARTESIAN_POINT ( 'NONE',  ( -5.656854249492381470, 21.74999999590322375, 5.656854249492379694 ) ) ;
#9347 = CARTESIAN_POINT ( 'NONE',  ( -7.320508075688773708, 168.7499999931720822, -7.320508075688774596 ) ) ;
#9348 = CARTESIAN_POINT ( 'NONE',  ( 3.000000000000001332, -45.00000000000001421, 139.1455027589170470 ) ) ;
#9349 = CARTESIAN_POINT ( 'NONE',  ( -8.311093377946836114, 72.96874999658602690, -8.311093377946837890 ) ) ;
#9350 = CARTESIAN_POINT ( 'NONE',  ( 6.676582343750001591, 293.9531250017069510, -8.176455196517173205E-16 ) ) ;
#9351 = CARTESIAN_POINT ( 'NONE',  ( 10.18810118750000093, -4.220049686691933033, 106.1875000020483810 ) ) ;
#9352 = CARTESIAN_POINT ( 'NONE',  ( -8.311093377946836114, 212.6562499965860411, -8.311093377946837890 ) ) ;
#9353 = ORIENTED_EDGE ( 'NONE', *, *, #70144, .T. ) ;
#9354 = CARTESIAN_POINT ( 'NONE',  ( -5.656854249492373476, -5.656854249492376141, 26.70530278392014623 ) ) ;
#9355 = CARTESIAN_POINT ( 'NONE',  ( -4.193030820682224658, -60.66866849074650503, -23.17095654502674762 ) ) ;
#9356 = CARTESIAN_POINT ( 'NONE',  ( 5.000000000000000000, 65.19475225706599986, 23.98307544245006184 ) ) ;
#9358 = CARTESIAN_POINT ( 'NONE',  ( 11.35316468750000141, 205.7812499965860411, 0.000000000000000000 ) ) ;
#9357 = DIRECTION ( 'NONE',  ( -0.000000000000000000, -0.000000000000000000, 1.000000000000000000 ) ) ;
#9359 = AXIS2_PLACEMENT_3D ( 'NONE', #16267, #17022, #4605 ) ;
#9360 = CARTESIAN_POINT ( 'NONE',  ( 9.999999999999998224, 225.8333333401612606, -2.679491924311229401 ) ) ;
#9361 = CARTESIAN_POINT ( 'NONE',  ( -8.660254037844385522, 253.5416666734946602, 5.000000000000004441 ) ) ;
#9362 = ORIENTED_EDGE ( 'NONE', *, *, #40761, .F. ) ;
#9363 = CARTESIAN_POINT ( 'NONE',  ( -9.832129032723420536, 199.0104166632526983, 5.676582343749997150 ) ) ;
#9364 = CARTESIAN_POINT ( 'NONE',  ( 2.977408999572650927, -7.188101187499990274, 13.95530278187175455 ) ) ;
#9365 = CARTESIAN_POINT ( 'NONE',  ( 7.999999999981424637, 1.723583929636134980E-05, 16.76780327155163874 ) ) ;
#9366 = CARTESIAN_POINT ( 'NONE',  ( 3.313708498984762496, 8.718750000000000000, 7.999999999999998224 ) ) ;
#9367 = VERTEX_POINT ( 'NONE', #34022 ) ;
#9368 = CARTESIAN_POINT ( 'NONE',  ( -8.000000000000000000, 89.18750000409677625, 0.000000000000000000 ) ) ;
#9369 = CARTESIAN_POINT ( 'NONE',  ( 49.70177871865296026, 134.0000000000000284, 57.99999999999998579 ) ) ;
#9370 = AXIS2_PLACEMENT_3D ( 'NONE', #29831, #40412, #64533 ) ;
#9371 = ORIENTED_EDGE ( 'NONE', *, *, #43052, .F. ) ;
#9372 = CARTESIAN_POINT ( 'NONE',  ( -2.828427124746190735, 14.37500000000000000, -2.828427124746191623 ) ) ;
#9373 = CARTESIAN_POINT ( 'NONE',  ( 3.211159895383560947, 21.18749999863440792, 3.211159895383562723 ) ) ;
#9374 = CARTESIAN_POINT ( 'NONE',  ( -3.313708498984758943, -7.999999999999989342, 8.799052783920144449 ) ) ;
#9375 =( BOUNDED_CURVE ( )  B_SPLINE_CURVE ( 2, ( #39953, #73531, #33568, #22211, #21839, #27505, #26763, #28259, #21105, #67509, #10165, #68250, #68620 ),
 .UNSPECIFIED., .F., .F. ) 
 B_SPLINE_CURVE_WITH_KNOTS ( ( 3, 2, 2, 2, 2, 2, 3 ),
 ( 0.7228260869565217295, 0.7246376811594202882, 0.7264492753623188470, 0.7282608695652172948, 0.7300724637681158535, 0.7318840579710144123, 0.7336956521739129711 ),
 .UNSPECIFIED. ) 
 CURVE ( )  GEOMETRIC_REPRESENTATION_ITEM ( )  RATIONAL_B_SPLINE_CURVE ( ( 1.000000000000000000, 0.9659258262890683122, 1.000000000000000000, 0.9659258262890683122, 1.000000000000000000, 0.9659258262890683122, 1.000000000000000000, 0.9659258262890683122, 1.000000000000000000, 0.9659258262890683122, 1.000000000000000000, 0.9659258262890704216, 0.9999999999999978906 ) ) 
 REPRESENTATION_ITEM ( '' )  );
#9376 = CARTESIAN_POINT ( 'NONE',  ( -5.656854249492375253, 5.656854249492375253, 18.83030278392014623 ) ) ;
#9377 = EDGE_CURVE ( 'NONE', #21890, #56060, #36958, .T. ) ;
#9378 = ORIENTED_EDGE ( 'NONE', *, *, #15678, .F. ) ;
#9379 = CARTESIAN_POINT ( 'NONE',  ( 6.000000000000003553, 293.5000000034140157, 2.485281374238571317 ) ) ;
#9380 = CARTESIAN_POINT ( 'NONE',  ( -2.977408999572651815, 89.93750000204840944, 7.188101187500000933 ) ) ;
#9383 = CARTESIAN_POINT ( 'NONE',  ( 2.995737153982844347, -51.55860531535523705, 48.67776149471320934 ) ) ;
#9382 = CARTESIAN_POINT ( 'NONE',  ( -8.311093377946834337, 259.5312500034139589, 8.311093377946837890 ) ) ;
#9381 = CYLINDRICAL_SURFACE ( 'NONE', #15685, 3.999999999999976019 ) ;
#9384 = CARTESIAN_POINT ( 'NONE',  ( 1393.688200795887269, 596.9677537767817057, 960.3421604560587639 ) ) ;
#9385 = VERTEX_POINT ( 'NONE', #7915 ) ;
#9386 = CARTESIAN_POINT ( 'NONE',  ( 9.832129032723416984, 257.1354166700806445, -5.676582343750003368 ) ) ;
#9387 = CARTESIAN_POINT ( 'NONE',  ( 2.977408999572646486, 7.188101187499991163, 16.01780278187175455 ) ) ;
#9388 = ORIENTED_EDGE ( 'NONE', *, *, #25724, .T. ) ;
#9389 = ORIENTED_EDGE ( 'NONE', *, *, #43195, .T. ) ;
#9390 = CARTESIAN_POINT ( 'NONE',  ( 7.204075437095968759, -7.204075437095966983, 80.21875000204836681 ) ) ;
#9391 = CARTESIAN_POINT ( 'NONE',  ( 3.042071309553167069, 77.13541666325266988, -11.35316468749999785 ) ) ;
#9392 = DIRECTION ( 'NONE',  ( 0.000000000000000000, -1.000000000000000000, -0.000000000000000000 ) ) ;
#9393 = CARTESIAN_POINT ( 'NONE',  ( -6.735557395310442023E-16, 11.00000000000000000, 92.12499999999998579 ) ) ;
#9396 = CARTESIAN_POINT ( 'NONE',  ( -4.721056650415998313, 289.7343750017069510, 4.721056650416000089 ) ) ;
#9395 = CARTESIAN_POINT ( 'NONE',  ( 24.00000000000000355, 198.9375000027312126, 171.6568542494923122 ) ) ;
#9394 = FACE_OUTER_BOUND ( 'NONE', #47730, .T. ) ;
#9397 = EDGE_CURVE ( 'NONE', #28738, #23461, #52053, .T. ) ;
#9398 = CARTESIAN_POINT ( 'NONE',  ( 0.000000000000000000, -3.149999999999999911, 18.50000000000000000 ) ) ;
#9399 = CARTESIAN_POINT ( 'NONE',  ( 2.828427124746153876, 209.0000000027312126, 144.8284271247462129 ) ) ;
#9400 = CIRCLE ( 'NONE', #21414, 30.99999999999997158 ) ;
#9401 = CARTESIAN_POINT ( 'NONE',  ( 1.432654583217662481, 200.3750000013656063, 194.5412658750000219 ) ) ;
#9402 =( BOUNDED_CURVE ( )  B_SPLINE_CURVE ( 2, ( #28283, #23359, #46738, #34705, #34339, #73929, #51289, #16568, #379 ),
 .UNSPECIFIED., .F., .F. ) 
 B_SPLINE_CURVE_WITH_KNOTS ( ( 3, 2, 2, 2, 3 ),
 ( 0.8068181818181818787, 0.8125000000000001110, 0.8181818181818183433, 0.8238636363636363535, 0.8295454545454545858 ),
 .UNSPECIFIED. ) 
 CURVE ( )  GEOMETRIC_REPRESENTATION_ITEM ( )  RATIONAL_B_SPLINE_CURVE ( ( 0.9999999999999985567, 0.9238795325112881818, 1.000000000000000000, 0.9238795325112867385, 1.000000000000000000, 0.9238795325112867385, 1.000000000000000000, 0.9238795325112867385, 1.000000000000000000 ) ) 
 REPRESENTATION_ITEM ( '' )  );
#9403 = CARTESIAN_POINT ( 'NONE',  ( -1.469576158976823947E-15, 8.437499995903221972, 8.000000000000000000 ) ) ;
#9404 = VERTEX_POINT ( 'NONE', #13919 ) ;
#9405 = CARTESIAN_POINT ( 'NONE',  ( 24.54126587500000412, 208.3750000013656063, 168.5673454167822172 ) ) ;
#9406 = VECTOR ( 'NONE', #64889, 1000.000000000000000 ) ;
#9407 = CARTESIAN_POINT ( 'NONE',  ( -5.082755093536325042, 11.90624999795161010, -5.082755093536325930 ) ) ;
#9408 = CARTESIAN_POINT ( 'NONE',  ( -3.313708498984758943, -7.999999999999989342, 25.29905278392014623 ) ) ;
#9409 = CARTESIAN_POINT ( 'NONE',  ( -3.313708498984815343, 105.2187500000000000, -7.999999999999944933 ) ) ;
#9410 = CARTESIAN_POINT ( 'NONE',  ( 7.188101187500000933, 110.3750000020484094, -2.977408999572651371 ) ) ;
#9412 = CARTESIAN_POINT ( 'NONE',  ( 1.296342370383407161, -49.95006747298835847, -40.70914535207442952 ) ) ;
#9411 = CARTESIAN_POINT ( 'NONE',  ( -2.485281374238916374, 292.8750000034140157, -5.999999999999657163 ) ) ;
#9413 = CARTESIAN_POINT ( 'NONE',  ( 2.679491924308573747, 133.9583333333331154, 10.00000000000153655 ) ) ;
#9414 = CARTESIAN_POINT ( 'NONE',  ( 25.55430564589119768, 207.3125000013656063, 167.5543056458910485 ) ) ;
#9415 = CARTESIAN_POINT ( 'NONE',  ( 2.977408999572646486, 7.188101187499991163, 13.39280278187175455 ) ) ;
#9416 = CARTESIAN_POINT ( 'NONE',  ( 3.999999999999960032, 207.0625000027311842, 143.6568542494924543 ) ) ;
#9417 = CARTESIAN_POINT ( 'NONE',  ( -3.042071309553173730, 39.32291666325268409, 11.35316468749999785 ) ) ;
#9418 = DIRECTION ( 'NONE',  ( -0.000000000000000000, 1.000000000000000000, 4.476705744456276341E-16 ) ) ;
#9419 = CARTESIAN_POINT ( 'NONE',  ( -10.00000000000000000, 24.16666665983869677, -2.679491924311229845 ) ) ;
#9420 = CARTESIAN_POINT ( 'NONE',  ( 4.556349186104052151, -10.99999999999999822, 71.96874999999998579 ) ) ;
#9421 = ORIENTED_EDGE ( 'NONE', *, *, #65946, .F. ) ;
#9422 = FACE_OUTER_BOUND ( 'NONE', #73137, .T. ) ;
#9423 = DIRECTION ( 'NONE',  ( 0.000000000000000000, -0.000000000000000000, 1.000000000000000000 ) ) ;
#9424 = CARTESIAN_POINT ( 'NONE',  ( 9.832129032723416984, 55.36458332991934839, 5.676582343750006032 ) ) ;
#9425 = VECTOR ( 'NONE', #4971, 1000.000000000000000 ) ;
#9426 = CARTESIAN_POINT ( 'NONE',  ( 4.556349186104051263, -10.99999999999999822, 78.15625000409677625 ) ) ;
#9427 = CARTESIAN_POINT ( 'NONE',  ( -3.458734125000016757, 205.1250000013656347, 140.5673454167823593 ) ) ;
#9428 = CARTESIAN_POINT ( 'NONE',  ( 1.836970198721029589E-15, 261.2500000000000568, 10.00000000000000000 ) ) ;
#9429 = CARTESIAN_POINT ( 'NONE',  ( 38.00000000000000000, 63.00000000000000000, 15.00000000000000178 ) ) ;
#9431 = CARTESIAN_POINT ( 'NONE',  ( 8.311093377946834337, 45.15624999658601268, 8.311093377946839666 ) ) ;
#9430 = CARTESIAN_POINT ( 'NONE',  ( -7.188101187500000044, 98.65625000204838102, 0.000000000000000000 ) ) ;
#9432 = ADVANCED_FACE ( 'NONE', ( #59242 ), #65993, .F. ) ;
#9433 = CARTESIAN_POINT ( 'NONE',  ( 1.469576158976822172E-15, -7.999999999999991118, 7.205302779823365533 ) ) ;
#9434 = CARTESIAN_POINT ( 'NONE',  ( -2.085542519210945728E-15, 159.5312499965860127, 11.35316468750000141 ) ) ;
#9435 = PRESENTATION_LAYER_ASSIGNMENT (  '', '', ( #56399 ) ) ;
#9436 = EDGE_CURVE ( 'NONE', #46215, #48362, #57348, .T. ) ;
#9437 = CARTESIAN_POINT ( 'NONE',  ( 4.999999999999993783, 126.0416666598387110, 8.660254037844390851 ) ) ;
#9438 = CARTESIAN_POINT ( 'NONE',  ( 2.977408999572654480, 102.5000000020483810, 7.188101187499999156 ) ) ;
#9439 = EDGE_LOOP ( 'NONE', ( #45727, #52248, #10643, #50672 ) ) ;
#9440 = FACE_OUTER_BOUND ( 'NONE', #35406, .T. ) ;
#9441 = CARTESIAN_POINT ( 'NONE',  ( 5.676582343749993598, 40.26041666325268409, 9.832129032723422313 ) ) ;
#9442 = DIRECTION ( 'NONE',  ( -0.000000000000000000, 1.000000000000000000, -0.000000000000000000 ) ) ;
#9443 = ORIENTED_EDGE ( 'NONE', *, *, #59841, .F. ) ;
#9444 = DIRECTION ( 'NONE',  ( -1.000000000000000000, 0.000000000000000000, 0.000000000000000000 ) ) ;
#9445 = CARTESIAN_POINT ( 'NONE',  ( 10.18810118749999916, 4.220049686691935698, 76.00000000204838102 ) ) ;
#9446 = DIRECTION ( 'NONE',  ( 0.9884788384745426537, 6.483116892092363099E-18, -0.1513591288559071046 ) ) ;
#9448 = CARTESIAN_POINT ( 'NONE',  ( -9.832129032723418760, 167.8645833299193555, -5.676582343750004256 ) ) ;
#9447 = CARTESIAN_POINT ( 'NONE',  ( 0.000000000000000000, 0.000000000000000000, 118.0000000000000000 ) ) ;
#9449 = CARTESIAN_POINT ( 'NONE',  ( -30.93541659651595310, 271.9999999999999432, 167.9999999999998295 ) ) ;
#9450 = CARTESIAN_POINT ( 'NONE',  ( -7.999999999999991118, 3.313708498984756723, 14.29280278432982598 ) ) ;
#9451 = EDGE_CURVE ( 'NONE', #36272, #34184, #14863, .T. ) ;
#9452 = CARTESIAN_POINT ( 'NONE',  ( -19.99999999999993960, -31.42446164168984879, 193.6854385646540777 ) ) ;
#9453 = CARTESIAN_POINT ( 'NONE',  ( -11.35316468749999785, 228.6979166700806729, -3.042071309553164848 ) ) ;
#9454 = CARTESIAN_POINT ( 'NONE',  ( -4.220049686691937474, -10.18810118749999738, 86.31250000204838102 ) ) ;
#9455 = VERTEX_POINT ( 'NONE', #53206 ) ;
#9456 = ADVANCED_FACE ( 'NONE', ( #72019 ), #30920, .F. ) ;
#9457 = CARTESIAN_POINT ( 'NONE',  ( -4.999999999999998224, 118.5416666598386968, -8.660254037844389075 ) ) ;
#9458 = CARTESIAN_POINT ( 'NONE',  ( -1.656854249492382358, 204.1875000000000284, 202.0000000000000000 ) ) ;
#9459 = CARTESIAN_POINT ( 'NONE',  ( 11.35316468750000141, 101.0937499965860127, 0.000000000000000000 ) ) ;
#9460 = CARTESIAN_POINT ( 'NONE',  ( -10.18810118749999738, -4.220049686691941915, 97.75000000204838102 ) ) ;
#9461 = CARTESIAN_POINT ( 'NONE',  ( 3.211159895383561835, 19.56249999863440436, -3.211159895383561835 ) ) ;
#9462 = ORIENTED_EDGE ( 'NONE', *, *, #472, .F. ) ;
#9463 = ORIENTED_EDGE ( 'NONE', *, *, #38256, .T. ) ;
#9464 = CARTESIAN_POINT ( 'NONE',  ( 3.211159895383561835, 4.562499998634407028, -3.211159895383561835 ) ) ;
#9465 = CARTESIAN_POINT ( 'NONE',  ( 5.082755093536325930, 8.156249997951611874, -5.082755093536325930 ) ) ;
#9466 = CARTESIAN_POINT ( 'NONE',  ( -5.656854249492378806, 114.8750000040967905, 5.656854249492381470 ) ) ;
#9467 = CARTESIAN_POINT ( 'NONE',  ( 10.18810118749999916, 4.220049686691935698, 92.87500000204838102 ) ) ;
#9468 = CARTESIAN_POINT ( 'NONE',  ( -31.45873412500001010, 203.8750000013656063, 168.5673454167827572 ) ) ;
#9469 = AXIS2_PLACEMENT_3D ( 'NONE', #23327, #46339, #26939 ) ;
#9470 = PRESENTATION_STYLE_ASSIGNMENT (( #45555 ) ) ;
#9471 = CARTESIAN_POINT ( 'NONE',  ( -2.828427124746192067, 5.625000000000000000, 2.828427124746190735 ) ) ;
#9472 = CARTESIAN_POINT ( 'NONE',  ( -2.828427124746192067, 18.37499999726881583, 2.828427124746190735 ) ) ;
#9473 = CARTESIAN_POINT ( 'NONE',  ( -1.881053915767121776, 6.624999998634407916, -4.541265875000002339 ) ) ;
#9474 = CARTESIAN_POINT ( 'NONE',  ( -4.000000000000015987, 201.5000000000000000, 142.0000000000000568 ) ) ;
#9475 = VERTEX_POINT ( 'NONE', #31675 ) ;
#9476 = CARTESIAN_POINT ( 'NONE',  ( -28.00000000000003197, 209.0000000000000284, 166.0000000000003695 ) ) ;
#9477 = ADVANCED_FACE ( 'NONE', ( #36591 ), #64885, .T. ) ;
#9479 = CARTESIAN_POINT ( 'NONE',  ( -1.469576158976823947E-15, 16.12500000000000355, 8.000000000000000000 ) ) ;
#9478 = CARTESIAN_POINT ( 'NONE',  ( -29.43265458321771177, 198.5000000013656347, 166.5412658750003914 ) ) ;
#9480 =( NAMED_UNIT ( * ) PLANE_ANGLE_UNIT ( ) SI_UNIT ( $, .RADIAN. ) );
#9481 = VECTOR ( 'NONE', #54321, 1000.000000000000000 ) ;
#9482 = CARTESIAN_POINT ( 'NONE',  ( -4.541265875000002339, 18.81249999863440436, -5.561446717895856393E-16 ) ) ;
#9483 = CARTESIAN_POINT ( 'NONE',  ( -4.088227598258586603E-16, 299.2031250017070079, -6.676582343750001591 ) ) ;
#9484 = CARTESIAN_POINT ( 'NONE',  ( -7.188101187499991163, 2.977408999572646930, 7.392802781871750994 ) ) ;
#9485 = VERTEX_POINT ( 'NONE', #48266 ) ;
#9486 = EDGE_CURVE ( 'NONE', #7137, #25962, #66695, .T. ) ;
#9487 = ORIENTED_EDGE ( 'NONE', *, *, #41732, .T. ) ;
#9488 = CARTESIAN_POINT ( 'NONE',  ( 4.220049686691934809, 10.18810118749999916, 98.68750000204838102 ) ) ;
#9489 = CARTESIAN_POINT ( 'NONE',  ( 2.752039609470550924E-11, 41.24999999999786127, -9.999999999999998224 ) ) ;
#9490 = CARTESIAN_POINT ( 'NONE',  ( -30.44569435410883429, 198.8125000013656063, 167.5543056458915885 ) ) ;
#9491 = CARTESIAN_POINT ( 'NONE',  ( 4.556349186104045934, 11.00000000000000000, 105.5312500000000142 ) ) ;
#9492 = CARTESIAN_POINT ( 'NONE',  ( 2.754378923186476579E-14, 206.4375000013656063, 194.5412658750000219 ) ) ;
#9493 = CARTESIAN_POINT ( 'NONE',  ( 10.00000000000007816, 60.20833333333337833, -2.679491924311247608 ) ) ;
#9494 = CARTESIAN_POINT ( 'NONE',  ( -7.320508075688773708, 101.8750000000000000, -7.320508075688774596 ) ) ;
#9495 = CARTESIAN_POINT ( 'NONE',  ( 3.313708498984765161, 110.4687500000000000, 7.999999999999998224 ) ) ;
#9496 = CARTESIAN_POINT ( 'NONE',  ( 6.676582343750004256, 292.0468750017070079, 2.765530957081995478 ) ) ;
#9497 = CARTESIAN_POINT ( 'NONE',  ( 2.977408999572650927, -7.188101187499990274, 14.33030278187175277 ) ) ;
#9498 = ORIENTED_EDGE ( 'NONE', *, *, #72416, .T. ) ;
#9499 = CARTESIAN_POINT ( 'NONE',  ( 5.656854249492378806, 19.31250000000000355, 5.656854249492381470 ) ) ;
#9500 = ADVANCED_FACE ( 'NONE', ( #25984 ), #70337, .F. ) ;
#9501 = CARTESIAN_POINT ( 'NONE',  ( -27.99999999999999645, 210.0000000000000284, 170.0000000000003695 ) ) ;
#9502 = CARTESIAN_POINT ( 'NONE',  ( 3.313708498984762496, 22.03124999590322375, 7.999999999999998224 ) ) ;
#9503 = CARTESIAN_POINT ( 'NONE',  ( -1.432654583217662481, 204.1250000013656063, 145.4587341250000634 ) ) ;
#9504 = DIRECTION ( 'NONE',  ( 0.000000000000000000, 0.000000000000000000, 1.000000000000000000 ) ) ;
#9506 = CARTESIAN_POINT ( 'NONE',  ( 3.458734124999959469, 203.7500000013656063, 140.5673454167824161 ) ) ;
#9505 = CARTESIAN_POINT ( 'NONE',  ( 5.000000000000000000, -18.53862685874495853, -23.57305537018139674 ) ) ;
#9507 = CARTESIAN_POINT ( 'NONE',  ( -3.042071309553166181, 258.1770833367473301, -11.35316468749999608 ) ) ;
#9508 = LINE ( 'NONE', #32523, #30149 ) ;
#9509 = CARTESIAN_POINT ( 'NONE',  ( -2.679491924311235174, 95.41666665983869677, 10.00000000000000000 ) ) ;
#9510 =( BOUNDED_CURVE ( )  B_SPLINE_CURVE ( 2, ( #72037, #43371, #24627, #47638, #37734, #6923, #18977, #58989, #26381 ),
 .UNSPECIFIED., .F., .F. ) 
 B_SPLINE_CURVE_WITH_KNOTS ( ( 3, 2, 2, 2, 3 ),
 ( 0.4431818181818181768, 0.4488636363636363535, 0.4545454545454545858, 0.4602272727272727626, 0.4659090909090909394 ),
 .UNSPECIFIED. ) 
 CURVE ( )  GEOMETRIC_REPRESENTATION_ITEM ( )  RATIONAL_B_SPLINE_CURVE ( ( 1.000000000000000000, 0.9238795325112867385, 1.000000000000000000, 0.9238795325112867385, 1.000000000000000000, 0.9238795325112867385, 1.000000000000000000, 0.9238795325112859613, 1.000000000000000666 ) ) 
 REPRESENTATION_ITEM ( '' )  );
#9511 = CARTESIAN_POINT ( 'NONE',  ( 6.951808397369818766E-16, 2.031249996586016682, -11.35316468750000141 ) ) ;
#9512 = CARTESIAN_POINT ( 'NONE',  ( 7.188101187499992051, 2.977408999572647819, 7.205302781871755435 ) ) ;
#9513 = CARTESIAN_POINT ( 'NONE',  ( 3.042071309553159519, 200.0520833299193839, 11.35316468750000141 ) ) ;
#9514 = CARTESIAN_POINT ( 'NONE',  ( -7.320508075688778149, 134.9999999931720538, 7.320508075688769267 ) ) ;
#9515 = CARTESIAN_POINT ( 'NONE',  ( 4.541265875000002339, 7.374999998634408804, -1.881053915767121554 ) ) ;
#9516 = LINE ( 'NONE', #43832, #599 ) ;
#9518 = CARTESIAN_POINT ( 'NONE',  ( 38.00000000000000000, 205.0000000000000284, 3.504937291764267425E-14 ) ) ;
#9517 = CARTESIAN_POINT ( 'NONE',  ( -5.656854249492380582, 107.0000000040967763, -5.656854249492380582 ) ) ;
#9519 = ORIENTED_EDGE ( 'NONE', *, *, #70375, .F. ) ;
#9520 = CARTESIAN_POINT ( 'NONE',  ( -1.432654583217664701, 206.0000000013656347, 138.5412658750000787 ) ) ;
#9521 = CARTESIAN_POINT ( 'NONE',  ( -2.085542519210945728E-15, 4.531249996586016238, 11.35316468750000141 ) ) ;
#9522 = CARTESIAN_POINT ( 'NONE',  ( 4.556349186104051263, -10.99999999999999822, 97.65625000409680467 ) ) ;
#9523 = DIRECTION ( 'NONE',  ( -0.000000000000000000, -0.000000000000000000, 1.000000000000000000 ) ) ;
#9524 = CARTESIAN_POINT ( 'NONE',  ( -30.44569435410886982, 200.5625000013656063, 167.5543056458916169 ) ) ;
#9525 = CYLINDRICAL_SURFACE ( 'NONE', #32243, 10.00000000000000178 ) ;
#9527 = CARTESIAN_POINT ( 'NONE',  ( -5.676582343749998039, 2.447916663252682756, -9.832129032723420536 ) ) ;
#9526 = CARTESIAN_POINT ( 'NONE',  ( 5.082755093536326818, 120.2187500020483952, 5.082755093536325042 ) ) ;
#9528 = CARTESIAN_POINT ( 'NONE',  ( -3.313708498984757167, 7.999999999999991118, 29.04905277982337353 ) ) ;
#9529 = CARTESIAN_POINT ( 'NONE',  ( 8.311093377946837890, 116.4062499965860269, -8.311093377946837890 ) ) ;
#9530 = EDGE_CURVE ( 'NONE', #41332, #33110, #15052, .T. ) ;
#9531 = CARTESIAN_POINT ( 'NONE',  ( 5.000000000000001776, 87.70833332650538239, -8.660254037844389075 ) ) ;
#9532 = CARTESIAN_POINT ( 'NONE',  ( 2.977408999572654480, 91.62500000204838102, 7.188101187499999156 ) ) ;
#9533 = CARTESIAN_POINT ( 'NONE',  ( -4.541265875000003227, 18.99999999863440436, 1.881053915767121110 ) ) ;
#9534 = CARTESIAN_POINT ( 'NONE',  ( -10.00000000000000178, 199.3749999931720538, -1.224646799147353454E-15 ) ) ;
#9535 = FACE_OUTER_BOUND ( 'NONE', #63849, .T. ) ;
#9536 = EDGE_LOOP ( 'NONE', ( #21225, #7796, #50705, #56140 ) ) ;
#9537 = CARTESIAN_POINT ( 'NONE',  ( -6.607029887627752451, 225.9999999999999716, -7.535050054892760585 ) ) ;
#9538 =( BOUNDED_CURVE ( )  B_SPLINE_CURVE ( 2, ( #43148, #66532, #37883, #9201, #60879, #3546, #67943, #16237, #39274, #62275, #10603, #24509, #40753 ),
 .UNSPECIFIED., .F., .F. ) 
 B_SPLINE_CURVE_WITH_KNOTS ( ( 3, 2, 2, 2, 2, 2, 3 ),
 ( 1.585692104212438336, 1.590924485345288186, 1.596156866478138037, 1.601389247610987887, 1.606621628743837960, 1.611854009876687810, 1.617086391009537660 ),
 .UNSPECIFIED. ) 
 CURVE ( )  GEOMETRIC_REPRESENTATION_ITEM ( )  RATIONAL_B_SPLINE_CURVE ( ( 1.000000000000000000, 0.9659258262890683122, 1.000000000000000000, 0.9659258262890683122, 1.000000000000000000, 0.9659258262890683122, 1.000000000000000000, 0.9659258262890683122, 1.000000000000000000, 0.9659258262890683122, 1.000000000000000000, 0.9659258262890474400, 1.000000000000020872 ) ) 
 REPRESENTATION_ITEM ( '' )  );
#9539 = CARTESIAN_POINT ( 'NONE',  ( -6.676582343750000703, 288.6718750017069510, 2.765530957082001251 ) ) ;
#9540 = CARTESIAN_POINT ( 'NONE',  ( -1.656854249492381248, 12.06249999726881406, -4.000000000000001776 ) ) ;
#9541 = CARTESIAN_POINT ( 'NONE',  ( -7.999999999999991118, 3.313708498984756723, 2.424052783920144005 ) ) ;
#9542 = CARTESIAN_POINT ( 'NONE',  ( -1.656854249492263564, 200.9375000027312694, 194.0000000000000000 ) ) ;
#9543 = AXIS2_PLACEMENT_3D ( 'NONE', #12048, #52048, #40720 ) ;
#9544 = CARTESIAN_POINT ( 'NONE',  ( -5.000000000000005329, 210.2083333265053682, 8.660254037844387298 ) ) ;
#9545 = CARTESIAN_POINT ( 'NONE',  ( -1.469576158976823947E-15, 5.625000000000000888, 8.000000000000000000 ) ) ;
#9546 = CARTESIAN_POINT ( 'NONE',  ( 4.220049686691934809, 10.18810118749999916, 103.5625000020483668 ) ) ;
#9547 = EDGE_LOOP ( 'NONE', ( #62629, #58293, #44144, #45059 ) ) ;
#9548 = CARTESIAN_POINT ( 'NONE',  ( 0.000000000000000000, 265.0000000000000000, 0.000000000000000000 ) ) ;
#9549 = CARTESIAN_POINT ( 'NONE',  ( -11.35316468750000141, 158.5937499965860127, -1.390361679473963753E-15 ) ) ;
#9550 = CARTESIAN_POINT ( 'NONE',  ( -1.432654583217607192, 195.2500000013656063, 194.5412658750000219 ) ) ;
#9551 = CARTESIAN_POINT ( 'NONE',  ( 1.432654583217664701, 207.0000000013655779, 201.4587341250000065 ) ) ;
#9552 = CARTESIAN_POINT ( 'NONE',  ( 2.326828918379972154E-15, 0.000000000000000000, 19.00000000000000000 ) ) ;
#9553 = CARTESIAN_POINT ( 'NONE',  ( -9.832129032723420536, 64.01041666325268409, 5.676582343749997150 ) ) ;
#9554 = VERTEX_POINT ( 'NONE', #37713 ) ;
#9555 = CARTESIAN_POINT ( 'NONE',  ( 10.18810118749999916, 1.247682550866122264E-15, 113.4062500020483810 ) ) ;
#9556 = CARTESIAN_POINT ( 'NONE',  ( -4.541265875000002339, 7.874999998634407028, -1.881053915767121998 ) ) ;
#9557 = ORIENTED_EDGE ( 'NONE', *, *, #6088, .F. ) ;
#9558 = CARTESIAN_POINT ( 'NONE',  ( 5.082755093536324154, 18.28124999795161187, 5.082755093536326818 ) ) ;
#9559 = CARTESIAN_POINT ( 'NONE',  ( 4.242640687119285658, 289.6875000034139589, -4.242640687119286547 ) ) ;
#9560 = CARTESIAN_POINT ( 'NONE',  ( 0.000000000000000000, 75.00000000000000000, 0.000000000000000000 ) ) ;
#9561 = CARTESIAN_POINT ( 'NONE',  ( -7.188101187500001821, 17.99999999795161898, -2.977408999572651371 ) ) ;
#9562 = CARTESIAN_POINT ( 'NONE',  ( -5.082755093536319713, 5.082755093536319713, 2.799052781871750994 ) ) ;
#9563 = CARTESIAN_POINT ( 'NONE',  ( -10.18810118749999916, 0.000000000000000000, 107.0312500020483810 ) ) ;
#9564 = DIRECTION ( 'NONE',  ( -0.000000000000000000, 1.000000000000000000, -1.563033456626094573E-30 ) ) ;
#9565 = CARTESIAN_POINT ( 'NONE',  ( 2.828427124746191623, 5.874999997268813168, -2.828427124746191623 ) ) ;
#9566 = CARTESIAN_POINT ( 'NONE',  ( -25.17157287525386167, 208.0000000027312126, 167.1715728752541281 ) ) ;
#9567 = EDGE_LOOP ( 'NONE', ( #11864, #8611, #55785, #32027 ) ) ;
#9568 = CARTESIAN_POINT ( 'NONE',  ( -2.445694354108783664, 208.3125000013656063, 195.5543056458912190 ) ) ;
#9569 = ADVANCED_FACE ( 'NONE', ( #27873 ), #49770, .T. ) ;
#9570 = CARTESIAN_POINT ( 'NONE',  ( -28.00000000000007461, 209.4375000013656063, 166.5412658750003629 ) ) ;
#9571 = CARTESIAN_POINT ( 'NONE',  ( 4.220049686691934809, 10.18810118749999916, 70.56250000204836681 ) ) ;
#9572 = CARTESIAN_POINT ( 'NONE',  ( 1.881053915767122664, 6.124999998634407916, 4.541265875000001451 ) ) ;
#9573 = CONICAL_SURFACE ( 'NONE', #32472, 12.00000000000000000, 1.047197551196596077 ) ;
#9574 = CARTESIAN_POINT ( 'NONE',  ( -4.242640687119285658, 290.1249999999999432, 4.242640687119287435 ) ) ;
#9575 = CARTESIAN_POINT ( 'NONE',  ( -5.082755093536317936, -5.082755093536320601, 25.67405278187175810 ) ) ;
#9576 = EDGE_LOOP ( 'NONE', ( #41413, #25121, #17541, #36349 ) ) ;
#9577 = ADVANCED_FACE ( 'NONE', ( #49385 ), #72787, .T. ) ;
#9578 = CARTESIAN_POINT ( 'NONE',  ( -4.000000000000001776, 21.50000000000000000, -4.898587196589415787E-16 ) ) ;
#9579 = EDGE_LOOP ( 'NONE', ( #63358, #10502, #8307, #59673, #42515, #59466 ) ) ;
#9580 = CARTESIAN_POINT ( 'NONE',  ( -5.000000000000002665, 3.333333333333331261, 8.660254037844383745 ) ) ;
#9581 = CARTESIAN_POINT ( 'NONE',  ( -3.458734124999959914, 203.3750000013656063, 196.5673454167823877 ) ) ;
#9582 = CARTESIAN_POINT ( 'NONE',  ( 24.54126587499999346, 200.1875000013656063, 169.9999999999999432 ) ) ;
#9583 = CARTESIAN_POINT ( 'NONE',  ( -10.00000000000000355, 67.70833333333334281, 2.679491924311223183 ) ) ;
#9584 = VECTOR ( 'NONE', #58617, 1000.000000000000000 ) ;
#9585 = CARTESIAN_POINT ( 'NONE',  ( 5.082755093536325042, 92.46875000204838102, -5.082755093536325930 ) ) ;
#9586 = CARTESIAN_POINT ( 'NONE',  ( -6.000000000000001776, 294.0000000000000000, 0.000000000000000000 ) ) ;
#9587 = CARTESIAN_POINT ( 'NONE',  ( 26.34314575050758833, 207.6875000027311842, 165.9999999999998863 ) ) ;
#9588 = ORIENTED_EDGE ( 'NONE', *, *, #66589, .T. ) ;
#9589 = CARTESIAN_POINT ( 'NONE',  ( -12.00000000000000000, -6.928203230275542523, -1.071796769724504550 ) ) ;
#9590 = CARTESIAN_POINT ( 'NONE',  ( 7.999999999999998224, 11.90625000000000355, 3.313708498984766049 ) ) ;
#9591 = CARTESIAN_POINT ( 'NONE',  ( -1.656854249492405451, 200.4375000027311842, 138.0000000000000568 ) ) ;
#9592 = CARTESIAN_POINT ( 'NONE',  ( -4.898587196589407898E-16, 7.999999999999991118, 24.64280278392014978 ) ) ;
#9593 = FACE_OUTER_BOUND ( 'NONE', #9579, .T. ) ;
#9594 = CARTESIAN_POINT ( 'NONE',  ( -2.679491924311222295, 251.0416666666665719, 10.00000000000000178 ) ) ;
#9595 = FACE_OUTER_BOUND ( 'NONE', #10185, .T. ) ;
#9596 = CARTESIAN_POINT ( 'NONE',  ( -2.679491924311225848, 181.4583333333333428, -10.00000000000000178 ) ) ;
#9597 = CARTESIAN_POINT ( 'NONE',  ( 11.00000000000000000, 1.347111479062088405E-15, 76.93750000409677625 ) ) ;
#9598 = CARTESIAN_POINT ( 'NONE',  ( 2.977408999572646486, 7.188101187499992051, 23.89280278187175810 ) ) ;
#9599 = CARTESIAN_POINT ( 'NONE',  ( 9.832129032723420536, 151.5104166632526699, -5.676582343749999815 ) ) ;
#9600 = CARTESIAN_POINT ( 'NONE',  ( 1.469576158976823947E-15, 113.5625000040967905, 8.000000000000000000 ) ) ;
#9601 = DIRECTION ( 'NONE',  ( 1.000000000000000000, -0.000000000000000000, 0.000000000000000000 ) ) ;
#9602 = CARTESIAN_POINT ( 'NONE',  ( 5.499987861550171608, 9.526286449755788865, 67.99927393035380874 ) ) ;
#9604 = DIRECTION ( 'NONE',  ( 2.168404344971008868E-16, -1.000000000000000000, 0.000000000000000000 ) ) ;
#9603 = CARTESIAN_POINT ( 'NONE',  ( -8.660254037844387298, 83.95833332650536818, -5.000000000000004441 ) ) ;
#9605 = EDGE_LOOP ( 'NONE', ( #13872, #1919, #39821 ) ) ;
#9606 = CARTESIAN_POINT ( 'NONE',  ( -11.35316468750000141, 28.59374999658601624, -1.390361679473963753E-15 ) ) ;
#9607 = FACE_BOUND ( 'NONE', #8852, .T. ) ;
#9609 = CARTESIAN_POINT ( 'NONE',  ( 7.456155213531538095, -10.23501372118566444, -65.47700548259878417 ) ) ;
#9608 = CARTESIAN_POINT ( 'NONE',  ( -6.062591786044946751, -5.219672483564715471, -0.3118205092643556720 ) ) ;
#9610 = CARTESIAN_POINT ( 'NONE',  ( -2.828427124746153876, 196.0000000027312126, 195.1715728752538439 ) ) ;
#9611 = CARTESIAN_POINT ( 'NONE',  ( 3.458734124999959914, 203.3750000013656063, 143.4326545832176976 ) ) ;
#9612 = CARTESIAN_POINT ( 'NONE',  ( -4.999999999999998224, 48.54166665983870388, -8.660254037844389075 ) ) ;
#9613 = CARTESIAN_POINT ( 'NONE',  ( -7.188101187499999156, 109.2500000020483952, 2.977408999572654924 ) ) ;
#9614 = CARTESIAN_POINT ( 'NONE',  ( 4.541265875000001451, 8.374999998634406140, 1.881053915767124440 ) ) ;
#9615 = LINE ( 'NONE', #60536, #49354 ) ;
#9616 = CARTESIAN_POINT ( 'NONE',  ( -3.313708498984757167, 7.999999999999991118, 9.549052779823362869 ) ) ;
#9618 = CARTESIAN_POINT ( 'NONE',  ( -2.828427124746190735, 4.124999997268813168, -2.828427124746191623 ) ) ;
#9617 = CARTESIAN_POINT ( 'NONE',  ( 1.469576158976823947E-15, 110.3750000000000000, 8.000000000000000000 ) ) ;
#9619 = ORIENTED_EDGE ( 'NONE', *, *, #9313, .F. ) ;
#9620 = ORIENTED_EDGE ( 'NONE', *, *, #64417, .T. ) ;
#9621 = CARTESIAN_POINT ( 'NONE',  ( -4.999999999999999112, -67.66743717231497612, 22.54291394824926442 ) ) ;
#9622 = CARTESIAN_POINT ( 'NONE',  ( 0.000000000000000000, 0.000000000000000000, 28.00000000000000000 ) ) ;
#9623 = CARTESIAN_POINT ( 'NONE',  ( -5.656854249492375253, 5.656854249492375253, 14.33030278392014800 ) ) ;
#9624 = CARTESIAN_POINT ( 'NONE',  ( 0.000000000000000000, 125.0000000000000000, 8.000000000000000000 ) ) ;
#9625 = CARTESIAN_POINT ( 'NONE',  ( -11.35316468749999785, 123.0729166632526983, -3.042071309553167513 ) ) ;
#9626 = ORIENTED_EDGE ( 'NONE', *, *, #36970, .T. ) ;
#9627 = CARTESIAN_POINT ( 'NONE',  ( -4.242640687119285658, 298.1250000000000000, 4.242640687119287435 ) ) ;
#9628 = CARTESIAN_POINT ( 'NONE',  ( -4.220049686691935698, 10.18810118749999916, 91.37500000204838102 ) ) ;
#9629 = CARTESIAN_POINT ( 'NONE',  ( 7.999999999999991118, -2.975320552349488356E-08, 19.76780278304987348 ) ) ;
#9630 = CARTESIAN_POINT ( 'NONE',  ( 1.656854249492403008, 209.6875000000000284, 194.0000000000000853 ) ) ;
#9632 = CARTESIAN_POINT ( 'NONE',  ( -9.832129032723420536, 128.6979166632526983, 5.676582343749997150 ) ) ;
#9631 = CARTESIAN_POINT ( 'NONE',  ( -3.313708498984816231, 95.28124999999998579, 7.999999999999943157 ) ) ;
#9633 = DIRECTION ( 'NONE',  ( 0.000000000000000000, 0.000000000000000000, -1.000000000000000000 ) ) ;
#9634 = VERTEX_POINT ( 'NONE', #66746 ) ;
#9635 =( BOUNDED_CURVE ( )  B_SPLINE_CURVE ( 2, ( #67948, #4957, #69066, #17370, #63392, #10610, #56642, #27959, #6066 ),
 .UNSPECIFIED., .F., .F. ) 
 B_SPLINE_CURVE_WITH_KNOTS ( ( 3, 2, 2, 2, 3 ),
 ( 0.7395833333333334814, 0.7447916666666667407, 0.7500000000000001110, 0.7552083333333334814, 0.7604166666666667407 ),
 .UNSPECIFIED. ) 
 CURVE ( )  GEOMETRIC_REPRESENTATION_ITEM ( )  RATIONAL_B_SPLINE_CURVE ( ( 0.9999999999999983347, 0.9238795325112884038, 1.000000000000000000, 0.9238795325112867385, 1.000000000000000000, 0.9238795325112867385, 1.000000000000000000, 0.9238795325112850731, 1.000000000000001554 ) ) 
 REPRESENTATION_ITEM ( '' )  );
#9636 = CARTESIAN_POINT ( 'NONE',  ( -7.999999999999998224, 110.0937499999999858, 3.313708498984766049 ) ) ;
#9637 = FACE_OUTER_BOUND ( 'NONE', #812, .T. ) ;
#9638 = CARTESIAN_POINT ( 'NONE',  ( -3.042071309553173730, 119.6354166632526841, 11.35316468749999785 ) ) ;
#9639 = CARTESIAN_POINT ( 'NONE',  ( 2.754378923186476579E-14, 205.1875000013656063, 194.5412658750000219 ) ) ;
#9640 = CARTESIAN_POINT ( 'NONE',  ( 7.188101187500000044, 17.34374999795161543, 0.000000000000000000 ) ) ;
#9641 = CARTESIAN_POINT ( 'NONE',  ( 1.871523826299183495E-15, -10.18810118749999916, 84.90625000204838102 ) ) ;
#9642 = CARTESIAN_POINT ( 'NONE',  ( 8.311093377946834337, 20.46874999658601624, 8.311093377946839666 ) ) ;
#9643 = ORIENTED_EDGE ( 'NONE', *, *, #9317, .T. ) ;
#9644 = CARTESIAN_POINT ( 'NONE',  ( -4.000000000000002665, 4.562500000000001776, 1.656854249492380582 ) ) ;
#9645 = CARTESIAN_POINT ( 'NONE',  ( -5.662595241051935346, 5.662595241051935346, 21.82561528394063188 ) ) ;
#9646 = CARTESIAN_POINT ( 'NONE',  ( 8.660254037844385522, 237.9166666666666572, -5.000000000000003553 ) ) ;
#9647 = AXIS2_PLACEMENT_3D ( 'NONE', #66370, #14676, #3378 ) ;
#9648 = DIRECTION ( 'NONE',  ( -0.000000000000000000, 0.000000000000000000, -1.000000000000000000 ) ) ;
#9649 = CARTESIAN_POINT ( 'NONE',  ( -5.082755093536326818, 2.906249997951610098, 5.082755093536325042 ) ) ;
#9650 = CARTESIAN_POINT ( 'NONE',  ( 2.765530957082001251, 289.7656250017069510, 6.676582343750000703 ) ) ;
#9651 = CARTESIAN_POINT ( 'NONE',  ( 10.00000000000000178, 111.8749999931720396, 0.000000000000000000 ) ) ;
#9652 = CARTESIAN_POINT ( 'NONE',  ( -28.00000000000003197, 207.0000000000000284, 166.0000000000003695 ) ) ;
#9653 = ORIENTED_EDGE ( 'NONE', *, *, #13403, .T. ) ;
#9654 = EDGE_CURVE ( 'NONE', #14438, #29935, #39054, .T. ) ;
#9655 = CARTESIAN_POINT ( 'NONE',  ( -11.35316468749999785, 143.3854166632526983, -3.042071309553167513 ) ) ;
#9656 = CARTESIAN_POINT ( 'NONE',  ( 7.204075437095968759, -7.204075437095966983, 78.71875000204836681 ) ) ;
#9657 = CARTESIAN_POINT ( 'NONE',  ( -26.56734541678232375, 195.0000000013656063, 173.4587341250003760 ) ) ;
#9658 = PLANE ( 'NONE',  #29413 ) ;
#9659 = CARTESIAN_POINT ( 'NONE',  ( 4.541265875000002339, 16.49999999863440436, -1.881053915767121554 ) ) ;
#9660 = ORIENTED_EDGE ( 'NONE', *, *, #19932, .T. ) ;
#9661 = CARTESIAN_POINT ( 'NONE',  ( -1.656854249492347719, 201.9375000027311842, 194.0000000000000853 ) ) ;
#9662 = EDGE_CURVE ( 'NONE', #50631, #45507, #3339, .T. ) ;
#9663 = CARTESIAN_POINT ( 'NONE',  ( -4.000000000000015099, 209.5625000000000000, 143.6568542494924543 ) ) ;
#9664 = CARTESIAN_POINT ( 'NONE',  ( -23.99999999999999289, 205.8750000027312126, 170.0000000000002842 ) ) ;
#9665 = CARTESIAN_POINT ( 'NONE',  ( -10.99999999999992006, -31.99999999999978684, 205.0000000000000284 ) ) ;
#9666 = EDGE_CURVE ( 'NONE', #66256, #43772, #36623, .T. ) ;
#9667 = ORIENTED_EDGE ( 'NONE', *, *, #62486, .T. ) ;
#9668 = CARTESIAN_POINT ( 'NONE',  ( 5.082755093536324154, 13.78124999795161010, 5.082755093536326818 ) ) ;
#9669 = CARTESIAN_POINT ( 'NONE',  ( -23.07384334584684638, -13.62583975325536478, 190.7206728506874924 ) ) ;
#9670 = CARTESIAN_POINT ( 'NONE',  ( 11.00000000000000355, -4.556349186104044158, 73.84375000409676204 ) ) ;
#9671 = CARTESIAN_POINT ( 'NONE',  ( -9.832129032723420536, 183.6979166632526983, 5.676582343749997150 ) ) ;
#9672 = CARTESIAN_POINT ( 'NONE',  ( -7.188101187500001821, 110.9375000020483810, -2.977408999572650483 ) ) ;
#9673 = FACE_OUTER_BOUND ( 'NONE', #45046, .T. ) ;
#9674 = CARTESIAN_POINT ( 'NONE',  ( -6.676582343750002480, 289.3906250017070079, -2.765530957081996810 ) ) ;
#9676 = LINE ( 'NONE', #32697, #33803 ) ;
#9675 = CARTESIAN_POINT ( 'NONE',  ( -11.35316468749999608, 219.1145833367473017, 3.042071309553173730 ) ) ;
#9677 = ORIENTED_EDGE ( 'NONE', *, *, #2424, .F. ) ;
#9679 = CARTESIAN_POINT ( 'NONE',  ( 5.676582343750005144, 260.5729166700806445, 9.832129032723416984 ) ) ;
#9678 = AXIS2_PLACEMENT_3D ( 'NONE', #36583, #71264, #12815 ) ;
#9680 = CARTESIAN_POINT ( 'NONE',  ( 2.977408999572646486, 7.188101187499991163, 22.39280278187175810 ) ) ;
#9681 = CARTESIAN_POINT ( 'NONE',  ( 8.660254037844389075, 167.2916666598387110, -5.000000000000000000 ) ) ;
#9682 = CARTESIAN_POINT ( 'NONE',  ( -1.469576158976823947E-15, 18.93749999590322020, 8.000000000000000000 ) ) ;
#9683 = CARTESIAN_POINT ( 'NONE',  ( -1.925929944387235853E-31, 16.00000000000000000, 3.497325839728428143 ) ) ;
#9684 = LINE ( 'NONE', #22095, #18598 ) ;
#9685 = FACE_OUTER_BOUND ( 'NONE', #30806, .T. ) ;
#9686 = DIRECTION ( 'NONE',  ( -0.000000000000000000, -0.9659258262890698665, -0.2588190451025146332 ) ) ;
#9687 = CARTESIAN_POINT ( 'NONE',  ( 3.313708498984760720, 94.53125000000001421, -8.000000000000000000 ) ) ;
#9688 = CARTESIAN_POINT ( 'NONE',  ( 6.951808397369818766E-16, 112.3437499965860127, -11.35316468750000141 ) ) ;
#9689 = CARTESIAN_POINT ( 'NONE',  ( 12.00000000000000178, -28.00000000000000000, 0.000000000000000000 ) ) ;
#9690 = CARTESIAN_POINT ( 'NONE',  ( 11.00000000000000000, 1.347111479062088405E-15, 73.74999999999998579 ) ) ;
#9693 = CARTESIAN_POINT ( 'NONE',  ( -1.469576158976823947E-15, 13.12500000000000355, 8.000000000000000000 ) ) ;
#9692 = CARTESIAN_POINT ( 'NONE',  ( 31.45873412499997812, 200.7500000013656347, 168.5673454167822172 ) ) ;
#9691 = CARTESIAN_POINT ( 'NONE',  ( 28.00000000000001776, 197.1875000013655779, 166.5412658749999082 ) ) ;
#9694 = ORIENTED_EDGE ( 'NONE', *, *, #57006, .T. ) ;
#9695 = CARTESIAN_POINT ( 'NONE',  ( 6.042744113992383426, 224.2641768943893794, 7.989819569021650025 ) ) ;
#9696 = CARTESIAN_POINT ( 'NONE',  ( -4.556349186104048599, -10.99999999999999822, 113.9687500040968047 ) ) ;
#9697 = CARTESIAN_POINT ( 'NONE',  ( -1.432654583217662481, 197.1250000013656347, 145.4587341250000634 ) ) ;
#9698 = CARTESIAN_POINT ( 'NONE',  ( 25.55430564589115150, 199.5625000013656063, 172.4456943541086957 ) ) ;
#9699 = CARTESIAN_POINT ( 'NONE',  ( -11.35316468749999785, 213.3854166632526983, -3.042071309553167513 ) ) ;
#9700 = CARTESIAN_POINT ( 'NONE',  ( -11.00000000000000000, 0.000000000000000000, 69.99999999999998579 ) ) ;
#9701 = DIRECTION ( 'NONE',  ( 0.000000000000000000, 0.000000000000000000, 1.000000000000000000 ) ) ;
#9702 = CARTESIAN_POINT ( 'NONE',  ( 1.881053915767121776, 18.49999999863440436, -4.541265875000002339 ) ) ;
#9703 = CARTESIAN_POINT ( 'NONE',  ( 30.44569435410883074, 196.0625000013656063, 167.5543056458911053 ) ) ;
#9704 = CARTESIAN_POINT ( 'NONE',  ( -5.447323953993864265, -4.689931814214729933, 0.5319290643893268555 ) ) ;
#9706 = CYLINDRICAL_SURFACE ( 'NONE', #53216, 3.999999999999976019 ) ;
#9705 = DIRECTION ( 'NONE',  ( 0.000000000000000000, 1.000000000000000000, 0.000000000000000000 ) ) ;
#9707 = CARTESIAN_POINT ( 'NONE',  ( 3.042071309553167069, 91.82291666325269830, -11.35316468749999785 ) ) ;
#9708 = VERTEX_POINT ( 'NONE', #6371 ) ;
#9709 = CARTESIAN_POINT ( 'NONE',  ( 4.401442555609581635E-16, 21.84374999795161543, -7.188101187500000044 ) ) ;
#9710 = FACE_OUTER_BOUND ( 'NONE', #70896, .T. ) ;
#9711 = CARTESIAN_POINT ( 'NONE',  ( -3.042071309553159075, 260.2604166700805877, 11.35316468749999963 ) ) ;
#9712 = CARTESIAN_POINT ( 'NONE',  ( 3.042071309553159519, 89.73958332991935549, 11.35316468750000141 ) ) ;
#9713 = VERTEX_POINT ( 'NONE', #29377 ) ;
#9714 = CARTESIAN_POINT ( 'NONE',  ( 23.99999999999998579, 196.8750000027312126, 169.9999999999999432 ) ) ;
#9715 = CARTESIAN_POINT ( 'NONE',  ( 10.18810118749999916, 1.247682550866122264E-15, 108.9062500020483668 ) ) ;
#9716 = DIRECTION ( 'NONE',  ( -1.000000000000000000, 0.000000000000000000, 0.000000000000000000 ) ) ;
#9717 = CARTESIAN_POINT ( 'NONE',  ( 2.754378923186476579E-14, 205.4375000013656063, 194.5412658750000219 ) ) ;
#9718 = CARTESIAN_POINT ( 'NONE',  ( -30.82842712474624491, 201.2500000027312126, 167.1715728752542418 ) ) ;
#9720 = CARTESIAN_POINT ( 'NONE',  ( 5.676582343750001591, 86.61458332991936970, -9.832129032723420536 ) ) ;
#9719 = CARTESIAN_POINT ( 'NONE',  ( -26.34314575050755991, 206.6875000027312126, 174.0000000000003979 ) ) ;
#9721 = CARTESIAN_POINT ( 'NONE',  ( -7.999999999999991118, 0.000000000000000000, 20.51780278392014623 ) ) ;
#9722 = CARTESIAN_POINT ( 'NONE',  ( -25.55430564589115150, 201.3125000013656063, 172.4456943541091789 ) ) ;
#9723 = DIRECTION ( 'NONE',  ( 0.000000000000000000, 0.000000000000000000, -1.000000000000000000 ) ) ;
#9724 = AXIS2_PLACEMENT_3D ( 'NONE', #27752, #61722, #32316 ) ;
#9725 = CARTESIAN_POINT ( 'NONE',  ( 8.660254037844389075, 177.2916666598387110, -5.000000000000000000 ) ) ;
#9726 = CARTESIAN_POINT ( 'NONE',  ( 2.846894273155695654, -45.96635398628109925, 139.1309070811473418 ) ) ;
#9727 = CARTESIAN_POINT ( 'NONE',  ( -3.042071309553173730, 74.63541666325268409, 11.35316468749999785 ) ) ;
#9728 = CARTESIAN_POINT ( 'NONE',  ( 4.721056650416000089, 294.8281250017069510, 4.721056650415999201 ) ) ;
#9729 = CARTESIAN_POINT ( 'NONE',  ( -10.18810118749999916, 4.220049686691934809, 100.9375000020483810 ) ) ;
#9730 = CARTESIAN_POINT ( 'NONE',  ( 9.832129032723416984, 210.3645833299193555, 5.676582343750006032 ) ) ;
#9731 = ORIENTED_EDGE ( 'NONE', *, *, #6089, .F. ) ;
#9732 = FACE_OUTER_BOUND ( 'NONE', #59974, .T. ) ;
#9733 = CARTESIAN_POINT ( 'NONE',  ( -3.369429374625359852, -60.49191766694055872, -23.06312700027871898 ) ) ;
#9734 = LINE ( 'NONE', #43680, #16613 ) ;
#9736 = CARTESIAN_POINT ( 'NONE',  ( -3.042071309553163960, 212.2395833299193839, -11.35316468749999963 ) ) ;
#9735 = DIRECTION ( 'NONE',  ( -0.000000000000000000, 1.000000000000000000, -1.563033456626094573E-30 ) ) ;
#9737 = CARTESIAN_POINT ( 'NONE',  ( 5.000000000000004441, 219.7916666734946318, 8.660254037844385522 ) ) ;
#9738 = CARTESIAN_POINT ( 'NONE',  ( -2.765530957081996810, 299.2656250017070647, -6.676582343750003368 ) ) ;
#9739 = ORIENTED_EDGE ( 'NONE', *, *, #27453, .F. ) ;
#9740 = CARTESIAN_POINT ( 'NONE',  ( 9.832129032723416984, 195.6770833299193839, 5.676582343750006032 ) ) ;
#9741 = CIRCLE ( 'NONE', #42188, 8.000000000000000000 ) ;
#9742 = CARTESIAN_POINT ( 'NONE',  ( -7.188101187499992051, 2.977408999572646930, 13.39280278187175277 ) ) ;
#9743 =( BOUNDED_CURVE ( )  B_SPLINE_CURVE ( 2, ( #64813, #53870, #36150, #24806, #59895, #12753, #30117, #64453, #19154, #24073, #13114, #36520, #7842 ),
 .UNSPECIFIED., .F., .F. ) 
 B_SPLINE_CURVE_WITH_KNOTS ( ( 3, 2, 2, 2, 2, 2, 3 ),
 ( 0.5808961537982215706, 0.5861285976204262393, 0.5913610414426307971, 0.5965934852648355768, 0.6018259290870402456, 0.6070583729092448033, 0.6122908167314494721 ),
 .UNSPECIFIED. ) 
 CURVE ( )  GEOMETRIC_REPRESENTATION_ITEM ( )  RATIONAL_B_SPLINE_CURVE ( ( 1.000000000000001110, 0.9659258262890673130, 1.000000000000000000, 0.9659258262890683122, 1.000000000000000000, 0.9659258262890683122, 1.000000000000000000, 0.9659258262890683122, 1.000000000000000000, 0.9659258262890683122, 1.000000000000000000, 0.9659258262890584312, 1.000000000000009992 ) ) 
 REPRESENTATION_ITEM ( '' )  );
#9744 = CARTESIAN_POINT ( 'NONE',  ( 5.656854249492380582, 18.18750000000000355, -5.656854249492380582 ) ) ;
#9745 =( BOUNDED_CURVE ( )  B_SPLINE_CURVE ( 2, ( #28427, #17097, #23882, #11084, #158, #6540, #29546, #11821, #34858 ),
 .UNSPECIFIED., .F., .F. ) 
 B_SPLINE_CURVE_WITH_KNOTS ( ( 3, 2, 2, 2, 3 ),
 ( 0.03409090909090908839, 0.03977272727272727210, 0.04545454545454545581, 0.05113636363636364646, 0.05681818181818182323 ),
 .UNSPECIFIED. ) 
 CURVE ( )  GEOMETRIC_REPRESENTATION_ITEM ( )  RATIONAL_B_SPLINE_CURVE ( ( 1.000000000000000000, 0.9238795325112867385, 1.000000000000000000, 0.9238795325112867385, 1.000000000000000000, 0.9238795325112867385, 1.000000000000000000, 0.9238795325112866275, 1.000000000000000000 ) ) 
 REPRESENTATION_ITEM ( '' )  );
#9746 = CARTESIAN_POINT ( 'NONE',  ( 4.898587196589412829E-16, 9.375000000000001776, -8.000000000000000000 ) ) ;
#9747 = ORIENTED_EDGE ( 'NONE', *, *, #44016, .T. ) ;
#9748 = EDGE_CURVE ( 'NONE', #13929, #30170, #50059, .T. ) ;
#9749 = VECTOR ( 'NONE', #17678, 1000.000000000000000 ) ;
#9750 = CARTESIAN_POINT ( 'NONE',  ( 5.656854249492381470, 91.25000000409677625, 5.656854249492379694 ) ) ;
#9751 = CARTESIAN_POINT ( 'NONE',  ( 7.320508075688771044, 14.37500000000000178, 7.320508075688775484 ) ) ;
#9752 = CARTESIAN_POINT ( 'NONE',  ( -7.204075437095967871, 7.204075437095967871, 81.34375000204838102 ) ) ;
#9753 = ORIENTED_EDGE ( 'NONE', *, *, #19987, .T. ) ;
#9754 = CARTESIAN_POINT ( 'NONE',  ( 1.656854249492381914, 20.81250000000000000, 4.000000000000000888 ) ) ;
#9755 = CARTESIAN_POINT ( 'NONE',  ( -3.211159895383561391, 19.68749999863440436, -3.211159895383561835 ) ) ;
#9756 = CARTESIAN_POINT ( 'NONE',  ( 5.656854249492374365, 5.656854249492375253, 6.455302783920143561 ) ) ;
#9757 = CARTESIAN_POINT ( 'NONE',  ( 0.000000000000000000, 0.000000000000000000, 6.938893903907228378E-15 ) ) ;
#9758 = VERTEX_POINT ( 'NONE', #5992 ) ;
#9759 = CARTESIAN_POINT ( 'NONE',  ( -5.082755093536325930, 93.96875000204838102, -5.082755093536325930 ) ) ;
#9760 = EDGE_CURVE ( 'NONE', #16864, #9554, #52493, .T. ) ;
#9763 = CARTESIAN_POINT ( 'NONE',  ( 1.656854249492521136, 197.6874999999999432, 194.0000000000001990 ) ) ;
#9762 = CARTESIAN_POINT ( 'NONE',  ( -5.676582343749992710, 254.7395833367473301, 9.832129032723422313 ) ) ;
#9761 = CARTESIAN_POINT ( 'NONE',  ( 5.656854249492374365, 5.656854249492375253, 12.26780277982336642 ) ) ;
#9764 = DIRECTION ( 'NONE',  ( 0.000000000000000000, 0.000000000000000000, 1.000000000000000000 ) ) ;
#9765 = ORIENTED_EDGE ( 'NONE', *, *, #54026, .T. ) ;
#9766 = CARTESIAN_POINT ( 'NONE',  ( -5.676582343750000703, 248.3854166700806445, -9.832129032723418760 ) ) ;
#9767 = CARTESIAN_POINT ( 'NONE',  ( 5.082755093536320601, -5.082755093536318824, 12.54905278187175277 ) ) ;
#9768 = EDGE_LOOP ( 'NONE', ( #44265, #28243, #50661, #391 ) ) ;
#9769 = B_SPLINE_CURVE_WITH_KNOTS ( 'NONE', 3,
 ( #40957, #16804, #17187, #28139, #57956, #6263, #39467, #74161, #29267, #10792, #52279, #45485, #50776, #5887, #40206, #73790, #33828, #39832, #56825, #11172 ),
 .UNSPECIFIED., .F., .F.,
 ( 4, 2, 2, 2, 2, 2, 2, 2, 2, 4 ),
 ( 0.000000000000000000, 0.001156441540184007140, 0.001734662310276010493, 0.002312883080368014280, 0.003469324620552016215, 0.004625766160736019018, 0.005782207700920020954, 0.006938649241104022890, 0.008095090781288024825, 0.009251532321472025894 ),
 .UNSPECIFIED. ) ;
#9770 = VERTEX_POINT ( 'NONE', #19787 ) ;
#9771 = CARTESIAN_POINT ( 'NONE',  ( 4.220049686691934809, 10.18810118749999916, 71.68750000204838102 ) ) ;
#9772 = CARTESIAN_POINT ( 'NONE',  ( -8.311093377946841443, 74.21874999658601268, 8.311093377946830785 ) ) ;
#9773 = CARTESIAN_POINT ( 'NONE',  ( 3.313708498984762496, -7.999999999999989342, 23.98655278392014978 ) ) ;
#9774 = CARTESIAN_POINT ( 'NONE',  ( -6.735557395310442023E-16, 11.00000000000000000, 90.62499999999998579 ) ) ;
#9777 = CARTESIAN_POINT ( 'NONE',  ( -2.765530957081996810, 289.4218750017069510, -6.676582343750002480 ) ) ;
#9776 = CARTESIAN_POINT ( 'NONE',  ( 25.17157287525381903, 198.0000000027312126, 172.8284271247460993 ) ) ;
#9775 = CARTESIAN_POINT ( 'NONE',  ( -28.00000000000007816, 199.1250000027312126, 166.0000000000003695 ) ) ;
#9778 = CARTESIAN_POINT ( 'NONE',  ( 0.000000000000000000, 0.000000000000000000, 0.000000000000000000 ) ) ;
#9779 = CARTESIAN_POINT ( 'NONE',  ( 30.64284399271078740, 38.00000000000000711, 174.6921329945330115 ) ) ;
#9780 = CARTESIAN_POINT ( 'NONE',  ( 2.445694354108839175, 198.3125000013656063, 195.5543056458912190 ) ) ;
#9781 = CARTESIAN_POINT ( 'NONE',  ( -1.469576158976823947E-15, 9.937499995903220196, 8.000000000000000000 ) ) ;
#9782 = VERTEX_POINT ( 'NONE', #48456 ) ;
#9783 = CARTESIAN_POINT ( 'NONE',  ( 26.56734541678232375, 195.3750000013656063, 173.4587341249998929 ) ) ;
#9784 = CARTESIAN_POINT ( 'NONE',  ( 7.188101187500001821, 17.43749999795161543, -2.977408999572650483 ) ) ;
#9785 = CARTESIAN_POINT ( 'NONE',  ( -11.35316468750000141, 173.8020833299193839, 3.042071309553159963 ) ) ;
#9786 = FACE_BOUND ( 'NONE', #39775, .T. ) ;
#9787 = CARTESIAN_POINT ( 'NONE',  ( 5.082755093536326818, 102.5937500020483810, 5.082755093536325042 ) ) ;
#9788 = CARTESIAN_POINT ( 'NONE',  ( 0.3752463838824673381, -55.62178951997624665, -43.80327721769167226 ) ) ;
#9789 = CARTESIAN_POINT ( 'NONE',  ( 30.44569435410879521, 207.8125000013656063, 172.4456943541087526 ) ) ;
#9790 = CARTESIAN_POINT ( 'NONE',  ( -5.082755093536317936, -5.082755093536320601, 14.04905278187175455 ) ) ;
#9791 = CARTESIAN_POINT ( 'NONE',  ( -2.828427124746208943, 207.7500000027312126, 144.8284271247462129 ) ) ;
#9792 = CARTESIAN_POINT ( 'NONE',  ( 11.35316468749999963, 60.98958332991935549, -3.042071309553165293 ) ) ;
#9793 = DIRECTION ( 'NONE',  ( -1.000000000000000000, -0.000000000000000000, -0.000000000000000000 ) ) ;
#9794 = CARTESIAN_POINT ( 'NONE',  ( -8.660254037844387298, 23.95833332650536462, -5.000000000000004441 ) ) ;
#9795 = CARTESIAN_POINT ( 'NONE',  ( -6.735557395310442023E-16, 11.00000000000000000, 111.8125000040967763 ) ) ;
#9796 = ORIENTED_EDGE ( 'NONE', *, *, #6220, .F. ) ;
#9797 = LINE ( 'NONE', #56571, #47109 ) ;
#9798 = CARTESIAN_POINT ( 'NONE',  ( -5.676582343750006032, 44.11458332991934839, 9.832129032723418760 ) ) ;
#9799 = CARTESIAN_POINT ( 'NONE',  ( -11.00000000000000000, 0.000000000000000000, 77.68750000409677625 ) ) ;
#9800 = CARTESIAN_POINT ( 'NONE',  ( 1.432654583217608080, 198.8750000013656063, 138.5412658750000503 ) ) ;
#9802 = VECTOR ( 'NONE', #20837, 1000.000000000000000 ) ;
#9801 = CARTESIAN_POINT ( 'NONE',  ( 2.620431783929502600, 10.11675809140012383, 70.36490484707876192 ) ) ;
#9803 = CARTESIAN_POINT ( 'NONE',  ( -4.000000000000015987, 196.6250000027312126, 142.0000000000000568 ) ) ;
#9805 = CARTESIAN_POINT ( 'NONE',  ( 11.35316468750000141, 40.78124999658601268, 0.000000000000000000 ) ) ;
#9804 = CARTESIAN_POINT ( 'NONE',  ( -7.188101187500000933, 100.0625000020483810, -2.977408999572650483 ) ) ;
#9806 = CARTESIAN_POINT ( 'NONE',  ( -3.313708498984757167, 7.999999999999991118, 8.049052779823362869 ) ) ;
#9807 = CARTESIAN_POINT ( 'NONE',  ( -7.999999999999991118, 3.313708498984757167, 21.92405278392014978 ) ) ;
#9808 = CARTESIAN_POINT ( 'NONE',  ( -8.311093377946836114, 167.6562499965860411, -8.311093377946837890 ) ) ;
#9809 = CARTESIAN_POINT ( 'NONE',  ( 10.00000000000000178, 147.0833333265053682, -2.679491924311226736 ) ) ;
#9810 = CARTESIAN_POINT ( 'NONE',  ( -7.188101187500000044, 103.5312500020483810, 0.000000000000000000 ) ) ;
#9811 = CARTESIAN_POINT ( 'NONE',  ( -0.1959015630264571983, -48.00000000000003553, 139.0000000000000853 ) ) ;
#9812 = CARTESIAN_POINT ( 'NONE',  ( -11.35316468749999785, 38.38541666325268409, -3.042071309553167957 ) ) ;
#9813 = ORIENTED_EDGE ( 'NONE', *, *, #683, .T. ) ;
#9814 = CARTESIAN_POINT ( 'NONE',  ( -28.00000000000002842, 204.0000000000000284, 166.0000000000003695 ) ) ;
#9815 = CARTESIAN_POINT ( 'NONE',  ( -7.204075437095967871, 7.204075437095967871, 79.46875000204836681 ) ) ;
#9817 = CARTESIAN_POINT ( 'NONE',  ( -11.35316468750000141, 168.2812499965860411, -1.390361679473963753E-15 ) ) ;
#9816 = DIRECTION ( 'NONE',  ( -0.000000000000000000, 1.000000000000000000, -0.000000000000000000 ) ) ;
#9818 = AXIS2_PLACEMENT_3D ( 'NONE', #38184, #9132, #4230 ) ;
#9819 = CARTESIAN_POINT ( 'NONE',  ( -7.999999999999991118, 0.000000000000000000, 14.38655278432982598 ) ) ;
#9820 = ADVANCED_FACE ( 'NONE', ( #31110 ), #42426, .T. ) ;
#9821 = DIRECTION ( 'NONE',  ( -0.000000000000000000, 1.000000000000000000, -0.000000000000000000 ) ) ;
#9822 = CARTESIAN_POINT ( 'NONE',  ( 7.320508075688776373, 260.0000000068279746, 7.320508075688767491 ) ) ;
#9823 = CARTESIAN_POINT ( 'NONE',  ( -3.228176881619808647, 50.21013539028093220, -40.85102191503846569 ) ) ;
#9824 = CARTESIAN_POINT ( 'NONE',  ( 7.204075437095968759, -7.204075437095966983, 85.09375000204836681 ) ) ;
#9825 = ORIENTED_EDGE ( 'NONE', *, *, #47443, .T. ) ;
#9826 = CARTESIAN_POINT ( 'NONE',  ( 5.656854249492380582, 20.99999999590322375, -5.656854249492380582 ) ) ;
#9827 = CARTESIAN_POINT ( 'NONE',  ( -3.999999999999960032, 204.1250000027312126, 198.0000000000000284 ) ) ;
#9828 = CARTESIAN_POINT ( 'NONE',  ( -3.042071309553164404, 122.5520833299193413, -11.35316468749999963 ) ) ;
#9829 = CARTESIAN_POINT ( 'NONE',  ( 4.220049686691941027, -10.18810118749999738, 96.62500000204838102 ) ) ;
#9830 = CARTESIAN_POINT ( 'NONE',  ( 3.211159895383560947, 19.31249999863440436, 3.211159895383562723 ) ) ;
#9831 = ORIENTED_EDGE ( 'NONE', *, *, #57824, .T. ) ;
#9832 = VERTEX_POINT ( 'NONE', #61281 ) ;
#9833 = AXIS2_PLACEMENT_3D ( 'NONE', #5158, #10803, #28150 ) ;
#9834 = CARTESIAN_POINT ( 'NONE',  ( 4.541265875000001451, 4.374999998634407028, 1.881053915767124440 ) ) ;
#9835 = EDGE_CURVE ( 'NONE', #55737, #6572, #71095, .T. ) ;
#9836 = CARTESIAN_POINT ( 'NONE',  ( -5.082755093536326818, 5.906249997951610986, 5.082755093536325042 ) ) ;
#9837 = CARTESIAN_POINT ( 'NONE',  ( -8.000000000000000000, 111.6875000040967905, 0.000000000000000000 ) ) ;
#9838 = CARTESIAN_POINT ( 'NONE',  ( 1.871523826299183495E-15, -10.18810118749999916, 93.90625000204836681 ) ) ;
#9839 = EDGE_CURVE ( 'NONE', #71315, #37264, #58307, .T. ) ;
#9840 = CARTESIAN_POINT ( 'NONE',  ( -24.54126587499998280, 201.3750000013656347, 171.4326545832179818 ) ) ;
#9841 = CARTESIAN_POINT ( 'NONE',  ( 4.000000000000001776, 5.000000000000000000, 0.000000000000000000 ) ) ;
#9842 = CARTESIAN_POINT ( 'NONE',  ( -7.347880794884122694E-16, 19.49999999726881228, 4.000000000000001776 ) ) ;
#9843 = CARTESIAN_POINT ( 'NONE',  ( -4.541265875000003227, 7.874999998634407028, 1.881053915767121110 ) ) ;
#9844 = CARTESIAN_POINT ( 'NONE',  ( 1.656854249492347719, 203.8125000000000284, 146.0000000000000284 ) ) ;
#9845 = ORIENTED_EDGE ( 'NONE', *, *, #24394, .T. ) ;
#9846 = TOROIDAL_SURFACE ( 'NONE', #28959, 5.000000000000000000, 7.000000000000000000 ) ;
#9847 = EDGE_CURVE ( 'NONE', #26719, #13652, #13739, .T. ) ;
#9849 = CARTESIAN_POINT ( 'NONE',  ( -3.313708498984757611, 7.999999999999991118, 17.04905277982336642 ) ) ;
#9848 = CARTESIAN_POINT ( 'NONE',  ( -25.55430564589111597, 196.0625000013656063, 172.4456943541091505 ) ) ;
#9850 =( BOUNDED_CURVE ( )  B_SPLINE_CURVE ( 2, ( #15797, #50883, #74647, #22576, #33934, #5991, #62948, #27493, #61835 ),
 .UNSPECIFIED., .F., .F. ) 
 B_SPLINE_CURVE_WITH_KNOTS ( ( 3, 2, 2, 2, 3 ),
 ( 0.7613636363636363535, 0.7670454545454545858, 0.7727272727272727071, 0.7784090909090909394, 0.7840909090909090606 ),
 .UNSPECIFIED. ) 
 CURVE ( )  GEOMETRIC_REPRESENTATION_ITEM ( )  RATIONAL_B_SPLINE_CURVE ( ( 1.000000000000000000, 0.9238795325112867385, 1.000000000000000000, 0.9238795325112867385, 1.000000000000000000, 0.9238795325112867385, 1.000000000000000000, 0.9238795325112867385, 1.000000000000000000 ) ) 
 REPRESENTATION_ITEM ( '' )  );
#9851 = CARTESIAN_POINT ( 'NONE',  ( -3.211159895383561391, 19.68749999863440436, -3.211159895383561835 ) ) ;
#9852 = CARTESIAN_POINT ( 'NONE',  ( 10.00000000000000178, 72.08333332650536818, -2.679491924311226736 ) ) ;
#9853 = CARTESIAN_POINT ( 'NONE',  ( 5.082755093536318824, 5.082755093536319713, 27.92405278187175455 ) ) ;
#9854 = ORIENTED_EDGE ( 'NONE', *, *, #45601, .F. ) ;
#9855 = ORIENTED_EDGE ( 'NONE', *, *, #6114, .T. ) ;
#9856 = CARTESIAN_POINT ( 'NONE',  ( 10.18810118749999916, 4.220049686691935698, 98.50000000204838102 ) ) ;
#9857 = CARTESIAN_POINT ( 'NONE',  ( 5.656854249492374365, 5.656854249492375253, 19.76780277982336642 ) ) ;
#9858 = CARTESIAN_POINT ( 'NONE',  ( -24.54126587500000412, 200.5000000013656063, 168.5673454167827003 ) ) ;
#9859 = CARTESIAN_POINT ( 'NONE',  ( -11.00000000000000000, 4.556349186104045934, 107.4062500000000000 ) ) ;
#9860 = CARTESIAN_POINT ( 'NONE',  ( 3.458734125000016757, 206.1250000013655779, 199.4326545832176691 ) ) ;
#9861 = CARTESIAN_POINT ( 'NONE',  ( 2.449293598294707893E-16, 3.999999997268813168, -4.000000000000001776 ) ) ;
#9862 = CARTESIAN_POINT ( 'NONE',  ( 10.00000000000000000, 114.7916666666666856, 2.679491924311236062 ) ) ;
#9863 = CARTESIAN_POINT ( 'NONE',  ( 1.469576158976823947E-15, 105.8750000000000000, 8.000000000000000000 ) ) ;
#9864 = CARTESIAN_POINT ( 'NONE',  ( 2.765530957082001251, 290.9218750017070647, 6.676582343750000703 ) ) ;
#9865 = CARTESIAN_POINT ( 'NONE',  ( -7.188101187499990274, -2.977408999572651371, 12.45530278187175277 ) ) ;
#9866 = EDGE_LOOP ( 'NONE', ( #69993, #21675, #57527, #43714, #25649 ) ) ;
#9867 = CARTESIAN_POINT ( 'NONE',  ( 7.999999999999998224, 19.40625000000000355, 3.313708498984766049 ) ) ;
#9869 = EDGE_CURVE ( 'NONE', #6496, #36295, #54922, .T. ) ;
#9868 = CARTESIAN_POINT ( 'NONE',  ( 26.56734541678238415, 206.0000000013656347, 166.5412658749999650 ) ) ;
#9870 = CARTESIAN_POINT ( 'NONE',  ( -1.469576158976823947E-15, 20.43749999590322375, 8.000000000000000000 ) ) ;
#9871 =( BOUNDED_CURVE ( )  B_SPLINE_CURVE ( 2, ( #39785, #44711, #61319, #26602, #27345, #50361, #21685, #3990, #49624 ),
 .UNSPECIFIED., .F., .F. ) 
 B_SPLINE_CURVE_WITH_KNOTS ( ( 3, 2, 2, 2, 3 ),
 ( 0.7395833333333334814, 0.7447916666666667407, 0.7500000000000001110, 0.7552083333333334814, 0.7604166666666667407 ),
 .UNSPECIFIED. ) 
 CURVE ( )  GEOMETRIC_REPRESENTATION_ITEM ( )  RATIONAL_B_SPLINE_CURVE ( ( 0.9999999999999983347, 0.9238795325112884038, 1.000000000000000000, 0.9238795325112867385, 1.000000000000000000, 0.9238795325112867385, 1.000000000000000000, 0.9238795325112850731, 1.000000000000001554 ) ) 
 REPRESENTATION_ITEM ( '' )  );
#9872 = CARTESIAN_POINT ( 'NONE',  ( -3.458734125000016313, 199.8750000013655779, 140.5673454167824161 ) ) ;
#9873 = CARTESIAN_POINT ( 'NONE',  ( 7.188101187500002709, 119.1875000020483952, 2.977408999572649151 ) ) ;
#9874 = CARTESIAN_POINT ( 'NONE',  ( -2.445694354108839175, 203.3125000013656063, 144.4456943541088663 ) ) ;
#9875 = CARTESIAN_POINT ( 'NONE',  ( 2.085542519210945334E-15, 250.4687500034140157, 11.35316468749999963 ) ) ;
#9876 = LINE ( 'NONE', #26842, #72302 ) ;
#9877 = CARTESIAN_POINT ( 'NONE',  ( -38.00000000000000000, 272.0000000000000000, 20.00000000000003553 ) ) ;
#9878 = CARTESIAN_POINT ( 'NONE',  ( 7.320508075688774596, 225.6249999999999716, -7.320508075688774596 ) ) ;
#9879 = CARTESIAN_POINT ( 'NONE',  ( 5.082755093536318824, 5.082755093536319713, 7.299052781871751883 ) ) ;
#9880 = CARTESIAN_POINT ( 'NONE',  ( 8.311093377946834337, 210.4687499965859843, 8.311093377946839666 ) ) ;
#9881 = CARTESIAN_POINT ( 'NONE',  ( -28.00000000000007816, 203.1250000027312126, 166.0000000000003695 ) ) ;
#9882 = CARTESIAN_POINT ( 'NONE',  ( -1.881053915767121554, 7.624999998634408804, -4.541265875000002339 ) ) ;
#9884 = CARTESIAN_POINT ( 'NONE',  ( 11.00000000000000000, 1.347111479062088405E-15, 118.0000000000000000 ) ) ;
#9883 = CARTESIAN_POINT ( 'NONE',  ( 11.00000000000000000, 1.347111479062088405E-15, 70.93750000409676204 ) ) ;
#9885 = ORIENTED_EDGE ( 'NONE', *, *, #3523, .F. ) ;
#9886 = VECTOR ( 'NONE', #36621, 1000.000000000000000 ) ;
#9887 = CARTESIAN_POINT ( 'NONE',  ( 3.458734124999959469, 198.7500000013656063, 140.5673454167824161 ) ) ;
#9888 = CARTESIAN_POINT ( 'NONE',  ( 8.311093377946837890, 11.40624999658601624, -8.311093377946837890 ) ) ;
#9889 = CARTESIAN_POINT ( 'NONE',  ( -7.778174593052020747, -7.778174593052023411, 98.87500000409676204 ) ) ;
#9890 = CARTESIAN_POINT ( 'NONE',  ( -26.56734541678228112, 197.0000000013656063, 173.4587341250003476 ) ) ;
#9891 = FACE_OUTER_BOUND ( 'NONE', #11630, .T. ) ;
#9893 = CARTESIAN_POINT ( 'NONE',  ( -6.123233995736766282E-16, 228.7500000000000000, -10.00000000000000000 ) ) ;
#9892 = CARTESIAN_POINT ( 'NONE',  ( 7.188101187500002709, 117.3125000020483952, 2.977408999572649151 ) ) ;
#9894 = CARTESIAN_POINT ( 'NONE',  ( -7.999999999999991118, 0.000000000000000000, 27.83030277982336642 ) ) ;
#9895 = CARTESIAN_POINT ( 'NONE',  ( -3.042071309553164404, 117.2395833299193555, -11.35316468749999963 ) ) ;
#9896 = CARTESIAN_POINT ( 'NONE',  ( 4.999999999999993783, 96.04166665983871098, 8.660254037844390851 ) ) ;
#9897 = CARTESIAN_POINT ( 'NONE',  ( -7.188101187499999156, 120.1250000020483952, 2.977408999572654924 ) ) ;
#9898 = CARTESIAN_POINT ( 'NONE',  ( -4.541265875000002339, 21.93749999863440792, -5.561446717895856393E-16 ) ) ;
#9899 = CARTESIAN_POINT ( 'NONE',  ( -10.00000000000000000, 199.1666666598386826, -2.679491924311229845 ) ) ;
#9900 = CARTESIAN_POINT ( 'NONE',  ( 6.123233995736767268E-16, 38.12499999317203958, -10.00000000000000178 ) ) ;
#9901 = ORIENTED_EDGE ( 'NONE', *, *, #23453, .T. ) ;
#9902 = CARTESIAN_POINT ( 'NONE',  ( -3.223881452105937573, -60.47365957010883619, 23.05198836891605652 ) ) ;
#9903 = CARTESIAN_POINT ( 'NONE',  ( 1.226468279477575784E-15, 290.8593750017070079, 6.676582343750001591 ) ) ;
#9904 = CARTESIAN_POINT ( 'NONE',  ( -4.898587196589407898E-16, 7.999999999999991118, 0.6428027839201454485 ) ) ;
#9905 = CARTESIAN_POINT ( 'NONE',  ( 11.00000000000000000, 1.347111479062088405E-15, 84.43750000409677625 ) ) ;
#9906 = CARTESIAN_POINT ( 'NONE',  ( -9.832129032723415207, 259.3229166700806445, 5.676582343750005144 ) ) ;
#9907 = CARTESIAN_POINT ( 'NONE',  ( -10.18810118749999916, 0.000000000000000000, 101.0312500020483810 ) ) ;
#9908 = ORIENTED_EDGE ( 'NONE', *, *, #52687, .T. ) ;
#9909 = AXIS2_PLACEMENT_3D ( 'NONE', #34176, #22447, #62817 ) ;
#9910 = CARTESIAN_POINT ( 'NONE',  ( 6.123233995736767268E-16, 88.12499999317203958, -10.00000000000000178 ) ) ;
#9911 = CARTESIAN_POINT ( 'NONE',  ( -8.311093377946841443, 149.2187499965860127, 8.311093377946834337 ) ) ;
#9912 = CARTESIAN_POINT ( 'NONE',  ( 2.445694354108839175, 205.3125000013656063, 195.5543056458912190 ) ) ;
#9913 = CARTESIAN_POINT ( 'NONE',  ( 5.094044972490348933, 8.823157690132404696, 67.53052377765949643 ) ) ;
#9914 = CARTESIAN_POINT ( 'NONE',  ( 11.35316468749999785, 75.88541666325268409, 3.042071309553174174 ) ) ;
#9915 = ORIENTED_EDGE ( 'NONE', *, *, #41924, .F. ) ;
#9916 = CARTESIAN_POINT ( 'NONE',  ( -10.18810118749999916, 0.000000000000000000, 115.6562500020483810 ) ) ;
#9917 = CARTESIAN_POINT ( 'NONE',  ( -3.211159895383561391, 9.812499998634406140, -3.211159895383561835 ) ) ;
#9918 = ORIENTED_EDGE ( 'NONE', *, *, #73576, .F. ) ;
#9919 = B_SPLINE_CURVE_WITH_KNOTS ( 'NONE', 1,
 ( #67932, #39263 ),
 .UNSPECIFIED., .F., .F.,
 ( 2, 2 ),
 ( 0.000000000000000000, 1.000000000000000000 ),
 .UNSPECIFIED. ) ;
#9920 = CARTESIAN_POINT ( 'NONE',  ( -2.977408999572650039, 20.43749999795161187, -7.188101187500001821 ) ) ;
#9921 = CARTESIAN_POINT ( 'NONE',  ( -2.485281374238572649, 290.2500000034139589, 6.000000000000002665 ) ) ;
#9922 = DIRECTION ( 'NONE',  ( -0.000000000000000000, 1.000000000000000000, 4.689100369878284071E-30 ) ) ;
#9923 = CARTESIAN_POINT ( 'NONE',  ( 4.401442555609581635E-16, 17.71874999795161187, -7.188101187500000044 ) ) ;
#9924 = CARTESIAN_POINT ( 'NONE',  ( 1.656854249492246467, 199.8125000000000284, 146.0000000000001421 ) ) ;
#9925 = CARTESIAN_POINT ( 'NONE',  ( -7.204075437095967871, 7.204075437095967871, 111.3437500020483810 ) ) ;
#9926 = EDGE_CURVE ( 'NONE', #68962, #53267, #42596, .T. ) ;
#9927 = AXIS2_PLACEMENT_3D ( 'NONE', #61489, #10553, #50167 ) ;
#9928 = CARTESIAN_POINT ( 'NONE',  ( 0.000000000000000000, 125.0000000000000000, 8.000000000000000000 ) ) ;
#9929 = CARTESIAN_POINT ( 'NONE',  ( -4.000000000000001776, 5.187499997268813168, -1.656854249492381470 ) ) ;
#9930 = CARTESIAN_POINT ( 'NONE',  ( 4.541265875000002339, 0.4374999986344068059, 0.000000000000000000 ) ) ;
#9931 = ORIENTED_EDGE ( 'NONE', *, *, #45089, .T. ) ;
#9932 = CARTESIAN_POINT ( 'NONE',  ( 3.458734125000015425, 203.9375000013656063, 198.0000000000000284 ) ) ;
#9933 = VECTOR ( 'NONE', #8590, 1000.000000000000000 ) ;
#9934 = CARTESIAN_POINT ( 'NONE',  ( -24.54126587499996504, 209.1250000013656631, 171.4326545832179534 ) ) ;
#9935 = CARTESIAN_POINT ( 'NONE',  ( -7.204075437095965206, -7.204075437095968759, 68.21875000204836681 ) ) ;
#9936 = EDGE_CURVE ( 'NONE', #60340, #8511, #37150, .T. ) ;
#9937 = CARTESIAN_POINT ( 'NONE',  ( -4.541265875000002339, 5.812499998634406140, -5.561446717895856393E-16 ) ) ;
#9938 = CARTESIAN_POINT ( 'NONE',  ( -2.485281374238875962, 289.8125000000000000, -5.999999999999697131 ) ) ;
#9939 = CARTESIAN_POINT ( 'NONE',  ( -2.977408999572647819, 7.188101187499991163, 22.20530278187175455 ) ) ;
#9940 = ORIENTED_EDGE ( 'NONE', *, *, #51623, .T. ) ;
#9941 =( BOUNDED_CURVE ( )  B_SPLINE_CURVE ( 2, ( #36531, #7854, #30861, #31982, #55007, #15358, #3685, #26299, #16098 ),
 .UNSPECIFIED., .F., .F. ) 
 B_SPLINE_CURVE_WITH_KNOTS ( ( 3, 2, 2, 2, 3 ),
 ( 0.8333333333333340365, 0.8416666666666673402, 0.8500000000000006439, 0.8583333333333339477, 0.8666666666666673624 ),
 .UNSPECIFIED. ) 
 CURVE ( )  GEOMETRIC_REPRESENTATION_ITEM ( )  RATIONAL_B_SPLINE_CURVE ( ( 0.9999999999999938938, 0.9238795325112928447, 1.000000000000000000, 0.9238795325112867385, 1.000000000000000000, 0.9238795325112867385, 1.000000000000000000, 0.9238795325112806323, 1.000000000000005995 ) ) 
 REPRESENTATION_ITEM ( '' )  );
#9942 = EDGE_CURVE ( 'NONE', #7527, #61049, #42326, .T. ) ;
#9943 = CARTESIAN_POINT ( 'NONE',  ( 2.485281374238152097, 299.6875000000000568, -6.000000000000420997 ) ) ;
#9944 = EDGE_LOOP ( 'NONE', ( #54448, #28486, #13719, #20920 ) ) ;
#9945 = CARTESIAN_POINT ( 'NONE',  ( -4.999999999999995559, 1.666666666666664520, -8.660254037844385522 ) ) ;
#9946 = CARTESIAN_POINT ( 'NONE',  ( 7.778174593052021635, 7.778174593052023411, 96.62500000409676204 ) ) ;
#9947 = CARTESIAN_POINT ( 'NONE',  ( -1.432654583217607192, 205.2500000013655779, 194.5412658750000219 ) ) ;
#9948 = CARTESIAN_POINT ( 'NONE',  ( 31.45873412499999944, 199.6250000013656063, 171.4326545832175555 ) ) ;
#9949 = CARTESIAN_POINT ( 'NONE',  ( 10.00000000000000178, 65.20833333333334281, -2.679491924311226736 ) ) ;
#9950 = CARTESIAN_POINT ( 'NONE',  ( -8.000000000000000000, 123.5000000000000000, 0.000000000000000000 ) ) ;
#9951 = CARTESIAN_POINT ( 'NONE',  ( 6.000000000000003553, 293.5625000000001137, -2.485281374238571761 ) ) ;
#9952 = CARTESIAN_POINT ( 'NONE',  ( 28.00000000000002132, 204.1250000027312126, 173.9999999999999147 ) ) ;
#9953 = ORIENTED_EDGE ( 'NONE', *, *, #46309, .T. ) ;
#9954 = CARTESIAN_POINT ( 'NONE',  ( 4.898587196589412829E-16, 9.187499995903221972, -8.000000000000000000 ) ) ;
#9955 = CARTESIAN_POINT ( 'NONE',  ( 6.350741970897364085E-13, 216.2499999999999432, -9.999999999999998224 ) ) ;
#9956 = CARTESIAN_POINT ( 'NONE',  ( -4.000000000000015099, 196.6875000027312126, 143.6568542494924543 ) ) ;
#9957 = DIRECTION ( 'NONE',  ( 0.000000000000000000, 0.000000000000000000, 1.000000000000000000 ) ) ;
#9958 = FACE_OUTER_BOUND ( 'NONE', #3145, .T. ) ;
#9959 = CARTESIAN_POINT ( 'NONE',  ( 7.320508075688771044, 248.1250000000000284, -7.320508075688771932 ) ) ;
#9960 = ADVANCED_FACE ( 'NONE', ( #42795 ), #501, .F. ) ;
#9961 = LINE ( 'NONE', #62008, #16207 ) ;
#9962 = CARTESIAN_POINT ( 'NONE',  ( -2.679491924311225848, 191.4583333333333428, -10.00000000000000178 ) ) ;
#9963 =( BOUNDED_CURVE ( )  B_SPLINE_CURVE ( 2, ( #69188, #12208, #35246, #52216, #29204, #17501, #64271, #549, #35608, #40518, #23531, #46544, #51089 ),
 .UNSPECIFIED., .F., .F. ) 
 B_SPLINE_CURVE_WITH_KNOTS ( ( 3, 2, 2, 2, 2, 2, 3 ),
 ( 0.1684782608695652162, 0.1702898550724637750, 0.1721014492753623060, 0.1739130434782608647, 0.1757246376811594235, 0.1775362318840579823, 0.1793478260869565133 ),
 .UNSPECIFIED. ) 
 CURVE ( )  GEOMETRIC_REPRESENTATION_ITEM ( )  RATIONAL_B_SPLINE_CURVE ( ( 1.000000000000000000, 0.9659258262890683122, 1.000000000000000000, 0.9659258262890683122, 1.000000000000000000, 0.9659258262890683122, 1.000000000000000000, 0.9659258262890683122, 1.000000000000000000, 0.9659258262890683122, 1.000000000000000000, 0.9659258262890683122, 1.000000000000000000 ) ) 
 REPRESENTATION_ITEM ( '' )  );
#9964 = CARTESIAN_POINT ( 'NONE',  ( -11.00000000000000000, 0.000000000000000000, 110.4999999999999858 ) ) ;
#9965 = CARTESIAN_POINT ( 'NONE',  ( 1.320432766682872962E-15, -7.188101187499992051, 24.73655278187175810 ) ) ;
#9966 = CARTESIAN_POINT ( 'NONE',  ( -9.832129032723420536, 164.0104166632526983, 5.676582343749997150 ) ) ;
#9967 = CARTESIAN_POINT ( 'NONE',  ( -3.999999999999960032, 208.0625000027312410, 196.3431457505076594 ) ) ;
#9968 = DIRECTION ( 'NONE',  ( 0.000000000000000000, 0.000000000000000000, 1.000000000000000000 ) ) ;
#9969 = DIRECTION ( 'NONE',  ( -0.000000000000000000, 1.000000000000000000, -0.000000000000000000 ) ) ;
#9971 = CARTESIAN_POINT ( 'NONE',  ( 0.000000000000000000, 2.143131898507868248E-15, 17.50000000000000000 ) ) ;
#9970 = PRESENTATION_STYLE_ASSIGNMENT (( #45777 ) ) ;
#9972 = ORIENTED_EDGE ( 'NONE', *, *, #66470, .F. ) ;
#9973 = CARTESIAN_POINT ( 'NONE',  ( -8.311093377946841443, 29.21874999658601979, 8.311093377946830785 ) ) ;
#9974 = CARTESIAN_POINT ( 'NONE',  ( 7.999999999999992895, -9.797174393178815797E-16, 0.000000000000000000 ) ) ;
#9976 = CARTESIAN_POINT ( 'NONE',  ( 1.781595147088347098, -16.42277972782010309, -68.70049804031377505 ) ) ;
#9975 = CYLINDRICAL_SURFACE ( 'NONE', #14289, 10.00000000000000178 ) ;
#9977 = CARTESIAN_POINT ( 'NONE',  ( -23.79522946727241361, -50.66010755326980330, 189.8747476470669255 ) ) ;
#9978 = CARTESIAN_POINT ( 'NONE',  ( -2.445694354108839619, 204.8125000013656063, 139.5543056458912190 ) ) ;
#9979 = VECTOR ( 'NONE', #13843, 1000.000000000000000 ) ;
#9980 = CARTESIAN_POINT ( 'NONE',  ( -10.00000000000000178, 44.37499999317203248, -1.224646799147353454E-15 ) ) ;
#9981 = CARTESIAN_POINT ( 'NONE',  ( 2.977408999572654480, 102.1250000020483810, 7.188101187499999156 ) ) ;
#9982 = CARTESIAN_POINT ( 'NONE',  ( -4.541265875000003227, 8.999999998634406140, 1.881053915767121110 ) ) ;
#9983 = CARTESIAN_POINT ( 'NONE',  ( 2.449293598294707893E-16, 1.999999997268813168, -4.000000000000001776 ) ) ;
#9984 = CARTESIAN_POINT ( 'NONE',  ( 3.313708498984756279, 7.999999999999991118, 7.861552779823362869 ) ) ;
#9985 = CARTESIAN_POINT ( 'NONE',  ( 4.000000000000000888, 0.9375000000000001110, 1.656854249492384135 ) ) ;
#9986 = ORIENTED_EDGE ( 'NONE', *, *, #27826, .T. ) ;
#9987 = VERTEX_POINT ( 'NONE', #62753 ) ;
#9988 = CARTESIAN_POINT ( 'NONE',  ( -5.000000000000000888, -65.19475225706635513, 23.98307544244917011 ) ) ;
#9989 = CARTESIAN_POINT ( 'NONE',  ( -7.999999999999991118, 1.438550051402736141E-05, 14.51780237693182052 ) ) ;
#9990 = CARTESIAN_POINT ( 'NONE',  ( -4.000000000000015987, 196.5625000000000284, 143.6568542494924259 ) ) ;
#9991 = EDGE_CURVE ( 'NONE', #38797, #28093, #61026, .T. ) ;
#9992 = CARTESIAN_POINT ( 'NONE',  ( 5.676582343749997150, 222.5520833367473017, -9.832129032723418760 ) ) ;
#9993 = VECTOR ( 'NONE', #21132, 1000.000000000000000 ) ;
#9994 = CARTESIAN_POINT ( 'NONE',  ( 3.042071309553167069, 146.8229166632527267, -11.35316468749999785 ) ) ;
#9995 = ORIENTED_EDGE ( 'NONE', *, *, #53722, .T. ) ;
#9996 = CARTESIAN_POINT ( 'NONE',  ( -15.99999999999999645, 15.99999999999999645, 20.00000000000000000 ) ) ;
#9997 = CARTESIAN_POINT ( 'NONE',  ( -6.238412754330611322E-16, 10.18810118749999916, 91.28125000204836681 ) ) ;
#9998 = CARTESIAN_POINT ( 'NONE',  ( -7.999999999999991118, 0.000000000000000000, 20.51780278392014623 ) ) ;
#9999 = CARTESIAN_POINT ( 'NONE',  ( -1.656854249492348607, 209.1875000000000000, 202.0000000000000284 ) ) ;
#10001 = CARTESIAN_POINT ( 'NONE',  ( -11.35316468750000141, 128.2812499965860127, -1.390361679473963753E-15 ) ) ;
#10000 = CARTESIAN_POINT ( 'NONE',  ( 2.828427124746190291, 14.62499999726881406, 2.828427124746192067 ) ) ;
#10002 = EDGE_CURVE ( 'NONE', #24721, #10215, #46750, .T. ) ;
#10003 = CARTESIAN_POINT ( 'NONE',  ( 0.000000000000000000, 0.000000000000000000, 0.000000000000000000 ) ) ;
#10004 = ORIENTED_EDGE ( 'NONE', *, *, #11817, .F. ) ;
#10005 = CARTESIAN_POINT ( 'NONE',  ( 6.123233995736767268E-16, 23.12499999317203603, -10.00000000000000178 ) ) ;
#10006 = CARTESIAN_POINT ( 'NONE',  ( -30.92609751906903881, 178.6226547574352992, 173.1060824877128255 ) ) ;
#10007 = CARTESIAN_POINT ( 'NONE',  ( 5.676582343749993598, 120.2604166632526841, 9.832129032723422313 ) ) ;
#10008 = CARTESIAN_POINT ( 'NONE',  ( 2.754378923186476579E-14, 204.1875000013656063, 194.5412658750000219 ) ) ;
#10009 = CARTESIAN_POINT ( 'NONE',  ( 7.188101187500000044, 15.84374999795161365, 0.000000000000000000 ) ) ;
#10011 = ADVANCED_FACE ( 'NONE', ( #38655 ), #46901, .F. ) ;
#10010 = CARTESIAN_POINT ( 'NONE',  ( 7.204075437095966983, 7.204075437095967871, 80.96875000204836681 ) ) ;
#10012 = CARTESIAN_POINT ( 'NONE',  ( -9.832129032723420536, 29.01041666325268764, 5.676582343749997150 ) ) ;
#10013 = EDGE_LOOP ( 'NONE', ( #36358, #31435, #62778, #66756 ) ) ;
#10014 = DIRECTION ( 'NONE',  ( -0.000000000000000000, 1.000000000000000000, -0.000000000000000000 ) ) ;
#10015 = CARTESIAN_POINT ( 'NONE',  ( -8.008118988124991233, 3.317071493978878127, 18.91936528394063544 ) ) ;
#10016 = CARTESIAN_POINT ( 'NONE',  ( 38.00000000000000000, -53.00000000000000711, 9.999999999999991118 ) ) ;
#10017 = DIRECTION ( 'NONE',  ( -0.000000000000000000, 1.000000000000000000, -4.476705744456276341E-16 ) ) ;
#10018 = CARTESIAN_POINT ( 'NONE',  ( 5.082755093536324154, 4.781249997951610986, 5.082755093536326818 ) ) ;
#10019 = CARTESIAN_POINT ( 'NONE',  ( 6.676582343750003368, 288.0156250017069510, -2.765530957081997254 ) ) ;
#10020 = CARTESIAN_POINT ( 'NONE',  ( -5.447321192899549303, -4.689935021205116961, 0.1569292013794422458 ) ) ;
#10021 = CARTESIAN_POINT ( 'NONE',  ( -5.082755093536326818, 1.781249997951610098, 5.082755093536325042 ) ) ;
#10022 = ORIENTED_EDGE ( 'NONE', *, *, #4435, .F. ) ;
#10023 = CARTESIAN_POINT ( 'NONE',  ( -5.676582343750006032, 149.4270833299193555, 9.832129032723418760 ) ) ;
#10024 = CARTESIAN_POINT ( 'NONE',  ( -7.204075437095965206, -7.204075437095968759, 78.34375000204838102 ) ) ;
#10025 = CARTESIAN_POINT ( 'NONE',  ( -30.44569435410883074, 196.5625000013656063, 167.5543056458915885 ) ) ;
#10026 = DIRECTION ( 'NONE',  ( 1.000000000000000000, -0.000000000000000000, 0.000000000000000000 ) ) ;
#10027 = CARTESIAN_POINT ( 'NONE',  ( -3.211159895383561391, 16.81249999863440436, -3.211159895383561835 ) ) ;
#10028 = ORIENTED_EDGE ( 'NONE', *, *, #14560, .F. ) ;
#10029 = CARTESIAN_POINT ( 'NONE',  ( -2.828427124746152987, 205.2500000027312126, 200.8284271247462129 ) ) ;
#10030 = CARTESIAN_POINT ( 'NONE',  ( -4.000000000000015987, 209.4375000000000284, 140.3431457505076594 ) ) ;
#10031 = CARTESIAN_POINT ( 'NONE',  ( -30.82842712474624847, 206.2500000027312126, 167.1715728752542418 ) ) ;
#10032 = CARTESIAN_POINT ( 'NONE',  ( -1.469576158976823947E-15, 23.62500000000000355, 8.000000000000000000 ) ) ;
#10033 = ORIENTED_EDGE ( 'NONE', *, *, #67632, .T. ) ;
#10034 = CARTESIAN_POINT ( 'NONE',  ( 7.188101187500000044, 9.468749997951610098, 0.000000000000000000 ) ) ;
#10035 = CARTESIAN_POINT ( 'NONE',  ( -7.999999999946576068, -3.313708499038175770, 8.611552783922281407 ) ) ;
#10036 = CARTESIAN_POINT ( 'NONE',  ( 4.999999999999999112, 52.28182290968099011, -42.43119126381003525 ) ) ;
#10037 = AXIS2_PLACEMENT_3D ( 'NONE', #33906, #39545, #35386 ) ;
#10038 = CARTESIAN_POINT ( 'NONE',  ( 11.35316468749999785, 180.5729166632526983, 3.042071309553174174 ) ) ;
#10039 = CARTESIAN_POINT ( 'NONE',  ( -4.401442555609581635E-16, 115.1562500020483810, -7.188101187500000044 ) ) ;
#10040 = CARTESIAN_POINT ( 'NONE',  ( -4.721056650415999201, 288.3281250017069510, -4.721056650415999201 ) ) ;
#10042 = CARTESIAN_POINT ( 'NONE',  ( -4.898587196589412829E-16, 105.1250000000000000, -8.000000000000000000 ) ) ;
#10041 = DIRECTION ( 'NONE',  ( 0.000000000000000000, 0.000000000000000000, 1.000000000000000000 ) ) ;
#10043 = ORIENTED_EDGE ( 'NONE', *, *, #10370, .F. ) ;
#10044 = CARTESIAN_POINT ( 'NONE',  ( -8.311093377946834337, 259.5312500034139589, 8.311093377946837890 ) ) ;
#10045 = CARTESIAN_POINT ( 'NONE',  ( -4.401442555609577197E-16, 7.188101187499992051, 20.98655278187175455 ) ) ;
#10046 = CARTESIAN_POINT ( 'NONE',  ( -1.656854249492382580, 2.062499997268813168, -4.000000000000000000 ) ) ;
#10047 = CARTESIAN_POINT ( 'NONE',  ( 8.572527594031473190E-16, 0.000000000000000000, -7.000000000000000000 ) ) ;
#10048 = CARTESIAN_POINT ( 'NONE',  ( -3.511653767256468051, -68.04552192806512778, -20.40125235306675222 ) ) ;
#10049 = CARTESIAN_POINT ( 'NONE',  ( -3.458734124999959469, 194.7500000013656063, 199.4326545832176691 ) ) ;
#10050 = CARTESIAN_POINT ( 'NONE',  ( 8.660254037844385522, 144.5833333333333428, 5.000000000000005329 ) ) ;
#10051 = ORIENTED_EDGE ( 'NONE', *, *, #66274, .F. ) ;
#10052 = CARTESIAN_POINT ( 'NONE',  ( -4.500000000000007994, 7.794228634059939154, 0.000000000000000000 ) ) ;
#10053 = CARTESIAN_POINT ( 'NONE',  ( -5.656854249492380582, 94.81250000000000000, -5.656854249492380582 ) ) ;
#10054 = CARTESIAN_POINT ( 'NONE',  ( -11.35316468749999785, 113.3854166632526841, -3.042071309553167513 ) ) ;
#10055 = CARTESIAN_POINT ( 'NONE',  ( -4.999999999999995559, -15.86406185656355916, -69.92615499037641769 ) ) ;
#10056 = CARTESIAN_POINT ( 'NONE',  ( -7.778174593052020747, -7.778174593052023411, 68.68749999999998579 ) ) ;
#10059 = CARTESIAN_POINT ( 'NONE',  ( 28.00000000000002487, 206.1250000027312126, 173.9999999999999147 ) ) ;
#10058 = CARTESIAN_POINT ( 'NONE',  ( 26.56734541678232731, 202.0000000013656063, 166.5412658749999650 ) ) ;
#10057 = CARTESIAN_POINT ( 'NONE',  ( 25.55430564589119413, 198.3125000013656063, 167.5543056458910485 ) ) ;
#10060 = ORIENTED_EDGE ( 'NONE', *, *, #19650, .T. ) ;
#10061 = B_SPLINE_CURVE_WITH_KNOTS ( 'NONE', 3,
 ( #69480, #59278, #47198, #30225, #12497, #70227, #12856, #40804, #36631, #58540, #46461, #52500, #6486, #53979, #41181, #36262, #59638, #18902, #1926, #53245, #63813, #41909, #838, #13593, #64561, #23824 ),
 .UNSPECIFIED., .F., .F.,
 ( 4, 2, 2, 2, 2, 2, 2, 2, 2, 2, 2, 2, 4 ),
 ( 0.000000000000000000, 0.005942507281089738809, 0.008913760921634568749, 0.01039938774190698328, 0.01188501456217939782, 0.01782752184326906117, 0.02377002912435872972, 0.02674128276490356226, 0.02971253640544839134, 0.03565504368653799050, 0.04159755096762760007, 0.04456880460817239098, 0.04754005824871718189 ),
 .UNSPECIFIED. ) ;
#10062 = CARTESIAN_POINT ( 'NONE',  ( 9.969536597484252027, 224.9231957930772410, 0.9796593664695627535 ) ) ;
#10063 = CARTESIAN_POINT ( 'NONE',  ( 6.951808397369818766E-16, 222.0312499965860127, -11.35316468750000141 ) ) ;
#10064 =( BOUNDED_CURVE ( )  B_SPLINE_CURVE ( 2, ( #12544, #35572, #7264, #1615, #18947, #41951, #64959, #9117, #49472, #61912, #32134, #50218, #66074 ),
 .UNSPECIFIED., .F., .F. ) 
 B_SPLINE_CURVE_WITH_KNOTS ( ( 3, 2, 2, 2, 2, 2, 3 ),
 ( 0.7445652173913043237, 0.7463768115942028825, 0.7481884057971014412, 0.7500000000000000000, 0.7518115942028985588, 0.7536231884057971175, 0.7554347826086956763 ),
 .UNSPECIFIED. ) 
 CURVE ( )  GEOMETRIC_REPRESENTATION_ITEM ( )  RATIONAL_B_SPLINE_CURVE ( ( 1.000000000000000000, 0.9659258262890683122, 1.000000000000000000, 0.9659258262890683122, 1.000000000000000000, 0.9659258262890683122, 1.000000000000000000, 0.9659258262890683122, 1.000000000000000000, 0.9659258262890683122, 1.000000000000000000, 0.9659258262890683122, 1.000000000000000000 ) ) 
 REPRESENTATION_ITEM ( '' )  );
#10065 = CARTESIAN_POINT ( 'NONE',  ( 25.55430564589114795, 197.5625000013656063, 172.4456943541086957 ) ) ;
#10066 = CARTESIAN_POINT ( 'NONE',  ( -8.311093377946841443, 204.2187499965860411, 8.311093377946830785 ) ) ;
#10067 = AXIS2_PLACEMENT_3D ( 'NONE', #61116, #66778, #26018 ) ;
#10068 = CARTESIAN_POINT ( 'NONE',  ( -7.188101187499999156, 119.7500000020483810, 2.977408999572654924 ) ) ;
#10069 = CARTESIAN_POINT ( 'NONE',  ( 4.541265875000001451, 18.24999999863440792, 1.881053915767124440 ) ) ;
#10070 = CARTESIAN_POINT ( 'NONE',  ( 27.99999999999996092, 195.6875000013655779, 173.4587341249998929 ) ) ;
#10071 = CARTESIAN_POINT ( 'NONE',  ( 3.313708498984762496, -7.999999999999989342, 26.79905277982337353 ) ) ;
#10073 = DIRECTION ( 'NONE',  ( -0.000000000000000000, 1.000000000000000000, -0.000000000000000000 ) ) ;
#10072 = CARTESIAN_POINT ( 'NONE',  ( 8.660254037844383745, 185.4166666666666856, -4.999999999999997335 ) ) ;
#10074 = CARTESIAN_POINT ( 'NONE',  ( -11.35316468750000141, 98.48958332991936970, 3.042071309553159963 ) ) ;
#10075 = ORIENTED_EDGE ( 'NONE', *, *, #52584, .F. ) ;
#10076 = CYLINDRICAL_SURFACE ( 'NONE', #3803, 4.000000000000001776 ) ;
#10077 = CARTESIAN_POINT ( 'NONE',  ( 4.401442555609581635E-16, 18.84374999795161187, -7.188101187500000044 ) ) ;
#10078 = CARTESIAN_POINT ( 'NONE',  ( -5.656854249492380582, 108.5000000040967763, -5.656854249492380582 ) ) ;
#10079 = CARTESIAN_POINT ( 'NONE',  ( -8.311093377946836114, 253.5937500034139873, -8.311093377946836114 ) ) ;
#10080 = CARTESIAN_POINT ( 'NONE',  ( 9.832129032723416984, 105.3645833299193555, 5.676582343750006032 ) ) ;
#10081 = ORIENTED_EDGE ( 'NONE', *, *, #29708, .T. ) ;
#10082 = DIRECTION ( 'NONE',  ( -0.000000000000000000, -0.000000000000000000, 1.000000000000000000 ) ) ;
#10083 = CARTESIAN_POINT ( 'NONE',  ( -7.204075437095965206, -7.204075437095968759, 105.3437500020483810 ) ) ;
#10084 = CARTESIAN_POINT ( 'NONE',  ( -28.00000000000001776, 194.6875000013655779, 166.5412658750003629 ) ) ;
#10085 = CARTESIAN_POINT ( 'NONE',  ( -3.458734124999959469, 206.7500000013655779, 199.4326545832176691 ) ) ;
#10086 = CARTESIAN_POINT ( 'NONE',  ( 0.000000000000000000, 30.78460969082653875, -20.69999999999999929 ) ) ;
#10088 = CARTESIAN_POINT ( 'NONE',  ( -11.35316468750000141, 83.48958332991935549, 3.042071309553159963 ) ) ;
#10087 = CARTESIAN_POINT ( 'NONE',  ( -8.000000000000003553, 22.99999999999999645, -1.000000000000000000 ) ) ;
#10089 = CARTESIAN_POINT ( 'NONE',  ( -7.999999999999991118, 0.000000000000000000, 13.01780278392014623 ) ) ;
#10090 = CARTESIAN_POINT ( 'NONE',  ( -29.43265458321760519, 199.1250000013656347, 173.4587341250003760 ) ) ;
#10091 = EDGE_CURVE ( 'NONE', #3422, #54835, #69888, .T. ) ;
#10092 = CARTESIAN_POINT ( 'NONE',  ( 0.000000000000000000, 0.000000000000000000, 30.00000000000000000 ) ) ;
#10093 = CARTESIAN_POINT ( 'NONE',  ( -2.679491924311235618, 180.4166666598387394, 10.00000000000000000 ) ) ;
#10094 = CARTESIAN_POINT ( 'NONE',  ( -28.00000000000002487, 197.0000000000000000, 166.0000000000003695 ) ) ;
#10095 = CARTESIAN_POINT ( 'NONE',  ( -2.085542519210945728E-15, 69.84374999658601268, 11.35316468750000141 ) ) ;
#10096 = CARTESIAN_POINT ( 'NONE',  ( -2.765530957081998586, 290.6406250017069510, 6.676582343750001591 ) ) ;
#10098 = ADVANCED_FACE ( 'NONE', ( #34869 ), #23145, .T. ) ;
#10097 = CARTESIAN_POINT ( 'NONE',  ( -7.204075437095965206, -7.204075437095968759, 102.7187500020483668 ) ) ;
#10099 = CARTESIAN_POINT ( 'NONE',  ( 11.35316468750000141, 210.7812499965860411, 0.000000000000000000 ) ) ;
#10100 = ORIENTED_EDGE ( 'NONE', *, *, #67238, .T. ) ;
#10101 = CARTESIAN_POINT ( 'NONE',  ( -4.000000000000001776, 1.187499997268813390, -1.656854249492381470 ) ) ;
#10102 = LINE ( 'NONE', #4822, #24347 ) ;
#10103 = CARTESIAN_POINT ( 'NONE',  ( -3.729367062499960195, 209.2812500020483810, 198.0000000000000284 ) ) ;
#10104 = CARTESIAN_POINT ( 'NONE',  ( -3.042071309553173730, 209.3229166632526983, 11.35316468749999785 ) ) ;
#10105 = AXIS2_PLACEMENT_3D ( 'NONE', #12574, #58618, #28071 ) ;
#10106 = CARTESIAN_POINT ( 'NONE',  ( -9.999999999999998224, 223.3333333401613174, 2.679491924311235618 ) ) ;
#10107 = CARTESIAN_POINT ( 'NONE',  ( -9.999999999999998224, 253.3333333401613174, 2.679491924311235174 ) ) ;
#10108 = ORIENTED_EDGE ( 'NONE', *, *, #64781, .F. ) ;
#10109 = CARTESIAN_POINT ( 'NONE',  ( -5.676582343750006032, 189.4270833299193555, 9.832129032723418760 ) ) ;
#10110 = CARTESIAN_POINT ( 'NONE',  ( -5.082755093536319713, 5.082755093536319713, 13.29905278187175277 ) ) ;
#10111 = CARTESIAN_POINT ( 'NONE',  ( -31.45873412500001010, 208.6250000013655779, 168.5673454167827572 ) ) ;
#10112 = CARTESIAN_POINT ( 'NONE',  ( -1.469576158976823947E-15, 14.62500000000000178, 8.000000000000000000 ) ) ;
#10113 = ORIENTED_EDGE ( 'NONE', *, *, #65766, .T. ) ;
#10114 = CARTESIAN_POINT ( 'NONE',  ( 1.469576158976823947E-15, 94.06250000409677625, 8.000000000000000000 ) ) ;
#10115 = CARTESIAN_POINT ( 'NONE',  ( -4.999999999999998224, 16.66666666666666785, -8.660254037844389075 ) ) ;
#10116 = AXIS2_PLACEMENT_3D ( 'NONE', #43125, #50282, #14071 ) ;
#10117 = CARTESIAN_POINT ( 'NONE',  ( 7.204075437095966983, 7.204075437095967871, 82.46875000204836681 ) ) ;
#10118 = EDGE_LOOP ( 'NONE', ( #37873, #56927, #71962, #20003 ) ) ;
#10119 = CARTESIAN_POINT ( 'NONE',  ( -2.828427124746190735, 20.37500000000000000, -2.828427124746191623 ) ) ;
#10120 = CARTESIAN_POINT ( 'NONE',  ( -4.541265875000002339, 20.81249999863440436, -5.561446717895856393E-16 ) ) ;
#10121 = CARTESIAN_POINT ( 'NONE',  ( 30.65744098404905671, 194.5307006980096673, 172.3354755555894542 ) ) ;
#10122 = ORIENTED_EDGE ( 'NONE', *, *, #6206, .T. ) ;
#10123 = CARTESIAN_POINT ( 'NONE',  ( 27.99999999999999645, 210.0000000000000284, 169.9999999999999147 ) ) ;
#10124 = CARTESIAN_POINT ( 'NONE',  ( -7.188101187499999156, 91.25000000204838102, 2.977408999572654924 ) ) ;
#10127 = DIRECTION ( 'NONE',  ( 1.000000000000000000, 0.000000000000000000, 0.000000000000000000 ) ) ;
#10126 = CARTESIAN_POINT ( 'NONE',  ( -27.99999999999991118, 204.6250000027312126, 174.0000000000003695 ) ) ;
#10125 = CARTESIAN_POINT ( 'NONE',  ( 3.313708498984756279, 7.999999999999991118, 12.36155277982336820 ) ) ;
#10128 = PRODUCT_CONTEXT ( 'NONE', #28395, 'mechanical' ) ;
#10129 = ORIENTED_EDGE ( 'NONE', *, *, #50105, .T. ) ;
#10130 = CARTESIAN_POINT ( 'NONE',  ( 11.35316468749999963, 256.7187500034139589, -1.390361679473963556E-15 ) ) ;
#10131 = CARTESIAN_POINT ( 'NONE',  ( 7.188101187499991163, 2.977408999572648707, 11.33030278187175632 ) ) ;
#10132 = ORIENTED_EDGE ( 'NONE', *, *, #29784, .F. ) ;
#10133 = EDGE_LOOP ( 'NONE', ( #63669, #45840, #22603, #41258, #68474, #73357 ) ) ;
#10134 = CARTESIAN_POINT ( 'NONE',  ( -10.18810118749999916, 4.220049686691934809, 73.56250000204836681 ) ) ;
#10135 = CARTESIAN_POINT ( 'NONE',  ( 11.35316468749999963, 71.30208332991932707, -3.042071309553165293 ) ) ;
#10136 = CARTESIAN_POINT ( 'NONE',  ( 7.999999999999991118, 9.797174393178815797E-16, 18.08030277982336642 ) ) ;
#10137 = CARTESIAN_POINT ( 'NONE',  ( 2.020667218593132706E-15, -11.00000000000000000, 91.37499999999998579 ) ) ;
#10140 = CARTESIAN_POINT ( 'NONE',  ( 2.765530957082001251, 291.9218750017069510, 6.676582343749999815 ) ) ;
#10139 = CARTESIAN_POINT ( 'NONE',  ( 29.65685424949240101, 195.1875000027312410, 173.9999999999999147 ) ) ;
#10138 = DIRECTION ( 'NONE',  ( -0.000000000000000000, -0.000000000000000000, 1.000000000000000000 ) ) ;
#10141 = CIRCLE ( 'NONE', #14918, 12.00000000000000000 ) ;
#10142 = DIRECTION ( 'NONE',  ( -1.000000000000000000, 0.000000000000000000, 0.000000000000000000 ) ) ;
#10143 = CARTESIAN_POINT ( 'NONE',  ( -27.99999999999991118, 204.6250000027312126, 174.0000000000003695 ) ) ;
#10144 = CARTESIAN_POINT ( 'NONE',  ( -3.458734124999959469, 199.7500000013656063, 199.4326545832176976 ) ) ;
#10145 = ADVANCED_FACE ( 'NONE', ( #51823 ), #35961, .T. ) ;
#10146 = CARTESIAN_POINT ( 'NONE',  ( -5.656854249492379694, 6.374999995903221084, -5.656854249492380582 ) ) ;
#10147 = EDGE_CURVE ( 'NONE', #58040, #47682, #57505, .T. ) ;
#10148 = ORIENTED_EDGE ( 'NONE', *, *, #44836, .T. ) ;
#10149 = CARTESIAN_POINT ( 'NONE',  ( 28.00000000000002487, 209.1875000013656063, 166.5412658749999082 ) ) ;
#10150 = CARTESIAN_POINT ( 'NONE',  ( -7.188101187500000044, 18.09374999795161187, -8.802885111219163269E-16 ) ) ;
#10151 = CARTESIAN_POINT ( 'NONE',  ( -5.676582343750006032, 169.4270833299193555, 9.832129032723418760 ) ) ;
#10152 = CARTESIAN_POINT ( 'NONE',  ( -8.000000000000000000, 105.5000000000000000, 0.000000000000000000 ) ) ;
#10153 = CARTESIAN_POINT ( 'NONE',  ( 1.320432766682874540E-15, 105.4062500020483810, 7.188101187500000044 ) ) ;
#10155 = CARTESIAN_POINT ( 'NONE',  ( -2.679491924311193429, 236.0416666666666572, 10.00000000000001954 ) ) ;
#10154 = CARTESIAN_POINT ( 'NONE',  ( 1.656854249492381248, 16.93749999726881583, -4.000000000000001776 ) ) ;
#10156 = CARTESIAN_POINT ( 'NONE',  ( 24.54126587500000767, 208.3750000013656063, 168.5673454167822172 ) ) ;
#10157 = CARTESIAN_POINT ( 'NONE',  ( -2.977408999572647819, 7.188101187499991163, 15.08030278187175455 ) ) ;
#10158 = FACE_OUTER_BOUND ( 'NONE', #19768, .T. ) ;
#10159 = CARTESIAN_POINT ( 'NONE',  ( 11.35316468749999963, 50.98958332991934839, -3.042071309553165293 ) ) ;
#10160 = CARTESIAN_POINT ( 'NONE',  ( -2.696190831617548245, -43.66988855560286709, 139.1173792546188110 ) ) ;
#10161 = CARTESIAN_POINT ( 'NONE',  ( 10.00000000000000178, 16.87499999317203248, 0.000000000000000000 ) ) ;
#10162 = FACE_OUTER_BOUND ( 'NONE', #6136, .T. ) ;
#10163 = ORIENTED_EDGE ( 'NONE', *, *, #19393, .F. ) ;
#10164 = LINE ( 'NONE', #33201, #41097 ) ;
#10165 = CARTESIAN_POINT ( 'NONE',  ( -5.000000000000005329, 170.2083333265053682, 8.660254037844387298 ) ) ;
#10166 = EDGE_CURVE ( 'NONE', #73412, #73226, #53316, .T. ) ;
#10167 = CARTESIAN_POINT ( 'NONE',  ( -9.832129032723420536, 48.69791666325268409, 5.676582343749997150 ) ) ;
#10168 = CARTESIAN_POINT ( 'NONE',  ( 11.00000000000000000, 1.347111479062088405E-15, 75.43750000409676204 ) ) ;
#10169 = CARTESIAN_POINT ( 'NONE',  ( -2.445694354108839175, 199.3125000013656063, 144.4456943541088663 ) ) ;
#10170 = CARTESIAN_POINT ( 'NONE',  ( 6.891449706541182607, 10.24244278380985662, 65.16993756079884292 ) ) ;
#10171 = CARTESIAN_POINT ( 'NONE',  ( -7.320508075688779037, 13.12500000000000355, 7.320508075688770155 ) ) ;
#10173 = CARTESIAN_POINT ( 'NONE',  ( -5.676582343750006032, 44.11458332991934839, 9.832129032723418760 ) ) ;
#10172 = CARTESIAN_POINT ( 'NONE',  ( -2.977408999572650927, 99.87500000204838102, -7.188101187500000933 ) ) ;
#10174 = CARTESIAN_POINT ( 'NONE',  ( -7.999999999999989342, -3.313708498984762496, 8.424052779823362869 ) ) ;
#10175 = CARTESIAN_POINT ( 'NONE',  ( -4.898587196589407898E-16, 7.999999999999991118, 21.64280278392014623 ) ) ;
#10176 = CARTESIAN_POINT ( 'NONE',  ( -11.35316468750000141, 178.2812499965860411, -1.390361679473963753E-15 ) ) ;
#10178 = CARTESIAN_POINT ( 'NONE',  ( 6.123233995736767268E-16, 138.1249999931720538, -10.00000000000000178 ) ) ;
#10177 = PRODUCT_DEFINITION_SHAPE ( 'NONE', 'NONE',  #74661 ) ;
#10179 = CARTESIAN_POINT ( 'NONE',  ( -5.082755093536325930, 103.3437500020483668, -5.082755093536325930 ) ) ;
#10180 = AXIS2_PLACEMENT_3D ( 'NONE', #41567, #35913, #42292 ) ;
#10181 = CARTESIAN_POINT ( 'NONE',  ( 5.000000000000000000, 10.00000000000000000, 75.19090595827292134 ) ) ;
#10182 = CARTESIAN_POINT ( 'NONE',  ( -8.311093377946841443, 34.21874999658601268, 8.311093377946834337 ) ) ;
#10183 =( BOUNDED_CURVE ( )  B_SPLINE_CURVE ( 2, ( #7389, #1006, #70027, #12662, #1375, #65079, #53781, #30760, #1737 ),
 .UNSPECIFIED., .F., .F. ) 
 B_SPLINE_CURVE_WITH_KNOTS ( ( 3, 2, 2, 2, 3 ),
 ( 0.4270833333333332593, 0.4322916666666666297, 0.4374999999999998890, 0.4427083333333332038, 0.4479166666666665741 ),
 .UNSPECIFIED. ) 
 CURVE ( )  GEOMETRIC_REPRESENTATION_ITEM ( )  RATIONAL_B_SPLINE_CURVE ( ( 1.000000000000000888, 0.9238795325112859613, 1.000000000000000000, 0.9238795325112867385, 1.000000000000000000, 0.9238795325112867385, 1.000000000000000000, 0.9238795325112884038, 0.9999999999999983347 ) ) 
 REPRESENTATION_ITEM ( '' )  );
#10184 = CARTESIAN_POINT ( 'NONE',  ( -8.660254037844390851, 79.79166665983871098, 4.999999999999998224 ) ) ;
#10185 = EDGE_LOOP ( 'NONE', ( #847, #18597, #30637, #40077 ) ) ;
#10187 =( BOUNDED_CURVE ( )  B_SPLINE_CURVE ( 2, ( #43338, #21451, #37324, #33179, #14661, #37702, #71632, #9022, #61451 ),
 .UNSPECIFIED., .F., .F. ) 
 B_SPLINE_CURVE_WITH_KNOTS ( ( 3, 2, 2, 2, 3 ),
 ( 0.6250000000000000000, 0.6306818181818182323, 0.6363636363636363535, 0.6420454545454545858, 0.6477272727272727071 ),
 .UNSPECIFIED. ) 
 CURVE ( )  GEOMETRIC_REPRESENTATION_ITEM ( )  RATIONAL_B_SPLINE_CURVE ( ( 1.000000000000000000, 0.9238795325112867385, 1.000000000000000000, 0.9238795325112867385, 1.000000000000000000, 0.9238795325112867385, 1.000000000000000000, 0.9238795325112867385, 1.000000000000000000 ) ) 
 REPRESENTATION_ITEM ( '' )  );
#10186 = FACE_OUTER_BOUND ( 'NONE', #29060, .T. ) ;
#10188 = CARTESIAN_POINT ( 'NONE',  ( 10.18810118749999916, 1.247682550866122264E-15, 72.90625000204836681 ) ) ;
#10189 = CARTESIAN_POINT ( 'NONE',  ( -5.000000000000000000, -18.53862685874495142, 23.57305537018116581 ) ) ;
#10191 = CARTESIAN_POINT ( 'NONE',  ( 11.35316468749999963, 170.9895833299193839, -3.042071309553165293 ) ) ;
#10190 = CARTESIAN_POINT ( 'NONE',  ( 7.999978819527651552, -3.313729679457098065, 3.174051936482769953 ) ) ;
#10192 = CARTESIAN_POINT ( 'NONE',  ( -5.656854249492373476, -5.656854249492376141, 10.07405278432982421 ) ) ;
#10193 = CARTESIAN_POINT ( 'NONE',  ( 3.999999999999960032, 208.1250000027312126, 142.0000000000000568 ) ) ;
#10194 = CARTESIAN_POINT ( 'NONE',  ( -9.832129032723418760, 223.4895833367473301, -5.676582343749998927 ) ) ;
#10195 = CARTESIAN_POINT ( 'NONE',  ( 0.7581620860261992778, 55.63814191976882029, -43.81219804999550149 ) ) ;
#10196 = ADVANCED_FACE ( 'NONE', ( #6182 ), #18971, .T. ) ;
#10197 = CARTESIAN_POINT ( 'NONE',  ( -10.18810118749999916, 0.000000000000000000, 78.53125000204836681 ) ) ;
#10198 = VERTEX_POINT ( 'NONE', #24621 ) ;
#10199 = CARTESIAN_POINT ( 'NONE',  ( 2.751064625579944321E-14, 203.7500000000000284, 194.0000000000000568 ) ) ;
#10200 = CARTESIAN_POINT ( 'NONE',  ( 11.35316468749999963, 121.3020833299193697, -3.042071309553165293 ) ) ;
#10201 = CARTESIAN_POINT ( 'NONE',  ( 4.999999999999993783, 11.04166665983870033, 8.660254037844390851 ) ) ;
#10202 = ORIENTED_EDGE ( 'NONE', *, *, #43967, .T. ) ;
#10203 = ORIENTED_EDGE ( 'NONE', *, *, #57385, .F. ) ;
#10204 = VECTOR ( 'NONE', #54874, 1000.000000000000000 ) ;
#10205 = CARTESIAN_POINT ( 'NONE',  ( -3.211159895383562723, 8.062499998634406140, 3.211159895383561391 ) ) ;
#10206 = CARTESIAN_POINT ( 'NONE',  ( -2.977408999572650039, 6.937499997951610986, -7.188101187500001821 ) ) ;
#10207 = CARTESIAN_POINT ( 'NONE',  ( 5.656854249492381470, 110.7500000040967763, 5.656854249492379694 ) ) ;
#10208 = EDGE_CURVE ( 'NONE', #27914, #12427, #57874, .T. ) ;
#10209 = CARTESIAN_POINT ( 'NONE',  ( 4.220049686691941027, -10.18810118749999738, 92.50000000204838102 ) ) ;
#10210 = CARTESIAN_POINT ( 'NONE',  ( -26.56734541678238060, 202.6250000013656063, 166.5412658750003629 ) ) ;
#10211 = CARTESIAN_POINT ( 'NONE',  ( 4.000000000000000888, 6.937500000000000000, 1.656854249492384135 ) ) ;
#10212 = DIRECTION ( 'NONE',  ( 1.000000000000000000, 0.000000000000000000, -0.000000000000000000 ) ) ;
#10213 = CARTESIAN_POINT ( 'NONE',  ( -1.881053915767121776, 9.624999998634404363, -4.541265875000002339 ) ) ;
#10214 = CARTESIAN_POINT ( 'NONE',  ( -4.000000000000015987, 199.4375000000000284, 140.3431457505076594 ) ) ;
#10215 = VERTEX_POINT ( 'NONE', #46157 ) ;
#10216 = CARTESIAN_POINT ( 'NONE',  ( 7.999999999999991118, 3.313708498984758055, 9.361552783920146226 ) ) ;
#10217 = AXIS2_PLACEMENT_3D ( 'NONE', #66847, #15521, #3473 ) ;
#10219 = CARTESIAN_POINT ( 'NONE',  ( -25.17157287525377640, 199.6250000000000284, 172.8284271247465256 ) ) ;
#10218 = CARTESIAN_POINT ( 'NONE',  ( -29.43265458321771177, 196.5000000013656063, 166.5412658750003914 ) ) ;
#10220 = CARTESIAN_POINT ( 'NONE',  ( 4.541265875000002339, 21.37499999863441147, -1.881053915767121554 ) ) ;
#10221 = AXIS2_PLACEMENT_3D ( 'NONE', #1057, #51981, #17636 ) ;
#10222 = CARTESIAN_POINT ( 'NONE',  ( 7.188101187499992051, 8.802885111219154394E-16, 27.73655278187175455 ) ) ;
#10223 = ORIENTED_EDGE ( 'NONE', *, *, #28344, .F. ) ;
#10224 = VERTEX_POINT ( 'NONE', #168 ) ;
#10225 = CARTESIAN_POINT ( 'NONE',  ( 1.871523826299183495E-15, -10.18810118749999916, 90.53125000204836681 ) ) ;
#10226 = CARTESIAN_POINT ( 'NONE',  ( 29.65685424949238325, 204.5625000027312126, 165.9999999999999147 ) ) ;
#10227 = CARTESIAN_POINT ( 'NONE',  ( -30.44569435410883429, 200.8125000013656063, 167.5543056458915885 ) ) ;
#10228 = CARTESIAN_POINT ( 'NONE',  ( 11.00000000000000355, -4.556349186104045046, 108.1562500000000000 ) ) ;
#10229 = CARTESIAN_POINT ( 'NONE',  ( -1.432654583217607414, 207.5000000013655779, 194.5412658750000219 ) ) ;
#10230 = CARTESIAN_POINT ( 'NONE',  ( 4.000000000000015987, 203.6875000027311842, 196.3431457505076594 ) ) ;
#10231 = CARTESIAN_POINT ( 'NONE',  ( -4.999999999999998224, 126.6666666666666714, -8.660254037844389075 ) ) ;
#10232 = EDGE_CURVE ( 'NONE', #11931, #13626, #54470, .T. ) ;
#10233 = CARTESIAN_POINT ( 'NONE',  ( 8.000000000000000000, 107.8437500000000000, -3.313708498984762496 ) ) ;
#10234 = CARTESIAN_POINT ( 'NONE',  ( 2.765530957081996366, 293.2968750017069510, -6.676582343750003368 ) ) ;
#10235 = CARTESIAN_POINT ( 'NONE',  ( 2.977408999572646486, 7.188101187499991163, 4.392802781871752771 ) ) ;
#10236 = ORIENTED_EDGE ( 'NONE', *, *, #69038, .F. ) ;
#10237 = DIRECTION ( 'NONE',  ( -0.000000000000000000, -1.000000000000000000, -4.283267841918042741E-17 ) ) ;
#10238 = EDGE_CURVE ( 'NONE', #31431, #31876, #46530, .T. ) ;
#10239 = CARTESIAN_POINT ( 'NONE',  ( 25.55430564589115150, 205.3125000013656063, 172.4456943541086957 ) ) ;
#10240 = CARTESIAN_POINT ( 'NONE',  ( 7.999999999999998224, 26.71874999590322375, 3.313708498984766493 ) ) ;
#10241 = CARTESIAN_POINT ( 'NONE',  ( -2.445694354108839619, 197.8125000013656063, 139.5543056458912190 ) ) ;
#10242 = CARTESIAN_POINT ( 'NONE',  ( 7.188101187500000044, 120.7812500020483810, -8.802885111219163269E-16 ) ) ;
#10244 = CARTESIAN_POINT ( 'NONE',  ( -2.839093476692135984E-14, 204.9375000013656063, 138.5412658750000503 ) ) ;
#10243 = DIRECTION ( 'NONE',  ( -0.000000000000000000, -1.000000000000000000, -0.000000000000000000 ) ) ;
#10245 = CARTESIAN_POINT ( 'NONE',  ( -11.35316468749999785, 239.0104166700806161, -3.042071309553164848 ) ) ;
#10246 = LINE ( 'NONE', #55160, #7430 ) ;
#10247 = DIRECTION ( 'NONE',  ( -0.000000000000000000, 1.000000000000000000, -0.000000000000000000 ) ) ;
#10248 = CARTESIAN_POINT ( 'NONE',  ( -11.35316468750000141, 18.28124999658601624, -1.390361679473963753E-15 ) ) ;
#10249 = CARTESIAN_POINT ( 'NONE',  ( -7.188101187499992051, 2.977408999572646930, 1.767802781871753437 ) ) ;
#10250 = CARTESIAN_POINT ( 'NONE',  ( 5.676582343750001591, 211.9270833299193555, -9.832129032723420536 ) ) ;
#10251 = CARTESIAN_POINT ( 'NONE',  ( 0.000000000000000000, 0.000000000000000000, -10.00000000000000000 ) ) ;
#10252 = CARTESIAN_POINT ( 'NONE',  ( 2.485281374238266672, 290.6874999999999432, -6.000000000000306422 ) ) ;
#10254 = CYLINDRICAL_SURFACE ( 'NONE', #54354, 6.000000000000001776 ) ;
#10253 = CARTESIAN_POINT ( 'NONE',  ( 2.751064625579944321E-14, 208.7500000000000284, 194.0000000000000568 ) ) ;
#10255 = ORIENTED_EDGE ( 'NONE', *, *, #311, .F. ) ;
#10257 = EDGE_CURVE ( 'NONE', #12072, #4470, #18607, .T. ) ;
#10256 = CARTESIAN_POINT ( 'NONE',  ( 3.458734124999959469, 200.7500000013656347, 140.5673454167824161 ) ) ;
#10258 = EDGE_CURVE ( 'NONE', #71793, #24215, #44339, .T. ) ;
#10259 = CARTESIAN_POINT ( 'NONE',  ( 3.042071309553159519, 14.73958332991935016, 11.35316468750000141 ) ) ;
#10260 = CARTESIAN_POINT ( 'NONE',  ( 7.778174593052021635, 7.778174593052023411, 93.62500000409677625 ) ) ;
#10261 = CARTESIAN_POINT ( 'NONE',  ( 6.000000000000003553, 292.5625000000000000, -2.485281374238571761 ) ) ;
#10262 = CARTESIAN_POINT ( 'NONE',  ( -29.43265458321755190, 196.8750000013656347, 173.4587341250004044 ) ) ;
#10263 = CYLINDRICAL_SURFACE ( 'NONE', #14174, 3.999999999999976019 ) ;
#10265 = CARTESIAN_POINT ( 'NONE',  ( 6.951808397369818766E-16, 12.03124999658601801, -11.35316468750000141 ) ) ;
#10264 = CARTESIAN_POINT ( 'NONE',  ( -7.188101187500000933, 115.0625000020483810, -2.977408999572650483 ) ) ;
#10266 = CARTESIAN_POINT ( 'NONE',  ( -4.898587196589407898E-16, 7.999999999999991118, 28.95530277982336642 ) ) ;
#10267 = CARTESIAN_POINT ( 'NONE',  ( -11.35316468749999785, 128.0729166632526983, -3.042071309553167513 ) ) ;
#10268 = EDGE_CURVE ( 'NONE', #52001, #60988, #20065, .T. ) ;
#10269 = CARTESIAN_POINT ( 'NONE',  ( -1.836970198721029983E-15, 100.6249999931720396, 10.00000000000000178 ) ) ;
#10270 = CARTESIAN_POINT ( 'NONE',  ( 7.188101187500002709, 123.6875000020484094, 2.977408999572649151 ) ) ;
#10271 = CARTESIAN_POINT ( 'NONE',  ( -4.541265875000002339, 19.93749999863440436, -5.561446717895856393E-16 ) ) ;
#10272 = CARTESIAN_POINT ( 'NONE',  ( -4.999999999999998224, 198.5416666598387110, -8.660254037844389075 ) ) ;
#10273 = CARTESIAN_POINT ( 'NONE',  ( 0.000000000000000000, 1.132798289211301698E-14, 92.50000000000000000 ) ) ;
#10274 = VERTEX_POINT ( 'NONE', #66474 ) ;
#10275 = CARTESIAN_POINT ( 'NONE',  ( 1.506524674528582741, -65.82790954190812727, 26.31843049628270848 ) ) ;
#10276 = CARTESIAN_POINT ( 'NONE',  ( -2.765530957081996810, 288.4218750017070079, -6.676582343750003368 ) ) ;
#10277 = CARTESIAN_POINT ( 'NONE',  ( 5.000000000000001776, 53.53067326687830985, 46.58593137613159030 ) ) ;
#10278 = CARTESIAN_POINT ( 'NONE',  ( 3.313708498984762496, -7.999999999999989342, 26.85530278432982598 ) ) ;
#10279 = LINE ( 'NONE', #56683, #21259 ) ;
#10280 = CARTESIAN_POINT ( 'NONE',  ( -8.311093377946836114, 263.2812500034139020, -8.311093377946836114 ) ) ;
#10281 = ADVANCED_FACE ( 'NONE', ( #72129 ), #2735, .T. ) ;
#10282 = CARTESIAN_POINT ( 'NONE',  ( -10.18810118749999916, 4.220049686691934809, 94.93750000204838102 ) ) ;
#10283 = VERTEX_POINT ( 'NONE', #43083 ) ;
#10284 =( BOUNDED_CURVE ( )  B_SPLINE_CURVE ( 2, ( #10848, #23654, #74593, #40261, #46661, #69680, #11588, #28195, #17993, #33507, #50833, #73844, #56882 ),
 .UNSPECIFIED., .F., .F. ) 
 B_SPLINE_CURVE_WITH_KNOTS ( ( 3, 2, 2, 2, 2, 2, 3 ),
 ( 0.4184782608695651884, 0.4202898550724636917, 0.4221014492753622505, 0.4239130434782608092, 0.4257246376811593680, 0.4275362318840579268, 0.4293478260869564855 ),
 .UNSPECIFIED. ) 
 CURVE ( )  GEOMETRIC_REPRESENTATION_ITEM ( )  RATIONAL_B_SPLINE_CURVE ( ( 1.000000000000001110, 0.9659258262890673130, 1.000000000000000000, 0.9659258262890683122, 1.000000000000000000, 0.9659258262890683122, 1.000000000000000000, 0.9659258262890683122, 1.000000000000000000, 0.9659258262890683122, 1.000000000000000000, 0.9659258262890693114, 0.9999999999999990008 ) ) 
 REPRESENTATION_ITEM ( '' )  );
#10285 = COLOUR_RGB ( '',0.7921568627450980005, 0.8196078431372548767, 0.9333333333333333481 ) ;
#10286 = DIRECTION ( 'NONE',  ( 1.000000000000000000, -0.000000000000000000, -0.000000000000000000 ) ) ;
#10287 = CARTESIAN_POINT ( 'NONE',  ( 8.311093377946837890, 151.7187499965860127, -8.311093377946837890 ) ) ;
#10288 = CARTESIAN_POINT ( 'NONE',  ( -2.445694354108783219, 203.8125000013656063, 200.4456943541088663 ) ) ;
#10289 = CARTESIAN_POINT ( 'NONE',  ( 4.999999999999997335, 231.4583333401613174, -8.660254037844387298 ) ) ;
#10290 = CARTESIAN_POINT ( 'NONE',  ( 9.832129032723420536, 81.51041666325268409, -5.676582343749999815 ) ) ;
#10291 = VERTEX_POINT ( 'NONE', #8019 ) ;
#10292 = CARTESIAN_POINT ( 'NONE',  ( 10.18810118749999916, 4.220049686691935698, 112.0000000020483668 ) ) ;
#10293 = CARTESIAN_POINT ( 'NONE',  ( 1.881053915767122664, 7.249999998634407916, 4.541265875000001451 ) ) ;
#10294 = VERTEX_POINT ( 'NONE', #20443 ) ;
#10295 = CARTESIAN_POINT ( 'NONE',  ( 7.188101187499999156, 27.37499999795161187, 2.977408999572654924 ) ) ;
#10296 = DIRECTION ( 'NONE',  ( -0.000000000000000000, 1.000000000000000000, -1.563033456626094573E-30 ) ) ;
#10297 = CARTESIAN_POINT ( 'NONE',  ( 4.999999999999993783, 66.04166665983871098, 8.660254037844390851 ) ) ;
#10298 = CARTESIAN_POINT ( 'NONE',  ( -2.977408999572654480, 18.37499999795161187, 7.188101187499999156 ) ) ;
#10299 = CARTESIAN_POINT ( 'NONE',  ( 0.000000000000000000, 0.000000000000000000, -20.69999999999999929 ) ) ;
#10300 =( BOUNDED_CURVE ( )  B_SPLINE_CURVE ( 2, ( #24243, #1630, #70641, #47256, #12557, #70283, #64973, #60806, #48360 ),
 .UNSPECIFIED., .F., .F. ) 
 B_SPLINE_CURVE_WITH_KNOTS ( ( 3, 2, 2, 2, 3 ),
 ( 0.3833333333333335813, 0.3916666666666669405, 0.4000000000000003553, 0.4083333333333337145, 0.4166666666666671293 ),
 .UNSPECIFIED. ) 
 CURVE ( )  GEOMETRIC_REPRESENTATION_ITEM ( )  RATIONAL_B_SPLINE_CURVE ( ( 0.9999999999999980016, 0.9238795325112887369, 1.000000000000000000, 0.9238795325112867385, 1.000000000000000000, 0.9238795325112867385, 1.000000000000000000, 0.9238795325112826307, 1.000000000000003997 ) ) 
 REPRESENTATION_ITEM ( '' )  );
#10301 = CARTESIAN_POINT ( 'NONE',  ( -10.18810118749999738, -4.220049686691941915, 108.6250000020483668 ) ) ;
#10302 = CARTESIAN_POINT ( 'NONE',  ( 2.849036369511732440E-14, 204.2500000000000284, 202.0000000000000000 ) ) ;
#10303 = CARTESIAN_POINT ( 'NONE',  ( 2.449293598294707893E-16, 7.999999997268813168, -4.000000000000001776 ) ) ;
#10304 = CARTESIAN_POINT ( 'NONE',  ( 2.828427124746190291, 17.87500000000000355, 2.828427124746192067 ) ) ;
#10305 = VERTEX_POINT ( 'NONE', #65725 ) ;
#10306 = CARTESIAN_POINT ( 'NONE',  ( 2.445694354108838731, 201.0625000013656063, 195.5543056458912190 ) ) ;
#10307 = CARTESIAN_POINT ( 'NONE',  ( -30.44569435410876324, 207.8125000013656063, 172.4456943541092642 ) ) ;
#10308 = CARTESIAN_POINT ( 'NONE',  ( 4.000000000000001776, 12.81249999726881406, -1.656854249492381248 ) ) ;
#10309 = CARTESIAN_POINT ( 'NONE',  ( -4.541265875000002339, 6.749999998634407916, -1.881053915767121998 ) ) ;
#10310 = CARTESIAN_POINT ( 'NONE',  ( 54.00000000000000000, 272.0000000000000000, 4.085831468968142743E-14 ) ) ;
#10311 = CARTESIAN_POINT ( 'NONE',  ( -7.188101187499992051, 0.000000000000000000, 19.48655278187175455 ) ) ;
#10312 = ORIENTED_EDGE ( 'NONE', *, *, #23603, .T. ) ;
#10313 = CARTESIAN_POINT ( 'NONE',  ( 10.99999999999989342, 4.556349186104152515, 90.34375000000000000 ) ) ;
#10314 = ORIENTED_EDGE ( 'NONE', *, *, #53452, .T. ) ;
#10315 = CARTESIAN_POINT ( 'NONE',  ( -7.204075437095965206, -7.204075437095968759, 112.8437500020483810 ) ) ;
#10316 = CARTESIAN_POINT ( 'NONE',  ( -4.556349186104045934, 11.00000000000000000, 96.90625000409677625 ) ) ;
#10317 = CARTESIAN_POINT ( 'NONE',  ( 3.458734125000015425, 204.0000000013656347, 196.5673454167823877 ) ) ;
#10318 = CARTESIAN_POINT ( 'NONE',  ( 28.00000000000001776, 198.4375000013655779, 173.4587341249998929 ) ) ;
#10319 = CARTESIAN_POINT ( 'NONE',  ( -1.836970198721029983E-15, 83.75000000000000000, 10.00000000000000178 ) ) ;
#10320 = EDGE_CURVE ( 'NONE', #69933, #73724, #43459, .T. ) ;
#10321 = CARTESIAN_POINT ( 'NONE',  ( -5.656854249492380582, 123.3125000000000000, -5.656854249492380582 ) ) ;
#10322 = CARTESIAN_POINT ( 'NONE',  ( 6.000000000000003553, 291.5625000000000000, -2.485281374238571761 ) ) ;
#10323 = AXIS2_PLACEMENT_3D ( 'NONE', #43002, #49799, #65651 ) ;
#10324 = CARTESIAN_POINT ( 'NONE',  ( 28.00000000000002487, 207.1250000027312126, 173.9999999999999147 ) ) ;
#10325 = VERTEX_POINT ( 'NONE', #31780 ) ;
#10326 = CARTESIAN_POINT ( 'NONE',  ( 3.042071309553173286, 220.3645833367472733, 11.35316468749999608 ) ) ;
#10327 = VECTOR ( 'NONE', #64678, 1000.000000000000000 ) ;
#10328 = CARTESIAN_POINT ( 'NONE',  ( 5.107860025165524398, -10.26152767799308840, 64.38109526789187953 ) ) ;
#10329 = CARTESIAN_POINT ( 'NONE',  ( -1.656854249492403008, 195.8125000027312126, 146.0000000000000284 ) ) ;
#10330 = CARTESIAN_POINT ( 'NONE',  ( -4.556349186104048599, -10.99999999999999822, 91.28125000000000000 ) ) ;
#10331 = DIRECTION ( 'NONE',  ( 0.000000000000000000, -2.238352872228138170E-16, 1.000000000000000000 ) ) ;
#10332 = CARTESIAN_POINT ( 'NONE',  ( -4.999999999999992895, 255.8333333333333712, 8.660254037844390851 ) ) ;
#10333 = LINE ( 'NONE', #66925, #4182 ) ;
#10334 = CARTESIAN_POINT ( 'NONE',  ( -10.00000000000000000, 197.2916666666666856, -2.679491924311229845 ) ) ;
#10335 = DIRECTION ( 'NONE',  ( 1.734723475976998196E-15, -1.000000000000000000, -0.000000000000000000 ) ) ;
#10336 = CARTESIAN_POINT ( 'NONE',  ( 2.977408999572646486, 7.188101187499992051, 14.89280278187175455 ) ) ;
#10337 = CARTESIAN_POINT ( 'NONE',  ( -9.832129032723420536, 169.0104166632526983, 5.676582343749997150 ) ) ;
#10338 = CARTESIAN_POINT ( 'NONE',  ( -1.656854249492336173, 208.3125000027312126, 202.0000000000000284 ) ) ;
#10339 = CARTESIAN_POINT ( 'NONE',  ( -5.000000000000000000, 52.84347807771100491, 43.21644271080270983 ) ) ;
#10340 = CARTESIAN_POINT ( 'NONE',  ( 10.00000000000018119, 154.7916666666667993, 2.679491924311284468 ) ) ;
#10342 = CARTESIAN_POINT ( 'NONE',  ( -1.656854249492381248, 7.062499997268814056, -4.000000000000001776 ) ) ;
#10341 = DIRECTION ( 'NONE',  ( -0.1513591288559071046, 0.000000000000000000, -0.9884788384745426537 ) ) ;
#10343 = VERTEX_POINT ( 'NONE', #71015 ) ;
#10344 = CARTESIAN_POINT ( 'NONE',  ( 3.042071309553167069, 17.13541666325268409, -11.35316468749999785 ) ) ;
#10345 = CARTESIAN_POINT ( 'NONE',  ( 2.841757666793575255E-14, 194.6037658790967839, 201.6037658790967839 ) ) ;
#10347 = CARTESIAN_POINT ( 'NONE',  ( -1.506524674531949826, -10.12152537343867031, -70.16785718946157147 ) ) ;
#10346 = DIRECTION ( 'NONE',  ( 0.000000000000000000, 0.000000000000000000, 1.000000000000000000 ) ) ;
#10348 = FACE_OUTER_BOUND ( 'NONE', #47276, .T. ) ;
#10349 = CARTESIAN_POINT ( 'NONE',  ( 3.458734124999958581, 204.5000000013655779, 140.5673454167823593 ) ) ;
#10350 = EDGE_CURVE ( 'NONE', #69421, #62787, #44777, .T. ) ;
#10351 = CARTESIAN_POINT ( 'NONE',  ( 7.320508075688774596, 57.49999999317203958, -7.320508075688774596 ) ) ;
#10352 = CARTESIAN_POINT ( 'NONE',  ( 7.188101187500000044, 105.4062500020483810, -8.802885111219163269E-16 ) ) ;
#10353 = CARTESIAN_POINT ( 'NONE',  ( 4.541265875000001451, 7.374999998634408804, 1.881053915767124440 ) ) ;
#10354 = DIRECTION ( 'NONE',  ( 0.000000000000000000, 0.000000000000000000, -1.000000000000000000 ) ) ;
#10355 = CARTESIAN_POINT ( 'NONE',  ( 3.313708498984756279, 7.999999999999991118, 4.861552779823364645 ) ) ;
#10356 = CARTESIAN_POINT ( 'NONE',  ( 1.469576158976822172E-15, -7.999999999999991118, 20.89280278392014623 ) ) ;
#10357 = ORIENTED_EDGE ( 'NONE', *, *, #50193, .F. ) ;
#10358 = VERTEX_POINT ( 'NONE', #26096 ) ;
#10359 = CARTESIAN_POINT ( 'NONE',  ( -10.00000000000000355, 222.7083333333333428, 2.679491924311223183 ) ) ;
#10360 = CARTESIAN_POINT ( 'NONE',  ( 1.479685137562080274E-15, 225.9999999999999432, -10.00000000000000178 ) ) ;
#10361 = CARTESIAN_POINT ( 'NONE',  ( -7.778174593052023411, 7.778174593052023411, 104.3124999999999858 ) ) ;
#10362 = CARTESIAN_POINT ( 'NONE',  ( -6.951808397369817780E-16, 222.9687500034139873, -11.35316468749999963 ) ) ;
#10363 = CARTESIAN_POINT ( 'NONE',  ( -11.35316468750000141, 143.4895833299193839, 3.042071309553159963 ) ) ;
#10364 = VERTEX_POINT ( 'NONE', #7658 ) ;
#10365 = CARTESIAN_POINT ( 'NONE',  ( -7.204075437095965206, -7.204075437095968759, 87.34375000204836681 ) ) ;
#10366 = LINE ( 'NONE', #60549, #39328 ) ;
#10367 = CARTESIAN_POINT ( 'NONE',  ( 1.656854249492405451, 208.3125000000000000, 202.0000000000000284 ) ) ;
#10368 = CARTESIAN_POINT ( 'NONE',  ( -2.828427124746152987, 205.1250000000000284, 200.8284271247462129 ) ) ;
#10369 = CARTESIAN_POINT ( 'NONE',  ( 8.000000000000001776, 116.8437500040967905, 3.313708498984759387 ) ) ;
#10370 = EDGE_CURVE ( 'NONE', #66034, #29121, #62166, .T. ) ;
#10371 = CARTESIAN_POINT ( 'NONE',  ( 9.000000000000000000, 5.196152422706622254, -10.20000000000000284 ) ) ;
#10372 = ORIENTED_EDGE ( 'NONE', *, *, #74483, .F. ) ;
#10373 = EDGE_CURVE ( 'NONE', #44389, #62325, #25356, .T. ) ;
#10374 = CARTESIAN_POINT ( 'NONE',  ( 30.72172046173767512, -37.42303466342836060, 174.1770155974127476 ) ) ;
#10375 = CARTESIAN_POINT ( 'NONE',  ( -24.84350201213867848, 176.4274895007661996, 151.3179989103983587 ) ) ;
#10376 = CARTESIAN_POINT ( 'NONE',  ( 11.35316468750000141, 121.0937499965860269, 0.000000000000000000 ) ) ;
#10377 = CARTESIAN_POINT ( 'NONE',  ( -1.432654583217607192, 204.2500000013655779, 194.5412658750000219 ) ) ;
#10378 = CARTESIAN_POINT ( 'NONE',  ( -1.320432766682874540E-15, 19.96874999795161543, 7.188101187500000044 ) ) ;
#10379 = CARTESIAN_POINT ( 'NONE',  ( 10.18810118749999916, 1.247682550866122264E-15, 82.28125000204838102 ) ) ;
#10380 = CARTESIAN_POINT ( 'NONE',  ( 3.042071309553167069, 37.13541666325268409, -11.35316468749999785 ) ) ;
#10381 = ORIENTED_EDGE ( 'NONE', *, *, #62110, .F. ) ;
#10382 = CARTESIAN_POINT ( 'NONE',  ( 2.449293598294707893E-16, 4.250000000000000000, -4.000000000000001776 ) ) ;
#10383 = CARTESIAN_POINT ( 'NONE',  ( 1.471067592899761672E-15, -8.008118988124991233, 19.38811528394063188 ) ) ;
#10384 = CARTESIAN_POINT ( 'NONE',  ( 1.432654583217607414, 209.5000000013656063, 145.4587341250000634 ) ) ;
#10385 = CARTESIAN_POINT ( 'NONE',  ( -2.828427124746192067, 7.625000000000000000, 2.828427124746190735 ) ) ;
#10386 = CARTESIAN_POINT ( 'NONE',  ( 5.082755093536325930, 11.15624999795161187, -5.082755093536325930 ) ) ;
#10387 = CARTESIAN_POINT ( 'NONE',  ( -4.242640687119285658, 296.1875000034139589, 4.242640687119287435 ) ) ;
#10388 = VECTOR ( 'NONE', #10014, 1000.000000000000000 ) ;
#10389 = DIRECTION ( 'NONE',  ( -0.000000000000000000, -0.000000000000000000, -1.000000000000000000 ) ) ;
#10390 = DIRECTION ( 'NONE',  ( -0.000000000000000000, 1.000000000000000000, -0.000000000000000000 ) ) ;
#10391 = ORIENTED_EDGE ( 'NONE', *, *, #44076, .T. ) ;
#10392 = CARTESIAN_POINT ( 'NONE',  ( -5.676582343749998039, 152.7604166632526983, -9.832129032723420536 ) ) ;
#10393 = CARTESIAN_POINT ( 'NONE',  ( -4.220049686691937474, -10.18810118749999738, 78.43750000204838102 ) ) ;
#10394 = EDGE_CURVE ( 'NONE', #21159, #24629, #29357, .T. ) ;
#10395 =( BOUNDED_CURVE ( )  B_SPLINE_CURVE ( 2, ( #58824, #54646, #42184, #7135, #24833, #64838, #13871, #30143, #2953, #25943, #31248 ),
 .UNSPECIFIED., .F., .F. ) 
 B_SPLINE_CURVE_WITH_KNOTS ( ( 3, 2, 2, 2, 2, 3 ),
 ( 0.5559351258181921551, 0.5559351490943722496, 0.5625534246788289616, 0.5691717002632856737, 0.5757899758477422747, 0.5824082574719842142 ),
 .UNSPECIFIED. ) 
 CURVE ( )  GEOMETRIC_REPRESENTATION_ITEM ( )  RATIONAL_B_SPLINE_CURVE ( ( 0.9999994645773038204, 0.9999997322877103301, 1.000000000000000000, 0.9238795325112867385, 1.000000000000000000, 0.9238795325112867385, 1.000000000000000000, 0.9238795325112867385, 1.000000000000000000, 0.9238795325112867385, 1.000000000000000000 ) ) 
 REPRESENTATION_ITEM ( '' )  );
#10396 = CARTESIAN_POINT ( 'NONE',  ( -28.00000000000001776, 196.4375000013655779, 166.5412658750003629 ) ) ;
#10397 = CARTESIAN_POINT ( 'NONE',  ( 4.541265875000002339, 17.49999999863440436, -1.881053915767121554 ) ) ;
#10398 = ORIENTED_EDGE ( 'NONE', *, *, #71055, .T. ) ;
#10399 = CARTESIAN_POINT ( 'NONE',  ( -2.828427124746152987, 200.2500000027312126, 200.8284271247462129 ) ) ;
#10400 = CARTESIAN_POINT ( 'NONE',  ( 2.445694354108784108, 196.5625000013656063, 144.4456943541088663 ) ) ;
#10401 = CARTESIAN_POINT ( 'NONE',  ( -25.17157287525385811, 205.0000000027312126, 167.1715728752541281 ) ) ;
#10402 = AXIS2_PLACEMENT_3D ( 'NONE', #32336, #43636, #14582 ) ;
#10403 = CARTESIAN_POINT ( 'NONE',  ( -3.313708498984805573, 22.03125000000000000, 7.999999999999956479 ) ) ;
#10404 = ORIENTED_EDGE ( 'NONE', *, *, #64986, .T. ) ;
#10405 = CARTESIAN_POINT ( 'NONE',  ( -7.188101187500002709, 11.81249999795161187, 2.977408999572649151 ) ) ;
#10406 = DIRECTION ( 'NONE',  ( 0.000000000000000000, 0.000000000000000000, 1.000000000000000000 ) ) ;
#10407 = CARTESIAN_POINT ( 'NONE',  ( 6.123233995736767268E-16, 46.25000000000000711, -10.00000000000000178 ) ) ;
#10408 = CARTESIAN_POINT ( 'NONE',  ( -2.977408999572651815, 103.8125000020483952, 7.188101187500000933 ) ) ;
#10409 = CARTESIAN_POINT ( 'NONE',  ( -28.00000000000002487, 206.6875000013656063, 166.5412658750003629 ) ) ;
#10410 = CARTESIAN_POINT ( 'NONE',  ( -4.088227598258586603E-16, 289.2031250017069510, -6.676582343750001591 ) ) ;
#10411 = EDGE_CURVE ( 'NONE', #33509, #65401, #13453, .T. ) ;
#10412 = CARTESIAN_POINT ( 'NONE',  ( 2.679491924311227624, 96.04166666666665719, -9.999999999999994671 ) ) ;
#10413 = ORIENTED_EDGE ( 'NONE', *, *, #11225, .T. ) ;
#10414 = CARTESIAN_POINT ( 'NONE',  ( -3.042071309553166181, 257.8645833367473301, -11.35316468749999608 ) ) ;
#10415 = CARTESIAN_POINT ( 'NONE',  ( -4.401442555609577197E-16, 7.188101187499992051, 25.48655278187175810 ) ) ;
#10416 = CARTESIAN_POINT ( 'NONE',  ( -4.737866951563840523, 52.21905653845793438, 48.93292554254848881 ) ) ;
#10417 = CARTESIAN_POINT ( 'NONE',  ( -6.000000000000000000, 0.000000000000000000, -10.77459999999999951 ) ) ;
#10418 = CARTESIAN_POINT ( 'NONE',  ( -6.308070865144149053, -61.28915309314432847, -23.54949267152977299 ) ) ;
#10420 = ADVANCED_FACE ( 'NONE', ( #13418 ), #65107, .F. ) ;
#10419 = CARTESIAN_POINT ( 'NONE',  ( -3.458734124999960358, 196.6875000013655779, 198.0000000000000284 ) ) ;
#10421 = CARTESIAN_POINT ( 'NONE',  ( -7.320508075688773708, 146.8749999999999716, -7.320508075688774596 ) ) ;
#10422 = ORIENTED_EDGE ( 'NONE', *, *, #4109, .T. ) ;
#10423 = CARTESIAN_POINT ( 'NONE',  ( -1.474731560294321397, 9.540868182094907723, -0.3570196857253543077 ) ) ;
#10424 = CARTESIAN_POINT ( 'NONE',  ( -4.898587196589412829E-16, 90.12500000000000000, -8.000000000000000000 ) ) ;
#10425 = CARTESIAN_POINT ( 'NONE',  ( -8.311093377946841443, 129.2187499965860127, 8.311093377946830785 ) ) ;
#10426 = CARTESIAN_POINT ( 'NONE',  ( 8.000000000000000000, 98.74999999999998579, -9.797174393178825657E-16 ) ) ;
#10427 = CARTESIAN_POINT ( 'NONE',  ( -10.99999999999999822, -4.556349186104052151, 73.09375000000000000 ) ) ;
#10430 = DIRECTION ( 'NONE',  ( -0.000000000000000000, 1.000000000000000000, -1.563033456626094573E-30 ) ) ;
#10429 = CARTESIAN_POINT ( 'NONE',  ( 25.55430564589119058, 198.3125000013656063, 172.4456943541087526 ) ) ;
#10428 = CARTESIAN_POINT ( 'NONE',  ( 23.99999999999998224, 208.8125000000000000, 171.6568542494922553 ) ) ;
#10431 = EDGE_LOOP ( 'NONE', ( #21780, #66726, #40140, #32818 ) ) ;
#10432 = CARTESIAN_POINT ( 'NONE',  ( 9.543466050813522727, 224.7571304811999937, 3.001353285571292773 ) ) ;
#10433 = AXIS2_PLACEMENT_3D ( 'NONE', #41483, #1865, #47870 ) ;
#10434 = CARTESIAN_POINT ( 'NONE',  ( 0.000000000000000000, 300.0000000000000000, 0.000000000000000000 ) ) ;
#10435 = CARTESIAN_POINT ( 'NONE',  ( 30.44569435410883429, 200.0625000013656063, 167.5543056458911053 ) ) ;
#10436 = EDGE_CURVE ( 'NONE', #32560, #39397, #62614, .T. ) ;
#10437 = CARTESIAN_POINT ( 'NONE',  ( 5.676582343749993598, 205.2604166632526983, 9.832129032723422313 ) ) ;
#10438 = CARTESIAN_POINT ( 'NONE',  ( 5.082755093536326818, 120.2187500020483952, 5.082755093536325042 ) ) ;
#10439 = CARTESIAN_POINT ( 'NONE',  ( -1.881053915767121554, 19.62499999863441147, -4.541265875000002339 ) ) ;
#10440 = CARTESIAN_POINT ( 'NONE',  ( 25.55430564589119058, 195.3125000013656063, 167.5543056458910485 ) ) ;
#10441 = CARTESIAN_POINT ( 'NONE',  ( -5.272366635369878374, -4.893143551702760163, 0.5406094755204297053 ) ) ;
#10443 = CARTESIAN_POINT ( 'NONE',  ( -26.34314575050765228, 202.5625000000000000, 174.0000000000004547 ) ) ;
#10442 = CARTESIAN_POINT ( 'NONE',  ( -49.70177871865296026, 49.37974222467917684, 57.99999999999997868 ) ) ;
#10444 = CARTESIAN_POINT ( 'NONE',  ( 8.311093377946837890, 96.40624999658602690, -8.311093377946837890 ) ) ;
#10445 = ORIENTED_EDGE ( 'NONE', *, *, #395, .T. ) ;
#10446 = CARTESIAN_POINT ( 'NONE',  ( 23.99999999999997868, 204.8125000027312126, 168.3431457505075457 ) ) ;
#10447 = CARTESIAN_POINT ( 'NONE',  ( 2.977408999572651815, 18.18749999795161187, 7.188101187500000933 ) ) ;
#10448 = CARTESIAN_POINT ( 'NONE',  ( -3.313708498984759387, -7.999999999999989342, 8.611552779823364645 ) ) ;
#10449 = CARTESIAN_POINT ( 'NONE',  ( -11.35316468749999785, 259.0104166700807014, -3.042071309553164848 ) ) ;
#10450 = CARTESIAN_POINT ( 'NONE',  ( -3.042071309553173730, 104.3229166632526983, 11.35316468749999785 ) ) ;
#10451 = ORIENTED_EDGE ( 'NONE', *, *, #11068, .F. ) ;
#10452 = CARTESIAN_POINT ( 'NONE',  ( -4.220049686691935698, 10.18810118749999916, 107.8750000020483668 ) ) ;
#10453 = CARTESIAN_POINT ( 'NONE',  ( -24.54126587499999701, 196.5000000013656063, 168.5673454167827003 ) ) ;
#10454 = CARTESIAN_POINT ( 'NONE',  ( -2.445694354108783219, 202.8125000013656063, 200.4456943541088663 ) ) ;
#10455 = CARTESIAN_POINT ( 'NONE',  ( -27.99999999999991118, 201.6250000027312126, 174.0000000000003695 ) ) ;
#10457 = CARTESIAN_POINT ( 'NONE',  ( -11.35316468750000141, 88.48958332991934128, 3.042071309553159963 ) ) ;
#10456 = CARTESIAN_POINT ( 'NONE',  ( -30.82842712474615965, 202.3750000000000284, 172.8284271247465824 ) ) ;
#10458 = CARTESIAN_POINT ( 'NONE',  ( 5.656854249492376141, -5.656854249492374365, 12.08030278392014445 ) ) ;
#10459 = CARTESIAN_POINT ( 'NONE',  ( -26.56734541678232375, 201.2500000013656063, 173.4587341250003760 ) ) ;
#10460 = CARTESIAN_POINT ( 'NONE',  ( 0.000000000000000000, 0.000000000000000000, 0.000000000000000000 ) ) ;
#10461 = AXIS2_PLACEMENT_3D ( 'NONE', #28286, #46004, #62605 ) ;
#10462 = CARTESIAN_POINT ( 'NONE',  ( 10.00000000000000178, 182.0833333265053682, -2.679491924311226736 ) ) ;
#10463 = EDGE_CURVE ( 'NONE', #48525, #74324, #55942, .T. ) ;
#10464 = CARTESIAN_POINT ( 'NONE',  ( 5.656854249492379694, 115.4375000000000000, -5.656854249492380582 ) ) ;
#10465 = CARTESIAN_POINT ( 'NONE',  ( 6.000000000000003553, 296.6250000034139589, -2.485281374238571761 ) ) ;
#10466 = CARTESIAN_POINT ( 'NONE',  ( -5.676582343750006032, 69.42708332991935549, 9.832129032723418760 ) ) ;
#10467 = CARTESIAN_POINT ( 'NONE',  ( 4.721056650416000089, 290.8281250017069510, 4.721056650415999201 ) ) ;
#10468 = CARTESIAN_POINT ( 'NONE',  ( 7.204075437095966983, 7.204075437095967871, 101.9687500020483668 ) ) ;
#10469 = CARTESIAN_POINT ( 'NONE',  ( -11.35316468749999785, 223.0729166632527267, -3.042071309553167513 ) ) ;
#10470 = ORIENTED_EDGE ( 'NONE', *, *, #40303, .T. ) ;
#10471 = CARTESIAN_POINT ( 'NONE',  ( 0.000000000000000000, -3.149999999999999911, 0.000000000000000000 ) ) ;
#10472 = CARTESIAN_POINT ( 'NONE',  ( 1.148106374200643592E-15, 45.00000000000000000, 8.749999999999998224 ) ) ;
#10473 = CARTESIAN_POINT ( 'NONE',  ( 2.775557561562891351E-14, 210.0000000000000284, 202.0000000000000000 ) ) ;
#10474 = CARTESIAN_POINT ( 'NONE',  ( -11.35316468749999785, 203.0729166632526699, -3.042071309553167957 ) ) ;
#10475 = CARTESIAN_POINT ( 'NONE',  ( 2.679491924311235174, 224.5833333401613174, 9.999999999999998224 ) ) ;
#10476 = CARTESIAN_POINT ( 'NONE',  ( -25.17157287525374443, 207.7500000027312126, 172.8284271247464972 ) ) ;
#10477 = CARTESIAN_POINT ( 'NONE',  ( 6.676582343750003368, 299.0156250017069510, -2.765530957081997254 ) ) ;
#10478 = ORIENTED_EDGE ( 'NONE', *, *, #30261, .F. ) ;
#10479 = CARTESIAN_POINT ( 'NONE',  ( 3.042071309553167513, 192.1354166632526130, -11.35316468749999785 ) ) ;
#10480 = CARTESIAN_POINT ( 'NONE',  ( 2.977408999572646486, 7.188101187499992051, 16.01780278187175099 ) ) ;
#10481 = CARTESIAN_POINT ( 'NONE',  ( -24.54126587499998635, 206.1250000013655779, 171.4326545832179818 ) ) ;
#10482 = CARTESIAN_POINT ( 'NONE',  ( -8.000000000000001776, 12.84375000000000178, 3.313708498984759387 ) ) ;
#10483 = CIRCLE ( 'NONE', #20101, 5.000000000000000888 ) ;
#10484 = ORIENTED_EDGE ( 'NONE', *, *, #39807, .T. ) ;
#10485 = PRODUCT_DEFINITION_FORMATION_WITH_SPECIFIED_SOURCE ( 'ANY', '', #20355, .NOT_KNOWN. ) ;
#10486 = CARTESIAN_POINT ( 'NONE',  ( -8.000000000000000000, 90.68750000409677625, 0.000000000000000000 ) ) ;
#10487 = CARTESIAN_POINT ( 'NONE',  ( -7.320508075688778149, 13.12500000000000178, 7.320508075688769267 ) ) ;
#10488 = CARTESIAN_POINT ( 'NONE',  ( -10.18810118749999738, -4.220049686691941915, 81.62500000204836681 ) ) ;
#10489 = ORIENTED_EDGE ( 'NONE', *, *, #1410, .T. ) ;
#10490 = CARTESIAN_POINT ( 'NONE',  ( 2.449293598294707893E-16, 19.25000000000000000, -4.000000000000001776 ) ) ;
#10491 = CARTESIAN_POINT ( 'NONE',  ( -3.211159895383561391, 21.68749999863440792, -3.211159895383561835 ) ) ;
#10492 = FACE_OUTER_BOUND ( 'NONE', #62120, .T. ) ;
#10493 = ORIENTED_EDGE ( 'NONE', *, *, #16036, .T. ) ;
#10494 = FACE_OUTER_BOUND ( 'NONE', #51606, .T. ) ;
#10495 = CARTESIAN_POINT ( 'NONE',  ( -4.999999999999999112, -14.31098243164692008, 69.87317657433686691 ) ) ;
#10496 = EDGE_CURVE ( 'NONE', #5834, #21207, #23618, .T. ) ;
#10499 = CARTESIAN_POINT ( 'NONE',  ( -2.319934922699201535E-11, 23.74999999999819522, 10.00000000000000178 ) ) ;
#10498 = CARTESIAN_POINT ( 'NONE',  ( 11.35316468749999963, 251.4062500034139873, -1.390361679473963556E-15 ) ) ;
#10497 = CARTESIAN_POINT ( 'NONE',  ( 26.56734541678233441, 207.0000000013655779, 166.5412658749999650 ) ) ;
#10500 = SHAPE_DEFINITION_REPRESENTATION ( #45734, #68567 ) ;
#10501 =( BOUNDED_CURVE ( )  B_SPLINE_CURVE ( 2, ( #31333, #43774, #48678, #20005, #15092 ),
 .UNSPECIFIED., .F., .F. ) 
 B_SPLINE_CURVE_WITH_KNOTS ( ( 3, 2, 3 ),
 ( 0.000000000000000000, 0.006944444444444445794, 0.01388888888888889159 ),
 .UNSPECIFIED. ) 
 CURVE ( )  GEOMETRIC_REPRESENTATION_ITEM ( )  RATIONAL_B_SPLINE_CURVE ( ( 1.000000000000000000, 0.9238795325112867385, 1.000000000000000000, 0.9238795325112867385, 1.000000000000000000 ) ) 
 REPRESENTATION_ITEM ( '' )  );
#10502 = ORIENTED_EDGE ( 'NONE', *, *, #19686, .T. ) ;
#10503 = AXIS2_PLACEMENT_3D ( 'NONE', #16596, #73958, #63750 ) ;
#10504 = CARTESIAN_POINT ( 'NONE',  ( -11.35316468749999785, 259.0104166700807014, -3.042071309553164848 ) ) ;
#10505 = CARTESIAN_POINT ( 'NONE',  ( 7.188101187499991163, 2.977408999572648707, 9.830302781871752771 ) ) ;
#10506 = ORIENTED_EDGE ( 'NONE', *, *, #48693, .F. ) ;
#10507 = EDGE_CURVE ( 'NONE', #69483, #502, #30422, .T. ) ;
#10508 = ORIENTED_EDGE ( 'NONE', *, *, #20267, .T. ) ;
#10509 = CARTESIAN_POINT ( 'NONE',  ( -6.238412754330611322E-16, 10.18810118749999916, 74.78125000204836681 ) ) ;
#10510 = CARTESIAN_POINT ( 'NONE',  ( 8.311093377946837890, 86.71874999658601268, -8.311093377946837890 ) ) ;
#10511 = CARTESIAN_POINT ( 'NONE',  ( -5.656854249492373476, -5.656854249492376141, 23.70530278392014978 ) ) ;
#10512 = CARTESIAN_POINT ( 'NONE',  ( -4.556349186104047710, -10.99999999999999822, 89.78125000000000000 ) ) ;
#10515 = CARTESIAN_POINT ( 'NONE',  ( 2.765530957081996366, 291.2968750017069510, -6.676582343750002480 ) ) ;
#10514 = CARTESIAN_POINT ( 'NONE',  ( 30.44569435410879876, 207.8125000013656063, 167.5543056458910485 ) ) ;
#10513 = CARTESIAN_POINT ( 'NONE',  ( 29.43265458321761585, 208.7500000013656063, 173.4587341249998929 ) ) ;
#10516 = CARTESIAN_POINT ( 'NONE',  ( -57.81176970334891507, 213.7280777717725186, 47.88999329079207001 ) ) ;
#10517 = CARTESIAN_POINT ( 'NONE',  ( -7.999999999999991118, 9.797174393178815797E-16, 30.00000000000000000 ) ) ;
#10518 = CARTESIAN_POINT ( 'NONE',  ( 9.832129032723420536, 206.1979166632526983, -5.676582343749999815 ) ) ;
#10519 = CARTESIAN_POINT ( 'NONE',  ( 8.000000000000000000, 8.906249995903221972, -3.313708498984761608 ) ) ;
#10520 = ORIENTED_EDGE ( 'NONE', *, *, #13878, .T. ) ;
#10521 = CARTESIAN_POINT ( 'NONE',  ( 24.54126587499998635, 209.5000000013656063, 171.4326545832175555 ) ) ;
#10522 = CARTESIAN_POINT ( 'NONE',  ( 7.188101187500001821, 20.43749999795161187, -2.977408999572650483 ) ) ;
#10523 = CARTESIAN_POINT ( 'NONE',  ( -9.832129032723418760, 173.1770833299193555, -5.676582343750004256 ) ) ;
#10524 = DIRECTION ( 'NONE',  ( 0.000000000000000000, -0.000000000000000000, 1.000000000000000000 ) ) ;
#10525 = CARTESIAN_POINT ( 'NONE',  ( 2.977408999572654480, 107.0000000020483810, 7.188101187499999156 ) ) ;
#10527 = CARTESIAN_POINT ( 'NONE',  ( 2.436599634630353783, -51.42120007173177498, -48.62500384162233047 ) ) ;
#10526 = CARTESIAN_POINT ( 'NONE',  ( -9.999999999999992895, 207.2916666666666856, -2.679491924311228512 ) ) ;
#10528 = CARTESIAN_POINT ( 'NONE',  ( 30.44569435410883784, 207.0625000013656063, 167.5543056458911053 ) ) ;
#10529 = CARTESIAN_POINT ( 'NONE',  ( 7.188101187499993827, -2.977408999572645598, 14.51780278187175455 ) ) ;
#10530 = CARTESIAN_POINT ( 'NONE',  ( 11.35316468750000141, 60.78124999658601979, 0.000000000000000000 ) ) ;
#10531 = CARTESIAN_POINT ( 'NONE',  ( -1.331154411942331306, -42.30442036676597439, 139.0280677962163622 ) ) ;
#10532 = CARTESIAN_POINT ( 'NONE',  ( -7.320508075688778149, 19.99999999317203603, 7.320508075688769267 ) ) ;
#10533 = CARTESIAN_POINT ( 'NONE',  ( 4.000000000000001776, 17.06250000000000000, -1.656854249492381248 ) ) ;
#10534 = EDGE_LOOP ( 'NONE', ( #44254, #17406, #59187, #41194, #17869 ) ) ;
#10535 = CIRCLE ( 'NONE', #22529, 3.999999999999976019 ) ;
#10536 = DIRECTION ( 'NONE',  ( 1.000000000000000000, -0.000000000000000000, -0.000000000000000000 ) ) ;
#10537 = CARTESIAN_POINT ( 'NONE',  ( -6.735557395310442023E-16, 11.00000000000000000, 80.31250000409677625 ) ) ;
#10538 = CARTESIAN_POINT ( 'NONE',  ( 9.832129032723420536, 61.19791666325267698, -5.676582343749999815 ) ) ;
#10539 = CARTESIAN_POINT ( 'NONE',  ( -11.00000000000000000, 4.556349186104045934, 77.59375000409676204 ) ) ;
#10540 = CARTESIAN_POINT ( 'NONE',  ( -1.432654583217662481, 199.3750000013656063, 145.4587341250000350 ) ) ;
#10541 = FACE_BOUND ( 'NONE', #60079, .T. ) ;
#10542 = CARTESIAN_POINT ( 'NONE',  ( -9.999999999999998224, 245.2083333333333428, 2.679491924311235174 ) ) ;
#10544 = CARTESIAN_POINT ( 'NONE',  ( 5.676582343750001591, 41.61458332991934839, -9.832129032723420536 ) ) ;
#10543 = CARTESIAN_POINT ( 'NONE',  ( 5.082755093536325042, 96.59375000204838102, -5.082755093536325930 ) ) ;
#10545 = CARTESIAN_POINT ( 'NONE',  ( 5.656854249492374365, 5.656854249492375253, 4.767802779823363757 ) ) ;
#10546 = CARTESIAN_POINT ( 'NONE',  ( 10.99999999999994849, 4.556349186104097448, 98.03125000409677625 ) ) ;
#10547 = CARTESIAN_POINT ( 'NONE',  ( -9.832129032723420536, 173.6979166632526983, 5.676582343749997150 ) ) ;
#10548 = CARTESIAN_POINT ( 'NONE',  ( 4.999999999999993783, 136.0416666598387110, 8.660254037844390851 ) ) ;
#10549 = CLOSED_SHELL ( 'NONE', ( #4293, #44739, #22738, #13893, #24172, #13786, #22942, #53767, #54158, #73543, #52607, #46390, #43184, #58468, #61337, #62622, #45549, #1987, #74407, #53589, #11294, #29844, #37509, #55152, #60621, #37771, #26007, #30832, #44347, #5823 ) ) ;
#10550 = CARTESIAN_POINT ( 'NONE',  ( 7.188101187500001821, 104.3750000020483952, -2.977408999572651371 ) ) ;
#10551 = CARTESIAN_POINT ( 'NONE',  ( 30.64284399271082293, 178.3875230420589446, 174.6921329945330683 ) ) ;
#10552 = CARTESIAN_POINT ( 'NONE',  ( -3.042071309553173730, 29.63541666325268409, 11.35316468749999785 ) ) ;
#10553 = DIRECTION ( 'NONE',  ( 1.000000000000000000, -0.000000000000000000, -0.000000000000000000 ) ) ;
#10554 = CARTESIAN_POINT ( 'NONE',  ( 11.35316468749999785, 165.5729166632526415, 3.042071309553174174 ) ) ;
#10555 = ORIENTED_EDGE ( 'NONE', *, *, #18102, .T. ) ;
#10556 = CARTESIAN_POINT ( 'NONE',  ( 49.70177871865296026, 134.0000000000000284, 57.99999999999998579 ) ) ;
#10557 = CARTESIAN_POINT ( 'NONE',  ( -10.18810118749999738, -4.220049686691941915, 69.25000000204836681 ) ) ;
#10558 = CARTESIAN_POINT ( 'NONE',  ( -1.656854249492348607, 196.1875000000000568, 202.0000000000000284 ) ) ;
#10559 = CARTESIAN_POINT ( 'NONE',  ( 8.000000000000000000, 16.50000000000000355, 0.000000000000000000 ) ) ;
#10561 = CARTESIAN_POINT ( 'NONE',  ( 5.676582343750001591, 166.6145833299193555, -9.832129032723420536 ) ) ;
#10560 = CARTESIAN_POINT ( 'NONE',  ( -37.99999999999999289, 37.00000000000000000, 0.000000000000000000 ) ) ;
#10562 = CARTESIAN_POINT ( 'NONE',  ( 5.656854249492376141, -5.656854249492374365, 7.449052784329822430 ) ) ;
#10563 = CARTESIAN_POINT ( 'NONE',  ( -7.999999999999948486, 3.313708498984799355, 5.236552779823361981 ) ) ;
#10564 = CARTESIAN_POINT ( 'NONE',  ( 5.676582343749997150, 227.2395833367473301, -9.832129032723418760 ) ) ;
#10565 = CARTESIAN_POINT ( 'NONE',  ( -1.882291019712828861, 55.75505015263576070, -43.87597576788949993 ) ) ;
#10566 = CARTESIAN_POINT ( 'NONE',  ( 10.18810118749999916, 1.247682550866122264E-15, 82.28125000204838102 ) ) ;
#10567 = ORIENTED_EDGE ( 'NONE', *, *, #40479, .F. ) ;
#10568 = VECTOR ( 'NONE', #10341, 1000.000000000000114 ) ;
#10569 = CARTESIAN_POINT ( 'NONE',  ( -3.999999999999960032, 203.9375000000000000, 196.3431457505076594 ) ) ;
#10570 = CARTESIAN_POINT ( 'NONE',  ( -3.042071309553164404, 117.5520833299193413, -11.35316468749999963 ) ) ;
#10571 = DIRECTION ( 'NONE',  ( 1.000000000000000000, -0.000000000000000000, -0.000000000000000000 ) ) ;
#10572 = EDGE_LOOP ( 'NONE', ( #20197, #49414, #47455, #18746 ) ) ;
#10573 = EDGE_LOOP ( 'NONE', ( #24785, #31253, #44161, #14218 ) ) ;
#10574 = CARTESIAN_POINT ( 'NONE',  ( 1.881053915767122664, 7.249999998634408804, 4.541265875000001451 ) ) ;
#10575 = CARTESIAN_POINT ( 'NONE',  ( 7.188101187500001821, 12.56249999795161365, -2.977408999572650483 ) ) ;
#10576 = CARTESIAN_POINT ( 'NONE',  ( -3.313708498984762496, 108.9687500040967905, 7.999999999999998224 ) ) ;
#10577 = EDGE_CURVE ( 'NONE', #6677, #65401, #67305, .T. ) ;
#10578 = CARTESIAN_POINT ( 'NONE',  ( -29.43265458321760519, 199.1250000013656347, 173.4587341250003760 ) ) ;
#10579 = ADVANCED_FACE ( 'NONE', ( #2859 ), #30055, .T. ) ;
#10580 = CARTESIAN_POINT ( 'NONE',  ( -1.656854249492381248, 9.312499999999998224, -4.000000000000001776 ) ) ;
#10581 = CARTESIAN_POINT ( 'NONE',  ( -1.656854249492383691, 21.43749999726881228, 4.000000000000000888 ) ) ;
#10582 = CARTESIAN_POINT ( 'NONE',  ( -4.541265875000002339, 7.812499998634407028, -5.561446717895856393E-16 ) ) ;
#10583 = CARTESIAN_POINT ( 'NONE',  ( 2.828427124746152987, 200.1250000000000284, 139.1715728752538723 ) ) ;
#10584 = ORIENTED_EDGE ( 'NONE', *, *, #5374, .T. ) ;
#10585 = PRESENTATION_STYLE_ASSIGNMENT (( #27556 ) ) ;
#10586 = CARTESIAN_POINT ( 'NONE',  ( -7.188101187499999156, 107.7500000020483810, 2.977408999572654924 ) ) ;
#10587 = AXIS2_PLACEMENT_3D ( 'NONE', #39046, #28830, #22413 ) ;
#10588 = EDGE_CURVE ( 'NONE', #44710, #71315, #71876, .T. ) ;
#10590 = CARTESIAN_POINT ( 'NONE',  ( -2.828427124746208943, 209.6250000000000284, 144.8284271247462129 ) ) ;
#10589 = DIRECTION ( 'NONE',  ( 0.000000000000000000, 0.000000000000000000, 1.000000000000000000 ) ) ;
#10591 =( NAMED_UNIT ( * ) PLANE_ANGLE_UNIT ( ) SI_UNIT ( $, .RADIAN. ) );
#10592 = CARTESIAN_POINT ( 'NONE',  ( -7.999999999999991118, 0.000000000000000000, 3.830302779823362869 ) ) ;
#10593 = CARTESIAN_POINT ( 'NONE',  ( -7.188101187499990274, -2.977408999572651371, 1.580302781871753437 ) ) ;
#10594 = ORIENTED_EDGE ( 'NONE', *, *, #8491, .T. ) ;
#10595 =( BOUNDED_CURVE ( )  B_SPLINE_CURVE ( 2, ( #21212, #65743, #66869, #43474, #15177, #66115, #44239 ),
 .UNSPECIFIED., .F., .F. ) 
 B_SPLINE_CURVE_WITH_KNOTS ( ( 3, 2, 2, 3 ),
 ( 0.9166666666666674068, 0.9250000000000005995, 0.9333333333333335702, 0.9416666668637480031 ),
 .UNSPECIFIED. ) 
 CURVE ( )  GEOMETRIC_REPRESENTATION_ITEM ( )  RATIONAL_B_SPLINE_CURVE ( ( 0.9999999999999928946, 0.9238795325112938439, 1.000000000000000000, 0.9238795325112867385, 1.000000000000000000, 0.9238795325112867385, 1.000000000000000000 ) ) 
 REPRESENTATION_ITEM ( '' )  );
#10596 = EDGE_LOOP ( 'NONE', ( #15558, #52591, #59222, #6783 ) ) ;
#10597 = CARTESIAN_POINT ( 'NONE',  ( -7.204075437095965206, -7.204075437095968759, 93.34375000204838102 ) ) ;
#10598 = DIRECTION ( 'NONE',  ( 2.771571441169508074E-17, 1.000000000000000000, 2.238352872228138663E-16 ) ) ;
#10599 = CARTESIAN_POINT ( 'NONE',  ( -26.56734541678238060, 201.6250000013656063, 166.5412658750003629 ) ) ;
#10600 = CARTESIAN_POINT ( 'NONE',  ( -7.778174593052020747, -7.778174593052023411, 104.6874999999999858 ) ) ;
#10601 = CARTESIAN_POINT ( 'NONE',  ( -3.458734124999960358, 207.6875000013656063, 198.0000000000000284 ) ) ;
#10603 = CARTESIAN_POINT ( 'NONE',  ( -5.000000000000008882, 128.3333333333333428, 8.660254037844390851 ) ) ;
#10602 = CARTESIAN_POINT ( 'NONE',  ( -8.000000000000000000, 111.5000000000000000, 0.000000000000000000 ) ) ;
#10604 = CARTESIAN_POINT ( 'NONE',  ( -8.660254037844387298, 122.0833333333333286, -5.000000000000004441 ) ) ;
#10605 = CARTESIAN_POINT ( 'NONE',  ( 3.313708498984765161, 104.4687500000000000, 7.999999999999998224 ) ) ;
#10606 = CIRCLE ( 'NONE', #51584, 15.99999999999998579 ) ;
#10607 = CYLINDRICAL_SURFACE ( 'NONE', #41667, 37.00000000000000711 ) ;
#10608 = CARTESIAN_POINT ( 'NONE',  ( -5.082755093536317936, -5.082755093536320601, 6.549052781871754547 ) ) ;
#10609 = COLOUR_RGB ( '',0.7921568627450980005, 0.8196078431372548767, 0.9333333333333333481 ) ;
#10610 = CARTESIAN_POINT ( 'NONE',  ( -8.000000000000000000, 97.90625000000000000, -3.313708498984761164 ) ) ;
#10611 = CARTESIAN_POINT ( 'NONE',  ( 31.45873412500001010, 206.7500000013655779, 168.5673454167822740 ) ) ;
#10612 = CARTESIAN_POINT ( 'NONE',  ( -1.469576158976823947E-15, 24.93749999590322375, 8.000000000000000000 ) ) ;
#10613 = CARTESIAN_POINT ( 'NONE',  ( 2.445694354108783664, 198.3125000013656063, 144.4456943541088663 ) ) ;
#10614 = CARTESIAN_POINT ( 'NONE',  ( 5.082755093536325042, 122.4687500020483952, -5.082755093536325930 ) ) ;
#10616 = CARTESIAN_POINT ( 'NONE',  ( -2.754378923186476579E-14, 203.4375000013656063, 145.4587341250000350 ) ) ;
#10615 = DIRECTION ( 'NONE',  ( 0.000000000000000000, -1.000000000000000000, 0.000000000000000000 ) ) ;
#10617 = CARTESIAN_POINT ( 'NONE',  ( 5.676582343750005144, 235.8854166700806729, 9.832129032723416984 ) ) ;
#10618 = CYLINDRICAL_SURFACE ( 'NONE', #52026, 7.999999999999991118 ) ;
#10619 = CARTESIAN_POINT ( 'NONE',  ( 27.99999999999996803, 203.0000000000000000, 173.9999999999999147 ) ) ;
#10620 = CARTESIAN_POINT ( 'NONE',  ( 9.832129032723416984, 15.36458332991935016, 5.676582343750006032 ) ) ;
#10621 =( BOUNDED_SURFACE ( )  B_SPLINE_SURFACE ( 1, 2, ( 
 ( #42031, #37499, #65414, #30718, #66525, #31463, #30352, #2050, #37123, #54107, #71066, #14836, #1696, #24675, #54488, #19760, #14462, #71809, #19384, #47685, #31837, #2793, #43142, #59038, #2419, #53373, #13711, #48428, #25780, #25037, #48800, #72184, #25413, #66157, #3167, #36755, #60499, #65038, #65784, #59769, #8078, #8826, #31079, #13347, #54856, #70706, #20497, #19025, #59400, #71431, #26156, #7714, #26531, #32216, #61628, #44277, #56721, #21252, #38990, #3539, #33343, #43899, #27658, #38627, #32599, #21623, #55980, #9947, #15216, #38246, #66911, #51047, #33719, #3925, #73684, #49555, #67662, #15961, #61250, #61995, #4664, #50666, #5039, #27282, #67288, #44647, #32979, #10317, #16323, #21997, #28036, #26915, #56345, #15587, #4290, #45023, #72574, #9581, #20878, #50299, #68029, #74057, #55607, #39358, #49929, #62355, #72944, #73320, #10686, #9195, #22356, #45381, #55234, #68396, #37876, #60872, #46871, #41218, #57845, #11065, #34093, #17452, #39726, #46127, #28775, #29896, #45755, #51790, #875, #23861, #40845, #506, #138, #6885, #63853, #24221, #23114, #69517, #6520, #58219, #34838, #69893, #69145, #46497, #52909, #57089, #17831, #63478, #12168, #58577, #63106, #29527, #5779, #35202, #1243, #52537, #18205, #5405, #52174, #6150, #64226, #11800, #23485, #12534, #28407, #74429, #40473, #62727, #29156, #35564, #47234, #11432, #16694, #51415, #22735, #68768, #17079, #40101, #34469, #57473, #54018, #2328, #43048, #30630, #65693, #70619, #53652, #26062, #1962, #13993, #41945, #24592, #70262, #31748, #37034, #70985, #47597, #24953, #47970, #18574, #8353, #54398, #60035, #66067, #60409, #31370, #25692, #71719, #48712, #64953, #18939, #30996, #2704, #41584, #25324, #48340, #14374, #19301, #20034, #13263, #42311, #64599, #65326, #37408, #36300, #59317, #12896, #54768, #8735, #13631, #7623, #36669, #59679, #35932, #3077, #58949, #7256, #30267, #53283, #1608, #7990 ),
 ( #71347, #19669, #42681, #26827, #32124, #73596, #56636, #62273, #49083, #37789, #43810, #21537, #14748, #60785, #43426, #72859, #55518, #67941, #32506, #50211, #9109, #44560, #55144, #38902, #49840, #66825, #32888, #67201, #21164, #26438, #49463, #3449, #10601, #44934, #15127, #10229, #72483, #4204, #27194, #20790, #73231, #15870, #61905, #16235, #38536, #3830, #44188, #15499, #4950, #66440, #38159, #67573, #9492, #61160, #56257, #33257, #61537, #9860, #21904, #4573, #55890, #27571, #39272, #50579, #33629, #72096, #20410, #24420, #16989, #30086, #42131, #22274, #11342, #1792, #10974, #28319, #5688, #34009, #57003, #41774, #53105, #68310, #22645, #1439, #65143, #47427, #5317, #40016, #70451, #51328, #7451, #34378, #74337, #64784, #45665, #13086, #70814, #68680, #19125, #36490, #57378, #18767, #63018, #36121, #13452, #45296, #28686, #24776, #51700, #46, #23031, #46039, #70091, #59142, #30458, #16607, #18397, #53475, #59504, #47790, #41412, #64423, #27949, #12721, #50956, #35754, #58772, #73968, #39644, #62641, #7080, #60605, #2896, #71538, #15313, #25146, #48163, #8929, #43247, #37981, #20607, #19862, #71171, #55338, #37605, #43624, #38349, #25882, #67014, #14193, #71915, #3272, #25518, #26259, #20983, #48901, #31940, #26641, #37230, #60980, #13815, #66263, #42868, #60227, #72294, #8553, #65522, #32325, #7816, #44007, #30819, #19489, #2526, #54963, #42505, #36859, #2153, #31567, #54591, #49663, #65887, #49279, #59867, #66635, #8180, #14942, #20228, #48530, #14569, #9301, #3642, #31190, #54216, #72679, #53842, #57194, #27385, #22461, #73048, #16427, #39462, #15691, #62460, #28135, #51148, #28509, #50772, #67766, #10419, #4768, #68873, #4028, #27021, #10789, #21723, #61730, #68499, #74157, #50033, #33086, #11168, #45481, #39094, #44379, #34191, #17183, #74533, #61357, #21355, #56082, #33824, #67389, #38733, #55713, #33450, #16060, #5509, #44753, #56821, #10049, #5142 ) ),
 .UNSPECIFIED., .F., .F., .F. ) 
 B_SPLINE_SURFACE_WITH_KNOTS ( ( 2, 2 ),
 ( 3, 2, 2, 2, 2, 2, 2, 2, 2, 2, 2, 2, 2, 2, 2, 2, 2, 2, 2, 2, 2, 2, 2, 2, 2, 2, 2, 2, 2, 2, 2, 2, 2, 2, 2, 2, 2, 2, 2, 2, 2, 2, 2, 2, 2, 2, 2, 2, 2, 2, 2, 2, 2, 2, 2, 2, 2, 2, 2, 2, 2, 2, 2, 2, 2, 2, 2, 2, 2, 2, 2, 2, 2, 2, 2, 2, 2, 2, 2, 2, 2, 2, 2, 2, 2, 2, 2, 2, 2, 2, 2, 2, 2, 2, 2, 2, 2, 2, 2, 2, 2, 2, 2, 2, 2, 2, 2, 2, 2, 2, 2, 2, 2, 2, 2, 2, 2, 2, 2, 2, 3 ),
 ( 0.000000000000000000, 1.000000000000000000 ),
 ( 0.000000000000000000, 0.008333333333333333218, 0.01666666666666666644, 0.02500000000000000139, 0.03333333333333333287, 0.04166666666666666435, 0.05000000000000000278, 0.05833333333333333426, 0.06666666666666666574, 0.07499999999999999722, 0.08333333333333332871, 0.09166666666666666019, 0.1000000000000000056, 0.1083333333333333370, 0.1166666666666666685, 0.1250000000000000000, 0.1333333333333333315, 0.1416666666666666630, 0.1499999999999999944, 0.1583333333333333259, 0.1666666666666666574, 0.1749999999999999889, 0.1833333333333333204, 0.1916666666666666796, 0.2000000000000000111, 0.2083333333333333426, 0.2166666666666666741, 0.2250000000000000056, 0.2333333333333333370, 0.2416666666666666685, 0.2500000000000000000, 0.2583333333333333592, 0.2666666666666666630, 0.2750000000000000222, 0.2833333333333333259, 0.2916666666666666852, 0.2999999999999999889, 0.3083333333333333481, 0.3166666666666666519, 0.3250000000000000111, 0.3333333333333333148, 0.3416666666666666741, 0.3499999999999999778, 0.3583333333333333370, 0.3666666666666666408, 0.3750000000000000000, 0.3833333333333333592, 0.3916666666666666630, 0.4000000000000000222, 0.4083333333333333259, 0.4166666666666666852, 0.4249999999999999889, 0.4333333333333333481, 0.4416666666666666519, 0.4500000000000000111, 0.4583333333333333148, 0.4666666666666666741, 0.4749999999999999778, 0.4833333333333333370, 0.4916666666666666408, 0.5000000000000000000, 0.5083333333333333037, 0.5166666666666667185, 0.5250000000000000222, 0.5333333333333333259, 0.5416666666666666297, 0.5500000000000000444, 0.5583333333333333481, 0.5666666666666666519, 0.5749999999999999556, 0.5833333333333333703, 0.5916666666666666741, 0.5999999999999999778, 0.6083333333333332815, 0.6166666666666666963, 0.6250000000000000000, 0.6333333333333333037, 0.6416666666666667185, 0.6500000000000000222, 0.6583333333333333259, 0.6666666666666666297, 0.6750000000000000444, 0.6833333333333333481, 0.6916666666666666519, 0.6999999999999999556, 0.7083333333333333703, 0.7166666666666666741, 0.7249999999999999778, 0.7333333333333332815, 0.7416666666666666963, 0.7500000000000000000, 0.7583333333333333037, 0.7666666666666667185, 0.7750000000000000222, 0.7833333333333333259, 0.7916666666666666297, 0.8000000000000000444, 0.8083333333333333481, 0.8166666666666666519, 0.8249999999999999556, 0.8333333333333333703, 0.8416666666666666741, 0.8499999999999999778, 0.8583333333333332815, 0.8666666666666666963, 0.8750000000000000000, 0.8833333333333333037, 0.8916666666666667185, 0.9000000000000000222, 0.9083333333333333259, 0.9166666666666666297, 0.9250000000000000444, 0.9333333333333333481, 0.9416666666666666519, 0.9499999999999999556, 0.9583333333333333703, 0.9666666666666666741, 0.9749999999999999778, 0.9833333333333332815, 0.9916666666666666963, 1.000000000000000000 ),
 .UNSPECIFIED. ) 
 GEOMETRIC_REPRESENTATION_ITEM ( )  RATIONAL_B_SPLINE_SURFACE ( (
 ( 1.000000000000000000, 0.9238795325112867385, 1.000000000000000000, 0.9238795325112867385, 1.000000000000000000, 0.9238795325112867385, 1.000000000000000000, 0.9238795325112867385, 1.000000000000000000, 0.9238795325112867385, 1.000000000000000000, 0.9238795325112867385, 1.000000000000000000, 0.9238795325112867385, 1.000000000000000000, 0.9238795325112867385, 1.000000000000000000, 0.9238795325112867385, 1.000000000000000000, 0.9238795325112867385, 1.000000000000000000, 0.9238795325112867385, 1.000000000000000000, 0.9238795325112867385, 1.000000000000000000, 0.9238795325112867385, 1.000000000000000000, 0.9238795325112867385, 1.000000000000000000, 0.9238795325112867385, 1.000000000000000000, 0.9238795325112867385, 1.000000000000000000, 0.9238795325112867385, 1.000000000000000000, 0.9238795325112867385, 1.000000000000000000, 0.9238795325112867385, 1.000000000000000000, 0.9238795325112867385, 1.000000000000000000, 0.9238795325112867385, 1.000000000000000000, 0.9238795325112867385, 1.000000000000000000, 0.9238795325112867385, 1.000000000000000000, 0.9238795325112867385, 1.000000000000000000, 0.9238795325112867385, 1.000000000000000000, 0.9238795325112867385, 1.000000000000000000, 0.9238795325112867385, 1.000000000000000000, 0.9238795325112867385, 1.000000000000000000, 0.9238795325112867385, 1.000000000000000000, 0.9238795325112867385, 1.000000000000000000, 0.9238795325112867385, 1.000000000000000000, 0.9238795325112867385, 1.000000000000000000, 0.9238795325112867385, 1.000000000000000000, 0.9238795325112867385, 1.000000000000000000, 0.9238795325112867385, 1.000000000000000000, 0.9238795325112867385, 1.000000000000000000, 0.9238795325112867385, 1.000000000000000000, 0.9238795325112867385, 1.000000000000000000, 0.9238795325112867385, 1.000000000000000000, 0.9238795325112867385, 1.000000000000000000, 0.9238795325112867385, 1.000000000000000000, 0.9238795325112867385, 1.000000000000000000, 0.9238795325112867385, 1.000000000000000000, 0.9238795325112867385, 1.000000000000000000, 0.9238795325112867385, 1.000000000000000000, 0.9238795325112867385, 1.000000000000000000, 0.9238795325112867385, 1.000000000000000000, 0.9238795325112867385, 1.000000000000000000, 0.9238795325112867385, 1.000000000000000000, 0.9238795325112867385, 1.000000000000000000, 0.9238795325112867385, 1.000000000000000000, 0.9238795325112867385, 1.000000000000000000, 0.9238795325112867385, 1.000000000000000000, 0.9238795325112867385, 1.000000000000000000, 0.9238795325112867385, 1.000000000000000000, 0.9238795325112867385, 1.000000000000000000, 0.9238795325112867385, 1.000000000000000000, 0.9238795325112867385, 1.000000000000000000, 0.9238795325112867385, 1.000000000000000000, 0.9238795325112867385, 1.000000000000000000, 0.9238795325112867385, 1.000000000000000000, 0.9238795325112867385, 1.000000000000000000, 0.9238795325112867385, 1.000000000000000000, 0.9238795325112867385, 1.000000000000000000, 0.9238795325112867385, 1.000000000000000000, 0.9238795325112867385, 1.000000000000000000, 0.9238795325112867385, 1.000000000000000000, 0.9238795325112867385, 1.000000000000000000, 0.9238795325112867385, 1.000000000000000000, 0.9238795325112867385, 1.000000000000000000, 0.9238795325112867385, 1.000000000000000000, 0.9238795325112867385, 1.000000000000000000, 0.9238795325112867385, 1.000000000000000000, 0.9238795325112867385, 1.000000000000000000, 0.9238795325112867385, 1.000000000000000000, 0.9238795325112867385, 1.000000000000000000, 0.9238795325112867385, 1.000000000000000000, 0.9238795325112867385, 1.000000000000000000, 0.9238795325112867385, 1.000000000000000000, 0.9238795325112867385, 1.000000000000000000, 0.9238795325112867385, 1.000000000000000000, 0.9238795325112867385, 1.000000000000000000, 0.9238795325112867385, 1.000000000000000000, 0.9238795325112867385, 1.000000000000000000, 0.9238795325112867385, 1.000000000000000000, 0.9238795325112867385, 1.000000000000000000, 0.9238795325112867385, 1.000000000000000000, 0.9238795325112867385, 1.000000000000000000, 0.9238795325112867385, 1.000000000000000000, 0.9238795325112867385, 1.000000000000000000, 0.9238795325112867385, 1.000000000000000000, 0.9238795325112867385, 1.000000000000000000, 0.9238795325112867385, 1.000000000000000000, 0.9238795325112867385, 1.000000000000000000, 0.9238795325112867385, 1.000000000000000000, 0.9238795325112867385, 1.000000000000000000, 0.9238795325112867385, 1.000000000000000000, 0.9238795325112867385, 1.000000000000000000, 0.9238795325112867385, 1.000000000000000000, 0.9238795325112867385, 1.000000000000000000, 0.9238795325112867385, 1.000000000000000000, 0.9238795325112867385, 1.000000000000000000, 0.9238795325112867385, 1.000000000000000000, 0.9238795325112867385, 1.000000000000000000, 0.9238795325112867385, 1.000000000000000000, 0.9238795325112867385, 1.000000000000000000, 0.9238795325112867385, 1.000000000000000000, 0.9238795325112867385, 1.000000000000000000, 0.9238795325112867385, 1.000000000000000000, 0.9238795325112867385, 1.000000000000000000, 0.9238795325112867385, 1.000000000000000000, 0.9238795325112867385, 1.000000000000000000, 0.9238795325112867385, 1.000000000000000000, 0.9238795325112867385, 1.000000000000000000, 0.9238795325112867385, 1.000000000000000000, 0.9238795325112867385, 1.000000000000000000, 0.9238795325112867385, 1.000000000000000000, 0.9238795325112867385, 1.000000000000000000, 0.9238795325112867385, 1.000000000000000000, 0.9238795325112867385, 1.000000000000000000),
 ( 1.000000000000000000, 0.9238795325112867385, 1.000000000000000000, 0.9238795325112867385, 1.000000000000000000, 0.9238795325112867385, 1.000000000000000000, 0.9238795325112867385, 1.000000000000000000, 0.9238795325112867385, 1.000000000000000000, 0.9238795325112867385, 1.000000000000000000, 0.9238795325112867385, 1.000000000000000000, 0.9238795325112867385, 1.000000000000000000, 0.9238795325112867385, 1.000000000000000000, 0.9238795325112867385, 1.000000000000000000, 0.9238795325112867385, 1.000000000000000000, 0.9238795325112867385, 1.000000000000000000, 0.9238795325112867385, 1.000000000000000000, 0.9238795325112867385, 1.000000000000000000, 0.9238795325112867385, 1.000000000000000000, 0.9238795325112867385, 1.000000000000000000, 0.9238795325112867385, 1.000000000000000000, 0.9238795325112867385, 1.000000000000000000, 0.9238795325112867385, 1.000000000000000000, 0.9238795325112867385, 1.000000000000000000, 0.9238795325112867385, 1.000000000000000000, 0.9238795325112867385, 1.000000000000000000, 0.9238795325112867385, 1.000000000000000000, 0.9238795325112867385, 1.000000000000000000, 0.9238795325112867385, 1.000000000000000000, 0.9238795325112867385, 1.000000000000000000, 0.9238795325112867385, 1.000000000000000000, 0.9238795325112867385, 1.000000000000000000, 0.9238795325112867385, 1.000000000000000000, 0.9238795325112867385, 1.000000000000000000, 0.9238795325112867385, 1.000000000000000000, 0.9238795325112867385, 1.000000000000000000, 0.9238795325112867385, 1.000000000000000000, 0.9238795325112867385, 1.000000000000000000, 0.9238795325112867385, 1.000000000000000000, 0.9238795325112867385, 1.000000000000000000, 0.9238795325112867385, 1.000000000000000000, 0.9238795325112867385, 1.000000000000000000, 0.9238795325112867385, 1.000000000000000000, 0.9238795325112867385, 1.000000000000000000, 0.9238795325112867385, 1.000000000000000000, 0.9238795325112867385, 1.000000000000000000, 0.9238795325112867385, 1.000000000000000000, 0.9238795325112867385, 1.000000000000000000, 0.9238795325112867385, 1.000000000000000000, 0.9238795325112867385, 1.000000000000000000, 0.9238795325112867385, 1.000000000000000000, 0.9238795325112867385, 1.000000000000000000, 0.9238795325112867385, 1.000000000000000000, 0.9238795325112867385, 1.000000000000000000, 0.9238795325112867385, 1.000000000000000000, 0.9238795325112867385, 1.000000000000000000, 0.9238795325112867385, 1.000000000000000000, 0.9238795325112867385, 1.000000000000000000, 0.9238795325112867385, 1.000000000000000000, 0.9238795325112867385, 1.000000000000000000, 0.9238795325112867385, 1.000000000000000000, 0.9238795325112867385, 1.000000000000000000, 0.9238795325112867385, 1.000000000000000000, 0.9238795325112867385, 1.000000000000000000, 0.9238795325112867385, 1.000000000000000000, 0.9238795325112867385, 1.000000000000000000, 0.9238795325112867385, 1.000000000000000000, 0.9238795325112867385, 1.000000000000000000, 0.9238795325112867385, 1.000000000000000000, 0.9238795325112867385, 1.000000000000000000, 0.9238795325112867385, 1.000000000000000000, 0.9238795325112867385, 1.000000000000000000, 0.9238795325112867385, 1.000000000000000000, 0.9238795325112867385, 1.000000000000000000, 0.9238795325112867385, 1.000000000000000000, 0.9238795325112867385, 1.000000000000000000, 0.9238795325112867385, 1.000000000000000000, 0.9238795325112867385, 1.000000000000000000, 0.9238795325112867385, 1.000000000000000000, 0.9238795325112867385, 1.000000000000000000, 0.9238795325112867385, 1.000000000000000000, 0.9238795325112867385, 1.000000000000000000, 0.9238795325112867385, 1.000000000000000000, 0.9238795325112867385, 1.000000000000000000, 0.9238795325112867385, 1.000000000000000000, 0.9238795325112867385, 1.000000000000000000, 0.9238795325112867385, 1.000000000000000000, 0.9238795325112867385, 1.000000000000000000, 0.9238795325112867385, 1.000000000000000000, 0.9238795325112867385, 1.000000000000000000, 0.9238795325112867385, 1.000000000000000000, 0.9238795325112867385, 1.000000000000000000, 0.9238795325112867385, 1.000000000000000000, 0.9238795325112867385, 1.000000000000000000, 0.9238795325112867385, 1.000000000000000000, 0.9238795325112867385, 1.000000000000000000, 0.9238795325112867385, 1.000000000000000000, 0.9238795325112867385, 1.000000000000000000, 0.9238795325112867385, 1.000000000000000000, 0.9238795325112867385, 1.000000000000000000, 0.9238795325112867385, 1.000000000000000000, 0.9238795325112867385, 1.000000000000000000, 0.9238795325112867385, 1.000000000000000000, 0.9238795325112867385, 1.000000000000000000, 0.9238795325112867385, 1.000000000000000000, 0.9238795325112867385, 1.000000000000000000, 0.9238795325112867385, 1.000000000000000000, 0.9238795325112867385, 1.000000000000000000, 0.9238795325112867385, 1.000000000000000000, 0.9238795325112867385, 1.000000000000000000, 0.9238795325112867385, 1.000000000000000000, 0.9238795325112867385, 1.000000000000000000, 0.9238795325112867385, 1.000000000000000000, 0.9238795325112867385, 1.000000000000000000, 0.9238795325112867385, 1.000000000000000000, 0.9238795325112867385, 1.000000000000000000, 0.9238795325112867385, 1.000000000000000000, 0.9238795325112867385, 1.000000000000000000, 0.9238795325112867385, 1.000000000000000000, 0.9238795325112867385, 1.000000000000000000, 0.9238795325112867385, 1.000000000000000000, 0.9238795325112867385, 1.000000000000000000, 0.9238795325112867385, 1.000000000000000000, 0.9238795325112867385, 1.000000000000000000) ) ) 
 REPRESENTATION_ITEM ( '' )  SURFACE ( )  );
#10622 = DIRECTION ( 'NONE',  ( -0.000000000000000000, 1.000000000000000000, -0.000000000000000000 ) ) ;
#10623 = CARTESIAN_POINT ( 'NONE',  ( 8.311093377946837890, 211.7187499965860127, -8.311093377946837890 ) ) ;
#10624 = FACE_OUTER_BOUND ( 'NONE', #57710, .T. ) ;
#10625 = CARTESIAN_POINT ( 'NONE',  ( 5.204170427930421283E-15, 10.39230484541327293, -0.8038475772933779684 ) ) ;
#10626 = CARTESIAN_POINT ( 'NONE',  ( 2.020667218593132706E-15, -11.00000000000000000, 88.37499999999998579 ) ) ;
#10627 = ORIENTED_EDGE ( 'NONE', *, *, #2596, .T. ) ;
#10628 = CARTESIAN_POINT ( 'NONE',  ( -2.445694354108839175, 200.3125000013656063, 144.4456943541088663 ) ) ;
#10629 = CARTESIAN_POINT ( 'NONE',  ( -5.676582343750006032, 24.11458332991935194, 9.832129032723418760 ) ) ;
#10630 = CARTESIAN_POINT ( 'NONE',  ( -6.735557395310442023E-16, 11.00000000000000000, 90.81250000409676204 ) ) ;
#10631 = LINE ( 'NONE', #56664, #47956 ) ;
#10632 = CARTESIAN_POINT ( 'NONE',  ( -29.43265458321770822, 198.5000000013656063, 166.5412658750003914 ) ) ;
#10633 = SPHERICAL_SURFACE ( 'NONE', #9359, 10.00000000000001243 ) ;
#10635 = CARTESIAN_POINT ( 'NONE',  ( 9.832129032723416984, 10.36458332991935016, 5.676582343750006032 ) ) ;
#10634 = CARTESIAN_POINT ( 'NONE',  ( -7.188101187499999156, 112.2500000020483952, 2.977408999572654924 ) ) ;
#10636 = CARTESIAN_POINT ( 'NONE',  ( -7.999999999999991118, 0.000000000000000000, 18.83030277982336642 ) ) ;
#10637 = CARTESIAN_POINT ( 'NONE',  ( 8.311093377946837890, 141.4062499965860127, -8.311093377946837890 ) ) ;
#10638 = CARTESIAN_POINT ( 'NONE',  ( 2.679491924311222739, 105.8333333265053824, 10.00000000000000355 ) ) ;
#10639 = CARTESIAN_POINT ( 'NONE',  ( -5.082755093536325930, 122.8437500020483952, -5.082755093536325930 ) ) ;
#10640 = CARTESIAN_POINT ( 'NONE',  ( 0.4368895104463361156, 67.59332269699999074, -20.03478791450181973 ) ) ;
#10641 = CARTESIAN_POINT ( 'NONE',  ( -26.56734541678232731, 209.2500000013655779, 173.4587341250003760 ) ) ;
#10642 = CARTESIAN_POINT ( 'NONE',  ( -5.000000000000000000, 51.30401030464796008, -41.49390406301998269 ) ) ;
#10643 = ORIENTED_EDGE ( 'NONE', *, *, #54285, .T. ) ;
#10644 = CARTESIAN_POINT ( 'NONE',  ( 2.069125466538022096, -65.90280720053424091, 26.36412295902750103 ) ) ;
#10645 = CARTESIAN_POINT ( 'NONE',  ( 2.765530957081996366, 291.2968750017069510, -6.676582343750003368 ) ) ;
#10646 = CARTESIAN_POINT ( 'NONE',  ( 0.000000000000000000, 0.000000000000000000, 41.99999999999999289 ) ) ;
#10647 = CARTESIAN_POINT ( 'NONE',  ( -5.656854249492373476, -5.656854249492376141, 1.205302783920146004 ) ) ;
#10648 = CARTESIAN_POINT ( 'NONE',  ( -3.313708498984719864, 18.46875000000000000, -8.000000000000040856 ) ) ;
#10649 = CARTESIAN_POINT ( 'NONE',  ( 5.676582343750005144, 260.5729166700806445, 9.832129032723416984 ) ) ;
#10650 = CARTESIAN_POINT ( 'NONE',  ( -7.204075437095965206, -7.204075437095968759, 96.71875000204838102 ) ) ;
#10651 = ORIENTED_EDGE ( 'NONE', *, *, #4462, .T. ) ;
#10652 = EDGE_CURVE ( 'NONE', #21157, #72571, #31764, .T. ) ;
#10653 = CARTESIAN_POINT ( 'NONE',  ( 5.000000000000000000, 11.32881245867859121, 67.85521288293392672 ) ) ;
#10654 = CYLINDRICAL_SURFACE ( 'NONE', #54450, 8.000000000000000000 ) ;
#10655 = CARTESIAN_POINT ( 'NONE',  ( -2.445694354108783219, 202.8125000013656063, 200.4456943541088663 ) ) ;
#10656 = CARTESIAN_POINT ( 'NONE',  ( 5.676582343750001591, 76.92708332991935549, -9.832129032723420536 ) ) ;
#10657 = EDGE_LOOP ( 'NONE', ( #24976, #10203, #43677, #26538 ) ) ;
#10658 = CARTESIAN_POINT ( 'NONE',  ( 7.204075437095966983, 7.204075437095967871, 110.5937500020483810 ) ) ;
#10659 = CARTESIAN_POINT ( 'NONE',  ( 4.541265875000002339, 12.43749999863440792, 0.000000000000000000 ) ) ;
#10660 = ORIENTED_EDGE ( 'NONE', *, *, #45936, .F. ) ;
#10661 = CARTESIAN_POINT ( 'NONE',  ( -3.313708498984765161, 1.031250000000000000, 7.999999999999998224 ) ) ;
#10662 = CARTESIAN_POINT ( 'NONE',  ( -3.313708498984681672, 110.4687500040967763, 8.000000000000078160 ) ) ;
#10663 = VECTOR ( 'NONE', #50949, 1000.000000000000000 ) ;
#10664 = CARTESIAN_POINT ( 'NONE',  ( -10.99999999999989164, -4.556349186104158733, 76.28125000409679046 ) ) ;
#10665 = CARTESIAN_POINT ( 'NONE',  ( -7.188101187500002709, 25.68749999795162253, 2.977408999572649151 ) ) ;
#10666 = CARTESIAN_POINT ( 'NONE',  ( 0.000000000000000000, -16.70329308849007077, 0.000000000000000000 ) ) ;
#10667 = AXIS2_PLACEMENT_3D ( 'NONE', #28619, #68985, #51632 ) ;
#10668 = CARTESIAN_POINT ( 'NONE',  ( -6.238412754330611322E-16, 10.18810118749999916, 109.6562500020483668 ) ) ;
#10669 = CARTESIAN_POINT ( 'NONE',  ( 7.999999999999991118, 9.797174393178815797E-16, 6.080302779823364645 ) ) ;
#10670 = CARTESIAN_POINT ( 'NONE',  ( -2.828427124746190735, 9.124999997268814056, -2.828427124746191623 ) ) ;
#10671 = DIRECTION ( 'NONE',  ( -1.734723475976805517E-15, 1.000000000000000000, 0.000000000000000000 ) ) ;
#10672 = VERTEX_POINT ( 'NONE', #19456 ) ;
#10673 = EDGE_CURVE ( 'NONE', #8182, #39667, #41742, .T. ) ;
#10674 = EDGE_CURVE ( 'NONE', #25965, #38243, #8625, .T. ) ;
#10675 = CARTESIAN_POINT ( 'NONE',  ( 2.839093476692135984E-14, 202.6875000013656063, 201.4587341250000350 ) ) ;
#10676 = CARTESIAN_POINT ( 'NONE',  ( -29.43265458321771533, 207.5000000013655779, 166.5412658750003914 ) ) ;
#10677 = LINE ( 'NONE', #17070, #35704 ) ;
#10678 = CARTESIAN_POINT ( 'NONE',  ( 4.541265875000002339, 8.374999998634406140, -1.881053915767121554 ) ) ;
#10679 = CARTESIAN_POINT ( 'NONE',  ( -7.347880794884122694E-16, 10.49999999726881406, 4.000000000000001776 ) ) ;
#10680 = CARTESIAN_POINT ( 'NONE',  ( -7.188101187499991163, 2.977408999572646930, 16.39280278187175455 ) ) ;
#10681 = ORIENTED_EDGE ( 'NONE', *, *, #31191, .T. ) ;
#10682 = CARTESIAN_POINT ( 'NONE',  ( 1.469576158976823947E-15, 104.5625000040967763, 8.000000000000000000 ) ) ;
#10683 = ORIENTED_EDGE ( 'NONE', *, *, #65730, .T. ) ;
#10684 = CARTESIAN_POINT ( 'NONE',  ( -4.220049686691937474, -10.18810118749999738, 109.9375000020483810 ) ) ;
#10685 = CARTESIAN_POINT ( 'NONE',  ( 37.99999999999999289, 50.00000000000000711, 69.99999999999998579 ) ) ;
#10686 = CARTESIAN_POINT ( 'NONE',  ( 2.839093476692135984E-14, 202.6875000013656063, 201.4587341250000350 ) ) ;
#10687 = CARTESIAN_POINT ( 'NONE',  ( 26.56734541678233086, 200.0000000013656063, 166.5412658749999650 ) ) ;
#10688 = CARTESIAN_POINT ( 'NONE',  ( 5.000000000000001776, 80.83333333333334281, -8.660254037844389075 ) ) ;
#10689 = CARTESIAN_POINT ( 'NONE',  ( -5.656854249492380582, 124.8125000000000000, -5.656854249492380582 ) ) ;
#10690 = CARTESIAN_POINT ( 'NONE',  ( 4.242640687119285658, 290.6249999999999432, -4.242640687119286547 ) ) ;
#10691 = EDGE_CURVE ( 'NONE', #9385, #10672, #16387, .T. ) ;
#10692 = CARTESIAN_POINT ( 'NONE',  ( 27.99999999999996803, 206.6250000027312126, 165.9999999999998863 ) ) ;
#10693 = EDGE_LOOP ( 'NONE', ( #2679, #3162, #51756, #2709 ) ) ;
#10694 = CARTESIAN_POINT ( 'NONE',  ( 4.999999999999997335, 253.3333333333333428, -8.660254037844387298 ) ) ;
#10695 = AXIS2_PLACEMENT_3D ( 'NONE', #1826, #49316, #48197 ) ;
#10696 = CARTESIAN_POINT ( 'NONE',  ( 2.828427124746153876, 198.0000000027312126, 144.8284271247462129 ) ) ;
#10697 = CARTESIAN_POINT ( 'NONE',  ( 0.000000000000000000, 300.0000000000000000, 6.000000000000001776 ) ) ;
#10698 = CARTESIAN_POINT ( 'NONE',  ( 3.313708498984720308, 13.59374999590322552, -8.000000000000040856 ) ) ;
#10699 = CARTESIAN_POINT ( 'NONE',  ( -10.00000000000000000, 239.7916666666666288, -2.679491924311226292 ) ) ;
#10700 = CARTESIAN_POINT ( 'NONE',  ( 10.00000000000000178, 205.0000000000000284, 0.000000000000000000 ) ) ;
#10701 = CARTESIAN_POINT ( 'NONE',  ( 5.082755093536320601, -5.082755093536318824, 18.92405278187175455 ) ) ;
#10702 = CARTESIAN_POINT ( 'NONE',  ( -3.042071309553164404, 167.5520833299193271, -11.35316468749999963 ) ) ;
#10703 = CARTESIAN_POINT ( 'NONE',  ( -3.166186134455097228E-13, 211.2500000000000568, -9.999999999999998224 ) ) ;
#10704 = CARTESIAN_POINT ( 'NONE',  ( -2.382792795851246037, -43.16662372679000015, 151.1496796732567702 ) ) ;
#10706 = LINE ( 'NONE', #159, #71232 ) ;
#10705 = CARTESIAN_POINT ( 'NONE',  ( -10.59405059374999958, 0.000000000000000000, 117.7656250010241905 ) ) ;
#10707 = ORIENTED_EDGE ( 'NONE', *, *, #59477, .F. ) ;
#10708 = VECTOR ( 'NONE', #46006, 1000.000000000000000 ) ;
#10709 = CARTESIAN_POINT ( 'NONE',  ( -9.832129032723420536, 24.01041666325268409, 5.676582343749997150 ) ) ;
#10710 = CARTESIAN_POINT ( 'NONE',  ( 2.020667218593132706E-15, -11.00000000000000000, 109.5625000040967763 ) ) ;
#10711 = CARTESIAN_POINT ( 'NONE',  ( 6.123233995736767268E-16, 133.1249999931720254, -10.00000000000000178 ) ) ;
#10712 = DIRECTION ( 'NONE',  ( 0.000000000000000000, 0.000000000000000000, 1.000000000000000000 ) ) ;
#10713 = DIRECTION ( 'NONE',  ( -0.000000000000000000, 1.000000000000000000, -0.000000000000000000 ) ) ;
#10714 = CARTESIAN_POINT ( 'NONE',  ( -2.445694354108839619, 201.8125000013656063, 139.5543056458912190 ) ) ;
#10715 =( BOUNDED_CURVE ( )  B_SPLINE_CURVE ( 2, ( #29633, #23224, #17562, #982, #6993, #46972, #5512, #23594, #47343 ),
 .UNSPECIFIED., .F., .F. ) 
 B_SPLINE_CURVE_WITH_KNOTS ( ( 3, 2, 2, 2, 3 ),
 ( 0.1562500000000001110, 0.1614583333333334536, 0.1666666666666667407, 0.1718750000000000833, 0.1770833333333334259 ),
 .UNSPECIFIED. ) 
 CURVE ( )  GEOMETRIC_REPRESENTATION_ITEM ( )  RATIONAL_B_SPLINE_CURVE ( ( 0.9999999999999983347, 0.9238795325112884038, 1.000000000000000000, 0.9238795325112867385, 1.000000000000000000, 0.9238795325112867385, 1.000000000000000000, 0.9238795325112855172, 1.000000000000001110 ) ) 
 REPRESENTATION_ITEM ( '' )  );
#10716 = AXIS2_PLACEMENT_3D ( 'NONE', #47810, #52383, #718 ) ;
#10717 = CARTESIAN_POINT ( 'NONE',  ( 4.999999999999993783, 66.04166665983871098, 8.660254037844390851 ) ) ;
#10718 = CARTESIAN_POINT ( 'NONE',  ( 7.188101187500001821, 104.0000000020483810, -2.977408999572651371 ) ) ;
#10719 = CARTESIAN_POINT ( 'NONE',  ( -3.211159895383562723, 14.06249999863440614, 3.211159895383561391 ) ) ;
#10720 = CARTESIAN_POINT ( 'NONE',  ( 2.679491924311236506, 63.95833333333336412, 10.00000000000005507 ) ) ;
#10721 = CARTESIAN_POINT ( 'NONE',  ( 7.692636802427458953, 0.1926368024274620616, -0.5153151192473633957 ) ) ;
#10722 = CARTESIAN_POINT ( 'NONE',  ( 7.320508075688774596, 165.6250000000000568, -7.320508075688774596 ) ) ;
#10723 = ORIENTED_EDGE ( 'NONE', *, *, #17685, .T. ) ;
#10724 = EDGE_LOOP ( 'NONE', ( #46469, #32167, #108, #71539 ) ) ;
#10725 = CARTESIAN_POINT ( 'NONE',  ( 5.000000000000000000, -50.64189880742087269, -41.08656465431914029 ) ) ;
#10726 = DIRECTION ( 'NONE',  ( 0.000000000000000000, 0.000000000000000000, 1.000000000000000000 ) ) ;
#10727 = CARTESIAN_POINT ( 'NONE',  ( -11.00000000000000000, 0.000000000000000000, 104.5000000000000000 ) ) ;
#10728 = CARTESIAN_POINT ( 'NONE',  ( -9.832129032723415207, 219.6354166700806445, 5.676582343750005144 ) ) ;
#10729 = CARTESIAN_POINT ( 'NONE',  ( 11.35316468749999963, 135.9895833299193271, -3.042071309553165293 ) ) ;
#10730 = ORIENTED_EDGE ( 'NONE', *, *, #37000, .F. ) ;
#10731 = DIRECTION ( 'NONE',  ( -0.000000000000000000, 1.000000000000000000, 0.000000000000000000 ) ) ;
#10732 = CARTESIAN_POINT ( 'NONE',  ( 10.18810118750000093, -4.220049686691933921, 86.31250000204838102 ) ) ;
#10733 = FACE_OUTER_BOUND ( 'NONE', #48043, .T. ) ;
#10734 = CARTESIAN_POINT ( 'NONE',  ( -1.656854249492347719, 208.8125000000000000, 194.0000000000000853 ) ) ;
#10735 = CARTESIAN_POINT ( 'NONE',  ( 1.656854249492381248, 14.93749999726881406, -4.000000000000001776 ) ) ;
#10736 = LINE ( 'NONE', #69195, #76 ) ;
#10737 = CARTESIAN_POINT ( 'NONE',  ( -4.220049686691935698, 10.18810118749999916, 114.2500000020483952 ) ) ;
#10738 = VERTEX_POINT ( 'NONE', #61694 ) ;
#10739 =( BOUNDED_CURVE ( )  B_SPLINE_CURVE ( 2, ( #41696, #1354, #1720, #30010, #42053, #65060, #986, #13371, #620 ),
 .UNSPECIFIED., .F., .F. ) 
 B_SPLINE_CURVE_WITH_KNOTS ( ( 3, 2, 2, 2, 3 ),
 ( 0.3854166666666665741, 0.3906249999999998890, 0.3958333333333332038, 0.4010416666666665741, 0.4062499999999998890 ),
 .UNSPECIFIED. ) 
 CURVE ( )  GEOMETRIC_REPRESENTATION_ITEM ( )  RATIONAL_B_SPLINE_CURVE ( ( 1.000000000000001554, 0.9238795325112850731, 1.000000000000000000, 0.9238795325112867385, 1.000000000000000000, 0.9238795325112867385, 1.000000000000000000, 0.9238795325112884038, 0.9999999999999983347 ) ) 
 REPRESENTATION_ITEM ( '' )  );
#10740 = CARTESIAN_POINT ( 'NONE',  ( 36.75679849373859298, -4.490207463336263416, 134.7638201841734826 ) ) ;
#10741 = CARTESIAN_POINT ( 'NONE',  ( 21.92274966597144115, 176.8557779607809550, 147.9630726404944880 ) ) ;
#10742 = CARTESIAN_POINT ( 'NONE',  ( 5.676582343750001591, 131.9270833299193555, -9.832129032723420536 ) ) ;
#10743 = CARTESIAN_POINT ( 'NONE',  ( -3.458734124999959914, 203.3750000013656063, 196.5673454167823877 ) ) ;
#10744 = CARTESIAN_POINT ( 'NONE',  ( 5.082755093536324154, 23.15624999795161543, 5.082755093536326818 ) ) ;
#10745 = CARTESIAN_POINT ( 'NONE',  ( -10.18810118749999738, -4.220049686691941915, 81.62500000204836681 ) ) ;
#10746 = CARTESIAN_POINT ( 'NONE',  ( -11.35316468749999785, 33.38541666325269119, -3.042071309553167513 ) ) ;
#10747 = VERTEX_POINT ( 'NONE', #61321 ) ;
#10748 = DIRECTION ( 'NONE',  ( 0.000000000000000000, 0.000000000000000000, 1.000000000000000000 ) ) ;
#10749 = CARTESIAN_POINT ( 'NONE',  ( 3.211159895383560947, 2.312499998634407028, 3.211159895383562723 ) ) ;
#10750 = CARTESIAN_POINT ( 'NONE',  ( 5.662595241051934458, 5.662595241051935346, 18.45061528394063188 ) ) ;
#10751 = CARTESIAN_POINT ( 'NONE',  ( -2.445694354108840063, 208.0625000013656063, 139.5543056458912190 ) ) ;
#10752 = ADVANCED_FACE ( 'NONE', ( #67728 ), #55676, .T. ) ;
#10753 = CARTESIAN_POINT ( 'NONE',  ( 7.188101187499999156, 10.87499999795161187, 2.977408999572654924 ) ) ;
#10754 = CARTESIAN_POINT ( 'NONE',  ( -3.673940397442060854E-16, 296.8125000034140157, -6.000000000000001776 ) ) ;
#10755 = CARTESIAN_POINT ( 'NONE',  ( 6.123233995736767268E-16, 113.1249999931720396, -10.00000000000000178 ) ) ;
#10756 = CARTESIAN_POINT ( 'NONE',  ( 6.951808397369818766E-16, 157.3437499965860127, -11.35316468750000141 ) ) ;
#10757 = CARTESIAN_POINT ( 'NONE',  ( -7.204075437095965206, -7.204075437095968759, 75.34375000204838102 ) ) ;
#10758 = CIRCLE ( 'NONE', #5928, 10.00000000000000178 ) ;
#10759 = CARTESIAN_POINT ( 'NONE',  ( -26.56734541678237704, 196.3750000013656063, 166.5412658750003629 ) ) ;
#10760 = CARTESIAN_POINT ( 'NONE',  ( 11.00000000000007994, 4.556349186103967774, 109.8437500000000000 ) ) ;
#10761 = CARTESIAN_POINT ( 'NONE',  ( 1.881053915767122664, 18.24999999863440792, 4.541265875000001451 ) ) ;
#10762 = ORIENTED_EDGE ( 'NONE', *, *, #67678, .F. ) ;
#10763 = CONICAL_SURFACE ( 'NONE', #27663, 6.000000000000000000, 0.9599310885968792562 ) ;
#10764 = EDGE_CURVE ( 'NONE', #8328, #14438, #2897, .T. ) ;
#10765 = CARTESIAN_POINT ( 'NONE',  ( 1.656854249492403008, 197.8125000027312126, 194.0000000000000853 ) ) ;
#10766 = CARTESIAN_POINT ( 'NONE',  ( 3.458734124999959469, 194.7500000013656063, 140.5673454167824161 ) ) ;
#10767 = CARTESIAN_POINT ( 'NONE',  ( -32.00000000000003553, 206.3125000027312126, 168.3431457505080573 ) ) ;
#10768 = EDGE_CURVE ( 'NONE', #50397, #35571, #4729, .T. ) ;
#10769 = CARTESIAN_POINT ( 'NONE',  ( 2.751064625579944321E-14, 204.8750000027312126, 194.0000000000000568 ) ) ;
#10770 = VERTEX_POINT ( 'NONE', #27347 ) ;
#10771 = CARTESIAN_POINT ( 'NONE',  ( 5.082755093536324154, 16.78124999795161543, 5.082755093536326818 ) ) ;
#10772 = CARTESIAN_POINT ( 'NONE',  ( 1.102182119232618108E-15, 298.3125000034140157, 6.000000000000001776 ) ) ;
#10773 = DIRECTION ( 'NONE',  ( -1.000000000000000000, 0.000000000000000000, 0.000000000000000000 ) ) ;
#10774 = CARTESIAN_POINT ( 'NONE',  ( -4.999999999999998224, 36.66666666666666430, -8.660254037844389075 ) ) ;
#10775 = CARTESIAN_POINT ( 'NONE',  ( -5.082755093536325930, 107.8437500020483810, -5.082755093536325930 ) ) ;
#10776 = CARTESIAN_POINT ( 'NONE',  ( -31.45873412499999944, 207.9375000013656063, 170.0000000000003979 ) ) ;
#10777 = CARTESIAN_POINT ( 'NONE',  ( 6.676582343750001591, 288.9531250017069510, -8.176455196517173205E-16 ) ) ;
#10778 = EDGE_CURVE ( 'NONE', #68055, #40831, #50363, .T. ) ;
#10780 = CARTESIAN_POINT ( 'NONE',  ( 8.660254037844389075, 197.2916666598387110, -5.000000000000000000 ) ) ;
#10779 = CARTESIAN_POINT ( 'NONE',  ( 8.660254037844385522, 35.41666666666665719, -4.999999999999998224 ) ) ;
#10781 = ORIENTED_EDGE ( 'NONE', *, *, #23627, .T. ) ;
#10782 = CARTESIAN_POINT ( 'NONE',  ( 11.35316468749999963, 256.4062500034140157, -1.390361679473963556E-15 ) ) ;
#10783 = PRODUCT_DEFINITION_SHAPE ( 'NONE', 'NONE',  #6285 ) ;
#10784 = CARTESIAN_POINT ( 'NONE',  ( -7.188101187499991163, 2.977408999572646930, 21.26780278187175810 ) ) ;
#10785 = CARTESIAN_POINT ( 'NONE',  ( -3.734423912261892298, 56.16062404875953007, 44.09723116535829490 ) ) ;
#10786 = CARTESIAN_POINT ( 'NONE',  ( -8.224976990608492855, 220.0000000000001421, 7.304091559116764110 ) ) ;
#10787 = CARTESIAN_POINT ( 'NONE',  ( -5.000000000000005329, 148.3333333333333428, 8.660254037844387298 ) ) ;
#10788 = B_SPLINE_CURVE_WITH_KNOTS ( 'NONE', 3,
 ( #55906, #61552, #66453, #14761, #37801, #27206, #60796, #3462, #4217, #9121 ),
 .UNSPECIFIED., .F., .F.,
 ( 4, 2, 2, 2, 4 ),
 ( 8.481999574322108800E-16, 0.0007742087911299071071, 0.001548417582258966151, 0.002322626373388024870, 0.003096835164517084023 ),
 .UNSPECIFIED. ) ;
#10789 = CARTESIAN_POINT ( 'NONE',  ( 1.432654583217662481, 196.3750000013656063, 194.5412658750000219 ) ) ;
#10790 = CARTESIAN_POINT ( 'NONE',  ( -7.320508075688773708, 166.8750000000000284, -7.320508075688774596 ) ) ;
#10791 = CARTESIAN_POINT ( 'NONE',  ( 9.381899668004557213, 15.36796739199404094, 2.518546589542255271E-15 ) ) ;
#10792 = CARTESIAN_POINT ( 'NONE',  ( 5.000000000000000000, -53.55923425356098733, -45.42020841079093429 ) ) ;
#10793 = CARTESIAN_POINT ( 'NONE',  ( 8.311093377946834337, 130.4687499965860127, 8.311093377946839666 ) ) ;
#10794 = DIRECTION ( 'NONE',  ( 0.000000000000000000, 0.02418647091589873691, 0.9997074645238147594 ) ) ;
#10795 = CARTESIAN_POINT ( 'NONE',  ( -5.656854249492381470, 5.437500000000000888, 5.656854249492379694 ) ) ;
#10798 = CARTESIAN_POINT ( 'NONE',  ( 3.313708498984711426, 118.1562500040967905, 8.000000000000053291 ) ) ;
#10797 = CARTESIAN_POINT ( 'NONE',  ( 25.55430564589118703, 195.3125000013656063, 172.4456943541087526 ) ) ;
#10796 = CARTESIAN_POINT ( 'NONE',  ( 25.55430564589119058, 196.3125000013656063, 167.5543056458910485 ) ) ;
#10799 = EDGE_LOOP ( 'NONE', ( #71111, #39489, #16601, #30567 ) ) ;
#10800 = ADVANCED_FACE ( 'NONE', ( #44713 ), #60189, .F. ) ;
#10801 = CARTESIAN_POINT ( 'NONE',  ( -8.000000000000000000, 20.25000000000000355, -9.797174393178825657E-16 ) ) ;
#10802 = DIRECTION ( 'NONE',  ( -0.000000000000000000, -1.000000000000000000, -0.000000000000000000 ) ) ;
#10803 = DIRECTION ( 'NONE',  ( -1.000000000000000000, 0.000000000000000000, 0.000000000000000000 ) ) ;
#10804 = CARTESIAN_POINT ( 'NONE',  ( 31.45873412499999944, 200.0000000013656347, 168.5673454167822740 ) ) ;
#10805 = AXIS2_PLACEMENT_3D ( 'NONE', #55254, #38267, #61271 ) ;
#10806 = EDGE_CURVE ( 'NONE', #46685, #1819, #46395, .T. ) ;
#10807 = CARTESIAN_POINT ( 'NONE',  ( -11.35316468750000141, 208.5937499965860411, -1.390361679473963753E-15 ) ) ;
#10808 = CARTESIAN_POINT ( 'NONE',  ( -7.188101187500000044, 121.1562500020483810, 0.000000000000000000 ) ) ;
#10809 = CARTESIAN_POINT ( 'NONE',  ( 3.211159895383560947, 19.18749999863440436, 3.211159895383562723 ) ) ;
#10810 = CARTESIAN_POINT ( 'NONE',  ( 31.45873412499999944, 196.0000000013656063, 168.5673454167822740 ) ) ;
#10811 = CARTESIAN_POINT ( 'NONE',  ( 3.313708498984762496, -7.999999999999989342, 22.29905277982336287 ) ) ;
#10812 = CARTESIAN_POINT ( 'NONE',  ( -5.656854249492379694, 12.56250000000000178, -5.656854249492380582 ) ) ;
#10813 = CARTESIAN_POINT ( 'NONE',  ( -5.676582343750006032, 94.11458332991935549, 9.832129032723418760 ) ) ;
#10814 = ORIENTED_EDGE ( 'NONE', *, *, #35420, .T. ) ;
#10815 = DIRECTION ( 'NONE',  ( -0.000000000000000000, 1.000000000000000000, -0.000000000000000000 ) ) ;
#10816 = CARTESIAN_POINT ( 'NONE',  ( 7.188101187500000044, 25.96874999795161543, 0.000000000000000000 ) ) ;
#10817 = CARTESIAN_POINT ( 'NONE',  ( 5.656854249492376141, -5.656854249492374365, 8.892802779823364645 ) ) ;
#10818 = CARTESIAN_POINT ( 'NONE',  ( 11.35316468749999963, 251.7187500034139873, -1.390361679473963556E-15 ) ) ;
#10819 = CARTESIAN_POINT ( 'NONE',  ( -9.832129032723420536, 103.6979166632526841, 5.676582343749997150 ) ) ;
#10820 = VERTEX_POINT ( 'NONE', #24491 ) ;
#10821 = DIRECTION ( 'NONE',  ( -0.5000000000000012212, 0.8660254037844380415, 0.000000000000000000 ) ) ;
#10822 = VECTOR ( 'NONE', #29196, 1000.000000000000000 ) ;
#10823 = CARTESIAN_POINT ( 'NONE',  ( 7.204075437095968759, -7.204075437095966983, 108.7187500020483810 ) ) ;
#10824 = CARTESIAN_POINT ( 'NONE',  ( -8.660254037844387298, 223.9583333265053966, -5.000000000000004441 ) ) ;
#10825 = CARTESIAN_POINT ( 'NONE',  ( 3.458734125000016757, 205.1250000013656347, 199.4326545832176691 ) ) ;
#10826 = CARTESIAN_POINT ( 'NONE',  ( 3.313708498984762496, -7.999999999999989342, 11.79905277982336465 ) ) ;
#10828 = CARTESIAN_POINT ( 'NONE',  ( -5.676582343750006032, 94.11458332991935549, 9.832129032723418760 ) ) ;
#10827 = DIRECTION ( 'NONE',  ( -1.000000000000000000, 0.000000000000000000, -0.000000000000000000 ) ) ;
#10829 = CARTESIAN_POINT ( 'NONE',  ( 7.999999999999991118, 9.797174393178815797E-16, 15.26780278392014623 ) ) ;
#10830 = CARTESIAN_POINT ( 'NONE',  ( -29.43265458321766559, 200.7500000013656347, 166.5412658750003629 ) ) ;
#10831 = CARTESIAN_POINT ( 'NONE',  ( -5.656854249492379694, 27.37499999590322375, -5.656854249492380582 ) ) ;
#10832 = ORIENTED_EDGE ( 'NONE', *, *, #49430, .T. ) ;
#10833 = CARTESIAN_POINT ( 'NONE',  ( 2.679491924311228956, 177.9166666598387110, -10.00000000000000000 ) ) ;
#10834 = CARTESIAN_POINT ( 'NONE',  ( -1.469576158976823947E-15, 4.125000000000000888, 8.000000000000000000 ) ) ;
#10835 = CARTESIAN_POINT ( 'NONE',  ( 1.102182119232618108E-15, 296.3125000034140157, 6.000000000000001776 ) ) ;
#10836 = CARTESIAN_POINT ( 'NONE',  ( -11.35316468750000141, 78.59374999658601268, -1.390361679473963753E-15 ) ) ;
#10837 = CARTESIAN_POINT ( 'NONE',  ( -2.765530957081996810, 288.2656250017069510, -6.676582343750003368 ) ) ;
#10838 = CARTESIAN_POINT ( 'NONE',  ( -7.188101187500000933, 4.499999997951610098, -2.977408999572651371 ) ) ;
#10839 =( BOUNDED_CURVE ( )  B_SPLINE_CURVE ( 2, ( #64962, #46882, #29170, #30276, #1254, #52185, #17841, #18217, #57855, #887, #58589, #6895, #18585 ),
 .UNSPECIFIED., .F., .F. ) 
 B_SPLINE_CURVE_WITH_KNOTS ( ( 3, 2, 2, 2, 2, 2, 3 ),
 ( 1.051889995858769966, 1.057123116408781094, 1.062356236958792222, 1.067589357508803127, 1.072822478058814255, 1.078055598608825383, 1.083288719158836511 ),
 .UNSPECIFIED. ) 
 CURVE ( )  GEOMETRIC_REPRESENTATION_ITEM ( )  RATIONAL_B_SPLINE_CURVE ( ( 1.000000000000000000, 0.9659258262890683122, 1.000000000000000000, 0.9659258262890683122, 1.000000000000000000, 0.9659258262890683122, 1.000000000000000000, 0.9659258262890683122, 1.000000000000000000, 0.9659258262890683122, 1.000000000000000000, 0.9659258262890578761, 1.000000000000010436 ) ) 
 REPRESENTATION_ITEM ( '' )  );
#10840 = CARTESIAN_POINT ( 'NONE',  ( 10.18810118749999916, 4.220049686691935698, 98.87500000204838102 ) ) ;
#10841 = CARTESIAN_POINT ( 'NONE',  ( 9.832129032723416984, 220.3645833299193839, 5.676582343750006032 ) ) ;
#10842 = ORIENTED_EDGE ( 'NONE', *, *, #39892, .T. ) ;
#10843 = CARTESIAN_POINT ( 'NONE',  ( 6.123233995736767268E-16, 68.12499999317203958, -10.00000000000000178 ) ) ;
#10844 = CARTESIAN_POINT ( 'NONE',  ( -4.898587196589412829E-16, 115.8125000040967763, -8.000000000000000000 ) ) ;
#10845 = CARTESIAN_POINT ( 'NONE',  ( 2.485281374238247132, 291.6874999999999432, -6.000000000000325961 ) ) ;
#10846 = CARTESIAN_POINT ( 'NONE',  ( 5.676582343750001591, 211.6145833299193555, -9.832129032723420536 ) ) ;
#10847 = CARTESIAN_POINT ( 'NONE',  ( 7.320508075688776373, 230.0000000068279178, 7.320508075688767491 ) ) ;
#10848 = CARTESIAN_POINT ( 'NONE',  ( 6.123233995736767268E-16, 98.12499999317203958, -10.00000000000000178 ) ) ;
#10849 = CARTESIAN_POINT ( 'NONE',  ( 4.721056650416000089, 296.8281250017069510, 4.721056650415999201 ) ) ;
#10850 = ORIENTED_EDGE ( 'NONE', *, *, #9343, .F. ) ;
#10851 = CARTESIAN_POINT ( 'NONE',  ( -9.832129032723418760, 193.1770833299193555, -5.676582343750004256 ) ) ;
#10852 = EDGE_CURVE ( 'NONE', #57316, #46585, #67911, .T. ) ;
#10853 = CARTESIAN_POINT ( 'NONE',  ( -28.00000000000002132, 205.4375000013656063, 166.5412658750003629 ) ) ;
#10854 = CARTESIAN_POINT ( 'NONE',  ( -3.313708498984760720, 15.46875000000000533, -8.000000000000000000 ) ) ;
#10855 = ORIENTED_EDGE ( 'NONE', *, *, #69600, .T. ) ;
#10856 = CARTESIAN_POINT ( 'NONE',  ( -3.313708498984762052, 91.90625000409677625, -8.000000000000000000 ) ) ;
#10857 = SURFACE_SIDE_STYLE ('',( #45188 ) ) ;
#10858 = CARTESIAN_POINT ( 'NONE',  ( 8.660254037844389075, 20.41666666666666785, -5.000000000000000000 ) ) ;
#10859 = ADVANCED_FACE ( 'NONE', ( #13156 ), #64119, .T. ) ;
#10860 = CONICAL_SURFACE ( 'NONE', #25271, 8.999999999999998224, 1.047197551196595855 ) ;
#10861 = CARTESIAN_POINT ( 'NONE',  ( -10.18810118749999738, -4.220049686691941915, 78.62500000204838102 ) ) ;
#10862 = VERTEX_POINT ( 'NONE', #58473 ) ;
#10863 = CARTESIAN_POINT ( 'NONE',  ( 2.828427124746190291, 18.87500000000000000, 2.828427124746192067 ) ) ;
#10864 = CARTESIAN_POINT ( 'NONE',  ( -4.541265875000002339, 21.81249999863440792, -5.561446717895856393E-16 ) ) ;
#10865 = PRODUCT_RELATED_PRODUCT_CATEGORY ( 'part', '', ( #15569 ) ) ;
#10866 = CARTESIAN_POINT ( 'NONE',  ( 29.96114510722324198, 194.5054840307575148, 172.9142663285536230 ) ) ;
#10867 = CIRCLE ( 'NONE', #49424, 10.19999999999999396 ) ;
#10868 = CARTESIAN_POINT ( 'NONE',  ( 1.656854249492388576, 4.562499997268813168, 3.999999999999994671 ) ) ;
#10869 = CARTESIAN_POINT ( 'NONE',  ( -4.999999999999999112, -15.47455834364811622, 69.96446835377025764 ) ) ;
#10870 = LINE ( 'NONE', #69328, #6441 ) ;
#10873 = CARTESIAN_POINT ( 'NONE',  ( 9.797174393178825657E-16, 125.0000000000000000, -8.000000000000000000 ) ) ;
#10872 = CARTESIAN_POINT ( 'NONE',  ( -11.35316468749999963, 243.9062500034140157, 0.000000000000000000 ) ) ;
#10871 = CARTESIAN_POINT ( 'NONE',  ( 24.54126587499999701, 208.1875000013656063, 169.9999999999999432 ) ) ;
#10874 = SHAPE_DEFINITION_REPRESENTATION ( #43243, #64301 ) ;
#10875 = ORIENTED_EDGE ( 'NONE', *, *, #36995, .F. ) ;
#10876 = EDGE_CURVE ( 'NONE', #60165, #12530, #11061, .T. ) ;
#10877 = CARTESIAN_POINT ( 'NONE',  ( -11.35316468749999785, 249.0104166700806445, -3.042071309553164848 ) ) ;
#10878 = CARTESIAN_POINT ( 'NONE',  ( 7.188101187499992051, 8.802885111219154394E-16, 11.23655278187175455 ) ) ;
#10879 = ORIENTED_EDGE ( 'NONE', *, *, #32204, .T. ) ;
#10880 = EDGE_CURVE ( 'NONE', #34923, #24630, #47127, .T. ) ;
#10881 = ORIENTED_EDGE ( 'NONE', *, *, #51498, .F. ) ;
#10882 = CARTESIAN_POINT ( 'NONE',  ( 10.18810118749999916, 4.220049686691935698, 73.00000000204836681 ) ) ;
#10883 = CARTESIAN_POINT ( 'NONE',  ( -11.35316468749999785, 93.38541666325269830, -3.042071309553167513 ) ) ;
#10884 = CARTESIAN_POINT ( 'NONE',  ( 1.469576158976822172E-15, -7.999999999999991118, 23.89280278392014978 ) ) ;
#10885 = CARTESIAN_POINT ( 'NONE',  ( -4.556349186104045934, 11.00000000000000000, 90.71874999999998579 ) ) ;
#10888 = CARTESIAN_POINT ( 'NONE',  ( -6.676582343750002480, 290.5468750017070647, -2.765530957081996810 ) ) ;
#10887 = CARTESIAN_POINT ( 'NONE',  ( 27.99999999999996092, 194.6250000027311842, 165.9999999999998863 ) ) ;
#10886 = CARTESIAN_POINT ( 'NONE',  ( 31.45873412499999944, 206.9375000013656063, 169.9999999999999432 ) ) ;
#10889 = CARTESIAN_POINT ( 'NONE',  ( -51.66389186761343666, 201.9365919821820228, 54.51100076282494200 ) ) ;
#10890 = LINE ( 'NONE', #9779, #46780 ) ;
#10891 = VECTOR ( 'NONE', #12264, 1000.000000000000000 ) ;
#10892 = CARTESIAN_POINT ( 'NONE',  ( 11.35316468750000141, 200.7812499965860411, 0.000000000000000000 ) ) ;
#10893 = CARTESIAN_POINT ( 'NONE',  ( 8.000000000000000000, 11.81249999590322197, 0.000000000000000000 ) ) ;
#10894 = VERTEX_POINT ( 'NONE', #52066 ) ;
#10895 = CARTESIAN_POINT ( 'NONE',  ( 31.45873412499999944, 208.9375000013656063, 169.9999999999999432 ) ) ;
#10896 = CARTESIAN_POINT ( 'NONE',  ( -7.188101187500002709, 16.68749999795161543, 2.977408999572649151 ) ) ;
#10897 = CARTESIAN_POINT ( 'NONE',  ( 11.35316468749999963, 161.3020833299193555, -3.042071309553165293 ) ) ;
#10898 = CARTESIAN_POINT ( 'NONE',  ( 28.00000000000002132, 198.1250000027312126, 173.9999999999999147 ) ) ;
#10899 = CARTESIAN_POINT ( 'NONE',  ( 7.188101187500000933, 101.3750000020483952, -2.977408999572651371 ) ) ;
#10901 = CARTESIAN_POINT ( 'NONE',  ( -5.000000000000001776, 113.3333333333333286, 8.660254037844381969 ) ) ;
#10900 = CARTESIAN_POINT ( 'NONE',  ( 3.178432602446558121E-13, 206.2500000000000000, -10.00000000000000533 ) ) ;
#10902 = CARTESIAN_POINT ( 'NONE',  ( 25.55430564589115150, 205.5625000013656063, 172.4456943541086957 ) ) ;
#10903 = CARTESIAN_POINT ( 'NONE',  ( 2.977408999572650927, -7.188101187499990274, 8.330302781871752771 ) ) ;
#10904 = CARTESIAN_POINT ( 'NONE',  ( 9.832129032723416984, 55.36458332991934839, 5.676582343750006032 ) ) ;
#10905 = EDGE_CURVE ( 'NONE', #68143, #1009, #6230, .T. ) ;
#10906 = CARTESIAN_POINT ( 'NONE',  ( -6.000000000000000000, 7.347880794884119736E-16, 0.000000000000000000 ) ) ;
#10907 = CARTESIAN_POINT ( 'NONE',  ( 7.999999999999991118, 9.797174393178815797E-16, 1.636552784329821097 ) ) ;
#10908 = VERTEX_POINT ( 'NONE', #54661 ) ;
#10909 = CARTESIAN_POINT ( 'NONE',  ( -11.00000000000000000, 0.000000000000000000, 74.49999999999998579 ) ) ;
#10910 = CARTESIAN_POINT ( 'NONE',  ( -7.778174593052023411, 7.778174593052023411, 80.50000000409676204 ) ) ;
#10911 = CARTESIAN_POINT ( 'NONE',  ( -9.832129032723418760, 57.86458332991935549, -5.676582343750004256 ) ) ;
#10912 = CARTESIAN_POINT ( 'NONE',  ( 11.00000000000000000, 1.347111479062088405E-15, 72.43750000409676204 ) ) ;
#10913 = CARTESIAN_POINT ( 'NONE',  ( -1.432654583217662481, 200.3750000013656063, 145.4587341250000350 ) ) ;
#10914 = CARTESIAN_POINT ( 'NONE',  ( -4.850062511589670794E-16, 124.5792468245269475, -7.920753175473082663 ) ) ;
#10915 = CARTESIAN_POINT ( 'NONE',  ( -7.347880794884122694E-16, 1.499999997268813168, 4.000000000000001776 ) ) ;
#10917 = CARTESIAN_POINT ( 'NONE',  ( 11.35316468750000141, 45.78124999658601979, 0.000000000000000000 ) ) ;
#10916 = CARTESIAN_POINT ( 'NONE',  ( -5.082755093536324154, 94.34375000204838102, 5.082755093536326818 ) ) ;
#10918 = CARTESIAN_POINT ( 'NONE',  ( -9.121419926064122663, -1.666886344965055722, 0.8643199637478004016 ) ) ;
#10919 = CARTESIAN_POINT ( 'NONE',  ( -7.778174593052023411, 7.778174593052023411, 98.50000000409677625 ) ) ;
#10920 = CARTESIAN_POINT ( 'NONE',  ( -5.676582343749998039, 172.4479166632526983, -9.832129032723420536 ) ) ;
#10921 = CARTESIAN_POINT ( 'NONE',  ( -2.679491924311225848, 138.3333333265053966, -10.00000000000000178 ) ) ;
#10922 = CARTESIAN_POINT ( 'NONE',  ( 1.320432766682874540E-15, 100.9062500020483810, 7.188101187500000044 ) ) ;
#10923 = CARTESIAN_POINT ( 'NONE',  ( 2.775557559380704872E-14, -48.00000000000001421, 139.0000000000000568 ) ) ;
#10924 = CARTESIAN_POINT ( 'NONE',  ( 9.832129032723420536, 41.51041666325268409, -5.676582343749999815 ) ) ;
#10925 = DIRECTION ( 'NONE',  ( -0.000000000000000000, 1.000000000000000000, -0.000000000000000000 ) ) ;
#10926 = CARTESIAN_POINT ( 'NONE',  ( 8.311093377946834337, 180.1562499965859843, 8.311093377946839666 ) ) ;
#10927 = ORIENTED_EDGE ( 'NONE', *, *, #7464, .F. ) ;
#10928 = CARTESIAN_POINT ( 'NONE',  ( 5.099999999999999645, 0.000000000000000000, -10.80000000000000071 ) ) ;
#10929 = CARTESIAN_POINT ( 'NONE',  ( -6.238412754330611322E-16, 10.18810118749999916, 68.78125000204838102 ) ) ;
#10930 = CARTESIAN_POINT ( 'NONE',  ( -2.828427124746153876, 195.8750000000000284, 195.1715728752538439 ) ) ;
#10931 = CARTESIAN_POINT ( 'NONE',  ( 5.656854249492378806, 16.31250000000000355, 5.656854249492381470 ) ) ;
#10933 = CARTESIAN_POINT ( 'NONE',  ( -8.311093377946841443, 163.9062499965859843, 8.311093377946834337 ) ) ;
#10932 = CARTESIAN_POINT ( 'NONE',  ( -1.999122618766013604, 194.9741652105598746, 194.5555752659067252 ) ) ;
#10934 = CARTESIAN_POINT ( 'NONE',  ( 7.999999999999991118, 9.797174393178815797E-16, 4.636552784329823318 ) ) ;
#10935 = EDGE_CURVE ( 'NONE', #471, #22871, #60682, .T. ) ;
#10936 = CARTESIAN_POINT ( 'NONE',  ( -1.469576158976823947E-15, 8.625000000000000000, 8.000000000000000000 ) ) ;
#10937 = AXIS2_PLACEMENT_3D ( 'NONE', #14161, #42471, #54185 ) ;
#10938 = CARTESIAN_POINT ( 'NONE',  ( 5.676582343750005144, 225.5729166700806729, 9.832129032723416984 ) ) ;
#10939 = FACE_OUTER_BOUND ( 'NONE', #60914, .T. ) ;
#10940 = AXIS2_PLACEMENT_3D ( 'NONE', #4057, #67044, #2925 ) ;
#10941 = CARTESIAN_POINT ( 'NONE',  ( -6.238412754330611322E-16, 10.18810118749999916, 82.65625000204838102 ) ) ;
#10942 = VERTEX_POINT ( 'NONE', #26718 ) ;
#10943 = EDGE_CURVE ( 'NONE', #63554, #71456, #20300, .T. ) ;
#10944 = CARTESIAN_POINT ( 'NONE',  ( -1.656854249492280440, 203.9375000027312126, 194.0000000000000284 ) ) ;
#10945 = CARTESIAN_POINT ( 'NONE',  ( 5.676582343750001591, 116.9270833299193555, -9.832129032723420536 ) ) ;
#10946 = EDGE_CURVE ( 'NONE', #29054, #51609, #950, .T. ) ;
#10947 = CARTESIAN_POINT ( 'NONE',  ( 8.660254037844389075, 12.29166665983870033, -5.000000000000000000 ) ) ;
#10948 = ORIENTED_EDGE ( 'NONE', *, *, #21868, .T. ) ;
#10949 = CARTESIAN_POINT ( 'NONE',  ( 2.780723358947928197E-16, 9.687499998634406140, -4.541265875000002339 ) ) ;
#10950 = CARTESIAN_POINT ( 'NONE',  ( -2.977408999572654480, 13.49999999795161187, 7.188101187499999156 ) ) ;
#10951 = CARTESIAN_POINT ( 'NONE',  ( -5.656854249492380582, 110.0000000040967763, -5.656854249492380582 ) ) ;
#10952 = CONICAL_SURFACE ( 'NONE', #67550, 7.949999999999993960, 0.04496966185232758456 ) ;
#10953 =( BOUNDED_CURVE ( )  B_SPLINE_CURVE ( 2, ( #49896, #55200, #27248, #66878, #26494, #56309, #38213, #61218, #38954 ),
 .UNSPECIFIED., .F., .F. ) 
 B_SPLINE_CURVE_WITH_KNOTS ( ( 3, 2, 2, 2, 3 ),
 ( 0.7166666666666671182, 0.7250000000000005329, 0.7333333333333338366, 0.7416666666666673624, 0.7500000000000006661 ),
 .UNSPECIFIED. ) 
 CURVE ( )  GEOMETRIC_REPRESENTATION_ITEM ( )  RATIONAL_B_SPLINE_CURVE ( ( 0.9999999999999958922, 0.9238795325112908463, 1.000000000000000000, 0.9238795325112867385, 1.000000000000000000, 0.9238795325112867385, 1.000000000000000000, 0.9238795325112806323, 1.000000000000005995 ) ) 
 REPRESENTATION_ITEM ( '' )  );
#10954 = CARTESIAN_POINT ( 'NONE',  ( -30.44569435410879166, 198.0625000013656063, 172.4456943541092357 ) ) ;
#10955 = EDGE_CURVE ( 'NONE', #41098, #18106, #49622, .T. ) ;
#10956 = CARTESIAN_POINT ( 'NONE',  ( 1.656854249492381914, 7.812500000000000000, 4.000000000000000888 ) ) ;
#10957 = CARTESIAN_POINT ( 'NONE',  ( 4.000000000000001776, 20.74999999726881583, 0.000000000000000000 ) ) ;
#10958 = CARTESIAN_POINT ( 'NONE',  ( -1.881053915767124440, 5.999999998634406140, 4.541265875000001451 ) ) ;
#10959 = CARTESIAN_POINT ( 'NONE',  ( 2.828427124746153876, 197.8750000000000284, 144.8284271247462129 ) ) ;
#10960 = ORIENTED_EDGE ( 'NONE', *, *, #11791, .F. ) ;
#10961 = CARTESIAN_POINT ( 'NONE',  ( 7.320508075688771044, 223.1250000000000284, -7.320508075688771932 ) ) ;
#10962 = CARTESIAN_POINT ( 'NONE',  ( 2.977408999572650039, 102.6875000020483810, -7.188101187500001821 ) ) ;
#10964 = CARTESIAN_POINT ( 'NONE',  ( 4.242640687119285658, 293.6249999999999432, -4.242640687119286547 ) ) ;
#10963 = CARTESIAN_POINT ( 'NONE',  ( 38.00000000000000000, 1.110223024625156540E-13, 2.626867384171069243E-14 ) ) ;
#10965 = CARTESIAN_POINT ( 'NONE',  ( -5.126106709314341536, 16.23426604260439632, -69.90716554747308464 ) ) ;
#10966 = CARTESIAN_POINT ( 'NONE',  ( -2.977408999572648707, -7.188101187499990274, 1.767802781871753881 ) ) ;
#10967 = ORIENTED_EDGE ( 'NONE', *, *, #30430, .T. ) ;
#10968 = EDGE_CURVE ( 'NONE', #37658, #67176, #8247, .T. ) ;
#10969 = ORIENTED_EDGE ( 'NONE', *, *, #59737, .F. ) ;
#10970 = CARTESIAN_POINT ( 'NONE',  ( 10.18810118749999916, 4.220049686691935698, 92.50000000204838102 ) ) ;
#10971 = CARTESIAN_POINT ( 'NONE',  ( 5.656854249492381470, 91.25000000409677625, 5.656854249492379694 ) ) ;
#10972 = CARTESIAN_POINT ( 'NONE',  ( -29.43265458321766914, 198.7500000013656063, 166.5412658750003629 ) ) ;
#10973 = CARTESIAN_POINT ( 'NONE',  ( -4.556349186104047710, -10.99999999999999822, 107.7812500000000000 ) ) ;
#10974 = CARTESIAN_POINT ( 'NONE',  ( 2.445694354108840063, 205.0625000013656063, 200.4456943541088663 ) ) ;
#10976 = DIRECTION ( 'NONE',  ( -1.084202172485504434E-16, 1.000000000000000000, 0.000000000000000000 ) ) ;
#10975 = CARTESIAN_POINT ( 'NONE',  ( -4.242640687119285658, 290.1875000034139589, 4.242640687119287435 ) ) ;
#10977 = CARTESIAN_POINT ( 'NONE',  ( -2.679491924311235618, 118.5416666666666572, 10.00000000000000000 ) ) ;
#10978 = CARTESIAN_POINT ( 'NONE',  ( -8.000000000000000000, 108.5000000000000000, 0.000000000000000000 ) ) ;
#10979 = CARTESIAN_POINT ( 'NONE',  ( -2.765530957081998586, 287.7968750017070079, 6.676582343750001591 ) ) ;
#10980 = VECTOR ( 'NONE', #33478, 1000.000000000000000 ) ;
#10981 = CARTESIAN_POINT ( 'NONE',  ( -7.188101187499990274, -2.977408999572651371, 7.955302781871752771 ) ) ;
#10982 = CARTESIAN_POINT ( 'NONE',  ( -2.849036369511732440E-14, 196.2500000000000000, 138.0000000000000568 ) ) ;
#10983 = CARTESIAN_POINT ( 'NONE',  ( 29.43265458321766559, 207.8750000013656063, 166.5412658749999650 ) ) ;
#10984 = CARTESIAN_POINT ( 'NONE',  ( 5.656854249492380582, 26.99999999590322375, -5.656854249492380582 ) ) ;
#10985 = AXIS2_PLACEMENT_3D ( 'NONE', #73653, #61959, #39330 ) ;
#10986 = CARTESIAN_POINT ( 'NONE',  ( 3.458734124999959914, 200.3750000013656063, 143.4326545832176976 ) ) ;
#10987 = CARTESIAN_POINT ( 'NONE',  ( -7.188101187499999156, 120.1250000020484094, 2.977408999572654924 ) ) ;
#10989 = CARTESIAN_POINT ( 'NONE',  ( -1.432654583217662481, 201.3750000013656347, 145.4587341250000634 ) ) ;
#10988 = CARTESIAN_POINT ( 'NONE',  ( 28.00000000000001776, 195.1250000027311842, 173.9999999999999147 ) ) ;
#10990 = CARTESIAN_POINT ( 'NONE',  ( 5.676582343750005144, 240.8854166700806445, 9.832129032723416984 ) ) ;
#10991 = CARTESIAN_POINT ( 'NONE',  ( -7.778174593052023411, 7.778174593052023411, 86.31249999999998579 ) ) ;
#10992 = CARTESIAN_POINT ( 'NONE',  ( 31.99999999999997868, 197.1875000000000284, 171.6568542494923122 ) ) ;
#10993 = CARTESIAN_POINT ( 'NONE',  ( 11.35316468749999785, 20.57291666325268409, 3.042071309553174174 ) ) ;
#10994 = CARTESIAN_POINT ( 'NONE',  ( 0.000000000000000000, 300.0000000000000000, 0.000000000000000000 ) ) ;
#10995 = CARTESIAN_POINT ( 'NONE',  ( -9.832129032723418760, 203.1770833299193555, -5.676582343750004256 ) ) ;
#10996 = CARTESIAN_POINT ( 'NONE',  ( 0.000000000000000000, 130.3999865490244190, 45.94057108883949070 ) ) ;
#10997 = DIRECTION ( 'NONE',  ( 0.000000000000000000, 0.000000000000000000, 1.000000000000000000 ) ) ;
#10999 = DIRECTION ( 'NONE',  ( 0.000000000000000000, 0.000000000000000000, -1.000000000000000000 ) ) ;
#10998 = CARTESIAN_POINT ( 'NONE',  ( -26.34314575050761320, 205.5624999999999716, 174.0000000000003411 ) ) ;
#11000 = AXIS2_PLACEMENT_3D ( 'NONE', #18691, #47711, #36780 ) ;
#11001 = EDGE_LOOP ( 'NONE', ( #18035, #39176 ) ) ;
#11002 = CARTESIAN_POINT ( 'NONE',  ( 3.458734124999960358, 198.6250000013655779, 143.4326545832176976 ) ) ;
#11003 = CARTESIAN_POINT ( 'NONE',  ( 11.35316468749999963, 15.98958332991934839, -3.042071309553165293 ) ) ;
#11004 = CARTESIAN_POINT ( 'NONE',  ( -4.556349186104045934, 11.00000000000000000, 95.40625000409677625 ) ) ;
#11005 = CARTESIAN_POINT ( 'NONE',  ( 6.000000000000001776, 292.5000000000000000, -7.347880794884121708E-16 ) ) ;
#11006 = CARTESIAN_POINT ( 'NONE',  ( -24.54126587499995793, 196.1250000013656063, 171.4326545832179534 ) ) ;
#11007 = CARTESIAN_POINT ( 'NONE',  ( -8.999999999999998224, 0.000000000000000000, 0.000000000000000000 ) ) ;
#11009 = CARTESIAN_POINT ( 'NONE',  ( 11.35316468750000141, 5.781249996586016238, 0.000000000000000000 ) ) ;
#11008 = CARTESIAN_POINT ( 'NONE',  ( 7.188101187500002709, 114.3125000020483668, 2.977408999572649151 ) ) ;
#11010 = CARTESIAN_POINT ( 'NONE',  ( -7.999999999999989342, -3.313708498984762496, 20.42405277982336642 ) ) ;
#11011 = CARTESIAN_POINT ( 'NONE',  ( 11.35316468749999785, 130.5729166632526983, 3.042071309553174174 ) ) ;
#11012 = EDGE_CURVE ( 'NONE', #63081, #64865, #72775, .T. ) ;
#11013 = B_SPLINE_CURVE_WITH_KNOTS ( 'NONE', 3,
 ( #47648, #59000, #46550, #53331, #35613, #64277, #25000, #64647, #65376, #12945 ),
 .UNSPECIFIED., .F., .F.,
 ( 4, 2, 2, 2, 4 ),
 ( 0.01051554819734978365, 0.01182504667393343735, 0.01313454515051709279, 0.01575354210368439672, 0.02099153601001901154 ),
 .UNSPECIFIED. ) ;
#11014 = CARTESIAN_POINT ( 'NONE',  ( 7.320508075688771044, 96.24999999317202537, 7.320508075688775484 ) ) ;
#11015 = CARTESIAN_POINT ( 'NONE',  ( -2.977408999572651815, 120.3125000020483668, 7.188101187500000933 ) ) ;
#11016 = CARTESIAN_POINT ( 'NONE',  ( 0.8721677472516105034, 67.61512445009731209, -20.05250736213323748 ) ) ;
#11017 = CARTESIAN_POINT ( 'NONE',  ( -31.45873412500001010, 208.8750000013656347, 168.5673454167827572 ) ) ;
#11018 = CARTESIAN_POINT ( 'NONE',  ( 7.999999999999991118, 9.797174393178815797E-16, 0.2678027839201451155 ) ) ;
#11019 = VERTEX_POINT ( 'NONE', #71610 ) ;
#11020 = CARTESIAN_POINT ( 'NONE',  ( -7.320508075688777261, 116.8750000000000000, -7.320508075688778149 ) ) ;
#11021 = LINE ( 'NONE', #57425, #32972 ) ;
#11022 = CARTESIAN_POINT ( 'NONE',  ( -2.765530957081998586, 290.7968750017069510, 6.676582343750001591 ) ) ;
#11023 = SURFACE_STYLE_FILL_AREA ( #50255 ) ;
#11024 = CARTESIAN_POINT ( 'NONE',  ( 7.999999999999991118, 9.797174393178815797E-16, 21.13655278432982243 ) ) ;
#11025 = AXIS2_PLACEMENT_3D ( 'NONE', #73555, #20749, #66779 ) ;
#11026 = CARTESIAN_POINT ( 'NONE',  ( 7.320508075688771044, 226.2500000068279746, -7.320508075688771932 ) ) ;
#11027 = CARTESIAN_POINT ( 'NONE',  ( -11.35316468749999608, 259.1145833367473301, 3.042071309553173730 ) ) ;
#11028 = CARTESIAN_POINT ( 'NONE',  ( 10.18810118750000093, -4.220049686691933921, 100.1875000020483668 ) ) ;
#11029 = VERTEX_POINT ( 'NONE', #21058 ) ;
#11030 = ADVANCED_FACE ( 'NONE', ( #44082 ), #67093, .F. ) ;
#11031 = CARTESIAN_POINT ( 'NONE',  ( 5.000000000000000888, 11.44657803507906024, 68.01244171956641082 ) ) ;
#11032 = CARTESIAN_POINT ( 'NONE',  ( 8.000000000000001776, 3.313708498984747397, 24.17405277982336997 ) ) ;
#11033 = CARTESIAN_POINT ( 'NONE',  ( -1.432654583217607414, 203.5000000013655779, 194.5412658750000219 ) ) ;
#11034 = CARTESIAN_POINT ( 'NONE',  ( -5.676582343749998039, 82.76041666325268409, -9.832129032723420536 ) ) ;
#11035 = ORIENTED_EDGE ( 'NONE', *, *, #33182, .T. ) ;
#11036 = CARTESIAN_POINT ( 'NONE',  ( 10.18810118749999916, 4.220049686691935698, 106.0000000020483668 ) ) ;
#11037 = ADVANCED_FACE ( 'NONE', ( #36558 ), #25219, .F. ) ;
#11038 = CARTESIAN_POINT ( 'NONE',  ( 3.211159895383560947, 13.31249999863440792, 3.211159895383562723 ) ) ;
#11039 = EDGE_LOOP ( 'NONE', ( #6708, #38418, #46396, #73797 ) ) ;
#11040 = CARTESIAN_POINT ( 'NONE',  ( 8.000000000000000000, -1.084202172485504434E-16, 0.000000000000000000 ) ) ;
#11041 = CARTESIAN_POINT ( 'NONE',  ( -7.999999999999998224, 107.0937500000000142, 3.313708498984766049 ) ) ;
#11042=STYLED_ITEM('',(#74685),#16907);
#11043 = CARTESIAN_POINT ( 'NONE',  ( -4.999999999999999112, -67.66364885638941473, -22.52891795222312865 ) ) ;
#11044 = CARTESIAN_POINT ( 'NONE',  ( -5.082755093536326818, 21.28124999795161543, 5.082755093536325042 ) ) ;
#11045 = LINE ( 'NONE', #57072, #50838 ) ;
#11046 = CARTESIAN_POINT ( 'NONE',  ( -7.204075437095965206, -7.204075437095968759, 108.7187500020483810 ) ) ;
#11047 = AXIS2_PLACEMENT_3D ( 'NONE', #10994, #10622, #5338 ) ;
#11048 =( BOUNDED_CURVE ( )  B_SPLINE_CURVE ( 3, ( #64020, #63261, #58013, #51574 ),
 .UNSPECIFIED., .F., .F. ) 
 B_SPLINE_CURVE_WITH_KNOTS ( ( 4, 4 ),
 ( 1.697769116408975654, 2.139598793936698939 ),
 .UNSPECIFIED. ) 
 CURVE ( )  GEOMETRIC_REPRESENTATION_ITEM ( )  RATIONAL_B_SPLINE_CURVE ( ( 1.000000000000000000, 0.9837982640406375268, 0.9837982640406375268, 1.000000000000000000 ) ) 
 REPRESENTATION_ITEM ( '' )  );
#11049 = DIRECTION ( 'NONE',  ( -0.000000000000000000, -1.000000000000000000, -0.000000000000000000 ) ) ;
#11050 = CARTESIAN_POINT ( 'NONE',  ( 1.656854249492381914, 9.562499997268814056, 4.000000000000000888 ) ) ;
#11051 = DIRECTION ( 'NONE',  ( -0.000000000000000000, 1.000000000000000000, -0.000000000000000000 ) ) ;
#11052 = VECTOR ( 'NONE', #10073, 1000.000000000000000 ) ;
#11053 = ORIENTED_EDGE ( 'NONE', *, *, #51498, .T. ) ;
#11054 = CARTESIAN_POINT ( 'NONE',  ( 3.458734125000016313, 201.8750000013656063, 199.4326545832176691 ) ) ;
#11055 = CARTESIAN_POINT ( 'NONE',  ( -30.44569435410886982, 204.5625000013656063, 167.5543056458916169 ) ) ;
#11056 = CARTESIAN_POINT ( 'NONE',  ( -8.342170076843785083E-16, 9.062499998634407916, 4.541265875000002339 ) ) ;
#11057 = CARTESIAN_POINT ( 'NONE',  ( -2.828427124746192067, 10.37499999726881406, 2.828427124746190735 ) ) ;
#11058 = CARTESIAN_POINT ( 'NONE',  ( 1.320432766682872962E-15, -7.188101187499992051, 19.86155278187175455 ) ) ;
#11059 = ORIENTED_EDGE ( 'NONE', *, *, #5122, .F. ) ;
#11061 =( BOUNDED_CURVE ( )  B_SPLINE_CURVE ( 2, ( #29791, #46758, #30526, #53544, #403, #52801, #1859, #24845, #1135, #47863, #70884, #24113, #42200 ),
 .UNSPECIFIED., .F., .F. ) 
 B_SPLINE_CURVE_WITH_KNOTS ( ( 3, 2, 2, 2, 2, 2, 3 ),
 ( 2.339288409473456287, 2.344521723505997635, 2.349755037538538982, 2.354988351571080329, 2.360221665603621677, 2.365454979636163024, 2.370688293668704372 ),
 .UNSPECIFIED. ) 
 CURVE ( )  GEOMETRIC_REPRESENTATION_ITEM ( )  RATIONAL_B_SPLINE_CURVE ( ( 1.000000000000008438, 0.9659258262890599855, 1.000000000000000000, 0.9659258262890683122, 1.000000000000000000, 0.9659258262890683122, 1.000000000000000000, 0.9659258262890683122, 1.000000000000000000, 0.9659258262890683122, 1.000000000000000000, 0.9659258262890662028, 1.000000000000001998 ) ) 
 REPRESENTATION_ITEM ( '' )  );
#11060 = DIRECTION ( 'NONE',  ( -0.000000000000000000, 1.000000000000000000, -4.476705744456276341E-16 ) ) ;
#11062 = VERTEX_POINT ( 'NONE', #42940 ) ;
#11063 = CARTESIAN_POINT ( 'NONE',  ( -7.204075437095967871, 7.204075437095967871, 110.9687500020483810 ) ) ;
#11064 = CARTESIAN_POINT ( 'NONE',  ( 0.000000000000000000, 195.0000000000000284, 170.0000000000000284 ) ) ;
#11065 = CARTESIAN_POINT ( 'NONE',  ( 3.458734125000015425, 202.0000000013656063, 196.5673454167823877 ) ) ;
#11066 = CARTESIAN_POINT ( 'NONE',  ( 24.54126587499998990, 197.1875000013655779, 169.9999999999999432 ) ) ;
#11067 = CARTESIAN_POINT ( 'NONE',  ( -1.836970198721029983E-15, 78.75000000000000000, 10.00000000000000178 ) ) ;
#11068 = EDGE_CURVE ( 'NONE', #48454, #49614, #51002, .T. ) ;
#11069 = VECTOR ( 'NONE', #45509, 1000.000000000000114 ) ;
#11070 = CARTESIAN_POINT ( 'NONE',  ( 7.188101187500002709, 90.68750000204838102, 2.977408999572649151 ) ) ;
#11071 = CARTESIAN_POINT ( 'NONE',  ( -4.242640687119286547, 289.8750000000000000, -4.242640687119286547 ) ) ;
#11072 = EDGE_LOOP ( 'NONE', ( #74566, #73098, #39123, #21897, #24947, #35764 ) ) ;
#11073 = CARTESIAN_POINT ( 'NONE',  ( 11.00000000000000000, 1.347111479062088405E-15, 109.7499999999999858 ) ) ;
#11074 = CARTESIAN_POINT ( 'NONE',  ( 0.6474643998439180148, -10.28110762191874983, 63.57179091896463063 ) ) ;
#11075 = CARTESIAN_POINT ( 'NONE',  ( -4.000000000000015987, 196.5625000027312126, 140.3431457505076594 ) ) ;
#11076 = CARTESIAN_POINT ( 'NONE',  ( 0.000000000000000000, 300.0000000000000000, 10.00000000000000178 ) ) ;
#11077 = CARTESIAN_POINT ( 'NONE',  ( -7.999999999999976019, -3.611371706259009353E-07, 26.51781575558936055 ) ) ;
#11078 = CARTESIAN_POINT ( 'NONE',  ( -5.000000000000000888, 239.1666666666666572, -8.660254037844387298 ) ) ;
#11079 = CARTESIAN_POINT ( 'NONE',  ( -5.000000000000023093, 78.33333333333335702, 8.660254037844417496 ) ) ;
#11080 = CARTESIAN_POINT ( 'NONE',  ( 2.679491924311228956, 206.0416666666666856, -10.00000000000000000 ) ) ;
#11081 = CARTESIAN_POINT ( 'NONE',  ( -5.082755093536317936, -5.082755093536320601, 18.54905278187175455 ) ) ;
#11082 = CARTESIAN_POINT ( 'NONE',  ( -2.085542519210945728E-15, 169.8437499965860127, 11.35316468750000141 ) ) ;
#11083 = PLANE ( 'NONE',  #50550 ) ;
#11084 = CARTESIAN_POINT ( 'NONE',  ( 4.000000000000000888, 1.687499997268813168, 1.656854249492384135 ) ) ;
#11086 = CARTESIAN_POINT ( 'NONE',  ( -6.000000000000003553, 297.0000000034139589, -2.485281374238571317 ) ) ;
#11085 =( LENGTH_UNIT ( ) NAMED_UNIT ( * ) SI_UNIT ( .MILLI., .METRE. ) );
#11087 = ORIENTED_EDGE ( 'NONE', *, *, #13355, .T. ) ;
#11088 = CARTESIAN_POINT ( 'NONE',  ( -2.754378923186476579E-14, 199.1875000013655779, 145.4587341250000350 ) ) ;
#11089 = CARTESIAN_POINT ( 'NONE',  ( 8.311093377946837890, 31.71874999658601624, -8.311093377946837890 ) ) ;
#11090 = CARTESIAN_POINT ( 'NONE',  ( -4.556349186104047710, -10.99999999999999822, 109.4687500040967763 ) ) ;
#11091 = CARTESIAN_POINT ( 'NONE',  ( -30.44569435410876324, 207.8125000013656063, 172.4456943541092642 ) ) ;
#11092 = CARTESIAN_POINT ( 'NONE',  ( 24.00000000000000711, 207.9375000027312126, 171.6568542494923122 ) ) ;
#11094 = CARTESIAN_POINT ( 'NONE',  ( 3.369429374625374951, 10.27270496052241278, -63.91910092334653370 ) ) ;
#11093 = CARTESIAN_POINT ( 'NONE',  ( -11.00000000000000533, 11.00000000000000000, 20.00000000000000000 ) ) ;
#11095 = CARTESIAN_POINT ( 'NONE',  ( -30.99999999999992895, -31.99999999999978684, 167.9999999999997726 ) ) ;
#11096 = CARTESIAN_POINT ( 'NONE',  ( -2.754378923186476579E-14, 200.1875000013656063, 145.4587341250000350 ) ) ;
#11097 = EDGE_CURVE ( 'NONE', #45475, #31249, #45564, .T. ) ;
#11098 = EDGE_CURVE ( 'NONE', #62698, #72148, #74235, .T. ) ;
#11099 = CARTESIAN_POINT ( 'NONE',  ( 8.660254037844389075, 62.29166665983869677, -5.000000000000000000 ) ) ;
#11100 = CIRCLE ( 'NONE', #21959, 20.00000000000000355 ) ;
#11101 = CARTESIAN_POINT ( 'NONE',  ( 7.188101187500001821, 102.5000000020483810, -2.977408999572651371 ) ) ;
#11102 = CARTESIAN_POINT ( 'NONE',  ( 4.541265875000001451, 13.37499999863440969, 1.881053915767124440 ) ) ;
#11103 = LINE ( 'NONE', #63889, #10822 ) ;
#11104 = CARTESIAN_POINT ( 'NONE',  ( -7.999999999999989342, -3.313708498984762496, 3.924052779823362425 ) ) ;
#11105 = CARTESIAN_POINT ( 'NONE',  ( 10.00000000000000000, 101.6666666598386826, 2.679491924311235618 ) ) ;
#11106 = EDGE_LOOP ( 'NONE', ( #19011, #29358, #24276, #49518 ) ) ;
#11107 = ORIENTED_EDGE ( 'NONE', *, *, #54143, .T. ) ;
#11108 = CARTESIAN_POINT ( 'NONE',  ( -7.999999999999991118, 0.000000000000000000, 11.33030277982336642 ) ) ;
#11109 = CARTESIAN_POINT ( 'NONE',  ( 1.714505518806294638E-15, -2.500000000000000444, -14.00000000000000000 ) ) ;
#11110 = CYLINDRICAL_SURFACE ( 'NONE', #1417, 3.999999999999976019 ) ;
#11111 = CARTESIAN_POINT ( 'NONE',  ( -30.87166940467751175, -42.99943612658631764, 167.0139770318099011 ) ) ;
#11112 = CARTESIAN_POINT ( 'NONE',  ( 3.042071309553159519, 144.7395833299193839, 11.35316468750000141 ) ) ;
#11113 = CARTESIAN_POINT ( 'NONE',  ( -5.656854249492381470, 0.9375000000000001110, 5.656854249492379694 ) ) ;
#11114 = EDGE_CURVE ( 'NONE', #27000, #37291, #8181, .T. ) ;
#11115 = CARTESIAN_POINT ( 'NONE',  ( -6.238412754330611322E-16, 10.18810118749999916, 86.78125000204836681 ) ) ;
#11116 = CARTESIAN_POINT ( 'NONE',  ( 2.828427124746208943, 204.6250000000000284, 195.1715728752538439 ) ) ;
#11117 = CARTESIAN_POINT ( 'NONE',  ( -1.656854249492374143, 205.1875000000001137, 202.0000000000000000 ) ) ;
#11118 = CARTESIAN_POINT ( 'NONE',  ( -28.00000000000007461, 197.1250000027312126, 166.0000000000003695 ) ) ;
#11119 = CARTESIAN_POINT ( 'NONE',  ( -4.220049686691935698, 10.18810118749999916, 117.2500000020484094 ) ) ;
#11120 = ORIENTED_EDGE ( 'NONE', *, *, #45759, .T. ) ;
#11121 = CARTESIAN_POINT ( 'NONE',  ( 8.000000000000000000, 106.5312500040968189, -3.313708498984762496 ) ) ;
#11122 = AXIS2_PLACEMENT_3D ( 'NONE', #70666, #64642, #8686 ) ;
#11123 = CARTESIAN_POINT ( 'NONE',  ( 36.08150342469466665, 173.9980443334483766, 170.3486527213212867 ) ) ;
#11124 = CARTESIAN_POINT ( 'NONE',  ( 11.35316468749999785, 130.8854166632526699, 3.042071309553174174 ) ) ;
#11125 = CARTESIAN_POINT ( 'NONE',  ( -3.458734124999958581, 201.5000000013655779, 199.4326545832176976 ) ) ;
#11126 = CARTESIAN_POINT ( 'NONE',  ( 7.188101187500000933, 21.93749999795161187, -2.977408999572650483 ) ) ;
#11127 = CARTESIAN_POINT ( 'NONE',  ( -4.220049686691937474, -10.18810118749999738, 77.31250000204836681 ) ) ;
#11128 = CARTESIAN_POINT ( 'NONE',  ( 11.35316468749999963, 36.30208332991935549, -3.042071309553165293 ) ) ;
#11129 = VERTEX_POINT ( 'NONE', #73124 ) ;
#11130 = DIRECTION ( 'NONE',  ( 0.000000000000000000, -0.000000000000000000, 1.000000000000000000 ) ) ;
#11131 = CARTESIAN_POINT ( 'NONE',  ( -1.836970198721029983E-15, 43.75000000000000711, 10.00000000000000178 ) ) ;
#11132 = CARTESIAN_POINT ( 'NONE',  ( 8.008118988124991233, 3.317071493978879015, 18.35686528394063188 ) ) ;
#11133 = CARTESIAN_POINT ( 'NONE',  ( 2.445694354108783219, 207.8125000013656063, 139.5543056458912190 ) ) ;
#11134 = CARTESIAN_POINT ( 'NONE',  ( 4.401442555609581635E-16, 8.343749997951611874, -7.188101187500000044 ) ) ;
#11135 = CARTESIAN_POINT ( 'NONE',  ( -4.242640687119286547, 296.9375000034140157, -4.242640687119286547 ) ) ;
#11136 = EDGE_CURVE ( 'NONE', #52491, #50334, #16127, .T. ) ;
#11137 = CARTESIAN_POINT ( 'NONE',  ( -47.51267804510742110, 144.7530392445062830, 64.63931512073762065 ) ) ;
#11138 = CARTESIAN_POINT ( 'NONE',  ( -7.188101187500001821, 7.499999997951610986, -2.977408999572651371 ) ) ;
#11139 = CIRCLE ( 'NONE', #2671, 10.50000000000000000 ) ;
#11140 = CARTESIAN_POINT ( 'NONE',  ( -3.042071309553173730, 159.6354166632526983, 11.35316468749999785 ) ) ;
#11141 = CARTESIAN_POINT ( 'NONE',  ( -7.204075437095967871, 7.204075437095967871, 74.96875000204836681 ) ) ;
#11142 = CARTESIAN_POINT ( 'NONE',  ( -25.55430564589119768, 209.5625000013656063, 167.5543056458915316 ) ) ;
#11143 = CARTESIAN_POINT ( 'NONE',  ( 1.881053915767122664, 19.24999999863440436, 4.541265875000001451 ) ) ;
#11144 = ORIENTED_EDGE ( 'NONE', *, *, #32337, .T. ) ;
#11145 = CARTESIAN_POINT ( 'NONE',  ( 1.656854249492403008, 200.8125000027311842, 194.0000000000000853 ) ) ;
#11146 = CARTESIAN_POINT ( 'NONE',  ( 3.999999999999960032, 208.0000000000000284, 142.0000000000000568 ) ) ;
#11147 = CARTESIAN_POINT ( 'NONE',  ( -29.65685424949245785, 202.1875000027311842, 166.0000000000004263 ) ) ;
#11148 = VECTOR ( 'NONE', #17829, 1000.000000000000000 ) ;
#11149 = CARTESIAN_POINT ( 'NONE',  ( -4.898587196589407898E-16, 7.999999999999991118, 5.142802783920146226 ) ) ;
#11150 = ORIENTED_EDGE ( 'NONE', *, *, #12710, .F. ) ;
#11151 = CARTESIAN_POINT ( 'NONE',  ( -1.320432766682874540E-15, 19.59374999795161543, 7.188101187500000044 ) ) ;
#11152 = CARTESIAN_POINT ( 'NONE',  ( -27.99999999999990763, 196.6250000027312126, 174.0000000000003695 ) ) ;
#11153 = CARTESIAN_POINT ( 'NONE',  ( -1.329076325591744601, -47.69661646533484145, 151.0456795691926857 ) ) ;
#11154 = CARTESIAN_POINT ( 'NONE',  ( 2.679491924311228956, 41.04166666666667851, -10.00000000000000000 ) ) ;
#11155 = CARTESIAN_POINT ( 'NONE',  ( -4.401442555609581635E-16, 109.1562500020483810, -7.188101187500000044 ) ) ;
#11156 = CARTESIAN_POINT ( 'NONE',  ( -31.45873412499998523, 208.0000000013656063, 171.4326545832180386 ) ) ;
#11157 = CARTESIAN_POINT ( 'NONE',  ( -3.673940397442060854E-16, 299.7500000000000000, -6.000000000000001776 ) ) ;
#11159 = DIRECTION ( 'NONE',  ( -0.000000000000000000, 1.000000000000000000, 4.689100369878284071E-30 ) ) ;
#11158 = CARTESIAN_POINT ( 'NONE',  ( 5.000000000000058620, 80.83333333333341386, -8.660254037844484998 ) ) ;
#11160 =( BOUNDED_CURVE ( )  B_SPLINE_CURVE ( 2, ( #8216, #7849, #43662, #38016, #13849, #31604, #54625, #36892, #25920 ),
 .UNSPECIFIED., .F., .F. ) 
 B_SPLINE_CURVE_WITH_KNOTS ( ( 3, 2, 2, 2, 3 ),
 ( 0.1666666666666668239, 0.1750000000000001554, 0.1833333333333334869, 0.1916666666666668462, 0.2000000000000001776 ),
 .UNSPECIFIED. ) 
 CURVE ( )  GEOMETRIC_REPRESENTATION_ITEM ( )  RATIONAL_B_SPLINE_CURVE ( ( 0.9999999999999984457, 0.9238795325112882928, 1.000000000000000000, 0.9238795325112867385, 1.000000000000000000, 0.9238795325112867385, 1.000000000000000000, 0.9238795325112851842, 1.000000000000001554 ) ) 
 REPRESENTATION_ITEM ( '' )  );
#11161 = ORIENTED_EDGE ( 'NONE', *, *, #56540, .F. ) ;
#11162 = CARTESIAN_POINT ( 'NONE',  ( -11.35316468749999608, 239.1145833367473301, 3.042071309553173730 ) ) ;
#11163 = CIRCLE ( 'NONE', #36472, 8.999999999999998224 ) ;
#11164 = CARTESIAN_POINT ( 'NONE',  ( -7.188101187499991163, 2.977408999572646930, 19.76780278187175455 ) ) ;
#11165 = CARTESIAN_POINT ( 'NONE',  ( -1.781595147095501597, 51.28498669165002610, 48.57279346520133601 ) ) ;
#11166 = CARTESIAN_POINT ( 'NONE',  ( 0.000000000000000000, 0.000000000000000000, 7.000000000000000000 ) ) ;
#11167 = CARTESIAN_POINT ( 'NONE',  ( 4.000000000000016875, 198.5625000027312126, 199.6568542494924259 ) ) ;
#11168 = CARTESIAN_POINT ( 'NONE',  ( 2.839093476692135984E-14, 195.9375000013655779, 201.4587341250000350 ) ) ;
#11169 = CARTESIAN_POINT ( 'NONE',  ( 4.999999999999993783, 159.1666666666666856, 8.660254037844390851 ) ) ;
#11170 = DIRECTION ( 'NONE',  ( -0.000000000000000000, -1.000000000000000000, -4.283267841918042741E-17 ) ) ;
#11171 = DIRECTION ( 'NONE',  ( -0.000000000000000000, 1.000000000000000000, -0.000000000000000000 ) ) ;
#11172 = CARTESIAN_POINT ( 'NONE',  ( 5.000000000000000000, -50.64189880742087269, -41.08656465431914029 ) ) ;
#11173 = CARTESIAN_POINT ( 'NONE',  ( 11.35316468750000141, 126.0937499965860127, 0.000000000000000000 ) ) ;
#11174 = CARTESIAN_POINT ( 'NONE',  ( -36.10814071610730736, 271.9999999999999432, 139.0000000000000000 ) ) ;
#11175 = DIRECTION ( 'NONE',  ( 0.000000000000000000, 0.000000000000000000, -1.000000000000000000 ) ) ;
#11178 = CARTESIAN_POINT ( 'NONE',  ( -2.849036369511732440E-14, 202.2500000000000000, 138.0000000000000568 ) ) ;
#11177 = CARTESIAN_POINT ( 'NONE',  ( 31.45873412499999944, 194.6250000013655779, 171.4326545832175555 ) ) ;
#11176 = CARTESIAN_POINT ( 'NONE',  ( 25.55430564589114795, 196.5625000013656063, 172.4456943541086957 ) ) ;
#11179 = VERTEX_POINT ( 'NONE', #73487 ) ;
#11180 = CARTESIAN_POINT ( 'NONE',  ( 2.828427124746190291, 1.875000000000000222, 2.828427124746192067 ) ) ;
#11181 = CARTESIAN_POINT ( 'NONE',  ( 5.000000000000000000, 0.000000000000000000, 0.000000000000000000 ) ) ;
#11182 =( BOUNDED_CURVE ( )  B_SPLINE_CURVE ( 2, ( #26700, #53895, #42561, #65572, #13869, #36912, #74491, #40909, #34154, #68460, #22799, #28095, #33784 ),
 .UNSPECIFIED., .F., .F. ) 
 B_SPLINE_CURVE_WITH_KNOTS ( ( 3, 2, 2, 2, 2, 2, 3 ),
 ( 0.8315217391304348116, 0.8333333333333333703, 0.8351449275362319291, 0.8369565217391304879, 0.8387681159420289356, 0.8405797101449274944, 0.8423913043478260532 ),
 .UNSPECIFIED. ) 
 CURVE ( )  GEOMETRIC_REPRESENTATION_ITEM ( )  RATIONAL_B_SPLINE_CURVE ( ( 1.000000000000000000, 0.9659258262890683122, 1.000000000000000000, 0.9659258262890683122, 1.000000000000000000, 0.9659258262890683122, 1.000000000000000000, 0.9659258262890683122, 1.000000000000000000, 0.9659258262890683122, 1.000000000000000000, 0.9659258262890683122, 1.000000000000000000 ) ) 
 REPRESENTATION_ITEM ( '' )  );
#11183 = CARTESIAN_POINT ( 'NONE',  ( 18.00000000000000355, 0.000000000000000000, -21.50000000000000000 ) ) ;
#11184 = CARTESIAN_POINT ( 'NONE',  ( 5.676582343750001591, 216.9270833299193555, -9.832129032723420536 ) ) ;
#11185 = CARTESIAN_POINT ( 'NONE',  ( 2.977408999572650039, 119.1875000020483810, -7.188101187500001821 ) ) ;
#11186 = CARTESIAN_POINT ( 'NONE',  ( 1.881053915767121776, 1.624999998634407028, -4.541265875000002339 ) ) ;
#11187 = CARTESIAN_POINT ( 'NONE',  ( -2.591411123066599487, 60.37037679142435564, -22.98897912932020660 ) ) ;
#11188 = CARTESIAN_POINT ( 'NONE',  ( 5.656854249492376141, -5.656854249492374365, 22.39280277982336997 ) ) ;
#11189 = FACE_OUTER_BOUND ( 'NONE', #66898, .T. ) ;
#11190 = CARTESIAN_POINT ( 'NONE',  ( 3.042071309553167069, 96.82291666325269830, -11.35316468749999785 ) ) ;
#11191 = ORIENTED_EDGE ( 'NONE', *, *, #11782, .T. ) ;
#11192 = CARTESIAN_POINT ( 'NONE',  ( -5.082755093536326818, 25.40624999795161543, 5.082755093536325042 ) ) ;
#11193 = CARTESIAN_POINT ( 'NONE',  ( -7.999999999999991118, 0.000000000000000000, 8.330302779823362869 ) ) ;
#11194 = CARTESIAN_POINT ( 'NONE',  ( 9.832129032723420536, 241.3020833367473301, 5.676582343749996262 ) ) ;
#11195 = CARTESIAN_POINT ( 'NONE',  ( 11.35316468750000141, 100.7812499965860269, 0.000000000000000000 ) ) ;
#11196 = EDGE_LOOP ( 'NONE', ( #45935, #23638, #51313 ) ) ;
#11197 = CARTESIAN_POINT ( 'NONE',  ( -27.99999999999996092, 208.5000000000000284, 174.0000000000003695 ) ) ;
#11198 = EDGE_CURVE ( 'NONE', #24196, #17730, #10141, .T. ) ;
#11199 = CARTESIAN_POINT ( 'NONE',  ( 10.18810118749999916, 4.220049686691935698, 109.0000000020483810 ) ) ;
#11200 = CARTESIAN_POINT ( 'NONE',  ( -7.320508075688778149, 219.9999999931720538, 7.320508075688769267 ) ) ;
#11201 = CARTESIAN_POINT ( 'NONE',  ( 1.432654583217664701, 204.0000000013656347, 201.4587341250000065 ) ) ;
#11202 = CARTESIAN_POINT ( 'NONE',  ( -3.673940397442060854E-16, 297.7500000000000000, -6.000000000000001776 ) ) ;
#11204 = CARTESIAN_POINT ( 'NONE',  ( -11.35316468750000141, 93.28124999658602690, -1.390361679473963753E-15 ) ) ;
#11203 = CARTESIAN_POINT ( 'NONE',  ( 28.00000000000002132, 205.1250000027312126, 173.9999999999999147 ) ) ;
#11205 = CARTESIAN_POINT ( 'NONE',  ( -3.313708498984757167, 7.999999999999991118, 11.23655278392014445 ) ) ;
#11206 = CARTESIAN_POINT ( 'NONE',  ( -29.43265458321766559, 198.7500000013656063, 166.5412658750003629 ) ) ;
#11207 = CARTESIAN_POINT ( 'NONE',  ( -8.000000000000000000, 27.46874999590322375, -3.313708498984762496 ) ) ;
#11208 = ORIENTED_EDGE ( 'NONE', *, *, #16153, .T. ) ;
#11209 = ADVANCED_FACE ( 'NONE', ( #10492 ), #4844, .T. ) ;
#11210 = CARTESIAN_POINT ( 'NONE',  ( 8.660254037844389075, 192.2916666598387110, -5.000000000000000000 ) ) ;
#11211 = CARTESIAN_POINT ( 'NONE',  ( 27.99999999999996803, 201.0000000000000000, 173.9999999999999147 ) ) ;
#11212 = CARTESIAN_POINT ( 'NONE',  ( 5.676582343750001591, 81.92708332991935549, -9.832129032723420536 ) ) ;
#11213 = CARTESIAN_POINT ( 'NONE',  ( -2.765530957081998586, 291.6406250017068942, 6.676582343750001591 ) ) ;
#11214 = CARTESIAN_POINT ( 'NONE',  ( -5.082755093536326818, 7.781249997951610986, 5.082755093536325042 ) ) ;
#11215 = CARTESIAN_POINT ( 'NONE',  ( -7.204075437095965206, -7.204075437095968759, 98.21875000204838102 ) ) ;
#11216 = CARTESIAN_POINT ( 'NONE',  ( -5.676582343750006032, 224.1145833299193839, 9.832129032723418760 ) ) ;
#11217 = EDGE_LOOP ( 'NONE', ( #24178, #55048, #59119, #67105, #6429, #52653, #1780, #41270, #56885, #68108, #5079, #34283, #31814, #48468, #47333, #21121 ) ) ;
#11218 = CARTESIAN_POINT ( 'NONE',  ( -10.00000000000000355, 69.58333332650538239, 2.679491924311223183 ) ) ;
#11219 = CARTESIAN_POINT ( 'NONE',  ( 5.656854249492381470, 115.2500000040967905, 5.656854249492379694 ) ) ;
#11220 = CARTESIAN_POINT ( 'NONE',  ( 1.102182119232618108E-15, 291.2500000000000000, 6.000000000000001776 ) ) ;
#11221 = CARTESIAN_POINT ( 'NONE',  ( 10.92737078412413787, 225.9999999999999147, -3.080083792328916825 ) ) ;
#11222 = CARTESIAN_POINT ( 'NONE',  ( 8.660254037844385522, 46.45833332650536818, 5.000000000000005329 ) ) ;
#11223 = CARTESIAN_POINT ( 'NONE',  ( 7.320508075688771044, 199.3750000000000000, 7.320508075688775484 ) ) ;
#11224 = CARTESIAN_POINT ( 'NONE',  ( -4.088227598258586603E-16, 297.2031250017070079, -6.676582343750001591 ) ) ;
#11225 = EDGE_CURVE ( 'NONE', #10747, #40213, #41107, .T. ) ;
#11226 = ORIENTED_EDGE ( 'NONE', *, *, #2505, .T. ) ;
#11227 = CARTESIAN_POINT ( 'NONE',  ( 1.656854249492337949, 199.3125000000001137, 202.0000000000000853 ) ) ;
#11228 = CARTESIAN_POINT ( 'NONE',  ( 3.042071309553167513, 212.1354166632526983, -11.35316468749999785 ) ) ;
#11229 = CARTESIAN_POINT ( 'NONE',  ( 10.18810118749999916, 1.247682550866122264E-15, 96.90625000204838102 ) ) ;
#11230 = CARTESIAN_POINT ( 'NONE',  ( -29.43265458321766559, 207.5000000013655779, 166.5412658750003629 ) ) ;
#11231 = CARTESIAN_POINT ( 'NONE',  ( 4.898587196589412829E-16, 18.37500000000000355, -8.000000000000000000 ) ) ;
#11232 = ORIENTED_EDGE ( 'NONE', *, *, #16301, .T. ) ;
#11233 = VECTOR ( 'NONE', #65661, 1000.000000000000000 ) ;
#11234 = CARTESIAN_POINT ( 'NONE',  ( 5.082755093536325042, 120.5937500020483952, -5.082755093536325930 ) ) ;
#11235 = CARTESIAN_POINT ( 'NONE',  ( -62.39047978708157416, 272.0000000000000000, 45.00000000000000000 ) ) ;
#11236 = CARTESIAN_POINT ( 'NONE',  ( 5.000000000000001776, 10.83333333333333393, -8.660254037844389075 ) ) ;
#11237 = CARTESIAN_POINT ( 'NONE',  ( -3.999999999999960032, 209.9375000000000000, 196.3431457505076594 ) ) ;
#11238 = CARTESIAN_POINT ( 'NONE',  ( 7.204075437095968759, -7.204075437095966983, 83.59375000204838102 ) ) ;
#11239 = ORIENTED_EDGE ( 'NONE', *, *, #56245, .T. ) ;
#11240 = CARTESIAN_POINT ( 'NONE',  ( -2.828427124746192067, 19.62500000000000000, 2.828427124746190735 ) ) ;
#11241 = CARTESIAN_POINT ( 'NONE',  ( 5.082755093536325930, 2.156249997951610098, -5.082755093536325930 ) ) ;
#11242 = CARTESIAN_POINT ( 'NONE',  ( 23.99999999999999645, 198.9375000027312126, 171.6568542494923122 ) ) ;
#11243 = CARTESIAN_POINT ( 'NONE',  ( -7.188101187500000044, 123.0312500020483810, 0.000000000000000000 ) ) ;
#11244 = CARTESIAN_POINT ( 'NONE',  ( 4.999999999999999112, -68.33088307291114916, 21.57589723056470987 ) ) ;
#11245 = CARTESIAN_POINT ( 'NONE',  ( 2.980365356358375628, -45.39492263488825330, 151.2351675614557962 ) ) ;
#11248 = CARTESIAN_POINT ( 'NONE',  ( -4.000000000000015987, 199.6250000027312126, 142.0000000000000568 ) ) ;
#11247 = CARTESIAN_POINT ( 'NONE',  ( -6.951808397369817780E-16, 247.6562500034140157, -11.35316468749999963 ) ) ;
#11246 = CARTESIAN_POINT ( 'NONE',  ( 24.54126587499998635, 207.1250000013656347, 168.5673454167822740 ) ) ;
#11249 = PRODUCT_CONTEXT ( 'NONE', #14382, 'mechanical' ) ;
#11250 = EDGE_LOOP ( 'NONE', ( #29670, #31509, #14743, #73941 ) ) ;
#11251 = CARTESIAN_POINT ( 'NONE',  ( 5.676582343749997150, 242.5520833367473301, -9.832129032723418760 ) ) ;
#11252 = CARTESIAN_POINT ( 'NONE',  ( 2.977408999572646486, 7.188101187499991163, 11.51780278187175810 ) ) ;
#11253 = VECTOR ( 'NONE', #65652, 1000.000000000000000 ) ;
#11254 = ORIENTED_EDGE ( 'NONE', *, *, #55753, .T. ) ;
#11255 = ORIENTED_EDGE ( 'NONE', *, *, #17034, .T. ) ;
#11256 = CARTESIAN_POINT ( 'NONE',  ( 1.871523826299183495E-15, -10.18810118749999916, 74.03125000204836681 ) ) ;
#11257 = CARTESIAN_POINT ( 'NONE',  ( -8.311093377946841443, 94.21874999658601268, 8.311093377946830785 ) ) ;
#11258 = CARTESIAN_POINT ( 'NONE',  ( 1.704527592502766531, 60.27089976682777461, 22.92829164824435395 ) ) ;
#11259 = CARTESIAN_POINT ( 'NONE',  ( 2.020667218593132706E-15, -11.00000000000000000, 83.87499999999998579 ) ) ;
#11262 = CARTESIAN_POINT ( 'NONE',  ( 2.679491924311591333, 68.95833333333338544, 9.999999999999793943 ) ) ;
#11261 = CARTESIAN_POINT ( 'NONE',  ( 31.45873412499998523, 208.7500000013656063, 168.5673454167822172 ) ) ;
#11260 = CARTESIAN_POINT ( 'NONE',  ( 29.43265458321766559, 205.1250000013656347, 166.5412658749999650 ) ) ;
#11263 = CARTESIAN_POINT ( 'NONE',  ( -3.313708498984654138, 114.7812500000000142, 8.000000000000106581 ) ) ;
#11264 = CARTESIAN_POINT ( 'NONE',  ( 5.656854249492379694, 101.9375000000000000, -5.656854249492380582 ) ) ;
#11265 = CARTESIAN_POINT ( 'NONE',  ( -9.832129032723418760, 202.8645833299193555, -5.676582343750004256 ) ) ;
#11266 = CARTESIAN_POINT ( 'NONE',  ( -3.458734125000016313, 203.8750000013656063, 140.5673454167824161 ) ) ;
#11267 = CARTESIAN_POINT ( 'NONE',  ( 30.44569435410883784, 207.0625000013656063, 167.5543056458911053 ) ) ;
#11268 = CARTESIAN_POINT ( 'NONE',  ( 5.082755093536325930, 19.03124999795161543, -5.082755093536325930 ) ) ;
#11269 = CARTESIAN_POINT ( 'NONE',  ( -5.676582343749998039, 167.7604166632526983, -9.832129032723420536 ) ) ;
#11270 = CARTESIAN_POINT ( 'NONE',  ( 0.000000000000000000, 125.0000000000000000, 0.000000000000000000 ) ) ;
#11271 = CARTESIAN_POINT ( 'NONE',  ( -2.977408999572652260, 102.3125000020483952, 7.188101187500000044 ) ) ;
#11273 = CARTESIAN_POINT ( 'NONE',  ( -8.660254037844381969, 107.0833333333333428, -5.000000000000002665 ) ) ;
#11272 = CARTESIAN_POINT ( 'NONE',  ( 4.000000000000001776, 16.81249999726881583, -1.656854249492381248 ) ) ;
#11274 = CARTESIAN_POINT ( 'NONE',  ( 4.541265875000002339, 10.37499999863440792, -1.881053915767121554 ) ) ;
#11275 = CARTESIAN_POINT ( 'NONE',  ( 28.00000000000002132, 204.1875000013656063, 166.5412658749999082 ) ) ;
#11276 = CARTESIAN_POINT ( 'NONE',  ( -5.082755093536317936, -5.082755093536320601, 12.54905278187175277 ) ) ;
#11277 = CARTESIAN_POINT ( 'NONE',  ( 9.832129032723420536, 56.19791666325269119, -5.676582343749999815 ) ) ;
#11278 =( BOUNDED_CURVE ( )  B_SPLINE_CURVE ( 2, ( #68306, #72856, #55887, #22642, #39641, #62638, #10971, #21161, #34006 ),
 .UNSPECIFIED., .F., .F. ) 
 B_SPLINE_CURVE_WITH_KNOTS ( ( 3, 2, 2, 2, 3 ),
 ( 0.8854166666666669627, 0.8906250000000003331, 0.8958333333333337034, 0.9010416666666668517, 0.9062500000000002220 ),
 .UNSPECIFIED. ) 
 CURVE ( )  GEOMETRIC_REPRESENTATION_ITEM ( )  RATIONAL_B_SPLINE_CURVE ( ( 0.9999999999999951150, 0.9238795325112916235, 1.000000000000000000, 0.9238795325112867385, 1.000000000000000000, 0.9238795325112867385, 1.000000000000000000, 0.9238795325112835188, 1.000000000000003331 ) ) 
 REPRESENTATION_ITEM ( '' )  );
#11279 = CARTESIAN_POINT ( 'NONE',  ( 2.128287106641264010E-14, -42.00000000000000711, 139.0000000000000568 ) ) ;
#11280 = CARTESIAN_POINT ( 'NONE',  ( 7.999999999999991118, 9.797174393178815797E-16, 0.1365527843298230681 ) ) ;
#11281 = ORIENTED_EDGE ( 'NONE', *, *, #41105, .T. ) ;
#11282 = CARTESIAN_POINT ( 'NONE',  ( 8.032507269244971937, 9.218836226384805599, -0.1233701403699331844 ) ) ;
#11284 = CARTESIAN_POINT ( 'NONE',  ( 10.99999999999989342, 4.556349186104152515, 80.03125000409677625 ) ) ;
#11283 = AXIS2_PLACEMENT_3D ( 'NONE', #66368, #60713, #15798 ) ;
#11285 = CARTESIAN_POINT ( 'NONE',  ( 3.042071309553167069, 61.82291666325266988, -11.35316468749999785 ) ) ;
#11286 = CARTESIAN_POINT ( 'NONE',  ( 7.778174593052023411, -7.778174593052021635, 72.25000000409677625 ) ) ;
#11287 = CARTESIAN_POINT ( 'NONE',  ( 1.432654583217608080, 201.8750000013656063, 138.5412658750000503 ) ) ;
#11288 = FACE_OUTER_BOUND ( 'NONE', #72755, .T. ) ;
#11290 = CARTESIAN_POINT ( 'NONE',  ( -5.676582343749998039, 57.44791666325268409, -9.832129032723420536 ) ) ;
#11289 = CARTESIAN_POINT ( 'NONE',  ( -7.188101187500000044, 92.65625000204838102, 0.000000000000000000 ) ) ;
#11291 = CARTESIAN_POINT ( 'NONE',  ( 3.313708498984756279, 7.999999999999991118, 1.861552779823364423 ) ) ;
#11292 = CYLINDRICAL_SURFACE ( 'NONE', #15590, 6.000000000000001776 ) ;
#11293 = CARTESIAN_POINT ( 'NONE',  ( -5.676582343750006032, 174.1145833299193555, 9.832129032723418760 ) ) ;
#11294 = ADVANCED_FACE ( 'NONE', ( #58031 ), #64412, .T. ) ;
#11295 = CARTESIAN_POINT ( 'NONE',  ( 2.679491924311222739, 145.8333333265053398, 10.00000000000000355 ) ) ;
#11296 = CARTESIAN_POINT ( 'NONE',  ( -7.188101187499999156, 96.12500000204836681, 2.977408999572654924 ) ) ;
#11297 = CARTESIAN_POINT ( 'NONE',  ( -5.000000000000005329, 55.20833332650536818, 8.660254037844387298 ) ) ;
#11298 = CARTESIAN_POINT ( 'NONE',  ( 5.676582343749993598, 50.26041666325269119, 9.832129032723422313 ) ) ;
#11299 = CARTESIAN_POINT ( 'NONE',  ( -10.00000000000000178, 79.37499999317202537, -1.224646799147353454E-15 ) ) ;
#11300 = CARTESIAN_POINT ( 'NONE',  ( -2.085542519210945728E-15, 179.5312499965860411, 11.35316468750000141 ) ) ;
#11301 = ORIENTED_EDGE ( 'NONE', *, *, #5155, .T. ) ;
#11302 = DIRECTION ( 'NONE',  ( -0.000000000000000000, 1.000000000000000000, 4.476705744456276341E-16 ) ) ;
#11303 = CARTESIAN_POINT ( 'NONE',  ( -6.238412754330611322E-16, 10.18810118749999916, 73.28125000204838102 ) ) ;
#11304 = CARTESIAN_POINT ( 'NONE',  ( -1.656854249492347719, 195.8125000000000284, 194.0000000000000853 ) ) ;
#11305 = CARTESIAN_POINT ( 'NONE',  ( 31.94577087304961083, 43.09522593965584036, 65.00000000000000000 ) ) ;
#11307 = CARTESIAN_POINT ( 'NONE',  ( -9.832129032723420536, 183.6979166632526983, 5.676582343749997150 ) ) ;
#11306 = LINE ( 'NONE', #41091, #67623 ) ;
#11308 = CARTESIAN_POINT ( 'NONE',  ( -3.313708498984758943, -7.999999999999989342, 8.667802784329824206 ) ) ;
#11309 = CARTESIAN_POINT ( 'NONE',  ( 27.99999999999996447, 198.6250000027312126, 165.9999999999998863 ) ) ;
#11310 = CARTESIAN_POINT ( 'NONE',  ( -10.00000000000000000, 262.9166666734946034, -2.679491924311226292 ) ) ;
#11311 = LINE ( 'NONE', #52419, #10708 ) ;
#11312 = VERTEX_POINT ( 'NONE', #68951 ) ;
#11313 = EDGE_CURVE ( 'NONE', #55577, #41775, #28910, .T. ) ;
#11314 = VECTOR ( 'NONE', #73304, 1000.000000000000000 ) ;
#11315 = CARTESIAN_POINT ( 'NONE',  ( 2.977408999572650927, -7.188101187499990274, 27.45530278187175455 ) ) ;
#11316 = CARTESIAN_POINT ( 'NONE',  ( -11.35316468750000141, 113.8020833299193555, 3.042071309553159963 ) ) ;
#11317 = EDGE_CURVE ( 'NONE', #30893, #64535, #18769, .T. ) ;
#11318 = CARTESIAN_POINT ( 'NONE',  ( -3.733333029993816776, -8.236864015571837783, -6.823697423080643532E-15 ) ) ;
#11319 = VERTEX_POINT ( 'NONE', #1426 ) ;
#11320 = CARTESIAN_POINT ( 'NONE',  ( 1.881053915767122664, 9.249999998634406140, 4.541265875000001451 ) ) ;
#11321 = CARTESIAN_POINT ( 'NONE',  ( -5.082755093536326818, 11.90624999795161010, 5.082755093536325042 ) ) ;
#11322 = CARTESIAN_POINT ( 'NONE',  ( 8.000000000000000000, 112.5312500040967905, -3.313708498984762496 ) ) ;
#11323 = CARTESIAN_POINT ( 'NONE',  ( -30.44569435410879166, 200.0625000013656063, 172.4456943541092357 ) ) ;
#11324 = EDGE_CURVE ( 'NONE', #72156, #34067, #70080, .T. ) ;
#11325 = CARTESIAN_POINT ( 'NONE',  ( 1.656854249492381248, 6.187500000000000888, -4.000000000000001776 ) ) ;
#11326 = CARTESIAN_POINT ( 'NONE',  ( -4.000000000000001776, 22.24999999726881583, -4.898587196589415787E-16 ) ) ;
#11327 = CARTESIAN_POINT ( 'NONE',  ( 4.541265875000002339, 10.31249999863440792, 0.000000000000000000 ) ) ;
#11328 = CARTESIAN_POINT ( 'NONE',  ( -4.000000000000015987, 197.4375000000000000, 140.3431457505076594 ) ) ;
#11329 = ORIENTED_EDGE ( 'NONE', *, *, #74547, .F. ) ;
#11330 = CARTESIAN_POINT ( 'NONE',  ( -4.898587196589407898E-16, 7.999999999999991118, 9.642802783920146226 ) ) ;
#11331 = CARTESIAN_POINT ( 'NONE',  ( -7.188101187500001821, 104.5625000020483668, -2.977408999572650483 ) ) ;
#11333 = FACE_OUTER_BOUND ( 'NONE', #48841, .T. ) ;
#11332 = DIRECTION ( 'NONE',  ( -0.000000000000000000, -6.938893903907228378E-16, 1.000000000000000000 ) ) ;
#11334 = CARTESIAN_POINT ( 'NONE',  ( -1.881053915767124440, 21.99999999863440792, 4.541265875000001451 ) ) ;
#11335 = CARTESIAN_POINT ( 'NONE',  ( -2.977408999572648707, -7.188101187499990274, 0.2678027818717523822 ) ) ;
#11336 = ORIENTED_EDGE ( 'NONE', *, *, #58546, .T. ) ;
#11337 = B_SPLINE_CURVE_WITH_KNOTS ( 'NONE', 3,
 ( #53826, #7802, #48145, #1778, #25865, #47773, #31173, #59124, #65504, #54198, #71154, #25127, #43230, #2136, #37212, #37586, #36844, #70795, #8534, #48885 ),
 .UNSPECIFIED., .F., .F.,
 ( 4, 2, 2, 2, 2, 2, 2, 2, 2, 4 ),
 ( 0.000000000000000000, 0.001156441540183998683, 0.001734662310276000301, 0.002312883080368001703, 0.003469324620552004506, 0.004625766160736007743, 0.005782207700920009678, 0.006938649241104013349, 0.008095090781288016152, 0.009251532321472018955 ),
 .UNSPECIFIED. ) ;
#11338 = ORIENTED_EDGE ( 'NONE', *, *, #53117, .F. ) ;
#11339 = CARTESIAN_POINT ( 'NONE',  ( -10.18810118749999738, -4.220049686691941915, 90.25000000204838102 ) ) ;
#11340 = CARTESIAN_POINT ( 'NONE',  ( -30.44569435410878810, 197.0625000013656063, 172.4456943541092357 ) ) ;
#11341 = CARTESIAN_POINT ( 'NONE',  ( 4.556349186104051263, -10.99999999999999822, 101.9687500000000000 ) ) ;
#11342 = CARTESIAN_POINT ( 'NONE',  ( 3.458734125000015869, 205.1875000013656063, 198.0000000000000284 ) ) ;
#11344 = DIRECTION ( 'NONE',  ( -1.000000000000000000, -9.955163135201253416E-17, 0.000000000000000000 ) ) ;
#11343 = CARTESIAN_POINT ( 'NONE',  ( 11.00000000000010836, -4.556349186103939353, 87.15625000000000000 ) ) ;
#11345 = EDGE_CURVE ( 'NONE', #832, #66991, #63281, .T. ) ;
#11346 = CARTESIAN_POINT ( 'NONE',  ( 8.660254037844389075, 115.4166666666666714, -5.000000000000000000 ) ) ;
#11347 = CARTESIAN_POINT ( 'NONE',  ( -8.000000000000000000, 104.0000000000000000, 0.000000000000000000 ) ) ;
#11348 = CARTESIAN_POINT ( 'NONE',  ( -4.721056650415999201, 289.4843750017070079, -4.721056650415999201 ) ) ;
#11349 = CARTESIAN_POINT ( 'NONE',  ( -7.188101187499991163, 2.977408999572646930, 4.767802781871753659 ) ) ;
#11350 = ADVANCED_FACE ( 'NONE', ( #12350 ), #69701, .T. ) ;
#11351 = LINE ( 'NONE', #33636, #32580 ) ;
#11352 = CARTESIAN_POINT ( 'NONE',  ( 24.54126587499999701, 207.1875000013656063, 169.9999999999998863 ) ) ;
#11353 = CARTESIAN_POINT ( 'NONE',  ( 3.313708498984762052, 24.09374999590322020, -8.000000000000000000 ) ) ;
#11354 = CARTESIAN_POINT ( 'NONE',  ( -3.458734125000015425, 201.0000000013655779, 143.4326545832176976 ) ) ;
#11355 = CARTESIAN_POINT ( 'NONE',  ( -5.082755093536325930, 124.3437500020483952, -5.082755093536325930 ) ) ;
#11357 = CARTESIAN_POINT ( 'NONE',  ( 5.000000000000000000, 60.11723469343052528, 46.25570701698154608 ) ) ;
#11356 = CARTESIAN_POINT ( 'NONE',  ( 11.00000000000000000, 1.347111479062088405E-15, 111.2499999999999858 ) ) ;
#11358 = CARTESIAN_POINT ( 'NONE',  ( 5.676582343749997150, 237.5520833367473301, -9.832129032723418760 ) ) ;
#11359 = CARTESIAN_POINT ( 'NONE',  ( -2.977408999572648707, -7.188101187499990274, 27.64280278187175810 ) ) ;
#11360 = CARTESIAN_POINT ( 'NONE',  ( 30.82842712474616675, 197.1250000000000284, 172.8284271247460993 ) ) ;
#11361 = CARTESIAN_POINT ( 'NONE',  ( -2.085542519210945728E-15, 9.531249996586018014, 11.35316468750000141 ) ) ;
#11362 = EDGE_CURVE ( 'NONE', #49698, #56133, #29344, .T. ) ;
#11363 = CARTESIAN_POINT ( 'NONE',  ( 8.000000000000000000, 122.8437500000000000, -3.313708498984762496 ) ) ;
#11364 = CARTESIAN_POINT ( 'NONE',  ( 5.676582343750001591, 206.9270833299193555, -9.832129032723420536 ) ) ;
#11365 = CARTESIAN_POINT ( 'NONE',  ( -31.99999999999997868, 196.3125000000000284, 171.6568542494928238 ) ) ;
#11366 = CYLINDRICAL_SURFACE ( 'NONE', #11460, 3.999999999999976019 ) ;
#11368 = DIRECTION ( 'NONE',  ( -0.000000000000000000, 1.000000000000000000, -0.000000000000000000 ) ) ;
#11367 = CARTESIAN_POINT ( 'NONE',  ( -1.469576158976823947E-15, 26.43749999590322375, 8.000000000000000000 ) ) ;
#11369 = ORIENTED_EDGE ( 'NONE', *, *, #45345, .T. ) ;
#11370 = CARTESIAN_POINT ( 'NONE',  ( -2.445694354108840063, 199.0625000013656063, 139.5543056458912190 ) ) ;
#11371 = CARTESIAN_POINT ( 'NONE',  ( -3.042071309553164404, 27.23958332991934839, -11.35316468749999963 ) ) ;
#11372 = CARTESIAN_POINT ( 'NONE',  ( -11.00000000000000000, 0.000000000000000000, 94.18750000409677625 ) ) ;
#11373 = CARTESIAN_POINT ( 'NONE',  ( 4.999999999999994671, 209.1666666666666572, 8.660254037844390851 ) ) ;
#11374 = CARTESIAN_POINT ( 'NONE',  ( -24.54126587499996148, 198.1250000013656063, 171.4326545832179534 ) ) ;
#11375 = CARTESIAN_POINT ( 'NONE',  ( 8.000000000000000000, 7.312499995903221084, 0.000000000000000000 ) ) ;
#11377 = CARTESIAN_POINT ( 'NONE',  ( 5.676582343749993598, 14.94791666325268409, 9.832129032723422313 ) ) ;
#11376 = CARTESIAN_POINT ( 'NONE',  ( -5.082755093536325930, 110.4687500020483810, -5.082755093536325930 ) ) ;
#11378 = CARTESIAN_POINT ( 'NONE',  ( -3.313708498984758943, -7.999999999999989342, 20.61155277982337353 ) ) ;
#11379 = CARTESIAN_POINT ( 'NONE',  ( -2.085542519210945728E-15, 129.5312499965860127, 11.35316468750000141 ) ) ;
#11380 = CARTESIAN_POINT ( 'NONE',  ( 4.999999999999993783, 101.0416666598386968, 8.660254037844390851 ) ) ;
#11381 = CARTESIAN_POINT ( 'NONE',  ( -2.977408999572650927, 116.7500000020483810, -7.188101187500001821 ) ) ;
#11382 = CARTESIAN_POINT ( 'NONE',  ( -3.313708498984744732, 14.34374999590322552, 8.000000000000019540 ) ) ;
#11383 = CARTESIAN_POINT ( 'NONE',  ( -27.99999999999996803, 207.1875000013656063, 173.4587341250003760 ) ) ;
#11384 = CARTESIAN_POINT ( 'NONE',  ( 7.999999999714877852, 6.754118554053788561E-05, 0.2678047518895779744 ) ) ;
#11385 = ORIENTED_EDGE ( 'NONE', *, *, #45931, .T. ) ;
#11386 = CARTESIAN_POINT ( 'NONE',  ( -2.679491924311088624, 118.5416666666666714, 10.00000000000009237 ) ) ;
#11387 = DIRECTION ( 'NONE',  ( 0.000000000000000000, 0.000000000000000000, 1.000000000000000000 ) ) ;
#11388 = CARTESIAN_POINT ( 'NONE',  ( -4.088227598258586603E-16, 299.2031250017070079, -6.676582343750001591 ) ) ;
#11389 = CARTESIAN_POINT ( 'NONE',  ( 11.35316468749999963, 130.9895833299193555, -3.042071309553165293 ) ) ;
#11390 = CARTESIAN_POINT ( 'NONE',  ( 5.000000000000000000, 51.30401030464707901, 41.49390406302104850 ) ) ;
#11391 = CARTESIAN_POINT ( 'NONE',  ( -3.313708498984757167, 7.999999999999991118, 21.60530278432982954 ) ) ;
#11392 = VECTOR ( 'NONE', #61265, 1000.000000000000000 ) ;
#11393 = CARTESIAN_POINT ( 'NONE',  ( 1.656854249492309972, 206.9375000027311842, 146.0000000000001137 ) ) ;
#11394 = CARTESIAN_POINT ( 'NONE',  ( 5.676582343750005144, 255.5729166700806445, 9.832129032723416984 ) ) ;
#11395 = CARTESIAN_POINT ( 'NONE',  ( 4.220049686691934809, 10.18810118749999916, 96.06250000204836681 ) ) ;
#11396 = ORIENTED_EDGE ( 'NONE', *, *, #22684, .T. ) ;
#11397 =( BOUNDED_CURVE ( )  B_SPLINE_CURVE ( 2, ( #40638, #28945, #74596, #47400, #53074, #64396, #63266, #35727, #58381 ),
 .UNSPECIFIED., .F., .F. ) 
 B_SPLINE_CURVE_WITH_KNOTS ( ( 3, 2, 2, 2, 3 ),
 ( 0.5294117647058820264, 0.5330882352941173075, 0.5367647058823526995, 0.5404411764705880916, 0.5441176470588233727 ),
 .UNSPECIFIED. ) 
 CURVE ( )  GEOMETRIC_REPRESENTATION_ITEM ( )  RATIONAL_B_SPLINE_CURVE ( ( 1.000000000000006883, 0.9238795325112798551, 1.000000000000000000, 0.9238795325112867385, 1.000000000000000000, 0.9238795325112867385, 1.000000000000000000, 0.9238795325112890700, 0.9999999999999976685 ) ) 
 REPRESENTATION_ITEM ( '' )  );
#11398 = EDGE_CURVE ( 'NONE', #17643, #53551, #53090, .T. ) ;
#11399 = CARTESIAN_POINT ( 'NONE',  ( 38.00000000000000000, 0.000000000000000000, 20.00000000000001066 ) ) ;
#11400 = CARTESIAN_POINT ( 'NONE',  ( -10.99999999999989164, -4.556349186104158733, 100.2812500040967478 ) ) ;
#11401 = CARTESIAN_POINT ( 'NONE',  ( -3.458734124999959469, 201.7500000013655779, 199.4326545832176976 ) ) ;
#11402 = CARTESIAN_POINT ( 'NONE',  ( 8.311093377946837890, 71.71874999658601268, -8.311093377946837890 ) ) ;
#11403 = ORIENTED_EDGE ( 'NONE', *, *, #49676, .F. ) ;
#11404 = CARTESIAN_POINT ( 'NONE',  ( 10.18810118750000093, -4.220049686691933921, 107.3125000020483668 ) ) ;
#11405 = CARTESIAN_POINT ( 'NONE',  ( -8.342170076843785083E-16, 11.18749999863440792, 4.541265875000002339 ) ) ;
#11406 = ORIENTED_EDGE ( 'NONE', *, *, #32746, .F. ) ;
#11407 = CARTESIAN_POINT ( 'NONE',  ( -7.188101187500000044, 25.21874999795161543, -8.802885111219163269E-16 ) ) ;
#11408 = LINE ( 'NONE', #23092, #32417 ) ;
#11409 = LINE ( 'NONE', #11777, #12448 ) ;
#11410 = CARTESIAN_POINT ( 'NONE',  ( 4.401442555609581635E-16, 25.21874999795161543, -7.188101187500000044 ) ) ;
#11411 = DIRECTION ( 'NONE',  ( 1.000000000000000000, 0.000000000000000000, -0.000000000000000000 ) ) ;
#11412 = CARTESIAN_POINT ( 'NONE',  ( -10.18810118749999916, 4.220049686691934809, 103.9375000020483810 ) ) ;
#11413 = PRODUCT ( 'clamping lever', 'clamping lever', '', ( #62923 ) ) ;
#11414 = CONICAL_SURFACE ( 'NONE', #74091, 18.00000000000000355, 1.047197551196596965 ) ;
#11415 = CARTESIAN_POINT ( 'NONE',  ( 0.000000000000000000, 0.000000000000000000, 0.000000000000000000 ) ) ;
#11416 = CARTESIAN_POINT ( 'NONE',  ( -2.828427124746192067, 11.37499999726881406, 2.828427124746190735 ) ) ;
#11417 = LINE ( 'NONE', #28391, #21614 ) ;
#11418 = ORIENTED_EDGE ( 'NONE', *, *, #2410, .F. ) ;
#11419 = CARTESIAN_POINT ( 'NONE',  ( 0.000000000000000000, 0.000000000000000000, 0.000000000000000000 ) ) ;
#11420 = CARTESIAN_POINT ( 'NONE',  ( 2.445694354108838731, 203.0625000013656063, 195.5543056458912190 ) ) ;
#11421 = CARTESIAN_POINT ( 'NONE',  ( -24.54126587499999346, 204.1875000013656063, 170.0000000000002842 ) ) ;
#11422 = DIRECTION ( 'NONE',  ( 0.000000000000000000, 0.000000000000000000, 1.000000000000000000 ) ) ;
#11423 = CARTESIAN_POINT ( 'NONE',  ( 3.211159895383561835, 9.437499998634406140, -3.211159895383561835 ) ) ;
#11424 = CARTESIAN_POINT ( 'NONE',  ( 17.99999999999999645, 0.000000000000000000, 19.00000000000000355 ) ) ;
#11425 = CARTESIAN_POINT ( 'NONE',  ( 5.082755093536318824, 5.082755093536319713, 17.42405278187175810 ) ) ;
#11426 = VERTEX_POINT ( 'NONE', #24409 ) ;
#11427 = DIRECTION ( 'NONE',  ( 0.000000000000000000, 0.000000000000000000, 1.000000000000000000 ) ) ;
#11428 = ORIENTED_EDGE ( 'NONE', *, *, #19016, .F. ) ;
#11429 = CARTESIAN_POINT ( 'NONE',  ( 1.871523826299183495E-15, -10.18810118749999916, 113.0312500020483810 ) ) ;
#11430 = CARTESIAN_POINT ( 'NONE',  ( -1.967015505459129087E-11, 198.7499999999984936, 10.00000000000000533 ) ) ;
#11431 = CARTESIAN_POINT ( 'NONE',  ( -30.82842712474621294, 206.1250000000000284, 167.1715728752542134 ) ) ;
#11432 = CARTESIAN_POINT ( 'NONE',  ( 1.432654583217664479, 198.7500000013656063, 201.4587341250000065 ) ) ;
#11433 = CARTESIAN_POINT ( 'NONE',  ( 31.45873412499999944, 195.6250000013656063, 171.4326545832175555 ) ) ;
#11434 = CARTESIAN_POINT ( 'NONE',  ( 10.00000000000000178, 80.00000000000000000, 0.000000000000000000 ) ) ;
#11435 = CARTESIAN_POINT ( 'NONE',  ( 5.656854249492381470, 122.5625000000000000, 5.656854249492379694 ) ) ;
#11436 = CARTESIAN_POINT ( 'NONE',  ( 2.765530957082001251, 298.9218750017070647, 6.676582343750000703 ) ) ;
#11437 = EDGE_CURVE ( 'NONE', #64507, #57691, #47415, .T. ) ;
#11438 = ORIENTED_EDGE ( 'NONE', *, *, #23025, .T. ) ;
#11439 = DIRECTION ( 'NONE',  ( -0.000000000000000000, 1.000000000000000000, 4.689100369878284071E-30 ) ) ;
#11440 = FACE_OUTER_BOUND ( 'NONE', #12646, .T. ) ;
#11441 = CARTESIAN_POINT ( 'NONE',  ( 2.828427124746153876, 197.0000000027312126, 144.8284271247462129 ) ) ;
#11442 = CARTESIAN_POINT ( 'NONE',  ( -5.000000000000000000, 63.85408791058048905, 24.15552328276567806 ) ) ;
#11443 = CARTESIAN_POINT ( 'NONE',  ( 3.313708498984761608, 6.093749995903221084, -8.000000000000000000 ) ) ;
#11444 = CARTESIAN_POINT ( 'NONE',  ( 2.679491924311235174, 241.4583333333333144, 9.999999999999998224 ) ) ;
#11445 = DIRECTION ( 'NONE',  ( -0.000000000000000000, -1.000000000000000000, -0.000000000000000000 ) ) ;
#11446 = CARTESIAN_POINT ( 'NONE',  ( -6.238412754330611322E-16, 10.18810118749999916, 67.65625000204836681 ) ) ;
#11447 = CARTESIAN_POINT ( 'NONE',  ( -8.660254037844387298, 197.0833333333333428, -5.000000000000004441 ) ) ;
#11448 = EDGE_CURVE ( 'NONE', #39015, #6516, #64772, .T. ) ;
#11449 = B_SPLINE_CURVE_WITH_KNOTS ( 'NONE', 3,
 ( #66020, #9064, #32076, #18620, #6930, #61112, #32459, #29940 ),
 .UNSPECIFIED., .F., .F.,
 ( 4, 2, 2, 4 ),
 ( 0.005257893453559919252, 0.006567392922673248590, 0.007876892391786578795, 0.01049589133001323574 ),
 .UNSPECIFIED. ) ;
#11450 = CARTESIAN_POINT ( 'NONE',  ( -7.188101187499992051, 2.977408999572646930, 15.26780278187175455 ) ) ;
#11451 = CARTESIAN_POINT ( 'NONE',  ( 5.676582343750001591, 166.9270833299193555, -9.832129032723420536 ) ) ;
#11452 = CYLINDRICAL_SURFACE ( 'NONE', #63796, 3.999999999999976019 ) ;
#11453 = DIRECTION ( 'NONE',  ( -0.000000000000000000, -0.000000000000000000, -1.000000000000000000 ) ) ;
#11455 = CARTESIAN_POINT ( 'NONE',  ( 6.123233995736767268E-16, 88.12499999317203958, -10.00000000000000178 ) ) ;
#11454 = CARTESIAN_POINT ( 'NONE',  ( 5.000000000000000000, 8.780967503833453037E-15, 71.70204102886728492 ) ) ;
#11456 = ORIENTED_EDGE ( 'NONE', *, *, #26854, .T. ) ;
#11457 = CARTESIAN_POINT ( 'NONE',  ( 1.432654583217607192, 198.2500000013656347, 145.4587341250000634 ) ) ;
#11458 = CARTESIAN_POINT ( 'NONE',  ( 9.832129032723420536, 31.51041666325268764, -5.676582343749999815 ) ) ;
#11459 = CARTESIAN_POINT ( 'NONE',  ( 11.00000000000000000, 1.347111479062088405E-15, 108.4375000040967763 ) ) ;
#11460 = AXIS2_PLACEMENT_3D ( 'NONE', #58152, #12468, #35499 ) ;
#11461 = CARTESIAN_POINT ( 'NONE',  ( -3.160135233961579360, 194.4900331791218662, 199.4960084917820495 ) ) ;
#11462 = FACE_OUTER_BOUND ( 'NONE', #28002, .T. ) ;
#11464 = CARTESIAN_POINT ( 'NONE',  ( 0.8997857290925440621, -16.44125064681548309, -68.58473395859590482 ) ) ;
#11463 = CARTESIAN_POINT ( 'NONE',  ( 0.000000000000000000, 125.0000000000000000, 0.000000000000000000 ) ) ;
#11465 = CARTESIAN_POINT ( 'NONE',  ( -2.986204309486589110E-14, 67.59332269700053075, 20.03478791450399399 ) ) ;
#11466 = CARTESIAN_POINT ( 'NONE',  ( -1.432654583217662259, 198.1250000013656063, 145.4587341250000350 ) ) ;
#11467 = CARTESIAN_POINT ( 'NONE',  ( 10.00000000000000178, 67.08333332650536818, -2.679491924311226736 ) ) ;
#11468 = CIRCLE ( 'NONE', #60883, 20.00000000000001066 ) ;
#11469 = CARTESIAN_POINT ( 'NONE',  ( 7.188101187500001821, 105.5000000020483810, -2.977408999572651371 ) ) ;
#11470 = CARTESIAN_POINT ( 'NONE',  ( -4.541265875000003227, 10.99999999863440969, 1.881053915767121110 ) ) ;
#11471 = CARTESIAN_POINT ( 'NONE',  ( 7.320508075688811900, 65.62500000000002842, -7.320508075688811900 ) ) ;
#11472 = CARTESIAN_POINT ( 'NONE',  ( -5.656854249492373476, -5.656854249492376141, 4.017802779823362869 ) ) ;
#11473 = CARTESIAN_POINT ( 'NONE',  ( -7.347880794884122694E-16, 7.499999997268813168, 4.000000000000001776 ) ) ;
#11474 = ORIENTED_EDGE ( 'NONE', *, *, #2670, .T. ) ;
#11475 = ORIENTED_EDGE ( 'NONE', *, *, #50261, .T. ) ;
#11476 = CARTESIAN_POINT ( 'NONE',  ( -3.999999999999960032, 205.1250000027312126, 198.0000000000000284 ) ) ;
#11477 = CARTESIAN_POINT ( 'NONE',  ( 1.226468279477575784E-15, 296.8593750017070079, 6.676582343750001591 ) ) ;
#11478 = LINE ( 'NONE', #57887, #33948 ) ;
#11479 = CARTESIAN_POINT ( 'NONE',  ( 28.00000000000002132, 209.5000000000000284, 165.9999999999998863 ) ) ;
#11480 = CARTESIAN_POINT ( 'NONE',  ( -8.311093377946841443, 148.9062499965860127, 8.311093377946830785 ) ) ;
#11481 = DIRECTION ( 'NONE',  ( 1.000000000000000000, 0.000000000000000000, 0.000000000000000000 ) ) ;
#11482 = CARTESIAN_POINT ( 'NONE',  ( 10.18810118750000093, -4.220049686691933921, 81.81250000204838102 ) ) ;
#11483 = CARTESIAN_POINT ( 'NONE',  ( -27.99999999999999289, 194.7622595281507358, 173.7622595281509916 ) ) ;
#11484 = CARTESIAN_POINT ( 'NONE',  ( 4.000000000000015987, 202.4375000000000568, 199.6568542494924259 ) ) ;
#11485 = CARTESIAN_POINT ( 'NONE',  ( -27.99999999999991118, 197.6250000027312126, 174.0000000000003695 ) ) ;
#11486 = CARTESIAN_POINT ( 'NONE',  ( -8.000000000000000000, 100.9062500000000000, -3.313708498984761164 ) ) ;
#11487 = ORIENTED_EDGE ( 'NONE', *, *, #68085, .T. ) ;
#11488 = DIRECTION ( 'NONE',  ( -0.000000000000000000, 1.000000000000000000, -4.476705744456276341E-16 ) ) ;
#11489 = CARTESIAN_POINT ( 'NONE',  ( 8.901020801757749012, 183.4979971941716883, 140.2200920701691587 ) ) ;
#11490 = CARTESIAN_POINT ( 'NONE',  ( -9.832129032723420536, 134.0104166632526983, 5.676582343749997150 ) ) ;
#11491 = CARTESIAN_POINT ( 'NONE',  ( 1.432654583217664479, 202.7500000013655779, 201.4587341250000065 ) ) ;
#11492 = CARTESIAN_POINT ( 'NONE',  ( -2.977408999572650039, 23.81249999795161543, -7.188101187500000933 ) ) ;
#11493 =( BOUNDED_CURVE ( )  B_SPLINE_CURVE ( 1, ( #37807, #25710 ),
 .UNSPECIFIED., .F., .F. ) 
 B_SPLINE_CURVE_WITH_KNOTS ( ( 2, 2 ),
 ( 0.000000000000000000, 1.000000000000000000 ),
 .UNSPECIFIED. ) 
 CURVE ( )  GEOMETRIC_REPRESENTATION_ITEM ( )  RATIONAL_B_SPLINE_CURVE ( ( 0.9660722070829144137, 0.9660722070829144137 ) ) 
 REPRESENTATION_ITEM ( '' )  );
#11494 = CARTESIAN_POINT ( 'NONE',  ( 7.204075437095968759, -7.204075437095966983, 74.59375000204838102 ) ) ;
#11495 = CARTESIAN_POINT ( 'NONE',  ( -2.085542519210945728E-15, 34.84374999658601268, 11.35316468750000141 ) ) ;
#11496 = EDGE_LOOP ( 'NONE', ( #58530, #24482, #31743, #15773 ) ) ;
#11497 = CARTESIAN_POINT ( 'NONE',  ( -4.556349186104048599, -10.99999999999999822, 94.46875000409677625 ) ) ;
#11498 = CARTESIAN_POINT ( 'NONE',  ( 7.999999999999991118, 3.313708498984758055, 7.861552783920144449 ) ) ;
#11499 = CARTESIAN_POINT ( 'NONE',  ( -8.008118988124989457, -3.317071493978883900, 13.10686528394062833 ) ) ;
#11500 = CARTESIAN_POINT ( 'NONE',  ( -3.458734125000015869, 206.1875000013656063, 142.0000000000000568 ) ) ;
#11501 = CARTESIAN_POINT ( 'NONE',  ( 5.082755093536324154, 7.781249997951611874, 5.082755093536326818 ) ) ;
#11502 = CARTESIAN_POINT ( 'NONE',  ( 6.000000000000003553, 297.5000000034139589, 2.485281374238571317 ) ) ;
#11503 = CARTESIAN_POINT ( 'NONE',  ( -48.25721876928390230, 142.6802110789813867, 61.69279049735354903 ) ) ;
#11504 = CARTESIAN_POINT ( 'NONE',  ( 2.977408999572651815, 5.062499997951609210, 7.188101187500000933 ) ) ;
#11505 = CARTESIAN_POINT ( 'NONE',  ( 3.042071309553159519, 160.0520833299193555, 11.35316468750000141 ) ) ;
#11506 = CARTESIAN_POINT ( 'NONE',  ( -6.238412754330611322E-16, 10.18810118749999916, 68.78125000204838102 ) ) ;
#11507 = CARTESIAN_POINT ( 'NONE',  ( -29.43265458321766559, 207.7500000013656063, 166.5412658750003629 ) ) ;
#11508 =( BOUNDED_CURVE ( )  B_SPLINE_CURVE ( 2, ( #33016, #22032, #45057, #68069, #61666, #56017, #27318, #60912, #32257 ),
 .UNSPECIFIED., .F., .F. ) 
 B_SPLINE_CURVE_WITH_KNOTS ( ( 3, 2, 2, 2, 3 ),
 ( 0.1931818181818181768, 0.1988636363636363535, 0.2045454545454545581, 0.2102272727272727348, 0.2159090909090909116 ),
 .UNSPECIFIED. ) 
 CURVE ( )  GEOMETRIC_REPRESENTATION_ITEM ( )  RATIONAL_B_SPLINE_CURVE ( ( 1.000000000000000000, 0.9238795325112867385, 1.000000000000000000, 0.9238795325112867385, 1.000000000000000000, 0.9238795325112867385, 1.000000000000000000, 0.9238795325112867385, 1.000000000000000000 ) ) 
 REPRESENTATION_ITEM ( '' )  );
#11509 = CARTESIAN_POINT ( 'NONE',  ( 33.48318503342264307, 175.8115626168855385, 156.1427595010632956 ) ) ;
#11510 = CARTESIAN_POINT ( 'NONE',  ( 2.780723358947928197E-16, 19.68749999863440436, -4.541265875000002339 ) ) ;
#11511 = VERTEX_POINT ( 'NONE', #13075 ) ;
#11512 = CARTESIAN_POINT ( 'NONE',  ( 4.000000000000015987, 199.6250000027312126, 198.0000000000000284 ) ) ;
#11513 = VECTOR ( 'NONE', #33218, 999.9999999999998863 ) ;
#11514 = CARTESIAN_POINT ( 'NONE',  ( 1.656854249492347719, 205.8125000000000000, 146.0000000000000284 ) ) ;
#11515 = CARTESIAN_POINT ( 'NONE',  ( -25.17157287525374088, 200.7500000027312126, 172.8284271247464972 ) ) ;
#11516 = ADVANCED_FACE ( 'NONE', ( #36110 ), #59128, .T. ) ;
#11517 = EDGE_CURVE ( 'NONE', #15561, #27901, #40653, .T. ) ;
#11518 = CARTESIAN_POINT ( 'NONE',  ( 7.347880794884121708E-16, 300.0000000000000000, -6.000000000000001776 ) ) ;
#11519 = CARTESIAN_POINT ( 'NONE',  ( 5.656854249492376141, -5.656854249492374365, 7.580302783920144449 ) ) ;
#11520 = EDGE_LOOP ( 'NONE', ( #55968, #58846, #10100, #37231 ) ) ;
#11521 = CARTESIAN_POINT ( 'NONE',  ( 5.082755093536325930, 15.65624999795161365, -5.082755093536325930 ) ) ;
#11522 = CARTESIAN_POINT ( 'NONE',  ( -7.320508075688773708, 43.74999999317202537, -7.320508075688774596 ) ) ;
#11523 = CARTESIAN_POINT ( 'NONE',  ( 5.000000000000001776, 35.83333333333333570, -8.660254037844389075 ) ) ;
#11524 = CARTESIAN_POINT ( 'NONE',  ( -7.188101187500000044, 106.5312500020483810, 0.000000000000000000 ) ) ;
#11525 = CARTESIAN_POINT ( 'NONE',  ( -24.54126587499999701, 207.4375000013656063, 170.0000000000003411 ) ) ;
#11526 = CARTESIAN_POINT ( 'NONE',  ( 6.000000000000003553, 298.4375000000000000, 2.485281374238571317 ) ) ;
#11528 = CARTESIAN_POINT ( 'NONE',  ( 10.00000000000000000, 196.6666666598386826, 2.679491924311235618 ) ) ;
#11527 = DIRECTION ( 'NONE',  ( -0.000000000000000000, 1.000000000000000000, -0.000000000000000000 ) ) ;
#11529 = ORIENTED_EDGE ( 'NONE', *, *, #22844, .T. ) ;
#11530 = CARTESIAN_POINT ( 'NONE',  ( -11.35316468749999963, 248.9062500034139873, 0.000000000000000000 ) ) ;
#11531 = CARTESIAN_POINT ( 'NONE',  ( 7.188101187499992051, 8.802885111219154394E-16, 16.11155278187175455 ) ) ;
#11532 = CARTESIAN_POINT ( 'NONE',  ( -3.223881452105235024, 50.20043732027804850, 40.84573126306825230 ) ) ;
#11533 = CARTESIAN_POINT ( 'NONE',  ( -2.485281374238308860, 287.2500000034139589, 6.000000000000264677 ) ) ;
#11534 = DIRECTION ( 'NONE',  ( 1.000000000000000000, -0.000000000000000000, 0.000000000000000000 ) ) ;
#11535 = CARTESIAN_POINT ( 'NONE',  ( 8.660254037844385522, 201.4583333265053682, 5.000000000000005329 ) ) ;
#11536 = CARTESIAN_POINT ( 'NONE',  ( 2.679491924311228956, 161.0416666666666288, -10.00000000000000000 ) ) ;
#11537 = FACE_OUTER_BOUND ( 'NONE', #59002, .T. ) ;
#11538 = CARTESIAN_POINT ( 'NONE',  ( -6.123233995736766282E-16, 263.7500000000000568, -10.00000000000000000 ) ) ;
#11539 = CARTESIAN_POINT ( 'NONE',  ( -3.313708498984762052, 90.21874999999998579, -8.000000000000000000 ) ) ;
#11540 = CARTESIAN_POINT ( 'NONE',  ( -9.832129032723418760, 123.1770833299193555, -5.676582343750004256 ) ) ;
#11541 = FACE_OUTER_BOUND ( 'NONE', #69691, .T. ) ;
#11544 = CARTESIAN_POINT ( 'NONE',  ( 2.828427124746153876, 201.8750000000000284, 144.8284271247462129 ) ) ;
#11543 = CARTESIAN_POINT ( 'NONE',  ( 24.54126587499999701, 197.2500000013656063, 171.4326545832175839 ) ) ;
#11542 = CARTESIAN_POINT ( 'NONE',  ( 27.99999999999996092, 195.6875000013655779, 173.4587341249998929 ) ) ;
#11545 = ORIENTED_EDGE ( 'NONE', *, *, #69448, .T. ) ;
#11546 = CARTESIAN_POINT ( 'NONE',  ( 4.204081362154476587, 225.9042189071305700, -9.092352784983953384 ) ) ;
#11547 = CARTESIAN_POINT ( 'NONE',  ( 30.82842712474620939, 202.2500000027312126, 172.8284271247460424 ) ) ;
#11548 = CARTESIAN_POINT ( 'NONE',  ( -4.264261133003372173, -6.795089700395649857, -0.000000000000000000 ) ) ;
#11549 = LINE ( 'NONE', #5899, #70193 ) ;
#11550 = CARTESIAN_POINT ( 'NONE',  ( 11.35316468749999963, 226.3020833299193555, -3.042071309553165293 ) ) ;
#11551 = CARTESIAN_POINT ( 'NONE',  ( 5.082755093536326818, 123.2187500020483952, 5.082755093536325042 ) ) ;
#11552 = CARTESIAN_POINT ( 'NONE',  ( -4.541265875000002339, 21.81249999863440792, -5.561446717895856393E-16 ) ) ;
#11553 = CARTESIAN_POINT ( 'NONE',  ( 2.824543433528785410E-14, 210.0000000000000284, 194.0000000000000568 ) ) ;
#11554 = CARTESIAN_POINT ( 'NONE',  ( -3.313708498984758943, -7.999999999999989342, 22.11155277982336997 ) ) ;
#11556 = CARTESIAN_POINT ( 'NONE',  ( -10.00000000000000000, 225.0000000000000000, 0.000000000000000000 ) ) ;
#11555 = FACE_OUTER_BOUND ( 'NONE', #43241, .T. ) ;
#11557 = CARTESIAN_POINT ( 'NONE',  ( 5.676582343750001591, 111.6145833299193555, -9.832129032723420536 ) ) ;
#11558 = ORIENTED_EDGE ( 'NONE', *, *, #59665, .T. ) ;
#11559 = CYLINDRICAL_SURFACE ( 'NONE', #38762, 4.000000000000001776 ) ;
#11560 = CARTESIAN_POINT ( 'NONE',  ( -7.188101187500001821, 26.62499999795161543, -2.977408999572651371 ) ) ;
#11561 = CARTESIAN_POINT ( 'NONE',  ( 3.490152628695403868E-12, 151.2499999999997442, -10.00000000000000178 ) ) ;
#11562 = CARTESIAN_POINT ( 'NONE',  ( -6.951808397369817780E-16, 247.9687500034140157, -11.35316468749999963 ) ) ;
#11563 = CARTESIAN_POINT ( 'NONE',  ( 3.042071309553159519, 104.7395833299193555, 11.35316468750000141 ) ) ;
#11564 = ORIENTED_EDGE ( 'NONE', *, *, #57363, .F. ) ;
#11565 = CARTESIAN_POINT ( 'NONE',  ( -4.220049686691935698, 10.18810118749999916, 101.8750000020483810 ) ) ;
#11566 = CARTESIAN_POINT ( 'NONE',  ( 10.00000000000000178, 217.0833333265053682, -2.679491924311226736 ) ) ;
#11567 = CARTESIAN_POINT ( 'NONE',  ( 3.458734125000015869, 200.1875000013656063, 198.0000000000000284 ) ) ;
#11568 = DIRECTION ( 'NONE',  ( -0.000000000000000000, 1.000000000000000000, 4.476705744456276341E-16 ) ) ;
#11570 = CARTESIAN_POINT ( 'NONE',  ( -3.042071309553173730, 104.3229166632526841, 11.35316468749999785 ) ) ;
#11569 = CARTESIAN_POINT ( 'NONE',  ( -1.656854249492352604, 206.3125000027312410, 202.0000000000000284 ) ) ;
#11571 = CIRCLE ( 'NONE', #56157, 8.000000000000000000 ) ;
#11572 = CARTESIAN_POINT ( 'NONE',  ( 7.999999999999992895, -3.313708498984756279, 10.67405278392014623 ) ) ;
#11573 = CARTESIAN_POINT ( 'NONE',  ( -30.44569435410878810, 195.0625000013656063, 172.4456943541092357 ) ) ;
#11574 = CARTESIAN_POINT ( 'NONE',  ( 2.679491924305209327, 173.9583333333328312, 10.00000000000357581 ) ) ;
#11575 = EDGE_LOOP ( 'NONE', ( #11369, #40807, #22516, #28916 ) ) ;
#11576 = CARTESIAN_POINT ( 'NONE',  ( -10.00000000000000178, 194.3749999931720254, -1.224646799147353454E-15 ) ) ;
#11577 = AXIS2_PLACEMENT_3D ( 'NONE', #32147, #69080, #18138 ) ;
#11578 = CARTESIAN_POINT ( 'NONE',  ( 3.042071309553159519, 85.05208332991934128, 11.35316468750000141 ) ) ;
#11579 = CARTESIAN_POINT ( 'NONE',  ( -2.765530957081996810, 291.2656250017070079, -6.676582343750003368 ) ) ;
#11580 = CARTESIAN_POINT ( 'NONE',  ( 5.082755093536324154, 6.656249997951610986, 5.082755093536326818 ) ) ;
#11581 = CARTESIAN_POINT ( 'NONE',  ( 10.18810118749999916, 1.247682550866122264E-15, 92.78125000204836681 ) ) ;
#11582 = CARTESIAN_POINT ( 'NONE',  ( 11.35316468749999785, 220.5729166632526983, 3.042071309553174174 ) ) ;
#11583 = ORIENTED_EDGE ( 'NONE', *, *, #30252, .T. ) ;
#11584 = CARTESIAN_POINT ( 'NONE',  ( 3.313708498984763828, 123.2187500040967763, -7.999999999999996447 ) ) ;
#11585 = CARTESIAN_POINT ( 'NONE',  ( 3.313708498984711426, 98.65625000409679046, 8.000000000000053291 ) ) ;
#11586 = CARTESIAN_POINT ( 'NONE',  ( -11.35316468749999785, 218.0729166632526699, -3.042071309553167957 ) ) ;
#11587 = CARTESIAN_POINT ( 'NONE',  ( 0.000000000000000000, 0.000000000000000000, 29.33030277982336642 ) ) ;
#11588 = CARTESIAN_POINT ( 'NONE',  ( -10.00000000000000178, 99.37499999317203958, -1.224646799147353454E-15 ) ) ;
#11589 = CARTESIAN_POINT ( 'NONE',  ( -4.721056650415999201, 295.3281250017069510, -4.721056650415999201 ) ) ;
#11590 = ORIENTED_EDGE ( 'NONE', *, *, #37503, .T. ) ;
#11591 = DIRECTION ( 'NONE',  ( 0.000000000000000000, -0.8536788251726021848, -0.5207998305029730712 ) ) ;
#11592 = CARTESIAN_POINT ( 'NONE',  ( 5.676582343750001591, 211.9270833299193555, -9.832129032723420536 ) ) ;
#11593 = CIRCLE ( 'NONE', #18844, 19.00000000000000355 ) ;
#11594 = CARTESIAN_POINT ( 'NONE',  ( -6.238412754330611322E-16, 10.18810118749999916, 97.28125000204838102 ) ) ;
#11595 = EDGE_CURVE ( 'NONE', #1389, #73500, #35384, .T. ) ;
#11596 = CARTESIAN_POINT ( 'NONE',  ( -26.56734541678232731, 209.0000000013655779, 173.4587341250003760 ) ) ;
#11597 = CARTESIAN_POINT ( 'NONE',  ( 7.999999999999998224, 16.40625000000000355, 3.313708498984766493 ) ) ;
#11598 = VERTEX_POINT ( 'NONE', #9287 ) ;
#11599 = PRODUCT_DEFINITION_CONTEXT ( 'detailed design', #72242, 'design' ) ;
#11600 = CARTESIAN_POINT ( 'NONE',  ( 5.082755093536325042, 123.5937500020483952, -5.082755093536325930 ) ) ;
#11601 = LINE ( 'NONE', #34637, #17538 ) ;
#11602 =( BOUNDED_CURVE ( )  B_SPLINE_CURVE ( 2, ( #9428, #55455, #48651, #43748, #71659, #14688, #37729, #60727, #9049, #68624, #44500, #21843, #33947 ),
 .UNSPECIFIED., .F., .F. ) 
 B_SPLINE_CURVE_WITH_KNOTS ( ( 3, 2, 2, 2, 2, 2, 3 ),
 ( 0.08333333333333278747, 0.09259259259259206010, 0.1018518518518513188, 0.1111111111111105776, 0.1203703703703698502, 0.1296296296296291228, 0.1388888888888883955 ),
 .UNSPECIFIED. ) 
 CURVE ( )  GEOMETRIC_REPRESENTATION_ITEM ( )  RATIONAL_B_SPLINE_CURVE ( ( 1.000000000000001998, 0.9659258262890662028, 1.000000000000000000, 0.9659258262890683122, 1.000000000000000000, 0.9659258262890683122, 1.000000000000000000, 0.9659258262890683122, 1.000000000000000000, 0.9659258262890683122, 1.000000000000000000, 0.9659258262890701996, 0.9999999999999981126 ) ) 
 REPRESENTATION_ITEM ( '' )  );
#11603 = CARTESIAN_POINT ( 'NONE',  ( -5.000000000000005329, 23.33333333333333570, 8.660254037844387298 ) ) ;
#11604 = CARTESIAN_POINT ( 'NONE',  ( -6.238412754330611322E-16, 10.18810118749999916, 72.15625000204836681 ) ) ;
#11605 = VERTEX_POINT ( 'NONE', #2882 ) ;
#11606 = CARTESIAN_POINT ( 'NONE',  ( 1.881053915767122664, 3.124999998634407028, 4.541265875000001451 ) ) ;
#11607 = CARTESIAN_POINT ( 'NONE',  ( 2.977408999572652260, 1.687499997951610098, 7.188101187500000044 ) ) ;
#11608 = CARTESIAN_POINT ( 'NONE',  ( 18.00000000000000000, 10.39230484541325161, -20.69999999999999929 ) ) ;
#11609 = EDGE_CURVE ( 'NONE', #67709, #60791, #1699, .T. ) ;
#11610 = EDGE_CURVE ( 'NONE', #38403, #7966, #26457, .T. ) ;
#11611 = CARTESIAN_POINT ( 'NONE',  ( -5.000000000000000888, -10.54112798502250214, 66.30787999718575065 ) ) ;
#11612 = CARTESIAN_POINT ( 'NONE',  ( 10.00000000000000000, 151.6666666598387110, 2.679491924311235618 ) ) ;
#11613 = CARTESIAN_POINT ( 'NONE',  ( -2.765530957081998142, 294.6406250017069510, 6.676582343750000703 ) ) ;
#11616 = CARTESIAN_POINT ( 'NONE',  ( -4.556349186104048599, -10.99999999999999822, 88.46875000409677625 ) ) ;
#11615 = CARTESIAN_POINT ( 'NONE',  ( 8.311093377946834337, 252.0312500034139873, -8.311093377946836114 ) ) ;
#11614 = CARTESIAN_POINT ( 'NONE',  ( 31.45873412500001010, 207.6250000013656063, 171.4326545832175555 ) ) ;
#11617 = APPLICATION_PROTOCOL_DEFINITION ( 'draft international standard', 'automotive_design', 1998, #48113 ) ;
#11618 = EDGE_LOOP ( 'NONE', ( #32871, #27831, #23424 ) ) ;
#11619 = ADVANCED_FACE ( 'NONE', ( #31179 ), #25506, .T. ) ;
#11620 = CARTESIAN_POINT ( 'NONE',  ( -5.676582343750000703, 238.3854166700806445, -9.832129032723418760 ) ) ;
#11621 = CARTESIAN_POINT ( 'NONE',  ( 7.188101187499991163, 2.977408999572648707, 6.830302781871755435 ) ) ;
#11622 = ORIENTED_EDGE ( 'NONE', *, *, #5842, .F. ) ;
#11623 = CARTESIAN_POINT ( 'NONE',  ( 10.18810118749999916, 1.247682550866122264E-15, 71.40625000204836681 ) ) ;
#11624 = CARTESIAN_POINT ( 'NONE',  ( -8.311093377946836114, 82.96874999658601268, -8.311093377946837890 ) ) ;
#11625 = DIRECTION ( 'NONE',  ( -0.000000000000000000, 1.000000000000000000, 0.000000000000000000 ) ) ;
#11626 = CARTESIAN_POINT ( 'NONE',  ( 11.00000000000000355, -4.556349186104045046, 85.65625000000001421 ) ) ;
#11629 = DIRECTION ( 'NONE',  ( -0.000000000000000000, -0.000000000000000000, -1.000000000000000000 ) ) ;
#11628 = CARTESIAN_POINT ( 'NONE',  ( 24.54126587500000412, 208.2500000013656063, 171.4326545832175839 ) ) ;
#11627 = CARTESIAN_POINT ( 'NONE',  ( 26.56734541678238415, 207.2500000013655779, 166.5412658749999650 ) ) ;
#11630 = EDGE_LOOP ( 'NONE', ( #65062, #67478, #15391, #5602 ) ) ;
#11631 = FACE_OUTER_BOUND ( 'NONE', #56961, .T. ) ;
#11632 = CARTESIAN_POINT ( 'NONE',  ( 0.000000000000000000, 0.000000000000000000, 118.0000000000000000 ) ) ;
#11633 = ADVANCED_FACE ( 'NONE', ( #48889 ), #8915, .F. ) ;
#11634 = CARTESIAN_POINT ( 'NONE',  ( 5.676582343750001591, 196.6145833299193839, -9.832129032723420536 ) ) ;
#11635 = CARTESIAN_POINT ( 'NONE',  ( -1.432654583217664479, 206.7500000013655779, 138.5412658750000787 ) ) ;
#11636 = VECTOR ( 'NONE', #2960, 1000.000000000000114 ) ;
#11637 = CARTESIAN_POINT ( 'NONE',  ( 29.43265458321761230, 205.7500000013656063, 173.4587341249998929 ) ) ;
#11638 = CARTESIAN_POINT ( 'NONE',  ( -2.977408999572650039, 25.31249999795161543, -7.188101187500001821 ) ) ;
#11639 = CARTESIAN_POINT ( 'NONE',  ( 11.35316468749999785, 180.8854166632526699, 3.042071309553174174 ) ) ;
#11640 = DIRECTION ( 'NONE',  ( 0.000000000000000000, 0.000000000000000000, 1.000000000000000000 ) ) ;
#11641 = CARTESIAN_POINT ( 'NONE',  ( -2.977408999572650927, 98.75000000204838102, -7.188101187500000933 ) ) ;
#11643 = CARTESIAN_POINT ( 'NONE',  ( -8.660254037844387298, 234.5833333333333428, -4.999999999999999112 ) ) ;
#11642 = DIRECTION ( 'NONE',  ( -0.000000000000000000, 1.000000000000000000, -0.000000000000000000 ) ) ;
#11644 = CARTESIAN_POINT ( 'NONE',  ( 4.541265875000001451, 12.24999999863440969, 1.881053915767124440 ) ) ;
#11645 = CARTESIAN_POINT ( 'NONE',  ( 30.44569435410883429, 201.0625000013656063, 167.5543056458911053 ) ) ;
#11646 = CARTESIAN_POINT ( 'NONE',  ( -7.188101187499991163, 2.977408999572646930, 10.76780278187175632 ) ) ;
#11647 = CARTESIAN_POINT ( 'NONE',  ( 8.311093377946834337, 65.15624999658602690, 8.311093377946839666 ) ) ;
#11648 = CARTESIAN_POINT ( 'NONE',  ( 0.000000000000000000, 0.000000000000000000, 118.0000000000000000 ) ) ;
#11649 = CARTESIAN_POINT ( 'NONE',  ( -7.999999999999991118, 3.313708498984756723, 2.292802784329821986 ) ) ;
#11650 = EDGE_LOOP ( 'NONE', ( #33716, #34334, #23090, #26492 ) ) ;
#11651 = DIRECTION ( 'NONE',  ( -0.000000000000000000, -0.000000000000000000, -1.000000000000000000 ) ) ;
#11652 = CARTESIAN_POINT ( 'NONE',  ( 11.00000000000000000, 1.347111479062088405E-15, 117.2500000000000000 ) ) ;
#11653 = CARTESIAN_POINT ( 'NONE',  ( -8.311093377946836114, 57.65624999658601979, -8.311093377946837890 ) ) ;
#11654 = CARTESIAN_POINT ( 'NONE',  ( 7.778174593052021635, 7.778174593052023411, 75.62500000409677625 ) ) ;
#11655 = CARTESIAN_POINT ( 'NONE',  ( -2.839093476692135984E-14, 196.9375000013655779, 138.5412658750000503 ) ) ;
#11656 = CARTESIAN_POINT ( 'NONE',  ( 1.656854249492394349, 8.562499997268817609, 3.999999999999988898 ) ) ;
#11658 = CARTESIAN_POINT ( 'NONE',  ( -2.085542519210945728E-15, 59.53124999658601979, 11.35316468750000141 ) ) ;
#11657 = CARTESIAN_POINT ( 'NONE',  ( 2.977408999572654480, 94.62500000204838102, 7.188101187499999156 ) ) ;
#11659 = CARTESIAN_POINT ( 'NONE',  ( 1.469576158976822172E-15, -7.999999999999991118, 1.205302779823363979 ) ) ;
#11660 = CARTESIAN_POINT ( 'NONE',  ( -5.000000000000005329, 15.20833332650536640, 8.660254037844387298 ) ) ;
#11661 = CARTESIAN_POINT ( 'NONE',  ( 2.679491924311228956, 157.9166666598386826, -10.00000000000000000 ) ) ;
#11662 = CARTESIAN_POINT ( 'NONE',  ( -7.188101187500001821, 97.43750000204839523, -2.977408999572650483 ) ) ;
#11663 = CARTESIAN_POINT ( 'NONE',  ( 7.778174593052021635, 7.778174593052023411, 108.4374999999999858 ) ) ;
#11664 = CARTESIAN_POINT ( 'NONE',  ( -5.676582343749998039, 42.76041666325268409, -9.832129032723420536 ) ) ;
#11665 = CARTESIAN_POINT ( 'NONE',  ( -10.18810118749999916, 0.000000000000000000, 113.0312500020483810 ) ) ;
#11666 = CARTESIAN_POINT ( 'NONE',  ( -11.35316468750000141, 178.2812499965860411, -1.390361679473963753E-15 ) ) ;
#11667 = ORIENTED_EDGE ( 'NONE', *, *, #45373, .F. ) ;
#11668 = CARTESIAN_POINT ( 'NONE',  ( 0.3794862803195203083, 65.74576272852577574, 26.26831557574585219 ) ) ;
#11669 = CARTESIAN_POINT ( 'NONE',  ( 7.204075437095968759, -7.204075437095966983, 72.71875000204838102 ) ) ;
#11670 = CARTESIAN_POINT ( 'NONE',  ( -3.999999999999959144, 195.0625000000000284, 199.6568542494924259 ) ) ;
#11672 = CARTESIAN_POINT ( 'NONE',  ( 11.35316468749999963, 185.9895833299193555, -3.042071309553165293 ) ) ;
#11671 = CARTESIAN_POINT ( 'NONE',  ( -2.435013580646407494, 194.9873243428586704, 194.8320309108055142 ) ) ;
#11673 = CARTESIAN_POINT ( 'NONE',  ( 7.999999999999991118, 3.313708498984757611, 4.730302784329824206 ) ) ;
#11674 = CARTESIAN_POINT ( 'NONE',  ( 1.656854249492318409, 207.9375000027311842, 146.0000000000000568 ) ) ;
#11675 = CARTESIAN_POINT ( 'NONE',  ( -9.999999999999998224, 248.3333333401613174, 2.679491924311235618 ) ) ;
#11676 = CARTESIAN_POINT ( 'NONE',  ( -29.65685424949237259, 206.0624999999999716, 166.0000000000003695 ) ) ;
#11677 = CARTESIAN_POINT ( 'NONE',  ( 3.042071309553159519, 174.7395833299193555, 11.35316468750000141 ) ) ;
#11678 = ORIENTED_EDGE ( 'NONE', *, *, #11751, .T. ) ;
#11679 = CARTESIAN_POINT ( 'NONE',  ( 3.042071309553159519, 165.0520833299193839, 11.35316468750000141 ) ) ;
#11680 = CARTESIAN_POINT ( 'NONE',  ( -2.977408999572647819, 7.188101187499992051, 28.20530278187175810 ) ) ;
#11681 = CARTESIAN_POINT ( 'NONE',  ( -9.832129032723420536, 124.0104166632526841, 5.676582343749997150 ) ) ;
#11682 = CARTESIAN_POINT ( 'NONE',  ( -1.347111479062088207E-15, 0.000000000000000000, 0.000000000000000000 ) ) ;
#11683 = ORIENTED_EDGE ( 'NONE', *, *, #30607, .T. ) ;
#11684 = ADVANCED_FACE ( 'NONE', ( #19479 ), #49265, .T. ) ;
#11685 = CARTESIAN_POINT ( 'NONE',  ( -4.541265875000002339, 10.93749999863440792, -5.561446717895856393E-16 ) ) ;
#11686 = CARTESIAN_POINT ( 'NONE',  ( -2.977408999572650039, 15.93749999795161543, -7.188101187500001821 ) ) ;
#11687 = CARTESIAN_POINT ( 'NONE',  ( -8.000000000000000000, 104.0937500040967905, -3.313708498984761608 ) ) ;
#11688 = CARTESIAN_POINT ( 'NONE',  ( -24.54126587500000056, 198.5000000013656347, 168.5673454167827003 ) ) ;
#11689 = CARTESIAN_POINT ( 'NONE',  ( 4.000000000000001776, 9.062499999999998224, -1.656854249492381248 ) ) ;
#11690 = FACE_OUTER_BOUND ( 'NONE', #3297, .T. ) ;
#11691 = CARTESIAN_POINT ( 'NONE',  ( -3.211159895383561391, 12.68749999863440792, -3.211159895383561835 ) ) ;
#11692 = CARTESIAN_POINT ( 'NONE',  ( 7.999999999999992895, -3.313708498984756279, 21.17405278392015333 ) ) ;
#11693 = CARTESIAN_POINT ( 'NONE',  ( 1.656854249492347719, 197.8125000000000284, 146.0000000000000284 ) ) ;
#11695 = ADVANCED_FACE ( 'NONE', ( #43234 ), #20592, .T. ) ;
#11694 = ORIENTED_EDGE ( 'NONE', *, *, #472, .T. ) ;
#11696 = CARTESIAN_POINT ( 'NONE',  ( 1.656854249492374143, 205.1875000000001137, 138.0000000000000568 ) ) ;
#11697 = CARTESIAN_POINT ( 'NONE',  ( -2.977408999572651815, 103.4375000020483668, 7.188101187500000933 ) ) ;
#11698 = CARTESIAN_POINT ( 'NONE',  ( -5.656854249492381470, 15.74999999590322197, 5.656854249492379694 ) ) ;
#11699 = ORIENTED_EDGE ( 'NONE', *, *, #44091, .F. ) ;
#11700 = DIRECTION ( 'NONE',  ( 0.000000000000000000, -1.000000000000000000, 0.000000000000000000 ) ) ;
#11701 = CARTESIAN_POINT ( 'NONE',  ( -5.082755093536319713, 5.082755093536319713, 23.79905278187175455 ) ) ;
#11702 = ORIENTED_EDGE ( 'NONE', *, *, #43051, .F. ) ;
#11703 =( BOUNDED_CURVE ( )  B_SPLINE_CURVE ( 2, ( #33276, #17009, #27971, #11363, #50975, #27588, #40035, #57398, #5706 ),
 .UNSPECIFIED., .F., .F. ) 
 B_SPLINE_CURVE_WITH_KNOTS ( ( 3, 2, 2, 2, 3 ),
 ( 0.05208333333333337034, 0.05729166666666669905, 0.06250000000000004163, 0.06770833333333337034, 0.07291666666666671293 ),
 .UNSPECIFIED. ) 
 CURVE ( )  GEOMETRIC_REPRESENTATION_ITEM ( )  RATIONAL_B_SPLINE_CURVE ( ( 0.9999999999999994449, 0.9238795325112872936, 1.000000000000000000, 0.9238795325112867385, 1.000000000000000000, 0.9238795325112867385, 1.000000000000000000, 0.9238795325112861834, 1.000000000000000666 ) ) 
 REPRESENTATION_ITEM ( '' )  );
#11704 = ORIENTED_EDGE ( 'NONE', *, *, #882, .F. ) ;
#11705 = CARTESIAN_POINT ( 'NONE',  ( -4.220049686691935698, 10.18810118749999916, 92.87500000204838102 ) ) ;
#11706 = CARTESIAN_POINT ( 'NONE',  ( -11.00000000000000000, 0.000000000000000000, 92.49999999999998579 ) ) ;
#11707 = CARTESIAN_POINT ( 'NONE',  ( -30.44569435410878810, 195.0625000013656063, 172.4456943541092357 ) ) ;
#11708 = CARTESIAN_POINT ( 'NONE',  ( -4.556349186104045934, 11.00000000000000000, 101.2187500000000000 ) ) ;
#11709 = CONICAL_SURFACE ( 'NONE', #920, 10.49999999999998224, 0.7853981633974378429 ) ;
#11711 = CARTESIAN_POINT ( 'NONE',  ( -4.088227598258586603E-16, 297.3593750017070079, -6.676582343750001591 ) ) ;
#11710 = CARTESIAN_POINT ( 'NONE',  ( -28.00000000000007816, 201.1250000027312126, 166.0000000000003695 ) ) ;
#11712 = CARTESIAN_POINT ( 'NONE',  ( -2.679491924311225848, 136.4583333333333428, -10.00000000000000178 ) ) ;
#11713 = CARTESIAN_POINT ( 'NONE',  ( 8.000000000000000000, 101.8437499999999858, -3.313708498984762496 ) ) ;
#11714 = CARTESIAN_POINT ( 'NONE',  ( 2.020667218593132706E-15, -11.00000000000000000, 87.06250000409676204 ) ) ;
#11715 = CARTESIAN_POINT ( 'NONE',  ( 5.082755093536318824, 5.082755093536319713, 2.799052781871750994 ) ) ;
#11716 = ADVANCED_FACE ( 'NONE', ( #14181 ), #8169, .T. ) ;
#11717 = CARTESIAN_POINT ( 'NONE',  ( 1.522769729196201526E-11, 196.2499999999988063, -10.00000000000000178 ) ) ;
#11718 = ADVANCED_FACE ( 'NONE', ( #14554 ), #14926, .T. ) ;
#11719 = CARTESIAN_POINT ( 'NONE',  ( 26.56734541678232375, 204.3750000013656063, 173.4587341249998929 ) ) ;
#11720 = CLOSED_SHELL ( 'NONE', ( #57920, #21422, #53345, #23794, #33069, #14802, #27539, #26325, #21847, #60599, #24559, #68848, #29143, #59130, #3912, #11037, #50058 ) ) ;
#11721 = CARTESIAN_POINT ( 'NONE',  ( -3.313708498984760720, 24.28124999590322020, -8.000000000000000000 ) ) ;
#11722 = CARTESIAN_POINT ( 'NONE',  ( 1.471067592899761672E-15, -8.008118988124991233, 2.888115283940627886 ) ) ;
#11723 = CARTESIAN_POINT ( 'NONE',  ( 3.458734124999959025, 196.5000000013656063, 140.5673454167824161 ) ) ;
#11724 = CARTESIAN_POINT ( 'NONE',  ( -5.082755093536324154, 118.7187500020483810, 5.082755093536326818 ) ) ;
#11726 = CARTESIAN_POINT ( 'NONE',  ( 3.563081508477182968, 194.7984481092557019, 196.6609801925580996 ) ) ;
#11725 = CARTESIAN_POINT ( 'NONE',  ( -2.828427124746209831, 204.3750000000000284, 139.1715728752538723 ) ) ;
#11727 = CARTESIAN_POINT ( 'NONE',  ( -11.35316468749999963, 239.2187500034139873, 0.000000000000000000 ) ) ;
#11728 = CARTESIAN_POINT ( 'NONE',  ( -32.38898301269489366, 42.28296087153265859, 65.00000000000000000 ) ) ;
#11729 = CARTESIAN_POINT ( 'NONE',  ( -7.188101187499991163, 2.977408999572646930, 27.26780278187175099 ) ) ;
#11730 = CARTESIAN_POINT ( 'NONE',  ( 28.00000000000001421, 196.5000000000000000, 165.9999999999998863 ) ) ;
#11731 = CARTESIAN_POINT ( 'NONE',  ( 3.042071309553167069, 11.82291666325268231, -11.35316468749999785 ) ) ;
#11732 = CARTESIAN_POINT ( 'NONE',  ( 3.464965446656449899, -11.85590772719120878, -0.1959795092987934584 ) ) ;
#11733 = CARTESIAN_POINT ( 'NONE',  ( -3.042071309553173730, 219.6354166632526699, 11.35316468749999785 ) ) ;
#11734 = CARTESIAN_POINT ( 'NONE',  ( -2.679491924311087736, 220.4166666598387110, 10.00000000000008349 ) ) ;
#11736 = CARTESIAN_POINT ( 'NONE',  ( -3.426202465283580523, 194.4587341250000350, 198.4732635780662235 ) ) ;
#11735 = CARTESIAN_POINT ( 'NONE',  ( 1.836970198721029589E-15, 234.3750000068279746, 10.00000000000000000 ) ) ;
#11737 = ORIENTED_EDGE ( 'NONE', *, *, #56350, .F. ) ;
#11738 = ADVANCED_FACE ( 'NONE', ( #48519 ), #66620, .T. ) ;
#11739 = EDGE_CURVE ( 'NONE', #62422, #7527, #21182, .T. ) ;
#11740 = CARTESIAN_POINT ( 'NONE',  ( -2.445694354108840063, 196.0625000013656063, 139.5543056458912190 ) ) ;
#11741 = CARTESIAN_POINT ( 'NONE',  ( -11.35316468750000141, 18.48958332991934483, 3.042071309553159963 ) ) ;
#11742 = CARTESIAN_POINT ( 'NONE',  ( -4.556349186104045934, 11.00000000000000000, 92.40625000409676204 ) ) ;
#11743 = CARTESIAN_POINT ( 'NONE',  ( -46.67364751762348618, 38.00000000000001421, 69.99999999999997158 ) ) ;
#11744 = DIRECTION ( 'NONE',  ( -0.000000000000000000, 1.000000000000000000, -0.000000000000000000 ) ) ;
#11745 = LINE ( 'NONE', #56287, #51504 ) ;
#11747 = CARTESIAN_POINT ( 'NONE',  ( -9.832129032723420536, 13.69791666325268409, 5.676582343749997150 ) ) ;
#11746 = CARTESIAN_POINT ( 'NONE',  ( 5.082755093536325042, 111.5937500020483810, -5.082755093536325930 ) ) ;
#11748 = CARTESIAN_POINT ( 'NONE',  ( -7.999999999999991118, 0.000000000000000000, 21.83030277982336997 ) ) ;
#11749 = CARTESIAN_POINT ( 'NONE',  ( 5.676582343750001591, 136.6145833299193555, -9.832129032723420536 ) ) ;
#11750 = CARTESIAN_POINT ( 'NONE',  ( -10.00000000000000178, 109.3749999931720396, -1.224646799147353454E-15 ) ) ;
#11751 = EDGE_CURVE ( 'NONE', #25916, #653, #29490, .T. ) ;
#11752 = CARTESIAN_POINT ( 'NONE',  ( 2.977408999572650039, 115.0625000020483952, -7.188101187500001821 ) ) ;
#11753 = CARTESIAN_POINT ( 'NONE',  ( -3.313708498984800688, 13.78124999590322552, -7.999999999999958256 ) ) ;
#11754 = CARTESIAN_POINT ( 'NONE',  ( -31.45873412499999944, 206.9375000013656063, 170.0000000000003979 ) ) ;
#11755 = CARTESIAN_POINT ( 'NONE',  ( -4.999999999999999112, -53.57153130924464079, -46.19535935661085091 ) ) ;
#11756 = ORIENTED_EDGE ( 'NONE', *, *, #42196, .T. ) ;
#11757 = CARTESIAN_POINT ( 'NONE',  ( -5.676582343750006032, 4.427083329919350163, 9.832129032723418760 ) ) ;
#11758 = LINE ( 'NONE', #9247, #23309 ) ;
#11759 = CARTESIAN_POINT ( 'NONE',  ( -4.721056650415998313, 296.5781250017069510, 4.721056650416000089 ) ) ;
#11760 = CARTESIAN_POINT ( 'NONE',  ( -11.35316468750000141, 138.2812499965860411, -1.390361679473963753E-15 ) ) ;
#11761 =( LENGTH_UNIT ( ) NAMED_UNIT ( * ) SI_UNIT ( .MILLI., .METRE. ) );
#11762 = CARTESIAN_POINT ( 'NONE',  ( -5.656854249492375253, 5.656854249492375253, 24.69905278432982598 ) ) ;
#11763 = CARTESIAN_POINT ( 'NONE',  ( -2.986204309486589110E-14, 67.59332269700053075, 20.03478791450399399 ) ) ;
#11764 = CARTESIAN_POINT ( 'NONE',  ( 9.832129032723416984, 246.8229166700806729, -5.676582343750003368 ) ) ;
#11765 = CARTESIAN_POINT ( 'NONE',  ( -6.238412754330611322E-16, 10.18810118749999916, 99.15625000204838102 ) ) ;
#11766 = ORIENTED_EDGE ( 'NONE', *, *, #14207, .T. ) ;
#11767 = CARTESIAN_POINT ( 'NONE',  ( 2.679491924311370177, 215.8333333265053682, 9.999999999999918288 ) ) ;
#11768 = CARTESIAN_POINT ( 'NONE',  ( -4.556349186104048599, -10.99999999999999822, 100.4687500040967763 ) ) ;
#11769 = CARTESIAN_POINT ( 'NONE',  ( 8.311093377946837890, 86.71874999658601268, -8.311093377946837890 ) ) ;
#11770 = ORIENTED_EDGE ( 'NONE', *, *, #1017, .F. ) ;
#11771 = CARTESIAN_POINT ( 'NONE',  ( -4.220049686691935698, 10.18810118749999916, 106.3750000020483668 ) ) ;
#11772 = CARTESIAN_POINT ( 'NONE',  ( 4.541265875000002339, 14.43749999863440792, 0.000000000000000000 ) ) ;
#11773 = VERTEX_POINT ( 'NONE', #49649 ) ;
#11774 = VERTEX_POINT ( 'NONE', #50017 ) ;
#11775 = CARTESIAN_POINT ( 'NONE',  ( -8.000000000000000000, 6.656250000000000888, -3.313708498984762496 ) ) ;
#11776 = CARTESIAN_POINT ( 'NONE',  ( 1.469576158976823947E-15, 110.5625000040967905, 8.000000000000000000 ) ) ;
#11777 = CARTESIAN_POINT ( 'NONE',  ( -5.000000000000000000, -29.68417822476653711, -4.268394125863121502 ) ) ;
#11778 = CARTESIAN_POINT ( 'NONE',  ( -7.188101187500002709, 24.18749999795161543, 2.977408999572649151 ) ) ;
#11779 = CARTESIAN_POINT ( 'NONE',  ( 8.000000000000000000, 119.9375000040967763, -9.797174393178825657E-16 ) ) ;
#11780 = VECTOR ( 'NONE', #11488, 1000.000000000000000 ) ;
#11781 = CARTESIAN_POINT ( 'NONE',  ( -7.204075437095967871, 7.204075437095967871, 103.8437500020483810 ) ) ;
#11782 = EDGE_CURVE ( 'NONE', #12782, #36860, #34218, .T. ) ;
#11783 = B_SPLINE_CURVE_WITH_KNOTS ( 'NONE', 3,
 ( #8748, #49853, #54407, #31758, #55532, #21175, #72871, #15139, #72494, #3842, #2714, #31381 ),
 .UNSPECIFIED., .F., .F.,
 ( 4, 2, 2, 2, 2, 4 ),
 ( 0.04207017064022902653, 0.04374078687342293492, 0.04541140310661684332, 0.04708201933981074477, 0.04791732745640769897, 0.04875263557300465317 ),
 .UNSPECIFIED. ) ;
#11784 = CARTESIAN_POINT ( 'NONE',  ( 4.999999999999999112, 110.8333333333333428, -8.660254037844383745 ) ) ;
#11785 = CARTESIAN_POINT ( 'NONE',  ( -4.000000000000002665, 9.312499997268814056, 1.656854249492380804 ) ) ;
#11786 = CARTESIAN_POINT ( 'NONE',  ( 4.541265875000002339, 1.374999998634407250, -1.881053915767121776 ) ) ;
#11787 = ORIENTED_EDGE ( 'NONE', *, *, #27274, .F. ) ;
#11788 = DIRECTION ( 'NONE',  ( -0.000000000000000000, -1.000000000000000000, -0.000000000000000000 ) ) ;
#11789 = CARTESIAN_POINT ( 'NONE',  ( -3.458734124999959914, 198.4375000013655779, 198.0000000000000284 ) ) ;
#11790 = CARTESIAN_POINT ( 'NONE',  ( -28.00000000000007105, 204.4375000013656063, 166.5412658750003629 ) ) ;
#11791 = EDGE_CURVE ( 'NONE', #8182, #65581, #17413, .T. ) ;
#11792 = CARTESIAN_POINT ( 'NONE',  ( -8.342170076843785083E-16, 12.06249999863440614, 4.541265875000002339 ) ) ;
#11793 = CARTESIAN_POINT ( 'NONE',  ( 1.656854249492381248, 16.18750000000000000, -4.000000000000001776 ) ) ;
#11794 = CARTESIAN_POINT ( 'NONE',  ( -5.082755093536317936, -5.082755093536320601, 18.17405278187175455 ) ) ;
#11795 = ORIENTED_EDGE ( 'NONE', *, *, #26071, .F. ) ;
#11796 = ORIENTED_EDGE ( 'NONE', *, *, #54912, .T. ) ;
#11797 = CARTESIAN_POINT ( 'NONE',  ( 4.220049686691941027, -10.18810118749999738, 110.1250000020483810 ) ) ;
#11798 = CYLINDRICAL_SURFACE ( 'NONE', #57456, 3.999999999999976019 ) ;
#11799 = CARTESIAN_POINT ( 'NONE',  ( -31.99999999999998579, 203.3125000000000284, 171.6568542494928238 ) ) ;
#11800 = CARTESIAN_POINT ( 'NONE',  ( -3.458734124999959914, 199.3750000013656063, 196.5673454167823877 ) ) ;
#11801 = LINE ( 'NONE', #40102, #66324 ) ;
#11802 = CARTESIAN_POINT ( 'NONE',  ( 5.000000000000001776, 85.83333333333334281, -8.660254037844389075 ) ) ;
#11803 = CARTESIAN_POINT ( 'NONE',  ( 1.469576158976823947E-15, 116.3750000000000000, 8.000000000000000000 ) ) ;
#11804 = CARTESIAN_POINT ( 'NONE',  ( 11.35316468749999963, 66.30208332991935549, -3.042071309553165293 ) ) ;
#11805 = CARTESIAN_POINT ( 'NONE',  ( 6.000000000000003553, 288.5625000000000000, -2.485281374238571761 ) ) ;
#11806 = ORIENTED_EDGE ( 'NONE', *, *, #23306, .F. ) ;
#11807 = DIRECTION ( 'NONE',  ( 0.000000000000000000, 0.000000000000000000, 1.000000000000000000 ) ) ;
#11808 = EDGE_CURVE ( 'NONE', #4330, #17054, #660, .T. ) ;
#11809 = CARTESIAN_POINT ( 'NONE',  ( -2.216418498320922748, -67.77535163244887428, 20.18253627485176693 ) ) ;
#11810 = CARTESIAN_POINT ( 'NONE',  ( -3.458734125000015425, 207.0000000013656063, 143.4326545832176976 ) ) ;
#11811 = CARTESIAN_POINT ( 'NONE',  ( 7.778174593052023411, -7.778174593052021635, 91.56249999999998579 ) ) ;
#11812 = CARTESIAN_POINT ( 'NONE',  ( 28.47326357806521813, 194.4587341250000350, 173.4262024652836658 ) ) ;
#11813 = CARTESIAN_POINT ( 'NONE',  ( -7.320508075688771932, 244.3750000000000000, -7.320508075688771932 ) ) ;
#11814 = FACE_OUTER_BOUND ( 'NONE', #5135, .T. ) ;
#11815 = CARTESIAN_POINT ( 'NONE',  ( -6.238412754330611322E-16, 10.18810118749999916, 70.65625000204836681 ) ) ;
#11816 = CARTESIAN_POINT ( 'NONE',  ( 10.00000000000000178, 205.2083333333333428, -2.679491924311226736 ) ) ;
#11817 = EDGE_CURVE ( 'NONE', #24834, #50950, #51134, .T. ) ;
#11818 = CARTESIAN_POINT ( 'NONE',  ( 1.320432766682872962E-15, -7.188101187499992051, 18.73655278187175455 ) ) ;
#11819 = CARTESIAN_POINT ( 'NONE',  ( 8.311093377946837890, 176.7187499965860127, -8.311093377946837890 ) ) ;
#11820 = CARTESIAN_POINT ( 'NONE',  ( 105.0000000000000000, 146.0000000000000000, 139.0000000000000000 ) ) ;
#11821 = CARTESIAN_POINT ( 'NONE',  ( 1.656854249492379472, 1.937499997268812946, -4.000000000000002665 ) ) ;
#11823 = CARTESIAN_POINT ( 'NONE',  ( 2.679491924311228956, 87.91666665983868256, -10.00000000000000000 ) ) ;
#11822 = CARTESIAN_POINT ( 'NONE',  ( -9.999999999999998224, 228.3333333401613174, 2.679491924311235174 ) ) ;
#11824 = ORIENTED_EDGE ( 'NONE', *, *, #24458, .T. ) ;
#11825 = CARTESIAN_POINT ( 'NONE',  ( -2.754378923186476579E-14, 198.1875000013655779, 145.4587341250000350 ) ) ;
#11826 = CARTESIAN_POINT ( 'NONE',  ( -5.676582343749998039, 32.76041666325269119, -9.832129032723420536 ) ) ;
#11827 = CARTESIAN_POINT ( 'NONE',  ( -6.735557395310442023E-16, 11.00000000000000000, 111.8125000040967763 ) ) ;
#11828 = CARTESIAN_POINT ( 'NONE',  ( -28.00000000000007461, 208.4375000013656063, 166.5412658750003629 ) ) ;
#11829 = DIRECTION ( 'NONE',  ( -0.000000000000000000, 1.000000000000000000, 2.238352872228138170E-16 ) ) ;
#11831 = CARTESIAN_POINT ( 'NONE',  ( -2.679491924311220519, 101.4583333333333286, -9.999999999999978684 ) ) ;
#11830 = DIRECTION ( 'NONE',  ( 1.000000000000000000, 0.000000000000000000, 0.000000000000000000 ) ) ;
#11832 = CARTESIAN_POINT ( 'NONE',  ( 6.123233995736767268E-16, 68.12499999317203958, -10.00000000000000178 ) ) ;
#11833 = CARTESIAN_POINT ( 'NONE',  ( 3.458734124999958581, 199.5000000013656063, 140.5673454167823593 ) ) ;
#11834 =( BOUNDED_CURVE ( )  B_SPLINE_CURVE ( 2, ( #73443, #60634, #56478, #67417, #73813, #66663, #73074, #44404, #14969 ),
 .UNSPECIFIED., .F., .F. ) 
 B_SPLINE_CURVE_WITH_KNOTS ( ( 3, 2, 2, 2, 3 ),
 ( 0.7058823529411764053, 0.7095588235294116863, 0.7132352941176469674, 0.7169117647058823595, 0.7205882352941176405 ),
 .UNSPECIFIED. ) 
 CURVE ( )  GEOMETRIC_REPRESENTATION_ITEM ( )  RATIONAL_B_SPLINE_CURVE ( ( 1.000000000000002220, 0.9238795325112844070, 1.000000000000000000, 0.9238795325112867385, 1.000000000000000000, 0.9238795325112867385, 1.000000000000000000, 0.9238795325112867385, 1.000000000000000000 ) ) 
 REPRESENTATION_ITEM ( '' )  );
#11835 = CIRCLE ( 'NONE', #56428, 14.00000000000000000 ) ;
#11836 = CARTESIAN_POINT ( 'NONE',  ( -7.320508075688778149, 59.99999999317203248, 7.320508075688769267 ) ) ;
#11837 = CARTESIAN_POINT ( 'NONE',  ( 2.977408999572650039, 98.18750000204838102, -7.188101187500001821 ) ) ;
#11838 = CARTESIAN_POINT ( 'NONE',  ( 4.541265875000002339, 12.49999999863440969, -1.881053915767121554 ) ) ;
#11839 = CARTESIAN_POINT ( 'NONE',  ( 3.313708498984756279, 7.999999999999991118, 1.861552779823364423 ) ) ;
#11840 = ORIENTED_EDGE ( 'NONE', *, *, #46837, .T. ) ;
#11842 = EDGE_CURVE ( 'NONE', #72356, #20252, #51124, .T. ) ;
#11841 = ORIENTED_EDGE ( 'NONE', *, *, #11610, .F. ) ;
#11843 = CARTESIAN_POINT ( 'NONE',  ( -2.124081043562911830, -50.03790111639190741, -40.75706181777510295 ) ) ;
#11844 = CARTESIAN_POINT ( 'NONE',  ( 6.676582343750001591, 298.1093750017069510, -8.176455196517173205E-16 ) ) ;
#11845 = CARTESIAN_POINT ( 'NONE',  ( -7.320508075688787919, 163.1250000000000568, 7.320508075688779925 ) ) ;
#11846 = CARTESIAN_POINT ( 'NONE',  ( -2.170320029193735234, 51.35721532638135045, -48.60044191894100862 ) ) ;
#11847 = CARTESIAN_POINT ( 'NONE',  ( 3.042071309553167069, 156.8229166632526983, -11.35316468749999785 ) ) ;
#11848 = CARTESIAN_POINT ( 'NONE',  ( 8.660254037844376640, 105.4166666666666714, -4.999999999999992895 ) ) ;
#11849 = CARTESIAN_POINT ( 'NONE',  ( -6.238412754330611322E-16, 10.18810118749999916, 80.78125000204838102 ) ) ;
#11850 = CARTESIAN_POINT ( 'NONE',  ( 4.898587196589412829E-16, 4.875000000000000888, -8.000000000000000000 ) ) ;
#11851 = CIRCLE ( 'NONE', #34754, 19.00000000000000355 ) ;
#11852 = CARTESIAN_POINT ( 'NONE',  ( 4.000000000000015987, 202.5000000000000000, 198.0000000000000284 ) ) ;
#11853 = CARTESIAN_POINT ( 'NONE',  ( 5.622403371994028731, -5.703161834202245650, -0.000000000000000000 ) ) ;
#11854 = CARTESIAN_POINT ( 'NONE',  ( -6.238412754330611322E-16, 10.18810118749999916, 117.1562500020483810 ) ) ;
#11855 = ORIENTED_EDGE ( 'NONE', *, *, #5591, .T. ) ;
#11856 = CIRCLE ( 'NONE', #56443, 18.99999999999998934 ) ;
#11857 = CARTESIAN_POINT ( 'NONE',  ( 35.10848717540839914, -10.41162500814705361, 145.5284226875257332 ) ) ;
#11858 = CARTESIAN_POINT ( 'NONE',  ( 35.44037136445330560, 174.9968844453804024, 162.5244051778536800 ) ) ;
#11859 = CARTESIAN_POINT ( 'NONE',  ( 5.676582343749993598, 130.2604166632526983, 9.832129032723422313 ) ) ;
#11860 = CARTESIAN_POINT ( 'NONE',  ( 2.839093476692135984E-14, 198.6875000013655779, 201.4587341250000350 ) ) ;
#11861 = CARTESIAN_POINT ( 'NONE',  ( -7.188101187500002709, 25.68749999795162253, 2.977408999572649151 ) ) ;
#11862 = CARTESIAN_POINT ( 'NONE',  ( 7.204075437095968759, -7.204075437095966983, 79.09375000204838102 ) ) ;
#11863 = CARTESIAN_POINT ( 'NONE',  ( -2.085542519210945728E-15, 39.84374999658601979, 11.35316468750000141 ) ) ;
#11864 = ORIENTED_EDGE ( 'NONE', *, *, #19334, .F. ) ;
#11865 = CARTESIAN_POINT ( 'NONE',  ( 6.123233995736767268E-16, 38.12499999317203958, -10.00000000000000178 ) ) ;
#11866 = DIRECTION ( 'NONE',  ( -0.000000000000000000, -0.000000000000000000, 1.000000000000000000 ) ) ;
#11867 = CARTESIAN_POINT ( 'NONE',  ( 8.008118988124993010, -3.317071493978877239, 16.66936528394062833 ) ) ;
#11868 = CARTESIAN_POINT ( 'NONE',  ( 3.458734124999960358, 206.6875000013656063, 142.0000000000000568 ) ) ;
#11869 = CARTESIAN_POINT ( 'NONE',  ( 7.188101187499999156, 6.374999997951610986, 2.977408999572654924 ) ) ;
#11870 = CARTESIAN_POINT ( 'NONE',  ( 2.485281374238571317, 294.7500000034140157, -6.000000000000003553 ) ) ;
#11871 = CARTESIAN_POINT ( 'NONE',  ( -22.47208635730043724, -13.90457062485806539, 137.3734879024097211 ) ) ;
#11872 = CARTESIAN_POINT ( 'NONE',  ( -1.320432766682874540E-15, 4.968749997951610986, 7.188101187500000044 ) ) ;
#11873 = CARTESIAN_POINT ( 'NONE',  ( 7.188101187499992051, 2.977408999572647819, 12.83030278187175277 ) ) ;
#11874 = EDGE_CURVE ( 'NONE', #70240, #23624, #67754, .T. ) ;
#11875 = CARTESIAN_POINT ( 'NONE',  ( -7.204075437095965206, -7.204075437095968759, 72.34375000204836681 ) ) ;
#11876 = CARTESIAN_POINT ( 'NONE',  ( -27.99999999999996803, 207.1875000013656063, 173.4587341250003760 ) ) ;
#11877 = EDGE_CURVE ( 'NONE', #65410, #59936, #41464, .T. ) ;
#11878 = DIRECTION ( 'NONE',  ( 0.000000000000000000, 0.000000000000000000, -1.000000000000000000 ) ) ;
#11879 = CARTESIAN_POINT ( 'NONE',  ( -4.541265875000002339, 20.87499999863441147, -1.881053915767121998 ) ) ;
#11880 = UNCERTAINTY_MEASURE_WITH_UNIT (LENGTH_MEASURE( 1.000000000000000082E-05 ), #57835, 'distance_accuracy_value', 'NONE');
#11881 = ORIENTED_EDGE ( 'NONE', *, *, #41331, .T. ) ;
#11882 = CARTESIAN_POINT ( 'NONE',  ( 4.000000000000015987, 198.6250000027312126, 198.0000000000000284 ) ) ;
#11883 = CARTESIAN_POINT ( 'NONE',  ( 3.999999999999960032, 204.9375000000000284, 143.6568542494924543 ) ) ;
#11884 = CARTESIAN_POINT ( 'NONE',  ( -30.82842712474624491, 203.2500000027312126, 167.1715728752542418 ) ) ;
#11886 = CARTESIAN_POINT ( 'NONE',  ( 5.082755093536326818, 118.7187500020483810, 5.082755093536325042 ) ) ;
#11885 = VECTOR ( 'NONE', #12312, 1000.000000000000000 ) ;
#11887 = CARTESIAN_POINT ( 'NONE',  ( -11.00000000000000000, 0.000000000000000000, 74.68750000409676204 ) ) ;
#11888 = CARTESIAN_POINT ( 'NONE',  ( -3.313708498984758943, -7.999999999999989342, 5.799052783920146226 ) ) ;
#11889 = ORIENTED_EDGE ( 'NONE', *, *, #4731, .T. ) ;
#11890 = CARTESIAN_POINT ( 'NONE',  ( 5.082755093536324154, 18.28124999795161187, 5.082755093536326818 ) ) ;
#11891 = VERTEX_POINT ( 'NONE', #5869 ) ;
#11892 = CARTESIAN_POINT ( 'NONE',  ( 29.65685424949250404, 200.4375000000000568, 165.9999999999999716 ) ) ;
#11893 = CARTESIAN_POINT ( 'NONE',  ( -0.8419854211627032514, -10.28111362163632769, -63.57154293063803152 ) ) ;
#11894 = CARTESIAN_POINT ( 'NONE',  ( -5.000000000000005329, 38.33333333333333570, 8.660254037844387298 ) ) ;
#11895 = CARTESIAN_POINT ( 'NONE',  ( 5.082755093536326818, 104.0937500020483810, 5.082755093536325042 ) ) ;
#11896 = CARTESIAN_POINT ( 'NONE',  ( -25.55430564589119768, 208.5625000013656063, 167.5543056458915316 ) ) ;
#11897 = CARTESIAN_POINT ( 'NONE',  ( -23.99999999999998579, 196.7500000000000000, 170.0000000000003411 ) ) ;
#11899 = CARTESIAN_POINT ( 'NONE',  ( 7.320508075688774596, 197.4999999931720254, -7.320508075688774596 ) ) ;
#11898 = CARTESIAN_POINT ( 'NONE',  ( -7.320508075688773708, 33.74999999317202537, -7.320508075688774596 ) ) ;
#11900 = ORIENTED_EDGE ( 'NONE', *, *, #35816, .T. ) ;
#11901 = AXIS2_PLACEMENT_3D ( 'NONE', #33558, #58425, #53125 ) ;
#11902 = CARTESIAN_POINT ( 'NONE',  ( -5.676582343749992710, 249.7395833367473301, 9.832129032723422313 ) ) ;
#11903 = CARTESIAN_POINT ( 'NONE',  ( -5.082755093536317936, -5.082755093536320601, 20.04905278187175455 ) ) ;
#11904 = CARTESIAN_POINT ( 'NONE',  ( 3.228176881614417848, 50.21013539027831030, 40.85102191503853675 ) ) ;
#11905 = CARTESIAN_POINT ( 'NONE',  ( 28.00000000000002132, 206.5000000000000284, 165.9999999999998863 ) ) ;
#11906 = CARTESIAN_POINT ( 'NONE',  ( 105.0000000000000000, 205.0000000000000284, 0.000000000000000000 ) ) ;
#11907 = DIRECTION ( 'NONE',  ( 0.000000000000000000, -1.000000000000000000, 0.000000000000000000 ) ) ;
#11908 = CARTESIAN_POINT ( 'NONE',  ( 8.660254037844385522, 159.5833333333333428, 5.000000000000005329 ) ) ;
#11909 = DIRECTION ( 'NONE',  ( -0.000000000000000000, -0.000000000000000000, 1.000000000000000000 ) ) ;
#11910 = LINE ( 'NONE', #57197, #30728 ) ;
#11911 = DIRECTION ( 'NONE',  ( 1.000000000000000000, 0.000000000000000000, 0.000000000000000000 ) ) ;
#11912 = CARTESIAN_POINT ( 'NONE',  ( -9.832129032723418760, 133.1770833299193555, -5.676582343750004256 ) ) ;
#11913 = CARTESIAN_POINT ( 'NONE',  ( -4.242640687119285658, 294.1875000034139589, 4.242640687119287435 ) ) ;
#11914 = CARTESIAN_POINT ( 'NONE',  ( 4.615726161707415010, -16.27701803902728273, -69.62876280158644704 ) ) ;
#11917 = CARTESIAN_POINT ( 'NONE',  ( 5.000000000000000000, 60.90295814858271939, -23.31388853594749833 ) ) ;
#11916 = CARTESIAN_POINT ( 'NONE',  ( 30.44569435410882718, 195.5625000013656063, 172.4456943541086957 ) ) ;
#11915 = CARTESIAN_POINT ( 'NONE',  ( 31.99999999999998579, 209.1875000000000000, 171.6568542494923122 ) ) ;
#11918 = ORIENTED_EDGE ( 'NONE', *, *, #29775, .T. ) ;
#11919 = CARTESIAN_POINT ( 'NONE',  ( -3.042071309553164404, 2.552083329919349275, -11.35316468749999963 ) ) ;
#11920 = FACE_OUTER_BOUND ( 'NONE', #71891, .T. ) ;
#11921 = CARTESIAN_POINT ( 'NONE',  ( 26.34314575050753149, 196.0625000027312126, 173.9999999999997726 ) ) ;
#11922 = CARTESIAN_POINT ( 'NONE',  ( 5.000000000000001776, -62.69487254116403108, -24.02505537902060695 ) ) ;
#11923 = CARTESIAN_POINT ( 'NONE',  ( -10.00000000000000000, 19.16666665983869322, -2.679491924311229845 ) ) ;
#11924 = CARTESIAN_POINT ( 'NONE',  ( 1.320432766682874540E-15, 115.5312500020483952, 7.188101187500000044 ) ) ;
#11925 = CARTESIAN_POINT ( 'NONE',  ( -8.342170076843785083E-16, 22.06249999863440792, 4.541265875000002339 ) ) ;
#11926 = CARTESIAN_POINT ( 'NONE',  ( -0.8912353796373138071, -51.17464048784082564, 48.53058040617325020 ) ) ;
#11927 = CARTESIAN_POINT ( 'NONE',  ( -5.656854249492375253, 5.656854249492375253, 21.64280277982336997 ) ) ;
#11929 = CARTESIAN_POINT ( 'NONE',  ( -6.123233995736766282E-16, 238.7500000000000284, -10.00000000000000000 ) ) ;
#11928 = FACE_OUTER_BOUND ( 'NONE', #3581, .T. ) ;
#11930 = CARTESIAN_POINT ( 'NONE',  ( 8.311093377946834337, 115.1562499965859985, 8.311093377946839666 ) ) ;
#11931 = VERTEX_POINT ( 'NONE', #68858 ) ;
#11932 =( BOUNDED_CURVE ( )  B_SPLINE_CURVE ( 2, ( #8133, #58722, #31136, #7033, #54168, #48485, #49229, #62046, #38301, #60554, #44329, #26209, #31891 ),
 .UNSPECIFIED., .F., .F. ) 
 B_SPLINE_CURVE_WITH_KNOTS ( ( 3, 2, 2, 2, 2, 2, 3 ),
 ( 0.6250000000000001110, 0.6268115942028986698, 0.6286231884057972286, 0.6304347826086957873, 0.6322463768115942351, 0.6340579710144927938, 0.6358695652173913526 ),
 .UNSPECIFIED. ) 
 CURVE ( )  GEOMETRIC_REPRESENTATION_ITEM ( )  RATIONAL_B_SPLINE_CURVE ( ( 0.9999999999999978906, 0.9659258262890704216, 1.000000000000000000, 0.9659258262890683122, 1.000000000000000000, 0.9659258262890683122, 1.000000000000000000, 0.9659258262890683122, 1.000000000000000000, 0.9659258262890683122, 1.000000000000000000, 0.9659258262890683122, 1.000000000000000000 ) ) 
 REPRESENTATION_ITEM ( '' )  );
#11933 = CARTESIAN_POINT ( 'NONE',  ( -14.00000000000000178, -2.250000000005106138, 10.23492587299426404 ) ) ;
#11934 = CARTESIAN_POINT ( 'NONE',  ( 0.000000000000000000, 300.0000000000000000, 0.000000000000000000 ) ) ;
#11935 = LINE ( 'NONE', #45147, #10980 ) ;
#11936 = CARTESIAN_POINT ( 'NONE',  ( -9.832129032723418760, 238.8020833367473301, -5.676582343749998927 ) ) ;
#11937 = CARTESIAN_POINT ( 'NONE',  ( 3.042071309553159519, 114.7395833299193555, 11.35316468750000141 ) ) ;
#11938 = VERTEX_POINT ( 'NONE', #23948 ) ;
#11939 = CARTESIAN_POINT ( 'NONE',  ( 5.000000000000000000, -10.26105934116143459, 64.40045319026695836 ) ) ;
#11940 = CARTESIAN_POINT ( 'NONE',  ( -4.220049686691937474, -10.18810118749999738, 102.4375000020483810 ) ) ;
#11941 = CARTESIAN_POINT ( 'NONE',  ( -10.00000000000000000, 224.1666666598386826, -2.679491924311229845 ) ) ;
#11942 = CARTESIAN_POINT ( 'NONE',  ( 2.445694354108840063, 199.0625000013656063, 200.4456943541088663 ) ) ;
#11943 = DIRECTION ( 'NONE',  ( 0.000000000000000000, 0.000000000000000000, 1.000000000000000000 ) ) ;
#11945 = CARTESIAN_POINT ( 'NONE',  ( -5.676582343749998039, 97.44791666325269830, -9.832129032723420536 ) ) ;
#11944 = CARTESIAN_POINT ( 'NONE',  ( -2.679491924311519835, 181.4583333333333428, -9.999999999999827693 ) ) ;
#11946 = CARTESIAN_POINT ( 'NONE',  ( 5.656854249492376141, -5.656854249492374365, 4.580302783920145338 ) ) ;
#11947 = CARTESIAN_POINT ( 'NONE',  ( -31.45873412499999233, 197.9375000013655779, 170.0000000000003979 ) ) ;
#11948 = CARTESIAN_POINT ( 'NONE',  ( -1.836970198721029983E-15, 63.75000000000000000, 10.00000000000000178 ) ) ;
#11949 = ORIENTED_EDGE ( 'NONE', *, *, #27916, .F. ) ;
#11950 = EDGE_CURVE ( 'NONE', #35159, #53828, #17169, .T. ) ;
#11951 = CARTESIAN_POINT ( 'NONE',  ( 10.00000000000000178, 191.8749999931720254, 0.000000000000000000 ) ) ;
#11952 = AXIS2_PLACEMENT_3D ( 'NONE', #17650, #51240, #74251 ) ;
#11953 = CARTESIAN_POINT ( 'NONE',  ( 3.313708498984873518, 114.9687500000000142, 7.999999999999890754 ) ) ;
#11954 = DIRECTION ( 'NONE',  ( -0.000000000000000000, 1.000000000000000000, -4.476705744456276341E-16 ) ) ;
#11955 = CARTESIAN_POINT ( 'NONE',  ( -11.35316468750000141, 93.80208332991935549, 3.042071309553159963 ) ) ;
#11956 = CARTESIAN_POINT ( 'NONE',  ( 3.458734125000015425, 208.9375000013656063, 198.0000000000000284 ) ) ;
#11957 = CARTESIAN_POINT ( 'NONE',  ( 7.188101187500000044, 8.343749997951611874, 0.000000000000000000 ) ) ;
#11958 = CARTESIAN_POINT ( 'NONE',  ( -7.204075437095965206, -7.204075437095968759, 92.21875000204838102 ) ) ;
#11959 = CARTESIAN_POINT ( 'NONE',  ( -5.676582343749998039, 2.760416663252683644, -9.832129032723420536 ) ) ;
#11961 = ORIENTED_EDGE ( 'NONE', *, *, #2410, .T. ) ;
#11960 =( BOUNDED_CURVE ( )  B_SPLINE_CURVE ( 2, ( #72120, #33281, #8760, #55918, #49108, #3855, #56280, #20432, #20056 ),
 .UNSPECIFIED., .F., .F. ) 
 B_SPLINE_CURVE_WITH_KNOTS ( ( 3, 2, 2, 2, 3 ),
 ( 0.2166666666666669516, 0.2250000000000002554, 0.2333333333333335313, 0.2416666666666668073, 0.2500000000000001110 ),
 .UNSPECIFIED. ) 
 CURVE ( )  GEOMETRIC_REPRESENTATION_ITEM ( )  RATIONAL_B_SPLINE_CURVE ( ( 0.9999999999999974465, 0.9238795325112892920, 1.000000000000000000, 0.9238795325112867385, 1.000000000000000000, 0.9238795325112867385, 1.000000000000000000, 0.9238795325112857393, 1.000000000000001110 ) ) 
 REPRESENTATION_ITEM ( '' )  );
#11962 = CARTESIAN_POINT ( 'NONE',  ( 8.000000000000000000, 123.0312500040967905, -3.313708498984762496 ) ) ;
#11963 = CARTESIAN_POINT ( 'NONE',  ( 3.000000000000001332, -44.80415277035162092, 139.1455027589170470 ) ) ;
#11964 = CARTESIAN_POINT ( 'NONE',  ( -9.832129032723420536, 223.6979166632526983, 5.676582343749997150 ) ) ;
#11965 = CARTESIAN_POINT ( 'NONE',  ( 0.000000000000000000, 300.0000000000000000, 0.000000000000000000 ) ) ;
#11966 = CARTESIAN_POINT ( 'NONE',  ( -27.99999999999991473, 207.6250000027312126, 174.0000000000003695 ) ) ;
#11967 = CARTESIAN_POINT ( 'NONE',  ( -2.765530957081996810, 296.2656250017069510, -6.676582343750003368 ) ) ;
#11968 = EDGE_LOOP ( 'NONE', ( #63092, #4211, #33598, #49729 ) ) ;
#11969 = CARTESIAN_POINT ( 'NONE',  ( -8.660254037844390851, 119.7916666598386968, 4.999999999999998224 ) ) ;
#11970 = CARTESIAN_POINT ( 'NONE',  ( -11.35316468750000141, 213.5937499965860411, -1.390361679473963753E-15 ) ) ;
#11971 = EDGE_CURVE ( 'NONE', #18291, #21807, #57641, .T. ) ;
#11972 = CARTESIAN_POINT ( 'NONE',  ( 4.220049686691934809, 10.18810118749999916, 89.68750000204836681 ) ) ;
#11973 = EDGE_CURVE ( 'NONE', #29697, #47641, #25848, .T. ) ;
#11974 = CARTESIAN_POINT ( 'NONE',  ( -25.55430564589119413, 203.3125000013656063, 167.5543056458915316 ) ) ;
#11975 = CARTESIAN_POINT ( 'NONE',  ( 3.313708498984762052, 15.28125000000000355, -8.000000000000000000 ) ) ;
#11976 = ORIENTED_EDGE ( 'NONE', *, *, #48891, .T. ) ;
#11977 = CARTESIAN_POINT ( 'NONE',  ( 7.188101187500001821, 120.5000000020483810, -2.977408999572651371 ) ) ;
#11978 = CARTESIAN_POINT ( 'NONE',  ( -26.34314575050763096, 200.0625000027311842, 166.0000000000004263 ) ) ;
#11979 = CARTESIAN_POINT ( 'NONE',  ( -7.320508075688773708, 21.87500000000000355, -7.320508075688774596 ) ) ;
#11980 = DIRECTION ( 'NONE',  ( 0.000000000000000000, 0.000000000000000000, -1.000000000000000000 ) ) ;
#11981 = CARTESIAN_POINT ( 'NONE',  ( -10.18810118749999916, 0.000000000000000000, 75.53125000204836681 ) ) ;
#11982 = VERTEX_POINT ( 'NONE', #34556 ) ;
#11983 = CARTESIAN_POINT ( 'NONE',  ( 9.000000000000000000, -3.485479754112952300, -0.3552645118408620517 ) ) ;
#11984 = CARTESIAN_POINT ( 'NONE',  ( -11.00000000000000000, 0.000000000000000000, 111.9999999999999858 ) ) ;
#11985 = DIRECTION ( 'NONE',  ( 0.000000000000000000, 0.000000000000000000, 1.000000000000000000 ) ) ;
#11986 = CARTESIAN_POINT ( 'NONE',  ( -5.082755093536325930, 122.8437500020483952, -5.082755093536325930 ) ) ;
#11987 = CARTESIAN_POINT ( 'NONE',  ( -6.676582343750002480, 297.3906250017069510, -2.765530957081996810 ) ) ;
#11989 = DIRECTION ( 'NONE',  ( 1.000000000000000000, -0.000000000000000000, -0.000000000000000000 ) ) ;
#11988 = CARTESIAN_POINT ( 'NONE',  ( 5.676582343749997150, 242.2395833367473301, -9.832129032723418760 ) ) ;
#11990 = CONTEXT_DEPENDENT_SHAPE_REPRESENTATION ( #42381, #73414 ) ;
#11991 = EDGE_LOOP ( 'NONE', ( #565, #29255, #31544, #5118 ) ) ;
#11992 = CARTESIAN_POINT ( 'NONE',  ( 8.311093377946839666, 246.0937500034139873, 8.311093377946829008 ) ) ;
#11993 = CARTESIAN_POINT ( 'NONE',  ( 7.188101187499992051, 8.802885111219154394E-16, 8.236552781871752771 ) ) ;
#11994 = ADVANCED_BREP_SHAPE_REPRESENTATION ( '', ( #65418, #57354 ), #17638 ) ;
#11995 = AXIS2_PLACEMENT_3D ( 'NONE', #29808, #59588, #53560 ) ;
#11996 = ORIENTED_EDGE ( 'NONE', *, *, #73976, .F. ) ;
#11997 = CARTESIAN_POINT ( 'NONE',  ( -10.18810118749999738, -4.220049686691941915, 70.75000000204836681 ) ) ;
#11998 = CARTESIAN_POINT ( 'NONE',  ( -8.311093377946836114, 92.96874999658602690, -8.311093377946837890 ) ) ;
#11999 = PLANE ( 'NONE',  #2293 ) ;
#12000 = CARTESIAN_POINT ( 'NONE',  ( -11.00000000000000000, 0.000000000000000000, 81.99999999999998579 ) ) ;
#12003 = CARTESIAN_POINT ( 'NONE',  ( -31.66756539373098178, -12.01114419369879016, 167.9999999999997726 ) ) ;
#12002 = CARTESIAN_POINT ( 'NONE',  ( 28.00000000000002132, 208.4375000013656063, 173.4587341249998929 ) ) ;
#12001 = CARTESIAN_POINT ( 'NONE',  ( 29.43265458321761230, 205.7500000013656063, 173.4587341249998929 ) ) ;
#12004 = ORIENTED_EDGE ( 'NONE', *, *, #72604, .T. ) ;
#12005 = CIRCLE ( 'NONE', #62558, 4.000000000000003553 ) ;
#12006 = CARTESIAN_POINT ( 'NONE',  ( -8.000000000000000000, 114.4062500000000000, -3.313708498984761164 ) ) ;
#12007 = CARTESIAN_POINT ( 'NONE',  ( 27.99999999999999645, 210.0000000000000284, 173.9999999999998863 ) ) ;
#12008 = CARTESIAN_POINT ( 'NONE',  ( 5.676582343749993598, 204.9479166632526983, 9.832129032723422313 ) ) ;
#12009 = CARTESIAN_POINT ( 'NONE',  ( 1.432654583217607192, 203.2500000013656063, 145.4587341250000634 ) ) ;
#12010 = CARTESIAN_POINT ( 'NONE',  ( 25.55430564589115150, 205.5625000013656063, 172.4456943541086957 ) ) ;
#12011 = CARTESIAN_POINT ( 'NONE',  ( 7.188101187500000044, 23.34374999795161543, 0.000000000000000000 ) ) ;
#12012 = CARTESIAN_POINT ( 'NONE',  ( -5.676582343749998039, 177.7604166632526699, -9.832129032723420536 ) ) ;
#12013 = CARTESIAN_POINT ( 'NONE',  ( -7.188101187500000044, 97.53125000204838102, 0.000000000000000000 ) ) ;
#12015 = CARTESIAN_POINT ( 'NONE',  ( -5.000000000000003553, 108.3333333333333570, 8.660254037844381969 ) ) ;
#12014 = CARTESIAN_POINT ( 'NONE',  ( -5.000000000000000888, 63.46295559274128806, -24.14151313015300104 ) ) ;
#12016 = CARTESIAN_POINT ( 'NONE',  ( -4.541265875000003227, 8.874999998634407916, 1.881053915767121110 ) ) ;
#12017 = CARTESIAN_POINT ( 'NONE',  ( 26.56734541678232731, 202.6250000013656063, 173.4587341249998929 ) ) ;
#12018 = CARTESIAN_POINT ( 'NONE',  ( 2.977408999572650927, -7.188101187499990274, 9.830302781871752771 ) ) ;
#12019 = CARTESIAN_POINT ( 'NONE',  ( -5.676582343749998039, 67.44791666325268409, -9.832129032723420536 ) ) ;
#12020 = DIRECTION ( 'NONE',  ( -1.000000000000000000, 0.000000000000000000, 0.000000000000000000 ) ) ;
#12021 = CARTESIAN_POINT ( 'NONE',  ( 5.656854249492376141, -5.656854249492374365, 1.449052784329824428 ) ) ;
#12022 = ORIENTED_EDGE ( 'NONE', *, *, #2609, .F. ) ;
#12023 = LINE ( 'NONE', #17302, #9749 ) ;
#12024 = CARTESIAN_POINT ( 'NONE',  ( 32.00000000000000711, 206.3125000027312126, 171.6568542494922553 ) ) ;
#12025 = CARTESIAN_POINT ( 'NONE',  ( -3.042071309553173730, 59.32291666325267698, 11.35316468749999785 ) ) ;
#12026 = CARTESIAN_POINT ( 'NONE',  ( -4.556349186104047710, -10.99999999999999822, 67.46875000409676204 ) ) ;
#12027 = CARTESIAN_POINT ( 'NONE',  ( 2.445694354108783219, 194.8125000013656063, 139.5543056458912190 ) ) ;
#12028 = DIRECTION ( 'NONE',  ( 0.000000000000000000, 0.000000000000000000, -1.000000000000000000 ) ) ;
#12030 = CARTESIAN_POINT ( 'NONE',  ( 3.042071309553159519, 54.73958332991934839, 11.35316468750000141 ) ) ;
#12029 = CARTESIAN_POINT ( 'NONE',  ( -5.082755093536325930, 92.46875000204838102, -5.082755093536325930 ) ) ;
#12031 = CARTESIAN_POINT ( 'NONE',  ( 1.469576158976822172E-15, -7.999999999999991118, 5.705302779823364645 ) ) ;
#12033 = CARTESIAN_POINT ( 'NONE',  ( -8.660254037844390851, 159.7916666598387110, 4.999999999999998224 ) ) ;
#12032 = PRODUCT_DEFINITION_SHAPE ( 'NONE', 'NONE',  #74656 ) ;
#12034 = CARTESIAN_POINT ( 'NONE',  ( -7.188101187499999156, 97.62500000204836681, 2.977408999572654924 ) ) ;
#12035 = DIRECTION ( 'NONE',  ( 1.000000000000000000, 0.000000000000000000, 0.000000000000000000 ) ) ;
#12036 = CARTESIAN_POINT ( 'NONE',  ( 3.042071309553159519, 50.05208332991935549, 11.35316468750000141 ) ) ;
#12037 = CARTESIAN_POINT ( 'NONE',  ( -10.18810118749999738, -4.220049686691941915, 114.6250000020483810 ) ) ;
#12038 = CARTESIAN_POINT ( 'NONE',  ( 11.35316468749999785, 180.5729166632526983, 3.042071309553174174 ) ) ;
#12039 = VERTEX_POINT ( 'NONE', #46957 ) ;
#12040 = CARTESIAN_POINT ( 'NONE',  ( 4.471435261917194204, 60.74652839096584955, 23.21845616858769645 ) ) ;
#12041 = CARTESIAN_POINT ( 'NONE',  ( -7.204075437095965206, -7.204075437095968759, 67.84375000204836681 ) ) ;
#12042 = DIRECTION ( 'NONE',  ( -1.000000000000000000, -0.000000000000000000, -0.000000000000000000 ) ) ;
#12044 = CARTESIAN_POINT ( 'NONE',  ( 9.832129032723420536, 176.1979166632526983, -5.676582343749999815 ) ) ;
#12043 = CARTESIAN_POINT ( 'NONE',  ( -3.034644841523098859E-11, -67.59332269700080076, 20.03478791450305962 ) ) ;
#12045 = DIRECTION ( 'NONE',  ( 0.000000000000000000, 0.8536788251726095123, -0.5207998305029611918 ) ) ;
#12046 = EDGE_CURVE ( 'NONE', #53794, #18299, #13885, .T. ) ;
#12047 = CARTESIAN_POINT ( 'NONE',  ( -8.660254037844385522, 248.5416666734946318, 5.000000000000004441 ) ) ;
#12048 = CARTESIAN_POINT ( 'NONE',  ( 0.000000000000000000, 0.000000000000000000, 0.000000000000000000 ) ) ;
#12049 = VERTEX_POINT ( 'NONE', #46587 ) ;
#12050 = CARTESIAN_POINT ( 'NONE',  ( -3.042071309553163960, 162.5520833299193555, -11.35316468749999963 ) ) ;
#12051 =( BOUNDED_CURVE ( )  B_SPLINE_CURVE ( 2, ( #44114, #51255, #38084, #27123, #61833, #56186, #44483, #33189, #22574 ),
 .UNSPECIFIED., .F., .F. ) 
 B_SPLINE_CURVE_WITH_KNOTS ( ( 3, 2, 2, 2, 3 ),
 ( 0.2638888888888888951, 0.2708333333333333148, 0.2777777777777777346, 0.2847222222222221544, 0.2916666666666666297 ),
 .UNSPECIFIED. ) 
 CURVE ( )  GEOMETRIC_REPRESENTATION_ITEM ( )  RATIONAL_B_SPLINE_CURVE ( ( 1.000000000000000000, 0.9238795325112867385, 1.000000000000000000, 0.9238795325112867385, 1.000000000000000000, 0.9238795325112867385, 1.000000000000000000, 0.9238795325112872936, 0.9999999999999994449 ) ) 
 REPRESENTATION_ITEM ( '' )  );
#12052 = CARTESIAN_POINT ( 'NONE',  ( -5.082755093536317936, -5.082755093536320601, 25.67405278187175810 ) ) ;
#12053 = CARTESIAN_POINT ( 'NONE',  ( 11.35316468749999785, 135.8854166632526983, 3.042071309553174174 ) ) ;
#12054 = CARTESIAN_POINT ( 'NONE',  ( 0.000000000000000000, 0.000000000000000000, 118.0000000000000000 ) ) ;
#12055 = ORIENTED_EDGE ( 'NONE', *, *, #61047, .F. ) ;
#12056 = EDGE_CURVE ( 'NONE', #58393, #38666, #12258, .T. ) ;
#12057 = CARTESIAN_POINT ( 'NONE',  ( 8.000000000000000000, 106.5312500040967905, -3.313708498984762496 ) ) ;
#12058 = CARTESIAN_POINT ( 'NONE',  ( 2.828427124746191623, 10.12500000000000000, -2.828427124746191623 ) ) ;
#12059 = CARTESIAN_POINT ( 'NONE',  ( 105.0000000000000000, 242.0000000000000284, 0.000000000000000000 ) ) ;
#12060 = CARTESIAN_POINT ( 'NONE',  ( 1.881053915767121998, 12.49999999863440969, -4.541265875000002339 ) ) ;
#12061 = CARTESIAN_POINT ( 'NONE',  ( 5.656854249492376141, -5.656854249492374365, 18.08030278392014623 ) ) ;
#12062 = CARTESIAN_POINT ( 'NONE',  ( 3.999999999999960032, 195.9375000000000000, 143.6568542494924543 ) ) ;
#12063 = ORIENTED_EDGE ( 'NONE', *, *, #16301, .F. ) ;
#12064 = CARTESIAN_POINT ( 'NONE',  ( -4.898587196589412829E-16, 112.8125000040967905, -8.000000000000000000 ) ) ;
#12065 = CARTESIAN_POINT ( 'NONE',  ( -2.977408999572650927, 104.3750000020483952, -7.188101187500001821 ) ) ;
#12067 = CARTESIAN_POINT ( 'NONE',  ( -4.000000000000015987, 209.5625000000000000, 143.6568542494924259 ) ) ;
#12066 = FACE_OUTER_BOUND ( 'NONE', #62925, .T. ) ;
#12068 = CARTESIAN_POINT ( 'NONE',  ( 1424.688200795887269, 828.9677537767817057, 969.8421604560587639 ) ) ;
#12069 = ORIENTED_EDGE ( 'NONE', *, *, #13442, .T. ) ;
#12070 = CARTESIAN_POINT ( 'NONE',  ( 1.558072418983080354, 16.42747873774318990, -68.67104701338824668 ) ) ;
#12071 = CARTESIAN_POINT ( 'NONE',  ( -7.188101187499990274, -2.977408999572651371, 25.58030278187175810 ) ) ;
#12072 = VERTEX_POINT ( 'NONE', #17545 ) ;
#12073 = ORIENTED_EDGE ( 'NONE', *, *, #64674, .T. ) ;
#12074 = CARTESIAN_POINT ( 'NONE',  ( -10.18810118749999916, 4.220049686691934809, 84.06250000204838102 ) ) ;
#12075 = CARTESIAN_POINT ( 'NONE',  ( -6.735557395310442023E-16, 11.00000000000000000, 92.12499999999998579 ) ) ;
#12076 = CARTESIAN_POINT ( 'NONE',  ( -25.55430564589119058, 196.5625000013656063, 167.5543056458915316 ) ) ;
#12077 = CARTESIAN_POINT ( 'NONE',  ( -4.556349186104047710, -10.99999999999999822, 100.2812499999999858 ) ) ;
#12080 = CARTESIAN_POINT ( 'NONE',  ( 4.721056650416000089, 296.9843750017070079, 4.721056650415999201 ) ) ;
#12079 = CARTESIAN_POINT ( 'NONE',  ( 31.99999999999998579, 204.4375000027311842, 168.3431457505075173 ) ) ;
#12078 = FACE_OUTER_BOUND ( 'NONE', #5303, .T. ) ;
#12081 = CARTESIAN_POINT ( 'NONE',  ( -10.00000000000000178, 132.5000000000000000, -1.224646799147353454E-15 ) ) ;
#12082 = CARTESIAN_POINT ( 'NONE',  ( -3.313708498984762052, 100.7187499999999858, -8.000000000000000000 ) ) ;
#12083 = CARTESIAN_POINT ( 'NONE',  ( 2.710081836398223309, 225.9999999999999716, 9.633870074142324214 ) ) ;
#12084 = CARTESIAN_POINT ( 'NONE',  ( 7.778174593052021635, 7.778174593052023411, 78.43750000000000000 ) ) ;
#12085 = CARTESIAN_POINT ( 'NONE',  ( -37.99999999999999289, 0.000000000000000000, 0.000000000000000000 ) ) ;
#12086 = CARTESIAN_POINT ( 'NONE',  ( 30.44569435410883429, 203.8125000013656063, 167.5543056458911053 ) ) ;
#12087 = CARTESIAN_POINT ( 'NONE',  ( 2.977408999572650927, 4.124999997951610986, -7.188101187500001821 ) ) ;
#12088 = CARTESIAN_POINT ( 'NONE',  ( 3.317071493978877683, 8.008118988124991233, 0.5443652839406293298 ) ) ;
#12089 = CARTESIAN_POINT ( 'NONE',  ( -1.432654583217664479, 194.7500000013656063, 138.5412658750000787 ) ) ;
#12090 = CARTESIAN_POINT ( 'NONE',  ( 5.082755093536325042, 117.9687500020483810, -5.082755093536325930 ) ) ;
#12092 = CARTESIAN_POINT ( 'NONE',  ( 5.656854249492376141, -5.656854249492374365, 7.392802779823366421 ) ) ;
#12091 = CARTESIAN_POINT ( 'NONE',  ( -2.849036369511732440E-14, 204.2500000000000284, 138.0000000000000568 ) ) ;
#12093 = CARTESIAN_POINT ( 'NONE',  ( 11.35316468749999963, 226.5104166700806445, 3.042071309553159519 ) ) ;
#12094 = CARTESIAN_POINT ( 'NONE',  ( -5.656854249492378806, 90.68750000000000000, 5.656854249492381470 ) ) ;
#12095 = CARTESIAN_POINT ( 'NONE',  ( -5.082755093536319713, 5.082755093536319713, 25.67405278187175810 ) ) ;
#12096 = CARTESIAN_POINT ( 'NONE',  ( 31.99999999999997868, 198.1875000000000853, 171.6568542494923122 ) ) ;
#12097 = CARTESIAN_POINT ( 'NONE',  ( 8.311093377946834337, 30.15624999658601624, 8.311093377946839666 ) ) ;
#12098 = CARTESIAN_POINT ( 'NONE',  ( -29.65685424949231219, 199.0625000000000284, 166.0000000000003411 ) ) ;
#12099 = CARTESIAN_POINT ( 'NONE',  ( 3.508297656242422846, 227.0932911785184842, -10.79750878567371153 ) ) ;
#12100 = DIRECTION ( 'NONE',  ( -0.000000000000000000, 1.000000000000000000, -0.000000000000000000 ) ) ;
#12102 = CARTESIAN_POINT ( 'NONE',  ( -5.656854249492375253, 5.656854249492375253, 29.14280277982336642 ) ) ;
#12101 = CARTESIAN_POINT ( 'NONE',  ( -30.99999999999992895, -31.99999999999978684, 205.0000000000000284 ) ) ;
#12103 = VERTEX_POINT ( 'NONE', #53000 ) ;
#12104 = CIRCLE ( 'NONE', #45823, 7.000000000000000000 ) ;
#12105 = CARTESIAN_POINT ( 'NONE',  ( -2.754378923186476579E-14, 197.4375000013655779, 145.4587341250000350 ) ) ;
#12106 = CARTESIAN_POINT ( 'NONE',  ( -3.042071309553173730, 24.32291666325268764, 11.35316468749999785 ) ) ;
#12107 = CARTESIAN_POINT ( 'NONE',  ( -7.778174593052023411, 7.778174593052023411, 86.50000000409677625 ) ) ;
#12108 = CARTESIAN_POINT ( 'NONE',  ( -2.754378923186476579E-14, 206.4375000013656063, 145.4587341250000350 ) ) ;
#12109 = CARTESIAN_POINT ( 'NONE',  ( 1.102182119232618108E-15, 295.3125000034140157, 6.000000000000001776 ) ) ;
#12110 = DIRECTION ( 'NONE',  ( -0.000000000000000000, 1.000000000000000000, -0.000000000000000000 ) ) ;
#12112 = CARTESIAN_POINT ( 'NONE',  ( -8.311093377946836114, 17.65624999658601624, -8.311093377946837890 ) ) ;
#12111 = CARTESIAN_POINT ( 'NONE',  ( 5.082755093536325042, 113.0937500020483810, -5.082755093536325930 ) ) ;
#12113 = CARTESIAN_POINT ( 'NONE',  ( -4.898587196589407898E-16, 7.999999999999991118, 19.95530277982336642 ) ) ;
#12114 = CARTESIAN_POINT ( 'NONE',  ( -9.832129032723418760, 142.8645833299193555, -5.676582343750004256 ) ) ;
#12115 = CARTESIAN_POINT ( 'NONE',  ( 6.123233995736767268E-16, 118.1249999931720396, -10.00000000000000178 ) ) ;
#12116 = CARTESIAN_POINT ( 'NONE',  ( 7.188101187500002709, 116.1875000020483952, 2.977408999572649151 ) ) ;
#12117 = CYLINDRICAL_SURFACE ( 'NONE', #40920, 10.00000000000000178 ) ;
#12118 = CARTESIAN_POINT ( 'NONE',  ( -46.67364751762349329, 146.0000000000000000, 69.99999999999997158 ) ) ;
#12119 = ORIENTED_EDGE ( 'NONE', *, *, #49843, .F. ) ;
#12120 = CARTESIAN_POINT ( 'NONE',  ( -11.35316468750000141, 13.59374999658601801, -1.390361679473963753E-15 ) ) ;
#12121 = ORIENTED_EDGE ( 'NONE', *, *, #19874, .T. ) ;
#12122 = DIRECTION ( 'NONE',  ( 3.469446951953619612E-16, 0.000000000000000000, 1.000000000000000000 ) ) ;
#12123 = CARTESIAN_POINT ( 'NONE',  ( 4.721056650416000089, 295.8281250017069510, 4.721056650415999201 ) ) ;
#12124 = CARTESIAN_POINT ( 'NONE',  ( -3.042071309553173730, 139.3229166632526699, 11.35316468749999785 ) ) ;
#12125 = DIRECTION ( 'NONE',  ( -0.000000000000000000, -1.000000000000000000, -0.000000000000000000 ) ) ;
#12126 = CARTESIAN_POINT ( 'NONE',  ( -7.999999999999991118, 0.000000000000000000, 26.38655278432982243 ) ) ;
#12127 = CARTESIAN_POINT ( 'NONE',  ( -11.00000000000000000, 0.000000000000000000, 91.18750000409677625 ) ) ;
#12128 = EDGE_CURVE ( 'NONE', #5844, #32408, #16319, .T. ) ;
#12129 = CARTESIAN_POINT ( 'NONE',  ( -11.35316468749999963, 243.9062500034140157, 0.000000000000000000 ) ) ;
#12130 = CARTESIAN_POINT ( 'NONE',  ( -7.204075437095965206, -7.204075437095968759, 93.71875000204838102 ) ) ;
#12131 = ORIENTED_EDGE ( 'NONE', *, *, #40761, .T. ) ;
#12132 = EDGE_CURVE ( 'NONE', #6596, #4443, #51505, .T. ) ;
#12133 = CARTESIAN_POINT ( 'NONE',  ( 0.000000000000000000, 0.000000000000000000, 118.0000000000000000 ) ) ;
#12134 = LINE ( 'NONE', #46836, #15861 ) ;
#12135 = UNCERTAINTY_MEASURE_WITH_UNIT (LENGTH_MEASURE( 1.000000000000000082E-05 ), #5423, 'distance_accuracy_value', 'NONE');
#12136 = CARTESIAN_POINT ( 'NONE',  ( 11.35316468750000141, 96.09374999658601268, 0.000000000000000000 ) ) ;
#12137 = ORIENTED_EDGE ( 'NONE', *, *, #43289, .F. ) ;
#12138 = CARTESIAN_POINT ( 'NONE',  ( 10.18810118749999916, 1.247682550866122264E-15, 110.4062500020483668 ) ) ;
#12139 = CARTESIAN_POINT ( 'NONE',  ( -3.211159895383561391, 14.81249999863440792, -3.211159895383561835 ) ) ;
#12140 = ORIENTED_EDGE ( 'NONE', *, *, #66470, .T. ) ;
#12141 = EDGE_LOOP ( 'NONE', ( #6776, #24937, #29484 ) ) ;
#12142 = CARTESIAN_POINT ( 'NONE',  ( -8.000000000000000000, 6.750000000000000888, -9.797174393178825657E-16 ) ) ;
#12143 = CARTESIAN_POINT ( 'NONE',  ( -8.000000000000000000, 11.15625000000000178, -3.313708498984762496 ) ) ;
#12144 = CARTESIAN_POINT ( 'NONE',  ( 5.082755093536325930, 23.53124999795161543, -5.082755093536325930 ) ) ;
#12145 = EDGE_CURVE ( 'NONE', #14276, #55396, #15890, .T. ) ;
#12146 = CARTESIAN_POINT ( 'NONE',  ( 8.000000000000000000, 122.9375000040967905, -9.797174393178825657E-16 ) ) ;
#12147 = CARTESIAN_POINT ( 'NONE',  ( 10.18810118749999916, 1.247682550866122264E-15, 104.7812500020483810 ) ) ;
#12148 = VECTOR ( 'NONE', #35114, 1000.000000000000000 ) ;
#12149 =( BOUNDED_CURVE ( )  B_SPLINE_CURVE ( 2, ( #1651, #14794, #43471, #61210, #26109, #60830, #32171, #48386, #37078, #15544, #49510, #54815, #2373 ),
 .UNSPECIFIED., .F., .F. ) 
 B_SPLINE_CURVE_WITH_KNOTS ( ( 3, 2, 2, 2, 2, 2, 3 ),
 ( 0.7989130434782609758, 0.8007246376811595345, 0.8025362318840579823, 0.8043478260869565410, 0.8061594202898550998, 0.8079710144927535476, 0.8097826086956521063 ),
 .UNSPECIFIED. ) 
 CURVE ( )  GEOMETRIC_REPRESENTATION_ITEM ( )  RATIONAL_B_SPLINE_CURVE ( ( 0.9999999999999978906, 0.9659258262890704216, 1.000000000000000000, 0.9659258262890683122, 1.000000000000000000, 0.9659258262890683122, 1.000000000000000000, 0.9659258262890683122, 1.000000000000000000, 0.9659258262890683122, 1.000000000000000000, 0.9659258262890704216, 0.9999999999999978906 ) ) 
 REPRESENTATION_ITEM ( '' )  );
#12150 = CARTESIAN_POINT ( 'NONE',  ( -7.347880794884122694E-16, 1.750000000000000222, 4.000000000000001776 ) ) ;
#12151 = CARTESIAN_POINT ( 'NONE',  ( -7.347880794884122694E-16, 8.499999997268814056, 4.000000000000001776 ) ) ;
#12152 =( BOUNDED_CURVE ( )  B_SPLINE_CURVE ( 2, ( #26429, #44552, #3441, #15491, #39912, #15119, #72088, #9852, #50203, #32878, #38527, #3069, #27186 ),
 .UNSPECIFIED., .F., .F. ) 
 B_SPLINE_CURVE_WITH_KNOTS ( ( 3, 2, 2, 2, 2, 2, 3 ),
 ( 0.2989130434782608647, 0.3007246376811594235, 0.3025362318840579823, 0.3043478260869565410, 0.3061594202898551553, 0.3079710144927536586, 0.3097826086956522174 ),
 .UNSPECIFIED. ) 
 CURVE ( )  GEOMETRIC_REPRESENTATION_ITEM ( )  RATIONAL_B_SPLINE_CURVE ( ( 1.000000000000000000, 0.9659258262890683122, 1.000000000000000000, 0.9659258262890683122, 1.000000000000000000, 0.9659258262890683122, 1.000000000000000000, 0.9659258262890683122, 1.000000000000000000, 0.9659258262890683122, 1.000000000000000000, 0.9659258262890673130, 1.000000000000001110 ) ) 
 REPRESENTATION_ITEM ( '' )  );
#12153 = CARTESIAN_POINT ( 'NONE',  ( -1.881053915767121776, 0.6249999986344065839, -4.541265875000002339 ) ) ;
#12154 = VERTEX_POINT ( 'NONE', #43512 ) ;
#12155 = CARTESIAN_POINT ( 'NONE',  ( 0.000000000000000000, 0.000000000000000000, 30.00000000000000000 ) ) ;
#12156 = CARTESIAN_POINT ( 'NONE',  ( 2.445694354108839619, 197.8125000013656063, 200.4456943541088663 ) ) ;
#12157 = VECTOR ( 'NONE', #10536, 1000.000000000000000 ) ;
#12158 = CARTESIAN_POINT ( 'NONE',  ( -24.54126587499996504, 206.1250000013655779, 171.4326545832179534 ) ) ;
#12159 = CARTESIAN_POINT ( 'NONE',  ( 4.541265875000002339, 10.31249999863440792, 0.000000000000000000 ) ) ;
#12160 = EDGE_CURVE ( 'NONE', #2698, #23527, #6597, .T. ) ;
#12161 = CARTESIAN_POINT ( 'NONE',  ( 7.188101187499992051, 8.802885111219154394E-16, 15.73655278187175632 ) ) ;
#12162 = EDGE_LOOP ( 'NONE', ( #13766, #48827, #8640, #62956 ) ) ;
#12163 = ORIENTED_EDGE ( 'NONE', *, *, #15375, .F. ) ;
#12164 = CARTESIAN_POINT ( 'NONE',  ( 10.18810118749999916, 4.220049686691935698, 104.5000000020483668 ) ) ;
#12165 = CARTESIAN_POINT ( 'NONE',  ( -4.999999999999992895, 220.8333333333333428, 8.660254037844390851 ) ) ;
#12166 = VECTOR ( 'NONE', #49488, 1000.000000000000000 ) ;
#12167 = CARTESIAN_POINT ( 'NONE',  ( -24.00000000000001066, 203.8125000000000284, 168.3431457505080004 ) ) ;
#12168 = CARTESIAN_POINT ( 'NONE',  ( 2.754378923186476579E-14, 200.1875000013656063, 194.5412658750000219 ) ) ;
#12169 = CARTESIAN_POINT ( 'NONE',  ( 29.62416036582268219, 194.5118150472865466, 173.2672283423948443 ) ) ;
#12170 = CARTESIAN_POINT ( 'NONE',  ( 8.660254037844389075, 95.41666666666667140, -5.000000000000000000 ) ) ;
#12171 = CARTESIAN_POINT ( 'NONE',  ( -4.898587196589412829E-16, 115.6250000000000000, -8.000000000000000000 ) ) ;
#12172 = CARTESIAN_POINT ( 'NONE',  ( -3.042071309553173730, 64.63541666325269830, 11.35316468749999785 ) ) ;
#12173 = CARTESIAN_POINT ( 'NONE',  ( 6.676582343750001591, 299.1093750017069510, -8.176455196517173205E-16 ) ) ;
#12174 = EDGE_LOOP ( 'NONE', ( #21258, #9918, #14434, #58629 ) ) ;
#12175 = CARTESIAN_POINT ( 'NONE',  ( 5.656854249492378806, 16.12499999590322375, 5.656854249492381470 ) ) ;
#12176 = CARTESIAN_POINT ( 'NONE',  ( -3.458734125000016313, 208.8750000013656347, 140.5673454167824161 ) ) ;
#12177 = CARTESIAN_POINT ( 'NONE',  ( 5.656854249492378806, 11.62499999590322197, 5.656854249492381470 ) ) ;
#12178 = CARTESIAN_POINT ( 'NONE',  ( 8.660254037844385522, 232.9166666666666572, -5.000000000000003553 ) ) ;
#12179 = DIRECTION ( 'NONE',  ( -0.000000000000000000, -1.000000000000000000, -0.000000000000000000 ) ) ;
#12180 = CARTESIAN_POINT ( 'NONE',  ( 7.204075437095966983, 7.204075437095967871, 70.46875000204836681 ) ) ;
#12181 = CARTESIAN_POINT ( 'NONE',  ( -8.660254037844390851, 217.9166666666666856, 4.999999999999998224 ) ) ;
#12182 = CARTESIAN_POINT ( 'NONE',  ( 2.977408999572650927, -7.188101187499990274, 11.33030278187175455 ) ) ;
#12183 = CARTESIAN_POINT ( 'NONE',  ( 6.951808397369818766E-16, 187.3437499965860127, -11.35316468750000141 ) ) ;
#12184 = CARTESIAN_POINT ( 'NONE',  ( -5.000000000000003553, 38.33333333333333570, 8.660254037844385522 ) ) ;
#12185 = CARTESIAN_POINT ( 'NONE',  ( -2.845105320593860121, -44.02866216854777548, 151.2140713481509806 ) ) ;
#12187 = CYLINDRICAL_SURFACE ( 'NONE', #1374, 3.999999999999976019 ) ;
#12186 = CARTESIAN_POINT ( 'NONE',  ( 7.999999999999991118, 9.797174393178815797E-16, 21.08030277982336642 ) ) ;
#12188 = ORIENTED_EDGE ( 'NONE', *, *, #25066, .T. ) ;
#12189 = CARTESIAN_POINT ( 'NONE',  ( 2.445694354108784108, 207.5625000013656063, 144.4456943541088663 ) ) ;
#12190 = CARTESIAN_POINT ( 'NONE',  ( 11.35316468750000141, 31.09374999658601979, 0.000000000000000000 ) ) ;
#12191 = CARTESIAN_POINT ( 'NONE',  ( 11.00000000000000000, 4.556349186104045934, 111.5312500040968047 ) ) ;
#12192 = CARTESIAN_POINT ( 'NONE',  ( -24.54126587500002543, 207.2500000013655779, 168.5673454167826435 ) ) ;
#12193 = CARTESIAN_POINT ( 'NONE',  ( 6.123233995736767268E-16, 11.25000000000000178, -10.00000000000000178 ) ) ;
#12195 = CARTESIAN_POINT ( 'NONE',  ( 0.000000000000000000, 300.0000000000000000, 0.000000000000000000 ) ) ;
#12194 = CARTESIAN_POINT ( 'NONE',  ( 2.775557561562891351E-14, 210.0000000000000284, 198.0000000000000284 ) ) ;
#12196 = CARTESIAN_POINT ( 'NONE',  ( -3.458734125000015425, 198.9375000013655779, 142.0000000000000568 ) ) ;
#12197 = CARTESIAN_POINT ( 'NONE',  ( 2.679491924311228956, 77.91666665983871098, -10.00000000000000000 ) ) ;
#12198 = CARTESIAN_POINT ( 'NONE',  ( -7.188101187500000044, 100.1562500020483810, 0.000000000000000000 ) ) ;
#12199 = CARTESIAN_POINT ( 'NONE',  ( 2.780723358947928197E-16, 11.68749999863440614, -4.541265875000002339 ) ) ;
#12200 = CARTESIAN_POINT ( 'NONE',  ( -30.82842712474612767, 206.5000000027312126, 172.8284271247466108 ) ) ;
#12201 = CARTESIAN_POINT ( 'NONE',  ( -1.836970198721029983E-15, 150.6249999931720538, 10.00000000000000178 ) ) ;
#12202 = CARTESIAN_POINT ( 'NONE',  ( 5.000000000000000000, -50.64189880742116401, 41.08656465431877791 ) ) ;
#12203 = ORIENTED_EDGE ( 'NONE', *, *, #39052, .T. ) ;
#12204 = ORIENTED_EDGE ( 'NONE', *, *, #60595, .F. ) ;
#12205 = CARTESIAN_POINT ( 'NONE',  ( 5.204170427930421283E-15, 10.39230484541327293, -0.8038475772933779684 ) ) ;
#12206 = CARTESIAN_POINT ( 'NONE',  ( -6.676582343750001591, 296.6093750017069510, 0.000000000000000000 ) ) ;
#12207 = CARTESIAN_POINT ( 'NONE',  ( 5.000000000000000000, 70.11723469343073134, 28.93519894129288517 ) ) ;
#12208 = CARTESIAN_POINT ( 'NONE',  ( 2.679491924311222739, 40.83333332650536818, 10.00000000000000355 ) ) ;
#12209 = CARTESIAN_POINT ( 'NONE',  ( -11.35316468750000141, 158.4895833299193839, 3.042071309553159963 ) ) ;
#12210 = CARTESIAN_POINT ( 'NONE',  ( 7.204075437095966983, 7.204075437095967871, 80.59375000204838102 ) ) ;
#12211 = CARTESIAN_POINT ( 'NONE',  ( 8.660254037844389075, 2.291666659838699438, -5.000000000000000000 ) ) ;
#12212 = CARTESIAN_POINT ( 'NONE',  ( 2.849036369511732440E-14, 204.2500000000000284, 202.0000000000000000 ) ) ;
#12213 = CARTESIAN_POINT ( 'NONE',  ( 0.000000000000000000, 125.0000000000000000, 0.000000000000000000 ) ) ;
#12214 = VECTOR ( 'NONE', #48757, 1000.000000000000000 ) ;
#12215 = ADVANCED_FACE ( 'NONE', ( #14088 ), #10621, .F. ) ;
#12216 = CARTESIAN_POINT ( 'NONE',  ( -10.18810118749999916, 4.220049686691934809, 112.9375000020483810 ) ) ;
#12217 = ORIENTED_EDGE ( 'NONE', *, *, #53092, .F. ) ;
#12218 = EDGE_CURVE ( 'NONE', #56773, #35916, #24342, .T. ) ;
#12219 = CARTESIAN_POINT ( 'NONE',  ( -5.656854249492380582, 112.8125000000000000, -5.656854249492380582 ) ) ;
#12220 = AXIS2_PLACEMENT_3D ( 'NONE', #53338, #65752, #24645 ) ;
#12221 = CARTESIAN_POINT ( 'NONE',  ( 25.17741886377238814, 181.7850574557842549, 151.7745050278317649 ) ) ;
#12222 = CARTESIAN_POINT ( 'NONE',  ( 3.042071309553159519, 130.0520833299193555, 11.35316468750000141 ) ) ;
#12223 = CARTESIAN_POINT ( 'NONE',  ( 3.458734125000015425, 199.9375000013656063, 198.0000000000000284 ) ) ;
#12224 = CARTESIAN_POINT ( 'NONE',  ( 4.401442555609581635E-16, 25.21874999795161543, -7.188101187500000044 ) ) ;
#12225 = CARTESIAN_POINT ( 'NONE',  ( -7.204075437095965206, -7.204075437095968759, 75.71875000204836681 ) ) ;
#12226 = CARTESIAN_POINT ( 'NONE',  ( -3.042071309553164404, 52.55208332991934839, -11.35316468749999963 ) ) ;
#12227 = ORIENTED_EDGE ( 'NONE', *, *, #47466, .F. ) ;
#12228 = PLANE ( 'NONE',  #23634 ) ;
#12229 = CARTESIAN_POINT ( 'NONE',  ( -1.881053915767121776, 1.749999998634407250, -4.541265875000002339 ) ) ;
#12230 = CARTESIAN_POINT ( 'NONE',  ( -8.008118988124991233, 3.317071493978878127, 11.41936528394062833 ) ) ;
#12231 = CARTESIAN_POINT ( 'NONE',  ( -3.458734125000016757, 207.1250000013656347, 140.5673454167824161 ) ) ;
#12232 = AXIS2_PLACEMENT_3D ( 'NONE', #8576, #24156, #70201 ) ;
#12233 = CARTESIAN_POINT ( 'NONE',  ( -7.188101187500000044, 17.71874999795161187, -8.802885111219163269E-16 ) ) ;
#12234 = CARTESIAN_POINT ( 'NONE',  ( -4.242640687119286547, 290.9375000034140157, -4.242640687119286547 ) ) ;
#12235 = CARTESIAN_POINT ( 'NONE',  ( -25.08437354053939927, -12.87872738848815146, 138.2120169791296007 ) ) ;
#12236 = CARTESIAN_POINT ( 'NONE',  ( -7.188101187500002709, 4.687499997951610986, 2.977408999572649151 ) ) ;
#12237 = CARTESIAN_POINT ( 'NONE',  ( 2.977408999572646486, 7.188101187499992051, 8.517802781871756324 ) ) ;
#12238 = CARTESIAN_POINT ( 'NONE',  ( 1.871523826299183495E-15, -10.18810118749999916, 74.03125000204836681 ) ) ;
#12239 = EDGE_CURVE ( 'NONE', #68967, #70895, #9684, .T. ) ;
#12240 = CARTESIAN_POINT ( 'NONE',  ( -27.99999999999996803, 208.1875000013656063, 173.4587341250003760 ) ) ;
#12241 = EDGE_CURVE ( 'NONE', #69323, #15401, #59750, .T. ) ;
#12242 = DIRECTION ( 'NONE',  ( -0.000000000000000000, -0.000000000000000000, 1.000000000000000000 ) ) ;
#12243 = CARTESIAN_POINT ( 'NONE',  ( -4.541265875000002339, 19.87499999863440792, -1.881053915767121998 ) ) ;
#12244 = EDGE_LOOP ( 'NONE', ( #53160, #53081, #11529, #26959 ) ) ;
#12245 =( BOUNDED_CURVE ( )  B_SPLINE_CURVE ( 2, ( #51231, #5220, #24041, #16892, #11248, #63289, #39915, #57281, #69708 ),
 .UNSPECIFIED., .F., .F. ) 
 B_SPLINE_CURVE_WITH_KNOTS ( ( 3, 2, 2, 2, 3 ),
 ( 0.6166666666666672514, 0.6250000000000005551, 0.6333333333333337478, 0.6416666666666671626, 0.6500000000000004663 ),
 .UNSPECIFIED. ) 
 CURVE ( )  GEOMETRIC_REPRESENTATION_ITEM ( )  RATIONAL_B_SPLINE_CURVE ( ( 0.9999999999999948930, 0.9238795325112918455, 1.000000000000000000, 0.9238795325112867385, 1.000000000000000000, 0.9238795325112867385, 1.000000000000000000, 0.9238795325112826307, 1.000000000000003997 ) ) 
 REPRESENTATION_ITEM ( '' )  );
#12246 = CARTESIAN_POINT ( 'NONE',  ( -2.445694354108783664, 209.3125000013656063, 195.5543056458912190 ) ) ;
#12247 = CARTESIAN_POINT ( 'NONE',  ( -4.000000000000015987, 207.5000000000000284, 142.0000000000000568 ) ) ;
#12248 = CARTESIAN_POINT ( 'NONE',  ( -26.34314575050769491, 201.0625000027312126, 166.0000000000003695 ) ) ;
#12249 = CARTESIAN_POINT ( 'NONE',  ( -4.401442555609581635E-16, 117.7812500020483810, -7.188101187500000044 ) ) ;
#12250 = ADVANCED_FACE ( 'NONE', ( #40203 ), #69623, .T. ) ;
#12251 = CARTESIAN_POINT ( 'NONE',  ( -6.735557395310442023E-16, 11.00000000000000000, 93.81250000409677625 ) ) ;
#12252 = CARTESIAN_POINT ( 'NONE',  ( -7.999999999999991118, 3.313708498984756723, 0.9240527839201456706 ) ) ;
#12253 = ORIENTED_EDGE ( 'NONE', *, *, #4040, .F. ) ;
#12254 = EDGE_CURVE ( 'NONE', #6516, #338, #64330, .T. ) ;
#12255 = CARTESIAN_POINT ( 'NONE',  ( -5.082755093536325042, 19.03124999795161543, -5.082755093536325930 ) ) ;
#12256 = VERTEX_POINT ( 'NONE', #24329 ) ;
#12257 = CARTESIAN_POINT ( 'NONE',  ( 31.99999999999997868, 198.1875000000000853, 171.6568542494923122 ) ) ;
#12258 = LINE ( 'NONE', #57939, #5367 ) ;
#12259 = CARTESIAN_POINT ( 'NONE',  ( 10.00000000000000000, 49.79166666666667140, 2.679491924311236062 ) ) ;
#12260 = CARTESIAN_POINT ( 'NONE',  ( 1.320432766682874540E-15, 97.90625000204839523, 7.188101187500000044 ) ) ;
#12261 = CARTESIAN_POINT ( 'NONE',  ( -31.45873412500001010, 202.8750000013656063, 168.5673454167827572 ) ) ;
#12262 = CARTESIAN_POINT ( 'NONE',  ( 3.999999999999960032, 205.0625000027312126, 143.6568542494924259 ) ) ;
#12264 = DIRECTION ( 'NONE',  ( -0.000000000000000000, -0.000000000000000000, -1.000000000000000000 ) ) ;
#12263 = CARTESIAN_POINT ( 'NONE',  ( -4.898587196589412829E-16, 111.3125000040967905, -8.000000000000000000 ) ) ;
#12265 = VERTEX_POINT ( 'NONE', #35667 ) ;
#12266 =( BOUNDED_CURVE ( )  B_SPLINE_CURVE ( 2, ( #53970, #48294, #31699, #54721, #3028, #72042, #43376, #14701, #37739, #52579, #9060, #32074, #69936 ),
 .UNSPECIFIED., .F., .F. ) 
 B_SPLINE_CURVE_WITH_KNOTS ( ( 3, 2, 2, 2, 2, 2, 3 ),
 ( 0.08152173913043478382, 0.08333333333333332871, 0.08514492753623188748, 0.08695652173913043237, 0.08876811594202899114, 0.09057971014492753603, 0.09239130434782608092 ),
 .UNSPECIFIED. ) 
 CURVE ( )  GEOMETRIC_REPRESENTATION_ITEM ( )  RATIONAL_B_SPLINE_CURVE ( ( 1.000000000000000000, 0.9659258262890683122, 1.000000000000000000, 0.9659258262890683122, 1.000000000000000000, 0.9659258262890683122, 1.000000000000000000, 0.9659258262890683122, 1.000000000000000000, 0.9659258262890683122, 1.000000000000000000, 0.9659258262890683122, 1.000000000000000000 ) ) 
 REPRESENTATION_ITEM ( '' )  );
#12267 = CARTESIAN_POINT ( 'NONE',  ( -5.676582343749992710, 244.7395833367473301, 9.832129032723422313 ) ) ;
#12268 = CARTESIAN_POINT ( 'NONE',  ( -2.977408999572648707, -7.188101187499990274, 17.14280278187175455 ) ) ;
#12269 = VECTOR ( 'NONE', #244, 1000.000000000000000 ) ;
#12270 = CARTESIAN_POINT ( 'NONE',  ( -3.313708498984765161, 14.53125000000000178, 7.999999999999998224 ) ) ;
#12271 = CARTESIAN_POINT ( 'NONE',  ( -5.000000000000005329, 75.20833332650536818, 8.660254037844387298 ) ) ;
#12272 = CARTESIAN_POINT ( 'NONE',  ( -5.000000000000000000, -11.14555136602166208, 27.84144949604419494 ) ) ;
#12273 = CARTESIAN_POINT ( 'NONE',  ( 10.00000000000000000, 201.6666666598387110, 2.679491924311235618 ) ) ;
#12274 = CARTESIAN_POINT ( 'NONE',  ( 10.00000000000000178, 160.2083333333333144, -2.679491924311226736 ) ) ;
#12275 = DIRECTION ( 'NONE',  ( -0.000000000000000000, 1.000000000000000000, 4.689100369878284071E-30 ) ) ;
#12276 = CARTESIAN_POINT ( 'NONE',  ( -31.81200641282667263, 176.5294866793762765, 167.0567011592689823 ) ) ;
#12277 = CARTESIAN_POINT ( 'NONE',  ( -2.977408999572647819, -7.188101187499990274, 26.14280278187176165 ) ) ;
#12278 = CARTESIAN_POINT ( 'NONE',  ( -9.832129032723420536, 139.0104166632526983, 5.676582343749997150 ) ) ;
#12279 = CARTESIAN_POINT ( 'NONE',  ( 23.99999999999998934, 198.7500000000000000, 169.9999999999998863 ) ) ;
#12280 = CARTESIAN_POINT ( 'NONE',  ( 4.999999999999993783, 26.04166665983870388, 8.660254037844390851 ) ) ;
#12283 = DIRECTION ( 'NONE',  ( -0.000000000000000000, 1.000000000000000000, 4.476705744456276341E-16 ) ) ;
#12282 = CARTESIAN_POINT ( 'NONE',  ( 6.123233995736767268E-16, 108.1249999931720396, -10.00000000000000178 ) ) ;
#12281 = CARTESIAN_POINT ( 'NONE',  ( 24.00000000000000355, 204.6875000000000284, 168.3431457505075173 ) ) ;
#12284 = EDGE_CURVE ( 'NONE', #54079, #9758, #611, .T. ) ;
#12285 = ORIENTED_EDGE ( 'NONE', *, *, #2306, .F. ) ;
#12286 = CARTESIAN_POINT ( 'NONE',  ( 0.000000000000000000, 0.000000000000000000, 118.0000000000000000 ) ) ;
#12287 = EDGE_CURVE ( 'NONE', #63012, #29054, #18332, .T. ) ;
#12288 = CARTESIAN_POINT ( 'NONE',  ( -9.000000000000000000, -5.196152422706648899, -0.8038475772933779684 ) ) ;
#12289 = CARTESIAN_POINT ( 'NONE',  ( 36.10814071610729314, 133.9999999999999716, 139.0000000000000000 ) ) ;
#12290 = CARTESIAN_POINT ( 'NONE',  ( 29.43265458321760519, 194.7500000013656063, 173.4587341249998929 ) ) ;
#12291 = CARTESIAN_POINT ( 'NONE',  ( -5.000000000000005329, 35.20833332650536818, 8.660254037844387298 ) ) ;
#12292 = CARTESIAN_POINT ( 'NONE',  ( -7.188101187500001821, 115.0625000020483952, -2.977408999572650483 ) ) ;
#12293 = CARTESIAN_POINT ( 'NONE',  ( 4.541265875000002339, 1.437499998634406806, 0.000000000000000000 ) ) ;
#12294 = DIRECTION ( 'NONE',  ( 1.000000000000000000, 0.000000000000000000, 0.000000000000000000 ) ) ;
#12295 = CARTESIAN_POINT ( 'NONE',  ( 7.999999999999992895, -3.313708498984756279, 23.98655277982336642 ) ) ;
#12297 = CARTESIAN_POINT ( 'NONE',  ( -7.320508075688771932, 224.3750000000000000, -7.320508075688771932 ) ) ;
#12296 = CARTESIAN_POINT ( 'NONE',  ( -11.00000000000000000, 0.000000000000000000, 101.6875000040967763 ) ) ;
#12298 = ORIENTED_EDGE ( 'NONE', *, *, #30125, .F. ) ;
#12299 = EDGE_CURVE ( 'NONE', #7034, #42039, #72832, .T. ) ;
#12300 = B_SPLINE_CURVE_WITH_KNOTS ( 'NONE', 3,
 ( #66289, #26284, #19515, #24803, #36517, #60588, #31552, #48518, #14552, #37216, #54575, #48888, #15675, #37967, #60213, #43990, #55323, #71524, #65872, #21343, #49264, #32308, #31177, #67000, #72279, #9669, #8914, #73032, #50016, #67376, #42855, #60966, #15298, #38336, #8538, #9285, #72662, #2881 ),
 .UNSPECIFIED., .F., .F.,
 ( 4, 2, 2, 2, 2, 2, 2, 2, 2, 2, 2, 2, 2, 2, 2, 2, 2, 2, 4 ),
 ( 0.1434430299490632998, 0.1461315498160218884, 0.1474758097495011688, 0.1488200696829804492, 0.1515085895499390101, 0.1541971094168975431, 0.1555413693503768235, 0.1568856292838561040, 0.1595741491508146093, 0.1622626690177731423, 0.1649511888847316476, 0.1662954488182109003, 0.1676397087516901807, 0.1703282286186486583, 0.1730167484856071081, 0.1757052683525655579, 0.1810823080864824297, 0.1837708279534408795, 0.1864593478203993016 ),
 .UNSPECIFIED. ) ;
#12301 = CARTESIAN_POINT ( 'NONE',  ( 1.656854249492381248, 15.93749999726881406, -4.000000000000001776 ) ) ;
#12302 = CARTESIAN_POINT ( 'NONE',  ( 4.401442555609581635E-16, 23.34374999795161543, -7.188101187500000044 ) ) ;
#12303 = PLANE ( 'NONE',  #23001 ) ;
#12304 = CARTESIAN_POINT ( 'NONE',  ( 8.311093377946839666, 241.0937500034139873, 8.311093377946830785 ) ) ;
#12305 = VECTOR ( 'NONE', #21490, 1000.000000000000000 ) ;
#12306 = CARTESIAN_POINT ( 'NONE',  ( 9.832129032723420536, 121.1979166632526983, -5.676582343749999815 ) ) ;
#12307 = ORIENTED_EDGE ( 'NONE', *, *, #30530, .T. ) ;
#12308 = CARTESIAN_POINT ( 'NONE',  ( -10.55165312886146367, 1.890739080934536576, 117.7907753267484878 ) ) ;
#12309 = CARTESIAN_POINT ( 'NONE',  ( -7.204075437095967871, 7.204075437095967871, 100.4687500020483668 ) ) ;
#12310 = CARTESIAN_POINT ( 'NONE',  ( 7.320508075688771044, 216.2499999931720538, 7.320508075688775484 ) ) ;
#12311 = CARTESIAN_POINT ( 'NONE',  ( 2.839093476692135984E-14, 199.9375000013656063, 201.4587341250000350 ) ) ;
#12312 = DIRECTION ( 'NONE',  ( -1.000000000000000000, -0.000000000000000000, -0.000000000000000000 ) ) ;
#12314 = CARTESIAN_POINT ( 'NONE',  ( 11.35316468750000141, 100.7812499965860269, 0.000000000000000000 ) ) ;
#12313 = DIRECTION ( 'NONE',  ( -0.000000000000000000, 1.000000000000000000, -0.000000000000000000 ) ) ;
#12315 = CARTESIAN_POINT ( 'NONE',  ( 7.999999999999991118, 9.797174393178815797E-16, 6.267802783920147114 ) ) ;
#12316 = CARTESIAN_POINT ( 'NONE',  ( -30.44569435410883074, 197.8125000013656063, 167.5543056458915885 ) ) ;
#12317 = CARTESIAN_POINT ( 'NONE',  ( 10.00000000000009059, 175.2083333333333997, -2.679491924311250273 ) ) ;
#12318 = ORIENTED_EDGE ( 'NONE', *, *, #61021, .F. ) ;
#12319 = AXIS2_PLACEMENT_3D ( 'NONE', #55375, #14608, #73085 ) ;
#12320 = CARTESIAN_POINT ( 'NONE',  ( 2.679491924311222739, 190.8333333265053682, 10.00000000000000355 ) ) ;
#12321 = CARTESIAN_POINT ( 'NONE',  ( 10.99999999999989697, -4.556349186104149851, 73.65625000000000000 ) ) ;
#12322 = CARTESIAN_POINT ( 'NONE',  ( 32.00000000000000711, 202.3125000000000000, 168.3431457505075457 ) ) ;
#12323 = CARTESIAN_POINT ( 'NONE',  ( 11.35316468749999785, 90.88541666325266988, 3.042071309553174174 ) ) ;
#12324 = CARTESIAN_POINT ( 'NONE',  ( 2.828427124746208943, 205.6250000000000284, 195.1715728752538439 ) ) ;
#12325 = CARTESIAN_POINT ( 'NONE',  ( 7.188101187500000933, 5.437499997951610098, -2.977408999572650483 ) ) ;
#12326 = CARTESIAN_POINT ( 'NONE',  ( 4.220049686691941027, -10.18810118749999738, 97.00000000204838102 ) ) ;
#12327 = CARTESIAN_POINT ( 'NONE',  ( -3.042071309553164404, 7.552083329919349275, -11.35316468749999963 ) ) ;
#12328 = VERTEX_POINT ( 'NONE', #40953 ) ;
#12329 = CARTESIAN_POINT ( 'NONE',  ( 8.000000000000001776, 98.84375000409680467, 3.313708498984759387 ) ) ;
#12330 = CARTESIAN_POINT ( 'NONE',  ( 5.676582343750001591, 221.6145833299193839, -9.832129032723420536 ) ) ;
#12331 = CARTESIAN_POINT ( 'NONE',  ( 7.204075437095966983, 7.204075437095967871, 82.46875000204836681 ) ) ;
#12332 = CARTESIAN_POINT ( 'NONE',  ( -4.898587196589407898E-16, 7.999999999999991118, 11.14280278392014800 ) ) ;
#12333 = CARTESIAN_POINT ( 'NONE',  ( 8.660254037844389075, 200.4166666666666856, -5.000000000000000000 ) ) ;
#12334 = CARTESIAN_POINT ( 'NONE',  ( 6.676582343750001591, 297.9531250017069510, -8.176455196517173205E-16 ) ) ;
#12335 = ORIENTED_EDGE ( 'NONE', *, *, #5214, .T. ) ;
#12336 = CARTESIAN_POINT ( 'NONE',  ( 2.726951573962122902E-14, -51.14729664189338365, -48.52014062455057797 ) ) ;
#12337 = CARTESIAN_POINT ( 'NONE',  ( 5.676582343749993598, 205.2604166632526983, 9.832129032723422313 ) ) ;
#12338 = CARTESIAN_POINT ( 'NONE',  ( -4.220049686691937474, -10.18810118749999738, 87.43750000204838102 ) ) ;
#12339 = VECTOR ( 'NONE', #23576, 1000.000000000000000 ) ;
#12340 = CARTESIAN_POINT ( 'NONE',  ( -26.56734541678238060, 202.3750000013655779, 166.5412658750003629 ) ) ;
#12341 = CARTESIAN_POINT ( 'NONE',  ( -8.000000000000000000, 18.75000000000000355, -9.797174393178825657E-16 ) ) ;
#12342 = ORIENTED_EDGE ( 'NONE', *, *, #28115, .T. ) ;
#12343 = CARTESIAN_POINT ( 'NONE',  ( -5.082755093536324154, 119.8437500020483810, 5.082755093536326818 ) ) ;
#12344 = CARTESIAN_POINT ( 'NONE',  ( 4.000000000000015099, 205.6875000027312126, 196.3431457505076594 ) ) ;
#12345 = CARTESIAN_POINT ( 'NONE',  ( 8.660254037844385522, 24.58333333333333570, 5.000000000000005329 ) ) ;
#12346 = CARTESIAN_POINT ( 'NONE',  ( -4.999999999999997335, 15.86406185656356271, 69.92615499037644611 ) ) ;
#12347 = CARTESIAN_POINT ( 'NONE',  ( -7.204075437095967871, 7.204075437095967871, 73.84375000204838102 ) ) ;
#12348 = ORIENTED_EDGE ( 'NONE', *, *, #33443, .F. ) ;
#12349 = CARTESIAN_POINT ( 'NONE',  ( 0.000000000000000000, 300.0000000000000000, 10.00000000000000178 ) ) ;
#12350 = FACE_OUTER_BOUND ( 'NONE', #11072, .T. ) ;
#12351 = VECTOR ( 'NONE', #20845, 1000.000000000000000 ) ;
#12352 = CARTESIAN_POINT ( 'NONE',  ( 5.082755093536325042, 119.4687500020483810, -5.082755093536325930 ) ) ;
#12353 = CARTESIAN_POINT ( 'NONE',  ( -5.000000000000000000, -60.11723469343085213, -46.25570701698114107 ) ) ;
#12354 = CARTESIAN_POINT ( 'NONE',  ( 4.721056650415999201, 296.0781250017069510, -4.721056650415999201 ) ) ;
#12356 = DIRECTION ( 'NONE',  ( 0.000000000000000000, 0.000000000000000000, -1.000000000000000000 ) ) ;
#12355 = CARTESIAN_POINT ( 'NONE',  ( -11.35316468749999785, 228.6979166700806445, -3.042071309553164848 ) ) ;
#12357 = AXIS2_PLACEMENT_3D ( 'NONE', #61409, #37286, #71966 ) ;
#12358 = VERTEX_POINT ( 'NONE', #30368 ) ;
#12359 = CARTESIAN_POINT ( 'NONE',  ( 11.35316468749999963, 241.7187500034139873, -1.390361679473963556E-15 ) ) ;
#12360 = CARTESIAN_POINT ( 'NONE',  ( -7.188101187499990274, -2.977408999572651371, 9.080302781871752771 ) ) ;
#12361 =( BOUNDED_SURFACE ( )  B_SPLINE_SURFACE ( 1, 2, ( 
 ( #22044, #51845, #34890, #11119, #11854, #57895, #5092, #28460, #46179, #45807, #57526, #22787, #190, #23166, #5833, #57142, #74111, #68086, #16374, #34521, #39413, #6571, #5458, #28827, #40155, #69196, #6204, #62411, #34143, #40524, #28084, #29211, #52224, #69570, #17508, #10737, #56772, #51098, #51467, #45433, #16749, #74480, #68818, #556, #23539, #68446, #46551, #63159, #40898, #12216, #35252, #58270, #65746, #41269, #36348, #42362, #13677, #35614, #7675, #71030, #58628, #30682, #19348, #23910, #59001, #53700, #48019, #6936, #41992, #69945, #65377, #13311, #41637, #29947, #30313, #71395, #24638, #36716, #64648, #52961, #29578, #59363, #927, #46920, #1295, #24275, #2012, #19721, #8037, #59728, #42732, #18627, #47286, #54069, #25001, #14048, #25374, #2378, #31044, #35984, #48391, #37085, #60089, #64279, #47650, #52590, #70311, #18253, #12585, #12946, #7306, #53332, #1658, #70671, #18988, #65002, #54447, #54822, #21586, #72147, #49517, #20458, #43860, #66118, #31420, #8407, #38588, #38211, #15550, #44611, #43478, #66490, #38952, #8788, #25743, #14800, #14427, #67626, #15921, #26115, #50259, #37460, #21214, #32559, #48763, #43101, #73282, #26491, #26878, #9546, #71771, #67255, #55198, #3132, #2755, #20087, #55569, #60458, #27243, #3883, #72536, #61215, #15180, #31801, #49135, #9160, #37839, #60837, #32177, #49893, #3503, #20842, #66873, #72907, #44242, #61588, #9907, #32939, #55946, #4255, #74019, #69482, #17416, #33308, #23080, #11028, #45718, #51010, #34060, #73649, #470, #57056, #23451, #51755, #39690, #44984, #11765, #5370, #68363, #67990, #46463, #68729, #57432, #28370, #51378, #28737, #69108, #16286, #34431, #45347, #63072, #27621, #5739, #21956, #4623, #34803, #56306, #17044, #74390, #62689, #39326, #62324, #10650, #61955, #40067, #50630, #33682, #56685, #5003, #11395, #29120, #40439, #46089, #52138, #22321, #28001, #57809, #101, #16658, #17793, #22700, #10282, #63438, #6115, #18169, #30961, #7224, #29493, #13228, #69857, #840, #53981, #70949, #1577, #12130, #35169, #70230, #58543, #6488, #19265, #65290, #30227, #58183, #35530, #64195, #7589, #6847, #12499, #24187, #47932, #47200, #52503, #41911, #24916, #1206, #1929, #42277, #41184, #18540, #36264, #35897, #47565, #12858, #64919, #59280, #70588, #41547, #29862, #23826, #46831, #24557, #52874, #71314, #64564, #18904, #53247, #30596, #13595, #40806, #58914, #53615, #36633, #59640, #7957, #2291, #25288, #63816, #48305, #2668, #3042, #42647, #60372, #43391, #66406, #3415, #20756, #19633, #32470, #60752, #72823, #72056, #61501, #38499, #55858, #31331, #26400, #55480, #3792, #25659, #72448, #61123, #48675, #43771, #9454, #13957, #49048, #66785, #38124, #71682, #32088, #60004, #26792, #49428, #31712, #20002, #20373, #9824, #14714, #49807, #54735, #43012, #9075, #21130, #37752, #32850, #4174, #27161, #54358, #15089, #44152, #67167, #66033, #15462, #50178, #14340, #65659, #36998, #8320, #55108, #37371, #8698, #26026, #10941, #38869, #12331, #58011, #10566, #4539, #73935, #41379, #68279, #58375, #33597, #50546, #73196, #6317, #44523, #15835, #73562, #21872, #23652, #64390, #52700, #6681, #12688, #62239, #16200, #24014, #52330, #39240, #30056, #33226, #7048, #56603, #69678, #44900, #35722, #39611, #61875, #46659, #27534, #56225, #58737, #29683, #33976, #67538, #10197, #27913, #4919, #67906, #1034, #47023, #62609, #50923, #22238, #45268, #41009, #16574, #29321, #667, #70055, #17991, #64018, #35364, #18365, #21504, #54184, #25481, #36089, #13419, #59833, #7783, #71134, #30788, #13779, #42470, #19457, #65108, #30423, #47396, #24388, #48128, #70418, #2860, #42096, #65487, #2118, #36823, #2489, #53069, #70780, #48498, #7415, #71502, #19826, #37193, #8147, #1403, #64753, #53443, #59471, #41743, #36457, #25111, #31152, #42831, #65850, #18735, #14160, #60193, #19092, #53808, #8515, #13051, #59108, #1764, #24745, #31531, #54553, #47756, #47250, #57489, #63868, #23876, #40488, #24236, #18589, #52552, #46886, #64615, #11815, #891, #12180, #1624, #17092, #17468, #58964, #34853, #35217, #57859, #6535, #28791, #68782, #45771, #1258, #69909, #52925, #7271, #6165, #29174, #40114, #46142, #63120, #52189, #51806, #30279, #53299, #63493, #12911, #154, #58593, #18220, #11446, #5794, #35944 ),
 ( #41234, #34482, #23130, #46514, #69159, #520, #23500, #64241, #69533, #17845, #40861, #35579, #58236, #29541, #12551, #6899, #29910, #41600, #70277, #32140, #54782, #70635, #60425, #48353, #8369, #13644, #71359, #36314, #37803, #19684, #60799, #14391, #2344, #7640, #49099, #42694, #31009, #30645, #9124, #31385, #20047, #65706, #14011, #66081, #31762, #53664, #71733, #8002, #25706, #64965, #43065, #59330, #41958, #72112, #18954, #54411, #37047, #1976, #24604, #2718, #13275, #24968, #47984, #70997, #48726, #66456, #3093, #8752, #14764, #36682, #42324, #20425, #37425, #65342, #55161, #19313, #47611, #54034, #26078, #59694, #25338, #60048, #43441, #38901, #55517, #33256, #3829, #61159, #16606, #38158, #27570, #61904, #44559, #21163, #44186, #72858, #57002, #39643, #62640, #50955, #50209, #16234, #34008, #45295, #26826, #10228, #21903, #38535, #22273, #10973, #50578, #44933, #5316, #9859, #73595, #56255, #74335, #15126, #15498, #28318, #32887, #4572, #55889, #67940, #49839, #66824, #43809, #73967, #39271, #68308, #51327, #4203, #27193, #9491, #67200, #32505, #73230, #61536, #21536, #67572, #15869, #62271, #10600, #56635, #33628, #4949, #27948, #12809, #40750, #41128, #23770, #40015, #6796, #69426, #17363, #7168, #63017, #46774, #51699, #41494, #69798, #63759, #787, #29438, #68679, #35841, #23397, #16988, #57753, #46038, #18114, #11341, #58856, #30173, #12443, #6058, #69058, #34377, #34749, #11708, #70175, #29064, #53190, #52817, #57377, #6436, #64135, #22644, #35475, #12077, #1152, #417, #64511, #45664, #5686, #28685, #52449, #58489, #29806, #45, #24130, #47144, #23030, #18484, #40386, #63385, #52085, #46412, #17734, #35113, #58127, #41858, #14281, #59949, #13535, #7537, #2239, #43333, #71257, #60316, #36574, #53559, #1526, #8264, #47510, #18851, #1875, #24861, #25607, #66353, #54679, #8644, #14657, #65231, #19214, #25969, #54306, #42219, #32032, #36208, #9018, #59587, #71627, #47880, #37698, #42591, #70899, #37319, #65606, #24506, #60698, #31658, #36944, #70536, #64869, #30906, #7901, #13172, #2985, #48992, #13905, #59225, #53926, #25233, #42958, #48250, #19576, #31278, #72002, #2617, #30543, #48620, #20317, #19949, #65977, #62185, #9393, #32793, #50491, #50125, #61819, #27110, #4486, #56173, #10137, #61447, #3735, #72387, #26349, #38819, #49370, #10885, #9774, #33175, #44470, #15782, #16142, #55052, #44101, #44844, #32413, #10512, #33544, #73883, #27477, #3359, #20700, #38072, #38444, #43718, #21077, #4117, #73141, #73504, #66731, #68223, #55801, #15036, #15404, #26734, #21811, #61071, #16520, #39560, #67851, #21447, #49754, #55426, #67109, #67483, #27858, #39181, #62554, #56545, #72771, #4862, #50867, #22187, #45212, #57667, #45581, #47059, #5974, #70096, #23687, #11626, #16902, #58411, #28977, #40297, #39928, #18402, #17651, #29362, #334, #23315, #704, #41047, #62934, #6358, #68971, #51997, #68595, #46327, #11259, #51241, #6717, #28233, #40670, #69341, #34664, #34288, #57292, #5606, #41417, #29724, #52738, #64055, #63298, #52368, #24050, #35401, #28604, #63673, #12000, #51615, #12366, #1072, #35032, #58044, #64429, #74631, #46693, #69717, #33919, #5232, #22947, #56919, #45954, #18031, #17280, #74252, #22560, #35760, #12728, #42874, #42511, #19868, #25888, #1797, #47796, #43253, #13091, #30091, #70819, #18774, #48907, #71921, #30463, #54597, #41779, #25524, #36865, #53110, #47432, #2903, #30824, #31197, #13821, #1444, #71544, #59508, #7456, #20234, #24425, #59873, #64790, #31573, #8186, #53846, #65528, #24781, #36495, #70456, #58777, #7821, #7085, #2532, #65148, #36126, #37236, #2159, #19131, #59147, #53480, #71177, #54222, #25153, #48169, #48536, #65893, #42135, #14199, #13457, #19495, #60234, #8559, #26265, #8935, #39101, #60611, #50039, #9690, #67022, #43631, #66641, #20613, #4775, #62104, #10427, #73425, #72686, #38740, #56458, #67773, #3278, #32710, #44385, #60985, #44760, #33457, #73053, #67396, #27767, #32331, #21361, #55719, #22102, #37612, #37987, #50779, #55344, #4034, #3647, #27028, #49285, #14576, #66269, #21729, #15698, #16067, #73793, #26647, #49669, #31946, #14948, #54969, #20988, #72301, #9307, #44012, #15319, #38355, #61363, #4399, #61739, #10056, #33093, #56090, #27391, #50411, #46238, #62467, #29270, #17190 ) ),
 .UNSPECIFIED., .F., .F., .F. ) 
 B_SPLINE_SURFACE_WITH_KNOTS ( ( 2, 2 ),
 ( 3, 2, 2, 2, 2, 2, 2, 2, 2, 2, 2, 2, 2, 2, 2, 2, 2, 2, 2, 2, 2, 2, 2, 2, 2, 2, 2, 2, 2, 2, 2, 2, 2, 2, 2, 2, 2, 2, 2, 2, 2, 2, 2, 2, 2, 2, 2, 2, 2, 2, 2, 2, 2, 2, 2, 2, 2, 2, 2, 2, 2, 2, 2, 2, 2, 2, 2, 2, 2, 2, 2, 2, 2, 2, 2, 2, 2, 2, 2, 2, 2, 2, 2, 2, 2, 2, 2, 2, 2, 2, 2, 2, 2, 2, 2, 2, 2, 2, 2, 2, 2, 2, 2, 2, 2, 2, 2, 2, 2, 2, 2, 2, 2, 2, 2, 2, 2, 2, 2, 2, 2, 2, 2, 2, 2, 2, 2, 2, 2, 2, 2, 2, 2, 2, 2, 2, 2, 2, 2, 2, 2, 2, 2, 2, 2, 2, 2, 2, 2, 2, 2, 2, 2, 2, 2, 2, 2, 2, 2, 2, 2, 2, 2, 2, 2, 2, 2, 2, 2, 2, 2, 2, 2, 2, 2, 2, 2, 2, 2, 2, 2, 2, 2, 2, 2, 2, 2, 2, 2, 2, 2, 2, 2, 2, 2, 2, 2, 2, 2, 2, 2, 2, 2, 2, 2, 2, 2, 2, 2, 2, 2, 2, 2, 2, 2, 2, 2, 2, 2, 2, 2, 2, 2, 2, 2, 2, 2, 2, 2, 2, 2, 2, 2, 2, 2, 2, 2, 2, 2, 2, 2, 2, 2, 2, 2, 2, 2, 2, 2, 2, 2, 2, 2, 2, 2, 2, 2, 2, 2, 2, 2, 2, 2, 2, 2, 2, 2, 3 ),
 ( 0.000000000000000000, 1.000000000000000000 ),
 ( 0.000000000000000000, 0.003676470588235294067, 0.007352941176470588133, 0.01102941176470588307, 0.01470588235294117627, 0.01838235294117647120, 0.02205882352941176613, 0.02573529411764705760, 0.02941176470588235253, 0.03308823529411764747, 0.03676470588235294240, 0.04044117647058823733, 0.04411764705882353227, 0.04779411764705882026, 0.05147058823529411520, 0.05514705882352941013, 0.05882352941176470507, 0.06250000000000000000, 0.06617647058823529493, 0.06985294117647058987, 0.07352941176470588480, 0.07720588235294117974, 0.08088235294117647467, 0.08455882352941176960, 0.08823529411764706454, 0.09191176470588235947, 0.09558823529411764053, 0.09926470588235293546, 0.1029411764705882304, 0.1066176470588235253, 0.1102941176470588203, 0.1139705882352941152, 0.1176470588235294101, 0.1213235294117647051, 0.1250000000000000000, 0.1286764705882352811, 0.1323529411764705899, 0.1360294117647058709, 0.1397058823529411797, 0.1433823529411764608, 0.1470588235294117696, 0.1507352941176470507, 0.1544117647058823595, 0.1580882352941176405, 0.1617647058823529493, 0.1654411764705882304, 0.1691176470588235392, 0.1727941176470588203, 0.1764705882352941291, 0.1801470588235294101, 0.1838235294117647189, 0.1875000000000000000, 0.1911764705882352811, 0.1948529411764705899, 0.1985294117647058709, 0.2022058823529411797, 0.2058823529411764608, 0.2095588235294117696, 0.2132352941176470507, 0.2169117647058823595, 0.2205882352941176405, 0.2242647058823529493, 0.2279411764705882304, 0.2316176470588235392, 0.2352941176470588203, 0.2389705882352941291, 0.2426470588235294101, 0.2463235294117647189, 0.2500000000000000000, 0.2536764705882352811, 0.2573529411764705621, 0.2610294117647058987, 0.2647058823529411797, 0.2683823529411764608, 0.2720588235294117418, 0.2757352941176470784, 0.2794117647058823595, 0.2830882352941176405, 0.2867647058823529216, 0.2904411764705882582, 0.2941176470588235392, 0.2977941176470588203, 0.3014705882352941013, 0.3051470588235294379, 0.3088235294117647189, 0.3125000000000000000, 0.3161764705882352811, 0.3198529411764705621, 0.3235294117647058987, 0.3272058823529411797, 0.3308823529411764608, 0.3345588235294117418, 0.3382352941176470784, 0.3419117647058823595, 0.3455882352941176405, 0.3492647058823529216, 0.3529411764705882582, 0.3566176470588235392, 0.3602941176470588203, 0.3639705882352941013, 0.3676470588235294379, 0.3713235294117647189, 0.3750000000000000000, 0.3786764705882352811, 0.3823529411764705621, 0.3860294117647058987, 0.3897058823529411797, 0.3933823529411764608, 0.3970588235294117418, 0.4007352941176470784, 0.4044117647058823595, 0.4080882352941176405, 0.4117647058823529216, 0.4154411764705882582, 0.4191176470588235392, 0.4227941176470588203, 0.4264705882352941013, 0.4301470588235294379, 0.4338235294117647189, 0.4375000000000000000, 0.4411764705882352811, 0.4448529411764705621, 0.4485294117647058987, 0.4522058823529411797, 0.4558823529411764608, 0.4595588235294117418, 0.4632352941176470784, 0.4669117647058823595, 0.4705882352941176405, 0.4742647058823529216, 0.4779411764705882582, 0.4816176470588235392, 0.4852941176470588203, 0.4889705882352941013, 0.4926470588235294379, 0.4963235294117647189, 0.5000000000000000000, 0.5036764705882352811, 0.5073529411764705621, 0.5110294117647058432, 0.5147058823529411242, 0.5183823529411765163, 0.5220588235294117974, 0.5257352941176470784, 0.5294117647058823595, 0.5330882352941176405, 0.5367647058823529216, 0.5404411764705882026, 0.5441176470588234837, 0.5477941176470588758, 0.5514705882352941568, 0.5551470588235294379, 0.5588235294117647189, 0.5625000000000000000, 0.5661764705882352811, 0.5698529411764705621, 0.5735294117647058432, 0.5772058823529411242, 0.5808823529411765163, 0.5845588235294117974, 0.5882352941176470784, 0.5919117647058823595, 0.5955882352941176405, 0.5992647058823529216, 0.6029411764705882026, 0.6066176470588234837, 0.6102941176470588758, 0.6139705882352941568, 0.6176470588235294379, 0.6213235294117647189, 0.6250000000000000000, 0.6286764705882352811, 0.6323529411764705621, 0.6360294117647058432, 0.6397058823529411242, 0.6433823529411765163, 0.6470588235294117974, 0.6507352941176470784, 0.6544117647058823595, 0.6580882352941176405, 0.6617647058823529216, 0.6654411764705882026, 0.6691176470588234837, 0.6727941176470588758, 0.6764705882352941568, 0.6801470588235294379, 0.6838235294117647189, 0.6875000000000000000, 0.6911764705882352811, 0.6948529411764705621, 0.6985294117647058432, 0.7022058823529411242, 0.7058823529411765163, 0.7095588235294117974, 0.7132352941176470784, 0.7169117647058823595, 0.7205882352941176405, 0.7242647058823529216, 0.7279411764705882026, 0.7316176470588234837, 0.7352941176470588758, 0.7389705882352941568, 0.7426470588235294379, 0.7463235294117647189, 0.7500000000000000000, 0.7536764705882352811, 0.7573529411764705621, 0.7610294117647058432, 0.7647058823529411242, 0.7683823529411765163, 0.7720588235294117974, 0.7757352941176470784, 0.7794117647058823595, 0.7830882352941176405, 0.7867647058823529216, 0.7904411764705882026, 0.7941176470588234837, 0.7977941176470588758, 0.8014705882352941568, 0.8051470588235294379, 0.8088235294117647189, 0.8125000000000000000, 0.8161764705882352811, 0.8198529411764705621, 0.8235294117647058432, 0.8272058823529411242, 0.8308823529411765163, 0.8345588235294117974, 0.8382352941176470784, 0.8419117647058823595, 0.8455882352941176405, 0.8492647058823529216, 0.8529411764705882026, 0.8566176470588234837, 0.8602941176470588758, 0.8639705882352941568, 0.8676470588235294379, 0.8713235294117647189, 0.8750000000000000000, 0.8786764705882352811, 0.8823529411764705621, 0.8860294117647058432, 0.8897058823529411242, 0.8933823529411765163, 0.8970588235294117974, 0.9007352941176470784, 0.9044117647058823595, 0.9080882352941176405, 0.9117647058823529216, 0.9154411764705882026, 0.9191176470588234837, 0.9227941176470588758, 0.9264705882352941568, 0.9301470588235294379, 0.9338235294117647189, 0.9375000000000000000, 0.9411764705882352811, 0.9448529411764705621, 0.9485294117647058432, 0.9522058823529411242, 0.9558823529411765163, 0.9595588235294117974, 0.9632352941176470784, 0.9669117647058823595, 0.9705882352941176405, 0.9742647058823529216, 0.9779411764705882026, 0.9803851213646477269 ),
 .UNSPECIFIED. ) 
 GEOMETRIC_REPRESENTATION_ITEM ( )  RATIONAL_B_SPLINE_SURFACE ( (
 ( 1.000000000000000000, 0.9238795325112867385, 1.000000000000000000, 0.9238795325112867385, 1.000000000000000000, 0.9238795325112867385, 1.000000000000000000, 0.9238795325112867385, 1.000000000000000000, 0.9238795325112867385, 1.000000000000000000, 0.9238795325112867385, 1.000000000000000000, 0.9238795325112867385, 1.000000000000000000, 0.9238795325112867385, 1.000000000000000000, 0.9238795325112867385, 1.000000000000000000, 0.9238795325112867385, 1.000000000000000000, 0.9238795325112867385, 1.000000000000000000, 0.9238795325112867385, 1.000000000000000000, 0.9238795325112867385, 1.000000000000000000, 0.9238795325112867385, 1.000000000000000000, 0.9238795325112867385, 1.000000000000000000, 0.9238795325112867385, 1.000000000000000000, 0.9238795325112867385, 1.000000000000000000, 0.9238795325112867385, 1.000000000000000000, 0.9238795325112867385, 1.000000000000000000, 0.9238795325112867385, 1.000000000000000000, 0.9238795325112867385, 1.000000000000000000, 0.9238795325112867385, 1.000000000000000000, 0.9238795325112867385, 1.000000000000000000, 0.9238795325112867385, 1.000000000000000000, 0.9238795325112867385, 1.000000000000000000, 0.9238795325112867385, 1.000000000000000000, 0.9238795325112867385, 1.000000000000000000, 0.9238795325112867385, 1.000000000000000000, 0.9238795325112867385, 1.000000000000000000, 0.9238795325112867385, 1.000000000000000000, 0.9238795325112867385, 1.000000000000000000, 0.9238795325112867385, 1.000000000000000000, 0.9238795325112867385, 1.000000000000000000, 0.9238795325112867385, 1.000000000000000000, 0.9238795325112867385, 1.000000000000000000, 0.9238795325112867385, 1.000000000000000000, 0.9238795325112867385, 1.000000000000000000, 0.9238795325112867385, 1.000000000000000000, 0.9238795325112867385, 1.000000000000000000, 0.9238795325112867385, 1.000000000000000000, 0.9238795325112867385, 1.000000000000000000, 0.9238795325112867385, 1.000000000000000000, 0.9238795325112867385, 1.000000000000000000, 0.9238795325112867385, 1.000000000000000000, 0.9238795325112867385, 1.000000000000000000, 0.9238795325112867385, 1.000000000000000000, 0.9238795325112867385, 1.000000000000000000, 0.9238795325112867385, 1.000000000000000000, 0.9238795325112867385, 1.000000000000000000, 0.9238795325112867385, 1.000000000000000000, 0.9238795325112867385, 1.000000000000000000, 0.9238795325112867385, 1.000000000000000000, 0.9238795325112867385, 1.000000000000000000, 0.9238795325112867385, 1.000000000000000000, 0.9238795325112867385, 1.000000000000000000, 0.9238795325112867385, 1.000000000000000000, 0.9238795325112867385, 1.000000000000000000, 0.9238795325112867385, 1.000000000000000000, 0.9238795325112867385, 1.000000000000000000, 0.9238795325112867385, 1.000000000000000000, 0.9238795325112867385, 1.000000000000000000, 0.9238795325112867385, 1.000000000000000000, 0.9238795325112867385, 1.000000000000000000, 0.9238795325112867385, 1.000000000000000000, 0.9238795325112867385, 1.000000000000000000, 0.9238795325112867385, 1.000000000000000000, 0.9238795325112867385, 1.000000000000000000, 0.9238795325112867385, 1.000000000000000000, 0.9238795325112867385, 1.000000000000000000, 0.9238795325112867385, 1.000000000000000000, 0.9238795325112867385, 1.000000000000000000, 0.9238795325112867385, 1.000000000000000000, 0.9238795325112867385, 1.000000000000000000, 0.9238795325112867385, 1.000000000000000000, 0.9238795325112867385, 1.000000000000000000, 0.9238795325112867385, 1.000000000000000000, 0.9238795325112867385, 1.000000000000000000, 0.9238795325112867385, 1.000000000000000000, 0.9238795325112867385, 1.000000000000000000, 0.9238795325112867385, 1.000000000000000000, 0.9238795325112867385, 1.000000000000000000, 0.9238795325112867385, 1.000000000000000000, 0.9238795325112867385, 1.000000000000000000, 0.9238795325112867385, 1.000000000000000000, 0.9238795325112867385, 1.000000000000000000, 0.9238795325112867385, 1.000000000000000000, 0.9238795325112867385, 1.000000000000000000, 0.9238795325112867385, 1.000000000000000000, 0.9238795325112867385, 1.000000000000000000, 0.9238795325112867385, 1.000000000000000000, 0.9238795325112867385, 1.000000000000000000, 0.9238795325112867385, 1.000000000000000000, 0.9238795325112867385, 1.000000000000000000, 0.9238795325112867385, 1.000000000000000000, 0.9238795325112867385, 1.000000000000000000, 0.9238795325112867385, 1.000000000000000000, 0.9238795325112867385, 1.000000000000000000, 0.9238795325112867385, 1.000000000000000000, 0.9238795325112867385, 1.000000000000000000, 0.9238795325112867385, 1.000000000000000000, 0.9238795325112867385, 1.000000000000000000, 0.9238795325112867385, 1.000000000000000000, 0.9238795325112867385, 1.000000000000000000, 0.9238795325112867385, 1.000000000000000000, 0.9238795325112867385, 1.000000000000000000, 0.9238795325112867385, 1.000000000000000000, 0.9238795325112867385, 1.000000000000000000, 0.9238795325112867385, 1.000000000000000000, 0.9238795325112867385, 1.000000000000000000, 0.9238795325112867385, 1.000000000000000000, 0.9238795325112867385, 1.000000000000000000, 0.9238795325112867385, 1.000000000000000000, 0.9238795325112867385, 1.000000000000000000, 0.9238795325112867385, 1.000000000000000000, 0.9238795325112867385, 1.000000000000000000, 0.9238795325112867385, 1.000000000000000000, 0.9238795325112867385, 1.000000000000000000, 0.9238795325112867385, 1.000000000000000000, 0.9238795325112867385, 1.000000000000000000, 0.9238795325112867385, 1.000000000000000000, 0.9238795325112867385, 1.000000000000000000, 0.9238795325112867385, 1.000000000000000000, 0.9238795325112867385, 1.000000000000000000, 0.9238795325112867385, 1.000000000000000000, 0.9238795325112867385, 1.000000000000000000, 0.9238795325112867385, 1.000000000000000000, 0.9238795325112867385, 1.000000000000000000, 0.9238795325112867385, 1.000000000000000000, 0.9238795325112867385, 1.000000000000000000, 0.9238795325112867385, 1.000000000000000000, 0.9238795325112867385, 1.000000000000000000, 0.9238795325112867385, 1.000000000000000000, 0.9238795325112867385, 1.000000000000000000, 0.9238795325112867385, 1.000000000000000000, 0.9238795325112867385, 1.000000000000000000, 0.9238795325112867385, 1.000000000000000000, 0.9238795325112867385, 1.000000000000000000, 0.9238795325112867385, 1.000000000000000000, 0.9238795325112867385, 1.000000000000000000, 0.9238795325112867385, 1.000000000000000000, 0.9238795325112867385, 1.000000000000000000, 0.9238795325112867385, 1.000000000000000000, 0.9238795325112867385, 1.000000000000000000, 0.9238795325112867385, 1.000000000000000000, 0.9238795325112867385, 1.000000000000000000, 0.9238795325112867385, 1.000000000000000000, 0.9238795325112867385, 1.000000000000000000, 0.9238795325112867385, 1.000000000000000000, 0.9238795325112867385, 1.000000000000000000, 0.9238795325112867385, 1.000000000000000000, 0.9238795325112867385, 1.000000000000000000, 0.9238795325112867385, 1.000000000000000000, 0.9238795325112867385, 1.000000000000000000, 0.9238795325112867385, 1.000000000000000000, 0.9238795325112867385, 1.000000000000000000, 0.9238795325112867385, 1.000000000000000000, 0.9238795325112867385, 1.000000000000000000, 0.9238795325112867385, 1.000000000000000000, 0.9238795325112867385, 1.000000000000000000, 0.9238795325112867385, 1.000000000000000000, 0.9238795325112867385, 1.000000000000000000, 0.9238795325112867385, 1.000000000000000000, 0.9238795325112867385, 1.000000000000000000, 0.9238795325112867385, 1.000000000000000000, 0.9238795325112867385, 1.000000000000000000, 0.9238795325112867385, 1.000000000000000000, 0.9238795325112867385, 1.000000000000000000, 0.9238795325112867385, 1.000000000000000000, 0.9238795325112867385, 1.000000000000000000, 0.9238795325112867385, 1.000000000000000000, 0.9238795325112867385, 1.000000000000000000, 0.9238795325112867385, 1.000000000000000000, 0.9238795325112867385, 1.000000000000000000, 0.9238795325112867385, 1.000000000000000000, 0.9238795325112867385, 1.000000000000000000, 0.9238795325112867385, 1.000000000000000000, 0.9238795325112867385, 1.000000000000000000, 0.9238795325112867385, 1.000000000000000000, 0.9238795325112867385, 1.000000000000000000, 0.9238795325112867385, 1.000000000000000000, 0.9238795325112867385, 1.000000000000000000, 0.9238795325112867385, 1.000000000000000000, 0.9238795325112867385, 1.000000000000000000, 0.9238795325112867385, 1.000000000000000000, 0.9238795325112867385, 1.000000000000000000, 0.9238795325112867385, 1.000000000000000000, 0.9238795325112867385, 1.000000000000000000, 0.9238795325112867385, 1.000000000000000000, 0.9238795325112867385, 1.000000000000000000, 0.9238795325112867385, 1.000000000000000000, 0.9238795325112867385, 1.000000000000000000, 0.9238795325112867385, 1.000000000000000000, 0.9238795325112867385, 1.000000000000000000, 0.9238795325112867385, 1.000000000000000000, 0.9238795325112867385, 1.000000000000000000, 0.9238795325112867385, 1.000000000000000000, 0.9238795325112867385, 1.000000000000000000, 0.9238795325112867385, 1.000000000000000000, 0.9238795325112867385, 1.000000000000000000, 0.9238795325112867385, 1.000000000000000000, 0.9238795325112867385, 1.000000000000000000, 0.9238795325112867385, 1.000000000000000000, 0.9238795325112867385, 1.000000000000000000, 0.9238795325112867385, 1.000000000000000000, 0.9238795325112867385, 1.000000000000000000, 0.9238795325112867385, 1.000000000000000000, 0.9238795325112867385, 1.000000000000000000, 0.9238795325112867385, 1.000000000000000000, 0.9238795325112867385, 1.000000000000000000, 0.9238795325112867385, 1.000000000000000000, 0.9238795325112867385, 1.000000000000000000, 0.9238795325112867385, 1.000000000000000000, 0.9238795325112867385, 1.000000000000000000, 0.9238795325112867385, 1.000000000000000000, 0.9238795325112867385, 1.000000000000000000, 0.9238795325112867385, 1.000000000000000000, 0.9238795325112867385, 1.000000000000000000, 0.9238795325112867385, 1.000000000000000000, 0.9238795325112867385, 1.000000000000000000, 0.9238795325112867385, 1.000000000000000000, 0.9238795325112867385, 1.000000000000000000, 0.9238795325112867385, 1.000000000000000000, 0.9238795325112867385, 1.000000000000000000, 0.9238795325112867385, 1.000000000000000000, 0.9238795325112867385, 1.000000000000000000, 0.9238795325112867385, 1.000000000000000000, 0.9238795325112867385, 1.000000000000000000, 0.9238795325112867385, 1.000000000000000000, 0.9238795325112867385, 1.000000000000000000, 0.9238795325112867385, 1.000000000000000000, 0.9238795325112867385, 1.000000000000000000, 0.9238795325112867385, 1.000000000000000000, 0.9238795325112867385, 1.000000000000000000, 0.9238795325112867385, 1.000000000000000000, 0.9238795325112867385, 1.000000000000000000, 0.9238795325112867385, 1.000000000000000000, 0.9238795325112867385, 1.000000000000000000, 0.9238795325112867385, 1.000000000000000000, 0.9238795325112867385, 1.000000000000000000, 0.9238795325112867385, 1.000000000000000000, 0.9238795325112867385, 1.000000000000000000, 0.9238795325112867385, 1.000000000000000000, 0.9238795325112867385, 1.000000000000000000, 0.9238795325112867385, 1.000000000000000000, 0.9238795325112867385, 1.000000000000000000, 0.9238795325112867385, 1.000000000000000000, 0.9238795325112867385, 1.000000000000000000, 0.9238795325112867385, 1.000000000000000000, 0.9238795325112867385, 1.000000000000000000, 0.9238795325112867385, 1.000000000000000000, 0.9238795325112867385, 1.000000000000000000, 0.9238795325112867385, 1.000000000000000000, 0.9238795325112867385, 1.000000000000000000, 0.9238795325112867385, 1.000000000000000000, 0.9238795325112867385, 1.000000000000000000, 0.9238795325112867385, 1.000000000000000000, 0.9238795325112867385, 1.000000000000000000, 0.9238795325112867385, 1.000000000000000000, 0.9238795325112867385, 1.000000000000000000, 0.9238795325112867385, 1.000000000000000000, 0.9238795325112867385, 1.000000000000000000, 0.9238795325112867385, 1.000000000000000000, 0.9238795325112867385, 1.000000000000000000, 0.9238795325112867385, 1.000000000000000000, 0.9238795325112867385, 1.000000000000000000, 0.9238795325112867385, 1.000000000000000000, 0.9493986900241293547, 0.9660721264009082265),
 ( 1.000000000000000000, 0.9238795325112867385, 1.000000000000000000, 0.9238795325112867385, 1.000000000000000000, 0.9238795325112867385, 1.000000000000000000, 0.9238795325112867385, 1.000000000000000000, 0.9238795325112867385, 1.000000000000000000, 0.9238795325112867385, 1.000000000000000000, 0.9238795325112867385, 1.000000000000000000, 0.9238795325112867385, 1.000000000000000000, 0.9238795325112867385, 1.000000000000000000, 0.9238795325112867385, 1.000000000000000000, 0.9238795325112867385, 1.000000000000000000, 0.9238795325112867385, 1.000000000000000000, 0.9238795325112867385, 1.000000000000000000, 0.9238795325112867385, 1.000000000000000000, 0.9238795325112867385, 1.000000000000000000, 0.9238795325112867385, 1.000000000000000000, 0.9238795325112867385, 1.000000000000000000, 0.9238795325112867385, 1.000000000000000000, 0.9238795325112867385, 1.000000000000000000, 0.9238795325112867385, 1.000000000000000000, 0.9238795325112867385, 1.000000000000000000, 0.9238795325112867385, 1.000000000000000000, 0.9238795325112867385, 1.000000000000000000, 0.9238795325112867385, 1.000000000000000000, 0.9238795325112867385, 1.000000000000000000, 0.9238795325112867385, 1.000000000000000000, 0.9238795325112867385, 1.000000000000000000, 0.9238795325112867385, 1.000000000000000000, 0.9238795325112867385, 1.000000000000000000, 0.9238795325112867385, 1.000000000000000000, 0.9238795325112867385, 1.000000000000000000, 0.9238795325112867385, 1.000000000000000000, 0.9238795325112867385, 1.000000000000000000, 0.9238795325112867385, 1.000000000000000000, 0.9238795325112867385, 1.000000000000000000, 0.9238795325112867385, 1.000000000000000000, 0.9238795325112867385, 1.000000000000000000, 0.9238795325112867385, 1.000000000000000000, 0.9238795325112867385, 1.000000000000000000, 0.9238795325112867385, 1.000000000000000000, 0.9238795325112867385, 1.000000000000000000, 0.9238795325112867385, 1.000000000000000000, 0.9238795325112867385, 1.000000000000000000, 0.9238795325112867385, 1.000000000000000000, 0.9238795325112867385, 1.000000000000000000, 0.9238795325112867385, 1.000000000000000000, 0.9238795325112867385, 1.000000000000000000, 0.9238795325112867385, 1.000000000000000000, 0.9238795325112867385, 1.000000000000000000, 0.9238795325112867385, 1.000000000000000000, 0.9238795325112867385, 1.000000000000000000, 0.9238795325112867385, 1.000000000000000000, 0.9238795325112867385, 1.000000000000000000, 0.9238795325112867385, 1.000000000000000000, 0.9238795325112867385, 1.000000000000000000, 0.9238795325112867385, 1.000000000000000000, 0.9238795325112867385, 1.000000000000000000, 0.9238795325112867385, 1.000000000000000000, 0.9238795325112867385, 1.000000000000000000, 0.9238795325112867385, 1.000000000000000000, 0.9238795325112867385, 1.000000000000000000, 0.9238795325112867385, 1.000000000000000000, 0.9238795325112867385, 1.000000000000000000, 0.9238795325112867385, 1.000000000000000000, 0.9238795325112867385, 1.000000000000000000, 0.9238795325112867385, 1.000000000000000000, 0.9238795325112867385, 1.000000000000000000, 0.9238795325112867385, 1.000000000000000000, 0.9238795325112867385, 1.000000000000000000, 0.9238795325112867385, 1.000000000000000000, 0.9238795325112867385, 1.000000000000000000, 0.9238795325112867385, 1.000000000000000000, 0.9238795325112867385, 1.000000000000000000, 0.9238795325112867385, 1.000000000000000000, 0.9238795325112867385, 1.000000000000000000, 0.9238795325112867385, 1.000000000000000000, 0.9238795325112867385, 1.000000000000000000, 0.9238795325112867385, 1.000000000000000000, 0.9238795325112867385, 1.000000000000000000, 0.9238795325112867385, 1.000000000000000000, 0.9238795325112867385, 1.000000000000000000, 0.9238795325112867385, 1.000000000000000000, 0.9238795325112867385, 1.000000000000000000, 0.9238795325112867385, 1.000000000000000000, 0.9238795325112867385, 1.000000000000000000, 0.9238795325112867385, 1.000000000000000000, 0.9238795325112867385, 1.000000000000000000, 0.9238795325112867385, 1.000000000000000000, 0.9238795325112867385, 1.000000000000000000, 0.9238795325112867385, 1.000000000000000000, 0.9238795325112867385, 1.000000000000000000, 0.9238795325112867385, 1.000000000000000000, 0.9238795325112867385, 1.000000000000000000, 0.9238795325112867385, 1.000000000000000000, 0.9238795325112867385, 1.000000000000000000, 0.9238795325112867385, 1.000000000000000000, 0.9238795325112867385, 1.000000000000000000, 0.9238795325112867385, 1.000000000000000000, 0.9238795325112867385, 1.000000000000000000, 0.9238795325112867385, 1.000000000000000000, 0.9238795325112867385, 1.000000000000000000, 0.9238795325112867385, 1.000000000000000000, 0.9238795325112867385, 1.000000000000000000, 0.9238795325112867385, 1.000000000000000000, 0.9238795325112867385, 1.000000000000000000, 0.9238795325112867385, 1.000000000000000000, 0.9238795325112867385, 1.000000000000000000, 0.9238795325112867385, 1.000000000000000000, 0.9238795325112867385, 1.000000000000000000, 0.9238795325112867385, 1.000000000000000000, 0.9238795325112867385, 1.000000000000000000, 0.9238795325112867385, 1.000000000000000000, 0.9238795325112867385, 1.000000000000000000, 0.9238795325112867385, 1.000000000000000000, 0.9238795325112867385, 1.000000000000000000, 0.9238795325112867385, 1.000000000000000000, 0.9238795325112867385, 1.000000000000000000, 0.9238795325112867385, 1.000000000000000000, 0.9238795325112867385, 1.000000000000000000, 0.9238795325112867385, 1.000000000000000000, 0.9238795325112867385, 1.000000000000000000, 0.9238795325112867385, 1.000000000000000000, 0.9238795325112867385, 1.000000000000000000, 0.9238795325112867385, 1.000000000000000000, 0.9238795325112867385, 1.000000000000000000, 0.9238795325112867385, 1.000000000000000000, 0.9238795325112867385, 1.000000000000000000, 0.9238795325112867385, 1.000000000000000000, 0.9238795325112867385, 1.000000000000000000, 0.9238795325112867385, 1.000000000000000000, 0.9238795325112867385, 1.000000000000000000, 0.9238795325112867385, 1.000000000000000000, 0.9238795325112867385, 1.000000000000000000, 0.9238795325112867385, 1.000000000000000000, 0.9238795325112867385, 1.000000000000000000, 0.9238795325112867385, 1.000000000000000000, 0.9238795325112867385, 1.000000000000000000, 0.9238795325112867385, 1.000000000000000000, 0.9238795325112867385, 1.000000000000000000, 0.9238795325112867385, 1.000000000000000000, 0.9238795325112867385, 1.000000000000000000, 0.9238795325112867385, 1.000000000000000000, 0.9238795325112867385, 1.000000000000000000, 0.9238795325112867385, 1.000000000000000000, 0.9238795325112867385, 1.000000000000000000, 0.9238795325112867385, 1.000000000000000000, 0.9238795325112867385, 1.000000000000000000, 0.9238795325112867385, 1.000000000000000000, 0.9238795325112867385, 1.000000000000000000, 0.9238795325112867385, 1.000000000000000000, 0.9238795325112867385, 1.000000000000000000, 0.9238795325112867385, 1.000000000000000000, 0.9238795325112867385, 1.000000000000000000, 0.9238795325112867385, 1.000000000000000000, 0.9238795325112867385, 1.000000000000000000, 0.9238795325112867385, 1.000000000000000000, 0.9238795325112867385, 1.000000000000000000, 0.9238795325112867385, 1.000000000000000000, 0.9238795325112867385, 1.000000000000000000, 0.9238795325112867385, 1.000000000000000000, 0.9238795325112867385, 1.000000000000000000, 0.9238795325112867385, 1.000000000000000000, 0.9238795325112867385, 1.000000000000000000, 0.9238795325112867385, 1.000000000000000000, 0.9238795325112867385, 1.000000000000000000, 0.9238795325112867385, 1.000000000000000000, 0.9238795325112867385, 1.000000000000000000, 0.9238795325112867385, 1.000000000000000000, 0.9238795325112867385, 1.000000000000000000, 0.9238795325112867385, 1.000000000000000000, 0.9238795325112867385, 1.000000000000000000, 0.9238795325112867385, 1.000000000000000000, 0.9238795325112867385, 1.000000000000000000, 0.9238795325112867385, 1.000000000000000000, 0.9238795325112867385, 1.000000000000000000, 0.9238795325112867385, 1.000000000000000000, 0.9238795325112867385, 1.000000000000000000, 0.9238795325112867385, 1.000000000000000000, 0.9238795325112867385, 1.000000000000000000, 0.9238795325112867385, 1.000000000000000000, 0.9238795325112867385, 1.000000000000000000, 0.9238795325112867385, 1.000000000000000000, 0.9238795325112867385, 1.000000000000000000, 0.9238795325112867385, 1.000000000000000000, 0.9238795325112867385, 1.000000000000000000, 0.9238795325112867385, 1.000000000000000000, 0.9238795325112867385, 1.000000000000000000, 0.9238795325112867385, 1.000000000000000000, 0.9238795325112867385, 1.000000000000000000, 0.9238795325112867385, 1.000000000000000000, 0.9238795325112867385, 1.000000000000000000, 0.9238795325112867385, 1.000000000000000000, 0.9238795325112867385, 1.000000000000000000, 0.9238795325112867385, 1.000000000000000000, 0.9238795325112867385, 1.000000000000000000, 0.9238795325112867385, 1.000000000000000000, 0.9238795325112867385, 1.000000000000000000, 0.9238795325112867385, 1.000000000000000000, 0.9238795325112867385, 1.000000000000000000, 0.9238795325112867385, 1.000000000000000000, 0.9238795325112867385, 1.000000000000000000, 0.9238795325112867385, 1.000000000000000000, 0.9238795325112867385, 1.000000000000000000, 0.9238795325112867385, 1.000000000000000000, 0.9238795325112867385, 1.000000000000000000, 0.9238795325112867385, 1.000000000000000000, 0.9238795325112867385, 1.000000000000000000, 0.9238795325112867385, 1.000000000000000000, 0.9238795325112867385, 1.000000000000000000, 0.9238795325112867385, 1.000000000000000000, 0.9238795325112867385, 1.000000000000000000, 0.9238795325112867385, 1.000000000000000000, 0.9238795325112867385, 1.000000000000000000, 0.9238795325112867385, 1.000000000000000000, 0.9238795325112867385, 1.000000000000000000, 0.9238795325112867385, 1.000000000000000000, 0.9238795325112867385, 1.000000000000000000, 0.9238795325112867385, 1.000000000000000000, 0.9238795325112867385, 1.000000000000000000, 0.9238795325112867385, 1.000000000000000000, 0.9238795325112867385, 1.000000000000000000, 0.9238795325112867385, 1.000000000000000000, 0.9238795325112867385, 1.000000000000000000, 0.9238795325112867385, 1.000000000000000000, 0.9238795325112867385, 1.000000000000000000, 0.9238795325112867385, 1.000000000000000000, 0.9238795325112867385, 1.000000000000000000, 0.9238795325112867385, 1.000000000000000000, 0.9238795325112867385, 1.000000000000000000, 0.9238795325112867385, 1.000000000000000000, 0.9238795325112867385, 1.000000000000000000, 0.9238795325112867385, 1.000000000000000000, 0.9238795325112867385, 1.000000000000000000, 0.9238795325112867385, 1.000000000000000000, 0.9238795325112867385, 1.000000000000000000, 0.9238795325112867385, 1.000000000000000000, 0.9238795325112867385, 1.000000000000000000, 0.9238795325112867385, 1.000000000000000000, 0.9238795325112867385, 1.000000000000000000, 0.9238795325112867385, 1.000000000000000000, 0.9238795325112867385, 1.000000000000000000, 0.9238795325112867385, 1.000000000000000000, 0.9238795325112867385, 1.000000000000000000, 0.9238795325112867385, 1.000000000000000000, 0.9238795325112867385, 1.000000000000000000, 0.9238795325112867385, 1.000000000000000000, 0.9238795325112867385, 1.000000000000000000, 0.9238795325112867385, 1.000000000000000000, 0.9238795325112867385, 1.000000000000000000, 0.9238795325112867385, 1.000000000000000000, 0.9238795325112867385, 1.000000000000000000, 0.9238795325112867385, 1.000000000000000000, 0.9238795325112867385, 1.000000000000000000, 0.9238795325112867385, 1.000000000000000000, 0.9238795325112867385, 1.000000000000000000, 0.9238795325112867385, 1.000000000000000000, 0.9238795325112867385, 1.000000000000000000, 0.9238795325112867385, 1.000000000000000000, 0.9238795325112867385, 1.000000000000000000, 0.9238795325112867385, 1.000000000000000000, 0.9238795325112867385, 1.000000000000000000, 0.9238795325112867385, 1.000000000000000000, 0.9238795325112867385, 1.000000000000000000, 0.9238795325112867385, 1.000000000000000000, 0.9238795325112867385, 1.000000000000000000, 0.9238795325112867385, 1.000000000000000000, 0.9493986900241293547, 0.9660721264009082265) ) ) 
 REPRESENTATION_ITEM ( '' )  SURFACE ( )  );
#12362 = ORIENTED_EDGE ( 'NONE', *, *, #4855, .F. ) ;
#12363 = CARTESIAN_POINT ( 'NONE',  ( -4.220049686691935698, 10.18810118749999916, 70.37500000204838102 ) ) ;
#12364 = CARTESIAN_POINT ( 'NONE',  ( -5.676582343749998039, 97.76041666325269830, -9.832129032723420536 ) ) ;
#12365 = CARTESIAN_POINT ( 'NONE',  ( 11.00000000000000000, 0.000000000000000000, 0.000000000000000000 ) ) ;
#12366 = CARTESIAN_POINT ( 'NONE',  ( -7.778174593052023411, 7.778174593052023411, 81.81249999999998579 ) ) ;
#12368 = CARTESIAN_POINT ( 'NONE',  ( 26.56734541678232731, 204.0000000013656347, 166.5412658749999650 ) ) ;
#12367 = CARTESIAN_POINT ( 'NONE',  ( 24.54126587499998280, 201.5000000013655779, 171.4326545832175555 ) ) ;
#12369 = ORIENTED_EDGE ( 'NONE', *, *, #63840, .T. ) ;
#12370 = CARTESIAN_POINT ( 'NONE',  ( -1.469576158976823947E-15, 20.62500000000000355, 8.000000000000000000 ) ) ;
#12371 = CARTESIAN_POINT ( 'NONE',  ( 4.000000000000015987, 202.6250000027312126, 198.0000000000000284 ) ) ;
#12372 = EDGE_CURVE ( 'NONE', #3444, #25788, #47340, .T. ) ;
#12373 = CARTESIAN_POINT ( 'NONE',  ( -5.676582343750006032, 209.1145833299193555, 9.832129032723418760 ) ) ;
#12374 = CARTESIAN_POINT ( 'NONE',  ( 1.432654583217607858, 206.6250000013656063, 138.5412658750000787 ) ) ;
#12375 = CARTESIAN_POINT ( 'NONE',  ( 24.54126587499998635, 206.5000000013655779, 171.4326545832175555 ) ) ;
#12376 = CARTESIAN_POINT ( 'NONE',  ( -7.188101187500001821, 20.99999999795161898, -2.977408999572651371 ) ) ;
#12377 = CARTESIAN_POINT ( 'NONE',  ( -3.042071309553173730, 174.6354166632526983, 11.35316468749999785 ) ) ;
#12378 = CARTESIAN_POINT ( 'NONE',  ( -7.188101187500000933, 97.43750000204839523, -2.977408999572650483 ) ) ;
#12380 = CARTESIAN_POINT ( 'NONE',  ( -7.320508075688768379, 111.8750000000000000, -7.320508075688769267 ) ) ;
#12379 = CARTESIAN_POINT ( 'NONE',  ( -3.673940397442060854E-16, 295.8125000034140157, -6.000000000000001776 ) ) ;
#12381 = CARTESIAN_POINT ( 'NONE',  ( -3.211159895383562723, 11.93749999863440614, 3.211159895383561391 ) ) ;
#12382 = CARTESIAN_POINT ( 'NONE',  ( 24.54126587499999346, 202.4375000013656063, 169.9999999999998863 ) ) ;
#12383 = CARTESIAN_POINT ( 'NONE',  ( -5.082755093536319713, 5.082755093536319713, 9.174052781871752771 ) ) ;
#12384 = CARTESIAN_POINT ( 'NONE',  ( 11.35316468749999785, 65.57291666325269830, 3.042071309553174174 ) ) ;
#12385 = EDGE_CURVE ( 'NONE', #68967, #10283, #31320, .T. ) ;
#12387 =( BOUNDED_CURVE ( )  B_SPLINE_CURVE ( 2, ( #68523, #67789, #16080, #39487, #39115, #62118, #33847, #10443, #33473 ),
 .UNSPECIFIED., .F., .F. ) 
 B_SPLINE_CURVE_WITH_KNOTS ( ( 3, 2, 2, 2, 3 ),
 ( 0.4666666666666670626, 0.4750000000000003664, 0.4833333333333337256, 0.4916666666666670849, 0.5000000000000004441 ),
 .UNSPECIFIED. ) 
 CURVE ( )  GEOMETRIC_REPRESENTATION_ITEM ( )  RATIONAL_B_SPLINE_CURVE ( ( 0.9999999999999964473, 0.9238795325112902912, 1.000000000000000000, 0.9238795325112867385, 1.000000000000000000, 0.9238795325112867385, 1.000000000000000000, 0.9238795325112826307, 1.000000000000003997 ) ) 
 REPRESENTATION_ITEM ( '' )  );
#12386 = CARTESIAN_POINT ( 'NONE',  ( -28.00000000000003197, 207.0000000000000284, 166.0000000000003695 ) ) ;
#12388 = CARTESIAN_POINT ( 'NONE',  ( 5.656854249492376141, -5.656854249492374365, -0.05094721567017711228 ) ) ;
#12389 = ORIENTED_EDGE ( 'NONE', *, *, #57418, .T. ) ;
#12390 = CARTESIAN_POINT ( 'NONE',  ( 0.000000000000000000, 125.0000000000000000, 8.000000000000000000 ) ) ;
#12391 = CARTESIAN_POINT ( 'NONE',  ( -11.00000000000000000, 0.000000000000000000, 80.68750000409677625 ) ) ;
#12392 = CARTESIAN_POINT ( 'NONE',  ( -3.042071309553173730, 79.32291666325271251, 11.35316468749999785 ) ) ;
#12393 = CARTESIAN_POINT ( 'NONE',  ( -6.735557395310442023E-16, 11.00000000000000000, 69.81250000409677625 ) ) ;
#12394 = FACE_OUTER_BOUND ( 'NONE', #59299, .T. ) ;
#12395 = DIRECTION ( 'NONE',  ( -0.000000000000000000, 1.000000000000000000, -0.000000000000000000 ) ) ;
#12397 = CARTESIAN_POINT ( 'NONE',  ( -5.676582343750006032, 54.11458332991934839, 9.832129032723418760 ) ) ;
#12396 = CARTESIAN_POINT ( 'NONE',  ( -28.00000000000007816, 202.1250000027312126, 166.0000000000003695 ) ) ;
#12398 = CARTESIAN_POINT ( 'NONE',  ( -7.999999999999989342, -3.313708498984762496, 22.11155278392014623 ) ) ;
#12399 = CARTESIAN_POINT ( 'NONE',  ( -3.257047731941386637, 194.8184057345648625, 144.0082042844364025 ) ) ;
#12400 = CARTESIAN_POINT ( 'NONE',  ( -5.000000000000005329, 150.2083333265053682, 8.660254037844387298 ) ) ;
#12401 = CARTESIAN_POINT ( 'NONE',  ( 7.188101187500002709, 95.18750000204838102, 2.977408999572649151 ) ) ;
#12402 = CARTESIAN_POINT ( 'NONE',  ( -1.836970198721029983E-15, 10.62499999317203425, 10.00000000000000178 ) ) ;
#12403 = CARTESIAN_POINT ( 'NONE',  ( 5.676582343750001591, 41.92708332991934839, -9.832129032723420536 ) ) ;
#12404 = CARTESIAN_POINT ( 'NONE',  ( -7.204075437095967871, 7.204075437095967871, 112.8437500020483810 ) ) ;
#12405 = CARTESIAN_POINT ( 'NONE',  ( 11.35316468749999785, 190.5729166632526699, 3.042071309553174174 ) ) ;
#12406 = ORIENTED_EDGE ( 'NONE', *, *, #36186, .T. ) ;
#12407 = CARTESIAN_POINT ( 'NONE',  ( 1.656854249492388576, 3.812500000000000888, 3.999999999999994671 ) ) ;
#12408 = CARTESIAN_POINT ( 'NONE',  ( -28.00000000000007816, 199.1250000027312126, 166.0000000000003695 ) ) ;
#12409 = CARTESIAN_POINT ( 'NONE',  ( -1.656854249492195619, 195.8125000000000568, 193.9999999999999147 ) ) ;
#12411 = CARTESIAN_POINT ( 'NONE',  ( -3.042071309553163960, 182.2395833299193555, -11.35316468749999963 ) ) ;
#12410 = CYLINDRICAL_SURFACE ( 'NONE', #17040, 3.999999999999976019 ) ;
#12412 = CYLINDRICAL_SURFACE ( 'NONE', #50191, 10.00000000000000000 ) ;
#12413 = CARTESIAN_POINT ( 'NONE',  ( 2.679491924311225848, 256.6666666734946602, -10.00000000000000000 ) ) ;
#12414 = CYLINDRICAL_SURFACE ( 'NONE', #29985, 4.999999999999997335 ) ;
#12415 = ORIENTED_EDGE ( 'NONE', *, *, #68019, .F. ) ;
#12416 = CARTESIAN_POINT ( 'NONE',  ( 9.832129032723416984, 170.6770833299193555, 5.676582343750006032 ) ) ;
#12417 = CARTESIAN_POINT ( 'NONE',  ( -7.999999999961178609, -1.665943300379353739E-05, 2.518425711869641592 ) ) ;
#12418 = CARTESIAN_POINT ( 'NONE',  ( -11.35316468750000141, 128.8020833299193555, 3.042071309553159963 ) ) ;
#12419 = CARTESIAN_POINT ( 'NONE',  ( -8.000000000000001776, 3.656249995903220640, 3.313708498984759387 ) ) ;
#12420 = EDGE_LOOP ( 'NONE', ( #44568, #15584, #31713, #71761 ) ) ;
#12421 = CARTESIAN_POINT ( 'NONE',  ( 5.656854249492379694, 106.6250000040967763, -5.656854249492380582 ) ) ;
#12422 = CARTESIAN_POINT ( 'NONE',  ( -4.000000000000001776, 12.43750000000000000, -1.656854249492381470 ) ) ;
#12423 = FACE_OUTER_BOUND ( 'NONE', #8797, .T. ) ;
#12424 = CARTESIAN_POINT ( 'NONE',  ( 4.541265875000001451, 12.24999999863440792, 1.881053915767124440 ) ) ;
#12425 = CARTESIAN_POINT ( 'NONE',  ( -7.999999999999991118, 0.000000000000000000, 20.51780278392014623 ) ) ;
#12426 = CARTESIAN_POINT ( 'NONE',  ( 0.000000000000000000, 125.0000000000000000, 0.000000000000000000 ) ) ;
#12427 = VERTEX_POINT ( 'NONE', #18680 ) ;
#12428 = CARTESIAN_POINT ( 'NONE',  ( 6.326249034914468552E-13, 178.7500000000000853, 10.00000000000000533 ) ) ;
#12429 = CARTESIAN_POINT ( 'NONE',  ( 2.977408999572654480, 105.1250000020483668, 7.188101187499999156 ) ) ;
#12431 = CARTESIAN_POINT ( 'NONE',  ( 2.449293598294707893E-16, 6.999999997268813168, -4.000000000000001776 ) ) ;
#12430 = CARTESIAN_POINT ( 'NONE',  ( -5.656854249492378806, 92.37500000409677625, 5.656854249492381470 ) ) ;
#12432 = DIRECTION ( 'NONE',  ( 0.000000000000000000, 0.000000000000000000, 1.000000000000000000 ) ) ;
#12434 = ADVANCED_FACE ( 'NONE', ( #52643 ), #51899, .T. ) ;
#12433 = VERTEX_POINT ( 'NONE', #46969 ) ;
#12435 = EDGE_CURVE ( 'NONE', #37130, #73625, #56899, .T. ) ;
#12436 = CARTESIAN_POINT ( 'NONE',  ( -6.298842414732201078, 10.24914933418224194, -64.89273347874026854 ) ) ;
#12437 = CARTESIAN_POINT ( 'NONE',  ( 5.082755093536320601, -5.082755093536318824, 26.04905278187175810 ) ) ;
#12438 = ORIENTED_EDGE ( 'NONE', *, *, #39801, .F. ) ;
#12439 = ORIENTED_EDGE ( 'NONE', *, *, #40150, .F. ) ;
#12440 = CARTESIAN_POINT ( 'NONE',  ( -10.18810118749999916, 0.000000000000000000, 84.15625000204838102 ) ) ;
#12441 = PRODUCT_DEFINITION_CONTEXT ( 'detailed design', #50548, 'design' ) ;
#12442 = CARTESIAN_POINT ( 'NONE',  ( -24.54126587500000056, 197.5000000013656063, 168.5673454167827003 ) ) ;
#12443 = CARTESIAN_POINT ( 'NONE',  ( -7.778174593052020747, -7.778174593052023411, 101.6874999999999858 ) ) ;
#12446 = CARTESIAN_POINT ( 'NONE',  ( 4.721056650416000089, 298.9843750017070079, 4.721056650415999201 ) ) ;
#12445 = CARTESIAN_POINT ( 'NONE',  ( 25.17157287525378351, 206.7500000027312126, 167.1715728752537586 ) ) ;
#12444 = CARTESIAN_POINT ( 'NONE',  ( -5.999999999999999112, 290.1250000034140157, 2.485281374238575314 ) ) ;
#12447 = CARTESIAN_POINT ( 'NONE',  ( 10.00000000000000178, 135.2083333333333144, -2.679491924311226736 ) ) ;
#12448 = VECTOR ( 'NONE', #34816, 1000.000000000000000 ) ;
#12449 = AXIS2_PLACEMENT_3D ( 'NONE', #37449, #43090, #66107 ) ;
#12451 = EDGE_CURVE ( 'NONE', #61992, #33914, #71446, .T. ) ;
#12450 = CARTESIAN_POINT ( 'NONE',  ( -7.999999999999998224, 98.09375000000001421, 3.313708498984766493 ) ) ;
#12452 = CARTESIAN_POINT ( 'NONE',  ( 26.34314575050757057, 200.0625000027311842, 173.9999999999998295 ) ) ;
#12453 = CARTESIAN_POINT ( 'NONE',  ( 2.775557561562891351E-14, -37.99999999999997868, 170.0000000000000284 ) ) ;
#12454 = CARTESIAN_POINT ( 'NONE',  ( 6.000000000000001776, 290.5625000034140157, -7.347880794884121708E-16 ) ) ;
#12455 = CARTESIAN_POINT ( 'NONE',  ( 24.54126587499998280, 203.2500000013656063, 171.4326545832175555 ) ) ;
#12456 = CARTESIAN_POINT ( 'NONE',  ( -5.082755093536326818, 3.281249997951610542, 5.082755093536325042 ) ) ;
#12457 = CARTESIAN_POINT ( 'NONE',  ( 3.317071493978883456, -8.008118988124989457, 4.481865283940629219 ) ) ;
#12458 = CARTESIAN_POINT ( 'NONE',  ( -3.458734125000016313, 194.8750000013656063, 140.5673454167824161 ) ) ;
#12459 = CARTESIAN_POINT ( 'NONE',  ( -7.188101187500000933, 118.4375000020483952, -2.977408999572650483 ) ) ;
#12460 = CYLINDRICAL_SURFACE ( 'NONE', #26320, 27.99999999999998224 ) ;
#12461 = CARTESIAN_POINT ( 'NONE',  ( -6.951808397369817780E-16, 232.9687500034139873, -11.35316468749999963 ) ) ;
#12462 = CARTESIAN_POINT ( 'NONE',  ( -35.59712740376152595, 39.55325799726388425, 64.99999999999998579 ) ) ;
#12463 = CARTESIAN_POINT ( 'NONE',  ( 7.188101187499991163, 2.977408999572648707, 26.70530278187175455 ) ) ;
#12464 = CARTESIAN_POINT ( 'NONE',  ( 23.99999999999998934, 199.7500000000000000, 169.9999999999998863 ) ) ;
#12465 = CARTESIAN_POINT ( 'NONE',  ( -3.042071309553164404, 27.23958332991934839, -11.35316468749999963 ) ) ;
#12466 = CARTESIAN_POINT ( 'NONE',  ( 6.123233995736767268E-16, 26.25000000000000355, -10.00000000000000178 ) ) ;
#12467 = CARTESIAN_POINT ( 'NONE',  ( 11.35316468750000141, 216.0937499965860411, 0.000000000000000000 ) ) ;
#12468 = DIRECTION ( 'NONE',  ( -0.000000000000000000, 1.000000000000000000, -4.476705744456276341E-16 ) ) ;
#12470 = CARTESIAN_POINT ( 'NONE',  ( -8.000000000000000000, 96.40625000000000000, -3.313708498984761164 ) ) ;
#12469 = DIRECTION ( 'NONE',  ( -1.000000000000000000, -1.224646799147353207E-16, 0.000000000000000000 ) ) ;
#12471 = ORIENTED_EDGE ( 'NONE', *, *, #20266, .T. ) ;
#12472 = CARTESIAN_POINT ( 'NONE',  ( 1.432654583217607414, 196.5000000013656063, 145.4587341250000634 ) ) ;
#12473 = CARTESIAN_POINT ( 'NONE',  ( -8.311093377946836114, 37.65624999658601268, -8.311093377946837890 ) ) ;
#12474 = CARTESIAN_POINT ( 'NONE',  ( 4.556349186104045934, 11.00000000000000000, 87.71875000409677625 ) ) ;
#12475 = CARTESIAN_POINT ( 'NONE',  ( -2.754378923186476579E-14, 208.4375000013656063, 145.4587341250000350 ) ) ;
#12476 = EDGE_CURVE ( 'NONE', #9987, #12049, #68032, .T. ) ;
#12477 = CARTESIAN_POINT ( 'NONE',  ( 27.99999999999999645, 210.0000000000000284, 165.9999999999999147 ) ) ;
#12479 = CARTESIAN_POINT ( 'NONE',  ( -9.832129032723418760, 22.86458332991934839, -5.676582343750004256 ) ) ;
#12478 = CARTESIAN_POINT ( 'NONE',  ( 2.977408999572650039, 104.1875000020483810, -7.188101187500000933 ) ) ;
#12480 = CARTESIAN_POINT ( 'NONE',  ( -5.656854249492373476, -5.656854249492376141, 13.01780277982336465 ) ) ;
#12481 =( BOUNDED_CURVE ( )  B_SPLINE_CURVE ( 2, ( #17065, #67647, #10304, #33331, #74413, #62712, #22722, #49915, #45737 ),
 .UNSPECIFIED., .F., .F. ) 
 B_SPLINE_CURVE_WITH_KNOTS ( ( 3, 2, 2, 2, 3 ),
 ( 0.8068181818181818787, 0.8125000000000001110, 0.8181818181818183433, 0.8238636363636363535, 0.8295454545454545858 ),
 .UNSPECIFIED. ) 
 CURVE ( )  GEOMETRIC_REPRESENTATION_ITEM ( )  RATIONAL_B_SPLINE_CURVE ( ( 0.9999999999999985567, 0.9238795325112881818, 1.000000000000000000, 0.9238795325112867385, 1.000000000000000000, 0.9238795325112867385, 1.000000000000000000, 0.9238795325112867385, 1.000000000000000000 ) ) 
 REPRESENTATION_ITEM ( '' )  );
#12482 = CARTESIAN_POINT ( 'NONE',  ( -5.676582343749998039, 147.4479166632526983, -9.832129032723420536 ) ) ;
#12483 = CARTESIAN_POINT ( 'NONE',  ( 10.00000000000000178, 121.8749999931720396, 0.000000000000000000 ) ) ;
#12484 = CARTESIAN_POINT ( 'NONE',  ( -5.082755093536324154, 115.7187500020483810, 5.082755093536326818 ) ) ;
#12485 = DIRECTION ( 'NONE',  ( 0.000000000000000000, -1.000000000000000000, 0.000000000000000000 ) ) ;
#12486 = CARTESIAN_POINT ( 'NONE',  ( -31.45873412499999944, 203.9375000013656063, 170.0000000000003979 ) ) ;
#12487 = VECTOR ( 'NONE', #59273, 1000.000000000000000 ) ;
#12488 = VERTEX_POINT ( 'NONE', #7727 ) ;
#12489 = CARTESIAN_POINT ( 'NONE',  ( -11.35316468750000141, 3.593749996586016682, -1.390361679473963753E-15 ) ) ;
#12490 = ORIENTED_EDGE ( 'NONE', *, *, #60922, .T. ) ;
#12491 = CARTESIAN_POINT ( 'NONE',  ( 2.020667218593132706E-15, -11.00000000000000000, 100.3749999999999858 ) ) ;
#12492 = CARTESIAN_POINT ( 'NONE',  ( 6.676582343750001591, 297.9531250017069510, -8.176455196517173205E-16 ) ) ;
#12494 = CARTESIAN_POINT ( 'NONE',  ( 11.35316468749999785, 140.5729166632526983, 3.042071309553174174 ) ) ;
#12493 = CARTESIAN_POINT ( 'NONE',  ( -3.999999999999959144, 205.0625000000000568, 199.6568542494924259 ) ) ;
#12495 = CARTESIAN_POINT ( 'NONE',  ( -2.828427124746190735, 3.375000000000000000, -2.828427124746191623 ) ) ;
#12496 = CARTESIAN_POINT ( 'NONE',  ( 1.469576158976822172E-15, -7.999999999999991118, 26.76155278432982598 ) ) ;
#12497 = CARTESIAN_POINT ( 'NONE',  ( 61.13545642015998283, 221.8209763507006187, 45.67084927140797390 ) ) ;
#12498 = CARTESIAN_POINT ( 'NONE',  ( 8.311093377946834337, 242.0312500034140157, -8.311093377946836114 ) ) ;
#12499 = CARTESIAN_POINT ( 'NONE',  ( 4.220049686691941027, -10.18810118749999738, 92.50000000204838102 ) ) ;
#12500 = ORIENTED_EDGE ( 'NONE', *, *, #35639, .F. ) ;
#12501 = CARTESIAN_POINT ( 'NONE',  ( 2.679491924311371065, 118.9583333333333570, 9.999999999999920064 ) ) ;
#12502 = DIRECTION ( 'NONE',  ( 0.000000000000000000, 1.000000000000000000, 0.000000000000000000 ) ) ;
#12503 = CARTESIAN_POINT ( 'NONE',  ( 9.832129032723416984, 85.67708332991935549, 5.676582343750006032 ) ) ;
#12504 = CARTESIAN_POINT ( 'NONE',  ( 10.18810118749999916, 4.220049686691935698, 109.0000000020483810 ) ) ;
#12505 = CARTESIAN_POINT ( 'NONE',  ( 3.211159895383561835, 15.56249999863440614, -3.211159895383561835 ) ) ;
#12506 = ORIENTED_EDGE ( 'NONE', *, *, #2954, .T. ) ;
#12507 = ORIENTED_EDGE ( 'NONE', *, *, #26143, .T. ) ;
#12508 = AXIS2_PLACEMENT_3D ( 'NONE', #45415, #57512, #51451 ) ;
#12509 = CARTESIAN_POINT ( 'NONE',  ( -5.656854249492381470, 3.937500000000000888, 5.656854249492379694 ) ) ;
#12510 = CARTESIAN_POINT ( 'NONE',  ( -1.881053915767124440, 1.124999998634406584, 4.541265875000001451 ) ) ;
#12511 = CARTESIAN_POINT ( 'NONE',  ( -5.082755093536325042, 2.531249997951610542, -5.082755093536325930 ) ) ;
#12512 = CARTESIAN_POINT ( 'NONE',  ( 5.656854249492379694, 123.1250000040967905, -5.656854249492380582 ) ) ;
#12513 = CARTESIAN_POINT ( 'NONE',  ( -4.220049686691937474, -10.18810118749999738, 104.3125000020483810 ) ) ;
#12514 = ADVANCED_FACE ( 'NONE', ( #36401 ), #8091, .F. ) ;
#12515 = CARTESIAN_POINT ( 'NONE',  ( 27.99999999999997158, 208.0000000000000284, 173.9999999999999147 ) ) ;
#12516 = CARTESIAN_POINT ( 'NONE',  ( -2.828427124746192067, 12.37499999726881406, 2.828427124746190735 ) ) ;
#12517 = CARTESIAN_POINT ( 'NONE',  ( 2.449293598294707893E-16, 13.99999999726881406, -4.000000000000001776 ) ) ;
#12518 = EDGE_LOOP ( 'NONE', ( #45950, #48424, #46910, #53725 ) ) ;
#12519 = ADVANCED_FACE ( 'NONE', ( #71823 ), #19398, .T. ) ;
#12520 = CARTESIAN_POINT ( 'NONE',  ( 0.000000000000000000, 22.00000000000000355, 0.000000000000000000 ) ) ;
#12521 = CARTESIAN_POINT ( 'NONE',  ( 1.432654583217664479, 197.7500000013656063, 201.4587341250000065 ) ) ;
#12522 =( REPRESENTATION_RELATIONSHIP ('NONE','NONE', #46008, #15137 ) REPRESENTATION_RELATIONSHIP_WITH_TRANSFORMATION ( #72673 )SHAPE_REPRESENTATION_RELATIONSHIP( ) );
#12524 = CARTESIAN_POINT ( 'NONE',  ( 38.00000000000000000, 63.00000000000000000, 10.00000000000006217 ) ) ;
#12523 = CARTESIAN_POINT ( 'NONE',  ( -31.45873412499999944, 205.6875000013656063, 170.0000000000004547 ) ) ;
#12525 = CARTESIAN_POINT ( 'NONE',  ( 3.211159895383561835, 12.43749999863440792, -3.211159895383561835 ) ) ;
#12526 = CARTESIAN_POINT ( 'NONE',  ( 4.000000000000001776, 12.06250000000000000, -1.656854249492381248 ) ) ;
#12527 = AXIS2_PLACEMENT_3D ( 'NONE', #37108, #60110, #25765 ) ;
#12528 = CARTESIAN_POINT ( 'NONE',  ( 1.320432766682872962E-15, -7.188101187499992051, 10.86155278187175455 ) ) ;
#12529 = ORIENTED_EDGE ( 'NONE', *, *, #34553, .F. ) ;
#12530 = VERTEX_POINT ( 'NONE', #42782 ) ;
#12531 = CARTESIAN_POINT ( 'NONE',  ( 4.220049686691941027, -10.18810118749999738, 104.1250000020483810 ) ) ;
#12532 = DIRECTION ( 'NONE',  ( -0.000000000000000000, 1.000000000000000000, 4.476705744456276341E-16 ) ) ;
#12533 = CARTESIAN_POINT ( 'NONE',  ( -30.82842712474616320, 206.3750000000000284, 172.8284271247465824 ) ) ;
#12534 = CARTESIAN_POINT ( 'NONE',  ( -1.432654583217607192, 199.2500000013656063, 194.5412658750000219 ) ) ;
#12535 = CARTESIAN_POINT ( 'NONE',  ( 31.45873412499999233, 195.6875000013655779, 169.9999999999998863 ) ) ;
#12536 = CARTESIAN_POINT ( 'NONE',  ( -7.320508075688778149, 93.12500000000000000, 7.320508075688769267 ) ) ;
#12537 = ADVANCED_FACE ( 'NONE', ( #20512 ), #26170, .T. ) ;
#12538 = ADVANCED_FACE ( 'NONE', ( #65052 ), #60515, .T. ) ;
#12539 = CARTESIAN_POINT ( 'NONE',  ( 8.000000000000001776, 115.1562500000000000, 3.313708498984759387 ) ) ;
#12540 = CARTESIAN_POINT ( 'NONE',  ( -3.042071309553164404, 57.55208332991936260, -11.35316468749999963 ) ) ;
#12541 = CARTESIAN_POINT ( 'NONE',  ( 6.676582343750001591, 298.1093750017069510, -8.176455196517173205E-16 ) ) ;
#12542 = ORIENTED_EDGE ( 'NONE', *, *, #2226, .F. ) ;
#12543 = ADVANCED_FACE ( 'NONE', ( #54123 ), #49189, .F. ) ;
#12544 = CARTESIAN_POINT ( 'NONE',  ( 6.123233995736767268E-16, 173.1249999931720538, -10.00000000000000178 ) ) ;
#12545 = CARTESIAN_POINT ( 'NONE',  ( 3.313708498984762052, 15.09374999590322020, -8.000000000000000000 ) ) ;
#12546 = CARTESIAN_POINT ( 'NONE',  ( 1.432654583217607858, 208.6250000013655779, 138.5412658750000787 ) ) ;
#12547 = CARTESIAN_POINT ( 'NONE',  ( 7.999999999999998224, 11.71874999590322197, 3.313708498984766049 ) ) ;
#12548 = DIRECTION ( 'NONE',  ( -0.000000000000000000, -1.000000000000000000, -4.283267841918042741E-17 ) ) ;
#12549 = CARTESIAN_POINT ( 'NONE',  ( -7.320508075688771932, 224.3749999999999716, -7.320508075688771932 ) ) ;
#12550 = DIRECTION ( 'NONE',  ( 0.000000000000000000, 0.000000000000000000, 1.000000000000000000 ) ) ;
#12551 = CARTESIAN_POINT ( 'NONE',  ( -7.778174593052020747, -7.778174593052023411, 116.6875000000000000 ) ) ;
#12552 = CARTESIAN_POINT ( 'NONE',  ( 2.679491924311228956, 221.0416666666667140, -10.00000000000000000 ) ) ;
#12553 = CARTESIAN_POINT ( 'NONE',  ( -7.188101187499992051, 2.977408999572646930, 12.26780278187175455 ) ) ;
#12554 = CARTESIAN_POINT ( 'NONE',  ( 11.35316468750000141, 186.0937499965860411, 0.000000000000000000 ) ) ;
#12555 = CARTESIAN_POINT ( 'NONE',  ( -8.342170076843785083E-16, 4.062499998634407028, 4.541265875000002339 ) ) ;
#12556 = CARTESIAN_POINT ( 'NONE',  ( 2.679491924311228956, 177.9166666598387110, -10.00000000000000000 ) ) ;
#12558 = CARTESIAN_POINT ( 'NONE',  ( 4.898587196589412829E-16, 10.68749999590322020, -8.000000000000000000 ) ) ;
#12557 = CARTESIAN_POINT ( 'NONE',  ( -3.999999999999960032, 203.1250000027312126, 198.0000000000000284 ) ) ;
#12559 = ORIENTED_EDGE ( 'NONE', *, *, #59652, .F. ) ;
#12560 = VECTOR ( 'NONE', #27459, 1000.000000000000000 ) ;
#12561 = CARTESIAN_POINT ( 'NONE',  ( 3.458734124999960358, 208.6875000013656063, 142.0000000000000568 ) ) ;
#12562 = CARTESIAN_POINT ( 'NONE',  ( -11.35316468749999785, 43.38541666325269119, -3.042071309553167513 ) ) ;
#12563 = CARTESIAN_POINT ( 'NONE',  ( -7.778174593052020747, -7.778174593052023411, 103.3750000040967763 ) ) ;
#12564 = EDGE_CURVE ( 'NONE', #61043, #63531, #67463, .T. ) ;
#12565 = CARTESIAN_POINT ( 'NONE',  ( -30.44569435410886982, 203.5625000013656063, 167.5543056458916169 ) ) ;
#12567 = CARTESIAN_POINT ( 'NONE',  ( -2.679491924318369911, 103.5416666666660319, 9.999999999995861089 ) ) ;
#12566 = DIRECTION ( 'NONE',  ( 0.000000000000000000, 0.000000000000000000, -1.000000000000000000 ) ) ;
#12568 = CARTESIAN_POINT ( 'NONE',  ( -3.458734125000015425, 196.9375000013655779, 142.0000000000000568 ) ) ;
#12569 = CARTESIAN_POINT ( 'NONE',  ( -7.320508075688778149, 79.99999999317203958, 7.320508075688769267 ) ) ;
#12570 = CARTESIAN_POINT ( 'NONE',  ( -5.082755093536325930, 96.96875000204838102, -5.082755093536325930 ) ) ;
#12571 = CARTESIAN_POINT ( 'NONE',  ( 4.541265875000002339, 16.49999999863440436, -1.881053915767121554 ) ) ;
#12572 = CARTESIAN_POINT ( 'NONE',  ( 2.828427124746190291, 10.87500000000000178, 2.828427124746192067 ) ) ;
#12573 = CARTESIAN_POINT ( 'NONE',  ( 2.775557561562891351E-14, -37.99999999999992184, 139.0000000000000568 ) ) ;
#12574 = CARTESIAN_POINT ( 'NONE',  ( -56.00000000000004974, 5.999999999999977796, 167.9999999999997726 ) ) ;
#12575 = ORIENTED_EDGE ( 'NONE', *, *, #49584, .T. ) ;
#12576 = VERTEX_POINT ( 'NONE', #8459 ) ;
#12577 = CARTESIAN_POINT ( 'NONE',  ( 6.676582343750003368, 298.1718750017070079, -2.765530957081997254 ) ) ;
#12578 = DIRECTION ( 'NONE',  ( -1.000000000000000000, 0.000000000000000000, 0.000000000000000000 ) ) ;
#12579 = CARTESIAN_POINT ( 'NONE',  ( 1.656854249492416109, 198.3125000027312126, 138.0000000000000853 ) ) ;
#12580 = CARTESIAN_POINT ( 'NONE',  ( -8.311093377946836114, 157.6562499965860411, -8.311093377946837890 ) ) ;
#12581 = CARTESIAN_POINT ( 'NONE',  ( -4.220049686691935698, 10.18810118749999916, 82.37500000204838102 ) ) ;
#12582 = CARTESIAN_POINT ( 'NONE',  ( 5.656854249492374365, 5.656854249492375253, 9.267802779823364645 ) ) ;
#12583 = CARTESIAN_POINT ( 'NONE',  ( -3.999999999999959144, 204.0625000000000000, 199.6568542494924259 ) ) ;
#12584 = DIRECTION ( 'NONE',  ( -0.000000000000000000, -0.000000000000000000, 1.000000000000000000 ) ) ;
#12585 = CARTESIAN_POINT ( 'NONE',  ( 1.871523826299183495E-15, -10.18810118749999916, 107.4062500020483668 ) ) ;
#12586 = VERTEX_POINT ( 'NONE', #31479 ) ;
#12587 = CARTESIAN_POINT ( 'NONE',  ( 4.898587196589412829E-16, 18.18749999590322020, -8.000000000000000000 ) ) ;
#12588 = VECTOR ( 'NONE', #62521, 1000.000000000000000 ) ;
#12589 = CARTESIAN_POINT ( 'NONE',  ( -11.00000000000000000, 0.000000000000000000, 109.1875000040967763 ) ) ;
#12590 = CARTESIAN_POINT ( 'NONE',  ( -11.35316468750000141, 143.8020833299193555, 3.042071309553159963 ) ) ;
#12591 = CARTESIAN_POINT ( 'NONE',  ( -2.445694354108782775, 196.5625000013656063, 200.4456943541088663 ) ) ;
#12592 = CARTESIAN_POINT ( 'NONE',  ( -2.445694354108784108, 209.5625000013656063, 195.5543056458912190 ) ) ;
#12593 = CARTESIAN_POINT ( 'NONE',  ( -10.18810118749999916, 0.000000000000000000, 75.53125000204836681 ) ) ;
#12594 = CARTESIAN_POINT ( 'NONE',  ( -8.311093377946841443, 44.21874999658602690, 8.311093377946830785 ) ) ;
#12596 = EDGE_LOOP ( 'NONE', ( #52306, #65838, #54584, #72321 ) ) ;
#12595 =( BOUNDED_CURVE ( )  B_SPLINE_CURVE ( 2, ( #47928, #24553, #12495, #34798, #47559, #41907, #57803, #52498, #64915 ),
 .UNSPECIFIED., .F., .F. ) 
 B_SPLINE_CURVE_WITH_KNOTS ( ( 3, 2, 2, 2, 3 ),
 ( 0.1477272727272727348, 0.1534090909090909116, 0.1590909090909091161, 0.1647727272727272929, 0.1704545454545454697 ),
 .UNSPECIFIED. ) 
 CURVE ( )  GEOMETRIC_REPRESENTATION_ITEM ( )  RATIONAL_B_SPLINE_CURVE ( ( 1.000000000000000000, 0.9238795325112867385, 1.000000000000000000, 0.9238795325112867385, 1.000000000000000000, 0.9238795325112867385, 1.000000000000000000, 0.9238795325112864054, 1.000000000000000444 ) ) 
 REPRESENTATION_ITEM ( '' )  );
#12597 = CARTESIAN_POINT ( 'NONE',  ( -7.320508075688779037, 26.87500000000001066, -7.320508075688779037 ) ) ;
#12599 = CARTESIAN_POINT ( 'NONE',  ( 1.881053915767121998, 4.624999998634407028, -4.541265875000002339 ) ) ;
#12598 =( BOUNDED_CURVE ( )  B_SPLINE_CURVE ( 2, ( #22920, #17256, #6334, #24029, #12707, #35012, #69697, #52718, #28955 ),
 .UNSPECIFIED., .F., .F. ) 
 B_SPLINE_CURVE_WITH_KNOTS ( ( 3, 2, 2, 2, 3 ),
 ( 0.8000000000000007105, 0.8083333333333340143, 0.8166666666666673180, 0.8250000000000006217, 0.8333333333333340365 ),
 .UNSPECIFIED. ) 
 CURVE ( )  GEOMETRIC_REPRESENTATION_ITEM ( )  RATIONAL_B_SPLINE_CURVE ( ( 0.9999999999999938938, 0.9238795325112928447, 1.000000000000000000, 0.9238795325112867385, 1.000000000000000000, 0.9238795325112867385, 1.000000000000000000, 0.9238795325112806323, 1.000000000000005995 ) ) 
 REPRESENTATION_ITEM ( '' )  );
#12600 = CARTESIAN_POINT ( 'NONE',  ( -5.662595241051935346, 5.662595241051935346, 17.32561528394063188 ) ) ;
#12601 = CARTESIAN_POINT ( 'NONE',  ( -5.082755093536326818, 17.90624999795161187, 5.082755093536325042 ) ) ;
#12602 = CARTESIAN_POINT ( 'NONE',  ( 2.485281374238575314, 292.3750000034139589, 6.000000000000000888 ) ) ;
#12603 = CARTESIAN_POINT ( 'NONE',  ( -17.31735666187940126, -17.38929073870280462, 137.2212251797212446 ) ) ;
#12604 = CARTESIAN_POINT ( 'NONE',  ( -5.082755093536325042, 5.906249997951610986, -5.082755093536325930 ) ) ;
#12605 = CARTESIAN_POINT ( 'NONE',  ( 7.188101187499992051, 2.977408999572647819, 9.830302781871754547 ) ) ;
#12606 = CARTESIAN_POINT ( 'NONE',  ( -10.18810118749999916, 0.000000000000000000, 72.15625000204836681 ) ) ;
#12607 = CARTESIAN_POINT ( 'NONE',  ( -25.55430564589119413, 205.5625000013656063, 167.5543056458915316 ) ) ;
#12608 = FACE_OUTER_BOUND ( 'NONE', #15191, .T. ) ;
#12609 = CARTESIAN_POINT ( 'NONE',  ( 4.000000000000000888, 1.687499997268813168, 1.656854249492384135 ) ) ;
#12610 = ORIENTED_EDGE ( 'NONE', *, *, #16376, .T. ) ;
#12611 = EDGE_CURVE ( 'NONE', #44635, #10894, #55249, .T. ) ;
#12612 = CARTESIAN_POINT ( 'NONE',  ( 2.754378923186476579E-14, 209.1875000013656063, 194.5412658750000219 ) ) ;
#12613 = CARTESIAN_POINT ( 'NONE',  ( 3.999999999999959144, 207.0625000000000568, 140.3431457505076594 ) ) ;
#12614 = CARTESIAN_POINT ( 'NONE',  ( -26.34314575050769491, 200.0625000027312410, 166.0000000000003695 ) ) ;
#12615 = CARTESIAN_POINT ( 'NONE',  ( 7.188101187500002709, 117.3125000020483810, 2.977408999572649151 ) ) ;
#12616 = CARTESIAN_POINT ( 'NONE',  ( 4.898587196589414801E-16, 1.806524977843537691E-16, 4.000000000000000000 ) ) ;
#12617 = CARTESIAN_POINT ( 'NONE',  ( -6.062598230945730471, -5.219664997883827873, -0.3118207965721654928 ) ) ;
#12618 = ORIENTED_EDGE ( 'NONE', *, *, #10652, .T. ) ;
#12619 = CARTESIAN_POINT ( 'NONE',  ( -5.082755093536325042, 23.53124999795161543, -5.082755093536325930 ) ) ;
#12620 = EDGE_LOOP ( 'NONE', ( #27361, #26318, #6945, #42792 ) ) ;
#12621 = CYLINDRICAL_SURFACE ( 'NONE', #44856, 4.000000000000001776 ) ;
#12622 = CARTESIAN_POINT ( 'NONE',  ( -1.836970198721029983E-15, 48.75000000000000000, 10.00000000000000178 ) ) ;
#12623 = CARTESIAN_POINT ( 'NONE',  ( 7.188101187500002709, 101.1875000020483810, 2.977408999572649151 ) ) ;
#12624 = CARTESIAN_POINT ( 'NONE',  ( 1.102182119232618108E-15, 299.2500000000000000, 6.000000000000001776 ) ) ;
#12625 = AXIS2_PLACEMENT_3D ( 'NONE', #66397, #71673, #61114 ) ;
#12627 = CARTESIAN_POINT ( 'NONE',  ( -21.22593267006811146, -37.05473098918513841, 192.5941682686834326 ) ) ;
#12626 = DIRECTION ( 'NONE',  ( 1.000000000000000000, -0.000000000000000000, -0.000000000000000000 ) ) ;
#12628 = ORIENTED_EDGE ( 'NONE', *, *, #22011, .T. ) ;
#12629 = ORIENTED_EDGE ( 'NONE', *, *, #56034, .T. ) ;
#12630 = CARTESIAN_POINT ( 'NONE',  ( -3.042071309553159075, 239.9479166700806729, 11.35316468749999963 ) ) ;
#12631 = CARTESIAN_POINT ( 'NONE',  ( 2.977408999572646486, 7.188101187499991163, 16.39280278187175455 ) ) ;
#12632 = VECTOR ( 'NONE', #15315, 1000.000000000000000 ) ;
#12633 = CARTESIAN_POINT ( 'NONE',  ( -1.469576158976823947E-15, 14.62500000000000178, 8.000000000000000000 ) ) ;
#12634 = CARTESIAN_POINT ( 'NONE',  ( 7.347880794884121708E-16, 300.0000000000000000, -6.000000000000001776 ) ) ;
#12635 = CARTESIAN_POINT ( 'NONE',  ( 27.99999999999996092, 194.7622595281506790, 166.2377404718492357 ) ) ;
#12636 = CARTESIAN_POINT ( 'NONE',  ( -5.656854249492373476, -5.656854249492376141, 19.20530278392014978 ) ) ;
#12637 = CARTESIAN_POINT ( 'NONE',  ( -8.660254037844387298, 177.0833333333333428, -5.000000000000004441 ) ) ;
#12638 = CARTESIAN_POINT ( 'NONE',  ( -32.64477921267295102, 175.7392199487970856, 161.6181240735822939 ) ) ;
#12639 = CARTESIAN_POINT ( 'NONE',  ( 2.020667218593132706E-15, -11.00000000000000000, 69.06250000409677625 ) ) ;
#12640 = CARTESIAN_POINT ( 'NONE',  ( 11.35316468749999785, 135.8854166632526983, 3.042071309553174174 ) ) ;
#12641 = CARTESIAN_POINT ( 'NONE',  ( -11.00000000000010658, 4.556349186103942017, 76.09375000409676204 ) ) ;
#12642 = LINE ( 'NONE', #25434, #55410 ) ;
#12645 = CARTESIAN_POINT ( 'NONE',  ( 9.000000000000001776, 0.000000000000000000, 0.000000000000000000 ) ) ;
#12644 = CARTESIAN_POINT ( 'NONE',  ( -7.999999999999991118, 0.000000000000000000, 26.33030277982336997 ) ) ;
#12643 = CARTESIAN_POINT ( 'NONE',  ( 28.00000000000001776, 205.5000000000000284, 165.9999999999998863 ) ) ;
#12646 = EDGE_LOOP ( 'NONE', ( #1704, #13636, #5010, #19322, #12500 ) ) ;
#12647 = EDGE_CURVE ( 'NONE', #31217, #54743, #48816, .T. ) ;
#12648 = CARTESIAN_POINT ( 'NONE',  ( -3.999999999999960032, 209.0625000027312126, 196.3431457505076594 ) ) ;
#12649 = CARTESIAN_POINT ( 'NONE',  ( 7.320508075688852756, 195.6250000000001421, -7.320508075688852756 ) ) ;
#12650 = CARTESIAN_POINT ( 'NONE',  ( 5.000000000000000888, -61.58609660504367866, -23.68302032025107806 ) ) ;
#12651 = ADVANCED_FACE ( 'NONE', ( #8840 ), #53752, .T. ) ;
#12652 = CARTESIAN_POINT ( 'NONE',  ( 10.00000000000000000, 31.66666665983870033, 2.679491924311236062 ) ) ;
#12653 = CARTESIAN_POINT ( 'NONE',  ( 1.320432766682874540E-15, 112.5312500020483952, 7.188101187500000044 ) ) ;
#12654 = CARTESIAN_POINT ( 'NONE',  ( 1.881053915767121776, 0.6249999986344068059, -4.541265875000002339 ) ) ;
#12655 = CARTESIAN_POINT ( 'NONE',  ( -4.898587196589412829E-16, 117.3125000040967763, -8.000000000000000000 ) ) ;
#12656 = CARTESIAN_POINT ( 'NONE',  ( 7.999999999999992895, -3.313708498984756279, 16.48655277982336642 ) ) ;
#12658 = CARTESIAN_POINT ( 'NONE',  ( -8.000000000000000000, 24.46874999590322375, -3.313708498984762496 ) ) ;
#12657 = CARTESIAN_POINT ( 'NONE',  ( -7.320508075688771932, 237.5000000068279746, -7.320508075688771932 ) ) ;
#12659 = ORIENTED_EDGE ( 'NONE', *, *, #70739, .T. ) ;
#12660 = CARTESIAN_POINT ( 'NONE',  ( 1.469576158976823947E-15, 122.3750000000000000, 8.000000000000000000 ) ) ;
#12661 = CARTESIAN_POINT ( 'NONE',  ( -6.101342341038383132, 225.9999999999999716, -7.950158476763387938 ) ) ;
#12662 = CARTESIAN_POINT ( 'NONE',  ( 8.000000000000000000, 109.3437499999999858, -3.313708498984762496 ) ) ;
#12663 = CARTESIAN_POINT ( 'NONE',  ( 11.35316468749999608, 246.9270833367473017, -3.042071309553167513 ) ) ;
#12664 = CARTESIAN_POINT ( 'NONE',  ( -5.676582343750006032, 119.1145833299193697, 9.832129032723418760 ) ) ;
#12665 = VERTEX_POINT ( 'NONE', #31851 ) ;
#12666 = CARTESIAN_POINT ( 'NONE',  ( 5.000000000000002665, -14.32120916179451697, 69.86289779849465731 ) ) ;
#12667 = CARTESIAN_POINT ( 'NONE',  ( 4.220049686691941027, -10.18810118749999738, 101.1250000020483810 ) ) ;
#12668 = DIRECTION ( 'NONE',  ( 0.8191520442889906883, 1.003171929053523391E-16, -0.5735764363510477137 ) ) ;
#12669 = CARTESIAN_POINT ( 'NONE',  ( -3.458734124999960358, 199.6250000013656063, 196.5673454167823877 ) ) ;
#12670 = FACE_OUTER_BOUND ( 'NONE', #14790, .T. ) ;
#12671 = CARTESIAN_POINT ( 'NONE',  ( 9.832129032723416984, 115.3645833299193555, 5.676582343750006032 ) ) ;
#12672 = CARTESIAN_POINT ( 'NONE',  ( 3.313708498984756279, 7.999999999999991118, 9.549052783920146226 ) ) ;
#12673 = CARTESIAN_POINT ( 'NONE',  ( -30.44569435410878810, 196.0625000013656063, 172.4456943541092357 ) ) ;
#12674 = CARTESIAN_POINT ( 'NONE',  ( 5.656854249492374365, 5.656854249492375253, 6.455302783920143561 ) ) ;
#12675 = ORIENTED_EDGE ( 'NONE', *, *, #37673, .T. ) ;
#12676 = CARTESIAN_POINT ( 'NONE',  ( -10.00000000000000000, 199.1666666598386826, -2.679491924311229845 ) ) ;
#12677 = ADVANCED_FACE ( 'NONE', ( #48073 ), #65430, .F. ) ;
#12678 = CARTESIAN_POINT ( 'NONE',  ( 0.3946985168883124784, -47.98037922302377467, 139.0019161614035852 ) ) ;
#12679 = CARTESIAN_POINT ( 'NONE',  ( -5.676582343750006032, 89.42708332991934128, 9.832129032723418760 ) ) ;
#12680 = CARTESIAN_POINT ( 'NONE',  ( -3.458734124999959914, 209.3750000013656063, 196.5673454167823877 ) ) ;
#12681 = CARTESIAN_POINT ( 'NONE',  ( -5.082755093536326818, 13.78124999795161187, 5.082755093536325042 ) ) ;
#12682 = CARTESIAN_POINT ( 'NONE',  ( -10.18810118749999738, -4.220049686691941915, 93.62500000204838102 ) ) ;
#12683 = CARTESIAN_POINT ( 'NONE',  ( 8.311093377946834337, 5.468749996586017126, 8.311093377946839666 ) ) ;
#12684 = ORIENTED_EDGE ( 'NONE', *, *, #17599, .F. ) ;
#12685 = CARTESIAN_POINT ( 'NONE',  ( -2.679491924330377639, 138.5416666666649803, 9.999999999988961719 ) ) ;
#12686 = CYLINDRICAL_SURFACE ( 'NONE', #7061, 11.00000000000000000 ) ;
#12687 = CARTESIAN_POINT ( 'NONE',  ( 11.35316468749999785, 215.5729166632526699, 3.042071309553174174 ) ) ;
#12688 = CARTESIAN_POINT ( 'NONE',  ( 7.204075437095968759, -7.204075437095966983, 80.59375000204838102 ) ) ;
#12689 = CARTESIAN_POINT ( 'NONE',  ( 2.679491924311192097, 47.91666665983871098, -10.00000000000002309 ) ) ;
#12690 = CARTESIAN_POINT ( 'NONE',  ( 1.469576158976823947E-15, 94.06250000409677625, 8.000000000000000000 ) ) ;
#12691 = CARTESIAN_POINT ( 'NONE',  ( -6.676582343750000703, 294.5156250017069510, 2.765530957082001251 ) ) ;
#12692 = CIRCLE ( 'NONE', #60877, 37.00000000000000711 ) ;
#12693 = VERTEX_POINT ( 'NONE', #50680 ) ;
#12694 = CARTESIAN_POINT ( 'NONE',  ( 0.000000000000000000, 0.000000000000000000, -10.20000000000000462 ) ) ;
#12695 = CARTESIAN_POINT ( 'NONE',  ( 8.311093377946837890, 206.7187499965859843, -8.311093377946837890 ) ) ;
#12696 =( BOUNDED_CURVE ( )  B_SPLINE_CURVE ( 2, ( #61248, #32977, #9945, #14086, #37121, #2791, #66155, #72942, #60123, #49172, #9580, #32597, #60870 ),
 .UNSPECIFIED., .F., .F. ) 
 B_SPLINE_CURVE_WITH_KNOTS ( ( 3, 2, 2, 2, 2, 2, 3 ),
 ( 0.01569808486621994056, 0.02093092178115263380, 0.02616375869608532703, 0.03139659561101801333, 0.03662943252595071697, 0.04186226944088339980, 0.04709510635581609650 ),
 .UNSPECIFIED. ) 
 CURVE ( )  GEOMETRIC_REPRESENTATION_ITEM ( )  RATIONAL_B_SPLINE_CURVE ( ( 0.9999999999999127365, 0.9659258262891555757, 1.000000000000000000, 0.9659258262890683122, 1.000000000000000000, 0.9659258262890683122, 1.000000000000000000, 0.9659258262890683122, 1.000000000000000000, 0.9659258262890683122, 1.000000000000000000, 0.9659258262890683122, 1.000000000000000000 ) ) 
 REPRESENTATION_ITEM ( '' )  );
#12697 = CARTESIAN_POINT ( 'NONE',  ( -4.220049686691937474, -10.18810118749999738, 91.93750000204836681 ) ) ;
#12698 =( GEOMETRIC_REPRESENTATION_CONTEXT ( 3 ) GLOBAL_UNCERTAINTY_ASSIGNED_CONTEXT ( ( #46574 ) ) GLOBAL_UNIT_ASSIGNED_CONTEXT ( ( #67017, #28512, #18311 ) ) REPRESENTATION_CONTEXT ( 'NONE', 'WORKASPACE' ) );
#12699 = CARTESIAN_POINT ( 'NONE',  ( -24.54126587499998280, 201.1250000013656347, 171.4326545832179818 ) ) ;
#12700 = CARTESIAN_POINT ( 'NONE',  ( -3.313708498984760720, 21.46875000000000355, -8.000000000000000000 ) ) ;
#12701 = ORIENTED_EDGE ( 'NONE', *, *, #15604, .T. ) ;
#12702 = CARTESIAN_POINT ( 'NONE',  ( 0.000000000000000000, 0.000000000000000000, 0.000000000000000000 ) ) ;
#12703 = CARTESIAN_POINT ( 'NONE',  ( 1.656854249492405451, 206.4375000027311842, 202.0000000000000284 ) ) ;
#12704 = EDGE_CURVE ( 'NONE', #33755, #47208, #41902, .T. ) ;
#12705 = CARTESIAN_POINT ( 'NONE',  ( -1.836970198721029983E-15, 23.75000000000000000, 10.00000000000000178 ) ) ;
#12706 =( BOUNDED_CURVE ( )  B_SPLINE_CURVE ( 2, ( #12644, #42420, #58690, #70008, #18317, #41330, #64340, #8850, #49198 ),
 .UNSPECIFIED., .F., .F. ) 
 B_SPLINE_CURVE_WITH_KNOTS ( ( 3, 2, 2, 2, 3 ),
 ( 0.1052631578947368085, 0.1118421052631578816, 0.1184210526315789269, 0.1250000000000000000, 0.1315789473684210453 ),
 .UNSPECIFIED. ) 
 CURVE ( )  GEOMETRIC_REPRESENTATION_ITEM ( )  RATIONAL_B_SPLINE_CURVE ( ( 1.000000000000000222, 0.9238795325112864054, 1.000000000000000000, 0.9238795325112867385, 1.000000000000000000, 0.9238795325112867385, 1.000000000000000000, 0.9238795325112867385, 1.000000000000000000 ) ) 
 REPRESENTATION_ITEM ( '' )  );
#12707 = CARTESIAN_POINT ( 'NONE',  ( -23.99999999999998579, 197.7500000000000000, 170.0000000000003411 ) ) ;
#12708 = CARTESIAN_POINT ( 'NONE',  ( -10.18810118749999738, -4.220049686691941915, 72.62500000204836681 ) ) ;
#12709 = ORIENTED_EDGE ( 'NONE', *, *, #61700, .F. ) ;
#12710 = EDGE_CURVE ( 'NONE', #48053, #16277, #65022, .T. ) ;
#12711 = CARTESIAN_POINT ( 'NONE',  ( -3.211159895383562723, 21.93749999863440792, 3.211159895383561391 ) ) ;
#12712 = CARTESIAN_POINT ( 'NONE',  ( -2.977408999572650927, 116.7500000020483810, -7.188101187500001821 ) ) ;
#12713 = CARTESIAN_POINT ( 'NONE',  ( -2.786452729588720256, 21.99999999999999289, -3.148080783184952658 ) ) ;
#12714 = CARTESIAN_POINT ( 'NONE',  ( -2.765530957081996810, 298.2656250017069510, -6.676582343750002480 ) ) ;
#12716 = DIRECTION ( 'NONE',  ( -0.000000000000000000, 1.000000000000000000, -0.000000000000000000 ) ) ;
#12715 = CARTESIAN_POINT ( 'NONE',  ( -8.311093377946836114, 228.2812500034139589, -8.311093377946836114 ) ) ;
#12717 = ORIENTED_EDGE ( 'NONE', *, *, #42112, .F. ) ;
#12718 = EDGE_CURVE ( 'NONE', #13626, #21890, #72751, .T. ) ;
#12719 = CARTESIAN_POINT ( 'NONE',  ( 11.35316468749999963, 236.7187500034139873, -1.390361679473963556E-15 ) ) ;
#12720 = CARTESIAN_POINT ( 'NONE',  ( 5.082755093536318824, 5.082755093536319713, 6.924052781871750994 ) ) ;
#12721 = CARTESIAN_POINT ( 'NONE',  ( 1.432654583217664701, 202.0000000013656063, 201.4587341250000065 ) ) ;
#12722 = ORIENTED_EDGE ( 'NONE', *, *, #55857, .T. ) ;
#12723 = EDGE_CURVE ( 'NONE', #26888, #71806, #9961, .T. ) ;
#12724 = CARTESIAN_POINT ( 'NONE',  ( 10.18810118749999916, 1.247682550866122264E-15, 69.90625000204836681 ) ) ;
#12725 = CARTESIAN_POINT ( 'NONE',  ( 9.832129032723420536, 106.5104166632526841, -5.676582343749999815 ) ) ;
#12726 = CARTESIAN_POINT ( 'NONE',  ( -27.99999999999999289, 194.7622595281507358, 173.7622595281509916 ) ) ;
#12727 = PRODUCT_RELATED_PRODUCT_CATEGORY ( 'part', '', ( #4157 ) ) ;
#12728 = CARTESIAN_POINT ( 'NONE',  ( -6.735557395310442023E-16, 11.00000000000000000, 80.12499999999998579 ) ) ;
#12731 = CARTESIAN_POINT ( 'NONE',  ( -1.836970198721029983E-15, 195.6249999931720254, 10.00000000000000178 ) ) ;
#12730 = CARTESIAN_POINT ( 'NONE',  ( 24.54126587500000056, 203.2500000013656063, 171.4326545832175839 ) ) ;
#12729 = CARTESIAN_POINT ( 'NONE',  ( 27.99999999999996447, 203.6875000013656063, 173.4587341249998929 ) ) ;
#12732 = ORIENTED_EDGE ( 'NONE', *, *, #46613, .F. ) ;
#12733 = CARTESIAN_POINT ( 'NONE',  ( 4.000000000000001776, 19.00000000000000000, 0.000000000000000000 ) ) ;
#12734 = CARTESIAN_POINT ( 'NONE',  ( 1.224646799147353454E-15, 300.0000000000000000, -10.00000000000000178 ) ) ;
#12735 = AXIS2_PLACEMENT_3D ( 'NONE', #69955, #51479, #18265 ) ;
#12736 = CARTESIAN_POINT ( 'NONE',  ( 8.311093377946837890, 211.4062499965860411, -8.311093377946837890 ) ) ;
#12737 = CARTESIAN_POINT ( 'NONE',  ( 2.445694354108782775, 206.5625000013656063, 139.5543056458912190 ) ) ;
#12738 = CARTESIAN_POINT ( 'NONE',  ( 28.00000000000002487, 208.1875000013656063, 166.5412658749999082 ) ) ;
#12739 = EDGE_CURVE ( 'NONE', #12586, #70885, #10333, .T. ) ;
#12740 = CARTESIAN_POINT ( 'NONE',  ( 2.977408999572651815, 26.06249999795161543, 7.188101187500000933 ) ) ;
#12741 = VECTOR ( 'NONE', #32487, 1000.000000000000000 ) ;
#12742 = CARTESIAN_POINT ( 'NONE',  ( 6.951808397369818766E-16, 182.3437499965860411, -11.35316468750000141 ) ) ;
#12743 = CARTESIAN_POINT ( 'NONE',  ( -5.082755093536324154, 100.7187500020483810, 5.082755093536326818 ) ) ;
#12744 = CARTESIAN_POINT ( 'NONE',  ( -5.000000000000000000, 66.10919140998015564, -23.67639547905944752 ) ) ;
#12745 = CARTESIAN_POINT ( 'NONE',  ( -29.65685424949233706, 196.4375000000000568, 174.0000000000004547 ) ) ;
#12746 = CARTESIAN_POINT ( 'NONE',  ( -4.541265875000002339, 10.74999999863440969, -1.881053915767121998 ) ) ;
#12747 = CARTESIAN_POINT ( 'NONE',  ( 30.44569435410879166, 201.8125000013656063, 172.4456943541087526 ) ) ;
#12748 = CARTESIAN_POINT ( 'NONE',  ( 7.188101187499991163, 2.977408999572648707, 5.705302781871753659 ) ) ;
#12749 = CARTESIAN_POINT ( 'NONE',  ( 8.311093377946834337, 70.15624999658602690, 8.311093377946839666 ) ) ;
#12750 = CARTESIAN_POINT ( 'NONE',  ( 0.000000000000000000, -16.70329308849007077, 0.000000000000000000 ) ) ;
#12751 = CARTESIAN_POINT ( 'NONE',  ( 4.000000000000015987, 209.5625000000000000, 196.3431457505076594 ) ) ;
#12752 = VERTEX_POINT ( 'NONE', #15230 ) ;
#12753 = CARTESIAN_POINT ( 'NONE',  ( -10.00000000000002665, 47.29166666666668561, -2.679491924311236950 ) ) ;
#12754 = CARTESIAN_POINT ( 'NONE',  ( -7.778174593052020747, -7.778174593052023411, 80.87500000409677625 ) ) ;
#12755 = CARTESIAN_POINT ( 'NONE',  ( 11.35316468749999785, 70.57291666325269830, 3.042071309553174174 ) ) ;
#12756 = CARTESIAN_POINT ( 'NONE',  ( -6.735557395310442023E-16, 11.00000000000000000, 66.81250000409677625 ) ) ;
#12757 = CARTESIAN_POINT ( 'NONE',  ( 3.458734124999960358, 195.6250000013656063, 143.4326545832176976 ) ) ;
#12758 = CARTESIAN_POINT ( 'NONE',  ( 2.449293598294707893E-16, 8.999999997268814056, -4.000000000000001776 ) ) ;
#12760 = CARTESIAN_POINT ( 'NONE',  ( -11.35316468750000141, 58.28124999658601268, -1.390361679473963753E-15 ) ) ;
#12759 = CARTESIAN_POINT ( 'NONE',  ( -2.751064625579944321E-14, 207.8750000027312126, 146.0000000000000284 ) ) ;
#12761 = CARTESIAN_POINT ( 'NONE',  ( 1.469576158976822172E-15, -7.999999999999991118, 22.39280278392014623 ) ) ;
#12762 = CARTESIAN_POINT ( 'NONE',  ( -3.735655735689777934, 194.7783520383262896, 142.6174758718100293 ) ) ;
#12763 = CARTESIAN_POINT ( 'NONE',  ( -7.320508075688778149, 154.9999999931720538, 7.320508075688769267 ) ) ;
#12764 = CARTESIAN_POINT ( 'NONE',  ( -4.401442555609581635E-16, 94.15625000204838102, -7.188101187500000044 ) ) ;
#12765 = CARTESIAN_POINT ( 'NONE',  ( -7.778174593052023411, 7.778174593052023411, 108.8124999999999858 ) ) ;
#12766 = CARTESIAN_POINT ( 'NONE',  ( -3.042071309553173730, 54.63541666325268409, 11.35316468749999785 ) ) ;
#12767 = CARTESIAN_POINT ( 'NONE',  ( 1.871523826299183495E-15, -10.18810118749999916, 111.9062500020483810 ) ) ;
#12768 = CARTESIAN_POINT ( 'NONE',  ( 8.311093377946837890, 191.4062499965860127, -8.311093377946837890 ) ) ;
#12769 = ORIENTED_EDGE ( 'NONE', *, *, #28552, .F. ) ;
#12770 = CARTESIAN_POINT ( 'NONE',  ( 1.656854249492381248, 4.187500000000000000, -4.000000000000001776 ) ) ;
#12771 = CARTESIAN_POINT ( 'NONE',  ( 5.094040948422622783, 8.823160013426731396, 67.15552388843440212 ) ) ;
#12772 = DIRECTION ( 'NONE',  ( -0.8660254037844401509, 0.4999999999999973910, 0.000000000000000000 ) ) ;
#12774 = CARTESIAN_POINT ( 'NONE',  ( -9.832129032723420536, 178.6979166632526983, 5.676582343749997150 ) ) ;
#12773 = CARTESIAN_POINT ( 'NONE',  ( 8.660254037844389075, 262.0833333333333144, 4.999999999999997335 ) ) ;
#12775 = CARTESIAN_POINT ( 'NONE',  ( 0.000000000000000000, 125.0000000000000000, 8.000000000000000000 ) ) ;
#12776 = CARTESIAN_POINT ( 'NONE',  ( -9.999999999999998224, 258.3333333401612890, 2.679491924311235618 ) ) ;
#12777 = DIRECTION ( 'NONE',  ( -1.734723475976998196E-15, -1.000000000000000000, -0.000000000000000000 ) ) ;
#12778 = ORIENTED_EDGE ( 'NONE', *, *, #71796, .T. ) ;
#12779 = CARTESIAN_POINT ( 'NONE',  ( -8.311093377946836114, 172.9687499965860127, -8.311093377946837890 ) ) ;
#12780 = CARTESIAN_POINT ( 'NONE',  ( -2.977408999572647819, 7.188101187499992051, 25.20530278187175810 ) ) ;
#12781 = CARTESIAN_POINT ( 'NONE',  ( -1.469576158976823947E-15, 3.937499995903220640, 8.000000000000000000 ) ) ;
#12782 = VERTEX_POINT ( 'NONE', #39374 ) ;
#12783 = CONICAL_SURFACE ( 'NONE', #28412, 7.500000000000020428, 0.7853981633974552734 ) ;
#12784 = CARTESIAN_POINT ( 'NONE',  ( -8.000000000000000000, 105.6875000040967763, 0.000000000000000000 ) ) ;
#12785 = EDGE_CURVE ( 'NONE', #5775, #11982, #73204, .T. ) ;
#12786 =( BOUNDED_CURVE ( )  B_SPLINE_CURVE ( 2, ( #38555, #67958, #55537, #4966, #27967, #68326, #38920, #66841, #38176, #61179, #21553, #9509, #44205 ),
 .UNSPECIFIED., .F., .F. ) 
 B_SPLINE_CURVE_WITH_KNOTS ( ( 3, 2, 2, 2, 2, 2, 3 ),
 ( 0.3967391304347826497, 0.3985507246376812085, 0.4003623188405797673, 0.4021739130434782705, 0.4039855072463768293, 0.4057971014492753881, 0.4076086956521738913 ),
 .UNSPECIFIED. ) 
 CURVE ( )  GEOMETRIC_REPRESENTATION_ITEM ( )  RATIONAL_B_SPLINE_CURVE ( ( 0.9999999999999990008, 0.9659258262890693114, 1.000000000000000000, 0.9659258262890683122, 1.000000000000000000, 0.9659258262890683122, 1.000000000000000000, 0.9659258262890683122, 1.000000000000000000, 0.9659258262890683122, 1.000000000000000000, 0.9659258262890683122, 1.000000000000000000 ) ) 
 REPRESENTATION_ITEM ( '' )  );
#12787 = B_SPLINE_CURVE_WITH_KNOTS ( 'NONE', 3,
 ( #50038, #10055, #50778, #44011, #15318, #38354, #66640, #73792, #26264, #14947, #4033, #72685, #73052, #21360, #8934, #44384, #66268, #67395, #38739, #14575 ),
 .UNSPECIFIED., .F., .F.,
 ( 4, 2, 2, 2, 2, 2, 2, 2, 2, 4 ),
 ( 0.000000000000000000, 0.001156441540183929945, 0.001734662310275897085, 0.002312883080367864226, 0.003469324620551793303, 0.004625766160735722381, 0.005782207700919650591, 0.006938649241103580535, 0.008095090781287509613, 0.009251532321471437822 ),
 .UNSPECIFIED. ) ;
#12788 = EDGE_CURVE ( 'NONE', #37917, #22266, #16709, .T. ) ;
#12789 = CARTESIAN_POINT ( 'NONE',  ( -2.828427124746190735, 11.37500000000000000, -2.828427124746191623 ) ) ;
#12790 = CARTESIAN_POINT ( 'NONE',  ( 9.000000000000000000, 5.196152422706648899, -0.8038475772933779684 ) ) ;
#12791 = CARTESIAN_POINT ( 'NONE',  ( -1.881053915767121776, 13.62499999863440792, -4.541265875000002339 ) ) ;
#12792 = CARTESIAN_POINT ( 'NONE',  ( -5.656854249492375253, 5.656854249492375253, 20.33030278392014623 ) ) ;
#12793 = CARTESIAN_POINT ( 'NONE',  ( 3.999999999999960032, 196.0000000000000000, 142.0000000000000568 ) ) ;
#12794 = EDGE_LOOP ( 'NONE', ( #9915, #55277, #62764, #42201 ) ) ;
#12795 = FACE_OUTER_BOUND ( 'NONE', #45192, .T. ) ;
#12796 = CARTESIAN_POINT ( 'NONE',  ( 2.977408999572650039, 98.18750000204838102, -7.188101187500001821 ) ) ;
#12798 = DIRECTION ( 'NONE',  ( -0.000000000000000000, 1.000000000000000000, -0.000000000000000000 ) ) ;
#12797 = CARTESIAN_POINT ( 'NONE',  ( -3.313708498984870410, 92.46875000409679046, 7.999999999999890754 ) ) ;
#12799 = SHAPE_REPRESENTATION_RELATIONSHIP ( 'NONE' , 'NONE' ,  #69137, #72247 ) ;
#12800 = EDGE_LOOP ( 'NONE', ( #14368, #72795, #3801, #68458 ) ) ;
#12801 = CARTESIAN_POINT ( 'NONE',  ( -0.7581620860332122236, 10.12340554704894657, -70.09014334687758208 ) ) ;
#12802 = DIRECTION ( 'NONE',  ( 0.000000000000000000, 0.000000000000000000, 1.000000000000000000 ) ) ;
#12803 = CARTESIAN_POINT ( 'NONE',  ( -2.977408999572647819, 7.188101187499991163, 23.70530278187175810 ) ) ;
#12804 = ORIENTED_EDGE ( 'NONE', *, *, #12564, .T. ) ;
#12805 =( BOUNDED_SURFACE ( )  B_SPLINE_SURFACE ( 3, 2, ( 
 ( #66537, #66168, #20507 ),
 ( #55616, #43522, #37886 ),
 ( #60884, #3933, #9206 ),
 ( #32226, #55244, #3550 ),
 ( #21261, #26540, #44285 ),
 ( #49565, #15225, #67299 ),
 ( #27292, #61638, #32988 ),
 ( #29168, #68776, #23124 ),
 ( #38999, #514, #17086 ),
 ( #22366, #148, #11074 ),
 ( #74066, #68404, #6159 ),
 ( #46136, #5412, #62003 ),
 ( #74436, #57097, #28785 ),
 ( #56354, #57483, #62365 ),
 ( #63487, #33353, #4673 ),
 ( #52183, #5049, #10328 ),
 ( #27669, #67671, #16331 ),
 ( #22744, #23494, #69153 ) ),
 .UNSPECIFIED., .F., .F., .T. ) 
 B_SPLINE_SURFACE_WITH_KNOTS ( ( 4, 2, 2, 2, 2, 2, 2, 2, 4 ),
 ( 3, 3 ),
 ( 0.04202945594034821625, 0.04396162471218456602, 0.04589379348402090886, 0.04782596225585725169, 0.04975813102769359453, 0.05169029979952993736, 0.05265638418544810878, 0.05362246857136628020, 0.05748680611503896587 ),
 ( 0.000000000000000000, 1.000000000000000000 ),
 .UNSPECIFIED. ) 
 GEOMETRIC_REPRESENTATION_ITEM ( )  RATIONAL_B_SPLINE_SURFACE ( (
 ( 1.000000000000000000, 0.6241276099607504513, 1.000000000000000000),
 ( 1.000000000000000000, 0.6218761496800573330, 1.000000000000000000),
 ( 1.000000000000000000, 0.6198047272362451343, 1.000000000000000000),
 ( 1.000000000000000000, 0.6161935119825044938, 1.000000000000000000),
 ( 1.000000000000000000, 0.6146642324079192310, 1.000000000000000000),
 ( 1.000000000000000000, 0.6121850116872262770, 1.000000000000000000),
 ( 1.000000000000000000, 0.6112350889398914244, 1.000000000000000000),
 ( 1.000000000000000000, 0.6099522725973434145, 1.000000000000000000),
 ( 1.000000000000000000, 0.6096208180308361202, 1.000000000000000000),
 ( 1.000000000000000000, 0.6096183796348998429, 1.000000000000000000),
 ( 1.000000000000000000, 0.6099422200101185521, 1.000000000000000000),
 ( 1.000000000000000000, 0.6109087447823760009, 1.000000000000000000),
 ( 1.000000000000000000, 0.6113123981688344255, 1.000000000000000000),
 ( 1.000000000000000000, 0.6122677719809430652, 1.000000000000000000),
 ( 1.000000000000000000, 0.6128199619021360567, 1.000000000000000000),
 ( 1.000000000000000000, 0.6159350830264649357, 1.000000000000000000),
 ( 1.000000000000000000, 0.6195556778516543295, 1.000000000000000000),
 ( 1.000000000000000000, 0.6241278272307883013, 1.000000000000000000) ) ) 
 REPRESENTATION_ITEM ( '' )  SURFACE ( )  );
#12806 = ORIENTED_EDGE ( 'NONE', *, *, #54172, .F. ) ;
#12807 = CARTESIAN_POINT ( 'NONE',  ( -7.204075437095967871, 7.204075437095967871, 88.46875000204838102 ) ) ;
#12808 = CARTESIAN_POINT ( 'NONE',  ( -29.43265458321766914, 194.7500000013656063, 166.5412658750003629 ) ) ;
#12809 = CARTESIAN_POINT ( 'NONE',  ( -4.556349186104045934, 11.00000000000000000, 104.2187500000000000 ) ) ;
#12811 = CARTESIAN_POINT ( 'NONE',  ( 23.99999999999998934, 201.8750000027312126, 169.9999999999999432 ) ) ;
#12810 = CARTESIAN_POINT ( 'NONE',  ( -4.556349186104048599, -10.99999999999999822, 104.7812499999999858 ) ) ;
#12812 = CARTESIAN_POINT ( 'NONE',  ( 7.320508075688771044, 129.3750000000000000, 7.320508075688775484 ) ) ;
#12813 = CARTESIAN_POINT ( 'NONE',  ( -25.17157287525377640, 203.6250000000000284, 172.8284271247465256 ) ) ;
#12814 = DIRECTION ( 'NONE',  ( 0.000000000000000000, 1.224646799147353700E-16, 1.000000000000000000 ) ) ;
#12815 = DIRECTION ( 'NONE',  ( -0.4999978731667203413, -0.8660266317087230714, 0.000000000000000000 ) ) ;
#12816 = CARTESIAN_POINT ( 'NONE',  ( 30.44569435410879166, 204.5625000013656063, 172.4456943541087526 ) ) ;
#12817 = CARTESIAN_POINT ( 'NONE',  ( -5.082755093536326818, 4.781249997951610986, 5.082755093536325042 ) ) ;
#12818 = CARTESIAN_POINT ( 'NONE',  ( -3.317071493978880348, -8.008118988124989457, 4.294365283940629219 ) ) ;
#12819 = CARTESIAN_POINT ( 'NONE',  ( 3.458734124999959914, 195.4375000013655779, 142.0000000000000568 ) ) ;
#12820 = CARTESIAN_POINT ( 'NONE',  ( 2.977408999572650039, 118.0625000020483952, -7.188101187500000933 ) ) ;
#12822 = CARTESIAN_POINT ( 'NONE',  ( -4.465349678524266785, -56.41423509509906609, -44.23558526901030774 ) ) ;
#12821 = LINE ( 'NONE', #35856, #41995 ) ;
#12823 = CARTESIAN_POINT ( 'NONE',  ( -9.832129032723415207, 234.6354166700806445, 5.676582343750005144 ) ) ;
#12824 = CYLINDRICAL_SURFACE ( 'NONE', #62619, 3.999999999999976019 ) ;
#12825 = CARTESIAN_POINT ( 'NONE',  ( 2.679491924311228956, 52.91666665983869677, -10.00000000000000000 ) ) ;
#12826 = CARTESIAN_POINT ( 'NONE',  ( 28.00000000000001421, 195.5000000000000000, 165.9999999999998863 ) ) ;
#12827 = CARTESIAN_POINT ( 'NONE',  ( 3.042071309553167069, 26.82291666325268054, -11.35316468749999785 ) ) ;
#12828 = CARTESIAN_POINT ( 'NONE',  ( 0.9790701977573584847, -13.29114001832031633, -0.7454400371385776491 ) ) ;
#12829 = CARTESIAN_POINT ( 'NONE',  ( 5.676582343749993598, 220.2604166632526983, 9.832129032723422313 ) ) ;
#12830 = DIRECTION ( 'NONE',  ( 0.000000000000000000, -0.000000000000000000, 1.000000000000000000 ) ) ;
#12831 = CARTESIAN_POINT ( 'NONE',  ( 11.00000000000000000, 1.347111479062088405E-15, 99.24999999999998579 ) ) ;
#12832 = ORIENTED_EDGE ( 'NONE', *, *, #57616, .F. ) ;
#12833 = CARTESIAN_POINT ( 'NONE',  ( -3.458734125000016757, 195.1250000013656063, 140.5673454167824161 ) ) ;
#12834 = CARTESIAN_POINT ( 'NONE',  ( -9.832129032723420536, 38.69791666325268409, 5.676582343749997150 ) ) ;
#12835 = CARTESIAN_POINT ( 'NONE',  ( 4.556349186104051263, -10.99999999999999822, 87.15625000409677625 ) ) ;
#12836 = CARTESIAN_POINT ( 'NONE',  ( -3.458734125000015425, 209.2500000013656063, 143.4326545832176976 ) ) ;
#12837 = CARTESIAN_POINT ( 'NONE',  ( 4.556349186104052151, -10.99999999999999822, 111.1562500040967620 ) ) ;
#12838 = DIRECTION ( 'NONE',  ( 8.881784197001248379E-16, 0.000000000000000000, 1.000000000000000000 ) ) ;
#12840 = CARTESIAN_POINT ( 'NONE',  ( 8.311093377946834337, 25.15624999658601268, 8.311093377946839666 ) ) ;
#12839 = CARTESIAN_POINT ( 'NONE',  ( -2.977408999572650927, 104.3750000020483952, -7.188101187500000933 ) ) ;
#12841 = CARTESIAN_POINT ( 'NONE',  ( 1.469576158976822172E-15, -7.999999999999991118, 13.20530277982336465 ) ) ;
#12842 = CARTESIAN_POINT ( 'NONE',  ( 9.832129032723420536, 146.1979166632526983, -5.676582343749999815 ) ) ;
#12843 = CARTESIAN_POINT ( 'NONE',  ( 10.00000000000000178, 117.0833333265053682, -2.679491924311226736 ) ) ;
#12844 = CARTESIAN_POINT ( 'NONE',  ( 5.082755093536325042, 111.9687500020483810, -5.082755093536325930 ) ) ;
#12845 = CARTESIAN_POINT ( 'NONE',  ( 8.660254037844385522, 171.4583333265053682, 5.000000000000005329 ) ) ;
#12846 = CARTESIAN_POINT ( 'NONE',  ( -31.45873412500001010, 204.8750000013656063, 168.5673454167827572 ) ) ;
#12847 = ORIENTED_EDGE ( 'NONE', *, *, #64497, .T. ) ;
#12848 = CARTESIAN_POINT ( 'NONE',  ( 8.311093377946837890, 6.718749996586015349, -8.311093377946837890 ) ) ;
#12849 = ORIENTED_EDGE ( 'NONE', *, *, #49032, .T. ) ;
#12850 = DIRECTION ( 'NONE',  ( -0.000000000000000000, 1.000000000000000000, -0.000000000000000000 ) ) ;
#12851 = CARTESIAN_POINT ( 'NONE',  ( -2.765530957081996810, 299.2656250017070647, -6.676582343750003368 ) ) ;
#12853 = CARTESIAN_POINT ( 'NONE',  ( -11.35316468749999785, 138.0729166632526699, -3.042071309553167957 ) ) ;
#12852 = CARTESIAN_POINT ( 'NONE',  ( -20.85263231745901535, -27.74477033172298235, 145.1903991576613748 ) ) ;
#12854 = CARTESIAN_POINT ( 'NONE',  ( -32.00000000000000000, 207.3750000027312126, 170.0000000000004547 ) ) ;
#12855 = CARTESIAN_POINT ( 'NONE',  ( -3.313708498984758943, -7.999999999999989342, 17.66780278432982598 ) ) ;
#12856 = CARTESIAN_POINT ( 'NONE',  ( 60.49709665278108872, 219.9546912311418509, 46.04782487784429179 ) ) ;
#12857 = CARTESIAN_POINT ( 'NONE',  ( -9.832129032723415207, 249.3229166700806729, 5.676582343750005144 ) ) ;
#12858 = CARTESIAN_POINT ( 'NONE',  ( 7.204075437095968759, -7.204075437095966983, 91.09375000204838102 ) ) ;
#12859 = EDGE_LOOP ( 'NONE', ( #42744, #973, #13480, #10028, #55954, #61653, #66021, #74506, #56352, #42117 ) ) ;
#12860 = EDGE_CURVE ( 'NONE', #50104, #70051, #38262, .T. ) ;
#12862 = B_SPLINE_CURVE_WITH_KNOTS ( 'NONE', 3,
 ( #15638, #66963, #3979, #43954, #21307, #72999 ),
 .UNSPECIFIED., .F., .F.,
 ( 4, 2, 4 ),
 ( 2.380729645499014578E-07, 0.003505341553885837295, 0.007010445034807124762 ),
 .UNSPECIFIED. ) ;
#12861 = AXIS2_PLACEMENT_3D ( 'NONE', #22242, #45272, #5292 ) ;
#12863 = ADVANCED_FACE ( 'NONE', ( #9595 ), #32614, .T. ) ;
#12864 = CARTESIAN_POINT ( 'NONE',  ( -8.660254037844390851, 204.7916666598387110, 4.999999999999998224 ) ) ;
#12865 = CARTESIAN_POINT ( 'NONE',  ( 4.999999999999999112, 67.91007042436142171, -22.22893179987901746 ) ) ;
#12866 = CARTESIAN_POINT ( 'NONE',  ( 3.042071309553167069, 92.13541666325266988, -11.35316468749999785 ) ) ;
#12867 = CARTESIAN_POINT ( 'NONE',  ( 4.220049686691934809, 10.18810118749999916, 98.68750000204838102 ) ) ;
#12868 = CARTESIAN_POINT ( 'NONE',  ( -3.211159895383561391, 15.81249999863440436, -3.211159895383561835 ) ) ;
#12869 = EDGE_LOOP ( 'NONE', ( #49109, #51052, #43851, #38876 ) ) ;
#12870 = ORIENTED_EDGE ( 'NONE', *, *, #12299, .T. ) ;
#12871 = CARTESIAN_POINT ( 'NONE',  ( -3.313708498984765161, 4.031250000000000888, 7.999999999999998224 ) ) ;
#12872 = CARTESIAN_POINT ( 'NONE',  ( -7.999999999999991118, 9.797174393178815797E-16, 30.00000000000000000 ) ) ;
#12873 = CARTESIAN_POINT ( 'NONE',  ( -2.977408999572654480, 1.499999997951610542, 7.188101187499999156 ) ) ;
#12874 = CARTESIAN_POINT ( 'NONE',  ( -8.000000000000000000, 119.1875000040967763, 0.000000000000000000 ) ) ;
#12875 = EDGE_CURVE ( 'NONE', #36860, #15625, #64594, .T. ) ;
#12876 = CARTESIAN_POINT ( 'NONE',  ( 10.18810118750000093, -4.220049686691933921, 106.1875000020483810 ) ) ;
#12877 = CARTESIAN_POINT ( 'NONE',  ( 2.828427073549516724, 195.0000000000000284, 144.8284271759428634 ) ) ;
#12878 = CARTESIAN_POINT ( 'NONE',  ( 1.656854249492381914, 13.56249999726881583, 4.000000000000000888 ) ) ;
#12879 = CARTESIAN_POINT ( 'NONE',  ( -8.342170076843785083E-16, 1.062499998634406584, 4.541265875000002339 ) ) ;
#12880 = ORIENTED_EDGE ( 'NONE', *, *, #35464, .F. ) ;
#12881 = VECTOR ( 'NONE', #37404, 1000.000000000000000 ) ;
#12882 = CARTESIAN_POINT ( 'NONE',  ( 7.778174593052023411, -7.778174593052021635, 81.06249999999998579 ) ) ;
#12883 = CARTESIAN_POINT ( 'NONE',  ( -3.458734124999959914, 199.4375000013655779, 198.0000000000000284 ) ) ;
#12884 = PRODUCT_DEFINITION_FORMATION_WITH_SPECIFIED_SOURCE ( 'ANY', '', #62589, .NOT_KNOWN. ) ;
#12886 = CARTESIAN_POINT ( 'NONE',  ( 4.898587196589412829E-16, 13.68749999590322375, -8.000000000000000000 ) ) ;
#12885 = CARTESIAN_POINT ( 'NONE',  ( -24.54126587500002188, 202.2500000013656063, 168.5673454167826435 ) ) ;
#12887 = SHAPE_REPRESENTATION_RELATIONSHIP ( 'NONE' , 'NONE' ,  #63845, #58002 ) ;
#12888 = CARTESIAN_POINT ( 'NONE',  ( -4.541265875000003227, 13.87499999863440969, 1.881053915767121110 ) ) ;
#12889 = CARTESIAN_POINT ( 'NONE',  ( 2.947433605447500327, 11.00000000000000000, 68.06435453820057546 ) ) ;
#12890 = CARTESIAN_POINT ( 'NONE',  ( -2.977408999572648707, -7.188101187499990274, 13.76780278187175455 ) ) ;
#12891 = ORIENTED_EDGE ( 'NONE', *, *, #48476, .F. ) ;
#12892 = EDGE_LOOP ( 'NONE', ( #37753, #33855, #1566, #45320 ) ) ;
#12893 = CARTESIAN_POINT ( 'NONE',  ( -4.220049686691937474, -10.18810118749999738, 105.4375000020483810 ) ) ;
#12894 = FACE_OUTER_BOUND ( 'NONE', #12244, .T. ) ;
#12895 = CARTESIAN_POINT ( 'NONE',  ( -30.82842712474615965, 205.3750000000000284, 172.8284271247465824 ) ) ;
#12896 = CARTESIAN_POINT ( 'NONE',  ( -2.445694354108783664, 195.3125000013656063, 195.5543056458912190 ) ) ;
#12897 = CARTESIAN_POINT ( 'NONE',  ( -4.999999999999996447, 31.66666666666666785, -8.660254037844385522 ) ) ;
#12898 = CARTESIAN_POINT ( 'NONE',  ( 6.123233995736767268E-16, 101.2500000000000000, -10.00000000000000178 ) ) ;
#12899 = CARTESIAN_POINT ( 'NONE',  ( -5.656854249492378806, 120.6875000000000000, 5.656854249492381470 ) ) ;
#12900 = CARTESIAN_POINT ( 'NONE',  ( -4.721056650415998313, 296.7343750017069510, 4.721056650416000089 ) ) ;
#12901 = EDGE_LOOP ( 'NONE', ( #12318, #13528, #47726, #24206 ) ) ;
#12902 =( BOUNDED_CURVE ( )  B_SPLINE_CURVE ( 2, ( #38544, #61546, #55899, #4212, #43057, #51707, #51336, #23405, #40024 ),
 .UNSPECIFIED., .F., .F. ) 
 B_SPLINE_CURVE_WITH_KNOTS ( ( 3, 2, 2, 2, 3 ),
 ( 0.5729166666666666297, 0.5781250000000000000, 0.5833333333333333703, 0.5885416666666666297, 0.5937500000000000000 ),
 .UNSPECIFIED. ) 
 CURVE ( )  GEOMETRIC_REPRESENTATION_ITEM ( )  RATIONAL_B_SPLINE_CURVE ( ( 1.000000000000000000, 0.9238795325112867385, 1.000000000000000000, 0.9238795325112867385, 1.000000000000000000, 0.9238795325112867385, 1.000000000000000000, 0.9238795325112867385, 1.000000000000000000 ) ) 
 REPRESENTATION_ITEM ( '' )  );
#12903 = VECTOR ( 'NONE', #44413, 1000.000000000000000 ) ;
#12904 = DIRECTION ( 'NONE',  ( 0.000000000000000000, 0.000000000000000000, 1.000000000000000000 ) ) ;
#12905 = CARTESIAN_POINT ( 'NONE',  ( -5.656854249492381470, 12.74999999590322197, 5.656854249492379694 ) ) ;
#12906 = CARTESIAN_POINT ( 'NONE',  ( -1.432654583217662481, 206.1250000013655779, 145.4587341250000634 ) ) ;
#12907 = CARTESIAN_POINT ( 'NONE',  ( -7.320508075688773708, 103.7499999931720396, -7.320508075688774596 ) ) ;
#12908 = CARTESIAN_POINT ( 'NONE',  ( 0.000000000000000000, 284.0000000000000000, 0.000000000000000000 ) ) ;
#12909 = CARTESIAN_POINT ( 'NONE',  ( -10.00000000000000000, 230.0000000000000000, 0.000000000000000000 ) ) ;
#12910 = CARTESIAN_POINT ( 'NONE',  ( -5.000000000000000000, 0.000000000000000000, 0.000000000000000000 ) ) ;
#12911 = CARTESIAN_POINT ( 'NONE',  ( -10.18810118749999916, 0.000000000000000000, 68.03125000204838102 ) ) ;
#12912 = CARTESIAN_POINT ( 'NONE',  ( 7.320508075688771044, 209.3750000000000000, 7.320508075688775484 ) ) ;
#12913 = CARTESIAN_POINT ( 'NONE',  ( 5.082755093536320601, -5.082755093536318824, 9.924052781871754547 ) ) ;
#12914 = CARTESIAN_POINT ( 'NONE',  ( 9.832129032723416984, 185.6770833299193555, 5.676582343750006032 ) ) ;
#12915 = CARTESIAN_POINT ( 'NONE',  ( -1.881053915767121554, 2.624999998634406584, -4.541265875000002339 ) ) ;
#12916 = CARTESIAN_POINT ( 'NONE',  ( -7.999999999999998224, 99.78125000409676204, 3.313708498984766049 ) ) ;
#12918 = DIRECTION ( 'NONE',  ( -0.000000000000000000, -0.000000000000000000, 1.000000000000000000 ) ) ;
#12917 = DIRECTION ( 'NONE',  ( 0.000000000000000000, 0.000000000000000000, 1.000000000000000000 ) ) ;
#12919 = ORIENTED_EDGE ( 'NONE', *, *, #53389, .T. ) ;
#12920 = CARTESIAN_POINT ( 'NONE',  ( 1.432654583217608080, 206.8750000013656347, 138.5412658750000503 ) ) ;
#12921 = CARTESIAN_POINT ( 'NONE',  ( 9.832129032723420536, 46.51041666325269119, -5.676582343749999815 ) ) ;
#12922 = CARTESIAN_POINT ( 'NONE',  ( -4.556349186104045934, 11.00000000000000000, 105.9062500040967763 ) ) ;
#12923 = CARTESIAN_POINT ( 'NONE',  ( 11.35316468749999963, 216.3020833299193555, -3.042071309553165293 ) ) ;
#12924 = CARTESIAN_POINT ( 'NONE',  ( -24.54126587500001833, 205.2500000013655779, 168.5673454167826435 ) ) ;
#12925 = CARTESIAN_POINT ( 'NONE',  ( 8.660254037844385522, 9.583333333333333925, 5.000000000000006217 ) ) ;
#12927 = DIRECTION ( 'NONE',  ( -0.000000000000000000, -0.000000000000000000, -1.000000000000000000 ) ) ;
#12926 = CARTESIAN_POINT ( 'NONE',  ( 4.556349186104045934, 11.00000000000000000, 71.21875000409676204 ) ) ;
#12928 = DIRECTION ( 'NONE',  ( -0.000000000000000000, -0.000000000000000000, -1.000000000000000000 ) ) ;
#12929 = ADVANCED_FACE ( 'NONE', ( #6534 ), #69158, .T. ) ;
#12930 = CARTESIAN_POINT ( 'NONE',  ( 7.320508075688771044, 71.24999999317203958, 7.320508075688775484 ) ) ;
#12931 = CARTESIAN_POINT ( 'NONE',  ( -5.082755093536324154, 97.34375000204838102, 5.082755093536326818 ) ) ;
#12932 = CARTESIAN_POINT ( 'NONE',  ( -4.541265875000002339, 16.87499999863440436, -1.881053915767121998 ) ) ;
#12933 = CARTESIAN_POINT ( 'NONE',  ( 4.000000000000001776, 11.00000000000000000, 0.000000000000000000 ) ) ;
#12934 = DIRECTION ( 'NONE',  ( -0.000000000000000000, 1.000000000000000000, 0.000000000000000000 ) ) ;
#12935 = CARTESIAN_POINT ( 'NONE',  ( 1.836970198721029589E-15, 254.3750000068280031, 10.00000000000000000 ) ) ;
#12936 = EDGE_LOOP ( 'NONE', ( #2468, #14324, #35188, #42191 ) ) ;
#12937 = ORIENTED_EDGE ( 'NONE', *, *, #2739, .T. ) ;
#12938 = CARTESIAN_POINT ( 'NONE',  ( 6.676582343750003368, 297.1718750017071216, -2.765530957081997254 ) ) ;
#12939 = CARTESIAN_POINT ( 'NONE',  ( -8.660254037844401509, 142.9166666666666572, 5.000000000000004441 ) ) ;
#12940 = VECTOR ( 'NONE', #4304, 1000.000000000000000 ) ;
#12941 = CARTESIAN_POINT ( 'NONE',  ( -3.042071309553164404, 157.2395833299193555, -11.35316468749999963 ) ) ;
#12942 = CARTESIAN_POINT ( 'NONE',  ( 1.871523826299183495E-15, -10.18810118749999916, 86.03125000204836681 ) ) ;
#12943 = CARTESIAN_POINT ( 'NONE',  ( 4.999999999999994671, 4.166666666666666963, 8.660254037844390851 ) ) ;
#12944 = CARTESIAN_POINT ( 'NONE',  ( 2.828427124746209831, 201.3750000000000284, 200.8284271247462129 ) ) ;
#12945 = CARTESIAN_POINT ( 'NONE',  ( -5.204170427930421283E-15, 20.78460969082654231, -1.607695154586745501 ) ) ;
#12946 = CARTESIAN_POINT ( 'NONE',  ( -4.220049686691937474, -10.18810118749999738, 107.3125000020483668 ) ) ;
#12947 = VERTEX_POINT ( 'NONE', #23875 ) ;
#12948 = DIRECTION ( 'NONE',  ( 0.000000000000000000, 0.000000000000000000, -1.000000000000000000 ) ) ;
#12949 = CARTESIAN_POINT ( 'NONE',  ( -9.832129032723420536, 139.0104166632526983, 5.676582343749997150 ) ) ;
#12950 = CARTESIAN_POINT ( 'NONE',  ( 1.432654583217664479, 199.7500000013656063, 201.4587341250000065 ) ) ;
#12951 = CARTESIAN_POINT ( 'NONE',  ( -3.673940397442060854E-16, 290.7500000000000000, -6.000000000000001776 ) ) ;
#12952 = CARTESIAN_POINT ( 'NONE',  ( -7.204075437095967871, 7.204075437095967871, 70.84375000204836681 ) ) ;
#12953 = CARTESIAN_POINT ( 'NONE',  ( 11.35316468750000141, 46.09374999658602690, 0.000000000000000000 ) ) ;
#12954 = ORIENTED_EDGE ( 'NONE', *, *, #5284, .F. ) ;
#12955 = DIRECTION ( 'NONE',  ( 0.000000000000000000, -1.000000000000000000, 0.000000000000000000 ) ) ;
#12956 = CARTESIAN_POINT ( 'NONE',  ( -8.342170076843785083E-16, 6.187499998634407028, 4.541265875000002339 ) ) ;
#12957 = CARTESIAN_POINT ( 'NONE',  ( 3.317071493978883456, -8.008118988124989457, 13.48186528394063011 ) ) ;
#12958 = ADVANCED_FACE ( 'NONE', ( #519 ), #58963, .T. ) ;
#12959 = EDGE_CURVE ( 'NONE', #57671, #70231, #57799, .T. ) ;
#12960 = CARTESIAN_POINT ( 'NONE',  ( -7.188101187500000044, 13.21874999795161187, -8.802885111219163269E-16 ) ) ;
#12961 = CARTESIAN_POINT ( 'NONE',  ( -2.485281374238571761, 290.8750000034140157, -6.000000000000003553 ) ) ;
#12962 = CARTESIAN_POINT ( 'NONE',  ( -7.999999999999998224, 117.7812500040967763, 3.313708498984766049 ) ) ;
#12963 = CARTESIAN_POINT ( 'NONE',  ( 7.188101187500000044, 14.34374999795161187, 0.000000000000000000 ) ) ;
#12964 = CARTESIAN_POINT ( 'NONE',  ( -5.082755093536317936, -5.082755093536320601, 9.174052781871752771 ) ) ;
#12965 = AXIS2_PLACEMENT_3D ( 'NONE', #52195, #59337, #63874 ) ;
#12966 = CARTESIAN_POINT ( 'NONE',  ( -7.204075437095967871, 7.204075437095967871, 68.96875000204836681 ) ) ;
#12967 = CARTESIAN_POINT ( 'NONE',  ( -30.44569435410879521, 206.0625000013656063, 172.4456943541092357 ) ) ;
#12968 = CARTESIAN_POINT ( 'NONE',  ( 11.00000000000000000, 1.347111479062088405E-15, 85.93750000409677625 ) ) ;
#12969 = CARTESIAN_POINT ( 'NONE',  ( -4.000000000000002665, 3.312499997268814056, 1.656854249492380804 ) ) ;
#12970 = ORIENTED_EDGE ( 'NONE', *, *, #39918, .F. ) ;
#12971 = CARTESIAN_POINT ( 'NONE',  ( 4.000000000000015987, 194.5625000027311842, 199.6568542494924259 ) ) ;
#12972 = ADVANCED_FACE ( 'NONE', ( #11814 ), #57858, .F. ) ;
#12973 = CARTESIAN_POINT ( 'NONE',  ( 1.656854249492348607, 204.1875000000000568, 138.0000000000000568 ) ) ;
#12974 = CARTESIAN_POINT ( 'NONE',  ( -26.34314575050769491, 198.0625000027312410, 166.0000000000003695 ) ) ;
#12975 = CARTESIAN_POINT ( 'NONE',  ( -3.211159895383561391, 1.687499998634406584, -3.211159895383561835 ) ) ;
#12976 = CARTESIAN_POINT ( 'NONE',  ( -5.082755093536324154, 115.3437500020483810, 5.082755093536326818 ) ) ;
#12977 = LINE ( 'NONE', #36014, #71756 ) ;
#12978 = CARTESIAN_POINT ( 'NONE',  ( -4.401442555609577197E-16, 7.188101187499992051, 28.11155278187175455 ) ) ;
#12979 = ORIENTED_EDGE ( 'NONE', *, *, #20996, .T. ) ;
#12980 = CARTESIAN_POINT ( 'NONE',  ( -7.188101187500000044, 25.21874999795161543, -8.802885111219163269E-16 ) ) ;
#12981 = ORIENTED_EDGE ( 'NONE', *, *, #70602, .F. ) ;
#12982 = CARTESIAN_POINT ( 'NONE',  ( 8.660254037844385522, 256.0416666734946602, -5.000000000000003553 ) ) ;
#12983 = CARTESIAN_POINT ( 'NONE',  ( 0.8588954341814353244, -10.28066745654381720, -63.58998442112848437 ) ) ;
#12984 = CARTESIAN_POINT ( 'NONE',  ( 25.55430564589115860, 207.0625000013656063, 167.5543056458911053 ) ) ;
#12985 = CARTESIAN_POINT ( 'NONE',  ( 4.999999999999993783, 54.16666666666667140, 8.660254037844390851 ) ) ;
#12986 = CARTESIAN_POINT ( 'NONE',  ( 2.977408999572650039, 100.0625000020483952, -7.188101187500001821 ) ) ;
#12987 = CARTESIAN_POINT ( 'NONE',  ( -2.485281374238571761, 297.8124999999999432, -6.000000000000003553 ) ) ;
#12988 = CIRCLE ( 'NONE', #32299, 7.000000000000006217 ) ;
#12990 = CARTESIAN_POINT ( 'NONE',  ( -29.89941891291018905, -42.94590694075801451, 178.2112019679211130 ) ) ;
#12989 = DIRECTION ( 'NONE',  ( 0.000000000000000000, 0.000000000000000000, 1.000000000000000000 ) ) ;
#12991 = ORIENTED_EDGE ( 'NONE', *, *, #4894, .T. ) ;
#12992 = CARTESIAN_POINT ( 'NONE',  ( 3.042071309553163960, 237.4479166700806729, -11.35316468749999785 ) ) ;
#12993 = CARTESIAN_POINT ( 'NONE',  ( 5.082755093536320601, -5.082755093536318824, 12.92405278187175277 ) ) ;
#12994 = CARTESIAN_POINT ( 'NONE',  ( -27.99999999999999645, 210.0000000000000284, 170.0000000000003695 ) ) ;
#12995 = CARTESIAN_POINT ( 'NONE',  ( -2.679491924311300011, 73.33333332650538239, -9.999999999999959144 ) ) ;
#12996 = CARTESIAN_POINT ( 'NONE',  ( 1.656854249492433206, 197.3125000027311557, 138.0000000000001705 ) ) ;
#12997 = FACE_OUTER_BOUND ( 'NONE', #73680, .T. ) ;
#12998 = CARTESIAN_POINT ( 'NONE',  ( -8.660254037844390851, 139.7916666598387110, 4.999999999999998224 ) ) ;
#12999 = CARTESIAN_POINT ( 'NONE',  ( 4.999999999999993783, 174.1666666666666572, 8.660254037844390851 ) ) ;
#13000 = CARTESIAN_POINT ( 'NONE',  ( 25.55430564589115505, 209.3125000013656063, 172.4456943541086957 ) ) ;
#13001 = CARTESIAN_POINT ( 'NONE',  ( -31.10877240494261287, 177.5931723900570489, 171.6493011599653755 ) ) ;
#13002 = CARTESIAN_POINT ( 'NONE',  ( 4.556349186104052151, -10.99999999999999822, 69.15625000409676204 ) ) ;
#13003 = CARTESIAN_POINT ( 'NONE',  ( -8.311093377946836114, 137.9687499965860411, -8.311093377946837890 ) ) ;
#13004 = CARTESIAN_POINT ( 'NONE',  ( -14.00000000000000178, -2.250000000005106138, 10.23492587299426404 ) ) ;
#13005 = DIRECTION ( 'NONE',  ( 0.000000000000000000, 0.000000000000000000, 1.000000000000000000 ) ) ;
#13007 = CARTESIAN_POINT ( 'NONE',  ( 25.17157287525381548, 203.6250000000000284, 167.1715728752537018 ) ) ;
#13006 = CARTESIAN_POINT ( 'NONE',  ( 24.00000000000001066, 207.6875000000000000, 168.3431457505075173 ) ) ;
#13008 = ORIENTED_EDGE ( 'NONE', *, *, #11324, .T. ) ;
#13009 = VECTOR ( 'NONE', #30650, 1000.000000000000000 ) ;
#13010 = CARTESIAN_POINT ( 'NONE',  ( -3.999999999999959144, 206.0625000000000000, 199.6568542494924259 ) ) ;
#13011 = CARTESIAN_POINT ( 'NONE',  ( -37.99999999999999289, 205.0000000000000284, 20.00000000000000000 ) ) ;
#13012 = CARTESIAN_POINT ( 'NONE',  ( -24.00000000000001421, 209.8125000000000000, 168.3431457505080289 ) ) ;
#13013 = CARTESIAN_POINT ( 'NONE',  ( -2.445694354108839619, 208.8125000013656063, 139.5543056458912190 ) ) ;
#13014 = CARTESIAN_POINT ( 'NONE',  ( 0.000000000000000000, 0.5000000000000004441, 8.000000000000000000 ) ) ;
#13015 = CARTESIAN_POINT ( 'NONE',  ( 4.999999999999993783, 36.04166665983870388, 8.660254037844390851 ) ) ;
#13016 = CARTESIAN_POINT ( 'NONE',  ( -5.082755093536324154, 116.8437500020483810, 5.082755093536326818 ) ) ;
#13017 = CARTESIAN_POINT ( 'NONE',  ( -1.881053915767124440, 5.124999998634406140, 4.541265875000001451 ) ) ;
#13018 = CARTESIAN_POINT ( 'NONE',  ( 2.219371606097240601, 67.78152867896243094, -20.18750705526135647 ) ) ;
#13019 = CARTESIAN_POINT ( 'NONE',  ( 5.656854249492374365, 5.656854249492375253, 16.76780277982336287 ) ) ;
#13021 = CARTESIAN_POINT ( 'NONE',  ( 7.999999999521839378, -8.746674989952265200E-05, 18.26780030933659305 ) ) ;
#13020 = CARTESIAN_POINT ( 'NONE',  ( -30.82842712474621294, 203.1250000000000284, 167.1715728752542134 ) ) ;
#13022 = ORIENTED_EDGE ( 'NONE', *, *, #9666, .T. ) ;
#13023 =( BOUNDED_CURVE ( )  B_SPLINE_CURVE ( 2, ( #20166, #44319, #20544, #33022, #56024, #4333, #54525, #49602, #55652 ),
 .UNSPECIFIED., .F., .F. ) 
 B_SPLINE_CURVE_WITH_KNOTS ( ( 3, 2, 2, 2, 3 ),
 ( 0.9473684210526316374, 0.9539473684210527660, 0.9605263157894736725, 0.9671052631578946901, 0.9736842105263158187 ),
 .UNSPECIFIED. ) 
 CURVE ( )  GEOMETRIC_REPRESENTATION_ITEM ( )  RATIONAL_B_SPLINE_CURVE ( ( 0.9999999999999986677, 0.9238795325112880708, 1.000000000000000000, 0.9238795325112867385, 1.000000000000000000, 0.9238795325112867385, 1.000000000000000000, 0.9238795325112867385, 1.000000000000000000 ) ) 
 REPRESENTATION_ITEM ( '' )  );
#13024 = DIRECTION ( 'NONE',  ( -0.000000000000000000, 1.000000000000000000, 4.476705744456276341E-16 ) ) ;
#13025 = CARTESIAN_POINT ( 'NONE',  ( -2.250000000000000000, 300.0000000000000000, 7.677076266392047543 ) ) ;
#13026 = CARTESIAN_POINT ( 'NONE',  ( 5.676582343749997150, 227.5520833367473017, -9.832129032723418760 ) ) ;
#13027 = CARTESIAN_POINT ( 'NONE',  ( 3.042071309553167069, 116.8229166632526983, -11.35316468749999785 ) ) ;
#13028 = ORIENTED_EDGE ( 'NONE', *, *, #19334, .T. ) ;
#13029 = EDGE_CURVE ( 'NONE', #16856, #52326, #74441, .T. ) ;
#13030 = DIRECTION ( 'NONE',  ( -0.000000000000000000, -1.000000000000000000, -0.000000000000000000 ) ) ;
#13031 = CARTESIAN_POINT ( 'NONE',  ( -7.204075437095965206, -7.204075437095968759, 102.3437500020483668 ) ) ;
#13032 = LINE ( 'NONE', #41356, #38080 ) ;
#13033 = CARTESIAN_POINT ( 'NONE',  ( 2.445694354108839175, 199.3125000013656063, 195.5543056458912190 ) ) ;
#13034 = DIRECTION ( 'NONE',  ( 0.000000000000000000, 0.000000000000000000, 1.000000000000000000 ) ) ;
#13036 = CARTESIAN_POINT ( 'NONE',  ( -9.832129032723420536, 108.6979166632526983, 5.676582343749997150 ) ) ;
#13035 = DIRECTION ( 'NONE',  ( -0.000000000000000000, 1.000000000000000000, -0.000000000000000000 ) ) ;
#13037 = CARTESIAN_POINT ( 'NONE',  ( -26.34314575050764873, 207.9375000000000000, 166.0000000000003695 ) ) ;
#13038 = CARTESIAN_POINT ( 'NONE',  ( -1.300830538084598961E-11, 173.7499999999989768, 10.00000000000000178 ) ) ;
#13039 = VERTEX_POINT ( 'NONE', #51429 ) ;
#13040 = CARTESIAN_POINT ( 'NONE',  ( -5.000000000000005329, 205.2083333265053682, 8.660254037844387298 ) ) ;
#13041 = CARTESIAN_POINT ( 'NONE',  ( 8.000000000000000000, 22.50000000000000355, 0.000000000000000000 ) ) ;
#13042 = CARTESIAN_POINT ( 'NONE',  ( -11.35316468750000141, 98.80208332991934128, 3.042071309553159963 ) ) ;
#13043 = DIRECTION ( 'NONE',  ( -0.000000000000000000, -1.000000000000000000, -0.000000000000000000 ) ) ;
#13044 = CARTESIAN_POINT ( 'NONE',  ( 4.401442555609581635E-16, 14.71874999795161187, -7.188101187500000044 ) ) ;
#13045 = CARTESIAN_POINT ( 'NONE',  ( -7.204075437095967871, 7.204075437095967871, 94.84375000204838102 ) ) ;
#13046 = CARTESIAN_POINT ( 'NONE',  ( 9.832129032723416984, 10.67708332991935016, 5.676582343750006032 ) ) ;
#13047 = EDGE_LOOP ( 'NONE', ( #69119, #36007, #68372, #55199 ) ) ;
#13048 = DIRECTION ( 'NONE',  ( 0.000000000000000000, 0.000000000000000000, 1.000000000000000000 ) ) ;
#13049 = DIRECTION ( 'NONE',  ( -1.000000000000000000, 0.000000000000000000, 0.000000000000000000 ) ) ;
#13050 = DIRECTION ( 'NONE',  ( -0.000000000000000000, -0.000000000000000000, 1.000000000000000000 ) ) ;
#13051 = CARTESIAN_POINT ( 'NONE',  ( -4.220049686691935698, 10.18810118749999916, 72.25000000204836681 ) ) ;
#13052 = EDGE_CURVE ( 'NONE', #37692, #50334, #41599, .T. ) ;
#13053 = DIRECTION ( 'NONE',  ( -0.000000000000000000, 1.000000000000000000, -0.000000000000000000 ) ) ;
#13054 = CARTESIAN_POINT ( 'NONE',  ( -7.320508075688771932, 264.3750000000000000, -7.320508075688771932 ) ) ;
#13055 = CARTESIAN_POINT ( 'NONE',  ( -6.676582343750000703, 293.5156250017070647, 2.765530957082001251 ) ) ;
#13056 = CYLINDRICAL_SURFACE ( 'NONE', #23233, 8.000000000000000000 ) ;
#13057 = CARTESIAN_POINT ( 'NONE',  ( -8.311093377946841443, 224.2187499965860411, 8.311093377946834337 ) ) ;
#13058 = EDGE_CURVE ( 'NONE', #28738, #43761, #23499, .T. ) ;
#13059 = CARTESIAN_POINT ( 'NONE',  ( 4.220049686691941027, -10.18810118749999738, 90.62500000204836681 ) ) ;
#13060 = AXIS2_PLACEMENT_3D ( 'NONE', #39215, #33573, #61477 ) ;
#13061 = CARTESIAN_POINT ( 'NONE',  ( -31.45873412499998523, 203.7500000013656063, 171.4326545832180386 ) ) ;
#13062 = CARTESIAN_POINT ( 'NONE',  ( 5.656854249492380582, 25.68750000000000711, -5.656854249492380582 ) ) ;
#13063 = CARTESIAN_POINT ( 'NONE',  ( 4.541265875000002339, 11.43749999863440614, 0.000000000000000000 ) ) ;
#13064 = EDGE_LOOP ( 'NONE', ( #409, #49248, #53180, #55977 ) ) ;
#13065 = CARTESIAN_POINT ( 'NONE',  ( -14.80971666716479085, -43.85485428142018804, 142.7495589859527172 ) ) ;
#13066 = AXIS2_PLACEMENT_3D ( 'NONE', #46699, #40305, #69348 ) ;
#13067 = CARTESIAN_POINT ( 'NONE',  ( 2.828427124746209831, 208.5000000027312126, 200.8284271247462129 ) ) ;
#13068 = EDGE_CURVE ( 'NONE', #24245, #4661, #47561, .T. ) ;
#13069 = CARTESIAN_POINT ( 'NONE',  ( 3.458734124999960358, 197.6875000013655779, 142.0000000000000568 ) ) ;
#13070 = VECTOR ( 'NONE', #50223, 1000.000000000000000 ) ;
#13071 = CARTESIAN_POINT ( 'NONE',  ( -5.000000000000054179, 173.3333333333333712, 8.660254037844469011 ) ) ;
#13072 = CARTESIAN_POINT ( 'NONE',  ( -6.238412754330611322E-16, 10.18810118749999916, 73.65625000204836681 ) ) ;
#13073 = ORIENTED_EDGE ( 'NONE', *, *, #32847, .F. ) ;
#13074 = CARTESIAN_POINT ( 'NONE',  ( 7.188101187499999156, 4.874999997951610986, 2.977408999572654924 ) ) ;
#13075 = CARTESIAN_POINT ( 'NONE',  ( 2.449293598294707893E-16, 12.99999999726881406, -4.000000000000001776 ) ) ;
#13076 = CARTESIAN_POINT ( 'NONE',  ( -5.082755093536324154, 115.7187500020483810, 5.082755093536326818 ) ) ;
#13077 = CARTESIAN_POINT ( 'NONE',  ( 2.295000000000000373, 278.5679999999998699, 5.413230550749199566 ) ) ;
#13078 = CARTESIAN_POINT ( 'NONE',  ( 2.765530957082001251, 290.7656250017070079, 6.676582343749999815 ) ) ;
#13080 = FACE_OUTER_BOUND ( 'NONE', #25412, .T. ) ;
#13079 = CARTESIAN_POINT ( 'NONE',  ( 11.35316468749999963, 226.4062500034139873, -1.390361679473963556E-15 ) ) ;
#13081 = ITEM_DEFINED_TRANSFORMATION ( 'NONE', 'NONE', #32087,  #57354 ) ;
#13082 = ORIENTED_EDGE ( 'NONE', *, *, #2517, .T. ) ;
#13083 = CARTESIAN_POINT ( 'NONE',  ( -9.832129032723418760, 223.8020833367473301, -5.676582343749998927 ) ) ;
#13084 = EDGE_CURVE ( 'NONE', #68115, #44173, #26013, .T. ) ;
#13085 = CARTESIAN_POINT ( 'NONE',  ( -7.188101187499992051, 0.000000000000000000, 8.986552781871752771 ) ) ;
#13086 = CARTESIAN_POINT ( 'NONE',  ( -3.458734124999959469, 203.7500000013656063, 199.4326545832176691 ) ) ;
#13087 = ORIENTED_EDGE ( 'NONE', *, *, #18005, .T. ) ;
#13088 = CARTESIAN_POINT ( 'NONE',  ( -7.204075437095965206, -7.204075437095968759, 70.84375000204836681 ) ) ;
#13089 = CARTESIAN_POINT ( 'NONE',  ( -11.35316468750000141, 103.8020833299193413, 3.042071309553159963 ) ) ;
#13090 = CARTESIAN_POINT ( 'NONE',  ( 2.849036369511732440E-14, 209.2500000000000284, 202.0000000000000000 ) ) ;
#13091 = CARTESIAN_POINT ( 'NONE',  ( 2.020667218593132706E-15, -11.00000000000000000, 79.37499999999998579 ) ) ;
#13094 = DIRECTION ( 'NONE',  ( -0.000000000000000000, -0.000000000000000000, 1.000000000000000000 ) ) ;
#13093 = CARTESIAN_POINT ( 'NONE',  ( 25.55430564589115505, 205.0625000013656063, 167.5543056458911053 ) ) ;
#13092 = CARTESIAN_POINT ( 'NONE',  ( 26.56734541678232375, 204.6250000013655779, 173.4587341249998929 ) ) ;
#13095 = ORIENTED_EDGE ( 'NONE', *, *, #53528, .F. ) ;
#13096 = DIRECTION ( 'NONE',  ( -0.000000000000000000, 1.000000000000000000, -4.476705744456276341E-16 ) ) ;
#13097 = CARTESIAN_POINT ( 'NONE',  ( -2.679491924311235174, 180.4166666598387110, 10.00000000000000000 ) ) ;
#13098 = CARTESIAN_POINT ( 'NONE',  ( 11.35316468749999963, 215.9895833299192986, -3.042071309553165293 ) ) ;
#13099 = CARTESIAN_POINT ( 'NONE',  ( 3.458734124999959914, 199.4375000013655779, 142.0000000000000568 ) ) ;
#13100 = CARTESIAN_POINT ( 'NONE',  ( 24.54126587499999346, 202.4375000013656063, 169.9999999999998863 ) ) ;
#13101 = AXIS2_PLACEMENT_3D ( 'NONE', #47431, #42510, #71920 ) ;
#13102 = CARTESIAN_POINT ( 'NONE',  ( 2.977408999572650927, 25.12499999795161187, -7.188101187500001821 ) ) ;
#13103 = CARTESIAN_POINT ( 'NONE',  ( -2.085542519210945728E-15, 179.8437499965860411, 11.35316468750000141 ) ) ;
#13104 = CARTESIAN_POINT ( 'NONE',  ( -2.977408999572650927, 95.75000000204838102, -7.188101187500000933 ) ) ;
#13105 = CARTESIAN_POINT ( 'NONE',  ( -4.999999999999999112, 65.74990953740004329, -23.82322416715241431 ) ) ;
#13106 = CARTESIAN_POINT ( 'NONE',  ( -25.17157287525381903, 196.8750000000000284, 167.1715728752541565 ) ) ;
#13107 = CARTESIAN_POINT ( 'NONE',  ( -4.541265875000003227, 14.87499999863441147, 1.881053915767121110 ) ) ;
#13108 = CARTESIAN_POINT ( 'NONE',  ( 31.45873412499999944, 199.0000000013656063, 168.5673454167822740 ) ) ;
#13109 = CARTESIAN_POINT ( 'NONE',  ( 7.188101187499991163, 2.977408999572648707, 2.705302781871750994 ) ) ;
#13110 = CARTESIAN_POINT ( 'NONE',  ( -5.676582343750006032, 64.11458332991935549, 9.832129032723418760 ) ) ;
#13111 = CARTESIAN_POINT ( 'NONE',  ( 9.000000000000023093, -15.58845726811988541, 0.000000000000000000 ) ) ;
#13112 = CARTESIAN_POINT ( 'NONE',  ( -54.00000000000000711, 242.0000000000000284, 0.000000000000000000 ) ) ;
#13113 = EDGE_LOOP ( 'NONE', ( #44776, #6515, #15841, #62164, #44588, #55044, #18361 ) ) ;
#13114 = CARTESIAN_POINT ( 'NONE',  ( -5.000000000000018652, 48.33333333333334991, 8.660254037844408614 ) ) ;
#13115 = DIRECTION ( 'NONE',  ( -0.000000000000000000, 1.000000000000000000, -4.476705744456276341E-16 ) ) ;
#13116 = CARTESIAN_POINT ( 'NONE',  ( 3.042071309553167069, 71.82291666325269830, -11.35316468749999785 ) ) ;
#13117 = VECTOR ( 'NONE', #14254, 1000.000000000000000 ) ;
#13118 = CARTESIAN_POINT ( 'NONE',  ( -11.00000000000000000, 4.556349186104045934, 67.09375000409677625 ) ) ;
#13119 = CARTESIAN_POINT ( 'NONE',  ( 2.445694354108784108, 196.5625000013656063, 144.4456943541088663 ) ) ;
#13120 = CARTESIAN_POINT ( 'NONE',  ( -2.849036369511732440E-14, 203.3750000027312126, 138.0000000000000568 ) ) ;
#13122 = CARTESIAN_POINT ( 'NONE',  ( 8.311093377946834337, 70.15624999658602690, 8.311093377946839666 ) ) ;
#13121 = CARTESIAN_POINT ( 'NONE',  ( 2.449293598294707893E-16, 12.99999999726881406, -4.000000000000001776 ) ) ;
#13123 = CARTESIAN_POINT ( 'NONE',  ( 5.656854249492376141, -5.656854249492374365, 24.08030278392014978 ) ) ;
#13124 = CARTESIAN_POINT ( 'NONE',  ( 4.999999999999993783, 129.1666666666666856, 8.660254037844390851 ) ) ;
#13125 =( BOUNDED_SURFACE ( )  B_SPLINE_SURFACE ( 1, 2, ( 
 ( #1590, #1945, #64581, #58562, #6866, #69501, #40828, #30977, #52892, #1224, #69874, #24934, #47580, #47951, #17811, #18921, #41927, #53998, #24203, #47214, #64936, #23844, #2309, #46481, #36280, #59296, #7605, #63834, #12150, #6504, #46851, #18186, #41202, #64210, #67183, #20018, #43028, #37772, #2688, #43791, #19651, #13974, #31729, #72075, #66050, #60768, #55872, #14358, #49064, #8337, #25306, #9094, #32488, #20393, #37390, #60391, #48323, #42664, #15480, #8717, #54751, #48694, #3811, #66421, #26809, #71330, #32108, #20772, #49823, #3061, #26044, #43407, #31349, #61518, #65675, #14733, #55126, #3429, #26420, #49446, #9841, #54379, #37016, #72464, #66806, #38516, #15109, #38141, #61141, #25674, #9471, #71700, #55499, #32867, #44169, #60018, #72840, #21147, #4555, #11325, #50194, #62253, #74320, #45645, #73949, #22252, #51309, #68661, #22626, #16972, #73213, #10211, #45280, #57358, #39998, #21521, #63001, #5298, #44543, #4188, #44915, #68290, #28300, #23012, #56240, #10956, #50937, #56985, #5669, #15849, #34357, #28666, #51680, #16587, #25, #27550, #46019, #39626, #27930, #69040, #63364, #62625, #21886, #17343, #40364, #11689, #34728, #50563, #27177, #10580, #67553, #38884, #61888, #33240, #73578, #67922, #16215, #39255, #33991, #33611, #56618, #4933, #12058, #52062, #29786, #52797, #24109, #29420, #6414, #70880, #1507, #1131, #59206, #1855, #18463, #63740, #47123, #70156, #41839, #58836, #41473, #18094, #12789, #6038, #24486, #57733, #64489, #13152, #47489, #399, #35821, #40730, #41108, #35092, #6779, #47859, #58103, #7147, #64115, #12422, #30152, #766, #53169, #64848, #70512, #18832, #23752, #35456, #24841, #46754, #52429, #7516, #69777, #58469, #36190, #30522, #53539, #19194, #42197, #65212, #29043, #13517, #23378, #46391, #69409, #17715, #3338, #48970, #2219, #72367, #9372, #48603, #61050, #31637, #66712, #72750, #15014, #8624, #54658, #31256, #42937, #26329, #21055, #59932, #2966, #65586, #44078, #13884, #32013, #25951, #49350, #71984, #53906, #54286, #20297, #60295, #26715, #36924, #48231, #25215, #43315, #66332, #14636, #25587, #19927, #71606, #37679, #20678, #30888, #43697, #8244, #2597, #60678, #8998, #55032, #38050, #32392, #55407, #67090, #71239, #3716, #49735, #36555, #65958, #19559, #59568, #7883, #42573, #14262, #37299, #5586, #39163, #4097, #21428, #16125, #16500, #62165, #68203, #16882, #27090, #33900, #45562, #10863, #27839, #22539, #15759, #51223, #4842, #10490, #74233, #74610, #50846, #33157, #68575, #11240, #39905, #62911, #38798, #34268, #73485, #57271, #28585, #51593, #39540, #22923, #44451, #10119, #62536, #73860, #45937, #22167, #33525, #67462, #9754, #56525, #45193, #56898, #61801, #32773, #50106, #21791, #5211, #56151, #28211, #15387, #4467, #38423, #73120, #61427, #55781, #27456, #50471, #44821 ),
 ( #67833, #30710, #65406, #48420, #24666, #70698, #19017, #1323, #31454, #25770, #7337, #42022, #36376, #47677, #65030, #54479, #52991, #68949, #71058, #2042, #37113, #64676, #12975, #7704, #47318, #13703, #18656, #36747, #60115, #14078, #17259, #40279, #6965, #70344, #2411, #63279, #53362, #59759, #8069, #13339, #59391, #42390, #31070, #54098, #25406, #11606, #24306, #53730, #71423, #19751, #34643, #42758, #19376, #57649, #29974, #36011, #25029, #65775, #8434, #41665, #48049, #2784, #59030, #30343, #1688, #27275, #67281, #20118, #44269, #49921, #43132, #48791, #14827, #66903, #72936, #67653, #26146, #55598, #20869, #26905, #50291, #60490, #15577, #4282, #38618, #61242, #55972, #49165, #9937, #38238, #72566, #32969, #33336, #9572, #66515, #73312, #44639, #21613, #15953, #72174, #38979, #32206, #61986, #10309, #56337, #21245, #4656, #3157, #43504, #61621, #32591, #71798, #3916, #49547, #20486, #66147, #43891, #15207, #14453, #37868, #37489, #8816, #55225, #31828, #60863, #54847, #9185, #3530, #26522, #10678, #58210, #63098, #34830, #51406, #39717, #62719, #50658, #21988, #69510, #68388, #11056, #51038, #6141, #68760, #29147, #73677, #11423, #23106, #52166, #57081, #28399, #74419, #33710, #63843, #27649, #34085, #22727, #17071, #5396, #45746, #12159, #56713, #45014, #28765, #34460, #17822, #22347, #45372, #40093, #5030, #46119, #74047, #69136, #40836, #46489, #68020, #16313, #39350, #28028, #57836, #62347, #57463, #17444, #40465, #5768, #51781, #130, #63468, #11792, #497, #23477, #35194, #16686, #41937, #12525, #70611, #1600, #65317, #7615, #18931, #41576, #36290, #29519, #24944, #6512, #64945, #36659, #47961, #867, #13255, #64218, #64590, #35557, #30256, #71337, #58569, #59306, #12888, #35924, #30622, #24213, #53644, #13621, #1954, #70976, #47225, #58941, #25313, #70254, #6877, #30988, #29888, #52900, #19290, #1234, #18565, #42300, #59670, #7981, #52529, #54007, #37025, #53273, #24584, #19659, #2319, #48330, #46861, #42672, #65684, #7246, #13984, #47588, #23853, #69883, #18196, #41209, #55134, #54758, #66430, #26817, #44551, #8725, #32115, #14365, #21528, #37398, #55508, #26428, #49831, #20780, #2695, #3068, #3440, #9101, #50202, #60399, #71709, #48701, #49454, #72473, #43801, #49074, #43414, #72087, #66815, #44178, #54387, #21154, #31738, #26052, #15118, #38148, #61151, #67192, #15490, #9482, #67562, #20026, #3820, #72849, #32497, #20401, #43038, #15859, #60026, #38526, #61528, #73222, #8344, #9851, #66058, #14740, #60775, #32876, #37780, #31359, #55881, #4196, #27185, #25683, #23390, #21894, #69419, #40006, #45657, #6050, #33621, #56627, #51320, #16226, #57369, #62264, #34368, #29057, #57746, #61897, #10220, #50571, #39264, #46031, #33249, #22263, #5679, #28677, #34000, #56995, #11334, #51691, #38, #23023, #56248, #44926 ) ),
 .UNSPECIFIED., .F., .F., .F. ) 
 B_SPLINE_SURFACE_WITH_KNOTS ( ( 2, 2 ),
 ( 3, 2, 2, 2, 2, 2, 2, 2, 2, 2, 2, 2, 2, 2, 2, 2, 2, 2, 2, 2, 2, 2, 2, 2, 2, 2, 2, 2, 2, 2, 2, 2, 2, 2, 2, 2, 2, 2, 2, 2, 2, 2, 2, 2, 2, 2, 2, 2, 2, 2, 2, 2, 2, 2, 2, 2, 2, 2, 2, 2, 2, 2, 2, 2, 2, 2, 2, 2, 2, 2, 2, 2, 2, 2, 2, 2, 2, 2, 2, 2, 2, 2, 2, 2, 2, 2, 2, 2, 2, 2, 2, 2, 2, 2, 2, 2, 2, 2, 2, 2, 2, 2, 2, 2, 2, 2, 2, 2, 2, 2, 2, 2, 2, 2, 2, 2, 2, 2, 2, 2, 2, 2, 2, 2, 2, 2, 2, 2, 2, 2, 2, 2, 2, 2, 2, 2, 2, 2, 2, 2, 2, 2, 2, 2, 2, 2, 2, 2, 2, 2, 2, 2, 2, 2, 2, 2, 2, 2, 2, 2, 2, 2, 2, 2, 2, 2, 2, 2, 2, 2, 2, 2, 2, 2, 2, 2, 3 ),
 ( 0.000000000000000000, 1.000000000000000000 ),
 ( 0.000000000000000000, 0.005681818181818181976, 0.01136363636363636395, 0.01704545454545454419, 0.02272727272727272790, 0.02840909090909090814, 0.03409090909090908839, 0.03977272727272727210, 0.04545454545454545581, 0.05113636363636363952, 0.05681818181818181629, 0.06250000000000000000, 0.06818181818181817677, 0.07386363636363636742, 0.07954545454545454419, 0.08522727272727272096, 0.09090909090909091161, 0.09659090909090908839, 0.1022727272727272790, 0.1079545454545454558, 0.1136363636363636326, 0.1193181818181818232, 0.1250000000000000000, 0.1306818181818181768, 0.1363636363636363535, 0.1420454545454545581, 0.1477272727272727348, 0.1534090909090909116, 0.1590909090909090884, 0.1647727272727272652, 0.1704545454545454419, 0.1761363636363636465, 0.1818181818181818232, 0.1875000000000000000, 0.1931818181818181768, 0.1988636363636363535, 0.2045454545454545581, 0.2102272727272727348, 0.2159090909090909116, 0.2215909090909090884, 0.2272727272727272652, 0.2329545454545454419, 0.2386363636363636465, 0.2443181818181818232, 0.2500000000000000000, 0.2556818181818181768, 0.2613636363636363535, 0.2670454545454545303, 0.2727272727272727071, 0.2784090909090908839, 0.2840909090909091161, 0.2897727272727272929, 0.2954545454545454697, 0.3011363636363636465, 0.3068181818181818232, 0.3125000000000000000, 0.3181818181818181768, 0.3238636363636363535, 0.3295454545454545303, 0.3352272727272727071, 0.3409090909090908839, 0.3465909090909091161, 0.3522727272727272929, 0.3579545454545454697, 0.3636363636363636465, 0.3693181818181818232, 0.3750000000000000000, 0.3806818181818181768, 0.3863636363636363535, 0.3920454545454545303, 0.3977272727272727071, 0.4034090909090908839, 0.4090909090909091161, 0.4147727272727272929, 0.4204545454545454697, 0.4261363636363636465, 0.4318181818181818232, 0.4375000000000000000, 0.4431818181818181768, 0.4488636363636363535, 0.4545454545454545303, 0.4602272727272727071, 0.4659090909090908839, 0.4715909090909091161, 0.4772727272727272929, 0.4829545454545454697, 0.4886363636363636465, 0.4943181818181818232, 0.5000000000000000000, 0.5056818181818182323, 0.5113636363636363535, 0.5170454545454545858, 0.5227272727272727071, 0.5284090909090909394, 0.5340909090909090606, 0.5397727272727272929, 0.5454545454545454142, 0.5511363636363636465, 0.5568181818181817677, 0.5625000000000000000, 0.5681818181818182323, 0.5738636363636363535, 0.5795454545454545858, 0.5852272727272727071, 0.5909090909090909394, 0.5965909090909090606, 0.6022727272727272929, 0.6079545454545454142, 0.6136363636363636465, 0.6193181818181817677, 0.6250000000000000000, 0.6306818181818182323, 0.6363636363636363535, 0.6420454545454545858, 0.6477272727272727071, 0.6534090909090909394, 0.6590909090909090606, 0.6647727272727272929, 0.6704545454545454142, 0.6761363636363636465, 0.6818181818181817677, 0.6875000000000000000, 0.6931818181818182323, 0.6988636363636363535, 0.7045454545454545858, 0.7102272727272727071, 0.7159090909090909394, 0.7215909090909090606, 0.7272727272727272929, 0.7329545454545454142, 0.7386363636363636465, 0.7443181818181817677, 0.7500000000000000000, 0.7556818181818182323, 0.7613636363636363535, 0.7670454545454545858, 0.7727272727272727071, 0.7784090909090909394, 0.7840909090909090606, 0.7897727272727272929, 0.7954545454545454142, 0.8011363636363636465, 0.8068181818181817677, 0.8125000000000000000, 0.8181818181818182323, 0.8238636363636363535, 0.8295454545454545858, 0.8352272727272727071, 0.8409090909090909394, 0.8465909090909090606, 0.8522727272727272929, 0.8579545454545454142, 0.8636363636363636465, 0.8693181818181817677, 0.8750000000000000000, 0.8806818181818182323, 0.8863636363636363535, 0.8920454545454545858, 0.8977272727272727071, 0.9034090909090909394, 0.9090909090909090606, 0.9147727272727272929, 0.9204545454545454142, 0.9261363636363636465, 0.9318181818181817677, 0.9375000000000000000, 0.9431818181818182323, 0.9488636363636363535, 0.9545454545454545858, 0.9602272727272727071, 0.9659090909090909394, 0.9715909090909090606, 0.9772727272727272929, 0.9829545454545454142, 0.9886363636363636465, 0.9943181818181817677, 1.000000000000000000 ),
 .UNSPECIFIED. ) 
 GEOMETRIC_REPRESENTATION_ITEM ( )  RATIONAL_B_SPLINE_SURFACE ( (
 ( 1.000000000000000000, 0.9238795325112867385, 1.000000000000000000, 0.9238795325112867385, 1.000000000000000000, 0.9238795325112867385, 1.000000000000000000, 0.9238795325112867385, 1.000000000000000000, 0.9238795325112867385, 1.000000000000000000, 0.9238795325112867385, 1.000000000000000000, 0.9238795325112867385, 1.000000000000000000, 0.9238795325112867385, 1.000000000000000000, 0.9238795325112867385, 1.000000000000000000, 0.9238795325112867385, 1.000000000000000000, 0.9238795325112867385, 1.000000000000000000, 0.9238795325112867385, 1.000000000000000000, 0.9238795325112867385, 1.000000000000000000, 0.9238795325112867385, 1.000000000000000000, 0.9238795325112867385, 1.000000000000000000, 0.9238795325112867385, 1.000000000000000000, 0.9238795325112867385, 1.000000000000000000, 0.9238795325112867385, 1.000000000000000000, 0.9238795325112867385, 1.000000000000000000, 0.9238795325112867385, 1.000000000000000000, 0.9238795325112867385, 1.000000000000000000, 0.9238795325112867385, 1.000000000000000000, 0.9238795325112867385, 1.000000000000000000, 0.9238795325112867385, 1.000000000000000000, 0.9238795325112867385, 1.000000000000000000, 0.9238795325112867385, 1.000000000000000000, 0.9238795325112867385, 1.000000000000000000, 0.9238795325112867385, 1.000000000000000000, 0.9238795325112867385, 1.000000000000000000, 0.9238795325112867385, 1.000000000000000000, 0.9238795325112867385, 1.000000000000000000, 0.9238795325112867385, 1.000000000000000000, 0.9238795325112867385, 1.000000000000000000, 0.9238795325112867385, 1.000000000000000000, 0.9238795325112867385, 1.000000000000000000, 0.9238795325112867385, 1.000000000000000000, 0.9238795325112867385, 1.000000000000000000, 0.9238795325112867385, 1.000000000000000000, 0.9238795325112867385, 1.000000000000000000, 0.9238795325112867385, 1.000000000000000000, 0.9238795325112867385, 1.000000000000000000, 0.9238795325112867385, 1.000000000000000000, 0.9238795325112867385, 1.000000000000000000, 0.9238795325112867385, 1.000000000000000000, 0.9238795325112867385, 1.000000000000000000, 0.9238795325112867385, 1.000000000000000000, 0.9238795325112867385, 1.000000000000000000, 0.9238795325112867385, 1.000000000000000000, 0.9238795325112867385, 1.000000000000000000, 0.9238795325112867385, 1.000000000000000000, 0.9238795325112867385, 1.000000000000000000, 0.9238795325112867385, 1.000000000000000000, 0.9238795325112867385, 1.000000000000000000, 0.9238795325112867385, 1.000000000000000000, 0.9238795325112867385, 1.000000000000000000, 0.9238795325112867385, 1.000000000000000000, 0.9238795325112867385, 1.000000000000000000, 0.9238795325112867385, 1.000000000000000000, 0.9238795325112867385, 1.000000000000000000, 0.9238795325112867385, 1.000000000000000000, 0.9238795325112867385, 1.000000000000000000, 0.9238795325112867385, 1.000000000000000000, 0.9238795325112867385, 1.000000000000000000, 0.9238795325112867385, 1.000000000000000000, 0.9238795325112867385, 1.000000000000000000, 0.9238795325112867385, 1.000000000000000000, 0.9238795325112867385, 1.000000000000000000, 0.9238795325112867385, 1.000000000000000000, 0.9238795325112867385, 1.000000000000000000, 0.9238795325112867385, 1.000000000000000000, 0.9238795325112867385, 1.000000000000000000, 0.9238795325112867385, 1.000000000000000000, 0.9238795325112867385, 1.000000000000000000, 0.9238795325112867385, 1.000000000000000000, 0.9238795325112867385, 1.000000000000000000, 0.9238795325112867385, 1.000000000000000000, 0.9238795325112867385, 1.000000000000000000, 0.9238795325112867385, 1.000000000000000000, 0.9238795325112867385, 1.000000000000000000, 0.9238795325112867385, 1.000000000000000000, 0.9238795325112867385, 1.000000000000000000, 0.9238795325112867385, 1.000000000000000000, 0.9238795325112867385, 1.000000000000000000, 0.9238795325112867385, 1.000000000000000000, 0.9238795325112867385, 1.000000000000000000, 0.9238795325112867385, 1.000000000000000000, 0.9238795325112867385, 1.000000000000000000, 0.9238795325112867385, 1.000000000000000000, 0.9238795325112867385, 1.000000000000000000, 0.9238795325112867385, 1.000000000000000000, 0.9238795325112867385, 1.000000000000000000, 0.9238795325112867385, 1.000000000000000000, 0.9238795325112867385, 1.000000000000000000, 0.9238795325112867385, 1.000000000000000000, 0.9238795325112867385, 1.000000000000000000, 0.9238795325112867385, 1.000000000000000000, 0.9238795325112867385, 1.000000000000000000, 0.9238795325112867385, 1.000000000000000000, 0.9238795325112867385, 1.000000000000000000, 0.9238795325112867385, 1.000000000000000000, 0.9238795325112867385, 1.000000000000000000, 0.9238795325112867385, 1.000000000000000000, 0.9238795325112867385, 1.000000000000000000, 0.9238795325112867385, 1.000000000000000000, 0.9238795325112867385, 1.000000000000000000, 0.9238795325112867385, 1.000000000000000000, 0.9238795325112867385, 1.000000000000000000, 0.9238795325112867385, 1.000000000000000000, 0.9238795325112867385, 1.000000000000000000, 0.9238795325112867385, 1.000000000000000000, 0.9238795325112867385, 1.000000000000000000, 0.9238795325112867385, 1.000000000000000000, 0.9238795325112867385, 1.000000000000000000, 0.9238795325112867385, 1.000000000000000000, 0.9238795325112867385, 1.000000000000000000, 0.9238795325112867385, 1.000000000000000000, 0.9238795325112867385, 1.000000000000000000, 0.9238795325112867385, 1.000000000000000000, 0.9238795325112867385, 1.000000000000000000, 0.9238795325112867385, 1.000000000000000000, 0.9238795325112867385, 1.000000000000000000, 0.9238795325112867385, 1.000000000000000000, 0.9238795325112867385, 1.000000000000000000, 0.9238795325112867385, 1.000000000000000000, 0.9238795325112867385, 1.000000000000000000, 0.9238795325112867385, 1.000000000000000000, 0.9238795325112867385, 1.000000000000000000, 0.9238795325112867385, 1.000000000000000000, 0.9238795325112867385, 1.000000000000000000, 0.9238795325112867385, 1.000000000000000000, 0.9238795325112867385, 1.000000000000000000, 0.9238795325112867385, 1.000000000000000000, 0.9238795325112867385, 1.000000000000000000, 0.9238795325112867385, 1.000000000000000000, 0.9238795325112867385, 1.000000000000000000, 0.9238795325112867385, 1.000000000000000000, 0.9238795325112867385, 1.000000000000000000, 0.9238795325112867385, 1.000000000000000000, 0.9238795325112867385, 1.000000000000000000, 0.9238795325112867385, 1.000000000000000000, 0.9238795325112867385, 1.000000000000000000, 0.9238795325112867385, 1.000000000000000000, 0.9238795325112867385, 1.000000000000000000, 0.9238795325112867385, 1.000000000000000000, 0.9238795325112867385, 1.000000000000000000, 0.9238795325112867385, 1.000000000000000000, 0.9238795325112867385, 1.000000000000000000, 0.9238795325112867385, 1.000000000000000000, 0.9238795325112867385, 1.000000000000000000, 0.9238795325112867385, 1.000000000000000000, 0.9238795325112867385, 1.000000000000000000, 0.9238795325112867385, 1.000000000000000000, 0.9238795325112867385, 1.000000000000000000, 0.9238795325112867385, 1.000000000000000000, 0.9238795325112867385, 1.000000000000000000, 0.9238795325112867385, 1.000000000000000000, 0.9238795325112867385, 1.000000000000000000, 0.9238795325112867385, 1.000000000000000000, 0.9238795325112867385, 1.000000000000000000, 0.9238795325112867385, 1.000000000000000000, 0.9238795325112867385, 1.000000000000000000, 0.9238795325112867385, 1.000000000000000000, 0.9238795325112867385, 1.000000000000000000, 0.9238795325112867385, 1.000000000000000000, 0.9238795325112867385, 1.000000000000000000, 0.9238795325112867385, 1.000000000000000000, 0.9238795325112867385, 1.000000000000000000, 0.9238795325112867385, 1.000000000000000000, 0.9238795325112867385, 1.000000000000000000, 0.9238795325112867385, 1.000000000000000000, 0.9238795325112867385, 1.000000000000000000, 0.9238795325112867385, 1.000000000000000000, 0.9238795325112867385, 1.000000000000000000, 0.9238795325112867385, 1.000000000000000000, 0.9238795325112867385, 1.000000000000000000, 0.9238795325112867385, 1.000000000000000000),
 ( 1.000000000000000000, 0.9238795325112867385, 1.000000000000000000, 0.9238795325112867385, 1.000000000000000000, 0.9238795325112867385, 1.000000000000000000, 0.9238795325112867385, 1.000000000000000000, 0.9238795325112867385, 1.000000000000000000, 0.9238795325112867385, 1.000000000000000000, 0.9238795325112867385, 1.000000000000000000, 0.9238795325112867385, 1.000000000000000000, 0.9238795325112867385, 1.000000000000000000, 0.9238795325112867385, 1.000000000000000000, 0.9238795325112867385, 1.000000000000000000, 0.9238795325112867385, 1.000000000000000000, 0.9238795325112867385, 1.000000000000000000, 0.9238795325112867385, 1.000000000000000000, 0.9238795325112867385, 1.000000000000000000, 0.9238795325112867385, 1.000000000000000000, 0.9238795325112867385, 1.000000000000000000, 0.9238795325112867385, 1.000000000000000000, 0.9238795325112867385, 1.000000000000000000, 0.9238795325112867385, 1.000000000000000000, 0.9238795325112867385, 1.000000000000000000, 0.9238795325112867385, 1.000000000000000000, 0.9238795325112867385, 1.000000000000000000, 0.9238795325112867385, 1.000000000000000000, 0.9238795325112867385, 1.000000000000000000, 0.9238795325112867385, 1.000000000000000000, 0.9238795325112867385, 1.000000000000000000, 0.9238795325112867385, 1.000000000000000000, 0.9238795325112867385, 1.000000000000000000, 0.9238795325112867385, 1.000000000000000000, 0.9238795325112867385, 1.000000000000000000, 0.9238795325112867385, 1.000000000000000000, 0.9238795325112867385, 1.000000000000000000, 0.9238795325112867385, 1.000000000000000000, 0.9238795325112867385, 1.000000000000000000, 0.9238795325112867385, 1.000000000000000000, 0.9238795325112867385, 1.000000000000000000, 0.9238795325112867385, 1.000000000000000000, 0.9238795325112867385, 1.000000000000000000, 0.9238795325112867385, 1.000000000000000000, 0.9238795325112867385, 1.000000000000000000, 0.9238795325112867385, 1.000000000000000000, 0.9238795325112867385, 1.000000000000000000, 0.9238795325112867385, 1.000000000000000000, 0.9238795325112867385, 1.000000000000000000, 0.9238795325112867385, 1.000000000000000000, 0.9238795325112867385, 1.000000000000000000, 0.9238795325112867385, 1.000000000000000000, 0.9238795325112867385, 1.000000000000000000, 0.9238795325112867385, 1.000000000000000000, 0.9238795325112867385, 1.000000000000000000, 0.9238795325112867385, 1.000000000000000000, 0.9238795325112867385, 1.000000000000000000, 0.9238795325112867385, 1.000000000000000000, 0.9238795325112867385, 1.000000000000000000, 0.9238795325112867385, 1.000000000000000000, 0.9238795325112867385, 1.000000000000000000, 0.9238795325112867385, 1.000000000000000000, 0.9238795325112867385, 1.000000000000000000, 0.9238795325112867385, 1.000000000000000000, 0.9238795325112867385, 1.000000000000000000, 0.9238795325112867385, 1.000000000000000000, 0.9238795325112867385, 1.000000000000000000, 0.9238795325112867385, 1.000000000000000000, 0.9238795325112867385, 1.000000000000000000, 0.9238795325112867385, 1.000000000000000000, 0.9238795325112867385, 1.000000000000000000, 0.9238795325112867385, 1.000000000000000000, 0.9238795325112867385, 1.000000000000000000, 0.9238795325112867385, 1.000000000000000000, 0.9238795325112867385, 1.000000000000000000, 0.9238795325112867385, 1.000000000000000000, 0.9238795325112867385, 1.000000000000000000, 0.9238795325112867385, 1.000000000000000000, 0.9238795325112867385, 1.000000000000000000, 0.9238795325112867385, 1.000000000000000000, 0.9238795325112867385, 1.000000000000000000, 0.9238795325112867385, 1.000000000000000000, 0.9238795325112867385, 1.000000000000000000, 0.9238795325112867385, 1.000000000000000000, 0.9238795325112867385, 1.000000000000000000, 0.9238795325112867385, 1.000000000000000000, 0.9238795325112867385, 1.000000000000000000, 0.9238795325112867385, 1.000000000000000000, 0.9238795325112867385, 1.000000000000000000, 0.9238795325112867385, 1.000000000000000000, 0.9238795325112867385, 1.000000000000000000, 0.9238795325112867385, 1.000000000000000000, 0.9238795325112867385, 1.000000000000000000, 0.9238795325112867385, 1.000000000000000000, 0.9238795325112867385, 1.000000000000000000, 0.9238795325112867385, 1.000000000000000000, 0.9238795325112867385, 1.000000000000000000, 0.9238795325112867385, 1.000000000000000000, 0.9238795325112867385, 1.000000000000000000, 0.9238795325112867385, 1.000000000000000000, 0.9238795325112867385, 1.000000000000000000, 0.9238795325112867385, 1.000000000000000000, 0.9238795325112867385, 1.000000000000000000, 0.9238795325112867385, 1.000000000000000000, 0.9238795325112867385, 1.000000000000000000, 0.9238795325112867385, 1.000000000000000000, 0.9238795325112867385, 1.000000000000000000, 0.9238795325112867385, 1.000000000000000000, 0.9238795325112867385, 1.000000000000000000, 0.9238795325112867385, 1.000000000000000000, 0.9238795325112867385, 1.000000000000000000, 0.9238795325112867385, 1.000000000000000000, 0.9238795325112867385, 1.000000000000000000, 0.9238795325112867385, 1.000000000000000000, 0.9238795325112867385, 1.000000000000000000, 0.9238795325112867385, 1.000000000000000000, 0.9238795325112867385, 1.000000000000000000, 0.9238795325112867385, 1.000000000000000000, 0.9238795325112867385, 1.000000000000000000, 0.9238795325112867385, 1.000000000000000000, 0.9238795325112867385, 1.000000000000000000, 0.9238795325112867385, 1.000000000000000000, 0.9238795325112867385, 1.000000000000000000, 0.9238795325112867385, 1.000000000000000000, 0.9238795325112867385, 1.000000000000000000, 0.9238795325112867385, 1.000000000000000000, 0.9238795325112867385, 1.000000000000000000, 0.9238795325112867385, 1.000000000000000000, 0.9238795325112867385, 1.000000000000000000, 0.9238795325112867385, 1.000000000000000000, 0.9238795325112867385, 1.000000000000000000, 0.9238795325112867385, 1.000000000000000000, 0.9238795325112867385, 1.000000000000000000, 0.9238795325112867385, 1.000000000000000000, 0.9238795325112867385, 1.000000000000000000, 0.9238795325112867385, 1.000000000000000000, 0.9238795325112867385, 1.000000000000000000, 0.9238795325112867385, 1.000000000000000000, 0.9238795325112867385, 1.000000000000000000, 0.9238795325112867385, 1.000000000000000000, 0.9238795325112867385, 1.000000000000000000, 0.9238795325112867385, 1.000000000000000000, 0.9238795325112867385, 1.000000000000000000, 0.9238795325112867385, 1.000000000000000000, 0.9238795325112867385, 1.000000000000000000, 0.9238795325112867385, 1.000000000000000000, 0.9238795325112867385, 1.000000000000000000, 0.9238795325112867385, 1.000000000000000000, 0.9238795325112867385, 1.000000000000000000, 0.9238795325112867385, 1.000000000000000000, 0.9238795325112867385, 1.000000000000000000, 0.9238795325112867385, 1.000000000000000000, 0.9238795325112867385, 1.000000000000000000, 0.9238795325112867385, 1.000000000000000000, 0.9238795325112867385, 1.000000000000000000, 0.9238795325112867385, 1.000000000000000000, 0.9238795325112867385, 1.000000000000000000, 0.9238795325112867385, 1.000000000000000000, 0.9238795325112867385, 1.000000000000000000, 0.9238795325112867385, 1.000000000000000000, 0.9238795325112867385, 1.000000000000000000, 0.9238795325112867385, 1.000000000000000000, 0.9238795325112867385, 1.000000000000000000, 0.9238795325112867385, 1.000000000000000000, 0.9238795325112867385, 1.000000000000000000, 0.9238795325112867385, 1.000000000000000000, 0.9238795325112867385, 1.000000000000000000, 0.9238795325112867385, 1.000000000000000000, 0.9238795325112867385, 1.000000000000000000, 0.9238795325112867385, 1.000000000000000000, 0.9238795325112867385, 1.000000000000000000, 0.9238795325112867385, 1.000000000000000000, 0.9238795325112867385, 1.000000000000000000, 0.9238795325112867385, 1.000000000000000000, 0.9238795325112867385, 1.000000000000000000, 0.9238795325112867385, 1.000000000000000000, 0.9238795325112867385, 1.000000000000000000, 0.9238795325112867385, 1.000000000000000000, 0.9238795325112867385, 1.000000000000000000, 0.9238795325112867385, 1.000000000000000000) ) ) 
 REPRESENTATION_ITEM ( '' )  SURFACE ( )  );
#13126 = CARTESIAN_POINT ( 'NONE',  ( -8.660254037844387298, 153.9583333265053682, -5.000000000000004441 ) ) ;
#13127 = CARTESIAN_POINT ( 'NONE',  ( -5.082755093536325930, 89.84375000204839523, -5.082755093536325930 ) ) ;
#13128 = FACE_OUTER_BOUND ( 'NONE', #65498, .T. ) ;
#13129 = CARTESIAN_POINT ( 'NONE',  ( 3.042071309553167513, 57.13541666325268409, -11.35316468749999785 ) ) ;
#13130 = EDGE_CURVE ( 'NONE', #30828, #47406, #24046, .T. ) ;
#13131 = CARTESIAN_POINT ( 'NONE',  ( -10.18810118749999738, -4.220049686691941915, 111.6250000020483810 ) ) ;
#13132 = CARTESIAN_POINT ( 'NONE',  ( -2.085542519210945728E-15, 199.5312499965860411, 11.35316468750000141 ) ) ;
#13133 = VERTEX_POINT ( 'NONE', #2717 ) ;
#13134 = CARTESIAN_POINT ( 'NONE',  ( -0.4451317748866090995, 67.59323688304503719, 20.03471819849916002 ) ) ;
#13135 = CARTESIAN_POINT ( 'NONE',  ( 8.660254037844385522, 61.45833332650536818, 5.000000000000005329 ) ) ;
#13137 = CARTESIAN_POINT ( 'NONE',  ( 5.676582343750001591, 186.6145833299193839, -9.832129032723420536 ) ) ;
#13136 = CARTESIAN_POINT ( 'NONE',  ( 1.836970198721029589E-15, 261.2500000000000568, 10.00000000000000000 ) ) ;
#13138 = CARTESIAN_POINT ( 'NONE',  ( -1.469576158976823947E-15, 2.437499995903220196, 8.000000000000000000 ) ) ;
#13139 = CARTESIAN_POINT ( 'NONE',  ( -8.660254037844387298, 252.7083333401612890, -4.999999999999999112 ) ) ;
#13140 = CARTESIAN_POINT ( 'NONE',  ( -1.836970198721029983E-15, 190.6249999931720254, 10.00000000000000178 ) ) ;
#13141 = VERTEX_POINT ( 'NONE', #70634 ) ;
#13142 = CARTESIAN_POINT ( 'NONE',  ( -9.832129032723420536, 164.0104166632526983, 5.676582343749997150 ) ) ;
#13143 =( BOUNDED_CURVE ( )  B_SPLINE_CURVE ( 2, ( #53878, #70126, #53509, #59177, #6748 ),
 .UNSPECIFIED., .F., .F. ) 
 B_SPLINE_CURVE_WITH_KNOTS ( ( 3, 2, 3 ),
 ( 0.000000000000000000, 0.005208333333333336514, 0.01041666666666667303 ),
 .UNSPECIFIED. ) 
 CURVE ( )  GEOMETRIC_REPRESENTATION_ITEM ( )  RATIONAL_B_SPLINE_CURVE ( ( 1.000000000000000000, 0.9238795325112867385, 1.000000000000000000, 0.9238795325112866275, 1.000000000000000000 ) ) 
 REPRESENTATION_ITEM ( '' )  );
#13144 = EDGE_CURVE ( 'NONE', #40937, #8912, #43440, .T. ) ;
#13145 = CARTESIAN_POINT ( 'NONE',  ( 7.188101187499992051, 2.977408999572647819, 21.83030278187175810 ) ) ;
#13146 = CARTESIAN_POINT ( 'NONE',  ( 5.994779237468493172, 226.0000000000000000, -8.522275728953271567 ) ) ;
#13147 = VERTEX_POINT ( 'NONE', #20046 ) ;
#13148 = CARTESIAN_POINT ( 'NONE',  ( -5.656854249492378806, 101.3750000040967905, 5.656854249492381470 ) ) ;
#13149 = ADVANCED_FACE ( 'NONE', ( #47610 ), #13274, .T. ) ;
#13150 = AXIS2_PLACEMENT_3D ( 'NONE', #12365, #11625, #56918 ) ;
#13151 = EDGE_CURVE ( 'NONE', #851, #68055, #33781, .T. ) ;
#13152 = CARTESIAN_POINT ( 'NONE',  ( -1.656854249492383691, 11.68750000000000000, 4.000000000000000888 ) ) ;
#13153 = CYLINDRICAL_SURFACE ( 'NONE', #3542, 3.999999999999976019 ) ;
#13154 = CARTESIAN_POINT ( 'NONE',  ( -4.541265875000002339, 14.81249999863440792, -5.561446717895856393E-16 ) ) ;
#13155 = CARTESIAN_POINT ( 'NONE',  ( -3.313708498984758943, -7.999999999999989342, 13.29905278392014800 ) ) ;
#13156 = FACE_OUTER_BOUND ( 'NONE', #9536, .T. ) ;
#13157 = AXIS2_PLACEMENT_3D ( 'NONE', #66387, #24260, #3397 ) ;
#13158 = ORIENTED_EDGE ( 'NONE', *, *, #44244, .T. ) ;
#13159 = CARTESIAN_POINT ( 'NONE',  ( -7.320508075688813676, 176.8750000000000568, -7.320508075688814564 ) ) ;
#13160 = CARTESIAN_POINT ( 'NONE',  ( 7.188101187500002709, 99.31250000204839523, 2.977408999572649151 ) ) ;
#13162 = CARTESIAN_POINT ( 'NONE',  ( -7.999999999961182162, -1.665870058181487338E-05, 5.518425684709454160 ) ) ;
#13161 = CARTESIAN_POINT ( 'NONE',  ( 8.660254037844431707, 179.5833333333333712, 5.000000000000031974 ) ) ;
#13163 = DIRECTION ( 'NONE',  ( -1.000000000000000000, -2.444036937190193349E-14, -3.491481338843133355E-15 ) ) ;
#13164 = ORIENTED_EDGE ( 'NONE', *, *, #15516, .F. ) ;
#13165 = CARTESIAN_POINT ( 'NONE',  ( -3.313708498984815343, 103.9062500040968047, -7.999999999999944933 ) ) ;
#13166 = CARTESIAN_POINT ( 'NONE',  ( 5.082755093536320601, -5.082755093536318824, 23.04905278187175455 ) ) ;
#13167 = ORIENTED_EDGE ( 'NONE', *, *, #2314, .T. ) ;
#13168 = EDGE_CURVE ( 'NONE', #59211, #56591, #41470, .T. ) ;
#13169 = VERTEX_POINT ( 'NONE', #54410 ) ;
#13170 = CARTESIAN_POINT ( 'NONE',  ( 10.18810118750000093, -4.220049686691933033, 89.31250000204838102 ) ) ;
#13171 = CARTESIAN_POINT ( 'NONE',  ( -32.68481389732080800, -12.04511711863264978, 161.3566701468946007 ) ) ;
#13172 = CARTESIAN_POINT ( 'NONE',  ( -11.00000000000000000, 4.556349186104045934, 93.90625000000000000 ) ) ;
#13175 = CARTESIAN_POINT ( 'NONE',  ( 4.721056650416000089, 294.9843750017070079, 4.721056650415999201 ) ) ;
#13174 = CARTESIAN_POINT ( 'NONE',  ( 23.99999999999997868, 200.8125000027311842, 168.3431457505075741 ) ) ;
#13173 = DIRECTION ( 'NONE',  ( 0.000000000000000000, -1.000000000000000000, -0.000000000000000000 ) ) ;
#13176 = CARTESIAN_POINT ( 'NONE',  ( 8.660254037844389075, 135.4166666666666856, -5.000000000000000000 ) ) ;
#13177 = DIRECTION ( 'NONE',  ( -0.000000000000000000, 1.000000000000000000, -0.000000000000000000 ) ) ;
#13178 = LINE ( 'NONE', #36214, #20283 ) ;
#13179 = PLANE ( 'NONE',  #51848 ) ;
#13180 = CARTESIAN_POINT ( 'NONE',  ( 3.313708498984756279, 7.999999999999991118, 0.5490527839201453375 ) ) ;
#13181 = CARTESIAN_POINT ( 'NONE',  ( 26.56734541678238060, 198.0000000013656063, 166.5412658749999650 ) ) ;
#13182 = CARTESIAN_POINT ( 'NONE',  ( -2.977408999572650039, 2.812499997951610542, -7.188101187500001821 ) ) ;
#13183 = CARTESIAN_POINT ( 'NONE',  ( 5.662595241051934458, 5.662595241051935346, 3.450615283940628775 ) ) ;
#13184 = CARTESIAN_POINT ( 'NONE',  ( -3.458734125000016313, 195.8750000013655779, 140.5673454167824161 ) ) ;
#13185 = CARTESIAN_POINT ( 'NONE',  ( -5.082755093536324154, 114.2187500020483810, 5.082755093536326818 ) ) ;
#13186 = CARTESIAN_POINT ( 'NONE',  ( -4.330454160167402478, -52.03352386568571575, -48.86100738216764228 ) ) ;
#13187 = CARTESIAN_POINT ( 'NONE',  ( 2.085542519210945334E-15, 225.4687500034139873, 11.35316468749999963 ) ) ;
#13188 = CARTESIAN_POINT ( 'NONE',  ( -36.77445904156687106, 39.18007991166720672, 65.00000000000001421 ) ) ;
#13189 = CARTESIAN_POINT ( 'NONE',  ( 5.082755093536318824, 5.082755093536319713, 23.79905278187175455 ) ) ;
#13190 = CARTESIAN_POINT ( 'NONE',  ( 31.99999999999997868, 195.1875000000000000, 171.6568542494923122 ) ) ;
#13191 = CARTESIAN_POINT ( 'NONE',  ( 11.35316468749999785, 30.57291666325268409, 3.042071309553174174 ) ) ;
#13192 = CARTESIAN_POINT ( 'NONE',  ( 3.967492730755045383, -11.56577346444175269, -0.1233701403699556803 ) ) ;
#13193 = CARTESIAN_POINT ( 'NONE',  ( 8.311093377946834337, 225.4687499965860411, 8.311093377946839666 ) ) ;
#13194 = CARTESIAN_POINT ( 'NONE',  ( 5.656854249492381470, 112.0625000000000000, 5.656854249492379694 ) ) ;
#13195 = LINE ( 'NONE', #34775, #57588 ) ;
#13196 = VERTEX_POINT ( 'NONE', #65341 ) ;
#13197 = EDGE_CURVE ( 'NONE', #67176, #43329, #72295, .T. ) ;
#13198 = DIRECTION ( 'NONE',  ( 0.000000000000000000, 1.000000000000000000, 4.283267841918042741E-17 ) ) ;
#13199 = CARTESIAN_POINT ( 'NONE',  ( -1.432654583217664701, 195.0000000013656063, 138.5412658750000787 ) ) ;
#13200 = CARTESIAN_POINT ( 'NONE',  ( 9.832129032723416984, 35.36458332991934839, 5.676582343750006032 ) ) ;
#13201 = CARTESIAN_POINT ( 'NONE',  ( 11.00000000000000000, 1.347111479062088405E-15, 88.93750000409677625 ) ) ;
#13202 = CARTESIAN_POINT ( 'NONE',  ( 1.432654583217608080, 208.8750000013656063, 138.5412658750000503 ) ) ;
#13203 = CARTESIAN_POINT ( 'NONE',  ( -28.00000000000006750, 195.4375000013655779, 166.5412658750003629 ) ) ;
#13204 = CARTESIAN_POINT ( 'NONE',  ( -2.849036369511732440E-14, 201.3750000027312126, 138.0000000000000568 ) ) ;
#13206 = CARTESIAN_POINT ( 'NONE',  ( 3.042071309553159519, 34.73958332991934839, 11.35316468750000141 ) ) ;
#13205 = CARTESIAN_POINT ( 'NONE',  ( 7.188101187500000933, 108.5000000020483810, -2.977408999572651371 ) ) ;
#13208 = ADVANCED_FACE ( 'NONE', ( #72111 ), #71358, .F. ) ;
#13207 = CARTESIAN_POINT ( 'NONE',  ( -3.313708498984757167, 7.999999999999991118, 14.04905277982336465 ) ) ;
#13209 = CARTESIAN_POINT ( 'NONE',  ( -3.042071309553173730, 144.3229166632527267, 11.35316468749999785 ) ) ;
#13210 = VECTOR ( 'NONE', #26932, 1000.000000000000000 ) ;
#13211 = CARTESIAN_POINT ( 'NONE',  ( -7.320508075688773708, 118.7499999931720396, -7.320508075688774596 ) ) ;
#13212 = CARTESIAN_POINT ( 'NONE',  ( 7.188101187500001821, 107.3750000020484094, -2.977408999572651371 ) ) ;
#13213 = DIRECTION ( 'NONE',  ( 0.000000000000000000, 0.000000000000000000, -1.000000000000000000 ) ) ;
#13214 = CARTESIAN_POINT ( 'NONE',  ( -30.44569435410879166, 205.0625000013656063, 172.4456943541092357 ) ) ;
#13215 = ORIENTED_EDGE ( 'NONE', *, *, #57173, .T. ) ;
#13216 = CARTESIAN_POINT ( 'NONE',  ( -3.042071309553163960, 22.55208332991935194, -11.35316468749999963 ) ) ;
#13217 = ADVANCED_FACE ( 'NONE', ( #30278 ), #1623, .F. ) ;
#13218 = ORIENTED_EDGE ( 'NONE', *, *, #20370, .F. ) ;
#13219 = CARTESIAN_POINT ( 'NONE',  ( -5.656854249492381470, 6.749999995903220196, 5.656854249492379694 ) ) ;
#13220 = CARTESIAN_POINT ( 'NONE',  ( 1.469576158976823947E-15, 107.3750000000000000, 8.000000000000000000 ) ) ;
#13222 = CARTESIAN_POINT ( 'NONE',  ( 3.042071309553159519, 144.7395833299193839, 11.35316468750000141 ) ) ;
#13221 = CARTESIAN_POINT ( 'NONE',  ( -24.43732893277740459, -23.15729197918710369, 146.3325141974158328 ) ) ;
#13223 = DIRECTION ( 'NONE',  ( -0.000000000000000000, 1.000000000000000000, -0.000000000000000000 ) ) ;
#13224 = CARTESIAN_POINT ( 'NONE',  ( 5.656854249492376141, -5.656854249492374365, 17.94905278432982243 ) ) ;
#13225 = CARTESIAN_POINT ( 'NONE',  ( -4.556349186104045934, 11.00000000000000000, 90.90625000409677625 ) ) ;
#13226 = VECTOR ( 'NONE', #15268, 1000.000000000000000 ) ;
#13227 = CARTESIAN_POINT ( 'NONE',  ( 11.35316468749999963, 251.1979166700807014, 3.042071309553159519 ) ) ;
#13228 = CARTESIAN_POINT ( 'NONE',  ( 10.18810118749999916, 1.247682550866122264E-15, 94.28125000204836681 ) ) ;
#13229 = ORIENTED_EDGE ( 'NONE', *, *, #22758, .F. ) ;
#13230 = CARTESIAN_POINT ( 'NONE',  ( 8.660254037844389075, 119.5833333333333428, 5.000000000000007105 ) ) ;
#13231 = LINE ( 'NONE', #48309, #52033 ) ;
#13232 = EDGE_CURVE ( 'NONE', #32201, #60988, #49159, .T. ) ;
#13233 = CARTESIAN_POINT ( 'NONE',  ( 11.35316468749999963, 91.30208332991934128, -3.042071309553165293 ) ) ;
#13235 = EDGE_CURVE ( 'NONE', #112, #16071, #49857, .T. ) ;
#13234 =( BOUNDED_CURVE ( )  B_SPLINE_CURVE ( 2, ( #50091, #26317, #56139, #38785, #32380, #38037, #44065, #62153, #15374 ),
 .UNSPECIFIED., .F., .F. ) 
 B_SPLINE_CURVE_WITH_KNOTS ( ( 3, 2, 2, 2, 3 ),
 ( 0.8676470588235294379, 0.8713235294117647189, 0.8750000000000000000, 0.8786764705882352811, 0.8823529411764705621 ),
 .UNSPECIFIED. ) 
 CURVE ( )  GEOMETRIC_REPRESENTATION_ITEM ( )  RATIONAL_B_SPLINE_CURVE ( ( 1.000000000000000000, 0.9238795325112867385, 1.000000000000000000, 0.9238795325112867385, 1.000000000000000000, 0.9238795325112867385, 1.000000000000000000, 0.9238795325112867385, 1.000000000000000000 ) ) 
 REPRESENTATION_ITEM ( '' )  );
#13236 = CARTESIAN_POINT ( 'NONE',  ( 10.18810118750000093, -4.220049686691933921, 102.8125000020483952 ) ) ;
#13237 = CARTESIAN_POINT ( 'NONE',  ( 3.211159895383561835, 18.56249999863440436, -3.211159895383561835 ) ) ;
#13238 = ORIENTED_EDGE ( 'NONE', *, *, #30497, .F. ) ;
#13239 = ORIENTED_EDGE ( 'NONE', *, *, #41291, .F. ) ;
#13240 = CARTESIAN_POINT ( 'NONE',  ( 7.999999999999998224, 5.906250000000000000, 3.313708498984766493 ) ) ;
#13241 = CARTESIAN_POINT ( 'NONE',  ( 28.00000000000002132, 199.1250000027312126, 173.9999999999999147 ) ) ;
#13242 = CARTESIAN_POINT ( 'NONE',  ( 4.401442555609581635E-16, 3.843749997951610098, -7.188101187500000044 ) ) ;
#13243 = CARTESIAN_POINT ( 'NONE',  ( 5.656854249492381470, 122.7500000040967905, 5.656854249492379694 ) ) ;
#13244 = B_SPLINE_CURVE_WITH_KNOTS ( 'NONE', 3,
 ( #22476, #46617, #69264, #46244, #11548, #34206, #30016, #35681, #70014, #45874, #18322, #57209, #46982, #68887, #58334, #23236, #23606, #17199, #58696, #16815 ),
 .UNSPECIFIED., .F., .F.,
 ( 4, 2, 1, 2, 2, 1, 2, 2, 1, 1, 2, 4 ),
 ( 0.6132134907475605967, 0.6391986578402925057, 0.6651838249330244146, 0.6781764084793903136, 0.6911689920257563235, 0.7171541591184882325, 0.7431393262112202525, 0.7561319097575862624, 0.7691244933039521614, 0.7951096603966840703, 0.8081022439430500803, 0.8210948274894160903 ),
 .UNSPECIFIED. ) ;
#13245 = CARTESIAN_POINT ( 'NONE',  ( -10.18810118749999916, 0.000000000000000000, 95.03125000204836681 ) ) ;
#13246 = CARTESIAN_POINT ( 'NONE',  ( 29.65685424949233706, 208.0624999999999432, 173.9999999999999147 ) ) ;
#13247 = EDGE_CURVE ( 'NONE', #44612, #3824, #32139, .T. ) ;
#13248 = CARTESIAN_POINT ( 'NONE',  ( 1.656854249492381914, 15.56249999726881406, 4.000000000000000888 ) ) ;
#13249 = CARTESIAN_POINT ( 'NONE',  ( 23.99999999999999289, 209.7500000000000284, 169.9999999999998863 ) ) ;
#13250 = EDGE_LOOP ( 'NONE', ( #15524, #43299, #93, #17711 ) ) ;
#13251 = CARTESIAN_POINT ( 'NONE',  ( -2.445694354108839619, 208.8125000013656063, 139.5543056458912190 ) ) ;
#13252 = CARTESIAN_POINT ( 'NONE',  ( 2.839093476692135984E-14, 198.6875000013655779, 201.4587341250000350 ) ) ;
#13254 = CARTESIAN_POINT ( 'NONE',  ( -4.999999999999998224, 223.5416666598387110, -8.660254037844389075 ) ) ;
#13253 = CARTESIAN_POINT ( 'NONE',  ( -29.43265458321755901, 201.8750000013656063, 173.4587341250004044 ) ) ;
#13255 = CARTESIAN_POINT ( 'NONE',  ( 4.541265875000002339, 13.37499999863440792, -1.881053915767121554 ) ) ;
#13256 = VECTOR ( 'NONE', #11060, 1000.000000000000000 ) ;
#13257 = CARTESIAN_POINT ( 'NONE',  ( 7.188101187499991163, 2.977408999572648707, 14.33030278187175277 ) ) ;
#13258 = EDGE_LOOP ( 'NONE', ( #43486, #36018, #72952, #20851 ) ) ;
#13259 = ORIENTED_EDGE ( 'NONE', *, *, #44836, .F. ) ;
#13260 = CARTESIAN_POINT ( 'NONE',  ( 7.204075437095966983, 7.204075437095967871, 103.0937500020483668 ) ) ;
#13261 = CARTESIAN_POINT ( 'NONE',  ( -4.556349186104048599, -10.99999999999999822, 103.2812499999999858 ) ) ;
#13262 = CARTESIAN_POINT ( 'NONE',  ( -27.99999999999995737, 199.5000000000000000, 174.0000000000003695 ) ) ;
#13263 = CARTESIAN_POINT ( 'NONE',  ( 1.432654583217664479, 195.7500000013656063, 201.4587341250000065 ) ) ;
#13264 = DIRECTION ( 'NONE',  ( -0.000000000000000000, -1.000000000000000000, -0.000000000000000000 ) ) ;
#13265 = CARTESIAN_POINT ( 'NONE',  ( 7.320508075688774596, 90.62499999999998579, -7.320508075688774596 ) ) ;
#13266 = CARTESIAN_POINT ( 'NONE',  ( -3.313708498984762496, 117.7812500000000000, 7.999999999999998224 ) ) ;
#13267 = CARTESIAN_POINT ( 'NONE',  ( -2.765530957081996810, 297.4218750017069510, -6.676582343750003368 ) ) ;
#13268 = VERTEX_POINT ( 'NONE', #38919 ) ;
#13269 = CARTESIAN_POINT ( 'NONE',  ( -1.469576158976823947E-15, 17.43749999590322375, 8.000000000000000000 ) ) ;
#13270 = CARTESIAN_POINT ( 'NONE',  ( -3.458734125000015425, 208.9375000013656063, 142.0000000000000568 ) ) ;
#13271 = CARTESIAN_POINT ( 'NONE',  ( -10.00000000000000355, 52.50000000000000711, -1.224646799147353651E-15 ) ) ;
#13272 = LINE ( 'NONE', #47608, #46746 ) ;
#13273 = CARTESIAN_POINT ( 'NONE',  ( -6.123233995736766282E-16, 228.7500000000000000, -10.00000000000000000 ) ) ;
#13274 = CYLINDRICAL_SURFACE ( 'NONE', #57223, 4.000000000000001776 ) ;
#13275 = CARTESIAN_POINT ( 'NONE',  ( 2.020667218593132706E-15, -11.00000000000000000, 112.3749999999999858 ) ) ;
#13276 = CARTESIAN_POINT ( 'NONE',  ( -8.660254037844387298, 217.0833333333333428, -5.000000000000004441 ) ) ;
#13277 = CARTESIAN_POINT ( 'NONE',  ( -5.082755093536319713, 5.082755093536319713, 12.17405278187175277 ) ) ;
#13278 = CARTESIAN_POINT ( 'NONE',  ( -9.832129032723418760, 183.1770833299193555, -5.676582343750004256 ) ) ;
#13279 = DIRECTION ( 'NONE',  ( -1.000000000000000000, 0.000000000000000000, 0.000000000000000000 ) ) ;
#13280 = CARTESIAN_POINT ( 'NONE',  ( 3.211159895383561835, 2.437499998634407028, -3.211159895383561835 ) ) ;
#13281 = LINE ( 'NONE', #19691, #6778 ) ;
#13283 = DIRECTION ( 'NONE',  ( -0.000000000000000000, -0.000000000000000000, 1.000000000000000000 ) ) ;
#13282 = DIRECTION ( 'NONE',  ( 0.000000000000000000, 0.000000000000000000, 1.000000000000000000 ) ) ;
#13284 = ORIENTED_EDGE ( 'NONE', *, *, #29937, .T. ) ;
#13285 = CARTESIAN_POINT ( 'NONE',  ( 1.432654583217607414, 209.5000000013656063, 145.4587341250000634 ) ) ;
#13286 = CARTESIAN_POINT ( 'NONE',  ( -2.085542519210945728E-15, 49.84374999658601268, 11.35316468750000141 ) ) ;
#13287 = CARTESIAN_POINT ( 'NONE',  ( 4.556349186104051263, -10.99999999999999822, 106.6562500040967905 ) ) ;
#13288 = CARTESIAN_POINT ( 'NONE',  ( -5.676582343749998039, 222.7604166632526983, -9.832129032723420536 ) ) ;
#13289 = CARTESIAN_POINT ( 'NONE',  ( -25.55430564589122966, 204.3125000013656063, 167.5543056458915032 ) ) ;
#13290 = CARTESIAN_POINT ( 'NONE',  ( 7.320508075688771932, 9.375000000000001776, 7.320508075688776373 ) ) ;
#13292 = DIRECTION ( 'NONE',  ( -0.000000000000000000, -1.000000000000000000, -0.000000000000000000 ) ) ;
#13291 = CARTESIAN_POINT ( 'NONE',  ( -11.00000000000000000, 4.556349186104045934, 71.59375000409676204 ) ) ;
#13294 = EDGE_CURVE ( 'NONE', #29130, #63012, #9508, .T. ) ;
#13293 = CARTESIAN_POINT ( 'NONE',  ( 3.458734124999959914, 196.4375000013655779, 142.0000000000000568 ) ) ;
#13295 = VECTOR ( 'NONE', #68584, 1000.000000000000000 ) ;
#13296 = CARTESIAN_POINT ( 'NONE',  ( -11.35316468749999785, 113.0729166632526841, -3.042071309553167513 ) ) ;
#13297 = CARTESIAN_POINT ( 'NONE',  ( 5.000000000000001776, 77.70833332650536818, -8.660254037844389075 ) ) ;
#13298 = CARTESIAN_POINT ( 'NONE',  ( -7.188101187499999156, 95.75000000204836681, 2.977408999572654924 ) ) ;
#13299 = CARTESIAN_POINT ( 'NONE',  ( -4.541265875000003227, 14.99999999863440969, 1.881053915767121110 ) ) ;
#13300 = DIRECTION ( 'NONE',  ( 0.000000000000000000, 0.000000000000000000, 1.000000000000000000 ) ) ;
#13301 = CARTESIAN_POINT ( 'NONE',  ( 5.656854249492376141, -5.656854249492374365, 23.89280277982336642 ) ) ;
#13302 = ORIENTED_EDGE ( 'NONE', *, *, #41016, .F. ) ;
#13303 = VERTEX_POINT ( 'NONE', #21552 ) ;
#13304 = EDGE_CURVE ( 'NONE', #41375, #33835, #27004, .T. ) ;
#13305 = CARTESIAN_POINT ( 'NONE',  ( -2.765530957081998586, 291.7968750017070079, 6.676582343750001591 ) ) ;
#13306 = CYLINDRICAL_SURFACE ( 'NONE', #8610, 3.999999999999976019 ) ;
#13307 = CARTESIAN_POINT ( 'NONE',  ( 11.35316468749999963, 150.9895833299193271, -3.042071309553165293 ) ) ;
#13308 = CARTESIAN_POINT ( 'NONE',  ( 7.320508075688774596, 2.499999993172032031, -7.320508075688774596 ) ) ;
#13309 = CARTESIAN_POINT ( 'NONE',  ( -2.828427124746153876, 199.8750000000000284, 195.1715728752538439 ) ) ;
#13310 = CARTESIAN_POINT ( 'NONE',  ( -30.82842712474615965, 201.3750000000000284, 172.8284271247465824 ) ) ;
#13311 = CARTESIAN_POINT ( 'NONE',  ( 10.18810118749999916, 4.220049686691935698, 110.8750000020483810 ) ) ;
#13312 = ORIENTED_EDGE ( 'NONE', *, *, #24290, .F. ) ;
#13313 = CARTESIAN_POINT ( 'NONE',  ( -3.999999999999959144, 202.1875000027311842, 199.6568542494924259 ) ) ;
#13314 = CARTESIAN_POINT ( 'NONE',  ( 2.020667218593132706E-15, -11.00000000000000000, 109.5625000040967763 ) ) ;
#13315 = CARTESIAN_POINT ( 'NONE',  ( -5.676582343749998039, 147.7604166632526699, -9.832129032723420536 ) ) ;
#13316 = CARTESIAN_POINT ( 'NONE',  ( 2.754378923186476579E-14, 199.1875000013655779, 194.5412658750000219 ) ) ;
#13317 = CARTESIAN_POINT ( 'NONE',  ( -1.432654583217608080, 208.8750000013656063, 201.4587341250000350 ) ) ;
#13318 = CARTESIAN_POINT ( 'NONE',  ( -4.220049686691935698, 10.18810118749999916, 72.25000000204836681 ) ) ;
#13319 = CARTESIAN_POINT ( 'NONE',  ( 8.311093377946834337, 55.46874999658601268, 8.311093377946839666 ) ) ;
#13320 = VERTEX_POINT ( 'NONE', #44578 ) ;
#13321 = DIRECTION ( 'NONE',  ( 1.000000000000000000, 0.000000000000000000, 0.000000000000000000 ) ) ;
#13322 = CARTESIAN_POINT ( 'NONE',  ( -8.342170076843785083E-16, 4.187499998634407028, 4.541265875000002339 ) ) ;
#13323 = CARTESIAN_POINT ( 'NONE',  ( 5.662595241051936235, -5.662595241051934458, 7.575615283940628331 ) ) ;
#13324 = VECTOR ( 'NONE', #53809, 1000.000000000000227 ) ;
#13325 = CARTESIAN_POINT ( 'NONE',  ( -2.977408999572654480, 16.49999999795161543, 7.188101187499999156 ) ) ;
#13326 = CARTESIAN_POINT ( 'NONE',  ( 4.242640687119285658, 293.6875000034139589, -4.242640687119286547 ) ) ;
#13327 = CIRCLE ( 'NONE', #56771, 36.00000000000000000 ) ;
#13328 = CARTESIAN_POINT ( 'NONE',  ( 0.000000000000000000, 0.000000000000000000, 6.938893903907228378E-15 ) ) ;
#13329 = CARTESIAN_POINT ( 'NONE',  ( -1.320432766682874540E-15, 12.46874999795161187, 7.188101187500000044 ) ) ;
#13330 = CARTESIAN_POINT ( 'NONE',  ( 2.977408999572646486, 7.188101187499992051, 11.51780278187175632 ) ) ;
#13331 = CARTESIAN_POINT ( 'NONE',  ( -4.220049686691935698, 10.18810118749999916, 67.37500000204838102 ) ) ;
#13332 = CARTESIAN_POINT ( 'NONE',  ( 0.000000000000000000, 0.000000000000000000, 0.000000000000000000 ) ) ;
#13333 = CARTESIAN_POINT ( 'NONE',  ( 1.656854249492381248, 3.937499997268813168, -4.000000000000001776 ) ) ;
#13334 = ORIENTED_EDGE ( 'NONE', *, *, #50919, .T. ) ;
#13335 = CARTESIAN_POINT ( 'NONE',  ( -1.656854249492347719, 194.9375000027312126, 194.0000000000000853 ) ) ;
#13336 = CARTESIAN_POINT ( 'NONE',  ( -2.849036369511732440E-14, 204.2500000000000284, 138.0000000000000568 ) ) ;
#13338 =( BOUNDED_CURVE ( )  B_SPLINE_CURVE ( 2, ( #24919, #52507, #36267, #58185, #24560, #35900, #52878, #64567, #7591 ),
 .UNSPECIFIED., .F., .F. ) 
 B_SPLINE_CURVE_WITH_KNOTS ( ( 3, 2, 2, 2, 3 ),
 ( 0.8166666666666674290, 0.8250000000000006217, 0.8333333333333340365, 0.8416666666666672292, 0.8500000000000005329 ),
 .UNSPECIFIED. ) 
 CURVE ( )  GEOMETRIC_REPRESENTATION_ITEM ( )  RATIONAL_B_SPLINE_CURVE ( ( 0.9999999999999928946, 0.9238795325112938439, 1.000000000000000000, 0.9238795325112867385, 1.000000000000000000, 0.9238795325112867385, 1.000000000000000000, 0.9238795325112816315, 1.000000000000005107 ) ) 
 REPRESENTATION_ITEM ( '' )  );
#13337 = CARTESIAN_POINT ( 'NONE',  ( -31.99999999999995737, 198.4375000027312126, 171.6568542494928522 ) ) ;
#13339 = CARTESIAN_POINT ( 'NONE',  ( -4.541265875000002339, 2.749999998634406584, -1.881053915767121998 ) ) ;
#13340 = CARTESIAN_POINT ( 'NONE',  ( 7.188101187500001821, 119.0000000020483810, -2.977408999572651371 ) ) ;
#13341 = DIRECTION ( 'NONE',  ( -0.000000000000000000, 1.000000000000000000, -4.476705744456276341E-16 ) ) ;
#13342 = CARTESIAN_POINT ( 'NONE',  ( 3.313708498984762496, -7.999999999999989342, 1.486552783920146448 ) ) ;
#13343 = ORIENTED_EDGE ( 'NONE', *, *, #70067, .F. ) ;
#13344 = CARTESIAN_POINT ( 'NONE',  ( -5.082755093536326818, 23.90624999795161543, 5.082755093536325042 ) ) ;
#13345 = ORIENTED_EDGE ( 'NONE', *, *, #22371, .F. ) ;
#13346 = CARTESIAN_POINT ( 'NONE',  ( 0.000000000000000000, 0.000000000000000000, -4.000000000000001776 ) ) ;
#13347 = CARTESIAN_POINT ( 'NONE',  ( 1.432654583217664479, 206.7500000013655779, 201.4587341250000065 ) ) ;
#13348 = CARTESIAN_POINT ( 'NONE',  ( 26.56734541678237704, 204.3750000013656063, 173.4587341249998929 ) ) ;
#13349 = CARTESIAN_POINT ( 'NONE',  ( -4.999999999999998224, 51.66666666666667140, -8.660254037844389075 ) ) ;
#13350 = CARTESIAN_POINT ( 'NONE',  ( 7.188101187500002709, 99.68750000204838102, 2.977408999572649151 ) ) ;
#13351 = CARTESIAN_POINT ( 'NONE',  ( 6.000000000000003553, 297.5625000000000568, -2.485281374238571761 ) ) ;
#13353 = CARTESIAN_POINT ( 'NONE',  ( -23.65306228329526306, -40.20135459992185645, 190.0452978749128761 ) ) ;
#13352 = CARTESIAN_POINT ( 'NONE',  ( -5.656854249492380582, 89.00000000409677625, -5.656854249492380582 ) ) ;
#13354 = ORIENTED_EDGE ( 'NONE', *, *, #56867, .T. ) ;
#13355 = EDGE_CURVE ( 'NONE', #10224, #4458, #9876, .T. ) ;
#13356 = ADVANCED_FACE ( 'NONE', ( #21179 ), #44204, .F. ) ;
#13357 = CARTESIAN_POINT ( 'NONE',  ( 11.35316468749999963, 231.4062500034139873, -1.390361679473963556E-15 ) ) ;
#13358 = CARTESIAN_POINT ( 'NONE',  ( 4.465384415997338152, 56.41424811512310811, 44.23559237191029325 ) ) ;
#13359 = CARTESIAN_POINT ( 'NONE',  ( -5.000000000000000000, -16.14408868864072844, 27.96238185062368586 ) ) ;
#13360 = CARTESIAN_POINT ( 'NONE',  ( 0.000000000000000000, 0.000000000000000000, 0.000000000000000000 ) ) ;
#13361 = CARTESIAN_POINT ( 'NONE',  ( 26.50088068719039214, 194.8029862363522682, 166.4839507087883703 ) ) ;
#13362 = CARTESIAN_POINT ( 'NONE',  ( -6.735557395310442023E-16, 11.00000000000000000, 116.3125000040967763 ) ) ;
#13363 = CARTESIAN_POINT ( 'NONE',  ( -8.660254037844387298, 172.0833333333333428, -5.000000000000004441 ) ) ;
#13364 = CARTESIAN_POINT ( 'NONE',  ( -8.000000000000033751, -3.313708498984719864, 5.424052779823364645 ) ) ;
#13365 = CARTESIAN_POINT ( 'NONE',  ( 4.556349186104052151, -10.99999999999999822, 89.96875000000000000 ) ) ;
#13366 = CARTESIAN_POINT ( 'NONE',  ( -7.999999999999991118, 0.000000000000000000, 3.830302779823362869 ) ) ;
#13367 = CARTESIAN_POINT ( 'NONE',  ( 8.311093377946834337, 140.4687499965859843, 8.311093377946839666 ) ) ;
#13368 = CARTESIAN_POINT ( 'NONE',  ( 25.17157287525378351, 201.8750000000000284, 172.8284271247460424 ) ) ;
#13369 = LINE ( 'NONE', #71088, #36132 ) ;
#13372 = CARTESIAN_POINT ( 'NONE',  ( -10.00000000000000178, 167.2916666666666856, -2.679491924311230733 ) ) ;
#13371 = CARTESIAN_POINT ( 'NONE',  ( 3.313708498984819339, 110.4687500000000000, 7.999999999999943157 ) ) ;
#13370 = CARTESIAN_POINT ( 'NONE',  ( 23.99999999999997868, 205.8125000000000000, 171.6568542494922553 ) ) ;
#13373 = ORIENTED_EDGE ( 'NONE', *, *, #39301, .F. ) ;
#13374 = ADVANCED_FACE ( 'NONE', ( #38554 ), #15887, .F. ) ;
#13375 = CARTESIAN_POINT ( 'NONE',  ( -11.35316468749999785, 13.38541666325268409, -3.042071309553167513 ) ) ;
#13376 = PRESENTATION_LAYER_ASSIGNMENT (  '', '', ( #11042 ) ) ;
#13377 = FACE_OUTER_BOUND ( 'NONE', #44919, .T. ) ;
#13378 = CARTESIAN_POINT ( 'NONE',  ( 3.313708498984762496, -7.999999999999989342, 25.29905277982336287 ) ) ;
#13379 = CARTESIAN_POINT ( 'NONE',  ( 1.432654583217607858, 208.6250000013656063, 138.5412658750000787 ) ) ;
#13380 = CARTESIAN_POINT ( 'NONE',  ( -2.751064625579944321E-14, 207.7500000000000284, 146.0000000000000284 ) ) ;
#13381 = CARTESIAN_POINT ( 'NONE',  ( 8.660254037844385522, 36.45833332650536818, 5.000000000000005329 ) ) ;
#13382 = AXIS2_PLACEMENT_3D ( 'NONE', #24737, #1026, #42088 ) ;
#13383 = CARTESIAN_POINT ( 'NONE',  ( -4.401442555609581635E-16, 114.7812500020483952, -7.188101187500000044 ) ) ;
#13384 = CARTESIAN_POINT ( 'NONE',  ( 3.211159895383561835, 4.562499998634407028, -3.211159895383561835 ) ) ;
#13385 = CARTESIAN_POINT ( 'NONE',  ( -11.00000000000000000, 0.000000000000000000, 94.18750000409677625 ) ) ;
#13386 = CARTESIAN_POINT ( 'NONE',  ( -3.313708498984757167, 7.999999999999991118, 17.04905277982336642 ) ) ;
#13388 = CARTESIAN_POINT ( 'NONE',  ( 7.320508075688771044, 6.249999993172032475, 7.320508075688775484 ) ) ;
#13387 = CARTESIAN_POINT ( 'NONE',  ( 7.778174593052021635, 7.778174593052023411, 101.1250000040967763 ) ) ;
#13389 = ORIENTED_EDGE ( 'NONE', *, *, #42601, .T. ) ;
#13390 = DIRECTION ( 'NONE',  ( 0.000000000000000000, 0.000000000000000000, 1.000000000000000000 ) ) ;
#13391 = VECTOR ( 'NONE', #26464, 1000.000000000000000 ) ;
#13392 = CARTESIAN_POINT ( 'NONE',  ( 27.99999999999999645, 210.0000000000000284, 169.9999999999999147 ) ) ;
#13393 = CARTESIAN_POINT ( 'NONE',  ( -5.676582343749992710, 230.0520833367473017, 9.832129032723422313 ) ) ;
#13394 = CARTESIAN_POINT ( 'NONE',  ( 9.832129032723420536, 116.1979166632526841, -5.676582343749999815 ) ) ;
#13395 = EDGE_LOOP ( 'NONE', ( #66669, #29494, #40711, #51000, #47428 ) ) ;
#13396 = CARTESIAN_POINT ( 'NONE',  ( -4.000000000000016875, 200.4375000000000568, 140.3431457505076594 ) ) ;
#13397 = CARTESIAN_POINT ( 'NONE',  ( -4.220049686691937474, -10.18810118749999738, 97.93750000204836681 ) ) ;
#13398 = DIRECTION ( 'NONE',  ( 0.000000000000000000, 0.000000000000000000, -1.000000000000000000 ) ) ;
#13399 = CARTESIAN_POINT ( 'NONE',  ( 3.458734125000015869, 195.1875000013655779, 198.0000000000000284 ) ) ;
#13400 = CARTESIAN_POINT ( 'NONE',  ( 0.000000000000000000, 0.000000000000000000, -10.77459999999999951 ) ) ;
#13402 = CARTESIAN_POINT ( 'NONE',  ( -8.311093377946836114, 117.6562499965860269, -8.311093377946837890 ) ) ;
#13401 = CARTESIAN_POINT ( 'NONE',  ( -1.656854249492305531, 205.9375000027311842, 194.0000000000000284 ) ) ;
#13403 = EDGE_CURVE ( 'NONE', #24477, #14040, #39288, .T. ) ;
#13404 = CARTESIAN_POINT ( 'NONE',  ( -29.65685424949234772, 208.4375000000000853, 174.0000000000004547 ) ) ;
#13405 = CARTESIAN_POINT ( 'NONE',  ( -3.313708498984757611, 7.999999999999991118, 6.736552783920143561 ) ) ;
#13406 = ORIENTED_EDGE ( 'NONE', *, *, #30419, .T. ) ;
#13407 = CARTESIAN_POINT ( 'NONE',  ( -2.679491924311235618, 205.4166666598387394, 10.00000000000000000 ) ) ;
#13408 = CARTESIAN_POINT ( 'NONE',  ( 7.999999999999998224, 22.40625000000000355, 3.313708498984766049 ) ) ;
#13409 = DIRECTION ( 'NONE',  ( 0.000000000000000000, 0.000000000000000000, -1.000000000000000000 ) ) ;
#13410 = CARTESIAN_POINT ( 'NONE',  ( -11.35316468749999785, 103.3854166632526699, -3.042071309553167957 ) ) ;
#13411 = FACE_OUTER_BOUND ( 'NONE', #60291, .T. ) ;
#13412 = CARTESIAN_POINT ( 'NONE',  ( 7.188101187499999156, 11.24999999795161187, 2.977408999572654924 ) ) ;
#13413 = CARTESIAN_POINT ( 'NONE',  ( 4.220049686691934809, 10.18810118749999916, 88.56250000204838102 ) ) ;
#13414 = CARTESIAN_POINT ( 'NONE',  ( 8.311093377946837890, 11.71874999658601801, -8.311093377946837890 ) ) ;
#13415 = ORIENTED_EDGE ( 'NONE', *, *, #32678, .T. ) ;
#13416 = LINE ( 'NONE', #36454, #48872 ) ;
#13417 = CARTESIAN_POINT ( 'NONE',  ( 5.662595241051934458, 5.662595241051935346, 27.45061528394063188 ) ) ;
#13418 = FACE_OUTER_BOUND ( 'NONE', #58099, .T. ) ;
#13419 = CARTESIAN_POINT ( 'NONE',  ( 10.18810118749999916, 4.220049686691935698, 76.37500000204838102 ) ) ;
#13420 = VECTOR ( 'NONE', #61382, 1000.000000000000000 ) ;
#13421 = CARTESIAN_POINT ( 'NONE',  ( 0.5061642150818620456, 21.99999999999999289, 4.376614538100004559 ) ) ;
#13422 = FACE_OUTER_BOUND ( 'NONE', #39076, .T. ) ;
#13423 = CARTESIAN_POINT ( 'NONE',  ( -4.088227598258586603E-16, 292.2031250017069510, -6.676582343750001591 ) ) ;
#13424 = CARTESIAN_POINT ( 'NONE',  ( 6.123233995736767268E-16, 128.1249999931720254, -10.00000000000000178 ) ) ;
#13425 = CARTESIAN_POINT ( 'NONE',  ( -11.35316468750000141, 223.5937499965860127, -1.390361679473963753E-15 ) ) ;
#13426 = CARTESIAN_POINT ( 'NONE',  ( 10.18810118750000093, -4.220049686691933921, 83.31250000204836681 ) ) ;
#13427 = CARTESIAN_POINT ( 'NONE',  ( -30.44569435410883429, 201.5625000013656063, 167.5543056458915885 ) ) ;
#13428 = CARTESIAN_POINT ( 'NONE',  ( 8.000000000000000000, 22.59375000000000355, -3.313708498984761608 ) ) ;
#13429 = CARTESIAN_POINT ( 'NONE',  ( 4.541265875000001451, 13.37499999863440969, 1.881053915767124440 ) ) ;
#13430 = ORIENTED_EDGE ( 'NONE', *, *, #21229, .T. ) ;
#13431 = CARTESIAN_POINT ( 'NONE',  ( -12.46529734028881720, -39.55870005852607107, 141.6141688283849760 ) ) ;
#13432 = AXIS2_PLACEMENT_3D ( 'NONE', #3199, #26562, #49206 ) ;
#13433 = CARTESIAN_POINT ( 'NONE',  ( -1.656854249492348607, 206.3125000027312126, 202.0000000000000284 ) ) ;
#13434 = CARTESIAN_POINT ( 'NONE',  ( -2.445694354108839175, 200.3125000013656063, 144.4456943541088663 ) ) ;
#13435 = CARTESIAN_POINT ( 'NONE',  ( 1.656854249492347719, 203.9375000027311842, 146.0000000000000284 ) ) ;
#13436 = CARTESIAN_POINT ( 'NONE',  ( -5.000000000000000000, 11.00774715070965470, 67.37702390743054082 ) ) ;
#13437 = LINE ( 'NONE', #7803, #48913 ) ;
#13439 = ORIENTED_EDGE ( 'NONE', *, *, #61208, .F. ) ;
#13438 =( BOUNDED_CURVE ( )  B_SPLINE_CURVE ( 2, ( #71115, #7763, #37172, #53420, #64733, #65465, #47372, #54162, #2472 ),
 .UNSPECIFIED., .F., .F. ) 
 B_SPLINE_CURVE_WITH_KNOTS ( ( 3, 2, 2, 2, 3 ),
 ( 0.5882352941176468564, 0.5919117647058821374, 0.5955882352941175295, 0.5992647058823528106, 0.6029411764705880916 ),
 .UNSPECIFIED. ) 
 CURVE ( )  GEOMETRIC_REPRESENTATION_ITEM ( )  RATIONAL_B_SPLINE_CURVE ( ( 1.000000000000004663, 0.9238795325112821866, 1.000000000000000000, 0.9238795325112867385, 1.000000000000000000, 0.9238795325112867385, 1.000000000000000000, 0.9238795325112890700, 0.9999999999999976685 ) ) 
 REPRESENTATION_ITEM ( '' )  );
#13440 = CARTESIAN_POINT ( 'NONE',  ( 7.188101187500000044, 7.968749997951610986, 0.000000000000000000 ) ) ;
#13441 = CARTESIAN_POINT ( 'NONE',  ( 2.828427124746191623, 20.12500000000000000, -2.828427124746191623 ) ) ;
#13442 = EDGE_CURVE ( 'NONE', #42724, #60791, #10246, .T. ) ;
#13443 = CARTESIAN_POINT ( 'NONE',  ( 2.977408999572650039, 116.5625000020483810, -7.188101187500001821 ) ) ;
#13444 = CARTESIAN_POINT ( 'NONE',  ( 5.951239500248227898, -17.34865996334632143, -0.1850551574587783465 ) ) ;
#13445 = CARTESIAN_POINT ( 'NONE',  ( 4.721056650415999201, 292.0781250017069510, -4.721056650415999201 ) ) ;
#13447 = CARTESIAN_POINT ( 'NONE',  ( -1.450627696953363260E-15, 11.84527406565996621, 27.11488387514485154 ) ) ;
#13446 = CARTESIAN_POINT ( 'NONE',  ( -9.832129032723415207, 234.3229166700806445, 5.676582343750005144 ) ) ;
#13448 = ORIENTED_EDGE ( 'NONE', *, *, #31951, .T. ) ;
#13449 = CARTESIAN_POINT ( 'NONE',  ( -8.311093377946834337, 229.8437500034140157, 8.311093377946837890 ) ) ;
#13450 = CARTESIAN_POINT ( 'NONE',  ( -7.188101187499990274, -2.977408999572651371, 1.580302781871753437 ) ) ;
#13451 = CARTESIAN_POINT ( 'NONE',  ( -31.99999999999999289, 195.3750000027311842, 170.0000000000004547 ) ) ;
#13452 = CARTESIAN_POINT ( 'NONE',  ( 3.458734125000015869, 203.1875000013656063, 198.0000000000000284 ) ) ;
#13453 =( BOUNDED_CURVE ( )  B_SPLINE_CURVE ( 2, ( #32923, #22681, #16269, #38193, #55929, #67974, #45699, #15532, #9527, #4240, #55553, #39310, #50613, #45330, #27985, #27227, #3866, #62674, #44968, #50990, #15162, #74002, #22305, #4984, #11009, #5350, #16642, #39675, #34042, #57039, #50243, #67236, #73633, #28351, #21938, #61938, #62308, #51360, #74370, #61197, #73265, #26861, #49876, #72891, #21198, #21569, #10635, #44223, #38573, #44596, #67608, #33662, #15905, #38936, #10265, #56289, #33292, #4607, #27602, #53227, #6830, #23432, #11747, #34411, #24167, #18520, #35150, #63052, #11377, #69464, #17024, #46446, #6096, #7203, #23062, #29102, #52854, #1186, #18150, #52484, #52121, #12112, #1559, #57414, #46811, #58523, #35510, #58165, #47179, #17772, #23808, #5720, #30207, #29842, #6471, #41528, #64543, #40787, #35877, #29474, #57788, #46071, #40048, #28720, #821, #453, #12479, #51735, #24538, #70211, #69835, #41165, #63793, #69091, #17397, #40421, #68713, #12840, #34785, #58894, #85, #64175, #63419, #1909, #7936, #31692, #54712, #71662, #31311, #30941, #37732, #19983, #55087, #59621, #25639, #37351, #14316, #65641, #3019, #2274, #2650, #42256, #48287, #26002, #36611, #43368, #25268, #59984, #48654, #60350, #72035, #24897, #60730, #66010, #49027, #20351, #8677, #30576, #47914, #71292, #53598, #66385, #42992, #13206, #65268, #14691, #9052, #32066, #70933, #53961, #3395, #19245, #47546, #19613, #13573, #70570, #18886, #41892, #42626, #64902, #36245, #13937, #36979, #8300, #59260, #54339, #7572, #26379, #62585, #21846, #27142, #3770, #9805, #32827, #49403, #39218, #10544, #67884, #22218, #16552, #62218, #39589, #44503, #50523, #45245, #55837, #4892, #32449, #10173, #38477, #4153, #16175, #50158, #9431, #50899, #33951, #10917, #72424, #15069, #21112, #73538, #67515, #49789, #20733, #73175, #61102, #38102, #68257, #15814, #21482, #38849, #61853, #56949, #43751, #66765, #56205, #61480, #26771, #33576, #56579, #55458, #72803, #44135, #27889, #33209, #73914, #67145, #4518, #15440, #27513, #44878, #28635, #41448, #6749, #63705, #58439, #12397, #35430, #52028, #12030, #58076, #34320, #18062, #29393, #45613, #21306, #52400, #64460, #736, #62965, #17309, #6387, #11290, #29752, #63332, #51649, #12760, #23718, #28266, #22980, #46722, #365, #11658, #57324, #40328, #69748, #45986, #5635, #5265, #35792, #41077, #6008, #69002, #34692, #57700, #51273, #64087, #52766, #1103, #24080, #70127, #47089, #18433, #23347, #74283, #22593, #29009, #68627, #46357, #35063, #69374, #17684, #16936, #40701, #39961, #8591, #66302, #71950, #58806, #47464, #53510, #70487, #25186, #7488, #7118, #42166, #18806, #41810, #36158, #24455, #64820, #7851, #42905, #13122, #59178, #53141, #13490, #1828, #30493, #14229, #31605, #20263, #54627, #24815, #19899, #47830, #13851, #36894, #70851, #59904, #25554, #48568, #37271, #65925, #48940, #19164, #8218, #65179, #30858, #60264, #36529, #31230, #59539, #53879, #2189, #48199, #54254, #2936, #30124, #71208, #19526, #42544, #2565, #1474, #43287, #71577, #65557, #25922, #14609, #14981, #38017, #4067, #31980, #55004, #38390, #60646, #67056, #49705, #50814, #66676, #72718, #21762, #44791, #61770, #21394, #21022, #27801, #10088, #45158, #44046, #15728, #15355, #61017, #67804, #4429, #3310, #9342, #32362, #61394, #16095, #26681, #33488, #9720, #50072, #38769, #50439, #62134, #55376, #73825, #56120, #39130, #10457, #56490, #32741, #44417, #33126, #26297, #20649, #55750, #8967, #27060, #73086, #73455, #3682, #67431, #49318, #27424, #4807, #22132, #68168, #37648, #72334, #43664, #39504, #11204, #69288, #23996, #16842, #10828, #34231, #56862, #17598, #51940, #46640, #29303, #5545, #5178, #63999, #46269, #52313, #47006, #1016, #22886, #5921, #11945, #57233, #34977, #29666, #34604, #40616, #35346, #45898, #69660, #22500, #278, #28547, #51554, #17222, #17973, #74573, #12314, #68912, #58358, #28924, #40242, #39869, #52682, #40992, #23260, #6663, #23633, #16467, #63244, #63618, #57993, #33863, #74195, #11570, #62499, #57611, #6297, #28175, #649, #45522, #51187, #68538, #62871, #48483, #53424, #41725, #2843, #71119, #18346, #64737, #48109, #25833, #70402, #64370, #13036, #35703, #19440, #24369, #70037, #31516, #65469, #70761, #47376, #1747, #24728, #41360, #8131, #54166, #36807, #65834, #60177, #31134, #25466, #71485, #19811, #36072, #18717, #42817, #1385, #53791, #7399, #47737, #59817, #19077, #53053, #14141, #12671, #8499, #58719, #7030, #59090, #42451, #30037, #30406, #42081, #65091, #13763, #13402, #36440, #59453, #7767, #30769, #2474, #2100, #25094, #37176, #54537, #66585, #14515, #5364, #74383, #15267, #43193, #66210, #49612, #71861, #3592, #26965, #3220, #49981, #15637, #38678, #17037, #38300, #55288, #72627, #66962, #57427, #37553, #60553, #3978, #9249, #49228, #56033, #61680, #8877, #20555, #31890, #60928, #72998, #68724, #20175, #54911, #61308, #32271, #67341, #26208, #34425, #10001, #32652, #9632, #20931, #72239, #43568, #14889, #63067, #45712, #43953, #37928, #26588, #55661, #11389, #21305, #44328, #33031, #28364, #51373, #22694, #40062, #5734, #48852, #36260, #40801, #6843, #18534, #70224, #46826, #41541, #46085, #466, #23444, #29487, #58909, #17788, #24552, #6484, #41179, #29857, #64557, #53240, #57802, #18899, #47193, #7220, #30222, #12853, #11760, #35524, #52869, #23075, #34797, #12124, #51748, #52497, #63808, #35892, #46459, #12494, #97, #1201, #6109, #58536, #1571, #35162, #69104, #24182, #47558, #69477, #70582, #59275, #29114, #17411, #58178, #40433, #41906, #64189, #64914, #13222, #835, #63433, #28732, #52133, #23822, #69851, #18163, #66780, #13950, #3410, #72441, #43384, #37747, #9070, #60747, #2286, #59634, #43006, #14709, #66026, #54352, #37366, #32082, #66401, #20750, #71308, #8692, #65654, #2662, #70945, #25282, #54730, #47927, #19260, #7585, #42272, #48300, #3037, #65284, #13590, #36628, #19628, #31707, #26394, #30590, #7950, #48670, #42642, #26020, #30955, #53976, #1923, #36991, #59998, #8315, #55102, #49419, #71677, #24911, #31325, #25654, #53610, #19998, #14334, #43766, #60366, #49043, #15084, #38119, #72050, #20367, #51290, #33592, #68644, #73191, #39234, #50916, #27907, #4534, #45261, #15829, #16193, #55472, #22609, #22235, #27529, #33970, #56967, #38864, #62234, #73930, #10933, #15457, #74301, #4913, #39606, #62603, #68273, #44147, #61495, #61868, #67162, #38492, #16569, #10561, #26786, #55852, #56597, #45630, #44894, #9448, #5282, #9817, #28284, #16953, #21499, #32465, #67901, #61118, #3785, #44518, #49803, #56220, #67530, #32842, #10191, #72819, #4169, #27156, #21126, #50173, #33222, #50541, #73556, #21865, #70502, #35078, #24471, #46375, #29407, #35445, #57715, #58456, #53156, #58090, #64101, #58821, #69390, #18449, #23734, #12044, #69763, #41463, #24095, #30140, #29025, #41092, #23360, #1490, #1119, #70142, #64477, #12774, #34706, #17324, #751, #47104, #46739, #6401, #17698, #29767, #40716, #22995, #35806, #47478, #39977, #62984, #28650, #6021, #12411, #5649, #51665, #8, #52044, #6763, #7132, #11307, #46002, #52415, #63722, #34340, #69020, #40345, #57340, #18076, #380, #63347, #11672, #52781, #59919, #13137, #36172, #19542, #41824, #48214, #30875, #31998, #47846, #53893, #60280, #60661, #8234, #25201, #42559, #36911, #26313, #59192, #7502, #48583, #2205, #19178, #25940, #8606, #30508, #65193, #13504, #65571, #48957, #7869, #14624, #71222, #8983, #31245, #13868, #42181, #55018, #20281, #2581, #71967, #43303, #66318, #54271, #25570, #71593, #53526, #1844, #19915, #64834, #42923, #65942, #3325, #14250, #24830, #37287, #31621, #70867, #37663, #54642, #36543, #49336, #2950, #59554, #18821, #50453, #5196, #72734, #66693, #67072, #38034, #44062, #26699, #72352, #33880, #67818, #73103, #49719, #55766, #4082, #20664, #10474, #56507, #39147, #68189, #27076, #15371, #61033, #27821, #22148, #38783, #16485, #38408, #33505, #9358, #27438, #73469, #21038, #21778, #62151, #4824, #39522, #61786, #50089, #21410, #15744, #28193, #14996, #32377, #44805, #32758, #10104, #50831, #44432, #16110, #55392, #56880, #73842, #33142, #45176, #62518, #67447, #10846, #56137, #61410, #9736, #43682, #3701, #4447, #29682, #58374, #34249, #51573, #28940, #57251, #5564, #64017, #666, #16860, #45916, #23651, #12687, #46658, #28565, #63260, #52329, #74590, #52699, #34621, #22904, #58736, #34995, #24013, #11586, #58010, #46284, #57627, #68928, #5940, #69677, #17239, #40258, #51204, #35721, #17990, #51959, #296, #23276, #69304, #74215, #12330, #41008, #47022, #41378, #35363, #6680, #1033, #70054, #17615, #40633, #11964, #18364, #6316, #63633, #29320, #64389, #7047, #22520, #45540, #68557, #39885, #62888, #11221 ),
 .UNSPECIFIED., .F., .F. ) 
 B_SPLINE_CURVE_WITH_KNOTS ( ( 3, 2, 2, 2, 2, 2, 2, 2, 2, 2, 2, 2, 2, 2, 2, 2, 2, 2, 2, 2, 2, 2, 2, 2, 2, 2, 2, 2, 2, 2, 2, 2, 2, 2, 2, 2, 2, 2, 2, 2, 2, 2, 2, 2, 2, 2, 2, 2, 2, 2, 2, 2, 2, 2, 2, 2, 2, 2, 2, 2, 2, 2, 2, 2, 2, 2, 2, 2, 2, 2, 2, 2, 2, 2, 2, 2, 2, 2, 2, 2, 2, 2, 2, 2, 2, 2, 2, 2, 2, 2, 2, 2, 2, 2, 2, 2, 2, 2, 2, 2, 2, 2, 2, 2, 2, 2, 2, 2, 2, 2, 2, 2, 2, 2, 2, 2, 2, 2, 2, 2, 2, 2, 2, 2, 2, 2, 2, 2, 2, 2, 2, 2, 2, 2, 2, 2, 2, 2, 2, 2, 2, 2, 2, 2, 2, 2, 2, 2, 2, 2, 2, 2, 2, 2, 2, 2, 2, 2, 2, 2, 2, 2, 2, 2, 2, 2, 2, 2, 2, 2, 2, 2, 2, 2, 2, 2, 2, 2, 2, 2, 2, 2, 2, 2, 2, 2, 2, 2, 2, 2, 2, 2, 2, 2, 2, 2, 2, 2, 2, 2, 2, 2, 2, 2, 2, 2, 2, 2, 2, 2, 2, 2, 2, 2, 2, 2, 2, 2, 2, 2, 2, 2, 2, 2, 2, 2, 2, 2, 2, 2, 2, 2, 2, 2, 2, 2, 2, 2, 2, 2, 2, 2, 2, 2, 2, 2, 2, 2, 2, 2, 2, 2, 2, 2, 2, 2, 2, 2, 2, 2, 2, 2, 2, 2, 2, 2, 2, 2, 2, 2, 2, 2, 2, 2, 2, 2, 2, 2, 2, 2, 2, 2, 2, 2, 2, 2, 2, 2, 2, 2, 2, 2, 2, 2, 2, 2, 2, 2, 2, 2, 2, 2, 2, 2, 2, 2, 2, 2, 2, 2, 2, 2, 2, 2, 2, 2, 2, 2, 2, 2, 2, 2, 2, 2, 2, 2, 2, 2, 2, 2, 2, 2, 2, 2, 2, 2, 2, 2, 2, 2, 2, 2, 2, 2, 2, 2, 2, 2, 2, 2, 2, 2, 2, 2, 2, 2, 2, 2, 2, 2, 2, 2, 2, 2, 2, 2, 2, 2, 2, 2, 2, 2, 2, 2, 2, 2, 2, 2, 2, 2, 2, 2, 2, 2, 2, 2, 2, 2, 2, 2, 2, 2, 2, 2, 2, 2, 2, 2, 2, 2, 2, 2, 2, 2, 2, 2, 2, 2, 2, 2, 2, 2, 2, 2, 2, 2, 2, 2, 2, 2, 2, 2, 2, 2, 2, 2, 2, 2, 2, 2, 2, 2, 2, 2, 2, 2, 2, 2, 2, 2, 2, 2, 2, 2, 2, 2, 2, 2, 2, 2, 2, 2, 2, 2, 2, 2, 2, 2, 2, 2, 2, 2, 2, 2, 2, 2, 2, 2, 2, 2, 2, 2, 2, 2, 2, 2, 2, 2, 2, 2, 2, 2, 2, 2, 2, 2, 2, 2, 2, 2, 2, 2, 2, 2, 2, 2, 2, 2, 2, 2, 2, 2, 2, 2, 2, 2, 2, 2, 2, 2, 2, 2, 2, 2, 2, 2, 2, 2, 2, 2, 2, 2, 2, 2, 2, 2, 2, 2, 2, 2, 2, 2, 2, 2, 2, 2, 2, 2, 2, 2, 2, 3 ),
 ( 0.000000000000000000, 0.001843655950715879319, 0.003687311901431758639, 0.005530967852147637524, 0.007374623802863517277, 0.009218279753579396163, 0.01106193570429527505, 0.01290559165501115740, 0.01474924760572703455, 0.01659290355644291171, 0.01843655950715879233, 0.02028021545787467295, 0.02212387140859055010, 0.02396752735930643072, 0.02581118331002231481, 0.02765483926073818849, 0.02949849521145406911, 0.03134215116216994973, 0.03318580711288582341, 0.03502946306360171097, 0.03687311901431758465, 0.03871677496503346527, 0.04056043091574934589, 0.04240408686646521957, 0.04424774281718110019, 0.04609139876789698775, 0.04793505471861286144, 0.04977871066932874206, 0.05162236662004462961, 0.05346602257076049636, 0.05530967852147637698, 0.05715333447219225760, 0.05899699042290813822, 0.06084064637362401884, 0.06268430232433989946, 0.06452795827505578008, 0.06637161422577164682, 0.06821527017648754132, 0.07005892612720342194, 0.07190258207791928868, 0.07374623802863516930, 0.07558989397935104992, 0.07743354993006693054, 0.07927720588078279729, 0.08112086183149869179, 0.08296451778221457241, 0.08480817373293043915, 0.08665182968364633365, 0.08849548563436220039, 0.09033914158507809489, 0.09218279753579397551, 0.09402645348650984225, 0.09587010943722572287, 0.09771376538794160349, 0.09955742133865748411, 0.1014010772893733647, 0.1032447332400892592, 0.1050883891908051260, 0.1069320451415209927, 0.1087757010922368733, 0.1106193570429527540, 0.1124630129936686485, 0.1143066689443845152, 0.1161503248951003958, 0.1179939808458162764, 0.1198376367965321432, 0.1216812927472480377, 0.1235249486979639183, 0.1253686046486797989, 0.1272122605993956657, 0.1290559165501115602, 0.1308995725008274269, 0.1327432284515432936, 0.1345868844022591881, 0.1364305403529750826, 0.1382741963036909494, 0.1401178522544068439, 0.1419615082051227106, 0.1438051641558385774, 0.1456488201065544441, 0.1474924760572703386, 0.1493361320079862609, 0.1511797879587020998, 0.1530234439094179943, 0.1548670998601338611, 0.1567107558108497278, 0.1585544117615655946, 0.1603980677122815168, 0.1622417236629973836, 0.1640853796137132503, 0.1659290355644291448, 0.1677726915151450116, 0.1696163474658608783, 0.1714600034165768006, 0.1733036593672926673, 0.1751473153180085340, 0.1769909712687244008, 0.1788346272194402953, 0.1806782831701561898, 0.1825219391208720288, 0.1843655950715879510, 0.1862092510223038178, 0.1880529069730196845, 0.1898965629237355512, 0.1917402188744514457, 0.1935838748251673402, 0.1954275307758832070, 0.1972711867265991015, 0.1991148426773149682, 0.2009584986280308350, 0.2028021545787467295, 0.2046458105294625962, 0.2064894664801785185, 0.2083331224308943574, 0.2101767783816102519, 0.2120204343323261187, 0.2138640902830419854, 0.2157077462337578799, 0.2175514021844737467, 0.2193950581351896689, 0.2212387140859055079, 0.2230823700366214024, 0.2249260259873372969, 0.2267696819380531359, 0.2286133378887690304, 0.2304569938394849249, 0.2323006497902007916, 0.2341443057409166861, 0.2359879616916325529, 0.2378316176423484474, 0.2396752735930642864, 0.2415189295437801809, 0.2433625854944960754, 0.2452062414452119421, 0.2470498973959278366, 0.2488935533466437033, 0.2507372092973595978, 0.2525808652480754368, 0.2544245211987913313, 0.2562681771495072258, 0.2581118331002231203, 0.2599554890509390148, 0.2617991450016548538, 0.2636428009523706928, 0.2654864569030865873, 0.2673301128538024818, 0.2691737688045183763, 0.2710174247552342708, 0.2728610807059501653, 0.2747047366566660043, 0.2765483926073818988, 0.2783920485580977933, 0.2802357045088136878, 0.2820793604595295268, 0.2839230164102454212, 0.2857666723609613157, 0.2876103283116771547, 0.2894539842623930492, 0.2912976402131088882, 0.2931412961638247827, 0.2949849521145406772, 0.2968286080652566272, 0.2986722640159725217, 0.3005159199666883052, 0.3023595759174041997, 0.3042032318681200942, 0.3060468878188359887, 0.3078905437695518832, 0.3097341997202677222, 0.3115778556709836167, 0.3134215116216994557, 0.3152651675724153502, 0.3171088235231311891, 0.3189524794738471392, 0.3207961354245630337, 0.3226397913752789282, 0.3244834473259947671, 0.3263271032767106061, 0.3281707592274265006, 0.3300144151781423951, 0.3318580711288582896, 0.3337017270795741841, 0.3355453830302900231, 0.3373890389810058621, 0.3392326949317217566, 0.3410763508824376511, 0.3429200068331536011, 0.3447636627838694401, 0.3466073187345853346, 0.3484509746853012291, 0.3502946306360170681, 0.3521382865867329626, 0.3539819425374488016, 0.3558255984881646961, 0.3576692544388805906, 0.3595129103895964851, 0.3613565663403123795, 0.3632002222910281630, 0.3650438782417440575, 0.3668875341924600075, 0.3687311901431759020, 0.3705748460938917410, 0.3724185020446076355, 0.3742621579953235300, 0.3761058139460393690, 0.3779494698967552635, 0.3797931258474711025, 0.3816367817981869970, 0.3834804377489028915, 0.3853240936996187860, 0.3871677496503346805, 0.3890114056010504640, 0.3908550615517664140, 0.3926987175024823085, 0.3945423734531982030, 0.3963860294039140975, 0.3982296853546299364, 0.4000733413053458309, 0.4019169972560616699, 0.4037606532067775644, 0.4056043091574934589, 0.4074479651082092979, 0.4092916210589251924, 0.4111352770096410869, 0.4129789329603570369, 0.4148225889110728759, 0.4166662448617887149, 0.4185099008125046094, 0.4203535567632205039, 0.4221972127139363984, 0.4240408686646522374, 0.4258845246153681319, 0.4277281805660839709, 0.4295718365167998654, 0.4314154924675157599, 0.4332591484182315988, 0.4351028043689474933, 0.4369464603196634434, 0.4387901162703793378, 0.4406337722210951768, 0.4424774281718110158, 0.4443210841225269103, 0.4461647400732428048, 0.4480083960239586993, 0.4498520519746745938, 0.4516957079253903773, 0.4535393638761062718, 0.4553830198268221663, 0.4572266757775380608, 0.4590703317282539553, 0.4609139876789698498, 0.4627576436296857443, 0.4646012995804015833, 0.4664449555311174778, 0.4682886114818333723, 0.4701322674325492113, 0.4719759233832651057, 0.4738195793339810002, 0.4756632352846968947, 0.4775068912354127337, 0.4793505471861285727, 0.4811942031368444672, 0.4830378590875603617, 0.4848815150382763117, 0.4867251709889921507, 0.4885688269397080452, 0.4904124828904238842, 0.4922561388411397787, 0.4940997947918556732, 0.4959434507425715122, 0.4977871066932874067, 0.4996307626440033012, 0.5014744185947191957, 0.5033180745454350902, 0.5051617304961508736, 0.5070053864468667681, 0.5088490423975826626, 0.5106926983482985571, 0.5125363542990144516, 0.5143800102497303461, 0.5162236662004462406, 0.5180673221511620241, 0.5199109781018780296, 0.5217546340525938131, 0.5235982900033097076, 0.5254419459540256021, 0.5272856019047413856, 0.5291292578554573911, 0.5309729138061731746, 0.5328165697568891801, 0.5346602257076049636, 0.5365038816583208581, 0.5383475376090367526, 0.5401911935597526471, 0.5420348495104685416, 0.5438785054611844361, 0.5457221614119003306, 0.5475658173626161140, 0.5494094733133320085, 0.5512531292640479030, 0.5530967852147637975, 0.5549404411654795810, 0.5567840971161955865, 0.5586277530669113700, 0.5604714090176273755, 0.5623150649683431590, 0.5641587209190590535, 0.5660023768697749480, 0.5678460328204908425, 0.5696896887712068480, 0.5715333447219226315, 0.5733770006726384150, 0.5752206566233543095, 0.5770643125740702040, 0.5789079685247860985, 0.5807516244755019930, 0.5825952804262177764, 0.5844389363769337820, 0.5862825923276495654, 0.5881262482783655710, 0.5899699042290813544, 0.5918135601797972489, 0.5936572161305132544, 0.5955008720812290379, 0.5973445280319450434, 0.5991881839826607159, 0.6010318399333766104, 0.6028754958840925049, 0.6047191518348083994, 0.6065628077855242939, 0.6084064637362401884, 0.6102501196869559719, 0.6120937756376719774, 0.6139374315883877609, 0.6157810875391037664, 0.6176247434898196609, 0.6194683994405354444, 0.6213120553912514499, 0.6231557113419672334, 0.6249993672926830168, 0.6268430232433989113, 0.6286866791941148058, 0.6305303351448307003, 0.6323739910955465948, 0.6342176470462623783, 0.6360613029969783838, 0.6379049589476942783, 0.6397486148984101728, 0.6415922708491260673, 0.6434359267998418508, 0.6452795827505578563, 0.6471232387012736398, 0.6489668946519895343, 0.6508105506027053178, 0.6526542065534212123, 0.6544978625041371068, 0.6563415184548530013, 0.6581851744055688958, 0.6600288303562847902, 0.6618724863070006847, 0.6637161422577165792, 0.6655597982084324737, 0.6674034541591483682, 0.6692471101098642627, 0.6710907660605800462, 0.6729344220112960517, 0.6747780779620117242, 0.6766217339127277297, 0.6784653898634435132, 0.6803090458141594077, 0.6821527017648753022, 0.6839963577155911967, 0.6858400136663072022, 0.6876836696170229857, 0.6895273255677388802, 0.6913709815184547747, 0.6932146374691706692, 0.6950582934198865637, 0.6969019493706024582, 0.6987456053213182416, 0.7005892612720341361, 0.7024329172227499196, 0.7042765731734659251, 0.7061202291241817086, 0.7079638850748976031, 0.7098075410256136086, 0.7116511969763293921, 0.7134948529270453976, 0.7153385088777611811, 0.7171821648284770756, 0.7190258207791929701, 0.7208694767299088646, 0.7227131326806247591, 0.7245567886313406536, 0.7264004445820563260, 0.7282441005327723316, 0.7300877564834881150, 0.7319314124342041206, 0.7337750683849200151, 0.7356187243356357985, 0.7374623802863518041, 0.7393060362370675875, 0.7411496921877834820, 0.7429933481384993765, 0.7448370040892152710, 0.7466806600399311655, 0.7485243159906470600, 0.7503679719413628435, 0.7522116278920787380, 0.7540552838427945215, 0.7558989397935105270, 0.7577425957442264215, 0.7595862516949422050, 0.7614299076456582105, 0.7632735635963739940, 0.7651172195470899995, 0.7669608754978057830, 0.7688045314485216775, 0.7706481873992375720, 0.7724918433499534665, 0.7743354993006693610, 0.7761791552513851444, 0.7780228112021009279, 0.7798664671528169334, 0.7817101231035328279, 0.7835537790542487224, 0.7853974350049646169, 0.7872410909556804004, 0.7890847469063964059, 0.7909284028571121894, 0.7927720588078281949, 0.7946157147585439784, 0.7964593707092598729, 0.7983030266599757674, 0.8001466826106916619, 0.8019903385614074454, 0.8038339945121233399, 0.8056776504628392344, 0.8075213064135551289, 0.8093649623642710234, 0.8112086183149869179, 0.8130522742657028124, 0.8148959302164185958, 0.8167395861671346013, 0.8185832421178503848, 0.8204268980685663903, 0.8222705540192821738, 0.8241142099699980683, 0.8259578659207140738, 0.8278015218714297463, 0.8296451778221457518, 0.8314888337728615353, 0.8333324897235774298, 0.8351761456742933243, 0.8370198016250092188, 0.8388634575757251133, 0.8407071135264410078, 0.8425507694771567913, 0.8443944254278727968, 0.8462380813785885803, 0.8480817373293044747, 0.8499253932800204803, 0.8517690492307362637, 0.8536127051814521582, 0.8554563611321679417, 0.8573000170828838362, 0.8591436730335997307, 0.8609873289843156252, 0.8628309849350315197, 0.8646746408857474142, 0.8665182968364631977, 0.8683619527871792032, 0.8702056087378949867, 0.8720492646886109922, 0.8738929206393268867, 0.8757365765900426702, 0.8775802325407586757, 0.8794238884914743482, 0.8812675444421903537, 0.8831112003929061371, 0.8849548563436220316, 0.8867985122943379261, 0.8886421682450538206, 0.8904858241957697151, 0.8923294801464856096, 0.8941731360972013931, 0.8960167920479173986, 0.8978604479986332931, 0.8997041039493491876, 0.9015477599000650821, 0.9033914158507807546, 0.9052350718014967601, 0.9070787277522125436, 0.9089223837029285491, 0.9107660396536443326, 0.9126096956043602271, 0.9144533515550761216, 0.9162970075057920161, 0.9181406634565079106, 0.9199843194072238051, 0.9218279753579396996, 0.9236716313086555941, 0.9255152872593714886, 0.9273589432100873831, 0.9292025991608031665, 0.9310462551115189500, 0.9328899110622349555, 0.9347335670129507390, 0.9365772229636667445, 0.9384208789143825280, 0.9402645348650984225, 0.9421081908158143170, 0.9439518467665302115, 0.9457955027172462170, 0.9476391586679620005, 0.9494828146186778950, 0.9513264705693937895, 0.9531701265201096840, 0.9550137824708254675, 0.9568574384215413620, 0.9587010943722571454, 0.9605447503229731510, 0.9623884062736889344, 0.9642320622244048289, 0.9660757181751207234, 0.9679193741258366179, 0.9697630300765526234, 0.9716066860272684069, 0.9734503419779843014, 0.9752939979287001959, 0.9771376538794160904, 0.9789813098301319849, 0.9808249657808477684, 0.9826686217315635519, 0.9845122776822795574, 0.9863559336329953409, 0.9881995895837113464, 0.9900432455344271299, 0.9918869014851430244, 0.9937305574358590299, 0.9955742133865748134, 0.9965413494093805502 ),
 .UNSPECIFIED. ) 
 CURVE ( )  GEOMETRIC_REPRESENTATION_ITEM ( )  RATIONAL_B_SPLINE_CURVE ( ( 1.000000000000000000, 0.9659258262890683122, 1.000000000000000000, 0.9659258262890683122, 1.000000000000000000, 0.9659258262890683122, 1.000000000000000000, 0.9659258262890683122, 1.000000000000000000, 0.9659258262890683122, 1.000000000000000000, 0.9659258262890683122, 1.000000000000000000, 0.9659258262890683122, 1.000000000000000000, 0.9659258262890683122, 1.000000000000000000, 0.9659258262890683122, 1.000000000000000000, 0.9659258262890683122, 1.000000000000000000, 0.9659258262890683122, 1.000000000000000000, 0.9659258262890683122, 1.000000000000000000, 0.9659258262890683122, 1.000000000000000000, 0.9659258262890683122, 1.000000000000000000, 0.9659258262890683122, 1.000000000000000000, 0.9659258262890683122, 1.000000000000000000, 0.9659258262890683122, 1.000000000000000000, 0.9659258262890683122, 1.000000000000000000, 0.9659258262890683122, 1.000000000000000000, 0.9659258262890683122, 1.000000000000000000, 0.9659258262890683122, 1.000000000000000000, 0.9659258262890683122, 1.000000000000000000, 0.9659258262890683122, 1.000000000000000000, 0.9659258262890683122, 1.000000000000000000, 0.9659258262890683122, 1.000000000000000000, 0.9659258262890683122, 1.000000000000000000, 0.9659258262890683122, 1.000000000000000000, 0.9659258262890683122, 1.000000000000000000, 0.9659258262890683122, 1.000000000000000000, 0.9659258262890683122, 1.000000000000000000, 0.9659258262890683122, 1.000000000000000000, 0.9659258262890683122, 1.000000000000000000, 0.9659258262890683122, 1.000000000000000000, 0.9659258262890683122, 1.000000000000000000, 0.9659258262890683122, 1.000000000000000000, 0.9659258262890683122, 1.000000000000000000, 0.9659258262890683122, 1.000000000000000000, 0.9659258262890683122, 1.000000000000000000, 0.9659258262890683122, 1.000000000000000000, 0.9659258262890683122, 1.000000000000000000, 0.9659258262890683122, 1.000000000000000000, 0.9659258262890683122, 1.000000000000000000, 0.9659258262890683122, 1.000000000000000000, 0.9659258262890683122, 1.000000000000000000, 0.9659258262890683122, 1.000000000000000000, 0.9659258262890683122, 1.000000000000000000, 0.9659258262890683122, 1.000000000000000000, 0.9659258262890683122, 1.000000000000000000, 0.9659258262890683122, 1.000000000000000000, 0.9659258262890683122, 1.000000000000000000, 0.9659258262890683122, 1.000000000000000000, 0.9659258262890683122, 1.000000000000000000, 0.9659258262890683122, 1.000000000000000000, 0.9659258262890683122, 1.000000000000000000, 0.9659258262890683122, 1.000000000000000000, 0.9659258262890683122, 1.000000000000000000, 0.9659258262890683122, 1.000000000000000000, 0.9659258262890683122, 1.000000000000000000, 0.9659258262890683122, 1.000000000000000000, 0.9659258262890683122, 1.000000000000000000, 0.9659258262890683122, 1.000000000000000000, 0.9659258262890683122, 1.000000000000000000, 0.9659258262890683122, 1.000000000000000000, 0.9659258262890683122, 1.000000000000000000, 0.9659258262890683122, 1.000000000000000000, 0.9659258262890683122, 1.000000000000000000, 0.9659258262890683122, 1.000000000000000000, 0.9659258262890683122, 1.000000000000000000, 0.9659258262890683122, 1.000000000000000000, 0.9659258262890683122, 1.000000000000000000, 0.9659258262890683122, 1.000000000000000000, 0.9659258262890683122, 1.000000000000000000, 0.9659258262890683122, 1.000000000000000000, 0.9659258262890683122, 1.000000000000000000, 0.9659258262890683122, 1.000000000000000000, 0.9659258262890683122, 1.000000000000000000, 0.9659258262890683122, 1.000000000000000000, 0.9659258262890683122, 1.000000000000000000, 0.9659258262890683122, 1.000000000000000000, 0.9659258262890683122, 1.000000000000000000, 0.9659258262890683122, 1.000000000000000000, 0.9659258262890683122, 1.000000000000000000, 0.9659258262890683122, 1.000000000000000000, 0.9659258262890683122, 1.000000000000000000, 0.9659258262890683122, 1.000000000000000000, 0.9659258262890683122, 1.000000000000000000, 0.9659258262890683122, 1.000000000000000000, 0.9659258262890683122, 1.000000000000000000, 0.9659258262890683122, 1.000000000000000000, 0.9659258262890683122, 1.000000000000000000, 0.9659258262890683122, 1.000000000000000000, 0.9659258262890683122, 1.000000000000000000, 0.9659258262890683122, 1.000000000000000000, 0.9659258262890683122, 1.000000000000000000, 0.9659258262890683122, 1.000000000000000000, 0.9659258262890683122, 1.000000000000000000, 0.9659258262890683122, 1.000000000000000000, 0.9659258262890683122, 1.000000000000000000, 0.9659258262890683122, 1.000000000000000000, 0.9659258262890683122, 1.000000000000000000, 0.9659258262890683122, 1.000000000000000000, 0.9659258262890683122, 1.000000000000000000, 0.9659258262890683122, 1.000000000000000000, 0.9659258262890683122, 1.000000000000000000, 0.9659258262890683122, 1.000000000000000000, 0.9659258262890683122, 1.000000000000000000, 0.9659258262890683122, 1.000000000000000000, 0.9659258262890683122, 1.000000000000000000, 0.9659258262890683122, 1.000000000000000000, 0.9659258262890683122, 1.000000000000000000, 0.9659258262890683122, 1.000000000000000000, 0.9659258262890683122, 1.000000000000000000, 0.9659258262890683122, 1.000000000000000000, 0.9659258262890683122, 1.000000000000000000, 0.9659258262890683122, 1.000000000000000000, 0.9659258262890683122, 1.000000000000000000, 0.9659258262890683122, 1.000000000000000000, 0.9659258262890683122, 1.000000000000000000, 0.9659258262890683122, 1.000000000000000000, 0.9659258262890683122, 1.000000000000000000, 0.9659258262890683122, 1.000000000000000000, 0.9659258262890683122, 1.000000000000000000, 0.9659258262890683122, 1.000000000000000000, 0.9659258262890683122, 1.000000000000000000, 0.9659258262890683122, 1.000000000000000000, 0.9659258262890683122, 1.000000000000000000, 0.9659258262890683122, 1.000000000000000000, 0.9659258262890683122, 1.000000000000000000, 0.9659258262890683122, 1.000000000000000000, 0.9659258262890683122, 1.000000000000000000, 0.9659258262890683122, 1.000000000000000000, 0.9659258262890683122, 1.000000000000000000, 0.9659258262890683122, 1.000000000000000000, 0.9659258262890683122, 1.000000000000000000, 0.9659258262890683122, 1.000000000000000000, 0.9659258262890683122, 1.000000000000000000, 0.9659258262890683122, 1.000000000000000000, 0.9659258262890683122, 1.000000000000000000, 0.9659258262890683122, 1.000000000000000000, 0.9659258262890683122, 1.000000000000000000, 0.9659258262890683122, 1.000000000000000000, 0.9659258262890683122, 1.000000000000000000, 0.9659258262890683122, 1.000000000000000000, 0.9659258262890683122, 1.000000000000000000, 0.9659258262890683122, 1.000000000000000000, 0.9659258262890683122, 1.000000000000000000, 0.9659258262890683122, 1.000000000000000000, 0.9659258262890683122, 1.000000000000000000, 0.9659258262890683122, 1.000000000000000000, 0.9659258262890683122, 1.000000000000000000, 0.9659258262890683122, 1.000000000000000000, 0.9659258262890683122, 1.000000000000000000, 0.9659258262890683122, 1.000000000000000000, 0.9659258262890683122, 1.000000000000000000, 0.9659258262890683122, 1.000000000000000000, 0.9659258262890683122, 1.000000000000000000, 0.9659258262890683122, 1.000000000000000000, 0.9659258262890683122, 1.000000000000000000, 0.9659258262890683122, 1.000000000000000000, 0.9659258262890683122, 1.000000000000000000, 0.9659258262890683122, 1.000000000000000000, 0.9659258262890683122, 1.000000000000000000, 0.9659258262890683122, 1.000000000000000000, 0.9659258262890683122, 1.000000000000000000, 0.9659258262890683122, 1.000000000000000000, 0.9659258262890683122, 1.000000000000000000, 0.9659258262890683122, 1.000000000000000000, 0.9659258262890683122, 1.000000000000000000, 0.9659258262890683122, 1.000000000000000000, 0.9659258262890683122, 1.000000000000000000, 0.9659258262890683122, 1.000000000000000000, 0.9659258262890683122, 1.000000000000000000, 0.9659258262890683122, 1.000000000000000000, 0.9659258262890683122, 1.000000000000000000, 0.9659258262890683122, 1.000000000000000000, 0.9659258262890683122, 1.000000000000000000, 0.9659258262890683122, 1.000000000000000000, 0.9659258262890683122, 1.000000000000000000, 0.9659258262890683122, 1.000000000000000000, 0.9659258262890683122, 1.000000000000000000, 0.9659258262890683122, 1.000000000000000000, 0.9659258262890683122, 1.000000000000000000, 0.9659258262890683122, 1.000000000000000000, 0.9659258262890683122, 1.000000000000000000, 0.9659258262890683122, 1.000000000000000000, 0.9659258262890683122, 1.000000000000000000, 0.9659258262890683122, 1.000000000000000000, 0.9659258262890683122, 1.000000000000000000, 0.9659258262890683122, 1.000000000000000000, 0.9659258262890683122, 1.000000000000000000, 0.9659258262890683122, 1.000000000000000000, 0.9659258262890683122, 1.000000000000000000, 0.9659258262890683122, 1.000000000000000000, 0.9659258262890683122, 1.000000000000000000, 0.9659258262890683122, 1.000000000000000000, 0.9659258262890683122, 1.000000000000000000, 0.9659258262890683122, 1.000000000000000000, 0.9659258262890683122, 1.000000000000000000, 0.9659258262890683122, 1.000000000000000000, 0.9659258262890683122, 1.000000000000000000, 0.9659258262890683122, 1.000000000000000000, 0.9659258262890683122, 1.000000000000000000, 0.9659258262890683122, 1.000000000000000000, 0.9659258262890683122, 1.000000000000000000, 0.9659258262890683122, 1.000000000000000000, 0.9659258262890683122, 1.000000000000000000, 0.9659258262890683122, 1.000000000000000000, 0.9659258262890683122, 1.000000000000000000, 0.9659258262890683122, 1.000000000000000000, 0.9659258262890683122, 1.000000000000000000, 0.9659258262890683122, 1.000000000000000000, 0.9659258262890683122, 1.000000000000000000, 0.9659258262890683122, 1.000000000000000000, 0.9659258262890683122, 1.000000000000000000, 0.9659258262890683122, 1.000000000000000000, 0.9659258262890683122, 1.000000000000000000, 0.9659258262890683122, 1.000000000000000000, 0.9659258262890683122, 1.000000000000000000, 0.9659258262890683122, 1.000000000000000000, 0.9659258262890683122, 1.000000000000000000, 0.9659258262890683122, 1.000000000000000000, 0.9659258262890683122, 1.000000000000000000, 0.9659258262890683122, 1.000000000000000000, 0.9659258262890683122, 1.000000000000000000, 0.9659258262890683122, 1.000000000000000000, 0.9659258262890683122, 1.000000000000000000, 0.9659258262890683122, 1.000000000000000000, 0.9659258262890683122, 1.000000000000000000, 0.9659258262890683122, 1.000000000000000000, 0.9659258262890683122, 1.000000000000000000, 0.9659258262890683122, 1.000000000000000000, 0.9659258262890683122, 1.000000000000000000, 0.9659258262890683122, 1.000000000000000000, 0.9659258262890683122, 1.000000000000000000, 0.9659258262890683122, 1.000000000000000000, 0.9659258262890683122, 1.000000000000000000, 0.9659258262890683122, 1.000000000000000000, 0.9659258262890683122, 1.000000000000000000, 0.9659258262890683122, 1.000000000000000000, 0.9659258262890683122, 1.000000000000000000, 0.9659258262890683122, 1.000000000000000000, 0.9659258262890683122, 1.000000000000000000, 0.9659258262890683122, 1.000000000000000000, 0.9659258262890683122, 1.000000000000000000, 0.9659258262890683122, 1.000000000000000000, 0.9659258262890683122, 1.000000000000000000, 0.9659258262890683122, 1.000000000000000000, 0.9659258262890683122, 1.000000000000000000, 0.9659258262890683122, 1.000000000000000000, 0.9659258262890683122, 1.000000000000000000, 0.9659258262890683122, 1.000000000000000000, 0.9659258262890683122, 1.000000000000000000, 0.9659258262890683122, 1.000000000000000000, 0.9659258262890683122, 1.000000000000000000, 0.9659258262890683122, 1.000000000000000000, 0.9659258262890683122, 1.000000000000000000, 0.9659258262890683122, 1.000000000000000000, 0.9659258262890683122, 1.000000000000000000, 0.9659258262890683122, 1.000000000000000000, 0.9659258262890683122, 1.000000000000000000, 0.9659258262890683122, 1.000000000000000000, 0.9659258262890683122, 1.000000000000000000, 0.9659258262890683122, 1.000000000000000000, 0.9659258262890683122, 1.000000000000000000, 0.9659258262890683122, 1.000000000000000000, 0.9659258262890683122, 1.000000000000000000, 0.9659258262890683122, 1.000000000000000000, 0.9659258262890683122, 1.000000000000000000, 0.9659258262890683122, 1.000000000000000000, 0.9659258262890683122, 1.000000000000000000, 0.9659258262890683122, 1.000000000000000000, 0.9659258262890683122, 1.000000000000000000, 0.9659258262890683122, 1.000000000000000000, 0.9659258262890683122, 1.000000000000000000, 0.9659258262890683122, 1.000000000000000000, 0.9659258262890683122, 1.000000000000000000, 0.9659258262890683122, 1.000000000000000000, 0.9659258262890683122, 1.000000000000000000, 0.9659258262890683122, 1.000000000000000000, 0.9659258262890683122, 1.000000000000000000, 0.9659258262890683122, 1.000000000000000000, 0.9659258262890683122, 1.000000000000000000, 0.9659258262890683122, 1.000000000000000000, 0.9659258262890683122, 1.000000000000000000, 0.9659258262890683122, 1.000000000000000000, 0.9659258262890683122, 1.000000000000000000, 0.9659258262890683122, 1.000000000000000000, 0.9659258262890683122, 1.000000000000000000, 0.9659258262890683122, 1.000000000000000000, 0.9659258262890683122, 1.000000000000000000, 0.9659258262890683122, 1.000000000000000000, 0.9659258262890683122, 1.000000000000000000, 0.9659258262890683122, 1.000000000000000000, 0.9659258262890683122, 1.000000000000000000, 0.9659258262890683122, 1.000000000000000000, 0.9659258262890683122, 1.000000000000000000, 0.9659258262890683122, 1.000000000000000000, 0.9659258262890683122, 1.000000000000000000, 0.9659258262890683122, 1.000000000000000000, 0.9659258262890683122, 1.000000000000000000, 0.9659258262890683122, 1.000000000000000000, 0.9659258262890683122, 1.000000000000000000, 0.9659258262890683122, 1.000000000000000000, 0.9659258262890683122, 1.000000000000000000, 0.9659258262890683122, 1.000000000000000000, 0.9659258262890683122, 1.000000000000000000, 0.9659258262890683122, 1.000000000000000000, 0.9659258262890683122, 1.000000000000000000, 0.9659258262890683122, 1.000000000000000000, 0.9659258262890683122, 1.000000000000000000, 0.9659258262890683122, 1.000000000000000000, 0.9659258262890683122, 1.000000000000000000, 0.9659258262890683122, 1.000000000000000000, 0.9659258262890683122, 1.000000000000000000, 0.9659258262890683122, 1.000000000000000000, 0.9659258262890683122, 1.000000000000000000, 0.9659258262890683122, 1.000000000000000000, 0.9659258262890683122, 1.000000000000000000, 0.9659258262890683122, 1.000000000000000000, 0.9659258262890683122, 1.000000000000000000, 0.9659258262890683122, 1.000000000000000000, 0.9659258262890683122, 1.000000000000000000, 0.9659258262890683122, 1.000000000000000000, 0.9659258262890683122, 1.000000000000000000, 0.9659258262890683122, 1.000000000000000000, 0.9659258262890683122, 1.000000000000000000, 0.9659258262890683122, 1.000000000000000000, 0.9659258262890683122, 1.000000000000000000, 0.9659258262890683122, 1.000000000000000000, 0.9659258262890683122, 1.000000000000000000, 0.9659258262890683122, 1.000000000000000000, 0.9659258262890683122, 1.000000000000000000, 0.9659258262890683122, 1.000000000000000000, 0.9659258262890683122, 1.000000000000000000, 0.9659258262890683122, 1.000000000000000000, 0.9659258262890683122, 1.000000000000000000, 0.9659258262890683122, 1.000000000000000000, 0.9659258262890683122, 1.000000000000000000, 0.9659258262890683122, 1.000000000000000000, 0.9659258262890683122, 1.000000000000000000, 0.9659258262890683122, 1.000000000000000000, 0.9659258262890683122, 1.000000000000000000, 0.9659258262890683122, 1.000000000000000000, 0.9659258262890683122, 1.000000000000000000, 0.9659258262890683122, 1.000000000000000000, 0.9659258262890683122, 1.000000000000000000, 0.9659258262890683122, 1.000000000000000000, 0.9659258262890683122, 1.000000000000000000, 0.9659258262890683122, 1.000000000000000000, 0.9659258262890683122, 1.000000000000000000, 0.9659258262890683122, 1.000000000000000000, 0.9659258262890683122, 1.000000000000000000, 0.9659258262890683122, 1.000000000000000000, 0.9659258262890683122, 1.000000000000000000, 0.9659258262890683122, 1.000000000000000000, 0.9659258262890683122, 1.000000000000000000, 0.9659258262890683122, 1.000000000000000000, 0.9659258262890683122, 1.000000000000000000, 0.9659258262890683122, 1.000000000000000000, 0.9659258262890683122, 1.000000000000000000, 0.9659258262890683122, 1.000000000000000000, 0.9659258262890683122, 1.000000000000000000, 0.9659258262890683122, 1.000000000000000000, 0.9659258262890683122, 1.000000000000000000, 0.9659258262890683122, 1.000000000000000000, 0.9659258262890683122, 1.000000000000000000, 0.9659258262890683122, 1.000000000000000000, 0.9659258262890683122, 1.000000000000000000, 0.9659258262890683122, 1.000000000000000000, 0.9659258262890683122, 1.000000000000000000, 0.9659258262890683122, 1.000000000000000000, 0.9659258262890683122, 1.000000000000000000, 0.9659258262890683122, 1.000000000000000000, 0.9659258262890683122, 1.000000000000000000, 0.9659258262890683122, 1.000000000000000000, 0.9659258262890683122, 1.000000000000000000, 0.9659258262890683122, 1.000000000000000000, 0.9659258262890683122, 1.000000000000000000, 0.9659258262890683122, 1.000000000000000000, 0.9659258262890683122, 1.000000000000000000, 0.9659258262890683122, 1.000000000000000000, 0.9659258262890683122, 1.000000000000000000, 0.9659258262890683122, 1.000000000000000000, 0.9659258262890683122, 1.000000000000000000, 0.9659258262890683122, 1.000000000000000000, 0.9659258262890683122, 1.000000000000000000, 0.9659258262890683122, 1.000000000000000000, 0.9659258262890683122, 1.000000000000000000, 0.9659258262890683122, 1.000000000000000000, 0.9659258262890683122, 1.000000000000000000, 0.9659258262890683122, 1.000000000000000000, 0.9659258262890683122, 1.000000000000000000, 0.9659258262890683122, 1.000000000000000000, 0.9659258262890683122, 1.000000000000000000, 0.9659258262890683122, 1.000000000000000000, 0.9659258262890683122, 1.000000000000000000, 0.9659258262890683122, 1.000000000000000000, 0.9659258262890683122, 1.000000000000000000, 0.9659258262890683122, 1.000000000000000000, 0.9659258262890683122, 1.000000000000000000, 0.9659258262890683122, 1.000000000000000000, 0.9659258262890683122, 1.000000000000000000, 0.9659258262890683122, 1.000000000000000000, 0.9659258262890683122, 1.000000000000000000, 0.9659258262890683122, 1.000000000000000000, 0.9659258262890683122, 1.000000000000000000, 0.9659258262890683122, 1.000000000000000000, 0.9659258262890683122, 1.000000000000000000, 0.9659258262890683122, 1.000000000000000000, 0.9659258262890683122, 1.000000000000000000, 0.9659258262890683122, 1.000000000000000000, 0.9659258262890683122, 1.000000000000000000, 0.9659258262890683122, 1.000000000000000000, 0.9659258262890683122, 1.000000000000000000, 0.9659258262890683122, 1.000000000000000000, 0.9659258262890683122, 1.000000000000000000, 0.9659258262890683122, 1.000000000000000000, 0.9659258262890683122, 1.000000000000000000, 0.9659258262890683122, 1.000000000000000000, 0.9659258262890683122, 1.000000000000000000, 0.9659258262890683122, 1.000000000000000000, 0.9659258262890683122, 1.000000000000000000, 0.9659258262890683122, 1.000000000000000000, 0.9659258262890683122, 1.000000000000000000, 0.9659258262890683122, 1.000000000000000000, 0.9659258262890683122, 1.000000000000000000, 0.9659258262890683122, 1.000000000000000000, 0.9659258262890683122, 1.000000000000000000, 0.9659258262890683122, 1.000000000000000000, 0.9659258262890683122, 1.000000000000000000, 0.9659258262890683122, 1.000000000000000000, 0.9659258262890683122, 1.000000000000000000, 0.9659258262890683122, 1.000000000000000000, 0.9659258262890683122, 1.000000000000000000, 0.9659258262890683122, 1.000000000000000000, 0.9659258262890683122, 1.000000000000000000, 0.9659258262890683122, 1.000000000000000000, 0.9659258262890683122, 1.000000000000000000, 0.9659258262890683122, 1.000000000000000000, 0.9659258262890683122, 1.000000000000000000, 0.9659258262890683122, 1.000000000000000000, 0.9659258262890683122, 1.000000000000000000, 0.9659258262890683122, 1.000000000000000000, 0.9659258262890683122, 1.000000000000000000, 0.9659258262890683122, 1.000000000000000000, 0.9659258262890683122, 1.000000000000000000, 0.9659258262890683122, 1.000000000000000000, 0.9659258262890683122, 1.000000000000000000, 0.9659258262890683122, 1.000000000000000000, 0.9659258262890683122, 1.000000000000000000, 0.9659258262890683122, 1.000000000000000000, 0.9659258262890683122, 1.000000000000000000, 0.9659258262890683122, 1.000000000000000000, 0.9659258262890683122, 1.000000000000000000, 0.9659258262890683122, 1.000000000000000000, 0.9659258262890683122, 1.000000000000000000, 0.9659258262890683122, 1.000000000000000000, 0.9659258262890683122, 1.000000000000000000, 0.9659258262890683122, 1.000000000000000000, 0.9659258262890683122, 1.000000000000000000, 0.9659258262890683122, 1.000000000000000000, 0.9659258262890683122, 1.000000000000000000, 0.9659258262890683122, 1.000000000000000000, 0.9659258262890683122, 1.000000000000000000, 0.9659258262890683122, 1.000000000000000000, 0.9659258262890683122, 1.000000000000000000, 0.9659258262890683122, 1.000000000000000000, 0.9659258262890683122, 1.000000000000000000, 0.9659258262890683122, 1.000000000000000000, 0.9659258262890683122, 1.000000000000000000, 0.9659258262890683122, 1.000000000000000000, 0.9659258262890683122, 1.000000000000000000, 0.9659258262890683122, 1.000000000000000000, 0.9659258262890683122, 1.000000000000000000, 0.9659258262890683122, 1.000000000000000000, 0.9659258262890683122, 1.000000000000000000, 0.9659258262890683122, 1.000000000000000000, 0.9659258262890683122, 1.000000000000000000, 0.9659258262890683122, 1.000000000000000000, 0.9659258262890683122, 1.000000000000000000, 0.9659258262890683122, 1.000000000000000000, 0.9659258262890683122, 1.000000000000000000, 0.9659258262890683122, 1.000000000000000000, 0.9659258262890683122, 1.000000000000000000, 0.9659258262890683122, 1.000000000000000000, 0.9659258262890683122, 1.000000000000000000, 0.9659258262890683122, 1.000000000000000000, 0.9659258262890683122, 1.000000000000000000, 0.9659258262890683122, 1.000000000000000000, 0.9659258262890683122, 1.000000000000000000, 0.9659258262890683122, 1.000000000000000000, 0.9659258262890683122, 1.000000000000000000, 0.9659258262890683122, 1.000000000000000000, 0.9659258262890683122, 1.000000000000000000, 0.9659258262890683122, 1.000000000000000000, 0.9659258262890683122, 1.000000000000000000, 0.9659258262890683122, 1.000000000000000000, 0.9659258262890683122, 1.000000000000000000, 0.9659258262890683122, 1.000000000000000000, 0.9659258262890683122, 1.000000000000000000, 0.9659258262890683122, 1.000000000000000000, 0.9659258262890683122, 1.000000000000000000, 0.9659258262890683122, 1.000000000000000000, 0.9659258262890683122, 1.000000000000000000, 0.9659258262890683122, 1.000000000000000000, 0.9659258262890683122, 1.000000000000000000, 0.9659258262890683122, 1.000000000000000000, 0.9659258262890683122, 1.000000000000000000, 0.9659258262890683122, 1.000000000000000000, 0.9659258262890683122, 1.000000000000000000, 0.9659258262890683122, 1.000000000000000000, 0.9659258262890683122, 1.000000000000000000, 0.9659258262890683122, 1.000000000000000000, 0.9659258262890683122, 1.000000000000000000, 0.9659258262890683122, 1.000000000000000000, 0.9659258262890683122, 1.000000000000000000, 0.9659258262890683122, 1.000000000000000000, 0.9659258262890683122, 1.000000000000000000, 0.9659258262890683122, 1.000000000000000000, 0.9659258262890683122, 1.000000000000000000, 0.9659258262890683122, 1.000000000000000000, 0.9659258262890683122, 1.000000000000000000, 0.9659258262890683122, 1.000000000000000000, 0.9659258262890683122, 1.000000000000000000, 0.9659258262890683122, 1.000000000000000000, 0.9659258262890683122, 1.000000000000000000, 0.9659258262890683122, 1.000000000000000000, 0.9659258262890683122, 1.000000000000000000, 0.9659258262890683122, 1.000000000000000000, 0.9659258262890683122, 1.000000000000000000, 0.9659258262890683122, 1.000000000000000000, 0.9659258262890683122, 1.000000000000000000, 0.9659258262890683122, 1.000000000000000000, 0.9659258262890683122, 1.000000000000000000, 0.9659258262890683122, 1.000000000000000000, 0.9659258262890683122, 1.000000000000000000, 0.9659258262890683122, 1.000000000000000000, 0.9659258262890683122, 1.000000000000000000, 0.9659258262890683122, 1.000000000000000000, 0.9659258262890683122, 1.000000000000000000, 0.9821255365837726625, 0.9830040703864066920 ) ) 
 REPRESENTATION_ITEM ( '' )  );
#13454 = ORIENTED_EDGE ( 'NONE', *, *, #29775, .F. ) ;
#13455 = DIRECTION ( 'NONE',  ( 0.000000000000000000, 0.000000000000000000, -1.000000000000000000 ) ) ;
#13456 = CARTESIAN_POINT ( 'NONE',  ( -5.676582343750006032, 104.4270833299193555, 9.832129032723418760 ) ) ;
#13457 = CARTESIAN_POINT ( 'NONE',  ( -10.99999999999999822, -4.556349186104052151, 74.59374999999998579 ) ) ;
#13460 = CARTESIAN_POINT ( 'NONE',  ( 0.000000000000000000, 0.000000000000000000, -10.80000000000000071 ) ) ;
#13459 = CARTESIAN_POINT ( 'NONE',  ( 28.00000000000001776, 203.4375000013656063, 173.4587341249998929 ) ) ;
#13458 = CARTESIAN_POINT ( 'NONE',  ( 30.44569435410879166, 201.8125000013656063, 172.4456943541087526 ) ) ;
#13461 = ORIENTED_EDGE ( 'NONE', *, *, #4625, .F. ) ;
#13462 = ADVANCED_FACE ( 'NONE', ( #56272, #4591 ), #3465, .T. ) ;
#13463 = CARTESIAN_POINT ( 'NONE',  ( 2.828427124746190291, 18.87500000000000000, 2.828427124746192067 ) ) ;
#13464 = CARTESIAN_POINT ( 'NONE',  ( 1.469576158976823947E-15, 99.87499999999998579, 8.000000000000000000 ) ) ;
#13465 = CARTESIAN_POINT ( 'NONE',  ( -11.35316468750000141, 208.2812499965860411, -1.390361679473963753E-15 ) ) ;
#13467 = ADVANCED_FACE ( 'NONE', ( #62289 ), #10618, .F. ) ;
#13466 = CARTESIAN_POINT ( 'NONE',  ( -2.445694354108839619, 200.8125000013656063, 139.5543056458912190 ) ) ;
#13468 = CARTESIAN_POINT ( 'NONE',  ( 25.55430564589115150, 200.5625000013656063, 172.4456943541086957 ) ) ;
#13469 = CARTESIAN_POINT ( 'NONE',  ( -4.556349186104045934, 11.00000000000000000, 116.4062500040967905 ) ) ;
#13470 = CARTESIAN_POINT ( 'NONE',  ( -3.042071309553164404, 192.5520833299193271, -11.35316468749999963 ) ) ;
#13471 = CARTESIAN_POINT ( 'NONE',  ( -7.188101187500000044, 93.03125000204836681, 0.000000000000000000 ) ) ;
#13472 = CARTESIAN_POINT ( 'NONE',  ( 11.00000000000000000, 1.347111479062088405E-15, 118.0000000000000000 ) ) ;
#13473 = CARTESIAN_POINT ( 'NONE',  ( -31.99999999999997868, 198.3125000000000284, 171.6568542494928238 ) ) ;
#13474 = CARTESIAN_POINT ( 'NONE',  ( 4.541265875000002339, 16.31249999863440436, 0.000000000000000000 ) ) ;
#13475 = CARTESIAN_POINT ( 'NONE',  ( 25.55430564589119058, 197.3125000013656063, 167.5543056458910485 ) ) ;
#13476 = CARTESIAN_POINT ( 'NONE',  ( 7.188101187499991163, 2.977408999572648707, 4.205302781871751883 ) ) ;
#13477 = CARTESIAN_POINT ( 'NONE',  ( 6.951808397369818766E-16, 77.03124999658601268, -11.35316468750000141 ) ) ;
#13478 = DIRECTION ( 'NONE',  ( 0.8660254037844381525, 0.5000000000000008882, 0.000000000000000000 ) ) ;
#13479 = CARTESIAN_POINT ( 'NONE',  ( -15.99999999999999645, -16.00000000000000355, 20.00000000000000000 ) ) ;
#13480 = ORIENTED_EDGE ( 'NONE', *, *, #51476, .F. ) ;
#13481 = CARTESIAN_POINT ( 'NONE',  ( -3.034644841523098859E-11, -67.59332269700080076, 20.03478791450305962 ) ) ;
#13482 = CARTESIAN_POINT ( 'NONE',  ( -3.999999999999960032, 206.9375000000000284, 196.3431457505076594 ) ) ;
#13483 = CARTESIAN_POINT ( 'NONE',  ( -9.832129032723420536, 73.69791666325268409, 5.676582343749997150 ) ) ;
#13484 = ORIENTED_EDGE ( 'NONE', *, *, #16881, .F. ) ;
#13485 = CARTESIAN_POINT ( 'NONE',  ( -4.220049686691935698, 10.18810118749999916, 85.75000000204838102 ) ) ;
#13486 = CARTESIAN_POINT ( 'NONE',  ( -11.00000000000000000, 4.556349186104045934, 70.09375000409676204 ) ) ;
#13487 = CARTESIAN_POINT ( 'NONE',  ( 3.458734125000016757, 209.1250000013656631, 199.4326545832176691 ) ) ;
#13488 = CARTESIAN_POINT ( 'NONE',  ( 8.660254037844415720, 75.41666666666669983, -5.000000000000016875 ) ) ;
#13490 = CARTESIAN_POINT ( 'NONE',  ( 11.35316468750000141, 70.78124999658602690, 0.000000000000000000 ) ) ;
#13489 = CARTESIAN_POINT ( 'NONE',  ( -1.656854249492383468, 13.43749999726881406, 4.000000000000000888 ) ) ;
#13491 = EDGE_CURVE ( 'NONE', #69151, #22422, #20807, .T. ) ;
#13492 = CARTESIAN_POINT ( 'NONE',  ( -5.656854249492373476, -5.656854249492376141, 23.70530278392014978 ) ) ;
#13493 = CARTESIAN_POINT ( 'NONE',  ( 10.00000000000000178, 171.8749999931720538, 0.000000000000000000 ) ) ;
#13494 = CARTESIAN_POINT ( 'NONE',  ( 7.188101187500001821, 92.37500000204839523, -2.977408999572651371 ) ) ;
#13495 = AXIS2_PLACEMENT_3D ( 'NONE', #5495, #62083, #10406 ) ;
#13496 = CARTESIAN_POINT ( 'NONE',  ( -27.23973938214595947, 194.7821183710415482, 173.7247389417105978 ) ) ;
#13497 = CARTESIAN_POINT ( 'NONE',  ( 8.311093377946837890, 66.71874999658601268, -8.311093377946837890 ) ) ;
#13498 = CARTESIAN_POINT ( 'NONE',  ( -10.18810118749999916, 4.220049686691934809, 106.9375000020483810 ) ) ;
#13499 = CARTESIAN_POINT ( 'NONE',  ( 11.35316468750000141, 200.7812499965860411, 0.000000000000000000 ) ) ;
#13500 = ORIENTED_EDGE ( 'NONE', *, *, #11098, .T. ) ;
#13501 = LINE ( 'NONE', #53523, #18381 ) ;
#13502 = CARTESIAN_POINT ( 'NONE',  ( 7.320508075688774596, 62.49999999317203248, -7.320508075688774596 ) ) ;
#13504 = CARTESIAN_POINT ( 'NONE',  ( 3.042071309553167513, 191.8229166632526699, -11.35316468749999785 ) ) ;
#13503 = DIRECTION ( 'NONE',  ( -0.000000000000000000, 1.000000000000000000, -0.000000000000000000 ) ) ;
#13505 = CARTESIAN_POINT ( 'NONE',  ( -2.751064625579944321E-14, 203.7500000000000284, 146.0000000000000284 ) ) ;
#13506 = CARTESIAN_POINT ( 'NONE',  ( 1.836970198721029589E-15, 239.3750000068279746, 10.00000000000000000 ) ) ;
#13507 = VERTEX_POINT ( 'NONE', #36923 ) ;
#13508 = CARTESIAN_POINT ( 'NONE',  ( -9.832129032723418760, 178.1770833299193555, -5.676582343750004256 ) ) ;
#13509 = VECTOR ( 'NONE', #4163, 1000.000000000000000 ) ;
#13510 = CARTESIAN_POINT ( 'NONE',  ( -7.188101187499992051, 2.977408999572646930, 22.39280278187175810 ) ) ;
#13511 = CARTESIAN_POINT ( 'NONE',  ( 7.999999999999998224, 17.90625000000000355, 3.313708498984766049 ) ) ;
#13512 = ORIENTED_EDGE ( 'NONE', *, *, #8255, .T. ) ;
#13513 = VECTOR ( 'NONE', #48023, 1000.000000000000000 ) ;
#13514 = CARTESIAN_POINT ( 'NONE',  ( -3.313708498984762052, 99.40625000409676204, -8.000000000000000000 ) ) ;
#13515 = VECTOR ( 'NONE', #60927, 1000.000000000000000 ) ;
#13516 = CARTESIAN_POINT ( 'NONE',  ( -7.320508075688778149, 3.125000000000000444, 7.320508075688769267 ) ) ;
#13517 = CARTESIAN_POINT ( 'NONE',  ( 1.656854249492381914, 13.81250000000000000, 4.000000000000000888 ) ) ;
#13518 = CARTESIAN_POINT ( 'NONE',  ( -1.881053915767121776, 17.62499999863440436, -4.541265875000002339 ) ) ;
#13519 = CARTESIAN_POINT ( 'NONE',  ( 7.999999999999991118, 9.797174393178815797E-16, 13.76780278392014623 ) ) ;
#13520 = DIRECTION ( 'NONE',  ( -0.000000000000000000, 1.000000000000000000, -0.000000000000000000 ) ) ;
#13521 = EDGE_CURVE ( 'NONE', #64126, #57841, #34659, .T. ) ;
#13522 = ORIENTED_EDGE ( 'NONE', *, *, #42848, .F. ) ;
#13523 = FACE_OUTER_BOUND ( 'NONE', #3837, .T. ) ;
#13524 = CARTESIAN_POINT ( 'NONE',  ( 7.188101187500000044, 99.40625000204838102, -8.802885111219163269E-16 ) ) ;
#13526 = DIRECTION ( 'NONE',  ( 0.000000000000000000, 0.000000000000000000, -1.000000000000000000 ) ) ;
#13525 = CARTESIAN_POINT ( 'NONE',  ( 5.656854249492378806, 16.12499999590322375, 5.656854249492381470 ) ) ;
#13527 = DIRECTION ( 'NONE',  ( 1.000000000000000000, 0.000000000000000000, 0.000000000000000000 ) ) ;
#13528 = ORIENTED_EDGE ( 'NONE', *, *, #22351, .F. ) ;
#13529 = CARTESIAN_POINT ( 'NONE',  ( -0.8419854211626224272, 49.91401432488780188, -40.68947704084985872 ) ) ;
#13530 = CARTESIAN_POINT ( 'NONE',  ( -2.977408999572648707, -7.188101187499990274, 18.26780278187175455 ) ) ;
#13531 = ORIENTED_EDGE ( 'NONE', *, *, #69826, .T. ) ;
#13532 = VERTEX_POINT ( 'NONE', #9369 ) ;
#13533 = CARTESIAN_POINT ( 'NONE',  ( 7.204075437095966983, 7.204075437095967871, 80.59375000204838102 ) ) ;
#13534 = CARTESIAN_POINT ( 'NONE',  ( 5.952395412842803601, 17.34799259689864570, -0.1532218116813576225 ) ) ;
#13535 = CARTESIAN_POINT ( 'NONE',  ( 7.778174593052021635, 7.778174593052023411, 97.93749999999998579 ) ) ;
#13538 = CARTESIAN_POINT ( 'NONE',  ( 2.765530957082001251, 294.9218750017070647, 6.676582343749999815 ) ) ;
#13537 = CARTESIAN_POINT ( 'NONE',  ( 24.00000000000000355, 201.9375000027311842, 171.6568542494923122 ) ) ;
#13536 = CARTESIAN_POINT ( 'NONE',  ( 31.99999999999997868, 196.4375000027312410, 168.3431457505074889 ) ) ;
#13539 = CARTESIAN_POINT ( 'NONE',  ( 10.00000000000000000, 149.7916666666666856, 2.679491924311236062 ) ) ;
#13540 = CARTESIAN_POINT ( 'NONE',  ( 11.00000000000000000, 1.347111479062088405E-15, 105.4375000040967763 ) ) ;
#13541 = FACE_OUTER_BOUND ( 'NONE', #23481, .T. ) ;
#13542 =( BOUNDED_CURVE ( )  B_SPLINE_CURVE ( 2, ( #55340, #49281, #7818, #31193, #59869, #43627, #2899, #42133, #37607 ),
 .UNSPECIFIED., .F., .F. ) 
 B_SPLINE_CURVE_WITH_KNOTS ( ( 3, 2, 2, 2, 3 ),
 ( 0.8750000000000000000, 0.8819444444444444198, 0.8888888888888888395, 0.8958333333333332593, 0.9027777777777776791 ),
 .UNSPECIFIED. ) 
 CURVE ( )  GEOMETRIC_REPRESENTATION_ITEM ( )  RATIONAL_B_SPLINE_CURVE ( ( 1.000000000000000000, 0.9238795325112867385, 1.000000000000000000, 0.9238795325112867385, 1.000000000000000000, 0.9238795325112867385, 1.000000000000000000, 0.9238795325112879597, 0.9999999999999987788 ) ) 
 REPRESENTATION_ITEM ( '' )  );
#13543 = CARTESIAN_POINT ( 'NONE',  ( -9.999999999999998224, 233.3333333401613174, 2.679491924311235174 ) ) ;
#13544 = CARTESIAN_POINT ( 'NONE',  ( -1.469576158976823947E-15, 5.437499995903221084, 8.000000000000000000 ) ) ;
#13545 = EDGE_CURVE ( 'NONE', #35360, #19306, #48229, .T. ) ;
#13547 = CARTESIAN_POINT ( 'NONE',  ( 29.43265458321761230, 198.5000000013656347, 173.4587341249998929 ) ) ;
#13546 = CIRCLE ( 'NONE', #1533, 7.949999999999993960 ) ;
#13548 = CARTESIAN_POINT ( 'NONE',  ( 7.188101187499999156, 6.749999997951610986, 2.977408999572654924 ) ) ;
#13549 = CARTESIAN_POINT ( 'NONE',  ( -5.656854249492373476, -5.656854249492376141, 26.70530278392014623 ) ) ;
#13550 = CARTESIAN_POINT ( 'NONE',  ( 0.000000000000000000, 300.0000000000000000, 0.000000000000000000 ) ) ;
#13551 = CARTESIAN_POINT ( 'NONE',  ( 5.082755093536326818, 108.5937500020483810, 5.082755093536325042 ) ) ;
#13553 = DIRECTION ( 'NONE',  ( 0.000000000000000000, 0.000000000000000000, 1.000000000000000000 ) ) ;
#13552 = CARTESIAN_POINT ( 'NONE',  ( -2.679491924311315110, 248.9583333333333428, -9.999999999999950262 ) ) ;
#13554 = CARTESIAN_POINT ( 'NONE',  ( -6.951808397369817780E-16, 227.9687500034139873, -11.35316468749999963 ) ) ;
#13555 = CARTESIAN_POINT ( 'NONE',  ( -2.828427124746190735, 12.37500000000000000, -2.828427124746191623 ) ) ;
#13556 = CARTESIAN_POINT ( 'NONE',  ( 2.977408999572646486, 7.188101187499991163, 20.89280278187176521 ) ) ;
#13557 = CARTESIAN_POINT ( 'NONE',  ( 23.99999999999999645, 195.6875000000000284, 168.3431457505075173 ) ) ;
#13558 = CARTESIAN_POINT ( 'NONE',  ( 9.832129032723416984, 25.36458332991935194, 5.676582343750006032 ) ) ;
#13559 = CARTESIAN_POINT ( 'NONE',  ( 5.000000000000003553, 150.8333333333333428, -8.660254037844390851 ) ) ;
#13560 = CARTESIAN_POINT ( 'NONE',  ( -5.000000000000005329, 10.20833332650536640, 8.660254037844387298 ) ) ;
#13561 = PLANE ( 'NONE',  #5429 ) ;
#13562 = CARTESIAN_POINT ( 'NONE',  ( 1.530808498934191719E-15, 11.84527406565996976, 27.11488387514484444 ) ) ;
#13563 = VERTEX_POINT ( 'NONE', #48969 ) ;
#13564 = CARTESIAN_POINT ( 'NONE',  ( -2.679491924311382611, 130.4166666598386541, 9.999999999999914735 ) ) ;
#13565 = VECTOR ( 'NONE', #11591, 1000.000000000000227 ) ;
#13566 = CARTESIAN_POINT ( 'NONE',  ( -2.828427124746192067, 8.374999997268814056, 2.828427124746190735 ) ) ;
#13567 = CARTESIAN_POINT ( 'NONE',  ( 6.951808397369818766E-16, 32.03124999658601268, -11.35316468750000141 ) ) ;
#13568 = CARTESIAN_POINT ( 'NONE',  ( 4.556349186104045934, 11.00000000000000000, 84.71875000409676204 ) ) ;
#13569 = CARTESIAN_POINT ( 'NONE',  ( 1.432654583217607414, 206.5000000013655779, 145.4587341250000350 ) ) ;
#13570 = CARTESIAN_POINT ( 'NONE',  ( -3.673940397442060854E-16, 298.7500000000000000, -6.000000000000001776 ) ) ;
#13571 = CARTESIAN_POINT ( 'NONE',  ( -1.836970198721029983E-15, 175.6249999931720538, 10.00000000000000178 ) ) ;
#13573 = CARTESIAN_POINT ( 'NONE',  ( 6.951808397369818766E-16, 37.03124999658601979, -11.35316468750000141 ) ) ;
#13572 = CARTESIAN_POINT ( 'NONE',  ( -7.188101187499999156, 107.7500000020483810, 2.977408999572654924 ) ) ;
#13574 = CARTESIAN_POINT ( 'NONE',  ( 7.999999999999992895, -3.313708498984756279, 13.48655277982336465 ) ) ;
#13575 = CARTESIAN_POINT ( 'NONE',  ( -9.832129032723420536, 153.6979166632526983, 5.676582343749997150 ) ) ;
#13576 =( BOUNDED_CURVE ( )  B_SPLINE_CURVE ( 2, ( #63436, #10648, #29118, #33679, #27618, #34428, #62687, #17414, #5368 ),
 .UNSPECIFIED., .F., .F. ) 
 B_SPLINE_CURVE_WITH_KNOTS ( ( 3, 2, 2, 2, 3 ),
 ( 0.6805555555555554692, 0.6874999999999998890, 0.6944444444444443088, 0.7013888888888887285, 0.7083333333333332593 ),
 .UNSPECIFIED. ) 
 CURVE ( )  GEOMETRIC_REPRESENTATION_ITEM ( )  RATIONAL_B_SPLINE_CURVE ( ( 1.000000000000001110, 0.9238795325112855172, 1.000000000000000000, 0.9238795325112867385, 1.000000000000000000, 0.9238795325112867385, 1.000000000000000000, 0.9238795325112879597, 0.9999999999999987788 ) ) 
 REPRESENTATION_ITEM ( '' )  );
#13577 = ADVANCED_FACE ( 'NONE', ( #38046 ), #59566, .T. ) ;
#13578 = CARTESIAN_POINT ( 'NONE',  ( 5.000000000000001776, 122.7083333265053682, -8.660254037844389075 ) ) ;
#13579 = CARTESIAN_POINT ( 'NONE',  ( 7.188101187500000044, 110.2812500020483810, -8.802885111219163269E-16 ) ) ;
#13580 = LINE ( 'NONE', #36617, #54170 ) ;
#13581 = CARTESIAN_POINT ( 'NONE',  ( -29.43265458321760519, 203.1250000013656347, 173.4587341250003760 ) ) ;
#13582 = ORIENTED_EDGE ( 'NONE', *, *, #18017, .F. ) ;
#13583 = LINE ( 'NONE', #58260, #9886 ) ;
#13584 = CARTESIAN_POINT ( 'NONE',  ( 8.311093377946837890, 26.71874999658601624, -8.311093377946837890 ) ) ;
#13585 = ADVANCED_FACE ( 'NONE', ( #66330 ), #65482, .F. ) ;
#13586 = ORIENTED_EDGE ( 'NONE', *, *, #56789, .T. ) ;
#13587 = CARTESIAN_POINT ( 'NONE',  ( -3.979266480698733677, 0.4999999999999095723, -6.940132439340586323 ) ) ;
#13588 = CARTESIAN_POINT ( 'NONE',  ( 7.778174593052023411, -7.778174593052021635, 100.5625000000000000 ) ) ;
#13590 = CARTESIAN_POINT ( 'NONE',  ( -11.35316468749999785, 153.0729166632526983, -3.042071309553167957 ) ) ;
#13589 = CARTESIAN_POINT ( 'NONE',  ( -20.65215481363291161, -28.25858978279028833, 145.2053689099807059 ) ) ;
#13591 = CARTESIAN_POINT ( 'NONE',  ( 2.977408999572650927, 1.124999997951610098, -7.188101187500000933 ) ) ;
#13592 = CARTESIAN_POINT ( 'NONE',  ( -7.999999999999991118, 3.313708498984756723, 15.79280278432982421 ) ) ;
#13593 = CARTESIAN_POINT ( 'NONE',  ( 47.61592578303785928, 192.8061930999018614, 64.10259711995320231 ) ) ;
#13594 = CARTESIAN_POINT ( 'NONE',  ( 5.676582343750005144, 230.5729166700806729, 9.832129032723416984 ) ) ;
#13595 = CARTESIAN_POINT ( 'NONE',  ( 10.18810118750000093, -4.220049686691933921, 89.68750000204836681 ) ) ;
#13596 = ORIENTED_EDGE ( 'NONE', *, *, #58404, .F. ) ;
#13597 = EDGE_CURVE ( 'NONE', #7250, #62397, #21620, .T. ) ;
#13598 = CARTESIAN_POINT ( 'NONE',  ( -1.836970198721029983E-15, 205.6249999931720538, 10.00000000000000178 ) ) ;
#13599 = CARTESIAN_POINT ( 'NONE',  ( -1.656854249492416109, 199.3125000027311842, 201.9999999999999432 ) ) ;
#13600 = CARTESIAN_POINT ( 'NONE',  ( 9.832129032723420536, 106.5104166632526841, -5.676582343749999815 ) ) ;
#13601 = CARTESIAN_POINT ( 'NONE',  ( -4.220049686691937474, -10.18810118749999738, 99.43750000204836681 ) ) ;
#13602 = CARTESIAN_POINT ( 'NONE',  ( 1.881053915767121998, 18.62499999863441147, -4.541265875000002339 ) ) ;
#13603 = ORIENTED_EDGE ( 'NONE', *, *, #24311, .T. ) ;
#13604 = EDGE_LOOP ( 'NONE', ( #58259, #72327, #15956, #13164 ) ) ;
#13605 = CARTESIAN_POINT ( 'NONE',  ( -3.313708498984760720, 12.46875000000000178, -8.000000000000000000 ) ) ;
#13606 = CARTESIAN_POINT ( 'NONE',  ( 1.881053915767121776, 0.6249999986344068059, -4.541265875000002339 ) ) ;
#13607 = CARTESIAN_POINT ( 'NONE',  ( -2.977408999572654480, 4.499999997951610986, 7.188101187499999156 ) ) ;
#13608 = CARTESIAN_POINT ( 'NONE',  ( -7.999999999999998224, 114.7812500040967763, 3.313708498984766493 ) ) ;
#13609 = CARTESIAN_POINT ( 'NONE',  ( -4.220049686691937474, -10.18810118749999738, 98.31250000204836681 ) ) ;
#13610 = CARTESIAN_POINT ( 'NONE',  ( -8.000000000000000000, 6.656250000000000888, -3.313708498984762496 ) ) ;
#13611 = CARTESIAN_POINT ( 'NONE',  ( -7.347880794884122694E-16, 12.49999999726881406, 4.000000000000001776 ) ) ;
#13612 = CARTESIAN_POINT ( 'NONE',  ( -4.541265875000002339, 3.749999998634407028, -1.881053915767121998 ) ) ;
#13613 = ORIENTED_EDGE ( 'NONE', *, *, #15324, .F. ) ;
#13614 = EDGE_CURVE ( 'NONE', #28203, #38699, #37049, .T. ) ;
#13615 = AXIS2_PLACEMENT_3D ( 'NONE', #12694, #57632, #62894 ) ;
#13616 = FACE_OUTER_BOUND ( 'NONE', #30435, .T. ) ;
#13617 = DIRECTION ( 'NONE',  ( -0.000000000000000000, -1.000000000000000000, -0.000000000000000000 ) ) ;
#13618 = EDGE_CURVE ( 'NONE', #51583, #37575, #62821, .T. ) ;
#13620 = FACE_OUTER_BOUND ( 'NONE', #56416, .T. ) ;
#13619 = CARTESIAN_POINT ( 'NONE',  ( -27.99999999999991829, 201.9375000013656063, 173.4587341250003760 ) ) ;
#13621 = CARTESIAN_POINT ( 'NONE',  ( 3.211159895383560947, 14.18749999863440792, 3.211159895383562723 ) ) ;
#13622 = CARTESIAN_POINT ( 'NONE',  ( -2.828427124746153876, 200.0000000027312126, 195.1715728752538439 ) ) ;
#13623 = CARTESIAN_POINT ( 'NONE',  ( -7.188101187499992051, 0.000000000000000000, 13.48655278187175455 ) ) ;
#13624 = ORIENTED_EDGE ( 'NONE', *, *, #17818, .T. ) ;
#13625 = EDGE_CURVE ( 'NONE', #39246, #55774, #65899, .T. ) ;
#13626 = VERTEX_POINT ( 'NONE', #43637 ) ;
#13627 = CARTESIAN_POINT ( 'NONE',  ( -6.238412754330611322E-16, 10.18810118749999916, 104.7812500020483810 ) ) ;
#13628 = DIRECTION ( 'NONE',  ( 0.000000000000000000, 0.000000000000000000, 1.000000000000000000 ) ) ;
#13629 = CARTESIAN_POINT ( 'NONE',  ( -29.43265458321766914, 204.7500000013655779, 166.5412658750003629 ) ) ;
#13630 = CARTESIAN_POINT ( 'NONE',  ( -32.00000000000000711, 202.1875000000000568, 168.3431457505080004 ) ) ;
#13631 = CARTESIAN_POINT ( 'NONE',  ( 1.432654583217662481, 195.1250000013656063, 194.5412658750000219 ) ) ;
#13632 = CARTESIAN_POINT ( 'NONE',  ( 5.656854249492381470, 104.5625000000000000, 5.656854249492379694 ) ) ;
#13633 = CARTESIAN_POINT ( 'NONE',  ( -1.836970198721029983E-15, 98.75000000000000000, 10.00000000000000178 ) ) ;
#13634 = CARTESIAN_POINT ( 'NONE',  ( -5.656854249492380582, 114.3125000000000000, -5.656854249492380582 ) ) ;
#13635 = CARTESIAN_POINT ( 'NONE',  ( -4.721056650415999201, 294.4843750017070079, -4.721056650415999201 ) ) ;
#13636 = ORIENTED_EDGE ( 'NONE', *, *, #45759, .F. ) ;
#13637 = CARTESIAN_POINT ( 'NONE',  ( -7.778174593052020747, -7.778174593052023411, 109.1875000000000000 ) ) ;
#13638 = CARTESIAN_POINT ( 'NONE',  ( 8.000000000000000000, 17.90624999590322375, -3.313708498984761608 ) ) ;
#13639 = CARTESIAN_POINT ( 'NONE',  ( 3.458734124999959914, 202.3750000013655779, 143.4326545832176976 ) ) ;
#13640 = CARTESIAN_POINT ( 'NONE',  ( -2.751064625579944321E-14, 205.7500000000000284, 146.0000000000000284 ) ) ;
#13641 = LINE ( 'NONE', #52922, #14188 ) ;
#13642 = CARTESIAN_POINT ( 'NONE',  ( -2.679491924311222295, 231.0416666666666856, 10.00000000000000178 ) ) ;
#13643 = DIRECTION ( 'NONE',  ( -0.000000000000000000, -1.000000000000000000, -0.000000000000000000 ) ) ;
#13644 = CARTESIAN_POINT ( 'NONE',  ( 11.00000000000000355, -4.556349186104045046, 115.6562500000000000 ) ) ;
#13645 = CARTESIAN_POINT ( 'NONE',  ( 10.00000000000000178, 210.2083333333333428, -2.679491924311226736 ) ) ;
#13646 = CARTESIAN_POINT ( 'NONE',  ( -7.188101187499990274, -2.977408999572651815, 9.455302781871752771 ) ) ;
#13647 = CARTESIAN_POINT ( 'NONE',  ( -2.085542519210945728E-15, 194.8437499965860127, 11.35316468750000141 ) ) ;
#13648 = CARTESIAN_POINT ( 'NONE',  ( -2.849036369511732440E-14, 198.2500000000000000, 138.0000000000000568 ) ) ;
#13649 = CARTESIAN_POINT ( 'NONE',  ( 3.211159895383561835, 3.437499998634407028, -3.211159895383561835 ) ) ;
#13651 = FACE_OUTER_BOUND ( 'NONE', #37379, .T. ) ;
#13650 = CARTESIAN_POINT ( 'NONE',  ( -4.000000000000002665, 14.31249999726881406, 1.656854249492380582 ) ) ;
#13652 = VERTEX_POINT ( 'NONE', #57586 ) ;
#13653 = CARTESIAN_POINT ( 'NONE',  ( -1.432654583217662481, 209.3750000013656063, 145.4587341250000634 ) ) ;
#13654 = CARTESIAN_POINT ( 'NONE',  ( -3.042071309553173730, 54.63541666325268409, 11.35316468749999785 ) ) ;
#13655 = CARTESIAN_POINT ( 'NONE',  ( -4.556349186104047710, -10.99999999999999822, 103.4687500040967763 ) ) ;
#13656 = CARTESIAN_POINT ( 'NONE',  ( -11.35316468750000141, 223.8020833299192986, 3.042071309553159963 ) ) ;
#13657 = CARTESIAN_POINT ( 'NONE',  ( -25.55430564589111953, 206.0625000013656063, 172.4456943541091505 ) ) ;
#13659 = CARTESIAN_POINT ( 'NONE',  ( 1.469576158976823947E-15, 119.3750000000000000, 8.000000000000000000 ) ) ;
#13658 = CARTESIAN_POINT ( 'NONE',  ( -5.082755093536325930, 122.4687500020483952, -5.082755093536325930 ) ) ;
#13660 = CARTESIAN_POINT ( 'NONE',  ( 0.000000000000000000, 0.000000000000000000, 118.0000000000000000 ) ) ;
#13661 = CARTESIAN_POINT ( 'NONE',  ( 11.35316468749999963, 110.9895833299193697, -3.042071309553165293 ) ) ;
#13662 = ADVANCED_FACE ( 'NONE', ( #34205 ), #16813, .T. ) ;
#13663 = CARTESIAN_POINT ( 'NONE',  ( -4.999999999999998224, 73.54166665983869677, -8.660254037844389075 ) ) ;
#13664 = CARTESIAN_POINT ( 'NONE',  ( 1.926045908305006327, 89.22060438569889129, -7.188101187499999156 ) ) ;
#13665 = CARTESIAN_POINT ( 'NONE',  ( 4.541265875000002339, 17.43749999863440792, 0.000000000000000000 ) ) ;
#13666 = FACE_OUTER_BOUND ( 'NONE', #71341, .T. ) ;
#13667 = CARTESIAN_POINT ( 'NONE',  ( 4.556349186104052151, -10.99999999999999822, 67.65625000409677625 ) ) ;
#13668 = ORIENTED_EDGE ( 'NONE', *, *, #41704, .T. ) ;
#13669 = VERTEX_POINT ( 'NONE', #28149 ) ;
#13670 =( BOUNDED_CURVE ( )  B_SPLINE_CURVE ( 2, ( #785, #23768, #2152, #19488, #46772, #59503, #42130, #30818, #69056 ),
 .UNSPECIFIED., .F., .F. ) 
 B_SPLINE_CURVE_WITH_KNOTS ( ( 3, 2, 2, 2, 3 ),
 ( 0.09722222222222220989, 0.1041666666666666574, 0.1111111111111111049, 0.1180555555555555525, 0.1250000000000000000 ),
 .UNSPECIFIED. ) 
 CURVE ( )  GEOMETRIC_REPRESENTATION_ITEM ( )  RATIONAL_B_SPLINE_CURVE ( ( 1.000000000000000222, 0.9238795325112866275, 1.000000000000000000, 0.9238795325112867385, 1.000000000000000000, 0.9238795325112867385, 1.000000000000000000, 0.9238795325112867385, 1.000000000000000000 ) ) 
 REPRESENTATION_ITEM ( '' )  );
#13671 = CARTESIAN_POINT ( 'NONE',  ( -4.088227598258586603E-16, 295.3593750017070079, -6.676582343750001591 ) ) ;
#13672 = DIRECTION ( 'NONE',  ( -0.000000000000000000, -0.000000000000000000, -1.000000000000000000 ) ) ;
#13673 = CARTESIAN_POINT ( 'NONE',  ( 9.832129032723416984, 170.3645833299193555, 5.676582343750006032 ) ) ;
#13674 = LINE ( 'NONE', #52587, #29692 ) ;
#13675 = CARTESIAN_POINT ( 'NONE',  ( 2.751064625579944321E-14, 201.7500000000000000, 194.0000000000000568 ) ) ;
#13676 = CARTESIAN_POINT ( 'NONE',  ( 1.332431167089188095E-11, 191.2499999999989768, -10.00000000000000533 ) ) ;
#13677 = CARTESIAN_POINT ( 'NONE',  ( 10.18810118749999916, 1.247682550866122264E-15, 112.2812500020483810 ) ) ;
#13678 = ORIENTED_EDGE ( 'NONE', *, *, #18839, .T. ) ;
#13679 = CARTESIAN_POINT ( 'NONE',  ( 30.64415807102239953, 173.4395964365057239, 174.7231612473719053 ) ) ;
#13680 = CARTESIAN_POINT ( 'NONE',  ( 9.832129032723416984, 135.6770833299193555, 5.676582343750006032 ) ) ;
#13681 = CARTESIAN_POINT ( 'NONE',  ( -3.458734124999959914, 195.4375000013655779, 198.0000000000000284 ) ) ;
#13682 = CARTESIAN_POINT ( 'NONE',  ( 2.445694354108840063, 208.0625000013656063, 200.4456943541088663 ) ) ;
#13683 = CARTESIAN_POINT ( 'NONE',  ( -4.220049686691937474, -10.18810118749999738, 69.81250000204835260 ) ) ;
#13684 = CARTESIAN_POINT ( 'NONE',  ( -5.676582343750006032, 59.42708332991934839, 9.832129032723418760 ) ) ;
#13685 = ORIENTED_EDGE ( 'NONE', *, *, #51692, .F. ) ;
#13686 = CARTESIAN_POINT ( 'NONE',  ( 1.469576158976823947E-15, 120.8750000000000000, 8.000000000000000000 ) ) ;
#13687 = CARTESIAN_POINT ( 'NONE',  ( -4.541265875000003227, 4.999999998634407028, 1.881053915767121110 ) ) ;
#13688 = CARTESIAN_POINT ( 'NONE',  ( 8.008118988124991233, 9.807117285998411148E-16, 7.763115283940629219 ) ) ;
#13689 = B_SPLINE_CURVE_WITH_KNOTS ( 'NONE', 3,
 ( #30345, #42392, #70347, #2044, #65408, #25031 ),
 .UNSPECIFIED., .F., .F.,
 ( 4, 2, 4 ),
 ( 2.380730968220417642E-07, 0.002629065763328348321, 0.005257893453559874149 ),
 .UNSPECIFIED. ) ;
#13690 = CARTESIAN_POINT ( 'NONE',  ( 7.188101187500001821, 17.06249999795161543, -2.977408999572650483 ) ) ;
#13691 = CARTESIAN_POINT ( 'NONE',  ( 4.242640687119285658, 290.6875000034139589, -4.242640687119286547 ) ) ;
#13692 = CARTESIAN_POINT ( 'NONE',  ( 0.3459307087059793062, 124.5729800877406461, -7.927019912259368972 ) ) ;
#13693 = CARTESIAN_POINT ( 'NONE',  ( -2.977408999572654480, 9.374999997951610098, 7.188101187499999156 ) ) ;
#13694 = CARTESIAN_POINT ( 'NONE',  ( -7.188101187499992051, 2.977408999572646930, 2.892802781871751439 ) ) ;
#13695 = CARTESIAN_POINT ( 'NONE',  ( 4.220049686691941027, -10.18810118749999738, 115.0000000020483668 ) ) ;
#13696 = CARTESIAN_POINT ( 'NONE',  ( 4.000000000000001776, 9.000000000000001776, 0.000000000000000000 ) ) ;
#13697 = CARTESIAN_POINT ( 'NONE',  ( 2.828427124746191623, 2.874999997268813168, -2.828427124746191623 ) ) ;
#13698 = EDGE_LOOP ( 'NONE', ( #14194, #2790, #28031, #21190, #20057 ) ) ;
#13699 = CARTESIAN_POINT ( 'NONE',  ( -2.828427124746153876, 195.0000000027312126, 195.1715728752538439 ) ) ;
#13700 = EDGE_CURVE ( 'NONE', #67076, #33995, #21738, .T. ) ;
#13701 = CARTESIAN_POINT ( 'NONE',  ( -1.656854249492403008, 203.6875000000000000, 146.0000000000000284 ) ) ;
#13702 = CARTESIAN_POINT ( 'NONE',  ( -29.65685424949245785, 198.1875000027312126, 166.0000000000004263 ) ) ;
#13703 = CARTESIAN_POINT ( 'NONE',  ( -4.541265875000003227, 1.874999998634406806, 1.881053915767121110 ) ) ;
#13704 = CARTESIAN_POINT ( 'NONE',  ( 5.082755093536326818, 112.7187500020483810, 5.082755093536325042 ) ) ;
#13705 = CARTESIAN_POINT ( 'NONE',  ( 37.99999999999999289, 82.00000000000001421, 57.99999999999999289 ) ) ;
#13706 = CARTESIAN_POINT ( 'NONE',  ( -7.188101187499992051, 0.000000000000000000, 28.48655278187175810 ) ) ;
#13707 = EDGE_LOOP ( 'NONE', ( #40429, #19341, #23683, #11456 ) ) ;
#13708 = EDGE_CURVE ( 'NONE', #51761, #34174, #31367, .T. ) ;
#13709 = CARTESIAN_POINT ( 'NONE',  ( 7.188101187500000933, 24.56249999795161543, -2.977408999572650483 ) ) ;
#13710 = ORIENTED_EDGE ( 'NONE', *, *, #3253, .F. ) ;
#13711 = CARTESIAN_POINT ( 'NONE',  ( 2.445694354108839619, 207.8125000013656063, 200.4456943541088663 ) ) ;
#13712 = CARTESIAN_POINT ( 'NONE',  ( 31.45873412500001010, 202.6250000013656063, 171.4326545832175555 ) ) ;
#13713 = CARTESIAN_POINT ( 'NONE',  ( -10.00000000000000178, 57.50000000000000000, -1.224646799147353454E-15 ) ) ;
#13714 = AXIS2_PLACEMENT_3D ( 'NONE', #42830, #71501, #48127 ) ;
#13715 = CARTESIAN_POINT ( 'NONE',  ( -2.977408999572651815, 100.8125000020484094, 7.188101187500000933 ) ) ;
#13716 = CARTESIAN_POINT ( 'NONE',  ( 1.102182119232618108E-15, 298.2500000000000000, 6.000000000000001776 ) ) ;
#13718 = CARTESIAN_POINT ( 'NONE',  ( -26.73865209873909166, -42.14721765163382372, 185.6978372118126970 ) ) ;
#13717 = CARTESIAN_POINT ( 'NONE',  ( 26.34314575050764162, 209.0625000027312126, 173.9999999999999147 ) ) ;
#13719 = ORIENTED_EDGE ( 'NONE', *, *, #34980, .T. ) ;
#13720 = CARTESIAN_POINT ( 'NONE',  ( -11.35316468749999608, 234.1145833367473017, 3.042071309553173730 ) ) ;
#13721 = CARTESIAN_POINT ( 'NONE',  ( 1.656854249492347719, 201.9375000027311842, 146.0000000000000284 ) ) ;
#13722 = CARTESIAN_POINT ( 'NONE',  ( 10.00000000000000178, 0.000000000000000000, 0.000000000000000000 ) ) ;
#13723 = CARTESIAN_POINT ( 'NONE',  ( 10.99999999999995026, -4.556349186104096560, 94.65625000000001421 ) ) ;
#13724 = CARTESIAN_POINT ( 'NONE',  ( -10.00000000000000000, 265.0000000000000000, 0.000000000000000000 ) ) ;
#13725 = CARTESIAN_POINT ( 'NONE',  ( 0.000000000000000000, 0.000000000000000000, -4.000000000000001776 ) ) ;
#13726 = CARTESIAN_POINT ( 'NONE',  ( -5.000000000000005329, 173.3333333333333428, 8.660254037844387298 ) ) ;
#13727 = DIRECTION ( 'NONE',  ( -0.000000000000000000, -1.000000000000000000, -0.000000000000000000 ) ) ;
#13728 = DIRECTION ( 'NONE',  ( -0.000000000000000000, 1.000000000000000000, -1.563033456626094573E-30 ) ) ;
#13729 = CARTESIAN_POINT ( 'NONE',  ( 5.082755093536318824, 5.082755093536319713, 26.79905278187175455 ) ) ;
#13730 = CARTESIAN_POINT ( 'NONE',  ( -9.832129032723418760, 138.1770833299193555, -5.676582343750004256 ) ) ;
#13731 = CARTESIAN_POINT ( 'NONE',  ( -3.673940397442060854E-16, 294.8125000034140157, -6.000000000000001776 ) ) ;
#13732 = CARTESIAN_POINT ( 'NONE',  ( 8.660254037844385522, 26.45833332650536818, 5.000000000000005329 ) ) ;
#13735 = CARTESIAN_POINT ( 'NONE',  ( 26.34314575050754215, 203.9375000000000568, 173.9999999999998863 ) ) ;
#13734 = CARTESIAN_POINT ( 'NONE',  ( 2.679491924311222739, 105.8333333265053540, 10.00000000000000355 ) ) ;
#13733 = CARTESIAN_POINT ( 'NONE',  ( 30.82842712474620583, 208.3750000000000284, 167.1715728752537586 ) ) ;
#13736 = VERTEX_POINT ( 'NONE', #16073 ) ;
#13737 = CARTESIAN_POINT ( 'NONE',  ( 9.832129032723420536, 11.51041666325268409, -5.676582343749999815 ) ) ;
#13738 = CYLINDRICAL_SURFACE ( 'NONE', #2195, 11.00000000000000000 ) ;
#13739 = LINE ( 'NONE', #19414, #72736 ) ;
#13740 = CARTESIAN_POINT ( 'NONE',  ( -1.656854249492327735, 208.9375000027311842, 194.0000000000000568 ) ) ;
#13741 = CARTESIAN_POINT ( 'NONE',  ( 1.432654583217607192, 208.2500000013656063, 145.4587341250000350 ) ) ;
#13742 = B_SPLINE_CURVE_WITH_KNOTS ( 'NONE', 3,
 ( #66717, #55038, #60684, #2224, #26334, #31263, #9004, #15021, #38055, #31643, #3344, #7888, #19564, #43322, #8630, #61055, #66337, #54291, #25222, #47865, #42942, #42579 ),
 .UNSPECIFIED., .F., .F.,
 ( 4, 2, 2, 2, 2, 2, 2, 2, 2, 2, 4 ),
 ( 0.000000000000000000, 0.001156727053362478904, 0.001735090580043718465, 0.002313454106724957809, 0.003470181160087434762, 0.004048544686768671720, 0.004626908213449908679, 0.005783635266812357442, 0.006940362320174807073, 0.008097089373537256704, 0.009253816426899704600 ),
 .UNSPECIFIED. ) ;
#13743 = CARTESIAN_POINT ( 'NONE',  ( -7.692623880995575369, 124.8073761190044166, -0.5146232510360394530 ) ) ;
#13744 = CARTESIAN_POINT ( 'NONE',  ( -10.00000000000000355, 29.58333332650536818, 2.679491924311223183 ) ) ;
#13745 = AXIS2_PLACEMENT_3D ( 'NONE', #8721, #71704, #31734 ) ;
#13746 = CARTESIAN_POINT ( 'NONE',  ( 5.082755093536326818, 111.2187500020483810, 5.082755093536325042 ) ) ;
#13747 = CARTESIAN_POINT ( 'NONE',  ( -4.541265875000002339, 2.874999998634407028, -1.881053915767121998 ) ) ;
#13748 = CARTESIAN_POINT ( 'NONE',  ( 1.506524674528596730, 65.82790954191280264, -26.31843049628337639 ) ) ;
#13749 = CARTESIAN_POINT ( 'NONE',  ( -5.656854249492375253, 5.656854249492375253, 17.14280277982336287 ) ) ;
#13750 = CARTESIAN_POINT ( 'NONE',  ( 4.898587196589412829E-16, 25.87500000000000711, -8.000000000000000000 ) ) ;
#13751 = EDGE_LOOP ( 'NONE', ( #53902, #11558, #4945, #29317 ) ) ;
#13752 = CARTESIAN_POINT ( 'NONE',  ( 10.00000000000000711, 30.00000000000000711, 0.000000000000000000 ) ) ;
#13753 = CARTESIAN_POINT ( 'NONE',  ( -2.679491924324933105, 61.45833333333461468, -9.999999999992150279 ) ) ;
#13754 = CARTESIAN_POINT ( 'NONE',  ( -5.676582343749992710, 235.0520833367473301, 9.832129032723422313 ) ) ;
#13755 = CARTESIAN_POINT ( 'NONE',  ( -9.832129032723418760, 127.8645833299193697, -5.676582343750004256 ) ) ;
#13756 = VERTEX_POINT ( 'NONE', #39107 ) ;
#13757 = CARTESIAN_POINT ( 'NONE',  ( -7.999999999999991118, 3.313708498984757167, 5.424052783920146226 ) ) ;
#13758 = CARTESIAN_POINT ( 'NONE',  ( -6.238412754330611322E-16, 10.18810118749999916, 95.78125000204836681 ) ) ;
#13759 = CARTESIAN_POINT ( 'NONE',  ( 2.265596578422603396E-15, 0.000000000000000000, -18.50000000000000000 ) ) ;
#13760 = CARTESIAN_POINT ( 'NONE',  ( 2.839093476692135984E-14, 195.9375000013655779, 201.4587341250000350 ) ) ;
#13761 = CARTESIAN_POINT ( 'NONE',  ( -1.836970198721029983E-15, 130.6249999931720254, 10.00000000000000178 ) ) ;
#13763 = CARTESIAN_POINT ( 'NONE',  ( -5.676582343749998039, 117.4479166632526841, -9.832129032723420536 ) ) ;
#13762 = CARTESIAN_POINT ( 'NONE',  ( 5.000000000000006217, 44.16666666666667851, 8.660254037844412167 ) ) ;
#13764 = CARTESIAN_POINT ( 'NONE',  ( -25.17157287525377996, 208.6250000000000284, 172.8284271247465256 ) ) ;
#13765 = CARTESIAN_POINT ( 'NONE',  ( 7.999999999999991118, 9.797174393178815797E-16, 6.267802783920147114 ) ) ;
#13766 = ORIENTED_EDGE ( 'NONE', *, *, #67583, .F. ) ;
#13767 = CARTESIAN_POINT ( 'NONE',  ( 6.123233995736767268E-16, 213.1249999931720538, -10.00000000000000178 ) ) ;
#13768 = DIRECTION ( 'NONE',  ( 0.000000000000000000, 0.000000000000000000, -1.000000000000000000 ) ) ;
#13769 = DIRECTION ( 'NONE',  ( 1.000000000000000000, 0.000000000000000000, 0.000000000000000000 ) ) ;
#13770 = CARTESIAN_POINT ( 'NONE',  ( 5.676582343749993598, 95.26041666325268409, 9.832129032723422313 ) ) ;
#13771 = CARTESIAN_POINT ( 'NONE',  ( 3.458734125000016313, 206.8750000013656347, 199.4326545832176976 ) ) ;
#13772 = CARTESIAN_POINT ( 'NONE',  ( -2.977408999572650039, 10.31249999795161187, -7.188101187500000933 ) ) ;
#13773 = CARTESIAN_POINT ( 'NONE',  ( 10.18810118750000093, -4.220049686691933033, 88.18750000204838102 ) ) ;
#13774 = CARTESIAN_POINT ( 'NONE',  ( -9.832129032723420536, 4.010416663252683200, 5.676582343749997150 ) ) ;
#13775 = ORIENTED_EDGE ( 'NONE', *, *, #35396, .T. ) ;
#13776 = CARTESIAN_POINT ( 'NONE',  ( 4.000000000000001776, 20.74999999726881583, 0.000000000000000000 ) ) ;
#13777 = CARTESIAN_POINT ( 'NONE',  ( 3.317071493978883456, -8.008118988124989457, 26.98186528394063188 ) ) ;
#13778 = CARTESIAN_POINT ( 'NONE',  ( -4.556349186104048599, -10.99999999999999822, 101.9687500040967620 ) ) ;
#13779 = CARTESIAN_POINT ( 'NONE',  ( 1.871523826299183495E-15, -10.18810118749999916, 75.90625000204836681 ) ) ;
#13780 = CARTESIAN_POINT ( 'NONE',  ( -3.313708498984707429, 97.90625000409677625, -8.000000000000055067 ) ) ;
#13781 = CARTESIAN_POINT ( 'NONE',  ( -8.660254037844387298, 148.9583333265053682, -5.000000000000004441 ) ) ;
#13782 = CARTESIAN_POINT ( 'NONE',  ( 6.676582343750004256, 290.8906250017069510, 2.765530957081995478 ) ) ;
#13783 = CARTESIAN_POINT ( 'NONE',  ( 2.828427124746208943, 204.7500000027312126, 195.1715728752538439 ) ) ;
#13784 = CARTESIAN_POINT ( 'NONE',  ( -12.00000000000000000, 6.928203230275504332, -14.00000000000000178 ) ) ;
#13785 =( BOUNDED_CURVE ( )  B_SPLINE_CURVE ( 2, ( #60105, #8423, #19738, #64662, #53716, #71787, #31058, #18644, #24293 ),
 .UNSPECIFIED., .F., .F. ) 
 B_SPLINE_CURVE_WITH_KNOTS ( ( 3, 2, 2, 2, 3 ),
 ( 0.4833333333333338366, 0.4916666666666670849, 0.5000000000000004441, 0.5083333333333336368, 0.5166666666666670515 ),
 .UNSPECIFIED. ) 
 CURVE ( )  GEOMETRIC_REPRESENTATION_ITEM ( )  RATIONAL_B_SPLINE_CURVE ( ( 0.9999999999999954481, 0.9238795325112912904, 1.000000000000000000, 0.9238795325112867385, 1.000000000000000000, 0.9238795325112867385, 1.000000000000000000, 0.9238795325112837409, 1.000000000000003109 ) ) 
 REPRESENTATION_ITEM ( '' )  );
#13786 = ADVANCED_FACE ( 'NONE', ( #51530 ), #68513, .F. ) ;
#13787 = ADVANCED_FACE ( 'NONE', ( #33463 ), #5522, .T. ) ;
#13788 = CARTESIAN_POINT ( 'NONE',  ( 3.042071309553167069, 127.1354166632526699, -11.35316468749999785 ) ) ;
#13789 = CARTESIAN_POINT ( 'NONE',  ( -6.238412754330611322E-16, 10.18810118749999916, 85.28125000204836681 ) ) ;
#13790 = CARTESIAN_POINT ( 'NONE',  ( -26.56734541678232375, 200.0000000013656347, 173.4587341250003760 ) ) ;
#13791 = CARTESIAN_POINT ( 'NONE',  ( -5.656854249492381470, 24.93750000000000355, 5.656854249492379694 ) ) ;
#13792 = CARTESIAN_POINT ( 'NONE',  ( 3.211159895383561835, 12.56249999863440792, -3.211159895383561835 ) ) ;
#13793 = ORIENTED_EDGE ( 'NONE', *, *, #66704, .F. ) ;
#13794 = DIRECTION ( 'NONE',  ( 0.000000000000000000, 0.000000000000000000, -1.000000000000000000 ) ) ;
#13795 = CARTESIAN_POINT ( 'NONE',  ( -1.656854249492347719, 208.9375000027312410, 194.0000000000000853 ) ) ;
#13796 = CIRCLE ( 'NONE', #56005, 17.50000000000000000 ) ;
#13797 = CARTESIAN_POINT ( 'NONE',  ( -3.458734125000015869, 198.1875000013655779, 142.0000000000000568 ) ) ;
#13798 = CARTESIAN_POINT ( 'NONE',  ( 1.656854249492347719, 202.9375000027312410, 146.0000000000000284 ) ) ;
#13799 = VECTOR ( 'NONE', #58032, 1000.000000000000000 ) ;
#13800 = CARTESIAN_POINT ( 'NONE',  ( -5.000000000000000000, 10.53354221205070829, 66.31578581128123062 ) ) ;
#13801 = CARTESIAN_POINT ( 'NONE',  ( 7.204075437095968759, -7.204075437095966983, 70.09375000204836681 ) ) ;
#13802 = VERTEX_POINT ( 'NONE', #62845 ) ;
#13803 = CARTESIAN_POINT ( 'NONE',  ( 5.082755093536324154, 6.281249997951610986, 5.082755093536326818 ) ) ;
#13804 = DIRECTION ( 'NONE',  ( -0.000000000000000000, 1.000000000000000000, -0.000000000000000000 ) ) ;
#13805 = CARTESIAN_POINT ( 'NONE',  ( 5.082755093536326818, 116.0937500020483810, 5.082755093536325042 ) ) ;
#13806 = CARTESIAN_POINT ( 'NONE',  ( 0.4589999999999999636, 255.7199999999997715, 5.818592113973279467 ) ) ;
#13807 = CARTESIAN_POINT ( 'NONE',  ( 4.721056650416000089, 291.8281250017069510, 4.721056650415999201 ) ) ;
#13809 = CARTESIAN_POINT ( 'NONE',  ( 2.679491924311228956, 137.9166666598387110, -10.00000000000000000 ) ) ;
#13808 = CARTESIAN_POINT ( 'NONE',  ( 3.042071309553163516, 222.4479166700806729, -11.35316468749999785 ) ) ;
#13810 = CONTEXT_DEPENDENT_SHAPE_REPRESENTATION ( #54956, #28875 ) ;
#13811 = ORIENTED_EDGE ( 'NONE', *, *, #67745, .F. ) ;
#13812 = CARTESIAN_POINT ( 'NONE',  ( 9.832129032723420536, 226.3020833367473301, 5.676582343749996262 ) ) ;
#13813 = CARTESIAN_POINT ( 'NONE',  ( 7.188101187499992051, 8.802885111219154394E-16, 28.11155278187175455 ) ) ;
#13814 = LINE ( 'NONE', #59866, #53830 ) ;
#13815 = CARTESIAN_POINT ( 'NONE',  ( -3.458734124999960358, 199.6875000013656063, 198.0000000000000284 ) ) ;
#13816 = ORIENTED_EDGE ( 'NONE', *, *, #57548, .T. ) ;
#13817 = CARTESIAN_POINT ( 'NONE',  ( 9.797174393178825657E-16, 0.000000000000000000, -8.000000000000000000 ) ) ;
#13818 = CARTESIAN_POINT ( 'NONE',  ( 8.000000000000000000, 97.34375000000000000, -3.313708498984762496 ) ) ;
#13819 = CARTESIAN_POINT ( 'NONE',  ( -3.042071309553164404, 102.5520833299193555, -11.35316468749999963 ) ) ;
#13820 = FACE_OUTER_BOUND ( 'NONE', #67328, .T. ) ;
#13821 = CARTESIAN_POINT ( 'NONE',  ( 2.020667218593132706E-15, -11.00000000000000000, 77.87499999999998579 ) ) ;
#13824 = LINE ( 'NONE', #36129, #25358 ) ;
#13823 = CARTESIAN_POINT ( 'NONE',  ( 30.44569435410879521, 203.8125000013656063, 167.5543056458910485 ) ) ;
#13822 = CARTESIAN_POINT ( 'NONE',  ( 31.45873412500001010, 205.0000000013655779, 168.5673454167822740 ) ) ;
#13825 = ORIENTED_EDGE ( 'NONE', *, *, #18214, .T. ) ;
#13826 = CARTESIAN_POINT ( 'NONE',  ( 5.676582343750001591, 216.6145833299193555, -9.832129032723420536 ) ) ;
#13827 = CARTESIAN_POINT ( 'NONE',  ( -3.458734125000015425, 203.0000000013655779, 143.4326545832176976 ) ) ;
#13828 = CARTESIAN_POINT ( 'NONE',  ( 30.44569435410879166, 200.8125000013656063, 172.4456943541087526 ) ) ;
#13829 = CARTESIAN_POINT ( 'NONE',  ( 7.188101187500000044, 27.84374999795161543, 0.000000000000000000 ) ) ;
#13830 = CARTESIAN_POINT ( 'NONE',  ( -3.042071309553173730, 199.6354166632526699, 11.35316468749999785 ) ) ;
#13831 = CARTESIAN_POINT ( 'NONE',  ( 1.320432766682874540E-15, 91.90625000204838102, 7.188101187500000044 ) ) ;
#13832 = CARTESIAN_POINT ( 'NONE',  ( -29.65685424949240812, 197.0625000000000000, 166.0000000000004263 ) ) ;
#13833 = CARTESIAN_POINT ( 'NONE',  ( -4.541265875000002339, 12.74999999863440969, -1.881053915767121998 ) ) ;
#13834 = CARTESIAN_POINT ( 'NONE',  ( 31.45873412499999944, 197.0000000013656063, 168.5673454167822740 ) ) ;
#13835 = ADVANCED_BREP_SHAPE_REPRESENTATION ( '', ( #41611, #57354 ), #58583 ) ;
#13836 = CARTESIAN_POINT ( 'NONE',  ( -7.188101187499992051, 0.000000000000000000, 3.361552781871751883 ) ) ;
#13837 = DIRECTION ( 'NONE',  ( 0.8660254037844389297, -0.4999999999999994449, 0.000000000000000000 ) ) ;
#13838 = CARTESIAN_POINT ( 'NONE',  ( 6.951808397369818766E-16, 87.03124999658602690, -11.35316468750000141 ) ) ;
#13839 = EDGE_LOOP ( 'NONE', ( #7995, #14223, #15506, #53248, #31721 ) ) ;
#13840 = CARTESIAN_POINT ( 'NONE',  ( -29.65685424949240812, 195.0625000000000000, 166.0000000000003979 ) ) ;
#13841 = CARTESIAN_POINT ( 'NONE',  ( 1.656854249492418107, 209.3125000000000000, 202.0000000000000000 ) ) ;
#13842 = FACE_OUTER_BOUND ( 'NONE', #9329, .T. ) ;
#13843 = DIRECTION ( 'NONE',  ( 0.8191520442889911324, 0.000000000000000000, 0.5735764363510471586 ) ) ;
#13844 = CARTESIAN_POINT ( 'NONE',  ( 5.676582343749993598, 74.94791666325269830, 9.832129032723422313 ) ) ;
#13845 = EDGE_LOOP ( 'NONE', ( #35994, #65228, #9237, #72271 ) ) ;
#13846 = CARTESIAN_POINT ( 'NONE',  ( -10.18810118749999916, 0.000000000000000000, 87.53125000204836681 ) ) ;
#13847 = CARTESIAN_POINT ( 'NONE',  ( 7.204075437095968759, -7.204075437095966983, 111.7187500020483810 ) ) ;
#13848 = CARTESIAN_POINT ( 'NONE',  ( 2.754378923186476579E-14, 209.4375000013656063, 194.5412658750000219 ) ) ;
#13849 = CARTESIAN_POINT ( 'NONE',  ( 32.00000000000000000, 207.2500000000000284, 169.9999999999999432 ) ) ;
#13851 = CARTESIAN_POINT ( 'NONE',  ( -9.832129032723418760, 72.86458332991935549, -5.676582343750004256 ) ) ;
#13850 = CARTESIAN_POINT ( 'NONE',  ( -3.428378827827393671, 68.02396499344679626, 20.38382289158802863 ) ) ;
#13852 = AXIS2_PLACEMENT_3D ( 'NONE', #24154, #1175, #19601 ) ;
#13853 = CARTESIAN_POINT ( 'NONE',  ( -7.999999999999991118, 3.313708498984756723, 17.42405278392014623 ) ) ;
#13854 = DIRECTION ( 'NONE',  ( 0.000000000000000000, 0.000000000000000000, 1.000000000000000000 ) ) ;
#13855 = CARTESIAN_POINT ( 'NONE',  ( 10.00000000000000178, 172.0833333265053398, -2.679491924311226736 ) ) ;
#13856 = CARTESIAN_POINT ( 'NONE',  ( -4.401442555609581635E-16, 92.65625000204838102, -7.188101187500000044 ) ) ;
#13857 = ADVANCED_FACE ( 'NONE', ( #11920 ), #28523, .T. ) ;
#13858 = COLOUR_RGB ( '',0.7921568627450980005, 0.8196078431372548767, 0.9333333333333333481 ) ;
#13859 = DIRECTION ( 'NONE',  ( -0.000000000000000000, -0.000000000000000000, -1.000000000000000000 ) ) ;
#13860 = CARTESIAN_POINT ( 'NONE',  ( -9.832129032723420536, 64.01041666325268409, 5.676582343749997150 ) ) ;
#13861 = CARTESIAN_POINT ( 'NONE',  ( 10.18810118750000093, -4.220049686691933033, 107.6875000020483810 ) ) ;
#13862 = CARTESIAN_POINT ( 'NONE',  ( 11.35316468749999785, 195.5729166632526983, 3.042071309553174174 ) ) ;
#13863 = VERTEX_POINT ( 'NONE', #68145 ) ;
#13864 = CARTESIAN_POINT ( 'NONE',  ( -2.997005883569024753, 66.06021892604954360, 26.46015439093776322 ) ) ;
#13865 = CARTESIAN_POINT ( 'NONE',  ( 4.193070328474952646, -60.66867996115637851, -23.17096354272581493 ) ) ;
#13866 = CARTESIAN_POINT ( 'NONE',  ( 1.688721909672346033, 49.97488762307308718, 40.72268565194335110 ) ) ;
#13868 = CARTESIAN_POINT ( 'NONE',  ( -11.35316468750000141, 193.4895833299193271, 3.042071309553159963 ) ) ;
#13867 = CARTESIAN_POINT ( 'NONE',  ( -26.34314575050760254, 200.6875000027312410, 174.0000000000004547 ) ) ;
#13869 = CARTESIAN_POINT ( 'NONE',  ( -8.660254037844387298, 193.9583333265053966, -5.000000000000004441 ) ) ;
#13870 = CARTESIAN_POINT ( 'NONE',  ( 7.320508075688771044, 236.2500000068279746, -7.320508075688771932 ) ) ;
#13871 = CARTESIAN_POINT ( 'NONE',  ( 1.469576158976822172E-15, -7.999999999999991118, 11.89280278392014445 ) ) ;
#13872 = ORIENTED_EDGE ( 'NONE', *, *, #58885, .T. ) ;
#13873 = CARTESIAN_POINT ( 'NONE',  ( -11.35316468750000141, 183.5937499965860411, -1.390361679473963753E-15 ) ) ;
#13874 = CARTESIAN_POINT ( 'NONE',  ( 7.188101187499992051, 8.802885111219154394E-16, 18.73655278187175455 ) ) ;
#13875 =( BOUNDED_CURVE ( )  B_SPLINE_CURVE ( 2, ( #65983, #14288, #37325, #56924, #74638, #56178, #68228, #32798, #15787 ),
 .UNSPECIFIED., .F., .F. ) 
 B_SPLINE_CURVE_WITH_KNOTS ( ( 3, 2, 2, 2, 3 ),
 ( 0.6500000000000004663, 0.6583333333333338810, 0.6666666666666671848, 0.6750000000000007105, 0.6833333333333340143 ),
 .UNSPECIFIED. ) 
 CURVE ( )  GEOMETRIC_REPRESENTATION_ITEM ( )  RATIONAL_B_SPLINE_CURVE ( ( 0.9999999999999958922, 0.9238795325112908463, 1.000000000000000000, 0.9238795325112867385, 1.000000000000000000, 0.9238795325112867385, 1.000000000000000000, 0.9238795325112806323, 1.000000000000005995 ) ) 
 REPRESENTATION_ITEM ( '' )  );
#13876 = CARTESIAN_POINT ( 'NONE',  ( -7.999999999998400391, 3.416934844025491914E-06, 16.01767659775488184 ) ) ;
#13877 = EDGE_LOOP ( 'NONE', ( #10129, #54297, #18570, #59323 ) ) ;
#13878 = EDGE_CURVE ( 'NONE', #8905, #29247, #51861, .T. ) ;
#13879 = EDGE_CURVE ( 'NONE', #59499, #72853, #5896, .T. ) ;
#13880 = CARTESIAN_POINT ( 'NONE',  ( -8.000000000000000000, 96.68750000409679046, 0.000000000000000000 ) ) ;
#13881 = B_SPLINE_CURVE_WITH_KNOTS ( 'NONE', 3,
 ( #4911, #67899, #56595, #50171, #27154, #4532, #51288, #16951, #74299, #5280, #56218, #68642, #21863, #22607, #39975, #11305, #45259, #73928, #45628, #15827, #34338, #21497, #56965, #73554, #27527, #44893 ),
 .UNSPECIFIED., .F., .F.,
 ( 4, 2, 2, 2, 2, 2, 2, 2, 2, 2, 2, 2, 4 ),
 ( 0.000000000000000000, 0.001829763450930076358, 0.002744645176395114211, 0.003659526901860152715, 0.004574408627325191219, 0.005489290352790228422, 0.006404172078255266493, 0.007319053803720305430, 0.008233935529185342633, 0.009148817254650382438, 0.01097858070558046205, 0.01280834415651054339, 0.01463810760744062647 ),
 .UNSPECIFIED. ) ;
#13883 = ADVANCED_FACE ( 'NONE', ( #4781 ), #9846, .F. ) ;
#13882 = CARTESIAN_POINT ( 'NONE',  ( 4.999999999999993783, 4.166666666666666963, 8.660254037844390851 ) ) ;
#13884 = CARTESIAN_POINT ( 'NONE',  ( -4.000000000000001776, 15.43749999999999822, -1.656854249492381470 ) ) ;
#13885 =( BOUNDED_CURVE ( )  B_SPLINE_CURVE ( 2, ( #18293, #40189, #41309, #11522, #64317, #29249, #23207, #63948, #23577, #52261, #28866, #46219, #69236 ),
 .UNSPECIFIED., .F., .F. ) 
 B_SPLINE_CURVE_WITH_KNOTS ( ( 3, 2, 2, 2, 2, 2, 3 ),
 ( 0.1793478260869565133, 0.1811594202898550721, 0.1829710144927536308, 0.1847826086956521618, 0.1865942028985506929, 0.1884057971014492516, 0.1902173913043478104 ),
 .UNSPECIFIED. ) 
 CURVE ( )  GEOMETRIC_REPRESENTATION_ITEM ( )  RATIONAL_B_SPLINE_CURVE ( ( 1.000000000000000000, 0.9659258262890683122, 1.000000000000000000, 0.9659258262890683122, 1.000000000000000000, 0.9659258262890683122, 1.000000000000000000, 0.9659258262890683122, 1.000000000000000000, 0.9659258262890683122, 1.000000000000000000, 0.9659258262890688673, 0.9999999999999994449 ) ) 
 REPRESENTATION_ITEM ( '' )  );
#13886 = CARTESIAN_POINT ( 'NONE',  ( 1.881053915767121998, 14.49999999863440969, -4.541265875000002339 ) ) ;
#13887 = CARTESIAN_POINT ( 'NONE',  ( 3.313708498984756279, 7.999999999999991118, 14.04905278392014978 ) ) ;
#13888 = CARTESIAN_POINT ( 'NONE',  ( 7.999999999999991118, -4.373337617987190320E-05, 18.26780154663448386 ) ) ;
#13889 = ORIENTED_EDGE ( 'NONE', *, *, #39004, .T. ) ;
#13890 = DIRECTION ( 'NONE',  ( 0.000000000000000000, 6.938893903907228378E-16, 1.000000000000000000 ) ) ;
#13891 = CARTESIAN_POINT ( 'NONE',  ( -7.188101187499999156, 100.2500000020483952, 2.977408999572654924 ) ) ;
#13892 = VECTOR ( 'NONE', #32461, 1000.000000000000000 ) ;
#13893 = ADVANCED_FACE ( 'NONE', ( #57208 ), #74548, .T. ) ;
#13894 = CARTESIAN_POINT ( 'NONE',  ( -7.347880794884122694E-16, 13.49999999726881406, 4.000000000000001776 ) ) ;
#13895 = CARTESIAN_POINT ( 'NONE',  ( 1424.688200795887269, 427.4838061919900838, 997.8421604560587639 ) ) ;
#13896 = ORIENTED_EDGE ( 'NONE', *, *, #50675, .F. ) ;
#13897 = CARTESIAN_POINT ( 'NONE',  ( 0.4320110153365225858, 49.91454558246021378, -40.68976686129062870 ) ) ;
#13898 = VECTOR ( 'NONE', #48793, 1000.000000000000000 ) ;
#13899 = CARTESIAN_POINT ( 'NONE',  ( 5.082755093536320601, -5.082755093536318824, 21.54905278187175455 ) ) ;
#13900 = ORIENTED_EDGE ( 'NONE', *, *, #61775, .T. ) ;
#13901 = ORIENTED_EDGE ( 'NONE', *, *, #69535, .F. ) ;
#13902 = CARTESIAN_POINT ( 'NONE',  ( 4.220049686691941027, -10.18810118749999738, 78.62500000204838102 ) ) ;
#13903 = CARTESIAN_POINT ( 'NONE',  ( 11.35316468749999785, 55.88541666325266988, 3.042071309553174174 ) ) ;
#13904 = CYLINDRICAL_SURFACE ( 'NONE', #44463, 3.999999999999988010 ) ;
#13905 = CARTESIAN_POINT ( 'NONE',  ( -6.735557395310442023E-16, 11.00000000000000000, 93.62499999999998579 ) ) ;
#13908 = CARTESIAN_POINT ( 'NONE',  ( 2.765530957081996366, 295.2968750017070079, -6.676582343750002480 ) ) ;
#13907 = CARTESIAN_POINT ( 'NONE',  ( 26.34314575050758833, 199.6875000027312126, 165.9999999999998863 ) ) ;
#13906 = CARTESIAN_POINT ( 'NONE',  ( 28.00000000000001776, 196.1250000027311842, 173.9999999999999147 ) ) ;
#13909 = CARTESIAN_POINT ( 'NONE',  ( -4.999999999999998224, 141.6666666666666572, -8.660254037844389075 ) ) ;
#13910 = CARTESIAN_POINT ( 'NONE',  ( 3.999999999999960032, 209.0625000027312126, 143.6568542494924259 ) ) ;
#13911 = CARTESIAN_POINT ( 'NONE',  ( -4.898587196589407898E-16, 7.999999999999991118, 15.45530277982336642 ) ) ;
#13912 = CARTESIAN_POINT ( 'NONE',  ( 8.000000000000000000, 1.312499995903220196, 0.000000000000000000 ) ) ;
#13913 = CARTESIAN_POINT ( 'NONE',  ( 29.43265458321761230, 199.5000000013656063, 173.4587341249998929 ) ) ;
#13914 = CARTESIAN_POINT ( 'NONE',  ( -1.320432766682874540E-15, 9.468749997951610098, 7.188101187500000044 ) ) ;
#13915 = CARTESIAN_POINT ( 'NONE',  ( 7.999999999999991118, 3.313708498984757611, 27.36155278392014978 ) ) ;
#13916 = CARTESIAN_POINT ( 'NONE',  ( -1.469576158976823947E-15, 11.62500000000000178, 8.000000000000000000 ) ) ;
#13917 = CARTESIAN_POINT ( 'NONE',  ( -5.082755093536325930, 107.8437500020483810, -5.082755093536325930 ) ) ;
#13919 = CARTESIAN_POINT ( 'NONE',  ( 7.999999999999992895, -7.224685084787812073E-14, 27.26780278391845513 ) ) ;
#13918 = CARTESIAN_POINT ( 'NONE',  ( 12.00000000000000000, 28.00000000000000000, -3.999999999999986233 ) ) ;
#13920 = CARTESIAN_POINT ( 'NONE',  ( 4.999999999999995559, 134.1666666666666856, 8.660254037844392627 ) ) ;
#13921 = CARTESIAN_POINT ( 'NONE',  ( -7.347880794884122694E-16, 0.7500000000000002220, 4.000000000000001776 ) ) ;
#13922 = CARTESIAN_POINT ( 'NONE',  ( -7.188101187499990274, -2.977408999572651371, 24.45530278187175455 ) ) ;
#13923 = CARTESIAN_POINT ( 'NONE',  ( 27.99999999999996447, 200.6250000027312126, 165.9999999999998863 ) ) ;
#13924 = CARTESIAN_POINT ( 'NONE',  ( -8.311093377946836114, 37.65624999658601979, -8.311093377946837890 ) ) ;
#13925 = CYLINDRICAL_SURFACE ( 'NONE', #54497, 17.50000000000000000 ) ;
#13926 = CARTESIAN_POINT ( 'NONE',  ( 6.123233995736767268E-16, 13.12499999317203425, -10.00000000000000178 ) ) ;
#13927 = DIRECTION ( 'NONE',  ( 1.000000000000000000, 0.000000000000000000, -0.000000000000000000 ) ) ;
#13928 = DIRECTION ( 'NONE',  ( -0.000000000000000000, 1.000000000000000000, -0.000000000000000000 ) ) ;
#13929 = VERTEX_POINT ( 'NONE', #73801 ) ;
#13930 = CARTESIAN_POINT ( 'NONE',  ( -4.000000000000001776, 14.50000000000000000, -4.898587196589415787E-16 ) ) ;
#13931 = CARTESIAN_POINT ( 'NONE',  ( 11.35316468750000141, 35.78124999658601268, 0.000000000000000000 ) ) ;
#13932 = CARTESIAN_POINT ( 'NONE',  ( 11.00000000000000355, -4.556349186104045046, 78.34375000409677625 ) ) ;
#13933 = CARTESIAN_POINT ( 'NONE',  ( -2.445694354108840063, 206.0625000013656063, 139.5543056458912190 ) ) ;
#13934 = FACE_OUTER_BOUND ( 'NONE', #49902, .T. ) ;
#13935 = CARTESIAN_POINT ( 'NONE',  ( -2.828427124746208943, 195.6250000000000284, 144.8284271247462129 ) ) ;
#13937 = CARTESIAN_POINT ( 'NONE',  ( -11.35316468750000141, 38.48958332991934839, 3.042071309553159963 ) ) ;
#13936 = CARTESIAN_POINT ( 'NONE',  ( 1.320432766682874540E-15, 108.0312500020483810, 7.188101187500000044 ) ) ;
#13938 = CARTESIAN_POINT ( 'NONE',  ( -5.656854249492375253, 5.656854249492375253, 12.64280277982336287 ) ) ;
#13939 = APPLICATION_CONTEXT ( 'automotive_design' ) ;
#13940 = CARTESIAN_POINT ( 'NONE',  ( -11.35316468750000141, 163.4895833299193271, 3.042071309553159963 ) ) ;
#13941 = CARTESIAN_POINT ( 'NONE',  ( 2.679491924311222739, 125.8333333265053682, 10.00000000000000355 ) ) ;
#13942 = CARTESIAN_POINT ( 'NONE',  ( 7.188101187500002709, 108.6875000020483952, 2.977408999572649151 ) ) ;
#13943 = VERTEX_POINT ( 'NONE', #22108 ) ;
#13944 = CARTESIAN_POINT ( 'NONE',  ( 5.000000000000000000, -68.60357193678697740, -20.85024232999374050 ) ) ;
#13945 = CARTESIAN_POINT ( 'NONE',  ( -5.676582343749998039, 27.76041666325268409, -9.832129032723420536 ) ) ;
#13946 = ORIENTED_EDGE ( 'NONE', *, *, #5862, .T. ) ;
#13947 = DIRECTION ( 'NONE',  ( -0.000000000000000000, -1.000000000000000000, -4.283267841918042741E-17 ) ) ;
#13948 = LINE ( 'NONE', #3408, #71491 ) ;
#13950 = CARTESIAN_POINT ( 'NONE',  ( 5.676582343750001591, 146.6145833299193555, -9.832129032723420536 ) ) ;
#13949 = CARTESIAN_POINT ( 'NONE',  ( -26.04552021810898310, -22.17630871065499321, 147.4484293028725119 ) ) ;
#13951 = LINE ( 'NONE', #42643, #59199 ) ;
#13952 = CARTESIAN_POINT ( 'NONE',  ( 3.313708498984756279, 7.999999999999991118, 18.41780278432982598 ) ) ;
#13953 = EDGE_CURVE ( 'NONE', #47258, #26574, #39490, .T. ) ;
#13954 = CARTESIAN_POINT ( 'NONE',  ( -2.849036369511732440E-14, 208.3750000027312126, 138.0000000000000568 ) ) ;
#13955 = CARTESIAN_POINT ( 'NONE',  ( 2.085542519210945334E-15, 235.1562500034140157, 11.35316468749999963 ) ) ;
#13956 = AXIS2_PLACEMENT_3D ( 'NONE', #30693, #42741, #25385 ) ;
#13957 = CARTESIAN_POINT ( 'NONE',  ( -7.204075437095965206, -7.204075437095968759, 86.21875000204836681 ) ) ;
#13958 = ORIENTED_EDGE ( 'NONE', *, *, #51032, .F. ) ;
#13959 = AXIS2_PLACEMENT_3D ( 'NONE', #4866, #56923, #28982 ) ;
#13960 = LINE ( 'NONE', #53620, #67696 ) ;
#13961 = CARTESIAN_POINT ( 'NONE',  ( 6.951808397369818766E-16, 97.34374999658601268, -11.35316468750000141 ) ) ;
#13962 = CARTESIAN_POINT ( 'NONE',  ( -7.204075437095965206, -7.204075437095968759, 100.8437500020483668 ) ) ;
#13963 = CARTESIAN_POINT ( 'NONE',  ( 2.780723358947928197E-16, 16.68749999863440436, -4.541265875000002339 ) ) ;
#13964 = VERTEX_POINT ( 'NONE', #62473 ) ;
#13965 = EDGE_LOOP ( 'NONE', ( #50723, #544, #10357 ) ) ;
#13966 = CARTESIAN_POINT ( 'NONE',  ( -8.000000000000000000, 11.15625000000000178, -3.313708498984762496 ) ) ;
#13967 = CARTESIAN_POINT ( 'NONE',  ( -8.342170076843785083E-16, 3.187499998634407028, 4.541265875000002339 ) ) ;
#13968 = EDGE_CURVE ( 'NONE', #34597, #6793, #47188, .T. ) ;
#13969 = CARTESIAN_POINT ( 'NONE',  ( 7.188101187500001821, 5.062499997951610098, -2.977408999572650483 ) ) ;
#13970 = CARTESIAN_POINT ( 'NONE',  ( 5.656854249492379694, 117.1250000040967905, -5.656854249492380582 ) ) ;
#13971 = CARTESIAN_POINT ( 'NONE',  ( 7.204075437095968759, -7.204075437095966983, 97.09375000204836681 ) ) ;
#13972 = AXIS2_PLACEMENT_3D ( 'NONE', #26875, #27241, #49890 ) ;
#13973 = CYLINDRICAL_SURFACE ( 'NONE', #9093, 8.000000000000000000 ) ;
#13974 = CARTESIAN_POINT ( 'NONE',  ( -4.000000000000002665, 2.562500000000000444, 1.656854249492380804 ) ) ;
#13975 = CARTESIAN_POINT ( 'NONE',  ( -2.828427124746192067, 17.37499999726881583, 2.828427124746190735 ) ) ;
#13976 = CARTESIAN_POINT ( 'NONE',  ( 3.211159895383561835, 2.437499998634407028, -3.211159895383561835 ) ) ;
#13977 = CARTESIAN_POINT ( 'NONE',  ( -1.432654583217662481, 209.1250000013656631, 145.4587341250000634 ) ) ;
#13978 = CARTESIAN_POINT ( 'NONE',  ( 3.458734125000016313, 195.8750000013655779, 199.4326545832176691 ) ) ;
#13979 = ADVANCED_FACE ( 'NONE', ( #65065 ), #38612, .F. ) ;
#13982 = CARTESIAN_POINT ( 'NONE',  ( 6.123233995736767268E-16, 223.1249999931720254, -10.00000000000000178 ) ) ;
#13981 = CARTESIAN_POINT ( 'NONE',  ( -29.43265458321755901, 200.8750000013656063, 173.4587341250004044 ) ) ;
#13980 =( BOUNDED_SURFACE ( )  B_SPLINE_SURFACE ( 3, 2, ( 
 ( #22840, #63577, #4765 ),
 ( #10416, #17556, #33447 ),
 ( #45478, #10785, #16797 ),
 ( #39091, #39825, #62094 ),
 ( #28506, #62829, #40200 ),
 ( #44749, #67763, #11532 ),
 ( #11165, #56446, #46229 ),
 ( #27757, #50769, #34187 ),
 ( #57191, #34565, #73783 ),
 ( #51515, #33821, #74530 ),
 ( #45118, #68129, #57571 ),
 ( #45853, #39458, #62457 ),
 ( #68870, #69246, #56818 ),
 ( #5881, #28877, #11904 ),
 ( #69996, #23959, #19037 ),
 ( #976, #41319, #53748 ),
 ( #1343, #6623, #29260 ),
 ( #47696, #13358, #34937 ) ),
 .UNSPECIFIED., .F., .F., .F. ) 
 B_SPLINE_SURFACE_WITH_KNOTS ( ( 4, 2, 2, 2, 2, 2, 2, 2, 4 ),
 ( 3, 3 ),
 ( 0.04202945594032910653, 0.04396162471216781553, 0.04589379348400653147, 0.04782596225584524741, 0.04975813102768396334, 0.05169029979952267928, 0.05265638418544203725, 0.05362246857136139522, 0.05748680611503882015 ),
 ( 0.000000000000000000, 1.000000000000000000 ),
 .UNSPECIFIED. ) 
 GEOMETRIC_REPRESENTATION_ITEM ( )  RATIONAL_B_SPLINE_SURFACE ( (
 ( 1.000000000000000000, 0.6241276099608161765, 1.000000000000000000),
 ( 1.000000000000000000, 0.6218761496803369981, 1.000000000000000000),
 ( 1.000000000000000000, 0.6198047272360041049, 1.000000000000000000),
 ( 1.000000000000000000, 0.6161935119828376717, 1.000000000000000000),
 ( 1.000000000000000000, 0.6146642324084842235, 1.000000000000000000),
 ( 1.000000000000000000, 0.6121850116867159075, 1.000000000000000000),
 ( 1.000000000000000000, 0.6112350889402272669, 1.000000000000000000),
 ( 1.000000000000000000, 0.6099522725970315529, 1.000000000000000000),
 ( 1.000000000000000000, 0.6096208180308009261, 1.000000000000000000),
 ( 1.000000000000000000, 0.6096183796349370354, 1.000000000000000000),
 ( 1.000000000000000000, 0.6099422200101830560, 1.000000000000000000),
 ( 1.000000000000000000, 0.6109087447823331463, 1.000000000000000000),
 ( 1.000000000000000000, 0.6113123981686992003, 1.000000000000000000),
 ( 1.000000000000000000, 0.6122677719810616370, 1.000000000000000000),
 ( 1.000000000000000000, 0.6128199619022168809, 1.000000000000000000),
 ( 1.000000000000000000, 0.6159350830261014487, 1.000000000000000000),
 ( 1.000000000000000000, 0.6195556778519170082, 1.000000000000000000),
 ( 1.000000000000000000, 0.6241278272307890784, 1.000000000000000000) ) ) 
 REPRESENTATION_ITEM ( '' )  SURFACE ( )  );
#13983 = EDGE_CURVE ( 'NONE', #19989, #74609, #19471, .T. ) ;
#13984 = CARTESIAN_POINT ( 'NONE',  ( -1.881053915767124440, 15.99999999863440614, 4.541265875000001451 ) ) ;
#13985 = CYLINDRICAL_SURFACE ( 'NONE', #28416, 37.00000000000000711 ) ;
#13986 = CARTESIAN_POINT ( 'NONE',  ( 7.188101187499992051, 8.802885111219154394E-16, 9.736552781871754547 ) ) ;
#13987 = ORIENTED_EDGE ( 'NONE', *, *, #68470, .T. ) ;
#13988 = ORIENTED_EDGE ( 'NONE', *, *, #49600, .T. ) ;
#13989 = CARTESIAN_POINT ( 'NONE',  ( -10.18810118749999916, 0.000000000000000000, 96.15625000204838102 ) ) ;
#13990 = CARTESIAN_POINT ( 'NONE',  ( 0.000000000000000000, 0.000000000000000000, -4.000000000000001776 ) ) ;
#13991 = CARTESIAN_POINT ( 'NONE',  ( -26.56734541678232731, 202.2500000013655779, 173.4587341250003760 ) ) ;
#13992 = CARTESIAN_POINT ( 'NONE',  ( -29.65685424949241167, 201.0625000000000000, 166.0000000000004263 ) ) ;
#13993 = CARTESIAN_POINT ( 'NONE',  ( -1.432654583217607858, 197.6250000013656063, 201.4587341250000065 ) ) ;
#13994 = CARTESIAN_POINT ( 'NONE',  ( 2.997893585525398702E-11, 31.24999999999767653, -10.00000000000000178 ) ) ;
#13995 = CARTESIAN_POINT ( 'NONE',  ( -1.836970198721029983E-15, 113.7500000000000000, 10.00000000000000178 ) ) ;
#13996 = EDGE_CURVE ( 'NONE', #58474, #26634, #51149, .T. ) ;
#13997 = EDGE_CURVE ( 'NONE', #50322, #64865, #8120, .T. ) ;
#13998 = CARTESIAN_POINT ( 'NONE',  ( -7.999999999999998224, 113.0937500000000000, 3.313708498984766493 ) ) ;
#13999 = CARTESIAN_POINT ( 'NONE',  ( 6.676582343750004256, 298.0468750017070647, 2.765530957081995478 ) ) ;
#14000 =( GEOMETRIC_REPRESENTATION_CONTEXT ( 3 ) GLOBAL_UNCERTAINTY_ASSIGNED_CONTEXT ( ( #7166 ) ) GLOBAL_UNIT_ASSIGNED_CONTEXT ( ( #1518, #24496, #18105 ) ) REPRESENTATION_CONTEXT ( 'NONE', 'WORKASPACE' ) );
#14001 = ORIENTED_EDGE ( 'NONE', *, *, #67751, .T. ) ;
#14003 =( BOUNDED_CURVE ( )  B_SPLINE_CURVE ( 2, ( #57154, #34902, #29221, #5470, #62424, #6216, #51480, #6583, #52235, #45819, #40535, #46190, #56783, #567, #68830, #17142, #29589, #40167, #69583, #63172, #34531, #12229, #52602, #63918, #57537, #57908, #5846, #51858, #23550, #15372, #10749, #940, #17896, #202, #63541, #23180, #35266, #17519, #58281, #23922, #31054, #65014, #25012, #58639, #64291, #19733, #69956, #8418, #42374, #19360, #6947, #48403, #48031, #29959, #65389, #14060, #36360, #59013, #1670, #71040, #13322, #18639, #42005, #7686, #70324, #30694, #47300, #12599, #30325, #52972, #31433, #53712, #60100, #13687, #54460, #2389, #36728, #24650, #59375, #2025, #1305, #18266, #41281, #47660, #35625, #70682, #53343, #41648, #46931, #64658, #24287, #59741, #12956, #35996, #8049, #7320, #18999, #54081, #65757, #37096, #25386, #71408, #42742, #2767, #66886, #3894, #3143, #26887, #15193, #10293, #38221, #31812, #67265, #26503, #32188, #8799, #55208, #44253, #3513, #9556, #15560, #66131, #37469, #9170, #56317, #33319, #60850, #44622, #61227, #32949, #54833, #73294, #20853, #43871, #49904, #60470, #43112, #21596, #48775, #61965, #21227, #72918, #32570, #67637, #55579, #38599, #49527, #61598, #25754, #72548, #9917, #55956, #4266, #72158, #27256, #50272, #49146, #15932, #26126, #14436, #38962, #71782, #20468, #43488, #20098, #66500, #14811, #37852, #5747, #6124, #63080, #51388, #11405, #56697, #5378, #69118, #74027, #28747, #27633, #17802, #45726, #28010, #50641, #40076, #39335, #22330, #22709, #39700, #34069, #62332, #23460, #46472, #10659, #33692, #16295, #29129, #5012, #23088, #57441, #74400, #68740, #63823, #17053, #51019, #46100, #28379, #11038, #45357, #4636, #34442, #73659, #21968, #57065, #68371, #44995, #16669, #57817, #62700, #17424, #40448, #51763, #63447, #40817, #110, #11772, #67999, #34810, #52145, #69492, #479, #12139, #35176, #7595, #65665, #7965, #24194, #24924, #48313, #2297, #71320, #53987, #29869, #12505, #25295, #30601, #58552, #12868, #35537, #19641, #7231, #41917, #47206, #30235, #47571, #29502, #42654, #70238, #6495, #6857, #41192, #13963, #52513, #70955, #18547, #58191, #19273, #35905, #53623, #36271, #23835, #42283, #52883, #1215, #850, #41553, #36639, #18177, #64202, #64571, #46841, #69864, #58923, #1935, #53253, #64928, #47938, #1581, #24565, #70594, #65297, #13237, #13602, #18911, #59647, #59287, #30968, #72063, #21136, #43780, #55116, #4179, #54367, #9830, #60009, #73205, #32477, #9461, #48683, #38507, #15097, #71689, #55486, #27166, #26407, #49055, #66411, #38130, #3420, #3800, #26799, #66793, #60378, #20762, #37377, #2678, #20381, #43018, #21510, #61131, #50183, #49813, #44532, #67174, #72829, #14721, #32096, #49435, #66040, #44160, #8327, #31337, #31720, #15470, #25665, #67543, #72454, #43397 ),
 .UNSPECIFIED., .F., .F. ) 
 B_SPLINE_CURVE_WITH_KNOTS ( ( 3, 2, 2, 2, 2, 2, 2, 2, 2, 2, 2, 2, 2, 2, 2, 2, 2, 2, 2, 2, 2, 2, 2, 2, 2, 2, 2, 2, 2, 2, 2, 2, 2, 2, 2, 2, 2, 2, 2, 2, 2, 2, 2, 2, 2, 2, 2, 2, 2, 2, 2, 2, 2, 2, 2, 2, 2, 2, 2, 2, 2, 2, 2, 2, 2, 2, 2, 2, 2, 2, 2, 2, 2, 2, 2, 2, 2, 2, 2, 2, 2, 2, 2, 2, 2, 2, 2, 2, 2, 2, 2, 2, 2, 2, 2, 2, 2, 2, 2, 2, 2, 2, 2, 2, 2, 2, 2, 2, 2, 2, 2, 2, 2, 2, 2, 2, 2, 2, 2, 2, 2, 2, 2, 2, 2, 2, 2, 2, 2, 2, 2, 2, 2, 2, 2, 2, 2, 2, 2, 2, 2, 2, 2, 2, 2, 2, 2, 2, 2, 2, 2, 2, 2, 2, 2, 2, 2, 2, 2, 2, 2, 2, 2, 2, 2, 2, 2, 2, 2, 2, 2, 2, 2, 3 ),
 ( 0.000000000000000000, 0.005681818181818181976, 0.01136363636363636395, 0.01704545454545454419, 0.02272727272727272790, 0.02840909090909090814, 0.03409090909090908839, 0.03977272727272727210, 0.04545454545454545581, 0.05113636363636363952, 0.05681818181818181629, 0.06250000000000000000, 0.06818181818181817677, 0.07386363636363636742, 0.07954545454545454419, 0.08522727272727272096, 0.09090909090909091161, 0.09659090909090908839, 0.1022727272727272790, 0.1079545454545454558, 0.1136363636363636326, 0.1193181818181818232, 0.1250000000000000000, 0.1306818181818181768, 0.1363636363636363535, 0.1420454545454545581, 0.1477272727272727348, 0.1534090909090909116, 0.1590909090909090884, 0.1647727272727272652, 0.1704545454545454419, 0.1761363636363636465, 0.1818181818181818232, 0.1875000000000000000, 0.1931818181818181768, 0.1988636363636363535, 0.2045454545454545581, 0.2102272727272727348, 0.2159090909090909116, 0.2215909090909090884, 0.2272727272727272652, 0.2329545454545454419, 0.2386363636363636465, 0.2443181818181818232, 0.2500000000000000000, 0.2556818181818181768, 0.2613636363636363535, 0.2670454545454545303, 0.2727272727272727071, 0.2784090909090908839, 0.2840909090909091161, 0.2897727272727272929, 0.2954545454545454697, 0.3011363636363636465, 0.3068181818181818232, 0.3125000000000000000, 0.3181818181818181768, 0.3238636363636363535, 0.3295454545454545303, 0.3352272727272727071, 0.3409090909090908839, 0.3465909090909091161, 0.3522727272727272929, 0.3579545454545454697, 0.3636363636363636465, 0.3693181818181818232, 0.3750000000000000000, 0.3806818181818181768, 0.3863636363636363535, 0.3920454545454545303, 0.3977272727272727071, 0.4034090909090908839, 0.4090909090909091161, 0.4147727272727272929, 0.4204545454545454697, 0.4261363636363636465, 0.4318181818181818232, 0.4375000000000000000, 0.4431818181818181768, 0.4488636363636363535, 0.4545454545454545303, 0.4602272727272727071, 0.4659090909090908839, 0.4715909090909091161, 0.4772727272727272929, 0.4829545454545454697, 0.4886363636363636465, 0.4943181818181818232, 0.5000000000000000000, 0.5056818181818182323, 0.5113636363636363535, 0.5170454545454545858, 0.5227272727272727071, 0.5284090909090909394, 0.5340909090909090606, 0.5397727272727272929, 0.5454545454545454142, 0.5511363636363636465, 0.5568181818181817677, 0.5625000000000001110, 0.5681818181818182323, 0.5738636363636363535, 0.5795454545454545858, 0.5852272727272727071, 0.5909090909090909394, 0.5965909090909090606, 0.6022727272727272929, 0.6079545454545454142, 0.6136363636363636465, 0.6193181818181817677, 0.6250000000000000000, 0.6306818181818182323, 0.6363636363636363535, 0.6420454545454545858, 0.6477272727272727071, 0.6534090909090909394, 0.6590909090909090606, 0.6647727272727272929, 0.6704545454545454142, 0.6761363636363636465, 0.6818181818181817677, 0.6874999999999998890, 0.6931818181818182323, 0.6988636363636363535, 0.7045454545454545858, 0.7102272727272727071, 0.7159090909090909394, 0.7215909090909090606, 0.7272727272727272929, 0.7329545454545454142, 0.7386363636363636465, 0.7443181818181817677, 0.7500000000000000000, 0.7556818181818182323, 0.7613636363636363535, 0.7670454545454545858, 0.7727272727272727071, 0.7784090909090909394, 0.7840909090909090606, 0.7897727272727272929, 0.7954545454545454142, 0.8011363636363636465, 0.8068181818181817677, 0.8125000000000001110, 0.8181818181818182323, 0.8238636363636363535, 0.8295454545454545858, 0.8352272727272727071, 0.8409090909090909394, 0.8465909090909090606, 0.8522727272727272929, 0.8579545454545454142, 0.8636363636363636465, 0.8693181818181817677, 0.8750000000000000000, 0.8806818181818182323, 0.8863636363636363535, 0.8920454545454545858, 0.8977272727272727071, 0.9034090909090909394, 0.9090909090909090606, 0.9147727272727272929, 0.9204545454545454142, 0.9261363636363636465, 0.9318181818181817677, 0.9374999999999998890, 0.9431818181818182323, 0.9488636363636363535, 0.9545454545454545858, 0.9602272727272727071, 0.9659090909090909394, 0.9715909090909090606, 0.9772727272727272929, 0.9801136364233462572 ),
 .UNSPECIFIED. ) 
 CURVE ( )  GEOMETRIC_REPRESENTATION_ITEM ( )  RATIONAL_B_SPLINE_CURVE ( ( 1.000000000000000000, 0.9238795325112867385, 1.000000000000000000, 0.9238795325112867385, 1.000000000000000000, 0.9238795325112867385, 1.000000000000000000, 0.9238795325112867385, 1.000000000000000000, 0.9238795325112867385, 1.000000000000000000, 0.9238795325112867385, 1.000000000000000000, 0.9238795325112867385, 1.000000000000000000, 0.9238795325112867385, 1.000000000000000000, 0.9238795325112867385, 1.000000000000000000, 0.9238795325112867385, 1.000000000000000000, 0.9238795325112867385, 1.000000000000000000, 0.9238795325112867385, 1.000000000000000000, 0.9238795325112867385, 1.000000000000000000, 0.9238795325112867385, 1.000000000000000000, 0.9238795325112867385, 1.000000000000000000, 0.9238795325112867385, 1.000000000000000000, 0.9238795325112867385, 1.000000000000000000, 0.9238795325112867385, 1.000000000000000000, 0.9238795325112867385, 1.000000000000000000, 0.9238795325112867385, 1.000000000000000000, 0.9238795325112867385, 1.000000000000000000, 0.9238795325112867385, 1.000000000000000000, 0.9238795325112867385, 1.000000000000000000, 0.9238795325112867385, 1.000000000000000000, 0.9238795325112867385, 1.000000000000000000, 0.9238795325112867385, 1.000000000000000000, 0.9238795325112867385, 1.000000000000000000, 0.9238795325112867385, 1.000000000000000000, 0.9238795325112867385, 1.000000000000000000, 0.9238795325112867385, 1.000000000000000000, 0.9238795325112867385, 1.000000000000000000, 0.9238795325112867385, 1.000000000000000000, 0.9238795325112867385, 1.000000000000000000, 0.9238795325112867385, 1.000000000000000000, 0.9238795325112867385, 1.000000000000000000, 0.9238795325112867385, 1.000000000000000000, 0.9238795325112867385, 1.000000000000000000, 0.9238795325112867385, 1.000000000000000000, 0.9238795325112867385, 1.000000000000000000, 0.9238795325112867385, 1.000000000000000000, 0.9238795325112867385, 1.000000000000000000, 0.9238795325112867385, 1.000000000000000000, 0.9238795325112867385, 1.000000000000000000, 0.9238795325112867385, 1.000000000000000000, 0.9238795325112867385, 1.000000000000000000, 0.9238795325112867385, 1.000000000000000000, 0.9238795325112867385, 1.000000000000000000, 0.9238795325112867385, 1.000000000000000000, 0.9238795325112867385, 1.000000000000000000, 0.9238795325112867385, 1.000000000000000000, 0.9238795325112867385, 1.000000000000000000, 0.9238795325112867385, 1.000000000000000000, 0.9238795325112867385, 1.000000000000000000, 0.9238795325112867385, 1.000000000000000000, 0.9238795325112867385, 1.000000000000000000, 0.9238795325112867385, 1.000000000000000000, 0.9238795325112867385, 1.000000000000000000, 0.9238795325112867385, 1.000000000000000000, 0.9238795325112867385, 1.000000000000000000, 0.9238795325112867385, 1.000000000000000000, 0.9238795325112867385, 1.000000000000000000, 0.9238795325112867385, 1.000000000000000000, 0.9238795325112867385, 1.000000000000000000, 0.9238795325112867385, 1.000000000000000000, 0.9238795325112867385, 1.000000000000000000, 0.9238795325112867385, 1.000000000000000000, 0.9238795325112867385, 1.000000000000000000, 0.9238795325112867385, 1.000000000000000000, 0.9238795325112867385, 1.000000000000000000, 0.9238795325112867385, 1.000000000000000000, 0.9238795325112867385, 1.000000000000000000, 0.9238795325112867385, 1.000000000000000000, 0.9238795325112867385, 1.000000000000000000, 0.9238795325112867385, 1.000000000000000000, 0.9238795325112867385, 1.000000000000000000, 0.9238795325112867385, 1.000000000000000000, 0.9238795325112867385, 1.000000000000000000, 0.9238795325112867385, 1.000000000000000000, 0.9238795325112867385, 1.000000000000000000, 0.9238795325112867385, 1.000000000000000000, 0.9238795325112867385, 1.000000000000000000, 0.9238795325112867385, 1.000000000000000000, 0.9238795325112867385, 1.000000000000000000, 0.9238795325112867385, 1.000000000000000000, 0.9238795325112867385, 1.000000000000000000, 0.9238795325112867385, 1.000000000000000000, 0.9238795325112867385, 1.000000000000000000, 0.9238795325112867385, 1.000000000000000000, 0.9238795325112867385, 1.000000000000000000, 0.9238795325112867385, 1.000000000000000000, 0.9238795325112867385, 1.000000000000000000, 0.9238795325112867385, 1.000000000000000000, 0.9238795325112867385, 1.000000000000000000, 0.9238795325112867385, 1.000000000000000000, 0.9238795325112867385, 1.000000000000000000, 0.9238795325112867385, 1.000000000000000000, 0.9238795325112867385, 1.000000000000000000, 0.9238795325112867385, 1.000000000000000000, 0.9238795325112867385, 1.000000000000000000, 0.9238795325112867385, 1.000000000000000000, 0.9238795325112867385, 1.000000000000000000, 0.9238795325112867385, 1.000000000000000000, 0.9238795325112867385, 1.000000000000000000, 0.9238795325112867385, 1.000000000000000000, 0.9238795325112867385, 1.000000000000000000, 0.9238795325112867385, 1.000000000000000000, 0.9238795325112867385, 1.000000000000000000, 0.9238795325112867385, 1.000000000000000000, 0.9238795325112867385, 1.000000000000000000, 0.9238795325112867385, 1.000000000000000000, 0.9238795325112867385, 1.000000000000000000, 0.9238795325112867385, 1.000000000000000000, 0.9238795325112867385, 1.000000000000000000, 0.9238795325112867385, 1.000000000000000000, 0.9238795325112867385, 1.000000000000000000, 0.9238795325112867385, 1.000000000000000000, 0.9238795325112867385, 1.000000000000000000, 0.9238795325112867385, 1.000000000000000000, 0.9238795325112867385, 1.000000000000000000, 0.9238795325112867385, 1.000000000000000000, 0.9238795325112867385, 1.000000000000000000, 0.9238795325112867385, 1.000000000000000000, 0.9238795325112867385, 1.000000000000000000, 0.9238795325112867385, 1.000000000000000000, 0.9238795325112867385, 1.000000000000000000, 0.9238795325112867385, 1.000000000000000000, 0.9238795325112867385, 1.000000000000000000, 0.9238795325112867385, 1.000000000000000000, 0.9238795325112867385, 1.000000000000000000, 0.9238795325112867385, 1.000000000000000000, 0.9238795325112867385, 1.000000000000000000, 0.9238795325112867385, 1.000000000000000000, 0.9238795325112867385, 1.000000000000000000, 0.9238795325112867385, 1.000000000000000000, 0.9238795325112867385, 1.000000000000000000, 0.9238795325112867385, 1.000000000000000000, 0.9238795325112867385, 1.000000000000000000, 0.9238795325112867385, 1.000000000000000000, 0.9238795325112867385, 1.000000000000000000, 0.9238795325112867385, 1.000000000000000000, 0.9238795325112867385, 1.000000000000000000, 0.9238795325112867385, 1.000000000000000000, 0.9238795325112867385, 1.000000000000000000, 0.9238795325112867385, 1.000000000000000000, 0.9238795325112867385, 1.000000000000000000, 0.9238795325112867385, 1.000000000000000000, 0.9238795325112867385, 1.000000000000000000, 0.9238795325112867385, 1.000000000000000000, 0.9238795325112867385, 1.000000000000000000, 0.9238795325112867385, 1.000000000000000000, 0.9238795325112867385, 1.000000000000000000, 0.9238795325112867385, 1.000000000000000000, 0.9238795325112867385, 1.000000000000000000, 0.9238795325112867385, 1.000000000000000000, 0.9238795325112867385, 1.000000000000000000, 0.9238795325112867385, 1.000000000000000000, 0.9238795325112867385, 1.000000000000000000, 0.9238795325112867385, 1.000000000000000000, 0.9238795325112867385, 1.000000000000000000, 0.9238795325112867385, 1.000000000000000000, 0.9238795325112867385, 1.000000000000000000, 0.9238795325112867385, 1.000000000000000000, 0.9238795325112867385, 1.000000000000000000, 0.9238795325112867385, 1.000000000000000000, 0.9238795325112867385, 1.000000000000000000, 0.9238795325112867385, 1.000000000000000000, 0.9238795325112867385, 1.000000000000000000, 0.9238795325112867385, 1.000000000000000000, 0.9238795325112867385, 1.000000000000000000, 0.9238795325112867385, 1.000000000000000000, 0.9238795325112867385, 1.000000000000000000, 0.9238795325112867385, 1.000000000000000000, 0.9619397654556977040, 0.9619397662556433692 ) ) 
 REPRESENTATION_ITEM ( '' )  );
#14002 = CARTESIAN_POINT ( 'NONE',  ( -4.999999999999998224, 143.5416666598386826, -8.660254037844389075 ) ) ;
#14004 = EDGE_CURVE ( 'NONE', #49749, #68115, #624, .T. ) ;
#14005 = CARTESIAN_POINT ( 'NONE',  ( 4.898587196589412829E-16, 22.68749999590322375, -8.000000000000000000 ) ) ;
#14006 = CARTESIAN_POINT ( 'NONE',  ( 3.458734124999959914, 203.3750000013656063, 143.4326545832176976 ) ) ;
#14007 = CARTESIAN_POINT ( 'NONE',  ( -38.00000000000000000, -53.00000000000000000, 15.00000000000000178 ) ) ;
#14008 = DIRECTION ( 'NONE',  ( -0.000000000000000000, 1.000000000000000000, 4.476705744456276341E-16 ) ) ;
#14009 = CARTESIAN_POINT ( 'NONE',  ( 10.00000000000000178, 227.2916666666666572, 2.679491924311222739 ) ) ;
#14010 = CARTESIAN_POINT ( 'NONE',  ( 1.469576158976823947E-15, 115.0625000040967905, 8.000000000000000000 ) ) ;
#14011 = CARTESIAN_POINT ( 'NONE',  ( 7.778174593052023411, -7.778174593052021635, 114.0625000000000000 ) ) ;
#14012 = CARTESIAN_POINT ( 'NONE',  ( 8.660254037844385522, 224.5833333333333712, 5.000000000000005329 ) ) ;
#14013 = CARTESIAN_POINT ( 'NONE',  ( -5.082755093536317936, -5.082755093536320601, 6.549052781871754547 ) ) ;
#14014 = CARTESIAN_POINT ( 'NONE',  ( -11.35316468750000141, 198.5937499965860127, -1.390361679473963753E-15 ) ) ;
#14015 = CARTESIAN_POINT ( 'NONE',  ( 9.797174393178825657E-16, 125.0000000000000000, -8.000000000000000000 ) ) ;
#14016 = CARTESIAN_POINT ( 'NONE',  ( -4.541265875000002339, 7.812499998634407028, -5.561446717895856393E-16 ) ) ;
#14017 = CARTESIAN_POINT ( 'NONE',  ( 2.751549872419338751E-14, 194.9207531772044888, 194.0792468227953975 ) ) ;
#14019 = CARTESIAN_POINT ( 'NONE',  ( 2.485281374238175189, 297.6875000000000568, -6.000000000000396128 ) ) ;
#14018 = CARTESIAN_POINT ( 'NONE',  ( -2.775557561562891351E-14, 210.0000000000000284, 146.0000000000000284 ) ) ;
#14020 = ORIENTED_EDGE ( 'NONE', *, *, #52857, .T. ) ;
#14021 = CARTESIAN_POINT ( 'NONE',  ( 2.445694354108784108, 205.5625000013656063, 144.4456943541088663 ) ) ;
#14022 = CARTESIAN_POINT ( 'NONE',  ( 3.042071309553159519, 50.05208332991935549, 11.35316468750000141 ) ) ;
#14023 = CARTESIAN_POINT ( 'NONE',  ( -7.778174593052023411, 7.778174593052023411, 103.0000000040967763 ) ) ;
#14024 = CARTESIAN_POINT ( 'NONE',  ( -4.000000000000016875, 205.4375000000000284, 140.3431457505076594 ) ) ;
#14025 = CARTESIAN_POINT ( 'NONE',  ( -31.45873412500002786, 202.6250000013656063, 168.5673454167828140 ) ) ;
#14026 = DIRECTION ( 'NONE',  ( -6.308085367188386297E-16, 0.000000000000000000, -1.000000000000000000 ) ) ;
#14028 = CARTESIAN_POINT ( 'NONE',  ( -4.999999999999998224, 58.54166665983870388, -8.660254037844389075 ) ) ;
#14027 = CARTESIAN_POINT ( 'NONE',  ( 7.188101187500000044, 121.9062500020483810, -8.802885111219163269E-16 ) ) ;
#14029 = CARTESIAN_POINT ( 'NONE',  ( 1.432654583217607192, 195.2500000013656063, 145.4587341250000350 ) ) ;
#14030 = CARTESIAN_POINT ( 'NONE',  ( 9.832129032723420536, 106.1979166632526983, -5.676582343749999815 ) ) ;
#14031 = AXIS2_PLACEMENT_3D ( 'NONE', #59555, #26314, #7870 ) ;
#14032 = CARTESIAN_POINT ( 'NONE',  ( -2.679491924311235618, 85.41666665983869677, 10.00000000000000000 ) ) ;
#14033 = CARTESIAN_POINT ( 'NONE',  ( -5.082755093536325930, 93.96875000204838102, -5.082755093536325930 ) ) ;
#14034 = CARTESIAN_POINT ( 'NONE',  ( 4.541265875000002339, 17.49999999863440436, -1.881053915767121554 ) ) ;
#14035 = CARTESIAN_POINT ( 'NONE',  ( 2.828427124746191623, 11.12500000000000000, -2.828427124746191623 ) ) ;
#14036 = AXIS2_PLACEMENT_3D ( 'NONE', #5511, #34193, #45483 ) ;
#14037 = CARTESIAN_POINT ( 'NONE',  ( -11.00000000000000000, 0.000000000000000000, 67.18750000409676204 ) ) ;
#14038 = ORIENTED_EDGE ( 'NONE', *, *, #46301, .T. ) ;
#14039 = CARTESIAN_POINT ( 'NONE',  ( -1.656854249492487607, 200.8125000027312126, 145.9999999999999716 ) ) ;
#14040 = VERTEX_POINT ( 'NONE', #58695 ) ;
#14041 = CARTESIAN_POINT ( 'NONE',  ( -6.676582343750001591, 295.6093750017069510, 0.000000000000000000 ) ) ;
#14042 = CARTESIAN_POINT ( 'NONE',  ( 0.000000000000000000, 0.000000000000000000, 118.0000000000000000 ) ) ;
#14043 = CARTESIAN_POINT ( 'NONE',  ( 1.469576158976822172E-15, -7.999999999999991118, 8.892802783920146226 ) ) ;
#14044 = CARTESIAN_POINT ( 'NONE',  ( 8.311093377946837890, 166.4062499965860127, -8.311093377946837890 ) ) ;
#14045 = LINE ( 'NONE', #21583, #58611 ) ;
#14046 = CARTESIAN_POINT ( 'NONE',  ( 2.828427124746208943, 199.6250000000000284, 195.1715728752538439 ) ) ;
#14047 = CARTESIAN_POINT ( 'NONE',  ( 9.000000000000000000, 5.196152422706648899, -0.8038475772933779684 ) ) ;
#14048 = CARTESIAN_POINT ( 'NONE',  ( -10.18810118749999738, -4.220049686691941915, 108.6250000020483668 ) ) ;
#14049 = VERTEX_POINT ( 'NONE', #59066 ) ;
#14050 = CARTESIAN_POINT ( 'NONE',  ( -5.107860025166923279, 50.62490018645984691, -41.07729128472220026 ) ) ;
#14051 = DIRECTION ( 'NONE',  ( 0.000000000000000000, 0.000000000000000000, 1.000000000000000000 ) ) ;
#14052 = CARTESIAN_POINT ( 'NONE',  ( 11.35316468750000141, 136.0937499965860127, 0.000000000000000000 ) ) ;
#14053 = DIRECTION ( 'NONE',  ( 6.308085367188386297E-16, 0.000000000000000000, 1.000000000000000000 ) ) ;
#14054 = CARTESIAN_POINT ( 'NONE',  ( -3.458734124999960358, 204.6875000013656063, 198.0000000000000284 ) ) ;
#14056 = EDGE_CURVE ( 'NONE', #60791, #10325, #41029, .T. ) ;
#14055 = CARTESIAN_POINT ( 'NONE',  ( -6.238412754330611322E-16, 10.18810118749999916, 70.65625000204836681 ) ) ;
#14057 = CARTESIAN_POINT ( 'NONE',  ( -11.35316468750000141, 68.59374999658601268, -1.390361679473963753E-15 ) ) ;
#14058 = EDGE_LOOP ( 'NONE', ( #58841, #15777, #62453, #42216 ) ) ;
#14059 = CARTESIAN_POINT ( 'NONE',  ( -1.836970198721029983E-15, 28.75000000000000000, 10.00000000000000178 ) ) ;
#14060 = CARTESIAN_POINT ( 'NONE',  ( -4.541265875000002339, 3.874999998634407028, -1.881053915767121998 ) ) ;
#14061 = CARTESIAN_POINT ( 'NONE',  ( 3.317071493978877683, 8.008118988124991233, 9.544365283940628331 ) ) ;
#14062 = ORIENTED_EDGE ( 'NONE', *, *, #55105, .T. ) ;
#14063 = CARTESIAN_POINT ( 'NONE',  ( -5.082755093536326818, 20.90624999795161543, 5.082755093536325042 ) ) ;
#14064 = DIRECTION ( 'NONE',  ( -0.000000000000000000, -1.000000000000000000, -0.000000000000000000 ) ) ;
#14065 = FACE_OUTER_BOUND ( 'NONE', #29802, .T. ) ;
#14066 = CARTESIAN_POINT ( 'NONE',  ( 38.00000000000000000, 0.000000000000000000, 20.00000000000001066 ) ) ;
#14067 = CARTESIAN_POINT ( 'NONE',  ( 7.188101187500001821, 11.43749999795161010, -2.977408999572650483 ) ) ;
#14068 = CARTESIAN_POINT ( 'NONE',  ( 1.320432766682872962E-15, -7.188101187499992051, 0.3615527818717524378 ) ) ;
#14069 = CARTESIAN_POINT ( 'NONE',  ( 10.18810118749999916, 4.220049686691935698, 116.8750000020483668 ) ) ;
#14070 = EDGE_CURVE ( 'NONE', #66510, #15239, #23974, .T. ) ;
#14071 = DIRECTION ( 'NONE',  ( -0.4999969897303749300, 0.000000000000000000, 0.8660271417574413322 ) ) ;
#14072 = CARTESIAN_POINT ( 'NONE',  ( -1.656854249492383691, 1.437499997268813390, 4.000000000000000888 ) ) ;
#14073 = ORIENTED_EDGE ( 'NONE', *, *, #26003, .T. ) ;
#14074 = CARTESIAN_POINT ( 'NONE',  ( 2.839093476692135984E-14, 208.6875000013656063, 201.4587341250000350 ) ) ;
#14075 = CARTESIAN_POINT ( 'NONE',  ( -30.82842712474612057, 196.5000000027312126, 172.8284271247466108 ) ) ;
#14076 = AXIS2_PLACEMENT_3D ( 'NONE', #47587, #47223, #31357 ) ;
#14077 = EDGE_CURVE ( 'NONE', #4744, #74182, #7754, .T. ) ;
#14078 = CARTESIAN_POINT ( 'NONE',  ( 1.881053915767122664, 2.124999998634406584, 4.541265875000001451 ) ) ;
#14079 = CARTESIAN_POINT ( 'NONE',  ( -2.977408999572651815, 109.4375000020483810, 7.188101187500000933 ) ) ;
#14080 = CARTESIAN_POINT ( 'NONE',  ( 27.99999999999996803, 209.5625000013656063, 173.4587341249998929 ) ) ;
#14081 = CARTESIAN_POINT ( 'NONE',  ( -7.188101187499991163, 2.977408999572646930, 22.39280278187175810 ) ) ;
#14082 = ORIENTED_EDGE ( 'NONE', *, *, #69784, .F. ) ;
#14083 = ADVANCED_FACE ( 'NONE', ( #53769 ), #53402, .T. ) ;
#14084 = CARTESIAN_POINT ( 'NONE',  ( -7.188101187500000933, 20.62499999795161543, -2.977408999572651371 ) ) ;
#14085 = ORIENTED_EDGE ( 'NONE', *, *, #10935, .T. ) ;
#14086 = CARTESIAN_POINT ( 'NONE',  ( -7.320508075688770155, 1.874999999999997780, -7.320508075688771044 ) ) ;
#14087 = CARTESIAN_POINT ( 'NONE',  ( -7.320508075688773708, 201.8750000000000000, -7.320508075688774596 ) ) ;
#14088 = FACE_OUTER_BOUND ( 'NONE', #40382, .T. ) ;
#14089 = CARTESIAN_POINT ( 'NONE',  ( 24.54126587500000412, 203.2500000013655495, 171.4326545832176123 ) ) ;
#14090 = CARTESIAN_POINT ( 'NONE',  ( -10.00000000000000178, 72.50000000000001421, -1.224646799147353454E-15 ) ) ;
#14091 = CARTESIAN_POINT ( 'NONE',  ( -5.082755093536324154, 96.21875000204838102, 5.082755093536326818 ) ) ;
#14092 = CARTESIAN_POINT ( 'NONE',  ( -6.000000000000001776, 296.0000000000000000, 0.000000000000000000 ) ) ;
#14094 = CARTESIAN_POINT ( 'NONE',  ( -11.00000000000000000, 0.000000000000000000, 101.5000000000000000 ) ) ;
#14093 = CARTESIAN_POINT ( 'NONE',  ( 1.739508062077475881, -51.27839935804492910, -48.57027215863523395 ) ) ;
#14095 = ORIENTED_EDGE ( 'NONE', *, *, #60680, .T. ) ;
#14096 = CARTESIAN_POINT ( 'NONE',  ( 3.042071309553173286, 225.3645833367473301, 11.35316468749999608 ) ) ;
#14097 = DIRECTION ( 'NONE',  ( -0.000000000000000000, -0.000000000000000000, -1.000000000000000000 ) ) ;
#14098 = CARTESIAN_POINT ( 'NONE',  ( -4.000000000000015987, 198.6250000027312126, 142.0000000000000568 ) ) ;
#14099 = CARTESIAN_POINT ( 'NONE',  ( 7.999999999999991118, 3.313708498984758055, 24.36155278392014978 ) ) ;
#14100 = CARTESIAN_POINT ( 'NONE',  ( 2.449293598294707893E-16, 9.250000000000000000, -4.000000000000001776 ) ) ;
#14101 = CARTESIAN_POINT ( 'NONE',  ( 24.74639540312131558, 194.8627345059741458, 167.9092417302315425 ) ) ;
#14102 = EDGE_CURVE ( 'NONE', #53531, #41098, #7316, .T. ) ;
#14103 = DIRECTION ( 'NONE',  ( -1.000000000000000000, 0.000000000000000000, 0.000000000000000000 ) ) ;
#14104 =( BOUNDED_CURVE ( )  B_SPLINE_CURVE ( 2, ( #38989, #41216, #52907, #6883, #46125, #13261, #873, #69143, #35200 ),
 .UNSPECIFIED., .F., .F. ) 
 B_SPLINE_CURVE_WITH_KNOTS ( ( 3, 2, 2, 2, 3 ),
 ( 0.2794117647058823040, 0.2830882352941175850, 0.2867647058823528661, 0.2904411764705882026, 0.2941176470588234837 ),
 .UNSPECIFIED. ) 
 CURVE ( )  GEOMETRIC_REPRESENTATION_ITEM ( )  RATIONAL_B_SPLINE_CURVE ( ( 1.000000000000001110, 0.9238795325112856283, 1.000000000000000000, 0.9238795325112867385, 1.000000000000000000, 0.9238795325112867385, 1.000000000000000000, 0.9238795325112878487, 0.9999999999999988898 ) ) 
 REPRESENTATION_ITEM ( '' )  );
#14105 = CARTESIAN_POINT ( 'NONE',  ( 4.999999999999993783, 179.1666666666666572, 8.660254037844390851 ) ) ;
#14106 = SURFACE_STYLE_FILL_AREA ( #54126 ) ;
#14107 = CARTESIAN_POINT ( 'NONE',  ( 7.188101187499992051, 8.802885111219154394E-16, 22.11155278187175455 ) ) ;
#14108 = CARTESIAN_POINT ( 'NONE',  ( 9.832129032723416984, 150.6770833299193555, 5.676582343750006032 ) ) ;
#14109 = CARTESIAN_POINT ( 'NONE',  ( 1.102182119232618108E-15, 294.3125000034140157, 6.000000000000001776 ) ) ;
#14110 = LINE ( 'NONE', #31101, #22880 ) ;
#14113 = DIRECTION ( 'NONE',  ( 0.8660254037844377084, -0.5000000000000017764, 0.000000000000000000 ) ) ;
#14112 = CARTESIAN_POINT ( 'NONE',  ( -4.999999999999998224, 83.54166665983869677, -8.660254037844389075 ) ) ;
#14111 = CARTESIAN_POINT ( 'NONE',  ( 30.82842712474617031, 204.1250000000000284, 172.8284271247460993 ) ) ;
#14114 = EDGE_LOOP ( 'NONE', ( #63352, #49238, #67568, #18111 ) ) ;
#14115 = CARTESIAN_POINT ( 'NONE',  ( 11.35316468750000141, 16.09374999658601979, 0.000000000000000000 ) ) ;
#14116 = CARTESIAN_POINT ( 'NONE',  ( -1.656854249492416109, 199.1875000000000000, 201.9999999999999432 ) ) ;
#14117 = CARTESIAN_POINT ( 'NONE',  ( 3.496982156810621412, -16.35094707925534863, -69.15443034746733986 ) ) ;
#14118 = DIRECTION ( 'NONE',  ( -0.000000000000000000, -0.000000000000000000, 1.000000000000000000 ) ) ;
#14119 = CARTESIAN_POINT ( 'NONE',  ( -2.839093476692135984E-14, 207.6875000013656063, 138.5412658750000503 ) ) ;
#14120 = CARTESIAN_POINT ( 'NONE',  ( -7.514277766361627364, 124.7823509838186169, -1.778518646698914241 ) ) ;
#14121 = CLOSED_SHELL ( 'NONE', ( #13979, #59263, #67102, #6260, #69395, #22569, #20635, #37842, #24238, #63861, #24981, #53763, #54567, #43887, #41347, #61140, #14959, #16969, #40555, #42669, #907, #60473, #33034, #23517, #19852, #21492, #19121, #66805, #50343, #22442, #15594, #31974, #61953, #70100, #61431, #72266, #28224, #43996, #29759, #61974, #21329, #19558, #53167, #1805, #6984, #70966, #13356, #44159, #46448, #16115, #5935, #8814, #49073, #27536, #49939, #29700, #69882, #66031, #72723, #46193, #22802, #64278, #13374, #16410, #19635, #38967, #29928, #63940, #44766, #47777, #26918, #25305, #71112, #4124, #27375, #54021, #25863, #57462, #3060, #74393, #16697, #50189, #7262, #54974, #15909, #37310, #34990, #46286, #43579, #71150, #38049, #47701, #68231, #73057, #58313, #18539, #11633, #69969, #66120, #12514, #29867, #45927, #18648, #14728, #55830, #57807, #47750, #63556, #52676, #8621, #33896, #17311, #12677, #33494, #690, #50, #52360, #62799, #8061, #47119, #52421, #64506, #24429, #56671, #5046, #17253, #53590, #3235, #1928, #9432, #13217, #72154, #63282, #33112, #43123, #398, #61130, #42345, #33961, #45368, #43788, #39034, #27705, #62716, #35352, #9054, #49933, #34480, #15479, #5289, #31983, #28755, #39846, #8012, #164, #8599, #12543, #27445, #60485, #57105, #18359, #10420, #61606, #41565, #41271, #13208, #42756, #317, #1208, #7226, #27247, #70734, #24229, #52865, #5154, #54866, #57351, #39988, #681, #17661, #29281, #24057, #27174, #28571, #66711, #40172, #71238, #67078, #69773, #50342, #34437, #3365, #38545, #72370, #20976, #44730, #31020, #64785, #8711, #44323, #59682, #69022, #3900, #22250, #13883, #63648, #43905, #31585, #50047, #60059, #14083, #12215, #65208, #57966, #33516, #74200, #49958, #4554, #61011, #698, #39984, #11718, #59577, #43545, #1231, #59758, #54944, #10800, #56037, #38530, #57838, #68233, #30998 ) ) ;
#14122 = CARTESIAN_POINT ( 'NONE',  ( 7.320508075688774596, 47.49999999317203958, -7.320508075688774596 ) ) ;
#14123 = CARTESIAN_POINT ( 'NONE',  ( 7.188101187500001821, 107.0000000020483810, -2.977408999572651371 ) ) ;
#14124 = CARTESIAN_POINT ( 'NONE',  ( -8.342170076843785083E-16, 3.187499998634407028, 4.541265875000002339 ) ) ;
#14125 = CARTESIAN_POINT ( 'NONE',  ( 3.511653767258104963, 68.04552192806764310, -20.40125235305975337 ) ) ;
#14126 = CARTESIAN_POINT ( 'NONE',  ( 5.656854249492374365, 5.656854249492375253, 13.76780277982336465 ) ) ;
#14128 = CARTESIAN_POINT ( 'NONE',  ( 8.660254037844385522, 6.458333326505366401, 5.000000000000005329 ) ) ;
#14127 = CARTESIAN_POINT ( 'NONE',  ( 3.240027456986572574, 194.4836769270507375, 140.7027311861366456 ) ) ;
#14129 = ORIENTED_EDGE ( 'NONE', *, *, #17919, .F. ) ;
#14130 = CARTESIAN_POINT ( 'NONE',  ( -4.898587196589412829E-16, 93.31250000409677625, -8.000000000000000000 ) ) ;
#14131 = CARTESIAN_POINT ( 'NONE',  ( 7.999999999932789763, 3.279097096261179525E-05, 13.76780373625499010 ) ) ;
#14132 = CARTESIAN_POINT ( 'NONE',  ( 8.311093377946834337, 232.3437500034140442, -8.311093377946836114 ) ) ;
#14133 = CARTESIAN_POINT ( 'NONE',  ( -11.35316468750000141, 133.4895833299193839, 3.042071309553159963 ) ) ;
#14134 = ORIENTED_EDGE ( 'NONE', *, *, #44436, .F. ) ;
#14135 = CARTESIAN_POINT ( 'NONE',  ( -1.656854249492337949, 200.3125000000000000, 138.0000000000000000 ) ) ;
#14136 = CARTESIAN_POINT ( 'NONE',  ( -4.220049686691937474, -10.18810118749999738, 93.43750000204836681 ) ) ;
#14137 = CARTESIAN_POINT ( 'NONE',  ( 4.089761226760953328, 227.7900538254533558, -9.185780638600787640 ) ) ;
#14138 = CARTESIAN_POINT ( 'NONE',  ( -3.458734124999959469, 196.7500000013656063, 199.4326545832176691 ) ) ;
#14139 = CARTESIAN_POINT ( 'NONE',  ( 2.449293598294707893E-16, 17.25000000000000000, -4.000000000000001776 ) ) ;
#14141 = CARTESIAN_POINT ( 'NONE',  ( 8.311093377946834337, 115.1562499965859985, 8.311093377946839666 ) ) ;
#14140 = DIRECTION ( 'NONE',  ( -1.000000000000000000, 0.000000000000000000, 0.000000000000000000 ) ) ;
#14142 = CARTESIAN_POINT ( 'NONE',  ( -25.17157287525382614, 209.8750000000000284, 167.1715728752541565 ) ) ;
#14143 = ADVANCED_FACE ( 'NONE', ( #3572 ), #8857, .F. ) ;
#14144 = CARTESIAN_POINT ( 'NONE',  ( 7.320508075688771044, 81.24999999317202537, 7.320508075688775484 ) ) ;
#14145 = ORIENTED_EDGE ( 'NONE', *, *, #45349, .F. ) ;
#14146 = AXIS2_PLACEMENT_3D ( 'NONE', #58970, #1264, #12917 ) ;
#14147 = CARTESIAN_POINT ( 'NONE',  ( 1.224646799147353454E-15, 300.0000000000000000, -10.00000000000000178 ) ) ;
#14148 = CARTESIAN_POINT ( 'NONE',  ( 29.65685424949229088, 202.0625000000000568, 174.0000000000000284 ) ) ;
#14149 = CARTESIAN_POINT ( 'NONE',  ( 5.676582343750001591, 106.9270833299193413, -9.832129032723420536 ) ) ;
#14150 = CARTESIAN_POINT ( 'NONE',  ( -3.458734124999959914, 205.3750000013656063, 196.5673454167823877 ) ) ;
#14151 = CARTESIAN_POINT ( 'NONE',  ( 2.977408999572652260, 14.06249999795161365, 7.188101187500000044 ) ) ;
#14153 = ADVANCED_FACE ( 'NONE', ( #71463 ), #26187, .F. ) ;
#14152 = CARTESIAN_POINT ( 'NONE',  ( -10.18810118749999738, -4.220049686691941915, 87.62500000204836681 ) ) ;
#14154 = B_SPLINE_CURVE_WITH_KNOTS ( 'NONE', 3,
 ( #19403, #31098, #36405, #59418, #70725, #70369, #47344, #53019, #24694 ),
 .UNSPECIFIED., .F., .F.,
 ( 4, 2, 1, 2, 4 ),
 ( 0.000000000000000000, 0.001314083742615069009, 0.002628167485230138017, 0.003942251227845207026, 0.005256334970460276035 ),
 .UNSPECIFIED. ) ;
#14155 = CARTESIAN_POINT ( 'NONE',  ( -3.042071309553164404, 27.55208332991935194, -11.35316468749999963 ) ) ;
#14156 = ORIENTED_EDGE ( 'NONE', *, *, #13068, .F. ) ;
#14157 = CARTESIAN_POINT ( 'NONE',  ( 6.123233995736767268E-16, 183.1249999931720538, -10.00000000000000178 ) ) ;
#14158 = CARTESIAN_POINT ( 'NONE',  ( 3.317071493978877683, 8.008118988124991233, 26.04436528394063188 ) ) ;
#14159 = CARTESIAN_POINT ( 'NONE',  ( -1.836970198721029983E-15, 115.6249999931720396, 10.00000000000000178 ) ) ;
#14160 = CARTESIAN_POINT ( 'NONE',  ( -7.204075437095965206, -7.204075437095968759, 72.71875000204838102 ) ) ;
#14161 = CARTESIAN_POINT ( 'NONE',  ( 0.000000000000000000, 0.000000000000000000, 0.000000000000000000 ) ) ;
#14162 = CARTESIAN_POINT ( 'NONE',  ( 7.188101187500001821, 0.5624999979516098758, -2.977408999572650483 ) ) ;
#14163 = CARTESIAN_POINT ( 'NONE',  ( 6.676582343750004256, 292.8906250017068942, 2.765530957081995478 ) ) ;
#14164 = FACE_OUTER_BOUND ( 'NONE', #70890, .T. ) ;
#14165 = CARTESIAN_POINT ( 'NONE',  ( 11.35316468749999963, 221.3020833299193271, -3.042071309553165293 ) ) ;
#14166 = CARTESIAN_POINT ( 'NONE',  ( 8.311093377946837890, 126.7187499965860269, -8.311093377946837890 ) ) ;
#14167 = CARTESIAN_POINT ( 'NONE',  ( -6.238412754330611322E-16, 10.18810118749999916, 82.28125000204838102 ) ) ;
#14168 = EDGE_CURVE ( 'NONE', #33244, #64315, #66188, .T. ) ;
#14169 = CARTESIAN_POINT ( 'NONE',  ( -29.43265458321760519, 200.8750000013656063, 173.4587341250003760 ) ) ;
#14170 = CARTESIAN_POINT ( 'NONE',  ( 5.656854249492380582, 21.18750000000000355, -5.656854249492380582 ) ) ;
#14171 = CARTESIAN_POINT ( 'NONE',  ( 3.211159895383561835, 13.56249999863440614, -3.211159895383561835 ) ) ;
#14172 = VERTEX_POINT ( 'NONE', #19788 ) ;
#14173 = CARTESIAN_POINT ( 'NONE',  ( -3.999999999999960032, 204.1250000027312126, 198.0000000000000284 ) ) ;
#14174 = AXIS2_PLACEMENT_3D ( 'NONE', #44594, #22303, #4982 ) ;
#14175 = CARTESIAN_POINT ( 'NONE',  ( 3.458734124999960358, 200.6875000013656063, 142.0000000000000568 ) ) ;
#14176 = CARTESIAN_POINT ( 'NONE',  ( -4.000000000000015987, 203.5625000027312126, 140.3431457505076594 ) ) ;
#14177 = CARTESIAN_POINT ( 'NONE',  ( -4.999999999999999112, 10.82378452496245735, 67.02990231369408036 ) ) ;
#14178 = CARTESIAN_POINT ( 'NONE',  ( -4.220049686691937474, -10.18810118749999738, 68.31250000204838102 ) ) ;
#14179 = ORIENTED_EDGE ( 'NONE', *, *, #58752, .F. ) ;
#14180 = CARTESIAN_POINT ( 'NONE',  ( -1.320432766682874540E-15, 7.593749997951611874, 7.188101187500000044 ) ) ;
#14181 = FACE_OUTER_BOUND ( 'NONE', #7708, .T. ) ;
#14182 = CARTESIAN_POINT ( 'NONE',  ( 7.188101187500002709, 111.6875000020483810, 2.977408999572649151 ) ) ;
#14183 = CARTESIAN_POINT ( 'NONE',  ( 1.377000000000000002, 278.5679999999998699, 5.673918265505059289 ) ) ;
#14184 = CARTESIAN_POINT ( 'NONE',  ( 6.676582343750002480, 294.0156250017068942, -2.765530957081997254 ) ) ;
#14186 = CARTESIAN_POINT ( 'NONE',  ( 5.000000000000001776, 137.7083333265053682, -8.660254037844389075 ) ) ;
#14185 = CARTESIAN_POINT ( 'NONE',  ( 10.00000000000000178, 131.8749999931720254, 0.000000000000000000 ) ) ;
#14187 = EDGE_LOOP ( 'NONE', ( #28377, #69634, #41304, #37667 ) ) ;
#14188 = VECTOR ( 'NONE', #65704, 1000.000000000000000 ) ;
#14189 = CARTESIAN_POINT ( 'NONE',  ( 3.042071309553173286, 220.6770833367472733, 11.35316468749999608 ) ) ;
#14190 = CARTESIAN_POINT ( 'NONE',  ( 1.320432766682872962E-15, -7.188101187499992051, 1.861552781871753881 ) ) ;
#14191 = DIRECTION ( 'NONE',  ( 0.000000000000000000, 1.000000000000000000, 0.000000000000000000 ) ) ;
#14192 = LINE ( 'NONE', #11166, #4457 ) ;
#14193 = CARTESIAN_POINT ( 'NONE',  ( 1.432654583217662481, 200.3750000013656063, 194.5412658750000219 ) ) ;
#14194 = ORIENTED_EDGE ( 'NONE', *, *, #74053, .T. ) ;
#14195 = DIRECTION ( 'NONE',  ( -1.000000000000000000, 0.000000000000000000, 0.000000000000000000 ) ) ;
#14196 = CARTESIAN_POINT ( 'NONE',  ( -8.000000000000000000, 97.90625000000000000, -3.313708498984761608 ) ) ;
#14197 = CARTESIAN_POINT ( 'NONE',  ( -9.832129032723418760, 113.1770833299193555, -5.676582343750004256 ) ) ;
#14198 = CARTESIAN_POINT ( 'NONE',  ( 4.999999999999993783, 211.0416666598387110, 8.660254037844390851 ) ) ;
#14199 = CARTESIAN_POINT ( 'NONE',  ( -7.778174593052020747, -7.778174593052023411, 74.68749999999998579 ) ) ;
#14202 = CARTESIAN_POINT ( 'NONE',  ( 28.00000000000001776, 204.5000000000000284, 165.9999999999998863 ) ) ;
#14201 = CARTESIAN_POINT ( 'NONE',  ( 26.56734541678232731, 200.0000000013656347, 166.5412658749999650 ) ) ;
#14200 = CARTESIAN_POINT ( 'NONE',  ( 31.45873412499997812, 199.8750000013655779, 171.4326545832175839 ) ) ;
#14203 = EDGE_LOOP ( 'NONE', ( #74379, #60112, #4285, #40440 ) ) ;
#14204 = CARTESIAN_POINT ( 'NONE',  ( 2.828427124746209831, 202.5000000027312126, 200.8284271247462129 ) ) ;
#14205 = CARTESIAN_POINT ( 'NONE',  ( 4.242640687119285658, 287.6875000034139589, -4.242640687119286547 ) ) ;
#14206 = CARTESIAN_POINT ( 'NONE',  ( -2.839093476692135984E-14, 202.6875000013656063, 138.5412658750000503 ) ) ;
#14207 = EDGE_CURVE ( 'NONE', #20933, #27944, #48705, .T. ) ;
#14208 = CARTESIAN_POINT ( 'NONE',  ( 25.55430564589119413, 202.3125000013656063, 167.5543056458910485 ) ) ;
#14209 = CARTESIAN_POINT ( 'NONE',  ( 7.188101187499999156, 27.74999999795161543, 2.977408999572654924 ) ) ;
#14210 = CARTESIAN_POINT ( 'NONE',  ( 5.676582343750001591, 191.9270833299193555, -9.832129032723420536 ) ) ;
#14211 = CARTESIAN_POINT ( 'NONE',  ( 2.977408999572654480, 95.00000000204838102, 7.188101187499999156 ) ) ;
#14212 = CYLINDRICAL_SURFACE ( 'NONE', #50654, 8.000000000000000000 ) ;
#14213 = CARTESIAN_POINT ( 'NONE',  ( 3.211159895383560947, 14.18749999863440792, 3.211159895383562723 ) ) ;
#14214 = CARTESIAN_POINT ( 'NONE',  ( 26.56734541678232731, 199.6250000013656063, 173.4587341249998929 ) ) ;
#14215 = CARTESIAN_POINT ( 'NONE',  ( -2.977408999572647819, 7.188101187499991163, 6.080302781871753659 ) ) ;
#14216 = LINE ( 'NONE', #60250, #15830 ) ;
#14217 = CARTESIAN_POINT ( 'NONE',  ( 3.042071309553159519, 84.73958332991936970, 11.35316468750000141 ) ) ;
#14218 = ORIENTED_EDGE ( 'NONE', *, *, #18195, .T. ) ;
#14219 = CARTESIAN_POINT ( 'NONE',  ( -29.65685424949245430, 195.4374999999999716, 174.0000000000002842 ) ) ;
#14220 = CARTESIAN_POINT ( 'NONE',  ( 4.000000000000016875, 209.4375000000000284, 199.6568542494924259 ) ) ;
#14221 = CARTESIAN_POINT ( 'NONE',  ( -6.123233995736766282E-16, 233.7500000000000000, -10.00000000000000000 ) ) ;
#14222 = CARTESIAN_POINT ( 'NONE',  ( -5.676582343750006032, 94.11458332991935549, 9.832129032723418760 ) ) ;
#14223 = ORIENTED_EDGE ( 'NONE', *, *, #12723, .T. ) ;
#14224 = CARTESIAN_POINT ( 'NONE',  ( -7.204075437095967871, 7.204075437095967871, 87.34375000204836681 ) ) ;
#14225 = CARTESIAN_POINT ( 'NONE',  ( 7.204075437095966983, 7.204075437095967871, 112.0937500020483810 ) ) ;
#14226 = CARTESIAN_POINT ( 'NONE',  ( -3.313708498984762496, 102.7812499999999858, 7.999999999999998224 ) ) ;
#14227 = CARTESIAN_POINT ( 'NONE',  ( 5.656854249492380582, 23.99999999590322375, -5.656854249492380582 ) ) ;
#14229 = CARTESIAN_POINT ( 'NONE',  ( 8.311093377946837890, 71.40624999658602690, -8.311093377946837890 ) ) ;
#14228 = CARTESIAN_POINT ( 'NONE',  ( -23.99999999999996092, 206.8125000027312126, 171.6568542494926817 ) ) ;
#14231 = VECTOR ( 'NONE', #6624, 1000.000000000000000 ) ;
#14230 = CARTESIAN_POINT ( 'NONE',  ( 3.313708498984762496, -7.999999999999989342, 19.48655278392014978 ) ) ;
#14232 = ADVANCED_FACE ( 'NONE', ( #20530 ), #9227, .T. ) ;
#14233 = FACE_OUTER_BOUND ( 'NONE', #50818, .T. ) ;
#14234 =( BOUNDED_CURVE ( )  B_SPLINE_CURVE ( 2, ( #29406, #62602, #17323, #40344, #68272, #57339, #39976, #29024, #40715 ),
 .UNSPECIFIED., .F., .F. ) 
 B_SPLINE_CURVE_WITH_KNOTS ( ( 3, 2, 2, 2, 3 ),
 ( 0.4333333333333336812, 0.4416666666666669849, 0.4500000000000003997, 0.4583333333333337034, 0.4666666666666670626 ),
 .UNSPECIFIED. ) 
 CURVE ( )  GEOMETRIC_REPRESENTATION_ITEM ( )  RATIONAL_B_SPLINE_CURVE ( ( 0.9999999999999970024, 0.9238795325112897361, 1.000000000000000000, 0.9238795325112867385, 1.000000000000000000, 0.9238795325112867385, 1.000000000000000000, 0.9238795325112831858, 1.000000000000003553 ) ) 
 REPRESENTATION_ITEM ( '' )  );
#14235 = CARTESIAN_POINT ( 'NONE',  ( -2.679491924311235618, 175.4166666598387110, 10.00000000000000000 ) ) ;
#14236 = CARTESIAN_POINT ( 'NONE',  ( -2.977408999572650927, 91.25000000204838102, -7.188101187500001821 ) ) ;
#14237 = AXIS2_PLACEMENT_3D ( 'NONE', #63314, #57306, #5617 ) ;
#14238 = CARTESIAN_POINT ( 'NONE',  ( 36.10814071610729314, 141.0294372515228645, 139.0000000000000000 ) ) ;
#14239 = CARTESIAN_POINT ( 'NONE',  ( -11.35316468749999785, 68.38541666325268409, -3.042071309553167957 ) ) ;
#14240 = CARTESIAN_POINT ( 'NONE',  ( -2.765530957081996810, 292.2656250017069510, -6.676582343750003368 ) ) ;
#14243 = EDGE_CURVE ( 'NONE', #59936, #59221, #72976, .T. ) ;
#14242 = CARTESIAN_POINT ( 'NONE',  ( -10.18810118749999916, 0.000000000000000000, 108.5312500020483810 ) ) ;
#14241 = B_SPLINE_CURVE_WITH_KNOTS ( 'NONE', 3,
 ( #68694, #57393, #45679, #23413, #28700, #28334, #40402, #61, #46053, #63400, #74350, #11726, #57768, #18130, #22660, #34766, #51341, #46428, #69442, #58145, #6452, #52464, #802, #69814, #23788, #58503, #6809, #29822, #52834, #1167, #70190, #64524 ),
 .UNSPECIFIED., .F., .F.,
 ( 4, 2, 2, 2, 2, 2, 2, 2, 2, 2, 2, 2, 2, 2, 2, 4 ),
 ( 0.003096835164517359844, 0.003832390200801030506, 0.004567945237084701168, 0.006039055309652006931, 0.006774610345935660680, 0.007510165382219314428, 0.008245720418502968177, 0.008981275454786621926, 0.009716830491070273940, 0.01045238552735392769, 0.01118794056363758144, 0.01192349559992123345, 0.01265905063620488893, 0.01339460567248854095, 0.01413016070877219643, 0.01486571574505584845 ),
 .UNSPECIFIED. ) ;
#14244 = CARTESIAN_POINT ( 'NONE',  ( 6.951808397369818766E-16, 212.0312499965860411, -11.35316468750000141 ) ) ;
#14245 = ORIENTED_EDGE ( 'NONE', *, *, #4382, .T. ) ;
#14246 = CARTESIAN_POINT ( 'NONE',  ( -3.544144923083014653, 60.54353712382538077, 23.09461823984563011 ) ) ;
#14247 = CARTESIAN_POINT ( 'NONE',  ( 2.828427124746153876, 206.0000000027312126, 144.8284271247462129 ) ) ;
#14248 = CARTESIAN_POINT ( 'NONE',  ( 5.000000000000000000, 67.91996363552645732, 22.23680535815963921 ) ) ;
#14250 = CARTESIAN_POINT ( 'NONE',  ( -3.042071309553163960, 197.2395833299193555, -11.35316468749999963 ) ) ;
#14249 = CARTESIAN_POINT ( 'NONE',  ( -27.99999999999999645, 210.0000000000000284, 166.0000000000003979 ) ) ;
#14251 = CARTESIAN_POINT ( 'NONE',  ( 0.000000000000000000, 125.0000000000000000, 0.000000000000000000 ) ) ;
#14252 = AXIS2_PLACEMENT_3D ( 'NONE', #50497, #68600, #16908 ) ;
#14253 = CARTESIAN_POINT ( 'NONE',  ( 8.660254037844389075, 245.2083333401613174, 4.999999999999997335 ) ) ;
#14254 = DIRECTION ( 'NONE',  ( -0.000000000000000000, -0.000000000000000000, -1.000000000000000000 ) ) ;
#14255 = ORIENTED_EDGE ( 'NONE', *, *, #72486, .T. ) ;
#14256 = CARTESIAN_POINT ( 'NONE',  ( -9.832129032723420536, 184.0104166632526983, 5.676582343749997150 ) ) ;
#14257 = CARTESIAN_POINT ( 'NONE',  ( 5.082755093536318824, 5.082755093536319713, 23.42405278187175455 ) ) ;
#14258 = LINE ( 'NONE', #8992, #11636 ) ;
#14259 = ORIENTED_EDGE ( 'NONE', *, *, #36582, .T. ) ;
#14260 = CARTESIAN_POINT ( 'NONE',  ( -5.656854249492380582, 98.00000000409677625, -5.656854249492380582 ) ) ;
#14261 = CARTESIAN_POINT ( 'NONE',  ( -7.320508075688773708, 6.874999999999999112, -7.320508075688774596 ) ) ;
#14262 = CARTESIAN_POINT ( 'NONE',  ( 4.000000000000001776, 18.00000000000000355, 0.000000000000000000 ) ) ;
#14263 = CARTESIAN_POINT ( 'NONE',  ( 1.881053915767121998, 16.49999999863440436, -4.541265875000002339 ) ) ;
#14264 = CARTESIAN_POINT ( 'NONE',  ( -7.999999999999989342, -3.313708498984762496, 14.61155278392014800 ) ) ;
#14265 = EDGE_CURVE ( 'NONE', #728, #26967, #30312, .T. ) ;
#14266 = CARTESIAN_POINT ( 'NONE',  ( 7.999999999999991118, 3.313708498984758055, 18.36155278392014623 ) ) ;
#14267 = ORIENTED_EDGE ( 'NONE', *, *, #17240, .F. ) ;
#14268 = CARTESIAN_POINT ( 'NONE',  ( 7.778174593052021635, 7.778174593052023411, 72.43749999999998579 ) ) ;
#14269 = CARTESIAN_POINT ( 'NONE',  ( 1.320432766682874540E-15, 96.03125000204838102, 7.188101187500000044 ) ) ;
#14271 = CARTESIAN_POINT ( 'NONE',  ( 9.832129032723420536, 260.9895833367473301, 5.676582343749996262 ) ) ;
#14270 = CARTESIAN_POINT ( 'NONE',  ( -9.999999999999998224, 258.3333333401612890, 2.679491924311235174 ) ) ;
#14272 = ORIENTED_EDGE ( 'NONE', *, *, #15324, .T. ) ;
#14274 = CARTESIAN_POINT ( 'NONE',  ( 4.193070328474947317, 50.40098303874201235, -40.95513628906619630 ) ) ;
#14273 = AXIS2_PLACEMENT_3D ( 'NONE', #46638, #47004, #11943 ) ;
#14275 = CARTESIAN_POINT ( 'NONE',  ( 7.188101187499991163, 2.977408999572648707, 18.83030278187175099 ) ) ;
#14276 = VERTEX_POINT ( 'NONE', #31865 ) ;
#14277 = EDGE_LOOP ( 'NONE', ( #22943, #71427, #34491, #22312 ) ) ;
#14278 = CARTESIAN_POINT ( 'NONE',  ( 10.18810118749999916, 4.220049686691935698, 77.50000000204839523 ) ) ;
#14279 = CARTESIAN_POINT ( 'NONE',  ( -3.042071309553164404, 62.55208332991934839, -11.35316468749999963 ) ) ;
#14280 = CARTESIAN_POINT ( 'NONE',  ( -8.660254037844387298, 113.9583333265053682, -5.000000000000004441 ) ) ;
#14281 = CARTESIAN_POINT ( 'NONE',  ( -6.735557395310442023E-16, 11.00000000000000000, 98.12499999999998579 ) ) ;
#14284 = CARTESIAN_POINT ( 'NONE',  ( -6.676582343750002480, 293.5468750017070079, -2.765530957081996810 ) ) ;
#14283 = CARTESIAN_POINT ( 'NONE',  ( 29.65685424949240456, 199.1875000027312694, 173.9999999999999147 ) ) ;
#14282 = CARTESIAN_POINT ( 'NONE',  ( 4.556349186104052151, -10.99999999999999822, 104.9687500000000000 ) ) ;
#14285 = CARTESIAN_POINT ( 'NONE',  ( 10.00000000000000000, 144.7916666666666572, 2.679491924311236062 ) ) ;
#14286 = AXIS2_PLACEMENT_3D ( 'NONE', #29771, #46379, #6405 ) ;
#14287 = CARTESIAN_POINT ( 'NONE',  ( -50.57310678023845441, 199.7857410358465131, 56.30867738842443515 ) ) ;
#14288 = CARTESIAN_POINT ( 'NONE',  ( -1.656854249492416109, 200.1875000000000284, 201.9999999999999432 ) ) ;
#14289 = AXIS2_PLACEMENT_3D ( 'NONE', #33371, #56372, #4692 ) ;
#14290 = DIRECTION ( 'NONE',  ( -0.000000000000000000, 1.000000000000000000, -4.476705744456276341E-16 ) ) ;
#14291 = CARTESIAN_POINT ( 'NONE',  ( 7.999999999999998224, 4.218749995903220196, 3.313708498984766493 ) ) ;
#14292 = CARTESIAN_POINT ( 'NONE',  ( 30.44569435410879166, 199.5625000013656063, 172.4456943541087526 ) ) ;
#14293 = CARTESIAN_POINT ( 'NONE',  ( 7.188101187500001821, 9.937499997951610098, -2.977408999572650483 ) ) ;
#14294 = CARTESIAN_POINT ( 'NONE',  ( -5.656854249492375253, 5.656854249492375253, 26.33030278392014623 ) ) ;
#14295 = CARTESIAN_POINT ( 'NONE',  ( -8.660254037844387298, 242.7083333401613174, -4.999999999999999112 ) ) ;
#14296 = CARTESIAN_POINT ( 'NONE',  ( -4.401442555609581635E-16, 110.6562500020483810, -7.188101187500000044 ) ) ;
#14298 = CARTESIAN_POINT ( 'NONE',  ( -2.679491924313885054, 133.5416666666664298, 9.999999999998470557 ) ) ;
#14297 = CARTESIAN_POINT ( 'NONE',  ( 2.828427124746209831, 201.3750000000000284, 200.8284271247462129 ) ) ;
#14299 = CARTESIAN_POINT ( 'NONE',  ( -11.00000000000000000, 0.000000000000000000, 112.1875000040967763 ) ) ;
#14300 = DIRECTION ( 'NONE',  ( 0.000000000000000000, 0.000000000000000000, 1.000000000000000000 ) ) ;
#14301 = CARTESIAN_POINT ( 'NONE',  ( 7.188101187499993827, -2.977408999572645598, 25.01780278187175455 ) ) ;
#14302 = CARTESIAN_POINT ( 'NONE',  ( 30.82842712474616675, 196.1250000000000284, 172.8284271247460993 ) ) ;
#14303 = CARTESIAN_POINT ( 'NONE',  ( -9.832129032723420536, 43.69791666325269119, 5.676582343749997150 ) ) ;
#14304 = CARTESIAN_POINT ( 'NONE',  ( 3.490152628695403868E-12, 151.2499999999997442, -10.00000000000000178 ) ) ;
#14305 = CARTESIAN_POINT ( 'NONE',  ( 7.320508075688774596, 7.499999993172031587, -7.320508075688774596 ) ) ;
#14306 = ORIENTED_EDGE ( 'NONE', *, *, #14207, .F. ) ;
#14307 = CARTESIAN_POINT ( 'NONE',  ( -38.00000000000000000, 53.00000000000000711, 9.999999999999991118 ) ) ;
#14308 = CARTESIAN_POINT ( 'NONE',  ( 0.000000000000000000, 0.000000000000000000, -14.00000000000000178 ) ) ;
#14309 = EDGE_CURVE ( 'NONE', #67735, #47641, #14868, .T. ) ;
#14310 = CARTESIAN_POINT ( 'NONE',  ( 11.35316468749999785, 45.57291666325266988, 3.042071309553174174 ) ) ;
#14311 = CARTESIAN_POINT ( 'NONE',  ( -6.735557395310442023E-16, 11.00000000000000000, 78.81250000409677625 ) ) ;
#14312 = CARTESIAN_POINT ( 'NONE',  ( -1.432654583217662481, 203.3750000013656063, 145.4587341250000350 ) ) ;
#14313 = CARTESIAN_POINT ( 'NONE',  ( 27.99999999999996803, 203.0000000000000000, 173.9999999999999147 ) ) ;
#14314 = DIRECTION ( 'NONE',  ( -0.000000000000000000, -0.000000000000000000, 1.000000000000000000 ) ) ;
#14316 = CARTESIAN_POINT ( 'NONE',  ( -5.676582343750006032, 29.11458332991935194, 9.832129032723418760 ) ) ;
#14315 = CARTESIAN_POINT ( 'NONE',  ( 5.082755093536326818, 102.2187500020483810, 5.082755093536325042 ) ) ;
#14317 = CARTESIAN_POINT ( 'NONE',  ( -5.656854249492375253, 5.656854249492375253, 6.642802779823365533 ) ) ;
#14318 = DIRECTION ( 'NONE',  ( 1.000000000000000000, 0.000000000000000000, 0.000000000000000000 ) ) ;
#14319 = CARTESIAN_POINT ( 'NONE',  ( 3.042071309553159519, 159.7395833299193839, 11.35316468750000141 ) ) ;
#14320 = B_SPLINE_CURVE_WITH_KNOTS ( 'NONE', 3,
 ( #45751, #24499, #41488, #47137 ),
 .UNSPECIFIED., .F., .F.,
 ( 4, 4 ),
 ( 0.05130768332321102021, 0.06449425364950420181 ),
 .UNSPECIFIED. ) ;
#14322 = CARTESIAN_POINT ( 'NONE',  ( -10.00000000000000355, 129.5833333265053966, 2.679491924311223183 ) ) ;
#14321 = B_SPLINE_SURFACE_WITH_KNOTS ( 'NONE', 5, 5, ( 
 ( #6704, #16889, #18390, #13806, #25508, #64774 ),
 ( #47781, #42496, #8543, #58762, #31181, #70802 ),
 ( #59134, #19481, #37220, #1430, #24769, #7072 ),
 ( #30078, #53096, #59495, #36481, #2142, #25136 ),
 ( #1784, #36112, #60218, #7808, #14183, #13077 ),
 ( #47048, #30810, #52725, #19116, #30450, #47418 ) ),
 .UNSPECIFIED., .F., .F., .F.,
 ( 6, 6 ),
 ( 6, 6 ),
 ( -14.28000000000008640, 14.28000000000005976 ),
 ( -2.294999999999999485, 2.295000000000000373 ),
 .UNSPECIFIED. ) ;
#14323 = CARTESIAN_POINT ( 'NONE',  ( 7.188101187500000044, 107.2812500020483810, -8.802885111219163269E-16 ) ) ;
#14324 = ORIENTED_EDGE ( 'NONE', *, *, #3174, .T. ) ;
#14325 = CARTESIAN_POINT ( 'NONE',  ( -1.347111479062088207E-15, 0.000000000000000000, 0.000000000000000000 ) ) ;
#14326 = CARTESIAN_POINT ( 'NONE',  ( 11.35316468749999963, 16.30208332991935194, -3.042071309553165293 ) ) ;
#14327 =( BOUNDED_CURVE ( )  B_SPLINE_CURVE ( 2, ( #57580, #5890, #22468, #247, #52650, #46607, #10795, #6266, #68880 ),
 .UNSPECIFIED., .F., .F. ) 
 B_SPLINE_CURVE_WITH_KNOTS ( ( 3, 2, 2, 2, 3 ),
 ( 0.1805555555555555525, 0.1875000000000000000, 0.1944444444444444198, 0.2013888888888888673, 0.2083333333333333148 ),
 .UNSPECIFIED. ) 
 CURVE ( )  GEOMETRIC_REPRESENTATION_ITEM ( )  RATIONAL_B_SPLINE_CURVE ( ( 1.000000000000000000, 0.9238795325112867385, 1.000000000000000000, 0.9238795325112867385, 1.000000000000000000, 0.9238795325112867385, 1.000000000000000000, 0.9238795325112870716, 0.9999999999999996669 ) ) 
 REPRESENTATION_ITEM ( '' )  );
#14328 = CARTESIAN_POINT ( 'NONE',  ( -5.394762896564973355E-12, 18.74999999999958433, 10.00000000000000178 ) ) ;
#14329 = ORIENTED_EDGE ( 'NONE', *, *, #47764, .F. ) ;
#14330 = CARTESIAN_POINT ( 'NONE',  ( -30.82842712474612767, 205.5000000027312126, 172.8284271247466108 ) ) ;
#14331 = CARTESIAN_POINT ( 'NONE',  ( 10.18810118750000093, -4.220049686691933921, 75.81250000204838102 ) ) ;
#14332 = DIRECTION ( 'NONE',  ( -0.000000000000000000, 1.000000000000000000, 4.689100369878284071E-30 ) ) ;
#14334 = CARTESIAN_POINT ( 'NONE',  ( -11.35316468749999785, 158.0729166632526699, -3.042071309553167957 ) ) ;
#14333 = CARTESIAN_POINT ( 'NONE',  ( -22.20752581988981689, -25.36715512050907151, 145.3755878121157821 ) ) ;
#14335 = CARTESIAN_POINT ( 'NONE',  ( -1.320432766682874540E-15, 1.968749997951610320, 7.188101187500000044 ) ) ;
#14336 = CARTESIAN_POINT ( 'NONE',  ( 7.999999999999991118, 3.313708498984757611, 19.73030278432982598 ) ) ;
#14337 = CARTESIAN_POINT ( 'NONE',  ( 7.999999999999950262, -3.313708498984798467, 16.48655277982336287 ) ) ;
#14338 = CARTESIAN_POINT ( 'NONE',  ( -8.311093377946834337, 239.5312500034140157, 8.311093377946837890 ) ) ;
#14339 = EDGE_CURVE ( 'NONE', #10291, #870, #2461, .T. ) ;
#14340 = CARTESIAN_POINT ( 'NONE',  ( 1.871523826299183495E-15, -10.18810118749999916, 83.40625000204838102 ) ) ;
#14341 = ORIENTED_EDGE ( 'NONE', *, *, #36982, .T. ) ;
#14342 = AXIS2_PLACEMENT_3D ( 'NONE', #48906, #64789, #19494 ) ;
#14343 = FACE_OUTER_BOUND ( 'NONE', #9003, .T. ) ;
#14344 = CARTESIAN_POINT ( 'NONE',  ( 25.17157282405715435, 195.0000000000000284, 172.8284270735494772 ) ) ;
#14345 = CARTESIAN_POINT ( 'NONE',  ( -8.311093377946841443, 109.2187499965860269, 8.311093377946830785 ) ) ;
#14346 = CARTESIAN_POINT ( 'NONE',  ( -10.18810118749999738, -4.220049686691941915, 103.7500000020483668 ) ) ;
#14347 =( BOUNDED_CURVE ( )  B_SPLINE_CURVE ( 2, ( #65061, #59061, #19783, #31104, #35676, #13372, #37145, #30011, #58691, #42791, #2073, #7000, #8101 ),
 .UNSPECIFIED., .F., .F. ) 
 B_SPLINE_CURVE_WITH_KNOTS ( ( 3, 2, 2, 2, 2, 2, 3 ),
 ( 2.088085437352556362, 2.093319447082276685, 2.098553456811997009, 2.103787466541717777, 2.109021476271438100, 2.114255486001158424, 2.119489495730878748 ),
 .UNSPECIFIED. ) 
 CURVE ( )  GEOMETRIC_REPRESENTATION_ITEM ( )  RATIONAL_B_SPLINE_CURVE ( ( 1.000000000000267342, 0.9659258262888009705, 1.000000000000000000, 0.9659258262890683122, 1.000000000000000000, 0.9659258262890683122, 1.000000000000000000, 0.9659258262890683122, 1.000000000000000000, 0.9659258262890683122, 1.000000000000000000, 0.9659258262890829672, 0.9999999999999853451 ) ) 
 REPRESENTATION_ITEM ( '' )  );
#14348 = CARTESIAN_POINT ( 'NONE',  ( 7.320508075688778149, 14.37500000000000533, 7.320508075688781702 ) ) ;
#14349 = ORIENTED_EDGE ( 'NONE', *, *, #40352, .F. ) ;
#14350 = ORIENTED_EDGE ( 'NONE', *, *, #33685, .F. ) ;
#14351 = CARTESIAN_POINT ( 'NONE',  ( 3.211159895383561835, 5.562499998634407028, -3.211159895383561835 ) ) ;
#14352 = CIRCLE ( 'NONE', #58973, 11.00000000000000000 ) ;
#14353 = CARTESIAN_POINT ( 'NONE',  ( -7.188101187500001821, 8.624999997951611874, -2.977408999572651371 ) ) ;
#14354 = CARTESIAN_POINT ( 'NONE',  ( -4.898587196589412829E-16, 114.3125000040967905, -8.000000000000000000 ) ) ;
#14355 = CARTESIAN_POINT ( 'NONE',  ( 7.204075437095966983, 7.204075437095967871, 95.96875000204838102 ) ) ;
#14356 = CARTESIAN_POINT ( 'NONE',  ( -31.45873412499999944, 202.9375000013656063, 170.0000000000003979 ) ) ;
#14357 = CARTESIAN_POINT ( 'NONE',  ( -4.999999999999998224, 158.5416666598387110, -8.660254037844389075 ) ) ;
#14358 = CARTESIAN_POINT ( 'NONE',  ( 4.000000000000000888, 2.937500000000000444, 1.656854249492384135 ) ) ;
#14359 = CARTESIAN_POINT ( 'NONE',  ( 2.828427124746190291, 19.62499999726881228, 2.828427124746192067 ) ) ;
#14360 = CARTESIAN_POINT ( 'NONE',  ( 4.541265875000002339, 4.312499998634407028, 0.000000000000000000 ) ) ;
#14361 = CARTESIAN_POINT ( 'NONE',  ( -2.754378923186476579E-14, 208.1875000013656063, 145.4587341250000350 ) ) ;
#14362 = CARTESIAN_POINT ( 'NONE',  ( 1.432654583217664479, 195.7500000013656063, 201.4587341250000065 ) ) ;
#14364 = CARTESIAN_POINT ( 'NONE',  ( -11.00000000000000000, 0.000000000000000000, 95.68750000409677625 ) ) ;
#14363 = CARTESIAN_POINT ( 'NONE',  ( -31.45873412500001720, 201.6250000013656063, 168.5673454167828140 ) ) ;
#14365 = CARTESIAN_POINT ( 'NONE',  ( -4.541265875000002339, 16.81249999863440436, -5.561446717895856393E-16 ) ) ;
#14366 = CARTESIAN_POINT ( 'NONE',  ( -6.676582343749999815, 298.5156250017069510, 2.765530957082001251 ) ) ;
#14367 = CARTESIAN_POINT ( 'NONE',  ( -7.188101187499992051, 0.000000000000000000, 8.986552781871752771 ) ) ;
#14368 = ORIENTED_EDGE ( 'NONE', *, *, #59669, .F. ) ;
#14369 = ORIENTED_EDGE ( 'NONE', *, *, #27919, .T. ) ;
#14370 = CARTESIAN_POINT ( 'NONE',  ( -7.204075437095965206, -7.204075437095968759, 96.34375000204836681 ) ) ;
#14371 = CARTESIAN_POINT ( 'NONE',  ( 11.00000000000000000, 11.00000000000000000, -6.938893903907228378E-15 ) ) ;
#14372 = CARTESIAN_POINT ( 'NONE',  ( -26.56734541678232731, 205.2500000013655779, 173.4587341250003760 ) ) ;
#14373 = CARTESIAN_POINT ( 'NONE',  ( -29.65685424949234061, 202.4375000000000568, 174.0000000000004547 ) ) ;
#14374 = CARTESIAN_POINT ( 'NONE',  ( 3.458734125000015425, 195.9375000013655779, 198.0000000000000284 ) ) ;
#14375 = CARTESIAN_POINT ( 'NONE',  ( 1.469576158976823947E-15, 104.3750000000000000, 8.000000000000000000 ) ) ;
#14376 = CARTESIAN_POINT ( 'NONE',  ( -7.320508075688778149, 103.1249999999999858, 7.320508075688769267 ) ) ;
#14377 = EDGE_CURVE ( 'NONE', #9171, #50622, #56450, .T. ) ;
#14378 = CARTESIAN_POINT ( 'NONE',  ( 5.656854249492381470, 112.0625000000000000, 5.656854249492379694 ) ) ;
#14379 = CARTESIAN_POINT ( 'NONE',  ( 6.676582343750003368, 291.1718750017069510, -2.765530957081997254 ) ) ;
#14380 = CARTESIAN_POINT ( 'NONE',  ( 1.320432766682872962E-15, -7.188101187499992051, 11.23655278187175455 ) ) ;
#14381 = ORIENTED_EDGE ( 'NONE', *, *, #69806, .F. ) ;
#14382 = APPLICATION_CONTEXT ( 'automotive_design' ) ;
#14383 = FACE_OUTER_BOUND ( 'NONE', #7194, .T. ) ;
#14384 = AXIS2_PLACEMENT_3D ( 'NONE', #31856, #27302, #55627 ) ;
#14385 = CARTESIAN_POINT ( 'NONE',  ( -5.656854249492381470, 20.24999999590322375, 5.656854249492379694 ) ) ;
#14386 = CARTESIAN_POINT ( 'NONE',  ( 2.445694354108783664, 205.3125000013656063, 144.4456943541088663 ) ) ;
#14387 = CARTESIAN_POINT ( 'NONE',  ( -1.656854249492383468, 5.687500000000000000, 4.000000000000000888 ) ) ;
#14388 = CARTESIAN_POINT ( 'NONE',  ( 0.000000000000000000, 0.000000000000000000, 0.000000000000000000 ) ) ;
#14389 = CARTESIAN_POINT ( 'NONE',  ( -9.832129032723418760, 258.8020833367473301, -5.676582343749998927 ) ) ;
#14390 = CARTESIAN_POINT ( 'NONE',  ( -4.000000000000016875, 207.4375000000000284, 140.3431457505076594 ) ) ;
#14391 = CARTESIAN_POINT ( 'NONE',  ( -10.99999999999999822, -4.556349186104052151, 115.0937500000000000 ) ) ;
#14392 = CARTESIAN_POINT ( 'NONE',  ( -24.05663304117221557, 228.2939914580040863, -18.33101321549810692 ) ) ;
#14393 = CARTESIAN_POINT ( 'NONE',  ( 2.977408999572646486, 7.188101187499992051, 2.892802781871751439 ) ) ;
#14394 = CARTESIAN_POINT ( 'NONE',  ( 3.042071309553167069, 197.1354166632526415, -11.35316468749999785 ) ) ;
#14395 = CARTESIAN_POINT ( 'NONE',  ( 10.00000000000000178, 192.0833333265053682, -2.679491924311226736 ) ) ;
#14396 = CARTESIAN_POINT ( 'NONE',  ( -3.211159895383562723, 4.937499998634407028, 3.211159895383561391 ) ) ;
#14397 = CARTESIAN_POINT ( 'NONE',  ( -11.00000000000000000, 0.000000000000000000, 118.0000000000000000 ) ) ;
#14399 = CARTESIAN_POINT ( 'NONE',  ( 16.00000000000000711, 16.00000000000000355, 20.00000000000000000 ) ) ;
#14398 = CARTESIAN_POINT ( 'NONE',  ( 5.000000000000000000, -10.00000000000000000, -75.19090595827292134 ) ) ;
#14400 = ORIENTED_EDGE ( 'NONE', *, *, #67619, .T. ) ;
#14401 = VECTOR ( 'NONE', #26569, 1000.000000000000000 ) ;
#14403 = EDGE_CURVE ( 'NONE', #71172, #33552, #26138, .T. ) ;
#14402 = CARTESIAN_POINT ( 'NONE',  ( -3.458734125000015869, 205.1875000013656063, 142.0000000000000568 ) ) ;
#14404 = CARTESIAN_POINT ( 'NONE',  ( -7.778174593052023411, 7.778174593052023411, 100.0000000040967763 ) ) ;
#14405 = CARTESIAN_POINT ( 'NONE',  ( 2.020667218593132706E-15, -11.00000000000000000, 106.5625000040967763 ) ) ;
#14406 = CARTESIAN_POINT ( 'NONE',  ( -31.45873412499999233, 199.6875000013656063, 170.0000000000004547 ) ) ;
#14407 = LINE ( 'NONE', #66855, #16543 ) ;
#14409 = CARTESIAN_POINT ( 'NONE',  ( 3.999999999999959144, 204.0625000000000000, 140.3431457505076594 ) ) ;
#14408 = CARTESIAN_POINT ( 'NONE',  ( 5.082755093536326818, 123.2187500020483952, 5.082755093536325042 ) ) ;
#14410 = CARTESIAN_POINT ( 'NONE',  ( -5.656854249492375253, 5.656854249492375253, 26.14280277982336997 ) ) ;
#14411 = CARTESIAN_POINT ( 'NONE',  ( 11.35316468749999963, 120.9895833299193413, -3.042071309553165293 ) ) ;
#14412 = EDGE_CURVE ( 'NONE', #338, #70161, #16351, .T. ) ;
#14413 = CARTESIAN_POINT ( 'NONE',  ( -2.679491924311235618, 90.41666665983869677, 10.00000000000000000 ) ) ;
#14414 = CARTESIAN_POINT ( 'NONE',  ( -7.188101187500000044, 89.65625000204838102, 0.000000000000000000 ) ) ;
#14415 = CARTESIAN_POINT ( 'NONE',  ( -3.211159895383561391, 19.81249999863440436, -3.211159895383561835 ) ) ;
#14416 = CARTESIAN_POINT ( 'NONE',  ( -28.00000000000002842, 205.0000000000000284, 166.0000000000003695 ) ) ;
#14417 = DIRECTION ( 'NONE',  ( -0.1501682406780870394, -0.1251959390492823898, 0.9807015225527165869 ) ) ;
#14418 = ORIENTED_EDGE ( 'NONE', *, *, #19012, .F. ) ;
#14419 = ORIENTED_EDGE ( 'NONE', *, *, #30771, .F. ) ;
#14420 = CARTESIAN_POINT ( 'NONE',  ( 2.765530957081996366, 294.2968750017070079, -6.676582343750003368 ) ) ;
#14421 = CARTESIAN_POINT ( 'NONE',  ( -3.313708498984758943, -7.999999999999989342, 5.799052783920146226 ) ) ;
#14422 = CARTESIAN_POINT ( 'NONE',  ( -8.311093377946836114, 167.6562499965860411, -8.311093377946837890 ) ) ;
#14423 = CARTESIAN_POINT ( 'NONE',  ( -2.828427124746153876, 201.0000000027312126, 195.1715728752538439 ) ) ;
#14424 = CARTESIAN_POINT ( 'NONE',  ( 4.000000000000015987, 200.5000000000000000, 198.0000000000000284 ) ) ;
#14425 = CARTESIAN_POINT ( 'NONE',  ( 3.313708498984760276, 103.5312500000000000, -8.000000000000000000 ) ) ;
#14426 = EDGE_CURVE ( 'NONE', #18054, #55487, #22925, .T. ) ;
#14427 = CARTESIAN_POINT ( 'NONE',  ( 10.18810118749999916, 1.247682550866122264E-15, 104.7812500020483810 ) ) ;
#14428 = ORIENTED_EDGE ( 'NONE', *, *, #44420, .F. ) ;
#14429 = CARTESIAN_POINT ( 'NONE',  ( -11.35316468749999785, 153.3854166632526699, -3.042071309553167957 ) ) ;
#14430 = CARTESIAN_POINT ( 'NONE',  ( 2.445694354108839619, 195.8125000013656063, 200.4456943541088663 ) ) ;
#14431 = CARTESIAN_POINT ( 'NONE',  ( -2.445694354108783219, 205.8125000013656063, 200.4456943541088663 ) ) ;
#14432 = CARTESIAN_POINT ( 'NONE',  ( -10.18810118749999916, 0.000000000000000000, 71.03125000204838102 ) ) ;
#14433 = CARTESIAN_POINT ( 'NONE',  ( -5.676582343750006032, 69.42708332991935549, 9.832129032723418760 ) ) ;
#14434 = ORIENTED_EDGE ( 'NONE', *, *, #21484, .F. ) ;
#14435 = DIRECTION ( 'NONE',  ( -0.000000000000000000, -0.000000000000000000, 1.000000000000000000 ) ) ;
#14436 = CARTESIAN_POINT ( 'NONE',  ( 4.541265875000001451, 10.37499999863440969, 1.881053915767124440 ) ) ;
#14437 = CARTESIAN_POINT ( 'NONE',  ( -4.903558642999205574E-16, 8.008118988124991233, 9.638115283940630107 ) ) ;
#14438 = VERTEX_POINT ( 'NONE', #22765 ) ;
#14439 = CARTESIAN_POINT ( 'NONE',  ( -2.977408999572650039, 23.43749999795161898, -7.188101187500001821 ) ) ;
#14440 = CARTESIAN_POINT ( 'NONE',  ( -6.000000000000000888, 288.1250000034140157, 2.485281374238575758 ) ) ;
#14441 = CARTESIAN_POINT ( 'NONE',  ( 75.00000000000001421, 0.000000000000000000, 20.00000000000002132 ) ) ;
#14442 = CARTESIAN_POINT ( 'NONE',  ( -7.188101187500000044, 9.093749997951611874, -8.802885111219163269E-16 ) ) ;
#14443 = CARTESIAN_POINT ( 'NONE',  ( -7.188101187499992051, 0.000000000000000000, 5.986552781871753659 ) ) ;
#14444 =( BOUNDED_CURVE ( )  B_SPLINE_CURVE ( 2, ( #6093, #29099, #18517, #12837, #23429, #46808, #18147, #41162, #17769 ),
 .UNSPECIFIED., .F., .F. ) 
 B_SPLINE_CURVE_WITH_KNOTS ( ( 3, 2, 2, 2, 3 ),
 ( 0.1029411764705882998, 0.1066176470588235947, 0.1102941176470588897, 0.1139705882352941846, 0.1176470588235294795 ),
 .UNSPECIFIED. ) 
 CURVE ( )  GEOMETRIC_REPRESENTATION_ITEM ( )  RATIONAL_B_SPLINE_CURVE ( ( 0.9999999999999985567, 0.9238795325112881818, 1.000000000000000000, 0.9238795325112867385, 1.000000000000000000, 0.9238795325112867385, 1.000000000000000000, 0.9238795325112852952, 1.000000000000001332 ) ) 
 REPRESENTATION_ITEM ( '' )  );
#14445 = CARTESIAN_POINT ( 'NONE',  ( 10.18810118749999916, 1.247682550866122264E-15, 113.7812500020483810 ) ) ;
#14446 = EDGE_CURVE ( 'NONE', #32492, #55577, #45788, .T. ) ;
#14447 = CARTESIAN_POINT ( 'NONE',  ( 2.903844486065115582, -44.22102027988700712, 151.2231735565142969 ) ) ;
#14448 = CARTESIAN_POINT ( 'NONE',  ( 4.000000000000001776, 6.812499997268813168, -1.656854249492381248 ) ) ;
#14449 = ORIENTED_EDGE ( 'NONE', *, *, #39997, .T. ) ;
#14450 = AXIS2_PLACEMENT_3D ( 'NONE', #54435, #31408, #2743 ) ;
#14451 = CARTESIAN_POINT ( 'NONE',  ( -3.458734124999959025, 205.5000000013655779, 199.4326545832176691 ) ) ;
#14452 = CARTESIAN_POINT ( 'NONE',  ( -30.82842712474612412, 198.5000000027312126, 172.8284271247466108 ) ) ;
#14453 = CARTESIAN_POINT ( 'NONE',  ( -3.211159895383561391, 7.687499998634407028, -3.211159895383561835 ) ) ;
#14454 = CARTESIAN_POINT ( 'NONE',  ( -4.401442555609581635E-16, 108.7812500020483810, -7.188101187500000044 ) ) ;
#14455 = CARTESIAN_POINT ( 'NONE',  ( -2.485281374238268004, 290.1875000000000000, 6.000000000000304645 ) ) ;
#14456 = CARTESIAN_POINT ( 'NONE',  ( -2.977408999572647819, 7.188101187499991163, 26.70530278187175455 ) ) ;
#14457 = VERTEX_POINT ( 'NONE', #11465 ) ;
#14458 = CARTESIAN_POINT ( 'NONE',  ( 4.242640687119285658, 299.6250000000000000, -4.242640687119286547 ) ) ;
#14459 = EDGE_LOOP ( 'NONE', ( #34655, #23393 ) ) ;
#14460 = CARTESIAN_POINT ( 'NONE',  ( -10.18810118749999738, -4.220049686691941915, 114.2500000020483952 ) ) ;
#14461 = CARTESIAN_POINT ( 'NONE',  ( 2.775557561562891351E-14, -37.99999999999997868, 170.0000000000000284 ) ) ;
#14462 = CARTESIAN_POINT ( 'NONE',  ( -3.458734124999959914, 208.4375000013656063, 198.0000000000000284 ) ) ;
#14463 = CARTESIAN_POINT ( 'NONE',  ( 25.55430564589119058, 202.3125000013656063, 172.4456943541087526 ) ) ;
#14464 = CARTESIAN_POINT ( 'NONE',  ( -4.999999999999998224, 66.66666666666667140, -8.660254037844389075 ) ) ;
#14465 = CARTESIAN_POINT ( 'NONE',  ( -7.188101187500000044, 91.53125000204836681, 0.000000000000000000 ) ) ;
#14466 = CARTESIAN_POINT ( 'NONE',  ( -6.000000000000001776, 298.0000000000000000, 0.000000000000000000 ) ) ;
#14468 = CARTESIAN_POINT ( 'NONE',  ( 0.000000000000000000, 125.0000000000000000, 0.000000000000000000 ) ) ;
#14467 = CARTESIAN_POINT ( 'NONE',  ( 3.428378827827396336, -51.66489094708061458, -48.71857030467509020 ) ) ;
#14469 = VECTOR ( 'NONE', #58765, 1000.000000000000000 ) ;
#14470 = ORIENTED_EDGE ( 'NONE', *, *, #32396, .F. ) ;
#14471 = CARTESIAN_POINT ( 'NONE',  ( 11.35316468749999963, 236.4062500034140157, -1.390361679473963556E-15 ) ) ;
#14472 = CARTESIAN_POINT ( 'NONE',  ( -1.469576158976823947E-15, 11.62500000000000178, 8.000000000000000000 ) ) ;
#14473 = CARTESIAN_POINT ( 'NONE',  ( 1.656854249492348607, 200.3125000027312126, 138.0000000000000568 ) ) ;
#14474 = LINE ( 'NONE', #2805, #40739 ) ;
#14475 = DIRECTION ( 'NONE',  ( -0.000000000000000000, 1.000000000000000000, 4.476705744456276341E-16 ) ) ;
#14476 = CARTESIAN_POINT ( 'NONE',  ( 8.660254037844385522, 252.9166666666666856, -5.000000000000003553 ) ) ;
#14477 = CARTESIAN_POINT ( 'NONE',  ( -2.775557561562891351E-14, 210.0000000000000284, 142.0000000000000568 ) ) ;
#14478 = CARTESIAN_POINT ( 'NONE',  ( -8.660254037844387298, 182.0833333333333428, -5.000000000000004441 ) ) ;
#14479 = CARTESIAN_POINT ( 'NONE',  ( 4.999999999999997335, 241.4583333401613174, -8.660254037844387298 ) ) ;
#14480 = CARTESIAN_POINT ( 'NONE',  ( -7.188101187499992051, 0.000000000000000000, 22.86155278187175455 ) ) ;
#14481 = CARTESIAN_POINT ( 'NONE',  ( -8.311093377946836114, 157.9687499965860127, -8.311093377946837890 ) ) ;
#14482 = CARTESIAN_POINT ( 'NONE',  ( 2.751064625579944321E-14, 207.8750000027312126, 194.0000000000000568 ) ) ;
#14483 = CARTESIAN_POINT ( 'NONE',  ( -5.000000000000000000, 50.98531617258460358, 41.27391139027680111 ) ) ;
#14485 = DIRECTION ( 'NONE',  ( 1.000000000000000000, 0.000000000000000000, 0.000000000000000000 ) ) ;
#14484 = CARTESIAN_POINT ( 'NONE',  ( 30.82842712474617031, 203.1250000000000284, 172.8284271247460993 ) ) ;
#14486 = ORIENTED_EDGE ( 'NONE', *, *, #58294, .F. ) ;
#14487 = CARTESIAN_POINT ( 'NONE',  ( 8.311093377946837890, 11.71874999658601801, -8.311093377946837890 ) ) ;
#14488 = CARTESIAN_POINT ( 'NONE',  ( 8.660254037844385522, 96.45833332650536818, 5.000000000000005329 ) ) ;
#14489 = CARTESIAN_POINT ( 'NONE',  ( -3.999999999999960032, 207.9375000000000000, 196.3431457505076594 ) ) ;
#14490 = CARTESIAN_POINT ( 'NONE',  ( -8.000000000000000000, 115.9999999999999858, 0.000000000000000000 ) ) ;
#14491 = CARTESIAN_POINT ( 'NONE',  ( 2.445694354108782775, 207.5625000013656063, 139.5543056458912190 ) ) ;
#14492 = EDGE_CURVE ( 'NONE', #3547, #28168, #39958, .T. ) ;
#14493 = VECTOR ( 'NONE', #60686, 1000.000000000000000 ) ;
#14494 = CARTESIAN_POINT ( 'NONE',  ( -10.00000000000000000, 54.16666665983869677, -2.679491924311229845 ) ) ;
#14495 = CARTESIAN_POINT ( 'NONE',  ( 7.188101187500001821, 110.0000000020483668, -2.977408999572651371 ) ) ;
#14496 = CARTESIAN_POINT ( 'NONE',  ( -4.541265875000002339, 3.937499998634406584, -5.561446717895856393E-16 ) ) ;
#14497 = CARTESIAN_POINT ( 'NONE',  ( -11.30585650302948864, -35.52092734576367405, 141.0516638859361933 ) ) ;
#14498 = CARTESIAN_POINT ( 'NONE',  ( -4.898587196589407898E-16, 7.999999999999991118, 7.955302779823362869 ) ) ;
#14500 = CARTESIAN_POINT ( 'NONE',  ( 5.000000000000002665, 159.1666666666666856, 8.660254037844406838 ) ) ;
#14499 = DIRECTION ( 'NONE',  ( 0.000000000000000000, 0.000000000000000000, 1.000000000000000000 ) ) ;
#14501 = ORIENTED_EDGE ( 'NONE', *, *, #62864, .F. ) ;
#14502 = CARTESIAN_POINT ( 'NONE',  ( -3.673940397442060854E-16, 289.7500000000000000, -6.000000000000001776 ) ) ;
#14503 = CIRCLE ( 'NONE', #4914, 9.999999999999998224 ) ;
#14504 = CARTESIAN_POINT ( 'NONE',  ( 7.999999999999998224, 26.90625000000000355, 3.313708498984766049 ) ) ;
#14505 = CARTESIAN_POINT ( 'NONE',  ( 9.832129032723420536, 231.3020833367473301, 5.676582343749996262 ) ) ;
#14506 = CARTESIAN_POINT ( 'NONE',  ( -11.35316468749999785, 133.0729166632526983, -3.042071309553167513 ) ) ;
#14507 = ORIENTED_EDGE ( 'NONE', *, *, #14560, .T. ) ;
#14508 = CARTESIAN_POINT ( 'NONE',  ( -5.656854249492375253, 5.656854249492375253, 5.330302783920146226 ) ) ;
#14509 = AXIS2_PLACEMENT_3D ( 'NONE', #15334, #43266, #8572 ) ;
#14510 = CARTESIAN_POINT ( 'NONE',  ( -10.18810118749999916, 4.220049686691934809, 97.56250000204836681 ) ) ;
#14511 = CARTESIAN_POINT ( 'NONE',  ( 4.556349186104045934, 11.00000000000000000, 93.53125000000000000 ) ) ;
#14512 = CARTESIAN_POINT ( 'NONE',  ( -3.458734124999960358, 195.6875000013655779, 198.0000000000000284 ) ) ;
#14513 = CARTESIAN_POINT ( 'NONE',  ( -10.67658234375000070, 218.5156250051209668, 0.000000000000000000 ) ) ;
#14515 = CARTESIAN_POINT ( 'NONE',  ( 5.676582343749993598, 119.9479166632526841, 9.832129032723422313 ) ) ;
#14514 = CARTESIAN_POINT ( 'NONE',  ( 23.99999999999998579, 197.7500000000000000, 169.9999999999998863 ) ) ;
#14516 = LINE ( 'NONE', #3222, #13226 ) ;
#14517 = ORIENTED_EDGE ( 'NONE', *, *, #21229, .F. ) ;
#14518 = EDGE_CURVE ( 'NONE', #26574, #13652, #38152, .T. ) ;
#14519 = CARTESIAN_POINT ( 'NONE',  ( -10.00000000000000178, 24.37499999317203603, -1.224646799147353454E-15 ) ) ;
#14520 = CARTESIAN_POINT ( 'NONE',  ( -23.97073152254930406, 177.5684002068723828, 142.3808650461662921 ) ) ;
#14521 = CARTESIAN_POINT ( 'NONE',  ( 9.832129032723416984, 110.6770833299193555, 5.676582343750006032 ) ) ;
#14522 = CARTESIAN_POINT ( 'NONE',  ( -3.458734124999959914, 207.3750000013656063, 196.5673454167823877 ) ) ;
#14523 = CARTESIAN_POINT ( 'NONE',  ( 2.977408999572652260, 17.06249999795161543, 7.188101187500000044 ) ) ;
#14524 = CARTESIAN_POINT ( 'NONE',  ( -10.18810118749999916, 4.220049686691934809, 90.43750000204838102 ) ) ;
#14525 = ADVANCED_FACE ( 'NONE', ( #10348 ), #56374, .T. ) ;
#14526 = CARTESIAN_POINT ( 'NONE',  ( -5.676582343750006032, 19.42708332991934839, 9.832129032723418760 ) ) ;
#14527 = EDGE_LOOP ( 'NONE', ( #54512, #63272, #52225, #43358 ) ) ;
#14528 = CARTESIAN_POINT ( 'NONE',  ( 2.679491924311222739, 180.8333333265053966, 10.00000000000000355 ) ) ;
#14529 = CARTESIAN_POINT ( 'NONE',  ( 5.662595241051934458, 5.662595241051935346, 25.95061528394063188 ) ) ;
#14530 = CARTESIAN_POINT ( 'NONE',  ( 1.978034651643857389, 21.99999999999999645, 3.835510656344423452 ) ) ;
#14531 = CARTESIAN_POINT ( 'NONE',  ( 7.188101187500000044, 4.968749997951610986, 0.000000000000000000 ) ) ;
#14532 = CARTESIAN_POINT ( 'NONE',  ( 2.765530957081996366, 288.1406250017070647, -6.676582343750003368 ) ) ;
#14533 = CARTESIAN_POINT ( 'NONE',  ( -5.000000000000000000, 52.35862550122891435, 48.98731492261470777 ) ) ;
#14535 = VERTEX_POINT ( 'NONE', #19975 ) ;
#14534 = CIRCLE ( 'NONE', #21767, 15.99999999999998579 ) ;
#14536 = CARTESIAN_POINT ( 'NONE',  ( 6.951808397369818766E-16, 137.3437499965860127, -11.35316468750000141 ) ) ;
#14537 = CARTESIAN_POINT ( 'NONE',  ( 4.220049686691934809, 10.18810118749999916, 82.18750000204836681 ) ) ;
#14538 = ADVANCED_FACE ( 'NONE', ( #25631 ), #63510, .F. ) ;
#14539 = EDGE_CURVE ( 'NONE', #60403, #24263, #31684, .T. ) ;
#14540 = CARTESIAN_POINT ( 'NONE',  ( -28.00000000000002132, 199.4375000013655779, 166.5412658750003629 ) ) ;
#14541 = DIRECTION ( 'NONE',  ( -1.000000000000000000, 0.000000000000000000, 0.000000000000000000 ) ) ;
#14542 = CARTESIAN_POINT ( 'NONE',  ( -4.541265875000003227, 17.99999999863440436, 1.881053915767121110 ) ) ;
#14543 = VERTEX_POINT ( 'NONE', #11832 ) ;
#14544 = CARTESIAN_POINT ( 'NONE',  ( 4.000000000000015987, 203.5625000027312126, 199.6568542494924259 ) ) ;
#14545 = CARTESIAN_POINT ( 'NONE',  ( 1.432654583217607414, 200.5000000013656063, 145.4587341250000634 ) ) ;
#14546 = CARTESIAN_POINT ( 'NONE',  ( -2.828427124746208943, 204.7500000027312126, 144.8284271247462129 ) ) ;
#14547 = CARTESIAN_POINT ( 'NONE',  ( 0.000000000000000000, 15.08051212944140218, 15.04081104653146994 ) ) ;
#14548 = EDGE_LOOP ( 'NONE', ( #8953, #17236 ) ) ;
#14549 =( BOUNDED_CURVE ( )  B_SPLINE_CURVE ( 2, ( #23595, #28885, #46604, #48447, #29634, #65055, #18312, #8095, #13366 ),
 .UNSPECIFIED., .F., .F. ) 
 B_SPLINE_CURVE_WITH_KNOTS ( ( 3, 2, 2, 2, 3 ),
 ( 0.8684210526315789824, 0.8750000000000000000, 0.8815789473684210176, 0.8881578947368422572, 0.8947368421052632748 ),
 .UNSPECIFIED. ) 
 CURVE ( )  GEOMETRIC_REPRESENTATION_ITEM ( )  RATIONAL_B_SPLINE_CURVE ( ( 1.000000000000000000, 0.9238795325112867385, 1.000000000000000000, 0.9238795325112867385, 1.000000000000000000, 0.9238795325112867385, 1.000000000000000000, 0.9238795325112854062, 1.000000000000001332 ) ) 
 REPRESENTATION_ITEM ( '' )  );
#14550 = CARTESIAN_POINT ( 'NONE',  ( -5.082755093536325042, 7.031249997951611874, -5.082755093536325930 ) ) ;
#14551 =( BOUNDED_SURFACE ( )  B_SPLINE_SURFACE ( 1, 2, ( 
 ( #71781, #20097, #43111, #66129, #37468, #60469, #8798, #31811, #15559, #67264, #33691, #43870, #50640, #55955, #38220, #60849, #9916, #32569, #26886, #55578, #73658, #56316, #51018, #4265, #66885, #15192, #27255, #38598, #3893, #44994, #50271, #74026, #49903, #72917, #61225, #73293, #15931, #56694, #61597, #21226, #9555, #44252, #32948, #43487, #5011, #21595, #32186, #49526, #55207, #66499, #44621, #14810, #67636, #38961, #61964, #10292, #33318, #4635, #28009, #67998, #26502, #27631, #21967, #16294, #39334, #62331, #72547, #3512, #37851, #9169, #10658, #20852, #12138, #51386, #68739, #74399, #28746, #17423, #45725, #69863, #17052, #478, #28378, #34809, #23458, #40447, #69116, #12504, #46098, #58190, #6855, #57816, #40074, #52511, #18176, #849, #6494, #63079, #41191, #5746, #35535, #46840, #22708, #29501, #23834, #11404, #34441, #46471, #6123, #57064, #29868, #29128, #57440, #16668, #63446, #11771, #52144, #51762, #39699, #11036, #109, #69491, #23087, #17801, #40815, #64201, #34068, #52882, #22329, #63822, #35175, #68370, #58551, #45356, #62699, #5377, #43017, #41916, #36270, #24564, #18910, #7964, #25664, #14346, #36638, #71319, #54366, #30600, #1934, #24922, #7230, #37376, #31718, #13236, #47937, #42282, #31336, #30233, #60377, #30967, #1214, #2296, #53986, #66039, #48681, #19638, #59286, #25294, #42653, #47570, #65664, #8704, #58922, #53252, #13962, #59646, #1580, #8326, #47205, #7594, #64926, #70237, #53622, #70954, #19271, #37005, #48311, #24193, #65296, #13601, #60008, #64570, #2676, #71688, #20008, #18546, #41552, #12867, #35903, #70593, #72453, #61507, #5574, #68935, #15468, #51212, #34257, #9460, #55485, #3798, #60758, #17246, #11594, #66792, #26798, #21135, #11229, #9080, #40268, #9829, #54740, #56887, #32857, #22911, #28573, #74222, #38129, #5202, #22526, #3419, #45547, #45923, #37759, #32094, #68564, #38506, #55115, #62896, #26033, #61129, #20761, #49054, #32476, #49812, #72828, #16866, #28199, #63268, #43778, #44158, #15095, #43396, #39891, #57259, #26406, #66410, #72062, #3048, #67173, #51579, #74598, #49434, #20380, #14720, #41018, #29693, #58019, #7423, #29328, #12697, #40640, #47031, #35729, #52708, #6689, #24752, #58383, #70425, #19099, #70065, #52337, #64759, #30431, #13059, #18742, #6324, #53450, #18001, #47763, #59114, #63643, #41751, #36098, #11972, #675, #58746, #18372, #69313, #42104, #41387, #35004, #28947, #1041, #24021, #64398, #23661, #51966, #23283, #64026, #7055, #46666, #30064, #69686, #1770, #46293, #65116, #34630, #12338, #35371, #5948, #70785, #53077, #57636, #1412, #303, #24396, #47402, #17623, #60953, #31914, #71511, #66235, #54935, #36832, #8901, #55308, #71143, #19465, #3244, #48876, #13789, #20579, #59479, #19834, #54190, #7791, #65859, #37200, #31539, #26230, #71886, #72651, #2497, #60199, #25491, #2123, #37577, #60577, #42478, #25117, #30794, #13426, #48505, #54561, #49250, #65494, #59840, #8154, #42840, #8524, #31160, #9272, #14167, #14537, #2868, #25855, #72265, #20199, #43217, #3616, #43592, #66607, #20953, #14913, #37953, #32293, #26611, #49635, #43975, #36463, #53815, #48135, #57162, #16769, #73020, #28104, #51119, #21331, #61703, #45091, #27733, #26989, #74499, #4739, #44352, #61328, #39066, #62068, #33419, #38702, #9656, #55685, #73391, #10393, #10024, #50743, #33056, #62801, #4000, #22808, #66986, #56055, #4364, #38323, #27356, #74131, #73758, #50373, #34162, #21696, #44722, #15660, #67739, #22065, #39796, #5479, #68105, #62432, #45452, #16034, #56418, #16395, #67362, #28481, #15287, #39432, #10757, #33796, #56794, #5113, #11141, #22433, #50003, #68469, #51490, #32676, #46938, #52980, #35634, #68842, #12238, #36003, #63550, #59020, #17155, #948, #69967, #40545, #57546, #18647, #57919, #70332, #40919, #34910, #5854, #23929, #45829, #63928, #11875, #52243, #12606, #30334, #69217, #17904, #212, #7329, #23191, #41290, #35276, #41655, #64299, #6227, #577, #58289, #69592, #53353, #46203, #1313, #6591, #29231, #63179, #29598, #23559, #46570, #52612, #24297, #58648, #1677, #18275, #17528, #6956, #29966, #47308, #64665, #12966, #40176, #11506, #34539, #28848, #51871, #31444, #71790, #14818, #71417, #54089, #25021, #59748, #19368, #32196, #37860, #48411, #13331, #30701, #36367, #55217 ),
 ( #47668, #43122, #24657, #8426, #54841, #66140, #19008, #14069, #7696, #8060, #53719, #48039, #70689, #31821, #54469, #31062, #2399, #48783, #42382, #2033, #60479, #60108, #42014, #65398, #25397, #43496, #71048, #13695, #2776, #25762, #59383, #65020, #37106, #36739, #37479, #19742, #42750, #49157, #65767, #20110, #14445, #8809, #3150, #26137, #72165, #20476, #66507, #60857, #9178, #21235, #68379, #49536, #33326, #27640, #72925, #15200, #51027, #15568, #28016, #73303, #67274, #38229, #56325, #3522, #21603, #44261, #9925, #45004, #62708, #26895, #50281, #32579, #39707, #55587, #73667, #44629, #74035, #21975, #38605, #32958, #67643, #27263, #16678, #3903, #10668, #15940, #61607, #20861, #38969, #55963, #4273, #61973, #33699, #16303, #11046, #10301, #49911, #4647, #50647, #68007, #39341, #5021, #62339, #34076, #56704, #22337, #45364, #26510, #72555, #43878, #66894, #61235, #9563, #17432, #51771, #64578, #47212, #6131, #45733, #63088, #68747, #12876, #118, #57073, #28758, #46480, #23096, #17810, #40826, #40456, #18555, #6864, #40083, #63455, #69128, #41200, #12147, #5385, #857, #28387, #63832, #12513, #23843, #51395, #69500, #11412, #11781, #34449, #57450, #74410, #64209, #35183, #34819, #57826, #46108, #17061, #58198, #22717, #52153, #29137, #488, #46850, #41564, #5756, #23468, #6503, #29510, #52520, #69871, #18184, #29877, #35545, #58561, #52891, #1222, #24201, #70246, #36279, #43025, #48321, #30610, #53261, #2305, #24931, #19280, #47947, #66048, #48690, #43404, #71327, #59294, #7602, #19648, #59656, #70964, #37385, #42662, #66418, #42290, #65304, #53632, #65673, #8333, #26040, #7973, #13609, #1942, #36647, #30976, #35912, #49061, #53994, #24574, #41925, #47578, #58931, #25303, #7238, #13971, #37014, #60016, #31344, #54375, #2684, #72070, #60385, #18918, #25672, #71696, #20014, #14355, #30242, #8712, #1588, #31726, #54748, #3057, #70601, #20390, #64935, #13245, #49443, #43786, #37768, #61886, #55870, #55495, #26806, #27172, #38136, #72461, #15847, #9838, #60766, #61137, #55122, #38881, #14727, #15105, #50560, #66802, #20768, #67551, #9467, #32485, #21517, #56236, #10209, #32103, #32865, #16213, #3808, #39251, #3426, #50190, #44538, #49819, #72836, #73574, #21143, #21884, #38514, #73211, #9089, #4186, #44166, #15476, #4552, #26415, #33238, #44913, #27546, #67180, #67919, #61516, #48562, #54998, #2930, #42539, #36889, #54249, #31224, #72328, #7846, #14603, #19894, #2185, #24810, #71572, #71203, #65552, #19521, #37642, #20258, #14976, #42900, #30853, #53874, #65920, #2560, #13846, #8961, #14224, #38012, #59899, #8213, #25180, #37265, #54622, #20643, #25549, #60259, #48194, #8586, #31601, #7483, #43658, #25917, #70846, #13485, #19158, #30488, #48935, #53505, #71947, #43280, #66296, #60640, #31973, #3305, #66670, #26291, #65173, #49311, #1823, #47825, #42161, #36524, #59534, #34266, #33155, #45560, #11238, #68573, #74231, #38796, #62909, #73483, #5584, #39902, #21426, #51221, #22537, #44449, #10117, #68201, #50844, #50103, #22921, #27837, #16879, #57269, #4095, #10488, #56523, #61799, #9752, #27088, #21789, #62163, #56149, #73858, #4464, #28583, #73118, #45934, #15385, #27454, #50468, #61425, #44819, #51591, #22165, #67831, #74608, #16123, #39161, #33522, #4840, #45190, #16498, #39538, #62533, #38421, #67460, #10861, #32771, #55778, #33898, #15757, #56896, #5209, #28209, #17631, #41760, #52349, #59125, #18751, #315, #30072, #53087, #23293, #63655, #47041, #29703, #28956, #1779, #6698, #1422, #36107, #57647, #64036, #35381, #40650, #63277, #5955, #685, #41027, #11981, #52719, #35013, #64769, #51976, #24764, #68947, #58027, #6335, #40277, #29338, #24406, #1052, #23669, #7436, #46675, #69698, #18012, #12347, #24030, #13072, #30442, #70076, #64408, #47412, #58392, #18383, #41396, #46304, #53461, #17257, #12708, #35738, #58755, #70436, #69322, #11604, #7066, #34640, #49920, #55596, #15951, #21612, #67280, #31174, #26904, #15576, #71155, #44268, #38977, #30805, #53827, #38617, #9571, #48146, #55971, #19111, #54199, #13801, #42116, #25502, #71521, #65869, #61619, #32590, #33335, #36845, #19845, #59852, #36474, #72934, #21244, #2137, #59490, #65128, #47774, #8165, #14178, #9935, #25128, #19476, #42489, #2508, #42852, #65505, #44638, #48515 ) ),
 .UNSPECIFIED., .F., .F., .T. ) 
 B_SPLINE_SURFACE_WITH_KNOTS ( ( 2, 2 ),
 ( 3, 2, 2, 2, 2, 2, 2, 2, 2, 2, 2, 2, 2, 2, 2, 2, 2, 2, 2, 2, 2, 2, 2, 2, 2, 2, 2, 2, 2, 2, 2, 2, 2, 2, 2, 2, 2, 2, 2, 2, 2, 2, 2, 2, 2, 2, 2, 2, 2, 2, 2, 2, 2, 2, 2, 2, 2, 2, 2, 2, 2, 2, 2, 2, 2, 2, 2, 2, 2, 2, 2, 2, 2, 2, 2, 2, 2, 2, 2, 2, 2, 2, 2, 2, 2, 2, 2, 2, 2, 2, 2, 2, 2, 2, 2, 2, 2, 2, 2, 2, 2, 2, 2, 2, 2, 2, 2, 2, 2, 2, 2, 2, 2, 2, 2, 2, 2, 2, 2, 2, 2, 2, 2, 2, 2, 2, 2, 2, 2, 2, 2, 2, 2, 2, 2, 2, 2, 2, 2, 2, 2, 2, 2, 2, 2, 2, 2, 2, 2, 2, 2, 2, 2, 2, 2, 2, 2, 2, 2, 2, 2, 2, 2, 2, 2, 2, 2, 2, 2, 2, 2, 2, 2, 2, 2, 2, 2, 2, 2, 2, 2, 2, 2, 2, 2, 2, 2, 2, 2, 2, 2, 2, 2, 2, 2, 2, 2, 2, 2, 2, 2, 2, 2, 2, 2, 2, 2, 2, 2, 2, 2, 2, 2, 2, 2, 2, 2, 2, 2, 2, 2, 2, 2, 2, 2, 2, 2, 2, 2, 2, 2, 2, 2, 2, 2, 2, 2, 2, 2, 2, 2, 2, 2, 2, 2, 2, 2, 2, 2, 2, 2, 2, 2, 2, 2, 2, 2, 2, 2, 2, 2, 2, 2, 2, 2, 2, 2, 3 ),
 ( 0.000000000000000000, 1.000000000000000000 ),
 ( 0.000000000000000000, 0.003676470588235294067, 0.007352941176470588133, 0.01102941176470588307, 0.01470588235294117627, 0.01838235294117647120, 0.02205882352941176613, 0.02573529411764705760, 0.02941176470588235253, 0.03308823529411764747, 0.03676470588235294240, 0.04044117647058823733, 0.04411764705882353227, 0.04779411764705882026, 0.05147058823529411520, 0.05514705882352941013, 0.05882352941176470507, 0.06250000000000000000, 0.06617647058823529493, 0.06985294117647058987, 0.07352941176470588480, 0.07720588235294117974, 0.08088235294117647467, 0.08455882352941176960, 0.08823529411764706454, 0.09191176470588235947, 0.09558823529411764053, 0.09926470588235293546, 0.1029411764705882304, 0.1066176470588235253, 0.1102941176470588203, 0.1139705882352941152, 0.1176470588235294101, 0.1213235294117647051, 0.1250000000000000000, 0.1286764705882352811, 0.1323529411764705899, 0.1360294117647058709, 0.1397058823529411797, 0.1433823529411764608, 0.1470588235294117696, 0.1507352941176470507, 0.1544117647058823595, 0.1580882352941176405, 0.1617647058823529493, 0.1654411764705882304, 0.1691176470588235392, 0.1727941176470588203, 0.1764705882352941291, 0.1801470588235294101, 0.1838235294117647189, 0.1875000000000000000, 0.1911764705882352811, 0.1948529411764705899, 0.1985294117647058709, 0.2022058823529411797, 0.2058823529411764608, 0.2095588235294117696, 0.2132352941176470507, 0.2169117647058823595, 0.2205882352941176405, 0.2242647058823529493, 0.2279411764705882304, 0.2316176470588235392, 0.2352941176470588203, 0.2389705882352941291, 0.2426470588235294101, 0.2463235294117647189, 0.2500000000000000000, 0.2536764705882352811, 0.2573529411764705621, 0.2610294117647058987, 0.2647058823529411797, 0.2683823529411764608, 0.2720588235294117418, 0.2757352941176470784, 0.2794117647058823595, 0.2830882352941176405, 0.2867647058823529216, 0.2904411764705882582, 0.2941176470588235392, 0.2977941176470588203, 0.3014705882352941013, 0.3051470588235294379, 0.3088235294117647189, 0.3125000000000000000, 0.3161764705882352811, 0.3198529411764705621, 0.3235294117647058987, 0.3272058823529411797, 0.3308823529411764608, 0.3345588235294117418, 0.3382352941176470784, 0.3419117647058823595, 0.3455882352941176405, 0.3492647058823529216, 0.3529411764705882582, 0.3566176470588235392, 0.3602941176470588203, 0.3639705882352941013, 0.3676470588235294379, 0.3713235294117647189, 0.3750000000000000000, 0.3786764705882352811, 0.3823529411764705621, 0.3860294117647058987, 0.3897058823529411797, 0.3933823529411764608, 0.3970588235294117418, 0.4007352941176470784, 0.4044117647058823595, 0.4080882352941176405, 0.4117647058823529216, 0.4154411764705882582, 0.4191176470588235392, 0.4227941176470588203, 0.4264705882352941013, 0.4301470588235294379, 0.4338235294117647189, 0.4375000000000000000, 0.4411764705882352811, 0.4448529411764705621, 0.4485294117647058987, 0.4522058823529411797, 0.4558823529411764608, 0.4595588235294117418, 0.4632352941176470784, 0.4669117647058823595, 0.4705882352941176405, 0.4742647058823529216, 0.4779411764705882582, 0.4816176470588235392, 0.4852941176470588203, 0.4889705882352941013, 0.4926470588235294379, 0.4963235294117647189, 0.5000000000000000000, 0.5036764705882352811, 0.5073529411764705621, 0.5110294117647058432, 0.5147058823529411242, 0.5183823529411765163, 0.5220588235294117974, 0.5257352941176470784, 0.5294117647058823595, 0.5330882352941176405, 0.5367647058823529216, 0.5404411764705882026, 0.5441176470588234837, 0.5477941176470588758, 0.5514705882352941568, 0.5551470588235294379, 0.5588235294117647189, 0.5625000000000000000, 0.5661764705882352811, 0.5698529411764705621, 0.5735294117647058432, 0.5772058823529411242, 0.5808823529411765163, 0.5845588235294117974, 0.5882352941176470784, 0.5919117647058823595, 0.5955882352941176405, 0.5992647058823529216, 0.6029411764705882026, 0.6066176470588234837, 0.6102941176470588758, 0.6139705882352941568, 0.6176470588235294379, 0.6213235294117647189, 0.6250000000000000000, 0.6286764705882352811, 0.6323529411764705621, 0.6360294117647058432, 0.6397058823529411242, 0.6433823529411765163, 0.6470588235294117974, 0.6507352941176470784, 0.6544117647058823595, 0.6580882352941176405, 0.6617647058823529216, 0.6654411764705882026, 0.6691176470588234837, 0.6727941176470588758, 0.6764705882352941568, 0.6801470588235294379, 0.6838235294117647189, 0.6875000000000000000, 0.6911764705882352811, 0.6948529411764705621, 0.6985294117647058432, 0.7022058823529411242, 0.7058823529411765163, 0.7095588235294117974, 0.7132352941176470784, 0.7169117647058823595, 0.7205882352941176405, 0.7242647058823529216, 0.7279411764705882026, 0.7316176470588234837, 0.7352941176470588758, 0.7389705882352941568, 0.7426470588235294379, 0.7463235294117647189, 0.7500000000000000000, 0.7536764705882352811, 0.7573529411764705621, 0.7610294117647058432, 0.7647058823529411242, 0.7683823529411765163, 0.7720588235294117974, 0.7757352941176470784, 0.7794117647058823595, 0.7830882352941176405, 0.7867647058823529216, 0.7904411764705882026, 0.7941176470588234837, 0.7977941176470588758, 0.8014705882352941568, 0.8051470588235294379, 0.8088235294117647189, 0.8125000000000000000, 0.8161764705882352811, 0.8198529411764705621, 0.8235294117647058432, 0.8272058823529411242, 0.8308823529411765163, 0.8345588235294117974, 0.8382352941176470784, 0.8419117647058823595, 0.8455882352941176405, 0.8492647058823529216, 0.8529411764705882026, 0.8566176470588234837, 0.8602941176470588758, 0.8639705882352941568, 0.8676470588235294379, 0.8713235294117647189, 0.8750000000000000000, 0.8786764705882352811, 0.8823529411764705621, 0.8860294117647058432, 0.8897058823529411242, 0.8933823529411765163, 0.8970588235294117974, 0.9007352941176470784, 0.9044117647058823595, 0.9080882352941176405, 0.9117647058823529216, 0.9154411764705882026, 0.9191176470588234837, 0.9227941176470588758, 0.9264705882352941568, 0.9301470588235294379, 0.9338235294117647189, 0.9375000000000000000, 0.9411764705882352811, 0.9448529411764705621, 0.9485294117647058432, 0.9522058823529411242, 0.9558823529411765163, 0.9595588235294117974, 0.9632352941176470784, 0.9669117647058823595, 0.9705882352941176405, 0.9742647058823529216, 0.9779411764705882026, 0.9803851272776890058 ),
 .UNSPECIFIED. ) 
 GEOMETRIC_REPRESENTATION_ITEM ( )  RATIONAL_B_SPLINE_SURFACE ( (
 ( 1.000000000000000000, 0.9238795325112867385, 1.000000000000000000, 0.9238795325112867385, 1.000000000000000000, 0.9238795325112867385, 1.000000000000000000, 0.9238795325112867385, 1.000000000000000000, 0.9238795325112867385, 1.000000000000000000, 0.9238795325112867385, 1.000000000000000000, 0.9238795325112867385, 1.000000000000000000, 0.9238795325112867385, 1.000000000000000000, 0.9238795325112867385, 1.000000000000000000, 0.9238795325112867385, 1.000000000000000000, 0.9238795325112867385, 1.000000000000000000, 0.9238795325112867385, 1.000000000000000000, 0.9238795325112867385, 1.000000000000000000, 0.9238795325112867385, 1.000000000000000000, 0.9238795325112867385, 1.000000000000000000, 0.9238795325112867385, 1.000000000000000000, 0.9238795325112867385, 1.000000000000000000, 0.9238795325112867385, 1.000000000000000000, 0.9238795325112867385, 1.000000000000000000, 0.9238795325112867385, 1.000000000000000000, 0.9238795325112867385, 1.000000000000000000, 0.9238795325112867385, 1.000000000000000000, 0.9238795325112867385, 1.000000000000000000, 0.9238795325112867385, 1.000000000000000000, 0.9238795325112867385, 1.000000000000000000, 0.9238795325112867385, 1.000000000000000000, 0.9238795325112867385, 1.000000000000000000, 0.9238795325112867385, 1.000000000000000000, 0.9238795325112867385, 1.000000000000000000, 0.9238795325112867385, 1.000000000000000000, 0.9238795325112867385, 1.000000000000000000, 0.9238795325112867385, 1.000000000000000000, 0.9238795325112867385, 1.000000000000000000, 0.9238795325112867385, 1.000000000000000000, 0.9238795325112867385, 1.000000000000000000, 0.9238795325112867385, 1.000000000000000000, 0.9238795325112867385, 1.000000000000000000, 0.9238795325112867385, 1.000000000000000000, 0.9238795325112867385, 1.000000000000000000, 0.9238795325112867385, 1.000000000000000000, 0.9238795325112867385, 1.000000000000000000, 0.9238795325112867385, 1.000000000000000000, 0.9238795325112867385, 1.000000000000000000, 0.9238795325112867385, 1.000000000000000000, 0.9238795325112867385, 1.000000000000000000, 0.9238795325112867385, 1.000000000000000000, 0.9238795325112867385, 1.000000000000000000, 0.9238795325112867385, 1.000000000000000000, 0.9238795325112867385, 1.000000000000000000, 0.9238795325112867385, 1.000000000000000000, 0.9238795325112867385, 1.000000000000000000, 0.9238795325112867385, 1.000000000000000000, 0.9238795325112867385, 1.000000000000000000, 0.9238795325112867385, 1.000000000000000000, 0.9238795325112867385, 1.000000000000000000, 0.9238795325112867385, 1.000000000000000000, 0.9238795325112867385, 1.000000000000000000, 0.9238795325112867385, 1.000000000000000000, 0.9238795325112867385, 1.000000000000000000, 0.9238795325112867385, 1.000000000000000000, 0.9238795325112867385, 1.000000000000000000, 0.9238795325112867385, 1.000000000000000000, 0.9238795325112867385, 1.000000000000000000, 0.9238795325112867385, 1.000000000000000000, 0.9238795325112867385, 1.000000000000000000, 0.9238795325112867385, 1.000000000000000000, 0.9238795325112867385, 1.000000000000000000, 0.9238795325112867385, 1.000000000000000000, 0.9238795325112867385, 1.000000000000000000, 0.9238795325112867385, 1.000000000000000000, 0.9238795325112867385, 1.000000000000000000, 0.9238795325112867385, 1.000000000000000000, 0.9238795325112867385, 1.000000000000000000, 0.9238795325112867385, 1.000000000000000000, 0.9238795325112867385, 1.000000000000000000, 0.9238795325112867385, 1.000000000000000000, 0.9238795325112867385, 1.000000000000000000, 0.9238795325112867385, 1.000000000000000000, 0.9238795325112867385, 1.000000000000000000, 0.9238795325112867385, 1.000000000000000000, 0.9238795325112867385, 1.000000000000000000, 0.9238795325112867385, 1.000000000000000000, 0.9238795325112867385, 1.000000000000000000, 0.9238795325112867385, 1.000000000000000000, 0.9238795325112867385, 1.000000000000000000, 0.9238795325112867385, 1.000000000000000000, 0.9238795325112867385, 1.000000000000000000, 0.9238795325112867385, 1.000000000000000000, 0.9238795325112867385, 1.000000000000000000, 0.9238795325112867385, 1.000000000000000000, 0.9238795325112867385, 1.000000000000000000, 0.9238795325112867385, 1.000000000000000000, 0.9238795325112867385, 1.000000000000000000, 0.9238795325112867385, 1.000000000000000000, 0.9238795325112867385, 1.000000000000000000, 0.9238795325112867385, 1.000000000000000000, 0.9238795325112867385, 1.000000000000000000, 0.9238795325112867385, 1.000000000000000000, 0.9238795325112867385, 1.000000000000000000, 0.9238795325112867385, 1.000000000000000000, 0.9238795325112867385, 1.000000000000000000, 0.9238795325112867385, 1.000000000000000000, 0.9238795325112867385, 1.000000000000000000, 0.9238795325112867385, 1.000000000000000000, 0.9238795325112867385, 1.000000000000000000, 0.9238795325112867385, 1.000000000000000000, 0.9238795325112867385, 1.000000000000000000, 0.9238795325112867385, 1.000000000000000000, 0.9238795325112867385, 1.000000000000000000, 0.9238795325112867385, 1.000000000000000000, 0.9238795325112867385, 1.000000000000000000, 0.9238795325112867385, 1.000000000000000000, 0.9238795325112867385, 1.000000000000000000, 0.9238795325112867385, 1.000000000000000000, 0.9238795325112867385, 1.000000000000000000, 0.9238795325112867385, 1.000000000000000000, 0.9238795325112867385, 1.000000000000000000, 0.9238795325112867385, 1.000000000000000000, 0.9238795325112867385, 1.000000000000000000, 0.9238795325112867385, 1.000000000000000000, 0.9238795325112867385, 1.000000000000000000, 0.9238795325112867385, 1.000000000000000000, 0.9238795325112867385, 1.000000000000000000, 0.9238795325112867385, 1.000000000000000000, 0.9238795325112867385, 1.000000000000000000, 0.9238795325112867385, 1.000000000000000000, 0.9238795325112867385, 1.000000000000000000, 0.9238795325112867385, 1.000000000000000000, 0.9238795325112867385, 1.000000000000000000, 0.9238795325112867385, 1.000000000000000000, 0.9238795325112867385, 1.000000000000000000, 0.9238795325112867385, 1.000000000000000000, 0.9238795325112867385, 1.000000000000000000, 0.9238795325112867385, 1.000000000000000000, 0.9238795325112867385, 1.000000000000000000, 0.9238795325112867385, 1.000000000000000000, 0.9238795325112867385, 1.000000000000000000, 0.9238795325112867385, 1.000000000000000000, 0.9238795325112867385, 1.000000000000000000, 0.9238795325112867385, 1.000000000000000000, 0.9238795325112867385, 1.000000000000000000, 0.9238795325112867385, 1.000000000000000000, 0.9238795325112867385, 1.000000000000000000, 0.9238795325112867385, 1.000000000000000000, 0.9238795325112867385, 1.000000000000000000, 0.9238795325112867385, 1.000000000000000000, 0.9238795325112867385, 1.000000000000000000, 0.9238795325112867385, 1.000000000000000000, 0.9238795325112867385, 1.000000000000000000, 0.9238795325112867385, 1.000000000000000000, 0.9238795325112867385, 1.000000000000000000, 0.9238795325112867385, 1.000000000000000000, 0.9238795325112867385, 1.000000000000000000, 0.9238795325112867385, 1.000000000000000000, 0.9238795325112867385, 1.000000000000000000, 0.9238795325112867385, 1.000000000000000000, 0.9238795325112867385, 1.000000000000000000, 0.9238795325112867385, 1.000000000000000000, 0.9238795325112867385, 1.000000000000000000, 0.9238795325112867385, 1.000000000000000000, 0.9238795325112867385, 1.000000000000000000, 0.9238795325112867385, 1.000000000000000000, 0.9238795325112867385, 1.000000000000000000, 0.9238795325112867385, 1.000000000000000000, 0.9238795325112867385, 1.000000000000000000, 0.9238795325112867385, 1.000000000000000000, 0.9238795325112867385, 1.000000000000000000, 0.9238795325112867385, 1.000000000000000000, 0.9238795325112867385, 1.000000000000000000, 0.9238795325112867385, 1.000000000000000000, 0.9238795325112867385, 1.000000000000000000, 0.9238795325112867385, 1.000000000000000000, 0.9238795325112867385, 1.000000000000000000, 0.9238795325112867385, 1.000000000000000000, 0.9238795325112867385, 1.000000000000000000, 0.9238795325112867385, 1.000000000000000000, 0.9238795325112867385, 1.000000000000000000, 0.9238795325112867385, 1.000000000000000000, 0.9238795325112867385, 1.000000000000000000, 0.9238795325112867385, 1.000000000000000000, 0.9238795325112867385, 1.000000000000000000, 0.9238795325112867385, 1.000000000000000000, 0.9238795325112867385, 1.000000000000000000, 0.9238795325112867385, 1.000000000000000000, 0.9238795325112867385, 1.000000000000000000, 0.9238795325112867385, 1.000000000000000000, 0.9238795325112867385, 1.000000000000000000, 0.9238795325112867385, 1.000000000000000000, 0.9238795325112867385, 1.000000000000000000, 0.9238795325112867385, 1.000000000000000000, 0.9238795325112867385, 1.000000000000000000, 0.9238795325112867385, 1.000000000000000000, 0.9238795325112867385, 1.000000000000000000, 0.9238795325112867385, 1.000000000000000000, 0.9238795325112867385, 1.000000000000000000, 0.9238795325112867385, 1.000000000000000000, 0.9238795325112867385, 1.000000000000000000, 0.9238795325112867385, 1.000000000000000000, 0.9238795325112867385, 1.000000000000000000, 0.9238795325112867385, 1.000000000000000000, 0.9238795325112867385, 1.000000000000000000, 0.9238795325112867385, 1.000000000000000000, 0.9238795325112867385, 1.000000000000000000, 0.9238795325112867385, 1.000000000000000000, 0.9238795325112867385, 1.000000000000000000, 0.9238795325112867385, 1.000000000000000000, 0.9238795325112867385, 1.000000000000000000, 0.9238795325112867385, 1.000000000000000000, 0.9238795325112867385, 1.000000000000000000, 0.9238795325112867385, 1.000000000000000000, 0.9238795325112867385, 1.000000000000000000, 0.9238795325112867385, 1.000000000000000000, 0.9238795325112867385, 1.000000000000000000, 0.9238795325112867385, 1.000000000000000000, 0.9238795325112867385, 1.000000000000000000, 0.9238795325112867385, 1.000000000000000000, 0.9238795325112867385, 1.000000000000000000, 0.9238795325112867385, 1.000000000000000000, 0.9238795325112867385, 1.000000000000000000, 0.9238795325112867385, 1.000000000000000000, 0.9238795325112867385, 1.000000000000000000, 0.9238795325112867385, 1.000000000000000000, 0.9238795325112867385, 1.000000000000000000, 0.9238795325112867385, 1.000000000000000000, 0.9238795325112867385, 1.000000000000000000, 0.9238795325112867385, 1.000000000000000000, 0.9238795325112867385, 1.000000000000000000, 0.9238795325112867385, 1.000000000000000000, 0.9238795325112867385, 1.000000000000000000, 0.9238795325112867385, 1.000000000000000000, 0.9238795325112867385, 1.000000000000000000, 0.9238795325112867385, 1.000000000000000000, 0.9238795325112867385, 1.000000000000000000, 0.9238795325112867385, 1.000000000000000000, 0.9238795325112867385, 1.000000000000000000, 0.9238795325112867385, 1.000000000000000000, 0.9238795325112867385, 1.000000000000000000, 0.9238795325112867385, 1.000000000000000000, 0.9238795325112867385, 1.000000000000000000, 0.9238795325112867385, 1.000000000000000000, 0.9238795325112867385, 1.000000000000000000, 0.9238795325112867385, 1.000000000000000000, 0.9238795325112867385, 1.000000000000000000, 0.9238795325112867385, 1.000000000000000000, 0.9238795325112867385, 1.000000000000000000, 0.9238795325112867385, 1.000000000000000000, 0.9238795325112867385, 1.000000000000000000, 0.9238795325112867385, 1.000000000000000000, 0.9238795325112867385, 1.000000000000000000, 0.9238795325112867385, 1.000000000000000000, 0.9238795325112867385, 1.000000000000000000, 0.9238795325112867385, 1.000000000000000000, 0.9238795325112867385, 1.000000000000000000, 0.9238795325112867385, 1.000000000000000000, 0.9238795325112867385, 1.000000000000000000, 0.9238795325112867385, 1.000000000000000000, 0.9238795325112867385, 1.000000000000000000, 0.9238795325112867385, 1.000000000000000000, 0.9238795325112867385, 1.000000000000000000, 0.9238795325112867385, 1.000000000000000000, 0.9238795325112867385, 1.000000000000000000, 0.9238795325112867385, 1.000000000000000000, 0.9238795325112867385, 1.000000000000000000, 0.9238795325112867385, 1.000000000000000000, 0.9238795325112867385, 1.000000000000000000, 0.9238795325112867385, 1.000000000000000000, 0.9493985675959865089, 0.9660722070829228514),
 ( 1.000000000000000000, 0.9238795325112867385, 1.000000000000000000, 0.9238795325112867385, 1.000000000000000000, 0.9238795325112867385, 1.000000000000000000, 0.9238795325112867385, 1.000000000000000000, 0.9238795325112867385, 1.000000000000000000, 0.9238795325112867385, 1.000000000000000000, 0.9238795325112867385, 1.000000000000000000, 0.9238795325112867385, 1.000000000000000000, 0.9238795325112867385, 1.000000000000000000, 0.9238795325112867385, 1.000000000000000000, 0.9238795325112867385, 1.000000000000000000, 0.9238795325112867385, 1.000000000000000000, 0.9238795325112867385, 1.000000000000000000, 0.9238795325112867385, 1.000000000000000000, 0.9238795325112867385, 1.000000000000000000, 0.9238795325112867385, 1.000000000000000000, 0.9238795325112867385, 1.000000000000000000, 0.9238795325112867385, 1.000000000000000000, 0.9238795325112867385, 1.000000000000000000, 0.9238795325112867385, 1.000000000000000000, 0.9238795325112867385, 1.000000000000000000, 0.9238795325112867385, 1.000000000000000000, 0.9238795325112867385, 1.000000000000000000, 0.9238795325112867385, 1.000000000000000000, 0.9238795325112867385, 1.000000000000000000, 0.9238795325112867385, 1.000000000000000000, 0.9238795325112867385, 1.000000000000000000, 0.9238795325112867385, 1.000000000000000000, 0.9238795325112867385, 1.000000000000000000, 0.9238795325112867385, 1.000000000000000000, 0.9238795325112867385, 1.000000000000000000, 0.9238795325112867385, 1.000000000000000000, 0.9238795325112867385, 1.000000000000000000, 0.9238795325112867385, 1.000000000000000000, 0.9238795325112867385, 1.000000000000000000, 0.9238795325112867385, 1.000000000000000000, 0.9238795325112867385, 1.000000000000000000, 0.9238795325112867385, 1.000000000000000000, 0.9238795325112867385, 1.000000000000000000, 0.9238795325112867385, 1.000000000000000000, 0.9238795325112867385, 1.000000000000000000, 0.9238795325112867385, 1.000000000000000000, 0.9238795325112867385, 1.000000000000000000, 0.9238795325112867385, 1.000000000000000000, 0.9238795325112867385, 1.000000000000000000, 0.9238795325112867385, 1.000000000000000000, 0.9238795325112867385, 1.000000000000000000, 0.9238795325112867385, 1.000000000000000000, 0.9238795325112867385, 1.000000000000000000, 0.9238795325112867385, 1.000000000000000000, 0.9238795325112867385, 1.000000000000000000, 0.9238795325112867385, 1.000000000000000000, 0.9238795325112867385, 1.000000000000000000, 0.9238795325112867385, 1.000000000000000000, 0.9238795325112867385, 1.000000000000000000, 0.9238795325112867385, 1.000000000000000000, 0.9238795325112867385, 1.000000000000000000, 0.9238795325112867385, 1.000000000000000000, 0.9238795325112867385, 1.000000000000000000, 0.9238795325112867385, 1.000000000000000000, 0.9238795325112867385, 1.000000000000000000, 0.9238795325112867385, 1.000000000000000000, 0.9238795325112867385, 1.000000000000000000, 0.9238795325112867385, 1.000000000000000000, 0.9238795325112867385, 1.000000000000000000, 0.9238795325112867385, 1.000000000000000000, 0.9238795325112867385, 1.000000000000000000, 0.9238795325112867385, 1.000000000000000000, 0.9238795325112867385, 1.000000000000000000, 0.9238795325112867385, 1.000000000000000000, 0.9238795325112867385, 1.000000000000000000, 0.9238795325112867385, 1.000000000000000000, 0.9238795325112867385, 1.000000000000000000, 0.9238795325112867385, 1.000000000000000000, 0.9238795325112867385, 1.000000000000000000, 0.9238795325112867385, 1.000000000000000000, 0.9238795325112867385, 1.000000000000000000, 0.9238795325112867385, 1.000000000000000000, 0.9238795325112867385, 1.000000000000000000, 0.9238795325112867385, 1.000000000000000000, 0.9238795325112867385, 1.000000000000000000, 0.9238795325112867385, 1.000000000000000000, 0.9238795325112867385, 1.000000000000000000, 0.9238795325112867385, 1.000000000000000000, 0.9238795325112867385, 1.000000000000000000, 0.9238795325112867385, 1.000000000000000000, 0.9238795325112867385, 1.000000000000000000, 0.9238795325112867385, 1.000000000000000000, 0.9238795325112867385, 1.000000000000000000, 0.9238795325112867385, 1.000000000000000000, 0.9238795325112867385, 1.000000000000000000, 0.9238795325112867385, 1.000000000000000000, 0.9238795325112867385, 1.000000000000000000, 0.9238795325112867385, 1.000000000000000000, 0.9238795325112867385, 1.000000000000000000, 0.9238795325112867385, 1.000000000000000000, 0.9238795325112867385, 1.000000000000000000, 0.9238795325112867385, 1.000000000000000000, 0.9238795325112867385, 1.000000000000000000, 0.9238795325112867385, 1.000000000000000000, 0.9238795325112867385, 1.000000000000000000, 0.9238795325112867385, 1.000000000000000000, 0.9238795325112867385, 1.000000000000000000, 0.9238795325112867385, 1.000000000000000000, 0.9238795325112867385, 1.000000000000000000, 0.9238795325112867385, 1.000000000000000000, 0.9238795325112867385, 1.000000000000000000, 0.9238795325112867385, 1.000000000000000000, 0.9238795325112867385, 1.000000000000000000, 0.9238795325112867385, 1.000000000000000000, 0.9238795325112867385, 1.000000000000000000, 0.9238795325112867385, 1.000000000000000000, 0.9238795325112867385, 1.000000000000000000, 0.9238795325112867385, 1.000000000000000000, 0.9238795325112867385, 1.000000000000000000, 0.9238795325112867385, 1.000000000000000000, 0.9238795325112867385, 1.000000000000000000, 0.9238795325112867385, 1.000000000000000000, 0.9238795325112867385, 1.000000000000000000, 0.9238795325112867385, 1.000000000000000000, 0.9238795325112867385, 1.000000000000000000, 0.9238795325112867385, 1.000000000000000000, 0.9238795325112867385, 1.000000000000000000, 0.9238795325112867385, 1.000000000000000000, 0.9238795325112867385, 1.000000000000000000, 0.9238795325112867385, 1.000000000000000000, 0.9238795325112867385, 1.000000000000000000, 0.9238795325112867385, 1.000000000000000000, 0.9238795325112867385, 1.000000000000000000, 0.9238795325112867385, 1.000000000000000000, 0.9238795325112867385, 1.000000000000000000, 0.9238795325112867385, 1.000000000000000000, 0.9238795325112867385, 1.000000000000000000, 0.9238795325112867385, 1.000000000000000000, 0.9238795325112867385, 1.000000000000000000, 0.9238795325112867385, 1.000000000000000000, 0.9238795325112867385, 1.000000000000000000, 0.9238795325112867385, 1.000000000000000000, 0.9238795325112867385, 1.000000000000000000, 0.9238795325112867385, 1.000000000000000000, 0.9238795325112867385, 1.000000000000000000, 0.9238795325112867385, 1.000000000000000000, 0.9238795325112867385, 1.000000000000000000, 0.9238795325112867385, 1.000000000000000000, 0.9238795325112867385, 1.000000000000000000, 0.9238795325112867385, 1.000000000000000000, 0.9238795325112867385, 1.000000000000000000, 0.9238795325112867385, 1.000000000000000000, 0.9238795325112867385, 1.000000000000000000, 0.9238795325112867385, 1.000000000000000000, 0.9238795325112867385, 1.000000000000000000, 0.9238795325112867385, 1.000000000000000000, 0.9238795325112867385, 1.000000000000000000, 0.9238795325112867385, 1.000000000000000000, 0.9238795325112867385, 1.000000000000000000, 0.9238795325112867385, 1.000000000000000000, 0.9238795325112867385, 1.000000000000000000, 0.9238795325112867385, 1.000000000000000000, 0.9238795325112867385, 1.000000000000000000, 0.9238795325112867385, 1.000000000000000000, 0.9238795325112867385, 1.000000000000000000, 0.9238795325112867385, 1.000000000000000000, 0.9238795325112867385, 1.000000000000000000, 0.9238795325112867385, 1.000000000000000000, 0.9238795325112867385, 1.000000000000000000, 0.9238795325112867385, 1.000000000000000000, 0.9238795325112867385, 1.000000000000000000, 0.9238795325112867385, 1.000000000000000000, 0.9238795325112867385, 1.000000000000000000, 0.9238795325112867385, 1.000000000000000000, 0.9238795325112867385, 1.000000000000000000, 0.9238795325112867385, 1.000000000000000000, 0.9238795325112867385, 1.000000000000000000, 0.9238795325112867385, 1.000000000000000000, 0.9238795325112867385, 1.000000000000000000, 0.9238795325112867385, 1.000000000000000000, 0.9238795325112867385, 1.000000000000000000, 0.9238795325112867385, 1.000000000000000000, 0.9238795325112867385, 1.000000000000000000, 0.9238795325112867385, 1.000000000000000000, 0.9238795325112867385, 1.000000000000000000, 0.9238795325112867385, 1.000000000000000000, 0.9238795325112867385, 1.000000000000000000, 0.9238795325112867385, 1.000000000000000000, 0.9238795325112867385, 1.000000000000000000, 0.9238795325112867385, 1.000000000000000000, 0.9238795325112867385, 1.000000000000000000, 0.9238795325112867385, 1.000000000000000000, 0.9238795325112867385, 1.000000000000000000, 0.9238795325112867385, 1.000000000000000000, 0.9238795325112867385, 1.000000000000000000, 0.9238795325112867385, 1.000000000000000000, 0.9238795325112867385, 1.000000000000000000, 0.9238795325112867385, 1.000000000000000000, 0.9238795325112867385, 1.000000000000000000, 0.9238795325112867385, 1.000000000000000000, 0.9238795325112867385, 1.000000000000000000, 0.9238795325112867385, 1.000000000000000000, 0.9238795325112867385, 1.000000000000000000, 0.9238795325112867385, 1.000000000000000000, 0.9238795325112867385, 1.000000000000000000, 0.9238795325112867385, 1.000000000000000000, 0.9238795325112867385, 1.000000000000000000, 0.9238795325112867385, 1.000000000000000000, 0.9238795325112867385, 1.000000000000000000, 0.9238795325112867385, 1.000000000000000000, 0.9238795325112867385, 1.000000000000000000, 0.9238795325112867385, 1.000000000000000000, 0.9238795325112867385, 1.000000000000000000, 0.9238795325112867385, 1.000000000000000000, 0.9238795325112867385, 1.000000000000000000, 0.9238795325112867385, 1.000000000000000000, 0.9238795325112867385, 1.000000000000000000, 0.9238795325112867385, 1.000000000000000000, 0.9238795325112867385, 1.000000000000000000, 0.9238795325112867385, 1.000000000000000000, 0.9238795325112867385, 1.000000000000000000, 0.9238795325112867385, 1.000000000000000000, 0.9238795325112867385, 1.000000000000000000, 0.9238795325112867385, 1.000000000000000000, 0.9238795325112867385, 1.000000000000000000, 0.9238795325112867385, 1.000000000000000000, 0.9238795325112867385, 1.000000000000000000, 0.9238795325112867385, 1.000000000000000000, 0.9238795325112867385, 1.000000000000000000, 0.9238795325112867385, 1.000000000000000000, 0.9238795325112867385, 1.000000000000000000, 0.9238795325112867385, 1.000000000000000000, 0.9238795325112867385, 1.000000000000000000, 0.9238795325112867385, 1.000000000000000000, 0.9238795325112867385, 1.000000000000000000, 0.9238795325112867385, 1.000000000000000000, 0.9238795325112867385, 1.000000000000000000, 0.9238795325112867385, 1.000000000000000000, 0.9238795325112867385, 1.000000000000000000, 0.9238795325112867385, 1.000000000000000000, 0.9238795325112867385, 1.000000000000000000, 0.9238795325112867385, 1.000000000000000000, 0.9238795325112867385, 1.000000000000000000, 0.9238795325112867385, 1.000000000000000000, 0.9238795325112867385, 1.000000000000000000, 0.9238795325112867385, 1.000000000000000000, 0.9238795325112867385, 1.000000000000000000, 0.9238795325112867385, 1.000000000000000000, 0.9238795325112867385, 1.000000000000000000, 0.9238795325112867385, 1.000000000000000000, 0.9238795325112867385, 1.000000000000000000, 0.9238795325112867385, 1.000000000000000000, 0.9238795325112867385, 1.000000000000000000, 0.9238795325112867385, 1.000000000000000000, 0.9238795325112867385, 1.000000000000000000, 0.9238795325112867385, 1.000000000000000000, 0.9238795325112867385, 1.000000000000000000, 0.9238795325112867385, 1.000000000000000000, 0.9238795325112867385, 1.000000000000000000, 0.9238795325112867385, 1.000000000000000000, 0.9238795325112867385, 1.000000000000000000, 0.9238795325112867385, 1.000000000000000000, 0.9238795325112867385, 1.000000000000000000, 0.9238795325112867385, 1.000000000000000000, 0.9238795325112867385, 1.000000000000000000, 0.9238795325112867385, 1.000000000000000000, 0.9238795325112867385, 1.000000000000000000, 0.9238795325112867385, 1.000000000000000000, 0.9238795325112867385, 1.000000000000000000, 0.9238795325112867385, 1.000000000000000000, 0.9493985675959865089, 0.9660722070829228514) ) ) 
 REPRESENTATION_ITEM ( '' )  SURFACE ( )  );
#14552 = CARTESIAN_POINT ( 'NONE',  ( -12.27346345387604032, -24.92146970284692387, 198.4694471900890278 ) ) ;
#14553 = ADVANCED_FACE ( 'NONE', ( #19237 ), #1900, .F. ) ;
#14554 = FACE_OUTER_BOUND ( 'NONE', #48615, .T. ) ;
#14555 = CARTESIAN_POINT ( 'NONE',  ( 8.311093377946837890, 186.4062499965860411, -8.311093377946837890 ) ) ;
#14556 = CARTESIAN_POINT ( 'NONE',  ( -5.082755093536324154, 114.2187500020483810, 5.082755093536326818 ) ) ;
#14557 = AXIS2_PLACEMENT_3D ( 'NONE', #8209, #19517, #70842 ) ;
#14558 = CARTESIAN_POINT ( 'NONE',  ( 2.751064625579944321E-14, 201.8750000027312126, 194.0000000000000568 ) ) ;
#14559 = CARTESIAN_POINT ( 'NONE',  ( 6.676582343750003368, 290.8906250017069510, 2.765530957081995478 ) ) ;
#14560 = EDGE_CURVE ( 'NONE', #5894, #64638, #14503, .T. ) ;
#14562 = CARTESIAN_POINT ( 'NONE',  ( -5.000000000000000000, 66.66666666666667140, -8.660254037844390851 ) ) ;
#14561 = CARTESIAN_POINT ( 'NONE',  ( -28.00000000000003197, 209.0000000000000284, 166.0000000000003695 ) ) ;
#14563 = VERTEX_POINT ( 'NONE', #54704 ) ;
#14564 = CARTESIAN_POINT ( 'NONE',  ( 11.35316468749999963, 231.7187500034139873, -1.390361679473963556E-15 ) ) ;
#14565 = CARTESIAN_POINT ( 'NONE',  ( -5.082755093536319713, 5.082755093536319713, 1.299052781871753215 ) ) ;
#14566 = AXIS2_PLACEMENT_3D ( 'NONE', #9622, #10726, #56023 ) ;
#14567 = CARTESIAN_POINT ( 'NONE',  ( 5.000000000000001776, 167.7083333265053682, -8.660254037844389075 ) ) ;
#14568 = DIRECTION ( 'NONE',  ( -0.000000000000000000, -1.000000000000000000, -4.283267841918042741E-17 ) ) ;
#14570 = ADVANCED_FACE ( 'NONE', ( #8292 ), #42983, .T. ) ;
#14569 = CARTESIAN_POINT ( 'NONE',  ( 2.839093476692135984E-14, 197.9375000013655779, 201.4587341250000350 ) ) ;
#14571 = DIRECTION ( 'NONE',  ( -0.000000000000000000, 1.000000000000000000, -0.000000000000000000 ) ) ;
#14572 = DIRECTION ( 'NONE',  ( 0.000000000000000000, 0.000000000000000000, 1.000000000000000000 ) ) ;
#14573 = CARTESIAN_POINT ( 'NONE',  ( 8.000000000000000000, 91.25000000000000000, -9.797174393178825657E-16 ) ) ;
#14574 = CARTESIAN_POINT ( 'NONE',  ( 8.311093377946834337, 120.4687499965860269, 8.311093377946839666 ) ) ;
#14575 = CARTESIAN_POINT ( 'NONE',  ( -5.000000000000000000, -10.26105934116142215, -64.40045319026754100 ) ) ;
#14576 = CARTESIAN_POINT ( 'NONE',  ( 7.778174593052023411, -7.778174593052021635, 70.56249999999998579 ) ) ;
#14577 = AXIS2_PLACEMENT_3D ( 'NONE', #32623, #14861, #3566 ) ;
#14580 = CARTESIAN_POINT ( 'NONE',  ( 3.313708498984800688, 118.7187500040967905, -7.999999999999958256 ) ) ;
#14579 = CARTESIAN_POINT ( 'NONE',  ( 24.54126587500000056, 200.2500000013656631, 171.4326545832175839 ) ) ;
#14578 = CARTESIAN_POINT ( 'NONE',  ( 27.99999999999996092, 197.6875000013655779, 173.4587341249998929 ) ) ;
#14581 = ORIENTED_EDGE ( 'NONE', *, *, #12723, .F. ) ;
#14582 = DIRECTION ( 'NONE',  ( 0.000000000000000000, 0.000000000000000000, -1.000000000000000000 ) ) ;
#14583 = CARTESIAN_POINT ( 'NONE',  ( 5.676582343750001591, 221.6145833299193839, -9.832129032723420536 ) ) ;
#14584 = CARTESIAN_POINT ( 'NONE',  ( 3.458734124999959914, 202.4375000013656063, 142.0000000000000568 ) ) ;
#14585 = CARTESIAN_POINT ( 'NONE',  ( 25.55430564589119413, 203.3125000013656063, 167.5543056458910485 ) ) ;
#14586 = CARTESIAN_POINT ( 'NONE',  ( -9.832129032723418760, 193.1770833299193555, -5.676582343750004256 ) ) ;
#14587 = CARTESIAN_POINT ( 'NONE',  ( -5.082755093536324154, 90.21875000204838102, 5.082755093536326818 ) ) ;
#14588 = CARTESIAN_POINT ( 'NONE',  ( 0.000000000000000000, 51.05255888325788050, 0.000000000000000000 ) ) ;
#14589 = CARTESIAN_POINT ( 'NONE',  ( 3.211159895383561835, 15.43749999863440614, -3.211159895383561835 ) ) ;
#14590 = CARTESIAN_POINT ( 'NONE',  ( 29.43265458321766914, 200.1250000013656063, 166.5412658749999650 ) ) ;
#14591 = CARTESIAN_POINT ( 'NONE',  ( 5.656854249492376141, -5.656854249492374365, 28.39280277982336642 ) ) ;
#14592 = DIRECTION ( 'NONE',  ( -1.000000000000000000, 0.000000000000000000, 0.000000000000000000 ) ) ;
#14593 = CARTESIAN_POINT ( 'NONE',  ( 9.832129032723420536, 81.19791666325269830, -5.676582343749999815 ) ) ;
#14594 = ORIENTED_EDGE ( 'NONE', *, *, #57275, .T. ) ;
#14595 = CARTESIAN_POINT ( 'NONE',  ( -5.000000000000000000, -53.57132521838729389, 46.19376297453487012 ) ) ;
#14596 = CARTESIAN_POINT ( 'NONE',  ( 5.000000000000000000, -16.14408868864072844, -27.96238185062390613 ) ) ;
#14597 = CARTESIAN_POINT ( 'NONE',  ( -7.188101187500000044, 20.71874999795161543, -8.802885111219163269E-16 ) ) ;
#14598 = CARTESIAN_POINT ( 'NONE',  ( 7.999999999999991118, 9.797174393178815797E-16, 15.08030277982336642 ) ) ;
#14599 = CARTESIAN_POINT ( 'NONE',  ( 8.660254037844385522, 232.9166666666666572, -5.000000000000003553 ) ) ;
#14600 = CIRCLE ( 'NONE', #2710, 18.50000000000000000 ) ;
#14601 = CARTESIAN_POINT ( 'NONE',  ( 9.832129032723420536, 91.19791666325269830, -5.676582343749999815 ) ) ;
#14602 = ORIENTED_EDGE ( 'NONE', *, *, #34723, .F. ) ;
#14603 = CARTESIAN_POINT ( 'NONE',  ( -10.18810118749999916, 0.000000000000000000, 89.03125000204836681 ) ) ;
#14604 = CARTESIAN_POINT ( 'NONE',  ( -4.220049686691937474, -10.18810118749999738, 115.9375000020483668 ) ) ;
#14605 = CARTESIAN_POINT ( 'NONE',  ( -29.43265458321760164, 196.1250000013655779, 173.4587341250003760 ) ) ;
#14606 = CARTESIAN_POINT ( 'NONE',  ( -3.458734124999960358, 209.6875000013656063, 198.0000000000000284 ) ) ;
#14607 = CARTESIAN_POINT ( 'NONE',  ( 4.500000000000013323, 7.794228634059940930, -10.20000000000000462 ) ) ;
#14609 = CARTESIAN_POINT ( 'NONE',  ( -2.085542519210945728E-15, 79.53124999658602690, 11.35316468750000141 ) ) ;
#14608 = DIRECTION ( 'NONE',  ( -0.000000000000000000, 1.000000000000000000, 2.238352872228138170E-16 ) ) ;
#14610 = CARTESIAN_POINT ( 'NONE',  ( 5.656854249492376141, -5.656854249492374365, 18.08030278392014623 ) ) ;
#14611 = CARTESIAN_POINT ( 'NONE',  ( 6.123233995736767268E-16, 131.2500000000000000, -10.00000000000000178 ) ) ;
#14612 = CARTESIAN_POINT ( 'NONE',  ( -7.320508075688773708, 163.7499999931720538, -7.320508075688774596 ) ) ;
#14613 = CARTESIAN_POINT ( 'NONE',  ( 2.977408999572654480, 93.50000000204838102, 7.188101187499999156 ) ) ;
#14614 = CARTESIAN_POINT ( 'NONE',  ( -7.999999999999991118, 0.000000000000000000, 14.33030277982336465 ) ) ;
#14615 = CARTESIAN_POINT ( 'NONE',  ( 11.35316468749999785, 65.88541666325268409, 3.042071309553174174 ) ) ;
#14616 = CARTESIAN_POINT ( 'NONE',  ( -4.721056650415998313, 292.5781250017069510, 4.721056650416000089 ) ) ;
#14617 = CARTESIAN_POINT ( 'NONE',  ( 10.18810118749999916, 1.247682550866122264E-15, 106.2812500020483810 ) ) ;
#14618 = CARTESIAN_POINT ( 'NONE',  ( 8.311093377946834337, 205.1562499965859843, 8.311093377946839666 ) ) ;
#14619 = ORIENTED_EDGE ( 'NONE', *, *, #18513, .T. ) ;
#14620 = CARTESIAN_POINT ( 'NONE',  ( 3.999999999999960032, 202.9375000000000284, 143.6568542494924259 ) ) ;
#14621 = CARTESIAN_POINT ( 'NONE',  ( 1.704527592502762756, -60.27089976682793093, -22.92829164824393118 ) ) ;
#14622 = CARTESIAN_POINT ( 'NONE',  ( -6.000000000000001776, 288.0000000000000000, 0.000000000000000000 ) ) ;
#14624 = CARTESIAN_POINT ( 'NONE',  ( -8.311093377946836114, 192.6562499965860127, -8.311093377946837890 ) ) ;
#14623 = CARTESIAN_POINT ( 'NONE',  ( -4.000000000000002665, 11.31249999726881406, 1.656854249492380582 ) ) ;
#14625 = CARTESIAN_POINT ( 'NONE',  ( -7.320508075688770155, 238.7500000068279462, 7.320508075688774596 ) ) ;
#14626 = CARTESIAN_POINT ( 'NONE',  ( -6.123233995736766282E-16, 251.8750000068280031, -10.00000000000000000 ) ) ;
#14627 = VECTOR ( 'NONE', #34133, 1000.000000000000000 ) ;
#14628 = ORIENTED_EDGE ( 'NONE', *, *, #64384, .T. ) ;
#14629 = CARTESIAN_POINT ( 'NONE',  ( 9.832129032723416984, 185.6770833299193555, 5.676582343750006032 ) ) ;
#14630 = CARTESIAN_POINT ( 'NONE',  ( 2.977408999572650927, -7.188101187499990274, 19.95530278187175455 ) ) ;
#14631 = CARTESIAN_POINT ( 'NONE',  ( -28.00000000000002487, 209.4375000013656063, 166.5412658750003629 ) ) ;
#14632 = CIRCLE ( 'NONE', #64039, 8.000000000000000000 ) ;
#14633 = ORIENTED_EDGE ( 'NONE', *, *, #68500, .T. ) ;
#14634 = CARTESIAN_POINT ( 'NONE',  ( 1.469576158976823947E-15, 98.56250000409677625, 8.000000000000000000 ) ) ;
#14635 = CARTESIAN_POINT ( 'NONE',  ( -10.00000000000000000, 2.291666666666666963, -2.679491924311229845 ) ) ;
#14636 = CARTESIAN_POINT ( 'NONE',  ( -2.828427124746190735, 16.37500000000000000, -2.828427124746191623 ) ) ;
#14637 = CARTESIAN_POINT ( 'NONE',  ( -3.211159895383562723, 14.93749999863440792, 3.211159895383561391 ) ) ;
#14638 = CARTESIAN_POINT ( 'NONE',  ( 7.999999999999991118, 3.313708498984757611, 15.36155278392014623 ) ) ;
#14639 =( BOUNDED_CURVE ( )  B_SPLINE_CURVE ( 2, ( #11652, #29003, #730, #57693, #47458, #359, #23712, #70121, #23341 ),
 .UNSPECIFIED., .F., .F. ) 
 B_SPLINE_CURVE_WITH_KNOTS ( ( 3, 2, 2, 2, 3 ),
 ( 0.01470588235294118667, 0.01838235294117648508, 0.02205882352941178348, 0.02573529411764707842, 0.02941176470588237335 ),
 .UNSPECIFIED. ) 
 CURVE ( )  GEOMETRIC_REPRESENTATION_ITEM ( )  RATIONAL_B_SPLINE_CURVE ( ( 0.9999999999999998890, 0.9238795325112869605, 1.000000000000000000, 0.9238795325112867385, 1.000000000000000000, 0.9238795325112867385, 1.000000000000000000, 0.9238795325112862944, 1.000000000000000444 ) ) 
 REPRESENTATION_ITEM ( '' )  );
#14640 = DIRECTION ( 'NONE',  ( -0.000000000000000000, -1.000000000000000000, -0.000000000000000000 ) ) ;
#14641 = AXIS2_PLACEMENT_3D ( 'NONE', #51147, #57193, #22460 ) ;
#14642 = ORIENTED_EDGE ( 'NONE', *, *, #59880, .T. ) ;
#14643 = CARTESIAN_POINT ( 'NONE',  ( 0.000000000000000000, 0.000000000000000000, -21.50000000000000000 ) ) ;
#14644 = CARTESIAN_POINT ( 'NONE',  ( 5.082755093536325042, 95.09375000204838102, -5.082755093536325930 ) ) ;
#14645 = EDGE_CURVE ( 'NONE', #4091, #8398, #60290, .T. ) ;
#14647 = CARTESIAN_POINT ( 'NONE',  ( -3.042071309553166625, 262.8645833367473301, -11.35316468749999608 ) ) ;
#14646 = FACE_OUTER_BOUND ( 'NONE', #672, .T. ) ;
#14648 = DIRECTION ( 'NONE',  ( 1.000000000000000000, 0.000000000000000000, 0.000000000000000000 ) ) ;
#14649 = ORIENTED_EDGE ( 'NONE', *, *, #73603, .F. ) ;
#14650 = CARTESIAN_POINT ( 'NONE',  ( 5.082755093536318824, 5.082755093536319713, 20.42405278187175455 ) ) ;
#14651 = ORIENTED_EDGE ( 'NONE', *, *, #65153, .T. ) ;
#14652 = EDGE_CURVE ( 'NONE', #28748, #61990, #53581, .T. ) ;
#14653 = ORIENTED_EDGE ( 'NONE', *, *, #9839, .F. ) ;
#14654 = CARTESIAN_POINT ( 'NONE',  ( -4.220049686691937474, -10.18810118749999738, 81.43750000204836681 ) ) ;
#14655 = CARTESIAN_POINT ( 'NONE',  ( -5.676582343750006032, 79.42708332991935549, 9.832129032723418760 ) ) ;
#14656 = CARTESIAN_POINT ( 'NONE',  ( 6.123233995736767268E-16, 93.12499999317203958, -10.00000000000000178 ) ) ;
#14657 = CARTESIAN_POINT ( 'NONE',  ( 11.00000000000000000, 1.347111479062088405E-15, 96.24999999999998579 ) ) ;
#14660 = CARTESIAN_POINT ( 'NONE',  ( -4.088227598258586603E-16, 293.3593750017070079, -6.676582343750001591 ) ) ;
#14659 = CARTESIAN_POINT ( 'NONE',  ( 28.00000000000001776, 196.1250000027311842, 173.9999999999999147 ) ) ;
#14658 = LINE ( 'NONE', #38073, #20270 ) ;
#14661 = CARTESIAN_POINT ( 'NONE',  ( 4.000000000000001776, 14.00000000000000000, 0.000000000000000000 ) ) ;
#14662 = DIRECTION ( 'NONE',  ( 0.000000000000000000, -0.000000000000000000, 1.000000000000000000 ) ) ;
#14663 = CARTESIAN_POINT ( 'NONE',  ( 2.754378923186476579E-14, 198.4375000013655779, 194.5412658750000219 ) ) ;
#14665 =( BOUNDED_CURVE ( )  B_SPLINE_CURVE ( 2, ( #2924, #38758, #21750, #72706, #44034, #67042, #49306, #4794, #54992 ),
 .UNSPECIFIED., .F., .F. ) 
 B_SPLINE_CURVE_WITH_KNOTS ( ( 3, 2, 2, 2, 3 ),
 ( 0.8854166666666669627, 0.8906250000000003331, 0.8958333333333337034, 0.9010416666666668517, 0.9062500000000002220 ),
 .UNSPECIFIED. ) 
 CURVE ( )  GEOMETRIC_REPRESENTATION_ITEM ( )  RATIONAL_B_SPLINE_CURVE ( ( 0.9999999999999951150, 0.9238795325112916235, 1.000000000000000000, 0.9238795325112867385, 1.000000000000000000, 0.9238795325112867385, 1.000000000000000000, 0.9238795325112835188, 1.000000000000003331 ) ) 
 REPRESENTATION_ITEM ( '' )  );
#14664 = CARTESIAN_POINT ( 'NONE',  ( 3.999999999999960032, 198.9375000000000568, 143.6568542494924259 ) ) ;
#14666 = CARTESIAN_POINT ( 'NONE',  ( -4.898587196589407898E-16, 7.999999999999991118, 0.6428027839201454485 ) ) ;
#14667 = CARTESIAN_POINT ( 'NONE',  ( 25.55430564589115150, 200.3125000013656063, 172.4456943541086957 ) ) ;
#14668 = CARTESIAN_POINT ( 'NONE',  ( -5.082755093536326818, 13.78124999795161187, 5.082755093536325042 ) ) ;
#14669 = VECTOR ( 'NONE', #25173, 1000.000000000000000 ) ;
#14670 = CARTESIAN_POINT ( 'NONE',  ( 8.008118988124993010, -3.317071493978877239, 0.1693652839406289412 ) ) ;
#14671 = CARTESIAN_POINT ( 'NONE',  ( 0.000000000000000000, 125.0000000000000000, 0.000000000000000000 ) ) ;
#14672 = CARTESIAN_POINT ( 'NONE',  ( -7.188101187500000044, 111.0312500020483810, 0.000000000000000000 ) ) ;
#14674 = CARTESIAN_POINT ( 'NONE',  ( 4.465384415997316836, -56.41424811512342785, -44.23559237190989535 ) ) ;
#14673 = CARTESIAN_POINT ( 'NONE',  ( 4.000000000000015987, 201.5000000000000000, 198.0000000000000284 ) ) ;
#14675 = CARTESIAN_POINT ( 'NONE',  ( 9.832129032723420536, 221.3020833367473301, 5.676582343749996262 ) ) ;
#14676 = DIRECTION ( 'NONE',  ( 1.000000000000000000, -0.000000000000000000, -0.000000000000000000 ) ) ;
#14677 = CARTESIAN_POINT ( 'NONE',  ( 2.977408999572646486, 7.188101187499991163, 17.89280278187175455 ) ) ;
#14678 = CARTESIAN_POINT ( 'NONE',  ( 2.828427124746152987, 207.2500000027312126, 139.1715728752538723 ) ) ;
#14679 = CARTESIAN_POINT ( 'NONE',  ( 3.042071309553159519, 39.73958332991934128, 11.35316468750000141 ) ) ;
#14680 = CYLINDRICAL_SURFACE ( 'NONE', #27941, 3.999999999999976019 ) ;
#14681 = CARTESIAN_POINT ( 'NONE',  ( -8.660254037844390851, 9.791666659838700326, 4.999999999999998224 ) ) ;
#14682 = ORIENTED_EDGE ( 'NONE', *, *, #7002, .T. ) ;
#14683 = DIRECTION ( 'NONE',  ( -0.000000000000000000, 1.000000000000000000, -0.000000000000000000 ) ) ;
#14684 = CARTESIAN_POINT ( 'NONE',  ( -11.00000000000010658, 4.556349186103942017, 80.59375000409677625 ) ) ;
#14685 = CARTESIAN_POINT ( 'NONE',  ( -2.085542519210945728E-15, 54.53124999658601979, 11.35316468750000141 ) ) ;
#14686 = CARTESIAN_POINT ( 'NONE',  ( -7.778174593052020747, -7.778174593052023411, 82.37500000409677625 ) ) ;
#14687 = CARTESIAN_POINT ( 'NONE',  ( -2.445694354108839175, 205.3125000013656063, 144.4456943541088663 ) ) ;
#14688 = CARTESIAN_POINT ( 'NONE',  ( -9.999999999999998224, 260.2083333333333144, 2.679491924311235174 ) ) ;
#14689 = LINE ( 'NONE', #8298, #56371 ) ;
#14691 = CARTESIAN_POINT ( 'NONE',  ( 8.311093377946834337, 35.15624999658601268, 8.311093377946839666 ) ) ;
#14690 = CARTESIAN_POINT ( 'NONE',  ( -5.082755093536324154, 98.84375000204838102, 5.082755093536326818 ) ) ;
#14692 = CARTESIAN_POINT ( 'NONE',  ( -5.656854249492373476, -5.656854249492376141, 8.517802779823362869 ) ) ;
#14694 = CARTESIAN_POINT ( 'NONE',  ( 27.99999999999999645, 210.0000000000000284, 173.9999999999998863 ) ) ;
#14693 = B_SPLINE_CURVE_WITH_KNOTS ( 'NONE', 3,
 ( #28566, #57629, #298, #28942, #5943, #56510, #16487, #5566 ),
 .UNSPECIFIED., .F., .F.,
 ( 4, 2, 2, 4 ),
 ( 0.005256334970490767269, 0.006570121696662000604, 0.007883908422833233939, 0.01051148187517570234 ),
 .UNSPECIFIED. ) ;
#14695 = CARTESIAN_POINT ( 'NONE',  ( 5.676582343749993598, 164.9479166632526983, 9.832129032723422313 ) ) ;
#14696 = CARTESIAN_POINT ( 'NONE',  ( -10.00000000000000355, 134.5833333265053966, 2.679491924311223183 ) ) ;
#14697 = AXIS2_PLACEMENT_3D ( 'NONE', #23731, #35075, #6398 ) ;
#14698 = CARTESIAN_POINT ( 'NONE',  ( 2.977408999572654480, 111.5000000020483810, 7.188101187499999156 ) ) ;
#14699 =( BOUNDED_CURVE ( )  B_SPLINE_CURVE ( 2, ( #10843, #5193, #28190, #44058, #22517, #16857, #62885, #11218, #34246, #57248, #21034, #38404, #61406 ),
 .UNSPECIFIED., .F., .F. ) 
 B_SPLINE_CURVE_WITH_KNOTS ( ( 3, 2, 2, 2, 2, 2, 3 ),
 ( 0.2880434782608695676, 0.2898550724637681264, 0.2916666666666666852, 0.2934782608695652439, 0.2952898550724637472, 0.2971014492753623060, 0.2989130434782608647 ),
 .UNSPECIFIED. ) 
 CURVE ( )  GEOMETRIC_REPRESENTATION_ITEM ( )  RATIONAL_B_SPLINE_CURVE ( ( 1.000000000000000000, 0.9659258262890683122, 1.000000000000000000, 0.9659258262890683122, 1.000000000000000000, 0.9659258262890683122, 1.000000000000000000, 0.9659258262890683122, 1.000000000000000000, 0.9659258262890683122, 1.000000000000000000, 0.9659258262890683122, 1.000000000000000000 ) ) 
 REPRESENTATION_ITEM ( '' )  );
#14700 = EDGE_LOOP ( 'NONE', ( #51412, #38234, #7943, #73829 ) ) ;
#14701 = CARTESIAN_POINT ( 'NONE',  ( 10.00000000000000178, 22.08333332650536818, -2.679491924311226736 ) ) ;
#14702 = CARTESIAN_POINT ( 'NONE',  ( -3.042071309553173730, 19.63541666325268764, 11.35316468749999785 ) ) ;
#14703 = CARTESIAN_POINT ( 'NONE',  ( 2.828427124746153876, 198.0000000027312126, 144.8284271247462129 ) ) ;
#14704 = EDGE_LOOP ( 'NONE', ( #29567, #6105, #56686, #21033 ) ) ;
#14705 = CYLINDRICAL_SURFACE ( 'NONE', #10323, 6.000000000000001776 ) ;
#14706 = CARTESIAN_POINT ( 'NONE',  ( 10.18810118749999916, 1.247682550866122264E-15, 78.90625000204836681 ) ) ;
#14707 = CARTESIAN_POINT ( 'NONE',  ( 6.000000000000029310, -10.39230484541328714, -14.00000000000000178 ) ) ;
#14709 = CARTESIAN_POINT ( 'NONE',  ( -9.832129032723420536, 148.6979166632526983, 5.676582343749997150 ) ) ;
#14708 = CARTESIAN_POINT ( 'NONE',  ( 2.828427124746190291, 21.87500000000000355, 2.828427124746192067 ) ) ;
#14710 = CARTESIAN_POINT ( 'NONE',  ( 7.188101187500000044, 2.343749997951610098, 0.000000000000000000 ) ) ;
#14711 = CARTESIAN_POINT ( 'NONE',  ( 5.656854249492374365, 5.656854249492375253, 13.82405278432982421 ) ) ;
#14712 = CARTESIAN_POINT ( 'NONE',  ( -22.08061828530267690, -25.55732291036708759, 191.7597596367724861 ) ) ;
#14713 = CARTESIAN_POINT ( 'NONE',  ( 11.35316468749999963, 236.1979166700806445, 3.042071309553159519 ) ) ;
#14714 = CARTESIAN_POINT ( 'NONE',  ( 4.220049686691941027, -10.18810118749999738, 85.00000000204838102 ) ) ;
#14715 = ORIENTED_EDGE ( 'NONE', *, *, #20387, .T. ) ;
#14716 = VECTOR ( 'NONE', #49802, 1000.000000000000000 ) ;
#14717 = CARTESIAN_POINT ( 'NONE',  ( 0.000000000000000000, 55.00000000000000000, 8.000000000000000000 ) ) ;
#14718 = DIRECTION ( 'NONE',  ( 1.000000000000000000, -1.486057055854349470E-32, 3.469446951953617147E-16 ) ) ;
#14719 = CARTESIAN_POINT ( 'NONE',  ( -3.042071309553164404, 97.55208332991932707, -11.35316468749999963 ) ) ;
#14720 = CARTESIAN_POINT ( 'NONE',  ( 10.18810118749999916, 4.220049686691935698, 92.50000000204838102 ) ) ;
#14721 = CARTESIAN_POINT ( 'NONE',  ( 3.211159895383560947, 21.31249999863440792, 3.211159895383562723 ) ) ;
#14722 = ORIENTED_EDGE ( 'NONE', *, *, #2908, .T. ) ;
#14723 = ORIENTED_EDGE ( 'NONE', *, *, #74053, .F. ) ;
#14724 = CARTESIAN_POINT ( 'NONE',  ( -4.541265875000002339, 5.937499998634407028, -5.561446717895856393E-16 ) ) ;
#14725 = CARTESIAN_POINT ( 'NONE',  ( 5.082755093536325930, 9.656249997951610098, -5.082755093536325930 ) ) ;
#14726 = CARTESIAN_POINT ( 'NONE',  ( -5.656854249492380582, 116.0000000040967905, -5.656854249492380582 ) ) ;
#14728 = ADVANCED_FACE ( 'NONE', ( #40505 ), #60341, .F. ) ;
#14727 = CARTESIAN_POINT ( 'NONE',  ( -10.18810118749999916, 4.220049686691934809, 93.43750000204836681 ) ) ;
#14729 = EDGE_CURVE ( 'NONE', #46864, #24549, #51594, .T. ) ;
#14730 = CARTESIAN_POINT ( 'NONE',  ( -25.55430564589115150, 201.3125000013656063, 172.4456943541091789 ) ) ;
#14731 =( LENGTH_UNIT ( ) NAMED_UNIT ( * ) SI_UNIT ( .MILLI., .METRE. ) );
#14732 = VECTOR ( 'NONE', #28773, 1000.000000000000227 ) ;
#14733 = CARTESIAN_POINT ( 'NONE',  ( -1.656854249492383691, 4.687500000000000888, 4.000000000000000888 ) ) ;
#14734 = CARTESIAN_POINT ( 'NONE',  ( 4.000000000000000888, 19.68749999726881228, 1.656854249492384135 ) ) ;
#14735 = CARTESIAN_POINT ( 'NONE',  ( 1.881053915767122664, 5.124999998634407028, 4.541265875000001451 ) ) ;
#14736 = CARTESIAN_POINT ( 'NONE',  ( 1.469576158976823947E-15, 95.37499999999998579, 8.000000000000000000 ) ) ;
#14737 = CARTESIAN_POINT ( 'NONE',  ( -3.458734124999959025, 196.5000000013656063, 199.4326545832176691 ) ) ;
#14739 = CARTESIAN_POINT ( 'NONE',  ( 6.123233995736767268E-16, 96.25000000000000000, -10.00000000000000178 ) ) ;
#14738 = CARTESIAN_POINT ( 'NONE',  ( -31.45873412499995680, 197.7500000013656063, 171.4326545832181239 ) ) ;
#14740 = CARTESIAN_POINT ( 'NONE',  ( -4.541265875000002339, 19.81249999863440436, -5.561446717895856393E-16 ) ) ;
#14741 = CARTESIAN_POINT ( 'NONE',  ( -6.676582343750001591, 299.4531250017069510, 0.000000000000000000 ) ) ;
#14742 = CARTESIAN_POINT ( 'NONE',  ( 7.188101187499993827, -2.977408999572645598, 8.142802781871750994 ) ) ;
#14743 = ORIENTED_EDGE ( 'NONE', *, *, #36067, .T. ) ;
#14744 = ORIENTED_EDGE ( 'NONE', *, *, #18285, .T. ) ;
#14745 = CARTESIAN_POINT ( 'NONE',  ( 4.220049686691941027, -10.18810118749999738, 96.62500000204838102 ) ) ;
#14746 = CARTESIAN_POINT ( 'NONE',  ( -26.56734541678232731, 204.2500000013655779, 173.4587341250003760 ) ) ;
#14747 = CARTESIAN_POINT ( 'NONE',  ( -28.00000000000002842, 202.0000000000000000, 166.0000000000003695 ) ) ;
#14748 = CARTESIAN_POINT ( 'NONE',  ( 2.839093476692135984E-14, 208.9375000013656063, 201.4587341250000350 ) ) ;
#14749 = CARTESIAN_POINT ( 'NONE',  ( 2.449293598294707893E-16, 20.99999999726881583, -4.000000000000001776 ) ) ;
#14750 = CARTESIAN_POINT ( 'NONE',  ( -10.00000000000000000, 107.2916666666666856, -2.679491924311229845 ) ) ;
#14751 = AXIS2_PLACEMENT_3D ( 'NONE', #29951, #52964, #14051 ) ;
#14752 = CARTESIAN_POINT ( 'NONE',  ( -5.656854249492378806, 111.6875000000000000, 5.656854249492381470 ) ) ;
#14753 = CARTESIAN_POINT ( 'NONE',  ( 6.676582343750001591, 290.1093750017069510, -8.176455196517173205E-16 ) ) ;
#14754 = EDGE_CURVE ( 'NONE', #22353, #59630, #64895, .T. ) ;
#14755 = CARTESIAN_POINT ( 'NONE',  ( -2.977408999572647819, 7.188101187499991163, 9.080302781871752771 ) ) ;
#14756 = VERTEX_POINT ( 'NONE', #36236 ) ;
#14757 = DIRECTION ( 'NONE',  ( -0.000000000000000000, 1.000000000000000000, -0.000000000000000000 ) ) ;
#14758 = CARTESIAN_POINT ( 'NONE',  ( -8.000000000000001776, 20.15624999590322375, 3.313708498984759387 ) ) ;
#14759 = CARTESIAN_POINT ( 'NONE',  ( -2.445694354108838731, 202.0625000013656063, 144.4456943541088663 ) ) ;
#14760 = CARTESIAN_POINT ( 'NONE',  ( -7.320508075688773708, 183.7499999931720254, -7.320508075688774596 ) ) ;
#14761 = CARTESIAN_POINT ( 'NONE',  ( 1.999122618765707404, 194.9741652105599599, 145.4444247340934453 ) ) ;
#14762 = CARTESIAN_POINT ( 'NONE',  ( 5.676582343750005144, 260.8854166700806445, 9.832129032723416984 ) ) ;
#14763 = CARTESIAN_POINT ( 'NONE',  ( -2.828427124746152987, 207.2500000027312126, 200.8284271247462129 ) ) ;
#14764 = CARTESIAN_POINT ( 'NONE',  ( -6.735557395310442023E-16, 11.00000000000000000, 111.6249999999999858 ) ) ;
#14765 =( BOUNDED_CURVE ( )  B_SPLINE_CURVE ( 2, ( #18132, #47160, #53208, #70552, #49387, #32049, #9036, #43352, #42610 ),
 .UNSPECIFIED., .F., .F. ) 
 B_SPLINE_CURVE_WITH_KNOTS ( ( 3, 2, 2, 2, 3 ),
 ( 0.1333333333333334425, 0.1416666666666667740, 0.1500000000000001332, 0.1583333333333334925, 0.1666666666666668239 ),
 .UNSPECIFIED. ) 
 CURVE ( )  GEOMETRIC_REPRESENTATION_ITEM ( )  RATIONAL_B_SPLINE_CURVE ( ( 0.9999999999999990008, 0.9238795325112877377, 1.000000000000000000, 0.9238795325112867385, 1.000000000000000000, 0.9238795325112867385, 1.000000000000000000, 0.9238795325112851842, 1.000000000000001554 ) ) 
 REPRESENTATION_ITEM ( '' )  );
#14766 = CARTESIAN_POINT ( 'NONE',  ( 8.311093377946837890, 6.406249996586016238, -8.311093377946837890 ) ) ;
#14767 = CARTESIAN_POINT ( 'NONE',  ( 1.320432766682872962E-15, -7.188101187499992051, 6.736552781871754547 ) ) ;
#14768 = CARTESIAN_POINT ( 'NONE',  ( 9.832129032723416984, 200.6770833299193555, 5.676582343750006032 ) ) ;
#14769 = CARTESIAN_POINT ( 'NONE',  ( -2.849036369511732440E-14, 197.3750000027312126, 138.0000000000000568 ) ) ;
#14770 = CARTESIAN_POINT ( 'NONE',  ( 4.541265875000002339, 5.374999998634406140, -1.881053915767121554 ) ) ;
#14771 = CARTESIAN_POINT ( 'NONE',  ( -11.00000000000000000, 11.00000000000000000, 25.00000000000000000 ) ) ;
#14773 = DIRECTION ( 'NONE',  ( -0.000000000000000000, -0.000000000000000000, -1.000000000000000000 ) ) ;
#14772 = CARTESIAN_POINT ( 'NONE',  ( -4.000000000000001776, 14.18749999726881406, -1.656854249492381470 ) ) ;
#14774 = ORIENTED_EDGE ( 'NONE', *, *, #34232, .F. ) ;
#14775 = CARTESIAN_POINT ( 'NONE',  ( -3.458734125000015869, 206.1875000013656063, 142.0000000000000568 ) ) ;
#14776 = CARTESIAN_POINT ( 'NONE',  ( -11.35316468750000141, 3.281249996586016238, -1.390361679473963753E-15 ) ) ;
#14777 = CARTESIAN_POINT ( 'NONE',  ( 11.00000000000000000, 1.347111479062088405E-15, 100.9375000040967763 ) ) ;
#14778 = CARTESIAN_POINT ( 'NONE',  ( -11.00000000000012967, -4.556349186103920701, 106.2812500040967763 ) ) ;
#14779 = CARTESIAN_POINT ( 'NONE',  ( -26.56734541678243033, 201.3750000013656347, 166.5412658750003345 ) ) ;
#14780 = CARTESIAN_POINT ( 'NONE',  ( 4.898587196589412829E-16, 4.687499995903220196, -8.000000000000000000 ) ) ;
#14782 = CARTESIAN_POINT ( 'NONE',  ( 2.828427124746153876, 203.8750000000000284, 144.8284271247462129 ) ) ;
#14781 = CARTESIAN_POINT ( 'NONE',  ( -2.977408999572652260, 119.9375000020483952, 7.188101187500000044 ) ) ;
#14783 = CARTESIAN_POINT ( 'NONE',  ( -3.313708498984758943, -7.999999999999989342, 28.11155277982336642 ) ) ;
#14784 = CARTESIAN_POINT ( 'NONE',  ( 6.951808397369818766E-16, 122.0312499965860269, -11.35316468750000141 ) ) ;
#14785 = CARTESIAN_POINT ( 'NONE',  ( -4.999999999999998224, 83.54166665983869677, -8.660254037844389075 ) ) ;
#14786 = CARTESIAN_POINT ( 'NONE',  ( -7.188101187500001821, 124.4375000020483810, -2.977408999572650483 ) ) ;
#14787 = CARTESIAN_POINT ( 'NONE',  ( -1.881053915767121554, 20.74999999863440436, -4.541265875000002339 ) ) ;
#14788 = DIRECTION ( 'NONE',  ( -0.000000000000000000, -0.000000000000000000, 1.000000000000000000 ) ) ;
#14789 = LINE ( 'NONE', #21947, #39016 ) ;
#14790 = EDGE_LOOP ( 'NONE', ( #69317, #24000, #45151, #57372, #32471, #44444, #44745, #64839 ) ) ;
#14791 = CARTESIAN_POINT ( 'NONE',  ( 1.656854249492318409, 208.8125000000000000, 146.0000000000000568 ) ) ;
#14792 =( BOUNDED_CURVE ( )  B_SPLINE_CURVE ( 2, ( #66272, #14580, #45130, #67776, #32714, #61366, #33834, #10798, #44763 ),
 .UNSPECIFIED., .F., .F. ) 
 B_SPLINE_CURVE_WITH_KNOTS ( ( 3, 2, 2, 2, 3 ),
 ( 0.1354166666666667407, 0.1406250000000000833, 0.1458333333333334259, 0.1510416666666667684, 0.1562500000000001110 ),
 .UNSPECIFIED. ) 
 CURVE ( )  GEOMETRIC_REPRESENTATION_ITEM ( )  RATIONAL_B_SPLINE_CURVE ( ( 0.9999999999999987788, 0.9238795325112879597, 1.000000000000000000, 0.9238795325112867385, 1.000000000000000000, 0.9238795325112867385, 1.000000000000000000, 0.9238795325112850731, 1.000000000000001554 ) ) 
 REPRESENTATION_ITEM ( '' )  );
#14793 = CARTESIAN_POINT ( 'NONE',  ( 2.765530957082001251, 292.9218750017069510, 6.676582343750000703 ) ) ;
#14794 = CARTESIAN_POINT ( 'NONE',  ( 2.679491924311370177, 185.8333333265053966, 9.999999999999918288 ) ) ;
#14795 = CARTESIAN_POINT ( 'NONE',  ( 5.656854249492376141, -5.656854249492374365, 1.580302783920146226 ) ) ;
#14796 = CARTESIAN_POINT ( 'NONE',  ( -5.676582343750006032, 169.1145833299193555, 9.832129032723418760 ) ) ;
#14797 = DIRECTION ( 'NONE',  ( -0.000000000000000000, -1.000000000000000000, -0.000000000000000000 ) ) ;
#14798 = CARTESIAN_POINT ( 'NONE',  ( 4.000000000000015987, 197.5000000000000000, 198.0000000000000284 ) ) ;
#14799 = CARTESIAN_POINT ( 'NONE',  ( 4.556349186104052151, -10.99999999999999822, 70.65625000409676204 ) ) ;
#14800 = CARTESIAN_POINT ( 'NONE',  ( 10.18810118749999916, 4.220049686691935698, 104.8750000020483668 ) ) ;
#14801 = EDGE_LOOP ( 'NONE', ( #36939, #67717, #7215, #24501 ) ) ;
#14802 = ADVANCED_FACE ( 'NONE', ( #30568 ), #53588, .T. ) ;
#14803 = CARTESIAN_POINT ( 'NONE',  ( -28.00000000000007816, 199.1250000027312126, 166.0000000000003695 ) ) ;
#14804 = CARTESIAN_POINT ( 'NONE',  ( 8.311093377946837890, 161.7187499965860411, -8.311093377946837890 ) ) ;
#14805 = CARTESIAN_POINT ( 'NONE',  ( 1.432654583217664479, 195.7500000013656063, 201.4587341250000065 ) ) ;
#14806 = CARTESIAN_POINT ( 'NONE',  ( 3.458734125000016757, 207.1250000013656347, 199.4326545832176976 ) ) ;
#14807 = CARTESIAN_POINT ( 'NONE',  ( 10.00000000000000178, 230.4166666734946034, 2.679491924311222739 ) ) ;
#14808 = CARTESIAN_POINT ( 'NONE',  ( 5.676582343750001591, 61.92708332991934839, -9.832129032723420536 ) ) ;
#14809 = VERTEX_POINT ( 'NONE', #4510 ) ;
#14810 = CARTESIAN_POINT ( 'NONE',  ( -4.220049686691935698, 10.18810118749999916, 112.3750000020483810 ) ) ;
#14811 = CARTESIAN_POINT ( 'NONE',  ( -3.211159895383561391, 10.81249999863440792, -3.211159895383561835 ) ) ;
#14812 = ORIENTED_EDGE ( 'NONE', *, *, #62889, .T. ) ;
#14813 = AXIS2_PLACEMENT_3D ( 'NONE', #49245, #21326, #26985 ) ;
#14814 = CARTESIAN_POINT ( 'NONE',  ( 5.082755093536325930, 21.65624999795161543, -5.082755093536325930 ) ) ;
#14815 = CARTESIAN_POINT ( 'NONE',  ( -27.99999999999999645, 210.0000000000000284, 170.0000000000003695 ) ) ;
#14816 = CARTESIAN_POINT ( 'NONE',  ( -5.082755093536326818, 19.78124999795161543, 5.082755093536325042 ) ) ;
#14817 = CARTESIAN_POINT ( 'NONE',  ( -7.188101187499990274, -2.977408999572651815, 3.080302781871751439 ) ) ;
#14818 = CARTESIAN_POINT ( 'NONE',  ( 7.204075437095968759, -7.204075437095966983, 68.21875000204836681 ) ) ;
#14819 = PLANE ( 'NONE',  #10116 ) ;
#14820 = CARTESIAN_POINT ( 'NONE',  ( 2.449293598294707893E-16, 6.999999997268813168, -4.000000000000001776 ) ) ;
#14821 = ORIENTED_EDGE ( 'NONE', *, *, #6304, .F. ) ;
#14822 = EDGE_CURVE ( 'NONE', #15401, #44635, #25578, .T. ) ;
#14823 = ADVANCED_FACE ( 'NONE', ( #67137 ), #127, .T. ) ;
#14824 = CARTESIAN_POINT ( 'NONE',  ( 1.432654583217664479, 206.7500000013655779, 201.4587341250000065 ) ) ;
#14825 = CARTESIAN_POINT ( 'NONE',  ( -32.00000000000002842, 195.3125000027311842, 168.3431457505080573 ) ) ;
#14826 = EDGE_CURVE ( 'NONE', #49563, #1603, #15431, .T. ) ;
#14827 = CARTESIAN_POINT ( 'NONE',  ( -4.541265875000002339, 4.812499998634407028, -5.561446717895856393E-16 ) ) ;
#14828 = CARTESIAN_POINT ( 'NONE',  ( -7.188101187500001821, 109.0625000020483810, -2.977408999572650483 ) ) ;
#14829 = CARTESIAN_POINT ( 'NONE',  ( 23.99999999999999645, 204.6875000000000284, 168.3431457505074889 ) ) ;
#14830 = CARTESIAN_POINT ( 'NONE',  ( 1.320432766682872962E-15, -7.188101187499992051, 24.36155278187175810 ) ) ;
#14831 = ORIENTED_EDGE ( 'NONE', *, *, #58814, .F. ) ;
#14832 = CARTESIAN_POINT ( 'NONE',  ( 2.449293598294707893E-16, 21.25000000000000000, -4.000000000000001776 ) ) ;
#14833 = ORIENTED_EDGE ( 'NONE', *, *, #71533, .F. ) ;
#14834 = CARTESIAN_POINT ( 'NONE',  ( -4.220049686691937474, -10.18810118749999738, 115.9375000020483810 ) ) ;
#14835 = CARTESIAN_POINT ( 'NONE',  ( 11.00000000000000000, 1.347111479062088405E-15, 84.43750000409677625 ) ) ;
#14836 = CARTESIAN_POINT ( 'NONE',  ( 1.432654583217664479, 208.7500000013656063, 201.4587341250000065 ) ) ;
#14837 = CARTESIAN_POINT ( 'NONE',  ( 30.44569435410879521, 201.8125000013656063, 167.5543056458910485 ) ) ;
#14838 = CARTESIAN_POINT ( 'NONE',  ( -10.00000000000000000, 72.29166666666667140, -2.679491924311229845 ) ) ;
#14839 = CARTESIAN_POINT ( 'NONE',  ( -4.401442555609581635E-16, 92.65625000204838102, -7.188101187500000044 ) ) ;
#14840 = CARTESIAN_POINT ( 'NONE',  ( 6.000000000000001776, 290.5000000000000000, -7.347880794884121708E-16 ) ) ;
#14841 = EDGE_CURVE ( 'NONE', #36620, #46386, #9797, .T. ) ;
#14843 = CARTESIAN_POINT ( 'NONE',  ( 0.000000000000000000, 0.000000000000000000, -14.80000000000000071 ) ) ;
#14842 = DIRECTION ( 'NONE',  ( -0.000000000000000000, 1.000000000000000000, -0.000000000000000000 ) ) ;
#14844 = ORIENTED_EDGE ( 'NONE', *, *, #31146, .T. ) ;
#14845 = CARTESIAN_POINT ( 'NONE',  ( -11.35316468749999785, 223.6979166700806445, -3.042071309553164848 ) ) ;
#14846 = LINE ( 'NONE', #4302, #42431 ) ;
#14847 = CARTESIAN_POINT ( 'NONE',  ( -2.751064625579944321E-14, 198.8750000027312126, 146.0000000000000284 ) ) ;
#14848 = FACE_OUTER_BOUND ( 'NONE', #30799, .T. ) ;
#14849 = CARTESIAN_POINT ( 'NONE',  ( -7.999999999999989342, -3.313708498984762496, 21.92405277982336642 ) ) ;
#14850 = CARTESIAN_POINT ( 'NONE',  ( 7.320508075688776373, 251.8750000000000000, 7.320508075688767491 ) ) ;
#14851 = CARTESIAN_POINT ( 'NONE',  ( 8.000000000000000000, 108.0312500040967905, -3.313708498984762496 ) ) ;
#14852 = CARTESIAN_POINT ( 'NONE',  ( 6.123233995736767268E-16, 191.2500000000000000, -10.00000000000000178 ) ) ;
#14853 = SURFACE_SIDE_STYLE ('',( #39376 ) ) ;
#14854 = CARTESIAN_POINT ( 'NONE',  ( -7.188101187499990274, -2.977408999572651815, 21.45530278187175810 ) ) ;
#14855 = CARTESIAN_POINT ( 'NONE',  ( 3.042071309553159519, 150.0520833299193555, 11.35316468750000141 ) ) ;
#14856 = CARTESIAN_POINT ( 'NONE',  ( 0.000000000000000000, 300.0000000000000000, 0.000000000000000000 ) ) ;
#14857 = CARTESIAN_POINT ( 'NONE',  ( 1.836970198721029589E-15, 259.3750000068280315, 10.00000000000000000 ) ) ;
#14858 = DIRECTION ( 'NONE',  ( -0.000000000000000000, 1.000000000000000000, 4.476705744456276341E-16 ) ) ;
#14861 = DIRECTION ( 'NONE',  ( -0.000000000000000000, -0.000000000000000000, -1.000000000000000000 ) ) ;
#14860 = DIRECTION ( 'NONE',  ( 0.000000000000000000, 0.000000000000000000, -1.000000000000000000 ) ) ;
#14859 = CARTESIAN_POINT ( 'NONE',  ( 25.17157287525378351, 203.8750000000000284, 172.8284271247460424 ) ) ;
#14862 = ORIENTED_EDGE ( 'NONE', *, *, #71991, .F. ) ;
#14863 = CIRCLE ( 'NONE', #36579, 68.99999999999994316 ) ;
#14864 = CARTESIAN_POINT ( 'NONE',  ( 11.35316468750000141, 11.09374999658601624, 0.000000000000000000 ) ) ;
#14865 = CARTESIAN_POINT ( 'NONE',  ( -6.062687379811042554, -5.219768740853823807, 2.519839246067225784E-12 ) ) ;
#14867 = CARTESIAN_POINT ( 'NONE',  ( -3.999999999999959144, 208.0625000000000000, 199.6568542494924259 ) ) ;
#14866 = CYLINDRICAL_SURFACE ( 'NONE', #69751, 8.000000000000000000 ) ;
#14868 = LINE ( 'NONE', #20910, #23093 ) ;
#14869 = CARTESIAN_POINT ( 'NONE',  ( -1.432654583217662259, 203.1250000013656347, 145.4587341250000350 ) ) ;
#14870 = CARTESIAN_POINT ( 'NONE',  ( -5.000000000000005329, 55.20833332650536818, 8.660254037844387298 ) ) ;
#14871 = CARTESIAN_POINT ( 'NONE',  ( 7.188101187500001821, 108.5000000020483810, -2.977408999572651371 ) ) ;
#14872 = CARTESIAN_POINT ( 'NONE',  ( 1.881053915767122664, 10.24999999863440792, 4.541265875000001451 ) ) ;
#14873 = CARTESIAN_POINT ( 'NONE',  ( 2.679491924311232953, 221.0416666666666856, -10.00000000000001066 ) ) ;
#14874 = CARTESIAN_POINT ( 'NONE',  ( -3.313708498984758943, -7.999999999999989342, 10.11155277982336820 ) ) ;
#14876 = CARTESIAN_POINT ( 'NONE',  ( 10.00000000000001954, 160.0000000000000000, 0.000000000000000000 ) ) ;
#14875 = CARTESIAN_POINT ( 'NONE',  ( 0.000000000000000000, 0.000000000000000000, 118.0000000000000000 ) ) ;
#14877 = ORIENTED_EDGE ( 'NONE', *, *, #40394, .F. ) ;
#14878 = VERTEX_POINT ( 'NONE', #73167 ) ;
#14879 = FACE_OUTER_BOUND ( 'NONE', #31412, .T. ) ;
#14880 = CARTESIAN_POINT ( 'NONE',  ( -3.313708498984816231, 99.78124999999997158, 7.999999999999943157 ) ) ;
#14881 = CARTESIAN_POINT ( 'NONE',  ( 6.951808397369818766E-16, 127.0312499965860269, -11.35316468750000141 ) ) ;
#14882 = ORIENTED_EDGE ( 'NONE', *, *, #26302, .F. ) ;
#14883 = CARTESIAN_POINT ( 'NONE',  ( 27.99999999999996803, 201.0000000000000000, 173.9999999999999147 ) ) ;
#14884 = CARTESIAN_POINT ( 'NONE',  ( -4.220049686691935698, 10.18810118749999916, 94.37500000204839523 ) ) ;
#14885 = FACE_OUTER_BOUND ( 'NONE', #70077, .T. ) ;
#14886 = CARTESIAN_POINT ( 'NONE',  ( 3.458734125000015425, 198.2500000013656347, 196.5673454167823877 ) ) ;
#14887 = CARTESIAN_POINT ( 'NONE',  ( -4.898587196589412829E-16, 117.1250000000000000, -8.000000000000000000 ) ) ;
#14889 = CARTESIAN_POINT ( 'NONE',  ( -2.085542519210945728E-15, 129.5312499965860127, 11.35316468750000141 ) ) ;
#14888 = CARTESIAN_POINT ( 'NONE',  ( -8.000000000000000000, 95.00000000000000000, 0.000000000000000000 ) ) ;
#14890 = DIRECTION ( 'NONE',  ( -0.000000000000000000, -1.000000000000000000, -0.000000000000000000 ) ) ;
#14891 = ORIENTED_EDGE ( 'NONE', *, *, #69981, .T. ) ;
#14892 =( BOUNDED_CURVE ( )  B_SPLINE_CURVE ( 2, ( #59420, #12641, #70005, #30007, #42050, #2440, #25433, #36776, #6996 ),
 .UNSPECIFIED., .F., .F. ) 
 B_SPLINE_CURVE_WITH_KNOTS ( ( 3, 2, 2, 2, 3 ),
 ( 0.7941176470588233727, 0.7977941176470587648, 0.8014705882352940458, 0.8051470588235293269, 0.8088235294117646079 ),
 .UNSPECIFIED. ) 
 CURVE ( )  GEOMETRIC_REPRESENTATION_ITEM ( )  RATIONAL_B_SPLINE_CURVE ( ( 1.000000000000002220, 0.9238795325112844070, 1.000000000000000000, 0.9238795325112867385, 1.000000000000000000, 0.9238795325112867385, 1.000000000000000000, 0.9238795325112890700, 0.9999999999999976685 ) ) 
 REPRESENTATION_ITEM ( '' )  );
#14893 = DIRECTION ( 'NONE',  ( -0.000000000000000000, 1.000000000000000000, -0.000000000000000000 ) ) ;
#14894 = AXIS2_PLACEMENT_3D ( 'NONE', #56796, #12242, #68472 ) ;
#14895 = CARTESIAN_POINT ( 'NONE',  ( 48.45866277005245593, 41.96974402280773120, 61.07789613012150909 ) ) ;
#14896 = CARTESIAN_POINT ( 'NONE',  ( 9.832129032723420536, 116.5104166632526841, -5.676582343749999815 ) ) ;
#14897 = CARTESIAN_POINT ( 'NONE',  ( -2.445694354108782775, 205.5625000013656063, 200.4456943541088663 ) ) ;
#14898 = CARTESIAN_POINT ( 'NONE',  ( 5.082755093536325930, 20.53124999795161543, -5.082755093536325930 ) ) ;
#14899 = CARTESIAN_POINT ( 'NONE',  ( 1.871523826299183495E-15, -10.18810118749999916, 90.90625000204838102 ) ) ;
#14900 = CARTESIAN_POINT ( 'NONE',  ( -9.832129032723420536, 24.01041666325268409, 5.676582343749997150 ) ) ;
#14901 = ORIENTED_EDGE ( 'NONE', *, *, #10880, .F. ) ;
#14902 = CARTESIAN_POINT ( 'NONE',  ( -2.804140485925949776E-11, 67.59332269700094287, -20.03478791450258001 ) ) ;
#14903 = CARTESIAN_POINT ( 'NONE',  ( -5.662595241051933570, -5.662595241051936235, 23.70061528394063188 ) ) ;
#14904 = CARTESIAN_POINT ( 'NONE',  ( 5.000000000000004441, 236.6666666666666856, 8.660254037844385522 ) ) ;
#14905 = EDGE_CURVE ( 'NONE', #18289, #70531, #25131, .T. ) ;
#14906 = CARTESIAN_POINT ( 'NONE',  ( -7.347880794884122694E-16, 7.750000000000000000, 4.000000000000001776 ) ) ;
#14907 = CARTESIAN_POINT ( 'NONE',  ( 4.401442555609581635E-16, 3.843749997951610098, -7.188101187500000044 ) ) ;
#14908 = CARTESIAN_POINT ( 'NONE',  ( 2.485281374238571317, 298.7500000034140157, -6.000000000000003553 ) ) ;
#14909 = CARTESIAN_POINT ( 'NONE',  ( -49.36289658985559470, 138.1946914039819774, 58.74035077246725933 ) ) ;
#14910 = CARTESIAN_POINT ( 'NONE',  ( 5.082755093536325930, 1.031249997951609876, -5.082755093536325930 ) ) ;
#14911 = EDGE_LOOP ( 'NONE', ( #32178, #881, #16287, #7127 ) ) ;
#14912 = CARTESIAN_POINT ( 'NONE',  ( -9.832129032723420536, 139.0104166632526983, 5.676582343749997150 ) ) ;
#14913 = CARTESIAN_POINT ( 'NONE',  ( -10.18810118749999738, -4.220049686691941915, 81.25000000204836681 ) ) ;
#14914 = CARTESIAN_POINT ( 'NONE',  ( -24.54126587499999346, 200.1875000013656063, 170.0000000000003411 ) ) ;
#14915 = LINE ( 'NONE', #62072, #4094 ) ;
#14916 = CARTESIAN_POINT ( 'NONE',  ( 3.211159895383560947, 16.31249999863440436, 3.211159895383562723 ) ) ;
#14917 = EDGE_LOOP ( 'NONE', ( #58711, #1436, #44820, #39508, #10148 ) ) ;
#14918 = AXIS2_PLACEMENT_3D ( 'NONE', #9757, #21430, #44823 ) ;
#14919 = CARTESIAN_POINT ( 'NONE',  ( -2.828427124746153876, 204.0000000027312126, 195.1715728752538439 ) ) ;
#14920 = CARTESIAN_POINT ( 'NONE',  ( -3.458734125000015425, 196.2500000013656631, 143.4326545832176976 ) ) ;
#14921 = CARTESIAN_POINT ( 'NONE',  ( -30.82842712474612412, 204.5000000027312126, 172.8284271247466108 ) ) ;
#14922 = DIRECTION ( 'NONE',  ( -0.000000000000000000, -0.000000000000000000, 1.000000000000000000 ) ) ;
#14923 = VERTEX_POINT ( 'NONE', #55450 ) ;
#14924 = CARTESIAN_POINT ( 'NONE',  ( 7.188101187500000933, 9.562499997951608322, -2.977408999572650483 ) ) ;
#14925 = LINE ( 'NONE', #19850, #3885 ) ;
#14926 = PLANE ( 'NONE',  #45148 ) ;
#14927 = CARTESIAN_POINT ( 'NONE',  ( -11.35316468750000141, 188.4895833299193555, 3.042071309553159963 ) ) ;
#14928 = CARTESIAN_POINT ( 'NONE',  ( 5.082755093536325042, 114.9687500020483810, -5.082755093536325930 ) ) ;
#14929 = CARTESIAN_POINT ( 'NONE',  ( -4.242640687119285658, 291.1875000034139589, 4.242640687119287435 ) ) ;
#14930 = CARTESIAN_POINT ( 'NONE',  ( 6.676582343750003368, 288.8906250017070079, 2.765530957081995478 ) ) ;
#14931 = EDGE_CURVE ( 'NONE', #48188, #65462, #49780, .T. ) ;
#14933 = CARTESIAN_POINT ( 'NONE',  ( 7.320508075688766603, 94.37500000000000000, 7.320508075688770155 ) ) ;
#14932 = CARTESIAN_POINT ( 'NONE',  ( 11.35316468749999608, 221.6145833367473017, -3.042071309553167513 ) ) ;
#14934 = CONTEXT_DEPENDENT_SHAPE_REPRESENTATION ( #12522, #605 ) ;
#14935 = ORIENTED_EDGE ( 'NONE', *, *, #7604, .T. ) ;
#14936 = EDGE_CURVE ( 'NONE', #47682, #72263, #22540, .T. ) ;
#14937 = CARTESIAN_POINT ( 'NONE',  ( -6.951808397369817780E-16, 257.6562500034140157, -11.35316468749999963 ) ) ;
#14938 = CARTESIAN_POINT ( 'NONE',  ( -5.447323953993864265, -4.689931814214729933, 0.1569290643893266057 ) ) ;
#14939 = VECTOR ( 'NONE', #62916, 1000.000000000000000 ) ;
#14940 = CARTESIAN_POINT ( 'NONE',  ( -28.00000000000002842, 204.0000000000000284, 166.0000000000003695 ) ) ;
#14941 = DIRECTION ( 'NONE',  ( -0.000000000000000000, 1.000000000000000000, -0.000000000000000000 ) ) ;
#14942 = CARTESIAN_POINT ( 'NONE',  ( 3.458734125000016757, 198.1250000013656063, 199.4326545832176691 ) ) ;
#14943 = DIRECTION ( 'NONE',  ( -0.000000000000000000, 1.000000000000000000, -0.000000000000000000 ) ) ;
#14944 = LINE ( 'NONE', #25520, #19843 ) ;
#14945 = CARTESIAN_POINT ( 'NONE',  ( 8.000000000000000000, 92.84375000000000000, -3.313708498984762496 ) ) ;
#14946 = CARTESIAN_POINT ( 'NONE',  ( -5.676582343750006032, 109.4270833299193555, 9.832129032723418760 ) ) ;
#14947 = CARTESIAN_POINT ( 'NONE',  ( -5.000000000000000888, -12.55543720214795478, -69.09376167622117748 ) ) ;
#14948 = CARTESIAN_POINT ( 'NONE',  ( -4.556349186104045934, 11.00000000000000000, 69.71875000000000000 ) ) ;
#14951 = DIRECTION ( 'NONE',  ( -0.000000000000000000, -1.000000000000000000, -0.000000000000000000 ) ) ;
#14950 = CARTESIAN_POINT ( 'NONE',  ( 24.54126587499998280, 200.1250000013656063, 168.5673454167822740 ) ) ;
#14949 = CARTESIAN_POINT ( 'NONE',  ( 25.55430564589115150, 198.5625000013656063, 172.4456943541086957 ) ) ;
#14952 = ADVANCED_FACE ( 'NONE', ( #27504 ), #32441, .T. ) ;
#14953 = ORIENTED_EDGE ( 'NONE', *, *, #18349, .F. ) ;
#14954 = CARTESIAN_POINT ( 'NONE',  ( 3.153939666463620179E-13, 158.7500000000000284, 9.999999999999998224 ) ) ;
#14955 = CARTESIAN_POINT ( 'NONE',  ( -3.042071309553164404, 222.2395833299193555, -11.35316468749999963 ) ) ;
#14956 = CARTESIAN_POINT ( 'NONE',  ( -2.839093476692135984E-14, 197.6875000013655779, 138.5412658750000503 ) ) ;
#14957 = CARTESIAN_POINT ( 'NONE',  ( 25.55430564589119413, 199.3125000013656063, 167.5543056458910485 ) ) ;
#14958 = CARTESIAN_POINT ( 'NONE',  ( -4.556349186104045934, 11.00000000000000000, 114.9062500040967763 ) ) ;
#14959 = ADVANCED_FACE ( 'NONE', ( #9422 ), #27880, .F. ) ;
#14960 = CARTESIAN_POINT ( 'NONE',  ( -9.832129032723420536, 189.0104166632526983, 5.676582343749997150 ) ) ;
#14961 = CARTESIAN_POINT ( 'NONE',  ( -7.320508075688773708, 123.7499999931720396, -7.320508075688774596 ) ) ;
#14962 = DIRECTION ( 'NONE',  ( 1.577021341797097560E-16, -1.000000000000000000, 0.000000000000000000 ) ) ;
#14963 = CARTESIAN_POINT ( 'NONE',  ( -8.342170076843785083E-16, 20.06249999863440436, 4.541265875000002339 ) ) ;
#14964 = CARTESIAN_POINT ( 'NONE',  ( 24.54126587499998990, 195.4375000013655779, 169.9999999999998863 ) ) ;
#14965 = CARTESIAN_POINT ( 'NONE',  ( 5.656854249492374365, 5.656854249492375253, 28.76780277982336642 ) ) ;
#14966 = LINE ( 'NONE', #6462, #66437 ) ;
#14967 = CARTESIAN_POINT ( 'NONE',  ( -8.311093377946836114, 77.65624999658602690, -8.311093377946837890 ) ) ;
#14968 = ORIENTED_EDGE ( 'NONE', *, *, #31139, .F. ) ;
#14969 = CARTESIAN_POINT ( 'NONE',  ( 11.00000000000000000, 1.347111479062088405E-15, 81.24999999999998579 ) ) ;
#14970 = CARTESIAN_POINT ( 'NONE',  ( 2.977408999572650927, 20.24999999795161898, -7.188101187500001821 ) ) ;
#14971 = CARTESIAN_POINT ( 'NONE',  ( -7.320508075688770155, 223.7500000068279746, 7.320508075688774596 ) ) ;
#14973 = DIRECTION ( 'NONE',  ( 0.000000000000000000, 0.000000000000000000, 1.000000000000000000 ) ) ;
#14972 = AXIS2_PLACEMENT_3D ( 'NONE', #37591, #31927, #47778 ) ;
#14974 = CARTESIAN_POINT ( 'NONE',  ( 9.832129032723416984, 95.36458332991935549, 5.676582343750006032 ) ) ;
#14975 = ORIENTED_EDGE ( 'NONE', *, *, #56884, .F. ) ;
#14976 = CARTESIAN_POINT ( 'NONE',  ( 7.204075437095968759, -7.204075437095966983, 88.09375000204836681 ) ) ;
#14977 = CARTESIAN_POINT ( 'NONE',  ( 4.220049686691941027, -10.18810118749999738, 116.1250000020483810 ) ) ;
#14978 = CARTESIAN_POINT ( 'NONE',  ( -31.45873412499999233, 196.9375000013655779, 170.0000000000003979 ) ) ;
#14979 = CARTESIAN_POINT ( 'NONE',  ( 3.458734125000016757, 207.1250000013656347, 199.4326545832176691 ) ) ;
#14981 = CARTESIAN_POINT ( 'NONE',  ( 3.042071309553159519, 79.73958332991934128, 11.35316468750000141 ) ) ;
#14980 = CARTESIAN_POINT ( 'NONE',  ( -23.99999999999999289, 206.8750000027312126, 170.0000000000002842 ) ) ;
#14982 = CARTESIAN_POINT ( 'NONE',  ( 3.313708498984762496, -7.999999999999989342, 16.48655278392014623 ) ) ;
#14983 = CARTESIAN_POINT ( 'NONE',  ( -24.54126587499998280, 203.3750000013656063, 171.4326545832179818 ) ) ;
#14984 = CARTESIAN_POINT ( 'NONE',  ( 2.828427124746190291, 14.87500000000000178, 2.828427124746192067 ) ) ;
#14985 = CARTESIAN_POINT ( 'NONE',  ( 10.00000000000000178, 166.8749999931720538, 0.000000000000000000 ) ) ;
#14986 = CARTESIAN_POINT ( 'NONE',  ( 4.242640687119287435, 296.4375000034140157, 4.242640687119285658 ) ) ;
#14987 = CARTESIAN_POINT ( 'NONE',  ( -9.832129032723420536, 79.01041666325268409, 5.676582343749997150 ) ) ;
#14988 = CARTESIAN_POINT ( 'NONE',  ( -6.676582343750001591, 292.4531250017069510, 0.000000000000000000 ) ) ;
#14989 = CARTESIAN_POINT ( 'NONE',  ( 4.220049686691941027, -10.18810118749999738, 107.5000000020483668 ) ) ;
#14990 = CARTESIAN_POINT ( 'NONE',  ( -9.832129032723420536, 203.6979166632526983, 5.676582343749997150 ) ) ;
#14991 = ORIENTED_EDGE ( 'NONE', *, *, #36552, .F. ) ;
#14992 = FACE_OUTER_BOUND ( 'NONE', #44808, .T. ) ;
#14993 = CARTESIAN_POINT ( 'NONE',  ( -0.8419854211626188745, -60.19512794652365528, -22.88206588978800582 ) ) ;
#14994 = DIRECTION ( 'NONE',  ( -0.8660254037844380415, -0.5000000000000012212, 0.000000000000000000 ) ) ;
#14996 = CARTESIAN_POINT ( 'NONE',  ( -11.35316468750000141, 208.4895833299193839, 3.042071309553159963 ) ) ;
#14995 = CARTESIAN_POINT ( 'NONE',  ( -2.828427124746192067, 19.62500000000000000, 2.828427124746190735 ) ) ;
#14997 = CARTESIAN_POINT ( 'NONE',  ( -4.000000000000015987, 203.5000000000000000, 142.0000000000000568 ) ) ;
#14998 = CARTESIAN_POINT ( 'NONE',  ( 8.660254037844385522, 226.0416666734946602, -5.000000000000003553 ) ) ;
#14999 = CARTESIAN_POINT ( 'NONE',  ( -7.347880794884122694E-16, 20.75000000000000000, 4.000000000000001776 ) ) ;
#15000 = ORIENTED_EDGE ( 'NONE', *, *, #4440, .F. ) ;
#15001 = EDGE_CURVE ( 'NONE', #45416, #18291, #10164, .T. ) ;
#15002 = CARTESIAN_POINT ( 'NONE',  ( 6.951808397369818766E-16, 182.3437499965860411, -11.35316468750000141 ) ) ;
#15003 = AXIS2_PLACEMENT_3D ( 'NONE', #42507, #37232, #2156 ) ;
#15004 = CARTESIAN_POINT ( 'NONE',  ( 7.188101187499992051, 8.802885111219154394E-16, 17.23655278187175810 ) ) ;
#15005 = EDGE_CURVE ( 'NONE', #5945, #42039, #39208, .T. ) ;
#15006 =( BOUNDED_CURVE ( )  B_SPLINE_CURVE ( 2, ( #20255, #38380, #55740, #66665, #43276, #38008, #10078, #71943, #4419 ),
 .UNSPECIFIED., .F., .F. ) 
 B_SPLINE_CURVE_WITH_KNOTS ( ( 3, 2, 2, 2, 3 ),
 ( 0.4062499999999998890, 0.4114583333333332038, 0.4166666666666666297, 0.4218749999999999445, 0.4270833333333332593 ),
 .UNSPECIFIED. ) 
 CURVE ( )  GEOMETRIC_REPRESENTATION_ITEM ( )  RATIONAL_B_SPLINE_CURVE ( ( 1.000000000000001554, 0.9238795325112850731, 1.000000000000000000, 0.9238795325112867385, 1.000000000000000000, 0.9238795325112867385, 1.000000000000000000, 0.9238795325112875156, 0.9999999999999992228 ) ) 
 REPRESENTATION_ITEM ( '' )  );
#15007 = CARTESIAN_POINT ( 'NONE',  ( -4.999999999999994671, 91.66666666666665719, -8.660254037844383745 ) ) ;
#15008 =( BOUNDED_CURVE ( )  B_SPLINE_CURVE ( 2, ( #2469, #53785, #48103, #42811, #36434, #1741, #54531, #54160, #41719 ),
 .UNSPECIFIED., .F., .F. ) 
 B_SPLINE_CURVE_WITH_KNOTS ( ( 3, 2, 2, 2, 3 ),
 ( 0.7500000000000006661, 0.7583333333333339699, 0.7666666666666672736, 0.7750000000000005773, 0.7833333333333338810 ),
 .UNSPECIFIED. ) 
 CURVE ( )  GEOMETRIC_REPRESENTATION_ITEM ( )  RATIONAL_B_SPLINE_CURVE ( ( 0.9999999999999938938, 0.9238795325112928447, 1.000000000000000000, 0.9238795325112867385, 1.000000000000000000, 0.9238795325112867385, 1.000000000000000000, 0.9238795325112816315, 1.000000000000005107 ) ) 
 REPRESENTATION_ITEM ( '' )  );
#15009 = ORIENTED_EDGE ( 'NONE', *, *, #33684, .F. ) ;
#15010 = CARTESIAN_POINT ( 'NONE',  ( -3.313708498984762496, 89.46875000409677625, 7.999999999999998224 ) ) ;
#15011 = DIRECTION ( 'NONE',  ( -0.000000000000000000, 1.000000000000000000, -0.000000000000000000 ) ) ;
#15012 = EDGE_CURVE ( 'NONE', #24662, #46560, #358, .T. ) ;
#15013 = VERTEX_POINT ( 'NONE', #68249 ) ;
#15014 = CARTESIAN_POINT ( 'NONE',  ( -7.347880794884122694E-16, 14.75000000000000178, 4.000000000000001776 ) ) ;
#15015 = CARTESIAN_POINT ( 'NONE',  ( 1.881053915767121998, 18.49999999863440436, -4.541265875000002339 ) ) ;
#15016 = CARTESIAN_POINT ( 'NONE',  ( -7.999999999999991118, 3.313708498984756723, 6.924052783920144449 ) ) ;
#15017 = PRODUCT_DEFINITION ( 'UNKNOWN', '', #61044, #68940 ) ;
#15019 = DIRECTION ( 'NONE',  ( -0.000000000000000000, -0.000000000000000000, 1.000000000000000000 ) ) ;
#15018 = AXIS2_PLACEMENT_3D ( 'NONE', #12910, #34481, #46513 ) ;
#15020 = ORIENTED_EDGE ( 'NONE', *, *, #17815, .T. ) ;
#15021 = CARTESIAN_POINT ( 'NONE',  ( 5.000000000000000888, -10.82431413986195956, -67.03128830763427004 ) ) ;
#15022 = CARTESIAN_POINT ( 'NONE',  ( 1.320432766682874540E-15, 94.53125000204836681, 7.188101187500000044 ) ) ;
#15025 = CARTESIAN_POINT ( 'NONE',  ( -2.751064625579944321E-14, 196.7500000000000000, 146.0000000000000284 ) ) ;
#15024 = CARTESIAN_POINT ( 'NONE',  ( 3.042071309553163516, 252.4479166700806445, -11.35316468749999785 ) ) ;
#15023 = CARTESIAN_POINT ( 'NONE',  ( -10.00000000000011546, 82.29166666666672825, -2.679491924311261375 ) ) ;
#15026 = DIRECTION ( 'NONE',  ( 1.000000000000000000, 0.000000000000000000, 0.000000000000000000 ) ) ;
#15027 = ORIENTED_EDGE ( 'NONE', *, *, #26589, .F. ) ;
#15028 = EDGE_CURVE ( 'NONE', #72263, #73846, #54899, .T. ) ;
#15029 = CARTESIAN_POINT ( 'NONE',  ( 1.469576158976823947E-15, 101.5625000040967763, 8.000000000000000000 ) ) ;
#15030 = CARTESIAN_POINT ( 'NONE',  ( -4.401442555609577197E-16, 7.188101187499992051, 16.11155278187175455 ) ) ;
#15031 = ORIENTED_EDGE ( 'NONE', *, *, #30348, .T. ) ;
#15032 = ORIENTED_EDGE ( 'NONE', *, *, #70153, .T. ) ;
#15033 = CARTESIAN_POINT ( 'NONE',  ( 7.204075437095968759, -7.204075437095966983, 81.71875000204836681 ) ) ;
#15034 = CARTESIAN_POINT ( 'NONE',  ( -8.311093377946841443, 69.21874999658602690, 8.311093377946830785 ) ) ;
#15035 = DIRECTION ( 'NONE',  ( 1.000000000000000000, 0.000000000000000000, 0.000000000000000000 ) ) ;
#15036 = CARTESIAN_POINT ( 'NONE',  ( -4.556349186104047710, -10.99999999999999822, 88.28124999999998579 ) ) ;
#15039 = CARTESIAN_POINT ( 'NONE',  ( -6.676582343750001591, 291.6093750017069510, 0.000000000000000000 ) ) ;
#15038 = CARTESIAN_POINT ( 'NONE',  ( 29.65685424949240101, 196.1875000027312126, 173.9999999999999147 ) ) ;
#15037 = CARTESIAN_POINT ( 'NONE',  ( -1.836970198721029983E-15, 70.62499999317203958, 10.00000000000000178 ) ) ;
#15040 = CARTESIAN_POINT ( 'NONE',  ( -23.99999999999995026, 203.8125000027312126, 171.6568542494926817 ) ) ;
#15041 = CARTESIAN_POINT ( 'NONE',  ( 2.957351242930898602E-11, 51.14729664189404446, -48.52014062454985321 ) ) ;
#15042 = AXIS2_PLACEMENT_3D ( 'NONE', #3973, #10731, #61302 ) ;
#15043 = CARTESIAN_POINT ( 'NONE',  ( 3.458734125000015869, 199.1875000013655779, 198.0000000000000284 ) ) ;
#15044 = CARTESIAN_POINT ( 'NONE',  ( 8.000000000000000000, 7.406249995903221972, -3.313708498984761608 ) ) ;
#15045 = CARTESIAN_POINT ( 'NONE',  ( 30.44569435410878810, 195.5625000013656063, 172.4456943541087526 ) ) ;
#15046 = CARTESIAN_POINT ( 'NONE',  ( 7.188101187499999156, 12.74999999795161187, 2.977408999572654924 ) ) ;
#15047 = MECHANICAL_DESIGN_GEOMETRIC_PRESENTATION_REPRESENTATION (  '', ( #23520 ), #39195 ) ;
#15048 = CARTESIAN_POINT ( 'NONE',  ( -7.999999999999991118, 0.000000000000000000, 23.51780278392014978 ) ) ;
#15049 = CYLINDRICAL_SURFACE ( 'NONE', #43151, 7.000000000000000000 ) ;
#15050 = CARTESIAN_POINT ( 'NONE',  ( 7.188101187500000933, 107.3750000020483952, -2.977408999572651371 ) ) ;
#15052 = LINE ( 'NONE', #20716, #67926 ) ;
#15051 = CYLINDRICAL_SURFACE ( 'NONE', #48021, 3.999999999999976019 ) ;
#15053 = CARTESIAN_POINT ( 'NONE',  ( 0.000000000000000000, 0.000000000000000000, 24.00000000000001421 ) ) ;
#15054 = CARTESIAN_POINT ( 'NONE',  ( 29.43265458321766914, 208.1250000013656063, 166.5412658749999650 ) ) ;
#15055 = CARTESIAN_POINT ( 'NONE',  ( 2.977408999572646486, 7.188101187499991163, 14.89280278187175455 ) ) ;
#15056 = CARTESIAN_POINT ( 'NONE',  ( -1.656854249492403008, 207.8125000027312410, 146.0000000000000284 ) ) ;
#15057 = CARTESIAN_POINT ( 'NONE',  ( 8.311093377946837890, 46.40624999658601268, -8.311093377946837890 ) ) ;
#15058 = CARTESIAN_POINT ( 'NONE',  ( -7.320508075688778149, 4.999999993172032475, 7.320508075688769267 ) ) ;
#15059 = CARTESIAN_POINT ( 'NONE',  ( 4.000000000000001776, 17.00000000000000000, 0.000000000000000000 ) ) ;
#15060 = ORIENTED_EDGE ( 'NONE', *, *, #10232, .T. ) ;
#15061 = DIRECTION ( 'NONE',  ( -0.000000000000000000, 1.000000000000000000, -0.000000000000000000 ) ) ;
#15062 = CARTESIAN_POINT ( 'NONE',  ( -4.000000000000001776, 8.187499997268814056, -1.656854249492381470 ) ) ;
#15063 = CARTESIAN_POINT ( 'NONE',  ( -5.676582343749998039, 52.44791666325268409, -9.832129032723420536 ) ) ;
#15064 = CARTESIAN_POINT ( 'NONE',  ( 11.00000000000000000, 1.347111479062088405E-15, 78.43750000409677625 ) ) ;
#15065 = CARTESIAN_POINT ( 'NONE',  ( 3.458734124999960358, 205.6250000013656063, 143.4326545832176976 ) ) ;
#15066 = LINE ( 'NONE', #3766, #41975 ) ;
#15067 = CARTESIAN_POINT ( 'NONE',  ( 3.313708498984802020, 25.59374999590322375, -7.999999999999958256 ) ) ;
#15069 = CARTESIAN_POINT ( 'NONE',  ( 9.832129032723420536, 46.19791666325268409, -5.676582343749999815 ) ) ;
#15068 = CARTESIAN_POINT ( 'NONE',  ( 5.082755093536326818, 97.71875000204838102, 5.082755093536325042 ) ) ;
#15070 = CARTESIAN_POINT ( 'NONE',  ( -7.999999999999989342, -3.313708498984762496, 9.924052779823364645 ) ) ;
#15071 = DIRECTION ( 'NONE',  ( 0.000000000000000000, 1.000000000000000000, -1.224646799147353207E-16 ) ) ;
#15072 = CARTESIAN_POINT ( 'NONE',  ( -9.832129032723418760, 157.8645833299193839, -5.676582343750004256 ) ) ;
#15073 = CARTESIAN_POINT ( 'NONE',  ( 6.123233995736767268E-16, 128.1249999931720254, -10.00000000000000178 ) ) ;
#15074 = CARTESIAN_POINT ( 'NONE',  ( 7.188101187500000044, 104.2812500020483810, -8.802885111219163269E-16 ) ) ;
#15075 = EDGE_LOOP ( 'NONE', ( #3715, #19547, #43187, #28655 ) ) ;
#15076 = CYLINDRICAL_SURFACE ( 'NONE', #36431, 10.00000000000000178 ) ;
#15077 = CARTESIAN_POINT ( 'NONE',  ( 8.311093377946834337, 35.46874999658600558, 8.311093377946839666 ) ) ;
#15078 = CARTESIAN_POINT ( 'NONE',  ( -3.999999999999960032, 197.0000000000000000, 198.0000000000000284 ) ) ;
#15079 = ORIENTED_EDGE ( 'NONE', *, *, #7528, .T. ) ;
#15080 = CARTESIAN_POINT ( 'NONE',  ( 0.000000000000000000, 300.0000000000000000, 0.000000000000000000 ) ) ;
#15081 = CARTESIAN_POINT ( 'NONE',  ( 10.18810118749999916, 4.220049686691935698, 79.00000000204838102 ) ) ;
#15082 = LINE ( 'NONE', #38117, #66654 ) ;
#15084 = CARTESIAN_POINT ( 'NONE',  ( -8.311093377946841443, 158.9062499965860411, 8.311093377946834337 ) ) ;
#15083 = CYLINDRICAL_SURFACE ( 'NONE', #5000, 11.00000000000000000 ) ;
#15085 = CARTESIAN_POINT ( 'NONE',  ( -7.188101187500002709, 3.187499997951610542, 2.977408999572649151 ) ) ;
#15086 = CARTESIAN_POINT ( 'NONE',  ( -5.656854249492373476, -5.656854249492376141, 11.57405278432982243 ) ) ;
#15087 = CARTESIAN_POINT ( 'NONE',  ( -24.11868154898130712, -23.40756885739441273, 189.4818584164396498 ) ) ;
#15088 = CARTESIAN_POINT ( 'NONE',  ( 3.042071309553173286, 240.3645833367473301, 11.35316468749999608 ) ) ;
#15089 = CARTESIAN_POINT ( 'NONE',  ( 7.204075437095966983, 7.204075437095967871, 83.96875000204836681 ) ) ;
#15090 = ORIENTED_EDGE ( 'NONE', *, *, #28200, .F. ) ;
#15091 = EDGE_CURVE ( 'NONE', #3980, #832, #35082, .T. ) ;
#15092 = CARTESIAN_POINT ( 'NONE',  ( 4.898587196589412829E-16, 1.687499995903220196, -8.000000000000000000 ) ) ;
#15093 = CARTESIAN_POINT ( 'NONE',  ( -11.00000000000010658, 4.556349186103942017, 105.9062500000000142 ) ) ;
#15094 = CARTESIAN_POINT ( 'NONE',  ( 3.042071309553167069, 102.1354166632526983, -11.35316468749999785 ) ) ;
#15095 = CARTESIAN_POINT ( 'NONE',  ( 7.204075437095968759, -7.204075437095966983, 93.71875000204838102 ) ) ;
#15096 = ADVANCED_FACE ( 'NONE', ( #28258 ), #73905, .F. ) ;
#15097 = CARTESIAN_POINT ( 'NONE',  ( -1.881053915767121776, 19.74999999863440081, -4.541265875000002339 ) ) ;
#15098 = ORIENTED_EDGE ( 'NONE', *, *, #41732, .F. ) ;
#15099 = EDGE_LOOP ( 'NONE', ( #1003, #72241 ) ) ;
#15100 = CARTESIAN_POINT ( 'NONE',  ( -4.541265875000002339, 4.874999998634407916, -1.881053915767121998 ) ) ;
#15101 = CARTESIAN_POINT ( 'NONE',  ( -2.977408999572650039, 8.437499997951611874, -7.188101187500001821 ) ) ;
#15102 = AXIS2_PLACEMENT_3D ( 'NONE', #65484, #71499, #43207 ) ;
#15103 = CARTESIAN_POINT ( 'NONE',  ( 5.656854249492379694, 115.6250000040967905, -5.656854249492380582 ) ) ;
#15104 =( BOUNDED_CURVE ( )  B_SPLINE_CURVE ( 2, ( #28767, #63846, #16687, #39719, #34461, #74048, #40466, #45374, #17445 ),
 .UNSPECIFIED., .F., .F. ) 
 B_SPLINE_CURVE_WITH_KNOTS ( ( 3, 2, 2, 2, 3 ),
 ( 0.1500000000000002442, 0.1583333333333335202, 0.1666666666666667962, 0.1750000000000000722, 0.1833333333333333481 ),
 .UNSPECIFIED. ) 
 CURVE ( )  GEOMETRIC_REPRESENTATION_ITEM ( )  RATIONAL_B_SPLINE_CURVE ( ( 0.9999999999999976685, 0.9238795325112890700, 1.000000000000000000, 0.9238795325112867385, 1.000000000000000000, 0.9238795325112867385, 1.000000000000000000, 0.9238795325112865164, 1.000000000000000222 ) ) 
 REPRESENTATION_ITEM ( '' )  );
#15105 = CARTESIAN_POINT ( 'NONE',  ( -7.204075437095967871, 7.204075437095967871, 93.34375000204838102 ) ) ;
#15106 = CARTESIAN_POINT ( 'NONE',  ( -26.56734541678232375, 203.2500000013656063, 173.4587341250003760 ) ) ;
#15107 = CARTESIAN_POINT ( 'NONE',  ( -12.00000000000000000, -6.928203230275542523, -1.071796769724504550 ) ) ;
#15108 = VECTOR ( 'NONE', #1690, 1000.000000000000000 ) ;
#15109 = CARTESIAN_POINT ( 'NONE',  ( -2.828427124746190735, 5.375000000000000000, -2.828427124746191623 ) ) ;
#15110 = CARTESIAN_POINT ( 'NONE',  ( -7.347880794884122694E-16, 16.49999999726881228, 4.000000000000001776 ) ) ;
#15111 = CARTESIAN_POINT ( 'NONE',  ( -4.541265875000003227, 2.874999998634407028, 1.881053915767121110 ) ) ;
#15112 = CARTESIAN_POINT ( 'NONE',  ( 1.656854249492347719, 202.8125000000000000, 146.0000000000000284 ) ) ;
#15113 = ORIENTED_EDGE ( 'NONE', *, *, #34298, .F. ) ;
#15114 = CARTESIAN_POINT ( 'NONE',  ( -2.445694354108782775, 194.5625000013656063, 200.4456943541088663 ) ) ;
#15116 = CARTESIAN_POINT ( 'NONE',  ( 9.999999999999998224, 235.8333333401613174, -2.679491924311229401 ) ) ;
#15115 = CARTESIAN_POINT ( 'NONE',  ( -28.00000000000006750, 196.4375000013655779, 166.5412658750003629 ) ) ;
#15117 =( BOUNDED_CURVE ( )  B_SPLINE_CURVE ( 2, ( #4428, #45897, #27800, #56119, #22499, #67803, #50813, #28174, #68167 ),
 .UNSPECIFIED., .F., .F. ) 
 B_SPLINE_CURVE_WITH_KNOTS ( ( 3, 2, 2, 2, 3 ),
 ( 0.3970588235294117418, 0.4007352941176470784, 0.4044117647058823595, 0.4080882352941176405, 0.4117647058823529216 ),
 .UNSPECIFIED. ) 
 CURVE ( )  GEOMETRIC_REPRESENTATION_ITEM ( )  RATIONAL_B_SPLINE_CURVE ( ( 1.000000000000000000, 0.9238795325112867385, 1.000000000000000000, 0.9238795325112867385, 1.000000000000000000, 0.9238795325112867385, 1.000000000000000000, 0.9238795325112867385, 1.000000000000000000 ) ) 
 REPRESENTATION_ITEM ( '' )  );
#15118 = CARTESIAN_POINT ( 'NONE',  ( 1.881053915767121776, 18.49999999863440436, -4.541265875000002339 ) ) ;
#15119 = CARTESIAN_POINT ( 'NONE',  ( 10.00000000000000000, 71.66666665983869677, 2.679491924311235618 ) ) ;
#15120 = CARTESIAN_POINT ( 'NONE',  ( -7.188101187499990274, -2.977408999572651371, 4.580302781871752771 ) ) ;
#15121 = EDGE_LOOP ( 'NONE', ( #54117, #55937, #48209, #68828, #41316 ) ) ;
#15122 = ORIENTED_EDGE ( 'NONE', *, *, #14931, .F. ) ;
#15123 = CARTESIAN_POINT ( 'NONE',  ( 7.204075437095966983, 7.204075437095967871, 95.59375000204836681 ) ) ;
#15124 = CARTESIAN_POINT ( 'NONE',  ( 5.000000000000002665, 125.8333333333333570, -8.660254037844390851 ) ) ;
#15125 = CARTESIAN_POINT ( 'NONE',  ( -24.54126587499999346, 200.4375000013656063, 170.0000000000003411 ) ) ;
#15126 = CARTESIAN_POINT ( 'NONE',  ( 4.556349186104045934, 11.00000000000000000, 107.0312500000000000 ) ) ;
#15127 = CARTESIAN_POINT ( 'NONE',  ( -2.445694354108784108, 207.5625000013656063, 195.5543056458912190 ) ) ;
#15128 = LINE ( 'NONE', #40751, #12148 ) ;
#15129 = CARTESIAN_POINT ( 'NONE',  ( -4.999999999999998224, 101.6666666666666714, -8.660254037844389075 ) ) ;
#15130 = CARTESIAN_POINT ( 'NONE',  ( 1.469576158976823947E-15, 111.8750000000000000, 8.000000000000000000 ) ) ;
#15131 = CARTESIAN_POINT ( 'NONE',  ( -4.721056650415999201, 290.4843750017070079, -4.721056650415999201 ) ) ;
#15132 = CARTESIAN_POINT ( 'NONE',  ( 7.188101187499991163, 2.977408999572648707, 11.70530278187175455 ) ) ;
#15133 = ORIENTED_EDGE ( 'NONE', *, *, #6696, .T. ) ;
#15134 = PLANE ( 'NONE',  #65068 ) ;
#15135 = LINE ( 'NONE', #36038, #23703 ) ;
#15136 = CARTESIAN_POINT ( 'NONE',  ( -5.656854249492379694, 21.37499999590322375, -5.656854249492380582 ) ) ;
#15137 = SHAPE_REPRESENTATION ( 'hexagon nut style 1_is_IS 1364-3 - M24-W-N', ( #57354 ), #17638 ) ;
#15138 = CARTESIAN_POINT ( 'NONE',  ( 3.458734124999959914, 205.3750000013656063, 143.4326545832176976 ) ) ;
#15139 = CARTESIAN_POINT ( 'NONE',  ( -21.14973805123842965, -36.90291134455131328, 147.3140804305565155 ) ) ;
#15141 = CARTESIAN_POINT ( 'NONE',  ( -1.432654583217662481, 204.3750000013656063, 145.4587341250000634 ) ) ;
#15140 = LINE ( 'NONE', #44575, #13070 ) ;
#15142 = CARTESIAN_POINT ( 'NONE',  ( 11.35316468749999963, 251.5104166700806729, 3.042071309553159519 ) ) ;
#15143 = CARTESIAN_POINT ( 'NONE',  ( -7.999999999999998224, 114.7812500040967763, 3.313708498984766049 ) ) ;
#15144 = CARTESIAN_POINT ( 'NONE',  ( -2.679491924311087736, 215.4166666598387110, 10.00000000000008349 ) ) ;
#15145 = CARTESIAN_POINT ( 'NONE',  ( -2.679491924311225848, 221.4583333333333428, -10.00000000000000178 ) ) ;
#15146 = CARTESIAN_POINT ( 'NONE',  ( 7.188101187499993827, -2.977408999572645598, 7.017802781871754547 ) ) ;
#15147 = CARTESIAN_POINT ( 'NONE',  ( -9.832129032723418760, 188.1770833299193555, -5.676582343750004256 ) ) ;
#15148 = DIRECTION ( 'NONE',  ( -0.000000000000000000, -0.000000000000000000, -1.000000000000000000 ) ) ;
#15149 = CARTESIAN_POINT ( 'NONE',  ( -1.881053915767124440, 4.999999998634406140, 4.541265875000001451 ) ) ;
#15150 = CARTESIAN_POINT ( 'NONE',  ( -8.031737012268317599, 9.219280934457623644, -0.1021479564361138237 ) ) ;
#15152 = CARTESIAN_POINT ( 'NONE',  ( 54.00000000000000000, 272.0000000000000000, 4.085831468968142743E-14 ) ) ;
#15151 = CARTESIAN_POINT ( 'NONE',  ( 8.248616681371277227E-12, 116.2499999999993747, -10.00000000000000178 ) ) ;
#15153 = ORIENTED_EDGE ( 'NONE', *, *, #50026, .T. ) ;
#15154 = CARTESIAN_POINT ( 'NONE',  ( 3.458734124999960358, 205.6250000013656063, 143.4326545832176976 ) ) ;
#15155 = CARTESIAN_POINT ( 'NONE',  ( -8.311093377946836114, 2.656249996586016238, -8.311093377946837890 ) ) ;
#15156 = CARTESIAN_POINT ( 'NONE',  ( -7.778174593052023411, 7.778174593052023411, 101.5000000040967763 ) ) ;
#15157 = VECTOR ( 'NONE', #63917, 1000.000000000000000 ) ;
#15158 = CARTESIAN_POINT ( 'NONE',  ( 1.656854249492381914, 19.56249999726881228, 4.000000000000000888 ) ) ;
#15159 = CARTESIAN_POINT ( 'NONE',  ( -31.45873412499999233, 200.6875000013656063, 170.0000000000004547 ) ) ;
#15160 = DIRECTION ( 'NONE',  ( 0.000000000000000000, 0.000000000000000000, 1.000000000000000000 ) ) ;
#15162 = CARTESIAN_POINT ( 'NONE',  ( 5.676582343749993598, 4.947916663252683200, 9.832129032723422313 ) ) ;
#15161 = CARTESIAN_POINT ( 'NONE',  ( -2.977408999572650927, 114.8750000020483810, -7.188101187500000933 ) ) ;
#15163 = CARTESIAN_POINT ( 'NONE',  ( 7.999999999999991118, 9.797174393178815797E-16, 27.08030277982336642 ) ) ;
#15164 = CARTESIAN_POINT ( 'NONE',  ( 11.35316468749999785, 115.5729166632526841, 3.042071309553174174 ) ) ;
#15165 = ADVANCED_FACE ( 'NONE', ( #64080 ), #22973, .F. ) ;
#15166 = CARTESIAN_POINT ( 'NONE',  ( -4.999999999999998224, 88.54166665983869677, -8.660254037844389075 ) ) ;
#15167 = VECTOR ( 'NONE', #18779, 1000.000000000000000 ) ;
#15168 = CARTESIAN_POINT ( 'NONE',  ( 7.188101187500001821, 90.50000000204840944, -2.977408999572651371 ) ) ;
#15169 = CARTESIAN_POINT ( 'NONE',  ( -3.211159895383561391, 18.81249999863440436, -3.211159895383561835 ) ) ;
#15170 = CARTESIAN_POINT ( 'NONE',  ( -3.426202465283580523, 194.4587341250000350, 198.4732635780662235 ) ) ;
#15171 = CARTESIAN_POINT ( 'NONE',  ( -30.64284399271078740, -12.00318926462334801, 174.6921329945331536 ) ) ;
#15172 = ORIENTED_EDGE ( 'NONE', *, *, #26239, .F. ) ;
#15173 = CARTESIAN_POINT ( 'NONE',  ( 1.479685137562080274E-15, 225.9999999999999432, -10.00000000000000178 ) ) ;
#15174 = CARTESIAN_POINT ( 'NONE',  ( 6.676582343750004256, 291.0468750017070079, 2.765530957081995478 ) ) ;
#15175 = CARTESIAN_POINT ( 'NONE',  ( -2.828427124746192067, 12.37499999726881406, 2.828427124746190735 ) ) ;
#15176 = CARTESIAN_POINT ( 'NONE',  ( -9.121419926064122663, -1.666886344965055722, -0.4481800321554205713 ) ) ;
#15177 = CARTESIAN_POINT ( 'NONE',  ( -3.999999999999960032, 195.1250000027311842, 198.0000000000000284 ) ) ;
#15178 = CARTESIAN_POINT ( 'NONE',  ( -2.679491924311225848, 208.3333333265053966, -10.00000000000000178 ) ) ;
#15179 = CARTESIAN_POINT ( 'NONE',  ( 0.000000000000000000, 0.000000000000000000, 30.00000000000000000 ) ) ;
#15180 = CARTESIAN_POINT ( 'NONE',  ( -7.204075437095967871, 7.204075437095967871, 102.3437500020483668 ) ) ;
#15181 = ORIENTED_EDGE ( 'NONE', *, *, #43669, .T. ) ;
#15182 = EDGE_CURVE ( 'NONE', #66596, #60057, #12023, .T. ) ;
#15183 = AXIS2_PLACEMENT_3D ( 'NONE', #46917, #64999, #18623 ) ;
#15184 = CARTESIAN_POINT ( 'NONE',  ( -9.832129032723420536, 159.0104166632526983, 5.676582343749997150 ) ) ;
#15185 = CARTESIAN_POINT ( 'NONE',  ( -2.679491924311236506, 218.5416666666667140, 10.00000000000000355 ) ) ;
#15186 = EDGE_CURVE ( 'NONE', #31074, #4353, #39581, .T. ) ;
#15187 = CARTESIAN_POINT ( 'NONE',  ( 3.458734125000015869, 205.1875000013656063, 198.0000000000000284 ) ) ;
#15188 = B_SPLINE_CURVE_WITH_KNOTS ( 'NONE', 3,
 ( #18046, #70833, #1458, #70471, #69358, #17668, #18789, #12014, #35047, #24064, #47074, #58059, #64443, #13105, #12744, #41794, #65161, #64803, #6370, #7471, #30476, #53493 ),
 .UNSPECIFIED., .F., .F.,
 ( 4, 2, 2, 2, 2, 2, 2, 2, 2, 2, 4 ),
 ( 0.000000000000000000, 0.001156727053362452667, 0.001735090580043686806, 0.002313454106724920946, 0.003470181160087388791, 0.004048544686768622280, 0.004626908213449855770, 0.005783635266812325350, 0.006940362320174795797, 0.008097089373537265378, 0.009253816426899735825 ),
 .UNSPECIFIED. ) ;
#15189 = CARTESIAN_POINT ( 'NONE',  ( -30.99999999999992895, -31.99999999999978684, 167.9999999999997726 ) ) ;
#15190 = CARTESIAN_POINT ( 'NONE',  ( -8.311093377946841443, 59.21874999658601979, 8.311093377946830785 ) ) ;
#15191 = EDGE_LOOP ( 'NONE', ( #13229, #20740, #18201, #13613 ) ) ;
#15192 = CARTESIAN_POINT ( 'NONE',  ( 10.18810118750000093, -4.220049686691933921, 114.8125000020483668 ) ) ;
#15193 = CARTESIAN_POINT ( 'NONE',  ( -8.342170076843785083E-16, 7.187499998634407028, 4.541265875000002339 ) ) ;
#15194 = ORIENTED_EDGE ( 'NONE', *, *, #24961, .T. ) ;
#15195 = CARTESIAN_POINT ( 'NONE',  ( -1.320432766682874540E-15, 19.59374999795161543, 7.188101187500000044 ) ) ;
#15196 = CARTESIAN_POINT ( 'NONE',  ( -6.000000000000003553, 288.0000000034140157, -2.485281374238571317 ) ) ;
#15197 = CARTESIAN_POINT ( 'NONE',  ( -8.660254037844387298, 247.7083333401613174, -4.999999999999999112 ) ) ;
#15198 = CARTESIAN_POINT ( 'NONE',  ( 5.082755093536325930, 17.53124999795161543, -5.082755093536325930 ) ) ;
#15199 = CARTESIAN_POINT ( 'NONE',  ( -7.188101187499992051, 0.000000000000000000, 2.986552781871751439 ) ) ;
#15200 = CARTESIAN_POINT ( 'NONE',  ( 10.18810118749999916, 4.220049686691935698, 112.3750000020483810 ) ) ;
#15201 = DIRECTION ( 'NONE',  ( 0.000000000000000000, 0.000000000000000000, 1.000000000000000000 ) ) ;
#15202 = CARTESIAN_POINT ( 'NONE',  ( 4.000000000000001776, 6.749999997268813168, 0.000000000000000000 ) ) ;
#15203 = CARTESIAN_POINT ( 'NONE',  ( -30.82842712474624847, 208.2500000027312126, 167.1715728752542418 ) ) ;
#15204 = EDGE_LOOP ( 'NONE', ( #3355, #36839, #33079, #45103 ) ) ;
#15205 = CARTESIAN_POINT ( 'NONE',  ( 2.839093476692135984E-14, 205.6875000013656063, 201.4587341250000350 ) ) ;
#15206 = CARTESIAN_POINT ( 'NONE',  ( -25.55430564589111953, 208.0625000013656063, 172.4456943541091505 ) ) ;
#15207 = CARTESIAN_POINT ( 'NONE',  ( -1.881053915767121554, 7.624999998634408804, -4.541265875000002339 ) ) ;
#15208 = CARTESIAN_POINT ( 'NONE',  ( -6.000000000000003553, 289.9375000000000000, -2.485281374238571317 ) ) ;
#15209 = CARTESIAN_POINT ( 'NONE',  ( 7.188101187499993827, -2.977408999572645598, 26.14280278187175455 ) ) ;
#15210 = ORIENTED_EDGE ( 'NONE', *, *, #11225, .F. ) ;
#15211 =( BOUNDED_CURVE ( )  B_SPLINE_CURVE ( 2, ( #69930, #71021, #24626, #7664, #35601, #8026, #53690, #64264, #31034 ),
 .UNSPECIFIED., .F., .F. ) 
 B_SPLINE_CURVE_WITH_KNOTS ( ( 3, 2, 2, 2, 3 ),
 ( 0.3000000000000002109, 0.3083333333333335702, 0.3166666666666669294, 0.3250000000000002887, 0.3333333333333336479 ),
 .UNSPECIFIED. ) 
 CURVE ( )  GEOMETRIC_REPRESENTATION_ITEM ( )  RATIONAL_B_SPLINE_CURVE ( ( 0.9999999999999980016, 0.9238795325112887369, 1.000000000000000000, 0.9238795325112867385, 1.000000000000000000, 0.9238795325112867385, 1.000000000000000000, 0.9238795325112837409, 1.000000000000003109 ) ) 
 REPRESENTATION_ITEM ( '' )  );
#15212 = CARTESIAN_POINT ( 'NONE',  ( -7.347880794884122694E-16, 21.75000000000000355, 4.000000000000001776 ) ) ;
#15213 = VERTEX_POINT ( 'NONE', #45605 ) ;
#15214 = CARTESIAN_POINT ( 'NONE',  ( -4.220049686691935698, 10.18810118749999916, 115.3750000020483810 ) ) ;
#15215 = CARTESIAN_POINT ( 'NONE',  ( -4.556349186104048599, -10.99999999999999822, 83.96875000409677625 ) ) ;
#15216 = CARTESIAN_POINT ( 'NONE',  ( 2.754378923186476579E-14, 205.1875000013656063, 194.5412658750000219 ) ) ;
#15217 = CARTESIAN_POINT ( 'NONE',  ( 29.43265458321766914, 199.5000000013656063, 173.4587341249998929 ) ) ;
#15218 = CARTESIAN_POINT ( 'NONE',  ( 7.320508075688771044, 69.37499999999998579, 7.320508075688775484 ) ) ;
#15219 = CARTESIAN_POINT ( 'NONE',  ( 1.320432766682874540E-15, 94.90625000204838102, 7.188101187500000044 ) ) ;
#15220 = CARTESIAN_POINT ( 'NONE',  ( -6.000000000000003553, 293.9374999999999432, -2.485281374238571317 ) ) ;
#15221 = CARTESIAN_POINT ( 'NONE',  ( 30.82842712474621294, 207.2500000027312126, 172.8284271247460424 ) ) ;
#15222 = VERTEX_POINT ( 'NONE', #46715 ) ;
#15223 = AXIS2_PLACEMENT_3D ( 'NONE', #40436, #68361, #34801 ) ;
#15224 = DIRECTION ( 'NONE',  ( -0.000000000000000000, 1.000000000000000000, -0.000000000000000000 ) ) ;
#15225 = CARTESIAN_POINT ( 'NONE',  ( -1.877992804776299263, -10.12031740952197545, 70.21778636471883317 ) ) ;
#15226 = CARTESIAN_POINT ( 'NONE',  ( -1.656854249492403008, 200.8125000027311842, 146.0000000000000284 ) ) ;
#15227 = CARTESIAN_POINT ( 'NONE',  ( 2.020667218593132706E-15, -11.00000000000000000, 77.87499999999998579 ) ) ;
#15228 = CARTESIAN_POINT ( 'NONE',  ( -3.313708498984759387, -7.999999999999989342, 22.11155277982336997 ) ) ;
#15229 = CARTESIAN_POINT ( 'NONE',  ( 10.00000000000000178, 252.2916666666666856, 2.679491924311222739 ) ) ;
#15230 = CARTESIAN_POINT ( 'NONE',  ( -11.00000000000000000, 0.000000000000000000, 104.5000000000000000 ) ) ;
#15231 = CARTESIAN_POINT ( 'NONE',  ( -2.679491924311225848, 186.4583333333332860, -10.00000000000000178 ) ) ;
#15232 =( BOUNDED_CURVE ( )  B_SPLINE_CURVE ( 2, ( #62768, #28075, #68810, #57888, #34134, #28452, #5824, #5450, #6565, #63524, #34883, #17874, #74471 ),
 .UNSPECIFIED., .F., .F. ) 
 B_SPLINE_CURVE_WITH_KNOTS ( ( 3, 2, 2, 2, 2, 2, 3 ),
 ( 1.083288719158836511, 1.088522722798160647, 1.093756726437484783, 1.098990730076808697, 1.104224733716132612, 1.109458737355456748, 1.114692740994780884 ),
 .UNSPECIFIED. ) 
 CURVE ( )  GEOMETRIC_REPRESENTATION_ITEM ( )  RATIONAL_B_SPLINE_CURVE ( ( 0.9999999999999895639, 0.9659258262890787483, 1.000000000000000000, 0.9659258262890683122, 1.000000000000000000, 0.9659258262890683122, 1.000000000000000000, 0.9659258262890683122, 1.000000000000000000, 0.9659258262890683122, 1.000000000000000000, 0.9659258262890725311, 0.9999999999999957812 ) ) 
 REPRESENTATION_ITEM ( '' )  );
#15233 = CARTESIAN_POINT ( 'NONE',  ( 9.797174393178825657E-16, 125.0000000000000000, -8.000000000000000000 ) ) ;
#15234 = CARTESIAN_POINT ( 'NONE',  ( 7.188101187499992051, 2.977408999572647819, 23.70530278187175455 ) ) ;
#15235 = CARTESIAN_POINT ( 'NONE',  ( 11.35316468749999963, 151.3020833299193555, -3.042071309553165293 ) ) ;
#15236 = CYLINDRICAL_SURFACE ( 'NONE', #14384, 17.50000000000000000 ) ;
#15237 = CARTESIAN_POINT ( 'NONE',  ( -31.04077938110227208, 46.94736917785515118, 64.99999999999998579 ) ) ;
#15238 = CARTESIAN_POINT ( 'NONE',  ( -1.502569866548080446, -42.39601903919200510, 151.0587995217003652 ) ) ;
#15239 = VERTEX_POINT ( 'NONE', #62957 ) ;
#15240 = CARTESIAN_POINT ( 'NONE',  ( -3.042071309553164404, 17.55208332991935194, -11.35316468749999963 ) ) ;
#15241 = CARTESIAN_POINT ( 'NONE',  ( 4.000000000000015987, 200.6250000027312126, 198.0000000000000284 ) ) ;
#15243 = CARTESIAN_POINT ( 'NONE',  ( -38.00000000000002132, 50.00000000000000711, 65.00000000000000000 ) ) ;
#15242 = DIRECTION ( 'NONE',  ( 0.000000000000000000, 0.000000000000000000, 1.000000000000000000 ) ) ;
#15244 = CARTESIAN_POINT ( 'NONE',  ( -3.999999999999960032, 196.1250000027311842, 198.0000000000000284 ) ) ;
#15245 = CARTESIAN_POINT ( 'NONE',  ( 3.458734124999959914, 201.4375000013656063, 142.0000000000000568 ) ) ;
#15246 = CARTESIAN_POINT ( 'NONE',  ( -7.320508075688773708, 43.74999999317202537, -7.320508075688774596 ) ) ;
#15247 = CARTESIAN_POINT ( 'NONE',  ( 2.977408999572654480, 109.6250000020483952, 7.188101187499999156 ) ) ;
#15248 = CARTESIAN_POINT ( 'NONE',  ( -8.342170076843785083E-16, 9.187499998634407916, 4.541265875000002339 ) ) ;
#15249 = CARTESIAN_POINT ( 'NONE',  ( 7.320508075688767491, 54.37500000000000000, 7.320508075688771044 ) ) ;
#15250 = CARTESIAN_POINT ( 'NONE',  ( -3.313708498984758943, -7.999999999999989342, 8.611552779823366421 ) ) ;
#15252 = CARTESIAN_POINT ( 'NONE',  ( -9.000000000000000000, -5.196152422706644458, -10.80000000000000071 ) ) ;
#15251 = CARTESIAN_POINT ( 'NONE',  ( 3.403184810911259017, 194.4648993367464982, 141.3150426067872445 ) ) ;
#15253 = EDGE_LOOP ( 'NONE', ( #62317, #22350, #13816, #61456 ) ) ;
#15254 = ORIENTED_EDGE ( 'NONE', *, *, #2585, .T. ) ;
#15255 = CARTESIAN_POINT ( 'NONE',  ( -6.000000000000015099, 10.39230484541326227, -14.00000000000000178 ) ) ;
#15256 = CARTESIAN_POINT ( 'NONE',  ( -4.000000000000015987, 196.5000000000000000, 142.0000000000000568 ) ) ;
#15257 = CARTESIAN_POINT ( 'NONE',  ( -22.27202332600456103, -38.70770797676598107, 148.4337101287379426 ) ) ;
#15258 = CARTESIAN_POINT ( 'NONE',  ( 3.042071309553159519, 134.7395833299193839, 11.35316468750000141 ) ) ;
#15259 = ORIENTED_EDGE ( 'NONE', *, *, #45905, .F. ) ;
#15260 = CARTESIAN_POINT ( 'NONE',  ( 30.82842712474617031, 201.1250000000000284, 172.8284271247460993 ) ) ;
#15261 = EDGE_CURVE ( 'NONE', #54743, #71172, #30204, .T. ) ;
#15262 = CARTESIAN_POINT ( 'NONE',  ( -6.238412754330611322E-16, 10.18810118749999916, 89.78125000204836681 ) ) ;
#15263 = CARTESIAN_POINT ( 'NONE',  ( -3.313708498984757611, 7.999999999999991118, 20.23655278392014978 ) ) ;
#15264 = CARTESIAN_POINT ( 'NONE',  ( -2.828427124746152987, 207.1250000000000284, 200.8284271247462129 ) ) ;
#15265 = CARTESIAN_POINT ( 'NONE',  ( -11.00000000000000000, 0.000000000000000000, 72.99999999999998579 ) ) ;
#15267 = CARTESIAN_POINT ( 'NONE',  ( 11.35316468749999785, 120.5729166632526841, 3.042071309553174174 ) ) ;
#15266 = CARTESIAN_POINT ( 'NONE',  ( 5.292292394482791984, 220.0000000000000568, 8.892157229669562568 ) ) ;
#15268 = DIRECTION ( 'NONE',  ( -0.000000000000000000, 1.000000000000000000, 4.689100369878284071E-30 ) ) ;
#15269 = ORIENTED_EDGE ( 'NONE', *, *, #20477, .F. ) ;
#15270 = CARTESIAN_POINT ( 'NONE',  ( 47.32259252271278882, 38.77329591270031983, 65.76194439203456454 ) ) ;
#15271 = CARTESIAN_POINT ( 'NONE',  ( 11.35316468749999785, 115.8854166632526983, 3.042071309553174174 ) ) ;
#15272 = CARTESIAN_POINT ( 'NONE',  ( 3.458734125000015425, 204.9375000013656063, 198.0000000000000284 ) ) ;
#15273 = CARTESIAN_POINT ( 'NONE',  ( -2.977408999572650039, 19.31249999795161543, -7.188101187500000933 ) ) ;
#15274 = CARTESIAN_POINT ( 'NONE',  ( 4.220049686691934809, 10.18810118749999916, 81.06250000204836681 ) ) ;
#15275 = CARTESIAN_POINT ( 'NONE',  ( -3.042071309553173730, 24.63541666325268054, 11.35316468749999785 ) ) ;
#15276 = ORIENTED_EDGE ( 'NONE', *, *, #35813, .F. ) ;
#15277 = CARTESIAN_POINT ( 'NONE',  ( 3.317071493978877683, 8.008118988124991233, 23.04436528394063544 ) ) ;
#15278 = CARTESIAN_POINT ( 'NONE',  ( 7.999999999842164478, 5.025161467855852442E-05, 22.76780420562571905 ) ) ;
#15279 = CARTESIAN_POINT ( 'NONE',  ( -10.99999999999978684, -4.556349186104264426, 85.28125000409679046 ) ) ;
#15280 = CARTESIAN_POINT ( 'NONE',  ( 2.977408999572650927, 3.749999997951610542, -7.188101187500001821 ) ) ;
#15281 = CARTESIAN_POINT ( 'NONE',  ( -2.765530957081998586, 287.6406250017069510, 6.676582343750001591 ) ) ;
#15282 = ADVANCED_FACE ( 'NONE', ( #57317 ), #68619, .T. ) ;
#15283 = DIRECTION ( 'NONE',  ( -0.000000000000000000, -1.000000000000000000, -0.000000000000000000 ) ) ;
#15284 = CARTESIAN_POINT ( 'NONE',  ( 12.00000000000000000, -28.00000000000000000, 0.000000000000000000 ) ) ;
#15285 = ORIENTED_EDGE ( 'NONE', *, *, #10943, .F. ) ;
#15286 = CARTESIAN_POINT ( 'NONE',  ( 11.35316468749999785, 140.8854166632526415, 3.042071309553174174 ) ) ;
#15287 = CARTESIAN_POINT ( 'NONE',  ( 1.871523826299183495E-15, -10.18810118749999916, 75.53125000204836681 ) ) ;
#15288 = CARTESIAN_POINT ( 'NONE',  ( -24.54126587499998990, 197.1875000013655779, 170.0000000000003411 ) ) ;
#15289 = CARTESIAN_POINT ( 'NONE',  ( 0.000000000000000000, 0.000000000000000000, 0.000000000000000000 ) ) ;
#15290 = CARTESIAN_POINT ( 'NONE',  ( 2.780723358947928197E-16, 17.68749999863440792, -4.541265875000002339 ) ) ;
#15291 = ORIENTED_EDGE ( 'NONE', *, *, #43108, .T. ) ;
#15292 = CARTESIAN_POINT ( 'NONE',  ( -3.999999999999960032, 202.1250000027312126, 198.0000000000000284 ) ) ;
#15293 = CARTESIAN_POINT ( 'NONE',  ( -1.656854249492405451, 209.3125000000000568, 138.0000000000000568 ) ) ;
#15294 = CARTESIAN_POINT ( 'NONE',  ( -31.99999999999996447, 207.4375000027311842, 171.6568542494928522 ) ) ;
#15295 = DIRECTION ( 'NONE',  ( 1.000000000000000000, 0.000000000000000000, 0.000000000000000000 ) ) ;
#15296 = ORIENTED_EDGE ( 'NONE', *, *, #3283, .T. ) ;
#15297 = CARTESIAN_POINT ( 'NONE',  ( -1.320432766682874540E-15, 10.59374999795161187, 7.188101187500000044 ) ) ;
#15298 = CARTESIAN_POINT ( 'NONE',  ( -28.77118861177961051, -12.11599118489504612, 181.6832355153309209 ) ) ;
#15299 = VECTOR ( 'NONE', #26542, 1000.000000000000000 ) ;
#15300 = CARTESIAN_POINT ( 'NONE',  ( -1.836970198721029983E-15, 30.62499999317203248, 10.00000000000000178 ) ) ;
#15301 = CARTESIAN_POINT ( 'NONE',  ( 5.676582343749993598, 184.9479166632526983, 9.832129032723422313 ) ) ;
#15302 = CARTESIAN_POINT ( 'NONE',  ( -7.188101187499999156, 109.6250000020483952, 2.977408999572654924 ) ) ;
#15303 = LINE ( 'NONE', #32694, #2818 ) ;
#15304 = CARTESIAN_POINT ( 'NONE',  ( -6.676582343750002480, 290.3906250017070647, -2.765530957081996810 ) ) ;
#15306 = CARTESIAN_POINT ( 'NONE',  ( -18.00000000000000355, 0.000000000000000000, 0.000000000000000000 ) ) ;
#15305 = CARTESIAN_POINT ( 'NONE',  ( -5.676582343749992710, 219.7395833367473301, 9.832129032723422313 ) ) ;
#15307 = ORIENTED_EDGE ( 'NONE', *, *, #50261, .F. ) ;
#15308 = CARTESIAN_POINT ( 'NONE',  ( -9.832129032723415207, 259.3229166700806445, 5.676582343750005144 ) ) ;
#15309 = CARTESIAN_POINT ( 'NONE',  ( 7.188101187499991163, 2.977408999572648707, 23.70530278187175810 ) ) ;
#15310 = CARTESIAN_POINT ( 'NONE',  ( -11.00000000000010303, -4.556349186103947346, 92.59374999999997158 ) ) ;
#15311 = CARTESIAN_POINT ( 'NONE',  ( 0.000000000000000000, 0.000000000000000000, 0.000000000000000000 ) ) ;
#15312 = CARTESIAN_POINT ( 'NONE',  ( 3.223881452105731515, -60.47365957010915594, -23.05198836891676351 ) ) ;
#15313 = CARTESIAN_POINT ( 'NONE',  ( 2.445694354108839175, 201.3125000013656063, 195.5543056458912190 ) ) ;
#15314 = CARTESIAN_POINT ( 'NONE',  ( 4.556349186104052151, -10.99999999999999822, 115.6562500040967905 ) ) ;
#15315 = DIRECTION ( 'NONE',  ( -0.000000000000000000, 1.000000000000000000, -0.000000000000000000 ) ) ;
#15316 = CARTESIAN_POINT ( 'NONE',  ( -5.656854249492378806, 96.68750000000000000, 5.656854249492381470 ) ) ;
#15317 = CARTESIAN_POINT ( 'NONE',  ( -2.085542519210945728E-15, 114.8437499965860127, 11.35316468750000141 ) ) ;
#15318 = CARTESIAN_POINT ( 'NONE',  ( -5.000000000000000000, -14.70421557449315486, -69.92631206022691970 ) ) ;
#15319 = CARTESIAN_POINT ( 'NONE',  ( 11.00000000000000355, -4.556349186104045046, 69.15624999999998579 ) ) ;
#15322 = CARTESIAN_POINT ( 'NONE',  ( 6.000000000000003553, 298.4375000000000000, 2.485281374238571317 ) ) ;
#15321 = CARTESIAN_POINT ( 'NONE',  ( 30.44569435410883074, 199.5625000013656063, 172.4456943541086957 ) ) ;
#15320 = CARTESIAN_POINT ( 'NONE',  ( 26.56734541678238060, 199.2500000013656063, 166.5412658749999650 ) ) ;
#15323 = ORIENTED_EDGE ( 'NONE', *, *, #3253, .T. ) ;
#15324 = EDGE_CURVE ( 'NONE', #26210, #17226, #59312, .T. ) ;
#15325 = CARTESIAN_POINT ( 'NONE',  ( 9.627422524176592944, 224.7807405533921212, 2.720186965506536936 ) ) ;
#15326 = CARTESIAN_POINT ( 'NONE',  ( -8.311093377946836114, 222.6562499965860411, -8.311093377946837890 ) ) ;
#15327 =( BOUNDED_CURVE ( )  B_SPLINE_CURVE ( 2, ( #26900, #72928, #44264, #15572, #27266, #4650, #35187, #6506, #29513 ),
 .UNSPECIFIED., .F., .F. ) 
 B_SPLINE_CURVE_WITH_KNOTS ( ( 3, 2, 2, 2, 3 ),
 ( 0.1333333333333334425, 0.1416666666666667740, 0.1500000000000001332, 0.1583333333333334925, 0.1666666666666668239 ),
 .UNSPECIFIED. ) 
 CURVE ( )  GEOMETRIC_REPRESENTATION_ITEM ( )  RATIONAL_B_SPLINE_CURVE ( ( 0.9999999999999990008, 0.9238795325112877377, 1.000000000000000000, 0.9238795325112867385, 1.000000000000000000, 0.9238795325112867385, 1.000000000000000000, 0.9238795325112851842, 1.000000000000001554 ) ) 
 REPRESENTATION_ITEM ( '' )  );
#15328 = CARTESIAN_POINT ( 'NONE',  ( 3.458734124999959025, 197.5000000013656063, 140.5673454167824161 ) ) ;
#15329 = VECTOR ( 'NONE', #70358, 1000.000000000000000 ) ;
#15330 = CARTESIAN_POINT ( 'NONE',  ( 28.00000000000002132, 198.1875000013655779, 166.5412658749999082 ) ) ;
#15331 = CARTESIAN_POINT ( 'NONE',  ( -4.556349186104045934, 11.00000000000000000, 108.9062500040967763 ) ) ;
#15332 = CARTESIAN_POINT ( 'NONE',  ( 5.676582343750001591, 201.9270833299193555, -9.832129032723420536 ) ) ;
#15333 = CARTESIAN_POINT ( 'NONE',  ( 17.99999999999998934, 0.000000000000000000, 0.000000000000000000 ) ) ;
#15334 = CARTESIAN_POINT ( 'NONE',  ( 2.775557561562891351E-14, 271.9999999999999432, 170.0000000000000284 ) ) ;
#15335 = CARTESIAN_POINT ( 'NONE',  ( -3.211159895383562723, 16.93749999863440436, 3.211159895383561391 ) ) ;
#15336 = CARTESIAN_POINT ( 'NONE',  ( 6.891449706512932316, -51.31760009880697027, 41.45518442799505721 ) ) ;
#15337 = CARTESIAN_POINT ( 'NONE',  ( 1.469576158976822172E-15, -7.999999999999991118, 25.20530277982336642 ) ) ;
#15339 = DIRECTION ( 'NONE',  ( 0.000000000000000000, 0.000000000000000000, 1.000000000000000000 ) ) ;
#15338 = CARTESIAN_POINT ( 'NONE',  ( 4.999999999999999112, 185.8333333333333428, -8.660254037844383745 ) ) ;
#15340 = CARTESIAN_POINT ( 'NONE',  ( 8.311093377946834337, 90.15624999658604111, 8.311093377946839666 ) ) ;
#15341 = ORIENTED_EDGE ( 'NONE', *, *, #18006, .F. ) ;
#15342 = LINE ( 'NONE', #3299, #30338 ) ;
#15343 = CARTESIAN_POINT ( 'NONE',  ( -5.082755093536325042, 19.03124999795161543, -5.082755093536325930 ) ) ;
#15344 = DIRECTION ( 'NONE',  ( 0.000000000000000000, 0.000000000000000000, 1.000000000000000000 ) ) ;
#15345 = CARTESIAN_POINT ( 'NONE',  ( 3.042071309553163516, 262.7604166700806445, -11.35316468749999785 ) ) ;
#15346 = CARTESIAN_POINT ( 'NONE',  ( 5.676582343749993598, 89.94791666325269830, 9.832129032723422313 ) ) ;
#15347 = ORIENTED_EDGE ( 'NONE', *, *, #15752, .T. ) ;
#15348 = DIRECTION ( 'NONE',  ( -0.000000000000000000, 1.000000000000000000, -0.000000000000000000 ) ) ;
#15349 = EDGE_CURVE ( 'NONE', #54725, #3504, #61731, .T. ) ;
#15350 = CARTESIAN_POINT ( 'NONE',  ( 7.204075437095968759, -7.204075437095966983, 114.7187500020483810 ) ) ;
#15351 = CARTESIAN_POINT ( 'NONE',  ( -26.56734541678232375, 196.2500000013656631, 173.4587341250003760 ) ) ;
#15352 = CARTESIAN_POINT ( 'NONE',  ( -1.432654583217608080, 203.8750000013656063, 201.4587341250000350 ) ) ;
#15353 = DIRECTION ( 'NONE',  ( -0.000000000000000000, -0.000000000000000000, 1.000000000000000000 ) ) ;
#15355 = CARTESIAN_POINT ( 'NONE',  ( -3.042071309553173730, 84.32291666325268409, 11.35316468749999785 ) ) ;
#15354 = CARTESIAN_POINT ( 'NONE',  ( -4.898587196589412829E-16, 121.8125000040967763, -8.000000000000000000 ) ) ;
#15356 = CARTESIAN_POINT ( 'NONE',  ( 1.469576158976822172E-15, -7.999999999999991118, 20.89280278392014623 ) ) ;
#15357 = CARTESIAN_POINT ( 'NONE',  ( -31.45873412500001010, 202.8750000013656347, 168.5673454167827572 ) ) ;
#15358 = CARTESIAN_POINT ( 'NONE',  ( -32.00000000000002842, 196.3125000027312126, 168.3431457505080857 ) ) ;
#15359 = EDGE_CURVE ( 'NONE', #24466, #32974, #35785, .T. ) ;
#15360 = CARTESIAN_POINT ( 'NONE',  ( -1.836970198721029983E-15, 180.6249999931720538, 10.00000000000000178 ) ) ;
#15361 = CARTESIAN_POINT ( 'NONE',  ( 4.999999999999999112, -53.09993190648272332, 43.73864582539214751 ) ) ;
#15362 = CARTESIAN_POINT ( 'NONE',  ( 5.676582343750001591, 76.92708332991935549, -9.832129032723420536 ) ) ;
#15363 = CARTESIAN_POINT ( 'NONE',  ( -4.721056650415998313, 294.5781250017069510, 4.721056650416000089 ) ) ;
#15364 = CARTESIAN_POINT ( 'NONE',  ( 7.204075437095966983, 7.204075437095967871, 103.4687500020483668 ) ) ;
#15365 = CARTESIAN_POINT ( 'NONE',  ( -11.35316468750000141, 203.2812499965860411, -1.390361679473963753E-15 ) ) ;
#15366 = EDGE_LOOP ( 'NONE', ( #45752, #39600, #44890 ) ) ;
#15367 = CARTESIAN_POINT ( 'NONE',  ( -8.000000000000005329, -3.313708498984745621, 27.92405277982336287 ) ) ;
#15368 = CARTESIAN_POINT ( 'NONE',  ( -27.99999999999991473, 206.6250000027312126, 174.0000000000003695 ) ) ;
#15369 = CARTESIAN_POINT ( 'NONE',  ( 5.000000000000000888, 64.42874436516095216, 24.11656705754242580 ) ) ;
#15371 = CARTESIAN_POINT ( 'NONE',  ( -5.676582343750006032, 204.1145833299193555, 9.832129032723418760 ) ) ;
#15370 = CARTESIAN_POINT ( 'NONE',  ( -1.469576158976823947E-15, 21.93749999590322375, 8.000000000000000000 ) ) ;
#15372 = CARTESIAN_POINT ( 'NONE',  ( 1.881053915767122664, 2.249999998634407028, 4.541265875000001451 ) ) ;
#15373 = CARTESIAN_POINT ( 'NONE',  ( 7.320508075688771044, 221.2500000068280031, -7.320508075688771932 ) ) ;
#15374 = CARTESIAN_POINT ( 'NONE',  ( -11.00000000000000000, 0.000000000000000000, 71.68750000409676204 ) ) ;
#15375 = EDGE_CURVE ( 'NONE', #62362, #30042, #52760, .T. ) ;
#15376 = VERTEX_POINT ( 'NONE', #58799 ) ;
#15377 = CARTESIAN_POINT ( 'NONE',  ( -9.832129032723420536, 189.0104166632526983, 5.676582343749997150 ) ) ;
#15378 = CARTESIAN_POINT ( 'NONE',  ( -2.977408999572647819, 7.188101187499992051, 13.20530278187175277 ) ) ;
#15379 = CARTESIAN_POINT ( 'NONE',  ( -8.660254037844385522, 92.91666666666667140, 4.999999999999994671 ) ) ;
#15380 = CARTESIAN_POINT ( 'NONE',  ( -3.313708498984765161, 14.53125000000000178, 7.999999999999998224 ) ) ;
#15381 = EDGE_LOOP ( 'NONE', ( #7897, #16927, #10122, #68819, #49992, #49364 ) ) ;
#15382 = CARTESIAN_POINT ( 'NONE',  ( -5.656854249492380582, 92.00000000409677625, -5.656854249492380582 ) ) ;
#15383 = CARTESIAN_POINT ( 'NONE',  ( -5.000000000000005329, 18.33333333333333215, 8.660254037844387298 ) ) ;
#15384 = EDGE_CURVE ( 'NONE', #46331, #72211, #7480, .T. ) ;
#15385 = CARTESIAN_POINT ( 'NONE',  ( 1.871523826299183495E-15, -10.18810118749999916, 80.40625000204838102 ) ) ;
#15386 = ORIENTED_EDGE ( 'NONE', *, *, #5486, .T. ) ;
#15387 = CARTESIAN_POINT ( 'NONE',  ( -4.000000000000001776, 21.50000000000000000, -4.898587196589415787E-16 ) ) ;
#15388 = CARTESIAN_POINT ( 'NONE',  ( 1.881053915767121998, 19.49999999863440436, -4.541265875000002339 ) ) ;
#15389 = CARTESIAN_POINT ( 'NONE',  ( 7.999999999999992895, -3.313708498984756279, 7.674052783920145338 ) ) ;
#15390 = CARTESIAN_POINT ( 'NONE',  ( 9.797174393178825657E-16, 125.0000000000000000, -8.000000000000000000 ) ) ;
#15391 = ORIENTED_EDGE ( 'NONE', *, *, #21571, .F. ) ;
#15392 = CARTESIAN_POINT ( 'NONE',  ( 7.320508075688774596, 17.49999999317202892, -7.320508075688774596 ) ) ;
#15393 = CARTESIAN_POINT ( 'NONE',  ( -2.977408999572651815, 94.43750000204838102, 7.188101187500000933 ) ) ;
#15396 = CARTESIAN_POINT ( 'NONE',  ( 29.65685424949236904, 207.5625000027312126, 165.9999999999999432 ) ) ;
#15395 = CARTESIAN_POINT ( 'NONE',  ( -11.35316468749999785, 263.6979166700807014, -3.042071309553164848 ) ) ;
#15394 = CARTESIAN_POINT ( 'NONE',  ( -10.68301270189220098, 0.000000000000000000, 117.8169872981077617 ) ) ;
#15397 = ORIENTED_EDGE ( 'NONE', *, *, #72663, .F. ) ;
#15398 = CARTESIAN_POINT ( 'NONE',  ( -5.676582343749992710, 250.0520833367473301, 9.832129032723422313 ) ) ;
#15399 = CARTESIAN_POINT ( 'NONE',  ( -7.188101187499990274, -2.977408999572651371, 10.58030278187175455 ) ) ;
#15400 = EDGE_LOOP ( 'NONE', ( #26833, #65919, #50260, #8440 ) ) ;
#15401 = VERTEX_POINT ( 'NONE', #7110 ) ;
#15402 = CARTESIAN_POINT ( 'NONE',  ( 10.18810118749999916, 1.247682550866122264E-15, 77.40625000204836681 ) ) ;
#15403 = CARTESIAN_POINT ( 'NONE',  ( -3.042071309553173730, 69.63541666325268409, 11.35316468749999785 ) ) ;
#15404 = CARTESIAN_POINT ( 'NONE',  ( -7.778174593052020747, -7.778174593052023411, 88.18749999999998579 ) ) ;
#15407 = CARTESIAN_POINT ( 'NONE',  ( 2.765530957082001251, 288.9218750017069510, 6.676582343749999815 ) ) ;
#15406 = CARTESIAN_POINT ( 'NONE',  ( 29.65685424949234772, 195.5625000027311842, 165.9999999999998863 ) ) ;
#15405 = DIRECTION ( 'NONE',  ( 1.000000000000000000, 0.000000000000000000, 0.000000000000000000 ) ) ;
#15408 = CARTESIAN_POINT ( 'NONE',  ( -9.000000000000000000, 5.196152422706624918, -10.20000000000000284 ) ) ;
#15409 = CARTESIAN_POINT ( 'NONE',  ( -8.660254037844387298, 163.9583333265053966, -5.000000000000004441 ) ) ;
#15410 = VECTOR ( 'NONE', #12110, 1000.000000000000000 ) ;
#15411 = CARTESIAN_POINT ( 'NONE',  ( -2.445694354108784108, 196.5625000013656063, 195.5543056458912190 ) ) ;
#15412 = CARTESIAN_POINT ( 'NONE',  ( 3.313708498984762052, 9.093749995903223748, -8.000000000000000000 ) ) ;
#15413 = ORIENTED_EDGE ( 'NONE', *, *, #22400, .T. ) ;
#15414 = CARTESIAN_POINT ( 'NONE',  ( 28.00000000000001776, 194.9375000013655779, 166.5412658749999082 ) ) ;
#15415 = AXIS2_PLACEMENT_3D ( 'NONE', #50881, #33932, #55438 ) ;
#15416 = CARTESIAN_POINT ( 'NONE',  ( 7.188101187499999156, 15.74999999795161543, 2.977408999572654924 ) ) ;
#15417 = CARTESIAN_POINT ( 'NONE',  ( -9.832129032723420536, 169.0104166632526983, 5.676582343749997150 ) ) ;
#15418 = DIRECTION ( 'NONE',  ( -0.000000000000000000, 1.000000000000000000, -0.000000000000000000 ) ) ;
#15419 = CARTESIAN_POINT ( 'NONE',  ( -2.977408999572650927, 103.2500000020483810, -7.188101187500000933 ) ) ;
#15421 = CARTESIAN_POINT ( 'NONE',  ( -3.223881452104699008, -50.20043732027927774, -40.84573126306842283 ) ) ;
#15420 = CARTESIAN_POINT ( 'NONE',  ( 2.485281374238878627, 289.3750000034139589, 5.999999999999694467 ) ) ;
#15422 = CARTESIAN_POINT ( 'NONE',  ( 28.00000000000002487, 208.1875000013656063, 166.5412658749999082 ) ) ;
#15423 = CARTESIAN_POINT ( 'NONE',  ( 1.320432766682872962E-15, -7.188101187499992051, 14.23655278187175455 ) ) ;
#15424 = CARTESIAN_POINT ( 'NONE',  ( -1.656854249492405451, 208.4375000027311842, 138.0000000000000568 ) ) ;
#15425 = CARTESIAN_POINT ( 'NONE',  ( 5.676582343750001591, 46.61458332991935549, -9.832129032723420536 ) ) ;
#15426 = ADVANCED_FACE ( 'NONE', ( #13842 ), #65916, .T. ) ;
#15427 = CARTESIAN_POINT ( 'NONE',  ( 5.656854249492378806, 20.81250000000000355, 5.656854249492381470 ) ) ;
#15428 = CARTESIAN_POINT ( 'NONE',  ( -10.00000000000000355, 24.58333332650536462, 2.679491924311223183 ) ) ;
#15429 = CARTESIAN_POINT ( 'NONE',  ( -7.347880794884122694E-16, 16.75000000000000000, 4.000000000000001776 ) ) ;
#15430 = ORIENTED_EDGE ( 'NONE', *, *, #51754, .F. ) ;
#15431 = LINE ( 'NONE', #38842, #63974 ) ;
#15432 = CARTESIAN_POINT ( 'NONE',  ( -8.000000000000000000, 19.96874999590322020, -3.313708498984762496 ) ) ;
#15433 = CARTESIAN_POINT ( 'NONE',  ( -11.35316468749999785, 43.07291666325267698, -3.042071309553167513 ) ) ;
#15434 = VECTOR ( 'NONE', #71001, 1000.000000000000000 ) ;
#15435 = CARTESIAN_POINT ( 'NONE',  ( -7.778174593052020747, -7.778174593052023411, 77.87500000409677625 ) ) ;
#15436 = CARTESIAN_POINT ( 'NONE',  ( 1.432654583217608080, 202.8750000013656063, 138.5412658750000503 ) ) ;
#15437 = CARTESIAN_POINT ( 'NONE',  ( 3.734423912265155465, 10.10901040137928852, 70.68514270129381316 ) ) ;
#15438 = CARTESIAN_POINT ( 'NONE',  ( 0.000000000000000000, 0.000000000000000000, 30.00000000000000000 ) ) ;
#15440 = CARTESIAN_POINT ( 'NONE',  ( -5.676582343749998039, 52.44791666325268409, -9.832129032723420536 ) ) ;
#15439 = CARTESIAN_POINT ( 'NONE',  ( 7.188101187500002709, 102.3125000020483952, 2.977408999572649151 ) ) ;
#15441 = CARTESIAN_POINT ( 'NONE',  ( -3.313708498984758943, -7.999999999999989342, 8.611552779823366421 ) ) ;
#15442 = CARTESIAN_POINT ( 'NONE',  ( 7.778174593052021635, 7.778174593052023411, 98.12500000409676204 ) ) ;
#15443 = CARTESIAN_POINT ( 'NONE',  ( 3.042071309553167069, 166.8229166632526699, -11.35316468749999785 ) ) ;
#15444 = VECTOR ( 'NONE', #59611, 1000.000000000000000 ) ;
#15445 = EDGE_CURVE ( 'NONE', #36060, #8118, #9743, .T. ) ;
#15446 = CARTESIAN_POINT ( 'NONE',  ( -8.660254037844390851, 139.7916666598387110, 4.999999999999998224 ) ) ;
#15447 = CARTESIAN_POINT ( 'NONE',  ( 2.977408999572650039, 103.0625000020483810, -7.188101187500001821 ) ) ;
#15448 = CARTESIAN_POINT ( 'NONE',  ( 1.224646799147353454E-15, 300.0000000000000000, -10.00000000000000178 ) ) ;
#15449 = CARTESIAN_POINT ( 'NONE',  ( 8.311093377946837890, 36.71874999658601979, -8.311093377946837890 ) ) ;
#15450 =( BOUNDED_CURVE ( )  B_SPLINE_CURVE ( 3, ( #29293, #22875, #16831, #16457 ),
 .UNSPECIFIED., .F., .F. ) 
 B_SPLINE_CURVE_WITH_KNOTS ( ( 4, 4 ),
 ( 1.570796326794896780, 3.141592653589792228 ),
 .UNSPECIFIED. ) 
 CURVE ( )  GEOMETRIC_REPRESENTATION_ITEM ( )  RATIONAL_B_SPLINE_CURVE ( ( 1.000000000000000000, 0.8047378541243652705, 0.8047378541243652705, 1.000000000000000000 ) ) 
 REPRESENTATION_ITEM ( '' )  );
#15451 = ORIENTED_EDGE ( 'NONE', *, *, #55111, .T. ) ;
#15453 = DIRECTION ( 'NONE',  ( -0.000000000000000000, 1.000000000000000000, -0.000000000000000000 ) ) ;
#15452 =( BOUNDED_CURVE ( )  B_SPLINE_CURVE ( 2, ( #47475, #70138, #46735, #30503, #29403, #41088, #52777, #69386, #64098 ),
 .UNSPECIFIED., .F., .F. ) 
 B_SPLINE_CURVE_WITH_KNOTS ( ( 3, 2, 2, 2, 3 ),
 ( 0.2166666666666669516, 0.2250000000000002554, 0.2333333333333335313, 0.2416666666666668073, 0.2500000000000001110 ),
 .UNSPECIFIED. ) 
 CURVE ( )  GEOMETRIC_REPRESENTATION_ITEM ( )  RATIONAL_B_SPLINE_CURVE ( ( 0.9999999999999974465, 0.9238795325112892920, 1.000000000000000000, 0.9238795325112867385, 1.000000000000000000, 0.9238795325112867385, 1.000000000000000000, 0.9238795325112857393, 1.000000000000001110 ) ) 
 REPRESENTATION_ITEM ( '' )  );
#15454 = CARTESIAN_POINT ( 'NONE',  ( -6.238412754330611322E-16, 10.18810118749999916, 79.28125000204836681 ) ) ;
#15455 = CARTESIAN_POINT ( 'NONE',  ( -2.775557561562891351E-14, 210.0000000000000284, 146.0000000000000284 ) ) ;
#15457 = CARTESIAN_POINT ( 'NONE',  ( -5.676582343750006032, 164.1145833299193555, 9.832129032723418760 ) ) ;
#15456 = CARTESIAN_POINT ( 'NONE',  ( -1.836970198721029983E-15, 8.750000000000000000, 10.00000000000000178 ) ) ;
#15458 = CARTESIAN_POINT ( 'NONE',  ( 3.313708498984762496, -7.999999999999989342, 11.85530278432982243 ) ) ;
#15459 = DIRECTION ( 'NONE',  ( 0.000000000000000000, 0.000000000000000000, -1.000000000000000000 ) ) ;
#15460 = CARTESIAN_POINT ( 'NONE',  ( -6.123233995736766282E-16, 261.8750000068280315, -10.00000000000000000 ) ) ;
#15461 = CARTESIAN_POINT ( 'NONE',  ( 1.877992804776344338, 55.75022808459620904, -43.87334515337072105 ) ) ;
#15462 = CARTESIAN_POINT ( 'NONE',  ( 7.204075437095968759, -7.204075437095966983, 83.59375000204838102 ) ) ;
#15463 = ORIENTED_EDGE ( 'NONE', *, *, #32095, .T. ) ;
#15464 = EDGE_CURVE ( 'NONE', #5966, #3175, #70012, .T. ) ;
#15465 = CARTESIAN_POINT ( 'NONE',  ( -10.00000000000000000, 119.1666666598386968, -2.679491924311229845 ) ) ;
#15466 = CARTESIAN_POINT ( 'NONE',  ( 7.594050593750000466, 0.2343749989758049379, 0.000000000000000000 ) ) ;
#15467 = CARTESIAN_POINT ( 'NONE',  ( -3.042071309553173730, 109.6354166632526557, 11.35316468749999785 ) ) ;
#15468 = CARTESIAN_POINT ( 'NONE',  ( 1.871523826299183495E-15, -10.18810118749999916, 98.03125000204838102 ) ) ;
#15469 = ADVANCED_FACE ( 'NONE', ( #59171 ), #30849, .T. ) ;
#15470 = CARTESIAN_POINT ( 'NONE',  ( -3.211159895383561391, 21.81249999863440792, -3.211159895383561835 ) ) ;
#15471 = VERTEX_POINT ( 'NONE', #41441 ) ;
#15472 = EDGE_LOOP ( 'NONE', ( #50168, #58303, #60312, #51993 ) ) ;
#15473 = CARTESIAN_POINT ( 'NONE',  ( -1.881053915767121554, 2.749999998634406584, -4.541265875000002339 ) ) ;
#15474 = CARTESIAN_POINT ( 'NONE',  ( -5.082755093536325042, 11.53124999795161010, -5.082755093536325930 ) ) ;
#15475 = CARTESIAN_POINT ( 'NONE',  ( -8.000000000000000000, 110.1875000040967905, 0.000000000000000000 ) ) ;
#15476 = CARTESIAN_POINT ( 'NONE',  ( -7.204075437095965206, -7.204075437095968759, 90.71875000204838102 ) ) ;
#15477 = CARTESIAN_POINT ( 'NONE',  ( -30.44569435410883429, 203.8125000013656063, 167.5543056458915885 ) ) ;
#15478 = AXIS2_PLACEMENT_3D ( 'NONE', #43285, #26295, #47828 ) ;
#15479 = ADVANCED_FACE ( 'NONE', ( #53501, #71199, #1820, #59530, #54247, #47821 ), #2181, .F. ) ;
#15480 = CARTESIAN_POINT ( 'NONE',  ( -2.828427124746192067, 3.625000000000000000, 2.828427124746190735 ) ) ;
#15481 = CARTESIAN_POINT ( 'NONE',  ( 4.000000000000000888, 18.68749999726881583, 1.656854249492384135 ) ) ;
#15482 = CARTESIAN_POINT ( 'NONE',  ( 1.881053915767122664, 8.124999998634406140, 4.541265875000001451 ) ) ;
#15483 = CARTESIAN_POINT ( 'NONE',  ( -4.000000000000015987, 200.5000000000000000, 142.0000000000000568 ) ) ;
#15484 = CIRCLE ( 'NONE', #51644, 7.000000000000000000 ) ;
#15485 = VERTEX_POINT ( 'NONE', #65169 ) ;
#15486 = CARTESIAN_POINT ( 'NONE',  ( 2.679491924311206308, 221.4583333333333144, 10.00000000000001421 ) ) ;
#15488 = CARTESIAN_POINT ( 'NONE',  ( -7.999999999999927169, 3.313708498984821116, 17.23655277982336642 ) ) ;
#15487 = CARTESIAN_POINT ( 'NONE',  ( -25.55430564589122611, 196.3125000013656063, 167.5543056458915032 ) ) ;
#15489 = AXIS2_PLACEMENT_3D ( 'NONE', #55533, #25703, #48723 ) ;
#15490 = CARTESIAN_POINT ( 'NONE',  ( -4.541265875000002339, 18.74999999863440436, -1.881053915767121998 ) ) ;
#15491 = CARTESIAN_POINT ( 'NONE',  ( 7.320508075688771044, 71.24999999317203958, 7.320508075688775484 ) ) ;
#15492 = CARTESIAN_POINT ( 'NONE',  ( 1.224646799147353454E-15, 300.0000000000000000, -10.00000000000000178 ) ) ;
#15493 = VERTEX_POINT ( 'NONE', #13481 ) ;
#15494 = ORIENTED_EDGE ( 'NONE', *, *, #6099, .F. ) ;
#15495 = CARTESIAN_POINT ( 'NONE',  ( 10.18810118749999916, 1.247682550866122264E-15, 99.90625000204838102 ) ) ;
#15496 = CARTESIAN_POINT ( 'NONE',  ( 30.82842712474620939, 204.2500000027312126, 172.8284271247460424 ) ) ;
#15497 = CARTESIAN_POINT ( 'NONE',  ( -29.43265458321760519, 201.1250000013656347, 173.4587341250003760 ) ) ;
#15498 = CARTESIAN_POINT ( 'NONE',  ( 7.778174593052021635, 7.778174593052023411, 106.9374999999999858 ) ) ;
#15499 = CARTESIAN_POINT ( 'NONE',  ( -3.458734124999959469, 206.7500000013655779, 199.4326545832176691 ) ) ;
#15500 = EDGE_CURVE ( 'NONE', #17357, #31653, #69449, .T. ) ;
#15501 = CARTESIAN_POINT ( 'NONE',  ( -8.660254037844390851, 112.9166666666666856, 4.999999999999998224 ) ) ;
#15502 = CARTESIAN_POINT ( 'NONE',  ( 3.313708498984765161, 107.4687500000000000, 7.999999999999998224 ) ) ;
#15503 = CARTESIAN_POINT ( 'NONE',  ( -4.721056650415998313, 292.7343750017069510, 4.721056650416000089 ) ) ;
#15504 = CARTESIAN_POINT ( 'NONE',  ( -4.401442555609577197E-16, 7.188101187499992051, 8.986552781871752771 ) ) ;
#15505 = EDGE_CURVE ( 'NONE', #46331, #56463, #64157, .T. ) ;
#15506 = ORIENTED_EDGE ( 'NONE', *, *, #5237, .F. ) ;
#15507 = CARTESIAN_POINT ( 'NONE',  ( 25.55430564589115505, 206.3125000013656063, 172.4456943541086957 ) ) ;
#15508 = CARTESIAN_POINT ( 'NONE',  ( -5.656854249492379694, 18.37499999590322020, -5.656854249492380582 ) ) ;
#15509 = CARTESIAN_POINT ( 'NONE',  ( -3.458734125000015425, 200.0000000013656347, 143.4326545832176976 ) ) ;
#15510 = CARTESIAN_POINT ( 'NONE',  ( 5.082755093536326818, 119.0937500020483810, 5.082755093536325042 ) ) ;
#15512 = CARTESIAN_POINT ( 'NONE',  ( -2.754378923186476579E-14, 202.4375000013656063, 145.4587341250000350 ) ) ;
#15511 = CARTESIAN_POINT ( 'NONE',  ( -5.000000000000000000, 50.64189880742059557, 41.08656465431948845 ) ) ;
#15513 = CARTESIAN_POINT ( 'NONE',  ( -6.951808397369817780E-16, 252.9687500034140157, -11.35316468749999963 ) ) ;
#15514 = CARTESIAN_POINT ( 'NONE',  ( -5.447319899895621376, -4.689936522885654213, 0.2819290645437558807 ) ) ;
#15515 = CARTESIAN_POINT ( 'NONE',  ( -5.676582343750006032, 4.114583329919350163, 9.832129032723418760 ) ) ;
#15516 = EDGE_CURVE ( 'NONE', #44642, #8416, #13327, .T. ) ;
#15517 = CARTESIAN_POINT ( 'NONE',  ( -2.977408999572647819, -7.188101187499990274, 2.142802781871754103 ) ) ;
#15518 = CARTESIAN_POINT ( 'NONE',  ( -11.35316468750000141, 208.5937499965860411, -1.390361679473963753E-15 ) ) ;
#15519 = FACE_OUTER_BOUND ( 'NONE', #59940, .T. ) ;
#15520 = CARTESIAN_POINT ( 'NONE',  ( 4.541265875000001451, 5.249999998634406140, 1.881053915767124440 ) ) ;
#15521 = DIRECTION ( 'NONE',  ( -0.000000000000000000, -0.000000000000000000, 1.000000000000000000 ) ) ;
#15523 = DIRECTION ( 'NONE',  ( 0.000000000000000000, 0.000000000000000000, 1.000000000000000000 ) ) ;
#15522 = CARTESIAN_POINT ( 'NONE',  ( -8.000000000000001776, 26.15624999590322730, 3.313708498984759387 ) ) ;
#15524 = ORIENTED_EDGE ( 'NONE', *, *, #37103, .T. ) ;
#15525 = CARTESIAN_POINT ( 'NONE',  ( -2.839093476692135984E-14, 199.9375000013656063, 138.5412658750000503 ) ) ;
#15526 = CARTESIAN_POINT ( 'NONE',  ( 3.042071309553159519, 4.739583329919349275, 11.35316468750000141 ) ) ;
#15527 = CARTESIAN_POINT ( 'NONE',  ( 11.00000000000000000, 1.347111479062088405E-15, 96.43750000409677625 ) ) ;
#15528 = CARTESIAN_POINT ( 'NONE',  ( 2.775557561562891351E-14, 210.0000000000000284, 198.0000000000000284 ) ) ;
#15529 = CARTESIAN_POINT ( 'NONE',  ( -25.55430564589111953, 200.0625000013656063, 172.4456943541091505 ) ) ;
#15530 = FACE_OUTER_BOUND ( 'NONE', #60029, .T. ) ;
#15532 = CARTESIAN_POINT ( 'NONE',  ( -3.042071309553163960, 2.239583329919349719, -11.35316468749999963 ) ) ;
#15531 = CARTESIAN_POINT ( 'NONE',  ( -5.082755093536324154, 118.3437500020483810, 5.082755093536326818 ) ) ;
#15533 = CARTESIAN_POINT ( 'NONE',  ( 7.999999999999991118, 9.797174393178815797E-16, 28.58030277982336642 ) ) ;
#15534 = CARTESIAN_POINT ( 'NONE',  ( 6.951808397369818766E-16, 117.0312499965860269, -11.35316468750000141 ) ) ;
#15535 = AXIS2_PLACEMENT_3D ( 'NONE', #73503, #9392, #67850 ) ;
#15536 = CARTESIAN_POINT ( 'NONE',  ( 2.679491924311228956, 87.91666665983868256, -10.00000000000000000 ) ) ;
#15537 = CARTESIAN_POINT ( 'NONE',  ( -2.977408999572650927, 121.2500000020483952, -7.188101187500001821 ) ) ;
#15538 = CARTESIAN_POINT ( 'NONE',  ( 1.881053915767122664, 19.24999999863440436, 4.541265875000001451 ) ) ;
#15539 = CARTESIAN_POINT ( 'NONE',  ( 0.7343025909353769753, -9.968355046870113867, -0.5590800469813878015 ) ) ;
#15540 = CARTESIAN_POINT ( 'NONE',  ( -12.00000000000000178, 2.352228297136951252, -0.1238145317436992882 ) ) ;
#15541 = EDGE_LOOP ( 'NONE', ( #41570, #71865, #26652 ) ) ;
#15542 = CARTESIAN_POINT ( 'NONE',  ( -5.000000000000007994, 118.3333333333333428, 8.660254037844390851 ) ) ;
#15543 = CARTESIAN_POINT ( 'NONE',  ( -4.088227598258586603E-16, 289.3593750017070079, -6.676582343750001591 ) ) ;
#15544 = CARTESIAN_POINT ( 'NONE',  ( 7.320508075688774596, 187.4999999931720254, -7.320508075688774596 ) ) ;
#15545 = CARTESIAN_POINT ( 'NONE',  ( -5.656854249492375253, 5.656854249492375253, 0.8303027839201455595 ) ) ;
#15546 = CARTESIAN_POINT ( 'NONE',  ( -1.656854249492399234, 201.3125000027311842, 201.9999999999999432 ) ) ;
#15547 = CIRCLE ( 'NONE', #49256, 12.00000000000000000 ) ;
#15548 = CARTESIAN_POINT ( 'NONE',  ( -7.320508075688778149, 209.9999999931719969, 7.320508075688769267 ) ) ;
#15549 = CARTESIAN_POINT ( 'NONE',  ( -9.832129032723418760, 258.4895833367473301, -5.676582343749998927 ) ) ;
#15550 = CARTESIAN_POINT ( 'NONE',  ( -10.18810118749999916, 0.000000000000000000, 105.5312500020483810 ) ) ;
#15551 = ORIENTED_EDGE ( 'NONE', *, *, #19674, .F. ) ;
#15552 =( BOUNDED_CURVE ( )  B_SPLINE_CURVE ( 2, ( #65048, #42407, #65425, #29996, #69620, #41685, #30729, #12270, #12633 ),
 .UNSPECIFIED., .F., .F. ) 
 B_SPLINE_CURVE_WITH_KNOTS ( ( 3, 2, 2, 2, 3 ),
 ( 0.5138888888888888395, 0.5208333333333333703, 0.5277777777777777901, 0.5347222222222222099, 0.5416666666666666297 ),
 .UNSPECIFIED. ) 
 CURVE ( )  GEOMETRIC_REPRESENTATION_ITEM ( )  RATIONAL_B_SPLINE_CURVE ( ( 1.000000000000000000, 0.9238795325112867385, 1.000000000000000000, 0.9238795325112867385, 1.000000000000000000, 0.9238795325112867385, 1.000000000000000000, 0.9238795325112867385, 1.000000000000000000 ) ) 
 REPRESENTATION_ITEM ( '' )  );
#15553 = CARTESIAN_POINT ( 'NONE',  ( 8.660254037844385522, 156.4583333265053966, 5.000000000000005329 ) ) ;
#15554 = CARTESIAN_POINT ( 'NONE',  ( -5.676582343750006032, 159.4270833299193555, 9.832129032723418760 ) ) ;
#15555 = SURFACE_STYLE_USAGE ( .BOTH. , #56690 ) ;
#15556 = CARTESIAN_POINT ( 'NONE',  ( 2.445694354108840063, 206.0625000013656063, 200.4456943541088663 ) ) ;
#15557 = CARTESIAN_POINT ( 'NONE',  ( -3.042071309553173730, 74.63541666325268409, 11.35316468749999785 ) ) ;
#15558 = ORIENTED_EDGE ( 'NONE', *, *, #22614, .F. ) ;
#15559 = CARTESIAN_POINT ( 'NONE',  ( 10.18810118749999916, 1.247682550866122264E-15, 116.4062500020483810 ) ) ;
#15560 = CARTESIAN_POINT ( 'NONE',  ( -4.541265875000002339, 7.937499998634407028, -5.561446717895856393E-16 ) ) ;
#15561 = VERTEX_POINT ( 'NONE', #21383 ) ;
#15562 = CARTESIAN_POINT ( 'NONE',  ( 7.188101187499999156, 18.37499999795161187, 2.977408999572654924 ) ) ;
#15563 = CARTESIAN_POINT ( 'NONE',  ( -6.000000000000000888, 287.1250000034140157, 2.485281374238575758 ) ) ;
#15564 = CYLINDRICAL_SURFACE ( 'NONE', #25677, 3.999999999999976019 ) ;
#15565 = CARTESIAN_POINT ( 'NONE',  ( 7.188101187499999156, 17.24999999795162253, 2.977408999572654924 ) ) ;
#15566 = CARTESIAN_POINT ( 'NONE',  ( 11.00000000000013323, -4.556349186103911819, 103.8437500040967763 ) ) ;
#15567 =( BOUNDED_CURVE ( )  B_SPLINE_CURVE ( 2, ( #32241, #66181, #26935, #37524, #60524, #31859, #43536, #48825, #54883 ),
 .UNSPECIFIED., .F., .F. ) 
 B_SPLINE_CURVE_WITH_KNOTS ( ( 3, 2, 2, 2, 3 ),
 ( 0.6166666666666672514, 0.6250000000000005551, 0.6333333333333337478, 0.6416666666666671626, 0.6500000000000004663 ),
 .UNSPECIFIED. ) 
 CURVE ( )  GEOMETRIC_REPRESENTATION_ITEM ( )  RATIONAL_B_SPLINE_CURVE ( ( 0.9999999999999948930, 0.9238795325112918455, 1.000000000000000000, 0.9238795325112867385, 1.000000000000000000, 0.9238795325112867385, 1.000000000000000000, 0.9238795325112826307, 1.000000000000003997 ) ) 
 REPRESENTATION_ITEM ( '' )  );
#15568 = CARTESIAN_POINT ( 'NONE',  ( 10.18810118750000093, -4.220049686691933921, 112.1875000020483810 ) ) ;
#15569 = PRODUCT ( 'barrel', 'barrel', '', ( #21802 ) ) ;
#15570 = CARTESIAN_POINT ( 'NONE',  ( 0.000000000000000000, 125.0000000000000000, 0.000000000000000000 ) ) ;
#15571 = CARTESIAN_POINT ( 'NONE',  ( -4.000000000000001776, 6.187499997268813168, -1.656854249492381470 ) ) ;
#15572 = CARTESIAN_POINT ( 'NONE',  ( 24.00000000000000711, 206.9375000027312410, 171.6568542494923122 ) ) ;
#15573 = ORIENTED_EDGE ( 'NONE', *, *, #40363, .T. ) ;
#15574 = CARTESIAN_POINT ( 'NONE',  ( 3.458734125000016313, 206.8750000013656347, 199.4326545832176691 ) ) ;
#15575 = CARTESIAN_POINT ( 'NONE',  ( -28.00000000000007461, 195.1250000027311842, 166.0000000000003695 ) ) ;
#15576 = CARTESIAN_POINT ( 'NONE',  ( -7.204075437095965206, -7.204075437095968759, 71.21875000204836681 ) ) ;
#15577 = CARTESIAN_POINT ( 'NONE',  ( 3.211159895383561835, 5.437499998634407028, -3.211159895383561835 ) ) ;
#15578 = AXIS2_PLACEMENT_3D ( 'NONE', #11820, #17849, #34857 ) ;
#15579 = CARTESIAN_POINT ( 'NONE',  ( 3.313708498984815343, 94.71875000409676204, -7.999999999999944933 ) ) ;
#15580 = CARTESIAN_POINT ( 'NONE',  ( 5.082755093536320601, -5.082755093536318824, 23.04905278187175455 ) ) ;
#15581 = ADVANCED_BREP_SHAPE_REPRESENTATION ( '', ( #67429, #57354 ), #40540 ) ;
#15582 = ORIENTED_EDGE ( 'NONE', *, *, #25290, .T. ) ;
#15583 = CARTESIAN_POINT ( 'NONE',  ( -1.656854249492381248, 21.31250000000000000, -4.000000000000001776 ) ) ;
#15584 = ORIENTED_EDGE ( 'NONE', *, *, #9847, .T. ) ;
#15585 = CARTESIAN_POINT ( 'NONE',  ( -10.18810118749999916, 4.220049686691934809, 114.0625000020483668 ) ) ;
#15586 = CARTESIAN_POINT ( 'NONE',  ( -2.828427124746190735, 18.37500000000000000, -2.828427124746191623 ) ) ;
#15587 = CARTESIAN_POINT ( 'NONE',  ( -1.432654583217607858, 203.6250000013656063, 201.4587341250000065 ) ) ;
#15588 = CARTESIAN_POINT ( 'NONE',  ( 24.54126587499998280, 201.1250000013656347, 168.5673454167822740 ) ) ;
#15589 = CARTESIAN_POINT ( 'NONE',  ( 5.000000000000001776, 70.83333333333332860, -8.660254037844389075 ) ) ;
#15590 = AXIS2_PLACEMENT_3D ( 'NONE', #41450, #58442, #63707 ) ;
#15591 = CARTESIAN_POINT ( 'NONE',  ( 2.977408999572650039, 97.06250000204838102, -7.188101187500001821 ) ) ;
#15592 = CARTESIAN_POINT ( 'NONE',  ( -6.000000000000001776, 291.0000000000000000, 0.000000000000000000 ) ) ;
#15593 = CARTESIAN_POINT ( 'NONE',  ( 23.99999999999999289, 205.8750000027312126, 169.9999999999999432 ) ) ;
#15594 = ADVANCED_FACE ( 'NONE', ( #9710 ), #54618, .F. ) ;
#15595 = VERTEX_POINT ( 'NONE', #44406 ) ;
#15596 = CARTESIAN_POINT ( 'NONE',  ( -5.676582343749992710, 219.7395833367473301, 9.832129032723422313 ) ) ;
#15597 = CARTESIAN_POINT ( 'NONE',  ( -7.778174593052023411, 7.778174593052023411, 88.00000000409677625 ) ) ;
#15598 = CARTESIAN_POINT ( 'NONE',  ( -2.751064625579944321E-14, 194.8750000027311842, 146.0000000000000284 ) ) ;
#15599 = DIRECTION ( 'NONE',  ( 8.659560562354941486E-17, 0.7071067811865469066, -0.7071067811865482389 ) ) ;
#15600 = CARTESIAN_POINT ( 'NONE',  ( 4.898587196589412829E-16, 22.87500000000000355, -8.000000000000000000 ) ) ;
#15601 = CARTESIAN_POINT ( 'NONE',  ( -7.320508075688771932, 254.3750000000000284, -7.320508075688771932 ) ) ;
#15602 = CARTESIAN_POINT ( 'NONE',  ( -7.320508075688801242, 76.87500000000002842, -7.320508075688802130 ) ) ;
#15603 = CARTESIAN_POINT ( 'NONE',  ( -1.836970198721029983E-15, 188.7500000000000000, 10.00000000000000178 ) ) ;
#15604 = EDGE_CURVE ( 'NONE', #69825, #59062, #6139, .T. ) ;
#15605 = CARTESIAN_POINT ( 'NONE',  ( -7.188101187499992051, 2.977408999572646930, 21.26780278187175810 ) ) ;
#15606 = CARTESIAN_POINT ( 'NONE',  ( -8.311093377946841443, 154.2187499965859843, 8.311093377946830785 ) ) ;
#15607 = DIRECTION ( 'NONE',  ( -0.000000000000000000, -1.000000000000000000, -0.000000000000000000 ) ) ;
#15608 = CARTESIAN_POINT ( 'NONE',  ( -12.00000000000000000, -6.928203230275527424, -14.00000000000000178 ) ) ;
#15609 = CARTESIAN_POINT ( 'NONE',  ( 7.320508075688905159, 154.3750000000001137, 7.320508075688908711 ) ) ;
#15611 = CARTESIAN_POINT ( 'NONE',  ( 1.469576158976823947E-15, 109.0625000040967905, 8.000000000000000000 ) ) ;
#15610 = CARTESIAN_POINT ( 'NONE',  ( -4.000000000000015987, 202.6250000027312126, 142.0000000000000568 ) ) ;
#15612 = ORIENTED_EDGE ( 'NONE', *, *, #23367, .T. ) ;
#15613 = CARTESIAN_POINT ( 'NONE',  ( -11.35316468750000141, 28.80208332991935194, 3.042071309553159963 ) ) ;
#15614 = CARTESIAN_POINT ( 'NONE',  ( 10.00000000000000178, 97.08333332650536818, -2.679491924311226736 ) ) ;
#15616 = CARTESIAN_POINT ( 'NONE',  ( 28.00000000000001776, 199.5000000000000000, 165.9999999999998863 ) ) ;
#15615 = CARTESIAN_POINT ( 'NONE',  ( -10.18810118749999916, 0.000000000000000000, 117.1562500020483810 ) ) ;
#15617 = CARTESIAN_POINT ( 'NONE',  ( -4.556349186104048599, -10.99999999999999822, 79.28125000000000000 ) ) ;
#15618 = CARTESIAN_POINT ( 'NONE',  ( 1.432654583217607858, 201.6250000013656063, 138.5412658750000787 ) ) ;
#15619 = CARTESIAN_POINT ( 'NONE',  ( -7.320508075688773708, 53.74999999317203248, -7.320508075688774596 ) ) ;
#15620 = CARTESIAN_POINT ( 'NONE',  ( 5.082755093536326818, 103.7187500020483810, 5.082755093536325042 ) ) ;
#15621 = CARTESIAN_POINT ( 'NONE',  ( 3.211159895383561835, 8.562499998634407916, -3.211159895383561835 ) ) ;
#15622 = CARTESIAN_POINT ( 'NONE',  ( -6.000000000000001776, 299.5312500017070079, 0.000000000000000000 ) ) ;
#15623 = CARTESIAN_POINT ( 'NONE',  ( 3.313708498984762496, -7.999999999999989342, 10.29905277982336465 ) ) ;
#15624 = CARTESIAN_POINT ( 'NONE',  ( 5.000000000000001776, 165.8333333333333428, -8.660254037844389075 ) ) ;
#15625 = VERTEX_POINT ( 'NONE', #38760 ) ;
#15626 = ORIENTED_EDGE ( 'NONE', *, *, #66984, .F. ) ;
#15627 = CARTESIAN_POINT ( 'NONE',  ( -2.679491924311226292, 221.4583333333333428, -10.00000000000000178 ) ) ;
#15628 = CARTESIAN_POINT ( 'NONE',  ( -3.458734124999960358, 194.6875000013655779, 198.0000000000000284 ) ) ;
#15629 = DIRECTION ( 'NONE',  ( 0.000000000000000000, 0.000000000000000000, -1.000000000000000000 ) ) ;
#15630 = CARTESIAN_POINT ( 'NONE',  ( 11.35316468749999963, 221.5104166700806161, 3.042071309553159519 ) ) ;
#15631 = CARTESIAN_POINT ( 'NONE',  ( 11.35316468750000141, 140.7812499965860411, 0.000000000000000000 ) ) ;
#15632 = ORIENTED_EDGE ( 'NONE', *, *, #10674, .T. ) ;
#15633 = CARTESIAN_POINT ( 'NONE',  ( 7.999999999667481099, -7.293937043860970585E-05, 4.767800658666735636 ) ) ;
#15634 = CARTESIAN_POINT ( 'NONE',  ( -10.18810118749999738, -4.220049686691941915, 91.75000000204836681 ) ) ;
#15635 = CARTESIAN_POINT ( 'NONE',  ( -3.999999999999960032, 207.0000000000000284, 198.0000000000000284 ) ) ;
#15637 = CARTESIAN_POINT ( 'NONE',  ( -5.676582343749998039, 122.4479166632526983, -9.832129032723420536 ) ) ;
#15636 = CARTESIAN_POINT ( 'NONE',  ( 8.660254037844385522, 247.9166666666666856, -5.000000000000003553 ) ) ;
#15638 = CARTESIAN_POINT ( 'NONE',  ( 12.00000000000000355, -6.928203230275539859, -1.071796769724504550 ) ) ;
#15639 = EDGE_LOOP ( 'NONE', ( #62403, #45291, #14953, #23691 ) ) ;
#15640 = AXIS2_PLACEMENT_3D ( 'NONE', #68775, #69526, #29534 ) ;
#15641 = LINE ( 'NONE', #27336, #23842 ) ;
#15642 = CARTESIAN_POINT ( 'NONE',  ( 48.25721876928392362, 41.31978892101862755, 61.69279049735350640 ) ) ;
#15643 = CARTESIAN_POINT ( 'NONE',  ( 8.311093377946837890, 116.7187499965859985, -8.311093377946837890 ) ) ;
#15644 = CARTESIAN_POINT ( 'NONE',  ( 3.458734125000016313, 203.8750000013656063, 199.4326545832176976 ) ) ;
#15645 = CARTESIAN_POINT ( 'NONE',  ( -7.188101187500000044, 18.09374999795161187, -8.802885111219163269E-16 ) ) ;
#15646 = CARTESIAN_POINT ( 'NONE',  ( -7.204075437095967871, 7.204075437095967871, 84.34375000204836681 ) ) ;
#15647 = CARTESIAN_POINT ( 'NONE',  ( -11.35316468750000141, 28.80208332991935194, 3.042071309553159963 ) ) ;
#15648 = ORIENTED_EDGE ( 'NONE', *, *, #25302, .T. ) ;
#15649 = CARTESIAN_POINT ( 'NONE',  ( -4.977777815167797826, -10.98248509899778291, -1.005597514980305363E-14 ) ) ;
#15650 = CARTESIAN_POINT ( 'NONE',  ( -8.008118988124989457, -3.317071493978883900, 17.60686528394063188 ) ) ;
#15651 = CARTESIAN_POINT ( 'NONE',  ( -7.999999999999991118, 3.313708498984757167, 23.42405278392015333 ) ) ;
#15652 = AXIS2_PLACEMENT_3D ( 'NONE', #27693, #37912, #33014 ) ;
#15653 = CARTESIAN_POINT ( 'NONE',  ( 2.828427124746152987, 201.1250000000000284, 139.1715728752538723 ) ) ;
#15654 = CARTESIAN_POINT ( 'NONE',  ( -2.977408999572654480, 4.499999997951610986, 7.188101187499999156 ) ) ;
#15655 = CARTESIAN_POINT ( 'NONE',  ( -6.676582343750003368, 290.3906250017070647, -2.765530957081996810 ) ) ;
#15656 = CARTESIAN_POINT ( 'NONE',  ( 0.000000000000000000, 0.000000000000000000, 0.000000000000000000 ) ) ;
#15657 = CARTESIAN_POINT ( 'NONE',  ( -2.977408999572650039, 1.312499997951610098, -7.188101187500001821 ) ) ;
#15658 = ORIENTED_EDGE ( 'NONE', *, *, #43477, .T. ) ;
#15659 = CARTESIAN_POINT ( 'NONE',  ( -11.35316468750000141, 148.5937499965860411, -1.390361679473963753E-15 ) ) ;
#15660 = CARTESIAN_POINT ( 'NONE',  ( -10.18810118749999738, -4.220049686691941915, 76.75000000204838102 ) ) ;
#15661 =( BOUNDED_CURVE ( )  B_SPLINE_CURVE ( 2, ( #4813, #51948, #22893, #51193, #45166, #39875, #6305, #34238, #23266 ),
 .UNSPECIFIED., .F., .F. ) 
 B_SPLINE_CURVE_WITH_KNOTS ( ( 3, 2, 2, 2, 3 ),
 ( 0.2613636363636363535, 0.2670454545454545303, 0.2727272727272727071, 0.2784090909090908839, 0.2840909090909091161 ),
 .UNSPECIFIED. ) 
 CURVE ( )  GEOMETRIC_REPRESENTATION_ITEM ( )  RATIONAL_B_SPLINE_CURVE ( ( 1.000000000000000000, 0.9238795325112867385, 1.000000000000000000, 0.9238795325112867385, 1.000000000000000000, 0.9238795325112867385, 1.000000000000000000, 0.9238795325112867385, 1.000000000000000000 ) ) 
 REPRESENTATION_ITEM ( '' )  );
#15662 = CARTESIAN_POINT ( 'NONE',  ( -31.45873412500001010, 208.8750000013656347, 168.5673454167827572 ) ) ;
#15663 = CARTESIAN_POINT ( 'NONE',  ( -30.64284399271078740, 5.999999999999950262, 174.6921329945331536 ) ) ;
#15664 = CARTESIAN_POINT ( 'NONE',  ( -1.881053915767124440, 14.12499999863440969, 4.541265875000001451 ) ) ;
#15665 = VERTEX_POINT ( 'NONE', #55366 ) ;
#15666 = CARTESIAN_POINT ( 'NONE',  ( -3.999999999999960032, 202.0625000027312410, 196.3431457505076594 ) ) ;
#15667 = CARTESIAN_POINT ( 'NONE',  ( -2.828427124746208943, 209.6250000000000284, 144.8284271247462129 ) ) ;
#15668 = CARTESIAN_POINT ( 'NONE',  ( -25.17157287525386167, 207.0000000027312126, 167.1715728752541281 ) ) ;
#15669 = EDGE_CURVE ( 'NONE', #46255, #33515, #43654, .T. ) ;
#15670 = EDGE_CURVE ( 'NONE', #4192, #61043, #15006, .T. ) ;
#15671 = B_SPLINE_CURVE_WITH_KNOTS ( 'NONE', 1,
 ( #17225, #57996 ),
 .UNSPECIFIED., .F., .F.,
 ( 2, 2 ),
 ( 0.000000000000000000, 1.000000000000000000 ),
 .UNSPECIFIED. ) ;
#15672 = CARTESIAN_POINT ( 'NONE',  ( 0.000000000000000000, 300.0000000000000000, 10.00000000000000178 ) ) ;
#15673 = ORIENTED_EDGE ( 'NONE', *, *, #18285, .F. ) ;
#15674 = CARTESIAN_POINT ( 'NONE',  ( -2.977408999572654480, 10.49999999795161010, 7.188101187499999156 ) ) ;
#15675 = CARTESIAN_POINT ( 'NONE',  ( -14.29549407509282410, -20.99323513088765836, 197.5084943229587964 ) ) ;
#15676 = DIRECTION ( 'NONE',  ( -0.000000000000000000, -1.000000000000000000, -4.283267841918042741E-17 ) ) ;
#15677 = CARTESIAN_POINT ( 'NONE',  ( 11.35316468749999963, 185.9895833299193839, -3.042071309553165293 ) ) ;
#15678 = EDGE_CURVE ( 'NONE', #65025, #21899, #27414, .T. ) ;
#15679 = CARTESIAN_POINT ( 'NONE',  ( -2.977408999572650927, 110.7500000020483668, -7.188101187500001821 ) ) ;
#15680 = LINE ( 'NONE', #49268, #42560 ) ;
#15681 = CARTESIAN_POINT ( 'NONE',  ( -2.765530957081998142, 289.6406250017069510, 6.676582343750000703 ) ) ;
#15683 = CARTESIAN_POINT ( 'NONE',  ( -5.000000000000007105, 68.33333333333335702, 8.660254037844389075 ) ) ;
#15682 = CARTESIAN_POINT ( 'NONE',  ( -8.000000000000000000, 111.5937500040967905, -3.313708498984761164 ) ) ;
#15684 = ORIENTED_EDGE ( 'NONE', *, *, #25100, .T. ) ;
#15686 = CARTESIAN_POINT ( 'NONE',  ( 9.832129032723420536, 260.9895833367473301, 5.676582343749996262 ) ) ;
#15685 = AXIS2_PLACEMENT_3D ( 'NONE', #3723, #3346, #50112 ) ;
#15687 = CARTESIAN_POINT ( 'NONE',  ( -7.188101187499992051, 0.000000000000000000, 25.86155278187175810 ) ) ;
#15688 = CARTESIAN_POINT ( 'NONE',  ( -7.778174593052020747, -7.778174593052023411, 92.68749999999998579 ) ) ;
#15689 = CARTESIAN_POINT ( 'NONE',  ( -8.000000000000005329, 0.000000000000000000, -14.77459999999999951 ) ) ;
#15690 = DIRECTION ( 'NONE',  ( 1.000000000000000000, -0.000000000000000000, -0.000000000000000000 ) ) ;
#15691 = CARTESIAN_POINT ( 'NONE',  ( 3.458734125000016757, 197.1250000013656347, 199.4326545832176691 ) ) ;
#15692 = CARTESIAN_POINT ( 'NONE',  ( -10.00000000000000000, 142.2916666666666856, -2.679491924311229845 ) ) ;
#15693 = CARTESIAN_POINT ( 'NONE',  ( 10.99999999999999467, -4.556349186104053040, 115.8437500040967763 ) ) ;
#15694 = FACE_OUTER_BOUND ( 'NONE', #43375, .T. ) ;
#15695 = CARTESIAN_POINT ( 'NONE',  ( 5.656854249492381470, 94.06250000000000000, 5.656854249492379694 ) ) ;
#15696 = CARTESIAN_POINT ( 'NONE',  ( 3.042071309553159519, 115.0520833299193555, 11.35316468750000141 ) ) ;
#15697 = CARTESIAN_POINT ( 'NONE',  ( 6.123233995736767268E-16, 213.1249999931720538, -10.00000000000000178 ) ) ;
#15698 = CARTESIAN_POINT ( 'NONE',  ( -4.556349186104047710, -10.99999999999999822, 70.28124999999998579 ) ) ;
#15701 = FACE_OUTER_BOUND ( 'NONE', #69866, .T. ) ;
#15700 = CARTESIAN_POINT ( 'NONE',  ( 28.00000000000001776, 202.4375000013656063, 173.4587341249998929 ) ) ;
#15699 = CARTESIAN_POINT ( 'NONE',  ( 28.00000000000002132, 199.1875000013655779, 166.5412658749999082 ) ) ;
#15702 = ORIENTED_EDGE ( 'NONE', *, *, #41485, .T. ) ;
#15703 = CARTESIAN_POINT ( 'NONE',  ( -8.000000000000000000, 20.15625000000000355, -3.313708498984762496 ) ) ;
#15704 = EDGE_CURVE ( 'NONE', #69862, #4108, #44036, .T. ) ;
#15705 = CARTESIAN_POINT ( 'NONE',  ( 2.485281374238838215, 287.3750000034139020, 5.999999999999736211 ) ) ;
#15706 = CARTESIAN_POINT ( 'NONE',  ( 28.00000000000002132, 200.1875000013656063, 166.5412658749999082 ) ) ;
#15707 = CARTESIAN_POINT ( 'NONE',  ( 11.35316468749999963, 201.3020833299193839, -3.042071309553165293 ) ) ;
#15708 = DIRECTION ( 'NONE',  ( -0.000000000000000000, 1.000000000000000000, -0.000000000000000000 ) ) ;
#15709 = CARTESIAN_POINT ( 'NONE',  ( 1.881053915767121776, 16.49999999863440436, -4.541265875000002339 ) ) ;
#15710 = CARTESIAN_POINT ( 'NONE',  ( 4.471435261904115777, -50.48103707412492724, 40.99880869399019190 ) ) ;
#15711 = CARTESIAN_POINT ( 'NONE',  ( -3.313708498984758943, -7.999999999999989342, 25.11155277982337353 ) ) ;
#15713 = LINE ( 'NONE', #61379, #1425 ) ;
#15712 = CARTESIAN_POINT ( 'NONE',  ( 7.320508075688767491, 184.3750000000000000, 7.320508075688771044 ) ) ;
#15714 = CARTESIAN_POINT ( 'NONE',  ( -3.042071309553173730, 89.32291666325268409, 11.35316468749999785 ) ) ;
#15715 = ORIENTED_EDGE ( 'NONE', *, *, #64606, .T. ) ;
#15716 = FACE_OUTER_BOUND ( 'NONE', #42555, .T. ) ;
#15717 = CARTESIAN_POINT ( 'NONE',  ( -7.188101187500000044, 17.71874999795161187, -8.802885111219163269E-16 ) ) ;
#15718 = CARTESIAN_POINT ( 'NONE',  ( -9.999999999999998224, 223.3333333401613174, 2.679491924311235174 ) ) ;
#15719 = CARTESIAN_POINT ( 'NONE',  ( 5.676582343749997150, 257.5520833367473301, -9.832129032723418760 ) ) ;
#15720 = CARTESIAN_POINT ( 'NONE',  ( 8.311093377946834337, 95.15624999658601268, 8.311093377946839666 ) ) ;
#15721 = VERTEX_POINT ( 'NONE', #25913 ) ;
#15722 = CARTESIAN_POINT ( 'NONE',  ( 8.660254037844385522, 206.4583333265053682, 5.000000000000005329 ) ) ;
#15723 = CARTESIAN_POINT ( 'NONE',  ( 1.871523826299183495E-15, -10.18810118749999916, 110.0312500020483668 ) ) ;
#15724 = CARTESIAN_POINT ( 'NONE',  ( -29.43265458321766559, 196.7500000013656063, 166.5412658750003629 ) ) ;
#15725 = CARTESIAN_POINT ( 'NONE',  ( -2.445694354108784108, 203.5625000013656063, 195.5543056458912190 ) ) ;
#15726 = CARTESIAN_POINT ( 'NONE',  ( -2.751064625579944321E-14, 203.8750000027312126, 146.0000000000000284 ) ) ;
#15728 = CARTESIAN_POINT ( 'NONE',  ( -5.676582343750006032, 84.11458332991935549, 9.832129032723418760 ) ) ;
#15727 = CARTESIAN_POINT ( 'NONE',  ( -28.00000000000008171, 207.1250000027312126, 166.0000000000003695 ) ) ;
#15729 = CARTESIAN_POINT ( 'NONE',  ( 7.999999999999991118, 3.313708498984757611, 12.36155278392014445 ) ) ;
#15730 = CARTESIAN_POINT ( 'NONE',  ( -24.54126587499999346, 202.4375000013656063, 170.0000000000003411 ) ) ;
#15731 = FACE_OUTER_BOUND ( 'NONE', #42740, .T. ) ;
#15732 = AXIS2_PLACEMENT_3D ( 'NONE', #74634, #58414, #69720 ) ;
#15733 = EDGE_CURVE ( 'NONE', #14756, #49450, #71848, .T. ) ;
#15734 = CARTESIAN_POINT ( 'NONE',  ( -2.679491924311225848, 188.3333333265053682, -10.00000000000000178 ) ) ;
#15735 = CARTESIAN_POINT ( 'NONE',  ( 4.242640687119285658, 296.6875000034139589, -4.242640687119286547 ) ) ;
#15736 = CARTESIAN_POINT ( 'NONE',  ( -3.042071309553173730, 79.63541666325268409, 11.35316468749999785 ) ) ;
#15737 = CARTESIAN_POINT ( 'NONE',  ( -6.676582343750000703, 292.5156250017068942, 2.765530957082001251 ) ) ;
#15738 = CARTESIAN_POINT ( 'NONE',  ( -4.220049686691937474, -10.18810118749999738, 98.31250000204836681 ) ) ;
#15739 = CARTESIAN_POINT ( 'NONE',  ( -11.35316468750000141, 213.4895833299193839, 3.042071309553159963 ) ) ;
#15740 = ORIENTED_EDGE ( 'NONE', *, *, #40052, .T. ) ;
#15741 = CARTESIAN_POINT ( 'NONE',  ( -7.999999999961167951, -1.666173683171983354E-05, 1.018425797410095646 ) ) ;
#15742 = DIRECTION ( 'NONE',  ( 1.577021341797097560E-16, -1.000000000000000000, 0.000000000000000000 ) ) ;
#15743 = CARTESIAN_POINT ( 'NONE',  ( -3.673940397442060854E-16, 291.7500000000000000, -6.000000000000001776 ) ) ;
#15744 = CARTESIAN_POINT ( 'NONE',  ( -11.35316468749999785, 208.0729166632526983, -3.042071309553167957 ) ) ;
#15745 = CARTESIAN_POINT ( 'NONE',  ( -7.320508075688771932, 227.5000000068279462, -7.320508075688771932 ) ) ;
#15746 = ORIENTED_EDGE ( 'NONE', *, *, #20482, .F. ) ;
#15747 = CARTESIAN_POINT ( 'NONE',  ( -11.35316468749999785, 193.3854166632526415, -3.042071309553167957 ) ) ;
#15748 = CARTESIAN_POINT ( 'NONE',  ( 1.320432766682872962E-15, -7.188101187499992051, 16.86155278187175810 ) ) ;
#15749 = CARTESIAN_POINT ( 'NONE',  ( -24.54126587500000412, 207.2500000013655779, 168.5673454167827003 ) ) ;
#15750 = CARTESIAN_POINT ( 'NONE',  ( -5.656854249492379694, 14.06250000000000178, -5.656854249492380582 ) ) ;
#15751 = ORIENTED_EDGE ( 'NONE', *, *, #69177, .F. ) ;
#15752 = EDGE_CURVE ( 'NONE', #54774, #21472, #66, .T. ) ;
#15753 = AXIS2_PLACEMENT_3D ( 'NONE', #56480, #4796, #40231 ) ;
#15754 = CARTESIAN_POINT ( 'NONE',  ( 5.656854249492381470, 89.75000000409677625, 5.656854249492379694 ) ) ;
#15755 = CARTESIAN_POINT ( 'NONE',  ( -10.00000000000000000, 12.29166666666666785, -2.679491924311229845 ) ) ;
#15756 = EDGE_CURVE ( 'NONE', #14923, #58023, #58878, .T. ) ;
#15757 = CARTESIAN_POINT ( 'NONE',  ( -4.220049686691935698, 10.18810118749999916, 78.25000000204836681 ) ) ;
#15758 = VERTEX_POINT ( 'NONE', #5169 ) ;
#15759 = CARTESIAN_POINT ( 'NONE',  ( 4.000000000000001776, 19.06250000000000000, -1.656854249492381248 ) ) ;
#15760 = CARTESIAN_POINT ( 'NONE',  ( 4.541265875000002339, 19.31249999863440436, 0.000000000000000000 ) ) ;
#15761 = AXIS2_PLACEMENT_3D ( 'NONE', #30654, #47992, #65351 ) ;
#15762 = CARTESIAN_POINT ( 'NONE',  ( 31.54067435258301444, 194.6262042466636331, 169.1852728244599007 ) ) ;
#15764 = VERTEX_POINT ( 'NONE', #11561 ) ;
#15763 = EDGE_CURVE ( 'NONE', #2415, #41608, #46258, .T. ) ;
#15765 = ADVANCED_FACE ( 'NONE', ( #50802 ), #33852, .T. ) ;
#15766 = CARTESIAN_POINT ( 'NONE',  ( 4.000000000000001776, 4.812499997268813168, -1.656854249492381248 ) ) ;
#15767 = CARTESIAN_POINT ( 'NONE',  ( 2.977408999572654480, 91.62500000204838102, 7.188101187499999156 ) ) ;
#15770 = LINE ( 'NONE', #70086, #44613 ) ;
#15769 = CARTESIAN_POINT ( 'NONE',  ( -8.311093377946834337, 254.5312500034139873, 8.311093377946837890 ) ) ;
#15768 = CYLINDRICAL_SURFACE ( 'NONE', #72358, 8.000000000000000000 ) ;
#15771 = SHAPE_DEFINITION_REPRESENTATION ( #45115, #22268 ) ;
#15772 =( BOUNDED_CURVE ( )  B_SPLINE_CURVE ( 2, ( #33092, #62103, #44759, #49668, #10426, #56089, #16066, #20612, #67772 ),
 .UNSPECIFIED., .F., .F. ) 
 B_SPLINE_CURVE_WITH_KNOTS ( ( 3, 2, 2, 2, 3 ),
 ( 0.7187500000000001110, 0.7239583333333334814, 0.7291666666666667407, 0.7343750000000001110, 0.7395833333333334814 ),
 .UNSPECIFIED. ) 
 CURVE ( )  GEOMETRIC_REPRESENTATION_ITEM ( )  RATIONAL_B_SPLINE_CURVE ( ( 0.9999999999999983347, 0.9238795325112884038, 1.000000000000000000, 0.9238795325112867385, 1.000000000000000000, 0.9238795325112867385, 1.000000000000000000, 0.9238795325112850731, 1.000000000000001554 ) ) 
 REPRESENTATION_ITEM ( '' )  );
#15773 = ORIENTED_EDGE ( 'NONE', *, *, #52687, .F. ) ;
#15774 = EDGE_CURVE ( 'NONE', #10747, #34668, #59133, .T. ) ;
#15775 = CARTESIAN_POINT ( 'NONE',  ( 11.35316468749999963, 251.5104166700806729, 3.042071309553159519 ) ) ;
#15776 = CARTESIAN_POINT ( 'NONE',  ( -2.977408999572647819, 7.188101187499991163, 14.70530278187175455 ) ) ;
#15777 = ORIENTED_EDGE ( 'NONE', *, *, #21054, .F. ) ;
#15778 = VERTEX_POINT ( 'NONE', #22122 ) ;
#15779 = CARTESIAN_POINT ( 'NONE',  ( -4.220049686691937474, -10.18810118749999738, 76.93750000204838102 ) ) ;
#15780 = CARTESIAN_POINT ( 'NONE',  ( -9.832129032723420536, 79.01041666325268409, 5.676582343749997150 ) ) ;
#15781 = LINE ( 'NONE', #21446, #16770 ) ;
#15782 = CARTESIAN_POINT ( 'NONE',  ( 11.00000000000000000, 4.556349186104045934, 90.34375000000000000 ) ) ;
#15784 = CARTESIAN_POINT ( 'NONE',  ( 6.676582343750001591, 291.1093750017069510, -8.176455196517173205E-16 ) ) ;
#15783 = CARTESIAN_POINT ( 'NONE',  ( 32.00000000000000000, 195.3125000027311842, 171.6568542494922553 ) ) ;
#15785 = VECTOR ( 'NONE', #63721, 1000.000000000000000 ) ;
#15786 = FACE_OUTER_BOUND ( 'NONE', #44299, .T. ) ;
#15787 = CARTESIAN_POINT ( 'NONE',  ( 2.751064625579944321E-14, 199.7500000000000000, 194.0000000000000568 ) ) ;
#15788 = EDGE_CURVE ( 'NONE', #72148, #19, #74563, .T. ) ;
#15789 = CARTESIAN_POINT ( 'NONE',  ( 1.432654583217664701, 198.0000000013656063, 201.4587341250000065 ) ) ;
#15790 = CARTESIAN_POINT ( 'NONE',  ( -8.000000000000001776, 8.156249995903221972, 3.313708498984759387 ) ) ;
#15791 = ORIENTED_EDGE ( 'NONE', *, *, #34820, .F. ) ;
#15792 = CARTESIAN_POINT ( 'NONE',  ( 24.54126587499997925, 195.2500000013656063, 171.4326545832175555 ) ) ;
#15793 = CARTESIAN_POINT ( 'NONE',  ( -2.977408999572650039, 17.81249999795161543, -7.188101187500001821 ) ) ;
#15794 = CARTESIAN_POINT ( 'NONE',  ( 8.311093377946837890, 161.7187499965860411, -8.311093377946837890 ) ) ;
#15795 = CARTESIAN_POINT ( 'NONE',  ( 26.34314575050753859, 198.0625000027312126, 173.9999999999997726 ) ) ;
#15796 = CARTESIAN_POINT ( 'NONE',  ( 7.188101187500000933, 105.8750000020483668, -2.977408999572651371 ) ) ;
#15798 = DIRECTION ( 'NONE',  ( 0.000000000000000000, 0.000000000000000000, 1.000000000000000000 ) ) ;
#15797 = CARTESIAN_POINT ( 'NONE',  ( -7.347880794884122694E-16, 17.49999999726881583, 4.000000000000001776 ) ) ;
#15799 = CARTESIAN_POINT ( 'NONE',  ( 24.54126587499999346, 205.4375000013656063, 169.9999999999998863 ) ) ;
#15800 = CARTESIAN_POINT ( 'NONE',  ( -5.082755093536317936, -5.082755093536320601, 17.04905278187175810 ) ) ;
#15801 = CARTESIAN_POINT ( 'NONE',  ( 2.828427124746152987, 206.2500000027312126, 139.1715728752538723 ) ) ;
#15802 = CARTESIAN_POINT ( 'NONE',  ( -3.042071309553173730, 49.32291666325266988, 11.35316468749999785 ) ) ;
#15803 = CARTESIAN_POINT ( 'NONE',  ( 38.00000000000000000, 53.00000000000000711, 9.999999999999991118 ) ) ;
#15804 = CARTESIAN_POINT ( 'NONE',  ( 2.679491924311228956, 22.91666665983870033, -10.00000000000000000 ) ) ;
#15805 = CARTESIAN_POINT ( 'NONE',  ( 30.82842712474620228, 199.3750000000000284, 167.1715728752537586 ) ) ;
#15806 = ORIENTED_EDGE ( 'NONE', *, *, #64987, .F. ) ;
#15807 = CARTESIAN_POINT ( 'NONE',  ( 4.898587196589412829E-16, 22.68749999590322375, -8.000000000000000000 ) ) ;
#15808 = CARTESIAN_POINT ( 'NONE',  ( -8.311093377946836114, 52.65624999658601268, -8.311093377946837890 ) ) ;
#15809 = CARTESIAN_POINT ( 'NONE',  ( -11.00000000000000000, 4.556349186104045934, 73.09375000409676204 ) ) ;
#15810 = CARTESIAN_POINT ( 'NONE',  ( 3.458734124999960358, 198.6875000013655779, 142.0000000000000568 ) ) ;
#15811 = PLANE ( 'NONE',  #19100 ) ;
#15812 = CARTESIAN_POINT ( 'NONE',  ( -1.656854249492321074, 196.4375000027312126, 137.9999999999999716 ) ) ;
#15814 = CARTESIAN_POINT ( 'NONE',  ( -11.35316468750000141, 48.28124999658601268, -1.390361679473963753E-15 ) ) ;
#15813 = CARTESIAN_POINT ( 'NONE',  ( -5.082755093536324154, 100.3437500020483810, 5.082755093536326818 ) ) ;
#15815 = CARTESIAN_POINT ( 'NONE',  ( 5.656854249492376141, -5.656854249492374365, 11.89280277982336642 ) ) ;
#15816 = CARTESIAN_POINT ( 'NONE',  ( -5.656854249492375253, 5.656854249492375253, 21.83030278392014623 ) ) ;
#15817 = CARTESIAN_POINT ( 'NONE',  ( 3.042071309553167069, 176.8229166632526415, -11.35316468749999785 ) ) ;
#15818 = CARTESIAN_POINT ( 'NONE',  ( 10.00000000000000000, 146.6666666598386826, 2.679491924311236062 ) ) ;
#15819 = CARTESIAN_POINT ( 'NONE',  ( 1.320432766682874540E-15, 102.4062500020483810, 7.188101187500000044 ) ) ;
#15820 = AXIS2_PLACEMENT_3D ( 'NONE', #53241, #13223, #17789 ) ;
#15821 = CARTESIAN_POINT ( 'NONE',  ( -2.259052278473090869, -46.98367307418688199, 139.0821099909463499 ) ) ;
#15822 = CARTESIAN_POINT ( 'NONE',  ( 3.042071309553159519, 30.05208332991934839, 11.35316468750000141 ) ) ;
#15823 = CARTESIAN_POINT ( 'NONE',  ( -3.999999999999960032, 201.0000000000000000, 198.0000000000000284 ) ) ;
#15824 = ORIENTED_EDGE ( 'NONE', *, *, #39510, .F. ) ;
#15825 = CARTESIAN_POINT ( 'NONE',  ( 48.25549907375997094, 142.6778302163886849, 61.70628817261103904 ) ) ;
#15826 = CARTESIAN_POINT ( 'NONE',  ( -10.18810118749999738, -4.220049686691941915, 76.75000000204838102 ) ) ;
#15827 = CARTESIAN_POINT ( 'NONE',  ( 31.26628500697347590, 45.12997455106602018, 65.00000000000000000 ) ) ;
#15829 = CARTESIAN_POINT ( 'NONE',  ( 5.676582343750001591, 161.6145833299193839, -9.832129032723420536 ) ) ;
#15828 = CARTESIAN_POINT ( 'NONE',  ( -5.000000000000008882, 8.333333333333337478, 8.660254037844390851 ) ) ;
#15830 = VECTOR ( 'NONE', #60629, 1000.000000000000000 ) ;
#15831 = CARTESIAN_POINT ( 'NONE',  ( 7.999999999999991118, 3.313708498984757611, 10.73030278432982598 ) ) ;
#15832 = CARTESIAN_POINT ( 'NONE',  ( 4.898587196589412829E-16, 9.375000000000001776, -8.000000000000000000 ) ) ;
#15833 = CARTESIAN_POINT ( 'NONE',  ( 11.35316468749999608, 226.6145833367473301, -3.042071309553167069 ) ) ;
#15834 = CARTESIAN_POINT ( 'NONE',  ( 3.074111742560642124, 51.58078258920254910, -48.68628732315515606 ) ) ;
#15835 = CARTESIAN_POINT ( 'NONE',  ( -4.220049686691935698, 10.18810118749999916, 81.25000000204836681 ) ) ;
#15836 = ORIENTED_EDGE ( 'NONE', *, *, #56536, .T. ) ;
#15837 = CARTESIAN_POINT ( 'NONE',  ( 2.828427124746152987, 202.2500000027312126, 139.1715728752538723 ) ) ;
#15838 = CARTESIAN_POINT ( 'NONE',  ( 11.00000000000000000, 1.347111479062088405E-15, 96.24999999999998579 ) ) ;
#15839 = CARTESIAN_POINT ( 'NONE',  ( 11.35316468749999963, 111.3020833299193271, -3.042071309553165293 ) ) ;
#15840 = CARTESIAN_POINT ( 'NONE',  ( -2.249999999999999556, 255.9999999999998295, 5.427273995024871844 ) ) ;
#15841 = ORIENTED_EDGE ( 'NONE', *, *, #42502, .F. ) ;
#15842 = EDGE_LOOP ( 'NONE', ( #25667, #67826, #73448, #60357 ) ) ;
#15843 = ADVANCED_FACE ( 'NONE', ( #23621 ), #45872, .T. ) ;
#15844 = CARTESIAN_POINT ( 'NONE',  ( 3.211159895383560947, 7.312499998634407028, 3.211159895383562723 ) ) ;
#15845 = CARTESIAN_POINT ( 'NONE',  ( -7.188101187500000044, 10.21874999795161187, -8.802885111219163269E-16 ) ) ;
#15846 = CARTESIAN_POINT ( 'NONE',  ( -4.898587196589412829E-16, 111.3125000040967905, -8.000000000000000000 ) ) ;
#15847 = CARTESIAN_POINT ( 'NONE',  ( 4.220049686691941027, -10.18810118749999738, 94.00000000204838102 ) ) ;
#15848 = CARTESIAN_POINT ( 'NONE',  ( -25.55430564589119413, 200.5625000013656063, 167.5543056458915316 ) ) ;
#15849 = CARTESIAN_POINT ( 'NONE',  ( 4.000000000000001776, 8.062500000000000000, -1.656854249492381248 ) ) ;
#15850 = CARTESIAN_POINT ( 'NONE',  ( -30.64284399271078740, -12.00318926462334801, 174.6921329945331536 ) ) ;
#15851 = CARTESIAN_POINT ( 'NONE',  ( 3.211159895383561835, 9.437499998634406140, -3.211159895383561835 ) ) ;
#15852 = CARTESIAN_POINT ( 'NONE',  ( -4.000000000000015099, 198.5625000000000000, 143.6568542494924543 ) ) ;
#15853 = VERTEX_POINT ( 'NONE', #57983 ) ;
#15854 = CARTESIAN_POINT ( 'NONE',  ( 7.999999999996472155, 7.505344305739403062E-06, 9.267802996260090964 ) ) ;
#15856 = CARTESIAN_POINT ( 'NONE',  ( -25.17157287525382259, 199.8750000000000284, 167.1715728752541565 ) ) ;
#15855 = CARTESIAN_POINT ( 'NONE',  ( -24.54126587499995793, 196.1250000013655779, 171.4326545832179534 ) ) ;
#15857 =( NAMED_UNIT ( * ) SI_UNIT ( $, .STERADIAN. ) SOLID_ANGLE_UNIT ( ) );
#15858 = EDGE_CURVE ( 'NONE', #29990, #38241, #11935, .T. ) ;
#15859 = CARTESIAN_POINT ( 'NONE',  ( 4.541265875000002339, 19.31249999863440436, 0.000000000000000000 ) ) ;
#15860 = CARTESIAN_POINT ( 'NONE',  ( -11.00000000000000000, 0.000000000000000000, 118.0000000000000000 ) ) ;
#15861 = VECTOR ( 'NONE', #64198, 1000.000000000000000 ) ;
#15862 = CARTESIAN_POINT ( 'NONE',  ( -5.447321192899549303, -4.689935021205116961, 0.1569292013794422458 ) ) ;
#15863 = ORIENTED_EDGE ( 'NONE', *, *, #44122, .T. ) ;
#15864 =( BOUNDED_CURVE ( )  B_SPLINE_CURVE ( 2, ( #1120, #24831, #24473, #35079, #34710, #65194, #752, #58091, #35809 ),
 .UNSPECIFIED., .F., .F. ) 
 B_SPLINE_CURVE_WITH_KNOTS ( ( 3, 2, 2, 2, 3 ),
 ( 0.3472222222222222099, 0.3541666666666666852, 0.3611111111111111049, 0.3680555555555555802, 0.3750000000000000000 ),
 .UNSPECIFIED. ) 
 CURVE ( )  GEOMETRIC_REPRESENTATION_ITEM ( )  RATIONAL_B_SPLINE_CURVE ( ( 1.000000000000000000, 0.9238795325112867385, 1.000000000000000000, 0.9238795325112867385, 1.000000000000000000, 0.9238795325112867385, 1.000000000000000000, 0.9238795325112867385, 1.000000000000000000 ) ) 
 REPRESENTATION_ITEM ( '' )  );
#15865 = ORIENTED_EDGE ( 'NONE', *, *, #15756, .T. ) ;
#15866 = CARTESIAN_POINT ( 'NONE',  ( 10.18810118749999916, 1.247682550866122264E-15, 90.90625000204836681 ) ) ;
#15867 = LINE ( 'NONE', #56633, #31084 ) ;
#15868 = CARTESIAN_POINT ( 'NONE',  ( -29.43265458321766914, 200.7500000013656063, 166.5412658750003629 ) ) ;
#15869 = CARTESIAN_POINT ( 'NONE',  ( 2.020667218593132706E-15, -11.00000000000000000, 104.8750000000000000 ) ) ;
#15870 = CARTESIAN_POINT ( 'NONE',  ( 3.458734125000016757, 207.1250000013656347, 199.4326545832176691 ) ) ;
#15871 = CARTESIAN_POINT ( 'NONE',  ( 0.000000000000000000, 0.000000000000000000, -10.20000000000000462 ) ) ;
#15872 = CARTESIAN_POINT ( 'NONE',  ( 6.123233995736767268E-16, 121.2500000000000142, -10.00000000000000178 ) ) ;
#15873 = CARTESIAN_POINT ( 'NONE',  ( 8.000000000000001776, 103.1562500000000142, 3.313708498984759387 ) ) ;
#15874 = CARTESIAN_POINT ( 'NONE',  ( -6.676582343750000703, 292.6718750017069510, 2.765530957082001251 ) ) ;
#15875 = CARTESIAN_POINT ( 'NONE',  ( -5.082755093536317936, -5.082755093536320601, 5.049052781871752771 ) ) ;
#15876 = EDGE_CURVE ( 'NONE', #53073, #55780, #15450, .T. ) ;
#15877 = ORIENTED_EDGE ( 'NONE', *, *, #42246, .F. ) ;
#15878 = CARTESIAN_POINT ( 'NONE',  ( 8.000000000000000000, 19.50000000000000355, 0.000000000000000000 ) ) ;
#15879 = EDGE_CURVE ( 'NONE', #47128, #15485, #29030, .T. ) ;
#15880 = CARTESIAN_POINT ( 'NONE',  ( 25.55430564589119413, 205.0625000013656063, 167.5543056458910485 ) ) ;
#15881 = CARTESIAN_POINT ( 'NONE',  ( -8.000000000000000000, 26.06249999590322375, -9.797174393178825657E-16 ) ) ;
#15882 = CARTESIAN_POINT ( 'NONE',  ( -2.839093476692135984E-14, 199.6875000013656063, 138.5412658750000503 ) ) ;
#15883 = CARTESIAN_POINT ( 'NONE',  ( 1.320432766682874540E-15, 123.4062500020483810, 7.188101187500000044 ) ) ;
#15885 = CARTESIAN_POINT ( 'NONE',  ( -2.445694354108840063, 201.0625000013656063, 139.5543056458912190 ) ) ;
#15884 = CARTESIAN_POINT ( 'NONE',  ( 4.556349186104045934, 11.00000000000000000, 111.5312500000000142 ) ) ;
#15886 = CARTESIAN_POINT ( 'NONE',  ( 3.042071309553173286, 260.6770833367473301, 11.35316468749999608 ) ) ;
#15887 = CYLINDRICAL_SURFACE ( 'NONE', #25321, 3.999999999999976019 ) ;
#15888 = CARTESIAN_POINT ( 'NONE',  ( 0.000000000000000000, 0.000000000000000000, 0.000000000000000000 ) ) ;
#15889 = CARTESIAN_POINT ( 'NONE',  ( -8.311093377946841443, 8.906249996586018014, 8.311093377946830785 ) ) ;
#15890 =( BOUNDED_CURVE ( )  B_SPLINE_CURVE ( 2, ( #22827, #41675, #64684, #20127, #53739, #42768, #7345, #60125, #36385 ),
 .UNSPECIFIED., .F., .F. ) 
 B_SPLINE_CURVE_WITH_KNOTS ( ( 3, 2, 2, 2, 3 ),
 ( 0.2708333333333312609, 0.2812499999999979461, 0.2916666666666646313, 0.3020833333333312609, 0.3124999999999979461 ),
 .UNSPECIFIED. ) 
 CURVE ( )  GEOMETRIC_REPRESENTATION_ITEM ( )  RATIONAL_B_SPLINE_CURVE ( ( 1.000000000000015099, 0.9238795325112717505, 1.000000000000000000, 0.9238795325112867385, 1.000000000000000000, 0.9238795325112867385, 1.000000000000000000, 0.9238795325113017265, 0.9999999999999850120 ) ) 
 REPRESENTATION_ITEM ( '' )  );
#15891 = CARTESIAN_POINT ( 'NONE',  ( 9.735942053221449011E-16, 101.0525588832578734, 7.949999999999993960 ) ) ;
#15892 = CARTESIAN_POINT ( 'NONE',  ( -8.311093377946841443, 209.2187499965859843, 8.311093377946830785 ) ) ;
#15893 = CARTESIAN_POINT ( 'NONE',  ( -24.00000000000002487, 202.9375000027312126, 168.3431457505079152 ) ) ;
#15894 = DIRECTION ( 'NONE',  ( -0.000000000000000000, 1.000000000000000000, -0.000000000000000000 ) ) ;
#15896 = FACE_OUTER_BOUND ( 'NONE', #48242, .T. ) ;
#15895 = CARTESIAN_POINT ( 'NONE',  ( 4.898587196589415787E-16, 0.000000000000000000, 4.000000000000001776 ) ) ;
#15897 = ORIENTED_EDGE ( 'NONE', *, *, #37012, .F. ) ;
#15898 = CARTESIAN_POINT ( 'NONE',  ( -2.754378923186476579E-14, 200.4375000013656063, 145.4587341250000350 ) ) ;
#15899 = CARTESIAN_POINT ( 'NONE',  ( -2.085542519210945728E-15, 14.53124999658601624, 11.35316468750000141 ) ) ;
#15900 = CARTESIAN_POINT ( 'NONE',  ( -7.778174593052020747, -7.778174593052023411, 97.37500000409676204 ) ) ;
#15901 = CARTESIAN_POINT ( 'NONE',  ( 2.485281374238247132, 292.6875000000001137, -6.000000000000325961 ) ) ;
#15902 = CARTESIAN_POINT ( 'NONE',  ( -25.55430564589122966, 199.3125000013656063, 167.5543056458915032 ) ) ;
#15903 = CARTESIAN_POINT ( 'NONE',  ( 27.99999999999999645, 210.0000000000000284, 165.9999999999999147 ) ) ;
#15905 = CARTESIAN_POINT ( 'NONE',  ( 5.676582343750001591, 11.61458332991935016, -9.832129032723420536 ) ) ;
#15904 = CARTESIAN_POINT ( 'NONE',  ( -5.082755093536324154, 116.8437500020483810, 5.082755093536326818 ) ) ;
#15906 = CARTESIAN_POINT ( 'NONE',  ( -7.999999999999991118, 0.000000000000000000, 29.33030277982336642 ) ) ;
#15907 = CARTESIAN_POINT ( 'NONE',  ( -5.676582343749998039, 127.4479166632526983, -9.832129032723420536 ) ) ;
#15908 = CARTESIAN_POINT ( 'NONE',  ( -5.000000000000005329, 105.2083333265053824, 8.660254037844387298 ) ) ;
#15909 = ADVANCED_FACE ( 'NONE', ( #74185 ), #68158, .F. ) ;
#15910 = CARTESIAN_POINT ( 'NONE',  ( 5.082755093536325042, 117.9687500020483810, -5.082755093536325930 ) ) ;
#15911 = CARTESIAN_POINT ( 'NONE',  ( 1.881053915767121776, 20.62499999863441147, -4.541265875000002339 ) ) ;
#15912 = CARTESIAN_POINT ( 'NONE',  ( 6.123233995736767268E-16, 183.1249999931720538, -10.00000000000000178 ) ) ;
#15913 = CARTESIAN_POINT ( 'NONE',  ( -1.836970198721029983E-15, 5.624999993172032475, 10.00000000000000178 ) ) ;
#15914 = ORIENTED_EDGE ( 'NONE', *, *, #5400, .T. ) ;
#15915 = CARTESIAN_POINT ( 'NONE',  ( 11.35316468749999963, 1.302083329919349941, -3.042071309553165293 ) ) ;
#15916 = CARTESIAN_POINT ( 'NONE',  ( -4.721056650415998313, 289.7343750017069510, 4.721056650416000089 ) ) ;
#15917 = DIRECTION ( 'NONE',  ( -0.000000000000000000, 1.000000000000000000, -0.000000000000000000 ) ) ;
#15918 = CARTESIAN_POINT ( 'NONE',  ( 7.999999999999992895, -3.313708498984756279, 0.1740527839201450044 ) ) ;
#15919 = FACE_OUTER_BOUND ( 'NONE', #23526, .T. ) ;
#15920 = CARTESIAN_POINT ( 'NONE',  ( -11.35316468749999785, 258.6979166700807014, -3.042071309553164848 ) ) ;
#15921 = CARTESIAN_POINT ( 'NONE',  ( 7.204075437095968759, -7.204075437095966983, 104.5937500020483810 ) ) ;
#15922 = ORIENTED_EDGE ( 'NONE', *, *, #48790, .F. ) ;
#15923 = VECTOR ( 'NONE', #63566, 1000.000000000000000 ) ;
#15924 = CARTESIAN_POINT ( 'NONE',  ( 1.836970198721029589E-15, 251.2500000000000284, 10.00000000000000000 ) ) ;
#15925 = CARTESIAN_POINT ( 'NONE',  ( -8.311093377946836114, 157.9687499965860411, -8.311093377946837890 ) ) ;
#15926 = CARTESIAN_POINT ( 'NONE',  ( -5.000000000000000000, 29.68417822476651580, 4.268394125863321342 ) ) ;
#15927 = CARTESIAN_POINT ( 'NONE',  ( -3.458734124999959469, 200.7500000013656063, 199.4326545832176976 ) ) ;
#15928 = DIRECTION ( 'NONE',  ( -1.000000000000000000, -0.000000000000000000, -0.000000000000000000 ) ) ;
#15929 = CARTESIAN_POINT ( 'NONE',  ( -8.311093377946841443, 79.21874999658601268, 8.311093377946830785 ) ) ;
#15930 = ORIENTED_EDGE ( 'NONE', *, *, #6769, .F. ) ;
#15931 = CARTESIAN_POINT ( 'NONE',  ( -6.238412754330611322E-16, 10.18810118749999916, 113.7812500020483810 ) ) ;
#15932 = CARTESIAN_POINT ( 'NONE',  ( 1.881053915767122664, 10.24999999863440792, 4.541265875000001451 ) ) ;
#15933 = EDGE_LOOP ( 'NONE', ( #72455, #14381, #14341, #60762 ) ) ;
#15934 = CARTESIAN_POINT ( 'NONE',  ( -1.320432766682874540E-15, 25.59374999795161543, 7.188101187500000044 ) ) ;
#15935 = CARTESIAN_POINT ( 'NONE',  ( -11.00000000000000000, 0.000000000000000000, 95.49999999999998579 ) ) ;
#15936 = CARTESIAN_POINT ( 'NONE',  ( -2.679491924311280471, 249.1666666734946887, 9.999999999999971578 ) ) ;
#15937 = CARTESIAN_POINT ( 'NONE',  ( -5.082755093536326818, 18.28124999795161187, 5.082755093536325042 ) ) ;
#15938 = PLANE ( 'NONE',  #65243 ) ;
#15939 = ADVANCED_FACE ( 'NONE', ( #62489 ), #45511, .F. ) ;
#15940 = CARTESIAN_POINT ( 'NONE',  ( 4.220049686691934809, 10.18810118749999916, 109.5625000020483810 ) ) ;
#15941 = VECTOR ( 'NONE', #38781, 1000.000000000000114 ) ;
#15942 = EDGE_CURVE ( 'NONE', #64958, #9708, #67578, .T. ) ;
#15943 = CARTESIAN_POINT ( 'NONE',  ( 7.320508075688766603, 109.3750000000000000, 7.320508075688770155 ) ) ;
#15944 = CARTESIAN_POINT ( 'NONE',  ( 2.828427124746190291, 7.624999997268813168, 2.828427124746192067 ) ) ;
#15945 = CARTESIAN_POINT ( 'NONE',  ( -2.751064625579944321E-14, 208.8750000027312126, 146.0000000000000284 ) ) ;
#15946 = ORIENTED_EDGE ( 'NONE', *, *, #46311, .T. ) ;
#15947 = VECTOR ( 'NONE', #6119, 1000.000000000000000 ) ;
#15948 = CARTESIAN_POINT ( 'NONE',  ( -2.445694354108782775, 202.5625000013656063, 200.4456943541088663 ) ) ;
#15949 = AXIS2_PLACEMENT_3D ( 'NONE', #9209, #44661, #45035 ) ;
#15950 = CARTESIAN_POINT ( 'NONE',  ( -25.55430564589123321, 208.3125000013656063, 167.5543056458915032 ) ) ;
#15951 = CARTESIAN_POINT ( 'NONE',  ( 10.18810118750000093, -4.220049686691933921, 71.68750000204836681 ) ) ;
#15952 = EDGE_CURVE ( 'NONE', #68916, #28711, #67015, .T. ) ;
#15953 = CARTESIAN_POINT ( 'NONE',  ( 3.211159895383561835, 6.437499998634407028, -3.211159895383561835 ) ) ;
#15954 = CARTESIAN_POINT ( 'NONE',  ( 11.00000000000000000, 1.347111479062088405E-15, 72.24999999999998579 ) ) ;
#15955 = CARTESIAN_POINT ( 'NONE',  ( -4.401442555609577197E-16, 7.188101187499992051, 17.61155278187175810 ) ) ;
#15956 = ORIENTED_EDGE ( 'NONE', *, *, #57207, .T. ) ;
#15957 = CARTESIAN_POINT ( 'NONE',  ( 1.102182119232618108E-15, 299.2500000000000000, 6.000000000000001776 ) ) ;
#15958 = ORIENTED_EDGE ( 'NONE', *, *, #20770, .F. ) ;
#15959 = CARTESIAN_POINT ( 'NONE',  ( 10.18810118749999916, 1.247682550866122264E-15, 110.4062500020483668 ) ) ;
#15960 = CARTESIAN_POINT ( 'NONE',  ( -7.347880794884122694E-16, 10.75000000000000000, 4.000000000000001776 ) ) ;
#15961 = CARTESIAN_POINT ( 'NONE',  ( -1.432654583217607858, 204.6250000013655779, 201.4587341250000065 ) ) ;
#15962 = CARTESIAN_POINT ( 'NONE',  ( 27.99999999999996803, 198.9375000013655779, 166.5412658749999082 ) ) ;
#15963 = CARTESIAN_POINT ( 'NONE',  ( -7.320508075688778149, 83.12499999999998579, 7.320508075688769267 ) ) ;
#15964 = CARTESIAN_POINT ( 'NONE',  ( 7.188101187500001821, 90.87500000204838102, -2.977408999572651371 ) ) ;
#15965 = CARTESIAN_POINT ( 'NONE',  ( -6.000000000000000888, 291.0625000000000000, 2.485281374238575758 ) ) ;
#15966 = CARTESIAN_POINT ( 'NONE',  ( 24.00000000000000355, 203.9375000027311842, 171.6568542494923122 ) ) ;
#15967 = VERTEX_POINT ( 'NONE', #35336 ) ;
#15968 = LINE ( 'NONE', #61258, #59069 ) ;
#15969 = EDGE_CURVE ( 'NONE', #42125, #65387, #36242, .T. ) ;
#15970 = CARTESIAN_POINT ( 'NONE',  ( -7.999999999999948486, 3.313708498984799355, 8.236552779823361092 ) ) ;
#15971 = CARTESIAN_POINT ( 'NONE',  ( -2.828427124746208943, 196.7500000027312126, 144.8284271247462129 ) ) ;
#15972 = CARTESIAN_POINT ( 'NONE',  ( 2.679491924311228956, 57.91666665983870388, -10.00000000000000000 ) ) ;
#15973 = CARTESIAN_POINT ( 'NONE',  ( 0.000000000000000000, 125.0000000000000000, 0.000000000000000000 ) ) ;
#15974 = CARTESIAN_POINT ( 'NONE',  ( -7.320508075688770155, 250.6249999999999432, 7.320508075688774596 ) ) ;
#15975 = CARTESIAN_POINT ( 'NONE',  ( -10.00000000000003908, 77.29166666666669983, -2.679491924311240947 ) ) ;
#15976 = CARTESIAN_POINT ( 'NONE',  ( 4.999999999999993783, 194.1666666666666856, 8.660254037844390851 ) ) ;
#15977 = LINE ( 'NONE', #21640, #5438 ) ;
#15978 = CARTESIAN_POINT ( 'NONE',  ( 1.320432766682872962E-15, -7.188101187499992051, 17.23655278187175810 ) ) ;
#15979 = CARTESIAN_POINT ( 'NONE',  ( 8.311093377946837890, 161.7187499965860411, -8.311093377946837890 ) ) ;
#15980 = CARTESIAN_POINT ( 'NONE',  ( -2.828427124746209831, 204.5000000027312126, 139.1715728752538723 ) ) ;
#15981 = CARTESIAN_POINT ( 'NONE',  ( 10.00000000000000178, 260.4166666734946034, 2.679491924311222739 ) ) ;
#15982 = CARTESIAN_POINT ( 'NONE',  ( -3.673940397442060854E-16, 292.7500000000000000, -6.000000000000001776 ) ) ;
#15984 = CARTESIAN_POINT ( 'NONE',  ( 16.00000000000000711, -16.00000000000000000, 7.387219678533747391 ) ) ;
#15983 = LINE ( 'NONE', #62016, #16576 ) ;
#15985 = ORIENTED_EDGE ( 'NONE', *, *, #12056, .T. ) ;
#15986 = CARTESIAN_POINT ( 'NONE',  ( -3.042071309553164404, 22.55208332991935194, -11.35316468749999963 ) ) ;
#15987 = CARTESIAN_POINT ( 'NONE',  ( -25.17157287525382259, 200.8750000000000284, 167.1715728752541565 ) ) ;
#15989 = CARTESIAN_POINT ( 'NONE',  ( 3.223881452092225430, -10.27322224982958687, -63.89771963198325011 ) ) ;
#15988 = FACE_OUTER_BOUND ( 'NONE', #9944, .T. ) ;
#15990 = CARTESIAN_POINT ( 'NONE',  ( 23.99999999999997868, 201.8125000027312126, 168.3431457505075457 ) ) ;
#15991 = CARTESIAN_POINT ( 'NONE',  ( 1.432654583217607858, 202.6250000013656063, 138.5412658750000787 ) ) ;
#15992 =( BOUNDED_CURVE ( )  B_SPLINE_CURVE ( 2, ( #68560, #39887, #62891, #11223, #65110, #53445, #24390, #19094, #12333, #7786, #64021, #47758, #19460 ),
 .UNSPECIFIED., .F., .F. ) 
 B_SPLINE_CURVE_WITH_KNOTS ( ( 3, 2, 2, 2, 2, 2, 3 ),
 ( 2.496284451484902078, 2.501517587813307131, 2.506750724141712183, 2.511983860470117236, 2.517216996798521844, 2.522450133126926897, 2.527683269455331949 ),
 .UNSPECIFIED. ) 
 CURVE ( )  GEOMETRIC_REPRESENTATION_ITEM ( )  RATIONAL_B_SPLINE_CURVE ( ( 1.000000000000129452, 0.9659258262889388602, 1.000000000000000000, 0.9659258262890683122, 1.000000000000000000, 0.9659258262890683122, 1.000000000000000000, 0.9659258262890683122, 1.000000000000000000, 0.9659258262890683122, 1.000000000000000000, 0.9659258262892875813, 0.9999999999997807310 ) ) 
 REPRESENTATION_ITEM ( '' )  );
#15993 = CARTESIAN_POINT ( 'NONE',  ( -4.999999999999998224, 58.54166665983870388, -8.660254037844389075 ) ) ;
#15994 = CARTESIAN_POINT ( 'NONE',  ( 2.977408999572650039, 104.1875000020483668, -7.188101187500001821 ) ) ;
#15995 = CARTESIAN_POINT ( 'NONE',  ( 4.541265875000001451, 9.374999998634407916, 1.881053915767124440 ) ) ;
#15996 = CARTESIAN_POINT ( 'NONE',  ( -11.00000000000000000, 0.000000000000000000, 118.0000000000000000 ) ) ;
#15997 = CARTESIAN_POINT ( 'NONE',  ( -7.999999999999991118, 3.313708498984756723, 2.236552779823365533 ) ) ;
#15998 = CARTESIAN_POINT ( 'NONE',  ( 5.656854249492376141, -5.656854249492374365, 21.08030278392014623 ) ) ;
#15999 = VERTEX_POINT ( 'NONE', #59079 ) ;
#16000 = ORIENTED_EDGE ( 'NONE', *, *, #68966, .T. ) ;
#16001 = CARTESIAN_POINT ( 'NONE',  ( 7.320508075688778149, 30.62500000000000711, -7.320508075688778149 ) ) ;
#16002 = CARTESIAN_POINT ( 'NONE',  ( 2.775557559380704872E-14, -48.00000000000001421, 139.0000000000000568 ) ) ;
#16003 = DIRECTION ( 'NONE',  ( -0.000000000000000000, -0.000000000000000000, 1.000000000000000000 ) ) ;
#16004 = CARTESIAN_POINT ( 'NONE',  ( -28.38078951492683544, -42.68542688325498347, 157.5190196697000999 ) ) ;
#16005 = VECTOR ( 'NONE', #31156, 1000.000000000000000 ) ;
#16006 = CARTESIAN_POINT ( 'NONE',  ( 11.35316468750000141, 135.7812499965860411, 0.000000000000000000 ) ) ;
#16007 = ORIENTED_EDGE ( 'NONE', *, *, #26577, .T. ) ;
#16008 = CARTESIAN_POINT ( 'NONE',  ( -5.000000000000000000, 11.00479820989369806, -67.37201579502529114 ) ) ;
#16009 = CARTESIAN_POINT ( 'NONE',  ( 10.18810118750000093, -4.220049686691933921, 87.81250000204838102 ) ) ;
#16010 = CARTESIAN_POINT ( 'NONE',  ( 4.898587196589412829E-16, 6.187499995903221084, -8.000000000000000000 ) ) ;
#16011 = CARTESIAN_POINT ( 'NONE',  ( -1.656854249492347719, 209.8125000000000000, 194.0000000000000853 ) ) ;
#16012 = CARTESIAN_POINT ( 'NONE',  ( -5.656854249492381470, 18.74999999590322020, 5.656854249492379694 ) ) ;
#16013 = CYLINDRICAL_SURFACE ( 'NONE', #3607, 9.999999999999996447 ) ;
#16014 = ORIENTED_EDGE ( 'NONE', *, *, #49092, .T. ) ;
#16015 =( BOUNDED_CURVE ( )  B_SPLINE_CURVE ( 2, ( #924, #59725, #12943, #6933, #42729, #41988, #29943, #59360, #24271, #47282, #70308, #8034, #35980 ),
 .UNSPECIFIED., .F., .T. ) 
 B_SPLINE_CURVE_WITH_KNOTS ( ( 3, 2, 2, 2, 2, 2, 3 ),
 ( 0.04709510635581609650, 0.05232794973517845838, 0.05756079311454082026, 0.06279363649390318214, 0.06802647987326554402, 0.07325932325262790590, 0.07849216663199026778 ),
 .UNSPECIFIED. ) 
 CURVE ( )  GEOMETRIC_REPRESENTATION_ITEM ( )  RATIONAL_B_SPLINE_CURVE ( ( 1.000000000000000000, 0.9659258262890683122, 1.000000000000000000, 0.9659258262890683122, 1.000000000000000000, 0.9659258262890683122, 1.000000000000000000, 0.9659258262890683122, 1.000000000000000000, 0.9659258262890683122, 1.000000000000000000, 0.9659258262893161140, 0.9999999999997521982 ) ) 
 REPRESENTATION_ITEM ( '' )  );
#16016 = CARTESIAN_POINT ( 'NONE',  ( 11.00000000000000000, 1.347111479062088405E-15, 108.4375000040967763 ) ) ;
#16017 = CARTESIAN_POINT ( 'NONE',  ( 47.51267804510744952, 39.24696075549372409, 64.63931512073757801 ) ) ;
#16018 = CARTESIAN_POINT ( 'NONE',  ( -11.35316468750000141, 118.8020833299193413, 3.042071309553159963 ) ) ;
#16019 = CARTESIAN_POINT ( 'NONE',  ( -3.458734124999958581, 200.5000000013655779, 199.4326545832176976 ) ) ;
#16020 = CARTESIAN_POINT ( 'NONE',  ( 7.188101187500000933, 18.93749999795161543, -2.977408999572650483 ) ) ;
#16021 = CARTESIAN_POINT ( 'NONE',  ( -10.18810118749999738, -4.220049686691941915, 83.12500000204836681 ) ) ;
#16022 = CARTESIAN_POINT ( 'NONE',  ( 5.676582343749993598, 40.26041666325268409, 9.832129032723422313 ) ) ;
#16023 = ORIENTED_EDGE ( 'NONE', *, *, #42423, .F. ) ;
#16024 = CARTESIAN_POINT ( 'NONE',  ( 8.008118988124991233, 9.807117285998411148E-16, 19.76311528394062833 ) ) ;
#16025 = CARTESIAN_POINT ( 'NONE',  ( 3.458734124999960358, 209.6875000013656063, 142.0000000000000568 ) ) ;
#16026 = LINE ( 'NONE', #61322, #21476 ) ;
#16027 = CARTESIAN_POINT ( 'NONE',  ( 7.188101187500001821, 11.06249999795161187, -2.977408999572650483 ) ) ;
#16028 = CARTESIAN_POINT ( 'NONE',  ( -4.088227598258586603E-16, 290.2031250017069510, -6.676582343750001591 ) ) ;
#16029 = FACE_OUTER_BOUND ( 'NONE', #56315, .T. ) ;
#16030 = CARTESIAN_POINT ( 'NONE',  ( 5.082755093536324154, 2.156249997951610098, 5.082755093536326818 ) ) ;
#16031 = ADVANCED_FACE ( 'NONE', ( #70392 ), #12303, .T. ) ;
#16032 = VERTEX_POINT ( 'NONE', #53414 ) ;
#16033 = CARTESIAN_POINT ( 'NONE',  ( 5.676582343749993598, 155.2604166632526983, 9.832129032723422313 ) ) ;
#16034 = CARTESIAN_POINT ( 'NONE',  ( 10.18810118749999916, 4.220049686691935698, 76.00000000204838102 ) ) ;
#16035 = CARTESIAN_POINT ( 'NONE',  ( -25.55430564589119768, 208.5625000013656063, 167.5543056458915316 ) ) ;
#16036 = EDGE_CURVE ( 'NONE', #40449, #4004, #2090, .T. ) ;
#16037 = DIRECTION ( 'NONE',  ( 0.000000000000000000, 0.000000000000000000, -1.000000000000000000 ) ) ;
#16038 = CARTESIAN_POINT ( 'NONE',  ( 3.211159895383561835, 14.56249999863440792, -3.211159895383561835 ) ) ;
#16039 = ORIENTED_EDGE ( 'NONE', *, *, #30517, .T. ) ;
#16040 = CARTESIAN_POINT ( 'NONE',  ( 1.656854249492405451, 199.4375000027312410, 202.0000000000000284 ) ) ;
#16041 = CARTESIAN_POINT ( 'NONE',  ( 3.999999999999960032, 209.9375000000000000, 143.6568542494924543 ) ) ;
#16042 = CARTESIAN_POINT ( 'NONE',  ( -32.00000000000000000, 207.3750000027312126, 170.0000000000004547 ) ) ;
#16043 = VERTEX_POINT ( 'NONE', #46995 ) ;
#16044 = CARTESIAN_POINT ( 'NONE',  ( -2.977408999572654480, 11.99999999795161187, 7.188101187499999156 ) ) ;
#16045 = CARTESIAN_POINT ( 'NONE',  ( -23.99999999999995026, 196.8125000027312410, 171.6568542494926817 ) ) ;
#16046 = CARTESIAN_POINT ( 'NONE',  ( -2.258718157965394546, -46.98403154167964146, 151.1342229724999129 ) ) ;
#16047 = CIRCLE ( 'NONE', #10037, 10.00000000000000000 ) ;
#16048 = CARTESIAN_POINT ( 'NONE',  ( -10.00000000000000355, 47.70833333333333570, 2.679491924311223183 ) ) ;
#16049 = CARTESIAN_POINT ( 'NONE',  ( -2.977408999572651815, 106.8125000020484094, 7.188101187500000933 ) ) ;
#16050 = CARTESIAN_POINT ( 'NONE',  ( -5.999999999999999112, 291.1250000034140157, 2.485281374238575314 ) ) ;
#16051 = DIRECTION ( 'NONE',  ( 0.000000000000000000, 0.000000000000000000, -1.000000000000000000 ) ) ;
#16053 = CARTESIAN_POINT ( 'NONE',  ( 2.828427124746153876, 201.0000000027312126, 144.8284271247462129 ) ) ;
#16052 = CARTESIAN_POINT ( 'NONE',  ( 7.320508075688770155, 34.37500000000000711, 7.320508075688773708 ) ) ;
#16054 = ORIENTED_EDGE ( 'NONE', *, *, #15349, .F. ) ;
#16055 = CARTESIAN_POINT ( 'NONE',  ( -8.311093377946834337, 219.8437500034139873, 8.311093377946837890 ) ) ;
#16056 = CARTESIAN_POINT ( 'NONE',  ( 7.188101187499991163, 2.977408999572648707, 25.20530278187175810 ) ) ;
#16057 = CARTESIAN_POINT ( 'NONE',  ( -2.679491924311235174, 10.41666665983869855, 10.00000000000000000 ) ) ;
#16058 = CARTESIAN_POINT ( 'NONE',  ( -9.628968395985378237, 219.9999999999999716, 4.435878529719882835 ) ) ;
#16059 = CARTESIAN_POINT ( 'NONE',  ( 0.3794862803195819256, -65.74576272852144143, -26.26831557574764986 ) ) ;
#16060 = CARTESIAN_POINT ( 'NONE',  ( 1.432654583217664701, 195.0000000013656063, 201.4587341250000065 ) ) ;
#16061 = CARTESIAN_POINT ( 'NONE',  ( 2.679491924311228956, 151.0416666666666856, -10.00000000000000000 ) ) ;
#16062 = CARTESIAN_POINT ( 'NONE',  ( 7.778174593052023411, -7.778174593052021635, 115.7500000040967905 ) ) ;
#16063 = CYLINDRICAL_SURFACE ( 'NONE', #60777, 11.99999999999999645 ) ;
#16064 = CARTESIAN_POINT ( 'NONE',  ( -8.000000000000000000, 91.90625000000000000, -3.313708498984761608 ) ) ;
#16065 = CARTESIAN_POINT ( 'NONE',  ( 3.042071309553167069, 127.1354166632526699, -11.35316468749999785 ) ) ;
#16066 = CARTESIAN_POINT ( 'NONE',  ( 5.656854249492381470, 98.56250000000000000, 5.656854249492379694 ) ) ;
#16067 = CARTESIAN_POINT ( 'NONE',  ( -7.778174593052020747, -7.778174593052023411, 70.18749999999998579 ) ) ;
#16070 = DIRECTION ( 'NONE',  ( 0.000000000000000000, 0.000000000000000000, 1.000000000000000000 ) ) ;
#16069 = CARTESIAN_POINT ( 'NONE',  ( 25.55430564589118703, 197.3125000013656063, 172.4456943541087526 ) ) ;
#16068 = CARTESIAN_POINT ( 'NONE',  ( 23.99999999999999289, 208.7500000000000284, 169.9999999999998863 ) ) ;
#16071 = VERTEX_POINT ( 'NONE', #52670 ) ;
#16072 = CARTESIAN_POINT ( 'NONE',  ( 2.449293598294707893E-16, 2.250000000000000444, -4.000000000000001776 ) ) ;
#16073 = CARTESIAN_POINT ( 'NONE',  ( -2.849036369511732440E-14, 206.2500000000000284, 138.0000000000000568 ) ) ;
#16074 = CARTESIAN_POINT ( 'NONE',  ( 24.54126587500000056, 198.3750000013655779, 168.5673454167822172 ) ) ;
#16075 = CARTESIAN_POINT ( 'NONE',  ( -2.085542519210945728E-15, 204.8437499965860411, 11.35316468750000141 ) ) ;
#16076 = CARTESIAN_POINT ( 'NONE',  ( -4.401442555609581635E-16, 123.7812500020483810, -7.188101187500000044 ) ) ;
#16077 = CARTESIAN_POINT ( 'NONE',  ( 1.881053915767122664, 19.12499999863441147, 4.541265875000001451 ) ) ;
#16078 = CARTESIAN_POINT ( 'NONE',  ( 0.6547826978324309266, -49.91450260127135863, 40.68974341348022961 ) ) ;
#16079 = CARTESIAN_POINT ( 'NONE',  ( 5.656854249492374365, 5.656854249492375253, 27.26780277982336642 ) ) ;
#16080 = CARTESIAN_POINT ( 'NONE',  ( -25.17157287525382259, 202.8750000000000284, 167.1715728752541565 ) ) ;
#16081 = CARTESIAN_POINT ( 'NONE',  ( 3.042071309553159519, 94.73958332991934128, 11.35316468750000141 ) ) ;
#16082 = ORIENTED_EDGE ( 'NONE', *, *, #6220, .T. ) ;
#16083 = CARTESIAN_POINT ( 'NONE',  ( 0.000000000000000000, 0.000000000000000000, 0.000000000000000000 ) ) ;
#16084 = CARTESIAN_POINT ( 'NONE',  ( 4.401442555609581635E-16, 17.34374999795161187, -7.188101187500000044 ) ) ;
#16085 = CARTESIAN_POINT ( 'NONE',  ( -8.000000000000033751, -3.313708498984719864, 14.42405277982336465 ) ) ;
#16086 = CARTESIAN_POINT ( 'NONE',  ( -9.832129032723418760, 253.8020833367473017, -5.676582343749998927 ) ) ;
#16087 = CARTESIAN_POINT ( 'NONE',  ( 6.951808397369818766E-16, 107.0312499965860269, -11.35316468750000141 ) ) ;
#16088 = EDGE_LOOP ( 'NONE', ( #58312, #70789, #10004, #10723 ) ) ;
#16089 = CARTESIAN_POINT ( 'NONE',  ( -1.970469249063935269E-15, 20.78460969082654231, -21.50000000000000000 ) ) ;
#16090 = CARTESIAN_POINT ( 'NONE',  ( 4.220049686691941027, -10.18810118749999738, 110.1250000020483810 ) ) ;
#16091 = CARTESIAN_POINT ( 'NONE',  ( -7.320508075689014404, 21.87500000000019540, -7.320508075689014404 ) ) ;
#16092 = CARTESIAN_POINT ( 'NONE',  ( -2.445694354108784108, 206.5625000013656063, 195.5543056458912190 ) ) ;
#16093 = CARTESIAN_POINT ( 'NONE',  ( -3.313708498984759387, -7.999999999999989342, 11.61155277982336820 ) ) ;
#16095 = CARTESIAN_POINT ( 'NONE',  ( 11.35316468749999963, 85.98958332991938391, -3.042071309553165293 ) ) ;
#16094 = CARTESIAN_POINT ( 'NONE',  ( 0.000000000000000000, 4.408728476930470856E-15, -36.00000000000000000 ) ) ;
#16096 = CARTESIAN_POINT ( 'NONE',  ( -3.313708498984758943, -7.999999999999989342, 14.79905278392014978 ) ) ;
#16097 = CARTESIAN_POINT ( 'NONE',  ( -29.43265458321766559, 199.7500000013656063, 166.5412658750003629 ) ) ;
#16098 = CARTESIAN_POINT ( 'NONE',  ( -28.00000000000007461, 196.1250000027311842, 166.0000000000003695 ) ) ;
#16099 = EDGE_CURVE ( 'NONE', #35953, #54549, #10183, .T. ) ;
#16100 = CARTESIAN_POINT ( 'NONE',  ( 10.00000000000000178, 177.0833333265053966, -2.679491924311226736 ) ) ;
#16101 = CARTESIAN_POINT ( 'NONE',  ( 11.35316468749999785, 80.88541666325268409, 3.042071309553174174 ) ) ;
#16102 = CARTESIAN_POINT ( 'NONE',  ( -4.721056650415999201, 291.3281250017069510, -4.721056650415999201 ) ) ;
#16103 =( BOUNDED_CURVE ( )  B_SPLINE_CURVE ( 2, ( #33035, #3224, #26211, #9636, #48856, #72631, #26593, #49231, #20180 ),
 .UNSPECIFIED., .F., .F. ) 
 B_SPLINE_CURVE_WITH_KNOTS ( ( 3, 2, 2, 2, 3 ),
 ( 0.4062499999999998890, 0.4114583333333332038, 0.4166666666666666297, 0.4218749999999999445, 0.4270833333333332593 ),
 .UNSPECIFIED. ) 
 CURVE ( )  GEOMETRIC_REPRESENTATION_ITEM ( )  RATIONAL_B_SPLINE_CURVE ( ( 1.000000000000001554, 0.9238795325112850731, 1.000000000000000000, 0.9238795325112867385, 1.000000000000000000, 0.9238795325112867385, 1.000000000000000000, 0.9238795325112875156, 0.9999999999999992228 ) ) 
 REPRESENTATION_ITEM ( '' )  );
#16104 = CARTESIAN_POINT ( 'NONE',  ( -6.238412754330611322E-16, 10.18810118749999916, 103.6562500020483810 ) ) ;
#16105 = CARTESIAN_POINT ( 'NONE',  ( 11.35316468749999963, 215.9895833299192986, -3.042071309553165293 ) ) ;
#16106 = ORIENTED_EDGE ( 'NONE', *, *, #32337, .F. ) ;
#16107 = CARTESIAN_POINT ( 'NONE',  ( 1.469576158976822172E-15, -7.999999999999991118, 28.20530277982336642 ) ) ;
#16108 = CARTESIAN_POINT ( 'NONE',  ( 6.000000000000011546, -10.39230484541325694, 0.000000000000000000 ) ) ;
#16109 = DIRECTION ( 'NONE',  ( 0.000000000000000000, 0.000000000000000000, 1.000000000000000000 ) ) ;
#16110 = CARTESIAN_POINT ( 'NONE',  ( 5.676582343749993598, 209.9479166632526983, 9.832129032723422313 ) ) ;
#16111 = CARTESIAN_POINT ( 'NONE',  ( -7.320508075688770155, 223.7500000068280031, 7.320508075688774596 ) ) ;
#16112 = CARTESIAN_POINT ( 'NONE',  ( 6.123233995736767268E-16, 98.12499999317203958, -10.00000000000000178 ) ) ;
#16113 = ORIENTED_EDGE ( 'NONE', *, *, #9869, .T. ) ;
#16114 = CARTESIAN_POINT ( 'NONE',  ( 6.951808397369818766E-16, 197.3437499965860127, -11.35316468750000141 ) ) ;
#16115 = ADVANCED_FACE ( 'NONE', ( #47366 ), #19067, .F. ) ;
#16116 = CARTESIAN_POINT ( 'NONE',  ( -2.977408999572647819, -7.188101187499990274, 16.76780278187175455 ) ) ;
#16117 = CARTESIAN_POINT ( 'NONE',  ( -26.56734541678232731, 208.0000000013656347, 173.4587341250003760 ) ) ;
#16118 = CARTESIAN_POINT ( 'NONE',  ( -1.469576158976823947E-15, 10.12500000000000178, 8.000000000000000000 ) ) ;
#16119 = ORIENTED_EDGE ( 'NONE', *, *, #16438, .F. ) ;
#16120 = CARTESIAN_POINT ( 'NONE',  ( -8.000000000000000000, 93.59375000409679046, -3.313708498984761608 ) ) ;
#16121 = CARTESIAN_POINT ( 'NONE',  ( 8.660254037844385522, 19.58333333333333570, 5.000000000000005329 ) ) ;
#16122 = AXIS2_PLACEMENT_3D ( 'NONE', #71077, #17934, #18676 ) ;
#16123 = CARTESIAN_POINT ( 'NONE',  ( 4.220049686691934809, 10.18810118749999916, 79.56250000204836681 ) ) ;
#16124 = EDGE_LOOP ( 'NONE', ( #9643, #72361, #16054, #56494 ) ) ;
#16125 = CARTESIAN_POINT ( 'NONE',  ( -2.828427124746190735, 18.37500000000000000, -2.828427124746191623 ) ) ;
#16126 = CARTESIAN_POINT ( 'NONE',  ( 2.780723358947928197E-16, 21.56249999863440792, -4.541265875000002339 ) ) ;
#16127 = LINE ( 'NONE', #62914, #73952 ) ;
#16128 = ORIENTED_EDGE ( 'NONE', *, *, #46092, .F. ) ;
#16129 = CARTESIAN_POINT ( 'NONE',  ( -4.401442555609581635E-16, 93.78125000204836681, -7.188101187500000044 ) ) ;
#16132 = CARTESIAN_POINT ( 'NONE',  ( 4.000000000000015987, 197.5625000000000568, 196.3431457505076594 ) ) ;
#16131 = CARTESIAN_POINT ( 'NONE',  ( 11.35316468749999608, 251.6145833367473585, -3.042071309553167513 ) ) ;
#16130 = CARTESIAN_POINT ( 'NONE',  ( 31.45873412499998523, 208.7500000013656063, 168.5673454167822172 ) ) ;
#16133 = APPLICATION_PROTOCOL_DEFINITION ( 'draft international standard', 'automotive_design', 1998, #73674 ) ;
#16134 = ORIENTED_EDGE ( 'NONE', *, *, #44067, .T. ) ;
#16135 = CARTESIAN_POINT ( 'NONE',  ( -8.311093377946834337, 249.8437500034139589, 8.311093377946837890 ) ) ;
#16136 = CARTESIAN_POINT ( 'NONE',  ( -2.977408999572648707, -7.188101187499990274, 12.26780278187175455 ) ) ;
#16137 = ORIENTED_EDGE ( 'NONE', *, *, #18609, .F. ) ;
#16138 = ORIENTED_EDGE ( 'NONE', *, *, #15186, .T. ) ;
#16139 = CARTESIAN_POINT ( 'NONE',  ( 1.871523826299183495E-15, -10.18810118749999916, 77.03125000204836681 ) ) ;
#16140 = CARTESIAN_POINT ( 'NONE',  ( -9.832129032723420536, 89.01041666325268409, 5.676582343749997150 ) ) ;
#16141 = CARTESIAN_POINT ( 'NONE',  ( -2.250000000000000888, 2.250000000000000000, 28.00000000000000000 ) ) ;
#16142 = CARTESIAN_POINT ( 'NONE',  ( 11.00000000000000000, 1.347111479062088405E-15, 90.25000000000000000 ) ) ;
#16145 = CARTESIAN_POINT ( 'NONE',  ( -4.721056650415999201, 288.4843750017070079, -4.721056650415999201 ) ) ;
#16144 = CARTESIAN_POINT ( 'NONE',  ( 25.55430564589119413, 208.3125000013656063, 172.4456943541087526 ) ) ;
#16143 = CARTESIAN_POINT ( 'NONE',  ( 28.00000000000002487, 209.1875000013656063, 166.5412658749999082 ) ) ;
#16146 = AXIS2_PLACEMENT_3D ( 'NONE', #72754, #60298, #48606 ) ;
#16147 = CARTESIAN_POINT ( 'NONE',  ( -8.000000000000000000, 114.4999999999999858, 0.000000000000000000 ) ) ;
#16148 = CARTESIAN_POINT ( 'NONE',  ( 3.313708498984815343, 102.0312499999999574, -7.999999999999944933 ) ) ;
#16149 = CARTESIAN_POINT ( 'NONE',  ( 2.445694354108840063, 197.0625000013656063, 200.4456943541088663 ) ) ;
#16150 = CARTESIAN_POINT ( 'NONE',  ( 4.898587196589412829E-16, 10.68749999590322020, -8.000000000000000000 ) ) ;
#16151 = VERTEX_POINT ( 'NONE', #23986 ) ;
#16152 = CARTESIAN_POINT ( 'NONE',  ( 30.44569435410878810, 196.5625000013656063, 172.4456943541087526 ) ) ;
#16153 = EDGE_CURVE ( 'NONE', #23017, #43686, #24718, .T. ) ;
#16154 = CARTESIAN_POINT ( 'NONE',  ( 2.977408999572651815, 20.06249999795161543, 7.188101187500000933 ) ) ;
#16155 = CARTESIAN_POINT ( 'NONE',  ( -2.085542519210945728E-15, 164.8437499965860127, 11.35316468750000141 ) ) ;
#16156 = CARTESIAN_POINT ( 'NONE',  ( 23.99999999999999645, 197.9375000027312126, 171.6568542494923122 ) ) ;
#16157 = CARTESIAN_POINT ( 'NONE',  ( 7.188101187500002709, 102.6875000020483810, 2.977408999572649151 ) ) ;
#16159 = CARTESIAN_POINT ( 'NONE',  ( 1.317228840344440322, -55.68607278123021587, -43.83834608838390068 ) ) ;
#16158 = DIRECTION ( 'NONE',  ( 0.000000000000000000, 0.000000000000000000, 1.000000000000000000 ) ) ;
#16160 = CARTESIAN_POINT ( 'NONE',  ( 28.00000000000002132, 205.1875000013656063, 166.5412658749999082 ) ) ;
#16161 = CARTESIAN_POINT ( 'NONE',  ( -5.082755093536319713, 5.082755093536319713, 16.67405278187175810 ) ) ;
#16162 = CARTESIAN_POINT ( 'NONE',  ( -9.832129032723420536, 53.69791666325268409, 5.676582343749997150 ) ) ;
#16163 = CARTESIAN_POINT ( 'NONE',  ( -2.386700107840288521, -43.17188096653440255, 139.0918205410118560 ) ) ;
#16164 = CARTESIAN_POINT ( 'NONE',  ( 2.679491924311222739, 15.83333332650536640, 10.00000000000000355 ) ) ;
#16165 = CARTESIAN_POINT ( 'NONE',  ( -30.82842712474624491, 200.2500000027312126, 167.1715728752542418 ) ) ;
#16166 = ORIENTED_EDGE ( 'NONE', *, *, #19639, .T. ) ;
#16167 = CARTESIAN_POINT ( 'NONE',  ( 8.660254037844389075, 142.2916666598386826, -5.000000000000000000 ) ) ;
#16168 = CARTESIAN_POINT ( 'NONE',  ( 4.556349186104052151, -10.99999999999999822, 81.15625000409676204 ) ) ;
#16169 = CARTESIAN_POINT ( 'NONE',  ( -11.35316468750000141, 63.28124999658601979, -1.390361679473963753E-15 ) ) ;
#16170 = CARTESIAN_POINT ( 'NONE',  ( -6.735557395310442023E-16, 11.00000000000000000, 75.81250000409677625 ) ) ;
#16171 = CARTESIAN_POINT ( 'NONE',  ( 3.458734124999960358, 200.6875000013656063, 142.0000000000000568 ) ) ;
#16172 = CARTESIAN_POINT ( 'NONE',  ( 18.00000000000000000, 10.39230484541325161, -21.50000000000000000 ) ) ;
#16173 = CARTESIAN_POINT ( 'NONE',  ( 2.849036369511732440E-14, 207.2500000000000284, 202.0000000000000000 ) ) ;
#16175 = CARTESIAN_POINT ( 'NONE',  ( 3.042071309553159519, 44.73958332991934839, 11.35316468750000141 ) ) ;
#16174 = CARTESIAN_POINT ( 'NONE',  ( 5.082755093536326818, 91.71875000204838102, 5.082755093536325042 ) ) ;
#16176 = CARTESIAN_POINT ( 'NONE',  ( -7.999999999999991118, 0.000000000000000000, 28.01780278392014978 ) ) ;
#16177 = CARTESIAN_POINT ( 'NONE',  ( 8.660254037844383745, 204.5833333333333428, 5.000000000000004441 ) ) ;
#16178 = CARTESIAN_POINT ( 'NONE',  ( 3.042071309553159519, 179.7395833299193555, 11.35316468750000141 ) ) ;
#16180 = CARTESIAN_POINT ( 'NONE',  ( 7.320508075688774596, 142.4999999931720538, -7.320508075688774596 ) ) ;
#16179 = PRODUCT_DEFINITION_SHAPE ( 'NONE', 'NONE',  #29780 ) ;
#16181 = CARTESIAN_POINT ( 'NONE',  ( -4.401442555609581635E-16, 104.6562500020483810, -7.188101187500000044 ) ) ;
#16182 = CIRCLE ( 'NONE', #65578, 12.00000000000000355 ) ;
#16183 = CARTESIAN_POINT ( 'NONE',  ( 0.000000000000000000, 0.000000000000000000, 0.000000000000000000 ) ) ;
#16184 = CARTESIAN_POINT ( 'NONE',  ( -11.35316468750000141, 38.80208332991934839, 3.042071309553159963 ) ) ;
#16185 = CARTESIAN_POINT ( 'NONE',  ( -1.656854249492263564, 200.8125000000000284, 194.0000000000000000 ) ) ;
#16186 = CARTESIAN_POINT ( 'NONE',  ( 11.35316468749999963, 170.9895833299193839, -3.042071309553165293 ) ) ;
#16187 = EDGE_LOOP ( 'NONE', ( #3304, #59648, #45719, #9192 ) ) ;
#16188 = CARTESIAN_POINT ( 'NONE',  ( 48.32285594383907323, 142.4683213782394944, 61.49255443819184563 ) ) ;
#16189 = CARTESIAN_POINT ( 'NONE',  ( 4.220049686691941027, -10.18810118749999738, 69.62500000204838102 ) ) ;
#16190 = CARTESIAN_POINT ( 'NONE',  ( 2.828427124746209831, 197.3750000000000284, 200.8284271247462129 ) ) ;
#16191 = CARTESIAN_POINT ( 'NONE',  ( 6.123233995736767268E-16, 218.1249999931720538, -10.00000000000000178 ) ) ;
#16193 = CARTESIAN_POINT ( 'NONE',  ( 3.042071309553167513, 161.8229166632527267, -11.35316468749999785 ) ) ;
#16192 = CARTESIAN_POINT ( 'NONE',  ( -5.656854249492373476, -5.656854249492376141, 2.705302783920143561 ) ) ;
#16194 = CARTESIAN_POINT ( 'NONE',  ( 7.999999999999992895, -3.313708498984756279, 4.542802784329823318 ) ) ;
#16195 = CARTESIAN_POINT ( 'NONE',  ( -27.99999999999999645, 195.0000000000000000, 174.0000000000003411 ) ) ;
#16196 = EDGE_CURVE ( 'NONE', #8706, #15013, #30444, .T. ) ;
#16197 = EDGE_CURVE ( 'NONE', #69954, #29602, #54011, .T. ) ;
#16198 = CARTESIAN_POINT ( 'NONE',  ( 11.35316468749999608, 221.6145833367472733, -3.042071309553167069 ) ) ;
#16199 = CARTESIAN_POINT ( 'NONE',  ( 6.298842414715673854, 51.07418104650354707, -41.32239042994763878 ) ) ;
#16200 = CARTESIAN_POINT ( 'NONE',  ( 1.871523826299183495E-15, -10.18810118749999916, 80.40625000204838102 ) ) ;
#16201 = ORIENTED_EDGE ( 'NONE', *, *, #15349, .T. ) ;
#16202 = CARTESIAN_POINT ( 'NONE',  ( -2.849036369511732440E-14, 198.3750000027312126, 138.0000000000000568 ) ) ;
#16203 = CARTESIAN_POINT ( 'NONE',  ( 11.35316468750000141, 116.0937499965860127, 0.000000000000000000 ) ) ;
#16204 = CARTESIAN_POINT ( 'NONE',  ( 6.123233995736767268E-16, 13.12499999317203425, -10.00000000000000178 ) ) ;
#16205 = ORIENTED_EDGE ( 'NONE', *, *, #35947, .T. ) ;
#16206 = ORIENTED_EDGE ( 'NONE', *, *, #18839, .F. ) ;
#16207 = VECTOR ( 'NONE', #5054, 1000.000000000000000 ) ;
#16208 = CARTESIAN_POINT ( 'NONE',  ( -8.342170076843785083E-16, 8.187499998634406140, 4.541265875000002339 ) ) ;
#16209 = CARTESIAN_POINT ( 'NONE',  ( -1.320432766682874540E-15, 16.59374999795161543, 7.188101187500000044 ) ) ;
#16210 = EDGE_CURVE ( 'NONE', #4336, #57316, #45857, .T. ) ;
#16211 = CARTESIAN_POINT ( 'NONE',  ( -8.000000000000000000, 107.1875000040967905, 0.000000000000000000 ) ) ;
#16212 =( BOUNDED_CURVE ( )  B_SPLINE_CURVE ( 2, ( #29311, #28931, #51949, #45906, #39876, #64378, #70045, #29674, #28556 ),
 .UNSPECIFIED., .F., .F. ) 
 B_SPLINE_CURVE_WITH_KNOTS ( ( 3, 2, 2, 2, 3 ),
 ( 0.3977272727272727626, 0.4034090909090909394, 0.4090909090909091717, 0.4147727272727272929, 0.4204545454545454697 ),
 .UNSPECIFIED. ) 
 CURVE ( )  GEOMETRIC_REPRESENTATION_ITEM ( )  RATIONAL_B_SPLINE_CURVE ( ( 0.9999999999999992228, 0.9238795325112875156, 1.000000000000000000, 0.9238795325112867385, 1.000000000000000000, 0.9238795325112867385, 1.000000000000000000, 0.9238795325112867385, 1.000000000000000000 ) ) 
 REPRESENTATION_ITEM ( '' )  );
#16213 = CARTESIAN_POINT ( 'NONE',  ( -7.204075437095965206, -7.204075437095968759, 92.21875000204838102 ) ) ;
#16214 = CARTESIAN_POINT ( 'NONE',  ( -28.00000000000002132, 198.6875000013655779, 166.5412658750003629 ) ) ;
#16215 = CARTESIAN_POINT ( 'NONE',  ( -7.347880794884122694E-16, 9.750000000000000000, 4.000000000000001776 ) ) ;
#16216 = CARTESIAN_POINT ( 'NONE',  ( 2.449293598294707893E-16, 20.99999999726881583, -4.000000000000001776 ) ) ;
#16217 = CARTESIAN_POINT ( 'NONE',  ( 4.541265875000002339, 6.312499998634407028, 0.000000000000000000 ) ) ;
#16218 = B_SPLINE_CURVE_WITH_KNOTS ( 'NONE', 3,
 ( #44105, #42963, #65982, #38450, #32797, #27114, #14287, #63304, #5238, #10889, #74256, #27862, #52003, #73887, #57296, #10516, #16906, #5610, #22564, #51245, #69347, #27481, #22952, #4490 ),
 .UNSPECIFIED., .F., .F.,
 ( 4, 2, 2, 2, 2, 2, 2, 2, 2, 2, 2, 4 ),
 ( 1.551583845779545699E-17, 0.005931354918227581437, 0.01186270983645514726, 0.01334554856601203460, 0.01482838729556891846, 0.01779406475468268620, 0.02372541967291023554, 0.02965677459113778142, 0.03262245205025155609, 0.03558812950936532382, 0.04151948442759286623, 0.04745083934582040169 ),
 .UNSPECIFIED. ) ;
#16219 = CARTESIAN_POINT ( 'NONE',  ( 2.828427124746153876, 196.8750000000000284, 144.8284271247462129 ) ) ;
#16220 = ORIENTED_EDGE ( 'NONE', *, *, #18092, .T. ) ;
#16221 = CARTESIAN_POINT ( 'NONE',  ( -6.123233995736766282E-16, 223.7500000000000000, -10.00000000000000000 ) ) ;
#16222 = CARTESIAN_POINT ( 'NONE',  ( 5.082755093536326818, 108.2187500020483810, 5.082755093536325042 ) ) ;
#16223 = AXIS2_PLACEMENT_3D ( 'NONE', #66462, #4972, #49106 ) ;
#16225 = CARTESIAN_POINT ( 'NONE',  ( -1.656854249492422992, 209.6875000000000000, 146.0000000000000284 ) ) ;
#16224 = CARTESIAN_POINT ( 'NONE',  ( -4.556349186104045934, 11.00000000000000000, 78.90625000409676204 ) ) ;
#16226 = CARTESIAN_POINT ( 'NONE',  ( -3.211159895383562723, 20.93749999863440436, 3.211159895383561391 ) ) ;
#16227 = VECTOR ( 'NONE', #70816, 1000.000000000000000 ) ;
#16228 = DIRECTION ( 'NONE',  ( -0.000000000000000000, 1.000000000000000000, 2.238352872228138170E-16 ) ) ;
#16229 = ORIENTED_EDGE ( 'NONE', *, *, #56516, .F. ) ;
#16230 = EDGE_LOOP ( 'NONE', ( #19490, #50449, #38582, #39353 ) ) ;
#16231 = CARTESIAN_POINT ( 'NONE',  ( 4.220049686691934809, 10.18810118749999916, 94.18750000204836681 ) ) ;
#16232 = CARTESIAN_POINT ( 'NONE',  ( -10.99999999999999822, 219.6309830641437202, 2.947441116742358425 ) ) ;
#16233 = CARTESIAN_POINT ( 'NONE',  ( -27.99999999999996447, 199.1875000013655779, 173.4587341250003760 ) ) ;
#16234 = CARTESIAN_POINT ( 'NONE',  ( 4.556349186104045934, 11.00000000000000000, 108.5312500000000142 ) ) ;
#16235 = CARTESIAN_POINT ( 'NONE',  ( 1.432654583217664701, 207.0000000013656063, 201.4587341250000065 ) ) ;
#16237 = CARTESIAN_POINT ( 'NONE',  ( -10.00000000000000888, 127.7083333333333570, 2.679491924311224960 ) ) ;
#16236 = CARTESIAN_POINT ( 'NONE',  ( 2.751064625579944321E-14, 203.8750000027312126, 194.0000000000000568 ) ) ;
#16238 = CARTESIAN_POINT ( 'NONE',  ( 10.00000000000000178, 125.2083333333333428, -2.679491924311226736 ) ) ;
#16239 = CARTESIAN_POINT ( 'NONE',  ( -8.000000000000000000, 106.9062500000000000, -3.313708498984761608 ) ) ;
#16240 = CARTESIAN_POINT ( 'NONE',  ( 3.084418934648133437, 225.9999999999999716, 9.520615687278169759 ) ) ;
#16241 = CARTESIAN_POINT ( 'NONE',  ( -2.977408999572648707, -7.188101187499990274, 3.642802781871751883 ) ) ;
#16242 = CARTESIAN_POINT ( 'NONE',  ( 3.313708498984762496, 1.218750000000000222, 7.999999999999998224 ) ) ;
#16243 = CARTESIAN_POINT ( 'NONE',  ( 26.56734541678238060, 205.0000000013655779, 166.5412658749999650 ) ) ;
#16244 = CARTESIAN_POINT ( 'NONE',  ( -1.320432766682874540E-15, 1.968749997951610320, 7.188101187500000044 ) ) ;
#16245 = CARTESIAN_POINT ( 'NONE',  ( -1.432654583217664479, 198.7500000013656063, 138.5412658750000787 ) ) ;
#16246 = CARTESIAN_POINT ( 'NONE',  ( 7.188101187500002709, 123.6875000020483952, 2.977408999572649151 ) ) ;
#16248 = CARTESIAN_POINT ( 'NONE',  ( 3.458734124999960358, 201.6875000013656063, 142.0000000000000568 ) ) ;
#16247 = DIRECTION ( 'NONE',  ( 0.000000000000000000, -1.000000000000000000, -6.938893903907228378E-16 ) ) ;
#16249 = CARTESIAN_POINT ( 'NONE',  ( 5.676582343749997150, 247.5520833367473301, -9.832129032723418760 ) ) ;
#16250 = CARTESIAN_POINT ( 'NONE',  ( -5.656854249492380582, 114.5000000040967763, -5.656854249492380582 ) ) ;
#16251 = CARTESIAN_POINT ( 'NONE',  ( -8.660254037844387298, 213.9583333265053682, -5.000000000000004441 ) ) ;
#16252 = CARTESIAN_POINT ( 'NONE',  ( 29.65685424949240101, 200.4375000000000568, 165.9999999999998863 ) ) ;
#16253 = CARTESIAN_POINT ( 'NONE',  ( -3.042071309553173730, 14.32291666325268231, 11.35316468749999785 ) ) ;
#16254 = CARTESIAN_POINT ( 'NONE',  ( 7.188101187499992051, 8.802885111219154394E-16, 1.111552781871753215 ) ) ;
#16255 = CARTESIAN_POINT ( 'NONE',  ( -5.676582343749998039, 202.7604166632526983, -9.832129032723420536 ) ) ;
#16256 = CARTESIAN_POINT ( 'NONE',  ( -23.99999999999998934, 202.8750000027312126, 170.0000000000002842 ) ) ;
#16257 = CARTESIAN_POINT ( 'NONE',  ( 12.00000000000000000, 6.928203230275491009, -14.00000000000000178 ) ) ;
#16259 = CARTESIAN_POINT ( 'NONE',  ( 7.999999999999991118, 9.797174393178815797E-16, 28.58030277982336642 ) ) ;
#16258 = LINE ( 'NONE', #15895, #64780 ) ;
#16260 = ORIENTED_EDGE ( 'NONE', *, *, #68183, .T. ) ;
#16261 = EDGE_CURVE ( 'NONE', #73165, #33251, #13023, .T. ) ;
#16262 = CARTESIAN_POINT ( 'NONE',  ( -1.432654583217664701, 199.0000000013656063, 138.5412658750000787 ) ) ;
#16263 = CARTESIAN_POINT ( 'NONE',  ( -8.311093377946841443, 3.906249996586016682, 8.311093377946830785 ) ) ;
#16264 = CARTESIAN_POINT ( 'NONE',  ( -11.00000000000000000, 4.556349186104045934, 95.59375000409677625 ) ) ;
#16265 = CARTESIAN_POINT ( 'NONE',  ( 1.102182119232618108E-15, 292.2500000000000000, 6.000000000000001776 ) ) ;
#16266 = CARTESIAN_POINT ( 'NONE',  ( -30.44569435410886626, 195.5625000013656063, 167.5543056458916169 ) ) ;
#16267 = CARTESIAN_POINT ( 'NONE',  ( 0.000000000000000000, 15.99999999999998579, 0.000000000000000000 ) ) ;
#16269 = CARTESIAN_POINT ( 'NONE',  ( 9.832129032723420536, 1.197916663252682756, -5.676582343749999815 ) ) ;
#16268 = CARTESIAN_POINT ( 'NONE',  ( 5.082755093536325042, 117.5937500020483810, -5.082755093536325930 ) ) ;
#16270 = CARTESIAN_POINT ( 'NONE',  ( -7.999999999999989342, -3.313708498984762496, 18.92405277982336642 ) ) ;
#16271 = CARTESIAN_POINT ( 'NONE',  ( -8.311093377946841443, 138.9062499965859843, 8.311093377946830785 ) ) ;
#16272 = CARTESIAN_POINT ( 'NONE',  ( 8.660254037844389075, 107.2916666598387110, -5.000000000000000000 ) ) ;
#16273 = CARTESIAN_POINT ( 'NONE',  ( 5.082755093536326818, 122.0937500020483952, 5.082755093536325042 ) ) ;
#16274 = CARTESIAN_POINT ( 'NONE',  ( -8.000000000000000000, 13.96874999590322375, -3.313708498984762496 ) ) ;
#16275 = CARTESIAN_POINT ( 'NONE',  ( -24.54126587499999701, 207.4375000013656063, 170.0000000000003411 ) ) ;
#16276 = DIRECTION ( 'NONE',  ( 0.000000000000000000, 0.000000000000000000, -1.000000000000000000 ) ) ;
#16277 = VERTEX_POINT ( 'NONE', #38669 ) ;
#16278 = CARTESIAN_POINT ( 'NONE',  ( -1.506680654955288245, -65.82403019918164944, 26.31606384388981112 ) ) ;
#16279 = CARTESIAN_POINT ( 'NONE',  ( -6.676582343750003368, 290.5468750017071216, -2.765530957081996810 ) ) ;
#16280 = CARTESIAN_POINT ( 'NONE',  ( -1.656854249492432318, 207.8125000027312410, 146.0000000000000284 ) ) ;
#16281 = CARTESIAN_POINT ( 'NONE',  ( -7.999999999999991118, 3.313708498984756723, 0.9240527839201456706 ) ) ;
#16282 = CARTESIAN_POINT ( 'NONE',  ( 1.656854249492229592, 197.8125000000000000, 146.0000000000001421 ) ) ;
#16283 = EDGE_CURVE ( 'NONE', #60666, #55449, #66570, .T. ) ;
#16284 = CARTESIAN_POINT ( 'NONE',  ( 3.042071309553163960, 257.4479166700806445, -11.35316468749999785 ) ) ;
#16285 = AXIS2_PLACEMENT_3D ( 'NONE', #59994, #15453, #8311 ) ;
#16286 = CARTESIAN_POINT ( 'NONE',  ( -10.18810118749999738, -4.220049686691941915, 98.12500000204836681 ) ) ;
#16287 = ORIENTED_EDGE ( 'NONE', *, *, #61872, .T. ) ;
#16288 = VECTOR ( 'NONE', #66804, 1000.000000000000000 ) ;
#16289 = CYLINDRICAL_SURFACE ( 'NONE', #41333, 11.00000000000000000 ) ;
#16290 = CARTESIAN_POINT ( 'NONE',  ( -6.735557395310442023E-16, 11.00000000000000000, 98.12499999999998579 ) ) ;
#16291 = CARTESIAN_POINT ( 'NONE',  ( -3.458734124999960358, 202.6250000013656063, 196.5673454167823877 ) ) ;
#16292 = CARTESIAN_POINT ( 'NONE',  ( 11.35316468749999785, 80.88541666325269830, 3.042071309553174174 ) ) ;
#16293 = ORIENTED_EDGE ( 'NONE', *, *, #3790, .T. ) ;
#16294 = CARTESIAN_POINT ( 'NONE',  ( -10.18810118749999738, -4.220049686691941915, 111.2500000020483952 ) ) ;
#16295 = CARTESIAN_POINT ( 'NONE',  ( 3.211159895383561835, 12.56249999863440792, -3.211159895383561835 ) ) ;
#16296 = ORIENTED_EDGE ( 'NONE', *, *, #63430, .T. ) ;
#16297 = CARTESIAN_POINT ( 'NONE',  ( 2.977408999572651815, 25.68749999795162253, 7.188101187500000933 ) ) ;
#16298 = CARTESIAN_POINT ( 'NONE',  ( 1.567784982238203817E-13, 113.7500000000000284, 10.00000000000000533 ) ) ;
#16299 = CARTESIAN_POINT ( 'NONE',  ( 5.000000000000001776, 67.70833332650536818, -8.660254037844389075 ) ) ;
#16300 = CARTESIAN_POINT ( 'NONE',  ( 2.977408999572651815, 17.06249999795161543, 7.188101187500000933 ) ) ;
#16301 = EDGE_CURVE ( 'NONE', #49646, #54702, #61294, .T. ) ;
#16302 = DIRECTION ( 'NONE',  ( 0.8660254037844379305, 0.5000000000000011102, 0.000000000000000000 ) ) ;
#16303 = CARTESIAN_POINT ( 'NONE',  ( -4.220049686691937474, -10.18810118749999738, 108.8125000020484094 ) ) ;
#16304 =( BOUNDED_CURVE ( )  B_SPLINE_CURVE ( 2, ( #55568, #14425, #37459, #60457, #28000, #28368, #23079, #56305, #57055 ),
 .UNSPECIFIED., .F., .F. ) 
 B_SPLINE_CURVE_WITH_KNOTS ( ( 3, 2, 2, 2, 3 ),
 ( 0.5937500000000000000, 0.5989583333333333703, 0.6041666666666666297, 0.6093750000000000000, 0.6145833333333333703 ),
 .UNSPECIFIED. ) 
 CURVE ( )  GEOMETRIC_REPRESENTATION_ITEM ( )  RATIONAL_B_SPLINE_CURVE ( ( 1.000000000000000000, 0.9238795325112867385, 1.000000000000000000, 0.9238795325112867385, 1.000000000000000000, 0.9238795325112867385, 1.000000000000000000, 0.9238795325112867385, 1.000000000000000000 ) ) 
 REPRESENTATION_ITEM ( '' )  );
#16305 = CARTESIAN_POINT ( 'NONE',  ( 1.656854249492381914, 8.562499997268814056, 4.000000000000000888 ) ) ;
#16306 = DIRECTION ( 'NONE',  ( 0.000000000000000000, 0.000000000000000000, 1.000000000000000000 ) ) ;
#16307 = ORIENTED_EDGE ( 'NONE', *, *, #23310, .F. ) ;
#16308 = ADVANCED_FACE ( 'NONE', ( #60542 ), #67332, .T. ) ;
#16309 = EDGE_CURVE ( 'NONE', #70218, #71597, #5337, .T. ) ;
#16310 = CARTESIAN_POINT ( 'NONE',  ( -3.458734124999959914, 202.3750000013655779, 196.5673454167823877 ) ) ;
#16311 = CARTESIAN_POINT ( 'NONE',  ( -24.00000000000002132, 194.9375000027312126, 168.3431457505079152 ) ) ;
#16312 = CARTESIAN_POINT ( 'NONE',  ( 27.99999999999996447, 199.6250000027312126, 165.9999999999998863 ) ) ;
#16313 = CARTESIAN_POINT ( 'NONE',  ( 4.541265875000002339, 11.31249999863440614, 0.000000000000000000 ) ) ;
#16314 = EDGE_CURVE ( 'NONE', #26730, #42029, #72228, .T. ) ;
#16315 = CARTESIAN_POINT ( 'NONE',  ( -2.828427124746190735, 10.12499999726881406, -2.828427124746191623 ) ) ;
#16316 = CARTESIAN_POINT ( 'NONE',  ( -5.082755093536319713, 5.082755093536319713, 17.79905278187175455 ) ) ;
#16317 = VERTEX_POINT ( 'NONE', #72989 ) ;
#16319 =( BOUNDED_CURVE ( )  B_SPLINE_CURVE ( 2, ( #35652, #40564, #6973, #29982, #1333, #24315, #47326, #69608, #17923 ),
 .UNSPECIFIED., .F., .F. ) 
 B_SPLINE_CURVE_WITH_KNOTS ( ( 3, 2, 2, 2, 3 ),
 ( 0.4861111111111111049, 0.4930555555555555802, 0.5000000000000000000, 0.5069444444444444198, 0.5138888888888888395 ),
 .UNSPECIFIED. ) 
 CURVE ( )  GEOMETRIC_REPRESENTATION_ITEM ( )  RATIONAL_B_SPLINE_CURVE ( ( 1.000000000000000000, 0.9238795325112867385, 1.000000000000000000, 0.9238795325112867385, 1.000000000000000000, 0.9238795325112867385, 1.000000000000000000, 0.9238795325112867385, 1.000000000000000000 ) ) 
 REPRESENTATION_ITEM ( '' )  );
#16318 = CARTESIAN_POINT ( 'NONE',  ( 1.224646799147353256E-15, 0.000000000000000000, 10.00000000000000000 ) ) ;
#16320 = ORIENTED_EDGE ( 'NONE', *, *, #21579, .T. ) ;
#16321 = CARTESIAN_POINT ( 'NONE',  ( 10.18810118750000093, -4.220049686691933033, 108.8125000020483952 ) ) ;
#16322 = LINE ( 'NONE', #50298, #14732 ) ;
#16323 = CARTESIAN_POINT ( 'NONE',  ( 3.458734125000015425, 203.9375000013656063, 198.0000000000000284 ) ) ;
#16324 = CARTESIAN_POINT ( 'NONE',  ( 31.45873412499999944, 197.6250000013656063, 171.4326545832175555 ) ) ;
#16325 = CARTESIAN_POINT ( 'NONE',  ( 8.660254037844389075, 80.41666666666667140, -5.000000000000000000 ) ) ;
#16326 = CARTESIAN_POINT ( 'NONE',  ( 8.000000000000000000, 124.3437500000000000, -3.313708498984762496 ) ) ;
#16327 = CARTESIAN_POINT ( 'NONE',  ( 2.485281374238575314, 291.3125000000000000, 6.000000000000000888 ) ) ;
#16328 = CARTESIAN_POINT ( 'NONE',  ( 32.00000000000000000, 205.3750000027312126, 169.9999999999998863 ) ) ;
#16329 = EDGE_LOOP ( 'NONE', ( #45604, #30, #51130, #54134 ) ) ;
#16330 = CIRCLE ( 'NONE', #58547, 11.00000000000000000 ) ;
#16331 = CARTESIAN_POINT ( 'NONE',  ( 6.308070865109145053, -10.25011764679052995, 64.85270989093093874 ) ) ;
#16332 = CARTESIAN_POINT ( 'NONE',  ( 2.828427124746152987, 194.2500000027312126, 139.1715728752538723 ) ) ;
#16333 = CARTESIAN_POINT ( 'NONE',  ( -5.000000000000000888, 66.79063484153765273, 23.29724706625453479 ) ) ;
#16334 = CARTESIAN_POINT ( 'NONE',  ( 8.000000000000000000, 13.31249999590322375, 0.000000000000000000 ) ) ;
#16335 = CARTESIAN_POINT ( 'NONE',  ( -5.000000000000000888, 244.1666666666666572, -8.660254037844387298 ) ) ;
#16336 = CARTESIAN_POINT ( 'NONE',  ( 28.00000000000002132, 203.1250000027312126, 173.9999999999999147 ) ) ;
#16337 = CARTESIAN_POINT ( 'NONE',  ( -1.836970198721029983E-15, 198.7500000000000000, 10.00000000000000178 ) ) ;
#16338 = VECTOR ( 'NONE', #18927, 1000.000000000000227 ) ;
#16339 = LINE ( 'NONE', #26548, #7860 ) ;
#16340 = CARTESIAN_POINT ( 'NONE',  ( 2.977408999572650927, -7.188101187499990274, 14.33030278187175277 ) ) ;
#16341 = CARTESIAN_POINT ( 'NONE',  ( -11.35316468749999785, 163.3854166632526983, -3.042071309553167513 ) ) ;
#16342 = CARTESIAN_POINT ( 'NONE',  ( -5.000000000000000000, -16.14408868864072844, 27.96238185062368586 ) ) ;
#16343 = FACE_OUTER_BOUND ( 'NONE', #56307, .T. ) ;
#16345 = CARTESIAN_POINT ( 'NONE',  ( -4.242640687119285658, 297.1875000034139589, 4.242640687119287435 ) ) ;
#16344 = CARTESIAN_POINT ( 'NONE',  ( 2.775557561562891351E-14, -70.00000000000000000, 139.0000000000000568 ) ) ;
#16346 = VERTEX_POINT ( 'NONE', #60168 ) ;
#16347 = CARTESIAN_POINT ( 'NONE',  ( -9.832129032723420536, 19.01041666325268409, 5.676582343749997150 ) ) ;
#16348 = CARTESIAN_POINT ( 'NONE',  ( -24.54126587499999701, 209.1875000013656063, 170.0000000000002842 ) ) ;
#16350 = CARTESIAN_POINT ( 'NONE',  ( -5.000000000000000000, 10.26105934116143281, -64.40045319026697257 ) ) ;
#16349 = CARTESIAN_POINT ( 'NONE',  ( -7.999999999999992895, -1.544684865728715588E-05, 17.51780322093567577 ) ) ;
#16351 = LINE ( 'NONE', #51075, #35016 ) ;
#16352 = CARTESIAN_POINT ( 'NONE',  ( -2.839093476692135984E-14, 203.6875000013656063, 138.5412658750000503 ) ) ;
#16353 = CARTESIAN_POINT ( 'NONE',  ( -10.00000000000000000, 64.16666665983869677, -2.679491924311229845 ) ) ;
#16354 = CARTESIAN_POINT ( 'NONE',  ( -4.401442555609581635E-16, 101.2812500020483810, -7.188101187500000044 ) ) ;
#16355 = CARTESIAN_POINT ( 'NONE',  ( -3.211159895383561391, 13.81249999863440614, -3.211159895383561835 ) ) ;
#16356 = CARTESIAN_POINT ( 'NONE',  ( 5.000000000000104805, 214.1666666666667993, 8.660254037844582697 ) ) ;
#16357 = CARTESIAN_POINT ( 'NONE',  ( -4.898587196589407898E-16, 7.999999999999991118, 1.955302779823364645 ) ) ;
#16358 = CARTESIAN_POINT ( 'NONE',  ( 3.313708498984762496, -7.999999999999989342, 20.98655278392014978 ) ) ;
#16359 = ORIENTED_EDGE ( 'NONE', *, *, #17785, .T. ) ;
#16360 = ORIENTED_EDGE ( 'NONE', *, *, #21030, .T. ) ;
#16361 = EDGE_CURVE ( 'NONE', #8939, #12433, #32881, .T. ) ;
#16362 = CARTESIAN_POINT ( 'NONE',  ( -5.000000000000000000, -50.64189880742087269, -41.08656465431914029 ) ) ;
#16363 = CARTESIAN_POINT ( 'NONE',  ( 1.432654583217662481, 195.3750000013656063, 194.5412658750000219 ) ) ;
#16364 = CARTESIAN_POINT ( 'NONE',  ( -10.00000000000001599, 162.7083333333333712, 2.679491924311226292 ) ) ;
#16365 = CARTESIAN_POINT ( 'NONE',  ( -5.656854249492380582, 99.31250000000000000, -5.656854249492380582 ) ) ;
#16366 = CARTESIAN_POINT ( 'NONE',  ( -8.311093377946836114, 137.6562499965859558, -8.311093377946837890 ) ) ;
#16367 = EDGE_LOOP ( 'NONE', ( #62929, #68036, #57926, #43379, #32950, #18369, #71092, #38067, #17176, #17301, #70662, #28893, #53237, #28229, #44066, #28085, #11474, #1659, #74097, #71254, #4009, #51067, #28073, #64452 ) ) ;
#16368 = CARTESIAN_POINT ( 'NONE',  ( 29.65685424949246851, 201.4375000000000284, 165.9999999999999716 ) ) ;
#16369 = CARTESIAN_POINT ( 'NONE',  ( -4.220049686691937474, -10.18810118749999738, 87.43750000204838102 ) ) ;
#16370 = CARTESIAN_POINT ( 'NONE',  ( -29.53044679813742945, 194.7194814984362381, 173.3976864218442415 ) ) ;
#16371 = CARTESIAN_POINT ( 'NONE',  ( 1.656854249492405451, 209.3125000000000568, 202.0000000000000284 ) ) ;
#16372 = CARTESIAN_POINT ( 'NONE',  ( -5.656854249492379694, 18.37499999590322020, -5.656854249492380582 ) ) ;
#16373 = CARTESIAN_POINT ( 'NONE',  ( 11.00000000000000000, 1.347111479062088405E-15, 112.7499999999999858 ) ) ;
#16374 = CARTESIAN_POINT ( 'NONE',  ( -7.204075437095967871, 7.204075437095967871, 115.8437500020483810 ) ) ;
#16375 = VERTEX_POINT ( 'NONE', #6194 ) ;
#16376 = EDGE_CURVE ( 'NONE', #728, #6516, #51456, .T. ) ;
#16377 = CARTESIAN_POINT ( 'NONE',  ( 37.76477820665567720, -2.162727750835041984, 128.1810218861025419 ) ) ;
#16378 = CARTESIAN_POINT ( 'NONE',  ( 17.06637649524319400, 182.9342320177482009, 144.0228969870551339 ) ) ;
#16379 = CARTESIAN_POINT ( 'NONE',  ( 11.35316468749999963, 131.3020833299193555, -3.042071309553165293 ) ) ;
#16380 = CARTESIAN_POINT ( 'NONE',  ( -2.445694354108783664, 203.3125000013656063, 195.5543056458912190 ) ) ;
#16381 = CARTESIAN_POINT ( 'NONE',  ( -2.977408999572654480, 25.87499999795161543, 7.188101187499999156 ) ) ;
#16382 = CARTESIAN_POINT ( 'NONE',  ( 7.204075437095966983, 7.204075437095967871, 85.46875000204836681 ) ) ;
#16383 = CARTESIAN_POINT ( 'NONE',  ( 9.832129032723416984, 35.67708332991935549, 5.676582343750006032 ) ) ;
#16384 = ORIENTED_EDGE ( 'NONE', *, *, #12959, .T. ) ;
#16385 = LINE ( 'NONE', #33783, #41662 ) ;
#16386 = CARTESIAN_POINT ( 'NONE',  ( 5.662595241051936235, -5.662595241051934458, 19.57561528394063188 ) ) ;
#16387 = LINE ( 'NONE', #38315, #7717 ) ;
#16388 = PRODUCT_RELATED_PRODUCT_CATEGORY ( 'part', '', ( #25763 ) ) ;
#16389 = CARTESIAN_POINT ( 'NONE',  ( -2.977408999572650039, 9.937499997951610098, -7.188101187500001821 ) ) ;
#16390 = CARTESIAN_POINT ( 'NONE',  ( -4.242640687119285658, 298.1875000034139589, 4.242640687119287435 ) ) ;
#16391 =( GEOMETRIC_REPRESENTATION_CONTEXT ( 3 ) GLOBAL_UNCERTAINTY_ASSIGNED_CONTEXT ( ( #57925 ) ) GLOBAL_UNIT_ASSIGNED_CONTEXT ( ( #46118, #17443, #40092 ) ) REPRESENTATION_CONTEXT ( 'NONE', 'WORKASPACE' ) );
#16392 = CARTESIAN_POINT ( 'NONE',  ( 8.660254037844389075, 112.2916666598387110, -5.000000000000000000 ) ) ;
#16393 = CARTESIAN_POINT ( 'NONE',  ( -5.082755093536325042, 2.906249997951610542, -5.082755093536325930 ) ) ;
#16394 = CARTESIAN_POINT ( 'NONE',  ( -8.311093377946836114, 152.9687499965859558, -8.311093377946837890 ) ) ;
#16395 = CARTESIAN_POINT ( 'NONE',  ( 10.18810118750000093, -4.220049686691933921, 75.81250000204838102 ) ) ;
#16396 = EDGE_CURVE ( 'NONE', #12752, #68202, #71405, .T. ) ;
#16397 = CIRCLE ( 'NONE', #46507, 8.000000000000000000 ) ;
#16398 = CARTESIAN_POINT ( 'NONE',  ( -31.45873412499999233, 195.6875000013655779, 170.0000000000003979 ) ) ;
#16399 = EDGE_CURVE ( 'NONE', #7225, #338, #56386, .T. ) ;
#16400 = CARTESIAN_POINT ( 'NONE',  ( 12.00000000000000178, 4.898587196589402968E-16, 31.99999999999998579 ) ) ;
#16401 = CARTESIAN_POINT ( 'NONE',  ( 3.211159895383561835, 19.56249999863440436, -3.211159895383561835 ) ) ;
#16402 = ORIENTED_EDGE ( 'NONE', *, *, #6051, .F. ) ;
#16403 = MANIFOLD_SOLID_BREP ( 'EndChamfer', #16557 ) ;
#16404 = CARTESIAN_POINT ( 'NONE',  ( 2.751064625579944321E-14, 200.8750000027312126, 194.0000000000000568 ) ) ;
#16405 = CARTESIAN_POINT ( 'NONE',  ( -3.458734125000015869, 195.1875000013655779, 142.0000000000000568 ) ) ;
#16406 = CARTESIAN_POINT ( 'NONE',  ( -28.00000000000008171, 207.1250000027312126, 166.0000000000003695 ) ) ;
#16407 = VECTOR ( 'NONE', #1381, 1000.000000000000000 ) ;
#16408 = CARTESIAN_POINT ( 'NONE',  ( 4.898587196589412829E-16, 21.37500000000000355, -8.000000000000000000 ) ) ;
#16409 = ORIENTED_EDGE ( 'NONE', *, *, #2542, .F. ) ;
#16410 = ADVANCED_FACE ( 'NONE', ( #5449 ), #11110, .F. ) ;
#16411 = CARTESIAN_POINT ( 'NONE',  ( 7.188101187500000044, 10.96874999795161187, 0.000000000000000000 ) ) ;
#16412 = CARTESIAN_POINT ( 'NONE',  ( -8.660254037844390851, 209.7916666598387110, 4.999999999999998224 ) ) ;
#16413 = CARTESIAN_POINT ( 'NONE',  ( 5.000000000000000000, 53.55895565990340401, -45.41404144516010888 ) ) ;
#16414 = CARTESIAN_POINT ( 'NONE',  ( -10.00000000000000355, 37.70833333333333570, 2.679491924311223183 ) ) ;
#16415 = CARTESIAN_POINT ( 'NONE',  ( 7.188101187500000044, 104.2812500020483810, -8.802885111219163269E-16 ) ) ;
#16416 = CARTESIAN_POINT ( 'NONE',  ( -26.56734541678233086, 206.2500000013655779, 173.4587341250003760 ) ) ;
#16417 = CARTESIAN_POINT ( 'NONE',  ( -5.656854249492373476, -5.656854249492376141, 2.517802779823365089 ) ) ;
#16419 = CARTESIAN_POINT ( 'NONE',  ( -8.000072035430726203, -0.9604724192222298118, 0.000000000000000000 ) ) ;
#16418 = DIRECTION ( 'NONE',  ( 0.000000000000000000, 0.000000000000000000, 1.000000000000000000 ) ) ;
#16420 =( BOUNDED_CURVE ( )  B_SPLINE_CURVE ( 2, ( #71461, #14116, #37528, #31863, #3197, #26184, #49203, #45405, #33370 ),
 .UNSPECIFIED., .F., .F. ) 
 B_SPLINE_CURVE_WITH_KNOTS ( ( 3, 2, 2, 2, 3 ),
 ( 0.7166666666666671182, 0.7250000000000005329, 0.7333333333333338366, 0.7416666666666673624, 0.7500000000000006661 ),
 .UNSPECIFIED. ) 
 CURVE ( )  GEOMETRIC_REPRESENTATION_ITEM ( )  RATIONAL_B_SPLINE_CURVE ( ( 0.9999999999999958922, 0.9238795325112908463, 1.000000000000000000, 0.9238795325112867385, 1.000000000000000000, 0.9238795325112867385, 1.000000000000000000, 0.9238795325112806323, 1.000000000000005995 ) ) 
 REPRESENTATION_ITEM ( '' )  );
#16421 = ORIENTED_EDGE ( 'NONE', *, *, #22684, .F. ) ;
#16422 = CARTESIAN_POINT ( 'NONE',  ( 3.042071309553173286, 255.3645833367473301, 11.35316468749999608 ) ) ;
#16423 = CARTESIAN_POINT ( 'NONE',  ( 7.188101187499993827, -2.977408999572645598, 23.51780278187175455 ) ) ;
#16424 = CARTESIAN_POINT ( 'NONE',  ( -11.00000000000000000, 0.000000000000000000, 92.49999999999998579 ) ) ;
#16425 = CARTESIAN_POINT ( 'NONE',  ( 1.102182119232618108E-15, 287.3125000034140157, 6.000000000000001776 ) ) ;
#16426 = CARTESIAN_POINT ( 'NONE',  ( 1.781595147095572207, -67.70776641946376628, -20.12770457511637190 ) ) ;
#16427 = CARTESIAN_POINT ( 'NONE',  ( 3.458734125000015425, 197.2500000013656063, 196.5673454167823877 ) ) ;
#16428 = CARTESIAN_POINT ( 'NONE',  ( 5.000000000000001776, 160.8333333333333428, -8.660254037844389075 ) ) ;
#16429 = CARTESIAN_POINT ( 'NONE',  ( 37.99999999999999289, 205.0000000000000284, 20.00000000000000000 ) ) ;
#16430 = DIRECTION ( 'NONE',  ( 1.000000000000000000, 0.000000000000000000, 0.000000000000000000 ) ) ;
#16431 = DIRECTION ( 'NONE',  ( -0.000000000000000000, -1.000000000000000000, -0.000000000000000000 ) ) ;
#16432 = CARTESIAN_POINT ( 'NONE',  ( 8.311093377946837890, 121.7187499965860411, -8.311093377946837890 ) ) ;
#16433 = CARTESIAN_POINT ( 'NONE',  ( -2.143145793903030439E-12, 53.74999999999984368, 9.999999999999998224 ) ) ;
#16434 = CARTESIAN_POINT ( 'NONE',  ( 1.224646799147353256E-15, 0.000000000000000000, 10.00000000000000000 ) ) ;
#16437 = CARTESIAN_POINT ( 'NONE',  ( -6.735557395310442023E-16, 11.00000000000000000, 110.3125000040967763 ) ) ;
#16436 = CARTESIAN_POINT ( 'NONE',  ( 28.00000000000001421, 195.4375000013655779, 173.4587341249998929 ) ) ;
#16435 = CARTESIAN_POINT ( 'NONE',  ( 23.99999999999998224, 209.8125000000000000, 171.6568542494922553 ) ) ;
#16438 = EDGE_CURVE ( 'NONE', #71834, #46180, #74470, .T. ) ;
#16439 = ORIENTED_EDGE ( 'NONE', *, *, #35816, .F. ) ;
#16440 = CARTESIAN_POINT ( 'NONE',  ( 0.000000000000000000, 0.000000000000000000, -92.50000000000000000 ) ) ;
#16441 = EDGE_CURVE ( 'NONE', #60482, #69418, #57133, .T. ) ;
#16442 = CARTESIAN_POINT ( 'NONE',  ( 10.99999999999999822, 1.347111479062088405E-15, 112.9375000040967763 ) ) ;
#16443 =( BOUNDED_CURVE ( )  B_SPLINE_CURVE ( 2, ( #42645, #60370, #8318 ),
 .UNSPECIFIED., .F., .F. ) 
 B_SPLINE_CURVE_WITH_KNOTS ( ( 3, 3 ),
 ( 0.9728260869565217295, 0.9744508335588618619 ),
 .UNSPECIFIED. ) 
 CURVE ( )  GEOMETRIC_REPRESENTATION_ITEM ( )  RATIONAL_B_SPLINE_CURVE ( ( 1.000000000000000000, 0.9694402323236602781, 0.9936961387326025408 ) ) 
 REPRESENTATION_ITEM ( '' )  );
#16444 = CARTESIAN_POINT ( 'NONE',  ( 31.45873412499997812, 199.8750000013655779, 171.4326545832175839 ) ) ;
#16445 = CARTESIAN_POINT ( 'NONE',  ( 6.951808397369818766E-16, 202.3437499965860127, -11.35316468750000141 ) ) ;
#16446 = CARTESIAN_POINT ( 'NONE',  ( 7.188101187500000044, 121.9062500020483810, -8.802885111219163269E-16 ) ) ;
#16447 = CARTESIAN_POINT ( 'NONE',  ( 1.881053915767122664, 18.12499999863440792, 4.541265875000001451 ) ) ;
#16448 = CARTESIAN_POINT ( 'NONE',  ( 7.456155213531532766, -51.58724325107078812, 41.60228463192836301 ) ) ;
#16449 = CARTESIAN_POINT ( 'NONE',  ( -7.999999999999991118, 3.313708498984756723, 23.23655277982336642 ) ) ;
#16451 = CARTESIAN_POINT ( 'NONE',  ( 1.425702245604163669E-12, 48.75000000000012079, 10.00000000000000178 ) ) ;
#16450 = CARTESIAN_POINT ( 'NONE',  ( 3.499857865026532622, -7.193933550196781823, 0.0006324257780546024528 ) ) ;
#16452 = CARTESIAN_POINT ( 'NONE',  ( 3.042071309553159519, 89.73958332991935549, 11.35316468750000141 ) ) ;
#16453 = EDGE_LOOP ( 'NONE', ( #65660, #9498, #47921, #11428, #12119, #27866, #74313, #57851, #10567, #38011, #3920 ) ) ;
#16454 = EDGE_CURVE ( 'NONE', #832, #2971, #72421, .T. ) ;
#16455 = CARTESIAN_POINT ( 'NONE',  ( -2.849036369511732440E-14, 205.3750000027312126, 138.0000000000000568 ) ) ;
#16456 = CARTESIAN_POINT ( 'NONE',  ( -2.977408999572654480, 25.49999999795161898, 7.188101187499999156 ) ) ;
#16457 = CARTESIAN_POINT ( 'NONE',  ( 36.10814071610729314, 49.99999999999998579, 139.0000000000000000 ) ) ;
#16458 = CARTESIAN_POINT ( 'NONE',  ( 5.676582343750005144, 260.8854166700806445, 9.832129032723416984 ) ) ;
#16459 = CARTESIAN_POINT ( 'NONE',  ( 9.832129032723420536, 101.1979166632526841, -5.676582343749999815 ) ) ;
#16460 = ORIENTED_EDGE ( 'NONE', *, *, #15969, .F. ) ;
#16461 = CARTESIAN_POINT ( 'NONE',  ( 10.00000000000000178, 206.8749999931720538, 0.000000000000000000 ) ) ;
#16462 = CARTESIAN_POINT ( 'NONE',  ( -4.220049686691935698, 10.18810118749999916, 109.3750000020483810 ) ) ;
#16463 = CARTESIAN_POINT ( 'NONE',  ( 5.000000000000001776, 217.7083333265053682, -8.660254037844389075 ) ) ;
#16464 = CARTESIAN_POINT ( 'NONE',  ( -2.445694354108783219, 203.8125000013656063, 200.4456943541088663 ) ) ;
#16465 = PLANE ( 'NONE',  #74510 ) ;
#16467 = CARTESIAN_POINT ( 'NONE',  ( -11.35316468749999785, 103.0729166632526841, -3.042071309553167957 ) ) ;
#16466 = CARTESIAN_POINT ( 'NONE',  ( 27.99999999999999645, 210.0000000000000284, 173.9999999999998863 ) ) ;
#16468 = CARTESIAN_POINT ( 'NONE',  ( 7.999999999999991118, 9.797174393178815797E-16, 13.76780278392014623 ) ) ;
#16469 = CARTESIAN_POINT ( 'NONE',  ( -31.45873412499998523, 202.0000000013656063, 171.4326545832180386 ) ) ;
#16470 = CARTESIAN_POINT ( 'NONE',  ( 4.000000000000015987, 208.6250000027312126, 198.0000000000000284 ) ) ;
#16471 = VERTEX_POINT ( 'NONE', #40146 ) ;
#16472 = CARTESIAN_POINT ( 'NONE',  ( 7.320508075688771044, 181.2499999931720254, 7.320508075688775484 ) ) ;
#16473 = CARTESIAN_POINT ( 'NONE',  ( 2.828427124746152987, 208.1250000000000284, 139.1715728752538723 ) ) ;
#16474 = DIRECTION ( 'NONE',  ( -0.000000000000000000, 1.000000000000000000, -0.000000000000000000 ) ) ;
#16475 = CARTESIAN_POINT ( 'NONE',  ( -11.35316468750000141, 68.59374999658601268, -1.390361679473963753E-15 ) ) ;
#16476 = CARTESIAN_POINT ( 'NONE',  ( -6.676582343750003368, 288.3906250017069510, -2.765530957081996810 ) ) ;
#16477 = CARTESIAN_POINT ( 'NONE',  ( -7.188101187500000933, 7.499999997951610986, -2.977408999572651371 ) ) ;
#16478 = EDGE_CURVE ( 'NONE', #50841, #28168, #11478, .T. ) ;
#16479 = CARTESIAN_POINT ( 'NONE',  ( 4.220049686691941027, -10.18810118749999738, 103.0000000020483668 ) ) ;
#16480 = CARTESIAN_POINT ( 'NONE',  ( 9.832129032723420536, 1.510416663252683422, -5.676582343749999815 ) ) ;
#16481 = ORIENTED_EDGE ( 'NONE', *, *, #69935, .T. ) ;
#16482 = CARTESIAN_POINT ( 'NONE',  ( -7.999999999999991118, 0.000000000000000000, 27.83030277982336642 ) ) ;
#16483 = CARTESIAN_POINT ( 'NONE',  ( -5.656854249492379694, 1.874999995903220196, -5.656854249492380582 ) ) ;
#16484 = CARTESIAN_POINT ( 'NONE',  ( 2.449293598294707893E-16, 0.9999999972688131678, -4.000000000000001776 ) ) ;
#16485 = CARTESIAN_POINT ( 'NONE',  ( 8.311093377946834337, 205.1562499965859843, 8.311093377946839666 ) ) ;
#16486 = CARTESIAN_POINT ( 'NONE',  ( -5.000000000000000888, 232.2916666734946602, -8.660254037844387298 ) ) ;
#16487 = CARTESIAN_POINT ( 'NONE',  ( -4.231687259407054036, -16.30907003467246597, -69.42009600258494117 ) ) ;
#16488 = CARTESIAN_POINT ( 'NONE',  ( -6.676582343750003368, 296.3906250017069510, -2.765530957081996810 ) ) ;
#16489 = ORIENTED_EDGE ( 'NONE', *, *, #27773, .F. ) ;
#16490 = CARTESIAN_POINT ( 'NONE',  ( -8.311093377946841443, 199.2187499965860411, 8.311093377946834337 ) ) ;
#16491 = CARTESIAN_POINT ( 'NONE',  ( -27.99999999999996803, 208.9375000013656063, 173.4587341250003760 ) ) ;
#16492 = CARTESIAN_POINT ( 'NONE',  ( 3.313708498984762496, 19.21875000000000000, 7.999999999999998224 ) ) ;
#16493 = CIRCLE ( 'NONE', #36968, 10.00000000000000178 ) ;
#16494 = ORIENTED_EDGE ( 'NONE', *, *, #5155, .F. ) ;
#16495 = AXIS2_PLACEMENT_3D ( 'NONE', #40832, #6509, #35552 ) ;
#16496 = CARTESIAN_POINT ( 'NONE',  ( -3.313708498984762496, 92.46875000409679046, 7.999999999999998224 ) ) ;
#16497 = CARTESIAN_POINT ( 'NONE',  ( -8.660254037844387298, 17.08333333333333570, -5.000000000000004441 ) ) ;
#16498 = CARTESIAN_POINT ( 'NONE',  ( 7.204075437095968759, -7.204075437095966983, 79.09375000204838102 ) ) ;
#16499 = ORIENTED_EDGE ( 'NONE', *, *, #14841, .F. ) ;
#16500 = CARTESIAN_POINT ( 'NONE',  ( -4.000000000000001776, 18.43749999999999645, -1.656854249492381470 ) ) ;
#16501 = CARTESIAN_POINT ( 'NONE',  ( -4.541265875000003227, 19.87499999863441147, 1.881053915767121110 ) ) ;
#16502 = CARTESIAN_POINT ( 'NONE',  ( 26.34314575050768426, 198.6875000027312126, 165.9999999999998010 ) ) ;
#16503 = CARTESIAN_POINT ( 'NONE',  ( 2.828427124746190291, 4.624999997268813168, 2.828427124746192067 ) ) ;
#16504 = CARTESIAN_POINT ( 'NONE',  ( -5.000000000000000000, -11.32881245867859121, 67.85521288293392672 ) ) ;
#16505 = CARTESIAN_POINT ( 'NONE',  ( 4.231687259402825418, 51.96503165405418656, 48.83411696341816821 ) ) ;
#16508 = CARTESIAN_POINT ( 'NONE',  ( 4.615726161707419450, -52.16176840074130183, 48.91069252044830051 ) ) ;
#16507 = CARTESIAN_POINT ( 'NONE',  ( -11.35316468749999608, 244.1145833367473017, 3.042071309553173730 ) ) ;
#16506 = CARTESIAN_POINT ( 'NONE',  ( 29.43265458321766914, 206.5000000013655779, 173.4587341249998929 ) ) ;
#16509 = APPLICATION_PROTOCOL_DEFINITION ( 'draft international standard', 'automotive_design', 1998, #36116 ) ;
#16510 = ORIENTED_EDGE ( 'NONE', *, *, #55945, .T. ) ;
#16511 = ADVANCED_FACE ( 'NONE', ( #21665 ), #7300, .F. ) ;
#16512 = VECTOR ( 'NONE', #14842, 1000.000000000000000 ) ;
#16513 = CARTESIAN_POINT ( 'NONE',  ( -3.042071309553159075, 255.2604166700806445, 11.35316468749999963 ) ) ;
#16514 = CARTESIAN_POINT ( 'NONE',  ( -5.082755093536319713, 5.082755093536319713, 11.79905278187175277 ) ) ;
#16515 = ORIENTED_EDGE ( 'NONE', *, *, #60484, .T. ) ;
#16516 = EDGE_LOOP ( 'NONE', ( #14991, #3416, #16205, #38811 ) ) ;
#16517 = CARTESIAN_POINT ( 'NONE',  ( -10.18810118749999916, 0.000000000000000000, 73.65625000204836681 ) ) ;
#16518 = CARTESIAN_POINT ( 'NONE',  ( 3.042071309553159519, 90.05208332991932707, 11.35316468750000141 ) ) ;
#16519 = CARTESIAN_POINT ( 'NONE',  ( 1.102182119232618108E-15, 297.2500000000000000, 6.000000000000001776 ) ) ;
#16520 = CARTESIAN_POINT ( 'NONE',  ( -7.778174593052023411, 7.778174593052023411, 87.81249999999998579 ) ) ;
#16523 = CARTESIAN_POINT ( 'NONE',  ( 4.721056650415999201, 289.2343750017069510, -4.721056650415999201 ) ) ;
#16522 = CARTESIAN_POINT ( 'NONE',  ( 31.45873412499999944, 207.6875000013656063, 169.9999999999998863 ) ) ;
#16521 = CARTESIAN_POINT ( 'NONE',  ( 29.43265458321761585, 207.7500000013656063, 173.4587341249998929 ) ) ;
#16524 = CARTESIAN_POINT ( 'NONE',  ( 0.000000000000000000, 0.000000000000000000, 20.00000000000000000 ) ) ;
#16525 = EDGE_CURVE ( 'NONE', #24773, #50622, #64270, .T. ) ;
#16526 = CARTESIAN_POINT ( 'NONE',  ( -8.311093377946841443, 198.9062499965860695, 8.311093377946830785 ) ) ;
#16527 = CARTESIAN_POINT ( 'NONE',  ( 5.656854249492378806, 10.12499999590322020, 5.656854249492381470 ) ) ;
#16528 = VERTEX_POINT ( 'NONE', #59723 ) ;
#16529 = CARTESIAN_POINT ( 'NONE',  ( 31.45873412499997812, 195.6250000013656063, 171.4326545832175839 ) ) ;
#16530 = CARTESIAN_POINT ( 'NONE',  ( 5.082755093536324154, 17.15624999795161543, 5.082755093536326818 ) ) ;
#16531 = CARTESIAN_POINT ( 'NONE',  ( 6.951808397369818766E-16, 172.3437499965860127, -11.35316468750000141 ) ) ;
#16532 = CARTESIAN_POINT ( 'NONE',  ( -4.556349186104048599, -10.99999999999999822, 98.96875000409676204 ) ) ;
#16533 = CARTESIAN_POINT ( 'NONE',  ( -7.188101187499999156, 102.1250000020483810, 2.977408999572654924 ) ) ;
#16534 = CARTESIAN_POINT ( 'NONE',  ( -7.320508075688768379, 206.8750000000000000, -7.320508075688769267 ) ) ;
#16535 = CARTESIAN_POINT ( 'NONE',  ( 24.54126587500000767, 206.3750000013656063, 168.5673454167822172 ) ) ;
#16536 = CARTESIAN_POINT ( 'NONE',  ( -2.977408999572647819, 7.188101187499991163, 9.080302781871752771 ) ) ;
#16537 = CARTESIAN_POINT ( 'NONE',  ( -8.311093377946841443, 48.90624999658601268, 8.311093377946830785 ) ) ;
#16538 =( BOUNDED_CURVE ( )  B_SPLINE_CURVE ( 2, ( #47697, #64697, #1709, #30365, #69621, #36767, #24326, #17935, #58678 ),
 .UNSPECIFIED., .F., .F. ) 
 B_SPLINE_CURVE_WITH_KNOTS ( ( 3, 2, 2, 2, 3 ),
 ( 0.8947368421052632748, 0.9013157894736842923, 0.9078947368421054209, 0.9144736842105264385, 0.9210526315789474561 ),
 .UNSPECIFIED. ) 
 CURVE ( )  GEOMETRIC_REPRESENTATION_ITEM ( )  RATIONAL_B_SPLINE_CURVE ( ( 0.9999999999999986677, 0.9238795325112880708, 1.000000000000000000, 0.9238795325112867385, 1.000000000000000000, 0.9238795325112867385, 1.000000000000000000, 0.9238795325112854062, 1.000000000000001332 ) ) 
 REPRESENTATION_ITEM ( '' )  );
#16539 = ADVANCED_FACE ( 'NONE', ( #40890 ), #24996, .T. ) ;
#16540 = CARTESIAN_POINT ( 'NONE',  ( 3.313708498984762496, -7.999999999999989342, 1.486552783920146448 ) ) ;
#16541 = CARTESIAN_POINT ( 'NONE',  ( 2.449293598294707893E-16, 17.25000000000000000, -4.000000000000001776 ) ) ;
#16542 = EDGE_LOOP ( 'NONE', ( #67461, #23680, #31269, #39531 ) ) ;
#16543 = VECTOR ( 'NONE', #72515, 1000.000000000000000 ) ;
#16544 = DIRECTION ( 'NONE',  ( -0.000000000000000000, 1.000000000000000000, -0.000000000000000000 ) ) ;
#16545 = CARTESIAN_POINT ( 'NONE',  ( -2.751064625579944321E-14, 202.8750000027312126, 146.0000000000000284 ) ) ;
#16546 = CARTESIAN_POINT ( 'NONE',  ( -8.311093377946836114, 62.65624999658601268, -8.311093377946837890 ) ) ;
#16547 = CARTESIAN_POINT ( 'NONE',  ( -4.556349186104045934, 11.00000000000000000, 75.90625000409677625 ) ) ;
#16548 = CARTESIAN_POINT ( 'NONE',  ( -1.432654583217662481, 201.3750000013656347, 145.4587341250000350 ) ) ;
#16549 = CARTESIAN_POINT ( 'NONE',  ( 0.3794862803194714584, 10.12385276103914222, 70.07165850195889334 ) ) ;
#16550 = CARTESIAN_POINT ( 'NONE',  ( -10.00000000000000000, 244.7916666666666856, -2.679491924311226292 ) ) ;
#16552 = CARTESIAN_POINT ( 'NONE',  ( -3.042071309553163960, 42.23958332991934128, -11.35316468749999963 ) ) ;
#16551 = CARTESIAN_POINT ( 'NONE',  ( 1.320432766682874540E-15, 94.53125000204836681, 7.188101187500000044 ) ) ;
#16553 = CARTESIAN_POINT ( 'NONE',  ( 3.313708498984762496, -7.999999999999989342, 4.299052779823363757 ) ) ;
#16554 = CARTESIAN_POINT ( 'NONE',  ( 4.556349186104045934, 11.00000000000000000, 98.21875000409679046 ) ) ;
#16555 = CARTESIAN_POINT ( 'NONE',  ( -8.311093377946836114, 177.6562499965859843, -8.311093377946837890 ) ) ;
#16556 = CARTESIAN_POINT ( 'NONE',  ( 8.660254037844389075, 137.2916666598387110, -5.000000000000000000 ) ) ;
#16557 = CLOSED_SHELL ( 'NONE', ( #1515, #28479, #37854, #40935, #59749, #49548, #27065, #54263, #47197, #59563, #60882, #23372, #46160, #23722, #48818, #3549, #2837, #38195, #57544, #55316, #59564, #73284, #57011, #15843, #50673, #36153, #7709, #30639, #54587, #17777 ) ) ;
#16558 = CARTESIAN_POINT ( 'NONE',  ( -7.188101187500001821, 104.9375000020483810, -2.977408999572650483 ) ) ;
#16559 = LINE ( 'NONE', #15448, #64112 ) ;
#16560 = CARTESIAN_POINT ( 'NONE',  ( 11.35316468750000141, 41.09374999658601979, 0.000000000000000000 ) ) ;
#16561 = CARTESIAN_POINT ( 'NONE',  ( 4.242640687119285658, 295.6875000034139589, -4.242640687119286547 ) ) ;
#16562 = CARTESIAN_POINT ( 'NONE',  ( 5.676582343750001591, 181.6145833299193555, -9.832129032723420536 ) ) ;
#16563 = ORIENTED_EDGE ( 'NONE', *, *, #47441, .F. ) ;
#16564 = CARTESIAN_POINT ( 'NONE',  ( 47.49838633794698950, 144.7933162453838349, 64.61389030631686126 ) ) ;
#16565 = CARTESIAN_POINT ( 'NONE',  ( -10.18810118749999738, -4.220049686691941915, 72.25000000204836681 ) ) ;
#16566 = CARTESIAN_POINT ( 'NONE',  ( -2.828427124746153876, 195.8750000000000284, 195.1715728752538439 ) ) ;
#16567 = CARTESIAN_POINT ( 'NONE',  ( 12.00000000000000178, 0.000000000000000000, 28.00000000000000000 ) ) ;
#16569 = CARTESIAN_POINT ( 'NONE',  ( 8.311093377946837890, 166.4062499965860127, -8.311093377946837890 ) ) ;
#16568 = CARTESIAN_POINT ( 'NONE',  ( 1.656854249492381248, 18.93749999726881228, -4.000000000000001776 ) ) ;
#16570 = CARTESIAN_POINT ( 'NONE',  ( -4.898587196589407898E-16, 7.999999999999991118, 5.011552784329824206 ) ) ;
#16571 = CARTESIAN_POINT ( 'NONE',  ( -36.10814071610730736, 133.9999999999999716, 139.0000000000000000 ) ) ;
#16572 = CARTESIAN_POINT ( 'NONE',  ( 5.676582343750005144, 220.5729166700806729, 9.832129032723416984 ) ) ;
#16573 = DIRECTION ( 'NONE',  ( -1.000000000000000000, -0.000000000000000000, -0.000000000000000000 ) ) ;
#16574 = CARTESIAN_POINT ( 'NONE',  ( 4.220049686691941027, -10.18810118749999738, 77.50000000204839523 ) ) ;
#16575 = ORIENTED_EDGE ( 'NONE', *, *, #47622, .T. ) ;
#16576 = VECTOR ( 'NONE', #68053, 1000.000000000000000 ) ;
#16577 = DIRECTION ( 'NONE',  ( 1.000000000000000000, -0.000000000000000000, -0.000000000000000000 ) ) ;
#16578 = CARTESIAN_POINT ( 'NONE',  ( 11.35316468750000141, 111.0937499965860127, 0.000000000000000000 ) ) ;
#16579 = CARTESIAN_POINT ( 'NONE',  ( -1.836970198721029983E-15, 10.62499999317203425, 10.00000000000000178 ) ) ;
#16580 = ORIENTED_EDGE ( 'NONE', *, *, #1596, .T. ) ;
#16581 = ORIENTED_EDGE ( 'NONE', *, *, #60228, .T. ) ;
#16582 = ADVANCED_FACE ( 'NONE', ( #35245 ), #52581, .F. ) ;
#16583 = CARTESIAN_POINT ( 'NONE',  ( 2.780723358947928197E-16, 7.687499998634407028, -4.541265875000002339 ) ) ;
#16584 = CARTESIAN_POINT ( 'NONE',  ( -2.977408999572650039, 14.43749999795161365, -7.188101187500001821 ) ) ;
#16585 = CARTESIAN_POINT ( 'NONE',  ( -3.313708498984762496, 111.9687500040967905, 7.999999999999998224 ) ) ;
#16586 = CARTESIAN_POINT ( 'NONE',  ( -24.54126587499999346, 198.4375000013655779, 170.0000000000003411 ) ) ;
#16587 = CARTESIAN_POINT ( 'NONE',  ( -1.656854249492381248, 8.312500000000000000, -4.000000000000001776 ) ) ;
#16588 = CARTESIAN_POINT ( 'NONE',  ( -2.828427124746153876, 197.8750000000000284, 195.1715728752538439 ) ) ;
#16589 = CARTESIAN_POINT ( 'NONE',  ( 4.541265875000001451, 7.249999998634407916, 1.881053915767124440 ) ) ;
#16590 = CARTESIAN_POINT ( 'NONE',  ( 3.999999999999959144, 198.0625000000000284, 140.3431457505076594 ) ) ;
#16591 = ORIENTED_EDGE ( 'NONE', *, *, #20196, .T. ) ;
#16592 = CARTESIAN_POINT ( 'NONE',  ( 9.999999999999998224, 222.7083333333333428, -2.679491924311229401 ) ) ;
#16593 = CARTESIAN_POINT ( 'NONE',  ( -5.082755093536325930, 102.9687500020483810, -5.082755093536325930 ) ) ;
#16594 = CIRCLE ( 'NONE', #22633, 5.000000000000000888 ) ;
#16596 = CARTESIAN_POINT ( 'NONE',  ( 0.000000000000000000, 0.000000000000000000, 0.000000000000000000 ) ) ;
#16595 = CARTESIAN_POINT ( 'NONE',  ( -6.735557395310442023E-16, 11.00000000000000000, 78.81250000409677625 ) ) ;
#16597 = ADVANCED_FACE ( 'NONE', ( #36343 ), #8031, .T. ) ;
#16598 = ADVANCED_FACE ( 'NONE', ( #59358 ), #65372, .T. ) ;
#16599 = CARTESIAN_POINT ( 'NONE',  ( -3.734423912265298018, 10.10901040137928852, -70.68514270129381316 ) ) ;
#16600 = CARTESIAN_POINT ( 'NONE',  ( -7.188101187499992051, 0.000000000000000000, 28.48655278187175810 ) ) ;
#16601 = ORIENTED_EDGE ( 'NONE', *, *, #59841, .T. ) ;
#16602 = ORIENTED_EDGE ( 'NONE', *, *, #17162, .T. ) ;
#16603 = CARTESIAN_POINT ( 'NONE',  ( 10.18810118749999916, 1.247682550866122264E-15, 93.90625000204836681 ) ) ;
#16604 = CARTESIAN_POINT ( 'NONE',  ( -4.898587196589407898E-16, 7.999999999999991118, 19.95530277982336642 ) ) ;
#16605 = CARTESIAN_POINT ( 'NONE',  ( -30.44569435410879166, 201.0625000013656063, 172.4456943541092357 ) ) ;
#16606 = CARTESIAN_POINT ( 'NONE',  ( 11.00000000000000000, 1.347111479062088405E-15, 109.7499999999999858 ) ) ;
#16607 = CARTESIAN_POINT ( 'NONE',  ( -1.432654583217607414, 202.5000000013656063, 194.5412658750000219 ) ) ;
#16609 = CARTESIAN_POINT ( 'NONE',  ( -7.778174593052023411, 7.778174593052023411, 113.5000000040967763 ) ) ;
#16608 = CARTESIAN_POINT ( 'NONE',  ( 23.99999999999999645, 202.9375000027312126, 171.6568542494923122 ) ) ;
#16610 = CARTESIAN_POINT ( 'NONE',  ( 10.00000000000000000, 119.7916666666666714, 2.679491924311236062 ) ) ;
#16611 = EDGE_CURVE ( 'NONE', #53065, #54420, #35120, .T. ) ;
#16612 = CARTESIAN_POINT ( 'NONE',  ( 5.656854249492381470, 104.5625000000000000, 5.656854249492379694 ) ) ;
#16613 = VECTOR ( 'NONE', #14994, 999.9999999999998863 ) ;
#16614 = CARTESIAN_POINT ( 'NONE',  ( -6.676582343750003368, 289.5468750017069510, -2.765530957081996810 ) ) ;
#16615 = CARTESIAN_POINT ( 'NONE',  ( -7.188101187499992051, 0.000000000000000000, 3.361552781871751883 ) ) ;
#16616 = CARTESIAN_POINT ( 'NONE',  ( 5.656854249492378806, 1.312500000000000222, 5.656854249492381470 ) ) ;
#16617 = CARTESIAN_POINT ( 'NONE',  ( 29.43265458321761585, 208.5000000013656063, 173.4587341249998929 ) ) ;
#16618 = CARTESIAN_POINT ( 'NONE',  ( 7.188101187500001821, 2.437499997951610542, -2.977408999572650483 ) ) ;
#16619 = CARTESIAN_POINT ( 'NONE',  ( 3.458734124999959914, 198.3750000013655779, 143.4326545832176976 ) ) ;
#16620 = CARTESIAN_POINT ( 'NONE',  ( -2.977408999572650927, 124.2500000020484094, -7.188101187500000933 ) ) ;
#16622 = CARTESIAN_POINT ( 'NONE',  ( -2.445694354108840063, 202.0625000013656063, 139.5543056458912190 ) ) ;
#16621 = DIRECTION ( 'NONE',  ( 0.000000000000000000, 0.000000000000000000, 1.000000000000000000 ) ) ;
#16623 = CARTESIAN_POINT ( 'NONE',  ( 9.832129032723420536, 241.3020833367473301, 5.676582343749996262 ) ) ;
#16624 = CARTESIAN_POINT ( 'NONE',  ( -38.00000000000000000, 242.0000000000000284, 20.00000000000003553 ) ) ;
#16625 = CARTESIAN_POINT ( 'NONE',  ( 29.65685424949235482, 201.0625000000000000, 173.9999999999999147 ) ) ;
#16626 = CARTESIAN_POINT ( 'NONE',  ( -9.832129032723420536, 18.69791666325268409, 5.676582343749997150 ) ) ;
#16627 = CARTESIAN_POINT ( 'NONE',  ( -5.082755093536317936, -5.082755093536320601, 0.5490527818717526598 ) ) ;
#16628 = CARTESIAN_POINT ( 'NONE',  ( 3.042071309553159519, 210.0520833299193555, 11.35316468750000141 ) ) ;
#16629 = CARTESIAN_POINT ( 'NONE',  ( -1.656854249492321074, 197.4375000027312410, 137.9999999999999716 ) ) ;
#16630 = CARTESIAN_POINT ( 'NONE',  ( 1.836970198721029589E-15, 241.2500000000000284, 10.00000000000000000 ) ) ;
#16632 = DIRECTION ( 'NONE',  ( -0.000000000000000000, 1.000000000000000000, -0.000000000000000000 ) ) ;
#16631 = CARTESIAN_POINT ( 'NONE',  ( 3.999999999999959144, 203.1875000027311842, 140.3431457505076594 ) ) ;
#16633 = ORIENTED_EDGE ( 'NONE', *, *, #71284, .T. ) ;
#16634 = CARTESIAN_POINT ( 'NONE',  ( 3.458734124999960358, 200.6875000013656063, 142.0000000000000568 ) ) ;
#16635 = CARTESIAN_POINT ( 'NONE',  ( -11.35316468749999785, 18.07291666325267698, -3.042071309553167513 ) ) ;
#16636 = CARTESIAN_POINT ( 'NONE',  ( 11.00000000000000000, 4.556349186104045934, 95.03125000409677625 ) ) ;
#16637 = DIRECTION ( 'NONE',  ( -0.000000000000000000, 1.000000000000000000, -0.000000000000000000 ) ) ;
#16638 = ADVANCED_FACE ( 'NONE', ( #64997 ), #24632, .F. ) ;
#16639 = CARTESIAN_POINT ( 'NONE',  ( -24.54126587499998990, 196.1875000013655779, 170.0000000000002842 ) ) ;
#16640 = CARTESIAN_POINT ( 'NONE',  ( -9.000000000000000000, 3.504753767550377930, -0.3593172728154441775 ) ) ;
#16642 = CARTESIAN_POINT ( 'NONE',  ( 9.832129032723420536, 6.197916663252683200, -5.676582343749999815 ) ) ;
#16641 = CARTESIAN_POINT ( 'NONE',  ( -5.082755093536324154, 109.3437500020483810, 5.082755093536326818 ) ) ;
#16643 = CARTESIAN_POINT ( 'NONE',  ( -3.313708498984758943, -7.999999999999989342, 22.11155277982336997 ) ) ;
#16644 = CARTESIAN_POINT ( 'NONE',  ( 8.311093377946834337, 135.1562499965860411, 8.311093377946839666 ) ) ;
#16645 = CARTESIAN_POINT ( 'NONE',  ( -10.00000000000000178, 99.37499999317203958, -1.224646799147353454E-15 ) ) ;
#16646 = CARTESIAN_POINT ( 'NONE',  ( -7.188101187500000044, 123.0312500020483810, 0.000000000000000000 ) ) ;
#16647 = CARTESIAN_POINT ( 'NONE',  ( -5.656854249492378806, 120.8750000040967905, 5.656854249492381470 ) ) ;
#16648 = CARTESIAN_POINT ( 'NONE',  ( -11.00000000000000000, 0.000000000000000000, 69.99999999999998579 ) ) ;
#16649 = CARTESIAN_POINT ( 'NONE',  ( 1.224646799147353454E-15, 300.0000000000000000, -10.00000000000000178 ) ) ;
#16650 = VERTEX_POINT ( 'NONE', #42356 ) ;
#16651 = CARTESIAN_POINT ( 'NONE',  ( 1.296342370383565035, -60.23018777774463217, 22.90345467631815168 ) ) ;
#16652 = CARTESIAN_POINT ( 'NONE',  ( -7.347880794884122694E-16, 20.49999999726881583, 4.000000000000001776 ) ) ;
#16653 = CARTESIAN_POINT ( 'NONE',  ( -6.676582343750001591, 290.6093750017069510, 0.000000000000000000 ) ) ;
#16654 = DIRECTION ( 'NONE',  ( 1.000000000000000000, 0.000000000000000000, 0.000000000000000000 ) ) ;
#16655 = CARTESIAN_POINT ( 'NONE',  ( -3.313708498984757167, 7.999999999999991118, 26.10530278432982598 ) ) ;
#16656 = CARTESIAN_POINT ( 'NONE',  ( -25.17157287525382259, 198.8750000000000284, 167.1715728752541565 ) ) ;
#16657 = CARTESIAN_POINT ( 'NONE',  ( 38.00000000000000000, 0.000000000000000000, 2.626867384171068612E-14 ) ) ;
#16658 = CARTESIAN_POINT ( 'NONE',  ( -7.204075437095965206, -7.204075437095968759, 95.21875000204838102 ) ) ;
#16659 = ORIENTED_EDGE ( 'NONE', *, *, #21321, .T. ) ;
#16660 =( BOUNDED_CURVE ( )  B_SPLINE_CURVE ( 2, ( #2831, #27321, #4331, #61296, #3966 ),
 .UNSPECIFIED., .F., .F. ) 
 B_SPLINE_CURVE_WITH_KNOTS ( ( 3, 2, 3 ),
 ( 0.9861111111111110494, 0.9930555555555555802, 1.000000000000000000 ),
 .UNSPECIFIED. ) 
 CURVE ( )  GEOMETRIC_REPRESENTATION_ITEM ( )  RATIONAL_B_SPLINE_CURVE ( ( 1.000000000000001110, 0.9238795325112855172, 1.000000000000000000, 0.9238795325112867385, 1.000000000000000000 ) ) 
 REPRESENTATION_ITEM ( '' )  );
#16661 = AXIS2_PLACEMENT_3D ( 'NONE', #11270, #62946, #11640 ) ;
#16662 = CARTESIAN_POINT ( 'NONE',  ( 7.320508075688771044, 216.2499999931720538, 7.320508075688775484 ) ) ;
#16663 = FACE_OUTER_BOUND ( 'NONE', #4718, .T. ) ;
#16664 = CARTESIAN_POINT ( 'NONE',  ( -3.458734124999960358, 203.6875000013656063, 198.0000000000000284 ) ) ;
#16665 = CARTESIAN_POINT ( 'NONE',  ( -2.085542519210945728E-15, 74.84374999658602690, 11.35316468750000141 ) ) ;
#16666 = B_SPLINE_CURVE_WITH_KNOTS ( 'NONE', 5,
 ( #57412, #33660, #74368, #62306, #73631, #27225 ),
 .UNSPECIFIED., .F., .F.,
 ( 6, 6 ),
 ( 0.000000000000000000, 4.840251854566806067 ),
 .UNSPECIFIED. ) ;
#16667 = ORIENTED_EDGE ( 'NONE', *, *, #21816, .F. ) ;
#16668 = CARTESIAN_POINT ( 'NONE',  ( -10.18810118749999916, 4.220049686691934809, 106.5625000020483668 ) ) ;
#16669 = CARTESIAN_POINT ( 'NONE',  ( -4.541265875000002339, 13.87499999863440792, -1.881053915767121998 ) ) ;
#16670 = ORIENTED_EDGE ( 'NONE', *, *, #40352, .T. ) ;
#16671 = CARTESIAN_POINT ( 'NONE',  ( -7.188101187500001821, 25.12499999795161187, -2.977408999572651371 ) ) ;
#16672 = CARTESIAN_POINT ( 'NONE',  ( -3.313708498984762496, 107.2812500000000000, 7.999999999999998224 ) ) ;
#16673 = VECTOR ( 'NONE', #7174, 1000.000000000000000 ) ;
#16674 = CARTESIAN_POINT ( 'NONE',  ( -1.656854249492433206, 197.3125000027311557, 201.9999999999999432 ) ) ;
#16675 = CARTESIAN_POINT ( 'NONE',  ( -7.188101187500000044, 21.09374999795161543, -8.802885111219163269E-16 ) ) ;
#16676 = DIRECTION ( 'NONE',  ( 0.5000000000000012212, -0.8660254037844380415, 0.000000000000000000 ) ) ;
#16677 = CONICAL_SURFACE ( 'NONE', #64877, 10.00000000000000000, 0.02777063659342106361 ) ;
#16678 = CARTESIAN_POINT ( 'NONE',  ( -7.204075437095967871, 7.204075437095967871, 109.8437500020483810 ) ) ;
#16679 = LINE ( 'NONE', #51773, #30584 ) ;
#16680 = CARTESIAN_POINT ( 'NONE',  ( 4.000000000000000888, 10.68749999726881406, 1.656854249492384135 ) ) ;
#16681 = LINE ( 'NONE', #56328, #22861 ) ;
#16682 = ORIENTED_EDGE ( 'NONE', *, *, #28574, .F. ) ;
#16683 = ADVANCED_FACE ( 'NONE', ( #46913 ), #69938, .T. ) ;
#16684 = CARTESIAN_POINT ( 'NONE',  ( 1.432654583217662481, 202.1250000013656063, 194.5412658750000219 ) ) ;
#16685 = CARTESIAN_POINT ( 'NONE',  ( -31.45873412499996746, 205.7500000013656063, 171.4326545832181239 ) ) ;
#16686 = CARTESIAN_POINT ( 'NONE',  ( 4.541265875000002339, 12.31249999863440792, 0.000000000000000000 ) ) ;
#16687 = CARTESIAN_POINT ( 'NONE',  ( -2.828427124746208943, 206.7500000027312126, 144.8284271247462129 ) ) ;
#16688 = CARTESIAN_POINT ( 'NONE',  ( -7.188101187499990274, -2.977408999572651371, 21.08030278187175810 ) ) ;
#16689 = ORIENTED_EDGE ( 'NONE', *, *, #39997, .F. ) ;
#16690 = CARTESIAN_POINT ( 'NONE',  ( 0.000000000000000000, 300.0000000000000000, 0.000000000000000000 ) ) ;
#16691 = VERTEX_POINT ( 'NONE', #17873 ) ;
#16692 = CARTESIAN_POINT ( 'NONE',  ( 10.18810118749999916, 4.220049686691935698, 112.0000000020483810 ) ) ;
#16693 = CARTESIAN_POINT ( 'NONE',  ( 0.000000000000000000, 125.0000000000000000, 8.000000000000000000 ) ) ;
#16694 = CARTESIAN_POINT ( 'NONE',  ( 2.839093476692135984E-14, 198.6875000013655779, 201.4587341250000350 ) ) ;
#16695 = CARTESIAN_POINT ( 'NONE',  ( 29.43265458321761230, 200.8750000013656063, 166.5412658749999650 ) ) ;
#16696 = CARTESIAN_POINT ( 'NONE',  ( 2.679491924311228956, 86.04166666666667140, -10.00000000000000000 ) ) ;
#16697 = ADVANCED_FACE ( 'NONE', ( #48013 ), #13306, .F. ) ;
#16698 = CARTESIAN_POINT ( 'NONE',  ( -3.313708498984762052, 121.7187500000000000, -8.000000000000000000 ) ) ;
#16699 = CARTESIAN_POINT ( 'NONE',  ( -4.721056650415998313, 298.7343750017069510, 4.721056650416000089 ) ) ;
#16700 = ORIENTED_EDGE ( 'NONE', *, *, #65153, .F. ) ;
#16701 = EDGE_CURVE ( 'NONE', #39904, #34004, #36182, .T. ) ;
#16702 = CARTESIAN_POINT ( 'NONE',  ( -11.00000000000000000, 0.000000000000000000, 113.4999999999999858 ) ) ;
#16703 = AXIS2_PLACEMENT_3D ( 'NONE', #62132, #33124, #56488 ) ;
#16704 = CARTESIAN_POINT ( 'NONE',  ( -5.656854249492375253, 5.656854249492375253, 8.142802779823362869 ) ) ;
#16705 = CARTESIAN_POINT ( 'NONE',  ( 3.999999999999960032, 197.0625000027311842, 143.6568542494924543 ) ) ;
#16706 = FACE_OUTER_BOUND ( 'NONE', #31240, .T. ) ;
#16707 = CARTESIAN_POINT ( 'NONE',  ( 3.313708498984762496, 5.531249995903220196, 7.999999999999998224 ) ) ;
#16708 = CARTESIAN_POINT ( 'NONE',  ( 1.836970198721029589E-15, 236.2500000000000284, 10.00000000000000000 ) ) ;
#16709 = LINE ( 'NONE', #39739, #28237 ) ;
#16710 = CARTESIAN_POINT ( 'NONE',  ( 4.999999999999993783, 204.1666666666666856, 8.660254037844390851 ) ) ;
#16711 = CARTESIAN_POINT ( 'NONE',  ( -4.401442555609577197E-16, 7.188101187499992051, 16.48655278187175810 ) ) ;
#16712 = CARTESIAN_POINT ( 'NONE',  ( 5.676582343749993598, 165.2604166632526983, 9.832129032723422313 ) ) ;
#16713 = CARTESIAN_POINT ( 'NONE',  ( 4.898587196589412829E-16, 7.687499995903221084, -8.000000000000000000 ) ) ;
#16714 = CYLINDRICAL_SURFACE ( 'NONE', #39315, 4.000000000000001776 ) ;
#16716 = CARTESIAN_POINT ( 'NONE',  ( -27.99999999999997158, 191.0000000000000284, 170.0000000000003695 ) ) ;
#16715 = SURFACE_STYLE_USAGE ( .BOTH. , #68415 ) ;
#16717 = EDGE_LOOP ( 'NONE', ( #66935, #23934, #61245, #21597 ) ) ;
#16718 = VECTOR ( 'NONE', #6861, 1000.000000000000000 ) ;
#16719 = CARTESIAN_POINT ( 'NONE',  ( 3.458734124999959914, 198.3750000013655779, 143.4326545832176976 ) ) ;
#16720 = CARTESIAN_POINT ( 'NONE',  ( -8.311093377946836114, 27.96874999658601624, -8.311093377946837890 ) ) ;
#16721 = CARTESIAN_POINT ( 'NONE',  ( 7.778174593052023411, -7.778174593052021635, 109.7500000040967763 ) ) ;
#16722 = EDGE_CURVE ( 'NONE', #10942, #58121, #12149, .T. ) ;
#16723 = CARTESIAN_POINT ( 'NONE',  ( -29.43265458321771533, 208.5000000013656063, 166.5412658750003914 ) ) ;
#16724 = CARTESIAN_POINT ( 'NONE',  ( 26.34314575050763096, 208.0625000027312126, 173.9999999999999147 ) ) ;
#16726 = CARTESIAN_POINT ( 'NONE',  ( -1.296342370391218246, -10.28012030475504268, -63.61260002839784278 ) ) ;
#16725 = CARTESIAN_POINT ( 'NONE',  ( 7.320508075688774596, 222.4999999931720254, -7.320508075688774596 ) ) ;
#16727 = CARTESIAN_POINT ( 'NONE',  ( -11.01764313090027869, -32.97031354457840280, 198.9760758422500544 ) ) ;
#16728 = CARTESIAN_POINT ( 'NONE',  ( 1.432654583217607858, 198.6250000013656063, 138.5412658750000787 ) ) ;
#16729 = CARTESIAN_POINT ( 'NONE',  ( 10.00000000000000178, 61.87499999317203958, 0.000000000000000000 ) ) ;
#16730 = CARTESIAN_POINT ( 'NONE',  ( -7.188101187500001821, 104.5625000020483668, -2.977408999572650483 ) ) ;
#16731 = CARTESIAN_POINT ( 'NONE',  ( -1.881053915767121554, 12.74999999863440969, -4.541265875000002339 ) ) ;
#16732 = CARTESIAN_POINT ( 'NONE',  ( 10.00000000000022382, 215.0000000000001421, 0.000000000000000000 ) ) ;
#16733 = CARTESIAN_POINT ( 'NONE',  ( 7.454948327196666114, 0.2228442467353887457, -2.032657377778160690 ) ) ;
#16734 = CARTESIAN_POINT ( 'NONE',  ( -3.369429374625374063, -50.21921270641836088, 40.85597392306797815 ) ) ;
#16735 = VERTEX_POINT ( 'NONE', #26485 ) ;
#16736 = ORIENTED_EDGE ( 'NONE', *, *, #62692, .T. ) ;
#16737 = CARTESIAN_POINT ( 'NONE',  ( -10.99999999999997868, 4.556349186104065474, 116.4062499999999716 ) ) ;
#16738 = CARTESIAN_POINT ( 'NONE',  ( -1.432654583217607414, 196.5000000013656063, 194.5412658750000219 ) ) ;
#16739 = CARTESIAN_POINT ( 'NONE',  ( 38.00000000000000000, -52.99999999999999289, 25.00000000000000000 ) ) ;
#16740 = CARTESIAN_POINT ( 'NONE',  ( 3.999999999999960032, 198.1250000027312126, 142.0000000000000568 ) ) ;
#16741 = CARTESIAN_POINT ( 'NONE',  ( 9.832129032723420536, 146.1979166632526983, -5.676582343749999815 ) ) ;
#16742 = ORIENTED_EDGE ( 'NONE', *, *, #42007, .T. ) ;
#16743 = DIRECTION ( 'NONE',  ( -0.000000000000000000, -0.000000000000000000, 1.000000000000000000 ) ) ;
#16744 = CARTESIAN_POINT ( 'NONE',  ( 10.18810118749999916, 1.247682550866122264E-15, 87.90625000204838102 ) ) ;
#16745 = LINE ( 'NONE', #17505, #48943 ) ;
#16746 = CARTESIAN_POINT ( 'NONE',  ( 2.828427124746209831, 206.3750000000000284, 200.8284271247462129 ) ) ;
#16747 = CARTESIAN_POINT ( 'NONE',  ( 0.000000000000000000, 300.0000000000000000, 0.000000000000000000 ) ) ;
#16748 = CARTESIAN_POINT ( 'NONE',  ( -50.99999999999994316, -31.99999999999978684, 205.0000000000000284 ) ) ;
#16749 = CARTESIAN_POINT ( 'NONE',  ( 10.18810118749999916, 1.247682550866122264E-15, 113.7812500020483810 ) ) ;
#16750 = ORIENTED_EDGE ( 'NONE', *, *, #9011, .F. ) ;
#16751 = CARTESIAN_POINT ( 'NONE',  ( 3.313708498984706985, 106.7187500040967763, -8.000000000000055067 ) ) ;
#16752 = CARTESIAN_POINT ( 'NONE',  ( -14.81870148747846727, 177.5301863014532273, 142.6802073051195521 ) ) ;
#16753 = CARTESIAN_POINT ( 'NONE',  ( -5.676582343750006032, 124.4270833299193555, 9.832129032723418760 ) ) ;
#16754 = CARTESIAN_POINT ( 'NONE',  ( -3.458734124999958581, 203.5000000013655779, 199.4326545832176976 ) ) ;
#16755 = CARTESIAN_POINT ( 'NONE',  ( 7.188101187500000044, 26.34374999795161543, 0.000000000000000000 ) ) ;
#16756 =( BOUNDED_CURVE ( )  B_SPLINE_CURVE ( 3, ( #70033, #58715, #59086, #47002 ),
 .UNSPECIFIED., .F., .F. ) 
 B_SPLINE_CURVE_WITH_KNOTS ( ( 4, 4 ),
 ( 4.712388980384693227, 5.073347664490325926 ),
 .UNSPECIFIED. ) 
 CURVE ( )  GEOMETRIC_REPRESENTATION_ITEM ( )  RATIONAL_B_SPLINE_CURVE ( ( 1.000000000000000000, 0.9891718422399167210, 0.9891718422399167210, 1.000000000000000000 ) ) 
 REPRESENTATION_ITEM ( '' )  );
#16757 = CARTESIAN_POINT ( 'NONE',  ( 10.18810118750000093, -4.220049686691933033, 83.68750000204836681 ) ) ;
#16758 = CARTESIAN_POINT ( 'NONE',  ( 3.042071309553167069, 32.13541666325269119, -11.35316468749999785 ) ) ;
#16759 = ORIENTED_EDGE ( 'NONE', *, *, #15704, .T. ) ;
#16760 = DIRECTION ( 'NONE',  ( -0.000000000000000000, 1.000000000000000000, -0.000000000000000000 ) ) ;
#16761 = CARTESIAN_POINT ( 'NONE',  ( -5.656854249492375253, 5.656854249492375253, 8.330302783920144449 ) ) ;
#16762 = CARTESIAN_POINT ( 'NONE',  ( 8.008118988124993010, -3.317071493978877239, 21.16936528394063899 ) ) ;
#16763 = CARTESIAN_POINT ( 'NONE',  ( 2.445694354108784108, 205.5625000013656063, 144.4456943541088663 ) ) ;
#16764 = CARTESIAN_POINT ( 'NONE',  ( -7.188101187500001821, 7.124999997951610098, -2.977408999572651371 ) ) ;
#16765 = CARTESIAN_POINT ( 'NONE',  ( -2.485281374238572649, 298.2500000034139589, 6.000000000000002665 ) ) ;
#16766 = CARTESIAN_POINT ( 'NONE',  ( -11.25337967316606758, -28.72254143076221311, 139.8939584852003293 ) ) ;
#16767 = CARTESIAN_POINT ( 'NONE',  ( 7.188101187500001821, 3.937499997951610986, -2.977408999572650483 ) ) ;
#16768 = CARTESIAN_POINT ( 'NONE',  ( -5.676582343750006032, 154.4270833299193555, 9.832129032723418760 ) ) ;
#16769 = CARTESIAN_POINT ( 'NONE',  ( 10.18810118750000093, -4.220049686691933921, 80.31250000204836681 ) ) ;
#16770 = VECTOR ( 'NONE', #38071, 1000.000000000000000 ) ;
#16771 = CARTESIAN_POINT ( 'NONE',  ( -24.54126587499998635, 209.3750000013656063, 171.4326545832179818 ) ) ;
#16772 =( BOUNDED_CURVE ( )  B_SPLINE_CURVE ( 2, ( #7279, #30286, #2352, #64974, #24975, #1631, #18962, #24611, #41965, #36323, #7649, #42333, #65715 ),
 .UNSPECIFIED., .F., .F. ) 
 B_SPLINE_CURVE_WITH_KNOTS ( ( 3, 2, 2, 2, 2, 2, 3 ),
 ( 0.8471392367758522335, 0.8471392748104720205, 0.8537575503949288436, 0.8603758259793856666, 0.8669941015638423787, 0.8736123771482992018, 0.8736124324192364732 ),
 .UNSPECIFIED. ) 
 CURVE ( )  GEOMETRIC_REPRESENTATION_ITEM ( )  RATIONAL_B_SPLINE_CURVE ( ( 0.9999991250904070039, 0.9999995625426895129, 1.000000000000000000, 0.9238795325112867385, 1.000000000000000000, 0.9238795325112867385, 1.000000000000000000, 0.9238795325112867385, 1.000000000000000000, 0.9238795325112867385, 1.000000000000000000, 0.9999993642982181186, 0.9999987286070540771 ) ) 
 REPRESENTATION_ITEM ( '' )  );
#16773 = FACE_OUTER_BOUND ( 'NONE', #26116, .T. ) ;
#16774 = CARTESIAN_POINT ( 'NONE',  ( -4.541265875000002339, 21.93749999863440792, -5.561446717895856393E-16 ) ) ;
#16775 = ORIENTED_EDGE ( 'NONE', *, *, #42502, .T. ) ;
#16776 = VECTOR ( 'NONE', #73248, 1000.000000000000000 ) ;
#16777 = CARTESIAN_POINT ( 'NONE',  ( 1.656854249492403008, 199.8125000027312410, 194.0000000000000853 ) ) ;
#16778 = CARTESIAN_POINT ( 'NONE',  ( 3.999999999999960032, 205.0000000000000284, 142.0000000000000568 ) ) ;
#16779 = CARTESIAN_POINT ( 'NONE',  ( -31.99999999999996447, 201.4375000027311842, 171.6568542494928522 ) ) ;
#16780 = VECTOR ( 'NONE', #3098, 1000.000000000000000 ) ;
#16781 = CARTESIAN_POINT ( 'NONE',  ( 1.836970198721029589E-15, 249.3750000068279746, 10.00000000000000000 ) ) ;
#16782 = CARTESIAN_POINT ( 'NONE',  ( -7.999999999999991118, 3.313708498984756723, 5.424052783920145338 ) ) ;
#16783 = ORIENTED_EDGE ( 'NONE', *, *, #36897, .T. ) ;
#16784 = CARTESIAN_POINT ( 'NONE',  ( -7.188101187500000933, 17.62499999795161187, -2.977408999572651371 ) ) ;
#16785 = CARTESIAN_POINT ( 'NONE',  ( -6.000000000000003553, 298.0000000034140157, -2.485281374238571317 ) ) ;
#16786 = DIRECTION ( 'NONE',  ( 1.000000000000000000, 0.000000000000000000, 3.016910393003145324E-16 ) ) ;
#16787 = CARTESIAN_POINT ( 'NONE',  ( -2.679491924311225848, 36.45833333333333570, -10.00000000000000178 ) ) ;
#16788 = CARTESIAN_POINT ( 'NONE',  ( -2.977408999572650927, 104.7500000020483810, -7.188101187500001821 ) ) ;
#16789 = CARTESIAN_POINT ( 'NONE',  ( -30.44569435410883784, 208.8125000013656063, 167.5543056458915885 ) ) ;
#16790 = CARTESIAN_POINT ( 'NONE',  ( -6.000000000000003553, 299.9374999999999432, -2.485281374238571317 ) ) ;
#16791 = CARTESIAN_POINT ( 'NONE',  ( 5.000000000000001776, 197.7083333265053966, -8.660254037844389075 ) ) ;
#16792 = VERTEX_POINT ( 'NONE', #71389 ) ;
#16793 = EDGE_CURVE ( 'NONE', #40550, #32674, #72529, .T. ) ;
#16794 = CARTESIAN_POINT ( 'NONE',  ( -8.311093377946834337, 239.5312500034140157, 8.311093377946837890 ) ) ;
#16795 = PRODUCT_DEFINITION_SHAPE ( 'NONE', 'NONE',  #37611 ) ;
#16796 = CARTESIAN_POINT ( 'NONE',  ( 5.082755093536320601, -5.082755093536318824, 20.42405278187175810 ) ) ;
#16797 = CARTESIAN_POINT ( 'NONE',  ( -6.298842414731628203, 51.07418104650923851, 41.32239042995228573 ) ) ;
#16798 = DIRECTION ( 'NONE',  ( -0.000000000000000000, -1.000000000000000000, -0.000000000000000000 ) ) ;
#16799 = SPHERICAL_SURFACE ( 'NONE', #2601, 15.99999999999998579 ) ;
#16800 = CARTESIAN_POINT ( 'NONE',  ( -3.425306192931087068, 22.00000000000000355, 2.996540939710079954 ) ) ;
#16801 = CARTESIAN_POINT ( 'NONE',  ( -8.660254037844390851, 167.9166666666666856, 4.999999999999998224 ) ) ;
#16802 = LINE ( 'NONE', #57576, #55845 ) ;
#16803 = PRESENTATION_STYLE_ASSIGNMENT (( #45484 ) ) ;
#16804 = CARTESIAN_POINT ( 'NONE',  ( 4.999999999999992895, -52.62579568235199190, -48.70175807018021885 ) ) ;
#16805 = CARTESIAN_POINT ( 'NONE',  ( 9.832129032723420536, 121.5104166632526841, -5.676582343749999815 ) ) ;
#16806 = DIRECTION ( 'NONE',  ( -1.000000000000000000, 0.000000000000000000, 0.000000000000000000 ) ) ;
#16807 = CARTESIAN_POINT ( 'NONE',  ( -3.313708498984757611, 7.999999999999991118, 27.73655278392014978 ) ) ;
#16810 = FACE_OUTER_BOUND ( 'NONE', #35210, .T. ) ;
#16809 = CARTESIAN_POINT ( 'NONE',  ( 31.45873412499999944, 196.6250000013656063, 171.4326545832175555 ) ) ;
#16808 = CARTESIAN_POINT ( 'NONE',  ( 29.43265458321760519, 196.7500000013656063, 173.4587341249998929 ) ) ;
#16811 = ORIENTED_EDGE ( 'NONE', *, *, #10778, .T. ) ;
#16812 = CARTESIAN_POINT ( 'NONE',  ( 9.255284998869608870, 224.6865538138296756, 3.831861534692823756 ) ) ;
#16813 = CYLINDRICAL_SURFACE ( 'NONE', #54279, 10.00000000000000178 ) ;
#16815 = CARTESIAN_POINT ( 'NONE',  ( 3.459103461385761413, -7.213501455148458419, -0.0001169852011744028255 ) ) ;
#16814 = APPLICATION_CONTEXT ( 'automotive_design' ) ;
#16816 = DIRECTION ( 'NONE',  ( 0.000000000000000000, 1.000000000000000000, 0.000000000000000000 ) ) ;
#16817 = EDGE_CURVE ( 'NONE', #67743, #33552, #66867, .T. ) ;
#16818 = AXIS2_PLACEMENT_3D ( 'NONE', #53603, #70216, #30213 ) ;
#16819 = CARTESIAN_POINT ( 'NONE',  ( 8.311093377946834337, 215.4687499965860411, 8.311093377946839666 ) ) ;
#16820 = CARTESIAN_POINT ( 'NONE',  ( 5.082755093536326818, 121.7187500020483952, 5.082755093536325042 ) ) ;
#16821 = CARTESIAN_POINT ( 'NONE',  ( 4.541265875000002339, 0.4374999986344068059, 0.000000000000000000 ) ) ;
#16822 = CARTESIAN_POINT ( 'NONE',  ( 0.000000000000000000, 0.000000000000000000, 30.00000000000000000 ) ) ;
#16823 = CARTESIAN_POINT ( 'NONE',  ( 7.999999999999991118, 9.797174393178815797E-16, 24.08030277982336642 ) ) ;
#16825 = CARTESIAN_POINT ( 'NONE',  ( 27.99999999999996447, 197.0000000000000000, 173.9999999999999147 ) ) ;
#16824 =( LENGTH_UNIT ( ) NAMED_UNIT ( * ) SI_UNIT ( .MILLI., .METRE. ) );
#16826 = CARTESIAN_POINT ( 'NONE',  ( -11.35316468750000141, 98.28124999658602690, -1.390361679473963753E-15 ) ) ;
#16827 = EDGE_LOOP ( 'NONE', ( #54601, #6329, #57186, #5093 ) ) ;
#16828 = EDGE_CURVE ( 'NONE', #9367, #26574, #72902, .T. ) ;
#16829 = PLANE ( 'NONE',  #269 ) ;
#16830 = CARTESIAN_POINT ( 'NONE',  ( -2.977408999572654480, 26.99999999795161187, 7.188101187499999156 ) ) ;
#16831 = CARTESIAN_POINT ( 'NONE',  ( 36.10814071610729314, 42.97056274847713553, 139.0000000000000000 ) ) ;
#16832 = CARTESIAN_POINT ( 'NONE',  ( -9.832129032723418760, 243.8020833367473301, -5.676582343749998927 ) ) ;
#16833 = CARTESIAN_POINT ( 'NONE',  ( -5.676582343749998039, 97.44791666325269830, -9.832129032723420536 ) ) ;
#16834 = ORIENTED_EDGE ( 'NONE', *, *, #32959, .T. ) ;
#16835 = CARTESIAN_POINT ( 'NONE',  ( 28.00000000000002487, 208.1250000027312126, 173.9999999999999147 ) ) ;
#16836 = AXIS2_PLACEMENT_3D ( 'NONE', #10003, #61309, #49982 ) ;
#16837 = CARTESIAN_POINT ( 'NONE',  ( -7.204075437095965206, -7.204075437095968759, 108.3437500020483810 ) ) ;
#16838 = CARTESIAN_POINT ( 'NONE',  ( 2.679491924311222739, 220.8333333265053966, 10.00000000000000355 ) ) ;
#16839 = CARTESIAN_POINT ( 'NONE',  ( -1.432654583217608080, 205.8750000013656063, 201.4587341250000350 ) ) ;
#16840 = CARTESIAN_POINT ( 'NONE',  ( -8.000000000000033751, -3.313708498984719864, 11.42405277982336642 ) ) ;
#16842 = CARTESIAN_POINT ( 'NONE',  ( -8.311093377946841443, 93.90624999658599847, 8.311093377946834337 ) ) ;
#16841 = CARTESIAN_POINT ( 'NONE',  ( -28.00000000000002842, 202.0000000000000000, 166.0000000000003695 ) ) ;
#16843 = CARTESIAN_POINT ( 'NONE',  ( -5.656854249492375253, 5.656854249492375253, 11.33030278392014445 ) ) ;
#16844 = CARTESIAN_POINT ( 'NONE',  ( -25.55430564589115150, 199.3125000013656063, 172.4456943541091789 ) ) ;
#16845 = CARTESIAN_POINT ( 'NONE',  ( 5.000000000000038192, 174.1666666666666856, 8.660254037844467234 ) ) ;
#16846 = VERTEX_POINT ( 'NONE', #43854 ) ;
#16847 = CARTESIAN_POINT ( 'NONE',  ( 8.660254037844385522, 186.4583333265053682, 5.000000000000005329 ) ) ;
#16848 = CARTESIAN_POINT ( 'NONE',  ( 26.34314575050757057, 201.0625000027311842, 173.9999999999998295 ) ) ;
#16849 = ADVANCED_FACE ( 'NONE', ( #26873 ), #55191, .T. ) ;
#16850 = CYLINDRICAL_SURFACE ( 'NONE', #73798, 11.00000000000000000 ) ;
#16851 = CARTESIAN_POINT ( 'NONE',  ( -9.832129032723420536, 84.01041666325268409, 5.676582343749997150 ) ) ;
#16852 = CARTESIAN_POINT ( 'NONE',  ( -6.676582343750001591, 291.4531250017069510, 0.000000000000000000 ) ) ;
#16853 = CARTESIAN_POINT ( 'NONE',  ( -1.320432766682874540E-15, 6.468749997951610098, 7.188101187500000044 ) ) ;
#16854 = CARTESIAN_POINT ( 'NONE',  ( 4.220049686691941027, -10.18810118749999738, 98.50000000204838102 ) ) ;
#16855 = CARTESIAN_POINT ( 'NONE',  ( 6.951808397369818766E-16, 217.0312499965860411, -11.35316468750000141 ) ) ;
#16856 = VERTEX_POINT ( 'NONE', #3497 ) ;
#16857 = CARTESIAN_POINT ( 'NONE',  ( -10.00000000000000000, 69.16666665983868256, -2.679491924311229845 ) ) ;
#16858 = CARTESIAN_POINT ( 'NONE',  ( 8.000000000000000000, 115.5312500040968047, -3.313708498984762496 ) ) ;
#16859 = CARTESIAN_POINT ( 'NONE',  ( -0.4369882809721274963, -16.44602605510714710, 68.55492853905352035 ) ) ;
#16860 = CARTESIAN_POINT ( 'NONE',  ( 5.676582343749993598, 214.9479166632526983, 9.832129032723422313 ) ) ;
#16861 = DIRECTION ( 'NONE',  ( 0.000000000000000000, -0.000000000000000000, 1.000000000000000000 ) ) ;
#16862 = CARTESIAN_POINT ( 'NONE',  ( -2.679491924311137030, 158.5416666666667425, 10.00000000000026823 ) ) ;
#16863 = CARTESIAN_POINT ( 'NONE',  ( -4.721056650415998313, 298.5781250017069510, 4.721056650416000089 ) ) ;
#16864 = VERTEX_POINT ( 'NONE', #32554 ) ;
#16865 = CARTESIAN_POINT ( 'NONE',  ( 6.951808397369818766E-16, 207.3437499965860411, -11.35316468750000141 ) ) ;
#16866 = CARTESIAN_POINT ( 'NONE',  ( 4.220049686691934809, 10.18810118749999916, 94.18750000204836681 ) ) ;
#16867 = CARTESIAN_POINT ( 'NONE',  ( -28.00000000000002487, 206.4375000013656063, 166.5412658750003629 ) ) ;
#16868 = CARTESIAN_POINT ( 'NONE',  ( -5.656854249492381470, 18.93750000000000355, 5.656854249492379694 ) ) ;
#16869 = ORIENTED_EDGE ( 'NONE', *, *, #64781, .T. ) ;
#16870 = EDGE_CURVE ( 'NONE', #41608, #28042, #17892, .T. ) ;
#16871 = PRODUCT_DEFINITION_CONTEXT ( 'detailed design', #1435, 'design' ) ;
#16872 = CARTESIAN_POINT ( 'NONE',  ( -4.898587196589412829E-16, 88.81250000409677625, -8.000000000000000000 ) ) ;
#16873 = CARTESIAN_POINT ( 'NONE',  ( -24.00000000000002487, 199.9375000027312126, 168.3431457505079152 ) ) ;
#16874 = EDGE_CURVE ( 'NONE', #3720, #9276, #45928, .T. ) ;
#16875 =( BOUNDED_CURVE ( )  B_SPLINE_CURVE ( 2, ( #5318, #28320, #64136, #16608, #58128, #51329, #5689, #52450, #69059 ),
 .UNSPECIFIED., .F., .F. ) 
 B_SPLINE_CURVE_WITH_KNOTS ( ( 3, 2, 2, 2, 3 ),
 ( 0.4000000000000003553, 0.4083333333333336590, 0.4166666666666670182, 0.4250000000000003220, 0.4333333333333336812 ),
 .UNSPECIFIED. ) 
 CURVE ( )  GEOMETRIC_REPRESENTATION_ITEM ( )  RATIONAL_B_SPLINE_CURVE ( ( 0.9999999999999970024, 0.9238795325112897361, 1.000000000000000000, 0.9238795325112867385, 1.000000000000000000, 0.9238795325112867385, 1.000000000000000000, 0.9238795325112837409, 1.000000000000003109 ) ) 
 REPRESENTATION_ITEM ( '' )  );
#16876 = CARTESIAN_POINT ( 'NONE',  ( -7.320508075688778149, 18.12500000000000355, 7.320508075688769267 ) ) ;
#16877 = AXIS2_PLACEMENT_3D ( 'NONE', #3086, #14757, #37418 ) ;
#16878 = CARTESIAN_POINT ( 'NONE',  ( -5.000000000000000888, 13.57926339724869536, 69.65188861886714733 ) ) ;
#16879 = CARTESIAN_POINT ( 'NONE',  ( 1.871523826299183495E-15, -10.18810118749999916, 81.90625000204838102 ) ) ;
#16880 = ORIENTED_EDGE ( 'NONE', *, *, #56330, .F. ) ;
#16881 = EDGE_CURVE ( 'NONE', #13756, #70510, #21210, .T. ) ;
#16882 = CARTESIAN_POINT ( 'NONE',  ( -2.828427124746192067, 18.62500000000000000, 2.828427124746190735 ) ) ;
#16883 = CARTESIAN_POINT ( 'NONE',  ( 0.000000000000000000, 192.0000000000000284, 170.0000000000000284 ) ) ;
#16884 = VECTOR ( 'NONE', #15011, 1000.000000000000000 ) ;
#16885 = CARTESIAN_POINT ( 'NONE',  ( 28.92188847141878227, 194.4720194171913761, 173.3550665274295568 ) ) ;
#16886 = AXIS2_PLACEMENT_3D ( 'NONE', #18976, #41980, #13300 ) ;
#16887 = CARTESIAN_POINT ( 'NONE',  ( 10.00000000000000178, 17.08333332650536818, -2.679491924311226736 ) ) ;
#16888 = CARTESIAN_POINT ( 'NONE',  ( -2.977408999572650927, 122.7500000020483952, -7.188101187500001821 ) ) ;
#16889 = CARTESIAN_POINT ( 'NONE',  ( -1.377000000000000002, 255.7199999999997715, 5.684444333912885838 ) ) ;
#16892 = CARTESIAN_POINT ( 'NONE',  ( -4.000000000000015987, 199.6875000027312126, 143.6568542494924259 ) ) ;
#16891 = CARTESIAN_POINT ( 'NONE',  ( -3.042071309553159075, 244.9479166700806445, 11.35316468749999963 ) ) ;
#16890 = CARTESIAN_POINT ( 'NONE',  ( 29.43265458321766914, 208.5000000013656063, 173.4587341249998929 ) ) ;
#16893 = SHAPE_DEFINITION_REPRESENTATION ( #2891, #15137 ) ;
#16894 = ORIENTED_EDGE ( 'NONE', *, *, #35904, .F. ) ;
#16895 = CARTESIAN_POINT ( 'NONE',  ( -9.832129032723418760, 258.8020833367473301, -5.676582343749998927 ) ) ;
#16896 = CARTESIAN_POINT ( 'NONE',  ( -2.977408999572648707, -7.188101187499990274, 15.26780278187175455 ) ) ;
#16897 = VERTEX_POINT ( 'NONE', #72141 ) ;
#16898 = ORIENTED_EDGE ( 'NONE', *, *, #48033, .T. ) ;
#16899 = CARTESIAN_POINT ( 'NONE',  ( -6.238412754330611322E-16, 10.18810118749999916, 76.28125000204836681 ) ) ;
#16900 = CARTESIAN_POINT ( 'NONE',  ( -9.832129032723418760, 83.17708332991935549, -5.676582343750004256 ) ) ;
#16901 = DIRECTION ( 'NONE',  ( -0.000000000000000000, 1.000000000000000000, -0.000000000000000000 ) ) ;
#16902 = CARTESIAN_POINT ( 'NONE',  ( 7.778174593052023411, -7.778174593052021635, 85.56249999999998579 ) ) ;
#16905 = CARTESIAN_POINT ( 'NONE',  ( -3.313708498984770934, 2.531250000000000000, 7.999999999999992895 ) ) ;
#16904 = CARTESIAN_POINT ( 'NONE',  ( 31.45873412499998523, 206.7500000013655779, 168.5673454167822172 ) ) ;
#16903 = CARTESIAN_POINT ( 'NONE',  ( 30.44569435410883784, 206.0625000013656063, 167.5543056458911053 ) ) ;
#16906 = CARTESIAN_POINT ( 'NONE',  ( -58.22573788689760477, 214.5877240280044873, 47.57528612463626416 ) ) ;
#16907 = MANIFOLD_SOLID_BREP ( 'Revolve1', #23782 ) ;
#16908 = DIRECTION ( 'NONE',  ( 0.000000000000000000, 0.000000000000000000, 1.000000000000000000 ) ) ;
#16909 = AXIS2_PLACEMENT_3D ( 'NONE', #33164, #45201, #73494 ) ;
#16910 = CARTESIAN_POINT ( 'NONE',  ( 5.676582343749993598, 194.9479166632526983, 9.832129032723422313 ) ) ;
#16911 = CARTESIAN_POINT ( 'NONE',  ( -2.445694354108838731, 206.0625000013656063, 144.4456943541088663 ) ) ;
#16912 = ORIENTED_EDGE ( 'NONE', *, *, #21736, .T. ) ;
#16913 = CARTESIAN_POINT ( 'NONE',  ( 26.56734541678232375, 205.6250000013656063, 173.4587341249998929 ) ) ;
#16914 = EDGE_CURVE ( 'NONE', #44182, #40831, #33327, .T. ) ;
#16915 = CARTESIAN_POINT ( 'NONE',  ( 5.082755093536324154, 18.65624999795161187, 5.082755093536326818 ) ) ;
#16916 = CARTESIAN_POINT ( 'NONE',  ( 9.832129032723420536, 161.5104166632526983, -5.676582343749999815 ) ) ;
#16917 = CARTESIAN_POINT ( 'NONE',  ( -38.00000000000000000, 272.0000000000000000, 3.791916237172779019E-14 ) ) ;
#16918 = CARTESIAN_POINT ( 'NONE',  ( -4.401442555609581635E-16, 106.1562500020483810, -7.188101187500000044 ) ) ;
#16920 = CARTESIAN_POINT ( 'NONE',  ( -7.320508075688778149, 89.99999999317203958, 7.320508075688769267 ) ) ;
#16919 = CARTESIAN_POINT ( 'NONE',  ( -2.679491924311077522, 206.4583333333333144, -10.00000000000007816 ) ) ;
#16921 = CARTESIAN_POINT ( 'NONE',  ( -4.541265875000002339, 11.74999999863440792, -1.881053915767121998 ) ) ;
#16922 = CARTESIAN_POINT ( 'NONE',  ( 31.45873412499999944, 203.9375000013656063, 169.9999999999999432 ) ) ;
#16923 = CARTESIAN_POINT ( 'NONE',  ( -4.401442555609577197E-16, 7.188101187499992051, 10.48655278187175455 ) ) ;
#16924 = CARTESIAN_POINT ( 'NONE',  ( 9.832129032723420536, 51.19791666325268409, -5.676582343749999815 ) ) ;
#16925 = LINE ( 'NONE', #62574, #5072 ) ;
#16926 = CARTESIAN_POINT ( 'NONE',  ( -3.313708498984757167, 7.999999999999991118, 2.105302784329821542 ) ) ;
#16927 = ORIENTED_EDGE ( 'NONE', *, *, #11791, .T. ) ;
#16928 = DIRECTION ( 'NONE',  ( -0.000000000000000000, -1.000000000000000000, -0.000000000000000000 ) ) ;
#16929 = CARTESIAN_POINT ( 'NONE',  ( 11.00000000000000000, 1.347111479062088405E-15, 79.93750000409677625 ) ) ;
#16930 = CARTESIAN_POINT ( 'NONE',  ( -11.35316468749999785, 68.07291666325266988, -3.042071309553167513 ) ) ;
#16931 = CARTESIAN_POINT ( 'NONE',  ( 7.778174593052023411, -7.778174593052021635, 73.75000000409676204 ) ) ;
#16932 = CARTESIAN_POINT ( 'NONE',  ( 2.445694354108783219, 201.8125000013656063, 139.5543056458912190 ) ) ;
#16933 = DIRECTION ( 'NONE',  ( 0.000000000000000000, -1.000000000000000000, 0.000000000000000000 ) ) ;
#16934 = CARTESIAN_POINT ( 'NONE',  ( -6.123233995736766282E-16, 243.7500000000000284, -10.00000000000000000 ) ) ;
#16936 = CARTESIAN_POINT ( 'NONE',  ( 11.35316468750000141, 65.78124999658602690, 0.000000000000000000 ) ) ;
#16935 = CARTESIAN_POINT ( 'NONE',  ( -5.082755093536324154, 92.84375000204838102, 5.082755093536326818 ) ) ;
#16937 = CARTESIAN_POINT ( 'NONE',  ( -7.999999999999991118, 0.000000000000000000, 2.330302779823365089 ) ) ;
#16938 = CARTESIAN_POINT ( 'NONE',  ( -8.660254037844390851, 14.79166665983870210, 4.999999999999998224 ) ) ;
#16939 = CARTESIAN_POINT ( 'NONE',  ( 5.676582343750001591, 171.6145833299193555, -9.832129032723420536 ) ) ;
#16940 = VECTOR ( 'NONE', #50945, 1000.000000000000000 ) ;
#16941 = CARTESIAN_POINT ( 'NONE',  ( -2.679491924311235618, 145.4166666598386826, 10.00000000000000000 ) ) ;
#16942 = CARTESIAN_POINT ( 'NONE',  ( 5.082755093536325042, 98.46875000204838102, -5.082755093536325930 ) ) ;
#16943 = CARTESIAN_POINT ( 'NONE',  ( 11.00000000000013145, 4.556349186103913596, 108.3437499999999716 ) ) ;
#16944 = CARTESIAN_POINT ( 'NONE',  ( -2.085542519210945728E-15, 49.84374999658601268, 11.35316468750000141 ) ) ;
#16945 = DIRECTION ( 'NONE',  ( -0.000000000000000000, 1.000000000000000000, -0.000000000000000000 ) ) ;
#16946 = CARTESIAN_POINT ( 'NONE',  ( 3.042071309553167069, 181.8229166632526983, -11.35316468749999785 ) ) ;
#16947 = ORIENTED_EDGE ( 'NONE', *, *, #24474, .F. ) ;
#16948 = CARTESIAN_POINT ( 'NONE',  ( -11.00000000000000533, -11.00000000000000355, 41.99999999999999289 ) ) ;
#16949 = CARTESIAN_POINT ( 'NONE',  ( 4.220049686691934809, 10.18810118749999916, 71.68750000204836681 ) ) ;
#16950 = CARTESIAN_POINT ( 'NONE',  ( -3.999999999999960032, 196.0000000000000000, 198.0000000000000284 ) ) ;
#16951 = CARTESIAN_POINT ( 'NONE',  ( 34.26476665131792032, 40.28315359274959917, 65.00000000000001421 ) ) ;
#16953 = CARTESIAN_POINT ( 'NONE',  ( -9.832129032723420536, 168.6979166632526983, 5.676582343749997150 ) ) ;
#16952 = DIRECTION ( 'NONE',  ( 0.000000000000000000, 0.000000000000000000, -1.000000000000000000 ) ) ;
#16954 = CARTESIAN_POINT ( 'NONE',  ( -4.898587196589407898E-16, 7.999999999999991118, 6.511552784329821542 ) ) ;
#16955 = CARTESIAN_POINT ( 'NONE',  ( 3.313708498984761608, 9.281250000000001776, -8.000000000000000000 ) ) ;
#16956 = CIRCLE ( 'NONE', #10937, 11.00000000000000000 ) ;
#16957 = ADVANCED_FACE ( 'NONE', ( #40063 ), #44980, .T. ) ;
#16958 = CARTESIAN_POINT ( 'NONE',  ( 10.00000000000000000, 260.6250000068279746, -1.224646799147353256E-15 ) ) ;
#16959 = DIRECTION ( 'NONE',  ( 0.000000000000000000, 0.000000000000000000, 1.000000000000000000 ) ) ;
#16960 = AXIS2_PLACEMENT_3D ( 'NONE', #34221, #57222, #45888 ) ;
#16961 = VERTEX_POINT ( 'NONE', #63434 ) ;
#16962 = FACE_OUTER_BOUND ( 'NONE', #33171, .T. ) ;
#16963 = CARTESIAN_POINT ( 'NONE',  ( -5.676582343749998039, 112.7604166632526841, -9.832129032723420536 ) ) ;
#16964 = CARTESIAN_POINT ( 'NONE',  ( 27.99999999999996447, 195.0000000000000000, 173.9999999999999147 ) ) ;
#16965 = ORIENTED_EDGE ( 'NONE', *, *, #23692, .T. ) ;
#16966 = CARTESIAN_POINT ( 'NONE',  ( 4.541265875000001451, 9.374999998634407916, 1.881053915767124440 ) ) ;
#16967 = CARTESIAN_POINT ( 'NONE',  ( 7.188101187499999156, 12.37499999795161010, 2.977408999572654924 ) ) ;
#16968 = CARTESIAN_POINT ( 'NONE',  ( -3.313708498984762052, 108.4062500040967905, -8.000000000000000000 ) ) ;
#16969 = ADVANCED_FACE ( 'NONE', ( #61949 ), #74015, .F. ) ;
#16970 = CARTESIAN_POINT ( 'NONE',  ( -24.54126587499997925, 197.3750000013656063, 171.4326545832179818 ) ) ;
#16971 = EDGE_CURVE ( 'NONE', #74244, #39873, #39896, .T. ) ;
#16972 = CARTESIAN_POINT ( 'NONE',  ( 1.656854249492381914, 6.812500000000000000, 4.000000000000000888 ) ) ;
#16973 = CARTESIAN_POINT ( 'NONE',  ( -1.656854249492381248, 21.06249999726881583, -4.000000000000001776 ) ) ;
#16974 = CARTESIAN_POINT ( 'NONE',  ( 2.780723358947928197E-16, 13.56249999863440614, -4.541265875000002339 ) ) ;
#16975 = CARTESIAN_POINT ( 'NONE',  ( -2.849036369511732440E-14, 198.2500000000000000, 138.0000000000000568 ) ) ;
#16976 = ORIENTED_EDGE ( 'NONE', *, *, #7146, .F. ) ;
#16977 = CARTESIAN_POINT ( 'NONE',  ( -7.188101187500001821, 106.0625000020483668, -2.977408999572650483 ) ) ;
#16979 = CARTESIAN_POINT ( 'NONE',  ( 4.898587196589412829E-16, 15.18749999590322197, -8.000000000000000000 ) ) ;
#16978 = CARTESIAN_POINT ( 'NONE',  ( 38.00000000000000000, 52.99999999999999289, 25.00000000000000000 ) ) ;
#16980 = CARTESIAN_POINT ( 'NONE',  ( 9.000000000000014211, 15.58845726811988541, -20.69999999999999929 ) ) ;
#16981 = CARTESIAN_POINT ( 'NONE',  ( 5.082755093536320601, -5.082755093536318824, 3.549052781871751883 ) ) ;
#16982 = ORIENTED_EDGE ( 'NONE', *, *, #12128, .T. ) ;
#16983 =( BOUNDED_CURVE ( )  B_SPLINE_CURVE ( 2, ( #56356, #5790, #68406, #28419, #51426, #67673, #74438, #22746, #40110, #57485, #51802, #15972, #40857 ),
 .UNSPECIFIED., .F., .F. ) 
 B_SPLINE_CURVE_WITH_KNOTS ( ( 3, 2, 2, 2, 2, 2, 3 ),
 ( 0.2336956521739130821, 0.2355072463768116131, 0.2373188405797101719, 0.2391304347826087029, 0.2409420289855072339, 0.2427536231884057927, 0.2445652173913043514 ),
 .UNSPECIFIED. ) 
 CURVE ( )  GEOMETRIC_REPRESENTATION_ITEM ( )  RATIONAL_B_SPLINE_CURVE ( ( 0.9999999999999994449, 0.9659258262890688673, 1.000000000000000000, 0.9659258262890683122, 1.000000000000000000, 0.9659258262890683122, 1.000000000000000000, 0.9659258262890683122, 1.000000000000000000, 0.9659258262890683122, 1.000000000000000000, 0.9659258262890683122, 1.000000000000000000 ) ) 
 REPRESENTATION_ITEM ( '' )  );
#16984 = ORIENTED_EDGE ( 'NONE', *, *, #32853, .T. ) ;
#16985 = CARTESIAN_POINT ( 'NONE',  ( -7.204075437095965206, -7.204075437095968759, 90.34375000204838102 ) ) ;
#16986 = CARTESIAN_POINT ( 'NONE',  ( 0.000000000000000000, 0.000000000000000000, 0.000000000000000000 ) ) ;
#16987 = CARTESIAN_POINT ( 'NONE',  ( -31.45873412499997812, 195.0000000013656063, 171.4326545832180386 ) ) ;
#16988 = CARTESIAN_POINT ( 'NONE',  ( 11.00000000000000000, 4.556349186104045934, 102.3437499999999858 ) ) ;
#16989 = CARTESIAN_POINT ( 'NONE',  ( 2.754378923186476579E-14, 205.4375000013656063, 194.5412658750000219 ) ) ;
#16991 = CARTESIAN_POINT ( 'NONE',  ( -4.999999999999992895, 255.8333333333333712, 8.660254037844390851 ) ) ;
#16990 = CARTESIAN_POINT ( 'NONE',  ( -28.00000000000008171, 206.1250000027312126, 166.0000000000003695 ) ) ;
#16992 = CARTESIAN_POINT ( 'NONE',  ( 5.000000000000001776, 120.8333333333333286, -8.660254037844389075 ) ) ;
#16993 = CARTESIAN_POINT ( 'NONE',  ( 5.656854249492381470, 106.0625000000000000, 5.656854249492379694 ) ) ;
#16994 = CARTESIAN_POINT ( 'NONE',  ( -2.765530957081998586, 288.7968750017069510, 6.676582343750001591 ) ) ;
#16995 = AXIS2_PLACEMENT_3D ( 'NONE', #27997, #21952, #40434 ) ;
#16996 = CARTESIAN_POINT ( 'NONE',  ( 7.188101187499992051, 8.802885111219154394E-16, 5.611552781871753659 ) ) ;
#16997 = CARTESIAN_POINT ( 'NONE',  ( 2.828427124746208943, 200.6250000000000284, 195.1715728752538439 ) ) ;
#16998 = CARTESIAN_POINT ( 'NONE',  ( 24.54126587500000412, 206.1250000013655779, 168.5673454167822172 ) ) ;
#16999 = CARTESIAN_POINT ( 'NONE',  ( 4.898587196589412829E-16, 25.68749999590322375, -8.000000000000000000 ) ) ;
#17000 = PRESENTATION_LAYER_ASSIGNMENT (  '', '', ( #53162 ) ) ;
#17001 = CARTESIAN_POINT ( 'NONE',  ( 1.432654583217607858, 199.6250000013656063, 138.5412658750000787 ) ) ;
#17002 = CARTESIAN_POINT ( 'NONE',  ( -4.401442555609581635E-16, 119.6562500020483810, -7.188101187500000044 ) ) ;
#17004 = LINE ( 'NONE', #57019, #33003 ) ;
#17003 = CARTESIAN_POINT ( 'NONE',  ( 29.65685424949227311, 195.1875000027312126, 174.0000000000000000 ) ) ;
#17005 = CARTESIAN_POINT ( 'NONE',  ( 9.832129032723416984, 242.1354166700806445, -5.676582343750003368 ) ) ;
#17006 = CARTESIAN_POINT ( 'NONE',  ( 6.123233995736767268E-16, 53.12499999317203958, -10.00000000000000178 ) ) ;
#17007 = CARTESIAN_POINT ( 'NONE',  ( 31.99999999999999289, 200.2500000000000000, 169.9999999999999432 ) ) ;
#17008 = CARTESIAN_POINT ( 'NONE',  ( 5.676582343749993598, 14.94791666325268409, 9.832129032723422313 ) ) ;
#17009 = CARTESIAN_POINT ( 'NONE',  ( 3.313708498984777595, 123.0312499999999858, -7.999999999999983125 ) ) ;
#17010 = CARTESIAN_POINT ( 'NONE',  ( 8.311093377946837890, 201.7187499965860411, -8.311093377946837890 ) ) ;
#17011 = CARTESIAN_POINT ( 'NONE',  ( -28.00000000000002487, 196.0000000000000000, 166.0000000000003695 ) ) ;
#17012 = LINE ( 'NONE', #40775, #68057 ) ;
#17014 = CARTESIAN_POINT ( 'NONE',  ( -8.660254037844529407, 42.08333333333342097, -5.000000000000087041 ) ) ;
#17013 = CARTESIAN_POINT ( 'NONE',  ( 0.000000000000000000, 0.000000000000000000, 0.000000000000000000 ) ) ;
#17015 = VECTOR ( 'NONE', #48361, 1000.000000000000000 ) ;
#17016 = ORIENTED_EDGE ( 'NONE', *, *, #53272, .F. ) ;
#17017 = CARTESIAN_POINT ( 'NONE',  ( -1.432654583217664701, 200.0000000013656347, 138.5412658750000787 ) ) ;
#17018 = CARTESIAN_POINT ( 'NONE',  ( -11.35316468749999785, 28.07291666325268054, -3.042071309553167513 ) ) ;
#17019 = CARTESIAN_POINT ( 'NONE',  ( -10.99999999999999822, -4.556349186104052151, 92.78125000409679046 ) ) ;
#17020 = CARTESIAN_POINT ( 'NONE',  ( 7.320508075688771044, 228.1250000000000000, -7.320508075688771932 ) ) ;
#17021 = CARTESIAN_POINT ( 'NONE',  ( -31.45873412499995680, 197.7500000013656063, 171.4326545832181239 ) ) ;
#17022 = DIRECTION ( 'NONE',  ( -1.000000000000000000, -0.000000000000000000, 0.000000000000000000 ) ) ;
#17024 = CARTESIAN_POINT ( 'NONE',  ( 9.832129032723416984, 15.36458332991935016, 5.676582343750006032 ) ) ;
#17023 = CARTESIAN_POINT ( 'NONE',  ( -2.977408999572652260, 113.9375000020483952, 7.188101187500000044 ) ) ;
#17025 = CARTESIAN_POINT ( 'NONE',  ( 5.656854249492376141, -5.656854249492374365, 23.89280277982336642 ) ) ;
#17026 = CARTESIAN_POINT ( 'NONE',  ( 3.042071309553159519, 139.7395833299193555, 11.35316468750000141 ) ) ;
#17027 = CARTESIAN_POINT ( 'NONE',  ( 2.679491924311222739, 95.83333332650535397, 10.00000000000000355 ) ) ;
#17028 = CARTESIAN_POINT ( 'NONE',  ( -7.188101187500000044, 121.5312500020483810, 0.000000000000000000 ) ) ;
#17029 = CARTESIAN_POINT ( 'NONE',  ( -2.804140485925949776E-11, 67.59332269700094287, -20.03478791450258001 ) ) ;
#17030 = CARTESIAN_POINT ( 'NONE',  ( -27.99999999999991118, 203.6250000027312126, 174.0000000000003695 ) ) ;
#17031 = CARTESIAN_POINT ( 'NONE',  ( -4.999999999999999112, -53.36732872257274352, -44.46877392682785057 ) ) ;
#17032 = ORIENTED_EDGE ( 'NONE', *, *, #22159, .F. ) ;
#17033 = CARTESIAN_POINT ( 'NONE',  ( 2.997005883566703055, -66.06021892604988466, 26.46015439093906352 ) ) ;
#17034 = EDGE_CURVE ( 'NONE', #45651, #72830, #62953, .T. ) ;
#17035 = DIRECTION ( 'NONE',  ( 0.000000000000000000, 0.000000000000000000, 1.000000000000000000 ) ) ;
#17036 = CARTESIAN_POINT ( 'NONE',  ( -6.676582343750000703, 297.5156250017070079, 2.765530957082001251 ) ) ;
#17037 = CARTESIAN_POINT ( 'NONE',  ( -9.832129032723418760, 122.8645833299193555, -5.676582343750004256 ) ) ;
#17038 = SURFACE_STYLE_USAGE ( .BOTH. , #22695 ) ;
#17039 = CARTESIAN_POINT ( 'NONE',  ( 5.656854249492374365, 5.656854249492375253, 25.82405278432982243 ) ) ;
#17040 = AXIS2_PLACEMENT_3D ( 'NONE', #7501, #53525, #54270 ) ;
#17041 = CARTESIAN_POINT ( 'NONE',  ( 4.217983994790206914, 68.29231466825460473, 20.60018752343912141 ) ) ;
#17042 = CARTESIAN_POINT ( 'NONE',  ( -9.832129032723418760, 263.4895833367473301, -5.676582343749998927 ) ) ;
#17043 = MANIFOLD_SOLID_BREP ( 'Cut-Revolve1', #9296 ) ;
#17044 = CARTESIAN_POINT ( 'NONE',  ( 10.18810118750000093, -4.220049686691933921, 97.18750000204836681 ) ) ;
#17045 = EDGE_LOOP ( 'NONE', ( #52885, #58915, #1649, #30603, #6543, #13500 ) ) ;
#17046 = EDGE_CURVE ( 'NONE', #61381, #42656, #52134, .T. ) ;
#17047 = EDGE_CURVE ( 'NONE', #60780, #51815, #66391, .T. ) ;
#17048 = DIRECTION ( 'NONE',  ( -0.000000000000000000, -0.000000000000000000, -1.000000000000000000 ) ) ;
#17049 = CARTESIAN_POINT ( 'NONE',  ( -2.445694354108783219, 201.8125000013656063, 200.4456943541088663 ) ) ;
#17050 = CARTESIAN_POINT ( 'NONE',  ( 3.042071309553167069, 77.13541666325266988, -11.35316468749999785 ) ) ;
#17051 = ORIENTED_EDGE ( 'NONE', *, *, #64579, .F. ) ;
#17052 = CARTESIAN_POINT ( 'NONE',  ( -10.18810118749999916, 0.000000000000000000, 109.6562500020483668 ) ) ;
#17053 = CARTESIAN_POINT ( 'NONE',  ( -3.211159895383562723, 13.06249999863440792, 3.211159895383561391 ) ) ;
#17054 = VERTEX_POINT ( 'NONE', #58537 ) ;
#17055 = CARTESIAN_POINT ( 'NONE',  ( 7.188101187499999156, 24.37499999795161543, 2.977408999572654924 ) ) ;
#17056 = LINE ( 'NONE', #21971, #52888 ) ;
#17057 = AXIS2_PLACEMENT_3D ( 'NONE', #51914, #63591, #6272 ) ;
#17058 = CARTESIAN_POINT ( 'NONE',  ( -4.999999999999999112, -65.00666015986166713, -24.03732210400576008 ) ) ;
#17059 = CARTESIAN_POINT ( 'NONE',  ( 5.082755093536324154, 23.15624999795161543, 5.082755093536326818 ) ) ;
#17060 = DIRECTION ( 'NONE',  ( 1.000000000000000000, 0.000000000000000000, 0.000000000000000000 ) ) ;
#17061 = CARTESIAN_POINT ( 'NONE',  ( 4.220049686691941027, -10.18810118749999738, 103.0000000020483668 ) ) ;
#17062 = CIRCLE ( 'NONE', #32763, 18.00000000000000355 ) ;
#17063 = CARTESIAN_POINT ( 'NONE',  ( 2.849036369511732440E-14, 201.3750000027312126, 202.0000000000000000 ) ) ;
#17064 = CARTESIAN_POINT ( 'NONE',  ( -2.828427124746192067, 9.374999997268814056, 2.828427124746190735 ) ) ;
#17065 = CARTESIAN_POINT ( 'NONE',  ( -7.347880794884122694E-16, 17.75000000000000355, 4.000000000000001776 ) ) ;
#17066 = ORIENTED_EDGE ( 'NONE', *, *, #64167, .F. ) ;
#17067 = DIRECTION ( 'NONE',  ( -0.000000000000000000, 1.000000000000000000, -0.000000000000000000 ) ) ;
#17068 = CARTESIAN_POINT ( 'NONE',  ( 2.445694354108839619, 203.8125000013656063, 200.4456943541088663 ) ) ;
#17069 = CARTESIAN_POINT ( 'NONE',  ( -28.00000000000007105, 205.4375000013656063, 166.5412658750003629 ) ) ;
#17070 = CARTESIAN_POINT ( 'NONE',  ( 7.594050593750000466, 28.07812499692741781, 0.000000000000000000 ) ) ;
#17071 = CARTESIAN_POINT ( 'NONE',  ( 1.881053915767122664, 10.12499999863440792, 4.541265875000001451 ) ) ;
#17072 = LINE ( 'NONE', #22348, #74204 ) ;
#17073 = CARTESIAN_POINT ( 'NONE',  ( 5.082755093536318824, 5.082755093536319713, 18.92405278187175455 ) ) ;
#17074 = EDGE_LOOP ( 'NONE', ( #18934, #28969, #61545, #34280 ) ) ;
#17075 = CARTESIAN_POINT ( 'NONE',  ( -2.485281374238227592, 292.1875000000000568, 6.000000000000345501 ) ) ;
#17076 = ORIENTED_EDGE ( 'NONE', *, *, #72067, .F. ) ;
#17077 = CARTESIAN_POINT ( 'NONE',  ( 10.18810118749999916, 4.220049686691935698, 109.0000000020483810 ) ) ;
#17078 = CARTESIAN_POINT ( 'NONE',  ( 23.99999999999999289, 208.8750000027312126, 169.9999999999999432 ) ) ;
#17079 = CARTESIAN_POINT ( 'NONE',  ( -3.458734124999959914, 198.4375000013655779, 198.0000000000000284 ) ) ;
#17080 = CARTESIAN_POINT ( 'NONE',  ( 31.45873412499999944, 196.6250000013656063, 171.4326545832175555 ) ) ;
#17081 = CARTESIAN_POINT ( 'NONE',  ( -5.000000000000005329, 83.33333333333334281, 8.660254037844387298 ) ) ;
#17082 = CARTESIAN_POINT ( 'NONE',  ( 1.469576158976823947E-15, 123.8750000000000000, 8.000000000000000000 ) ) ;
#17083 = CARTESIAN_POINT ( 'NONE',  ( 6.000000000000001776, 289.5000000000000000, -7.347880794884121708E-16 ) ) ;
#17084 = ORIENTED_EDGE ( 'NONE', *, *, #30340, .F. ) ;
#17085 = CARTESIAN_POINT ( 'NONE',  ( 10.00000000000000000, 252.5000000000000000, -1.224646799147353256E-15 ) ) ;
#17086 = CARTESIAN_POINT ( 'NONE',  ( -0.6547826978331323655, -10.28110016890870071, 63.57209897671329912 ) ) ;
#17087 = CARTESIAN_POINT ( 'NONE',  ( -2.828427124746208943, 195.7500000027312126, 144.8284271247462129 ) ) ;
#17088 = CARTESIAN_POINT ( 'NONE',  ( -5.000000000000000000, 62.69792629052177091, 24.03557775816959463 ) ) ;
#17089 = CARTESIAN_POINT ( 'NONE',  ( -5.656854249492375253, 5.656854249492375253, 26.33030278392014623 ) ) ;
#17090 = CARTESIAN_POINT ( 'NONE',  ( -7.320508075688770155, 240.6249999999999716, 7.320508075688774596 ) ) ;
#17091 = CARTESIAN_POINT ( 'NONE',  ( 0.000000000000000000, 300.0000000000000000, 0.000000000000000000 ) ) ;
#17092 = CARTESIAN_POINT ( 'NONE',  ( 10.18810118749999916, 1.247682550866122264E-15, 70.28125000204838102 ) ) ;
#17093 = CARTESIAN_POINT ( 'NONE',  ( 7.320508075688774596, 200.6250000000000000, -7.320508075688774596 ) ) ;
#17094 = CARTESIAN_POINT ( 'NONE',  ( -2.977408999572647819, -7.188101187499990274, 17.14280278187175455 ) ) ;
#17095 = CARTESIAN_POINT ( 'NONE',  ( -8.311093377946841443, 174.2187499965860127, 8.311093377946830785 ) ) ;
#17096 = CARTESIAN_POINT ( 'NONE',  ( 3.729367062499960195, 209.8437500006828031, 142.0000000000000568 ) ) ;
#17097 = CARTESIAN_POINT ( 'NONE',  ( 1.656854249492381914, 1.562499997268813390, 4.000000000000000888 ) ) ;
#17098 = DIRECTION ( 'NONE',  ( 1.000000000000000000, 0.000000000000000000, -0.000000000000000000 ) ) ;
#17099 = ORIENTED_EDGE ( 'NONE', *, *, #27268, .F. ) ;
#17100 = CARTESIAN_POINT ( 'NONE',  ( 1.432654583217607192, 196.2500000013656631, 145.4587341250000634 ) ) ;
#17101 = CARTESIAN_POINT ( 'NONE',  ( 3.042071309553167069, 32.13541666325269119, -11.35316468749999785 ) ) ;
#17102 = CARTESIAN_POINT ( 'NONE',  ( -7.778174593052020747, -7.778174593052023411, 112.3750000040967763 ) ) ;
#17103 = CARTESIAN_POINT ( 'NONE',  ( -0.8361131105014090181, 194.5804128891768983, 201.4878662614913765 ) ) ;
#17104 = DIRECTION ( 'NONE',  ( 0.000000000000000000, 0.000000000000000000, 1.000000000000000000 ) ) ;
#17106 = CARTESIAN_POINT ( 'NONE',  ( -3.228176881619507999, -10.27295505383823304, -63.90876373295927237 ) ) ;
#17105 = CARTESIAN_POINT ( 'NONE',  ( -18.00000000000000000, 1.759986210487456626, -0.03733711119006485196 ) ) ;
#17107 = DIRECTION ( 'NONE',  ( 0.000000000000000000, 0.000000000000000000, 1.000000000000000000 ) ) ;
#17108 = CARTESIAN_POINT ( 'NONE',  ( -3.458734125000016313, 198.8750000013656063, 140.5673454167823593 ) ) ;
#17109 =( BOUNDED_CURVE ( )  B_SPLINE_CURVE ( 2, ( #65050, #54121, #65797, #31092, #48071, #43155, #20139, #7358, #53750, #42780, #25425, #71444, #47338 ),
 .UNSPECIFIED., .F., .F. ) 
 B_SPLINE_CURVE_WITH_KNOTS ( ( 3, 2, 2, 2, 2, 2, 3 ),
 ( 0.9000854414465758735, 0.9000854794861264940, 0.9067037550705827620, 0.9133220306550392520, 0.9199403062394955199, 0.9265585818239518989, 0.9265586498208127075 ),
 .UNSPECIFIED. ) 
 CURVE ( )  GEOMETRIC_REPRESENTATION_ITEM ( )  RATIONAL_B_SPLINE_CURVE ( ( 0.9999991249769839552, 0.9999995624859773224, 1.000000000000000000, 0.9238795325112867385, 1.000000000000000000, 0.9238795325112867385, 1.000000000000000000, 0.9238795325112867385, 1.000000000000000000, 0.9238795325112867385, 1.000000000000000000, 0.9999992179302951145, 0.9999984358766603743 ) ) 
 REPRESENTATION_ITEM ( '' )  );
#17110 = EDGE_CURVE ( 'NONE', #68741, #74274, #74291, .T. ) ;
#17111 = CARTESIAN_POINT ( 'NONE',  ( -2.679491924311225848, 63.33333332650536818, -10.00000000000000178 ) ) ;
#17112 = CIRCLE ( 'NONE', #67748, 12.00000000000000178 ) ;
#17113 = CARTESIAN_POINT ( 'NONE',  ( 5.082755093536326818, 100.7187500020483810, 5.082755093536325042 ) ) ;
#17114 = CARTESIAN_POINT ( 'NONE',  ( 4.541265875000002339, 10.49999999863440792, -1.881053915767121554 ) ) ;
#17115 = DIRECTION ( 'NONE',  ( -0.000000000000000000, 1.000000000000000000, -1.563033456626094573E-30 ) ) ;
#17116 = CARTESIAN_POINT ( 'NONE',  ( -3.313708498984757167, 7.999999999999991118, 5.049052779823364645 ) ) ;
#17117 = CARTESIAN_POINT ( 'NONE',  ( 2.679491924311228956, 102.9166666598386826, -10.00000000000000000 ) ) ;
#17118 = ORIENTED_EDGE ( 'NONE', *, *, #52743, .T. ) ;
#17119 = ORIENTED_EDGE ( 'NONE', *, *, #48588, .F. ) ;
#17120 = CARTESIAN_POINT ( 'NONE',  ( 11.00000000000000000, 1.347111479062088405E-15, 115.7499999999999858 ) ) ;
#17121 = CARTESIAN_POINT ( 'NONE',  ( 2.839093476692135984E-14, 194.9375000013655779, 201.4587341250000350 ) ) ;
#17122 = CARTESIAN_POINT ( 'NONE',  ( -0.8721677472503426287, 51.17354301023129892, -48.53016177276298038 ) ) ;
#17123 = CARTESIAN_POINT ( 'NONE',  ( 11.35316468749999785, 140.5729166632526983, 3.042071309553174174 ) ) ;
#17124 = B_SPLINE_CURVE_WITH_KNOTS ( 'NONE', 3,
 ( #33231, #23373, #34351, #74312, #11318, #38874 ),
 .UNSPECIFIED., .F., .F.,
 ( 4, 2, 4 ),
 ( 2.380730968676944577E-07, 0.002629065763328393424, 0.005257893453559919252 ),
 .UNSPECIFIED. ) ;
#17125 = CARTESIAN_POINT ( 'NONE',  ( 18.00000000000000355, 0.000000000000000000, 0.000000000000000000 ) ) ;
#17126 = CARTESIAN_POINT ( 'NONE',  ( -4.220049686691937474, -10.18810118749999738, 82.93750000204838102 ) ) ;
#17127 = CARTESIAN_POINT ( 'NONE',  ( 3.313708498984761608, 4.781250000000000888, -8.000000000000000000 ) ) ;
#17128 = CARTESIAN_POINT ( 'NONE',  ( -3.999999999999960032, 202.9375000000000000, 196.3431457505076594 ) ) ;
#17129 = CARTESIAN_POINT ( 'NONE',  ( -29.65685424949239390, 197.5625000027312126, 174.0000000000003126 ) ) ;
#17130 = CARTESIAN_POINT ( 'NONE',  ( -7.999999999999998224, 101.0937500000000142, 3.313708498984766049 ) ) ;
#17131 = ORIENTED_EDGE ( 'NONE', *, *, #40917, .F. ) ;
#17132 = CARTESIAN_POINT ( 'NONE',  ( -7.778174593052023411, 7.778174593052023411, 109.0000000040967763 ) ) ;
#17133 = CIRCLE ( 'NONE', #23169, 36.00000000000000000 ) ;
#17134 = CARTESIAN_POINT ( 'NONE',  ( 16.73219239634777011, 177.3864488911898150, 143.8061503520119118 ) ) ;
#17135 = CARTESIAN_POINT ( 'NONE',  ( -9.832129032723418760, 133.1770833299193555, -5.676582343750004256 ) ) ;
#17136 = CARTESIAN_POINT ( 'NONE',  ( -3.458734124999959914, 201.3750000013656347, 196.5673454167823877 ) ) ;
#17137 = CARTESIAN_POINT ( 'NONE',  ( -5.082755093536326818, 27.28124999795161543, 5.082755093536325042 ) ) ;
#17138 = CARTESIAN_POINT ( 'NONE',  ( -10.18810118749999738, -4.220049686691941915, 77.12500000204838102 ) ) ;
#17139 = CARTESIAN_POINT ( 'NONE',  ( -3.042071309553173730, 34.63541666325269119, 11.35316468749999785 ) ) ;
#17140 = ORIENTED_EDGE ( 'NONE', *, *, #2011, .T. ) ;
#17141 = LINE ( 'NONE', #52234, #762 ) ;
#17142 = CARTESIAN_POINT ( 'NONE',  ( 4.541265875000001451, 1.374999998634407250, 1.881053915767124440 ) ) ;
#17143 = CARTESIAN_POINT ( 'NONE',  ( 5.662595241051936235, -5.662595241051934458, 12.07561528394063011 ) ) ;
#17144 = CARTESIAN_POINT ( 'NONE',  ( -1.432654583217664701, 206.0000000013656347, 138.5412658750000787 ) ) ;
#17145 = VECTOR ( 'NONE', #8973, 1000.000000000000000 ) ;
#17146 = EDGE_CURVE ( 'NONE', #43761, #3011, #4903, .T. ) ;
#17147 = ADVANCED_FACE ( 'NONE', ( #42273 ), #30223, .T. ) ;
#17148 = CARTESIAN_POINT ( 'NONE',  ( -1.320432766682874540E-15, 7.593749997951611874, 7.188101187500000044 ) ) ;
#17149 = CARTESIAN_POINT ( 'NONE',  ( -6.000000000000001776, 297.0625000034140157, 0.000000000000000000 ) ) ;
#17150 = CARTESIAN_POINT ( 'NONE',  ( 2.449293598294707893E-16, 0.2500000000000001665, -4.000000000000001776 ) ) ;
#17151 = CARTESIAN_POINT ( 'NONE',  ( 5.082755093536325930, 7.031249997951610986, -5.082755093536325930 ) ) ;
#17152 = CONICAL_SURFACE ( 'NONE', #36444, 8.000000000000005329, 0.9599310885968794782 ) ;
#17153 = EDGE_CURVE ( 'NONE', #282, #31861, #12595, .T. ) ;
#17154 = CARTESIAN_POINT ( 'NONE',  ( -2.085542519210945728E-15, 154.8437499965860127, 11.35316468750000141 ) ) ;
#17155 = CARTESIAN_POINT ( 'NONE',  ( -10.18810118749999916, 0.000000000000000000, 73.65625000204836681 ) ) ;
#17156 = CARTESIAN_POINT ( 'NONE',  ( -24.54126587499998280, 205.3750000013656063, 171.4326545832179818 ) ) ;
#17157 = FACE_OUTER_BOUND ( 'NONE', #62995, .T. ) ;
#17158 = CARTESIAN_POINT ( 'NONE',  ( 4.541265875000001451, 19.37499999863440792, 1.881053915767124440 ) ) ;
#17159 = ORIENTED_EDGE ( 'NONE', *, *, #2392, .F. ) ;
#17160 = MANIFOLD_SOLID_BREP ( 'Cut-Extrude1', #65951 ) ;
#17161 = CARTESIAN_POINT ( 'NONE',  ( 4.000000000000015099, 200.6875000027312126, 196.3431457505076594 ) ) ;
#17162 = EDGE_CURVE ( 'NONE', #71456, #38888, #21854, .T. ) ;
#17163 = CARTESIAN_POINT ( 'NONE',  ( -2.828427124746209831, 207.3750000000000284, 139.1715728752538723 ) ) ;
#17164 = CARTESIAN_POINT ( 'NONE',  ( -23.99999999999998934, 202.8750000027312126, 170.0000000000002842 ) ) ;
#17165 = FACE_OUTER_BOUND ( 'NONE', #62893, .T. ) ;
#17166 = CARTESIAN_POINT ( 'NONE',  ( 5.656854249492374365, 5.656854249492375253, 4.955302783920146226 ) ) ;
#17167 = ORIENTED_EDGE ( 'NONE', *, *, #29684, .F. ) ;
#17168 = CARTESIAN_POINT ( 'NONE',  ( 7.188101187500000933, 20.06249999795161543, -2.977408999572650483 ) ) ;
#17169 = LINE ( 'NONE', #34927, #30656 ) ;
#17170 = CARTESIAN_POINT ( 'NONE',  ( 8.660254037844389075, 35.41666666666666430, -5.000000000000000000 ) ) ;
#17171 = CARTESIAN_POINT ( 'NONE',  ( 7.188101187500002709, 105.6875000020483952, 2.977408999572649151 ) ) ;
#17172 = CARTESIAN_POINT ( 'NONE',  ( -24.54126587499999701, 208.4375000013656063, 170.0000000000003411 ) ) ;
#17173 = CARTESIAN_POINT ( 'NONE',  ( -2.124081043562909610, -10.27770035960974582, 63.71262442773669932 ) ) ;
#17175 = FACE_OUTER_BOUND ( 'NONE', #6419, .T. ) ;
#17174 = CARTESIAN_POINT ( 'NONE',  ( -28.00000000000002842, 202.0000000000000000, 166.0000000000003695 ) ) ;
#17176 = ORIENTED_EDGE ( 'NONE', *, *, #68024, .T. ) ;
#17177 = CARTESIAN_POINT ( 'NONE',  ( 11.35316468749999963, 241.1979166700806729, 3.042071309553159519 ) ) ;
#17178 = VECTOR ( 'NONE', #7929, 1000.000000000000000 ) ;
#17179 = CARTESIAN_POINT ( 'NONE',  ( -5.082755093536317936, -5.082755093536320601, 17.04905278187175810 ) ) ;
#17180 = CARTESIAN_POINT ( 'NONE',  ( -2.679491924311226292, 8.333333326505366401, -10.00000000000000178 ) ) ;
#17181 = CARTESIAN_POINT ( 'NONE',  ( 2.775557561562891351E-14, 183.6788756342477029, 139.0000000000000568 ) ) ;
#17182 = FACE_OUTER_BOUND ( 'NONE', #50859, .T. ) ;
#17183 = CARTESIAN_POINT ( 'NONE',  ( -3.458734124999960358, 195.6250000013656063, 196.5673454167823877 ) ) ;
#17184 = CARTESIAN_POINT ( 'NONE',  ( -4.999999999999998224, 161.6666666666666856, -8.660254037844389075 ) ) ;
#17185 = CARTESIAN_POINT ( 'NONE',  ( 7.999999999999991118, 9.797174393178815797E-16, 24.08030277982336642 ) ) ;
#17186 = DIRECTION ( 'NONE',  ( -0.000000000000000000, 1.000000000000000000, 4.476705744456276341E-16 ) ) ;
#17187 = CARTESIAN_POINT ( 'NONE',  ( 4.999999999999998224, -52.85071664756681287, -48.38833198888288223 ) ) ;
#17188 = CARTESIAN_POINT ( 'NONE',  ( 9.832129032723416984, 125.6770833299193697, 5.676582343750006032 ) ) ;
#17189 = CARTESIAN_POINT ( 'NONE',  ( 28.00000000000001776, 205.5000000000000284, 165.9999999999998863 ) ) ;
#17190 = CARTESIAN_POINT ( 'NONE',  ( 5.499987861550172497, 9.526286449755788865, 67.99927393035380874 ) ) ;
#17193 = CARTESIAN_POINT ( 'NONE',  ( 2.828427124746152987, 202.1250000000000284, 139.1715728752538723 ) ) ;
#17192 = CARTESIAN_POINT ( 'NONE',  ( 25.55430564589115150, 196.0625000013656063, 167.5543056458911053 ) ) ;
#17191 = CARTESIAN_POINT ( 'NONE',  ( 29.65685424949235482, 209.0625000000000568, 173.9999999999999147 ) ) ;
#17194 = ORIENTED_EDGE ( 'NONE', *, *, #45223, .F. ) ;
#17195 = AXIS2_PLACEMENT_3D ( 'NONE', #46093, #17048, #44986 ) ;
#17196 = FACE_OUTER_BOUND ( 'NONE', #43042, .T. ) ;
#17197 = AXIS2_PLACEMENT_3D ( 'NONE', #34455, #46485, #69506 ) ;
#17198 = DIRECTION ( 'NONE',  ( 0.000000000000000000, 0.000000000000000000, 1.000000000000000000 ) ) ;
#17199 = CARTESIAN_POINT ( 'NONE',  ( 3.058894802626711318, -7.395264550195966180, -0.000000000000000000 ) ) ;
#17200 = CARTESIAN_POINT ( 'NONE',  ( -4.000000000000001776, 11.43750000000000000, -1.656854249492381470 ) ) ;
#17201 = CARTESIAN_POINT ( 'NONE',  ( -3.042071309553164404, 222.5520833299192986, -11.35316468749999963 ) ) ;
#17202 = CARTESIAN_POINT ( 'NONE',  ( -2.977408999572650927, 123.8750000020483810, -7.188101187500001821 ) ) ;
#17203 = CARTESIAN_POINT ( 'NONE',  ( 4.541265875000001451, 21.24999999863440436, 1.881053915767124440 ) ) ;
#17204 = FACE_OUTER_BOUND ( 'NONE', #38005, .T. ) ;
#17205 = CARTESIAN_POINT ( 'NONE',  ( -5.656854249492373476, -5.656854249492376141, 20.51780277982336642 ) ) ;
#17206 = LINE ( 'NONE', #62854, #38741 ) ;
#17207 = CARTESIAN_POINT ( 'NONE',  ( -11.35316468750000141, 108.4895833299193413, 3.042071309553159963 ) ) ;
#17208 = ORIENTED_EDGE ( 'NONE', *, *, #29903, .T. ) ;
#17209 =( BOUNDED_CURVE ( )  B_SPLINE_CURVE ( 2, ( #73916, #22220, #45247, #68259, #5268, #73177, #21485, #38851, #61855 ),
 .UNSPECIFIED., .F., .F. ) 
 B_SPLINE_CURVE_WITH_KNOTS ( ( 3, 2, 2, 2, 3 ),
 ( 0.8206662513146789628, 0.8272844480571014403, 0.8339027236415583744, 0.8405209992260151974, 0.8471392367758522335 ),
 .UNSPECIFIED. ) 
 CURVE ( )  GEOMETRIC_REPRESENTATION_ITEM ( )  RATIONAL_B_SPLINE_CURVE ( ( 0.9999981864094533712, 0.9238804393173626339, 1.000000000000000000, 0.9238795325112867385, 1.000000000000000000, 0.9238795325112867385, 1.000000000000000000, 0.9238799699685972255, 0.9999991250904070039 ) ) 
 REPRESENTATION_ITEM ( '' )  );
#17210 = CARTESIAN_POINT ( 'NONE',  ( 4.000000000000000888, 15.68749999726881406, 1.656854249492384135 ) ) ;
#17211 = CARTESIAN_POINT ( 'NONE',  ( 7.188101187499999156, 25.87499999795161543, 2.977408999572654924 ) ) ;
#17212 = CARTESIAN_POINT ( 'NONE',  ( -1.966770576099810657E-11, 61.25000000000153477, -9.999999999999998224 ) ) ;
#17213 = CARTESIAN_POINT ( 'NONE',  ( -3.042071309553166625, 243.1770833367473017, -11.35316468749999608 ) ) ;
#17214 = CARTESIAN_POINT ( 'NONE',  ( -5.676582343750006032, 99.11458332991935549, 9.832129032723418760 ) ) ;
#17215 = ORIENTED_EDGE ( 'NONE', *, *, #16611, .T. ) ;
#17216 = EDGE_CURVE ( 'NONE', #21786, #27460, #33897, .T. ) ;
#17217 = CARTESIAN_POINT ( 'NONE',  ( -32.00000000000001421, 208.1875000000000853, 168.3431457505080289 ) ) ;
#17218 = CARTESIAN_POINT ( 'NONE',  ( 4.220049686691934809, 10.18810118749999916, 107.6875000020483810 ) ) ;
#17219 = CARTESIAN_POINT ( 'NONE',  ( -5.000000000000005329, 225.2083333265053966, 8.660254037844387298 ) ) ;
#17220 = CARTESIAN_POINT ( 'NONE',  ( 3.458734125000015425, 202.2500000013656063, 196.5673454167823877 ) ) ;
#17222 = CARTESIAN_POINT ( 'NONE',  ( 8.311093377946834337, 100.1562499965860127, 8.311093377946839666 ) ) ;
#17221 = CARTESIAN_POINT ( 'NONE',  ( 0.000000000000000000, 0.000000000000000000, -4.000000000000001776 ) ) ;
#17223 = CARTESIAN_POINT ( 'NONE',  ( -5.656854249492375253, 5.656854249492375253, 15.83030278392014800 ) ) ;
#17224 = CARTESIAN_POINT ( 'NONE',  ( -26.56734541678232375, 198.2500000013656347, 173.4587341250003760 ) ) ;
#17225 = CARTESIAN_POINT ( 'NONE',  ( -7.999999999999991118, 0.000000000000000000, 28.01780278392014978 ) ) ;
#17226 = VERTEX_POINT ( 'NONE', #43007 ) ;
#17227 = CARTESIAN_POINT ( 'NONE',  ( -10.00000000000000355, 194.5833333265053966, 2.679491924311223183 ) ) ;
#17228 = CARTESIAN_POINT ( 'NONE',  ( 28.00000000000002132, 200.1250000027312126, 173.9999999999999147 ) ) ;
#17229 = CARTESIAN_POINT ( 'NONE',  ( 1.829776888832211235, -47.38538817230226385, 139.0536211277514838 ) ) ;
#17230 = CARTESIAN_POINT ( 'NONE',  ( -8.311093377946836114, 87.96874999658602690, -8.311093377946837890 ) ) ;
#17231 = CARTESIAN_POINT ( 'NONE',  ( -4.721056650415998313, 289.5781250017069510, 4.721056650416000089 ) ) ;
#17232 = CARTESIAN_POINT ( 'NONE',  ( -7.188101187500002709, 4.687499997951610986, 2.977408999572649151 ) ) ;
#17233 = CARTESIAN_POINT ( 'NONE',  ( 10.18810118750000093, -4.220049686691933033, 92.68750000204838102 ) ) ;
#17234 = CARTESIAN_POINT ( 'NONE',  ( 9.832129032723420536, 221.1979166632526983, -5.676582343749999815 ) ) ;
#17236 = ORIENTED_EDGE ( 'NONE', *, *, #4040, .T. ) ;
#17235 =( BOUNDED_CURVE ( )  B_SPLINE_CURVE ( 2, ( #39027, #44313, #67327, #49215, #72224, #56381, #62395, #27695, #44685, #10722, #15624, #38664, #50704 ),
 .UNSPECIFIED., .F., .F. ) 
 B_SPLINE_CURVE_WITH_KNOTS ( ( 3, 2, 2, 2, 2, 2, 3 ),
 ( 2.056685274044849354, 2.061918634596133781, 2.067151995147418209, 2.072385355698702636, 2.077618716249987063, 2.082852076801271934, 2.088085437352556362 ),
 .UNSPECIFIED. ) 
 CURVE ( )  GEOMETRIC_REPRESENTATION_ITEM ( )  RATIONAL_B_SPLINE_CURVE ( ( 0.9999999999999895639, 0.9659258262890787483, 1.000000000000000000, 0.9659258262890683122, 1.000000000000000000, 0.9659258262890683122, 1.000000000000000000, 0.9659258262890683122, 1.000000000000000000, 0.9659258262890683122, 1.000000000000000000, 0.9659258262893356539, 0.9999999999997326583 ) ) 
 REPRESENTATION_ITEM ( '' )  );
#17237 = DIRECTION ( 'NONE',  ( 0.5000000000000009992, -0.8660254037844380415, 0.000000000000000000 ) ) ;
#17238 = CARTESIAN_POINT ( 'NONE',  ( 4.242640687119287435, 291.3750000000000000, 4.242640687119285658 ) ) ;
#17239 = CARTESIAN_POINT ( 'NONE',  ( -2.085542519210945728E-15, 219.5312499965860411, 11.35316468750000141 ) ) ;
#17240 = EDGE_CURVE ( 'NONE', #24115, #5172, #30956, .T. ) ;
#17241 = FACE_BOUND ( 'NONE', #38672, .T. ) ;
#17242 = CARTESIAN_POINT ( 'NONE',  ( -6.676582343750001591, 295.4531250017069510, 0.000000000000000000 ) ) ;
#17243 = ORIENTED_EDGE ( 'NONE', *, *, #10852, .F. ) ;
#17244 = CARTESIAN_POINT ( 'NONE',  ( -4.615726161707376818, -52.16176840074092524, -48.91069252044866289 ) ) ;
#17245 = CARTESIAN_POINT ( 'NONE',  ( -3.042071309553163960, 207.5520833299193271, -11.35316468749999963 ) ) ;
#17246 = CARTESIAN_POINT ( 'NONE',  ( -4.220049686691935698, 10.18810118749999916, 97.37500000204839523 ) ) ;
#17247 = CARTESIAN_POINT ( 'NONE',  ( -25.55430564589115150, 205.0625000013656063, 172.4456943541091789 ) ) ;
#17248 = CARTESIAN_POINT ( 'NONE',  ( 5.656854249492378806, 16.31250000000000355, 5.656854249492381470 ) ) ;
#17249 = VERTEX_POINT ( 'NONE', #43385 ) ;
#17250 = VECTOR ( 'NONE', #54362, 1000.000000000000000 ) ;
#17251 = CARTESIAN_POINT ( 'NONE',  ( -2.977408999572650927, 120.8750000020483810, -7.188101187500001821 ) ) ;
#17252 = CARTESIAN_POINT ( 'NONE',  ( -25.17157287525374088, 199.7500000027312126, 172.8284271247464972 ) ) ;
#17253 = ADVANCED_FACE ( 'NONE', ( #2287 ), #38120, .F. ) ;
#17254 = CARTESIAN_POINT ( 'NONE',  ( -5.000000000000005329, 33.33333333333333570, 8.660254037844387298 ) ) ;
#17255 = ADVANCED_FACE ( 'NONE', ( #8693 ), #71309, .F. ) ;
#17256 = CARTESIAN_POINT ( 'NONE',  ( -26.34314575050754215, 197.9375000000000000, 166.0000000000004263 ) ) ;
#17257 = CARTESIAN_POINT ( 'NONE',  ( -7.204075437095965206, -7.204075437095968759, 72.71875000204838102 ) ) ;
#17258 = ORIENTED_EDGE ( 'NONE', *, *, #7928, .F. ) ;
#17259 = CARTESIAN_POINT ( 'NONE',  ( 3.211159895383560947, 2.187499998634407028, 3.211159895383562723 ) ) ;
#17260 = CARTESIAN_POINT ( 'NONE',  ( -7.188101187500002709, 1.312499997951610098, 2.977408999572649151 ) ) ;
#17261 = EDGE_CURVE ( 'NONE', #34052, #6656, #13951, .T. ) ;
#17262 = CARTESIAN_POINT ( 'NONE',  ( 7.778174593052023411, -7.778174593052021635, 112.5625000000000000 ) ) ;
#17263 = EDGE_CURVE ( 'NONE', #31616, #61881, #32083, .T. ) ;
#17264 = CARTESIAN_POINT ( 'NONE',  ( 7.188101187500000044, 122.2812500020483810, -8.802885111219163269E-16 ) ) ;
#17265 = CARTESIAN_POINT ( 'NONE',  ( 7.320508075688774596, 152.4999999931720538, -7.320508075688774596 ) ) ;
#17266 = CARTESIAN_POINT ( 'NONE',  ( 1.226468279477575784E-15, 294.7031250017069510, 6.676582343750001591 ) ) ;
#17269 = CARTESIAN_POINT ( 'NONE',  ( -4.242640687119285658, 289.1875000034139589, 4.242640687119287435 ) ) ;
#17268 = CARTESIAN_POINT ( 'NONE',  ( 11.35316468749999963, 241.4062500034140157, -1.390361679473963556E-15 ) ) ;
#17267 = CARTESIAN_POINT ( 'NONE',  ( 26.56734541678238060, 208.3750000013656063, 173.4587341249998929 ) ) ;
#17270 = SHAPE_DEFINITION_REPRESENTATION ( #16179, #30147 ) ;
#17271 = VERTEX_POINT ( 'NONE', #36992 ) ;
#17272 = CARTESIAN_POINT ( 'NONE',  ( 8.311093377946834337, 242.3437500034139873, -8.311093377946836114 ) ) ;
#17273 = EDGE_CURVE ( 'NONE', #52335, #12328, #73835, .T. ) ;
#17274 = CARTESIAN_POINT ( 'NONE',  ( 5.082755093536318824, 5.082755093536319713, 8.424052781871752771 ) ) ;
#17275 = CIRCLE ( 'NONE', #20871, 3.999999999999989786 ) ;
#17276 = ORIENTED_EDGE ( 'NONE', *, *, #34100, .T. ) ;
#17277 = CARTESIAN_POINT ( 'NONE',  ( -7.204075437095967871, 7.204075437095967871, 67.46875000204836681 ) ) ;
#17278 = CARTESIAN_POINT ( 'NONE',  ( 11.35316468749999963, 86.30208332991936970, -3.042071309553165293 ) ) ;
#17279 = CARTESIAN_POINT ( 'NONE',  ( -3.673940397442060854E-16, 294.8125000034140157, -6.000000000000001776 ) ) ;
#17280 = CARTESIAN_POINT ( 'NONE',  ( -11.00000000000000000, 0.000000000000000000, 80.49999999999998579 ) ) ;
#17283 = CARTESIAN_POINT ( 'NONE',  ( 4.999999999999995559, 69.16666666666667140, 8.660254037844392627 ) ) ;
#17282 = CARTESIAN_POINT ( 'NONE',  ( 26.56734541678233086, 208.0000000013656347, 166.5412658749999650 ) ) ;
#17281 = CARTESIAN_POINT ( 'NONE',  ( 30.44569435410879521, 206.8125000013656063, 172.4456943541087526 ) ) ;
#17284 = ORIENTED_EDGE ( 'NONE', *, *, #3458, .T. ) ;
#17285 = CARTESIAN_POINT ( 'NONE',  ( 5.499987861550171608, 9.526286449755788865, 67.99927393035380874 ) ) ;
#17286 = DIRECTION ( 'NONE',  ( -1.000000000000000000, 0.000000000000000000, 0.000000000000000000 ) ) ;
#17287 = CARTESIAN_POINT ( 'NONE',  ( -11.35316468750000141, 203.2812499965860411, -1.390361679473963753E-15 ) ) ;
#17288 = CARTESIAN_POINT ( 'NONE',  ( 3.458734124999959025, 203.5000000013655779, 140.5673454167824161 ) ) ;
#17289 = CARTESIAN_POINT ( 'NONE',  ( 30.44569435410879521, 207.8125000013656063, 172.4456943541087526 ) ) ;
#17290 = CARTESIAN_POINT ( 'NONE',  ( 2.977408999572650927, 23.62499999795161543, -7.188101187500001821 ) ) ;
#17291 = CARTESIAN_POINT ( 'NONE',  ( 6.951808397369818766E-16, 177.3437499965860411, -11.35316468750000141 ) ) ;
#17292 = LINE ( 'NONE', #57681, #56496 ) ;
#17293 = CARTESIAN_POINT ( 'NONE',  ( 7.188101187500000933, 99.87500000204838102, -2.977408999572651371 ) ) ;
#17295 = CARTESIAN_POINT ( 'NONE',  ( 2.828427124746190291, 9.875000000000000000, 2.828427124746192067 ) ) ;
#17294 = DIRECTION ( 'NONE',  ( -1.000000000000000000, 0.000000000000000000, 0.000000000000000000 ) ) ;
#17296 = CARTESIAN_POINT ( 'NONE',  ( 2.780723358947928197E-16, 9.562499998634406140, -4.541265875000002339 ) ) ;
#17297 = CARTESIAN_POINT ( 'NONE',  ( 31.45873412500001010, 204.0000000013656063, 168.5673454167822740 ) ) ;
#17298 = CARTESIAN_POINT ( 'NONE',  ( -2.977408999572647819, 7.188101187499991163, 7.580302781871751883 ) ) ;
#17299 = CARTESIAN_POINT ( 'NONE',  ( -2.085542519210945728E-15, 59.53124999658601979, 11.35316468750000141 ) ) ;
#17300 = FACE_OUTER_BOUND ( 'NONE', #39245, .T. ) ;
#17301 = ORIENTED_EDGE ( 'NONE', *, *, #52389, .T. ) ;
#17302 = CARTESIAN_POINT ( 'NONE',  ( 0.000000000000000000, 125.0000000000000000, 8.000000000000000000 ) ) ;
#17303 = CARTESIAN_POINT ( 'NONE',  ( 27.99999999999996803, 206.6250000027312126, 165.9999999999998863 ) ) ;
#17304 = CARTESIAN_POINT ( 'NONE',  ( 11.35316468749999785, 65.57291666325269830, 3.042071309553174174 ) ) ;
#17305 = CARTESIAN_POINT ( 'NONE',  ( -10.99999999999999822, -4.556349186104052151, 71.78125000409679046 ) ) ;
#17306 = CARTESIAN_POINT ( 'NONE',  ( -3.458734125000015425, 201.2500000013656063, 143.4326545832176976 ) ) ;
#17307 = CARTESIAN_POINT ( 'NONE',  ( -3.511653767256416092, 16.35475815725936499, 69.12977678000893889 ) ) ;
#17309 = CARTESIAN_POINT ( 'NONE',  ( 6.951808397369818766E-16, 57.03124999658601268, -11.35316468750000141 ) ) ;
#17308 = CARTESIAN_POINT ( 'NONE',  ( 2.977408999572654480, 91.62500000204836681, 7.188101187499999156 ) ) ;
#17311 = ADVANCED_FACE ( 'NONE', ( #27813 ), #31326, .F. ) ;
#17310 = CARTESIAN_POINT ( 'NONE',  ( -3.313708498984758943, -7.999999999999989342, 2.611552779823365977 ) ) ;
#17312 = CARTESIAN_POINT ( 'NONE',  ( 6.123233995736767268E-16, 13.12499999317203425, -10.00000000000000178 ) ) ;
#17313 = CARTESIAN_POINT ( 'NONE',  ( -2.679491924311225848, 153.3333333265053682, -10.00000000000000178 ) ) ;
#17314 = CARTESIAN_POINT ( 'NONE',  ( 7.188101187500002709, 99.68750000204838102, 2.977408999572649151 ) ) ;
#17315 = CARTESIAN_POINT ( 'NONE',  ( 0.000000000000000000, 15.99999999999998579, -1.000000000000000000 ) ) ;
#17316 = CARTESIAN_POINT ( 'NONE',  ( 11.35316468750000141, 51.09374999658601268, 0.000000000000000000 ) ) ;
#17317 = EDGE_CURVE ( 'NONE', #29688, #61043, #7951, .T. ) ;
#17318 = CARTESIAN_POINT ( 'NONE',  ( -2.828427124746153876, 200.8750000000000284, 195.1715728752538439 ) ) ;
#17319 = CARTESIAN_POINT ( 'NONE',  ( 5.676582343750001591, 186.6145833299193839, -9.832129032723420536 ) ) ;
#17320 = VERTEX_POINT ( 'NONE', #50824 ) ;
#17321 = CARTESIAN_POINT ( 'NONE',  ( 7.204075437095966983, 7.204075437095967871, 73.09375000204838102 ) ) ;
#17322 = CARTESIAN_POINT ( 'NONE',  ( 2.828427124746208943, 195.6250000000000284, 195.1715728752538439 ) ) ;
#17324 = CARTESIAN_POINT ( 'NONE',  ( -5.676582343750006032, 179.1145833299193555, 9.832129032723418760 ) ) ;
#17323 = CARTESIAN_POINT ( 'NONE',  ( 30.82842712474620228, 203.3750000000000284, 167.1715728752537586 ) ) ;
#17325 = CARTESIAN_POINT ( 'NONE',  ( 3.313708498984762496, -7.999999999999989342, 5.855302784329825094 ) ) ;
#17326 = LINE ( 'NONE', #16195, #8022 ) ;
#17327 = CARTESIAN_POINT ( 'NONE',  ( 8.660254037844389075, 250.2083333401612890, 4.999999999999997335 ) ) ;
#17328 = FACE_BOUND ( 'NONE', #68218, .T. ) ;
#17329 = ORIENTED_EDGE ( 'NONE', *, *, #5651, .T. ) ;
#17330 = CARTESIAN_POINT ( 'NONE',  ( -11.35316468750000141, 163.8020833299193555, 3.042071309553159963 ) ) ;
#17331 =( BOUNDED_CURVE ( )  B_SPLINE_CURVE ( 2, ( #52828, #30551, #1160, #24868, #12454, #18122, #47887, #19583, #64517 ),
 .UNSPECIFIED., .F., .F. ) 
 B_SPLINE_CURVE_WITH_KNOTS ( ( 3, 2, 2, 2, 3 ),
 ( 0.6874999999999982236, 0.6979166666666648533, 0.7083333333333317050, 0.7187499999999983347, 0.7291666666666649643 ),
 .UNSPECIFIED. ) 
 CURVE ( )  GEOMETRIC_REPRESENTATION_ITEM ( )  RATIONAL_B_SPLINE_CURVE ( ( 1.000000000000012879, 0.9238795325112737489, 1.000000000000000000, 0.9238795325112867385, 1.000000000000000000, 0.9238795325112867385, 1.000000000000000000, 0.9238795325112989509, 0.9999999999999877875 ) ) 
 REPRESENTATION_ITEM ( '' )  );
#17332 = EDGE_CURVE ( 'NONE', #22422, #61351, #4453, .T. ) ;
#17333 = CARTESIAN_POINT ( 'NONE',  ( 7.188101187499992051, 2.977408999572647819, 26.33030278187176165 ) ) ;
#17334 = CARTESIAN_POINT ( 'NONE',  ( -11.35316468750000141, 133.5937499965860127, -1.390361679473963753E-15 ) ) ;
#17335 = CYLINDRICAL_SURFACE ( 'NONE', #41788, 3.999999999999976019 ) ;
#17336 = VERTEX_POINT ( 'NONE', #29954 ) ;
#17337 = CARTESIAN_POINT ( 'NONE',  ( 1.881053915767121776, 7.624999998634408804, -4.541265875000002339 ) ) ;
#17338 = CARTESIAN_POINT ( 'NONE',  ( -2.977408999572654480, 11.99999999795161187, 7.188101187499999156 ) ) ;
#17339 = CARTESIAN_POINT ( 'NONE',  ( -8.000000000000000000, 101.0937500040968047, -3.313708498984761608 ) ) ;
#17340 = CARTESIAN_POINT ( 'NONE',  ( -31.45873412499997812, 197.0000000013656347, 171.4326545832180386 ) ) ;
#17341 = EDGE_CURVE ( 'NONE', #65897, #24662, #20290, .T. ) ;
#17342 = B_SPLINE_CURVE_WITH_KNOTS ( 'NONE', 3,
 ( #45198, #35021, #11244, #39911, #5592, #64043, #62918, #6342, #22174, #51228, #74239, #22545, #23300, #34649, #28964, #28589, #23676, #57654, #74615, #29712 ),
 .UNSPECIFIED., .F., .F.,
 ( 4, 2, 2, 2, 2, 2, 2, 2, 2, 4 ),
 ( 2.797157557069881010E-17, 0.001156441540184017982, 0.001734662310276006807, 0.002312883080367995198, 0.003469324620551979786, 0.004625766160735963507, 0.005782207700919948096, 0.006938649241103932684, 0.008095090781287915538, 0.009251532321471899259 ),
 .UNSPECIFIED. ) ;
#17343 = CARTESIAN_POINT ( 'NONE',  ( 4.000000000000000888, 8.937500000000001776, 1.656854249492384135 ) ) ;
#17344 = CARTESIAN_POINT ( 'NONE',  ( -7.347880794884122694E-16, 21.49999999726881583, 4.000000000000001776 ) ) ;
#17345 = CARTESIAN_POINT ( 'NONE',  ( -1.881053915767121776, 10.62499999863440969, -4.541265875000002339 ) ) ;
#17346 = CARTESIAN_POINT ( 'NONE',  ( 7.999999999999991118, 3.313708498984757611, 19.86155278392014978 ) ) ;
#17348 = AXIS2_PLACEMENT_3D ( 'NONE', #52944, #13292, #35595 ) ;
#17347 = CARTESIAN_POINT ( 'NONE',  ( 1.656854249492347719, 198.8125000000000284, 146.0000000000000284 ) ) ;
#17349 = ORIENTED_EDGE ( 'NONE', *, *, #66662, .F. ) ;
#17350 = CARTESIAN_POINT ( 'NONE',  ( -8.000000000000000000, 24.75000000000000355, -9.797174393178825657E-16 ) ) ;
#17351 = CARTESIAN_POINT ( 'NONE',  ( 2.977408999572650039, 105.6875000020483952, -7.188101187500001821 ) ) ;
#17353 = CARTESIAN_POINT ( 'NONE',  ( -5.656854249492379694, 15.37499999590322197, -5.656854249492380582 ) ) ;
#17352 = CARTESIAN_POINT ( 'NONE',  ( -31.45873412500001720, 194.6250000013655779, 168.5673454167828140 ) ) ;
#17354 =( LENGTH_UNIT ( ) NAMED_UNIT ( * ) SI_UNIT ( .MILLI., .METRE. ) );
#17355 = ORIENTED_EDGE ( 'NONE', *, *, #49425, .F. ) ;
#17356 = CARTESIAN_POINT ( 'NONE',  ( 5.082755093536318824, 5.082755093536319713, 23.42405278187175455 ) ) ;
#17357 = VERTEX_POINT ( 'NONE', #35260 ) ;
#17358 = ADVANCED_FACE ( 'NONE', ( #71402 ), #31049, .T. ) ;
#17359 = ORIENTED_EDGE ( 'NONE', *, *, #49692, .T. ) ;
#17360 = CARTESIAN_POINT ( 'NONE',  ( -7.204075437095967871, 7.204075437095967871, 92.96875000204838102 ) ) ;
#17361 = CARTESIAN_POINT ( 'NONE',  ( -4.556349186104045934, 11.00000000000000000, 92.21874999999998579 ) ) ;
#17362 = CARTESIAN_POINT ( 'NONE',  ( -26.56734541678232731, 196.2500000013656347, 173.4587341250003760 ) ) ;
#17363 = CARTESIAN_POINT ( 'NONE',  ( 7.778174593052023411, -7.778174593052021635, 103.5624999999999858 ) ) ;
#17365 = CARTESIAN_POINT ( 'NONE',  ( 1.226468279477575784E-15, 298.8593750017070079, 6.676582343750001591 ) ) ;
#17364 = DIRECTION ( 'NONE',  ( -0.000000000000000000, 1.000000000000000000, 4.476705744456276341E-16 ) ) ;
#17366 = CARTESIAN_POINT ( 'NONE',  ( 2.679491924311222739, 128.9583333333333428, 10.00000000000000355 ) ) ;
#17367 = CARTESIAN_POINT ( 'NONE',  ( 5.656854249492381470, 100.0625000000000000, 5.656854249492379694 ) ) ;
#17368 = CARTESIAN_POINT ( 'NONE',  ( -6.676582343750001591, 287.6093750017069510, 0.000000000000000000 ) ) ;
#17369 = CARTESIAN_POINT ( 'NONE',  ( -4.401442555609577197E-16, 7.188101187499992051, 2.986552781871751439 ) ) ;
#17370 = CARTESIAN_POINT ( 'NONE',  ( -7.999999999999998224, 98.09375000000001421, 3.313708498984766049 ) ) ;
#17371 = CARTESIAN_POINT ( 'NONE',  ( 25.55430564589119413, 203.0625000013656063, 167.5543056458910485 ) ) ;
#17372 = CARTESIAN_POINT ( 'NONE',  ( 5.656854249492378806, 25.12499999590322375, 5.656854249492381470 ) ) ;
#17373 = AXIS2_PLACEMENT_3D ( 'NONE', #56623, #38521, #38889 ) ;
#17374 = CARTESIAN_POINT ( 'NONE',  ( 8.008118988124991233, 9.807117285998411148E-16, 3.263115283940628331 ) ) ;
#17375 = CARTESIAN_POINT ( 'NONE',  ( 12.00000000000000178, -2.333919766284219488, -0.1006330532450328968 ) ) ;
#17376 = CARTESIAN_POINT ( 'NONE',  ( -2.977408999572652260, 117.3125000020483952, 7.188101187500000044 ) ) ;
#17378 = CARTESIAN_POINT ( 'NONE',  ( -7.999999999999989342, -3.313708498984762496, 6.924052779823365533 ) ) ;
#17377 = CARTESIAN_POINT ( 'NONE',  ( -6.676582343750001591, 299.5312500017070079, 0.000000000000000000 ) ) ;
#17379 = CARTESIAN_POINT ( 'NONE',  ( -8.311093377946836114, 243.5937500034140157, -8.311093377946836114 ) ) ;
#17380 = CARTESIAN_POINT ( 'NONE',  ( -8.000000000000000000, 90.50000000000000000, 0.000000000000000000 ) ) ;
#17381 = CARTESIAN_POINT ( 'NONE',  ( -3.673940397442060854E-16, 291.8125000034140157, -6.000000000000001776 ) ) ;
#17382 = CARTESIAN_POINT ( 'NONE',  ( 25.17157287525381193, 196.6250000000000284, 167.1715728752537018 ) ) ;
#17383 = CARTESIAN_POINT ( 'NONE',  ( 9.832129032723420536, 21.19791666325268409, -5.676582343749999815 ) ) ;
#17384 = LINE ( 'NONE', #73989, #27896 ) ;
#17385 = CARTESIAN_POINT ( 'NONE',  ( -5.676582343750006032, 224.4270833299193555, 9.832129032723418760 ) ) ;
#17386 = CARTESIAN_POINT ( 'NONE',  ( 6.123233995736767268E-16, 218.1249999931720538, -10.00000000000000178 ) ) ;
#17388 = CARTESIAN_POINT ( 'NONE',  ( -5.000000000000087930, 43.33333333333343518, 8.660254037844529407 ) ) ;
#17387 = FACE_OUTER_BOUND ( 'NONE', #44524, .T. ) ;
#17389 = VERTEX_POINT ( 'NONE', #47293 ) ;
#17390 = CARTESIAN_POINT ( 'NONE',  ( 3.458734124999960358, 197.6250000013656063, 143.4326545832176976 ) ) ;
#17391 = CARTESIAN_POINT ( 'NONE',  ( 3.042071309553159519, 19.73958332991934483, 11.35316468750000141 ) ) ;
#17392 = CARTESIAN_POINT ( 'NONE',  ( 11.00000000000000355, -4.556349186104045046, 94.84375000409679046 ) ) ;
#17393 = CARTESIAN_POINT ( 'NONE',  ( 2.124081043562865201, 10.27770035960974582, 63.71262442773669221 ) ) ;
#17394 = CARTESIAN_POINT ( 'NONE',  ( -10.00000000000001066, 152.7083333333333428, 2.679491924311225404 ) ) ;
#17395 = CARTESIAN_POINT ( 'NONE',  ( 5.656854249492380582, 7.499999995903221084, -5.656854249492380582 ) ) ;
#17397 = CARTESIAN_POINT ( 'NONE',  ( -2.085542519210945728E-15, 24.53124999658601624, 11.35316468750000141 ) ) ;
#17396 = CARTESIAN_POINT ( 'NONE',  ( -2.977408999572650927, 110.3750000020484094, -7.188101187500000933 ) ) ;
#17399 = EDGE_CURVE ( 'NONE', #63756, #32479, #17434, .T. ) ;
#17398 = CARTESIAN_POINT ( 'NONE',  ( 5.656854249492374365, 5.656854249492375253, 19.76780277982336642 ) ) ;
#17400 = CARTESIAN_POINT ( 'NONE',  ( 9.832129032723416984, 130.3645833299193555, 5.676582343750006032 ) ) ;
#17401 = CARTESIAN_POINT ( 'NONE',  ( -8.660254037844390851, 104.7916666598386968, 4.999999999999998224 ) ) ;
#17402 = CARTESIAN_POINT ( 'NONE',  ( 7.188101187500000044, 114.7812500020483952, -8.802885111219163269E-16 ) ) ;
#17403 = CARTESIAN_POINT ( 'NONE',  ( -4.898587196589412829E-16, 120.3125000040967763, -8.000000000000000000 ) ) ;
#17404 = CARTESIAN_POINT ( 'NONE',  ( -24.54126587500000412, 207.5000000013655779, 168.5673454167827003 ) ) ;
#17405 = CARTESIAN_POINT ( 'NONE',  ( -5.000000000000000000, -52.63864145287891461, -42.88977517748093504 ) ) ;
#17406 = ORIENTED_EDGE ( 'NONE', *, *, #61527, .F. ) ;
#17407 = CARTESIAN_POINT ( 'NONE',  ( -5.676582343749998039, 12.76041666325268409, -9.832129032723420536 ) ) ;
#17408 = EDGE_CURVE ( 'NONE', #74050, #40814, #22718, .T. ) ;
#17409 = CARTESIAN_POINT ( 'NONE',  ( -10.00000000000000000, 154.1666666598387110, -2.679491924311229845 ) ) ;
#17410 = CARTESIAN_POINT ( 'NONE',  ( 6.676582343750003368, 298.0156250017070079, -2.765530957081997254 ) ) ;
#17411 = CARTESIAN_POINT ( 'NONE',  ( -11.35316468750000141, 143.4895833299193839, 3.042071309553159963 ) ) ;
#17412 = CARTESIAN_POINT ( 'NONE',  ( 5.656854249492376141, -5.656854249492374365, 23.94905278432982598 ) ) ;
#17413 = CIRCLE ( 'NONE', #53543, 9.000000000000001776 ) ;
#17414 = CARTESIAN_POINT ( 'NONE',  ( -3.313708498984805573, 19.03125000000000000, 7.999999999999956479 ) ) ;
#17415 = CARTESIAN_POINT ( 'NONE',  ( -6.951808397369817780E-16, 252.6562500034140157, -11.35316468749999963 ) ) ;
#17416 = CARTESIAN_POINT ( 'NONE',  ( 7.204075437095966983, 7.204075437095967871, 100.4687500020483810 ) ) ;
#17417 = ORIENTED_EDGE ( 'NONE', *, *, #49537, .F. ) ;
#17418 = CARTESIAN_POINT ( 'NONE',  ( 5.000000000000000000, 12.55023575007693104, 69.09043692422063998 ) ) ;
#17419 = FACE_OUTER_BOUND ( 'NONE', #60494, .T. ) ;
#17420 = CARTESIAN_POINT ( 'NONE',  ( 1.432654583217664701, 201.0000000013655779, 201.4587341250000065 ) ) ;
#17421 = CARTESIAN_POINT ( 'NONE',  ( 6.951808397369818766E-16, 87.34374999658602690, -11.35316468750000141 ) ) ;
#17422 = VERTEX_POINT ( 'NONE', #68808 ) ;
#17423 = CARTESIAN_POINT ( 'NONE',  ( -4.220049686691937474, -10.18810118749999738, 109.9375000020483952 ) ) ;
#17424 = CARTESIAN_POINT ( 'NONE',  ( -3.211159895383562723, 14.06249999863440614, 3.211159895383561391 ) ) ;
#17425 = ORIENTED_EDGE ( 'NONE', *, *, #6176, .F. ) ;
#17426 = ORIENTED_EDGE ( 'NONE', *, *, #14168, .T. ) ;
#17427 = CARTESIAN_POINT ( 'NONE',  ( 3.313708498984762052, 1.781250000000000444, -8.000000000000000000 ) ) ;
#17428 = DIRECTION ( 'NONE',  ( -0.000000000000000000, 1.000000000000000000, -0.000000000000000000 ) ) ;
#17429 = CARTESIAN_POINT ( 'NONE',  ( -5.000000000000000000, -65.75515815785537654, -23.82162496270666452 ) ) ;
#17430 = CARTESIAN_POINT ( 'NONE',  ( 7.188101187500001821, 21.93749999795161543, -2.977408999572650483 ) ) ;
#17431 = CARTESIAN_POINT ( 'NONE',  ( 5.656854249492381470, 119.7500000040967905, 5.656854249492379694 ) ) ;
#17432 = CARTESIAN_POINT ( 'NONE',  ( -10.18810118749999916, 4.220049686691934809, 106.9375000020483810 ) ) ;
#17433 = AXIS2_PLACEMENT_3D ( 'NONE', #48165, #20230, #66637 ) ;
#17434 =( BOUNDED_CURVE ( )  B_SPLINE_CURVE ( 2, ( #59008, #41276, #36723, #47656, #7681, #19727, #52597, #65008, #70318 ),
 .UNSPECIFIED., .F., .F. ) 
 B_SPLINE_CURVE_WITH_KNOTS ( ( 3, 2, 2, 2, 3 ),
 ( 0.02083333333333103887, 0.03124999999999771363, 0.04166666666666438146, 0.05208333333333105969, 0.06249999999999773792 ),
 .UNSPECIFIED. ) 
 CURVE ( )  GEOMETRIC_REPRESENTATION_ITEM ( )  RATIONAL_B_SPLINE_CURVE ( ( 1.000000000000016653, 0.9238795325112698631, 1.000000000000000000, 0.9238795325112867385, 1.000000000000000000, 0.9238795325112867385, 1.000000000000000000, 0.9238795325113032808, 0.9999999999999834577 ) ) 
 REPRESENTATION_ITEM ( '' )  );
#17435 = CARTESIAN_POINT ( 'NONE',  ( 1.656854249492478948, 201.8125000027312410, 194.0000000000001705 ) ) ;
#17436 = CARTESIAN_POINT ( 'NONE',  ( 4.000000000000001776, 10.74999999726881406, 0.000000000000000000 ) ) ;
#17437 =( BOUNDED_CURVE ( )  B_SPLINE_CURVE ( 2, ( #60209, #25501, #48514, #71520, #64768, #66245, #19844, #60585, #42851, #65868, #13071, #31549, #1421 ),
 .UNSPECIFIED., .F., .T. ) 
 B_SPLINE_CURVE_WITH_KNOTS ( ( 3, 2, 2, 2, 2, 2, 3 ),
 ( 2.150888710979840468, 2.156121240787547411, 2.161353770595253909, 2.166586300402960852, 2.171818830210667794, 2.177051360018374293, 2.182283889826081236 ),
 .UNSPECIFIED. ) 
 CURVE ( )  GEOMETRIC_REPRESENTATION_ITEM ( )  RATIONAL_B_SPLINE_CURVE ( ( 0.9999999999999978906, 0.9659258262890704216, 1.000000000000000000, 0.9659258262890683122, 1.000000000000000000, 0.9659258262890683122, 1.000000000000000000, 0.9659258262890683122, 1.000000000000000000, 0.9659258262890683122, 1.000000000000000000, 0.9659258262891539104, 0.9999999999999144018 ) ) 
 REPRESENTATION_ITEM ( '' )  );
#17438 = CARTESIAN_POINT ( 'NONE',  ( 3.211159895383561835, 1.437499998634406806, -3.211159895383561835 ) ) ;
#17439 = VERTEX_POINT ( 'NONE', #38668 ) ;
#17440 = CARTESIAN_POINT ( 'NONE',  ( 2.751064625579944321E-14, 198.8750000027312126, 194.0000000000000568 ) ) ;
#17441 = CARTESIAN_POINT ( 'NONE',  ( -1.432654583217607858, 204.6250000013655779, 201.4587341250000065 ) ) ;
#17442 = CARTESIAN_POINT ( 'NONE',  ( -30.44569435410875968, 204.8125000013656063, 172.4456943541092642 ) ) ;
#17443 =( NAMED_UNIT ( * ) PLANE_ANGLE_UNIT ( ) SI_UNIT ( $, .RADIAN. ) );
#17444 = CARTESIAN_POINT ( 'NONE',  ( -3.211159895383561391, 11.68749999863440614, -3.211159895383561835 ) ) ;
#17445 = CARTESIAN_POINT ( 'NONE',  ( -2.849036369511732440E-14, 206.3750000027312126, 138.0000000000000568 ) ) ;
#17446 = CARTESIAN_POINT ( 'NONE',  ( -7.188101187499991163, 2.977408999572646930, 19.39280278187176165 ) ) ;
#17447 = ORIENTED_EDGE ( 'NONE', *, *, #8996, .T. ) ;
#17448 = EDGE_LOOP ( 'NONE', ( #33156, #15060, #49289, #64374 ) ) ;
#17449 = CARTESIAN_POINT ( 'NONE',  ( -10.18810118749999916, 0.000000000000000000, 112.6562500020483810 ) ) ;
#17450 = CARTESIAN_POINT ( 'NONE',  ( -9.765709903158434457, -15.14637444941025635, -0.009429105422181003823 ) ) ;
#17451 = CARTESIAN_POINT ( 'NONE',  ( -25.17157287525377996, 206.6250000000000284, 172.8284271247465256 ) ) ;
#17452 = CARTESIAN_POINT ( 'NONE',  ( 3.458734125000016313, 201.8750000013656063, 199.4326545832176691 ) ) ;
#17453 = CARTESIAN_POINT ( 'NONE',  ( -1.734723475976807094E-15, 13.85640646055103886, -14.80000000000000071 ) ) ;
#17454 = CARTESIAN_POINT ( 'NONE',  ( -10.00000000000000000, 77.29166666666665719, -2.679491924311229845 ) ) ;
#17455 = CARTESIAN_POINT ( 'NONE',  ( 8.000000000000001776, 124.1562499999999858, 3.313708498984759387 ) ) ;
#17456 = CARTESIAN_POINT ( 'NONE',  ( 8.311093377946834337, 65.46874999658601268, 8.311093377946839666 ) ) ;
#17457 = CARTESIAN_POINT ( 'NONE',  ( -6.000000000000003553, 288.9375000000000000, -2.485281374238571317 ) ) ;
#17458 = VERTEX_POINT ( 'NONE', #11109 ) ;
#17459 = EDGE_CURVE ( 'NONE', #37555, #70218, #28018, .T. ) ;
#17460 = CARTESIAN_POINT ( 'NONE',  ( 4.000000000000015987, 203.5625000000000000, 196.3431457505076594 ) ) ;
#17461 = CARTESIAN_POINT ( 'NONE',  ( -6.891449706547808418, -61.56004288259260449, 23.71475313280533115 ) ) ;
#17462 = CARTESIAN_POINT ( 'NONE',  ( 3.458734124999959025, 208.5000000013656063, 140.5673454167824161 ) ) ;
#17463 = CARTESIAN_POINT ( 'NONE',  ( 1.102182119232618108E-15, 288.2500000000000000, 6.000000000000001776 ) ) ;
#17464 = CARTESIAN_POINT ( 'NONE',  ( -4.898587196589412829E-16, 97.62499999999998579, -8.000000000000000000 ) ) ;
#17465 = B_SPLINE_CURVE_WITH_KNOTS ( 'NONE', 3,
 ( #43964, #21318, #66973, #32284, #15649, #55298 ),
 .UNSPECIFIED., .F., .F.,
 ( 4, 2, 4 ),
 ( 2.380729646213380196E-07, 0.003505341553885911888, 0.007010445034807201957 ),
 .UNSPECIFIED. ) ;
#17466 = CARTESIAN_POINT ( 'NONE',  ( 8.660254037844389075, 242.0833333333333428, 4.999999999999997335 ) ) ;
#17467 = DIRECTION ( 'NONE',  ( -0.000000000000000000, 1.000000000000000000, -0.000000000000000000 ) ) ;
#17468 = CARTESIAN_POINT ( 'NONE',  ( 10.18810118750000093, -4.220049686691933921, 70.18750000204838102 ) ) ;
#17469 = CARTESIAN_POINT ( 'NONE',  ( -10.00000000000000000, 207.2916666666666856, -2.679491924311229845 ) ) ;
#17470 = CARTESIAN_POINT ( 'NONE',  ( -2.977408999572647819, 7.188101187499992051, 15.08030278187175455 ) ) ;
#17471 = CARTESIAN_POINT ( 'NONE',  ( -11.35316468750000141, 178.5937499965860411, -1.390361679473963753E-15 ) ) ;
#17472 = CARTESIAN_POINT ( 'NONE',  ( -10.00000000000000355, 37.70833333333333570, 2.679491924311223183 ) ) ;
#17473 = CARTESIAN_POINT ( 'NONE',  ( 10.00000000000000178, 177.0833333265053966, -2.679491924311226736 ) ) ;
#17475 = CARTESIAN_POINT ( 'NONE',  ( 2.751064625579944321E-14, 207.8750000027312126, 194.0000000000000568 ) ) ;
#17474 = CARTESIAN_POINT ( 'NONE',  ( -8.660254037844385522, 228.5416666734946602, 5.000000000000004441 ) ) ;
#17476 = VERTEX_POINT ( 'NONE', #5448 ) ;
#17477 = CARTESIAN_POINT ( 'NONE',  ( -2.445694354108838731, 198.0625000013656063, 144.4456943541088663 ) ) ;
#17478 = CARTESIAN_POINT ( 'NONE',  ( 8.311093377946834337, 30.46874999658601979, 8.311093377946839666 ) ) ;
#17479 = CARTESIAN_POINT ( 'NONE',  ( 7.778174593052023411, -7.778174593052021635, 108.2500000040967763 ) ) ;
#17480 = AXIS2_PLACEMENT_3D ( 'NONE', #46674, #68572, #64035 ) ;
#17481 = CARTESIAN_POINT ( 'NONE',  ( -2.968631558800673975, 194.5024059583198550, 199.8703579010459350 ) ) ;
#17482 = DIRECTION ( 'NONE',  ( 0.000000000000000000, 0.000000000000000000, -1.000000000000000000 ) ) ;
#17484 = CARTESIAN_POINT ( 'NONE',  ( 4.556349186104052151, -10.99999999999999822, 108.1562500040967763 ) ) ;
#17483 = CYLINDRICAL_SURFACE ( 'NONE', #58102, 18.99999999999998934 ) ;
#17485 = CARTESIAN_POINT ( 'NONE',  ( -27.29358557349494419, -51.67046305750793778, 184.8225746511350280 ) ) ;
#17487 = ADVANCED_FACE ( 'NONE', ( #67705 ), #62399, .T. ) ;
#17486 = CARTESIAN_POINT ( 'NONE',  ( 2.445694354108783664, 199.3125000013656063, 144.4456943541088663 ) ) ;
#17488 = CARTESIAN_POINT ( 'NONE',  ( -8.660254037844390851, 64.79166665983871098, 4.999999999999998224 ) ) ;
#17489 = VECTOR ( 'NONE', #25799, 1000.000000000000000 ) ;
#17490 = CARTESIAN_POINT ( 'NONE',  ( 7.188101187500000044, 96.40625000204838102, -8.802885111219163269E-16 ) ) ;
#17491 = CARTESIAN_POINT ( 'NONE',  ( -4.541265875000002339, 12.87499999863440969, -1.881053915767121998 ) ) ;
#17492 = CARTESIAN_POINT ( 'NONE',  ( -29.65685424949231930, 206.5625000027312410, 174.0000000000003695 ) ) ;
#17493 = CARTESIAN_POINT ( 'NONE',  ( -3.313708498984758943, -7.999999999999989342, 2.611552779823365977 ) ) ;
#17494 = ADVANCED_FACE ( 'NONE', ( #28450 ), #74469, .F. ) ;
#17495 = CARTESIAN_POINT ( 'NONE',  ( 6.123233995736767268E-16, 103.1249999931720396, -10.00000000000000178 ) ) ;
#17496 = ORIENTED_EDGE ( 'NONE', *, *, #41976, .F. ) ;
#17497 = ORIENTED_EDGE ( 'NONE', *, *, #8504, .T. ) ;
#17498 = CARTESIAN_POINT ( 'NONE',  ( -4.193070328474953534, -50.40098303874145103, -40.95513628906691395 ) ) ;
#17499 = CARTESIAN_POINT ( 'NONE',  ( -6.676582343750001591, 298.6093750017069510, 0.000000000000000000 ) ) ;
#17500 = DIRECTION ( 'NONE',  ( -0.000000000000000000, 1.000000000000000000, -1.563033456626094573E-30 ) ) ;
#17501 = CARTESIAN_POINT ( 'NONE',  ( 10.00000000000000000, 41.66666665983870388, 2.679491924311235618 ) ) ;
#17502 = CARTESIAN_POINT ( 'NONE',  ( -2.085542519210945728E-15, 149.5312499965860411, 11.35316468750000141 ) ) ;
#17503 = CARTESIAN_POINT ( 'NONE',  ( -3.673940397442060854E-16, 297.7500000000000000, -6.000000000000001776 ) ) ;
#17504 = CARTESIAN_POINT ( 'NONE',  ( -10.18810118749999738, -4.220049686691941915, 81.25000000204836681 ) ) ;
#17505 = CARTESIAN_POINT ( 'NONE',  ( -11.00000000000000000, 0.000000000000000000, 118.0000000000000000 ) ) ;
#17506 = CARTESIAN_POINT ( 'NONE',  ( 4.000000000000015987, 205.4375000000000000, 199.6568542494924259 ) ) ;
#17507 = CARTESIAN_POINT ( 'NONE',  ( -4.898587196589412829E-16, 117.3125000040967763, -8.000000000000000000 ) ) ;
#17508 = CARTESIAN_POINT ( 'NONE',  ( -7.204075437095967871, 7.204075437095967871, 114.3437500020483810 ) ) ;
#17509 = VERTEX_POINT ( 'NONE', #16002 ) ;
#17510 = CARTESIAN_POINT ( 'NONE',  ( 0.000000000000000000, 0.000000000000000000, 0.000000000000000000 ) ) ;
#17511 = CARTESIAN_POINT ( 'NONE',  ( 4.503730643507597442, 183.6423555172976592, 139.2463417149559746 ) ) ;
#17512 = CARTESIAN_POINT ( 'NONE',  ( -5.676582343749998039, 122.7604166632526841, -9.832129032723420536 ) ) ;
#17513 = CARTESIAN_POINT ( 'NONE',  ( 1.432654583217662259, 200.1250000013656063, 194.5412658750000219 ) ) ;
#17514 = CARTESIAN_POINT ( 'NONE',  ( -2.977408999572650039, 22.31249999795161543, -7.188101187500000933 ) ) ;
#17515 = CARTESIAN_POINT ( 'NONE',  ( -10.18810118749999916, 0.000000000000000000, 77.03125000204836681 ) ) ;
#17516 = CARTESIAN_POINT ( 'NONE',  ( 5.676582343749993598, 30.26041666325268409, 9.832129032723422313 ) ) ;
#17517 = ORIENTED_EDGE ( 'NONE', *, *, #63465, .T. ) ;
#17518 = CARTESIAN_POINT ( 'NONE',  ( 2.679491924311185880, 35.83333332650536107, 10.00000000000002487 ) ) ;
#17519 = CARTESIAN_POINT ( 'NONE',  ( -1.881053915767121776, 2.749999998634407028, -4.541265875000002339 ) ) ;
#17520 = CARTESIAN_POINT ( 'NONE',  ( 5.662595241051936235, -5.662595241051934458, 13.57561528394063011 ) ) ;
#17521 = CARTESIAN_POINT ( 'NONE',  ( -2.754378923186476579E-14, 207.4375000013656063, 145.4587341250000350 ) ) ;
#17522 = CARTESIAN_POINT ( 'NONE',  ( -7.188101187500000044, 10.21874999795161187, -8.802885111219163269E-16 ) ) ;
#17523 = CARTESIAN_POINT ( 'NONE',  ( 2.485281374238571317, 297.7500000034140157, -6.000000000000003553 ) ) ;
#17524 = CARTESIAN_POINT ( 'NONE',  ( -48.92004685705027356, 140.3555003654597328, 59.80336641654271546 ) ) ;
#17525 = CARTESIAN_POINT ( 'NONE',  ( 7.188101187500001821, 6.937499997951610098, -2.977408999572650483 ) ) ;
#17526 = CARTESIAN_POINT ( 'NONE',  ( -2.977408999572647819, -7.188101187499990274, 13.76780278187175455 ) ) ;
#17527 = CARTESIAN_POINT ( 'NONE',  ( 6.951808397369818766E-16, 152.3437499965860411, -11.35316468750000141 ) ) ;
#17528 = CARTESIAN_POINT ( 'NONE',  ( -4.220049686691937474, -10.18810118749999738, 69.43750000204838102 ) ) ;
#17529 = CARTESIAN_POINT ( 'NONE',  ( -28.00000000000002487, 206.6875000013656063, 166.5412658750003629 ) ) ;
#17530 = CARTESIAN_POINT ( 'NONE',  ( -2.828427124746190735, 15.37500000000000000, -2.828427124746191623 ) ) ;
#17531 = CARTESIAN_POINT ( 'NONE',  ( -1.881053915767124440, 21.12499999863441147, 4.541265875000001451 ) ) ;
#17532 = ORIENTED_EDGE ( 'NONE', *, *, #59025, .T. ) ;
#17533 =( BOUNDED_CURVE ( )  B_SPLINE_CURVE ( 2, ( #31791, #37451, #60449, #72139, #43469, #37831, #66483, #14791, #60828 ),
 .UNSPECIFIED., .F., .F. ) 
 B_SPLINE_CURVE_WITH_KNOTS ( ( 3, 2, 2, 2, 3 ),
 ( 0.04999999999999991951, 0.05833333333333332038, 0.06666666666666672125, 0.07500000000000012212, 0.08333333333333352300 ),
 .UNSPECIFIED. ) 
 CURVE ( )  GEOMETRIC_REPRESENTATION_ITEM ( )  RATIONAL_B_SPLINE_CURVE ( ( 1.000000000000000666, 0.9238795325112859613, 1.000000000000000000, 0.9238795325112867385, 1.000000000000000000, 0.9238795325112867385, 1.000000000000000000, 0.9238795325112849621, 1.000000000000001776 ) ) 
 REPRESENTATION_ITEM ( '' )  );
#17534 = CARTESIAN_POINT ( 'NONE',  ( 1.656854249492405451, 200.4375000027311842, 202.0000000000000284 ) ) ;
#17535 = CARTESIAN_POINT ( 'NONE',  ( -2.849036369511732440E-14, 205.2500000000000284, 138.0000000000000568 ) ) ;
#17536 = CARTESIAN_POINT ( 'NONE',  ( -29.65685424949245785, 203.1875000027312126, 166.0000000000004263 ) ) ;
#17537 = CARTESIAN_POINT ( 'NONE',  ( 1.320432766682874540E-15, 117.0312500020483810, 7.188101187500000044 ) ) ;
#17538 = VECTOR ( 'NONE', #57643, 1000.000000000000000 ) ;
#17539 = CARTESIAN_POINT ( 'NONE',  ( -6.123233995736766282E-16, 251.8750000068280031, -10.00000000000000000 ) ) ;
#17540 = CARTESIAN_POINT ( 'NONE',  ( 3.313708498984756279, 7.999999999999991118, 8.049052783920146226 ) ) ;
#17541 = ORIENTED_EDGE ( 'NONE', *, *, #5214, .F. ) ;
#17542 = CARTESIAN_POINT ( 'NONE',  ( -7.188101187500000044, 17.71874999795161187, -8.802885111219163269E-16 ) ) ;
#17543 = ORIENTED_EDGE ( 'NONE', *, *, #13545, .T. ) ;
#17544 = CARTESIAN_POINT ( 'NONE',  ( -5.000000000000005329, 210.2083333265053682, 8.660254037844387298 ) ) ;
#17545 = CARTESIAN_POINT ( 'NONE',  ( -47.32259252271279593, 191.7059220763548240, 65.76194439203463560 ) ) ;
#17546 = CARTESIAN_POINT ( 'NONE',  ( -2.679491924311225848, 46.45833333333334281, -10.00000000000000178 ) ) ;
#17547 = CARTESIAN_POINT ( 'NONE',  ( -5.082755093536325930, 104.8437500020483810, -5.082755093536325930 ) ) ;
#17548 = CARTESIAN_POINT ( 'NONE',  ( -25.55430564589115505, 209.3125000013656063, 172.4456943541091789 ) ) ;
#17549 = CARTESIAN_POINT ( 'NONE',  ( -4.193070328474945541, -10.26769692241485643, 64.12609983179220308 ) ) ;
#17551 = LINE ( 'NONE', #28502, #10891 ) ;
#17550 = CARTESIAN_POINT ( 'NONE',  ( -5.000000000000005329, 35.20833332650536818, 8.660254037844387298 ) ) ;
#17552 = ORIENTED_EDGE ( 'NONE', *, *, #26417, .T. ) ;
#17553 =( BOUNDED_CURVE ( )  B_SPLINE_CURVE ( 2, ( #22669, #44958, #39297, #27975, #32912, #15522, #45688, #21188, #11367 ),
 .UNSPECIFIED., .F., .F. ) 
 B_SPLINE_CURVE_WITH_KNOTS ( ( 3, 2, 2, 2, 3 ),
 ( 0.9027777777777776791, 0.9097222222222220989, 0.9166666666666665186, 0.9236111111111110494, 0.9305555555555554692 ),
 .UNSPECIFIED. ) 
 CURVE ( )  GEOMETRIC_REPRESENTATION_ITEM ( )  RATIONAL_B_SPLINE_CURVE ( ( 1.000000000000001110, 0.9238795325112855172, 1.000000000000000000, 0.9238795325112867385, 1.000000000000000000, 0.9238795325112867385, 1.000000000000000000, 0.9238795325112879597, 0.9999999999999987788 ) ) 
 REPRESENTATION_ITEM ( '' )  );
#17554 = CARTESIAN_POINT ( 'NONE',  ( 11.35316468749999963, 251.1979166700807014, 3.042071309553159519 ) ) ;
#17555 = CARTESIAN_POINT ( 'NONE',  ( -5.082755093536319713, 5.082755093536319713, 15.17405278187175455 ) ) ;
#17556 = CARTESIAN_POINT ( 'NONE',  ( -4.104248244567547665, 56.27889056303344262, 44.16174987545375785 ) ) ;
#17557 = CARTESIAN_POINT ( 'NONE',  ( -33.73481160478831953, 181.3810825260465833, 154.4994655493011919 ) ) ;
#17558 = CARTESIAN_POINT ( 'NONE',  ( 24.35042252706871935, 194.9613588559977302, 171.5521228611845288 ) ) ;
#17559 = DIRECTION ( 'NONE',  ( 1.000000000000000000, -0.000000000000000000, -0.000000000000000000 ) ) ;
#17560 = CARTESIAN_POINT ( 'NONE',  ( 10.00000000000000178, 155.0000000000000000, 0.000000000000000000 ) ) ;
#17561 = CARTESIAN_POINT ( 'NONE',  ( -27.99999999999999645, 210.0000000000000284, 170.0000000000003695 ) ) ;
#17562 = CARTESIAN_POINT ( 'NONE',  ( -5.656854249492378806, 119.1875000000000000, 5.656854249492381470 ) ) ;
#17563 = CARTESIAN_POINT ( 'NONE',  ( 27.99999999999999645, 210.0000000000000284, 173.9999999999998863 ) ) ;
#17564 = CARTESIAN_POINT ( 'NONE',  ( -5.676582343749998039, 122.7604166632526841, -9.832129032723420536 ) ) ;
#17565 = LINE ( 'NONE', #5889, #51679 ) ;
#17566 = CARTESIAN_POINT ( 'NONE',  ( 0.8761883848702571864, -16.44150283900215825, -68.58316157020809101 ) ) ;
#17569 = CARTESIAN_POINT ( 'NONE',  ( 4.242640687119287435, 298.3750000000000000, 4.242640687119285658 ) ) ;
#17568 = CARTESIAN_POINT ( 'NONE',  ( 30.44569435410879166, 194.8125000013656063, 167.5543056458910485 ) ) ;
#17567 = CARTESIAN_POINT ( 'NONE',  ( 26.56734541678237704, 195.2500000013656063, 166.5412658749999650 ) ) ;
#17570 = VERTEX_POINT ( 'NONE', #10360 ) ;
#17571 = EDGE_CURVE ( 'NONE', #40096, #21431, #73726, .T. ) ;
#17572 = CARTESIAN_POINT ( 'NONE',  ( -4.500000000000007994, 7.794228634059939154, 0.000000000000000000 ) ) ;
#17573 = CARTESIAN_POINT ( 'NONE',  ( 28.00000000000002132, 202.1250000027312126, 173.9999999999999147 ) ) ;
#17574 = CARTESIAN_POINT ( 'NONE',  ( 27.99999999999996092, 195.6250000027311842, 165.9999999999998863 ) ) ;
#17575 = CARTESIAN_POINT ( 'NONE',  ( 4.999999999999999112, -61.23691386381950252, -23.51762333030244534 ) ) ;
#17577 = CARTESIAN_POINT ( 'NONE',  ( 7.320508075688771044, 16.24999999317203248, 7.320508075688775484 ) ) ;
#17576 =( BOUNDED_CURVE ( )  B_SPLINE_CURVE ( 2, ( #65756, #60099, #8417, #42373, #1669, #24649, #65388, #31432, #54459 ),
 .UNSPECIFIED., .F., .T. ) 
 B_SPLINE_CURVE_WITH_KNOTS ( ( 3, 2, 2, 2, 3 ),
 ( 0.000000000000000000, 0.008333333333333340157, 0.01666666666666668031, 0.02500000000000002220, 0.03333333333333336063 ),
 .UNSPECIFIED. ) 
 CURVE ( )  GEOMETRIC_REPRESENTATION_ITEM ( )  RATIONAL_B_SPLINE_CURVE ( ( 1.000000000000000000, 0.9238795325112867385, 1.000000000000000000, 0.9238795325112867385, 1.000000000000000000, 0.9238795325112867385, 1.000000000000000000, 0.9238795325112865164, 1.000000000000000222 ) ) 
 REPRESENTATION_ITEM ( '' )  );
#17578 = CARTESIAN_POINT ( 'NONE',  ( -7.188101187500000044, 124.1562500020483810, 0.000000000000000000 ) ) ;
#17579 = CARTESIAN_POINT ( 'NONE',  ( -1.881053915767124440, 20.99999999863440792, 4.541265875000001451 ) ) ;
#17580 = CARTESIAN_POINT ( 'NONE',  ( -6.891449706532799979, 61.56004288261516422, -23.71475313281856501 ) ) ;
#17581 = CARTESIAN_POINT ( 'NONE',  ( 7.999999999999991118, 9.797174393178815797E-16, 19.58030277982336642 ) ) ;
#17583 = DIRECTION ( 'NONE',  ( 0.000000000000000000, 0.000000000000000000, 1.000000000000000000 ) ) ;
#17582 = SURFACE_SIDE_STYLE ('',( #62853 ) ) ;
#17584 = CARTESIAN_POINT ( 'NONE',  ( 5.676582343749993598, 109.9479166632526983, 9.832129032723422313 ) ) ;
#17585 = ORIENTED_EDGE ( 'NONE', *, *, #56540, .T. ) ;
#17586 = CARTESIAN_POINT ( 'NONE',  ( -7.347880794884122694E-16, 15.49999999726881406, 4.000000000000001776 ) ) ;
#17587 = CARTESIAN_POINT ( 'NONE',  ( -3.979266480698733677, 0.4999999999999095723, -6.940132439340585435 ) ) ;
#17588 = CARTESIAN_POINT ( 'NONE',  ( 10.00000000000016165, 40.20833333333342807, -2.679491924311269813 ) ) ;
#17589 = CARTESIAN_POINT ( 'NONE',  ( -6.951808397369817780E-16, 242.9687500034140157, -11.35316468749999963 ) ) ;
#17590 = CARTESIAN_POINT ( 'NONE',  ( -8.311093377946836114, 107.6562499965860127, -8.311093377946837890 ) ) ;
#17591 = ORIENTED_EDGE ( 'NONE', *, *, #25734, .T. ) ;
#17592 = LINE ( 'NONE', #35340, #59654 ) ;
#17593 = CARTESIAN_POINT ( 'NONE',  ( -10.18810118749999738, -4.220049686691941915, 99.25000000204838102 ) ) ;
#17594 = CARTESIAN_POINT ( 'NONE',  ( 2.679491924311222739, 215.8333333265053682, 10.00000000000000355 ) ) ;
#17595 = CARTESIAN_POINT ( 'NONE',  ( -1.432654583217608080, 200.8750000013656063, 201.4587341250000350 ) ) ;
#17596 = CARTESIAN_POINT ( 'NONE',  ( -4.000000000000001776, 6.249999997268812280, -4.898587196589415787E-16 ) ) ;
#17598 = CARTESIAN_POINT ( 'NONE',  ( 3.042071309553159519, 94.73958332991934128, 11.35316468750000141 ) ) ;
#17597 = CARTESIAN_POINT ( 'NONE',  ( 6.123233995736767268E-16, 143.1249999931720538, -10.00000000000000178 ) ) ;
#17599 = EDGE_CURVE ( 'NONE', #47573, #62856, #30258, .T. ) ;
#17600 = CARTESIAN_POINT ( 'NONE',  ( 5.656854249492374365, 5.656854249492375253, 4.955302783920146226 ) ) ;
#17601 = CARTESIAN_POINT ( 'NONE',  ( -27.99999999999996447, 198.1875000013655779, 173.4587341250003760 ) ) ;
#17602 = CARTESIAN_POINT ( 'NONE',  ( 1.656854249492418107, 208.4375000027312410, 202.0000000000000000 ) ) ;
#17603 = EDGE_LOOP ( 'NONE', ( #8253, #46123, #45958, #21873 ) ) ;
#17604 = CARTESIAN_POINT ( 'NONE',  ( 8.660254037844385522, 201.4583333265053682, 5.000000000000005329 ) ) ;
#17605 = CARTESIAN_POINT ( 'NONE',  ( 3.999999999999959144, 208.0625000000000000, 140.3431457505076594 ) ) ;
#17606 = CARTESIAN_POINT ( 'NONE',  ( 0.1958068277149552505, -48.00000000000002132, 139.0000000000000568 ) ) ;
#17607 = CARTESIAN_POINT ( 'NONE',  ( -11.35316468749999785, 93.38541666325268409, -3.042071309553167957 ) ) ;
#17608 = CARTESIAN_POINT ( 'NONE',  ( -6.676582343750001591, 288.4531250017069510, 0.000000000000000000 ) ) ;
#17609 = CARTESIAN_POINT ( 'NONE',  ( -7.188101187500000044, 7.593749997951610986, -8.802885111219163269E-16 ) ) ;
#17610 = CARTESIAN_POINT ( 'NONE',  ( -6.238412754330611322E-16, 10.18810118749999916, 97.65625000204838102 ) ) ;
#17611 = CARTESIAN_POINT ( 'NONE',  ( 8.311093377946837890, 226.4062499965860411, -8.311093377946837890 ) ) ;
#17612 = ORIENTED_EDGE ( 'NONE', *, *, #68094, .F. ) ;
#17613 = DIRECTION ( 'NONE',  ( 1.000000000000000000, 0.000000000000000000, 0.000000000000000000 ) ) ;
#17614 = CARTESIAN_POINT ( 'NONE',  ( 1.469576158976823947E-15, 98.56250000409677625, 8.000000000000000000 ) ) ;
#17615 = CARTESIAN_POINT ( 'NONE',  ( -11.35316468750000141, 223.2812499965860127, -1.390361679473963753E-15 ) ) ;
#17616 = CARTESIAN_POINT ( 'NONE',  ( 8.660254037844389075, 47.29166665983870388, -5.000000000000000000 ) ) ;
#17617 = CYLINDRICAL_SURFACE ( 'NONE', #18567, 10.00000000000000178 ) ;
#17618 = CARTESIAN_POINT ( 'NONE',  ( -4.088227598258586603E-16, 295.2031250017069510, -6.676582343750001591 ) ) ;
#17619 = ORIENTED_EDGE ( 'NONE', *, *, #61872, .F. ) ;
#17620 = CARTESIAN_POINT ( 'NONE',  ( -4.999999999999953815, -52.35862550122923409, -48.98731492261434539 ) ) ;
#17621 = CARTESIAN_POINT ( 'NONE',  ( -3.042071309553173730, 209.6354166632526699, 11.35316468749999785 ) ) ;
#17622 = VECTOR ( 'NONE', #72904, 1000.000000000000114 ) ;
#17623 = CARTESIAN_POINT ( 'NONE',  ( 10.18810118749999916, 4.220049686691935698, 86.50000000204838102 ) ) ;
#17624 = CARTESIAN_POINT ( 'NONE',  ( -24.54126587499999346, 203.1875000013656063, 170.0000000000003411 ) ) ;
#17625 = CARTESIAN_POINT ( 'NONE',  ( -3.313708498984765161, 20.53125000000001066, 7.999999999999998224 ) ) ;
#17626 = ORIENTED_EDGE ( 'NONE', *, *, #12128, .F. ) ;
#17627 = CARTESIAN_POINT ( 'NONE',  ( -7.188101187499999156, 121.2500000020483952, 2.977408999572654924 ) ) ;
#17628 = DIRECTION ( 'NONE',  ( -0.000000000000000000, 1.000000000000000000, 4.689100369878284071E-30 ) ) ;
#17629 = CARTESIAN_POINT ( 'NONE',  ( -2.679491924311225848, 21.45833333333333925, -10.00000000000000178 ) ) ;
#17630 = CARTESIAN_POINT ( 'NONE',  ( 5.000000000000000000, -32.28817737728140003, -1.075528555105620399E-13 ) ) ;
#17631 = CARTESIAN_POINT ( 'NONE',  ( 10.18810118749999916, 4.220049686691935698, 77.87500000204838102 ) ) ;
#17632 = ORIENTED_EDGE ( 'NONE', *, *, #4278, .T. ) ;
#17633 = CARTESIAN_POINT ( 'NONE',  ( 2.977408999572650927, 0.7499999979516099868, -7.188101187500000933 ) ) ;
#17634 = DIRECTION ( 'NONE',  ( -0.8660254037844696828, 0.4999999999999462097, -0.000000000000000000 ) ) ;
#17635 = ADVANCED_FACE ( 'NONE', ( #29202 ), #40577, .F. ) ;
#17636 = DIRECTION ( 'NONE',  ( 0.000000000000000000, 0.000000000000000000, 1.000000000000000000 ) ) ;
#17637 = FACE_OUTER_BOUND ( 'NONE', #66908, .T. ) ;
#17638 =( GEOMETRIC_REPRESENTATION_CONTEXT ( 3 ) GLOBAL_UNCERTAINTY_ASSIGNED_CONTEXT ( ( #29804 ) ) GLOBAL_UNIT_ASSIGNED_CONTEXT ( ( #17354, #69417, #4563 ) ) REPRESENTATION_CONTEXT ( 'NONE', 'WORKASPACE' ) );
#17639 = CARTESIAN_POINT ( 'NONE',  ( 8.660254037844385522, 151.4583333265053682, 5.000000000000005329 ) ) ;
#17640 = CARTESIAN_POINT ( 'NONE',  ( -4.721056650415998313, 296.5781250017069510, 4.721056650416000089 ) ) ;
#17642 = DIRECTION ( 'NONE',  ( -0.000000000000000000, 1.000000000000000000, 4.476705744456276341E-16 ) ) ;
#17641 = CARTESIAN_POINT ( 'NONE',  ( -11.35316468749999963, 238.9062500034140157, 0.000000000000000000 ) ) ;
#17643 = VERTEX_POINT ( 'NONE', #29313 ) ;
#17644 = CARTESIAN_POINT ( 'NONE',  ( 8.311093377946839666, 241.0937500034139873, 8.311093377946829008 ) ) ;
#17645 = CARTESIAN_POINT ( 'NONE',  ( 1.320432766682872962E-15, -7.188101187499992051, 9.361552781871752771 ) ) ;
#17646 =( BOUNDED_CURVE ( )  B_SPLINE_CURVE ( 2, ( #70129, #57326, #41079, #52402, #68629, #62968, #18436, #46360, #46726 ),
 .UNSPECIFIED., .F., .F. ) 
 B_SPLINE_CURVE_WITH_KNOTS ( ( 3, 2, 2, 2, 3 ),
 ( 0.3437499999999998335, 0.3489583333333331483, 0.3541666666666665186, 0.3593749999999998335, 0.3645833333333331483 ),
 .UNSPECIFIED. ) 
 CURVE ( )  GEOMETRIC_REPRESENTATION_ITEM ( )  RATIONAL_B_SPLINE_CURVE ( ( 1.000000000000002442, 0.9238795325112842960, 1.000000000000000000, 0.9238795325112867385, 1.000000000000000000, 0.9238795325112867385, 1.000000000000000000, 0.9238795325112891810, 0.9999999999999975575 ) ) 
 REPRESENTATION_ITEM ( '' )  );
#17647 = VERTEX_POINT ( 'NONE', #70047 ) ;
#17648 = CARTESIAN_POINT ( 'NONE',  ( 7.204075437095968759, -7.204075437095966983, 69.71875000204836681 ) ) ;
#17649 = CARTESIAN_POINT ( 'NONE',  ( 11.35316468750000141, 86.09374999658601268, 0.000000000000000000 ) ) ;
#17650 = CARTESIAN_POINT ( 'NONE',  ( 2.775557561562891351E-14, 271.9999999999999432, 170.0000000000000284 ) ) ;
#17651 = CARTESIAN_POINT ( 'NONE',  ( -11.00000000000000000, 0.000000000000000000, 84.99999999999998579 ) ) ;
#17654 = CARTESIAN_POINT ( 'NONE',  ( 10.00000000000000355, 70.20833333333331439, -2.679491924311227180 ) ) ;
#17653 = CARTESIAN_POINT ( 'NONE',  ( 25.55430564589115860, 208.0625000013656063, 167.5543056458911053 ) ) ;
#17652 = CARTESIAN_POINT ( 'NONE',  ( 24.54126587499998635, 206.5000000013655779, 171.4326545832175555 ) ) ;
#17655 = EDGE_LOOP ( 'NONE', ( #57364, #4726, #70376, #14968 ) ) ;
#17656 = EDGE_CURVE ( 'NONE', #37508, #49656, #58003, .T. ) ;
#17657 = CARTESIAN_POINT ( 'NONE',  ( -50.99999999999994316, -31.99999999999978684, 205.0000000000000284 ) ) ;
#17658 = CARTESIAN_POINT ( 'NONE',  ( -8.660254037844387298, 178.9583333265053682, -5.000000000000004441 ) ) ;
#17659 = CARTESIAN_POINT ( 'NONE',  ( -2.085542519210945728E-15, 204.5312499965860411, 11.35316468750000141 ) ) ;
#17661 = ADVANCED_FACE ( 'NONE', ( #13411 ), #65100, .F. ) ;
#17660 = CARTESIAN_POINT ( 'NONE',  ( -3.458734125000015425, 205.0000000013655779, 143.4326545832176976 ) ) ;
#17662 = AXIS2_PLACEMENT_3D ( 'NONE', #72735, #2951, #19543 ) ;
#17663 = CARTESIAN_POINT ( 'NONE',  ( 29.43265458321761585, 206.7500000013655779, 173.4587341249998929 ) ) ;
#17664 = CARTESIAN_POINT ( 'NONE',  ( -7.188101187500002709, 24.18749999795161543, 2.977408999572649151 ) ) ;
#17665 = CARTESIAN_POINT ( 'NONE',  ( -11.35316468750000141, 178.8020833299193271, 3.042071309553159963 ) ) ;
#17666 = CARTESIAN_POINT ( 'NONE',  ( 11.00000000000000355, -11.00000000000000000, 25.00000000000000000 ) ) ;
#17667 = CARTESIAN_POINT ( 'NONE',  ( 1.320432766682874540E-15, 96.40625000204838102, 7.188101187500000044 ) ) ;
#17669 = CARTESIAN_POINT ( 'NONE',  ( 6.123233995736767268E-16, 88.12499999317203958, -10.00000000000000178 ) ) ;
#17668 = CARTESIAN_POINT ( 'NONE',  ( -5.000000000000001776, 62.69487254116438635, -24.02505537901974009 ) ) ;
#17670 = CARTESIAN_POINT ( 'NONE',  ( 3.211159895383560947, 9.187499998634407916, 3.211159895383562723 ) ) ;
#17671 = CARTESIAN_POINT ( 'NONE',  ( 31.45873412500001010, 202.0000000013656063, 168.5673454167822740 ) ) ;
#17672 = CARTESIAN_POINT ( 'NONE',  ( 2.977408999572646486, 7.188101187499991163, 8.892802781871754547 ) ) ;
#17673 = CARTESIAN_POINT ( 'NONE',  ( -5.676582343750006032, 74.11458332991935549, 9.832129032723418760 ) ) ;
#17675 =( BOUNDED_CURVE ( )  B_SPLINE_CURVE ( 2, ( #66774, #44143, #24268, #67156, #26388, #35977, #7301, #19992, #1652, #43000, #58996, #37741, #14328 ),
 .UNSPECIFIED., .F., .F. ) 
 B_SPLINE_CURVE_WITH_KNOTS ( ( 3, 2, 2, 2, 2, 2, 3 ),
 ( 0.2040931733865910258, 0.2093271569598113002, 0.2145611405330315191, 0.2197951241062517935, 0.2250291076794720402, 0.2302630912526922591, 0.2354970748259125335 ),
 .UNSPECIFIED. ) 
 CURVE ( )  GEOMETRIC_REPRESENTATION_ITEM ( )  RATIONAL_B_SPLINE_CURVE ( ( 0.9999999999999992228, 0.9659258262890690894, 1.000000000000000000, 0.9659258262890683122, 1.000000000000000000, 0.9659258262890683122, 1.000000000000000000, 0.9659258262890683122, 1.000000000000000000, 0.9659258262890683122, 1.000000000000000000, 0.9659258262891544655, 0.9999999999999138467 ) ) 
 REPRESENTATION_ITEM ( '' )  );
#17674 = CARTESIAN_POINT ( 'NONE',  ( 23.99999999999998224, 205.8125000027312126, 168.3431457505075457 ) ) ;
#17676 = CARTESIAN_POINT ( 'NONE',  ( 3.313708498984756279, 7.999999999999991118, 0.4178027843298233734 ) ) ;
#17677 = EDGE_LOOP ( 'NONE', ( #22570, #19537, #14082, #31037, #14833, #60380 ) ) ;
#17678 = DIRECTION ( 'NONE',  ( -0.000000000000000000, 1.000000000000000000, -0.000000000000000000 ) ) ;
#17679 = CARTESIAN_POINT ( 'NONE',  ( -11.35316468750000141, 68.28124999658602690, -1.390361679473963753E-15 ) ) ;
#17680 = CARTESIAN_POINT ( 'NONE',  ( 11.00000000000000355, -4.556349186104045046, 69.34375000409679046 ) ) ;
#17681 = CARTESIAN_POINT ( 'NONE',  ( -1.432654583217662481, 197.3750000013656063, 145.4587341250000350 ) ) ;
#17682 = CARTESIAN_POINT ( 'NONE',  ( 0.000000000000000000, 23.85640646055104241, -14.00000000000000178 ) ) ;
#17684 = CARTESIAN_POINT ( 'NONE',  ( 11.35316468749999785, 65.57291666325268409, 3.042071309553174174 ) ) ;
#17683 = CARTESIAN_POINT ( 'NONE',  ( -7.188101187499999156, 94.25000000204838102, 2.977408999572654924 ) ) ;
#17685 = EDGE_CURVE ( 'NONE', #24834, #71723, #36449, .T. ) ;
#17686 = CARTESIAN_POINT ( 'NONE',  ( -3.313708498984758943, -7.999999999999989342, 4.111552779823362869 ) ) ;
#17687 = CARTESIAN_POINT ( 'NONE',  ( -2.303252245372783058, 194.8562092600116671, 145.1314104344461668 ) ) ;
#17688 = CARTESIAN_POINT ( 'NONE',  ( -10.00000000000000178, 154.3749999931720254, -1.224646799147353454E-15 ) ) ;
#17689 = CARTESIAN_POINT ( 'NONE',  ( 7.188101187500001821, 96.87500000204836681, -2.977408999572651371 ) ) ;
#17690 = CARTESIAN_POINT ( 'NONE',  ( -1.836970198721029983E-15, 55.62499999317203958, 10.00000000000000178 ) ) ;
#17691 = CARTESIAN_POINT ( 'NONE',  ( 6.951808397369818766E-16, 42.34374999658601979, -11.35316468750000141 ) ) ;
#17692 = CARTESIAN_POINT ( 'NONE',  ( 4.220049686691934809, 10.18810118749999916, 112.5625000020483810 ) ) ;
#17693 = CARTESIAN_POINT ( 'NONE',  ( 8.311093377946834337, 185.1562499965860411, 8.311093377946839666 ) ) ;
#17694 = ORIENTED_EDGE ( 'NONE', *, *, #71509, .F. ) ;
#17695 = CARTESIAN_POINT ( 'NONE',  ( -4.220049686691937474, -10.18810118749999738, 73.93750000204838102 ) ) ;
#17696 = CARTESIAN_POINT ( 'NONE',  ( 10.00000000000000178, 161.8749999931720254, 0.000000000000000000 ) ) ;
#17698 = CARTESIAN_POINT ( 'NONE',  ( 8.311093377946834337, 180.1562499965860127, 8.311093377946839666 ) ) ;
#17697 = CARTESIAN_POINT ( 'NONE',  ( -4.999999999999944045, 68.60357193678724741, -20.85024232999276350 ) ) ;
#17699 = CARTESIAN_POINT ( 'NONE',  ( -3.313708498984758943, -7.999999999999989342, 5.667802784329825094 ) ) ;
#17700 = VECTOR ( 'NONE', #16798, 1000.000000000000000 ) ;
#17701 = CARTESIAN_POINT ( 'NONE',  ( 5.000000000000000000, 70.11723469343132820, -28.93519894129142145 ) ) ;
#17702 = CARTESIAN_POINT ( 'NONE',  ( -4.999999999999992895, 258.9583333401613459, 8.660254037844390851 ) ) ;
#17703 = DIRECTION ( 'NONE',  ( -1.000000000000000000, 0.000000000000000000, -0.000000000000000000 ) ) ;
#17704 = PRODUCT_DEFINITION_FORMATION_WITH_SPECIFIED_SOURCE ( 'ANY', '', #1223, .NOT_KNOWN. ) ;
#17705 = ORIENTED_EDGE ( 'NONE', *, *, #48975, .T. ) ;
#17706 = CARTESIAN_POINT ( 'NONE',  ( 11.35316468749999785, 165.8854166632526130, 3.042071309553174174 ) ) ;
#17707 = EDGE_CURVE ( 'NONE', #61795, #45464, #17983, .T. ) ;
#17708 = CARTESIAN_POINT ( 'NONE',  ( -7.188101187499992051, 2.977408999572646930, 26.89280278187175455 ) ) ;
#17709 = CARTESIAN_POINT ( 'NONE',  ( 9.832129032723420536, 126.5104166632526841, -5.676582343749999815 ) ) ;
#17710 = CARTESIAN_POINT ( 'NONE',  ( 0.000000000000000000, 300.0000000000000000, 10.00000000000000178 ) ) ;
#17711 = ORIENTED_EDGE ( 'NONE', *, *, #68278, .F. ) ;
#17712 = CARTESIAN_POINT ( 'NONE',  ( 1.881053915767121776, 11.62499999863440969, -4.541265875000002339 ) ) ;
#17713 = CARTESIAN_POINT ( 'NONE',  ( -4.898587196589412829E-16, 103.8125000040967763, -8.000000000000000000 ) ) ;
#17714 = VECTOR ( 'NONE', #48433, 1000.000000000000000 ) ;
#17715 = CARTESIAN_POINT ( 'NONE',  ( 4.000000000000001776, 14.06249999999999822, -1.656854249492381248 ) ) ;
#17716 = DIRECTION ( 'NONE',  ( 3.469446951953619612E-16, 0.000000000000000000, 1.000000000000000000 ) ) ;
#17717 = CARTESIAN_POINT ( 'NONE',  ( 1.881053915767122664, 11.12499999863440969, 4.541265875000001451 ) ) ;
#17718 = CARTESIAN_POINT ( 'NONE',  ( 3.313708498984762496, -7.999999999999989342, 17.98655278392014978 ) ) ;
#17719 = CARTESIAN_POINT ( 'NONE',  ( 11.00000000000010836, -4.556349186103939353, 78.34375000409676204 ) ) ;
#17720 = ORIENTED_EDGE ( 'NONE', *, *, #13151, .T. ) ;
#17721 = CARTESIAN_POINT ( 'NONE',  ( -8.000000000000001776, 24.84375000000000355, 3.313708498984759387 ) ) ;
#17722 = CARTESIAN_POINT ( 'NONE',  ( -7.188101187500000044, 101.6562500020483810, 0.000000000000000000 ) ) ;
#17724 = CARTESIAN_POINT ( 'NONE',  ( -2.751064625579944321E-14, 209.7500000000000284, 146.0000000000000284 ) ) ;
#17723 = CARTESIAN_POINT ( 'NONE',  ( 0.000000000000000000, 300.0000000000000000, 0.000000000000000000 ) ) ;
#17725 = DIRECTION ( 'NONE',  ( 0.000000000000000000, 0.000000000000000000, 1.000000000000000000 ) ) ;
#17726 = VERTEX_POINT ( 'NONE', #59099 ) ;
#17727 = CARTESIAN_POINT ( 'NONE',  ( 3.511653767256929459, 16.35475815725939341, -69.12977678000905257 ) ) ;
#17728 = CARTESIAN_POINT ( 'NONE',  ( 2.977408999572646486, 7.188101187499991163, 23.51780278187175455 ) ) ;
#17729 = ORIENTED_EDGE ( 'NONE', *, *, #11842, .F. ) ;
#17730 = VERTEX_POINT ( 'NONE', #59462 ) ;
#17731 = CARTESIAN_POINT ( 'NONE',  ( -4.220049686691937474, -10.18810118749999738, 87.43750000204838102 ) ) ;
#17732 = CARTESIAN_POINT ( 'NONE',  ( -1.656854249492371034, 9.437499997268814056, 4.000000000000013323 ) ) ;
#17733 = CARTESIAN_POINT ( 'NONE',  ( -24.54126587499997569, 197.3750000013656063, 171.4326545832179818 ) ) ;
#17734 = CARTESIAN_POINT ( 'NONE',  ( -11.00000000000000000, 0.000000000000000000, 98.49999999999998579 ) ) ;
#17735 = AXIS2_PLACEMENT_3D ( 'NONE', #40127, #46528, #49683 ) ;
#17738 = CARTESIAN_POINT ( 'NONE',  ( -2.765530957081998142, 298.7968750017070079, 6.676582343750000703 ) ) ;
#17737 = CARTESIAN_POINT ( 'NONE',  ( 25.17157287525381903, 205.0000000027312126, 172.8284271247460993 ) ) ;
#17736 = CARTESIAN_POINT ( 'NONE',  ( 2.775557561562891351E-14, 210.0000000000000284, 202.0000000000000000 ) ) ;
#17739 = CARTESIAN_POINT ( 'NONE',  ( 5.000000000000001776, 135.8333333333333428, -8.660254037844389075 ) ) ;
#17740 = CARTESIAN_POINT ( 'NONE',  ( 5.656854249492381470, 103.0625000000000000, 5.656854249492379694 ) ) ;
#17741 = CARTESIAN_POINT ( 'NONE',  ( 0.7835476670742943517, 225.9999999999999716, 9.977056579405376269 ) ) ;
#17743 = EDGE_CURVE ( 'NONE', #51478, #47672, #35740, .T. ) ;
#17742 = FACE_BOUND ( 'NONE', #14548, .T. ) ;
#17744 = CARTESIAN_POINT ( 'NONE',  ( -25.17157287525382614, 208.8750000000000284, 167.1715728752541565 ) ) ;
#17745 = ADVANCED_FACE ( 'NONE', ( #34987 ), #53061, .F. ) ;
#17746 = CARTESIAN_POINT ( 'NONE',  ( 31.45873412499998523, 204.6250000013655779, 171.4326545832175839 ) ) ;
#17747 = CLOSED_SHELL ( 'NONE', ( #24296, #63736, #48144, #39313, #954, #72931, #70333, #37115, #17999, #57284, #16308, #34847, #28328, #1056, #26412, #3185, #47867, #20965, #45163, #61930, #54657, #42944, #49772, #13857, #24299, #64488, #20822, #12929, #26228, #13149, #54244, #33519, #12519, #65084, #60109, #46262, #26743, #54374, #22810, #70477, #31108, #53866, #344, #20568, #53917, #60157, #12972, #10196, #11619, #44567, #68075, #40408, #55036, #64689, #27096, #18641 ) ) ;
#17748 = CARTESIAN_POINT ( 'NONE',  ( -7.188101187500000044, 4.593749997951610098, -8.802885111219163269E-16 ) ) ;
#17749 = CARTESIAN_POINT ( 'NONE',  ( 8.008118988124991233, 3.317071493978879015, 1.856865283940626998 ) ) ;
#17750 = CARTESIAN_POINT ( 'NONE',  ( -2.839093476692135984E-14, 196.6875000013655779, 138.5412658750000503 ) ) ;
#17751 = CARTESIAN_POINT ( 'NONE',  ( 7.188101187500000933, 116.3750000020483810, -2.977408999572651371 ) ) ;
#17753 = DIRECTION ( 'NONE',  ( -0.000000000000000000, 1.000000000000000000, -0.000000000000000000 ) ) ;
#17752 = CARTESIAN_POINT ( 'NONE',  ( 32.00000000000000000, 195.3125000027312126, 171.6568542494922553 ) ) ;
#17754 = CARTESIAN_POINT ( 'NONE',  ( 5.676582343749997150, 242.5520833367473301, -9.832129032723418760 ) ) ;
#17755 = CARTESIAN_POINT ( 'NONE',  ( -33.54549332286219965, 40.87151432623902281, 65.00000000000000000 ) ) ;
#17756 = CARTESIAN_POINT ( 'NONE',  ( 7.188101187499992051, 8.802885111219154394E-16, 25.11155278187175810 ) ) ;
#17757 = CARTESIAN_POINT ( 'NONE',  ( 29.65685424949235482, 199.0625000000000284, 173.9999999999999147 ) ) ;
#17758 = CARTESIAN_POINT ( 'NONE',  ( 8.311093377946837890, 26.40624999658601268, -8.311093377946837890 ) ) ;
#17759 = CARTESIAN_POINT ( 'NONE',  ( -8.000000000000001776, 9.843750000000000000, 3.313708498984759387 ) ) ;
#17760 = CARTESIAN_POINT ( 'NONE',  ( -8.311093377946836114, 217.9687499965860127, -8.311093377946837890 ) ) ;
#17761 = FACE_OUTER_BOUND ( 'NONE', #22106, .T. ) ;
#17763 = CARTESIAN_POINT ( 'NONE',  ( -3.313708498984757611, 7.999999999999991118, 29.04905277982336997 ) ) ;
#17762 = CARTESIAN_POINT ( 'NONE',  ( -5.000000000000000000, 52.35862550122891435, 48.98731492261470777 ) ) ;
#17764 = ORIENTED_EDGE ( 'NONE', *, *, #22786, .F. ) ;
#17765 = CARTESIAN_POINT ( 'NONE',  ( -2.839093476692135984E-14, 195.9375000013655779, 138.5412658750000503 ) ) ;
#17766 = CARTESIAN_POINT ( 'NONE',  ( -2.085542519210945728E-15, 24.53124999658601624, 11.35316468750000141 ) ) ;
#17767 = CARTESIAN_POINT ( 'NONE',  ( -7.778174593052020747, -7.778174593052023411, 88.37500000409677625 ) ) ;
#17768 = CARTESIAN_POINT ( 'NONE',  ( 2.445694354108783219, 206.8125000013656063, 139.5543056458912190 ) ) ;
#17769 = CARTESIAN_POINT ( 'NONE',  ( -11.00000000000000000, 0.000000000000000000, 110.6875000040967763 ) ) ;
#17770 = CARTESIAN_POINT ( 'NONE',  ( -6.123233995736766282E-16, 228.7500000000000000, -10.00000000000000000 ) ) ;
#17772 = CARTESIAN_POINT ( 'NONE',  ( -3.042071309553173730, 19.32291666325268409, 11.35316468749999785 ) ) ;
#17771 = CARTESIAN_POINT ( 'NONE',  ( 1.320432766682874540E-15, 114.0312500020483952, 7.188101187500000044 ) ) ;
#17773 = CARTESIAN_POINT ( 'NONE',  ( 7.999999999999991118, 3.313708498984757611, 21.17405277982336642 ) ) ;
#17774 =( BOUNDED_SURFACE ( )  B_SPLINE_SURFACE ( 1, 2, ( 
 ( #5421, #46890, #18959, #42699, #47254, #41963, #19318, #58597, #8007, #18593, #47616, #35950, #1628, #64619, #70639, #31014, #18224, #2349, #52931, #47989, #71364, #59335, #64245, #29545, #7276, #30283, #53668, #64971, #35221, #25344, #24608, #53304, #41239, #42330, #13280, #23881, #6539, #12915, #65712, #36320, #65348, #58968, #70281, #41604, #58241, #52556, #48358, #1262, #7646, #6903, #13649, #30651, #36688, #895, #1981, #24973, #59699, #71002, #54039, #19690, #12555, #69914, #35583, #29914, #24241, #72117, #54787, #20430, #32910, #3099, #21186, #37053, #43070, #66086, #14396, #15149, #49485, #43831, #43446, #15520, #32146, #14770, #44584, #60804, #55166, #4227, #55542, #26461, #54416, #49863, #61561, #26084, #38560, #9129, #44211, #50232, #67224, #3472, #72504, #8757, #66461, #3852, #73253, #37430, #20813, #60430, #37808, #31768, #49105, #66846, #38181, #26848, #61185, #9515, #32530, #72880, #21558, #9882, #55915, #27215, #14016, #60053, #31390, #8374, #2723, #25711, #48732, #71738, #20053, #28995, #40687, #46343, #63318, #52013, #63689, #52753, #29738, #12016, #1089, #68612, #18048, #35049, #17670, #57685, #5621, #1460, #7102, #41433, #17296, #64445, #35416, #30110, #45972, #58061, #69360, #69733, #40314, #53127, #62949, #6372, #57310, #11274, #29378, #74649, #52385, #720, #58426, #12746, #47076, #351, #35777, #6734, #18419, #51634, #70113, #34306, #58792, #24441, #23704, #22964, #23331, #68987, #46708, #16921, #41063, #64073, #12381, #24066, #39944, #28621, #34679, #11644, #5993, #59522, #64805, #2546, #8948, #7835, #31589, #13833, #70835, #30840, #19510, #25167, #42150, #53861, #42528, #54610, #8573, #65542, #2917, #47449, #71560, #36879, #71191, #36513, #59164, #54985, #60626, #20247, #19147, #43267, #14213, #31960, #24798, #59887, #48184, #48550, #65163, #3292, #41796, #8200, #36143, #13107, #31212, #53495, #54237, #25537, #37251, #66282, #25905, #2173, #14589, #60247, #71935, #30478, #48922, #7473, #37628, #70473, #19882, #1812, #42888, #47812, #65907, #18791, #13474, #67411, #73067, #15709, #22114, #27406, #67036, #72316, #39111, #38370, #15335, #32723, #45138, #61375, #33469, #49299, #55357, #3662, #26662, #50421, #61751, #56101, #55731, #27780, #44397, #27040, #56841, #21373, #38751, #16447, #67785, #10069, #66656, #62115, #73806, #9702, #50793, #33104, #56471, #62479, #4787, #4410, #73435, #21001, #4048, #16077, #10809, #49685, #21743, #72700, #50051, #44027, #44771, #10439, #68150, #39483, #33843, #26278, #20629, #43645, #14963, #38000, #60998, #9324, #32344, #23241, #34586, #6644, #46249, #5902, #35685, #51920, #69268, #70020, #46621, #17579, #45501, #40973, #52662, #17203, #29647, #258, #35328, #41341, #58340, #40597, #63598, #74553, #11552, #69641, #64351, #28528, #11925, #34211, #28902, #57213, #5527 ),
 ( #16821, #39849, #998, #12654, #34957, #57972, #23979, #46987, #5162, #17955, #28156, #62850, #6278, #18326, #63980, #630, #12293, #29284, #52294, #11186, #23611, #51167, #68519, #74176, #51536, #22480, #22865, #45879, #68893, #40222, #63225, #57592, #8113, #70385, #1365, #31118, #2826, #36055, #65450, #13747, #7381, #53034, #53407, #2455, #14124, #54146, #71101, #66192, #43176, #30388, #2083, #65817, #25448, #19794, #18700, #42434, #14496, #70743, #36790, #42801, #1730, #31499, #42063, #19421, #59436, #25075, #13384, #59800, #54520, #41707, #25817, #24710, #71468, #20159, #48463, #13017, #24350, #30753, #53774, #37158, #60160, #58700, #48836, #48092, #8479, #64721, #71842, #59072, #7011, #30020, #47722, #47359, #19061, #65071, #36422, #7748, #49966, #45055, #22029, #60908, #55643, #44682, #4326, #73353, #49211, #21286, #68066, #49592, #44309, #21657, #9231, #10353, #20914, #72980, #38282, #3958, #66944, #67324, #33377, #20535, #4699, #55271, #50331, #73719, #61663, #66563, #31871, #9614, #32634, #56014, #15621, #37535, #27692, #26947, #38661, #43549, #67698, #9982, #26191, #8861, #15248, #60535, #33013, #15995, #61287, #72608, #43935, #54892, #3203, #50701, #3576, #27315, #32253, #39025, #62029, #56378, #72220, #14872, #37911, #26568, #45792, #17114, #40136, #22392, #52573, #28068, #45412, #57509, #74461, #11470, #5815, #33751, #63142, #35237, #34504, #68802, #17865, #5074, #51079, #74093, #12199, #910, #28810, #51828, #58255, #40882, #23896, #57879, #46905, #68428, #174, #63888, #6186, #11838, #29195, #23150, #46163, #16731, #69180, #17491, #39757, #62392, #62759, #40510, #69554, #6556, #52207, #11102, #63514, #29562, #34873, #34125, #56754, #540, #16355, #23522, #46536, #39393, #10719, #57125, #5440, #28442, #51448, #22769, #31033, #42719, #7293, #19706, #64990, #25362, #31407, #48379, #41979, #13299, #64635, #1644, #36705, #54434, #18612, #36337, #24258, #70658, #47271, #70297, #2000, #59352, #59717, #35968, #7663, #18975, #53320, #2742, #41623, #65732, #42349, #65366, #30669, #12571, #24990, #25728, #30301, #54058, #53689, #12932, #24625, #48007, #47636, #58988, #71020, #19337, #2367, #71382, #13665, #14034, #69929, #8025, #37071, #60074, #8393, #6921, #18239, #41254, #64263, #35600, #58615, #29932, #52948, #1281, #43848, #49504, #49881, #72135, #61943, #43088, #15169, #37447, #66105, #9533, #54807, #38199, #66861, #15538, #21575, #27233, #32164, #44601, #38579, #73271, #31787, #50249, #14415, #67614, #10271, #61202, #3118, #55185, #26103, #3491, #33298, #32548, #55558, #20831, #3871, #15911, #72896, #14787, #20072, #61579, #60824, #37827, #26479, #38942, #9147, #55934, #71758, #49123, #20448, #43465, #21204, #26867, #44231, #72523, #67242, #60445, #9898, #56296, #32928, #4245, #4612, #66479, #48749, #8775, #5356 ) ),
 .UNSPECIFIED., .F., .F., .F. ) 
 B_SPLINE_SURFACE_WITH_KNOTS ( ( 2, 2 ),
 ( 3, 2, 2, 2, 2, 2, 2, 2, 2, 2, 2, 2, 2, 2, 2, 2, 2, 2, 2, 2, 2, 2, 2, 2, 2, 2, 2, 2, 2, 2, 2, 2, 2, 2, 2, 2, 2, 2, 2, 2, 2, 2, 2, 2, 2, 2, 2, 2, 2, 2, 2, 2, 2, 2, 2, 2, 2, 2, 2, 2, 2, 2, 2, 2, 2, 2, 2, 2, 2, 2, 2, 2, 2, 2, 2, 2, 2, 2, 2, 2, 2, 2, 2, 2, 2, 2, 2, 2, 2, 2, 2, 2, 2, 2, 2, 2, 2, 2, 2, 2, 2, 2, 2, 2, 2, 2, 2, 2, 2, 2, 2, 2, 2, 2, 2, 2, 2, 2, 2, 2, 2, 2, 2, 2, 2, 2, 2, 2, 2, 2, 2, 2, 2, 2, 2, 2, 2, 2, 2, 2, 2, 2, 2, 2, 2, 2, 2, 2, 2, 2, 2, 2, 2, 2, 2, 2, 2, 2, 2, 2, 2, 2, 2, 2, 2, 2, 2, 2, 2, 2, 2, 2, 2, 2, 2, 2, 3 ),
 ( 0.000000000000000000, 1.000000000000000000 ),
 ( 0.000000000000000000, 0.005681818181818181976, 0.01136363636363636395, 0.01704545454545454419, 0.02272727272727272790, 0.02840909090909090814, 0.03409090909090908839, 0.03977272727272727210, 0.04545454545454545581, 0.05113636363636363952, 0.05681818181818181629, 0.06250000000000000000, 0.06818181818181817677, 0.07386363636363636742, 0.07954545454545454419, 0.08522727272727272096, 0.09090909090909091161, 0.09659090909090908839, 0.1022727272727272790, 0.1079545454545454558, 0.1136363636363636326, 0.1193181818181818232, 0.1250000000000000000, 0.1306818181818181768, 0.1363636363636363535, 0.1420454545454545581, 0.1477272727272727348, 0.1534090909090909116, 0.1590909090909090884, 0.1647727272727272652, 0.1704545454545454419, 0.1761363636363636465, 0.1818181818181818232, 0.1875000000000000000, 0.1931818181818181768, 0.1988636363636363535, 0.2045454545454545581, 0.2102272727272727348, 0.2159090909090909116, 0.2215909090909090884, 0.2272727272727272652, 0.2329545454545454419, 0.2386363636363636465, 0.2443181818181818232, 0.2500000000000000000, 0.2556818181818181768, 0.2613636363636363535, 0.2670454545454545303, 0.2727272727272727071, 0.2784090909090908839, 0.2840909090909091161, 0.2897727272727272929, 0.2954545454545454697, 0.3011363636363636465, 0.3068181818181818232, 0.3125000000000000000, 0.3181818181818181768, 0.3238636363636363535, 0.3295454545454545303, 0.3352272727272727071, 0.3409090909090908839, 0.3465909090909091161, 0.3522727272727272929, 0.3579545454545454697, 0.3636363636363636465, 0.3693181818181818232, 0.3750000000000000000, 0.3806818181818181768, 0.3863636363636363535, 0.3920454545454545303, 0.3977272727272727071, 0.4034090909090908839, 0.4090909090909091161, 0.4147727272727272929, 0.4204545454545454697, 0.4261363636363636465, 0.4318181818181818232, 0.4375000000000000000, 0.4431818181818181768, 0.4488636363636363535, 0.4545454545454545303, 0.4602272727272727071, 0.4659090909090908839, 0.4715909090909091161, 0.4772727272727272929, 0.4829545454545454697, 0.4886363636363636465, 0.4943181818181818232, 0.5000000000000000000, 0.5056818181818182323, 0.5113636363636363535, 0.5170454545454545858, 0.5227272727272727071, 0.5284090909090909394, 0.5340909090909090606, 0.5397727272727272929, 0.5454545454545454142, 0.5511363636363636465, 0.5568181818181817677, 0.5625000000000000000, 0.5681818181818182323, 0.5738636363636363535, 0.5795454545454545858, 0.5852272727272727071, 0.5909090909090909394, 0.5965909090909090606, 0.6022727272727272929, 0.6079545454545454142, 0.6136363636363636465, 0.6193181818181817677, 0.6250000000000000000, 0.6306818181818182323, 0.6363636363636363535, 0.6420454545454545858, 0.6477272727272727071, 0.6534090909090909394, 0.6590909090909090606, 0.6647727272727272929, 0.6704545454545454142, 0.6761363636363636465, 0.6818181818181817677, 0.6875000000000000000, 0.6931818181818182323, 0.6988636363636363535, 0.7045454545454545858, 0.7102272727272727071, 0.7159090909090909394, 0.7215909090909090606, 0.7272727272727272929, 0.7329545454545454142, 0.7386363636363636465, 0.7443181818181817677, 0.7500000000000000000, 0.7556818181818182323, 0.7613636363636363535, 0.7670454545454545858, 0.7727272727272727071, 0.7784090909090909394, 0.7840909090909090606, 0.7897727272727272929, 0.7954545454545454142, 0.8011363636363636465, 0.8068181818181817677, 0.8125000000000000000, 0.8181818181818182323, 0.8238636363636363535, 0.8295454545454545858, 0.8352272727272727071, 0.8409090909090909394, 0.8465909090909090606, 0.8522727272727272929, 0.8579545454545454142, 0.8636363636363636465, 0.8693181818181817677, 0.8750000000000000000, 0.8806818181818182323, 0.8863636363636363535, 0.8920454545454545858, 0.8977272727272727071, 0.9034090909090909394, 0.9090909090909090606, 0.9147727272727272929, 0.9204545454545454142, 0.9261363636363636465, 0.9318181818181817677, 0.9375000000000000000, 0.9431818181818182323, 0.9488636363636363535, 0.9545454545454545858, 0.9602272727272727071, 0.9659090909090909394, 0.9715909090909090606, 0.9772727272727272929, 0.9829545454545454142, 0.9886363636363636465, 0.9943181818181817677, 1.000000000000000000 ),
 .UNSPECIFIED. ) 
 GEOMETRIC_REPRESENTATION_ITEM ( )  RATIONAL_B_SPLINE_SURFACE ( (
 ( 1.000000000000000000, 0.9238795325112867385, 1.000000000000000000, 0.9238795325112867385, 1.000000000000000000, 0.9238795325112867385, 1.000000000000000000, 0.9238795325112867385, 1.000000000000000000, 0.9238795325112867385, 1.000000000000000000, 0.9238795325112867385, 1.000000000000000000, 0.9238795325112867385, 1.000000000000000000, 0.9238795325112867385, 1.000000000000000000, 0.9238795325112867385, 1.000000000000000000, 0.9238795325112867385, 1.000000000000000000, 0.9238795325112867385, 1.000000000000000000, 0.9238795325112867385, 1.000000000000000000, 0.9238795325112867385, 1.000000000000000000, 0.9238795325112867385, 1.000000000000000000, 0.9238795325112867385, 1.000000000000000000, 0.9238795325112867385, 1.000000000000000000, 0.9238795325112867385, 1.000000000000000000, 0.9238795325112867385, 1.000000000000000000, 0.9238795325112867385, 1.000000000000000000, 0.9238795325112867385, 1.000000000000000000, 0.9238795325112867385, 1.000000000000000000, 0.9238795325112867385, 1.000000000000000000, 0.9238795325112867385, 1.000000000000000000, 0.9238795325112867385, 1.000000000000000000, 0.9238795325112867385, 1.000000000000000000, 0.9238795325112867385, 1.000000000000000000, 0.9238795325112867385, 1.000000000000000000, 0.9238795325112867385, 1.000000000000000000, 0.9238795325112867385, 1.000000000000000000, 0.9238795325112867385, 1.000000000000000000, 0.9238795325112867385, 1.000000000000000000, 0.9238795325112867385, 1.000000000000000000, 0.9238795325112867385, 1.000000000000000000, 0.9238795325112867385, 1.000000000000000000, 0.9238795325112867385, 1.000000000000000000, 0.9238795325112867385, 1.000000000000000000, 0.9238795325112867385, 1.000000000000000000, 0.9238795325112867385, 1.000000000000000000, 0.9238795325112867385, 1.000000000000000000, 0.9238795325112867385, 1.000000000000000000, 0.9238795325112867385, 1.000000000000000000, 0.9238795325112867385, 1.000000000000000000, 0.9238795325112867385, 1.000000000000000000, 0.9238795325112867385, 1.000000000000000000, 0.9238795325112867385, 1.000000000000000000, 0.9238795325112867385, 1.000000000000000000, 0.9238795325112867385, 1.000000000000000000, 0.9238795325112867385, 1.000000000000000000, 0.9238795325112867385, 1.000000000000000000, 0.9238795325112867385, 1.000000000000000000, 0.9238795325112867385, 1.000000000000000000, 0.9238795325112867385, 1.000000000000000000, 0.9238795325112867385, 1.000000000000000000, 0.9238795325112867385, 1.000000000000000000, 0.9238795325112867385, 1.000000000000000000, 0.9238795325112867385, 1.000000000000000000, 0.9238795325112867385, 1.000000000000000000, 0.9238795325112867385, 1.000000000000000000, 0.9238795325112867385, 1.000000000000000000, 0.9238795325112867385, 1.000000000000000000, 0.9238795325112867385, 1.000000000000000000, 0.9238795325112867385, 1.000000000000000000, 0.9238795325112867385, 1.000000000000000000, 0.9238795325112867385, 1.000000000000000000, 0.9238795325112867385, 1.000000000000000000, 0.9238795325112867385, 1.000000000000000000, 0.9238795325112867385, 1.000000000000000000, 0.9238795325112867385, 1.000000000000000000, 0.9238795325112867385, 1.000000000000000000, 0.9238795325112867385, 1.000000000000000000, 0.9238795325112867385, 1.000000000000000000, 0.9238795325112867385, 1.000000000000000000, 0.9238795325112867385, 1.000000000000000000, 0.9238795325112867385, 1.000000000000000000, 0.9238795325112867385, 1.000000000000000000, 0.9238795325112867385, 1.000000000000000000, 0.9238795325112867385, 1.000000000000000000, 0.9238795325112867385, 1.000000000000000000, 0.9238795325112867385, 1.000000000000000000, 0.9238795325112867385, 1.000000000000000000, 0.9238795325112867385, 1.000000000000000000, 0.9238795325112867385, 1.000000000000000000, 0.9238795325112867385, 1.000000000000000000, 0.9238795325112867385, 1.000000000000000000, 0.9238795325112867385, 1.000000000000000000, 0.9238795325112867385, 1.000000000000000000, 0.9238795325112867385, 1.000000000000000000, 0.9238795325112867385, 1.000000000000000000, 0.9238795325112867385, 1.000000000000000000, 0.9238795325112867385, 1.000000000000000000, 0.9238795325112867385, 1.000000000000000000, 0.9238795325112867385, 1.000000000000000000, 0.9238795325112867385, 1.000000000000000000, 0.9238795325112867385, 1.000000000000000000, 0.9238795325112867385, 1.000000000000000000, 0.9238795325112867385, 1.000000000000000000, 0.9238795325112867385, 1.000000000000000000, 0.9238795325112867385, 1.000000000000000000, 0.9238795325112867385, 1.000000000000000000, 0.9238795325112867385, 1.000000000000000000, 0.9238795325112867385, 1.000000000000000000, 0.9238795325112867385, 1.000000000000000000, 0.9238795325112867385, 1.000000000000000000, 0.9238795325112867385, 1.000000000000000000, 0.9238795325112867385, 1.000000000000000000, 0.9238795325112867385, 1.000000000000000000, 0.9238795325112867385, 1.000000000000000000, 0.9238795325112867385, 1.000000000000000000, 0.9238795325112867385, 1.000000000000000000, 0.9238795325112867385, 1.000000000000000000, 0.9238795325112867385, 1.000000000000000000, 0.9238795325112867385, 1.000000000000000000, 0.9238795325112867385, 1.000000000000000000, 0.9238795325112867385, 1.000000000000000000, 0.9238795325112867385, 1.000000000000000000, 0.9238795325112867385, 1.000000000000000000, 0.9238795325112867385, 1.000000000000000000, 0.9238795325112867385, 1.000000000000000000, 0.9238795325112867385, 1.000000000000000000, 0.9238795325112867385, 1.000000000000000000, 0.9238795325112867385, 1.000000000000000000, 0.9238795325112867385, 1.000000000000000000, 0.9238795325112867385, 1.000000000000000000, 0.9238795325112867385, 1.000000000000000000, 0.9238795325112867385, 1.000000000000000000, 0.9238795325112867385, 1.000000000000000000, 0.9238795325112867385, 1.000000000000000000, 0.9238795325112867385, 1.000000000000000000, 0.9238795325112867385, 1.000000000000000000, 0.9238795325112867385, 1.000000000000000000, 0.9238795325112867385, 1.000000000000000000, 0.9238795325112867385, 1.000000000000000000, 0.9238795325112867385, 1.000000000000000000, 0.9238795325112867385, 1.000000000000000000, 0.9238795325112867385, 1.000000000000000000, 0.9238795325112867385, 1.000000000000000000, 0.9238795325112867385, 1.000000000000000000, 0.9238795325112867385, 1.000000000000000000, 0.9238795325112867385, 1.000000000000000000, 0.9238795325112867385, 1.000000000000000000, 0.9238795325112867385, 1.000000000000000000, 0.9238795325112867385, 1.000000000000000000, 0.9238795325112867385, 1.000000000000000000, 0.9238795325112867385, 1.000000000000000000, 0.9238795325112867385, 1.000000000000000000, 0.9238795325112867385, 1.000000000000000000, 0.9238795325112867385, 1.000000000000000000, 0.9238795325112867385, 1.000000000000000000, 0.9238795325112867385, 1.000000000000000000, 0.9238795325112867385, 1.000000000000000000, 0.9238795325112867385, 1.000000000000000000, 0.9238795325112867385, 1.000000000000000000, 0.9238795325112867385, 1.000000000000000000, 0.9238795325112867385, 1.000000000000000000, 0.9238795325112867385, 1.000000000000000000, 0.9238795325112867385, 1.000000000000000000, 0.9238795325112867385, 1.000000000000000000, 0.9238795325112867385, 1.000000000000000000, 0.9238795325112867385, 1.000000000000000000, 0.9238795325112867385, 1.000000000000000000, 0.9238795325112867385, 1.000000000000000000, 0.9238795325112867385, 1.000000000000000000, 0.9238795325112867385, 1.000000000000000000, 0.9238795325112867385, 1.000000000000000000, 0.9238795325112867385, 1.000000000000000000, 0.9238795325112867385, 1.000000000000000000, 0.9238795325112867385, 1.000000000000000000, 0.9238795325112867385, 1.000000000000000000, 0.9238795325112867385, 1.000000000000000000, 0.9238795325112867385, 1.000000000000000000, 0.9238795325112867385, 1.000000000000000000, 0.9238795325112867385, 1.000000000000000000, 0.9238795325112867385, 1.000000000000000000, 0.9238795325112867385, 1.000000000000000000, 0.9238795325112867385, 1.000000000000000000, 0.9238795325112867385, 1.000000000000000000),
 ( 1.000000000000000000, 0.9238795325112867385, 1.000000000000000000, 0.9238795325112867385, 1.000000000000000000, 0.9238795325112867385, 1.000000000000000000, 0.9238795325112867385, 1.000000000000000000, 0.9238795325112867385, 1.000000000000000000, 0.9238795325112867385, 1.000000000000000000, 0.9238795325112867385, 1.000000000000000000, 0.9238795325112867385, 1.000000000000000000, 0.9238795325112867385, 1.000000000000000000, 0.9238795325112867385, 1.000000000000000000, 0.9238795325112867385, 1.000000000000000000, 0.9238795325112867385, 1.000000000000000000, 0.9238795325112867385, 1.000000000000000000, 0.9238795325112867385, 1.000000000000000000, 0.9238795325112867385, 1.000000000000000000, 0.9238795325112867385, 1.000000000000000000, 0.9238795325112867385, 1.000000000000000000, 0.9238795325112867385, 1.000000000000000000, 0.9238795325112867385, 1.000000000000000000, 0.9238795325112867385, 1.000000000000000000, 0.9238795325112867385, 1.000000000000000000, 0.9238795325112867385, 1.000000000000000000, 0.9238795325112867385, 1.000000000000000000, 0.9238795325112867385, 1.000000000000000000, 0.9238795325112867385, 1.000000000000000000, 0.9238795325112867385, 1.000000000000000000, 0.9238795325112867385, 1.000000000000000000, 0.9238795325112867385, 1.000000000000000000, 0.9238795325112867385, 1.000000000000000000, 0.9238795325112867385, 1.000000000000000000, 0.9238795325112867385, 1.000000000000000000, 0.9238795325112867385, 1.000000000000000000, 0.9238795325112867385, 1.000000000000000000, 0.9238795325112867385, 1.000000000000000000, 0.9238795325112867385, 1.000000000000000000, 0.9238795325112867385, 1.000000000000000000, 0.9238795325112867385, 1.000000000000000000, 0.9238795325112867385, 1.000000000000000000, 0.9238795325112867385, 1.000000000000000000, 0.9238795325112867385, 1.000000000000000000, 0.9238795325112867385, 1.000000000000000000, 0.9238795325112867385, 1.000000000000000000, 0.9238795325112867385, 1.000000000000000000, 0.9238795325112867385, 1.000000000000000000, 0.9238795325112867385, 1.000000000000000000, 0.9238795325112867385, 1.000000000000000000, 0.9238795325112867385, 1.000000000000000000, 0.9238795325112867385, 1.000000000000000000, 0.9238795325112867385, 1.000000000000000000, 0.9238795325112867385, 1.000000000000000000, 0.9238795325112867385, 1.000000000000000000, 0.9238795325112867385, 1.000000000000000000, 0.9238795325112867385, 1.000000000000000000, 0.9238795325112867385, 1.000000000000000000, 0.9238795325112867385, 1.000000000000000000, 0.9238795325112867385, 1.000000000000000000, 0.9238795325112867385, 1.000000000000000000, 0.9238795325112867385, 1.000000000000000000, 0.9238795325112867385, 1.000000000000000000, 0.9238795325112867385, 1.000000000000000000, 0.9238795325112867385, 1.000000000000000000, 0.9238795325112867385, 1.000000000000000000, 0.9238795325112867385, 1.000000000000000000, 0.9238795325112867385, 1.000000000000000000, 0.9238795325112867385, 1.000000000000000000, 0.9238795325112867385, 1.000000000000000000, 0.9238795325112867385, 1.000000000000000000, 0.9238795325112867385, 1.000000000000000000, 0.9238795325112867385, 1.000000000000000000, 0.9238795325112867385, 1.000000000000000000, 0.9238795325112867385, 1.000000000000000000, 0.9238795325112867385, 1.000000000000000000, 0.9238795325112867385, 1.000000000000000000, 0.9238795325112867385, 1.000000000000000000, 0.9238795325112867385, 1.000000000000000000, 0.9238795325112867385, 1.000000000000000000, 0.9238795325112867385, 1.000000000000000000, 0.9238795325112867385, 1.000000000000000000, 0.9238795325112867385, 1.000000000000000000, 0.9238795325112867385, 1.000000000000000000, 0.9238795325112867385, 1.000000000000000000, 0.9238795325112867385, 1.000000000000000000, 0.9238795325112867385, 1.000000000000000000, 0.9238795325112867385, 1.000000000000000000, 0.9238795325112867385, 1.000000000000000000, 0.9238795325112867385, 1.000000000000000000, 0.9238795325112867385, 1.000000000000000000, 0.9238795325112867385, 1.000000000000000000, 0.9238795325112867385, 1.000000000000000000, 0.9238795325112867385, 1.000000000000000000, 0.9238795325112867385, 1.000000000000000000, 0.9238795325112867385, 1.000000000000000000, 0.9238795325112867385, 1.000000000000000000, 0.9238795325112867385, 1.000000000000000000, 0.9238795325112867385, 1.000000000000000000, 0.9238795325112867385, 1.000000000000000000, 0.9238795325112867385, 1.000000000000000000, 0.9238795325112867385, 1.000000000000000000, 0.9238795325112867385, 1.000000000000000000, 0.9238795325112867385, 1.000000000000000000, 0.9238795325112867385, 1.000000000000000000, 0.9238795325112867385, 1.000000000000000000, 0.9238795325112867385, 1.000000000000000000, 0.9238795325112867385, 1.000000000000000000, 0.9238795325112867385, 1.000000000000000000, 0.9238795325112867385, 1.000000000000000000, 0.9238795325112867385, 1.000000000000000000, 0.9238795325112867385, 1.000000000000000000, 0.9238795325112867385, 1.000000000000000000, 0.9238795325112867385, 1.000000000000000000, 0.9238795325112867385, 1.000000000000000000, 0.9238795325112867385, 1.000000000000000000, 0.9238795325112867385, 1.000000000000000000, 0.9238795325112867385, 1.000000000000000000, 0.9238795325112867385, 1.000000000000000000, 0.9238795325112867385, 1.000000000000000000, 0.9238795325112867385, 1.000000000000000000, 0.9238795325112867385, 1.000000000000000000, 0.9238795325112867385, 1.000000000000000000, 0.9238795325112867385, 1.000000000000000000, 0.9238795325112867385, 1.000000000000000000, 0.9238795325112867385, 1.000000000000000000, 0.9238795325112867385, 1.000000000000000000, 0.9238795325112867385, 1.000000000000000000, 0.9238795325112867385, 1.000000000000000000, 0.9238795325112867385, 1.000000000000000000, 0.9238795325112867385, 1.000000000000000000, 0.9238795325112867385, 1.000000000000000000, 0.9238795325112867385, 1.000000000000000000, 0.9238795325112867385, 1.000000000000000000, 0.9238795325112867385, 1.000000000000000000, 0.9238795325112867385, 1.000000000000000000, 0.9238795325112867385, 1.000000000000000000, 0.9238795325112867385, 1.000000000000000000, 0.9238795325112867385, 1.000000000000000000, 0.9238795325112867385, 1.000000000000000000, 0.9238795325112867385, 1.000000000000000000, 0.9238795325112867385, 1.000000000000000000, 0.9238795325112867385, 1.000000000000000000, 0.9238795325112867385, 1.000000000000000000, 0.9238795325112867385, 1.000000000000000000, 0.9238795325112867385, 1.000000000000000000, 0.9238795325112867385, 1.000000000000000000, 0.9238795325112867385, 1.000000000000000000, 0.9238795325112867385, 1.000000000000000000, 0.9238795325112867385, 1.000000000000000000, 0.9238795325112867385, 1.000000000000000000, 0.9238795325112867385, 1.000000000000000000, 0.9238795325112867385, 1.000000000000000000, 0.9238795325112867385, 1.000000000000000000, 0.9238795325112867385, 1.000000000000000000, 0.9238795325112867385, 1.000000000000000000, 0.9238795325112867385, 1.000000000000000000, 0.9238795325112867385, 1.000000000000000000, 0.9238795325112867385, 1.000000000000000000, 0.9238795325112867385, 1.000000000000000000, 0.9238795325112867385, 1.000000000000000000, 0.9238795325112867385, 1.000000000000000000, 0.9238795325112867385, 1.000000000000000000, 0.9238795325112867385, 1.000000000000000000, 0.9238795325112867385, 1.000000000000000000, 0.9238795325112867385, 1.000000000000000000, 0.9238795325112867385, 1.000000000000000000, 0.9238795325112867385, 1.000000000000000000, 0.9238795325112867385, 1.000000000000000000, 0.9238795325112867385, 1.000000000000000000, 0.9238795325112867385, 1.000000000000000000, 0.9238795325112867385, 1.000000000000000000, 0.9238795325112867385, 1.000000000000000000, 0.9238795325112867385, 1.000000000000000000, 0.9238795325112867385, 1.000000000000000000, 0.9238795325112867385, 1.000000000000000000, 0.9238795325112867385, 1.000000000000000000, 0.9238795325112867385, 1.000000000000000000, 0.9238795325112867385, 1.000000000000000000, 0.9238795325112867385, 1.000000000000000000) ) ) 
 REPRESENTATION_ITEM ( '' )  SURFACE ( )  );
#17775 = CARTESIAN_POINT ( 'NONE',  ( -2.085542519210945728E-15, 139.5312499965860411, 11.35316468750000141 ) ) ;
#17776 =( GEOMETRIC_REPRESENTATION_CONTEXT ( 3 ) GLOBAL_UNCERTAINTY_ASSIGNED_CONTEXT ( ( #40812 ) ) GLOBAL_UNIT_ASSIGNED_CONTEXT ( ( #11085, #27682, #63126 ) ) REPRESENTATION_CONTEXT ( 'NONE', 'WORKASPACE' ) );
#17777 = ADVANCED_FACE ( 'NONE', ( #30779 ), #70410, .F. ) ;
#17778 = CARTESIAN_POINT ( 'NONE',  ( -2.679491924311235618, 110.4166666598387110, 10.00000000000000000 ) ) ;
#17779 = CARTESIAN_POINT ( 'NONE',  ( 7.188101187500002709, 113.1875000020483810, 2.977408999572649151 ) ) ;
#17780 = CARTESIAN_POINT ( 'NONE',  ( 2.679491924311075302, 170.8333333265053398, 10.00000000000008704 ) ) ;
#17781 = CARTESIAN_POINT ( 'NONE',  ( 4.556349186104045934, 11.00000000000000000, 102.7187500040967620 ) ) ;
#17782 = CARTESIAN_POINT ( 'NONE',  ( -5.000000000000001776, 53.12474899268234907, -47.87640533067806814 ) ) ;
#17783 = VERTEX_POINT ( 'NONE', #47015 ) ;
#17784 = CARTESIAN_POINT ( 'NONE',  ( -9.832129032723420536, 14.01041666325268409, 5.676582343749997150 ) ) ;
#17785 = EDGE_CURVE ( 'NONE', #20313, #35739, #41371, .T. ) ;
#17786 = LINE ( 'NONE', #7217, #12487 ) ;
#17787 = CARTESIAN_POINT ( 'NONE',  ( -4.721056650415999201, 296.3281250017069510, -4.721056650415999201 ) ) ;
#17788 = CARTESIAN_POINT ( 'NONE',  ( 11.35316468749999785, 135.5729166632526983, 3.042071309553174174 ) ) ;
#17789 = DIRECTION ( 'NONE',  ( 0.000000000000000000, 0.000000000000000000, 1.000000000000000000 ) ) ;
#17790 = CARTESIAN_POINT ( 'NONE',  ( 7.999999999999991118, 9.797174393178815797E-16, 25.63655278432982954 ) ) ;
#17791 = CARTESIAN_POINT ( 'NONE',  ( 7.320508075688776373, 225.0000000068280315, 7.320508075688767491 ) ) ;
#17792 = CARTESIAN_POINT ( 'NONE',  ( -8.311093377946834337, 244.5312500034139589, 8.311093377946837890 ) ) ;
#17793 = CARTESIAN_POINT ( 'NONE',  ( -10.18810118749999738, -4.220049686691941915, 95.12500000204836681 ) ) ;
#17794 = VERTEX_POINT ( 'NONE', #24380 ) ;
#17795 = EDGE_CURVE ( 'NONE', #49471, #30705, #43880, .T. ) ;
#17796 = LINE ( 'NONE', #57812, #53346 ) ;
#17797 = CARTESIAN_POINT ( 'NONE',  ( 0.000000000000000000, 125.0000000000000000, 0.000000000000000000 ) ) ;
#17798 = EDGE_CURVE ( 'NONE', #16650, #6283, #25748, .T. ) ;
#17799 = CARTESIAN_POINT ( 'NONE',  ( 9.832129032723416984, 95.67708332991935549, 5.676582343750006032 ) ) ;
#17800 = ORIENTED_EDGE ( 'NONE', *, *, #50993, .T. ) ;
#17801 = CARTESIAN_POINT ( 'NONE',  ( 4.220049686691941027, -10.18810118749999738, 105.6250000020483668 ) ) ;
#17802 = CARTESIAN_POINT ( 'NONE',  ( 1.881053915767121998, 11.62499999863440792, -4.541265875000002339 ) ) ;
#17803 = EDGE_LOOP ( 'NONE', ( #37795, #38145, #30585, #47566, #37784 ) ) ;
#17804 = ORIENTED_EDGE ( 'NONE', *, *, #73012, .T. ) ;
#17805 = CARTESIAN_POINT ( 'NONE',  ( -8.000000000000001776, 3.843750000000000888, 3.313708498984759387 ) ) ;
#17806 = CARTESIAN_POINT ( 'NONE',  ( -4.999999999999999112, -63.85408791058067379, -24.15552328276524463 ) ) ;
#17807 = CARTESIAN_POINT ( 'NONE',  ( 4.401442555609581635E-16, 26.71874999795161543, -7.188101187500000044 ) ) ;
#17808 = CARTESIAN_POINT ( 'NONE',  ( 11.00000000000005151, 4.556349186103993532, 96.34374999999998579 ) ) ;
#17809 = VECTOR ( 'NONE', #39216, 1000.000000000000000 ) ;
#17810 = CARTESIAN_POINT ( 'NONE',  ( -10.18810118749999738, -4.220049686691941915, 105.6250000020483668 ) ) ;
#17811 = CARTESIAN_POINT ( 'NONE',  ( 2.828427124746190291, 0.8750000000000002220, 2.828427124746192067 ) ) ;
#17812 = CARTESIAN_POINT ( 'NONE',  ( -2.828427124746190735, 12.12499999726881406, -2.828427124746191623 ) ) ;
#17813 = CARTESIAN_POINT ( 'NONE',  ( -7.999999999999861444, -9.580972845112835701E-07, 13.01783880491507261 ) ) ;
#17814 = ORIENTED_EDGE ( 'NONE', *, *, #68172, .T. ) ;
#17815 = EDGE_CURVE ( 'NONE', #43329, #40040, #43419, .T. ) ;
#17816 = CYLINDRICAL_SURFACE ( 'NONE', #34342, 7.999999999999991118 ) ;
#17817 = CARTESIAN_POINT ( 'NONE',  ( 2.445694354108839619, 198.8125000013656063, 200.4456943541088663 ) ) ;
#17818 = EDGE_CURVE ( 'NONE', #2879, #27850, #31427, .T. ) ;
#17819 = CARTESIAN_POINT ( 'NONE',  ( -27.99999999999992184, 206.9375000013656063, 173.4587341250003760 ) ) ;
#17820 = CARTESIAN_POINT ( 'NONE',  ( 1.656854249492352604, 207.1875000000000568, 138.0000000000000853 ) ) ;
#17821 = AXIS2_PLACEMENT_3D ( 'NONE', #71471, #29650, #25451 ) ;
#17822 = CARTESIAN_POINT ( 'NONE',  ( -1.881053915767121554, 10.62499999863440792, -4.541265875000002339 ) ) ;
#17823 = CARTESIAN_POINT ( 'NONE',  ( -2.828427124746192067, 18.37499999726881583, 2.828427124746190735 ) ) ;
#17824 = CARTESIAN_POINT ( 'NONE',  ( 5.082755093536320601, -5.082755093536318824, 15.54905278187175455 ) ) ;
#17825 = EDGE_LOOP ( 'NONE', ( #59764, #5820 ) ) ;
#17826 = EDGE_CURVE ( 'NONE', #3534, #45065, #48272, .T. ) ;
#17827 = VERTEX_POINT ( 'NONE', #25006 ) ;
#17828 = CARTESIAN_POINT ( 'NONE',  ( 7.204075437095968759, -7.204075437095966983, 107.2187500020483810 ) ) ;
#17829 = DIRECTION ( 'NONE',  ( -0.000000000000000000, 1.000000000000000000, -4.476705744456276341E-16 ) ) ;
#17830 = CARTESIAN_POINT ( 'NONE',  ( -32.00000000000001421, 205.1875000000000000, 168.3431457505080004 ) ) ;
#17831 = CARTESIAN_POINT ( 'NONE',  ( -2.445694354108783664, 200.3125000013656063, 195.5543056458912190 ) ) ;
#17832 = CARTESIAN_POINT ( 'NONE',  ( 28.00000000000001421, 195.4375000013655779, 173.4587341249998929 ) ) ;
#17833 = CARTESIAN_POINT ( 'NONE',  ( 6.123233995736767268E-16, 96.25000000000000000, -10.00000000000000178 ) ) ;
#17834 = CARTESIAN_POINT ( 'NONE',  ( -3.313708498984762052, 118.7187499999999858, -8.000000000000000000 ) ) ;
#17835 = CARTESIAN_POINT ( 'NONE',  ( 5.676582343749993598, 55.26041666325268409, 9.832129032723422313 ) ) ;
#17836 = CARTESIAN_POINT ( 'NONE',  ( 4.242640687119287435, 288.3750000000000000, 4.242640687119285658 ) ) ;
#17837 = ORIENTED_EDGE ( 'NONE', *, *, #28984, .T. ) ;
#17838 = CARTESIAN_POINT ( 'NONE',  ( 8.660254037844389075, 252.0833333333333144, 4.999999999999997335 ) ) ;
#17839 = CARTESIAN_POINT ( 'NONE',  ( -5.656854249492379694, 13.87499999590322375, -5.656854249492380582 ) ) ;
#17840 = CARTESIAN_POINT ( 'NONE',  ( -1.432654583217664479, 205.7500000013656063, 138.5412658750000787 ) ) ;
#17841 = CARTESIAN_POINT ( 'NONE',  ( 10.00000000000001243, 85.00000000000000000, 0.000000000000000000 ) ) ;
#17842 = CARTESIAN_POINT ( 'NONE',  ( 5.656854249492381470, 97.06250000000000000, 5.656854249492379694 ) ) ;
#17843 = CARTESIAN_POINT ( 'NONE',  ( 2.679491924311225848, 243.5416666666666572, -10.00000000000000000 ) ) ;
#17844 = CARTESIAN_POINT ( 'NONE',  ( -30.82842712474612412, 202.5000000027312126, 172.8284271247466108 ) ) ;
#17845 = CARTESIAN_POINT ( 'NONE',  ( 11.00000000000000355, -4.556349186104045046, 117.1562499999999858 ) ) ;
#17846 = CARTESIAN_POINT ( 'NONE',  ( -5.000000000000005329, 198.3333333333333428, 8.660254037844387298 ) ) ;
#17847 = CARTESIAN_POINT ( 'NONE',  ( -4.401442555609577197E-16, 7.188101187499992051, 8.986552781871752771 ) ) ;
#17848 = CARTESIAN_POINT ( 'NONE',  ( 8.311093377946834337, 185.4687499965860127, 8.311093377946839666 ) ) ;
#17849 = DIRECTION ( 'NONE',  ( 0.000000000000000000, -1.000000000000000000, 0.000000000000000000 ) ) ;
#17850 = CARTESIAN_POINT ( 'NONE',  ( 28.00000000000001776, 197.1250000027312126, 173.9999999999999147 ) ) ;
#17851 = CARTESIAN_POINT ( 'NONE',  ( -11.00000000000000533, -11.00000000000000355, 41.99999999999999289 ) ) ;
#17852 = ORIENTED_EDGE ( 'NONE', *, *, #42405, .T. ) ;
#17853 = CARTESIAN_POINT ( 'NONE',  ( 3.458734124999960358, 207.6875000013656063, 142.0000000000000568 ) ) ;
#17854 = CARTESIAN_POINT ( 'NONE',  ( -11.35316468750000141, 38.80208332991934839, 3.042071309553159963 ) ) ;
#17855 = CARTESIAN_POINT ( 'NONE',  ( 11.00000000000000000, 4.556349186104045934, 110.0312500040967620 ) ) ;
#17856 = CARTESIAN_POINT ( 'NONE',  ( -24.54126587500001833, 204.2500000013655779, 168.5673454167826435 ) ) ;
#17857 = VECTOR ( 'NONE', #23395, 1000.000000000000000 ) ;
#17858 = CARTESIAN_POINT ( 'NONE',  ( 3.313708498984761608, 4.593749995903220196, -8.000000000000000000 ) ) ;
#17860 = CARTESIAN_POINT ( 'NONE',  ( -4.999999999999987566, 101.6666666666666572, -8.660254037844371311 ) ) ;
#17859 = CARTESIAN_POINT ( 'NONE',  ( -5.656854249492378806, 116.3750000040967905, 5.656854249492381470 ) ) ;
#17861 = CARTESIAN_POINT ( 'NONE',  ( 2.445694354108783664, 197.3125000013656063, 144.4456943541088663 ) ) ;
#17862 = VECTOR ( 'NONE', #1724, 1000.000000000000000 ) ;
#17863 = CARTESIAN_POINT ( 'NONE',  ( -8.660254037844390851, 74.79166665983871098, 4.999999999999998224 ) ) ;
#17864 = CARTESIAN_POINT ( 'NONE',  ( 5.082755093536325042, 95.09375000204838102, -5.082755093536325930 ) ) ;
#17865 = CARTESIAN_POINT ( 'NONE',  ( 4.541265875000002339, 11.43749999863440614, 0.000000000000000000 ) ) ;
#17866 = DIRECTION ( 'NONE',  ( -1.000000000000000000, 0.000000000000000000, 0.000000000000000000 ) ) ;
#17867 = CARTESIAN_POINT ( 'NONE',  ( 5.836461775160671550, 0.2934486527655157939, -5.189590606809809437 ) ) ;
#17868 = DIRECTION ( 'NONE',  ( 0.000000000000000000, 0.000000000000000000, -1.000000000000000000 ) ) ;
#17869 = ORIENTED_EDGE ( 'NONE', *, *, #33288, .F. ) ;
#17870 = EDGE_LOOP ( 'NONE', ( #1340, #28682, #11487, #28078 ) ) ;
#17871 = CARTESIAN_POINT ( 'NONE',  ( 1.881637226502129035E-11, 6.249999999998538058, -10.00000000000000178 ) ) ;
#17872 = CARTESIAN_POINT ( 'NONE',  ( 4.721056650415999201, 299.2343750017069510, -4.721056650415999201 ) ) ;
#17873 = CARTESIAN_POINT ( 'NONE',  ( 1.102182119232618108E-15, 290.3125000034140157, 6.000000000000001776 ) ) ;
#17874 = CARTESIAN_POINT ( 'NONE',  ( -2.679491924311529161, 88.54166666666665719, 9.999999999999831246 ) ) ;
#17875 = CARTESIAN_POINT ( 'NONE',  ( -9.832129032723418760, 157.8645833299193839, -5.676582343750004256 ) ) ;
#17876 = CARTESIAN_POINT ( 'NONE',  ( 7.320508075688760385, 104.3750000000000000, 7.320508075688763938 ) ) ;
#17877 = CARTESIAN_POINT ( 'NONE',  ( -10.18810118749999916, 4.220049686691934809, 82.56250000204836681 ) ) ;
#17878 = CARTESIAN_POINT ( 'NONE',  ( -28.89281933948912595, 194.7383503587969074, 173.6371172511951215 ) ) ;
#17879 = VECTOR ( 'NONE', #31202, 1000.000000000000000 ) ;
#17880 = CARTESIAN_POINT ( 'NONE',  ( 2.828427124746209831, 204.3750000000000284, 200.8284271247462129 ) ) ;
#17881 = DIRECTION ( 'NONE',  ( -1.000000000000000000, 0.000000000000000000, 0.000000000000000000 ) ) ;
#17882 = FACE_OUTER_BOUND ( 'NONE', #27471, .T. ) ;
#17883 = ORIENTED_EDGE ( 'NONE', *, *, #27362, .T. ) ;
#17884 = AXIS2_PLACEMENT_3D ( 'NONE', #73609, #40767, #16621 ) ;
#17885 = CARTESIAN_POINT ( 'NONE',  ( -1.656854249492271780, 201.9375000027311842, 193.9999999999999716 ) ) ;
#17886 = CARTESIAN_POINT ( 'NONE',  ( 35.84459951466202909, 174.6650488676636712, 165.1237838699680083 ) ) ;
#17887 = CARTESIAN_POINT ( 'NONE',  ( -3.042071309553163960, 127.5520833299193555, -11.35316468749999963 ) ) ;
#17888 = CARTESIAN_POINT ( 'NONE',  ( 1.432654583217662259, 197.1250000013656347, 194.5412658750000219 ) ) ;
#17889 = CARTESIAN_POINT ( 'NONE',  ( -5.082755093536325042, 22.40624999795161543, -5.082755093536325930 ) ) ;
#17890 = CARTESIAN_POINT ( 'NONE',  ( 1.871523826299183495E-15, -10.18810118749999916, 77.40625000204836681 ) ) ;
#17891 = CARTESIAN_POINT ( 'NONE',  ( -2.085542519210945728E-15, 54.84374999658601979, 11.35316468750000141 ) ) ;
#17893 = VERTEX_POINT ( 'NONE', #45352 ) ;
#17892 =( BOUNDED_CURVE ( )  B_SPLINE_CURVE ( 2, ( #31414, #9540, #3877, #20453, #54441, #55564, #15175, #43095, #49887 ),
 .UNSPECIFIED., .F., .F. ) 
 B_SPLINE_CURVE_WITH_KNOTS ( ( 3, 2, 2, 2, 3 ),
 ( 0.5113636363636363535, 0.5170454545454545858, 0.5227272727272727071, 0.5284090909090909394, 0.5340909090909090606 ),
 .UNSPECIFIED. ) 
 CURVE ( )  GEOMETRIC_REPRESENTATION_ITEM ( )  RATIONAL_B_SPLINE_CURVE ( ( 1.000000000000000000, 0.9238795325112867385, 1.000000000000000000, 0.9238795325112867385, 1.000000000000000000, 0.9238795325112867385, 1.000000000000000000, 0.9238795325112867385, 1.000000000000000000 ) ) 
 REPRESENTATION_ITEM ( '' )  );
#17894 = CARTESIAN_POINT ( 'NONE',  ( 11.00000000000000000, 1.347111479062088405E-15, 94.93750000409677625 ) ) ;
#17896 = CARTESIAN_POINT ( 'NONE',  ( 4.541265875000002339, 2.437499998634407028, 0.000000000000000000 ) ) ;
#17895 =( BOUNDED_CURVE ( )  B_SPLINE_CURVE ( 2, ( #63678, #57672, #68599, #34294, #22192, #33924, #68976, #21817, #45216, #74637, #33548, #44848, #56551 ),
 .UNSPECIFIED., .F., .F. ) 
 B_SPLINE_CURVE_WITH_KNOTS ( ( 3, 2, 2, 2, 2, 2, 3 ),
 ( 0.3206521739130435145, 0.3224637681159420732, 0.3242753623188406320, 0.3260869565217391353, 0.3278985507246376940, 0.3297101449275362528, 0.3315217391304347561 ),
 .UNSPECIFIED. ) 
 CURVE ( )  GEOMETRIC_REPRESENTATION_ITEM ( )  RATIONAL_B_SPLINE_CURVE ( ( 0.9999999999999990008, 0.9659258262890693114, 1.000000000000000000, 0.9659258262890683122, 1.000000000000000000, 0.9659258262890683122, 1.000000000000000000, 0.9659258262890683122, 1.000000000000000000, 0.9659258262890683122, 1.000000000000000000, 0.9659258262890683122, 1.000000000000000000 ) ) 
 REPRESENTATION_ITEM ( '' )  );
#17897 = CARTESIAN_POINT ( 'NONE',  ( 1.471067592899761672E-15, -8.008118988124991233, 16.38811528394063188 ) ) ;
#17898 = CARTESIAN_POINT ( 'NONE',  ( -1.432654583217664701, 205.0000000013655779, 138.5412658750000787 ) ) ;
#17899 = CARTESIAN_POINT ( 'NONE',  ( 7.188101187500001821, 12.56249999795161365, -2.977408999572650483 ) ) ;
#17900 = CARTESIAN_POINT ( 'NONE',  ( -2.485281374238572649, 295.2500000034139589, 6.000000000000002665 ) ) ;
#17901 = CARTESIAN_POINT ( 'NONE',  ( -47.86415381379093503, 143.8221353245225771, 63.07999174420056221 ) ) ;
#17902 = CARTESIAN_POINT ( 'NONE',  ( -5.082755093536325042, 7.406249997951610986, -5.082755093536325930 ) ) ;
#17903 = CARTESIAN_POINT ( 'NONE',  ( 2.977408999572650927, -7.188101187499990274, 10.95530278187175455 ) ) ;
#17904 = CARTESIAN_POINT ( 'NONE',  ( -4.220049686691935698, 10.18810118749999916, 71.87500000204836681 ) ) ;
#17905 = CARTESIAN_POINT ( 'NONE',  ( -31.45873412500001010, 205.8750000013656063, 168.5673454167827572 ) ) ;
#17906 = CARTESIAN_POINT ( 'NONE',  ( 11.00000000000000000, 1.347111479062088405E-15, 109.7499999999999858 ) ) ;
#17907 = CARTESIAN_POINT ( 'NONE',  ( 3.211159895383561835, 20.56249999863440436, -3.211159895383561835 ) ) ;
#17908 = UNCERTAINTY_MEASURE_WITH_UNIT (LENGTH_MEASURE( 1.000000000000000082E-05 ), #14731, 'distance_accuracy_value', 'NONE');
#17909 = EDGE_LOOP ( 'NONE', ( #39951, #60848, #30683, #53869 ) ) ;
#17910 = CARTESIAN_POINT ( 'NONE',  ( -2.828427124746152987, 194.2500000027312126, 200.8284271247462129 ) ) ;
#17911 = ADVANCED_FACE ( 'NONE', ( #22704, #4630 ), #50635, .T. ) ;
#17912 = CARTESIAN_POINT ( 'NONE',  ( -2.751064625579944321E-14, 205.7500000000000284, 146.0000000000000284 ) ) ;
#17913 = CARTESIAN_POINT ( 'NONE',  ( -32.00000000000003553, 203.3125000027311842, 168.3431457505080573 ) ) ;
#17915 = CARTESIAN_POINT ( 'NONE',  ( -2.977408999572651815, 113.9375000020483952, 7.188101187500000933 ) ) ;
#17914 = CONICAL_SURFACE ( 'NONE', #8256, 12.00000000000000000, 1.047197551196596077 ) ;
#17916 = CARTESIAN_POINT ( 'NONE',  ( -4.556349186104045934, 11.00000000000000000, 93.90625000409679046 ) ) ;
#17917 = CARTESIAN_POINT ( 'NONE',  ( 3.313708498984762496, -7.999999999999989342, 2.986552783920144449 ) ) ;
#17918 = ORIENTED_EDGE ( 'NONE', *, *, #36982, .F. ) ;
#17919 = EDGE_CURVE ( 'NONE', #65387, #42125, #32701, .T. ) ;
#17920 = CARTESIAN_POINT ( 'NONE',  ( 7.188101187500000933, 17.06249999795161543, -2.977408999572650483 ) ) ;
#17921 = ORIENTED_EDGE ( 'NONE', *, *, #7273, .F. ) ;
#17922 = CARTESIAN_POINT ( 'NONE',  ( 28.00000000000001776, 200.5000000000000000, 165.9999999999998863 ) ) ;
#17923 = CARTESIAN_POINT ( 'NONE',  ( 4.898587196589412829E-16, 13.87500000000000178, -8.000000000000000000 ) ) ;
#17924 = CARTESIAN_POINT ( 'NONE',  ( 8.660254037844389075, 50.41666666666667140, -5.000000000000000000 ) ) ;
#17925 = AXIS2_PLACEMENT_3D ( 'NONE', #6679, #23275, #13049 ) ;
#17926 = CARTESIAN_POINT ( 'NONE',  ( 7.188101187500000044, 99.78125000204838102, -8.802885111219163269E-16 ) ) ;
#17927 = CARTESIAN_POINT ( 'NONE',  ( -24.54126587499998635, 207.3750000013656063, 171.4326545832179818 ) ) ;
#17928 = CARTESIAN_POINT ( 'NONE',  ( -6.000000000000001776, 299.0000000000000000, 0.000000000000000000 ) ) ;
#17930 = CARTESIAN_POINT ( 'NONE',  ( 6.123233995736767268E-16, 198.1249999931720538, -10.00000000000000178 ) ) ;
#17929 = CARTESIAN_POINT ( 'NONE',  ( -8.000000000000000000, 89.18750000409677625, 0.000000000000000000 ) ) ;
#17931 = ORIENTED_EDGE ( 'NONE', *, *, #10002, .F. ) ;
#17932 = CARTESIAN_POINT ( 'NONE',  ( 3.042071309553173286, 240.3645833367473301, 11.35316468749999608 ) ) ;
#17933 = CARTESIAN_POINT ( 'NONE',  ( 2.977408999572650927, -7.188101187499990274, 20.33030278187175455 ) ) ;
#17934 = DIRECTION ( 'NONE',  ( -0.000000000000000000, 1.000000000000000000, -0.000000000000000000 ) ) ;
#17935 = CARTESIAN_POINT ( 'NONE',  ( 8.000000000000035527, 3.313708498984715423, 3.174052779823360648 ) ) ;
#17936 = CARTESIAN_POINT ( 'NONE',  ( 2.751064625579944321E-14, 198.8750000027312126, 194.0000000000000568 ) ) ;
#17937 = DIRECTION ( 'NONE',  ( 0.000000000000000000, 0.000000000000000000, -1.000000000000000000 ) ) ;
#17938 = CARTESIAN_POINT ( 'NONE',  ( 10.00000000000000000, 164.7916666666666572, 2.679491924311236062 ) ) ;
#17939 = CARTESIAN_POINT ( 'NONE',  ( -30.64284399271078740, 271.9999999999999432, 174.6921329945331536 ) ) ;
#17940 = CARTESIAN_POINT ( 'NONE',  ( 2.775557561562891351E-14, 210.0000000000000284, 198.0000000000000284 ) ) ;
#17941 = CARTESIAN_POINT ( 'NONE',  ( 9.000000000000014211, 15.58845726811988719, 0.000000000000000000 ) ) ;
#17942 = CARTESIAN_POINT ( 'NONE',  ( 8.311093377946834337, 135.4687499965860411, 8.311093377946839666 ) ) ;
#17943 = CARTESIAN_POINT ( 'NONE',  ( 1.102182119232618108E-15, 294.3125000034140157, 6.000000000000001776 ) ) ;
#17944 = DIRECTION ( 'NONE',  ( -0.000000000000000000, 1.000000000000000000, 0.000000000000000000 ) ) ;
#17947 = CARTESIAN_POINT ( 'NONE',  ( -30.93541659651597797, 271.9999999999999432, 171.9999999999998295 ) ) ;
#17946 = CARTESIAN_POINT ( 'NONE',  ( 11.00000000000000000, 11.00000000000000000, 25.00000000000000000 ) ) ;
#17945 = CARTESIAN_POINT ( 'NONE',  ( 23.99999999999999289, 206.7500000000000284, 169.9999999999998863 ) ) ;
#17948 = ORIENTED_EDGE ( 'NONE', *, *, #9839, .T. ) ;
#17949 = CARTESIAN_POINT ( 'NONE',  ( -9.832129032723418760, 3.177083329919349719, -5.676582343750004256 ) ) ;
#17950 = CARTESIAN_POINT ( 'NONE',  ( 11.00000000000000000, 4.556349186104045934, 68.03125000409676204 ) ) ;
#17951 = CARTESIAN_POINT ( 'NONE',  ( 3.458734124999959914, 209.3750000013656063, 143.4326545832176976 ) ) ;
#17952 = CARTESIAN_POINT ( 'NONE',  ( 31.45873412499999944, 196.0000000013656347, 168.5673454167822740 ) ) ;
#17953 = CARTESIAN_POINT ( 'NONE',  ( 2.679491924311222739, 20.83333332650536462, 10.00000000000000355 ) ) ;
#17954 = CARTESIAN_POINT ( 'NONE',  ( 7.188101187500000044, 117.4062500020483810, -8.802885111219163269E-16 ) ) ;
#17955 = CARTESIAN_POINT ( 'NONE',  ( -4.541265875000003227, 0.9999999986344068059, 1.881053915767121110 ) ) ;
#17956 = CARTESIAN_POINT ( 'NONE',  ( -3.544144923088103472, -50.27229464832340966, 40.88493206427740745 ) ) ;
#17957 = CARTESIAN_POINT ( 'NONE',  ( -5.656854249492375253, 5.656854249492375253, 23.14280277982336642 ) ) ;
#17958 = CARTESIAN_POINT ( 'NONE',  ( -6.123233995736766282E-16, 223.7500000000000000, -10.00000000000000000 ) ) ;
#17959 = CARTESIAN_POINT ( 'NONE',  ( 8.311093377946837890, 111.4062499965860269, -8.311093377946837890 ) ) ;
#17960 = VERTEX_POINT ( 'NONE', #15926 ) ;
#17961 = DIRECTION ( 'NONE',  ( 0.000000000000000000, 0.000000000000000000, -1.000000000000000000 ) ) ;
#17962 = CARTESIAN_POINT ( 'NONE',  ( -7.999999999999991118, 9.797174393178815797E-16, 30.00000000000000000 ) ) ;
#17963 = DIRECTION ( 'NONE',  ( 0.000000000000000000, 0.000000000000000000, 1.000000000000000000 ) ) ;
#17964 = CARTESIAN_POINT ( 'NONE',  ( 3.042071309553163516, 247.7604166700806445, -11.35316468749999785 ) ) ;
#17965 = CARTESIAN_POINT ( 'NONE',  ( 8.311093377946834337, 115.1562499965859985, 8.311093377946839666 ) ) ;
#17966 = ORIENTED_EDGE ( 'NONE', *, *, #23867, .T. ) ;
#17967 = CARTESIAN_POINT ( 'NONE',  ( -1.469576158976823947E-15, 25.12500000000000355, 8.000000000000000000 ) ) ;
#17968 = CARTESIAN_POINT ( 'NONE',  ( -6.238412754330611322E-16, 10.18810118749999916, 101.7812500020483810 ) ) ;
#17969 = CARTESIAN_POINT ( 'NONE',  ( -10.00000000000000178, 219.3749999931720538, -1.224646799147353454E-15 ) ) ;
#17970 = CARTESIAN_POINT ( 'NONE',  ( -3.458734124999959469, 200.7500000013656347, 199.4326545832176691 ) ) ;
#17971 = CYLINDRICAL_SURFACE ( 'NONE', #1084, 4.000000000000001776 ) ;
#17973 = CARTESIAN_POINT ( 'NONE',  ( 9.832129032723416984, 100.3645833299193697, 5.676582343750006032 ) ) ;
#17972 = CYLINDRICAL_SURFACE ( 'NONE', #6348, 3.999999999999976019 ) ;
#17974 = CARTESIAN_POINT ( 'NONE',  ( 7.999999999999991118, 3.313708498984757611, 7.861552783920145338 ) ) ;
#17975 = CARTESIAN_POINT ( 'NONE',  ( -29.43265458321766559, 197.7500000013656063, 166.5412658750003629 ) ) ;
#17976 = DIRECTION ( 'NONE',  ( 0.000000000000000000, -1.000000000000000000, 0.000000000000000000 ) ) ;
#17977 = ORIENTED_EDGE ( 'NONE', *, *, #56464, .T. ) ;
#17978 = CARTESIAN_POINT ( 'NONE',  ( -10.00000000000000178, 189.3749999931720254, -1.224646799147353454E-15 ) ) ;
#17979 = CIRCLE ( 'NONE', #24002, 3.999999999999989786 ) ;
#17980 = DIRECTION ( 'NONE',  ( -0.000000000000000000, 1.000000000000000000, -0.000000000000000000 ) ) ;
#17981 = CARTESIAN_POINT ( 'NONE',  ( 30.82842712474620228, 202.3750000000000284, 167.1715728752537586 ) ) ;
#17982 = CARTESIAN_POINT ( 'NONE',  ( 3.042071309553159519, 95.05208332991935549, 11.35316468750000141 ) ) ;
#17983 = LINE ( 'NONE', #658, #65202 ) ;
#17984 = CARTESIAN_POINT ( 'NONE',  ( 7.188101187499999156, 3.749999997951610542, 2.977408999572654924 ) ) ;
#17985 = CARTESIAN_POINT ( 'NONE',  ( 4.220049686691941027, -10.18810118749999738, 95.50000000204838102 ) ) ;
#17986 = CARTESIAN_POINT ( 'NONE',  ( -8.311093377946836114, 2.968749996586016238, -8.311093377946837890 ) ) ;
#17987 = ORIENTED_EDGE ( 'NONE', *, *, #48541, .T. ) ;
#17988 = CARTESIAN_POINT ( 'NONE',  ( 11.00000000000000000, 11.00000000000000000, -6.938893903907228378E-15 ) ) ;
#17989 = CARTESIAN_POINT ( 'NONE',  ( 5.656854249492381470, 98.75000000409677625, 5.656854249492379694 ) ) ;
#17990 = CARTESIAN_POINT ( 'NONE',  ( 9.832129032723416984, 220.3645833299193839, 5.676582343750006032 ) ) ;
#17991 = CARTESIAN_POINT ( 'NONE',  ( -10.18810118749999738, -4.220049686691941915, 77.12500000204838102 ) ) ;
#17992 = CARTESIAN_POINT ( 'NONE',  ( 5.000000000000001776, 47.70833332650536818, -8.660254037844389075 ) ) ;
#17993 = CARTESIAN_POINT ( 'NONE',  ( -8.660254037844390851, 99.79166665983871098, 4.999999999999998224 ) ) ;
#17994 = CARTESIAN_POINT ( 'NONE',  ( 6.676582343750001591, 294.9531250017069510, -8.176455196517173205E-16 ) ) ;
#17995 = ORIENTED_EDGE ( 'NONE', *, *, #67048, .T. ) ;
#17996 = CARTESIAN_POINT ( 'NONE',  ( 0.000000000000000000, 0.000000000000000000, 0.000000000000000000 ) ) ;
#17997 = CARTESIAN_POINT ( 'NONE',  ( 3.042071309553159519, 215.0520833299193555, 11.35316468750000141 ) ) ;
#17998 =( BOUNDED_SURFACE ( )  B_SPLINE_SURFACE ( 1, 2, ( 
 ( #53457, #6694, #2131, #13795, #53083, #36841, #36104, #71149, #2502, #19472, #13067, #59121, #35734, #47409, #7798, #25496, #64405, #7431, #70073, #48511, #18379, #36469, #30437, #30801, #24760, #58388, #58751, #47770, #64765, #31169, #41393, #52715, #29699, #70791, #19106, #42111, #30069, #24402, #1418, #65122, #25124, #35378, #42484, #12703, #7062, #13433, #59486, #53823, #59847, #8161, #54195, #71516, #1048, #41024, #64032, #12344, #70431, #24027, #18748, #41756, #50008, #61334, #10029, #33064, #43598, #8530, #25860, #20585, #20960, #43226, #56061, #38328, #37959, #21336, #38708, #3622, #3249, #4369, #44357, #9277, #14173, #66612, #14919, #60959, #66241, #37208, #31545, #26237, #32298, #14544, #55315, #50378, #8907, #26618, #2874, #19839, #49641, #26996, #72657, #31919, #54941, #42847, #60206, #61708, #60582, #49257, #37582, #73026, #43981, #67369, #65865, #66992, #15292, #15666, #72272, #9661, #32683, #48882, #27363, #54566, #55691, #4005, #71892, #20206, #68475, #57927, #56424, #29238, #74507, #5484, #40551, #68109, #16404, #11145, #50749, #17161, #22071, #68849, #63555, #17534, #21701, #44727, #10399, #73763, #5859, #67744, #56800, #40181, #63184, #16777, #39802, #45835, #11512, #34545, #57552, #16040, #4746, #62808, #51877, #28857, #39072, #218, #22818, #62075, #73397, #39438, #34168, #23197, #11882, #45098, #28487, #45459, #51495, #46209, #33425, #62437, #69225, #27738, #57169, #34916, #6235, #10765, #33801, #22438, #5119, #28110, #51125, #74137, #7701, #48045, #30706, #36372, #955, #25026, #35640, #59387, #71054, #19372, #30339, #53726, #6599, #46944, #53359, #36008, #42387, #59027, #52987, #29603, #47673, #1684, #23564, #52250, #18282, #70341, #24663, #65402, #52618, #7333, #24303, #70694, #2038, #63936, #69973, #19013, #58295, #64671, #13699, #13335, #35283, #36744, #1318, #59755, #8065, #12971, #41297, #584, #46576, #69597, #17910, #23935, #40928 ),
 ( #64307, #42018, #12246, #65027, #12612, #58654, #6962, #29971, #47314, #18652, #41661, #60113, #14074, #3528, #8432, #31451, #32202, #55222, #9568, #31067, #43502, #61615, #3154, #49163, #21240, #72563, #66513, #71421, #66899, #3913, #43129, #55594, #26142, #61240, #67278, #32588, #72170, #20484, #25768, #37487, #20867, #15574, #54475, #14824, #2781, #38614, #48788, #26519, #37865, #43888, #60861, #48417, #71794, #9182, #54845, #44266, #20115, #42755, #19748, #49545, #15205, #38235, #66145, #14451, #60486, #26902, #49918, #25402, #72932, #8813, #31826, #54095, #2407, #65772, #37111, #45742, #56710, #17441, #21610, #28394, #51402, #33705, #73673, #44636, #40462, #46116, #40090, #74416, #9932, #45369, #17068, #5027, #21983, #45010, #32967, #4279, #51778, #50655, #68015, #33333, #63094, #51033, #11420, #55969, #68384, #5393, #34456, #39346, #10675, #28024, #15948, #69134, #27270, #16310, #74043, #22343, #62343, #16684, #50286, #67649, #73308, #11054, #39715, #126, #4652, #27646, #62715, #61983, #22725, #56332, #68756, #23104, #28763, #38975, #10306, #34083, #57079, #57458, #5764, #46857, #58938, #30250, #58566, #6873, #35919, #53269, #7243, #1595, #34826, #69507, #29883, #41933, #24580, #57832, #47585, #64587, #6138, #63463, #29516, #52897, #12883, #7611, #40833, #70252, #35553, #41572, #64941, #495, #58207, #70608, #17817, #1230, #13252, #18928, #46486, #18561, #11789, #36285, #29145, #47219, #59302, #30617, #52162, #24208, #63839, #69879, #12156, #12521, #53640, #35190, #1950, #23849, #18191, #24940, #6510, #47958, #70972, #19286, #23475, #52526, #41207, #863, #64216, #19655, #66812, #71334, #25310, #14737, #42668, #65679, #43411, #66425, #20777, #42297, #54755, #37777, #61147, #13978, #49069, #14362, #20397, #43797, #54003, #37021, #60772, #48327, #3065, #9098, #60395, #37394, #32493, #66054, #3434, #26814, #26048, #60023, #72469, #38146, #15114, #26424, #8341 ) ),
 .UNSPECIFIED., .F., .F., .F. ) 
 B_SPLINE_SURFACE_WITH_KNOTS ( ( 2, 2 ),
 ( 3, 2, 2, 2, 2, 2, 2, 2, 2, 2, 2, 2, 2, 2, 2, 2, 2, 2, 2, 2, 2, 2, 2, 2, 2, 2, 2, 2, 2, 2, 2, 2, 2, 2, 2, 2, 2, 2, 2, 2, 2, 2, 2, 2, 2, 2, 2, 2, 2, 2, 2, 2, 2, 2, 2, 2, 2, 2, 2, 2, 2, 2, 2, 2, 2, 2, 2, 2, 2, 2, 2, 2, 2, 2, 2, 2, 2, 2, 2, 2, 2, 2, 2, 2, 2, 2, 2, 2, 2, 2, 2, 2, 2, 2, 2, 2, 2, 2, 2, 2, 2, 2, 2, 2, 2, 2, 2, 2, 2, 2, 2, 2, 2, 2, 2, 2, 2, 2, 2, 2, 3 ),
 ( 0.000000000000000000, 1.000000000000000000 ),
 ( 0.000000000000000000, 0.008333333333333333218, 0.01666666666666666644, 0.02500000000000000139, 0.03333333333333333287, 0.04166666666666666435, 0.05000000000000000278, 0.05833333333333333426, 0.06666666666666666574, 0.07499999999999999722, 0.08333333333333332871, 0.09166666666666666019, 0.1000000000000000056, 0.1083333333333333370, 0.1166666666666666685, 0.1250000000000000000, 0.1333333333333333315, 0.1416666666666666630, 0.1499999999999999944, 0.1583333333333333259, 0.1666666666666666574, 0.1749999999999999889, 0.1833333333333333204, 0.1916666666666666796, 0.2000000000000000111, 0.2083333333333333426, 0.2166666666666666741, 0.2250000000000000056, 0.2333333333333333370, 0.2416666666666666685, 0.2500000000000000000, 0.2583333333333333592, 0.2666666666666666630, 0.2750000000000000222, 0.2833333333333333259, 0.2916666666666666852, 0.2999999999999999889, 0.3083333333333333481, 0.3166666666666666519, 0.3250000000000000111, 0.3333333333333333148, 0.3416666666666666741, 0.3499999999999999778, 0.3583333333333333370, 0.3666666666666666408, 0.3750000000000000000, 0.3833333333333333592, 0.3916666666666666630, 0.4000000000000000222, 0.4083333333333333259, 0.4166666666666666852, 0.4249999999999999889, 0.4333333333333333481, 0.4416666666666666519, 0.4500000000000000111, 0.4583333333333333148, 0.4666666666666666741, 0.4749999999999999778, 0.4833333333333333370, 0.4916666666666666408, 0.5000000000000000000, 0.5083333333333333037, 0.5166666666666667185, 0.5250000000000000222, 0.5333333333333333259, 0.5416666666666666297, 0.5500000000000000444, 0.5583333333333333481, 0.5666666666666666519, 0.5749999999999999556, 0.5833333333333333703, 0.5916666666666666741, 0.5999999999999999778, 0.6083333333333332815, 0.6166666666666666963, 0.6250000000000000000, 0.6333333333333333037, 0.6416666666666667185, 0.6500000000000000222, 0.6583333333333333259, 0.6666666666666666297, 0.6750000000000000444, 0.6833333333333333481, 0.6916666666666666519, 0.6999999999999999556, 0.7083333333333333703, 0.7166666666666666741, 0.7249999999999999778, 0.7333333333333332815, 0.7416666666666666963, 0.7500000000000000000, 0.7583333333333333037, 0.7666666666666667185, 0.7750000000000000222, 0.7833333333333333259, 0.7916666666666666297, 0.8000000000000000444, 0.8083333333333333481, 0.8166666666666666519, 0.8249999999999999556, 0.8333333333333333703, 0.8416666666666666741, 0.8499999999999999778, 0.8583333333333332815, 0.8666666666666666963, 0.8750000000000000000, 0.8833333333333333037, 0.8916666666666667185, 0.9000000000000000222, 0.9083333333333333259, 0.9166666666666666297, 0.9250000000000000444, 0.9333333333333333481, 0.9416666666666666519, 0.9499999999999999556, 0.9583333333333333703, 0.9666666666666666741, 0.9749999999999999778, 0.9833333333333332815, 0.9916666666666666963, 1.000000000000000000 ),
 .UNSPECIFIED. ) 
 GEOMETRIC_REPRESENTATION_ITEM ( )  RATIONAL_B_SPLINE_SURFACE ( (
 ( 1.000000000000000000, 0.9238795325112867385, 1.000000000000000000, 0.9238795325112867385, 1.000000000000000000, 0.9238795325112867385, 1.000000000000000000, 0.9238795325112867385, 1.000000000000000000, 0.9238795325112867385, 1.000000000000000000, 0.9238795325112867385, 1.000000000000000000, 0.9238795325112867385, 1.000000000000000000, 0.9238795325112867385, 1.000000000000000000, 0.9238795325112867385, 1.000000000000000000, 0.9238795325112867385, 1.000000000000000000, 0.9238795325112867385, 1.000000000000000000, 0.9238795325112867385, 1.000000000000000000, 0.9238795325112867385, 1.000000000000000000, 0.9238795325112867385, 1.000000000000000000, 0.9238795325112867385, 1.000000000000000000, 0.9238795325112867385, 1.000000000000000000, 0.9238795325112867385, 1.000000000000000000, 0.9238795325112867385, 1.000000000000000000, 0.9238795325112867385, 1.000000000000000000, 0.9238795325112867385, 1.000000000000000000, 0.9238795325112867385, 1.000000000000000000, 0.9238795325112867385, 1.000000000000000000, 0.9238795325112867385, 1.000000000000000000, 0.9238795325112867385, 1.000000000000000000, 0.9238795325112867385, 1.000000000000000000, 0.9238795325112867385, 1.000000000000000000, 0.9238795325112867385, 1.000000000000000000, 0.9238795325112867385, 1.000000000000000000, 0.9238795325112867385, 1.000000000000000000, 0.9238795325112867385, 1.000000000000000000, 0.9238795325112867385, 1.000000000000000000, 0.9238795325112867385, 1.000000000000000000, 0.9238795325112867385, 1.000000000000000000, 0.9238795325112867385, 1.000000000000000000, 0.9238795325112867385, 1.000000000000000000, 0.9238795325112867385, 1.000000000000000000, 0.9238795325112867385, 1.000000000000000000, 0.9238795325112867385, 1.000000000000000000, 0.9238795325112867385, 1.000000000000000000, 0.9238795325112867385, 1.000000000000000000, 0.9238795325112867385, 1.000000000000000000, 0.9238795325112867385, 1.000000000000000000, 0.9238795325112867385, 1.000000000000000000, 0.9238795325112867385, 1.000000000000000000, 0.9238795325112867385, 1.000000000000000000, 0.9238795325112867385, 1.000000000000000000, 0.9238795325112867385, 1.000000000000000000, 0.9238795325112867385, 1.000000000000000000, 0.9238795325112867385, 1.000000000000000000, 0.9238795325112867385, 1.000000000000000000, 0.9238795325112867385, 1.000000000000000000, 0.9238795325112867385, 1.000000000000000000, 0.9238795325112867385, 1.000000000000000000, 0.9238795325112867385, 1.000000000000000000, 0.9238795325112867385, 1.000000000000000000, 0.9238795325112867385, 1.000000000000000000, 0.9238795325112867385, 1.000000000000000000, 0.9238795325112867385, 1.000000000000000000, 0.9238795325112867385, 1.000000000000000000, 0.9238795325112867385, 1.000000000000000000, 0.9238795325112867385, 1.000000000000000000, 0.9238795325112867385, 1.000000000000000000, 0.9238795325112867385, 1.000000000000000000, 0.9238795325112867385, 1.000000000000000000, 0.9238795325112867385, 1.000000000000000000, 0.9238795325112867385, 1.000000000000000000, 0.9238795325112867385, 1.000000000000000000, 0.9238795325112867385, 1.000000000000000000, 0.9238795325112867385, 1.000000000000000000, 0.9238795325112867385, 1.000000000000000000, 0.9238795325112867385, 1.000000000000000000, 0.9238795325112867385, 1.000000000000000000, 0.9238795325112867385, 1.000000000000000000, 0.9238795325112867385, 1.000000000000000000, 0.9238795325112867385, 1.000000000000000000, 0.9238795325112867385, 1.000000000000000000, 0.9238795325112867385, 1.000000000000000000, 0.9238795325112867385, 1.000000000000000000, 0.9238795325112867385, 1.000000000000000000, 0.9238795325112867385, 1.000000000000000000, 0.9238795325112867385, 1.000000000000000000, 0.9238795325112867385, 1.000000000000000000, 0.9238795325112867385, 1.000000000000000000, 0.9238795325112867385, 1.000000000000000000, 0.9238795325112867385, 1.000000000000000000, 0.9238795325112867385, 1.000000000000000000, 0.9238795325112867385, 1.000000000000000000, 0.9238795325112867385, 1.000000000000000000, 0.9238795325112867385, 1.000000000000000000, 0.9238795325112867385, 1.000000000000000000, 0.9238795325112867385, 1.000000000000000000, 0.9238795325112867385, 1.000000000000000000, 0.9238795325112867385, 1.000000000000000000, 0.9238795325112867385, 1.000000000000000000, 0.9238795325112867385, 1.000000000000000000, 0.9238795325112867385, 1.000000000000000000, 0.9238795325112867385, 1.000000000000000000, 0.9238795325112867385, 1.000000000000000000, 0.9238795325112867385, 1.000000000000000000, 0.9238795325112867385, 1.000000000000000000, 0.9238795325112867385, 1.000000000000000000, 0.9238795325112867385, 1.000000000000000000, 0.9238795325112867385, 1.000000000000000000, 0.9238795325112867385, 1.000000000000000000, 0.9238795325112867385, 1.000000000000000000, 0.9238795325112867385, 1.000000000000000000, 0.9238795325112867385, 1.000000000000000000, 0.9238795325112867385, 1.000000000000000000, 0.9238795325112867385, 1.000000000000000000, 0.9238795325112867385, 1.000000000000000000, 0.9238795325112867385, 1.000000000000000000, 0.9238795325112867385, 1.000000000000000000, 0.9238795325112867385, 1.000000000000000000, 0.9238795325112867385, 1.000000000000000000, 0.9238795325112867385, 1.000000000000000000, 0.9238795325112867385, 1.000000000000000000, 0.9238795325112867385, 1.000000000000000000, 0.9238795325112867385, 1.000000000000000000, 0.9238795325112867385, 1.000000000000000000, 0.9238795325112867385, 1.000000000000000000),
 ( 1.000000000000000000, 0.9238795325112867385, 1.000000000000000000, 0.9238795325112867385, 1.000000000000000000, 0.9238795325112867385, 1.000000000000000000, 0.9238795325112867385, 1.000000000000000000, 0.9238795325112867385, 1.000000000000000000, 0.9238795325112867385, 1.000000000000000000, 0.9238795325112867385, 1.000000000000000000, 0.9238795325112867385, 1.000000000000000000, 0.9238795325112867385, 1.000000000000000000, 0.9238795325112867385, 1.000000000000000000, 0.9238795325112867385, 1.000000000000000000, 0.9238795325112867385, 1.000000000000000000, 0.9238795325112867385, 1.000000000000000000, 0.9238795325112867385, 1.000000000000000000, 0.9238795325112867385, 1.000000000000000000, 0.9238795325112867385, 1.000000000000000000, 0.9238795325112867385, 1.000000000000000000, 0.9238795325112867385, 1.000000000000000000, 0.9238795325112867385, 1.000000000000000000, 0.9238795325112867385, 1.000000000000000000, 0.9238795325112867385, 1.000000000000000000, 0.9238795325112867385, 1.000000000000000000, 0.9238795325112867385, 1.000000000000000000, 0.9238795325112867385, 1.000000000000000000, 0.9238795325112867385, 1.000000000000000000, 0.9238795325112867385, 1.000000000000000000, 0.9238795325112867385, 1.000000000000000000, 0.9238795325112867385, 1.000000000000000000, 0.9238795325112867385, 1.000000000000000000, 0.9238795325112867385, 1.000000000000000000, 0.9238795325112867385, 1.000000000000000000, 0.9238795325112867385, 1.000000000000000000, 0.9238795325112867385, 1.000000000000000000, 0.9238795325112867385, 1.000000000000000000, 0.9238795325112867385, 1.000000000000000000, 0.9238795325112867385, 1.000000000000000000, 0.9238795325112867385, 1.000000000000000000, 0.9238795325112867385, 1.000000000000000000, 0.9238795325112867385, 1.000000000000000000, 0.9238795325112867385, 1.000000000000000000, 0.9238795325112867385, 1.000000000000000000, 0.9238795325112867385, 1.000000000000000000, 0.9238795325112867385, 1.000000000000000000, 0.9238795325112867385, 1.000000000000000000, 0.9238795325112867385, 1.000000000000000000, 0.9238795325112867385, 1.000000000000000000, 0.9238795325112867385, 1.000000000000000000, 0.9238795325112867385, 1.000000000000000000, 0.9238795325112867385, 1.000000000000000000, 0.9238795325112867385, 1.000000000000000000, 0.9238795325112867385, 1.000000000000000000, 0.9238795325112867385, 1.000000000000000000, 0.9238795325112867385, 1.000000000000000000, 0.9238795325112867385, 1.000000000000000000, 0.9238795325112867385, 1.000000000000000000, 0.9238795325112867385, 1.000000000000000000, 0.9238795325112867385, 1.000000000000000000, 0.9238795325112867385, 1.000000000000000000, 0.9238795325112867385, 1.000000000000000000, 0.9238795325112867385, 1.000000000000000000, 0.9238795325112867385, 1.000000000000000000, 0.9238795325112867385, 1.000000000000000000, 0.9238795325112867385, 1.000000000000000000, 0.9238795325112867385, 1.000000000000000000, 0.9238795325112867385, 1.000000000000000000, 0.9238795325112867385, 1.000000000000000000, 0.9238795325112867385, 1.000000000000000000, 0.9238795325112867385, 1.000000000000000000, 0.9238795325112867385, 1.000000000000000000, 0.9238795325112867385, 1.000000000000000000, 0.9238795325112867385, 1.000000000000000000, 0.9238795325112867385, 1.000000000000000000, 0.9238795325112867385, 1.000000000000000000, 0.9238795325112867385, 1.000000000000000000, 0.9238795325112867385, 1.000000000000000000, 0.9238795325112867385, 1.000000000000000000, 0.9238795325112867385, 1.000000000000000000, 0.9238795325112867385, 1.000000000000000000, 0.9238795325112867385, 1.000000000000000000, 0.9238795325112867385, 1.000000000000000000, 0.9238795325112867385, 1.000000000000000000, 0.9238795325112867385, 1.000000000000000000, 0.9238795325112867385, 1.000000000000000000, 0.9238795325112867385, 1.000000000000000000, 0.9238795325112867385, 1.000000000000000000, 0.9238795325112867385, 1.000000000000000000, 0.9238795325112867385, 1.000000000000000000, 0.9238795325112867385, 1.000000000000000000, 0.9238795325112867385, 1.000000000000000000, 0.9238795325112867385, 1.000000000000000000, 0.9238795325112867385, 1.000000000000000000, 0.9238795325112867385, 1.000000000000000000, 0.9238795325112867385, 1.000000000000000000, 0.9238795325112867385, 1.000000000000000000, 0.9238795325112867385, 1.000000000000000000, 0.9238795325112867385, 1.000000000000000000, 0.9238795325112867385, 1.000000000000000000, 0.9238795325112867385, 1.000000000000000000, 0.9238795325112867385, 1.000000000000000000, 0.9238795325112867385, 1.000000000000000000, 0.9238795325112867385, 1.000000000000000000, 0.9238795325112867385, 1.000000000000000000, 0.9238795325112867385, 1.000000000000000000, 0.9238795325112867385, 1.000000000000000000, 0.9238795325112867385, 1.000000000000000000, 0.9238795325112867385, 1.000000000000000000, 0.9238795325112867385, 1.000000000000000000, 0.9238795325112867385, 1.000000000000000000, 0.9238795325112867385, 1.000000000000000000, 0.9238795325112867385, 1.000000000000000000, 0.9238795325112867385, 1.000000000000000000, 0.9238795325112867385, 1.000000000000000000, 0.9238795325112867385, 1.000000000000000000, 0.9238795325112867385, 1.000000000000000000, 0.9238795325112867385, 1.000000000000000000, 0.9238795325112867385, 1.000000000000000000, 0.9238795325112867385, 1.000000000000000000, 0.9238795325112867385, 1.000000000000000000, 0.9238795325112867385, 1.000000000000000000, 0.9238795325112867385, 1.000000000000000000) ) ) 
 REPRESENTATION_ITEM ( '' )  SURFACE ( )  );
#17999 = ADVANCED_FACE ( 'NONE', ( #16663 ), #21220, .T. ) ;
#18000 = ADVANCED_FACE ( 'NONE', ( #68735 ), #43497, .T. ) ;
#18001 = CARTESIAN_POINT ( 'NONE',  ( -10.18810118749999738, -4.220049686691941915, 90.25000000204838102 ) ) ;
#18002 = CARTESIAN_POINT ( 'NONE',  ( -24.54126587499999346, 204.1875000013656063, 170.0000000000003411 ) ) ;
#18003 = CARTESIAN_POINT ( 'NONE',  ( -8.000000000000000000, 15.65625000000000355, -3.313708498984762496 ) ) ;
#18004 = VERTEX_POINT ( 'NONE', #74022 ) ;
#18005 = EDGE_CURVE ( 'NONE', #74545, #69418, #69011, .T. ) ;
#18006 = EDGE_CURVE ( 'NONE', #6793, #471, #56020, .T. ) ;
#18007 = CARTESIAN_POINT ( 'NONE',  ( 2.977408999572650039, 123.6875000020484094, -7.188101187500001821 ) ) ;
#18008 = DIRECTION ( 'NONE',  ( 0.8660254037844312691, -0.5000000000000128786, -0.000000000000000000 ) ) ;
#18009 = CARTESIAN_POINT ( 'NONE',  ( -10.00000000000000355, 22.70833333333333215, 2.679491924311223183 ) ) ;
#18010 =( BOUNDED_CURVE ( )  B_SPLINE_CURVE ( 2, ( #56474, #50796, #45504, #68522, #58343, #70388, #23982, #6647, #18329 ),
 .UNSPECIFIED., .F., .F. ) 
 B_SPLINE_CURVE_WITH_KNOTS ( ( 3, 2, 2, 2, 3 ),
 ( 0.05681818181818182323, 0.06250000000000000000, 0.06818181818181817677, 0.07386363636363636742, 0.07954545454545454419 ),
 .UNSPECIFIED. ) 
 CURVE ( )  GEOMETRIC_REPRESENTATION_ITEM ( )  RATIONAL_B_SPLINE_CURVE ( ( 0.9999999999999998890, 0.9238795325112868495, 1.000000000000000000, 0.9238795325112867385, 1.000000000000000000, 0.9238795325112867385, 1.000000000000000000, 0.9238795325112867385, 1.000000000000000000 ) ) 
 REPRESENTATION_ITEM ( '' )  );
#18011 = LINE ( 'NONE', #45933, #50009 ) ;
#18012 = CARTESIAN_POINT ( 'NONE',  ( -10.18810118749999916, 4.220049686691934809, 73.93750000204838102 ) ) ;
#18013 = ORIENTED_EDGE ( 'NONE', *, *, #40922, .T. ) ;
#18014 = CARTESIAN_POINT ( 'NONE',  ( 1.656854249492381914, 2.562499997268814056, 4.000000000000000888 ) ) ;
#18015 = CARTESIAN_POINT ( 'NONE',  ( -2.250000000000000888, 2.250000000000000000, 28.00000000000000000 ) ) ;
#18016 = CARTESIAN_POINT ( 'NONE',  ( -2.977408999572650927, 121.2500000020483952, -7.188101187500001821 ) ) ;
#18017 = EDGE_CURVE ( 'NONE', #69504, #36412, #2021, .T. ) ;
#18018 = DIRECTION ( 'NONE',  ( -0.000000000000000000, 1.000000000000000000, -0.000000000000000000 ) ) ;
#18019 = CARTESIAN_POINT ( 'NONE',  ( 1.226468279477575784E-15, 296.7031250017070079, 6.676582343750001591 ) ) ;
#18021 = CYLINDRICAL_SURFACE ( 'NONE', #73510, 10.00000000000000000 ) ;
#18020 = CARTESIAN_POINT ( 'NONE',  ( -11.35316468749999608, 234.1145833367473017, 3.042071309553173730 ) ) ;
#18022 = ORIENTED_EDGE ( 'NONE', *, *, #26447, .F. ) ;
#18024 = AXIS2_PLACEMENT_3D ( 'NONE', #31100, #47707, #36042 ) ;
#18023 = CARTESIAN_POINT ( 'NONE',  ( 9.832129032723420536, 241.3020833367473301, 5.676582343749996262 ) ) ;
#18026 = CARTESIAN_POINT ( 'NONE',  ( -5.082755093536317936, -5.082755093536320601, 7.674052781871751883 ) ) ;
#18025 =( BOUNDED_CURVE ( )  B_SPLINE_CURVE ( 2, ( #4281, #27273, #61985, #50289, #73310, #10308, #56335, #4655, #70796 ),
 .UNSPECIFIED., .F., .F. ) 
 B_SPLINE_CURVE_WITH_KNOTS ( ( 3, 2, 2, 2, 3 ),
 ( 0.5340909090909090606, 0.5397727272727272929, 0.5454545454545454142, 0.5511363636363637575, 0.5568181818181818787 ),
 .UNSPECIFIED. ) 
 CURVE ( )  GEOMETRIC_REPRESENTATION_ITEM ( )  RATIONAL_B_SPLINE_CURVE ( ( 1.000000000000000000, 0.9238795325112867385, 1.000000000000000000, 0.9238795325112867385, 1.000000000000000000, 0.9238795325112867385, 1.000000000000000000, 0.9238795325112852952, 1.000000000000001554 ) ) 
 REPRESENTATION_ITEM ( '' )  );
#18027 = VERTEX_POINT ( 'NONE', #34064 ) ;
#18028 = CARTESIAN_POINT ( 'NONE',  ( 4.220049686691941027, -10.18810118749999738, 69.62500000204836681 ) ) ;
#18029 = CARTESIAN_POINT ( 'NONE',  ( -11.35316468750000141, 98.59374999658601268, -1.390361679473963753E-15 ) ) ;
#18030 = FACE_OUTER_BOUND ( 'NONE', #4362, .T. ) ;
#18031 = CARTESIAN_POINT ( 'NONE',  ( -10.99999999999999822, -4.556349186104052151, 80.59374999999998579 ) ) ;
#18034 = CARTESIAN_POINT ( 'NONE',  ( 6.123233995736767268E-16, 56.25000000000000000, -10.00000000000000178 ) ) ;
#18033 = CARTESIAN_POINT ( 'NONE',  ( 28.00000000000001776, 204.4375000013656063, 173.4587341249998929 ) ) ;
#18032 = CARTESIAN_POINT ( 'NONE',  ( 26.56734541678232375, 205.6250000013656063, 173.4587341249998929 ) ) ;
#18035 = ORIENTED_EDGE ( 'NONE', *, *, #11751, .F. ) ;
#18036 = AXIS2_PLACEMENT_3D ( 'NONE', #61397, #27804, #9723 ) ;
#18037 = LINE ( 'NONE', #60522, #44093 ) ;
#18038 = MANIFOLD_SOLID_BREP ( 'Cut-Extrude1', #33445 ) ;
#18039 = DIRECTION ( 'NONE',  ( -0.000000000000000000, -0.000000000000000000, 1.000000000000000000 ) ) ;
#18040 = CARTESIAN_POINT ( 'NONE',  ( -9.832129032723418760, 217.8645833299193839, -5.676582343750004256 ) ) ;
#18041 = CARTESIAN_POINT ( 'NONE',  ( -3.458734125000015425, 206.9375000013656063, 142.0000000000000568 ) ) ;
#18042 = CARTESIAN_POINT ( 'NONE',  ( 31.45873412499998523, 206.8750000013656347, 171.4326545832175839 ) ) ;
#18043 = CARTESIAN_POINT ( 'NONE',  ( 4.401442555609581635E-16, 22.21874999795161543, -7.188101187500000044 ) ) ;
#18044 = CARTESIAN_POINT ( 'NONE',  ( 6.951808397369818766E-16, 187.3437499965860127, -11.35316468750000141 ) ) ;
#18045 = CARTESIAN_POINT ( 'NONE',  ( -7.188101187500000933, 100.4375000020483810, -2.977408999572650483 ) ) ;
#18047 = CARTESIAN_POINT ( 'NONE',  ( -2.679491924311234730, 108.5416666666666714, 9.999999999999996447 ) ) ;
#18046 = CARTESIAN_POINT ( 'NONE',  ( -5.000000000000000000, 60.90295814858271939, -23.31388853594749833 ) ) ;
#18048 = CARTESIAN_POINT ( 'NONE',  ( -8.342170076843785083E-16, 9.062499998634407916, 4.541265875000002339 ) ) ;
#18049 = CARTESIAN_POINT ( 'NONE',  ( 29.43265458321766914, 204.1250000013656063, 166.5412658749999650 ) ) ;
#18050 = CARTESIAN_POINT ( 'NONE',  ( -7.188101187499990274, -2.977408999572651371, 12.45530278187175277 ) ) ;
#18051 = CARTESIAN_POINT ( 'NONE',  ( -11.35316468750000141, 63.28124999658601979, -1.390361679473963753E-15 ) ) ;
#18052 = DIRECTION ( 'NONE',  ( -0.000000000000000000, -0.000000000000000000, 1.000000000000000000 ) ) ;
#18053 = CARTESIAN_POINT ( 'NONE',  ( 3.313708498984762496, -7.999999999999989342, 2.855302784329822430 ) ) ;
#18054 = VERTEX_POINT ( 'NONE', #70235 ) ;
#18055 = CARTESIAN_POINT ( 'NONE',  ( -3.313708498984759387, -7.999999999999989342, 7.299052783920144449 ) ) ;
#18056 = CARTESIAN_POINT ( 'NONE',  ( -4.000000000000015987, 203.6250000027312126, 142.0000000000000568 ) ) ;
#18057 = CARTESIAN_POINT ( 'NONE',  ( 3.042071309553167069, 76.82291666325269830, -11.35316468749999785 ) ) ;
#18058 = CARTESIAN_POINT ( 'NONE',  ( -6.238412754330611322E-16, 10.18810118749999916, 116.7812500020483810 ) ) ;
#18059 = CARTESIAN_POINT ( 'NONE',  ( -11.00000000000000000, 0.000000000000000000, 118.0000000000000000 ) ) ;
#18060 = CARTESIAN_POINT ( 'NONE',  ( 2.751064625579944321E-14, 196.7500000000000000, 194.0000000000000568 ) ) ;
#18062 = CARTESIAN_POINT ( 'NONE',  ( 9.832129032723416984, 55.36458332991934839, 5.676582343750006032 ) ) ;
#18061 = CARTESIAN_POINT ( 'NONE',  ( 3.594044162775203777, 89.15552387383502264, -6.225081946264263699 ) ) ;
#18063 = CARTESIAN_POINT ( 'NONE',  ( 5.656854249492374365, 5.656854249492375253, 24.45530278392014978 ) ) ;
#18064 = CARTESIAN_POINT ( 'NONE',  ( -2.679491924311217410, 13.33333332650536640, -10.00000000000000711 ) ) ;
#18065 = CARTESIAN_POINT ( 'NONE',  ( 8.660254037844389075, 152.2916666598387110, -5.000000000000000000 ) ) ;
#18066 = CARTESIAN_POINT ( 'NONE',  ( 2.977408999572650039, 97.06250000204838102, -7.188101187500001821 ) ) ;
#18067 = CARTESIAN_POINT ( 'NONE',  ( 27.99999999999999645, 210.0000000000000284, 165.9999999999999147 ) ) ;
#18068 = CARTESIAN_POINT ( 'NONE',  ( 8.311093377946834337, 45.46874999658601979, 8.311093377946839666 ) ) ;
#18069 = CARTESIAN_POINT ( 'NONE',  ( 10.18810118750000093, -4.220049686691933033, 115.1875000020483668 ) ) ;
#18070 = CARTESIAN_POINT ( 'NONE',  ( -11.35316468750000141, 183.4895833299193839, 3.042071309553159963 ) ) ;
#18071 = ORIENTED_EDGE ( 'NONE', *, *, #44909, .T. ) ;
#18072 = CARTESIAN_POINT ( 'NONE',  ( 2.828427124746191623, 4.125000000000000000, -2.828427124746191623 ) ) ;
#18073 = DIRECTION ( 'NONE',  ( 0.000000000000000000, 0.000000000000000000, -1.000000000000000000 ) ) ;
#18074 = CARTESIAN_POINT ( 'NONE',  ( -10.99999999999992184, -31.99999999999978684, 198.9827534923788619 ) ) ;
#18076 = CARTESIAN_POINT ( 'NONE',  ( 9.832129032723416984, 185.3645833299193555, 5.676582343750006032 ) ) ;
#18075 = CARTESIAN_POINT ( 'NONE',  ( 27.99999999999999645, 210.0000000000000284, 165.9999999999999147 ) ) ;
#18077 = ADVANCED_FACE ( 'NONE', ( #17419 ), #10654, .T. ) ;
#18078 = DIRECTION ( 'NONE',  ( 1.000000000000000000, -0.000000000000000000, -0.000000000000000000 ) ) ;
#18079 = CARTESIAN_POINT ( 'NONE',  ( -8.660254037844387298, 257.7083333401612890, -4.999999999999999112 ) ) ;
#18080 = DIRECTION ( 'NONE',  ( -0.000000000000000000, -1.000000000000000000, -4.283267841918042741E-17 ) ) ;
#18081 = ORIENTED_EDGE ( 'NONE', *, *, #8892, .T. ) ;
#18082 = CARTESIAN_POINT ( 'NONE',  ( -9.832129032723418760, 163.1770833299193839, -5.676582343750004256 ) ) ;
#18083 = AXIS2_PLACEMENT_3D ( 'NONE', #34269, #64410, #5587 ) ;
#18084 = CARTESIAN_POINT ( 'NONE',  ( 11.00000000000000000, 1.347111479062088405E-15, 105.2500000000000000 ) ) ;
#18085 = CARTESIAN_POINT ( 'NONE',  ( -5.676582343749998039, 127.7604166632526841, -9.832129032723420536 ) ) ;
#18086 = CARTESIAN_POINT ( 'NONE',  ( 25.17157287525381903, 204.0000000027312126, 172.8284271247460993 ) ) ;
#18087 = ORIENTED_EDGE ( 'NONE', *, *, #15969, .T. ) ;
#18088 = VECTOR ( 'NONE', #65995, 1000.000000000000000 ) ;
#18089 = ADVANCED_FACE ( 'NONE', ( #69860, #18543 ), #1210, .F. ) ;
#18090 = EDGE_CURVE ( 'NONE', #63637, #66203, #20743, .T. ) ;
#18091 = CARTESIAN_POINT ( 'NONE',  ( 8.000000000000000000, 106.4375000040967763, -9.797174393178825657E-16 ) ) ;
#18092 = EDGE_CURVE ( 'NONE', #62884, #61795, #63713, .T. ) ;
#18093 =( BOUNDED_CURVE ( )  B_SPLINE_CURVE ( 2, ( #1973, #58960, #24232, #12907, #41597, #6161, #47980, #35575, #516, #69905, #58232, #6531, #63864 ),
 .UNSPECIFIED., .F., .F. ) 
 B_SPLINE_CURVE_WITH_KNOTS ( ( 3, 2, 2, 2, 2, 2, 3 ),
 ( 0.4402173913043478382, 0.4420289855072463969, 0.4438405797101449002, 0.4456521739130434590, 0.4474637681159420177, 0.4492753623188405765, 0.4510869565217391353 ),
 .UNSPECIFIED. ) 
 CURVE ( )  GEOMETRIC_REPRESENTATION_ITEM ( )  RATIONAL_B_SPLINE_CURVE ( ( 1.000000000000000000, 0.9659258262890683122, 1.000000000000000000, 0.9659258262890683122, 1.000000000000000000, 0.9659258262890683122, 1.000000000000000000, 0.9659258262890683122, 1.000000000000000000, 0.9659258262890683122, 1.000000000000000000, 0.9659258262890683122, 1.000000000000000000 ) ) 
 REPRESENTATION_ITEM ( '' )  );
#18094 = CARTESIAN_POINT ( 'NONE',  ( -1.656854249492381248, 11.31249999999999822, -4.000000000000001776 ) ) ;
#18095 = CARTESIAN_POINT ( 'NONE',  ( -10.00000000000000000, 220.0000000000000000, 0.000000000000000000 ) ) ;
#18096 = CARTESIAN_POINT ( 'NONE',  ( -4.541265875000002339, 10.74999999863440969, -1.881053915767121998 ) ) ;
#18097 = CARTESIAN_POINT ( 'NONE',  ( -7.999999999999991118, 0.000000000000000000, 22.01780278392014623 ) ) ;
#18098 = CARTESIAN_POINT ( 'NONE',  ( 2.828427124746153876, 195.8750000000000284, 144.8284271247462129 ) ) ;
#18099 = ORIENTED_EDGE ( 'NONE', *, *, #71135, .F. ) ;
#18100 = CYLINDRICAL_SURFACE ( 'NONE', #29450, 7.999999999999991118 ) ;
#18101 = CARTESIAN_POINT ( 'NONE',  ( 7.188101187500000044, 106.9062500020483810, -8.802885111219163269E-16 ) ) ;
#18102 = EDGE_CURVE ( 'NONE', #15485, #47128, #23097, .T. ) ;
#18104 = CARTESIAN_POINT ( 'NONE',  ( 1.656854249492381248, 6.937499997268813168, -4.000000000000001776 ) ) ;
#18103 = CARTESIAN_POINT ( 'NONE',  ( 2.849036369511732440E-14, 196.2500000000000000, 202.0000000000000000 ) ) ;
#18105 =( NAMED_UNIT ( * ) SI_UNIT ( $, .STERADIAN. ) SOLID_ANGLE_UNIT ( ) );
#18106 = VERTEX_POINT ( 'NONE', #41188 ) ;
#18107 = CARTESIAN_POINT ( 'NONE',  ( -8.660254037844545394, 157.0833333333334565, -5.000000000000096811 ) ) ;
#18108 = CARTESIAN_POINT ( 'NONE',  ( -2.977408999572647819, 7.188101187499991163, 26.70530278187175455 ) ) ;
#18109 = EDGE_LOOP ( 'NONE', ( #58007, #63459, #73569, #3085 ) ) ;
#18110 =( BOUNDED_CURVE ( )  B_SPLINE_CURVE ( 2, ( #27252, #50267, #10289, #55952, #43867, #4262, #43484, #14807, #37848, #73290, #21592, #73655, #66882 ),
 .UNSPECIFIED., .F., .F. ) 
 B_SPLINE_CURVE_WITH_KNOTS ( ( 3, 2, 2, 2, 2, 2, 3 ),
 ( 0.6944444444444444198, 0.7037037037037037202, 0.7129629629629629095, 0.7222222222222222099, 0.7314814814814815103, 0.7407407407407406996, 0.7500000000000000000 ),
 .UNSPECIFIED. ) 
 CURVE ( )  GEOMETRIC_REPRESENTATION_ITEM ( )  RATIONAL_B_SPLINE_CURVE ( ( 1.000000000000000000, 0.9659258262890683122, 1.000000000000000000, 0.9659258262890683122, 1.000000000000000000, 0.9659258262890683122, 1.000000000000000000, 0.9659258262890683122, 1.000000000000000000, 0.9659258262890683122, 1.000000000000000000, 0.9659258262890683122, 1.000000000000000000 ) ) 
 REPRESENTATION_ITEM ( '' )  );
#18111 = ORIENTED_EDGE ( 'NONE', *, *, #43195, .F. ) ;
#18112 = CARTESIAN_POINT ( 'NONE',  ( 7.204075437095968759, -7.204075437095966983, 87.71875000204836681 ) ) ;
#18113 = CARTESIAN_POINT ( 'NONE',  ( -26.56734541678237704, 195.6250000013656063, 166.5412658750003629 ) ) ;
#18114 = CARTESIAN_POINT ( 'NONE',  ( 7.778174593052023411, -7.778174593052021635, 102.0624999999999858 ) ) ;
#18117 = CARTESIAN_POINT ( 'NONE',  ( -2.765530957081996810, 298.4218750017068942, -6.676582343750002480 ) ) ;
#18116 = CARTESIAN_POINT ( 'NONE',  ( 26.34314575050758833, 203.6875000027311842, 165.9999999999998863 ) ) ;
#18115 = DIRECTION ( 'NONE',  ( 1.000000000000000000, 0.000000000000000000, 0.000000000000000000 ) ) ;
#18118 = CARTESIAN_POINT ( 'NONE',  ( 8.660254037844385522, 129.5833333333333144, 5.000000000000005329 ) ) ;
#18119 = CARTESIAN_POINT ( 'NONE',  ( 5.656854249492381470, 101.5625000000000000, 5.656854249492379694 ) ) ;
#18120 = CARTESIAN_POINT ( 'NONE',  ( -9.000000000000000000, 5.196152422706624918, -10.20000000000000284 ) ) ;
#18121 = CARTESIAN_POINT ( 'NONE',  ( 7.188101187499992051, 8.802885111219154394E-16, 2.611552781871750994 ) ) ;
#18122 = CARTESIAN_POINT ( 'NONE',  ( 6.000000000000003553, 290.5000000034140726, 2.485281374238571317 ) ) ;
#18123 = VECTOR ( 'NONE', #11332, 1000.000000000000000 ) ;
#18124 = CARTESIAN_POINT ( 'NONE',  ( 30.44569435410879166, 201.5625000013656063, 172.4456943541087526 ) ) ;
#18125 = CARTESIAN_POINT ( 'NONE',  ( 7.188101187500001821, 6.937499997951610098, -2.977408999572650483 ) ) ;
#18126 = CARTESIAN_POINT ( 'NONE',  ( 8.008118988124991233, 9.807117285998411148E-16, 6.263115283940630995 ) ) ;
#18127 = CARTESIAN_POINT ( 'NONE',  ( -3.458734125000015425, 194.9375000013655779, 142.0000000000000568 ) ) ;
#18128 = CARTESIAN_POINT ( 'NONE',  ( 7.188101187500000044, 114.7812500020483952, -8.802885111219163269E-16 ) ) ;
#18130 = CARTESIAN_POINT ( 'NONE',  ( 3.735655735689753509, 194.7783520383262328, 197.3825241281900560 ) ) ;
#18129 = DIRECTION ( 'NONE',  ( 0.000000000000000000, 0.000000000000000000, -1.000000000000000000 ) ) ;
#18131 = CARTESIAN_POINT ( 'NONE',  ( 3.042071309553173286, 230.6770833367473585, 11.35316468749999608 ) ) ;
#18132 = CARTESIAN_POINT ( 'NONE',  ( -28.00000000000003197, 208.0000000000000284, 166.0000000000003695 ) ) ;
#18133 = CARTESIAN_POINT ( 'NONE',  ( -2.977408999572647819, 7.188101187499991163, 27.08030278187175810 ) ) ;
#18134 = CARTESIAN_POINT ( 'NONE',  ( 28.00000000000001421, 197.5000000000000000, 165.9999999999998863 ) ) ;
#18135 = CARTESIAN_POINT ( 'NONE',  ( 3.042071309553167069, 31.82291666325268054, -11.35316468749999785 ) ) ;
#18136 = CARTESIAN_POINT ( 'NONE',  ( 2.679491924311317330, 26.04166666666685259, -10.00000000000032863 ) ) ;
#18137 = CARTESIAN_POINT ( 'NONE',  ( -11.35316468749999785, 218.3854166632526415, -3.042071309553167513 ) ) ;
#18138 = DIRECTION ( 'NONE',  ( 0.000000000000000000, 0.000000000000000000, 1.000000000000000000 ) ) ;
#18140 = CARTESIAN_POINT ( 'NONE',  ( 0.000000000000000000, 0.000000000000000000, 30.00000000000000000 ) ) ;
#18139 = CARTESIAN_POINT ( 'NONE',  ( 28.00000000000002132, 206.5000000000000284, 165.9999999999998863 ) ) ;
#18141 = ORIENTED_EDGE ( 'NONE', *, *, #61106, .T. ) ;
#18142 = AXIS2_PLACEMENT_3D ( 'NONE', #25904, #54609, #72699 ) ;
#18143 = CARTESIAN_POINT ( 'NONE',  ( 1.432654583217608080, 196.8750000013656063, 138.5412658750000503 ) ) ;
#18144 = CARTESIAN_POINT ( 'NONE',  ( -9.832129032723418760, 22.86458332991934839, -5.676582343750004256 ) ) ;
#18145 = CARTESIAN_POINT ( 'NONE',  ( 4.556349186104045934, 11.00000000000000000, 89.21875000409680467 ) ) ;
#18146 = CARTESIAN_POINT ( 'NONE',  ( 3.458734124999960358, 208.6875000013656063, 142.0000000000000568 ) ) ;
#18147 = CARTESIAN_POINT ( 'NONE',  ( -7.778174593052020747, -7.778174593052023411, 110.8750000040967763 ) ) ;
#18148 = DIRECTION ( 'NONE',  ( -0.000000000000000000, 1.000000000000000000, -0.000000000000000000 ) ) ;
#18150 = CARTESIAN_POINT ( 'NONE',  ( 6.951808397369818766E-16, 17.03124999658601624, -11.35316468750000141 ) ) ;
#18149 = CARTESIAN_POINT ( 'NONE',  ( 7.188101187500002709, 105.3125000020483810, 2.977408999572649151 ) ) ;
#18151 = CARTESIAN_POINT ( 'NONE',  ( 1.469576158976822172E-15, -7.999999999999991118, 14.70530277982336642 ) ) ;
#18152 = CARTESIAN_POINT ( 'NONE',  ( 9.832129032723416984, 145.3645833299193555, 5.676582343750006032 ) ) ;
#18153 = CARTESIAN_POINT ( 'NONE',  ( -2.679491924311225848, 113.3333333265053682, -10.00000000000000178 ) ) ;
#18154 = CARTESIAN_POINT ( 'NONE',  ( -2.977408999572651815, 117.3125000020483810, 7.188101187500000933 ) ) ;
#18155 = FACE_OUTER_BOUND ( 'NONE', #5748, .T. ) ;
#18156 = CARTESIAN_POINT ( 'NONE',  ( -27.99999999999996447, 204.1875000013656063, 173.4587341250003760 ) ) ;
#18157 = ORIENTED_EDGE ( 'NONE', *, *, #39189, .F. ) ;
#18158 = CARTESIAN_POINT ( 'NONE',  ( 3.042071309553159519, 15.05208332991935194, 11.35316468750000141 ) ) ;
#18159 = ORIENTED_EDGE ( 'NONE', *, *, #4838, .T. ) ;
#18160 = DIRECTION ( 'NONE',  ( -0.000000000000000000, 1.000000000000000000, -0.000000000000000000 ) ) ;
#18161 = CARTESIAN_POINT ( 'NONE',  ( -6.676582343750001591, 297.4531250017069510, 0.000000000000000000 ) ) ;
#18163 = CARTESIAN_POINT ( 'NONE',  ( 9.832129032723420536, 146.1979166632526983, -5.676582343749999815 ) ) ;
#18162 = CARTESIAN_POINT ( 'NONE',  ( 1.656854249492381914, 14.56249999726881583, 4.000000000000000888 ) ) ;
#18164 = DIRECTION ( 'NONE',  ( 1.000000000000000000, 0.000000000000000000, 0.000000000000000000 ) ) ;
#18165 = CARTESIAN_POINT ( 'NONE',  ( -4.898587196589407898E-16, 7.999999999999991118, 21.51155278432982243 ) ) ;
#18166 = EDGE_CURVE ( 'NONE', #24578, #6205, #21380, .T. ) ;
#18167 = CARTESIAN_POINT ( 'NONE',  ( 4.898587196589412829E-16, 15.37500000000000355, -8.000000000000000000 ) ) ;
#18168 = CARTESIAN_POINT ( 'NONE',  ( 5.676582343749997150, 242.2395833367473301, -9.832129032723418760 ) ) ;
#18169 = CARTESIAN_POINT ( 'NONE',  ( -6.238412754330611322E-16, 10.18810118749999916, 94.65625000204836681 ) ) ;
#18170 = ORIENTED_EDGE ( 'NONE', *, *, #12718, .F. ) ;
#18171 = AXIS2_PLACEMENT_3D ( 'NONE', #56461, #38744, #4402 ) ;
#18172 = CARTESIAN_POINT ( 'NONE',  ( 8.000000000000000000, 20.90624999590322375, -3.313708498984761164 ) ) ;
#18173 = CARTESIAN_POINT ( 'NONE',  ( 7.778174593052023411, -7.778174593052021635, 100.7500000040967763 ) ) ;
#18174 = CARTESIAN_POINT ( 'NONE',  ( 3.042071309553159519, 85.05208332991934128, 11.35316468750000141 ) ) ;
#18175 = ORIENTED_EDGE ( 'NONE', *, *, #58641, .T. ) ;
#18176 = CARTESIAN_POINT ( 'NONE',  ( -7.204075437095965206, -7.204075437095968759, 108.3437500020483810 ) ) ;
#18177 = CARTESIAN_POINT ( 'NONE',  ( 2.780723358947928197E-16, 17.68749999863440792, -4.541265875000002339 ) ) ;
#18178 = ORIENTED_EDGE ( 'NONE', *, *, #62454, .T. ) ;
#18179 = ORIENTED_EDGE ( 'NONE', *, *, #49760, .F. ) ;
#18180 = CARTESIAN_POINT ( 'NONE',  ( 3.313708498984762052, 7.781250000000001776, -8.000000000000000000 ) ) ;
#18181 = CARTESIAN_POINT ( 'NONE',  ( 38.00000000000000000, 52.99999999999992895, -6.791607979884335933E-15 ) ) ;
#18182 = CARTESIAN_POINT ( 'NONE',  ( 5.082755093536324154, 1.781249997951610098, 5.082755093536326818 ) ) ;
#18183 = CARTESIAN_POINT ( 'NONE',  ( 8.000000000000000000, 120.0312500040967763, -3.313708498984762496 ) ) ;
#18184 = CARTESIAN_POINT ( 'NONE',  ( 10.18810118750000093, -4.220049686691933921, 101.6875000020483810 ) ) ;
#18185 = EDGE_CURVE ( 'NONE', #20942, #2612, #12134, .T. ) ;
#18186 = CARTESIAN_POINT ( 'NONE',  ( 4.000000000000000888, 1.937500000000000222, 1.656854249492384135 ) ) ;
#18187 = CARTESIAN_POINT ( 'NONE',  ( 4.000000000000001776, 12.81249999726881406, -1.656854249492381248 ) ) ;
#18188 = CARTESIAN_POINT ( 'NONE',  ( 25.17157287525378706, 209.8750000000000284, 172.8284271247460424 ) ) ;
#18189 = ORIENTED_EDGE ( 'NONE', *, *, #59396, .F. ) ;
#18190 = LINE ( 'NONE', #51777, #22531 ) ;
#18191 = CARTESIAN_POINT ( 'NONE',  ( -3.458734124999959914, 197.4375000013655779, 198.0000000000000284 ) ) ;
#18192 = VECTOR ( 'NONE', #40321, 1000.000000000000000 ) ;
#18193 = ADVANCED_FACE ( 'NONE', ( #52141 ), #46467, .T. ) ;
#18194 = CARTESIAN_POINT ( 'NONE',  ( -27.99999999999991829, 204.9375000013656063, 173.4587341250003760 ) ) ;
#18195 = EDGE_CURVE ( 'NONE', #2977, #45738, #19847, .T. ) ;
#18196 = CARTESIAN_POINT ( 'NONE',  ( 4.541265875000001451, 16.24999999863440436, 1.881053915767124440 ) ) ;
#18197 = CARTESIAN_POINT ( 'NONE',  ( 0.000000000000000000, 210.0000000000000284, 170.0000000000000284 ) ) ;
#18198 = VECTOR ( 'NONE', #37463, 1000.000000000000227 ) ;
#18199 = CARTESIAN_POINT ( 'NONE',  ( -7.188101187499991163, 2.977408999572646930, 14.89280278187175455 ) ) ;
#18200 = ORIENTED_EDGE ( 'NONE', *, *, #41182, .T. ) ;
#18201 = ORIENTED_EDGE ( 'NONE', *, *, #70693, .T. ) ;
#18202 = CARTESIAN_POINT ( 'NONE',  ( -7.204075437095965206, -7.204075437095968759, 102.3437500020483668 ) ) ;
#18203 = CARTESIAN_POINT ( 'NONE',  ( -12.80255146922223375, -13.39305315375707295, -0.2939692054342312177 ) ) ;
#18204 = CARTESIAN_POINT ( 'NONE',  ( -24.00000000000001421, 206.8125000000000000, 168.3431457505080004 ) ) ;
#18205 = CARTESIAN_POINT ( 'NONE',  ( 2.839093476692135984E-14, 199.6875000013656063, 201.4587341250000350 ) ) ;
#18206 = CARTESIAN_POINT ( 'NONE',  ( 26.56734541678232731, 197.0000000013656063, 166.5412658749999650 ) ) ;
#18207 = CARTESIAN_POINT ( 'NONE',  ( -10.00000000000000178, 97.50000000000000000, -1.224646799147353454E-15 ) ) ;
#18208 = CARTESIAN_POINT ( 'NONE',  ( -3.313708498984762052, 120.2187500000000000, -8.000000000000000000 ) ) ;
#18209 = CARTESIAN_POINT ( 'NONE',  ( 9.832129032723420536, 56.51041666325268409, -5.676582343749999815 ) ) ;
#18210 = CARTESIAN_POINT ( 'NONE',  ( -2.485281374238571761, 289.8125000000000000, -6.000000000000003553 ) ) ;
#18211 = EDGE_LOOP ( 'NONE', ( #19624, #21443, #8502, #60721 ) ) ;
#18212 =( BOUNDED_CURVE ( )  B_SPLINE_CURVE ( 2, ( #21347, #55327, #14929, #16050, #3262, #56071, #4018, #27008, #49652 ),
 .UNSPECIFIED., .F., .F. ) 
 B_SPLINE_CURVE_WITH_KNOTS ( ( 3, 2, 2, 2, 3 ),
 ( 0.6458333333333314830, 0.6562499999999981126, 0.6666666666666647423, 0.6770833333333315940, 0.6874999999999982236 ),
 .UNSPECIFIED. ) 
 CURVE ( )  GEOMETRIC_REPRESENTATION_ITEM ( )  RATIONAL_B_SPLINE_CURVE ( ( 1.000000000000013767, 0.9238795325112729717, 1.000000000000000000, 0.9238795325112867385, 1.000000000000000000, 0.9238795325112867385, 1.000000000000000000, 0.9238795325112997281, 0.9999999999999870104 ) ) 
 REPRESENTATION_ITEM ( '' )  );
#18213 = CARTESIAN_POINT ( 'NONE',  ( -11.00000000000000533, 11.00000000000000000, 41.99999999999999289 ) ) ;
#18214 = EDGE_CURVE ( 'NONE', #44928, #27622, #27564, .T. ) ;
#18215 = CARTESIAN_POINT ( 'NONE',  ( 8.000000000000000000, 16.40624999590322375, -3.313708498984761608 ) ) ;
#18216 = CARTESIAN_POINT ( 'NONE',  ( -1.432654583217662481, 208.1250000013656063, 145.4587341250000634 ) ) ;
#18217 = CARTESIAN_POINT ( 'NONE',  ( 10.00000000000001066, 85.20833333333337123, -2.679491924311228956 ) ) ;
#18218 = DIRECTION ( 'NONE',  ( 0.000000000000000000, 0.000000000000000000, 1.000000000000000000 ) ) ;
#18219 = CARTESIAN_POINT ( 'NONE',  ( -8.311093377946836114, 263.5937500034140157, -8.311093377946836114 ) ) ;
#18220 = CARTESIAN_POINT ( 'NONE',  ( -4.220049686691935698, 10.18810118749999916, 67.75000000204836681 ) ) ;
#18221 = CARTESIAN_POINT ( 'NONE',  ( 8.660254037844385522, 219.5833333333333428, 5.000000000000005329 ) ) ;
#18222 = CARTESIAN_POINT ( 'NONE',  ( 2.977408999572646486, 7.188101187499992051, 11.89280278187175810 ) ) ;
#18223 = CARTESIAN_POINT ( 'NONE',  ( 5.676582343750001591, 186.9270833299193555, -9.832129032723420536 ) ) ;
#18224 = CARTESIAN_POINT ( 'NONE',  ( 4.541265875000002339, 1.312499998634406584, 0.000000000000000000 ) ) ;
#18225 = CARTESIAN_POINT ( 'NONE',  ( 31.99999999999999289, 197.3750000027312126, 169.9999999999998863 ) ) ;
#18226 = CARTESIAN_POINT ( 'NONE',  ( 12.00000000000000178, 28.00000000000000000, -3.999999999999986233 ) ) ;
#18227 = ORIENTED_EDGE ( 'NONE', *, *, #59819, .F. ) ;
#18228 = VECTOR ( 'NONE', #32376, 1000.000000000000000 ) ;
#18229 = CARTESIAN_POINT ( 'NONE',  ( -2.839093476692135984E-14, 206.9375000013656063, 138.5412658750000503 ) ) ;
#18230 = CARTESIAN_POINT ( 'NONE',  ( 9.832129032723416984, 30.67708332991935194, 5.676582343750006032 ) ) ;
#18231 = CARTESIAN_POINT ( 'NONE',  ( -4.556349186104045934, 11.00000000000000000, 107.4062500040967620 ) ) ;
#18232 = CARTESIAN_POINT ( 'NONE',  ( -25.55430564589111953, 207.0625000013656063, 172.4456943541091505 ) ) ;
#18233 = CARTESIAN_POINT ( 'NONE',  ( 2.679491924311184103, 11.04166666666667140, -10.00000000000002487 ) ) ;
#18235 = CARTESIAN_POINT ( 'NONE',  ( -2.679491924311226292, 58.33333332650537528, -10.00000000000000178 ) ) ;
#18234 = FACE_OUTER_BOUND ( 'NONE', #46150, .T. ) ;
#18236 = CARTESIAN_POINT ( 'NONE',  ( 3.458734124999958581, 200.5000000013655779, 140.5673454167823593 ) ) ;
#18237 = CARTESIAN_POINT ( 'NONE',  ( 10.00000000000000178, 76.87499999317203958, 0.000000000000000000 ) ) ;
#18238 = CARTESIAN_POINT ( 'NONE',  ( -2.977408999572650927, 99.87500000204838102, -7.188101187500001821 ) ) ;
#18239 = CARTESIAN_POINT ( 'NONE',  ( -4.541265875000002339, 17.93749999863440792, -5.561446717895856393E-16 ) ) ;
#18240 = CARTESIAN_POINT ( 'NONE',  ( 1.567784982238203817E-13, 73.75000000000002842, 10.00000000000000533 ) ) ;
#18241 = CARTESIAN_POINT ( 'NONE',  ( 6.123233995736767268E-16, 48.12499999317203958, -10.00000000000000178 ) ) ;
#18242 = FACE_BOUND ( 'NONE', #57584, .T. ) ;
#18243 = ORIENTED_EDGE ( 'NONE', *, *, #39807, .F. ) ;
#18244 = VERTEX_POINT ( 'NONE', #37374 ) ;
#18245 = CARTESIAN_POINT ( 'NONE',  ( -2.765530957081998586, 296.7968750017070079, 6.676582343750001591 ) ) ;
#18246 = CARTESIAN_POINT ( 'NONE',  ( 0.000000000000000000, 0.000000000000000000, 118.0000000000000000 ) ) ;
#18247 = DIRECTION ( 'NONE',  ( 0.000000000000000000, -1.387778780781445676E-15, 1.000000000000000000 ) ) ;
#18248 = CARTESIAN_POINT ( 'NONE',  ( 8.311093377946834337, 160.1562499965860411, 8.311093377946839666 ) ) ;
#18249 = CARTESIAN_POINT ( 'NONE',  ( -10.18810118749999916, 0.000000000000000000, 82.65625000204838102 ) ) ;
#18250 = CARTESIAN_POINT ( 'NONE',  ( -3.999999999999960032, 205.0000000000000284, 198.0000000000000284 ) ) ;
#18251 = CARTESIAN_POINT ( 'NONE',  ( 0.000000000000000000, 125.0000000000000000, 0.000000000000000000 ) ) ;
#18252 = EDGE_CURVE ( 'NONE', #19945, #20745, #30598, .T. ) ;
#18253 = CARTESIAN_POINT ( 'NONE',  ( 4.220049686691941027, -10.18810118749999738, 107.5000000020483668 ) ) ;
#18254 = ORIENTED_EDGE ( 'NONE', *, *, #58896, .T. ) ;
#18255 = DIRECTION ( 'NONE',  ( -0.000000000000000000, -1.000000000000000000, -0.000000000000000000 ) ) ;
#18256 = AXIS2_PLACEMENT_3D ( 'NONE', #56975, #39614, #38872 ) ;
#18257 = CARTESIAN_POINT ( 'NONE',  ( -4.000000000000001776, 17.50000000000000000, -4.898587196589415787E-16 ) ) ;
#18258 = CARTESIAN_POINT ( 'NONE',  ( 3.042071309553167513, 142.1354166632526415, -11.35316468749999785 ) ) ;
#18259 = CARTESIAN_POINT ( 'NONE',  ( 2.445694354108839619, 196.8125000013656063, 200.4456943541088663 ) ) ;
#18260 = CARTESIAN_POINT ( 'NONE',  ( -4.242640687119286547, 290.8750000000000000, -4.242640687119286547 ) ) ;
#18262 = EDGE_CURVE ( 'NONE', #42176, #2370, #13960, .T. ) ;
#18261 = CARTESIAN_POINT ( 'NONE',  ( 7.204075437095968759, -7.204075437095966983, 77.59375000204838102 ) ) ;
#18263 = CARTESIAN_POINT ( 'NONE',  ( 11.35316468749999963, 51.30208332991936260, -3.042071309553165293 ) ) ;
#18264 = ORIENTED_EDGE ( 'NONE', *, *, #13708, .T. ) ;
#18265 = DIRECTION ( 'NONE',  ( 0.000000000000000000, 0.000000000000000000, 1.000000000000000000 ) ) ;
#18266 = CARTESIAN_POINT ( 'NONE',  ( 4.541265875000002339, 5.499999998634407028, -1.881053915767121776 ) ) ;
#18267 = CARTESIAN_POINT ( 'NONE',  ( 5.662595241051934458, 5.662595241051935346, 13.95061528394063011 ) ) ;
#18268 = AXIS2_PLACEMENT_3D ( 'NONE', #45319, #16632, #4974 ) ;
#18269 = CARTESIAN_POINT ( 'NONE',  ( 2.977408999572651815, 16.68749999795161543, 7.188101187500000933 ) ) ;
#18270 = CARTESIAN_POINT ( 'NONE',  ( -3.673940397442060854E-16, 293.8125000034140157, -6.000000000000001776 ) ) ;
#18271 = CARTESIAN_POINT ( 'NONE',  ( -31.52641926705831210, -12.00051207543326193, 143.3285058911732506 ) ) ;
#18272 = CARTESIAN_POINT ( 'NONE',  ( 5.082755093536324154, 5.156249997951610098, 5.082755093536326818 ) ) ;
#18273 = CARTESIAN_POINT ( 'NONE',  ( 1.320432766682872962E-15, -7.188101187499992051, 10.86155278187175455 ) ) ;
#18274 = APPLICATION_CONTEXT ( 'automotive_design' ) ;
#18275 = CARTESIAN_POINT ( 'NONE',  ( 1.871523826299183495E-15, -10.18810118749999916, 69.53125000204838102 ) ) ;
#18276 = EDGE_CURVE ( 'NONE', #46734, #55139, #13231, .T. ) ;
#18277 = CARTESIAN_POINT ( 'NONE',  ( -30.44569435410883784, 206.8125000013656063, 167.5543056458915885 ) ) ;
#18278 = DIRECTION ( 'NONE',  ( -1.000000000000000000, 0.000000000000000000, 0.000000000000000000 ) ) ;
#18279 = CARTESIAN_POINT ( 'NONE',  ( -7.347880794884122694E-16, 2.499999997268813168, 4.000000000000001776 ) ) ;
#18280 = PRODUCT_RELATED_PRODUCT_CATEGORY ( 'part', '', ( #51772 ) ) ;
#18281 = ORIENTED_EDGE ( 'NONE', *, *, #58228, .F. ) ;
#18282 = CARTESIAN_POINT ( 'NONE',  ( 2.751064625579944321E-14, 195.8750000027311842, 194.0000000000000568 ) ) ;
#18283 = CARTESIAN_POINT ( 'NONE',  ( -4.000000000000015987, 205.4375000000000000, 140.3431457505076594 ) ) ;
#18284 = CARTESIAN_POINT ( 'NONE',  ( -30.82842712474624491, 200.2500000027312126, 167.1715728752542418 ) ) ;
#18285 = EDGE_CURVE ( 'NONE', #62597, #69992, #35307, .T. ) ;
#18286 = CARTESIAN_POINT ( 'NONE',  ( -7.188101187500000044, 113.6562500020483810, 0.000000000000000000 ) ) ;
#18287 = CARTESIAN_POINT ( 'NONE',  ( 8.660254037844385522, 251.0416666734946318, -5.000000000000003553 ) ) ;
#18288 = CARTESIAN_POINT ( 'NONE',  ( -7.999999999999989342, -3.313708498984762496, 1.111552783920146004 ) ) ;
#18289 = VERTEX_POINT ( 'NONE', #72451 ) ;
#18290 = CARTESIAN_POINT ( 'NONE',  ( 2.977408999572652260, 25.68749999795162253, 7.188101187500000044 ) ) ;
#18291 = VERTEX_POINT ( 'NONE', #53984 ) ;
#18292 = FACE_OUTER_BOUND ( 'NONE', #14058, .T. ) ;
#18293 = CARTESIAN_POINT ( 'NONE',  ( 6.123233995736767268E-16, 43.12499999317203248, -10.00000000000000178 ) ) ;
#18294 = CARTESIAN_POINT ( 'NONE',  ( 2.679491924311228956, 61.04166666666665719, -10.00000000000000000 ) ) ;
#18295 = CARTESIAN_POINT ( 'NONE',  ( 7.188101187500002709, 102.6875000020483810, 2.977408999572649151 ) ) ;
#18296 = CARTESIAN_POINT ( 'NONE',  ( 4.242640687119285658, 299.6250000000000000, -4.242640687119286547 ) ) ;
#18298 = CARTESIAN_POINT ( 'NONE',  ( 4.000000000000016875, 197.5625000027312126, 199.6568542494924259 ) ) ;
#18297 = DIRECTION ( 'NONE',  ( -0.000000000000000000, 1.000000000000000000, -0.000000000000000000 ) ) ;
#18299 = VERTEX_POINT ( 'NONE', #66037 ) ;
#18300 = VERTEX_POINT ( 'NONE', #14344 ) ;
#18301 = CARTESIAN_POINT ( 'NONE',  ( 3.042071309553173286, 245.3645833367472733, 11.35316468749999608 ) ) ;
#18302 = CARTESIAN_POINT ( 'NONE',  ( -5.082755093536319713, 5.082755093536319713, 18.17405278187175455 ) ) ;
#18303 = AXIS2_PLACEMENT_3D ( 'NONE', #34075, #68746, #51026 ) ;
#18304 = CARTESIAN_POINT ( 'NONE',  ( 8.660254037844371311, 89.58333333333332860, 4.999999999999997335 ) ) ;
#18305 = DIRECTION ( 'NONE',  ( 0.000000000000000000, 2.081668171172168119E-15, 1.000000000000000000 ) ) ;
#18306 = CARTESIAN_POINT ( 'NONE',  ( 4.000000000000015987, 198.6250000027312126, 198.0000000000000284 ) ) ;
#18307 =( BOUNDED_CURVE ( )  B_SPLINE_CURVE ( 2, ( #51751, #44609, #45715, #22318, #68727, #44982, #23078, #11393, #38950 ),
 .UNSPECIFIED., .F., .F. ) 
 B_SPLINE_CURVE_WITH_KNOTS ( ( 3, 2, 2, 2, 3 ),
 ( 0.1166666666666666546, 0.1250000000000000555, 0.1333333333333334425, 0.1416666666666668573, 0.1500000000000002442 ),
 .UNSPECIFIED. ) 
 CURVE ( )  GEOMETRIC_REPRESENTATION_ITEM ( )  RATIONAL_B_SPLINE_CURVE ( ( 1.000000000000000222, 0.9238795325112867385, 1.000000000000000000, 0.9238795325112867385, 1.000000000000000000, 0.9238795325112867385, 1.000000000000000000, 0.9238795325112844070, 1.000000000000002220 ) ) 
 REPRESENTATION_ITEM ( '' )  );
#18308 = DIRECTION ( 'NONE',  ( 0.8660254037844389297, 0.4999999999999994449, -0.000000000000000000 ) ) ;
#18309 = CARTESIAN_POINT ( 'NONE',  ( -2.679491924311225848, 176.4583333333333428, -10.00000000000000178 ) ) ;
#18310 = CARTESIAN_POINT ( 'NONE',  ( 27.99999999999996803, 209.4375000013656063, 173.4587341249998929 ) ) ;
#18311 =( NAMED_UNIT ( * ) SI_UNIT ( $, .STERADIAN. ) SOLID_ANGLE_UNIT ( ) );
#18312 = CARTESIAN_POINT ( 'NONE',  ( -5.656854249492373476, -5.656854249492376141, 4.017802779823362869 ) ) ;
#18313 = CARTESIAN_POINT ( 'NONE',  ( 6.951808397369818766E-16, 137.3437499965860127, -11.35316468750000141 ) ) ;
#18314 = CARTESIAN_POINT ( 'NONE',  ( 0.000000000000000000, 0.000000000000000000, 0.000000000000000000 ) ) ;
#18315 = CARTESIAN_POINT ( 'NONE',  ( -5.656854249492378806, 117.6875000000000000, 5.656854249492381470 ) ) ;
#18318 = CARTESIAN_POINT ( 'NONE',  ( 3.999999999999960032, 201.9375000000000000, 143.6568542494924259 ) ) ;
#18317 = CARTESIAN_POINT ( 'NONE',  ( -4.898587196589407898E-16, 7.999999999999991118, 25.95530277982336997 ) ) ;
#18316 = CARTESIAN_POINT ( 'NONE',  ( 26.34314575050758833, 205.9375000000000284, 173.9999999999999147 ) ) ;
#18319 = ORIENTED_EDGE ( 'NONE', *, *, #21337, .F. ) ;
#18320 = CARTESIAN_POINT ( 'NONE',  ( 4.898587196589412829E-16, 10.87500000000000178, -8.000000000000000000 ) ) ;
#18321 = CARTESIAN_POINT ( 'NONE',  ( 7.778174593052021635, 7.778174593052023411, 68.12500000409677625 ) ) ;
#18322 = CARTESIAN_POINT ( 'NONE',  ( -0.7855267195163277982, -7.974084888391890225, -0.000000000000000000 ) ) ;
#18323 = CARTESIAN_POINT ( 'NONE',  ( 5.000000000000000000, -68.32828612846148530, -21.58087353894176275 ) ) ;
#18324 = CARTESIAN_POINT ( 'NONE',  ( -8.660254037844390851, 34.79166665983870388, 4.999999999999998224 ) ) ;
#18325 = CARTESIAN_POINT ( 'NONE',  ( -7.188101187499999156, 116.7500000020483810, 2.977408999572654924 ) ) ;
#18326 = CARTESIAN_POINT ( 'NONE',  ( 1.881053915767122664, 1.249999998634407028, 4.541265875000001451 ) ) ;
#18327 = CARTESIAN_POINT ( 'NONE',  ( -5.107860025166927720, -50.62490018645955558, 41.07729128472254843 ) ) ;
#18328 = CARTESIAN_POINT ( 'NONE',  ( 7.999999999999991118, 3.313708498984757611, 13.67405277982336287 ) ) ;
#18330 = CARTESIAN_POINT ( 'NONE',  ( 4.898587196589412829E-16, 24.18749999590322375, -8.000000000000000000 ) ) ;
#18329 = CARTESIAN_POINT ( 'NONE',  ( -7.347880794884122694E-16, 1.750000000000000222, 4.000000000000001776 ) ) ;
#18331 = ORIENTED_EDGE ( 'NONE', *, *, #34911, .F. ) ;
#18332 =( BOUNDED_CURVE ( )  B_SPLINE_CURVE ( 2, ( #29630, #58681, #57952, #6990, #1712, #58319, #12636, #59052, #46600 ),
 .UNSPECIFIED., .F., .F. ) 
 B_SPLINE_CURVE_WITH_KNOTS ( ( 3, 2, 2, 2, 3 ),
 ( 0.2912041257482609335, 0.2978224013005510984, 0.3044406768850113632, 0.3110589524694716279, 0.3176771498271482308 ),
 .UNSPECIFIED. ) 
 CURVE ( )  GEOMETRIC_REPRESENTATION_ITEM ( )  RATIONAL_B_SPLINE_CURVE ( ( 1.000000000000000000, 0.9238795325112867385, 1.000000000000000000, 0.9238795325112867385, 1.000000000000000000, 0.9238795325112867385, 1.000000000000000000, 0.9238804322410221204, 0.9999982005617984449 ) ) 
 REPRESENTATION_ITEM ( '' )  );
#18333 = CARTESIAN_POINT ( 'NONE',  ( 2.250000000000000444, 283.9999999999998863, 5.427273995025124975 ) ) ;
#18334 = CARTESIAN_POINT ( 'NONE',  ( -3.220591000267885917, 225.9999999999999432, 9.489952148308894664 ) ) ;
#18335 = CARTESIAN_POINT ( 'NONE',  ( 2.824543433528785410E-14, 210.0000000000000284, 194.0000000000000568 ) ) ;
#18336 = CARTESIAN_POINT ( 'NONE',  ( -3.042071309553159075, 245.2604166700806729, 11.35316468749999963 ) ) ;
#18337 = VECTOR ( 'NONE', #8225, 1000.000000000000000 ) ;
#18338 = CARTESIAN_POINT ( 'NONE',  ( 6.951808397369818766E-16, 112.0312499965860269, -11.35316468750000141 ) ) ;
#18339 = EDGE_LOOP ( 'NONE', ( #17814, #1519, #43206, #32133 ) ) ;
#18340 = CARTESIAN_POINT ( 'NONE',  ( -6.911667950094911639, 8.332266638136186288, 117.6845864511994932 ) ) ;
#18341 = CARTESIAN_POINT ( 'NONE',  ( 4.220049686691934809, 10.18810118749999916, 98.68750000204838102 ) ) ;
#18342 = CARTESIAN_POINT ( 'NONE',  ( 7.347880794884121708E-16, 300.0000000000000000, -6.000000000000001776 ) ) ;
#18343 = CARTESIAN_POINT ( 'NONE',  ( 2.754378923186476579E-14, 201.4375000013656063, 194.5412658750000219 ) ) ;
#18344 = CARTESIAN_POINT ( 'NONE',  ( -4.556349186104048599, -10.99999999999999822, 68.78125000000000000 ) ) ;
#18346 = CARTESIAN_POINT ( 'NONE',  ( -5.676582343749998039, 107.4479166632526983, -9.832129032723420536 ) ) ;
#18345 = CARTESIAN_POINT ( 'NONE',  ( -4.999999999999997335, 181.6666666666666856, -8.660254037844387298 ) ) ;
#18347 = CARTESIAN_POINT ( 'NONE',  ( -7.999999999999989342, -3.313708498984762496, 7.111552783920144449 ) ) ;
#18348 = CARTESIAN_POINT ( 'NONE',  ( -24.54126587499997925, 197.3750000013656063, 171.4326545832179818 ) ) ;
#18349 = EDGE_CURVE ( 'NONE', #7251, #1076, #42978, .T. ) ;
#18350 = CARTESIAN_POINT ( 'NONE',  ( 4.999999999999996447, 49.16666666666667140, 8.660254037844394404 ) ) ;
#18351 = VERTEX_POINT ( 'NONE', #54738 ) ;
#18352 = AXIS2_PLACEMENT_3D ( 'NONE', #26680, #65924, #55003 ) ;
#18353 = CARTESIAN_POINT ( 'NONE',  ( 6.123233995736767268E-16, 198.1249999931720538, -10.00000000000000178 ) ) ;
#18354 = CARTESIAN_POINT ( 'NONE',  ( 1.656854249492297093, 205.8125000000000284, 146.0000000000000853 ) ) ;
#18355 = DIRECTION ( 'NONE',  ( 0.000000000000000000, 0.000000000000000000, 1.000000000000000000 ) ) ;
#18356 = CARTESIAN_POINT ( 'NONE',  ( -5.676582343749998039, 82.76041666325268409, -9.832129032723420536 ) ) ;
#18357 = CARTESIAN_POINT ( 'NONE',  ( -7.188101187500000044, 15.09374999795161187, -8.802885111219163269E-16 ) ) ;
#18359 = ADVANCED_FACE ( 'NONE', ( #7961 ), #20378, .F. ) ;
#18358 = CARTESIAN_POINT ( 'NONE',  ( -6.238412754330611322E-16, 10.18810118749999916, 94.65625000204836681 ) ) ;
#18360 = CARTESIAN_POINT ( 'NONE',  ( 11.35316468750000141, 6.093749996586017126, 0.000000000000000000 ) ) ;
#18361 = ORIENTED_EDGE ( 'NONE', *, *, #42074, .F. ) ;
#18362 = CARTESIAN_POINT ( 'NONE',  ( 7.999999999999967137, -3.313708498984783368, 26.98655277982336997 ) ) ;
#18363 = CARTESIAN_POINT ( 'NONE',  ( 2.904064318449610216, -44.22191370252287612, 139.1363011946421295 ) ) ;
#18364 = CARTESIAN_POINT ( 'NONE',  ( -8.311093377946841443, 223.9062499965860411, 8.311093377946834337 ) ) ;
#18365 = CARTESIAN_POINT ( 'NONE',  ( -7.204075437095967871, 7.204075437095967871, 76.84375000204838102 ) ) ;
#18366 = CYLINDRICAL_SURFACE ( 'NONE', #45870, 10.00000000000000178 ) ;
#18367 = CARTESIAN_POINT ( 'NONE',  ( -10.00000000000000000, 265.0000000000000000, 0.000000000000000000 ) ) ;
#18368 = CARTESIAN_POINT ( 'NONE',  ( -2.765530957081998586, 294.6406250017069510, 6.676582343750001591 ) ) ;
#18369 = ORIENTED_EDGE ( 'NONE', *, *, #58332, .T. ) ;
#18370 = CARTESIAN_POINT ( 'NONE',  ( -2.751064625579944321E-14, 201.8750000027312126, 146.0000000000000284 ) ) ;
#18371 = CARTESIAN_POINT ( 'NONE',  ( 11.35316468750000141, 206.0937499965860411, 0.000000000000000000 ) ) ;
#18372 = CARTESIAN_POINT ( 'NONE',  ( 10.18810118749999916, 1.247682550866122264E-15, 89.40625000204838102 ) ) ;
#18373 = AXIS2_PLACEMENT_3D ( 'NONE', #32437, #9418, #26758 ) ;
#18374 = CARTESIAN_POINT ( 'NONE',  ( -24.54126587500000056, 202.2500000013656063, 168.5673454167827003 ) ) ;
#18375 = CARTESIAN_POINT ( 'NONE',  ( -3.313708498984765161, 22.03125000000000355, 7.999999999999998224 ) ) ;
#18376 = ORIENTED_EDGE ( 'NONE', *, *, #26029, .F. ) ;
#18377 = CARTESIAN_POINT ( 'NONE',  ( -15.79467996801232132, -45.08104900353366418, 143.2946372208209311 ) ) ;
#18378 = CARTESIAN_POINT ( 'NONE',  ( -5.082755093536325930, 123.9687500020483952, -5.082755093536325930 ) ) ;
#18379 = CARTESIAN_POINT ( 'NONE',  ( 2.751064625579944321E-14, 207.8750000027312126, 194.0000000000000568 ) ) ;
#18380 = CARTESIAN_POINT ( 'NONE',  ( 8.660254037844385522, 29.58333333333333570, 5.000000000000005329 ) ) ;
#18381 = VECTOR ( 'NONE', #7499, 1000.000000000000000 ) ;
#18382 = CARTESIAN_POINT ( 'NONE',  ( -5.000000000000000000, 14.89980876190746351, 69.94558486267358433 ) ) ;
#18383 = CARTESIAN_POINT ( 'NONE',  ( 7.204075437095968759, -7.204075437095966983, 73.09375000204838102 ) ) ;
#18384 = ORIENTED_EDGE ( 'NONE', *, *, #22072, .T. ) ;
#18385 = CARTESIAN_POINT ( 'NONE',  ( 7.188101187500000044, 1.968749997951610320, 0.000000000000000000 ) ) ;
#18386 = CARTESIAN_POINT ( 'NONE',  ( -6.338291171875001240, 287.2578125025604550, 0.000000000000000000 ) ) ;
#18387 = VECTOR ( 'NONE', #64283, 1000.000000000000000 ) ;
#18388 = LINE ( 'NONE', #53093, #52406 ) ;
#18389 = CARTESIAN_POINT ( 'NONE',  ( 2.977408999572654480, 120.5000000020483810, 7.188101187499999156 ) ) ;
#18390 = CARTESIAN_POINT ( 'NONE',  ( -0.4590000000000000746, 255.7199999999997715, 5.818583442785218551 ) ) ;
#18391 = CARTESIAN_POINT ( 'NONE',  ( -6.676582343750002480, 296.3906250017069510, -2.765530957081996810 ) ) ;
#18393 = CARTESIAN_POINT ( 'NONE',  ( 2.828427124746208943, 206.6250000000000284, 195.1715728752538439 ) ) ;
#18392 = CARTESIAN_POINT ( 'NONE',  ( 11.35316468749999963, 231.4062500034139873, -1.390361679473963556E-15 ) ) ;
#18394 = VERTEX_POINT ( 'NONE', #20759 ) ;
#18395 = CARTESIAN_POINT ( 'NONE',  ( -5.676582343749992710, 235.0520833367473301, 9.832129032723422313 ) ) ;
#18396 = CARTESIAN_POINT ( 'NONE',  ( 2.977408999572650927, -7.188101187499990274, 7.955302781871752771 ) ) ;
#18397 = CARTESIAN_POINT ( 'NONE',  ( 2.754378923186476579E-14, 202.4375000013656063, 194.5412658750000219 ) ) ;
#18398 = ORIENTED_EDGE ( 'NONE', *, *, #41437, .T. ) ;
#18399 = CARTESIAN_POINT ( 'NONE',  ( 8.000000000000000000, 104.9375000040967763, -9.797174393178825657E-16 ) ) ;
#18400 = CARTESIAN_POINT ( 'NONE',  ( -11.35316468749999785, 98.38541666325268409, -3.042071309553167513 ) ) ;
#18401 = CYLINDRICAL_SURFACE ( 'NONE', #69776, 15.99999999999998579 ) ;
#18402 = CARTESIAN_POINT ( 'NONE',  ( -10.99999999999999822, -4.556349186104052151, 85.09375000000000000 ) ) ;
#18405 = CARTESIAN_POINT ( 'NONE',  ( 11.00000000000000000, 1.347111479062088405E-15, 114.2499999999999858 ) ) ;
#18404 = CARTESIAN_POINT ( 'NONE',  ( 26.56734541678232731, 205.0000000013655779, 166.5412658749999650 ) ) ;
#18403 = CARTESIAN_POINT ( 'NONE',  ( 31.45873412499999944, 203.9375000013656063, 169.9999999999999432 ) ) ;
#18406 = ORIENTED_EDGE ( 'NONE', *, *, #24158, .T. ) ;
#18407 = DIRECTION ( 'NONE',  ( 0.000000000000000000, -1.000000000000000000, 0.000000000000000000 ) ) ;
#18408 = CYLINDRICAL_SURFACE ( 'NONE', #13066, 11.00000000000000000 ) ;
#18409 = CARTESIAN_POINT ( 'NONE',  ( 5.676582343749993598, 209.9479166632526983, 9.832129032723422313 ) ) ;
#18410 = CARTESIAN_POINT ( 'NONE',  ( -3.458734125000016313, 206.8750000013656347, 140.5673454167824161 ) ) ;
#18411 = EDGE_CURVE ( 'NONE', #70531, #29624, #28469, .T. ) ;
#18412 = CARTESIAN_POINT ( 'NONE',  ( 30.44569435410879521, 206.8125000013656063, 172.4456943541087526 ) ) ;
#18413 = EDGE_CURVE ( 'NONE', #783, #10198, #23176, .T. ) ;
#18414 = CARTESIAN_POINT ( 'NONE',  ( 2.977408999572651815, 24.56249999795161543, 7.188101187500000933 ) ) ;
#18415 = CARTESIAN_POINT ( 'NONE',  ( -11.35316468749999785, 178.3854166632526983, -3.042071309553167513 ) ) ;
#18416 = CARTESIAN_POINT ( 'NONE',  ( 1.320432766682874540E-15, 97.90625000204839523, 7.188101187500000044 ) ) ;
#18417 = CARTESIAN_POINT ( 'NONE',  ( 3.999999999999960032, 196.0625000027312126, 143.6568542494924259 ) ) ;
#18418 = CARTESIAN_POINT ( 'NONE',  ( -23.99999999999998579, 196.7500000000000000, 170.0000000000003411 ) ) ;
#18419 = CARTESIAN_POINT ( 'NONE',  ( -8.342170076843785083E-16, 11.06249999863440792, 4.541265875000002339 ) ) ;
#18420 = CARTESIAN_POINT ( 'NONE',  ( 31.45873412499997812, 201.8750000013656063, 171.4326545832176123 ) ) ;
#18421 = CARTESIAN_POINT ( 'NONE',  ( 5.082755093536320601, -5.082755093536318824, 3.924052781871752327 ) ) ;
#18422 = CARTESIAN_POINT ( 'NONE',  ( -2.085542519210945728E-15, 69.53124999658602690, 11.35316468750000141 ) ) ;
#18423 = LINE ( 'NONE', #41800, #35235 ) ;
#18424 = CARTESIAN_POINT ( 'NONE',  ( 1.469576158976823947E-15, 119.5625000040967763, 8.000000000000000000 ) ) ;
#18425 = ORIENTED_EDGE ( 'NONE', *, *, #68470, .F. ) ;
#18426 = DIRECTION ( 'NONE',  ( -0.000000000000000000, 1.000000000000000000, -0.000000000000000000 ) ) ;
#18427 = CARTESIAN_POINT ( 'NONE',  ( -10.99999999999989342, 4.556349186104152515, 67.09375000409677625 ) ) ;
#18428 = CARTESIAN_POINT ( 'NONE',  ( -3.042071309553164404, 77.23958332991935549, -11.35316468749999963 ) ) ;
#18429 = CARTESIAN_POINT ( 'NONE',  ( 11.00000000000000000, 4.556349186104045934, 68.03125000409676204 ) ) ;
#18430 = CARTESIAN_POINT ( 'NONE',  ( 2.445694354108783219, 196.8125000013656063, 139.5543056458912190 ) ) ;
#18431 = CARTESIAN_POINT ( 'NONE',  ( 3.999980467337267864, 125.0000000000000000, -6.928214507426884161 ) ) ;
#18433 = CARTESIAN_POINT ( 'NONE',  ( -9.832129032723420536, 63.69791666325269830, 5.676582343749997150 ) ) ;
#18432 = DIRECTION ( 'NONE',  ( -0.000000000000000000, 1.000000000000000000, -1.563033456626094573E-30 ) ) ;
#18434 = CARTESIAN_POINT ( 'NONE',  ( 1.469576158976822172E-15, -7.999999999999991118, 26.89280278392014623 ) ) ;
#18435 = ADVANCED_FACE ( 'NONE', ( #67171 ), #26796, .T. ) ;
#18436 = CARTESIAN_POINT ( 'NONE',  ( 5.656854249492381470, 110.7500000040967763, 5.656854249492379694 ) ) ;
#18437 =( BOUNDED_SURFACE ( )  B_SPLINE_SURFACE ( 3, 2, ( 
 ( #10965, #5308, #73960 ),
 ( #45289, #68300, #28310 ),
 ( #410, #16599, #12436 ),
 ( #52441, #42211, #64501 ),
 ( #24123, #35468, #58481 ),
 ( #63753, #1867, #64127 ),
 ( #69791, #36201, #18475 ),
 ( #40743, #12801, #1520 ),
 ( #29798, #1143, #47136 ),
 ( #41487, #35832, #58847 ),
 ( #6789, #52809, #70167 ),
 ( #12070, #6427, #46766 ),
 ( #35106, #7160, #24498 ),
 ( #30165, #19206, #29431 ),
 ( #47502, #53182, #70527 ),
 ( #17727, #58118, #70891 ),
 ( #778, #23763, #18843 ),
 ( #41851, #64860, #30536 ) ),
 .UNSPECIFIED., .F., .F., .F. ) 
 B_SPLINE_SURFACE_WITH_KNOTS ( ( 4, 2, 2, 2, 2, 2, 2, 2, 4 ),
 ( 3, 3 ),
 ( 0.04202945594032914123, 0.04396162471216785717, 0.04589379348400656616, 0.04782596225584527516, 0.04975813102768399110, 0.05169029979952270704, 0.05265638418544206500, 0.05362246857136142297, 0.05748680611503884791 ),
 ( 0.000000000000000000, 1.000000000000000000 ),
 .UNSPECIFIED. ) 
 GEOMETRIC_REPRESENTATION_ITEM ( )  RATIONAL_B_SPLINE_SURFACE ( (
 ( 1.000000000000000000, 0.6241276099608163985, 1.000000000000000000),
 ( 1.000000000000000000, 0.6218761496800119248, 1.000000000000000000),
 ( 1.000000000000000000, 0.6198047272364380911, 1.000000000000000000),
 ( 1.000000000000000000, 0.6161935119824036855, 1.000000000000000000),
 ( 1.000000000000000000, 0.6146642324079838460, 1.000000000000000000),
 ( 1.000000000000000000, 0.6121850116872165071, 1.000000000000000000),
 ( 1.000000000000000000, 0.6112350889399397191, 1.000000000000000000),
 ( 1.000000000000000000, 0.6099522725973182125, 1.000000000000000000),
 ( 1.000000000000000000, 0.6096208180308724245, 1.000000000000000000),
 ( 1.000000000000000000, 0.6096183796348639827, 1.000000000000000000),
 ( 1.000000000000000000, 0.6099422200103278291, 1.000000000000000000),
 ( 1.000000000000000000, 0.6109087447822608707, 1.000000000000000000),
 ( 1.000000000000000000, 0.6113123981687891284, 1.000000000000000000),
 ( 1.000000000000000000, 0.6122677719809712649, 1.000000000000000000),
 ( 1.000000000000000000, 0.6128199619020906486, 1.000000000000000000),
 ( 1.000000000000000000, 0.6159350830266026033, 1.000000000000000000),
 ( 1.000000000000000000, 0.6195556778515390883, 1.000000000000000000),
 ( 1.000000000000000000, 0.6241278272307889674, 1.000000000000000000) ) ) 
 REPRESENTATION_ITEM ( '' )  SURFACE ( )  );
#18438 = CARTESIAN_POINT ( 'NONE',  ( -2.679491924311235618, 150.4166666598387110, 10.00000000000000000 ) ) ;
#18439 = CARTESIAN_POINT ( 'NONE',  ( 2.977408999572650039, 95.56250000204838102, -7.188101187500001821 ) ) ;
#18440 = CARTESIAN_POINT ( 'NONE',  ( 4.999999999999998224, 19.16666666666667140, 8.660254037844396180 ) ) ;
#18441 = CARTESIAN_POINT ( 'NONE',  ( 11.35316468749999785, 45.88541666325267698, 3.042071309553174174 ) ) ;
#18442 = CARTESIAN_POINT ( 'NONE',  ( 10.18810118749999916, 4.220049686691935698, 113.8750000020483810 ) ) ;
#18443 = CARTESIAN_POINT ( 'NONE',  ( -5.676582343750006032, 199.1145833299193555, 9.832129032723418760 ) ) ;
#18444 = ORIENTED_EDGE ( 'NONE', *, *, #10768, .F. ) ;
#18445 = CARTESIAN_POINT ( 'NONE',  ( 1.877992804784440972, 65.87054549411425342, 26.34444121134915662 ) ) ;
#18446 = CARTESIAN_POINT ( 'NONE',  ( 2.729887517050593182, 10.18810118749999916, 67.22060451829246119 ) ) ;
#18447 = LINE ( 'NONE', #53524, #25064 ) ;
#18449 = CARTESIAN_POINT ( 'NONE',  ( 11.35316468750000141, 175.7812499965860411, 0.000000000000000000 ) ) ;
#18448 = CARTESIAN_POINT ( 'NONE',  ( 4.000000000000016875, 195.4375000000000000, 199.6568542494924259 ) ) ;
#18450 = CIRCLE ( 'NONE', #53399, 18.00000000000000000 ) ;
#18451 = DIRECTION ( 'NONE',  ( 0.000000000000000000, 0.000000000000000000, 1.000000000000000000 ) ) ;
#18452 = CARTESIAN_POINT ( 'NONE',  ( 9.999999999999998224, 255.8333333401613459, -2.679491924311229401 ) ) ;
#18453 = CARTESIAN_POINT ( 'NONE',  ( 7.999999999999991118, 0.000000000000000000, 30.00000000000000000 ) ) ;
#18454 = ORIENTED_EDGE ( 'NONE', *, *, #23183, .T. ) ;
#18455 = CARTESIAN_POINT ( 'NONE',  ( 5.676582343750001591, 161.9270833299193555, -9.832129032723420536 ) ) ;
#18456 =( BOUNDED_CURVE ( )  B_SPLINE_CURVE ( 2, ( #1539, #58871, #41145, #58144, #53574, #52463, #47894, #24519, #65622, #47524, #64150, #13552, #70549 ),
 .UNSPECIFIED., .F., .F. ) 
 B_SPLINE_CURVE_WITH_KNOTS ( ( 3, 2, 2, 2, 2, 2, 3 ),
 ( 0.3055555555555551916, 0.3148148148148144365, 0.3240740740740736814, 0.3333333333333329263, 0.3425925925925922821, 0.3518518518518515270, 0.3611111111111107719 ),
 .UNSPECIFIED. ) 
 CURVE ( )  GEOMETRIC_REPRESENTATION_ITEM ( )  RATIONAL_B_SPLINE_CURVE ( ( 1.000000000000001332, 0.9659258262890668689, 1.000000000000000000, 0.9659258262890683122, 1.000000000000000000, 0.9659258262890683122, 1.000000000000000000, 0.9659258262890683122, 1.000000000000000000, 0.9659258262890683122, 1.000000000000000000, 0.9659258262890695335, 0.9999999999999987788 ) ) 
 REPRESENTATION_ITEM ( '' )  );
#18457 = CARTESIAN_POINT ( 'NONE',  ( -2.977408999572647819, -7.188101187499990274, 25.76780278187175810 ) ) ;
#18458 = CARTESIAN_POINT ( 'NONE',  ( -3.042071309553173730, 129.6354166632526415, 11.35316468749999785 ) ) ;
#18459 = CARTESIAN_POINT ( 'NONE',  ( -5.656854249492379694, 3.374999995903220640, -5.656854249492380582 ) ) ;
#18460 = ORIENTED_EDGE ( 'NONE', *, *, #71666, .T. ) ;
#18461 = CARTESIAN_POINT ( 'NONE',  ( -5.656854249492380582, 104.0000000040967905, -5.656854249492380582 ) ) ;
#18462 = VECTOR ( 'NONE', #51371, 1000.000000000000000 ) ;
#18463 = CARTESIAN_POINT ( 'NONE',  ( 2.828427124746190291, 10.87500000000000178, 2.828427124746192067 ) ) ;
#18464 = DIRECTION ( 'NONE',  ( -0.000000000000000000, 1.000000000000000000, -1.563033456626094573E-30 ) ) ;
#18465 = CARTESIAN_POINT ( 'NONE',  ( -1.881053915767124440, 10.99999999863440969, 4.541265875000001451 ) ) ;
#18466 = CARTESIAN_POINT ( 'NONE',  ( 7.999999999999991118, 3.313708498984757611, 21.36155278392014978 ) ) ;
#18467 = CARTESIAN_POINT ( 'NONE',  ( 11.00000000000000000, 1.347111479062088405E-15, 78.43750000409677625 ) ) ;
#18468 = ORIENTED_EDGE ( 'NONE', *, *, #19433, .F. ) ;
#18469 = CARTESIAN_POINT ( 'NONE',  ( 2.828427124746153876, 204.8750000000000284, 144.8284271247462129 ) ) ;
#18470 = CARTESIAN_POINT ( 'NONE',  ( -7.188101187499999156, 95.75000000204836681, 2.977408999572654924 ) ) ;
#18472 = DIRECTION ( 'NONE',  ( 0.000000000000000000, 0.000000000000000000, 1.000000000000000000 ) ) ;
#18471 = CARTESIAN_POINT ( 'NONE',  ( 4.898587196589412829E-16, 16.68749999590322375, -8.000000000000000000 ) ) ;
#18473 = CARTESIAN_POINT ( 'NONE',  ( 0.000000000000000000, 0.000000000000000000, 0.000000000000000000 ) ) ;
#18474 = ORIENTED_EDGE ( 'NONE', *, *, #255, .F. ) ;
#18475 = CARTESIAN_POINT ( 'NONE',  ( -2.591411123065824551, 10.27614846265000637, -63.77676950207272455 ) ) ;
#18476 = CARTESIAN_POINT ( 'NONE',  ( -8.000000000000000000, 104.1875000040967763, 0.000000000000000000 ) ) ;
#18477 = EDGE_CURVE ( 'NONE', #31066, #3802, #50551, .T. ) ;
#18478 = CARTESIAN_POINT ( 'NONE',  ( -5.082755093536319713, 5.082755093536319713, 25.29905278187175810 ) ) ;
#18479 = VERTEX_POINT ( 'NONE', #67909 ) ;
#18480 = ORIENTED_EDGE ( 'NONE', *, *, #74600, .T. ) ;
#18481 = CARTESIAN_POINT ( 'NONE',  ( 10.18810118750000093, -4.220049686691933033, 87.81250000204838102 ) ) ;
#18482 = UNCERTAINTY_MEASURE_WITH_UNIT (LENGTH_MEASURE( 1.000000000000000082E-05 ), #3438, 'distance_accuracy_value', 'NONE');
#18483 = CARTESIAN_POINT ( 'NONE',  ( -31.45873412499999944, 196.8750000013656347, 168.5673454167827572 ) ) ;
#18484 = CARTESIAN_POINT ( 'NONE',  ( 4.556349186104051263, -10.99999999999999822, 98.96875000000000000 ) ) ;
#18487 = FACE_OUTER_BOUND ( 'NONE', #24400, .T. ) ;
#18486 = CARTESIAN_POINT ( 'NONE',  ( 26.34314575050763807, 201.0625000027312126, 173.9999999999999147 ) ) ;
#18485 = CARTESIAN_POINT ( 'NONE',  ( -27.99999999999991118, 198.6250000027312126, 174.0000000000003695 ) ) ;
#18488 = CARTESIAN_POINT ( 'NONE',  ( -1.836970198721029983E-15, 133.7500000000000000, 10.00000000000000178 ) ) ;
#18489 = AXIS2_PLACEMENT_3D ( 'NONE', #46792, #17753, #52101 ) ;
#18490 = CARTESIAN_POINT ( 'NONE',  ( -28.00000000000007816, 204.1250000027312126, 166.0000000000003695 ) ) ;
#18491 = FACE_OUTER_BOUND ( 'NONE', #72477, .T. ) ;
#18492 = CYLINDRICAL_SURFACE ( 'NONE', #3707, 7.999999999999991118 ) ;
#18493 = CARTESIAN_POINT ( 'NONE',  ( 29.43265458321766559, 202.8750000013656347, 166.5412658749999650 ) ) ;
#18494 = CARTESIAN_POINT ( 'NONE',  ( -5.082755093536326818, 7.781249997951610986, 5.082755093536325042 ) ) ;
#18495 = CARTESIAN_POINT ( 'NONE',  ( -5.662595241051933570, -5.662595241051936235, 2.700615283940627886 ) ) ;
#18496 = CARTESIAN_POINT ( 'NONE',  ( 3.458734124999959914, 196.3750000013656063, 143.4326545832176976 ) ) ;
#18497 = CARTESIAN_POINT ( 'NONE',  ( 2.977408999572650039, 115.0625000020483810, -7.188101187500000933 ) ) ;
#18499 = CYLINDRICAL_SURFACE ( 'NONE', #18489, 10.00000000000000178 ) ;
#18498 = CARTESIAN_POINT ( 'NONE',  ( 4.898587196589412829E-16, 6.375000000000000888, -8.000000000000000000 ) ) ;
#18500 = CARTESIAN_POINT ( 'NONE',  ( 9.832129032723420536, 231.3020833367473301, 5.676582343749996262 ) ) ;
#18501 = CARTESIAN_POINT ( 'NONE',  ( -34.01307589418283328, 40.47055483369444318, 65.00000000000000000 ) ) ;
#18502 = CARTESIAN_POINT ( 'NONE',  ( -4.401442555609577197E-16, 7.188101187499992051, 28.48655278187175810 ) ) ;
#18503 = CARTESIAN_POINT ( 'NONE',  ( 28.00000000000001776, 198.5000000000000000, 165.9999999999998863 ) ) ;
#18504 = CARTESIAN_POINT ( 'NONE',  ( -11.35316468750000141, 33.28124999658601979, -1.390361679473963753E-15 ) ) ;
#18505 = CARTESIAN_POINT ( 'NONE',  ( -5.656854249492379694, 9.562500000000001776, -5.656854249492380582 ) ) ;
#18506 = CARTESIAN_POINT ( 'NONE',  ( -8.311093377946841443, 219.2187499965859843, 8.311093377946830785 ) ) ;
#18507 = CARTESIAN_POINT ( 'NONE',  ( 28.00000000000002132, 201.1250000027312126, 173.9999999999999147 ) ) ;
#18509 = DIRECTION ( 'NONE',  ( 0.000000000000000000, 0.000000000000000000, 1.000000000000000000 ) ) ;
#18508 = CARTESIAN_POINT ( 'NONE',  ( 0.8721677472748811111, -16.44158143986581777, 68.58266913489941885 ) ) ;
#18510 = ORIENTED_EDGE ( 'NONE', *, *, #47743, .F. ) ;
#18512 = EDGE_CURVE ( 'NONE', #30899, #54369, #32855, .T. ) ;
#18511 = CARTESIAN_POINT ( 'NONE',  ( 1.432654583217607414, 197.5000000013656063, 145.4587341250000634 ) ) ;
#18513 = EDGE_CURVE ( 'NONE', #57615, #11773, #37533, .T. ) ;
#18514 = CARTESIAN_POINT ( 'NONE',  ( 3.042071309553159519, 34.73958332991934839, 11.35316468750000141 ) ) ;
#18515 = CARTESIAN_POINT ( 'NONE',  ( 11.00000000000000000, 1.347111479062088405E-15, 87.43750000409677625 ) ) ;
#18516 = CARTESIAN_POINT ( 'NONE',  ( -2.754378923186476579E-14, 207.4375000013656063, 145.4587341250000350 ) ) ;
#18517 = CARTESIAN_POINT ( 'NONE',  ( 7.778174593052023411, -7.778174593052021635, 111.2500000040967763 ) ) ;
#18518 = DIRECTION ( 'NONE',  ( -0.000000000000000000, 1.000000000000000000, -0.000000000000000000 ) ) ;
#18520 = CARTESIAN_POINT ( 'NONE',  ( -3.042071309553173730, 14.32291666325268231, 11.35316468749999785 ) ) ;
#18519 = CARTESIAN_POINT ( 'NONE',  ( -7.188101187500000933, 106.0625000020483668, -2.977408999572650483 ) ) ;
#18521 = CARTESIAN_POINT ( 'NONE',  ( -4.898587196589407898E-16, 7.999999999999991118, 16.95530277982336287 ) ) ;
#18522 = CARTESIAN_POINT ( 'NONE',  ( 5.676582343749993598, 149.9479166632526983, 9.832129032723422313 ) ) ;
#18523 = CARTESIAN_POINT ( 'NONE',  ( 8.660254037844385522, 116.4583333265053824, 5.000000000000005329 ) ) ;
#18524 = CARTESIAN_POINT ( 'NONE',  ( 2.977408999572650039, 113.5625000020483668, -7.188101187500001821 ) ) ;
#18525 = PLANE ( 'NONE',  #57791 ) ;
#18526 = CARTESIAN_POINT ( 'NONE',  ( -30.44569435410883429, 205.8125000013656063, 167.5543056458915885 ) ) ;
#18527 = AXIS2_PLACEMENT_3D ( 'NONE', #53356, #47670, #48413 ) ;
#18528 = VERTEX_POINT ( 'NONE', #15838 ) ;
#18529 = CARTESIAN_POINT ( 'NONE',  ( -11.35316468750000141, 8.593749996586016238, -1.390361679473963753E-15 ) ) ;
#18530 = EDGE_LOOP ( 'NONE', ( #48855, #69847, #6252, #40946 ) ) ;
#18531 = DIRECTION ( 'NONE',  ( 0.000000000000000000, 0.000000000000000000, 1.000000000000000000 ) ) ;
#18532 = CARTESIAN_POINT ( 'NONE',  ( -6.676582343750003368, 299.3906250017069510, -2.765530957081996810 ) ) ;
#18534 = CARTESIAN_POINT ( 'NONE',  ( -9.832129032723420536, 133.6979166632526983, 5.676582343749997150 ) ) ;
#18533 = CARTESIAN_POINT ( 'NONE',  ( -8.000000000000000000, 108.5000000000000000, 0.000000000000000000 ) ) ;
#18535 = CARTESIAN_POINT ( 'NONE',  ( -4.000000000000001776, 16.18749999726881228, -1.656854249492381470 ) ) ;
#18536 = CARTESIAN_POINT ( 'NONE',  ( -7.999999999999989342, -3.313708498984762496, 17.48030278432982598 ) ) ;
#18537 = FACE_OUTER_BOUND ( 'NONE', #43330, .T. ) ;
#18538 = CARTESIAN_POINT ( 'NONE',  ( -5.676582343749992710, 244.7395833367473301, 9.832129032723422313 ) ) ;
#18539 = ADVANCED_FACE ( 'NONE', ( #33229 ), #55483, .F. ) ;
#18540 = CARTESIAN_POINT ( 'NONE',  ( 7.204075437095966983, 7.204075437095967871, 91.46875000204838102 ) ) ;
#18541 = ORIENTED_EDGE ( 'NONE', *, *, #4346, .T. ) ;
#18542 = CARTESIAN_POINT ( 'NONE',  ( -7.320508075688773708, 203.7499999931720538, -7.320508075688774596 ) ) ;
#18543 = FACE_OUTER_BOUND ( 'NONE', #51385, .T. ) ;
#18544 = CARTESIAN_POINT ( 'NONE',  ( 9.832129032723416984, 90.67708332991934128, 5.676582343750006032 ) ) ;
#18545 =( BOUNDED_CURVE ( )  B_SPLINE_CURVE ( 2, ( #42624, #55456, #65639, #42990, #71660, #49401, #59982, #15067, #61100 ),
 .UNSPECIFIED., .F., .F. ) 
 B_SPLINE_CURVE_WITH_KNOTS ( ( 3, 2, 2, 2, 3 ),
 ( 0.8750000000000000000, 0.8819444444444444198, 0.8888888888888888395, 0.8958333333333332593, 0.9027777777777776791 ),
 .UNSPECIFIED. ) 
 CURVE ( )  GEOMETRIC_REPRESENTATION_ITEM ( )  RATIONAL_B_SPLINE_CURVE ( ( 1.000000000000000000, 0.9238795325112867385, 1.000000000000000000, 0.9238795325112867385, 1.000000000000000000, 0.9238795325112867385, 1.000000000000000000, 0.9238795325112879597, 0.9999999999999987788 ) ) 
 REPRESENTATION_ITEM ( '' )  );
#18546 = CARTESIAN_POINT ( 'NONE',  ( -4.220049686691935698, 10.18810118749999916, 98.87500000204836681 ) ) ;
#18547 = CARTESIAN_POINT ( 'NONE',  ( -4.541265875000002339, 16.87499999863440436, -1.881053915767121998 ) ) ;
#18548 = ORIENTED_EDGE ( 'NONE', *, *, #55893, .T. ) ;
#18549 = ORIENTED_EDGE ( 'NONE', *, *, #5736, .F. ) ;
#18550 = VECTOR ( 'NONE', #35017, 1000.000000000000000 ) ;
#18551 = CARTESIAN_POINT ( 'NONE',  ( 3.313708498984762496, 5.718750000000000888, 7.999999999999998224 ) ) ;
#18552 = CARTESIAN_POINT ( 'NONE',  ( 2.780723358947928197E-16, 1.687499998634406806, -4.541265875000002339 ) ) ;
#18553 = CARTESIAN_POINT ( 'NONE',  ( -1.320432766682874540E-15, 1.593749997951610098, 7.188101187500000044 ) ) ;
#18554 = CARTESIAN_POINT ( 'NONE',  ( 4.556349186104045934, 11.00000000000000000, 96.53125000000000000 ) ) ;
#18555 = CARTESIAN_POINT ( 'NONE',  ( -7.204075437095967871, 7.204075437095967871, 105.3437500020483810 ) ) ;
#18556 = LINE ( 'NONE', #52521, #19744 ) ;
#18557 = CARTESIAN_POINT ( 'NONE',  ( 2.828427124746191623, 12.87499999726881406, -2.828427124746191623 ) ) ;
#18558 = CARTESIAN_POINT ( 'NONE',  ( 24.00000000000000711, 209.6875000000000284, 168.3431457505074889 ) ) ;
#18559 = ORIENTED_EDGE ( 'NONE', *, *, #4346, .F. ) ;
#18560 = CARTESIAN_POINT ( 'NONE',  ( -2.679491924311383499, 262.0833333401613459, -9.999999999999909406 ) ) ;
#18561 = CARTESIAN_POINT ( 'NONE',  ( -3.458734124999959025, 198.5000000013656347, 199.4326545832176691 ) ) ;
#18563 = FACE_OUTER_BOUND ( 'NONE', #57439, .T. ) ;
#18562 = CARTESIAN_POINT ( 'NONE',  ( -24.54126587499996148, 199.1250000013656347, 171.4326545832179534 ) ) ;
#18564 =( NAMED_UNIT ( * ) SI_UNIT ( $, .STERADIAN. ) SOLID_ANGLE_UNIT ( ) );
#18565 = CARTESIAN_POINT ( 'NONE',  ( -1.881053915767124440, 14.99999999863440969, 4.541265875000001451 ) ) ;
#18566 = CARTESIAN_POINT ( 'NONE',  ( 2.828427124746191623, 12.12500000000000000, -2.828427124746191623 ) ) ;
#18567 = AXIS2_PLACEMENT_3D ( 'NONE', #4826, #46288, #33882 ) ;
#18568 = CARTESIAN_POINT ( 'NONE',  ( -2.977408999572647819, 7.188101187499991163, 14.70530278187175455 ) ) ;
#18569 = VERTEX_POINT ( 'NONE', #28290 ) ;
#18570 = ORIENTED_EDGE ( 'NONE', *, *, #56439, .F. ) ;
#18571 = CARTESIAN_POINT ( 'NONE',  ( -4.220049686691935698, 10.18810118749999916, 104.8750000020483668 ) ) ;
#18572 = CARTESIAN_POINT ( 'NONE',  ( -9.999999999999987566, 97.29166666666667140, -2.679491924311226736 ) ) ;
#18573 = CARTESIAN_POINT ( 'NONE',  ( -32.00000000000001421, 206.1875000000000568, 168.3431457505080004 ) ) ;
#18574 = CARTESIAN_POINT ( 'NONE',  ( 3.458734125000015425, 197.0000000013656347, 196.5673454167823877 ) ) ;
#18575 = LINE ( 'NONE', #41585, #42228 ) ;
#18576 = CARTESIAN_POINT ( 'NONE',  ( 8.660254037844385522, 89.58333333333332860, 5.000000000000005329 ) ) ;
#18577 = ADVANCED_FACE ( 'NONE', ( #56227 ), #21133, .T. ) ;
#18578 = CARTESIAN_POINT ( 'NONE',  ( 1.469576158976823947E-15, 119.3750000000000000, 8.000000000000000000 ) ) ;
#18579 = CARTESIAN_POINT ( 'NONE',  ( -11.35316468749999785, 58.38541666325268409, -3.042071309553167513 ) ) ;
#18580 = CARTESIAN_POINT ( 'NONE',  ( 1.226468279477575784E-15, 294.8593750017070079, 6.676582343750001591 ) ) ;
#18581 = ORIENTED_EDGE ( 'NONE', *, *, #69806, .T. ) ;
#18582 = CARTESIAN_POINT ( 'NONE',  ( -10.00000000000000178, 144.3749999931720538, -1.224646799147353454E-15 ) ) ;
#18583 = CARTESIAN_POINT ( 'NONE',  ( 8.000000000000000000, 13.40624999590322375, -3.313708498984761608 ) ) ;
#18584 = CARTESIAN_POINT ( 'NONE',  ( 1.432654583217607192, 206.2500000013656063, 145.4587341250000634 ) ) ;
#18585 = CARTESIAN_POINT ( 'NONE',  ( -1.744157829248402118E-12, 86.25000000000015632, -10.00000000000000533 ) ) ;
#18586 = CARTESIAN_POINT ( 'NONE',  ( 4.000000000000001776, 8.000000000000000000, 0.000000000000000000 ) ) ;
#18587 = CARTESIAN_POINT ( 'NONE',  ( -9.999999999999998224, 230.2083333333333428, 2.679491924311235618 ) ) ;
#18588 = CARTESIAN_POINT ( 'NONE',  ( 11.00000000000000000, 4.556349186104045934, 72.53125000409677625 ) ) ;
#18589 = CARTESIAN_POINT ( 'NONE',  ( -10.18810118749999916, 0.000000000000000000, 71.03125000204838102 ) ) ;
#18590 = CARTESIAN_POINT ( 'NONE',  ( 2.679491924311228956, 211.0416666666666572, -10.00000000000000000 ) ) ;
#18591 = CARTESIAN_POINT ( 'NONE',  ( -7.188101187499990274, -2.977408999572651815, 10.95530278187175455 ) ) ;
#18592 = CARTESIAN_POINT ( 'NONE',  ( 11.35316468750000141, 181.0937499965860411, 0.000000000000000000 ) ) ;
#18593 = CARTESIAN_POINT ( 'NONE',  ( -4.541265875000003227, 0.8749999986344069169, 1.881053915767121110 ) ) ;
#18594 = CARTESIAN_POINT ( 'NONE',  ( -3.313708498984762496, 99.96875000409676204, 7.999999999999998224 ) ) ;
#18596 = CARTESIAN_POINT ( 'NONE',  ( 2.828427124746190291, 4.875000000000000000, 2.828427124746192067 ) ) ;
#18595 = CARTESIAN_POINT ( 'NONE',  ( -5.656854249492373476, -5.656854249492376141, 20.51780277982336642 ) ) ;
#18597 = ORIENTED_EDGE ( 'NONE', *, *, #52290, .T. ) ;
#18598 = VECTOR ( 'NONE', #39828, 1000.000000000000000 ) ;
#18600 = EDGE_CURVE ( 'NONE', #66108, #28197, #30882, .T. ) ;
#18599 = CARTESIAN_POINT ( 'NONE',  ( 2.445694354108783219, 206.8125000013656063, 139.5543056458912190 ) ) ;
#18601 = CARTESIAN_POINT ( 'NONE',  ( -5.676582343750006032, 34.42708332991935549, 9.832129032723418760 ) ) ;
#18602 = CARTESIAN_POINT ( 'NONE',  ( 4.556349186104045934, 11.00000000000000000, 104.2187500040968047 ) ) ;
#18603 = CARTESIAN_POINT ( 'NONE',  ( 4.643183940729320724, 227.0088029853575620, -10.42876187888753847 ) ) ;
#18604 = CARTESIAN_POINT ( 'NONE',  ( -25.55430564589122966, 205.3125000013656063, 167.5543056458915032 ) ) ;
#18605 = CARTESIAN_POINT ( 'NONE',  ( 8.000000000000000000, 4.312499995903220196, 0.000000000000000000 ) ) ;
#18607 = LINE ( 'NONE', #69549, #528 ) ;
#18606 = CARTESIAN_POINT ( 'NONE',  ( -7.188101187500000044, 121.1562500020483810, 0.000000000000000000 ) ) ;
#18608 = CARTESIAN_POINT ( 'NONE',  ( -3.458734125000015425, 195.0000000013656063, 143.4326545832176976 ) ) ;
#18609 = EDGE_CURVE ( 'NONE', #45292, #49304, #38607, .T. ) ;
#18610 = CARTESIAN_POINT ( 'NONE',  ( 10.00000000000000178, 82.08333332650535397, -2.679491924311226736 ) ) ;
#18611 = CARTESIAN_POINT ( 'NONE',  ( 2.977408999572654480, 94.62500000204838102, 7.188101187499999156 ) ) ;
#18612 = CARTESIAN_POINT ( 'NONE',  ( 3.211159895383560947, 15.31249999863440792, 3.211159895383562723 ) ) ;
#18613 = CARTESIAN_POINT ( 'NONE',  ( 0.000000000000000000, 0.000000000000000000, 118.0000000000000000 ) ) ;
#18614 = CARTESIAN_POINT ( 'NONE',  ( 5.117192270959802336, 0.3122852236289677674, -5.908609428792219731 ) ) ;
#18615 = DIRECTION ( 'NONE',  ( -0.000000000000000000, 1.000000000000000000, -0.000000000000000000 ) ) ;
#18616 = ORIENTED_EDGE ( 'NONE', *, *, #31532, .F. ) ;
#18617 = ORIENTED_EDGE ( 'NONE', *, *, #51557, .F. ) ;
#18618 = CARTESIAN_POINT ( 'NONE',  ( -6.676582343750001591, 297.6093750017069510, 0.000000000000000000 ) ) ;
#18619 = CARTESIAN_POINT ( 'NONE',  ( 0.000000000000000000, 0.000000000000000000, -14.00000000000000178 ) ) ;
#18620 = CARTESIAN_POINT ( 'NONE',  ( -6.024380653971853405, -6.914127053141861268, -0.09252763182293101407 ) ) ;
#18621 = CARTESIAN_POINT ( 'NONE',  ( 11.35316468749999963, 160.9895833299193839, -3.042071309553165293 ) ) ;
#18622 = CARTESIAN_POINT ( 'NONE',  ( 10.18810118750000093, -4.220049686691933921, 80.31250000204836681 ) ) ;
#18623 = DIRECTION ( 'NONE',  ( 0.000000000000000000, 0.000000000000000000, 1.000000000000000000 ) ) ;
#18624 = CARTESIAN_POINT ( 'NONE',  ( 4.000000000000015099, 202.5625000000000000, 196.3431457505076594 ) ) ;
#18625 = DIRECTION ( 'NONE',  ( 0.000000000000000000, 0.000000000000000000, 1.000000000000000000 ) ) ;
#18626 = EDGE_CURVE ( 'NONE', #15222, #20958, #66431, .T. ) ;
#18627 = CARTESIAN_POINT ( 'NONE',  ( 4.220049686691941027, -10.18810118749999738, 109.0000000020483810 ) ) ;
#18628 = VERTEX_POINT ( 'NONE', #12417 ) ;
#18629 = CARTESIAN_POINT ( 'NONE',  ( -3.999999999999960032, 202.1250000027312126, 198.0000000000000284 ) ) ;
#18630 = VECTOR ( 'NONE', #30528, 1000.000000000000000 ) ;
#18631 = CARTESIAN_POINT ( 'NONE',  ( 2.775557561562891351E-14, 210.0000000000000284, 198.0000000000000284 ) ) ;
#18632 = CARTESIAN_POINT ( 'NONE',  ( 11.35316468750000141, 141.0937499965860127, 0.000000000000000000 ) ) ;
#18633 = CARTESIAN_POINT ( 'NONE',  ( -3.458734124999959914, 200.4375000013656063, 198.0000000000000284 ) ) ;
#18634 = CARTESIAN_POINT ( 'NONE',  ( -6.000000000000001776, 291.0000000000000000, 0.000000000000000000 ) ) ;
#18635 = CARTESIAN_POINT ( 'NONE',  ( 10.18810118749999916, 4.220049686691935698, 76.37500000204838102 ) ) ;
#18636 = CARTESIAN_POINT ( 'NONE',  ( 9.832129032723416984, 50.67708332991935549, 5.676582343750006032 ) ) ;
#18637 = ORIENTED_EDGE ( 'NONE', *, *, #42173, .T. ) ;
#18638 = CARTESIAN_POINT ( 'NONE',  ( -11.00000000000000000, 0.000000000000000000, 94.18750000409677625 ) ) ;
#18639 = CARTESIAN_POINT ( 'NONE',  ( 1.881053915767122664, 4.249999998634407028, 4.541265875000001451 ) ) ;
#18640 = CARTESIAN_POINT ( 'NONE',  ( 8.008118988124993010, -3.317071493978877239, 12.16936528394062833 ) ) ;
#18641 = ADVANCED_FACE ( 'NONE', ( #16962 ), #53163, .T. ) ;
#18642 = CARTESIAN_POINT ( 'NONE',  ( -5.082755093536326818, 14.90624999795161187, 5.082755093536325042 ) ) ;
#18643 = CARTESIAN_POINT ( 'NONE',  ( -6.000000000000003553, 292.0000000034139589, -2.485281374238571317 ) ) ;
#18644 = CARTESIAN_POINT ( 'NONE',  ( 1.656854249492354825, 202.3125000000000000, 202.0000000000000853 ) ) ;
#18645 = CARTESIAN_POINT ( 'NONE',  ( 4.401442555609581635E-16, 13.21874999795161187, -7.188101187500000044 ) ) ;
#18646 = CARTESIAN_POINT ( 'NONE',  ( -7.188101187499992051, 2.977408999572646930, 10.39280278187175632 ) ) ;
#18647 = CARTESIAN_POINT ( 'NONE',  ( 4.220049686691934809, 10.18810118749999916, 73.18750000204838102 ) ) ;
#18648 = ADVANCED_FACE ( 'NONE', ( #52051 ), #23745, .F. ) ;
#18649 = CARTESIAN_POINT ( 'NONE',  ( -25.55430564589119768, 206.5625000013656063, 167.5543056458915316 ) ) ;
#18650 = CARTESIAN_POINT ( 'NONE',  ( 2.828427124746191623, 1.874999997268813390, -2.828427124746191623 ) ) ;
#18651 = ORIENTED_EDGE ( 'NONE', *, *, #2333, .T. ) ;
#18652 = CARTESIAN_POINT ( 'NONE',  ( 3.458734125000016313, 208.8750000013656347, 199.4326545832176691 ) ) ;
#18653 = CARTESIAN_POINT ( 'NONE',  ( 3.999999999999959144, 202.0625000000000284, 140.3431457505076594 ) ) ;
#18655 =( BOUNDED_CURVE ( )  B_SPLINE_CURVE ( 2, ( #60949, #44348, #22060, #39062, #4735, #4360, #33052, #3611, #26607 ),
 .UNSPECIFIED., .F., .F. ) 
 B_SPLINE_CURVE_WITH_KNOTS ( ( 3, 2, 2, 2, 3 ),
 ( 0.2291666666666645480, 0.2395833333333312609, 0.2499999999999979183, 0.2604166666666646313, 0.2708333333333312609 ),
 .UNSPECIFIED. ) 
 CURVE ( )  GEOMETRIC_REPRESENTATION_ITEM ( )  RATIONAL_B_SPLINE_CURVE ( ( 1.000000000000015321, 0.9238795325112713064, 1.000000000000000000, 0.9238795325112867385, 1.000000000000000000, 0.9238795325112867385, 1.000000000000000000, 0.9238795325113017265, 0.9999999999999850120 ) ) 
 REPRESENTATION_ITEM ( '' )  );
#18654 = CARTESIAN_POINT ( 'NONE',  ( -28.00000000000007816, 199.1250000027312126, 166.0000000000003695 ) ) ;
#18656 = CARTESIAN_POINT ( 'NONE',  ( -3.211159895383562723, 1.937499998634406806, 3.211159895383561391 ) ) ;
#18657 = CARTESIAN_POINT ( 'NONE',  ( 7.188101187500002709, 115.8125000020484094, 2.977408999572649151 ) ) ;
#18658 = CARTESIAN_POINT ( 'NONE',  ( 0.000000000000000000, 300.0000000000000000, 10.00000000000000178 ) ) ;
#18659 = CARTESIAN_POINT ( 'NONE',  ( -7.188101187499991163, 2.977408999572646930, 28.39280278187175810 ) ) ;
#18660 = VERTEX_POINT ( 'NONE', #69769 ) ;
#18661 = CARTESIAN_POINT ( 'NONE',  ( -7.188101187500000044, 22.21874999795161187, -8.802885111219163269E-16 ) ) ;
#18662 = EDGE_LOOP ( 'NONE', ( #52364, #7534, #21859, #42490 ) ) ;
#18663 = CARTESIAN_POINT ( 'NONE',  ( 7.320508075688771044, 256.2500000068279746, -7.320508075688771932 ) ) ;
#18664 = DIRECTION ( 'NONE',  ( -0.000000000000000000, 1.000000000000000000, -0.000000000000000000 ) ) ;
#18665 = CARTESIAN_POINT ( 'NONE',  ( 24.54126587500000767, 207.2500000013655779, 171.4326545832176123 ) ) ;
#18666 = CARTESIAN_POINT ( 'NONE',  ( 5.000000000000001776, 50.83333333333333570, -8.660254037844389075 ) ) ;
#18667 = CARTESIAN_POINT ( 'NONE',  ( -2.977408999572651815, 102.3125000020483810, 7.188101187500000933 ) ) ;
#18668 = CARTESIAN_POINT ( 'NONE',  ( 1.102182119232618108E-15, 297.2500000000000000, 6.000000000000001776 ) ) ;
#18669 = AXIS2_PLACEMENT_3D ( 'NONE', #17630, #63654, #11980 ) ;
#18671 = CARTESIAN_POINT ( 'NONE',  ( -22.95497581444661250, -39.50625172345834812, 190.8358528039529460 ) ) ;
#18670 = CARTESIAN_POINT ( 'NONE',  ( -3.313708498984761608, 88.90625000409677625, -8.000000000000000000 ) ) ;
#18672 = ORIENTED_EDGE ( 'NONE', *, *, #52380, .F. ) ;
#18673 = CARTESIAN_POINT ( 'NONE',  ( -9.832129032723415207, 234.3229166700806445, 5.676582343750005144 ) ) ;
#18674 = CARTESIAN_POINT ( 'NONE',  ( -5.082755093536317936, -5.082755093536320601, 11.04905278187175455 ) ) ;
#18675 = VECTOR ( 'NONE', #24778, 1000.000000000000000 ) ;
#18676 = DIRECTION ( 'NONE',  ( 0.000000000000000000, 0.000000000000000000, 1.000000000000000000 ) ) ;
#18677 = DIRECTION ( 'NONE',  ( -0.000000000000000000, 1.000000000000000000, 4.476705744456276341E-16 ) ) ;
#18678 = CARTESIAN_POINT ( 'NONE',  ( -2.828427124746192067, 17.37499999726881583, 2.828427124746190735 ) ) ;
#18679 = CARTESIAN_POINT ( 'NONE',  ( -5.000000000000000888, 264.1666666666666856, -8.660254037844387298 ) ) ;
#18681 = EDGE_CURVE ( 'NONE', #2593, #33835, #46306, .T. ) ;
#18680 = CARTESIAN_POINT ( 'NONE',  ( -2.849036369511732440E-14, 195.3750000027311842, 138.0000000000000568 ) ) ;
#18682 = CARTESIAN_POINT ( 'NONE',  ( -1.836970198721029983E-15, 173.7500000000000284, 10.00000000000000178 ) ) ;
#18683 = CARTESIAN_POINT ( 'NONE',  ( 4.242640687119287435, 297.4375000034140157, 4.242640687119285658 ) ) ;
#18684 = CARTESIAN_POINT ( 'NONE',  ( -30.99999999999992895, -31.99999999999978684, 205.0000000000000284 ) ) ;
#18685 = CARTESIAN_POINT ( 'NONE',  ( 5.082755093536320601, -5.082755093536318824, 27.92405278187175455 ) ) ;
#18686 = CARTESIAN_POINT ( 'NONE',  ( 9.832129032723420536, 146.5104166632526699, -5.676582343749999815 ) ) ;
#18687 = CARTESIAN_POINT ( 'NONE',  ( 4.242640687119285658, 294.6875000034139589, -4.242640687119286547 ) ) ;
#18688 = LINE ( 'NONE', #19780, #31329 ) ;
#18691 = CARTESIAN_POINT ( 'NONE',  ( 0.000000000000000000, 0.000000000000000000, -20.69999999999999929 ) ) ;
#18690 = CARTESIAN_POINT ( 'NONE',  ( 0.000000000000000000, 125.0000000000000000, 8.000000000000000000 ) ) ;
#18689 = CARTESIAN_POINT ( 'NONE',  ( 25.17157287525378706, 207.8750000000000284, 172.8284271247460424 ) ) ;
#18692 = ORIENTED_EDGE ( 'NONE', *, *, #20294, .T. ) ;
#18693 = CARTESIAN_POINT ( 'NONE',  ( 3.090148520752590944, 225.9998984954551418, -9.510618362637927703 ) ) ;
#18694 = CARTESIAN_POINT ( 'NONE',  ( -6.735557395310442023E-16, 11.00000000000000000, 68.31250000409677625 ) ) ;
#18695 = CARTESIAN_POINT ( 'NONE',  ( -2.754378923186476579E-14, 205.1875000013656063, 145.4587341250000350 ) ) ;
#18696 = CARTESIAN_POINT ( 'NONE',  ( -4.000000000000015987, 202.5000000000000000, 142.0000000000000568 ) ) ;
#18697 = EDGE_CURVE ( 'NONE', #15721, #53176, #65674, .T. ) ;
#18698 = CARTESIAN_POINT ( 'NONE',  ( -10.00000000000000355, 34.58333332650536107, 2.679491924311223183 ) ) ;
#18699 = CARTESIAN_POINT ( 'NONE',  ( -2.977408999572651815, 115.4375000020483810, 7.188101187500000933 ) ) ;
#18700 = CARTESIAN_POINT ( 'NONE',  ( -3.211159895383561391, 3.812499998634407028, -3.211159895383561835 ) ) ;
#18701 = CARTESIAN_POINT ( 'NONE',  ( 9.000000000000000000, 5.196152422706622254, -10.20000000000000284 ) ) ;
#18702 = CARTESIAN_POINT ( 'NONE',  ( -5.656854249492373476, -5.656854249492376141, 16.01780277982336642 ) ) ;
#18704 = CARTESIAN_POINT ( 'NONE',  ( -1.836970198721029983E-15, 5.624999993172032475, 10.00000000000000178 ) ) ;
#18703 = CARTESIAN_POINT ( 'NONE',  ( -10.00000000000000000, 237.9166666734946602, -2.679491924311226292 ) ) ;
#18705 = EDGE_LOOP ( 'NONE', ( #46663, #56442, #71243 ) ) ;
#18706 = CARTESIAN_POINT ( 'NONE',  ( 5.656854249492381470, 92.75000000409677625, 5.656854249492379694 ) ) ;
#18707 = CARTESIAN_POINT ( 'NONE',  ( -10.00000000000005329, 62.50000000000002842, -1.224646799147359765E-15 ) ) ;
#18708 = CARTESIAN_POINT ( 'NONE',  ( 3.042071309553163516, 227.7604166700806445, -11.35316468749999785 ) ) ;
#18709 = CARTESIAN_POINT ( 'NONE',  ( 5.676582343750001591, 116.6145833299193697, -9.832129032723420536 ) ) ;
#18710 = ORIENTED_EDGE ( 'NONE', *, *, #31139, .T. ) ;
#18711 = CARTESIAN_POINT ( 'NONE',  ( 3.294287002270811282, 10.47076035885145018, 117.5334525074227798 ) ) ;
#18712 = CARTESIAN_POINT ( 'NONE',  ( 10.18810118749999916, 4.220049686691935698, 101.5000000020483810 ) ) ;
#18713 = LINE ( 'NONE', #18342, #21218 ) ;
#18714 = CARTESIAN_POINT ( 'NONE',  ( 3.458734125000016757, 199.1250000013656347, 199.4326545832176691 ) ) ;
#18715 = CARTESIAN_POINT ( 'NONE',  ( 1.102182119232618108E-15, 294.3125000034140157, 6.000000000000001776 ) ) ;
#18717 = CARTESIAN_POINT ( 'NONE',  ( -11.35316468750000141, 113.2812499965860269, -1.390361679473963753E-15 ) ) ;
#18716 = CARTESIAN_POINT ( 'NONE',  ( 2.080949416610004210, 225.9999999999999716, -9.795045780231548704 ) ) ;
#18718 = CARTESIAN_POINT ( 'NONE',  ( -28.00000000000003197, 208.0000000000000284, 166.0000000000003695 ) ) ;
#18719 = CARTESIAN_POINT ( 'NONE',  ( -7.999987529518498341, 3.313720969466249500, 6.924052284972249005 ) ) ;
#18720 = ORIENTED_EDGE ( 'NONE', *, *, #643, .F. ) ;
#18721 = CARTESIAN_POINT ( 'NONE',  ( -5.000000000000005329, 195.2083333265053966, 8.660254037844387298 ) ) ;
#18722 = ADVANCED_FACE ( 'NONE', ( #44628 ), #61972, .T. ) ;
#18723 = CARTESIAN_POINT ( 'NONE',  ( -11.00000000000000000, 0.000000000000000000, 72.99999999999998579 ) ) ;
#18724 = CARTESIAN_POINT ( 'NONE',  ( -1.040834085586084257E-14, 82.00000000000001421, 57.99999999999999289 ) ) ;
#18725 = CARTESIAN_POINT ( 'NONE',  ( 9.832129032723416984, 95.67708332991935549, 5.676582343750006032 ) ) ;
#18726 = CARTESIAN_POINT ( 'NONE',  ( -3.458734124999959914, 209.4375000013656063, 198.0000000000000284 ) ) ;
#18727 = CARTESIAN_POINT ( 'NONE',  ( 7.188101187499999156, 14.24999999795161187, 2.977408999572654924 ) ) ;
#18728 = CARTESIAN_POINT ( 'NONE',  ( -7.204075437095965206, -7.204075437095968759, 93.71875000204838102 ) ) ;
#18729 = ADVANCED_FACE ( 'NONE', ( #62706 ), #15938, .T. ) ;
#18730 = CARTESIAN_POINT ( 'NONE',  ( -11.35316468750000141, 8.802083329919348387, 3.042071309553159963 ) ) ;
#18731 = EDGE_LOOP ( 'NONE', ( #37633, #21365, #71233 ) ) ;
#18732 = CARTESIAN_POINT ( 'NONE',  ( 5.656854249492379694, 123.1250000040967905, -5.656854249492380582 ) ) ;
#18733 = DIRECTION ( 'NONE',  ( 1.000000000000000000, 0.000000000000000000, 0.000000000000000000 ) ) ;
#18734 = CARTESIAN_POINT ( 'NONE',  ( 0.000000000000000000, 125.0000000000000000, 0.000000000000000000 ) ) ;
#18735 = CARTESIAN_POINT ( 'NONE',  ( -4.220049686691937474, -10.18810118749999738, 72.81250000204836681 ) ) ;
#18736 = CARTESIAN_POINT ( 'NONE',  ( -0.01139559756449873805, 21.99999999999999645, 4.447709176919010687 ) ) ;
#18737 = CARTESIAN_POINT ( 'NONE',  ( -30.99999999999992895, -31.99999999999978684, 135.0000000000000000 ) ) ;
#18738 = CARTESIAN_POINT ( 'NONE',  ( 4.721056650416000089, 292.8281250017069510, 4.721056650415999201 ) ) ;
#18739 = AXIS2_PLACEMENT_3D ( 'NONE', #71589, #61030, #54267 ) ;
#18740 = CARTESIAN_POINT ( 'NONE',  ( 0.000000000000000000, 0.000000000000000000, 118.0000000000000000 ) ) ;
#18741 = CARTESIAN_POINT ( 'NONE',  ( -9.832129032723418760, 218.1770833299193555, -5.676582343750004256 ) ) ;
#18742 = CARTESIAN_POINT ( 'NONE',  ( 1.871523826299183495E-15, -10.18810118749999916, 90.53125000204836681 ) ) ;
#18743 = ADVANCED_FACE ( 'NONE', ( #73666 ), #67272, .T. ) ;
#18744 = CARTESIAN_POINT ( 'NONE',  ( -24.54126587500000056, 204.2500000013655779, 168.5673454167827003 ) ) ;
#18745 = CARTESIAN_POINT ( 'NONE',  ( -3.313708498984760720, 25.96875000000001066, -8.000000000000000000 ) ) ;
#18746 = ORIENTED_EDGE ( 'NONE', *, *, #2836, .F. ) ;
#18747 = CARTESIAN_POINT ( 'NONE',  ( -23.99999999999999289, 207.8750000027312126, 170.0000000000002842 ) ) ;
#18748 = CARTESIAN_POINT ( 'NONE',  ( 2.828427124746209831, 205.5000000027312126, 200.8284271247462129 ) ) ;
#18749 = CARTESIAN_POINT ( 'NONE',  ( -7.320508075688773708, 31.87500000000000000, -7.320508075688774596 ) ) ;
#18750 = CARTESIAN_POINT ( 'NONE',  ( 30.82842712474617031, 208.5000000027312126, 167.1715728752537018 ) ) ;
#18751 = CARTESIAN_POINT ( 'NONE',  ( 4.220049686691941027, -10.18810118749999738, 77.50000000204839523 ) ) ;
#18753 = ORIENTED_EDGE ( 'NONE', *, *, #48982, .T. ) ;
#18752 =( BOUNDED_CURVE ( )  B_SPLINE_CURVE ( 3, ( #8516, #31153, #7785, #71136 ),
 .UNSPECIFIED., .F., .T. ) 
 B_SPLINE_CURVE_WITH_KNOTS ( ( 4, 4 ),
 ( 1.570796326794898556, 1.931755010900532588 ),
 .UNSPECIFIED. ) 
 CURVE ( )  GEOMETRIC_REPRESENTATION_ITEM ( )  RATIONAL_B_SPLINE_CURVE ( ( 1.000000000000000000, 0.9891718422399164989, 0.9891718422399164989, 1.000000000000000000 ) ) 
 REPRESENTATION_ITEM ( '' )  );
#18754 = CARTESIAN_POINT ( 'NONE',  ( 4.401442555609581635E-16, 3.843749997951610098, -7.188101187500000044 ) ) ;
#18755 = EDGE_CURVE ( 'NONE', #23729, #17439, #11045, .T. ) ;
#18756 = CARTESIAN_POINT ( 'NONE',  ( 5.000000000000000000, 16.24494643555759410, -69.83755725260752456 ) ) ;
#18757 = CARTESIAN_POINT ( 'NONE',  ( -7.188101187500001821, 115.4375000020483810, -2.977408999572650483 ) ) ;
#18758 = CARTESIAN_POINT ( 'NONE',  ( -1.388913554731741051, 22.00000000000001776, -3.856217111854652657 ) ) ;
#18759 = CARTESIAN_POINT ( 'NONE',  ( 1.226468279477575784E-15, 297.7031250017070079, 6.676582343750001591 ) ) ;
#18760 = EDGE_CURVE ( 'NONE', #69933, #43418, #2628, .T. ) ;
#18762 = CARTESIAN_POINT ( 'NONE',  ( -4.000000000000001776, 15.18749999726881406, -1.656854249492381470 ) ) ;
#18761 = CARTESIAN_POINT ( 'NONE',  ( 8.311093377946834337, 227.0312500034140157, -8.311093377946836114 ) ) ;
#18763 = ITEM_DEFINED_TRANSFORMATION ( 'NONE', 'NONE', #29711,  #57354 ) ;
#18764 = ORIENTED_EDGE ( 'NONE', *, *, #17707, .T. ) ;
#18765 = CARTESIAN_POINT ( 'NONE',  ( -3.042071309553159075, 240.2604166700806729, 11.35316468749999963 ) ) ;
#18766 = CARTESIAN_POINT ( 'NONE',  ( -4.401442555609577197E-16, 7.188101187499992051, 7.111552781871751883 ) ) ;
#18768 = EDGE_CURVE ( 'NONE', #6516, #64786, #17062, .T. ) ;
#18767 = CARTESIAN_POINT ( 'NONE',  ( 1.432654583217662481, 203.3750000013656063, 194.5412658750000219 ) ) ;
#18769 =( BOUNDED_CURVE ( )  B_SPLINE_CURVE ( 2, ( #46678, #51980, #41764, #1782, #7439, #40281, #57651, #63658, #41399 ),
 .UNSPECIFIED., .F., .F. ) 
 B_SPLINE_CURVE_WITH_KNOTS ( ( 3, 2, 2, 2, 3 ),
 ( 0.7894736842105263275, 0.7960526315789473450, 0.8026315789473685847, 0.8092105263157896022, 0.8157894736842106198 ),
 .UNSPECIFIED. ) 
 CURVE ( )  GEOMETRIC_REPRESENTATION_ITEM ( )  RATIONAL_B_SPLINE_CURVE ( ( 1.000000000000000000, 0.9238795325112867385, 1.000000000000000000, 0.9238795325112867385, 1.000000000000000000, 0.9238795325112867385, 1.000000000000000000, 0.9238795325112854062, 1.000000000000001332 ) ) 
 REPRESENTATION_ITEM ( '' )  );
#18770 = ORIENTED_EDGE ( 'NONE', *, *, #18102, .F. ) ;
#18771 = CARTESIAN_POINT ( 'NONE',  ( 1.469576158976823947E-15, 104.5625000040967763, 8.000000000000000000 ) ) ;
#18772 = CARTESIAN_POINT ( 'NONE',  ( -3.042071309553173730, 99.63541666325268409, 11.35316468749999785 ) ) ;
#18773 = DIRECTION ( 'NONE',  ( 0.000000000000000000, 0.000000000000000000, 1.000000000000000000 ) ) ;
#18774 = CARTESIAN_POINT ( 'NONE',  ( -10.99999999999999822, -4.556349186104052151, 79.09375000000000000 ) ) ;
#18777 = LINE ( 'NONE', #65151, #33866 ) ;
#18776 = CARTESIAN_POINT ( 'NONE',  ( 24.54126587499999346, 205.1875000013656063, 169.9999999999999432 ) ) ;
#18775 = CARTESIAN_POINT ( 'NONE',  ( 25.55430564589119413, 201.3125000013656063, 167.5543056458910485 ) ) ;
#18778 = ORIENTED_EDGE ( 'NONE', *, *, #12385, .T. ) ;
#18779 = DIRECTION ( 'NONE',  ( 0.000000000000000000, 0.000000000000000000, 1.000000000000000000 ) ) ;
#18780 = DIRECTION ( 'NONE',  ( -0.000000000000000000, 1.000000000000000000, -0.000000000000000000 ) ) ;
#18781 =( GEOMETRIC_REPRESENTATION_CONTEXT ( 3 ) GLOBAL_UNCERTAINTY_ASSIGNED_CONTEXT ( ( #23933 ) ) GLOBAL_UNIT_ASSIGNED_CONTEXT ( ( #53643, #69881, #15857 ) ) REPRESENTATION_CONTEXT ( 'NONE', 'WORKASPACE' ) );
#18782 = CARTESIAN_POINT ( 'NONE',  ( -11.35316468750000141, 213.2812499965860411, -1.390361679473963753E-15 ) ) ;
#18783 = CARTESIAN_POINT ( 'NONE',  ( 1.432654583217607858, 199.6250000013656063, 138.5412658750000787 ) ) ;
#18784 = CARTESIAN_POINT ( 'NONE',  ( 29.43265458321766559, 204.1250000013656063, 166.5412658749999650 ) ) ;
#18785 = CARTESIAN_POINT ( 'NONE',  ( -5.082755093536326818, 24.28124999795161543, 5.082755093536325042 ) ) ;
#18786 = AXIS2_PLACEMENT_3D ( 'NONE', #7542, #31283, #41134 ) ;
#18787 = CARTESIAN_POINT ( 'NONE',  ( 3.042071309553167069, 182.1354166632526699, -11.35316468749999785 ) ) ;
#18788 = CARTESIAN_POINT ( 'NONE',  ( -7.188101187499999156, 96.12500000204838102, 2.977408999572654924 ) ) ;
#18789 = CARTESIAN_POINT ( 'NONE',  ( -5.000000000000000888, 62.88740100213682638, -24.06179116403683338 ) ) ;
#18790 = CARTESIAN_POINT ( 'NONE',  ( -29.65685424949234061, 198.4375000000000568, 174.0000000000004547 ) ) ;
#18791 = CARTESIAN_POINT ( 'NONE',  ( 4.541265875000001451, 16.24999999863440436, 1.881053915767124440 ) ) ;
#18792 = CARTESIAN_POINT ( 'NONE',  ( 31.45873412499997812, 197.8750000013656063, 171.4326545832176123 ) ) ;
#18793 = CARTESIAN_POINT ( 'NONE',  ( 5.082755093536318824, 5.082755093536319713, 2.799052781871750994 ) ) ;
#18794 = CARTESIAN_POINT ( 'NONE',  ( -8.311093377946841443, 63.90624999658601979, 8.311093377946830785 ) ) ;
#18795 = ADVANCED_FACE ( 'NONE', ( #45363, #40082 ), #57447, .F. ) ;
#18796 = DIRECTION ( 'NONE',  ( 1.224646799147353207E-16, -1.000000000000000000, 0.000000000000000000 ) ) ;
#18797 = DIRECTION ( 'NONE',  ( -0.000000000000000000, 1.000000000000000000, -4.476705744456276341E-16 ) ) ;
#18798 = EDGE_LOOP ( 'NONE', ( #26994, #67847, #14486, #6125, #50252 ) ) ;
#18799 = CARTESIAN_POINT ( 'NONE',  ( -2.679491924311222295, 224.1666666734946318, 10.00000000000000178 ) ) ;
#18800 = CARTESIAN_POINT ( 'NONE',  ( -6.735557395310442023E-16, 11.00000000000000000, 66.81250000409677625 ) ) ;
#18801 = CARTESIAN_POINT ( 'NONE',  ( -5.676582343750006032, 79.11458332991935549, 9.832129032723418760 ) ) ;
#18802 = CARTESIAN_POINT ( 'NONE',  ( 10.18810118749999916, 1.247682550866122264E-15, 116.4062500020483810 ) ) ;
#18803 = CARTESIAN_POINT ( 'NONE',  ( -3.458734125000015869, 197.1875000013655779, 142.0000000000000568 ) ) ;
#18804 = CARTESIAN_POINT ( 'NONE',  ( -7.347880794884122694E-16, 8.499999997268814056, 4.000000000000001776 ) ) ;
#18806 = CARTESIAN_POINT ( 'NONE',  ( -9.832129032723420536, 68.69791666325268409, 5.676582343749997150 ) ) ;
#18805 = CARTESIAN_POINT ( 'NONE',  ( -4.000000000000001776, 13.24999999726881406, -4.898587196589415787E-16 ) ) ;
#18807 = CARTESIAN_POINT ( 'NONE',  ( 3.313708498984756279, 7.999999999999991118, 27.54905278392014623 ) ) ;
#18808 = CARTESIAN_POINT ( 'NONE',  ( 5.000000000000001776, 130.8333333333333428, -8.660254037844389075 ) ) ;
#18809 = CARTESIAN_POINT ( 'NONE',  ( 8.660254037844385522, 161.4583333265053966, 5.000000000000005329 ) ) ;
#18810 = CARTESIAN_POINT ( 'NONE',  ( 2.977408999572654480, 92.00000000204838102, 7.188101187499999156 ) ) ;
#18811 = CARTESIAN_POINT ( 'NONE',  ( -24.35042252706858079, 194.9613588559978155, 168.4478771388161817 ) ) ;
#18812 = CARTESIAN_POINT ( 'NONE',  ( 8.311093377946837890, 56.71874999658601979, -8.311093377946837890 ) ) ;
#18813 = CARTESIAN_POINT ( 'NONE',  ( 4.220049686691941027, -10.18810118749999738, 113.5000000020483810 ) ) ;
#18814 = CARTESIAN_POINT ( 'NONE',  ( -11.35316468750000141, 198.4895833299193555, 3.042071309553159963 ) ) ;
#18815 = ORIENTED_EDGE ( 'NONE', *, *, #51126, .F. ) ;
#18816 = EDGE_CURVE ( 'NONE', #51832, #64185, #45002, .T. ) ;
#18817 = CARTESIAN_POINT ( 'NONE',  ( 0.4501631047671865726, 67.59340899456755380, 20.03485802339891109 ) ) ;
#18818 = CARTESIAN_POINT ( 'NONE',  ( -4.220049686691937474, -10.18810118749999738, 67.93750000204838102 ) ) ;
#18819 = CARTESIAN_POINT ( 'NONE',  ( -1.836970198721029983E-15, 120.6249999931720396, 10.00000000000000178 ) ) ;
#18821 = CARTESIAN_POINT ( 'NONE',  ( -2.085542519210945728E-15, 199.5312499965860411, 11.35316468750000141 ) ) ;
#18820 = CARTESIAN_POINT ( 'NONE',  ( 27.99999999999999645, 195.0000000000000000, 165.9999999999999147 ) ) ;
#18822 = CARTESIAN_POINT ( 'NONE',  ( 0.000000000000000000, 300.0000000000000000, 0.000000000000000000 ) ) ;
#18823 = CARTESIAN_POINT ( 'NONE',  ( -2.679491924311222295, 254.1666666734946318, 10.00000000000000178 ) ) ;
#18824 = CARTESIAN_POINT ( 'NONE',  ( -8.660254037844390851, 189.7916666598387110, 4.999999999999998224 ) ) ;
#18825 = VERTEX_POINT ( 'NONE', #68005 ) ;
#18826 = CARTESIAN_POINT ( 'NONE',  ( 3.042071309553167513, 172.1354166632526983, -11.35316468749999785 ) ) ;
#18827 = CARTESIAN_POINT ( 'NONE',  ( -2.977408999572647819, -7.188101187499990274, 18.26780278187175455 ) ) ;
#18828 = LINE ( 'NONE', #7878, #51421 ) ;
#18829 = VERTEX_POINT ( 'NONE', #56324 ) ;
#18830 = CARTESIAN_POINT ( 'NONE',  ( 3.313708498984760720, 105.2187500040967905, -8.000000000000000000 ) ) ;
#18831 = EDGE_CURVE ( 'NONE', #27541, #60310, #51770, .T. ) ;
#18832 = CARTESIAN_POINT ( 'NONE',  ( 1.656854249492381914, 12.81250000000000000, 4.000000000000000888 ) ) ;
#18833 = FACE_OUTER_BOUND ( 'NONE', #56019, .T. ) ;
#18834 = CARTESIAN_POINT ( 'NONE',  ( 3.211159895383560947, 17.18749999863440792, 3.211159895383562723 ) ) ;
#18835 = CARTESIAN_POINT ( 'NONE',  ( 3.313708498984756279, 7.999999999999991118, 17.04905278392014623 ) ) ;
#18836 = ORIENTED_EDGE ( 'NONE', *, *, #13996, .T. ) ;
#18837 = CARTESIAN_POINT ( 'NONE',  ( 0.000000000000000000, 125.0000000000000000, 0.000000000000000000 ) ) ;
#18838 = CARTESIAN_POINT ( 'NONE',  ( 5.082755093536325042, 98.09375000204838102, -5.082755093536325930 ) ) ;
#18839 = EDGE_CURVE ( 'NONE', #24549, #71006, #24265, .T. ) ;
#18841 = CARTESIAN_POINT ( 'NONE',  ( 8.000000000000000000, 120.0312500040967905, -3.313708498984762496 ) ) ;
#18840 = CARTESIAN_POINT ( 'NONE',  ( 4.000000000000016875, 196.4375000000000568, 199.6568542494924259 ) ) ;
#18842 = ORIENTED_EDGE ( 'NONE', *, *, #70623, .T. ) ;
#18844 = AXIS2_PLACEMENT_3D ( 'NONE', #60924, #48848, #66206 ) ;
#18843 = CARTESIAN_POINT ( 'NONE',  ( 6.308070865145555040, 10.25011764679231341, -64.85270989085731230 ) ) ;
#18845 = CARTESIAN_POINT ( 'NONE',  ( -5.082755093536317936, -5.082755093536320601, 25.67405278187175810 ) ) ;
#18846 = VERTEX_POINT ( 'NONE', #21974 ) ;
#18847 = EDGE_CURVE ( 'NONE', #48495, #74465, #62338, .T. ) ;
#18848 = EDGE_LOOP ( 'NONE', ( #3494, #73389, #67895, #46540 ) ) ;
#18849 = CARTESIAN_POINT ( 'NONE',  ( -10.18810118749999916, 0.000000000000000000, 87.15625000204838102 ) ) ;
#18850 = CARTESIAN_POINT ( 'NONE',  ( -33.69651738014277953, -12.15649368946403364, 154.7495530794294325 ) ) ;
#18851 = CARTESIAN_POINT ( 'NONE',  ( -11.00000000000000000, 4.556349186104045934, 96.90624999999998579 ) ) ;
#18854 = CARTESIAN_POINT ( 'NONE',  ( -2.765530957081996810, 296.4218750017069510, -6.676582343750002480 ) ) ;
#18853 = CARTESIAN_POINT ( 'NONE',  ( 23.99999999999998934, 200.8750000027312126, 169.9999999999999432 ) ) ;
#18852 = CARTESIAN_POINT ( 'NONE',  ( 2.020667218593132706E-15, -11.00000000000000000, 104.8750000000000000 ) ) ;
#18855 = CARTESIAN_POINT ( 'NONE',  ( -7.320508075688778149, 128.1250000000000000, 7.320508075688769267 ) ) ;
#18856 = CARTESIAN_POINT ( 'NONE',  ( -6.735557395310442023E-16, 11.00000000000000000, 105.8125000040967763 ) ) ;
#18857 = CARTESIAN_POINT ( 'NONE',  ( -5.082755093536317936, -5.082755093536320601, 0.5490527818717526598 ) ) ;
#18858 =( BOUNDED_CURVE ( )  B_SPLINE_CURVE ( 2, ( #21020, #61015, #67802, #10826, #9340, #16093, #32739, #16840, #39128 ),
 .UNSPECIFIED., .F., .F. ) 
 B_SPLINE_CURVE_WITH_KNOTS ( ( 3, 2, 2, 2, 3 ),
 ( 0.6052631578947368363, 0.6118421052631578538, 0.6184210526315789824, 0.6250000000000001110, 0.6315789473684211286 ),
 .UNSPECIFIED. ) 
 CURVE ( )  GEOMETRIC_REPRESENTATION_ITEM ( )  RATIONAL_B_SPLINE_CURVE ( ( 1.000000000000000000, 0.9238795325112867385, 1.000000000000000000, 0.9238795325112867385, 1.000000000000000000, 0.9238795325112867385, 1.000000000000000000, 0.9238795325112854062, 1.000000000000001332 ) ) 
 REPRESENTATION_ITEM ( '' )  );
#18859 = DIRECTION ( 'NONE',  ( -0.000000000000000000, -0.000000000000000000, 1.000000000000000000 ) ) ;
#18860 = CARTESIAN_POINT ( 'NONE',  ( 24.54126587499999346, 203.1875000013656063, 169.9999999999998863 ) ) ;
#18861 = CARTESIAN_POINT ( 'NONE',  ( 7.188101187500001821, 3.937499997951610986, -2.977408999572650483 ) ) ;
#18862 = CARTESIAN_POINT ( 'NONE',  ( -8.008118988124991233, 0.000000000000000000, 1.013115283940629663 ) ) ;
#18863 = CARTESIAN_POINT ( 'NONE',  ( -2.445694354108838731, 195.0625000013656063, 144.4456943541088663 ) ) ;
#18864 = CARTESIAN_POINT ( 'NONE',  ( -5.082755093536324154, 117.2187500020483810, 5.082755093536326818 ) ) ;
#18866 = CARTESIAN_POINT ( 'NONE',  ( -27.99999999999999645, 210.0000000000000284, 170.0000000000003695 ) ) ;
#18865 = DIRECTION ( 'NONE',  ( -0.000000000000000000, -1.000000000000000000, -0.000000000000000000 ) ) ;
#18867 = CARTESIAN_POINT ( 'NONE',  ( -8.311093377946836114, 223.5937500034139589, -8.311093377946836114 ) ) ;
#18868 = DIRECTION ( 'NONE',  ( 0.000000000000000000, 0.000000000000000000, 1.000000000000000000 ) ) ;
#18869 = CARTESIAN_POINT ( 'NONE',  ( 1.320432766682872962E-15, -7.188101187499992051, 23.23655278187175455 ) ) ;
#18870 = LINE ( 'NONE', #70919, #39569 ) ;
#18871 = CARTESIAN_POINT ( 'NONE',  ( 5.676582343749993598, 29.94791666325268409, 9.832129032723422313 ) ) ;
#18872 = CARTESIAN_POINT ( 'NONE',  ( -29.65685424949244364, 199.4375000000000000, 174.0000000000003126 ) ) ;
#18873 = CARTESIAN_POINT ( 'NONE',  ( 11.35316468750000141, 226.0937499965860127, 0.000000000000000000 ) ) ;
#18874 = LINE ( 'NONE', #2263, #41560 ) ;
#18875 = LINE ( 'NONE', #7193, #5766 ) ;
#18876 = ORIENTED_EDGE ( 'NONE', *, *, #45345, .F. ) ;
#18877 = CARTESIAN_POINT ( 'NONE',  ( 4.556349186104045934, 11.00000000000000000, 104.2187500040967905 ) ) ;
#18878 = CARTESIAN_POINT ( 'NONE',  ( 3.458734124999960358, 197.6875000013655779, 142.0000000000000568 ) ) ;
#18879 = CARTESIAN_POINT ( 'NONE',  ( -5.676582343750006032, 29.11458332991935194, 9.832129032723418760 ) ) ;
#18880 = CARTESIAN_POINT ( 'NONE',  ( -11.00000000000000000, 0.000000000000000000, 85.18750000409677625 ) ) ;
#18881 = AXIS2_PLACEMENT_3D ( 'NONE', #42947, #25961, #65967 ) ;
#18882 = CARTESIAN_POINT ( 'NONE',  ( -3.458734125000015869, 206.1875000013656063, 142.0000000000000568 ) ) ;
#18883 = CARTESIAN_POINT ( 'NONE',  ( -7.320508075688784366, 153.1250000000000000, 7.320508075688776373 ) ) ;
#18884 = CARTESIAN_POINT ( 'NONE',  ( -2.828427124746208943, 201.7500000027312126, 144.8284271247462129 ) ) ;
#18886 = CARTESIAN_POINT ( 'NONE',  ( -5.676582343749998039, 37.44791666325267698, -9.832129032723420536 ) ) ;
#18885 = CARTESIAN_POINT ( 'NONE',  ( -7.188101187500000933, 104.5625000020483810, -2.977408999572650483 ) ) ;
#18887 = CARTESIAN_POINT ( 'NONE',  ( -7.999999999999989342, -3.313708498984762496, 14.42405277982336465 ) ) ;
#18888 = CARTESIAN_POINT ( 'NONE',  ( 8.311093377946834337, 150.1562499965859843, 8.311093377946839666 ) ) ;
#18889 =( BOUNDED_CURVE ( )  B_SPLINE_CURVE ( 2, ( #8235, #20282, #37664, #44063, #38035, #2582, #8984, #43683, #32000 ),
 .UNSPECIFIED., .F., .F. ) 
 B_SPLINE_CURVE_WITH_KNOTS ( ( 3, 2, 2, 2, 3 ),
 ( 0.9333333333333341253, 0.9416666666666674290, 0.9500000000000007327, 0.9583333333333341475, 0.9666666666666674512 ),
 .UNSPECIFIED. ) 
 CURVE ( )  GEOMETRIC_REPRESENTATION_ITEM ( )  RATIONAL_B_SPLINE_CURVE ( ( 0.9999999999999928946, 0.9238795325112938439, 1.000000000000000000, 0.9238795325112867385, 1.000000000000000000, 0.9238795325112867385, 1.000000000000000000, 0.9238795325112796331, 1.000000000000007105 ) ) 
 REPRESENTATION_ITEM ( '' )  );
#18890 = CARTESIAN_POINT ( 'NONE',  ( 5.000000000000001776, 117.7083333265053824, -8.660254037844389075 ) ) ;
#18891 = CARTESIAN_POINT ( 'NONE',  ( 7.188101187500002709, 117.6875000020484094, 2.977408999572649151 ) ) ;
#18892 = CARTESIAN_POINT ( 'NONE',  ( 7.320508075688771044, 171.2499999931719969, 7.320508075688775484 ) ) ;
#18893 = CARTESIAN_POINT ( 'NONE',  ( -31.45873412499998523, 206.0000000013656347, 171.4326545832180386 ) ) ;
#18894 = ORIENTED_EDGE ( 'NONE', *, *, #58712, .T. ) ;
#18895 = CARTESIAN_POINT ( 'NONE',  ( 11.35316468750000141, 6.093749996586017126, 0.000000000000000000 ) ) ;
#18896 = ORIENTED_EDGE ( 'NONE', *, *, #5676, .F. ) ;
#18897 = CARTESIAN_POINT ( 'NONE',  ( 0.000000000000000000, 125.0000000000000000, 0.000000000000000000 ) ) ;
#18899 = CARTESIAN_POINT ( 'NONE',  ( -3.042071309553163960, 137.2395833299193271, -11.35316468749999963 ) ) ;
#18898 = CARTESIAN_POINT ( 'NONE',  ( -20.32014887409041037, -29.30880718903640414, 145.2752703588716940 ) ) ;
#18900 = CARTESIAN_POINT ( 'NONE',  ( -4.000000000000001776, 16.24999999726881228, -4.898587196589415787E-16 ) ) ;
#18901 = CARTESIAN_POINT ( 'NONE',  ( -7.999999999999991118, 3.313708498984756723, 18.79280278432982598 ) ) ;
#18902 = CARTESIAN_POINT ( 'NONE',  ( 51.66394966539462530, 201.9441476707329741, 54.47058887522228332 ) ) ;
#18903 = CARTESIAN_POINT ( 'NONE',  ( -11.35316468749999608, 249.1145833367473017, 3.042071309553173730 ) ) ;
#18904 = CARTESIAN_POINT ( 'NONE',  ( 7.204075437095966983, 7.204075437095967871, 89.96875000204838102 ) ) ;
#18905 = ORIENTED_EDGE ( 'NONE', *, *, #68172, .F. ) ;
#18906 = VECTOR ( 'NONE', #47115, 1000.000000000000000 ) ;
#18907 = CARTESIAN_POINT ( 'NONE',  ( 3.153939666463620179E-13, 118.7500000000000426, 9.999999999999998224 ) ) ;
#18908 = DIRECTION ( 'NONE',  ( 0.000000000000000000, 0.000000000000000000, 1.000000000000000000 ) ) ;
#18909 = CARTESIAN_POINT ( 'NONE',  ( -11.35316468750000141, 83.59374999658601268, -1.390361679473963753E-15 ) ) ;
#18910 = CARTESIAN_POINT ( 'NONE',  ( 1.871523826299183495E-15, -10.18810118749999916, 104.0312500020483810 ) ) ;
#18911 = CARTESIAN_POINT ( 'NONE',  ( 2.780723358947928197E-16, 18.68749999863440436, -4.541265875000002339 ) ) ;
#18912 = ORIENTED_EDGE ( 'NONE', *, *, #54378, .F. ) ;
#18913 = ORIENTED_EDGE ( 'NONE', *, *, #63218, .T. ) ;
#18914 = CARTESIAN_POINT ( 'NONE',  ( -3.313708498984765161, 5.531250000000000888, 7.999999999999998224 ) ) ;
#18915 = CARTESIAN_POINT ( 'NONE',  ( 2.780723358947928197E-16, 0.6874999986344068059, -4.541265875000002339 ) ) ;
#18916 = CARTESIAN_POINT ( 'NONE',  ( -5.082755093536326818, 2.906249997951610098, 5.082755093536325042 ) ) ;
#18917 = CARTESIAN_POINT ( 'NONE',  ( -5.656854249492380582, 122.0000000040967905, -5.656854249492380582 ) ) ;
#18919 = EDGE_CURVE ( 'NONE', #40106, #18528, #68116, .T. ) ;
#18918 = CARTESIAN_POINT ( 'NONE',  ( -7.204075437095967871, 7.204075437095967871, 96.34375000204836681 ) ) ;
#18920 = ADVANCED_FACE ( 'NONE', ( #24573 ), #47403, .T. ) ;
#18921 = CARTESIAN_POINT ( 'NONE',  ( 4.000000000000000888, 0.9375000000000001110, 1.656854249492384135 ) ) ;
#18922 = CARTESIAN_POINT ( 'NONE',  ( -4.000000000000001776, 13.18749999726881583, -1.656854249492381470 ) ) ;
#18923 = CARTESIAN_POINT ( 'NONE',  ( 7.999999999971009856, 2.153409470846384379E-05, 12.26780339315719814 ) ) ;
#18924 = ORIENTED_EDGE ( 'NONE', *, *, #61971, .F. ) ;
#18925 = AXIS2_PLACEMENT_3D ( 'NONE', #23126, #63489, #40484 ) ;
#18926 = EDGE_CURVE ( 'NONE', #44017, #25179, #62803, .T. ) ;
#18927 = DIRECTION ( 'NONE',  ( 0.1513591288559072157, 0.000000000000000000, -0.9884788384745425427 ) ) ;
#18928 = CARTESIAN_POINT ( 'NONE',  ( -1.432654583217607858, 198.6250000013655779, 201.4587341250000065 ) ) ;
#18930 = DIRECTION ( 'NONE',  ( -0.000000000000000000, 1.000000000000000000, -0.000000000000000000 ) ) ;
#18929 = CARTESIAN_POINT ( 'NONE',  ( -28.00000000000007105, 202.4375000013656063, 166.5412658750003629 ) ) ;
#18931 = CARTESIAN_POINT ( 'NONE',  ( -4.541265875000002339, 12.74999999863440969, -1.881053915767121998 ) ) ;
#18932 = CARTESIAN_POINT ( 'NONE',  ( 7.320508075688771044, 121.2499999931720254, 7.320508075688775484 ) ) ;
#18933 = CARTESIAN_POINT ( 'NONE',  ( 7.188101187499993827, -2.977408999572645598, 15.64280278187175277 ) ) ;
#18934 = ORIENTED_EDGE ( 'NONE', *, *, #10320, .F. ) ;
#18935 = ORIENTED_EDGE ( 'NONE', *, *, #30328, .F. ) ;
#18936 = CARTESIAN_POINT ( 'NONE',  ( -6.238412754330611322E-16, 10.18810118749999916, 106.2812500020483810 ) ) ;
#18937 = CARTESIAN_POINT ( 'NONE',  ( -4.898587196589412829E-16, 123.3125000040967905, -8.000000000000000000 ) ) ;
#18938 = CARTESIAN_POINT ( 'NONE',  ( -26.34314575050758123, 203.5625000000000000, 174.0000000000003411 ) ) ;
#18939 = CARTESIAN_POINT ( 'NONE',  ( -2.445694354108783664, 196.3125000013656063, 195.5543056458912190 ) ) ;
#18940 = LINE ( 'NONE', #64954, #53085 ) ;
#18941 = CARTESIAN_POINT ( 'NONE',  ( 5.000000000000001776, 90.83333333333332860, -8.660254037844389075 ) ) ;
#18942 = CARTESIAN_POINT ( 'NONE',  ( -5.656854249492380582, 120.3125000000000000, -5.656854249492380582 ) ) ;
#18943 = CARTESIAN_POINT ( 'NONE',  ( 4.721056650416000089, 295.9843750017070079, 4.721056650415999201 ) ) ;
#18944 = ADVANCED_FACE ( 'NONE', ( #17637 ), #53148, .T. ) ;
#18945 = ORIENTED_EDGE ( 'NONE', *, *, #2585, .F. ) ;
#18946 = AXIS2_PLACEMENT_3D ( 'NONE', #71336, #65316, #53642 ) ;
#18947 = CARTESIAN_POINT ( 'NONE',  ( -8.660254037844387298, 173.9583333265053682, -5.000000000000004441 ) ) ;
#18948 = CARTESIAN_POINT ( 'NONE',  ( -5.656854249492381470, 17.24999999590322375, 5.656854249492379694 ) ) ;
#18949 = CARTESIAN_POINT ( 'NONE',  ( -2.445694354108839619, 205.8125000013656063, 139.5543056458912190 ) ) ;
#18950 = CARTESIAN_POINT ( 'NONE',  ( -8.660254037844390851, 52.08333333333333570, -5.000000000000005329 ) ) ;
#18951 = DIRECTION ( 'NONE',  ( -1.000000000000000000, -0.000000000000000000, -0.000000000000000000 ) ) ;
#18952 = CARTESIAN_POINT ( 'NONE',  ( 5.000000000000004441, 226.6666666666666856, 8.660254037844385522 ) ) ;
#18953 = CARTESIAN_POINT ( 'NONE',  ( -7.347880794884122694E-16, 3.499999997268812724, 4.000000000000001776 ) ) ;
#18954 = CARTESIAN_POINT ( 'NONE',  ( 7.778174593052021635, 7.778174593052023411, 112.9375000000000000 ) ) ;
#18955 = CARTESIAN_POINT ( 'NONE',  ( -4.999999999999998224, 211.6666666666666572, -8.660254037844389075 ) ) ;
#18956 = CARTESIAN_POINT ( 'NONE',  ( -2.977408999572647819, 7.188101187499992051, 9.080302781871752771 ) ) ;
#18957 = CARTESIAN_POINT ( 'NONE',  ( 9.832129032723416984, 175.6770833299193555, 5.676582343750006032 ) ) ;
#18958 = CARTESIAN_POINT ( 'NONE',  ( 7.320508075688771044, 191.2499999931720538, 7.320508075688775484 ) ) ;
#18959 = CARTESIAN_POINT ( 'NONE',  ( 3.211159895383561835, 0.4374999986344066949, -3.211159895383561835 ) ) ;
#18960 = CARTESIAN_POINT ( 'NONE',  ( 1.836970198721029589E-15, 241.2500000000000284, 10.00000000000000000 ) ) ;
#18962 = CARTESIAN_POINT ( 'NONE',  ( -4.898587196589407898E-16, 7.999999999999991118, 3.642802783920144449 ) ) ;
#18961 = DIRECTION ( 'NONE',  ( -0.000000000000000000, -1.000000000000000000, -0.000000000000000000 ) ) ;
#18963 = ORIENTED_EDGE ( 'NONE', *, *, #5242, .F. ) ;
#18964 = CARTESIAN_POINT ( 'NONE',  ( -2.445694354108838731, 195.0625000013656063, 144.4456943541088663 ) ) ;
#18965 = CARTESIAN_POINT ( 'NONE',  ( 6.951808397369818766E-16, 52.34374999658601979, -11.35316468750000141 ) ) ;
#18966 = CARTESIAN_POINT ( 'NONE',  ( 2.020667218593132706E-15, -11.00000000000000000, 105.0625000040967763 ) ) ;
#18967 = CARTESIAN_POINT ( 'NONE',  ( 9.832129032723416984, 215.6770833299193555, 5.676582343750006032 ) ) ;
#18968 = CARTESIAN_POINT ( 'NONE',  ( -30.44569435410886982, 204.5625000013656063, 167.5543056458916169 ) ) ;
#18969 = CARTESIAN_POINT ( 'NONE',  ( 10.00000000000000178, 10.20833333333333570, -2.679491924311227180 ) ) ;
#18971 = CYLINDRICAL_SURFACE ( 'NONE', #17348, 4.000000000000001776 ) ;
#18970 = CARTESIAN_POINT ( 'NONE',  ( -7.188101187500000933, 121.0625000020483810, -2.977408999572650483 ) ) ;
#18972 = CARTESIAN_POINT ( 'NONE',  ( -7.778174593052023411, 7.778174593052023411, 87.81249999999998579 ) ) ;
#18973 = CARTESIAN_POINT ( 'NONE',  ( 2.679491924311222739, 70.83333332650536818, 10.00000000000000355 ) ) ;
#18974 = CARTESIAN_POINT ( 'NONE',  ( -5.082755093536324154, 98.84375000204838102, 5.082755093536326818 ) ) ;
#18975 = CARTESIAN_POINT ( 'NONE',  ( -4.541265875000003227, 15.99999999863440614, 1.881053915767121110 ) ) ;
#18976 = CARTESIAN_POINT ( 'NONE',  ( 7.000000000000000000, 0.000000000000000000, 0.000000000000000000 ) ) ;
#18977 = CARTESIAN_POINT ( 'NONE',  ( 2.828427124746191623, 10.87499999726881406, -2.828427124746191623 ) ) ;
#18978 = CARTESIAN_POINT ( 'NONE',  ( 3.313708498984762496, -7.999999999999989342, 23.79905277982336287 ) ) ;
#18979 = ORIENTED_EDGE ( 'NONE', *, *, #33443, .T. ) ;
#18980 = VERTEX_POINT ( 'NONE', #28513 ) ;
#18981 =( BOUNDED_CURVE ( )  B_SPLINE_CURVE ( 2, ( #52535, #58947, #63476, #24590, #64951, #18572, #36297, #58217, #41582, #69891, #29894, #46869, #24219 ),
 .UNSPECIFIED., .F., .F. ) 
 B_SPLINE_CURVE_WITH_KNOTS ( ( 3, 2, 2, 2, 2, 2, 3 ),
 ( 1.208890027026519931, 1.214123945856841358, 1.219357864687163007, 1.224591783517484433, 1.229825702347806082, 1.235059621178127509, 1.240293540008449158 ),
 .UNSPECIFIED. ) 
 CURVE ( )  GEOMETRIC_REPRESENTATION_ITEM ( )  RATIONAL_B_SPLINE_CURVE ( ( 1.000000000000000000, 0.9659258262890683122, 1.000000000000000000, 0.9659258262890683122, 1.000000000000000000, 0.9659258262890683122, 1.000000000000000000, 0.9659258262890683122, 1.000000000000000000, 0.9659258262890683122, 1.000000000000000000, 0.9659258262889941493, 1.000000000000074163 ) ) 
 REPRESENTATION_ITEM ( '' )  );
#18982 = CARTESIAN_POINT ( 'NONE',  ( 6.676582343750004256, 292.0468750017070079, 2.765530957081995478 ) ) ;
#18983 = CARTESIAN_POINT ( 'NONE',  ( -11.00000000000000000, 0.000000000000000000, 118.0000000000000000 ) ) ;
#18984 = CARTESIAN_POINT ( 'NONE',  ( -3.042071309553173730, 154.3229166632527267, 11.35316468749999785 ) ) ;
#18985 = CARTESIAN_POINT ( 'NONE',  ( 0.000000000000000000, 125.0000000000000000, 0.000000000000000000 ) ) ;
#18986 = CARTESIAN_POINT ( 'NONE',  ( -3.999999999999959144, 202.0625000000000284, 199.6568542494924259 ) ) ;
#18987 = DIRECTION ( 'NONE',  ( -0.000000000000000000, -0.000000000000000000, -1.000000000000000000 ) ) ;
#18988 = CARTESIAN_POINT ( 'NONE',  ( -7.204075437095967871, 7.204075437095967871, 106.8437500020483810 ) ) ;
#18989 = ORIENTED_EDGE ( 'NONE', *, *, #37951, .F. ) ;
#18990 = CARTESIAN_POINT ( 'NONE',  ( -8.000000000000000000, 113.0000000000000000, 0.000000000000000000 ) ) ;
#18991 = DIRECTION ( 'NONE',  ( -0.000000000000000000, 1.000000000000000000, 4.476705744456276341E-16 ) ) ;
#18992 = CARTESIAN_POINT ( 'NONE',  ( -3.042071309553163960, 142.5520833299193271, -11.35316468749999963 ) ) ;
#18993 = CARTESIAN_POINT ( 'NONE',  ( 2.445694354108839619, 198.8125000013656063, 200.4456943541088663 ) ) ;
#18994 = CARTESIAN_POINT ( 'NONE',  ( 1.102182119232618108E-15, 291.2500000000000000, 6.000000000000001776 ) ) ;
#18995 = CARTESIAN_POINT ( 'NONE',  ( 10.18810118749999916, 4.220049686691935698, 68.87500000204838102 ) ) ;
#18996 = CARTESIAN_POINT ( 'NONE',  ( -3.042071309553173730, 54.63541666325268409, 11.35316468749999785 ) ) ;
#18997 = ORIENTED_EDGE ( 'NONE', *, *, #29970, .F. ) ;
#18998 = PLANE ( 'NONE',  #13956 ) ;
#18999 = CARTESIAN_POINT ( 'NONE',  ( 4.541265875000002339, 6.437499998634407028, 0.000000000000000000 ) ) ;
#19000 = CARTESIAN_POINT ( 'NONE',  ( 5.662595241051934458, 5.662595241051935346, 6.450615283940627442 ) ) ;
#19001 = EDGE_CURVE ( 'NONE', #48097, #20942, #71268, .T. ) ;
#19002 = CARTESIAN_POINT ( 'NONE',  ( 7.188101187500000044, 13.96874999795161187, 0.000000000000000000 ) ) ;
#19003 = CARTESIAN_POINT ( 'NONE',  ( 6.000000000000003553, 292.5000000034140157, 2.485281374238571317 ) ) ;
#19004 = CARTESIAN_POINT ( 'NONE',  ( 1.377103048673011143, 124.5535323524340896, -7.833776318515874415 ) ) ;
#19005 = CARTESIAN_POINT ( 'NONE',  ( 7.188101187499999156, 9.749999997951611874, 2.977408999572654924 ) ) ;
#19006 = CARTESIAN_POINT ( 'NONE',  ( -7.188101187499992051, 0.000000000000000000, 7.486552781871751883 ) ) ;
#19007 = AXIS2_PLACEMENT_3D ( 'NONE', #38183, #48734, #49107 ) ;
#19008 = CARTESIAN_POINT ( 'NONE',  ( 7.204075437095966983, 7.204075437095967871, 116.9687500020483810 ) ) ;
#19009 = CARTESIAN_POINT ( 'NONE',  ( -10.00000000000000000, 64.16666665983869677, -2.679491924311229845 ) ) ;
#19010 = CARTESIAN_POINT ( 'NONE',  ( 4.000000000000001776, 3.749999997268813168, 0.000000000000000000 ) ) ;
#19011 = ORIENTED_EDGE ( 'NONE', *, *, #40010, .F. ) ;
#19012 = EDGE_CURVE ( 'NONE', #29523, #73780, #46235, .T. ) ;
#19013 = CARTESIAN_POINT ( 'NONE',  ( -3.999999999999959144, 195.1875000027312410, 199.6568542494924259 ) ) ;
#19014 = CARTESIAN_POINT ( 'NONE',  ( -1.656854249492405451, 202.3125000000000000, 138.0000000000000568 ) ) ;
#19015 = CARTESIAN_POINT ( 'NONE',  ( -26.34314575050753149, 199.6875000027312126, 174.0000000000003411 ) ) ;
#19016 = EDGE_CURVE ( 'NONE', #17509, #40533, #69627, .T. ) ;
#19017 = CARTESIAN_POINT ( 'NONE',  ( -3.211159895383561391, 0.6874999986344068059, -3.211159895383561835 ) ) ;
#19018 = CARTESIAN_POINT ( 'NONE',  ( 1.320432766682874540E-15, 114.0312500020483952, 7.188101187500000044 ) ) ;
#19019 = DIRECTION ( 'NONE',  ( 1.000000000000000000, 0.000000000000000000, 0.000000000000000000 ) ) ;
#19020 = CARTESIAN_POINT ( 'NONE',  ( 7.999999999999991118, 3.313708498984757611, 4.861552783920145338 ) ) ;
#19021 = ORIENTED_EDGE ( 'NONE', *, *, #70566, .F. ) ;
#19022 = CARTESIAN_POINT ( 'NONE',  ( 7.188101187499999156, 22.87499999795161543, 2.977408999572654924 ) ) ;
#19023 = VERTEX_POINT ( 'NONE', #17941 ) ;
#19024 = CARTESIAN_POINT ( 'NONE',  ( 10.00000000000000000, 255.6250000068279746, -1.224646799147353256E-15 ) ) ;
#19025 = CARTESIAN_POINT ( 'NONE',  ( -3.458734124999959025, 206.5000000013655779, 199.4326545832176691 ) ) ;
#19026 = CARTESIAN_POINT ( 'NONE',  ( 27.99999999999996803, 201.9375000013656063, 166.5412658749999082 ) ) ;
#19027 = CARTESIAN_POINT ( 'NONE',  ( -1.836970198721029983E-15, 58.75000000000000711, 10.00000000000000178 ) ) ;
#19028 = CARTESIAN_POINT ( 'NONE',  ( -2.977408999572650927, 98.75000000204838102, -7.188101187500001821 ) ) ;
#19029 = CARTESIAN_POINT ( 'NONE',  ( 6.000000000000001776, 296.5000000000000000, -7.347880794884121708E-16 ) ) ;
#19030 = EDGE_CURVE ( 'NONE', #8029, #22020, #51904, .T. ) ;
#19031 = CIRCLE ( 'NONE', #73219, 71.70204102886728492 ) ;
#19033 = CARTESIAN_POINT ( 'NONE',  ( 4.000000000000015987, 197.6875000027312126, 196.3431457505076594 ) ) ;
#19032 = DIRECTION ( 'NONE',  ( 0.000000000000000000, 2.891205793294679411E-15, 1.000000000000000000 ) ) ;
#19034 = ORIENTED_EDGE ( 'NONE', *, *, #66138, .T. ) ;
#19035 = CARTESIAN_POINT ( 'NONE',  ( 11.35316468749999608, 231.6145833367473017, -3.042071309553167069 ) ) ;
#19036 = CARTESIAN_POINT ( 'NONE',  ( -5.082755093536317936, -5.082755093536320601, 12.54905278187175277 ) ) ;
#19037 = CARTESIAN_POINT ( 'NONE',  ( 3.544144923083259791, 50.27229464832175410, 40.88493206427750692 ) ) ;
#19038 = DIRECTION ( 'NONE',  ( 0.000000000000000000, 0.000000000000000000, 1.000000000000000000 ) ) ;
#19039 = DIRECTION ( 'NONE',  ( 0.000000000000000000, 0.000000000000000000, 1.000000000000000000 ) ) ;
#19040 = CARTESIAN_POINT ( 'NONE',  ( -27.99999999999999645, 210.0000000000000284, 170.0000000000003695 ) ) ;
#19041 = DIRECTION ( 'NONE',  ( 0.000000000000000000, 0.000000000000000000, -1.000000000000000000 ) ) ;
#19042 = CARTESIAN_POINT ( 'NONE',  ( 7.320508075688771044, 179.3750000000000284, 7.320508075688775484 ) ) ;
#19043 = CARTESIAN_POINT ( 'NONE',  ( 24.54126587500000412, 209.1250000013656631, 168.5673454167822172 ) ) ;
#19044 = CARTESIAN_POINT ( 'NONE',  ( 7.188101187499993827, -2.977408999572645598, 28.01780278187175455 ) ) ;
#19045 = CARTESIAN_POINT ( 'NONE',  ( 9.832129032723420536, 136.5104166632526983, -5.676582343749999815 ) ) ;
#19046 = DIRECTION ( 'NONE',  ( 0.000000000000000000, 0.000000000000000000, -1.000000000000000000 ) ) ;
#19047 = CARTESIAN_POINT ( 'NONE',  ( 8.660254037844389075, 27.29166665983870033, -5.000000000000000000 ) ) ;
#19050 = CARTESIAN_POINT ( 'NONE',  ( 18.00000000000000000, 4.406054334071555445, -0.2960025734007551979 ) ) ;
#19049 = CARTESIAN_POINT ( 'NONE',  ( -1.836970198721029983E-15, 105.6249999931720396, 10.00000000000000178 ) ) ;
#19048 = CARTESIAN_POINT ( 'NONE',  ( 29.65685424949240101, 207.4375000000000284, 165.9999999999998863 ) ) ;
#19051 = ORIENTED_EDGE ( 'NONE', *, *, #61420, .T. ) ;
#19052 = CONICAL_SURFACE ( 'NONE', #5829, 10.35000000000000142, 0.9599310885968800333 ) ;
#19053 = CARTESIAN_POINT ( 'NONE',  ( -9.832129032723418760, 13.17708332991935194, -5.676582343750004256 ) ) ;
#19054 = CARTESIAN_POINT ( 'NONE',  ( 5.000000000000000000, -18.53862685874497274, -23.57305537018140384 ) ) ;
#19055 = CARTESIAN_POINT ( 'NONE',  ( -4.556349186104045934, 11.00000000000000000, 68.40625000409677625 ) ) ;
#19056 = CARTESIAN_POINT ( 'NONE',  ( 3.458734124999959914, 206.4375000013656063, 142.0000000000000568 ) ) ;
#19057 = VECTOR ( 'NONE', #51539, 1000.000000000000000 ) ;
#19058 = CYLINDRICAL_SURFACE ( 'NONE', #37761, 7.999999999999991118 ) ;
#19059 = CARTESIAN_POINT ( 'NONE',  ( 7.320508075688771044, 36.24999999317202537, 7.320508075688775484 ) ) ;
#19060 = CARTESIAN_POINT ( 'NONE',  ( 2.977408999572650039, 116.1875000020483952, -7.188101187500001821 ) ) ;
#19061 = CARTESIAN_POINT ( 'NONE',  ( -8.342170076843785083E-16, 6.187499998634407028, 4.541265875000002339 ) ) ;
#19062 = CARTESIAN_POINT ( 'NONE',  ( 2.020667218593132706E-15, -11.00000000000000000, 85.37499999999997158 ) ) ;
#19063 = CARTESIAN_POINT ( 'NONE',  ( -5.656854249492373476, -5.656854249492376141, 17.51780277982336287 ) ) ;
#19064 = CARTESIAN_POINT ( 'NONE',  ( 5.000000000000000000, -18.53862685874495142, 23.57305537018116581 ) ) ;
#19065 = VERTEX_POINT ( 'NONE', #34944 ) ;
#19066 = CARTESIAN_POINT ( 'NONE',  ( 7.071067751884405617, 220.0000000000000284, 7.071067871846544506 ) ) ;
#19067 = CYLINDRICAL_SURFACE ( 'NONE', #49531, 3.999999999999976019 ) ;
#19068 = CARTESIAN_POINT ( 'NONE',  ( 5.676582343750005144, 225.8854166700806729, 9.832129032723416984 ) ) ;
#19069 = CARTESIAN_POINT ( 'NONE',  ( -11.35316468750000141, 113.4895833299193413, 3.042071309553159963 ) ) ;
#19070 = ORIENTED_EDGE ( 'NONE', *, *, #71486, .F. ) ;
#19071 = CARTESIAN_POINT ( 'NONE',  ( -2.751064625579944321E-14, 200.7500000000000000, 146.0000000000000284 ) ) ;
#19072 = CARTESIAN_POINT ( 'NONE',  ( 10.18810118750000093, -4.220049686691933921, 95.31250000204838102 ) ) ;
#19073 = CARTESIAN_POINT ( 'NONE',  ( -11.00000000000000000, 0.000000000000000000, 118.0000000000000000 ) ) ;
#19074 = CARTESIAN_POINT ( 'NONE',  ( -2.445694354108784108, 196.5625000013656063, 195.5543056458912190 ) ) ;
#19075 = DIRECTION ( 'NONE',  ( -1.000000000000000000, -0.000000000000000000, -0.000000000000000000 ) ) ;
#19077 = CARTESIAN_POINT ( 'NONE',  ( 3.042071309553159519, 114.7395833299193413, 11.35316468750000141 ) ) ;
#19076 = DIRECTION ( 'NONE',  ( 0.000000000000000000, 0.000000000000000000, 1.000000000000000000 ) ) ;
#19078 = CARTESIAN_POINT ( 'NONE',  ( -29.65685424949241877, 207.0625000000000568, 166.0000000000004263 ) ) ;
#19079 = CARTESIAN_POINT ( 'NONE',  ( -7.999999999971585396, 1.424435121157765920E-05, 7.017269882810325932 ) ) ;
#19080 = EDGE_LOOP ( 'NONE', ( #67479, #60827, #17552, #53333 ) ) ;
#19081 = CARTESIAN_POINT ( 'NONE',  ( 2.679491924311222739, 210.8333333265053682, 10.00000000000000355 ) ) ;
#19082 = CARTESIAN_POINT ( 'NONE',  ( 4.898587196589412829E-16, 22.87500000000000355, -8.000000000000000000 ) ) ;
#19083 = DIRECTION ( 'NONE',  ( -0.000000000000000000, -0.000000000000000000, 1.000000000000000000 ) ) ;
#19084 = CARTESIAN_POINT ( 'NONE',  ( 11.35316468749999785, 95.88541666325268409, 3.042071309553174174 ) ) ;
#19085 = CARTESIAN_POINT ( 'NONE',  ( 2.445694354108839619, 208.8125000013656063, 200.4456943541088663 ) ) ;
#19086 = CARTESIAN_POINT ( 'NONE',  ( -5.082755093536325042, 11.90624999795161010, -5.082755093536325930 ) ) ;
#19087 = CARTESIAN_POINT ( 'NONE',  ( -7.204075437095967871, 7.204075437095967871, 88.84375000204838102 ) ) ;
#19088 = CARTESIAN_POINT ( 'NONE',  ( -11.35316468750000141, 8.593749996586016238, -1.390361679473963753E-15 ) ) ;
#19089 = ORIENTED_EDGE ( 'NONE', *, *, #35833, .F. ) ;
#19090 = CARTESIAN_POINT ( 'NONE',  ( 9.797174393178825657E-16, 125.0000000000000000, -8.000000000000000000 ) ) ;
#19091 = CARTESIAN_POINT ( 'NONE',  ( 49.70177871865296026, 50.00000000000000711, 57.99999999999999289 ) ) ;
#19092 = CARTESIAN_POINT ( 'NONE',  ( -10.18810118749999916, 0.000000000000000000, 72.53125000204838102 ) ) ;
#19093 = ADVANCED_FACE ( 'NONE', ( #27764 ), #45124, .T. ) ;
#19094 = CARTESIAN_POINT ( 'NONE',  ( 10.00000000000000178, 200.2083333333333144, -2.679491924311226736 ) ) ;
#19095 = CARTESIAN_POINT ( 'NONE',  ( 1.226468279477575784E-15, 292.7031250017069510, 6.676582343750001591 ) ) ;
#19096 = CARTESIAN_POINT ( 'NONE',  ( 7.999999999521839378, -8.746674989952265200E-05, 18.26780030933659305 ) ) ;
#19097 = CARTESIAN_POINT ( 'NONE',  ( -3.042071309553173730, 224.6354166632526983, 11.35316468749999785 ) ) ;
#19098 =( BOUNDED_CURVE ( )  B_SPLINE_CURVE ( 2, ( #39206, #55075, #61092, #9420, #32439, #33199, #67506, #56195, #61470 ),
 .UNSPECIFIED., .F., .F. ) 
 B_SPLINE_CURVE_WITH_KNOTS ( ( 3, 2, 2, 2, 3 ),
 ( 0.8970588235294119084, 0.9007352941176471894, 0.9044117647058824705, 0.9080882352941177516, 0.9117647058823530326 ),
 .UNSPECIFIED. ) 
 CURVE ( )  GEOMETRIC_REPRESENTATION_ITEM ( )  RATIONAL_B_SPLINE_CURVE ( ( 0.9999999999999976685, 0.9238795325112890700, 1.000000000000000000, 0.9238795325112867385, 1.000000000000000000, 0.9238795325112867385, 1.000000000000000000, 0.9238795325112844070, 1.000000000000002220 ) ) 
 REPRESENTATION_ITEM ( '' )  );
#19099 = CARTESIAN_POINT ( 'NONE',  ( 7.204075437095966983, 7.204075437095967871, 91.09375000204838102 ) ) ;
#19100 = AXIS2_PLACEMENT_3D ( 'NONE', #56202, #16933, #38847 ) ;
#19101 = CARTESIAN_POINT ( 'NONE',  ( -24.54126587499998280, 204.1250000013656063, 171.4326545832179818 ) ) ;
#19102 = CARTESIAN_POINT ( 'NONE',  ( 5.656854249492380582, 22.68750000000000355, -5.656854249492380582 ) ) ;
#19103 = CARTESIAN_POINT ( 'NONE',  ( 1.881053915767121776, 13.62499999863440792, -4.541265875000002339 ) ) ;
#19104 = EDGE_LOOP ( 'NONE', ( #25883, #20659, #6396, #2046 ) ) ;
#19105 = CARTESIAN_POINT ( 'NONE',  ( -12.17000663722010678, -38.79110389607787113, 141.4874838486608155 ) ) ;
#19106 = CARTESIAN_POINT ( 'NONE',  ( -2.828427124746153876, 207.0000000027312126, 195.1715728752538439 ) ) ;
#19107 = CARTESIAN_POINT ( 'NONE',  ( -3.458734125000015869, 200.1875000013656063, 142.0000000000000568 ) ) ;
#19108 = CARTESIAN_POINT ( 'NONE',  ( 3.999999999999960032, 204.0625000027312410, 143.6568542494924543 ) ) ;
#19109 = EDGE_CURVE ( 'NONE', #29247, #27168, #9769, .T. ) ;
#19110 = CARTESIAN_POINT ( 'NONE',  ( -5.000000000000000000, 10.25161785469021680, 64.79070129774557074 ) ) ;
#19111 = CARTESIAN_POINT ( 'NONE',  ( 10.18810118749999916, 1.247682550866122264E-15, 70.28125000204838102 ) ) ;
#19112 = ORIENTED_EDGE ( 'NONE', *, *, #14645, .F. ) ;
#19113 = CARTESIAN_POINT ( 'NONE',  ( 7.188101187499999156, 7.874999997951610986, 2.977408999572654924 ) ) ;
#19114 = CARTESIAN_POINT ( 'NONE',  ( -7.347880794884122694E-16, 19.75000000000000000, 4.000000000000001776 ) ) ;
#19115 = CARTESIAN_POINT ( 'NONE',  ( -5.082755093536324154, 118.7187500020483810, 5.082755093536326818 ) ) ;
#19116 = CARTESIAN_POINT ( 'NONE',  ( 0.4589999999999999636, 284.2799999999998590, 5.818583442781865678 ) ) ;
#19117 = CARTESIAN_POINT ( 'NONE',  ( 2.765530957081996366, 294.1406250017069510, -6.676582343750002480 ) ) ;
#19119 = CARTESIAN_POINT ( 'NONE',  ( -2.828427124746190735, 15.12499999726881406, -2.828427124746191623 ) ) ;
#19118 = CARTESIAN_POINT ( 'NONE',  ( -5.676582343749992710, 229.7395833367473301, 9.832129032723422313 ) ) ;
#19120 = ORIENTED_EDGE ( 'NONE', *, *, #25130, .T. ) ;
#19121 = ADVANCED_FACE ( 'NONE', ( #5146 ), #5513, .F. ) ;
#19122 = CARTESIAN_POINT ( 'NONE',  ( 9.832129032723416984, 222.1354166700806729, -5.676582343750003368 ) ) ;
#19123 = CARTESIAN_POINT ( 'NONE',  ( -5.082755093536317936, -5.082755093536320601, 3.174052781871751439 ) ) ;
#19124 = CARTESIAN_POINT ( 'NONE',  ( 11.00000000000010658, 4.556349186103942017, 91.84374999999998579 ) ) ;
#19125 = CARTESIAN_POINT ( 'NONE',  ( -2.445694354108784108, 203.5625000013656063, 195.5543056458912190 ) ) ;
#19126 = EDGE_CURVE ( 'NONE', #28973, #64740, #14549, .T. ) ;
#19127 = ORIENTED_EDGE ( 'NONE', *, *, #56468, .T. ) ;
#19128 = LINE ( 'NONE', #26261, #18675 ) ;
#19129 = CARTESIAN_POINT ( 'NONE',  ( -8.311093377946836114, 97.96874999658599847, -8.311093377946837890 ) ) ;
#19130 = CARTESIAN_POINT ( 'NONE',  ( 27.99999999999999645, 210.0000000000000284, 169.9999999999999147 ) ) ;
#19131 = CARTESIAN_POINT ( 'NONE',  ( -6.735557395310442023E-16, 11.00000000000000000, 75.62499999999998579 ) ) ;
#19134 = CARTESIAN_POINT ( 'NONE',  ( -30.82842712474621294, 205.1250000000000284, 167.1715728752542134 ) ) ;
#19133 = CARTESIAN_POINT ( 'NONE',  ( 30.44569435410883074, 204.5625000013656063, 172.4456943541086957 ) ) ;
#19132 = CARTESIAN_POINT ( 'NONE',  ( 31.45873412499997812, 201.8750000013656063, 171.4326545832175839 ) ) ;
#19135 = EDGE_LOOP ( 'NONE', ( #67627, #70497, #35638, #40496 ) ) ;
#19136 = LINE ( 'NONE', #1802, #15167 ) ;
#19137 = CARTESIAN_POINT ( 'NONE',  ( 1.224646799147353454E-15, 300.0000000000000000, -10.00000000000000178 ) ) ;
#19138 = CARTESIAN_POINT ( 'NONE',  ( -9.832129032723420536, 208.6979166632526983, 5.676582343749997150 ) ) ;
#19139 = CARTESIAN_POINT ( 'NONE',  ( 2.445694354108782775, 202.5625000013656063, 139.5543056458912190 ) ) ;
#19140 = CARTESIAN_POINT ( 'NONE',  ( 25.55430564589115150, 201.5625000013656063, 172.4456943541086957 ) ) ;
#19141 = CARTESIAN_POINT ( 'NONE',  ( -11.00000000000000000, 0.000000000000000000, 116.6875000040967763 ) ) ;
#19142 = ADVANCED_FACE ( 'NONE', ( #53756 ), #7364, .F. ) ;
#19143 = CARTESIAN_POINT ( 'NONE',  ( 11.35316468749999963, 196.3020833299193271, -3.042071309553165293 ) ) ;
#19144 = CARTESIAN_POINT ( 'NONE',  ( 7.188101187500002709, 93.68750000204838102, 2.977408999572649151 ) ) ;
#19145 = CARTESIAN_POINT ( 'NONE',  ( -2.849036369511732440E-14, 196.3750000027311842, 138.0000000000000568 ) ) ;
#19146 = CARTESIAN_POINT ( 'NONE',  ( -23.99999999999998934, 198.7500000000000000, 170.0000000000003411 ) ) ;
#19147 = CARTESIAN_POINT ( 'NONE',  ( -8.342170076843785083E-16, 14.06249999863440614, 4.541265875000002339 ) ) ;
#19148 = CARTESIAN_POINT ( 'NONE',  ( 26.56734541678232731, 197.6250000013656063, 173.4587341249998929 ) ) ;
#19149 = CARTESIAN_POINT ( 'NONE',  ( -7.188101187499990274, -2.977408999572651371, 4.955302781871753659 ) ) ;
#19150 = CARTESIAN_POINT ( 'NONE',  ( -11.35316468750000141, 73.48958332991932707, 3.042071309553159963 ) ) ;
#19151 = CARTESIAN_POINT ( 'NONE',  ( -5.000000000000000000, -50.64189880742115690, 41.08656465431877791 ) ) ;
#19152 = DIRECTION ( 'NONE',  ( -1.000000000000000000, -1.084202172485504434E-16, 0.000000000000000000 ) ) ;
#19153 = ORIENTED_EDGE ( 'NONE', *, *, #35751, .T. ) ;
#19154 = CARTESIAN_POINT ( 'NONE',  ( -8.660254037844412167, 47.91666666666668561, 5.000000000000011546 ) ) ;
#19155 = CARTESIAN_POINT ( 'NONE',  ( -3.999999999999959144, 207.0625000000000568, 199.6568542494924259 ) ) ;
#19156 = CARTESIAN_POINT ( 'NONE',  ( -11.35316468749999785, 78.07291666325269830, -3.042071309553167513 ) ) ;
#19157 = ORIENTED_EDGE ( 'NONE', *, *, #29659, .F. ) ;
#19158 = CARTESIAN_POINT ( 'NONE',  ( -6.238412754330611322E-16, 10.18810118749999916, 85.65625000204838102 ) ) ;
#19159 = CIRCLE ( 'NONE', #37207, 30.99999999999997158 ) ;
#19160 = CARTESIAN_POINT ( 'NONE',  ( 5.499989586027935751, 9.526285454130809072, 66.68677389048281157 ) ) ;
#19161 = CARTESIAN_POINT ( 'NONE',  ( -2.445694354108783219, 207.8125000013656063, 200.4456943541088663 ) ) ;
#19162 = CARTESIAN_POINT ( 'NONE',  ( -0.4368895104719995870, 16.44602605510714710, 68.55492853905352035 ) ) ;
#19164 = CARTESIAN_POINT ( 'NONE',  ( 3.042071309553159519, 74.73958332991934128, 11.35316468750000141 ) ) ;
#19163 = CARTESIAN_POINT ( 'NONE',  ( -0.8721677472748841087, 67.61512445009852001, 20.05250736213596952 ) ) ;
#19165 = CARTESIAN_POINT ( 'NONE',  ( 7.999999999999992895, -3.313708498984756279, 27.17405278392014978 ) ) ;
#19166 = CYLINDRICAL_SURFACE ( 'NONE', #56550, 3.999999999999976019 ) ;
#19167 = CARTESIAN_POINT ( 'NONE',  ( 2.679491924311228956, 167.9166666598387110, -10.00000000000000000 ) ) ;
#19168 = CARTESIAN_POINT ( 'NONE',  ( -7.188101187500000044, 91.53125000204836681, 0.000000000000000000 ) ) ;
#19169 = CARTESIAN_POINT ( 'NONE',  ( -25.51922947296871413, 194.8335204809880281, 172.9287957184589857 ) ) ;
#19170 = CARTESIAN_POINT ( 'NONE',  ( 5.676582343750001591, 66.92708332991935549, -9.832129032723420536 ) ) ;
#19171 = CARTESIAN_POINT ( 'NONE',  ( -7.204075437095965206, -7.204075437095968759, 108.7187500020483810 ) ) ;
#19172 = CARTESIAN_POINT ( 'NONE',  ( 11.35316468750000141, 190.7812499965860127, 0.000000000000000000 ) ) ;
#19173 = ORIENTED_EDGE ( 'NONE', *, *, #28766, .F. ) ;
#19174 = CARTESIAN_POINT ( 'NONE',  ( -1.558072418983263985, 67.68461058694082055, 20.10890959968151748 ) ) ;
#19175 = CARTESIAN_POINT ( 'NONE',  ( -25.17157287525374088, 198.7500000027312126, 172.8284271247464972 ) ) ;
#19176 = CARTESIAN_POINT ( 'NONE',  ( 6.123233995736767268E-16, 163.1249999931720254, -10.00000000000000178 ) ) ;
#19178 = CARTESIAN_POINT ( 'NONE',  ( 11.35316468750000141, 190.7812499965860127, 0.000000000000000000 ) ) ;
#19177 = LINE ( 'NONE', #18820, #33923 ) ;
#19179 = EDGE_CURVE ( 'NONE', #20924, #15493, #14154, .T. ) ;
#19180 = CARTESIAN_POINT ( 'NONE',  ( 4.000000000000001776, 21.74999999726881583, 0.000000000000000000 ) ) ;
#19181 = CARTESIAN_POINT ( 'NONE',  ( 2.679491924311225848, 236.6666666734946602, -10.00000000000000000 ) ) ;
#19182 = CARTESIAN_POINT ( 'NONE',  ( 0.000000000000000000, 0.000000000000000000, -10.14441321561125520 ) ) ;
#19183 = ORIENTED_EDGE ( 'NONE', *, *, #45455, .F. ) ;
#19184 = EDGE_CURVE ( 'NONE', #15561, #58474, #4011, .T. ) ;
#19185 = CARTESIAN_POINT ( 'NONE',  ( 11.35316468750000141, 186.0937499965860411, 0.000000000000000000 ) ) ;
#19186 = CARTESIAN_POINT ( 'NONE',  ( 2.977408999572650927, -7.188101187499990274, 22.95530278187175455 ) ) ;
#19187 =( BOUNDED_CURVE ( )  B_SPLINE_CURVE ( 2, ( #1117, #46737, #65191, #30138, #7867, #53154, #17696, #69761, #59552, #40714, #1488, #29405, #19176 ),
 .UNSPECIFIED., .F., .F. ) 
 B_SPLINE_CURVE_WITH_KNOTS ( ( 3, 2, 2, 2, 2, 2, 3 ),
 ( 0.6902173913043477826, 0.6920289855072463414, 0.6938405797101449002, 0.6956521739130434590, 0.6974637681159420177, 0.6992753623188405765, 0.7010869565217391353 ),
 .UNSPECIFIED. ) 
 CURVE ( )  GEOMETRIC_REPRESENTATION_ITEM ( )  RATIONAL_B_SPLINE_CURVE ( ( 1.000000000000000000, 0.9659258262890683122, 1.000000000000000000, 0.9659258262890683122, 1.000000000000000000, 0.9659258262890683122, 1.000000000000000000, 0.9659258262890683122, 1.000000000000000000, 0.9659258262890683122, 1.000000000000000000, 0.9659258262890683122, 1.000000000000000000 ) ) 
 REPRESENTATION_ITEM ( '' )  );
#19188 = EDGE_CURVE ( 'NONE', #69617, #41375, #44992, .T. ) ;
#19189 = CARTESIAN_POINT ( 'NONE',  ( -1.469576158976823947E-15, 17.62500000000000000, 8.000000000000000000 ) ) ;
#19190 = ORIENTED_EDGE ( 'NONE', *, *, #27269, .T. ) ;
#19191 = CARTESIAN_POINT ( 'NONE',  ( 5.656854249492379694, 97.62500000409677625, -5.656854249492380582 ) ) ;
#19192 = CARTESIAN_POINT ( 'NONE',  ( 10.00000000000000178, 0.2083333333333333703, -2.679491924311226736 ) ) ;
#19193 = CIRCLE ( 'NONE', #28850, 10.50000000000000000 ) ;
#19194 = CARTESIAN_POINT ( 'NONE',  ( -4.000000000000002665, 13.56250000000000000, 1.656854249492380804 ) ) ;
#19195 =( BOUNDED_CURVE ( )  B_SPLINE_CURVE ( 2, ( #67701, #55275, #49596, #9985, #72612, #43939, #33754, #73356, #9235 ),
 .UNSPECIFIED., .F., .F. ) 
 B_SPLINE_CURVE_WITH_KNOTS ( ( 3, 2, 2, 2, 3 ),
 ( 0.03409090909090908839, 0.03977272727272727210, 0.04545454545454545581, 0.05113636363636364646, 0.05681818181818182323 ),
 .UNSPECIFIED. ) 
 CURVE ( )  GEOMETRIC_REPRESENTATION_ITEM ( )  RATIONAL_B_SPLINE_CURVE ( ( 1.000000000000000000, 0.9238795325112867385, 1.000000000000000000, 0.9238795325112867385, 1.000000000000000000, 0.9238795325112867385, 1.000000000000000000, 0.9238795325112866275, 1.000000000000000000 ) ) 
 REPRESENTATION_ITEM ( '' )  );
#19196 = CARTESIAN_POINT ( 'NONE',  ( -1.881053915767124440, 13.99999999863440792, 4.541265875000001451 ) ) ;
#19197 = CARTESIAN_POINT ( 'NONE',  ( -5.656854249492375253, 5.656854249492375253, 12.83030278392014623 ) ) ;
#19198 = CARTESIAN_POINT ( 'NONE',  ( -4.000000000000015099, 195.5625000000000568, 143.6568542494924543 ) ) ;
#19199 = EDGE_LOOP ( 'NONE', ( #72347, #53166, #74559, #29773 ) ) ;
#19200 = DIRECTION ( 'NONE',  ( -0.000000000000000000, -0.000000000000000000, -1.000000000000000000 ) ) ;
#19201 = CARTESIAN_POINT ( 'NONE',  ( -4.401442555609581635E-16, 96.78125000204838102, -7.188101187500000044 ) ) ;
#19203 = CARTESIAN_POINT ( 'NONE',  ( 4.000000000000001776, 6.749999997268813168, 0.000000000000000000 ) ) ;
#19202 = CARTESIAN_POINT ( 'NONE',  ( 2.679491924310949180, 181.0416666666667425, -10.00000000000022204 ) ) ;
#19204 = CARTESIAN_POINT ( 'NONE',  ( 1424.688200795887951, 594.9677537767815920, 997.8421604560580818 ) ) ;
#19205 = VERTEX_POINT ( 'NONE', #74355 ) ;
#19206 = CARTESIAN_POINT ( 'NONE',  ( 1.882291019709046553, 10.12018455450524002, -70.22327770540687197 ) ) ;
#19207 = EDGE_CURVE ( 'NONE', #26465, #12947, #62660, .T. ) ;
#19208 = CARTESIAN_POINT ( 'NONE',  ( 0.000000000000000000, 192.0000000000000284, 170.0000000000000284 ) ) ;
#19209 = CARTESIAN_POINT ( 'NONE',  ( 2.977408999572650927, -7.188101187499990274, 18.45530278187175455 ) ) ;
#19210 = ORIENTED_EDGE ( 'NONE', *, *, #1678, .F. ) ;
#19211 = ORIENTED_EDGE ( 'NONE', *, *, #70963, .T. ) ;
#19212 = CARTESIAN_POINT ( 'NONE',  ( -4.220049686691935698, 10.18810118749999916, 86.87500000204836681 ) ) ;
#19213 = CARTESIAN_POINT ( 'NONE',  ( -7.320508075688778149, 114.9999999931720254, 7.320508075688769267 ) ) ;
#19214 = CARTESIAN_POINT ( 'NONE',  ( 7.778174593052023411, -7.778174593052021635, 96.06250000000000000 ) ) ;
#19217 = CARTESIAN_POINT ( 'NONE',  ( 6.676582343750002480, 293.1718750017071216, -2.765530957081997254 ) ) ;
#19216 = CARTESIAN_POINT ( 'NONE',  ( 24.00000000000000355, 202.9375000027312410, 171.6568542494923122 ) ) ;
#19215 = CARTESIAN_POINT ( 'NONE',  ( 27.99999999999999645, 210.0000000000000284, 173.9999999999998863 ) ) ;
#19218 = CARTESIAN_POINT ( 'NONE',  ( 8.660254037844389075, 150.4166666666666572, -5.000000000000000000 ) ) ;
#19219 = CARTESIAN_POINT ( 'NONE',  ( 23.99999999999998934, 199.8750000027312126, 169.9999999999999432 ) ) ;
#19220 = CARTESIAN_POINT ( 'NONE',  ( 2.977408999572646486, 7.188101187499991163, 1.392802781871753437 ) ) ;
#19221 = LINE ( 'NONE', #29815, #47039 ) ;
#19222 = CARTESIAN_POINT ( 'NONE',  ( -8.000000000000000000, 5.062499995903221084, -9.797174393178825657E-16 ) ) ;
#19223 = CARTESIAN_POINT ( 'NONE',  ( 30.44569435410878810, 197.5625000013656063, 172.4456943541087526 ) ) ;
#19224 = CARTESIAN_POINT ( 'NONE',  ( -2.977408999572654480, 3.374999997951610986, 7.188101187499999156 ) ) ;
#19225 = CARTESIAN_POINT ( 'NONE',  ( 7.999999999999991118, 9.797174393178815797E-16, 27.26780278392014978 ) ) ;
#19226 = FACE_OUTER_BOUND ( 'NONE', #32801, .T. ) ;
#19227 = CARTESIAN_POINT ( 'NONE',  ( 7.188101187500000933, 108.8750000020483952, -2.977408999572651371 ) ) ;
#19229 = DIRECTION ( 'NONE',  ( -0.000000000000000000, 1.000000000000000000, 0.000000000000000000 ) ) ;
#19228 = DIRECTION ( 'NONE',  ( 0.000000000000000000, 0.000000000000000000, -1.000000000000000000 ) ) ;
#19230 = CARTESIAN_POINT ( 'NONE',  ( 8.311093377946834337, 232.3437500034140157, -8.311093377946836114 ) ) ;
#19231 = CARTESIAN_POINT ( 'NONE',  ( -4.401442555609577197E-16, 7.188101187499992051, 23.98655278187175455 ) ) ;
#19232 = FACE_OUTER_BOUND ( 'NONE', #32931, .T. ) ;
#19233 = CARTESIAN_POINT ( 'NONE',  ( 5.676582343749993598, 34.94791666325268409, 9.832129032723422313 ) ) ;
#19234 = CARTESIAN_POINT ( 'NONE',  ( 2.849036369511732440E-14, 203.2500000000000000, 202.0000000000000000 ) ) ;
#19235 = CARTESIAN_POINT ( 'NONE',  ( -2.679491924311225848, 8.333333326505366401, -10.00000000000000178 ) ) ;
#19236 = ORIENTED_EDGE ( 'NONE', *, *, #56605, .F. ) ;
#19237 = FACE_OUTER_BOUND ( 'NONE', #29340, .T. ) ;
#19238 = CARTESIAN_POINT ( 'NONE',  ( -1.656854249492381248, 8.062499997268814056, -4.000000000000001776 ) ) ;
#19239 = CARTESIAN_POINT ( 'NONE',  ( 11.35316468749999963, 40.98958332991935549, -3.042071309553165293 ) ) ;
#19240 = CARTESIAN_POINT ( 'NONE',  ( 2.020667218593132706E-15, -11.00000000000000000, 85.56250000409676204 ) ) ;
#19241 = CARTESIAN_POINT ( 'NONE',  ( -3.458734125000015425, 208.2500000013656063, 143.4326545832176976 ) ) ;
#19242 = CARTESIAN_POINT ( 'NONE',  ( -2.485281374238979879, 298.8125000000000000, -5.999999999999594991 ) ) ;
#19243 = CARTESIAN_POINT ( 'NONE',  ( -3.673940397442060854E-16, 290.7500000000000000, -6.000000000000001776 ) ) ;
#19245 = CARTESIAN_POINT ( 'NONE',  ( 8.311093377946837890, 36.40624999658601979, -8.311093377946837890 ) ) ;
#19244 = CARTESIAN_POINT ( 'NONE',  ( -2.977408999572650927, 107.3750000020483952, -7.188101187500000933 ) ) ;
#19246 = CARTESIAN_POINT ( 'NONE',  ( 7.999999999999991118, 9.797174393178815797E-16, 16.58030277982336287 ) ) ;
#19247 = CARTESIAN_POINT ( 'NONE',  ( -5.676582343749998039, 152.4479166632526983, -9.832129032723420536 ) ) ;
#19248 = AXIS2_PLACEMENT_3D ( 'NONE', #68318, #68687, #50963 ) ;
#19249 = CARTESIAN_POINT ( 'NONE',  ( -10.00000000000000355, 109.5833333265053540, 2.679491924311223183 ) ) ;
#19250 = CARTESIAN_POINT ( 'NONE',  ( 7.188101187500001821, 105.8750000020483952, -2.977408999572651371 ) ) ;
#19251 = CARTESIAN_POINT ( 'NONE',  ( 2.849036369511732440E-14, 199.2500000000000000, 202.0000000000000000 ) ) ;
#19252 = CARTESIAN_POINT ( 'NONE',  ( -26.56734541678232375, 203.2500000013656063, 173.4587341250003760 ) ) ;
#19253 = ORIENTED_EDGE ( 'NONE', *, *, #40888, .T. ) ;
#19254 = PLANE ( 'NONE',  #67729 ) ;
#19255 = CARTESIAN_POINT ( 'NONE',  ( -9.832129032723420536, 24.01041666325268409, 5.676582343749997150 ) ) ;
#19256 = EDGE_LOOP ( 'NONE', ( #61029, #66407, #42132, #59549 ) ) ;
#19257 = CARTESIAN_POINT ( 'NONE',  ( 8.660254037844373087, 104.5833333333333286, 4.999999999999998224 ) ) ;
#19258 = FACE_OUTER_BOUND ( 'NONE', #21774, .T. ) ;
#19260 = CARTESIAN_POINT ( 'NONE',  ( 3.042071309553167513, 151.8229166632526699, -11.35316468749999785 ) ) ;
#19259 = CARTESIAN_POINT ( 'NONE',  ( -27.96822672120047670, -21.40302687707136897, 149.2371148674697849 ) ) ;
#19261 = CARTESIAN_POINT ( 'NONE',  ( 7.999999999999991118, 9.797174393178815797E-16, 19.63655278432982243 ) ) ;
#19262 = CARTESIAN_POINT ( 'NONE',  ( 7.999999999999998224, 14.90625000000000355, 3.313708498984766049 ) ) ;
#19263 = AXIS2_PLACEMENT_3D ( 'NONE', #41694, #65804, #53022 ) ;
#19264 = CARTESIAN_POINT ( 'NONE',  ( -11.35316468749999963, 238.9062500034140157, 0.000000000000000000 ) ) ;
#19265 = CARTESIAN_POINT ( 'NONE',  ( -4.220049686691935698, 10.18810118749999916, 93.25000000204838102 ) ) ;
#19266 = ORIENTED_EDGE ( 'NONE', *, *, #53219, .F. ) ;
#19267 = ADVANCED_FACE ( 'NONE', ( #22665 ), #45684, .T. ) ;
#19268 = DIRECTION ( 'NONE',  ( -0.000000000000000000, -1.000000000000000000, -0.000000000000000000 ) ) ;
#19269 = CARTESIAN_POINT ( 'NONE',  ( 30.82842712474620228, 205.3750000000000284, 167.1715728752537586 ) ) ;
#19270 = CARTESIAN_POINT ( 'NONE',  ( -9.832129032723420536, 99.01041666325269830, 5.676582343749997150 ) ) ;
#19271 = CARTESIAN_POINT ( 'NONE',  ( 10.18810118749999916, 1.247682550866122264E-15, 99.90625000204838102 ) ) ;
#19272 = EDGE_CURVE ( 'NONE', #23374, #5520, #62815, .T. ) ;
#19273 = CARTESIAN_POINT ( 'NONE',  ( -4.541265875000003227, 16.99999999863440436, 1.881053915767121110 ) ) ;
#19274 = ORIENTED_EDGE ( 'NONE', *, *, #56766, .T. ) ;
#19275 = ORIENTED_EDGE ( 'NONE', *, *, #26231, .T. ) ;
#19276 = CARTESIAN_POINT ( 'NONE',  ( 8.000000000000000000, 3.093750000000001332, -3.313708498984761608 ) ) ;
#19277 = CARTESIAN_POINT ( 'NONE',  ( -3.313708498984719864, 10.96874999999999822, -8.000000000000040856 ) ) ;
#19278 = CARTESIAN_POINT ( 'NONE',  ( 5.082755093536325930, 5.156249997951610986, -5.082755093536325930 ) ) ;
#19279 = CARTESIAN_POINT ( 'NONE',  ( 8.000000000000000000, 114.0312500040967763, -3.313708498984762496 ) ) ;
#19280 = CARTESIAN_POINT ( 'NONE',  ( 10.18810118749999916, 1.247682550866122264E-15, 100.2812500020483810 ) ) ;
#19281 = CARTESIAN_POINT ( 'NONE',  ( -5.656854249492381470, 6.937500000000000888, 5.656854249492379694 ) ) ;
#19282 = CARTESIAN_POINT ( 'NONE',  ( 2.449293598294707893E-16, 13.99999999726881406, -4.000000000000001776 ) ) ;
#19283 = CARTESIAN_POINT ( 'NONE',  ( -4.541265875000002339, 4.749999998634407028, -1.881053915767121998 ) ) ;
#19284 = ORIENTED_EDGE ( 'NONE', *, *, #26599, .F. ) ;
#19285 = CARTESIAN_POINT ( 'NONE',  ( 2.445694354108783664, 207.3125000013656063, 144.4456943541088663 ) ) ;
#19286 = CARTESIAN_POINT ( 'NONE',  ( 1.432654583217662481, 197.1250000013656347, 194.5412658750000219 ) ) ;
#19289 = DIRECTION ( 'NONE',  ( -0.000000000000000000, 1.000000000000000000, -0.000000000000000000 ) ) ;
#19288 = CARTESIAN_POINT ( 'NONE',  ( -26.56734541678227757, 202.0000000013656063, 173.4587341250003476 ) ) ;
#19287 =( BOUNDED_CURVE ( )  B_SPLINE_CURVE ( 2, ( #2524, #60977, #27018, #25516, #9298, #71913, #33083, #37978, #9681, #26257, #14567, #37603, #48528 ),
 .UNSPECIFIED., .F., .F. ) 
 B_SPLINE_CURVE_WITH_KNOTS ( ( 3, 2, 2, 2, 2, 2, 3 ),
 ( 0.7119565217391303769, 0.7137681159420288246, 0.7155797101449273834, 0.7173913043478259421, 0.7192028985507246119, 0.7210144927536231707, 0.7228260869565217295 ),
 .UNSPECIFIED. ) 
 CURVE ( )  GEOMETRIC_REPRESENTATION_ITEM ( )  RATIONAL_B_SPLINE_CURVE ( ( 1.000000000000001998, 0.9659258262890662028, 1.000000000000000000, 0.9659258262890683122, 1.000000000000000000, 0.9659258262890683122, 1.000000000000000000, 0.9659258262890683122, 1.000000000000000000, 0.9659258262890683122, 1.000000000000000000, 0.9659258262890683122, 1.000000000000000000 ) ) 
 REPRESENTATION_ITEM ( '' )  );
#19290 = CARTESIAN_POINT ( 'NONE',  ( -4.541265875000003227, 14.87499999863441147, 1.881053915767121110 ) ) ;
#19291 = AXIS2_PLACEMENT_3D ( 'NONE', #28308, #68669, #57742 ) ;
#19292 = CARTESIAN_POINT ( 'NONE',  ( 10.00000000000000000, 121.6666666598386968, 2.679491924311235618 ) ) ;
#19293 = CARTESIAN_POINT ( 'NONE',  ( -5.082755093536319713, 5.082755093536319713, 11.79905278187175277 ) ) ;
#19294 = ORIENTED_EDGE ( 'NONE', *, *, #47649, .F. ) ;
#19295 = ORIENTED_EDGE ( 'NONE', *, *, #32090, .T. ) ;
#19296 = CARTESIAN_POINT ( 'NONE',  ( -4.220049686691935698, 10.18810118749999916, 101.8750000020483810 ) ) ;
#19297 = CARTESIAN_POINT ( 'NONE',  ( -4.556349186104045934, 11.00000000000000000, 114.9062500040967763 ) ) ;
#19298 = AXIS2_PLACEMENT_3D ( 'NONE', #11181, #253, #56466 ) ;
#19299 = CARTESIAN_POINT ( 'NONE',  ( -29.43265458321766914, 205.7500000013656063, 166.5412658750003629 ) ) ;
#19300 = CARTESIAN_POINT ( 'NONE',  ( -26.34314575050758123, 202.5625000000000000, 174.0000000000003411 ) ) ;
#19301 = CARTESIAN_POINT ( 'NONE',  ( 3.458734125000016313, 195.8750000013655779, 199.4326545832176691 ) ) ;
#19302 = CARTESIAN_POINT ( 'NONE',  ( -27.99999999999991118, 201.6250000027312126, 174.0000000000003695 ) ) ;
#19303 = CARTESIAN_POINT ( 'NONE',  ( 2.679491924311222739, 93.95833333333334281, 10.00000000000000355 ) ) ;
#19304 = CARTESIAN_POINT ( 'NONE',  ( 8.000000000000000000, 110.8437499999999858, -3.313708498984762496 ) ) ;
#19305 = CARTESIAN_POINT ( 'NONE',  ( 2.765530957081996366, 295.2968750017069510, -6.676582343750003368 ) ) ;
#19306 = VERTEX_POINT ( 'NONE', #23048 ) ;
#19307 = CARTESIAN_POINT ( 'NONE',  ( -11.00000000000000000, 0.000000000000000000, 74.49999999999998579 ) ) ;
#19308 = CARTESIAN_POINT ( 'NONE',  ( 5.656854249492380582, 13.49999999590322375, -5.656854249492380582 ) ) ;
#19309 = CARTESIAN_POINT ( 'NONE',  ( 2.445694354108782775, 204.5625000013656063, 139.5543056458912190 ) ) ;
#19310 = LINE ( 'NONE', #6896, #34758 ) ;
#19311 = CARTESIAN_POINT ( 'NONE',  ( -9.832129032723418760, 263.8020833367473301, -5.676582343749998927 ) ) ;
#19312 = CARTESIAN_POINT ( 'NONE',  ( -1.656854249492440978, 207.6875000000000284, 146.0000000000000000 ) ) ;
#19313 = CARTESIAN_POINT ( 'NONE',  ( 4.556349186104051263, -10.99999999999999822, 110.9687500000000142 ) ) ;
#19314 = CARTESIAN_POINT ( 'NONE',  ( 10.00000000000000178, 215.0000000000000284, 0.000000000000000000 ) ) ;
#19315 = CARTESIAN_POINT ( 'NONE',  ( 1.320432766682872962E-15, -7.188101187499992051, 8.236552781871752771 ) ) ;
#19316 = CARTESIAN_POINT ( 'NONE',  ( -5.676582343750006032, 189.4270833299193555, 9.832129032723418760 ) ) ;
#19317 = CARTESIAN_POINT ( 'NONE',  ( 3.008240453400888764E-14, -70.00000000000000000, 189.0000000000000000 ) ) ;
#19318 = CARTESIAN_POINT ( 'NONE',  ( -3.211159895383561391, 0.6874999986344068059, -3.211159895383561835 ) ) ;
#19319 = CARTESIAN_POINT ( 'NONE',  ( 8.660254037844389075, 242.0833333333333428, 4.999999999999997335 ) ) ;
#19321 = CARTESIAN_POINT ( 'NONE',  ( 0.000000000000000000, 0.000000000000000000, 0.000000000000000000 ) ) ;
#19320 = CARTESIAN_POINT ( 'NONE',  ( -3.458734124999960358, 194.6875000013655779, 198.0000000000000284 ) ) ;
#19322 = ORIENTED_EDGE ( 'NONE', *, *, #48597, .F. ) ;
#19323 = CARTESIAN_POINT ( 'NONE',  ( -3.458734125000015869, 209.1875000013656063, 142.0000000000000568 ) ) ;
#19324 = CARTESIAN_POINT ( 'NONE',  ( -9.832129032723420536, 54.01041666325268409, 5.676582343749997150 ) ) ;
#19325 = CARTESIAN_POINT ( 'NONE',  ( 7.778174593052021635, 7.778174593052023411, 105.6250000040967763 ) ) ;
#19326 = CARTESIAN_POINT ( 'NONE',  ( 8.311093377946834337, 220.4687499965859843, 8.311093377946839666 ) ) ;
#19327 = CARTESIAN_POINT ( 'NONE',  ( -29.43265458321755546, 203.8750000013656063, 173.4587341250004044 ) ) ;
#19328 = CARTESIAN_POINT ( 'NONE',  ( 11.00000000000000000, 4.556349186104045934, 95.03125000409677625 ) ) ;
#19330 = CARTESIAN_POINT ( 'NONE',  ( -7.320508075688773708, 58.74999999317203248, -7.320508075688774596 ) ) ;
#19329 = DIRECTION ( 'NONE',  ( 0.000000000000000000, 1.387778780781445676E-15, 1.000000000000000000 ) ) ;
#19331 = DIRECTION ( 'NONE',  ( 0.000000000000000000, 2.238352872228138170E-16, -1.000000000000000000 ) ) ;
#19332 = CARTESIAN_POINT ( 'NONE',  ( -3.042071309553164404, 107.2395833299193413, -11.35316468749999963 ) ) ;
#19333 = EDGE_CURVE ( 'NONE', #21298, #48333, #11703, .T. ) ;
#19334 = EDGE_CURVE ( 'NONE', #53057, #59077, #17384, .T. ) ;
#19335 = CARTESIAN_POINT ( 'NONE',  ( -8.660254037844387298, 73.95833332650536818, -5.000000000000004441 ) ) ;
#19336 = CARTESIAN_POINT ( 'NONE',  ( 2.977408999572654480, 93.12500000204836681, 7.188101187499999156 ) ) ;
#19337 = CARTESIAN_POINT ( 'NONE',  ( 1.881053915767122664, 17.24999999863440792, 4.541265875000001451 ) ) ;
#19338 = CARTESIAN_POINT ( 'NONE',  ( -2.679491924316527385, 71.45833333333379755, -9.999999999996944666 ) ) ;
#19339 = CARTESIAN_POINT ( 'NONE',  ( 2.020667218593132706E-15, -11.00000000000000000, 67.56250000409677625 ) ) ;
#19340 = ORIENTED_EDGE ( 'NONE', *, *, #21299, .F. ) ;
#19341 = ORIENTED_EDGE ( 'NONE', *, *, #25602, .F. ) ;
#19342 = CARTESIAN_POINT ( 'NONE',  ( -4.721056650415999201, 294.4843750017070079, -4.721056650415999201 ) ) ;
#19343 = CARTESIAN_POINT ( 'NONE',  ( -7.320508075688787919, 143.1250000000000284, 7.320508075688779925 ) ) ;
#19344 = CARTESIAN_POINT ( 'NONE',  ( -11.35316468750000141, 163.4895833299193271, 3.042071309553159963 ) ) ;
#19345 = CARTESIAN_POINT ( 'NONE',  ( 10.00000000000000178, 2.083333326505365957, -2.679491924311226736 ) ) ;
#19346 = CARTESIAN_POINT ( 'NONE',  ( 4.000000000000015099, 201.5625000000000853, 196.3431457505076594 ) ) ;
#19347 = DIRECTION ( 'NONE',  ( -0.000000000000000000, -0.000000000000000000, 1.000000000000000000 ) ) ;
#19348 = CARTESIAN_POINT ( 'NONE',  ( -7.204075437095965206, -7.204075437095968759, 111.7187500020483810 ) ) ;
#19349 = ORIENTED_EDGE ( 'NONE', *, *, #28386, .F. ) ;
#19350 = VECTOR ( 'NONE', #58857, 1000.000000000000000 ) ;
#19351 = CYLINDRICAL_SURFACE ( 'NONE', #50495, 7.999999999999991118 ) ;
#19352 = CARTESIAN_POINT ( 'NONE',  ( 0.000000000000000000, 0.000000000000000000, 118.0000000000000000 ) ) ;
#19353 = CARTESIAN_POINT ( 'NONE',  ( 3.042071309553159519, 140.0520833299193271, 11.35316468750000141 ) ) ;
#19354 = CARTESIAN_POINT ( 'NONE',  ( 3.458734125000015425, 195.9375000013655779, 198.0000000000000284 ) ) ;
#19355 = CARTESIAN_POINT ( 'NONE',  ( -3.458734124999960358, 208.6875000013656063, 198.0000000000000284 ) ) ;
#19356 = CARTESIAN_POINT ( 'NONE',  ( -7.204075437095967871, 7.204075437095967871, 73.84375000204838102 ) ) ;
#19357 = CARTESIAN_POINT ( 'NONE',  ( 8.311093377946837890, 51.71874999658601979, -8.311093377946837890 ) ) ;
#19358 = ORIENTED_EDGE ( 'NONE', *, *, #41587, .T. ) ;
#19359 = DIRECTION ( 'NONE',  ( 0.000000000000000000, 0.000000000000000000, 1.000000000000000000 ) ) ;
#19360 = CARTESIAN_POINT ( 'NONE',  ( 4.541265875000002339, 3.499999998634407028, -1.881053915767121776 ) ) ;
#19361 = CARTESIAN_POINT ( 'NONE',  ( -5.662595241051935346, 5.662595241051935346, 9.825615283940630107 ) ) ;
#19362 = CARTESIAN_POINT ( 'NONE',  ( 4.401442555609581635E-16, 15.84374999795161365, -7.188101187500000044 ) ) ;
#19363 = CARTESIAN_POINT ( 'NONE',  ( 4.242640687119287435, 291.4375000034140157, 4.242640687119285658 ) ) ;
#19364 = VECTOR ( 'NONE', #9044, 1000.000000000000000 ) ;
#19365 = CARTESIAN_POINT ( 'NONE',  ( -3.313708498984720308, 117.4062500040967763, -8.000000000000040856 ) ) ;
#19366 = CARTESIAN_POINT ( 'NONE',  ( -2.977408999572650039, 14.81249999795161543, -7.188101187500001821 ) ) ;
#19367 = CARTESIAN_POINT ( 'NONE',  ( 7.188101187499992051, 2.977408999572647819, 6.830302781871754547 ) ) ;
#19368 = CARTESIAN_POINT ( 'NONE',  ( -10.18810118749999738, -4.220049686691941915, 67.75000000204836681 ) ) ;
#19369 = CARTESIAN_POINT ( 'NONE',  ( 27.99999999999999645, 210.0000000000000284, 169.9999999999999147 ) ) ;
#19370 = CARTESIAN_POINT ( 'NONE',  ( -1.656854249492381248, 2.062499997268813612, -4.000000000000001776 ) ) ;
#19371 = ORIENTED_EDGE ( 'NONE', *, *, #26526, .F. ) ;
#19372 = CARTESIAN_POINT ( 'NONE',  ( 1.656854249492403008, 196.8125000027311842, 194.0000000000000853 ) ) ;
#19373 = CARTESIAN_POINT ( 'NONE',  ( 2.828427124746153876, 203.8750000000000284, 144.8284271247462129 ) ) ;
#19374 = B_SPLINE_CURVE_WITH_KNOTS ( 'NONE', 3,
 ( #35790, #363, #59176, #58804, #30122, #53139, #40699, #63703 ),
 .UNSPECIFIED., .F., .F.,
 ( 4, 2, 2, 4 ),
 ( 0.02466681279448781211, 0.02652623278167728915, 0.02838565276886676619, 0.03210449274324569946 ),
 .UNSPECIFIED. ) ;
#19375 = CARTESIAN_POINT ( 'NONE',  ( -26.34314575050753149, 197.6875000027312126, 174.0000000000003411 ) ) ;
#19376 = CARTESIAN_POINT ( 'NONE',  ( 2.780723358947928197E-16, 3.562499998634407028, -4.541265875000002339 ) ) ;
#19377 = CARTESIAN_POINT ( 'NONE',  ( -7.188101187500001821, 112.0625000020483810, -2.977408999572650483 ) ) ;
#19378 = CYLINDRICAL_SURFACE ( 'NONE', #38064, 10.00000000000000178 ) ;
#19379 = CARTESIAN_POINT ( 'NONE',  ( -3.313708498984758943, -7.999999999999989342, -0.2009472160798553009 ) ) ;
#19380 = ORIENTED_EDGE ( 'NONE', *, *, #17240, .T. ) ;
#19381 = CARTESIAN_POINT ( 'NONE',  ( -7.188101187500002709, 22.31249999795161187, 2.977408999572649151 ) ) ;
#19382 = ORIENTED_EDGE ( 'NONE', *, *, #30261, .T. ) ;
#19383 = CARTESIAN_POINT ( 'NONE',  ( -5.000000000000000000, 0.000000000000000000, 0.000000000000000000 ) ) ;
#19384 = CARTESIAN_POINT ( 'NONE',  ( -2.445694354108783664, 208.3125000013656063, 195.5543056458912190 ) ) ;
#19385 = CARTESIAN_POINT ( 'NONE',  ( 26.56734541678237704, 205.3750000013656063, 173.4587341249998929 ) ) ;
#19386 = CARTESIAN_POINT ( 'NONE',  ( 7.320508075688771044, 49.37500000000000000, 7.320508075688775484 ) ) ;
#19387 = CARTESIAN_POINT ( 'NONE',  ( 2.977408999572654480, 102.5000000020483810, 7.188101187499999156 ) ) ;
#19388 = CARTESIAN_POINT ( 'NONE',  ( 4.242640687119287435, 297.3750000000000000, 4.242640687119285658 ) ) ;
#19390 = DIRECTION ( 'NONE',  ( -0.000000000000000000, -0.000000000000000000, -1.000000000000000000 ) ) ;
#19389 = CARTESIAN_POINT ( 'NONE',  ( 28.00000000000002487, 209.1250000027312126, 173.9999999999999147 ) ) ;
#19391 = ORIENTED_EDGE ( 'NONE', *, *, #58921, .T. ) ;
#19392 = CARTESIAN_POINT ( 'NONE',  ( -5.676582343749992710, 234.7395833367473301, 9.832129032723422313 ) ) ;
#19393 = EDGE_CURVE ( 'NONE', #40745, #72853, #34879, .T. ) ;
#19394 = DIRECTION ( 'NONE',  ( -0.000000000000000000, 1.000000000000000000, -1.563033456626094573E-30 ) ) ;
#19395 = CARTESIAN_POINT ( 'NONE',  ( -10.00000000000000355, 74.58333332650535397, 2.679491924311223183 ) ) ;
#19396 = CARTESIAN_POINT ( 'NONE',  ( -6.123233995736766282E-16, 246.8750000068280031, -10.00000000000000000 ) ) ;
#19397 = CARTESIAN_POINT ( 'NONE',  ( -10.00000000000000000, 260.0000000000000000, 0.000000000000000000 ) ) ;
#19398 = CYLINDRICAL_SURFACE ( 'NONE', #19827, 4.000000000000001776 ) ;
#19399 =( BOUNDED_CURVE ( )  B_SPLINE_CURVE ( 2, ( #47165, #46434, #69450, #72792, #20721, #36598, #8288, #25255, #42614 ),
 .UNSPECIFIED., .F., .F. ) 
 B_SPLINE_CURVE_WITH_KNOTS ( ( 3, 2, 2, 2, 3 ),
 ( 0.6000000000000004219, 0.6083333333333338366, 0.6166666666666672514, 0.6250000000000006661, 0.6333333333333339699 ),
 .UNSPECIFIED. ) 
 CURVE ( )  GEOMETRIC_REPRESENTATION_ITEM ( )  RATIONAL_B_SPLINE_CURVE ( ( 0.9999999999999958922, 0.9238795325112908463, 1.000000000000000000, 0.9238795325112867385, 1.000000000000000000, 0.9238795325112867385, 1.000000000000000000, 0.9238795325112806323, 1.000000000000005995 ) ) 
 REPRESENTATION_ITEM ( '' )  );
#19400 = CARTESIAN_POINT ( 'NONE',  ( -4.999999999999998224, 176.6666666666666572, -8.660254037844389075 ) ) ;
#19401 = CARTESIAN_POINT ( 'NONE',  ( 0.000000000000000000, 0.000000000000000000, -4.000000000000001776 ) ) ;
#19402 =( LENGTH_UNIT ( ) NAMED_UNIT ( * ) SI_UNIT ( .MILLI., .METRE. ) );
#19403 = CARTESIAN_POINT ( 'NONE',  ( -4.999999999999952927, -68.60357193678709109, 20.85024232999324667 ) ) ;
#19404 = CARTESIAN_POINT ( 'NONE',  ( 11.35316468749999785, 145.8854166632526983, 3.042071309553174174 ) ) ;
#19405 = DIRECTION ( 'NONE',  ( -1.000000000000000000, 0.000000000000000000, 0.000000000000000000 ) ) ;
#19406 = LINE ( 'NONE', #36043, #73488 ) ;
#19409 = DIRECTION ( 'NONE',  ( -2.771571441169508074E-17, -1.000000000000000000, -2.238352872228138663E-16 ) ) ;
#19408 = DIRECTION ( 'NONE',  ( 0.000000000000000000, -8.566535683836083017E-17, 1.000000000000000000 ) ) ;
#19407 = CARTESIAN_POINT ( 'NONE',  ( 26.34314575050763452, 205.5625000000000284, 165.9999999999998863 ) ) ;
#19410 = ORIENTED_EDGE ( 'NONE', *, *, #40554, .T. ) ;
#19411 = CARTESIAN_POINT ( 'NONE',  ( -9.832129032723420536, 4.010416663252683200, 5.676582343749997150 ) ) ;
#19412 = AXIS2_PLACEMENT_3D ( 'NONE', #18619, #1288, #919 ) ;
#19413 = CYLINDRICAL_SURFACE ( 'NONE', #67298, 3.999999999999976019 ) ;
#19414 = CARTESIAN_POINT ( 'NONE',  ( 27.99999999999999645, 210.0000000000000284, 165.9999999999999147 ) ) ;
#19415 = CARTESIAN_POINT ( 'NONE',  ( -27.99999999999995381, 196.5000000000000000, 174.0000000000003695 ) ) ;
#19416 = CARTESIAN_POINT ( 'NONE',  ( 2.445694354108782775, 206.5625000013656063, 139.5543056458912190 ) ) ;
#19417 = CARTESIAN_POINT ( 'NONE',  ( -2.828427124746208943, 202.6250000000000284, 144.8284271247462129 ) ) ;
#19418 = CARTESIAN_POINT ( 'NONE',  ( -10.00000000000000355, 39.58333332650536107, 2.679491924311223183 ) ) ;
#19419 = PRESENTATION_LAYER_ASSIGNMENT (  '', '', ( #71226 ) ) ;
#19420 = CARTESIAN_POINT ( 'NONE',  ( 1.320432766682874540E-15, 114.0312500020483952, 7.188101187500000044 ) ) ;
#19421 = CARTESIAN_POINT ( 'NONE',  ( 4.541265875000001451, 4.374999998634407028, 1.881053915767124440 ) ) ;
#19422 = CARTESIAN_POINT ( 'NONE',  ( -11.00000000000000000, 0.000000000000000000, 84.99999999999998579 ) ) ;
#19423 = CARTESIAN_POINT ( 'NONE',  ( 3.313708498984756279, 7.999999999999991118, 12.36155277982336820 ) ) ;
#19425 = CARTESIAN_POINT ( 'NONE',  ( 8.660254037844389075, 7.291666659838699438, -5.000000000000000000 ) ) ;
#19424 = CARTESIAN_POINT ( 'NONE',  ( -31.99999999999998579, 203.3125000000000284, 171.6568542494928238 ) ) ;
#19426 = ORIENTED_EDGE ( 'NONE', *, *, #12160, .F. ) ;
#19427 = CARTESIAN_POINT ( 'NONE',  ( 5.000000000000000000, -32.28817737728140003, -1.075528555105620399E-13 ) ) ;
#19428 = AXIS2_PLACEMENT_3D ( 'NONE', #621, #12283, #46610 ) ;
#19429 = CARTESIAN_POINT ( 'NONE',  ( -7.320508075688818117, 63.12500000000004263, 7.320508075688810123 ) ) ;
#19430 = CARTESIAN_POINT ( 'NONE',  ( -11.35316468749999785, 234.0104166700806161, -3.042071309553164848 ) ) ;
#19431 = CARTESIAN_POINT ( 'NONE',  ( 11.35316468749999963, 115.9895833299193555, -3.042071309553165293 ) ) ;
#19432 = VERTEX_POINT ( 'NONE', #32907 ) ;
#19433 = EDGE_CURVE ( 'NONE', #27289, #51761, #30316, .T. ) ;
#19434 = EDGE_CURVE ( 'NONE', #22621, #38422, #67594, .T. ) ;
#19435 = CARTESIAN_POINT ( 'NONE',  ( -4.220049686691937474, -10.18810118749999738, 96.43750000204836681 ) ) ;
#19436 = DIRECTION ( 'NONE',  ( 1.000000000000000000, -0.000000000000000000, 0.000000000000000000 ) ) ;
#19437 = CARTESIAN_POINT ( 'NONE',  ( 3.458734125000015869, 196.1875000013655779, 198.0000000000000284 ) ) ;
#19438 = CYLINDRICAL_SURFACE ( 'NONE', #73937, 10.00000000000000178 ) ;
#19440 = CARTESIAN_POINT ( 'NONE',  ( -5.676582343750006032, 109.1145833299193555, 9.832129032723418760 ) ) ;
#19439 = CARTESIAN_POINT ( 'NONE',  ( 27.99999999999996447, 196.0000000000000000, 173.9999999999999147 ) ) ;
#19441 = CARTESIAN_POINT ( 'NONE',  ( -24.00000000000001421, 208.8125000000000000, 168.3431457505080004 ) ) ;
#19442 = CARTESIAN_POINT ( 'NONE',  ( 10.00000000000000711, 50.00000000000000711, 0.000000000000000000 ) ) ;
#19443 = VERTEX_POINT ( 'NONE', #7558 ) ;
#19444 = EDGE_CURVE ( 'NONE', #7158, #10862, #50707, .T. ) ;
#19445 = CARTESIAN_POINT ( 'NONE',  ( 8.660254037844389075, 212.2916666598387110, -5.000000000000000000 ) ) ;
#19446 = DIRECTION ( 'NONE',  ( -0.000000000000000000, 1.000000000000000000, -0.000000000000000000 ) ) ;
#19447 = DIRECTION ( 'NONE',  ( 0.000000000000000000, 0.000000000000000000, 1.000000000000000000 ) ) ;
#19448 = CARTESIAN_POINT ( 'NONE',  ( 6.951808397369818766E-16, 107.3437499965860269, -11.35316468750000141 ) ) ;
#19449 = CARTESIAN_POINT ( 'NONE',  ( 2.828427124746209831, 205.3750000000000284, 200.8284271247462129 ) ) ;
#19450 = CARTESIAN_POINT ( 'NONE',  ( -7.188101187500002709, 10.68749999795161187, 2.977408999572649151 ) ) ;
#19451 = CARTESIAN_POINT ( 'NONE',  ( 10.18810118749999916, 1.247682550866122264E-15, 88.28125000204836681 ) ) ;
#19452 = CARTESIAN_POINT ( 'NONE',  ( -11.35316468750000141, 13.59374999658601801, -1.390361679473963753E-15 ) ) ;
#19453 = VERTEX_POINT ( 'NONE', #64158 ) ;
#19454 = CARTESIAN_POINT ( 'NONE',  ( 4.000000000000000888, 20.68749999726881583, 1.656854249492384135 ) ) ;
#19455 = CARTESIAN_POINT ( 'NONE',  ( -4.903558642999205574E-16, 8.008118988124991233, 27.63811528394063188 ) ) ;
#19456 = CARTESIAN_POINT ( 'NONE',  ( -1.734723475976807489E-15, 11.00000000000000178, 41.99999999999999289 ) ) ;
#19457 = CARTESIAN_POINT ( 'NONE',  ( -7.204075437095965206, -7.204075437095968759, 75.71875000204836681 ) ) ;
#19458 = VECTOR ( 'NONE', #5523, 1000.000000000000114 ) ;
#19459 = CARTESIAN_POINT ( 'NONE',  ( -7.999999999999998224, 98.28125000409677625, 3.313708498984766049 ) ) ;
#19460 = CARTESIAN_POINT ( 'NONE',  ( 2.220677790255211837E-11, 201.2499999999982663, -9.999999999999998224 ) ) ;
#19461 = CARTESIAN_POINT ( 'NONE',  ( 2.765530957082001251, 291.7656250017069510, 6.676582343750000703 ) ) ;
#19462 = EDGE_CURVE ( 'NONE', #69889, #20696, #70532, .T. ) ;
#19463 = CARTESIAN_POINT ( 'NONE',  ( 10.00000000000000178, 127.0833333265053682, -2.679491924311226736 ) ) ;
#19464 = CARTESIAN_POINT ( 'NONE',  ( 8.311093377946834337, 215.4687499965860127, 8.311093377946839666 ) ) ;
#19465 = CARTESIAN_POINT ( 'NONE',  ( -10.18810118749999916, 4.220049686691934809, 85.56250000204838102 ) ) ;
#19466 = CARTESIAN_POINT ( 'NONE',  ( -25.55430564589115150, 200.0625000013656063, 172.4456943541091789 ) ) ;
#19467 = CARTESIAN_POINT ( 'NONE',  ( -8.000000000000000000, 24.75000000000000355, -9.797174393178825657E-16 ) ) ;
#19468 = CARTESIAN_POINT ( 'NONE',  ( -8.342170076843785083E-16, 11.18749999863440792, 4.541265875000002339 ) ) ;
#19469 = VERTEX_POINT ( 'NONE', #41514 ) ;
#19470 = CARTESIAN_POINT ( 'NONE',  ( -1.836970198721029983E-15, 85.62499999317203958, 10.00000000000000178 ) ) ;
#19471 = CIRCLE ( 'NONE', #36184, 16.70329308849007077 ) ;
#19472 = CARTESIAN_POINT ( 'NONE',  ( 4.000000000000015987, 208.5625000027312410, 199.6568542494924259 ) ) ;
#19473 = CARTESIAN_POINT ( 'NONE',  ( 1.432654583217608080, 200.8750000013656063, 138.5412658750000503 ) ) ;
#19474 = CARTESIAN_POINT ( 'NONE',  ( -4.000000000000015099, 204.6875000027312126, 143.6568542494924543 ) ) ;
#19475 = VECTOR ( 'NONE', #63454, 1000.000000000000000 ) ;
#19476 = CARTESIAN_POINT ( 'NONE',  ( -10.18810118749999916, 0.000000000000000000, 68.03125000204838102 ) ) ;
#19477 = ORIENTED_EDGE ( 'NONE', *, *, #8119, .T. ) ;
#19478 = CARTESIAN_POINT ( 'NONE',  ( -1.320432766682874540E-15, 3.093749997951610542, 7.188101187500000044 ) ) ;
#19479 = FACE_OUTER_BOUND ( 'NONE', #30673, .T. ) ;
#19480 = CARTESIAN_POINT ( 'NONE',  ( -5.082755093536325930, 118.3437500020483810, -5.082755093536325930 ) ) ;
#19481 = CARTESIAN_POINT ( 'NONE',  ( -1.377000000000000002, 267.1439999999997212, 5.668132533233856130 ) ) ;
#19482 = CARTESIAN_POINT ( 'NONE',  ( -6.676582343750001591, 294.4531250017069510, 0.000000000000000000 ) ) ;
#19484 = CARTESIAN_POINT ( 'NONE',  ( -7.347880794884122694E-16, 11.75000000000000000, 4.000000000000001776 ) ) ;
#19483 = CARTESIAN_POINT ( 'NONE',  ( 9.832129032723420536, 230.9895833367473301, 5.676582343749996262 ) ) ;
#19485 = VERTEX_POINT ( 'NONE', #52107 ) ;
#19486 = CARTESIAN_POINT ( 'NONE',  ( 8.311093377946839666, 221.0937500034139589, 8.311093377946829008 ) ) ;
#19487 = CARTESIAN_POINT ( 'NONE',  ( 5.082755093536318824, 5.082755093536319713, 0.9240527818717529929 ) ) ;
#19488 = CARTESIAN_POINT ( 'NONE',  ( 7.999999999999998224, 2.906250000000000888, 3.313708498984766049 ) ) ;
#19489 = CARTESIAN_POINT ( 'NONE',  ( 1.432654583217664701, 199.0000000013656063, 201.4587341250000065 ) ) ;
#19490 = ORIENTED_EDGE ( 'NONE', *, *, #56011, .F. ) ;
#19491 = PLANE ( 'NONE',  #15003 ) ;
#19492 = CARTESIAN_POINT ( 'NONE',  ( -8.000000000000000000, 99.49999999999998579, 0.000000000000000000 ) ) ;
#19493 = CARTESIAN_POINT ( 'NONE',  ( 5.676582343750001591, 106.9270833299193413, -9.832129032723420536 ) ) ;
#19494 = DIRECTION ( 'NONE',  ( 0.000000000000000000, 0.000000000000000000, -1.000000000000000000 ) ) ;
#19495 = CARTESIAN_POINT ( 'NONE',  ( -11.00000000000000000, 0.000000000000000000, 74.49999999999998579 ) ) ;
#19498 = CARTESIAN_POINT ( 'NONE',  ( 0.000000000000000000, 300.0000000000000000, 0.000000000000000000 ) ) ;
#19497 = CARTESIAN_POINT ( 'NONE',  ( 30.44569435410879521, 202.8125000013656063, 167.5543056458910485 ) ) ;
#19496 = CARTESIAN_POINT ( 'NONE',  ( 31.45873412499999944, 202.9375000013656063, 169.9999999999999432 ) ) ;
#19499 = ORIENTED_EDGE ( 'NONE', *, *, #30607, .F. ) ;
#19500 = VECTOR ( 'NONE', #13024, 1000.000000000000000 ) ;
#19501 = EDGE_CURVE ( 'NONE', #3350, #57691, #39292, .T. ) ;
#19502 = DIRECTION ( 'NONE',  ( -0.000000000000000000, 1.000000000000000000, -0.000000000000000000 ) ) ;
#19503 = CARTESIAN_POINT ( 'NONE',  ( 9.832129032723416984, 215.3645833299193555, 5.676582343750006032 ) ) ;
#19504 = CARTESIAN_POINT ( 'NONE',  ( -1.432654583217662481, 202.1250000013656063, 145.4587341250000634 ) ) ;
#19505 = CARTESIAN_POINT ( 'NONE',  ( 26.56734541678238060, 203.2500000013656063, 166.5412658749999650 ) ) ;
#19506 = CARTESIAN_POINT ( 'NONE',  ( 4.556349186104045934, 11.00000000000000000, 114.7187500040967620 ) ) ;
#19507 = CARTESIAN_POINT ( 'NONE',  ( -8.311093377946841443, 194.2187499965859843, 8.311093377946830785 ) ) ;
#19508 = CARTESIAN_POINT ( 'NONE',  ( -7.188101187500000044, 94.53125000204836681, 0.000000000000000000 ) ) ;
#19509 = CARTESIAN_POINT ( 'NONE',  ( -29.65685424949233706, 195.4375000000000000, 174.0000000000004547 ) ) ;
#19510 = CARTESIAN_POINT ( 'NONE',  ( -3.211159895383562723, 12.93749999863440792, 3.211159895383561391 ) ) ;
#19511 = CARTESIAN_POINT ( 'NONE',  ( 29.43265458321766204, 197.1250000013656347, 166.5412658749999650 ) ) ;
#19512 = CARTESIAN_POINT ( 'NONE',  ( -2.977408999572647819, 7.188101187499991163, 4.580302781871752771 ) ) ;
#19513 = CARTESIAN_POINT ( 'NONE',  ( 9.832129032723420536, 76.19791666325269830, -5.676582343749999815 ) ) ;
#19514 = ORIENTED_EDGE ( 'NONE', *, *, #59781, .T. ) ;
#19515 = CARTESIAN_POINT ( 'NONE',  ( -11.06147676142086667, -30.19208531610511415, 198.9596407016909438 ) ) ;
#19516 = PLANE ( 'NONE',  #68847 ) ;
#19517 = DIRECTION ( 'NONE',  ( -0.000000000000000000, 1.000000000000000000, -0.000000000000000000 ) ) ;
#19518 = DIRECTION ( 'NONE',  ( -0.000000000000000000, 1.000000000000000000, 4.689100369878284071E-30 ) ) ;
#19519 = CARTESIAN_POINT ( 'NONE',  ( 6.951808397369818766E-16, 82.03124999658602690, -11.35316468750000141 ) ) ;
#19520 = ORIENTED_EDGE ( 'NONE', *, *, #28114, .F. ) ;
#19521 = CARTESIAN_POINT ( 'NONE',  ( 10.18810118749999916, 4.220049686691935698, 88.37500000204839523 ) ) ;
#19522 = EDGE_CURVE ( 'NONE', #55282, #57640, #68565, .T. ) ;
#19523 = CARTESIAN_POINT ( 'NONE',  ( 10.18810118749999916, 1.247682550866122264E-15, 111.9062500020483810 ) ) ;
#19524 = CARTESIAN_POINT ( 'NONE',  ( -8.000000000000000000, 102.4062500000000000, -3.313708498984761164 ) ) ;
#19525 = CARTESIAN_POINT ( 'NONE',  ( 7.188101187500000044, 27.84374999795161543, 0.000000000000000000 ) ) ;
#19526 = CARTESIAN_POINT ( 'NONE',  ( -9.832129032723418760, 77.86458332991935549, -5.676582343750004256 ) ) ;
#19527 = CARTESIAN_POINT ( 'NONE',  ( 7.999999999999991118, 9.797174393178815797E-16, 24.26780278392014978 ) ) ;
#19528 = CARTESIAN_POINT ( 'NONE',  ( 0.000000000000000000, 0.000000000000000000, 0.000000000000000000 ) ) ;
#19529 =( BOUNDED_CURVE ( )  B_SPLINE_CURVE ( 2, ( #74468, #51834, #68072, #5447, #29201, #74099, #27698, #46168, #45420, #46542, #69186, #62765, #5821 ),
 .UNSPECIFIED., .F., .F. ) 
 B_SPLINE_CURVE_WITH_KNOTS ( ( 3, 2, 2, 2, 2, 2, 3 ),
 ( 2.464888983165918646, 2.470121561219082551, 2.475354139272246456, 2.480586717325410362, 2.485819295378574267, 2.491051873431738617, 2.496284451484902078 ),
 .UNSPECIFIED. ) 
 CURVE ( )  GEOMETRIC_REPRESENTATION_ITEM ( )  RATIONAL_B_SPLINE_CURVE ( ( 1.000000000000100142, 0.9659258262889679481, 1.000000000000000000, 0.9659258262890682012, 1.000000000000000000, 0.9659258262890682012, 1.000000000000000000, 0.9659258262890682012, 1.000000000000000000, 0.9659258262890682012, 1.000000000000000000, 0.9659258262891976532, 0.9999999999998705480 ) ) 
 REPRESENTATION_ITEM ( '' )  );
#19530 = CARTESIAN_POINT ( 'NONE',  ( -8.660254037844387298, 168.9583333265053682, -5.000000000000004441 ) ) ;
#19531 = CARTESIAN_POINT ( 'NONE',  ( 4.898587196589412829E-16, 1.687499995903220196, -8.000000000000000000 ) ) ;
#19532 = VECTOR ( 'NONE', #69607, 1000.000000000000000 ) ;
#19533 = CARTESIAN_POINT ( 'NONE',  ( 0.000000000000000000, 0.000000000000000000, 118.0000000000000000 ) ) ;
#19534 = CARTESIAN_POINT ( 'NONE',  ( 5.676582343750001591, 61.92708332991934839, -9.832129032723420536 ) ) ;
#19535 = CARTESIAN_POINT ( 'NONE',  ( -6.238412754330611322E-16, 10.18810118749999916, 105.1562500020483810 ) ) ;
#19536 = CARTESIAN_POINT ( 'NONE',  ( -3.042071309553173730, 189.3229166632526699, 11.35316468749999785 ) ) ;
#19537 = ORIENTED_EDGE ( 'NONE', *, *, #17263, .F. ) ;
#19538 = CARTESIAN_POINT ( 'NONE',  ( -2.436599634630237432, 67.82108862182660403, 20.21956363439100457 ) ) ;
#19539 = CARTESIAN_POINT ( 'NONE',  ( -23.99999999999995026, 198.8125000027312126, 171.6568542494926817 ) ) ;
#19540 = DIRECTION ( 'NONE',  ( -0.000000000000000000, 1.000000000000000000, 4.689100369878284071E-30 ) ) ;
#19542 = CARTESIAN_POINT ( 'NONE',  ( 6.951808397369818766E-16, 187.0312499965860127, -11.35316468750000141 ) ) ;
#19541 = CARTESIAN_POINT ( 'NONE',  ( -25.17157287525385811, 201.0000000027312126, 167.1715728752541281 ) ) ;
#19543 = DIRECTION ( 'NONE',  ( 1.000000000000000000, 0.000000000000000000, 0.000000000000000000 ) ) ;
#19544 = CARTESIAN_POINT ( 'NONE',  ( -2.679491924311222295, 234.1666666734946602, 10.00000000000000178 ) ) ;
#19545 = CARTESIAN_POINT ( 'NONE',  ( 30.64284399271082293, 178.3875230420589446, 174.6921329945330683 ) ) ;
#19546 = EDGE_CURVE ( 'NONE', #4267, #60284, #73402, .T. ) ;
#19547 = ORIENTED_EDGE ( 'NONE', *, *, #46194, .T. ) ;
#19548 = CARTESIAN_POINT ( 'NONE',  ( 3.042071309553159519, 185.0520833299193555, 11.35316468750000141 ) ) ;
#19549 = EDGE_CURVE ( 'NONE', #49884, #64213, #29087, .T. ) ;
#19550 = CARTESIAN_POINT ( 'NONE',  ( 2.977408999572650927, -7.188101187499990274, 21.45530278187175810 ) ) ;
#19551 = VERTEX_POINT ( 'NONE', #69820 ) ;
#19552 = EDGE_CURVE ( 'NONE', #25296, #43894, #19399, .T. ) ;
#19553 = AXIS2_PLACEMENT_3D ( 'NONE', #19352, #48395, #71399 ) ;
#19554 = EDGE_CURVE ( 'NONE', #65462, #15764, #27131, .T. ) ;
#19555 = CARTESIAN_POINT ( 'NONE',  ( -3.313708498984762052, 97.90625000409677625, -8.000000000000000000 ) ) ;
#19556 = CIRCLE ( 'NONE', #38871, 14.00000000000000000 ) ;
#19557 = CARTESIAN_POINT ( 'NONE',  ( 0.000000000000000000, 300.0000000000000000, 0.000000000000000000 ) ) ;
#19558 = ADVANCED_FACE ( 'NONE', ( #71651 ), #42979, .F. ) ;
#19559 = CARTESIAN_POINT ( 'NONE',  ( -7.347880794884122694E-16, 17.75000000000000355, 4.000000000000001776 ) ) ;
#19560 = CARTESIAN_POINT ( 'NONE',  ( -1.881053915767124440, 14.99999999863440969, 4.541265875000001451 ) ) ;
#19561 = CARTESIAN_POINT ( 'NONE',  ( -4.898587196589407898E-16, 7.999999999999991118, 12.64280278392014623 ) ) ;
#19562 = CARTESIAN_POINT ( 'NONE',  ( 3.313708498984756279, 7.999999999999991118, 18.54905278392014623 ) ) ;
#19563 = ORIENTED_EDGE ( 'NONE', *, *, #65954, .F. ) ;
#19564 = CARTESIAN_POINT ( 'NONE',  ( 5.000000000000000000, -11.82742353449333095, -68.45184936927694253 ) ) ;
#19565 = CARTESIAN_POINT ( 'NONE',  ( 7.188101187500002709, 100.8125000020484094, 2.977408999572649151 ) ) ;
#19567 = DIRECTION ( 'NONE',  ( -0.000000000000000000, -1.000000000000000000, -0.000000000000000000 ) ) ;
#19566 = CYLINDRICAL_SURFACE ( 'NONE', #27754, 6.000000000000001776 ) ;
#19568 = APPLICATION_PROTOCOL_DEFINITION ( 'draft international standard', 'automotive_design', 1998, #52979 ) ;
#19569 = ORIENTED_EDGE ( 'NONE', *, *, #36559, .T. ) ;
#19570 = CARTESIAN_POINT ( 'NONE',  ( 5.676582343749997150, 262.5520833367473301, -9.832129032723418760 ) ) ;
#19571 = CARTESIAN_POINT ( 'NONE',  ( 5.082755093536320601, -5.082755093536318824, 20.04905278187175455 ) ) ;
#19572 = ORIENTED_EDGE ( 'NONE', *, *, #22365, .F. ) ;
#19573 = EDGE_LOOP ( 'NONE', ( #6858, #67285, #39936, #8360 ) ) ;
#19574 = CARTESIAN_POINT ( 'NONE',  ( -4.220049686691935698, 10.18810118749999916, 82.37500000204838102 ) ) ;
#19575 = CARTESIAN_POINT ( 'NONE',  ( 30.64284399271078740, 146.0000000000000000, 174.6921329945330399 ) ) ;
#19576 = CARTESIAN_POINT ( 'NONE',  ( 7.778174593052023411, -7.778174593052021635, 93.06249999999998579 ) ) ;
#19579 = CARTESIAN_POINT ( 'NONE',  ( -2.765530957081996810, 295.4218750017069510, -6.676582343750002480 ) ) ;
#19578 = CARTESIAN_POINT ( 'NONE',  ( 23.99999999999997868, 199.8125000027312410, 168.3431457505075741 ) ) ;
#19577 = CARTESIAN_POINT ( 'NONE',  ( -28.00000000000007816, 198.1250000027312126, 166.0000000000003695 ) ) ;
#19580 = CARTESIAN_POINT ( 'NONE',  ( -5.000000000000005329, 143.3333333333333428, 8.660254037844387298 ) ) ;
#19581 = CARTESIAN_POINT ( 'NONE',  ( 38.00000000000000000, 205.0000000000000568, 3.504937291764268056E-14 ) ) ;
#19582 = CARTESIAN_POINT ( 'NONE',  ( -8.660254037844390851, 164.7916666598387110, 4.999999999999998224 ) ) ;
#19583 = CARTESIAN_POINT ( 'NONE',  ( 2.485281374238878627, 290.3750000034138452, 5.999999999999694467 ) ) ;
#19584 = CARTESIAN_POINT ( 'NONE',  ( 5.656854249492380582, 2.999999995903220196, -5.656854249492380582 ) ) ;
#19586 = CARTESIAN_POINT ( 'NONE',  ( 29.43265458321766559, 200.8750000013656063, 166.5412658749999650 ) ) ;
#19585 = CIRCLE ( 'NONE', #3955, 5.000000000000000000 ) ;
#19587 = CARTESIAN_POINT ( 'NONE',  ( -7.188101187500002709, 12.18749999795161187, 2.977408999572649151 ) ) ;
#19588 = CARTESIAN_POINT ( 'NONE',  ( -4.898587196589407898E-16, 7.999999999999991118, 24.64280278392014978 ) ) ;
#19589 = CARTESIAN_POINT ( 'NONE',  ( 0.000000000000000000, 0.000000000000000000, 0.000000000000000000 ) ) ;
#19590 = CARTESIAN_POINT ( 'NONE',  ( -7.188101187499999156, 108.1250000020483810, 2.977408999572654924 ) ) ;
#19592 = CARTESIAN_POINT ( 'NONE',  ( -7.320508075688773708, 131.8750000000000284, -7.320508075688774596 ) ) ;
#19591 =( NAMED_UNIT ( * ) SI_UNIT ( $, .STERADIAN. ) SOLID_ANGLE_UNIT ( ) );
#19593 = CARTESIAN_POINT ( 'NONE',  ( -3.042071309553159075, 235.2604166700806161, 11.35316468749999963 ) ) ;
#19594 = CARTESIAN_POINT ( 'NONE',  ( -1.656854249492405895, 12.31250000000000178, -3.999999999999976463 ) ) ;
#19595 = CARTESIAN_POINT ( 'NONE',  ( -2.977408999572647819, 7.188101187499991163, 22.58030278187175099 ) ) ;
#19596 = DIRECTION ( 'NONE',  ( 0.000000000000000000, 1.000000000000000000, 0.000000000000000000 ) ) ;
#19597 = CARTESIAN_POINT ( 'NONE',  ( 11.35316468750000141, 35.78124999658601979, 0.000000000000000000 ) ) ;
#19598 = EDGE_CURVE ( 'NONE', #27032, #45065, #2261, .T. ) ;
#19599 = CARTESIAN_POINT ( 'NONE',  ( 0.000000000000000000, 0.000000000000000000, 0.000000000000000000 ) ) ;
#19600 = CARTESIAN_POINT ( 'NONE',  ( 8.660254037844385522, 11.45833332650536640, 5.000000000000005329 ) ) ;
#19601 = DIRECTION ( 'NONE',  ( 0.000000000000000000, 1.000000000000000000, 0.000000000000000000 ) ) ;
#19602 = CARTESIAN_POINT ( 'NONE',  ( 9.999999999999996447, 185.0000000000000284, 0.000000000000000000 ) ) ;
#19603 = ORIENTED_EDGE ( 'NONE', *, *, #15756, .F. ) ;
#19604 = DIRECTION ( 'NONE',  ( -1.000000000000000000, -0.000000000000000000, -0.000000000000000000 ) ) ;
#19605 = AXIS2_PLACEMENT_3D ( 'NONE', #13328, #65763, #8056 ) ;
#19606 = CARTESIAN_POINT ( 'NONE',  ( 2.449293598294707893E-16, 7.999999997268813168, -4.000000000000001776 ) ) ;
#19607 = CARTESIAN_POINT ( 'NONE',  ( 11.35316468749999785, 35.57291666325267698, 3.042071309553174174 ) ) ;
#19608 = CARTESIAN_POINT ( 'NONE',  ( 11.00000000000000355, -4.556349186104045046, 81.34375000409677625 ) ) ;
#19609 = CARTESIAN_POINT ( 'NONE',  ( -3.458734125000015869, 205.1875000013656063, 142.0000000000000568 ) ) ;
#19610 = CARTESIAN_POINT ( 'NONE',  ( 28.00000000000001421, 197.5000000000000000, 165.9999999999998863 ) ) ;
#19611 = CARTESIAN_POINT ( 'NONE',  ( 0.000000000000000000, 0.000000000000000000, -4.000000000000001776 ) ) ;
#19613 = CARTESIAN_POINT ( 'NONE',  ( 3.042071309553167513, 36.82291666325267698, -11.35316468749999785 ) ) ;
#19612 = CARTESIAN_POINT ( 'NONE',  ( -5.082755093536325930, 107.4687500020483810, -5.082755093536325930 ) ) ;
#19614 = CARTESIAN_POINT ( 'NONE',  ( -7.999999999999991118, 0.000000000000000000, 12.83030277982336465 ) ) ;
#19615 = CARTESIAN_POINT ( 'NONE',  ( -5.676582343749998039, 142.4479166632526699, -9.832129032723420536 ) ) ;
#19616 = ADVANCED_FACE ( 'NONE', ( #26369 ), #13925, .T. ) ;
#19617 = CARTESIAN_POINT ( 'NONE',  ( -7.320508075688773708, 123.7499999931720396, -7.320508075688774596 ) ) ;
#19618 = CARTESIAN_POINT ( 'NONE',  ( -5.082755093536324154, 109.7187500020483810, 5.082755093536326818 ) ) ;
#19619 = CARTESIAN_POINT ( 'NONE',  ( -25.55430564589119768, 206.5625000013656063, 167.5543056458915316 ) ) ;
#19620 = EDGE_LOOP ( 'NONE', ( #57350, #11961 ) ) ;
#19621 = CARTESIAN_POINT ( 'NONE',  ( -2.978189300774432354E-14, -67.59332269700065865, -20.03478791450352858 ) ) ;
#19622 = CARTESIAN_POINT ( 'NONE',  ( 6.951808397369818766E-16, 17.34374999658601624, -11.35316468750000141 ) ) ;
#19623 =( BOUNDED_CURVE ( )  B_SPLINE_CURVE ( 2, ( #48823, #26933, #71830, #43163, #3190, #72206, #49952, #15981, #73340, #61649, #39011, #66548, #14857 ),
 .UNSPECIFIED., .F., .F. ) 
 B_SPLINE_CURVE_WITH_KNOTS ( ( 3, 2, 2, 2, 2, 2, 3 ),
 ( 0.02777777777777718296, 0.03703703703703645211, 0.04629629629629572474, 0.05555555555555498348, 0.06481481481481425611, 0.07407407407407351485, 0.08333333333333278747 ),
 .UNSPECIFIED. ) 
 CURVE ( )  GEOMETRIC_REPRESENTATION_ITEM ( )  RATIONAL_B_SPLINE_CURVE ( ( 1.000000000000002220, 0.9659258262890662028, 1.000000000000000000, 0.9659258262890683122, 1.000000000000000000, 0.9659258262890683122, 1.000000000000000000, 0.9659258262890683122, 1.000000000000000000, 0.9659258262890683122, 1.000000000000000000, 0.9659258262890703106, 0.9999999999999980016 ) ) 
 REPRESENTATION_ITEM ( '' )  );
#19624 = ORIENTED_EDGE ( 'NONE', *, *, #37503, .F. ) ;
#19625 = CARTESIAN_POINT ( 'NONE',  ( -29.65685424949239035, 204.4375000000000284, 174.0000000000003979 ) ) ;
#19626 = CARTESIAN_POINT ( 'NONE',  ( 54.00000000000000711, 242.0000000000000284, 20.00000000000001776 ) ) ;
#19628 = CARTESIAN_POINT ( 'NONE',  ( -11.35316468750000141, 153.4895833299193555, 3.042071309553159963 ) ) ;
#19627 = CARTESIAN_POINT ( 'NONE',  ( -31.04164783046611120, -20.98636254260840772, 153.7481747945847701 ) ) ;
#19629 = DIRECTION ( 'NONE',  ( 0.000000000000000000, 1.000000000000000000, 4.283267841918042741E-17 ) ) ;
#19630 = CARTESIAN_POINT ( 'NONE',  ( 1.469576158976822172E-15, -7.999999999999991118, 19.26155278432982598 ) ) ;
#19631 = CARTESIAN_POINT ( 'NONE',  ( -5.857508853935765814, -5.043084890513333640, 0.8444290630237344386 ) ) ;
#19632 = CARTESIAN_POINT ( 'NONE',  ( 11.35316468749999608, 236.6145833367473301, -3.042071309553167069 ) ) ;
#19633 = CARTESIAN_POINT ( 'NONE',  ( 1.871523826299183495E-15, -10.18810118749999916, 87.90625000204838102 ) ) ;
#19634 = ORIENTED_EDGE ( 'NONE', *, *, #70233, .F. ) ;
#19635 = ADVANCED_FACE ( 'NONE', ( #55447 ), #14680, .F. ) ;
#19636 = CARTESIAN_POINT ( 'NONE',  ( 4.999999999999999112, 13.22058908515350062, 69.49198671174478648 ) ) ;
#19637 = CARTESIAN_POINT ( 'NONE',  ( -9.832129032723418760, 108.1770833299193555, -5.676582343750004256 ) ) ;
#19638 = CARTESIAN_POINT ( 'NONE',  ( 4.220049686691934809, 10.18810118749999916, 101.6875000020483810 ) ) ;
#19639 = EDGE_CURVE ( 'NONE', #6173, #5243, #72961, .T. ) ;
#19640 =( BOUNDED_CURVE ( )  B_SPLINE_CURVE ( 2, ( #43180, #66196, #14500, #43553, #3962, #66948, #14876, #20918, #33380, #73722, #26951, #66567, #49969 ),
 .UNSPECIFIED., .F., .F. ) 
 B_SPLINE_CURVE_WITH_KNOTS ( ( 3, 2, 2, 2, 2, 2, 3 ),
 ( 1.993888113706278942, 1.999121869590356759, 2.004355625474434799, 2.009589381358512838, 2.014823137242590434, 2.020056893126668474, 2.025290649010746513 ),
 .UNSPECIFIED. ) 
 CURVE ( )  GEOMETRIC_REPRESENTATION_ITEM ( )  RATIONAL_B_SPLINE_CURVE ( ( 0.9999999999999978906, 0.9659258262890703106, 1.000000000000000000, 0.9659258262890682012, 1.000000000000000000, 0.9659258262890682012, 1.000000000000000000, 0.9659258262890682012, 1.000000000000000000, 0.9659258262890682012, 1.000000000000000000, 0.9659258262890682012, 1.000000000000000000 ) ) 
 REPRESENTATION_ITEM ( '' )  );
#19641 = CARTESIAN_POINT ( 'NONE',  ( -4.541265875000002339, 15.93749999863440436, -5.561446717895856393E-16 ) ) ;
#19642 = ORIENTED_EDGE ( 'NONE', *, *, #29970, .T. ) ;
#19643 = ORIENTED_EDGE ( 'NONE', *, *, #59179, .T. ) ;
#19644 = CARTESIAN_POINT ( 'NONE',  ( -8.000000000000001776, 11.34375000000000000, 3.313708498984759387 ) ) ;
#19645 = CARTESIAN_POINT ( 'NONE',  ( -1.881053915767124440, 3.124999998634407472, 4.541265875000001451 ) ) ;
#19646 = CARTESIAN_POINT ( 'NONE',  ( 2.977408999572650927, 2.249999997951610098, -7.188101187500001821 ) ) ;
#19647 = CARTESIAN_POINT ( 'NONE',  ( -3.313708498984762496, 114.9687500040967905, 7.999999999999998224 ) ) ;
#19648 = CARTESIAN_POINT ( 'NONE',  ( -10.18810118749999916, 0.000000000000000000, 99.53125000204838102 ) ) ;
#19649 = SURFACE_STYLE_USAGE ( .BOTH. , #14853 ) ;
#19650 = EDGE_CURVE ( 'NONE', #60656, #18569, #60937, .T. ) ;
#19651 = CARTESIAN_POINT ( 'NONE',  ( -4.000000000000001776, 2.500000000000000000, -4.898587196589415787E-16 ) ) ;
#19652 = CARTESIAN_POINT ( 'NONE',  ( -1.656854249492383691, 14.43749999726881406, 4.000000000000000888 ) ) ;
#19653 = CARTESIAN_POINT ( 'NONE',  ( 4.541265875000001451, 2.249999998634407028, 1.881053915767124440 ) ) ;
#19654 = VECTOR ( 'NONE', #60593, 1000.000000000000000 ) ;
#19655 = CARTESIAN_POINT ( 'NONE',  ( 1.432654583217664479, 196.7500000013656063, 201.4587341250000065 ) ) ;
#19657 = CARTESIAN_POINT ( 'NONE',  ( -2.679491924311078410, 223.3333333265053113, -10.00000000000008527 ) ) ;
#19656 = CARTESIAN_POINT ( 'NONE',  ( -24.54126587499999346, 201.1875000013656063, 170.0000000000002842 ) ) ;
#19658 = B_SPLINE_CURVE_WITH_KNOTS ( 'NONE', 3,
 ( #24910, #7584, #71307, #8314, #19627, #65283, #60365, #8691, #1570, #19259, #59997, #42641, #13949, #64556, #59633, #52868, #13221, #7949, #36990, #70581, #25653, #30589, #14333, #47926, #42271, #65653, #12852, #13589, #48669, #18898, #24181, #54351, #59274, #66025 ),
 .UNSPECIFIED., .F., .F.,
 ( 4, 2, 2, 2, 2, 2, 2, 2, 2, 2, 2, 2, 2, 2, 2, 2, 4 ),
 ( 0.01600311806101276102, 0.01926149963341478033, 0.02251988120581680311, 0.02414907199201781623, 0.02577826277821882936, 0.02903664435062079316, 0.02985123974372128758, 0.03066583513682177853, 0.03229502592302276043, 0.03310962131612327219, 0.03392421670922378396, 0.03555340749542482137, 0.03718259828162585878, 0.03799719367472638443, 0.03881178906782691007, 0.04044097985402796830, 0.04207017064022902653 ),
 .UNSPECIFIED. ) ;
#19659 = CARTESIAN_POINT ( 'NONE',  ( 2.780723358947928197E-16, 15.56249999863440614, -4.541265875000002339 ) ) ;
#19660 = CARTESIAN_POINT ( 'NONE',  ( 11.00000000000000000, 1.347111479062088405E-15, 84.24999999999998579 ) ) ;
#19661 = CARTESIAN_POINT ( 'NONE',  ( -5.082755093536317936, -5.082755093536320601, 7.674052781871751883 ) ) ;
#19662 = ORIENTED_EDGE ( 'NONE', *, *, #24212, .F. ) ;
#19663 = VECTOR ( 'NONE', #11170, 1000.000000000000000 ) ;
#19664 = VERTEX_POINT ( 'NONE', #66373 ) ;
#19665 = CARTESIAN_POINT ( 'NONE',  ( -6.238412754330611322E-16, 10.18810118749999916, 97.28125000204838102 ) ) ;
#19666 = CARTESIAN_POINT ( 'NONE',  ( 5.656854249492380582, 26.99999999590322375, -5.656854249492380582 ) ) ;
#19667 = CARTESIAN_POINT ( 'NONE',  ( -24.54126587499999346, 202.4375000013656063, 170.0000000000003411 ) ) ;
#19668 = CARTESIAN_POINT ( 'NONE',  ( -32.00000000000000711, 199.1875000000000000, 168.3431457505080004 ) ) ;
#19669 = CARTESIAN_POINT ( 'NONE',  ( -3.458734124999960358, 209.6250000013656063, 196.5673454167823877 ) ) ;
#19670 = CARTESIAN_POINT ( 'NONE',  ( -26.34314575050760254, 201.6875000027312410, 174.0000000000004547 ) ) ;
#19671 = CARTESIAN_POINT ( 'NONE',  ( -4.999999999999998224, 111.6666666666666714, -8.660254037844389075 ) ) ;
#19672 = CARTESIAN_POINT ( 'NONE',  ( 5.656854249492379694, 112.4375000000000000, -5.656854249492380582 ) ) ;
#19673 = CARTESIAN_POINT ( 'NONE',  ( 6.676582343750004256, 295.0468750017069510, 2.765530957081995478 ) ) ;
#19674 = EDGE_CURVE ( 'NONE', #41950, #15778, #67220, .T. ) ;
#19675 = ORIENTED_EDGE ( 'NONE', *, *, #20375, .T. ) ;
#19676 = APPLICATION_CONTEXT ( 'automotive_design' ) ;
#19677 = CARTESIAN_POINT ( 'NONE',  ( -8.000000000000000000, 21.56249999590322375, -9.797174393178825657E-16 ) ) ;
#19678 = AXIS2_PLACEMENT_3D ( 'NONE', #20226, #71536, #32322 ) ;
#19679 = CARTESIAN_POINT ( 'NONE',  ( 3.458734124999959025, 204.5000000013656063, 140.5673454167824161 ) ) ;
#19680 = CARTESIAN_POINT ( 'NONE',  ( -2.828427124746192067, 5.625000000000000000, 2.828427124746190735 ) ) ;
#19681 = FILL_AREA_STYLE ('',( #58590 ) ) ;
#19682 = CARTESIAN_POINT ( 'NONE',  ( -8.660254037844385522, 230.4166666666666856, 5.000000000000004441 ) ) ;
#19683 = DIRECTION ( 'NONE',  ( -0.000000000000000000, 1.000000000000000000, 4.689100369878284071E-30 ) ) ;
#19684 = CARTESIAN_POINT ( 'NONE',  ( -4.556349186104047710, -10.99999999999999822, 115.2812500000000000 ) ) ;
#19685 = CARTESIAN_POINT ( 'NONE',  ( -10.00000000000000355, 222.7083333333333428, 2.679491924311223183 ) ) ;
#19686 = EDGE_CURVE ( 'NONE', #56610, #52340, #63605, .T. ) ;
#19687 = CARTESIAN_POINT ( 'NONE',  ( -7.188101187499992051, 2.977408999572646930, 7.767802781871751883 ) ) ;
#19688 = CARTESIAN_POINT ( 'NONE',  ( -5.676582343749998039, 197.7604166632526983, -9.832129032723420536 ) ) ;
#19689 = CARTESIAN_POINT ( 'NONE',  ( 2.679491924311222739, 190.8333333265053682, 10.00000000000000355 ) ) ;
#19690 = CARTESIAN_POINT ( 'NONE',  ( -1.881053915767124440, 3.999999998634406140, 4.541265875000001451 ) ) ;
#19691 = CARTESIAN_POINT ( 'NONE',  ( 0.000000000000000000, 300.0000000000000000, 6.000000000000001776 ) ) ;
#19692 = DIRECTION ( 'NONE',  ( -0.000000000000000000, -0.000000000000000000, -1.000000000000000000 ) ) ;
#19693 = ORIENTED_EDGE ( 'NONE', *, *, #23459, .F. ) ;
#19694 = CARTESIAN_POINT ( 'NONE',  ( -3.458734125000016757, 203.1250000013656347, 140.5673454167824161 ) ) ;
#19695 = CARTESIAN_POINT ( 'NONE',  ( -3.042071309553173730, 49.63541666325267698, 11.35316468749999785 ) ) ;
#19696 = CARTESIAN_POINT ( 'NONE',  ( 11.00000000000000000, 1.347111479062088405E-15, 105.4375000040967763 ) ) ;
#19697 = CARTESIAN_POINT ( 'NONE',  ( 2.828427124746191623, 19.87499999726881228, -2.828427124746191623 ) ) ;
#19698 = CARTESIAN_POINT ( 'NONE',  ( -26.56734541678243033, 203.3750000013656063, 166.5412658750003345 ) ) ;
#19699 = CYLINDRICAL_SURFACE ( 'NONE', #74402, 10.99999999999999645 ) ;
#19701 = DIRECTION ( 'NONE',  ( 0.000000000000000000, 0.000000000000000000, 1.000000000000000000 ) ) ;
#19700 = CARTESIAN_POINT ( 'NONE',  ( 7.188101187500002709, 123.3125000020483810, 2.977408999572649151 ) ) ;
#19702 = CARTESIAN_POINT ( 'NONE',  ( 3.458734124999958581, 195.5000000013656347, 140.5673454167823593 ) ) ;
#19703 = CARTESIAN_POINT ( 'NONE',  ( -3.042071309553164404, 112.2395833299193697, -11.35316468749999963 ) ) ;
#19704 = CARTESIAN_POINT ( 'NONE',  ( 8.660254037844385522, 91.45833332650536818, 5.000000000000005329 ) ) ;
#19705 = CARTESIAN_POINT ( 'NONE',  ( -7.188101187500001821, 91.06250000204838102, -2.977408999572650483 ) ) ;
#19706 = CARTESIAN_POINT ( 'NONE',  ( 1.881053915767121776, 14.62499999863440969, -4.541265875000002339 ) ) ;
#19707 = CARTESIAN_POINT ( 'NONE',  ( -7.320508075688778149, 71.87500000000001421, -7.320508075688779037 ) ) ;
#19708 = FACE_OUTER_BOUND ( 'NONE', #42997, .T. ) ;
#19709 = ORIENTED_EDGE ( 'NONE', *, *, #61047, .T. ) ;
#19710 = CARTESIAN_POINT ( 'NONE',  ( -7.535050054895622296, 225.9999999999999716, 6.607029887625837539 ) ) ;
#19711 = ORIENTED_EDGE ( 'NONE', *, *, #831, .F. ) ;
#19712 = ADVANCED_FACE ( 'NONE', ( #73162 ), #27500, .T. ) ;
#19713 = CARTESIAN_POINT ( 'NONE',  ( -6.676582343750003368, 294.5468750017069510, -2.765530957081996810 ) ) ;
#19714 = DIRECTION ( 'NONE',  ( -0.000000000000000000, -1.000000000000000000, -4.283267841918042741E-17 ) ) ;
#19715 = CARTESIAN_POINT ( 'NONE',  ( -7.999999999999991118, 3.313708498984756723, 5.424052783920145338 ) ) ;
#19716 = CARTESIAN_POINT ( 'NONE',  ( -11.35316468749999785, 173.0729166632526983, -3.042071309553167513 ) ) ;
#19717 = CIRCLE ( 'NONE', #22083, 8.999999999999998224 ) ;
#19718 = LINE ( 'NONE', #52958, #47693 ) ;
#19719 = CARTESIAN_POINT ( 'NONE',  ( -3.999999999999960032, 201.0000000000000000, 198.0000000000000284 ) ) ;
#19720 = CARTESIAN_POINT ( 'NONE',  ( 11.00000000000000000, 1.347111479062088405E-15, 69.24999999999997158 ) ) ;
#19721 = CARTESIAN_POINT ( 'NONE',  ( 10.18810118749999916, 4.220049686691935698, 109.3750000020483810 ) ) ;
#19722 = ORIENTED_EDGE ( 'NONE', *, *, #49323, .T. ) ;
#19723 = CARTESIAN_POINT ( 'NONE',  ( -2.589639417659073573, 50.10293296561771115, -40.79253907059123208 ) ) ;
#19724 = CARTESIAN_POINT ( 'NONE',  ( 11.00000000000000000, 1.347111479062088405E-15, 90.25000000000000000 ) ) ;
#19725 = CARTESIAN_POINT ( 'NONE',  ( -8.311093377946836114, 137.9687499965860127, -8.311093377946837890 ) ) ;
#19726 = CARTESIAN_POINT ( 'NONE',  ( -3.458734124999959914, 195.3750000013656063, 196.5673454167823877 ) ) ;
#19727 = CARTESIAN_POINT ( 'NONE',  ( 6.000000000000003553, 298.5000000034139589, 2.485281374238571317 ) ) ;
#19728 = CARTESIAN_POINT ( 'NONE',  ( -10.18810118749999916, 0.000000000000000000, 72.53125000204838102 ) ) ;
#19729 = CARTESIAN_POINT ( 'NONE',  ( -5.676582343749998039, 62.76041666325269119, -9.832129032723420536 ) ) ;
#19730 = ORIENTED_EDGE ( 'NONE', *, *, #48588, .T. ) ;
#19731 = CARTESIAN_POINT ( 'NONE',  ( -2.679491924311236950, 28.54166666666667140, 10.00000000000000711 ) ) ;
#19732 = B_SPLINE_CURVE_WITH_KNOTS ( 'NONE', 3,
 ( #11736, #29091, #52111, #444 ),
 .UNSPECIFIED., .F., .F.,
 ( 4, 4 ),
 ( 6.677181410677363213E-16, 0.0004743803571052117697 ),
 .UNSPECIFIED. ) ;
#19733 = CARTESIAN_POINT ( 'NONE',  ( 1.881053915767122664, 3.249999998634407472, 4.541265875000001451 ) ) ;
#19734 = CARTESIAN_POINT ( 'NONE',  ( 5.662595241051934458, 5.662595241051935346, 10.95061528394063188 ) ) ;
#19735 = ORIENTED_EDGE ( 'NONE', *, *, #67147, .F. ) ;
#19736 = CARTESIAN_POINT ( 'NONE',  ( 7.188101187499999156, 22.87499999795161187, 2.977408999572654924 ) ) ;
#19737 = CARTESIAN_POINT ( 'NONE',  ( -6.000000000000001776, 292.0625000034140157, 0.000000000000000000 ) ) ;
#19738 = CARTESIAN_POINT ( 'NONE',  ( 2.828427124746208943, 202.6250000000000284, 195.1715728752538439 ) ) ;
#19739 = CARTESIAN_POINT ( 'NONE',  ( -1.320432766682874540E-15, 9.468749997951610098, 7.188101187500000044 ) ) ;
#19740 = CARTESIAN_POINT ( 'NONE',  ( 2.977408999572650927, -7.188101187499990274, 0.4553027818717525488 ) ) ;
#19741 =( BOUNDED_CURVE ( )  B_SPLINE_CURVE ( 2, ( #61392, #55374, #50812, #45156, #62497, #55748, #3680, #49703, #33861 ),
 .UNSPECIFIED., .F., .F. ) 
 B_SPLINE_CURVE_WITH_KNOTS ( ( 3, 2, 2, 2, 3 ),
 ( 0.1770833333333334259, 0.1822916666666667407, 0.1875000000000001110, 0.1927083333333334814, 0.1979166666666667962 ),
 .UNSPECIFIED. ) 
 CURVE ( )  GEOMETRIC_REPRESENTATION_ITEM ( )  RATIONAL_B_SPLINE_CURVE ( ( 0.9999999999999987788, 0.9238795325112879597, 1.000000000000000000, 0.9238795325112867385, 1.000000000000000000, 0.9238795325112867385, 1.000000000000000000, 0.9238795325112847401, 1.000000000000001998 ) ) 
 REPRESENTATION_ITEM ( '' )  );
#19742 = CARTESIAN_POINT ( 'NONE',  ( -4.220049686691935698, 10.18810118749999916, 114.2500000020483952 ) ) ;
#19743 = PRODUCT_DEFINITION_SHAPE ( 'NONE', 'NONE',  #43127 ) ;
#19744 = VECTOR ( 'NONE', #7975, 1000.000000000000000 ) ;
#19745 = CARTESIAN_POINT ( 'NONE',  ( 2.828427124746190291, 8.875000000000001776, 2.828427124746192067 ) ) ;
#19746 = CARTESIAN_POINT ( 'NONE',  ( -4.000000000000001776, 4.249999997268813168, -4.898587196589415787E-16 ) ) ;
#19747 = ORIENTED_EDGE ( 'NONE', *, *, #51917, .T. ) ;
#19748 = CARTESIAN_POINT ( 'NONE',  ( 2.445694354108839619, 205.8125000013656063, 200.4456943541088663 ) ) ;
#19749 = CARTESIAN_POINT ( 'NONE',  ( -25.17157287525373732, 196.7500000027312126, 172.8284271247464972 ) ) ;
#19750 = EDGE_CURVE ( 'NONE', #52951, #73226, #58020, .T. ) ;
#19751 = CARTESIAN_POINT ( 'NONE',  ( 4.541265875000002339, 3.374999998634406584, -1.881053915767121554 ) ) ;
#19752 = CARTESIAN_POINT ( 'NONE',  ( -2.977408999572650927, 113.3750000020483810, -7.188101187500001821 ) ) ;
#19753 = LINE ( 'NONE', #14080, #9145 ) ;
#19754 = CARTESIAN_POINT ( 'NONE',  ( -7.188101187499992051, 0.000000000000000000, 22.48655278187175455 ) ) ;
#19755 = ORIENTED_EDGE ( 'NONE', *, *, #18513, .F. ) ;
#19756 = CARTESIAN_POINT ( 'NONE',  ( 2.977408999572652260, 22.68749999795161187, 7.188101187500000044 ) ) ;
#19757 = ORIENTED_EDGE ( 'NONE', *, *, #47311, .F. ) ;
#19758 = SURFACE_SIDE_STYLE ('',( #70441 ) ) ;
#19759 = LINE ( 'NONE', #25779, #40007 ) ;
#19760 = CARTESIAN_POINT ( 'NONE',  ( -3.458734124999959025, 208.5000000013656063, 199.4326545832176691 ) ) ;
#19761 = CARTESIAN_POINT ( 'NONE',  ( 29.43265458321766914, 203.5000000013655779, 173.4587341249998929 ) ) ;
#19762 = CARTESIAN_POINT ( 'NONE',  ( -10.00000000000000000, 62.29166666666666430, -2.679491924311229845 ) ) ;
#19763 = AXIS2_PLACEMENT_3D ( 'NONE', #27842, #28213, #50848 ) ;
#19764 = CARTESIAN_POINT ( 'NONE',  ( 2.977408999572654480, 92.00000000204838102, 7.188101187499999156 ) ) ;
#19765 = CARTESIAN_POINT ( 'NONE',  ( 6.000000000000001776, 295.5000000000000000, -7.347880794884121708E-16 ) ) ;
#19766 = CARTESIAN_POINT ( 'NONE',  ( -30.20912146882930571, -42.97263271206719537, 176.9862772038617891 ) ) ;
#19767 = EDGE_CURVE ( 'NONE', #22710, #62930, #5625, .T. ) ;
#19768 = EDGE_LOOP ( 'NONE', ( #25859, #7825, #29792, #39895, #37565, #31561, #15323, #19804, #29220, #53026, #38344, #71122, #49605, #53555, #5681, #30393, #43181, #59126, #39580, #28304, #928, #61596, #18651, #73283, #9953, #12188, #15658, #8789, #46582, #16775, #32778, #4906, #16563, #19784 ) ) ;
#19769 = CARTESIAN_POINT ( 'NONE',  ( 11.35316468749999608, 236.6145833367473301, -3.042071309553167069 ) ) ;
#19770 = CARTESIAN_POINT ( 'NONE',  ( 3.999999999999959144, 200.1875000027312126, 140.3431457505076594 ) ) ;
#19771 = CARTESIAN_POINT ( 'NONE',  ( -11.35316468749999963, 264.0625000034140157, 0.000000000000000000 ) ) ;
#19772 = CARTESIAN_POINT ( 'NONE',  ( -2.828427124746190735, 17.12499999726881583, -2.828427124746191623 ) ) ;
#19773 = CARTESIAN_POINT ( 'NONE',  ( 9.999999999999998224, 262.7083333333333712, -2.679491924311229401 ) ) ;
#19774 = CARTESIAN_POINT ( 'NONE',  ( 4.556349186104045934, 11.00000000000000000, 116.2187500040967763 ) ) ;
#19775 = CARTESIAN_POINT ( 'NONE',  ( 7.320508075688774596, 170.6250000000000284, -7.320508075688774596 ) ) ;
#19776 = DIRECTION ( 'NONE',  ( 0.000000000000000000, 0.000000000000000000, -1.000000000000000000 ) ) ;
#19777 = CARTESIAN_POINT ( 'NONE',  ( -7.188101187499992051, 0.000000000000000000, 27.36155278187175455 ) ) ;
#19778 = CARTESIAN_POINT ( 'NONE',  ( 11.35316468749999963, 156.3020833299192986, -3.042071309553165293 ) ) ;
#19779 = CARTESIAN_POINT ( 'NONE',  ( 27.99999999999996803, 202.0000000000000000, 173.9999999999999147 ) ) ;
#19780 = CARTESIAN_POINT ( 'NONE',  ( -54.00000000000000000, 242.0000000000000284, 4.085831468968145267E-14 ) ) ;
#19783 = CARTESIAN_POINT ( 'NONE',  ( -5.000000000000000000, 166.6666666666666856, -8.660254037844390851 ) ) ;
#19782 = DIRECTION ( 'NONE',  ( 0.000000000000000000, 0.000000000000000000, -1.000000000000000000 ) ) ;
#19781 = CARTESIAN_POINT ( 'NONE',  ( 32.00000000000000711, 204.3125000000000000, 168.3431457505075741 ) ) ;
#19784 = ORIENTED_EDGE ( 'NONE', *, *, #32204, .F. ) ;
#19785 = CARTESIAN_POINT ( 'NONE',  ( -5.676582343750006032, 9.427083329919350163, 9.832129032723418760 ) ) ;
#19786 = CARTESIAN_POINT ( 'NONE',  ( -11.00000000000000000, 4.556349186104045934, 77.59375000409676204 ) ) ;
#19787 = CARTESIAN_POINT ( 'NONE',  ( -11.00000000000000000, 0.000000000000000000, 85.18750000409677625 ) ) ;
#19788 = CARTESIAN_POINT ( 'NONE',  ( -6.338495502905945601E-13, 181.2500000000000853, -10.00000000000000533 ) ) ;
#19789 = CARTESIAN_POINT ( 'NONE',  ( -2.445694354108838731, 208.0625000013656063, 144.4456943541088663 ) ) ;
#19790 = CARTESIAN_POINT ( 'NONE',  ( -1.656854249492354825, 202.3125000000000000, 138.0000000000000284 ) ) ;
#19791 = CARTESIAN_POINT ( 'NONE',  ( -8.660254037844390851, 49.79166665983870388, 4.999999999999998224 ) ) ;
#19792 = VECTOR ( 'NONE', #37304, 1000.000000000000227 ) ;
#19793 = CARTESIAN_POINT ( 'NONE',  ( -5.082755093536325930, 110.4687500020483810, -5.082755093536325930 ) ) ;
#19794 = CARTESIAN_POINT ( 'NONE',  ( -1.881053915767121554, 3.749999998634407028, -4.541265875000002339 ) ) ;
#19795 = CARTESIAN_POINT ( 'NONE',  ( 1.558072418983049268, 67.68461058694150267, -20.10890959967917624 ) ) ;
#19796 = CARTESIAN_POINT ( 'NONE',  ( 3.313708498984756279, 7.999999999999991118, 16.86155277982336642 ) ) ;
#19797 = CARTESIAN_POINT ( 'NONE',  ( 1.426884777062171983, 194.5622161278626265, 138.7293107566222261 ) ) ;
#19798 = ORIENTED_EDGE ( 'NONE', *, *, #53301, .F. ) ;
#19799 = CARTESIAN_POINT ( 'NONE',  ( 2.679491924311283579, 221.6666666734946887, -9.999999999999969802 ) ) ;
#19800 = CARTESIAN_POINT ( 'NONE',  ( -6.735557395310442023E-16, 11.00000000000000000, 81.81250000409677625 ) ) ;
#19801 = CIRCLE ( 'NONE', #42843, 8.000000000000003553 ) ;
#19802 = CARTESIAN_POINT ( 'NONE',  ( 5.676582343750005144, 235.8854166700806729, 9.832129032723416984 ) ) ;
#19803 = CARTESIAN_POINT ( 'NONE',  ( 5.676582343750001591, 126.6145833299193697, -9.832129032723420536 ) ) ;
#19804 = ORIENTED_EDGE ( 'NONE', *, *, #48243, .T. ) ;
#19805 = CARTESIAN_POINT ( 'NONE',  ( 0.9859162824928909830, 10.93016620314303999, 117.5662746148575906 ) ) ;
#19806 = CARTESIAN_POINT ( 'NONE',  ( 10.18810118750000093, -4.220049686691933921, 93.81250000204839523 ) ) ;
#19807 = CARTESIAN_POINT ( 'NONE',  ( 5.000000000000000000, 0.000000000000000000, 0.000000000000000000 ) ) ;
#19808 = CARTESIAN_POINT ( 'NONE',  ( -1.432654583217608080, 195.8750000013655779, 201.4587341250000350 ) ) ;
#19809 = DIRECTION ( 'NONE',  ( -0.000000000000000000, 1.000000000000000000, -0.000000000000000000 ) ) ;
#19811 = CARTESIAN_POINT ( 'NONE',  ( -9.832129032723418760, 112.8645833299193555, -5.676582343750004256 ) ) ;
#19810 = CARTESIAN_POINT ( 'NONE',  ( 10.00000000000002665, 45.00000000000001421, 0.000000000000000000 ) ) ;
#19812 = CARTESIAN_POINT ( 'NONE',  ( -26.34314575050764873, 209.9375000000000000, 166.0000000000003695 ) ) ;
#19813 = CARTESIAN_POINT ( 'NONE',  ( 7.320508075688774596, 82.49999999317202537, -7.320508075688774596 ) ) ;
#19814 = ORIENTED_EDGE ( 'NONE', *, *, #9203, .F. ) ;
#19815 = CARTESIAN_POINT ( 'NONE',  ( 11.00000000000000000, 4.556349186104045934, 76.84374999999998579 ) ) ;
#19816 = DIRECTION ( 'NONE',  ( -0.000000000000000000, 1.000000000000000000, -0.000000000000000000 ) ) ;
#19817 = CARTESIAN_POINT ( 'NONE',  ( -9.832129032723418760, 108.1770833299193555, -5.676582343750004256 ) ) ;
#19818 = CARTESIAN_POINT ( 'NONE',  ( 3.458734125000015425, 206.0000000013656063, 196.5673454167823877 ) ) ;
#19819 = CARTESIAN_POINT ( 'NONE',  ( -2.977408999572650039, 11.81249999795161187, -7.188101187500000933 ) ) ;
#19820 = CARTESIAN_POINT ( 'NONE',  ( -7.204075437095967871, 7.204075437095967871, 87.34375000204836681 ) ) ;
#19821 = CARTESIAN_POINT ( 'NONE',  ( 3.042071309553159519, 20.05208332991934839, 11.35316468750000141 ) ) ;
#19822 = ORIENTED_EDGE ( 'NONE', *, *, #46470, .F. ) ;
#19823 = CARTESIAN_POINT ( 'NONE',  ( -1.836970198721029983E-15, 180.6249999931720538, 10.00000000000000178 ) ) ;
#19824 = CARTESIAN_POINT ( 'NONE',  ( -8.008118988124989457, -3.317071493978883900, 23.60686528394063188 ) ) ;
#19825 = CARTESIAN_POINT ( 'NONE',  ( -11.00000000000000000, 0.000000000000000000, 101.6875000040967763 ) ) ;
#19826 = CARTESIAN_POINT ( 'NONE',  ( -10.18810118749999916, 0.000000000000000000, 74.03125000204838102 ) ) ;
#19827 = AXIS2_PLACEMENT_3D ( 'NONE', #2434, #25427, #19041 ) ;
#19828 = CARTESIAN_POINT ( 'NONE',  ( 38.00000000000000000, -53.00000000000000000, 15.00000000000000178 ) ) ;
#19829 = DIRECTION ( 'NONE',  ( -0.000000000000000000, 1.000000000000000000, -0.000000000000000000 ) ) ;
#19830 = CARTESIAN_POINT ( 'NONE',  ( -4.721056650415999201, 293.3281250017069510, -4.721056650415999201 ) ) ;
#19831 = DIRECTION ( 'NONE',  ( -1.000000000000000000, 0.000000000000000000, 0.000000000000000000 ) ) ;
#19832 = CARTESIAN_POINT ( 'NONE',  ( -9.832129032723420536, 224.0104166632526983, 5.676582343749997150 ) ) ;
#19833 = CARTESIAN_POINT ( 'NONE',  ( 9.832129032723416984, 130.6770833299193555, 5.676582343750006032 ) ) ;
#19834 = CARTESIAN_POINT ( 'NONE',  ( 10.18810118749999916, 4.220049686691935698, 85.00000000204838102 ) ) ;
#19835 = CARTESIAN_POINT ( 'NONE',  ( -31.45873412499997812, 197.7500000013656063, 171.4326545832180386 ) ) ;
#19836 = CARTESIAN_POINT ( 'NONE',  ( -8.000000000000001776, 24.84375000000000355, 3.313708498984759387 ) ) ;
#19837 = CARTESIAN_POINT ( 'NONE',  ( -1.881053915767124440, 11.12499999863440792, 4.541265875000001451 ) ) ;
#19838 = ORIENTED_EDGE ( 'NONE', *, *, #1599, .F. ) ;
#19839 = CARTESIAN_POINT ( 'NONE',  ( -3.999999999999959144, 203.1875000027312126, 199.6568542494924259 ) ) ;
#19840 = VECTOR ( 'NONE', #52744, 1000.000000000000000 ) ;
#19841 = CARTESIAN_POINT ( 'NONE',  ( 2.445694354108784108, 198.5625000013656063, 144.4456943541088663 ) ) ;
#19842 = CARTESIAN_POINT ( 'NONE',  ( -2.849036369511732440E-14, 204.3750000027312126, 138.0000000000000568 ) ) ;
#19843 = VECTOR ( 'NONE', #42870, 1000.000000000000000 ) ;
#19844 = CARTESIAN_POINT ( 'NONE',  ( -10.00000000000009948, 172.5000000000000568, -1.224646799147365089E-15 ) ) ;
#19845 = CARTESIAN_POINT ( 'NONE',  ( -4.220049686691935698, 10.18810118749999916, 69.25000000204836681 ) ) ;
#19846 = EDGE_LOOP ( 'NONE', ( #41043, #7298, #56281, #5645 ) ) ;
#19847 =( BOUNDED_CURVE ( )  B_SPLINE_CURVE ( 2, ( #43394, #65662, #32092, #9078, #26404, #1932, #71686, #3046, #60375 ),
 .UNSPECIFIED., .F., .F. ) 
 B_SPLINE_CURVE_WITH_KNOTS ( ( 3, 2, 2, 2, 3 ),
 ( 0.03125000000000002082, 0.03645833333333335646, 0.04166666666666669211, 0.04687500000000002776, 0.05208333333333337034 ),
 .UNSPECIFIED. ) 
 CURVE ( )  GEOMETRIC_REPRESENTATION_ITEM ( )  RATIONAL_B_SPLINE_CURVE ( ( 0.9999999999999996669, 0.9238795325112870716, 1.000000000000000000, 0.9238795325112867385, 1.000000000000000000, 0.9238795325112867385, 1.000000000000000000, 0.9238795325112861834, 1.000000000000000444 ) ) 
 REPRESENTATION_ITEM ( '' )  );
#19848 = CARTESIAN_POINT ( 'NONE',  ( -2.977408999572650039, 6.937499997951611874, -7.188101187500000933 ) ) ;
#19849 =( BOUNDED_CURVE ( )  B_SPLINE_CURVE ( 2, ( #33765, #16368, #56765, #49976, #5086, #72233, #15260, #66579, #14883 ),
 .UNSPECIFIED., .F., .F. ) 
 B_SPLINE_CURVE_WITH_KNOTS ( ( 3, 2, 2, 2, 3 ),
 ( 0.5666666666666670960, 0.5750000000000003997, 0.5833333333333338144, 0.5916666666666671182, 0.6000000000000004219 ),
 .UNSPECIFIED. ) 
 CURVE ( )  GEOMETRIC_REPRESENTATION_ITEM ( )  RATIONAL_B_SPLINE_CURVE ( ( 0.9999999999999958922, 0.9238795325112908463, 1.000000000000000000, 0.9238795325112867385, 1.000000000000000000, 0.9238795325112867385, 1.000000000000000000, 0.9238795325112826307, 1.000000000000003997 ) ) 
 REPRESENTATION_ITEM ( '' )  );
#19850 = CARTESIAN_POINT ( 'NONE',  ( -10.35000000000000142, 1.267509437117510795E-15, -1.155342438046016218 ) ) ;
#19851 = CARTESIAN_POINT ( 'NONE',  ( -27.99999999999999645, 210.0000000000000284, 170.0000000000003695 ) ) ;
#19852 = ADVANCED_FACE ( 'NONE', ( #28625 ), #61468, .F. ) ;
#19853 = CARTESIAN_POINT ( 'NONE',  ( 1.320432766682874540E-15, 109.9062500020483810, 7.188101187500000044 ) ) ;
#19854 = CARTESIAN_POINT ( 'NONE',  ( -2.644300734200176084, 21.99999999999999289, -3.253854384680795242 ) ) ;
#19855 = CARTESIAN_POINT ( 'NONE',  ( -6.676582343750001591, 292.4531250017069510, 0.000000000000000000 ) ) ;
#19856 = CARTESIAN_POINT ( 'NONE',  ( -9.832129032723415207, 219.3229166700806729, 5.676582343750005144 ) ) ;
#19857 = VERTEX_POINT ( 'NONE', #10906 ) ;
#19858 = CARTESIAN_POINT ( 'NONE',  ( -8.311093377946836114, 228.5937500034139873, -8.311093377946836114 ) ) ;
#19859 = CARTESIAN_POINT ( 'NONE',  ( 5.082755093536318824, 5.082755093536319713, 28.29905278187175810 ) ) ;
#19860 = CARTESIAN_POINT ( 'NONE',  ( -2.828427124746190735, 2.124999997268813168, -2.828427124746191623 ) ) ;
#19861 = CARTESIAN_POINT ( 'NONE',  ( -2.828427124746192067, 9.374999997268814056, 2.828427124746190735 ) ) ;
#19862 = CARTESIAN_POINT ( 'NONE',  ( -1.432654583217608080, 200.8750000013656063, 201.4587341250000350 ) ) ;
#19863 = VERTEX_POINT ( 'NONE', #4506 ) ;
#19864 = CARTESIAN_POINT ( 'NONE',  ( 28.00000000000002487, 209.2812500020483810, 173.7293670624999038 ) ) ;
#19865 = CARTESIAN_POINT ( 'NONE',  ( 1.469576158976823947E-15, 102.8750000000000000, 8.000000000000000000 ) ) ;
#19866 = CARTESIAN_POINT ( 'NONE',  ( 11.35316468750000141, 111.0937499965860127, 0.000000000000000000 ) ) ;
#19867 = CARTESIAN_POINT ( 'NONE',  ( -2.679491924312698004, 121.4583333333334707, -9.999999999999149125 ) ) ;
#19868 = CARTESIAN_POINT ( 'NONE',  ( 11.00000000000000000, 4.556349186104045934, 79.84374999999998579 ) ) ;
#19871 = CARTESIAN_POINT ( 'NONE',  ( 0.000000000000000000, 0.000000000000000000, 30.00000000000000000 ) ) ;
#19870 = CARTESIAN_POINT ( 'NONE',  ( 26.56734541678237704, 199.3750000013656063, 173.4587341249998929 ) ) ;
#19869 = CARTESIAN_POINT ( 'NONE',  ( 24.54126587499998280, 200.5000000013656063, 171.4326545832175555 ) ) ;
#19872 = ORIENTED_EDGE ( 'NONE', *, *, #63430, .F. ) ;
#19873 = FACE_OUTER_BOUND ( 'NONE', #64204, .T. ) ;
#19874 = EDGE_CURVE ( 'NONE', #44362, #15853, #8715, .T. ) ;
#19875 = CARTESIAN_POINT ( 'NONE',  ( 9.832129032723416984, 225.3645833299193839, 5.676582343750006032 ) ) ;
#19876 = CARTESIAN_POINT ( 'NONE',  ( 3.458734124999959914, 200.4375000013656063, 142.0000000000000568 ) ) ;
#19877 = CARTESIAN_POINT ( 'NONE',  ( 31.45873412500001010, 204.0000000013656347, 168.5673454167822740 ) ) ;
#19878 = DIRECTION ( 'NONE',  ( -0.000000000000000000, 1.000000000000000000, -0.000000000000000000 ) ) ;
#19879 = CARTESIAN_POINT ( 'NONE',  ( -5.676582343750006032, 199.4270833299193555, 9.832129032723418760 ) ) ;
#19880 = CARTESIAN_POINT ( 'NONE',  ( -2.977408999572652260, 93.31250000204838102, 7.188101187500000044 ) ) ;
#19881 = DIRECTION ( 'NONE',  ( -0.000000000000000000, -1.000000000000000000, -0.000000000000000000 ) ) ;
#19882 = CARTESIAN_POINT ( 'NONE',  ( -3.211159895383562723, 15.93749999863440436, 3.211159895383561391 ) ) ;
#19883 = CARTESIAN_POINT ( 'NONE',  ( 24.54126587499997569, 197.5000000013656063, 171.4326545832175555 ) ) ;
#19884 = CARTESIAN_POINT ( 'NONE',  ( 5.082755093536320601, -5.082755093536318824, 2.424052781871754103 ) ) ;
#19885 = CARTESIAN_POINT ( 'NONE',  ( -3.313708498984707429, 96.21875000000000000, -8.000000000000055067 ) ) ;
#19886 = CARTESIAN_POINT ( 'NONE',  ( 9.832129032723420536, 86.19791666325268409, -5.676582343749999815 ) ) ;
#19887 = ORIENTED_EDGE ( 'NONE', *, *, #57006, .F. ) ;
#19888 = CARTESIAN_POINT ( 'NONE',  ( 0.000000000000000000, -28.00000000000000000, 0.000000000000000000 ) ) ;
#19889 = CARTESIAN_POINT ( 'NONE',  ( 0.000000000000000000, 0.000000000000000000, 0.000000000000000000 ) ) ;
#19890 = CARTESIAN_POINT ( 'NONE',  ( -5.656854249492381470, 9.749999995903220196, 5.656854249492379694 ) ) ;
#19891 = CARTESIAN_POINT ( 'NONE',  ( 9.999999999999998224, 232.7083333333333428, -2.679491924311229401 ) ) ;
#19892 = CARTESIAN_POINT ( 'NONE',  ( 11.35316468750000141, 90.78124999658602690, 0.000000000000000000 ) ) ;
#19893 = EDGE_LOOP ( 'NONE', ( #52078, #13215, #18753, #10489, #35867, #2835 ) ) ;
#19894 = CARTESIAN_POINT ( 'NONE',  ( -10.18810118749999916, 4.220049686691934809, 88.93750000204839523 ) ) ;
#19895 = CARTESIAN_POINT ( 'NONE',  ( 7.204075437095966983, 7.204075437095967871, 110.5937500020483810 ) ) ;
#19896 = CARTESIAN_POINT ( 'NONE',  ( -1.432654583217607414, 207.5000000013655779, 194.5412658750000219 ) ) ;
#19897 = CARTESIAN_POINT ( 'NONE',  ( 4.898587196589412829E-16, 24.18749999590322375, -8.000000000000000000 ) ) ;
#19899 = CARTESIAN_POINT ( 'NONE',  ( -5.676582343749998039, 72.44791666325268409, -9.832129032723420536 ) ) ;
#19898 = CARTESIAN_POINT ( 'NONE',  ( 8.000000000000000000, 121.4375000040967763, -9.797174393178825657E-16 ) ) ;
#19900 = CIRCLE ( 'NONE', #37960, 4.000000000000000000 ) ;
#19901 = CARTESIAN_POINT ( 'NONE',  ( -5.656854249492375253, 5.656854249492375253, 21.83030278392014623 ) ) ;
#19902 = CARTESIAN_POINT ( 'NONE',  ( -3.003894787873372163, 194.6986583611033268, 139.8281716599198603 ) ) ;
#19903 = CARTESIAN_POINT ( 'NONE',  ( -5.000000000000005329, 175.2083333265053682, 8.660254037844387298 ) ) ;
#19904 = CARTESIAN_POINT ( 'NONE',  ( 1.656854249492263564, 199.9375000027312126, 146.0000000000001421 ) ) ;
#19905 = VECTOR ( 'NONE', #20515, 1000.000000000000000 ) ;
#19906 = CYLINDRICAL_SURFACE ( 'NONE', #68903, 5.099999999999999645 ) ;
#19907 = CARTESIAN_POINT ( 'NONE',  ( -5.676582343749998039, 67.76041666325268409, -9.832129032723420536 ) ) ;
#19908 = CARTESIAN_POINT ( 'NONE',  ( -4.088227598258586603E-16, 294.2031250017069510, -6.676582343750001591 ) ) ;
#19909 = CARTESIAN_POINT ( 'NONE',  ( 1.871523826299183495E-15, -10.18810118749999916, 108.9062500020483668 ) ) ;
#19910 = CARTESIAN_POINT ( 'NONE',  ( 3.042071309553159519, 199.7395833299193555, 11.35316468750000141 ) ) ;
#19911 = VERTEX_POINT ( 'NONE', #47780 ) ;
#19912 = CARTESIAN_POINT ( 'NONE',  ( -31.99999999999996447, 203.4375000027312126, 171.6568542494928522 ) ) ;
#19913 = CARTESIAN_POINT ( 'NONE',  ( 8.000000000000000000, 14.90624999590322197, -3.313708498984761164 ) ) ;
#19915 = CARTESIAN_POINT ( 'NONE',  ( 9.832129032723420536, 196.1979166632526983, -5.676582343749999815 ) ) ;
#19914 = FACE_OUTER_BOUND ( 'NONE', #21138, .T. ) ;
#19916 = DIRECTION ( 'NONE',  ( -0.000000000000000000, 1.000000000000000000, 2.238352872228138170E-16 ) ) ;
#19917 = CARTESIAN_POINT ( 'NONE',  ( 2.679491924311235174, 239.5833333401612606, 9.999999999999998224 ) ) ;
#19918 = CARTESIAN_POINT ( 'NONE',  ( -30.82842712474621294, 200.1250000000000284, 167.1715728752542134 ) ) ;
#19919 = VERTEX_POINT ( 'NONE', #22207 ) ;
#19920 = CARTESIAN_POINT ( 'NONE',  ( -8.311093377946841443, 184.2187499965860127, 8.311093377946834337 ) ) ;
#19921 = CARTESIAN_POINT ( 'NONE',  ( -7.188101187499992051, 0.000000000000000000, 19.48655278187175455 ) ) ;
#19922 = CARTESIAN_POINT ( 'NONE',  ( -9.999999999999994671, 92.50000000000001421, -1.224646799147352665E-15 ) ) ;
#19923 = ORIENTED_EDGE ( 'NONE', *, *, #66150, .T. ) ;
#19924 = B_SPLINE_CURVE_WITH_KNOTS ( 'NONE', 3,
 ( #25657, #9452, #26789, #32468, #2289, #26398, #31710, #49423, #2666, #55477, #20754, #14712, #43769, #3040, #66783, #25285, #26023, #15087, #38122, #37750, #48673, #9073, #38496, #54733, #66029, #61121, #54356, #3788, #49805, #21128 ),
 .UNSPECIFIED., .F., .F.,
 ( 4, 2, 2, 2, 2, 2, 2, 2, 2, 2, 2, 2, 2, 2, 4 ),
 ( 0.09613912281754555256, 0.09784836092776083571, 0.09955759903797611887, 0.1004122180930837605, 0.1012668371481914020, 0.1029760752584066574, 0.1038306943135142713, 0.1046853133686218990, 0.1063945514788370711, 0.1081037895890522432, 0.1098130276992674154, 0.1132315039196977735, 0.1166499801401281178, 0.1200684563605584620, 0.1234869325809888202 ),
 .UNSPECIFIED. ) ;
#19925 = CARTESIAN_POINT ( 'NONE',  ( 3.313708498984765161, 100.1562500040967905, 7.999999999999998224 ) ) ;
#19926 = CARTESIAN_POINT ( 'NONE',  ( -1.836970198721029983E-15, 3.750000000000000444, 10.00000000000000178 ) ) ;
#19927 = CARTESIAN_POINT ( 'NONE',  ( -4.000000000000001776, 16.50000000000000000, -4.898587196589415787E-16 ) ) ;
#19928 = CARTESIAN_POINT ( 'NONE',  ( 1.881053915767122664, 16.12499999863440436, 4.541265875000001451 ) ) ;
#19929 = CARTESIAN_POINT ( 'NONE',  ( 7.999999999999991118, 3.313708498984757611, 16.86155278392014623 ) ) ;
#19930 =( BOUNDED_CURVE ( )  B_SPLINE_CURVE ( 2, ( #42897, #71200, #60256, #19155, #65170, #13482, #8582, #54619, #72325 ),
 .UNSPECIFIED., .F., .F. ) 
 B_SPLINE_CURVE_WITH_KNOTS ( ( 3, 2, 2, 2, 3 ),
 ( 0.1833333333333333481, 0.1916666666666667629, 0.2000000000000001776, 0.2083333333333335646, 0.2166666666666669516 ),
 .UNSPECIFIED. ) 
 CURVE ( )  GEOMETRIC_REPRESENTATION_ITEM ( )  RATIONAL_B_SPLINE_CURVE ( ( 0.9999999999999997780, 0.9238795325112869605, 1.000000000000000000, 0.9238795325112867385, 1.000000000000000000, 0.9238795325112867385, 1.000000000000000000, 0.9238795325112841850, 1.000000000000002442 ) ) 
 REPRESENTATION_ITEM ( '' )  );
#19931 = DIRECTION ( 'NONE',  ( 0.000000000000000000, 0.000000000000000000, -1.000000000000000000 ) ) ;
#19933 = ORIENTED_EDGE ( 'NONE', *, *, #21942, .F. ) ;
#19932 = EDGE_CURVE ( 'NONE', #38109, #51876, #16925, .T. ) ;
#19934 = LINE ( 'NONE', #71989, #40275 ) ;
#19935 = CARTESIAN_POINT ( 'NONE',  ( 7.188101187500002709, 96.31250000204838102, 2.977408999572649151 ) ) ;
#19937 = CARTESIAN_POINT ( 'NONE',  ( -26.34314575050756346, 204.6875000027312126, 174.0000000000003411 ) ) ;
#19936 = CARTESIAN_POINT ( 'NONE',  ( 28.00000000000002132, 209.4375000013656063, 173.4587341249998929 ) ) ;
#19938 = DIRECTION ( 'NONE',  ( 0.000000000000000000, 0.000000000000000000, 1.000000000000000000 ) ) ;
#19939 = ORIENTED_EDGE ( 'NONE', *, *, #30497, .T. ) ;
#19940 = EDGE_CURVE ( 'NONE', #6126, #60666, #61841, .T. ) ;
#19941 = CARTESIAN_POINT ( 'NONE',  ( -1.688721909672344479, 49.97488762307396115, -40.72268565194232082 ) ) ;
#19942 = AXIS2_PLACEMENT_3D ( 'NONE', #40558, #221, #6604 ) ;
#19943 = CARTESIAN_POINT ( 'NONE',  ( 7.188101187499992051, 8.802885111219154394E-16, 15.73655278187175632 ) ) ;
#19944 = ORIENTED_EDGE ( 'NONE', *, *, #51126, .T. ) ;
#19945 = VERTEX_POINT ( 'NONE', #5254 ) ;
#19946 = CARTESIAN_POINT ( 'NONE',  ( -4.220049686691935698, 10.18810118749999916, 77.87500000204838102 ) ) ;
#19947 = CARTESIAN_POINT ( 'NONE',  ( 9.832129032723420536, 61.51041666325268409, -5.676582343749999815 ) ) ;
#19948 = CARTESIAN_POINT ( 'NONE',  ( 6.123233995736767268E-16, 113.1249999931720396, -10.00000000000000178 ) ) ;
#19949 = CARTESIAN_POINT ( 'NONE',  ( -11.00000000000000000, 4.556349186104045934, 92.40624999999998579 ) ) ;
#19952 = CARTESIAN_POINT ( 'NONE',  ( 2.765530957081996366, 294.2968750017070079, -6.676582343750002480 ) ) ;
#19951 = CARTESIAN_POINT ( 'NONE',  ( 30.82842712474616675, 202.5000000027312126, 167.1715728752537018 ) ) ;
#19950 = CARTESIAN_POINT ( 'NONE',  ( 0.000000000000000000, 0.000000000000000000, 7.000000000000000000 ) ) ;
#19953 = CARTESIAN_POINT ( 'NONE',  ( -7.320508075688773708, 141.8750000000000000, -7.320508075688774596 ) ) ;
#19954 = LINE ( 'NONE', #15408, #1869 ) ;
#19955 = CARTESIAN_POINT ( 'NONE',  ( -8.000000000000000000, 90.59375000409677625, -3.313708498984761164 ) ) ;
#19956 = EDGE_CURVE ( 'NONE', #69918, #29891, #57558, .T. ) ;
#19958 =( BOUNDED_CURVE ( )  B_SPLINE_CURVE ( 2, ( #41905, #53609, #1200, #47192, #18533, #35891, #58908, #30221, #53239 ),
 .UNSPECIFIED., .F., .F. ) 
 B_SPLINE_CURVE_WITH_KNOTS ( ( 3, 2, 2, 2, 3 ),
 ( 0.4479166666666665741, 0.4531249999999998890, 0.4583333333333332038, 0.4635416666666665741, 0.4687499999999998890 ),
 .UNSPECIFIED. ) 
 CURVE ( )  GEOMETRIC_REPRESENTATION_ITEM ( )  RATIONAL_B_SPLINE_CURVE ( ( 1.000000000000001554, 0.9238795325112850731, 1.000000000000000000, 0.9238795325112867385, 1.000000000000000000, 0.9238795325112867385, 1.000000000000000000, 0.9238795325112884038, 0.9999999999999983347 ) ) 
 REPRESENTATION_ITEM ( '' )  );
#19957 = LINE ( 'NONE', #42964, #62709 ) ;
#19959 = CARTESIAN_POINT ( 'NONE',  ( 4.898587196589412829E-16, 1.687499995903220196, -8.000000000000000000 ) ) ;
#19960 = CARTESIAN_POINT ( 'NONE',  ( 30.44569435410883429, 199.8125000013656063, 167.5543056458911053 ) ) ;
#19961 = CARTESIAN_POINT ( 'NONE',  ( 7.188101187500000044, 12.84374999795161187, 0.000000000000000000 ) ) ;
#19962 = CARTESIAN_POINT ( 'NONE',  ( -5.656854249492373476, -5.656854249492376141, 25.20530278392014978 ) ) ;
#19963 = DIRECTION ( 'NONE',  ( 1.000000000000000000, 3.154042683594195121E-16, 0.000000000000000000 ) ) ;
#19964 = CARTESIAN_POINT ( 'NONE',  ( -4.401442555609581635E-16, 112.1562500020483952, -7.188101187500000044 ) ) ;
#19966 = CARTESIAN_POINT ( 'NONE',  ( 6.123233995736767268E-16, 131.2500000000000000, -10.00000000000000178 ) ) ;
#19965 = FACE_OUTER_BOUND ( 'NONE', #55014, .T. ) ;
#19967 = CARTESIAN_POINT ( 'NONE',  ( -8.311093377946834337, 219.8437500034139873, 8.311093377946837890 ) ) ;
#19968 = CARTESIAN_POINT ( 'NONE',  ( 31.45873412499998523, 208.8750000013656063, 171.4326545832176123 ) ) ;
#19969 = CARTESIAN_POINT ( 'NONE',  ( 5.082755093536320601, -5.082755093536318824, 24.92405278187175810 ) ) ;
#19970 = CARTESIAN_POINT ( 'NONE',  ( 4.898587196589415787E-16, 0.000000000000000000, 4.000000000000001776 ) ) ;
#19971 = CARTESIAN_POINT ( 'NONE',  ( 11.35316468749999785, 35.57291666325267698, 3.042071309553174174 ) ) ;
#19972 = CARTESIAN_POINT ( 'NONE',  ( -2.828427124746192067, 6.625000000000000000, 2.828427124746190735 ) ) ;
#19973 = CARTESIAN_POINT ( 'NONE',  ( -5.000000000000005329, 15.20833332650536640, 8.660254037844387298 ) ) ;
#19974 = ORIENTED_EDGE ( 'NONE', *, *, #30782, .F. ) ;
#19975 = CARTESIAN_POINT ( 'NONE',  ( -6.123233995736766282E-16, 248.7500000000000284, -10.00000000000000000 ) ) ;
#19976 = DIRECTION ( 'NONE',  ( 3.552713678800499352E-15, 0.000000000000000000, 1.000000000000000000 ) ) ;
#19977 = CARTESIAN_POINT ( 'NONE',  ( 9.832129032723416984, 45.36458332991934839, 5.676582343750006032 ) ) ;
#19978 = CARTESIAN_POINT ( 'NONE',  ( 4.556349186104045934, 11.00000000000000000, 80.21875000409679046 ) ) ;
#19979 = CARTESIAN_POINT ( 'NONE',  ( 3.458734124999959469, 204.7500000013655779, 140.5673454167823593 ) ) ;
#19980 = CARTESIAN_POINT ( 'NONE',  ( -6.000000000000001776, 299.0000000000000000, 0.000000000000000000 ) ) ;
#19981 = DIRECTION ( 'NONE',  ( -0.000000000000000000, -0.000000000000000000, -1.000000000000000000 ) ) ;
#19983 = CARTESIAN_POINT ( 'NONE',  ( -11.35316468749999785, 28.07291666325268054, -3.042071309553167957 ) ) ;
#19982 = CARTESIAN_POINT ( 'NONE',  ( 7.188101187500002709, 99.31250000204838102, 2.977408999572649151 ) ) ;
#19984 = CARTESIAN_POINT ( 'NONE',  ( -5.656854249492373476, -5.656854249492376141, 11.51780277982336642 ) ) ;
#19985 = CARTESIAN_POINT ( 'NONE',  ( -5.676582343749998039, 157.4479166632526983, -9.832129032723420536 ) ) ;
#19986 = CARTESIAN_POINT ( 'NONE',  ( -8.660254037844387298, 128.9583333265053966, -5.000000000000004441 ) ) ;
#19987 = EDGE_CURVE ( 'NONE', #34174, #4709, #11100, .T. ) ;
#19988 = CARTESIAN_POINT ( 'NONE',  ( -4.401442555609581635E-16, 110.6562500020483810, -7.188101187500000044 ) ) ;
#19989 = VERTEX_POINT ( 'NONE', #12750 ) ;
#19990 = CARTESIAN_POINT ( 'NONE',  ( -4.242640687119285658, 289.1249999999999432, 4.242640687119287435 ) ) ;
#19991 = CARTESIAN_POINT ( 'NONE',  ( -11.35316468749999785, 23.38541666325268054, -3.042071309553167957 ) ) ;
#19992 = CARTESIAN_POINT ( 'NONE',  ( -10.00000000000001243, 17.70833333333333925, 2.679491924311226292 ) ) ;
#19993 = ORIENTED_EDGE ( 'NONE', *, *, #65427, .T. ) ;
#19994 = CARTESIAN_POINT ( 'NONE',  ( -7.999999999999991118, -1.288204405367768053E-10, 8.517802783929960597 ) ) ;
#19995 = CARTESIAN_POINT ( 'NONE',  ( -4.220049686691935698, 10.18810118749999916, 76.37500000204838102 ) ) ;
#19996 = CARTESIAN_POINT ( 'NONE',  ( 2.449293598294707893E-16, 8.250000000000000000, -4.000000000000001776 ) ) ;
#19998 = CARTESIAN_POINT ( 'NONE',  ( -9.832129032723418760, 157.8645833299193839, -5.676582343750004256 ) ) ;
#19997 = CYLINDRICAL_SURFACE ( 'NONE', #38810, 3.999999999999976019 ) ;
#19999 = CARTESIAN_POINT ( 'NONE',  ( 7.188101187500000933, 0.9374999979516102089, -2.977408999572650483 ) ) ;
#20000 = CARTESIAN_POINT ( 'NONE',  ( 3.313708498984762496, -7.999999999999989342, 19.35530278432982954 ) ) ;
#20001 = CARTESIAN_POINT ( 'NONE',  ( -5.676582343750000703, 233.0729166700806729, -9.832129032723418760 ) ) ;
#20002 = CARTESIAN_POINT ( 'NONE',  ( 10.18810118749999916, 1.247682550866122264E-15, 85.28125000204836681 ) ) ;
#20003 = ORIENTED_EDGE ( 'NONE', *, *, #10674, .F. ) ;
#20004 = AXIS2_PLACEMENT_3D ( 'NONE', #9778, #48997, #61823 ) ;
#20005 = CARTESIAN_POINT ( 'NONE',  ( 3.313708498984760276, 1.593749995903220196, -8.000000000000001776 ) ) ;
#20006 = CARTESIAN_POINT ( 'NONE',  ( 27.99999999999996803, 205.0000000000000284, 173.9999999999999147 ) ) ;
#20007 = CARTESIAN_POINT ( 'NONE',  ( 11.35316468749999785, 105.8854166632526983, 3.042071309553174174 ) ) ;
#20008 = CARTESIAN_POINT ( 'NONE',  ( -7.204075437095967871, 7.204075437095967871, 98.96875000204838102 ) ) ;
#20009 = ORIENTED_EDGE ( 'NONE', *, *, #8639, .T. ) ;
#20010 = VERTEX_POINT ( 'NONE', #47453 ) ;
#20011 = CARTESIAN_POINT ( 'NONE',  ( 2.780723358947928197E-16, 4.687499998634407028, -4.541265875000002339 ) ) ;
#20012 = CARTESIAN_POINT ( 'NONE',  ( -7.188101187500000044, 7.218749997951610986, -8.802885111219163269E-16 ) ) ;
#20013 = CARTESIAN_POINT ( 'NONE',  ( -3.313708498984762496, 117.9687500040968047, 7.999999999999998224 ) ) ;
#20014 = CARTESIAN_POINT ( 'NONE',  ( 4.220049686691934809, 10.18810118749999916, 96.06250000204836681 ) ) ;
#20015 = VECTOR ( 'NONE', #61304, 1000.000000000000000 ) ;
#20016 = CARTESIAN_POINT ( 'NONE',  ( -31.45873412499998523, 202.0000000013656063, 171.4326545832180386 ) ) ;
#20017 = DIRECTION ( 'NONE',  ( 1.000000000000000000, 1.991032627040250683E-16, 0.000000000000000000 ) ) ;
#20018 = CARTESIAN_POINT ( 'NONE',  ( 1.656854249492381248, 2.187500000000000444, -4.000000000000001776 ) ) ;
#20019 = CARTESIAN_POINT ( 'NONE',  ( -4.000000000000001776, 19.24999999726881228, -4.898587196589415787E-16 ) ) ;
#20020 = CARTESIAN_POINT ( 'NONE',  ( 2.780723358947928197E-16, 3.562499998634407028, -4.541265875000002339 ) ) ;
#20021 = CARTESIAN_POINT ( 'NONE',  ( 28.00000000000002132, 207.5000000000000284, 165.9999999999998863 ) ) ;
#20023 = CARTESIAN_POINT ( 'NONE',  ( -8.000000000000000000, 15.75000000000000355, -9.797174393178825657E-16 ) ) ;
#20022 = CARTESIAN_POINT ( 'NONE',  ( -30.44569435410875968, 200.8125000013656063, 172.4456943541092642 ) ) ;
#20024 =( NAMED_UNIT ( * ) SI_UNIT ( $, .STERADIAN. ) SOLID_ANGLE_UNIT ( ) );
#20025 = EDGE_CURVE ( 'NONE', #42017, #25822, #48438, .T. ) ;
#20026 = CARTESIAN_POINT ( 'NONE',  ( -3.211159895383562723, 18.93749999863440436, 3.211159895383561391 ) ) ;
#20027 = CARTESIAN_POINT ( 'NONE',  ( 4.721056650416000089, 298.8281250017069510, 4.721056650415999201 ) ) ;
#20028 = CARTESIAN_POINT ( 'NONE',  ( -5.082755093536319713, 5.082755093536319713, 5.799052781871753659 ) ) ;
#20029 = ORIENTED_EDGE ( 'NONE', *, *, #66198, .T. ) ;
#20030 = ORIENTED_EDGE ( 'NONE', *, *, #60921, .F. ) ;
#20031 = CARTESIAN_POINT ( 'NONE',  ( 10.18810118750000093, -4.220049686691933033, 101.3125000020483810 ) ) ;
#20032 = CARTESIAN_POINT ( 'NONE',  ( -30.44569435410883429, 204.8125000013656063, 167.5543056458915885 ) ) ;
#20033 = CARTESIAN_POINT ( 'NONE',  ( -31.99999999999999289, 201.2500000000000000, 170.0000000000003979 ) ) ;
#20034 = CARTESIAN_POINT ( 'NONE',  ( 2.445694354108839619, 195.8125000013656063, 200.4456943541088663 ) ) ;
#20035 = CARTESIAN_POINT ( 'NONE',  ( -25.17157287525374088, 201.7500000027312126, 172.8284271247464972 ) ) ;
#20036 = CARTESIAN_POINT ( 'NONE',  ( -2.679491924311235618, 108.5416666666666714, 10.00000000000000000 ) ) ;
#20037 = CARTESIAN_POINT ( 'NONE',  ( 8.000000000000000000, 110.7500000000000000, -9.797174393178825657E-16 ) ) ;
#20038 = CARTESIAN_POINT ( 'NONE',  ( -4.721056650415999201, 295.4843750017070079, -4.721056650415999201 ) ) ;
#20039 = ORIENTED_EDGE ( 'NONE', *, *, #37412, .T. ) ;
#20040 = ADVANCED_FACE ( 'NONE', ( #53131 ), #29742, .T. ) ;
#20041 = CARTESIAN_POINT ( 'NONE',  ( -8.000000000000000000, 23.06249999590322020, -9.797174393178825657E-16 ) ) ;
#20042 = CARTESIAN_POINT ( 'NONE',  ( -3.458734125000016313, 203.8750000013656063, 140.5673454167824161 ) ) ;
#20043 = CARTESIAN_POINT ( 'NONE',  ( 2.775557561562891351E-14, 210.0000000000000284, 198.0000000000000284 ) ) ;
#20044 = CARTESIAN_POINT ( 'NONE',  ( 8.000000000000000000, 121.2500000000000000, -9.797174393178825657E-16 ) ) ;
#20045 = CARTESIAN_POINT ( 'NONE',  ( -9.832129032723415207, 249.6354166700806445, 5.676582343750005144 ) ) ;
#20046 = CARTESIAN_POINT ( 'NONE',  ( 2.449293598294707893E-16, 0.9999999972688131678, -4.000000000000001776 ) ) ;
#20047 = CARTESIAN_POINT ( 'NONE',  ( 11.00000000000000000, 1.347111479062088405E-15, 114.2499999999999858 ) ) ;
#20048 =( BOUNDED_SURFACE ( )  B_SPLINE_SURFACE ( 1, 2, ( 
 ( #459, #45336, #40427, #63800, #51742, #6103, #51366, #10641, #35156, #69097, #34791, #33670, #91, #11017, #22688, #4991, #40056, #29108, #57045, #23438, #44975, #23069, #67980, #50997, #50620, #27991, #74009, #40794, #46452, #69471, #27610, #34050, #46078, #45706, #22310, #17404, #16275, #5727, #68353, #63059, #11383, #34418, #28726, #63426, #11754, #36252, #47552, #38020, #52490, #52861, #19619, #70217, #70576, #7212, #30582, #6477, #30214, #47920, #59267, #18893, #1193, #43666, #18526, #41534, #29481, #6836, #23816, #41899, #64550, #35884, #7579, #24544, #53604, #64908, #13214, #42263, #828, #12846, #70939, #58529, #36618, #59627, #25274, #1916, #46818, #69844, #64182, #58901, #18156, #41171, #24903, #53234, #12486, #35516, #29850, #53968, #66678, #7942, #1565, #48292, #71299, #14983, #24175, #19252, #65275, #13581, #47185, #30947, #2279, #15357, #39132, #27803, #55378, #68171, #61019, #62137, #15730, #73457, #26683, #73827, #44793, #3684, #22134, #16469, #49707, #56123, #45160, #73088, #38393, #9345, #67806, #32364, #72720, #61396, #9722, #10459, #28177, #39506, #62501, #51189, #50075, #27062, #21024, #10830, #21396, #4431, #44049, #74197, #32743, #56492, #55752, #22502, #27426, #4069, #33865, #50441, #68540, #56864, #67058, #16097, #44419, #38771, #67434, #45524, #33128, #5181, #16844, #21765, #61772, #10090, #33490, #50817, #4809, #34606, #46643, #11206, #68914, #34234, #40994, #23998, #280, #1019, #47008, #17224, #17601, #35348, #34979, #69662, #11947, #64001, #12316, #17975, #46271, #58360, #7032, #70039, #57235, #18348, #63620, #23636, #28926, #57995, #51556, #53055, #6299, #1387, #29668, #40618, #22888, #64372, #57613, #52684, #24371, #6665, #41362, #29305, #74575, #47378, #12673, #35706, #45900, #58721, #23262, #52315, #40244, #651, #30040, #69290, #70403, #5547, #39871, #28549, #63247, #62873, #11573, #5923, #51942, #31517, #8500, #65836, #30770 ),
 ( #36441, #19812, #14142, #1748, #53792, #25467, #48110, #36808, #71120, #54167, #8132, #59818, #2101, #2475, #2844, #42453, #59454, #25095, #31135, #19441, #48484, #65470, #13764, #42818, #43194, #13404, #71487, #24729, #37177, #60178, #54538, #25835, #18718, #13037, #53425, #7768, #64738, #30407, #48853, #71863, #41727, #47739, #70762, #20176, #36073, #59092, #7400, #19078, #42082, #65092, #23113, #18204, #24220, #70261, #17451, #64225, #52908, #40472, #12533, #1242, #5778, #18573, #11431, #35563, #40844, #23860, #51789, #47233, #69892, #28774, #41583, #64598, #137, #6519, #12895, #58948, #35931, #17830, #58576, #63852, #63477, #7255, #57472, #6884, #6149, #30266, #53282, #41217, #29895, #1607, #52173, #24591, #52536, #41944, #46126, #57844, #47596, #505, #874, #12167, #70618, #34468, #35201, #18938, #69144, #46870, #29155, #11799, #23484, #46496, #34837, #69516, #58218, #29526, #70984, #3448, #26437, #7989, #32123, #19300, #3076, #14373, #30629, #60408, #65692, #13630, #55143, #72095, #14747, #71718, #53651, #59678, #49462, #1961, #66066, #42310, #9108, #37407, #31369, #43047, #20033, #36299, #72482, #13992, #59316, #25323, #36668, #48339, #20789, #37788, #20409, #54767, #71346, #30995, #24952, #2703, #25691, #65325, #8734, #64952, #43425, #7622, #26061, #37033, #48711, #54017, #60034, #47969, #13262, #8352, #2327, #49082, #42680, #19668, #60784, #54397, #66439, #31747, #8199, #30477, #19146, #51721, #47811, #28707, #42527, #18790, #70, #13473, #41795, #59886, #25166, #45686, #7472, #63040, #30109, #5708, #65541, #24440, #7834, #2172, #64804, #68701, #53126, #34399, #48183, #70112, #65162, #13832, #1811, #47075, #13106, #51347, #18418, #42149, #59521, #57400, #24797, #12745, #47448, #11365, #36142, #53860, #7101, #30839, #17011, #70834, #40037, #24065, #74357, #41432, #64444, #36878, #71190, #19509, #22667, #58791, #36512, #1459, #35776, #70472, #59163 ) ),
 .UNSPECIFIED., .F., .F., .F. ) 
 B_SPLINE_SURFACE_WITH_KNOTS ( ( 2, 2 ),
 ( 3, 2, 2, 2, 2, 2, 2, 2, 2, 2, 2, 2, 2, 2, 2, 2, 2, 2, 2, 2, 2, 2, 2, 2, 2, 2, 2, 2, 2, 2, 2, 2, 2, 2, 2, 2, 2, 2, 2, 2, 2, 2, 2, 2, 2, 2, 2, 2, 2, 2, 2, 2, 2, 2, 2, 2, 2, 2, 2, 2, 2, 2, 2, 2, 2, 2, 2, 2, 2, 2, 2, 2, 2, 2, 2, 2, 2, 2, 2, 2, 2, 2, 2, 2, 2, 2, 2, 2, 2, 2, 2, 2, 2, 2, 2, 2, 2, 2, 2, 2, 2, 2, 2, 2, 2, 2, 2, 2, 2, 2, 2, 2, 2, 2, 2, 2, 2, 2, 2, 2, 3 ),
 ( 0.000000000000000000, 1.000000000000000000 ),
 ( 0.000000000000000000, 0.008333333333333333218, 0.01666666666666666644, 0.02500000000000000139, 0.03333333333333333287, 0.04166666666666666435, 0.05000000000000000278, 0.05833333333333333426, 0.06666666666666666574, 0.07499999999999999722, 0.08333333333333332871, 0.09166666666666666019, 0.1000000000000000056, 0.1083333333333333370, 0.1166666666666666685, 0.1250000000000000000, 0.1333333333333333315, 0.1416666666666666630, 0.1499999999999999944, 0.1583333333333333259, 0.1666666666666666574, 0.1749999999999999889, 0.1833333333333333204, 0.1916666666666666796, 0.2000000000000000111, 0.2083333333333333426, 0.2166666666666666741, 0.2250000000000000056, 0.2333333333333333370, 0.2416666666666666685, 0.2500000000000000000, 0.2583333333333333592, 0.2666666666666666630, 0.2750000000000000222, 0.2833333333333333259, 0.2916666666666666852, 0.2999999999999999889, 0.3083333333333333481, 0.3166666666666666519, 0.3250000000000000111, 0.3333333333333333148, 0.3416666666666666741, 0.3499999999999999778, 0.3583333333333333370, 0.3666666666666666408, 0.3750000000000000000, 0.3833333333333333592, 0.3916666666666666630, 0.4000000000000000222, 0.4083333333333333259, 0.4166666666666666852, 0.4249999999999999889, 0.4333333333333333481, 0.4416666666666666519, 0.4500000000000000111, 0.4583333333333333148, 0.4666666666666666741, 0.4749999999999999778, 0.4833333333333333370, 0.4916666666666666408, 0.5000000000000000000, 0.5083333333333333037, 0.5166666666666667185, 0.5250000000000000222, 0.5333333333333333259, 0.5416666666666666297, 0.5500000000000000444, 0.5583333333333333481, 0.5666666666666666519, 0.5749999999999999556, 0.5833333333333333703, 0.5916666666666666741, 0.5999999999999999778, 0.6083333333333332815, 0.6166666666666666963, 0.6250000000000000000, 0.6333333333333333037, 0.6416666666666667185, 0.6500000000000000222, 0.6583333333333333259, 0.6666666666666666297, 0.6750000000000000444, 0.6833333333333333481, 0.6916666666666666519, 0.6999999999999999556, 0.7083333333333333703, 0.7166666666666666741, 0.7249999999999999778, 0.7333333333333332815, 0.7416666666666666963, 0.7500000000000000000, 0.7583333333333333037, 0.7666666666666667185, 0.7750000000000000222, 0.7833333333333333259, 0.7916666666666666297, 0.8000000000000000444, 0.8083333333333333481, 0.8166666666666666519, 0.8249999999999999556, 0.8333333333333333703, 0.8416666666666666741, 0.8499999999999999778, 0.8583333333333332815, 0.8666666666666666963, 0.8750000000000000000, 0.8833333333333333037, 0.8916666666666667185, 0.9000000000000000222, 0.9083333333333333259, 0.9166666666666666297, 0.9250000000000000444, 0.9333333333333333481, 0.9416666666666666519, 0.9499999999999999556, 0.9583333333333333703, 0.9666666666666666741, 0.9749999999999999778, 0.9833333333333332815, 0.9916666666666666963, 1.000000000000000000 ),
 .UNSPECIFIED. ) 
 GEOMETRIC_REPRESENTATION_ITEM ( )  RATIONAL_B_SPLINE_SURFACE ( (
 ( 1.000000000000000000, 0.9238795325112867385, 1.000000000000000000, 0.9238795325112867385, 1.000000000000000000, 0.9238795325112867385, 1.000000000000000000, 0.9238795325112867385, 1.000000000000000000, 0.9238795325112867385, 1.000000000000000000, 0.9238795325112867385, 1.000000000000000000, 0.9238795325112867385, 1.000000000000000000, 0.9238795325112867385, 1.000000000000000000, 0.9238795325112867385, 1.000000000000000000, 0.9238795325112867385, 1.000000000000000000, 0.9238795325112867385, 1.000000000000000000, 0.9238795325112867385, 1.000000000000000000, 0.9238795325112867385, 1.000000000000000000, 0.9238795325112867385, 1.000000000000000000, 0.9238795325112867385, 1.000000000000000000, 0.9238795325112867385, 1.000000000000000000, 0.9238795325112867385, 1.000000000000000000, 0.9238795325112867385, 1.000000000000000000, 0.9238795325112867385, 1.000000000000000000, 0.9238795325112867385, 1.000000000000000000, 0.9238795325112867385, 1.000000000000000000, 0.9238795325112867385, 1.000000000000000000, 0.9238795325112867385, 1.000000000000000000, 0.9238795325112867385, 1.000000000000000000, 0.9238795325112867385, 1.000000000000000000, 0.9238795325112867385, 1.000000000000000000, 0.9238795325112867385, 1.000000000000000000, 0.9238795325112867385, 1.000000000000000000, 0.9238795325112867385, 1.000000000000000000, 0.9238795325112867385, 1.000000000000000000, 0.9238795325112867385, 1.000000000000000000, 0.9238795325112867385, 1.000000000000000000, 0.9238795325112867385, 1.000000000000000000, 0.9238795325112867385, 1.000000000000000000, 0.9238795325112867385, 1.000000000000000000, 0.9238795325112867385, 1.000000000000000000, 0.9238795325112867385, 1.000000000000000000, 0.9238795325112867385, 1.000000000000000000, 0.9238795325112867385, 1.000000000000000000, 0.9238795325112867385, 1.000000000000000000, 0.9238795325112867385, 1.000000000000000000, 0.9238795325112867385, 1.000000000000000000, 0.9238795325112867385, 1.000000000000000000, 0.9238795325112867385, 1.000000000000000000, 0.9238795325112867385, 1.000000000000000000, 0.9238795325112867385, 1.000000000000000000, 0.9238795325112867385, 1.000000000000000000, 0.9238795325112867385, 1.000000000000000000, 0.9238795325112867385, 1.000000000000000000, 0.9238795325112867385, 1.000000000000000000, 0.9238795325112867385, 1.000000000000000000, 0.9238795325112867385, 1.000000000000000000, 0.9238795325112867385, 1.000000000000000000, 0.9238795325112867385, 1.000000000000000000, 0.9238795325112867385, 1.000000000000000000, 0.9238795325112867385, 1.000000000000000000, 0.9238795325112867385, 1.000000000000000000, 0.9238795325112867385, 1.000000000000000000, 0.9238795325112867385, 1.000000000000000000, 0.9238795325112867385, 1.000000000000000000, 0.9238795325112867385, 1.000000000000000000, 0.9238795325112867385, 1.000000000000000000, 0.9238795325112867385, 1.000000000000000000, 0.9238795325112867385, 1.000000000000000000, 0.9238795325112867385, 1.000000000000000000, 0.9238795325112867385, 1.000000000000000000, 0.9238795325112867385, 1.000000000000000000, 0.9238795325112867385, 1.000000000000000000, 0.9238795325112867385, 1.000000000000000000, 0.9238795325112867385, 1.000000000000000000, 0.9238795325112867385, 1.000000000000000000, 0.9238795325112867385, 1.000000000000000000, 0.9238795325112867385, 1.000000000000000000, 0.9238795325112867385, 1.000000000000000000, 0.9238795325112867385, 1.000000000000000000, 0.9238795325112867385, 1.000000000000000000, 0.9238795325112867385, 1.000000000000000000, 0.9238795325112867385, 1.000000000000000000, 0.9238795325112867385, 1.000000000000000000, 0.9238795325112867385, 1.000000000000000000, 0.9238795325112867385, 1.000000000000000000, 0.9238795325112867385, 1.000000000000000000, 0.9238795325112867385, 1.000000000000000000, 0.9238795325112867385, 1.000000000000000000, 0.9238795325112867385, 1.000000000000000000, 0.9238795325112867385, 1.000000000000000000, 0.9238795325112867385, 1.000000000000000000, 0.9238795325112867385, 1.000000000000000000, 0.9238795325112867385, 1.000000000000000000, 0.9238795325112867385, 1.000000000000000000, 0.9238795325112867385, 1.000000000000000000, 0.9238795325112867385, 1.000000000000000000, 0.9238795325112867385, 1.000000000000000000, 0.9238795325112867385, 1.000000000000000000, 0.9238795325112867385, 1.000000000000000000, 0.9238795325112867385, 1.000000000000000000, 0.9238795325112867385, 1.000000000000000000, 0.9238795325112867385, 1.000000000000000000, 0.9238795325112867385, 1.000000000000000000, 0.9238795325112867385, 1.000000000000000000, 0.9238795325112867385, 1.000000000000000000, 0.9238795325112867385, 1.000000000000000000, 0.9238795325112867385, 1.000000000000000000, 0.9238795325112867385, 1.000000000000000000, 0.9238795325112867385, 1.000000000000000000, 0.9238795325112867385, 1.000000000000000000, 0.9238795325112867385, 1.000000000000000000, 0.9238795325112867385, 1.000000000000000000, 0.9238795325112867385, 1.000000000000000000, 0.9238795325112867385, 1.000000000000000000, 0.9238795325112867385, 1.000000000000000000, 0.9238795325112867385, 1.000000000000000000, 0.9238795325112867385, 1.000000000000000000, 0.9238795325112867385, 1.000000000000000000, 0.9238795325112867385, 1.000000000000000000, 0.9238795325112867385, 1.000000000000000000, 0.9238795325112867385, 1.000000000000000000, 0.9238795325112867385, 1.000000000000000000, 0.9238795325112867385, 1.000000000000000000, 0.9238795325112867385, 1.000000000000000000),
 ( 1.000000000000000000, 0.9238795325112867385, 1.000000000000000000, 0.9238795325112867385, 1.000000000000000000, 0.9238795325112867385, 1.000000000000000000, 0.9238795325112867385, 1.000000000000000000, 0.9238795325112867385, 1.000000000000000000, 0.9238795325112867385, 1.000000000000000000, 0.9238795325112867385, 1.000000000000000000, 0.9238795325112867385, 1.000000000000000000, 0.9238795325112867385, 1.000000000000000000, 0.9238795325112867385, 1.000000000000000000, 0.9238795325112867385, 1.000000000000000000, 0.9238795325112867385, 1.000000000000000000, 0.9238795325112867385, 1.000000000000000000, 0.9238795325112867385, 1.000000000000000000, 0.9238795325112867385, 1.000000000000000000, 0.9238795325112867385, 1.000000000000000000, 0.9238795325112867385, 1.000000000000000000, 0.9238795325112867385, 1.000000000000000000, 0.9238795325112867385, 1.000000000000000000, 0.9238795325112867385, 1.000000000000000000, 0.9238795325112867385, 1.000000000000000000, 0.9238795325112867385, 1.000000000000000000, 0.9238795325112867385, 1.000000000000000000, 0.9238795325112867385, 1.000000000000000000, 0.9238795325112867385, 1.000000000000000000, 0.9238795325112867385, 1.000000000000000000, 0.9238795325112867385, 1.000000000000000000, 0.9238795325112867385, 1.000000000000000000, 0.9238795325112867385, 1.000000000000000000, 0.9238795325112867385, 1.000000000000000000, 0.9238795325112867385, 1.000000000000000000, 0.9238795325112867385, 1.000000000000000000, 0.9238795325112867385, 1.000000000000000000, 0.9238795325112867385, 1.000000000000000000, 0.9238795325112867385, 1.000000000000000000, 0.9238795325112867385, 1.000000000000000000, 0.9238795325112867385, 1.000000000000000000, 0.9238795325112867385, 1.000000000000000000, 0.9238795325112867385, 1.000000000000000000, 0.9238795325112867385, 1.000000000000000000, 0.9238795325112867385, 1.000000000000000000, 0.9238795325112867385, 1.000000000000000000, 0.9238795325112867385, 1.000000000000000000, 0.9238795325112867385, 1.000000000000000000, 0.9238795325112867385, 1.000000000000000000, 0.9238795325112867385, 1.000000000000000000, 0.9238795325112867385, 1.000000000000000000, 0.9238795325112867385, 1.000000000000000000, 0.9238795325112867385, 1.000000000000000000, 0.9238795325112867385, 1.000000000000000000, 0.9238795325112867385, 1.000000000000000000, 0.9238795325112867385, 1.000000000000000000, 0.9238795325112867385, 1.000000000000000000, 0.9238795325112867385, 1.000000000000000000, 0.9238795325112867385, 1.000000000000000000, 0.9238795325112867385, 1.000000000000000000, 0.9238795325112867385, 1.000000000000000000, 0.9238795325112867385, 1.000000000000000000, 0.9238795325112867385, 1.000000000000000000, 0.9238795325112867385, 1.000000000000000000, 0.9238795325112867385, 1.000000000000000000, 0.9238795325112867385, 1.000000000000000000, 0.9238795325112867385, 1.000000000000000000, 0.9238795325112867385, 1.000000000000000000, 0.9238795325112867385, 1.000000000000000000, 0.9238795325112867385, 1.000000000000000000, 0.9238795325112867385, 1.000000000000000000, 0.9238795325112867385, 1.000000000000000000, 0.9238795325112867385, 1.000000000000000000, 0.9238795325112867385, 1.000000000000000000, 0.9238795325112867385, 1.000000000000000000, 0.9238795325112867385, 1.000000000000000000, 0.9238795325112867385, 1.000000000000000000, 0.9238795325112867385, 1.000000000000000000, 0.9238795325112867385, 1.000000000000000000, 0.9238795325112867385, 1.000000000000000000, 0.9238795325112867385, 1.000000000000000000, 0.9238795325112867385, 1.000000000000000000, 0.9238795325112867385, 1.000000000000000000, 0.9238795325112867385, 1.000000000000000000, 0.9238795325112867385, 1.000000000000000000, 0.9238795325112867385, 1.000000000000000000, 0.9238795325112867385, 1.000000000000000000, 0.9238795325112867385, 1.000000000000000000, 0.9238795325112867385, 1.000000000000000000, 0.9238795325112867385, 1.000000000000000000, 0.9238795325112867385, 1.000000000000000000, 0.9238795325112867385, 1.000000000000000000, 0.9238795325112867385, 1.000000000000000000, 0.9238795325112867385, 1.000000000000000000, 0.9238795325112867385, 1.000000000000000000, 0.9238795325112867385, 1.000000000000000000, 0.9238795325112867385, 1.000000000000000000, 0.9238795325112867385, 1.000000000000000000, 0.9238795325112867385, 1.000000000000000000, 0.9238795325112867385, 1.000000000000000000, 0.9238795325112867385, 1.000000000000000000, 0.9238795325112867385, 1.000000000000000000, 0.9238795325112867385, 1.000000000000000000, 0.9238795325112867385, 1.000000000000000000, 0.9238795325112867385, 1.000000000000000000, 0.9238795325112867385, 1.000000000000000000, 0.9238795325112867385, 1.000000000000000000, 0.9238795325112867385, 1.000000000000000000, 0.9238795325112867385, 1.000000000000000000, 0.9238795325112867385, 1.000000000000000000, 0.9238795325112867385, 1.000000000000000000, 0.9238795325112867385, 1.000000000000000000, 0.9238795325112867385, 1.000000000000000000, 0.9238795325112867385, 1.000000000000000000, 0.9238795325112867385, 1.000000000000000000, 0.9238795325112867385, 1.000000000000000000, 0.9238795325112867385, 1.000000000000000000, 0.9238795325112867385, 1.000000000000000000, 0.9238795325112867385, 1.000000000000000000, 0.9238795325112867385, 1.000000000000000000, 0.9238795325112867385, 1.000000000000000000, 0.9238795325112867385, 1.000000000000000000, 0.9238795325112867385, 1.000000000000000000, 0.9238795325112867385, 1.000000000000000000) ) ) 
 REPRESENTATION_ITEM ( '' )  SURFACE ( )  );
#20049 = CARTESIAN_POINT ( 'NONE',  ( -4.999999999999998224, 221.6666666666666856, -8.660254037844389075 ) ) ;
#20050 = EDGE_CURVE ( 'NONE', #33535, #31504, #17112, .T. ) ;
#20051 = CARTESIAN_POINT ( 'NONE',  ( 7.188101187499992051, 8.802885111219154394E-16, 5.611552781871753659 ) ) ;
#20052 = CARTESIAN_POINT ( 'NONE',  ( -8.311093377946841443, 199.2187499965860411, 8.311093377946830785 ) ) ;
#20053 = CARTESIAN_POINT ( 'NONE',  ( 4.541265875000002339, 8.312499998634407916, 0.000000000000000000 ) ) ;
#20054 = CARTESIAN_POINT ( 'NONE',  ( -8.000000000000000000, 99.59375000409679046, -3.313708498984761164 ) ) ;
#20056 = CARTESIAN_POINT ( 'NONE',  ( -2.849036369511732440E-14, 206.2500000000000284, 138.0000000000000568 ) ) ;
#20055 = DIRECTION ( 'NONE',  ( 1.000000000000000000, -3.552713678800500929E-15, 0.000000000000000000 ) ) ;
#20057 = ORIENTED_EDGE ( 'NONE', *, *, #39510, .T. ) ;
#20058 = CARTESIAN_POINT ( 'NONE',  ( 1.432654583217608080, 204.8750000013656063, 138.5412658750000503 ) ) ;
#20059 = CARTESIAN_POINT ( 'NONE',  ( -8.311093377946836114, 47.96874999658601268, -8.311093377946837890 ) ) ;
#20060 = CARTESIAN_POINT ( 'NONE',  ( -7.778174593052023411, 7.778174593052023411, 97.00000000409677625 ) ) ;
#20061 = FACE_OUTER_BOUND ( 'NONE', #7958, .T. ) ;
#20062 = CARTESIAN_POINT ( 'NONE',  ( -25.55430564589111953, 201.0625000013656063, 172.4456943541091505 ) ) ;
#20063 = FACE_OUTER_BOUND ( 'NONE', #19199, .T. ) ;
#20065 = LINE ( 'NONE', #42343, #43856 ) ;
#20064 = CARTESIAN_POINT ( 'NONE',  ( -7.188101187500000933, 122.5625000020483668, -2.977408999572650483 ) ) ;
#20066 = CARTESIAN_POINT ( 'NONE',  ( 10.99999999999989342, 4.556349186104152515, 87.34374999999998579 ) ) ;
#20067 = CARTESIAN_POINT ( 'NONE',  ( 5.676582343749993598, 124.9479166632526983, 9.832129032723422313 ) ) ;
#20068 = VECTOR ( 'NONE', #6023, 1000.000000000000000 ) ;
#20069 = CARTESIAN_POINT ( 'NONE',  ( -7.320508075688773708, 83.74999999317203958, -7.320508075688774596 ) ) ;
#20070 = ADVANCED_FACE ( 'NONE', ( #58796 ), #7106, .T. ) ;
#20071 = CARTESIAN_POINT ( 'NONE',  ( -2.977408999572650927, 90.87500000204838102, -7.188101187500001821 ) ) ;
#20072 = CARTESIAN_POINT ( 'NONE',  ( -3.211159895383561391, 20.81249999863440436, -3.211159895383561835 ) ) ;
#20073 = CARTESIAN_POINT ( 'NONE',  ( -4.076600168545496672E-14, -10.39230484541327471, -0.8038475772933779684 ) ) ;
#20074 = AXIS2_PLACEMENT_3D ( 'NONE', #17561, #12275, #40579 ) ;
#20075 = CARTESIAN_POINT ( 'NONE',  ( 7.999999999999992895, -3.313708498984756279, 1.486552779823364201 ) ) ;
#20076 = ORIENTED_EDGE ( 'NONE', *, *, #52505, .T. ) ;
#20077 = CARTESIAN_POINT ( 'NONE',  ( -30.99999999999992895, -31.99999999999978684, 135.0000000000000000 ) ) ;
#20079 = EDGE_CURVE ( 'NONE', #18054, #16151, #30114, .T. ) ;
#20078 = ORIENTED_EDGE ( 'NONE', *, *, #7139, .T. ) ;
#20080 =( BOUNDED_CURVE ( )  B_SPLINE_CURVE ( 2, ( #6083, #73994, #40777, #40413, #17014, #63785, #69082, #63043, #57779, #5711, #17388, #63410, #35138 ),
 .UNSPECIFIED., .F., .F. ) 
 B_SPLINE_CURVE_WITH_KNOTS ( ( 3, 2, 2, 2, 2, 2, 3 ),
 ( 0.5180902627193306742, 0.5233241472621503743, 0.5285580318049700743, 0.5337919163477896634, 0.5390258008906093634, 0.5442596854334290635, 0.5494935699762487635 ),
 .UNSPECIFIED. ) 
 CURVE ( )  GEOMETRIC_REPRESENTATION_ITEM ( )  RATIONAL_B_SPLINE_CURVE ( ( 1.000000000000308642, 0.9659258262887597812, 1.000000000000000000, 0.9659258262890683122, 1.000000000000000000, 0.9659258262890683122, 1.000000000000000000, 0.9659258262890683122, 1.000000000000000000, 0.9659258262890683122, 1.000000000000000000, 0.9659258262890683122, 1.000000000000000000 ) ) 
 REPRESENTATION_ITEM ( '' )  );
#20081 = CARTESIAN_POINT ( 'NONE',  ( -2.765530957081998586, 293.7968750017069510, 6.676582343750001591 ) ) ;
#20082 = CARTESIAN_POINT ( 'NONE',  ( -3.313708498984758943, -7.999999999999989342, 8.799052783920144449 ) ) ;
#20083 = CARTESIAN_POINT ( 'NONE',  ( -2.085542519210945728E-15, 164.5312499965860127, 11.35316468750000141 ) ) ;
#20084 = CARTESIAN_POINT ( 'NONE',  ( 6.123233995736767268E-16, 168.1249999931720538, -10.00000000000000178 ) ) ;
#20085 = CARTESIAN_POINT ( 'NONE',  ( 4.000000000000015987, 198.4375000000000568, 199.6568542494924259 ) ) ;
#20086 = CARTESIAN_POINT ( 'NONE',  ( -10.00000000000004619, 192.7083333333333428, 2.679491924311234730 ) ) ;
#20087 = CARTESIAN_POINT ( 'NONE',  ( 4.220049686691941027, -10.18810118749999738, 103.0000000020483668 ) ) ;
#20088 = VERTEX_POINT ( 'NONE', #1093 ) ;
#20089 = CARTESIAN_POINT ( 'NONE',  ( 2.775557561562891351E-14, -37.99999999999992184, 170.0000000000000284 ) ) ;
#20090 = CARTESIAN_POINT ( 'NONE',  ( 5.656854249492380582, 22.49999999590322375, -5.656854249492380582 ) ) ;
#20091 = CARTESIAN_POINT ( 'NONE',  ( 8.311093377946834337, 155.4687499965859843, 8.311093377946839666 ) ) ;
#20092 = CARTESIAN_POINT ( 'NONE',  ( 1.432654583217664479, 194.7500000013656063, 201.4587341250000065 ) ) ;
#20093 = CARTESIAN_POINT ( 'NONE',  ( -3.458734124999960358, 207.6250000013656063, 196.5673454167823877 ) ) ;
#20094 = CARTESIAN_POINT ( 'NONE',  ( -6.238412754330611322E-16, 10.18810118749999916, 72.15625000204836681 ) ) ;
#20095 = CARTESIAN_POINT ( 'NONE',  ( -8.311093377946841443, 69.21874999658602690, 8.311093377946830785 ) ) ;
#20096 = ORIENTED_EDGE ( 'NONE', *, *, #16399, .T. ) ;
#20097 = CARTESIAN_POINT ( 'NONE',  ( -10.18810118749999916, 4.220049686691934809, 117.0625000020483668 ) ) ;
#20098 = CARTESIAN_POINT ( 'NONE',  ( 2.780723358947928197E-16, 10.68749999863440792, -4.541265875000002339 ) ) ;
#20099 = CARTESIAN_POINT ( 'NONE',  ( -3.317071493978880348, -8.008118988124989457, 10.29436528394063011 ) ) ;
#20100 = VERTEX_POINT ( 'NONE', #64450 ) ;
#20101 = AXIS2_PLACEMENT_3D ( 'NONE', #13359, #6987, #18305 ) ;
#20102 = EDGE_CURVE ( 'NONE', #5945, #17476, #47213, .T. ) ;
#20103 = CARTESIAN_POINT ( 'NONE',  ( 7.188101187500000044, 19.96874999795161543, 0.000000000000000000 ) ) ;
#20104 = CARTESIAN_POINT ( 'NONE',  ( -4.242640687119285658, 289.1875000034139589, 4.242640687119287435 ) ) ;
#20105 = CARTESIAN_POINT ( 'NONE',  ( -12.18025451098408318, 1.885907279315492735, 0.7279601535489274022 ) ) ;
#20106 = CARTESIAN_POINT ( 'NONE',  ( 13.99999999999999822, 2.249999999994893862, 10.23492587299426404 ) ) ;
#20107 = CARTESIAN_POINT ( 'NONE',  ( -2.977408999572654480, 10.87499999795161187, 7.188101187499999156 ) ) ;
#20108 = CARTESIAN_POINT ( 'NONE',  ( -4.401442555609577197E-16, 7.188101187499992051, 1.111552781871753215 ) ) ;
#20109 = ADVANCED_FACE ( 'NONE', ( #17300 ), #64129, .T. ) ;
#20110 = CARTESIAN_POINT ( 'NONE',  ( 10.18810118749999916, 4.220049686691935698, 113.8750000020483668 ) ) ;
#20111 = EDGE_CURVE ( 'NONE', #6054, #58407, #65227, .T. ) ;
#20112 = DIRECTION ( 'NONE',  ( 0.000000000000000000, 0.000000000000000000, -1.000000000000000000 ) ) ;
#20113 = CARTESIAN_POINT ( 'NONE',  ( 4.000000000000000888, 5.687499997268812280, 1.656854249492384135 ) ) ;
#20114 = ORIENTED_EDGE ( 'NONE', *, *, #60670, .T. ) ;
#20115 = CARTESIAN_POINT ( 'NONE',  ( 3.458734125000015425, 205.9375000013656063, 198.0000000000000284 ) ) ;
#20116 = CARTESIAN_POINT ( 'NONE',  ( -32.00000000000002842, 197.3125000027312126, 168.3431457505080573 ) ) ;
#20117 = AXIS2_PLACEMENT_3D ( 'NONE', #30620, #19289, #64589 ) ;
#20118 = CARTESIAN_POINT ( 'NONE',  ( 1.881053915767121776, 4.499999998634407028, -4.541265875000002339 ) ) ;
#20119 = CARTESIAN_POINT ( 'NONE',  ( 1.320432766682874540E-15, 111.0312500020483810, 7.188101187500000044 ) ) ;
#20120 = CARTESIAN_POINT ( 'NONE',  ( -2.775557561562891351E-14, 210.0000000000000284, 142.0000000000000568 ) ) ;
#20121 = CARTESIAN_POINT ( 'NONE',  ( -5.082755093536317936, -5.082755093536320601, 22.67405278187175455 ) ) ;
#20122 = ORIENTED_EDGE ( 'NONE', *, *, #1616, .F. ) ;
#20123 = CARTESIAN_POINT ( 'NONE',  ( -2.828427124746192067, 21.62500000000000355, 2.828427124746190735 ) ) ;
#20124 = ORIENTED_EDGE ( 'NONE', *, *, #14070, .F. ) ;
#20125 = CARTESIAN_POINT ( 'NONE',  ( -10.18810118749999738, -4.220049686691941915, 115.7500000020483810 ) ) ;
#20126 = CARTESIAN_POINT ( 'NONE',  ( -10.49999999999998224, 0.000000000000000000, 118.0000000000000000 ) ) ;
#20127 = CARTESIAN_POINT ( 'NONE',  ( 6.000000000000003553, 296.5625000000000000, -2.485281374238571761 ) ) ;
#20128 = CARTESIAN_POINT ( 'NONE',  ( 24.54126587499998280, 203.1250000013656347, 168.5673454167822740 ) ) ;
#20129 = CARTESIAN_POINT ( 'NONE',  ( -7.320508075688773708, 71.87500000000001421, -7.320508075688774596 ) ) ;
#20130 = CARTESIAN_POINT ( 'NONE',  ( -5.082755093536325930, 95.84375000204838102, -5.082755093536325930 ) ) ;
#20131 = CARTESIAN_POINT ( 'NONE',  ( -2.485281374238571761, 294.8124999999999432, -6.000000000000003553 ) ) ;
#20133 = CARTESIAN_POINT ( 'NONE',  ( -6.735557395310442023E-16, 11.00000000000000000, 113.3125000040967763 ) ) ;
#20132 = DIRECTION ( 'NONE',  ( -0.000000000000000000, 1.000000000000000000, -1.563033456626094573E-30 ) ) ;
#20134 = ORIENTED_EDGE ( 'NONE', *, *, #45783, .F. ) ;
#20135 = CARTESIAN_POINT ( 'NONE',  ( 9.832129032723416984, 231.8229166700806445, -5.676582343750003368 ) ) ;
#20136 = DIRECTION ( 'NONE',  ( -1.000000000000000000, 0.000000000000000000, 0.000000000000000000 ) ) ;
#20137 = CARTESIAN_POINT ( 'NONE',  ( 2.828427124746153876, 200.0000000027312126, 144.8284271247462129 ) ) ;
#20138 = FACE_OUTER_BOUND ( 'NONE', #48314, .T. ) ;
#20139 = CARTESIAN_POINT ( 'NONE',  ( -4.898587196589407898E-16, 7.999999999999991118, 2.142802783920143117 ) ) ;
#20140 = CARTESIAN_POINT ( 'NONE',  ( 10.00000000000000000, 252.5000000000000000, -1.224646799147353256E-15 ) ) ;
#20141 = CARTESIAN_POINT ( 'NONE',  ( -50.99999999999994316, -31.99999999999978684, 205.0000000000000284 ) ) ;
#20142 = CARTESIAN_POINT ( 'NONE',  ( 10.00000000000000178, 185.0000000000000284, 0.000000000000000000 ) ) ;
#20143 = CARTESIAN_POINT ( 'NONE',  ( 1.836970198721029589E-15, 239.3750000068279746, 10.00000000000000000 ) ) ;
#20144 = CARTESIAN_POINT ( 'NONE',  ( 2.977408999572650927, -7.188101187499990274, 23.33030278187175455 ) ) ;
#20145 = CARTESIAN_POINT ( 'NONE',  ( -5.676582343749998039, 157.7604166632526983, -9.832129032723420536 ) ) ;
#20146 = FACE_OUTER_BOUND ( 'NONE', #8167, .T. ) ;
#20147 = CARTESIAN_POINT ( 'NONE',  ( -4.999999999999999112, 52.85372778481288947, 48.38359481482947899 ) ) ;
#20150 = CARTESIAN_POINT ( 'NONE',  ( 23.99999999999997868, 203.8125000000000000, 171.6568542494922553 ) ) ;
#20149 = CARTESIAN_POINT ( 'NONE',  ( -2.828427124746209831, 202.5000000027312126, 139.1715728752538723 ) ) ;
#20148 = CARTESIAN_POINT ( 'NONE',  ( 23.99999999999997868, 200.8125000000000284, 171.6568542494922553 ) ) ;
#20151 = ORIENTED_EDGE ( 'NONE', *, *, #72166, .F. ) ;
#20152 = CARTESIAN_POINT ( 'NONE',  ( 8.311093377946834337, 10.46874999658601624, 8.311093377946839666 ) ) ;
#20153 = CARTESIAN_POINT ( 'NONE',  ( 5.086519500874520539, -10.26068667857087391, -64.41585657734346171 ) ) ;
#20154 = CARTESIAN_POINT ( 'NONE',  ( -3.999999999999959144, 196.1875000027312126, 199.6568542494924259 ) ) ;
#20155 = CARTESIAN_POINT ( 'NONE',  ( 3.458734124999958581, 207.5000000013656063, 140.5673454167823593 ) ) ;
#20156 = VECTOR ( 'NONE', #4770, 1000.000000000000000 ) ;
#20157 = CARTESIAN_POINT ( 'NONE',  ( 2.679491924311222739, 50.83333332650537528, 10.00000000000000355 ) ) ;
#20158 = CARTESIAN_POINT ( 'NONE',  ( -2.977408999572650927, 110.3750000020484094, -7.188101187500001821 ) ) ;
#20159 = CARTESIAN_POINT ( 'NONE',  ( -4.541265875000003227, 4.999999998634406140, 1.881053915767121110 ) ) ;
#20160 = CARTESIAN_POINT ( 'NONE',  ( 7.999999999999991118, 1.639585202047151108E-05, 13.76780324778446385 ) ) ;
#20161 = CARTESIAN_POINT ( 'NONE',  ( 3.313708498984762496, -7.999999999999989342, 7.299052779823365533 ) ) ;
#20163 = CYLINDRICAL_SURFACE ( 'NONE', #61892, 6.000000000000001776 ) ;
#20162 = DIRECTION ( 'NONE',  ( -0.000000000000000000, -0.000000000000000000, -1.000000000000000000 ) ) ;
#20164 = VERTEX_POINT ( 'NONE', #68992 ) ;
#20165 = LINE ( 'NONE', #43182, #26788 ) ;
#20166 = CARTESIAN_POINT ( 'NONE',  ( -7.999999999999991118, 0.000000000000000000, 2.330302779823365089 ) ) ;
#20167 = CARTESIAN_POINT ( 'NONE',  ( 8.311093377946834337, 237.3437500034139589, -8.311093377946836114 ) ) ;
#20168 = CARTESIAN_POINT ( 'NONE',  ( -3.042071309553173730, 134.3229166632526983, 11.35316468749999785 ) ) ;
#20169 = EDGE_LOOP ( 'NONE', ( #27135, #53648, #60598, #38125 ) ) ;
#20170 = DIRECTION ( 'NONE',  ( 0.000000000000000000, 0.000000000000000000, 1.000000000000000000 ) ) ;
#20171 = CARTESIAN_POINT ( 'NONE',  ( 7.204075437095966983, 7.204075437095967871, 97.09375000204836681 ) ) ;
#20172 = DIRECTION ( 'NONE',  ( -1.000000000000000000, 0.000000000000000000, -0.000000000000000000 ) ) ;
#20173 = CARTESIAN_POINT ( 'NONE',  ( -2.445694354108783219, 195.8125000013656063, 200.4456943541088663 ) ) ;
#20175 = CARTESIAN_POINT ( 'NONE',  ( 3.042071309553167513, 126.8229166632526841, -11.35316468749999785 ) ) ;
#20174 = CARTESIAN_POINT ( 'NONE',  ( 1.921951731159528443, 219.9999999999999432, 10.68631426227777226 ) ) ;
#20176 = CARTESIAN_POINT ( 'NONE',  ( -31.99999999999998579, 207.3125000000000284, 171.6568542494928238 ) ) ;
#20177 = EDGE_LOOP ( 'NONE', ( #22239, #7089, #70151, #58515 ) ) ;
#20178 =( BOUNDED_CURVE ( )  B_SPLINE_CURVE ( 2, ( #14832, #15583, #27278, #67284, #9578, #71805, #20123, #20493, #15212 ),
 .UNSPECIFIED., .F., .F. ) 
 B_SPLINE_CURVE_WITH_KNOTS ( ( 3, 2, 2, 2, 3 ),
 ( 0.9659090909090909394, 0.9715909090909090606, 0.9772727272727272929, 0.9829545454545454142, 0.9886363636363636465 ),
 .UNSPECIFIED. ) 
 CURVE ( )  GEOMETRIC_REPRESENTATION_ITEM ( )  RATIONAL_B_SPLINE_CURVE ( ( 1.000000000000000000, 0.9238795325112867385, 1.000000000000000000, 0.9238795325112867385, 1.000000000000000000, 0.9238795325112867385, 1.000000000000000000, 0.9238795325112867385, 1.000000000000000000 ) ) 
 REPRESENTATION_ITEM ( '' )  );
#20179 = AXIS2_PLACEMENT_3D ( 'NONE', #69916, #64247, #13282 ) ;
#20180 = CARTESIAN_POINT ( 'NONE',  ( -4.898587196589412829E-16, 109.6250000000000000, -8.000000000000000000 ) ) ;
#20181 = CARTESIAN_POINT ( 'NONE',  ( -2.775557561562891351E-14, 210.0000000000000284, 142.0000000000000568 ) ) ;
#20182 = CARTESIAN_POINT ( 'NONE',  ( -11.35316468750000141, 103.8020833299193413, 3.042071309553159963 ) ) ;
#20183 = CARTESIAN_POINT ( 'NONE',  ( 1.432654583217664479, 206.7500000013655779, 201.4587341250000065 ) ) ;
#20184 = CARTESIAN_POINT ( 'NONE',  ( 7.188101187499999156, 20.24999999795161898, 2.977408999572654924 ) ) ;
#20185 = CARTESIAN_POINT ( 'NONE',  ( 10.18810118749999916, 4.220049686691935698, 86.87500000204836681 ) ) ;
#20186 = CARTESIAN_POINT ( 'NONE',  ( -8.311093377946841443, 29.21874999658601979, 8.311093377946830785 ) ) ;
#20187 = VERTEX_POINT ( 'NONE', #64077 ) ;
#20188 = CARTESIAN_POINT ( 'NONE',  ( 0.000000000000000000, 0.000000000000000000, -4.000000000000001776 ) ) ;
#20189 = CARTESIAN_POINT ( 'NONE',  ( 5.662595241051936235, -5.662595241051934458, 25.57561528394063544 ) ) ;
#20190 = CARTESIAN_POINT ( 'NONE',  ( -54.00000000000000000, 272.0000000000000000, 4.085831468968145267E-14 ) ) ;
#20191 = LINE ( 'NONE', #42098, #13324 ) ;
#20192 = CARTESIAN_POINT ( 'NONE',  ( -7.188101187500001821, 1.124999997951610098, -2.977408999572651371 ) ) ;
#20193 = CARTESIAN_POINT ( 'NONE',  ( -4.088227598258586603E-16, 289.2031250017069510, -6.676582343750001591 ) ) ;
#20194 = DIRECTION ( 'NONE',  ( 0.000000000000000000, 0.000000000000000000, -1.000000000000000000 ) ) ;
#20195 = CARTESIAN_POINT ( 'NONE',  ( 11.35316468749999963, 216.3020833299193555, -3.042071309553165293 ) ) ;
#20196 = EDGE_CURVE ( 'NONE', #53701, #23527, #18423, .T. ) ;
#20197 = ORIENTED_EDGE ( 'NONE', *, *, #10166, .F. ) ;
#20198 = CARTESIAN_POINT ( 'NONE',  ( 8.311093377946837890, 146.7187499965860411, -8.311093377946837890 ) ) ;
#20199 = CARTESIAN_POINT ( 'NONE',  ( 10.18810118750000093, -4.220049686691933921, 81.81250000204838102 ) ) ;
#20200 = CARTESIAN_POINT ( 'NONE',  ( -28.00000000000002132, 198.4375000013655779, 166.5412658750003629 ) ) ;
#20201 = ADVANCED_FACE ( 'NONE', ( #35053 ), #63693, .T. ) ;
#20202 = CARTESIAN_POINT ( 'NONE',  ( -4.000000000000016875, 198.4375000000000568, 140.3431457505076594 ) ) ;
#20203 = CARTESIAN_POINT ( 'NONE',  ( 1.881053915767122664, 12.24999999863440969, 4.541265875000001451 ) ) ;
#20204 = VERTEX_POINT ( 'NONE', #12386 ) ;
#20205 = B_SPLINE_CURVE_WITH_KNOTS ( 'NONE', 3,
 ( #71437, #8084, #37129, #1339, #19766, #12990, #69990, #47691, #64322, #42775, #53745, #70713, #13718, #31086, #60132, #36763, #48066, #31471, #972, #54115, #13353, #42038, #18671, #41314, #70359, #25420, #36391, #12627, #35658, #59406, #23953, #7721, #59044, #46961, #29989, #30725, #2426, #58672 ),
 .UNSPECIFIED., .F., .F.,
 ( 4, 2, 2, 2, 2, 2, 2, 2, 2, 2, 2, 2, 2, 2, 2, 2, 2, 2, 4 ),
 ( 0.06608201874815884669, 0.06983915675683202706, 0.07171772576116866582, 0.07359629476550530458, 0.07735343277417856822, 0.07923200177851524861, 0.08111057078285191513, 0.08298913978718858164, 0.08392842428935692878, 0.08486770879152527591, 0.08674627779586201182, 0.08768556229803037283, 0.08862484680019871996, 0.09050341580453541424, 0.09144270030670376137, 0.09238198480887212238, 0.09426055381320884441, 0.09519983831537720542, 0.09613912281754555256 ),
 .UNSPECIFIED. ) ;
#20206 = CARTESIAN_POINT ( 'NONE',  ( 1.656854249492405451, 201.4375000027311842, 202.0000000000000284 ) ) ;
#20207 = VECTOR ( 'NONE', #63162, 1000.000000000000000 ) ;
#20208 = CARTESIAN_POINT ( 'NONE',  ( -3.458734125000016757, 199.1250000013656347, 140.5673454167824161 ) ) ;
#20209 = CARTESIAN_POINT ( 'NONE',  ( -2.828427124746209831, 202.5000000027312126, 139.1715728752538723 ) ) ;
#20210 = CARTESIAN_POINT ( 'NONE',  ( -4.999999999999999112, 10.28276986844631935, 65.17752827135416283 ) ) ;
#20211 = ORIENTED_EDGE ( 'NONE', *, *, #44227, .T. ) ;
#20212 = CARTESIAN_POINT ( 'NONE',  ( -5.082755093536325042, 5.531249997951610986, -5.082755093536325930 ) ) ;
#20213 = CARTESIAN_POINT ( 'NONE',  ( -1.656854249492432318, 208.6875000000000000, 146.0000000000000284 ) ) ;
#20214 = CARTESIAN_POINT ( 'NONE',  ( 1.656854249492381914, 19.81250000000000000, 4.000000000000000888 ) ) ;
#20215 = CARTESIAN_POINT ( 'NONE',  ( 11.35316468749999963, 190.9895833299193271, -3.042071309553165293 ) ) ;
#20216 = VECTOR ( 'NONE', #41074, 1000.000000000000000 ) ;
#20217 = CARTESIAN_POINT ( 'NONE',  ( -7.188101187500001821, 112.4375000020483810, -2.977408999572650483 ) ) ;
#20218 = CARTESIAN_POINT ( 'NONE',  ( 37.94562015984923420, 38.00000000000001421, 127.0000000000000000 ) ) ;
#20219 = CARTESIAN_POINT ( 'NONE',  ( -6.676582343749999815, 292.5156250017070079, 2.765530957082001251 ) ) ;
#20221 = DIRECTION ( 'NONE',  ( -0.000000000000000000, -0.000000000000000000, 1.000000000000000000 ) ) ;
#20220 = CARTESIAN_POINT ( 'NONE',  ( -30.82842712474621649, 209.1250000000000284, 167.1715728752542134 ) ) ;
#20222 = ORIENTED_EDGE ( 'NONE', *, *, #22513, .F. ) ;
#20223 = AXIS2_PLACEMENT_3D ( 'NONE', #26194, #31006, #53296 ) ;
#20224 = CARTESIAN_POINT ( 'NONE',  ( 3.042071309553173286, 230.6770833367473585, 11.35316468749999608 ) ) ;
#20225 = CARTESIAN_POINT ( 'NONE',  ( -7.188101187499992051, 0.000000000000000000, 2.986552781871751439 ) ) ;
#20226 = CARTESIAN_POINT ( 'NONE',  ( 0.000000000000000000, 0.000000000000000000, 0.000000000000000000 ) ) ;
#20227 = CYLINDRICAL_SURFACE ( 'NONE', #58692, 7.999999999999991118 ) ;
#20228 = CARTESIAN_POINT ( 'NONE',  ( 2.445694354108840063, 198.0625000013656063, 200.4456943541088663 ) ) ;
#20229 = EDGE_LOOP ( 'NONE', ( #32381, #26182, #19944, #21706 ) ) ;
#20230 = DIRECTION ( 'NONE',  ( -0.000000000000000000, -1.000000000000000000, -0.000000000000000000 ) ) ;
#20231 = CARTESIAN_POINT ( 'NONE',  ( 3.313708498984765161, 92.46874999999998579, 7.999999999999998224 ) ) ;
#20232 = CARTESIAN_POINT ( 'NONE',  ( -5.676582343749998039, 117.7604166632526841, -9.832129032723420536 ) ) ;
#20233 = CARTESIAN_POINT ( 'NONE',  ( 0.000000000000000000, 125.0000000000000000, 0.000000000000000000 ) ) ;
#20234 = CARTESIAN_POINT ( 'NONE',  ( -11.00000000000000000, 4.556349186104045934, 77.40624999999997158 ) ) ;
#20237 = DIRECTION ( 'NONE',  ( 1.000000000000000000, 0.000000000000000000, 0.000000000000000000 ) ) ;
#20236 = CARTESIAN_POINT ( 'NONE',  ( 31.45873412499997812, 199.7500000013656063, 168.5673454167822172 ) ) ;
#20235 = CARTESIAN_POINT ( 'NONE',  ( 30.44569435410879166, 198.8125000013656063, 172.4456943541087526 ) ) ;
#20238 = ORIENTED_EDGE ( 'NONE', *, *, #29592, .F. ) ;
#20239 = CARTESIAN_POINT ( 'NONE',  ( 0.000000000000000000, 0.000000000000000000, 0.000000000000000000 ) ) ;
#20240 = CARTESIAN_POINT ( 'NONE',  ( -11.00000000000000000, 0.000000000000000000, 113.6875000040967763 ) ) ;
#20241 = CARTESIAN_POINT ( 'NONE',  ( -3.458734125000015425, 199.9375000013656063, 142.0000000000000568 ) ) ;
#20242 = CARTESIAN_POINT ( 'NONE',  ( 30.44569435410879166, 201.8125000013656063, 172.4456943541087526 ) ) ;
#20243 = CARTESIAN_POINT ( 'NONE',  ( 4.401442555609581635E-16, 26.71874999795161543, -7.188101187500000044 ) ) ;
#20244 = CARTESIAN_POINT ( 'NONE',  ( 11.35316468749999785, 190.8854166632526983, 3.042071309553174174 ) ) ;
#20245 = CARTESIAN_POINT ( 'NONE',  ( 2.977408999572654480, 90.50000000204839523, 7.188101187499999156 ) ) ;
#20246 = FACE_OUTER_BOUND ( 'NONE', #14917, .T. ) ;
#20247 = CARTESIAN_POINT ( 'NONE',  ( -1.881053915767124440, 13.99999999863440792, 4.541265875000001451 ) ) ;
#20248 = CARTESIAN_POINT ( 'NONE',  ( 24.54126587500000412, 200.3750000013656063, 168.5673454167822172 ) ) ;
#20249 = CARTESIAN_POINT ( 'NONE',  ( 3.313708498984756279, 7.999999999999991118, 28.86155277982336642 ) ) ;
#20250 = CYLINDRICAL_SURFACE ( 'NONE', #43557, 10.00000000000000178 ) ;
#20251 = CARTESIAN_POINT ( 'NONE',  ( -5.676582343749998039, 77.44791666325269830, -9.832129032723420536 ) ) ;
#20252 = VERTEX_POINT ( 'NONE', #13111 ) ;
#20253 = DIRECTION ( 'NONE',  ( 0.000000000000000000, 0.000000000000000000, 1.000000000000000000 ) ) ;
#20254 = CARTESIAN_POINT ( 'NONE',  ( 2.696524195522682164E-11, 156.2499999999978968, -10.00000000000000178 ) ) ;
#20255 = CARTESIAN_POINT ( 'NONE',  ( 1.469576158976823947E-15, 109.0625000040967905, 8.000000000000000000 ) ) ;
#20256 = CARTESIAN_POINT ( 'NONE',  ( 3.042071309553167069, 86.82291666325265567, -11.35316468749999785 ) ) ;
#20257 = ORIENTED_EDGE ( 'NONE', *, *, #7035, .F. ) ;
#20258 = CARTESIAN_POINT ( 'NONE',  ( 10.18810118750000093, -4.220049686691933921, 88.18750000204838102 ) ) ;
#20259 = CARTESIAN_POINT ( 'NONE',  ( -4.220049686691937474, -10.18810118749999738, 114.4375000020483668 ) ) ;
#20260 = CARTESIAN_POINT ( 'NONE',  ( 11.35316468750000141, 0.7812499965860163487, 0.000000000000000000 ) ) ;
#20261 = FACE_OUTER_BOUND ( 'NONE', #70560, .T. ) ;
#20263 = CARTESIAN_POINT ( 'NONE',  ( 3.042071309553167513, 71.82291666325268409, -11.35316468749999785 ) ) ;
#20262 = LINE ( 'NONE', #43286, #43638 ) ;
#20264 = CARTESIAN_POINT ( 'NONE',  ( 5.656854249492376141, -5.656854249492374365, 19.58030278392014978 ) ) ;
#20265 = CARTESIAN_POINT ( 'NONE',  ( 7.320508075688771044, 129.3750000000000284, 7.320508075688775484 ) ) ;
#20266 = EDGE_CURVE ( 'NONE', #57466, #71522, #26714, .T. ) ;
#20267 = EDGE_CURVE ( 'NONE', #42156, #39904, #42552, .T. ) ;
#20268 = CARTESIAN_POINT ( 'NONE',  ( -4.999999999999998224, 173.5416666598387110, -8.660254037844389075 ) ) ;
#20269 = CARTESIAN_POINT ( 'NONE',  ( -7.188101187500000044, 90.03125000204838102, 0.000000000000000000 ) ) ;
#20270 = VECTOR ( 'NONE', #72003, 1000.000000000000000 ) ;
#20271 = CARTESIAN_POINT ( 'NONE',  ( 18.00000000000000000, 10.39230484541325161, -21.50000000000000000 ) ) ;
#20272 = CARTESIAN_POINT ( 'NONE',  ( 3.042071309553159519, 65.05208332991934128, 11.35316468750000141 ) ) ;
#20273 = CARTESIAN_POINT ( 'NONE',  ( 6.676582343750004256, 294.8906250017069510, 2.765530957081995478 ) ) ;
#20274 = CARTESIAN_POINT ( 'NONE',  ( 4.220049686691934809, 10.18810118749999916, 109.5625000020483810 ) ) ;
#20275 = CARTESIAN_POINT ( 'NONE',  ( -3.042071309553164404, 207.2395833299193555, -11.35316468749999963 ) ) ;
#20276 = ORIENTED_EDGE ( 'NONE', *, *, #59688, .T. ) ;
#20277 = CARTESIAN_POINT ( 'NONE',  ( 2.828427124746152987, 203.1250000000000284, 139.1715728752538723 ) ) ;
#20278 = LINE ( 'NONE', #43301, #58138 ) ;
#20279 = CARTESIAN_POINT ( 'NONE',  ( -4.193070328474950870, 50.40098303874115260, 40.95513628906723369 ) ) ;
#20281 = CARTESIAN_POINT ( 'NONE',  ( -5.676582343750006032, 194.1145833299193839, 9.832129032723418760 ) ) ;
#20280 = CARTESIAN_POINT ( 'NONE',  ( -4.000000000000002665, 19.56250000000000000, 1.656854249492380582 ) ) ;
#20282 = CARTESIAN_POINT ( 'NONE',  ( 26.34314575050746754, 195.9375000000000000, 173.9999999999998010 ) ) ;
#20283 = VECTOR ( 'NONE', #47886, 1000.000000000000000 ) ;
#20284 = CARTESIAN_POINT ( 'NONE',  ( 10.00000000000000178, 235.4166666734946602, 2.679491924311222739 ) ) ;
#20285 = CARTESIAN_POINT ( 'NONE',  ( -2.679491924311337314, 252.0833333401613174, -9.999999999999936051 ) ) ;
#20286 = ORIENTED_EDGE ( 'NONE', *, *, #62906, .T. ) ;
#20287 = CARTESIAN_POINT ( 'NONE',  ( -9.832129032723418760, 183.1770833299193555, -5.676582343750004256 ) ) ;
#20288 = VECTOR ( 'NONE', #14008, 1000.000000000000000 ) ;
#20289 = CARTESIAN_POINT ( 'NONE',  ( -2.977408999572647819, -7.188101187499990274, 19.76780278187175455 ) ) ;
#20290 =( BOUNDED_CURVE ( )  B_SPLINE_CURVE ( 2, ( #18994, #48026, #48398, #29584, #18634, #8044, #18260, #35620, #12951 ),
 .UNSPECIFIED., .F., .F. ) 
 B_SPLINE_CURVE_WITH_KNOTS ( ( 3, 2, 2, 2, 3 ),
 ( 0.7291666666666649643, 0.7395833333333317050, 0.7499999999999983347, 0.7604166666666649643, 0.7708333333333317050 ),
 .UNSPECIFIED. ) 
 CURVE ( )  GEOMETRIC_REPRESENTATION_ITEM ( )  RATIONAL_B_SPLINE_CURVE ( ( 1.000000000000012212, 0.9238795325112745260, 1.000000000000000000, 0.9238795325112867385, 1.000000000000000000, 0.9238795325112867385, 1.000000000000000000, 0.9238795325112989509, 0.9999999999999877875 ) ) 
 REPRESENTATION_ITEM ( '' )  );
#20291 = CARTESIAN_POINT ( 'NONE',  ( -8.660254037844381969, 92.08333333333332860, -5.000000000000000888 ) ) ;
#20292 =( BOUNDED_CURVE ( )  B_SPLINE_CURVE ( 2, ( #51975, #23668, #40276, #57268, #35380, #58026, #22536, #63276, #5954 ),
 .UNSPECIFIED., .F., .F. ) 
 B_SPLINE_CURVE_WITH_KNOTS ( ( 3, 2, 2, 2, 3 ),
 ( 0.2916666666666666297, 0.2986111111111110494, 0.3055555555555555247, 0.3124999999999999445, 0.3194444444444443643 ),
 .UNSPECIFIED. ) 
 CURVE ( )  GEOMETRIC_REPRESENTATION_ITEM ( )  RATIONAL_B_SPLINE_CURVE ( ( 1.000000000000000666, 0.9238795325112861834, 1.000000000000000000, 0.9238795325112867385, 1.000000000000000000, 0.9238795325112867385, 1.000000000000000000, 0.9238795325112872936, 0.9999999999999994449 ) ) 
 REPRESENTATION_ITEM ( '' )  );
#20293 = ORIENTED_EDGE ( 'NONE', *, *, #67828, .F. ) ;
#20294 = EDGE_CURVE ( 'NONE', #19065, #22196, #3298, .T. ) ;
#20295 = CARTESIAN_POINT ( 'NONE',  ( -8.000000000000000000, 99.59375000409679046, -3.313708498984761608 ) ) ;
#20296 = DIRECTION ( 'NONE',  ( -0.000000000000000000, 1.000000000000000000, -0.000000000000000000 ) ) ;
#20297 = CARTESIAN_POINT ( 'NONE',  ( 2.828427124746190291, 15.87500000000000000, 2.828427124746192067 ) ) ;
#20298 = CARTESIAN_POINT ( 'NONE',  ( -1.881053915767121776, 14.62499999863440969, -4.541265875000002339 ) ) ;
#20299 = CARTESIAN_POINT ( 'NONE',  ( -7.999999999999989342, -3.313708498984762496, 16.11155278392014267 ) ) ;
#20300 = LINE ( 'NONE', #61053, #6544 ) ;
#20301 = EDGE_LOOP ( 'NONE', ( #71321, #21621, #4820, #60507 ) ) ;
#20302 = CARTESIAN_POINT ( 'NONE',  ( 11.00000000000000000, 1.347111479062088405E-15, 72.24999999999998579 ) ) ;
#20303 = CARTESIAN_POINT ( 'NONE',  ( -5.082755093536325930, 92.46875000204838102, -5.082755093536325930 ) ) ;
#20305 = CARTESIAN_POINT ( 'NONE',  ( 11.35316468749999963, 256.1979166700806445, 3.042071309553159519 ) ) ;
#20304 = CARTESIAN_POINT ( 'NONE',  ( -10.00000000000011724, 82.50000000000007105, -1.224646799147367456E-15 ) ) ;
#20306 = DIRECTION ( 'NONE',  ( 0.2541423529692226624, 0.9671668234732140323, 0.000000000000000000 ) ) ;
#20307 = B_SPLINE_CURVE_WITH_KNOTS ( 'NONE', 3,
 ( #12205, #59991, #65648, #7944, #71301, #37358 ),
 .UNSPECIFIED., .F., .F.,
 ( 4, 2, 4 ),
 ( 2.380730968267134156E-07, 0.002629065763328368270, 0.005257893453559909711 ),
 .UNSPECIFIED. ) ;
#20308 = ORIENTED_EDGE ( 'NONE', *, *, #8504, .F. ) ;
#20310 = CARTESIAN_POINT ( 'NONE',  ( -6.951808397369817780E-16, 262.9687500034140157, -11.35316468749999963 ) ) ;
#20309 = VECTOR ( 'NONE', #20730, 1000.000000000000000 ) ;
#20311 = CARTESIAN_POINT ( 'NONE',  ( -7.188101187499991163, 2.977408999572646930, 17.89280278187175455 ) ) ;
#20312 = ORIENTED_EDGE ( 'NONE', *, *, #58745, .T. ) ;
#20313 = VERTEX_POINT ( 'NONE', #71196 ) ;
#20314 = CARTESIAN_POINT ( 'NONE',  ( 10.18810118749999916, 4.220049686691935698, 79.00000000204838102 ) ) ;
#20315 = CARTESIAN_POINT ( 'NONE',  ( 9.832129032723416984, 70.67708332991935549, 5.676582343750006032 ) ) ;
#20316 = CARTESIAN_POINT ( 'NONE',  ( -3.313708498984759387, -7.999999999999989342, 5.799052783920146226 ) ) ;
#20317 = CARTESIAN_POINT ( 'NONE',  ( -11.00000000000000000, 0.000000000000000000, 92.49999999999998579 ) ) ;
#20320 = CARTESIAN_POINT ( 'NONE',  ( -2.765530957081996810, 294.4218750017069510, -6.676582343750002480 ) ) ;
#20319 = CARTESIAN_POINT ( 'NONE',  ( 26.34314575050758478, 195.6875000027312126, 165.9999999999998863 ) ) ;
#20318 = LINE ( 'NONE', #49755, #52810 ) ;
#20321 = CARTESIAN_POINT ( 'NONE',  ( 2.679491924311228956, 146.0416666666666288, -10.00000000000000000 ) ) ;
#20322 = AXIS2_PLACEMENT_3D ( 'NONE', #22613, #45634, #35811 ) ;
#20323 = CARTESIAN_POINT ( 'NONE',  ( 7.778174593052023411, -7.778174593052021635, 84.06249999999998579 ) ) ;
#20324 = CARTESIAN_POINT ( 'NONE',  ( 27.99999999999997158, 209.0000000000000284, 173.9999999999999147 ) ) ;
#20325 = CARTESIAN_POINT ( 'NONE',  ( 3.458734125000015869, 198.1875000013655779, 198.0000000000000284 ) ) ;
#20326 = CARTESIAN_POINT ( 'NONE',  ( -8.000000000000000000, 3.468749995903220196, -3.313708498984762496 ) ) ;
#20327 = CARTESIAN_POINT ( 'NONE',  ( 31.45873412499999944, 199.7500000013656063, 168.5673454167822740 ) ) ;
#20328 = EDGE_CURVE ( 'NONE', #48616, #44095, #56888, .T. ) ;
#20329 = CARTESIAN_POINT ( 'NONE',  ( 4.401442555609581635E-16, 13.21874999795161187, -7.188101187500000044 ) ) ;
#20330 = CARTESIAN_POINT ( 'NONE',  ( 5.656854249492374365, 5.656854249492375253, 22.95530278392014623 ) ) ;
#20331 = FACE_OUTER_BOUND ( 'NONE', #21427, .T. ) ;
#20332 = CARTESIAN_POINT ( 'NONE',  ( 7.188101187500002709, 110.1875000020483810, 2.977408999572649151 ) ) ;
#20333 = CARTESIAN_POINT ( 'NONE',  ( -1.836970198721029983E-15, 20.62499999317203603, 10.00000000000000178 ) ) ;
#20334 = DIRECTION ( 'NONE',  ( -0.000000000000000000, 1.000000000000000000, -0.000000000000000000 ) ) ;
#20335 = CARTESIAN_POINT ( 'NONE',  ( 29.43265458321761585, 208.7500000013656063, 173.4587341249998929 ) ) ;
#20336 = CARTESIAN_POINT ( 'NONE',  ( 7.188101187499993827, -2.977408999572645598, 22.01780278187175810 ) ) ;
#20337 = CARTESIAN_POINT ( 'NONE',  ( 25.17157287525377996, 195.8750000000000284, 172.8284271247460424 ) ) ;
#20338 = CARTESIAN_POINT ( 'NONE',  ( 3.042071309553167069, 36.82291666325268409, -11.35316468749999785 ) ) ;
#20339 = CARTESIAN_POINT ( 'NONE',  ( 2.995737153982848344, 16.37687539610414333, 68.98994273414960787 ) ) ;
#20340 = CARTESIAN_POINT ( 'NONE',  ( -2.679491924311225848, 3.333333326505365513, -10.00000000000000178 ) ) ;
#20341 = ORIENTED_EDGE ( 'NONE', *, *, #62277, .T. ) ;
#20342 = CARTESIAN_POINT ( 'NONE',  ( 1.656854249492416109, 199.3125000027311842, 138.0000000000000853 ) ) ;
#20343 = EDGE_CURVE ( 'NONE', #18106, #13268, #24690, .T. ) ;
#20344 = CARTESIAN_POINT ( 'NONE',  ( 0.000000000000000000, 300.0000000000000000, 10.00000000000000178 ) ) ;
#20345 = CARTESIAN_POINT ( 'NONE',  ( -11.35316468750000141, 53.48958332991935549, 3.042071309553159963 ) ) ;
#20346 = CARTESIAN_POINT ( 'NONE',  ( -7.778174593052023411, 7.778174593052023411, 83.50000000409677625 ) ) ;
#20347 = CARTESIAN_POINT ( 'NONE',  ( 2.445694354108784108, 204.5625000013656063, 144.4456943541088663 ) ) ;
#20348 = CARTESIAN_POINT ( 'NONE',  ( -3.428378827827395892, -68.02396499344693837, -20.38382289158757033 ) ) ;
#20349 = DIRECTION ( 'NONE',  ( -0.000000000000000000, -1.000000000000000000, -0.000000000000000000 ) ) ;
#20351 = CARTESIAN_POINT ( 'NONE',  ( -11.35316468749999785, 33.07291666325268409, -3.042071309553167957 ) ) ;
#20350 = CARTESIAN_POINT ( 'NONE',  ( 5.082755093536325042, 101.0937500020483810, -5.082755093536325930 ) ) ;
#20352 = CARTESIAN_POINT ( 'NONE',  ( 5.656854249492376141, -5.656854249492374365, 7.392802779823366421 ) ) ;
#20353 = CARTESIAN_POINT ( 'NONE',  ( -7.347880794884122694E-16, 5.499999997268813168, 4.000000000000001776 ) ) ;
#20354 = CARTESIAN_POINT ( 'NONE',  ( 6.951808397369818766E-16, 162.0312499965860127, -11.35316468750000141 ) ) ;
#20356 = CARTESIAN_POINT ( 'NONE',  ( 10.00000000000000000, 131.6666666598386541, 2.679491924311236062 ) ) ;
#20355 = PRODUCT ( 'plain washer (type a)_is_IS 2016 A- 16', 'plain washer (type a)_is_IS 2016 A- 16', '', ( #62175 ) ) ;
#20357 = CARTESIAN_POINT ( 'NONE',  ( 1.320432766682874540E-15, 111.4062500020483810, 7.188101187500000044 ) ) ;
#20358 = EDGE_LOOP ( 'NONE', ( #51200, #8076, #43279, #43326, #6960, #42899 ) ) ;
#20359 = CARTESIAN_POINT ( 'NONE',  ( -54.00000000000000000, 37.00000000000000711, 4.085831468968145267E-14 ) ) ;
#20360 = CARTESIAN_POINT ( 'NONE',  ( -8.311093377946836114, 22.96874999658601979, -8.311093377946837890 ) ) ;
#20361 = CARTESIAN_POINT ( 'NONE',  ( -3.999999999999959144, 197.0625000000000000, 199.6568542494924259 ) ) ;
#20362 = ORIENTED_EDGE ( 'NONE', *, *, #47390, .T. ) ;
#20363 = CARTESIAN_POINT ( 'NONE',  ( -11.00000000000000000, 0.000000000000000000, 118.0000000000000000 ) ) ;
#20364 = CARTESIAN_POINT ( 'NONE',  ( -4.220049686691937474, -10.18810118749999738, 76.93750000204839523 ) ) ;
#20365 = DIRECTION ( 'NONE',  ( 1.000000000000000000, -0.000000000000000000, -0.000000000000000000 ) ) ;
#20367 = CARTESIAN_POINT ( 'NONE',  ( -2.085542519210945728E-15, 159.5312499965860127, 11.35316468750000141 ) ) ;
#20366 = PLANE ( 'NONE',  #64019 ) ;
#20368 = CARTESIAN_POINT ( 'NONE',  ( 2.977408999572650927, 2.624999997951610542, -7.188101187500000933 ) ) ;
#20369 = CARTESIAN_POINT ( 'NONE',  ( -7.999999999999991118, 3.313708498984756723, 9.792802784329825982 ) ) ;
#20370 = EDGE_CURVE ( 'NONE', #72372, #25774, #36885, .T. ) ;
#20371 = EDGE_CURVE ( 'NONE', #37575, #33535, #59527, .T. ) ;
#20372 = CARTESIAN_POINT ( 'NONE',  ( 8.311093377946839666, 240.7812500034140157, 8.311093377946829008 ) ) ;
#20373 = CARTESIAN_POINT ( 'NONE',  ( 10.18810118750000093, -4.220049686691933921, 85.18750000204838102 ) ) ;
#20374 = ORIENTED_EDGE ( 'NONE', *, *, #62793, .T. ) ;
#20375 = EDGE_CURVE ( 'NONE', #33552, #9013, #12300, .T. ) ;
#20376 = AXIS2_PLACEMENT_3D ( 'NONE', #7733, #19405, #48449 ) ;
#20377 = CARTESIAN_POINT ( 'NONE',  ( 7.347880794884121708E-16, 300.0000000000000000, -6.000000000000001776 ) ) ;
#20378 = PLANE ( 'NONE',  #26706 ) ;
#20379 = CARTESIAN_POINT ( 'NONE',  ( 9.832129032723420536, 96.51041666325268409, -5.676582343749999815 ) ) ;
#20380 = CARTESIAN_POINT ( 'NONE',  ( 7.204075437095966983, 7.204075437095967871, 92.59375000204838102 ) ) ;
#20381 = CARTESIAN_POINT ( 'NONE',  ( -1.881053915767121776, 20.74999999863440436, -4.541265875000002339 ) ) ;
#20382 = VERTEX_POINT ( 'NONE', #61342 ) ;
#20383 = ORIENTED_EDGE ( 'NONE', *, *, #55931, .T. ) ;
#20384 = CARTESIAN_POINT ( 'NONE',  ( -1.881053915767124440, 4.124999998634407028, 4.541265875000001451 ) ) ;
#20385 = VECTOR ( 'NONE', #9055, 1000.000000000000000 ) ;
#20386 = CARTESIAN_POINT ( 'NONE',  ( 2.977408999572650927, 6.749999997951611874, -7.188101187500001821 ) ) ;
#20387 = EDGE_CURVE ( 'NONE', #64105, #17730, #14925, .T. ) ;
#20388 = CARTESIAN_POINT ( 'NONE',  ( 8.000000000000001776, 115.3437500040967763, 3.313708498984759387 ) ) ;
#20389 =( BOUNDED_CURVE ( )  B_SPLINE_CURVE ( 2, ( #36861, #31569, #54593, #32327, #25148 ),
 .UNSPECIFIED., .F., .F. ) 
 B_SPLINE_CURVE_WITH_KNOTS ( ( 3, 2, 3 ),
 ( 0.000000000000000000, 0.01041666666666551944, 0.02083333333333103887 ),
 .UNSPECIFIED. ) 
 CURVE ( )  GEOMETRIC_REPRESENTATION_ITEM ( )  RATIONAL_B_SPLINE_CURVE ( ( 1.000000000000000000, 0.9238795325112867385, 1.000000000000000000, 0.9238795325113035029, 0.9999999999999832356 ) ) 
 REPRESENTATION_ITEM ( '' )  );
#20390 = CARTESIAN_POINT ( 'NONE',  ( -7.204075437095965206, -7.204075437095968759, 95.21875000204838102 ) ) ;
#20391 = CARTESIAN_POINT ( 'NONE',  ( -29.43265458321760519, 203.1250000013656347, 173.4587341250003760 ) ) ;
#20392 = CARTESIAN_POINT ( 'NONE',  ( -10.00000000000000000, 159.1666666598386541, -2.679491924311229845 ) ) ;
#20393 = CARTESIAN_POINT ( 'NONE',  ( -1.656854249492381248, 3.312500000000000000, -4.000000000000001776 ) ) ;
#20394 = CARTESIAN_POINT ( 'NONE',  ( 2.828427124746190291, 16.62499999726881583, 2.828427124746192067 ) ) ;
#20395 = CARTESIAN_POINT ( 'NONE',  ( 1.881053915767122664, 4.124999998634407028, 4.541265875000001451 ) ) ;
#20396 = CARTESIAN_POINT ( 'NONE',  ( -4.898587196589412829E-16, 96.12499999999998579, -8.000000000000000000 ) ) ;
#20397 = CARTESIAN_POINT ( 'NONE',  ( 2.839093476692135984E-14, 195.6875000013655779, 201.4587341250000350 ) ) ;
#20399 = CARTESIAN_POINT ( 'NONE',  ( -23.99999999999998934, 199.7500000000000000, 170.0000000000003411 ) ) ;
#20398 = CARTESIAN_POINT ( 'NONE',  ( -27.99999999999991829, 198.9375000013655779, 173.4587341250003760 ) ) ;
#20400 =( BOUNDED_CURVE ( )  B_SPLINE_CURVE ( 2, ( #44485, #55440, #20715, #32429, #59963, #38460, #8281, #36957, #67498, #61083, #2632, #48634, #20333 ),
 .UNSPECIFIED., .F., .F. ) 
 B_SPLINE_CURVE_WITH_KNOTS ( ( 3, 2, 2, 2, 2, 2, 3 ),
 ( 0.07065217391304347283, 0.07246376811594203160, 0.07427536231884057649, 0.07608695652173913526, 0.07789855072463768015, 0.07971014492753622505, 0.08152173913043478382 ),
 .UNSPECIFIED. ) 
 CURVE ( )  GEOMETRIC_REPRESENTATION_ITEM ( )  RATIONAL_B_SPLINE_CURVE ( ( 1.000000000000000000, 0.9659258262890683122, 1.000000000000000000, 0.9659258262890683122, 1.000000000000000000, 0.9659258262890683122, 1.000000000000000000, 0.9659258262890683122, 1.000000000000000000, 0.9659258262890683122, 1.000000000000000000, 0.9659258262890683122, 1.000000000000000000 ) ) 
 REPRESENTATION_ITEM ( '' )  );
#20401 = CARTESIAN_POINT ( 'NONE',  ( 3.211159895383560947, 19.18749999863440436, 3.211159895383562723 ) ) ;
#20402 = CARTESIAN_POINT ( 'NONE',  ( 0.1959721802077262487, -48.00000000000002842, 151.0000000000000000 ) ) ;
#20403 = CARTESIAN_POINT ( 'NONE',  ( -2.977408999572648707, -7.188101187499990274, 6.267802781871754547 ) ) ;
#20404 = ORIENTED_EDGE ( 'NONE', *, *, #58933, .F. ) ;
#20405 = ORIENTED_EDGE ( 'NONE', *, *, #20935, .T. ) ;
#20406 = CARTESIAN_POINT ( 'NONE',  ( -7.204075437095965206, -7.204075437095968759, 100.8437500020483668 ) ) ;
#20407 = CARTESIAN_POINT ( 'NONE',  ( 3.313708498984721640, 26.53124999590322020, 8.000000000000039080 ) ) ;
#20408 = CARTESIAN_POINT ( 'NONE',  ( -24.54126587499998280, 202.3750000013656063, 171.4326545832179818 ) ) ;
#20409 = CARTESIAN_POINT ( 'NONE',  ( -25.17157287525377640, 200.6250000000000284, 172.8284271247465256 ) ) ;
#20410 = CARTESIAN_POINT ( 'NONE',  ( -2.445694354108784108, 205.5625000013656063, 195.5543056458912190 ) ) ;
#20411 = CARTESIAN_POINT ( 'NONE',  ( -5.000000000000000000, 10.00000000000000000, 75.19090595827292134 ) ) ;
#20412 = CARTESIAN_POINT ( 'NONE',  ( 8.660254037844389075, 110.4166666666666714, -5.000000000000000000 ) ) ;
#20413 = CARTESIAN_POINT ( 'NONE',  ( -7.999999999999998224, 111.5937499999999858, 3.313708498984766493 ) ) ;
#20414 = CARTESIAN_POINT ( 'NONE',  ( 6.676582343750004256, 294.0468750017070079, 2.765530957081995478 ) ) ;
#20415 = CARTESIAN_POINT ( 'NONE',  ( -7.188101187499992051, 0.000000000000000000, 9.361552781871752771 ) ) ;
#20416 = EDGE_LOOP ( 'NONE', ( #43817, #14715, #22505, #33849 ) ) ;
#20417 = DIRECTION ( 'NONE',  ( -1.000000000000000000, 0.000000000000000000, 0.000000000000000000 ) ) ;
#20418 = CARTESIAN_POINT ( 'NONE',  ( -8.000000000000000000, 21.46874999590322375, -3.313708498984762496 ) ) ;
#20419 = SHAPE_REPRESENTATION ( 'square bolt', ( #57354 ), #67028 ) ;
#20420 = CARTESIAN_POINT ( 'NONE',  ( 2.445694354108783664, 204.3125000013656063, 144.4456943541088663 ) ) ;
#20421 = DIRECTION ( 'NONE',  ( -0.000000000000000000, 1.000000000000000000, 4.476705744456276341E-16 ) ) ;
#20422 = CARTESIAN_POINT ( 'NONE',  ( 0.000000000000000000, 0.000000000000000000, 0.000000000000000000 ) ) ;
#20423 = CARTESIAN_POINT ( 'NONE',  ( -5.676582343749992710, 255.0520833367473301, 9.832129032723422313 ) ) ;
#20424 = CARTESIAN_POINT ( 'NONE',  ( -2.751064625579944321E-14, 207.7500000000000284, 146.0000000000000284 ) ) ;
#20425 = CARTESIAN_POINT ( 'NONE',  ( 11.00000000000000000, 4.556349186104045934, 111.3437499999999858 ) ) ;
#20426 = CARTESIAN_POINT ( 'NONE',  ( -1.836970198721029983E-15, 223.7500000000000000, 10.00000000000000178 ) ) ;
#20427 = CARTESIAN_POINT ( 'NONE',  ( 1.320432766682872962E-15, -7.188101187499992051, 5.236552781871753659 ) ) ;
#20428 = CARTESIAN_POINT ( 'NONE',  ( -11.35316468749999785, 193.3854166632526415, -3.042071309553167513 ) ) ;
#20429 = CARTESIAN_POINT ( 'NONE',  ( -11.00000000000000000, 0.000000000000000000, 101.5000000000000000 ) ) ;
#20430 = CARTESIAN_POINT ( 'NONE',  ( 1.881053915767121776, 4.499999998634407028, -4.541265875000002339 ) ) ;
#20432 = CARTESIAN_POINT ( 'NONE',  ( -1.656854249492388576, 206.3124999999999716, 138.0000000000000000 ) ) ;
#20431 = CARTESIAN_POINT ( 'NONE',  ( -2.849036369511732440E-14, 207.3750000027312126, 138.0000000000000568 ) ) ;
#20433 = ORIENTED_EDGE ( 'NONE', *, *, #7424, .T. ) ;
#20434 = EDGE_CURVE ( 'NONE', #47217, #50184, #40142, .T. ) ;
#20435 = AXIS2_PLACEMENT_3D ( 'NONE', #16822, #34958, #12294 ) ;
#20436 = CARTESIAN_POINT ( 'NONE',  ( -1.432654583217662481, 206.3750000013656063, 145.4587341250000634 ) ) ;
#20437 = CARTESIAN_POINT ( 'NONE',  ( 11.35316468750000141, 10.78124999658601624, 0.000000000000000000 ) ) ;
#20438 = CARTESIAN_POINT ( 'NONE',  ( 7.778174593052021635, 7.778174593052023411, 99.62500000409677625 ) ) ;
#20439 = CARTESIAN_POINT ( 'NONE',  ( -1.469576158976823947E-15, 25.12500000000000355, 8.000000000000000000 ) ) ;
#20440 = CARTESIAN_POINT ( 'NONE',  ( -30.44569435410875968, 202.8125000013656063, 172.4456943541092642 ) ) ;
#20441 = CARTESIAN_POINT ( 'NONE',  ( -30.93541659651595666, -70.00000000000001421, 167.9999999999997442 ) ) ;
#20443 = CARTESIAN_POINT ( 'NONE',  ( 4.898587196589412829E-16, 18.18749999590322020, -8.000000000000000000 ) ) ;
#20442 = CARTESIAN_POINT ( 'NONE',  ( 5.082755093536326818, 118.7187500020483810, 5.082755093536325042 ) ) ;
#20444 = CARTESIAN_POINT ( 'NONE',  ( 5.656854249492374365, 5.656854249492375253, 27.26780277982336642 ) ) ;
#20445 = CARTESIAN_POINT ( 'NONE',  ( 11.35316468749999963, 115.9895833299193555, -3.042071309553165293 ) ) ;
#20446 = CARTESIAN_POINT ( 'NONE',  ( -10.00000000000000000, 84.16666665983869677, -2.679491924311229845 ) ) ;
#20447 = CARTESIAN_POINT ( 'NONE',  ( 7.188101187500000044, 91.90625000204838102, -8.802885111219163269E-16 ) ) ;
#20448 = CARTESIAN_POINT ( 'NONE',  ( 4.541265875000002339, 21.43749999863440792, 0.000000000000000000 ) ) ;
#20449 = CARTESIAN_POINT ( 'NONE',  ( -8.660254037844387298, 198.9583333265053682, -5.000000000000004441 ) ) ;
#20450 = EDGE_LOOP ( 'NONE', ( #13073, #40002, #63217, #23757 ) ) ;
#20451 = CARTESIAN_POINT ( 'NONE',  ( -5.010062319353657756, 225.9999999999999716, -8.679233769287526101 ) ) ;
#20452 = CARTESIAN_POINT ( 'NONE',  ( 6.676582343750003368, 295.1718750017070079, -2.765530957081997254 ) ) ;
#20453 = CARTESIAN_POINT ( 'NONE',  ( -4.000000000000001776, 12.18749999726881406, -1.656854249492381470 ) ) ;
#20454 = CARTESIAN_POINT ( 'NONE',  ( -12.18025451098408318, 1.885907279315492735, -0.5845398423542953470 ) ) ;
#20455 = CARTESIAN_POINT ( 'NONE',  ( 9.832129032723416984, 175.3645833299193555, 5.676582343750006032 ) ) ;
#20456 = CARTESIAN_POINT ( 'NONE',  ( -3.999999999999960032, 197.0000000000000000, 198.0000000000000284 ) ) ;
#20457 = CARTESIAN_POINT ( 'NONE',  ( -28.00000000000002842, 201.0000000000000000, 166.0000000000003695 ) ) ;
#20458 = CARTESIAN_POINT ( 'NONE',  ( 10.18810118750000093, -4.220049686691933921, 106.1875000020483810 ) ) ;
#20459 = EDGE_LOOP ( 'NONE', ( #3051, #45378, #39712, #60951 ) ) ;
#20460 = CARTESIAN_POINT ( 'NONE',  ( -31.99999999999995737, 199.4375000027312126, 171.6568542494928522 ) ) ;
#20461 = CARTESIAN_POINT ( 'NONE',  ( 11.35316468749999963, 161.3020833299193555, -3.042071309553165293 ) ) ;
#20462 = CARTESIAN_POINT ( 'NONE',  ( 2.828427124746209831, 206.5000000027312126, 200.8284271247462129 ) ) ;
#20463 = CARTESIAN_POINT ( 'NONE',  ( -3.458734124999960358, 207.6875000013656063, 198.0000000000000284 ) ) ;
#20464 = CARTESIAN_POINT ( 'NONE',  ( -4.220049686691935698, 10.18810118749999916, 67.75000000204836681 ) ) ;
#20465 = CARTESIAN_POINT ( 'NONE',  ( 5.676582343750001591, 56.92708332991935549, -9.832129032723420536 ) ) ;
#20466 = VERTEX_POINT ( 'NONE', #55698 ) ;
#20467 = DIRECTION ( 'NONE',  ( -0.000000000000000000, -0.000000000000000000, -1.000000000000000000 ) ) ;
#20468 = CARTESIAN_POINT ( 'NONE',  ( 3.211159895383561835, 10.56249999863440792, -3.211159895383561835 ) ) ;
#20469 = ORIENTED_EDGE ( 'NONE', *, *, #16870, .T. ) ;
#20470 = CARTESIAN_POINT ( 'NONE',  ( 2.977408999572651815, 19.68749999795161543, 7.188101187500000933 ) ) ;
#20471 = CARTESIAN_POINT ( 'NONE',  ( 1.102182119232618108E-15, 290.3125000034140157, 6.000000000000001776 ) ) ;
#20472 = CARTESIAN_POINT ( 'NONE',  ( 7.320508075688774596, 67.49999999317201116, -7.320508075688774596 ) ) ;
#20473 = CARTESIAN_POINT ( 'NONE',  ( 7.188101187499999156, 18.74999999795161898, 2.977408999572654924 ) ) ;
#20474 = EDGE_CURVE ( 'NONE', #10274, #19945, #52709, .T. ) ;
#20475 = CARTESIAN_POINT ( 'NONE',  ( -5.082755093536317936, -5.082755093536320601, 3.174052781871751439 ) ) ;
#20476 = CARTESIAN_POINT ( 'NONE',  ( -4.220049686691937474, -10.18810118749999738, 113.3125000020483668 ) ) ;
#20477 = EDGE_CURVE ( 'NONE', #71023, #72561, #37279, .T. ) ;
#20478 = AXIS2_PLACEMENT_3D ( 'NONE', #55151, #38910, #43818 ) ;
#20479 = CARTESIAN_POINT ( 'NONE',  ( 2.775557561822899905E-14, -42.00000000000000711, 151.0000000000000284 ) ) ;
#20480 = CARTESIAN_POINT ( 'NONE',  ( -7.347880794884122694E-16, 7.499999997268813168, 4.000000000000001776 ) ) ;
#20481 = ORIENTED_EDGE ( 'NONE', *, *, #44070, .F. ) ;
#20482 = EDGE_CURVE ( 'NONE', #28033, #71925, #22267, .T. ) ;
#20483 = AXIS2_PLACEMENT_3D ( 'NONE', #18251, #6570, #555 ) ;
#20484 = CARTESIAN_POINT ( 'NONE',  ( 1.432654583217662481, 207.1250000013656347, 194.5412658750000219 ) ) ;
#20485 = CARTESIAN_POINT ( 'NONE',  ( -28.00000000000007461, 194.1250000027311842, 166.0000000000003695 ) ) ;
#20486 = CARTESIAN_POINT ( 'NONE',  ( 3.211159895383561835, 7.437499998634407028, -3.211159895383561835 ) ) ;
#20487 = CARTESIAN_POINT ( 'NONE',  ( -4.401442555609581635E-16, 110.2812500020483810, -7.188101187500000044 ) ) ;
#20488 = EDGE_CURVE ( 'NONE', #9455, #31077, #51133, .T. ) ;
#20489 = CARTESIAN_POINT ( 'NONE',  ( 8.000000000000000000, 94.53125000409676204, -3.313708498984762496 ) ) ;
#20490 = CARTESIAN_POINT ( 'NONE',  ( 5.082755093536320601, -5.082755093536318824, 24.54905278187175810 ) ) ;
#20491 = ORIENTED_EDGE ( 'NONE', *, *, #44850, .F. ) ;
#20492 =( BOUNDED_CURVE ( )  B_SPLINE_CURVE ( 2, ( #73986, #62657, #10991, #34024, #1170, #35132, #51716, #35494, #29825 ),
 .UNSPECIFIED., .F., .F. ) 
 B_SPLINE_CURVE_WITH_KNOTS ( ( 3, 2, 2, 2, 3 ),
 ( 0.6176470588235293269, 0.6213235294117646079, 0.6249999999999998890, 0.6286764705882351700, 0.6323529411764704511 ),
 .UNSPECIFIED. ) 
 CURVE ( )  GEOMETRIC_REPRESENTATION_ITEM ( )  RATIONAL_B_SPLINE_CURVE ( ( 1.000000000000002220, 0.9238795325112844070, 1.000000000000000000, 0.9238795325112867385, 1.000000000000000000, 0.9238795325112867385, 1.000000000000000000, 0.9238795325112890700, 0.9999999999999976685 ) ) 
 REPRESENTATION_ITEM ( '' )  );
#20493 = CARTESIAN_POINT ( 'NONE',  ( -1.656854249492383468, 21.68750000000000355, 4.000000000000000888 ) ) ;
#20494 = ORIENTED_EDGE ( 'NONE', *, *, #8623, .F. ) ;
#20495 = DIRECTION ( 'NONE',  ( 0.000000000000000000, 0.000000000000000000, 1.000000000000000000 ) ) ;
#20496 = DIRECTION ( 'NONE',  ( 0.000000000000000000, 0.000000000000000000, -1.000000000000000000 ) ) ;
#20497 = CARTESIAN_POINT ( 'NONE',  ( -2.445694354108782775, 206.5625000013656063, 200.4456943541088663 ) ) ;
#20498 = CARTESIAN_POINT ( 'NONE',  ( 26.56734541678233086, 203.0000000013655779, 166.5412658749999650 ) ) ;
#20499 = CARTESIAN_POINT ( 'NONE',  ( 8.660254037844385522, 69.58333333333334281, 5.000000000000005329 ) ) ;
#20500 = CARTESIAN_POINT ( 'NONE',  ( -5.082755093536325930, 92.84375000204838102, -5.082755093536325930 ) ) ;
#20501 = CARTESIAN_POINT ( 'NONE',  ( 6.000000000000003553, 291.4375000000000568, 2.485281374238571317 ) ) ;
#20503 = CARTESIAN_POINT ( 'NONE',  ( -10.99999999999996625, 4.556349186104079685, 113.5937500040967620 ) ) ;
#20502 = CARTESIAN_POINT ( 'NONE',  ( 30.64284399271082293, 178.3875230420589446, 174.6921329945330683 ) ) ;
#20504 = AXIS2_PLACEMENT_3D ( 'NONE', #15284, #20575, #67734 ) ;
#20505 = ORIENTED_EDGE ( 'NONE', *, *, #44581, .T. ) ;
#20506 = CARTESIAN_POINT ( 'NONE',  ( 11.35316468749999963, 221.1979166700806161, 3.042071309553159519 ) ) ;
#20507 = CARTESIAN_POINT ( 'NONE',  ( -7.456155213531540760, -10.23501372118566266, 65.47700548259878417 ) ) ;
#20508 = CARTESIAN_POINT ( 'NONE',  ( -4.000000000000015099, 201.6875000027312126, 143.6568542494924543 ) ) ;
#20509 = CARTESIAN_POINT ( 'NONE',  ( 7.999999999999991118, 9.797174393178815797E-16, 24.26780278392014978 ) ) ;
#20510 = CARTESIAN_POINT ( 'NONE',  ( -27.99999999999996092, 208.5000000000000284, 174.0000000000003695 ) ) ;
#20511 = CARTESIAN_POINT ( 'NONE',  ( 7.320508075688776373, 256.8750000000000000, 7.320508075688767491 ) ) ;
#20512 = FACE_OUTER_BOUND ( 'NONE', #16516, .T. ) ;
#20513 = CARTESIAN_POINT ( 'NONE',  ( 10.00000000000000178, 190.0000000000000000, 0.000000000000000000 ) ) ;
#20514 =( BOUNDED_SURFACE ( )  B_SPLINE_SURFACE ( 1, 2, ( 
 ( #48326, #42667, #65678, #3064, #24939, #13977, #43032, #60394, #43410, #2691, #13251, #31733, #37020, #70971, #30616, #37776, #30249, #60022, #53268, #24579, #14361, #8340, #31354, #48697, #66053, #26047, #49068, #72080, #47584, #36284, #59301, #7610, #1949, #53639, #19285, #42296, #6365, #1453, #23696, #52747, #18041, #18410, #39935, #11635, #28987, #12374, #12737, #58419, #41056, #35768, #52005, #69351, #24059, #58054, #16911, #35410, #52377, #35041, #6726, #64064, #34297, #29732, #40307, #713, #41426, #1081, #342, #57301, #47069, #57676, #62942, #17660, #5613, #70106, #40680, #28612, #64438, #58785, #51624, #74641, #34672, #7094, #30102, #53120, #29370, #46701, #45588, #68603, #63682, #11266, #22956, #45964, #63308, #5984, #68979, #17288, #69726, #23323, #46335, #12009, #70827, #65900, #66276, #13827, #30831, #65536, #47440, #60241, #14206, #36872, #19139, #25531, #14584, #42881, #53488, #24791, #36506, #19504, #37244, #2539, #43259, #53853, #8566, #24434, #47804, #31582, #48916, #1804, #37621, #36136, #70466, #65156, #54230, #7466, #42143, #2166, #30471, #54604, #13466, #25160, #2911, #59515, #8942, #31954, #19876, #7828, #25898, #71928, #8194, #59879, #54978, #48544, #20241, #71553, #60618, #71185, #59156, #18783, #41787, #64797, #13099, #48177, #42520, #31205, #11088, #74449, #51069, #55726, #34863, #57499, #51438, #60992, #32339, #44020, #40497, #46151, #34492, #16719, #57114, #11457, #11825, #22381, #17477, #43639, #66648, #20994, #67030, #40123, #14956, #34114, #5802, #15328, #68418, #49679, #45780, #69168, #39746, #9697, #45402, #26272, #63130, #68791, #62747, #72693, #5426, #63503, #22757, #55351, #3656, #38364, #74081, #17100, #28430, #23139, #32718, #28799, #3285, #26655, #51816, #161, #61371, #49292, #37994, #72309, #4042, #20623, #9316, #27035, #35588, #63877, #18964, #29551, #58602, #47621, #58245, #42336, #65353, #53309, #52560, #41967, #64977 ),
 ( #899, #1986, #529, #13285, #40872, #13653, #36325, #7651, #19323, #58974, #59339, #30657, #29183, #57868, #7281, #53674, #12561, #24977, #1267, #35954, #64251, #6908, #71008, #6175, #52198, #29919, #47994, #41244, #23508, #69543, #46524, #52937, #17853, #24247, #12189, #35226, #6545, #23886, #30289, #64624, #47259, #70286, #46895, #69919, #18229, #12920, #18599, #41609, #1633, #24614, #70644, #20818, #72509, #20436, #72122, #67229, #14775, #43836, #9134, #9520, #8763, #48365, #66851, #37815, #32151, #15154, #14021, #26853, #31773, #43451, #55172, #54793, #14402, #36693, #38186, #31019, #2728, #20058, #3477, #3859, #49491, #26467, #49868, #43076, #60434, #61190, #49110, #8013, #32535, #66466, #26090, #55546, #72884, #25349, #21191, #31395, #60810, #44216, #59704, #66092, #71369, #54044, #48737, #2355, #3104, #19694, #42705, #65717, #37059, #60058, #8380, #54422, #25716, #71743, #37435, #57406, #45691, #27978, #68337, #22672, #23055, #33655, #28713, #55920, #4232, #33283, #56282, #51352, #27220, #45322, #68706, #4600, #4977, #61931, #57032, #5713, #50983, #21931, #56661, #38566, #74363, #5344, #73996, #10256, #16634, #51726, #34035, #44589, #15898, #27595, #10628, #28345, #39668, #34404, #44961, #17017, #15525, #38929, #40041, #63045, #67601, #77, #50237, #61566, #50606, #62667, #73258, #73626, #67967, #21563, #11370, #16262, #39300, #46064, #62300, #9887, #32916, #11002, #22298, #46804, #23801, #23425, #63787, #446, #1179, #69084, #6087, #6464, #24160, #53591, #70562, #29094, #18878, #17390, #53220, #18511, #12105, #35141, #69828, #41158, #29467, #59253, #41520, #52114, #63412, #18143, #40415, #64166, #70204, #1901, #41885, #12472, #1552, #24531, #64536, #52847, #7196, #24889, #11740, #7565, #17765, #46439, #40781, #34778, #35503, #58516, #813, #64896, #58157, #6822, #30199, #47537, #30569, #12833, #69457, #13199, #29835, #52477, #47172, #57782, #35869 ) ),
 .UNSPECIFIED., .F., .F., .F. ) 
 B_SPLINE_SURFACE_WITH_KNOTS ( ( 2, 2 ),
 ( 3, 2, 2, 2, 2, 2, 2, 2, 2, 2, 2, 2, 2, 2, 2, 2, 2, 2, 2, 2, 2, 2, 2, 2, 2, 2, 2, 2, 2, 2, 2, 2, 2, 2, 2, 2, 2, 2, 2, 2, 2, 2, 2, 2, 2, 2, 2, 2, 2, 2, 2, 2, 2, 2, 2, 2, 2, 2, 2, 2, 2, 2, 2, 2, 2, 2, 2, 2, 2, 2, 2, 2, 2, 2, 2, 2, 2, 2, 2, 2, 2, 2, 2, 2, 2, 2, 2, 2, 2, 2, 2, 2, 2, 2, 2, 2, 2, 2, 2, 2, 2, 2, 2, 2, 2, 2, 2, 2, 2, 2, 2, 2, 2, 2, 2, 2, 2, 2, 2, 2, 3 ),
 ( 0.000000000000000000, 1.000000000000000000 ),
 ( 0.000000000000000000, 0.008333333333333333218, 0.01666666666666666644, 0.02500000000000000139, 0.03333333333333333287, 0.04166666666666666435, 0.05000000000000000278, 0.05833333333333333426, 0.06666666666666666574, 0.07499999999999999722, 0.08333333333333332871, 0.09166666666666666019, 0.1000000000000000056, 0.1083333333333333370, 0.1166666666666666685, 0.1250000000000000000, 0.1333333333333333315, 0.1416666666666666630, 0.1499999999999999944, 0.1583333333333333259, 0.1666666666666666574, 0.1749999999999999889, 0.1833333333333333204, 0.1916666666666666796, 0.2000000000000000111, 0.2083333333333333426, 0.2166666666666666741, 0.2250000000000000056, 0.2333333333333333370, 0.2416666666666666685, 0.2500000000000000000, 0.2583333333333333592, 0.2666666666666666630, 0.2750000000000000222, 0.2833333333333333259, 0.2916666666666666852, 0.2999999999999999889, 0.3083333333333333481, 0.3166666666666666519, 0.3250000000000000111, 0.3333333333333333148, 0.3416666666666666741, 0.3499999999999999778, 0.3583333333333333370, 0.3666666666666666408, 0.3750000000000000000, 0.3833333333333333592, 0.3916666666666666630, 0.4000000000000000222, 0.4083333333333333259, 0.4166666666666666852, 0.4249999999999999889, 0.4333333333333333481, 0.4416666666666666519, 0.4500000000000000111, 0.4583333333333333148, 0.4666666666666666741, 0.4749999999999999778, 0.4833333333333333370, 0.4916666666666666408, 0.5000000000000000000, 0.5083333333333333037, 0.5166666666666667185, 0.5250000000000000222, 0.5333333333333333259, 0.5416666666666666297, 0.5500000000000000444, 0.5583333333333333481, 0.5666666666666666519, 0.5749999999999999556, 0.5833333333333333703, 0.5916666666666666741, 0.5999999999999999778, 0.6083333333333332815, 0.6166666666666666963, 0.6250000000000000000, 0.6333333333333333037, 0.6416666666666667185, 0.6500000000000000222, 0.6583333333333333259, 0.6666666666666666297, 0.6750000000000000444, 0.6833333333333333481, 0.6916666666666666519, 0.6999999999999999556, 0.7083333333333333703, 0.7166666666666666741, 0.7249999999999999778, 0.7333333333333332815, 0.7416666666666666963, 0.7500000000000000000, 0.7583333333333333037, 0.7666666666666667185, 0.7750000000000000222, 0.7833333333333333259, 0.7916666666666666297, 0.8000000000000000444, 0.8083333333333333481, 0.8166666666666666519, 0.8249999999999999556, 0.8333333333333333703, 0.8416666666666666741, 0.8499999999999999778, 0.8583333333333332815, 0.8666666666666666963, 0.8750000000000000000, 0.8833333333333333037, 0.8916666666666667185, 0.9000000000000000222, 0.9083333333333333259, 0.9166666666666666297, 0.9250000000000000444, 0.9333333333333333481, 0.9416666666666666519, 0.9499999999999999556, 0.9583333333333333703, 0.9666666666666666741, 0.9749999999999999778, 0.9833333333333332815, 0.9916666666666666963, 1.000000000000000000 ),
 .UNSPECIFIED. ) 
 GEOMETRIC_REPRESENTATION_ITEM ( )  RATIONAL_B_SPLINE_SURFACE ( (
 ( 1.000000000000000000, 0.9238795325112867385, 1.000000000000000000, 0.9238795325112867385, 1.000000000000000000, 0.9238795325112867385, 1.000000000000000000, 0.9238795325112867385, 1.000000000000000000, 0.9238795325112867385, 1.000000000000000000, 0.9238795325112867385, 1.000000000000000000, 0.9238795325112867385, 1.000000000000000000, 0.9238795325112867385, 1.000000000000000000, 0.9238795325112867385, 1.000000000000000000, 0.9238795325112867385, 1.000000000000000000, 0.9238795325112867385, 1.000000000000000000, 0.9238795325112867385, 1.000000000000000000, 0.9238795325112867385, 1.000000000000000000, 0.9238795325112867385, 1.000000000000000000, 0.9238795325112867385, 1.000000000000000000, 0.9238795325112867385, 1.000000000000000000, 0.9238795325112867385, 1.000000000000000000, 0.9238795325112867385, 1.000000000000000000, 0.9238795325112867385, 1.000000000000000000, 0.9238795325112867385, 1.000000000000000000, 0.9238795325112867385, 1.000000000000000000, 0.9238795325112867385, 1.000000000000000000, 0.9238795325112867385, 1.000000000000000000, 0.9238795325112867385, 1.000000000000000000, 0.9238795325112867385, 1.000000000000000000, 0.9238795325112867385, 1.000000000000000000, 0.9238795325112867385, 1.000000000000000000, 0.9238795325112867385, 1.000000000000000000, 0.9238795325112867385, 1.000000000000000000, 0.9238795325112867385, 1.000000000000000000, 0.9238795325112867385, 1.000000000000000000, 0.9238795325112867385, 1.000000000000000000, 0.9238795325112867385, 1.000000000000000000, 0.9238795325112867385, 1.000000000000000000, 0.9238795325112867385, 1.000000000000000000, 0.9238795325112867385, 1.000000000000000000, 0.9238795325112867385, 1.000000000000000000, 0.9238795325112867385, 1.000000000000000000, 0.9238795325112867385, 1.000000000000000000, 0.9238795325112867385, 1.000000000000000000, 0.9238795325112867385, 1.000000000000000000, 0.9238795325112867385, 1.000000000000000000, 0.9238795325112867385, 1.000000000000000000, 0.9238795325112867385, 1.000000000000000000, 0.9238795325112867385, 1.000000000000000000, 0.9238795325112867385, 1.000000000000000000, 0.9238795325112867385, 1.000000000000000000, 0.9238795325112867385, 1.000000000000000000, 0.9238795325112867385, 1.000000000000000000, 0.9238795325112867385, 1.000000000000000000, 0.9238795325112867385, 1.000000000000000000, 0.9238795325112867385, 1.000000000000000000, 0.9238795325112867385, 1.000000000000000000, 0.9238795325112867385, 1.000000000000000000, 0.9238795325112867385, 1.000000000000000000, 0.9238795325112867385, 1.000000000000000000, 0.9238795325112867385, 1.000000000000000000, 0.9238795325112867385, 1.000000000000000000, 0.9238795325112867385, 1.000000000000000000, 0.9238795325112867385, 1.000000000000000000, 0.9238795325112867385, 1.000000000000000000, 0.9238795325112867385, 1.000000000000000000, 0.9238795325112867385, 1.000000000000000000, 0.9238795325112867385, 1.000000000000000000, 0.9238795325112867385, 1.000000000000000000, 0.9238795325112867385, 1.000000000000000000, 0.9238795325112867385, 1.000000000000000000, 0.9238795325112867385, 1.000000000000000000, 0.9238795325112867385, 1.000000000000000000, 0.9238795325112867385, 1.000000000000000000, 0.9238795325112867385, 1.000000000000000000, 0.9238795325112867385, 1.000000000000000000, 0.9238795325112867385, 1.000000000000000000, 0.9238795325112867385, 1.000000000000000000, 0.9238795325112867385, 1.000000000000000000, 0.9238795325112867385, 1.000000000000000000, 0.9238795325112867385, 1.000000000000000000, 0.9238795325112867385, 1.000000000000000000, 0.9238795325112867385, 1.000000000000000000, 0.9238795325112867385, 1.000000000000000000, 0.9238795325112867385, 1.000000000000000000, 0.9238795325112867385, 1.000000000000000000, 0.9238795325112867385, 1.000000000000000000, 0.9238795325112867385, 1.000000000000000000, 0.9238795325112867385, 1.000000000000000000, 0.9238795325112867385, 1.000000000000000000, 0.9238795325112867385, 1.000000000000000000, 0.9238795325112867385, 1.000000000000000000, 0.9238795325112867385, 1.000000000000000000, 0.9238795325112867385, 1.000000000000000000, 0.9238795325112867385, 1.000000000000000000, 0.9238795325112867385, 1.000000000000000000, 0.9238795325112867385, 1.000000000000000000, 0.9238795325112867385, 1.000000000000000000, 0.9238795325112867385, 1.000000000000000000, 0.9238795325112867385, 1.000000000000000000, 0.9238795325112867385, 1.000000000000000000, 0.9238795325112867385, 1.000000000000000000, 0.9238795325112867385, 1.000000000000000000, 0.9238795325112867385, 1.000000000000000000, 0.9238795325112867385, 1.000000000000000000, 0.9238795325112867385, 1.000000000000000000, 0.9238795325112867385, 1.000000000000000000, 0.9238795325112867385, 1.000000000000000000, 0.9238795325112867385, 1.000000000000000000, 0.9238795325112867385, 1.000000000000000000, 0.9238795325112867385, 1.000000000000000000, 0.9238795325112867385, 1.000000000000000000, 0.9238795325112867385, 1.000000000000000000, 0.9238795325112867385, 1.000000000000000000, 0.9238795325112867385, 1.000000000000000000, 0.9238795325112867385, 1.000000000000000000, 0.9238795325112867385, 1.000000000000000000, 0.9238795325112867385, 1.000000000000000000, 0.9238795325112867385, 1.000000000000000000, 0.9238795325112867385, 1.000000000000000000, 0.9238795325112867385, 1.000000000000000000, 0.9238795325112867385, 1.000000000000000000, 0.9238795325112867385, 1.000000000000000000, 0.9238795325112867385, 1.000000000000000000),
 ( 1.000000000000000000, 0.9238795325112867385, 1.000000000000000000, 0.9238795325112867385, 1.000000000000000000, 0.9238795325112867385, 1.000000000000000000, 0.9238795325112867385, 1.000000000000000000, 0.9238795325112867385, 1.000000000000000000, 0.9238795325112867385, 1.000000000000000000, 0.9238795325112867385, 1.000000000000000000, 0.9238795325112867385, 1.000000000000000000, 0.9238795325112867385, 1.000000000000000000, 0.9238795325112867385, 1.000000000000000000, 0.9238795325112867385, 1.000000000000000000, 0.9238795325112867385, 1.000000000000000000, 0.9238795325112867385, 1.000000000000000000, 0.9238795325112867385, 1.000000000000000000, 0.9238795325112867385, 1.000000000000000000, 0.9238795325112867385, 1.000000000000000000, 0.9238795325112867385, 1.000000000000000000, 0.9238795325112867385, 1.000000000000000000, 0.9238795325112867385, 1.000000000000000000, 0.9238795325112867385, 1.000000000000000000, 0.9238795325112867385, 1.000000000000000000, 0.9238795325112867385, 1.000000000000000000, 0.9238795325112867385, 1.000000000000000000, 0.9238795325112867385, 1.000000000000000000, 0.9238795325112867385, 1.000000000000000000, 0.9238795325112867385, 1.000000000000000000, 0.9238795325112867385, 1.000000000000000000, 0.9238795325112867385, 1.000000000000000000, 0.9238795325112867385, 1.000000000000000000, 0.9238795325112867385, 1.000000000000000000, 0.9238795325112867385, 1.000000000000000000, 0.9238795325112867385, 1.000000000000000000, 0.9238795325112867385, 1.000000000000000000, 0.9238795325112867385, 1.000000000000000000, 0.9238795325112867385, 1.000000000000000000, 0.9238795325112867385, 1.000000000000000000, 0.9238795325112867385, 1.000000000000000000, 0.9238795325112867385, 1.000000000000000000, 0.9238795325112867385, 1.000000000000000000, 0.9238795325112867385, 1.000000000000000000, 0.9238795325112867385, 1.000000000000000000, 0.9238795325112867385, 1.000000000000000000, 0.9238795325112867385, 1.000000000000000000, 0.9238795325112867385, 1.000000000000000000, 0.9238795325112867385, 1.000000000000000000, 0.9238795325112867385, 1.000000000000000000, 0.9238795325112867385, 1.000000000000000000, 0.9238795325112867385, 1.000000000000000000, 0.9238795325112867385, 1.000000000000000000, 0.9238795325112867385, 1.000000000000000000, 0.9238795325112867385, 1.000000000000000000, 0.9238795325112867385, 1.000000000000000000, 0.9238795325112867385, 1.000000000000000000, 0.9238795325112867385, 1.000000000000000000, 0.9238795325112867385, 1.000000000000000000, 0.9238795325112867385, 1.000000000000000000, 0.9238795325112867385, 1.000000000000000000, 0.9238795325112867385, 1.000000000000000000, 0.9238795325112867385, 1.000000000000000000, 0.9238795325112867385, 1.000000000000000000, 0.9238795325112867385, 1.000000000000000000, 0.9238795325112867385, 1.000000000000000000, 0.9238795325112867385, 1.000000000000000000, 0.9238795325112867385, 1.000000000000000000, 0.9238795325112867385, 1.000000000000000000, 0.9238795325112867385, 1.000000000000000000, 0.9238795325112867385, 1.000000000000000000, 0.9238795325112867385, 1.000000000000000000, 0.9238795325112867385, 1.000000000000000000, 0.9238795325112867385, 1.000000000000000000, 0.9238795325112867385, 1.000000000000000000, 0.9238795325112867385, 1.000000000000000000, 0.9238795325112867385, 1.000000000000000000, 0.9238795325112867385, 1.000000000000000000, 0.9238795325112867385, 1.000000000000000000, 0.9238795325112867385, 1.000000000000000000, 0.9238795325112867385, 1.000000000000000000, 0.9238795325112867385, 1.000000000000000000, 0.9238795325112867385, 1.000000000000000000, 0.9238795325112867385, 1.000000000000000000, 0.9238795325112867385, 1.000000000000000000, 0.9238795325112867385, 1.000000000000000000, 0.9238795325112867385, 1.000000000000000000, 0.9238795325112867385, 1.000000000000000000, 0.9238795325112867385, 1.000000000000000000, 0.9238795325112867385, 1.000000000000000000, 0.9238795325112867385, 1.000000000000000000, 0.9238795325112867385, 1.000000000000000000, 0.9238795325112867385, 1.000000000000000000, 0.9238795325112867385, 1.000000000000000000, 0.9238795325112867385, 1.000000000000000000, 0.9238795325112867385, 1.000000000000000000, 0.9238795325112867385, 1.000000000000000000, 0.9238795325112867385, 1.000000000000000000, 0.9238795325112867385, 1.000000000000000000, 0.9238795325112867385, 1.000000000000000000, 0.9238795325112867385, 1.000000000000000000, 0.9238795325112867385, 1.000000000000000000, 0.9238795325112867385, 1.000000000000000000, 0.9238795325112867385, 1.000000000000000000, 0.9238795325112867385, 1.000000000000000000, 0.9238795325112867385, 1.000000000000000000, 0.9238795325112867385, 1.000000000000000000, 0.9238795325112867385, 1.000000000000000000, 0.9238795325112867385, 1.000000000000000000, 0.9238795325112867385, 1.000000000000000000, 0.9238795325112867385, 1.000000000000000000, 0.9238795325112867385, 1.000000000000000000, 0.9238795325112867385, 1.000000000000000000, 0.9238795325112867385, 1.000000000000000000, 0.9238795325112867385, 1.000000000000000000, 0.9238795325112867385, 1.000000000000000000, 0.9238795325112867385, 1.000000000000000000, 0.9238795325112867385, 1.000000000000000000, 0.9238795325112867385, 1.000000000000000000, 0.9238795325112867385, 1.000000000000000000, 0.9238795325112867385, 1.000000000000000000, 0.9238795325112867385, 1.000000000000000000, 0.9238795325112867385, 1.000000000000000000, 0.9238795325112867385, 1.000000000000000000) ) ) 
 REPRESENTATION_ITEM ( '' )  SURFACE ( )  );
#20515 = DIRECTION ( 'NONE',  ( -0.000000000000000000, -1.000000000000000000, -0.000000000000000000 ) ) ;
#20516 = CARTESIAN_POINT ( 'NONE',  ( 2.977408999572650927, -7.188101187499990274, 24.83030278187175455 ) ) ;
#20517 = CARTESIAN_POINT ( 'NONE',  ( -3.042071309553164404, 157.5520833299193555, -11.35316468749999963 ) ) ;
#20518 = CARTESIAN_POINT ( 'NONE',  ( 7.999999999842164478, 5.025161467855852442E-05, 22.76780420562571905 ) ) ;
#20519 = CARTESIAN_POINT ( 'NONE',  ( -5.000000000000000000, 52.35862550122891435, 48.98731492261470777 ) ) ;
#20520 = CARTESIAN_POINT ( 'NONE',  ( 0.000000000000000000, 0.000000000000000000, -0.6301867843887376530 ) ) ;
#20523 = CARTESIAN_POINT ( 'NONE',  ( 3.313708498984706985, 109.7187500040968047, -8.000000000000055067 ) ) ;
#20522 = DIRECTION ( 'NONE',  ( -0.000000000000000000, 1.000000000000000000, -0.000000000000000000 ) ) ;
#20521 = CARTESIAN_POINT ( 'NONE',  ( 26.34314575050758833, 201.9375000000000284, 173.9999999999999147 ) ) ;
#20524 = ORIENTED_EDGE ( 'NONE', *, *, #43571, .F. ) ;
#20525 = CARTESIAN_POINT ( 'NONE',  ( 8.311093377946837890, 16.71874999658601268, -8.311093377946837890 ) ) ;
#20526 = CARTESIAN_POINT ( 'NONE',  ( 2.751064625579944321E-14, 200.8750000027312126, 194.0000000000000568 ) ) ;
#20527 = EDGE_CURVE ( 'NONE', #32479, #31223, #50269, .T. ) ;
#20529 = CARTESIAN_POINT ( 'NONE',  ( 4.898587196589415787E-16, 0.000000000000000000, 4.000000000000001776 ) ) ;
#20528 = CARTESIAN_POINT ( 'NONE',  ( -5.656854249492375253, 5.656854249492375253, 17.33030278392014623 ) ) ;
#20530 = FACE_OUTER_BOUND ( 'NONE', #35831, .T. ) ;
#20531 = CARTESIAN_POINT ( 'NONE',  ( -2.839093476692135984E-14, 201.6875000013656063, 138.5412658750000503 ) ) ;
#20532 = VECTOR ( 'NONE', #54313, 1000.000000000000000 ) ;
#20533 = CARTESIAN_POINT ( 'NONE',  ( -8.660254037844387298, 43.95833332650536818, -5.000000000000004441 ) ) ;
#20534 = CARTESIAN_POINT ( 'NONE',  ( -2.977408999572650927, 108.8750000020483810, -7.188101187500001821 ) ) ;
#20535 = CARTESIAN_POINT ( 'NONE',  ( -4.541265875000002339, 7.874999998634407028, -1.881053915767121998 ) ) ;
#20536 = CARTESIAN_POINT ( 'NONE',  ( 1.110124581937998163E-11, 98.75000000000088107, 10.00000000000000533 ) ) ;
#20537 = CARTESIAN_POINT ( 'NONE',  ( -3.313708498984757167, 7.999999999999991118, 11.04905277982336642 ) ) ;
#20539 = DIRECTION ( 'NONE',  ( 0.000000000000000000, 0.000000000000000000, 1.000000000000000000 ) ) ;
#20538 = CARTESIAN_POINT ( 'NONE',  ( 11.00000000000000000, 1.347111479062088405E-15, 118.0000000000000000 ) ) ;
#20540 = ORIENTED_EDGE ( 'NONE', *, *, #35871, .F. ) ;
#20541 = ORIENTED_EDGE ( 'NONE', *, *, #33953, .F. ) ;
#20542 = ADVANCED_FACE ( 'NONE', ( #67753 ), #225, .T. ) ;
#20543 = CARTESIAN_POINT ( 'NONE',  ( 9.797174393178825657E-16, 125.0000000000000000, -8.000000000000000000 ) ) ;
#20544 = CARTESIAN_POINT ( 'NONE',  ( -5.656854249492375253, 5.656854249492375253, 2.142802779823364645 ) ) ;
#20545 = DIRECTION ( 'NONE',  ( -0.000000000000000000, 1.000000000000000000, -0.000000000000000000 ) ) ;
#20546 = CARTESIAN_POINT ( 'NONE',  ( 9.832129032723416984, 125.3645833299193413, 5.676582343750006032 ) ) ;
#20547 = VERTEX_POINT ( 'NONE', #39812 ) ;
#20548 = CARTESIAN_POINT ( 'NONE',  ( -5.000000000000000000, 10.28295106684163684, -65.17663434001590872 ) ) ;
#20549 = AXIS2_PLACEMENT_3D ( 'NONE', #37194, #36091, #54927 ) ;
#20550 = CARTESIAN_POINT ( 'NONE',  ( -7.204075437095965206, -7.204075437095968759, 94.84375000204838102 ) ) ;
#20551 = DIRECTION ( 'NONE',  ( 0.000000000000000000, -0.000000000000000000, -1.000000000000000000 ) ) ;
#20552 = CARTESIAN_POINT ( 'NONE',  ( -3.458734124999960358, 198.6250000013655779, 196.5673454167823877 ) ) ;
#20553 = CARTESIAN_POINT ( 'NONE',  ( -1.836970198721029983E-15, 155.6249999931720254, 10.00000000000000178 ) ) ;
#20555 = CARTESIAN_POINT ( 'NONE',  ( 11.35316468750000141, 125.7812499965860127, 0.000000000000000000 ) ) ;
#20554 = LINE ( 'NONE', #32651, #13515 ) ;
#20556 = CYLINDRICAL_SURFACE ( 'NONE', #45758, 8.000000000000000000 ) ;
#20557 = ORIENTED_EDGE ( 'NONE', *, *, #49032, .F. ) ;
#20558 = ADVANCED_FACE ( 'NONE', ( #57178 ), #73404, .T. ) ;
#20559 = CARTESIAN_POINT ( 'NONE',  ( -1.836970198721029983E-15, 50.62499999317203248, 10.00000000000000178 ) ) ;
#20560 = CARTESIAN_POINT ( 'NONE',  ( -31.08702224745096032, 174.0168584738444792, 170.2012752884367899 ) ) ;
#20561 = CARTESIAN_POINT ( 'NONE',  ( -3.042071309553173730, 114.6354166632526983, 11.35316468749999785 ) ) ;
#20562 = CARTESIAN_POINT ( 'NONE',  ( 3.458734125000015425, 208.0000000013656063, 196.5673454167823877 ) ) ;
#20563 = CARTESIAN_POINT ( 'NONE',  ( -7.188101187500000933, 16.49999999795161543, -2.977408999572651371 ) ) ;
#20564 = CARTESIAN_POINT ( 'NONE',  ( -4.220049686691935698, 10.18810118749999916, 87.25000000204838102 ) ) ;
#20565 = CARTESIAN_POINT ( 'NONE',  ( 8.311093377946837890, 21.71874999658601268, -8.311093377946837890 ) ) ;
#20566 = ORIENTED_EDGE ( 'NONE', *, *, #4747, .F. ) ;
#20567 = LINE ( 'NONE', #20188, #4296 ) ;
#20568 = ADVANCED_FACE ( 'NONE', ( #28495 ), #68118, .T. ) ;
#20569 = CARTESIAN_POINT ( 'NONE',  ( 8.008118988124993010, -3.317071493978877239, 25.66936528394063188 ) ) ;
#20570 = CARTESIAN_POINT ( 'NONE',  ( 8.660254037844389075, 237.0833333333333428, 4.999999999999997335 ) ) ;
#20571 = CARTESIAN_POINT ( 'NONE',  ( -4.556349186104048599, -10.99999999999999822, 85.46875000409677625 ) ) ;
#20572 = CARTESIAN_POINT ( 'NONE',  ( -7.188101187500001821, 5.624999997951611874, -2.977408999572651371 ) ) ;
#20573 = CARTESIAN_POINT ( 'NONE',  ( -3.673940397442060854E-16, 298.8125000034140157, -6.000000000000001776 ) ) ;
#20574 = CARTESIAN_POINT ( 'NONE',  ( -5.857492637593530560, -5.043103725236133705, -0.1555707967503436318 ) ) ;
#20575 = DIRECTION ( 'NONE',  ( 1.000000000000000000, -0.000000000000000000, -0.000000000000000000 ) ) ;
#20577 = ORIENTED_EDGE ( 'NONE', *, *, #35781, .F. ) ;
#20576 = VECTOR ( 'NONE', #37990, 1000.000000000000000 ) ;
#20578 = CARTESIAN_POINT ( 'NONE',  ( 11.35316468750000141, 146.0937499965860411, 0.000000000000000000 ) ) ;
#20579 = CARTESIAN_POINT ( 'NONE',  ( 4.220049686691934809, 10.18810118749999916, 85.18750000204838102 ) ) ;
#20580 = EDGE_CURVE ( 'NONE', #51233, #45113, #6430, .T. ) ;
#20581 = CARTESIAN_POINT ( 'NONE',  ( -24.54126587499999346, 198.1875000013655779, 170.0000000000003411 ) ) ;
#20582 = CARTESIAN_POINT ( 'NONE',  ( 3.313708498984756279, 7.999999999999991118, 21.36155277982336642 ) ) ;
#20583 = CARTESIAN_POINT ( 'NONE',  ( 4.541265875000001451, 15.37499999863440969, 1.881053915767124440 ) ) ;
#20584 = ORIENTED_EDGE ( 'NONE', *, *, #8899, .T. ) ;
#20585 = CARTESIAN_POINT ( 'NONE',  ( -1.656854249492347719, 204.9375000027312410, 194.0000000000000853 ) ) ;
#20586 = CARTESIAN_POINT ( 'NONE',  ( -2.839093476692135984E-14, 200.9375000013656063, 138.5412658750000503 ) ) ;
#20587 = CARTESIAN_POINT ( 'NONE',  ( -4.000000000000015987, 202.6250000027312126, 142.0000000000000568 ) ) ;
#20588 = CARTESIAN_POINT ( 'NONE',  ( -5.656854249492375253, 5.656854249492375253, 14.14280277982336465 ) ) ;
#20589 = EDGE_LOOP ( 'NONE', ( #31363, #40735, #13, #57205 ) ) ;
#20590 = CARTESIAN_POINT ( 'NONE',  ( 2.977408999572652260, 13.68749999795161187, 7.188101187500000044 ) ) ;
#20591 = CARTESIAN_POINT ( 'NONE',  ( 11.00000000000000355, -4.556349186104044158, 76.65625000000000000 ) ) ;
#20592 = CYLINDRICAL_SURFACE ( 'NONE', #27050, 6.000000000000001776 ) ;
#20593 = CARTESIAN_POINT ( 'NONE',  ( 8.311093377946837890, 181.4062499965860411, -8.311093377946837890 ) ) ;
#20594 = CARTESIAN_POINT ( 'NONE',  ( -4.401442555609581635E-16, 110.6562500020483810, -7.188101187500000044 ) ) ;
#20595 = AXIS2_PLACEMENT_3D ( 'NONE', #12207, #58262, #31039 ) ;
#20596 = CARTESIAN_POINT ( 'NONE',  ( -5.000000000000000000, -60.90295814858238543, -23.31388853594834032 ) ) ;
#20597 = CARTESIAN_POINT ( 'NONE',  ( -6.676582343750002480, 291.3906250017070079, -2.765530957081996810 ) ) ;
#20599 = LINE ( 'NONE', #4384, #60267 ) ;
#20598 = CARTESIAN_POINT ( 'NONE',  ( -3.042071309553159075, 224.9479166700806445, 11.35316468749999963 ) ) ;
#20600 = VERTEX_POINT ( 'NONE', #4376 ) ;
#20601 = CARTESIAN_POINT ( 'NONE',  ( -3.042071309553159075, 259.9479166700807014, 11.35316468749999963 ) ) ;
#20602 = CARTESIAN_POINT ( 'NONE',  ( 7.188101187499993827, -2.977408999572645598, 0.6428027818717528818 ) ) ;
#20603 = MECHANICAL_DESIGN_GEOMETRIC_PRESENTATION_REPRESENTATION (  '', ( #53162 ), #39967 ) ;
#20604 = DIRECTION ( 'NONE',  ( 0.000000000000000000, 0.000000000000000000, 1.000000000000000000 ) ) ;
#20605 = CARTESIAN_POINT ( 'NONE',  ( 8.000000000000000000, 19.40624999590322375, -3.313708498984761164 ) ) ;
#20606 = FACE_OUTER_BOUND ( 'NONE', #861, .T. ) ;
#20607 = CARTESIAN_POINT ( 'NONE',  ( 2.839093476692135984E-14, 200.9375000013656063, 201.4587341250000350 ) ) ;
#20608 = DIRECTION ( 'NONE',  ( -0.000000000000000000, 1.000000000000000000, -0.000000000000000000 ) ) ;
#20609 = CARTESIAN_POINT ( 'NONE',  ( 11.00000000000005151, 4.556349186103993532, 114.3437500000000142 ) ) ;
#20610 = CARTESIAN_POINT ( 'NONE',  ( 8.000000000000001776, 95.65625000000002842, 3.313708498984759387 ) ) ;
#20611 = CARTESIAN_POINT ( 'NONE',  ( -11.35316468750000141, 108.8020833299193555, 3.042071309553159963 ) ) ;
#20612 = CARTESIAN_POINT ( 'NONE',  ( 3.313708498984711426, 98.46875000000001421, 8.000000000000053291 ) ) ;
#20613 = CARTESIAN_POINT ( 'NONE',  ( 2.020667218593132706E-15, -11.00000000000000000, 73.37500000000000000 ) ) ;
#20614 = CIRCLE ( 'NONE', #72443, 6.000000000000000000 ) ;
#20617 = CARTESIAN_POINT ( 'NONE',  ( 11.49999999999998046, 82.00000000000001421, 65.00000000000000000 ) ) ;
#20616 = CARTESIAN_POINT ( 'NONE',  ( 24.54126587499999346, 201.1875000013656063, 169.9999999999999432 ) ) ;
#20615 = CARTESIAN_POINT ( 'NONE',  ( 30.44569435410883429, 199.0625000013656063, 167.5543056458911053 ) ) ;
#20618 = ORIENTED_EDGE ( 'NONE', *, *, #52512, .F. ) ;
#20619 = CARTESIAN_POINT ( 'NONE',  ( 28.00000000000002132, 205.1250000027312126, 173.9999999999999147 ) ) ;
#20620 = ADVANCED_FACE ( 'NONE', ( #27369 ), #33809, .F. ) ;
#20621 = DIRECTION ( 'NONE',  ( -0.000000000000000000, -1.000000000000000000, -0.000000000000000000 ) ) ;
#20622 =( BOUNDED_CURVE ( )  B_SPLINE_CURVE ( 2, ( #63749, #69416, #22634, #16224, #16595, #45287, #34738, #63372, #46401 ),
 .UNSPECIFIED., .F., .F. ) 
 B_SPLINE_CURVE_WITH_KNOTS ( ( 3, 2, 2, 2, 3 ),
 ( 0.7352941176470587648, 0.7389705882352940458, 0.7426470588235293269, 0.7463235294117646079, 0.7499999999999998890 ),
 .UNSPECIFIED. ) 
 CURVE ( )  GEOMETRIC_REPRESENTATION_ITEM ( )  RATIONAL_B_SPLINE_CURVE ( ( 1.000000000000002220, 0.9238795325112844070, 1.000000000000000000, 0.9238795325112867385, 1.000000000000000000, 0.9238795325112867385, 1.000000000000000000, 0.9238795325112890700, 0.9999999999999976685 ) ) 
 REPRESENTATION_ITEM ( '' )  );
#20623 = CARTESIAN_POINT ( 'NONE',  ( 3.458734124999959914, 195.3750000013656063, 143.4326545832176976 ) ) ;
#20624 = CARTESIAN_POINT ( 'NONE',  ( 29.43265458321760519, 196.7500000013656063, 173.4587341249998929 ) ) ;
#20625 = CARTESIAN_POINT ( 'NONE',  ( 7.778174593052023411, -7.778174593052021635, 115.7500000040967905 ) ) ;
#20626 = CARTESIAN_POINT ( 'NONE',  ( -5.676582343749998039, 192.7604166632526983, -9.832129032723420536 ) ) ;
#20627 = CARTESIAN_POINT ( 'NONE',  ( 3.594042629939374400, 89.53052393364181683, -6.225082831242716885 ) ) ;
#20628 = CARTESIAN_POINT ( 'NONE',  ( 4.951454888531130472, 225.9999999999999716, 8.768144228917044813 ) ) ;
#20629 = CARTESIAN_POINT ( 'NONE',  ( -3.211159895383562723, 19.93749999863440436, 3.211159895383561391 ) ) ;
#20630 = CARTESIAN_POINT ( 'NONE',  ( 26.56734541678237704, 196.2500000013656347, 166.5412658749999650 ) ) ;
#20631 = CARTESIAN_POINT ( 'NONE',  ( -3.313708498984758943, -7.999999999999989342, 26.61155277982337708 ) ) ;
#20632 = FACE_OUTER_BOUND ( 'NONE', #66710, .T. ) ;
#20633 = CARTESIAN_POINT ( 'NONE',  ( 5.676582343750001591, 76.61458332991935549, -9.832129032723420536 ) ) ;
#20634 = ORIENTED_EDGE ( 'NONE', *, *, #49676, .T. ) ;
#20635 = ADVANCED_FACE ( 'NONE', ( #28119 ), #30717, .T. ) ;
#20636 = LINE ( 'NONE', #50060, #23077 ) ;
#20637 = CARTESIAN_POINT ( 'NONE',  ( 2.977408999572650927, 18.74999999795161898, -7.188101187500001821 ) ) ;
#20638 = CARTESIAN_POINT ( 'NONE',  ( 10.00000000000016165, 40.00000000000009948, 0.000000000000000000 ) ) ;
#20639 = CARTESIAN_POINT ( 'NONE',  ( -1.656854249492466735, 195.1875000000000000, 201.9999999999999147 ) ) ;
#20640 = CIRCLE ( 'NONE', #62807, 10.50000000000000000 ) ;
#20641 = CARTESIAN_POINT ( 'NONE',  ( 6.951808397369818766E-16, 87.03124999658602690, -11.35316468750000141 ) ) ;
#20642 = VERTEX_POINT ( 'NONE', #2049 ) ;
#20643 = CARTESIAN_POINT ( 'NONE',  ( 10.18810118750000093, -4.220049686691933921, 86.68750000204836681 ) ) ;
#20644 = CARTESIAN_POINT ( 'NONE',  ( 10.18810118749999916, 4.220049686691935698, 110.5000000020483810 ) ) ;
#20645 = CARTESIAN_POINT ( 'NONE',  ( -25.55430564589119058, 196.5625000013656063, 167.5543056458915316 ) ) ;
#20646 = DIRECTION ( 'NONE',  ( -0.000000000000000000, 1.000000000000000000, 4.689100369878284071E-30 ) ) ;
#20647 = DIRECTION ( 'NONE',  ( 1.000000000000000000, 0.000000000000000000, 0.000000000000000000 ) ) ;
#20649 = CARTESIAN_POINT ( 'NONE',  ( 3.042071309553159519, 89.73958332991935549, 11.35316468750000141 ) ) ;
#20648 = FACE_OUTER_BOUND ( 'NONE', #25956, .T. ) ;
#20650 = CARTESIAN_POINT ( 'NONE',  ( 7.999999999999991118, 3.313708498984757611, 16.86155278392014623 ) ) ;
#20651 = CARTESIAN_POINT ( 'NONE',  ( 4.000000000000000888, 14.93750000000000178, 1.656854249492384135 ) ) ;
#20652 = CARTESIAN_POINT ( 'NONE',  ( -10.00000000000000000, 169.1666666598387110, -2.679491924311229845 ) ) ;
#20653 = CARTESIAN_POINT ( 'NONE',  ( 7.999999999999706901, -2.135495361439877059E-06, 10.76780272350167245 ) ) ;
#20654 = CARTESIAN_POINT ( 'NONE',  ( 5.000000000000000000, -52.28182290968072010, 42.43119126381040473 ) ) ;
#20655 = CARTESIAN_POINT ( 'NONE',  ( 6.951808397369818766E-16, 77.34374999658601268, -11.35316468750000141 ) ) ;
#20656 = CARTESIAN_POINT ( 'NONE',  ( 6.676582343750003368, 293.0156250017070079, -2.765530957081997254 ) ) ;
#20657 = CARTESIAN_POINT ( 'NONE',  ( 10.18810118749999916, 1.247682550866122264E-15, 109.2812500020483668 ) ) ;
#20658 = CARTESIAN_POINT ( 'NONE',  ( 8.311093377946834337, 215.1562499965860127, 8.311093377946839666 ) ) ;
#20659 = ORIENTED_EDGE ( 'NONE', *, *, #17046, .T. ) ;
#20660 = CARTESIAN_POINT ( 'NONE',  ( 11.35316468750000141, 1.093749996586016682, 0.000000000000000000 ) ) ;
#20661 = CARTESIAN_POINT ( 'NONE',  ( 1.656854249492381914, 3.562499997268812724, 4.000000000000000888 ) ) ;
#20662 = CARTESIAN_POINT ( 'NONE',  ( 0.8419854211626158769, 49.91401432488694923, 40.68947704085089612 ) ) ;
#20664 = CARTESIAN_POINT ( 'NONE',  ( -9.832129032723418760, 202.8645833299193555, -5.676582343750004256 ) ) ;
#20663 = FACE_BOUND ( 'NONE', #45072, .T. ) ;
#20665 = CARTESIAN_POINT ( 'NONE',  ( -2.828427124746208943, 203.6250000000000284, 144.8284271247462129 ) ) ;
#20666 = CARTESIAN_POINT ( 'NONE',  ( 2.679491924311235174, 244.5833333401612606, 9.999999999999998224 ) ) ;
#20667 = CARTESIAN_POINT ( 'NONE',  ( -7.320508075688770155, 253.7500000068279462, 7.320508075688774596 ) ) ;
#20668 = EDGE_LOOP ( 'NONE', ( #46627, #54621 ) ) ;
#20669 = CARTESIAN_POINT ( 'NONE',  ( 3.042071309553167513, 182.1354166632526699, -11.35316468749999785 ) ) ;
#20670 = CARTESIAN_POINT ( 'NONE',  ( 5.082755093536320601, -5.082755093536318824, 17.04905278187175810 ) ) ;
#20671 = CARTESIAN_POINT ( 'NONE',  ( 4.898587196589412829E-16, 18.37500000000000355, -8.000000000000000000 ) ) ;
#20672 = VECTOR ( 'NONE', #14592, 1000.000000000000000 ) ;
#20673 = EDGE_LOOP ( 'NONE', ( #58619, #36547, #54194 ) ) ;
#20674 = CARTESIAN_POINT ( 'NONE',  ( 3.313708498984765161, 98.65625000409679046, 7.999999999999998224 ) ) ;
#20675 = APPLICATION_CONTEXT ( 'automotive_design' ) ;
#20676 = CARTESIAN_POINT ( 'NONE',  ( -4.999999999999998224, 6.666666666666666963, -8.660254037844389075 ) ) ;
#20677 = ORIENTED_EDGE ( 'NONE', *, *, #44825, .T. ) ;
#20678 = CARTESIAN_POINT ( 'NONE',  ( -1.656854249492383691, 16.68750000000000355, 4.000000000000000888 ) ) ;
#20679 = CARTESIAN_POINT ( 'NONE',  ( 2.780723358947928197E-16, 19.56249999863440436, -4.541265875000002339 ) ) ;
#20680 = CARTESIAN_POINT ( 'NONE',  ( 7.999999999999991118, 9.797174393178815797E-16, 12.26780278392014623 ) ) ;
#20681 = CARTESIAN_POINT ( 'NONE',  ( 7.999999999521839378, -8.746674989952265200E-05, 18.26780030933659305 ) ) ;
#20682 = VECTOR ( 'NONE', #29629, 1000.000000000000000 ) ;
#20683 = ORIENTED_EDGE ( 'NONE', *, *, #70313, .T. ) ;
#20684 = CARTESIAN_POINT ( 'NONE',  ( -4.556349186104045934, 11.00000000000000000, 72.71875000000000000 ) ) ;
#20685 = CARTESIAN_POINT ( 'NONE',  ( 2.977408999572650039, 92.18750000204838102, -7.188101187500001821 ) ) ;
#20688 = FACE_OUTER_BOUND ( 'NONE', #35157, .T. ) ;
#20687 = CARTESIAN_POINT ( 'NONE',  ( -6.951808397369817780E-16, 257.6562500034140157, -11.35316468749999963 ) ) ;
#20686 = CARTESIAN_POINT ( 'NONE',  ( -7.320508075688858085, 81.87500000000008527, -7.320508075688859861 ) ) ;
#20689 =( NAMED_UNIT ( * ) SI_UNIT ( $, .STERADIAN. ) SOLID_ANGLE_UNIT ( ) );
#20690 = ORIENTED_EDGE ( 'NONE', *, *, #51947, .T. ) ;
#20691 = EDGE_CURVE ( 'NONE', #53484, #13320, #72557, .T. ) ;
#20692 = CARTESIAN_POINT ( 'NONE',  ( 4.556349186104045934, 11.00000000000000000, 83.03124999999998579 ) ) ;
#20693 = EDGE_CURVE ( 'NONE', #50134, #8029, #60390, .T. ) ;
#20694 = CARTESIAN_POINT ( 'NONE',  ( -7.188101187499992051, 0.000000000000000000, 20.98655278187175455 ) ) ;
#20695 = ORIENTED_EDGE ( 'NONE', *, *, #32311, .F. ) ;
#20696 = VERTEX_POINT ( 'NONE', #6972 ) ;
#20697 = CARTESIAN_POINT ( 'NONE',  ( -10.18810118749999916, 0.000000000000000000, 79.65625000204836681 ) ) ;
#20698 = CARTESIAN_POINT ( 'NONE',  ( -2.085542519210945728E-15, 74.84374999658602690, 11.35316468750000141 ) ) ;
#20699 = CARTESIAN_POINT ( 'NONE',  ( -5.656854249492380582, 105.5000000040967905, -5.656854249492380582 ) ) ;
#20700 = CARTESIAN_POINT ( 'NONE',  ( -7.778174593052023411, 7.778174593052023411, 89.31249999999998579 ) ) ;
#20703 = CARTESIAN_POINT ( 'NONE',  ( 2.765530957082001251, 295.9218750017069510, 6.676582343749999815 ) ) ;
#20702 = CARTESIAN_POINT ( 'NONE',  ( 32.00000000000000000, 197.3125000027312126, 171.6568542494922553 ) ) ;
#20701 = CARTESIAN_POINT ( 'NONE',  ( 0.000000000000000000, 0.000000000000000000, 0.000000000000000000 ) ) ;
#20704 = CARTESIAN_POINT ( 'NONE',  ( -10.99999999999989164, -4.556349186104158733, 83.59375000000000000 ) ) ;
#20705 = LINE ( 'NONE', #72392, #29944 ) ;
#20706 = EDGE_CURVE ( 'NONE', #67442, #24245, #72538, .T. ) ;
#20707 = CARTESIAN_POINT ( 'NONE',  ( 3.458734125000016757, 199.1250000013656347, 199.4326545832176976 ) ) ;
#20708 = CARTESIAN_POINT ( 'NONE',  ( -8.000000000000001776, 5.156249995903220196, 3.313708498984759387 ) ) ;
#20709 = CARTESIAN_POINT ( 'NONE',  ( 30.44569435410883429, 197.8125000013656063, 167.5543056458911053 ) ) ;
#20710 = CARTESIAN_POINT ( 'NONE',  ( 7.188101187499999156, 11.24999999795161187, 2.977408999572654924 ) ) ;
#20711 = AXIS2_PLACEMENT_3D ( 'NONE', #52757, #52390, #58430 ) ;
#20712 = CARTESIAN_POINT ( 'NONE',  ( 7.999999999999991118, 3.313708498984757611, 25.86155278392014623 ) ) ;
#20713 = CARTESIAN_POINT ( 'NONE',  ( -10.00000000000000000, 242.9166666734946318, -2.679491924311226292 ) ) ;
#20714 = CARTESIAN_POINT ( 'NONE',  ( -4.401442555609581635E-16, 107.6562500020483810, -7.188101187500000044 ) ) ;
#20716 = CARTESIAN_POINT ( 'NONE',  ( 0.000000000000000000, 125.0000000000000000, 8.000000000000000000 ) ) ;
#20715 = CARTESIAN_POINT ( 'NONE',  ( -4.999999999999998224, 18.54166665983870033, -8.660254037844389075 ) ) ;
#20717 = CARTESIAN_POINT ( 'NONE',  ( 11.00000000000000000, 1.347111479062088405E-15, 99.43750000409677625 ) ) ;
#20718 = CARTESIAN_POINT ( 'NONE',  ( 2.977408999572650927, -7.188101187499990274, 15.83030278187175277 ) ) ;
#20719 = CARTESIAN_POINT ( 'NONE',  ( -1.656854249492403008, 208.8125000027312126, 146.0000000000000284 ) ) ;
#20720 = CARTESIAN_POINT ( 'NONE',  ( 9.832129032723416984, 40.36458332991934839, 5.676582343750006032 ) ) ;
#20721 = CARTESIAN_POINT ( 'NONE',  ( 23.99999999999998934, 200.7500000000000000, 169.9999999999998863 ) ) ;
#20722 = CARTESIAN_POINT ( 'NONE',  ( 7.320508075688774596, 2.499999993172032031, -7.320508075688774596 ) ) ;
#20723 = CARTESIAN_POINT ( 'NONE',  ( -10.99999999999996092, 4.556349186104085902, 112.0937500040967620 ) ) ;
#20724 = ORIENTED_EDGE ( 'NONE', *, *, #8155, .F. ) ;
#20725 = CARTESIAN_POINT ( 'NONE',  ( 10.00000000000000000, 141.6666666598387110, 2.679491924311235618 ) ) ;
#20726 = CARTESIAN_POINT ( 'NONE',  ( -11.00000000000000533, -11.00000000000000355, 20.00000000000000000 ) ) ;
#20727 = CARTESIAN_POINT ( 'NONE',  ( -11.35316468750000141, 48.28124999658601268, -1.390361679473963753E-15 ) ) ;
#20728 = CARTESIAN_POINT ( 'NONE',  ( -11.00000000000000000, 4.556349186104045934, 79.09375000409676204 ) ) ;
#20729 = CARTESIAN_POINT ( 'NONE',  ( 3.458734124999960358, 203.6250000013656063, 143.4326545832176976 ) ) ;
#20730 = DIRECTION ( 'NONE',  ( 0.000000000000000000, 0.000000000000000000, -1.000000000000000000 ) ) ;
#20731 = DIRECTION ( 'NONE',  ( -1.000000000000000000, 0.000000000000000000, 0.000000000000000000 ) ) ;
#20733 = CARTESIAN_POINT ( 'NONE',  ( -3.042071309553163960, 47.23958332991934839, -11.35316468749999963 ) ) ;
#20732 = CARTESIAN_POINT ( 'NONE',  ( 7.188101187500000933, 98.00000000204838102, -2.977408999572651371 ) ) ;
#20734 = CARTESIAN_POINT ( 'NONE',  ( 3.313708498984756279, 7.999999999999991118, 9.361552779823366421 ) ) ;
#20735 = DIRECTION ( 'NONE',  ( 1.000000000000000000, 0.000000000000000000, 0.000000000000000000 ) ) ;
#20736 = CARTESIAN_POINT ( 'NONE',  ( 11.35316468750000141, 160.7812499965860127, 0.000000000000000000 ) ) ;
#20737 = CARTESIAN_POINT ( 'NONE',  ( -8.660254037844387298, 123.9583333265053682, -5.000000000000004441 ) ) ;
#20738 = CIRCLE ( 'NONE', #62907, 19.00000000000000355 ) ;
#20739 = CARTESIAN_POINT ( 'NONE',  ( 5.082755093536326818, 110.0937500020483810, 5.082755093536325042 ) ) ;
#20740 = ORIENTED_EDGE ( 'NONE', *, *, #68045, .T. ) ;
#20741 = LINE ( 'NONE', #66393, #53286 ) ;
#20742 = CARTESIAN_POINT ( 'NONE',  ( -8.311093377946836114, 17.96874999658601624, -8.311093377946837890 ) ) ;
#20743 =( BOUNDED_CURVE ( )  B_SPLINE_CURVE ( 2, ( #47568, #23083, #18173, #24191, #6852, #11768, #40811, #11400, #6491 ),
 .UNSPECIFIED., .F., .F. ) 
 B_SPLINE_CURVE_WITH_KNOTS ( ( 3, 2, 2, 2, 3 ),
 ( 0.3088235294117646079, 0.3124999999999998890, 0.3161764705882351700, 0.3198529411764704511, 0.3235294117647057877 ),
 .UNSPECIFIED. ) 
 CURVE ( )  GEOMETRIC_REPRESENTATION_ITEM ( )  RATIONAL_B_SPLINE_CURVE ( ( 1.000000000000002220, 0.9238795325112844070, 1.000000000000000000, 0.9238795325112867385, 1.000000000000000000, 0.9238795325112867385, 1.000000000000000000, 0.9238795325112890700, 0.9999999999999976685 ) ) 
 REPRESENTATION_ITEM ( '' )  );
#20744 = CARTESIAN_POINT ( 'NONE',  ( -1.656854249492433206, 197.1875000000000284, 201.9999999999999432 ) ) ;
#20745 = VERTEX_POINT ( 'NONE', #29248 ) ;
#20746 = DIRECTION ( 'NONE',  ( -0.000000000000000000, -0.000000000000000000, -1.000000000000000000 ) ) ;
#20747 = CARTESIAN_POINT ( 'NONE',  ( 1.871523826299183495E-15, -10.18810118749999916, 77.03125000204836681 ) ) ;
#20748 = CARTESIAN_POINT ( 'NONE',  ( -31.05507224581699077, -34.98990058138039672, 171.9999999999997726 ) ) ;
#20750 = CARTESIAN_POINT ( 'NONE',  ( 5.676582343749993598, 149.9479166632526983, 9.832129032723422313 ) ) ;
#20749 = DIRECTION ( 'NONE',  ( -0.000000000000000000, -0.000000000000000000, 1.000000000000000000 ) ) ;
#20751 = CARTESIAN_POINT ( 'NONE',  ( -5.082755093536325042, 2.906249997951610542, -5.082755093536325930 ) ) ;
#20752 = CARTESIAN_POINT ( 'NONE',  ( -5.656854249492373476, -5.656854249492376141, 13.07405278432982421 ) ) ;
#20753 = VECTOR ( 'NONE', #50336, 1000.000000000000000 ) ;
#20754 = CARTESIAN_POINT ( 'NONE',  ( -21.65224809748203683, -26.17991689200315975, 192.1888153259819489 ) ) ;
#20755 = CARTESIAN_POINT ( 'NONE',  ( 8.311093377946839666, 230.7812500034139589, 8.311093377946829008 ) ) ;
#20756 = CARTESIAN_POINT ( 'NONE',  ( 4.220049686691941027, -10.18810118749999738, 88.00000000204836681 ) ) ;
#20757 = EDGE_LOOP ( 'NONE', ( #42295, #30030, #30272, #23002 ) ) ;
#20758 = DIRECTION ( 'NONE',  ( -1.000000000000000000, 0.000000000000000000, 0.000000000000000000 ) ) ;
#20759 = CARTESIAN_POINT ( 'NONE',  ( -1.836970198721029983E-15, 155.6249999931720254, 10.00000000000000178 ) ) ;
#20760 = CARTESIAN_POINT ( 'NONE',  ( 8.311093377946837890, 106.7187499965860269, -8.311093377946837890 ) ) ;
#20761 = CARTESIAN_POINT ( 'NONE',  ( -10.18810118749999916, 0.000000000000000000, 94.65625000204836681 ) ) ;
#20762 = CARTESIAN_POINT ( 'NONE',  ( 3.211159895383561835, 20.56249999863440436, -3.211159895383561835 ) ) ;
#20763 = ORIENTED_EDGE ( 'NONE', *, *, #61637, .T. ) ;
#20764 = ORIENTED_EDGE ( 'NONE', *, *, #34386, .F. ) ;
#20765 = CARTESIAN_POINT ( 'NONE',  ( 1.881053915767122664, 4.249999998634406140, 4.541265875000001451 ) ) ;
#20766 = CARTESIAN_POINT ( 'NONE',  ( 4.401442555609581635E-16, 8.343749997951611874, -7.188101187500000044 ) ) ;
#20767 = CARTESIAN_POINT ( 'NONE',  ( 3.313708498984765161, 115.1562500040967763, 7.999999999999998224 ) ) ;
#20768 = CARTESIAN_POINT ( 'NONE',  ( 4.220049686691934809, 10.18810118749999916, 93.06250000204839523 ) ) ;
#20769 = CARTESIAN_POINT ( 'NONE',  ( -25.55430564589115150, 202.3125000013656063, 172.4456943541091789 ) ) ;
#20770 = EDGE_CURVE ( 'NONE', #49077, #44710, #70352, .T. ) ;
#20771 = CARTESIAN_POINT ( 'NONE',  ( -5.000000000000005329, 160.2083333265053966, 8.660254037844387298 ) ) ;
#20772 = CARTESIAN_POINT ( 'NONE',  ( 1.656854249492381248, 4.187500000000000000, -4.000000000000001776 ) ) ;
#20773 = CARTESIAN_POINT ( 'NONE',  ( -4.000000000000002665, 16.31249999726881228, 1.656854249492380804 ) ) ;
#20774 = CARTESIAN_POINT ( 'NONE',  ( 3.211159895383560947, 4.187499998634407028, 3.211159895383562723 ) ) ;
#20775 = CARTESIAN_POINT ( 'NONE',  ( -2.828427124746208943, 203.6250000000000284, 144.8284271247462129 ) ) ;
#20776 = EDGE_LOOP ( 'NONE', ( #27523, #66144, #17032, #7628 ) ) ;
#20777 = CARTESIAN_POINT ( 'NONE',  ( 2.754378923186476579E-14, 196.1875000013655779, 194.5412658750000219 ) ) ;
#20779 = CARTESIAN_POINT ( 'NONE',  ( -18.00000000000000000, 0.000000000000000000, -20.69999999999999929 ) ) ;
#20778 = CARTESIAN_POINT ( 'NONE',  ( -29.43265458321755901, 198.8750000013656347, 173.4587341250004044 ) ) ;
#20780 = CARTESIAN_POINT ( 'NONE',  ( 3.211159895383560947, 17.18749999863440792, 3.211159895383562723 ) ) ;
#20781 = AXIS2_PLACEMENT_3D ( 'NONE', #14308, #36971, #8293 ) ;
#20782 = CARTESIAN_POINT ( 'NONE',  ( 2.385186104111669980, -46.83003044365979406, 151.1499900409714030 ) ) ;
#20783 = CARTESIAN_POINT ( 'NONE',  ( 1.320432766682872962E-15, -7.188101187499992051, 4.861552781871752771 ) ) ;
#20784 = ORIENTED_EDGE ( 'NONE', *, *, #38615, .F. ) ;
#20785 = ORIENTED_EDGE ( 'NONE', *, *, #24459, .F. ) ;
#20786 = CARTESIAN_POINT ( 'NONE',  ( -4.220049686691937474, -10.18810118749999738, 100.9375000020483810 ) ) ;
#20787 = CARTESIAN_POINT ( 'NONE',  ( 10.00000000000000178, 124.7916666666666572, 2.679491924311236062 ) ) ;
#20788 = CARTESIAN_POINT ( 'NONE',  ( -29.43265458321760519, 203.1250000013656347, 173.4587341250003760 ) ) ;
#20789 = CARTESIAN_POINT ( 'NONE',  ( -23.99999999999998934, 200.7500000000000000, 170.0000000000003411 ) ) ;
#20790 = CARTESIAN_POINT ( 'NONE',  ( 3.458734125000015425, 207.2500000013655779, 196.5673454167823877 ) ) ;
#20791 = CARTESIAN_POINT ( 'NONE',  ( 10.00000000000007638, 59.79166666666671404, 2.679491924311256490 ) ) ;
#20792 = CARTESIAN_POINT ( 'NONE',  ( 2.679491924311222739, 103.9583333333333144, 10.00000000000000355 ) ) ;
#20793 = VECTOR ( 'NONE', #52140, 1000.000000000000000 ) ;
#20794 = EDGE_CURVE ( 'NONE', #43772, #13303, #58666, .T. ) ;
#20795 = EDGE_CURVE ( 'NONE', #43894, #24721, #5997, .T. ) ;
#20796 = CARTESIAN_POINT ( 'NONE',  ( -3.313708498984762052, 112.7187499999999858, -8.000000000000000000 ) ) ;
#20797 = CARTESIAN_POINT ( 'NONE',  ( -6.676582343750000703, 291.6718750017069510, 2.765530957082001251 ) ) ;
#20798 = CARTESIAN_POINT ( 'NONE',  ( 5.082755093536318824, 5.082755093536319713, 8.799052781871752771 ) ) ;
#20799 = ORIENTED_EDGE ( 'NONE', *, *, #25214, .T. ) ;
#20800 = CARTESIAN_POINT ( 'NONE',  ( 4.898587196589412829E-16, 19.87500000000000355, -8.000000000000000000 ) ) ;
#20801 = CARTESIAN_POINT ( 'NONE',  ( -5.656854249492379694, 19.87499999590322020, -5.656854249492380582 ) ) ;
#20802 = CARTESIAN_POINT ( 'NONE',  ( 2.445694354108782775, 203.5625000013656063, 139.5543056458912190 ) ) ;
#20803 = DIRECTION ( 'NONE',  ( -0.000000000000000000, -1.000000000000000000, -0.000000000000000000 ) ) ;
#20805 = CARTESIAN_POINT ( 'NONE',  ( -3.458734125000015869, 203.1875000013656063, 142.0000000000000568 ) ) ;
#20804 = FACE_OUTER_BOUND ( 'NONE', #49673, .T. ) ;
#20806 = CARTESIAN_POINT ( 'NONE',  ( 11.35316468749999963, 256.5104166700807014, 3.042071309553159519 ) ) ;
#20807 = LINE ( 'NONE', #25950, #49582 ) ;
#20808 = DIRECTION ( 'NONE',  ( 0.000000000000000000, 0.000000000000000000, 1.000000000000000000 ) ) ;
#20809 = CARTESIAN_POINT ( 'NONE',  ( 9.832129032723420536, 1.197916663252682978, -5.676582343749999815 ) ) ;
#20810 = CARTESIAN_POINT ( 'NONE',  ( 7.188101187499992051, 2.977408999572647819, 4.205302781871752771 ) ) ;
#20811 = CARTESIAN_POINT ( 'NONE',  ( -3.042071309553173730, 199.6354166632526699, 11.35316468749999785 ) ) ;
#20812 = CARTESIAN_POINT ( 'NONE',  ( -8.660254037844390851, 134.7916666598387110, 4.999999999999998224 ) ) ;
#20813 = CARTESIAN_POINT ( 'NONE',  ( -4.541265875000002339, 6.812499998634407028, -5.561446717895856393E-16 ) ) ;
#20814 = CARTESIAN_POINT ( 'NONE',  ( -32.00000000000000711, 198.1875000000000853, 168.3431457505080289 ) ) ;
#20816 = DIRECTION ( 'NONE',  ( -1.000000000000000000, 0.000000000000000000, -1.836970198721037823E-16 ) ) ;
#20815 = DIRECTION ( 'NONE',  ( 0.000000000000000000, 0.000000000000000000, 1.000000000000000000 ) ) ;
#20817 = EDGE_LOOP ( 'NONE', ( #41390, #31892, #61691 ) ) ;
#20818 = CARTESIAN_POINT ( 'NONE',  ( 1.432654583217607414, 206.5000000013655779, 145.4587341250000634 ) ) ;
#20819 = CARTESIAN_POINT ( 'NONE',  ( 6.951808397369818766E-16, 12.03124999658601801, -11.35316468750000141 ) ) ;
#20820 = CARTESIAN_POINT ( 'NONE',  ( 4.556349186104045934, 11.00000000000000000, 96.71875000409677625 ) ) ;
#20821 = CARTESIAN_POINT ( 'NONE',  ( -1.656854249492453857, 205.6875000000000000, 146.0000000000000284 ) ) ;
#20822 = ADVANCED_FACE ( 'NONE', ( #18292 ), #12621, .T. ) ;
#20823 = CARTESIAN_POINT ( 'NONE',  ( -27.99999999999991829, 200.9375000013656063, 173.4587341250003760 ) ) ;
#20824 = CARTESIAN_POINT ( 'NONE',  ( 0.000000000000000000, 0.000000000000000000, -14.80000000000000071 ) ) ;
#20826 = DIRECTION ( 'NONE',  ( -0.000000000000000000, 1.000000000000000000, -4.476705744456276341E-16 ) ) ;
#20825 = CARTESIAN_POINT ( 'NONE',  ( 1.320432766682874540E-15, 115.5312500020483952, 7.188101187500000044 ) ) ;
#20827 = CARTESIAN_POINT ( 'NONE',  ( -4.898587196589407898E-16, 7.999999999999991118, 24.45530277982336642 ) ) ;
#20828 = CARTESIAN_POINT ( 'NONE',  ( 5.676582343750001591, 121.6145833299193555, -9.832129032723420536 ) ) ;
#20829 = CARTESIAN_POINT ( 'NONE',  ( -7.320508075688778149, 84.99999999317203958, 7.320508075688769267 ) ) ;
#20830 = CARTESIAN_POINT ( 'NONE',  ( 5.082755093536325042, 123.9687500020483952, -5.082755093536325930 ) ) ;
#20831 = CARTESIAN_POINT ( 'NONE',  ( 4.541265875000002339, 20.49999999863440436, -1.881053915767121554 ) ) ;
#20832 = CARTESIAN_POINT ( 'NONE',  ( 1.469576158976822172E-15, -7.999999999999991118, 25.39280278392014978 ) ) ;
#20833 = CARTESIAN_POINT ( 'NONE',  ( 4.999999999999997335, 144.1666666666666572, 8.660254037844396180 ) ) ;
#20834 = ORIENTED_EDGE ( 'NONE', *, *, #14936, .T. ) ;
#20835 = DIRECTION ( 'NONE',  ( 0.000000000000000000, 0.000000000000000000, 1.000000000000000000 ) ) ;
#20836 = CARTESIAN_POINT ( 'NONE',  ( 4.721056650416000089, 287.9843750017070079, 4.721056650415999201 ) ) ;
#20837 = DIRECTION ( 'NONE',  ( -0.000000000000000000, 1.000000000000000000, -1.563033456626094573E-30 ) ) ;
#20838 = CARTESIAN_POINT ( 'NONE',  ( -3.313708498984757167, 7.999999999999991118, 3.736552783920145338 ) ) ;
#20839 = LINE ( 'NONE', #67252, #57370 ) ;
#20840 = CARTESIAN_POINT ( 'NONE',  ( 10.00000000000000178, 207.0833333265053966, -2.679491924311226736 ) ) ;
#20841 = CARTESIAN_POINT ( 'NONE',  ( -10.99999999999978861, 4.556349186104256432, 69.90625000000000000 ) ) ;
#20842 = CARTESIAN_POINT ( 'NONE',  ( 4.220049686691941027, -10.18810118749999738, 101.5000000020483810 ) ) ;
#20843 = ORIENTED_EDGE ( 'NONE', *, *, #35143, .F. ) ;
#20844 =( BOUNDED_CURVE ( )  B_SPLINE_CURVE ( 2, ( #23201, #39808, #5124, #5864, #28860, #51881, #57174, #62812, #5490, #63560, #46213, #45462, #41302 ),
 .UNSPECIFIED., .F., .F. ) 
 B_SPLINE_CURVE_WITH_KNOTS ( ( 3, 2, 2, 2, 2, 2, 3 ),
 ( 0.7064942623220252793, 0.7117267818841473970, 0.7169593014462694036, 0.7221918210083915213, 0.7274243405705135279, 0.7326568601326356456, 0.7378893796947577632 ),
 .UNSPECIFIED. ) 
 CURVE ( )  GEOMETRIC_REPRESENTATION_ITEM ( )  RATIONAL_B_SPLINE_CURVE ( ( 1.000000000000000000, 0.9659258262890683122, 1.000000000000000000, 0.9659258262890683122, 1.000000000000000000, 0.9659258262890683122, 1.000000000000000000, 0.9659258262890683122, 1.000000000000000000, 0.9659258262890683122, 1.000000000000000000, 0.9659258262891518010, 0.9999999999999165112 ) ) 
 REPRESENTATION_ITEM ( '' )  );
#20845 = DIRECTION ( 'NONE',  ( 0.000000000000000000, -1.000000000000000000, 0.000000000000000000 ) ) ;
#20846 = CARTESIAN_POINT ( 'NONE',  ( 9.832129032723416984, 155.6770833299193555, 5.676582343750006032 ) ) ;
#20847 = CARTESIAN_POINT ( 'NONE',  ( -8.660254037844392627, 217.9166666666666856, 5.000000000000000000 ) ) ;
#20848 = CARTESIAN_POINT ( 'NONE',  ( -1.432654583217607414, 205.5000000013655779, 194.5412658750000219 ) ) ;
#20849 = CARTESIAN_POINT ( 'NONE',  ( -10.18810118749999916, 0.000000000000000000, 68.03125000204838102 ) ) ;
#20850 = CARTESIAN_POINT ( 'NONE',  ( -5.676582343750006032, 64.42708332991935549, 9.832129032723418760 ) ) ;
#20851 = ORIENTED_EDGE ( 'NONE', *, *, #22674, .F. ) ;
#20852 = CARTESIAN_POINT ( 'NONE',  ( 10.18810118749999916, 4.220049686691935698, 110.5000000020483810 ) ) ;
#20853 = CARTESIAN_POINT ( 'NONE',  ( 2.780723358947928197E-16, 8.687499998634407916, -4.541265875000002339 ) ) ;
#20854 = ORIENTED_EDGE ( 'NONE', *, *, #3468, .T. ) ;
#20855 = CARTESIAN_POINT ( 'NONE',  ( -2.977408999572650039, 18.93749999795161187, -7.188101187500001821 ) ) ;
#20856 = CARTESIAN_POINT ( 'NONE',  ( 2.485281374238571317, 289.7500000034140157, -6.000000000000003553 ) ) ;
#20857 = LINE ( 'NONE', #34446, #35376 ) ;
#20858 = CARTESIAN_POINT ( 'NONE',  ( 5.082755093536325930, 19.03124999795161543, -5.082755093536325930 ) ) ;
#20859 = CARTESIAN_POINT ( 'NONE',  ( -5.082755093536319713, 5.082755093536319713, 4.299052781871752771 ) ) ;
#20860 =( BOUNDED_CURVE ( )  B_SPLINE_CURVE ( 2, ( #73622, #21927, #33652, #38926, #10626, #56657, #21560, #5710, #61927 ),
 .UNSPECIFIED., .F., .F. ) 
 B_SPLINE_CURVE_WITH_KNOTS ( ( 3, 2, 2, 2, 3 ),
 ( 0.5735294117647057321, 0.5772058823529410132, 0.5808823529411764053, 0.5845588235294116863, 0.5882352941176469674 ),
 .UNSPECIFIED. ) 
 CURVE ( )  GEOMETRIC_REPRESENTATION_ITEM ( )  RATIONAL_B_SPLINE_CURVE ( ( 1.000000000000002220, 0.9238795325112844070, 1.000000000000000000, 0.9238795325112867385, 1.000000000000000000, 0.9238795325112867385, 1.000000000000000000, 0.9238795325112890700, 0.9999999999999976685 ) ) 
 REPRESENTATION_ITEM ( '' )  );
#20861 = CARTESIAN_POINT ( 'NONE',  ( 10.18810118749999916, 4.220049686691935698, 109.3750000020483810 ) ) ;
#20862 = FACE_OUTER_BOUND ( 'NONE', #42506, .T. ) ;
#20863 = CARTESIAN_POINT ( 'NONE',  ( 1.656854249492381248, 5.937499997268813168, -4.000000000000001776 ) ) ;
#20864 = CARTESIAN_POINT ( 'NONE',  ( -32.00000000000003553, 208.3125000027312126, 168.3431457505080573 ) ) ;
#20865 = ORIENTED_EDGE ( 'NONE', *, *, #11782, .F. ) ;
#20866 = EDGE_CURVE ( 'NONE', #27257, #17726, #29616, .T. ) ;
#20867 = CARTESIAN_POINT ( 'NONE',  ( 3.458734125000015425, 206.9375000013656063, 198.0000000000000284 ) ) ;
#20868 = CARTESIAN_POINT ( 'NONE',  ( -31.45873412499999944, 208.6875000013656063, 170.0000000000004547 ) ) ;
#20869 = CARTESIAN_POINT ( 'NONE',  ( 3.211159895383560947, 5.187499998634407028, 3.211159895383562723 ) ) ;
#20870 = CARTESIAN_POINT ( 'NONE',  ( -4.898587196589412829E-16, 94.81250000409677625, -8.000000000000000000 ) ) ;
#20871 = AXIS2_PLACEMENT_3D ( 'NONE', #16567, #39604, #8926 ) ;
#20872 = CARTESIAN_POINT ( 'NONE',  ( 7.188101187499992051, 8.802885111219154394E-16, 24.73655278187175810 ) ) ;
#20873 = ORIENTED_EDGE ( 'NONE', *, *, #19522, .F. ) ;
#20874 = CARTESIAN_POINT ( 'NONE',  ( -28.00000000000002132, 194.8437500006828031, 166.2706329375003804 ) ) ;
#20875 = ORIENTED_EDGE ( 'NONE', *, *, #7090, .F. ) ;
#20876 = CARTESIAN_POINT ( 'NONE',  ( -10.18810118749999916, 4.220049686691934809, 117.0625000020483668 ) ) ;
#20877 = CARTESIAN_POINT ( 'NONE',  ( 12.00000000000000000, 4.408728476930470856E-15, -36.00000000000000000 ) ) ;
#20878 = CARTESIAN_POINT ( 'NONE',  ( -2.445694354108783664, 203.3125000013656063, 195.5543056458912190 ) ) ;
#20879 = CARTESIAN_POINT ( 'NONE',  ( 27.99999999999996803, 197.9375000013655779, 166.5412658749999082 ) ) ;
#20880 = CARTESIAN_POINT ( 'NONE',  ( 2.679491924311228956, 66.04166666666667140, -10.00000000000000000 ) ) ;
#20881 = EDGE_CURVE ( 'NONE', #18106, #9832, #24314, .T. ) ;
#20882 = CARTESIAN_POINT ( 'NONE',  ( 2.977408999572654480, 96.50000000204838102, 7.188101187499999156 ) ) ;
#20883 = CARTESIAN_POINT ( 'NONE',  ( 4.242640687119285658, 292.6249999999999432, -4.242640687119286547 ) ) ;
#20885 = DIRECTION ( 'NONE',  ( -0.000000000000000000, 0.000000000000000000, -1.000000000000000000 ) ) ;
#20884 = CARTESIAN_POINT ( 'NONE',  ( 29.65685424949235482, 208.5625000027312410, 165.9999999999998863 ) ) ;
#20886 = ORIENTED_EDGE ( 'NONE', *, *, #30782, .T. ) ;
#20887 = EDGE_CURVE ( 'NONE', #9311, #8879, #9283, .T. ) ;
#20888 = CARTESIAN_POINT ( 'NONE',  ( 5.656854249492379694, 94.43750000000000000, -5.656854249492380582 ) ) ;
#20889 = CARTESIAN_POINT ( 'NONE',  ( -11.00000000000000000, 0.000000000000000000, 88.18750000409677625 ) ) ;
#20890 = CARTESIAN_POINT ( 'NONE',  ( -1.656854249492405451, 201.4375000027311842, 138.0000000000000568 ) ) ;
#20891 = CARTESIAN_POINT ( 'NONE',  ( -3.673940397442060854E-16, 290.8125000034140157, -6.000000000000001776 ) ) ;
#20892 = CARTESIAN_POINT ( 'NONE',  ( 10.00000000000000178, 257.2916666666666856, 2.679491924311222739 ) ) ;
#20893 = CARTESIAN_POINT ( 'NONE',  ( -7.778174593052023411, 7.778174593052023411, 107.5000000040967763 ) ) ;
#20894 = CARTESIAN_POINT ( 'NONE',  ( -10.00000000000000355, 187.7083333333332860, 2.679491924311223183 ) ) ;
#20895 = DIRECTION ( 'NONE',  ( -0.000000000000000000, 1.000000000000000000, -0.000000000000000000 ) ) ;
#20896 = CARTESIAN_POINT ( 'NONE',  ( -4.401442555609577197E-16, 7.188101187499992051, 23.98655278187175455 ) ) ;
#20897 = CARTESIAN_POINT ( 'NONE',  ( -9.832129032723420536, 149.0104166632526699, 5.676582343749997150 ) ) ;
#20898 = CARTESIAN_POINT ( 'NONE',  ( -3.999999999999960032, 208.1250000027312126, 198.0000000000000284 ) ) ;
#20899 = CARTESIAN_POINT ( 'NONE',  ( -30.99778939216234264, 48.77778670582096510, 65.00000000000000000 ) ) ;
#20900 = CARTESIAN_POINT ( 'NONE',  ( -0.3930886489264411865, -42.01943585830397865, 151.0030965166856731 ) ) ;
#20902 = LINE ( 'NONE', #43924, #38693 ) ;
#20901 = CARTESIAN_POINT ( 'NONE',  ( -4.000000000000015987, 202.6875000027311842, 143.6568542494924259 ) ) ;
#20903 = ORIENTED_EDGE ( 'NONE', *, *, #11097, .F. ) ;
#20904 = VECTOR ( 'NONE', #7552, 1000.000000000000000 ) ;
#20905 = CARTESIAN_POINT ( 'NONE',  ( -8.311093377946836114, 22.96874999658601624, -8.311093377946837890 ) ) ;
#20906 = EDGE_CURVE ( 'NONE', #48510, #55947, #53738, .T. ) ;
#20907 = CARTESIAN_POINT ( 'NONE',  ( 7.320508075688774596, 97.49999999317203958, -7.320508075688774596 ) ) ;
#20909 = CARTESIAN_POINT ( 'NONE',  ( 5.126106709302931996, -16.23426604260537331, -69.90716554746668976 ) ) ;
#20908 = CARTESIAN_POINT ( 'NONE',  ( 5.656854249492374365, 5.656854249492375253, 16.95530278392014978 ) ) ;
#20910 = CARTESIAN_POINT ( 'NONE',  ( -2.249999999999998668, 255.9999999999999432, 7.677076266392048431 ) ) ;
#20911 = CARTESIAN_POINT ( 'NONE',  ( -3.458734125000015425, 202.9375000013656063, 142.0000000000000568 ) ) ;
#20912 = CARTESIAN_POINT ( 'NONE',  ( 10.00000000000000178, 47.08333332650536107, -2.679491924311226736 ) ) ;
#20913 = CARTESIAN_POINT ( 'NONE',  ( -2.977408999572651815, 109.4375000020483810, 7.188101187500000933 ) ) ;
#20914 = CARTESIAN_POINT ( 'NONE',  ( 4.541265875000002339, 7.437499998634407028, 0.000000000000000000 ) ) ;
#20915 = CARTESIAN_POINT ( 'NONE',  ( 7.320508075688758609, 99.37499999999997158, 7.320508075688762162 ) ) ;
#20916 = CARTESIAN_POINT ( 'NONE',  ( 7.999999999999992895, -3.313708498984756279, 8.986552779823366421 ) ) ;
#20918 = CARTESIAN_POINT ( 'NONE',  ( 10.00000000000002132, 160.2083333333333712, -2.679491924311232953 ) ) ;
#20917 = CARTESIAN_POINT ( 'NONE',  ( 2.143195687315755826, 194.5378148448417335, 139.1774195764784849 ) ) ;
#20919 = EDGE_LOOP ( 'NONE', ( #50690, #57906, #32409, #72159 ) ) ;
#20920 = ORIENTED_EDGE ( 'NONE', *, *, #38495, .F. ) ;
#20921 = CARTESIAN_POINT ( 'NONE',  ( 2.679491924332284114, 31.04166666666478491, -9.999999999987847943 ) ) ;
#20922 = LINE ( 'NONE', #9624, #62971 ) ;
#20923 = CARTESIAN_POINT ( 'NONE',  ( 3.042071309553167069, 131.8229166632526983, -11.35316468749999785 ) ) ;
#20924 = VERTEX_POINT ( 'NONE', #32598 ) ;
#20925 = CARTESIAN_POINT ( 'NONE',  ( -5.000000000000000000, 11.82742353449332917, -68.45184936927694253 ) ) ;
#20926 = CARTESIAN_POINT ( 'NONE',  ( 7.204075437095968759, -7.204075437095966983, 90.71875000204838102 ) ) ;
#20927 = CARTESIAN_POINT ( 'NONE',  ( -5.656854249492380582, 93.31249999999998579, -5.656854249492380582 ) ) ;
#20928 = CARTESIAN_POINT ( 'NONE',  ( -2.828427124746153876, 208.8750000000000284, 195.1715728752538439 ) ) ;
#20929 = FACE_OUTER_BOUND ( 'NONE', #38219, .T. ) ;
#20931 = CARTESIAN_POINT ( 'NONE',  ( -8.311093377946841443, 128.9062499965860411, 8.311093377946834337 ) ) ;
#20930 = CARTESIAN_POINT ( 'NONE',  ( -1.836970198721029983E-15, 210.6249999931720538, 10.00000000000000178 ) ) ;
#20932 = CARTESIAN_POINT ( 'NONE',  ( -1.836970198721029983E-15, 125.6249999931720254, 10.00000000000000178 ) ) ;
#20933 = VERTEX_POINT ( 'NONE', #3166 ) ;
#20934 = CARTESIAN_POINT ( 'NONE',  ( 1.224646799147353454E-15, 300.0000000000000000, -10.00000000000000178 ) ) ;
#20935 = EDGE_CURVE ( 'NONE', #20958, #53065, #19759, .T. ) ;
#20936 = CARTESIAN_POINT ( 'NONE',  ( 49.36289658985558759, 45.80530859601807236, 58.74035077246724512 ) ) ;
#20937 = CARTESIAN_POINT ( 'NONE',  ( 3.042071309553167513, 112.1354166632526699, -11.35316468749999785 ) ) ;
#20938 = CARTESIAN_POINT ( 'NONE',  ( -2.445694354108783664, 205.3125000013656063, 195.5543056458912190 ) ) ;
#20939 = CARTESIAN_POINT ( 'NONE',  ( 7.188101187500000933, 17.43749999795161543, -2.977408999572650483 ) ) ;
#20940 = CARTESIAN_POINT ( 'NONE',  ( -7.204075437095965206, -7.204075437095968759, 81.71875000204836681 ) ) ;
#20941 = CARTESIAN_POINT ( 'NONE',  ( -11.35316468750000141, 23.80208332991934839, 3.042071309553159963 ) ) ;
#20942 = VERTEX_POINT ( 'NONE', #20126 ) ;
#20943 = DIRECTION ( 'NONE',  ( 0.000000000000000000, 0.000000000000000000, 1.000000000000000000 ) ) ;
#20944 = CARTESIAN_POINT ( 'NONE',  ( 8.008118988124991233, 3.317071493978879015, 27.35686528394063544 ) ) ;
#20945 = CARTESIAN_POINT ( 'NONE',  ( 2.445694354108784108, 208.5625000013656063, 144.4456943541088663 ) ) ;
#20946 = DIRECTION ( 'NONE',  ( 1.000000000000000000, 0.000000000000000000, -0.000000000000000000 ) ) ;
#20947 = CARTESIAN_POINT ( 'NONE',  ( -1.320432766682874540E-15, 3.093749997951610542, 7.188101187500000044 ) ) ;
#20948 = CARTESIAN_POINT ( 'NONE',  ( 6.000000000000003553, 298.5000000034140157, 2.485281374238571317 ) ) ;
#20949 = DIRECTION ( 'NONE',  ( -0.000000000000000000, 1.000000000000000000, -0.000000000000000000 ) ) ;
#20950 = CARTESIAN_POINT ( 'NONE',  ( 2.977408999572650927, 1.124999997951610098, -7.188101187500001821 ) ) ;
#20951 = ORIENTED_EDGE ( 'NONE', *, *, #18262, .F. ) ;
#20952 = CARTESIAN_POINT ( 'NONE',  ( 8.311093377946834337, 145.4687499965860411, 8.311093377946839666 ) ) ;
#20953 = CARTESIAN_POINT ( 'NONE',  ( -7.204075437095965206, -7.204075437095968759, 81.34375000204838102 ) ) ;
#20954 =( BOUNDED_CURVE ( )  B_SPLINE_CURVE ( 2, ( #34867, #533, #23513, #14961, #40876, #25354, #1272, #53314, #35231, #65358, #31025, #29924, #58607 ),
 .UNSPECIFIED., .F., .F. ) 
 B_SPLINE_CURVE_WITH_KNOTS ( ( 3, 2, 2, 2, 2, 2, 3 ),
 ( 0.5271739130434782705, 0.5289855072463768293, 0.5307971014492753881, 0.5326086956521739468, 0.5344202898550725056, 0.5362318840579710644, 0.5380434782608695121 ),
 .UNSPECIFIED. ) 
 CURVE ( )  GEOMETRIC_REPRESENTATION_ITEM ( )  RATIONAL_B_SPLINE_CURVE ( ( 1.000000000000000000, 0.9659258262890683122, 1.000000000000000000, 0.9659258262890683122, 1.000000000000000000, 0.9659258262890683122, 1.000000000000000000, 0.9659258262890683122, 1.000000000000000000, 0.9659258262890683122, 1.000000000000000000, 0.9659258262890683122, 1.000000000000000000 ) ) 
 REPRESENTATION_ITEM ( '' )  );
#20955 = CARTESIAN_POINT ( 'NONE',  ( -29.43265458321766559, 200.5000000013655779, 166.5412658750003629 ) ) ;
#20956 = CARTESIAN_POINT ( 'NONE',  ( -3.313708498984757611, 7.999999999999991118, 21.54905277982336642 ) ) ;
#20957 = CARTESIAN_POINT ( 'NONE',  ( -3.211159895383561391, 15.81249999863440436, -3.211159895383561835 ) ) ;
#20958 = VERTEX_POINT ( 'NONE', #2418 ) ;
#20959 = VECTOR ( 'NONE', #1274, 1000.000000000000000 ) ;
#20960 = CARTESIAN_POINT ( 'NONE',  ( 2.751064625579944321E-14, 204.8750000027312126, 194.0000000000000568 ) ) ;
#20961 = CARTESIAN_POINT ( 'NONE',  ( 3.458734124999959469, 196.7500000013656063, 140.5673454167824161 ) ) ;
#20962 = CARTESIAN_POINT ( 'NONE',  ( -25.17157287525374088, 203.7500000027312126, 172.8284271247464972 ) ) ;
#20963 = CARTESIAN_POINT ( 'NONE',  ( -5.656854249492380582, 103.8125000000000000, -5.656854249492380582 ) ) ;
#20964 = ORIENTED_EDGE ( 'NONE', *, *, #35755, .F. ) ;
#20965 = ADVANCED_FACE ( 'NONE', ( #32215 ), #72573, .T. ) ;
#20966 = CARTESIAN_POINT ( 'NONE',  ( 5.082755093536325930, 14.15624999795161187, -5.082755093536325930 ) ) ;
#20967 = CARTESIAN_POINT ( 'NONE',  ( 38.00000000000000000, 272.0000000000000000, 20.00000000000002132 ) ) ;
#20968 = CARTESIAN_POINT ( 'NONE',  ( 8.311093377946834337, 180.1562499965859843, 8.311093377946839666 ) ) ;
#20969 = CARTESIAN_POINT ( 'NONE',  ( 7.188101187500000044, 110.2812500020483810, -8.802885111219163269E-16 ) ) ;
#20970 = CARTESIAN_POINT ( 'NONE',  ( -28.00000000000002842, 201.0000000000000000, 166.0000000000003695 ) ) ;
#20971 = CARTESIAN_POINT ( 'NONE',  ( -2.765530957081996810, 290.2656250017069510, -6.676582343750002480 ) ) ;
#20973 = CARTESIAN_POINT ( 'NONE',  ( -7.320508075688776373, 66.87500000000000000, -7.320508075688777261 ) ) ;
#20972 = DIRECTION ( 'NONE',  ( 0.000000000000000000, -0.9480053216942907479, -0.3182544737145173164 ) ) ;
#20974 = ITEM_DEFINED_TRANSFORMATION ( 'NONE', 'NONE', #64605,  #57354 ) ;
#20975 = VERTEX_POINT ( 'NONE', #20877 ) ;
#20976 = ADVANCED_FACE ( 'NONE', ( #61249 ), #52075, .F. ) ;
#20977 = CARTESIAN_POINT ( 'NONE',  ( -11.35316468749999963, 258.9062500034140157, 0.000000000000000000 ) ) ;
#20978 = CARTESIAN_POINT ( 'NONE',  ( 7.188101187499993827, -2.977408999572645598, 26.51780278187175455 ) ) ;
#20979 = VECTOR ( 'NONE', #52068, 999.9999999999998863 ) ;
#20980 = CARTESIAN_POINT ( 'NONE',  ( 2.020667218593132706E-15, -11.00000000000000000, 92.87499999999998579 ) ) ;
#20981 = CARTESIAN_POINT ( 'NONE',  ( 5.656854249492374365, 5.656854249492375253, 15.45530278392014623 ) ) ;
#20982 = CARTESIAN_POINT ( 'NONE',  ( 2.990854866098545894, -66.07503719301321610, -26.46919450144743635 ) ) ;
#20983 = CARTESIAN_POINT ( 'NONE',  ( 2.445694354108840063, 200.0625000013656063, 200.4456943541088663 ) ) ;
#20984 = ORIENTED_EDGE ( 'NONE', *, *, #23603, .F. ) ;
#20985 = CARTESIAN_POINT ( 'NONE',  ( -3.313708498984762496, 92.28124999999998579, 7.999999999999998224 ) ) ;
#20986 = CARTESIAN_POINT ( 'NONE',  ( -11.35316468750000141, 113.8020833299193555, 3.042071309553159963 ) ) ;
#20987 = CARTESIAN_POINT ( 'NONE',  ( 8.660254037844385522, 211.4583333265053682, 5.000000000000005329 ) ) ;
#20988 = CARTESIAN_POINT ( 'NONE',  ( 4.556349186104045934, 11.00000000000000000, 69.53124999999998579 ) ) ;
#20991 = CARTESIAN_POINT ( 'NONE',  ( 6.000000000000001776, 298.5000000000000000, -7.347880794884121708E-16 ) ) ;
#20990 = CARTESIAN_POINT ( 'NONE',  ( 24.54126587499999346, 202.1875000013656063, 169.9999999999999432 ) ) ;
#20989 = CARTESIAN_POINT ( 'NONE',  ( 31.45873412499999233, 197.9375000013655779, 169.9999999999999432 ) ) ;
#20992 = ORIENTED_EDGE ( 'NONE', *, *, #25403, .T. ) ;
#20993 = CARTESIAN_POINT ( 'NONE',  ( -6.362988438888832046E-13, 223.7499999999999147, 9.999999999999998224 ) ) ;
#20994 = CARTESIAN_POINT ( 'NONE',  ( -3.458734125000016313, 197.8750000013656063, 140.5673454167824161 ) ) ;
#20995 = CARTESIAN_POINT ( 'NONE',  ( 27.99999999999996447, 199.6875000013656063, 173.4587341249998929 ) ) ;
#20996 = EDGE_CURVE ( 'NONE', #60631, #73412, #47296, .T. ) ;
#20997 = CARTESIAN_POINT ( 'NONE',  ( 7.778174593052021635, 7.778174593052023411, 108.6250000040967763 ) ) ;
#20998 = CARTESIAN_POINT ( 'NONE',  ( -3.042071309553173730, 209.6354166632526415, 11.35316468749999785 ) ) ;
#20999 = CARTESIAN_POINT ( 'NONE',  ( 28.00000000000002487, 208.1250000027312126, 173.9999999999999147 ) ) ;
#21000 = DIRECTION ( 'NONE',  ( -0.000000000000000000, 1.000000000000000000, -0.000000000000000000 ) ) ;
#21001 = CARTESIAN_POINT ( 'NONE',  ( -1.881053915767124440, 18.99999999863440436, 4.541265875000001451 ) ) ;
#21002 = CARTESIAN_POINT ( 'NONE',  ( 5.126106709302927555, -52.42424824936786365, 49.01286957842454939 ) ) ;
#21003 = CARTESIAN_POINT ( 'NONE',  ( 1.320432766682872962E-15, -7.188101187499992051, 0.7365527818717527708 ) ) ;
#21005 = CARTESIAN_POINT ( 'NONE',  ( -27.99999999999999645, 210.0000000000000284, 170.0000000000003695 ) ) ;
#21004 = CARTESIAN_POINT ( 'NONE',  ( 7.320508075688770155, 185.6249999999999716, -7.320508075688770155 ) ) ;
#21006 = CARTESIAN_POINT ( 'NONE',  ( 11.35316468749999785, 100.5729166632526699, 3.042071309553174174 ) ) ;
#21007 = ORIENTED_EDGE ( 'NONE', *, *, #46641, .F. ) ;
#21008 = EDGE_CURVE ( 'NONE', #36810, #46282, #73849, .T. ) ;
#21009 = CYLINDRICAL_SURFACE ( 'NONE', #5042, 8.000000000000000000 ) ;
#21010 = CARTESIAN_POINT ( 'NONE',  ( -7.188101187500000044, 22.21874999795161187, -8.802885111219163269E-16 ) ) ;
#21011 = CARTESIAN_POINT ( 'NONE',  ( 1.469576158976823947E-15, 0.000000000000000000, -12.00000000000000000 ) ) ;
#21013 = CARTESIAN_POINT ( 'NONE',  ( -6.951808397369817780E-16, 257.9687500034140157, -11.35316468749999963 ) ) ;
#21012 = AXIS2_PLACEMENT_3D ( 'NONE', #38337, #27746, #62084 ) ;
#21014 = CARTESIAN_POINT ( 'NONE',  ( -3.042071309553173730, 84.32291666325268409, 11.35316468749999785 ) ) ;
#21015 = ORIENTED_EDGE ( 'NONE', *, *, #27362, .F. ) ;
#21016 = CARTESIAN_POINT ( 'NONE',  ( 26.34314575050753149, 197.0625000027312410, 173.9999999999997726 ) ) ;
#21017 = CARTESIAN_POINT ( 'NONE',  ( -7.204075437095965206, -7.204075437095968759, 114.3437500020483810 ) ) ;
#21018 = CYLINDRICAL_SURFACE ( 'NONE', #50246, 10.99999999999999645 ) ;
#21019 = CARTESIAN_POINT ( 'NONE',  ( -1.432654583217607414, 205.5000000013655779, 194.5412658750000219 ) ) ;
#21020 = CARTESIAN_POINT ( 'NONE',  ( 7.999999999999991118, 9.797174393178815797E-16, 12.08030277982336642 ) ) ;
#21022 = CARTESIAN_POINT ( 'NONE',  ( -11.35316468749999785, 83.07291666325268409, -3.042071309553167957 ) ) ;
#21021 = CARTESIAN_POINT ( 'NONE',  ( 11.00000000000010836, -4.556349186103939353, 106.6562500000000000 ) ) ;
#21023 = CARTESIAN_POINT ( 'NONE',  ( 1.469576158976822172E-15, -7.999999999999991118, 17.89280278392014623 ) ) ;
#21024 = CARTESIAN_POINT ( 'NONE',  ( -30.44569435410883429, 200.8125000013656063, 167.5543056458915885 ) ) ;
#21025 = FACE_OUTER_BOUND ( 'NONE', #47787, .T. ) ;
#21026 = CARTESIAN_POINT ( 'NONE',  ( -2.679491924311235618, 185.4166666598386826, 10.00000000000000000 ) ) ;
#21027 = CARTESIAN_POINT ( 'NONE',  ( 2.696441184376675793, -46.32960594482928229, 139.1174011848989380 ) ) ;
#21028 = CARTESIAN_POINT ( 'NONE',  ( 9.832129032723420536, 71.51041666325268409, -5.676582343749999815 ) ) ;
#21029 = CARTESIAN_POINT ( 'NONE',  ( 6.676582343750004256, 293.8906250017069510, 2.765530957081995478 ) ) ;
#21030 = EDGE_CURVE ( 'NONE', #2370, #70895, #47837, .T. ) ;
#21031 = CARTESIAN_POINT ( 'NONE',  ( 7.204075437095968759, -7.204075437095966983, 101.5937500020483668 ) ) ;
#21032 = CARTESIAN_POINT ( 'NONE',  ( -5.676582343750006032, 204.1145833299193555, 9.832129032723418760 ) ) ;
#21033 = ORIENTED_EDGE ( 'NONE', *, *, #44665, .F. ) ;
#21034 = CARTESIAN_POINT ( 'NONE',  ( -5.000000000000005329, 70.20833332650538239, 8.660254037844387298 ) ) ;
#21035 = CARTESIAN_POINT ( 'NONE',  ( 2.124081043562902948, -60.31560147600172428, -22.95556260996213283 ) ) ;
#21036 = CARTESIAN_POINT ( 'NONE',  ( 4.999999999999999112, 63.46295559274079068, 24.14151313015431199 ) ) ;
#21038 = CARTESIAN_POINT ( 'NONE',  ( 8.311093377946837890, 206.4062499965860127, -8.311093377946837890 ) ) ;
#21037 = CARTESIAN_POINT ( 'NONE',  ( -11.00000000000000000, 0.000000000000000000, 71.49999999999998579 ) ) ;
#21039 = CARTESIAN_POINT ( 'NONE',  ( 2.249999999999999112, -2.249999999999999556, 28.00000000000000000 ) ) ;
#21040 = CARTESIAN_POINT ( 'NONE',  ( -7.320508075688770155, 228.7500000068279462, 7.320508075688774596 ) ) ;
#21041 = CARTESIAN_POINT ( 'NONE',  ( -2.828427124746192067, 20.62500000000000000, 2.828427124746190735 ) ) ;
#21042 = ORIENTED_EDGE ( 'NONE', *, *, #48914, .T. ) ;
#21043 = CARTESIAN_POINT ( 'NONE',  ( -9.832129032723418760, 198.1770833299193555, -5.676582343750004256 ) ) ;
#21044 = VECTOR ( 'NONE', #8555, 1000.000000000000114 ) ;
#21045 = CARTESIAN_POINT ( 'NONE',  ( 7.188101187499992051, 2.977408999572647819, 17.33030278187175455 ) ) ;
#21046 = CARTESIAN_POINT ( 'NONE',  ( 8.000000000000000000, 18.00000000000000355, 0.000000000000000000 ) ) ;
#21047 = CARTESIAN_POINT ( 'NONE',  ( -8.000000000000000000, 14.25000000000000178, -9.797174393178825657E-16 ) ) ;
#21048 = VERTEX_POINT ( 'NONE', #8442 ) ;
#21049 = EDGE_CURVE ( 'NONE', #53778, #3815, #71808, .T. ) ;
#21050 = CARTESIAN_POINT ( 'NONE',  ( -7.999999999999998224, 92.28125000409679046, 3.313708498984766493 ) ) ;
#21051 = EDGE_CURVE ( 'NONE', #70312, #31825, #55979, .T. ) ;
#21052 = CARTESIAN_POINT ( 'NONE',  ( -5.000000000000005329, 13.33333333333333393, 8.660254037844387298 ) ) ;
#21053 = EDGE_LOOP ( 'NONE', ( #25574, #37214, #25366, #3164 ) ) ;
#21054 = EDGE_CURVE ( 'NONE', #9782, #23983, #49822, .T. ) ;
#21055 = CARTESIAN_POINT ( 'NONE',  ( 2.828427124746191623, 15.12500000000000000, -2.828427124746191623 ) ) ;
#21056 = CARTESIAN_POINT ( 'NONE',  ( -4.541265875000003227, 18.87499999863441147, 1.881053915767121110 ) ) ;
#21057 = CARTESIAN_POINT ( 'NONE',  ( -7.999999999999991118, 3.313708498984756723, 8.424052783920146226 ) ) ;
#21058 = CARTESIAN_POINT ( 'NONE',  ( -11.00000000000000000, 0.000000000000000000, 70.18750000409676204 ) ) ;
#21059 = ORIENTED_EDGE ( 'NONE', *, *, #50549, .T. ) ;
#21060 = SURFACE_STYLE_FILL_AREA ( #72756 ) ;
#21061 = CARTESIAN_POINT ( 'NONE',  ( 5.082755093536325042, 92.09375000204838102, -5.082755093536325930 ) ) ;
#21064 = CARTESIAN_POINT ( 'NONE',  ( 2.849036369511732440E-14, 197.2500000000000000, 202.0000000000000000 ) ) ;
#21063 = CARTESIAN_POINT ( 'NONE',  ( -23.99999999999995026, 204.8125000027312126, 171.6568542494926817 ) ) ;
#21062 = CARTESIAN_POINT ( 'NONE',  ( 0.000000000000000000, 0.000000000000000000, -81.50000000000000000 ) ) ;
#21065 = APPLICATION_PROTOCOL_DEFINITION ( 'draft international standard', 'automotive_design', 1998, #37556 ) ;
#21066 =( BOUNDED_CURVE ( )  B_SPLINE_CURVE ( 2, ( #33174, #43717, #26348, #9773, #10884, #61818, #10511, #4116, #67108 ),
 .UNSPECIFIED., .F., .F. ) 
 B_SPLINE_CURVE_WITH_KNOTS ( ( 3, 2, 2, 2, 3 ),
 ( 0.1323655657721681533, 0.1389837872735831814, 0.1456020628580432796, 0.1522203384425033779, 0.1588385999027599471 ),
 .UNSPECIFIED. ) 
 CURVE ( )  GEOMETRIC_REPRESENTATION_ITEM ( )  RATIONAL_B_SPLINE_CURVE ( ( 0.9999987559318189723, 0.9238801545504604640, 1.000000000000000000, 0.9238795325112867385, 1.000000000000000000, 0.9238795325112867385, 1.000000000000000000, 0.9238796949616049359, 0.9999996751000569395 ) ) 
 REPRESENTATION_ITEM ( '' )  );
#21067 = VERTEX_POINT ( 'NONE', #68028 ) ;
#21068 = CARTESIAN_POINT ( 'NONE',  ( -11.35316468749999785, 254.0104166700806729, -3.042071309553164848 ) ) ;
#21069 = CARTESIAN_POINT ( 'NONE',  ( -5.082755093536319713, 5.082755093536319713, 14.79905278187175455 ) ) ;
#21070 = ORIENTED_EDGE ( 'NONE', *, *, #5757, .T. ) ;
#21071 = EDGE_CURVE ( 'NONE', #61413, #36324, #56720, .T. ) ;
#21072 = EDGE_CURVE ( 'NONE', #55117, #50952, #43670, .T. ) ;
#21073 = EDGE_LOOP ( 'NONE', ( #5878, #15451, #52600, #19183 ) ) ;
#21074 = CARTESIAN_POINT ( 'NONE',  ( 4.220049686691941027, -10.18810118749999738, 83.12500000204836681 ) ) ;
#21075 = CARTESIAN_POINT ( 'NONE',  ( -11.35316468750000141, 73.80208332991935549, 3.042071309553159963 ) ) ;
#21076 = CARTESIAN_POINT ( 'NONE',  ( 3.313708498984762496, -7.999999999999989342, 17.79905277982336997 ) ) ;
#21077 = CARTESIAN_POINT ( 'NONE',  ( 7.778174593052021635, 7.778174593052023411, 88.93749999999998579 ) ) ;
#21080 = CARTESIAN_POINT ( 'NONE',  ( 6.676582343750001591, 289.1093750017069510, -8.176455196517173205E-16 ) ) ;
#21079 = CARTESIAN_POINT ( 'NONE',  ( 30.82842712474620583, 197.2500000027312126, 172.8284271247460424 ) ) ;
#21078 = CARTESIAN_POINT ( 'NONE',  ( -28.00000000000008171, 206.1250000027312126, 166.0000000000003695 ) ) ;
#21081 = DIRECTION ( 'NONE',  ( 0.000000000000000000, 0.000000000000000000, -1.000000000000000000 ) ) ;
#21082 = CARTESIAN_POINT ( 'NONE',  ( -8.000000000000000000, 90.68750000409677625, 0.000000000000000000 ) ) ;
#21083 = VECTOR ( 'NONE', #22039, 1000.000000000000000 ) ;
#21084 = CARTESIAN_POINT ( 'NONE',  ( -1.432654583217608080, 196.8750000013656347, 201.4587341250000350 ) ) ;
#21085 = CARTESIAN_POINT ( 'NONE',  ( 3.313708498984762052, 7.593749995903221972, -8.000000000000000000 ) ) ;
#21086 = ORIENTED_EDGE ( 'NONE', *, *, #15879, .F. ) ;
#21087 = CARTESIAN_POINT ( 'NONE',  ( 25.55430564589114795, 196.3125000013656063, 172.4456943541086957 ) ) ;
#21088 = CARTESIAN_POINT ( 'NONE',  ( -5.082755093536326818, 10.78124999795161187, 5.082755093536325042 ) ) ;
#21089 = VECTOR ( 'NONE', #28884, 1000.000000000000000 ) ;
#21090 = CARTESIAN_POINT ( 'NONE',  ( 8.311093377946834337, 165.4687499965859843, 8.311093377946839666 ) ) ;
#21091 = CARTESIAN_POINT ( 'NONE',  ( -7.999999999999998224, 105.5937500000000000, 3.313708498984766049 ) ) ;
#21092 = CARTESIAN_POINT ( 'NONE',  ( 5.082755093536326818, 104.0937500020483810, 5.082755093536325042 ) ) ;
#21094 = CARTESIAN_POINT ( 'NONE',  ( 2.219371606097089611, -51.37365828841584658, -48.60677221569350337 ) ) ;
#21093 = CARTESIAN_POINT ( 'NONE',  ( -6.000000000000003553, 293.0000000034139589, -2.485281374238571317 ) ) ;
#21095 = CARTESIAN_POINT ( 'NONE',  ( 29.43265458321761585, 206.7500000013655779, 173.4587341249998929 ) ) ;
#21096 = CARTESIAN_POINT ( 'NONE',  ( 7.188101187499991163, 2.977408999572648707, 13.20530278187175277 ) ) ;
#21097 = DIRECTION ( 'NONE',  ( 0.000000000000000000, 0.000000000000000000, 1.000000000000000000 ) ) ;
#21098 = CARTESIAN_POINT ( 'NONE',  ( -9.832129032723418760, 47.86458332991935549, -5.676582343750004256 ) ) ;
#21099 = DIRECTION ( 'NONE',  ( 0.000000000000000000, 0.000000000000000000, 1.000000000000000000 ) ) ;
#21100 = EDGE_CURVE ( 'NONE', #71847, #58601, #16322, .T. ) ;
#21101 = CARTESIAN_POINT ( 'NONE',  ( 10.00000000000000000, 26.66666665983870033, 2.679491924311236062 ) ) ;
#21102 = CARTESIAN_POINT ( 'NONE',  ( 7.778174593052021635, 7.778174593052023411, 111.6250000040967763 ) ) ;
#21103 = ORIENTED_EDGE ( 'NONE', *, *, #73063, .T. ) ;
#21104 = CARTESIAN_POINT ( 'NONE',  ( 7.320508075688771044, 141.2499999931720254, 7.320508075688775484 ) ) ;
#21105 = CARTESIAN_POINT ( 'NONE',  ( -8.660254037844390851, 169.7916666598387110, 4.999999999999998224 ) ) ;
#21106 = CARTESIAN_POINT ( 'NONE',  ( 5.676582343750001591, 46.61458332991934839, -9.832129032723420536 ) ) ;
#21107 = CARTESIAN_POINT ( 'NONE',  ( -7.778174593052020747, -7.778174593052023411, 79.37500000409677625 ) ) ;
#21108 = CARTESIAN_POINT ( 'NONE',  ( -2.839093476692135984E-14, 203.9375000013656063, 138.5412658750000503 ) ) ;
#21109 = CARTESIAN_POINT ( 'NONE',  ( 4.330454160168551780, 16.29811171461319574, 69.49285720719198878 ) ) ;
#21110 = CYLINDRICAL_SURFACE ( 'NONE', #49134, 8.000000000000000000 ) ;
#21112 = CARTESIAN_POINT ( 'NONE',  ( 8.311093377946837890, 46.40624999658601268, -8.311093377946837890 ) ) ;
#21111 = CARTESIAN_POINT ( 'NONE',  ( 5.082755093536326818, 99.21875000204838102, 5.082755093536325042 ) ) ;
#21113 = CARTESIAN_POINT ( 'NONE',  ( 7.999999999999991118, 3.313708498984757611, 9.174052779823364645 ) ) ;
#21114 = CARTESIAN_POINT ( 'NONE',  ( 3.178432602446558121E-13, 206.2500000000000000, -10.00000000000000533 ) ) ;
#21115 = CARTESIAN_POINT ( 'NONE',  ( 11.35316468750000141, 165.7812499965860411, 0.000000000000000000 ) ) ;
#21116 = CARTESIAN_POINT ( 'NONE',  ( -10.00000000000000355, 139.5833333265053966, 2.679491924311223183 ) ) ;
#21117 = CARTESIAN_POINT ( 'NONE',  ( -2.977408999572651815, 105.3125000020483668, 7.188101187500000933 ) ) ;
#21118 = CARTESIAN_POINT ( 'NONE',  ( -2.846433909902065906, -45.96771706956180026, 139.1308643719709437 ) ) ;
#21119 = CARTESIAN_POINT ( 'NONE',  ( -8.311093377946836114, 37.96874999658601979, -8.311093377946837890 ) ) ;
#21120 = CARTESIAN_POINT ( 'NONE',  ( -2.849036369511732440E-14, 195.3750000027311842, 138.0000000000000568 ) ) ;
#21121 = ORIENTED_EDGE ( 'NONE', *, *, #683, .F. ) ;
#21122 = CARTESIAN_POINT ( 'NONE',  ( -3.313708498984765161, 1.031250000000000000, 7.999999999999998224 ) ) ;
#21123 = CARTESIAN_POINT ( 'NONE',  ( -4.220049686691937474, -10.18810118749999738, 75.43750000204836681 ) ) ;
#21124 = DIRECTION ( 'NONE',  ( 0.000000000000000000, -1.000000000000000000, 0.000000000000000000 ) ) ;
#21126 = CARTESIAN_POINT ( 'NONE',  ( 3.042071309553167513, 171.8229166632526983, -11.35316468749999785 ) ) ;
#21125 = DIRECTION ( 'NONE',  ( -1.000000000000000000, 0.000000000000000000, 0.000000000000000000 ) ) ;
#21127 = CARTESIAN_POINT ( 'NONE',  ( 5.656854249492376141, -5.656854249492374365, 8.949052784329824206 ) ) ;
#21128 = CARTESIAN_POINT ( 'NONE',  ( -30.64284399271078740, -21.00579972956345642, 174.6921329945331536 ) ) ;
#21129 = CARTESIAN_POINT ( 'NONE',  ( -9.832129032723415207, 219.3229166700806729, 5.676582343750005144 ) ) ;
#21130 = CARTESIAN_POINT ( 'NONE',  ( -10.18810118749999916, 0.000000000000000000, 84.53125000204836681 ) ) ;
#21131 = ORIENTED_EDGE ( 'NONE', *, *, #40215, .T. ) ;
#21132 = DIRECTION ( 'NONE',  ( -0.000000000000000000, 1.000000000000000000, -1.563033456626094573E-30 ) ) ;
#21133 = CYLINDRICAL_SURFACE ( 'NONE', #35184, 10.00000000000000178 ) ;
#21134 = CARTESIAN_POINT ( 'NONE',  ( 11.35316468749999963, 116.3020833299193413, -3.042071309553165293 ) ) ;
#21135 = CARTESIAN_POINT ( 'NONE',  ( 10.18810118749999916, 4.220049686691935698, 97.00000000204836681 ) ) ;
#21136 = CARTESIAN_POINT ( 'NONE',  ( -4.541265875000003227, 18.99999999863440436, 1.881053915767121110 ) ) ;
#21137 = ORIENTED_EDGE ( 'NONE', *, *, #60821, .F. ) ;
#21138 = EDGE_LOOP ( 'NONE', ( #20122, #37452, #35907, #13710 ) ) ;
#21139 = CARTESIAN_POINT ( 'NONE',  ( 4.541265875000001451, 2.374999998634407028, 1.881053915767124440 ) ) ;
#21140 = CARTESIAN_POINT ( 'NONE',  ( -2.977408999572650039, 11.43749999795161010, -7.188101187500001821 ) ) ;
#21141 = CARTESIAN_POINT ( 'NONE',  ( -7.999999999999998224, 107.2812500040967620, 3.313708498984766493 ) ) ;
#21142 = EDGE_CURVE ( 'NONE', #65735, #35174, #37719, .T. ) ;
#21143 = CARTESIAN_POINT ( 'NONE',  ( 10.18810118749999916, 4.220049686691935698, 91.37500000204838102 ) ) ;
#21144 = CARTESIAN_POINT ( 'NONE',  ( -26.56734541678232375, 202.2500000013656063, 173.4587341250003760 ) ) ;
#21145 = VECTOR ( 'NONE', #61339, 1000.000000000000000 ) ;
#21146 = EDGE_CURVE ( 'NONE', #1123, #39166, #66127, .T. ) ;
#21147 = CARTESIAN_POINT ( 'NONE',  ( 4.000000000000001776, 6.062500000000000000, -1.656854249492381248 ) ) ;
#21148 = CARTESIAN_POINT ( 'NONE',  ( -4.000000000000001776, 19.18749999726881228, -1.656854249492381470 ) ) ;
#21149 = CARTESIAN_POINT ( 'NONE',  ( 1.881053915767121998, 6.499999998634407916, -4.541265875000002339 ) ) ;
#21150 = CARTESIAN_POINT ( 'NONE',  ( 2.828427124746153876, 200.8750000000000284, 144.8284271247462129 ) ) ;
#21151 = ORIENTED_EDGE ( 'NONE', *, *, #68754, .T. ) ;
#21153 = CYLINDRICAL_SURFACE ( 'NONE', #62311, 3.999999999999976019 ) ;
#21152 = CARTESIAN_POINT ( 'NONE',  ( -30.44569435410886982, 198.5625000013656063, 167.5543056458916169 ) ) ;
#21154 = CARTESIAN_POINT ( 'NONE',  ( 4.541265875000002339, 18.31249999863440792, 0.000000000000000000 ) ) ;
#21155 = CARTESIAN_POINT ( 'NONE',  ( 2.765530957082001251, 298.7656250017070079, 6.676582343749999815 ) ) ;
#21156 = CARTESIAN_POINT ( 'NONE',  ( 1.320432766682872962E-15, -7.188101187499992051, 7.861552781871751883 ) ) ;
#21157 = VERTEX_POINT ( 'NONE', #28406 ) ;
#21158 =( BOUNDED_CURVE ( )  B_SPLINE_CURVE ( 2, ( #15743, #10845, #39146, #32756, #61785, #62887, #17238, #67817, #11220 ),
 .UNSPECIFIED., .F., .F. ) 
 B_SPLINE_CURVE_WITH_KNOTS ( ( 3, 2, 2, 2, 3 ),
 ( 0.6874999999999982236, 0.6979166666666648533, 0.7083333333333317050, 0.7187499999999983347, 0.7291666666666649643 ),
 .UNSPECIFIED. ) 
 CURVE ( )  GEOMETRIC_REPRESENTATION_ITEM ( )  RATIONAL_B_SPLINE_CURVE ( ( 1.000000000000012879, 0.9238795325112737489, 1.000000000000000000, 0.9238795325112867385, 1.000000000000000000, 0.9238795325112867385, 1.000000000000000000, 0.9238795325112989509, 0.9999999999999877875 ) ) 
 REPRESENTATION_ITEM ( '' )  );
#21159 = VERTEX_POINT ( 'NONE', #45380 ) ;
#21160 = CARTESIAN_POINT ( 'NONE',  ( -10.18810118749999916, 0.000000000000000000, 100.6562500020483810 ) ) ;
#21161 = CARTESIAN_POINT ( 'NONE',  ( 3.313708498984657247, 91.15625000409677625, 8.000000000000106581 ) ) ;
#21162 = CARTESIAN_POINT ( 'NONE',  ( -30.44569435410883429, 199.8125000013656063, 167.5543056458915885 ) ) ;
#21163 = CARTESIAN_POINT ( 'NONE',  ( -4.556349186104047710, -10.99999999999999822, 109.2812499999999858 ) ) ;
#21164 = CARTESIAN_POINT ( 'NONE',  ( 2.839093476692135984E-14, 207.9375000013656063, 201.4587341250000350 ) ) ;
#21165 = CARTESIAN_POINT ( 'NONE',  ( -1.269107444400135093E-11, 58.74999999999901945, 10.00000000000000178 ) ) ;
#21166 = CARTESIAN_POINT ( 'NONE',  ( 8.660254037844385522, 109.5833333333333428, 5.000000000000005329 ) ) ;
#21167 = CARTESIAN_POINT ( 'NONE',  ( -5.656854249492378806, 107.1874999999999858, 5.656854249492381470 ) ) ;
#21168 = CARTESIAN_POINT ( 'NONE',  ( 4.721056650415999201, 292.2343750017069510, -4.721056650415999201 ) ) ;
#21169 = CARTESIAN_POINT ( 'NONE',  ( -5.082755093536319713, 5.082755093536319713, 12.17405278187175277 ) ) ;
#21170 = VERTEX_POINT ( 'NONE', #15960 ) ;
#21171 = DIRECTION ( 'NONE',  ( -0.000000000000000000, 1.000000000000000000, -0.000000000000000000 ) ) ;
#21172 = CARTESIAN_POINT ( 'NONE',  ( 25.55430564589115505, 208.3125000013656063, 172.4456943541086957 ) ) ;
#21173 = CARTESIAN_POINT ( 'NONE',  ( 8.000000000000000000, 19.31249999590322020, 0.000000000000000000 ) ) ;
#21174 = CARTESIAN_POINT ( 'NONE',  ( -1.432654583217662481, 199.1250000013656347, 145.4587341250000634 ) ) ;
#21175 = CARTESIAN_POINT ( 'NONE',  ( -20.63330740556099485, -35.71676899851056675, 146.7756149186916446 ) ) ;
#21177 = CARTESIAN_POINT ( 'NONE',  ( -3.458734125000015425, 203.2500000013656063, 143.4326545832176976 ) ) ;
#21176 = CARTESIAN_POINT ( 'NONE',  ( 5.656854249492381470, 121.0625000000000000, 5.656854249492379694 ) ) ;
#21178 = CARTESIAN_POINT ( 'NONE',  ( 8.311093377946839666, 251.0937500034139873, 8.311093377946829008 ) ) ;
#21179 = FACE_OUTER_BOUND ( 'NONE', #14704, .T. ) ;
#21180 = FACE_OUTER_BOUND ( 'NONE', #45020, .T. ) ;
#21181 = CARTESIAN_POINT ( 'NONE',  ( -10.00000000000000000, 222.2916666666667140, -2.679491924311229845 ) ) ;
#21182 =( BOUNDED_CURVE ( )  B_SPLINE_CURVE ( 2, ( #60589, #54204, #65874, #36477, #7806, #36849, #59493, #37217, #30808, #53831, #60215, #8539, #15300 ),
 .UNSPECIFIED., .F., .F. ) 
 B_SPLINE_CURVE_WITH_KNOTS ( ( 3, 2, 2, 2, 2, 2, 3 ),
 ( 0.1141304347826086890, 0.1159420289855072478, 0.1177536231884057927, 0.1195652173913043514, 0.1213768115942028963, 0.1231884057971014551, 0.1250000000000000000 ),
 .UNSPECIFIED. ) 
 CURVE ( )  GEOMETRIC_REPRESENTATION_ITEM ( )  RATIONAL_B_SPLINE_CURVE ( ( 1.000000000000000000, 0.9659258262890683122, 1.000000000000000000, 0.9659258262890683122, 1.000000000000000000, 0.9659258262890683122, 1.000000000000000000, 0.9659258262890683122, 1.000000000000000000, 0.9659258262890683122, 1.000000000000000000, 0.9659258262890683122, 1.000000000000000000 ) ) 
 REPRESENTATION_ITEM ( '' )  );
#21183 = CARTESIAN_POINT ( 'NONE',  ( 2.977408999572650927, -7.188101187499990274, 2.330302781871754991 ) ) ;
#21184 = CARTESIAN_POINT ( 'NONE',  ( -3.042071309553164404, 207.5520833299193555, -11.35316468749999963 ) ) ;
#21185 = CARTESIAN_POINT ( 'NONE',  ( 6.951808397369818766E-16, 2.031249996586016238, -11.35316468750000141 ) ) ;
#21186 = CARTESIAN_POINT ( 'NONE',  ( -3.211159895383561391, 4.687499998634407028, -3.211159895383561835 ) ) ;
#21187 = CARTESIAN_POINT ( 'NONE',  ( 4.242640687119285658, 290.6249999999999432, -4.242640687119286547 ) ) ;
#21189 = CARTESIAN_POINT ( 'NONE',  ( -3.999999999999960032, 195.0000000000000000, 198.0000000000000284 ) ) ;
#21188 = CARTESIAN_POINT ( 'NONE',  ( -3.313708498984805573, 26.34374999590322020, 7.999999999999956479 ) ) ;
#21190 = ORIENTED_EDGE ( 'NONE', *, *, #25514, .F. ) ;
#21191 = CARTESIAN_POINT ( 'NONE',  ( 2.445694354108783219, 203.8125000013656063, 139.5543056458912190 ) ) ;
#21192 = CARTESIAN_POINT ( 'NONE',  ( -5.676582343749998039, 12.44791666325268409, -9.832129032723420536 ) ) ;
#21193 = CARTESIAN_POINT ( 'NONE',  ( 7.778174593052023411, -7.778174593052021635, 97.75000000409677625 ) ) ;
#21194 = DIRECTION ( 'NONE',  ( -0.7071067811865525687, -0.7071067811865425767, -0.000000000000000000 ) ) ;
#21195 = CARTESIAN_POINT ( 'NONE',  ( -24.54126587500001833, 200.2500000013656063, 168.5673454167826435 ) ) ;
#21196 = DIRECTION ( 'NONE',  ( -1.000000000000000000, -1.577021341797097560E-16, -0.000000000000000000 ) ) ;
#21198 = CARTESIAN_POINT ( 'NONE',  ( 5.676582343749993598, 9.947916663252682312, 9.832129032723422313 ) ) ;
#21197 = CARTESIAN_POINT ( 'NONE',  ( 1.320432766682874540E-15, 120.0312500020483810, 7.188101187500000044 ) ) ;
#21199 = CARTESIAN_POINT ( 'NONE',  ( 1.469576158976822172E-15, -7.999999999999991118, 28.20530277982336642 ) ) ;
#21200 = CARTESIAN_POINT ( 'NONE',  ( -9.832129032723418760, 122.8645833299193555, -5.676582343750004256 ) ) ;
#21201 = CARTESIAN_POINT ( 'NONE',  ( -7.320508075688773708, 93.74999999317202537, -7.320508075688774596 ) ) ;
#21202 = CIRCLE ( 'NONE', #71800, 6.000000000000005329 ) ;
#21203 = CARTESIAN_POINT ( 'NONE',  ( -5.082755093536325930, 118.3437500020483810, -5.082755093536325930 ) ) ;
#21204 = CARTESIAN_POINT ( 'NONE',  ( 3.211159895383561835, 21.56249999863440792, -3.211159895383561835 ) ) ;
#21205 = CARTESIAN_POINT ( 'NONE',  ( 2.975619346028165246, -8.674330214978068554, -0.09252763182293416433 ) ) ;
#21206 = FACE_OUTER_BOUND ( 'NONE', #71489, .T. ) ;
#21207 = VERTEX_POINT ( 'NONE', #74428 ) ;
#21208 = DIRECTION ( 'NONE',  ( -1.000000000000000000, -0.000000000000000000, -0.000000000000000000 ) ) ;
#21209 = CARTESIAN_POINT ( 'NONE',  ( 2.765530957081996366, 290.2968750017069510, -6.676582343750003368 ) ) ;
#21210 = LINE ( 'NONE', #25736, #12214 ) ;
#21211 = CARTESIAN_POINT ( 'NONE',  ( 7.999999999999991118, 3.313708498984757611, 0.3615527839201451710 ) ) ;
#21212 = CARTESIAN_POINT ( 'NONE',  ( 2.849036369511732440E-14, 195.3750000027311842, 202.0000000000000284 ) ) ;
#21213 = CARTESIAN_POINT ( 'NONE',  ( 7.320508075688774596, 207.4999999931720538, -7.320508075688774596 ) ) ;
#21214 = CARTESIAN_POINT ( 'NONE',  ( -7.204075437095965206, -7.204075437095968759, 104.2187500020483810 ) ) ;
#21215 = ORIENTED_EDGE ( 'NONE', *, *, #19109, .F. ) ;
#21216 = ADVANCED_FACE ( 'NONE', ( #45754 ), #68395, .F. ) ;
#21217 = EDGE_CURVE ( 'NONE', #58094, #7596, #47269, .T. ) ;
#21218 = VECTOR ( 'NONE', #47733, 1000.000000000000000 ) ;
#21219 = CARTESIAN_POINT ( 'NONE',  ( 5.676582343750001591, 156.9270833299193555, -9.832129032723420536 ) ) ;
#21220 = CYLINDRICAL_SURFACE ( 'NONE', #7379, 4.000000000000001776 ) ;
#21221 = B_SPLINE_CURVE_WITH_KNOTS ( 'NONE', 3,
 ( #34225, #40985, #63993, #12308, #58352, #52674, #1010, #23990, #46999, #70031, #18340, #41354, #7022, #30031, #53046, #1379, #40235, #57227, #5539, #28541, #60172, #19805, #64731, #18711, #59447, #36801, #8492, #47731 ),
 .UNSPECIFIED., .F., .F.,
 ( 4, 2, 2, 2, 2, 2, 2, 2, 2, 2, 2, 2, 2, 4 ),
 ( 0.000000000000000000, 0.001421530729010940649, 0.002843061458021881299, 0.005686122916043762597, 0.008529184374065643462, 0.009950715103076584328, 0.01137224583208752346, 0.01279377656109846259, 0.01421530729010940346, 0.01563683801912034085, 0.01705836874813127652, 0.01990143020615315478, 0.02132296093516409738, 0.02274449166417503651 ),
 .UNSPECIFIED. ) ;
#21222 = CARTESIAN_POINT ( 'NONE',  ( -1.432654583217608080, 205.8750000013656063, 201.4587341250000350 ) ) ;
#21223 = CARTESIAN_POINT ( 'NONE',  ( -7.999999999961167951, -1.666173683171983354E-05, 1.018425797410095646 ) ) ;
#21224 = CARTESIAN_POINT ( 'NONE',  ( -3.042071309553164404, 57.55208332991936260, -11.35316468749999963 ) ) ;
#21225 = ORIENTED_EDGE ( 'NONE', *, *, #40075, .F. ) ;
#21226 = CARTESIAN_POINT ( 'NONE',  ( 10.18810118749999916, 4.220049686691935698, 113.5000000020483810 ) ) ;
#21227 = CARTESIAN_POINT ( 'NONE',  ( -8.342170076843785083E-16, 9.187499998634407916, 4.541265875000002339 ) ) ;
#21228 = VERTEX_POINT ( 'NONE', #11430 ) ;
#21229 = EDGE_CURVE ( 'NONE', #24115, #22353, #32978, .T. ) ;
#21230 = CARTESIAN_POINT ( 'NONE',  ( 4.401442555609581635E-16, 20.34374999795161543, -7.188101187500000044 ) ) ;
#21231 = CARTESIAN_POINT ( 'NONE',  ( 2.485281374238575314, 290.3750000034139589, 6.000000000000000888 ) ) ;
#21232 = CARTESIAN_POINT ( 'NONE',  ( -6.123233995736766282E-16, 246.8750000068280031, -10.00000000000000000 ) ) ;
#21233 = CARTESIAN_POINT ( 'NONE',  ( -2.977408999572650039, 17.81249999795161543, -7.188101187500001821 ) ) ;
#21234 = CARTESIAN_POINT ( 'NONE',  ( 2.977408999572650927, -7.188101187499990274, 1.955302781871753881 ) ) ;
#21235 = CARTESIAN_POINT ( 'NONE',  ( -10.18810118749999916, 4.220049686691934809, 112.9375000020483810 ) ) ;
#21236 = CARTESIAN_POINT ( 'NONE',  ( 0.9682425964012644215, -42.15372691850105014, 151.0238124213164213 ) ) ;
#21237 = CARTESIAN_POINT ( 'NONE',  ( 1.656854249492381914, 5.562499997268813168, 4.000000000000000888 ) ) ;
#21238 = CARTESIAN_POINT ( 'NONE',  ( -4.000000000000016875, 208.5625000027311842, 140.3431457505076594 ) ) ;
#21239 = VERTEX_POINT ( 'NONE', #56344 ) ;
#21240 = CARTESIAN_POINT ( 'NONE',  ( 3.458734125000015425, 207.9375000013656063, 198.0000000000000284 ) ) ;
#21241 =( GEOMETRIC_REPRESENTATION_CONTEXT ( 3 ) GLOBAL_UNCERTAINTY_ASSIGNED_CONTEXT ( ( #47142 ) ) GLOBAL_UNIT_ASSIGNED_CONTEXT ( ( #67191, #9480, #20024 ) ) REPRESENTATION_CONTEXT ( 'NONE', 'WORKASPACE' ) );
#21242 = EDGE_CURVE ( 'NONE', #68202, #21157, #14104, .T. ) ;
#21243 = CARTESIAN_POINT ( 'NONE',  ( -27.99999999999990763, 195.6250000027311842, 174.0000000000003695 ) ) ;
#21244 = CARTESIAN_POINT ( 'NONE',  ( 10.18810118749999916, 4.220049686691935698, 68.87500000204838102 ) ) ;
#21245 = CARTESIAN_POINT ( 'NONE',  ( -4.541265875000003227, 6.874999998634407916, 1.881053915767121110 ) ) ;
#21246 = CARTESIAN_POINT ( 'NONE',  ( -7.999999999999989342, -3.313708498984762496, 9.924052779823364645 ) ) ;
#21247 = CARTESIAN_POINT ( 'NONE',  ( -7.188101187499990274, -2.977408999572651371, 24.08030278187175455 ) ) ;
#21248 = VERTEX_POINT ( 'NONE', #53281 ) ;
#21249 = DIRECTION ( 'NONE',  ( 0.000000000000000000, 0.000000000000000000, -1.000000000000000000 ) ) ;
#21250 = ORIENTED_EDGE ( 'NONE', *, *, #38242, .F. ) ;
#21251 = CARTESIAN_POINT ( 'NONE',  ( 7.204075437095966983, 7.204075437095967871, 116.5937500020483810 ) ) ;
#21252 = CARTESIAN_POINT ( 'NONE',  ( 3.458734125000016313, 205.8750000013656063, 199.4326545832176691 ) ) ;
#21253 = CARTESIAN_POINT ( 'NONE',  ( 30.44569435410883074, 200.5625000013656063, 172.4456943541086957 ) ) ;
#21254 = CARTESIAN_POINT ( 'NONE',  ( -8.660254037844390851, 62.91666666666667851, 4.999999999999998224 ) ) ;
#21255 = CARTESIAN_POINT ( 'NONE',  ( 7.188101187500002709, 95.18750000204838102, 2.977408999572649151 ) ) ;
#21256 = CARTESIAN_POINT ( 'NONE',  ( 1.102182119232618108E-15, 291.2500000000000000, 6.000000000000001776 ) ) ;
#21257 = CARTESIAN_POINT ( 'NONE',  ( 23.99999999999998224, 206.8125000027312126, 168.3431457505075741 ) ) ;
#21258 = ORIENTED_EDGE ( 'NONE', *, *, #39996, .T. ) ;
#21259 = VECTOR ( 'NONE', #57430, 1000.000000000000000 ) ;
#21260 = CARTESIAN_POINT ( 'NONE',  ( 11.35316468749999608, 221.6145833367472733, -3.042071309553167069 ) ) ;
#21261 = CARTESIAN_POINT ( 'NONE',  ( -3.074111742560043936, -16.37317034319901410, 69.01341173090899872 ) ) ;
#21262 = CARTESIAN_POINT ( 'NONE',  ( 1.656854249492347719, 198.9375000027312126, 146.0000000000000284 ) ) ;
#21263 = CARTESIAN_POINT ( 'NONE',  ( -10.99999999999999822, -4.556349186104053040, 77.59374999999998579 ) ) ;
#21264 = CARTESIAN_POINT ( 'NONE',  ( -15.99999999999999645, -16.00000000000000355, 20.00000000000000000 ) ) ;
#21265 = CARTESIAN_POINT ( 'NONE',  ( -2.679491924311228512, 248.9583333333333712, -9.999999999999998224 ) ) ;
#21266 = CARTESIAN_POINT ( 'NONE',  ( -8.660254037844421049, 77.91666666666668561, 5.000000000000016875 ) ) ;
#21267 = CARTESIAN_POINT ( 'NONE',  ( -10.00000000000000000, 187.2916666666666572, -2.679491924311229845 ) ) ;
#21268 = CARTESIAN_POINT ( 'NONE',  ( 12.00000000000000000, 6.928203230275491009, -14.00000000000000178 ) ) ;
#21269 = CARTESIAN_POINT ( 'NONE',  ( 5.082755093536320601, -5.082755093536318824, 24.92405278187175810 ) ) ;
#21270 = CARTESIAN_POINT ( 'NONE',  ( -5.676582343749998039, 152.7604166632526983, -9.832129032723420536 ) ) ;
#21271 = CARTESIAN_POINT ( 'NONE',  ( -4.000000000000015987, 204.6875000027312126, 143.6568542494924259 ) ) ;
#21272 = CARTESIAN_POINT ( 'NONE',  ( -31.17484967038609867, 45.73369785095819395, 65.00000000000000000 ) ) ;
#21273 = CARTESIAN_POINT ( 'NONE',  ( 0.000000000000000000, 220.0000000000000284, 11.00000000000000000 ) ) ;
#21275 = CARTESIAN_POINT ( 'NONE',  ( 28.00000000000001776, 195.1250000027311842, 173.9999999999999147 ) ) ;
#21274 = DIRECTION ( 'NONE',  ( 0.000000000000000000, 0.000000000000000000, 1.000000000000000000 ) ) ;
#21276 = ORIENTED_EDGE ( 'NONE', *, *, #74065, .F. ) ;
#21277 = CARTESIAN_POINT ( 'NONE',  ( 5.676582343750001591, 21.92708332991935194, -9.832129032723420536 ) ) ;
#21278 = CARTESIAN_POINT ( 'NONE',  ( -6.735557395310442023E-16, 11.00000000000000000, 77.31250000409677625 ) ) ;
#21280 = CARTESIAN_POINT ( 'NONE',  ( 0.4501631047601223345, -16.44600848780494218, -68.55503832938644848 ) ) ;
#21279 = CARTESIAN_POINT ( 'NONE',  ( 7.999999999999991118, 9.797174393178815797E-16, 21.08030277982336642 ) ) ;
#21281 = CARTESIAN_POINT ( 'NONE',  ( 11.00000000000000000, 1.347111479062088405E-15, 79.74999999999998579 ) ) ;
#21282 = CARTESIAN_POINT ( 'NONE',  ( -2.754378923186476579E-14, 203.1875000013656063, 145.4587341250000350 ) ) ;
#21283 =( BOUNDED_CURVE ( )  B_SPLINE_CURVE ( 2, ( #26043, #72074, #14357, #31728, #54750, #20392, #26419, #38140, #47950, #25304, #20771, #43790, #7603 ),
 .UNSPECIFIED., .F., .F. ) 
 B_SPLINE_CURVE_WITH_KNOTS ( ( 3, 2, 2, 2, 2, 2, 3 ),
 ( 0.6793478260869565410, 0.6811594202898550998, 0.6829710144927536586, 0.6847826086956522174, 0.6865942028985507761, 0.6884057971014492239, 0.6902173913043477826 ),
 .UNSPECIFIED. ) 
 CURVE ( )  GEOMETRIC_REPRESENTATION_ITEM ( )  RATIONAL_B_SPLINE_CURVE ( ( 1.000000000000000000, 0.9659258262890683122, 1.000000000000000000, 0.9659258262890683122, 1.000000000000000000, 0.9659258262890683122, 1.000000000000000000, 0.9659258262890683122, 1.000000000000000000, 0.9659258262890683122, 1.000000000000000000, 0.9659258262890683122, 1.000000000000000000 ) ) 
 REPRESENTATION_ITEM ( '' )  );
#21284 = CARTESIAN_POINT ( 'NONE',  ( 10.00000000000000178, 46.87499999317203958, 0.000000000000000000 ) ) ;
#21285 = CARTESIAN_POINT ( 'NONE',  ( -7.188101187499999156, 101.7500000020483810, 2.977408999572654924 ) ) ;
#21286 = CARTESIAN_POINT ( 'NONE',  ( -4.541265875000003227, 6.999999998634407916, 1.881053915767121110 ) ) ;
#21287 = CARTESIAN_POINT ( 'NONE',  ( 4.999999999999991118, 54.16666666666666430, 8.660254037844389075 ) ) ;
#21288 = CARTESIAN_POINT ( 'NONE',  ( 7.999999999999991118, 9.797174393178815797E-16, 10.58030277982336465 ) ) ;
#21290 = CARTESIAN_POINT ( 'NONE',  ( -7.999999999995399236, -5.826008446853342637E-06, 20.51801720710344767 ) ) ;
#21289 = CARTESIAN_POINT ( 'NONE',  ( 1.102182119232618108E-15, 291.3125000034140157, 6.000000000000001776 ) ) ;
#21291 = ORIENTED_EDGE ( 'NONE', *, *, #54232, .T. ) ;
#21292 = EDGE_LOOP ( 'NONE', ( #44097, #481, #67859, #72169 ) ) ;
#21293 = CARTESIAN_POINT ( 'NONE',  ( -2.679491924311529605, 223.5416666666666288, 9.999999999999831246 ) ) ;
#21294 = CARTESIAN_POINT ( 'NONE',  ( 2.445694354108839175, 196.3125000013656063, 195.5543056458912190 ) ) ;
#21295 = VECTOR ( 'NONE', #10598, 1000.000000000000000 ) ;
#21296 = CARTESIAN_POINT ( 'NONE',  ( -4.556349186104045934, 11.00000000000000000, 95.21874999999998579 ) ) ;
#21297 = CARTESIAN_POINT ( 'NONE',  ( 11.35316468749999963, 145.9895833299193839, -3.042071309553165293 ) ) ;
#21298 = VERTEX_POINT ( 'NONE', #7253 ) ;
#21299 = EDGE_CURVE ( 'NONE', #41754, #1378, #6815, .T. ) ;
#21300 = CARTESIAN_POINT ( 'NONE',  ( -4.999999999999996447, 16.24494643555759410, -69.83755725260752456 ) ) ;
#21301 = CARTESIAN_POINT ( 'NONE',  ( 10.18810118749999916, 4.220049686691935698, 88.00000000204836681 ) ) ;
#21302 = CARTESIAN_POINT ( 'NONE',  ( 11.00000000000000000, 1.347111479062088405E-15, 93.24999999999998579 ) ) ;
#21303 = CARTESIAN_POINT ( 'NONE',  ( 2.828427124746208943, 209.6250000000000284, 195.1715728752538439 ) ) ;
#21305 = CARTESIAN_POINT ( 'NONE',  ( 9.832129032723420536, 131.1979166632526983, -5.676582343749999815 ) ) ;
#21304 = CARTESIAN_POINT ( 'NONE',  ( -3.313708498984765161, 18.84374999590322020, 7.999999999999998224 ) ) ;
#21306 = CARTESIAN_POINT ( 'NONE',  ( 11.35316468749999963, 55.98958332991934128, -3.042071309553165293 ) ) ;
#21307 = CARTESIAN_POINT ( 'NONE',  ( 7.022222184832267011, -9.802124591828780709, -1.180763928472494673E-14 ) ) ;
#21308 = ORIENTED_EDGE ( 'NONE', *, *, #69399, .T. ) ;
#21309 =( BOUNDED_CURVE ( )  B_SPLINE_CURVE ( 2, ( #13954, #43387, #36994, #66404, #10193, #67903, #4171, #11674, #27158 ),
 .UNSPECIFIED., .F., .F. ) 
 B_SPLINE_CURVE_WITH_KNOTS ( ( 3, 2, 2, 2, 3 ),
 ( 0.04999999999999991951, 0.05833333333333332038, 0.06666666666666672125, 0.07500000000000012212, 0.08333333333333352300 ),
 .UNSPECIFIED. ) 
 CURVE ( )  GEOMETRIC_REPRESENTATION_ITEM ( )  RATIONAL_B_SPLINE_CURVE ( ( 1.000000000000000666, 0.9238795325112859613, 1.000000000000000000, 0.9238795325112867385, 1.000000000000000000, 0.9238795325112867385, 1.000000000000000000, 0.9238795325112849621, 1.000000000000001776 ) ) 
 REPRESENTATION_ITEM ( '' )  );
#21310 = CARTESIAN_POINT ( 'NONE',  ( -7.320508075688778149, 24.99999999317203603, 7.320508075688769267 ) ) ;
#21311 = FACE_OUTER_BOUND ( 'NONE', #4256, .T. ) ;
#21312 = CARTESIAN_POINT ( 'NONE',  ( -5.676582343750006032, 109.4270833299193555, 9.832129032723418760 ) ) ;
#21313 = CARTESIAN_POINT ( 'NONE',  ( 1.432654583217664479, 200.7500000013656063, 201.4587341250000065 ) ) ;
#21314 = CARTESIAN_POINT ( 'NONE',  ( 5.082755093536324154, 15.65624999795161365, 5.082755093536326818 ) ) ;
#21315 = CARTESIAN_POINT ( 'NONE',  ( -4.220049686691937474, -10.18810118749999738, 84.81250000204838102 ) ) ;
#21316 = CARTESIAN_POINT ( 'NONE',  ( 11.35316468749999963, 26.30208332991934839, -3.042071309553165293 ) ) ;
#21317 = ORIENTED_EDGE ( 'NONE', *, *, #13983, .F. ) ;
#21318 = CARTESIAN_POINT ( 'NONE',  ( -0.9815212833345903221, -13.28972488340249214, -0.7446230086126913728 ) ) ;
#21319 = CARTESIAN_POINT ( 'NONE',  ( -8.008118988124989457, -3.317071493978883900, 20.60686528394063188 ) ) ;
#21320 = DIRECTION ( 'NONE',  ( -0.000000000000000000, 1.000000000000000000, -0.000000000000000000 ) ) ;
#21321 = EDGE_CURVE ( 'NONE', #38928, #52317, #18981, .T. ) ;
#21322 = EDGE_CURVE ( 'NONE', #13943, #61247, #30264, .T. ) ;
#21323 = CARTESIAN_POINT ( 'NONE',  ( -14.00000000000000000, 0.000000000000000000, 17.50000000000000000 ) ) ;
#21324 = CARTESIAN_POINT ( 'NONE',  ( -7.188101187500002709, 2.812499997951610098, 2.977408999572649151 ) ) ;
#21325 = CARTESIAN_POINT ( 'NONE',  ( -6.676582343750003368, 288.3906250017069510, -2.765530957081996810 ) ) ;
#21326 = DIRECTION ( 'NONE',  ( -0.000000000000000000, 1.000000000000000000, -0.000000000000000000 ) ) ;
#21327 = CARTESIAN_POINT ( 'NONE',  ( -25.17157287525382614, 206.8750000000000284, 167.1715728752541565 ) ) ;
#21328 = ORIENTED_EDGE ( 'NONE', *, *, #46866, .F. ) ;
#21329 = ADVANCED_FACE ( 'NONE', ( #12894 ), #11798, .F. ) ;
#21330 = CARTESIAN_POINT ( 'NONE',  ( -9.832129032723418760, 148.1770833299193555, -5.676582343750004256 ) ) ;
#21331 = CARTESIAN_POINT ( 'NONE',  ( -4.220049686691937474, -10.18810118749999738, 79.93750000204839523 ) ) ;
#21332 = CARTESIAN_POINT ( 'NONE',  ( -28.00000000000002487, 209.6875000013656063, 166.5412658750003629 ) ) ;
#21333 = CARTESIAN_POINT ( 'NONE',  ( -4.000000000000015987, 198.5000000000000000, 142.0000000000000568 ) ) ;
#21334 = CARTESIAN_POINT ( 'NONE',  ( 1.881053915767121776, 17.62499999863440436, -4.541265875000002339 ) ) ;
#21335 = EDGE_LOOP ( 'NONE', ( #64573, #54062, #60860, #4540 ) ) ;
#21336 = CARTESIAN_POINT ( 'NONE',  ( 4.000000000000015987, 204.5625000027312126, 199.6568542494924259 ) ) ;
#21337 = EDGE_CURVE ( 'NONE', #66166, #30304, #35930, .T. ) ;
#21338 = CARTESIAN_POINT ( 'NONE',  ( 1.432654583217608080, 194.8750000013656063, 138.5412658750000503 ) ) ;
#21339 = CARTESIAN_POINT ( 'NONE',  ( -23.99999999999996447, 205.8125000027312126, 171.6568542494926817 ) ) ;
#21340 = CARTESIAN_POINT ( 'NONE',  ( 0.000000000000000000, 0.000000000000000000, -14.77459999999999951 ) ) ;
#21341 = ORIENTED_EDGE ( 'NONE', *, *, #29372, .F. ) ;
#21342 = CARTESIAN_POINT ( 'NONE',  ( -7.188101187500002709, 8.812499997951611874, 2.977408999572649151 ) ) ;
#21343 = CARTESIAN_POINT ( 'NONE',  ( -19.41584562021463967, -15.67795138002411903, 194.1789750200875346 ) ) ;
#21344 = CARTESIAN_POINT ( 'NONE',  ( 4.999999999999999112, 52.15374455614202276, -42.28282461816495186 ) ) ;
#21345 = CARTESIAN_POINT ( 'NONE',  ( 8.311093377946834337, 190.1562499965860127, 8.311093377946839666 ) ) ;
#21346 = CARTESIAN_POINT ( 'NONE',  ( -7.188101187499999156, 114.1250000020483952, 2.977408999572654924 ) ) ;
#21347 = CARTESIAN_POINT ( 'NONE',  ( 1.102182119232618108E-15, 291.3125000034140157, 6.000000000000001776 ) ) ;
#21348 = CARTESIAN_POINT ( 'NONE',  ( 7.320508075688774596, 132.4999999931720254, -7.320508075688774596 ) ) ;
#21349 = ORIENTED_EDGE ( 'NONE', *, *, #15500, .F. ) ;
#21350 = CARTESIAN_POINT ( 'NONE',  ( -11.35316468749999963, 219.2187500034139873, 0.000000000000000000 ) ) ;
#21351 = CARTESIAN_POINT ( 'NONE',  ( -7.188101187499990274, -2.977408999572651371, 22.95530278187175455 ) ) ;
#21352 = CARTESIAN_POINT ( 'NONE',  ( 5.656854249492381470, 106.0625000000000000, 5.656854249492379694 ) ) ;
#21353 = CARTESIAN_POINT ( 'NONE',  ( 62.39047978708148889, 272.0000000000000000, 45.00000000000000000 ) ) ;
#21354 = CARTESIAN_POINT ( 'NONE',  ( -1.780377099648641437, -67.71330631781127352, -20.13219356122175441 ) ) ;
#21355 = CARTESIAN_POINT ( 'NONE',  ( 2.754378923186476579E-14, 195.4375000013655779, 194.5412658750000219 ) ) ;
#21356 = ORIENTED_EDGE ( 'NONE', *, *, #1586, .F. ) ;
#21357 = FACE_OUTER_BOUND ( 'NONE', #35036, .T. ) ;
#21358 = CARTESIAN_POINT ( 'NONE',  ( -4.898587196589412829E-16, 91.62499999999998579, -8.000000000000000000 ) ) ;
#21359 = CARTESIAN_POINT ( 'NONE',  ( -9.832129032723418760, 118.1770833299193555, -5.676582343750004256 ) ) ;
#21360 = CARTESIAN_POINT ( 'NONE',  ( -5.000000000000000000, -11.00774715070965648, -67.37702390743055503 ) ) ;
#21361 = CARTESIAN_POINT ( 'NONE',  ( -10.99999999999999822, -4.556349186104052151, 71.59374999999998579 ) ) ;
#21364 = CARTESIAN_POINT ( 'NONE',  ( -11.00000000000000000, 0.000000000000000000, 110.6875000040967763 ) ) ;
#21363 = CARTESIAN_POINT ( 'NONE',  ( 25.55430564589119058, 200.3125000013656063, 172.4456943541087526 ) ) ;
#21362 = CARTESIAN_POINT ( 'NONE',  ( 24.54126587499999346, 199.4375000013655779, 169.9999999999998863 ) ) ;
#21365 = ORIENTED_EDGE ( 'NONE', *, *, #19686, .F. ) ;
#21366 = CARTESIAN_POINT ( 'NONE',  ( 0.5935108062425623610, 223.7964224127544242, 9.986736671522551845 ) ) ;
#21367 = CARTESIAN_POINT ( 'NONE',  ( 3.042071309553159519, 224.7395833299193555, 11.35316468750000141 ) ) ;
#21368 = AXIS2_PLACEMENT_3D ( 'NONE', #30285, #7648, #30653 ) ;
#21369 = CARTESIAN_POINT ( 'NONE',  ( 31.45873412499999233, 199.9375000013656063, 169.9999999999999432 ) ) ;
#21370 = CARTESIAN_POINT ( 'NONE',  ( -2.085542519210945728E-15, 209.8437499965860411, 11.35316468750000141 ) ) ;
#21371 = DIRECTION ( 'NONE',  ( 0.000000000000000000, 0.000000000000000000, -1.000000000000000000 ) ) ;
#21372 = CARTESIAN_POINT ( 'NONE',  ( 1.469576158976823947E-15, 90.87500000000000000, 8.000000000000000000 ) ) ;
#21373 = CARTESIAN_POINT ( 'NONE',  ( -1.881053915767124440, 17.99999999863440436, 4.541265875000001451 ) ) ;
#21374 = CARTESIAN_POINT ( 'NONE',  ( 24.54126587500000056, 195.3750000013656063, 168.5673454167822172 ) ) ;
#21375 = CARTESIAN_POINT ( 'NONE',  ( -7.999999999999991118, 3.313708498984756723, 29.23655277982336642 ) ) ;
#21377 = CARTESIAN_POINT ( 'NONE',  ( 4.898587196589412829E-16, 12.37500000000000178, -8.000000000000000000 ) ) ;
#21376 = CARTESIAN_POINT ( 'NONE',  ( 2.751064625579944321E-14, 204.7500000000000284, 194.0000000000000568 ) ) ;
#21378 = CARTESIAN_POINT ( 'NONE',  ( 9.832129032723420536, 101.1979166632526841, -5.676582343749999815 ) ) ;
#21379 = VERTEX_POINT ( 'NONE', #29154 ) ;
#21380 = B_SPLINE_CURVE_WITH_KNOTS ( 'NONE', 3,
 ( #29497, #64568, #69112, #23455, #12865, #63442, #6120, #34435, #105, #35901, #57813, #24561, #58918, #844, #23830, #475, #57436, #46094, #7228, #29124 ),
 .UNSPECIFIED., .F., .F.,
 ( 4, 2, 2, 2, 2, 2, 2, 2, 2, 4 ),
 ( 2.797157557069881010E-17, 0.001156441540184027089, 0.001734662310276020251, 0.002312883080368013412, 0.003469324620551992363, 0.004625766160735971314, 0.005782207700919949830, 0.006938649241103929215, 0.008095090781287906864, 0.009251532321471885381 ),
 .UNSPECIFIED. ) ;
#21381 = DIRECTION ( 'NONE',  ( 0.000000000000000000, 0.000000000000000000, -1.000000000000000000 ) ) ;
#21382 = CARTESIAN_POINT ( 'NONE',  ( -2.977408999572650039, 17.43749999795161187, -7.188101187500001821 ) ) ;
#21383 = CARTESIAN_POINT ( 'NONE',  ( 11.00000000000000000, 1.347111479062088405E-15, 69.43750000409676204 ) ) ;
#21384 = CARTESIAN_POINT ( 'NONE',  ( 9.832129032723420536, 256.3020833367473301, 5.676582343749996262 ) ) ;
#21385 = CARTESIAN_POINT ( 'NONE',  ( 8.311093377946834337, 90.15624999658604111, 8.311093377946839666 ) ) ;
#21386 = ORIENTED_EDGE ( 'NONE', *, *, #11595, .F. ) ;
#21387 = EDGE_CURVE ( 'NONE', #29800, #56053, #21833, .T. ) ;
#21388 = CARTESIAN_POINT ( 'NONE',  ( -1.836970198721029983E-15, 205.6249999931720538, 10.00000000000000178 ) ) ;
#21389 = CARTESIAN_POINT ( 'NONE',  ( 7.204075437095966983, 7.204075437095967871, 109.0937500020483810 ) ) ;
#21390 = CARTESIAN_POINT ( 'NONE',  ( -1.469576158976823947E-15, 17.62500000000000000, 8.000000000000000000 ) ) ;
#21391 = CARTESIAN_POINT ( 'NONE',  ( 3.458734125000015869, 203.1875000013656063, 198.0000000000000284 ) ) ;
#21392 = DIRECTION ( 'NONE',  ( -1.000000000000000000, 0.000000000000000000, -0.000000000000000000 ) ) ;
#21394 = CARTESIAN_POINT ( 'NONE',  ( -9.832129032723418760, 82.86458332991935549, -5.676582343750004256 ) ) ;
#21393 = CARTESIAN_POINT ( 'NONE',  ( 8.000000000000001776, 121.3437500040967763, 3.313708498984759387 ) ) ;
#21395 = CARTESIAN_POINT ( 'NONE',  ( -3.313708498984758943, -7.999999999999989342, 19.29905278392014978 ) ) ;
#21396 = CARTESIAN_POINT ( 'NONE',  ( -28.00000000000002132, 200.6875000013656063, 166.5412658750003629 ) ) ;
#21397 = CARTESIAN_POINT ( 'NONE',  ( 2.828427124746191623, 15.12500000000000000, -2.828427124746191623 ) ) ;
#21398 = CARTESIAN_POINT ( 'NONE',  ( -8.660254037844387298, 178.9583333265053682, -5.000000000000004441 ) ) ;
#21399 = CARTESIAN_POINT ( 'NONE',  ( 4.999999999999999112, -52.15374455614175275, 42.28282461816533555 ) ) ;
#21400 = CARTESIAN_POINT ( 'NONE',  ( -5.676582343749998039, 77.76041666325268409, -9.832129032723420536 ) ) ;
#21401 = CARTESIAN_POINT ( 'NONE',  ( -6.676582343750000703, 293.5156250017070647, 2.765530957082001251 ) ) ;
#21402 =( BOUNDED_CURVE ( )  B_SPLINE_CURVE ( 2, ( #655, #16848, #22138, #23641, #57240, #45528, #39511, #46648, #69666 ),
 .UNSPECIFIED., .F., .F. ) 
 B_SPLINE_CURVE_WITH_KNOTS ( ( 3, 2, 2, 2, 3 ),
 ( 0.5333333333333337700, 0.5416666666666670737, 0.5500000000000004885, 0.5583333333333337922, 0.5666666666666670960 ),
 .UNSPECIFIED. ) 
 CURVE ( )  GEOMETRIC_REPRESENTATION_ITEM ( )  RATIONAL_B_SPLINE_CURVE ( ( 0.9999999999999958922, 0.9238795325112908463, 1.000000000000000000, 0.9238795325112867385, 1.000000000000000000, 0.9238795325112867385, 1.000000000000000000, 0.9238795325112826307, 1.000000000000003997 ) ) 
 REPRESENTATION_ITEM ( '' )  );
#21403 = CARTESIAN_POINT ( 'NONE',  ( 10.18810118749999916, 1.247682550866122264E-15, 101.7812500020483810 ) ) ;
#21404 = CARTESIAN_POINT ( 'NONE',  ( -9.832129032723420536, 213.6979166632526983, 5.676582343749997150 ) ) ;
#21405 = VERTEX_POINT ( 'NONE', #18937 ) ;
#21406 = CARTESIAN_POINT ( 'NONE',  ( 1.102182119232618108E-15, 289.3125000034140157, 6.000000000000001776 ) ) ;
#21407 = DIRECTION ( 'NONE',  ( 8.659560562354994488E-17, -0.7071067811865425767, 0.7071067811865525687 ) ) ;
#21408 = DIRECTION ( 'NONE',  ( -0.000000000000000000, 1.000000000000000000, 4.476705744456276341E-16 ) ) ;
#21410 = CARTESIAN_POINT ( 'NONE',  ( -9.832129032723418760, 207.8645833299193555, -5.676582343750004256 ) ) ;
#21409 = CARTESIAN_POINT ( 'NONE',  ( 6.123233995736767268E-16, 23.12499999317203603, -10.00000000000000178 ) ) ;
#21411 = CARTESIAN_POINT ( 'NONE',  ( 1.836970198721029589E-15, 229.3750000068279746, 10.00000000000000000 ) ) ;
#21412 = CARTESIAN_POINT ( 'NONE',  ( -2.679491924311106832, 254.1666666734946318, 10.00000000000006928 ) ) ;
#21413 = EDGE_LOOP ( 'NONE', ( #22445, #10927, #29720, #28568 ) ) ;
#21414 = AXIS2_PLACEMENT_3D ( 'NONE', #35875, #53596, #12838 ) ;
#21415 = CARTESIAN_POINT ( 'NONE',  ( 11.35316468749999785, 190.8854166632526983, 3.042071309553174174 ) ) ;
#21416 = EDGE_CURVE ( 'NONE', #72211, #27344, #6865, .T. ) ;
#21417 = CARTESIAN_POINT ( 'NONE',  ( -2.977408999572647819, -7.188101187499990274, 15.26780278187175455 ) ) ;
#21418 = CARTESIAN_POINT ( 'NONE',  ( -31.45873412499998523, 207.7500000013656063, 171.4326545832180386 ) ) ;
#21419 = CARTESIAN_POINT ( 'NONE',  ( 4.898587196589412829E-16, 12.37500000000000178, -8.000000000000000000 ) ) ;
#21420 = ORIENTED_EDGE ( 'NONE', *, *, #50752, .F. ) ;
#21421 = CARTESIAN_POINT ( 'NONE',  ( -3.313708498984762052, 93.40625000409677625, -8.000000000000000000 ) ) ;
#21422 = ADVANCED_FACE ( 'NONE', ( #43807 ), #31366, .F. ) ;
#21423 = CARTESIAN_POINT ( 'NONE',  ( 8.660254037844385522, 14.58333333333333393, 5.000000000000005329 ) ) ;
#21424 = AXIS2_PLACEMENT_3D ( 'NONE', #633, #27783, #63601 ) ;
#21425 = EDGE_CURVE ( 'NONE', #28769, #50841, #34439, .T. ) ;
#21426 = CARTESIAN_POINT ( 'NONE',  ( -7.204075437095967871, 7.204075437095967871, 82.84375000204838102 ) ) ;
#21427 = EDGE_LOOP ( 'NONE', ( #1237, #33964, #45833, #26936, #7044 ) ) ;
#21428 = CARTESIAN_POINT ( 'NONE',  ( -1.656854249492381248, 18.31249999999999645, -4.000000000000001776 ) ) ;
#21429 = CARTESIAN_POINT ( 'NONE',  ( 4.541265875000001451, 19.24999999863440436, 1.881053915767124440 ) ) ;
#21430 = DIRECTION ( 'NONE',  ( -0.000000000000000000, -0.000000000000000000, 1.000000000000000000 ) ) ;
#21431 = VERTEX_POINT ( 'NONE', #54015 ) ;
#21432 = CARTESIAN_POINT ( 'NONE',  ( -32.49574984736388217, 174.9883334519788320, 162.5913879594992295 ) ) ;
#21433 = CARTESIAN_POINT ( 'NONE',  ( 2.977408999572650039, 93.68750000204838102, -7.188101187500001821 ) ) ;
#21436 = CARTESIAN_POINT ( 'NONE',  ( 28.00000000000002487, 207.1250000027312126, 173.9999999999999147 ) ) ;
#21435 = CARTESIAN_POINT ( 'NONE',  ( 2.085542519210945334E-15, 255.1562500034140157, 11.35316468749999963 ) ) ;
#21434 = CARTESIAN_POINT ( 'NONE',  ( -7.320508075688770155, 258.7500000068279746, 7.320508075688774596 ) ) ;
#21437 = APPLICATION_PROTOCOL_DEFINITION ( 'draft international standard', 'automotive_design', 1998, #58288 ) ;
#21438 = ORIENTED_EDGE ( 'NONE', *, *, #73161, .F. ) ;
#21439 = CARTESIAN_POINT ( 'NONE',  ( -6.951808397369817780E-16, 252.9687500034140157, -11.35316468749999963 ) ) ;
#21440 = EDGE_CURVE ( 'NONE', #38706, #28551, #60847, .T. ) ;
#21441 = CARTESIAN_POINT ( 'NONE',  ( 7.188101187499991163, 2.977408999572648707, 14.33030278187175277 ) ) ;
#21442 = EDGE_LOOP ( 'NONE', ( #44234, #9588, #42027, #49169 ) ) ;
#21443 = ORIENTED_EDGE ( 'NONE', *, *, #12046, .T. ) ;
#21444 = CARTESIAN_POINT ( 'NONE',  ( -7.204075437095967871, 7.204075437095967871, 73.46875000204838102 ) ) ;
#21445 = CARTESIAN_POINT ( 'NONE',  ( 5.676582343750001591, 76.92708332991935549, -9.832129032723420536 ) ) ;
#21446 = CARTESIAN_POINT ( 'NONE',  ( 0.000000000000000000, 300.0000000000000000, 10.00000000000000178 ) ) ;
#21447 = CARTESIAN_POINT ( 'NONE',  ( 4.556349186104045934, 11.00000000000000000, 87.53125000000000000 ) ) ;
#21450 = CARTESIAN_POINT ( 'NONE',  ( 6.676582343750002480, 292.1718750017070079, -2.765530957081997254 ) ) ;
#21449 = CARTESIAN_POINT ( 'NONE',  ( 32.00000000000000000, 196.3125000027312126, 171.6568542494922553 ) ) ;
#21448 = DIRECTION ( 'NONE',  ( -0.000000000000000000, 1.000000000000000000, -0.000000000000000000 ) ) ;
#21451 = CARTESIAN_POINT ( 'NONE',  ( 1.656854249492381914, 13.81250000000000000, 4.000000000000000888 ) ) ;
#21452 = FACE_OUTER_BOUND ( 'NONE', #29854, .T. ) ;
#21453 = VECTOR ( 'NONE', #14568, 1000.000000000000000 ) ;
#21454 = CARTESIAN_POINT ( 'NONE',  ( 2.754378923186476579E-14, 199.4375000013655779, 194.5412658750000219 ) ) ;
#21455 = CARTESIAN_POINT ( 'NONE',  ( -8.000000000000000000, 8.062499995903221972, -9.797174393178825657E-16 ) ) ;
#21456 = ORIENTED_EDGE ( 'NONE', *, *, #57024, .F. ) ;
#21457 = CARTESIAN_POINT ( 'NONE',  ( 29.43265458321766204, 196.8750000013656063, 166.5412658749999650 ) ) ;
#21458 = VECTOR ( 'NONE', #1544, 1000.000000000000000 ) ;
#21459 = CARTESIAN_POINT ( 'NONE',  ( -2.977408999572650039, 19.31249999795161543, -7.188101187500001821 ) ) ;
#21460 = CARTESIAN_POINT ( 'NONE',  ( -11.35316468750000141, 168.5937499965860127, -1.390361679473963753E-15 ) ) ;
#21461 = CYLINDRICAL_SURFACE ( 'NONE', #25048, 8.000000000000000000 ) ;
#21462 = CARTESIAN_POINT ( 'NONE',  ( -4.401442555609581635E-16, 101.6562500020483810, -7.188101187500000044 ) ) ;
#21464 = CARTESIAN_POINT ( 'NONE',  ( -0.6547826978428695766, -49.91450260127106731, -40.68974341348058488 ) ) ;
#21463 = LINE ( 'NONE', #26362, #44440 ) ;
#21465 = CARTESIAN_POINT ( 'NONE',  ( 31.45873412499999944, 205.9375000013656063, 169.9999999999999432 ) ) ;
#21466 = CARTESIAN_POINT ( 'NONE',  ( -4.401442555609577197E-16, 7.188101187499992051, 17.98655278187175810 ) ) ;
#21467 = CARTESIAN_POINT ( 'NONE',  ( -2.849036369511732440E-14, 208.3750000027312126, 138.0000000000000568 ) ) ;
#21468 = CARTESIAN_POINT ( 'NONE',  ( -11.35316468749999785, 53.07291666325267698, -3.042071309553167513 ) ) ;
#21469 = B_SPLINE_CURVE_WITH_KNOTS ( 'NONE', 3,
 ( #26481, #21576, #72137, #15540, #38581, #60826, #44603, #67616 ),
 .UNSPECIFIED., .F., .F.,
 ( 4, 2, 2, 4 ),
 ( 0.01936970057594187763, 0.02112296051615076067, 0.02287622045635964371, 0.02638274033677740979 ),
 .UNSPECIFIED. ) ;
#21470 = CARTESIAN_POINT ( 'NONE',  ( -12.00000000000000178, -4.647306338817279503, -0.4736860157878169386 ) ) ;
#21471 = CARTESIAN_POINT ( 'NONE',  ( 10.00000000000000178, 21.87499999317203248, 0.000000000000000000 ) ) ;
#21472 = VERTEX_POINT ( 'NONE', #9489 ) ;
#21473 = CARTESIAN_POINT ( 'NONE',  ( 2.828427124746152987, 199.2500000027312126, 139.1715728752538723 ) ) ;
#21474 = DIRECTION ( 'NONE',  ( -0.000000000000000000, 1.000000000000000000, -1.563033456626094573E-30 ) ) ;
#21475 = CARTESIAN_POINT ( 'NONE',  ( -11.35316468749999785, 48.07291666325268409, -3.042071309553167513 ) ) ;
#21476 = VECTOR ( 'NONE', #3993, 1000.000000000000000 ) ;
#21477 = CARTESIAN_POINT ( 'NONE',  ( -11.00000000000000000, 4.556349186104045934, 74.59375000409676204 ) ) ;
#21478 = CARTESIAN_POINT ( 'NONE',  ( 3.458734124999960358, 198.6250000013656063, 143.4326545832176976 ) ) ;
#21479 = CARTESIAN_POINT ( 'NONE',  ( 4.465349678524270338, 10.10202304668574413, 70.97395336192860782 ) ) ;
#21480 = CARTESIAN_POINT ( 'NONE',  ( -4.999999999999992895, 245.8333333333333428, 8.660254037844390851 ) ) ;
#21482 = CARTESIAN_POINT ( 'NONE',  ( -11.35316468750000141, 48.48958332991934839, 3.042071309553159963 ) ) ;
#21481 = CARTESIAN_POINT ( 'NONE',  ( -5.082755093536325930, 96.96875000204838102, -5.082755093536325930 ) ) ;
#21484 = EDGE_CURVE ( 'NONE', #24322, #55047, #37031, .T. ) ;
#21483 = CARTESIAN_POINT ( 'NONE',  ( -3.313708498984758943, -7.999999999999989342, 10.11155277982336820 ) ) ;
#21485 = CARTESIAN_POINT ( 'NONE',  ( -5.656854249492373476, -5.656854249492376141, 4.205302783920145338 ) ) ;
#21486 = CARTESIAN_POINT ( 'NONE',  ( -11.35316468750000141, 168.2812499965860411, -1.390361679473963753E-15 ) ) ;
#21487 = VECTOR ( 'NONE', #56648, 1000.000000000000000 ) ;
#21488 = CARTESIAN_POINT ( 'NONE',  ( -8.660254037844390851, 144.7916666598387110, 4.999999999999998224 ) ) ;
#21489 = CARTESIAN_POINT ( 'NONE',  ( 2.977408999572650039, 104.5625000020483668, -7.188101187500001821 ) ) ;
#21490 = DIRECTION ( 'NONE',  ( 0.000000000000000000, -1.000000000000000000, 0.000000000000000000 ) ) ;
#21491 = CARTESIAN_POINT ( 'NONE',  ( 3.042071309553167513, 32.13541666325269119, -11.35316468749999785 ) ) ;
#21492 = ADVANCED_FACE ( 'NONE', ( #2325 ), #55141, .F. ) ;
#21493 = CARTESIAN_POINT ( 'NONE',  ( 4.242640687119287435, 295.4375000034140157, 4.242640687119285658 ) ) ;
#21494 = ORIENTED_EDGE ( 'NONE', *, *, #45013, .F. ) ;
#21495 = CARTESIAN_POINT ( 'NONE',  ( 0.000000000000000000, 300.0000000000000000, 0.000000000000000000 ) ) ;
#21496 = CARTESIAN_POINT ( 'NONE',  ( 10.18810118750000093, -4.220049686691933921, 78.81250000204838102 ) ) ;
#21497 = CARTESIAN_POINT ( 'NONE',  ( 31.04121413973415144, 46.94134546260061569, 65.00000000000001421 ) ) ;
#21499 = CARTESIAN_POINT ( 'NONE',  ( -8.311093377946841443, 168.9062499965860411, 8.311093377946834337 ) ) ;
#21498 = CARTESIAN_POINT ( 'NONE',  ( -7.320508075688783478, 8.125000000000003553, 7.320508075688775484 ) ) ;
#21500 = CARTESIAN_POINT ( 'NONE',  ( -3.313708498984757167, 7.999999999999991118, 11.10530278432982065 ) ) ;
#21501 = CARTESIAN_POINT ( 'NONE',  ( -38.00000000000000000, -53.00000000000000000, 15.00000000000000178 ) ) ;
#21502 = CARTESIAN_POINT ( 'NONE',  ( 3.042071309553163960, 227.4479166700806729, -11.35316468749999785 ) ) ;
#21503 = CARTESIAN_POINT ( 'NONE',  ( 0.4501631047599979341, 51.14740050676149963, -48.52018030598747345 ) ) ;
#21504 = CARTESIAN_POINT ( 'NONE',  ( -4.220049686691935698, 10.18810118749999916, 76.75000000204838102 ) ) ;
#21505 = ORIENTED_EDGE ( 'NONE', *, *, #29237, .T. ) ;
#21506 = EDGE_CURVE ( 'NONE', #1549, #48531, #72480, .T. ) ;
#21507 = DIRECTION ( 'NONE',  ( 0.000000000000000000, 0.000000000000000000, -1.000000000000000000 ) ) ;
#21508 = CARTESIAN_POINT ( 'NONE',  ( 10.99999999999989342, 4.556349186104152515, 105.3437499999999858 ) ) ;
#21509 = CARTESIAN_POINT ( 'NONE',  ( -5.676582343750006032, 119.4270833299193555, 9.832129032723418760 ) ) ;
#21510 = CARTESIAN_POINT ( 'NONE',  ( -4.541265875000002339, 20.87499999863440792, -1.881053915767121998 ) ) ;
#21511 = ORIENTED_EDGE ( 'NONE', *, *, #16722, .T. ) ;
#21512 = ORIENTED_EDGE ( 'NONE', *, *, #28829, .F. ) ;
#21513 = CARTESIAN_POINT ( 'NONE',  ( 3.211159895383560947, 8.312499998634407916, 3.211159895383562723 ) ) ;
#21514 = CARTESIAN_POINT ( 'NONE',  ( 7.188101187500000044, 9.468749997951610098, 0.000000000000000000 ) ) ;
#21515 = CARTESIAN_POINT ( 'NONE',  ( -8.000000000000000000, 108.5937500040967905, -3.313708498984761608 ) ) ;
#21516 =( BOUNDED_CURVE ( )  B_SPLINE_CURVE ( 2, ( #32817, #4143, #15805, #38840, #4508, #27502, #40284, #69705, #322 ),
 .UNSPECIFIED., .F., .F. ) 
 B_SPLINE_CURVE_WITH_KNOTS ( ( 3, 2, 2, 2, 3 ),
 ( 0.7000000000000006217, 0.7083333333333340365, 0.7166666666666673402, 0.7250000000000006439, 0.7333333333333339477 ),
 .UNSPECIFIED. ) 
 CURVE ( )  GEOMETRIC_REPRESENTATION_ITEM ( )  RATIONAL_B_SPLINE_CURVE ( ( 0.9999999999999938938, 0.9238795325112928447, 1.000000000000000000, 0.9238795325112867385, 1.000000000000000000, 0.9238795325112867385, 1.000000000000000000, 0.9238795325112806323, 1.000000000000005995 ) ) 
 REPRESENTATION_ITEM ( '' )  );
#21517 = CARTESIAN_POINT ( 'NONE',  ( 10.18810118750000093, -4.220049686691933921, 92.68750000204838102 ) ) ;
#21518 = CARTESIAN_POINT ( 'NONE',  ( -26.56734541678238060, 200.6250000013655779, 166.5412658750003629 ) ) ;
#21519 = EDGE_CURVE ( 'NONE', #6173, #8238, #59676, .T. ) ;
#21520 = VECTOR ( 'NONE', #68910, 1000.000000000000000 ) ;
#21521 = CARTESIAN_POINT ( 'NONE',  ( 1.656854249492381248, 7.187500000000000000, -4.000000000000001776 ) ) ;
#21522 = CARTESIAN_POINT ( 'NONE',  ( 4.000000000000001776, 19.81249999726881583, -1.656854249492381248 ) ) ;
#21523 = CARTESIAN_POINT ( 'NONE',  ( -8.342170076843785083E-16, 6.062499998634407028, 4.541265875000002339 ) ) ;
#21524 = CARTESIAN_POINT ( 'NONE',  ( -2.751064625579944321E-14, 197.7500000000000000, 146.0000000000000284 ) ) ;
#21525 = AXIS2_PLACEMENT_3D ( 'NONE', #70778, #665, #53441 ) ;
#21526 = ORIENTED_EDGE ( 'NONE', *, *, #28863, .T. ) ;
#21527 = CARTESIAN_POINT ( 'NONE',  ( -31.45873412500001720, 195.6250000013656063, 168.5673454167828140 ) ) ;
#21528 = CARTESIAN_POINT ( 'NONE',  ( -4.541265875000003227, 16.87499999863440436, 1.881053915767121110 ) ) ;
#21529 = CARTESIAN_POINT ( 'NONE',  ( 0.7799470984957478370, -47.90347954939649355, 151.0150387940846031 ) ) ;
#21530 = CARTESIAN_POINT ( 'NONE',  ( 1.320432766682872962E-15, -7.188101187499992051, 1.861552781871753881 ) ) ;
#21531 = ORIENTED_EDGE ( 'NONE', *, *, #20477, .T. ) ;
#21532 = EDGE_LOOP ( 'NONE', ( #50535, #57557, #50001, #31192 ) ) ;
#21533 = CARTESIAN_POINT ( 'NONE',  ( 10.18810118749999916, 1.247682550866122264E-15, 92.40625000204836681 ) ) ;
#21534 = CARTESIAN_POINT ( 'NONE',  ( 6.000000000000001776, 288.5000000000000000, -7.347880794884121708E-16 ) ) ;
#21535 = CARTESIAN_POINT ( 'NONE',  ( -25.55430564589115150, 199.3125000013656063, 172.4456943541091789 ) ) ;
#21536 = CARTESIAN_POINT ( 'NONE',  ( 7.778174593052023411, -7.778174593052021635, 105.0624999999999858 ) ) ;
#21537 = CARTESIAN_POINT ( 'NONE',  ( 1.432654583217664701, 209.0000000013655779, 201.4587341250000065 ) ) ;
#21538 = CARTESIAN_POINT ( 'NONE',  ( -5.656854249492380582, 111.3125000000000000, -5.656854249492380582 ) ) ;
#21539 = CARTESIAN_POINT ( 'NONE',  ( 2.679491924311228956, 126.0416666666666572, -10.00000000000000000 ) ) ;
#21540 = CARTESIAN_POINT ( 'NONE',  ( 8.000000000000000000, 104.7500000000000000, -9.797174393178825657E-16 ) ) ;
#21541 = CARTESIAN_POINT ( 'NONE',  ( 2.765530957082001251, 292.9218750017069510, 6.676582343750000703 ) ) ;
#21542 = CARTESIAN_POINT ( 'NONE',  ( 7.188101187499992051, 8.802885111219154394E-16, 7.111552781871754547 ) ) ;
#21543 = VERTEX_POINT ( 'NONE', #26435 ) ;
#21544 = CARTESIAN_POINT ( 'NONE',  ( 2.751064625579944321E-14, 199.8750000027312126, 194.0000000000000568 ) ) ;
#21545 = CARTESIAN_POINT ( 'NONE',  ( 26.56734541678238415, 207.0000000013656063, 166.5412658749999650 ) ) ;
#21546 = CARTESIAN_POINT ( 'NONE',  ( 3.313708498984762496, 28.03124999590322020, 7.999999999999998224 ) ) ;
#21547 = CARTESIAN_POINT ( 'NONE',  ( -2.445694354108839619, 198.8125000013656063, 139.5543056458912190 ) ) ;
#21548 = CARTESIAN_POINT ( 'NONE',  ( -7.188101187500000933, 124.4375000020483810, -2.977408999572650483 ) ) ;
#21550 = CARTESIAN_POINT ( 'NONE',  ( -3.458734125000015869, 204.1875000013656063, 142.0000000000000568 ) ) ;
#21549 = CARTESIAN_POINT ( 'NONE',  ( 8.000000000000000000, 121.3437500000000000, -3.313708498984762496 ) ) ;
#21551 = CARTESIAN_POINT ( 'NONE',  ( 9.832129032723420536, 261.3020833367473301, 5.676582343749996262 ) ) ;
#21552 = CARTESIAN_POINT ( 'NONE',  ( 2.449293598294707893E-16, 9.999999997268814056, -4.000000000000001776 ) ) ;
#21553 = CARTESIAN_POINT ( 'NONE',  ( -5.000000000000005329, 95.20833332650536818, 8.660254037844387298 ) ) ;
#21554 = CARTESIAN_POINT ( 'NONE',  ( 6.951808397369818766E-16, 17.03124999658601624, -11.35316468750000141 ) ) ;
#21555 = DIRECTION ( 'NONE',  ( -1.000000000000000000, 0.000000000000000000, 0.000000000000000000 ) ) ;
#21556 = CARTESIAN_POINT ( 'NONE',  ( 9.832129032723420536, 201.5104166632526983, -5.676582343749999815 ) ) ;
#21557 = CARTESIAN_POINT ( 'NONE',  ( -2.751064625579944321E-14, 206.7500000000000284, 146.0000000000000284 ) ) ;
#21558 = CARTESIAN_POINT ( 'NONE',  ( 2.780723358947928197E-16, 7.562499998634407028, -4.541265875000002339 ) ) ;
#21559 = CARTESIAN_POINT ( 'NONE',  ( -12.00000000000000000, 6.928203230275504332, -1.071796769724504550 ) ) ;
#21561 = CARTESIAN_POINT ( 'NONE',  ( 8.000000000000000000, 101.9375000040967763, -9.797174393178825657E-16 ) ) ;
#21560 = CARTESIAN_POINT ( 'NONE',  ( -7.778174593052020747, -7.778174593052023411, 88.18749999999998579 ) ) ;
#21562 = ORIENTED_EDGE ( 'NONE', *, *, #7642, .F. ) ;
#21563 = CARTESIAN_POINT ( 'NONE',  ( -3.458734125000016757, 199.1250000013656347, 140.5673454167824161 ) ) ;
#21564 = CARTESIAN_POINT ( 'NONE',  ( -11.35316468749999785, 8.072916663252682312, -3.042071309553167513 ) ) ;
#21565 = CARTESIAN_POINT ( 'NONE',  ( -7.778174593052020747, -7.778174593052023411, 100.3750000040967763 ) ) ;
#21566 = CARTESIAN_POINT ( 'NONE',  ( -24.54126587499996148, 199.1250000013656347, 171.4326545832179534 ) ) ;
#21567 = CYLINDRICAL_SURFACE ( 'NONE', #38272, 10.00000000000000178 ) ;
#21569 = CARTESIAN_POINT ( 'NONE',  ( 8.311093377946834337, 10.15624999658601801, 8.311093377946839666 ) ) ;
#21568 = CARTESIAN_POINT ( 'NONE',  ( -7.188101187500000933, 118.0625000020483952, -2.977408999572650483 ) ) ;
#21571 = EDGE_CURVE ( 'NONE', #27411, #69483, #26059, .T. ) ;
#21570 = CARTESIAN_POINT ( 'NONE',  ( -7.999999999999991118, 3.313708498984756723, 27.73655277982336642 ) ) ;
#21572 = CARTESIAN_POINT ( 'NONE',  ( 9.832129032723416984, 125.3645833299193413, 5.676582343750006032 ) ) ;
#21573 = CARTESIAN_POINT ( 'NONE',  ( -2.679491924311235618, 100.4166666598386684, 10.00000000000000000 ) ) ;
#21574 = CARTESIAN_POINT ( 'NONE',  ( 2.977408999572654480, 122.0000000020483668, 7.188101187499999156 ) ) ;
#21575 = CARTESIAN_POINT ( 'NONE',  ( 3.211159895383560947, 19.31249999863440436, 3.211159895383562723 ) ) ;
#21576 = CARTESIAN_POINT ( 'NONE',  ( -11.99999999999999822, 0.5857239961182026944, 7.623296525288699970E-18 ) ) ;
#21577 = ORIENTED_EDGE ( 'NONE', *, *, #38361, .F. ) ;
#21578 = CARTESIAN_POINT ( 'NONE',  ( 3.511653767256979197, -68.04552192806536937, 20.40125235306631524 ) ) ;
#21579 = EDGE_CURVE ( 'NONE', #29704, #70940, #60032, .T. ) ;
#21580 = CARTESIAN_POINT ( 'NONE',  ( 2.765530957081996366, 288.2968750017070647, -6.676582343750003368 ) ) ;
#21581 = CARTESIAN_POINT ( 'NONE',  ( -2.751064625579944321E-14, 207.8750000027312126, 146.0000000000000284 ) ) ;
#21582 = CARTESIAN_POINT ( 'NONE',  ( 7.999999999999991118, 3.313708498984757611, 3.361552783920145338 ) ) ;
#21583 = CARTESIAN_POINT ( 'NONE',  ( 1.224646799147353454E-15, 300.0000000000000000, -10.00000000000000178 ) ) ;
#21584 = VECTOR ( 'NONE', #46755, 1000.000000000000000 ) ;
#21585 = CARTESIAN_POINT ( 'NONE',  ( -7.347880794884122694E-16, 3.750000000000000000, 4.000000000000001776 ) ) ;
#21586 = CARTESIAN_POINT ( 'NONE',  ( 7.204075437095966983, 7.204075437095967871, 106.4687500020483810 ) ) ;
#21587 = ORIENTED_EDGE ( 'NONE', *, *, #36658, .F. ) ;
#21588 = CARTESIAN_POINT ( 'NONE',  ( 7.320508075688774596, 157.4999999931720254, -7.320508075688774596 ) ) ;
#21589 = CARTESIAN_POINT ( 'NONE',  ( 11.35316468750000141, 156.0937499965860127, 0.000000000000000000 ) ) ;
#21590 = CARTESIAN_POINT ( 'NONE',  ( -30.78020999568549243, -21.00133727736589506, 173.7950388576106775 ) ) ;
#21591 = CARTESIAN_POINT ( 'NONE',  ( -3.458734124999959469, 206.7500000013655779, 199.4326545832176976 ) ) ;
#21592 = CARTESIAN_POINT ( 'NONE',  ( 5.000000000000004441, 229.7916666734946602, 8.660254037844385522 ) ) ;
#21593 = CARTESIAN_POINT ( 'NONE',  ( 5.676582343749993598, 70.26041666325268409, 9.832129032723422313 ) ) ;
#21594 = ORIENTED_EDGE ( 'NONE', *, *, #4278, .F. ) ;
#21595 = CARTESIAN_POINT ( 'NONE',  ( -4.220049686691937474, -10.18810118749999738, 112.9375000020483810 ) ) ;
#21596 = CARTESIAN_POINT ( 'NONE',  ( -4.541265875000003227, 8.999999998634407916, 1.881053915767121110 ) ) ;
#21597 = ORIENTED_EDGE ( 'NONE', *, *, #70627, .T. ) ;
#21598 = CARTESIAN_POINT ( 'NONE',  ( -8.000000000000000000, 2.156250000000000444, -3.313708498984762496 ) ) ;
#21599 = CARTESIAN_POINT ( 'NONE',  ( -7.320508075688773708, 108.7499999931720254, -7.320508075688774596 ) ) ;
#21600 = DIRECTION ( 'NONE',  ( 0.000000000000000000, 0.000000000000000000, 1.000000000000000000 ) ) ;
#21601 = CARTESIAN_POINT ( 'NONE',  ( 7.188101187500000044, 20.34374999795161543, 0.000000000000000000 ) ) ;
#21602 = CARTESIAN_POINT ( 'NONE',  ( -5.447321192899549303, -4.689935021205116961, 0.1569292013794422458 ) ) ;
#21603 = CARTESIAN_POINT ( 'NONE',  ( -10.18810118749999916, 0.000000000000000000, 111.5312500020483668 ) ) ;
#21604 = PRODUCT_DEFINITION_SHAPE ( 'NONE', 'NONE',  #49627 ) ;
#21605 =( BOUNDED_CURVE ( )  B_SPLINE_CURVE ( 2, ( #25568, #37661, #48581, #71591, #60278, #19913, #67070, #8604, #25938 ),
 .UNSPECIFIED., .F., .F. ) 
 B_SPLINE_CURVE_WITH_KNOTS ( ( 3, 2, 2, 2, 3 ),
 ( 0.4861111111111111605, 0.4930555555555556357, 0.5000000000000000000, 0.5069444444444444198, 0.5138888888888888395 ),
 .UNSPECIFIED. ) 
 CURVE ( )  GEOMETRIC_REPRESENTATION_ITEM ( )  RATIONAL_B_SPLINE_CURVE ( ( 0.9999999999999994449, 0.9238795325112872936, 1.000000000000000000, 0.9238795325112867385, 1.000000000000000000, 0.9238795325112867385, 1.000000000000000000, 0.9238795325112867385, 1.000000000000000000 ) ) 
 REPRESENTATION_ITEM ( '' )  );
#21606 = CARTESIAN_POINT ( 'NONE',  ( 2.751064625579944321E-14, 201.8750000027312126, 194.0000000000000568 ) ) ;
#21607 = CARTESIAN_POINT ( 'NONE',  ( 2.828427124746191623, 7.874999997268813168, -2.828427124746191623 ) ) ;
#21608 = CARTESIAN_POINT ( 'NONE',  ( 27.99999999999999645, 210.0000000000000284, 173.9999999999998863 ) ) ;
#21609 = ORIENTED_EDGE ( 'NONE', *, *, #71978, .F. ) ;
#21610 = CARTESIAN_POINT ( 'NONE',  ( -2.445694354108782775, 204.5625000013656063, 200.4456943541088663 ) ) ;
#21611 = CARTESIAN_POINT ( 'NONE',  ( -24.54126587499999701, 209.1875000013656063, 170.0000000000002842 ) ) ;
#21612 = CARTESIAN_POINT ( 'NONE',  ( 7.204075437095968759, -7.204075437095966983, 71.59375000204836681 ) ) ;
#21613 = CARTESIAN_POINT ( 'NONE',  ( 4.541265875000002339, 6.374999998634407028, -1.881053915767121554 ) ) ;
#21614 = VECTOR ( 'NONE', #10671, 1000.000000000000000 ) ;
#21615 = CARTESIAN_POINT ( 'NONE',  ( 0.000000000000000000, 0.000000000000000000, -10.20000000000000462 ) ) ;
#21616 = CARTESIAN_POINT ( 'NONE',  ( -5.082755093536317936, -5.082755093536320601, 19.67405278187175455 ) ) ;
#21617 = ORIENTED_EDGE ( 'NONE', *, *, #39191, .T. ) ;
#21620 =( BOUNDED_CURVE ( )  B_SPLINE_CURVE ( 2, ( #37619, #38363, #56096, #9315, #3655, #9696, #32717, #44392, #20240 ),
 .UNSPECIFIED., .F., .F. ) 
 B_SPLINE_CURVE_WITH_KNOTS ( ( 3, 2, 2, 2, 3 ),
 ( 0.04411764705882355309, 0.04779411764705884802, 0.05147058823529414295, 0.05514705882352943789, 0.05882352941176473976 ),
 .UNSPECIFIED. ) 
 CURVE ( )  GEOMETRIC_REPRESENTATION_ITEM ( )  RATIONAL_B_SPLINE_CURVE ( ( 0.9999999999999995559, 0.9238795325112871826, 1.000000000000000000, 0.9238795325112867385, 1.000000000000000000, 0.9238795325112867385, 1.000000000000000000, 0.9238795325112860723, 1.000000000000000666 ) ) 
 REPRESENTATION_ITEM ( '' )  );
#21619 = CARTESIAN_POINT ( 'NONE',  ( -7.188101187500000044, 26.71874999795161543, -8.802885111219163269E-16 ) ) ;
#21618 = AXIS2_PLACEMENT_3D ( 'NONE', #29078, #57390, #6806 ) ;
#21621 = ORIENTED_EDGE ( 'NONE', *, *, #72345, .T. ) ;
#21622 = CARTESIAN_POINT ( 'NONE',  ( 10.18810118749999916, 4.220049686691935698, 113.5000000020483810 ) ) ;
#21623 = CARTESIAN_POINT ( 'NONE',  ( -3.458734124999959914, 205.3750000013656063, 196.5673454167823877 ) ) ;
#21624 = CARTESIAN_POINT ( 'NONE',  ( 29.43265458321761230, 199.8750000013656063, 166.5412658749999650 ) ) ;
#21625 = CARTESIAN_POINT ( 'NONE',  ( -10.00000000000000000, 82.29166666666665719, -2.679491924311229845 ) ) ;
#21626 = CARTESIAN_POINT ( 'NONE',  ( 2.977408999572654480, 90.50000000204840944, 7.188101187499999156 ) ) ;
#21627 = CARTESIAN_POINT ( 'NONE',  ( 2.485281374238571317, 293.6875000000000000, -6.000000000000003553 ) ) ;
#21628 = CARTESIAN_POINT ( 'NONE',  ( 30.82842712474616675, 203.5000000027312126, 167.1715728752537018 ) ) ;
#21629 = ORIENTED_EDGE ( 'NONE', *, *, #34414, .F. ) ;
#21630 = EDGE_CURVE ( 'NONE', #45401, #7250, #70967, .T. ) ;
#21631 = EDGE_CURVE ( 'NONE', #11605, #1524, #3556, .T. ) ;
#21632 = CARTESIAN_POINT ( 'NONE',  ( -3.042071309553166181, 222.8645833367473301, -11.35316468749999608 ) ) ;
#21633 = CARTESIAN_POINT ( 'NONE',  ( 5.656854249492378806, 11.81250000000000178, 5.656854249492381470 ) ) ;
#21634 = CARTESIAN_POINT ( 'NONE',  ( -2.828427124746208943, 197.7500000027312126, 144.8284271247462129 ) ) ;
#21635 = CARTESIAN_POINT ( 'NONE',  ( 4.556349186104052151, -10.99999999999999822, 91.46874999999998579 ) ) ;
#21636 = CARTESIAN_POINT ( 'NONE',  ( -4.898587196589412829E-16, 88.81250000409677625, -8.000000000000000000 ) ) ;
#21637 = CARTESIAN_POINT ( 'NONE',  ( -7.320508075688770155, 245.6250000000000000, 7.320508075688774596 ) ) ;
#21638 = CARTESIAN_POINT ( 'NONE',  ( -10.00000000000003908, 77.50000000000002842, -1.224646799147357990E-15 ) ) ;
#21639 = CARTESIAN_POINT ( 'NONE',  ( 4.999999999999993783, 184.1666666666666856, 8.660254037844390851 ) ) ;
#21640 = CARTESIAN_POINT ( 'NONE',  ( 0.000000000000000000, 101.0525588832578734, -7.949999999999993960 ) ) ;
#21641 = CARTESIAN_POINT ( 'NONE',  ( -7.188101187499992051, 0.000000000000000000, 18.36155278187175455 ) ) ;
#21642 = CARTESIAN_POINT ( 'NONE',  ( 11.35316468749999963, 166.3020833299193271, -3.042071309553165293 ) ) ;
#21643 = CARTESIAN_POINT ( 'NONE',  ( 7.999999999999920064, -1.061780717098090627E-06, 7.767802753882760314 ) ) ;
#21644 = CARTESIAN_POINT ( 'NONE',  ( 11.00000000000021494, -4.556349186103832771, 82.84375000409677625 ) ) ;
#21646 = CARTESIAN_POINT ( 'NONE',  ( -5.656854249492381470, 17.43750000000000000, 5.656854249492379694 ) ) ;
#21645 = DIRECTION ( 'NONE',  ( -0.000000000000000000, -1.000000000000000000, -4.283267841918042741E-17 ) ) ;
#21647 = ORIENTED_EDGE ( 'NONE', *, *, #51176, .F. ) ;
#21648 = CARTESIAN_POINT ( 'NONE',  ( 3.042071309553159519, 30.05208332991934839, 11.35316468750000141 ) ) ;
#21649 = CARTESIAN_POINT ( 'NONE',  ( -27.99999999999995737, 200.5000000000000000, 174.0000000000003695 ) ) ;
#21651 = CARTESIAN_POINT ( 'NONE',  ( -2.219371606101216976, -16.40787039054615448, -68.79427927095674988 ) ) ;
#21650 = CARTESIAN_POINT ( 'NONE',  ( 3.594044162775203777, 89.15552387383502264, -6.225081946264263699 ) ) ;
#21652 = CARTESIAN_POINT ( 'NONE',  ( 25.17157287525381903, 202.0000000027312126, 172.8284271247460993 ) ) ;
#21654 = EDGE_CURVE ( 'NONE', #71873, #44162, #27483, .T. ) ;
#21653 = CARTESIAN_POINT ( 'NONE',  ( 3.458734124999959914, 204.3750000013656063, 143.4326545832176976 ) ) ;
#21655 = CARTESIAN_POINT ( 'NONE',  ( -10.00000000000000178, 59.37499999317203248, -1.224646799147353454E-15 ) ) ;
#21656 = CARTESIAN_POINT ( 'NONE',  ( -7.188101187500001821, 106.0625000020483668, -2.977408999572650483 ) ) ;
#21657 = CARTESIAN_POINT ( 'NONE',  ( 1.881053915767122664, 7.249999998634408804, 4.541265875000001451 ) ) ;
#21658 = CARTESIAN_POINT ( 'NONE',  ( 4.999999999999985789, 99.16666666666668561, 8.660254037844380193 ) ) ;
#21659 = CARTESIAN_POINT ( 'NONE',  ( 5.656854249492374365, 5.656854249492375253, 6.267802779823364645 ) ) ;
#21660 = CARTESIAN_POINT ( 'NONE',  ( -3.313708498984759387, -7.999999999999989342, 20.79905278392014978 ) ) ;
#21661 = ORIENTED_EDGE ( 'NONE', *, *, #36830, .T. ) ;
#21662 = EDGE_LOOP ( 'NONE', ( #23215, #70754, #35055, #37314, #41854, #53838, #12063, #16750 ) ) ;
#21663 = CARTESIAN_POINT ( 'NONE',  ( -5.000000000000000000, -65.00653492603748873, 24.02639942437790310 ) ) ;
#21664 = DIRECTION ( 'NONE',  ( -0.000000000000000000, 0.000000000000000000, 1.000000000000000000 ) ) ;
#21665 = FACE_OUTER_BOUND ( 'NONE', #67777, .T. ) ;
#21666 = CARTESIAN_POINT ( 'NONE',  ( -28.17728963097874129, -42.63396036855753835, 157.0662270391268862 ) ) ;
#21667 = CARTESIAN_POINT ( 'NONE',  ( 3.042071309553167069, 141.8229166632526983, -11.35316468749999785 ) ) ;
#21668 = ORIENTED_EDGE ( 'NONE', *, *, #35527, .T. ) ;
#21669 = FACE_OUTER_BOUND ( 'NONE', #13698, .T. ) ;
#21670 = CARTESIAN_POINT ( 'NONE',  ( -4.220049686691935698, 10.18810118749999916, 89.87500000204836681 ) ) ;
#21671 = DIRECTION ( 'NONE',  ( -1.000000000000000000, 0.000000000000000000, 0.000000000000000000 ) ) ;
#21672 = CARTESIAN_POINT ( 'NONE',  ( 4.000000000000015099, 206.5625000000000000, 196.3431457505076594 ) ) ;
#21673 = CARTESIAN_POINT ( 'NONE',  ( 1.836970198721029589E-15, 246.2500000000000284, 10.00000000000000000 ) ) ;
#21674 = LINE ( 'NONE', #10371, #27725 ) ;
#21675 = ORIENTED_EDGE ( 'NONE', *, *, #65683, .T. ) ;
#21676 = AXIS2_PLACEMENT_3D ( 'NONE', #19208, #66344, #3352 ) ;
#21677 = CARTESIAN_POINT ( 'NONE',  ( 1.469576158976823947E-15, 106.0625000040967763, 8.000000000000000000 ) ) ;
#21678 = CARTESIAN_POINT ( 'NONE',  ( 48.92004685705027356, 43.64449963454028847, 59.80336641654269414 ) ) ;
#21679 = CARTESIAN_POINT ( 'NONE',  ( 3.042071309553159519, 120.0520833299193555, 11.35316468750000141 ) ) ;
#21680 = CARTESIAN_POINT ( 'NONE',  ( 2.754378923186476579E-14, 201.1875000013656063, 194.5412658750000219 ) ) ;
#21681 = CARTESIAN_POINT ( 'NONE',  ( -7.188101187500000044, 19.59374999795161543, -8.802885111219163269E-16 ) ) ;
#21682 = CARTESIAN_POINT ( 'NONE',  ( -7.204075437095965206, -7.204075437095968759, 80.21875000204836681 ) ) ;
#21683 = CARTESIAN_POINT ( 'NONE',  ( 8.311093377946837890, 36.71874999658601979, -8.311093377946837890 ) ) ;
#21684 = EDGE_LOOP ( 'NONE', ( #47603, #19634, #67814, #23138 ) ) ;
#21685 = CARTESIAN_POINT ( 'NONE',  ( -5.656854249492380582, 96.50000000409677625, -5.656854249492380582 ) ) ;
#21686 = CARTESIAN_POINT ( 'NONE',  ( -5.662595241051933570, -5.662595241051936235, 19.20061528394063188 ) ) ;
#21687 = CARTESIAN_POINT ( 'NONE',  ( -2.726571689596997292E-14, 210.0000000000000284, 138.0000000000000568 ) ) ;
#21688 = VECTOR ( 'NONE', #26590, 1000.000000000000000 ) ;
#21689 = CARTESIAN_POINT ( 'NONE',  ( 11.00000000000000000, 1.347111479062088405E-15, 85.93750000409677625 ) ) ;
#21690 = CARTESIAN_POINT ( 'NONE',  ( 7.188101187499999156, 9.374999997951610098, 2.977408999572654924 ) ) ;
#21691 = CARTESIAN_POINT ( 'NONE',  ( 1.226468279477575784E-15, 290.7031250017069510, 6.676582343750001591 ) ) ;
#21692 = CARTESIAN_POINT ( 'NONE',  ( 0.000000000000000000, 0.000000000000000000, 0.000000000000000000 ) ) ;
#21693 = CARTESIAN_POINT ( 'NONE',  ( -27.99999999999996092, 206.5000000000000284, 174.0000000000003695 ) ) ;
#21694 = ORIENTED_EDGE ( 'NONE', *, *, #60568, .F. ) ;
#21695 = CARTESIAN_POINT ( 'NONE',  ( 9.832129032723420536, 146.5104166632526699, -5.676582343749999815 ) ) ;
#21696 = CARTESIAN_POINT ( 'NONE',  ( -4.220049686691937474, -10.18810118749999738, 76.93750000204839523 ) ) ;
#21697 = CARTESIAN_POINT ( 'NONE',  ( -30.44569435410883784, 208.8125000013656063, 167.5543056458915885 ) ) ;
#21698 = CYLINDRICAL_SURFACE ( 'NONE', #26971, 6.999999999999999112 ) ;
#21699 = CARTESIAN_POINT ( 'NONE',  ( 3.211159895383561835, 15.56249999863440614, -3.211159895383561835 ) ) ;
#21700 = ORIENTED_EDGE ( 'NONE', *, *, #60460, .T. ) ;
#21701 = CARTESIAN_POINT ( 'NONE',  ( 2.849036369511732440E-14, 200.3750000027312126, 202.0000000000000000 ) ) ;
#21702 = CARTESIAN_POINT ( 'NONE',  ( -3.458734125000015425, 195.2500000013656063, 143.4326545832176976 ) ) ;
#21703 = CARTESIAN_POINT ( 'NONE',  ( -29.65685424949229443, 205.5625000027311842, 174.0000000000004547 ) ) ;
#21704 = EDGE_CURVE ( 'NONE', #22089, #32761, #15867, .T. ) ;
#21705 = CARTESIAN_POINT ( 'NONE',  ( 5.656854249492380582, 6.187500000000000888, -5.656854249492380582 ) ) ;
#21706 = ORIENTED_EDGE ( 'NONE', *, *, #53851, .F. ) ;
#21707 = CARTESIAN_POINT ( 'NONE',  ( -7.188101187500000933, 11.62499999795160832, -2.977408999572651371 ) ) ;
#21708 = CARTESIAN_POINT ( 'NONE',  ( -6.000000000000001776, 298.0625000034140157, 0.000000000000000000 ) ) ;
#21709 = CARTESIAN_POINT ( 'NONE',  ( -2.904027776795585769, -45.77777928767888227, 151.2232026270691279 ) ) ;
#21710 = CARTESIAN_POINT ( 'NONE',  ( -5.676582343750006032, 189.1145833299193839, 9.832129032723418760 ) ) ;
#21711 = CARTESIAN_POINT ( 'NONE',  ( 5.082755093536325042, 108.9687500020483810, -5.082755093536325930 ) ) ;
#21712 = CARTESIAN_POINT ( 'NONE',  ( 4.242640687119287435, 295.3750000000000000, 4.242640687119285658 ) ) ;
#21713 = CARTESIAN_POINT ( 'NONE',  ( 6.676582343750002480, 288.0156250017069510, -2.765530957081997254 ) ) ;
#21714 = CARTESIAN_POINT ( 'NONE',  ( 8.660254037844481445, 79.58333333333339965, 5.000000000000061284 ) ) ;
#21715 =( BOUNDED_CURVE ( )  B_SPLINE_CURVE ( 2, ( #46966, #57950, #52272, #48069, #18304, #64327, #58316, #36396, #24325, #59410, #608, #70363, #30364 ),
 .UNSPECIFIED., .F., .T. ) 
 B_SPLINE_CURVE_WITH_KNOTS ( ( 3, 2, 2, 2, 2, 2, 3 ),
 ( 1.114692740994780884, 1.119926170633683604, 1.125159600272586102, 1.130393029911488822, 1.135626459550391321, 1.140859889189293819, 1.146093318828196539 ),
 .UNSPECIFIED. ) 
 CURVE ( )  GEOMETRIC_REPRESENTATION_ITEM ( )  RATIONAL_B_SPLINE_CURVE ( ( 1.000000000000003997, 0.9659258262890639823, 0.9999999999999998890, 0.9659258262890682012, 0.9999999999999998890, 0.9659258262890682012, 0.9999999999999998890, 0.9659258262890682012, 0.9999999999999998890, 0.9659258262890682012, 0.9999999999999998890, 0.9659258262890682012, 0.9999999999999998890 ) ) 
 REPRESENTATION_ITEM ( '' )  );
#21716 = ORIENTED_EDGE ( 'NONE', *, *, #8058, .T. ) ;
#21718 = CARTESIAN_POINT ( 'NONE',  ( 9.832129032723416984, 261.8229166700807014, -5.676582343750003368 ) ) ;
#21717 = AXIS2_PLACEMENT_3D ( 'NONE', #21062, #48978, #44086 ) ;
#21719 = CARTESIAN_POINT ( 'NONE',  ( 7.188101187499991163, 2.977408999572648707, 20.70530278187175455 ) ) ;
#21720 = CARTESIAN_POINT ( 'NONE',  ( -7.320508075688773708, 8.749999993172030699, -7.320508075688774596 ) ) ;
#21721 = CARTESIAN_POINT ( 'NONE',  ( -4.898587196589407898E-16, 7.999999999999991118, 15.64280278392014800 ) ) ;
#21722 = CARTESIAN_POINT ( 'NONE',  ( -1.882291019709504631, -65.87523470714120322, -26.34730193751288851 ) ) ;
#21723 = CARTESIAN_POINT ( 'NONE',  ( 2.445694354108839175, 196.3125000013656063, 195.5543056458912190 ) ) ;
#21724 = CARTESIAN_POINT ( 'NONE',  ( -7.320508075688778149, 148.1249999999999716, 7.320508075688769267 ) ) ;
#21725 = CARTESIAN_POINT ( 'NONE',  ( -4.556349186104048599, -10.99999999999999822, 115.4687500040967763 ) ) ;
#21726 = CARTESIAN_POINT ( 'NONE',  ( 0.000000000000000000, 0.000000000000000000, 30.00000000000000000 ) ) ;
#21727 = CARTESIAN_POINT ( 'NONE',  ( -5.656854249492380582, 93.31249999999998579, -5.656854249492380582 ) ) ;
#21728 = CARTESIAN_POINT ( 'NONE',  ( 9.832129032723420536, 126.5104166632526841, -5.676582343749999815 ) ) ;
#21729 = CARTESIAN_POINT ( 'NONE',  ( 2.020667218593132706E-15, -11.00000000000000000, 70.37500000000000000 ) ) ;
#21732 = LINE ( 'NONE', #73796, #20576 ) ;
#21731 = CARTESIAN_POINT ( 'NONE',  ( 30.44569435410879166, 197.8125000013656063, 167.5543056458910485 ) ) ;
#21730 = CARTESIAN_POINT ( 'NONE',  ( 30.82842712474617386, 209.1250000000000284, 172.8284271247460993 ) ) ;
#21733 = ORIENTED_EDGE ( 'NONE', *, *, #57363, .T. ) ;
#21734 = AXIS2_PLACEMENT_3D ( 'NONE', #29577, #23538, #47284 ) ;
#21735 = EDGE_CURVE ( 'NONE', #19469, #23110, #31990, .T. ) ;
#21736 = EDGE_CURVE ( 'NONE', #30305, #29130, #45419, .T. ) ;
#21737 = CARTESIAN_POINT ( 'NONE',  ( 4.000000000000001776, 2.000000000000000000, 0.000000000000000000 ) ) ;
#21738 = LINE ( 'NONE', #40217, #42361 ) ;
#21739 =( BOUNDED_CURVE ( )  B_SPLINE_CURVE ( 2, ( #16579, #51673, #10201, #39616, #23005, #69032, #28292, #62243, #10947, #51299, #39244, #63357, #16204 ),
 .UNSPECIFIED., .F., .F. ) 
 B_SPLINE_CURVE_WITH_KNOTS ( ( 3, 2, 2, 2, 2, 2, 3 ),
 ( 0.03804347826086956763, 0.03985507246376811252, 0.04166666666666666435, 0.04347826086956521618, 0.04528985507246376108, 0.04710144927536231291, 0.04891304347826086474 ),
 .UNSPECIFIED. ) 
 CURVE ( )  GEOMETRIC_REPRESENTATION_ITEM ( )  RATIONAL_B_SPLINE_CURVE ( ( 1.000000000000000000, 0.9659258262890683122, 1.000000000000000000, 0.9659258262890683122, 1.000000000000000000, 0.9659258262890683122, 1.000000000000000000, 0.9659258262890683122, 1.000000000000000000, 0.9659258262890683122, 1.000000000000000000, 0.9659258262890684232, 0.9999999999999998890 ) ) 
 REPRESENTATION_ITEM ( '' )  );
#21740 = CARTESIAN_POINT ( 'NONE',  ( 24.54126587499998280, 198.5000000013656347, 171.4326545832175555 ) ) ;
#21741 = CARTESIAN_POINT ( 'NONE',  ( 3.042071309553167069, 212.1354166632526983, -11.35316468749999785 ) ) ;
#21742 = CARTESIAN_POINT ( 'NONE',  ( 7.188101187500000044, 123.4062500020483810, -8.802885111219163269E-16 ) ) ;
#21743 = CARTESIAN_POINT ( 'NONE',  ( 4.541265875000002339, 19.31249999863440436, 0.000000000000000000 ) ) ;
#21744 = CARTESIAN_POINT ( 'NONE',  ( 4.465349678513689469, -56.41423509509540679, 44.23558526900774979 ) ) ;
#21745 = CARTESIAN_POINT ( 'NONE',  ( 7.999999999999991118, 3.313708498984757611, 24.17405277982336642 ) ) ;
#21747 = CARTESIAN_POINT ( 'NONE',  ( -1.469576158976823947E-15, 13.12500000000000355, 8.000000000000000000 ) ) ;
#21746 = CARTESIAN_POINT ( 'NONE',  ( -48.25549907375996384, 41.32216978361132220, 61.70628817261103194 ) ) ;
#21748 = CARTESIAN_POINT ( 'NONE',  ( 6.951808397369818766E-16, 92.03124999658602690, -11.35316468750000141 ) ) ;
#21749 = ORIENTED_EDGE ( 'NONE', *, *, #32302, .T. ) ;
#21750 = CARTESIAN_POINT ( 'NONE',  ( 5.656854249492379694, 92.93749999999998579, -5.656854249492380582 ) ) ;
#21751 = CARTESIAN_POINT ( 'NONE',  ( 7.188101187500000044, 19.96874999795161543, 0.000000000000000000 ) ) ;
#21752 = CARTESIAN_POINT ( 'NONE',  ( -3.313708498984759387, -7.999999999999989342, 14.61155277982336465 ) ) ;
#21753 = CARTESIAN_POINT ( 'NONE',  ( -5.676582343750000703, 263.3854166700806445, -9.832129032723418760 ) ) ;
#21754 = CARTESIAN_POINT ( 'NONE',  ( 9.832129032723420536, 106.1979166632526983, -5.676582343749999815 ) ) ;
#21755 = VERTEX_POINT ( 'NONE', #49837 ) ;
#21756 = DIRECTION ( 'NONE',  ( -0.000000000000000000, 0.000000000000000000, 1.000000000000000000 ) ) ;
#21757 = CARTESIAN_POINT ( 'NONE',  ( -4.220049686691935698, 10.18810118749999916, 104.8750000020483668 ) ) ;
#21758 = CARTESIAN_POINT ( 'NONE',  ( -5.000000000000163425, 21.66666666666685970, -8.660254037844673292 ) ) ;
#21759 = CARTESIAN_POINT ( 'NONE',  ( 2.445694354108840063, 204.0625000013656063, 200.4456943541088663 ) ) ;
#21760 = FACE_OUTER_BOUND ( 'NONE', #73641, .T. ) ;
#21762 = CARTESIAN_POINT ( 'NONE',  ( -3.042071309553163960, 82.23958332991935549, -11.35316468749999963 ) ) ;
#21761 = CARTESIAN_POINT ( 'NONE',  ( -7.999999999999960032, 3.313708498984789141, 23.23655277982336642 ) ) ;
#21763 = EDGE_CURVE ( 'NONE', #6788, #6283, #55576, .T. ) ;
#21764 = CARTESIAN_POINT ( 'NONE',  ( -7.999999999999989342, -3.313708498984762496, 14.61155278392014800 ) ) ;
#21765 = CARTESIAN_POINT ( 'NONE',  ( -26.56734541678232375, 199.2500000013656063, 173.4587341250003760 ) ) ;
#21766 = DIRECTION ( 'NONE',  ( 0.000000000000000000, 0.000000000000000000, -1.000000000000000000 ) ) ;
#21767 = AXIS2_PLACEMENT_3D ( 'NONE', #9310, #44015, #39104 ) ;
#21768 = CARTESIAN_POINT ( 'NONE',  ( -10.00000000000000178, 179.3749999931720538, -1.224646799147353454E-15 ) ) ;
#21769 = CARTESIAN_POINT ( 'NONE',  ( 5.000000000000000888, -52.62657404299726238, 48.70092614269855602 ) ) ;
#21770 = CARTESIAN_POINT ( 'NONE',  ( 11.35316468750000141, 76.09374999658602690, 0.000000000000000000 ) ) ;
#21771 = CARTESIAN_POINT ( 'NONE',  ( 4.721056650415999201, 289.0781250017069510, -4.721056650415999201 ) ) ;
#21772 = CARTESIAN_POINT ( 'NONE',  ( -4.220049686691935698, 10.18810118749999916, 103.7500000020483668 ) ) ;
#21773 = CARTESIAN_POINT ( 'NONE',  ( 5.676582343749993598, 209.9479166632526983, 9.832129032723422313 ) ) ;
#21774 = EDGE_LOOP ( 'NONE', ( #62267, #71910, #28289 ) ) ;
#21775 = CARTESIAN_POINT ( 'NONE',  ( 0.000000000000000000, -2.500000000000000000, 7.000000000000000000 ) ) ;
#21776 = DIRECTION ( 'NONE',  ( 0.000000000000000000, 0.000000000000000000, 1.000000000000000000 ) ) ;
#21777 = CARTESIAN_POINT ( 'NONE',  ( -4.615726161707419450, -16.27701803902728273, 69.62876280158647546 ) ) ;
#21778 = CARTESIAN_POINT ( 'NONE',  ( 5.676582343750001591, 206.6145833299193555, -9.832129032723420536 ) ) ;
#21779 = CARTESIAN_POINT ( 'NONE',  ( -5.000000000000000888, 227.2916666734946602, -8.660254037844387298 ) ) ;
#21780 = ORIENTED_EDGE ( 'NONE', *, *, #35455, .F. ) ;
#21781 = CARTESIAN_POINT ( 'NONE',  ( -5.676582343750006032, 199.4270833299193555, 9.832129032723418760 ) ) ;
#21782 = AXIS2_PLACEMENT_3D ( 'NONE', #25234, #42220, #37320 ) ;
#21783 = CARTESIAN_POINT ( 'NONE',  ( 5.082755093536318824, 5.082755093536319713, 15.92405278187175632 ) ) ;
#21784 = CARTESIAN_POINT ( 'NONE',  ( -31.45873412499999944, 206.6875000013656063, 170.0000000000003979 ) ) ;
#21785 = CARTESIAN_POINT ( 'NONE',  ( 5.656854249492378806, 10.31250000000000178, 5.656854249492381470 ) ) ;
#21786 = VERTEX_POINT ( 'NONE', #39269 ) ;
#21787 = CARTESIAN_POINT ( 'NONE',  ( -5.656854249492380582, 93.50000000409677625, -5.656854249492380582 ) ) ;
#21788 = CARTESIAN_POINT ( 'NONE',  ( 7.320508075688771044, 19.37499999999999289, 7.320508075688775484 ) ) ;
#21789 = CARTESIAN_POINT ( 'NONE',  ( -6.238412754330611322E-16, 10.18810118749999916, 81.15625000204838102 ) ) ;
#21790 = EDGE_LOOP ( 'NONE', ( #51453, #16783, #44996, #61326 ) ) ;
#21791 = CARTESIAN_POINT ( 'NONE',  ( 2.449293598294707893E-16, 21.25000000000000000, -4.000000000000001776 ) ) ;
#21792 = CARTESIAN_POINT ( 'NONE',  ( 1.881053915767121998, 20.49999999863440436, -4.541265875000002339 ) ) ;
#21793 = CIRCLE ( 'NONE', #60368, 12.00000000000000000 ) ;
#21794 = CARTESIAN_POINT ( 'NONE',  ( 30.10854392850819750, 194.7007961766996402, 166.9503307040869515 ) ) ;
#21795 = EDGE_CURVE ( 'NONE', #5560, #53849, #73965, .T. ) ;
#21796 = ORIENTED_EDGE ( 'NONE', *, *, #27499, .T. ) ;
#21797 = LINE ( 'NONE', #67469, #14939 ) ;
#21798 = CARTESIAN_POINT ( 'NONE',  ( -4.401442555609581635E-16, 92.28125000204836681, -7.188101187500000044 ) ) ;
#21801 = CARTESIAN_POINT ( 'NONE',  ( 5.000000000000000000, 50.64189880742144823, -41.08656465431842975 ) ) ;
#21800 = CARTESIAN_POINT ( 'NONE',  ( 11.35316468749999963, 246.1979166700806445, 3.042071309553159519 ) ) ;
#21799 = CARTESIAN_POINT ( 'NONE',  ( 29.43265458321761585, 208.8750000013656063, 166.5412658749999650 ) ) ;
#21802 = PRODUCT_CONTEXT ( 'NONE', #48113, 'mechanical' ) ;
#21803 = ORIENTED_EDGE ( 'NONE', *, *, #4986, .F. ) ;
#21804 = CARTESIAN_POINT ( 'NONE',  ( 11.35316468749999608, 251.9270833367473301, -3.042071309553167069 ) ) ;
#21805 = CARTESIAN_POINT ( 'NONE',  ( 2.977408999572646486, 7.188101187499991163, 10.01780278187175632 ) ) ;
#21806 = ORIENTED_EDGE ( 'NONE', *, *, #42196, .F. ) ;
#21807 = VERTEX_POINT ( 'NONE', #62269 ) ;
#21808 = CARTESIAN_POINT ( 'NONE',  ( -4.220049686691937474, -10.18810118749999738, 75.43750000204836681 ) ) ;
#21809 = CARTESIAN_POINT ( 'NONE',  ( 5.676582343749993598, 70.26041666325268409, 9.832129032723422313 ) ) ;
#21810 = CARTESIAN_POINT ( 'NONE',  ( -11.35316468749999963, 218.9062500034139873, 0.000000000000000000 ) ) ;
#21811 = CARTESIAN_POINT ( 'NONE',  ( -11.00000000000000000, 0.000000000000000000, 88.00000000000000000 ) ) ;
#21814 = CARTESIAN_POINT ( 'NONE',  ( -6.676582343750002480, 288.5468750017070079, -2.765530957081996810 ) ) ;
#21813 = CARTESIAN_POINT ( 'NONE',  ( 29.65685424949235127, 197.5625000027312126, 165.9999999999998863 ) ) ;
#21812 = CARTESIAN_POINT ( 'NONE',  ( 24.54126587499999701, 209.4375000013656063, 169.9999999999998863 ) ) ;
#21815 = AXIS2_PLACEMENT_3D ( 'NONE', #23127, #69530, #45391 ) ;
#21816 = EDGE_CURVE ( 'NONE', #31249, #4353, #11278, .T. ) ;
#21817 = CARTESIAN_POINT ( 'NONE',  ( 10.00000000000000178, 77.08333332650536818, -2.679491924311226736 ) ) ;
#21818 = CARTESIAN_POINT ( 'NONE',  ( -27.99999999999991473, 205.6250000027312126, 174.0000000000003695 ) ) ;
#21819 = CARTESIAN_POINT ( 'NONE',  ( -1.432654583217608080, 198.8750000013656063, 201.4587341250000350 ) ) ;
#21820 = CARTESIAN_POINT ( 'NONE',  ( 8.000000000000000000, 7.312499995903221084, 0.000000000000000000 ) ) ;
#21821 = ORIENTED_EDGE ( 'NONE', *, *, #49252, .F. ) ;
#21822 = CARTESIAN_POINT ( 'NONE',  ( 24.54126587499999701, 196.1250000013655779, 168.5673454167822172 ) ) ;
#21823 = CARTESIAN_POINT ( 'NONE',  ( -7.188101187500001821, 16.49999999795161543, -2.977408999572651371 ) ) ;
#21824 = CARTESIAN_POINT ( 'NONE',  ( 11.35316468749999963, 171.3020833299193555, -3.042071309553165293 ) ) ;
#21825 = CARTESIAN_POINT ( 'NONE',  ( -7.778174593052020747, -7.778174593052023411, 98.87500000409676204 ) ) ;
#21826 = CARTESIAN_POINT ( 'NONE',  ( -7.188101187500000044, 103.5312500020483810, 0.000000000000000000 ) ) ;
#21828 = CARTESIAN_POINT ( 'NONE',  ( -3.074111742570392547, -51.58078258920560444, -48.68628732315601582 ) ) ;
#21827 = CARTESIAN_POINT ( 'NONE',  ( 0.000000000000000000, 284.0000000000000000, 0.000000000000000000 ) ) ;
#21829 = CARTESIAN_POINT ( 'NONE',  ( 30.44569435410883784, 208.0625000013656063, 167.5543056458911053 ) ) ;
#21830 = CARTESIAN_POINT ( 'NONE',  ( 5.082755093536320601, -5.082755093536318824, 15.92405278187175632 ) ) ;
#21831 = CARTESIAN_POINT ( 'NONE',  ( -2.751064625579944321E-14, 208.8750000027312126, 146.0000000000000284 ) ) ;
#21832 = CARTESIAN_POINT ( 'NONE',  ( 8.311093377946837890, 61.40624999658602690, -8.311093377946837890 ) ) ;
#21833 =( BOUNDED_CURVE ( )  B_SPLINE_CURVE ( 2, ( #23483, #6147, #46495, #47232, #40843, #30628, #6518, #70617, #63851 ),
 .UNSPECIFIED., .F., .F. ) 
 B_SPLINE_CURVE_WITH_KNOTS ( ( 3, 2, 2, 2, 3 ),
 ( 0.7604166666666667407, 0.7656250000000001110, 0.7708333333333334814, 0.7760416666666667407, 0.7812500000000001110 ),
 .UNSPECIFIED. ) 
 CURVE ( )  GEOMETRIC_REPRESENTATION_ITEM ( )  RATIONAL_B_SPLINE_CURVE ( ( 0.9999999999999983347, 0.9238795325112884038, 1.000000000000000000, 0.9238795325112867385, 1.000000000000000000, 0.9238795325112867385, 1.000000000000000000, 0.9238795325112850731, 1.000000000000001554 ) ) 
 REPRESENTATION_ITEM ( '' )  );
#21834 = CARTESIAN_POINT ( 'NONE',  ( -0.3963979750082347042, -42.00000000000003553, 139.0000000000000000 ) ) ;
#21835 = CARTESIAN_POINT ( 'NONE',  ( -7.320508075688773708, 28.74999999317203248, -7.320508075688774596 ) ) ;
#21836 = CARTESIAN_POINT ( 'NONE',  ( 2.828427124746190291, 16.87500000000000000, 2.828427124746192067 ) ) ;
#21837 = ORIENTED_EDGE ( 'NONE', *, *, #29853, .T. ) ;
#21838 = DIRECTION ( 'NONE',  ( -1.000000000000000000, -0.000000000000000000, -0.000000000000000000 ) ) ;
#21839 = CARTESIAN_POINT ( 'NONE',  ( -8.660254037844387298, 168.9583333265053682, -5.000000000000004441 ) ) ;
#21840 = CARTESIAN_POINT ( 'NONE',  ( 9.832129032723420536, 66.19791666325268409, -5.676582343749999815 ) ) ;
#21841 = CARTESIAN_POINT ( 'NONE',  ( -4.556349186104047710, -10.99999999999999822, 71.96875000409677625 ) ) ;
#21842 = CARTESIAN_POINT ( 'NONE',  ( -1.432654583217664701, 202.0000000013656063, 138.5412658750000787 ) ) ;
#21843 = CARTESIAN_POINT ( 'NONE',  ( -2.679491924311358186, 258.9583333333333712, -9.999999999999923617 ) ) ;
#21844 = CARTESIAN_POINT ( 'NONE',  ( -4.000000000000015987, 196.6875000027312126, 143.6568542494924259 ) ) ;
#21846 = CARTESIAN_POINT ( 'NONE',  ( 8.311093377946834337, 40.15624999658601268, 8.311093377946839666 ) ) ;
#21845 = CARTESIAN_POINT ( 'NONE',  ( -2.977408999572650927, 92.37500000204838102, -7.188101187500000933 ) ) ;
#21847 = ADVANCED_FACE ( 'NONE', ( #51325 ), #27191, .T. ) ;
#21848 = CARTESIAN_POINT ( 'NONE',  ( -7.999999999999991118, -9.344071862984236532, 28.28216120211630624 ) ) ;
#21849 = CARTESIAN_POINT ( 'NONE',  ( -2.849036369511732440E-14, 195.2500000000000000, 138.0000000000000568 ) ) ;
#21850 = CARTESIAN_POINT ( 'NONE',  ( 9.832129032723416984, 170.3645833299193555, 5.676582343750006032 ) ) ;
#21851 = EDGE_CURVE ( 'NONE', #62422, #27943, #32503, .T. ) ;
#21852 = CARTESIAN_POINT ( 'NONE',  ( -2.679491924311225848, 143.3333333265053398, -10.00000000000000178 ) ) ;
#21853 = CARTESIAN_POINT ( 'NONE',  ( -5.082755093536324154, 103.7187500020483810, 5.082755093536326818 ) ) ;
#21854 = CIRCLE ( 'NONE', #47112, 4.999999999999997335 ) ;
#21855 = CARTESIAN_POINT ( 'NONE',  ( -2.712922267096666396, 0.4730691518507174065, -7.505356363334990455 ) ) ;
#21856 = CARTESIAN_POINT ( 'NONE',  ( 11.35316468750000141, 31.09374999658601979, 0.000000000000000000 ) ) ;
#21857 = CARTESIAN_POINT ( 'NONE',  ( -5.000000000000005329, 80.20833332650536818, 8.660254037844387298 ) ) ;
#21858 = CARTESIAN_POINT ( 'NONE',  ( 5.676582343749993598, 174.9479166632526699, 9.832129032723422313 ) ) ;
#21859 = ORIENTED_EDGE ( 'NONE', *, *, #73110, .T. ) ;
#21860 = DIRECTION ( 'NONE',  ( 0.000000000000000000, 0.000000000000000000, 1.000000000000000000 ) ) ;
#21861 = CARTESIAN_POINT ( 'NONE',  ( -10.18810118749999738, -4.220049686691941915, 70.75000000204836681 ) ) ;
#21862 = FACE_OUTER_BOUND ( 'NONE', #57963, .T. ) ;
#21863 = CARTESIAN_POINT ( 'NONE',  ( 32.73475104982897932, 41.77914142897400751, 65.00000000000001421 ) ) ;
#21865 = CARTESIAN_POINT ( 'NONE',  ( -9.832129032723418760, 172.8645833299193555, -5.676582343750004256 ) ) ;
#21864 = DIRECTION ( 'NONE',  ( -1.000000000000000000, 0.000000000000000000, 0.000000000000000000 ) ) ;
#21866 = CARTESIAN_POINT ( 'NONE',  ( -7.999999999999989342, -3.313708498984762496, 12.98030278432982243 ) ) ;
#21867 = EDGE_CURVE ( 'NONE', #69413, #10358, #63383, .T. ) ;
#21868 = EDGE_CURVE ( 'NONE', #9832, #22395, #1589, .T. ) ;
#21869 = CARTESIAN_POINT ( 'NONE',  ( -7.999999999999991118, 0.000000000000000000, 5.330302779823363757 ) ) ;
#21870 = CARTESIAN_POINT ( 'NONE',  ( 8.311093377946834337, 222.0312500034139873, -8.311093377946836114 ) ) ;
#21871 = DIRECTION ( 'NONE',  ( 0.000000000000000000, 0.000000000000000000, 1.000000000000000000 ) ) ;
#21872 = CARTESIAN_POINT ( 'NONE',  ( 4.220049686691934809, 10.18810118749999916, 81.06250000204836681 ) ) ;
#21873 = ORIENTED_EDGE ( 'NONE', *, *, #48975, .F. ) ;
#21874 = ADVANCED_FACE ( 'NONE', ( #34375 ), #34747, .T. ) ;
#21875 = CARTESIAN_POINT ( 'NONE',  ( 2.849036369511732440E-14, 204.3750000027312126, 202.0000000000000000 ) ) ;
#21876 = CARTESIAN_POINT ( 'NONE',  ( 8.311093377946834337, 120.4687499965860269, 8.311093377946839666 ) ) ;
#21877 = CARTESIAN_POINT ( 'NONE',  ( 29.65685424949251825, 195.4374999999999716, 166.0000000000000284 ) ) ;
#21878 = ORIENTED_EDGE ( 'NONE', *, *, #71554, .T. ) ;
#21879 = ORIENTED_EDGE ( 'NONE', *, *, #71713, .F. ) ;
#21880 = CIRCLE ( 'NONE', #50805, 18.00000000000000355 ) ;
#21881 = CARTESIAN_POINT ( 'NONE',  ( 1.881053915767122664, 6.249999998634407916, 4.541265875000001451 ) ) ;
#21882 = CARTESIAN_POINT ( 'NONE',  ( -7.188101187500000044, 16.21874999795161543, -8.802885111219163269E-16 ) ) ;
#21883 = CARTESIAN_POINT ( 'NONE',  ( -5.656854249492378806, 108.8750000040967763, 5.656854249492381470 ) ) ;
#21884 = CARTESIAN_POINT ( 'NONE',  ( 10.18810118749999916, 1.247682550866122264E-15, 91.28125000204836681 ) ) ;
#21885 = CARTESIAN_POINT ( 'NONE',  ( -26.56734541678232375, 199.2500000013656063, 173.4587341250003760 ) ) ;
#21886 = CARTESIAN_POINT ( 'NONE',  ( 2.828427124746190291, 8.875000000000001776, 2.828427124746192067 ) ) ;
#21887 = CARTESIAN_POINT ( 'NONE',  ( 1.656854249492381914, 22.56249999726881583, 4.000000000000000888 ) ) ;
#21888 = CARTESIAN_POINT ( 'NONE',  ( -3.211159895383562723, 6.937499998634407028, 3.211159895383561391 ) ) ;
#21889 = CARTESIAN_POINT ( 'NONE',  ( -2.849036369511732440E-14, 197.2500000000000000, 138.0000000000000568 ) ) ;
#21890 = VERTEX_POINT ( 'NONE', #29062 ) ;
#21891 = CARTESIAN_POINT ( 'NONE',  ( 5.082755093536326818, 109.7187500020483810, 5.082755093536325042 ) ) ;
#21893 = CARTESIAN_POINT ( 'NONE',  ( 4.556349186104052151, -10.99999999999999822, 96.15625000409677625 ) ) ;
#21892 = CARTESIAN_POINT ( 'NONE',  ( -31.45873412499995680, 195.7500000013656063, 171.4326545832181239 ) ) ;
#21894 = CARTESIAN_POINT ( 'NONE',  ( 3.211159895383561835, 20.43749999863440436, -3.211159895383561835 ) ) ;
#21895 = AXIS2_PLACEMENT_3D ( 'NONE', #73565, #73938, #22240 ) ;
#21896 = LINE ( 'NONE', #15492, #10663 ) ;
#21897 = ORIENTED_EDGE ( 'NONE', *, *, #71726, .F. ) ;
#21898 = EDGE_CURVE ( 'NONE', #33515, #10305, #42105, .T. ) ;
#21899 = VERTEX_POINT ( 'NONE', #46410 ) ;
#21900 = CARTESIAN_POINT ( 'NONE',  ( -6.238412754330611322E-16, 10.18810118749999916, 94.28125000204836681 ) ) ;
#21901 = CARTESIAN_POINT ( 'NONE',  ( 7.999999999999991118, 9.797174393178815797E-16, 19.58030277982336642 ) ) ;
#21902 = CARTESIAN_POINT ( 'NONE',  ( -24.54126587500000412, 199.5000000013656063, 168.5673454167827003 ) ) ;
#21903 = CARTESIAN_POINT ( 'NONE',  ( 7.778174593052023411, -7.778174593052021635, 108.0624999999999858 ) ) ;
#21904 = CARTESIAN_POINT ( 'NONE',  ( 2.445694354108840063, 206.0625000013656063, 200.4456943541088663 ) ) ;
#21905 = LINE ( 'NONE', #39273, #48221 ) ;
#21906 = CARTESIAN_POINT ( 'NONE',  ( 6.123233995736767268E-16, 116.2500000000000000, -10.00000000000000178 ) ) ;
#21907 = CARTESIAN_POINT ( 'NONE',  ( 3.313708498984765161, 108.9687500000000000, 7.999999999999998224 ) ) ;
#21908 = CARTESIAN_POINT ( 'NONE',  ( 2.765530957081996366, 292.2968750017070647, -6.676582343750003368 ) ) ;
#21909 = CARTESIAN_POINT ( 'NONE',  ( 1.320432766682872962E-15, -7.188101187499992051, 5.236552781871753659 ) ) ;
#21910 = CARTESIAN_POINT ( 'NONE',  ( 3.313708498984761608, 1.781250000000000222, -8.000000000000000000 ) ) ;
#21911 = EDGE_CURVE ( 'NONE', #32460, #70626, #26690, .T. ) ;
#21912 = CARTESIAN_POINT ( 'NONE',  ( 30.44569435410883784, 206.8125000013656063, 167.5543056458911053 ) ) ;
#21913 = CARTESIAN_POINT ( 'NONE',  ( -7.188101187500000044, 1.593749997951610320, -8.802885111219163269E-16 ) ) ;
#21914 = CARTESIAN_POINT ( 'NONE',  ( -2.754378923186476579E-14, 200.1875000013656063, 145.4587341250000350 ) ) ;
#21915 = CARTESIAN_POINT ( 'NONE',  ( 7.188101187500002709, 120.6875000020483952, 2.977408999572649151 ) ) ;
#21917 = CARTESIAN_POINT ( 'NONE',  ( -2.839093476692135984E-14, 203.9375000013656063, 138.5412658750000503 ) ) ;
#21916 = CARTESIAN_POINT ( 'NONE',  ( 30.82842712474620583, 195.2500000027312126, 172.8284271247460424 ) ) ;
#21918 = CARTESIAN_POINT ( 'NONE',  ( -6.951808397369817780E-16, 242.9687500034140157, -11.35316468749999963 ) ) ;
#21919 = CARTESIAN_POINT ( 'NONE',  ( -3.313708498984869966, 114.4062500040967763, -7.999999999999892530 ) ) ;
#21920 = CARTESIAN_POINT ( 'NONE',  ( 27.99999999999999645, 210.0000000000000284, 169.9999999999999147 ) ) ;
#21921 = CARTESIAN_POINT ( 'NONE',  ( 32.00000000000000000, 204.2500000000000284, 169.9999999999999432 ) ) ;
#21922 = CARTESIAN_POINT ( 'NONE',  ( 11.35316468750000141, 15.78124999658601979, 0.000000000000000000 ) ) ;
#21923 = CARTESIAN_POINT ( 'NONE',  ( 7.188101187499993827, -2.977408999572645598, 1.017802781871752993 ) ) ;
#21924 = CARTESIAN_POINT ( 'NONE',  ( 5.676582343749993598, 205.2604166632526983, 9.832129032723422313 ) ) ;
#21925 = CARTESIAN_POINT ( 'NONE',  ( -5.000000000000005329, 135.2083333265053682, 8.660254037844387298 ) ) ;
#21926 = LINE ( 'NONE', #44957, #62020 ) ;
#21928 = CARTESIAN_POINT ( 'NONE',  ( 5.656854249492381470, 101.7500000040967905, 5.656854249492379694 ) ) ;
#21927 = CARTESIAN_POINT ( 'NONE',  ( 11.00000000000010836, -4.556349186103939353, 88.65624999999998579 ) ) ;
#21929 = VERTEX_POINT ( 'NONE', #53841 ) ;
#21930 = AXIS2_PLACEMENT_3D ( 'NONE', #29653, #35334, #17961 ) ;
#21931 = CARTESIAN_POINT ( 'NONE',  ( -3.458734125000016757, 201.1250000013656347, 140.5673454167824161 ) ) ;
#21932 = CARTESIAN_POINT ( 'NONE',  ( 5.676582343750001591, 6.614583329919350163, -9.832129032723420536 ) ) ;
#21933 = CARTESIAN_POINT ( 'NONE',  ( 11.00000000000000355, -4.556349186104045046, 90.34375000409677625 ) ) ;
#21934 = CARTESIAN_POINT ( 'NONE',  ( -3.673940397442060854E-16, 292.7500000000000000, -6.000000000000001776 ) ) ;
#21935 = CARTESIAN_POINT ( 'NONE',  ( -29.43265458321755190, 195.8750000013655779, 173.4587341250004044 ) ) ;
#21936 = CARTESIAN_POINT ( 'NONE',  ( 11.00000000000000355, -11.00000000000000000, -6.938893903907228378E-15 ) ) ;
#21938 = CARTESIAN_POINT ( 'NONE',  ( -9.832129032723418760, 7.864583329919350163, -5.676582343750004256 ) ) ;
#21937 = CARTESIAN_POINT ( 'NONE',  ( -7.188101187500000044, 115.1562500020483810, 0.000000000000000000 ) ) ;
#21939 = CARTESIAN_POINT ( 'NONE',  ( -5.656854249492373476, -5.656854249492376141, 26.51780277982336997 ) ) ;
#21940 = AXIS2_PLACEMENT_3D ( 'NONE', #10087, #33125, #10827 ) ;
#21941 = CARTESIAN_POINT ( 'NONE',  ( 6.951808397369818766E-16, 137.0312499965860411, -11.35316468750000141 ) ) ;
#21942 = EDGE_CURVE ( 'NONE', #24630, #31077, #13670, .T. ) ;
#21943 = CARTESIAN_POINT ( 'NONE',  ( -7.320508075688773708, 98.74999999317205379, -7.320508075688774596 ) ) ;
#21944 = CARTESIAN_POINT ( 'NONE',  ( 5.082755093536326818, 120.5937500020483952, 5.082755093536325042 ) ) ;
#21945 = CARTESIAN_POINT ( 'NONE',  ( -10.00000000000000000, 4.166666659838700326, -2.679491924311229845 ) ) ;
#21946 = CARTESIAN_POINT ( 'NONE',  ( -11.00000000000000000, 0.000000000000000000, 103.1875000040967763 ) ) ;
#21947 = CARTESIAN_POINT ( 'NONE',  ( 0.000000000000000000, 125.0000000000000000, 8.000000000000000000 ) ) ;
#21948 = ORIENTED_EDGE ( 'NONE', *, *, #42675, .F. ) ;
#21949 = CARTESIAN_POINT ( 'NONE',  ( 8.311093377946837890, 1.718749996586016682, -8.311093377946837890 ) ) ;
#21950 = EDGE_CURVE ( 'NONE', #1142, #46323, #25145, .T. ) ;
#21951 = CARTESIAN_POINT ( 'NONE',  ( 4.721056650416000089, 289.9843750017070079, 4.721056650415999201 ) ) ;
#21952 = DIRECTION ( 'NONE',  ( -0.000000000000000000, 1.000000000000000000, 4.476705744456276341E-16 ) ) ;
#21953 = CARTESIAN_POINT ( 'NONE',  ( -3.313708498984758943, -7.999999999999989342, 1.299052783920146448 ) ) ;
#21954 = CARTESIAN_POINT ( 'NONE',  ( -26.34314575050768070, 198.5625000000000000, 174.0000000000004547 ) ) ;
#21955 = CARTESIAN_POINT ( 'NONE',  ( -5.676582343749992710, 259.7395833367473301, 9.832129032723422313 ) ) ;
#21956 = CARTESIAN_POINT ( 'NONE',  ( 4.220049686691934809, 10.18810118749999916, 97.56250000204836681 ) ) ;
#21957 = ORIENTED_EDGE ( 'NONE', *, *, #20375, .F. ) ;
#21958 =( BOUNDED_CURVE ( )  B_SPLINE_CURVE ( 2, ( #15600, #55991, #51427, #5791, #68779, #34478, #22747, #39737, #40111 ),
 .UNSPECIFIED., .F., .F. ) 
 B_SPLINE_CURVE_WITH_KNOTS ( ( 3, 2, 2, 2, 3 ),
 ( 0.8472222222222222099, 0.8541666666666666297, 0.8611111111111111605, 0.8680555555555555802, 0.8750000000000000000 ),
 .UNSPECIFIED. ) 
 CURVE ( )  GEOMETRIC_REPRESENTATION_ITEM ( )  RATIONAL_B_SPLINE_CURVE ( ( 1.000000000000000000, 0.9238795325112867385, 1.000000000000000000, 0.9238795325112867385, 1.000000000000000000, 0.9238795325112867385, 1.000000000000000000, 0.9238795325112867385, 1.000000000000000000 ) ) 
 REPRESENTATION_ITEM ( '' )  );
#21959 = AXIS2_PLACEMENT_3D ( 'NONE', #52017, #36147, #18796 ) ;
#21960 = CARTESIAN_POINT ( 'NONE',  ( 10.00000000000000178, 216.8749999931720538, 0.000000000000000000 ) ) ;
#21961 = CARTESIAN_POINT ( 'NONE',  ( -8.311093377946841443, 174.2187499965860127, 8.311093377946834337 ) ) ;
#21962 = CARTESIAN_POINT ( 'NONE',  ( 2.754378923186476579E-14, 202.4375000013656063, 194.5412658750000219 ) ) ;
#21963 = EDGE_CURVE ( 'NONE', #54549, #4192, #42504, .T. ) ;
#21964 = CARTESIAN_POINT ( 'NONE',  ( -5.000000000000000000, 60.90295814858222201, 23.31388853594875599 ) ) ;
#21965 = CARTESIAN_POINT ( 'NONE',  ( 3.042071309553159519, 75.05208332991935549, 11.35316468750000141 ) ) ;
#21966 = ORIENTED_EDGE ( 'NONE', *, *, #6431, .T. ) ;
#21967 = CARTESIAN_POINT ( 'NONE',  ( -7.204075437095965206, -7.204075437095968759, 111.3437500020483810 ) ) ;
#21968 = CARTESIAN_POINT ( 'NONE',  ( 1.881053915767121998, 13.62499999863440792, -4.541265875000002339 ) ) ;
#21969 = ORIENTED_EDGE ( 'NONE', *, *, #15670, .T. ) ;
#21970 = CARTESIAN_POINT ( 'NONE',  ( 5.082755093536324154, 27.28124999795161543, 5.082755093536326818 ) ) ;
#21971 = CARTESIAN_POINT ( 'NONE',  ( -2.775557561562891351E-14, 195.0000000000000000, 146.0000000000000284 ) ) ;
#21972 = CARTESIAN_POINT ( 'NONE',  ( 10.00000000000000178, 66.87499999317203958, 0.000000000000000000 ) ) ;
#21973 = CARTESIAN_POINT ( 'NONE',  ( -7.188101187500000044, 15.09374999795161187, -8.802885111219163269E-16 ) ) ;
#21974 = CARTESIAN_POINT ( 'NONE',  ( 11.00000000000000000, 1.347111479062088405E-15, 93.43750000409677625 ) ) ;
#21975 = CARTESIAN_POINT ( 'NONE',  ( -4.220049686691937474, -10.18810118749999738, 110.3125000020483810 ) ) ;
#21976 = VECTOR ( 'NONE', #10925, 1000.000000000000000 ) ;
#21977 = CARTESIAN_POINT ( 'NONE',  ( 2.828427124746208943, 201.7500000027312126, 195.1715728752538439 ) ) ;
#21978 = CARTESIAN_POINT ( 'NONE',  ( 4.000000000000000888, 9.687499997268815832, 1.656854249492384135 ) ) ;
#21979 = DIRECTION ( 'NONE',  ( -0.000000000000000000, 1.000000000000000000, -0.000000000000000000 ) ) ;
#21980 = ORIENTED_EDGE ( 'NONE', *, *, #35358, .T. ) ;
#21981 = EDGE_CURVE ( 'NONE', #71972, #66887, #13814, .T. ) ;
#21982 = AXIS2_PLACEMENT_3D ( 'NONE', #54543, #59460, #13409 ) ;
#21983 = CARTESIAN_POINT ( 'NONE',  ( 2.839093476692135984E-14, 203.6875000013656063, 201.4587341250000350 ) ) ;
#21984 = EDGE_CURVE ( 'NONE', #46282, #5598, #2525, .T. ) ;
#21985 = CIRCLE ( 'NONE', #11025, 12.00000000000000000 ) ;
#21986 = CARTESIAN_POINT ( 'NONE',  ( -24.54126587500002543, 208.2500000013656063, 168.5673454167826435 ) ) ;
#21987 = DIRECTION ( 'NONE',  ( -0.000000000000000000, -0.000000000000000000, 1.000000000000000000 ) ) ;
#21988 = CARTESIAN_POINT ( 'NONE',  ( -4.541265875000003227, 8.874999998634407916, 1.881053915767121110 ) ) ;
#21989 = CARTESIAN_POINT ( 'NONE',  ( 4.000000000000001776, 1.806524977843537691E-16, 0.000000000000000000 ) ) ;
#21990 = CARTESIAN_POINT ( 'NONE',  ( -2.977408999572647819, 7.188101187499991163, 19.20530278187175810 ) ) ;
#21991 = EDGE_LOOP ( 'NONE', ( #46541, #60120, #11438, #57057 ) ) ;
#21992 = ADVANCED_FACE ( 'NONE', ( #25881 ), #31938, .T. ) ;
#21993 = DIRECTION ( 'NONE',  ( -0.000000000000000000, 1.000000000000000000, -0.000000000000000000 ) ) ;
#21994 = ORIENTED_EDGE ( 'NONE', *, *, #18847, .T. ) ;
#21995 = CARTESIAN_POINT ( 'NONE',  ( -10.18810118749999738, -4.220049686691941915, 109.7500000020483810 ) ) ;
#21996 = CARTESIAN_POINT ( 'NONE',  ( -11.00000000000000000, 4.556349186104045934, 97.09375000409680467 ) ) ;
#21997 = CARTESIAN_POINT ( 'NONE',  ( 3.458734125000016313, 203.8750000013656063, 199.4326545832176691 ) ) ;
#21998 = CARTESIAN_POINT ( 'NONE',  ( 31.45873412499997812, 197.7500000013656063, 168.5673454167822172 ) ) ;
#21999 = CARTESIAN_POINT ( 'NONE',  ( -5.000000000000005329, 78.33333333333334281, 8.660254037844387298 ) ) ;
#22000 = CARTESIAN_POINT ( 'NONE',  ( -3.313708498984762496, 122.2812500000000000, 7.999999999999998224 ) ) ;
#22001 = CARTESIAN_POINT ( 'NONE',  ( -2.485281374238572649, 292.1875000000000000, 6.000000000000002665 ) ) ;
#22002 = CARTESIAN_POINT ( 'NONE',  ( 26.34314575050764162, 206.0625000027312694, 173.9999999999999147 ) ) ;
#22003 = EDGE_LOOP ( 'NONE', ( #23836, #65566, #61966 ) ) ;
#22004 = CARTESIAN_POINT ( 'NONE',  ( -3.042071309553159075, 219.9479166700806445, 11.35316468749999963 ) ) ;
#22005 = CARTESIAN_POINT ( 'NONE',  ( -3.313708498984757611, 7.999999999999991118, 8.049052779823362869 ) ) ;
#22006 = CARTESIAN_POINT ( 'NONE',  ( 3.999999999999960032, 196.0625000027312694, 143.6568542494924543 ) ) ;
#22007 = CARTESIAN_POINT ( 'NONE',  ( -9.000000000000000000, 5.196152422706624918, -0.8038475772933814101 ) ) ;
#22008 = CARTESIAN_POINT ( 'NONE',  ( -11.00000000000010303, -4.556349186103947346, 94.09375000000000000 ) ) ;
#22009 = CARTESIAN_POINT ( 'NONE',  ( -5.000000000000000888, 234.1666666666666856, -8.660254037844387298 ) ) ;
#22010 = CARTESIAN_POINT ( 'NONE',  ( 32.00000000000000000, 204.2500000000000284, 169.9999999999999432 ) ) ;
#22011 = EDGE_CURVE ( 'NONE', #43617, #59649, #16493, .T. ) ;
#22012 = CARTESIAN_POINT ( 'NONE',  ( 5.000000000000001776, 205.8333333333333428, -8.660254037844389075 ) ) ;
#22013 = CARTESIAN_POINT ( 'NONE',  ( 2.020667218593132706E-15, -11.00000000000000000, 110.8749999999999858 ) ) ;
#22014 = CARTESIAN_POINT ( 'NONE',  ( 7.188101187499992051, 8.802885111219154394E-16, 17.61155278187175810 ) ) ;
#22015 = CARTESIAN_POINT ( 'NONE',  ( 8.311093377946834337, 170.4687499965860127, 8.311093377946839666 ) ) ;
#22016 = CARTESIAN_POINT ( 'NONE',  ( -5.000000000000116351, 213.3333333333334849, 8.660254037844579145 ) ) ;
#22017 = CARTESIAN_POINT ( 'NONE',  ( -1.982524389443043544, -42.73998104797299646, 151.1032041038507145 ) ) ;
#22019 = DIRECTION ( 'NONE',  ( -0.000000000000000000, 1.000000000000000000, -0.000000000000000000 ) ) ;
#22018 = CARTESIAN_POINT ( 'NONE',  ( 0.000000000000000000, 300.0000000000000000, 0.000000000000000000 ) ) ;
#22020 = VERTEX_POINT ( 'NONE', #37229 ) ;
#22021 = CARTESIAN_POINT ( 'NONE',  ( 11.35316468749999785, 20.88541666325268764, 3.042071309553174174 ) ) ;
#22022 = CARTESIAN_POINT ( 'NONE',  ( -24.54126587500002543, 209.2500000013656063, 168.5673454167826435 ) ) ;
#22024 = CARTESIAN_POINT ( 'NONE',  ( -1.704527592502766309, 10.27896685065642934, -63.66027613114052031 ) ) ;
#22023 = CARTESIAN_POINT ( 'NONE',  ( 75.00000000000001421, 272.0000000000000000, 20.00000000000002132 ) ) ;
#22025 = CARTESIAN_POINT ( 'NONE',  ( -29.80118446747862038, -51.96544576618858713, 178.5910842456946739 ) ) ;
#22026 = CARTESIAN_POINT ( 'NONE',  ( -3.458734125000015425, 203.0000000013655779, 143.4326545832176976 ) ) ;
#22027 = CARTESIAN_POINT ( 'NONE',  ( -10.00000000000000000, 59.16666665983869677, -2.679491924311229845 ) ) ;
#22028 = CARTESIAN_POINT ( 'NONE',  ( -2.977408999572651815, 101.9375000020483810, 7.188101187500000933 ) ) ;
#22029 = CARTESIAN_POINT ( 'NONE',  ( 3.211159895383561835, 6.562499998634407028, -3.211159895383561835 ) ) ;
#22030 = PLANE ( 'NONE',  #43320 ) ;
#22031 = CARTESIAN_POINT ( 'NONE',  ( -7.999999999999989342, -3.313708498984762496, 5.424052779823364645 ) ) ;
#22032 = CARTESIAN_POINT ( 'NONE',  ( -1.656854249492381248, 5.062499997268813168, -4.000000000000001776 ) ) ;
#22033 = ORIENTED_EDGE ( 'NONE', *, *, #47309, .F. ) ;
#22034 = VERTEX_POINT ( 'NONE', #33084 ) ;
#22035 = CARTESIAN_POINT ( 'NONE',  ( 0.8419854211626223162, -49.91401432488723344, -40.68947704085055506 ) ) ;
#22036 = CARTESIAN_POINT ( 'NONE',  ( -38.00000000000000000, 52.99999999999999289, 25.00000000000000000 ) ) ;
#22037 = CARTESIAN_POINT ( 'NONE',  ( -8.311093377946836114, 147.6562499965860411, -8.311093377946837890 ) ) ;
#22038 = ORIENTED_EDGE ( 'NONE', *, *, #26049, .T. ) ;
#22039 = DIRECTION ( 'NONE',  ( -0.000000000000000000, 1.000000000000000000, -4.476705744456276341E-16 ) ) ;
#22040 = CARTESIAN_POINT ( 'NONE',  ( 1.871523826299183495E-15, -10.18810118749999916, 90.53125000204836681 ) ) ;
#22041 = CARTESIAN_POINT ( 'NONE',  ( 5.656854249492378806, 4.312500000000000000, 5.656854249492381470 ) ) ;
#22042 = CARTESIAN_POINT ( 'NONE',  ( -3.999999999999959144, 207.0625000000000568, 199.6568542494924259 ) ) ;
#22043 = CARTESIAN_POINT ( 'NONE',  ( 7.588356073042825223, -2.561989435426024198, 0.000000000000000000 ) ) ;
#22044 = CARTESIAN_POINT ( 'NONE',  ( -10.18810118749999916, 0.000000000000000000, 117.5312500020483810 ) ) ;
#22045 = VERTEX_POINT ( 'NONE', #15689 ) ;
#22046 = CARTESIAN_POINT ( 'NONE',  ( 33.25337153428351655, -20.05426479499426051, 157.6435991425960879 ) ) ;
#22047 = DIRECTION ( 'NONE',  ( -0.000000000000000000, 1.000000000000000000, -0.000000000000000000 ) ) ;
#22048 = CARTESIAN_POINT ( 'NONE',  ( 11.35316468749999785, 110.8854166632526699, 3.042071309553174174 ) ) ;
#22049 = CARTESIAN_POINT ( 'NONE',  ( 3.458734125000015425, 201.9375000013656063, 198.0000000000000284 ) ) ;
#22050 = CARTESIAN_POINT ( 'NONE',  ( -7.188101187500000933, 22.49999999795161187, -2.977408999572651371 ) ) ;
#22051 =( BOUNDED_CURVE ( )  B_SPLINE_CURVE ( 2, ( #28443, #68429, #16356, #23151, #62393, #33752, #16732, #39758, #40511, #58256, #69555, #541, #6557 ),
 .UNSPECIFIED., .F., .F. ) 
 B_SPLINE_CURVE_WITH_KNOTS ( ( 3, 2, 2, 2, 2, 2, 3 ),
 ( 2.684688080663935494, 2.689920760420000612, 2.695153440176065729, 2.700386119932130846, 2.705618799688195963, 2.710851479444261081, 2.716084159200326198 ),
 .UNSPECIFIED. ) 
 CURVE ( )  GEOMETRIC_REPRESENTATION_ITEM ( )  RATIONAL_B_SPLINE_CURVE ( ( 1.000000000000077272, 0.9659258262889910407, 1.000000000000000000, 0.9659258262890683122, 1.000000000000000000, 0.9659258262890683122, 1.000000000000000000, 0.9659258262890683122, 1.000000000000000000, 0.9659258262890683122, 1.000000000000000000, 0.9659258262890725311, 0.9999999999999957812 ) ) 
 REPRESENTATION_ITEM ( '' )  );
#22052 = CARTESIAN_POINT ( 'NONE',  ( 7.204075437095966983, 7.204075437095967871, 83.96875000204836681 ) ) ;
#22053 = CARTESIAN_POINT ( 'NONE',  ( 3.042071309553159519, 40.05208332991935549, 11.35316468750000141 ) ) ;
#22054 = ORIENTED_EDGE ( 'NONE', *, *, #29993, .T. ) ;
#22055 = CARTESIAN_POINT ( 'NONE',  ( -4.000000000000001776, 4.437500000000001776, -1.656854249492381470 ) ) ;
#22056 = CARTESIAN_POINT ( 'NONE',  ( -3.317071493978880348, -8.008118988124989457, 22.29436528394063188 ) ) ;
#22057 = CARTESIAN_POINT ( 'NONE',  ( -1.432654583217664701, 209.0000000013655779, 138.5412658750000787 ) ) ;
#22058 = CARTESIAN_POINT ( 'NONE',  ( 2.977408999572651815, 9.187499997951610098, 7.188101187500000933 ) ) ;
#22059 = CARTESIAN_POINT ( 'NONE',  ( 6.000000000000003553, 294.6250000034140157, -2.485281374238571761 ) ) ;
#22060 = CARTESIAN_POINT ( 'NONE',  ( -4.242640687119285658, 297.1250000000000000, 4.242640687119287435 ) ) ;
#22061 = CARTESIAN_POINT ( 'NONE',  ( -23.99999999999999289, 206.7500000000000284, 170.0000000000003411 ) ) ;
#22062 = B_SPLINE_CURVE_WITH_KNOTS ( 'NONE', 3,
 ( #60644, #19162, #42164, #59902, #8965, #31978, #53877, #2187 ),
 .UNSPECIFIED., .F., .F.,
 ( 4, 2, 2, 4 ),
 ( 0.005256334970490775943, 0.006570121696662011880, 0.007883908422833247817, 0.01051148187517572143 ),
 .UNSPECIFIED. ) ;
#22063 = ADVANCED_FACE ( 'NONE', ( #50402 ), #61727, .F. ) ;
#22064 = CARTESIAN_POINT ( 'NONE',  ( -11.35316468750000141, 153.8020833299192986, 3.042071309553159963 ) ) ;
#22065 = CARTESIAN_POINT ( 'NONE',  ( -10.18810118749999916, 4.220049686691934809, 76.56250000204836681 ) ) ;
#22066 = CARTESIAN_POINT ( 'NONE',  ( -31.45873412499999944, 195.6250000013656063, 168.5673454167827572 ) ) ;
#22067 =( BOUNDED_CURVE ( )  B_SPLINE_CURVE ( 2, ( #11178, #34200, #17193, #28519, #68883, #18318, #11544, #57204, #51527 ),
 .UNSPECIFIED., .F., .F. ) 
 B_SPLINE_CURVE_WITH_KNOTS ( ( 3, 2, 2, 2, 3 ),
 ( 0.5166666666666670515, 0.5250000000000003553, 0.5333333333333337700, 0.5416666666666671848, 0.5500000000000005995 ),
 .UNSPECIFIED. ) 
 CURVE ( )  GEOMETRIC_REPRESENTATION_ITEM ( )  RATIONAL_B_SPLINE_CURVE ( ( 0.9999999999999970024, 0.9238795325112897361, 1.000000000000000000, 0.9238795325112867385, 1.000000000000000000, 0.9238795325112867385, 1.000000000000000000, 0.9238795325112816315, 1.000000000000005107 ) ) 
 REPRESENTATION_ITEM ( '' )  );
#22068 = DIRECTION ( 'NONE',  ( 0.000000000000000000, 0.000000000000000000, 1.000000000000000000 ) ) ;
#22069 = CARTESIAN_POINT ( 'NONE',  ( -1.881053915767121554, 14.74999999863440969, -4.541265875000002339 ) ) ;
#22070 = ORIENTED_EDGE ( 'NONE', *, *, #68348, .F. ) ;
#22071 = CARTESIAN_POINT ( 'NONE',  ( 4.000000000000015987, 200.6250000027312126, 198.0000000000000284 ) ) ;
#22072 = EDGE_CURVE ( 'NONE', #3266, #37555, #29568, .T. ) ;
#22073 = CARTESIAN_POINT ( 'NONE',  ( 2.445694354108783219, 195.8125000013656063, 139.5543056458912190 ) ) ;
#22074 = CARTESIAN_POINT ( 'NONE',  ( -30.82842712474624491, 204.2500000027312126, 167.1715728752542418 ) ) ;
#22075 = CARTESIAN_POINT ( 'NONE',  ( -38.00000000000000000, -53.00000000000000711, 9.999999999999991118 ) ) ;
#22076 = VERTEX_POINT ( 'NONE', #54590 ) ;
#22077 = ADVANCED_FACE ( 'NONE', ( #67012 ), #20227, .F. ) ;
#22078 = CARTESIAN_POINT ( 'NONE',  ( 7.188101187499999156, 9.374999997951610098, 2.977408999572654924 ) ) ;
#22079 = CARTESIAN_POINT ( 'NONE',  ( 5.000000000000000000, 60.11723469343148452, -46.25570701698029552 ) ) ;
#22080 = CARTESIAN_POINT ( 'NONE',  ( 4.999999999999999112, 51.88457047716768500, -42.00159762951405895 ) ) ;
#22081 = CIRCLE ( 'NONE', #44997, 3.999999999999976019 ) ;
#22082 = CARTESIAN_POINT ( 'NONE',  ( 2.679491924311228956, 36.04166666666666430, -10.00000000000000000 ) ) ;
#22083 = AXIS2_PLACEMENT_3D ( 'NONE', #58990, #30303, #1284 ) ;
#22084 = CARTESIAN_POINT ( 'NONE',  ( -7.188101187500000044, 105.0312500020483810, 0.000000000000000000 ) ) ;
#22085 = DIRECTION ( 'NONE',  ( 0.000000000000000000, -1.000000000000000000, 0.000000000000000000 ) ) ;
#22086 = CARTESIAN_POINT ( 'NONE',  ( 1.226468279477575784E-15, 287.7031250017069510, 6.676582343750001591 ) ) ;
#22088 = DIRECTION ( 'NONE',  ( 0.000000000000000000, 0.000000000000000000, -1.000000000000000000 ) ) ;
#22087 = CARTESIAN_POINT ( 'NONE',  ( -1.604524386212670052E-13, 78.75000000000000000, 10.00000000000000178 ) ) ;
#22089 = VERTEX_POINT ( 'NONE', #65885 ) ;
#22090 = CARTESIAN_POINT ( 'NONE',  ( 3.042071309553173286, 260.3645833367473301, 11.35316468749999608 ) ) ;
#22091 = CARTESIAN_POINT ( 'NONE',  ( 5.082755093536318824, 5.082755093536319713, 22.29905278187175455 ) ) ;
#22092 = CARTESIAN_POINT ( 'NONE',  ( 0.000000000000000000, 0.000000000000000000, 30.00000000000000000 ) ) ;
#22093 = CARTESIAN_POINT ( 'NONE',  ( 31.99999999999998579, 206.1875000000000853, 171.6568542494923122 ) ) ;
#22094 = CARTESIAN_POINT ( 'NONE',  ( -2.069125466538180191, -65.90280720052957975, -26.36412295902851355 ) ) ;
#22095 = CARTESIAN_POINT ( 'NONE',  ( 0.000000000000000000, 300.0000000000000000, 10.00000000000000178 ) ) ;
#22096 = CARTESIAN_POINT ( 'NONE',  ( 4.999999999999993783, 164.1666666666666856, 8.660254037844390851 ) ) ;
#22097 = DIRECTION ( 'NONE',  ( 0.000000000000000000, 0.000000000000000000, 1.000000000000000000 ) ) ;
#22098 = DIRECTION ( 'NONE',  ( -0.000000000000000000, 1.000000000000000000, -0.000000000000000000 ) ) ;
#22099 = DIRECTION ( 'NONE',  ( -0.000000000000000000, 1.000000000000000000, -0.000000000000000000 ) ) ;
#22100 = CARTESIAN_POINT ( 'NONE',  ( -3.042071309553164404, 132.5520833299193555, -11.35316468749999963 ) ) ;
#22101 = CARTESIAN_POINT ( 'NONE',  ( -4.242640687119285658, 296.1250000000000000, 4.242640687119287435 ) ) ;
#22102 = CARTESIAN_POINT ( 'NONE',  ( -11.00000000000000000, 4.556349186104045934, 71.40624999999997158 ) ) ;
#22105 = CARTESIAN_POINT ( 'NONE',  ( -3.673940397442060854E-16, 298.7500000000000000, -6.000000000000001776 ) ) ;
#22104 = CARTESIAN_POINT ( 'NONE',  ( 31.45873412499997812, 196.7500000013656063, 168.5673454167822172 ) ) ;
#22103 = CARTESIAN_POINT ( 'NONE',  ( 25.55430564589114795, 195.5625000013656063, 172.4456943541086957 ) ) ;
#22106 = EDGE_LOOP ( 'NONE', ( #62436, #59271, #41013, #65971 ) ) ;
#22107 = CARTESIAN_POINT ( 'NONE',  ( -5.656854249492381470, 20.43750000000000355, 5.656854249492379694 ) ) ;
#22108 = CARTESIAN_POINT ( 'NONE',  ( -2.849036369511732440E-14, 203.2500000000000000, 138.0000000000000568 ) ) ;
#22110 = CARTESIAN_POINT ( 'NONE',  ( 9.832129032723416984, 222.1354166700806729, -5.676582343750003368 ) ) ;
#22109 =( REPRESENTATION_RELATIONSHIP ('NONE','NONE', #46008, #22268 ) REPRESENTATION_RELATIONSHIP_WITH_TRANSFORMATION ( #69709 )SHAPE_REPRESENTATION_RELATIONSHIP( ) );
#22111 = CARTESIAN_POINT ( 'NONE',  ( 26.56734541678232375, 199.6250000013656063, 173.4587341249998929 ) ) ;
#22112 = CARTESIAN_POINT ( 'NONE',  ( 3.042071309553167069, 207.1354166632526415, -11.35316468749999785 ) ) ;
#22113 = CARTESIAN_POINT ( 'NONE',  ( -7.188101187499999156, 121.2500000020483952, 2.977408999572654924 ) ) ;
#22114 = CARTESIAN_POINT ( 'NONE',  ( 2.780723358947928197E-16, 16.56249999863440436, -4.541265875000002339 ) ) ;
#22115 = CARTESIAN_POINT ( 'NONE',  ( -0.4451317748922283268, -51.14719335908487352, 48.52010116548744634 ) ) ;
#22116 = CARTESIAN_POINT ( 'NONE',  ( 5.656854249492376141, -5.656854249492374365, 20.89280277982336642 ) ) ;
#22117 = DIRECTION ( 'NONE',  ( -0.000000000000000000, -0.000000000000000000, 1.000000000000000000 ) ) ;
#22118 = CARTESIAN_POINT ( 'NONE',  ( -3.042071309553173730, 94.32291666325266988, 11.35316468749999785 ) ) ;
#22119 = ORIENTED_EDGE ( 'NONE', *, *, #17685, .F. ) ;
#22120 = CARTESIAN_POINT ( 'NONE',  ( 4.000000000000001776, 15.74999999726881406, 0.000000000000000000 ) ) ;
#22121 = CARTESIAN_POINT ( 'NONE',  ( 7.188101187500000044, 24.46874999795161543, 0.000000000000000000 ) ) ;
#22122 = CARTESIAN_POINT ( 'NONE',  ( 2.128287106641264010E-14, -42.00000000000000711, 139.0000000000000568 ) ) ;
#22123 = EDGE_CURVE ( 'NONE', #9236, #35837, #66262, .T. ) ;
#22124 = CARTESIAN_POINT ( 'NONE',  ( 5.676582343749997150, 252.5520833367473301, -9.832129032723418760 ) ) ;
#22125 = CARTESIAN_POINT ( 'NONE',  ( -11.35316468749999785, 98.07291666325269830, -3.042071309553167513 ) ) ;
#22126 = ORIENTED_EDGE ( 'NONE', *, *, #29718, .T. ) ;
#22127 = DIRECTION ( 'NONE',  ( 1.000000000000000000, 0.000000000000000000, 0.000000000000000000 ) ) ;
#22128 = CARTESIAN_POINT ( 'NONE',  ( -10.18810118749999916, 4.220049686691934809, 108.0625000020483810 ) ) ;
#22129 = CARTESIAN_POINT ( 'NONE',  ( 2.679491924311228956, 222.9166666598386826, -10.00000000000000000 ) ) ;
#22130 = CARTESIAN_POINT ( 'NONE',  ( 2.445694354108839175, 204.3125000013656063, 195.5543056458912190 ) ) ;
#22132 = CARTESIAN_POINT ( 'NONE',  ( 6.951808397369818766E-16, 92.03124999658602690, -11.35316468750000141 ) ) ;
#22131 = CARTESIAN_POINT ( 'NONE',  ( -11.00000000000000000, 0.000000000000000000, 106.0000000000000000 ) ) ;
#22133 = CARTESIAN_POINT ( 'NONE',  ( -3.313708498984757167, 7.999999999999991118, 12.73655278392014623 ) ) ;
#22134 = CARTESIAN_POINT ( 'NONE',  ( -30.44569435410879166, 202.0625000013656063, 172.4456943541092357 ) ) ;
#22135 = CARTESIAN_POINT ( 'NONE',  ( 2.751064625579944321E-14, 208.8750000027312126, 194.0000000000000568 ) ) ;
#22136 = ORIENTED_EDGE ( 'NONE', *, *, #7336, .T. ) ;
#22137 = CARTESIAN_POINT ( 'NONE',  ( -5.000000000000005329, 180.2083333265053682, 8.660254037844387298 ) ) ;
#22138 = CARTESIAN_POINT ( 'NONE',  ( 25.17157287525381903, 201.0000000027312126, 172.8284271247460993 ) ) ;
#22139 = CARTESIAN_POINT ( 'NONE',  ( -27.99999999999995737, 202.5000000000000000, 174.0000000000003695 ) ) ;
#22140 = CARTESIAN_POINT ( 'NONE',  ( 9.832129032723420536, 81.51041666325268409, -5.676582343749999815 ) ) ;
#22141 = CARTESIAN_POINT ( 'NONE',  ( 6.676582343750003368, 290.0156250017069510, -2.765530957081997254 ) ) ;
#22142 = CARTESIAN_POINT ( 'NONE',  ( 10.18810118749999916, 1.247682550866122264E-15, 100.2812500020483810 ) ) ;
#22143 = CARTESIAN_POINT ( 'NONE',  ( 9.832129032723420536, 226.1979166632526983, -5.676582343749999815 ) ) ;
#22144 = ORIENTED_EDGE ( 'NONE', *, *, #9250, .T. ) ;
#22145 = DIRECTION ( 'NONE',  ( 0.000000000000000000, 0.000000000000000000, 1.000000000000000000 ) ) ;
#22146 = DIRECTION ( 'NONE',  ( -0.000000000000000000, -0.000000000000000000, -1.000000000000000000 ) ) ;
#22147 = CARTESIAN_POINT ( 'NONE',  ( 1.469576158976823947E-15, 120.8750000000000000, 8.000000000000000000 ) ) ;
#22148 = CARTESIAN_POINT ( 'NONE',  ( 3.042071309553159519, 204.7395833299193555, 11.35316468750000141 ) ) ;
#22149 = AXIS2_PLACEMENT_3D ( 'NONE', #30447, #28960, #319 ) ;
#22150 = CARTESIAN_POINT ( 'NONE',  ( 2.679491924311235174, 229.5833333401612890, 9.999999999999998224 ) ) ;
#22151 = LINE ( 'NONE', #45178, #12588 ) ;
#22152 = CARTESIAN_POINT ( 'NONE',  ( -4.088227598258586603E-16, 296.2031250017070079, -6.676582343750001591 ) ) ;
#22153 = ORIENTED_EDGE ( 'NONE', *, *, #34386, .T. ) ;
#22154 = CARTESIAN_POINT ( 'NONE',  ( 5.676582343749993598, 190.2604166632526983, 9.832129032723422313 ) ) ;
#22155 = EDGE_CURVE ( 'NONE', #25822, #61881, #50030, .T. ) ;
#22156 = CARTESIAN_POINT ( 'NONE',  ( -26.56734541678232731, 206.0000000013656347, 173.4587341250003760 ) ) ;
#22157 = CARTESIAN_POINT ( 'NONE',  ( 5.656854249492380582, 9.187500000000001776, -5.656854249492380582 ) ) ;
#22158 = ORIENTED_EDGE ( 'NONE', *, *, #3252, .T. ) ;
#22159 = EDGE_CURVE ( 'NONE', #63554, #21755, #37604, .T. ) ;
#22160 = CARTESIAN_POINT ( 'NONE',  ( 8.000000000000001776, 94.34375000409679046, 3.313708498984759387 ) ) ;
#22161 = CARTESIAN_POINT ( 'NONE',  ( -4.898587196589412829E-16, 115.8125000040967763, -8.000000000000000000 ) ) ;
#22162 =( BOUNDED_CURVE ( )  B_SPLINE_CURVE ( 2, ( #12109, #6468, #29471, #35874, #52481, #58891, #41525, #23805, #69832 ),
 .UNSPECIFIED., .F., .F. ) 
 B_SPLINE_CURVE_WITH_KNOTS ( ( 3, 2, 2, 2, 3 ),
 ( 0.3124999999999979461, 0.3229166666666646313, 0.3333333333333312609, 0.3437499999999979461, 0.3541666666666646313 ),
 .UNSPECIFIED. ) 
 CURVE ( )  GEOMETRIC_REPRESENTATION_ITEM ( )  RATIONAL_B_SPLINE_CURVE ( ( 1.000000000000015099, 0.9238795325112717505, 1.000000000000000000, 0.9238795325112867385, 1.000000000000000000, 0.9238795325112867385, 1.000000000000000000, 0.9238795325113017265, 0.9999999999999850120 ) ) 
 REPRESENTATION_ITEM ( '' )  );
#22163 = CARTESIAN_POINT ( 'NONE',  ( 2.679491924311222739, 18.95833333333333215, 10.00000000000000355 ) ) ;
#22164 = AXIS2_PLACEMENT_3D ( 'NONE', #7698, #23931, #46940 ) ;
#22165 = CARTESIAN_POINT ( 'NONE',  ( -7.204075437095967871, 7.204075437095967871, 79.84375000204838102 ) ) ;
#22166 = ORIENTED_EDGE ( 'NONE', *, *, #12704, .T. ) ;
#22167 = CARTESIAN_POINT ( 'NONE',  ( -2.828427124746192067, 20.62500000000000000, 2.828427124746190735 ) ) ;
#22168 = CARTESIAN_POINT ( 'NONE',  ( 4.541265875000002339, 18.31249999863440792, 0.000000000000000000 ) ) ;
#22169 = DIRECTION ( 'NONE',  ( 1.000000000000000000, 9.637352644315595243E-17, 0.000000000000000000 ) ) ;
#22170 = ORIENTED_EDGE ( 'NONE', *, *, #30518, .F. ) ;
#22171 = CARTESIAN_POINT ( 'NONE',  ( -4.898587196589412829E-16, 120.1250000000000000, -8.000000000000000000 ) ) ;
#22172 = CARTESIAN_POINT ( 'NONE',  ( -7.188101187500001821, 121.4375000020483668, -2.977408999572650483 ) ) ;
#22173 = EDGE_CURVE ( 'NONE', #1217, #73206, #1147, .T. ) ;
#22174 = CARTESIAN_POINT ( 'NONE',  ( 5.000000000000000000, -66.79063484153797958, 23.29724706625358266 ) ) ;
#22177 = CARTESIAN_POINT ( 'NONE',  ( 1.736494649845411908, -51.27805538754646619, 48.57014059985625209 ) ) ;
#22176 = CARTESIAN_POINT ( 'NONE',  ( 11.35316468749999963, 241.1979166700806729, 3.042071309553159519 ) ) ;
#22175 = CARTESIAN_POINT ( 'NONE',  ( 24.54126587500000767, 206.2500000013655779, 171.4326545832176123 ) ) ;
#22178 = PRODUCT_CONTEXT ( 'NONE', #58288, 'mechanical' ) ;
#22179 = ORIENTED_EDGE ( 'NONE', *, *, #51458, .F. ) ;
#22180 = CARTESIAN_POINT ( 'NONE',  ( -6.951808397369817780E-16, 257.9687500034140157, -11.35316468749999963 ) ) ;
#22181 = CARTESIAN_POINT ( 'NONE',  ( 2.977408999572646486, 7.188101187499991163, 14.51780278187175455 ) ) ;
#22182 = EDGE_LOOP ( 'NONE', ( #47322, #63893, #1045, #39839 ) ) ;
#22183 = ORIENTED_EDGE ( 'NONE', *, *, #62809, .F. ) ;
#22184 = CARTESIAN_POINT ( 'NONE',  ( -4.220049686691937474, -10.18810118749999738, 73.93750000204838102 ) ) ;
#22185 = CARTESIAN_POINT ( 'NONE',  ( 11.35316468749999785, 90.88541666325266988, 3.042071309553174174 ) ) ;
#22186 = DIRECTION ( 'NONE',  ( 0.000000000000000000, 0.000000000000000000, 1.000000000000000000 ) ) ;
#22187 = CARTESIAN_POINT ( 'NONE',  ( -11.00000000000000000, 4.556349186104045934, 86.40624999999998579 ) ) ;
#22190 = CARTESIAN_POINT ( 'NONE',  ( -4.721056650415998313, 290.7343750017069510, 4.721056650416000089 ) ) ;
#22189 = CARTESIAN_POINT ( 'NONE',  ( 30.44569435410883429, 208.5625000013656063, 172.4456943541086957 ) ) ;
#22188 = CARTESIAN_POINT ( 'NONE',  ( 24.54126587500000412, 207.3750000013656063, 168.5673454167822172 ) ) ;
#22191 = AXIS2_PLACEMENT_3D ( 'NONE', #58758, #5957, #7069 ) ;
#22192 = CARTESIAN_POINT ( 'NONE',  ( 8.660254037844385522, 76.45833332650536818, 5.000000000000005329 ) ) ;
#22193 = LINE ( 'NONE', #64436, #45607 ) ;
#22194 = CARTESIAN_POINT ( 'NONE',  ( 8.311093377946834337, 195.1562499965860411, 8.311093377946839666 ) ) ;
#22195 = CARTESIAN_POINT ( 'NONE',  ( 3.313708498984762052, 6.093749995903220196, -8.000000000000000000 ) ) ;
#22196 = VERTEX_POINT ( 'NONE', #10047 ) ;
#22197 = CARTESIAN_POINT ( 'NONE',  ( 30.44569435410879521, 208.8125000013656063, 172.4456943541087526 ) ) ;
#22198 = CARTESIAN_POINT ( 'NONE',  ( 2.977408999572650927, 16.12499999795161187, -7.188101187500001821 ) ) ;
#22199 = CARTESIAN_POINT ( 'NONE',  ( -11.35316468750000141, 163.5937499965860127, -1.390361679473963753E-15 ) ) ;
#22200 = CARTESIAN_POINT ( 'NONE',  ( 2.020667218593132706E-15, -11.00000000000000000, 99.06250000409677625 ) ) ;
#22201 = CARTESIAN_POINT ( 'NONE',  ( 2.977408999572650039, 103.0625000020483810, -7.188101187500000933 ) ) ;
#22203 = CARTESIAN_POINT ( 'NONE',  ( 0.4451317748863459212, -51.14719335908540643, -48.52010116548649421 ) ) ;
#22202 = CARTESIAN_POINT ( 'NONE',  ( -7.347880794884122694E-16, 16.49999999726881228, 4.000000000000001776 ) ) ;
#22204 = CARTESIAN_POINT ( 'NONE',  ( 25.55430564589115505, 207.5625000013656063, 172.4456943541086957 ) ) ;
#22205 = CARTESIAN_POINT ( 'NONE',  ( -2.977408999572647819, 7.188101187499991163, 13.58030278187175277 ) ) ;
#22206 = CARTESIAN_POINT ( 'NONE',  ( 8.311093377946834337, 50.15624999658601979, 8.311093377946839666 ) ) ;
#22207 = CARTESIAN_POINT ( 'NONE',  ( -6.676582343750001591, 299.4531250017069510, 0.000000000000000000 ) ) ;
#22208 = CARTESIAN_POINT ( 'NONE',  ( 2.828427124746209831, 195.5000000027312126, 200.8284271247462129 ) ) ;
#22209 = ORIENTED_EDGE ( 'NONE', *, *, #22786, .T. ) ;
#22210 = CARTESIAN_POINT ( 'NONE',  ( 7.999999999999992895, -3.313708498984756279, 7.674052783920143561 ) ) ;
#22211 = CARTESIAN_POINT ( 'NONE',  ( -7.320508075688773708, 168.7499999931720822, -7.320508075688774596 ) ) ;
#22212 = CARTESIAN_POINT ( 'NONE',  ( -9.832129032723420536, 58.69791666325268409, 5.676582343749997150 ) ) ;
#22213 = CARTESIAN_POINT ( 'NONE',  ( -10.99999999999999822, -4.556349186104052151, 74.78125000409679046 ) ) ;
#22214 = CARTESIAN_POINT ( 'NONE',  ( 2.445694354108784108, 200.5625000013656063, 144.4456943541088663 ) ) ;
#22215 = CARTESIAN_POINT ( 'NONE',  ( 0.7581620860333473377, 10.12340554704894657, 70.09014334687759629 ) ) ;
#22216 = CARTESIAN_POINT ( 'NONE',  ( 1.656854249492440978, 207.6875000000000284, 194.0000000000001137 ) ) ;
#22218 = CARTESIAN_POINT ( 'NONE',  ( 6.951808397369818766E-16, 42.03124999658601268, -11.35316468750000141 ) ) ;
#22217 = CARTESIAN_POINT ( 'NONE',  ( 7.188101187500000044, 96.40625000204838102, -8.802885111219163269E-16 ) ) ;
#22219 = CARTESIAN_POINT ( 'NONE',  ( -7.999999999999989342, -3.313708498984762496, 2.424052779823365533 ) ) ;
#22220 = CARTESIAN_POINT ( 'NONE',  ( 7.999969786815256612, -3.313738712169494338, 4.674051575081102250 ) ) ;
#22221 = CARTESIAN_POINT ( 'NONE',  ( 3.042071309553167069, 171.8229166632526983, -11.35316468749999785 ) ) ;
#22222 = CARTESIAN_POINT ( 'NONE',  ( 2.679491924311222739, 140.8333333265053682, 10.00000000000000355 ) ) ;
#22223 = CARTESIAN_POINT ( 'NONE',  ( 7.188101187500001821, 99.87500000204838102, -2.977408999572651371 ) ) ;
#22224 =( GEOMETRIC_REPRESENTATION_CONTEXT ( 3 ) GLOBAL_UNCERTAINTY_ASSIGNED_CONTEXT ( ( #8051 ) ) GLOBAL_UNIT_ASSIGNED_CONTEXT ( ( #27935, #68666, #50199 ) ) REPRESENTATION_CONTEXT ( 'NONE', 'WORKASPACE' ) );
#22225 = CARTESIAN_POINT ( 'NONE',  ( -2.381929342090383095, 0.4663230313613501155, -7.609644401983861606 ) ) ;
#22226 = CARTESIAN_POINT ( 'NONE',  ( 3.042071309553159519, 35.05208332991935549, 11.35316468750000141 ) ) ;
#22227 = CARTESIAN_POINT ( 'NONE',  ( -4.220049686691935698, 10.18810118749999916, 117.2500000020483952 ) ) ;
#22228 = CARTESIAN_POINT ( 'NONE',  ( -5.676582343749998039, 187.4479166632526983, -9.832129032723420536 ) ) ;
#22229 = EDGE_LOOP ( 'NONE', ( #69243, #57568, #48401, #50386 ) ) ;
#22230 = DIRECTION ( 'NONE',  ( -0.000000000000000000, -1.000000000000000000, -0.000000000000000000 ) ) ;
#22231 = CARTESIAN_POINT ( 'NONE',  ( -7.204075437095967871, 7.204075437095967871, 70.46875000204836681 ) ) ;
#22232 = CARTESIAN_POINT ( 'NONE',  ( -3.999999999999960032, 195.9375000000000000, 196.3431457505076594 ) ) ;
#22233 = DIRECTION ( 'NONE',  ( 1.000000000000000000, 0.000000000000000000, 0.000000000000000000 ) ) ;
#22235 = CARTESIAN_POINT ( 'NONE',  ( -5.676582343749998039, 162.4479166632526983, -9.832129032723420536 ) ) ;
#22234 = CARTESIAN_POINT ( 'NONE',  ( -4.898587196589412829E-16, 121.8125000040967763, -8.000000000000000000 ) ) ;
#22236 = CARTESIAN_POINT ( 'NONE',  ( -7.999999999999991118, 0.000000000000000000, 6.886552784329822430 ) ) ;
#22237 = CARTESIAN_POINT ( 'NONE',  ( 5.676582343749997150, 222.2395833367473017, -9.832129032723418760 ) ) ;
#22238 = CARTESIAN_POINT ( 'NONE',  ( 10.18810118749999916, 1.247682550866122264E-15, 77.78125000204836681 ) ) ;
#22239 = ORIENTED_EDGE ( 'NONE', *, *, #24701, .F. ) ;
#22240 = DIRECTION ( 'NONE',  ( 0.000000000000000000, 0.000000000000000000, 1.000000000000000000 ) ) ;
#22241 = CARTESIAN_POINT ( 'NONE',  ( -2.085542519210945728E-15, 119.8437499965860269, 11.35316468750000141 ) ) ;
#22242 = CARTESIAN_POINT ( 'NONE',  ( 0.000000000000000000, 20.39230484541327471, -10.20000000000000284 ) ) ;
#22243 = ORIENTED_EDGE ( 'NONE', *, *, #73874, .T. ) ;
#22244 = ORIENTED_EDGE ( 'NONE', *, *, #70810, .T. ) ;
#22245 = AXIS2_PLACEMENT_3D ( 'NONE', #42492, #31553, #70800 ) ;
#22246 = CARTESIAN_POINT ( 'NONE',  ( -4.541265875000002339, 7.874999998634407028, -1.881053915767121998 ) ) ;
#22247 = ADVANCED_FACE ( 'NONE', ( #66633 ), #55335, .F. ) ;
#22248 = CARTESIAN_POINT ( 'NONE',  ( 7.188101187500001821, 15.56249999795161365, -2.977408999572650483 ) ) ;
#22249 = CARTESIAN_POINT ( 'NONE',  ( 1.469576158976823947E-15, 109.0625000040967905, 8.000000000000000000 ) ) ;
#22250 = ADVANCED_FACE ( 'NONE', ( #56080 ), #3640, .T. ) ;
#22251 = CARTESIAN_POINT ( 'NONE',  ( -26.56734541678238060, 198.6250000013655779, 166.5412658750003629 ) ) ;
#22252 = CARTESIAN_POINT ( 'NONE',  ( -4.000000000000002665, 6.562500000000000000, 1.656854249492380804 ) ) ;
#22253 = CARTESIAN_POINT ( 'NONE',  ( -3.999999999999960032, 198.0000000000000000, 198.0000000000000284 ) ) ;
#22254 = CARTESIAN_POINT ( 'NONE',  ( -4.541265875000003227, 5.874999998634406140, 1.881053915767121110 ) ) ;
#22255 = CARTESIAN_POINT ( 'NONE',  ( 3.999999999999960032, 200.0000000000000000, 142.0000000000000568 ) ) ;
#22256 = ORIENTED_EDGE ( 'NONE', *, *, #17795, .T. ) ;
#22257 = CARTESIAN_POINT ( 'NONE',  ( 5.082755093536326818, 102.2187500020483810, 5.082755093536325042 ) ) ;
#22258 = AXIS2_PLACEMENT_3D ( 'NONE', #16089, #10821, #74189 ) ;
#22259 = EDGE_CURVE ( 'NONE', #73307, #59151, #14192, .T. ) ;
#22261 = CARTESIAN_POINT ( 'NONE',  ( -3.313708498984744732, 123.2187500000000142, -8.000000000000019540 ) ) ;
#22260 = CARTESIAN_POINT ( 'NONE',  ( 28.00000000000002132, 208.5000000000000284, 165.9999999999998863 ) ) ;
#22262 = SHAPE_REPRESENTATION_RELATIONSHIP ( 'NONE' , 'NONE' ,  #20419, #22811 ) ;
#22263 = CARTESIAN_POINT ( 'NONE',  ( -3.211159895383561391, 21.68749999863440792, -3.211159895383561835 ) ) ;
#22264 = CIRCLE ( 'NONE', #43933, 11.00000000000000000 ) ;
#22265 = CARTESIAN_POINT ( 'NONE',  ( 2.977408999572650927, -7.188101187499990274, 3.455302781871751439 ) ) ;
#22266 = VERTEX_POINT ( 'NONE', #56819 ) ;
#22267 =( BOUNDED_CURVE ( )  B_SPLINE_CURVE ( 2, ( #56067, #68857, #22826, #33071, #68482, #16045, #44735, #62444, #11152 ),
 .UNSPECIFIED., .F., .F. ) 
 B_SPLINE_CURVE_WITH_KNOTS ( ( 3, 2, 2, 2, 3 ),
 ( 0.8000000000000007105, 0.8083333333333340143, 0.8166666666666673180, 0.8250000000000006217, 0.8333333333333340365 ),
 .UNSPECIFIED. ) 
 CURVE ( )  GEOMETRIC_REPRESENTATION_ITEM ( )  RATIONAL_B_SPLINE_CURVE ( ( 0.9999999999999938938, 0.9238795325112928447, 1.000000000000000000, 0.9238795325112867385, 1.000000000000000000, 0.9238795325112867385, 1.000000000000000000, 0.9238795325112806323, 1.000000000000005995 ) ) 
 REPRESENTATION_ITEM ( '' )  );
#22268 = SHAPE_REPRESENTATION ( 'body', ( #57354 ), #16391 ) ;
#22269 = ORIENTED_EDGE ( 'NONE', *, *, #50459, .T. ) ;
#22270 = CARTESIAN_POINT ( 'NONE',  ( 7.204075437095968759, -7.204075437095966983, 95.21875000204838102 ) ) ;
#22271 = CARTESIAN_POINT ( 'NONE',  ( 32.00000000000000000, 204.3750000027312126, 169.9999999999998863 ) ) ;
#22272 = CARTESIAN_POINT ( 'NONE',  ( -31.45873412499997812, 200.0000000013656063, 171.4326545832180386 ) ) ;
#22273 = CARTESIAN_POINT ( 'NONE',  ( 2.020667218593132706E-15, -11.00000000000000000, 107.8750000000000000 ) ) ;
#22274 = CARTESIAN_POINT ( 'NONE',  ( 3.458734125000015425, 205.2500000013655779, 196.5673454167823877 ) ) ;
#22276 = CYLINDRICAL_SURFACE ( 'NONE', #65115, 8.000000000000000000 ) ;
#22275 = CARTESIAN_POINT ( 'NONE',  ( -56.00000000000004974, 5.999999999999977796, 167.9999999999997726 ) ) ;
#22277 = CARTESIAN_POINT ( 'NONE',  ( 10.00000000000000178, 115.0000000000000000, 0.000000000000000000 ) ) ;
#22278 = CARTESIAN_POINT ( 'NONE',  ( -3.313708498984762052, 106.7187500000000000, -8.000000000000000000 ) ) ;
#22279 = CARTESIAN_POINT ( 'NONE',  ( -2.765530957081996810, 289.4218750017069510, -6.676582343750003368 ) ) ;
#22280 = CARTESIAN_POINT ( 'NONE',  ( -7.188101187499990274, -2.977408999572651371, 3.455302781871751439 ) ) ;
#22281 = CARTESIAN_POINT ( 'NONE',  ( 4.898587196589412829E-16, 1.875000000000000444, -8.000000000000000000 ) ) ;
#22282 = CARTESIAN_POINT ( 'NONE',  ( 31.45873412500001010, 207.7500000013656063, 168.5673454167822740 ) ) ;
#22283 = CARTESIAN_POINT ( 'NONE',  ( -5.656854249492381470, 24.74999999590322375, 5.656854249492379694 ) ) ;
#22284 = CARTESIAN_POINT ( 'NONE',  ( -3.458734125000015425, 198.0000000013656063, 143.4326545832176976 ) ) ;
#22285 = CARTESIAN_POINT ( 'NONE',  ( 1.320432766682874540E-15, 120.4062500020483810, 7.188101187500000044 ) ) ;
#22287 = CARTESIAN_POINT ( 'NONE',  ( -2.445694354108840063, 204.0625000013656063, 139.5543056458912190 ) ) ;
#22286 = CARTESIAN_POINT ( 'NONE',  ( -4.000000000000016875, 204.4375000000000568, 140.3431457505076594 ) ) ;
#22288 = CARTESIAN_POINT ( 'NONE',  ( -9.832129032723415207, 244.6354166700806445, 5.676582343750005144 ) ) ;
#22289 = CARTESIAN_POINT ( 'NONE',  ( -7.320508075688778149, 214.9999999931720822, 7.320508075688769267 ) ) ;
#22290 = CARTESIAN_POINT ( 'NONE',  ( 26.34314575050763452, 201.5625000000000853, 165.9999999999998863 ) ) ;
#22291 = CARTESIAN_POINT ( 'NONE',  ( -9.832129032723418760, 17.86458332991935194, -5.676582343750004256 ) ) ;
#22292 = CARTESIAN_POINT ( 'NONE',  ( 5.676582343749993598, 210.2604166632526699, 9.832129032723422313 ) ) ;
#22293 = CYLINDRICAL_SURFACE ( 'NONE', #56393, 11.00000000000000000 ) ;
#22294 = DIRECTION ( 'NONE',  ( -0.000000000000000000, 1.000000000000000000, -1.563033456626094573E-30 ) ) ;
#22296 = CARTESIAN_POINT ( 'NONE',  ( -7.999999999999991118, 0.000000000000000000, 29.33030277982336642 ) ) ;
#22295 = DIRECTION ( 'NONE',  ( -0.000000000000000000, -0.000000000000000000, 1.000000000000000000 ) ) ;
#22297 = ORIENTED_EDGE ( 'NONE', *, *, #61774, .F. ) ;
#22298 = CARTESIAN_POINT ( 'NONE',  ( 2.445694354108784108, 198.5625000013656063, 144.4456943541088663 ) ) ;
#22299 = CARTESIAN_POINT ( 'NONE',  ( 5.676582343749993598, 24.94791666325268764, 9.832129032723422313 ) ) ;
#22300 = CARTESIAN_POINT ( 'NONE',  ( 2.020667218593132706E-15, -11.00000000000000000, 94.56250000409677625 ) ) ;
#22301 = CARTESIAN_POINT ( 'NONE',  ( 7.320508075688774596, 210.6249999999999716, -7.320508075688774596 ) ) ;
#22302 = CARTESIAN_POINT ( 'NONE',  ( -29.43265458321770822, 196.5000000013656063, 166.5412658750003914 ) ) ;
#22303 = DIRECTION ( 'NONE',  ( -0.000000000000000000, 1.000000000000000000, 4.689100369878284071E-30 ) ) ;
#22305 = CARTESIAN_POINT ( 'NONE',  ( 9.832129032723416984, 5.364583329919349275, 5.676582343750006032 ) ) ;
#22304 = CARTESIAN_POINT ( 'NONE',  ( 1.320432766682874540E-15, 112.5312500020483952, 7.188101187500000044 ) ) ;
#22306 = CARTESIAN_POINT ( 'NONE',  ( -7.999999999999991118, 3.313708498984756723, 23.23655277982336642 ) ) ;
#22307 = CARTESIAN_POINT ( 'NONE',  ( -8.311093377946836114, 132.6562499965860411, -8.311093377946837890 ) ) ;
#22308 = CARTESIAN_POINT ( 'NONE',  ( 10.00000000000000178, 107.0833333265053540, -2.679491924311226736 ) ) ;
#22309 = CARTESIAN_POINT ( 'NONE',  ( 5.082755093536325042, 122.4687500020483952, -5.082755093536325930 ) ) ;
#22310 = CARTESIAN_POINT ( 'NONE',  ( -25.55430564589119768, 207.5625000013656063, 167.5543056458915316 ) ) ;
#22311 = CARTESIAN_POINT ( 'NONE',  ( -4.999999999999999112, -51.88457047716706683, -42.00159762951478370 ) ) ;
#22312 = ORIENTED_EDGE ( 'NONE', *, *, #58222, .F. ) ;
#22313 = CARTESIAN_POINT ( 'NONE',  ( -2.591411123065472832, -60.37037679142518698, 22.98897912932123688 ) ) ;
#22314 = DIRECTION ( 'NONE',  ( 1.000000000000000000, 0.000000000000000000, 1.836970198721037823E-16 ) ) ;
#22315 = CARTESIAN_POINT ( 'NONE',  ( -4.088227598258586603E-16, 291.3593750017070079, -6.676582343750001591 ) ) ;
#22316 = CARTESIAN_POINT ( 'NONE',  ( 5.000000000000000000, 52.35862550122891435, 48.98731492261470777 ) ) ;
#22317 = CARTESIAN_POINT ( 'NONE',  ( -3.313708498984758943, -7.999999999999989342, 25.16780278432982954 ) ) ;
#22318 = CARTESIAN_POINT ( 'NONE',  ( 3.999999999999959144, 207.1875000027312126, 140.3431457505076594 ) ) ;
#22319 = FACE_OUTER_BOUND ( 'NONE', #16367, .T. ) ;
#22320 = VECTOR ( 'NONE', #72254, 1000.000000000000000 ) ;
#22321 = CARTESIAN_POINT ( 'NONE',  ( 7.204075437095968759, -7.204075437095966983, 95.59375000204838102 ) ) ;
#22322 = ORIENTED_EDGE ( 'NONE', *, *, #43318, .F. ) ;
#22323 = VECTOR ( 'NONE', #39007, 1000.000000000000000 ) ;
#22324 = CARTESIAN_POINT ( 'NONE',  ( 5.000000000000000000, 10.25159769123454900, 64.79153472057838314 ) ) ;
#22325 = CARTESIAN_POINT ( 'NONE',  ( -4.898587196589407898E-16, 7.999999999999991118, 24.45530277982336642 ) ) ;
#22326 = CARTESIAN_POINT ( 'NONE',  ( -2.445694354108784108, 203.5625000013656063, 195.5543056458912190 ) ) ;
#22327 = CARTESIAN_POINT ( 'NONE',  ( -8.311093377946836114, 77.96874999658598426, -8.311093377946837890 ) ) ;
#22328 = VERTEX_POINT ( 'NONE', #5140 ) ;
#22329 = CARTESIAN_POINT ( 'NONE',  ( -10.18810118749999916, 0.000000000000000000, 105.1562500020483810 ) ) ;
#22330 = CARTESIAN_POINT ( 'NONE',  ( -4.541265875000003227, 11.99999999863440792, 1.881053915767121110 ) ) ;
#22331 = VERTEX_POINT ( 'NONE', #33822 ) ;
#22332 = CARTESIAN_POINT ( 'NONE',  ( 7.188101187500001821, 24.56249999795161543, -2.977408999572650483 ) ) ;
#22333 = CARTESIAN_POINT ( 'NONE',  ( -18.00000000000000355, 2.204364238465235822E-15, -21.50000000000000000 ) ) ;
#22334 = LINE ( 'NONE', #5753, #29332 ) ;
#22335 = CARTESIAN_POINT ( 'NONE',  ( 7.188101187500000044, 24.84374999795161543, 0.000000000000000000 ) ) ;
#22336 = CARTESIAN_POINT ( 'NONE',  ( -2.849036369511732440E-14, 200.2500000000000000, 138.0000000000000568 ) ) ;
#22337 = CARTESIAN_POINT ( 'NONE',  ( 10.18810118750000093, -4.220049686691933921, 107.6875000020483810 ) ) ;
#22338 = ADVANCED_FACE ( 'NONE', ( #62458 ), #39459, .T. ) ;
#22339 = CARTESIAN_POINT ( 'NONE',  ( 4.000000000000015987, 204.5625000000000000, 196.3431457505076594 ) ) ;
#22340 = CARTESIAN_POINT ( 'NONE',  ( 2.828427124746190291, 9.624999997268814056, 2.828427124746192067 ) ) ;
#22341 = LINE ( 'NONE', #39344, #68650 ) ;
#22342 = ORIENTED_EDGE ( 'NONE', *, *, #20050, .T. ) ;
#22343 = CARTESIAN_POINT ( 'NONE',  ( -1.432654583217607192, 202.2500000013656063, 194.5412658750000219 ) ) ;
#22344 = CARTESIAN_POINT ( 'NONE',  ( -29.43265458321755901, 204.8750000013656063, 173.4587341250004044 ) ) ;
#22345 = DIRECTION ( 'NONE',  ( -0.000000000000000000, 1.000000000000000000, 4.476705744456276341E-16 ) ) ;
#22346 = EDGE_CURVE ( 'NONE', #11179, #4744, #51516, .T. ) ;
#22347 = CARTESIAN_POINT ( 'NONE',  ( -3.211159895383561391, 10.68749999863440792, -3.211159895383561835 ) ) ;
#22348 = CARTESIAN_POINT ( 'NONE',  ( -9.000000000000000000, 5.196152422706624918, -10.20000000000000284 ) ) ;
#22349 = CARTESIAN_POINT ( 'NONE',  ( 7.188101187499993827, -2.977408999572645598, 20.14280278187176165 ) ) ;
#22350 = ORIENTED_EDGE ( 'NONE', *, *, #15012, .T. ) ;
#22351 = EDGE_CURVE ( 'NONE', #16528, #54702, #62095, .T. ) ;
#22352 = FACE_OUTER_BOUND ( 'NONE', #21442, .T. ) ;
#22353 = VERTEX_POINT ( 'NONE', #27758 ) ;
#22354 = CARTESIAN_POINT ( 'NONE',  ( -7.204075437095967871, 7.204075437095967871, 109.4687500020483810 ) ) ;
#22355 = CARTESIAN_POINT ( 'NONE',  ( 11.00000000000000000, 1.347111479062088405E-15, 96.43750000409677625 ) ) ;
#22356 = CARTESIAN_POINT ( 'NONE',  ( -2.445694354108782775, 202.5625000013656063, 200.4456943541088663 ) ) ;
#22358 =( BOUNDED_CURVE ( )  B_SPLINE_CURVE ( 2, ( #9652, #43589, #21327, #37949, #22061, #27352, #55682, #62064, #21693 ),
 .UNSPECIFIED., .F., .F. ) 
 B_SPLINE_CURVE_WITH_KNOTS ( ( 3, 2, 2, 2, 3 ),
 ( 0.2000000000000001776, 0.2083333333333335091, 0.2166666666666668406, 0.2250000000000001998, 0.2333333333333335313 ),
 .UNSPECIFIED. ) 
 CURVE ( )  GEOMETRIC_REPRESENTATION_ITEM ( )  RATIONAL_B_SPLINE_CURVE ( ( 0.9999999999999984457, 0.9238795325112882928, 1.000000000000000000, 0.9238795325112867385, 1.000000000000000000, 0.9238795325112867385, 1.000000000000000000, 0.9238795325112849621, 1.000000000000001776 ) ) 
 REPRESENTATION_ITEM ( '' )  );
#22357 = CARTESIAN_POINT ( 'NONE',  ( 28.00000000000001776, 199.4375000013655779, 173.4587341249998929 ) ) ;
#22359 = CARTESIAN_POINT ( 'NONE',  ( 2.679491924311228956, 81.04166666666668561, -10.00000000000000000 ) ) ;
#22360 = CARTESIAN_POINT ( 'NONE',  ( -8.000000000000000000, 123.4062500000000142, -3.313708498984761608 ) ) ;
#22361 = CARTESIAN_POINT ( 'NONE',  ( 6.676582343750004256, 299.0468750017069510, 2.765530957081995478 ) ) ;
#22362 = VERTEX_POINT ( 'NONE', #74531 ) ;
#22363 = DIRECTION ( 'NONE',  ( -0.000000000000000000, -0.000000000000000000, -1.000000000000000000 ) ) ;
#22365 = EDGE_CURVE ( 'NONE', #6788, #27344, #29695, .T. ) ;
#22364 = CIRCLE ( 'NONE', #18786, 11.00000000000000000 ) ;
#22366 = CARTESIAN_POINT ( 'NONE',  ( 0.4451317748927060558, -16.44604352396231661, 68.55481936398555831 ) ) ;
#22367 = CARTESIAN_POINT ( 'NONE',  ( -1.656854249492403008, 196.8125000027311842, 146.0000000000000284 ) ) ;
#22368 = DIRECTION ( 'NONE',  ( -0.000000000000000000, 1.000000000000000000, -0.000000000000000000 ) ) ;
#22369 = CYLINDRICAL_SURFACE ( 'NONE', #21815, 10.00000000000000178 ) ;
#22370 = CARTESIAN_POINT ( 'NONE',  ( -4.999999999999992895, 240.8333333333333428, 8.660254037844390851 ) ) ;
#22371 = EDGE_CURVE ( 'NONE', #38699, #49698, #32436, .T. ) ;
#22372 = CARTESIAN_POINT ( 'NONE',  ( 27.99999999999996803, 204.0000000000000284, 173.9999999999999147 ) ) ;
#22373 = CARTESIAN_POINT ( 'NONE',  ( 10.00000000000000000, 199.7916666666666288, 2.679491924311236062 ) ) ;
#22374 = CARTESIAN_POINT ( 'NONE',  ( 7.188101187499992051, 2.977408999572647819, 14.70530278187175455 ) ) ;
#22375 = CARTESIAN_POINT ( 'NONE',  ( -5.676582343750006032, 169.4270833299193555, 9.832129032723418760 ) ) ;
#22376 = FACE_OUTER_BOUND ( 'NONE', #48684, .T. ) ;
#22377 = CARTESIAN_POINT ( 'NONE',  ( 18.00000000000000355, -10.39230484541328892, -1.607695154586745501 ) ) ;
#22379 = DIRECTION ( 'NONE',  ( -0.000000000000000000, -0.000000000000000000, -1.000000000000000000 ) ) ;
#22378 = FACE_OUTER_BOUND ( 'NONE', #41173, .T. ) ;
#22380 = VERTEX_POINT ( 'NONE', #5507 ) ;
#22381 = CARTESIAN_POINT ( 'NONE',  ( -1.432654583217662481, 198.1250000013656063, 145.4587341250000634 ) ) ;
#22382 = CARTESIAN_POINT ( 'NONE',  ( -5.676582343750006032, 24.42708332991935194, 9.832129032723418760 ) ) ;
#22383 = CARTESIAN_POINT ( 'NONE',  ( 2.020667218593132706E-15, -11.00000000000000000, 111.0625000040967763 ) ) ;
#22384 = CARTESIAN_POINT ( 'NONE',  ( -30.44569435410887337, 208.5625000013656063, 167.5543056458916169 ) ) ;
#22386 = CARTESIAN_POINT ( 'NONE',  ( -0.3752463838877027058, -10.12385607954436573, -70.07152133708838448 ) ) ;
#22385 = DIRECTION ( 'NONE',  ( -0.000000000000000000, -1.000000000000000000, -4.283267841918042741E-17 ) ) ;
#22387 = CARTESIAN_POINT ( 'NONE',  ( -18.32121218117747574, -47.49102260074459991, 195.0186025512507229 ) ) ;
#22388 = CARTESIAN_POINT ( 'NONE',  ( 1.432654583217607192, 197.2500000013656063, 145.4587341250000350 ) ) ;
#22389 =( BOUNDED_CURVE ( )  B_SPLINE_CURVE ( 2, ( #6392, #41083, #12765, #371, #46365, #35797, #11663, #16943, #6754 ),
 .UNSPECIFIED., .F., .F. ) 
 B_SPLINE_CURVE_WITH_KNOTS ( ( 3, 2, 2, 2, 3 ),
 ( 0.1764705882352942401, 0.1801470588235295212, 0.1838235294117648300, 0.1875000000000001388, 0.1911764705882354198 ),
 .UNSPECIFIED. ) 
 CURVE ( )  GEOMETRIC_REPRESENTATION_ITEM ( )  RATIONAL_B_SPLINE_CURVE ( ( 0.9999999999999976685, 0.9238795325112890700, 1.000000000000000000, 0.9238795325112867385, 1.000000000000000000, 0.9238795325112867385, 1.000000000000000000, 0.9238795325112838519, 1.000000000000002887 ) ) 
 REPRESENTATION_ITEM ( '' )  );
#22390 = CARTESIAN_POINT ( 'NONE',  ( -2.679491924311235618, 60.41666665983869677, 10.00000000000000000 ) ) ;
#22391 = CARTESIAN_POINT ( 'NONE',  ( 7.188101187500001821, 101.0000000020483810, -2.977408999572651371 ) ) ;
#22392 = CARTESIAN_POINT ( 'NONE',  ( 1.881053915767121776, 10.62499999863440792, -4.541265875000002339 ) ) ;
#22393 = CARTESIAN_POINT ( 'NONE',  ( 3.313708498984756279, 7.999999999999991118, 3.361552779823362425 ) ) ;
#22394 = CARTESIAN_POINT ( 'NONE',  ( -5.000000000000000000, -50.64189880742115690, 41.08656465431877791 ) ) ;
#22395 = VERTEX_POINT ( 'NONE', #28507 ) ;
#22396 = ORIENTED_EDGE ( 'NONE', *, *, #52993, .F. ) ;
#22397 = CARTESIAN_POINT ( 'NONE',  ( -4.898587196589407898E-16, 7.999999999999991118, 10.95530277982336642 ) ) ;
#22398 = CARTESIAN_POINT ( 'NONE',  ( 5.656854249492376141, -5.656854249492374365, 15.08030278392014623 ) ) ;
#22399 = SURFACE_SIDE_STYLE ('',( #51836 ) ) ;
#22400 = EDGE_CURVE ( 'NONE', #32606, #38095, #8841, .T. ) ;
#22401 = CARTESIAN_POINT ( 'NONE',  ( -28.94435879072220885, -42.80757904149561455, 158.8884701151923764 ) ) ;
#22402 = CARTESIAN_POINT ( 'NONE',  ( -11.35316468750000141, 148.4895833299193555, 3.042071309553159963 ) ) ;
#22403 = ORIENTED_EDGE ( 'NONE', *, *, #23751, .F. ) ;
#22404 = CARTESIAN_POINT ( 'NONE',  ( 6.000000000000023093, 10.39230484541324984, 0.000000000000000000 ) ) ;
#22405 = CARTESIAN_POINT ( 'NONE',  ( 10.18810118750000093, -4.220049686691933921, 90.81250000204838102 ) ) ;
#22406 = CARTESIAN_POINT ( 'NONE',  ( -29.10842753010508943, 194.7321495122487818, 173.5710399323151307 ) ) ;
#22407 = CARTESIAN_POINT ( 'NONE',  ( 4.000000000000015987, 206.4375000000000568, 199.6568542494924259 ) ) ;
#22408 = FACE_OUTER_BOUND ( 'NONE', #63935, .T. ) ;
#22409 = CARTESIAN_POINT ( 'NONE',  ( 7.999999999999998224, -0.7555120169168165756, 0.000000000000000000 ) ) ;
#22410 = EDGE_CURVE ( 'NONE', #63061, #71873, #39092, .T. ) ;
#22411 = CARTESIAN_POINT ( 'NONE',  ( 1.469576158976823947E-15, 101.3750000000000000, 8.000000000000000000 ) ) ;
#22412 = ORIENTED_EDGE ( 'NONE', *, *, #60759, .F. ) ;
#22413 = DIRECTION ( 'NONE',  ( 0.000000000000000000, 0.000000000000000000, 1.000000000000000000 ) ) ;
#22414 = SHAPE_REPRESENTATION ( 'spindle bearing', ( #57354 ), #33286 ) ;
#22415 = CARTESIAN_POINT ( 'NONE',  ( 31.07018350459786049, 178.9577932314791155, 170.8454493558014633 ) ) ;
#22416 = CARTESIAN_POINT ( 'NONE',  ( 5.676582343750001591, 121.9270833299193413, -9.832129032723420536 ) ) ;
#22417 = CARTESIAN_POINT ( 'NONE',  ( -3.458734124999958581, 202.5000000013656063, 199.4326545832176976 ) ) ;
#22418 = CARTESIAN_POINT ( 'NONE',  ( 7.188101187500000933, 23.43749999795161187, -2.977408999572650483 ) ) ;
#22420 = EDGE_CURVE ( 'NONE', #41205, #55362, #30001, .T. ) ;
#22419 = CARTESIAN_POINT ( 'NONE',  ( 10.18810118750000093, -4.220049686691933033, 80.68750000204836681 ) ) ;
#22421 = CARTESIAN_POINT ( 'NONE',  ( 11.35316468749999963, 41.30208332991936260, -3.042071309553165293 ) ) ;
#22422 = VERTEX_POINT ( 'NONE', #33448 ) ;
#22423 = LINE ( 'NONE', #3604, #24788 ) ;
#22424 = CARTESIAN_POINT ( 'NONE',  ( 5.000000000000000000, -29.68417822476651580, -4.268394125863113509 ) ) ;
#22425 = CARTESIAN_POINT ( 'NONE',  ( -5.662595241051935346, 5.662595241051935346, 20.32561528394062833 ) ) ;
#22426 = CARTESIAN_POINT ( 'NONE',  ( -1.432654583217662481, 207.3750000013656063, 145.4587341250000634 ) ) ;
#22427 = CARTESIAN_POINT ( 'NONE',  ( -5.082755093536326818, 11.90624999795161010, 5.082755093536325042 ) ) ;
#22428 = CARTESIAN_POINT ( 'NONE',  ( -6.000000000000001776, 295.0625000034140157, 0.000000000000000000 ) ) ;
#22429 = AXIS2_PLACEMENT_3D ( 'NONE', #38061, #9764, #54296 ) ;
#22430 = CARTESIAN_POINT ( 'NONE',  ( -4.898587196589412829E-16, 114.1250000000000000, -8.000000000000000000 ) ) ;
#22431 = CARTESIAN_POINT ( 'NONE',  ( -7.188101187500002709, 3.187499997951610098, 2.977408999572649151 ) ) ;
#22432 = CARTESIAN_POINT ( 'NONE',  ( -11.35316468750000141, 158.8020833299193555, 3.042071309553159963 ) ) ;
#22433 = CARTESIAN_POINT ( 'NONE',  ( -4.220049686691935698, 10.18810118749999916, 74.87500000204836681 ) ) ;
#22434 = CARTESIAN_POINT ( 'NONE',  ( -30.44569435410878810, 194.8125000013656063, 172.4456943541092357 ) ) ;
#22435 = CARTESIAN_POINT ( 'NONE',  ( -2.828427124746192067, 15.62500000000000000, 2.828427124746190735 ) ) ;
#22436 = CARTESIAN_POINT ( 'NONE',  ( 1.881053915767121776, 18.62499999863440792, -4.541265875000002339 ) ) ;
#22437 = VERTEX_POINT ( 'NONE', #56447 ) ;
#22438 = CARTESIAN_POINT ( 'NONE',  ( 4.000000000000015099, 197.6875000027312126, 196.3431457505076594 ) ) ;
#22439 = CARTESIAN_POINT ( 'NONE',  ( 3.999999999999960032, 208.9375000000000284, 143.6568542494924543 ) ) ;
#22440 = CARTESIAN_POINT ( 'NONE',  ( -23.99999999999995737, 204.8125000027312126, 171.6568542494926817 ) ) ;
#22441 = VECTOR ( 'NONE', #19502, 1000.000000000000000 ) ;
#22442 = ADVANCED_FACE ( 'NONE', ( #4766 ), #45119, .F. ) ;
#22443 = CARTESIAN_POINT ( 'NONE',  ( 7.320508075688771044, 251.2500000068279178, -7.320508075688771932 ) ) ;
#22444 = CARTESIAN_POINT ( 'NONE',  ( -7.999999999999989342, -3.313708498984762496, 5.611552783920146226 ) ) ;
#22445 = ORIENTED_EDGE ( 'NONE', *, *, #69873, .F. ) ;
#22446 = CARTESIAN_POINT ( 'NONE',  ( -2.977408999572654480, 19.49999999795161898, 7.188101187499999156 ) ) ;
#22447 = DIRECTION ( 'NONE',  ( 0.000000000000000000, 0.000000000000000000, -1.000000000000000000 ) ) ;
#22448 = CARTESIAN_POINT ( 'NONE',  ( -2.980474262337753366, -45.39381609957544583, 151.2351853170876552 ) ) ;
#22449 = CARTESIAN_POINT ( 'NONE',  ( -10.00000000000000000, 42.29166666666667140, -2.679491924311229845 ) ) ;
#22450 = CARTESIAN_POINT ( 'NONE',  ( 1.320432766682874540E-15, 103.9062500020483810, 7.188101187500000044 ) ) ;
#22451 = CARTESIAN_POINT ( 'NONE',  ( -27.99999999999996803, 209.1875000013656063, 173.4587341250003760 ) ) ;
#22452 = CARTESIAN_POINT ( 'NONE',  ( 2.765530957082001251, 287.7656250017069510, 6.676582343749999815 ) ) ;
#22454 = CARTESIAN_POINT ( 'NONE',  ( -6.785933778205718525, -4.286164213032431114, -0.000000000000000000 ) ) ;
#22453 = CARTESIAN_POINT ( 'NONE',  ( 0.000000000000000000, 300.0000000000000000, 0.000000000000000000 ) ) ;
#22455 = ORIENTED_EDGE ( 'NONE', *, *, #33476, .T. ) ;
#22456 = CARTESIAN_POINT ( 'NONE',  ( 9.832129032723420536, 240.9895833367473301, 5.676582343749996262 ) ) ;
#22457 = CARTESIAN_POINT ( 'NONE',  ( -2.977408999572647819, 7.188101187499991163, 24.08030278187175455 ) ) ;
#22458 = CARTESIAN_POINT ( 'NONE',  ( -10.00000000000000355, 9.583333326505364624, 2.679491924311223183 ) ) ;
#22459 = DIRECTION ( 'NONE',  ( 0.000000000000000000, 0.000000000000000000, 1.000000000000000000 ) ) ;
#22460 = DIRECTION ( 'NONE',  ( 0.000000000000000000, 0.000000000000000000, 1.000000000000000000 ) ) ;
#22461 = CARTESIAN_POINT ( 'NONE',  ( 1.432654583217662481, 197.3750000013656063, 194.5412658750000219 ) ) ;
#22462 = CARTESIAN_POINT ( 'NONE',  ( -10.00000000000000178, 167.5000000000000000, -1.224646799147353454E-15 ) ) ;
#22463 = CARTESIAN_POINT ( 'NONE',  ( 9.000000000000001776, -5.196152422706648899, -0.8038475772933779684 ) ) ;
#22464 = DIRECTION ( 'NONE',  ( 1.000000000000000000, 0.000000000000000000, 0.000000000000000000 ) ) ;
#22465 = CARTESIAN_POINT ( 'NONE',  ( 2.775557561562891351E-14, 271.9999999999999432, 139.0000000000000568 ) ) ;
#22466 = CARTESIAN_POINT ( 'NONE',  ( 11.35316468749999785, 125.8854166632526983, 3.042071309553174174 ) ) ;
#22467 = CARTESIAN_POINT ( 'NONE',  ( -28.47326357806616315, 194.4587341250000350, 166.5737975347167321 ) ) ;
#22468 = CARTESIAN_POINT ( 'NONE',  ( -5.656854249492379694, 5.062500000000000888, -5.656854249492380582 ) ) ;
#22471 = CARTESIAN_POINT ( 'NONE',  ( -2.849036369511732440E-14, 197.2500000000000000, 138.0000000000000568 ) ) ;
#22470 = CARTESIAN_POINT ( 'NONE',  ( 24.54126587499998990, 195.1875000013655779, 169.9999999999999432 ) ) ;
#22469 = CARTESIAN_POINT ( 'NONE',  ( 31.45873412499997812, 194.8750000013656063, 171.4326545832175839 ) ) ;
#22472 = ORIENTED_EDGE ( 'NONE', *, *, #65405, .F. ) ;
#22473 = EDGE_CURVE ( 'NONE', #64740, #27089, #16538, .T. ) ;
#22474 = CARTESIAN_POINT ( 'NONE',  ( -5.656854249492379694, 20.06250000000000355, -5.656854249492380582 ) ) ;
#22475 = CARTESIAN_POINT ( 'NONE',  ( 27.99999999999996447, 202.6250000027312126, 165.9999999999998863 ) ) ;
#22476 = CARTESIAN_POINT ( 'NONE',  ( -6.062687379811042554, -5.219768740853823807, 2.519839246067225784E-12 ) ) ;
#22477 = CARTESIAN_POINT ( 'NONE',  ( 28.00000000000001776, 195.1875000013655779, 166.5412658749999082 ) ) ;
#22478 = CARTESIAN_POINT ( 'NONE',  ( 6.951808397369818766E-16, 207.3437499965860411, -11.35316468750000141 ) ) ;
#22479 = CARTESIAN_POINT ( 'NONE',  ( -5.082755093536324154, 121.3437500020483952, 5.082755093536326818 ) ) ;
#22480 = CARTESIAN_POINT ( 'NONE',  ( -4.541265875000003227, 1.999999998634407250, 1.881053915767121110 ) ) ;
#22481 = CARTESIAN_POINT ( 'NONE',  ( -7.456155213548138150, 61.82225697226427030, -23.87472085067443572 ) ) ;
#22482 = CARTESIAN_POINT ( 'NONE',  ( 5.656854249492374365, 5.656854249492375253, 18.26780277982336642 ) ) ;
#22484 = CARTESIAN_POINT ( 'NONE',  ( 0.000000000000000000, 300.0000000000000000, 10.00000000000000178 ) ) ;
#22483 = CARTESIAN_POINT ( 'NONE',  ( 16.00000000000000711, -16.00000000000000000, 20.00000000000000000 ) ) ;
#22485 = CARTESIAN_POINT ( 'NONE',  ( 9.832129032723420536, 96.19791666325269830, -5.676582343749999815 ) ) ;
#22486 = VERTEX_POINT ( 'NONE', #41320 ) ;
#22487 =( BOUNDED_CURVE ( )  B_SPLINE_CURVE ( 2, ( #20536, #3959, #21658, #20915, #9232, #43550, #4327, #66564, #32254, #55272, #66945, #27316, #4700 ),
 .UNSPECIFIED., .F., .F. ) 
 B_SPLINE_CURVE_WITH_KNOTS ( ( 3, 2, 2, 2, 2, 2, 3 ),
 ( 1.240293540008449158, 1.245526234162428691, 1.250758928316408003, 1.255991622470387314, 1.261224316624366848, 1.266457010778346159, 1.271689704932325693 ),
 .UNSPECIFIED. ) 
 CURVE ( )  GEOMETRIC_REPRESENTATION_ITEM ( )  RATIONAL_B_SPLINE_CURVE ( ( 0.9999999999999257261, 0.9659258262891424751, 0.9999999999999998890, 0.9659258262890683122, 0.9999999999999998890, 0.9659258262890683122, 0.9999999999999998890, 0.9659258262890683122, 0.9999999999999998890, 0.9659258262890683122, 0.9999999999999998890, 0.9659258262890683122, 0.9999999999999998890 ) ) 
 REPRESENTATION_ITEM ( '' )  );
#22488 = CARTESIAN_POINT ( 'NONE',  ( 2.449293598294707893E-16, 18.99999999726881228, -4.000000000000001776 ) ) ;
#22489 = CARTESIAN_POINT ( 'NONE',  ( 4.401442555609581635E-16, 26.34374999795161543, -7.188101187500000044 ) ) ;
#22490 = CARTESIAN_POINT ( 'NONE',  ( -38.00000000000000000, 53.00000000000000711, 9.999999999999991118 ) ) ;
#22491 = CARTESIAN_POINT ( 'NONE',  ( 8.311093377946839666, 256.0937500034140157, 8.311093377946830785 ) ) ;
#22492 = CARTESIAN_POINT ( 'NONE',  ( 3.042071309553167069, 106.8229166632526699, -11.35316468749999785 ) ) ;
#22493 = ORIENTED_EDGE ( 'NONE', *, *, #21736, .F. ) ;
#22494 = DIRECTION ( 'NONE',  ( 0.000000000000000000, 0.000000000000000000, -1.000000000000000000 ) ) ;
#22495 = CARTESIAN_POINT ( 'NONE',  ( 7.204075437095968759, -7.204075437095966983, 110.2187500020483810 ) ) ;
#22496 = CARTESIAN_POINT ( 'NONE',  ( 10.00000000000000000, 216.6666666598387110, 2.679491924311236062 ) ) ;
#22497 = CARTESIAN_POINT ( 'NONE',  ( -3.458734124999960358, 203.6250000013656063, 196.5673454167823877 ) ) ;
#22498 = CARTESIAN_POINT ( 'NONE',  ( 18.00000000000000000, -6.103439543526004485, -0.5706341627281751316 ) ) ;
#22500 = CARTESIAN_POINT ( 'NONE',  ( -3.042071309553173730, 99.32291666325271251, 11.35316468749999785 ) ) ;
#22499 = CARTESIAN_POINT ( 'NONE',  ( 2.020667218593132706E-15, -11.00000000000000000, 97.37499999999998579 ) ) ;
#22501 = CARTESIAN_POINT ( 'NONE',  ( -7.999999999999991118, 3.313708498984756723, 12.92405278392014800 ) ) ;
#22502 = CARTESIAN_POINT ( 'NONE',  ( -26.56734541678232375, 200.2500000013656631, 173.4587341250003760 ) ) ;
#22503 = EDGE_CURVE ( 'NONE', #23374, #33509, #69383, .T. ) ;
#22504 = CARTESIAN_POINT ( 'NONE',  ( 4.999999999999993783, 169.1666666666666856, 8.660254037844390851 ) ) ;
#22505 = ORIENTED_EDGE ( 'NONE', *, *, #52267, .T. ) ;
#22506 = CARTESIAN_POINT ( 'NONE',  ( 10.00000000000000178, 187.0833333265053398, -2.679491924311226736 ) ) ;
#22507 = CARTESIAN_POINT ( 'NONE',  ( 5.000000000000000000, -16.14408868864072844, -27.96238185062390613 ) ) ;
#22508 = CARTESIAN_POINT ( 'NONE',  ( 27.99999999999999645, 210.0000000000000284, 169.9999999999999147 ) ) ;
#22509 = CARTESIAN_POINT ( 'NONE',  ( 8.311093377946834337, 85.46874999658599847, 8.311093377946839666 ) ) ;
#22510 = CARTESIAN_POINT ( 'NONE',  ( 4.721056650415999201, 288.0781250017069510, -4.721056650415999201 ) ) ;
#22511 = CARTESIAN_POINT ( 'NONE',  ( 5.082755093536324154, 5.156249997951610098, 5.082755093536326818 ) ) ;
#22513 = EDGE_CURVE ( 'NONE', #62806, #23203, #68309, .T. ) ;
#22512 = CARTESIAN_POINT ( 'NONE',  ( 10.18810118750000093, -4.220049686691933033, 98.68750000204838102 ) ) ;
#22514 = CARTESIAN_POINT ( 'NONE',  ( -11.35316468750000141, 218.2812499965860411, -1.390361679473963753E-15 ) ) ;
#22516 = ORIENTED_EDGE ( 'NONE', *, *, #21911, .F. ) ;
#22515 =( BOUNDED_CURVE ( )  B_SPLINE_CURVE ( 2, ( #40495, #45778, #52196, #23506, #897, #46522, #63501, #68054, #35224, #69541, #5800, #11823, #11455 ),
 .UNSPECIFIED., .F., .F. ) 
 B_SPLINE_CURVE_WITH_KNOTS ( ( 3, 2, 2, 2, 2, 2, 3 ),
 ( 0.3641304347826087029, 0.3659420289855072617, 0.3677536231884058204, 0.3695652173913043237, 0.3713768115942028825, 0.3731884057971014412, 0.3750000000000000000 ),
 .UNSPECIFIED. ) 
 CURVE ( )  GEOMETRIC_REPRESENTATION_ITEM ( )  RATIONAL_B_SPLINE_CURVE ( ( 1.000000000000000000, 0.9659258262890683122, 1.000000000000000000, 0.9659258262890683122, 1.000000000000000000, 0.9659258262890683122, 1.000000000000000000, 0.9659258262890683122, 1.000000000000000000, 0.9659258262890683122, 1.000000000000000000, 0.9659258262890683122, 1.000000000000000000 ) ) 
 REPRESENTATION_ITEM ( '' )  );
#22517 = CARTESIAN_POINT ( 'NONE',  ( -8.660254037844387298, 68.95833332650536818, -5.000000000000004441 ) ) ;
#22518 = CARTESIAN_POINT ( 'NONE',  ( -5.656854249492381470, 2.249999995903220196, 5.656854249492379694 ) ) ;
#22519 = CARTESIAN_POINT ( 'NONE',  ( -0.8761883848702631816, -16.44150283900215825, 68.58316157020809101 ) ) ;
#22520 = CARTESIAN_POINT ( 'NONE',  ( 8.311093377946834337, 225.1562499965860411, 8.311093377946839666 ) ) ;
#22521 = CARTESIAN_POINT ( 'NONE',  ( -10.00000000000000000, 228.1250000068279746, 0.000000000000000000 ) ) ;
#22522 = FACE_OUTER_BOUND ( 'NONE', #26573, .T. ) ;
#22523 = CARTESIAN_POINT ( 'NONE',  ( 4.721056650416000089, 295.8281250017069510, 4.721056650415999201 ) ) ;
#22524 = ORIENTED_EDGE ( 'NONE', *, *, #19333, .F. ) ;
#22525 = CARTESIAN_POINT ( 'NONE',  ( 11.35316468750000141, 196.0937499965860127, 0.000000000000000000 ) ) ;
#22526 = CARTESIAN_POINT ( 'NONE',  ( -6.238412754330611322E-16, 10.18810118749999916, 95.78125000204836681 ) ) ;
#22527 = CARTESIAN_POINT ( 'NONE',  ( -31.45873412499999944, 205.6875000013656063, 170.0000000000003979 ) ) ;
#22528 = CARTESIAN_POINT ( 'NONE',  ( -8.000000000000000000, 17.25000000000000000, -9.797174393178825657E-16 ) ) ;
#22529 = AXIS2_PLACEMENT_3D ( 'NONE', #9139, #32156, #15160 ) ;
#22530 = VERTEX_POINT ( 'NONE', #53749 ) ;
#22531 = VECTOR ( 'NONE', #23103, 1000.000000000000000 ) ;
#22532 = PRODUCT_DEFINITION_FORMATION_WITH_SPECIFIED_SOURCE ( 'ANY', '', #15569, .NOT_KNOWN. ) ;
#22533 = CARTESIAN_POINT ( 'NONE',  ( 3.313708498984765161, 89.65625000409679046, 7.999999999999998224 ) ) ;
#22534 = CARTESIAN_POINT ( 'NONE',  ( -9.000000000000017764, -15.58845726811988719, 0.000000000000000000 ) ) ;
#22535 = CARTESIAN_POINT ( 'NONE',  ( 5.000000000000001776, 20.83333333333333570, -8.660254037844389075 ) ) ;
#22536 = CARTESIAN_POINT ( 'NONE',  ( -5.656854249492381470, 8.437500000000000000, 5.656854249492379694 ) ) ;
#22537 = CARTESIAN_POINT ( 'NONE',  ( -6.238412754330611322E-16, 10.18810118749999916, 82.65625000204838102 ) ) ;
#22538 = ORIENTED_EDGE ( 'NONE', *, *, #6616, .F. ) ;
#22539 = CARTESIAN_POINT ( 'NONE',  ( 4.000000000000001776, 19.00000000000000000, 0.000000000000000000 ) ) ;
#22540 = B_SPLINE_CURVE_WITH_KNOTS ( 'NONE', 3,
 ( #37724, #44127, #43359, #72796, #27136, #38097 ),
 .UNSPECIFIED., .F., .F.,
 ( 4, 2, 4 ),
 ( 2.380729645507424821E-07, 0.003505341553885866785, 0.007010445034807182875 ),
 .UNSPECIFIED. ) ;
#22541 = CARTESIAN_POINT ( 'NONE',  ( 5.656854249492379694, 113.9375000000000000, -5.656854249492380582 ) ) ;
#22542 = CARTESIAN_POINT ( 'NONE',  ( 31.57880696627679029, 194.6197631453349572, 169.4120265342146752 ) ) ;
#22543 = CARTESIAN_POINT ( 'NONE',  ( 1.102182119232618108E-15, 291.2500000000000000, 6.000000000000001776 ) ) ;
#22544 = CARTESIAN_POINT ( 'NONE',  ( 2.977408999572654480, 123.5000000020483952, 7.188101187499999156 ) ) ;
#22545 = CARTESIAN_POINT ( 'NONE',  ( 4.999999999999999112, -65.00666015986186608, 24.03732210400530178 ) ) ;
#22548 = FACE_OUTER_BOUND ( 'NONE', #19135, .T. ) ;
#22547 = CARTESIAN_POINT ( 'NONE',  ( 3.042071309553163516, 247.4479166700806445, -11.35316468749999785 ) ) ;
#22546 = CARTESIAN_POINT ( 'NONE',  ( 24.54126587499999701, 209.1875000013656063, 169.9999999999999432 ) ) ;
#22549 = SHAPE_DEFINITION_REPRESENTATION ( #56584, #48857 ) ;
#22550 = ORIENTED_EDGE ( 'NONE', *, *, #28852, .T. ) ;
#22551 = VECTOR ( 'NONE', #12798, 1000.000000000000000 ) ;
#22552 = CARTESIAN_POINT ( 'NONE',  ( 9.832129032723420536, 251.3020833367473017, 5.676582343749996262 ) ) ;
#22553 = CARTESIAN_POINT ( 'NONE',  ( -4.401442555609577197E-16, 7.188101187499992051, 10.11155278187175455 ) ) ;
#22554 = ORIENTED_EDGE ( 'NONE', *, *, #27003, .T. ) ;
#22555 = ADVANCED_FACE ( 'NONE', ( #24686 ), #41686, .T. ) ;
#22556 = VERTEX_POINT ( 'NONE', #1344 ) ;
#22557 = CARTESIAN_POINT ( 'NONE',  ( 7.204075437095966983, 7.204075437095967871, 76.09375000204838102 ) ) ;
#22558 = CARTESIAN_POINT ( 'NONE',  ( -9.832129032723420536, 94.01041666325268409, 5.676582343749997150 ) ) ;
#22559 = DIRECTION ( 'NONE',  ( -0.8660254037844374864, 0.5000000000000018874, 0.000000000000000000 ) ) ;
#22560 = CARTESIAN_POINT ( 'NONE',  ( -7.778174593052023411, 7.778174593052023411, 80.31249999999998579 ) ) ;
#22563 = CARTESIAN_POINT ( 'NONE',  ( -6.676582343749999815, 290.6718750017070079, 2.765530957082001251 ) ) ;
#22562 = CARTESIAN_POINT ( 'NONE',  ( 30.44569435410879876, 206.8125000013656063, 167.5543056458910485 ) ) ;
#22561 = CARTESIAN_POINT ( 'NONE',  ( 30.44569435410879166, 205.8125000013656063, 172.4456943541087526 ) ) ;
#22564 = CARTESIAN_POINT ( 'NONE',  ( -59.41372232231626782, 217.2107491953770193, 46.73504222628263705 ) ) ;
#22565 = FACE_OUTER_BOUND ( 'NONE', #3705, .T. ) ;
#22566 = CARTESIAN_POINT ( 'NONE',  ( -11.35316468749999785, 198.0729166632526983, -3.042071309553167513 ) ) ;
#22567 = EDGE_CURVE ( 'NONE', #12039, #61682, #39697, .T. ) ;
#22568 = CARTESIAN_POINT ( 'NONE',  ( 5.656854249492378806, 11.62499999590322197, 5.656854249492381470 ) ) ;
#22569 = ADVANCED_FACE ( 'NONE', ( #48070 ), #29768, .T. ) ;
#22570 = ORIENTED_EDGE ( 'NONE', *, *, #37058, .F. ) ;
#22571 = CARTESIAN_POINT ( 'NONE',  ( 24.54126587499999701, 208.4375000013656063, 169.9999999999998863 ) ) ;
#22572 = CARTESIAN_POINT ( 'NONE',  ( 7.188101187500001821, 15.93749999795161543, -2.977408999572650483 ) ) ;
#22573 = CARTESIAN_POINT ( 'NONE',  ( 8.311093377946834337, 170.4687499965860127, 8.311093377946839666 ) ) ;
#22574 = CARTESIAN_POINT ( 'NONE',  ( 4.898587196589412829E-16, 7.875000000000001776, -8.000000000000000000 ) ) ;
#22575 = CARTESIAN_POINT ( 'NONE',  ( -2.977408999572652260, 106.8125000020483952, 7.188101187500000044 ) ) ;
#22577 = CARTESIAN_POINT ( 'NONE',  ( -10.00000000000000000, 235.0000000000000284, 0.000000000000000000 ) ) ;
#22576 = CARTESIAN_POINT ( 'NONE',  ( 4.000000000000000888, 17.68749999726881583, 1.656854249492384135 ) ) ;
#22578 = CARTESIAN_POINT ( 'NONE',  ( 31.45873412500001010, 205.0000000013655779, 168.5673454167822740 ) ) ;
#22579 = CARTESIAN_POINT ( 'NONE',  ( 1.320432766682872962E-15, -7.188101187499992051, 11.23655278187175455 ) ) ;
#22580 = CARTESIAN_POINT ( 'NONE',  ( -3.042071309553164404, 52.23958332991934128, -11.35316468749999963 ) ) ;
#22581 = CARTESIAN_POINT ( 'NONE',  ( -0.7902249196973902823, -42.07972071773131972, 139.0079724672118857 ) ) ;
#22582 = CARTESIAN_POINT ( 'NONE',  ( 3.313708498984756279, 7.999999999999991118, 1.917802784329821320 ) ) ;
#22583 = ORIENTED_EDGE ( 'NONE', *, *, #39625, .T. ) ;
#22584 = VECTOR ( 'NONE', #36698, 1000.000000000000000 ) ;
#22585 = DIRECTION ( 'NONE',  ( -0.000000000000000000, 1.000000000000000000, -0.000000000000000000 ) ) ;
#22586 = DIRECTION ( 'NONE',  ( 1.000000000000000000, 0.000000000000000000, 0.000000000000000000 ) ) ;
#22587 = CARTESIAN_POINT ( 'NONE',  ( -3.042071309553164404, 67.23958332991935549, -11.35316468749999963 ) ) ;
#22588 = CARTESIAN_POINT ( 'NONE',  ( 11.00000000000000000, 1.347111479062088405E-15, 76.93750000409677625 ) ) ;
#22589 = CARTESIAN_POINT ( 'NONE',  ( 3.458734124999960358, 199.6250000013656063, 143.4326545832176976 ) ) ;
#22590 = CARTESIAN_POINT ( 'NONE',  ( 5.086519500888148748, 10.26068667857073358, 64.41585657734925974 ) ) ;
#22591 = CARTESIAN_POINT ( 'NONE',  ( -2.679491924311272477, 11.45833333333333925, -9.999999999999976907 ) ) ;
#22593 = CARTESIAN_POINT ( 'NONE',  ( -3.042071309553173730, 64.32291666325269830, 11.35316468749999785 ) ) ;
#22592 = CARTESIAN_POINT ( 'NONE',  ( 5.082755093536326818, 96.21875000204838102, 5.082755093536325042 ) ) ;
#22594 = CARTESIAN_POINT ( 'NONE',  ( 7.999999999999991118, 9.797174393178815797E-16, 3.080302779823361981 ) ) ;
#22595 = CARTESIAN_POINT ( 'NONE',  ( 0.000000000000000000, 116.0729912458811839, 42.10166426739785095 ) ) ;
#22596 = CARTESIAN_POINT ( 'NONE',  ( 5.676582343749993598, 169.9479166632526983, 9.832129032723422313 ) ) ;
#22597 = CARTESIAN_POINT ( 'NONE',  ( 6.123233995736767268E-16, 143.1249999931720538, -10.00000000000000178 ) ) ;
#22598 = CARTESIAN_POINT ( 'NONE',  ( -5.082755093536324154, 94.71875000204838102, 5.082755093536326818 ) ) ;
#22599 = CARTESIAN_POINT ( 'NONE',  ( -0.7779459922035416586, -47.90409571976934444, 139.0091576938756361 ) ) ;
#22600 = CARTESIAN_POINT ( 'NONE',  ( -3.042071309553163960, 32.55208332991934128, -11.35316468749999963 ) ) ;
#22601 = CARTESIAN_POINT ( 'NONE',  ( 1.871523826299183495E-15, -10.18810118749999916, 116.4062500020483810 ) ) ;
#22602 = CARTESIAN_POINT ( 'NONE',  ( 3.042071309553159519, 179.7395833299193555, 11.35316468750000141 ) ) ;
#22603 = ORIENTED_EDGE ( 'NONE', *, *, #36731, .F. ) ;
#22604 = DIRECTION ( 'NONE',  ( 0.000000000000000000, 0.000000000000000000, -1.000000000000000000 ) ) ;
#22605 = CARTESIAN_POINT ( 'NONE',  ( -7.204075437095967871, 7.204075437095967871, 71.96875000204836681 ) ) ;
#22606 = CARTESIAN_POINT ( 'NONE',  ( -2.828427124746152987, 198.1250000000000284, 200.8284271247462129 ) ) ;
#22607 = CARTESIAN_POINT ( 'NONE',  ( 32.38595303115080526, 42.28758863251563582, 65.00000000000002842 ) ) ;
#22609 = CARTESIAN_POINT ( 'NONE',  ( -3.042071309553163960, 162.2395833299192986, -11.35316468749999963 ) ) ;
#22608 = CARTESIAN_POINT ( 'NONE',  ( 2.751549872419338751E-14, 194.9207531772044888, 194.0792468227953975 ) ) ;
#22610 = CARTESIAN_POINT ( 'NONE',  ( 7.999999999999991118, 3.313708498984757611, 6.230302784329825982 ) ) ;
#22611 = DIRECTION ( 'NONE',  ( 0.000000000000000000, 0.000000000000000000, 1.000000000000000000 ) ) ;
#22612 = CARTESIAN_POINT ( 'NONE',  ( -5.676582343749992710, 219.7395833367473301, 9.832129032723422313 ) ) ;
#22613 = CARTESIAN_POINT ( 'NONE',  ( 0.000000000000000000, 300.0000000000000000, 0.000000000000000000 ) ) ;
#22614 = EDGE_CURVE ( 'NONE', #17271, #46951, #10483, .T. ) ;
#22615 = VERTEX_POINT ( 'NONE', #36397 ) ;
#22616 =( BOUNDED_CURVE ( )  B_SPLINE_CURVE ( 2, ( #24696, #10338, #62013, #26175, #20898, #9967, #44295, #38646, #14482 ),
 .UNSPECIFIED., .F., .F. ) 
 B_SPLINE_CURVE_WITH_KNOTS ( ( 3, 2, 2, 2, 3 ),
 ( 0.04999999999999991951, 0.05833333333333332038, 0.06666666666666672125, 0.07500000000000012212, 0.08333333333333352300 ),
 .UNSPECIFIED. ) 
 CURVE ( )  GEOMETRIC_REPRESENTATION_ITEM ( )  RATIONAL_B_SPLINE_CURVE ( ( 1.000000000000000666, 0.9238795325112859613, 1.000000000000000000, 0.9238795325112867385, 1.000000000000000000, 0.9238795325112867385, 1.000000000000000000, 0.9238795325112849621, 1.000000000000001776 ) ) 
 REPRESENTATION_ITEM ( '' )  );
#22617 = AXIS2_PLACEMENT_3D ( 'NONE', #61187, #71740, #20055 ) ;
#22618 = CARTESIAN_POINT ( 'NONE',  ( -4.401442555609577197E-16, 7.188101187499992051, 26.61155278187175455 ) ) ;
#22619 = CARTESIAN_POINT ( 'NONE',  ( 9.832129032723420536, 121.5104166632526841, -5.676582343749999815 ) ) ;
#22620 = CARTESIAN_POINT ( 'NONE',  ( 0.4499999999999975131, 255.9999999999997726, 5.815339556497987061 ) ) ;
#22621 = VERTEX_POINT ( 'NONE', #64328 ) ;
#22622 = CARTESIAN_POINT ( 'NONE',  ( 2.780723358947928197E-16, 6.687499998634407028, -4.541265875000002339 ) ) ;
#22623 = CARTESIAN_POINT ( 'NONE',  ( -7.188101187500002709, 16.31249999795161543, 2.977408999572649151 ) ) ;
#22624 = CARTESIAN_POINT ( 'NONE',  ( -4.898587196589412829E-16, 108.3125000040967905, -8.000000000000000000 ) ) ;
#22625 = CARTESIAN_POINT ( 'NONE',  ( -24.54126587499999701, 197.5000000013656063, 168.5673454167827003 ) ) ;
#22626 = CARTESIAN_POINT ( 'NONE',  ( -7.347880794884122694E-16, 6.750000000000000000, 4.000000000000001776 ) ) ;
#22627 = CARTESIAN_POINT ( 'NONE',  ( 105.0000000000000000, 50.00000000000000711, 69.99999999999998579 ) ) ;
#22628 = CARTESIAN_POINT ( 'NONE',  ( -3.211159895383562723, 7.937499998634407028, 3.211159895383561391 ) ) ;
#22629 = CARTESIAN_POINT ( 'NONE',  ( -1.656854249492403008, 196.6875000000000000, 146.0000000000000284 ) ) ;
#22630 = ORIENTED_EDGE ( 'NONE', *, *, #10373, .F. ) ;
#22631 = CARTESIAN_POINT ( 'NONE',  ( 4.531193156845207581E-15, 207.0000000000000568, 133.0000000000000284 ) ) ;
#22632 = CARTESIAN_POINT ( 'NONE',  ( -7.188101187499999156, 106.2500000020484094, 2.977408999572654924 ) ) ;
#22633 = AXIS2_PLACEMENT_3D ( 'NONE', #22507, #68546, #62877 ) ;
#22635 = CARTESIAN_POINT ( 'NONE',  ( -4.898587196589412829E-16, 97.81250000409677625, -8.000000000000000000 ) ) ;
#22634 = CARTESIAN_POINT ( 'NONE',  ( -7.778174593052023411, 7.778174593052023411, 79.00000000409676204 ) ) ;
#22636 = DIRECTION ( 'NONE',  ( 0.000000000000000000, -1.000000000000000000, 0.000000000000000000 ) ) ;
#22637 = EDGE_CURVE ( 'NONE', #49221, #55885, #73281, .T. ) ;
#22638 = CARTESIAN_POINT ( 'NONE',  ( 2.977408999572650927, -7.188101187499990274, 1.955302781871753881 ) ) ;
#22639 = ORIENTED_EDGE ( 'NONE', *, *, #58814, .T. ) ;
#22640 = ORIENTED_EDGE ( 'NONE', *, *, #27010, .F. ) ;
#22641 = CARTESIAN_POINT ( 'NONE',  ( -10.18810118749999738, -4.220049686691941915, 94.75000000204838102 ) ) ;
#22642 = CARTESIAN_POINT ( 'NONE',  ( 8.000000000000000000, 91.53125000409679046, -3.313708498984762496 ) ) ;
#22643 = CARTESIAN_POINT ( 'NONE',  ( -28.00000000000001776, 194.6875000013655779, 166.5412658750003629 ) ) ;
#22644 = CARTESIAN_POINT ( 'NONE',  ( 4.556349186104051263, -10.99999999999999822, 100.4687500000000000 ) ) ;
#22645 = CARTESIAN_POINT ( 'NONE',  ( -2.445694354108784108, 204.5625000013656063, 195.5543056458912190 ) ) ;
#22647 = CARTESIAN_POINT ( 'NONE',  ( 11.00000000000003908, 4.556349186104006854, 113.0312500040967905 ) ) ;
#22646 = CARTESIAN_POINT ( 'NONE',  ( 0.000000000000000000, 0.000000000000000000, 0.000000000000000000 ) ) ;
#22648 = CARTESIAN_POINT ( 'NONE',  ( -10.00000000000000355, 122.7083333333333144, 2.679491924311223183 ) ) ;
#22649 = B_SPLINE_CURVE_WITH_KNOTS ( 'NONE', 3,
 ( #38149, #20402, #73223, #21529, #67564, #61529, #26053, #62919, #37781, #72474, #20782, #32116, #49075, #26819, #2696, #11245, #55510, #61152 ),
 .UNSPECIFIED., .F., .F.,
 ( 4, 2, 2, 2, 2, 2, 2, 2, 4 ),
 ( 0.004698154390242427307, 0.005285142545816686604, 0.005872130701390945035, 0.006459118856965203465, 0.007046107012539462762, 0.007633095168113722059, 0.008220083323687982224, 0.008807071479262240654, 0.009394059634836499084 ),
 .UNSPECIFIED. ) ;
#22650 = CARTESIAN_POINT ( 'NONE',  ( 3.313708498984760720, 105.0312500000000000, -8.000000000000000000 ) ) ;
#22651 = VECTOR ( 'NONE', #10017, 1000.000000000000000 ) ;
#22652 = CARTESIAN_POINT ( 'NONE',  ( -7.188101187499990274, -2.977408999572651371, 4.955302781871753659 ) ) ;
#22653 = CIRCLE ( 'NONE', #20223, 6.000000000000000000 ) ;
#22654 = CARTESIAN_POINT ( 'NONE',  ( 4.000000000000016875, 200.4375000000000568, 199.6568542494924259 ) ) ;
#22655 = CARTESIAN_POINT ( 'NONE',  ( 31.45873412499999944, 205.6875000013656063, 169.9999999999999432 ) ) ;
#22656 = CARTESIAN_POINT ( 'NONE',  ( 5.656854249492378806, 28.12499999590322375, 5.656854249492381470 ) ) ;
#22657 = CARTESIAN_POINT ( 'NONE',  ( 3.458734124999959914, 201.4375000013656063, 142.0000000000000568 ) ) ;
#22658 = CARTESIAN_POINT ( 'NONE',  ( -7.188101187500000933, 119.9375000020483952, -2.977408999572650483 ) ) ;
#22660 = CARTESIAN_POINT ( 'NONE',  ( 3.761416977589076449, 194.7718537773878893, 197.6264434403084636 ) ) ;
#22659 = CARTESIAN_POINT ( 'NONE',  ( 0.000000000000000000, 220.0000000000000284, 0.000000000000000000 ) ) ;
#22661 = CARTESIAN_POINT ( 'NONE',  ( 8.311093377946839666, 241.0937500034139873, 8.311093377946829008 ) ) ;
#22662 = CARTESIAN_POINT ( 'NONE',  ( 5.082755093536318824, 5.082755093536319713, 26.79905278187175455 ) ) ;
#22663 = CARTESIAN_POINT ( 'NONE',  ( 30.82842712474620228, 199.3750000000000284, 167.1715728752537586 ) ) ;
#22664 = CARTESIAN_POINT ( 'NONE',  ( -8.311093377946841443, 13.90624999658601801, 8.311093377946830785 ) ) ;
#22665 = FACE_OUTER_BOUND ( 'NONE', #55847, .T. ) ;
#22666 = CARTESIAN_POINT ( 'NONE',  ( -11.35316468750000141, 203.8020833299193839, 3.042071309553159963 ) ) ;
#22667 = CARTESIAN_POINT ( 'NONE',  ( -30.82842712474615610, 195.3750000000000284, 172.8284271247465824 ) ) ;
#22668 = DIRECTION ( 'NONE',  ( -0.000000000000000000, 1.000000000000000000, -0.000000000000000000 ) ) ;
#22670 = CARTESIAN_POINT ( 'NONE',  ( 2.828427124746190291, 11.62499999726881406, 2.828427124746192067 ) ) ;
#22669 = CARTESIAN_POINT ( 'NONE',  ( 4.898587196589412829E-16, 25.68749999590322375, -8.000000000000000000 ) ) ;
#22671 = ORIENTED_EDGE ( 'NONE', *, *, #69959, .F. ) ;
#22673 = EDGE_CURVE ( 'NONE', #20547, #6191, #42042, .T. ) ;
#22672 = CARTESIAN_POINT ( 'NONE',  ( -3.458734125000015425, 202.2500000013656063, 143.4326545832176976 ) ) ;
#22674 = EDGE_CURVE ( 'NONE', #6157, #9404, #58317, .T. ) ;
#22675 = CARTESIAN_POINT ( 'NONE',  ( -8.311093377946841443, 23.90624999658601979, 8.311093377946830785 ) ) ;
#22676 = CARTESIAN_POINT ( 'NONE',  ( -11.00000000000000000, 0.000000000000000000, 89.68750000409677625 ) ) ;
#22677 = CARTESIAN_POINT ( 'NONE',  ( 4.999999999999997335, 228.3333333333333428, -8.660254037844387298 ) ) ;
#22678 = CARTESIAN_POINT ( 'NONE',  ( -25.55430564589122966, 198.3125000013656063, 167.5543056458915032 ) ) ;
#22679 = CARTESIAN_POINT ( 'NONE',  ( -9.000000000000001776, 0.8785859941773058734, -1.113001292692150251E-15 ) ) ;
#22681 = CARTESIAN_POINT ( 'NONE',  ( 11.35316468749999963, 0.9895833299193492749, -3.042071309553165293 ) ) ;
#22680 = CARTESIAN_POINT ( 'NONE',  ( 1.320432766682874540E-15, 111.0312500020483810, 7.188101187500000044 ) ) ;
#22682 = CARTESIAN_POINT ( 'NONE',  ( 3.313708498984756279, 7.999999999999991118, 18.36155277982337353 ) ) ;
#22683 = CARTESIAN_POINT ( 'NONE',  ( 8.311093377946837890, 136.4062499965859558, -8.311093377946837890 ) ) ;
#22684 = EDGE_CURVE ( 'NONE', #22486, #28203, #29628, .T. ) ;
#22685 = CARTESIAN_POINT ( 'NONE',  ( 5.000000000000001776, 97.70833332650536818, -8.660254037844389075 ) ) ;
#22686 = CARTESIAN_POINT ( 'NONE',  ( -7.188101187500000044, 118.5312500020483810, 0.000000000000000000 ) ) ;
#22687 = CARTESIAN_POINT ( 'NONE',  ( 4.231687259402619361, 68.27410168872769702, -20.58597903916443173 ) ) ;
#22688 = CARTESIAN_POINT ( 'NONE',  ( -30.44569435410883784, 208.8125000013656063, 167.5543056458915885 ) ) ;
#22689 = CARTESIAN_POINT ( 'NONE',  ( -5.000000000000000000, -53.31073972600171373, -44.28411094576001261 ) ) ;
#22690 = ORIENTED_EDGE ( 'NONE', *, *, #81, .F. ) ;
#22691 = CARTESIAN_POINT ( 'NONE',  ( 5.107860025160634088, -60.88642786446147426, 23.30380398316933110 ) ) ;
#22692 = CYLINDRICAL_SURFACE ( 'NONE', #45016, 10.00000000000000178 ) ;
#22693 = CARTESIAN_POINT ( 'NONE',  ( 6.676582343750001591, 295.9531250017069510, -8.176455196517173205E-16 ) ) ;
#22694 = CARTESIAN_POINT ( 'NONE',  ( -3.042071309553163960, 132.2395833299193555, -11.35316468749999963 ) ) ;
#22695 = SURFACE_SIDE_STYLE ('',( #11023 ) ) ;
#22696 = CARTESIAN_POINT ( 'NONE',  ( -3.313708498984758943, -7.999999999999989342, 23.66780278432982954 ) ) ;
#22697 = CARTESIAN_POINT ( 'NONE',  ( 1.736494649845414795, 67.70200331863051701, 20.12302832235323180 ) ) ;
#22698 = CARTESIAN_POINT ( 'NONE',  ( -8.311093377946834337, 259.5312500034139589, 8.311093377946837890 ) ) ;
#22699 = EDGE_CURVE ( 'NONE', #46484, #6848, #65049, .T. ) ;
#22700 = CARTESIAN_POINT ( 'NONE',  ( -10.18810118749999916, 0.000000000000000000, 95.03125000204836681 ) ) ;
#22701 = ORIENTED_EDGE ( 'NONE', *, *, #69117, .F. ) ;
#22702 = VECTOR ( 'NONE', #29391, 1000.000000000000000 ) ;
#22703 = CARTESIAN_POINT ( 'NONE',  ( 5.000000000000000888, 10.54112798502250214, 66.30787999718575065 ) ) ;
#22704 = FACE_OUTER_BOUND ( 'NONE', #27353, .T. ) ;
#22705 = CARTESIAN_POINT ( 'NONE',  ( -1.432654583217608080, 201.8750000013656063, 201.4587341250000350 ) ) ;
#22706 = CARTESIAN_POINT ( 'NONE',  ( 11.35316468749999963, 76.30208332991935549, -3.042071309553165293 ) ) ;
#22707 = ORIENTED_EDGE ( 'NONE', *, *, #47817, .T. ) ;
#22708 = CARTESIAN_POINT ( 'NONE',  ( 7.204075437095966983, 7.204075437095967871, 107.5937500020483810 ) ) ;
#22709 = CARTESIAN_POINT ( 'NONE',  ( -3.211159895383562723, 12.06249999863440614, 3.211159895383561391 ) ) ;
#22710 = VERTEX_POINT ( 'NONE', #3552 ) ;
#22711 = CARTESIAN_POINT ( 'NONE',  ( -3.313708498984760720, 0.4687499999999999445, -8.000000000000000000 ) ) ;
#22712 = CARTESIAN_POINT ( 'NONE',  ( 7.320508075688773708, 115.6249999999999858, -7.320508075688773708 ) ) ;
#22713 = CARTESIAN_POINT ( 'NONE',  ( 2.849036369511732440E-14, 200.2500000000000000, 202.0000000000000000 ) ) ;
#22714 = CARTESIAN_POINT ( 'NONE',  ( -7.188101187500001821, 23.99999999795161543, -2.977408999572651371 ) ) ;
#22715 = CARTESIAN_POINT ( 'NONE',  ( 3.999999999999960032, 199.9375000000000000, 143.6568542494924259 ) ) ;
#22716 = CIRCLE ( 'NONE', #7064, 11.00000000000000000 ) ;
#22717 = CARTESIAN_POINT ( 'NONE',  ( -4.220049686691937474, -10.18810118749999738, 102.8125000020483952 ) ) ;
#22718 =( BOUNDED_CURVE ( )  B_SPLINE_CURVE ( 2, ( #58634, #70677, #12592, #58276, #6578, #30688, #35991, #6942, #934, #52967, #7313, #1300, #71036, #13317, #2018, #25381, #19355, #65384, #59734, #23917, #25007, #42000, #2384, #24281, #42369, #41643, #13682, #46926, #69951, #71777, #38593, #9165, #20463, #20093, #73289, #8794, #61221, #54454, #2762, #49522, #49899, #14806, #25749, #9551, #43106, #48770, #54828, #21591, #44617, #37464, #8413, #43483, #31807, #66124, #44248, #61593, #55203, #31428, #15556, #72913, #3137, #21222, #14431, #32565, #55573, #60465, #26121, #20848, #37847, #49140, #9912, #3508, #15187, #27251, #72152, #43866, #66495, #60844, #72542, #32182, #14054, #4261, #26497, #66881, #38216, #3889, #26882, #50266, #67260, #32944, #55951, #37091, #60095, #40071, #10288, #62696, #16664, #63076, #22326, #11033, #57061, #50636, #45722, #5373, #33314, #56312, #106, #45353, #74396, #4631, #10655, #57437, #28375, #16291, #27627, #73654, #21962, #68367, #56691, #34065, #39695, #68736, #33688, #51383, #44989, #22705, #17049, #11401, #34436, #5742, #28743, #51759, #51014, #67995, #39331, #62328, #23084, #46095, #69113, #17420, #67631, #74023, #5008, #15927, #38957, #61960, #28006, #33183, #55807, #9401, #2994, #66359, #60705, #72394, #38452, #50131, #27117, #4125, #49000, #10144, #66738, #56179, #73147, #32038, #21454, #50498, #25975, #31666, #15043, #20707, #73511, #44107, #44477, #21819, #54686, #43724, #4492, #43340, #9025, #38078, #14663, #67491, #9780, #72010, #20325, #44851, #3741, #15789, #37704, #61076, #61454, #55058, #3367, #67857, #26355, #32799, #49376, #27484, #38824, #26740, #55432, #32421, #16149, #49761, #72778, #21084, #67117, #60323, #8651, #61826, #15411, #16738, #56385, #56761, #21294, #32642, #39400, #72988, #44318, #4332, #5081, #62766, #26955, #28074, #51087, #39032, #68434, #45062, #33384, #16363, #39764, #45421, #51455, #50337, #27322, #44689, #17121, #4705, #61670, #27699, #15628 ),
 .UNSPECIFIED., .F., .F. ) 
 B_SPLINE_CURVE_WITH_KNOTS ( ( 3, 2, 2, 2, 2, 2, 2, 2, 2, 2, 2, 2, 2, 2, 2, 2, 2, 2, 2, 2, 2, 2, 2, 2, 2, 2, 2, 2, 2, 2, 2, 2, 2, 2, 2, 2, 2, 2, 2, 2, 2, 2, 2, 2, 2, 2, 2, 2, 2, 2, 2, 2, 2, 2, 2, 2, 2, 2, 2, 2, 2, 2, 2, 2, 2, 2, 2, 2, 2, 2, 2, 2, 2, 2, 2, 2, 2, 2, 2, 2, 2, 2, 2, 2, 2, 2, 2, 2, 2, 2, 2, 2, 2, 2, 2, 2, 2, 2, 2, 2, 2, 2, 2, 2, 2, 2, 2, 2, 2, 2, 2, 2, 2, 2, 2, 2, 2, 2, 2, 2, 3 ),
 ( 0.000000000000000000, 0.008333333333333333218, 0.01666666666666666644, 0.02500000000000000139, 0.03333333333333333287, 0.04166666666666666435, 0.05000000000000000278, 0.05833333333333333426, 0.06666666666666666574, 0.07499999999999999722, 0.08333333333333332871, 0.09166666666666666019, 0.1000000000000000056, 0.1083333333333333370, 0.1166666666666666685, 0.1250000000000000000, 0.1333333333333333315, 0.1416666666666666630, 0.1499999999999999944, 0.1583333333333333259, 0.1666666666666666574, 0.1749999999999999889, 0.1833333333333333204, 0.1916666666666666796, 0.2000000000000000111, 0.2083333333333333426, 0.2166666666666666741, 0.2250000000000000056, 0.2333333333333333370, 0.2416666666666666685, 0.2500000000000000000, 0.2583333333333333592, 0.2666666666666666630, 0.2750000000000000222, 0.2833333333333333259, 0.2916666666666666852, 0.2999999999999999889, 0.3083333333333333481, 0.3166666666666666519, 0.3250000000000000111, 0.3333333333333333148, 0.3416666666666666741, 0.3499999999999999778, 0.3583333333333333370, 0.3666666666666666408, 0.3750000000000000000, 0.3833333333333333592, 0.3916666666666666630, 0.4000000000000000222, 0.4083333333333333259, 0.4166666666666666852, 0.4249999999999999889, 0.4333333333333333481, 0.4416666666666666519, 0.4500000000000000111, 0.4583333333333333148, 0.4666666666666666741, 0.4749999999999999778, 0.4833333333333333370, 0.4916666666666666408, 0.5000000000000000000, 0.5083333333333333037, 0.5166666666666667185, 0.5250000000000000222, 0.5333333333333333259, 0.5416666666666666297, 0.5500000000000000444, 0.5583333333333333481, 0.5666666666666666519, 0.5749999999999999556, 0.5833333333333333703, 0.5916666666666666741, 0.5999999999999999778, 0.6083333333333332815, 0.6166666666666666963, 0.6250000000000000000, 0.6333333333333333037, 0.6416666666666667185, 0.6500000000000000222, 0.6583333333333333259, 0.6666666666666666297, 0.6750000000000000444, 0.6833333333333333481, 0.6916666666666666519, 0.6999999999999999556, 0.7083333333333333703, 0.7166666666666666741, 0.7249999999999999778, 0.7333333333333332815, 0.7416666666666666963, 0.7500000000000000000, 0.7583333333333333037, 0.7666666666666667185, 0.7750000000000000222, 0.7833333333333333259, 0.7916666666666666297, 0.8000000000000000444, 0.8083333333333333481, 0.8166666666666666519, 0.8249999999999999556, 0.8333333333333333703, 0.8416666666666666741, 0.8499999999999999778, 0.8583333333333332815, 0.8666666666666666963, 0.8750000000000000000, 0.8833333333333333037, 0.8916666666666667185, 0.9000000000000000222, 0.9083333333333333259, 0.9166666666666666297, 0.9250000000000000444, 0.9333333333333333481, 0.9416666666666666519, 0.9499999999999999556, 0.9583333333333333703, 0.9666666666666666741, 0.9749999999999999778, 0.9833333333333332815, 0.9916666666666666963, 1.000000000000000000 ),
 .UNSPECIFIED. ) 
 CURVE ( )  GEOMETRIC_REPRESENTATION_ITEM ( )  RATIONAL_B_SPLINE_CURVE ( ( 1.000000000000000000, 0.9238795325112867385, 1.000000000000000000, 0.9238795325112867385, 1.000000000000000000, 0.9238795325112867385, 1.000000000000000000, 0.9238795325112867385, 1.000000000000000000, 0.9238795325112867385, 1.000000000000000000, 0.9238795325112867385, 1.000000000000000000, 0.9238795325112867385, 1.000000000000000000, 0.9238795325112867385, 1.000000000000000000, 0.9238795325112867385, 1.000000000000000000, 0.9238795325112867385, 1.000000000000000000, 0.9238795325112867385, 1.000000000000000000, 0.9238795325112867385, 1.000000000000000000, 0.9238795325112867385, 1.000000000000000000, 0.9238795325112867385, 1.000000000000000000, 0.9238795325112867385, 1.000000000000000000, 0.9238795325112867385, 1.000000000000000000, 0.9238795325112867385, 1.000000000000000000, 0.9238795325112867385, 1.000000000000000000, 0.9238795325112867385, 1.000000000000000000, 0.9238795325112867385, 1.000000000000000000, 0.9238795325112867385, 1.000000000000000000, 0.9238795325112867385, 1.000000000000000000, 0.9238795325112867385, 1.000000000000000000, 0.9238795325112867385, 1.000000000000000000, 0.9238795325112867385, 1.000000000000000000, 0.9238795325112867385, 1.000000000000000000, 0.9238795325112867385, 1.000000000000000000, 0.9238795325112867385, 1.000000000000000000, 0.9238795325112867385, 1.000000000000000000, 0.9238795325112867385, 1.000000000000000000, 0.9238795325112867385, 1.000000000000000000, 0.9238795325112867385, 1.000000000000000000, 0.9238795325112867385, 1.000000000000000000, 0.9238795325112867385, 1.000000000000000000, 0.9238795325112867385, 1.000000000000000000, 0.9238795325112867385, 1.000000000000000000, 0.9238795325112867385, 1.000000000000000000, 0.9238795325112867385, 1.000000000000000000, 0.9238795325112867385, 1.000000000000000000, 0.9238795325112867385, 1.000000000000000000, 0.9238795325112867385, 1.000000000000000000, 0.9238795325112867385, 1.000000000000000000, 0.9238795325112867385, 1.000000000000000000, 0.9238795325112867385, 1.000000000000000000, 0.9238795325112867385, 1.000000000000000000, 0.9238795325112867385, 1.000000000000000000, 0.9238795325112867385, 1.000000000000000000, 0.9238795325112867385, 1.000000000000000000, 0.9238795325112867385, 1.000000000000000000, 0.9238795325112867385, 1.000000000000000000, 0.9238795325112867385, 1.000000000000000000, 0.9238795325112867385, 1.000000000000000000, 0.9238795325112867385, 1.000000000000000000, 0.9238795325112867385, 1.000000000000000000, 0.9238795325112867385, 1.000000000000000000, 0.9238795325112867385, 1.000000000000000000, 0.9238795325112867385, 1.000000000000000000, 0.9238795325112867385, 1.000000000000000000, 0.9238795325112867385, 1.000000000000000000, 0.9238795325112867385, 1.000000000000000000, 0.9238795325112867385, 1.000000000000000000, 0.9238795325112867385, 1.000000000000000000, 0.9238795325112867385, 1.000000000000000000, 0.9238795325112867385, 1.000000000000000000, 0.9238795325112867385, 1.000000000000000000, 0.9238795325112867385, 1.000000000000000000, 0.9238795325112867385, 1.000000000000000000, 0.9238795325112867385, 1.000000000000000000, 0.9238795325112867385, 1.000000000000000000, 0.9238795325112867385, 1.000000000000000000, 0.9238795325112867385, 1.000000000000000000, 0.9238795325112867385, 1.000000000000000000, 0.9238795325112867385, 1.000000000000000000, 0.9238795325112867385, 1.000000000000000000, 0.9238795325112867385, 1.000000000000000000, 0.9238795325112867385, 1.000000000000000000, 0.9238795325112867385, 1.000000000000000000, 0.9238795325112867385, 1.000000000000000000, 0.9238795325112867385, 1.000000000000000000, 0.9238795325112867385, 1.000000000000000000, 0.9238795325112867385, 1.000000000000000000, 0.9238795325112867385, 1.000000000000000000, 0.9238795325112867385, 1.000000000000000000, 0.9238795325112867385, 1.000000000000000000, 0.9238795325112867385, 1.000000000000000000, 0.9238795325112867385, 1.000000000000000000, 0.9238795325112867385, 1.000000000000000000, 0.9238795325112867385, 1.000000000000000000, 0.9238795325112867385, 1.000000000000000000, 0.9238795325112867385, 1.000000000000000000, 0.9238795325112867385, 1.000000000000000000, 0.9238795325112867385, 1.000000000000000000, 0.9238795325112867385, 1.000000000000000000, 0.9238795325112867385, 1.000000000000000000, 0.9238795325112867385, 1.000000000000000000, 0.9238795325112867385, 1.000000000000000000, 0.9238795325112867385, 1.000000000000000000, 0.9238795325112867385, 1.000000000000000000, 0.9238795325112867385, 1.000000000000000000, 0.9238795325112867385, 1.000000000000000000, 0.9238795325112867385, 1.000000000000000000, 0.9238795325112867385, 1.000000000000000000, 0.9238795325112867385, 1.000000000000000000, 0.9238795325112867385, 1.000000000000000000, 0.9238795325112867385, 1.000000000000000000, 0.9238795325112867385, 1.000000000000000000, 0.9238795325112867385, 1.000000000000000000, 0.9238795325112867385, 1.000000000000000000, 0.9238795325112867385, 1.000000000000000000, 0.9238795325112867385, 1.000000000000000000, 0.9238795325112867385, 1.000000000000000000, 0.9238795325112867385, 1.000000000000000000, 0.9238795325112867385, 1.000000000000000000, 0.9238795325112867385, 1.000000000000000000, 0.9238795325112867385, 1.000000000000000000, 0.9238795325112867385, 1.000000000000000000, 0.9238795325112867385, 1.000000000000000000, 0.9238795325112867385, 1.000000000000000000, 0.9238795325112867385, 1.000000000000000000, 0.9238795325112867385, 1.000000000000000000 ) ) 
 REPRESENTATION_ITEM ( '' )  );
#22719 = CARTESIAN_POINT ( 'NONE',  ( 28.00000000000002132, 208.5000000000000284, 165.9999999999998863 ) ) ;
#22720 = CARTESIAN_POINT ( 'NONE',  ( 1.656854249492381248, 8.937499997268814056, -4.000000000000001776 ) ) ;
#22721 =( BOUNDED_CURVE ( )  B_SPLINE_CURVE ( 2, ( #19071, #43188, #65083, #24722, #65828, #13396, #7761, #14135, #48846 ),
 .UNSPECIFIED., .F., .T. ) 
 B_SPLINE_CURVE_WITH_KNOTS ( ( 3, 2, 2, 2, 3 ),
 ( 0.6166666666666672514, 0.6250000000000005551, 0.6333333333333337478, 0.6416666666666671626, 0.6500000000000004663 ),
 .UNSPECIFIED. ) 
 CURVE ( )  GEOMETRIC_REPRESENTATION_ITEM ( )  RATIONAL_B_SPLINE_CURVE ( ( 0.9999999999999948930, 0.9238795325112918455, 1.000000000000000000, 0.9238795325112867385, 1.000000000000000000, 0.9238795325112867385, 1.000000000000000000, 0.9238795325112826307, 1.000000000000003997 ) ) 
 REPRESENTATION_ITEM ( '' )  );
#22722 = CARTESIAN_POINT ( 'NONE',  ( 2.828427124746191623, 18.12500000000000000, -2.828427124746191623 ) ) ;
#22723 = ORIENTED_EDGE ( 'NONE', *, *, #27173, .F. ) ;
#22724 = CYLINDRICAL_SURFACE ( 'NONE', #53922, 4.000000000000001776 ) ;
#22725 = CARTESIAN_POINT ( 'NONE',  ( -3.458734124999959914, 201.4375000013656063, 198.0000000000000284 ) ) ;
#22726 = CARTESIAN_POINT ( 'NONE',  ( -31.45873412499996746, 206.7500000013655779, 171.4326545832181239 ) ) ;
#22727 = CARTESIAN_POINT ( 'NONE',  ( -8.342170076843785083E-16, 10.06249999863440614, 4.541265875000002339 ) ) ;
#22728 = CARTESIAN_POINT ( 'NONE',  ( -4.000000000000001776, 18.24999999726881583, -4.898587196589415787E-16 ) ) ;
#22729 = CARTESIAN_POINT ( 'NONE',  ( -7.188101187499992051, 0.000000000000000000, 20.98655278187175455 ) ) ;
#22730 = VERTEX_POINT ( 'NONE', #66170 ) ;
#22731 = CARTESIAN_POINT ( 'NONE',  ( -6.000000000000001776, 292.0000000000000000, 0.000000000000000000 ) ) ;
#22732 = ORIENTED_EDGE ( 'NONE', *, *, #25172, .T. ) ;
#22733 = CARTESIAN_POINT ( 'NONE',  ( -4.220049686691935698, 10.18810118749999916, 109.3750000020483810 ) ) ;
#22734 = DIRECTION ( 'NONE',  ( 0.000000000000000000, 0.000000000000000000, -1.000000000000000000 ) ) ;
#22735 = CARTESIAN_POINT ( 'NONE',  ( -2.445694354108782775, 198.5625000013656063, 200.4456943541088663 ) ) ;
#22736 = CARTESIAN_POINT ( 'NONE',  ( 25.55430564589118703, 195.3125000013656063, 172.4456943541087526 ) ) ;
#22737 = CARTESIAN_POINT ( 'NONE',  ( 10.00000000000000178, 75.20833333333334281, -2.679491924311226736 ) ) ;
#22738 = ADVANCED_FACE ( 'NONE', ( #20138 ), #50380, .F. ) ;
#22739 = CARTESIAN_POINT ( 'NONE',  ( 8.000000000000000000, 124.2500000000000000, -9.797174393178825657E-16 ) ) ;
#22740 = CARTESIAN_POINT ( 'NONE',  ( -4.721056650415999201, 299.4843750017070079, -4.721056650415999201 ) ) ;
#22741 = ORIENTED_EDGE ( 'NONE', *, *, #47564, .T. ) ;
#22742 = CARTESIAN_POINT ( 'NONE',  ( -11.00000000000000000, 0.000000000000000000, 77.49999999999998579 ) ) ;
#22743 = CONICAL_SURFACE ( 'NONE', #67363, 7.500000000000020428, 0.7853981633974552734 ) ;
#22744 = CARTESIAN_POINT ( 'NONE',  ( 5.126144196591232216, -16.23426282122703768, 69.90718656545267606 ) ) ;
#22745 = CARTESIAN_POINT ( 'NONE',  ( -2.828427124746209831, 196.5000000027312126, 139.1715728752538723 ) ) ;
#22746 = CARTESIAN_POINT ( 'NONE',  ( 10.00000000000000178, 57.08333332650536107, -2.679491924311226736 ) ) ;
#22747 = CARTESIAN_POINT ( 'NONE',  ( -5.656854249492381470, 23.43750000000000355, 5.656854249492379694 ) ) ;
#22748 = CARTESIAN_POINT ( 'NONE',  ( -8.660254037844385522, 235.4166666666666572, 5.000000000000004441 ) ) ;
#22749 = CARTESIAN_POINT ( 'NONE',  ( -4.999999999999998224, 206.6666666666666856, -8.660254037844389075 ) ) ;
#22750 = CARTESIAN_POINT ( 'NONE',  ( 5.082755093536318824, 5.082755093536319713, 16.29905278187175455 ) ) ;
#22751 = CARTESIAN_POINT ( 'NONE',  ( -3.042071309553164404, 172.5520833299193555, -11.35316468749999963 ) ) ;
#22752 = CARTESIAN_POINT ( 'NONE',  ( -1.522892193876115035E-11, 103.7499999999988205, 10.00000000000000178 ) ) ;
#22753 = CARTESIAN_POINT ( 'NONE',  ( -3.000000000000001332, -45.00000000000001421, 151.2383369607063344 ) ) ;
#22754 = LINE ( 'NONE', #16716, #32711 ) ;
#22755 = ORIENTED_EDGE ( 'NONE', *, *, #25290, .F. ) ;
#22756 = VECTOR ( 'NONE', #67075, 1000.000000000000000 ) ;
#22758 = EDGE_CURVE ( 'NONE', #69783, #26210, #14474, .T. ) ;
#22757 = CARTESIAN_POINT ( 'NONE',  ( 2.445694354108782775, 196.5625000013656063, 139.5543056458912190 ) ) ;
#22759 = CARTESIAN_POINT ( 'NONE',  ( -3.042071309553164404, 42.55208332991933418, -11.35316468749999963 ) ) ;
#22760 = CARTESIAN_POINT ( 'NONE',  ( -10.99999999999999822, -4.556349186104052151, 109.2812500040967620 ) ) ;
#22761 = CARTESIAN_POINT ( 'NONE',  ( -30.44569435410887337, 207.5625000013656063, 167.5543056458916169 ) ) ;
#22762 = DIRECTION ( 'NONE',  ( 0.000000000000000000, 0.000000000000000000, 1.000000000000000000 ) ) ;
#22764 = CARTESIAN_POINT ( 'NONE',  ( -2.069125466540922886, -10.11940336925128214, -70.25556669588459613 ) ) ;
#22763 = DIRECTION ( 'NONE',  ( -0.8191520442889924647, 1.003171929053525486E-16, 0.5735764363510451602 ) ) ;
#22765 = CARTESIAN_POINT ( 'NONE',  ( 1.836970198721029589E-15, 236.2500000000000284, 10.00000000000000000 ) ) ;
#22766 = CARTESIAN_POINT ( 'NONE',  ( -2.445694354108839619, 197.8125000013656063, 139.5543056458912190 ) ) ;
#22767 = CARTESIAN_POINT ( 'NONE',  ( -7.320508075688773708, 58.74999999317203958, -7.320508075688774596 ) ) ;
#22768 = CARTESIAN_POINT ( 'NONE',  ( -5.082755093536325930, 101.4687500020483810, -5.082755093536325930 ) ) ;
#22769 = CARTESIAN_POINT ( 'NONE',  ( 4.541265875000001451, 14.37499999863440969, 1.881053915767124440 ) ) ;
#22770 = FACE_OUTER_BOUND ( 'NONE', #25365, .T. ) ;
#22771 = CARTESIAN_POINT ( 'NONE',  ( 1.469576158976822172E-15, -7.999999999999991118, 5.705302779823364645 ) ) ;
#22772 = CARTESIAN_POINT ( 'NONE',  ( 10.00000000000000178, 101.8749999931720396, 0.000000000000000000 ) ) ;
#22773 = ORIENTED_EDGE ( 'NONE', *, *, #67540, .T. ) ;
#22774 = ORIENTED_EDGE ( 'NONE', *, *, #11609, .F. ) ;
#22775 = CARTESIAN_POINT ( 'NONE',  ( -4.556349186104045934, 11.00000000000000000, 116.2187500000000000 ) ) ;
#22776 = DIRECTION ( 'NONE',  ( -1.000000000000000000, 0.000000000000000000, -0.000000000000000000 ) ) ;
#22777 = CARTESIAN_POINT ( 'NONE',  ( 0.000000000000000000, 0.5000000000000004441, 0.000000000000000000 ) ) ;
#22778 = CARTESIAN_POINT ( 'NONE',  ( 2.957351242930898602E-11, 51.14729664189404446, -48.52014062454985321 ) ) ;
#22779 = CARTESIAN_POINT ( 'NONE',  ( -11.35316468750000141, 138.2812499965860411, -1.390361679473963753E-15 ) ) ;
#22780 = CARTESIAN_POINT ( 'NONE',  ( 1.656854249492381914, 6.812500000000000000, 4.000000000000000888 ) ) ;
#22781 = CARTESIAN_POINT ( 'NONE',  ( -4.220049686691937474, -10.18810118749999738, 84.43750000204838102 ) ) ;
#22782 = CARTESIAN_POINT ( 'NONE',  ( -28.92188847141967756, 194.4720194171914613, 166.6449334725710116 ) ) ;
#22783 = CARTESIAN_POINT ( 'NONE',  ( -1.656854249492347719, 203.8125000000000284, 194.0000000000000853 ) ) ;
#22784 = CARTESIAN_POINT ( 'NONE',  ( 5.000000000000004441, 246.6666666666666856, 8.660254037844385522 ) ) ;
#22785 = CARTESIAN_POINT ( 'NONE',  ( 3.313708498984697215, 116.6562500040967620, 8.000000000000063949 ) ) ;
#22786 = EDGE_CURVE ( 'NONE', #68143, #34951, #44287, .T. ) ;
#22787 = CARTESIAN_POINT ( 'NONE',  ( 4.220049686691941027, -10.18810118749999738, 116.5000000020483810 ) ) ;
#22788 = VERTEX_POINT ( 'NONE', #38638 ) ;
#22789 = EDGE_CURVE ( 'NONE', #46714, #22871, #55125, .T. ) ;
#22790 = CARTESIAN_POINT ( 'NONE',  ( 4.556349186104045934, 11.00000000000000000, 108.7187500040967763 ) ) ;
#22791 = CARTESIAN_POINT ( 'NONE',  ( -2.251907551946513930, 183.6788756342477029, 139.0000000000000853 ) ) ;
#22792 = CARTESIAN_POINT ( 'NONE',  ( -8.311093377946841443, 124.2187499965860127, 8.311093377946834337 ) ) ;
#22793 = CARTESIAN_POINT ( 'NONE',  ( -3.458734124999959914, 201.4375000013656063, 198.0000000000000284 ) ) ;
#22794 = CARTESIAN_POINT ( 'NONE',  ( -7.188101187500000044, 25.59374999795161543, -8.802885111219163269E-16 ) ) ;
#22795 = CARTESIAN_POINT ( 'NONE',  ( 7.204075437095966983, 7.204075437095967871, 74.96875000204836681 ) ) ;
#22796 = CARTESIAN_POINT ( 'NONE',  ( 8.311093377946837890, 31.71874999658601624, -8.311093377946837890 ) ) ;
#22797 = EDGE_LOOP ( 'NONE', ( #24588, #15285, #68417, #65299 ) ) ;
#22798 = DIRECTION ( 'NONE',  ( -0.000000000000000000, 1.000000000000000000, -0.000000000000000000 ) ) ;
#22799 = CARTESIAN_POINT ( 'NONE',  ( -5.000000000000005329, 195.2083333265053966, 8.660254037844387298 ) ) ;
#22800 = CARTESIAN_POINT ( 'NONE',  ( -5.662595241051935346, 5.662595241051935346, 15.82561528394063188 ) ) ;
#22801 = CARTESIAN_POINT ( 'NONE',  ( 3.458734124999960358, 206.6250000013656063, 143.4326545832176976 ) ) ;
#22802 = ADVANCED_FACE ( 'NONE', ( #2431 ), #71819, .F. ) ;
#22803 = CARTESIAN_POINT ( 'NONE',  ( -2.977408999572654480, 11.99999999795161187, 7.188101187499999156 ) ) ;
#22804 = CARTESIAN_POINT ( 'NONE',  ( 6.000000000000003553, 295.5000000034140157, 2.485281374238571317 ) ) ;
#22805 = CARTESIAN_POINT ( 'NONE',  ( -21.36469158609146035, -14.45462074387679152, 137.1624617011106295 ) ) ;
#22806 = CARTESIAN_POINT ( 'NONE',  ( 2.977408999572650927, 7.124999997951610098, -7.188101187500001821 ) ) ;
#22807 = CARTESIAN_POINT ( 'NONE',  ( -8.311093377946841443, 154.2187499965859843, 8.311093377946830785 ) ) ;
#22808 = CARTESIAN_POINT ( 'NONE',  ( -4.220049686691935698, 10.18810118749999916, 77.87500000204838102 ) ) ;
#22809 = AXIS2_PLACEMENT_3D ( 'NONE', #24902, #47184, #6476 ) ;
#22810 = ADVANCED_FACE ( 'NONE', ( #43524 ), #8837, .T. ) ;
#22811 = ADVANCED_BREP_SHAPE_REPRESENTATION ( '', ( #17043, #57354 ), #67028 ) ;
#22812 = B_SPLINE_CURVE_WITH_KNOTS ( 'NONE', 3,
 ( #4895, #4520, #56581, #62587 ),
 .UNSPECIFIED., .F., .F.,
 ( 4, 4 ),
 ( 0.04320970014224184003, 0.04620423721442659670 ),
 .UNSPECIFIED. ) ;
#22813 = CARTESIAN_POINT ( 'NONE',  ( -31.45873412499999944, 194.6250000013655779, 168.5673454167827572 ) ) ;
#22814 = CYLINDRICAL_SURFACE ( 'NONE', #14894, 7.999999999999991118 ) ;
#22815 = CARTESIAN_POINT ( 'NONE',  ( -3.211159895383561391, 19.81249999863440436, -3.211159895383561835 ) ) ;
#22816 = ORIENTED_EDGE ( 'NONE', *, *, #9654, .F. ) ;
#22817 = AXIS2_PLACEMENT_3D ( 'NONE', #56207, #15071, #38105 ) ;
#22818 = CARTESIAN_POINT ( 'NONE',  ( -2.828427124746153876, 199.0000000027312126, 195.1715728752538439 ) ) ;
#22819 =( BOUNDED_CURVE ( )  B_SPLINE_CURVE ( 2, ( #1955, #69885, #868, #41577, #24945, #35558, #13622, #7982, #1601 ),
 .UNSPECIFIED., .F., .F. ) 
 B_SPLINE_CURVE_WITH_KNOTS ( ( 3, 2, 2, 2, 3 ),
 ( 0.5833333333333337034, 0.5916666666666670071, 0.6000000000000004219, 0.6083333333333338366, 0.6166666666666672514 ),
 .UNSPECIFIED. ) 
 CURVE ( )  GEOMETRIC_REPRESENTATION_ITEM ( )  RATIONAL_B_SPLINE_CURVE ( ( 0.9999999999999970024, 0.9238795325112897361, 1.000000000000000000, 0.9238795325112867385, 1.000000000000000000, 0.9238795325112867385, 1.000000000000000000, 0.9238795325112816315, 1.000000000000005107 ) ) 
 REPRESENTATION_ITEM ( '' )  );
#22820 = CARTESIAN_POINT ( 'NONE',  ( 2.828427124746153876, 205.8750000000000284, 144.8284271247462129 ) ) ;
#22821 = CARTESIAN_POINT ( 'NONE',  ( -25.17157287525385811, 201.0000000027312126, 167.1715728752541281 ) ) ;
#22822 = CARTESIAN_POINT ( 'NONE',  ( -7.778174593052020747, -7.778174593052023411, 74.87500000409677625 ) ) ;
#22823 = CARTESIAN_POINT ( 'NONE',  ( -5.656854249492373476, -5.656854249492376141, 8.705302783920146226 ) ) ;
#22824 = VERTEX_POINT ( 'NONE', #25424 ) ;
#22825 = CARTESIAN_POINT ( 'NONE',  ( 7.188101187500000933, 15.56249999795161365, -2.977408999572650483 ) ) ;
#22826 = CARTESIAN_POINT ( 'NONE',  ( -25.17157287525385456, 197.0000000027312126, 167.1715728752541281 ) ) ;
#22827 = CARTESIAN_POINT ( 'NONE',  ( -3.673940397442060854E-16, 296.7500000000000000, -6.000000000000001776 ) ) ;
#22828 = CARTESIAN_POINT ( 'NONE',  ( 8.660254037844389075, 40.41666666666667140, -5.000000000000000000 ) ) ;
#22829 = CARTESIAN_POINT ( 'NONE',  ( 1.320432766682874540E-15, 106.9062500020483810, 7.188101187500000044 ) ) ;
#22830 = CARTESIAN_POINT ( 'NONE',  ( -24.54126587500000767, 207.5000000013656063, 168.5673454167827003 ) ) ;
#22831 = CARTESIAN_POINT ( 'NONE',  ( 6.000000000000003553, 298.5625000000000568, -2.485281374238571761 ) ) ;
#22832 = ADVANCED_FACE ( 'NONE', ( #31848 ), #26167, .F. ) ;
#22834 = CARTESIAN_POINT ( 'NONE',  ( 8.660254037844385522, 196.4583333265053966, 5.000000000000005329 ) ) ;
#22833 = CARTESIAN_POINT ( 'NONE',  ( 3.410844894484189267E-12, 36.24999999999974420, -10.00000000000000178 ) ) ;
#22835 = ORIENTED_EDGE ( 'NONE', *, *, #1502, .F. ) ;
#22836 =( BOUNDED_CURVE ( )  B_SPLINE_CURVE ( 2, ( #68059, #16349, #72601, #39387, #20528, #62386, #43541, #3570, #20908, #43928, #66938 ),
 .UNSPECIFIED., .F., .F. ) 
 B_SPLINE_CURVE_WITH_KNOTS ( ( 3, 2, 2, 2, 2, 3 ),
 ( 0.3706233993366209178, 0.3706234327295814812, 0.3772417083140383043, 0.3838599838984951274, 0.3904782594829518949, 0.3970965164372073364 ),
 .UNSPECIFIED. ) 
 CURVE ( )  GEOMETRIC_REPRESENTATION_ITEM ( )  RATIONAL_B_SPLINE_CURVE ( ( 0.9999992318618620146, 0.9999996159289931130, 1.000000000000000000, 0.9238795325112867385, 1.000000000000000000, 0.9238795325112867385, 1.000000000000000000, 0.9238795325112867385, 1.000000000000000000, 0.9238797467875916603, 0.9999995714485965248 ) ) 
 REPRESENTATION_ITEM ( '' )  );
#22837 = CARTESIAN_POINT ( 'NONE',  ( 11.35316468749999963, 246.4062500034139873, -1.390361679473963556E-15 ) ) ;
#22838 = PRODUCT_DEFINITION_SHAPE ( 'NONE', 'NONE',  #67598 ) ;
#22839 = CARTESIAN_POINT ( 'NONE',  ( 1.320432766682872962E-15, -7.188101187499992051, 17.23655278187175810 ) ) ;
#22840 = CARTESIAN_POINT ( 'NONE',  ( -5.126106709314333543, 52.42424824937320693, 49.01286957842763314 ) ) ;
#22841 = CARTESIAN_POINT ( 'NONE',  ( 0.000000000000000000, 300.0000000000000000, 0.000000000000000000 ) ) ;
#22842 = CARTESIAN_POINT ( 'NONE',  ( 24.08860760445115545, 194.9317364962657848, 170.4427657083653287 ) ) ;
#22844 = EDGE_CURVE ( 'NONE', #783, #66108, #9208, .T. ) ;
#22843 = CARTESIAN_POINT ( 'NONE',  ( -7.320508075688773708, 138.7499999931720254, -7.320508075688774596 ) ) ;
#22845 = CARTESIAN_POINT ( 'NONE',  ( -1.836970198721029983E-15, 158.7500000000000000, 10.00000000000000178 ) ) ;
#22846 = DIRECTION ( 'NONE',  ( 0.000000000000000000, 1.000000000000000000, 0.000000000000000000 ) ) ;
#22847 = CARTESIAN_POINT ( 'NONE',  ( 7.778174593052023411, -7.778174593052021635, 90.06249999999998579 ) ) ;
#22848 = CARTESIAN_POINT ( 'NONE',  ( 0.000000000000000000, 0.000000000000000000, -10.00000000000000000 ) ) ;
#22849 = CARTESIAN_POINT ( 'NONE',  ( 6.951808397369818766E-16, 132.3437499965860127, -11.35316468750000141 ) ) ;
#22850 = CARTESIAN_POINT ( 'NONE',  ( 28.00000000000001421, 196.5000000000000000, 165.9999999999998863 ) ) ;
#22851 = CARTESIAN_POINT ( 'NONE',  ( 3.407298021510787311, -16.35582233947175013, -69.12343428065700834 ) ) ;
#22854 = CARTESIAN_POINT ( 'NONE',  ( 1.656854249492212938, 196.8125000000000284, 146.0000000000001990 ) ) ;
#22853 = CARTESIAN_POINT ( 'NONE',  ( 29.43265458321766204, 196.5000000013656063, 173.4587341249998929 ) ) ;
#22852 = CARTESIAN_POINT ( 'NONE',  ( 24.00000000000001066, 209.6875000000000284, 168.3431457505075173 ) ) ;
#22855 = ORIENTED_EDGE ( 'NONE', *, *, #46697, .T. ) ;
#22856 = CARTESIAN_POINT ( 'NONE',  ( -5.266666970006217419, 7.351593252548062729, 4.363913744254155347E-15 ) ) ;
#22857 = CARTESIAN_POINT ( 'NONE',  ( 0.000000000000000000, 0.000000000000000000, 0.000000000000000000 ) ) ;
#22858 = CARTESIAN_POINT ( 'NONE',  ( 2.679491924311103723, 193.9583333333333997, 10.00000000000019362 ) ) ;
#22859 = CARTESIAN_POINT ( 'NONE',  ( 5.000000000000001776, -63.46295559274096831, -24.14151313015386080 ) ) ;
#22860 = ADVANCED_FACE ( 'NONE', ( #14848 ), #49186, .T. ) ;
#22861 = VECTOR ( 'NONE', #73306, 1000.000000000000000 ) ;
#22862 = CARTESIAN_POINT ( 'NONE',  ( 3.042071309553159519, 225.0520833299193555, 11.35316468750000141 ) ) ;
#22863 = SHAPE_REPRESENTATION ( 'hexagon nut style 1_is_IS 1364-3 - M12-W-N', ( #57354 ), #14000 ) ;
#22864 = CARTESIAN_POINT ( 'NONE',  ( 7.188101187500002709, 120.3125000020483668, 2.977408999572649151 ) ) ;
#22865 = CARTESIAN_POINT ( 'NONE',  ( -3.211159895383562723, 2.062499998634407028, 3.211159895383561391 ) ) ;
#22866 = CARTESIAN_POINT ( 'NONE',  ( -1.558072418987807239, -51.25713184919958110, 48.56213741370790160 ) ) ;
#22867 = CARTESIAN_POINT ( 'NONE',  ( 7.999999999999992895, -3.313708498984756279, 22.48655277982336287 ) ) ;
#22869 = CARTESIAN_POINT ( 'NONE',  ( -2.679491924311222295, 226.0416666666666288, 10.00000000000000178 ) ) ;
#22868 = FILL_AREA_STYLE ('',( #68896 ) ) ;
#22870 = CARTESIAN_POINT ( 'NONE',  ( -9.832129032723418760, 102.8645833299193697, -5.676582343750004256 ) ) ;
#22871 = VERTEX_POINT ( 'NONE', #37888 ) ;
#22872 = DIRECTION ( 'NONE',  ( -0.000000000000000000, -1.000000000000000000, -0.000000000000000000 ) ) ;
#22874 = CARTESIAN_POINT ( 'NONE',  ( -2.977408999572650039, 24.93749999795161543, -7.188101187500001821 ) ) ;
#22873 = PRODUCT_RELATED_PRODUCT_CATEGORY ( 'part', '', ( #54717 ) ) ;
#22875 = CARTESIAN_POINT ( 'NONE',  ( 36.86924962228698632, 38.00000000000000711, 134.0294372515228645 ) ) ;
#22876 = CARTESIAN_POINT ( 'NONE',  ( 3.042071309553163516, 242.7604166700806729, -11.35316468749999785 ) ) ;
#22877 = CARTESIAN_POINT ( 'NONE',  ( -11.35316468750000141, 103.2812499965860269, -1.390361679473963753E-15 ) ) ;
#22878 = ORIENTED_EDGE ( 'NONE', *, *, #20079, .F. ) ;
#22879 = CARTESIAN_POINT ( 'NONE',  ( 3.999999999999960032, 209.1250000027312126, 142.0000000000000568 ) ) ;
#22880 = VECTOR ( 'NONE', #23968, 1000.000000000000000 ) ;
#22881 = CARTESIAN_POINT ( 'NONE',  ( 10.18810118749999916, 1.247682550866122264E-15, 107.4062500020483668 ) ) ;
#22882 = CARTESIAN_POINT ( 'NONE',  ( 4.999999999999993783, 226.0416666598387110, 8.660254037844390851 ) ) ;
#22883 = CARTESIAN_POINT ( 'NONE',  ( 1.432654583217662481, 201.3750000013656347, 194.5412658750000219 ) ) ;
#22884 = CARTESIAN_POINT ( 'NONE',  ( 2.824543433528785410E-14, 210.0000000000000284, 194.0000000000000568 ) ) ;
#22886 = CARTESIAN_POINT ( 'NONE',  ( 6.951808397369818766E-16, 97.03124999658602690, -11.35316468750000141 ) ) ;
#22885 = CARTESIAN_POINT ( 'NONE',  ( -5.656854249492375253, 5.656854249492375253, 23.14280277982336642 ) ) ;
#22887 = CARTESIAN_POINT ( 'NONE',  ( -5.656854249492373476, -5.656854249492376141, 10.20530278392014623 ) ) ;
#22888 = CARTESIAN_POINT ( 'NONE',  ( -28.00000000000001776, 196.6875000013655779, 166.5412658750003629 ) ) ;
#22889 = CARTESIAN_POINT ( 'NONE',  ( -3.313708498984870410, 92.28124999999998579, 7.999999999999890754 ) ) ;
#22890 = ORIENTED_EDGE ( 'NONE', *, *, #66727, .T. ) ;
#22891 = CARTESIAN_POINT ( 'NONE',  ( 10.00000000000000178, 201.8749999931720538, 0.000000000000000000 ) ) ;
#22892 = EDGE_CURVE ( 'NONE', #18846, #11062, #60886, .T. ) ;
#22893 = CARTESIAN_POINT ( 'NONE',  ( 2.828427124746190291, 5.875000000000000000, 2.828427124746192067 ) ) ;
#22894 = CARTESIAN_POINT ( 'NONE',  ( 1.981233606127732916, -47.26140082806393394, 139.0630574121168479 ) ) ;
#22895 = CARTESIAN_POINT ( 'NONE',  ( 5.676582343750001591, 91.92708332991935549, -9.832129032723420536 ) ) ;
#22896 = CARTESIAN_POINT ( 'NONE',  ( -6.676582343750001591, 290.4531250017069510, 0.000000000000000000 ) ) ;
#22897 = CARTESIAN_POINT ( 'NONE',  ( 5.082755093536325930, 4.031249997951610986, -5.082755093536325930 ) ) ;
#22898 = CARTESIAN_POINT ( 'NONE',  ( 4.220049686691934809, 10.18810118749999916, 96.06250000204836681 ) ) ;
#22899 = CARTESIAN_POINT ( 'NONE',  ( -3.042071309553164404, 222.2395833299193555, -11.35316468749999963 ) ) ;
#22900 = ORIENTED_EDGE ( 'NONE', *, *, #23779, .T. ) ;
#22901 = CARTESIAN_POINT ( 'NONE',  ( 1.469576158976823947E-15, 122.5625000040967763, 8.000000000000000000 ) ) ;
#22902 = CYLINDRICAL_SURFACE ( 'NONE', #8726, 10.00000000000000178 ) ;
#22903 = CARTESIAN_POINT ( 'NONE',  ( -5.000000000000000000, -16.24494643555759410, 69.83755725260752456 ) ) ;
#22904 = CARTESIAN_POINT ( 'NONE',  ( -3.042071309553163960, 217.2395833299193271, -11.35316468749999963 ) ) ;
#22905 = CARTESIAN_POINT ( 'NONE',  ( -9.999999999999998224, 218.3333333401612606, 2.679491924311235618 ) ) ;
#22906 = CARTESIAN_POINT ( 'NONE',  ( -8.660254037844548947, 157.9166666666667993, 5.000000000000091482 ) ) ;
#22907 = CARTESIAN_POINT ( 'NONE',  ( 6.676582343750004256, 295.8906250017069510, 2.765530957081995478 ) ) ;
#22908 = ORIENTED_EDGE ( 'NONE', *, *, #66528, .F. ) ;
#22909 = CARTESIAN_POINT ( 'NONE',  ( 4.000000000000015987, 199.5625000000000568, 196.3431457505076594 ) ) ;
#22910 = CARTESIAN_POINT ( 'NONE',  ( -2.085542519210945728E-15, 209.8437499965860411, 11.35316468750000141 ) ) ;
#22911 = CARTESIAN_POINT ( 'NONE',  ( -10.18810118749999738, -4.220049686691941915, 96.25000000204838102 ) ) ;
#22912 = CARTESIAN_POINT ( 'NONE',  ( -24.54126587500000056, 205.2500000013655779, 168.5673454167827003 ) ) ;
#22913 = CARTESIAN_POINT ( 'NONE',  ( 7.999999999999998224, 17.90625000000000355, 3.313708498984766493 ) ) ;
#22914 = ORIENTED_EDGE ( 'NONE', *, *, #64844, .F. ) ;
#22915 = PRODUCT_DEFINITION_CONTEXT ( 'detailed design', #50101, 'design' ) ;
#22916 = CARTESIAN_POINT ( 'NONE',  ( 7.188101187500000044, 121.9062500020483810, -8.802885111219163269E-16 ) ) ;
#22917 = CARTESIAN_POINT ( 'NONE',  ( -27.99999999999999645, 210.0000000000000284, 174.0000000000003411 ) ) ;
#22918 = CARTESIAN_POINT ( 'NONE',  ( -5.000000000000005329, 28.33333333333333570, 8.660254037844387298 ) ) ;
#22919 = VECTOR ( 'NONE', #10237, 1000.000000000000000 ) ;
#22920 = CARTESIAN_POINT ( 'NONE',  ( -28.00000000000002487, 198.0000000000000000, 166.0000000000003695 ) ) ;
#22921 = CARTESIAN_POINT ( 'NONE',  ( 7.204075437095968759, -7.204075437095966983, 82.09375000204838102 ) ) ;
#22922 = VERTEX_POINT ( 'NONE', #32228 ) ;
#22923 = CARTESIAN_POINT ( 'NONE',  ( 2.449293598294707893E-16, 20.25000000000000000, -4.000000000000001776 ) ) ;
#22924 = CARTESIAN_POINT ( 'NONE',  ( 1.656854249492381248, 2.937499997268813612, -4.000000000000001776 ) ) ;
#22925 = CIRCLE ( 'NONE', #61655, 11.00000000000000000 ) ;
#22926 = CARTESIAN_POINT ( 'NONE',  ( 30.76847783166686767, 194.6767860410251387, 167.5700053143318939 ) ) ;
#22927 = CIRCLE ( 'NONE', #2470, 5.099999999999999645 ) ;
#22928 = CARTESIAN_POINT ( 'NONE',  ( -7.778174593052020747, -7.778174593052023411, 92.87500000409677625 ) ) ;
#22929 = CARTESIAN_POINT ( 'NONE',  ( -4.999999999999999112, -10.60557809245594463, 66.49298242784793445 ) ) ;
#22930 = FACE_OUTER_BOUND ( 'NONE', #33398, .T. ) ;
#22931 = CARTESIAN_POINT ( 'NONE',  ( 6.676582343750003368, 296.8906250017069510, 2.765530957081995478 ) ) ;
#22932 = EDGE_CURVE ( 'NONE', #34951, #56815, #58447, .T. ) ;
#22935 = LINE ( 'NONE', #47051, #4868 ) ;
#22934 = CARTESIAN_POINT ( 'NONE',  ( 11.35316468749999608, 241.6145833367473585, -3.042071309553167513 ) ) ;
#22933 = CARTESIAN_POINT ( 'NONE',  ( 30.44569435410883429, 205.5625000013656063, 172.4456943541086957 ) ) ;
#22936 = PRODUCT_CONTEXT ( 'NONE', #27400, 'mechanical' ) ;
#22937 = ORIENTED_EDGE ( 'NONE', *, *, #38478, .T. ) ;
#22938 = CARTESIAN_POINT ( 'NONE',  ( 8.311093377946839666, 236.0937500034139589, 8.311093377946829008 ) ) ;
#22939 = CARTESIAN_POINT ( 'NONE',  ( -7.188101187499990274, -2.977408999572651371, 6.080302781871753659 ) ) ;
#22940 = ORIENTED_EDGE ( 'NONE', *, *, #21898, .F. ) ;
#22941 =( BOUNDED_CURVE ( )  B_SPLINE_CURVE ( 2, ( #2567, #7490, #54629, #53512, #48201, #59907, #1831, #2938, #47832 ),
 .UNSPECIFIED., .F., .F. ) 
 B_SPLINE_CURVE_WITH_KNOTS ( ( 3, 2, 2, 2, 3 ),
 ( 0.5795454545454545858, 0.5852272727272727071, 0.5909090909090909394, 0.5965909090909090606, 0.6022727272727272929 ),
 .UNSPECIFIED. ) 
 CURVE ( )  GEOMETRIC_REPRESENTATION_ITEM ( )  RATIONAL_B_SPLINE_CURVE ( ( 1.000000000000000000, 0.9238795325112867385, 1.000000000000000000, 0.9238795325112867385, 1.000000000000000000, 0.9238795325112867385, 1.000000000000000000, 0.9238795325112867385, 1.000000000000000000 ) ) 
 REPRESENTATION_ITEM ( '' )  );
#22942 = ADVANCED_FACE ( 'NONE', ( #16706 ), #51056, .T. ) ;
#22943 = ORIENTED_EDGE ( 'NONE', *, *, #56168, .F. ) ;
#22944 = CARTESIAN_POINT ( 'NONE',  ( -7.204075437095967871, 7.204075437095967871, 74.96875000204836681 ) ) ;
#22945 = CARTESIAN_POINT ( 'NONE',  ( 9.832129032723420536, 86.51041666325268409, -5.676582343749999815 ) ) ;
#22946 = CARTESIAN_POINT ( 'NONE',  ( 0.000000000000000000, 265.0000000000000000, -19.00000000000003553 ) ) ;
#22947 = CARTESIAN_POINT ( 'NONE',  ( 2.020667218593132706E-15, -11.00000000000000000, 80.87499999999998579 ) ) ;
#22950 = CARTESIAN_POINT ( 'NONE',  ( -1.538508811358849613E-11, 71.25000000000120792, -10.00000000000000178 ) ) ;
#22949 = CARTESIAN_POINT ( 'NONE',  ( 25.55430564589119413, 207.3125000013656063, 172.4456943541087526 ) ) ;
#22948 = CARTESIAN_POINT ( 'NONE',  ( 31.45873412499999944, 207.9375000013656063, 169.9999999999999432 ) ) ;
#22951 = ORIENTED_EDGE ( 'NONE', *, *, #1902, .F. ) ;
#22952 = CARTESIAN_POINT ( 'NONE',  ( -62.39047978708156705, 227.6022213359290447, 44.99999999999999289 ) ) ;
#22953 = CARTESIAN_POINT ( 'NONE',  ( 6.000000000000000000, 0.000000000000000000, -25.03750572909317285 ) ) ;
#22954 = AXIS2_PLACEMENT_3D ( 'NONE', #56161, #33533, #32022 ) ;
#22955 = CARTESIAN_POINT ( 'NONE',  ( -5.676582343750006032, 194.1145833299193839, 9.832129032723418760 ) ) ;
#22956 = CARTESIAN_POINT ( 'NONE',  ( -2.445694354108839619, 203.8125000013656063, 139.5543056458912190 ) ) ;
#22957 = CARTESIAN_POINT ( 'NONE',  ( 24.54126587500000412, 206.3750000013656063, 168.5673454167822172 ) ) ;
#22958 = CARTESIAN_POINT ( 'NONE',  ( 2.977408999572651815, 15.56249999795161365, 7.188101187500000933 ) ) ;
#22959 = CARTESIAN_POINT ( 'NONE',  ( -3.042071309553164404, 182.5520833299193271, -11.35316468749999963 ) ) ;
#22960 = PLANE ( 'NONE',  #31161 ) ;
#22961 = CARTESIAN_POINT ( 'NONE',  ( 5.082755093536325042, 99.96875000204838102, -5.082755093536325930 ) ) ;
#22963 = CARTESIAN_POINT ( 'NONE',  ( -4.999999999999996447, 106.6666666666666714, -8.660254037844383745 ) ) ;
#22962 = CARTESIAN_POINT ( 'NONE',  ( 1.656854249492381914, 16.56249999726881228, 4.000000000000000888 ) ) ;
#22964 = CARTESIAN_POINT ( 'NONE',  ( 1.881053915767121776, 11.49999999863440792, -4.541265875000002339 ) ) ;
#22965 = CARTESIAN_POINT ( 'NONE',  ( 30.44569435410879166, 203.8125000013656063, 172.4456943541087526 ) ) ;
#22966 = B_SPLINE_CURVE_WITH_KNOTS ( 'NONE', 1,
 ( #72348, #20660 ),
 .UNSPECIFIED., .F., .F.,
 ( 2, 2 ),
 ( 0.000000000000000000, 1.000000000000000000 ),
 .UNSPECIFIED. ) ;
#22967 = CARTESIAN_POINT ( 'NONE',  ( -5.082755093536317936, -5.082755093536320601, 8.049052781871752771 ) ) ;
#22968 = CARTESIAN_POINT ( 'NONE',  ( 11.35316468749999785, 55.57291666325267698, 3.042071309553174174 ) ) ;
#22970 =( BOUNDED_CURVE ( )  B_SPLINE_CURVE ( 2, ( #49219, #26578, #62401, #21296, #56025, #67707, #44320, #26957, #72230 ),
 .UNSPECIFIED., .F., .F. ) 
 B_SPLINE_CURVE_WITH_KNOTS ( ( 3, 2, 2, 2, 3 ),
 ( 0.4411764705882353366, 0.4448529411764706176, 0.4485294117647059542, 0.4522058823529412352, 0.4558823529411765163 ),
 .UNSPECIFIED. ) 
 CURVE ( )  GEOMETRIC_REPRESENTATION_ITEM ( )  RATIONAL_B_SPLINE_CURVE ( ( 0.9999999999999988898, 0.9238795325112878487, 1.000000000000000000, 0.9238795325112867385, 1.000000000000000000, 0.9238795325112867385, 1.000000000000000000, 0.9238795325112856283, 1.000000000000001110 ) ) 
 REPRESENTATION_ITEM ( '' )  );
#22969 = DIRECTION ( 'NONE',  ( -0.000000000000000000, -0.000000000000000000, -1.000000000000000000 ) ) ;
#22971 = CARTESIAN_POINT ( 'NONE',  ( -5.656854249492375253, 5.656854249492375253, 3.699052784329822874 ) ) ;
#22972 = EDGE_LOOP ( 'NONE', ( #48247, #58271, #56529, #54573 ) ) ;
#22973 = CYLINDRICAL_SURFACE ( 'NONE', #2514, 10.00000000000000000 ) ;
#22974 = DIRECTION ( 'NONE',  ( -0.000000000000000000, 1.000000000000000000, 4.476705744456276341E-16 ) ) ;
#22975 = CARTESIAN_POINT ( 'NONE',  ( 11.35316468749999963, 55.98958332991934128, -3.042071309553165293 ) ) ;
#22976 = CARTESIAN_POINT ( 'NONE',  ( 11.00000000000000000, 4.556349186104045934, 72.53125000409676204 ) ) ;
#22977 = CARTESIAN_POINT ( 'NONE',  ( -2.445694354108839175, 200.3125000013656063, 144.4456943541088663 ) ) ;
#22978 = CARTESIAN_POINT ( 'NONE',  ( -6.308070865149355555, 10.25011764679247328, 64.85270989085067583 ) ) ;
#22980 = CARTESIAN_POINT ( 'NONE',  ( -8.311093377946841443, 58.90624999658600558, 8.311093377946834337 ) ) ;
#22979 = CARTESIAN_POINT ( 'NONE',  ( 7.188101187500000933, 93.50000000204838102, -2.977408999572651371 ) ) ;
#22981 = CARTESIAN_POINT ( 'NONE',  ( -5.656854249492375253, 5.656854249492375253, 5.142802779823363757 ) ) ;
#22982 = CARTESIAN_POINT ( 'NONE',  ( -28.00000000000007461, 197.1250000027312126, 166.0000000000003695 ) ) ;
#22983 = CARTESIAN_POINT ( 'NONE',  ( 8.311093377946834337, 175.1562499965860127, 8.311093377946839666 ) ) ;
#22984 = AXIS2_PLACEMENT_3D ( 'NONE', #12702, #24759, #13794 ) ;
#22985 = CARTESIAN_POINT ( 'NONE',  ( 10.00000000000000000, 161.6666666598386826, 2.679491924311236062 ) ) ;
#22986 = CARTESIAN_POINT ( 'NONE',  ( -2.977408999572650927, 95.75000000204836681, -7.188101187500001821 ) ) ;
#22987 = DIRECTION ( 'NONE',  ( -0.000000000000000000, 1.000000000000000000, -1.563033456626094573E-30 ) ) ;
#22988 = CARTESIAN_POINT ( 'NONE',  ( -3.042071309553173730, 49.63541666325268409, 11.35316468749999785 ) ) ;
#22989 = CARTESIAN_POINT ( 'NONE',  ( 4.220049686691941027, -10.18810118749999738, 116.5000000020483810 ) ) ;
#22990 = CARTESIAN_POINT ( 'NONE',  ( -8.311093377946836114, 177.6562499965859843, -8.311093377946837890 ) ) ;
#22991 = ORIENTED_EDGE ( 'NONE', *, *, #15858, .F. ) ;
#22992 = CARTESIAN_POINT ( 'NONE',  ( 2.824543433528785410E-14, 210.0000000000000284, 194.0000000000000568 ) ) ;
#22993 = CARTESIAN_POINT ( 'NONE',  ( 7.204075437095968759, -7.204075437095966983, 71.21875000204836681 ) ) ;
#22994 = CARTESIAN_POINT ( 'NONE',  ( -3.999999999999959144, 197.0625000000000000, 199.6568542494924259 ) ) ;
#22995 = CARTESIAN_POINT ( 'NONE',  ( 11.35316468750000141, 180.7812499965860411, 0.000000000000000000 ) ) ;
#22996 = CARTESIAN_POINT ( 'NONE',  ( 3.313708498984756279, 7.999999999999991118, 6.417802784329822430 ) ) ;
#22997 = CARTESIAN_POINT ( 'NONE',  ( 7.999999999999991118, 9.797174393178815797E-16, 4.580302779823363757 ) ) ;
#22998 = VECTOR ( 'NONE', #13053, 1000.000000000000000 ) ;
#22999 = CARTESIAN_POINT ( 'NONE',  ( -7.320508075688770155, 248.7500000068279746, 7.320508075688774596 ) ) ;
#23000 = CARTESIAN_POINT ( 'NONE',  ( -29.65685424949237259, 206.4375000000000000, 174.0000000000003411 ) ) ;
#23001 = AXIS2_PLACEMENT_3D ( 'NONE', #13025, #36062, #30027 ) ;
#23002 = ORIENTED_EDGE ( 'NONE', *, *, #51992, .F. ) ;
#23003 = CARTESIAN_POINT ( 'NONE',  ( 2.977408999572650927, -7.188101187499990274, 25.95530278187175455 ) ) ;
#23004 = CARTESIAN_POINT ( 'NONE',  ( -11.35316468750000141, 123.5937499965860269, -1.390361679473963753E-15 ) ) ;
#23005 = CARTESIAN_POINT ( 'NONE',  ( 8.660254037844385522, 11.45833332650536640, 5.000000000000005329 ) ) ;
#23006 = ORIENTED_EDGE ( 'NONE', *, *, #25083, .F. ) ;
#23007 = CARTESIAN_POINT ( 'NONE',  ( 1.881053915767121776, 9.624999998634404363, -4.541265875000002339 ) ) ;
#23008 = CARTESIAN_POINT ( 'NONE',  ( -7.188101187500002709, 11.81249999795161187, 2.977408999572649151 ) ) ;
#23009 = CARTESIAN_POINT ( 'NONE',  ( 8.000000000000000000, 103.4375000040967763, -9.797174393178825657E-16 ) ) ;
#23010 = EDGE_CURVE ( 'NONE', #23294, #21472, #4675, .T. ) ;
#23011 = CARTESIAN_POINT ( 'NONE',  ( -26.56734541678232375, 197.2500000013656063, 173.4587341250003760 ) ) ;
#23012 = CARTESIAN_POINT ( 'NONE',  ( -1.656854249492383691, 7.687500000000000000, 4.000000000000000888 ) ) ;
#23013 = CARTESIAN_POINT ( 'NONE',  ( -7.347880794884122694E-16, 22.49999999726881583, 4.000000000000001776 ) ) ;
#23014 = CARTESIAN_POINT ( 'NONE',  ( 2.780723358947928197E-16, 12.56249999863440792, -4.541265875000002339 ) ) ;
#23015 = CARTESIAN_POINT ( 'NONE',  ( 3.313708498984756279, 7.999999999999991118, 21.54905278392014623 ) ) ;
#23016 = CARTESIAN_POINT ( 'NONE',  ( -2.751064625579944321E-14, 199.7500000000000000, 146.0000000000000284 ) ) ;
#23017 = VERTEX_POINT ( 'NONE', #62736 ) ;
#23018 = CARTESIAN_POINT ( 'NONE',  ( -2.849036369511732440E-14, 205.2500000000000284, 138.0000000000000568 ) ) ;
#23019 = CARTESIAN_POINT ( 'NONE',  ( 2.977408999572654480, 102.1250000020483810, 7.188101187499999156 ) ) ;
#23020 = EDGE_CURVE ( 'NONE', #17783, #32479, #5051, .T. ) ;
#23022 = DIRECTION ( 'NONE',  ( -0.000000000000000000, -0.000000000000000000, 1.000000000000000000 ) ) ;
#23021 = DIRECTION ( 'NONE',  ( 1.000000000000000000, -0.000000000000000000, -0.000000000000000000 ) ) ;
#23023 = CARTESIAN_POINT ( 'NONE',  ( 3.211159895383560947, 22.18749999863440792, 3.211159895383562723 ) ) ;
#23024 = CARTESIAN_POINT ( 'NONE',  ( -4.401442555609577197E-16, 7.188101187499992051, 28.11155278187175455 ) ) ;
#23025 = EDGE_CURVE ( 'NONE', #15471, #70797, #46138, .T. ) ;
#23026 = ORIENTED_EDGE ( 'NONE', *, *, #6526, .F. ) ;
#23027 = ORIENTED_EDGE ( 'NONE', *, *, #51410, .T. ) ;
#23028 = CARTESIAN_POINT ( 'NONE',  ( -4.220049686691935698, 10.18810118749999916, 94.37500000204839523 ) ) ;
#23029 = CARTESIAN_POINT ( 'NONE',  ( -28.00000000000001776, 197.6875000013655779, 166.5412658750003629 ) ) ;
#23030 = CARTESIAN_POINT ( 'NONE',  ( 7.778174593052023411, -7.778174593052021635, 99.06250000000000000 ) ) ;
#23031 = CARTESIAN_POINT ( 'NONE',  ( -2.445694354108783219, 202.8125000013656063, 200.4456943541088663 ) ) ;
#23032 = CARTESIAN_POINT ( 'NONE',  ( -6.676582343749999815, 298.6718750017070079, 2.765530957082001251 ) ) ;
#23033 = CARTESIAN_POINT ( 'NONE',  ( -8.660254037844390851, 122.9166666666666714, 4.999999999999998224 ) ) ;
#23034 = CARTESIAN_POINT ( 'NONE',  ( 8.000000000000000000, 97.25000000000000000, -9.797174393178825657E-16 ) ) ;
#23035 = CARTESIAN_POINT ( 'NONE',  ( 6.676582343750001591, 288.1093750017069510, -8.176455196517173205E-16 ) ) ;
#23036 = CARTESIAN_POINT ( 'NONE',  ( 5.082755093536320601, -5.082755093536318824, 3.924052781871752327 ) ) ;
#23037 = CARTESIAN_POINT ( 'NONE',  ( 25.55430564589119413, 201.0625000013656063, 167.5543056458910485 ) ) ;
#23038 = CARTESIAN_POINT ( 'NONE',  ( 2.977408999572650927, 1.124999997951610098, -7.188101187500001821 ) ) ;
#23039 = CARTESIAN_POINT ( 'NONE',  ( 3.458734124999959025, 195.5000000013655779, 140.5673454167824161 ) ) ;
#23040 = CARTESIAN_POINT ( 'NONE',  ( 5.082755093536325042, 120.9687500020483952, -5.082755093536325930 ) ) ;
#23042 = CARTESIAN_POINT ( 'NONE',  ( 3.499857865026532622, -7.193933550196781823, 0.0006324257780546024528 ) ) ;
#23041 = CARTESIAN_POINT ( 'NONE',  ( -2.751064625579944321E-14, 204.7500000000000284, 146.0000000000000284 ) ) ;
#23043 = CARTESIAN_POINT ( 'NONE',  ( -8.311093377946834337, 244.8437500034140157, 8.311093377946837890 ) ) ;
#23044 = CARTESIAN_POINT ( 'NONE',  ( -8.000000000000001776, 3.843750000000000888, 3.313708498984759387 ) ) ;
#23045 = CARTESIAN_POINT ( 'NONE',  ( 5.000000000000001776, 52.70833332650536818, -8.660254037844389075 ) ) ;
#23046 = CARTESIAN_POINT ( 'NONE',  ( 25.17157287525377996, 196.8750000000000284, 172.8284271247460424 ) ) ;
#23047 = CARTESIAN_POINT ( 'NONE',  ( -3.042071309553173730, 9.322916663252685865, 11.35316468749999785 ) ) ;
#23048 = CARTESIAN_POINT ( 'NONE',  ( 0.000000000000000000, 0.000000000000000000, 8.000000000000000000 ) ) ;
#23049 = CARTESIAN_POINT ( 'NONE',  ( -11.35316468750000141, 218.5937499965860411, -1.390361679473963753E-15 ) ) ;
#23050 = CARTESIAN_POINT ( 'NONE',  ( -8.660254037844385522, 240.4166666666666572, 5.000000000000004441 ) ) ;
#23052 = CARTESIAN_POINT ( 'NONE',  ( 3.313708498984756279, 7.999999999999991118, 28.86155277982336642 ) ) ;
#23051 = CARTESIAN_POINT ( 'NONE',  ( 1.656854249492407449, 208.3125000000000000, 202.0000000000000000 ) ) ;
#23053 = AXIS2_PLACEMENT_3D ( 'NONE', #71741, #32913, #15523 ) ;
#23054 = ORIENTED_EDGE ( 'NONE', *, *, #27929, .T. ) ;
#23055 = CARTESIAN_POINT ( 'NONE',  ( -3.458734125000015869, 202.1875000013656063, 142.0000000000000568 ) ) ;
#23056 = CARTESIAN_POINT ( 'NONE',  ( 11.35316468750000141, 15.78124999658601624, 0.000000000000000000 ) ) ;
#23057 = CARTESIAN_POINT ( 'NONE',  ( -4.556349186104047710, -10.99999999999999822, 92.96875000409676204 ) ) ;
#23058 = CARTESIAN_POINT ( 'NONE',  ( 4.193070328474942876, 10.26769692241485643, 64.12609983179218887 ) ) ;
#23059 = CARTESIAN_POINT ( 'NONE',  ( -26.56734541678242678, 197.3750000013656063, 166.5412658750003345 ) ) ;
#23060 = CARTESIAN_POINT ( 'NONE',  ( 7.999999999999998224, 7.218749995903221972, 3.313708498984766049 ) ) ;
#23062 = CARTESIAN_POINT ( 'NONE',  ( 9.832129032723420536, 16.19791666325268054, -5.676582343749999815 ) ) ;
#23061 = CARTESIAN_POINT ( 'NONE',  ( 7.188101187500002709, 109.8125000020483952, 2.977408999572649151 ) ) ;
#23063 = CARTESIAN_POINT ( 'NONE',  ( 5.656854249492374365, 5.656854249492375253, 21.26780277982336642 ) ) ;
#23064 =( BOUNDED_CURVE ( )  B_SPLINE_CURVE ( 2, ( #40208, #63585, #57579, #68138, #12279, #34573, #63212, #51156, #29269 ),
 .UNSPECIFIED., .F., .F. ) 
 B_SPLINE_CURVE_WITH_KNOTS ( ( 3, 2, 2, 2, 3 ),
 ( 0.7333333333333339477, 0.7416666666666673624, 0.7500000000000006661, 0.7583333333333339699, 0.7666666666666673846 ),
 .UNSPECIFIED. ) 
 CURVE ( )  GEOMETRIC_REPRESENTATION_ITEM ( )  RATIONAL_B_SPLINE_CURVE ( ( 0.9999999999999938938, 0.9238795325112928447, 1.000000000000000000, 0.9238795325112867385, 1.000000000000000000, 0.9238795325112867385, 1.000000000000000000, 0.9238795325112806323, 1.000000000000005995 ) ) 
 REPRESENTATION_ITEM ( '' )  );
#23065 = CARTESIAN_POINT ( 'NONE',  ( 3.042071309553159519, 129.7395833299193555, 11.35316468750000141 ) ) ;
#23066 = CARTESIAN_POINT ( 'NONE',  ( -7.320508075688773708, 103.7499999931720396, -7.320508075688774596 ) ) ;
#23067 = CARTESIAN_POINT ( 'NONE',  ( 7.188101187500000044, 113.2812500020483952, -8.802885111219163269E-16 ) ) ;
#23068 = CARTESIAN_POINT ( 'NONE',  ( -7.999999999999998224, 120.7812500040967905, 3.313708498984766049 ) ) ;
#23069 = CARTESIAN_POINT ( 'NONE',  ( -24.54126587499998635, 208.3750000013656063, 171.4326545832179818 ) ) ;
#23070 = CARTESIAN_POINT ( 'NONE',  ( -5.000000000000000000, -52.15374455614144722, -42.28282461816569082 ) ) ;
#23071 = EDGE_LOOP ( 'NONE', ( #71531, #64948, #55743, #51785 ) ) ;
#23072 = CARTESIAN_POINT ( 'NONE',  ( -11.35316468749999785, 8.385416663252684089, -3.042071309553167957 ) ) ;
#23073 = CARTESIAN_POINT ( 'NONE',  ( -2.828427124746190735, 20.12499999726881228, -2.828427124746191623 ) ) ;
#23074 = CARTESIAN_POINT ( 'NONE',  ( -6.676582343750001591, 296.4531250017069510, 0.000000000000000000 ) ) ;
#23075 = CARTESIAN_POINT ( 'NONE',  ( -8.311093377946841443, 138.9062499965859843, 8.311093377946834337 ) ) ;
#23076 = CARTESIAN_POINT ( 'NONE',  ( -7.999999999999989342, -3.313708498984762496, 26.48030278432982954 ) ) ;
#23077 = VECTOR ( 'NONE', #50800, 1000.000000000000000 ) ;
#23078 = CARTESIAN_POINT ( 'NONE',  ( 2.828427124746153876, 207.0000000027312126, 144.8284271247462129 ) ) ;
#23079 = CARTESIAN_POINT ( 'NONE',  ( 5.656854249492381470, 103.0625000000000000, 5.656854249492379694 ) ) ;
#23080 = CARTESIAN_POINT ( 'NONE',  ( 10.18810118749999916, 1.247682550866122264E-15, 100.2812500020483810 ) ) ;
#23081 = ORIENTED_EDGE ( 'NONE', *, *, #35269, .F. ) ;
#23082 = CARTESIAN_POINT ( 'NONE',  ( 5.000000000000000000, 11.82742353449332917, 68.45184936927694253 ) ) ;
#23083 = CARTESIAN_POINT ( 'NONE',  ( 11.00000000000010836, -4.556349186103939353, 100.8437500040967763 ) ) ;
#23084 = CARTESIAN_POINT ( 'NONE',  ( 3.458734125000015869, 201.1875000013656063, 198.0000000000000284 ) ) ;
#23085 = CARTESIAN_POINT ( 'NONE',  ( 9.832129032723416984, 80.67708332991935549, 5.676582343750006032 ) ) ;
#23086 = ORIENTED_EDGE ( 'NONE', *, *, #1329, .T. ) ;
#23087 = CARTESIAN_POINT ( 'NONE',  ( 7.204075437095968759, -7.204075437095966983, 105.7187500020483810 ) ) ;
#23088 = CARTESIAN_POINT ( 'NONE',  ( -1.881053915767121776, 12.74999999863440969, -4.541265875000002339 ) ) ;
#23089 = ORIENTED_EDGE ( 'NONE', *, *, #31345, .T. ) ;
#23090 = ORIENTED_EDGE ( 'NONE', *, *, #62693, .T. ) ;
#23091 = CARTESIAN_POINT ( 'NONE',  ( 7.188101187500000044, 25.96874999795161543, 0.000000000000000000 ) ) ;
#23092 = CARTESIAN_POINT ( 'NONE',  ( 38.00000000000000000, 52.99999999999992895, -6.791607979884335933E-15 ) ) ;
#23093 = VECTOR ( 'NONE', #14118, 1000.000000000000000 ) ;
#23094 = CARTESIAN_POINT ( 'NONE',  ( -5.000000000000001776, -67.10993666412726100, -23.06595724273644876 ) ) ;
#23095 = CARTESIAN_POINT ( 'NONE',  ( 2.977408999572651815, 26.06249999795161543, 7.188101187500000933 ) ) ;
#23096 = CARTESIAN_POINT ( 'NONE',  ( -7.204075437095965206, -7.204075437095968759, 105.7187500020483810 ) ) ;
#23097 = CIRCLE ( 'NONE', #73717, 3.999999999999986233 ) ;
#23098 = CARTESIAN_POINT ( 'NONE',  ( 11.00000000000010658, 4.556349186103942017, 75.34374999999998579 ) ) ;
#23099 = CARTESIAN_POINT ( 'NONE',  ( -2.828427124746190735, 10.12499999726881406, -2.828427124746191623 ) ) ;
#23100 = CARTESIAN_POINT ( 'NONE',  ( 3.211159895383561835, 0.4374999986344066949, -3.211159895383561835 ) ) ;
#23101 = EDGE_LOOP ( 'NONE', ( #38897, #42931, #21526, #37939, #7460, #12891 ) ) ;
#23102 = EDGE_CURVE ( 'NONE', #70626, #34562, #63269, .T. ) ;
#23103 = DIRECTION ( 'NONE',  ( -0.000000000000000000, 1.000000000000000000, -4.476705744456276341E-16 ) ) ;
#23104 = CARTESIAN_POINT ( 'NONE',  ( -1.432654583217607192, 201.2500000013656063, 194.5412658750000219 ) ) ;
#23105 = CARTESIAN_POINT ( 'NONE',  ( -24.54126587499999701, 206.1875000013656063, 170.0000000000002842 ) ) ;
#23106 = CARTESIAN_POINT ( 'NONE',  ( 1.881053915767121776, 9.499999998634406140, -4.541265875000002339 ) ) ;
#23107 = CARTESIAN_POINT ( 'NONE',  ( -4.000000000000001776, 10.24999999726881406, -4.898587196589415787E-16 ) ) ;
#23108 = CARTESIAN_POINT ( 'NONE',  ( 7.188101187499991163, 2.977408999572648707, 21.83030278187175810 ) ) ;
#23109 = ORIENTED_EDGE ( 'NONE', *, *, #66003, .F. ) ;
#23110 = VERTEX_POINT ( 'NONE', #17463 ) ;
#23111 = CARTESIAN_POINT ( 'NONE',  ( 7.204075437095966983, 7.204075437095967871, 112.0937500020483810 ) ) ;
#23112 = CARTESIAN_POINT ( 'NONE',  ( -9.999999999999998224, 220.2083333333333428, 2.679491924311235174 ) ) ;
#23113 = CARTESIAN_POINT ( 'NONE',  ( -25.17157287525382614, 206.8750000000000284, 167.1715728752541565 ) ) ;
#23114 = CARTESIAN_POINT ( 'NONE',  ( 3.458734125000015425, 200.9375000013656063, 198.0000000000000284 ) ) ;
#23115 = CARTESIAN_POINT ( 'NONE',  ( 30.44569435410879166, 194.8125000013656063, 167.5543056458910485 ) ) ;
#23116 = CARTESIAN_POINT ( 'NONE',  ( 7.320508075688771044, 84.37499999999998579, 7.320508075688775484 ) ) ;
#23117 = AXIS2_PLACEMENT_3D ( 'NONE', #66018, #2281, #46911 ) ;
#23118 = CARTESIAN_POINT ( 'NONE',  ( 8.000000000000001776, 121.1562499999999858, 3.313708498984759387 ) ) ;
#23119 = CARTESIAN_POINT ( 'NONE',  ( 6.951808397369818766E-16, 62.34374999658602690, -11.35316468750000141 ) ) ;
#23120 = CARTESIAN_POINT ( 'NONE',  ( 4.242640687119285658, 289.6249999999999432, -4.242640687119286547 ) ) ;
#23121 = EDGE_CURVE ( 'NONE', #24215, #28711, #34104, .T. ) ;
#23122 = ORIENTED_EDGE ( 'NONE', *, *, #23692, .F. ) ;
#23123 = CARTESIAN_POINT ( 'NONE',  ( 2.828427124746208943, 203.6250000000000284, 195.1715728752538439 ) ) ;
#23124 = CARTESIAN_POINT ( 'NONE',  ( -1.308779242298911516, -10.28008949575750641, 63.61387346696258049 ) ) ;
#23125 = CARTESIAN_POINT ( 'NONE',  ( 2.828427124746153876, 195.0000000027312126, 144.8284271247462129 ) ) ;
#23126 = CARTESIAN_POINT ( 'NONE',  ( 5.841566664369303132E-15, 13.85640646055103531, -14.80000000000000071 ) ) ;
#23127 = CARTESIAN_POINT ( 'NONE',  ( 0.000000000000000000, 300.0000000000000000, 0.000000000000000000 ) ) ;
#23128 = CARTESIAN_POINT ( 'NONE',  ( -6.123233995736766282E-16, 243.7500000000000284, -10.00000000000000000 ) ) ;
#23129 = CARTESIAN_POINT ( 'NONE',  ( -7.778174593052023411, 7.778174593052023411, 73.00000000409677625 ) ) ;
#23130 = CARTESIAN_POINT ( 'NONE',  ( -7.778174593052023411, 7.778174593052023411, 117.8125000000000000 ) ) ;
#23131 = CARTESIAN_POINT ( 'NONE',  ( -8.660254037844390851, 202.9166666666666856, 4.999999999999998224 ) ) ;
#23132 = CARTESIAN_POINT ( 'NONE',  ( 7.188101187499992051, 2.977408999572647819, 17.70530278187175455 ) ) ;
#23133 = CARTESIAN_POINT ( 'NONE',  ( 11.35316468749999785, 165.8854166632526415, 3.042071309553174174 ) ) ;
#23134 = CARTESIAN_POINT ( 'NONE',  ( -9.999999999999998224, 37.50000000000000711, -1.224646799147353059E-15 ) ) ;
#23135 = CARTESIAN_POINT ( 'NONE',  ( 4.999999999999993783, 176.0416666598387110, 8.660254037844390851 ) ) ;
#23137 = DIRECTION ( 'NONE',  ( 0.000000000000000000, 0.000000000000000000, 1.000000000000000000 ) ) ;
#23136 = PLANE ( 'NONE',  #73199 ) ;
#23138 = ORIENTED_EDGE ( 'NONE', *, *, #7790, .F. ) ;
#23139 = CARTESIAN_POINT ( 'NONE',  ( -1.432654583217662481, 196.1250000013655779, 145.4587341250000634 ) ) ;
#23140 = CARTESIAN_POINT ( 'NONE',  ( 9.832129032723420536, 41.51041666325268409, -5.676582343749999815 ) ) ;
#23141 = CARTESIAN_POINT ( 'NONE',  ( 11.00000000000000000, 4.556349186104045934, 108.5312500040967905 ) ) ;
#23142 = CARTESIAN_POINT ( 'NONE',  ( -31.45873412499999944, 208.6875000013656063, 170.0000000000004547 ) ) ;
#23143 = DIRECTION ( 'NONE',  ( -0.000000000000000000, -1.000000000000000000, -0.000000000000000000 ) ) ;
#23145 = CYLINDRICAL_SURFACE ( 'NONE', #5302, 11.00000000000000000 ) ;
#23144 = CARTESIAN_POINT ( 'NONE',  ( -3.313708498984830442, 116.4687500040967763, 7.999999999999930722 ) ) ;
#23146 = CARTESIAN_POINT ( 'NONE',  ( -22.88006642067102092, -50.28934137640644053, 190.9374477509714438 ) ) ;
#23147 = CARTESIAN_POINT ( 'NONE',  ( -2.754378923186476579E-14, 199.1875000013655779, 145.4587341250000350 ) ) ;
#23148 = CARTESIAN_POINT ( 'NONE',  ( 7.320508075688774596, 62.49999999317202537, -7.320508075688774596 ) ) ;
#23149 = CARTESIAN_POINT ( 'NONE',  ( -4.401442555609581635E-16, 98.28125000204838102, -7.188101187500000044 ) ) ;
#23150 = CARTESIAN_POINT ( 'NONE',  ( 1.881053915767121776, 12.62499999863441147, -4.541265875000002339 ) ) ;
#23151 = CARTESIAN_POINT ( 'NONE',  ( 7.320508075688934468, 214.3750000000000853, 7.320508075688938909 ) ) ;
#23152 = CARTESIAN_POINT ( 'NONE',  ( 7.999999999999991118, 9.797174393178815797E-16, 4.580302779823363757 ) ) ;
#23153 = CARTESIAN_POINT ( 'NONE',  ( -4.000000000000002665, 4.312499997268813168, 1.656854249492380582 ) ) ;
#23154 = ORIENTED_EDGE ( 'NONE', *, *, #2363, .F. ) ;
#23155 = EDGE_LOOP ( 'NONE', ( #63342, #16515, #55098, #28761 ) ) ;
#23156 = CARTESIAN_POINT ( 'NONE',  ( -6.735557395310442023E-16, 11.00000000000000000, 116.1249999999999858 ) ) ;
#23157 = CARTESIAN_POINT ( 'NONE',  ( -4.088227598258586603E-16, 299.3593750017070079, -6.676582343750001591 ) ) ;
#23158 = FILL_AREA_STYLE ('',( #39765 ) ) ;
#23159 = CARTESIAN_POINT ( 'NONE',  ( 4.898587196589412829E-16, 15.37500000000000355, -8.000000000000000000 ) ) ;
#23160 = CARTESIAN_POINT ( 'NONE',  ( 9.832129032723416984, 150.3645833299193555, 5.676582343750006032 ) ) ;
#23161 = DIRECTION ( 'NONE',  ( -0.000000000000000000, 1.000000000000000000, 4.476705744456276341E-16 ) ) ;
#23162 = CARTESIAN_POINT ( 'NONE',  ( -4.220049686691937474, -10.18810118749999738, 81.43750000204836681 ) ) ;
#23163 = CARTESIAN_POINT ( 'NONE',  ( -30.65744098404955409, 194.5307006980096105, 167.6645244444113132 ) ) ;
#23164 = CARTESIAN_POINT ( 'NONE',  ( 2.751064625579944321E-14, 204.7500000000000284, 194.0000000000000568 ) ) ;
#23165 = CARTESIAN_POINT ( 'NONE',  ( -3.673940397442060854E-16, 297.8125000034140157, -6.000000000000001776 ) ) ;
#23166 = CARTESIAN_POINT ( 'NONE',  ( -4.220049686691937474, -10.18810118749999738, 116.3125000020483668 ) ) ;
#23167 = ORIENTED_EDGE ( 'NONE', *, *, #73025, .T. ) ;
#23168 = CARTESIAN_POINT ( 'NONE',  ( 30.95907247477800084, -35.68886171965652920, 172.6269442939296823 ) ) ;
#23169 = AXIS2_PLACEMENT_3D ( 'NONE', #32566, #15928, #9166 ) ;
#23170 = CARTESIAN_POINT ( 'NONE',  ( 14.81870148747585958, 177.5301863014532842, 142.6802073050831439 ) ) ;
#23171 = CARTESIAN_POINT ( 'NONE',  ( -11.35316468750000141, 133.5937499965860127, -1.390361679473963753E-15 ) ) ;
#23172 = CARTESIAN_POINT ( 'NONE',  ( -1.432654583217607858, 197.6250000013656063, 201.4587341250000065 ) ) ;
#23173 = CARTESIAN_POINT ( 'NONE',  ( 2.977408999572650927, 26.62499999795161543, -7.188101187500000933 ) ) ;
#23174 = CARTESIAN_POINT ( 'NONE',  ( -4.220049686691935698, 10.18810118749999916, 75.25000000204836681 ) ) ;
#23175 = CARTESIAN_POINT ( 'NONE',  ( -2.085542519210945728E-15, 29.84374999658601624, 11.35316468750000141 ) ) ;
#23177 = VERTEX_POINT ( 'NONE', #22007 ) ;
#23176 =( BOUNDED_CURVE ( )  B_SPLINE_CURVE ( 2, ( #44904, #9458, #62241, #4922, #56606, #10569, #33599, #27537, #10199 ),
 .UNSPECIFIED., .F., .F. ) 
 B_SPLINE_CURVE_WITH_KNOTS ( ( 3, 2, 2, 2, 3 ),
 ( 0.3833333333333335813, 0.3916666666666669405, 0.4000000000000003553, 0.4083333333333337145, 0.4166666666666671293 ),
 .UNSPECIFIED. ) 
 CURVE ( )  GEOMETRIC_REPRESENTATION_ITEM ( )  RATIONAL_B_SPLINE_CURVE ( ( 0.9999999999999980016, 0.9238795325112887369, 1.000000000000000000, 0.9238795325112867385, 1.000000000000000000, 0.9238795325112867385, 1.000000000000000000, 0.9238795325112826307, 1.000000000000003997 ) ) 
 REPRESENTATION_ITEM ( '' )  );
#23178 = CARTESIAN_POINT ( 'NONE',  ( 5.000000000000001776, 37.70833332650536818, -8.660254037844389075 ) ) ;
#23180 = CARTESIAN_POINT ( 'NONE',  ( 1.881053915767121998, 2.624999998634407028, -4.541265875000002339 ) ) ;
#23179 =( BOUNDED_CURVE ( )  B_SPLINE_CURVE ( 2, ( #28795, #40494, #46891, #57109, #18225, #34488, #5799, #69539, #17850 ),
 .UNSPECIFIED., .F., .F. ) 
 B_SPLINE_CURVE_WITH_KNOTS ( ( 3, 2, 2, 2, 3 ),
 ( 0.7666666666666673846, 0.7750000000000006883, 0.7833333333333339921, 0.7916666666666672958, 0.8000000000000007105 ),
 .UNSPECIFIED. ) 
 CURVE ( )  GEOMETRIC_REPRESENTATION_ITEM ( )  RATIONAL_B_SPLINE_CURVE ( ( 0.9999999999999938938, 0.9238795325112928447, 1.000000000000000000, 0.9238795325112867385, 1.000000000000000000, 0.9238795325112867385, 1.000000000000000000, 0.9238795325112806323, 1.000000000000005995 ) ) 
 REPRESENTATION_ITEM ( '' )  );
#23181 = CARTESIAN_POINT ( 'NONE',  ( 1.471067592899761672E-15, -8.008118988124991233, 14.88811528394063011 ) ) ;
#23182 = CARTESIAN_POINT ( 'NONE',  ( -2.839093476692135984E-14, 207.9375000013656063, 138.5412658750000503 ) ) ;
#23183 = EDGE_CURVE ( 'NONE', #5956, #2769, #45060, .T. ) ;
#23184 = CARTESIAN_POINT ( 'NONE',  ( 5.082755093536325930, 9.656249997951610098, -5.082755093536325930 ) ) ;
#23185 = CARTESIAN_POINT ( 'NONE',  ( 6.000000000000001776, 295.5625000034140157, -7.347880794884121708E-16 ) ) ;
#23186 = CARTESIAN_POINT ( 'NONE',  ( -48.72590952693009569, 141.0982348105912365, 60.31981441777212183 ) ) ;
#23187 = CARTESIAN_POINT ( 'NONE',  ( -7.188101187500001821, 5.999999997951610098, -2.977408999572651371 ) ) ;
#23188 = CARTESIAN_POINT ( 'NONE',  ( 1.320432766682872962E-15, -7.188101187499992051, 13.86155278187175455 ) ) ;
#23189 = AXIS2_PLACEMENT_3D ( 'NONE', #46825, #28458, #39772 ) ;
#23190 = CARTESIAN_POINT ( 'NONE',  ( -3.042071309553173730, 149.6354166632526983, 11.35316468749999785 ) ) ;
#23191 = CARTESIAN_POINT ( 'NONE',  ( 7.204075437095966983, 7.204075437095967871, 71.59375000204836681 ) ) ;
#23192 = CARTESIAN_POINT ( 'NONE',  ( -24.54126587500000412, 207.5000000013655779, 168.5673454167827003 ) ) ;
#23193 = CARTESIAN_POINT ( 'NONE',  ( -3.673940397442060854E-16, 298.8125000034140157, -6.000000000000001776 ) ) ;
#23194 = CARTESIAN_POINT ( 'NONE',  ( 4.541265875000001451, 20.37499999863441147, 1.881053915767124440 ) ) ;
#23195 = ORIENTED_EDGE ( 'NONE', *, *, #55597, .F. ) ;
#23196 = EDGE_CURVE ( 'NONE', #19863, #71793, #16983, .T. ) ;
#23197 = CARTESIAN_POINT ( 'NONE',  ( 4.000000000000015099, 198.6875000027312126, 196.3431457505076594 ) ) ;
#23198 = CARTESIAN_POINT ( 'NONE',  ( 1.656854249492348607, 206.1875000000000568, 138.0000000000000568 ) ) ;
#23199 = CARTESIAN_POINT ( 'NONE',  ( -25.17157287525385811, 200.0000000027312126, 167.1715728752541281 ) ) ;
#23200 = EDGE_CURVE ( 'NONE', #37587, #12265, #10839, .T. ) ;
#23201 = CARTESIAN_POINT ( 'NONE',  ( 6.123233995736767268E-16, 56.25000000000000000, -10.00000000000000178 ) ) ;
#23202 = CARTESIAN_POINT ( 'NONE',  ( -4.898587196589407898E-16, 7.999999999999991118, 8.142802783920144449 ) ) ;
#23203 = VERTEX_POINT ( 'NONE', #24601 ) ;
#23204 = CARTESIAN_POINT ( 'NONE',  ( -1.320432766682874540E-15, 16.59374999795161543, 7.188101187500000044 ) ) ;
#23205 = B_SPLINE_CURVE_WITH_KNOTS ( 'NONE', 3,
 ( #47279, #60360, #3779, #41631 ),
 .UNSPECIFIED., .F., .F.,
 ( 4, 4 ),
 ( 1.537509207123490056E-15, 0.0004743803571073818546 ),
 .UNSPECIFIED. ) ;
#23206 = CARTESIAN_POINT ( 'NONE',  ( -10.00000000000000178, 209.3749999931720538, -1.224646799147353454E-15 ) ) ;
#23207 = CARTESIAN_POINT ( 'NONE',  ( -10.00000000000000178, 44.37499999317203248, -1.224646799147353454E-15 ) ) ;
#23208 = CARTESIAN_POINT ( 'NONE',  ( -10.00000000000000355, 42.70833333333333570, 2.679491924311223183 ) ) ;
#23209 = CARTESIAN_POINT ( 'NONE',  ( 5.082755093536325042, 107.4687500020483952, -5.082755093536325930 ) ) ;
#23210 = CARTESIAN_POINT ( 'NONE',  ( -29.43265458321766914, 206.7500000013655779, 166.5412658750003629 ) ) ;
#23211 = CARTESIAN_POINT ( 'NONE',  ( 6.000000000000003553, 299.5625000000000000, -2.485281374238571761 ) ) ;
#23212 = EDGE_CURVE ( 'NONE', #9014, #47712, #18093, .T. ) ;
#23214 = FACE_OUTER_BOUND ( 'NONE', #53605, .T. ) ;
#23213 = CARTESIAN_POINT ( 'NONE',  ( 1.469576158976823947E-15, 112.0625000040967905, 8.000000000000000000 ) ) ;
#23215 = ORIENTED_EDGE ( 'NONE', *, *, #21425, .T. ) ;
#23216 = CARTESIAN_POINT ( 'NONE',  ( -11.35316468749999608, 244.1145833367472733, 3.042071309553173730 ) ) ;
#23217 = CIRCLE ( 'NONE', #20781, 12.00000000000000178 ) ;
#23218 = CARTESIAN_POINT ( 'NONE',  ( -7.188101187499991163, 2.977408999572646930, 15.26780278187175455 ) ) ;
#23219 = CARTESIAN_POINT ( 'NONE',  ( -5.000000000000005329, 10.20833332650536640, 8.660254037844387298 ) ) ;
#23220 = CARTESIAN_POINT ( 'NONE',  ( -10.04299372122919820, 220.0000000000001137, 2.556404203812648213 ) ) ;
#23221 = CARTESIAN_POINT ( 'NONE',  ( 1.491046635511791134E-11, 146.2499999999988631, -9.999999999999998224 ) ) ;
#23222 = CARTESIAN_POINT ( 'NONE',  ( -8.660254037844387298, 162.0833333333333712, -5.000000000000004441 ) ) ;
#23223 = CARTESIAN_POINT ( 'NONE',  ( 2.449293598294707893E-16, 3.250000000000000444, -4.000000000000001776 ) ) ;
#23224 = CARTESIAN_POINT ( 'NONE',  ( -3.313708498984816231, 119.2812499999999858, 7.999999999999943157 ) ) ;
#23225 = CARTESIAN_POINT ( 'NONE',  ( 2.143582570168941270, 90.06435469398866189, -8.000000000000000000 ) ) ;
#23226 = CARTESIAN_POINT ( 'NONE',  ( 3.042071309553167069, 122.1354166632526841, -11.35316468749999785 ) ) ;
#23227 = CYLINDRICAL_SURFACE ( 'NONE', #60116, 4.000000000000001776 ) ;
#23228 = CARTESIAN_POINT ( 'NONE',  ( 2.775557561562891351E-14, 5.999999999999950262, 170.0000000000000284 ) ) ;
#23231 = LINE ( 'NONE', #29273, #69974 ) ;
#23230 = CARTESIAN_POINT ( 'NONE',  ( 27.99999999999996803, 197.9375000013655779, 166.5412658749999082 ) ) ;
#23229 = CARTESIAN_POINT ( 'NONE',  ( 26.56734541678237704, 196.2500000013656631, 166.5412658749999650 ) ) ;
#23232 = ORIENTED_EDGE ( 'NONE', *, *, #40236, .T. ) ;
#23233 = AXIS2_PLACEMENT_3D ( 'NONE', #60572, #36095, #65854 ) ;
#23234 = CARTESIAN_POINT ( 'NONE',  ( -1.656854249492297093, 205.8125000000000284, 194.0000000000000568 ) ) ;
#23235 = DIRECTION ( 'NONE',  ( -1.000000000000000000, 0.000000000000000000, 0.000000000000000000 ) ) ;
#23236 = CARTESIAN_POINT ( 'NONE',  ( 2.028713400070581319, -7.761291288302830438, -0.000000000000000000 ) ) ;
#23237 = CARTESIAN_POINT ( 'NONE',  ( 5.000000000000000000, -64.62379132009250782, -24.09319349500408691 ) ) ;
#23238 = EDGE_CURVE ( 'NONE', #66596, #16961, #25775, .T. ) ;
#23239 = CARTESIAN_POINT ( 'NONE',  ( 10.00000000000000000, 16.66666665983870033, 2.679491924311236062 ) ) ;
#23240 = CARTESIAN_POINT ( 'NONE',  ( -4.401442555609581635E-16, 122.2812500020483810, -7.188101187500000044 ) ) ;
#23241 = CARTESIAN_POINT ( 'NONE',  ( 4.541265875000002339, 20.37499999863441147, -1.881053915767121554 ) ) ;
#23242 = CARTESIAN_POINT ( 'NONE',  ( -3.496982156821212939, 68.06496700477899253, -20.41687962716563121 ) ) ;
#23243 = CARTESIAN_POINT ( 'NONE',  ( 7.999999999999991118, 9.797174393178815797E-16, 21.08030277982336642 ) ) ;
#23245 = CARTESIAN_POINT ( 'NONE',  ( 2.449293598294707893E-16, 5.999999997268813168, -4.000000000000001776 ) ) ;
#23244 = CARTESIAN_POINT ( 'NONE',  ( 3.486804365889302648, -7.201712369346796372, 3.176373552203626272E-17 ) ) ;
#23246 = CARTESIAN_POINT ( 'NONE',  ( 11.35316468750000141, 110.7812499965860269, 0.000000000000000000 ) ) ;
#23247 = ORIENTED_EDGE ( 'NONE', *, *, #45465, .F. ) ;
#23248 = CARTESIAN_POINT ( 'NONE',  ( -2.828427124746190735, 19.12499999726881228, -2.828427124746191623 ) ) ;
#23249 = CARTESIAN_POINT ( 'NONE',  ( -1.320432766682874540E-15, 24.09374999795161543, 7.188101187500000044 ) ) ;
#23250 = CARTESIAN_POINT ( 'NONE',  ( 2.752039609470550924E-11, 41.24999999999786127, -9.999999999999998224 ) ) ;
#23251 = CARTESIAN_POINT ( 'NONE',  ( -11.35316468749999963, 249.2187500034139873, 0.000000000000000000 ) ) ;
#23252 = CARTESIAN_POINT ( 'NONE',  ( -11.35316468750000141, 108.2812499965860269, -1.390361679473963753E-15 ) ) ;
#23253 = EDGE_LOOP ( 'NONE', ( #21456, #41919, #7817, #42586 ) ) ;
#23254 = CARTESIAN_POINT ( 'NONE',  ( 0.000000000000000000, 265.0000000000000000, -10.00000000000000000 ) ) ;
#23255 = CARTESIAN_POINT ( 'NONE',  ( 4.220049686691934809, 10.18810118749999916, 101.6875000020483810 ) ) ;
#23256 = CARTESIAN_POINT ( 'NONE',  ( 10.00000000000000178, 226.8749999931720254, 0.000000000000000000 ) ) ;
#23257 = CARTESIAN_POINT ( 'NONE',  ( -3.458734124999960358, 201.6250000013656063, 196.5673454167823877 ) ) ;
#23258 = CARTESIAN_POINT ( 'NONE',  ( -38.00000000000002132, 39.09128788536428800, 65.00000000000000000 ) ) ;
#23260 = CARTESIAN_POINT ( 'NONE',  ( -5.676582343749998039, 102.4479166632526841, -9.832129032723420536 ) ) ;
#23259 = CARTESIAN_POINT ( 'NONE',  ( -32.00000000000000000, 202.2500000000000000, 170.0000000000003979 ) ) ;
#23261 = CARTESIAN_POINT ( 'NONE',  ( 3.313708498984756279, 7.999999999999991118, 15.54905278392014623 ) ) ;
#23262 = CARTESIAN_POINT ( 'NONE',  ( -30.44569435410883074, 195.8125000013656063, 167.5543056458915885 ) ) ;
#23263 = CARTESIAN_POINT ( 'NONE',  ( 8.660254037844389075, 170.4166666666666856, -5.000000000000000000 ) ) ;
#23264 = ORIENTED_EDGE ( 'NONE', *, *, #31719, .F. ) ;
#23265 = CARTESIAN_POINT ( 'NONE',  ( 10.00000000000000000, 196.6666666598386826, 2.679491924311236062 ) ) ;
#23266 = CARTESIAN_POINT ( 'NONE',  ( 2.449293598294707893E-16, 6.250000000000000000, -4.000000000000001776 ) ) ;
#23267 = FACE_OUTER_BOUND ( 'NONE', #49361, .T. ) ;
#23268 = CARTESIAN_POINT ( 'NONE',  ( 11.35316468749999963, 91.30208332991932707, -3.042071309553165293 ) ) ;
#23269 = CARTESIAN_POINT ( 'NONE',  ( 4.721056650415999201, 291.0781250017069510, -4.721056650415999201 ) ) ;
#23270 = CARTESIAN_POINT ( 'NONE',  ( 4.401442555609581635E-16, 7.218749997951610986, -7.188101187500000044 ) ) ;
#23271 = CARTESIAN_POINT ( 'NONE',  ( 4.220049686691941027, -10.18810118749999738, 92.50000000204838102 ) ) ;
#23272 = CARTESIAN_POINT ( 'NONE',  ( 5.676582343750001591, 226.6145833299193839, -9.832129032723420536 ) ) ;
#23273 = ORIENTED_EDGE ( 'NONE', *, *, #53513, .T. ) ;
#23274 = CARTESIAN_POINT ( 'NONE',  ( 5.656854249492376141, -5.656854249492374365, 26.89280277982336642 ) ) ;
#23275 = DIRECTION ( 'NONE',  ( -0.000000000000000000, -0.000000000000000000, -1.000000000000000000 ) ) ;
#23276 = CARTESIAN_POINT ( 'NONE',  ( 11.35316468749999963, 220.9895833299193555, -3.042071309553165293 ) ) ;
#23277 = DIRECTION ( 'NONE',  ( -0.000000000000000000, 1.000000000000000000, 0.000000000000000000 ) ) ;
#23278 = CARTESIAN_POINT ( 'NONE',  ( 6.676582343750004256, 294.8906250017069510, 2.765530957081995478 ) ) ;
#23279 = ORIENTED_EDGE ( 'NONE', *, *, #19552, .F. ) ;
#23280 = CARTESIAN_POINT ( 'NONE',  ( 1.656854249492390574, 202.3125000027312126, 138.0000000000000853 ) ) ;
#23281 = CARTESIAN_POINT ( 'NONE',  ( 11.35316468749999785, 205.8854166632526699, 3.042071309553174174 ) ) ;
#23282 =( BOUNDED_CURVE ( )  B_SPLINE_CURVE ( 2, ( #66989, #71889, #31916, #20956, #32295, #20582, #33060, #73393, #56058 ),
 .UNSPECIFIED., .F., .F. ) 
 B_SPLINE_CURVE_WITH_KNOTS ( ( 3, 2, 2, 2, 3 ),
 ( 0.2631578947368420907, 0.2697368421052631637, 0.2763157894736841813, 0.2828947368421051989, 0.2894736842105262720 ),
 .UNSPECIFIED. ) 
 CURVE ( )  GEOMETRIC_REPRESENTATION_ITEM ( )  RATIONAL_B_SPLINE_CURVE ( ( 1.000000000000000000, 0.9238795325112867385, 1.000000000000000000, 0.9238795325112867385, 1.000000000000000000, 0.9238795325112867385, 1.000000000000000000, 0.9238795325112874046, 0.9999999999999993339 ) ) 
 REPRESENTATION_ITEM ( '' )  );
#23283 = CARTESIAN_POINT ( 'NONE',  ( -4.220049686691935698, 10.18810118749999916, 88.37500000204839523 ) ) ;
#23284 = CARTESIAN_POINT ( 'NONE',  ( -27.99999999999996447, 204.9375000013656063, 173.4587341250003760 ) ) ;
#23285 = CARTESIAN_POINT ( 'NONE',  ( -8.000000000000000000, 18.65625000000000355, -3.313708498984762496 ) ) ;
#23286 = ORIENTED_EDGE ( 'NONE', *, *, #6738, .T. ) ;
#23287 = CIRCLE ( 'NONE', #65441, 8.000000000000003553 ) ;
#23288 = CARTESIAN_POINT ( 'NONE',  ( 7.188101187500002709, 123.3125000020483810, 2.977408999572649151 ) ) ;
#23289 = CARTESIAN_POINT ( 'NONE',  ( -10.00000000000000178, 32.50000000000000000, -1.224646799147353454E-15 ) ) ;
#23290 =( BOUNDED_CURVE ( )  B_SPLINE_CURVE ( 2, ( #19145, #6733, #59162, #46707, #24796, #18417, #29376, #69731, #7100 ),
 .UNSPECIFIED., .F., .F. ) 
 B_SPLINE_CURVE_WITH_KNOTS ( ( 3, 2, 2, 2, 3 ),
 ( 0.8500000000000005329, 0.8583333333333339477, 0.8666666666666673624, 0.8750000000000007772, 0.8833333333333341919 ),
 .UNSPECIFIED. ) 
 CURVE ( )  GEOMETRIC_REPRESENTATION_ITEM ( )  RATIONAL_B_SPLINE_CURVE ( ( 0.9999999999999948930, 0.9238795325112918455, 1.000000000000000000, 0.9238795325112867385, 1.000000000000000000, 0.9238795325112867385, 1.000000000000000000, 0.9238795325112786339, 1.000000000000008216 ) ) 
 REPRESENTATION_ITEM ( '' )  );
#23291 = EDGE_CURVE ( 'NONE', #55580, #54420, #23496, .T. ) ;
#23292 = CARTESIAN_POINT ( 'NONE',  ( -36.86924962228702185, 37.99999999999999289, 134.0294372515228360 ) ) ;
#23293 = CARTESIAN_POINT ( 'NONE',  ( -10.18810118749999738, -4.220049686691941915, 77.12500000204838102 ) ) ;
#23294 = VERTEX_POINT ( 'NONE', #64237 ) ;
#23295 = VECTOR ( 'NONE', #11909, 1000.000000000000000 ) ;
#23296 = CARTESIAN_POINT ( 'NONE',  ( 4.000000000000001776, 2.749999997268813168, 0.000000000000000000 ) ) ;
#23297 = DIRECTION ( 'NONE',  ( 1.000000000000000000, -0.000000000000000000, -0.000000000000000000 ) ) ;
#23298 = SURFACE_STYLE_USAGE ( .BOTH. , #19758 ) ;
#23299 = CARTESIAN_POINT ( 'NONE',  ( -4.999999999999999112, -13.22058908515350062, 69.49198671174478648 ) ) ;
#23300 = CARTESIAN_POINT ( 'NONE',  ( 4.999999999999999112, -64.62627855237444408, 24.10294814404683450 ) ) ;
#23301 = CARTESIAN_POINT ( 'NONE',  ( -2.765530957081998142, 296.6406250017069510, 6.676582343750000703 ) ) ;
#23303 = CARTESIAN_POINT ( 'NONE',  ( 7.778174593052023411, -7.778174593052021635, 88.75000000409677625 ) ) ;
#23302 = CARTESIAN_POINT ( 'NONE',  ( -8.311093377946834337, 239.5312500034139873, 8.311093377946837890 ) ) ;
#23304 = CONTEXT_DEPENDENT_SHAPE_REPRESENTATION ( #40967, #74036 ) ;
#23305 = ORIENTED_EDGE ( 'NONE', *, *, #52160, .F. ) ;
#23306 = EDGE_CURVE ( 'NONE', #71352, #53888, #46510, .T. ) ;
#23307 = CARTESIAN_POINT ( 'NONE',  ( -6.951808397369817780E-16, 242.9687500034140157, -11.35316468749999963 ) ) ;
#23308 = CARTESIAN_POINT ( 'NONE',  ( -7.188101187499992051, 0.000000000000000000, 4.486552781871752771 ) ) ;
#23309 = VECTOR ( 'NONE', #32269, 1000.000000000000000 ) ;
#23310 = EDGE_CURVE ( 'NONE', #63044, #71522, #64611, .T. ) ;
#23311 = ORIENTED_EDGE ( 'NONE', *, *, #47030, .T. ) ;
#23312 = CARTESIAN_POINT ( 'NONE',  ( -7.204075437095965206, -7.204075437095968759, 69.34375000204836681 ) ) ;
#23313 = CARTESIAN_POINT ( 'NONE',  ( 11.35316468750000141, 91.09374999658602690, 0.000000000000000000 ) ) ;
#23314 = CARTESIAN_POINT ( 'NONE',  ( 0.000000000000000000, 300.0000000000000000, 0.000000000000000000 ) ) ;
#23315 = CARTESIAN_POINT ( 'NONE',  ( -4.556349186104045934, 11.00000000000000000, 84.71874999999998579 ) ) ;
#23318 = CARTESIAN_POINT ( 'NONE',  ( 6.676582343750001591, 288.1093750017069510, -8.176455196517173205E-16 ) ) ;
#23317 = CARTESIAN_POINT ( 'NONE',  ( 27.99999999999997158, 208.9375000013656063, 166.5412658749999082 ) ) ;
#23316 = CARTESIAN_POINT ( 'NONE',  ( 31.45873412500001010, 206.0000000013656347, 168.5673454167822740 ) ) ;
#23319 = ORIENTED_EDGE ( 'NONE', *, *, #29592, .T. ) ;
#23320 = CARTESIAN_POINT ( 'NONE',  ( -27.99999999999995737, 199.5000000000000000, 174.0000000000003695 ) ) ;
#23321 = CARTESIAN_POINT ( 'NONE',  ( 2.828427124746208943, 202.7500000027312126, 195.1715728752538439 ) ) ;
#23322 = CARTESIAN_POINT ( 'NONE',  ( -8.311093377946836114, 202.6562499965860127, -8.311093377946837890 ) ) ;
#23323 = CARTESIAN_POINT ( 'NONE',  ( 3.458734124999959914, 203.3750000013656063, 143.4326545832176976 ) ) ;
#23324 = CARTESIAN_POINT ( 'NONE',  ( 31.45873412500001010, 208.0000000013656347, 168.5673454167822740 ) ) ;
#23325 = CARTESIAN_POINT ( 'NONE',  ( 7.188101187499999156, 23.24999999795161187, 2.977408999572654924 ) ) ;
#23326 = CARTESIAN_POINT ( 'NONE',  ( 11.35316468749999963, 186.3020833299193555, -3.042071309553165293 ) ) ;
#23327 = CARTESIAN_POINT ( 'NONE',  ( 0.000000000000000000, 0.000000000000000000, -21.50000000000000000 ) ) ;
#23328 = CARTESIAN_POINT ( 'NONE',  ( -5.082755093536324154, 97.71875000204838102, 5.082755093536326818 ) ) ;
#23330 = CARTESIAN_POINT ( 'NONE',  ( 4.000000000000001776, 10.00000000000000000, 0.000000000000000000 ) ) ;
#23329 = LINE ( 'NONE', #73897, #54006 ) ;
#23331 = CARTESIAN_POINT ( 'NONE',  ( 2.780723358947928197E-16, 11.56249999863440614, -4.541265875000002339 ) ) ;
#23332 = CARTESIAN_POINT ( 'NONE',  ( 25.55430564589119413, 204.3125000013656063, 167.5543056458910485 ) ) ;
#23333 = CARTESIAN_POINT ( 'NONE',  ( 7.188101187499992051, 8.802885111219154394E-16, 8.611552781871752771 ) ) ;
#23334 = CARTESIAN_POINT ( 'NONE',  ( 6.951808397369818766E-16, 62.03124999658601979, -11.35316468750000141 ) ) ;
#23335 = EDGE_CURVE ( 'NONE', #5410, #54290, #36834, .T. ) ;
#23336 = CARTESIAN_POINT ( 'NONE',  ( -5.000000000000000000, -53.34243969459512869, 47.33397984627169564 ) ) ;
#23337 = CARTESIAN_POINT ( 'NONE',  ( 7.999999999999992895, -3.313708498984756279, 1.542802784329821097 ) ) ;
#23338 = ORIENTED_EDGE ( 'NONE', *, *, #50615, .T. ) ;
#23339 = CARTESIAN_POINT ( 'NONE',  ( -11.00000000000010303, -4.556349186103947346, 74.59374999999997158 ) ) ;
#23341 = CARTESIAN_POINT ( 'NONE',  ( -11.00000000000000000, 0.000000000000000000, 116.4999999999999858 ) ) ;
#23340 = AXIS2_PLACEMENT_3D ( 'NONE', #2829, #71105, #54150 ) ;
#23342 = CARTESIAN_POINT ( 'NONE',  ( -11.35316468750000141, 68.48958332991935549, 3.042071309553159963 ) ) ;
#23343 = CARTESIAN_POINT ( 'NONE',  ( 11.00000000000000000, 1.347111479062088405E-15, 67.93750000409676204 ) ) ;
#23344 = CARTESIAN_POINT ( 'NONE',  ( -2.754378923186476579E-14, 195.4375000013655779, 145.4587341250000350 ) ) ;
#23345 = DIRECTION ( 'NONE',  ( 1.000000000000000000, 0.000000000000000000, 0.000000000000000000 ) ) ;
#23347 = CARTESIAN_POINT ( 'NONE',  ( -8.311093377946841443, 63.90624999658601979, 8.311093377946834337 ) ) ;
#23346 = CARTESIAN_POINT ( 'NONE',  ( 7.188101187500000933, 95.00000000204838102, -2.977408999572651371 ) ) ;
#23348 = CARTESIAN_POINT ( 'NONE',  ( 7.999999999999991118, 3.313708498984757611, 1.674052779823364423 ) ) ;
#23349 = DIRECTION ( 'NONE',  ( 0.000000000000000000, 0.000000000000000000, 1.000000000000000000 ) ) ;
#23350 = CARTESIAN_POINT ( 'NONE',  ( 5.000000000000001776, 152.7083333265053682, -8.660254037844389075 ) ) ;
#23351 = CARTESIAN_POINT ( 'NONE',  ( 2.977408999572650039, 98.56250000204838102, -7.188101187500001821 ) ) ;
#23352 = CARTESIAN_POINT ( 'NONE',  ( -8.660254037844390851, 54.79166665983869677, 4.999999999999998224 ) ) ;
#23353 = CARTESIAN_POINT ( 'NONE',  ( 11.35316468750000141, 46.09374999658602690, 0.000000000000000000 ) ) ;
#23354 = CARTESIAN_POINT ( 'NONE',  ( 10.18810118749999916, 4.220049686691935698, 115.3750000020483810 ) ) ;
#23355 = CARTESIAN_POINT ( 'NONE',  ( 5.676582343749993598, 179.9479166632526983, 9.832129032723422313 ) ) ;
#23356 = EDGE_LOOP ( 'NONE', ( #15386, #12369, #55095 ) ) ;
#23357 = CARTESIAN_POINT ( 'NONE',  ( -1.780377099649267381, 67.71330631781158615, 20.13219356122112913 ) ) ;
#23358 = CARTESIAN_POINT ( 'NONE',  ( -7.204075437095965206, -7.204075437095968759, 72.34375000204836681 ) ) ;
#23360 = CARTESIAN_POINT ( 'NONE',  ( -8.311093377946836114, 177.6562499965859843, -8.311093377946837890 ) ) ;
#23359 = CARTESIAN_POINT ( 'NONE',  ( 1.656854249492406783, 18.56249999726881583, 3.999999999999976019 ) ) ;
#23361 = CARTESIAN_POINT ( 'NONE',  ( 7.999999999999991118, 9.797174393178815797E-16, 6.136552784329825094 ) ) ;
#23362 = EDGE_CURVE ( 'NONE', #37342, #50104, #25702, .T. ) ;
#23363 = CARTESIAN_POINT ( 'NONE',  ( -2.849036369511732440E-14, 205.3750000027312126, 138.0000000000000568 ) ) ;
#23364 = CARTESIAN_POINT ( 'NONE',  ( 2.679491924311225848, 251.6666666734946602, -10.00000000000000000 ) ) ;
#23365 = CARTESIAN_POINT ( 'NONE',  ( -32.00000000000000000, 206.2500000000000284, 170.0000000000003979 ) ) ;
#23366 = ORIENTED_EDGE ( 'NONE', *, *, #71978, .T. ) ;
#23367 = EDGE_CURVE ( 'NONE', #60693, #38468, #37421, .T. ) ;
#23368 = CARTESIAN_POINT ( 'NONE',  ( -11.35316468749999785, 168.3854166632526699, -3.042071309553167957 ) ) ;
#23369 = VECTOR ( 'NONE', #46206, 1000.000000000000000 ) ;
#23370 = CARTESIAN_POINT ( 'NONE',  ( -2.977408999572647819, -7.188101187499990274, 24.26780278187175810 ) ) ;
#23371 = CARTESIAN_POINT ( 'NONE',  ( 6.951808397369818766E-16, 132.3437499965860127, -11.35316468750000141 ) ) ;
#23372 = ADVANCED_FACE ( 'NONE', ( #66836 ), #65703, .T. ) ;
#23373 = CARTESIAN_POINT ( 'NONE',  ( -0.7361406979141749130, -9.967293815311105476, -0.5584673446549270892 ) ) ;
#23374 = VERTEX_POINT ( 'NONE', #66077 ) ;
#23375 = CARTESIAN_POINT ( 'NONE',  ( 4.541265875000002339, 13.43749999863440792, 0.000000000000000000 ) ) ;
#23376 = CARTESIAN_POINT ( 'NONE',  ( 1.469576158976823947E-15, 103.0625000040967763, 8.000000000000000000 ) ) ;
#23377 =( BOUNDED_CURVE ( )  B_SPLINE_CURVE ( 2, ( #68322, #21548, #11355, #16620, #33640, #45308, #73982, #38550, #5699, #16246, #61551, #27581, #15883, #38915, #50222, #39284, #62286, #5330, #50590, #61917, #32900, #73243, #10614, #34390, #56647, #51340, #73608, #44574, #4216, #4962, #28698, #33269, #27963, #57391, #59, #51712, #45677, #74348, #23040, #56268, #10242, #21915, #67587, #67213, #22285, #62653, #39655, #10987, #34020, #22658, #28332, #68692, #17002, #40028, #55905, #63030, #27205, #9873, #15510, #40400, #29820, #63773, #11724, #1538, #70548, #12459, #63398, #40766, #69440, #12820, #12090, #64149, #35128, #24144, #58870, #23786, #30187, #17376, #18864, #7181, #53205, #64883, #58143, #1165, #35489, #1888, #34764, #17751, #59241, #6450, #58501, #29453, #6807, #29079, #69071, #46051, #24518, #47156, #47523, #70188, #52832, #18497, #57766, #41870, #18128, #52462, #30558, #6072, #41506, #431, #13185, #64522, #35855, #36223, #7550, #52099, #53573, #46790, #23411, #800, #69812, #46426, #41144, #54692, #37333, #65246, #37711, #8658, #36956, #30919, #25619, #66744, #19964, #9033, #59962, #2254, #36589, #42970, #38085, #65621, #65991, #2631, #25982, #8280, #14672, #48633, #7913, #49383, #14296, #31290, #53940, #9410, #31673, #20332, #60330, #3001, #66366, #32045, #25247, #72017, #54320, #48264, #59600, #61082, #55065, #49007, #70913, #19227, #71643, #42606, #13551, #3374, #72402, #43348, #42233, #19590, #71271, #60711, #13917, #26361, #20714, #24874, #43730, #15050, #32428, #55439, #47893, #10525, #56561, #22575, #44484, #33557, #44859, #34303, #49768, #50139, #16918, #67497, #67864, #15796, #39198, #62200, #72785, #3749, #10153, #4876, #44115, #74266, #39941, #38831, #61834, #68240, #55816, #33933, #56932, #45595, #27871, #26750, #21092, #61461, #33190, #67124, #38459, #68609, #21826, #73519, #50882, #15419, #73896, #22201, #62947, #56187, #45228, #16157, #9787, #32808, #73154, #11271, #4499, #16533, #27492, #4133, #39573, #27124, #21462, #50505, #62569, #10899, #5248, #28248, #51256, #46340, #47073, #34677, #12743, #35774, #1457, #18045, #57307, #51631, #40312, #6732, #22961, #17293, #47446, #717, #1087, #58424, #74646, #41430, #29375, #52010, #41793, #45970, #29736, #11641, #24438, #52751, #23701, #35414, #64070, #24063, #57682, #70110, #18416, #68984, #23328, #5990, #12013, #12378, #69730, #63315, #64442, #41060, #69357, #28992, #58058, #70470, #52382, #58789, #17667, #348, #46706, #18788, #40685, #7099, #64802, #13104, #5618, #30107, #53124, #28618, #63686, #35046, #6369, #14211, #53858, #66653, #70832, #43643, #19508, #2915, #43265, #42147, #8571, #42526, #37249, #1809, #31587, #19144, #53492, #8946, #30475, #19880, #54235, #36877, #13471, #36510, #65160, #49297, #31958, #59519, #25903, #30837, #2544, #2170, #60245, #48920, #13831, #59885, #7832, #25165, #48182, #72314, #54983, #3290, #66280, #65540, #54608, #71189, #8198, #71933, #31210, #20245, #7470, #60623, #14587, #37626, #25535, #48548, #26276, #71558, #42886, #65905, #20627 ),
 .UNSPECIFIED., .F., .F. ) 
 B_SPLINE_CURVE_WITH_KNOTS ( ( 3, 2, 2, 2, 2, 2, 2, 2, 2, 2, 2, 2, 2, 2, 2, 2, 2, 2, 2, 2, 2, 2, 2, 2, 2, 2, 2, 2, 2, 2, 2, 2, 2, 2, 2, 2, 2, 2, 2, 2, 2, 2, 2, 2, 2, 2, 2, 2, 2, 2, 2, 2, 2, 2, 2, 2, 2, 2, 2, 2, 2, 2, 2, 2, 2, 2, 2, 2, 2, 2, 2, 2, 2, 2, 2, 2, 2, 2, 2, 2, 2, 2, 2, 2, 2, 2, 2, 2, 2, 2, 2, 2, 2, 2, 2, 2, 2, 2, 2, 2, 2, 2, 2, 2, 2, 2, 2, 2, 2, 2, 2, 2, 2, 2, 2, 2, 2, 2, 2, 2, 2, 2, 2, 2, 2, 2, 2, 2, 2, 2, 2, 2, 2, 2, 2, 2, 2, 2, 2, 2, 2, 2, 2, 2, 2, 2, 2, 2, 2, 2, 2, 2, 2, 2, 2, 2, 2, 2, 2, 2, 2, 2, 2, 2, 2, 2, 2, 2, 2, 2, 2, 2, 2, 2, 2, 2, 2, 2, 2, 2, 2, 2, 2, 2, 2, 2, 2, 3 ),
 ( 0.000000000000000000, 0.005357197731506658372, 0.01071439546301331674, 0.01607159319451997859, 0.02142879092602663349, 0.02678598865753329533, 0.03214318638903995717, 0.03750038412054661208, 0.04285758185205326698, 0.04821477958355992882, 0.05357197731506659066, 0.05892917504657324557, 0.06428637277807991435, 0.06964357050958655537, 0.07500076824109322415, 0.08035796597259987906, 0.08571516370410653396, 0.09107236143561320274, 0.09642955916711985764, 0.1017867568986265125, 0.1071439546301331813, 0.1125011523616398362, 0.1178583500931464911, 0.1232155478246531599, 0.1285727455561598287, 0.1339299432876664975, 0.1392871410191731107, 0.1446443387506797795, 0.1500015364821864483, 0.1553587342136930893, 0.1607159319451997581, 0.1660731296767064269, 0.1714303274082130679, 0.1767875251397197367, 0.1821447228712264055, 0.1875019206027330465, 0.1928591183342397153, 0.1982163160657463841, 0.2035735137972530251, 0.2089307115287596939, 0.2142879092602663627, 0.2196451069917730037, 0.2250023047232796725, 0.2303595024547863412, 0.2357167001862929823, 0.2410738979177996510, 0.2464310956493063198, 0.2517882933808129886, 0.2571454911123196574, 0.2625026888438262707, 0.2678598865753329950, 0.2732170843068396082, 0.2785742820383462215, 0.2839314797698529458, 0.2892886775013595591, 0.2946458752328662278, 0.3000030729643728966, 0.3053602706958795654, 0.3107174684273861787, 0.3160746661588929030, 0.3214318638903995162, 0.3267890616219061850, 0.3321462593534128538, 0.3375034570849195226, 0.3428606548164261358, 0.3482178525479328601, 0.3535750502794394734, 0.3589322480109461422, 0.3642894457424528110, 0.3696466434739594797, 0.3750038412054660930, 0.3803610389369728173, 0.3857182366684794306, 0.3910754343999860994, 0.3964326321314927681, 0.4017898298629994369, 0.4071470275945060502, 0.4125042253260127745, 0.4178614230575193877, 0.4232186207890260565, 0.4285758185205327253, 0.4339330162520393941, 0.4392902139835460074, 0.4446474117150527317, 0.4500046094465593449, 0.4553618071780660137, 0.4607190049095726825, 0.4660762026410793513, 0.4714334003725859645, 0.4767905981040926888, 0.4821477958355993021, 0.4875049935671059709, 0.4928621912986126397, 0.4982193890301193084, 0.5035765867616259772, 0.5089337844931326460, 0.5142909822246393148, 0.5196481799561459836, 0.5250053776876525413, 0.5303625754191592101, 0.5357197731506659899, 0.5410769708821725477, 0.5464341686136792164, 0.5517913663451858852, 0.5571485640766924430, 0.5625057618081992228, 0.5678629595397058916, 0.5732201572712124493, 0.5785773550027191181, 0.5839345527342258979, 0.5892917504657324557, 0.5946489481972391244, 0.6000061459287457932, 0.6053633436602524620, 0.6107205413917591308, 0.6160777391232657996, 0.6214349368547723573, 0.6267921345862791371, 0.6321493323177858059, 0.6375065300492923637, 0.6428637277807990325, 0.6482209255123058123, 0.6535781232438123700, 0.6589353209753190388, 0.6642925187068257076, 0.6696497164383323764, 0.6750069141698390451, 0.6803641119013457139, 0.6857213096328522717, 0.6910785073643590515, 0.6964357050958657203, 0.7017929028273722780, 0.7071501005588789468, 0.7125072982903857266, 0.7178644960218922844, 0.7232216937533989531, 0.7285788914849056219, 0.7339360892164122907, 0.7392932869479189595, 0.7446504846794256283, 0.7500076824109321860, 0.7553648801424389658, 0.7607220778739456346, 0.7660792756054521924, 0.7714364733369588611, 0.7767936710684656409, 0.7821508687999721987, 0.7875080665314788675, 0.7928652642629855363, 0.7982224619944920940, 0.8035796597259988738, 0.8089368574575055426, 0.8142940551890121004, 0.8196512529205187692, 0.8250084506520255490, 0.8303656483835321067, 0.8357228461150387755, 0.8410800438465454443, 0.8464372415780521131, 0.8517944393095587818, 0.8571516370410654506, 0.8625088347725720084, 0.8678660325040787882, 0.8732232302355854570, 0.8785804279670920147, 0.8839376256985986835, 0.8892948234301054633, 0.8946520211616120211, 0.9000092188931186898, 0.9053664166246253586, 0.9107236143561320274, 0.9160808120876386962, 0.9214380098191453650, 0.9267952075506519227, 0.9321524052821587025, 0.9375096030136653713, 0.9428668007451719291, 0.9482239984766785978, 0.9535811962081853776, 0.9589383939396919354, 0.9642955916711986042, 0.9696527894027052730, 0.9750099871342119418, 0.9803671848657186105, 0.9857243825972252793, 0.9910815803287318371, 0.9964387780602386169, 1.000000000000000000 ),
 .UNSPECIFIED. ) 
 CURVE ( )  GEOMETRIC_REPRESENTATION_ITEM ( )  RATIONAL_B_SPLINE_CURVE ( ( 1.000000000000000000, 0.9238795325112867385, 1.000000000000000000, 0.9238795325112867385, 1.000000000000000000, 0.9238795325112867385, 1.000000000000000000, 0.9238795325112867385, 1.000000000000000000, 0.9238795325112867385, 1.000000000000000000, 0.9238795325112867385, 1.000000000000000000, 0.9238795325112867385, 1.000000000000000000, 0.9238795325112867385, 1.000000000000000000, 0.9238795325112867385, 1.000000000000000000, 0.9238795325112867385, 1.000000000000000000, 0.9238795325112867385, 1.000000000000000000, 0.9238795325112867385, 1.000000000000000000, 0.9238795325112867385, 1.000000000000000000, 0.9238795325112867385, 1.000000000000000000, 0.9238795325112867385, 1.000000000000000000, 0.9238795325112867385, 1.000000000000000000, 0.9238795325112867385, 1.000000000000000000, 0.9238795325112867385, 1.000000000000000000, 0.9238795325112867385, 1.000000000000000000, 0.9238795325112867385, 1.000000000000000000, 0.9238795325112867385, 1.000000000000000000, 0.9238795325112867385, 1.000000000000000000, 0.9238795325112867385, 1.000000000000000000, 0.9238795325112867385, 1.000000000000000000, 0.9238795325112867385, 1.000000000000000000, 0.9238795325112867385, 1.000000000000000000, 0.9238795325112867385, 1.000000000000000000, 0.9238795325112867385, 1.000000000000000000, 0.9238795325112867385, 1.000000000000000000, 0.9238795325112867385, 1.000000000000000000, 0.9238795325112867385, 1.000000000000000000, 0.9238795325112867385, 1.000000000000000000, 0.9238795325112867385, 1.000000000000000000, 0.9238795325112867385, 1.000000000000000000, 0.9238795325112867385, 1.000000000000000000, 0.9238795325112867385, 1.000000000000000000, 0.9238795325112867385, 1.000000000000000000, 0.9238795325112867385, 1.000000000000000000, 0.9238795325112867385, 1.000000000000000000, 0.9238795325112867385, 1.000000000000000000, 0.9238795325112867385, 1.000000000000000000, 0.9238795325112867385, 1.000000000000000000, 0.9238795325112867385, 1.000000000000000000, 0.9238795325112867385, 1.000000000000000000, 0.9238795325112867385, 1.000000000000000000, 0.9238795325112867385, 1.000000000000000000, 0.9238795325112867385, 1.000000000000000000, 0.9238795325112867385, 1.000000000000000000, 0.9238795325112867385, 1.000000000000000000, 0.9238795325112867385, 1.000000000000000000, 0.9238795325112867385, 1.000000000000000000, 0.9238795325112867385, 1.000000000000000000, 0.9238795325112867385, 1.000000000000000000, 0.9238795325112867385, 1.000000000000000000, 0.9238795325112867385, 1.000000000000000000, 0.9238795325112867385, 1.000000000000000000, 0.9238795325112867385, 1.000000000000000000, 0.9238795325112867385, 1.000000000000000000, 0.9238795325112867385, 1.000000000000000000, 0.9238795325112867385, 1.000000000000000000, 0.9238795325112867385, 1.000000000000000000, 0.9238795325112867385, 1.000000000000000000, 0.9238795325112867385, 1.000000000000000000, 0.9238795325112867385, 1.000000000000000000, 0.9238795325112867385, 1.000000000000000000, 0.9238795325112867385, 1.000000000000000000, 0.9238795325112867385, 1.000000000000000000, 0.9238795325112867385, 1.000000000000000000, 0.9238795325112867385, 1.000000000000000000, 0.9238795325112867385, 1.000000000000000000, 0.9238795325112867385, 1.000000000000000000, 0.9238795325112867385, 1.000000000000000000, 0.9238795325112867385, 1.000000000000000000, 0.9238795325112867385, 1.000000000000000000, 0.9238795325112867385, 1.000000000000000000, 0.9238795325112867385, 1.000000000000000000, 0.9238795325112867385, 1.000000000000000000, 0.9238795325112867385, 1.000000000000000000, 0.9238795325112867385, 1.000000000000000000, 0.9238795325112867385, 1.000000000000000000, 0.9238795325112867385, 1.000000000000000000, 0.9238795325112867385, 1.000000000000000000, 0.9238795325112867385, 1.000000000000000000, 0.9238795325112867385, 1.000000000000000000, 0.9238795325112867385, 1.000000000000000000, 0.9238795325112867385, 1.000000000000000000, 0.9238795325112867385, 1.000000000000000000, 0.9238795325112867385, 1.000000000000000000, 0.9238795325112867385, 1.000000000000000000, 0.9238795325112867385, 1.000000000000000000, 0.9238795325112867385, 1.000000000000000000, 0.9238795325112867385, 1.000000000000000000, 0.9238795325112867385, 1.000000000000000000, 0.9238795325112867385, 1.000000000000000000, 0.9238795325112867385, 1.000000000000000000, 0.9238795325112867385, 1.000000000000000000, 0.9238795325112867385, 1.000000000000000000, 0.9238795325112867385, 1.000000000000000000, 0.9238795325112867385, 1.000000000000000000, 0.9238795325112867385, 1.000000000000000000, 0.9238795325112867385, 1.000000000000000000, 0.9238795325112867385, 1.000000000000000000, 0.9238795325112867385, 1.000000000000000000, 0.9238795325112867385, 1.000000000000000000, 0.9238795325112867385, 1.000000000000000000, 0.9238795325112867385, 1.000000000000000000, 0.9238795325112867385, 1.000000000000000000, 0.9238795325112867385, 1.000000000000000000, 0.9238795325112867385, 1.000000000000000000, 0.9238795325112867385, 1.000000000000000000, 0.9238795325112867385, 1.000000000000000000, 0.9238795325112867385, 1.000000000000000000, 0.9238795325112867385, 1.000000000000000000, 0.9238795325112867385, 1.000000000000000000, 0.9238795325112867385, 1.000000000000000000, 0.9238795325112867385, 1.000000000000000000, 0.9238795325112867385, 1.000000000000000000, 0.9238795325112867385, 1.000000000000000000, 0.9238795325112867385, 1.000000000000000000, 0.9238795325112867385, 1.000000000000000000, 0.9238795325112867385, 1.000000000000000000, 0.9238795325112867385, 1.000000000000000000, 0.9238795325112867385, 1.000000000000000000, 0.9238795325112867385, 1.000000000000000000, 0.9238795325112867385, 1.000000000000000000, 0.9238795325112867385, 1.000000000000000000, 0.9238795325112867385, 1.000000000000000000, 0.9238795325112867385, 1.000000000000000000, 0.9238795325112867385, 1.000000000000000000, 0.9238795325112867385, 1.000000000000000000, 0.9238795325112867385, 1.000000000000000000, 0.9238795325112867385, 1.000000000000000000, 0.9238795325112867385, 1.000000000000000000, 0.9238795325112867385, 1.000000000000000000, 0.9238795325112867385, 1.000000000000000000, 0.9238795325112867385, 1.000000000000000000, 0.9238795325112867385, 1.000000000000000000, 0.9238795325112867385, 1.000000000000000000, 0.9238795325112867385, 1.000000000000000000, 0.9238795325112867385, 1.000000000000000000, 0.9238795325112867385, 1.000000000000000000, 0.9238795325112867385, 1.000000000000000000, 0.9238795325112867385, 1.000000000000000000, 0.9238795325112867385, 1.000000000000000000, 0.9238795325112867385, 1.000000000000000000, 0.9238795325112867385, 1.000000000000000000, 0.9238795325112867385, 1.000000000000000000, 0.9238795325112867385, 1.000000000000000000, 0.9238795325112867385, 1.000000000000000000, 0.9238795325112867385, 1.000000000000000000, 0.9238795325112867385, 1.000000000000000000, 0.9238795325112867385, 1.000000000000000000, 0.9238795325112867385, 1.000000000000000000, 0.9238795325112867385, 1.000000000000000000, 0.9238795325112867385, 1.000000000000000000, 0.9238795325112867385, 1.000000000000000000, 0.9238795325112867385, 1.000000000000000000, 0.9238795325112867385, 1.000000000000000000, 0.9238795325112867385, 1.000000000000000000, 0.9238795325112867385, 1.000000000000000000, 0.9238795325112867385, 1.000000000000000000, 0.9238795325112867385, 1.000000000000000000, 0.9238795325112867385, 1.000000000000000000, 0.9238795325112867385, 1.000000000000000000, 0.9238795325112867385, 1.000000000000000000, 0.9238795325112867385, 1.000000000000000000, 0.9238795325112867385, 1.000000000000000000, 0.9238795325112867385, 1.000000000000000000, 0.9238795325112867385, 1.000000000000000000, 0.9238795325112867385, 1.000000000000000000, 0.9238795325112867385, 1.000000000000000000, 0.9238795325112867385, 1.000000000000000000, 0.9238795325112867385, 1.000000000000000000, 0.9238795325112867385, 1.000000000000000000, 0.9238795325112867385, 1.000000000000000000, 0.9238795325112867385, 1.000000000000000000, 0.9238795325112867385, 1.000000000000000000, 0.9238795325112867385, 1.000000000000000000, 0.9238795325112867385, 1.000000000000000000, 0.9238795325112867385, 1.000000000000000000, 0.9238795325112867385, 1.000000000000000000, 0.9238795325112867385, 1.000000000000000000, 0.9238795325112867385, 1.000000000000000000, 0.9238795325112867385, 1.000000000000000000, 0.9238795325112867385, 1.000000000000000000, 0.9238795325112867385, 1.000000000000000000, 0.9493985675959992765, 0.9660722070829144137 ) ) 
 REPRESENTATION_ITEM ( '' )  );
#23378 = CARTESIAN_POINT ( 'NONE',  ( 2.828427124746190291, 13.87500000000000000, 2.828427124746192067 ) ) ;
#23379 = CARTESIAN_POINT ( 'NONE',  ( 4.000000000000000888, 21.68749999726881583, 1.656854249492384135 ) ) ;
#23380 = CARTESIAN_POINT ( 'NONE',  ( 4.541265875000002339, 13.31249999863440792, 0.000000000000000000 ) ) ;
#23381 = CARTESIAN_POINT ( 'NONE',  ( 3.313708498984756279, 7.999999999999991118, 20.04905278392014978 ) ) ;
#23383 = VECTOR ( 'NONE', #66225, 1000.000000000000000 ) ;
#23382 = CARTESIAN_POINT ( 'NONE',  ( -2.751064625579944321E-14, 195.7500000000000000, 146.0000000000000284 ) ) ;
#23384 = VERTEX_POINT ( 'NONE', #25334 ) ;
#23385 = LINE ( 'NONE', #69414, #63163 ) ;
#23386 = CARTESIAN_POINT ( 'NONE',  ( -2.977408999572650927, 102.8750000020483810, -7.188101187500001821 ) ) ;
#23388 = CARTESIAN_POINT ( 'NONE',  ( -8.000000000000000000, 123.4062500000000142, -3.313708498984761164 ) ) ;
#23387 = DIRECTION ( 'NONE',  ( 0.000000000000000000, 0.000000000000000000, 1.000000000000000000 ) ) ;
#23389 = ORIENTED_EDGE ( 'NONE', *, *, #47816, .F. ) ;
#23390 = CARTESIAN_POINT ( 'NONE',  ( 4.541265875000002339, 20.37499999863441147, -1.881053915767121554 ) ) ;
#23391 = CARTESIAN_POINT ( 'NONE',  ( 7.188101187499992051, 8.802885111219154394E-16, 23.23655278187175455 ) ) ;
#23392 = ORIENTED_EDGE ( 'NONE', *, *, #63680, .F. ) ;
#23393 = ORIENTED_EDGE ( 'NONE', *, *, #18626, .F. ) ;
#23394 = CARTESIAN_POINT ( 'NONE',  ( -10.18810118749999738, -4.220049686691941915, 88.75000000204836681 ) ) ;
#23395 = DIRECTION ( 'NONE',  ( -0.000000000000000000, 1.000000000000000000, -0.000000000000000000 ) ) ;
#23396 = CARTESIAN_POINT ( 'NONE',  ( -30.44569435410883074, 197.8125000013656063, 167.5543056458915885 ) ) ;
#23397 = CARTESIAN_POINT ( 'NONE',  ( 7.778174593052021635, 7.778174593052023411, 102.4374999999999858 ) ) ;
#23400 = CARTESIAN_POINT ( 'NONE',  ( -6.676582343750001591, 299.6093750017069510, 0.000000000000000000 ) ) ;
#23399 = CARTESIAN_POINT ( 'NONE',  ( 24.00000000000001066, 206.9375000027312410, 171.6568542494923122 ) ) ;
#23398 = CARTESIAN_POINT ( 'NONE',  ( -2.485281374238875962, 289.8750000034139020, -5.999999999999697131 ) ) ;
#23401 = CARTESIAN_POINT ( 'NONE',  ( 8.660254037844385522, 139.5833333333333428, 5.000000000000005329 ) ) ;
#23402 = CARTESIAN_POINT ( 'NONE',  ( 3.313708498984765161, 98.46875000000000000, 7.999999999999998224 ) ) ;
#23403 = CARTESIAN_POINT ( 'NONE',  ( 4.721056650416000089, 289.9843750017070079, 4.721056650415999201 ) ) ;
#23404 = PLANE ( 'NONE',  #68485 ) ;
#23405 = CARTESIAN_POINT ( 'NONE',  ( -3.313708498984761608, 102.4062500040967763, -8.000000000000000000 ) ) ;
#23406 = CARTESIAN_POINT ( 'NONE',  ( 31.45873412499999944, 202.6875000013656063, 169.9999999999999432 ) ) ;
#23407 = CARTESIAN_POINT ( 'NONE',  ( -2.977408999572650039, 5.812499997951610098, -7.188101187500001821 ) ) ;
#23408 = AXIS2_PLACEMENT_3D ( 'NONE', #18737, #41745, #64755 ) ;
#23409 = CARTESIAN_POINT ( 'NONE',  ( 5.662595241051936235, -5.662595241051934458, 6.075615283940630995 ) ) ;
#23410 = CARTESIAN_POINT ( 'NONE',  ( -1.432654583217662481, 197.1250000013656347, 145.4587341250000634 ) ) ;
#23411 = CARTESIAN_POINT ( 'NONE',  ( 5.082755093536325042, 113.4687500020483810, -5.082755093536325930 ) ) ;
#23413 = CARTESIAN_POINT ( 'NONE',  ( 0.9718321562519269818, 194.8957299692297624, 194.2193535421813806 ) ) ;
#23412 = CARTESIAN_POINT ( 'NONE',  ( 31.99999999999999289, 195.3750000027311842, 169.9999999999998863 ) ) ;
#23414 = CARTESIAN_POINT ( 'NONE',  ( -11.35316468749999608, 244.4270833367473017, 3.042071309553173730 ) ) ;
#23415 = FACE_OUTER_BOUND ( 'NONE', #72121, .T. ) ;
#23416 = CARTESIAN_POINT ( 'NONE',  ( -7.188101187499992051, 0.000000000000000000, 28.86155278187175810 ) ) ;
#23417 = CARTESIAN_POINT ( 'NONE',  ( 25.17157287525381548, 199.6250000000000284, 167.1715728752537018 ) ) ;
#23418 = CARTESIAN_POINT ( 'NONE',  ( -11.35316468749999785, 33.07291666325268409, -3.042071309553167513 ) ) ;
#23419 = CARTESIAN_POINT ( 'NONE',  ( -3.313708498984760276, 9.468750000000001776, -8.000000000000000000 ) ) ;
#23420 = CARTESIAN_POINT ( 'NONE',  ( 5.676582343750001591, 226.9270833299193839, -9.832129032723420536 ) ) ;
#23421 = CARTESIAN_POINT ( 'NONE',  ( -10.00000000000000178, 219.3749999931720538, -1.224646799147353454E-15 ) ) ;
#23423 = DIRECTION ( 'NONE',  ( -0.000000000000000000, 1.000000000000000000, -0.000000000000000000 ) ) ;
#23422 = FACE_OUTER_BOUND ( 'NONE', #4811, .T. ) ;
#23424 = ORIENTED_EDGE ( 'NONE', *, *, #19501, .F. ) ;
#23425 = CARTESIAN_POINT ( 'NONE',  ( -1.432654583217662481, 198.3750000013655779, 145.4587341250000634 ) ) ;
#23426 = CARTESIAN_POINT ( 'NONE',  ( 9.832129032723416984, 25.36458332991935194, 5.676582343750006032 ) ) ;
#23427 = CARTESIAN_POINT ( 'NONE',  ( 11.00000000000000000, 1.347111479062088405E-15, 91.93750000409677625 ) ) ;
#23428 = CARTESIAN_POINT ( 'NONE',  ( -2.445694354108840063, 208.0625000013656063, 139.5543056458912190 ) ) ;
#23429 = CARTESIAN_POINT ( 'NONE',  ( 2.020667218593132706E-15, -11.00000000000000000, 111.0625000040967763 ) ) ;
#23430 = LINE ( 'NONE', #36243, #72009 ) ;
#23432 = CARTESIAN_POINT ( 'NONE',  ( -11.35316468750000141, 13.48958332991935194, 3.042071309553159963 ) ) ;
#23431 = CARTESIAN_POINT ( 'NONE',  ( -5.082755093536325930, 111.9687500020483810, -5.082755093536325930 ) ) ;
#23433 = CARTESIAN_POINT ( 'NONE',  ( 5.656854249492374365, 5.656854249492375253, 24.26780277982336642 ) ) ;
#23434 = CARTESIAN_POINT ( 'NONE',  ( 11.35316468749999963, 130.9895833299193555, -3.042071309553165293 ) ) ;
#23435 = CARTESIAN_POINT ( 'NONE',  ( 8.660254037844389075, 112.2916666598387110, -5.000000000000000000 ) ) ;
#23436 = CARTESIAN_POINT ( 'NONE',  ( -5.082755093536325930, 115.3437500020483810, -5.082755093536325930 ) ) ;
#23437 = DIRECTION ( 'NONE',  ( -1.000000000000000000, 0.000000000000000000, 0.000000000000000000 ) ) ;
#23438 = CARTESIAN_POINT ( 'NONE',  ( -24.54126587500000412, 208.5000000013656063, 168.5673454167827003 ) ) ;
#23439 = CARTESIAN_POINT ( 'NONE',  ( -5.000000000000000000, -52.84347807771128203, -43.21644271080234745 ) ) ;
#23440 = ORIENTED_EDGE ( 'NONE', *, *, #71294, .F. ) ;
#23441 = CARTESIAN_POINT ( 'NONE',  ( -11.35316468749999785, 13.38541666325268409, -3.042071309553167957 ) ) ;
#23442 = CARTESIAN_POINT ( 'NONE',  ( -7.999999999953861796, 1.809871347124574913E-05, 10.01712378708029938 ) ) ;
#23443 = CARTESIAN_POINT ( 'NONE',  ( 2.765530957081996366, 297.1406250017070079, -6.676582343750003368 ) ) ;
#23444 = CARTESIAN_POINT ( 'NONE',  ( 5.676582343749993598, 134.9479166632526983, 9.832129032723422313 ) ) ;
#23445 = CARTESIAN_POINT ( 'NONE',  ( -1.656854249492381248, 16.06249999726881228, -4.000000000000001776 ) ) ;
#23446 = CARTESIAN_POINT ( 'NONE',  ( 7.999999999999991118, 3.313708498984757611, 24.23030278432982598 ) ) ;
#23447 = AXIS2_PLACEMENT_3D ( 'NONE', #52275, #53386, #69249 ) ;
#23448 = FACE_OUTER_BOUND ( 'NONE', #37029, .T. ) ;
#23449 = AXIS2_PLACEMENT_3D ( 'NONE', #41932, #1594, #54002 ) ;
#23450 = CARTESIAN_POINT ( 'NONE',  ( 9.832129032723420536, 245.9895833367473301, 5.676582343749996262 ) ) ;
#23451 = CARTESIAN_POINT ( 'NONE',  ( -10.18810118749999916, 0.000000000000000000, 99.53125000204838102 ) ) ;
#23452 = ORIENTED_EDGE ( 'NONE', *, *, #40655, .T. ) ;
#23453 = EDGE_CURVE ( 'NONE', #49983, #52626, #11783, .T. ) ;
#23454 = CARTESIAN_POINT ( 'NONE',  ( 2.679491924310934969, 217.9166666598387962, -10.00000000000017053 ) ) ;
#23455 = CARTESIAN_POINT ( 'NONE',  ( 4.999999999999999112, 68.02455775458950882, -22.06917953199437221 ) ) ;
#23456 = CARTESIAN_POINT ( 'NONE',  ( -3.042071309553164404, 87.55208332991936970, -11.35316468749999963 ) ) ;
#23457 = ORIENTED_EDGE ( 'NONE', *, *, #36836, .F. ) ;
#23458 = CARTESIAN_POINT ( 'NONE',  ( -6.238412754330611322E-16, 10.18810118749999916, 109.2812500020483668 ) ) ;
#23459 = EDGE_CURVE ( 'NONE', #48578, #34152, #31540, .T. ) ;
#23460 = CARTESIAN_POINT ( 'NONE',  ( 3.211159895383560947, 12.31249999863440792, 3.211159895383562723 ) ) ;
#23461 = VERTEX_POINT ( 'NONE', #54778 ) ;
#23462 = ORIENTED_EDGE ( 'NONE', *, *, #62624, .T. ) ;
#23463 = CARTESIAN_POINT ( 'NONE',  ( 8.000000000000000000, 4.500000000000000888, 0.000000000000000000 ) ) ;
#23464 = CARTESIAN_POINT ( 'NONE',  ( 0.000000000000000000, 125.0000000000000000, 8.000000000000000000 ) ) ;
#23465 = CARTESIAN_POINT ( 'NONE',  ( 7.778174593052023411, -7.778174593052021635, 76.75000000409676204 ) ) ;
#23466 = CARTESIAN_POINT ( 'NONE',  ( -2.977408999572654480, 22.87499999795161187, 7.188101187499999156 ) ) ;
#23467 = CARTESIAN_POINT ( 'NONE',  ( -4.898587196589412829E-16, 123.3125000040967905, -8.000000000000000000 ) ) ;
#23468 = CARTESIAN_POINT ( 'NONE',  ( -6.238412754330611322E-16, 10.18810118749999916, 102.1562500020483810 ) ) ;
#23469 = AXIS2_PLACEMENT_3D ( 'NONE', #46679, #58397, #5958 ) ;
#23470 = DIRECTION ( 'NONE',  ( -0.000000000000000000, 1.000000000000000000, 4.689100369878284071E-30 ) ) ;
#23471 = CARTESIAN_POINT ( 'NONE',  ( -1.656854249492381248, 12.06249999726881228, -4.000000000000001776 ) ) ;
#23472 = CARTESIAN_POINT ( 'NONE',  ( -4.541265875000002339, 1.749999998634406584, -1.881053915767121998 ) ) ;
#23473 = EDGE_LOOP ( 'NONE', ( #58279, #28950, #34578 ) ) ;
#23474 = CARTESIAN_POINT ( 'NONE',  ( 11.00000000000000355, -4.556349186104044158, 81.15625000000000000 ) ) ;
#23475 = CARTESIAN_POINT ( 'NONE',  ( 2.445694354108838731, 197.0625000013656063, 195.5543056458912190 ) ) ;
#23476 = CARTESIAN_POINT ( 'NONE',  ( -31.45873412499996746, 203.7500000013656063, 171.4326545832181239 ) ) ;
#23477 = CARTESIAN_POINT ( 'NONE',  ( 3.211159895383560947, 12.18749999863440614, 3.211159895383562723 ) ) ;
#23478 = CARTESIAN_POINT ( 'NONE',  ( -2.828427124746190735, 18.12499999726881583, -2.828427124746191623 ) ) ;
#23479 = CARTESIAN_POINT ( 'NONE',  ( 2.977408999572650927, -7.188101187499990274, 10.95530278187175455 ) ) ;
#23480 = ORIENTED_EDGE ( 'NONE', *, *, #58421, .F. ) ;
#23481 = EDGE_LOOP ( 'NONE', ( #6713, #66154, #34509, #68774, #36380, #67266, #32940 ) ) ;
#23482 = CARTESIAN_POINT ( 'NONE',  ( 10.18810118749999916, 4.220049686691935698, 101.5000000020483668 ) ) ;
#23483 = CARTESIAN_POINT ( 'NONE',  ( -4.898587196589412829E-16, 96.31250000409677625, -8.000000000000000000 ) ) ;
#23484 = CARTESIAN_POINT ( 'NONE',  ( -32.00000000000000000, 203.2500000000000000, 170.0000000000003979 ) ) ;
#23485 = CARTESIAN_POINT ( 'NONE',  ( -2.445694354108783664, 199.3125000013656063, 195.5543056458912190 ) ) ;
#23486 = CARTESIAN_POINT ( 'NONE',  ( 26.56734541678232731, 196.0000000013656063, 166.5412658749999650 ) ) ;
#23487 = CARTESIAN_POINT ( 'NONE',  ( 10.00000000000000000, 89.79166666666665719, 2.679491924311236062 ) ) ;
#23488 = CARTESIAN_POINT ( 'NONE',  ( -5.656854249492380582, 115.8125000000000000, -5.656854249492380582 ) ) ;
#23489 = CARTESIAN_POINT ( 'NONE',  ( 3.042071309553167069, 67.13541666325266988, -11.35316468749999785 ) ) ;
#23490 = CARTESIAN_POINT ( 'NONE',  ( -4.242640687119285658, 290.1249999999999432, 4.242640687119287435 ) ) ;
#23491 = VERTEX_POINT ( 'NONE', #13640 ) ;
#23492 =( BOUNDED_CURVE ( )  B_SPLINE_CURVE ( 2, ( #69295, #52690, #40624, #68919, #63624, #58000, #40250, #656, #41369 ),
 .UNSPECIFIED., .F., .F. ) 
 B_SPLINE_CURVE_WITH_KNOTS ( ( 3, 2, 2, 2, 3 ),
 ( 0.3235294117647057877, 0.3272058823529410687, 0.3308823529411763498, 0.3345588235294116308, 0.3382352941176469674 ),
 .UNSPECIFIED. ) 
 CURVE ( )  GEOMETRIC_REPRESENTATION_ITEM ( )  RATIONAL_B_SPLINE_CURVE ( ( 1.000000000000002220, 0.9238795325112844070, 1.000000000000000000, 0.9238795325112867385, 1.000000000000000000, 0.9238795325112867385, 1.000000000000000000, 0.9238795325112890700, 0.9999999999999976685 ) ) 
 REPRESENTATION_ITEM ( '' )  );
#23493 = CARTESIAN_POINT ( 'NONE',  ( 6.000000000000003553, 294.4375000000000000, 2.485281374238571317 ) ) ;
#23494 = CARTESIAN_POINT ( 'NONE',  ( 4.465384415997275092, -10.10202268796506253, 70.97396818905022542 ) ) ;
#23495 = CARTESIAN_POINT ( 'NONE',  ( 3.458734124999959914, 206.4375000013656063, 142.0000000000000568 ) ) ;
#23496 = LINE ( 'NONE', #69529, #3326 ) ;
#23497 = CARTESIAN_POINT ( 'NONE',  ( -7.999999999999991118, 3.313708498984757167, 26.42405278392014978 ) ) ;
#23498 = CARTESIAN_POINT ( 'NONE',  ( 4.999999999999997335, 233.3333333333333428, -8.660254037844387298 ) ) ;
#23499 = LINE ( 'NONE', #46885, #51177 ) ;
#23500 = CARTESIAN_POINT ( 'NONE',  ( 7.778174593052021635, 7.778174593052023411, 117.4375000000000000 ) ) ;
#23501 = CARTESIAN_POINT ( 'NONE',  ( 10.00000000000000178, 195.0000000000000000, 0.000000000000000000 ) ) ;
#23502 = CARTESIAN_POINT ( 'NONE',  ( 5.082755093536318824, 5.082755093536319713, 10.29905278187175455 ) ) ;
#23503 = CARTESIAN_POINT ( 'NONE',  ( -3.042071309553173730, 184.6354166632526983, 11.35316468749999785 ) ) ;
#23504 = DIRECTION ( 'NONE',  ( 0.000000000000000000, 0.000000000000000000, 1.000000000000000000 ) ) ;
#23505 = FACE_OUTER_BOUND ( 'NONE', #23155, .T. ) ;
#23506 = CARTESIAN_POINT ( 'NONE',  ( 7.320508075688771044, 86.24999999317203958, 7.320508075688775484 ) ) ;
#23507 = VERTEX_POINT ( 'NONE', #31005 ) ;
#23508 = CARTESIAN_POINT ( 'NONE',  ( -2.839093476692135984E-14, 207.9375000013656063, 138.5412658750000503 ) ) ;
#23509 = CARTESIAN_POINT ( 'NONE',  ( -9.832129032723420536, 39.01041666325268409, 5.676582343749997150 ) ) ;
#23510 = CARTESIAN_POINT ( 'NONE',  ( -7.778174593052020747, -7.778174593052023411, 107.8750000040967763 ) ) ;
#23511 = VECTOR ( 'NONE', #65463, 1000.000000000000000 ) ;
#23512 = CARTESIAN_POINT ( 'NONE',  ( -30.44569435410876324, 206.8125000013656063, 172.4456943541092642 ) ) ;
#23513 = CARTESIAN_POINT ( 'NONE',  ( -4.999999999999998224, 123.5416666598387110, -8.660254037844389075 ) ) ;
#23515 = CARTESIAN_POINT ( 'NONE',  ( -11.00000000000000000, 0.000000000000000000, 107.6875000040967763 ) ) ;
#23514 = CYLINDRICAL_SURFACE ( 'NONE', #40050, 15.99999999999998579 ) ;
#23516 = CARTESIAN_POINT ( 'NONE',  ( -2.445694354108838731, 199.0625000013656063, 144.4456943541088663 ) ) ;
#23517 = ADVANCED_FACE ( 'NONE', ( #61174 ), #3089, .F. ) ;
#23518 = EDGE_CURVE ( 'NONE', #30885, #10942, #28228, .T. ) ;
#23519 = CARTESIAN_POINT ( 'NONE',  ( 10.00000000000000000, 76.66666665983871098, 2.679491924311236062 ) ) ;
#23520=STYLED_ITEM('',(#74713),#67429);
#23521 = CARTESIAN_POINT ( 'NONE',  ( 1.320432766682874540E-15, 94.53125000204836681, 7.188101187500000044 ) ) ;
#23522 = CARTESIAN_POINT ( 'NONE',  ( -4.541265875000002339, 13.87499999863440969, -1.881053915767121998 ) ) ;
#23523 = CARTESIAN_POINT ( 'NONE',  ( 0.000000000000000000, 0.000000000000000000, 12.00000000000000000 ) ) ;
#23524 = CARTESIAN_POINT ( 'NONE',  ( 7.683012701892216079, 0.1830127018922207416, 0.000000000000000000 ) ) ;
#23525 = CARTESIAN_POINT ( 'NONE',  ( 0.4320110153365238070, -49.91454558245994377, 40.68976686129099818 ) ) ;
#23526 = EDGE_LOOP ( 'NONE', ( #52427, #27200, #42982, #8321 ) ) ;
#23527 = VERTEX_POINT ( 'NONE', #3461 ) ;
#23528 = CARTESIAN_POINT ( 'NONE',  ( 3.313708498984756279, 7.999999999999991118, 10.86155277982336820 ) ) ;
#23529 = CARTESIAN_POINT ( 'NONE',  ( 2.765530957081996366, 297.2968750017070079, -6.676582343750003368 ) ) ;
#23530 = CARTESIAN_POINT ( 'NONE',  ( -2.775557561562891351E-14, 210.0000000000000284, 142.0000000000000568 ) ) ;
#23531 = CARTESIAN_POINT ( 'NONE',  ( 5.000000000000001776, 42.70833332650536818, -8.660254037844389075 ) ) ;
#23532 = CARTESIAN_POINT ( 'NONE',  ( 8.311093377946834337, 150.1562499965859843, 8.311093377946839666 ) ) ;
#23533 = DIRECTION ( 'NONE',  ( -0.000000000000000000, -0.000000000000000000, -1.000000000000000000 ) ) ;
#23534 = EDGE_CURVE ( 'NONE', #1512, #13147, #36679, .T. ) ;
#23535 = CARTESIAN_POINT ( 'NONE',  ( -7.204075437095965206, -7.204075437095968759, 85.84375000204836681 ) ) ;
#23536 = DIRECTION ( 'NONE',  ( -0.000000000000000000, 1.000000000000000000, -0.000000000000000000 ) ) ;
#23537 = CARTESIAN_POINT ( 'NONE',  ( -1.656854249492347719, 205.8125000000000000, 194.0000000000000853 ) ) ;
#23538 = DIRECTION ( 'NONE',  ( -0.000000000000000000, 1.000000000000000000, -0.000000000000000000 ) ) ;
#23539 = CARTESIAN_POINT ( 'NONE',  ( 1.871523826299183495E-15, -10.18810118749999916, 113.4062500020483810 ) ) ;
#23540 = EDGE_LOOP ( 'NONE', ( #52524, #67422, #17417, #3476, #5712, #7984, #33867, #64221, #41408, #31594, #67913, #36551, #50294, #15027, #37008, #26694, #64794, #24904, #34834, #60672, #47019, #62713, #67907, #30467, #9059, #47871, #50604, #44533, #66831, #28771, #11564, #48845, #69647 ) ) ;
#23541 = DIRECTION ( 'NONE',  ( 1.000000000000000000, 0.000000000000000000, 0.000000000000000000 ) ) ;
#23542 = CARTESIAN_POINT ( 'NONE',  ( 30.70214559338596061, 176.5462824210880228, 150.3874543681437785 ) ) ;
#23543 = CARTESIAN_POINT ( 'NONE',  ( 8.311093377946837890, 126.7187499965860269, -8.311093377946837890 ) ) ;
#23544 = CARTESIAN_POINT ( 'NONE',  ( -3.458734124999959914, 198.4375000013655779, 198.0000000000000284 ) ) ;
#23545 = CARTESIAN_POINT ( 'NONE',  ( -2.977408999572654480, 24.37499999795161543, 7.188101187499999156 ) ) ;
#23546 = CARTESIAN_POINT ( 'NONE',  ( 7.204075437095966983, 7.204075437095967871, 77.96875000204836681 ) ) ;
#23547 = CARTESIAN_POINT ( 'NONE',  ( 5.676582343750001591, 51.92708332991935549, -9.832129032723420536 ) ) ;
#23548 = ORIENTED_EDGE ( 'NONE', *, *, #65344, .F. ) ;
#23549 = FACE_OUTER_BOUND ( 'NONE', #49280, .T. ) ;
#23550 = CARTESIAN_POINT ( 'NONE',  ( -8.342170076843785083E-16, 2.187499998634407028, 4.541265875000002339 ) ) ;
#23551 = CARTESIAN_POINT ( 'NONE',  ( -8.008118988124991233, 0.000000000000000000, 16.01311528394063188 ) ) ;
#23552 = CARTESIAN_POINT ( 'NONE',  ( 1.432654583217608080, 205.8750000013656063, 138.5412658750000503 ) ) ;
#23553 = CARTESIAN_POINT ( 'NONE',  ( -5.082755093536325042, 17.53124999795161187, -5.082755093536325930 ) ) ;
#23554 = CARTESIAN_POINT ( 'NONE',  ( 4.242640687119285658, 296.6875000034139589, -4.242640687119286547 ) ) ;
#23555 = EDGE_CURVE ( 'NONE', #21929, #38953, #32519, .T. ) ;
#23556 = CARTESIAN_POINT ( 'NONE',  ( -12.64026178104464293, -24.05726467898398013, 138.8162041664353694 ) ) ;
#23557 = CARTESIAN_POINT ( 'NONE',  ( 7.188101187499999156, 5.249999997951610098, 2.977408999572654924 ) ) ;
#23558 = CARTESIAN_POINT ( 'NONE',  ( -7.188101187499990274, -2.977408999572651815, 7.580302781871751883 ) ) ;
#23559 = CARTESIAN_POINT ( 'NONE',  ( 7.204075437095966983, 7.204075437095967871, 70.09375000204836681 ) ) ;
#23560 = CARTESIAN_POINT ( 'NONE',  ( -31.45873412500001010, 204.8750000013656063, 168.5673454167827572 ) ) ;
#23561 = DIRECTION ( 'NONE',  ( -0.000000000000000000, 1.000000000000000000, -1.563033456626094573E-30 ) ) ;
#23562 = CARTESIAN_POINT ( 'NONE',  ( -1.881053915767121554, 18.74999999863440436, -4.541265875000002339 ) ) ;
#23563 = ORIENTED_EDGE ( 'NONE', *, *, #21440, .F. ) ;
#23564 = CARTESIAN_POINT ( 'NONE',  ( -2.828427124746153876, 196.0000000027312126, 195.1715728752538439 ) ) ;
#23565 = CONICAL_SURFACE ( 'NONE', #44047, 18.00000000000000355, 1.047197551196596965 ) ;
#23566 = EDGE_CURVE ( 'NONE', #43896, #39105, #33433, .T. ) ;
#23567 = CARTESIAN_POINT ( 'NONE',  ( 2.828427124746153876, 204.8750000000000284, 144.8284271247462129 ) ) ;
#23568 = CARTESIAN_POINT ( 'NONE',  ( -24.00000000000002487, 200.9375000027312410, 168.3431457505079152 ) ) ;
#23569 = CARTESIAN_POINT ( 'NONE',  ( 7.188101187500001821, 116.0000000020483810, -2.977408999572651371 ) ) ;
#23570 = CIRCLE ( 'NONE', #54936, 9.999999999999996447 ) ;
#23571 = CARTESIAN_POINT ( 'NONE',  ( -7.778174593052023411, 7.778174593052023411, 94.00000000409677625 ) ) ;
#23572 = CARTESIAN_POINT ( 'NONE',  ( -5.656854249492375253, 5.656854249492375253, 6.830302783920143561 ) ) ;
#23573 = ORIENTED_EDGE ( 'NONE', *, *, #39948, .F. ) ;
#23574 = CARTESIAN_POINT ( 'NONE',  ( 2.977408999572650927, 15.74999999795161365, -7.188101187500000933 ) ) ;
#23575 = VERTEX_POINT ( 'NONE', #50968 ) ;
#23576 = DIRECTION ( 'NONE',  ( -1.000000000000000000, 0.000000000000000000, 0.000000000000000000 ) ) ;
#23577 = CARTESIAN_POINT ( 'NONE',  ( -8.660254037844390851, 44.79166665983870388, 4.999999999999998224 ) ) ;
#23578 = CARTESIAN_POINT ( 'NONE',  ( -2.679491924311225848, 41.45833333333332149, -10.00000000000000178 ) ) ;
#23579 = CARTESIAN_POINT ( 'NONE',  ( 7.188101187500000044, 98.28125000204838102, -8.802885111219163269E-16 ) ) ;
#23580 = CARTESIAN_POINT ( 'NONE',  ( -25.55430564589115505, 206.3125000013656063, 172.4456943541091789 ) ) ;
#23581 = CARTESIAN_POINT ( 'NONE',  ( 6.000000000000003553, 299.4375000000000000, 2.485281374238571317 ) ) ;
#23583 = CYLINDRICAL_SURFACE ( 'NONE', #1276, 3.999999999999976019 ) ;
#23582 = CARTESIAN_POINT ( 'NONE',  ( -8.660254037844387298, 33.95833332650536818, -5.000000000000004441 ) ) ;
#23584 = EDGE_LOOP ( 'NONE', ( #47369, #64920, #70577, #5026 ) ) ;
#23585 = CARTESIAN_POINT ( 'NONE',  ( -3.042071309553166181, 242.8645833367473017, -11.35316468749999608 ) ) ;
#23586 = CARTESIAN_POINT ( 'NONE',  ( 5.082755093536320601, -5.082755093536318824, 18.92405278187175455 ) ) ;
#23587 = LINE ( 'NONE', #29627, #61915 ) ;
#23588 = CARTESIAN_POINT ( 'NONE',  ( -38.00000000000002132, 82.00000000000001421, 65.00000000000000000 ) ) ;
#23589 = CARTESIAN_POINT ( 'NONE',  ( -11.00000000000000000, 0.000000000000000000, 104.6875000040967763 ) ) ;
#23590 =( BOUNDED_CURVE ( )  B_SPLINE_CURVE ( 2, ( #61498, #14337, #32845, #37369, #8696, #71312, #72054, #65657, #60750 ),
 .UNSPECIFIED., .F., .F. ) 
 B_SPLINE_CURVE_WITH_KNOTS ( ( 3, 2, 2, 2, 3 ),
 ( 0.4473684210526316929, 0.4539473684210527660, 0.4605263157894737835, 0.4671052631578948011, 0.4736842105263158187 ),
 .UNSPECIFIED. ) 
 CURVE ( )  GEOMETRIC_REPRESENTATION_ITEM ( )  RATIONAL_B_SPLINE_CURVE ( ( 0.9999999999999986677, 0.9238795325112880708, 1.000000000000000000, 0.9238795325112867385, 1.000000000000000000, 0.9238795325112867385, 1.000000000000000000, 0.9238795325112860723, 1.000000000000000666 ) ) 
 REPRESENTATION_ITEM ( '' )  );
#23591 = CARTESIAN_POINT ( 'NONE',  ( -27.99999999999999645, 210.0000000000000284, 174.0000000000003411 ) ) ;
#23592 = CARTESIAN_POINT ( 'NONE',  ( 10.00000000000000178, 155.2083333333333712, -2.679491924311226736 ) ) ;
#23593 = LINE ( 'NONE', #74159, #62252 ) ;
#23594 = CARTESIAN_POINT ( 'NONE',  ( -3.313708498984720308, 118.7187499999999716, -8.000000000000040856 ) ) ;
#23595 = CARTESIAN_POINT ( 'NONE',  ( 7.999999999999991118, 9.797174393178815797E-16, 4.580302779823363757 ) ) ;
#23596 = CARTESIAN_POINT ( 'NONE',  ( 5.676582343750001591, 141.9270833299193555, -9.832129032723420536 ) ) ;
#23597 = PLANE ( 'NONE',  #63739 ) ;
#23598 = CARTESIAN_POINT ( 'NONE',  ( 11.00000000000000000, 1.347111479062088405E-15, 106.7500000000000000 ) ) ;
#23601 = CARTESIAN_POINT ( 'NONE',  ( 7.999999999999991118, 9.797174393178815797E-16, 27.08030277982336642 ) ) ;
#23600 = LINE ( 'NONE', #17946, #47805 ) ;
#23599 = CARTESIAN_POINT ( 'NONE',  ( 25.17157287525378351, 205.8750000000000284, 172.8284271247460424 ) ) ;
#23602 = ORIENTED_EDGE ( 'NONE', *, *, #74221, .T. ) ;
#23603 = EDGE_CURVE ( 'NONE', #50120, #28645, #23377, .T. ) ;
#23604 = CARTESIAN_POINT ( 'NONE',  ( -8.263859302085863945, 5.621163452808790595, -0.5584673446549202058 ) ) ;
#23605 = CARTESIAN_POINT ( 'NONE',  ( -29.65685424949245430, 196.4375000000000284, 174.0000000000002842 ) ) ;
#23606 = CARTESIAN_POINT ( 'NONE',  ( 2.648895341738178200, -7.552205831922027990, -0.000000000000000000 ) ) ;
#23607 = CARTESIAN_POINT ( 'NONE',  ( 5.000000000000000888, -62.31673578527537671, -23.93255728291397944 ) ) ;
#23608 = EDGE_CURVE ( 'NONE', #8912, #30991, #38815, .T. ) ;
#23609 = CARTESIAN_POINT ( 'NONE',  ( -8.660254037844390851, 19.79166665983870033, 4.999999999999998224 ) ) ;
#23610 = CARTESIAN_POINT ( 'NONE',  ( -7.188101187499999156, 115.2500000020484094, 2.977408999572654924 ) ) ;
#23611 = CARTESIAN_POINT ( 'NONE',  ( 2.780723358947928197E-16, 1.687499998634406806, -4.541265875000002339 ) ) ;
#23612 = CARTESIAN_POINT ( 'NONE',  ( 0.3752463838824955378, 65.74564559952163734, -26.26824411940089021 ) ) ;
#23613 = CARTESIAN_POINT ( 'NONE',  ( 3.313708498984756279, 7.999999999999991118, 19.86155277982336997 ) ) ;
#23615 = CARTESIAN_POINT ( 'NONE',  ( 23.99999999999997513, 196.8125000000000284, 171.6568542494922553 ) ) ;
#23614 = CARTESIAN_POINT ( 'NONE',  ( -49.70177871865297448, 50.00000000000007105, 57.99999999999998579 ) ) ;
#23616 = CARTESIAN_POINT ( 'NONE',  ( -3.042071309553173730, 109.3229166632526983, 11.35316468749999785 ) ) ;
#23617 = ORIENTED_EDGE ( 'NONE', *, *, #12959, .F. ) ;
#23618 =( BOUNDED_CURVE ( )  B_SPLINE_CURVE ( 2, ( #14159, #25480, #36822, #7782, #43209, #48497, #60567, #30787, #31151, #65849, #37192, #71133, #31530 ),
 .UNSPECIFIED., .F., .F. ) 
 B_SPLINE_CURVE_WITH_KNOTS ( ( 3, 2, 2, 2, 2, 2, 3 ),
 ( 0.4945652173913043237, 0.4963768115942028825, 0.4981884057971014412, 0.5000000000000000000, 0.5018115942028985588, 0.5036231884057971175, 0.5054347826086956763 ),
 .UNSPECIFIED. ) 
 CURVE ( )  GEOMETRIC_REPRESENTATION_ITEM ( )  RATIONAL_B_SPLINE_CURVE ( ( 1.000000000000000000, 0.9659258262890683122, 1.000000000000000000, 0.9659258262890683122, 1.000000000000000000, 0.9659258262890683122, 1.000000000000000000, 0.9659258262890683122, 1.000000000000000000, 0.9659258262890683122, 1.000000000000000000, 0.9659258262890683122, 1.000000000000000000 ) ) 
 REPRESENTATION_ITEM ( '' )  );
#23619 = CARTESIAN_POINT ( 'NONE',  ( 0.000000000000000000, 0.000000000000000000, 0.000000000000000000 ) ) ;
#23620 = CARTESIAN_POINT ( 'NONE',  ( -1.469576158976823947E-15, 14.62500000000000178, 8.000000000000000000 ) ) ;
#23621 = FACE_OUTER_BOUND ( 'NONE', #18705, .T. ) ;
#23622 = CARTESIAN_POINT ( 'NONE',  ( 8.311093377946834337, 242.3437500034139873, -8.311093377946836114 ) ) ;
#23623 = CARTESIAN_POINT ( 'NONE',  ( -11.35316468749999785, 118.0729166632526983, -3.042071309553167513 ) ) ;
#23624 = VERTEX_POINT ( 'NONE', #68795 ) ;
#23625 = CARTESIAN_POINT ( 'NONE',  ( -32.00000000000000000, 208.2500000000000284, 170.0000000000003979 ) ) ;
#23626 = EDGE_CURVE ( 'NONE', #42754, #23901, #57103, .T. ) ;
#23627 = EDGE_CURVE ( 'NONE', #6788, #41315, #26181, .T. ) ;
#23628 = CARTESIAN_POINT ( 'NONE',  ( -4.220049686691937474, -10.18810118749999738, 100.9375000020483810 ) ) ;
#23629 = CARTESIAN_POINT ( 'NONE',  ( -10.00000000000000178, 224.3749999931720254, -1.224646799147353454E-15 ) ) ;
#23630 = CARTESIAN_POINT ( 'NONE',  ( 3.458734125000016757, 200.1250000013656063, 199.4326545832176691 ) ) ;
#23631 = DIRECTION ( 'NONE',  ( 0.000000000000000000, 0.8536788251725985210, 0.5207998305029790664 ) ) ;
#23633 = CARTESIAN_POINT ( 'NONE',  ( -9.832129032723418760, 102.8645833299193697, -5.676582343750004256 ) ) ;
#23632 = CARTESIAN_POINT ( 'NONE',  ( 10.99999999999999467, 11.00000000000000355, 41.99999999999999289 ) ) ;
#23634 = AXIS2_PLACEMENT_3D ( 'NONE', #29588, #52601, #11130 ) ;
#23635 = CARTESIAN_POINT ( 'NONE',  ( 3.313708498984762496, -7.999999999999989342, 4.486552783920144449 ) ) ;
#23636 = CARTESIAN_POINT ( 'NONE',  ( -26.56734541678232375, 197.2500000013656063, 173.4587341250003760 ) ) ;
#23637 = CARTESIAN_POINT ( 'NONE',  ( 5.000000000000046185, 175.8333333333333997, -8.660254037844465458 ) ) ;
#23638 = ORIENTED_EDGE ( 'NONE', *, *, #1996, .F. ) ;
#23639 = ADVANCED_FACE ( 'NONE', ( #32343 ), #11709, .T. ) ;
#23640 = CARTESIAN_POINT ( 'NONE',  ( 8.660254037844385522, 191.4583333265053966, 5.000000000000005329 ) ) ;
#23641 = CARTESIAN_POINT ( 'NONE',  ( 23.99999999999999645, 200.9375000027312126, 171.6568542494923122 ) ) ;
#23642 = CARTESIAN_POINT ( 'NONE',  ( 1.469576158976823947E-15, 112.0625000040967905, 8.000000000000000000 ) ) ;
#23643 = CARTESIAN_POINT ( 'NONE',  ( -3.042071309553173730, 94.63541666325268409, 11.35316468749999785 ) ) ;
#23644 = DIRECTION ( 'NONE',  ( 0.000000000000000000, 0.000000000000000000, 1.000000000000000000 ) ) ;
#23645 = CARTESIAN_POINT ( 'NONE',  ( 7.188101187499999156, 5.249999997951610098, 2.977408999572654924 ) ) ;
#23646 = CARTESIAN_POINT ( 'NONE',  ( -4.220049686691935698, 10.18810118749999916, 94.75000000204838102 ) ) ;
#23647 = CARTESIAN_POINT ( 'NONE',  ( -8.311093377946841443, 14.21874999658601979, 8.311093377946830785 ) ) ;
#23648 = ORIENTED_EDGE ( 'NONE', *, *, #32311, .T. ) ;
#23649 = LINE ( 'NONE', #17988, #5485 ) ;
#23650 = CARTESIAN_POINT ( 'NONE',  ( 3.000000000000001332, -45.00000000000001421, 139.1455027589170470 ) ) ;
#23651 = CARTESIAN_POINT ( 'NONE',  ( 9.832129032723416984, 215.3645833299193555, 5.676582343750006032 ) ) ;
#23652 = CARTESIAN_POINT ( 'NONE',  ( 7.204075437095966983, 7.204075437095967871, 80.96875000204836681 ) ) ;
#23653 = CARTESIAN_POINT ( 'NONE',  ( 3.901180567966413104, 22.00000000000000355, 1.216512768759604235 ) ) ;
#23654 = CARTESIAN_POINT ( 'NONE',  ( -2.679491924311152573, 98.33333332650535397, -10.00000000000004619 ) ) ;
#23655 = CARTESIAN_POINT ( 'NONE',  ( -6.676582343750000703, 298.5156250017070079, 2.765530957082001251 ) ) ;
#23656 = EDGE_CURVE ( 'NONE', #63859, #35319, #3660, .T. ) ;
#23657 = ORIENTED_EDGE ( 'NONE', *, *, #65174, .F. ) ;
#23658 = CARTESIAN_POINT ( 'NONE',  ( 2.751064625579944321E-14, 205.7500000000000284, 194.0000000000000568 ) ) ;
#23659 = CARTESIAN_POINT ( 'NONE',  ( -11.35316468749999785, 213.3854166632526983, -3.042071309553167957 ) ) ;
#23660 = AXIS2_PLACEMENT_3D ( 'NONE', #18985, #71392, #64645 ) ;
#23661 = CARTESIAN_POINT ( 'NONE',  ( -10.18810118749999916, 4.220049686691934809, 88.56250000204836681 ) ) ;
#23662 = CARTESIAN_POINT ( 'NONE',  ( -31.45873412500001010, 202.6250000013656063, 168.5673454167827572 ) ) ;
#23663 = CARTESIAN_POINT ( 'NONE',  ( 3.313708498984762496, 16.21875000000000355, 7.999999999999998224 ) ) ;
#23664 = ORIENTED_EDGE ( 'NONE', *, *, #51863, .F. ) ;
#23665 = CARTESIAN_POINT ( 'NONE',  ( -7.188101187500001821, 121.0625000020483668, -2.977408999572650483 ) ) ;
#23666 = CARTESIAN_POINT ( 'NONE',  ( -28.00000000000007816, 200.1250000027312126, 166.0000000000003695 ) ) ;
#23667 = CARTESIAN_POINT ( 'NONE',  ( 4.999999999999993783, 34.16666666666667140, 8.660254037844390851 ) ) ;
#23668 = CARTESIAN_POINT ( 'NONE',  ( -3.313708498984740292, 7.968750000000001776, -8.000000000000021316 ) ) ;
#23669 = CARTESIAN_POINT ( 'NONE',  ( -4.220049686691937474, -10.18810118749999738, 74.31250000204836681 ) ) ;
#23670 = ORIENTED_EDGE ( 'NONE', *, *, #29834, .T. ) ;
#23671 = CARTESIAN_POINT ( 'NONE',  ( 7.188101187499999156, 1.874999997951610320, 2.977408999572654924 ) ) ;
#23672 = DIRECTION ( 'NONE',  ( -0.000000000000000000, 1.000000000000000000, -0.000000000000000000 ) ) ;
#23673 = CYLINDRICAL_SURFACE ( 'NONE', #10221, 3.999999999999976019 ) ;
#23674 = CARTESIAN_POINT ( 'NONE',  ( -4.401442555609581635E-16, 122.6562500020483810, -7.188101187500000044 ) ) ;
#23675 = AXIS2_PLACEMENT_3D ( 'NONE', #64858, #17725, #30898 ) ;
#23676 = CARTESIAN_POINT ( 'NONE',  ( 5.000000000000000000, -62.32183698944616879, 23.94439461060377994 ) ) ;
#23677 = CARTESIAN_POINT ( 'NONE',  ( 4.721056650416000089, 296.8281250017069510, 4.721056650415999201 ) ) ;
#23679 = DIRECTION ( 'NONE',  ( -0.000000000000000000, -1.000000000000000000, -4.283267841918042741E-17 ) ) ;
#23678 = CARTESIAN_POINT ( 'NONE',  ( 11.35316468749999963, 236.1979166700806445, 3.042071309553159519 ) ) ;
#23680 = ORIENTED_EDGE ( 'NONE', *, *, #45573, .T. ) ;
#23681 = CARTESIAN_POINT ( 'NONE',  ( 11.35316468749999963, 241.5104166700806729, 3.042071309553159519 ) ) ;
#23682 = CARTESIAN_POINT ( 'NONE',  ( 5.082755093536320601, -5.082755093536318824, 5.049052781871752771 ) ) ;
#23683 = ORIENTED_EDGE ( 'NONE', *, *, #34546, .T. ) ;
#23684 = CARTESIAN_POINT ( 'NONE',  ( 1.871523826299183495E-15, -10.18810118749999916, 68.03125000204838102 ) ) ;
#23685 = CARTESIAN_POINT ( 'NONE',  ( -9.832129032723420536, 84.01041666325268409, 5.676582343749997150 ) ) ;
#23686 = CARTESIAN_POINT ( 'NONE',  ( 0.4320110153365303018, 60.19564456717396439, 22.88238106212169498 ) ) ;
#23687 = CARTESIAN_POINT ( 'NONE',  ( 11.00000000000000000, 1.347111479062088405E-15, 85.75000000000000000 ) ) ;
#23690 = FACE_OUTER_BOUND ( 'NONE', #37039, .T. ) ;
#23689 = CARTESIAN_POINT ( 'NONE',  ( 31.99999999999997868, 194.4375000027312126, 168.3431457505075173 ) ) ;
#23688 = CARTESIAN_POINT ( 'NONE',  ( 31.45873412499998523, 208.8750000013656347, 171.4326545832175839 ) ) ;
#23691 = ORIENTED_EDGE ( 'NONE', *, *, #41305, .F. ) ;
#23692 = EDGE_CURVE ( 'NONE', #60403, #61413, #73166, .T. ) ;
#23693 = CARTESIAN_POINT ( 'NONE',  ( 4.000000000000000888, 18.93750000000000000, 1.656854249492384135 ) ) ;
#23694 = DIRECTION ( 'NONE',  ( 0.000000000000000000, -1.000000000000000000, 0.000000000000000000 ) ) ;
#23695 = CARTESIAN_POINT ( 'NONE',  ( 11.35316468750000141, 205.7812499965860411, 0.000000000000000000 ) ) ;
#23696 = CARTESIAN_POINT ( 'NONE',  ( -2.445694354108838731, 207.0625000013656063, 144.4456943541088663 ) ) ;
#23697 = CONICAL_SURFACE ( 'NONE', #46579, 12.00000000000000000, 1.047197551196596077 ) ;
#23698 = CARTESIAN_POINT ( 'NONE',  ( 25.55430564589115505, 206.5625000013656063, 172.4456943541086957 ) ) ;
#23699 = CARTESIAN_POINT ( 'NONE',  ( 7.188101187500000044, 21.84374999795161543, 0.000000000000000000 ) ) ;
#23700 = CARTESIAN_POINT ( 'NONE',  ( -2.085542519210945728E-15, 184.8437499965860411, 11.35316468750000141 ) ) ;
#23701 = CARTESIAN_POINT ( 'NONE',  ( 5.082755093536325042, 98.46875000204838102, -5.082755093536325930 ) ) ;
#23702 = CARTESIAN_POINT ( 'NONE',  ( -10.00000000000000355, 89.58333332650535397, 2.679491924311223183 ) ) ;
#23703 = VECTOR ( 'NONE', #53017, 1000.000000000000000 ) ;
#23704 = CARTESIAN_POINT ( 'NONE',  ( 3.211159895383561835, 11.43749999863440614, -3.211159895383561835 ) ) ;
#23705 = CARTESIAN_POINT ( 'NONE',  ( 25.55430564589115150, 202.5625000013656063, 172.4456943541086957 ) ) ;
#23706 = CARTESIAN_POINT ( 'NONE',  ( -7.188101187499990274, -2.977408999572651371, 10.95530278187175455 ) ) ;
#23707 = CARTESIAN_POINT ( 'NONE',  ( 11.35316468750000141, 70.78124999658602690, 0.000000000000000000 ) ) ;
#23708 = CARTESIAN_POINT ( 'NONE',  ( 26.34314575050762031, 206.0625000027312126, 173.9999999999998863 ) ) ;
#23709 = CARTESIAN_POINT ( 'NONE',  ( 1.469576158976822172E-15, -7.999999999999991118, -0.2384472156701772649 ) ) ;
#23710 = VERTEX_POINT ( 'NONE', #60996 ) ;
#23711 = CARTESIAN_POINT ( 'NONE',  ( 10.99999999999989697, -4.556349186104149851, 75.15624999999998579 ) ) ;
#23712 = CARTESIAN_POINT ( 'NONE',  ( -7.778174593052020747, -7.778174593052023411, 116.6875000000000000 ) ) ;
#23713 = CARTESIAN_POINT ( 'NONE',  ( -3.042071309553173730, 69.32291666325268409, 11.35316468749999785 ) ) ;
#23714 = CARTESIAN_POINT ( 'NONE',  ( -11.00000000000000000, 0.000000000000000000, 68.68750000409676204 ) ) ;
#23715 = CARTESIAN_POINT ( 'NONE',  ( 2.445694354108784108, 195.5625000013656063, 144.4456943541088663 ) ) ;
#23716 = CARTESIAN_POINT ( 'NONE',  ( -1.558072418983094343, 16.42747873774318990, 68.67104701338824668 ) ) ;
#23718 = CARTESIAN_POINT ( 'NONE',  ( -11.35316468750000141, 58.48958332991933418, 3.042071309553159963 ) ) ;
#23717 = CARTESIAN_POINT ( 'NONE',  ( -7.188101187500000044, 89.65625000204838102, 0.000000000000000000 ) ) ;
#23719 = CARTESIAN_POINT ( 'NONE',  ( 5.656854249492376141, -5.656854249492374365, 25.58030278392014978 ) ) ;
#23720 = CARTESIAN_POINT ( 'NONE',  ( -30.99999999999992895, -31.99999999999978684, 205.0000000000000284 ) ) ;
#23721 =( BOUNDED_CURVE ( )  B_SPLINE_CURVE ( 2, ( #65023, #2402, #19745, #64304, #13696, #71418, #42752, #69970, #36741 ),
 .UNSPECIFIED., .F., .F. ) 
 B_SPLINE_CURVE_WITH_KNOTS ( ( 3, 2, 2, 2, 3 ),
 ( 0.3977272727272727626, 0.4034090909090909394, 0.4090909090909091717, 0.4147727272727272929, 0.4204545454545454697 ),
 .UNSPECIFIED. ) 
 CURVE ( )  GEOMETRIC_REPRESENTATION_ITEM ( )  RATIONAL_B_SPLINE_CURVE ( ( 0.9999999999999992228, 0.9238795325112875156, 1.000000000000000000, 0.9238795325112867385, 1.000000000000000000, 0.9238795325112867385, 1.000000000000000000, 0.9238795325112867385, 1.000000000000000000 ) ) 
 REPRESENTATION_ITEM ( '' )  );
#23722 = ADVANCED_FACE ( 'NONE', ( #50049, #73065 ), #6180, .T. ) ;
#23723 = CARTESIAN_POINT ( 'NONE',  ( 7.320508075688771044, 151.2499999931720538, 7.320508075688775484 ) ) ;
#23724 = CARTESIAN_POINT ( 'NONE',  ( 1.320432766682874540E-15, 99.40625000204838102, 7.188101187500000044 ) ) ;
#23725 = CARTESIAN_POINT ( 'NONE',  ( -10.00000000000000178, 54.37499999317203958, -1.224646799147353454E-15 ) ) ;
#23726 = CARTESIAN_POINT ( 'NONE',  ( 11.35316468749999963, 51.30208332991935549, -3.042071309553165293 ) ) ;
#23727 = CARTESIAN_POINT ( 'NONE',  ( -6.238412754330611322E-16, 10.18810118749999916, 115.6562500020483810 ) ) ;
#23728 = CARTESIAN_POINT ( 'NONE',  ( -3.042071309553173730, 184.3229166632526983, 11.35316468749999785 ) ) ;
#23729 = VERTEX_POINT ( 'NONE', #5807 ) ;
#23730 = CARTESIAN_POINT ( 'NONE',  ( 4.000000000000001776, 4.062500000000000000, -1.656854249492381248 ) ) ;
#23731 = CARTESIAN_POINT ( 'NONE',  ( 0.000000000000000000, 125.0000000000000000, 0.000000000000000000 ) ) ;
#23732 = CARTESIAN_POINT ( 'NONE',  ( -12.00000000000000178, 0.000000000000000000, -21.47459999999999525 ) ) ;
#23734 = CARTESIAN_POINT ( 'NONE',  ( 11.35316468749999963, 175.9895833299193555, -3.042071309553165293 ) ) ;
#23733 = CARTESIAN_POINT ( 'NONE',  ( -0.2583006032756743342, 194.9270552508774301, 194.0729447491228257 ) ) ;
#23735 = VECTOR ( 'NONE', #73416, 1000.000000000000000 ) ;
#23736 = CARTESIAN_POINT ( 'NONE',  ( 0.000000000000000000, 0.000000000000000000, -17.50000000000000000 ) ) ;
#23737 = CARTESIAN_POINT ( 'NONE',  ( -5.000000000000000888, 247.2916666734946318, -8.660254037844387298 ) ) ;
#23738 = CYLINDRICAL_SURFACE ( 'NONE', #40871, 4.000000000000001776 ) ;
#23739 = PRODUCT_DEFINITION_FORMATION_WITH_SPECIFIED_SOURCE ( 'ANY', '', #51143, .NOT_KNOWN. ) ;
#23740 = ADVANCED_FACE ( 'NONE', ( #67409 ), #62751, .T. ) ;
#23741 = ORIENTED_EDGE ( 'NONE', *, *, #15028, .F. ) ;
#23742 = CARTESIAN_POINT ( 'NONE',  ( -2.085542519210945728E-15, 169.8437499965860127, 11.35316468750000141 ) ) ;
#23743 =( BOUNDED_CURVE ( )  B_SPLINE_CURVE ( 2, ( #58940, #7245, #59305, #36656, #20023, #37023, #1598, #54005, #2694 ),
 .UNSPECIFIED., .F., .F. ) 
 B_SPLINE_CURVE_WITH_KNOTS ( ( 3, 2, 2, 2, 3 ),
 ( 0.5694444444444444198, 0.5763888888888888395, 0.5833333333333333703, 0.5902777777777777901, 0.5972222222222222099 ),
 .UNSPECIFIED. ) 
 CURVE ( )  GEOMETRIC_REPRESENTATION_ITEM ( )  RATIONAL_B_SPLINE_CURVE ( ( 1.000000000000000000, 0.9238795325112867385, 1.000000000000000000, 0.9238795325112867385, 1.000000000000000000, 0.9238795325112867385, 1.000000000000000000, 0.9238795325112867385, 1.000000000000000000 ) ) 
 REPRESENTATION_ITEM ( '' )  );
#23744 = ADVANCED_FACE ( 'NONE', ( #45785 ), #29188, .T. ) ;
#23745 = CYLINDRICAL_SURFACE ( 'NONE', #33958, 3.999999999999976019 ) ;
#23746 = CARTESIAN_POINT ( 'NONE',  ( -3.042071309553173730, 124.6354166632526699, 11.35316468749999785 ) ) ;
#23747 = CARTESIAN_POINT ( 'NONE',  ( 28.00000000000002132, 204.1250000027312126, 173.9999999999999147 ) ) ;
#23748 = ORIENTED_EDGE ( 'NONE', *, *, #34454, .T. ) ;
#23749 = CARTESIAN_POINT ( 'NONE',  ( 1.469576158976823947E-15, 106.0625000040967763, 8.000000000000000000 ) ) ;
#23750 = AXIS2_PLACEMENT_3D ( 'NONE', #64943, #18930, #54386 ) ;
#23751 = EDGE_CURVE ( 'NONE', #35837, #15758, #40644, .T. ) ;
#23752 = CARTESIAN_POINT ( 'NONE',  ( 2.828427124746190291, 12.87500000000000178, 2.828427124746192067 ) ) ;
#23753 = CARTESIAN_POINT ( 'NONE',  ( 54.00000000000000000, 272.0000000000000000, 4.085831468968142743E-14 ) ) ;
#23754 = CARTESIAN_POINT ( 'NONE',  ( -4.541265875000002339, 12.81249999863440792, -5.561446717895856393E-16 ) ) ;
#23755 = CARTESIAN_POINT ( 'NONE',  ( -4.898587196589407898E-16, 7.999999999999991118, 18.64280278392014623 ) ) ;
#23756 = CARTESIAN_POINT ( 'NONE',  ( 3.999999999999959144, 196.0625000000000284, 140.3431457505076594 ) ) ;
#23757 = ORIENTED_EDGE ( 'NONE', *, *, #68039, .F. ) ;
#23758 = CARTESIAN_POINT ( 'NONE',  ( -3.313708498984805573, 25.03125000000000000, 7.999999999999956479 ) ) ;
#23759 = CARTESIAN_POINT ( 'NONE',  ( 7.188101187500001821, 104.0000000020483810, -2.977408999572651371 ) ) ;
#23761 = CARTESIAN_POINT ( 'NONE',  ( 11.00000000000005329, -4.556349186103991755, 99.15624999999998579 ) ) ;
#23760 = CARTESIAN_POINT ( 'NONE',  ( -30.44569435410886626, 194.5625000013656063, 167.5543056458916169 ) ) ;
#23762 = ORIENTED_EDGE ( 'NONE', *, *, #63309, .T. ) ;
#23763 = CARTESIAN_POINT ( 'NONE',  ( 3.728321214226603786, 10.10963409588449835, -70.65936332831182654 ) ) ;
#23764 = CARTESIAN_POINT ( 'NONE',  ( -7.188101187499992051, 0.000000000000000000, 23.98655278187175455 ) ) ;
#23765 = ORIENTED_EDGE ( 'NONE', *, *, #124, .F. ) ;
#23766 = ORIENTED_EDGE ( 'NONE', *, *, #35142, .T. ) ;
#23767 = CARTESIAN_POINT ( 'NONE',  ( -7.204075437095967871, 7.204075437095967871, 83.96875000204836681 ) ) ;
#23768 = CARTESIAN_POINT ( 'NONE',  ( 3.313708498984757167, 2.718750000000000000, 8.000000000000001776 ) ) ;
#23769 = CARTESIAN_POINT ( 'NONE',  ( -30.44569435410883074, 195.8125000013656063, 167.5543056458915885 ) ) ;
#23770 = CARTESIAN_POINT ( 'NONE',  ( 7.778174593052021635, 7.778174593052023411, 103.9374999999999858 ) ) ;
#23771 = VECTOR ( 'NONE', #70993, 1000.000000000000000 ) ;
#23774 = CARTESIAN_POINT ( 'NONE',  ( -6.676582343749999815, 296.6718750017069510, 2.765530957082001251 ) ) ;
#23773 = CARTESIAN_POINT ( 'NONE',  ( 25.17157287525377996, 203.7500000027312126, 167.1715728752537586 ) ) ;
#23772 = DIRECTION ( 'NONE',  ( -0.000000000000000000, 1.000000000000000000, -0.000000000000000000 ) ) ;
#23775 = CARTESIAN_POINT ( 'NONE',  ( -4.999999999999998224, 136.6666666666666856, -8.660254037844389075 ) ) ;
#23776 = CARTESIAN_POINT ( 'NONE',  ( -5.656854249492378806, 98.18750000000000000, 5.656854249492381470 ) ) ;
#23777 = CARTESIAN_POINT ( 'NONE',  ( 4.529167459315944555, 225.9997407208379911, 8.915528146188176351 ) ) ;
#23778 = LINE ( 'NONE', #41136, #50391 ) ;
#23779 = EDGE_CURVE ( 'NONE', #27106, #56231, #46669, .T. ) ;
#23780 = CARTESIAN_POINT ( 'NONE',  ( -10.00000000000000000, 233.1250000068279746, 0.000000000000000000 ) ) ;
#23781 = CARTESIAN_POINT ( 'NONE',  ( 24.54126587499998280, 201.2500000013656063, 171.4326545832175555 ) ) ;
#23782 = CLOSED_SHELL ( 'NONE', ( #14823, #31453, #5767, #37438, #35107, #73617, #1082, #44738 ) ) ;
#23783 = CARTESIAN_POINT ( 'NONE',  ( 4.401442555609581635E-16, 5.718749997951610986, -7.188101187500000044 ) ) ;
#23784 = CARTESIAN_POINT ( 'NONE',  ( 8.008118988124993010, -3.317071493978877239, 4.669365283940630107 ) ) ;
#23785 = CARTESIAN_POINT ( 'NONE',  ( 2.445694354108783664, 197.3125000013656063, 144.4456943541088663 ) ) ;
#23786 = CARTESIAN_POINT ( 'NONE',  ( 2.977408999572654480, 117.5000000020483810, 7.188101187499999156 ) ) ;
#23788 = CARTESIAN_POINT ( 'NONE',  ( 2.306210152021531901, 194.6725217480081369, 200.8686854203639598 ) ) ;
#23787 = FACE_OUTER_BOUND ( 'NONE', #50807, .T. ) ;
#23789 = CARTESIAN_POINT ( 'NONE',  ( 5.676582343749997150, 227.5520833367473017, -9.832129032723418760 ) ) ;
#23790 = CARTESIAN_POINT ( 'NONE',  ( -35.88625983882946002, 39.44394675551369289, 64.99999999999998579 ) ) ;
#23791 = CARTESIAN_POINT ( 'NONE',  ( 1.320432766682872962E-15, -7.188101187499992051, 27.73655278187175455 ) ) ;
#23792 = CARTESIAN_POINT ( 'NONE',  ( 26.34314575050758833, 196.9375000000000284, 173.9999999999999147 ) ) ;
#23793 = CARTESIAN_POINT ( 'NONE',  ( 9.832129032723420536, 31.19791666325268409, -5.676582343749999815 ) ) ;
#23794 = ADVANCED_FACE ( 'NONE', ( #11462 ), #57503, .F. ) ;
#23795 = DIRECTION ( 'NONE',  ( -0.000000000000000000, -1.000000000000000000, -4.283267841918042741E-17 ) ) ;
#23796 = CARTESIAN_POINT ( 'NONE',  ( -5.676582343749998039, 222.7604166632526983, -9.832129032723420536 ) ) ;
#23797 = CARTESIAN_POINT ( 'NONE',  ( 3.313708498984755391, 123.9687500000000142, 8.000000000000008882 ) ) ;
#23799 = CARTESIAN_POINT ( 'NONE',  ( -4.898587196589412829E-16, 96.12499999999998579, -8.000000000000000000 ) ) ;
#23798 = CARTESIAN_POINT ( 'NONE',  ( 28.00000000000002487, 209.5625000013656063, 173.9999999999999147 ) ) ;
#23800 = ORIENTED_EDGE ( 'NONE', *, *, #17153, .T. ) ;
#23801 = CARTESIAN_POINT ( 'NONE',  ( -2.754378923186476579E-14, 198.4375000013655779, 145.4587341250000350 ) ) ;
#23802 = CARTESIAN_POINT ( 'NONE',  ( -5.676582343749998039, 17.44791666325268409, -9.832129032723420536 ) ) ;
#23803 = CARTESIAN_POINT ( 'NONE',  ( 7.778174593052023411, -7.778174593052021635, 84.25000000409677625 ) ) ;
#23804 = CARTESIAN_POINT ( 'NONE',  ( 3.458734124999959469, 206.7500000013655779, 140.5673454167823593 ) ) ;
#23805 = CARTESIAN_POINT ( 'NONE',  ( -2.485281374238947016, 294.8750000034140726, -5.999999999999626965 ) ) ;
#23806 = CARTESIAN_POINT ( 'NONE',  ( 12.00000000000000000, 2.937369556047708219, -0.1973350489338391855 ) ) ;
#23808 = CARTESIAN_POINT ( 'NONE',  ( -2.085542519210945728E-15, 19.53124999658601979, 11.35316468750000141 ) ) ;
#23807 = CARTESIAN_POINT ( 'NONE',  ( 7.188101187500002709, 111.3125000020483810, 2.977408999572649151 ) ) ;
#23809 = CARTESIAN_POINT ( 'NONE',  ( 5.656854249492374365, 5.656854249492375253, 16.76780277982336287 ) ) ;
#23810 = CARTESIAN_POINT ( 'NONE',  ( -8.311093377946841443, 143.9062499965860127, 8.311093377946830785 ) ) ;
#23811 = CIRCLE ( 'NONE', #22617, 11.00000000000000000 ) ;
#23812 = EDGE_CURVE ( 'NONE', #31972, #29110, #20954, .T. ) ;
#23813 = CARTESIAN_POINT ( 'NONE',  ( 6.123233995736767268E-16, 113.1249999931720396, -10.00000000000000178 ) ) ;
#23814 = CARTESIAN_POINT ( 'NONE',  ( -7.188101187499999156, 115.6250000020483810, 2.977408999572654924 ) ) ;
#23815 = CYLINDRICAL_SURFACE ( 'NONE', #33711, 11.00000000000000000 ) ;
#23816 = CARTESIAN_POINT ( 'NONE',  ( -25.55430564589119413, 205.5625000013656063, 167.5543056458915316 ) ) ;
#23817 = ORIENTED_EDGE ( 'NONE', *, *, #36731, .T. ) ;
#23818 = CARTESIAN_POINT ( 'NONE',  ( -5.676582343749998039, 7.760416663252684089, -9.832129032723420536 ) ) ;
#23819 = EDGE_LOOP ( 'NONE', ( #24373, #38542, #68383, #1399, #37738 ) ) ;
#23820 = CARTESIAN_POINT ( 'NONE',  ( 1.102182119232618108E-15, 289.2500000000000000, 6.000000000000001776 ) ) ;
#23821 = CARTESIAN_POINT ( 'NONE',  ( -2.765530957081996810, 298.2656250017068942, -6.676582343750003368 ) ) ;
#23822 = CARTESIAN_POINT ( 'NONE',  ( 11.35316468750000141, 145.7812499965860411, 0.000000000000000000 ) ) ;
#23823 = CARTESIAN_POINT ( 'NONE',  ( -7.999999999999991118, 0.000000000000000000, 24.88655278432982598 ) ) ;
#23824 = CARTESIAN_POINT ( 'NONE',  ( 47.32259252271278882, 191.7059220763548524, 65.76194439203457875 ) ) ;
#23825 = CARTESIAN_POINT ( 'NONE',  ( 11.35316468749999963, 251.4062500034139873, -1.390361679473963556E-15 ) ) ;
#23826 = CARTESIAN_POINT ( 'NONE',  ( -10.18810118749999916, 0.000000000000000000, 90.53125000204836681 ) ) ;
#23827 = ORIENTED_EDGE ( 'NONE', *, *, #73564, .F. ) ;
#23828 = EDGE_CURVE ( 'NONE', #46063, #8912, #26232, .T. ) ;
#23829 = CARTESIAN_POINT ( 'NONE',  ( 0.000000000000000000, 125.0000000000000000, 8.000000000000000000 ) ) ;
#23830 = CARTESIAN_POINT ( 'NONE',  ( 5.000000000000000000, 63.46149047932947695, -24.14127879314006719 ) ) ;
#23831 = CARTESIAN_POINT ( 'NONE',  ( -5.676582343750006032, 84.42708332991935549, 9.832129032723418760 ) ) ;
#23833 = VERTEX_POINT ( 'NONE', #47628 ) ;
#23832 =( BOUNDED_SURFACE ( )  B_SPLINE_SURFACE ( 3, 2, ( 
 ( #50545, #2758, #27160 ),
 ( #61874, #44899, #54072 ),
 ( #67905, #44150, #16199 ),
 ( #37088, #61500, #4538 ),
 ( #15834, #55856, #33225 ),
 ( #38868, #15461, #31424 ),
 ( #2380, #67537, #25377 ),
 ( #38498, #10195, #48394 ),
 ( #21503, #8409, #71773 ),
 ( #60091, #39238, #62238 ),
 ( #44522, #8040, #71397 ),
 ( #31046, #48765, #32849 ),
 ( #56224, #73561, #19723 ),
 ( #50177, #10565, #9823 ),
 ( #27912, #45267, #42734 ),
 ( #33596, #56602, #14050 ),
 ( #4918, #54449, #50922 ),
 ( #65748, #4173, #73934 ) ),
 .UNSPECIFIED., .F., .F., .F. ) 
 B_SPLINE_SURFACE_WITH_KNOTS ( ( 4, 2, 2, 2, 2, 2, 2, 2, 4 ),
 ( 3, 3 ),
 ( 0.04202945594034795951, 0.04396162471218430234, 0.04589379348402064518, 0.04782596225585698801, 0.04975813102769333085, 0.05169029979952967369, 0.05265638418544784510, 0.05362246857136601652, 0.05748680611503870913 ),
 ( 0.000000000000000000, 1.000000000000000000 ),
 .UNSPECIFIED. ) 
 GEOMETRIC_REPRESENTATION_ITEM ( )  RATIONAL_B_SPLINE_SURFACE ( (
 ( 1.000000000000000000, 0.6241276099607513395, 1.000000000000000000),
 ( 1.000000000000000000, 0.6218761496800012667, 1.000000000000000000),
 ( 1.000000000000000000, 0.6198047272363184090, 1.000000000000000000),
 ( 1.000000000000000000, 0.6161935119824332174, 1.000000000000000000),
 ( 1.000000000000000000, 0.6146642324076686537, 1.000000000000000000),
 ( 1.000000000000000000, 0.6121850116874761882, 1.000000000000000000),
 ( 1.000000000000000000, 0.6112350889399633669, 1.000000000000000000),
 ( 1.000000000000000000, 0.6099522725972716941, 1.000000000000000000),
 ( 1.000000000000000000, 0.6096208180308003710, 1.000000000000000000),
 ( 1.000000000000000000, 0.6096183796349364803, 1.000000000000000000),
 ( 1.000000000000000000, 0.6099422200104442915, 1.000000000000000000),
 ( 1.000000000000000000, 0.6109087447822132422, 1.000000000000000000),
 ( 1.000000000000000000, 0.6113123981686904296, 1.000000000000000000),
 ( 1.000000000000000000, 0.6122677719810877273, 1.000000000000000000),
 ( 1.000000000000000000, 0.6128199619020645583, 1.000000000000000000),
 ( 1.000000000000000000, 0.6159350830267519283, 1.000000000000000000),
 ( 1.000000000000000000, 0.6195556778514385021, 1.000000000000000000),
 ( 1.000000000000000000, 0.6241278272307897446, 1.000000000000000000) ) ) 
 REPRESENTATION_ITEM ( '' )  SURFACE ( )  );
#23834 = CARTESIAN_POINT ( 'NONE',  ( 10.18810118749999916, 1.247682550866122264E-15, 107.4062500020483668 ) ) ;
#23835 = CARTESIAN_POINT ( 'NONE',  ( 1.881053915767122664, 17.24999999863440792, 4.541265875000001451 ) ) ;
#23836 = ORIENTED_EDGE ( 'NONE', *, *, #59025, .F. ) ;
#23837 = ORIENTED_EDGE ( 'NONE', *, *, #42423, .T. ) ;
#23838 = CARTESIAN_POINT ( 'NONE',  ( -3.313708498984765161, 8.531250000000001776, 7.999999999999998224 ) ) ;
#23839 = CARTESIAN_POINT ( 'NONE',  ( -4.541265875000002339, 1.874999998634406806, -1.881053915767121998 ) ) ;
#23840 = CARTESIAN_POINT ( 'NONE',  ( 5.082755093536325930, 22.03124999795161543, -5.082755093536325930 ) ) ;
#23841 = CARTESIAN_POINT ( 'NONE',  ( -8.000000000000000000, 120.5937500040967763, -3.313708498984761608 ) ) ;
#23842 = VECTOR ( 'NONE', #71490, 1000.000000000000000 ) ;
#23843 = CARTESIAN_POINT ( 'NONE',  ( -7.204075437095965206, -7.204075437095968759, 104.2187500020483810 ) ) ;
#23844 = CARTESIAN_POINT ( 'NONE',  ( -1.656854249492381248, 1.312500000000000444, -4.000000000000001776 ) ) ;
#23845 = CARTESIAN_POINT ( 'NONE',  ( -4.000000000000001776, 14.18749999726881406, -1.656854249492381470 ) ) ;
#23846 = CARTESIAN_POINT ( 'NONE',  ( 3.313708498984756279, 7.999999999999991118, 12.54905278392014800 ) ) ;
#23847 = ORIENTED_EDGE ( 'NONE', *, *, #57260, .F. ) ;
#23848 = AXIS2_PLACEMENT_3D ( 'NONE', #15528, #37437, #72513 ) ;
#23849 = CARTESIAN_POINT ( 'NONE',  ( -3.458734124999959025, 197.5000000013656063, 199.4326545832176691 ) ) ;
#23850 = CARTESIAN_POINT ( 'NONE',  ( -26.56734541678242678, 203.3750000013656063, 166.5412658750003345 ) ) ;
#23851 = SHAPE_REPRESENTATION_RELATIONSHIP ( 'NONE' , 'NONE' ,  #30147, #13835 ) ;
#23852 = VECTOR ( 'NONE', #27043, 1000.000000000000114 ) ;
#23853 = CARTESIAN_POINT ( 'NONE',  ( 1.881053915767122664, 16.12499999863440792, 4.541265875000001451 ) ) ;
#23854 = CARTESIAN_POINT ( 'NONE',  ( -11.00000000000010658, 4.556349186103942017, 84.90624999999998579 ) ) ;
#23855 = CARTESIAN_POINT ( 'NONE',  ( -4.401442555609577197E-16, 7.188101187499992051, 11.61155278187175632 ) ) ;
#23856 = ORIENTED_EDGE ( 'NONE', *, *, #34457, .T. ) ;
#23857 = VERTEX_POINT ( 'NONE', #63881 ) ;
#23858 = CARTESIAN_POINT ( 'NONE',  ( 4.220049686691934809, 10.18810118749999916, 104.6875000020483810 ) ) ;
#23859 = CARTESIAN_POINT ( 'NONE',  ( -15.05053643744965264, -12.09517842721673553, -0.7140392532422581429 ) ) ;
#23860 = CARTESIAN_POINT ( 'NONE',  ( -26.34314575050764518, 205.9375000000000284, 166.0000000000003695 ) ) ;
#23861 = CARTESIAN_POINT ( 'NONE',  ( -3.458734124999959914, 201.3750000013656347, 196.5673454167823877 ) ) ;
#23862 = CARTESIAN_POINT ( 'NONE',  ( 26.56734541678232731, 195.0000000013656063, 166.5412658749999650 ) ) ;
#23863 = CARTESIAN_POINT ( 'NONE',  ( -2.679491924311225848, 96.45833333333331439, -10.00000000000000178 ) ) ;
#23864 = CARTESIAN_POINT ( 'NONE',  ( -8.000000000000000000, 115.9062500000000000, -3.313708498984761608 ) ) ;
#23865 = CARTESIAN_POINT ( 'NONE',  ( -5.676582343749998039, 67.76041666325268409, -9.832129032723420536 ) ) ;
#23866 = CARTESIAN_POINT ( 'NONE',  ( -6.676582343750000703, 298.6718750017070079, 2.765530957082001251 ) ) ;
#23867 = EDGE_CURVE ( 'NONE', #12154, #15376, #70117, .T. ) ;
#23868 = VERTEX_POINT ( 'NONE', #7286 ) ;
#23869 = DIRECTION ( 'NONE',  ( -1.000000000000000000, -1.577021341797097560E-16, -0.000000000000000000 ) ) ;
#23870 = CARTESIAN_POINT ( 'NONE',  ( -1.469576158976823947E-15, 14.43749999590322375, 8.000000000000000000 ) ) ;
#23871 = CARTESIAN_POINT ( 'NONE',  ( -2.839093476692135984E-14, 207.6875000013656063, 138.5412658750000503 ) ) ;
#23872 = CARTESIAN_POINT ( 'NONE',  ( 3.313708498984761608, 12.09374999590322197, -8.000000000000000000 ) ) ;
#23873 = CARTESIAN_POINT ( 'NONE',  ( 5.656854249492378806, 13.12499999590322197, 5.656854249492381470 ) ) ;
#23874 = CARTESIAN_POINT ( 'NONE',  ( -2.679491924311222295, 226.0416666666666288, 10.00000000000000178 ) ) ;
#23875 = CARTESIAN_POINT ( 'NONE',  ( -54.00000000000000711, 37.00000000000000000, 20.00000000000000000 ) ) ;
#23876 = CARTESIAN_POINT ( 'NONE',  ( -4.220049686691937474, -10.18810118749999738, 71.31250000204836681 ) ) ;
#23877 = CARTESIAN_POINT ( 'NONE',  ( -10.00000000000000178, 217.5000000000000284, -1.224646799147353454E-15 ) ) ;
#23878 = ADVANCED_FACE ( 'NONE', ( #59344 ), #2360, .T. ) ;
#23879 = CARTESIAN_POINT ( 'NONE',  ( -4.401442555609577197E-16, 7.188101187499992051, 10.48655278187175455 ) ) ;
#23880 = CARTESIAN_POINT ( 'NONE',  ( 3.042071309553167069, 187.1354166632526983, -11.35316468749999785 ) ) ;
#23881 = CARTESIAN_POINT ( 'NONE',  ( 1.881053915767121776, 2.499999998634407028, -4.541265875000002339 ) ) ;
#23882 = CARTESIAN_POINT ( 'NONE',  ( 2.828427124746190291, 1.624999997268813390, 2.828427124746192067 ) ) ;
#23884 = LINE ( 'NONE', #52558, #4975 ) ;
#23883 = CYLINDRICAL_SURFACE ( 'NONE', #20179, 10.00000000000000178 ) ;
#23885 = EDGE_LOOP ( 'NONE', ( #1021, #41028, #33200, #35605 ) ) ;
#23886 = CARTESIAN_POINT ( 'NONE',  ( -1.432654583217662481, 207.3750000013656063, 145.4587341250000634 ) ) ;
#23887 = CARTESIAN_POINT ( 'NONE',  ( 3.042071309553167069, 42.13541666325267698, -11.35316468749999785 ) ) ;
#23888 = CARTESIAN_POINT ( 'NONE',  ( 7.778174593052021635, 7.778174593052023411, 104.1250000040967763 ) ) ;
#23889 = CARTESIAN_POINT ( 'NONE',  ( -31.45873412499996391, 206.7500000013655779, 171.4326545832181239 ) ) ;
#23890 = CARTESIAN_POINT ( 'NONE',  ( 11.00000000000000000, 1.347111479062088405E-15, 70.74999999999998579 ) ) ;
#23892 = CARTESIAN_POINT ( 'NONE',  ( 0.000000000000000000, 0.000000000000000000, -4.000000000000001776 ) ) ;
#23891 = CARTESIAN_POINT ( 'NONE',  ( -5.000000000000000000, -10.26105934116143281, 64.40045319026697257 ) ) ;
#23893 = CARTESIAN_POINT ( 'NONE',  ( -2.445694354108839619, 199.8125000013656063, 139.5543056458912190 ) ) ;
#23894 = CARTESIAN_POINT ( 'NONE',  ( 8.660254037844385522, 71.45833332650538239, 5.000000000000005329 ) ) ;
#23895 = CARTESIAN_POINT ( 'NONE',  ( 5.082755093536326818, 96.21875000204838102, 5.082755093536325042 ) ) ;
#23896 = CARTESIAN_POINT ( 'NONE',  ( -3.211159895383562723, 12.06249999863440614, 3.211159895383561391 ) ) ;
#23897 = LINE ( 'NONE', #51829, #26466 ) ;
#23898 = DIRECTION ( 'NONE',  ( 0.000000000000000000, 0.000000000000000000, -1.000000000000000000 ) ) ;
#23899 = CARTESIAN_POINT ( 'NONE',  ( -7.999999999999015010, 2.678670460604446806E-06, 11.51770387648012317 ) ) ;
#23900 = ORIENTED_EDGE ( 'NONE', *, *, #44436, .T. ) ;
#23901 = VERTEX_POINT ( 'NONE', #6913 ) ;
#23902 = CARTESIAN_POINT ( 'NONE',  ( 1.736494649845410798, -67.70200331863067333, -20.12302832235276995 ) ) ;
#23903 = CARTESIAN_POINT ( 'NONE',  ( -4.088227598258586603E-16, 296.3593750017070079, -6.676582343750001591 ) ) ;
#23904 = CARTESIAN_POINT ( 'NONE',  ( 0.000000000000000000, 0.000000000000000000, 118.0000000000000000 ) ) ;
#23905 = CARTESIAN_POINT ( 'NONE',  ( 8.311093377946837890, 156.4062499965860411, -8.311093377946837890 ) ) ;
#23906 = CARTESIAN_POINT ( 'NONE',  ( 1.871523826299183495E-15, -10.18810118749999916, 81.53125000204838102 ) ) ;
#23907 = FACE_OUTER_BOUND ( 'NONE', #26201, .T. ) ;
#23908 = CARTESIAN_POINT ( 'NONE',  ( 2.751064625579944321E-14, 203.7500000000000284, 194.0000000000000568 ) ) ;
#23909 = FACE_OUTER_BOUND ( 'NONE', #38439, .T. ) ;
#23910 = CARTESIAN_POINT ( 'NONE',  ( -10.18810118749999738, -4.220049686691941915, 111.6250000020483810 ) ) ;
#23911 = ORIENTED_EDGE ( 'NONE', *, *, #6326, .F. ) ;
#23912 = CIRCLE ( 'NONE', #29949, 11.00000000000000355 ) ;
#23913 = CARTESIAN_POINT ( 'NONE',  ( 2.449293598294707893E-16, 7.250000000000000000, -4.000000000000001776 ) ) ;
#23914 = CARTESIAN_POINT ( 'NONE',  ( 2.199244671006358676, 177.9999999999999716, 139.0000000000001137 ) ) ;
#23915 = CARTESIAN_POINT ( 'NONE',  ( 11.35316468750000141, 126.0937499965860127, 0.000000000000000000 ) ) ;
#23916 = CARTESIAN_POINT ( 'NONE',  ( 2.754378923186476579E-14, 200.1875000013656063, 194.5412658750000219 ) ) ;
#23917 = CARTESIAN_POINT ( 'NONE',  ( -1.432654583217607414, 208.5000000013656063, 194.5412658750000219 ) ) ;
#23918 = CARTESIAN_POINT ( 'NONE',  ( -10.18810118749999916, 4.220049686691934809, 78.43750000204838102 ) ) ;
#23919 = CARTESIAN_POINT ( 'NONE',  ( -8.311093377946836114, 47.96874999658601268, -8.311093377946837890 ) ) ;
#23920 = ORIENTED_EDGE ( 'NONE', *, *, #35627, .F. ) ;
#23921 = FACE_OUTER_BOUND ( 'NONE', #34260, .T. ) ;
#23922 = CARTESIAN_POINT ( 'NONE',  ( -4.541265875000002339, 2.874999998634407028, -1.881053915767121998 ) ) ;
#23923 = CARTESIAN_POINT ( 'NONE',  ( 3.317071493978883456, -8.008118988124989457, 16.48186528394062833 ) ) ;
#23924 = CARTESIAN_POINT ( 'NONE',  ( -7.188101187500000044, 16.21874999795161543, -8.802885111219163269E-16 ) ) ;
#23925 = CARTESIAN_POINT ( 'NONE',  ( 6.000000000000001776, 293.5625000034140157, -7.347880794884121708E-16 ) ) ;
#23926 = CARTESIAN_POINT ( 'NONE',  ( -48.12321776826230035, 143.0819390673957798, 62.13366417131346253 ) ) ;
#23927 = CARTESIAN_POINT ( 'NONE',  ( 5.082755093536325930, 8.531249997951611874, -5.082755093536325930 ) ) ;
#23928 = CARTESIAN_POINT ( 'NONE',  ( 7.188101187499992051, 8.802885111219154394E-16, 6.736552781871754547 ) ) ;
#23929 = CARTESIAN_POINT ( 'NONE',  ( 4.220049686691941027, -10.18810118749999738, 72.62500000204836681 ) ) ;
#23930 = CARTESIAN_POINT ( 'NONE',  ( -31.45873412499998523, 208.0000000013656347, 171.4326545832180386 ) ) ;
#23931 = DIRECTION ( 'NONE',  ( -0.000000000000000000, -0.000000000000000000, -1.000000000000000000 ) ) ;
#23932 = CARTESIAN_POINT ( 'NONE',  ( -1.656854249492381248, 3.062499997268814056, -4.000000000000001776 ) ) ;
#23933 = UNCERTAINTY_MEASURE_WITH_UNIT (LENGTH_MEASURE( 1.000000000000000082E-05 ), #53643, 'distance_accuracy_value', 'NONE');
#23934 = ORIENTED_EDGE ( 'NONE', *, *, #2140, .F. ) ;
#23935 = CARTESIAN_POINT ( 'NONE',  ( -3.999999999999959144, 194.1875000027312126, 199.6568542494924259 ) ) ;
#23936 = CARTESIAN_POINT ( 'NONE',  ( -4.000000000000015987, 206.5000000000000284, 142.0000000000000568 ) ) ;
#23938 =( BOUNDED_CURVE ( )  B_SPLINE_CURVE ( 3, ( #31521, #1392, #49986, #44333 ),
 .UNSPECIFIED., .F., .F. ) 
 B_SPLINE_CURVE_WITH_KNOTS ( ( 4, 4 ),
 ( 1.001993859653092844, 1.443823537180817684 ),
 .UNSPECIFIED. ) 
 CURVE ( )  GEOMETRIC_REPRESENTATION_ITEM ( )  RATIONAL_B_SPLINE_CURVE ( ( 1.000000000000000000, 0.9837982640406375268, 0.9837982640406375268, 1.000000000000000000 ) ) 
 REPRESENTATION_ITEM ( '' )  );
#23937 = CARTESIAN_POINT ( 'NONE',  ( -28.00000000000007816, 201.1250000027312126, 166.0000000000003695 ) ) ;
#23939 = EDGE_CURVE ( 'NONE', #72729, #36393, #59944, .T. ) ;
#23940 = CARTESIAN_POINT ( 'NONE',  ( -5.082755093536325930, 117.9687500020483810, -5.082755093536325930 ) ) ;
#23941 = EDGE_CURVE ( 'NONE', #56214, #30314, #52942, .T. ) ;
#23942 = CARTESIAN_POINT ( 'NONE',  ( 7.320508075688776373, 250.0000000068279746, 7.320508075688767491 ) ) ;
#23943 = CARTESIAN_POINT ( 'NONE',  ( -5.656854249492373476, -5.656854249492376141, 4.205302783920145338 ) ) ;
#23944 = ORIENTED_EDGE ( 'NONE', *, *, #18697, .F. ) ;
#23945 = CARTESIAN_POINT ( 'NONE',  ( -1.320432766682874540E-15, 15.09374999795161187, 7.188101187500000044 ) ) ;
#23946 = ORIENTED_EDGE ( 'NONE', *, *, #19179, .T. ) ;
#23947 = CARTESIAN_POINT ( 'NONE',  ( 31.99999999999999289, 198.2500000000000000, 169.9999999999999432 ) ) ;
#23948 = CARTESIAN_POINT ( 'NONE',  ( 7.071067751884405617, 220.0000000000000284, 7.071067871846544506 ) ) ;
#23949 = CARTESIAN_POINT ( 'NONE',  ( 10.00000000000000178, 60.20833333333333570, -2.679491924311226736 ) ) ;
#23950 = CARTESIAN_POINT ( 'NONE',  ( 2.977408999572654480, 99.50000000204838102, 7.188101187499999156 ) ) ;
#23951 = CARTESIAN_POINT ( 'NONE',  ( -26.34314575050754215, 196.9375000000000284, 166.0000000000004263 ) ) ;
#23953 = CARTESIAN_POINT ( 'NONE',  ( -20.73527393640048189, -35.96581507776245701, 193.0448900011637363 ) ) ;
#23952 = CARTESIAN_POINT ( 'NONE',  ( 1.469576158976823947E-15, 89.56250000409677625, 8.000000000000000000 ) ) ;
#23954 = EDGE_CURVE ( 'NONE', #4200, #48510, #36381, .T. ) ;
#23955 = ORIENTED_EDGE ( 'NONE', *, *, #16197, .F. ) ;
#23956 = CIRCLE ( 'NONE', #63708, 3.999999999999986233 ) ;
#23957 = CARTESIAN_POINT ( 'NONE',  ( -11.35316468749999785, 248.6979166700806445, -3.042071309553164848 ) ) ;
#23958 = CARTESIAN_POINT ( 'NONE',  ( 7.188101187499993827, -2.977408999572645598, 20.51780278187175455 ) ) ;
#23959 = CARTESIAN_POINT ( 'NONE',  ( 2.069125466538506597, 55.78340383127927993, 43.89144373685476808 ) ) ;
#23960 = CARTESIAN_POINT ( 'NONE',  ( -7.320508075688773708, 73.74999999317202537, -7.320508075688774596 ) ) ;
#23961 = CARTESIAN_POINT ( 'NONE',  ( -7.320508075688778149, 148.1250000000000000, 7.320508075688770155 ) ) ;
#23962 = CARTESIAN_POINT ( 'NONE',  ( 7.320508075688774596, 202.4999999931720538, -7.320508075688774596 ) ) ;
#23963 = CARTESIAN_POINT ( 'NONE',  ( 7.320508075688774596, 175.6249999999999716, -7.320508075688774596 ) ) ;
#23964 = DIRECTION ( 'NONE',  ( 0.000000000000000000, 0.000000000000000000, 1.000000000000000000 ) ) ;
#23965 = CARTESIAN_POINT ( 'NONE',  ( -7.188101187499990274, -2.977408999572651815, 25.95530278187175810 ) ) ;
#23966 = CARTESIAN_POINT ( 'NONE',  ( 3.042071309553159519, 145.0520833299193555, 11.35316468750000141 ) ) ;
#23967 = FACE_OUTER_BOUND ( 'NONE', #28429, .T. ) ;
#23968 = DIRECTION ( 'NONE',  ( -0.000000000000000000, -1.000000000000000000, -0.000000000000000000 ) ) ;
#23971 = CARTESIAN_POINT ( 'NONE',  ( 3.999985685286083115, 88.68677412680158056, -6.928211494859723985 ) ) ;
#23970 = CYLINDRICAL_SURFACE ( 'NONE', #32205, 7.999999999999991118 ) ;
#23969 = CARTESIAN_POINT ( 'NONE',  ( 27.99999999999997158, 207.0000000000000284, 173.9999999999999147 ) ) ;
#23972 = ORIENTED_EDGE ( 'NONE', *, *, #4902, .T. ) ;
#23973 = CARTESIAN_POINT ( 'NONE',  ( 3.655473550591499698, 225.9517612578558783, -9.326890965111893195 ) ) ;
#23974 = LINE ( 'NONE', #70736, #6084 ) ;
#23975 = CARTESIAN_POINT ( 'NONE',  ( 23.99999999999999645, 195.9375000027312126, 171.6568542494923122 ) ) ;
#23976 = CARTESIAN_POINT ( 'NONE',  ( -2.828427124746190735, 11.37500000000000000, -2.828427124746191623 ) ) ;
#23977 = CARTESIAN_POINT ( 'NONE',  ( 7.320508075688774596, 37.49999999317203248, -7.320508075688774596 ) ) ;
#23978 = CARTESIAN_POINT ( 'NONE',  ( 2.977408999572654480, 114.1250000020483952, 7.188101187499999156 ) ) ;
#23979 = CARTESIAN_POINT ( 'NONE',  ( -3.211159895383561391, 0.8124999986344069169, -3.211159895383561835 ) ) ;
#23980 = CARTESIAN_POINT ( 'NONE',  ( -1.506524674532530916, -55.70638416847222629, 43.84942669317716479 ) ) ;
#23981 = CARTESIAN_POINT ( 'NONE',  ( 3.313708498984762496, -7.999999999999989342, 16.29905277982336642 ) ) ;
#23982 = CARTESIAN_POINT ( 'NONE',  ( -2.828427124746192067, 1.625000000000000444, 2.828427124746190735 ) ) ;
#23983 = VERTEX_POINT ( 'NONE', #32921 ) ;
#23984 = CARTESIAN_POINT ( 'NONE',  ( -1.836970198721029983E-15, 28.75000000000000000, 10.00000000000000178 ) ) ;
#23985 = CARTESIAN_POINT ( 'NONE',  ( -0.6568112349274827233, 225.9999999999999716, 10.00000000000000178 ) ) ;
#23986 = CARTESIAN_POINT ( 'NONE',  ( -30.93541659651596021, -37.99999999999992184, 167.9999999999998295 ) ) ;
#23987 = CARTESIAN_POINT ( 'NONE',  ( -5.676582343750000703, 243.3854166700806445, -9.832129032723418760 ) ) ;
#23988 = CARTESIAN_POINT ( 'NONE',  ( -3.042071309553173730, 114.3229166632526841, 11.35316468749999785 ) ) ;
#23989 = VERTEX_POINT ( 'NONE', #8386 ) ;
#23990 = CARTESIAN_POINT ( 'NONE',  ( -8.825921739425714563, 6.257269313017580714, 117.7228986236605692 ) ) ;
#23991 = CARTESIAN_POINT ( 'NONE',  ( 1.871523826299183495E-15, -10.18810118749999916, 101.0312500020483810 ) ) ;
#23992 = CARTESIAN_POINT ( 'NONE',  ( 8.660254037844389075, 227.2916666598387110, -5.000000000000000000 ) ) ;
#23993 = CARTESIAN_POINT ( 'NONE',  ( 3.458734125000015425, 200.2500000013656631, 196.5673454167823877 ) ) ;
#23994 = LINE ( 'NONE', #30035, #28740 ) ;
#23996 = CARTESIAN_POINT ( 'NONE',  ( -9.832129032723420536, 93.69791666325269830, 5.676582343749997150 ) ) ;
#23995 = CARTESIAN_POINT ( 'NONE',  ( -41.99999999999992895, -31.99999999999978684, 135.0000000000000000 ) ) ;
#23997 = CARTESIAN_POINT ( 'NONE',  ( -7.999999999999991118, 0.000000000000000000, 4.017802783920145338 ) ) ;
#23998 = CARTESIAN_POINT ( 'NONE',  ( -24.54126587500000056, 198.5000000013656347, 168.5673454167827003 ) ) ;
#23999 = CARTESIAN_POINT ( 'NONE',  ( 10.00000000000000178, 170.2083333333333428, -2.679491924311226736 ) ) ;
#24000 = ORIENTED_EDGE ( 'NONE', *, *, #14841, .T. ) ;
#24001 = CARTESIAN_POINT ( 'NONE',  ( -1.836970198721029983E-15, 195.6249999931720254, 10.00000000000000178 ) ) ;
#24002 = AXIS2_PLACEMENT_3D ( 'NONE', #9689, #72300, #50410 ) ;
#24003 = DIRECTION ( 'NONE',  ( -0.000000000000000000, 1.000000000000000000, -1.563033456626094573E-30 ) ) ;
#24004 = CARTESIAN_POINT ( 'NONE',  ( 2.261312374316987839, -46.98133456361588145, 139.0822677152125095 ) ) ;
#24005 = CARTESIAN_POINT ( 'NONE',  ( 3.042071309553167513, 92.13541666325266988, -11.35316468749999785 ) ) ;
#24006 = DIRECTION ( 'NONE',  ( -0.000000000000000000, -1.000000000000000000, -0.000000000000000000 ) ) ;
#24007 = CARTESIAN_POINT ( 'NONE',  ( -2.977408999572650039, 14.81249999795161365, -7.188101187500000933 ) ) ;
#24008 = CARTESIAN_POINT ( 'NONE',  ( -10.18810118749999738, -4.220049686691941915, 95.12500000204838102 ) ) ;
#24009 = CARTESIAN_POINT ( 'NONE',  ( -9.832129032723418760, 8.177083329919350163, -5.676582343750004256 ) ) ;
#24010 = ORIENTED_EDGE ( 'NONE', *, *, #28552, .T. ) ;
#24011 = CARTESIAN_POINT ( 'NONE',  ( -5.000000000000009770, 138.3333333333333712, 8.660254037844394404 ) ) ;
#24012 = CARTESIAN_POINT ( 'NONE',  ( -6.123233995736766282E-16, 246.8750000068280031, -10.00000000000000000 ) ) ;
#24013 = CARTESIAN_POINT ( 'NONE',  ( -9.832129032723418760, 217.8645833299193839, -5.676582343750004256 ) ) ;
#24014 = CARTESIAN_POINT ( 'NONE',  ( -4.220049686691937474, -10.18810118749999738, 80.31250000204836681 ) ) ;
#24015 = CARTESIAN_POINT ( 'NONE',  ( 5.656854249492374365, 5.656854249492375253, 10.95530278392014800 ) ) ;
#24016 = CARTESIAN_POINT ( 'NONE',  ( -1.836970198721029983E-15, 150.6249999931720538, 10.00000000000000178 ) ) ;
#24017 = CARTESIAN_POINT ( 'NONE',  ( -4.721056650415998313, 292.5781250017069510, 4.721056650416000089 ) ) ;
#24018 = ORIENTED_EDGE ( 'NONE', *, *, #1749, .T. ) ;
#24019 = CARTESIAN_POINT ( 'NONE',  ( -2.849036369511732440E-14, 202.3750000027312126, 138.0000000000000568 ) ) ;
#24020 = CARTESIAN_POINT ( 'NONE',  ( -8.311093377946836114, 202.9687499965860411, -8.311093377946837890 ) ) ;
#24021 = CARTESIAN_POINT ( 'NONE',  ( -10.18810118749999738, -4.220049686691941915, 88.75000000204836681 ) ) ;
#24022 = EDGE_CURVE ( 'NONE', #3793, #2879, #37820, .T. ) ;
#24023 = CARTESIAN_POINT ( 'NONE',  ( -27.99999999999996447, 201.9375000013656063, 173.4587341250003760 ) ) ;
#24024 = CARTESIAN_POINT ( 'NONE',  ( -8.000000000000000000, 26.15625000000000711, -3.313708498984762496 ) ) ;
#24025 = EDGE_LOOP ( 'NONE', ( #40370, #40525, #11545, #8176 ) ) ;
#24026 = CARTESIAN_POINT ( 'NONE',  ( 2.143584681480918963, 88.75185463835309463, -8.000000000000000000 ) ) ;
#24027 = CARTESIAN_POINT ( 'NONE',  ( 4.000000000000015987, 205.5625000027311842, 199.6568542494924259 ) ) ;
#24028 = CARTESIAN_POINT ( 'NONE',  ( 5.000000000000001776, 30.83333333333333570, -8.660254037844389075 ) ) ;
#24029 = CARTESIAN_POINT ( 'NONE',  ( -23.99999999999999645, 197.8125000000000284, 168.3431457505080289 ) ) ;
#24030 = CARTESIAN_POINT ( 'NONE',  ( -4.220049686691935698, 10.18810118749999916, 73.75000000204836681 ) ) ;
#24032 = ORIENTED_EDGE ( 'NONE', *, *, #18262, .T. ) ;
#24031 =( BOUNDED_CURVE ( )  B_SPLINE_CURVE ( 2, ( #60052, #19689, #43069, #18958, #42698, #8756, #66085, #14395, #65347, #55165, #8006, #25343, #41962 ),
 .UNSPECIFIED., .F., .F. ) 
 B_SPLINE_CURVE_WITH_KNOTS ( ( 3, 2, 2, 2, 2, 2, 3 ),
 ( 0.8206521739130434590, 0.8224637681159420177, 0.8242753623188405765, 0.8260869565217391353, 0.8278985507246376940, 0.8297101449275362528, 0.8315217391304348116 ),
 .UNSPECIFIED. ) 
 CURVE ( )  GEOMETRIC_REPRESENTATION_ITEM ( )  RATIONAL_B_SPLINE_CURVE ( ( 1.000000000000000000, 0.9659258262890683122, 1.000000000000000000, 0.9659258262890683122, 1.000000000000000000, 0.9659258262890683122, 1.000000000000000000, 0.9659258262890683122, 1.000000000000000000, 0.9659258262890683122, 1.000000000000000000, 0.9659258262890683122, 1.000000000000000000 ) ) 
 REPRESENTATION_ITEM ( '' )  );
#24033 = CARTESIAN_POINT ( 'NONE',  ( 11.00000000000000000, 1.347111479062088405E-15, 112.7499999999999858 ) ) ;
#24034 = EDGE_CURVE ( 'NONE', #63656, #63859, #54798, .T. ) ;
#24035 = EDGE_CURVE ( 'NONE', #29411, #27622, #37064, .T. ) ;
#24036 = CARTESIAN_POINT ( 'NONE',  ( 7.778174593052023411, -7.778174593052021635, 93.25000000409677625 ) ) ;
#24037 = CARTESIAN_POINT ( 'NONE',  ( -5.082755093536324154, 120.2187500020483952, 5.082755093536326818 ) ) ;
#24038 = CARTESIAN_POINT ( 'NONE',  ( -4.384251028818017204, 22.00000000000000711, 1.062498824860025781 ) ) ;
#24039 = CARTESIAN_POINT ( 'NONE',  ( -2.765530957081998142, 295.6406250017068942, 6.676582343750000703 ) ) ;
#24041 = CARTESIAN_POINT ( 'NONE',  ( -2.828427124746208943, 199.7500000027312126, 144.8284271247462129 ) ) ;
#24040 = CARTESIAN_POINT ( 'NONE',  ( -8.311093377946836114, 238.2812500034139873, -8.311093377946836114 ) ) ;
#24042 = ORIENTED_EDGE ( 'NONE', *, *, #44390, .F. ) ;
#24044 = CIRCLE ( 'NONE', #2337, 9.999999999999996447 ) ;
#24043 = CARTESIAN_POINT ( 'NONE',  ( 9.832129032723420536, 236.3020833367473301, 5.676582343749996262 ) ) ;
#24045 = CARTESIAN_POINT ( 'NONE',  ( -7.188101187499990274, -2.977408999572651371, 4.580302781871752771 ) ) ;
#24046 =( BOUNDED_CURVE ( )  B_SPLINE_CURVE ( 2, ( #45770, #53298, #59693, #31008, #47983, #54033, #66080, #48725, #71732 ),
 .UNSPECIFIED., .F., .F. ) 
 B_SPLINE_CURVE_WITH_KNOTS ( ( 3, 2, 2, 2, 3 ),
 ( 0.4852941176470588758, 0.4889705882352941568, 0.4926470588235294379, 0.4963235294117647189, 0.5000000000000000000 ),
 .UNSPECIFIED. ) 
 CURVE ( )  GEOMETRIC_REPRESENTATION_ITEM ( )  RATIONAL_B_SPLINE_CURVE ( ( 0.9999999999999988898, 0.9238795325112878487, 1.000000000000000000, 0.9238795325112867385, 1.000000000000000000, 0.9238795325112867385, 1.000000000000000000, 0.9238795325112867385, 1.000000000000000000 ) ) 
 REPRESENTATION_ITEM ( '' )  );
#24047 = EDGE_LOOP ( 'NONE', ( #73489, #6925, #2391, #24960 ) ) ;
#24048 = CARTESIAN_POINT ( 'NONE',  ( -9.832129032723420536, 99.01041666325269830, 5.676582343749997150 ) ) ;
#24049 = DIRECTION ( 'NONE',  ( -0.000000000000000000, 0.000000000000000000, 1.000000000000000000 ) ) ;
#24050 = CARTESIAN_POINT ( 'NONE',  ( 2.020667218593132706E-15, -11.00000000000000000, 82.37499999999998579 ) ) ;
#24053 = CARTESIAN_POINT ( 'NONE',  ( -2.849036369511732440E-14, 205.2500000000000284, 138.0000000000000568 ) ) ;
#24052 = CARTESIAN_POINT ( 'NONE',  ( 31.45873412500001010, 203.6250000013656063, 171.4326545832175555 ) ) ;
#24051 = CARTESIAN_POINT ( 'NONE',  ( 31.45873412499999944, 204.9375000013656063, 169.9999999999999432 ) ) ;
#24054 = ORIENTED_EDGE ( 'NONE', *, *, #40997, .T. ) ;
#24055 = DIRECTION ( 'NONE',  ( -0.000000000000000000, 1.000000000000000000, -0.000000000000000000 ) ) ;
#24056 = CARTESIAN_POINT ( 'NONE',  ( 0.000000000000000000, 101.0525588832578734, 0.000000000000000000 ) ) ;
#24057 = ADVANCED_FACE ( 'NONE', ( #15530 ), #49496, .F. ) ;
#24058 = CARTESIAN_POINT ( 'NONE',  ( 9.832129032723416984, 210.3645833299193555, 5.676582343750006032 ) ) ;
#24059 = CARTESIAN_POINT ( 'NONE',  ( -2.754378923186476579E-14, 206.1875000013656063, 145.4587341250000350 ) ) ;
#24060 = CARTESIAN_POINT ( 'NONE',  ( 24.54126587499999701, 206.4375000013656063, 169.9999999999998863 ) ) ;
#24061 = CARTESIAN_POINT ( 'NONE',  ( -5.082755093536325042, 23.90624999795161543, -5.082755093536325930 ) ) ;
#24062 = CARTESIAN_POINT ( 'NONE',  ( -11.35316468750000141, 183.5937499965860411, -1.390361679473963753E-15 ) ) ;
#24063 = CARTESIAN_POINT ( 'NONE',  ( 7.188101187500002709, 98.18750000204835260, 2.977408999572649151 ) ) ;
#24064 = CARTESIAN_POINT ( 'NONE',  ( -5.000000000000000000, 64.42874436516143533, -24.11656705754108998 ) ) ;
#24065 = CARTESIAN_POINT ( 'NONE',  ( -24.00000000000000355, 195.8125000000000284, 168.3431457505080004 ) ) ;
#24066 = CARTESIAN_POINT ( 'NONE',  ( -1.881053915767124440, 11.99999999863440969, 4.541265875000001451 ) ) ;
#24067 = CARTESIAN_POINT ( 'NONE',  ( 26.56734541678238060, 204.2500000013655779, 166.5412658749999650 ) ) ;
#24068 = CARTESIAN_POINT ( 'NONE',  ( -5.082755093536319713, 5.082755093536319713, 12.17405278187175277 ) ) ;
#24069 = CARTESIAN_POINT ( 'NONE',  ( 11.35316468749999785, 70.57291666325269830, 3.042071309553174174 ) ) ;
#24070 = CARTESIAN_POINT ( 'NONE',  ( 0.000000000000000000, 0.000000000000000000, 118.0000000000000000 ) ) ;
#24071 = CARTESIAN_POINT ( 'NONE',  ( -12.18025451098408318, 1.885907279315492735, -0.7157898419446178107 ) ) ;
#24072 = ORIENTED_EDGE ( 'NONE', *, *, #13403, .F. ) ;
#24073 = CARTESIAN_POINT ( 'NONE',  ( -7.320508075688796801, 48.12500000000000711, 7.320508075688789695 ) ) ;
#24074 = CARTESIAN_POINT ( 'NONE',  ( 29.65685424949238325, 206.1875000027311842, 173.9999999999999716 ) ) ;
#24075 = CARTESIAN_POINT ( 'NONE',  ( 9.832129032723420536, 81.19791666325269830, -5.676582343749999815 ) ) ;
#24076 = CARTESIAN_POINT ( 'NONE',  ( -10.99999999999999822, -4.556349186104052151, 68.78125000409679046 ) ) ;
#24077 = CARTESIAN_POINT ( 'NONE',  ( -2.754378923186476579E-14, 197.4375000013655779, 145.4587341250000350 ) ) ;
#24078 = CARTESIAN_POINT ( 'NONE',  ( -1.882291019709195545, 10.12018455450467869, 70.22327770540688618 ) ) ;
#24080 = CARTESIAN_POINT ( 'NONE',  ( -11.35316468749999785, 63.07291666325268409, -3.042071309553167957 ) ) ;
#24079 = CARTESIAN_POINT ( 'NONE',  ( 8.000000000000000000, 103.4375000040967763, -9.797174393178825657E-16 ) ) ;
#24081 = CARTESIAN_POINT ( 'NONE',  ( -5.656854249492375253, 5.656854249492375253, 23.33030278392014978 ) ) ;
#24082 = CARTESIAN_POINT ( 'NONE',  ( -3.637049425642493450, 194.7916240854007413, 143.0994274795365016 ) ) ;
#24084 = CARTESIAN_POINT ( 'NONE',  ( 2.679491924311222739, 150.8333333265053682, 10.00000000000000355 ) ) ;
#24083 = PRODUCT_DEFINITION_SHAPE ( 'NONE', 'NONE',  #41778 ) ;
#24085 = CARTESIAN_POINT ( 'NONE',  ( 5.082755093536326818, 96.59375000204838102, 5.082755093536325042 ) ) ;
#24086 = CARTESIAN_POINT ( 'NONE',  ( 7.320508075688777261, 19.37500000000000000, 7.320508075688779925 ) ) ;
#24087 = CARTESIAN_POINT ( 'NONE',  ( -9.832129032723418760, 53.17708332991935549, -5.676582343750004256 ) ) ;
#24088 = CARTESIAN_POINT ( 'NONE',  ( 7.204075437095966983, 7.204075437095967871, 113.9687500020483810 ) ) ;
#24089 = CARTESIAN_POINT ( 'NONE',  ( 8.311093377946834337, 195.1562499965860411, 8.311093377946839666 ) ) ;
#24090 = EDGE_LOOP ( 'NONE', ( #70479, #59217, #6606, #33876 ) ) ;
#24091 = CARTESIAN_POINT ( 'NONE',  ( -33.07484552657816579, -21.19745326134420083, 158.8094963175336432 ) ) ;
#24092 = CARTESIAN_POINT ( 'NONE',  ( -3.313708498984782924, 122.2812500000000142, 7.999999999999979572 ) ) ;
#24093 = CARTESIAN_POINT ( 'NONE',  ( 0.000000000000000000, -2.500000000000000444, 14.00000000000000000 ) ) ;
#24095 = CARTESIAN_POINT ( 'NONE',  ( 3.042071309553167513, 176.8229166632526699, -11.35316468749999785 ) ) ;
#24094 = CARTESIAN_POINT ( 'NONE',  ( 2.828427124746208943, 195.6250000000000284, 195.1715728752538439 ) ) ;
#24096 = DIRECTION ( 'NONE',  ( -0.000000000000000000, -1.000000000000000000, -0.000000000000000000 ) ) ;
#24097 = CARTESIAN_POINT ( 'NONE',  ( 4.999999999999997335, 251.4583333401613174, -8.660254037844387298 ) ) ;
#24098 = CARTESIAN_POINT ( 'NONE',  ( 0.000000000000000000, 0.000000000000000000, 11.00000000000000000 ) ) ;
#24099 = ORIENTED_EDGE ( 'NONE', *, *, #28999, .F. ) ;
#24100 = CARTESIAN_POINT ( 'NONE',  ( -11.35316468749999785, 173.3854166632526983, -3.042071309553167957 ) ) ;
#24101 = VECTOR ( 'NONE', #50674, 1000.000000000000000 ) ;
#24102 = CARTESIAN_POINT ( 'NONE',  ( -7.188101187499992051, 0.000000000000000000, 28.48655278187175810 ) ) ;
#24103 = CARTESIAN_POINT ( 'NONE',  ( -9.832129032723420536, 134.0104166632526983, 5.676582343749997150 ) ) ;
#24104 = CARTESIAN_POINT ( 'NONE',  ( 2.751064625579944321E-14, 205.8750000027312126, 194.0000000000000568 ) ) ;
#24105 = ORIENTED_EDGE ( 'NONE', *, *, #55138, .F. ) ;
#24106 = EDGE_CURVE ( 'NONE', #20547, #36985, #25721, .T. ) ;
#24107 = AXIS2_PLACEMENT_3D ( 'NONE', #25536, #19881, #67035 ) ;
#24108 = CARTESIAN_POINT ( 'NONE',  ( -3.313708498984762052, 102.4062500040967763, -8.000000000000000000 ) ) ;
#24109 = CARTESIAN_POINT ( 'NONE',  ( -2.828427124746190735, 10.37500000000000000, -2.828427124746191623 ) ) ;
#24110 = CARTESIAN_POINT ( 'NONE',  ( 9.797174393178825657E-16, 125.0000000000000000, -8.000000000000000000 ) ) ;
#24111 = CARTESIAN_POINT ( 'NONE',  ( 3.211159895383561835, 10.43749999863440792, -3.211159895383561835 ) ) ;
#24112 = CARTESIAN_POINT ( 'NONE',  ( 3.313708498984762496, -7.999999999999989342, 19.48655278392014978 ) ) ;
#24113 = CARTESIAN_POINT ( 'NONE',  ( -2.679491924311088624, 188.5416666666666856, 10.00000000000008704 ) ) ;
#24115 = VERTEX_POINT ( 'NONE', #20441 ) ;
#24114 = EDGE_CURVE ( 'NONE', #56133, #3444, #3110, .T. ) ;
#24116 = CARTESIAN_POINT ( 'NONE',  ( -8.660254037844438812, 177.9166666666666856, 5.000000000000024869 ) ) ;
#24117 = CARTESIAN_POINT ( 'NONE',  ( -5.082755093536324154, 97.34375000204838102, 5.082755093536326818 ) ) ;
#24120 = AXIS2_PLACEMENT_3D ( 'NONE', #63573, #33816, #34933 ) ;
#24119 = CARTESIAN_POINT ( 'NONE',  ( 1.469576158976823947E-15, 119.5625000040967763, 8.000000000000000000 ) ) ;
#24118 = CARTESIAN_POINT ( 'NONE',  ( 2.828427124746153876, 204.0000000027312126, 144.8284271247462129 ) ) ;
#24121 = ORIENTED_EDGE ( 'NONE', *, *, #12132, .T. ) ;
#24122 = EDGE_CURVE ( 'NONE', #64593, #28937, #10535, .T. ) ;
#24123 = CARTESIAN_POINT ( 'NONE',  ( -3.074111742571038697, 16.37317034319774223, -69.01341173091250880 ) ) ;
#24124 = CARTESIAN_POINT ( 'NONE',  ( -7.999999999999998224, 104.2812500040967905, 3.313708498984766049 ) ) ;
#24125 = CARTESIAN_POINT ( 'NONE',  ( -5.082755093536317936, -5.082755093536320601, 27.17405278187175455 ) ) ;
#24126 = VERTEX_POINT ( 'NONE', #49115 ) ;
#24127 = ORIENTED_EDGE ( 'NONE', *, *, #55402, .F. ) ;
#24128 = CARTESIAN_POINT ( 'NONE',  ( -4.220049686691937474, -10.18810118749999738, 85.93750000204839523 ) ) ;
#24129 = CARTESIAN_POINT ( 'NONE',  ( -29.43265458321760164, 197.1250000013656347, 173.4587341250003760 ) ) ;
#24130 = CARTESIAN_POINT ( 'NONE',  ( 11.00000000000000000, 1.347111479062088405E-15, 99.24999999999998579 ) ) ;
#24133 = CARTESIAN_POINT ( 'NONE',  ( 4.721056650415999201, 297.2343750017069510, -4.721056650415999201 ) ) ;
#24132 = CARTESIAN_POINT ( 'NONE',  ( 32.00000000000000000, 201.3750000027312126, 169.9999999999998863 ) ) ;
#24131 = FACE_OUTER_BOUND ( 'NONE', #28371, .T. ) ;
#24134 = CARTESIAN_POINT ( 'NONE',  ( -5.000000000000005329, 133.3333333333333428, 8.660254037844387298 ) ) ;
#24135 = DIRECTION ( 'NONE',  ( -0.000000000000000000, 1.000000000000000000, 4.689100369878284071E-30 ) ) ;
#24136 = EDGE_CURVE ( 'NONE', #49272, #33217, #31075, .T. ) ;
#24137 =( BOUNDED_SURFACE ( )  B_SPLINE_SURFACE ( 1, 2, ( 
 ( #25970, #56174, #50492, #4487, #21812, #44845, #67852, #48993, #16143, #39182, #8645, #6359, #56920, #23688, #62555, #10513, #4863, #45213, #73884, #57293, #35033, #51998, #57668, #28978, #5607, #28605, #68224, #51616, #22948, #50868, #33545, #16521, #74632, #40671, #63674, #52369, #45955, #22188, #705, #11627, #39561, #27859, #34665, #29363, #10886, #68972, #17281, #33920, #56546, #5233, #5975, #17652, #335, #40298, #69718, #46694, #28234, #63299, #16903, #23316, #51242, #74253, #22561, #12001, #58045, #18032, #46328, #45582, #62186, #68596, #69342, #39929, #62935, #11260, #34289, #13822, #24051, #8187, #2160, #41048, #65149, #13092, #64791, #30092, #52739, #48537, #1073, #64430, #35402, #53111, #7822, #2533, #18403, #36127, #41780, #42136, #12729, #54223, #58412, #7457, #29725, #6718, #1798, #47060, #30464, #59148, #30825, #36866, #19496, #24426, #53847, #53481, #59874, #35761, #24782, #71179, #59509, #70097, #47797, #41418, #47433, #58778, #70820, #31198, #7086, #19132, #13458, #36496, #25525, #25154, #1445, #12367, #48170, #70457, #18775, #42512, #71545, #65529, #64056, #44386, #48908, #2904, #33094, #65894, #4035, #25889, #67397, #19869, #3649, #66270, #50412, #55345, #27029, #43632, #31947, #54970, #42875, #14200, #61740, #60612, #3279, #43254, #73054, #60986, #21362, #37237, #26649, #15320, #15699, #49286, #20615, #66642, #71922, #56091, #20235, #50040, #49670, #38742, #14949, #9308, #60235, #37988, #10057, #32332, #72303, #4400, #72687, #8560, #20989, #26266, #44013, #27392, #14578, #31574, #37613, #54598, #8936, #67023, #38356, #61364, #9691, #32712, #55720, #40210, #68508, #29271, #45489, #16808, #63586, #63214, #11176, #39102, #34575, #46239, #10796, #23229, #39836, #28889, #34948, #51908, #62841, #34198, #68140, #5150, #11542, #57959, #22103, #57202, #27769, #5517, #50781, #17567, #28517, #51525, #57581, #39471, #74541, #22469, #56830, #6267, #45128 ),
 ( #5891, #62468, #248, #16435, #73426, #22852, #51157, #33832, #28143, #45866, #69257, #40586, #68881, #11915, #21730, #17191, #44761, #67774, #74165, #10428, #16068, #33458, #62105, #56459, #4776, #73794, #13733, #29638, #47348, #53023, #53395, #985, #65437, #46608, #18689, #40961, #69631, #13006, #58327, #41695, #70372, #19048, #25060, #30742, #35674, #65059, #64708, #48081, #23969, #36044, #7735, #70729, #17945, #59059, #35316, #58689, #6633, #1353, #42419, #52651, #7368, #24338, #30376, #71089, #1719, #18316, #23599, #13370, #64339, #41329, #6998, #19407, #12643, #46976, #2071, #70007, #30009, #36778, #63969, #36409, #24698, #59788, #47709, #42052, #59422, #12281, #53760, #8099, #52283, #619, #25435, #19781, #21921, #49197, #14111, #37143, #56652, #31102, #14859, #2814, #62658, #66550, #39290, #54882, #43164, #66180, #54131, #48451, #73987, #71831, #14484, #54509, #10619, #72208, #33646, #2442, #37899, #26554, #4967, #60523, #31858, #3192, #60146, #68327, #8466, #62291, #60897, #27968, #26178, #20521, #71453, #43535, #50973, #9219, #8849, #22290, #32240, #42789, #55257, #37523, #3564, #45313, #25804, #16625, #31486, #65805, #48824, #20148, #50596, #73614, #39660, #44952, #67959, #16252, #6077, #29085, #17007, #52105, #46432, #74353, #57022, #40033, #437, #64155, #12464, #1171, #23417, #45682, #24150, #35133, #22663, #28336, #58149, #29826, #63035, #17757, #40771, #34395, #5335, #5704, #29459, #41150, #6456, #69446, #18503, #70195, #57396, #63779, #40406, #12096, #51343, #68697, #28703, #35495, #6813, #58507, #69818, #51717, #52838, #69076, #18134, #47162, #41512, #52468, #805, #10992, #11360, #34025, #64, #23792, #23046, #46796, #46057, #57772, #17382, #63404, #11730, #34770, #54326, #7919, #47529, #70554, #14302, #64528, #48270, #36228, #20337, #25253, #71649, #13557, #1893, #24880, #12826, #58876, #31679, #30563, #47899, #13190, #42976, #30924, #65997 ) ),
 .UNSPECIFIED., .F., .F., .F. ) 
 B_SPLINE_SURFACE_WITH_KNOTS ( ( 2, 2 ),
 ( 3, 2, 2, 2, 2, 2, 2, 2, 2, 2, 2, 2, 2, 2, 2, 2, 2, 2, 2, 2, 2, 2, 2, 2, 2, 2, 2, 2, 2, 2, 2, 2, 2, 2, 2, 2, 2, 2, 2, 2, 2, 2, 2, 2, 2, 2, 2, 2, 2, 2, 2, 2, 2, 2, 2, 2, 2, 2, 2, 2, 2, 2, 2, 2, 2, 2, 2, 2, 2, 2, 2, 2, 2, 2, 2, 2, 2, 2, 2, 2, 2, 2, 2, 2, 2, 2, 2, 2, 2, 2, 2, 2, 2, 2, 2, 2, 2, 2, 2, 2, 2, 2, 2, 2, 2, 2, 2, 2, 2, 2, 2, 2, 2, 2, 2, 2, 2, 2, 2, 2, 3 ),
 ( 0.000000000000000000, 1.000000000000000000 ),
 ( 0.000000000000000000, 0.008333333333333333218, 0.01666666666666666644, 0.02500000000000000139, 0.03333333333333333287, 0.04166666666666666435, 0.05000000000000000278, 0.05833333333333333426, 0.06666666666666666574, 0.07499999999999999722, 0.08333333333333332871, 0.09166666666666666019, 0.1000000000000000056, 0.1083333333333333370, 0.1166666666666666685, 0.1250000000000000000, 0.1333333333333333315, 0.1416666666666666630, 0.1499999999999999944, 0.1583333333333333259, 0.1666666666666666574, 0.1749999999999999889, 0.1833333333333333204, 0.1916666666666666796, 0.2000000000000000111, 0.2083333333333333426, 0.2166666666666666741, 0.2250000000000000056, 0.2333333333333333370, 0.2416666666666666685, 0.2500000000000000000, 0.2583333333333333592, 0.2666666666666666630, 0.2750000000000000222, 0.2833333333333333259, 0.2916666666666666852, 0.2999999999999999889, 0.3083333333333333481, 0.3166666666666666519, 0.3250000000000000111, 0.3333333333333333148, 0.3416666666666666741, 0.3499999999999999778, 0.3583333333333333370, 0.3666666666666666408, 0.3750000000000000000, 0.3833333333333333592, 0.3916666666666666630, 0.4000000000000000222, 0.4083333333333333259, 0.4166666666666666852, 0.4249999999999999889, 0.4333333333333333481, 0.4416666666666666519, 0.4500000000000000111, 0.4583333333333333148, 0.4666666666666666741, 0.4749999999999999778, 0.4833333333333333370, 0.4916666666666666408, 0.5000000000000000000, 0.5083333333333333037, 0.5166666666666667185, 0.5250000000000000222, 0.5333333333333333259, 0.5416666666666666297, 0.5500000000000000444, 0.5583333333333333481, 0.5666666666666666519, 0.5749999999999999556, 0.5833333333333333703, 0.5916666666666666741, 0.5999999999999999778, 0.6083333333333332815, 0.6166666666666666963, 0.6250000000000000000, 0.6333333333333333037, 0.6416666666666667185, 0.6500000000000000222, 0.6583333333333333259, 0.6666666666666666297, 0.6750000000000000444, 0.6833333333333333481, 0.6916666666666666519, 0.6999999999999999556, 0.7083333333333333703, 0.7166666666666666741, 0.7249999999999999778, 0.7333333333333332815, 0.7416666666666666963, 0.7500000000000000000, 0.7583333333333333037, 0.7666666666666667185, 0.7750000000000000222, 0.7833333333333333259, 0.7916666666666666297, 0.8000000000000000444, 0.8083333333333333481, 0.8166666666666666519, 0.8249999999999999556, 0.8333333333333333703, 0.8416666666666666741, 0.8499999999999999778, 0.8583333333333332815, 0.8666666666666666963, 0.8750000000000000000, 0.8833333333333333037, 0.8916666666666667185, 0.9000000000000000222, 0.9083333333333333259, 0.9166666666666666297, 0.9250000000000000444, 0.9333333333333333481, 0.9416666666666666519, 0.9499999999999999556, 0.9583333333333333703, 0.9666666666666666741, 0.9749999999999999778, 0.9833333333333332815, 0.9916666666666666963, 1.000000000000000000 ),
 .UNSPECIFIED. ) 
 GEOMETRIC_REPRESENTATION_ITEM ( )  RATIONAL_B_SPLINE_SURFACE ( (
 ( 1.000000000000000000, 0.9238795325112867385, 1.000000000000000000, 0.9238795325112867385, 1.000000000000000000, 0.9238795325112867385, 1.000000000000000000, 0.9238795325112867385, 1.000000000000000000, 0.9238795325112867385, 1.000000000000000000, 0.9238795325112867385, 1.000000000000000000, 0.9238795325112867385, 1.000000000000000000, 0.9238795325112867385, 1.000000000000000000, 0.9238795325112867385, 1.000000000000000000, 0.9238795325112867385, 1.000000000000000000, 0.9238795325112867385, 1.000000000000000000, 0.9238795325112867385, 1.000000000000000000, 0.9238795325112867385, 1.000000000000000000, 0.9238795325112867385, 1.000000000000000000, 0.9238795325112867385, 1.000000000000000000, 0.9238795325112867385, 1.000000000000000000, 0.9238795325112867385, 1.000000000000000000, 0.9238795325112867385, 1.000000000000000000, 0.9238795325112867385, 1.000000000000000000, 0.9238795325112867385, 1.000000000000000000, 0.9238795325112867385, 1.000000000000000000, 0.9238795325112867385, 1.000000000000000000, 0.9238795325112867385, 1.000000000000000000, 0.9238795325112867385, 1.000000000000000000, 0.9238795325112867385, 1.000000000000000000, 0.9238795325112867385, 1.000000000000000000, 0.9238795325112867385, 1.000000000000000000, 0.9238795325112867385, 1.000000000000000000, 0.9238795325112867385, 1.000000000000000000, 0.9238795325112867385, 1.000000000000000000, 0.9238795325112867385, 1.000000000000000000, 0.9238795325112867385, 1.000000000000000000, 0.9238795325112867385, 1.000000000000000000, 0.9238795325112867385, 1.000000000000000000, 0.9238795325112867385, 1.000000000000000000, 0.9238795325112867385, 1.000000000000000000, 0.9238795325112867385, 1.000000000000000000, 0.9238795325112867385, 1.000000000000000000, 0.9238795325112867385, 1.000000000000000000, 0.9238795325112867385, 1.000000000000000000, 0.9238795325112867385, 1.000000000000000000, 0.9238795325112867385, 1.000000000000000000, 0.9238795325112867385, 1.000000000000000000, 0.9238795325112867385, 1.000000000000000000, 0.9238795325112867385, 1.000000000000000000, 0.9238795325112867385, 1.000000000000000000, 0.9238795325112867385, 1.000000000000000000, 0.9238795325112867385, 1.000000000000000000, 0.9238795325112867385, 1.000000000000000000, 0.9238795325112867385, 1.000000000000000000, 0.9238795325112867385, 1.000000000000000000, 0.9238795325112867385, 1.000000000000000000, 0.9238795325112867385, 1.000000000000000000, 0.9238795325112867385, 1.000000000000000000, 0.9238795325112867385, 1.000000000000000000, 0.9238795325112867385, 1.000000000000000000, 0.9238795325112867385, 1.000000000000000000, 0.9238795325112867385, 1.000000000000000000, 0.9238795325112867385, 1.000000000000000000, 0.9238795325112867385, 1.000000000000000000, 0.9238795325112867385, 1.000000000000000000, 0.9238795325112867385, 1.000000000000000000, 0.9238795325112867385, 1.000000000000000000, 0.9238795325112867385, 1.000000000000000000, 0.9238795325112867385, 1.000000000000000000, 0.9238795325112867385, 1.000000000000000000, 0.9238795325112867385, 1.000000000000000000, 0.9238795325112867385, 1.000000000000000000, 0.9238795325112867385, 1.000000000000000000, 0.9238795325112867385, 1.000000000000000000, 0.9238795325112867385, 1.000000000000000000, 0.9238795325112867385, 1.000000000000000000, 0.9238795325112867385, 1.000000000000000000, 0.9238795325112867385, 1.000000000000000000, 0.9238795325112867385, 1.000000000000000000, 0.9238795325112867385, 1.000000000000000000, 0.9238795325112867385, 1.000000000000000000, 0.9238795325112867385, 1.000000000000000000, 0.9238795325112867385, 1.000000000000000000, 0.9238795325112867385, 1.000000000000000000, 0.9238795325112867385, 1.000000000000000000, 0.9238795325112867385, 1.000000000000000000, 0.9238795325112867385, 1.000000000000000000, 0.9238795325112867385, 1.000000000000000000, 0.9238795325112867385, 1.000000000000000000, 0.9238795325112867385, 1.000000000000000000, 0.9238795325112867385, 1.000000000000000000, 0.9238795325112867385, 1.000000000000000000, 0.9238795325112867385, 1.000000000000000000, 0.9238795325112867385, 1.000000000000000000, 0.9238795325112867385, 1.000000000000000000, 0.9238795325112867385, 1.000000000000000000, 0.9238795325112867385, 1.000000000000000000, 0.9238795325112867385, 1.000000000000000000, 0.9238795325112867385, 1.000000000000000000, 0.9238795325112867385, 1.000000000000000000, 0.9238795325112867385, 1.000000000000000000, 0.9238795325112867385, 1.000000000000000000, 0.9238795325112867385, 1.000000000000000000, 0.9238795325112867385, 1.000000000000000000, 0.9238795325112867385, 1.000000000000000000, 0.9238795325112867385, 1.000000000000000000, 0.9238795325112867385, 1.000000000000000000, 0.9238795325112867385, 1.000000000000000000, 0.9238795325112867385, 1.000000000000000000, 0.9238795325112867385, 1.000000000000000000, 0.9238795325112867385, 1.000000000000000000, 0.9238795325112867385, 1.000000000000000000, 0.9238795325112867385, 1.000000000000000000, 0.9238795325112867385, 1.000000000000000000, 0.9238795325112867385, 1.000000000000000000, 0.9238795325112867385, 1.000000000000000000, 0.9238795325112867385, 1.000000000000000000, 0.9238795325112867385, 1.000000000000000000, 0.9238795325112867385, 1.000000000000000000, 0.9238795325112867385, 1.000000000000000000, 0.9238795325112867385, 1.000000000000000000, 0.9238795325112867385, 1.000000000000000000, 0.9238795325112867385, 1.000000000000000000, 0.9238795325112867385, 1.000000000000000000),
 ( 1.000000000000000000, 0.9238795325112867385, 1.000000000000000000, 0.9238795325112867385, 1.000000000000000000, 0.9238795325112867385, 1.000000000000000000, 0.9238795325112867385, 1.000000000000000000, 0.9238795325112867385, 1.000000000000000000, 0.9238795325112867385, 1.000000000000000000, 0.9238795325112867385, 1.000000000000000000, 0.9238795325112867385, 1.000000000000000000, 0.9238795325112867385, 1.000000000000000000, 0.9238795325112867385, 1.000000000000000000, 0.9238795325112867385, 1.000000000000000000, 0.9238795325112867385, 1.000000000000000000, 0.9238795325112867385, 1.000000000000000000, 0.9238795325112867385, 1.000000000000000000, 0.9238795325112867385, 1.000000000000000000, 0.9238795325112867385, 1.000000000000000000, 0.9238795325112867385, 1.000000000000000000, 0.9238795325112867385, 1.000000000000000000, 0.9238795325112867385, 1.000000000000000000, 0.9238795325112867385, 1.000000000000000000, 0.9238795325112867385, 1.000000000000000000, 0.9238795325112867385, 1.000000000000000000, 0.9238795325112867385, 1.000000000000000000, 0.9238795325112867385, 1.000000000000000000, 0.9238795325112867385, 1.000000000000000000, 0.9238795325112867385, 1.000000000000000000, 0.9238795325112867385, 1.000000000000000000, 0.9238795325112867385, 1.000000000000000000, 0.9238795325112867385, 1.000000000000000000, 0.9238795325112867385, 1.000000000000000000, 0.9238795325112867385, 1.000000000000000000, 0.9238795325112867385, 1.000000000000000000, 0.9238795325112867385, 1.000000000000000000, 0.9238795325112867385, 1.000000000000000000, 0.9238795325112867385, 1.000000000000000000, 0.9238795325112867385, 1.000000000000000000, 0.9238795325112867385, 1.000000000000000000, 0.9238795325112867385, 1.000000000000000000, 0.9238795325112867385, 1.000000000000000000, 0.9238795325112867385, 1.000000000000000000, 0.9238795325112867385, 1.000000000000000000, 0.9238795325112867385, 1.000000000000000000, 0.9238795325112867385, 1.000000000000000000, 0.9238795325112867385, 1.000000000000000000, 0.9238795325112867385, 1.000000000000000000, 0.9238795325112867385, 1.000000000000000000, 0.9238795325112867385, 1.000000000000000000, 0.9238795325112867385, 1.000000000000000000, 0.9238795325112867385, 1.000000000000000000, 0.9238795325112867385, 1.000000000000000000, 0.9238795325112867385, 1.000000000000000000, 0.9238795325112867385, 1.000000000000000000, 0.9238795325112867385, 1.000000000000000000, 0.9238795325112867385, 1.000000000000000000, 0.9238795325112867385, 1.000000000000000000, 0.9238795325112867385, 1.000000000000000000, 0.9238795325112867385, 1.000000000000000000, 0.9238795325112867385, 1.000000000000000000, 0.9238795325112867385, 1.000000000000000000, 0.9238795325112867385, 1.000000000000000000, 0.9238795325112867385, 1.000000000000000000, 0.9238795325112867385, 1.000000000000000000, 0.9238795325112867385, 1.000000000000000000, 0.9238795325112867385, 1.000000000000000000, 0.9238795325112867385, 1.000000000000000000, 0.9238795325112867385, 1.000000000000000000, 0.9238795325112867385, 1.000000000000000000, 0.9238795325112867385, 1.000000000000000000, 0.9238795325112867385, 1.000000000000000000, 0.9238795325112867385, 1.000000000000000000, 0.9238795325112867385, 1.000000000000000000, 0.9238795325112867385, 1.000000000000000000, 0.9238795325112867385, 1.000000000000000000, 0.9238795325112867385, 1.000000000000000000, 0.9238795325112867385, 1.000000000000000000, 0.9238795325112867385, 1.000000000000000000, 0.9238795325112867385, 1.000000000000000000, 0.9238795325112867385, 1.000000000000000000, 0.9238795325112867385, 1.000000000000000000, 0.9238795325112867385, 1.000000000000000000, 0.9238795325112867385, 1.000000000000000000, 0.9238795325112867385, 1.000000000000000000, 0.9238795325112867385, 1.000000000000000000, 0.9238795325112867385, 1.000000000000000000, 0.9238795325112867385, 1.000000000000000000, 0.9238795325112867385, 1.000000000000000000, 0.9238795325112867385, 1.000000000000000000, 0.9238795325112867385, 1.000000000000000000, 0.9238795325112867385, 1.000000000000000000, 0.9238795325112867385, 1.000000000000000000, 0.9238795325112867385, 1.000000000000000000, 0.9238795325112867385, 1.000000000000000000, 0.9238795325112867385, 1.000000000000000000, 0.9238795325112867385, 1.000000000000000000, 0.9238795325112867385, 1.000000000000000000, 0.9238795325112867385, 1.000000000000000000, 0.9238795325112867385, 1.000000000000000000, 0.9238795325112867385, 1.000000000000000000, 0.9238795325112867385, 1.000000000000000000, 0.9238795325112867385, 1.000000000000000000, 0.9238795325112867385, 1.000000000000000000, 0.9238795325112867385, 1.000000000000000000, 0.9238795325112867385, 1.000000000000000000, 0.9238795325112867385, 1.000000000000000000, 0.9238795325112867385, 1.000000000000000000, 0.9238795325112867385, 1.000000000000000000, 0.9238795325112867385, 1.000000000000000000, 0.9238795325112867385, 1.000000000000000000, 0.9238795325112867385, 1.000000000000000000, 0.9238795325112867385, 1.000000000000000000, 0.9238795325112867385, 1.000000000000000000, 0.9238795325112867385, 1.000000000000000000, 0.9238795325112867385, 1.000000000000000000, 0.9238795325112867385, 1.000000000000000000, 0.9238795325112867385, 1.000000000000000000, 0.9238795325112867385, 1.000000000000000000, 0.9238795325112867385, 1.000000000000000000, 0.9238795325112867385, 1.000000000000000000, 0.9238795325112867385, 1.000000000000000000, 0.9238795325112867385, 1.000000000000000000) ) ) 
 REPRESENTATION_ITEM ( '' )  SURFACE ( )  );
#24138 = DIRECTION ( 'NONE',  ( -0.000000000000000000, -1.000000000000000000, -4.283267841918042741E-17 ) ) ;
#24139 = AXIS2_PLACEMENT_3D ( 'NONE', #67097, #38431, #49358 ) ;
#24140 = CARTESIAN_POINT ( 'NONE',  ( 26.56734541678238060, 201.0000000013655779, 166.5412658749999650 ) ) ;
#24141 = CARTESIAN_POINT ( 'NONE',  ( 2.977408999572651815, 6.562499997951610098, 7.188101187500000933 ) ) ;
#24142 = CARTESIAN_POINT ( 'NONE',  ( 8.008118988124993010, -3.317071493978877239, 1.669365283940626998 ) ) ;
#24143 = CARTESIAN_POINT ( 'NONE',  ( -3.458734125000015425, 196.0000000013656347, 143.4326545832176976 ) ) ;
#24144 = CARTESIAN_POINT ( 'NONE',  ( 7.188101187500002709, 117.6875000020484237, 2.977408999572649151 ) ) ;
#24146 = CARTESIAN_POINT ( 'NONE',  ( 4.707324249721353659, -6.606384249263396846, 0.04231178935258603918 ) ) ;
#24145 = FACE_OUTER_BOUND ( 'NONE', #64120, .T. ) ;
#24147 = CARTESIAN_POINT ( 'NONE',  ( -3.042071309553166181, 233.1770833367473017, -11.35316468749999608 ) ) ;
#24148 = DIRECTION ( 'NONE',  ( -1.000000000000000000, 0.000000000000000000, 0.000000000000000000 ) ) ;
#24149 = CARTESIAN_POINT ( 'NONE',  ( 4.999999999999993783, 51.04166665983870388, 8.660254037844390851 ) ) ;
#24150 = CARTESIAN_POINT ( 'NONE',  ( 28.00000000000001776, 199.5000000000000000, 165.9999999999998863 ) ) ;
#24151 = CARTESIAN_POINT ( 'NONE',  ( -3.042071309553164404, 32.23958332991936260, -11.35316468749999963 ) ) ;
#24152 = CARTESIAN_POINT ( 'NONE',  ( 10.00000000000032863, 24.79166666666685614, 2.679491924311323547 ) ) ;
#24153 = CARTESIAN_POINT ( 'NONE',  ( -8.311093377946841443, 224.2187499965860411, 8.311093377946830785 ) ) ;
#24154 = CARTESIAN_POINT ( 'NONE',  ( 0.000000000000000000, 0.000000000000000000, 38.34805510287551300 ) ) ;
#24156 = DIRECTION ( 'NONE',  ( -0.000000000000000000, -0.000000000000000000, -1.000000000000000000 ) ) ;
#24155 = PLANE ( 'NONE',  #9370 ) ;
#24157 = VERTEX_POINT ( 'NONE', #66097 ) ;
#24158 = EDGE_CURVE ( 'NONE', #58023, #72561, #14407, .T. ) ;
#24159 = AXIS2_PLACEMENT_3D ( 'NONE', #24389, #58377, #46287 ) ;
#24160 = CARTESIAN_POINT ( 'NONE',  ( -2.839093476692135984E-14, 197.9375000013655779, 138.5412658750000503 ) ) ;
#24161 = CARTESIAN_POINT ( 'NONE',  ( -3.042071309553173730, 29.32291666325268764, 11.35316468749999785 ) ) ;
#24162 = CARTESIAN_POINT ( 'NONE',  ( -6.735557395310442023E-16, 11.00000000000000000, 86.31250000409676204 ) ) ;
#24163 = CARTESIAN_POINT ( 'NONE',  ( 2.445694354108784108, 206.5625000013656063, 144.4456943541088663 ) ) ;
#24164 = DIRECTION ( 'NONE',  ( 0.000000000000000000, 0.000000000000000000, 1.000000000000000000 ) ) ;
#24165 = CARTESIAN_POINT ( 'NONE',  ( 5.000000000000000000, 68.60357193678729004, -20.85024232999272087 ) ) ;
#24167 = CARTESIAN_POINT ( 'NONE',  ( -5.676582343750006032, 14.11458332991935016, 9.832129032723418760 ) ) ;
#24166 = CARTESIAN_POINT ( 'NONE',  ( -4.401442555609581635E-16, 105.7812500020483810, -7.188101187500000044 ) ) ;
#24168 = CARTESIAN_POINT ( 'NONE',  ( -4.898587196589407898E-16, 7.999999999999991118, 12.45530277982336642 ) ) ;
#24169 = CARTESIAN_POINT ( 'NONE',  ( 3.042071309553159519, 149.7395833299192986, 11.35316468750000141 ) ) ;
#24170 =( BOUNDED_CURVE ( )  B_SPLINE_CURVE ( 2, ( #55507, #15488, #66428, #9849, #3819, #50569, #26816, #72084, #32874 ),
 .UNSPECIFIED., .F., .F. ) 
 B_SPLINE_CURVE_WITH_KNOTS ( ( 3, 2, 2, 2, 3 ),
 ( 0.4210526315789475116, 0.4276315789473685847, 0.4342105263157896022, 0.4407894736842106198, 0.4473684210526316929 ),
 .UNSPECIFIED. ) 
 CURVE ( )  GEOMETRIC_REPRESENTATION_ITEM ( )  RATIONAL_B_SPLINE_CURVE ( ( 0.9999999999999981126, 0.9238795325112886259, 1.000000000000000000, 0.9238795325112867385, 1.000000000000000000, 0.9238795325112867385, 1.000000000000000000, 0.9238795325112854062, 1.000000000000001332 ) ) 
 REPRESENTATION_ITEM ( '' )  );
#24171 = CARTESIAN_POINT ( 'NONE',  ( 8.660254037844389075, 122.2916666598387110, -5.000000000000000000 ) ) ;
#24172 = ADVANCED_FACE ( 'NONE', ( #31400 ), #48742, .F. ) ;
#24173 = CARTESIAN_POINT ( 'NONE',  ( -5.082755093536324154, 114.2187500020483810, 5.082755093536326818 ) ) ;
#24174 = CARTESIAN_POINT ( 'NONE',  ( 6.123233995736767268E-16, 173.1249999931720538, -10.00000000000000178 ) ) ;
#24175 = CARTESIAN_POINT ( 'NONE',  ( -25.55430564589115150, 203.3125000013656063, 172.4456943541091789 ) ) ;
#24176 = ORIENTED_EDGE ( 'NONE', *, *, #58294, .T. ) ;
#24177 = CARTESIAN_POINT ( 'NONE',  ( 6.951808397369818766E-16, 7.343749996586017126, -11.35316468750000141 ) ) ;
#24178 = ORIENTED_EDGE ( 'NONE', *, *, #1196, .F. ) ;
#24179 = DIRECTION ( 'NONE',  ( -0.000000000000000000, 1.000000000000000000, -0.000000000000000000 ) ) ;
#24180 = CARTESIAN_POINT ( 'NONE',  ( 6.676582343750001591, 296.9531250017069510, -8.176455196517173205E-16 ) ) ;
#24182 = CARTESIAN_POINT ( 'NONE',  ( -3.042071309553163960, 142.2395833299193839, -11.35316468749999963 ) ) ;
#24181 = CARTESIAN_POINT ( 'NONE',  ( -20.20046711624723201, -29.84009366552084330, 145.3336601245884196 ) ) ;
#24183 = CARTESIAN_POINT ( 'NONE',  ( -30.82842712474624847, 207.2500000027312126, 167.1715728752542418 ) ) ;
#24184 = CARTESIAN_POINT ( 'NONE',  ( -7.999999999999989342, -3.313708498984762496, 15.98030278432982243 ) ) ;
#24185 = CARTESIAN_POINT ( 'NONE',  ( 3.313708498984762496, 14.71875000000000355, 7.999999999999998224 ) ) ;
#24186 = CARTESIAN_POINT ( 'NONE',  ( -5.676582343750000703, 253.0729166700807014, -9.832129032723418760 ) ) ;
#24187 = CARTESIAN_POINT ( 'NONE',  ( 1.871523826299183495E-15, -10.18810118749999916, 92.40625000204836681 ) ) ;
#24188 = VERTEX_POINT ( 'NONE', #32540 ) ;
#24189 = AXIS2_PLACEMENT_3D ( 'NONE', #34667, #11629, #7088 ) ;
#24190 = CARTESIAN_POINT ( 'NONE',  ( -10.00000000000000355, 204.5833333265053966, 2.679491924311223183 ) ) ;
#24191 = CARTESIAN_POINT ( 'NONE',  ( 4.556349186104052151, -10.99999999999999822, 100.6562500040967905 ) ) ;
#24192 = CARTESIAN_POINT ( 'NONE',  ( -2.085542519210945728E-15, 89.84374999658602690, 11.35316468750000141 ) ) ;
#24193 = CARTESIAN_POINT ( 'NONE',  ( 4.220049686691941027, -10.18810118749999738, 99.62500000204838102 ) ) ;
#24194 = CARTESIAN_POINT ( 'NONE',  ( -1.881053915767124440, 15.12499999863440792, 4.541265875000001451 ) ) ;
#24195 = ORIENTED_EDGE ( 'NONE', *, *, #51625, .F. ) ;
#24196 = VERTEX_POINT ( 'NONE', #8768 ) ;
#24197 = CARTESIAN_POINT ( 'NONE',  ( 4.898587196589412829E-16, 4.875000000000000888, -8.000000000000000000 ) ) ;
#24198 = CARTESIAN_POINT ( 'NONE',  ( 4.541265875000002339, 1.437499998634406806, 0.000000000000000000 ) ) ;
#24199 = CARTESIAN_POINT ( 'NONE',  ( 2.977408999572650927, 0.7499999979516099868, -7.188101187500001821 ) ) ;
#24200 = CARTESIAN_POINT ( 'NONE',  ( -3.313708498984762052, 121.9062500040967763, -8.000000000000000000 ) ) ;
#24201 = CARTESIAN_POINT ( 'NONE',  ( -10.18810118749999738, -4.220049686691941915, 101.1250000020483810 ) ) ;
#24202 = ADVANCED_FACE ( 'NONE', ( #20063 ), #9525, .T. ) ;
#24203 = CARTESIAN_POINT ( 'NONE',  ( 2.828427124746191623, 1.125000000000000444, -2.828427124746191623 ) ) ;
#24204 = CARTESIAN_POINT ( 'NONE',  ( -2.828427124746192067, 15.37499999726881406, 2.828427124746190735 ) ) ;
#24205 = CARTESIAN_POINT ( 'NONE',  ( -4.541265875000002339, 0.8124999986344066949, -5.561446717895856393E-16 ) ) ;
#24206 = ORIENTED_EDGE ( 'NONE', *, *, #35268, .F. ) ;
#24207 = CARTESIAN_POINT ( 'NONE',  ( 2.020667218593132706E-15, -11.00000000000000000, 80.87499999999998579 ) ) ;
#24208 = CARTESIAN_POINT ( 'NONE',  ( 3.458734125000015425, 198.0000000013656063, 196.5673454167823877 ) ) ;
#24209 = VECTOR ( 'NONE', #61760, 1000.000000000000000 ) ;
#24211 = FACE_OUTER_BOUND ( 'NONE', #70595, .T. ) ;
#24210 = CARTESIAN_POINT ( 'NONE',  ( -24.54126587500002188, 201.2500000013656063, 168.5673454167826435 ) ) ;
#24212 = EDGE_CURVE ( 'NONE', #17249, #43963, #49874, .T. ) ;
#24213 = CARTESIAN_POINT ( 'NONE',  ( -8.342170076843785083E-16, 14.06249999863440614, 4.541265875000002339 ) ) ;
#24214 = CARTESIAN_POINT ( 'NONE',  ( 2.977408999572646486, 7.188101187499991163, 10.01780278187175632 ) ) ;
#24215 = VERTEX_POINT ( 'NONE', #38571 ) ;
#24216 = ORIENTED_EDGE ( 'NONE', *, *, #68008, .F. ) ;
#24217 = CARTESIAN_POINT ( 'NONE',  ( 10.18810118749999916, 4.220049686691935698, 106.0000000020483668 ) ) ;
#24218 = PRODUCT_RELATED_PRODUCT_CATEGORY ( 'part', '', ( #32453 ) ) ;
#24219 = CARTESIAN_POINT ( 'NONE',  ( 1.110124581937998163E-11, 98.75000000000088107, 10.00000000000000533 ) ) ;
#24220 = CARTESIAN_POINT ( 'NONE',  ( -23.99999999999999289, 206.7500000000000284, 170.0000000000003411 ) ) ;
#24221 = CARTESIAN_POINT ( 'NONE',  ( 3.458734125000015425, 201.0000000013655779, 196.5673454167823877 ) ) ;
#24222 = CARTESIAN_POINT ( 'NONE',  ( 28.47326357806521813, 194.4587341250000350, 173.4262024652836658 ) ) ;
#24223 = CARTESIAN_POINT ( 'NONE',  ( 10.00000000000000178, 100.0000000000000000, 0.000000000000000000 ) ) ;
#24224 = CARTESIAN_POINT ( 'NONE',  ( -7.999999999999998224, 120.5937500000000000, 3.313708498984766493 ) ) ;
#24225 = CARTESIAN_POINT ( 'NONE',  ( -5.676582343749998039, 62.76041666325269119, -9.832129032723420536 ) ) ;
#24226 = CARTESIAN_POINT ( 'NONE',  ( 6.676582343750001591, 295.1093750017069510, -8.176455196517173205E-16 ) ) ;
#24227 = ORIENTED_EDGE ( 'NONE', *, *, #12788, .T. ) ;
#24228 = CARTESIAN_POINT ( 'NONE',  ( 2.020667218593132706E-15, -11.00000000000000000, 109.3750000000000000 ) ) ;
#24229 = ADVANCED_FACE ( 'NONE', ( #9891 ), #4238, .F. ) ;
#24230 = CARTESIAN_POINT ( 'NONE',  ( 8.000000000000000000, 14.90624999590322375, -3.313708498984761608 ) ) ;
#24231 = CARTESIAN_POINT ( 'NONE',  ( 3.458734124999959914, 206.3750000013656063, 143.4326545832176976 ) ) ;
#24232 = CARTESIAN_POINT ( 'NONE',  ( -4.999999999999998224, 103.5416666598386968, -8.660254037844389075 ) ) ;
#24233 = CARTESIAN_POINT ( 'NONE',  ( 105.0000000000000000, 205.0000000000000284, 20.00000000000000000 ) ) ;
#24234 = CARTESIAN_POINT ( 'NONE',  ( -4.999999999999992895, 225.8333333333333428, 8.660254037844390851 ) ) ;
#24235 = CARTESIAN_POINT ( 'NONE',  ( -4.242640687119286547, 292.8750000000000000, -4.242640687119286547 ) ) ;
#24236 = CARTESIAN_POINT ( 'NONE',  ( -10.18810118749999738, -4.220049686691941915, 71.12500000204836681 ) ) ;
#24237 = CARTESIAN_POINT ( 'NONE',  ( -10.00000000000000355, 217.7083333333333428, 2.679491924311223183 ) ) ;
#24238 = ADVANCED_FACE ( 'NONE', ( #43457 ), #19699, .F. ) ;
#24239 = CARTESIAN_POINT ( 'NONE',  ( -5.082755093536319713, 5.082755093536319713, 13.67405278187175455 ) ) ;
#24240 = CARTESIAN_POINT ( 'NONE',  ( 11.35316468750000141, 176.0937499965860411, 0.000000000000000000 ) ) ;
#24241 = CARTESIAN_POINT ( 'NONE',  ( 4.541265875000002339, 4.312499998634407028, 0.000000000000000000 ) ) ;
#24242 = CARTESIAN_POINT ( 'NONE',  ( 11.00000000000005329, -4.556349186103991755, 97.84375000409679046 ) ) ;
#24244 = CARTESIAN_POINT ( 'NONE',  ( 2.828427124746191623, 5.125000000000000000, -2.828427124746191623 ) ) ;
#24243 = CARTESIAN_POINT ( 'NONE',  ( 2.849036369511732440E-14, 203.3750000027312126, 202.0000000000000000 ) ) ;
#24245 = VERTEX_POINT ( 'NONE', #62672 ) ;
#24246 = AXIS2_PLACEMENT_3D ( 'NONE', #33221, #9816, #43765 ) ;
#24247 = CARTESIAN_POINT ( 'NONE',  ( 3.458734124999960358, 207.6250000013656347, 143.4326545832176976 ) ) ;
#24248 = CARTESIAN_POINT ( 'NONE',  ( 11.35316468750000141, 41.09374999658601979, 0.000000000000000000 ) ) ;
#24249 = CARTESIAN_POINT ( 'NONE',  ( -10.99999999999999822, -4.556349186104052151, 101.7812500040967620 ) ) ;
#24250 = CARTESIAN_POINT ( 'NONE',  ( 5.676582343750001591, 226.9270833299193839, -9.832129032723420536 ) ) ;
#24251 = CARTESIAN_POINT ( 'NONE',  ( -29.43265458321770822, 205.5000000013655779, 166.5412658750003914 ) ) ;
#24252 = CARTESIAN_POINT ( 'NONE',  ( 5.000000000000002665, 10.83333333333333570, -8.660254037844389075 ) ) ;
#24254 = CARTESIAN_POINT ( 'NONE',  ( -11.00000000000007816, -4.556349186103974880, 107.7812500040967905 ) ) ;
#24253 = CARTESIAN_POINT ( 'NONE',  ( -4.556349186104045934, 11.00000000000000000, 71.40625000409676204 ) ) ;
#24255 = CARTESIAN_POINT ( 'NONE',  ( -3.458734125000016313, 194.8750000013656347, 140.5673454167823593 ) ) ;
#24256 = CARTESIAN_POINT ( 'NONE',  ( -5.000000000000005329, 75.20833332650536818, 8.660254037844387298 ) ) ;
#24257 = CARTESIAN_POINT ( 'NONE',  ( 2.977408999572654480, 96.12500000204836681, 7.188101187499999156 ) ) ;
#24258 = CARTESIAN_POINT ( 'NONE',  ( 4.541265875000002339, 15.43749999863440614, 0.000000000000000000 ) ) ;
#24259 = FACE_OUTER_BOUND ( 'NONE', #30455, .T. ) ;
#24260 = DIRECTION ( 'NONE',  ( -0.000000000000000000, 1.000000000000000000, -0.000000000000000000 ) ) ;
#24261 = CARTESIAN_POINT ( 'NONE',  ( -28.00000000000007461, 195.1250000027311842, 166.0000000000003695 ) ) ;
#24262 = EDGE_LOOP ( 'NONE', ( #10493, #18175, #10879, #20276 ) ) ;
#24264 = EDGE_CURVE ( 'NONE', #64865, #23177, #72545, .T. ) ;
#24263 = VERTEX_POINT ( 'NONE', #40046 ) ;
#24265 =( BOUNDED_CURVE ( )  B_SPLINE_CURVE ( 2, ( #27262, #15566, #61605, #50280, #73300, #38968, #33325, #74033, #27639 ),
 .UNSPECIFIED., .F., .F. ) 
 B_SPLINE_CURVE_WITH_KNOTS ( ( 3, 2, 2, 2, 3 ),
 ( 0.2499999999999998612, 0.2536764705882351145, 0.2573529411764703956, 0.2610294117647057321, 0.2647058823529410132 ),
 .UNSPECIFIED. ) 
 CURVE ( )  GEOMETRIC_REPRESENTATION_ITEM ( )  RATIONAL_B_SPLINE_CURVE ( ( 1.000000000000002887, 0.9238795325112838519, 1.000000000000000000, 0.9238795325112867385, 1.000000000000000000, 0.9238795325112867385, 1.000000000000000000, 0.9238795325112901802, 0.9999999999999965583 ) ) 
 REPRESENTATION_ITEM ( '' )  );
#24266 = CARTESIAN_POINT ( 'NONE',  ( -2.765530957081996810, 299.4218750017070079, -6.676582343750003368 ) ) ;
#24267 = CARTESIAN_POINT ( 'NONE',  ( 5.000000000000000000, 10.00000000000000000, -75.19090595827292134 ) ) ;
#24268 = CARTESIAN_POINT ( 'NONE',  ( -5.000000000000002665, 16.66666666666667140, -8.660254037844394404 ) ) ;
#24269 = CARTESIAN_POINT ( 'NONE',  ( 3.042071309553159519, 149.7395833299192986, 11.35316468750000141 ) ) ;
#24270 = CARTESIAN_POINT ( 'NONE',  ( 4.220049686691934809, 10.18810118749999916, 83.68750000204836681 ) ) ;
#24271 = CARTESIAN_POINT ( 'NONE',  ( 8.660254037844389075, 5.416666666666666963, -5.000000000000000888 ) ) ;
#24272 = CARTESIAN_POINT ( 'NONE',  ( 4.000000000000015987, 203.4375000000000284, 199.6568542494924259 ) ) ;
#24273 = FACE_OUTER_BOUND ( 'NONE', #4926, .T. ) ;
#24274 = VECTOR ( 'NONE', #19714, 1000.000000000000000 ) ;
#24275 = CARTESIAN_POINT ( 'NONE',  ( 4.220049686691934809, 10.18810118749999916, 109.5625000020483810 ) ) ;
#24276 = ORIENTED_EDGE ( 'NONE', *, *, #68278, .T. ) ;
#24277 = CARTESIAN_POINT ( 'NONE',  ( -4.898587196589412829E-16, 112.6250000000000000, -8.000000000000000000 ) ) ;
#24278 = CARTESIAN_POINT ( 'NONE',  ( -4.000000000000002665, 17.56250000000000000, 1.656854249492380582 ) ) ;
#24279 = CARTESIAN_POINT ( 'NONE',  ( -9.832129032723418760, 143.1770833299193555, -5.676582343750004256 ) ) ;
#24280 = CARTESIAN_POINT ( 'NONE',  ( -3.458734124999959914, 197.3750000013656063, 196.5673454167823877 ) ) ;
#24281 = CARTESIAN_POINT ( 'NONE',  ( 3.458734125000015425, 208.2500000013656063, 196.5673454167823877 ) ) ;
#24282 = B_SPLINE_CURVE_WITH_KNOTS ( 'NONE', 3,
 ( #17762, #41517, #6082, #58883, #52474, #63409, #57778, #41155, #51723, #69081 ),
 .UNSPECIFIED., .F., .F.,
 ( 4, 2, 2, 2, 4 ),
 ( 0.000000000000000000, 0.001314083742615453250, 0.002628167485230906500, 0.003942251227846359750, 0.005256334970461813000 ),
 .UNSPECIFIED. ) ;
#24283 = CARTESIAN_POINT ( 'NONE',  ( -6.238412754330611322E-16, 10.18810118749999916, 75.15625000204836681 ) ) ;
#24284 = CARTESIAN_POINT ( 'NONE',  ( -9.832129032723418760, 48.17708332991934839, -5.676582343750004256 ) ) ;
#24285 = EDGE_LOOP ( 'NONE', ( #23573, #1331, #43479, #40087, #28402 ) ) ;
#24286 = CARTESIAN_POINT ( 'NONE',  ( -10.00000000000001066, 27.70833333333333570, 2.679491924311224960 ) ) ;
#24287 = CARTESIAN_POINT ( 'NONE',  ( -3.211159895383562723, 6.062499998634407028, 3.211159895383561391 ) ) ;
#24288 = CARTESIAN_POINT ( 'NONE',  ( 8.008118988124991233, 3.317071493978879015, 12.35686528394062833 ) ) ;
#24289 = VECTOR ( 'NONE', #41156, 1000.000000000000000 ) ;
#24290 = EDGE_CURVE ( 'NONE', #48426, #67846, #16666, .T. ) ;
#24291 = CARTESIAN_POINT ( 'NONE',  ( -5.082755093536325042, 14.53124999795161187, -5.082755093536325930 ) ) ;
#24292 = CARTESIAN_POINT ( 'NONE',  ( -6.000000000000001776, 291.0625000034140157, 0.000000000000000000 ) ) ;
#24293 = CARTESIAN_POINT ( 'NONE',  ( 2.849036369511732440E-14, 202.2500000000000000, 202.0000000000000000 ) ) ;
#24294 = CARTESIAN_POINT ( 'NONE',  ( -2.977408999572650039, 11.81249999795161187, -7.188101187500001821 ) ) ;
#24295 = CARTESIAN_POINT ( 'NONE',  ( 2.977408999572646486, 7.188101187499992051, 10.01780278187175632 ) ) ;
#24296 = ADVANCED_FACE ( 'NONE', ( #73263 ), #10633, .T. ) ;
#24297 = CARTESIAN_POINT ( 'NONE',  ( 10.18810118750000093, -4.220049686691933921, 69.81250000204835260 ) ) ;
#24298 = CARTESIAN_POINT ( 'NONE',  ( -25.55430564589119768, 207.5625000013656063, 167.5543056458915316 ) ) ;
#24299 = ADVANCED_FACE ( 'NONE', ( #56666 ), #34040, .T. ) ;
#24300 = DIRECTION ( 'NONE',  ( 0.000000000000000000, 0.000000000000000000, -1.000000000000000000 ) ) ;
#24301 = CARTESIAN_POINT ( 'NONE',  ( 1.656854249492381248, 2.937499997268813612, -4.000000000000001776 ) ) ;
#24302 = ORIENTED_EDGE ( 'NONE', *, *, #56083, .F. ) ;
#24303 = CARTESIAN_POINT ( 'NONE',  ( 2.828427124746209831, 195.5000000027312126, 200.8284271247462129 ) ) ;
#24304 = CARTESIAN_POINT ( 'NONE',  ( -4.000000000000015987, 202.4375000000000568, 140.3431457505076594 ) ) ;
#24305 = CARTESIAN_POINT ( 'NONE',  ( -25.17157287525374088, 199.7500000027312126, 172.8284271247464972 ) ) ;
#24306 = CARTESIAN_POINT ( 'NONE',  ( 3.211159895383560947, 3.187499998634407028, 3.211159895383562723 ) ) ;
#24307 = CARTESIAN_POINT ( 'NONE',  ( -7.188101187500001821, 118.0625000020483952, -2.977408999572650483 ) ) ;
#24308 = DIRECTION ( 'NONE',  ( 0.000000000000000000, 0.000000000000000000, 1.000000000000000000 ) ) ;
#24309 = CARTESIAN_POINT ( 'NONE',  ( 3.313708498984762496, -7.999999999999989342, 4.486552783920144449 ) ) ;
#24310 = ORIENTED_EDGE ( 'NONE', *, *, #58337, .F. ) ;
#24311 = EDGE_CURVE ( 'NONE', #58992, #300, #39673, .T. ) ;
#24312 = CARTESIAN_POINT ( 'NONE',  ( 7.188101187500000933, 26.06249999795161543, -2.977408999572650483 ) ) ;
#24313 = ORIENTED_EDGE ( 'NONE', *, *, #69110, .F. ) ;
#24314 = LINE ( 'NONE', #7713, #34001 ) ;
#24315 = CARTESIAN_POINT ( 'NONE',  ( 8.000000000000000000, 13.59375000000000178, -3.313708498984761164 ) ) ;
#24316 = CARTESIAN_POINT ( 'NONE',  ( 31.45873412499998523, 207.7500000013656063, 168.5673454167822172 ) ) ;
#24317 = CARTESIAN_POINT ( 'NONE',  ( -2.679491924311235618, 48.54166666666665719, 10.00000000000000000 ) ) ;
#24318 = CARTESIAN_POINT ( 'NONE',  ( -7.188101187500000044, 97.53125000204838102, 0.000000000000000000 ) ) ;
#24319 = CARTESIAN_POINT ( 'NONE',  ( -6.000000000000001776, 295.0000000000000000, 0.000000000000000000 ) ) ;
#24321 = CARTESIAN_POINT ( 'NONE',  ( 1.656854249492321074, 197.4375000027312410, 202.0000000000001137 ) ) ;
#24320 = LINE ( 'NONE', #53378, #15329 ) ;
#24322 = VERTEX_POINT ( 'NONE', #21936 ) ;
#24323 = CARTESIAN_POINT ( 'NONE',  ( 3.042071309553173286, 230.3645833367472733, 11.35316468749999608 ) ) ;
#24324 = CARTESIAN_POINT ( 'NONE',  ( -4.401442555609577197E-16, 7.188101187499992051, 16.48655278187175810 ) ) ;
#24325 = CARTESIAN_POINT ( 'NONE',  ( 8.660254037844374864, 90.41666666666665719, -4.999999999999992006 ) ) ;
#24326 = CARTESIAN_POINT ( 'NONE',  ( 5.656854249492374365, 5.656854249492375253, 3.267802779823362425 ) ) ;
#24327 = DIRECTION ( 'NONE',  ( 0.000000000000000000, 0.000000000000000000, -1.000000000000000000 ) ) ;
#24328 = CARTESIAN_POINT ( 'NONE',  ( -2.679491924311228512, 263.9583333333333144, -9.999999999999998224 ) ) ;
#24329 = CARTESIAN_POINT ( 'NONE',  ( 2.849036369511732440E-14, 201.2500000000000000, 202.0000000000000000 ) ) ;
#24330 = CARTESIAN_POINT ( 'NONE',  ( -4.999999999999998224, 171.6666666666666856, -8.660254037844389075 ) ) ;
#24331 = FACE_OUTER_BOUND ( 'NONE', #1936, .T. ) ;
#24332 = ADVANCED_FACE ( 'NONE', ( #50241 ), #21567, .T. ) ;
#24333 = CARTESIAN_POINT ( 'NONE',  ( -32.16795224899004779, 176.1252443050158831, 164.7321309179486093 ) ) ;
#24334 = CARTESIAN_POINT ( 'NONE',  ( 7.188101187499992051, 2.977408999572647819, 26.70530278187175455 ) ) ;
#24335 = CARTESIAN_POINT ( 'NONE',  ( -8.311093377946836114, 142.9687499965859843, -8.311093377946837890 ) ) ;
#24336 = CARTESIAN_POINT ( 'NONE',  ( 23.99999999999997868, 201.8125000000000000, 171.6568542494922553 ) ) ;
#24337 = LINE ( 'NONE', #2441, #50605 ) ;
#24340 = CARTESIAN_POINT ( 'NONE',  ( 18.00000000000000000, 1.759986210487464176, -0.03733711119006424134 ) ) ;
#24339 = CARTESIAN_POINT ( 'NONE',  ( 4.999999999999993783, 106.0416666598387110, 8.660254037844390851 ) ) ;
#24338 = CARTESIAN_POINT ( 'NONE',  ( 31.99999999999998579, 206.1875000000000568, 171.6568542494923122 ) ) ;
#24341 = ORIENTED_EDGE ( 'NONE', *, *, #3858, .F. ) ;
#24342 = B_SPLINE_CURVE_WITH_KNOTS ( 'NONE', 3,
 ( #73418, #62097, #4392, #16800, #50404, #56449, #27760, #73786 ),
 .UNSPECIFIED., .F., .F.,
 ( 4, 2, 2, 4 ),
 ( 0.000000000000000000, 0.001793316283962787623, 0.002689974425944181326, 0.003586632567925575246 ),
 .UNSPECIFIED. ) ;
#24343 = CARTESIAN_POINT ( 'NONE',  ( 9.832129032723420536, 1.510416663252683422, -5.676582343749999815 ) ) ;
#24344 = CARTESIAN_POINT ( 'NONE',  ( -27.99999999999999645, 195.0000000000000000, 170.0000000000003695 ) ) ;
#24345 = CARTESIAN_POINT ( 'NONE',  ( -3.458734125000015425, 206.0000000013656063, 143.4326545832176976 ) ) ;
#24346 = CARTESIAN_POINT ( 'NONE',  ( -2.502880839332534801, 124.6278065515491562, -7.481218951737261591 ) ) ;
#24347 = VECTOR ( 'NONE', #21407, 999.9999999999998863 ) ;
#24348 = CARTESIAN_POINT ( 'NONE',  ( 6.123233995736767268E-16, 33.12499999317203248, -10.00000000000000178 ) ) ;
#24349 = CARTESIAN_POINT ( 'NONE',  ( -7.188101187499999156, 112.2500000020483952, 2.977408999572654924 ) ) ;
#24350 = CARTESIAN_POINT ( 'NONE',  ( -8.342170076843785083E-16, 5.187499998634407028, 4.541265875000002339 ) ) ;
#24351 = CARTESIAN_POINT ( 'NONE',  ( -5.656854249492373476, -5.656854249492376141, 13.20530278392014623 ) ) ;
#24352 = CARTESIAN_POINT ( 'NONE',  ( 3.313708498984756279, 7.999999999999991118, 13.86155277982336465 ) ) ;
#24354 = CARTESIAN_POINT ( 'NONE',  ( 26.34314575050774820, 196.5625000000000000, 165.9999999999997442 ) ) ;
#24353 = CARTESIAN_POINT ( 'NONE',  ( -30.82842712474615965, 203.3750000000000284, 172.8284271247465824 ) ) ;
#24355 = EDGE_LOOP ( 'NONE', ( #13522, #51084, #36928, #21700 ) ) ;
#24356 = CARTESIAN_POINT ( 'NONE',  ( -1.656854249492383468, 19.43749999726880873, 4.000000000000000888 ) ) ;
#24357 = DIRECTION ( 'NONE',  ( 1.000000000000000000, 0.000000000000000000, 0.000000000000000000 ) ) ;
#24358 = DIRECTION ( 'NONE',  ( -0.000000000000000000, 1.000000000000000000, -0.000000000000000000 ) ) ;
#24359 = CARTESIAN_POINT ( 'NONE',  ( -8.311093377946836114, 248.5937500034139589, -8.311093377946836114 ) ) ;
#24360 = AXIS2_PLACEMENT_3D ( 'NONE', #66772, #32834, #38856 ) ;
#24361 = CARTESIAN_POINT ( 'NONE',  ( 11.35316468750000141, 110.7812499965860269, 0.000000000000000000 ) ) ;
#24362 = ORIENTED_EDGE ( 'NONE', *, *, #34736, .F. ) ;
#24363 = CARTESIAN_POINT ( 'NONE',  ( 4.999999999999999112, -10.28276986844625718, 65.17752827135362281 ) ) ;
#24364 = CARTESIAN_POINT ( 'NONE',  ( 10.18810118749999916, 4.220049686691935698, 103.0000000020483668 ) ) ;
#24365 = CARTESIAN_POINT ( 'NONE',  ( 10.00000000000000178, 227.0833333265053682, -2.679491924311226736 ) ) ;
#24366 = CARTESIAN_POINT ( 'NONE',  ( -1.432654583217607414, 200.5000000013656063, 194.5412658750000219 ) ) ;
#24367 = FACE_OUTER_BOUND ( 'NONE', #3241, .T. ) ;
#24369 = CARTESIAN_POINT ( 'NONE',  ( -3.042071309553173730, 109.3229166632526983, 11.35316468749999785 ) ) ;
#24368 = DIRECTION ( 'NONE',  ( 0.000000000000000000, 0.000000000000000000, 1.000000000000000000 ) ) ;
#24370 = CARTESIAN_POINT ( 'NONE',  ( 3.313708498984762496, -7.999999999999989342, 5.986552783920146226 ) ) ;
#24371 = CARTESIAN_POINT ( 'NONE',  ( -24.54126587499998990, 196.4375000013655779, 170.0000000000003411 ) ) ;
#24372 = CARTESIAN_POINT ( 'NONE',  ( 7.320508075688778149, 50.62500000000000000, -7.320508075688778149 ) ) ;
#24373 = ORIENTED_EDGE ( 'NONE', *, *, #58404, .T. ) ;
#24374 = CIRCLE ( 'NONE', #7514, 3.999999999999976019 ) ;
#24375 = EDGE_CURVE ( 'NONE', #4853, #45416, #51358, .T. ) ;
#24376 = CARTESIAN_POINT ( 'NONE',  ( -8.660254037844390851, 199.7916666598387110, 4.999999999999998224 ) ) ;
#24377 = CARTESIAN_POINT ( 'NONE',  ( 1.656854249492365705, 206.1875000000000853, 138.0000000000000853 ) ) ;
#24378 = DIRECTION ( 'NONE',  ( 0.000000000000000000, 0.000000000000000000, -1.000000000000000000 ) ) ;
#24379 = CARTESIAN_POINT ( 'NONE',  ( 11.35316468749999963, 96.30208332991935549, -3.042071309553165293 ) ) ;
#24380 = CARTESIAN_POINT ( 'NONE',  ( -2.751064625579944321E-14, 206.8750000027312126, 146.0000000000000284 ) ) ;
#24381 = CARTESIAN_POINT ( 'NONE',  ( 7.188101187500000933, 11.43749999795161187, -2.977408999572650483 ) ) ;
#24382 = CARTESIAN_POINT ( 'NONE',  ( -10.18810118749999738, -4.220049686691941915, 96.62500000204838102 ) ) ;
#24383 = CARTESIAN_POINT ( 'NONE',  ( -11.35316468749999785, 8.385416663252684089, -3.042071309553167513 ) ) ;
#24384 = ORIENTED_EDGE ( 'NONE', *, *, #73977, .T. ) ;
#24385 = CARTESIAN_POINT ( 'NONE',  ( 8.000000000000000000, 122.9375000040967905, -9.797174393178825657E-16 ) ) ;
#24386 = CARTESIAN_POINT ( 'NONE',  ( 0.000000000000000000, 0.000000000000000000, -20.69999999999999929 ) ) ;
#24387 = CARTESIAN_POINT ( 'NONE',  ( 4.556349186104045934, 11.00000000000000000, 102.5312500000000000 ) ) ;
#24388 = CARTESIAN_POINT ( 'NONE',  ( -7.204075437095967871, 7.204075437095967871, 75.34375000204838102 ) ) ;
#24389 = CARTESIAN_POINT ( 'NONE',  ( 2.775557561562891351E-14, 210.0000000000000284, 198.0000000000000284 ) ) ;
#24390 = CARTESIAN_POINT ( 'NONE',  ( 10.00000000000000178, 200.0000000000000000, 0.000000000000000000 ) ) ;
#24391 = CARTESIAN_POINT ( 'NONE',  ( -6.676582343750001591, 293.4531250017069510, 0.000000000000000000 ) ) ;
#24392 = CARTESIAN_POINT ( 'NONE',  ( -2.679491924311235174, 120.4166666598386826, 10.00000000000000000 ) ) ;
#24393 = CARTESIAN_POINT ( 'NONE',  ( -8.311093377946841443, 204.2187499965859843, 8.311093377946834337 ) ) ;
#24394 = EDGE_CURVE ( 'NONE', #24466, #55027, #54674, .T. ) ;
#24395 =( BOUNDED_CURVE ( )  B_SPLINE_CURVE ( 2, ( #65823, #42069, #65458, #31505, #53040, #54152, #65077, #41713, #7387 ),
 .UNSPECIFIED., .F., .F. ) 
 B_SPLINE_CURVE_WITH_KNOTS ( ( 3, 2, 2, 2, 3 ),
 ( 0.5208333333333314830, 0.5312499999999981126, 0.5416666666666647423, 0.5520833333333314830, 0.5624999999999981126 ),
 .UNSPECIFIED. ) 
 CURVE ( )  GEOMETRIC_REPRESENTATION_ITEM ( )  RATIONAL_B_SPLINE_CURVE ( ( 1.000000000000013767, 0.9238795325112729717, 1.000000000000000000, 0.9238795325112867385, 1.000000000000000000, 0.9238795325112867385, 1.000000000000000000, 0.9238795325113005052, 0.9999999999999862332 ) ) 
 REPRESENTATION_ITEM ( '' )  );
#24396 = CARTESIAN_POINT ( 'NONE',  ( 4.220049686691934809, 10.18810118749999916, 86.68750000204836681 ) ) ;
#24397 = CARTESIAN_POINT ( 'NONE',  ( -29.43265458321766559, 204.5000000013656063, 166.5412658750003629 ) ) ;
#24398 = EDGE_CURVE ( 'NONE', #63859, #2879, #11745, .T. ) ;
#24399 = CARTESIAN_POINT ( 'NONE',  ( -3.313708498984760720, 24.46875000000000711, -8.000000000000000000 ) ) ;
#24400 = EDGE_LOOP ( 'NONE', ( #62563, #57077, #61257, #61589 ) ) ;
#24401 = CARTESIAN_POINT ( 'NONE',  ( -23.04491212681691081, -50.35853896439172672, 149.2494701692645833 ) ) ;
#24402 = CARTESIAN_POINT ( 'NONE',  ( 1.656854249492403008, 206.8125000027312126, 194.0000000000000853 ) ) ;
#24403 = CARTESIAN_POINT ( 'NONE',  ( 7.320508075688771044, 29.37500000000000000, 7.320508075688775484 ) ) ;
#24404 = AXIS2_PLACEMENT_3D ( 'NONE', #47644, #43378, #1289 ) ;
#24405 = CARTESIAN_POINT ( 'NONE',  ( -5.000000000000000000, 11.43937387734372813, 68.01947305042941139 ) ) ;
#24406 = CARTESIAN_POINT ( 'NONE',  ( 4.220049686691941027, -10.18810118749999738, 74.50000000204838102 ) ) ;
#24407 = ORIENTED_EDGE ( 'NONE', *, *, #668, .F. ) ;
#24408 = CARTESIAN_POINT ( 'NONE',  ( -7.188101187500002709, 2.812499997951610098, 2.977408999572649151 ) ) ;
#24409 = CARTESIAN_POINT ( 'NONE',  ( -7.999999999999991118, 0.000000000000000000, 5.330302779823363757 ) ) ;
#24410 = AXIS2_PLACEMENT_3D ( 'NONE', #18631, #18991, #54451 ) ;
#24411 = CARTESIAN_POINT ( 'NONE',  ( 2.020667218593132706E-15, -11.00000000000000000, 93.06250000409677625 ) ) ;
#24412 = CARTESIAN_POINT ( 'NONE',  ( 7.188101187500000044, 119.2812500020483810, -8.802885111219163269E-16 ) ) ;
#24413 = CARTESIAN_POINT ( 'NONE',  ( -4.436061581686053579, 22.00000000000000000, 0.5394833180921509985 ) ) ;
#24414 = CARTESIAN_POINT ( 'NONE',  ( 4.721056650415999201, 295.0781250017069510, -4.721056650415999201 ) ) ;
#24416 = LINE ( 'NONE', #8174, #56688 ) ;
#24415 = CARTESIAN_POINT ( 'NONE',  ( -9.832129032723415207, 229.3229166700806729, 5.676582343750005144 ) ) ;
#24417 = ORIENTED_EDGE ( 'NONE', *, *, #26589, .T. ) ;
#24418 = CARTESIAN_POINT ( 'NONE',  ( 11.35316468749999963, 236.5104166700806161, 3.042071309553159519 ) ) ;
#24419 = CARTESIAN_POINT ( 'NONE',  ( -7.188101187499991163, 2.977408999572646930, 7.392802781871750994 ) ) ;
#24420 = CARTESIAN_POINT ( 'NONE',  ( -1.432654583217607414, 205.5000000013655779, 194.5412658750000219 ) ) ;
#24421 = ORIENTED_EDGE ( 'NONE', *, *, #59857, .F. ) ;
#24422 = CARTESIAN_POINT ( 'NONE',  ( -7.204075437095967871, 7.204075437095967871, 70.46875000204836681 ) ) ;
#24423 = CARTESIAN_POINT ( 'NONE',  ( 6.951808397369818766E-16, 97.34374999658601268, -11.35316468750000141 ) ) ;
#24424 = CYLINDRICAL_SURFACE ( 'NONE', #8322, 8.000000000000000000 ) ;
#24425 = CARTESIAN_POINT ( 'NONE',  ( -7.778174593052023411, 7.778174593052023411, 77.31249999999997158 ) ) ;
#24428 = CARTESIAN_POINT ( 'NONE',  ( 2.849036369511732440E-14, 202.2500000000000000, 202.0000000000000000 ) ) ;
#24427 = CARTESIAN_POINT ( 'NONE',  ( 26.56734541678237704, 205.3750000013656063, 173.4587341249998929 ) ) ;
#24426 = CARTESIAN_POINT ( 'NONE',  ( 31.45873412499998523, 202.8750000013656347, 171.4326545832175839 ) ) ;
#24429 = ADVANCED_FACE ( 'NONE', ( #57786 ), #10263, .F. ) ;
#24430 = ORIENTED_EDGE ( 'NONE', *, *, #69408, .T. ) ;
#24431 = CARTESIAN_POINT ( 'NONE',  ( -23.99999999999998579, 195.8750000027311842, 170.0000000000002842 ) ) ;
#24432 = CARTESIAN_POINT ( 'NONE',  ( -8.660254037844390851, 179.7916666598387110, 4.999999999999998224 ) ) ;
#24433 = CARTESIAN_POINT ( 'NONE',  ( -11.35316468749999785, 208.0729166632526983, -3.042071309553167513 ) ) ;
#24434 = CARTESIAN_POINT ( 'NONE',  ( -1.432654583217664479, 201.7500000013655779, 138.5412658750000787 ) ) ;
#24435 = CARTESIAN_POINT ( 'NONE',  ( 24.54126587500000056, 200.3750000013656063, 168.5673454167822172 ) ) ;
#24436 = CARTESIAN_POINT ( 'NONE',  ( 4.401442555609581635E-16, 20.71874999795161543, -7.188101187500000044 ) ) ;
#24437 = CARTESIAN_POINT ( 'NONE',  ( 11.35316468749999785, 175.8854166632527267, 3.042071309553174174 ) ) ;
#24438 = CARTESIAN_POINT ( 'NONE',  ( -4.401442555609581635E-16, 98.65625000204838102, -7.188101187500000044 ) ) ;
#24439 = CARTESIAN_POINT ( 'NONE',  ( 0.000000000000000000, 300.0000000000000000, 10.00000000000000178 ) ) ;
#24440 = CARTESIAN_POINT ( 'NONE',  ( -23.99999999999997158, 197.6875000000000000, 171.6568542494927385 ) ) ;
#24441 = CARTESIAN_POINT ( 'NONE',  ( 4.541265875000002339, 11.37499999863440969, -1.881053915767121554 ) ) ;
#24442 = CARTESIAN_POINT ( 'NONE',  ( 24.54126587499998280, 201.5000000013655779, 171.4326545832175555 ) ) ;
#24443 = CARTESIAN_POINT ( 'NONE',  ( -4.401442555609577197E-16, 7.188101187499992051, 4.486552781871752771 ) ) ;
#24444 = CARTESIAN_POINT ( 'NONE',  ( 9.832129032723420536, 66.19791666325268409, -5.676582343749999815 ) ) ;
#24445 = DIRECTION ( 'NONE',  ( -1.000000000000000000, -0.000000000000000000, -0.000000000000000000 ) ) ;
#24446 = FACE_OUTER_BOUND ( 'NONE', #43782, .T. ) ;
#24447 = ORIENTED_EDGE ( 'NONE', *, *, #25834, .T. ) ;
#24448 = CARTESIAN_POINT ( 'NONE',  ( -3.313708498984781148, 9.281249995903221972, -7.999999999999981348 ) ) ;
#24449 = CARTESIAN_POINT ( 'NONE',  ( 2.751064625579944321E-14, 199.7500000000000000, 194.0000000000000568 ) ) ;
#24450 = CARTESIAN_POINT ( 'NONE',  ( -2.085542519210945728E-15, 74.53124999658602690, 11.35316468750000141 ) ) ;
#24451 = CARTESIAN_POINT ( 'NONE',  ( -7.778174593052020747, -7.778174593052023411, 68.87500000409677625 ) ) ;
#24452 = CARTESIAN_POINT ( 'NONE',  ( 1.432654583217607414, 196.5000000013656063, 145.4587341250000350 ) ) ;
#24453 = CARTESIAN_POINT ( 'NONE',  ( -2.266287154880006316, 10.27715108473168470, 63.73532778936321108 ) ) ;
#24455 = CARTESIAN_POINT ( 'NONE',  ( -3.042071309553173730, 69.32291666325268409, 11.35316468749999785 ) ) ;
#24454 = CARTESIAN_POINT ( 'NONE',  ( 7.188101187500002709, 90.31250000204838102, 2.977408999572649151 ) ) ;
#24456 = CARTESIAN_POINT ( 'NONE',  ( -4.898587196589407898E-16, 7.999999999999991118, 26.14280278392014623 ) ) ;
#24457 = CARTESIAN_POINT ( 'NONE',  ( -0.4917886453872661323, 194.6170594543940240, 138.4079500870968502 ) ) ;
#24458 = EDGE_CURVE ( 'NONE', #5775, #11605, #67606, .T. ) ;
#24459 = EDGE_CURVE ( 'NONE', #26622, #48555, #55197, .T. ) ;
#24460 = CARTESIAN_POINT ( 'NONE',  ( 4.999999999999993783, 161.0416666598387110, 8.660254037844390851 ) ) ;
#24461 = CARTESIAN_POINT ( 'NONE',  ( -7.188101187499999156, 90.12500000204836681, 2.977408999572654924 ) ) ;
#24462 = FACE_OUTER_BOUND ( 'NONE', #8761, .T. ) ;
#24463 = CARTESIAN_POINT ( 'NONE',  ( 11.35316468749999963, 66.30208332991935549, -3.042071309553165293 ) ) ;
#24464 = CARTESIAN_POINT ( 'NONE',  ( -6.238412754330611322E-16, 10.18810118749999916, 114.1562500020483810 ) ) ;
#24465 = CARTESIAN_POINT ( 'NONE',  ( 8.311093377946834337, 190.1562499965860127, 8.311093377946839666 ) ) ;
#24466 = VERTEX_POINT ( 'NONE', #50988 ) ;
#24467 = CARTESIAN_POINT ( 'NONE',  ( -8.000000000000000000, 123.6875000040967905, 0.000000000000000000 ) ) ;
#24468 = CYLINDRICAL_SURFACE ( 'NONE', #60532, 3.999999999999976019 ) ;
#24469 = CARTESIAN_POINT ( 'NONE',  ( -31.66756539373098178, -21.02027521086719730, 167.9999999999997726 ) ) ;
#24471 = CARTESIAN_POINT ( 'NONE',  ( -11.35316468750000141, 173.4895833299193839, 3.042071309553159963 ) ) ;
#24470 = CARTESIAN_POINT ( 'NONE',  ( -28.00000000000007816, 201.1250000027312126, 166.0000000000003695 ) ) ;
#24472 = VECTOR ( 'NONE', #15283, 1000.000000000000000 ) ;
#24473 = CARTESIAN_POINT ( 'NONE',  ( -5.656854249492379694, 10.87499999590322020, -5.656854249492380582 ) ) ;
#24474 = EDGE_CURVE ( 'NONE', #62325, #50149, #44096, .T. ) ;
#24475 = CARTESIAN_POINT ( 'NONE',  ( -7.320508075688771932, 247.5000000068279746, -7.320508075688771932 ) ) ;
#24476 = CARTESIAN_POINT ( 'NONE',  ( 0.000000000000000000, 300.0000000000000000, 0.000000000000000000 ) ) ;
#24477 = VERTEX_POINT ( 'NONE', #64173 ) ;
#24478 = CARTESIAN_POINT ( 'NONE',  ( -2.085542519210945728E-15, 174.8437499965860411, 11.35316468750000141 ) ) ;
#24479 = CARTESIAN_POINT ( 'NONE',  ( -2.977408999572647819, 7.188101187499992051, 19.20530278187175455 ) ) ;
#24480 =( BOUNDED_CURVE ( )  B_SPLINE_CURVE ( 3, ( #710, #36134, #47065, #69723 ),
 .UNSPECIFIED., .F., .F. ) 
 B_SPLINE_CURVE_WITH_KNOTS ( ( 4, 4 ),
 ( 4.712388980384689674, 6.283185307179586232 ),
 .UNSPECIFIED. ) 
 CURVE ( )  GEOMETRIC_REPRESENTATION_ITEM ( )  RATIONAL_B_SPLINE_CURVE ( ( 1.000000000000000000, 0.8047378541243649375, 0.8047378541243649375, 1.000000000000000000 ) ) 
 REPRESENTATION_ITEM ( '' )  );
#24481 = CARTESIAN_POINT ( 'NONE',  ( 7.128595191980942047, 226.0000000000000000, -7.835617972993563995 ) ) ;
#24482 = ORIENTED_EDGE ( 'NONE', *, *, #26692, .T. ) ;
#24483 = EDGE_CURVE ( 'NONE', #42214, #73730, #23430, .T. ) ;
#24484 = CARTESIAN_POINT ( 'NONE',  ( 5.656854249492379694, 102.1250000040967763, -5.656854249492380582 ) ) ;
#24485 = VECTOR ( 'NONE', #64735, 1000.000000000000227 ) ;
#24486 = CARTESIAN_POINT ( 'NONE',  ( -4.000000000000001776, 11.50000000000000000, -4.898587196589415787E-16 ) ) ;
#24487 =( BOUNDED_CURVE ( )  B_SPLINE_CURVE ( 2, ( #42702, #14019, #3475, #31771, #54790, #38564, #49866, #66089, #37433 ),
 .UNSPECIFIED., .F., .F. ) 
 B_SPLINE_CURVE_WITH_KNOTS ( ( 3, 2, 2, 2, 3 ),
 ( 0.1874999999999978351, 0.1979166666666645202, 0.2083333333333312054, 0.2187499999999978906, 0.2291666666666645480 ),
 .UNSPECIFIED. ) 
 CURVE ( )  GEOMETRIC_REPRESENTATION_ITEM ( )  RATIONAL_B_SPLINE_CURVE ( ( 1.000000000000015765, 0.9238795325112709733, 1.000000000000000000, 0.9238795325112867385, 1.000000000000000000, 0.9238795325112867385, 1.000000000000000000, 0.9238795325113021706, 0.9999999999999845679 ) ) 
 REPRESENTATION_ITEM ( '' )  );
#24488 = CARTESIAN_POINT ( 'NONE',  ( -39.02194704011109394, -0.3136195155953672709, 119.9708478605673605 ) ) ;
#24489 = CARTESIAN_POINT ( 'NONE',  ( 4.541265875000001451, 13.24999999863440969, 1.881053915767124440 ) ) ;
#24490 = CARTESIAN_POINT ( 'NONE',  ( -4.898587196589407898E-16, 7.999999999999991118, 20.14280278392014623 ) ) ;
#24491 = CARTESIAN_POINT ( 'NONE',  ( -11.00000000000000000, 0.000000000000000000, 80.68750000409677625 ) ) ;
#24492 = ORIENTED_EDGE ( 'NONE', *, *, #23867, .F. ) ;
#24493 = CYLINDRICAL_SURFACE ( 'NONE', #45117, 11.00000000000000000 ) ;
#24494 = CARTESIAN_POINT ( 'NONE',  ( -5.082755093536325930, 98.46875000204838102, -5.082755093536325930 ) ) ;
#24495 = CARTESIAN_POINT ( 'NONE',  ( 2.250000000000000000, 300.0000000000000000, 7.677076266392047543 ) ) ;
#24496 =( NAMED_UNIT ( * ) PLANE_ANGLE_UNIT ( ) SI_UNIT ( $, .RADIAN. ) );
#24497 = ORIENTED_EDGE ( 'NONE', *, *, #34232, .T. ) ;
#24498 = CARTESIAN_POINT ( 'NONE',  ( 2.589639417653364806, 10.27590863719303904, -63.78668228762732184 ) ) ;
#24499 = CARTESIAN_POINT ( 'NONE',  ( -32.58747683752128665, -24.20310531112317065, 161.9923478528805276 ) ) ;
#24500 = CARTESIAN_POINT ( 'NONE',  ( -7.188101187499992051, 0.000000000000000000, 26.98655278187175455 ) ) ;
#24501 = ORIENTED_EDGE ( 'NONE', *, *, #73025, .F. ) ;
#24502 = ORIENTED_EDGE ( 'NONE', *, *, #39361, .T. ) ;
#24503 = CARTESIAN_POINT ( 'NONE',  ( 4.220049686691934809, 10.18810118749999916, 85.18750000204838102 ) ) ;
#24504 = UNCERTAINTY_MEASURE_WITH_UNIT (LENGTH_MEASURE( 1.000000000000000082E-05 ), #32402, 'distance_accuracy_value', 'NONE');
#24505 = CARTESIAN_POINT ( 'NONE',  ( -4.999999999999998224, 113.5416666598387110, -8.660254037844389075 ) ) ;
#24506 = CARTESIAN_POINT ( 'NONE',  ( 11.00000000000000355, -4.556349186104045046, 94.65625000000001421 ) ) ;
#24509 = CARTESIAN_POINT ( 'NONE',  ( -2.679491924309764350, 128.5416666666667993, 10.00000000000085620 ) ) ;
#24508 = CARTESIAN_POINT ( 'NONE',  ( 30.82842712474616675, 200.5000000027312126, 167.1715728752537018 ) ) ;
#24507 = DIRECTION ( 'NONE',  ( -0.000000000000000000, 1.000000000000000000, -4.476705744456276341E-16 ) ) ;
#24510 = CARTESIAN_POINT ( 'NONE',  ( -7.320508075688778149, 133.1249999999999716, 7.320508075688769267 ) ) ;
#24511 = CARTESIAN_POINT ( 'NONE',  ( -4.000000000000001776, 0.5000000000000002220, -4.898587196589415787E-16 ) ) ;
#24512 = CARTESIAN_POINT ( 'NONE',  ( 11.00000000000000000, 4.556349186104045934, 78.34374999999998579 ) ) ;
#24513 = CARTESIAN_POINT ( 'NONE',  ( 7.999999999999991118, 3.313708498984758055, 15.17405277982336642 ) ) ;
#24514 = CARTESIAN_POINT ( 'NONE',  ( 27.99999999999996447, 202.4375000013656063, 173.4587341249998929 ) ) ;
#24515 = CARTESIAN_POINT ( 'NONE',  ( 2.977408999572651815, 8.062499997951611874, 7.188101187500000933 ) ) ;
#24516 = CARTESIAN_POINT ( 'NONE',  ( -4.903558642999205574E-16, 8.008118988124991233, 3.638115283940628775 ) ) ;
#24517 = CARTESIAN_POINT ( 'NONE',  ( 1.432654583217607192, 195.2500000013656063, 145.4587341250000634 ) ) ;
#24518 = CARTESIAN_POINT ( 'NONE',  ( -7.188101187500000044, 115.5312500020483952, 0.000000000000000000 ) ) ;
#24520 = CARTESIAN_POINT ( 'NONE',  ( -4.104248244559628667, -56.27889056305081539, -44.16174987545170438 ) ) ;
#24519 = CARTESIAN_POINT ( 'NONE',  ( -10.00000000000000000, 249.7916666666666572, -2.679491924311226292 ) ) ;
#24521 = CARTESIAN_POINT ( 'NONE',  ( -5.676582343749992710, 235.0520833367473301, 9.832129032723422313 ) ) ;
#24522 = CYLINDRICAL_SURFACE ( 'NONE', #66227, 10.50000000000000000 ) ;
#24523 = CARTESIAN_POINT ( 'NONE',  ( 7.188101187499993827, -2.977408999572645598, 23.51780278187175455 ) ) ;
#24524 = CARTESIAN_POINT ( 'NONE',  ( 9.832129032723420536, 26.19791666325268409, -5.676582343749999815 ) ) ;
#24525 = CARTESIAN_POINT ( 'NONE',  ( -8.000000000000000000, 9.656250000000001776, -3.313708498984762496 ) ) ;
#24526 = CARTESIAN_POINT ( 'NONE',  ( -11.35316468749999785, 223.3854166632526699, -3.042071309553167513 ) ) ;
#24527 = FACE_OUTER_BOUND ( 'NONE', #31519, .T. ) ;
#24528 = CARTESIAN_POINT ( 'NONE',  ( 0.4368895104719971445, -16.44602605510715065, 68.55492853905350614 ) ) ;
#24529 = ORIENTED_EDGE ( 'NONE', *, *, #18477, .T. ) ;
#24530 = CARTESIAN_POINT ( 'NONE',  ( -4.999999999999998224, 128.5416666598387110, -8.660254037844389075 ) ) ;
#24531 = CARTESIAN_POINT ( 'NONE',  ( -1.432654583217662481, 196.3750000013656063, 145.4587341250000634 ) ) ;
#24532 = CARTESIAN_POINT ( 'NONE',  ( -11.35316468749999785, 38.07291666325268409, -3.042071309553167513 ) ) ;
#24533 = CARTESIAN_POINT ( 'NONE',  ( 2.020667218593132706E-15, -11.00000000000000000, 88.56250000409676204 ) ) ;
#24534 = CARTESIAN_POINT ( 'NONE',  ( 3.458734124999960358, 207.6250000013656063, 143.4326545832176976 ) ) ;
#24535 = CARTESIAN_POINT ( 'NONE',  ( -25.55430564589111597, 195.0625000013656063, 172.4456943541091505 ) ) ;
#24536 = CARTESIAN_POINT ( 'NONE',  ( 0.000000000000000000, 300.0000000000000000, 0.000000000000000000 ) ) ;
#24538 = CARTESIAN_POINT ( 'NONE',  ( -11.35316468750000141, 23.28124999658601979, -1.390361679473963753E-15 ) ) ;
#24537 = CARTESIAN_POINT ( 'NONE',  ( -7.188101187500000044, 106.1562500020483810, 0.000000000000000000 ) ) ;
#24539 = CARTESIAN_POINT ( 'NONE',  ( 3.313708498984762496, -7.999999999999989342, 16.29905277982336642 ) ) ;
#24540 = CARTESIAN_POINT ( 'NONE',  ( 8.311093377946837890, 151.4062499965859843, -8.311093377946837890 ) ) ;
#24541 = CARTESIAN_POINT ( 'NONE',  ( -7.320508075688778149, 109.9999999931720396, 7.320508075688769267 ) ) ;
#24542 = CARTESIAN_POINT ( 'NONE',  ( 5.082755093536325042, 116.4687500020483810, -5.082755093536325930 ) ) ;
#24543 = DIRECTION ( 'NONE',  ( -0.000000000000000000, -0.000000000000000000, 1.000000000000000000 ) ) ;
#24544 = CARTESIAN_POINT ( 'NONE',  ( -26.56734541678232375, 205.2500000013655779, 173.4587341250003760 ) ) ;
#24545 = AXIS2_PLACEMENT_3D ( 'NONE', #15289, #66609, #37579 ) ;
#24546 = ADVANCED_BREP_SHAPE_REPRESENTATION ( '', ( #67054, #57354 ), #57409 ) ;
#24547 = ORIENTED_EDGE ( 'NONE', *, *, #2609, .T. ) ;
#24548 = CARTESIAN_POINT ( 'NONE',  ( 6.951808397369818766E-16, 2.343749996586016682, -11.35316468750000141 ) ) ;
#24549 = VERTEX_POINT ( 'NONE', #1184 ) ;
#24550 = CARTESIAN_POINT ( 'NONE',  ( -3.673940397442060854E-16, 289.7500000000000000, -6.000000000000001776 ) ) ;
#24552 = CARTESIAN_POINT ( 'NONE',  ( 11.35316468750000141, 135.7812499965860411, 0.000000000000000000 ) ) ;
#24551 = DIRECTION ( 'NONE',  ( -0.000000000000000000, 1.000000000000000000, -0.000000000000000000 ) ) ;
#24553 = CARTESIAN_POINT ( 'NONE',  ( -1.656854249492381248, 3.312500000000000000, -4.000000000000001776 ) ) ;
#24554 = CARTESIAN_POINT ( 'NONE',  ( -7.999999999999991118, 0.000000000000000000, 18.88655278432982243 ) ) ;
#24555 = EDGE_CURVE ( 'NONE', #5227, #49057, #44542, .T. ) ;
#24556 = CARTESIAN_POINT ( 'NONE',  ( 11.35316468749999608, 251.6145833367473585, -3.042071309553167069 ) ) ;
#24557 = CARTESIAN_POINT ( 'NONE',  ( -7.204075437095967871, 7.204075437095967871, 90.34375000204838102 ) ) ;
#24558 = ORIENTED_EDGE ( 'NONE', *, *, #68963, .T. ) ;
#24559 = ADVANCED_FACE ( 'NONE', ( #30574 ), #41526, .T. ) ;
#24560 = CARTESIAN_POINT ( 'NONE',  ( -4.000000000000015987, 197.5000000000000000, 142.0000000000000568 ) ) ;
#24561 = CARTESIAN_POINT ( 'NONE',  ( 5.000000000000000000, 65.00666015986205082, -24.03732210400486125 ) ) ;
#24562 = CARTESIAN_POINT ( 'NONE',  ( -11.35316468750000141, 88.80208332991935549, 3.042071309553159963 ) ) ;
#24563 = B_SPLINE_CURVE_WITH_KNOTS ( 'NONE', 3,
 ( #10020, #37948, #20574, #55303 ),
 .UNSPECIFIED., .F., .F.,
 ( 4, 4 ),
 ( 0.000000000000000000, 1.000000000000000000 ),
 .UNSPECIFIED. ) ;
#24564 = CARTESIAN_POINT ( 'NONE',  ( 4.220049686691941027, -10.18810118749999738, 104.1250000020483810 ) ) ;
#24565 = CARTESIAN_POINT ( 'NONE',  ( 4.541265875000001451, 18.37499999863441147, 1.881053915767124440 ) ) ;
#24566 = ORIENTED_EDGE ( 'NONE', *, *, #41762, .T. ) ;
#24567 = VERTEX_POINT ( 'NONE', #29100 ) ;
#24568 = VECTOR ( 'NONE', #67465, 1000.000000000000114 ) ;
#24569 = CARTESIAN_POINT ( 'NONE',  ( -3.313708498984765161, 7.031250000000000888, 7.999999999999998224 ) ) ;
#24570 = FACE_OUTER_BOUND ( 'NONE', #38359, .T. ) ;
#24571 = CARTESIAN_POINT ( 'NONE',  ( 7.188101187500000044, 27.84374999795161543, 0.000000000000000000 ) ) ;
#24572 = EDGE_CURVE ( 'NONE', #16151, #52626, #9400, .T. ) ;
#24573 = FACE_OUTER_BOUND ( 'NONE', #47207, .T. ) ;
#24574 = CARTESIAN_POINT ( 'NONE',  ( -6.238412754330611322E-16, 10.18810118749999916, 97.65625000204838102 ) ) ;
#24575 = CARTESIAN_POINT ( 'NONE',  ( -8.000000000000000000, 6.750000000000000888, -9.797174393178825657E-16 ) ) ;
#24576 = CARTESIAN_POINT ( 'NONE',  ( -2.828427124746190735, 14.12499999726881406, -2.828427124746191623 ) ) ;
#24577 = CARTESIAN_POINT ( 'NONE',  ( 4.541265875000002339, 1.312499998634406584, 0.000000000000000000 ) ) ;
#24578 = VERTEX_POINT ( 'NONE', #24165 ) ;
#24579 = CARTESIAN_POINT ( 'NONE',  ( 1.432654583217607192, 208.2500000013656063, 145.4587341250000634 ) ) ;
#24580 = CARTESIAN_POINT ( 'NONE',  ( 3.458734125000015425, 199.9375000013656063, 198.0000000000000284 ) ) ;
#24583 = CARTESIAN_POINT ( 'NONE',  ( -8.660254037844675068, 22.91666666666685970, 5.000000000000163425 ) ) ;
#24582 = CARTESIAN_POINT ( 'NONE',  ( -29.43265458321755901, 202.8750000013656347, 173.4587341250004044 ) ) ;
#24581 =( BOUNDED_CURVE ( )  B_SPLINE_CURVE ( 2, ( #73969, #11343, #28687, #34379, #57379, #35843, #65978, #7169, #59950 ),
 .UNSPECIFIED., .F., .F. ) 
 B_SPLINE_CURVE_WITH_KNOTS ( ( 3, 2, 2, 2, 3 ),
 ( 0.6029411764705880916, 0.6066176470588233727, 0.6102941176470587648, 0.6139705882352940458, 0.6176470588235293269 ),
 .UNSPECIFIED. ) 
 CURVE ( )  GEOMETRIC_REPRESENTATION_ITEM ( )  RATIONAL_B_SPLINE_CURVE ( ( 1.000000000000002220, 0.9238795325112844070, 1.000000000000000000, 0.9238795325112867385, 1.000000000000000000, 0.9238795325112867385, 1.000000000000000000, 0.9238795325112890700, 0.9999999999999976685 ) ) 
 REPRESENTATION_ITEM ( '' )  );
#24584 = CARTESIAN_POINT ( 'NONE',  ( 1.881053915767121776, 15.49999999863440792, -4.541265875000002339 ) ) ;
#24585 = LINE ( 'NONE', #59671, #51308 ) ;
#24586 = CARTESIAN_POINT ( 'NONE',  ( 2.977408999572646486, 7.188101187499991163, 11.51780278187175810 ) ) ;
#24587 = ORIENTED_EDGE ( 'NONE', *, *, #66801, .F. ) ;
#24588 = ORIENTED_EDGE ( 'NONE', *, *, #17162, .F. ) ;
#24589 = CARTESIAN_POINT ( 'NONE',  ( -10.18810118749999916, 0.000000000000000000, 102.1562500020483810 ) ) ;
#24590 = CARTESIAN_POINT ( 'NONE',  ( -7.320508075688764826, 96.87499999999997158, -7.320508075688765715 ) ) ;
#24591 = CARTESIAN_POINT ( 'NONE',  ( -31.99999999999998579, 204.3125000000000000, 171.6568542494928238 ) ) ;
#24592 = CARTESIAN_POINT ( 'NONE',  ( -3.458734124999959025, 197.5000000013656063, 199.4326545832176691 ) ) ;
#24593 = CARTESIAN_POINT ( 'NONE',  ( 3.313708498984706985, 105.0312499999999858, -8.000000000000055067 ) ) ;
#24594 = CARTESIAN_POINT ( 'NONE',  ( -7.320508075688778149, 88.12500000000001421, 7.320508075688769267 ) ) ;
#24595 = CARTESIAN_POINT ( 'NONE',  ( 8.000000000000001776, 119.6562499999999858, 3.313708498984759387 ) ) ;
#24596 = CARTESIAN_POINT ( 'NONE',  ( -2.765530957081998586, 294.7968750017069510, 6.676582343750001591 ) ) ;
#24597 = EDGE_LOOP ( 'NONE', ( #28448, #4615, #24302, #61635, #9901 ) ) ;
#24598 = DIRECTION ( 'NONE',  ( -0.000000000000000000, 1.000000000000000000, -0.000000000000000000 ) ) ;
#24599 = CARTESIAN_POINT ( 'NONE',  ( -8.000000000000001776, 15.65624999590322197, 3.313708498984759387 ) ) ;
#24600 = CARTESIAN_POINT ( 'NONE',  ( -2.839093476692135984E-14, 208.6875000013656063, 138.5412658750000503 ) ) ;
#24601 = CARTESIAN_POINT ( 'NONE',  ( 0.000000000000000000, 237.9999999999999716, 15.99999999999998579 ) ) ;
#24602 = CARTESIAN_POINT ( 'NONE',  ( -9.999999999999998224, 225.2083333333333144, 2.679491924311235618 ) ) ;
#24603 = CARTESIAN_POINT ( 'NONE',  ( 11.00000000000000000, 1.347111479062088405E-15, 118.0000000000000000 ) ) ;
#24604 = CARTESIAN_POINT ( 'NONE',  ( 7.778174593052023411, -7.778174593052021635, 112.5625000000000000 ) ) ;
#24605 = CARTESIAN_POINT ( 'NONE',  ( -4.999999999999998224, 216.6666666666666856, -8.660254037844389075 ) ) ;
#24606 = CARTESIAN_POINT ( 'NONE',  ( 2.977408999572650927, -7.188101187499990274, 9.830302781871754547 ) ) ;
#24607 = CARTESIAN_POINT ( 'NONE',  ( -3.042071309553164404, 182.5520833299193271, -11.35316468749999963 ) ) ;
#24608 = CARTESIAN_POINT ( 'NONE',  ( 3.211159895383560947, 2.187499998634407028, 3.211159895383562723 ) ) ;
#24609 = DIRECTION ( 'NONE',  ( 0.000000000000000000, 0.000000000000000000, -1.000000000000000000 ) ) ;
#24611 = CARTESIAN_POINT ( 'NONE',  ( 3.313708498984756279, 7.999999999999991118, 3.549052783920144893 ) ) ;
#24610 =( NAMED_UNIT ( * ) PLANE_ANGLE_UNIT ( ) SI_UNIT ( $, .RADIAN. ) );
#24612 = ORIENTED_EDGE ( 'NONE', *, *, #19030, .F. ) ;
#24613 = VECTOR ( 'NONE', #2063, 1000.000000000000000 ) ;
#24614 = CARTESIAN_POINT ( 'NONE',  ( 3.458734124999960358, 206.6250000013656063, 143.4326545832176976 ) ) ;
#24615 = CARTESIAN_POINT ( 'NONE',  ( 5.676582343749993598, 45.26041666325268409, 9.832129032723422313 ) ) ;
#24616 = CARTESIAN_POINT ( 'NONE',  ( -4.556349186104047710, -10.99999999999999822, 106.4687500040967763 ) ) ;
#24617 = CARTESIAN_POINT ( 'NONE',  ( -11.35316468750000141, 218.8020833299193271, 3.042071309553159963 ) ) ;
#24618 = CARTESIAN_POINT ( 'NONE',  ( -31.45873412499999944, 204.6875000013656063, 170.0000000000004547 ) ) ;
#24619 = CARTESIAN_POINT ( 'NONE',  ( 10.00000000000000000, 9.791666666666667851, 2.679491924311236062 ) ) ;
#24621 = CARTESIAN_POINT ( 'NONE',  ( 2.751064625579944321E-14, 203.7500000000000284, 194.0000000000000568 ) ) ;
#24620 = CARTESIAN_POINT ( 'NONE',  ( 7.188101187500000933, 123.5000000020483810, -2.977408999572651371 ) ) ;
#24622 = CARTESIAN_POINT ( 'NONE',  ( -2.445694354108839619, 195.8125000013656063, 139.5543056458912190 ) ) ;
#24623 = CARTESIAN_POINT ( 'NONE',  ( -10.00000000000000355, 74.58333332650533976, 2.679491924311223183 ) ) ;
#24624 = CARTESIAN_POINT ( 'NONE',  ( 1.320432766682874540E-15, 97.53125000204838102, 7.188101187500000044 ) ) ;
#24625 = CARTESIAN_POINT ( 'NONE',  ( -4.541265875000002339, 16.93749999863440436, -5.561446717895856393E-16 ) ) ;
#24626 = CARTESIAN_POINT ( 'NONE',  ( -30.82842712474612412, 204.5000000027312126, 172.8284271247466108 ) ) ;
#24627 = CARTESIAN_POINT ( 'NONE',  ( 2.828427124746190291, 10.62499999726881406, 2.828427124746192067 ) ) ;
#24628 = CYLINDRICAL_SURFACE ( 'NONE', #2873, 3.999999999999976019 ) ;
#24629 = VERTEX_POINT ( 'NONE', #17770 ) ;
#24630 = VERTEX_POINT ( 'NONE', #53225 ) ;
#24631 = CARTESIAN_POINT ( 'NONE',  ( 2.765530957081996366, 298.2968750017069510, -6.676582343750003368 ) ) ;
#24632 = PLANE ( 'NONE',  #20595 ) ;
#24633 = CARTESIAN_POINT ( 'NONE',  ( 2.751064625579944321E-14, 196.7500000000000000, 194.0000000000000568 ) ) ;
#24634 = CARTESIAN_POINT ( 'NONE',  ( 3.042071309553167069, 161.8229166632526983, -11.35316468749999785 ) ) ;
#24635 = CARTESIAN_POINT ( 'NONE',  ( 8.000000000000000000, -2.500000000000000444, 0.000000000000000000 ) ) ;
#24636 = CARTESIAN_POINT ( 'NONE',  ( 2.828427124746208943, 198.6250000000000284, 195.1715728752538439 ) ) ;
#24637 = FACE_OUTER_BOUND ( 'NONE', #3780, .T. ) ;
#24638 = CARTESIAN_POINT ( 'NONE',  ( 1.871523826299183495E-15, -10.18810118749999916, 110.4062500020483668 ) ) ;
#24639 = ORIENTED_EDGE ( 'NONE', *, *, #40780, .T. ) ;
#24640 = EDGE_CURVE ( 'NONE', #40340, #38960, #1907, .T. ) ;
#24641 = CARTESIAN_POINT ( 'NONE',  ( 5.656854249492380582, 17.99999999590322375, -5.656854249492380582 ) ) ;
#24642 = CARTESIAN_POINT ( 'NONE',  ( -28.00000000000007461, 209.4375000013656063, 166.5412658750003629 ) ) ;
#24643 = CARTESIAN_POINT ( 'NONE',  ( 3.042071309553167513, 147.1354166632526983, -11.35316468749999785 ) ) ;
#24644 = CARTESIAN_POINT ( 'NONE',  ( -2.445694354108782775, 199.5625000013656063, 200.4456943541088663 ) ) ;
#24645 = DIRECTION ( 'NONE',  ( -1.000000000000000000, 0.000000000000000000, 0.000000000000000000 ) ) ;
#24646 = CARTESIAN_POINT ( 'NONE',  ( -10.18810118749999916, 0.000000000000000000, 74.03125000204838102 ) ) ;
#24647 = CARTESIAN_POINT ( 'NONE',  ( 8.311093377946834337, 45.46874999658601268, 8.311093377946839666 ) ) ;
#24648 = ORIENTED_EDGE ( 'NONE', *, *, #37558, .T. ) ;
#24649 = CARTESIAN_POINT ( 'NONE',  ( -23.99999999999996092, 208.8125000027312126, 171.6568542494926817 ) ) ;
#24650 = CARTESIAN_POINT ( 'NONE',  ( 1.881053915767122664, 5.249999998634407028, 4.541265875000001451 ) ) ;
#24651 = CARTESIAN_POINT ( 'NONE',  ( -5.662595241051933570, -5.662595241051936235, 7.200615283940628331 ) ) ;
#24652 = CARTESIAN_POINT ( 'NONE',  ( -2.977408999572654480, 14.99999999795161187, 7.188101187499999156 ) ) ;
#24653 = CARTESIAN_POINT ( 'NONE',  ( 2.485281374238571317, 291.7500000034140726, -6.000000000000003553 ) ) ;
#24654 = CARTESIAN_POINT ( 'NONE',  ( -12.00000000000000000, 0.000000000000000000, 0.000000000000000000 ) ) ;
#24655 = CARTESIAN_POINT ( 'NONE',  ( -7.188101187500001821, 14.99999999795161187, -2.977408999572651371 ) ) ;
#24656 = CARTESIAN_POINT ( 'NONE',  ( 5.082755093536320601, -5.082755093536318824, 8.049052781871752771 ) ) ;
#24657 = CARTESIAN_POINT ( 'NONE',  ( -7.204075437095967871, 7.204075437095967871, 117.3437500020483810 ) ) ;
#24658 = EDGE_CURVE ( 'NONE', #61990, #48362, #47544, .T. ) ;
#24659 = EDGE_CURVE ( 'NONE', #54565, #47572, #69462, .T. ) ;
#24660 = CARTESIAN_POINT ( 'NONE',  ( -1.538508811358849613E-11, 71.25000000000120792, -10.00000000000000178 ) ) ;
#24661 = CARTESIAN_POINT ( 'NONE',  ( 2.828427124746190291, 2.624999997268812724, 2.828427124746192067 ) ) ;
#24662 = VERTEX_POINT ( 'NONE', #19243 ) ;
#24663 = CARTESIAN_POINT ( 'NONE',  ( 2.828427124746208943, 195.7500000027312126, 195.1715728752538439 ) ) ;
#24664 = CARTESIAN_POINT ( 'NONE',  ( 2.828427124746152987, 201.1250000000000284, 139.1715728752538723 ) ) ;
#24665 = CARTESIAN_POINT ( 'NONE',  ( -30.82842712474612057, 197.5000000027312126, 172.8284271247466108 ) ) ;
#24666 = CARTESIAN_POINT ( 'NONE',  ( 2.780723358947928197E-16, 0.5624999986344066949, -4.541265875000002339 ) ) ;
#24667 = CARTESIAN_POINT ( 'NONE',  ( 2.977408999572654480, 117.1250000020483952, 7.188101187499999156 ) ) ;
#24668 = EDGE_CURVE ( 'NONE', #19863, #51786, #63791, .T. ) ;
#24669 = FACE_OUTER_BOUND ( 'NONE', #71385, .T. ) ;
#24670 = CARTESIAN_POINT ( 'NONE',  ( 7.999999999999992895, -3.313708498984756279, 3.174052783920144893 ) ) ;
#24671 = VERTEX_POINT ( 'NONE', #13571 ) ;
#24672 = CARTESIAN_POINT ( 'NONE',  ( 7.188101187500000933, 21.56249999795161543, -2.977408999572650483 ) ) ;
#24673 = ORIENTED_EDGE ( 'NONE', *, *, #52876, .F. ) ;
#24674 = CARTESIAN_POINT ( 'NONE',  ( 31.99999999999999289, 200.2500000000000000, 169.9999999999999432 ) ) ;
#24675 = CARTESIAN_POINT ( 'NONE',  ( -1.432654583217607858, 208.6250000013655779, 201.4587341250000065 ) ) ;
#24676 = CARTESIAN_POINT ( 'NONE',  ( 29.43265458321761230, 203.8750000013656063, 166.5412658749999650 ) ) ;
#24677 = CARTESIAN_POINT ( 'NONE',  ( 10.00000000000000000, 54.79166666666665719, 2.679491924311236062 ) ) ;
#24678 = CARTESIAN_POINT ( 'NONE',  ( -7.188101187500001821, 98.93750000204838102, -2.977408999572650483 ) ) ;
#24679 = CARTESIAN_POINT ( 'NONE',  ( -6.000000000000003553, 297.9375000000000000, -2.485281374238571317 ) ) ;
#24681 = CARTESIAN_POINT ( 'NONE',  ( 2.828427124746208943, 197.7500000027312126, 195.1715728752538439 ) ) ;
#24680 = CARTESIAN_POINT ( 'NONE',  ( 33.24289252269444006, 175.6592107545515944, 157.7120342695833699 ) ) ;
#24682 = ORIENTED_EDGE ( 'NONE', *, *, #12132, .F. ) ;
#24683 = CARTESIAN_POINT ( 'NONE',  ( 3.042071309553173286, 235.3645833367473017, 11.35316468749999608 ) ) ;
#24684 = CARTESIAN_POINT ( 'NONE',  ( 7.188101187499992051, 8.802885111219154394E-16, 14.61155278187175455 ) ) ;
#24685 = CARTESIAN_POINT ( 'NONE',  ( 2.828427124746152987, 195.2500000027312126, 139.1715728752538723 ) ) ;
#24686 = FACE_OUTER_BOUND ( 'NONE', #27387, .T. ) ;
#24687 = CARTESIAN_POINT ( 'NONE',  ( -1.656854249492383468, 17.43749999726881583, 4.000000000000000888 ) ) ;
#24688 = CARTESIAN_POINT ( 'NONE',  ( 24.85907736982385430, 194.8576601072064705, 167.7522730105956725 ) ) ;
#24689 = CARTESIAN_POINT ( 'NONE',  ( 12.00000000000000178, 28.00000000000000000, 0.000000000000000000 ) ) ;
#24690 =( BOUNDED_CURVE ( )  B_SPLINE_CURVE ( 2, ( #65913, #14219, #37259, #70839, #54991, #54245, #42154, #13840, #48189 ),
 .UNSPECIFIED., .F., .F. ) 
 B_SPLINE_CURVE_WITH_KNOTS ( ( 3, 2, 2, 2, 3 ),
 ( 0.9666666666666674512, 0.9750000000000005329, 0.9833333333333336146, 0.9916666666666669183, 1.000000000000000000 ),
 .UNSPECIFIED. ) 
 CURVE ( )  GEOMETRIC_REPRESENTATION_ITEM ( )  RATIONAL_B_SPLINE_CURVE ( ( 0.9999999999999928946, 0.9238795325112938439, 1.000000000000000000, 0.9238795325112867385, 1.000000000000000000, 0.9238795325112867385, 1.000000000000000000, 0.9238795325112867385, 1.000000000000000000 ) ) 
 REPRESENTATION_ITEM ( '' )  );
#24691 = CARTESIAN_POINT ( 'NONE',  ( 7.320508075688771044, 174.3749999999999716, 7.320508075688775484 ) ) ;
#24692 = CARTESIAN_POINT ( 'NONE',  ( 2.250000000000000000, 300.0000000000000000, 7.677076266392047543 ) ) ;
#24693 = CARTESIAN_POINT ( 'NONE',  ( 27.99999999999999645, 195.0000000000000000, 169.9999999999999147 ) ) ;
#24694 = CARTESIAN_POINT ( 'NONE',  ( -3.034644841523098859E-11, -67.59332269700080076, 20.03478791450305962 ) ) ;
#24695 = CARTESIAN_POINT ( 'NONE',  ( 6.951808397369818766E-16, 147.3437499965860411, -11.35316468750000141 ) ) ;
#24696 = CARTESIAN_POINT ( 'NONE',  ( 2.849036369511732440E-14, 208.3750000027312126, 202.0000000000000000 ) ) ;
#24697 = CARTESIAN_POINT ( 'NONE',  ( -5.656854249492380582, 117.3125000000000000, -5.656854249492380582 ) ) ;
#24700 = DIRECTION ( 'NONE',  ( 0.000000000000000000, 0.000000000000000000, 1.000000000000000000 ) ) ;
#24699 = CARTESIAN_POINT ( 'NONE',  ( -2.170320029210516033, -51.35721532638450526, 48.60044191894271393 ) ) ;
#24698 = CARTESIAN_POINT ( 'NONE',  ( 27.99999999999996803, 205.0000000000000284, 173.9999999999999147 ) ) ;
#24701 = EDGE_CURVE ( 'NONE', #47201, #35750, #6469, .T. ) ;
#24702 = ORIENTED_EDGE ( 'NONE', *, *, #48158, .T. ) ;
#24703 = CARTESIAN_POINT ( 'NONE',  ( -11.35316468750000141, 3.802083329919349275, 3.042071309553159963 ) ) ;
#24704 = EDGE_CURVE ( 'NONE', #5379, #73846, #30169, .T. ) ;
#24705 = DIRECTION ( 'NONE',  ( -1.000000000000000000, 0.000000000000000000, 0.000000000000000000 ) ) ;
#24706 = CARTESIAN_POINT ( 'NONE',  ( 3.458734124999959914, 208.4375000013656063, 142.0000000000000568 ) ) ;
#24707 = CARTESIAN_POINT ( 'NONE',  ( -3.313708498984760276, 4.781249995903220196, -8.000000000000000000 ) ) ;
#24708 = CARTESIAN_POINT ( 'NONE',  ( 10.00000000000000178, 32.08333332650536107, -2.679491924311226736 ) ) ;
#24709 = CARTESIAN_POINT ( 'NONE',  ( -5.082755093536325930, 116.4687500020483810, -5.082755093536325930 ) ) ;
#24710 = CARTESIAN_POINT ( 'NONE',  ( -4.541265875000002339, 4.874999998634407916, -1.881053915767121998 ) ) ;
#24711 = CARTESIAN_POINT ( 'NONE',  ( 11.00000000000010836, -4.556349186103939353, 85.65625000000000000 ) ) ;
#24712 = CARTESIAN_POINT ( 'NONE',  ( 1.469576158976822172E-15, -7.999999999999991118, 17.70530277982336642 ) ) ;
#24714 = CARTESIAN_POINT ( 'NONE',  ( 0.000000000000000000, 0.000000000000000000, 36.00000000000000000 ) ) ;
#24713 = CARTESIAN_POINT ( 'NONE',  ( -4.500000000000010658, -7.794228634059939154, 0.000000000000000000 ) ) ;
#24715 = ORIENTED_EDGE ( 'NONE', *, *, #65509, .F. ) ;
#24716 = ADVANCED_FACE ( 'NONE', ( #29840 ), #70209, .T. ) ;
#24717 = CARTESIAN_POINT ( 'NONE',  ( 4.999999999999997335, 221.4583333401612890, -8.660254037844387298 ) ) ;
#24718 = LINE ( 'NONE', #18335, #70071 ) ;
#24719 = CARTESIAN_POINT ( 'NONE',  ( -3.042071309553159075, 230.2604166700806445, 11.35316468749999963 ) ) ;
#24720 = CARTESIAN_POINT ( 'NONE',  ( -11.35316468750000141, 113.2812499965860269, -1.390361679473963753E-15 ) ) ;
#24721 = VERTEX_POINT ( 'NONE', #59619 ) ;
#24722 = CARTESIAN_POINT ( 'NONE',  ( -4.000000000000015987, 200.5625000000000284, 143.6568542494924259 ) ) ;
#24723 = CARTESIAN_POINT ( 'NONE',  ( -7.204075437095967871, 7.204075437095967871, 103.4687500020483668 ) ) ;
#24724 = LINE ( 'NONE', #19073, #32104 ) ;
#24725 = CARTESIAN_POINT ( 'NONE',  ( -1.432654583217607414, 197.5000000013656063, 194.5412658750000219 ) ) ;
#24726 = CYLINDRICAL_SURFACE ( 'NONE', #28105, 10.00000000000000178 ) ;
#24728 = CARTESIAN_POINT ( 'NONE',  ( 11.35316468750000141, 110.7812499965860269, 0.000000000000000000 ) ) ;
#24727 = CARTESIAN_POINT ( 'NONE',  ( 0.5249639094239428871, 225.9999999999999716, -9.999968502165486939 ) ) ;
#24729 = CARTESIAN_POINT ( 'NONE',  ( -31.99999999999998579, 208.3125000000000000, 171.6568542494928238 ) ) ;
#24730 = CARTESIAN_POINT ( 'NONE',  ( 10.00000000000000178, 81.87499999317203958, 0.000000000000000000 ) ) ;
#24731 = ORIENTED_EDGE ( 'NONE', *, *, #6769, .T. ) ;
#24732 = B_SPLINE_CURVE_WITH_KNOTS ( 'NONE', 3,
 ( #20748, #43382, #71306, #32463, #3783, #43004 ),
 .UNSPECIFIED., .F., .F.,
 ( 4, 2, 4 ),
 ( 0.07045737639677604469, 0.07247979437381202317, 0.07450221235084798777 ),
 .UNSPECIFIED. ) ;
#24733 = CARTESIAN_POINT ( 'NONE',  ( 6.123233995736767268E-16, 208.1249999931720538, -10.00000000000000178 ) ) ;
#24734 = CARTESIAN_POINT ( 'NONE',  ( 8.000000000000000000, 22.59375000000000355, -3.313708498984761164 ) ) ;
#24735 = CARTESIAN_POINT ( 'NONE',  ( -2.828427124746192067, 9.625000000000000000, 2.828427124746190735 ) ) ;
#24736 = CARTESIAN_POINT ( 'NONE',  ( -9.832129032723420536, 99.01041666325269830, 5.676582343749997150 ) ) ;
#24737 = CARTESIAN_POINT ( 'NONE',  ( 105.0000000000000000, 37.00000000000000000, 0.000000000000000000 ) ) ;
#24738 = CARTESIAN_POINT ( 'NONE',  ( 7.188101187500000044, 11.34374999795161187, 0.000000000000000000 ) ) ;
#24739 = CARTESIAN_POINT ( 'NONE',  ( -4.220049686691935698, 10.18810118749999916, 90.25000000204838102 ) ) ;
#24740 = CARTESIAN_POINT ( 'NONE',  ( -3.042071309553173730, 9.635416663252682312, 11.35316468749999785 ) ) ;
#24741 = ORIENTED_EDGE ( 'NONE', *, *, #4435, .T. ) ;
#24742 = CYLINDRICAL_SURFACE ( 'NONE', #42835, 6.000000000000001776 ) ;
#24743 = CARTESIAN_POINT ( 'NONE',  ( -27.99999999999996092, 206.5000000000000284, 174.0000000000003695 ) ) ;
#24744 = DIRECTION ( 'NONE',  ( 0.000000000000000000, 0.000000000000000000, 1.000000000000000000 ) ) ;
#24745 = CARTESIAN_POINT ( 'NONE',  ( 7.204075437095966983, 7.204075437095967871, 71.96875000204836681 ) ) ;
#24746 = CARTESIAN_POINT ( 'NONE',  ( 5.000000000000000000, 32.28817737728141424, 3.295974604355933479E-13 ) ) ;
#24747 = DIRECTION ( 'NONE',  ( -0.000000000000000000, -1.000000000000000000, -0.000000000000000000 ) ) ;
#24748 = CARTESIAN_POINT ( 'NONE',  ( 2.765530957081996366, 291.1406250017069510, -6.676582343750003368 ) ) ;
#24749 = AXIS2_PLACEMENT_3D ( 'NONE', #15080, #2658, #37362 ) ;
#24750 = CARTESIAN_POINT ( 'NONE',  ( 1.656854249492453857, 204.8125000027312410, 194.0000000000001421 ) ) ;
#24751 = CARTESIAN_POINT ( 'NONE',  ( -11.35316468749999785, 223.3854166632526699, -3.042071309553167957 ) ) ;
#24752 = CARTESIAN_POINT ( 'NONE',  ( -4.220049686691935698, 10.18810118749999916, 91.37500000204838102 ) ) ;
#24753 = EDGE_CURVE ( 'NONE', #46585, #27914, #35945, .T. ) ;
#24754 = VECTOR ( 'NONE', #8436, 1000.000000000000000 ) ;
#24755 = CARTESIAN_POINT ( 'NONE',  ( -25.55430564589119413, 202.3125000013656063, 167.5543056458915316 ) ) ;
#24756 = CARTESIAN_POINT ( 'NONE',  ( -8.000000000000000000, 21.65625000000000000, -3.313708498984762496 ) ) ;
#24757 = CARTESIAN_POINT ( 'NONE',  ( 2.780723358947928197E-16, 10.68749999863440792, -4.541265875000002339 ) ) ;
#24758 = ORIENTED_EDGE ( 'NONE', *, *, #18681, .F. ) ;
#24759 = DIRECTION ( 'NONE',  ( -0.000000000000000000, -1.000000000000000000, -0.000000000000000000 ) ) ;
#24760 = CARTESIAN_POINT ( 'NONE',  ( 4.000000000000015987, 207.6250000027312126, 198.0000000000000284 ) ) ;
#24761 = CARTESIAN_POINT ( 'NONE',  ( -2.754378923186476579E-14, 197.4375000013655779, 145.4587341250000350 ) ) ;
#24762 = CARTESIAN_POINT ( 'NONE',  ( -2.828427124746208943, 205.7500000027312126, 144.8284271247462129 ) ) ;
#24763 = FACE_OUTER_BOUND ( 'NONE', #73478, .T. ) ;
#24764 = CARTESIAN_POINT ( 'NONE',  ( 4.220049686691934809, 10.18810118749999916, 75.06250000204836681 ) ) ;
#24765 = ORIENTED_EDGE ( 'NONE', *, *, #22365, .T. ) ;
#24766 = CARTESIAN_POINT ( 'NONE',  ( -2.977408999572654480, 7.499999997951610986, 7.188101187499999156 ) ) ;
#24767 = DIRECTION ( 'NONE',  ( -1.000000000000000000, 0.000000000000000000, -0.000000000000000000 ) ) ;
#24768 = CARTESIAN_POINT ( 'NONE',  ( -5.082755093536325930, 119.8437500020483810, -5.082755093536325930 ) ) ;
#24769 = CARTESIAN_POINT ( 'NONE',  ( 1.377000000000000002, 267.1439999999997212, 5.668134320359001777 ) ) ;
#24770 = CARTESIAN_POINT ( 'NONE',  ( -6.676582343750001591, 291.4531250017069510, 0.000000000000000000 ) ) ;
#24772 = LINE ( 'NONE', #65880, #71073 ) ;
#24771 = CARTESIAN_POINT ( 'NONE',  ( 9.832129032723416984, 226.8229166700806729, -5.676582343750003368 ) ) ;
#24773 = VERTEX_POINT ( 'NONE', #49787 ) ;
#24774 = CARTESIAN_POINT ( 'NONE',  ( -6.951808397369817780E-16, 227.9687500034139873, -11.35316468749999963 ) ) ;
#24775 = CARTESIAN_POINT ( 'NONE',  ( 2.977408999572646486, 7.188101187499991163, 1.017802781871753215 ) ) ;
#24776 = CARTESIAN_POINT ( 'NONE',  ( 1.432654583217664701, 203.0000000013655779, 201.4587341250000065 ) ) ;
#24777 = ORIENTED_EDGE ( 'NONE', *, *, #16701, .T. ) ;
#24778 = DIRECTION ( 'NONE',  ( -0.000000000000000000, 1.000000000000000000, 4.476705744456276341E-16 ) ) ;
#24779 = CARTESIAN_POINT ( 'NONE',  ( 9.832129032723416984, 105.6770833299193413, 5.676582343750006032 ) ) ;
#24780 = CARTESIAN_POINT ( 'NONE',  ( -7.320508075688771932, 121.8750000000000142, -7.320508075688772820 ) ) ;
#24781 = CARTESIAN_POINT ( 'NONE',  ( 11.00000000000000355, -4.556349186104045046, 76.65625000000000000 ) ) ;
#24784 = CARTESIAN_POINT ( 'NONE',  ( -4.556349186104048599, -10.99999999999999822, 113.7812500000000142 ) ) ;
#24783 = CARTESIAN_POINT ( 'NONE',  ( 31.45873412499999944, 205.6875000013656063, 169.9999999999998863 ) ) ;
#24782 = CARTESIAN_POINT ( 'NONE',  ( 25.55430564589115150, 202.5625000013656063, 172.4456943541086957 ) ) ;
#24785 = ORIENTED_EDGE ( 'NONE', *, *, #39713, .F. ) ;
#24786 = CARTESIAN_POINT ( 'NONE',  ( 2.828427124746191623, 19.12500000000000000, -2.828427124746191623 ) ) ;
#24787 = CARTESIAN_POINT ( 'NONE',  ( 0.000000000000000000, 0.000000000000000000, -14.07439246179028203 ) ) ;
#24788 = VECTOR ( 'NONE', #45444, 1000.000000000000000 ) ;
#24789 = EDGE_CURVE ( 'NONE', #57749, #11511, #72801, .T. ) ;
#24790 = CARTESIAN_POINT ( 'NONE',  ( -8.311093377946841443, 218.9062499965860127, 8.311093377946830785 ) ) ;
#24791 = CARTESIAN_POINT ( 'NONE',  ( 1.432654583217607192, 202.2500000013656063, 145.4587341250000634 ) ) ;
#24792 = CARTESIAN_POINT ( 'NONE',  ( 26.56734541678238060, 201.2500000013656063, 166.5412658749999650 ) ) ;
#24793 = CARTESIAN_POINT ( 'NONE',  ( -7.188101187500001821, 23.99999999795161543, -2.977408999572651371 ) ) ;
#24794 = AXIS2_PLACEMENT_3D ( 'NONE', #46520, #11453, #34111 ) ;
#24795 = CARTESIAN_POINT ( 'NONE',  ( -3.042071309553173730, 194.6354166632526415, 11.35316468749999785 ) ) ;
#24796 = CARTESIAN_POINT ( 'NONE',  ( 3.999999999999960032, 196.1250000027311842, 142.0000000000000568 ) ) ;
#24797 = CARTESIAN_POINT ( 'NONE',  ( -27.99999999999995381, 196.5000000000000000, 174.0000000000003695 ) ) ;
#24798 = CARTESIAN_POINT ( 'NONE',  ( 4.541265875000002339, 14.31249999863440792, 0.000000000000000000 ) ) ;
#24799 = CARTESIAN_POINT ( 'NONE',  ( 28.00000000000002132, 198.1875000013655779, 166.5412658749999082 ) ) ;
#24800 = CARTESIAN_POINT ( 'NONE',  ( 7.188101187499993827, -2.977408999572645598, 2.517802781871750550 ) ) ;
#24801 = CARTESIAN_POINT ( 'NONE',  ( 3.042071309553167069, 71.82291666325269830, -11.35316468749999785 ) ) ;
#24802 = ADVANCED_FACE ( 'NONE', ( #55085 ), #21110, .T. ) ;
#24803 = CARTESIAN_POINT ( 'NONE',  ( -11.24419251898897798, -28.85176448099364421, 198.8889667351488129 ) ) ;
#24804 = CARTESIAN_POINT ( 'NONE',  ( 38.00000000000000000, 0.000000000000000000, 20.00000000000002132 ) ) ;
#24805 = ORIENTED_EDGE ( 'NONE', *, *, #68463, .T. ) ;
#24806 = CARTESIAN_POINT ( 'NONE',  ( -7.320508075688792360, 46.87500000000001421, -7.320508075688793248 ) ) ;
#24807 = CARTESIAN_POINT ( 'NONE',  ( 5.841566664369303132E-15, 13.85640646055103531, -14.00000000000000178 ) ) ;
#24808 = CARTESIAN_POINT ( 'NONE',  ( -9.832129032723420536, 78.69791666325269830, 5.676582343749997150 ) ) ;
#24809 = ORIENTED_EDGE ( 'NONE', *, *, #58641, .F. ) ;
#24810 = CARTESIAN_POINT ( 'NONE',  ( -4.220049686691935698, 10.18810118749999916, 88.75000000204836681 ) ) ;
#24811 = CARTESIAN_POINT ( 'NONE',  ( 7.778174593052021635, 7.778174593052023411, 68.12500000409677625 ) ) ;
#24812 = CARTESIAN_POINT ( 'NONE',  ( -2.839093476692135984E-14, 197.9375000013655779, 138.5412658750000503 ) ) ;
#24813 = CYLINDRICAL_SURFACE ( 'NONE', #46833, 7.999999999999991118 ) ;
#24815 = CARTESIAN_POINT ( 'NONE',  ( -3.042071309553163960, 72.23958332991935549, -11.35316468749999963 ) ) ;
#24814 = CARTESIAN_POINT ( 'NONE',  ( -2.828427124746192067, 13.37499999726881406, 2.828427124746190735 ) ) ;
#24816 = CARTESIAN_POINT ( 'NONE',  ( 7.999999999999991118, 3.313708498984757611, 24.36155278392014623 ) ) ;
#24817 = CARTESIAN_POINT ( 'NONE',  ( 10.00000000000000000, 129.7916666666666572, 2.679491924311235618 ) ) ;
#24818 =( BOUNDED_CURVE ( )  B_SPLINE_CURVE ( 2, ( #27075, #60279, #67071, #44061, #44431, #14623, #26698, #49718, #66317 ),
 .UNSPECIFIED., .F., .F. ) 
 B_SPLINE_CURVE_WITH_KNOTS ( ( 3, 2, 2, 2, 3 ),
 ( 0.4659090909090909394, 0.4715909090909091717, 0.4772727272727272929, 0.4829545454545454697, 0.4886363636363636465 ),
 .UNSPECIFIED. ) 
 CURVE ( )  GEOMETRIC_REPRESENTATION_ITEM ( )  RATIONAL_B_SPLINE_CURVE ( ( 0.9999999999999992228, 0.9238795325112875156, 1.000000000000000000, 0.9238795325112867385, 1.000000000000000000, 0.9238795325112867385, 1.000000000000000000, 0.9238795325112867385, 1.000000000000000000 ) ) 
 REPRESENTATION_ITEM ( '' )  );
#24819 = VECTOR ( 'NONE', #2164, 1000.000000000000000 ) ;
#24820 = CARTESIAN_POINT ( 'NONE',  ( -4.999999999999998224, 163.5416666598387110, -8.660254037844389075 ) ) ;
#24821 = CARTESIAN_POINT ( 'NONE',  ( 7.188101187500000044, 90.78125000204838102, -8.802885111219163269E-16 ) ) ;
#24822 = LINE ( 'NONE', #65562, #18337 ) ;
#24823 = CARTESIAN_POINT ( 'NONE',  ( 11.35316468750000141, 56.09374999658601979, 0.000000000000000000 ) ) ;
#24824 = CARTESIAN_POINT ( 'NONE',  ( -4.220049686691935698, 10.18810118749999916, 115.7500000020483810 ) ) ;
#24825 = CARTESIAN_POINT ( 'NONE',  ( 5.676582343750001591, 201.6145833299193555, -9.832129032723420536 ) ) ;
#24826 = ORIENTED_EDGE ( 'NONE', *, *, #49426, .F. ) ;
#24827 = CARTESIAN_POINT ( 'NONE',  ( 2.591411123066388100, 60.37037679141896973, 22.98897912931846932 ) ) ;
#24828 = CARTESIAN_POINT ( 'NONE',  ( 4.220049686691941027, -10.18810118749999738, 68.12500000204838102 ) ) ;
#24829 = CARTESIAN_POINT ( 'NONE',  ( -27.99999999999999645, 210.0000000000000284, 166.0000000000003979 ) ) ;
#24830 = CARTESIAN_POINT ( 'NONE',  ( -5.676582343749998039, 197.4479166632526983, -9.832129032723420536 ) ) ;
#24831 = CARTESIAN_POINT ( 'NONE',  ( -3.313708498984760276, 10.78124999590322197, -8.000000000000000000 ) ) ;
#24832 = CARTESIAN_POINT ( 'NONE',  ( -4.999999999999992895, 238.9583333401613174, 8.660254037844390851 ) ) ;
#24833 = CARTESIAN_POINT ( 'NONE',  ( 5.656854249492376141, -5.656854249492374365, 12.08030278392014445 ) ) ;
#24834 = VERTEX_POINT ( 'NONE', #25637 ) ;
#24835 = CARTESIAN_POINT ( 'NONE',  ( -11.35316468750000141, 178.8020833299193555, 3.042071309553159963 ) ) ;
#24836 = CARTESIAN_POINT ( 'NONE',  ( 7.188101187499992051, 8.802885111219154394E-16, 20.23655278187175099 ) ) ;
#24837 = CARTESIAN_POINT ( 'NONE',  ( -7.347880794884122694E-16, 19.75000000000000000, 4.000000000000001776 ) ) ;
#24838 = ORIENTED_EDGE ( 'NONE', *, *, #72930, .F. ) ;
#24839 = CARTESIAN_POINT ( 'NONE',  ( 1.469576158976823947E-15, 97.06250000409677625, 8.000000000000000000 ) ) ;
#24840 = CARTESIAN_POINT ( 'NONE',  ( 8.660254037844385522, 4.583333333333333037, 5.000000000000005329 ) ) ;
#24841 = CARTESIAN_POINT ( 'NONE',  ( 4.000000000000001776, 13.00000000000000178, 0.000000000000000000 ) ) ;
#24842 = DIRECTION ( 'NONE',  ( -0.000000000000000000, 1.000000000000000000, -0.000000000000000000 ) ) ;
#24843 = CARTESIAN_POINT ( 'NONE',  ( 3.211159895383561835, 17.43749999863440792, -3.211159895383561835 ) ) ;
#24844 = CARTESIAN_POINT ( 'NONE',  ( 5.656854249492374365, 5.656854249492375253, 15.45530278392014623 ) ) ;
#24845 = CARTESIAN_POINT ( 'NONE',  ( -10.00000000000000711, 187.7083333333333144, 2.679491924311224071 ) ) ;
#24846 = ORIENTED_EDGE ( 'NONE', *, *, #19207, .T. ) ;
#24847 = CARTESIAN_POINT ( 'NONE',  ( 54.00000000000000000, 205.0000000000000284, 0.000000000000000000 ) ) ;
#24848 = CARTESIAN_POINT ( 'NONE',  ( 5.082755093536325042, 101.0937500020483810, -5.082755093536325930 ) ) ;
#24850 = CARTESIAN_POINT ( 'NONE',  ( 0.000000000000000000, 125.0000000000000000, -7.500000000000020428 ) ) ;
#24849 = CARTESIAN_POINT ( 'NONE',  ( 1.469576158976823947E-15, 92.56250000409677625, 8.000000000000000000 ) ) ;
#24852 = EDGE_CURVE ( 'NONE', #5956, #3856, #19031, .T. ) ;
#24851 = ORIENTED_EDGE ( 'NONE', *, *, #71883, .F. ) ;
#24853 = ADVANCED_FACE ( 'NONE', ( #44133 ), #67143, .F. ) ;
#24854 = CARTESIAN_POINT ( 'NONE',  ( -5.000000000000091482, 156.6666666666667993, -8.660254037844547170 ) ) ;
#24855 = CARTESIAN_POINT ( 'NONE',  ( -3.369429374625380280, 50.21921270641865220, -40.85597392306764419 ) ) ;
#24856 = CARTESIAN_POINT ( 'NONE',  ( -5.082755093536317936, -5.082755093536320601, 22.67405278187175455 ) ) ;
#24857 = EDGE_LOOP ( 'NONE', ( #28540, #9854 ) ) ;
#24858 = ORIENTED_EDGE ( 'NONE', *, *, #29122, .F. ) ;
#24859 = CARTESIAN_POINT ( 'NONE',  ( -4.220049686691937474, -10.18810118749999738, 88.93750000204839523 ) ) ;
#24860 = CARTESIAN_POINT ( 'NONE',  ( 10.00000000000000000, 91.66666665983869677, 2.679491924311235618 ) ) ;
#24861 = CARTESIAN_POINT ( 'NONE',  ( -4.556349186104045934, 11.00000000000000000, 96.71874999999998579 ) ) ;
#24864 = CARTESIAN_POINT ( 'NONE',  ( 4.721056650415999201, 293.2343750017069510, -4.721056650415999201 ) ) ;
#24863 = CARTESIAN_POINT ( 'NONE',  ( 28.00000000000002132, 202.1250000027312126, 173.9999999999999147 ) ) ;
#24862 = CARTESIAN_POINT ( 'NONE',  ( 7.999999999667481099, -7.293937043860970585E-05, 4.767800658666735636 ) ) ;
#24865 = CARTESIAN_POINT ( 'NONE',  ( 10.00000000000000000, 139.7916666666666572, 2.679491924311236062 ) ) ;
#24866 = CARTESIAN_POINT ( 'NONE',  ( -4.000000000000002665, 0.5625000000000003331, 1.656854249492380582 ) ) ;
#24867 = CARTESIAN_POINT ( 'NONE',  ( -2.977408999572647819, 7.188101187499991163, 1.580302781871753437 ) ) ;
#24868 = CARTESIAN_POINT ( 'NONE',  ( 6.000000000000003553, 290.6250000034140157, -2.485281374238571761 ) ) ;
#24869 = CARTESIAN_POINT ( 'NONE',  ( 8.000000000000000000, 4.406249995903220196, -3.313708498984761608 ) ) ;
#24870 = CARTESIAN_POINT ( 'NONE',  ( 31.45873412499997812, 197.6250000013656063, 171.4326545832175839 ) ) ;
#24871 = CARTESIAN_POINT ( 'NONE',  ( 7.188101187500000044, 8.343749997951611874, 0.000000000000000000 ) ) ;
#24872 = CARTESIAN_POINT ( 'NONE',  ( -8.008118988124991233, 0.000000000000000000, 5.513115283940630107 ) ) ;
#24873 = CARTESIAN_POINT ( 'NONE',  ( -8.660254037844385522, 243.5416666734946318, 5.000000000000004441 ) ) ;
#24874 = CARTESIAN_POINT ( 'NONE',  ( 2.977408999572650039, 107.5625000020483810, -7.188101187500000933 ) ) ;
#24876 = DIRECTION ( 'NONE',  ( 0.000000000000000000, 0.000000000000000000, 1.000000000000000000 ) ) ;
#24875 = DIRECTION ( 'NONE',  ( 1.000000000000000000, -0.000000000000000000, -0.000000000000000000 ) ) ;
#24877 = CARTESIAN_POINT ( 'NONE',  ( -11.35316468749999963, 234.2187500034139873, 0.000000000000000000 ) ) ;
#24878 = CARTESIAN_POINT ( 'NONE',  ( 1.102182119232618108E-15, 288.3125000034140157, 6.000000000000001776 ) ) ;
#24879 = CARTESIAN_POINT ( 'NONE',  ( 1.320432766682872962E-15, -7.188101187499992051, 24.73655278187175810 ) ) ;
#24880 = CARTESIAN_POINT ( 'NONE',  ( 26.34314575050763452, 195.5625000000000568, 165.9999999999998863 ) ) ;
#24881 = CARTESIAN_POINT ( 'NONE',  ( -11.35316468750000141, 28.48958332991934839, 3.042071309553159963 ) ) ;
#24882 = CARTESIAN_POINT ( 'NONE',  ( -3.999999999999959144, 203.0625000000000000, 199.6568542494924259 ) ) ;
#24883 = CARTESIAN_POINT ( 'NONE',  ( -2.679491924311235618, 5.416666659838698550, 10.00000000000000000 ) ) ;
#24884 = LINE ( 'NONE', #47903, #25923 ) ;
#24885 = LINE ( 'NONE', #13562, #23852 ) ;
#24886 = VERTEX_POINT ( 'NONE', #49025 ) ;
#24887 = AXIS2_PLACEMENT_3D ( 'NONE', #49080, #71716, #60405 ) ;
#24888 = DIRECTION ( 'NONE',  ( -0.000000000000000000, -1.000000000000000000, -0.000000000000000000 ) ) ;
#24889 = CARTESIAN_POINT ( 'NONE',  ( -3.458734125000016757, 196.1250000013655779, 140.5673454167824161 ) ) ;
#24890 = CARTESIAN_POINT ( 'NONE',  ( 3.042071309553167069, 41.82291666325269119, -11.35316468749999785 ) ) ;
#24891 = CARTESIAN_POINT ( 'NONE',  ( -11.00000000000000000, 0.000000000000000000, 88.18750000409677625 ) ) ;
#24892 = AXIS2_PLACEMENT_3D ( 'NONE', #3726, #31268, #26725 ) ;
#24893 = CARTESIAN_POINT ( 'NONE',  ( 3.458734124999959469, 207.7500000013656063, 140.5673454167823593 ) ) ;
#24894 = CARTESIAN_POINT ( 'NONE',  ( -8.660254037844392627, 152.0833333333333712, -5.000000000000007994 ) ) ;
#24895 = CARTESIAN_POINT ( 'NONE',  ( 11.00000000000000000, 1.347111479062088405E-15, 100.7499999999999858 ) ) ;
#24897 = CARTESIAN_POINT ( 'NONE',  ( -3.042071309553163960, 32.23958332991934839, -11.35316468749999963 ) ) ;
#24896 = CARTESIAN_POINT ( 'NONE',  ( 5.082755093536325042, 105.5937500020483810, -5.082755093536325930 ) ) ;
#24898 = CARTESIAN_POINT ( 'NONE',  ( -3.313708498984758943, -7.999999999999989342, 17.61155277982336997 ) ) ;
#24899 = CARTESIAN_POINT ( 'NONE',  ( 11.35316468749999963, 150.9895833299193271, -3.042071309553165293 ) ) ;
#24900 = CARTESIAN_POINT ( 'NONE',  ( 4.999999999999993783, 111.0416666598387110, 8.660254037844390851 ) ) ;
#24901 = CARTESIAN_POINT ( 'NONE',  ( -2.977408999572650927, 106.2500000020484094, -7.188101187500001821 ) ) ;
#24902 = CARTESIAN_POINT ( 'NONE',  ( 0.000000000000000000, 300.0000000000000000, 0.000000000000000000 ) ) ;
#24903 = CARTESIAN_POINT ( 'NONE',  ( -30.44569435410879166, 204.0625000013656063, 172.4456943541092357 ) ) ;
#24904 = ORIENTED_EDGE ( 'NONE', *, *, #44540, .F. ) ;
#24905 = CARTESIAN_POINT ( 'NONE',  ( 8.311093377946834337, 15.46874999658601624, 8.311093377946839666 ) ) ;
#24906 =( BOUNDED_CURVE ( )  B_SPLINE_CURVE ( 2, ( #70404, #47380, #54539, #14144, #65837, #25468, #24730, #65471, #2845, #19813, #30041, #7769, #71121 ),
 .UNSPECIFIED., .F., .F. ) 
 B_SPLINE_CURVE_WITH_KNOTS ( ( 3, 2, 2, 2, 2, 2, 3 ),
 ( 0.3423913043478260532, 0.3442028985507245564, 0.3460144927536231152, 0.3478260869565217295, 0.3496376811594202882, 0.3514492753623188470, 0.3532608695652174058 ),
 .UNSPECIFIED. ) 
 CURVE ( )  GEOMETRIC_REPRESENTATION_ITEM ( )  RATIONAL_B_SPLINE_CURVE ( ( 1.000000000000001110, 0.9659258262890673130, 1.000000000000000000, 0.9659258262890683122, 1.000000000000000000, 0.9659258262890683122, 1.000000000000000000, 0.9659258262890683122, 1.000000000000000000, 0.9659258262890683122, 1.000000000000000000, 0.9659258262890683122, 1.000000000000000000 ) ) 
 REPRESENTATION_ITEM ( '' )  );
#24907 = VERTEX_POINT ( 'NONE', #48285 ) ;
#24908 = CARTESIAN_POINT ( 'NONE',  ( 1.656854249492381248, 7.187500000000000000, -4.000000000000001776 ) ) ;
#24909 = CARTESIAN_POINT ( 'NONE',  ( 2.485281374238266672, 289.6875000000000568, -6.000000000000306422 ) ) ;
#24911 = CARTESIAN_POINT ( 'NONE',  ( 6.951808397369818766E-16, 157.0312499965860127, -11.35316468750000141 ) ) ;
#24910 = CARTESIAN_POINT ( 'NONE',  ( -33.07484552657816579, -21.19745326134420083, 158.8094963175336432 ) ) ;
#24912 = CARTESIAN_POINT ( 'NONE',  ( -28.00000000000008171, 207.1250000027312126, 166.0000000000003695 ) ) ;
#24913 = CARTESIAN_POINT ( 'NONE',  ( -7.999999999999991118, 3.313708498984756723, 17.29280278432982598 ) ) ;
#24914 = CARTESIAN_POINT ( 'NONE',  ( 7.778174593052021635, 7.778174593052023411, 90.62500000409677625 ) ) ;
#24915 = CARTESIAN_POINT ( 'NONE',  ( 9.832129032723420536, 230.9895833367473301, 5.676582343749996262 ) ) ;
#24916 = CARTESIAN_POINT ( 'NONE',  ( -10.18810118749999916, 4.220049686691934809, 91.93750000204836681 ) ) ;
#24917 = ORIENTED_EDGE ( 'NONE', *, *, #63245, .T. ) ;
#24918 = AXIS2_PLACEMENT_3D ( 'NONE', #2815, #72596, #21274 ) ;
#24919 = CARTESIAN_POINT ( 'NONE',  ( -2.751064625579944321E-14, 197.7500000000000000, 146.0000000000000284 ) ) ;
#24920 = CARTESIAN_POINT ( 'NONE',  ( -2.828427124746153876, 199.0000000027312126, 195.1715728752538439 ) ) ;
#24921 = CARTESIAN_POINT ( 'NONE',  ( -11.35316468750000141, 98.80208332991932707, 3.042071309553159963 ) ) ;
#24922 = CARTESIAN_POINT ( 'NONE',  ( 4.220049686691934809, 10.18810118749999916, 103.1875000020483810 ) ) ;
#24923 =( BOUNDED_CURVE ( )  B_SPLINE_CURVE ( 2, ( #24261, #43850, #66863 ),
 .UNSPECIFIED., .F., .F. ) 
 B_SPLINE_CURVE_WITH_KNOTS ( ( 3, 3 ),
 ( 0.9333333333333341253, 0.9416666668637481141 ),
 .UNSPECIFIED. ) 
 CURVE ( )  GEOMETRIC_REPRESENTATION_ITEM ( )  RATIONAL_B_SPLINE_CURVE ( ( 0.9999999999999928946, 0.9238795325112938439, 1.000000000000000000 ) ) 
 REPRESENTATION_ITEM ( '' )  );
#24924 = CARTESIAN_POINT ( 'NONE',  ( -8.342170076843785083E-16, 15.18749999863440792, 4.541265875000002339 ) ) ;
#24925 = ORIENTED_EDGE ( 'NONE', *, *, #2757, .T. ) ;
#24926 = ORIENTED_EDGE ( 'NONE', *, *, #55653, .F. ) ;
#24927 = CARTESIAN_POINT ( 'NONE',  ( -5.656854249492379694, 3.562500000000000444, -5.656854249492380582 ) ) ;
#24928 = CARTESIAN_POINT ( 'NONE',  ( -4.541265875000002339, 1.937499998634406806, -5.561446717895856393E-16 ) ) ;
#24929 = CARTESIAN_POINT ( 'NONE',  ( 7.188101187500001821, 2.062499997951610098, -2.977408999572650483 ) ) ;
#24930 = CARTESIAN_POINT ( 'NONE',  ( -8.000000000000000000, 113.0937500040968047, -3.313708498984761608 ) ) ;
#24931 = CARTESIAN_POINT ( 'NONE',  ( 10.18810118749999916, 4.220049686691935698, 100.3750000020484094 ) ) ;
#24932 = EDGE_CURVE ( 'NONE', #72729, #26793, #3393, .T. ) ;
#24933 = DIRECTION ( 'NONE',  ( 2.168404344971008868E-16, -1.000000000000000000, 0.000000000000000000 ) ) ;
#24934 = CARTESIAN_POINT ( 'NONE',  ( -1.656854249492383691, 0.6875000000000003331, 4.000000000000000888 ) ) ;
#24935 = CARTESIAN_POINT ( 'NONE',  ( -4.000000000000002665, 12.31249999726881406, 1.656854249492380804 ) ) ;
#24936 = CARTESIAN_POINT ( 'NONE',  ( -4.541265875000002339, 4.812499998634407028, -5.561446717895856393E-16 ) ) ;
#24937 = ORIENTED_EDGE ( 'NONE', *, *, #48129, .T. ) ;
#24938 = VECTOR ( 'NONE', #9120, 1000.000000000000000 ) ;
#24939 = CARTESIAN_POINT ( 'NONE',  ( -2.754378923186476579E-14, 209.1875000013656063, 145.4587341250000350 ) ) ;
#24940 = CARTESIAN_POINT ( 'NONE',  ( -3.458734124999959914, 197.3750000013656063, 196.5673454167823877 ) ) ;
#24942 = LINE ( 'NONE', #2318, #26145 ) ;
#24941 = CARTESIAN_POINT ( 'NONE',  ( -25.55430564589111953, 203.0625000013656063, 172.4456943541091505 ) ) ;
#24943 = SHAPE_REPRESENTATION_RELATIONSHIP ( 'NONE' , 'NONE' ,  #43124, #52625 ) ;
#24944 = CARTESIAN_POINT ( 'NONE',  ( -1.881053915767124440, 12.99999999863440969, 4.541265875000001451 ) ) ;
#24945 = CARTESIAN_POINT ( 'NONE',  ( -3.999999999999960032, 200.1250000027312126, 198.0000000000000284 ) ) ;
#24946 = CARTESIAN_POINT ( 'NONE',  ( -7.188101187499991163, 2.977408999572646930, 11.89280278187175277 ) ) ;
#24947 = ORIENTED_EDGE ( 'NONE', *, *, #18768, .F. ) ;
#24948 = ORIENTED_EDGE ( 'NONE', *, *, #52826, .T. ) ;
#24949 = CARTESIAN_POINT ( 'NONE',  ( -10.18810118749999916, 4.220049686691934809, 106.5625000020483810 ) ) ;
#24950 = CARTESIAN_POINT ( 'NONE',  ( 3.313708498984802020, 27.09374999590321664, -7.999999999999958256 ) ) ;
#24951 = CARTESIAN_POINT ( 'NONE',  ( -24.54126587499999346, 203.4375000013656063, 170.0000000000003411 ) ) ;
#24952 = CARTESIAN_POINT ( 'NONE',  ( -30.82842712474615965, 200.3750000000000284, 172.8284271247465824 ) ) ;
#24953 = CARTESIAN_POINT ( 'NONE',  ( 1.432654583217662481, 197.1250000013656347, 194.5412658750000219 ) ) ;
#24954 = CARTESIAN_POINT ( 'NONE',  ( 4.898587196589415787E-16, 0.000000000000000000, 4.000000000000001776 ) ) ;
#24955 = CARTESIAN_POINT ( 'NONE',  ( -10.00000000000000355, 97.70833333333331439, 2.679491924311223183 ) ) ;
#24956 = EDGE_CURVE ( 'NONE', #41332, #61205, #18545, .T. ) ;
#24957 = EDGE_CURVE ( 'NONE', #32715, #70301, #14689, .T. ) ;
#24958 = CARTESIAN_POINT ( 'NONE',  ( 8.000000000000001776, 116.6562500000000000, 3.313708498984759387 ) ) ;
#24959 = CARTESIAN_POINT ( 'NONE',  ( -6.676582343750000703, 295.6718750017070079, 2.765530957082001251 ) ) ;
#24960 = ORIENTED_EDGE ( 'NONE', *, *, #18847, .F. ) ;
#24961 = EDGE_CURVE ( 'NONE', #38816, #68280, #66008, .T. ) ;
#24962 = CARTESIAN_POINT ( 'NONE',  ( -1.836970198721029983E-15, 145.6249999931720538, 10.00000000000000178 ) ) ;
#24963 = CARTESIAN_POINT ( 'NONE',  ( 4.898587196589412829E-16, 13.68749999590322375, -8.000000000000000000 ) ) ;
#24964 = CARTESIAN_POINT ( 'NONE',  ( -1.432654583217662481, 205.1250000013656347, 145.4587341250000634 ) ) ;
#24965 = CARTESIAN_POINT ( 'NONE',  ( 4.898587196589412829E-16, 12.18749999590322197, -8.000000000000000000 ) ) ;
#24966 = CARTESIAN_POINT ( 'NONE',  ( -7.320508075688770155, 220.6250000000000284, 7.320508075688774596 ) ) ;
#24967 = CARTESIAN_POINT ( 'NONE',  ( -1.656854249492309972, 206.9375000027311842, 194.0000000000000284 ) ) ;
#24968 = CARTESIAN_POINT ( 'NONE',  ( -4.556349186104047710, -10.99999999999999822, 112.2812499999999858 ) ) ;
#24969 = CARTESIAN_POINT ( 'NONE',  ( -10.00000000000000178, 212.5000000000000284, -1.224646799147353454E-15 ) ) ;
#24970 = CARTESIAN_POINT ( 'NONE',  ( 5.082755093536318824, 5.082755093536319713, 11.79905278187175632 ) ) ;
#24971 = CARTESIAN_POINT ( 'NONE',  ( 3.042071309553159519, 180.0520833299193271, 11.35316468750000141 ) ) ;
#24972 = CARTESIAN_POINT ( 'NONE',  ( -4.556349186104048599, -10.99999999999999822, 101.7812499999999858 ) ) ;
#24973 = CARTESIAN_POINT ( 'NONE',  ( -4.541265875000002339, 3.749999998634407028, -1.881053915767121998 ) ) ;
#24974 = CARTESIAN_POINT ( 'NONE',  ( 2.828427124746153876, 209.8750000000000284, 144.8284271247462129 ) ) ;
#24975 = CARTESIAN_POINT ( 'NONE',  ( -5.656854249492375253, 5.656854249492375253, 3.830302783920144893 ) ) ;
#24976 = ORIENTED_EDGE ( 'NONE', *, *, #47243, .F. ) ;
#24977 = CARTESIAN_POINT ( 'NONE',  ( 3.458734124999960358, 208.6250000013655779, 143.4326545832176976 ) ) ;
#24978 = CARTESIAN_POINT ( 'NONE',  ( -11.35316468750000141, 53.59374999658601979, -1.390361679473963753E-15 ) ) ;
#24979 = CARTESIAN_POINT ( 'NONE',  ( -7.778174593052023411, 7.778174593052023411, 104.5000000040967763 ) ) ;
#24980 = CARTESIAN_POINT ( 'NONE',  ( 5.676582343749993598, 215.2604166632526983, 9.832129032723422313 ) ) ;
#24981 = ADVANCED_FACE ( 'NONE', ( #26377 ), #8675, .F. ) ;
#24982 = CARTESIAN_POINT ( 'NONE',  ( -24.54126587500002543, 206.2500000013655779, 168.5673454167826435 ) ) ;
#24983 = CARTESIAN_POINT ( 'NONE',  ( -1.836970198721029983E-15, 8.750000000000000000, 10.00000000000000178 ) ) ;
#24985 = CARTESIAN_POINT ( 'NONE',  ( -1.836970198721029983E-15, 60.62499999317203958, 10.00000000000000178 ) ) ;
#24984 = CARTESIAN_POINT ( 'NONE',  ( 11.00000000000000000, 1.347111479062088405E-15, 70.93750000409676204 ) ) ;
#24986 = CARTESIAN_POINT ( 'NONE',  ( -1.432654583217664479, 194.7500000013656063, 138.5412658750000787 ) ) ;
#24987 = CARTESIAN_POINT ( 'NONE',  ( -11.35316468749999785, 108.0729166632526699, -3.042071309553167513 ) ) ;
#24988 = CARTESIAN_POINT ( 'NONE',  ( -10.00000000000000178, 69.37499999317203958, -1.224646799147353454E-15 ) ) ;
#24989 = CARTESIAN_POINT ( 'NONE',  ( 7.188101187500002709, 91.81250000204839523, 2.977408999572649151 ) ) ;
#24990 = CARTESIAN_POINT ( 'NONE',  ( 3.211159895383561835, 16.56249999863440436, -3.211159895383561835 ) ) ;
#24991 = LINE ( 'NONE', #25363, #33787 ) ;
#24992 = CARTESIAN_POINT ( 'NONE',  ( 32.49574984736388217, 174.9883334519788320, 162.5913879594991158 ) ) ;
#24993 = VERTEX_POINT ( 'NONE', #43749 ) ;
#24994 = ORIENTED_EDGE ( 'NONE', *, *, #33989, .F. ) ;
#24995 = CARTESIAN_POINT ( 'NONE',  ( -4.721056650415999201, 295.4843750017070079, -4.721056650415999201 ) ) ;
#24996 = CYLINDRICAL_SURFACE ( 'NONE', #27886, 11.00000000000000000 ) ;
#24997 = CARTESIAN_POINT ( 'NONE',  ( 8.311093377946834337, 165.1562499965860127, 8.311093377946839666 ) ) ;
#24998 = DIRECTION ( 'NONE',  ( -0.000000000000000000, -0.000000000000000000, -1.000000000000000000 ) ) ;
#24999 = CARTESIAN_POINT ( 'NONE',  ( 4.000000000000015987, 199.4375000000000284, 199.6568542494924259 ) ) ;
#25000 = CARTESIAN_POINT ( 'NONE',  ( -5.197448530777805331, 17.78386138248274051, -0.2939692054342110672 ) ) ;
#25001 = CARTESIAN_POINT ( 'NONE',  ( -7.204075437095965206, -7.204075437095968759, 108.7187500020483810 ) ) ;
#25002 = EDGE_LOOP ( 'NONE', ( #42092, #46676, #34963, #40630 ) ) ;
#25003 = CARTESIAN_POINT ( 'NONE',  ( -7.999999999994639843, -6.164467849698474977E-06, 23.51803407853789807 ) ) ;
#25004 = CARTESIAN_POINT ( 'NONE',  ( -11.00000000000000000, 0.000000000000000000, 118.0000000000000000 ) ) ;
#25005 = CARTESIAN_POINT ( 'NONE',  ( 8.311093377946834337, 135.4687499965860411, 8.311093377946839666 ) ) ;
#25006 = CARTESIAN_POINT ( 'NONE',  ( 1.102182119232618108E-15, 297.3125000034140157, 6.000000000000001776 ) ) ;
#25007 = CARTESIAN_POINT ( 'NONE',  ( 2.754378923186476579E-14, 208.4375000013656063, 194.5412658750000219 ) ) ;
#25008 = CARTESIAN_POINT ( 'NONE',  ( 7.204075437095966983, 7.204075437095967871, 70.46875000204836681 ) ) ;
#25009 = CARTESIAN_POINT ( 'NONE',  ( -9.832129032723420536, 54.01041666325268409, 5.676582343749997150 ) ) ;
#25010 = ORIENTED_EDGE ( 'NONE', *, *, #13235, .F. ) ;
#25011 = CARTESIAN_POINT ( 'NONE',  ( 0.000000000000000000, 0.000000000000000000, 3.469446951953614189E-15 ) ) ;
#25012 = CARTESIAN_POINT ( 'NONE',  ( -3.211159895383562723, 3.062499998634407028, 3.211159895383561391 ) ) ;
#25013 = CARTESIAN_POINT ( 'NONE',  ( -4.903558642999205574E-16, 8.008118988124991233, 6.638115283940628331 ) ) ;
#25014 = CARTESIAN_POINT ( 'NONE',  ( -7.188101187500001821, 16.12499999795161187, -2.977408999572651371 ) ) ;
#25015 = CARTESIAN_POINT ( 'NONE',  ( 6.000000000000001776, 291.5625000034140157, -7.347880794884121708E-16 ) ) ;
#25016 = CARTESIAN_POINT ( 'NONE',  ( -5.656854249492380582, 117.5000000040967905, -5.656854249492380582 ) ) ;
#25017 = CARTESIAN_POINT ( 'NONE',  ( 5.082755093536325930, 11.53124999795161187, -5.082755093536325930 ) ) ;
#25018 = CARTESIAN_POINT ( 'NONE',  ( 1.320432766682872962E-15, -7.188101187499992051, 6.361552781871754547 ) ) ;
#25019 =( BOUNDED_CURVE ( )  B_SPLINE_CURVE ( 2, ( #53566, #1882, #64143, #65239, #31284, #13543, #23780, #46784, #35483, #2624, #60324, #37327, #2995 ),
 .UNSPECIFIED., .F., .F. ) 
 B_SPLINE_CURVE_WITH_KNOTS ( ( 3, 2, 2, 2, 2, 2, 3 ),
 ( 0.6388888888888887285, 0.6481481481481480289, 0.6574074074074073293, 0.6666666666666665186, 0.6759259259259259300, 0.6851851851851852304, 0.6944444444444444198 ),
 .UNSPECIFIED. ) 
 CURVE ( )  GEOMETRIC_REPRESENTATION_ITEM ( )  RATIONAL_B_SPLINE_CURVE ( ( 1.000000000000000444, 0.9659258262890678681, 1.000000000000000000, 0.9659258262890683122, 1.000000000000000000, 0.9659258262890683122, 1.000000000000000000, 0.9659258262890683122, 1.000000000000000000, 0.9659258262890683122, 1.000000000000000000, 0.9659258262890683122, 1.000000000000000000 ) ) 
 REPRESENTATION_ITEM ( '' )  );
#25020 = VECTOR ( 'NONE', #20522, 1000.000000000000000 ) ;
#25021 = CARTESIAN_POINT ( 'NONE',  ( -4.220049686691937474, -10.18810118749999738, 67.93750000204838102 ) ) ;
#25022 = CARTESIAN_POINT ( 'NONE',  ( -47.32259252271278882, 0.000000000000000000, 65.76194439203462139 ) ) ;
#25023 = CARTESIAN_POINT ( 'NONE',  ( -3.211159895383562723, 22.06249999863440792, 3.211159895383561391 ) ) ;
#25024 = ORIENTED_EDGE ( 'NONE', *, *, #11973, .T. ) ;
#25025 = ADVANCED_FACE ( 'NONE', ( #37349 ), #32447, .F. ) ;
#25026 = CARTESIAN_POINT ( 'NONE',  ( -3.999999999999960032, 197.0625000027311842, 196.3431457505076594 ) ) ;
#25027 = CARTESIAN_POINT ( 'NONE',  ( -2.751064625579944321E-14, 202.7500000000000000, 146.0000000000000284 ) ) ;
#25028 = CARTESIAN_POINT ( 'NONE',  ( -23.99999999999995737, 197.8125000027312126, 171.6568542494926817 ) ) ;
#25029 = CARTESIAN_POINT ( 'NONE',  ( -4.541265875000002339, 3.812499998634407028, -5.561446717895856393E-16 ) ) ;
#25030 = CARTESIAN_POINT ( 'NONE',  ( 1.320432766682874540E-15, 115.5312500020483952, 7.188101187500000044 ) ) ;
#25031 = CARTESIAN_POINT ( 'NONE',  ( 4.500000000000006217, -7.794228634059941818, 0.000000000000000000 ) ) ;
#25032 = CARTESIAN_POINT ( 'NONE',  ( -7.999999999999991118, 0.000000000000000000, 4.017802783920145338 ) ) ;
#25033 = ORIENTED_EDGE ( 'NONE', *, *, #29161, .T. ) ;
#25034 = CARTESIAN_POINT ( 'NONE',  ( 7.188101187500000933, 23.06249999795161543, -2.977408999572650483 ) ) ;
#25035 = EDGE_LOOP ( 'NONE', ( #10043, #50485, #24502, #39442 ) ) ;
#25036 = CARTESIAN_POINT ( 'NONE',  ( 29.65685424949250404, 198.4375000000000568, 165.9999999999999716 ) ) ;
#25037 = CARTESIAN_POINT ( 'NONE',  ( -1.432654583217607858, 207.6250000013656347, 201.4587341250000065 ) ) ;
#25038 = CARTESIAN_POINT ( 'NONE',  ( 27.99999999999996803, 202.9375000013656063, 166.5412658749999082 ) ) ;
#25039 = CARTESIAN_POINT ( 'NONE',  ( 4.999999999999993783, 49.16666666666667140, 8.660254037844390851 ) ) ;
#25040 = EDGE_CURVE ( 'NONE', #15376, #32224, #39254, .T. ) ;
#25041 = CARTESIAN_POINT ( 'NONE',  ( -7.188101187500001821, 97.43750000204839523, -2.977408999572650483 ) ) ;
#25042 = CARTESIAN_POINT ( 'NONE',  ( 1.102182119232618108E-15, 295.2500000000000000, 6.000000000000001776 ) ) ;
#25043 = AXIS2_PLACEMENT_3D ( 'NONE', #5551, #28555, #51561 ) ;
#25045 = CARTESIAN_POINT ( 'NONE',  ( 6.123233995736767268E-16, 78.12499999317202537, -10.00000000000000178 ) ) ;
#25044 = CARTESIAN_POINT ( 'NONE',  ( 31.10901663185143562, 177.6010581990177855, 171.6477061908809105 ) ) ;
#25046 = VERTEX_POINT ( 'NONE', #73912 ) ;
#25047 = CARTESIAN_POINT ( 'NONE',  ( -11.35316468749999608, 229.1145833367473301, 3.042071309553173730 ) ) ;
#25048 = AXIS2_PLACEMENT_3D ( 'NONE', #67123, #15418, #62568 ) ;
#25049 = CARTESIAN_POINT ( 'NONE',  ( -7.320508075688778149, 74.99999999317202537, 7.320508075688769267 ) ) ;
#25050 = CARTESIAN_POINT ( 'NONE',  ( 24.00000000000000711, 206.6875000000000284, 168.3431457505074889 ) ) ;
#25051 = CARTESIAN_POINT ( 'NONE',  ( 24.07362206087093170, 194.9222032098518014, 170.0609456059559932 ) ) ;
#25052 = CARTESIAN_POINT ( 'NONE',  ( 0.000000000000000000, 0.000000000000000000, 0.000000000000000000 ) ) ;
#25053 = CARTESIAN_POINT ( 'NONE',  ( -2.679491924311235618, 168.5416666666666856, 10.00000000000000000 ) ) ;
#25054 = CYLINDRICAL_SURFACE ( 'NONE', #4436, 7.999999999999991118 ) ;
#25055 = CARTESIAN_POINT ( 'NONE',  ( -4.898587196589412829E-16, 90.12500000000000000, -8.000000000000000000 ) ) ;
#25056 = CARTESIAN_POINT ( 'NONE',  ( 7.188101187499992051, 8.802885111219154394E-16, 28.11155278187175455 ) ) ;
#25057 = CARTESIAN_POINT ( 'NONE',  ( 8.311093377946837890, 146.7187499965860411, -8.311093377946837890 ) ) ;
#25058 = PLANE ( 'NONE',  #30044 ) ;
#25059 = DIRECTION ( 'NONE',  ( -0.000000000000000000, 1.000000000000000000, -0.000000000000000000 ) ) ;
#25062 = CARTESIAN_POINT ( 'NONE',  ( 17.99999999999999645, 8.711927089654787792, -1.122611879773029120 ) ) ;
#25061 = DIRECTION ( 'NONE',  ( -0.000000000000000000, 1.000000000000000000, 8.566535683836083017E-17 ) ) ;
#25060 = CARTESIAN_POINT ( 'NONE',  ( 30.82842712474620583, 207.3750000000000284, 167.1715728752537586 ) ) ;
#25063 = ORIENTED_EDGE ( 'NONE', *, *, #6712, .F. ) ;
#25064 = VECTOR ( 'NONE', #52779, 1000.000000000000000 ) ;
#25065 = CARTESIAN_POINT ( 'NONE',  ( -2.085542519210945728E-15, 4.843749996586016238, 11.35316468750000141 ) ) ;
#25066 = EDGE_CURVE ( 'NONE', #46261, #44110, #67677, .T. ) ;
#25067 = CARTESIAN_POINT ( 'NONE',  ( 5.000000000000000000, 29.68417822476651580, 4.268394125863321342 ) ) ;
#25068 = CARTESIAN_POINT ( 'NONE',  ( 4.104248244540173118, -10.10575198619682524, -70.81982386214420444 ) ) ;
#25069 = CARTESIAN_POINT ( 'NONE',  ( 2.751064625579944321E-14, 208.8750000027312126, 194.0000000000000568 ) ) ;
#25070 = CARTESIAN_POINT ( 'NONE',  ( 3.458734124999959914, 207.4375000013656063, 142.0000000000000568 ) ) ;
#25071 = CARTESIAN_POINT ( 'NONE',  ( -1.016170450681134207, 124.5980567557549250, -7.852785628585370326 ) ) ;
#25072 = EDGE_CURVE ( 'NONE', #55545, #26674, #61947, .T. ) ;
#25073 = CARTESIAN_POINT ( 'NONE',  ( -4.999999999999998224, 38.54166665983869677, -8.660254037844389075 ) ) ;
#25074 = CARTESIAN_POINT ( 'NONE',  ( -7.188101187500000044, 118.1562500020483810, 0.000000000000000000 ) ) ;
#25075 = CARTESIAN_POINT ( 'NONE',  ( 4.541265875000002339, 4.499999998634407028, -1.881053915767121554 ) ) ;
#25076 = CARTESIAN_POINT ( 'NONE',  ( -4.556349186104048599, -10.99999999999999822, 85.28124999999998579 ) ) ;
#25077 = CARTESIAN_POINT ( 'NONE',  ( -7.999999999999989342, -3.313708498984762496, 12.92405277982336287 ) ) ;
#25079 = CARTESIAN_POINT ( 'NONE',  ( 1.469576158976822172E-15, -7.999999999999991118, 17.89280278392014623 ) ) ;
#25078 = CARTESIAN_POINT ( 'NONE',  ( -7.778174593052023411, 7.778174593052023411, 101.5000000040967763 ) ) ;
#25080 = ORIENTED_EDGE ( 'NONE', *, *, #9436, .F. ) ;
#25081 = CARTESIAN_POINT ( 'NONE',  ( 10.00000000000000355, 29.79166666666667140, 2.679491924311236950 ) ) ;
#25082 = DIRECTION ( 'NONE',  ( 0.000000000000000000, 0.000000000000000000, 1.000000000000000000 ) ) ;
#25083 = EDGE_CURVE ( 'NONE', #58992, #39682, #33949, .T. ) ;
#25084 = CARTESIAN_POINT ( 'NONE',  ( 2.085542519210945334E-15, 235.4687500034139873, 11.35316468749999963 ) ) ;
#25085 = CARTESIAN_POINT ( 'NONE',  ( 11.35316468749999963, 120.9895833299193413, -3.042071309553165293 ) ) ;
#25086 = ORIENTED_EDGE ( 'NONE', *, *, #4638, .F. ) ;
#25087 = EDGE_CURVE ( 'NONE', #36295, #37658, #52258, .T. ) ;
#25088 = CARTESIAN_POINT ( 'NONE',  ( -27.99999999999999645, 210.0000000000000284, 170.0000000000003695 ) ) ;
#25089 = CARTESIAN_POINT ( 'NONE',  ( 1.871523826299183495E-15, -10.18810118749999916, 93.53125000204836681 ) ) ;
#25090 = CARTESIAN_POINT ( 'NONE',  ( -30.93541659651598508, -70.00000000000001421, 171.9999999999997442 ) ) ;
#25091 = CARTESIAN_POINT ( 'NONE',  ( 2.445694354108839175, 198.3125000013656063, 195.5543056458912190 ) ) ;
#25092 = FACE_OUTER_BOUND ( 'NONE', #40377, .T. ) ;
#25094 = CARTESIAN_POINT ( 'NONE',  ( -5.676582343750006032, 119.1145833299193697, 9.832129032723418760 ) ) ;
#25093 = DIRECTION ( 'NONE',  ( -0.000000000000000000, 1.000000000000000000, -0.000000000000000000 ) ) ;
#25095 = CARTESIAN_POINT ( 'NONE',  ( -26.34314575050764873, 208.9375000000000284, 166.0000000000003695 ) ) ;
#25096 = CARTESIAN_POINT ( 'NONE',  ( 7.999999999732929190, -6.536825277765295045E-05, 6.267800880277100362 ) ) ;
#25097 = ORIENTED_EDGE ( 'NONE', *, *, #40655, .F. ) ;
#25098 = CARTESIAN_POINT ( 'NONE',  ( -1.836970198721029983E-15, 210.6249999931720538, 10.00000000000000178 ) ) ;
#25099 = CARTESIAN_POINT ( 'NONE',  ( -1.469576158976823947E-15, 22.12500000000000355, 8.000000000000000000 ) ) ;
#25100 = EDGE_CURVE ( 'NONE', #42017, #25226, #62216, .T. ) ;
#25101 = CARTESIAN_POINT ( 'NONE',  ( -7.778174593052023411, 7.778174593052023411, 83.50000000409677625 ) ) ;
#25102 = CARTESIAN_POINT ( 'NONE',  ( -2.085542519210945728E-15, 104.8437499965860269, 11.35316468750000141 ) ) ;
#25103 = CARTESIAN_POINT ( 'NONE',  ( 1.432654583217662259, 209.1250000013656347, 194.5412658750000219 ) ) ;
#25104 = CARTESIAN_POINT ( 'NONE',  ( -7.188101187500000933, 10.49999999795161010, -2.977408999572651371 ) ) ;
#25105 = CARTESIAN_POINT ( 'NONE',  ( -7.204075437095967871, 7.204075437095967871, 91.84375000204838102 ) ) ;
#25106 = CARTESIAN_POINT ( 'NONE',  ( -8.311093377946836114, 12.96874999658601446, -8.311093377946837890 ) ) ;
#25107 = VERTEX_POINT ( 'NONE', #10915 ) ;
#25108 = DIRECTION ( 'NONE',  ( -0.000000000000000000, -0.000000000000000000, 1.000000000000000000 ) ) ;
#25109 = CARTESIAN_POINT ( 'NONE',  ( 2.679491924311139250, 246.6666666734946887, -10.00000000000004796 ) ) ;
#25110 = CARTESIAN_POINT ( 'NONE',  ( 10.99999999999994849, 4.556349186104097448, 102.3437499999999858 ) ) ;
#25111 = CARTESIAN_POINT ( 'NONE',  ( 10.18810118750000093, -4.220049686691933921, 73.18750000204838102 ) ) ;
#25112 = DIRECTION ( 'NONE',  ( -0.8660254037844505870, 0.4999999999999792388, 0.000000000000000000 ) ) ;
#25113 = CARTESIAN_POINT ( 'NONE',  ( 6.123233995736767268E-16, 148.1249999931720538, -10.00000000000000178 ) ) ;
#25114 = CARTESIAN_POINT ( 'NONE',  ( -4.721056650415998313, 293.5781250017069510, 4.721056650416000089 ) ) ;
#25115 = CARTESIAN_POINT ( 'NONE',  ( 2.849036369511732440E-14, 204.3750000027312126, 202.0000000000000000 ) ) ;
#25116 = CARTESIAN_POINT ( 'NONE',  ( -9.832129032723418760, 223.1770833299193555, -5.676582343750004256 ) ) ;
#25117 = CARTESIAN_POINT ( 'NONE',  ( 10.18810118749999916, 4.220049686691935698, 83.50000000204840944 ) ) ;
#25118 = CARTESIAN_POINT ( 'NONE',  ( -29.43265458321766559, 198.5000000013656347, 166.5412658750003629 ) ) ;
#25119 = CARTESIAN_POINT ( 'NONE',  ( -8.000000000000000000, 21.75000000000000355, -9.797174393178825657E-16 ) ) ;
#25120 = CARTESIAN_POINT ( 'NONE',  ( 3.211159895383560947, 11.31249999863440792, 3.211159895383562723 ) ) ;
#25121 = ORIENTED_EDGE ( 'NONE', *, *, #67516, .F. ) ;
#25122 = CARTESIAN_POINT ( 'NONE',  ( -27.32854269605737585, -51.68009665483441495, 155.2724884860399186 ) ) ;
#25123 = AXIS2_PLACEMENT_3D ( 'NONE', #7463, #53486, #6363 ) ;
#25124 = CARTESIAN_POINT ( 'NONE',  ( 4.000000000000015987, 206.6250000027312126, 198.0000000000000284 ) ) ;
#25125 = CARTESIAN_POINT ( 'NONE',  ( -3.458734125000015869, 199.1875000013655779, 142.0000000000000568 ) ) ;
#25126 = CARTESIAN_POINT ( 'NONE',  ( 3.999999999999960032, 203.1250000027312126, 142.0000000000000568 ) ) ;
#25127 = CARTESIAN_POINT ( 'NONE',  ( 5.000000000000000000, 11.68639849891297366, -68.31608016562482533 ) ) ;
#25128 = CARTESIAN_POINT ( 'NONE',  ( -10.18810118749999738, -4.220049686691941915, 68.12500000204838102 ) ) ;
#25129 = ORIENTED_EDGE ( 'NONE', *, *, #34722, .F. ) ;
#25130 = EDGE_CURVE ( 'NONE', #34152, #6173, #15661, .T. ) ;
#25131 =( BOUNDED_CURVE ( )  B_SPLINE_CURVE ( 2, ( #67875, #20342, #21473, #60722, #32819, #66376, #44495, #43743, #66757 ),
 .UNSPECIFIED., .F., .F. ) 
 B_SPLINE_CURVE_WITH_KNOTS ( ( 3, 2, 2, 2, 3 ),
 ( 0.6500000000000004663, 0.6583333333333338810, 0.6666666666666671848, 0.6750000000000007105, 0.6833333333333340143 ),
 .UNSPECIFIED. ) 
 CURVE ( )  GEOMETRIC_REPRESENTATION_ITEM ( )  RATIONAL_B_SPLINE_CURVE ( ( 0.9999999999999958922, 0.9238795325112908463, 1.000000000000000000, 0.9238795325112867385, 1.000000000000000000, 0.9238795325112867385, 1.000000000000000000, 0.9238795325112806323, 1.000000000000005995 ) ) 
 REPRESENTATION_ITEM ( '' )  );
#25132 = CARTESIAN_POINT ( 'NONE',  ( -2.977408999572650039, 3.937499997951610986, -7.188101187500000933 ) ) ;
#25133 =( BOUNDED_CURVE ( )  B_SPLINE_CURVE ( 2, ( #54571, #70435, #18750, #41759, #7435, #30441, #53460, #49699, #16835 ),
 .UNSPECIFIED., .F., .T. ) 
 B_SPLINE_CURVE_WITH_KNOTS ( ( 3, 2, 2, 2, 3 ),
 ( 0.03333333333333336063, 0.04166666666666669905, 0.05000000000000004441, 0.05833333333333338283, 0.06666666666666672125 ),
 .UNSPECIFIED. ) 
 CURVE ( )  GEOMETRIC_REPRESENTATION_ITEM ( )  RATIONAL_B_SPLINE_CURVE ( ( 0.9999999999999997780, 0.9238795325112869605, 1.000000000000000000, 0.9238795325112867385, 1.000000000000000000, 0.9238795325112867385, 1.000000000000000000, 0.9238795325112861834, 1.000000000000000444 ) ) 
 REPRESENTATION_ITEM ( '' )  );
#25134 = DIRECTION ( 'NONE',  ( 0.000000000000000000, 0.000000000000000000, 1.000000000000000000 ) ) ;
#25135 = CARTESIAN_POINT ( 'NONE',  ( 5.082755093536325042, 120.9687500020483952, -5.082755093536325930 ) ) ;
#25136 = CARTESIAN_POINT ( 'NONE',  ( 2.295000000000000373, 272.8559999999997672, 5.415579320911188432 ) ) ;
#25137 = CARTESIAN_POINT ( 'NONE',  ( 2.765530957081996366, 292.1406250017070647, -6.676582343750002480 ) ) ;
#25139 = CARTESIAN_POINT ( 'NONE',  ( -3.464965446656449899, 11.85590772719117503, -0.1959795092987741960 ) ) ;
#25138 = CARTESIAN_POINT ( 'NONE',  ( -11.35316468749999608, 229.1145833367473585, 3.042071309553173730 ) ) ;
#25140 = EDGE_LOOP ( 'NONE', ( #8687, #37467, #25600, #3248 ) ) ;
#25141 = EDGE_CURVE ( 'NONE', #26953, #59338, #33493, .T. ) ;
#25142 = CARTESIAN_POINT ( 'NONE',  ( -11.35316468749999608, 229.4270833367473585, 3.042071309553173730 ) ) ;
#25143 = PRODUCT_DEFINITION_SHAPE ( 'NONE', 'NONE',  #33982 ) ;
#25144 = CARTESIAN_POINT ( 'NONE',  ( 5.082755093536320601, -5.082755093536318824, 3.549052781871751883 ) ) ;
#25145 = LINE ( 'NONE', #48162, #63639 ) ;
#25146 = CARTESIAN_POINT ( 'NONE',  ( 3.458734125000015425, 201.2500000013656063, 196.5673454167823877 ) ) ;
#25147 = VERTEX_POINT ( 'NONE', #17228 ) ;
#25148 = CARTESIAN_POINT ( 'NONE',  ( -3.673940397442060854E-16, 298.8125000034140157, -6.000000000000001776 ) ) ;
#25149 = CARTESIAN_POINT ( 'NONE',  ( -8.000000000000000000, 100.9999999999999858, 0.000000000000000000 ) ) ;
#25150 = CARTESIAN_POINT ( 'NONE',  ( -3.042071309553164404, 97.55208332991932707, -11.35316468749999963 ) ) ;
#25151 = CARTESIAN_POINT ( 'NONE',  ( 2.666560895877943341E-14, -16.44602605510714355, 68.55492853905353456 ) ) ;
#25152 = PRODUCT_DEFINITION ( 'UNKNOWN', '', #64713, #34261 ) ;
#25153 = CARTESIAN_POINT ( 'NONE',  ( 11.00000000000000355, -4.556349186104045046, 75.15624999999998579 ) ) ;
#25156 = CARTESIAN_POINT ( 'NONE',  ( -3.999999999999960032, 201.9375000000000000, 196.3431457505076594 ) ) ;
#25155 = CARTESIAN_POINT ( 'NONE',  ( 31.45873412499998523, 202.7500000013655779, 168.5673454167822172 ) ) ;
#25154 = CARTESIAN_POINT ( 'NONE',  ( 26.56734541678232375, 201.6250000013656063, 173.4587341249998929 ) ) ;
#25157 = VERTEX_POINT ( 'NONE', #56497 ) ;
#25158 = DIRECTION ( 'NONE',  ( 0.000000000000000000, 0.000000000000000000, 1.000000000000000000 ) ) ;
#25159 = CARTESIAN_POINT ( 'NONE',  ( -3.042071309553173730, 214.3229166632526983, 11.35316468749999785 ) ) ;
#25160 = CARTESIAN_POINT ( 'NONE',  ( -1.432654583217664479, 200.7500000013656347, 138.5412658750000787 ) ) ;
#25161 = CARTESIAN_POINT ( 'NONE',  ( 26.56734541678238060, 202.2500000013656063, 166.5412658749999650 ) ) ;
#25162 = EDGE_CURVE ( 'NONE', #19945, #851, #59101, .T. ) ;
#25163 = CARTESIAN_POINT ( 'NONE',  ( -4.556349186104047710, -10.99999999999999822, 115.4687500040967763 ) ) ;
#25164 = CARTESIAN_POINT ( 'NONE',  ( -9.832129032723418760, 188.1770833299193555, -5.676582343750004256 ) ) ;
#25165 = CARTESIAN_POINT ( 'NONE',  ( -7.188101187499999156, 91.62500000204836681, 2.977408999572654924 ) ) ;
#25166 = CARTESIAN_POINT ( 'NONE',  ( -30.82842712474620939, 198.1250000000000284, 167.1715728752542134 ) ) ;
#25167 = CARTESIAN_POINT ( 'NONE',  ( -1.881053915767124440, 12.99999999863440969, 4.541265875000001451 ) ) ;
#25168 = CARTESIAN_POINT ( 'NONE',  ( 28.00000000000002132, 200.1875000013656063, 166.5412658749999082 ) ) ;
#25169 = CARTESIAN_POINT ( 'NONE',  ( 7.188101187499992051, 8.802885111219154394E-16, 4.111552781871752771 ) ) ;
#25170 = CARTESIAN_POINT ( 'NONE',  ( 3.042071309553167069, 86.82291666325265567, -11.35316468749999785 ) ) ;
#25171 = EDGE_LOOP ( 'NONE', ( #35659, #37884, #34925, #45920 ) ) ;
#25172 = EDGE_CURVE ( 'NONE', #27944, #14878, #725, .T. ) ;
#25173 = DIRECTION ( 'NONE',  ( -0.000000000000000000, 1.000000000000000000, -0.000000000000000000 ) ) ;
#25174 = CARTESIAN_POINT ( 'NONE',  ( 2.751064625579944321E-14, 209.7500000000000284, 194.0000000000000568 ) ) ;
#25175 = VERTEX_POINT ( 'NONE', #52319 ) ;
#25176 = CARTESIAN_POINT ( 'NONE',  ( 9.797174393178825657E-16, 125.0000000000000000, -8.000000000000000000 ) ) ;
#25177 = CARTESIAN_POINT ( 'NONE',  ( -27.99999999999999645, 210.0000000000000284, 170.0000000000003695 ) ) ;
#25178 = CARTESIAN_POINT ( 'NONE',  ( 9.832129032723420536, 76.19791666325269830, -5.676582343749999815 ) ) ;
#25179 = VERTEX_POINT ( 'NONE', #50820 ) ;
#25180 = CARTESIAN_POINT ( 'NONE',  ( 7.204075437095966983, 7.204075437095967871, 86.96875000204836681 ) ) ;
#25181 = AXIS2_PLACEMENT_3D ( 'NONE', #29788, #24842, #52798 ) ;
#25182 = CARTESIAN_POINT ( 'NONE',  ( 7.204075437095968759, -7.204075437095966983, 113.2187500020483810 ) ) ;
#25183 = CARTESIAN_POINT ( 'NONE',  ( -4.898587196589412829E-16, 102.1250000000000000, -8.000000000000000000 ) ) ;
#25184 = CARTESIAN_POINT ( 'NONE',  ( 0.000000000000000000, 0.000000000000000000, 30.00000000000000000 ) ) ;
#25186 = CARTESIAN_POINT ( 'NONE',  ( -9.832129032723418760, 67.86458332991935549, -5.676582343750004256 ) ) ;
#25185 = CARTESIAN_POINT ( 'NONE',  ( 5.656854249492379694, 103.6250000040967763, -5.656854249492380582 ) ) ;
#25187 = CARTESIAN_POINT ( 'NONE',  ( -7.999999999999991118, 3.313708498984756723, 23.42405278392015333 ) ) ;
#25188 = CARTESIAN_POINT ( 'NONE',  ( -1.672792093224638288, 194.6518978316833000, 138.7444869999763739 ) ) ;
#25189 = CARTESIAN_POINT ( 'NONE',  ( 5.000000000000001776, 172.7083333265053682, -8.660254037844389075 ) ) ;
#25190 = CARTESIAN_POINT ( 'NONE',  ( -7.188101187500001821, 92.93750000204839523, -2.977408999572650483 ) ) ;
#25191 = CARTESIAN_POINT ( 'NONE',  ( -25.17157282405719343, 195.0000000000000284, 167.1715729264508354 ) ) ;
#25192 = CARTESIAN_POINT ( 'NONE',  ( 9.832129032723420536, 61.51041666325268409, -5.676582343749999815 ) ) ;
#25193 = EDGE_CURVE ( 'NONE', #16792, #74182, #34984, .T. ) ;
#25194 = CARTESIAN_POINT ( 'NONE',  ( 7.204075437095966983, 7.204075437095967871, 106.4687500020483810 ) ) ;
#25195 = CARTESIAN_POINT ( 'NONE',  ( -5.676582343750006032, 189.1145833299193839, 9.832129032723418760 ) ) ;
#25196 = ORIENTED_EDGE ( 'NONE', *, *, #51847, .F. ) ;
#25197 = CARTESIAN_POINT ( 'NONE',  ( 0.000000000000000000, 192.0000000000000284, 170.0000000000000284 ) ) ;
#25198 = CARTESIAN_POINT ( 'NONE',  ( -26.34314575050759544, 199.0625000027312126, 166.0000000000004263 ) ) ;
#25199 = CARTESIAN_POINT ( 'NONE',  ( 5.000000000000000000, 50.64189880742059557, 41.08656465431948845 ) ) ;
#25201 = CARTESIAN_POINT ( 'NONE',  ( -5.676582343750006032, 189.1145833299193839, 9.832129032723418760 ) ) ;
#25200 = CARTESIAN_POINT ( 'NONE',  ( 2.679491924311071749, 263.5416666666666856, -10.00000000000008704 ) ) ;
#25202 = CARTESIAN_POINT ( 'NONE',  ( -1.656854249492363040, 203.3125000000000000, 138.0000000000000000 ) ) ;
#25203 = CARTESIAN_POINT ( 'NONE',  ( -8.660254037844387298, 237.7083333401613174, -4.999999999999999112 ) ) ;
#25204 = CARTESIAN_POINT ( 'NONE',  ( -30.82842712474615965, 200.3750000000000284, 172.8284271247465824 ) ) ;
#25205 = ORIENTED_EDGE ( 'NONE', *, *, #62048, .F. ) ;
#25206 = CARTESIAN_POINT ( 'NONE',  ( 11.35316468750000141, 176.0937499965860411, 0.000000000000000000 ) ) ;
#25207 = CARTESIAN_POINT ( 'NONE',  ( 7.188101187499992051, 2.977408999572647819, 20.33030278187175810 ) ) ;
#25208 = CARTESIAN_POINT ( 'NONE',  ( 4.796365593505123037, 226.0000000000000284, -9.057459967333279849 ) ) ;
#25209 = ORIENTED_EDGE ( 'NONE', *, *, #70627, .F. ) ;
#25210 = CARTESIAN_POINT ( 'NONE',  ( 8.000000000000000000, 99.03125000409677625, -3.313708498984762496 ) ) ;
#25211 = EDGE_CURVE ( 'NONE', #1549, #14809, #68918, .T. ) ;
#25212 = CARTESIAN_POINT ( 'NONE',  ( 7.320508075688774596, 5.624999999999999112, -7.320508075688774596 ) ) ;
#25213 = VECTOR ( 'NONE', #70605, 1000.000000000000000 ) ;
#25214 = EDGE_CURVE ( 'NONE', #4993, #53804, #21402, .T. ) ;
#25215 = CARTESIAN_POINT ( 'NONE',  ( 1.656854249492381248, 16.18750000000000355, -4.000000000000001776 ) ) ;
#25216 = CARTESIAN_POINT ( 'NONE',  ( 4.541265875000002339, 15.31249999863440614, 0.000000000000000000 ) ) ;
#25217 = CARTESIAN_POINT ( 'NONE',  ( 5.656854249492376141, -5.656854249492374365, 16.58030278392014978 ) ) ;
#25218 =( BOUNDED_CURVE ( )  B_SPLINE_CURVE ( 2, ( #27848, #9763, #3725, #16132, #50479, #3348, #32783, #50856, #21064 ),
 .UNSPECIFIED., .F., .F. ) 
 B_SPLINE_CURVE_WITH_KNOTS ( ( 3, 2, 2, 2, 3 ),
 ( 0.8166666666666674290, 0.8250000000000006217, 0.8333333333333340365, 0.8416666666666672292, 0.8500000000000005329 ),
 .UNSPECIFIED. ) 
 CURVE ( )  GEOMETRIC_REPRESENTATION_ITEM ( )  RATIONAL_B_SPLINE_CURVE ( ( 0.9999999999999928946, 0.9238795325112938439, 1.000000000000000000, 0.9238795325112867385, 1.000000000000000000, 0.9238795325112867385, 1.000000000000000000, 0.9238795325112816315, 1.000000000000005107 ) ) 
 REPRESENTATION_ITEM ( '' )  );
#25219 = CYLINDRICAL_SURFACE ( 'NONE', #52331, 3.999999999999986233 ) ;
#25220 = AXIS2_PLACEMENT_3D ( 'NONE', #10460, #38772, #49708 ) ;
#25221 = EDGE_LOOP ( 'NONE', ( #72660, #37206, #9362, #59045 ) ) ;
#25222 = CARTESIAN_POINT ( 'NONE',  ( 4.999999999999999112, -14.70234347858786705, -69.93881661156081009 ) ) ;
#25223 = CARTESIAN_POINT ( 'NONE',  ( 5.082755093536325042, 96.59375000204838102, -5.082755093536325930 ) ) ;
#25225 = CARTESIAN_POINT ( 'NONE',  ( 2.828427124746191623, 6.874999997268813168, -2.828427124746191623 ) ) ;
#25224 = CARTESIAN_POINT ( 'NONE',  ( 7.999999999999998224, 16.21874999590322375, 3.313708498984766049 ) ) ;
#25226 = VERTEX_POINT ( 'NONE', #62140 ) ;
#25227 = DIRECTION ( 'NONE',  ( -1.000000000000000000, 0.000000000000000000, 0.000000000000000000 ) ) ;
#25228 = CARTESIAN_POINT ( 'NONE',  ( 5.082755093536320601, -5.082755093536318824, 18.54905278187175455 ) ) ;
#25229 = ORIENTED_EDGE ( 'NONE', *, *, #49121, .F. ) ;
#25230 = VERTEX_POINT ( 'NONE', #62507 ) ;
#25231 = CARTESIAN_POINT ( 'NONE',  ( 7.204075437095968759, -7.204075437095966983, 83.21875000204836681 ) ) ;
#25232 = DIRECTION ( 'NONE',  ( -0.1513591288559072157, 0.000000000000000000, 0.9884788384745425427 ) ) ;
#25233 = CARTESIAN_POINT ( 'NONE',  ( 11.00000000000000000, 4.556349186104045934, 93.34374999999998579 ) ) ;
#25236 = CARTESIAN_POINT ( 'NONE',  ( 1.226468279477575784E-15, 292.8593750017070079, 6.676582343750001591 ) ) ;
#25235 = CARTESIAN_POINT ( 'NONE',  ( 32.00000000000000711, 202.3125000027312410, 171.6568542494922553 ) ) ;
#25234 = CARTESIAN_POINT ( 'NONE',  ( 12.00000000000000000, 0.000000000000000000, 28.00000000000000000 ) ) ;
#25237 = CARTESIAN_POINT ( 'NONE',  ( 2.679491924311222739, 153.9583333333333428, 10.00000000000000355 ) ) ;
#25238 = CARTESIAN_POINT ( 'NONE',  ( -4.556349186104045934, 11.00000000000000000, 105.9062500040967763 ) ) ;
#25239 = CARTESIAN_POINT ( 'NONE',  ( -10.00000000000000178, 164.3749999931720254, -1.224646799147353454E-15 ) ) ;
#25241 =( BOUNDED_CURVE ( )  B_SPLINE_CURVE ( 2, ( #39763, #33383, #57131, #56384, #11476, #40516, #34511, #28817, #180 ),
 .UNSPECIFIED., .F., .F. ) 
 B_SPLINE_CURVE_WITH_KNOTS ( ( 3, 2, 2, 2, 3 ),
 ( 0.2500000000000001110, 0.2583333333333335258, 0.2666666666666668850, 0.2750000000000002998, 0.2833333333333336590 ),
 .UNSPECIFIED. ) 
 CURVE ( )  GEOMETRIC_REPRESENTATION_ITEM ( )  RATIONAL_B_SPLINE_CURVE ( ( 0.9999999999999990008, 0.9238795325112877377, 1.000000000000000000, 0.9238795325112867385, 1.000000000000000000, 0.9238795325112867385, 1.000000000000000000, 0.9238795325112837409, 1.000000000000003109 ) ) 
 REPRESENTATION_ITEM ( '' )  );
#25240 = CARTESIAN_POINT ( 'NONE',  ( -3.313708498984757611, 7.999999999999991118, 15.54905277982336642 ) ) ;
#25242 = CARTESIAN_POINT ( 'NONE',  ( -3.313708498984760720, 4.781249995903221084, -8.000000000000000000 ) ) ;
#25243 = CARTESIAN_POINT ( 'NONE',  ( 24.54126587499999701, 197.1250000013656347, 168.5673454167822172 ) ) ;
#25244 = CARTESIAN_POINT ( 'NONE',  ( -7.188101187500000044, 9.093749997951611874, -8.802885111219163269E-16 ) ) ;
#25245 = CARTESIAN_POINT ( 'NONE',  ( -7.999999999999991118, 0.000000000000000000, 26.51780278392014623 ) ) ;
#25246 = FACE_OUTER_BOUND ( 'NONE', #67750, .T. ) ;
#25247 = CARTESIAN_POINT ( 'NONE',  ( -5.082755093536324154, 109.7187500020483810, 5.082755093536326818 ) ) ;
#25249 = DIRECTION ( 'NONE',  ( -1.000000000000000000, 0.000000000000000000, 0.000000000000000000 ) ) ;
#25248 = DIRECTION ( 'NONE',  ( -0.000000000000000000, 1.000000000000000000, -0.000000000000000000 ) ) ;
#25250 = CARTESIAN_POINT ( 'NONE',  ( -11.35316468749999608, 234.4270833367473017, 3.042071309553173730 ) ) ;
#25251 = CARTESIAN_POINT ( 'NONE',  ( 24.54126587499999701, 209.4375000013656063, 169.9999999999998863 ) ) ;
#25252 = CARTESIAN_POINT ( 'NONE',  ( -7.188101187499991163, 2.977408999572646930, 19.76780278187175455 ) ) ;
#25253 = CARTESIAN_POINT ( 'NONE',  ( 23.99999999999997513, 195.8125000000000284, 171.6568542494922553 ) ) ;
#25254 = CARTESIAN_POINT ( 'NONE',  ( -11.35316468750000141, 48.28124999658601979, -1.390361679473963753E-15 ) ) ;
#25255 = CARTESIAN_POINT ( 'NONE',  ( 26.34314575050773755, 200.5625000000000284, 165.9999999999998010 ) ) ;
#25256 = CARTESIAN_POINT ( 'NONE',  ( 5.000000000000001776, 2.708333326505365957, -8.660254037844389075 ) ) ;
#25257 = CARTESIAN_POINT ( 'NONE',  ( 31.99999999999998579, 201.4375000027311842, 168.3431457505074889 ) ) ;
#25258 = CARTESIAN_POINT ( 'NONE',  ( 9.999999999999992895, 184.7916666666666572, 2.679491924311234285 ) ) ;
#25259 = VERTEX_POINT ( 'NONE', #10834 ) ;
#25260 = CARTESIAN_POINT ( 'NONE',  ( 10.99999999999986855, 4.556349186104178273, 104.0312500040967905 ) ) ;
#25261 = DIRECTION ( 'NONE',  ( -1.000000000000000000, 1.776356839400250465E-15, 0.000000000000000000 ) ) ;
#25262 = CARTESIAN_POINT ( 'NONE',  ( -8.311093377946841443, 38.90624999658599847, 8.311093377946830785 ) ) ;
#25263 = CARTESIAN_POINT ( 'NONE',  ( 11.00000000000000000, 4.556349186104045934, 89.03125000409677625 ) ) ;
#25264 = CARTESIAN_POINT ( 'NONE',  ( -3.458734125000016757, 204.1250000013656063, 140.5673454167823593 ) ) ;
#25265 = CARTESIAN_POINT ( 'NONE',  ( 26.34314575050770557, 202.5625000000000000, 165.9999999999998579 ) ) ;
#25266 = CARTESIAN_POINT ( 'NONE',  ( -2.751064625579944321E-14, 195.7500000000000000, 146.0000000000000284 ) ) ;
#25268 = CARTESIAN_POINT ( 'NONE',  ( 9.832129032723420536, 31.19791666325268409, -5.676582343749999815 ) ) ;
#25267 = CARTESIAN_POINT ( 'NONE',  ( 7.188101187500000933, 104.0000000020483810, -2.977408999572651371 ) ) ;
#25269 = CARTESIAN_POINT ( 'NONE',  ( 3.313708498984756279, 7.999999999999991118, 12.36155277982336820 ) ) ;
#25270 = CARTESIAN_POINT ( 'NONE',  ( -8.311093377946836114, 142.6562499965860127, -8.311093377946837890 ) ) ;
#25271 = AXIS2_PLACEMENT_3D ( 'NONE', #72104, #49848, #20417 ) ;
#25272 = CARTESIAN_POINT ( 'NONE',  ( -2.679491924311225848, 123.3333333265053540, -10.00000000000000178 ) ) ;
#25273 = CARTESIAN_POINT ( 'NONE',  ( 7.188101187500002709, 111.6875000020483810, 2.977408999572649151 ) ) ;
#25274 = CARTESIAN_POINT ( 'NONE',  ( -25.55430564589119413, 204.5625000013656063, 167.5543056458915316 ) ) ;
#25275 = VERTEX_POINT ( 'NONE', #33869 ) ;
#25276 = CARTESIAN_POINT ( 'NONE',  ( 0.000000000000000000, 300.0000000000000000, 6.000000000000001776 ) ) ;
#25277 = CARTESIAN_POINT ( 'NONE',  ( 6.951808397369818766E-16, 27.34374999658601979, -11.35316468750000141 ) ) ;
#25278 = EDGE_LOOP ( 'NONE', ( #29641, #53008, #31167, #36467 ) ) ;
#25279 = FACE_OUTER_BOUND ( 'NONE', #32273, .T. ) ;
#25280 = FACE_OUTER_BOUND ( 'NONE', #74261, .T. ) ;
#25282 = CARTESIAN_POINT ( 'NONE',  ( 9.832129032723420536, 151.1979166632526983, -5.676582343749999815 ) ) ;
#25281 = CARTESIAN_POINT ( 'NONE',  ( 7.778174593052021635, 7.778174593052023411, 92.12500000409677625 ) ) ;
#25283 = DIRECTION ( 'NONE',  ( -0.8191520442889885789, 1.003171929053520802E-16, 0.5735764363510507113 ) ) ;
#25284 = CARTESIAN_POINT ( 'NONE',  ( 7.999999999999992895, -3.313708498984756279, 15.04280278432982421 ) ) ;
#25285 = CARTESIAN_POINT ( 'NONE',  ( -23.15363648233483218, -24.27661738907943700, 190.6184822510991808 ) ) ;
#25286 = VECTOR ( 'NONE', #17115, 1000.000000000000000 ) ;
#25287 = CARTESIAN_POINT ( 'NONE',  ( 9.832129032723420536, 240.9895833367473301, 5.676582343749996262 ) ) ;
#25288 = CARTESIAN_POINT ( 'NONE',  ( -10.18810118749999916, 4.220049686691934809, 88.93750000204839523 ) ) ;
#25289 = EDGE_LOOP ( 'NONE', ( #68511, #9796 ) ) ;
#25290 = EDGE_CURVE ( 'NONE', #42334, #4853, #16594, .T. ) ;
#25291 = CARTESIAN_POINT ( 'NONE',  ( -10.00000000000000178, 204.3749999931720538, -1.224646799147353454E-15 ) ) ;
#25292 = CARTESIAN_POINT ( 'NONE',  ( 1.102182119232618108E-15, 292.3125000034140157, 6.000000000000001776 ) ) ;
#25293 = CARTESIAN_POINT ( 'NONE',  ( 3.042071309553167069, 107.1354166632526983, -11.35316468749999785 ) ) ;
#25294 = CARTESIAN_POINT ( 'NONE',  ( 10.18810118749999916, 4.220049686691935698, 101.5000000020483810 ) ) ;
#25295 = CARTESIAN_POINT ( 'NONE',  ( 1.881053915767121998, 15.62499999863440614, -4.541265875000002339 ) ) ;
#25296 = VERTEX_POINT ( 'NONE', #11211 ) ;
#25297 = ORIENTED_EDGE ( 'NONE', *, *, #68991, .T. ) ;
#25298 = CARTESIAN_POINT ( 'NONE',  ( 8.000000000000000000, 13.59375000000000178, -3.313708498984761608 ) ) ;
#25299 = CARTESIAN_POINT ( 'NONE',  ( 3.211159895383560947, 4.312499998634407028, 3.211159895383562723 ) ) ;
#25300 = CARTESIAN_POINT ( 'NONE',  ( -7.188101187500002709, 4.312499997951610986, 2.977408999572649151 ) ) ;
#25301 = CARTESIAN_POINT ( 'NONE',  ( -3.313708498984762052, 115.9062500040967763, -8.000000000000000000 ) ) ;
#25302 = EDGE_CURVE ( 'NONE', #73724, #30852, #34694, .T. ) ;
#25303 = CARTESIAN_POINT ( 'NONE',  ( 10.18810118749999916, 1.247682550866122264E-15, 97.28125000204838102 ) ) ;
#25304 = CARTESIAN_POINT ( 'NONE',  ( -7.320508075688778149, 159.9999999931720254, 7.320508075688769267 ) ) ;
#25305 = ADVANCED_FACE ( 'NONE', ( #6669 ), #35353, .F. ) ;
#25306 = CARTESIAN_POINT ( 'NONE',  ( 2.828427124746191623, 3.125000000000000000, -2.828427124746191623 ) ) ;
#25307 = CARTESIAN_POINT ( 'NONE',  ( 4.000000000000000888, 13.68749999726881406, 1.656854249492384135 ) ) ;
#25308 = CARTESIAN_POINT ( 'NONE',  ( -3.211159895383561391, 5.687499998634407028, -3.211159895383561835 ) ) ;
#25309 = CARTESIAN_POINT ( 'NONE',  ( 8.000000000000000000, 95.84374999999998579, -3.313708498984762496 ) ) ;
#25310 = CARTESIAN_POINT ( 'NONE',  ( -2.445694354108782775, 196.5625000013656063, 200.4456943541088663 ) ) ;
#25312 = CARTESIAN_POINT ( 'NONE',  ( -10.00000000000033396, 22.70833333333352044, 2.679491924311311557 ) ) ;
#25311 = CARTESIAN_POINT ( 'NONE',  ( -26.56734541678242678, 201.3750000013656347, 166.5412658750003345 ) ) ;
#25313 = CARTESIAN_POINT ( 'NONE',  ( 1.881053915767121776, 14.49999999863440969, -4.541265875000002339 ) ) ;
#25314 = AXIS2_PLACEMENT_3D ( 'NONE', #29428, #10589, #5677 ) ;
#25315 = CARTESIAN_POINT ( 'NONE',  ( -6.735557395310442023E-16, 11.00000000000000000, 84.62499999999997158 ) ) ;
#25316 = CARTESIAN_POINT ( 'NONE',  ( 2.977408999572650927, -7.188101187499990274, 4.955302781871753659 ) ) ;
#25317 = EDGE_LOOP ( 'NONE', ( #27306, #59364, #5276, #9269 ) ) ;
#25318 = ORIENTED_EDGE ( 'NONE', *, *, #66420, .F. ) ;
#25319 = CARTESIAN_POINT ( 'NONE',  ( -10.18810118749999738, -4.220049686691941915, 97.75000000204838102 ) ) ;
#25320 = CARTESIAN_POINT ( 'NONE',  ( -12.00000000000000000, -6.928203230275527424, -14.00000000000000178 ) ) ;
#25321 = AXIS2_PLACEMENT_3D ( 'NONE', #61555, #55909, #4220 ) ;
#25322 = CARTESIAN_POINT ( 'NONE',  ( -25.55430564589119413, 202.5625000013656063, 167.5543056458915316 ) ) ;
#25323 = CARTESIAN_POINT ( 'NONE',  ( -26.34314575050764518, 200.9375000000000284, 166.0000000000003695 ) ) ;
#25324 = CARTESIAN_POINT ( 'NONE',  ( 2.445694354108838731, 196.0625000013656063, 195.5543056458912190 ) ) ;
#25325 = CARTESIAN_POINT ( 'NONE',  ( -8.000000000000000000, 12.56249999590322197, -9.797174393178825657E-16 ) ) ;
#25326 = CARTESIAN_POINT ( 'NONE',  ( -2.679491924311225848, 101.4583333333333428, -10.00000000000000178 ) ) ;
#25327 = VECTOR ( 'NONE', #14788, 1000.000000000000000 ) ;
#25328 = CARTESIAN_POINT ( 'NONE',  ( -3.313708498984762496, 110.2812499999999858, 7.999999999999998224 ) ) ;
#25329 = CARTESIAN_POINT ( 'NONE',  ( 1.226468279477575784E-15, 295.8593750017070079, 6.676582343750001591 ) ) ;
#25330 = ORIENTED_EDGE ( 'NONE', *, *, #15028, .T. ) ;
#25331 = DIRECTION ( 'NONE',  ( 1.000000000000000000, 0.000000000000000000, 0.000000000000000000 ) ) ;
#25332 = CARTESIAN_POINT ( 'NONE',  ( 3.313708498984762496, 20.53124999590322020, 7.999999999999998224 ) ) ;
#25333 = CARTESIAN_POINT ( 'NONE',  ( -2.839093476692135984E-14, 201.6875000013656063, 138.5412658750000503 ) ) ;
#25334 = CARTESIAN_POINT ( 'NONE',  ( -6.123233995736766282E-16, 236.8750000068279746, -10.00000000000000000 ) ) ;
#25335 = CARTESIAN_POINT ( 'NONE',  ( 8.000000000000001776, 113.8437500040967905, 3.313708498984759387 ) ) ;
#25336 = CARTESIAN_POINT ( 'NONE',  ( 4.999999999999997335, 223.3333333333333144, -8.660254037844387298 ) ) ;
#25337 = CARTESIAN_POINT ( 'NONE',  ( -4.000000000000002665, 3.312499997268814056, 1.656854249492380582 ) ) ;
#25338 = CARTESIAN_POINT ( 'NONE',  ( -11.00000000000000000, 0.000000000000000000, 110.4999999999999858 ) ) ;
#25339 =( BOUNDED_CURVE ( )  B_SPLINE_CURVE ( 2, ( #69256, #51907, #51524, #16807, #33831, #56828, #28888, #5149, #45127 ),
 .UNSPECIFIED., .F., .F. ) 
 B_SPLINE_CURVE_WITH_KNOTS ( ( 3, 2, 2, 2, 3 ),
 ( 0.000000000000000000, 0.006618275584456850824, 0.01323655116891370165, 0.01985482675337055247, 0.02647310233782740330 ),
 .UNSPECIFIED. ) 
 CURVE ( )  GEOMETRIC_REPRESENTATION_ITEM ( )  RATIONAL_B_SPLINE_CURVE ( ( 1.000000000000000000, 0.9238795325112867385, 1.000000000000000000, 0.9238795325112867385, 1.000000000000000000, 0.9238795325112867385, 1.000000000000000000, 0.9238795325112849621, 1.000000000000001776 ) ) 
 REPRESENTATION_ITEM ( '' )  );
#25340 = CARTESIAN_POINT ( 'NONE',  ( 2.679491924311222739, 218.9583333333333428, 10.00000000000000355 ) ) ;
#25341 = CARTESIAN_POINT ( 'NONE',  ( 7.188101187499992051, 8.802885111219154394E-16, 7.111552781871754547 ) ) ;
#25342 = CARTESIAN_POINT ( 'NONE',  ( 8.311093377946834337, 190.4687499965860411, 8.311093377946839666 ) ) ;
#25343 = CARTESIAN_POINT ( 'NONE',  ( 2.679491924311228956, 192.9166666598387110, -10.00000000000000000 ) ) ;
#25344 = CARTESIAN_POINT ( 'NONE',  ( 1.881053915767122664, 2.124999998634406584, 4.541265875000001451 ) ) ;
#25345 = CARTESIAN_POINT ( 'NONE',  ( -2.751064625579944321E-14, 198.8750000027312126, 146.0000000000000284 ) ) ;
#25347 = FACE_OUTER_BOUND ( 'NONE', #51893, .T. ) ;
#25346 = CARTESIAN_POINT ( 'NONE',  ( 11.00000000000000000, 1.347111479062088405E-15, 118.0000000000000000 ) ) ;
#25348 = ORIENTED_EDGE ( 'NONE', *, *, #38985, .T. ) ;
#25349 = CARTESIAN_POINT ( 'NONE',  ( 1.432654583217608080, 203.8750000013656063, 138.5412658750000503 ) ) ;
#25350 = CARTESIAN_POINT ( 'NONE',  ( -9.832129032723420536, 49.01041666325269119, 5.676582343749997150 ) ) ;
#25351 = CARTESIAN_POINT ( 'NONE',  ( 7.778174593052023411, -7.778174593052021635, 102.2500000040967763 ) ) ;
#25352 = CARTESIAN_POINT ( 'NONE',  ( -8.311093377946841443, 224.2187499965860411, 8.311093377946830785 ) ) ;
#25353 = CARTESIAN_POINT ( 'NONE',  ( -31.45873412499996391, 201.7500000013655779, 171.4326545832181239 ) ) ;
#25354 = CARTESIAN_POINT ( 'NONE',  ( -10.00000000000000000, 124.1666666598387110, -2.679491924311229845 ) ) ;
#25356 = LINE ( 'NONE', #72517, #37835 ) ;
#25355 = CARTESIAN_POINT ( 'NONE',  ( -7.188101187499999156, 122.7500000020483668, 2.977408999572654924 ) ) ;
#25357 = CARTESIAN_POINT ( 'NONE',  ( -4.556349186104045934, 11.00000000000000000, 87.71874999999998579 ) ) ;
#25358 = VECTOR ( 'NONE', #2906, 1000.000000000000000 ) ;
#25359 = CARTESIAN_POINT ( 'NONE',  ( 9.832129032723420536, 111.1979166632526983, -5.676582343749999815 ) ) ;
#25360 = CARTESIAN_POINT ( 'NONE',  ( -10.00000000000000178, 84.37499999317203958, -1.224646799147353454E-15 ) ) ;
#25361 = CARTESIAN_POINT ( 'NONE',  ( 5.082755093536325042, 90.59375000204838102, -5.082755093536325930 ) ) ;
#25362 = CARTESIAN_POINT ( 'NONE',  ( -1.881053915767121554, 14.74999999863440969, -4.541265875000002339 ) ) ;
#25363 = CARTESIAN_POINT ( 'NONE',  ( 0.000000000000000000, 125.0000000000000000, 8.000000000000000000 ) ) ;
#25364 = CARTESIAN_POINT ( 'NONE',  ( 5.656854249492376141, -5.656854249492374365, 1.392802779823364201 ) ) ;
#25365 = EDGE_LOOP ( 'NONE', ( #21059, #11254, #1969, #27977 ) ) ;
#25366 = ORIENTED_EDGE ( 'NONE', *, *, #48717, .F. ) ;
#25367 =( BOUNDED_CURVE ( )  B_SPLINE_CURVE ( 2, ( #65568, #20661, #49717, #38031, #38405, #37660, #54268, #37284, #71964 ),
 .UNSPECIFIED., .F., .F. ) 
 B_SPLINE_CURVE_WITH_KNOTS ( ( 3, 2, 2, 2, 3 ),
 ( 0.1250000000000000000, 0.1306818181818181768, 0.1363636363636363535, 0.1420454545454545581, 0.1477272727272727348 ),
 .UNSPECIFIED. ) 
 CURVE ( )  GEOMETRIC_REPRESENTATION_ITEM ( )  RATIONAL_B_SPLINE_CURVE ( ( 1.000000000000000000, 0.9238795325112867385, 1.000000000000000000, 0.9238795325112867385, 1.000000000000000000, 0.9238795325112867385, 1.000000000000000000, 0.9238795325112867385, 1.000000000000000000 ) ) 
 REPRESENTATION_ITEM ( '' )  );
#25368 = CARTESIAN_POINT ( 'NONE',  ( -6.676582343750003368, 295.5468750017069510, -2.765530957081996810 ) ) ;
#25369 =( NAMED_UNIT ( * ) SI_UNIT ( $, .STERADIAN. ) SOLID_ANGLE_UNIT ( ) );
#25370 = CARTESIAN_POINT ( 'NONE',  ( -9.832129032723418760, 172.8645833299193555, -5.676582343750004256 ) ) ;
#25371 = CARTESIAN_POINT ( 'NONE',  ( 7.999999999999991118, 9.797174393178815797E-16, 9.080302779823364645 ) ) ;
#25372 = CARTESIAN_POINT ( 'NONE',  ( 2.751064625579944321E-14, 199.7500000000000000, 194.0000000000000568 ) ) ;
#25373 = CARTESIAN_POINT ( 'NONE',  ( -29.65685424949234772, 201.0625000000000568, 166.0000000000003126 ) ) ;
#25374 = CARTESIAN_POINT ( 'NONE',  ( -10.18810118749999916, 0.000000000000000000, 108.5312500020483810 ) ) ;
#25375 = ORIENTED_EDGE ( 'NONE', *, *, #35168, .F. ) ;
#25376 = AXIS2_PLACEMENT_3D ( 'NONE', #15871, #4574, #27572 ) ;
#25377 = CARTESIAN_POINT ( 'NONE',  ( 2.591411123053213750, 50.09422832877228871, -40.78779037274974684 ) ) ;
#25378 = FACE_OUTER_BOUND ( 'NONE', #37357, .T. ) ;
#25379 = CARTESIAN_POINT ( 'NONE',  ( 8.311093377946834337, 140.4687499965859843, 8.311093377946839666 ) ) ;
#25380 = CARTESIAN_POINT ( 'NONE',  ( 1.656854249492401232, 206.4375000027311842, 202.0000000000000000 ) ) ;
#25381 = CARTESIAN_POINT ( 'NONE',  ( -3.458734124999959469, 208.7500000013656063, 199.4326545832176976 ) ) ;
#25382 = CARTESIAN_POINT ( 'NONE',  ( -10.18810118749999738, -4.220049686691941915, 72.62500000204836681 ) ) ;
#25383 = CARTESIAN_POINT ( 'NONE',  ( 3.042071309553167069, 67.13541666325266988, -11.35316468749999785 ) ) ;
#25384 = ORIENTED_EDGE ( 'NONE', *, *, #59047, .T. ) ;
#25385 = DIRECTION ( 'NONE',  ( -1.000000000000000000, 0.000000000000000000, -0.000000000000000000 ) ) ;
#25386 = CARTESIAN_POINT ( 'NONE',  ( 2.780723358947928197E-16, 6.687499998634407028, -4.541265875000002339 ) ) ;
#25387 = CARTESIAN_POINT ( 'NONE',  ( -5.662595241051935346, 5.662595241051935346, 6.825615283940628331 ) ) ;
#25388 = UNCERTAINTY_MEASURE_WITH_UNIT (LENGTH_MEASURE( 1.000000000000000082E-05 ), #34272, 'distance_accuracy_value', 'NONE');
#25389 = ORIENTED_EDGE ( 'NONE', *, *, #31352, .T. ) ;
#25390 = EDGE_CURVE ( 'NONE', #493, #47140, #62371, .T. ) ;
#25391 = CARTESIAN_POINT ( 'NONE',  ( 2.977408999572650927, 21.74999999795162253, -7.188101187500001821 ) ) ;
#25392 = CARTESIAN_POINT ( 'NONE',  ( -6.000000000000003553, 294.0000000034140726, -2.485281374238571317 ) ) ;
#25393 = AXIS2_PLACEMENT_3D ( 'NONE', #53134, #42157, #1467 ) ;
#25394 = CARTESIAN_POINT ( 'NONE',  ( 0.3346513822855006759, 219.9760043661977420, 11.00000000000000000 ) ) ;
#25395 = CARTESIAN_POINT ( 'NONE',  ( 2.977408999572650927, 13.12499999795161187, -7.188101187500001821 ) ) ;
#25396 = CARTESIAN_POINT ( 'NONE',  ( 7.188101187499993827, -2.977408999572645598, 0.6428027818717527708 ) ) ;
#25397 = CARTESIAN_POINT ( 'NONE',  ( 10.18810118749999916, 1.247682550866122264E-15, 115.2812500020483810 ) ) ;
#25398 = CARTESIAN_POINT ( 'NONE',  ( -10.50000000000000000, 1.285879139104720831E-15, -1.050311307314560239 ) ) ;
#25399 = CARTESIAN_POINT ( 'NONE',  ( -2.828427124746190735, 4.124999997268813168, -2.828427124746191623 ) ) ;
#25400 = VECTOR ( 'NONE', #66464, 1000.000000000000000 ) ;
#25401 = ORIENTED_EDGE ( 'NONE', *, *, #6176, .T. ) ;
#25402 = CARTESIAN_POINT ( 'NONE',  ( -1.432654583217607192, 205.2500000013655779, 194.5412658750000219 ) ) ;
#25403 = EDGE_CURVE ( 'NONE', #55117, #2727, #12988, .T. ) ;
#25404 = CARTESIAN_POINT ( 'NONE',  ( -2.751064625579944321E-14, 201.7500000000000000, 146.0000000000000284 ) ) ;
#25405 = CARTESIAN_POINT ( 'NONE',  ( -30.82842712474624491, 199.2500000027312126, 167.1715728752542418 ) ) ;
#25406 = CARTESIAN_POINT ( 'NONE',  ( -8.342170076843785083E-16, 3.062499998634406584, 4.541265875000002339 ) ) ;
#25407 = CARTESIAN_POINT ( 'NONE',  ( -2.977408999572651815, 110.9375000020483810, 7.188101187500000933 ) ) ;
#25408 = CARTESIAN_POINT ( 'NONE',  ( -2.485281374238927032, 294.8125000000000000, -5.999999999999647393 ) ) ;
#25409 = CARTESIAN_POINT ( 'NONE',  ( 5.082755093536318824, 5.082755093536319713, 27.92405278187175455 ) ) ;
#25410 = ORIENTED_EDGE ( 'NONE', *, *, #32745, .T. ) ;
#25411 = CARTESIAN_POINT ( 'NONE',  ( 4.401442555609581635E-16, 21.84374999795161543, -7.188101187500000044 ) ) ;
#25412 = EDGE_LOOP ( 'NONE', ( #52129, #14306, #13415, #5926 ) ) ;
#25413 = CARTESIAN_POINT ( 'NONE',  ( -3.458734124999959914, 207.4375000013656063, 198.0000000000000284 ) ) ;
#25414 = CARTESIAN_POINT ( 'NONE',  ( 26.56734541678237704, 203.3750000013656063, 173.4587341249998929 ) ) ;
#25415 = CARTESIAN_POINT ( 'NONE',  ( 2.679491924311222739, 58.95833333333332149, 10.00000000000000355 ) ) ;
#25416 = VECTOR ( 'NONE', #69389, 1000.000000000000227 ) ;
#25417 = CARTESIAN_POINT ( 'NONE',  ( 2.977408999572650039, 94.06250000204838102, -7.188101187500001821 ) ) ;
#25418 = CARTESIAN_POINT ( 'NONE',  ( 4.242640687119287435, 296.3750000000000000, 4.242640687119285658 ) ) ;
#25420 = CARTESIAN_POINT ( 'NONE',  ( -21.94909796891680287, -38.27482514980722073, 191.8966109145765415 ) ) ;
#25419 = CARTESIAN_POINT ( 'NONE',  ( 26.34314575050758833, 208.6875000027312126, 165.9999999999998863 ) ) ;
#25421 = ORIENTED_EDGE ( 'NONE', *, *, #7633, .F. ) ;
#25422 = CARTESIAN_POINT ( 'NONE',  ( 11.35316468749999608, 226.6145833367473301, -3.042071309553167069 ) ) ;
#25423 = CARTESIAN_POINT ( 'NONE',  ( 3.999999999999960032, 199.1250000027312126, 142.0000000000000568 ) ) ;
#25424 = CARTESIAN_POINT ( 'NONE',  ( -11.00000000000000000, 0.000000000000000000, 74.68750000409676204 ) ) ;
#25425 = CARTESIAN_POINT ( 'NONE',  ( 7.999999999999991118, 9.797174393178815797E-16, 1.767802783920142895 ) ) ;
#25426 = CARTESIAN_POINT ( 'NONE',  ( 24.46046022537912279, 194.8779416066606984, 168.4043623937020868 ) ) ;
#25427 = DIRECTION ( 'NONE',  ( -0.000000000000000000, -1.000000000000000000, -0.000000000000000000 ) ) ;
#25428 = CARTESIAN_POINT ( 'NONE',  ( -10.00000000000000355, 177.7083333333333428, 2.679491924311223183 ) ) ;
#25429 = DIRECTION ( 'NONE',  ( 0.000000000000000000, -1.000000000000000000, -0.000000000000000000 ) ) ;
#25430 = CARTESIAN_POINT ( 'NONE',  ( 2.679491924311168560, 241.6666666734946602, -10.00000000000003375 ) ) ;
#25431 = CARTESIAN_POINT ( 'NONE',  ( -5.082755093536317936, -5.082755093536320601, 27.54905278187175455 ) ) ;
#25432 = CARTESIAN_POINT ( 'NONE',  ( -5.676582343750006032, 154.4270833299193555, 9.832129032723418760 ) ) ;
#25433 = CARTESIAN_POINT ( 'NONE',  ( 7.778174593052021635, 7.778174593052023411, 75.62500000409677625 ) ) ;
#25434 = CARTESIAN_POINT ( 'NONE',  ( 54.00000000000000000, 272.0000000000000000, 4.085831468968142743E-14 ) ) ;
#25436 = CARTESIAN_POINT ( 'NONE',  ( -6.000000000000001776, 294.0000000000000000, 0.000000000000000000 ) ) ;
#25435 = CARTESIAN_POINT ( 'NONE',  ( 30.82842712474620228, 204.3750000000000284, 167.1715728752537586 ) ) ;
#25437 = ORIENTED_EDGE ( 'NONE', *, *, #40888, .F. ) ;
#25438 = CARTESIAN_POINT ( 'NONE',  ( 11.35316468749999785, 15.88541666325268586, 3.042071309553174174 ) ) ;
#25439 = AXIS2_PLACEMENT_3D ( 'NONE', #548, #36711, #70665 ) ;
#25440 = CARTESIAN_POINT ( 'NONE',  ( 27.99999999999996447, 197.6250000027312126, 165.9999999999998863 ) ) ;
#25441 = CARTESIAN_POINT ( 'NONE',  ( 3.734423912254536848, -10.10901040137823514, -70.68514270129527688 ) ) ;
#25442 = CARTESIAN_POINT ( 'NONE',  ( -11.00000000000000000, 0.000000000000000000, 78.99999999999998579 ) ) ;
#25443 = CARTESIAN_POINT ( 'NONE',  ( -3.458734125000015425, 205.9375000013656063, 142.0000000000000568 ) ) ;
#25444 = CARTESIAN_POINT ( 'NONE',  ( -1.656854249492478948, 202.6875000000000568, 146.0000000000000000 ) ) ;
#25445 = CARTESIAN_POINT ( 'NONE',  ( 10.00000000000000178, 37.08333332650536107, -2.679491924311226736 ) ) ;
#25446 =( GEOMETRIC_REPRESENTATION_CONTEXT ( 3 ) GLOBAL_UNCERTAINTY_ASSIGNED_CONTEXT ( ( #52880 ) ) GLOBAL_UNIT_ASSIGNED_CONTEXT ( ( #11761, #29488, #836 ) ) REPRESENTATION_CONTEXT ( 'NONE', 'WORKASPACE' ) );
#25447 = CARTESIAN_POINT ( 'NONE',  ( 5.082755093536326818, 109.7187500020483810, 5.082755093536325042 ) ) ;
#25448 = CARTESIAN_POINT ( 'NONE',  ( 2.780723358947928197E-16, 3.687499998634407472, -4.541265875000002339 ) ) ;
#25449 = CARTESIAN_POINT ( 'NONE',  ( 0.8912353796323385646, 67.61603573606910800, -20.05324848891999068 ) ) ;
#25450 = CARTESIAN_POINT ( 'NONE',  ( -7.999999999999991118, 3.313708498984756723, 15.73655277982336642 ) ) ;
#25452 = DIRECTION ( 'NONE',  ( -0.000000000000000000, 1.000000000000000000, -0.000000000000000000 ) ) ;
#25451 = DIRECTION ( 'NONE',  ( 0.000000000000000000, 0.000000000000000000, 1.000000000000000000 ) ) ;
#25453 = ORIENTED_EDGE ( 'NONE', *, *, #47816, .T. ) ;
#25454 = CARTESIAN_POINT ( 'NONE',  ( 8.000000000000001776, 92.84375000409677625, 3.313708498984759387 ) ) ;
#25455 = AXIS2_PLACEMENT_3D ( 'NONE', #58514, #42891, #66659 ) ;
#25456 = CARTESIAN_POINT ( 'NONE',  ( -11.00000000000021139, 4.556349186103834548, 82.09375000409677625 ) ) ;
#25457 = CARTESIAN_POINT ( 'NONE',  ( 11.35316468749999963, 231.5104166700806445, 3.042071309553159519 ) ) ;
#25458 = CARTESIAN_POINT ( 'NONE',  ( 6.951808397369818766E-16, 132.0312499965860127, -11.35316468750000141 ) ) ;
#25459 = ORIENTED_EDGE ( 'NONE', *, *, #14309, .T. ) ;
#25460 = CARTESIAN_POINT ( 'NONE',  ( 3.090148520752590944, 225.9998984954551418, -9.510618362637927703 ) ) ;
#25461 = CARTESIAN_POINT ( 'NONE',  ( 10.18810118749999916, 1.247682550866122264E-15, 93.90625000204836681 ) ) ;
#25462 = LINE ( 'NONE', #8495, #16407 ) ;
#25463 = CARTESIAN_POINT ( 'NONE',  ( -2.445694354108783219, 194.8125000013656063, 200.4456943541088663 ) ) ;
#25464 = CARTESIAN_POINT ( 'NONE',  ( -5.656854249492375253, 5.656854249492375253, 27.64280277982336642 ) ) ;
#25466 = CARTESIAN_POINT ( 'NONE',  ( -5.676582343749998039, 112.4479166632526983, -9.832129032723420536 ) ) ;
#25465 = CARTESIAN_POINT ( 'NONE',  ( 25.17157287525377996, 197.8750000000000284, 172.8284271247460424 ) ) ;
#25467 = CARTESIAN_POINT ( 'NONE',  ( -23.99999999999997868, 209.6875000000000284, 171.6568542494927385 ) ) ;
#25468 = CARTESIAN_POINT ( 'NONE',  ( 10.00000000000000000, 81.66666665983869677, 2.679491924311235618 ) ) ;
#25469 = ORIENTED_EDGE ( 'NONE', *, *, #21054, .T. ) ;
#25470 =( BOUNDED_CURVE ( )  B_SPLINE_CURVE ( 2, ( #17813, #47216, #41929, #57829, #860, #23846, #6869, #29141, #18923 ),
 .UNSPECIFIED., .F., .F. ) 
 B_SPLINE_CURVE_WITH_KNOTS ( ( 3, 2, 2, 2, 3 ),
 ( 0.5294620445568896105, 0.5360803223410017804, 0.5426985979254586034, 0.5493168735099153155, 0.5559351258181921551 ),
 .UNSPECIFIED. ) 
 CURVE ( )  GEOMETRIC_REPRESENTATION_ITEM ( )  RATIONAL_B_SPLINE_CURVE ( ( 1.000000000000000000, 0.9238795325112867385, 1.000000000000000000, 0.9238795325112867385, 1.000000000000000000, 0.9238795325112867385, 1.000000000000000000, 0.9238798002235764084, 0.9999994645773038204 ) ) 
 REPRESENTATION_ITEM ( '' )  );
#25471 = CARTESIAN_POINT ( 'NONE',  ( -38.00000000000000000, -63.00000000000000000, 15.00000000000000178 ) ) ;
#25472 = CARTESIAN_POINT ( 'NONE',  ( 11.35316468750000141, 106.0937499965860269, 0.000000000000000000 ) ) ;
#25473 = CARTESIAN_POINT ( 'NONE',  ( -1.432654583217607192, 206.2500000013655779, 194.5412658750000219 ) ) ;
#25474 = CARTESIAN_POINT ( 'NONE',  ( -7.188101187500000044, 13.59374999795161187, -8.802885111219163269E-16 ) ) ;
#25475 = CARTESIAN_POINT ( 'NONE',  ( 7.204075437095968759, -7.204075437095966983, 88.09375000204836681 ) ) ;
#25476 = CARTESIAN_POINT ( 'NONE',  ( -3.042071309553173730, 19.63541666325268764, 11.35316468749999785 ) ) ;
#25477 = ORIENTED_EDGE ( 'NONE', *, *, #9942, .F. ) ;
#25478 = DIRECTION ( 'NONE',  ( 1.000000000000000000, 0.000000000000000000, 0.000000000000000000 ) ) ;
#25479 = CARTESIAN_POINT ( 'NONE',  ( 8.008118988124991233, 3.317071493978879015, 24.35686528394063188 ) ) ;
#25480 = CARTESIAN_POINT ( 'NONE',  ( 2.679491924311222739, 115.8333333265053682, 10.00000000000000355 ) ) ;
#25481 = CARTESIAN_POINT ( 'NONE',  ( 4.220049686691934809, 10.18810118749999916, 76.56250000204836681 ) ) ;
#25482 = VECTOR ( 'NONE', #30847, 1000.000000000000000 ) ;
#25483 = EDGE_CURVE ( 'NONE', #65546, #49924, #3123, .T. ) ;
#25484 = CARTESIAN_POINT ( 'NONE',  ( 9.797174393178825657E-16, 125.0000000000000000, -8.000000000000000000 ) ) ;
#25485 = CARTESIAN_POINT ( 'NONE',  ( -8.660254037844390851, 149.7916666598387110, 4.999999999999998224 ) ) ;
#25486 = CARTESIAN_POINT ( 'NONE',  ( -6.676582343750003368, 294.3906250017070079, -2.765530957081996810 ) ) ;
#25487 = CARTESIAN_POINT ( 'NONE',  ( -4.000000000000015987, 199.5625000000000568, 143.6568542494924259 ) ) ;
#25488 = CARTESIAN_POINT ( 'NONE',  ( 9.832129032723416984, 220.6770833299193555, 5.676582343750006032 ) ) ;
#25489 = ADVANCED_FACE ( 'NONE', ( #29672 ), #36446, .T. ) ;
#25490 = CARTESIAN_POINT ( 'NONE',  ( -8.311093377946841443, 134.2187499965860411, 8.311093377946830785 ) ) ;
#25491 = CARTESIAN_POINT ( 'NONE',  ( -7.204075437095967871, 7.204075437095967871, 83.96875000204836681 ) ) ;
#25492 = CARTESIAN_POINT ( 'NONE',  ( -31.45873412499997812, 198.7500000013656063, 171.4326545832180386 ) ) ;
#25493 = CARTESIAN_POINT ( 'NONE',  ( -1.469576158976823947E-15, 23.62500000000000355, 8.000000000000000000 ) ) ;
#25494 = CARTESIAN_POINT ( 'NONE',  ( -4.541265875000003227, 11.99999999863440969, 1.881053915767121110 ) ) ;
#25495 = ORIENTED_EDGE ( 'NONE', *, *, #17332, .T. ) ;
#25496 = CARTESIAN_POINT ( 'NONE',  ( -3.999999999999959144, 208.1875000027311842, 199.6568542494924259 ) ) ;
#25497 = EDGE_CURVE ( 'NONE', #13736, #23491, #7963, .T. ) ;
#25498 = CARTESIAN_POINT ( 'NONE',  ( -2.445694354108840063, 197.0625000013656063, 139.5543056458912190 ) ) ;
#25499 = CARTESIAN_POINT ( 'NONE',  ( 2.828427124746153876, 205.0000000027312126, 144.8284271247462129 ) ) ;
#25500 = AXIS2_PLACEMENT_3D ( 'NONE', #6408, #51671, #46009 ) ;
#25501 = CARTESIAN_POINT ( 'NONE',  ( -2.679491924311399043, 171.4583333333333428, -10.00000000000001421 ) ) ;
#25502 = CARTESIAN_POINT ( 'NONE',  ( 1.871523826299183495E-15, -10.18810118749999916, 69.90625000204836681 ) ) ;
#25503 = ORIENTED_EDGE ( 'NONE', *, *, #61971, .T. ) ;
#25504 = CARTESIAN_POINT ( 'NONE',  ( -5.082755093536326818, 5.906249997951610986, 5.082755093536325042 ) ) ;
#25505 = CARTESIAN_POINT ( 'NONE',  ( 5.656854249492376141, -5.656854249492374365, 9.080302783920146226 ) ) ;
#25506 = SPHERICAL_SURFACE ( 'NONE', #36642, 10.00000000000001243 ) ;
#25507 = CARTESIAN_POINT ( 'NONE',  ( 5.082755093536325042, 117.9687500020483810, -5.082755093536325930 ) ) ;
#25508 = CARTESIAN_POINT ( 'NONE',  ( 1.377000000000000002, 255.7199999999997715, 5.684453117602858541 ) ) ;
#25509 = CARTESIAN_POINT ( 'NONE',  ( 4.721056650415999201, 294.0781250017069510, -4.721056650415999201 ) ) ;
#25511 = CARTESIAN_POINT ( 'NONE',  ( -6.062599403785866592, -5.219663636056774081, 0.8834915628530353171 ) ) ;
#25510 = CARTESIAN_POINT ( 'NONE',  ( 11.35316468749999963, 221.4062500034139873, -1.390361679473963556E-15 ) ) ;
#25512 = ORIENTED_EDGE ( 'NONE', *, *, #17047, .T. ) ;
#25513 = CARTESIAN_POINT ( 'NONE',  ( 11.35316468749999963, 231.5104166700806445, 3.042071309553159519 ) ) ;
#25514 = EDGE_CURVE ( 'NONE', #9276, #22486, #64822, .T. ) ;
#25515 = CARTESIAN_POINT ( 'NONE',  ( 2.977408999572646486, 7.188101187499991163, 2.517802781871750550 ) ) ;
#25516 = CARTESIAN_POINT ( 'NONE',  ( 7.320508075688771044, 166.2499999931720538, 7.320508075688775484 ) ) ;
#25517 = CARTESIAN_POINT ( 'NONE',  ( -11.00000000000000000, 0.000000000000000000, 118.0000000000000000 ) ) ;
#25518 = CARTESIAN_POINT ( 'NONE',  ( 3.458734125000015869, 200.1875000013656063, 198.0000000000000284 ) ) ;
#25519 = VERTEX_POINT ( 'NONE', #59458 ) ;
#25520 = CARTESIAN_POINT ( 'NONE',  ( -6.000000000000001776, 287.5312500017070079, 0.000000000000000000 ) ) ;
#25521 = CARTESIAN_POINT ( 'NONE',  ( 1.469576158976823947E-15, 99.87499999999998579, 8.000000000000000000 ) ) ;
#25522 = CARTESIAN_POINT ( 'NONE',  ( 5.676582343749993598, 100.2604166632526841, 9.832129032723422313 ) ) ;
#25523 = CARTESIAN_POINT ( 'NONE',  ( -3.999999999999960032, 209.0000000000000284, 198.0000000000000284 ) ) ;
#25524 = CARTESIAN_POINT ( 'NONE',  ( 4.556349186104045934, 11.00000000000000000, 78.53124999999998579 ) ) ;
#25527 = CARTESIAN_POINT ( 'NONE',  ( -29.65685424949237614, 205.4375000000000284, 174.0000000000003695 ) ) ;
#25526 = CARTESIAN_POINT ( 'NONE',  ( 29.43265458321761230, 204.8750000013656063, 166.5412658749999650 ) ) ;
#25525 = CARTESIAN_POINT ( 'NONE',  ( 27.99999999999996447, 201.6875000013656063, 173.4587341249998929 ) ) ;
#25528 = ORIENTED_EDGE ( 'NONE', *, *, #54111, .T. ) ;
#25529 = VECTOR ( 'NONE', #7756, 1000.000000000000000 ) ;
#25530 = CARTESIAN_POINT ( 'NONE',  ( -9.832129032723420536, 213.6979166632526983, 5.676582343749997150 ) ) ;
#25531 = CARTESIAN_POINT ( 'NONE',  ( 3.458734124999959025, 202.5000000013656063, 140.5673454167824161 ) ) ;
#25532 = CARTESIAN_POINT ( 'NONE',  ( 31.45873412499999944, 201.9375000013656063, 169.9999999999999432 ) ) ;
#25533 = CARTESIAN_POINT ( 'NONE',  ( -7.188101187500000044, 27.09374999795161898, -8.802885111219163269E-16 ) ) ;
#25534 = CARTESIAN_POINT ( 'NONE',  ( 8.311093377946834337, 190.4687499965860411, 8.311093377946839666 ) ) ;
#25535 = CARTESIAN_POINT ( 'NONE',  ( -7.188101187500000044, 90.03125000204838102, 0.000000000000000000 ) ) ;
#25536 = CARTESIAN_POINT ( 'NONE',  ( 0.000000000000000000, 0.000000000000000000, 0.000000000000000000 ) ) ;
#25537 = CARTESIAN_POINT ( 'NONE',  ( 1.881053915767122664, 15.12499999863441147, 4.541265875000001451 ) ) ;
#25538 = CARTESIAN_POINT ( 'NONE',  ( 27.99999999999996447, 200.6875000013656063, 173.4587341249998929 ) ) ;
#25539 = CARTESIAN_POINT ( 'NONE',  ( 2.977408999572646486, 7.188101187499991163, 1.392802781871753437 ) ) ;
#25540 = FACE_OUTER_BOUND ( 'NONE', #20673, .T. ) ;
#25541 = CARTESIAN_POINT ( 'NONE',  ( -9.832129032723418760, 77.86458332991935549, -5.676582343750004256 ) ) ;
#25542 = ORIENTED_EDGE ( 'NONE', *, *, #5237, .T. ) ;
#25543 = CARTESIAN_POINT ( 'NONE',  ( -5.000000000000000888, -53.32026166094896524, 44.27875806161925709 ) ) ;
#25544 = CARTESIAN_POINT ( 'NONE',  ( -1.836970198721029983E-15, 105.6249999931720396, 10.00000000000000178 ) ) ;
#25545 = CARTESIAN_POINT ( 'NONE',  ( -5.656854249492379694, 9.374999995903223748, -5.656854249492380582 ) ) ;
#25546 = CYLINDRICAL_SURFACE ( 'NONE', #72605, 3.999999999999976019 ) ;
#25547 = CARTESIAN_POINT ( 'NONE',  ( 9.832129032723420536, 86.19791666325268409, -5.676582343749999815 ) ) ;
#25548 = VERTEX_POINT ( 'NONE', #41367 ) ;
#25549 = CARTESIAN_POINT ( 'NONE',  ( 7.204075437095968759, -7.204075437095966983, 86.59375000204836681 ) ) ;
#25550 = CARTESIAN_POINT ( 'NONE',  ( -7.204075437095967871, 7.204075437095967871, 110.9687500020483810 ) ) ;
#25551 = CARTESIAN_POINT ( 'NONE',  ( 3.458734125000015869, 207.1875000013656063, 198.0000000000000284 ) ) ;
#25552 = CARTESIAN_POINT ( 'NONE',  ( 10.00000000000003375, 75.20833333333334281, -2.679491924311235618 ) ) ;
#25554 = CARTESIAN_POINT ( 'NONE',  ( -9.832129032723420536, 73.69791666325268409, 5.676582343749997150 ) ) ;
#25553 = DIRECTION ( 'NONE',  ( -0.000000000000000000, -1.000000000000000000, -4.283267841918042741E-17 ) ) ;
#25555 = CARTESIAN_POINT ( 'NONE',  ( -7.999999999999991118, 3.313708498984756723, 21.92405278392015333 ) ) ;
#25556 = CARTESIAN_POINT ( 'NONE',  ( -1.216591630144965963, 194.6379550352074546, 138.5627246035448366 ) ) ;
#25557 = CARTESIAN_POINT ( 'NONE',  ( -10.00000000000000355, 164.5833333265053682, 2.679491924311223183 ) ) ;
#25558 = CARTESIAN_POINT ( 'NONE',  ( -7.188101187499999156, 93.12500000204836681, 2.977408999572654924 ) ) ;
#25559 = AXIS2_PLACEMENT_3D ( 'NONE', #68616, #50888, #38838 ) ;
#25560 = CARTESIAN_POINT ( 'NONE',  ( -24.90605898815371688, 194.9908001228991736, 167.4500973631702436 ) ) ;
#25561 = CARTESIAN_POINT ( 'NONE',  ( -3.042071309553163960, 67.55208332991935549, -11.35316468749999963 ) ) ;
#25562 = CARTESIAN_POINT ( 'NONE',  ( -6.676582343750000703, 295.5156250017070079, 2.765530957082001251 ) ) ;
#25563 = CARTESIAN_POINT ( 'NONE',  ( 4.220049686691941027, -10.18810118749999738, 109.0000000020483810 ) ) ;
#25564 = CARTESIAN_POINT ( 'NONE',  ( -8.311093377946836114, 197.6562499965860695, -8.311093377946837890 ) ) ;
#25565 = ORIENTED_EDGE ( 'NONE', *, *, #45349, .T. ) ;
#25566 = CARTESIAN_POINT ( 'NONE',  ( 7.188101187500000044, 0.6562499979516100979, 0.000000000000000000 ) ) ;
#25567 = CARTESIAN_POINT ( 'NONE',  ( -29.65685424949234417, 203.5625000027312126, 174.0000000000003979 ) ) ;
#25568 = CARTESIAN_POINT ( 'NONE',  ( -1.469576158976823947E-15, 14.43749999590322375, 8.000000000000000000 ) ) ;
#25570 = CARTESIAN_POINT ( 'NONE',  ( 9.832129032723416984, 195.3645833299193839, 5.676582343750006032 ) ) ;
#25569 = DIRECTION ( 'NONE',  ( 1.000000000000000000, 0.000000000000000000, -0.000000000000000000 ) ) ;
#25571 = CYLINDRICAL_SURFACE ( 'NONE', #48983, 20.00000000000001066 ) ;
#25572 = CARTESIAN_POINT ( 'NONE',  ( 2.679491924311235174, 234.5833333401613174, 9.999999999999998224 ) ) ;
#25573 = EDGE_CURVE ( 'NONE', #32089, #62341, #33990, .T. ) ;
#25574 = ORIENTED_EDGE ( 'NONE', *, *, #12435, .T. ) ;
#25575 = CARTESIAN_POINT ( 'NONE',  ( -11.35316468750000141, 178.5937499965860411, -1.390361679473963753E-15 ) ) ;
#25576 = EDGE_CURVE ( 'NONE', #72156, #30597, #74453, .T. ) ;
#25577 = CARTESIAN_POINT ( 'NONE',  ( 5.082755093536320601, -5.082755093536318824, 18.54905278187175455 ) ) ;
#25578 =( BOUNDED_CURVE ( )  B_SPLINE_CURVE ( 2, ( #32058, #4145, #38469, #21104, #72414, #20725, #49395, #33567, #16167, #61094, #56197, #55078, #50150 ),
 .UNSPECIFIED., .F., .F. ) 
 B_SPLINE_CURVE_WITH_KNOTS ( ( 3, 2, 2, 2, 2, 2, 3 ),
 ( 0.6032608695652174058, 0.6050724637681159646, 0.6068840579710145233, 0.6086956521739130821, 0.6105072463768117519, 0.6123188405797103107, 0.6141304347826087584 ),
 .UNSPECIFIED. ) 
 CURVE ( )  GEOMETRIC_REPRESENTATION_ITEM ( )  RATIONAL_B_SPLINE_CURVE ( ( 1.000000000000000000, 0.9659258262890683122, 1.000000000000000000, 0.9659258262890683122, 1.000000000000000000, 0.9659258262890683122, 1.000000000000000000, 0.9659258262890683122, 1.000000000000000000, 0.9659258262890683122, 1.000000000000000000, 0.9659258262890662028, 1.000000000000001998 ) ) 
 REPRESENTATION_ITEM ( '' )  );
#25579 = CARTESIAN_POINT ( 'NONE',  ( 3.178432602446558121E-13, 136.2499999999999716, -10.00000000000000533 ) ) ;
#25580 =( BOUNDED_CURVE ( )  B_SPLINE_CURVE ( 2, ( #14741, #66816, #71710, #60776, #9483, #9102, #55135, #49832, #32498, #72850, #20027, #21155, #43040, #66059, #67193, #14366, #29348, #64416, #70444, #12714, #6343, #69706, #29713, #35746, #63663, #35022, #58035, #40285, #18759, #64775, #46315, #52355, #693, #11987, #28965, #6705, #57278, #34275, #35387, #41037, #1431, #22931, #23677, #46682, #18019, #23301, #17640, #69329, #64044, #18391, #28590, #70084, #57655, #5961, #12354, #58400, #52726, #41403, #58763, #1060, #40659, #24039, #47049, #41767, #5593, #63286, #7073, #30079, #53097, #51601, #24414, #47419, #74616, #45943, #323, #68956, #17266, #11613, #34650, #51984, #19482, #36482, #60594, #7809, #65878, #19117, #25509, #14184, #31182, #59859, #3263, #36852, #48893, #72284, #48522, #30811, #43238, #8919, #66253, #71906, #59496, #42122, #8172, #26251, #70803, #71528, #48152, #42497, #37221, #53835, #65134, #20219, #19855, #36113, #2143, #65512, #31931, #25137, #13445, #37595, #71162, #1785, #13807, #54207, #2516, #42859, #60219, #54953, #24770, #20597, #43612, #8544, #53467, #31557, #54581, #2886, #25874, #14559, #49269, #13078, #59135, #7443, #30451, #47782, #51138, #15304, #38723, #20971, #28125, #43995, #62088, #33076, #72669, #27009, #56072, #33438, #61720, #15681, #56812, #67005, #3633, #9674, #4381, #38341, #10410, #61348, #56438, #33814, #10777, #14930, #37972, #26631, #32695, #73777, #60971, #50022, #4758, #27750, #10040, #27374, #50394, #55703, #73409, #21713, #4019, #49653, #74148, #22452, #22086, #50762, #5132, #66625, #44742 ),
 .UNSPECIFIED., .F., .F. ) 
 B_SPLINE_CURVE_WITH_KNOTS ( ( 3, 2, 2, 2, 2, 2, 2, 2, 2, 2, 2, 2, 2, 2, 2, 2, 2, 2, 2, 2, 2, 2, 2, 2, 2, 2, 2, 2, 2, 2, 2, 2, 2, 2, 2, 2, 2, 2, 2, 2, 2, 2, 2, 2, 2, 2, 2, 2, 2, 2, 2, 2, 2, 2, 2, 2, 2, 2, 2, 2, 2, 2, 2, 2, 2, 2, 2, 2, 2, 2, 2, 2, 2, 2, 2, 2, 2, 2, 2, 2, 2, 2, 2, 2, 2, 2, 2, 2, 2, 2, 2, 2, 2, 2, 2, 2, 3 ),
 ( 0.000000000000000000, 0.01041666666666666609, 0.02083333333333333218, 0.03125000000000000000, 0.04166666666666666435, 0.05208333333333333565, 0.06250000000000000000, 0.07291666666666667129, 0.08333333333333332871, 0.09375000000000000000, 0.1041666666666666713, 0.1145833333333333287, 0.1250000000000000000, 0.1354166666666666574, 0.1458333333333333426, 0.1562500000000000000, 0.1666666666666666574, 0.1770833333333333426, 0.1875000000000000000, 0.1979166666666666574, 0.2083333333333333426, 0.2187500000000000000, 0.2291666666666666574, 0.2395833333333333426, 0.2500000000000000000, 0.2604166666666666852, 0.2708333333333333148, 0.2812500000000000000, 0.2916666666666666852, 0.3020833333333333148, 0.3125000000000000000, 0.3229166666666666852, 0.3333333333333333148, 0.3437500000000000000, 0.3541666666666666852, 0.3645833333333333148, 0.3750000000000000000, 0.3854166666666666852, 0.3958333333333333148, 0.4062500000000000000, 0.4166666666666666852, 0.4270833333333333148, 0.4375000000000000000, 0.4479166666666666852, 0.4583333333333333148, 0.4687500000000000000, 0.4791666666666666852, 0.4895833333333333148, 0.5000000000000000000, 0.5104166666666666297, 0.5208333333333333703, 0.5312500000000000000, 0.5416666666666666297, 0.5520833333333333703, 0.5625000000000000000, 0.5729166666666666297, 0.5833333333333333703, 0.5937500000000000000, 0.6041666666666666297, 0.6145833333333333703, 0.6250000000000000000, 0.6354166666666666297, 0.6458333333333333703, 0.6562500000000000000, 0.6666666666666666297, 0.6770833333333333703, 0.6875000000000000000, 0.6979166666666666297, 0.7083333333333333703, 0.7187500000000000000, 0.7291666666666666297, 0.7395833333333333703, 0.7500000000000000000, 0.7604166666666666297, 0.7708333333333333703, 0.7812500000000000000, 0.7916666666666666297, 0.8020833333333333703, 0.8125000000000000000, 0.8229166666666666297, 0.8333333333333333703, 0.8437500000000000000, 0.8541666666666666297, 0.8645833333333333703, 0.8750000000000000000, 0.8854166666666666297, 0.8958333333333333703, 0.9062500000000000000, 0.9166666666666666297, 0.9270833333333333703, 0.9375000000000000000, 0.9479166666666666297, 0.9583333333333333703, 0.9687500000000000000, 0.9791666666666666297, 0.9895833333333333703, 1.000000000000000000 ),
 .UNSPECIFIED. ) 
 CURVE ( )  GEOMETRIC_REPRESENTATION_ITEM ( )  RATIONAL_B_SPLINE_CURVE ( ( 1.000000000000000000, 0.9238795325112867385, 1.000000000000000000, 0.9238795325112867385, 1.000000000000000000, 0.9238795325112867385, 1.000000000000000000, 0.9238795325112867385, 1.000000000000000000, 0.9238795325112867385, 1.000000000000000000, 0.9238795325112867385, 1.000000000000000000, 0.9238795325112867385, 1.000000000000000000, 0.9238795325112867385, 1.000000000000000000, 0.9238795325112867385, 1.000000000000000000, 0.9238795325112867385, 1.000000000000000000, 0.9238795325112867385, 1.000000000000000000, 0.9238795325112867385, 1.000000000000000000, 0.9238795325112867385, 1.000000000000000000, 0.9238795325112867385, 1.000000000000000000, 0.9238795325112867385, 1.000000000000000000, 0.9238795325112867385, 1.000000000000000000, 0.9238795325112867385, 1.000000000000000000, 0.9238795325112867385, 1.000000000000000000, 0.9238795325112867385, 1.000000000000000000, 0.9238795325112867385, 1.000000000000000000, 0.9238795325112867385, 1.000000000000000000, 0.9238795325112867385, 1.000000000000000000, 0.9238795325112867385, 1.000000000000000000, 0.9238795325112867385, 1.000000000000000000, 0.9238795325112867385, 1.000000000000000000, 0.9238795325112867385, 1.000000000000000000, 0.9238795325112867385, 1.000000000000000000, 0.9238795325112867385, 1.000000000000000000, 0.9238795325112867385, 1.000000000000000000, 0.9238795325112867385, 1.000000000000000000, 0.9238795325112867385, 1.000000000000000000, 0.9238795325112867385, 1.000000000000000000, 0.9238795325112867385, 1.000000000000000000, 0.9238795325112867385, 1.000000000000000000, 0.9238795325112867385, 1.000000000000000000, 0.9238795325112867385, 1.000000000000000000, 0.9238795325112867385, 1.000000000000000000, 0.9238795325112867385, 1.000000000000000000, 0.9238795325112867385, 1.000000000000000000, 0.9238795325112867385, 1.000000000000000000, 0.9238795325112867385, 1.000000000000000000, 0.9238795325112867385, 1.000000000000000000, 0.9238795325112867385, 1.000000000000000000, 0.9238795325112867385, 1.000000000000000000, 0.9238795325112867385, 1.000000000000000000, 0.9238795325112867385, 1.000000000000000000, 0.9238795325112867385, 1.000000000000000000, 0.9238795325112867385, 1.000000000000000000, 0.9238795325112867385, 1.000000000000000000, 0.9238795325112867385, 1.000000000000000000, 0.9238795325112867385, 1.000000000000000000, 0.9238795325112867385, 1.000000000000000000, 0.9238795325112867385, 1.000000000000000000, 0.9238795325112867385, 1.000000000000000000, 0.9238795325112867385, 1.000000000000000000, 0.9238795325112867385, 1.000000000000000000, 0.9238795325112867385, 1.000000000000000000, 0.9238795325112867385, 1.000000000000000000, 0.9238795325112867385, 1.000000000000000000, 0.9238795325112867385, 1.000000000000000000, 0.9238795325112867385, 1.000000000000000000, 0.9238795325112867385, 1.000000000000000000, 0.9238795325112867385, 1.000000000000000000, 0.9238795325112867385, 1.000000000000000000, 0.9238795325112867385, 1.000000000000000000, 0.9238795325112867385, 1.000000000000000000, 0.9238795325112867385, 1.000000000000000000, 0.9238795325112867385, 1.000000000000000000, 0.9238795325112867385, 1.000000000000000000, 0.9238795325112867385, 1.000000000000000000, 0.9238795325112867385, 1.000000000000000000, 0.9238795325112867385, 1.000000000000000000, 0.9238795325112867385, 1.000000000000000000, 0.9238795325112867385, 1.000000000000000000, 0.9238795325112867385, 1.000000000000000000, 0.9238795325112867385, 1.000000000000000000, 0.9238795325112867385, 1.000000000000000000, 0.9238795325112867385, 1.000000000000000000, 0.9238795325112867385, 1.000000000000000000, 0.9238795325112867385, 1.000000000000000000, 0.9238795325112867385, 1.000000000000000000, 0.9238795325112867385, 1.000000000000000000, 0.9238795325112867385, 1.000000000000000000, 0.9238795325112867385, 1.000000000000000000, 0.9238795325112867385, 1.000000000000000000, 0.9238795325112867385, 1.000000000000000000, 0.9238795325112867385, 1.000000000000000000, 0.9238795325112867385, 1.000000000000000000, 0.9238795325112867385, 1.000000000000000000, 0.9238795325112867385, 1.000000000000000000, 0.9238795325112867385, 1.000000000000000000, 0.9238795325112867385, 1.000000000000000000, 0.9238795325112867385, 1.000000000000000000, 0.9238795325112867385, 1.000000000000000000, 0.9238795325112867385, 1.000000000000000000, 0.9238795325112867385, 1.000000000000000000 ) ) 
 REPRESENTATION_ITEM ( '' )  );
#25581 = ORIENTED_EDGE ( 'NONE', *, *, #47379, .T. ) ;
#25582 = CIRCLE ( 'NONE', #69023, 10.99999999999998934 ) ;
#25583 = CARTESIAN_POINT ( 'NONE',  ( 8.000000000000000000, 97.53125000409676204, -3.313708498984762496 ) ) ;
#25584 = CARTESIAN_POINT ( 'NONE',  ( -2.679491924311235618, 3.541666666666666963, 10.00000000000000000 ) ) ;
#25585 = EDGE_CURVE ( 'NONE', #73780, #15595, #8399, .T. ) ;
#25586 = EDGE_CURVE ( 'NONE', #51233, #17320, #65839, .T. ) ;
#25587 = CARTESIAN_POINT ( 'NONE',  ( -4.000000000000001776, 16.43750000000000355, -1.656854249492381470 ) ) ;
#25588 = CARTESIAN_POINT ( 'NONE',  ( -3.211159895383561391, 15.68749999863440436, -3.211159895383561835 ) ) ;
#25589 = CARTESIAN_POINT ( 'NONE',  ( 5.656854249492376141, -5.656854249492374365, 12.08030278392014445 ) ) ;
#25590 = CARTESIAN_POINT ( 'NONE',  ( -7.999999999999991118, -3.618600720434140080E-05, 19.01780380767893064 ) ) ;
#25591 = ORIENTED_EDGE ( 'NONE', *, *, #19434, .F. ) ;
#25592 = CARTESIAN_POINT ( 'NONE',  ( 4.242640687119287435, 293.4375000034140157, 4.242640687119285658 ) ) ;
#25593 = CARTESIAN_POINT ( 'NONE',  ( 2.977408999572650039, 99.68750000204838102, -7.188101187500001821 ) ) ;
#25595 = CARTESIAN_POINT ( 'NONE',  ( -11.35316468749999608, 259.1145833367473301, 3.042071309553173730 ) ) ;
#25594 = CARTESIAN_POINT ( 'NONE',  ( -4.898587196589412829E-16, 91.81250000409677625, -8.000000000000000000 ) ) ;
#25596 = ORIENTED_EDGE ( 'NONE', *, *, #8272, .T. ) ;
#25597 = CARTESIAN_POINT ( 'NONE',  ( 5.000000000000000000, 50.64189880742144823, -41.08656465431842975 ) ) ;
#25598 = EDGE_CURVE ( 'NONE', #67076, #28600, #46515, .T. ) ;
#25599 = CARTESIAN_POINT ( 'NONE',  ( -2.977408999572647819, 7.188101187499991163, 16.20530278187175455 ) ) ;
#25600 = ORIENTED_EDGE ( 'NONE', *, *, #18276, .T. ) ;
#25601 = ADVANCED_BREP_SHAPE_REPRESENTATION ( '', ( #42204, #57354 ), #16391 ) ;
#25602 = EDGE_CURVE ( 'NONE', #42073, #35953, #16103, .T. ) ;
#25603 = ORIENTED_EDGE ( 'NONE', *, *, #35947, .F. ) ;
#25604 = CARTESIAN_POINT ( 'NONE',  ( -7.204075437095967871, 7.204075437095967871, 77.96875000204836681 ) ) ;
#25605 = CARTESIAN_POINT ( 'NONE',  ( -5.676582343750006032, 64.42708332991935549, 9.832129032723418760 ) ) ;
#25606 = CARTESIAN_POINT ( 'NONE',  ( -34.69679471024809203, -12.34462646322155699, 148.2170566195945298 ) ) ;
#25607 = CARTESIAN_POINT ( 'NONE',  ( -6.735557395310442023E-16, 11.00000000000000000, 96.62499999999998579 ) ) ;
#25610 = CARTESIAN_POINT ( 'NONE',  ( -2.765530957081996810, 292.4218750017069510, -6.676582343750002480 ) ) ;
#25609 = CARTESIAN_POINT ( 'NONE',  ( 29.65685424949235127, 199.5625000027311842, 165.9999999999998863 ) ) ;
#25608 = CARTESIAN_POINT ( 'NONE',  ( -31.99999999999999289, 198.3750000027312126, 170.0000000000004547 ) ) ;
#25611 = CARTESIAN_POINT ( 'NONE',  ( -2.679491924311235618, 143.5416666666666856, 10.00000000000000000 ) ) ;
#25612 = CARTESIAN_POINT ( 'NONE',  ( 10.99999999999989342, 4.556349186104152515, 88.84374999999998579 ) ) ;
#25613 = CARTESIAN_POINT ( 'NONE',  ( 1.656854249492246467, 198.8125000000000000, 146.0000000000001421 ) ) ;
#25614 = CARTESIAN_POINT ( 'NONE',  ( -3.313708498984760720, 3.281249995903220640, -8.000000000000000000 ) ) ;
#25615 = CARTESIAN_POINT ( 'NONE',  ( 24.54126587500000056, 200.1250000013656063, 168.5673454167822172 ) ) ;
#25616 = CARTESIAN_POINT ( 'NONE',  ( 2.977408999572650927, 11.62499999795161365, -7.188101187500001821 ) ) ;
#25617 = CARTESIAN_POINT ( 'NONE',  ( 3.313708498984762496, -7.999999999999989342, 25.48655278392014623 ) ) ;
#25618 = FACE_OUTER_BOUND ( 'NONE', #12620, .T. ) ;
#25619 = CARTESIAN_POINT ( 'NONE',  ( -5.082755093536325930, 112.3437500020483810, -5.082755093536325930 ) ) ;
#25621 = DIRECTION ( 'NONE',  ( 0.000000000000000000, -1.000000000000000000, 0.000000000000000000 ) ) ;
#25620 = CARTESIAN_POINT ( 'NONE',  ( -27.99999999999999645, 210.0000000000000284, 170.0000000000003695 ) ) ;
#25622 = CARTESIAN_POINT ( 'NONE',  ( 11.35316468749999963, 221.5104166700805877, 3.042071309553159519 ) ) ;
#25623 = CARTESIAN_POINT ( 'NONE',  ( 26.56734541678233086, 209.6250000013656063, 173.4587341249998929 ) ) ;
#25624 = CARTESIAN_POINT ( 'NONE',  ( -7.188101187499990274, -2.977408999572651371, 19.95530278187175810 ) ) ;
#25625 = CARTESIAN_POINT ( 'NONE',  ( 29.65685424949234061, 200.1875000027312126, 174.0000000000000284 ) ) ;
#25626 = CARTESIAN_POINT ( 'NONE',  ( 6.951808397369818766E-16, 42.03124999658601268, -11.35316468750000141 ) ) ;
#25627 = CARTESIAN_POINT ( 'NONE',  ( -4.000000000000001776, 6.500000000000000888, -4.898587196589415787E-16 ) ) ;
#25628 = CARTESIAN_POINT ( 'NONE',  ( -10.00000000000000355, 14.58333332650536462, 2.679491924311223183 ) ) ;
#25629 = ORIENTED_EDGE ( 'NONE', *, *, #65332, .T. ) ;
#25630 = EDGE_CURVE ( 'NONE', #2022, #16864, #55665, .T. ) ;
#25631 = FACE_OUTER_BOUND ( 'NONE', #62722, .T. ) ;
#25632 = CARTESIAN_POINT ( 'NONE',  ( -1.656854249492381248, 14.31250000000000000, -4.000000000000001776 ) ) ;
#25633 = CARTESIAN_POINT ( 'NONE',  ( 8.311093377946837890, 36.40624999658601979, -8.311093377946837890 ) ) ;
#25634 = CARTESIAN_POINT ( 'NONE',  ( 11.00000000000000000, 4.556349186104045934, 83.03125000409677625 ) ) ;
#25635 = CARTESIAN_POINT ( 'NONE',  ( 2.445694354108783219, 203.8125000013656063, 139.5543056458912190 ) ) ;
#25636 = CARTESIAN_POINT ( 'NONE',  ( -11.35316468749999963, 264.0625000034140157, 0.000000000000000000 ) ) ;
#25637 = CARTESIAN_POINT ( 'NONE',  ( 37.99999999999999289, 37.00000000000000000, 20.00000000000000000 ) ) ;
#25639 = CARTESIAN_POINT ( 'NONE',  ( -9.832129032723420536, 28.69791666325268409, 5.676582343749997150 ) ) ;
#25638 = CARTESIAN_POINT ( 'NONE',  ( 5.082755093536325042, 107.0937500020483810, -5.082755093536325930 ) ) ;
#25641 = EDGE_CURVE ( 'NONE', #46122, #28343, #46952, .T. ) ;
#25640 = CARTESIAN_POINT ( 'NONE',  ( -4.898587196589407898E-16, 7.999999999999991118, 7.955302779823362869 ) ) ;
#25642 = CARTESIAN_POINT ( 'NONE',  ( -8.311093377946836114, 162.6562499965859843, -8.311093377946837890 ) ) ;
#25643 = CARTESIAN_POINT ( 'NONE',  ( 8.660254037844385522, 131.4583333265053682, 5.000000000000005329 ) ) ;
#25644 = CARTESIAN_POINT ( 'NONE',  ( -5.082755093536325930, 110.8437500020483810, -5.082755093536325930 ) ) ;
#25645 = ORIENTED_EDGE ( 'NONE', *, *, #13232, .F. ) ;
#25646 = DIRECTION ( 'NONE',  ( 3.469446951953617147E-16, 0.000000000000000000, -1.000000000000000000 ) ) ;
#25647 = CARTESIAN_POINT ( 'NONE',  ( 9.832129032723420536, 21.51041666325268409, -5.676582343749999815 ) ) ;
#25648 = EDGE_CURVE ( 'NONE', #23461, #3011, #15641, .T. ) ;
#25649 = ORIENTED_EDGE ( 'NONE', *, *, #4462, .F. ) ;
#25650 = CARTESIAN_POINT ( 'NONE',  ( 3.155198069298570310E-14, 271.9999999999999432, 201.0000000000000000 ) ) ;
#25651 = CARTESIAN_POINT ( 'NONE',  ( 4.220049686691941027, -10.18810118749999738, 80.12500000204835260 ) ) ;
#25652 = CARTESIAN_POINT ( 'NONE',  ( -29.65685424949230864, 197.0625000000000000, 166.0000000000003411 ) ) ;
#25654 = CARTESIAN_POINT ( 'NONE',  ( -5.676582343749998039, 157.4479166632526983, -9.832129032723420536 ) ) ;
#25653 = CARTESIAN_POINT ( 'NONE',  ( -23.08212290065930361, -24.35949675673025183, 145.6763322512113348 ) ) ;
#25655 = CARTESIAN_POINT ( 'NONE',  ( -5.082755093536326818, 1.781249997951610098, 5.082755093536325042 ) ) ;
#25656 = CARTESIAN_POINT ( 'NONE',  ( -5.656854249492373476, -5.656854249492376141, 20.57405278432982243 ) ) ;
#25657 = CARTESIAN_POINT ( 'NONE',  ( -19.99999999999993250, -31.99999999999978684, 193.6854385646540209 ) ) ;
#25658 = CARTESIAN_POINT ( 'NONE',  ( -9.832129032723418760, 233.4895833367473301, -5.676582343749998927 ) ) ;
#25659 = CARTESIAN_POINT ( 'NONE',  ( 10.18810118749999916, 1.247682550866122264E-15, 86.78125000204836681 ) ) ;
#25660 = ORIENTED_EDGE ( 'NONE', *, *, #68399, .T. ) ;
#25661 = FACE_OUTER_BOUND ( 'NONE', #31527, .T. ) ;
#25662 = CARTESIAN_POINT ( 'NONE',  ( 2.751064625579944321E-14, 198.8750000027312126, 194.0000000000000568 ) ) ;
#25663 = CARTESIAN_POINT ( 'NONE',  ( 8.311093377946837890, 101.7187499965860269, -8.311093377946837890 ) ) ;
#25664 = CARTESIAN_POINT ( 'NONE',  ( -7.204075437095965206, -7.204075437095968759, 103.8437500020483810 ) ) ;
#25665 = CARTESIAN_POINT ( 'NONE',  ( -4.541265875000002339, 21.87499999863441147, -1.881053915767121998 ) ) ;
#25666 = ORIENTED_EDGE ( 'NONE', *, *, #6413, .T. ) ;
#25667 = ORIENTED_EDGE ( 'NONE', *, *, #41838, .T. ) ;
#25668 = CARTESIAN_POINT ( 'NONE',  ( -4.541265875000002339, 4.937499998634407916, -5.561446717895856393E-16 ) ) ;
#25669 = CARTESIAN_POINT ( 'NONE',  ( -5.082755093536326818, 27.28124999795161543, 5.082755093536325042 ) ) ;
#25670 = CARTESIAN_POINT ( 'NONE',  ( 8.000000000000001776, 113.8437500040967763, 3.313708498984759387 ) ) ;
#25671 =( BOUNDED_CURVE ( )  B_SPLINE_CURVE ( 2, ( #2528, #71917, #71173, #44381, #55715, #28138, #32706 ),
 .UNSPECIFIED., .F., .F. ) 
 B_SPLINE_CURVE_WITH_KNOTS ( ( 3, 2, 2, 3 ),
 ( 0.000000000000000000, 0.009259259259259305583, 0.01851851851851849667, 0.02777777777777780052 ),
 .UNSPECIFIED. ) 
 CURVE ( )  GEOMETRIC_REPRESENTATION_ITEM ( )  RATIONAL_B_SPLINE_CURVE ( ( 1.000000000000000000, 0.9659258262890684232, 1.000000000000000000, 0.9659258262890684232, 1.000000000000000000, 0.9659258262890684232, 1.000000000000000000 ) ) 
 REPRESENTATION_ITEM ( '' )  );
#25672 = CARTESIAN_POINT ( 'NONE',  ( -4.220049686691935698, 10.18810118749999916, 96.25000000204838102 ) ) ;
#25673 = CARTESIAN_POINT ( 'NONE',  ( -26.56734541678232375, 205.2500000013655779, 173.4587341250003760 ) ) ;
#25674 = CARTESIAN_POINT ( 'NONE',  ( -4.000000000000002665, 5.562500000000000000, 1.656854249492380804 ) ) ;
#25675 = CARTESIAN_POINT ( 'NONE',  ( -7.347880794884122694E-16, 18.49999999726881583, 4.000000000000001776 ) ) ;
#25676 = CARTESIAN_POINT ( 'NONE',  ( -4.541265875000002339, 2.749999998634407028, -1.881053915767121998 ) ) ;
#25677 = AXIS2_PLACEMENT_3D ( 'NONE', #14815, #9922, #32954 ) ;
#25678 = CARTESIAN_POINT ( 'NONE',  ( -11.00000000000000000, 11.00000000000000000, -6.938893903907228378E-15 ) ) ;
#25679 = CARTESIAN_POINT ( 'NONE',  ( 27.99999999999997158, 208.0000000000000284, 173.9999999999999147 ) ) ;
#25681 = CARTESIAN_POINT ( 'NONE',  ( -7.320508075689018845, 23.12500000000019540, 7.320508075689011740 ) ) ;
#25680 = CARTESIAN_POINT ( 'NONE',  ( -26.56734541678227757, 201.0000000013655779, 173.4587341250003476 ) ) ;
#25682 =( BOUNDED_CURVE ( )  B_SPLINE_CURVE ( 2, ( #38270, #48452, #14112, #61274, #9603, #32622, #55630, #3946, #49954, #8467, #31487, #54510, #33365 ),
 .UNSPECIFIED., .F., .F. ) 
 B_SPLINE_CURVE_WITH_KNOTS ( ( 3, 2, 2, 2, 2, 2, 3 ),
 ( 0.3532608695652174058, 0.3550724637681159646, 0.3568840579710144678, 0.3586956521739130266, 0.3605072463768115854, 0.3623188405797101441, 0.3641304347826087029 ),
 .UNSPECIFIED. ) 
 CURVE ( )  GEOMETRIC_REPRESENTATION_ITEM ( )  RATIONAL_B_SPLINE_CURVE ( ( 1.000000000000000000, 0.9659258262890683122, 1.000000000000000000, 0.9659258262890683122, 1.000000000000000000, 0.9659258262890683122, 1.000000000000000000, 0.9659258262890683122, 1.000000000000000000, 0.9659258262890683122, 1.000000000000000000, 0.9659258262890683122, 1.000000000000000000 ) ) 
 REPRESENTATION_ITEM ( '' )  );
#25683 = CARTESIAN_POINT ( 'NONE',  ( 4.541265875000002339, 20.31249999863440436, 0.000000000000000000 ) ) ;
#25684 = CARTESIAN_POINT ( 'NONE',  ( 8.000000000000000000, 1.312499995903220196, 0.000000000000000000 ) ) ;
#25685 = CARTESIAN_POINT ( 'NONE',  ( -2.977408999572648707, -7.188101187499990274, 7.767802781871751883 ) ) ;
#25686 = EDGE_LOOP ( 'NONE', ( #73738, #40011, #41115, #61667 ) ) ;
#25687 = EDGE_LOOP ( 'NONE', ( #6426, #68655, #18549, #44039 ) ) ;
#25688 = CARTESIAN_POINT ( 'NONE',  ( -7.204075437095967871, 7.204075437095967871, 98.96875000204838102 ) ) ;
#25689 = DIRECTION ( 'NONE',  ( 0.8660254037844377084, -0.5000000000000017764, 0.000000000000000000 ) ) ;
#25690 = CARTESIAN_POINT ( 'NONE',  ( -26.56734541678238060, 204.6250000013656063, 166.5412658750003629 ) ) ;
#25691 = CARTESIAN_POINT ( 'NONE',  ( -31.99999999999999289, 200.2500000000000000, 170.0000000000003979 ) ) ;
#25692 = CARTESIAN_POINT ( 'NONE',  ( -2.445694354108782775, 196.5625000013656063, 200.4456943541088663 ) ) ;
#25693 = CARTESIAN_POINT ( 'NONE',  ( 3.153939666463669656E-13, 33.75000000000002842, 9.999999999999998224 ) ) ;
#25694 = CARTESIAN_POINT ( 'NONE',  ( 8.660254037844385522, 114.5833333333333428, 5.000000000000005329 ) ) ;
#25695 = CARTESIAN_POINT ( 'NONE',  ( -8.000000000000000000, 111.4062500000000142, -3.313708498984761608 ) ) ;
#25696 = CARTESIAN_POINT ( 'NONE',  ( -4.721056650415999201, 296.4843750017070079, -4.721056650415999201 ) ) ;
#25697 = ORIENTED_EDGE ( 'NONE', *, *, #69485, .F. ) ;
#25698 = CARTESIAN_POINT ( 'NONE',  ( 7.320508075688800353, 189.3750000000000568, 7.320508075688803906 ) ) ;
#25699 = CARTESIAN_POINT ( 'NONE',  ( -3.313708498984760720, 22.78124999590322375, -8.000000000000000000 ) ) ;
#25700 = VECTOR ( 'NONE', #19394, 1000.000000000000000 ) ;
#25701 = CARTESIAN_POINT ( 'NONE',  ( 2.445694354108782775, 201.5625000013656063, 139.5543056458912190 ) ) ;
#25702 = LINE ( 'NONE', #14007, #24938 ) ;
#25703 = DIRECTION ( 'NONE',  ( -0.000000000000000000, 1.000000000000000000, -4.476705744456276341E-16 ) ) ;
#25704 = CARTESIAN_POINT ( 'NONE',  ( -5.676582343750000703, 258.3854166700806445, -9.832129032723418760 ) ) ;
#25705 = CARTESIAN_POINT ( 'NONE',  ( -1.656854249492346609, 207.3125000027312126, 202.0000000000000000 ) ) ;
#25706 = CARTESIAN_POINT ( 'NONE',  ( -11.00000000000000000, 0.000000000000000000, 113.4999999999999858 ) ) ;
#25707 = CARTESIAN_POINT ( 'NONE',  ( 3.042071309553167069, 1.822916663252682978, -11.35316468749999785 ) ) ;
#25708 = CARTESIAN_POINT ( 'NONE',  ( -2.977408999572647819, -7.188101187499990274, 3.642802781871751883 ) ) ;
#25709 = CARTESIAN_POINT ( 'NONE',  ( 5.676582343749993598, 195.2604166632526983, 9.832129032723422313 ) ) ;
#25710 = CARTESIAN_POINT ( 'NONE',  ( 3.594044162775203333, 89.15552387383502264, -6.225081946264263699 ) ) ;
#25711 = CARTESIAN_POINT ( 'NONE',  ( 1.881053915767122664, 8.124999998634407916, 4.541265875000001451 ) ) ;
#25712 = CARTESIAN_POINT ( 'NONE',  ( 1.656854249492327735, 209.8125000000000000, 146.0000000000000853 ) ) ;
#25714 = CARTESIAN_POINT ( 'NONE',  ( -1.469576158976823947E-15, 14.43749999590322375, 8.000000000000000000 ) ) ;
#25713 = FACE_OUTER_BOUND ( 'NONE', #48786, .T. ) ;
#25715 = ORIENTED_EDGE ( 'NONE', *, *, #26692, .F. ) ;
#25716 = CARTESIAN_POINT ( 'NONE',  ( 3.458734124999960358, 202.6875000013656063, 142.0000000000000568 ) ) ;
#25717 = CARTESIAN_POINT ( 'NONE',  ( 11.35316468749999963, 51.30208332991936260, -3.042071309553165293 ) ) ;
#25718 = CARTESIAN_POINT ( 'NONE',  ( -10.99999999999999822, -4.556349186104052151, 100.2812500040967620 ) ) ;
#25719 = DIRECTION ( 'NONE',  ( 0.000000000000000000, 0.000000000000000000, 1.000000000000000000 ) ) ;
#25720 = CARTESIAN_POINT ( 'NONE',  ( -25.55430564589111953, 202.0625000013656063, 172.4456943541091505 ) ) ;
#25721 = LINE ( 'NONE', #60815, #74336 ) ;
#25722 = CARTESIAN_POINT ( 'NONE',  ( 4.556349186104052151, -10.99999999999999822, 107.9687500000000000 ) ) ;
#25724 = EDGE_CURVE ( 'NONE', #37130, #31137, #38304, .T. ) ;
#25723 = CARTESIAN_POINT ( 'NONE',  ( -6.735557395310442023E-16, 11.00000000000000000, 87.62499999999998579 ) ) ;
#25725 = CARTESIAN_POINT ( 'NONE',  ( 3.042071309553167069, 121.8229166632526841, -11.35316468749999785 ) ) ;
#25726 = CARTESIAN_POINT ( 'NONE',  ( -10.00000000000000178, 94.37499999317203958, -1.224646799147353454E-15 ) ) ;
#25727 = CARTESIAN_POINT ( 'NONE',  ( -2.977408999572651815, 89.93750000204840944, 7.188101187500000933 ) ) ;
#25728 = CARTESIAN_POINT ( 'NONE',  ( 1.881053915767121776, 16.62499999863440436, -4.541265875000002339 ) ) ;
#25729 = DIRECTION ( 'NONE',  ( -1.000000000000000000, 0.000000000000000000, 0.000000000000000000 ) ) ;
#25730 = CARTESIAN_POINT ( 'NONE',  ( 6.123233995736767268E-16, 161.2500000000000000, -10.00000000000000178 ) ) ;
#25731 = ORIENTED_EDGE ( 'NONE', *, *, #23751, .T. ) ;
#25732 = CARTESIAN_POINT ( 'NONE',  ( -7.535105736103198559, 226.0000000000000000, -6.607085568838196643 ) ) ;
#25733 = ORIENTED_EDGE ( 'NONE', *, *, #1238, .T. ) ;
#25734 = EDGE_CURVE ( 'NONE', #56815, #47217, #54243, .T. ) ;
#25735 = CARTESIAN_POINT ( 'NONE',  ( -4.088227598258586603E-16, 293.3593750017070079, -6.676582343750001591 ) ) ;
#25736 = CARTESIAN_POINT ( 'NONE',  ( -7.999999999999991118, 9.797174393178815797E-16, 30.00000000000000000 ) ) ;
#25737 = CARTESIAN_POINT ( 'NONE',  ( -5.656854249492373476, -5.656854249492376141, 8.705302783920146226 ) ) ;
#25738 = CARTESIAN_POINT ( 'NONE',  ( 9.832129032723420536, 171.1979166632526983, -5.676582343749999815 ) ) ;
#25739 = AXIS2_PLACEMENT_3D ( 'NONE', #37906, #2821, #8107 ) ;
#25740 = DIRECTION ( 'NONE',  ( 0.000000000000000000, -0.2588190451025146332, 0.9659258262890699775 ) ) ;
#25741 = CARTESIAN_POINT ( 'NONE',  ( -1.656854249492347719, 198.8125000000000284, 194.0000000000000853 ) ) ;
#25742 = CYLINDRICAL_SURFACE ( 'NONE', #37411, 11.00000000000000000 ) ;
#25743 = CARTESIAN_POINT ( 'NONE',  ( 7.204075437095966983, 7.204075437095967871, 104.9687500020483810 ) ) ;
#25744 = VERTEX_POINT ( 'NONE', #20559 ) ;
#25745 = CARTESIAN_POINT ( 'NONE',  ( 5.000000000000000000, -16.14408868864072844, 27.96238185062368586 ) ) ;
#25746 = CARTESIAN_POINT ( 'NONE',  ( 4.898587196589412829E-16, 22.68749999590322375, -8.000000000000000000 ) ) ;
#25747 = CARTESIAN_POINT ( 'NONE',  ( 9.832129032723420536, 151.5104166632526699, -5.676582343749999815 ) ) ;
#25748 = LINE ( 'NONE', #71776, #18198 ) ;
#25749 = CARTESIAN_POINT ( 'NONE',  ( 2.445694354108840063, 207.0625000013656063, 200.4456943541088663 ) ) ;
#25750 = CARTESIAN_POINT ( 'NONE',  ( -4.220049686691937474, -10.18810118749999738, 72.81250000204838102 ) ) ;
#25751 = CARTESIAN_POINT ( 'NONE',  ( 9.832129032723416984, 65.67708332991935549, 5.676582343750006032 ) ) ;
#25752 = ORIENTED_EDGE ( 'NONE', *, *, #9486, .T. ) ;
#25753 = CARTESIAN_POINT ( 'NONE',  ( 0.000000000000000000, 125.0000000000000000, 0.000000000000000000 ) ) ;
#25754 = CARTESIAN_POINT ( 'NONE',  ( 2.780723358947928197E-16, 9.687499998634406140, -4.541265875000002339 ) ) ;
#25755 = CARTESIAN_POINT ( 'NONE',  ( 8.008118988124991233, 3.317071493978879015, 10.85686528394063188 ) ) ;
#25756 = ORIENTED_EDGE ( 'NONE', *, *, #23367, .F. ) ;
#25757 = CARTESIAN_POINT ( 'NONE',  ( 5.082755093536325930, 23.15624999795161543, -5.082755093536325930 ) ) ;
#25758 = CARTESIAN_POINT ( 'NONE',  ( 1.102182119232618108E-15, 287.3125000034140157, 6.000000000000001776 ) ) ;
#25759 = CARTESIAN_POINT ( 'NONE',  ( -4.898587196589412829E-16, 117.3125000040967763, -8.000000000000000000 ) ) ;
#25760 = CARTESIAN_POINT ( 'NONE',  ( 4.401442555609581635E-16, 14.71874999795161187, -7.188101187500000044 ) ) ;
#25761 = CARTESIAN_POINT ( 'NONE',  ( 5.082755093536318824, 5.082755093536319713, 2.424052781871750994 ) ) ;
#25762 = CARTESIAN_POINT ( 'NONE',  ( -4.220049686691937474, -10.18810118749999738, 114.8125000020483668 ) ) ;
#25763 = PRODUCT ( 'hexagon nut style 1_is_IS 1364-3 - M12-W-N', 'hexagon nut style 1_is_IS 1364-3 - M12-W-N', '', ( #71248 ) ) ;
#25764 = VECTOR ( 'NONE', #67741, 1000.000000000000000 ) ;
#25765 = DIRECTION ( 'NONE',  ( 0.000000000000000000, 0.000000000000000000, 1.000000000000000000 ) ) ;
#25766 = CARTESIAN_POINT ( 'NONE',  ( -4.000000000000001776, 8.187499997268812280, -1.656854249492381470 ) ) ;
#25767 = ORIENTED_EDGE ( 'NONE', *, *, #41913, .F. ) ;
#25768 = CARTESIAN_POINT ( 'NONE',  ( 2.445694354108838731, 207.0625000013656063, 195.5543056458912190 ) ) ;
#25769 = CARTESIAN_POINT ( 'NONE',  ( -30.82842712474624491, 198.2500000027312126, 167.1715728752542418 ) ) ;
#25770 = CARTESIAN_POINT ( 'NONE',  ( -4.541265875000003227, 0.8749999986344069169, 1.881053915767121110 ) ) ;
#25771 = CARTESIAN_POINT ( 'NONE',  ( 2.977408999572650039, 113.1875000020483810, -7.188101187500001821 ) ) ;
#25772 = CARTESIAN_POINT ( 'NONE',  ( -6.000000000000001776, 295.0000000000000000, 0.000000000000000000 ) ) ;
#25773 = CARTESIAN_POINT ( 'NONE',  ( 2.977408999572646486, 7.188101187499991163, 23.51780278187175455 ) ) ;
#25774 = VERTEX_POINT ( 'NONE', #43572 ) ;
#25775 =( BOUNDED_CURVE ( )  B_SPLINE_CURVE ( 2, ( #29537, #52548, #12177, #12547, #52921, #47607, #35941, #23872, #24965 ),
 .UNSPECIFIED., .F., .F. ) 
 B_SPLINE_CURVE_WITH_KNOTS ( ( 3, 2, 2, 2, 3 ),
 ( 0.3750000000000000000, 0.3819444444444444198, 0.3888888888888888951, 0.3958333333333333148, 0.4027777777777777901 ),
 .UNSPECIFIED. ) 
 CURVE ( )  GEOMETRIC_REPRESENTATION_ITEM ( )  RATIONAL_B_SPLINE_CURVE ( ( 1.000000000000000000, 0.9238795325112867385, 1.000000000000000000, 0.9238795325112867385, 1.000000000000000000, 0.9238795325112867385, 1.000000000000000000, 0.9238795325112867385, 1.000000000000000000 ) ) 
 REPRESENTATION_ITEM ( '' )  );
#25776 = CARTESIAN_POINT ( 'NONE',  ( -7.188101187500002709, 25.31249999795161543, 2.977408999572649151 ) ) ;
#25777 = ORIENTED_EDGE ( 'NONE', *, *, #57260, .T. ) ;
#25778 = CARTESIAN_POINT ( 'NONE',  ( 7.204075437095966983, 7.204075437095967871, 115.0937500020483810 ) ) ;
#25779 = CARTESIAN_POINT ( 'NONE',  ( 12.00000000000000355, 0.000000000000000000, 0.000000000000000000 ) ) ;
#25780 = CARTESIAN_POINT ( 'NONE',  ( 2.839093476692135984E-14, 207.6875000013656063, 201.4587341250000350 ) ) ;
#25781 = CARTESIAN_POINT ( 'NONE',  ( 24.54126587499998280, 202.1250000013656063, 168.5673454167822740 ) ) ;
#25782 = CARTESIAN_POINT ( 'NONE',  ( -2.679491924311225848, 61.45833333333332860, -10.00000000000000178 ) ) ;
#25783 = VECTOR ( 'NONE', #23672, 1000.000000000000000 ) ;
#25784 = CARTESIAN_POINT ( 'NONE',  ( -7.188101187499999156, 93.12500000204836681, 2.977408999572654924 ) ) ;
#25785 = CARTESIAN_POINT ( 'NONE',  ( -4.242640687119285658, 295.1249999999999432, 4.242640687119287435 ) ) ;
#25787 = CARTESIAN_POINT ( 'NONE',  ( 10.00000000000000178, 0.9374999965860164597, 0.000000000000000000 ) ) ;
#25786 = CARTESIAN_POINT ( 'NONE',  ( 27.99999999999996803, 207.6250000027312126, 165.9999999999998863 ) ) ;
#25788 = VERTEX_POINT ( 'NONE', #9253 ) ;
#25789 = EDGE_CURVE ( 'NONE', #47572, #9713, #41671, .T. ) ;
#25790 = ADVANCED_FACE ( 'NONE', ( #74113 ), #51101, .F. ) ;
#25791 = CARTESIAN_POINT ( 'NONE',  ( -5.676582343750000703, 233.0729166700806729, -9.832129032723418760 ) ) ;
#25792 = CARTESIAN_POINT ( 'NONE',  ( 1.656854249492348607, 201.3125000027312126, 138.0000000000000568 ) ) ;
#25793 = CARTESIAN_POINT ( 'NONE',  ( 5.656854249492374365, 5.656854249492375253, 24.45530278392014978 ) ) ;
#25794 = CARTESIAN_POINT ( 'NONE',  ( 2.828427124746152987, 197.2500000027312126, 139.1715728752538723 ) ) ;
#25795 = CARTESIAN_POINT ( 'NONE',  ( -6.123233995736766282E-16, 258.7500000000000568, -10.00000000000000000 ) ) ;
#25796 = CARTESIAN_POINT ( 'NONE',  ( 1.224646799147353454E-15, 300.0000000000000000, -10.00000000000000178 ) ) ;
#25797 = CARTESIAN_POINT ( 'NONE',  ( -8.660254037844390851, 187.9166666666666856, 4.999999999999998224 ) ) ;
#25798 =( BOUNDED_SURFACE ( )  B_SPLINE_SURFACE ( 1, 2, ( 
 ( #19141, #42883, #65158, #13469, #60620, #42524, #2913, #66651, #36508, #7830, #20625, #30834, #59883, #25163, #65903, #48179, #8944, #37247, #71187, #14958, #31956, #19506, #65538, #60243, #8569, #31584, #26274, #54606, #25901, #48918, #71931, #54981, #72312, #63132, #74451, #33742, #68420, #63505, #39385, #57501, #49681, #5804, #56745, #34116, #69170, #69545, #17102, #57116, #51440, #45782, #35229, #44022, #11827, #63879, #67032, #12191, #46153, #5064, #28060, #39748, #22383, #62749, #51071, #28801, #5428, #34865, #26658, #74083, #40500, #52200, #45404, #17855, #62382, #72695, #16721, #51819, #10710, #11090, #28432, #22760, #68793, #57870, #163, #15331, #40125, #58247, #20997, #23141, #11459, #34494, #17479, #6178, #29185, #531, #23510, #46526, #40874, #54046, #53311, #18231, #1269, #64626, #29921, #7283, #58604, #71371, #1635, #13287, #1989, #24616, #58976, #37061, #59706, #901, #47261, #12922, #47996, #48367, #19325, #53676, #19696, #35956, #30291, #8015, #18966, #52562, #71010, #36327, #70646, #42338, #24979, #69921, #42708, #18602, #23888, #47624, #41246, #65355, #41969, #64254, #2357, #13655, #12563, #35590, #70288, #65719, #14023, #36695, #64979, #59341, #7653, #30659, #6910, #31022, #25351, #6547, #52939, #41612, #29553, #24249, #46897, #8382, #15156, #66094, #66468, #26856, #27222, #49493, #14777, #9136, #3479, #67603, #2730, #44218, #21565, #25718, #44591, #3861, #14404, #60435, #72124, #54795, #20438, #37436, #38188, #37817, #67231, #60061, #8765, #72886, #9889, #31775, #50239, #71745, #31397, #26092, #61192, #43078, #3106, #60812, #49112, #43454, #21193, #9522, #48739, #32153, #15900, #54424, #55548, #55174, #20060, #26469, #66853, #20820, #72512, #32537, #15527, #49870, #32918, #43838, #38568, #61568, #55924, #4234, #73260, #16264, #29096, #11004, #45693, #34406, #34037, #16636, #69459, #17392, #33285, #4979, #22300, #5715, #6091, #51730, #11372, #52116, #45324, #62669, #40417, #51354, #10260, #28715, #68708, #28347, #79, #57408, #27597, #23057, #33657, #17019, #34780, #4602, #50608, #11742, #56284, #46066, #448, #73628, #23427, #69086, #67969, #39304, #50985, #56663, #73998, #62302, #40043, #68341, #63414, #38931, #10630, #57784, #46441, #27980, #61933, #21933, #44963, #39670, #63047, #57034, #5346, #74365, #22676, #46806, #30571, #41887, #58159, #18145, #2269, #25263, #13201, #41160, #52479, #48282, #24533, #53222, #17767, #70564, #24891, #64898, #65263, #64538, #29469, #12474, #1181, #64170, #18515, #69830, #7931, #12835, #47541, #36239, #35872, #70206, #40783, #70928, #12107, #58518, #24162, #59255, #59616, #53593, #7567, #30935, #47174, #41522, #19240, #30201, #63789, #1904, #18880, #7198, #47909, #42250, #6466, #13568, #35505, #36606, #53956, #815, #23803, #35145, #6824, #29837, #52849, #58889, #1554, #43746, #20346, #59979, #44130, #66760, #54334, #25634, #37346, #32822, #38472, #26766, #9047, #55081, #14686, #72030, #48649, #38099, #32061, #43363, #2645, #60344, #32444, #8295, #26374, #19608, #49398, #71657, #3015, #61097, #61475, #60725, #25997, #66379, #37727, #4148, #66006, #19978, #3390, #71288, #31306, #8672, #72418, #55832, #72798, #42986, #21107, #42621, #55453, #20728, #65636, #49022, #14311, #36973, #31687, #67140, #15064, #13932, #54707, #9426, #3764, #49784, #15435, #27138, #9799, #10539, #34316, #57320, #74278, #33945, #33571, #40324, #22588, #57696, #56200, #4513, #27883, #6004, #4887, #50894, #56574, #45982, #68622, #16547, #16170, #73909, #11654, #45608, #10168, #28631, #39585, #39213, #73533, #34688, #50153, #22213, #73170, #21477, #5631, #45240, #56944, #28261, #44498, #33204, #68252, #67511, #16931, #39955, #33395, #5260, #51645, #51268, #63328, #15809, #38845, #62960, #62580, #61848, #50518, #22976, #10912, #44873, #11286, #27508, #68998, #21841, #67879, #17305, #62213, #65175, #30120, #59174, #36154, #361, #36525, #53137, #7484, #58435, #30489, #47085, #7114, #35428, #29748, #42162, #29005, #13486, #1100, #1824, #12393, #53506, #40697, #59535, #52762, #17680, #6745, #52023, #35059, #6383, #24451, #24076, #23714, #64816, #70123, #58072, #69370, #732, #24811, #18429, #23343, #46353, #41444, #63701, #64456, #12026, #29389, #47826, #64083, #13118, #70847, #1470, #12756, #35788, #19160 ),
 ( #47460, #52396, #46718, #58802, #18058, #69744, #41073, #70483, #18802, #41806, #44041, #14977, #54623, #14604, #60641, #2186, #65553, #65921, #30854, #3306, #26292, #32357, #66297, #66671, #8962, #72713, #15350, #53875, #37643, #20259, #21017, #8214, #38013, #48936, #2561, #43282, #38385, #31602, #67050, #7847, #61012, #55371, #25182, #31975, #9337, #3677, #48195, #71204, #54999, #26676, #37267, #49700, #25918, #49313, #14225, #8587, #19523, #42540, #13847, #2932, #36890, #60260, #59900, #31226, #54250, #71948, #25550, #72329, #48564, #71573, #19895, #20644, #43659, #42901, #22495, #16090, #15723, #56115, #67425, #68163, #61389, #73081, #73451, #16462, #45893, #62866, #21389, #11199, #9715, #45517, #10823, #55745, #39125, #4424, #16837, #27796, #27419, #22128, #68907, #10452, #51550, #17218, #39864, #34226, #22881, #62494, #57228, #68533, #32736, #4062, #33858, #5540, #62129, #28542, #4803, #39499, #67799, #33483, #74568, #27055, #50067, #56485, #44412, #44786, #38766, #61765, #10083, #50809, #33121, #73820, #50436, #21757, #45153, #56857, #5174, #28170, #51182, #74190, #69284, #34972, #46264, #47001, #40237, #51935, #52308, #70032, #24723, #41720, #273, #64732, #63239, #24364, #64365, #34599, #69655, #57988, #5916, #11940, #13031, #63994, #57606, #28919, #40987, #11565, #17968, #23255, #47732, #18712, #644, #47371, #70397, #12667, #23991, #23628, #30401, #35698, #70756, #36068, #12309, #63613, #1380, #35341, #58353, #46635, #59085, #58714, #6658, #6292, #29661, #1742, #7025, #17593, #7394, #52677, #29298, #1011, #40611, #18341, #41355, #30032, #53048, #53419, #65829, #25828, #71856, #13397, #2095, #2471, #42076, #14510, #37549, #43563, #2838, #3215, #20171, #9244, #26583, #65086, #48847, #31511, #32266, #19435, #43189, #54532, #55284, #42446, #49224, #60173, #13758, #66205, #49607, #42812, #3588, #19072, #72234, #66580, #36435, #60548, #20550, #26203, #59448, #7762, #8872, #14884, #48478, #37923, #37171, #31885, #25461, #19806, #30765, #53786, #25089, #14136, #60923, #71480, #48104, #71114, #65464, #8494, #36802, #54906, #59812, #8126, #31129, #54161, #4338, #67337, #33766, #27329, #26961, #15634, #3974, #4712, #72622, #9628, #9997, #27706, #57137, #74106, #32648, #22405, #20926, #56767, #22040, #66958, #50345, #38674, #38295, #44324, #45427, #21670, #15262, #61303, #73367, #43948, #44695, #55658, #5453, #51093, #33027, #5087, #28080, #45067, #56391, #56029, #62771, #68080, #28455, #68440, #67711, #21301, #16744, #16009, #39039, #62041, #39769, #16369, #10365, #61676, #33391, #34138, #39406, #49977, #11115, #50716, #73732, #62405, #72994, #10732, #34886, #51461, #12942, #58625, #23535, #58266, #29574, #45803, #34517, #57891, #74474, #46916, #69941, #1291, #35248, #35610, #52586, #41633, #59995, #22781, #923, #6198, #52220, #64644, #68813, #35979, #46547, #24270, #29207, #6932, #63155, #8312, #552, #40151, #69566, #17126, #57522, #28823, #18249, #17877, #46175, #12581, #40894, #5827, #69192, #51840, #6567, #11482, #186, #63526, #23906, #23162, #52957, #17504, #47281, #40521, #29942, #41265, #11849, #63900, #12210, #64274, #70307, #18622, #55100, #25651, #48666, #32079, #54349, #60744, #71674, #38861, #9815, #66398, #15454, #38489, #55469, #15081, #14706, #21496, #3782, #61865, #4166, #9067, #54727, #67159, #3407, #26391, #37744, #27153, #49800, #72438, #72047, #49416, #67527, #26783, #66023, #32839, #20747, #20364, #3033, #15826, #31323, #43763, #2659, #19995, #61492, #66777, #38116, #9445, #43003, #14331, #61115, #37363, #72816, #21123, #55849, #32462, #50170, #44145, #44515, #60363, #8689, #73188, #31704, #26017, #49040, #43381, #51286, #4909, #45626, #17695, #33966, #377, #40713, #40342, #34703, #46372, #11303, #63344, #17321, #56216, #10188, #34336, #11669, #39602, #57712, #28280, #23358, #16565, #56963, #6018, #22605, #4530, #5, #16949, #74297, #45999, #28647, #73552, #22993, #27903, #39973, #29022, #50537, #21861, #52041, #69387, #22231, #27525, #5278, #44892, #57337, #68640, #67897, #33219, #5647, #16189, #39230, #50912, #62230, #10557, #33588, #62980, #51662, #69017, #10929, #56593, #73926, #45257, #68269, #62599, #29764, #24828, #748, #18818, #12041, #41821, #69760, #70139, #30504, #30872, #53153, #18446, #12771 ) ),
 .UNSPECIFIED., .F., .F., .F. ) 
 B_SPLINE_SURFACE_WITH_KNOTS ( ( 2, 2 ),
 ( 3, 2, 2, 2, 2, 2, 2, 2, 2, 2, 2, 2, 2, 2, 2, 2, 2, 2, 2, 2, 2, 2, 2, 2, 2, 2, 2, 2, 2, 2, 2, 2, 2, 2, 2, 2, 2, 2, 2, 2, 2, 2, 2, 2, 2, 2, 2, 2, 2, 2, 2, 2, 2, 2, 2, 2, 2, 2, 2, 2, 2, 2, 2, 2, 2, 2, 2, 2, 2, 2, 2, 2, 2, 2, 2, 2, 2, 2, 2, 2, 2, 2, 2, 2, 2, 2, 2, 2, 2, 2, 2, 2, 2, 2, 2, 2, 2, 2, 2, 2, 2, 2, 2, 2, 2, 2, 2, 2, 2, 2, 2, 2, 2, 2, 2, 2, 2, 2, 2, 2, 2, 2, 2, 2, 2, 2, 2, 2, 2, 2, 2, 2, 2, 2, 2, 2, 2, 2, 2, 2, 2, 2, 2, 2, 2, 2, 2, 2, 2, 2, 2, 2, 2, 2, 2, 2, 2, 2, 2, 2, 2, 2, 2, 2, 2, 2, 2, 2, 2, 2, 2, 2, 2, 2, 2, 2, 2, 2, 2, 2, 2, 2, 2, 2, 2, 2, 2, 2, 2, 2, 2, 2, 2, 2, 2, 2, 2, 2, 2, 2, 2, 2, 2, 2, 2, 2, 2, 2, 2, 2, 2, 2, 2, 2, 2, 2, 2, 2, 2, 2, 2, 2, 2, 2, 2, 2, 2, 2, 2, 2, 2, 2, 2, 2, 2, 2, 2, 2, 2, 2, 2, 2, 2, 2, 2, 2, 2, 2, 2, 2, 2, 2, 2, 2, 2, 2, 2, 2, 2, 2, 2, 2, 2, 2, 2, 2, 2, 3 ),
 ( 0.000000000000000000, 1.000000000000000000 ),
 ( 0.000000000000000000, 0.003676470588235294067, 0.007352941176470588133, 0.01102941176470588307, 0.01470588235294117627, 0.01838235294117647120, 0.02205882352941176613, 0.02573529411764705760, 0.02941176470588235253, 0.03308823529411764747, 0.03676470588235294240, 0.04044117647058823733, 0.04411764705882353227, 0.04779411764705882026, 0.05147058823529411520, 0.05514705882352941013, 0.05882352941176470507, 0.06250000000000000000, 0.06617647058823529493, 0.06985294117647058987, 0.07352941176470588480, 0.07720588235294117974, 0.08088235294117647467, 0.08455882352941176960, 0.08823529411764706454, 0.09191176470588235947, 0.09558823529411764053, 0.09926470588235293546, 0.1029411764705882304, 0.1066176470588235253, 0.1102941176470588203, 0.1139705882352941152, 0.1176470588235294101, 0.1213235294117647051, 0.1250000000000000000, 0.1286764705882352811, 0.1323529411764705899, 0.1360294117647058709, 0.1397058823529411797, 0.1433823529411764608, 0.1470588235294117696, 0.1507352941176470507, 0.1544117647058823595, 0.1580882352941176405, 0.1617647058823529493, 0.1654411764705882304, 0.1691176470588235392, 0.1727941176470588203, 0.1764705882352941291, 0.1801470588235294101, 0.1838235294117647189, 0.1875000000000000000, 0.1911764705882352811, 0.1948529411764705899, 0.1985294117647058709, 0.2022058823529411797, 0.2058823529411764608, 0.2095588235294117696, 0.2132352941176470507, 0.2169117647058823595, 0.2205882352941176405, 0.2242647058823529493, 0.2279411764705882304, 0.2316176470588235392, 0.2352941176470588203, 0.2389705882352941291, 0.2426470588235294101, 0.2463235294117647189, 0.2500000000000000000, 0.2536764705882352811, 0.2573529411764705621, 0.2610294117647058987, 0.2647058823529411797, 0.2683823529411764608, 0.2720588235294117418, 0.2757352941176470784, 0.2794117647058823595, 0.2830882352941176405, 0.2867647058823529216, 0.2904411764705882582, 0.2941176470588235392, 0.2977941176470588203, 0.3014705882352941013, 0.3051470588235294379, 0.3088235294117647189, 0.3125000000000000000, 0.3161764705882352811, 0.3198529411764705621, 0.3235294117647058987, 0.3272058823529411797, 0.3308823529411764608, 0.3345588235294117418, 0.3382352941176470784, 0.3419117647058823595, 0.3455882352941176405, 0.3492647058823529216, 0.3529411764705882582, 0.3566176470588235392, 0.3602941176470588203, 0.3639705882352941013, 0.3676470588235294379, 0.3713235294117647189, 0.3750000000000000000, 0.3786764705882352811, 0.3823529411764705621, 0.3860294117647058987, 0.3897058823529411797, 0.3933823529411764608, 0.3970588235294117418, 0.4007352941176470784, 0.4044117647058823595, 0.4080882352941176405, 0.4117647058823529216, 0.4154411764705882582, 0.4191176470588235392, 0.4227941176470588203, 0.4264705882352941013, 0.4301470588235294379, 0.4338235294117647189, 0.4375000000000000000, 0.4411764705882352811, 0.4448529411764705621, 0.4485294117647058987, 0.4522058823529411797, 0.4558823529411764608, 0.4595588235294117418, 0.4632352941176470784, 0.4669117647058823595, 0.4705882352941176405, 0.4742647058823529216, 0.4779411764705882582, 0.4816176470588235392, 0.4852941176470588203, 0.4889705882352941013, 0.4926470588235294379, 0.4963235294117647189, 0.5000000000000000000, 0.5036764705882352811, 0.5073529411764705621, 0.5110294117647058432, 0.5147058823529411242, 0.5183823529411765163, 0.5220588235294117974, 0.5257352941176470784, 0.5294117647058823595, 0.5330882352941176405, 0.5367647058823529216, 0.5404411764705882026, 0.5441176470588234837, 0.5477941176470588758, 0.5514705882352941568, 0.5551470588235294379, 0.5588235294117647189, 0.5625000000000000000, 0.5661764705882352811, 0.5698529411764705621, 0.5735294117647058432, 0.5772058823529411242, 0.5808823529411765163, 0.5845588235294117974, 0.5882352941176470784, 0.5919117647058823595, 0.5955882352941176405, 0.5992647058823529216, 0.6029411764705882026, 0.6066176470588234837, 0.6102941176470588758, 0.6139705882352941568, 0.6176470588235294379, 0.6213235294117647189, 0.6250000000000000000, 0.6286764705882352811, 0.6323529411764705621, 0.6360294117647058432, 0.6397058823529411242, 0.6433823529411765163, 0.6470588235294117974, 0.6507352941176470784, 0.6544117647058823595, 0.6580882352941176405, 0.6617647058823529216, 0.6654411764705882026, 0.6691176470588234837, 0.6727941176470588758, 0.6764705882352941568, 0.6801470588235294379, 0.6838235294117647189, 0.6875000000000000000, 0.6911764705882352811, 0.6948529411764705621, 0.6985294117647058432, 0.7022058823529411242, 0.7058823529411765163, 0.7095588235294117974, 0.7132352941176470784, 0.7169117647058823595, 0.7205882352941176405, 0.7242647058823529216, 0.7279411764705882026, 0.7316176470588234837, 0.7352941176470588758, 0.7389705882352941568, 0.7426470588235294379, 0.7463235294117647189, 0.7500000000000000000, 0.7536764705882352811, 0.7573529411764705621, 0.7610294117647058432, 0.7647058823529411242, 0.7683823529411765163, 0.7720588235294117974, 0.7757352941176470784, 0.7794117647058823595, 0.7830882352941176405, 0.7867647058823529216, 0.7904411764705882026, 0.7941176470588234837, 0.7977941176470588758, 0.8014705882352941568, 0.8051470588235294379, 0.8088235294117647189, 0.8125000000000000000, 0.8161764705882352811, 0.8198529411764705621, 0.8235294117647058432, 0.8272058823529411242, 0.8308823529411765163, 0.8345588235294117974, 0.8382352941176470784, 0.8419117647058823595, 0.8455882352941176405, 0.8492647058823529216, 0.8529411764705882026, 0.8566176470588234837, 0.8602941176470588758, 0.8639705882352941568, 0.8676470588235294379, 0.8713235294117647189, 0.8750000000000000000, 0.8786764705882352811, 0.8823529411764705621, 0.8860294117647058432, 0.8897058823529411242, 0.8933823529411765163, 0.8970588235294117974, 0.9007352941176470784, 0.9044117647058823595, 0.9080882352941176405, 0.9117647058823529216, 0.9154411764705882026, 0.9191176470588234837, 0.9227941176470588758, 0.9264705882352941568, 0.9301470588235294379, 0.9338235294117647189, 0.9375000000000000000, 0.9411764705882352811, 0.9448529411764705621, 0.9485294117647058432, 0.9522058823529411242, 0.9558823529411765163, 0.9595588235294117974, 0.9632352941176470784, 0.9669117647058823595, 0.9705882352941176405, 0.9742647058823529216, 0.9779411764705882026, 0.9803851222046974234 ),
 .UNSPECIFIED. ) 
 GEOMETRIC_REPRESENTATION_ITEM ( )  RATIONAL_B_SPLINE_SURFACE ( (
 ( 1.000000000000000000, 0.9238795325112867385, 1.000000000000000000, 0.9238795325112867385, 1.000000000000000000, 0.9238795325112867385, 1.000000000000000000, 0.9238795325112867385, 1.000000000000000000, 0.9238795325112867385, 1.000000000000000000, 0.9238795325112867385, 1.000000000000000000, 0.9238795325112867385, 1.000000000000000000, 0.9238795325112867385, 1.000000000000000000, 0.9238795325112867385, 1.000000000000000000, 0.9238795325112867385, 1.000000000000000000, 0.9238795325112867385, 1.000000000000000000, 0.9238795325112867385, 1.000000000000000000, 0.9238795325112867385, 1.000000000000000000, 0.9238795325112867385, 1.000000000000000000, 0.9238795325112867385, 1.000000000000000000, 0.9238795325112867385, 1.000000000000000000, 0.9238795325112867385, 1.000000000000000000, 0.9238795325112867385, 1.000000000000000000, 0.9238795325112867385, 1.000000000000000000, 0.9238795325112867385, 1.000000000000000000, 0.9238795325112867385, 1.000000000000000000, 0.9238795325112867385, 1.000000000000000000, 0.9238795325112867385, 1.000000000000000000, 0.9238795325112867385, 1.000000000000000000, 0.9238795325112867385, 1.000000000000000000, 0.9238795325112867385, 1.000000000000000000, 0.9238795325112867385, 1.000000000000000000, 0.9238795325112867385, 1.000000000000000000, 0.9238795325112867385, 1.000000000000000000, 0.9238795325112867385, 1.000000000000000000, 0.9238795325112867385, 1.000000000000000000, 0.9238795325112867385, 1.000000000000000000, 0.9238795325112867385, 1.000000000000000000, 0.9238795325112867385, 1.000000000000000000, 0.9238795325112867385, 1.000000000000000000, 0.9238795325112867385, 1.000000000000000000, 0.9238795325112867385, 1.000000000000000000, 0.9238795325112867385, 1.000000000000000000, 0.9238795325112867385, 1.000000000000000000, 0.9238795325112867385, 1.000000000000000000, 0.9238795325112867385, 1.000000000000000000, 0.9238795325112867385, 1.000000000000000000, 0.9238795325112867385, 1.000000000000000000, 0.9238795325112867385, 1.000000000000000000, 0.9238795325112867385, 1.000000000000000000, 0.9238795325112867385, 1.000000000000000000, 0.9238795325112867385, 1.000000000000000000, 0.9238795325112867385, 1.000000000000000000, 0.9238795325112867385, 1.000000000000000000, 0.9238795325112867385, 1.000000000000000000, 0.9238795325112867385, 1.000000000000000000, 0.9238795325112867385, 1.000000000000000000, 0.9238795325112867385, 1.000000000000000000, 0.9238795325112867385, 1.000000000000000000, 0.9238795325112867385, 1.000000000000000000, 0.9238795325112867385, 1.000000000000000000, 0.9238795325112867385, 1.000000000000000000, 0.9238795325112867385, 1.000000000000000000, 0.9238795325112867385, 1.000000000000000000, 0.9238795325112867385, 1.000000000000000000, 0.9238795325112867385, 1.000000000000000000, 0.9238795325112867385, 1.000000000000000000, 0.9238795325112867385, 1.000000000000000000, 0.9238795325112867385, 1.000000000000000000, 0.9238795325112867385, 1.000000000000000000, 0.9238795325112867385, 1.000000000000000000, 0.9238795325112867385, 1.000000000000000000, 0.9238795325112867385, 1.000000000000000000, 0.9238795325112867385, 1.000000000000000000, 0.9238795325112867385, 1.000000000000000000, 0.9238795325112867385, 1.000000000000000000, 0.9238795325112867385, 1.000000000000000000, 0.9238795325112867385, 1.000000000000000000, 0.9238795325112867385, 1.000000000000000000, 0.9238795325112867385, 1.000000000000000000, 0.9238795325112867385, 1.000000000000000000, 0.9238795325112867385, 1.000000000000000000, 0.9238795325112867385, 1.000000000000000000, 0.9238795325112867385, 1.000000000000000000, 0.9238795325112867385, 1.000000000000000000, 0.9238795325112867385, 1.000000000000000000, 0.9238795325112867385, 1.000000000000000000, 0.9238795325112867385, 1.000000000000000000, 0.9238795325112867385, 1.000000000000000000, 0.9238795325112867385, 1.000000000000000000, 0.9238795325112867385, 1.000000000000000000, 0.9238795325112867385, 1.000000000000000000, 0.9238795325112867385, 1.000000000000000000, 0.9238795325112867385, 1.000000000000000000, 0.9238795325112867385, 1.000000000000000000, 0.9238795325112867385, 1.000000000000000000, 0.9238795325112867385, 1.000000000000000000, 0.9238795325112867385, 1.000000000000000000, 0.9238795325112867385, 1.000000000000000000, 0.9238795325112867385, 1.000000000000000000, 0.9238795325112867385, 1.000000000000000000, 0.9238795325112867385, 1.000000000000000000, 0.9238795325112867385, 1.000000000000000000, 0.9238795325112867385, 1.000000000000000000, 0.9238795325112867385, 1.000000000000000000, 0.9238795325112867385, 1.000000000000000000, 0.9238795325112867385, 1.000000000000000000, 0.9238795325112867385, 1.000000000000000000, 0.9238795325112867385, 1.000000000000000000, 0.9238795325112867385, 1.000000000000000000, 0.9238795325112867385, 1.000000000000000000, 0.9238795325112867385, 1.000000000000000000, 0.9238795325112867385, 1.000000000000000000, 0.9238795325112867385, 1.000000000000000000, 0.9238795325112867385, 1.000000000000000000, 0.9238795325112867385, 1.000000000000000000, 0.9238795325112867385, 1.000000000000000000, 0.9238795325112867385, 1.000000000000000000, 0.9238795325112867385, 1.000000000000000000, 0.9238795325112867385, 1.000000000000000000, 0.9238795325112867385, 1.000000000000000000, 0.9238795325112867385, 1.000000000000000000, 0.9238795325112867385, 1.000000000000000000, 0.9238795325112867385, 1.000000000000000000, 0.9238795325112867385, 1.000000000000000000, 0.9238795325112867385, 1.000000000000000000, 0.9238795325112867385, 1.000000000000000000, 0.9238795325112867385, 1.000000000000000000, 0.9238795325112867385, 1.000000000000000000, 0.9238795325112867385, 1.000000000000000000, 0.9238795325112867385, 1.000000000000000000, 0.9238795325112867385, 1.000000000000000000, 0.9238795325112867385, 1.000000000000000000, 0.9238795325112867385, 1.000000000000000000, 0.9238795325112867385, 1.000000000000000000, 0.9238795325112867385, 1.000000000000000000, 0.9238795325112867385, 1.000000000000000000, 0.9238795325112867385, 1.000000000000000000, 0.9238795325112867385, 1.000000000000000000, 0.9238795325112867385, 1.000000000000000000, 0.9238795325112867385, 1.000000000000000000, 0.9238795325112867385, 1.000000000000000000, 0.9238795325112867385, 1.000000000000000000, 0.9238795325112867385, 1.000000000000000000, 0.9238795325112867385, 1.000000000000000000, 0.9238795325112867385, 1.000000000000000000, 0.9238795325112867385, 1.000000000000000000, 0.9238795325112867385, 1.000000000000000000, 0.9238795325112867385, 1.000000000000000000, 0.9238795325112867385, 1.000000000000000000, 0.9238795325112867385, 1.000000000000000000, 0.9238795325112867385, 1.000000000000000000, 0.9238795325112867385, 1.000000000000000000, 0.9238795325112867385, 1.000000000000000000, 0.9238795325112867385, 1.000000000000000000, 0.9238795325112867385, 1.000000000000000000, 0.9238795325112867385, 1.000000000000000000, 0.9238795325112867385, 1.000000000000000000, 0.9238795325112867385, 1.000000000000000000, 0.9238795325112867385, 1.000000000000000000, 0.9238795325112867385, 1.000000000000000000, 0.9238795325112867385, 1.000000000000000000, 0.9238795325112867385, 1.000000000000000000, 0.9238795325112867385, 1.000000000000000000, 0.9238795325112867385, 1.000000000000000000, 0.9238795325112867385, 1.000000000000000000, 0.9238795325112867385, 1.000000000000000000, 0.9238795325112867385, 1.000000000000000000, 0.9238795325112867385, 1.000000000000000000, 0.9238795325112867385, 1.000000000000000000, 0.9238795325112867385, 1.000000000000000000, 0.9238795325112867385, 1.000000000000000000, 0.9238795325112867385, 1.000000000000000000, 0.9238795325112867385, 1.000000000000000000, 0.9238795325112867385, 1.000000000000000000, 0.9238795325112867385, 1.000000000000000000, 0.9238795325112867385, 1.000000000000000000, 0.9238795325112867385, 1.000000000000000000, 0.9238795325112867385, 1.000000000000000000, 0.9238795325112867385, 1.000000000000000000, 0.9238795325112867385, 1.000000000000000000, 0.9238795325112867385, 1.000000000000000000, 0.9238795325112867385, 1.000000000000000000, 0.9238795325112867385, 1.000000000000000000, 0.9238795325112867385, 1.000000000000000000, 0.9238795325112867385, 1.000000000000000000, 0.9238795325112867385, 1.000000000000000000, 0.9238795325112867385, 1.000000000000000000, 0.9238795325112867385, 1.000000000000000000, 0.9238795325112867385, 1.000000000000000000, 0.9238795325112867385, 1.000000000000000000, 0.9238795325112867385, 1.000000000000000000, 0.9238795325112867385, 1.000000000000000000, 0.9238795325112867385, 1.000000000000000000, 0.9238795325112867385, 1.000000000000000000, 0.9238795325112867385, 1.000000000000000000, 0.9238795325112867385, 1.000000000000000000, 0.9238795325112867385, 1.000000000000000000, 0.9238795325112867385, 1.000000000000000000, 0.9238795325112867385, 1.000000000000000000, 0.9238795325112867385, 1.000000000000000000, 0.9238795325112867385, 1.000000000000000000, 0.9238795325112867385, 1.000000000000000000, 0.9238795325112867385, 1.000000000000000000, 0.9238795325112867385, 1.000000000000000000, 0.9238795325112867385, 1.000000000000000000, 0.9238795325112867385, 1.000000000000000000, 0.9238795325112867385, 1.000000000000000000, 0.9238795325112867385, 1.000000000000000000, 0.9238795325112867385, 1.000000000000000000, 0.9238795325112867385, 1.000000000000000000, 0.9238795325112867385, 1.000000000000000000, 0.9238795325112867385, 1.000000000000000000, 0.9238795325112867385, 1.000000000000000000, 0.9238795325112867385, 1.000000000000000000, 0.9238795325112867385, 1.000000000000000000, 0.9238795325112867385, 1.000000000000000000, 0.9238795325112867385, 1.000000000000000000, 0.9238795325112867385, 1.000000000000000000, 0.9238795325112867385, 1.000000000000000000, 0.9238795325112867385, 1.000000000000000000, 0.9238795325112867385, 1.000000000000000000, 0.9238795325112867385, 1.000000000000000000, 0.9238795325112867385, 1.000000000000000000, 0.9238795325112867385, 1.000000000000000000, 0.9238795325112867385, 1.000000000000000000, 0.9238795325112867385, 1.000000000000000000, 0.9238795325112867385, 1.000000000000000000, 0.9238795325112867385, 1.000000000000000000, 0.9238795325112867385, 1.000000000000000000, 0.9238795325112867385, 1.000000000000000000, 0.9238795325112867385, 1.000000000000000000, 0.9238795325112867385, 1.000000000000000000, 0.9238795325112867385, 1.000000000000000000, 0.9238795325112867385, 1.000000000000000000, 0.9238795325112867385, 1.000000000000000000, 0.9238795325112867385, 1.000000000000000000, 0.9238795325112867385, 1.000000000000000000, 0.9238795325112867385, 1.000000000000000000, 0.9238795325112867385, 1.000000000000000000, 0.9238795325112867385, 1.000000000000000000, 0.9238795325112867385, 1.000000000000000000, 0.9238795325112867385, 1.000000000000000000, 0.9238795325112867385, 1.000000000000000000, 0.9238795325112867385, 1.000000000000000000, 0.9238795325112867385, 1.000000000000000000, 0.9238795325112867385, 1.000000000000000000, 0.9238795325112867385, 1.000000000000000000, 0.9238795325112867385, 1.000000000000000000, 0.9238795325112867385, 1.000000000000000000, 0.9238795325112867385, 1.000000000000000000, 0.9238795325112867385, 1.000000000000000000, 0.9238795325112867385, 1.000000000000000000, 0.9238795325112867385, 1.000000000000000000, 0.9238795325112867385, 1.000000000000000000, 0.9238795325112867385, 1.000000000000000000, 0.9238795325112867385, 1.000000000000000000, 0.9238795325112867385, 1.000000000000000000, 0.9238795325112867385, 1.000000000000000000, 0.9238795325112867385, 1.000000000000000000, 0.9238795325112867385, 1.000000000000000000, 0.9238795325112867385, 1.000000000000000000, 0.9238795325112867385, 1.000000000000000000, 0.9238795325112867385, 1.000000000000000000, 0.9238795325112867385, 1.000000000000000000, 0.9238795325112867385, 1.000000000000000000, 0.9238795325112867385, 1.000000000000000000, 0.9238795325112867385, 1.000000000000000000, 0.9238795325112867385, 1.000000000000000000, 0.9238795325112867385, 1.000000000000000000, 0.9238795325112867385, 1.000000000000000000, 0.9493986726310960078, 0.9660721378631347278),
 ( 1.000000000000000000, 0.9238795325112867385, 1.000000000000000000, 0.9238795325112867385, 1.000000000000000000, 0.9238795325112867385, 1.000000000000000000, 0.9238795325112867385, 1.000000000000000000, 0.9238795325112867385, 1.000000000000000000, 0.9238795325112867385, 1.000000000000000000, 0.9238795325112867385, 1.000000000000000000, 0.9238795325112867385, 1.000000000000000000, 0.9238795325112867385, 1.000000000000000000, 0.9238795325112867385, 1.000000000000000000, 0.9238795325112867385, 1.000000000000000000, 0.9238795325112867385, 1.000000000000000000, 0.9238795325112867385, 1.000000000000000000, 0.9238795325112867385, 1.000000000000000000, 0.9238795325112867385, 1.000000000000000000, 0.9238795325112867385, 1.000000000000000000, 0.9238795325112867385, 1.000000000000000000, 0.9238795325112867385, 1.000000000000000000, 0.9238795325112867385, 1.000000000000000000, 0.9238795325112867385, 1.000000000000000000, 0.9238795325112867385, 1.000000000000000000, 0.9238795325112867385, 1.000000000000000000, 0.9238795325112867385, 1.000000000000000000, 0.9238795325112867385, 1.000000000000000000, 0.9238795325112867385, 1.000000000000000000, 0.9238795325112867385, 1.000000000000000000, 0.9238795325112867385, 1.000000000000000000, 0.9238795325112867385, 1.000000000000000000, 0.9238795325112867385, 1.000000000000000000, 0.9238795325112867385, 1.000000000000000000, 0.9238795325112867385, 1.000000000000000000, 0.9238795325112867385, 1.000000000000000000, 0.9238795325112867385, 1.000000000000000000, 0.9238795325112867385, 1.000000000000000000, 0.9238795325112867385, 1.000000000000000000, 0.9238795325112867385, 1.000000000000000000, 0.9238795325112867385, 1.000000000000000000, 0.9238795325112867385, 1.000000000000000000, 0.9238795325112867385, 1.000000000000000000, 0.9238795325112867385, 1.000000000000000000, 0.9238795325112867385, 1.000000000000000000, 0.9238795325112867385, 1.000000000000000000, 0.9238795325112867385, 1.000000000000000000, 0.9238795325112867385, 1.000000000000000000, 0.9238795325112867385, 1.000000000000000000, 0.9238795325112867385, 1.000000000000000000, 0.9238795325112867385, 1.000000000000000000, 0.9238795325112867385, 1.000000000000000000, 0.9238795325112867385, 1.000000000000000000, 0.9238795325112867385, 1.000000000000000000, 0.9238795325112867385, 1.000000000000000000, 0.9238795325112867385, 1.000000000000000000, 0.9238795325112867385, 1.000000000000000000, 0.9238795325112867385, 1.000000000000000000, 0.9238795325112867385, 1.000000000000000000, 0.9238795325112867385, 1.000000000000000000, 0.9238795325112867385, 1.000000000000000000, 0.9238795325112867385, 1.000000000000000000, 0.9238795325112867385, 1.000000000000000000, 0.9238795325112867385, 1.000000000000000000, 0.9238795325112867385, 1.000000000000000000, 0.9238795325112867385, 1.000000000000000000, 0.9238795325112867385, 1.000000000000000000, 0.9238795325112867385, 1.000000000000000000, 0.9238795325112867385, 1.000000000000000000, 0.9238795325112867385, 1.000000000000000000, 0.9238795325112867385, 1.000000000000000000, 0.9238795325112867385, 1.000000000000000000, 0.9238795325112867385, 1.000000000000000000, 0.9238795325112867385, 1.000000000000000000, 0.9238795325112867385, 1.000000000000000000, 0.9238795325112867385, 1.000000000000000000, 0.9238795325112867385, 1.000000000000000000, 0.9238795325112867385, 1.000000000000000000, 0.9238795325112867385, 1.000000000000000000, 0.9238795325112867385, 1.000000000000000000, 0.9238795325112867385, 1.000000000000000000, 0.9238795325112867385, 1.000000000000000000, 0.9238795325112867385, 1.000000000000000000, 0.9238795325112867385, 1.000000000000000000, 0.9238795325112867385, 1.000000000000000000, 0.9238795325112867385, 1.000000000000000000, 0.9238795325112867385, 1.000000000000000000, 0.9238795325112867385, 1.000000000000000000, 0.9238795325112867385, 1.000000000000000000, 0.9238795325112867385, 1.000000000000000000, 0.9238795325112867385, 1.000000000000000000, 0.9238795325112867385, 1.000000000000000000, 0.9238795325112867385, 1.000000000000000000, 0.9238795325112867385, 1.000000000000000000, 0.9238795325112867385, 1.000000000000000000, 0.9238795325112867385, 1.000000000000000000, 0.9238795325112867385, 1.000000000000000000, 0.9238795325112867385, 1.000000000000000000, 0.9238795325112867385, 1.000000000000000000, 0.9238795325112867385, 1.000000000000000000, 0.9238795325112867385, 1.000000000000000000, 0.9238795325112867385, 1.000000000000000000, 0.9238795325112867385, 1.000000000000000000, 0.9238795325112867385, 1.000000000000000000, 0.9238795325112867385, 1.000000000000000000, 0.9238795325112867385, 1.000000000000000000, 0.9238795325112867385, 1.000000000000000000, 0.9238795325112867385, 1.000000000000000000, 0.9238795325112867385, 1.000000000000000000, 0.9238795325112867385, 1.000000000000000000, 0.9238795325112867385, 1.000000000000000000, 0.9238795325112867385, 1.000000000000000000, 0.9238795325112867385, 1.000000000000000000, 0.9238795325112867385, 1.000000000000000000, 0.9238795325112867385, 1.000000000000000000, 0.9238795325112867385, 1.000000000000000000, 0.9238795325112867385, 1.000000000000000000, 0.9238795325112867385, 1.000000000000000000, 0.9238795325112867385, 1.000000000000000000, 0.9238795325112867385, 1.000000000000000000, 0.9238795325112867385, 1.000000000000000000, 0.9238795325112867385, 1.000000000000000000, 0.9238795325112867385, 1.000000000000000000, 0.9238795325112867385, 1.000000000000000000, 0.9238795325112867385, 1.000000000000000000, 0.9238795325112867385, 1.000000000000000000, 0.9238795325112867385, 1.000000000000000000, 0.9238795325112867385, 1.000000000000000000, 0.9238795325112867385, 1.000000000000000000, 0.9238795325112867385, 1.000000000000000000, 0.9238795325112867385, 1.000000000000000000, 0.9238795325112867385, 1.000000000000000000, 0.9238795325112867385, 1.000000000000000000, 0.9238795325112867385, 1.000000000000000000, 0.9238795325112867385, 1.000000000000000000, 0.9238795325112867385, 1.000000000000000000, 0.9238795325112867385, 1.000000000000000000, 0.9238795325112867385, 1.000000000000000000, 0.9238795325112867385, 1.000000000000000000, 0.9238795325112867385, 1.000000000000000000, 0.9238795325112867385, 1.000000000000000000, 0.9238795325112867385, 1.000000000000000000, 0.9238795325112867385, 1.000000000000000000, 0.9238795325112867385, 1.000000000000000000, 0.9238795325112867385, 1.000000000000000000, 0.9238795325112867385, 1.000000000000000000, 0.9238795325112867385, 1.000000000000000000, 0.9238795325112867385, 1.000000000000000000, 0.9238795325112867385, 1.000000000000000000, 0.9238795325112867385, 1.000000000000000000, 0.9238795325112867385, 1.000000000000000000, 0.9238795325112867385, 1.000000000000000000, 0.9238795325112867385, 1.000000000000000000, 0.9238795325112867385, 1.000000000000000000, 0.9238795325112867385, 1.000000000000000000, 0.9238795325112867385, 1.000000000000000000, 0.9238795325112867385, 1.000000000000000000, 0.9238795325112867385, 1.000000000000000000, 0.9238795325112867385, 1.000000000000000000, 0.9238795325112867385, 1.000000000000000000, 0.9238795325112867385, 1.000000000000000000, 0.9238795325112867385, 1.000000000000000000, 0.9238795325112867385, 1.000000000000000000, 0.9238795325112867385, 1.000000000000000000, 0.9238795325112867385, 1.000000000000000000, 0.9238795325112867385, 1.000000000000000000, 0.9238795325112867385, 1.000000000000000000, 0.9238795325112867385, 1.000000000000000000, 0.9238795325112867385, 1.000000000000000000, 0.9238795325112867385, 1.000000000000000000, 0.9238795325112867385, 1.000000000000000000, 0.9238795325112867385, 1.000000000000000000, 0.9238795325112867385, 1.000000000000000000, 0.9238795325112867385, 1.000000000000000000, 0.9238795325112867385, 1.000000000000000000, 0.9238795325112867385, 1.000000000000000000, 0.9238795325112867385, 1.000000000000000000, 0.9238795325112867385, 1.000000000000000000, 0.9238795325112867385, 1.000000000000000000, 0.9238795325112867385, 1.000000000000000000, 0.9238795325112867385, 1.000000000000000000, 0.9238795325112867385, 1.000000000000000000, 0.9238795325112867385, 1.000000000000000000, 0.9238795325112867385, 1.000000000000000000, 0.9238795325112867385, 1.000000000000000000, 0.9238795325112867385, 1.000000000000000000, 0.9238795325112867385, 1.000000000000000000, 0.9238795325112867385, 1.000000000000000000, 0.9238795325112867385, 1.000000000000000000, 0.9238795325112867385, 1.000000000000000000, 0.9238795325112867385, 1.000000000000000000, 0.9238795325112867385, 1.000000000000000000, 0.9238795325112867385, 1.000000000000000000, 0.9238795325112867385, 1.000000000000000000, 0.9238795325112867385, 1.000000000000000000, 0.9238795325112867385, 1.000000000000000000, 0.9238795325112867385, 1.000000000000000000, 0.9238795325112867385, 1.000000000000000000, 0.9238795325112867385, 1.000000000000000000, 0.9238795325112867385, 1.000000000000000000, 0.9238795325112867385, 1.000000000000000000, 0.9238795325112867385, 1.000000000000000000, 0.9238795325112867385, 1.000000000000000000, 0.9238795325112867385, 1.000000000000000000, 0.9238795325112867385, 1.000000000000000000, 0.9238795325112867385, 1.000000000000000000, 0.9238795325112867385, 1.000000000000000000, 0.9238795325112867385, 1.000000000000000000, 0.9238795325112867385, 1.000000000000000000, 0.9238795325112867385, 1.000000000000000000, 0.9238795325112867385, 1.000000000000000000, 0.9238795325112867385, 1.000000000000000000, 0.9238795325112867385, 1.000000000000000000, 0.9238795325112867385, 1.000000000000000000, 0.9238795325112867385, 1.000000000000000000, 0.9238795325112867385, 1.000000000000000000, 0.9238795325112867385, 1.000000000000000000, 0.9238795325112867385, 1.000000000000000000, 0.9238795325112867385, 1.000000000000000000, 0.9238795325112867385, 1.000000000000000000, 0.9238795325112867385, 1.000000000000000000, 0.9238795325112867385, 1.000000000000000000, 0.9238795325112867385, 1.000000000000000000, 0.9238795325112867385, 1.000000000000000000, 0.9238795325112867385, 1.000000000000000000, 0.9238795325112867385, 1.000000000000000000, 0.9238795325112867385, 1.000000000000000000, 0.9238795325112867385, 1.000000000000000000, 0.9238795325112867385, 1.000000000000000000, 0.9238795325112867385, 1.000000000000000000, 0.9238795325112867385, 1.000000000000000000, 0.9238795325112867385, 1.000000000000000000, 0.9238795325112867385, 1.000000000000000000, 0.9238795325112867385, 1.000000000000000000, 0.9238795325112867385, 1.000000000000000000, 0.9238795325112867385, 1.000000000000000000, 0.9238795325112867385, 1.000000000000000000, 0.9238795325112867385, 1.000000000000000000, 0.9238795325112867385, 1.000000000000000000, 0.9238795325112867385, 1.000000000000000000, 0.9238795325112867385, 1.000000000000000000, 0.9238795325112867385, 1.000000000000000000, 0.9238795325112867385, 1.000000000000000000, 0.9238795325112867385, 1.000000000000000000, 0.9238795325112867385, 1.000000000000000000, 0.9238795325112867385, 1.000000000000000000, 0.9238795325112867385, 1.000000000000000000, 0.9238795325112867385, 1.000000000000000000, 0.9238795325112867385, 1.000000000000000000, 0.9238795325112867385, 1.000000000000000000, 0.9238795325112867385, 1.000000000000000000, 0.9238795325112867385, 1.000000000000000000, 0.9238795325112867385, 1.000000000000000000, 0.9238795325112867385, 1.000000000000000000, 0.9238795325112867385, 1.000000000000000000, 0.9238795325112867385, 1.000000000000000000, 0.9238795325112867385, 1.000000000000000000, 0.9238795325112867385, 1.000000000000000000, 0.9238795325112867385, 1.000000000000000000, 0.9238795325112867385, 1.000000000000000000, 0.9238795325112867385, 1.000000000000000000, 0.9238795325112867385, 1.000000000000000000, 0.9238795325112867385, 1.000000000000000000, 0.9238795325112867385, 1.000000000000000000, 0.9238795325112867385, 1.000000000000000000, 0.9238795325112867385, 1.000000000000000000, 0.9238795325112867385, 1.000000000000000000, 0.9238795325112867385, 1.000000000000000000, 0.9238795325112867385, 1.000000000000000000, 0.9238795325112867385, 1.000000000000000000, 0.9493986726310960078, 0.9660721378631347278) ) ) 
 REPRESENTATION_ITEM ( '' )  SURFACE ( )  );
#25799 = DIRECTION ( 'NONE',  ( -0.000000000000000000, -0.000000000000000000, -1.000000000000000000 ) ) ;
#25800 = CARTESIAN_POINT ( 'NONE',  ( 2.977408999572646486, 7.188101187499992051, 22.39280278187175810 ) ) ;
#25801 = CARTESIAN_POINT ( 'NONE',  ( 11.35316468750000141, 161.0937499965860127, 0.000000000000000000 ) ) ;
#25802 = CARTESIAN_POINT ( 'NONE',  ( 7.999999999999991118, 2.512580743551133942E-05, 22.76780349476856458 ) ) ;
#25803 = CARTESIAN_POINT ( 'NONE',  ( -5.000000000000000000, 50.64189880742059557, 41.08656465431948845 ) ) ;
#25806 = CARTESIAN_POINT ( 'NONE',  ( -2.485281374238916374, 293.8125000000000000, -5.999999999999657163 ) ) ;
#25805 = CYLINDRICAL_SURFACE ( 'NONE', #74373, 45.00000000000000000 ) ;
#25804 = CARTESIAN_POINT ( 'NONE',  ( 30.82842712474617031, 201.1250000000000284, 172.8284271247460993 ) ) ;
#25807 = ORIENTED_EDGE ( 'NONE', *, *, #35656, .F. ) ;
#25808 = EDGE_CURVE ( 'NONE', #47864, #30692, #33774, .T. ) ;
#25809 = CARTESIAN_POINT ( 'NONE',  ( -5.676582343750006032, 4.427083329919350163, 9.832129032723418760 ) ) ;
#25810 = CARTESIAN_POINT ( 'NONE',  ( -7.778174593052023411, 7.778174593052023411, 77.50000000409676204 ) ) ;
#25811 = DIRECTION ( 'NONE',  ( -0.000000000000000000, 0.000000000000000000, 1.000000000000000000 ) ) ;
#25812 = CARTESIAN_POINT ( 'NONE',  ( 2.849036369511732440E-14, 196.3750000027311842, 202.0000000000000000 ) ) ;
#25813 = CARTESIAN_POINT ( 'NONE',  ( 1.432654583217607192, 206.2500000013655779, 145.4587341250000350 ) ) ;
#25814 = CARTESIAN_POINT ( 'NONE',  ( 10.00000000000000000, 51.66666665983870388, 2.679491924311236062 ) ) ;
#25815 = CIRCLE ( 'NONE', #23408, 20.00000000000001066 ) ;
#25816 = CARTESIAN_POINT ( 'NONE',  ( 2.977408999572654480, 106.6250000020483952, 7.188101187499999156 ) ) ;
#25817 = CARTESIAN_POINT ( 'NONE',  ( -3.211159895383561391, 4.812499998634407028, -3.211159895383561835 ) ) ;
#25818 = CARTESIAN_POINT ( 'NONE',  ( 5.656854249492376141, -5.656854249492374365, 13.58030278392014623 ) ) ;
#25819 = CARTESIAN_POINT ( 'NONE',  ( 7.999999999999991118, 9.797174393178815797E-16, 9.080302779823364645 ) ) ;
#25821 = CARTESIAN_POINT ( 'NONE',  ( -8.000000000000000000, 26.15625000000000711, -3.313708498984762496 ) ) ;
#25820 = CARTESIAN_POINT ( 'NONE',  ( 3.160135233961288037, 194.4900331791219514, 140.5039915082175526 ) ) ;
#25822 = VERTEX_POINT ( 'NONE', #62779 ) ;
#25823 = CARTESIAN_POINT ( 'NONE',  ( -5.000000000000000888, -63.46295559274116016, 24.14151313015344158 ) ) ;
#25824 = CARTESIAN_POINT ( 'NONE',  ( 5.676582343749997150, 237.5520833367473301, -9.832129032723418760 ) ) ;
#25825 = CARTESIAN_POINT ( 'NONE',  ( -2.085542519210945728E-15, 134.5312499965860411, 11.35316468750000141 ) ) ;
#25826 = VERTEX_POINT ( 'NONE', #57528 ) ;
#25827 = DIRECTION ( 'NONE',  ( -1.000000000000000000, 0.000000000000000000, 0.000000000000000000 ) ) ;
#25828 = CARTESIAN_POINT ( 'NONE',  ( 4.220049686691941027, -10.18810118749999738, 98.12500000204836681 ) ) ;
#25829 = DIRECTION ( 'NONE',  ( 0.000000000000000000, -1.000000000000000000, 0.000000000000000000 ) ) ;
#25830 = CARTESIAN_POINT ( 'NONE',  ( -3.458734124999960358, 196.6250000013656063, 196.5673454167823877 ) ) ;
#25831 = CARTESIAN_POINT ( 'NONE',  ( 31.99999999999997868, 197.1875000000000284, 171.6568542494923122 ) ) ;
#25833 = CARTESIAN_POINT ( 'NONE',  ( -11.35316468749999785, 108.0729166632526699, -3.042071309553167957 ) ) ;
#25832 = CARTESIAN_POINT ( 'NONE',  ( 4.508099642231537807, 219.9999999999999716, 9.452567682505941704 ) ) ;
#25834 = EDGE_CURVE ( 'NONE', #18351, #11931, #49365, .T. ) ;
#25835 = CARTESIAN_POINT ( 'NONE',  ( -29.65685424949241877, 208.0625000000000000, 166.0000000000004263 ) ) ;
#25836 = EDGE_LOOP ( 'NONE', ( #20677, #48661, #66001, #36884, #19923, #68304 ) ) ;
#25837 = CARTESIAN_POINT ( 'NONE',  ( -7.778174593052023411, 7.778174593052023411, 77.31249999999997158 ) ) ;
#25838 = CARTESIAN_POINT ( 'NONE',  ( 28.00000000000001776, 198.5000000000000000, 165.9999999999998863 ) ) ;
#25839 = CARTESIAN_POINT ( 'NONE',  ( 9.832129032723416984, 100.6770833299193555, 5.676582343750006032 ) ) ;
#25840 = CARTESIAN_POINT ( 'NONE',  ( 3.458734125000015425, 206.9375000013656063, 198.0000000000000284 ) ) ;
#25841 = CARTESIAN_POINT ( 'NONE',  ( 4.401442555609581635E-16, 20.71874999795161543, -7.188101187500000044 ) ) ;
#25842 = CARTESIAN_POINT ( 'NONE',  ( -10.18810118749999916, 0.000000000000000000, 92.03125000204836681 ) ) ;
#25843 = CARTESIAN_POINT ( 'NONE',  ( 9.832129032723416984, 25.67708332991935194, 5.676582343750006032 ) ) ;
#25844 = ORIENTED_EDGE ( 'NONE', *, *, #28662, .F. ) ;
#25845 = CARTESIAN_POINT ( 'NONE',  ( -2.584176286468218287, 67.83040016931262528, -20.22720298431334029 ) ) ;
#25846 = CARTESIAN_POINT ( 'NONE',  ( 3.317071493978883456, -8.008118988124989457, 25.48186528394063188 ) ) ;
#25847 = DIRECTION ( 'NONE',  ( 0.000000000000000000, 0.000000000000000000, 1.000000000000000000 ) ) ;
#25848 = CIRCLE ( 'NONE', #33116, 8.000000000000003553 ) ;
#25849 = CARTESIAN_POINT ( 'NONE',  ( 1.672363534939973917, 21.99999999999999289, 4.002810566133208958 ) ) ;
#25850 = CARTESIAN_POINT ( 'NONE',  ( 2.977408999572651815, 3.187499997951610098, 7.188101187500000933 ) ) ;
#25851 = CARTESIAN_POINT ( 'NONE',  ( -6.676582343750001591, 289.4531250017069510, 0.000000000000000000 ) ) ;
#25852 = CARTESIAN_POINT ( 'NONE',  ( 0.000000000000000000, 30.78460969082653875, -20.69999999999999929 ) ) ;
#25853 = CARTESIAN_POINT ( 'NONE',  ( 11.35316468750000141, 216.0937499965860411, 0.000000000000000000 ) ) ;
#25854 = CARTESIAN_POINT ( 'NONE',  ( 3.042071309553167069, 142.1354166632526415, -11.35316468749999785 ) ) ;
#25855 = CARTESIAN_POINT ( 'NONE',  ( 10.18810118749999916, 4.220049686691935698, 82.00000000204836681 ) ) ;
#25856 = CARTESIAN_POINT ( 'NONE',  ( -31.45873412499999944, 198.6250000013655779, 168.5673454167827572 ) ) ;
#25857 = FACE_OUTER_BOUND ( 'NONE', #44853, .T. ) ;
#25858 = CARTESIAN_POINT ( 'NONE',  ( 4.541265875000002339, 10.49999999863440792, -1.881053915767121554 ) ) ;
#25859 = ORIENTED_EDGE ( 'NONE', *, *, #34709, .T. ) ;
#25860 = CARTESIAN_POINT ( 'NONE',  ( -2.828427124746153876, 205.0000000027312126, 195.1715728752538439 ) ) ;
#25861 = CARTESIAN_POINT ( 'NONE',  ( -1.432654583217664701, 200.0000000013656347, 138.5412658750000787 ) ) ;
#25862 = CARTESIAN_POINT ( 'NONE',  ( -4.000000000000015987, 202.5625000027312126, 140.3431457505076594 ) ) ;
#25863 = ADVANCED_FACE ( 'NONE', ( #44703 ), #45810, .F. ) ;
#25864 = CONICAL_SURFACE ( 'NONE', #72851, 12.50000000000000178, 0.06208826691561822320 ) ;
#25865 = CARTESIAN_POINT ( 'NONE',  ( 5.000000000000000888, 14.70421557449305716, -69.92631206022691970 ) ) ;
#25866 = VERTEX_POINT ( 'NONE', #51849 ) ;
#25867 = CARTESIAN_POINT ( 'NONE',  ( 2.977408999572652260, 3.187499997951610098, 7.188101187500000044 ) ) ;
#25868 = CARTESIAN_POINT ( 'NONE',  ( -11.00000000000000000, 0.000000000000000000, 75.99999999999998579 ) ) ;
#25869 = DIRECTION ( 'NONE',  ( -0.000000000000000000, 1.000000000000000000, 4.689100369878284071E-30 ) ) ;
#25870 = EDGE_CURVE ( 'NONE', #25774, #327, #5461, .T. ) ;
#25871 = CARTESIAN_POINT ( 'NONE',  ( -3.042071309553173730, 189.3229166632526699, 11.35316468749999785 ) ) ;
#25872 = CARTESIAN_POINT ( 'NONE',  ( 1.320432766682874540E-15, 112.9062500020483952, 7.188101187500000044 ) ) ;
#25873 = PLANE ( 'NONE',  #32406 ) ;
#25874 = CARTESIAN_POINT ( 'NONE',  ( 6.676582343750001591, 290.9531250017069510, -8.176455196517173205E-16 ) ) ;
#25876 = CARTESIAN_POINT ( 'NONE',  ( -1.656854249492381248, 15.06249999726881406, -4.000000000000001776 ) ) ;
#25875 = CARTESIAN_POINT ( 'NONE',  ( -31.99999999999998579, 209.3125000000000284, 171.6568542494928238 ) ) ;
#25877 = ORIENTED_EDGE ( 'NONE', *, *, #44731, .F. ) ;
#25878 = CARTESIAN_POINT ( 'NONE',  ( -5.676582343749992710, 230.0520833367473017, 9.832129032723422313 ) ) ;
#25879 = CARTESIAN_POINT ( 'NONE',  ( -7.188101187499990274, -2.977408999572651371, 3.080302781871750994 ) ) ;
#25880 = CARTESIAN_POINT ( 'NONE',  ( -4.500000000000007994, 7.794228634059939154, 0.000000000000000000 ) ) ;
#25881 = FACE_OUTER_BOUND ( 'NONE', #47351, .T. ) ;
#25882 = CARTESIAN_POINT ( 'NONE',  ( -1.432654583217607414, 200.5000000013656063, 194.5412658750000219 ) ) ;
#25883 = ORIENTED_EDGE ( 'NONE', *, *, #53722, .F. ) ;
#25884 = LINE ( 'NONE', #65145, #28311 ) ;
#25885 = CARTESIAN_POINT ( 'NONE',  ( 8.000000000000000000, 95.84374999999998579, -3.313708498984762496 ) ) ;
#25886 = CARTESIAN_POINT ( 'NONE',  ( 11.35316468749999963, 111.3020833299193271, -3.042071309553165293 ) ) ;
#25887 = DIRECTION ( 'NONE',  ( -0.000000000000000000, 1.000000000000000000, -0.000000000000000000 ) ) ;
#25888 = CARTESIAN_POINT ( 'NONE',  ( 11.00000000000000000, 1.347111479062088405E-15, 79.74999999999998579 ) ) ;
#25891 = CARTESIAN_POINT ( 'NONE',  ( -31.99999999999998579, 205.3125000000000284, 171.6568542494928238 ) ) ;
#25890 = CARTESIAN_POINT ( 'NONE',  ( 31.45873412499998523, 201.7500000013655779, 168.5673454167822172 ) ) ;
#25889 = CARTESIAN_POINT ( 'NONE',  ( 26.56734541678232375, 200.6250000013655779, 173.4587341249998929 ) ) ;
#25892 = ORIENTED_EDGE ( 'NONE', *, *, #37164, .F. ) ;
#25893 = EDGE_CURVE ( 'NONE', #10274, #445, #28462, .T. ) ;
#25894 = EDGE_CURVE ( 'NONE', #30150, #36272, #1328, .T. ) ;
#25895 = DIRECTION ( 'NONE',  ( -0.000000000000000000, 1.000000000000000000, -0.000000000000000000 ) ) ;
#25896 = CARTESIAN_POINT ( 'NONE',  ( -2.085542519210945728E-15, 224.5312499965860127, 11.35316468750000141 ) ) ;
#25897 =( BOUNDED_CURVE ( )  B_SPLINE_CURVE ( 2, ( #40669, #333, #46692, #74630, #5973, #57666, #63297, #33918, #45953 ),
 .UNSPECIFIED., .F., .F. ) 
 B_SPLINE_CURVE_WITH_KNOTS ( ( 3, 2, 2, 2, 3 ),
 ( 0.9431818181818182323, 0.9488636363636363535, 0.9545454545454545858, 0.9602272727272727071, 0.9659090909090909394 ),
 .UNSPECIFIED. ) 
 CURVE ( )  GEOMETRIC_REPRESENTATION_ITEM ( )  RATIONAL_B_SPLINE_CURVE ( ( 1.000000000000000000, 0.9238795325112867385, 1.000000000000000000, 0.9238795325112867385, 1.000000000000000000, 0.9238795325112867385, 1.000000000000000000, 0.9238795325112867385, 1.000000000000000000 ) ) 
 REPRESENTATION_ITEM ( '' )  );
#25899 = EDGE_CURVE ( 'NONE', #40560, #8028, #42364, .T. ) ;
#25898 = CARTESIAN_POINT ( 'NONE',  ( 2.445694354108783664, 200.3125000013656063, 144.4456943541088663 ) ) ;
#25900 = CARTESIAN_POINT ( 'NONE',  ( 24.54126587500000056, 201.3750000013656347, 168.5673454167822172 ) ) ;
#25901 = CARTESIAN_POINT ( 'NONE',  ( 2.020667218593132706E-15, -11.00000000000000000, 114.0625000040967763 ) ) ;
#25902 = CARTESIAN_POINT ( 'NONE',  ( -5.676582343750006032, 189.4270833299193555, 9.832129032723418760 ) ) ;
#25903 = CARTESIAN_POINT ( 'NONE',  ( 5.082755093536325042, 92.46875000204838102, -5.082755093536325930 ) ) ;
#25904 = CARTESIAN_POINT ( 'NONE',  ( 0.000000000000000000, 0.000000000000000000, -20.69999999999999929 ) ) ;
#25905 = CARTESIAN_POINT ( 'NONE',  ( 4.541265875000002339, 15.31249999863440614, 0.000000000000000000 ) ) ;
#25906 = CARTESIAN_POINT ( 'NONE',  ( 26.56734541678238060, 200.2500000013656063, 166.5412658749999650 ) ) ;
#25907 = CARTESIAN_POINT ( 'NONE',  ( 7.999999999999991118, 9.797174393178815797E-16, 25.58030277982336997 ) ) ;
#25908 = DIRECTION ( 'NONE',  ( 1.000000000000000000, 0.000000000000000000, 0.000000000000000000 ) ) ;
#25909 = CARTESIAN_POINT ( 'NONE',  ( 11.35316468749999785, 75.57291666325269830, 3.042071309553174174 ) ) ;
#25910 = ORIENTED_EDGE ( 'NONE', *, *, #53918, .T. ) ;
#25911 = CARTESIAN_POINT ( 'NONE',  ( -5.000000000000000000, -53.50771145605706636, 45.03482491321309311 ) ) ;
#25912 = CARTESIAN_POINT ( 'NONE',  ( -4.000000000000015987, 201.5000000000000000, 142.0000000000000568 ) ) ;
#25913 = CARTESIAN_POINT ( 'NONE',  ( -2.849036369511732440E-14, 200.2500000000000000, 138.0000000000000568 ) ) ;
#25914 = CARTESIAN_POINT ( 'NONE',  ( 6.123233995736767268E-16, 153.1249999931720538, -10.00000000000000178 ) ) ;
#25915 = CARTESIAN_POINT ( 'NONE',  ( 8.311093377946837890, 86.40624999658601268, -8.311093377946837890 ) ) ;
#25916 = VERTEX_POINT ( 'NONE', #65379 ) ;
#25917 = CARTESIAN_POINT ( 'NONE',  ( -10.18810118749999916, 4.220049686691934809, 85.93750000204839523 ) ) ;
#25918 = CARTESIAN_POINT ( 'NONE',  ( -6.238412754330611322E-16, 10.18810118749999916, 112.2812500020483810 ) ) ;
#25919 = CARTESIAN_POINT ( 'NONE',  ( -8.000000000000000000, 102.5000000000000000, 0.000000000000000000 ) ) ;
#25920 = CARTESIAN_POINT ( 'NONE',  ( 27.99999999999997158, 207.0000000000000284, 173.9999999999999147 ) ) ;
#25922 = CARTESIAN_POINT ( 'NONE',  ( -3.042071309553173730, 79.32291666325269830, 11.35316468749999785 ) ) ;
#25921 = CARTESIAN_POINT ( 'NONE',  ( 5.656854249492381470, 121.2500000040967905, 5.656854249492379694 ) ) ;
#25923 = VECTOR ( 'NONE', #42243, 1000.000000000000000 ) ;
#25924 = EDGE_CURVE ( 'NONE', #56463, #16846, #69573, .T. ) ;
#25925 = CARTESIAN_POINT ( 'NONE',  ( 7.999999999999991118, 3.313708498984757611, 18.36155278392014623 ) ) ;
#25926 = CARTESIAN_POINT ( 'NONE',  ( -3.649821741245752094, 194.7395660307605283, 141.1495723825965456 ) ) ;
#25927 = CARTESIAN_POINT ( 'NONE',  ( -8.660254037844390851, 169.7916666598387110, 4.999999999999998224 ) ) ;
#25928 = CARTESIAN_POINT ( 'NONE',  ( 2.977408999572654480, 90.50000000204840944, 7.188101187499999156 ) ) ;
#25929 = AXIS2_PLACEMENT_3D ( 'NONE', #71698, #3428, #37388 ) ;
#25930 = DIRECTION ( 'NONE',  ( 1.110223029476700175E-14, -0.5000000000000113243, 0.8660254037844320463 ) ) ;
#25931 = CARTESIAN_POINT ( 'NONE',  ( 9.832129032723416984, 65.67708332991935549, 5.676582343750006032 ) ) ;
#25932 = CARTESIAN_POINT ( 'NONE',  ( 1.226468279477575784E-15, 291.7031250017069510, 6.676582343750001591 ) ) ;
#25933 = CARTESIAN_POINT ( 'NONE',  ( -10.18810118749999916, 0.000000000000000000, 110.0312500020483668 ) ) ;
#25934 = CARTESIAN_POINT ( 'NONE',  ( -5.676582343749998039, 212.4479166632526983, -9.832129032723420536 ) ) ;
#25935 = ORIENTED_EDGE ( 'NONE', *, *, #68183, .F. ) ;
#25936 = FACE_OUTER_BOUND ( 'NONE', #21790, .T. ) ;
#25937 = CARTESIAN_POINT ( 'NONE',  ( -5.000000000000000000, -60.90295814858238543, -23.31388853594834032 ) ) ;
#25938 = CARTESIAN_POINT ( 'NONE',  ( 4.898587196589412829E-16, 15.18749999590322197, -8.000000000000000000 ) ) ;
#25940 = CARTESIAN_POINT ( 'NONE',  ( 11.35316468749999963, 190.9895833299193271, -3.042071309553165293 ) ) ;
#25939 = CARTESIAN_POINT ( 'NONE',  ( 23.99999999999998224, 206.8125000000000000, 171.6568542494922553 ) ) ;
#25941 = CARTESIAN_POINT ( 'NONE',  ( 8.000000000000000000, 2.906249995903220640, -3.313708498984761164 ) ) ;
#25942 = CARTESIAN_POINT ( 'NONE',  ( 4.999999999999997335, 236.4583333401613174, -8.660254037844387298 ) ) ;
#25943 = CARTESIAN_POINT ( 'NONE',  ( -7.999999999999989342, -3.313708498984762496, 11.61155278392014445 ) ) ;
#25944 = ORIENTED_EDGE ( 'NONE', *, *, #72229, .T. ) ;
#25945 = CARTESIAN_POINT ( 'NONE',  ( -5.676582343749998039, 187.7604166632526983, -9.832129032723420536 ) ) ;
#25946 = CARTESIAN_POINT ( 'NONE',  ( -5.082755093536319713, 5.082755093536319713, 22.29905278187175455 ) ) ;
#25947 = CARTESIAN_POINT ( 'NONE',  ( -3.313708498984759387, -7.999999999999989342, 16.29905278392014623 ) ) ;
#25948 = ORIENTED_EDGE ( 'NONE', *, *, #32142, .F. ) ;
#25949 = CARTESIAN_POINT ( 'NONE',  ( -7.999999999999998224, 99.78125000409679046, 3.313708498984766493 ) ) ;
#25950 = CARTESIAN_POINT ( 'NONE',  ( 7.594050593750000466, 1.078124996927415147, 0.000000000000000000 ) ) ;
#25951 = CARTESIAN_POINT ( 'NONE',  ( -4.000000000000002665, 15.56250000000000000, 1.656854249492380804 ) ) ;
#25952 = CARTESIAN_POINT ( 'NONE',  ( 3.211159895383560947, 16.18749999863440436, 3.211159895383562723 ) ) ;
#25953 = CARTESIAN_POINT ( 'NONE',  ( 7.999999999999991118, 3.313708498984757611, 13.86155278392014623 ) ) ;
#25954 = CARTESIAN_POINT ( 'NONE',  ( 28.45294094728589940, 194.7504983042305184, 166.2701787046703430 ) ) ;
#25955 = EDGE_CURVE ( 'NONE', #17336, #26713, #33539, .T. ) ;
#25956 = EDGE_LOOP ( 'NONE', ( #12389, #65472, #61442, #62550, #36102, #51970, #55331 ) ) ;
#25957 = CARTESIAN_POINT ( 'NONE',  ( -10.99999999999989342, 4.556349186104152515, 72.90624999999995737 ) ) ;
#25958 = CARTESIAN_POINT ( 'NONE',  ( -7.188101187499999156, 94.25000000204838102, 2.977408999572654924 ) ) ;
#25960 = CARTESIAN_POINT ( 'NONE',  ( -9.832129032723418760, 263.4895833367473301, -5.676582343749998927 ) ) ;
#25959 = DIRECTION ( 'NONE',  ( -0.000000000000000000, 1.000000000000000000, -0.000000000000000000 ) ) ;
#25961 = DIRECTION ( 'NONE',  ( 0.000000000000000000, 0.000000000000000000, -1.000000000000000000 ) ) ;
#25962 = VERTEX_POINT ( 'NONE', #70314 ) ;
#25963 = CARTESIAN_POINT ( 'NONE',  ( 8.311093377946834337, 262.3437500034140157, -8.311093377946836114 ) ) ;
#25964 = CARTESIAN_POINT ( 'NONE',  ( 2.977408999572646486, 7.188101187499991163, 20.51780278187175455 ) ) ;
#25965 = VERTEX_POINT ( 'NONE', #25003 ) ;
#25966 = EDGE_LOOP ( 'NONE', ( #17948, #41440, #233, #38334 ) ) ;
#25967 = CARTESIAN_POINT ( 'NONE',  ( -10.18810118749999738, -4.220049686691941915, 81.25000000204838102 ) ) ;
#25968 = CARTESIAN_POINT ( 'NONE',  ( -11.35316468749999785, 78.38541666325266988, -3.042071309553167513 ) ) ;
#25969 = CARTESIAN_POINT ( 'NONE',  ( 4.556349186104051263, -10.99999999999999822, 95.96875000000000000 ) ) ;
#25972 = CARTESIAN_POINT ( 'NONE',  ( -6.676582343749999815, 295.6718750017070079, 2.765530957082001251 ) ) ;
#25971 = CARTESIAN_POINT ( 'NONE',  ( 31.99999999999997868, 198.4375000027312126, 168.3431457505075173 ) ) ;
#25970 = CARTESIAN_POINT ( 'NONE',  ( 27.99999999999996803, 209.6875000013656063, 173.4587341249998929 ) ) ;
#25973 = CARTESIAN_POINT ( 'NONE',  ( 8.660254037844389075, 145.4166666666666572, -5.000000000000000000 ) ) ;
#25974 = CARTESIAN_POINT ( 'NONE',  ( 29.65685424949241167, 209.4375000000000568, 165.9999999999999147 ) ) ;
#25975 = CARTESIAN_POINT ( 'NONE',  ( 2.445694354108839175, 199.3125000013656063, 195.5543056458912190 ) ) ;
#25976 = CARTESIAN_POINT ( 'NONE',  ( -30.99999999999992895, -31.99999999999978684, 171.9999999999997726 ) ) ;
#25977 = CARTESIAN_POINT ( 'NONE',  ( 3.313708498984762496, 2.531249995903220640, 7.999999999999998224 ) ) ;
#25978 = CARTESIAN_POINT ( 'NONE',  ( 31.45873412499999233, 198.6875000013655779, 169.9999999999999432 ) ) ;
#25979 = CARTESIAN_POINT ( 'NONE',  ( -2.977408999572650039, 13.31249999795161187, -7.188101187500001821 ) ) ;
#25980 = CARTESIAN_POINT ( 'NONE',  ( 7.999999999999992895, -3.313708498984756279, 25.67405278392015333 ) ) ;
#25981 = CARTESIAN_POINT ( 'NONE',  ( 4.000000000000001776, 5.812499997268813168, -1.656854249492381248 ) ) ;
#25982 = CARTESIAN_POINT ( 'NONE',  ( -5.082755093536324154, 111.2187500020483810, 5.082755093536326818 ) ) ;
#25984 = FACE_OUTER_BOUND ( 'NONE', #7946, .T. ) ;
#25983 = CARTESIAN_POINT ( 'NONE',  ( -6.000000000000001776, 293.0625000034140157, 0.000000000000000000 ) ) ;
#25985 = FACE_OUTER_BOUND ( 'NONE', #39365, .T. ) ;
#25986 = CARTESIAN_POINT ( 'NONE',  ( 30.44569435410879521, 208.8125000013656063, 172.4456943541087526 ) ) ;
#25987 = CARTESIAN_POINT ( 'NONE',  ( 2.977408999572650927, -7.188101187499990274, 24.83030278187175455 ) ) ;
#25989 =( BOUNDED_CURVE ( )  B_SPLINE_CURVE ( 2, ( #28081, #5454, #22041, #68081, #63527, #51462, #68814, #17127, #11850 ),
 .UNSPECIFIED., .F., .F. ) 
 B_SPLINE_CURVE_WITH_KNOTS ( ( 3, 2, 2, 2, 3 ),
 ( 0.1527777777777777901, 0.1597222222222222099, 0.1666666666666666574, 0.1736111111111111049, 0.1805555555555555525 ),
 .UNSPECIFIED. ) 
 CURVE ( )  GEOMETRIC_REPRESENTATION_ITEM ( )  RATIONAL_B_SPLINE_CURVE ( ( 1.000000000000000000, 0.9238795325112867385, 1.000000000000000000, 0.9238795325112867385, 1.000000000000000000, 0.9238795325112867385, 1.000000000000000000, 0.9238795325112867385, 1.000000000000000000 ) ) 
 REPRESENTATION_ITEM ( '' )  );
#25988 = FACE_BOUND ( 'NONE', #46744, .T. ) ;
#25990 = CARTESIAN_POINT ( 'NONE',  ( 11.35316468749999963, 45.98958332991934839, -3.042071309553165293 ) ) ;
#25991 = CARTESIAN_POINT ( 'NONE',  ( 2.160335347077980472, 16.41093803200691070, 68.77481055341485217 ) ) ;
#25992 = CARTESIAN_POINT ( 'NONE',  ( 4.999999999999993783, 6.041666659838699438, 8.660254037844390851 ) ) ;
#25993 = VERTEX_POINT ( 'NONE', #23913 ) ;
#25994 = DIRECTION ( 'NONE',  ( 0.000000000000000000, -0.000000000000000000, 1.000000000000000000 ) ) ;
#25995 = CARTESIAN_POINT ( 'NONE',  ( 0.000000000000000000, 0.000000000000000000, -10.00000000000000000 ) ) ;
#25996 = CARTESIAN_POINT ( 'NONE',  ( 5.676582343749993598, 49.94791666325268409, 9.832129032723422313 ) ) ;
#25997 = CARTESIAN_POINT ( 'NONE',  ( -11.00000000000000000, 0.000000000000000000, 80.68750000409677625 ) ) ;
#25998 = CARTESIAN_POINT ( 'NONE',  ( -2.754378923186476579E-14, 204.4375000013656063, 145.4587341250000350 ) ) ;
#25999 = CARTESIAN_POINT ( 'NONE',  ( -0.8721677472748857740, -67.61512445009864791, -20.05250736213550056 ) ) ;
#26000 = CARTESIAN_POINT ( 'NONE',  ( -4.000000000000016875, 195.4375000000000000, 140.3431457505076594 ) ) ;
#26002 = CARTESIAN_POINT ( 'NONE',  ( 11.35316468749999785, 30.57291666325268409, 3.042071309553174174 ) ) ;
#26001 = CARTESIAN_POINT ( 'NONE',  ( -2.977408999572652260, 101.9375000020483810, 7.188101187500000044 ) ) ;
#26003 = EDGE_CURVE ( 'NONE', #72648, #39873, #29950, .T. ) ;
#26004 = CARTESIAN_POINT ( 'NONE',  ( 7.999999999999992895, -3.313708498984756279, 11.98655277982336997 ) ) ;
#26005 = FACE_OUTER_BOUND ( 'NONE', #13047, .T. ) ;
#26006 = CARTESIAN_POINT ( 'NONE',  ( 5.676582343750001591, 161.6145833299193839, -9.832129032723420536 ) ) ;
#26007 = ADVANCED_FACE ( 'NONE', ( #29580 ), #61333, .T. ) ;
#26008 = CARTESIAN_POINT ( 'NONE',  ( -8.660254037844390851, 134.7916666598387110, 4.999999999999998224 ) ) ;
#26009 = CARTESIAN_POINT ( 'NONE',  ( 7.188101187500000044, 108.7812500020483810, -8.802885111219163269E-16 ) ) ;
#26010 = ORIENTED_EDGE ( 'NONE', *, *, #39714, .F. ) ;
#26011 = CARTESIAN_POINT ( 'NONE',  ( -6.000000000000001776, 289.0000000000000000, 0.000000000000000000 ) ) ;
#26012 = CARTESIAN_POINT ( 'NONE',  ( 3.042071309553159519, 20.05208332991934839, 11.35316468750000141 ) ) ;
#26013 =( BOUNDED_CURVE ( )  B_SPLINE_CURVE ( 2, ( #69532, #57488, #17844, #63867, #7270, #5793, #35216, #890, #58235 ),
 .UNSPECIFIED., .F., .F. ) 
 B_SPLINE_CURVE_WITH_KNOTS ( ( 3, 2, 2, 2, 3 ),
 ( 0.4333333333333336812, 0.4416666666666669849, 0.4500000000000003997, 0.4583333333333337034, 0.4666666666666670626 ),
 .UNSPECIFIED. ) 
 CURVE ( )  GEOMETRIC_REPRESENTATION_ITEM ( )  RATIONAL_B_SPLINE_CURVE ( ( 0.9999999999999970024, 0.9238795325112897361, 1.000000000000000000, 0.9238795325112867385, 1.000000000000000000, 0.9238795325112867385, 1.000000000000000000, 0.9238795325112831858, 1.000000000000003553 ) ) 
 REPRESENTATION_ITEM ( '' )  );
#26014 = CARTESIAN_POINT ( 'NONE',  ( 11.00000000000000000, 1.347111479062088405E-15, 94.74999999999998579 ) ) ;
#26015 = ORIENTED_EDGE ( 'NONE', *, *, #64986, .F. ) ;
#26016 = LINE ( 'NONE', #8688, #13892 ) ;
#26017 = CARTESIAN_POINT ( 'NONE',  ( 10.18810118749999916, 4.220049686691935698, 74.50000000204838102 ) ) ;
#26018 = DIRECTION ( 'NONE',  ( 0.000000000000000000, 0.000000000000000000, -1.000000000000000000 ) ) ;
#26020 = CARTESIAN_POINT ( 'NONE',  ( 5.676582343749993598, 154.9479166632526983, 9.832129032723422313 ) ) ;
#26019 = CARTESIAN_POINT ( 'NONE',  ( 1.656854249492381914, 21.81250000000000355, 4.000000000000000888 ) ) ;
#26021 = CARTESIAN_POINT ( 'NONE',  ( 5.082755093536325930, 2.531249997951610542, -5.082755093536325930 ) ) ;
#26022 = CARTESIAN_POINT ( 'NONE',  ( 1.469576158976822172E-15, -7.999999999999991118, 10.26155278432982598 ) ) ;
#26023 = CARTESIAN_POINT ( 'NONE',  ( -23.47315765520887609, -23.96700175019265444, 190.2549864653887255 ) ) ;
#26024 = CARTESIAN_POINT ( 'NONE',  ( 5.676582343749997150, 232.2395833367473301, -9.832129032723418760 ) ) ;
#26025 = AXIS2_PLACEMENT_3D ( 'NONE', #4727, #16760, #28094 ) ;
#26026 = CARTESIAN_POINT ( 'NONE',  ( -4.220049686691935698, 10.18810118749999916, 82.75000000204838102 ) ) ;
#26027 = ORIENTED_EDGE ( 'NONE', *, *, #73977, .F. ) ;
#26029 = EDGE_CURVE ( 'NONE', #3727, #53235, #64809, .T. ) ;
#26028 = VECTOR ( 'NONE', #53305, 1000.000000000000000 ) ;
#26030 = CYLINDRICAL_SURFACE ( 'NONE', #29275, 8.000000000000000000 ) ;
#26031 = CARTESIAN_POINT ( 'NONE',  ( -5.999999999999999112, 292.1250000034140157, 2.485281374238575314 ) ) ;
#26032 = CARTESIAN_POINT ( 'NONE',  ( -11.35316468750000141, 103.5937499965860269, -1.390361679473963753E-15 ) ) ;
#26033 = CARTESIAN_POINT ( 'NONE',  ( -7.204075437095965206, -7.204075437095968759, 94.84375000204838102 ) ) ;
#26034 = CARTESIAN_POINT ( 'NONE',  ( 8.660254037844394404, 15.41666666666667140, -5.000000000000004441 ) ) ;
#26035 = ORIENTED_EDGE ( 'NONE', *, *, #39415, .F. ) ;
#26036 = ORIENTED_EDGE ( 'NONE', *, *, #59819, .T. ) ;
#26037 = CARTESIAN_POINT ( 'NONE',  ( 1.881053915767121776, 3.624999998634407028, -4.541265875000002339 ) ) ;
#26038 = CARTESIAN_POINT ( 'NONE',  ( 2.977408999572651815, 7.687499997951611874, 7.188101187500000933 ) ) ;
#26039 = CARTESIAN_POINT ( 'NONE',  ( -5.656854249492380582, 117.5000000040967905, -5.656854249492380582 ) ) ;
#26040 = CARTESIAN_POINT ( 'NONE',  ( 4.220049686691941027, -10.18810118749999738, 98.50000000204838102 ) ) ;
#26041 = AXIS2_PLACEMENT_3D ( 'NONE', #12286, #28894, #6637 ) ;
#26042 = CARTESIAN_POINT ( 'NONE',  ( -29.43265458321760519, 202.1250000013656063, 173.4587341250003760 ) ) ;
#26043 = CARTESIAN_POINT ( 'NONE',  ( 6.123233995736767268E-16, 158.1249999931720254, -10.00000000000000178 ) ) ;
#26044 = CARTESIAN_POINT ( 'NONE',  ( -2.828427124746190735, 4.375000000000000000, -2.828427124746191623 ) ) ;
#26045 = CARTESIAN_POINT ( 'NONE',  ( -2.828427124746190735, 20.12499999726881228, -2.828427124746191623 ) ) ;
#26046 = CARTESIAN_POINT ( 'NONE',  ( 4.541265875000001451, 3.249999998634407472, 1.881053915767124440 ) ) ;
#26047 = CARTESIAN_POINT ( 'NONE',  ( -3.458734125000016313, 207.8750000013656063, 140.5673454167824161 ) ) ;
#26048 = CARTESIAN_POINT ( 'NONE',  ( 2.445694354108839619, 194.8125000013656063, 200.4456943541088663 ) ) ;
#26049 = EDGE_CURVE ( 'NONE', #663, #10294, #69671, .T. ) ;
#26050 = CARTESIAN_POINT ( 'NONE',  ( -24.54126587500002188, 195.2500000013656063, 168.5673454167826435 ) ) ;
#26051 =( LENGTH_UNIT ( ) NAMED_UNIT ( * ) SI_UNIT ( .MILLI., .METRE. ) );
#26052 = CARTESIAN_POINT ( 'NONE',  ( 3.211159895383561835, 18.43749999863440436, -3.211159895383561835 ) ) ;
#26053 = CARTESIAN_POINT ( 'NONE',  ( 1.505685307859701227, -47.60212024653139906, 151.0590535837835660 ) ) ;
#26054 = CARTESIAN_POINT ( 'NONE',  ( 2.977408999572646486, 7.188101187499991163, 4.017802781871751883 ) ) ;
#26055 = ORIENTED_EDGE ( 'NONE', *, *, #58642, .T. ) ;
#26056 = ADVANCED_FACE ( 'NONE', ( #70673 ), #19351, .F. ) ;
#26057 = ORIENTED_EDGE ( 'NONE', *, *, #27468, .T. ) ;
#26058 = CARTESIAN_POINT ( 'NONE',  ( 4.220049686691941027, -10.18810118749999738, 101.1250000020483810 ) ) ;
#26059 = LINE ( 'NONE', #72093, #69505 ) ;
#26060 = CARTESIAN_POINT ( 'NONE',  ( -30.44569435410879166, 204.0625000013656063, 172.4456943541092357 ) ) ;
#26061 = CARTESIAN_POINT ( 'NONE',  ( -25.17157287525382259, 199.8750000000000284, 167.1715728752541565 ) ) ;
#26062 = CARTESIAN_POINT ( 'NONE',  ( 1.432654583217664479, 197.7500000013656063, 201.4587341250000065 ) ) ;
#26063 = CARTESIAN_POINT ( 'NONE',  ( -5.000000000000003553, 33.33333333333333570, 8.660254037844383745 ) ) ;
#26064 = CARTESIAN_POINT ( 'NONE',  ( -8.660254037844387298, 102.0833333333333428, -5.000000000000004441 ) ) ;
#26065 = CARTESIAN_POINT ( 'NONE',  ( -8.000000000000000000, 111.5000000000000000, 0.000000000000000000 ) ) ;
#26066 = CARTESIAN_POINT ( 'NONE',  ( 2.765530957081996366, 291.2968750017069510, -6.676582343750003368 ) ) ;
#26067 = AXIS2_PLACEMENT_3D ( 'NONE', #38434, #44089, #15026 ) ;
#26068 = CARTESIAN_POINT ( 'NONE',  ( 1.320432766682872962E-15, -7.188101187499992051, 9.736552781871754547 ) ) ;
#26069 = ORIENTED_EDGE ( 'NONE', *, *, #39546, .F. ) ;
#26070 = DIRECTION ( 'NONE',  ( -1.000000000000000000, 0.000000000000000000, 0.000000000000000000 ) ) ;
#26071 = EDGE_CURVE ( 'NONE', #48097, #31332, #35255, .T. ) ;
#26072 = CARTESIAN_POINT ( 'NONE',  ( 5.656854249492378806, 19.12499999590322020, 5.656854249492381470 ) ) ;
#26073 = CARTESIAN_POINT ( 'NONE',  ( -2.754378923186476579E-14, 202.1875000013656063, 145.4587341250000350 ) ) ;
#26074 = CARTESIAN_POINT ( 'NONE',  ( 1.224646799147353454E-15, 300.0000000000000000, -10.00000000000000178 ) ) ;
#26075 = DIRECTION ( 'NONE',  ( -0.000000000000000000, 1.000000000000000000, -0.000000000000000000 ) ) ;
#26076 = CARTESIAN_POINT ( 'NONE',  ( 8.311093377946834337, 257.3437500034140157, -8.311093377946836114 ) ) ;
#26077 = CARTESIAN_POINT ( 'NONE',  ( -3.999999999999960032, 207.0625000027312126, 196.3431457505076594 ) ) ;
#26078 = CARTESIAN_POINT ( 'NONE',  ( -7.778174593052020747, -7.778174593052023411, 110.6875000000000000 ) ) ;
#26079 = CARTESIAN_POINT ( 'NONE',  ( 11.35316468749999963, 0.9895833299193496080, -3.042071309553165293 ) ) ;
#26080 = CARTESIAN_POINT ( 'NONE',  ( -2.977408999572647819, 7.188101187499992051, 7.580302781871751883 ) ) ;
#26081 = ADVANCED_FACE ( 'NONE', ( #58630 ), #41996, .T. ) ;
#26082 = CARTESIAN_POINT ( 'NONE',  ( -9.832129032723418760, 198.1770833299193555, -5.676582343750004256 ) ) ;
#26083 = CARTESIAN_POINT ( 'NONE',  ( -5.000000000000000000, 11.14555136602166741, -27.84144949604398889 ) ) ;
#26084 = CARTESIAN_POINT ( 'NONE',  ( -1.881053915767124440, 5.999999998634407028, 4.541265875000001451 ) ) ;
#26085 = CARTESIAN_POINT ( 'NONE',  ( 38.00000000000000000, 272.0000000000000000, 3.791916237172776494E-14 ) ) ;
#26086 = PRODUCT_DEFINITION ( 'UNKNOWN', '', #10485, #16871 ) ;
#26088 = CARTESIAN_POINT ( 'NONE',  ( 0.000000000000000000, 125.0000000000000000, 11.00000000000000000 ) ) ;
#26087 = CARTESIAN_POINT ( 'NONE',  ( -8.000000000000000000, 107.0937500040967905, -3.313708498984761164 ) ) ;
#26089 = ORIENTED_EDGE ( 'NONE', *, *, #35040, .T. ) ;
#26090 = CARTESIAN_POINT ( 'NONE',  ( -2.445694354108840063, 204.0625000013656063, 139.5543056458912190 ) ) ;
#26091 = CARTESIAN_POINT ( 'NONE',  ( -8.311093377946841443, 8.906249996586018014, 8.311093377946830785 ) ) ;
#26092 = CARTESIAN_POINT ( 'NONE',  ( -4.556349186104045934, 11.00000000000000000, 98.40625000409677625 ) ) ;
#26093 = CARTESIAN_POINT ( 'NONE',  ( -29.43265458321755546, 202.8750000013656063, 173.4587341250004044 ) ) ;
#26094 = DIRECTION ( 'NONE',  ( 0.000000000000000000, 0.000000000000000000, -1.000000000000000000 ) ) ;
#26096 = CARTESIAN_POINT ( 'NONE',  ( -1.183492779173324630E-13, 16.25000000000001066, -10.00000000000000178 ) ) ;
#26095 = CARTESIAN_POINT ( 'NONE',  ( -2.977408999572650927, 119.3750000020483810, -7.188101187500000933 ) ) ;
#26097 = CARTESIAN_POINT ( 'NONE',  ( -3.313708498984758943, -7.999999999999989342, 26.61155277982337708 ) ) ;
#26098 = CARTESIAN_POINT ( 'NONE',  ( 8.311093377946837890, 126.4062499965860269, -8.311093377946837890 ) ) ;
#26099 = CIRCLE ( 'NONE', #35769, 70.50000000000000000 ) ;
#26100 = ADVANCED_FACE ( 'NONE', ( #27533 ), #23832, .F. ) ;
#26101 = CARTESIAN_POINT ( 'NONE',  ( 5.000000000000001776, 92.70833332650536818, -8.660254037844389075 ) ) ;
#26102 = CARTESIAN_POINT ( 'NONE',  ( -7.188101187500001821, 94.06250000204838102, -2.977408999572650483 ) ) ;
#26103 = CARTESIAN_POINT ( 'NONE',  ( -8.342170076843785083E-16, 20.18749999863440436, 4.541265875000002339 ) ) ;
#26104 = CARTESIAN_POINT ( 'NONE',  ( -27.99999999999995737, 204.5000000000000284, 174.0000000000003695 ) ) ;
#26105 = CARTESIAN_POINT ( 'NONE',  ( -2.679491924311226292, 38.33333332650536818, -10.00000000000000178 ) ) ;
#26106 = ORIENTED_EDGE ( 'NONE', *, *, #1479, .T. ) ;
#26107 = CARTESIAN_POINT ( 'NONE',  ( -8.987711252924967198, 225.9999999999998863, 4.433107781483233367 ) ) ;
#26108 = CARTESIAN_POINT ( 'NONE',  ( -6.676582343750001591, 293.6093750017069510, 0.000000000000000000 ) ) ;
#26109 = CARTESIAN_POINT ( 'NONE',  ( 8.660254037844385522, 186.4583333265053682, 5.000000000000005329 ) ) ;
#26110 = CARTESIAN_POINT ( 'NONE',  ( -3.313708498984757167, 7.999999999999991118, 0.7365527839201455595 ) ) ;
#26111 = CARTESIAN_POINT ( 'NONE',  ( 8.311093377946834337, 170.1562499965860127, 8.311093377946839666 ) ) ;
#26112 = CARTESIAN_POINT ( 'NONE',  ( -27.99999999999999645, 210.0000000000000284, 166.0000000000003979 ) ) ;
#26113 = CARTESIAN_POINT ( 'NONE',  ( 2.849036369511732440E-14, 199.2500000000000000, 202.0000000000000000 ) ) ;
#26114 = CARTESIAN_POINT ( 'NONE',  ( 2.775557561562891351E-14, 210.0000000000000284, 202.0000000000000000 ) ) ;
#26115 = CARTESIAN_POINT ( 'NONE',  ( 4.220049686691941027, -10.18810118749999738, 104.5000000020483668 ) ) ;
#26116 = EDGE_LOOP ( 'NONE', ( #30409, #30763, #63733, #32500 ) ) ;
#26117 =( BOUNDED_CURVE ( )  B_SPLINE_CURVE ( 2, ( #30004, #1349, #40956, #63582, #51521, #53018, #63209, #34943, #69626 ),
 .UNSPECIFIED., .F., .T. ) 
 B_SPLINE_CURVE_WITH_KNOTS ( ( 3, 2, 2, 2, 3 ),
 ( 0.9270833333333335924, 0.9322916666666667407, 0.9375000000000000000, 0.9427083333333333703, 0.9479166666666665186 ),
 .UNSPECIFIED. ) 
 CURVE ( )  GEOMETRIC_REPRESENTATION_ITEM ( )  RATIONAL_B_SPLINE_CURVE ( ( 0.9999999999999967804, 0.9238795325112899581, 1.000000000000000000, 0.9238795325112867385, 1.000000000000000000, 0.9238795325112867385, 1.000000000000000000, 0.9238795325112884038, 0.9999999999999983347 ) ) 
 REPRESENTATION_ITEM ( '' )  );
#26118 = CARTESIAN_POINT ( 'NONE',  ( -31.99999999999999289, 199.3750000027312126, 170.0000000000004547 ) ) ;
#26119 = CARTESIAN_POINT ( 'NONE',  ( -8.311093377946841443, 159.2187499965860411, 8.311093377946834337 ) ) ;
#26120 = CARTESIAN_POINT ( 'NONE',  ( 3.458734125000015425, 196.0000000013656063, 196.5673454167823877 ) ) ;
#26121 = CARTESIAN_POINT ( 'NONE',  ( -2.445694354108784108, 205.5625000013656063, 195.5543056458912190 ) ) ;
#26122 = CARTESIAN_POINT ( 'NONE',  ( 10.18810118750000093, -4.220049686691933033, 73.18750000204838102 ) ) ;
#26123 = CARTESIAN_POINT ( 'NONE',  ( 3.042071309553159519, 60.05208332991934128, 11.35316468750000141 ) ) ;
#26124 = ORIENTED_EDGE ( 'NONE', *, *, #12451, .T. ) ;
#26125 = CARTESIAN_POINT ( 'NONE',  ( 0.000000000000000000, 0.000000000000000000, 118.0000000000000000 ) ) ;
#26126 = CARTESIAN_POINT ( 'NONE',  ( 3.211159895383560947, 10.31249999863440792, 3.211159895383562723 ) ) ;
#26127 = CARTESIAN_POINT ( 'NONE',  ( 1.471067592899761672E-15, -8.008118988124991233, 10.38811528394063188 ) ) ;
#26128 = VERTEX_POINT ( 'NONE', #68277 ) ;
#26129 = VECTOR ( 'NONE', #25689, 999.9999999999998863 ) ;
#26130 = CARTESIAN_POINT ( 'NONE',  ( 7.188101187500001821, 18.56249999795161187, -2.977408999572650483 ) ) ;
#26131 = CARTESIAN_POINT ( 'NONE',  ( 4.242640687119287435, 287.4375000034140157, 4.242640687119285658 ) ) ;
#26132 = CARTESIAN_POINT ( 'NONE',  ( 2.977408999572654480, 96.12500000204838102, 7.188101187499999156 ) ) ;
#26133 = FACE_OUTER_BOUND ( 'NONE', #42353, .T. ) ;
#26134 = CARTESIAN_POINT ( 'NONE',  ( -7.188101187500002709, 18.18749999795161187, 2.977408999572649151 ) ) ;
#26135 = CARTESIAN_POINT ( 'NONE',  ( 7.188101187499993827, -2.977408999572645598, 5.142802781871753659 ) ) ;
#26136 =( BOUNDED_CURVE ( )  B_SPLINE_CURVE ( 2, ( #41249, #23144, #17859, #40877, #63882, #63135, #6550, #52565, #62752 ),
 .UNSPECIFIED., .F., .F. ) 
 B_SPLINE_CURVE_WITH_KNOTS ( ( 3, 2, 2, 2, 3 ),
 ( 0.1979166666666667962, 0.2031250000000001388, 0.2083333333333334814, 0.2135416666666667962, 0.2187500000000001388 ),
 .UNSPECIFIED. ) 
 CURVE ( )  GEOMETRIC_REPRESENTATION_ITEM ( )  RATIONAL_B_SPLINE_CURVE ( ( 0.9999999999999980016, 0.9238795325112887369, 1.000000000000000000, 0.9238795325112867385, 1.000000000000000000, 0.9238795325112867385, 1.000000000000000000, 0.9238795325112847401, 1.000000000000001998 ) ) 
 REPRESENTATION_ITEM ( '' )  );
#26137 = CARTESIAN_POINT ( 'NONE',  ( 4.220049686691941027, -10.18810118749999738, 113.5000000020483810 ) ) ;
#26138 = B_SPLINE_CURVE_WITH_KNOTS ( 'NONE', 3,
 ( #45408, #68424, #34499, #22025, #57121, #62024, #45051, #17485, #63137, #169, #61659, #68061, #9977, #23146, #5434, #62388, #33008, #34120, #22387, #56009, #27687, #39753, #73348, #44678, #4694, #28437, #46158, #5068, #56749, #51444, #28064, #68798, #33746, #16727, #62754, #4322 ),
 .UNSPECIFIED., .F., .F.,
 ( 4, 2, 2, 2, 2, 2, 2, 2, 2, 2, 2, 2, 2, 2, 2, 2, 2, 4 ),
 ( 0.09762823107336830730, 0.1033550809328300790, 0.1062185058625610135, 0.1090819307922919479, 0.1148087806517538029, 0.1162404931166192701, 0.1176722055814847373, 0.1205356305112156717, 0.1233990554409466062, 0.1262624803706775267, 0.1291259053004084612, 0.1305576177652739422, 0.1319893302301394233, 0.1348527551598703855, 0.1377161800896013477, 0.1405796050193323099, 0.1420113174841978188, 0.1434430299490632998 ),
 .UNSPECIFIED. ) ;
#26139 = CARTESIAN_POINT ( 'NONE',  ( 27.99999999999997158, 207.0000000000000284, 173.9999999999999147 ) ) ;
#26140 = CARTESIAN_POINT ( 'NONE',  ( 4.000000000000000888, 6.687499997268813168, 1.656854249492384135 ) ) ;
#26141 = EDGE_LOOP ( 'NONE', ( #37599, #26822, #37169, #39117, #43691, #15863 ) ) ;
#26142 = CARTESIAN_POINT ( 'NONE',  ( -3.458734124999959914, 207.4375000013656063, 198.0000000000000284 ) ) ;
#26143 = EDGE_CURVE ( 'NONE', #30587, #6891, #42034, .T. ) ;
#26144 = CARTESIAN_POINT ( 'NONE',  ( -26.56734541678243033, 209.3750000013656063, 166.5412658750003345 ) ) ;
#26145 = VECTOR ( 'NONE', #1952, 1000.000000000000000 ) ;
#26146 = CARTESIAN_POINT ( 'NONE',  ( -8.342170076843785083E-16, 5.062499998634407028, 4.541265875000002339 ) ) ;
#26147 = CARTESIAN_POINT ( 'NONE',  ( -2.977408999572651815, 107.9375000020483810, 7.188101187500000933 ) ) ;
#26148 = CARTESIAN_POINT ( 'NONE',  ( -1.656854249492381248, 13.31250000000000000, -4.000000000000001776 ) ) ;
#26149 = CARTESIAN_POINT ( 'NONE',  ( -2.977408999572648707, -7.188101187499990274, 22.76780278187175455 ) ) ;
#26150 = ORIENTED_EDGE ( 'NONE', *, *, #32404, .T. ) ;
#26151 = EDGE_CURVE ( 'NONE', #38509, #27684, #19159, .T. ) ;
#26152 = CARTESIAN_POINT ( 'NONE',  ( -1.347111479062088207E-15, 0.000000000000000000, 0.000000000000000000 ) ) ;
#26153 = VERTEX_POINT ( 'NONE', #1122 ) ;
#26154 = CARTESIAN_POINT ( 'NONE',  ( -10.18810118749999916, 4.220049686691934809, 115.5625000020483810 ) ) ;
#26155 = DIRECTION ( 'NONE',  ( -0.000000000000000000, 1.000000000000000000, 0.000000000000000000 ) ) ;
#26156 = CARTESIAN_POINT ( 'NONE',  ( -2.445694354108783664, 206.3125000013656063, 195.5543056458912190 ) ) ;
#26157 = CARTESIAN_POINT ( 'NONE',  ( 31.45873412499998523, 203.7500000013656063, 168.5673454167822172 ) ) ;
#26158 = CARTESIAN_POINT ( 'NONE',  ( 2.679491924311228956, 71.04166666666664298, -10.00000000000000000 ) ) ;
#26159 = CARTESIAN_POINT ( 'NONE',  ( -2.977408999572651815, 93.31250000204838102, 7.188101187500000933 ) ) ;
#26160 = CARTESIAN_POINT ( 'NONE',  ( -3.673940397442060854E-16, 293.7500000000000000, -6.000000000000001776 ) ) ;
#26162 = FACE_OUTER_BOUND ( 'NONE', #50706, .T. ) ;
#26161 = CARTESIAN_POINT ( 'NONE',  ( 32.52547942292778060, 175.8139142074479651, 162.3972334572641785 ) ) ;
#26163 = ORIENTED_EDGE ( 'NONE', *, *, #41790, .F. ) ;
#26164 = CARTESIAN_POINT ( 'NONE',  ( 3.313708498984740736, 9.093749995903223748, -8.000000000000021316 ) ) ;
#26165 = DIRECTION ( 'NONE',  ( -0.000000000000000000, 1.000000000000000000, 4.689100369878284071E-30 ) ) ;
#26166 = CARTESIAN_POINT ( 'NONE',  ( -4.000000000000015987, 199.5625000027311842, 140.3431457505076594 ) ) ;
#26167 = PLANE ( 'NONE',  #5687 ) ;
#26168 = CARTESIAN_POINT ( 'NONE',  ( -7.778174593052020747, -7.778174593052023411, 94.18750000000000000 ) ) ;
#26169 = CARTESIAN_POINT ( 'NONE',  ( 8.660254037844389075, 247.0833333333333428, 4.999999999999997335 ) ) ;
#26170 = CYLINDRICAL_SURFACE ( 'NONE', #34292, 11.00000000000000000 ) ;
#26171 = CARTESIAN_POINT ( 'NONE',  ( -2.679491924311235618, 188.5416666666666572, 10.00000000000000000 ) ) ;
#26172 = PRESENTATION_STYLE_ASSIGNMENT (( #60517 ) ) ;
#26173 = CARTESIAN_POINT ( 'NONE',  ( -7.188101187499990274, -2.977408999572651815, 22.95530278187175455 ) ) ;
#26174 = CARTESIAN_POINT ( 'NONE',  ( -11.35316468750000141, 148.5937499965860411, -1.390361679473963753E-15 ) ) ;
#26175 = CARTESIAN_POINT ( 'NONE',  ( -3.999999999999959144, 208.1875000027311842, 199.6568542494924259 ) ) ;
#26176 = CARTESIAN_POINT ( 'NONE',  ( -1.040834085586084257E-14, 82.00000000000001421, 65.00000000000000000 ) ) ;
#26177 = CARTESIAN_POINT ( 'NONE',  ( 5.499989586027935751, 9.526285454130809072, 66.68677389048282578 ) ) ;
#26180 = CARTESIAN_POINT ( 'NONE',  ( 8.000000000000000000, 109.4375000040967905, -9.797174393178825657E-16 ) ) ;
#26179 = CARTESIAN_POINT ( 'NONE',  ( -27.99999999999995737, 200.5000000000000000, 174.0000000000003695 ) ) ;
#26178 = CARTESIAN_POINT ( 'NONE',  ( 27.99999999999996803, 202.0000000000000000, 173.9999999999999147 ) ) ;
#26181 = CIRCLE ( 'NONE', #57518, 11.00000000000000000 ) ;
#26182 = ORIENTED_EDGE ( 'NONE', *, *, #51396, .T. ) ;
#26183 = CARTESIAN_POINT ( 'NONE',  ( 11.35316468749999963, 16.30208332991935194, -3.042071309553165293 ) ) ;
#26184 = CARTESIAN_POINT ( 'NONE',  ( -3.999999999999960032, 198.9375000000000568, 196.3431457505076594 ) ) ;
#26186 = CARTESIAN_POINT ( 'NONE',  ( 0.000000000000000000, 0.000000000000000000, 41.99999999999999289 ) ) ;
#26185 = CYLINDRICAL_SURFACE ( 'NONE', #31171, 11.00000000000000000 ) ;
#26187 = CYLINDRICAL_SURFACE ( 'NONE', #13432, 5.000000000000000000 ) ;
#26188 = CARTESIAN_POINT ( 'NONE',  ( -3.458734125000016313, 202.8750000013656063, 140.5673454167823593 ) ) ;
#26189 = CARTESIAN_POINT ( 'NONE',  ( -7.320508075688778149, 54.99999999317203958, 7.320508075688769267 ) ) ;
#26190 = CARTESIAN_POINT ( 'NONE',  ( -4.401442555609581635E-16, 107.2812500020483810, -7.188101187500000044 ) ) ;
#26191 = CARTESIAN_POINT ( 'NONE',  ( -3.211159895383562723, 9.062499998634407916, 3.211159895383561391 ) ) ;
#26192 = CARTESIAN_POINT ( 'NONE',  ( 8.660254037844397956, 220.4166666666666856, -5.000000000000006217 ) ) ;
#26193 = CARTESIAN_POINT ( 'NONE',  ( 5.656854249492374365, 5.656854249492375253, 9.267802779823364645 ) ) ;
#26195 = FACE_OUTER_BOUND ( 'NONE', #13395, .T. ) ;
#26194 = CARTESIAN_POINT ( 'NONE',  ( 0.000000000000000000, 0.000000000000000000, 0.000000000000000000 ) ) ;
#26196 = ORIENTED_EDGE ( 'NONE', *, *, #38242, .T. ) ;
#26197 = LINE ( 'NONE', #20543, #44824 ) ;
#26198 = CARTESIAN_POINT ( 'NONE',  ( -11.00000000000000000, 0.000000000000000000, 81.99999999999998579 ) ) ;
#26199 = CARTESIAN_POINT ( 'NONE',  ( -6.951808397369817780E-16, 227.9687500034139873, -11.35316468749999963 ) ) ;
#26200 = CARTESIAN_POINT ( 'NONE',  ( 11.35316468749999963, 130.9895833299193555, -3.042071309553165293 ) ) ;
#26201 = EDGE_LOOP ( 'NONE', ( #32883, #56512 ) ) ;
#26202 = FACE_OUTER_BOUND ( 'NONE', #31302, .T. ) ;
#26203 = CARTESIAN_POINT ( 'NONE',  ( -10.18810118749999738, -4.220049686691941915, 94.75000000204838102 ) ) ;
#26204 = CARTESIAN_POINT ( 'NONE',  ( -4.556349186104045934, 11.00000000000000000, 93.71874999999998579 ) ) ;
#26205 = CARTESIAN_POINT ( 'NONE',  ( -1.432654583217607414, 195.5000000013655779, 194.5412658750000219 ) ) ;
#26206 = CARTESIAN_POINT ( 'NONE',  ( 28.00000000000001421, 197.5000000000000000, 165.9999999999998863 ) ) ;
#26208 = CARTESIAN_POINT ( 'NONE',  ( -9.832129032723418760, 127.8645833299193697, -5.676582343750004256 ) ) ;
#26207 = CARTESIAN_POINT ( 'NONE',  ( 31.99999999999997868, 196.1875000000000568, 171.6568542494923122 ) ) ;
#26209 = CARTESIAN_POINT ( 'NONE',  ( 2.679491924311228956, 147.9166666598387110, -10.00000000000000000 ) ) ;
#26210 = VERTEX_POINT ( 'NONE', #57720 ) ;
#26211 = CARTESIAN_POINT ( 'NONE',  ( -5.656854249492378806, 110.1875000000000000, 5.656854249492381470 ) ) ;
#26212 = CARTESIAN_POINT ( 'NONE',  ( 0.000000000000000000, 125.0000000000000000, 0.000000000000000000 ) ) ;
#26213 = CARTESIAN_POINT ( 'NONE',  ( -11.35316468749999785, 118.3854166632526699, -3.042071309553167957 ) ) ;
#26214 = CARTESIAN_POINT ( 'NONE',  ( -1.432654583217607858, 206.6250000013656063, 201.4587341250000065 ) ) ;
#26215 = CARTESIAN_POINT ( 'NONE',  ( 7.188101187499999156, 18.74999999795161543, 2.977408999572654924 ) ) ;
#26216 = CARTESIAN_POINT ( 'NONE',  ( -4.220049686691937474, -10.18810118749999738, 89.31250000204838102 ) ) ;
#26217 = CARTESIAN_POINT ( 'NONE',  ( 6.951808397369818766E-16, 27.34374999658601979, -11.35316468750000141 ) ) ;
#26218 = ORIENTED_EDGE ( 'NONE', *, *, #46301, .F. ) ;
#26219 = CARTESIAN_POINT ( 'NONE',  ( 8.660254037844389075, 182.2916666598387110, -5.000000000000000000 ) ) ;
#26220 = CARTESIAN_POINT ( 'NONE',  ( 5.000000000000004441, 244.7916666734946318, 8.660254037844385522 ) ) ;
#26221 = CARTESIAN_POINT ( 'NONE',  ( 4.999999999999997335, 238.3333333333333428, -8.660254037844387298 ) ) ;
#26222 = CARTESIAN_POINT ( 'NONE',  ( 2.020667218593132706E-15, -11.00000000000000000, 85.56250000409676204 ) ) ;
#26223 = CARTESIAN_POINT ( 'NONE',  ( 5.082755093536324154, 3.281249997951610098, 5.082755093536326818 ) ) ;
#26224 = CARTESIAN_POINT ( 'NONE',  ( -2.765530957081996810, 290.2656250017068942, -6.676582343750003368 ) ) ;
#26225 = CARTESIAN_POINT ( 'NONE',  ( -2.751064625579944321E-14, 199.7500000000000000, 146.0000000000000284 ) ) ;
#26226 = CARTESIAN_POINT ( 'NONE',  ( 11.35316468749999785, 215.8854166632526983, 3.042071309553174174 ) ) ;
#26227 = ORIENTED_EDGE ( 'NONE', *, *, #37588, .F. ) ;
#26228 = ADVANCED_FACE ( 'NONE', ( #29029 ), #6767, .T. ) ;
#26229 = CARTESIAN_POINT ( 'NONE',  ( -5.676582343749998039, 142.7604166632526699, -9.832129032723420536 ) ) ;
#26230 = CARTESIAN_POINT ( 'NONE',  ( -4.220049686691937474, -10.18810118749999738, 84.43750000204838102 ) ) ;
#26231 = EDGE_CURVE ( 'NONE', #63656, #27850, #12, .T. ) ;
#26232 =( BOUNDED_CURVE ( )  B_SPLINE_CURVE ( 2, ( #903, #54050, #1638, #64982, #35959, #58979, #36330, #1992, #23890 ),
 .UNSPECIFIED., .F., .F. ) 
 B_SPLINE_CURVE_WITH_KNOTS ( ( 3, 2, 2, 2, 3 ),
 ( 0.9117647058823530326, 0.9154411764705883137, 0.9191176470588235947, 0.9227941176470588758, 0.9264705882352941568 ),
 .UNSPECIFIED. ) 
 CURVE ( )  GEOMETRIC_REPRESENTATION_ITEM ( )  RATIONAL_B_SPLINE_CURVE ( ( 0.9999999999999976685, 0.9238795325112890700, 1.000000000000000000, 0.9238795325112867385, 1.000000000000000000, 0.9238795325112867385, 1.000000000000000000, 0.9238795325112867385, 1.000000000000000000 ) ) 
 REPRESENTATION_ITEM ( '' )  );
#26233 = CARTESIAN_POINT ( 'NONE',  ( -25.55430564589119413, 198.3125000013656063, 167.5543056458915316 ) ) ;
#26234 = DIRECTION ( 'NONE',  ( -0.000000000000000000, 1.000000000000000000, -0.000000000000000000 ) ) ;
#26235 = CARTESIAN_POINT ( 'NONE',  ( -3.211159895383561391, 14.81249999863440792, -3.211159895383561835 ) ) ;
#26236 = VERTEX_POINT ( 'NONE', #58093 ) ;
#26237 = CARTESIAN_POINT ( 'NONE',  ( 4.000000000000015099, 203.6875000027311842, 196.3431457505076594 ) ) ;
#26238 = VECTOR ( 'NONE', #47289, 1000.000000000000000 ) ;
#26239 = EDGE_CURVE ( 'NONE', #39682, #300, #36023, .T. ) ;
#26240 = CARTESIAN_POINT ( 'NONE',  ( -2.445694354108840063, 199.0625000013656063, 139.5543056458912190 ) ) ;
#26241 = CARTESIAN_POINT ( 'NONE',  ( -2.751064625579944321E-14, 205.8750000027312126, 146.0000000000000284 ) ) ;
#26242 = CARTESIAN_POINT ( 'NONE',  ( -7.999999999999948486, 3.313708498984799355, 14.23655277982336287 ) ) ;
#26243 = EDGE_LOOP ( 'NONE', ( #17329, #40381, #18376, #70447 ) ) ;
#26244 = CARTESIAN_POINT ( 'NONE',  ( -5.082755093536325042, 11.53124999795161010, -5.082755093536325930 ) ) ;
#26245 = CARTESIAN_POINT ( 'NONE',  ( -4.556349186104048599, -10.99999999999999822, 76.28125000000000000 ) ) ;
#26246 = DIRECTION ( 'NONE',  ( 0.000000000000000000, 0.000000000000000000, 1.000000000000000000 ) ) ;
#26247 = CARTESIAN_POINT ( 'NONE',  ( 8.311093377946837890, 191.4062499965860127, -8.311093377946837890 ) ) ;
#26248 = AXIS2_PLACEMENT_3D ( 'NONE', #26697, #19540, #42557 ) ;
#26249 = CARTESIAN_POINT ( 'NONE',  ( -2.977408999572650927, 112.2500000020483952, -7.188101187500001821 ) ) ;
#26250 = CARTESIAN_POINT ( 'NONE',  ( 1.224646799147353454E-15, 300.0000000000000000, -10.00000000000000178 ) ) ;
#26251 = CARTESIAN_POINT ( 'NONE',  ( 6.676582343750002480, 293.0156250017069510, -2.765530957081997254 ) ) ;
#26253 = CARTESIAN_POINT ( 'NONE',  ( 2.679491924305479333, 93.95833333333280279, 10.00000000000330935 ) ) ;
#26252 = CARTESIAN_POINT ( 'NONE',  ( -3.042071309553166625, 222.8645833367473301, -11.35316468749999608 ) ) ;
#26254 = ORIENTED_EDGE ( 'NONE', *, *, #7954, .T. ) ;
#26255 = CARTESIAN_POINT ( 'NONE',  ( 8.311093377946834337, 232.3437500034140157, -8.311093377946836114 ) ) ;
#26256 = CARTESIAN_POINT ( 'NONE',  ( 2.977408999572646486, 7.188101187499991163, 28.39280278187175810 ) ) ;
#26257 = CARTESIAN_POINT ( 'NONE',  ( 7.320508075688774596, 167.4999999931720538, -7.320508075688774596 ) ) ;
#26258 = CARTESIAN_POINT ( 'NONE',  ( -1.506524674528165075, -65.82790954191020205, -26.31843049628427877 ) ) ;
#26259 = CARTESIAN_POINT ( 'NONE',  ( 3.458734125000016757, 200.1250000013656063, 199.4326545832176691 ) ) ;
#26260 = CARTESIAN_POINT ( 'NONE',  ( 11.00000000000000000, 1.347111479062088405E-15, 115.9375000040967763 ) ) ;
#26261 = CARTESIAN_POINT ( 'NONE',  ( 2.775557561562891351E-14, 210.0000000000000284, 202.0000000000000000 ) ) ;
#26262 = CARTESIAN_POINT ( 'NONE',  ( -4.898587196589412829E-16, 94.62499999999998579, -8.000000000000000000 ) ) ;
#26263 = CARTESIAN_POINT ( 'NONE',  ( -9.832129032723418760, 108.1770833299193555, -5.676582343750004256 ) ) ;
#26264 = CARTESIAN_POINT ( 'NONE',  ( -4.999999999999999112, -13.21930962315088998, -69.49101004078880806 ) ) ;
#26265 = CARTESIAN_POINT ( 'NONE',  ( -4.556349186104045934, 11.00000000000000000, 74.21875000000001421 ) ) ;
#26268 = CARTESIAN_POINT ( 'NONE',  ( 4.556349186104045934, 11.00000000000000000, 110.2187500040967763 ) ) ;
#26267 = CARTESIAN_POINT ( 'NONE',  ( 27.99999999999996803, 201.9375000013656063, 166.5412658749999082 ) ) ;
#26266 = CARTESIAN_POINT ( 'NONE',  ( 31.45873412499997812, 197.8750000013656063, 171.4326545832175839 ) ) ;
#26269 = ORIENTED_EDGE ( 'NONE', *, *, #24264, .F. ) ;
#26270 = CARTESIAN_POINT ( 'NONE',  ( 0.000000000000000000, 195.0000000000000284, 170.0000000000000284 ) ) ;
#26271 = CARTESIAN_POINT ( 'NONE',  ( -8.311093377946841443, 223.9062499965860411, 8.311093377946830785 ) ) ;
#26272 = CARTESIAN_POINT ( 'NONE',  ( -3.458734125000015425, 197.0000000013656347, 143.4326545832176976 ) ) ;
#26273 = CARTESIAN_POINT ( 'NONE',  ( 30.44569435410879166, 198.8125000013656063, 172.4456943541087526 ) ) ;
#26274 = CARTESIAN_POINT ( 'NONE',  ( 7.778174593052023411, -7.778174593052021635, 114.2500000040967763 ) ) ;
#26275 = CARTESIAN_POINT ( 'NONE',  ( -8.311093377946841443, 199.2187499965860411, 8.311093377946830785 ) ) ;
#26276 = CARTESIAN_POINT ( 'NONE',  ( -5.082755093536325930, 89.84375000204839523, -5.082755093536325930 ) ) ;
#26277 = CYLINDRICAL_SURFACE ( 'NONE', #14509, 30.99999999999997158 ) ;
#26278 = CARTESIAN_POINT ( 'NONE',  ( -4.541265875000003227, 19.87499999863440792, 1.881053915767121110 ) ) ;
#26279 = CARTESIAN_POINT ( 'NONE',  ( 29.43265458321766204, 195.1250000013656063, 166.5412658749999650 ) ) ;
#26280 = CARTESIAN_POINT ( 'NONE',  ( 7.999999999999992895, -3.313708498984756279, 28.48655277982336642 ) ) ;
#26281 = LINE ( 'NONE', #31963, #8617 ) ;
#26282 = CARTESIAN_POINT ( 'NONE',  ( -2.085542519210945728E-15, 84.53124999658602690, 11.35316468750000141 ) ) ;
#26283 = VERTEX_POINT ( 'NONE', #24098 ) ;
#26284 = CARTESIAN_POINT ( 'NONE',  ( -10.99999999999992184, -31.09254642223693921, 198.9827534923788903 ) ) ;
#26285 = CARTESIAN_POINT ( 'NONE',  ( 23.99999999999999645, 204.9375000027312126, 171.6568542494923122 ) ) ;
#26286 = CARTESIAN_POINT ( 'NONE',  ( -7.188101187500002709, 17.81249999795161543, 2.977408999572649151 ) ) ;
#26287 = CARTESIAN_POINT ( 'NONE',  ( 8.660254037844522301, 39.58333333333343518, 5.000000000000085265 ) ) ;
#26288 = DIRECTION ( 'NONE',  ( 0.000000000000000000, -0.000000000000000000, 1.000000000000000000 ) ) ;
#26289 = CARTESIAN_POINT ( 'NONE',  ( 3.042071309553159519, 94.73958332991934128, 11.35316468750000141 ) ) ;
#26290 = ORIENTED_EDGE ( 'NONE', *, *, #32572, .T. ) ;
#26291 = CARTESIAN_POINT ( 'NONE',  ( -10.18810118749999738, -4.220049686691941915, 84.62500000204838102 ) ) ;
#26292 = CARTESIAN_POINT ( 'NONE',  ( -6.238412754330611322E-16, 10.18810118749999916, 115.2812500020483810 ) ) ;
#26293 = CARTESIAN_POINT ( 'NONE',  ( -30.44569435410883074, 195.8125000013656063, 167.5543056458915885 ) ) ;
#26294 = CARTESIAN_POINT ( 'NONE',  ( -3.458734124999960358, 207.6875000013656063, 198.0000000000000284 ) ) ;
#26295 = DIRECTION ( 'NONE',  ( -0.000000000000000000, 1.000000000000000000, 4.476705744456276341E-16 ) ) ;
#26297 = CARTESIAN_POINT ( 'NONE',  ( -2.085542519210945728E-15, 89.53124999658602690, 11.35316468750000141 ) ) ;
#26296 = DIRECTION ( 'NONE',  ( -0.000000000000000000, 1.000000000000000000, -4.476705744456276341E-16 ) ) ;
#26298 = CARTESIAN_POINT ( 'NONE',  ( -3.313708498984757167, 7.999999999999991118, 20.23655278392014978 ) ) ;
#26299 = CARTESIAN_POINT ( 'NONE',  ( -29.65685424949235838, 196.1875000027312126, 166.0000000000003411 ) ) ;
#26300 = CARTESIAN_POINT ( 'NONE',  ( -7.320508075688773708, 173.7499999931720254, -7.320508075688774596 ) ) ;
#26301 = CARTESIAN_POINT ( 'NONE',  ( 4.172829859562196653, -6.868037143713721981, 0.000000000000000000 ) ) ;
#26302 = EDGE_CURVE ( 'NONE', #12328, #55139, #11311, .T. ) ;
#26303 = DIRECTION ( 'NONE',  ( 0.000000000000000000, 0.000000000000000000, -1.000000000000000000 ) ) ;
#26304 = CARTESIAN_POINT ( 'NONE',  ( -8.311093377946841443, 69.21874999658601268, 8.311093377946834337 ) ) ;
#26305 = CARTESIAN_POINT ( 'NONE',  ( -4.721056650415999201, 293.3281250017069510, -4.721056650415999201 ) ) ;
#26306 = CARTESIAN_POINT ( 'NONE',  ( -7.204075437095967871, 7.204075437095967871, 109.8437500020483810 ) ) ;
#26307 = CARTESIAN_POINT ( 'NONE',  ( -11.35316468749999785, 213.0729166632527267, -3.042071309553167513 ) ) ;
#26308 = VERTEX_POINT ( 'NONE', #28288 ) ;
#26309 = CARTESIAN_POINT ( 'NONE',  ( -2.849036369511732440E-14, 203.2500000000000000, 138.0000000000000568 ) ) ;
#26310 = CARTESIAN_POINT ( 'NONE',  ( 3.999999999999959144, 206.1875000027312126, 140.3431457505076594 ) ) ;
#26311 = CARTESIAN_POINT ( 'NONE',  ( 5.000000000000000000, 65.74990953739953170, 23.82322416715377855 ) ) ;
#26313 = CARTESIAN_POINT ( 'NONE',  ( 3.042071309553159519, 189.7395833299193271, 11.35316468750000141 ) ) ;
#26312 = CARTESIAN_POINT ( 'NONE',  ( -4.000000000000001776, 19.43750000000000000, -1.656854249492381470 ) ) ;
#26314 = DIRECTION ( 'NONE',  ( -0.000000000000000000, 1.000000000000000000, -0.000000000000000000 ) ) ;
#26315 = VECTOR ( 'NONE', #45961, 1000.000000000000000 ) ;
#26316 = CARTESIAN_POINT ( 'NONE',  ( -10.00000000000000000, 232.9166666734946602, -2.679491924311226292 ) ) ;
#26317 = CARTESIAN_POINT ( 'NONE',  ( 11.00000000000000355, -4.556349186104044158, 72.34375000409677625 ) ) ;
#26318 = ORIENTED_EDGE ( 'NONE', *, *, #39713, .T. ) ;
#26319 = CARTESIAN_POINT ( 'NONE',  ( -11.35316468749999785, 188.3854166632526983, -3.042071309553167957 ) ) ;
#26320 = AXIS2_PLACEMENT_3D ( 'NONE', #64884, #6451, #29454 ) ;
#26321 = CARTESIAN_POINT ( 'NONE',  ( 5.082755093536320601, -5.082755093536318824, 12.54905278187175277 ) ) ;
#26322 = CARTESIAN_POINT ( 'NONE',  ( -7.999999999999989342, -3.313708498984762496, 16.11155278392014623 ) ) ;
#26323 = VERTEX_POINT ( 'NONE', #69394 ) ;
#26324 = ADVANCED_FACE ( 'NONE', ( #33975 ), #12414, .F. ) ;
#26325 = ADVANCED_FACE ( 'NONE', ( #34345, #57344, #5287, #17328, #5655, #28654 ), #62608, .T. ) ;
#26326 = CARTESIAN_POINT ( 'NONE',  ( -5.656854249492378806, 98.37500000409677625, 5.656854249492381470 ) ) ;
#26327 = CARTESIAN_POINT ( 'NONE',  ( -8.660254037844387298, 2.083333333333333481, -5.000000000000004441 ) ) ;
#26328 = EDGE_LOOP ( 'NONE', ( #72745, #47139, #23232, #54647 ) ) ;
#26329 = CARTESIAN_POINT ( 'NONE',  ( 4.000000000000001776, 15.06249999999999822, -1.656854249492381248 ) ) ;
#26330 = CARTESIAN_POINT ( 'NONE',  ( 1.881053915767122664, 17.12499999863440436, 4.541265875000001451 ) ) ;
#26331 = CARTESIAN_POINT ( 'NONE',  ( -5.656854249492375253, 5.656854249492375253, 11.33030278392014445 ) ) ;
#26332 = CARTESIAN_POINT ( 'NONE',  ( -10.99999999999999822, -4.556349186104053040, 77.78125000409680467 ) ) ;
#26333 = ORIENTED_EDGE ( 'NONE', *, *, #72345, .F. ) ;
#26334 = CARTESIAN_POINT ( 'NONE',  ( 5.000000000000000000, -10.43216530810821219, -65.93415491242824089 ) ) ;
#26335 = CARTESIAN_POINT ( 'NONE',  ( 5.082755093536326818, 94.71875000204838102, 5.082755093536325042 ) ) ;
#26336 = EDGE_CURVE ( 'NONE', #30502, #21899, #73396, .T. ) ;
#26339 = CARTESIAN_POINT ( 'NONE',  ( 29.65685424949239035, 207.1875000027312410, 173.9999999999999147 ) ) ;
#26338 = CARTESIAN_POINT ( 'NONE',  ( 8.311093377946839666, 260.7812500034140157, 8.311093377946830785 ) ) ;
#26337 = CARTESIAN_POINT ( 'NONE',  ( -6.123233995736766282E-16, 256.8750000068279746, -10.00000000000000000 ) ) ;
#26340 =( BOUNDED_CURVE ( )  B_SPLINE_CURVE ( 2, ( #58743, #29326, #35000, #22909, #1039, #69683, #5569, #11227, #46291 ),
 .UNSPECIFIED., .F., .F. ) 
 B_SPLINE_CURVE_WITH_KNOTS ( ( 3, 2, 2, 2, 3 ),
 ( 0.6833333333333340143, 0.6916666666666673180, 0.7000000000000005107, 0.7083333333333339255, 0.7166666666666671182 ),
 .UNSPECIFIED. ) 
 CURVE ( )  GEOMETRIC_REPRESENTATION_ITEM ( )  RATIONAL_B_SPLINE_CURVE ( ( 0.9999999999999938938, 0.9238795325112928447, 1.000000000000000000, 0.9238795325112867385, 1.000000000000000000, 0.9238795325112867385, 1.000000000000000000, 0.9238795325112826307, 1.000000000000003997 ) ) 
 REPRESENTATION_ITEM ( '' )  );
#26341 = ORIENTED_EDGE ( 'NONE', *, *, #70464, .F. ) ;
#26342 = CARTESIAN_POINT ( 'NONE',  ( 8.311093377946839666, 261.0937500034140157, 8.311093377946829008 ) ) ;
#26343 = CARTESIAN_POINT ( 'NONE',  ( -2.977408999572647819, 7.188101187499991163, 17.70530278187175455 ) ) ;
#26344 = ORIENTED_EDGE ( 'NONE', *, *, #53851, .T. ) ;
#26345 = ORIENTED_EDGE ( 'NONE', *, *, #30618, .F. ) ;
#26346 = CARTESIAN_POINT ( 'NONE',  ( -4.220049686691937474, -10.18810118749999738, 78.43750000204838102 ) ) ;
#26347 = CARTESIAN_POINT ( 'NONE',  ( 8.311093377946834337, 70.46874999658599847, 8.311093377946839666 ) ) ;
#26348 = CARTESIAN_POINT ( 'NONE',  ( 5.656854249492376141, -5.656854249492374365, 24.08030278392014978 ) ) ;
#26349 = CARTESIAN_POINT ( 'NONE',  ( -11.00000000000000000, 0.000000000000000000, 91.00000000000000000 ) ) ;
#26352 = CARTESIAN_POINT ( 'NONE',  ( -4.721056650415999201, 295.4843750017070079, -4.721056650415999201 ) ) ;
#26351 = CARTESIAN_POINT ( 'NONE',  ( 26.34314575050763807, 199.0625000027312126, 173.9999999999999147 ) ) ;
#26350 = DIRECTION ( 'NONE',  ( 1.000000000000000000, 0.000000000000000000, 0.000000000000000000 ) ) ;
#26353 = AXIS2_PLACEMENT_3D ( 'NONE', #47575, #35541, #46845 ) ;
#26354 = CARTESIAN_POINT ( 'NONE',  ( -11.00000000000010658, 4.556349186103942017, 89.40624999999998579 ) ) ;
#26355 = CARTESIAN_POINT ( 'NONE',  ( -2.445694354108784108, 197.5625000013656063, 195.5543056458912190 ) ) ;
#26356 = CARTESIAN_POINT ( 'NONE',  ( 8.000000000000000000, 2.906249995903220640, -3.313708498984761608 ) ) ;
#26357 = CARTESIAN_POINT ( 'NONE',  ( 28.00000000000002132, 197.9375000013655779, 166.5412658749999082 ) ) ;
#26358 = CARTESIAN_POINT ( 'NONE',  ( -1.320432766682874540E-15, 13.96874999795161187, 7.188101187500000044 ) ) ;
#26359 = CARTESIAN_POINT ( 'NONE',  ( -3.313708498984757167, 7.999999999999991118, 27.73655278392014978 ) ) ;
#26360 = CARTESIAN_POINT ( 'NONE',  ( 4.000000000000001776, 5.749999997268813168, 0.000000000000000000 ) ) ;
#26361 = CARTESIAN_POINT ( 'NONE',  ( -2.977408999572650927, 107.7500000020483810, -7.188101187500000933 ) ) ;
#26363 = CARTESIAN_POINT ( 'NONE',  ( 7.456209740496410276, -51.58726928745755202, -41.60229883573035892 ) ) ;
#26362 = CARTESIAN_POINT ( 'NONE',  ( -11.00000000000000000, 0.000000000000000000, 118.0000000000000000 ) ) ;
#26364 = DIRECTION ( 'NONE',  ( -0.000000000000000000, -0.000000000000000000, -1.000000000000000000 ) ) ;
#26365 = FACE_OUTER_BOUND ( 'NONE', #51846, .T. ) ;
#26366 = CARTESIAN_POINT ( 'NONE',  ( 7.188101187499991163, 2.977408999572648707, 16.20530278187175455 ) ) ;
#26367 = CARTESIAN_POINT ( 'NONE',  ( -4.000000000000015099, 208.6875000027312126, 143.6568542494924543 ) ) ;
#26368 = CARTESIAN_POINT ( 'NONE',  ( -11.35316468749999785, 38.07291666325269119, -3.042071309553167513 ) ) ;
#26369 = FACE_OUTER_BOUND ( 'NONE', #36177, .T. ) ;
#26370 = CARTESIAN_POINT ( 'NONE',  ( -2.679491924311225848, 13.33333332650536640, -10.00000000000000178 ) ) ;
#26371 = VERTEX_POINT ( 'NONE', #63726 ) ;
#26372 = DIRECTION ( 'NONE',  ( 0.000000000000000000, 0.000000000000000000, 1.000000000000000000 ) ) ;
#26373 = CARTESIAN_POINT ( 'NONE',  ( 3.042071309553167069, 46.82291666325267698, -11.35316468749999785 ) ) ;
#26374 = CARTESIAN_POINT ( 'NONE',  ( 11.00000000000000000, 1.347111479062088405E-15, 81.43750000409677625 ) ) ;
#26375 = CARTESIAN_POINT ( 'NONE',  ( -2.754378923186476579E-14, 203.4375000013656063, 145.4587341250000350 ) ) ;
#26376 = CARTESIAN_POINT ( 'NONE',  ( -5.999999999999999112, 299.0625000000000000, 2.485281374238575314 ) ) ;
#26377 = FACE_OUTER_BOUND ( 'NONE', #42674, .T. ) ;
#26379 = CARTESIAN_POINT ( 'NONE',  ( 3.042071309553159519, 39.73958332991934128, 11.35316468750000141 ) ) ;
#26378 = CARTESIAN_POINT ( 'NONE',  ( 7.188101187500000044, 102.4062500020483810, -8.802885111219163269E-16 ) ) ;
#26380 = CARTESIAN_POINT ( 'NONE',  ( -5.656854249492373476, -5.656854249492376141, 7.017802779823365533 ) ) ;
#26381 = CARTESIAN_POINT ( 'NONE',  ( 2.449293598294707893E-16, 10.99999999726881406, -4.000000000000001776 ) ) ;
#26382 = CARTESIAN_POINT ( 'NONE',  ( -3.042071309553164404, 167.2395833299193839, -11.35316468749999963 ) ) ;
#26383 = CARTESIAN_POINT ( 'NONE',  ( -10.00000000000000000, 124.1666666598387110, -2.679491924311229845 ) ) ;
#26384 = CARTESIAN_POINT ( 'NONE',  ( -7.188101187500000044, 108.0312500020483810, 0.000000000000000000 ) ) ;
#26385 = ORIENTED_EDGE ( 'NONE', *, *, #52826, .F. ) ;
#26386 = CYLINDRICAL_SURFACE ( 'NONE', #29159, 3.999999999999976019 ) ;
#26387 = CARTESIAN_POINT ( 'NONE',  ( 3.042071309553167513, 22.13541666325268409, -11.35316468749999785 ) ) ;
#26388 = CARTESIAN_POINT ( 'NONE',  ( -8.660254037844392627, 17.08333333333334281, -5.000000000000008882 ) ) ;
#26389 = VERTEX_POINT ( 'NONE', #40349 ) ;
#26390 = CARTESIAN_POINT ( 'NONE',  ( -30.82842712474624491, 205.2500000027312126, 167.1715728752542418 ) ) ;
#26391 = CARTESIAN_POINT ( 'NONE',  ( -10.18810118749999916, 4.220049686691934809, 78.06250000204838102 ) ) ;
#26392 = DIRECTION ( 'NONE',  ( -0.000000000000000000, -1.000000000000000000, -0.000000000000000000 ) ) ;
#26394 = CARTESIAN_POINT ( 'NONE',  ( -8.311093377946841443, 153.9062499965860411, 8.311093377946834337 ) ) ;
#26393 = CARTESIAN_POINT ( 'NONE',  ( 3.313708498984762496, -7.999999999999989342, 2.986552783920144893 ) ) ;
#26395 = DIRECTION ( 'NONE',  ( -0.000000000000000000, 1.000000000000000000, -0.000000000000000000 ) ) ;
#26396 = CARTESIAN_POINT ( 'NONE',  ( -3.313708498984757167, 7.999999999999991118, 14.10530278432982421 ) ) ;
#26397 = EDGE_CURVE ( 'NONE', #34236, #40301, #2675, .T. ) ;
#26398 = CARTESIAN_POINT ( 'NONE',  ( -20.61528569718738524, -28.36198039966152251, 193.1521699238367660 ) ) ;
#26399 = CARTESIAN_POINT ( 'NONE',  ( -11.35316468749999608, 229.1145833367473301, 3.042071309553173730 ) ) ;
#26400 = CARTESIAN_POINT ( 'NONE',  ( 4.220049686691934809, 10.18810118749999916, 87.06250000204838102 ) ) ;
#26401 = VERTEX_POINT ( 'NONE', #35081 ) ;
#26402 = AXIS2_PLACEMENT_3D ( 'NONE', #55425, #73882, #22186 ) ;
#26403 = DIRECTION ( 'NONE',  ( -0.000000000000000000, -0.000000000000000000, -1.000000000000000000 ) ) ;
#26404 = CARTESIAN_POINT ( 'NONE',  ( -8.000000000000000000, 122.1875000040967763, 0.000000000000000000 ) ) ;
#26405 = CARTESIAN_POINT ( 'NONE',  ( 9.832129032723420536, 101.5104166632526841, -5.676582343749999815 ) ) ;
#26406 = CARTESIAN_POINT ( 'NONE',  ( -7.204075437095965206, -7.204075437095968759, 93.34375000204838102 ) ) ;
#26407 = CARTESIAN_POINT ( 'NONE',  ( -4.541265875000003227, 19.99999999863440436, 1.881053915767121110 ) ) ;
#26408 = ORIENTED_EDGE ( 'NONE', *, *, #46866, .T. ) ;
#26409 = VERTEX_POINT ( 'NONE', #29410 ) ;
#26410 = CARTESIAN_POINT ( 'NONE',  ( -4.541265875000002339, 3.874999998634407028, -1.881053915767121998 ) ) ;
#26411 = AXIS2_PLACEMENT_3D ( 'NONE', #21920, #49858, #72876 ) ;
#26412 = ADVANCED_FACE ( 'NONE', ( #754 ), #23738, .T. ) ;
#26413 = CARTESIAN_POINT ( 'NONE',  ( -7.188101187500000044, 8.718749997951611874, -8.802885111219163269E-16 ) ) ;
#26414 = CARTESIAN_POINT ( 'NONE',  ( -5.656854249492378806, 116.3750000040967905, 5.656854249492381470 ) ) ;
#26415 = CARTESIAN_POINT ( 'NONE',  ( -10.18810118749999916, 0.000000000000000000, 90.53125000204836681 ) ) ;
#26416 = AXIS2_PLACEMENT_3D ( 'NONE', #32154, #2731, #25719 ) ;
#26417 = EDGE_CURVE ( 'NONE', #33251, #52951, #70146, .T. ) ;
#26418 = CARTESIAN_POINT ( 'NONE',  ( -30.44569435410879166, 201.0625000013656063, 172.4456943541092357 ) ) ;
#26419 = CARTESIAN_POINT ( 'NONE',  ( -10.00000000000000178, 159.3749999931720254, -1.224646799147353454E-15 ) ) ;
#26420 = CARTESIAN_POINT ( 'NONE',  ( 2.828427124746190291, 4.875000000000000000, 2.828427124746192067 ) ) ;
#26421 = CARTESIAN_POINT ( 'NONE',  ( 1.656854249492381248, 19.93749999726881228, -4.000000000000001776 ) ) ;
#26422 = CARTESIAN_POINT ( 'NONE',  ( 4.541265875000002339, 5.374999998634407028, -1.881053915767121776 ) ) ;
#26423 = ORIENTED_EDGE ( 'NONE', *, *, #43571, .T. ) ;
#26424 = CARTESIAN_POINT ( 'NONE',  ( -3.458734124999959025, 194.5000000013656063, 199.4326545832176691 ) ) ;
#26425 = ADVANCED_FACE ( 'NONE', ( #10939 ), #56972, .T. ) ;
#26427 = CARTESIAN_POINT ( 'NONE',  ( -30.99999999999992895, -31.99999999999978684, 205.0000000000000284 ) ) ;
#26426 = CARTESIAN_POINT ( 'NONE',  ( -26.56734541678227757, 198.0000000013656063, 173.4587341250003476 ) ) ;
#26428 = CARTESIAN_POINT ( 'NONE',  ( -8.342170076843785083E-16, 17.06249999863440792, 4.541265875000002339 ) ) ;
#26429 = CARTESIAN_POINT ( 'NONE',  ( -1.836970198721029983E-15, 70.62499999317203958, 10.00000000000000178 ) ) ;
#26430 = CARTESIAN_POINT ( 'NONE',  ( 5.082755093536318824, 5.082755093536319713, 8.424052781871752771 ) ) ;
#26431 = ORIENTED_EDGE ( 'NONE', *, *, #24483, .T. ) ;
#26432 =( BOUNDED_CURVE ( )  B_SPLINE_CURVE ( 2, ( #43455, #15158, #38189, #61193, #3108, #55549, #19697, #60813, #31776 ),
 .UNSPECIFIED., .F., .F. ) 
 B_SPLINE_CURVE_WITH_KNOTS ( ( 3, 2, 2, 2, 3 ),
 ( 0.8522727272727272929, 0.8579545454545454142, 0.8636363636363636465, 0.8693181818181817677, 0.8750000000000000000 ),
 .UNSPECIFIED. ) 
 CURVE ( )  GEOMETRIC_REPRESENTATION_ITEM ( )  RATIONAL_B_SPLINE_CURVE ( ( 1.000000000000000000, 0.9238795325112867385, 1.000000000000000000, 0.9238795325112867385, 1.000000000000000000, 0.9238795325112867385, 1.000000000000000000, 0.9238795325112867385, 1.000000000000000000 ) ) 
 REPRESENTATION_ITEM ( '' )  );
#26433 = ORIENTED_EDGE ( 'NONE', *, *, #59236, .T. ) ;
#26434 = CARTESIAN_POINT ( 'NONE',  ( 10.18810118749999916, 1.247682550866122264E-15, 98.40625000204838102 ) ) ;
#26435 = CARTESIAN_POINT ( 'NONE',  ( -12.00000000000000000, 6.928203230275504332, -1.071796769724504550 ) ) ;
#26436 = CARTESIAN_POINT ( 'NONE',  ( -29.43265458321766914, 203.7500000013656063, 166.5412658750003629 ) ) ;
#26437 = CARTESIAN_POINT ( 'NONE',  ( -23.99999999999998934, 202.7500000000000000, 170.0000000000003411 ) ) ;
#26438 = CARTESIAN_POINT ( 'NONE',  ( -1.432654583217608080, 207.8750000013656063, 201.4587341250000350 ) ) ;
#26439 = CARTESIAN_POINT ( 'NONE',  ( -4.000000000000002665, 21.31249999726881228, 1.656854249492380582 ) ) ;
#26440 = CARTESIAN_POINT ( 'NONE',  ( 7.320508075688771044, 104.3750000000000000, 7.320508075688775484 ) ) ;
#26441 = ADVANCED_FACE ( 'NONE', ( #48587 ), #2209, .T. ) ;
#26442 = CARTESIAN_POINT ( 'NONE',  ( 8.000000000000000000, 112.3437500000000000, -3.313708498984762496 ) ) ;
#26443 = CARTESIAN_POINT ( 'NONE',  ( 6.676582343750001591, 291.1093750017069510, -8.176455196517173205E-16 ) ) ;
#26444 = CARTESIAN_POINT ( 'NONE',  ( 2.977408999572650927, -7.188101187499990274, 12.83030278187175277 ) ) ;
#26445 = ORIENTED_EDGE ( 'NONE', *, *, #51410, .F. ) ;
#26446 = LINE ( 'NONE', #66832, #22919 ) ;
#26447 = EDGE_CURVE ( 'NONE', #63061, #59993, #54110, .T. ) ;
#26448 = CARTESIAN_POINT ( 'NONE',  ( 5.656854249492378806, 22.12499999590322375, 5.656854249492381470 ) ) ;
#26449 = CARTESIAN_POINT ( 'NONE',  ( 3.458734124999959914, 205.4375000013656063, 142.0000000000000568 ) ) ;
#26450 = CARTESIAN_POINT ( 'NONE',  ( -4.000000000000001776, 5.437500000000001776, -1.656854249492381470 ) ) ;
#26452 = CARTESIAN_POINT ( 'NONE',  ( 2.445694354108784108, 203.5625000013656063, 144.4456943541088663 ) ) ;
#26451 = CARTESIAN_POINT ( 'NONE',  ( -11.00000000000000000, 0.000000000000000000, 111.9999999999999858 ) ) ;
#26453 = CARTESIAN_POINT ( 'NONE',  ( 2.085542519210945334E-15, 255.4687500034140157, 11.35316468749999963 ) ) ;
#26454 = CARTESIAN_POINT ( 'NONE',  ( -5.447321926944742820, -4.689934168550192517, 0.4069290644665413681 ) ) ;
#26455 = CARTESIAN_POINT ( 'NONE',  ( -7.320508075688773708, 213.7499999931720254, -7.320508075688774596 ) ) ;
#26456 = CARTESIAN_POINT ( 'NONE',  ( 9.832129032723420536, 6.197916663252683200, -5.676582343749999815 ) ) ;
#26457 =( BOUNDED_CURVE ( )  B_SPLINE_CURVE ( 2, ( #19114, #20214, #54949, #42119, #2512, #65508, #13441, #3258, #72280 ),
 .UNSPECIFIED., .F., .F. ) 
 B_SPLINE_CURVE_WITH_KNOTS ( ( 3, 2, 2, 2, 3 ),
 ( 0.8977272727272727071, 0.9034090909090909394, 0.9090909090909091717, 0.9147727272727274039, 0.9204545454545455252 ),
 .UNSPECIFIED. ) 
 CURVE ( )  GEOMETRIC_REPRESENTATION_ITEM ( )  RATIONAL_B_SPLINE_CURVE ( ( 1.000000000000000000, 0.9238795325112867385, 1.000000000000000000, 0.9238795325112867385, 1.000000000000000000, 0.9238795325112867385, 1.000000000000000000, 0.9238795325112852952, 1.000000000000001554 ) ) 
 REPRESENTATION_ITEM ( '' )  );
#26458 = CARTESIAN_POINT ( 'NONE',  ( -5.082755093536319713, 5.082755093536319713, 4.674052781871752771 ) ) ;
#26459 = CARTESIAN_POINT ( 'NONE',  ( 9.832129032723420536, 196.5104166632526983, -5.676582343749999815 ) ) ;
#26460 = CARTESIAN_POINT ( 'NONE',  ( 11.00000000000000000, 1.347111479062088405E-15, 102.4375000040967763 ) ) ;
#26461 = CARTESIAN_POINT ( 'NONE',  ( -4.541265875000002339, 5.749999998634407028, -1.881053915767121998 ) ) ;
#26462 = CARTESIAN_POINT ( 'NONE',  ( -10.02978802437156425, 8.065705644765211346, -0.4750804646944142839 ) ) ;
#26464 = DIRECTION ( 'NONE',  ( -0.000000000000000000, -0.000000000000000000, -1.000000000000000000 ) ) ;
#26463 = CARTESIAN_POINT ( 'NONE',  ( 0.000000000000000000, 300.0000000000000000, 0.000000000000000000 ) ) ;
#26465 = VERTEX_POINT ( 'NONE', #47481 ) ;
#26466 = VECTOR ( 'NONE', #51449, 1000.000000000000114 ) ;
#26467 = CARTESIAN_POINT ( 'NONE',  ( 3.458734124999960358, 204.6250000013655779, 143.4326545832176976 ) ) ;
#26468 = CARTESIAN_POINT ( 'NONE',  ( -2.085542519210945728E-15, 9.531249996586018014, 11.35316468750000141 ) ) ;
#26469 = CARTESIAN_POINT ( 'NONE',  ( -4.556349186104045934, 11.00000000000000000, 96.90625000409677625 ) ) ;
#26470 = FACE_OUTER_BOUND ( 'NONE', #26243, .T. ) ;
#26471 = CARTESIAN_POINT ( 'NONE',  ( -24.54126587499996148, 203.1250000013656347, 171.4326545832179534 ) ) ;
#26472 = CARTESIAN_POINT ( 'NONE',  ( -6.676582343750001591, 287.5312500017070079, 0.000000000000000000 ) ) ;
#26474 = CARTESIAN_POINT ( 'NONE',  ( -2.849036369511732440E-14, 204.2500000000000284, 138.0000000000000568 ) ) ;
#26473 = CARTESIAN_POINT ( 'NONE',  ( 7.188101187500000933, 116.0000000020483810, -2.977408999572651371 ) ) ;
#26475 = CARTESIAN_POINT ( 'NONE',  ( -5.656854249492375253, 5.656854249492375253, 24.64280277982336642 ) ) ;
#26476 = CARTESIAN_POINT ( 'NONE',  ( -8.311093377946841443, 118.9062499965860269, 8.311093377946830785 ) ) ;
#26477 = CARTESIAN_POINT ( 'NONE',  ( -2.679491924311235618, 95.41666665983868256, 10.00000000000000000 ) ) ;
#26478 = CARTESIAN_POINT ( 'NONE',  ( -5.082755093536325930, 92.46875000204838102, -5.082755093536325930 ) ) ;
#26479 = CARTESIAN_POINT ( 'NONE',  ( -3.211159895383562723, 21.06249999863440792, 3.211159895383561391 ) ) ;
#26480 = CARTESIAN_POINT ( 'NONE',  ( 2.598723904613009950, -8.891930899535452681, -0.1469846612282645348 ) ) ;
#26481 = CARTESIAN_POINT ( 'NONE',  ( -12.00000000000000000, 0.000000000000000000, 0.000000000000000000 ) ) ;
#26482 = ORIENTED_EDGE ( 'NONE', *, *, #52389, .F. ) ;
#26483 = CARTESIAN_POINT ( 'NONE',  ( -5.010106067795776497, 225.9999999999999716, 8.679299243466562785 ) ) ;
#26484 = CARTESIAN_POINT ( 'NONE',  ( -2.765530957081996810, 294.4218750017069510, -6.676582343750003368 ) ) ;
#26485 = CARTESIAN_POINT ( 'NONE',  ( -10.99999999999999645, 11.00000000000000355, -6.791607979884335933E-15 ) ) ;
#26486 = CARTESIAN_POINT ( 'NONE',  ( 5.656854249492374365, 5.656854249492375253, 0.4553027839201452265 ) ) ;
#26487 = CARTESIAN_POINT ( 'NONE',  ( 3.042071309553159519, 169.7395833299193839, 11.35316468750000141 ) ) ;
#26488 = CARTESIAN_POINT ( 'NONE',  ( 3.999999999999959144, 198.0625000000000284, 140.3431457505076594 ) ) ;
#26489 = CARTESIAN_POINT ( 'NONE',  ( 10.00000000000000178, 206.8749999931720538, 0.000000000000000000 ) ) ;
#26490 = CARTESIAN_POINT ( 'NONE',  ( -5.000000000000026645, 193.3333333333333712, 8.660254037844424602 ) ) ;
#26491 = CARTESIAN_POINT ( 'NONE',  ( -4.220049686691935698, 10.18810118749999916, 103.7500000020483668 ) ) ;
#26492 = ORIENTED_EDGE ( 'NONE', *, *, #54048, .T. ) ;
#26493 = B_SPLINE_CURVE_WITH_KNOTS ( 'NONE', 3,
 ( #70881, #41109, #24488, #52430, #41840, #64849, #30523, #41474, #46392, #35094, #69778, #35457, #58104, #64116 ),
 .UNSPECIFIED., .F., .F.,
 ( 4, 2, 2, 2, 2, 2, 4 ),
 ( 1.413604231308014593E-17, 0.009367252303384981590, 0.01405087845507746458, 0.01639269153092370521, 0.01873450460676994930, 0.02810175691015468977, 0.03746900921353943370 ),
 .UNSPECIFIED. ) ;
#26494 = CARTESIAN_POINT ( 'NONE',  ( -3.999999999999960032, 198.1250000027312126, 198.0000000000000284 ) ) ;
#26495 = CARTESIAN_POINT ( 'NONE',  ( 5.676582343749993598, 155.2604166632526983, 9.832129032723422313 ) ) ;
#26496 = CARTESIAN_POINT ( 'NONE',  ( 2.445694354108839619, 194.8125000013656063, 200.4456943541088663 ) ) ;
#26497 = CARTESIAN_POINT ( 'NONE',  ( -2.445694354108784108, 204.5625000013656063, 195.5543056458912190 ) ) ;
#26499 = EDGE_CURVE ( 'NONE', #36393, #2485, #30511, .T. ) ;
#26498 = DIRECTION ( 'NONE',  ( 0.000000000000000000, 1.000000000000000000, 0.000000000000000000 ) ) ;
#26500 = CARTESIAN_POINT ( 'NONE',  ( -2.085542519210945728E-15, 59.84374999658602690, 11.35316468750000141 ) ) ;
#26501 = ORIENTED_EDGE ( 'NONE', *, *, #55230, .F. ) ;
#26502 = CARTESIAN_POINT ( 'NONE',  ( 1.871523826299183495E-15, -10.18810118749999916, 111.5312500020483668 ) ) ;
#26503 = CARTESIAN_POINT ( 'NONE',  ( 4.541265875000002339, 7.499999998634407916, -1.881053915767121776 ) ) ;
#26504 = ORIENTED_EDGE ( 'NONE', *, *, #45031, .F. ) ;
#26505 = CARTESIAN_POINT ( 'NONE',  ( -2.977408999572654480, 23.99999999795161543, 7.188101187499999156 ) ) ;
#26506 = CARTESIAN_POINT ( 'NONE',  ( -4.242640687119286547, 288.9375000034140157, -4.242640687119286547 ) ) ;
#26507 = DIRECTION ( 'NONE',  ( -0.000000000000000000, 1.000000000000000000, -0.000000000000000000 ) ) ;
#26508 = CARTESIAN_POINT ( 'NONE',  ( 2.977408999572650927, 19.12499999795161187, -7.188101187500001821 ) ) ;
#26509 = CARTESIAN_POINT ( 'NONE',  ( 1.320432766682872962E-15, -7.188101187499992051, 4.861552781871752771 ) ) ;
#26510 = CARTESIAN_POINT ( 'NONE',  ( 4.220049686691941027, -10.18810118749999738, 107.5000000020483668 ) ) ;
#26511 = EDGE_CURVE ( 'NONE', #53476, #17389, #1847, .T. ) ;
#26512 = AXIS2_PLACEMENT_3D ( 'NONE', #36202, #59219, #7530 ) ;
#26513 = CARTESIAN_POINT ( 'NONE',  ( -3.673940397442060854E-16, 294.7500000000000000, -6.000000000000001776 ) ) ;
#26514 = CARTESIAN_POINT ( 'NONE',  ( -2.828427124746190735, 7.124999997268813168, -2.828427124746191623 ) ) ;
#26515 = CARTESIAN_POINT ( 'NONE',  ( -30.58772083827739152, -51.99923150805006600, 164.6923585894454618 ) ) ;
#26516 = AXIS2_PLACEMENT_3D ( 'NONE', #54515, #37530, #38277 ) ;
#26517 = ORIENTED_EDGE ( 'NONE', *, *, #24956, .T. ) ;
#26518 = AXIS2_PLACEMENT_3D ( 'NONE', #66655, #37999, #60997 ) ;
#26519 = CARTESIAN_POINT ( 'NONE',  ( -3.458734124999959025, 206.5000000013655779, 199.4326545832176691 ) ) ;
#26520 = CARTESIAN_POINT ( 'NONE',  ( -25.55430564589123321, 209.3125000013656063, 167.5543056458915032 ) ) ;
#26521 = EDGE_CURVE ( 'NONE', #59338, #8699, #10395, .T. ) ;
#26522 = CARTESIAN_POINT ( 'NONE',  ( 4.541265875000002339, 8.312499998634407916, 0.000000000000000000 ) ) ;
#26523 = DIRECTION ( 'NONE',  ( 1.000000000000000000, 0.000000000000000000, 0.000000000000000000 ) ) ;
#26524 = CARTESIAN_POINT ( 'NONE',  ( -4.401442555609577197E-16, 7.188101187499992051, 22.11155278187175455 ) ) ;
#26525 = VERTEX_POINT ( 'NONE', #19545 ) ;
#26526 = EDGE_CURVE ( 'NONE', #58121, #15471, #29126, .T. ) ;
#26527 = CARTESIAN_POINT ( 'NONE',  ( -7.188101187500000933, 26.62499999795161543, -2.977408999572651371 ) ) ;
#26528 = ORIENTED_EDGE ( 'NONE', *, *, #6311, .T. ) ;
#26529 = CARTESIAN_POINT ( 'NONE',  ( 4.220049686691934809, 10.18810118749999916, 115.1875000020483668 ) ) ;
#26530 = CARTESIAN_POINT ( 'NONE',  ( 4.556349186104052151, -10.99999999999999822, 84.15625000409676204 ) ) ;
#26531 = CARTESIAN_POINT ( 'NONE',  ( 2.754378923186476579E-14, 206.1875000013656063, 194.5412658750000219 ) ) ;
#26532 = CARTESIAN_POINT ( 'NONE',  ( 31.45873412499999233, 198.6875000013655779, 169.9999999999998863 ) ) ;
#26533 = CARTESIAN_POINT ( 'NONE',  ( -8.660254037844387298, 67.08333333333334281, -5.000000000000004441 ) ) ;
#26534 = CARTESIAN_POINT ( 'NONE',  ( -7.188101187500001821, 91.43750000204838102, -2.977408999572650483 ) ) ;
#26535 = CARTESIAN_POINT ( 'NONE',  ( -6.000000000000000888, 292.0625000000000000, 2.485281374238575758 ) ) ;
#26536 = CARTESIAN_POINT ( 'NONE',  ( 23.99999999999999289, 207.8750000027312126, 169.9999999999999432 ) ) ;
#26537 = VECTOR ( 'NONE', #48524, 1000.000000000000000 ) ;
#26538 = ORIENTED_EDGE ( 'NONE', *, *, #32223, .T. ) ;
#26539 = CARTESIAN_POINT ( 'NONE',  ( -5.676582343749992710, 224.7395833367473301, 9.832129032723422313 ) ) ;
#26540 = CARTESIAN_POINT ( 'NONE',  ( -2.620431783921197244, -10.11675809139960869, 70.36490484706814641 ) ) ;
#26541 = CARTESIAN_POINT ( 'NONE',  ( 3.999999999999960032, 202.0625000027312410, 143.6568542494924543 ) ) ;
#26542 = DIRECTION ( 'NONE',  ( -0.000000000000000000, -0.000000000000000000, -1.000000000000000000 ) ) ;
#26543 = CARTESIAN_POINT ( 'NONE',  ( -11.00000000000000000, 0.000000000000000000, 118.0000000000000000 ) ) ;
#26544 = CARTESIAN_POINT ( 'NONE',  ( 5.000000000000004441, 251.6666666666667140, 8.660254037844385522 ) ) ;
#26545 = EDGE_CURVE ( 'NONE', #34061, #45912, #36546, .T. ) ;
#26546 = DIRECTION ( 'NONE',  ( -0.000000000000000000, 1.000000000000000000, -0.000000000000000000 ) ) ;
#26547 = CARTESIAN_POINT ( 'NONE',  ( -7.320508075688778149, 183.1250000000000284, 7.320508075688769267 ) ) ;
#26548 = CARTESIAN_POINT ( 'NONE',  ( 0.000000000000000000, 300.0000000000000000, 10.00000000000000178 ) ) ;
#26549 = CARTESIAN_POINT ( 'NONE',  ( -7.188101187499990274, -2.977408999572651815, 19.95530278187175455 ) ) ;
#26550 = CARTESIAN_POINT ( 'NONE',  ( 3.042071309553167069, 157.1354166632526983, -11.35316468749999785 ) ) ;
#26551 = DIRECTION ( 'NONE',  ( -0.000000000000000000, -0.000000000000000000, -1.000000000000000000 ) ) ;
#26552 = CYLINDRICAL_SURFACE ( 'NONE', #21, 3.999999999999976019 ) ;
#26553 = CARTESIAN_POINT ( 'NONE',  ( 11.00000000000000000, 1.347111479062088405E-15, 82.93750000409677625 ) ) ;
#26556 = CARTESIAN_POINT ( 'NONE',  ( -8.000000000000001776, 17.34375000000000000, 3.313708498984759387 ) ) ;
#26555 = CARTESIAN_POINT ( 'NONE',  ( -2.828427124746208943, 202.7500000027312126, 144.8284271247462129 ) ) ;
#26554 = CARTESIAN_POINT ( 'NONE',  ( 24.00000000000000355, 202.6875000000000284, 168.3431457505075173 ) ) ;
#26557 = ORIENTED_EDGE ( 'NONE', *, *, #10208, .T. ) ;
#26558 = CARTESIAN_POINT ( 'NONE',  ( 8.311093377946834337, 20.46874999658601624, 8.311093377946839666 ) ) ;
#26559 = CARTESIAN_POINT ( 'NONE',  ( 10.00000000000000178, 96.87499999317203958, 0.000000000000000000 ) ) ;
#26561 = CARTESIAN_POINT ( 'NONE',  ( 5.000000000000001776, 32.70833332650536107, -8.660254037844389075 ) ) ;
#26560 = CARTESIAN_POINT ( 'NONE',  ( 0.000000000000000000, 125.0000000000000000, 0.000000000000000000 ) ) ;
#26562 = DIRECTION ( 'NONE',  ( 1.000000000000000000, 0.000000000000000000, 0.000000000000000000 ) ) ;
#26563 = CARTESIAN_POINT ( 'NONE',  ( 1.432654583217607192, 202.2500000013655779, 145.4587341250000350 ) ) ;
#26564 =( BOUNDED_CURVE ( )  B_SPLINE_CURVE ( 2, ( #47714, #53766, #30746 ),
 .UNSPECIFIED., .F., .F. ) 
 B_SPLINE_CURVE_WITH_KNOTS ( ( 3, 3 ),
 ( 0.9687500000000000000, 0.9722122500602408124 ),
 .UNSPECIFIED. ) 
 CURVE ( )  GEOMETRIC_REPRESENTATION_ITEM ( )  RATIONAL_B_SPLINE_CURVE ( ( 1.000000000000000000, 0.9493987661155159907, 0.9660720762559202868 ) ) 
 REPRESENTATION_ITEM ( '' )  );
#26565 = AXIS2_PLACEMENT_3D ( 'NONE', #65500, #41392, #36468 ) ;
#26566 = CARTESIAN_POINT ( 'NONE',  ( 8.660254037844389075, 47.29166665983870388, -5.000000000000000000 ) ) ;
#26567 = CARTESIAN_POINT ( 'NONE',  ( 2.977408999572650039, 108.6875000020483952, -7.188101187500001821 ) ) ;
#26568 = CARTESIAN_POINT ( 'NONE',  ( 4.541265875000001451, 10.37499999863440792, 1.881053915767124440 ) ) ;
#26569 = DIRECTION ( 'NONE',  ( -0.000000000000000000, 1.000000000000000000, -0.000000000000000000 ) ) ;
#26570 = CARTESIAN_POINT ( 'NONE',  ( -5.656854249492373476, -5.656854249492376141, 8.517802779823362869 ) ) ;
#26572 = CARTESIAN_POINT ( 'NONE',  ( -7.347880794884122694E-16, 14.49999999726881406, 4.000000000000001776 ) ) ;
#26571 = CARTESIAN_POINT ( 'NONE',  ( 0.8361131105013063225, 194.5804128891767846, 138.5121337385087088 ) ) ;
#26573 = EDGE_LOOP ( 'NONE', ( #52673, #16602, #51295, #4509, #60252, #18454, #13896, #16134, #42569, #27455, #51944, #33152, #40726, #66221, #41580, #67791, #14156, #37991, #68161, #47052, #44427, #65138, #55348, #24851, #31127, #26445, #69877, #7015, #51323, #56150, #12471, #16307, #11796, #31317, #72711, #50566, #65321, #14774, #21878 ) ) ;
#26574 = VERTEX_POINT ( 'NONE', #70870 ) ;
#26575 = CARTESIAN_POINT ( 'NONE',  ( -8.660254037844390851, 222.9166666666666856, 4.999999999999998224 ) ) ;
#26576 = CARTESIAN_POINT ( 'NONE',  ( 1.224646799147353454E-15, 300.0000000000000000, -10.00000000000000178 ) ) ;
#26577 = EDGE_CURVE ( 'NONE', #16961, #64023, #65196, .T. ) ;
#26578 = CARTESIAN_POINT ( 'NONE',  ( -10.99999999999994849, 4.556349186104097448, 95.40625000000000000 ) ) ;
#26579 = CARTESIAN_POINT ( 'NONE',  ( -3.042071309553164404, 132.2395833299193555, -11.35316468749999963 ) ) ;
#26580 = ORIENTED_EDGE ( 'NONE', *, *, #72251, .T. ) ;
#26581 = CARTESIAN_POINT ( 'NONE',  ( -2.726571689596997292E-14, 210.0000000000000284, 138.0000000000000568 ) ) ;
#26582 = AXIS2_PLACEMENT_3D ( 'NONE', #24746, #48869, #59834 ) ;
#26583 = CARTESIAN_POINT ( 'NONE',  ( 10.18810118749999916, 1.247682550866122264E-15, 96.90625000204838102 ) ) ;
#26584 = CARTESIAN_POINT ( 'NONE',  ( -8.000000000000000000, 93.50000000000000000, 0.000000000000000000 ) ) ;
#26585 = CARTESIAN_POINT ( 'NONE',  ( 2.828427124746209831, 207.3750000000000284, 200.8284271247462129 ) ) ;
#26586 = CARTESIAN_POINT ( 'NONE',  ( -4.999999999999998224, 153.5416666598387110, -8.660254037844389075 ) ) ;
#26588 = CARTESIAN_POINT ( 'NONE',  ( 11.35316468749999785, 130.5729166632526983, 3.042071309553174174 ) ) ;
#26587 = CARTESIAN_POINT ( 'NONE',  ( 26.34314575050748530, 197.9375000000000000, 173.9999999999997726 ) ) ;
#26589 = EDGE_CURVE ( 'NONE', #40278, #32586, #72527, .T. ) ;
#26590 = DIRECTION ( 'NONE',  ( -0.000000000000000000, 1.000000000000000000, -0.000000000000000000 ) ) ;
#26591 = ORIENTED_EDGE ( 'NONE', *, *, #57274, .T. ) ;
#26592 =( BOUNDED_CURVE ( )  B_SPLINE_CURVE ( 2, ( #7157, #30161, #47499, #55416, #61058, #21063, #2606, #19937, #10126 ),
 .UNSPECIFIED., .F., .F. ) 
 B_SPLINE_CURVE_WITH_KNOTS ( ( 3, 2, 2, 2, 3 ),
 ( 0.2666666666666668850, 0.2750000000000002442, 0.2833333333333335480, 0.2916666666666669072, 0.3000000000000002109 ),
 .UNSPECIFIED. ) 
 CURVE ( )  GEOMETRIC_REPRESENTATION_ITEM ( )  RATIONAL_B_SPLINE_CURVE ( ( 0.9999999999999980016, 0.9238795325112887369, 1.000000000000000000, 0.9238795325112867385, 1.000000000000000000, 0.9238795325112867385, 1.000000000000000000, 0.9238795325112847401, 1.000000000000001998 ) ) 
 REPRESENTATION_ITEM ( '' )  );
#26593 = CARTESIAN_POINT ( 'NONE',  ( -5.656854249492380582, 109.8125000000000000, -5.656854249492380582 ) ) ;
#26594 = CARTESIAN_POINT ( 'NONE',  ( 49.70177871865297448, 48.76036930335158814, 58.00000000000000000 ) ) ;
#26595 = CARTESIAN_POINT ( 'NONE',  ( 8.311093377946834337, 115.4687499965860127, 8.311093377946839666 ) ) ;
#26596 = CARTESIAN_POINT ( 'NONE',  ( -2.445694354108783664, 206.3125000013656063, 195.5543056458912190 ) ) ;
#26597 = CARTESIAN_POINT ( 'NONE',  ( 2.977408999572652260, 18.56249999795161187, 7.188101187500000044 ) ) ;
#26599 = EDGE_CURVE ( 'NONE', #46523, #54990, #59923, .T. ) ;
#26598 = CARTESIAN_POINT ( 'NONE',  ( 4.220049686691934809, 10.18810118749999916, 85.56250000204838102 ) ) ;
#26600 = CARTESIAN_POINT ( 'NONE',  ( 5.676582343750001591, 21.92708332991935194, -9.832129032723420536 ) ) ;
#26601 = ORIENTED_EDGE ( 'NONE', *, *, #57418, .F. ) ;
#26602 = CARTESIAN_POINT ( 'NONE',  ( -7.999999999999998224, 96.78125000409679046, 3.313708498984766049 ) ) ;
#26603 = CARTESIAN_POINT ( 'NONE',  ( 3.317071493978877683, 8.008118988124991233, 24.54436528394063188 ) ) ;
#26604 = CARTESIAN_POINT ( 'NONE',  ( -2.839093476692135984E-14, 208.9375000013656063, 138.5412658750000503 ) ) ;
#26605 = CARTESIAN_POINT ( 'NONE',  ( -7.188101187500000044, 2.718749997951610098, -8.802885111219163269E-16 ) ) ;
#26606 = CARTESIAN_POINT ( 'NONE',  ( 4.242640687119285658, 298.6875000034139589, -4.242640687119286547 ) ) ;
#26607 = CARTESIAN_POINT ( 'NONE',  ( -3.673940397442060854E-16, 296.7500000000000000, -6.000000000000001776 ) ) ;
#26608 = CARTESIAN_POINT ( 'NONE',  ( -3.313708498984760276, 16.78124999590322375, -8.000000000000000000 ) ) ;
#26609 = ORIENTED_EDGE ( 'NONE', *, *, #2112, .T. ) ;
#26610 = CARTESIAN_POINT ( 'NONE',  ( -8.311093377946836114, 142.9687499965859843, -8.311093377946837890 ) ) ;
#26611 = CARTESIAN_POINT ( 'NONE',  ( -7.204075437095967871, 7.204075437095967871, 80.96875000204836681 ) ) ;
#26612 = EDGE_CURVE ( 'NONE', #8879, #44513, #5557, .T. ) ;
#26613 = EDGE_CURVE ( 'NONE', #55859, #3208, #61412, .T. ) ;
#26614 = CARTESIAN_POINT ( 'NONE',  ( -31.45873412499999944, 197.6250000013656063, 168.5673454167827572 ) ) ;
#26615 = DIRECTION ( 'NONE',  ( 0.000000000000000000, 0.000000000000000000, 1.000000000000000000 ) ) ;
#26616 = CARTESIAN_POINT ( 'NONE',  ( 4.541265875000002339, 16.43749999863440436, 0.000000000000000000 ) ) ;
#26617 = ORIENTED_EDGE ( 'NONE', *, *, #12718, .T. ) ;
#26618 = CARTESIAN_POINT ( 'NONE',  ( -1.656854249492348607, 203.3125000027311842, 202.0000000000000284 ) ) ;
#26619 = CARTESIAN_POINT ( 'NONE',  ( 3.458734124999960358, 194.6875000013655779, 142.0000000000000568 ) ) ;
#26620 = CARTESIAN_POINT ( 'NONE',  ( -23.99999999999998934, 203.8750000027312126, 170.0000000000002842 ) ) ;
#26621 = CARTESIAN_POINT ( 'NONE',  ( 3.313708498984756279, 7.999999999999991118, 13.86155277982336465 ) ) ;
#26622 = VERTEX_POINT ( 'NONE', #33508 ) ;
#26623 = CARTESIAN_POINT ( 'NONE',  ( -5.082755093536325042, 13.03124999795161187, -5.082755093536325930 ) ) ;
#26624 = EDGE_CURVE ( 'NONE', #1774, #50149, #37666, .T. ) ;
#26625 = CARTESIAN_POINT ( 'NONE',  ( -4.000000000000016875, 208.4375000000000853, 140.3431457505076594 ) ) ;
#26626 = CARTESIAN_POINT ( 'NONE',  ( 5.000000000000000000, 53.36732872257336169, -44.46877392682712582 ) ) ;
#26627 = CARTESIAN_POINT ( 'NONE',  ( -9.832129032723418760, 192.8645833299193839, -5.676582343750004256 ) ) ;
#26628 = CARTESIAN_POINT ( 'NONE',  ( 2.977408999572654480, 110.0000000020483668, 7.188101187499999156 ) ) ;
#26629 = VECTOR ( 'NONE', #50711, 1000.000000000000114 ) ;
#26630 = CARTESIAN_POINT ( 'NONE',  ( -7.240284387734133737E-08, 22.00000000000001066, -4.000000000000000888 ) ) ;
#26631 = CARTESIAN_POINT ( 'NONE',  ( 2.765530957082001251, 288.7656250017069510, 6.676582343749999815 ) ) ;
#26632 = CARTESIAN_POINT ( 'NONE',  ( 9.498558403365325509E-13, 68.75000000000008527, 10.00000000000000178 ) ) ;
#26633 = ITEM_DEFINED_TRANSFORMATION ( 'NONE', 'NONE', #41726,  #57354 ) ;
#26634 = VERTEX_POINT ( 'NONE', #56511 ) ;
#26635 = CARTESIAN_POINT ( 'NONE',  ( 5.676582343749997150, 257.2395833367473301, -9.832129032723418760 ) ) ;
#26636 = CARTESIAN_POINT ( 'NONE',  ( -7.188101187499992051, 0.000000000000000000, 22.86155278187175455 ) ) ;
#26637 = VECTOR ( 'NONE', #9071, 1000.000000000000000 ) ;
#26638 = DIRECTION ( 'NONE',  ( 0.000000000000000000, 0.000000000000000000, 1.000000000000000000 ) ) ;
#26639 = DIRECTION ( 'NONE',  ( 0.000000000000000000, 0.000000000000000000, 1.000000000000000000 ) ) ;
#26640 = CARTESIAN_POINT ( 'NONE',  ( 3.734423912262952783, -66.26963445014256138, -26.58791153593539036 ) ) ;
#26641 = CARTESIAN_POINT ( 'NONE',  ( -1.432654583217608080, 199.8750000013655779, 201.4587341250000350 ) ) ;
#26642 = FACE_OUTER_BOUND ( 'NONE', #58085, .T. ) ;
#26643 = CARTESIAN_POINT ( 'NONE',  ( 0.000000000000000000, 300.0000000000000000, 10.00000000000000178 ) ) ;
#26644 = CARTESIAN_POINT ( 'NONE',  ( -7.999999999999998224, 93.59375000000000000, 3.313708498984766493 ) ) ;
#26645 = CARTESIAN_POINT ( 'NONE',  ( -5.676582343750006032, 114.4270833299193555, 9.832129032723418760 ) ) ;
#26646 = CARTESIAN_POINT ( 'NONE',  ( 23.99999999999999645, 205.6875000000000284, 168.3431457505074889 ) ) ;
#26647 = CARTESIAN_POINT ( 'NONE',  ( -11.00000000000000000, 0.000000000000000000, 69.99999999999998579 ) ) ;
#26648 = AXIS2_PLACEMENT_3D ( 'NONE', #40963, #63971, #35318 ) ;
#26651 = CARTESIAN_POINT ( 'NONE',  ( 4.242640687119285658, 298.6250000000000000, -4.242640687119286547 ) ) ;
#26650 = CARTESIAN_POINT ( 'NONE',  ( 25.55430564589119058, 202.3125000013656063, 172.4456943541087526 ) ) ;
#26649 = CARTESIAN_POINT ( 'NONE',  ( 25.55430564589119413, 199.3125000013656063, 167.5543056458910485 ) ) ;
#26652 = ORIENTED_EDGE ( 'NONE', *, *, #7694, .T. ) ;
#26653 = CARTESIAN_POINT ( 'NONE',  ( 8.000000000000001776, 100.1562500000000000, 3.313708498984759387 ) ) ;
#26654 = CARTESIAN_POINT ( 'NONE',  ( 8.311093377946834337, 220.1562499965860127, 8.311093377946839666 ) ) ;
#26655 = CARTESIAN_POINT ( 'NONE',  ( -3.458734125000016313, 195.8750000013655779, 140.5673454167824161 ) ) ;
#26656 = ADVANCED_FACE ( 'NONE', ( #66697 ), #67449, .T. ) ;
#26657 = CARTESIAN_POINT ( 'NONE',  ( 27.99999999999996092, 197.6875000013655779, 173.4587341249998929 ) ) ;
#26658 = CARTESIAN_POINT ( 'NONE',  ( -7.778174593052023411, 7.778174593052023411, 110.5000000040967763 ) ) ;
#26659 = CARTESIAN_POINT ( 'NONE',  ( -5.676582343749998039, 212.7604166632526699, -9.832129032723420536 ) ) ;
#26660 = CARTESIAN_POINT ( 'NONE',  ( 26.34314575050760610, 207.6875000027312126, 165.9999999999998863 ) ) ;
#26661 = FACE_OUTER_BOUND ( 'NONE', #21662, .T. ) ;
#26662 = CARTESIAN_POINT ( 'NONE',  ( 3.211159895383561835, 17.43749999863440792, -3.211159895383561835 ) ) ;
#26663 = CARTESIAN_POINT ( 'NONE',  ( 31.45873412499997812, 194.8750000013656347, 171.4326545832176123 ) ) ;
#26664 = CARTESIAN_POINT ( 'NONE',  ( 7.999999999999992895, -3.313708498984756279, 25.48655277982336642 ) ) ;
#26665 = CARTESIAN_POINT ( 'NONE',  ( -29.65685424949230153, 208.5625000027312694, 174.0000000000004547 ) ) ;
#26666 = CARTESIAN_POINT ( 'NONE',  ( 9.832129032723416984, 85.36458332991936970, 5.676582343750006032 ) ) ;
#26667 = ORIENTED_EDGE ( 'NONE', *, *, #61705, .T. ) ;
#26668 = FACE_OUTER_BOUND ( 'NONE', #34634, .T. ) ;
#26669 = CARTESIAN_POINT ( 'NONE',  ( 7.188101187499999156, 21.37499999795161543, 2.977408999572654924 ) ) ;
#26670 = CARTESIAN_POINT ( 'NONE',  ( -7.320508075688771932, 222.5000000068279746, -7.320508075688771932 ) ) ;
#26671 = CARTESIAN_POINT ( 'NONE',  ( 9.832129032723416984, 262.1354166700806445, -5.676582343750003368 ) ) ;
#26672 = AXIS2_PLACEMENT_3D ( 'NONE', #44597, #49499, #38937 ) ;
#26673 = CARTESIAN_POINT ( 'NONE',  ( 5.676582343750001591, 91.61458332991935549, -9.832129032723420536 ) ) ;
#26674 = VERTEX_POINT ( 'NONE', #73105 ) ;
#26675 = CARTESIAN_POINT ( 'NONE',  ( 2.679491924311075302, 205.8333333265053682, 10.00000000000008704 ) ) ;
#26676 = CARTESIAN_POINT ( 'NONE',  ( -10.18810118749999916, 4.220049686691934809, 112.5625000020483810 ) ) ;
#26677 = CARTESIAN_POINT ( 'NONE',  ( -29.43265458321766559, 194.7500000013656063, 166.5412658750003629 ) ) ;
#26678 = FACE_OUTER_BOUND ( 'NONE', #53101, .T. ) ;
#26679 = CARTESIAN_POINT ( 'NONE',  ( 18.00000000000000355, -10.39230484541328892, -1.607695154586745501 ) ) ;
#26681 = CARTESIAN_POINT ( 'NONE',  ( 9.832129032723420536, 86.19791666325268409, -5.676582343749999815 ) ) ;
#26680 = CARTESIAN_POINT ( 'NONE',  ( -56.00000000000004974, 5.999999999999977796, 171.9999999999997726 ) ) ;
#26682 = CARTESIAN_POINT ( 'NONE',  ( 5.656854249492374365, 5.656854249492375253, 18.45530278392014623 ) ) ;
#26683 = CARTESIAN_POINT ( 'NONE',  ( -25.55430564589115150, 202.3125000013656063, 172.4456943541091789 ) ) ;
#26684 = EDGE_CURVE ( 'NONE', #7966, #61381, #41235, .T. ) ;
#26685 = CYLINDRICAL_SURFACE ( 'NONE', #25220, 10.00000000000000000 ) ;
#26686 = CARTESIAN_POINT ( 'NONE',  ( -10.00000000000000355, 179.5833333265053966, 2.679491924311223183 ) ) ;
#26687 = CARTESIAN_POINT ( 'NONE',  ( 2.485281374238175189, 296.7500000034139589, -6.000000000000396128 ) ) ;
#26688 = CARTESIAN_POINT ( 'NONE',  ( -2.085542519210945728E-15, 74.84374999658602690, 11.35316468750000141 ) ) ;
#26689 = CARTESIAN_POINT ( 'NONE',  ( -4.721056650415999201, 294.3281250017069510, -4.721056650415999201 ) ) ;
#26690 =( BOUNDED_CURVE ( )  B_SPLINE_CURVE ( 2, ( #11706, #43, #40748, #17361, #12075, #6434, #5684, #19124, #29436 ),
 .UNSPECIFIED., .F., .F. ) 
 B_SPLINE_CURVE_WITH_KNOTS ( ( 3, 2, 2, 2, 3 ),
 ( 0.5000000000000001110, 0.5036764705882353921, 0.5073529411764706731, 0.5110294117647059542, 0.5147058823529412352 ),
 .UNSPECIFIED. ) 
 CURVE ( )  GEOMETRIC_REPRESENTATION_ITEM ( )  RATIONAL_B_SPLINE_CURVE ( ( 0.9999999999999976685, 0.9238795325112890700, 1.000000000000000000, 0.9238795325112867385, 1.000000000000000000, 0.9238795325112867385, 1.000000000000000000, 0.9238795325112844070, 1.000000000000002220 ) ) 
 REPRESENTATION_ITEM ( '' )  );
#26692 = EDGE_CURVE ( 'NONE', #15625, #53323, #13234, .T. ) ;
#26691 = CARTESIAN_POINT ( 'NONE',  ( -6.238412754330611322E-16, 10.18810118749999916, 109.6562500020483668 ) ) ;
#26693 = CARTESIAN_POINT ( 'NONE',  ( 5.676582343749993598, 204.9479166632526983, 9.832129032723422313 ) ) ;
#26694 = ORIENTED_EDGE ( 'NONE', *, *, #31630, .F. ) ;
#26695 = DIRECTION ( 'NONE',  ( 0.000000000000000000, 0.000000000000000000, 1.000000000000000000 ) ) ;
#26696 = DIRECTION ( 'NONE',  ( 0.000000000000000000, 0.000000000000000000, -1.000000000000000000 ) ) ;
#26697 = CARTESIAN_POINT ( 'NONE',  ( -27.99999999999999645, 210.0000000000000284, 170.0000000000003695 ) ) ;
#26699 = CARTESIAN_POINT ( 'NONE',  ( 9.832129032723420536, 201.1979166632526983, -5.676582343749999815 ) ) ;
#26698 = CARTESIAN_POINT ( 'NONE',  ( -2.828427124746192067, 11.37499999726881406, 2.828427124746190735 ) ) ;
#26700 = CARTESIAN_POINT ( 'NONE',  ( 6.123233995736767268E-16, 193.1249999931720254, -10.00000000000000178 ) ) ;
#26701 = CARTESIAN_POINT ( 'NONE',  ( -6.123233995736766282E-16, 221.8750000068279746, -10.00000000000000000 ) ) ;
#26702 = CARTESIAN_POINT ( 'NONE',  ( -6.676582343750003368, 299.3906250017069510, -2.765530957081996810 ) ) ;
#26703 = AXIS2_PLACEMENT_3D ( 'NONE', #60154, #8474, #37151 ) ;
#26704 = EDGE_LOOP ( 'NONE', ( #72287, #58460, #13389, #18559 ) ) ;
#26705 = CARTESIAN_POINT ( 'NONE',  ( -5.676582343750006032, 194.4270833299193839, 9.832129032723418760 ) ) ;
#26706 = AXIS2_PLACEMENT_3D ( 'NONE', #36636, #14718, #60756 ) ;
#26707 = CARTESIAN_POINT ( 'NONE',  ( -7.188101187499992051, 2.977408999572646930, 14.89280278187175455 ) ) ;
#26708 = CARTESIAN_POINT ( 'NONE',  ( -24.54126587500000412, 209.2500000013655779, 168.5673454167827003 ) ) ;
#26709 = CARTESIAN_POINT ( 'NONE',  ( -3.313708498984760720, 13.96875000000000355, -8.000000000000000000 ) ) ;
#26710 = VERTEX_POINT ( 'NONE', #16112 ) ;
#26711 = CARTESIAN_POINT ( 'NONE',  ( 1.469576158976823947E-15, 89.56250000409677625, 8.000000000000000000 ) ) ;
#26712 = CARTESIAN_POINT ( 'NONE',  ( -1.836970198721029983E-15, 13.75000000000000000, 10.00000000000000178 ) ) ;
#26713 = VERTEX_POINT ( 'NONE', #61788 ) ;
#26714 = B_SPLINE_CURVE_WITH_KNOTS ( 'NONE', 3,
 ( #7477, #30482, #35421, #53499, #355, #23336, #29382, #34683, #14595, #2552, #25911, #25543, #47818, #42533, #2178, #1816, #60632, #8954, #31218, #19151 ),
 .UNSPECIFIED., .F., .F.,
 ( 4, 2, 2, 2, 2, 2, 2, 2, 2, 4 ),
 ( 0.000000000000000000, 0.001156441540184021885, 0.001734662310276033044, 0.002312883080368043770, 0.003469324620552040501, 0.004625766160736037233, 0.005782207700920033965, 0.006938649241104030696, 0.008095090781288028295, 0.009251532321472025894 ),
 .UNSPECIFIED. ) ;
#26715 = CARTESIAN_POINT ( 'NONE',  ( 4.000000000000001776, 16.00000000000000000, 0.000000000000000000 ) ) ;
#26716 = CARTESIAN_POINT ( 'NONE',  ( 3.211159895383560947, 20.18749999863440436, 3.211159895383562723 ) ) ;
#26717 = CARTESIAN_POINT ( 'NONE',  ( -7.999999999999991118, 0.000000000000000000, 10.01780278392014623 ) ) ;
#26718 = CARTESIAN_POINT ( 'NONE',  ( -1.836970198721029983E-15, 185.6249999931720538, 10.00000000000000178 ) ) ;
#26719 = VERTEX_POINT ( 'NONE', #61036 ) ;
#26720 = CARTESIAN_POINT ( 'NONE',  ( -1.040834085586084257E-14, 82.00000000000001421, 65.00000000000000000 ) ) ;
#26721 = CARTESIAN_POINT ( 'NONE',  ( -5.082755093536324154, 92.84375000204838102, 5.082755093536326818 ) ) ;
#26724 = FACE_OUTER_BOUND ( 'NONE', #8987, .T. ) ;
#26723 = CARTESIAN_POINT ( 'NONE',  ( 9.832129032723420536, 255.9895833367473301, 5.676582343749996262 ) ) ;
#26722 = CARTESIAN_POINT ( 'NONE',  ( -8.660254037844385522, 258.5416666734946602, 5.000000000000004441 ) ) ;
#26725 = DIRECTION ( 'NONE',  ( 1.000000000000000000, 0.000000000000000000, 0.000000000000000000 ) ) ;
#26726 = EDGE_LOOP ( 'NONE', ( #41214, #7241, #10223, #69664 ) ) ;
#26727 = CARTESIAN_POINT ( 'NONE',  ( 8.311093377946839666, 251.0937500034139873, 8.311093377946829008 ) ) ;
#26728 = CARTESIAN_POINT ( 'NONE',  ( -5.082755093536317936, -5.082755093536320601, 10.67405278187175455 ) ) ;
#26729 = EDGE_LOOP ( 'NONE', ( #20076, #49715, #74391, #43399 ) ) ;
#26730 = VERTEX_POINT ( 'NONE', #4449 ) ;
#26731 = CARTESIAN_POINT ( 'NONE',  ( -10.18810118749999916, 0.000000000000000000, 82.65625000204838102 ) ) ;
#26732 = CARTESIAN_POINT ( 'NONE',  ( 11.35316468749999963, 81.30208332991935549, -3.042071309553165293 ) ) ;
#26733 = CARTESIAN_POINT ( 'NONE',  ( -7.999999999999991118, 0.000000000000000000, 17.33030277982336287 ) ) ;
#26734 = CARTESIAN_POINT ( 'NONE',  ( -10.99999999999999822, -4.556349186104052151, 88.09375000000000000 ) ) ;
#26737 = CARTESIAN_POINT ( 'NONE',  ( 2.765530957081996366, 290.2968750017069510, -6.676582343750002480 ) ) ;
#26736 = CARTESIAN_POINT ( 'NONE',  ( 23.99999999999997513, 195.8125000027312126, 168.3431457505075741 ) ) ;
#26735 = CYLINDRICAL_SURFACE ( 'NONE', #40923, 10.00000000000000178 ) ;
#26738 = DIRECTION ( 'NONE',  ( 0.000000000000000000, -1.000000000000000000, 0.000000000000000000 ) ) ;
#26739 = CARTESIAN_POINT ( 'NONE',  ( 32.00000000000000711, 209.3125000000000284, 168.3431457505075457 ) ) ;
#26740 = CARTESIAN_POINT ( 'NONE',  ( 3.458734125000015425, 197.2500000013656063, 196.5673454167823877 ) ) ;
#26741 = ADVANCED_FACE ( 'NONE', ( #27440 ), #28665, .F. ) ;
#26742 = CARTESIAN_POINT ( 'NONE',  ( 8.000000000000000000, 10.40624999590322020, -3.313708498984761608 ) ) ;
#26743 = ADVANCED_FACE ( 'NONE', ( #38602 ), #31438, .T. ) ;
#26744 = EDGE_LOOP ( 'NONE', ( #42954, #42372, #56989, #62549 ) ) ;
#26745 = CARTESIAN_POINT ( 'NONE',  ( 26.56734541678237704, 196.0000000013656347, 166.5412658749999650 ) ) ;
#26746 = CARTESIAN_POINT ( 'NONE',  ( -5.082755093536325042, 13.40624999795161187, -5.082755093536325930 ) ) ;
#26747 = AXIS2_PLACEMENT_3D ( 'NONE', #19888, #71941, #20253 ) ;
#26748 = CARTESIAN_POINT ( 'NONE',  ( -2.085542519210945728E-15, 169.8437499965860127, 11.35316468750000141 ) ) ;
#26749 = CARTESIAN_POINT ( 'NONE',  ( -3.313708498984762496, 105.7812500000000000, 7.999999999999998224 ) ) ;
#26750 = CARTESIAN_POINT ( 'NONE',  ( 7.188101187500002709, 104.1875000020483810, 2.977408999572649151 ) ) ;
#26752 = CARTESIAN_POINT ( 'NONE',  ( 6.308070865158109441, -51.03903544633450906, -41.30321721932262591 ) ) ;
#26751 = CARTESIAN_POINT ( 'NONE',  ( -3.673940397442060854E-16, 292.8125000034140157, -6.000000000000001776 ) ) ;
#26753 = CARTESIAN_POINT ( 'NONE',  ( 0.000000000000000000, 125.0000000000000000, 0.000000000000000000 ) ) ;
#26754 = CARTESIAN_POINT ( 'NONE',  ( 24.54126587499998635, 206.5000000013655779, 171.4326545832175555 ) ) ;
#26755 = CARTESIAN_POINT ( 'NONE',  ( 5.082755093536320601, -5.082755093536318824, 14.42405278187175455 ) ) ;
#26756 = CARTESIAN_POINT ( 'NONE',  ( -2.828427124746209831, 206.5000000027312126, 139.1715728752538723 ) ) ;
#26757 = CARTESIAN_POINT ( 'NONE',  ( 3.042071309553167069, 46.82291666325267698, -11.35316468749999785 ) ) ;
#26758 = DIRECTION ( 'NONE',  ( 0.000000000000000000, 0.000000000000000000, 1.000000000000000000 ) ) ;
#26759 = CARTESIAN_POINT ( 'NONE',  ( -2.679491924311225848, 23.33333332650536818, -10.00000000000000178 ) ) ;
#26760 = CARTESIAN_POINT ( 'NONE',  ( -4.556349186104045934, 11.00000000000000000, 111.9062500040967763 ) ) ;
#26761 = EDGE_LOOP ( 'NONE', ( #22755, #46208, #24826, #60900 ) ) ;
#26762 = DIRECTION ( 'NONE',  ( -0.000000000000000000, 1.000000000000000000, 4.476705744456276341E-16 ) ) ;
#26763 = CARTESIAN_POINT ( 'NONE',  ( -10.00000000000000178, 169.3749999931720538, -1.224646799147353454E-15 ) ) ;
#26764 = EDGE_CURVE ( 'NONE', #2022, #73747, #51807, .T. ) ;
#26765 = CARTESIAN_POINT ( 'NONE',  ( -11.35316468750000141, 43.28124999658601268, -1.390361679473963753E-15 ) ) ;
#26766 = CARTESIAN_POINT ( 'NONE',  ( 4.556349186104051263, -10.99999999999999822, 82.65625000409677625 ) ) ;
#26767 = CARTESIAN_POINT ( 'NONE',  ( 2.445694354108783219, 202.8125000013656063, 139.5543056458912190 ) ) ;
#26768 = CARTESIAN_POINT ( 'NONE',  ( -2.485281374238159646, 299.1875000000000000, 6.000000000000414779 ) ) ;
#26769 = DIRECTION ( 'NONE',  ( -0.000000000000000000, 1.000000000000000000, -0.000000000000000000 ) ) ;
#26771 = CARTESIAN_POINT ( 'NONE',  ( 8.311093377946834337, 50.15624999658601268, 8.311093377946839666 ) ) ;
#26770 = CARTESIAN_POINT ( 'NONE',  ( -7.188101187500000933, 101.5625000020483952, -2.977408999572650483 ) ) ;
#26772 = CARTESIAN_POINT ( 'NONE',  ( 3.313708498984756279, 7.999999999999991118, 6.361552779823365533 ) ) ;
#26773 = CARTESIAN_POINT ( 'NONE',  ( 4.999999999999992895, 204.1666666666666856, 8.660254037844390851 ) ) ;
#26774 = CARTESIAN_POINT ( 'NONE',  ( 11.35316468749999785, 165.5729166632526415, 3.042071309553174174 ) ) ;
#26775 = CARTESIAN_POINT ( 'NONE',  ( 7.320508075688771044, 131.2499999931720254, 7.320508075688775484 ) ) ;
#26776 = AXIS2_PLACEMENT_3D ( 'NONE', #3612, #10390, #73388 ) ;
#26777 = CARTESIAN_POINT ( 'NONE',  ( 5.082755093536326818, 101.0937500020483810, 5.082755093536325042 ) ) ;
#26778 = CARTESIAN_POINT ( 'NONE',  ( -0.3459307087060433106, 0.4270199122593540952, -7.927019912259357426 ) ) ;
#26779 = CARTESIAN_POINT ( 'NONE',  ( 8.311093377946837890, 41.71874999658601979, -8.311093377946837890 ) ) ;
#26780 = CARTESIAN_POINT ( 'NONE',  ( -2.828427124746208943, 195.7500000027312126, 144.8284271247462129 ) ) ;
#26781 = ORIENTED_EDGE ( 'NONE', *, *, #27397, .T. ) ;
#26782 = CARTESIAN_POINT ( 'NONE',  ( 11.00000000000000000, 1.347111479062088405E-15, 81.24999999999998579 ) ) ;
#26783 = CARTESIAN_POINT ( 'NONE',  ( 10.18810118750000093, -4.220049686691933921, 77.31250000204836681 ) ) ;
#26784 = PLANE ( 'NONE',  #41368 ) ;
#26786 = CARTESIAN_POINT ( 'NONE',  ( 3.042071309553167513, 166.8229166632526983, -11.35316468749999785 ) ) ;
#26785 = CARTESIAN_POINT ( 'NONE',  ( 5.656854249492376141, -5.656854249492374365, 3.080302783920144005 ) ) ;
#26787 = CARTESIAN_POINT ( 'NONE',  ( 7.999999999999991118, 9.797174393178815797E-16, 10.63655278432982598 ) ) ;
#26788 = VECTOR ( 'NONE', #66199, 1000.000000000000000 ) ;
#26789 = CARTESIAN_POINT ( 'NONE',  ( -20.04493609933055254, -30.85035079005604075, 193.6477215188961054 ) ) ;
#26790 = CARTESIAN_POINT ( 'NONE',  ( 11.35316468749999963, 226.4062500034139873, -1.390361679473963556E-15 ) ) ;
#26791 = EDGE_CURVE ( 'NONE', #9554, #40886, #67247, .T. ) ;
#26792 = CARTESIAN_POINT ( 'NONE',  ( 4.220049686691934809, 10.18810118749999916, 85.56250000204838102 ) ) ;
#26793 = VERTEX_POINT ( 'NONE', #15935 ) ;
#26794 = TOROIDAL_SURFACE ( 'NONE', #6302, 38.00000000000000000, 7.000000000000000000 ) ;
#26795 = CARTESIAN_POINT ( 'NONE',  ( 3.313708498984802020, 21.09374999590322020, -7.999999999999958256 ) ) ;
#26796 = CYLINDRICAL_SURFACE ( 'NONE', #18256, 6.000000000000001776 ) ;
#26797 = CARTESIAN_POINT ( 'NONE',  ( -11.35316468749999785, 118.3854166632526557, -3.042071309553167513 ) ) ;
#26798 = CARTESIAN_POINT ( 'NONE',  ( 7.204075437095966983, 7.204075437095967871, 97.09375000204836681 ) ) ;
#26799 = CARTESIAN_POINT ( 'NONE',  ( 4.541265875000001451, 20.37499999863441147, 1.881053915767124440 ) ) ;
#26800 = VERTEX_POINT ( 'NONE', #34814 ) ;
#26801 = ORIENTED_EDGE ( 'NONE', *, *, #473, .T. ) ;
#26802 = CARTESIAN_POINT ( 'NONE',  ( 1.881053915767122664, 5.249999998634406140, 4.541265875000001451 ) ) ;
#26803 = CARTESIAN_POINT ( 'NONE',  ( -2.977408999572654480, 7.499999997951610986, 7.188101187499999156 ) ) ;
#26804 = CARTESIAN_POINT ( 'NONE',  ( 3.313708498984765161, 107.6562500040968189, 7.999999999999998224 ) ) ;
#26805 =( BOUNDED_CURVE ( )  B_SPLINE_CURVE ( 2, ( #44493, #62575, #32056, #3759, #50148, #3384, #16165, #72412, #43741 ),
 .UNSPECIFIED., .F., .F. ) 
 B_SPLINE_CURVE_WITH_KNOTS ( ( 3, 2, 2, 2, 3 ),
 ( 0.5666666666666670960, 0.5750000000000003997, 0.5833333333333338144, 0.5916666666666671182, 0.6000000000000004219 ),
 .UNSPECIFIED. ) 
 CURVE ( )  GEOMETRIC_REPRESENTATION_ITEM ( )  RATIONAL_B_SPLINE_CURVE ( ( 0.9999999999999958922, 0.9238795325112908463, 1.000000000000000000, 0.9238795325112867385, 1.000000000000000000, 0.9238795325112867385, 1.000000000000000000, 0.9238795325112826307, 1.000000000000003997 ) ) 
 REPRESENTATION_ITEM ( '' )  );
#26806 = CARTESIAN_POINT ( 'NONE',  ( 10.18810118749999916, 4.220049686691935698, 94.37500000204839523 ) ) ;
#26807 = CARTESIAN_POINT ( 'NONE',  ( -24.54126587499999346, 203.4375000013656063, 170.0000000000003411 ) ) ;
#26808 = CARTESIAN_POINT ( 'NONE',  ( 7.999999999999991118, 9.797174393178815797E-16, 19.58030277982336642 ) ) ;
#26809 = CARTESIAN_POINT ( 'NONE',  ( 4.000000000000001776, 4.000000000000000000, 0.000000000000000000 ) ) ;
#26810 = CARTESIAN_POINT ( 'NONE',  ( 1.656854249492381914, 18.56249999726882294, 4.000000000000000888 ) ) ;
#26811 = CARTESIAN_POINT ( 'NONE',  ( -1.881053915767124440, 6.999999998634407916, 4.541265875000001451 ) ) ;
#26812 = CARTESIAN_POINT ( 'NONE',  ( -4.000000000000015099, 200.5625000000000284, 143.6568542494924543 ) ) ;
#26813 = ORIENTED_EDGE ( 'NONE', *, *, #65271, .F. ) ;
#26814 = CARTESIAN_POINT ( 'NONE',  ( 3.458734125000016313, 194.8750000013656063, 199.4326545832176691 ) ) ;
#26816 = CARTESIAN_POINT ( 'NONE',  ( 5.656854249492374365, 5.656854249492375253, 16.76780277982336287 ) ) ;
#26815 = CARTESIAN_POINT ( 'NONE',  ( -26.56734541678227757, 199.0000000013656063, 173.4587341250003476 ) ) ;
#26817 = CARTESIAN_POINT ( 'NONE',  ( 2.780723358947928197E-16, 16.56249999863440436, -4.541265875000002339 ) ) ;
#26818 = VECTOR ( 'NONE', #2927, 1000.000000000000000 ) ;
#26819 = CARTESIAN_POINT ( 'NONE',  ( 2.846681722708030993, -45.96694654806373848, 151.2143091719884183 ) ) ;
#26820 = CARTESIAN_POINT ( 'NONE',  ( -2.977408999572648707, -7.188101187499990274, 9.267802781871756324 ) ) ;
#26821 = ORIENTED_EDGE ( 'NONE', *, *, #69688, .T. ) ;
#26822 = ORIENTED_EDGE ( 'NONE', *, *, #39141, .F. ) ;
#26823 = CARTESIAN_POINT ( 'NONE',  ( -6.238412754330611322E-16, 10.18810118749999916, 100.2812500020483810 ) ) ;
#26824 = CARTESIAN_POINT ( 'NONE',  ( -3.673940397442060854E-16, 288.7500000000000000, -6.000000000000001776 ) ) ;
#26825 = CARTESIAN_POINT ( 'NONE',  ( -25.55430564589115150, 198.3125000013656063, 172.4456943541091789 ) ) ;
#26826 = CARTESIAN_POINT ( 'NONE',  ( 11.00000000000000000, 1.347111479062088405E-15, 108.2499999999999858 ) ) ;
#26827 = CARTESIAN_POINT ( 'NONE',  ( -1.432654583217607414, 209.5000000013656063, 194.5412658750000219 ) ) ;
#26828 = CARTESIAN_POINT ( 'NONE',  ( 5.000000000000001776, 110.8333333333333428, -8.660254037844389075 ) ) ;
#26829 = EDGE_CURVE ( 'NONE', #47413, #55780, #73662, .T. ) ;
#26830 = CARTESIAN_POINT ( 'NONE',  ( -7.999999999999998224, 114.5937499999999858, 3.313708498984766493 ) ) ;
#26831 = CARTESIAN_POINT ( 'NONE',  ( 4.721056650416000089, 293.9843750017070079, 4.721056650415999201 ) ) ;
#26832 = CARTESIAN_POINT ( 'NONE',  ( -7.188101187499991163, 2.977408999572646930, 12.26780278187175455 ) ) ;
#26833 = ORIENTED_EDGE ( 'NONE', *, *, #51043, .F. ) ;
#26834 = CARTESIAN_POINT ( 'NONE',  ( 1.224646799147353454E-15, 300.0000000000000000, -10.00000000000000178 ) ) ;
#26835 = CARTESIAN_POINT ( 'NONE',  ( 29.43265458321766559, 206.8750000013656347, 166.5412658749999650 ) ) ;
#26836 = CARTESIAN_POINT ( 'NONE',  ( -8.000000000000001776, 23.15624999590322730, 3.313708498984759387 ) ) ;
#26837 = CARTESIAN_POINT ( 'NONE',  ( -2.754378923186476579E-14, 199.1875000013655779, 145.4587341250000350 ) ) ;
#26838 = DIRECTION ( 'NONE',  ( -1.000000000000000000, 0.000000000000000000, 0.000000000000000000 ) ) ;
#26840 = CARTESIAN_POINT ( 'NONE',  ( -3.458734125000016757, 201.1250000013656347, 140.5673454167824161 ) ) ;
#26839 = CARTESIAN_POINT ( 'NONE',  ( 0.000000000000000000, 255.9999999999999432, 0.000000000000000000 ) ) ;
#26841 = CARTESIAN_POINT ( 'NONE',  ( -8.311093377946834337, 259.8437500034140157, 8.311093377946837890 ) ) ;
#26842 = CARTESIAN_POINT ( 'NONE',  ( 3.000000000000001332, -45.00000000000001421, 201.0010000000000048 ) ) ;
#26843 = DIRECTION ( 'NONE',  ( -1.000000000000000000, 0.000000000000000000, 0.000000000000000000 ) ) ;
#26844 = CARTESIAN_POINT ( 'NONE',  ( 9.832129032723416984, 5.364583329919349275, 5.676582343750006032 ) ) ;
#26845 = CARTESIAN_POINT ( 'NONE',  ( 7.188101187499993827, -2.977408999572645598, 2.517802781871750994 ) ) ;
#26846 = CARTESIAN_POINT ( 'NONE',  ( 11.35316468749999963, 201.3020833299193839, -3.042071309553165293 ) ) ;
#26847 = CARTESIAN_POINT ( 'NONE',  ( 11.35316468750000141, 0.7812499965860162376, 0.000000000000000000 ) ) ;
#26848 = CARTESIAN_POINT ( 'NONE',  ( 4.541265875000001451, 7.249999998634408804, 1.881053915767124440 ) ) ;
#26849 = CARTESIAN_POINT ( 'NONE',  ( -28.00000000000002487, 198.0000000000000000, 166.0000000000003695 ) ) ;
#26851 = LINE ( 'NONE', #9884, #13391 ) ;
#26850 = CARTESIAN_POINT ( 'NONE',  ( 9.797174393178825657E-16, 125.0000000000000000, -8.000000000000000000 ) ) ;
#26852 = VERTEX_POINT ( 'NONE', #45729 ) ;
#26854 = EDGE_CURVE ( 'NONE', #38454, #53341, #59526, .T. ) ;
#26853 = CARTESIAN_POINT ( 'NONE',  ( 1.432654583217607414, 205.5000000013655779, 145.4587341250000634 ) ) ;
#26855 = CARTESIAN_POINT ( 'NONE',  ( 9.832129032723420536, 11.19791666325268409, -5.676582343749999815 ) ) ;
#26856 = CARTESIAN_POINT ( 'NONE',  ( 4.556349186104045934, 11.00000000000000000, 101.2187500040967905 ) ) ;
#26857 = CARTESIAN_POINT ( 'NONE',  ( -1.469576158976823947E-15, 7.125000000000000888, 8.000000000000000000 ) ) ;
#26858 = CARTESIAN_POINT ( 'NONE',  ( -31.45873412500002075, 200.6250000013656063, 168.5673454167828140 ) ) ;
#26859 = DIRECTION ( 'NONE',  ( 0.000000000000000000, 0.000000000000000000, 1.000000000000000000 ) ) ;
#26861 = CARTESIAN_POINT ( 'NONE',  ( -3.042071309553173730, 9.322916663252684089, 11.35316468749999785 ) ) ;
#26860 = CARTESIAN_POINT ( 'NONE',  ( 7.188101187500002709, 120.3125000020483810, 2.977408999572649151 ) ) ;
#26862 = CARTESIAN_POINT ( 'NONE',  ( 3.313708498984756279, 7.999999999999991118, 25.86155277982337353 ) ) ;
#26863 = CARTESIAN_POINT ( 'NONE',  ( 9.832129032723416984, 115.3645833299193555, 5.676582343750006032 ) ) ;
#26864 = EDGE_CURVE ( 'NONE', #55648, #20187, #17056, .T. ) ;
#26865 = CARTESIAN_POINT ( 'NONE',  ( 10.00000000000000178, 91.87499999317203958, 0.000000000000000000 ) ) ;
#26866 = CARTESIAN_POINT ( 'NONE',  ( 7.188101187500001821, 122.3750000020483952, -2.977408999572651371 ) ) ;
#26867 = CARTESIAN_POINT ( 'NONE',  ( 1.881053915767121776, 21.62499999863441502, -4.541265875000002339 ) ) ;
#26868 = CARTESIAN_POINT ( 'NONE',  ( -23.99999999999997513, 204.6875000000000284, 171.6568542494927385 ) ) ;
#26869 = CARTESIAN_POINT ( 'NONE',  ( 2.679491924311224516, 143.9583333333333428, 10.00000000000000888 ) ) ;
#26870 = ORIENTED_EDGE ( 'NONE', *, *, #39714, .T. ) ;
#26871 = CARTESIAN_POINT ( 'NONE',  ( -8.660254037844390851, 117.0833333333333570, -5.000000000000007105 ) ) ;
#26872 = CARTESIAN_POINT ( 'NONE',  ( 6.676582343750001591, 290.1093750017069510, -8.176455196517173205E-16 ) ) ;
#26873 = FACE_OUTER_BOUND ( 'NONE', #6301, .T. ) ;
#26874 = CARTESIAN_POINT ( 'NONE',  ( 5.656854249492376141, -5.656854249492374365, 3.080302783920144005 ) ) ;
#26875 = CARTESIAN_POINT ( 'NONE',  ( -2.250000000000000888, 2.250000000000000000, 28.00000000000000000 ) ) ;
#26876 = CARTESIAN_POINT ( 'NONE',  ( -2.679491924311235618, 210.4166666598386826, 10.00000000000000000 ) ) ;
#26877 = EDGE_CURVE ( 'NONE', #34844, #24188, #11408, .T. ) ;
#26878 = CARTESIAN_POINT ( 'NONE',  ( -6.238412754330611322E-16, 10.18810118749999916, 103.6562500020483810 ) ) ;
#26879 = ORIENTED_EDGE ( 'NONE', *, *, #56984, .F. ) ;
#26880 = LINE ( 'NONE', #72539, #12351 ) ;
#26881 = CARTESIAN_POINT ( 'NONE',  ( -3.042071309553173730, 159.6354166632526699, 11.35316468749999785 ) ) ;
#26882 = CARTESIAN_POINT ( 'NONE',  ( 2.445694354108839175, 204.3125000013656063, 195.5543056458912190 ) ) ;
#26883 = FACE_OUTER_BOUND ( 'NONE', #42352, .T. ) ;
#26884 = CARTESIAN_POINT ( 'NONE',  ( 6.951808397369818766E-16, 57.34374999658601979, -11.35316468750000141 ) ) ;
#26885 = ORIENTED_EDGE ( 'NONE', *, *, #15669, .T. ) ;
#26886 = CARTESIAN_POINT ( 'NONE',  ( -7.204075437095967871, 7.204075437095967871, 115.4687500020483810 ) ) ;
#26887 = CARTESIAN_POINT ( 'NONE',  ( -1.881053915767124440, 7.124999998634407916, 4.541265875000001451 ) ) ;
#26888 = VERTEX_POINT ( 'NONE', #57069 ) ;
#26889 = VECTOR ( 'NONE', #5110, 1000.000000000000000 ) ;
#26890 = CARTESIAN_POINT ( 'NONE',  ( -1.320432766682874540E-15, 22.59374999795161187, 7.188101187500000044 ) ) ;
#26891 = CARTESIAN_POINT ( 'NONE',  ( -2.485281374238571761, 289.8750000034139589, -6.000000000000003553 ) ) ;
#26892 = CARTESIAN_POINT ( 'NONE',  ( -10.00000000000000000, 247.9166666734946318, -2.679491924311226292 ) ) ;
#26893 = CARTESIAN_POINT ( 'NONE',  ( -7.188101187500000044, 16.59374999795161543, -8.802885111219163269E-16 ) ) ;
#26894 = CARTESIAN_POINT ( 'NONE',  ( 5.082755093536318824, 5.082755093536319713, 5.424052781871753659 ) ) ;
#26895 = CARTESIAN_POINT ( 'NONE',  ( 4.220049686691934809, 10.18810118749999916, 111.0625000020483810 ) ) ;
#26896 =( BOUNDED_CURVE ( )  B_SPLINE_CURVE ( 2, ( #7413, #295, #30054, #46283, #64016, #52328, #47754, #1032, #30421 ),
 .UNSPECIFIED., .F., .F. ) 
 B_SPLINE_CURVE_WITH_KNOTS ( ( 3, 2, 2, 2, 3 ),
 ( 0.8166666666666674290, 0.8250000000000006217, 0.8333333333333340365, 0.8416666666666672292, 0.8500000000000005329 ),
 .UNSPECIFIED. ) 
 CURVE ( )  GEOMETRIC_REPRESENTATION_ITEM ( )  RATIONAL_B_SPLINE_CURVE ( ( 0.9999999999999928946, 0.9238795325112938439, 1.000000000000000000, 0.9238795325112867385, 1.000000000000000000, 0.9238795325112867385, 1.000000000000000000, 0.9238795325112816315, 1.000000000000005107 ) ) 
 REPRESENTATION_ITEM ( '' )  );
#26897 = AXIS2_PLACEMENT_3D ( 'NONE', #72681, #38350, #61358 ) ;
#26898 = CARTESIAN_POINT ( 'NONE',  ( 2.384279753873915553, -43.16861503118958154, 151.1498700657236327 ) ) ;
#26899 = CARTESIAN_POINT ( 'NONE',  ( -4.000000000000002665, 6.312499997268812280, 1.656854249492380804 ) ) ;
#26900 = CARTESIAN_POINT ( 'NONE',  ( 28.00000000000002487, 207.1250000027312126, 173.9999999999999147 ) ) ;
#26901 = VERTEX_POINT ( 'NONE', #40452 ) ;
#26902 = CARTESIAN_POINT ( 'NONE',  ( -3.458734124999959914, 205.3750000013656063, 196.5673454167823877 ) ) ;
#26903 = CARTESIAN_POINT ( 'NONE',  ( -28.00000000000007461, 207.4375000013656063, 166.5412658750003629 ) ) ;
#26904 = CARTESIAN_POINT ( 'NONE',  ( -4.220049686691937474, -10.18810118749999738, 71.31250000204836681 ) ) ;
#26905 = CARTESIAN_POINT ( 'NONE',  ( 4.541265875000001451, 5.249999998634406140, 1.881053915767124440 ) ) ;
#26906 = DIRECTION ( 'NONE',  ( -0.000000000000000000, 1.000000000000000000, -1.563033456626094573E-30 ) ) ;
#26907 = VECTOR ( 'NONE', #14191, 1000.000000000000000 ) ;
#26908 = CARTESIAN_POINT ( 'NONE',  ( 2.977408999572646486, 7.188101187499991163, 26.51780278187175455 ) ) ;
#26909 = ORIENTED_EDGE ( 'NONE', *, *, #66787, .F. ) ;
#26911 =( BOUNDED_CURVE ( )  B_SPLINE_CURVE ( 2, ( #21275, #33001, #39014 ),
 .UNSPECIFIED., .F., .F. ) 
 B_SPLINE_CURVE_WITH_KNOTS ( ( 3, 3 ),
 ( 0.9333333333333341253, 0.9416666668637480031 ),
 .UNSPECIFIED. ) 
 CURVE ( )  GEOMETRIC_REPRESENTATION_ITEM ( )  RATIONAL_B_SPLINE_CURVE ( ( 0.9999999999999928946, 0.9238795325112938439, 1.000000000000000000 ) ) 
 REPRESENTATION_ITEM ( '' )  );
#26910 = DIRECTION ( 'NONE',  ( -0.000000000000000000, -1.000000000000000000, -0.000000000000000000 ) ) ;
#26912 = ORIENTED_EDGE ( 'NONE', *, *, #9317, .F. ) ;
#26913 = CARTESIAN_POINT ( 'NONE',  ( 12.00000000000000178, 0.000000000000000000, 24.00000000000001066 ) ) ;
#26914 = CARTESIAN_POINT ( 'NONE',  ( -6.985140028429535519, 4.041179811479543638, 0.000000000000000000 ) ) ;
#26915 = CARTESIAN_POINT ( 'NONE',  ( 1.432654583217664479, 203.7500000013656063, 201.4587341250000065 ) ) ;
#26916 = CARTESIAN_POINT ( 'NONE',  ( 25.55430564589119058, 200.3125000013656063, 172.4456943541087526 ) ) ;
#26917 = CARTESIAN_POINT ( 'NONE',  ( -7.320508075688773708, 61.87500000000000000, -7.320508075688774596 ) ) ;
#26918 = ADVANCED_FACE ( 'NONE', ( #63451 ), #44625, .F. ) ;
#26919 = CARTESIAN_POINT ( 'NONE',  ( -5.082755093536325930, 94.34375000204838102, -5.082755093536325930 ) ) ;
#26920 = CARTESIAN_POINT ( 'NONE',  ( -6.000000000000000888, 293.0625000000000000, 2.485281374238575758 ) ) ;
#26921 = CARTESIAN_POINT ( 'NONE',  ( 30.82842712474617031, 206.5000000027312126, 167.1715728752537018 ) ) ;
#26922 = ORIENTED_EDGE ( 'NONE', *, *, #28415, .F. ) ;
#26923 = CARTESIAN_POINT ( 'NONE',  ( -8.311093377946836114, 223.2812500034140157, -8.311093377946836114 ) ) ;
#26924 = CARTESIAN_POINT ( 'NONE',  ( -4.000000000000015099, 198.6875000027312126, 143.6568542494924543 ) ) ;
#26925 = DIRECTION ( 'NONE',  ( 1.000000000000000000, 0.000000000000000000, 0.000000000000000000 ) ) ;
#26926 = CARTESIAN_POINT ( 'NONE',  ( -7.999999999999991118, 0.000000000000000000, 21.83030277982336997 ) ) ;
#26927 = CARTESIAN_POINT ( 'NONE',  ( 5.000000000000004441, 256.6666666666666288, 8.660254037844385522 ) ) ;
#26928 = CARTESIAN_POINT ( 'NONE',  ( 7.320508075688774596, 185.6249999999999716, -7.320508075688774596 ) ) ;
#26929 = DIRECTION ( 'NONE',  ( -1.000000000000000000, 0.000000000000000000, 0.000000000000000000 ) ) ;
#26930 = CARTESIAN_POINT ( 'NONE',  ( -5.082755093536319713, 5.082755093536319713, 24.17405278187175455 ) ) ;
#26931 = CARTESIAN_POINT ( 'NONE',  ( 6.951808397369818766E-16, 157.3437499965860127, -11.35316468750000141 ) ) ;
#26932 = DIRECTION ( 'NONE',  ( -0.000000000000000000, -0.000000000000000000, -1.000000000000000000 ) ) ;
#26933 = CARTESIAN_POINT ( 'NONE',  ( 2.679491924311071749, 261.6666666734946602, -10.00000000000008704 ) ) ;
#26934 = PLANE ( 'NONE',  #36875 ) ;
#26935 = CARTESIAN_POINT ( 'NONE',  ( 2.828427124746208943, 199.7500000027312126, 195.1715728752538439 ) ) ;
#26936 = ORIENTED_EDGE ( 'NONE', *, *, #42716, .T. ) ;
#26937 = AXIS2_PLACEMENT_3D ( 'NONE', #11357, #29081, #64151 ) ;
#26938 = CARTESIAN_POINT ( 'NONE',  ( 9.832129032723416984, 25.67708332991935194, 5.676582343750006032 ) ) ;
#26939 = DIRECTION ( 'NONE',  ( 1.000000000000000000, 0.000000000000000000, 0.000000000000000000 ) ) ;
#26941 = CARTESIAN_POINT ( 'NONE',  ( -7.456209740496309024, -10.23501300384518053, -65.47703513267214248 ) ) ;
#26940 = DIRECTION ( 'NONE',  ( -0.000000000000000000, -1.000000000000000000, -4.283267841918042741E-17 ) ) ;
#26942 = CARTESIAN_POINT ( 'NONE',  ( 11.00000000000000355, -4.556349186104044158, 79.65625000000000000 ) ) ;
#26943 = CARTESIAN_POINT ( 'NONE',  ( -2.445694354108838731, 203.0625000013656063, 144.4456943541088663 ) ) ;
#26944 = EDGE_CURVE ( 'NONE', #41193, #65025, #15547, .T. ) ;
#26945 = CARTESIAN_POINT ( 'NONE',  ( 10.00000000000000178, 51.87499999317203248, 0.000000000000000000 ) ) ;
#26946 = CARTESIAN_POINT ( 'NONE',  ( 1.320432766682874540E-15, 109.5312500020483810, 7.188101187500000044 ) ) ;
#26947 = CARTESIAN_POINT ( 'NONE',  ( -1.881053915767121554, 8.749999998634406140, -4.541265875000002339 ) ) ;
#26948 = CARTESIAN_POINT ( 'NONE',  ( 2.679491924310263951, 53.95833333333325044, 10.00000000000055067 ) ) ;
#26949 = CARTESIAN_POINT ( 'NONE',  ( -3.313708498984757167, 7.999999999999991118, 8.049052779823362869 ) ) ;
#26951 = CARTESIAN_POINT ( 'NONE',  ( 5.000000000000010658, 160.8333333333333428, -8.660254037844403285 ) ) ;
#26950 = LINE ( 'NONE', #60911, #34716 ) ;
#26952 = EDGE_LOOP ( 'NONE', ( #60761, #32372, #55865, #58832, #44272, #66110, #73682, #72103, #32478, #20481, #25715, #71946, #20865, #11059, #70970, #18912, #46832, #48306, #5192, #59990, #62492, #46803, #6032, #23955, #36443, #65223, #69865, #33054, #16106, #65912, #62546, #65483, #35140, #41783, #56342, #8978, #49078, #18876, #63992, #18905, #55762, #30990, #55884, #59892, #9519, #3825, #43781, #31001, #61154, #500, #71854, #57726, #16206, #40290, #38185, #63258, #66392, #18170, #51222, #60417, #71691, #53988, #21137, #69274, #67544, #39917, #54344, #28162, #22690, #54997 ) ) ;
#26953 = VERTEX_POINT ( 'NONE', #28013 ) ;
#26954 = CARTESIAN_POINT ( 'NONE',  ( -5.000000000000001776, -62.69487254116422292, 24.02505537902018773 ) ) ;
#26955 = CARTESIAN_POINT ( 'NONE',  ( -2.445694354108783219, 195.8125000013656063, 200.4456943541088663 ) ) ;
#26956 = CARTESIAN_POINT ( 'NONE',  ( 0.000000000000000000, 0.000000000000000000, 0.000000000000000000 ) ) ;
#26957 = CARTESIAN_POINT ( 'NONE',  ( 11.00000000000005151, 4.556349186103993532, 94.84374999999997158 ) ) ;
#26958 = CARTESIAN_POINT ( 'NONE',  ( 11.35316468749999963, 125.9895833299193271, -3.042071309553165293 ) ) ;
#26959 = ORIENTED_EDGE ( 'NONE', *, *, #51623, .F. ) ;
#26960 = CARTESIAN_POINT ( 'NONE',  ( -3.313708498984759387, -7.999999999999989342, 10.29905278392014445 ) ) ;
#26961 = CARTESIAN_POINT ( 'NONE',  ( -7.204075437095965206, -7.204075437095968759, 91.84375000204838102 ) ) ;
#26962 = CARTESIAN_POINT ( 'NONE',  ( 11.00000000000010658, 4.556349186103942017, 93.34375000000000000 ) ) ;
#26963 = CARTESIAN_POINT ( 'NONE',  ( -2.828427124746153876, 206.8750000000000284, 195.1715728752538439 ) ) ;
#26965 = CARTESIAN_POINT ( 'NONE',  ( 3.042071309553167513, 121.8229166632526841, -11.35316468749999785 ) ) ;
#26964 = CARTESIAN_POINT ( 'NONE',  ( 0.000000000000000000, -2.500000000000000444, 0.000000000000000000 ) ) ;
#26966 = FACE_OUTER_BOUND ( 'NONE', #7402, .T. ) ;
#26967 = VERTEX_POINT ( 'NONE', #22333 ) ;
#26968 =( REPRESENTATION_RELATIONSHIP ('NONE','NONE', #46008, #43124 ) REPRESENTATION_RELATIONSHIP_WITH_TRANSFORMATION ( #18763 )SHAPE_REPRESENTATION_RELATIONSHIP( ) );
#26969 = EDGE_CURVE ( 'NONE', #72916, #54565, #290, .T. ) ;
#26970 = CARTESIAN_POINT ( 'NONE',  ( 1.836970198721029589E-15, 256.2500000000000568, 10.00000000000000000 ) ) ;
#26971 = AXIS2_PLACEMENT_3D ( 'NONE', #43595, #54938, #27359 ) ;
#26972 = CARTESIAN_POINT ( 'NONE',  ( -25.87252272011470566, 177.3363770347620516, 144.1983798943641375 ) ) ;
#26973 = CARTESIAN_POINT ( 'NONE',  ( -5.676582343749998039, 112.7604166632526841, -9.832129032723420536 ) ) ;
#26974 = CARTESIAN_POINT ( 'NONE',  ( 2.839093476692135984E-14, 205.6875000013656063, 201.4587341250000350 ) ) ;
#26975 = CARTESIAN_POINT ( 'NONE',  ( -5.082755093536326818, 21.28124999795161543, 5.082755093536325042 ) ) ;
#26976 = CARTESIAN_POINT ( 'NONE',  ( -10.18810118749999916, 4.220049686691934809, 82.93750000204838102 ) ) ;
#26977 = EDGE_CURVE ( 'NONE', #41903, #57937, #7599, .T. ) ;
#26978 = CARTESIAN_POINT ( 'NONE',  ( 3.042071309553167069, 17.13541666325268409, -11.35316468749999785 ) ) ;
#26979 = ORIENTED_EDGE ( 'NONE', *, *, #7189, .F. ) ;
#26980 = CARTESIAN_POINT ( 'NONE',  ( -8.008118988124989457, -3.317071493978883900, 19.10686528394063188 ) ) ;
#26981 = CARTESIAN_POINT ( 'NONE',  ( 10.00000000000000000, 237.5000000000000284, -1.224646799147353256E-15 ) ) ;
#26982 = LINE ( 'NONE', #61695, #55521 ) ;
#26983 = CARTESIAN_POINT ( 'NONE',  ( -5.082755093536325042, 2.531249997951610542, -5.082755093536325930 ) ) ;
#26984 = CARTESIAN_POINT ( 'NONE',  ( -2.765530957081996810, 289.2656250017069510, -6.676582343750003368 ) ) ;
#26985 = DIRECTION ( 'NONE',  ( 0.000000000000000000, 0.000000000000000000, 1.000000000000000000 ) ) ;
#26986 = DIRECTION ( 'NONE',  ( 1.000000000000000000, 0.000000000000000000, 0.000000000000000000 ) ) ;
#26987 = EDGE_LOOP ( 'NONE', ( #25196, #65036, #57167, #17119 ) ) ;
#26988 = CARTESIAN_POINT ( 'NONE',  ( 5.676582343749993598, 140.2604166632526983, 9.832129032723422313 ) ) ;
#26989 = CARTESIAN_POINT ( 'NONE',  ( -10.18810118749999916, 4.220049686691934809, 79.56250000204836681 ) ) ;
#26990 = EDGE_CURVE ( 'NONE', #24188, #5894, #35909, .T. ) ;
#26991 = CARTESIAN_POINT ( 'NONE',  ( -30.44569435410878810, 196.8125000013656063, 172.4456943541092357 ) ) ;
#26992 = DIRECTION ( 'NONE',  ( -0.000000000000000000, 1.000000000000000000, -0.000000000000000000 ) ) ;
#26993 = CARTESIAN_POINT ( 'NONE',  ( 1.881053915767121776, 15.62499999863440614, -4.541265875000002339 ) ) ;
#26994 = ORIENTED_EDGE ( 'NONE', *, *, #55529, .F. ) ;
#26995 = AXIS2_PLACEMENT_3D ( 'NONE', #69325, #52352, #24767 ) ;
#26996 = CARTESIAN_POINT ( 'NONE',  ( -3.999999999999960032, 203.0625000027311842, 196.3431457505076594 ) ) ;
#26997 = CARTESIAN_POINT ( 'NONE',  ( -2.839093476692135984E-14, 196.9375000013655779, 138.5412658750000503 ) ) ;
#26998 = CARTESIAN_POINT ( 'NONE',  ( -32.00000000000000000, 206.3750000027312126, 170.0000000000004547 ) ) ;
#26999 = CARTESIAN_POINT ( 'NONE',  ( 3.313708498984761608, 6.281250000000000888, -8.000000000000000000 ) ) ;
#27000 = VERTEX_POINT ( 'NONE', #13241 ) ;
#27001 = CARTESIAN_POINT ( 'NONE',  ( 7.188101187500000933, 11.06249999795161187, -2.977408999572650483 ) ) ;
#27002 = CARTESIAN_POINT ( 'NONE',  ( -2.849036369511732440E-14, 208.2500000000000284, 138.0000000000000568 ) ) ;
#27003 = EDGE_CURVE ( 'NONE', #6793, #46714, #59651, .T. ) ;
#27005 = DIRECTION ( 'NONE',  ( 1.652117596168387509E-16, 4.283267841918042741E-17, -1.000000000000000000 ) ) ;
#27004 = B_SPLINE_CURVE_WITH_KNOTS ( 'NONE', 3,
 ( #27585, #26454, #15514, #3846 ),
 .UNSPECIFIED., .F., .F.,
 ( 4, 4 ),
 ( 0.000000000000000000, 1.000000000000000000 ),
 .UNSPECIFIED. ) ;
#27006 = CARTESIAN_POINT ( 'NONE',  ( -11.35316468749999785, 188.0729166632526983, -3.042071309553167513 ) ) ;
#27007 = CARTESIAN_POINT ( 'NONE',  ( 5.082755093536325042, 111.9687500020483810, -5.082755093536325930 ) ) ;
#27008 = CARTESIAN_POINT ( 'NONE',  ( -2.485281374238895502, 290.8750000034139589, -5.999999999999677591 ) ) ;
#27009 = CARTESIAN_POINT ( 'NONE',  ( 6.676582343750003368, 289.8906250017069510, 2.765530957081995478 ) ) ;
#27010 = EDGE_CURVE ( 'NONE', #68569, #62240, #484, .T. ) ;
#27012 = CARTESIAN_POINT ( 'NONE',  ( -2.679491924310867912, 68.54166666666671404, 10.00000000000021494 ) ) ;
#27011 = CARTESIAN_POINT ( 'NONE',  ( 2.250000000000000000, 284.0000000000000000, 7.677076266392047543 ) ) ;
#27013 =( BOUNDED_SURFACE ( )  B_SPLINE_SURFACE ( 3, 2, ( 
 ( #56576, #21479, #5633 ),
 ( #56946, #4889, #10170 ),
 ( #21109, #15437, #34318 ),
 ( #33206, #73172, #22590 ),
 ( #45610, #9801, #27885 ),
 ( #57322, #27510, #50896 ),
 ( #4150, #49786, #32824 ),
 ( #73911, #22215, #45242 ),
 ( #68254, #16549, #5262 ),
 ( #27140, #39587, #62582 ),
 ( #47462, #58437, #70485 ),
 ( #23716, #28633, #24453 ),
 ( #63330, #51647, #64085 ),
 ( #52398, #24078, #70125 ),
 ( #46720, #34690, #69746 ),
 ( #17307, #28522, #57698 ),
 ( #7116, #47087, #22978 ),
 ( #29750, #45984, #69000 ) ),
 .UNSPECIFIED., .F., .F., .F. ) 
 B_SPLINE_SURFACE_WITH_KNOTS ( ( 4, 2, 2, 2, 2, 2, 2, 2, 4 ),
 ( 3, 3 ),
 ( 0.04202945594032935633, 0.04396162471216807227, 0.04589379348400678821, 0.04782596225584550415, 0.04975813102768422008, 0.05169029979952293602, 0.05265638418544229399, 0.05362246857136165196, 0.05748680611503908383 ),
 ( 0.000000000000000000, 1.000000000000000000 ),
 .UNSPECIFIED. ) 
 GEOMETRIC_REPRESENTATION_ITEM ( )  RATIONAL_B_SPLINE_SURFACE ( (
 ( 1.000000000000000000, 0.6241276099608165095, 1.000000000000000000),
 ( 1.000000000000000000, 0.6218761496800117028, 1.000000000000000000),
 ( 1.000000000000000000, 0.6198047272364380911, 1.000000000000000000),
 ( 1.000000000000000000, 0.6161935119824036855, 1.000000000000000000),
 ( 1.000000000000000000, 0.6146642324079838460, 1.000000000000000000),
 ( 1.000000000000000000, 0.6121850116872165071, 1.000000000000000000),
 ( 1.000000000000000000, 0.6112350889399397191, 1.000000000000000000),
 ( 1.000000000000000000, 0.6099522725973182125, 1.000000000000000000),
 ( 1.000000000000000000, 0.6096208180308724245, 1.000000000000000000),
 ( 1.000000000000000000, 0.6096183796348639827, 1.000000000000000000),
 ( 1.000000000000000000, 0.6099422200103279401, 1.000000000000000000),
 ( 1.000000000000000000, 0.6109087447822609818, 1.000000000000000000),
 ( 1.000000000000000000, 0.6113123981687891284, 1.000000000000000000),
 ( 1.000000000000000000, 0.6122677719809712649, 1.000000000000000000),
 ( 1.000000000000000000, 0.6128199619021086342, 1.000000000000000000),
 ( 1.000000000000000000, 0.6159350830265309940, 1.000000000000000000),
 ( 1.000000000000000000, 0.6195556778515928231, 1.000000000000000000),
 ( 1.000000000000000000, 0.6241278272307890784, 1.000000000000000000) ) ) 
 REPRESENTATION_ITEM ( '' )  SURFACE ( )  );
#27014 = EDGE_LOOP ( 'NONE', ( #28223, #12004, #17208, #20029, #49808 ) ) ;
#27015 = CARTESIAN_POINT ( 'NONE',  ( -11.35316468749999608, 259.1145833367473301, 3.042071309553173730 ) ) ;
#27016 = CARTESIAN_POINT ( 'NONE',  ( 2.977408999572646486, 7.188101187499991163, 23.89280278187176165 ) ) ;
#27017 = AXIS2_PLACEMENT_3D ( 'NONE', #10123, #55412, #67836 ) ;
#27018 = CARTESIAN_POINT ( 'NONE',  ( 4.999999999999993783, 166.0416666598387110, 8.660254037844390851 ) ) ;
#27019 = CARTESIAN_POINT ( 'NONE',  ( 0.000000000000000000, 0.000000000000000000, 0.000000000000000000 ) ) ;
#27020 = CYLINDRICAL_SURFACE ( 'NONE', #27923, 7.999999999999991118 ) ;
#27022 = EDGE_CURVE ( 'NONE', #73500, #60057, #48928, .T. ) ;
#27021 = CARTESIAN_POINT ( 'NONE',  ( 2.754378923186476579E-14, 196.4375000013655779, 194.5412658750000219 ) ) ;
#27023 = VERTEX_POINT ( 'NONE', #29506 ) ;
#27024 = DIRECTION ( 'NONE',  ( -3.469446951953617147E-16, 0.000000000000000000, 1.000000000000000000 ) ) ;
#27025 = CARTESIAN_POINT ( 'NONE',  ( 3.313708498984760720, 91.53125000000000000, -8.000000000000000000 ) ) ;
#27026 = CARTESIAN_POINT ( 'NONE',  ( -8.311093377946836114, 117.9687499965860127, -8.311093377946837890 ) ) ;
#27027 = CARTESIAN_POINT ( 'NONE',  ( 10.00000000000000000, 211.6666666598386826, 2.679491924311235618 ) ) ;
#27028 = CARTESIAN_POINT ( 'NONE',  ( 11.00000000000000000, 1.347111479062088405E-15, 70.74999999999998579 ) ) ;
#27031 = CARTESIAN_POINT ( 'NONE',  ( 11.00000000000007994, 4.556349186103967774, 110.0312500040967763 ) ) ;
#27030 = CARTESIAN_POINT ( 'NONE',  ( 25.55430564589119058, 199.3125000013656063, 172.4456943541087526 ) ) ;
#27029 = CARTESIAN_POINT ( 'NONE',  ( 28.00000000000002132, 200.1875000013656063, 166.5412658749999082 ) ) ;
#27032 = VERTEX_POINT ( 'NONE', #65301 ) ;
#27033 = CARTESIAN_POINT ( 'NONE',  ( 1.656854249492381914, 1.812500000000000222, 4.000000000000000888 ) ) ;
#27034 = CARTESIAN_POINT ( 'NONE',  ( 2.485281374238286656, 287.7500000034141294, -6.000000000000285105 ) ) ;
#27035 = CARTESIAN_POINT ( 'NONE',  ( 1.432654583217607192, 195.2500000013656063, 145.4587341250000634 ) ) ;
#27036 = CARTESIAN_POINT ( 'NONE',  ( 25.55430564589119058, 196.3125000013656063, 167.5543056458910485 ) ) ;
#27037 = CARTESIAN_POINT ( 'NONE',  ( 9.832129032723420536, 201.5104166632526983, -5.676582343749999815 ) ) ;
#27038 = CARTESIAN_POINT ( 'NONE',  ( 23.99999999999998224, 207.8125000027312410, 168.3431457505075457 ) ) ;
#27039 = CARTESIAN_POINT ( 'NONE',  ( 10.54825475571325022, 225.9999999999999716, 3.425896574385907112 ) ) ;
#27040 = CARTESIAN_POINT ( 'NONE',  ( -4.541265875000003227, 17.87499999863441147, 1.881053915767121110 ) ) ;
#27041 = CARTESIAN_POINT ( 'NONE',  ( 25.55430564589119058, 196.3125000013656063, 167.5543056458910485 ) ) ;
#27042 = CARTESIAN_POINT ( 'NONE',  ( 7.999999999999992895, -3.313708498984756279, 26.98655277982336997 ) ) ;
#27044 = LINE ( 'NONE', #73071, #56829 ) ;
#27043 = DIRECTION ( 'NONE',  ( 7.598735409842530687E-18, -0.9801239283673559566, -0.1983862017423140278 ) ) ;
#27045 = CARTESIAN_POINT ( 'NONE',  ( 11.35316468750000141, 100.7812499965860269, 0.000000000000000000 ) ) ;
#27046 = ORIENTED_EDGE ( 'NONE', *, *, #33346, .T. ) ;
#27047 = CARTESIAN_POINT ( 'NONE',  ( 27.99999999999996447, 204.6250000027312126, 165.9999999999998863 ) ) ;
#27048 = CARTESIAN_POINT ( 'NONE',  ( 7.188101187500000044, 18.46874999795161187, 0.000000000000000000 ) ) ;
#27049 = CARTESIAN_POINT ( 'NONE',  ( -10.00000000000000000, 223.1250000068279746, 0.000000000000000000 ) ) ;
#27051 = CARTESIAN_POINT ( 'NONE',  ( 3.042071309553173286, 260.6770833367473301, 11.35316468749999608 ) ) ;
#27050 = AXIS2_PLACEMENT_3D ( 'NONE', #43608, #13804, #48149 ) ;
#27052 = CARTESIAN_POINT ( 'NONE',  ( 11.35316468749999785, 95.57291666325269830, 3.042071309553174174 ) ) ;
#27053 = ORIENTED_EDGE ( 'NONE', *, *, #32012, .F. ) ;
#27054 = FACE_OUTER_BOUND ( 'NONE', #73257, .T. ) ;
#27055 = CARTESIAN_POINT ( 'NONE',  ( 10.18810118749999916, 4.220049686691935698, 106.0000000020483668 ) ) ;
#27056 = CARTESIAN_POINT ( 'NONE',  ( -24.54126587499997925, 196.3750000013656063, 171.4326545832179818 ) ) ;
#27057 = CARTESIAN_POINT ( 'NONE',  ( 3.458734125000015869, 205.1875000013656063, 198.0000000000000284 ) ) ;
#27058 = CARTESIAN_POINT ( 'NONE',  ( 18.00000000000000000, -8.694318397447183600, -1.139757812215642430 ) ) ;
#27060 = CARTESIAN_POINT ( 'NONE',  ( 9.832129032723416984, 90.36458332991935549, 5.676582343750006032 ) ) ;
#27059 = CARTESIAN_POINT ( 'NONE',  ( -25.17157287525386167, 207.0000000027312126, 167.1715728752541281 ) ) ;
#27061 = CARTESIAN_POINT ( 'NONE',  ( -3.313708498984757167, 7.999999999999991118, 18.73655278392014623 ) ) ;
#27062 = CARTESIAN_POINT ( 'NONE',  ( -31.45873412499999944, 200.8750000013656063, 168.5673454167827572 ) ) ;
#27063 = CARTESIAN_POINT ( 'NONE',  ( -8.000000000000000000, 21.46874999590322375, -3.313708498984762496 ) ) ;
#27064 = CARTESIAN_POINT ( 'NONE',  ( 2.679491924311228956, 187.9166666598387394, -10.00000000000000000 ) ) ;
#27065 = ADVANCED_FACE ( 'NONE', ( #24570 ), #29873, .T. ) ;
#27066 = CARTESIAN_POINT ( 'NONE',  ( 2.903636603592172793, -45.77934199174493557, 139.1362610670268509 ) ) ;
#27067 = CARTESIAN_POINT ( 'NONE',  ( -11.35316468749999785, 78.38541666325266988, -3.042071309553167957 ) ) ;
#27068 = CARTESIAN_POINT ( 'NONE',  ( -2.765530957081998586, 293.6406250017069510, 6.676582343750001591 ) ) ;
#27069 = CARTESIAN_POINT ( 'NONE',  ( 1.871523826299183495E-15, -10.18810118749999916, 102.9062500020483810 ) ) ;
#27070 = CARTESIAN_POINT ( 'NONE',  ( 8.311093377946837890, 211.4062499965860411, -8.311093377946837890 ) ) ;
#27071 = ORIENTED_EDGE ( 'NONE', *, *, #12647, .F. ) ;
#27072 = CARTESIAN_POINT ( 'NONE',  ( 3.313708498984762496, -7.999999999999989342, 28.29905277982337353 ) ) ;
#27073 = CARTESIAN_POINT ( 'NONE',  ( -32.00000000000003553, 203.3125000027312126, 168.3431457505080857 ) ) ;
#27074 = CARTESIAN_POINT ( 'NONE',  ( 1.656854249492381248, 0.9374999972688131678, -4.000000000000001776 ) ) ;
#27076 = CARTESIAN_POINT ( 'NONE',  ( -8.311093377946841443, 203.9062499965859843, 8.311093377946834337 ) ) ;
#27075 = CARTESIAN_POINT ( 'NONE',  ( 2.449293598294707893E-16, 10.99999999726881406, -4.000000000000001776 ) ) ;
#27077 = CARTESIAN_POINT ( 'NONE',  ( 2.679491924311225848, 221.6666666734946602, -10.00000000000000000 ) ) ;
#27078 = CARTESIAN_POINT ( 'NONE',  ( 7.347880794884121708E-16, 300.0000000000000000, -6.000000000000001776 ) ) ;
#27079 = ORIENTED_EDGE ( 'NONE', *, *, #45740, .F. ) ;
#27080 = CARTESIAN_POINT ( 'NONE',  ( 5.676582343749993598, 200.2604166632526983, 9.832129032723422313 ) ) ;
#27081 = VECTOR ( 'NONE', #27024, 1000.000000000000000 ) ;
#27082 = CARTESIAN_POINT ( 'NONE',  ( -5.082755093536317936, -5.082755093536320601, 13.67405278187175455 ) ) ;
#27083 = CARTESIAN_POINT ( 'NONE',  ( -30.44569435410883784, 208.5625000013656063, 167.5543056458915885 ) ) ;
#27084 = CARTESIAN_POINT ( 'NONE',  ( -8.000000000000000000, 11.25000000000000178, -9.797174393178825657E-16 ) ) ;
#27085 = VERTEX_POINT ( 'NONE', #30239 ) ;
#27086 = CARTESIAN_POINT ( 'NONE',  ( -8.000000000000000000, 92.18750000409679046, 0.000000000000000000 ) ) ;
#27087 = CARTESIAN_POINT ( 'NONE',  ( 4.999999999999993783, 9.166666666666666075, 8.660254037844390851 ) ) ;
#27088 = CARTESIAN_POINT ( 'NONE',  ( -4.220049686691935698, 10.18810118749999916, 81.25000000204836681 ) ) ;
#27089 = VERTEX_POINT ( 'NONE', #41558 ) ;
#27090 = CARTESIAN_POINT ( 'NONE',  ( -1.656854249492383691, 18.68750000000000000, 4.000000000000000888 ) ) ;
#27091 = CARTESIAN_POINT ( 'NONE',  ( -3.211159895383561391, 20.68749999863440436, -3.211159895383561835 ) ) ;
#27092 = CARTESIAN_POINT ( 'NONE',  ( 7.999999999999991118, 9.797174393178815797E-16, 7.767802783920144449 ) ) ;
#27093 = CARTESIAN_POINT ( 'NONE',  ( -3.255014963930524218E-15, -13.85640646055106728, -14.00000000000000178 ) ) ;
#27094 = EDGE_LOOP ( 'NONE', ( #73119, #23670, #2460, #62610 ) ) ;
#27095 = CARTESIAN_POINT ( 'NONE',  ( 2.977408999572650039, 95.18750000204838102, -7.188101187500001821 ) ) ;
#27096 = ADVANCED_FACE ( 'NONE', ( #64206 ), #56678, .F. ) ;
#27099 = CARTESIAN_POINT ( 'NONE',  ( 30.82842712474621294, 207.2500000027312126, 172.8284271247460424 ) ) ;
#27098 = CARTESIAN_POINT ( 'NONE',  ( -11.35316468749999785, 253.6979166700806729, -3.042071309553164848 ) ) ;
#27097 = CARTESIAN_POINT ( 'NONE',  ( 7.999999999999991118, 9.797174393178815797E-16, 12.08030277982336642 ) ) ;
#27100 = APPLICATION_PROTOCOL_DEFINITION ( 'draft international standard', 'automotive_design', 1998, #33707 ) ;
#27101 = ORIENTED_EDGE ( 'NONE', *, *, #20691, .T. ) ;
#27102 = CARTESIAN_POINT ( 'NONE',  ( 8.311093377946834337, 257.3437500034140157, -8.311093377946836114 ) ) ;
#27103 = CARTESIAN_POINT ( 'NONE',  ( -4.401442555609577197E-16, 7.188101187499992051, 14.61155278187175455 ) ) ;
#27104 = ORIENTED_EDGE ( 'NONE', *, *, #12372, .F. ) ;
#27105 = EDGE_CURVE ( 'NONE', #13133, #1142, #64382, .T. ) ;
#27106 = VERTEX_POINT ( 'NONE', #69041 ) ;
#27107 = CARTESIAN_POINT ( 'NONE',  ( 10.18810118749999916, 4.220049686691935698, 71.50000000204838102 ) ) ;
#27108 = CARTESIAN_POINT ( 'NONE',  ( -9.832129032723420536, 69.01041666325268409, 5.676582343749997150 ) ) ;
#27109 = CARTESIAN_POINT ( 'NONE',  ( 3.458734124999960358, 194.6875000013655779, 142.0000000000000568 ) ) ;
#27110 = CARTESIAN_POINT ( 'NONE',  ( 11.00000000000000355, -4.556349186104045046, 91.65625000000001421 ) ) ;
#27113 = CARTESIAN_POINT ( 'NONE',  ( -2.765530957081998142, 288.7968750017069510, 6.676582343750000703 ) ) ;
#27112 = CARTESIAN_POINT ( 'NONE',  ( 23.99999999999999645, 196.9375000027312410, 171.6568542494923122 ) ) ;
#27111 = CARTESIAN_POINT ( 'NONE',  ( -25.17157287525374443, 205.7500000027312126, 172.8284271247464972 ) ) ;
#27114 = CARTESIAN_POINT ( 'NONE',  ( -50.40052831295453473, 199.4366166527698567, 56.62108449863357151 ) ) ;
#27115 = DIRECTION ( 'NONE',  ( -0.000000000000000000, -0.000000000000000000, -1.000000000000000000 ) ) ;
#27116 = CONICAL_SURFACE ( 'NONE', #48805, 10.35000000000000142, 0.9599310885968800333 ) ;
#27117 = CARTESIAN_POINT ( 'NONE',  ( 2.839093476692135984E-14, 199.9375000013656063, 201.4587341250000350 ) ) ;
#27118 = CARTESIAN_POINT ( 'NONE',  ( -5.656854249492379694, 9.374999995903223748, -5.656854249492380582 ) ) ;
#27119 = VERTEX_POINT ( 'NONE', #57359 ) ;
#27120 = CARTESIAN_POINT ( 'NONE',  ( 24.54126587499999701, 195.1250000013656063, 168.5673454167822172 ) ) ;
#27121 = CARTESIAN_POINT ( 'NONE',  ( 7.188101187500000044, 18.84374999795161187, 0.000000000000000000 ) ) ;
#27122 = CARTESIAN_POINT ( 'NONE',  ( -11.35316468749999785, 163.3854166632526983, -3.042071309553167513 ) ) ;
#27123 = CARTESIAN_POINT ( 'NONE',  ( 7.999999999999998224, 7.406250000000001776, 3.313708498984766049 ) ) ;
#27124 = CARTESIAN_POINT ( 'NONE',  ( -2.977408999572650927, 101.7500000020483810, -7.188101187500000933 ) ) ;
#27126 = CARTESIAN_POINT ( 'NONE',  ( -0.8997857291006282621, -51.17549659652937777, -48.53090770943286714 ) ) ;
#27125 = CARTESIAN_POINT ( 'NONE',  ( -1.734723475976807094E-15, 13.85640646055103886, 0.000000000000000000 ) ) ;
#27127 = CARTESIAN_POINT ( 'NONE',  ( 26.56734541678238415, 208.2500000013656063, 166.5412658749999650 ) ) ;
#27128 = CARTESIAN_POINT ( 'NONE',  ( 5.082755093536318824, 5.082755093536319713, 14.79905278187175455 ) ) ;
#27129 = CARTESIAN_POINT ( 'NONE',  ( -2.828427124746209831, 208.5000000027312126, 139.1715728752538723 ) ) ;
#27130 = CARTESIAN_POINT ( 'NONE',  ( 9.832129032723416984, 50.36458332991934839, 5.676582343750006032 ) ) ;
#27131 =( BOUNDED_CURVE ( )  B_SPLINE_CURVE ( 2, ( #55073, #65628, #43738, #2639, #59608, #60719, #31681, #7921, #48273, #48642, #13559, #31298, #14304 ),
 .UNSPECIFIED., .F., .F. ) 
 B_SPLINE_CURVE_WITH_KNOTS ( ( 3, 2, 2, 2, 2, 2, 3 ),
 ( 1.868286558610450454, 1.873520558097138355, 1.878754557583826035, 1.883988557070513936, 1.889222556557201838, 1.894456556043889517, 1.899690555530577418 ),
 .UNSPECIFIED. ) 
 CURVE ( )  GEOMETRIC_REPRESENTATION_ITEM ( )  RATIONAL_B_SPLINE_CURVE ( ( 1.000000000000194289, 0.9659258262888741342, 1.000000000000000000, 0.9659258262890683122, 1.000000000000000000, 0.9659258262890683122, 1.000000000000000000, 0.9659258262890683122, 1.000000000000000000, 0.9659258262890683122, 1.000000000000000000, 0.9659258262890912938, 0.9999999999999770184 ) ) 
 REPRESENTATION_ITEM ( '' )  );
#27132 = CARTESIAN_POINT ( 'NONE',  ( 3.313708498984720308, 21.28125000000000711, -8.000000000000040856 ) ) ;
#27133 = CARTESIAN_POINT ( 'NONE',  ( 10.00000000000000178, 27.08333332650536462, -2.679491924311226736 ) ) ;
#27134 = CARTESIAN_POINT ( 'NONE',  ( -10.99999999999999822, 0.000000000000000000, 112.1875000040967763 ) ) ;
#27135 = ORIENTED_EDGE ( 'NONE', *, *, #58612, .F. ) ;
#27136 = CARTESIAN_POINT ( 'NONE',  ( 4.977777815167777398, 10.98248509899775982, 6.901624454228039163E-15 ) ) ;
#27137 = CARTESIAN_POINT ( 'NONE',  ( 8.311093377946837890, 51.40624999658601979, -8.311093377946837890 ) ) ;
#27138 = CARTESIAN_POINT ( 'NONE',  ( -10.99999999999999822, -4.556349186104052151, 77.78125000409680467 ) ) ;
#27139 = CARTESIAN_POINT ( 'NONE',  ( 1.432654583217607414, 199.5000000013656063, 145.4587341250000350 ) ) ;
#27140 = CARTESIAN_POINT ( 'NONE',  ( -0.4451317748865747936, 16.44604352396224911, 68.55481936398530252 ) ) ;
#27142 = CARTESIAN_POINT ( 'NONE',  ( 9.832129032723416984, 40.36458332991934839, 5.676582343750006032 ) ) ;
#27141 = CARTESIAN_POINT ( 'NONE',  ( -7.188101187499999156, 98.75000000204838102, 2.977408999572654924 ) ) ;
#27143 = CARTESIAN_POINT ( 'NONE',  ( 7.999999999999992895, -3.313708498984756279, 10.48655277982336642 ) ) ;
#27144 = CARTESIAN_POINT ( 'NONE',  ( -11.00000000000000000, 0.000000000000000000, 98.68750000409677625 ) ) ;
#27145 = CARTESIAN_POINT ( 'NONE',  ( -9.832129032723420536, 158.6979166632526983, 5.676582343749997150 ) ) ;
#27146 = CARTESIAN_POINT ( 'NONE',  ( 10.00000000000000178, 141.8749999931720538, 0.000000000000000000 ) ) ;
#27147 = CARTESIAN_POINT ( 'NONE',  ( 7.188101187500001821, 101.3750000020483952, -2.977408999572651371 ) ) ;
#27148 = CARTESIAN_POINT ( 'NONE',  ( -38.00000000000002132, 82.00000000000001421, 57.99999999999999289 ) ) ;
#27149 = CARTESIAN_POINT ( 'NONE',  ( 5.676582343750001591, 36.92708332991935549, -9.832129032723420536 ) ) ;
#27150 = CARTESIAN_POINT ( 'NONE',  ( -7.204075437095965206, -7.204075437095968759, 116.2187500020483810 ) ) ;
#27151 = EDGE_LOOP ( 'NONE', ( #16499, #40256, #16759, #62666 ) ) ;
#27152 = CARTESIAN_POINT ( 'NONE',  ( 5.000000000000000000, 50.64189880742059557, 41.08656465431948845 ) ) ;
#27153 = CARTESIAN_POINT ( 'NONE',  ( -4.220049686691935698, 10.18810118749999916, 77.87500000204838102 ) ) ;
#27154 = CARTESIAN_POINT ( 'NONE',  ( 35.60314802423817326, 39.55078242745623385, 65.00000000000000000 ) ) ;
#27156 = CARTESIAN_POINT ( 'NONE',  ( 5.676582343750001591, 171.6145833299193555, -9.832129032723420536 ) ) ;
#27155 = CARTESIAN_POINT ( 'NONE',  ( -5.000000000000001776, 6.666666666666670515, -8.660254037844392627 ) ) ;
#27157 = CARTESIAN_POINT ( 'NONE',  ( -7.999999999999991118, 3.313708498984756723, 11.29280278432982421 ) ) ;
#27158 = CARTESIAN_POINT ( 'NONE',  ( -2.751064625579944321E-14, 207.8750000027312126, 146.0000000000000284 ) ) ;
#27159 = CARTESIAN_POINT ( 'NONE',  ( 4.999999999999997335, 261.4583333401613459, -8.660254037844387298 ) ) ;
#27160 = CARTESIAN_POINT ( 'NONE',  ( 7.456155213531542536, 51.58724325107107944, -41.60228463192800774 ) ) ;
#27161 = CARTESIAN_POINT ( 'NONE',  ( -6.238412754330611322E-16, 10.18810118749999916, 84.15625000204838102 ) ) ;
#27162 = ORIENTED_EDGE ( 'NONE', *, *, #70346, .T. ) ;
#27163 = CARTESIAN_POINT ( 'NONE',  ( 10.99999999999989697, -4.556349186104149851, 90.34375000409677625 ) ) ;
#27164 = CARTESIAN_POINT ( 'NONE',  ( -6.735557395310442023E-16, 11.00000000000000000, 105.6250000000000000 ) ) ;
#27165 = CARTESIAN_POINT ( 'NONE',  ( -9.832129032723418760, 113.1770833299193555, -5.676582343750004256 ) ) ;
#27166 = CARTESIAN_POINT ( 'NONE',  ( -4.541265875000002339, 19.93749999863440436, -5.561446717895856393E-16 ) ) ;
#27167 = ORIENTED_EDGE ( 'NONE', *, *, #63642, .F. ) ;
#27168 = VERTEX_POINT ( 'NONE', #45281 ) ;
#27169 = CARTESIAN_POINT ( 'NONE',  ( 1.881053915767121776, 8.624999998634406140, -4.541265875000002339 ) ) ;
#27170 = CARTESIAN_POINT ( 'NONE',  ( 2.977408999572651815, 9.187499997951610098, 7.188101187500000933 ) ) ;
#27171 = CARTESIAN_POINT ( 'NONE',  ( -8.000000000000000000, 108.6875000040967905, 0.000000000000000000 ) ) ;
#27173 = EDGE_CURVE ( 'NONE', #9013, #53417, #72061, .T. ) ;
#27172 = CARTESIAN_POINT ( 'NONE',  ( 10.18810118749999916, 1.247682550866122264E-15, 94.28125000204836681 ) ) ;
#27174 = ADVANCED_FACE ( 'NONE', ( #39627 ), #61889, .F. ) ;
#27175 = CARTESIAN_POINT ( 'NONE',  ( -25.55430564589119413, 203.5625000013656063, 167.5543056458915316 ) ) ;
#27176 = VECTOR ( 'NONE', #39441, 1000.000000000000000 ) ;
#27177 = CARTESIAN_POINT ( 'NONE',  ( 2.449293598294707893E-16, 9.250000000000000000, -4.000000000000001776 ) ) ;
#27178 = CARTESIAN_POINT ( 'NONE',  ( 1.656854249492381914, 19.56249999726881228, 4.000000000000000888 ) ) ;
#27179 = CARTESIAN_POINT ( 'NONE',  ( -8.342170076843785083E-16, 9.062499998634407916, 4.541265875000002339 ) ) ;
#27180 = CARTESIAN_POINT ( 'NONE',  ( -4.000000000000015987, 196.5000000000000000, 142.0000000000000568 ) ) ;
#27181 = ORIENTED_EDGE ( 'NONE', *, *, #26990, .F. ) ;
#27182 = CARTESIAN_POINT ( 'NONE',  ( 10.00000000000000178, 222.2916666666666572, 2.679491924311222739 ) ) ;
#27184 = CARTESIAN_POINT ( 'NONE',  ( 7.778174593052023411, -7.778174593052021635, 96.25000000409677625 ) ) ;
#27183 = CARTESIAN_POINT ( 'NONE',  ( -30.44569435410875613, 195.8125000013656063, 172.4456943541092642 ) ) ;
#27185 = CARTESIAN_POINT ( 'NONE',  ( 4.541265875000001451, 20.24999999863440436, 1.881053915767124440 ) ) ;
#27186 = CARTESIAN_POINT ( 'NONE',  ( 6.123233995736767268E-16, 73.12499999317203958, -10.00000000000000178 ) ) ;
#27187 = CARTESIAN_POINT ( 'NONE',  ( -7.188101187499992051, 0.000000000000000000, 1.486552781871753437 ) ) ;
#27188 = ORIENTED_EDGE ( 'NONE', *, *, #28115, .F. ) ;
#27189 = ORIENTED_EDGE ( 'NONE', *, *, #764, .F. ) ;
#27190 = CARTESIAN_POINT ( 'NONE',  ( -10.18810118749999916, 4.220049686691934809, 94.56250000204838102 ) ) ;
#27191 = CYLINDRICAL_SURFACE ( 'NONE', #62272, 36.00000000000000000 ) ;
#27192 = CARTESIAN_POINT ( 'NONE',  ( -31.45873412499997812, 201.0000000013655779, 171.4326545832180386 ) ) ;
#27193 = CARTESIAN_POINT ( 'NONE',  ( -6.735557395310442023E-16, 11.00000000000000000, 105.6250000000000000 ) ) ;
#27194 = CARTESIAN_POINT ( 'NONE',  ( 2.445694354108839175, 207.3125000013656063, 195.5543056458912190 ) ) ;
#27195 = CARTESIAN_POINT ( 'NONE',  ( 9.797174393178825657E-16, 125.0000000000000000, -8.000000000000000000 ) ) ;
#27196 = CARTESIAN_POINT ( 'NONE',  ( 5.000000000000001776, 125.8333333333333570, -8.660254037844389075 ) ) ;
#27197 = CARTESIAN_POINT ( 'NONE',  ( -8.000000000000000000, 105.5000000000000000, 0.000000000000000000 ) ) ;
#27198 = CARTESIAN_POINT ( 'NONE',  ( 6.676582343750003368, 290.1718750017070079, -2.765530957081997254 ) ) ;
#27199 = CARTESIAN_POINT ( 'NONE',  ( -7.188101187499990274, -2.977408999572651371, 10.95530278187175455 ) ) ;
#27200 = ORIENTED_EDGE ( 'NONE', *, *, #25586, .T. ) ;
#27201 = PLANE ( 'NONE',  #20478 ) ;
#27202 = CARTESIAN_POINT ( 'NONE',  ( 26.56734541678232375, 205.3750000013656063, 173.4587341249998929 ) ) ;
#27203 = CARTESIAN_POINT ( 'NONE',  ( -8.000000000000001776, 26.15624999590322730, 3.313708498984759387 ) ) ;
#27204 = CARTESIAN_POINT ( 'NONE',  ( -2.445694354108839619, 199.8125000013656063, 139.5543056458912190 ) ) ;
#27205 = CARTESIAN_POINT ( 'NONE',  ( 7.188101187500000044, 119.2812500020483810, -8.802885111219163269E-16 ) ) ;
#27207 = CARTESIAN_POINT ( 'NONE',  ( 1.432654583217607414, 204.5000000013656063, 145.4587341250000634 ) ) ;
#27206 = CARTESIAN_POINT ( 'NONE',  ( 1.280032823142233767, 194.9537783487151898, 145.7498327385835921 ) ) ;
#27208 = CARTESIAN_POINT ( 'NONE',  ( -11.35316468749999963, 254.2187500034139873, 0.000000000000000000 ) ) ;
#27209 = CARTESIAN_POINT ( 'NONE',  ( 0.000000000000000000, 125.0000000000000000, 8.000000000000000000 ) ) ;
#27210 = LINE ( 'NONE', #50972, #16776 ) ;
#27211 = CARTESIAN_POINT ( 'NONE',  ( -11.35316468750000141, 8.489583329919350163, 3.042071309553159963 ) ) ;
#27212 = CARTESIAN_POINT ( 'NONE',  ( 0.000000000000000000, 0.000000000000000000, 29.33030277982336642 ) ) ;
#27213 = CARTESIAN_POINT ( 'NONE',  ( 6.951808397369818766E-16, 202.3437499965860127, -11.35316468750000141 ) ) ;
#27214 = CARTESIAN_POINT ( 'NONE',  ( -2.679491924311235174, 135.4166666598387110, 10.00000000000000000 ) ) ;
#27215 = CARTESIAN_POINT ( 'NONE',  ( -4.541265875000002339, 7.749999998634407916, -1.881053915767121998 ) ) ;
#27216 = CYLINDRICAL_SURFACE ( 'NONE', #6615, 11.00000000000000000 ) ;
#27218 = CARTESIAN_POINT ( 'NONE',  ( 5.499985535179889418, 9.526287792881966254, 118.0000000000000000 ) ) ;
#27217 = CARTESIAN_POINT ( 'NONE',  ( -26.34314575050760965, 205.9375000000000000, 166.0000000000003695 ) ) ;
#27219 = ORIENTED_EDGE ( 'NONE', *, *, #3951, .F. ) ;
#27220 = CARTESIAN_POINT ( 'NONE',  ( 3.458734124999960358, 201.6875000013656063, 142.0000000000000568 ) ) ;
#27221 = CARTESIAN_POINT ( 'NONE',  ( -5.676582343750006032, 14.11458332991935016, 9.832129032723418760 ) ) ;
#27222 = CARTESIAN_POINT ( 'NONE',  ( 7.778174593052021635, 7.778174593052023411, 101.1250000040967763 ) ) ;
#27223 = CARTESIAN_POINT ( 'NONE',  ( -1.656854249492379916, 205.3125000000000284, 138.0000000000000284 ) ) ;
#27224 = CARTESIAN_POINT ( 'NONE',  ( -28.00000000000006750, 196.4375000013655779, 166.5412658750003629 ) ) ;
#27225 = CARTESIAN_POINT ( 'NONE',  ( -2.249999999999998224, 283.9999999998748308, 5.427273999917394676 ) ) ;
#27227 = CARTESIAN_POINT ( 'NONE',  ( -8.311093377946841443, 3.906249996586016682, 8.311093377946834337 ) ) ;
#27226 = CARTESIAN_POINT ( 'NONE',  ( -7.188101187500000044, 116.6562500020483810, 0.000000000000000000 ) ) ;
#27228 = CARTESIAN_POINT ( 'NONE',  ( 3.313708498984756279, 7.999999999999991118, 28.86155277982336642 ) ) ;
#27229 = CARTESIAN_POINT ( 'NONE',  ( 11.35316468750000141, 120.7812499965860269, 0.000000000000000000 ) ) ;
#27230 = CARTESIAN_POINT ( 'NONE',  ( 8.660254037844389075, 97.29166665983871098, -5.000000000000000000 ) ) ;
#27231 = VECTOR ( 'NONE', #58416, 1000.000000000000000 ) ;
#27232 = CARTESIAN_POINT ( 'NONE',  ( 7.188101187500002709, 120.6875000020483952, 2.977408999572649151 ) ) ;
#27233 = CARTESIAN_POINT ( 'NONE',  ( 4.541265875000001451, 19.37499999863440792, 1.881053915767124440 ) ) ;
#27234 = CARTESIAN_POINT ( 'NONE',  ( 0.000000000000000000, 0.000000000000000000, -0.7702282920306856573 ) ) ;
#27235 = DIRECTION ( 'NONE',  ( -0.000000000000000000, 1.000000000000000000, -0.000000000000000000 ) ) ;
#27236 = ORIENTED_EDGE ( 'NONE', *, *, #45453, .T. ) ;
#27237 = CARTESIAN_POINT ( 'NONE',  ( 8.248616681371277227E-12, 116.2499999999993747, -10.00000000000000178 ) ) ;
#27238 = CARTESIAN_POINT ( 'NONE',  ( 2.765530957082001251, 290.9218750017070647, 6.676582343750000703 ) ) ;
#27239 = CARTESIAN_POINT ( 'NONE',  ( 4.999999999999998224, 52.84634075987080593, 43.22150062466589304 ) ) ;
#27240 = CARTESIAN_POINT ( 'NONE',  ( 3.313708498984756279, 7.999999999999991118, 0.5490527839201453375 ) ) ;
#27241 = DIRECTION ( 'NONE',  ( 0.000000000000000000, -1.000000000000000000, 0.000000000000000000 ) ) ;
#27242 = CARTESIAN_POINT ( 'NONE',  ( -5.676582343749992710, 254.7395833367473301, 9.832129032723422313 ) ) ;
#27243 = CARTESIAN_POINT ( 'NONE',  ( -7.204075437095965206, -7.204075437095968759, 102.7187500020483668 ) ) ;
#27244 = ORIENTED_EDGE ( 'NONE', *, *, #43886, .F. ) ;
#27245 =( BOUNDED_CURVE ( )  B_SPLINE_CURVE ( 2, ( #44327, #11117, #10368, #12493, #34141, #27709, #45430, #51096, #61679 ),
 .UNSPECIFIED., .F., .F. ) 
 B_SPLINE_CURVE_WITH_KNOTS ( ( 3, 2, 2, 2, 3 ),
 ( 0.3166666666666668184, 0.3250000000000002331, 0.3333333333333335924, 0.3416666666666670626, 0.3500000000000004219 ),
 .UNSPECIFIED. ) 
 CURVE ( )  GEOMETRIC_REPRESENTATION_ITEM ( )  RATIONAL_B_SPLINE_CURVE ( ( 0.9999999999999984457, 0.9238795325112882928, 1.000000000000000000, 0.9238795325112867385, 1.000000000000000000, 0.9238795325112867385, 1.000000000000000000, 0.9238795325112826307, 1.000000000000003997 ) ) 
 REPRESENTATION_ITEM ( '' )  );
#27246 = CIRCLE ( 'NONE', #4372, 12.50000000000000711 ) ;
#27247 = ADVANCED_FACE ( 'NONE', ( #11690 ), #58470, .F. ) ;
#27248 = CARTESIAN_POINT ( 'NONE',  ( -2.828427124746152987, 198.2500000027312126, 200.8284271247462129 ) ) ;
#27249 = CARTESIAN_POINT ( 'NONE',  ( -2.085542519210945728E-15, 159.8437499965860127, 11.35316468750000141 ) ) ;
#27250 =( NAMED_UNIT ( * ) PLANE_ANGLE_UNIT ( ) SI_UNIT ( $, .RADIAN. ) );
#27251 = CARTESIAN_POINT ( 'NONE',  ( 3.458734125000016757, 205.1250000013656347, 199.4326545832176976 ) ) ;
#27252 = CARTESIAN_POINT ( 'NONE',  ( -6.123233995736766282E-16, 231.8750000068279746, -10.00000000000000000 ) ) ;
#27253 = CARTESIAN_POINT ( 'NONE',  ( -11.35316468749999785, 78.38541666325266988, -3.042071309553167513 ) ) ;
#27254 = ORIENTED_EDGE ( 'NONE', *, *, #68944, .T. ) ;
#27255 = CARTESIAN_POINT ( 'NONE',  ( 7.204075437095968759, -7.204075437095966983, 114.7187500020483810 ) ) ;
#27256 = CARTESIAN_POINT ( 'NONE',  ( -3.211159895383562723, 10.06249999863440614, 3.211159895383561391 ) ) ;
#27257 = VERTEX_POINT ( 'NONE', #6415 ) ;
#27258 = CARTESIAN_POINT ( 'NONE',  ( -5.082755093536326818, 25.40624999795161543, 5.082755093536325042 ) ) ;
#27259 = CARTESIAN_POINT ( 'NONE',  ( -4.242640687119286547, 287.9375000034140157, -4.242640687119286547 ) ) ;
#27260 = DIRECTION ( 'NONE',  ( 0.000000000000000000, 0.000000000000000000, 1.000000000000000000 ) ) ;
#27261 = CARTESIAN_POINT ( 'NONE',  ( 7.188101187500000044, 18.84374999795161187, 0.000000000000000000 ) ) ;
#27262 = CARTESIAN_POINT ( 'NONE',  ( 11.00000000000000000, 1.347111479062088405E-15, 103.9375000040967763 ) ) ;
#27263 = CARTESIAN_POINT ( 'NONE',  ( -10.18810118749999916, 4.220049686691934809, 109.9375000020483952 ) ) ;
#27264 = CARTESIAN_POINT ( 'NONE',  ( 2.603172624180115857, -43.49592116648197049, 151.1788501740049071 ) ) ;
#27265 = CARTESIAN_POINT ( 'NONE',  ( 1.656854249492381914, 4.562499997268812280, 4.000000000000000888 ) ) ;
#27266 = CARTESIAN_POINT ( 'NONE',  ( 23.99999999999999289, 206.8750000027312126, 169.9999999999999432 ) ) ;
#27267 = ORIENTED_EDGE ( 'NONE', *, *, #36179, .T. ) ;
#27268 = EDGE_CURVE ( 'NONE', #6116, #1178, #70514, .T. ) ;
#27269 = EDGE_CURVE ( 'NONE', #13802, #31722, #49895, .T. ) ;
#27270 = CARTESIAN_POINT ( 'NONE',  ( -3.458734124999959914, 202.4375000013656063, 198.0000000000000284 ) ) ;
#27271 =( GEOMETRIC_REPRESENTATION_CONTEXT ( 3 ) GLOBAL_UNCERTAINTY_ASSIGNED_CONTEXT ( ( #35839 ) ) GLOBAL_UNIT_ASSIGNED_CONTEXT ( ( #53915, #30163, #47134 ) ) REPRESENTATION_CONTEXT ( 'NONE', 'WORKASPACE' ) );
#27272 = CARTESIAN_POINT ( 'NONE',  ( -28.00000000000007461, 208.4375000013656063, 166.5412658750003629 ) ) ;
#27273 = CARTESIAN_POINT ( 'NONE',  ( 1.656854249492381914, 12.56249999726881406, 4.000000000000000888 ) ) ;
#27274 = EDGE_CURVE ( 'NONE', #62863, #47640, #767, .T. ) ;
#27275 = CARTESIAN_POINT ( 'NONE',  ( 4.541265875000002339, 4.374999998634407028, -1.881053915767121554 ) ) ;
#27276 = CARTESIAN_POINT ( 'NONE',  ( -7.188101187499990274, -2.977408999572651371, 16.58030278187175455 ) ) ;
#27277 = ORIENTED_EDGE ( 'NONE', *, *, #4737, .T. ) ;
#27278 = CARTESIAN_POINT ( 'NONE',  ( -2.828427124746190735, 21.37500000000000000, -2.828427124746191623 ) ) ;
#27279 = ORIENTED_EDGE ( 'NONE', *, *, #35751, .F. ) ;
#27280 = CARTESIAN_POINT ( 'NONE',  ( 4.220049686691934809, 10.18810118749999916, 113.6875000020483810 ) ) ;
#27281 = DIRECTION ( 'NONE',  ( -1.000000000000000000, -0.000000000000000000, -0.000000000000000000 ) ) ;
#27282 = CARTESIAN_POINT ( 'NONE',  ( -1.432654583217607192, 204.2500000013655779, 194.5412658750000219 ) ) ;
#27283 = CARTESIAN_POINT ( 'NONE',  ( 31.45873412499997812, 200.7500000013656063, 168.5673454167822172 ) ) ;
#27284 = CARTESIAN_POINT ( 'NONE',  ( 10.00000000000000000, 74.79166666666667140, 2.679491924311236062 ) ) ;
#27285 = CARTESIAN_POINT ( 'NONE',  ( 5.082755093536326818, 90.59375000204839523, 5.082755093536325042 ) ) ;
#27286 = CARTESIAN_POINT ( 'NONE',  ( 2.485281374238571317, 292.6875000000001137, -6.000000000000003553 ) ) ;
#27287 = EDGE_CURVE ( 'NONE', #34184, #74626, #26493, .T. ) ;
#27288 = CARTESIAN_POINT ( 'NONE',  ( 27.99999999999996447, 203.6250000027312126, 165.9999999999998863 ) ) ;
#27289 = VERTEX_POINT ( 'NONE', #53170 ) ;
#27290 = CONICAL_SURFACE ( 'NONE', #64675, 12.00000000000000000, 1.047197551196596077 ) ;
#27291 = CARTESIAN_POINT ( 'NONE',  ( -6.951808397369817780E-16, 222.6562500034139873, -11.35316468749999963 ) ) ;
#27292 = CARTESIAN_POINT ( 'NONE',  ( -1.781595147088172792, -16.42277972781904083, 68.70049804031401663 ) ) ;
#27293 = CARTESIAN_POINT ( 'NONE',  ( -2.849036369511732440E-14, 197.3750000027312126, 138.0000000000000568 ) ) ;
#27294 = CARTESIAN_POINT ( 'NONE',  ( -5.000000000000000888, 64.62627855237413144, 24.10294814404773334 ) ) ;
#27295 = CARTESIAN_POINT ( 'NONE',  ( -11.00000000000000000, 0.000000000000000000, 93.99999999999998579 ) ) ;
#27296 = CARTESIAN_POINT ( 'NONE',  ( 1.836970198721029589E-15, 256.2500000000000568, 10.00000000000000000 ) ) ;
#27297 = CARTESIAN_POINT ( 'NONE',  ( 29.65685424949235838, 203.1875000027311842, 173.9999999999999432 ) ) ;
#27298 = CARTESIAN_POINT ( 'NONE',  ( -2.679491924311235618, 193.5416666666666856, 10.00000000000000000 ) ) ;
#27299 = CARTESIAN_POINT ( 'NONE',  ( -5.000000000000000000, -16.24494643555759410, -69.83755725260751035 ) ) ;
#27300 = CARTESIAN_POINT ( 'NONE',  ( 5.082755093536318824, 5.082755093536319713, 20.79905278187175455 ) ) ;
#27301 = CARTESIAN_POINT ( 'NONE',  ( 6.951808397369818766E-16, 172.3437499965860127, -11.35316468750000141 ) ) ;
#27302 = DIRECTION ( 'NONE',  ( 1.000000000000000000, -0.000000000000000000, -0.000000000000000000 ) ) ;
#27303 = CARTESIAN_POINT ( 'NONE',  ( 5.000000000000086153, 154.1666666666667993, 8.660254037844548947 ) ) ;
#27305 = CARTESIAN_POINT ( 'NONE',  ( 18.00000000000000000, 0.000000000000000000, -20.69999999999999929 ) ) ;
#27304 = CYLINDRICAL_SURFACE ( 'NONE', #35880, 10.00000000000000178 ) ;
#27306 = ORIENTED_EDGE ( 'NONE', *, *, #48601, .F. ) ;
#27307 = CARTESIAN_POINT ( 'NONE',  ( 9.832129032723420536, 21.51041666325268409, -5.676582343749999815 ) ) ;
#27308 = CARTESIAN_POINT ( 'NONE',  ( -29.43265458321755901, 208.8750000013656063, 173.4587341250004044 ) ) ;
#27310 = CARTESIAN_POINT ( 'NONE',  ( 0.6547826978328875613, -10.28110016890869893, -63.57209897671329912 ) ) ;
#27309 = CYLINDRICAL_SURFACE ( 'NONE', #1107, 8.000000000000000000 ) ;
#27311 = DIRECTION ( 'NONE',  ( -0.000000000000000000, -0.000000000000000000, -1.000000000000000000 ) ) ;
#27312 = CARTESIAN_POINT ( 'NONE',  ( 3.458734124999958581, 202.5000000013656063, 140.5673454167823593 ) ) ;
#27313 = CARTESIAN_POINT ( 'NONE',  ( -8.660254037844390851, 44.79166665983870388, 4.999999999999998224 ) ) ;
#27314 = CARTESIAN_POINT ( 'NONE',  ( -7.188101187499999156, 100.2500000020483952, 2.977408999572654924 ) ) ;
#27315 = CARTESIAN_POINT ( 'NONE',  ( -4.541265875000002339, 9.874999998634404363, -1.881053915767121998 ) ) ;
#27316 = CARTESIAN_POINT ( 'NONE',  ( 2.679491924311225404, 101.0416666666666714, -9.999999999999982236 ) ) ;
#27317 = CARTESIAN_POINT ( 'NONE',  ( -5.656854249492375253, 5.656854249492375253, 6.642802779823365533 ) ) ;
#27318 = CARTESIAN_POINT ( 'NONE',  ( -2.828427124746192067, 5.374999997268813168, 2.828427124746190735 ) ) ;
#27319 = ORIENTED_EDGE ( 'NONE', *, *, #50549, .F. ) ;
#27320 = ORIENTED_EDGE ( 'NONE', *, *, #45165, .F. ) ;
#27321 = CARTESIAN_POINT ( 'NONE',  ( 3.313708498984721640, 28.03124999590321664, 8.000000000000039080 ) ) ;
#27322 = CARTESIAN_POINT ( 'NONE',  ( 2.445694354108840063, 195.0625000013656063, 200.4456943541088663 ) ) ;
#27323 = CARTESIAN_POINT ( 'NONE',  ( 11.00000000000000000, 1.347111479062088405E-15, 82.74999999999998579 ) ) ;
#27324 = VECTOR ( 'NONE', #38731, 1000.000000000000000 ) ;
#27325 = CARTESIAN_POINT ( 'NONE',  ( -25.55513208947350279, -41.56254277292774901, 152.4454915852995498 ) ) ;
#27326 = CARTESIAN_POINT ( 'NONE',  ( 6.951808397369818766E-16, 137.0312499965860411, -11.35316468750000141 ) ) ;
#27327 = ORIENTED_EDGE ( 'NONE', *, *, #37312, .T. ) ;
#27328 = CARTESIAN_POINT ( 'NONE',  ( 7.999999999999706901, -2.135495361439877059E-06, 10.76780272350167245 ) ) ;
#27329 = CARTESIAN_POINT ( 'NONE',  ( -4.220049686691937474, -10.18810118749999738, 91.93750000204836681 ) ) ;
#27330 = LINE ( 'NONE', #49608, #20015 ) ;
#27331 = CARTESIAN_POINT ( 'NONE',  ( 2.849036369511732440E-14, 208.2500000000000284, 202.0000000000000000 ) ) ;
#27332 = FACE_OUTER_BOUND ( 'NONE', #6379, .T. ) ;
#27333 = PRODUCT_DEFINITION_FORMATION_WITH_SPECIFIED_SOURCE ( 'ANY', '', #54090, .NOT_KNOWN. ) ;
#27334 = CARTESIAN_POINT ( 'NONE',  ( -11.00000000000000000, 0.000000000000000000, 95.49999999999998579 ) ) ;
#27335 = EDGE_LOOP ( 'NONE', ( #43114, #54473, #15291, #45624 ) ) ;
#27336 = CARTESIAN_POINT ( 'NONE',  ( 4.898587196589415787E-16, 0.000000000000000000, 4.000000000000001776 ) ) ;
#27337 = CARTESIAN_POINT ( 'NONE',  ( -30.51809756383105920, 179.9566333433965895, 164.1079028600190099 ) ) ;
#27338 = CARTESIAN_POINT ( 'NONE',  ( 9.832129032723420536, 111.5104166632526841, -5.676582343749999815 ) ) ;
#27339 = CARTESIAN_POINT ( 'NONE',  ( -1.432654583217607192, 202.2500000013655779, 194.5412658750000219 ) ) ;
#27340 = CARTESIAN_POINT ( 'NONE',  ( -7.188101187500000044, 16.59374999795161543, -8.802885111219163269E-16 ) ) ;
#27341 =( BOUNDED_CURVE ( )  B_SPLINE_CURVE ( 1, ( #49576, #33364 ),
 .UNSPECIFIED., .F., .F. ) 
 B_SPLINE_CURVE_WITH_KNOTS ( ( 2, 2 ),
 ( 0.000000000000000000, 1.000000000000000000 ),
 .UNSPECIFIED. ) 
 CURVE ( )  GEOMETRIC_REPRESENTATION_ITEM ( )  RATIONAL_B_SPLINE_CURVE ( ( 0.9660722070829228514, 0.9660722070829228514 ) ) 
 REPRESENTATION_ITEM ( '' )  );
#27342 = CARTESIAN_POINT ( 'NONE',  ( 4.220049686691941027, -10.18810118749999738, 80.50000000204839523 ) ) ;
#27343 = CARTESIAN_POINT ( 'NONE',  ( 9.832129032723420536, 36.51041666325267698, -5.676582343749999815 ) ) ;
#27344 = VERTEX_POINT ( 'NONE', #18095 ) ;
#27345 = CARTESIAN_POINT ( 'NONE',  ( -8.000000000000000000, 96.68750000409679046, 0.000000000000000000 ) ) ;
#27346 = CARTESIAN_POINT ( 'NONE',  ( 3.317071493978883456, -8.008118988124989457, 19.48186528394063544 ) ) ;
#27347 = CARTESIAN_POINT ( 'NONE',  ( 12.00000000000000178, -28.00000000000000000, 3.999999999999989786 ) ) ;
#27348 = ADVANCED_FACE ( 'NONE', ( #12423 ), #6780, .T. ) ;
#27349 = CARTESIAN_POINT ( 'NONE',  ( -11.00000000000000000, 0.000000000000000000, 92.49999999999998579 ) ) ;
#27350 = CARTESIAN_POINT ( 'NONE',  ( -2.977408999572650039, 5.437499997951610986, -7.188101187500001821 ) ) ;
#27351 = CARTESIAN_POINT ( 'NONE',  ( 6.000000000000001776, 298.5625000034140157, -7.347880794884121708E-16 ) ) ;
#27352 = CARTESIAN_POINT ( 'NONE',  ( -23.99999999999997868, 206.6875000000000284, 171.6568542494927385 ) ) ;
#27353 = EDGE_LOOP ( 'NONE', ( #36920, #1500 ) ) ;
#27354 = CARTESIAN_POINT ( 'NONE',  ( -11.35316468750000141, 148.8020833299193555, 3.042071309553159963 ) ) ;
#27355 = AXIS2_PLACEMENT_3D ( 'NONE', #71090, #25061, #19408 ) ;
#27356 = CARTESIAN_POINT ( 'NONE',  ( 10.18810118749999916, 1.247682550866122264E-15, 77.40625000204836681 ) ) ;
#27357 = CARTESIAN_POINT ( 'NONE',  ( -24.54126587499998990, 196.1875000013655779, 170.0000000000003411 ) ) ;
#27358 =( BOUNDED_CURVE ( )  B_SPLINE_CURVE ( 2, ( #35971, #20075, #25364, #60076, #8395, #48381, #64637, #7296, #59354 ),
 .UNSPECIFIED., .F., .F. ) 
 B_SPLINE_CURVE_WITH_KNOTS ( ( 3, 2, 2, 2, 3 ),
 ( 0.9736842105263158187, 0.9802631578947368363, 0.9868421052631578538, 0.9934210526315789824, 0.9940576599040155115 ),
 .UNSPECIFIED. ) 
 CURVE ( )  GEOMETRIC_REPRESENTATION_ITEM ( )  RATIONAL_B_SPLINE_CURVE ( ( 1.000000000000000000, 0.9238795325112867385, 1.000000000000000000, 0.9238795325112867385, 1.000000000000000000, 0.9238795325112867385, 1.000000000000000000, 0.9926342558359432244, 0.9866939939076171395 ) ) 
 REPRESENTATION_ITEM ( '' )  );
#27359 = DIRECTION ( 'NONE',  ( 0.000000000000000000, 0.000000000000000000, -1.000000000000000000 ) ) ;
#27360 = CARTESIAN_POINT ( 'NONE',  ( -4.541265875000003227, 16.99999999863440792, 1.881053915767121110 ) ) ;
#27361 = ORIENTED_EDGE ( 'NONE', *, *, #42405, .F. ) ;
#27362 = EDGE_CURVE ( 'NONE', #55690, #64356, #1132, .T. ) ;
#27363 = CARTESIAN_POINT ( 'NONE',  ( 2.828427124746208943, 201.7500000027312126, 195.1715728752538439 ) ) ;
#27364 = CARTESIAN_POINT ( 'NONE',  ( 1.432654583217607414, 195.5000000013655779, 145.4587341250000634 ) ) ;
#27365 = CARTESIAN_POINT ( 'NONE',  ( -27.99999999999991473, 206.6250000027312126, 174.0000000000003695 ) ) ;
#27366 = CARTESIAN_POINT ( 'NONE',  ( 8.000000000000000000, 6.093750000000000888, -3.313708498984761164 ) ) ;
#27367 = ORIENTED_EDGE ( 'NONE', *, *, #7528, .F. ) ;
#27368 = CARTESIAN_POINT ( 'NONE',  ( 4.401442555609581635E-16, 11.34374999795161010, -7.188101187500000044 ) ) ;
#27369 = FACE_OUTER_BOUND ( 'NONE', #10013, .T. ) ;
#27370 = CARTESIAN_POINT ( 'NONE',  ( 5.000000000000000000, 53.57153130924530871, -46.19535935661008352 ) ) ;
#27371 = CARTESIAN_POINT ( 'NONE',  ( 8.311093377946834337, 185.1562499965860411, 8.311093377946839666 ) ) ;
#27372 = CARTESIAN_POINT ( 'NONE',  ( -7.188101187499999156, 112.6250000020483668, 2.977408999572654924 ) ) ;
#27373 = CARTESIAN_POINT ( 'NONE',  ( 4.242640687119285658, 295.6249999999999432, -4.242640687119286547 ) ) ;
#27374 = CARTESIAN_POINT ( 'NONE',  ( -2.765530957081996810, 288.2656250017069510, -6.676582343750002480 ) ) ;
#27375 = ADVANCED_FACE ( 'NONE', ( #18833 ), #13153, .F. ) ;
#27376 = CARTESIAN_POINT ( 'NONE',  ( -8.660254037844390851, 67.91666666666668561, 5.000000000000000000 ) ) ;
#27377 = EDGE_LOOP ( 'NONE', ( #54043, #5858, #46842, #50185 ) ) ;
#27378 = EDGE_CURVE ( 'NONE', #5483, #37641, #47490, .T. ) ;
#27379 = CARTESIAN_POINT ( 'NONE',  ( 11.35316468749999608, 256.6145833367473301, -3.042071309553167069 ) ) ;
#27380 = CLOSED_SHELL ( 'NONE', ( #23878, #30621, #42476, #42452, #22247, #49183, #55320, #14553, #37623, #69191, #15165, #60003, #42103, #29055, #29098, #4459, #28483, #28388, #11030, #51900, #17745, #25790, #70244, #21216, #18089, #8762, #33748, #71550, #31883, #62913, #35206, #22832, #56522, #47121, #31909 ) ) ;
#27381 = CARTESIAN_POINT ( 'NONE',  ( 2.977408999572650927, -7.188101187499990274, 24.83030278187175455 ) ) ;
#27382 = CARTESIAN_POINT ( 'NONE',  ( -8.660254037844387298, 8.958333326505366401, -5.000000000000004441 ) ) ;
#27383 = DIRECTION ( 'NONE',  ( 0.000000000000000000, 0.000000000000000000, 1.000000000000000000 ) ) ;
#27384 = CARTESIAN_POINT ( 'NONE',  ( -1.296342370383604559, -60.23018777774399268, -22.90345467631826182 ) ) ;
#27385 = CARTESIAN_POINT ( 'NONE',  ( 2.754378923186476579E-14, 197.4375000013655779, 194.5412658750000219 ) ) ;
#27386 = CARTESIAN_POINT ( 'NONE',  ( -1.836970198721029983E-15, 143.7500000000000284, 10.00000000000000178 ) ) ;
#27387 = EDGE_LOOP ( 'NONE', ( #20211, #18159, #43321, #57129, #35472, #15296 ) ) ;
#27388 = LINE ( 'NONE', #26643, #64466 ) ;
#27389 = CARTESIAN_POINT ( 'NONE',  ( 8.000000000000000000, 94.25000000000000000, -9.797174393178825657E-16 ) ) ;
#27390 = CARTESIAN_POINT ( 'NONE',  ( 3.042071309553159519, 125.0520833299193555, 11.35316468750000141 ) ) ;
#27391 = CARTESIAN_POINT ( 'NONE',  ( -11.00000000000000000, 4.556349186104045934, 68.40624999999998579 ) ) ;
#27394 = CARTESIAN_POINT ( 'NONE',  ( 12.04760458715722748, -13.82892193934116776, -0.1532218116813789111 ) ) ;
#27393 = CARTESIAN_POINT ( 'NONE',  ( 29.43265458321760519, 194.8750000013656063, 166.5412658749999650 ) ) ;
#27392 = CARTESIAN_POINT ( 'NONE',  ( 29.43265458321760519, 197.7500000013656063, 173.4587341249998929 ) ) ;
#27395 = EDGE_CURVE ( 'NONE', #27944, #67659, #1856, .T. ) ;
#27396 = ORIENTED_EDGE ( 'NONE', *, *, #34648, .F. ) ;
#27397 = EDGE_CURVE ( 'NONE', #59649, #23374, #4745, .T. ) ;
#27398 = CARTESIAN_POINT ( 'NONE',  ( 7.285275666675271822, 225.6005920617279799, -6.856447244518973250 ) ) ;
#27399 = CARTESIAN_POINT ( 'NONE',  ( 0.000000000000000000, 0.000000000000000000, -21.50000000000000000 ) ) ;
#27400 = APPLICATION_CONTEXT ( 'automotive_design' ) ;
#27401 = VECTOR ( 'NONE', #50602, 1000.000000000000000 ) ;
#27402 = CARTESIAN_POINT ( 'NONE',  ( 24.54126587499999346, 199.4375000013655779, 169.9999999999998863 ) ) ;
#27403 = EDGE_CURVE ( 'NONE', #41883, #17647, #61922, .T. ) ;
#27404 = CARTESIAN_POINT ( 'NONE',  ( 9.832129032723416984, 205.6770833299193555, 5.676582343750006032 ) ) ;
#27405 = CARTESIAN_POINT ( 'NONE',  ( -2.977408999572651815, 122.9375000020483810, 7.188101187500000933 ) ) ;
#27406 = CARTESIAN_POINT ( 'NONE',  ( -1.881053915767121554, 16.62499999863440436, -4.541265875000002339 ) ) ;
#27407 = CARTESIAN_POINT ( 'NONE',  ( 5.656854249492374365, 5.656854249492375253, 24.26780277982336642 ) ) ;
#27409 = CARTESIAN_POINT ( 'NONE',  ( -8.000000000000000000, 12.65625000000000178, -3.313708498984762496 ) ) ;
#27408 = SURFACE_SIDE_STYLE ('',( #61378 ) ) ;
#27410 = CARTESIAN_POINT ( 'NONE',  ( 3.042071309553167069, 101.8229166632526699, -11.35316468749999785 ) ) ;
#27411 = VERTEX_POINT ( 'NONE', #33274 ) ;
#27412 = DIRECTION ( 'NONE',  ( -0.000000000000000000, 1.000000000000000000, -0.000000000000000000 ) ) ;
#27413 = CARTESIAN_POINT ( 'NONE',  ( -2.977408999572650039, 21.93749999795161543, -7.188101187500001821 ) ) ;
#27414 = LINE ( 'NONE', #21011, #68757 ) ;
#27415 = CARTESIAN_POINT ( 'NONE',  ( 2.085542519210945334E-15, 260.4687500034140157, 11.35316468749999963 ) ) ;
#27416 = CARTESIAN_POINT ( 'NONE',  ( -9.832129032723420536, 98.69791666325269830, 5.676582343749997150 ) ) ;
#27417 = ORIENTED_EDGE ( 'NONE', *, *, #13052, .F. ) ;
#27418 = CARTESIAN_POINT ( 'NONE',  ( 0.000000000000000000, 125.0000000000000000, 8.000000000000000000 ) ) ;
#27419 = CARTESIAN_POINT ( 'NONE',  ( -10.18810118749999916, 0.000000000000000000, 108.1562500020483668 ) ) ;
#27420 = CARTESIAN_POINT ( 'NONE',  ( 1.102182119232618108E-15, 287.3125000034140157, 6.000000000000001776 ) ) ;
#27421 = CARTESIAN_POINT ( 'NONE',  ( -3.458734124999960358, 206.6875000013656063, 198.0000000000000284 ) ) ;
#27422 = CARTESIAN_POINT ( 'NONE',  ( -7.999999999999991118, 9.797174393178815797E-16, 30.00000000000000000 ) ) ;
#27424 = CARTESIAN_POINT ( 'NONE',  ( 5.676582343750001591, 91.61458332991935549, -9.832129032723420536 ) ) ;
#27423 = CARTESIAN_POINT ( 'NONE',  ( -27.99999999999995737, 202.5000000000000000, 174.0000000000003695 ) ) ;
#27425 = CARTESIAN_POINT ( 'NONE',  ( 1.469576158976822172E-15, -7.999999999999991118, 10.39280278392014800 ) ) ;
#27426 = CARTESIAN_POINT ( 'NONE',  ( -27.99999999999996447, 200.1875000013656063, 173.4587341250003760 ) ) ;
#27427 = FACE_OUTER_BOUND ( 'NONE', #20169, .T. ) ;
#27428 = CARTESIAN_POINT ( 'NONE',  ( -7.320508075688773708, 183.7499999931719969, -7.320508075688774596 ) ) ;
#27429 = CARTESIAN_POINT ( 'NONE',  ( 5.000000000000000000, -53.21762015693898462, 47.70201125340187787 ) ) ;
#27430 = CARTESIAN_POINT ( 'NONE',  ( 9.832129032723420536, 76.51041666325268409, -5.676582343749999815 ) ) ;
#27431 = CARTESIAN_POINT ( 'NONE',  ( 6.676582343750003368, 291.0156250017069510, -2.765530957081997254 ) ) ;
#27432 = CARTESIAN_POINT ( 'NONE',  ( 4.220049686691941027, -10.18810118749999738, 101.5000000020483668 ) ) ;
#27433 = CARTESIAN_POINT ( 'NONE',  ( 8.311093377946837890, 206.4062499965860127, -8.311093377946837890 ) ) ;
#27434 = ORIENTED_EDGE ( 'NONE', *, *, #49345, .T. ) ;
#27435 = CARTESIAN_POINT ( 'NONE',  ( -1.656854249492381248, 1.062499997268813168, -4.000000000000001776 ) ) ;
#27436 = CARTESIAN_POINT ( 'NONE',  ( -8.000000000000000000, 1.968749995903220196, -3.313708498984762496 ) ) ;
#27437 = CARTESIAN_POINT ( 'NONE',  ( -8.000000000000000000, 120.4062500000000000, -3.313708498984761164 ) ) ;
#27438 = CARTESIAN_POINT ( 'NONE',  ( 11.35316468749999963, 205.9895833299193555, -3.042071309553165293 ) ) ;
#27439 = CARTESIAN_POINT ( 'NONE',  ( -8.660254037844385522, 223.5416666734946602, 5.000000000000004441 ) ) ;
#27440 = FACE_OUTER_BOUND ( 'NONE', #63802, .T. ) ;
#27441 = ORIENTED_EDGE ( 'NONE', *, *, #12254, .T. ) ;
#27442 = VECTOR ( 'NONE', #35148, 1000.000000000000000 ) ;
#27443 = CARTESIAN_POINT ( 'NONE',  ( -3.042071309553173730, 194.6354166632526415, 11.35316468749999785 ) ) ;
#27444 = CARTESIAN_POINT ( 'NONE',  ( 7.188101187499993827, -2.977408999572645598, 17.14280278187175455 ) ) ;
#27445 = ADVANCED_FACE ( 'NONE', ( #67218 ), #56273, .F. ) ;
#27446 = CARTESIAN_POINT ( 'NONE',  ( -31.45873412499998523, 206.7500000013655779, 171.4326545832180386 ) ) ;
#27447 = CARTESIAN_POINT ( 'NONE',  ( -8.000000000000001776, 9.843750000000000000, 3.313708498984759387 ) ) ;
#27448 = EDGE_LOOP ( 'NONE', ( #53185, #48607, #56044, #50754 ) ) ;
#27449 = CARTESIAN_POINT ( 'NONE',  ( -4.898587196589412829E-16, 91.81250000409677625, -8.000000000000000000 ) ) ;
#27450 =( BOUNDED_CURVE ( )  B_SPLINE_CURVE ( 2, ( #61768, #7028, #5919, #276, #63242, #18344, #6295, #41358, #62869 ),
 .UNSPECIFIED., .F., .F. ) 
 B_SPLINE_CURVE_WITH_KNOTS ( ( 3, 2, 2, 2, 3 ),
 ( 0.9558823529411766273, 0.9595588235294119084, 0.9632352941176471894, 0.9669117647058825815, 0.9705882352941178626 ),
 .UNSPECIFIED. ) 
 CURVE ( )  GEOMETRIC_REPRESENTATION_ITEM ( )  RATIONAL_B_SPLINE_CURVE ( ( 0.9999999999999976685, 0.9238795325112890700, 1.000000000000000000, 0.9238795325112867385, 1.000000000000000000, 0.9238795325112867385, 1.000000000000000000, 0.9238795325112821866, 1.000000000000004663 ) ) 
 REPRESENTATION_ITEM ( '' )  );
#27451 = CARTESIAN_POINT ( 'NONE',  ( 4.999999999999993783, 19.16666666666666785, 8.660254037844390851 ) ) ;
#27452 = VECTOR ( 'NONE', #36058, 1000.000000000000000 ) ;
#27453 = EDGE_CURVE ( 'NONE', #24886, #27817, #72499, .T. ) ;
#27454 = CARTESIAN_POINT ( 'NONE',  ( -4.220049686691937474, -10.18810118749999738, 80.31250000204836681 ) ) ;
#27455 = ORIENTED_EDGE ( 'NONE', *, *, #43593, .T. ) ;
#27456 = CARTESIAN_POINT ( 'NONE',  ( 2.828427124746190291, 21.87500000000000355, 2.828427124746192067 ) ) ;
#27457 = CARTESIAN_POINT ( 'NONE',  ( 3.211159895383560947, 19.18749999863440436, 3.211159895383562723 ) ) ;
#27458 = PRODUCT_DEFINITION ( 'UNKNOWN', '', #32130, #55878 ) ;
#27459 = DIRECTION ( 'NONE',  ( -0.000000000000000000, 1.000000000000000000, -0.000000000000000000 ) ) ;
#27460 = VERTEX_POINT ( 'NONE', #44951 ) ;
#27461 = LINE ( 'NONE', #50475, #37861 ) ;
#27462 = CARTESIAN_POINT ( 'NONE',  ( -7.188101187499999156, 92.75000000204839523, 2.977408999572654924 ) ) ;
#27465 = CARTESIAN_POINT ( 'NONE',  ( 5.000000000000000000, -60.90295814858255596, 23.31388853594792110 ) ) ;
#27464 = CARTESIAN_POINT ( 'NONE',  ( 8.311093377946834337, 247.0312500034139589, -8.311093377946836114 ) ) ;
#27463 = CARTESIAN_POINT ( 'NONE',  ( 24.54126587499999701, 206.1875000013656063, 169.9999999999999432 ) ) ;
#27466 = APPLICATION_PROTOCOL_DEFINITION ( 'draft international standard', 'automotive_design', 1998, #16814 ) ;
#27467 = EDGE_LOOP ( 'NONE', ( #66998, #71621, #6336, #37902 ) ) ;
#27468 = EDGE_CURVE ( 'NONE', #66396, #9485, #27210, .T. ) ;
#27469 = CARTESIAN_POINT ( 'NONE',  ( 2.085542519210945334E-15, 255.4687500034140157, 11.35316468749999963 ) ) ;
#27470 = CARTESIAN_POINT ( 'NONE',  ( -5.082755093536319713, 5.082755093536319713, 13.29905278187175277 ) ) ;
#27471 = EDGE_LOOP ( 'NONE', ( #58620, #60448, #53398, #70680, #59398, #70714, #11855, #25389, #29762, #48664, #33740, #6560, #73879, #56915, #10391, #46217, #33690, #60133, #6980, #28380, #29613, #12618, #33018, #34440, #16736, #11881, #60102, #13087, #20505, #48020, #17837, #26609, #44985, #53735, #23762, #73496, #33977, #40675, #6880, #57031, #47840, #47229, #52147, #46819, #6507, #25297, #30418, #43055, #34608, #1866, #49489, #26801, #36640, #23856, #34090, #17591, #45144, #42305, #14272, #38376, #74011, #32391, #9908, #2299, #54280, #6145, #66073, #24558, #56503, #52533, #24176 ) ) ;
#27472 = EDGE_CURVE ( 'NONE', #28745, #27032, #5114, .T. ) ;
#27473 = VERTEX_POINT ( 'NONE', #33645 ) ;
#27474 = CARTESIAN_POINT ( 'NONE',  ( -4.220049686691935698, 10.18810118749999916, 76.37500000204838102 ) ) ;
#27475 = CARTESIAN_POINT ( 'NONE',  ( -3.042071309553164404, 77.55208332991932707, -11.35316468749999963 ) ) ;
#27476 = CARTESIAN_POINT ( 'NONE',  ( -27.99999999999995381, 196.5000000000000000, 174.0000000000003695 ) ) ;
#27477 = CARTESIAN_POINT ( 'NONE',  ( -11.00000000000000000, 0.000000000000000000, 89.50000000000000000 ) ) ;
#27480 = CARTESIAN_POINT ( 'NONE',  ( 4.721056650416000089, 288.9843750017070079, 4.721056650415999201 ) ) ;
#27479 = CARTESIAN_POINT ( 'NONE',  ( 26.34314575050758833, 197.6875000027312126, 165.9999999999998863 ) ) ;
#27478 = CARTESIAN_POINT ( 'NONE',  ( 0.000000000000000000, 0.000000000000000000, -10.20000000000000462 ) ) ;
#27481 = CARTESIAN_POINT ( 'NONE',  ( -62.11529995450147368, 225.6269371553590304, 45.13481720891326887 ) ) ;
#27482 = CARTESIAN_POINT ( 'NONE',  ( 38.00000000000000000, -53.00000000000000711, -5.204170427930421283E-15 ) ) ;
#27483 = CIRCLE ( 'NONE', #8052, 6.000000000000000000 ) ;
#27484 = CARTESIAN_POINT ( 'NONE',  ( 1.432654583217662481, 197.3750000013656063, 194.5412658750000219 ) ) ;
#27485 = CARTESIAN_POINT ( 'NONE',  ( -5.656854249492381470, 6.749999995903220196, 5.656854249492379694 ) ) ;
#27486 = ORIENTED_EDGE ( 'NONE', *, *, #33369, .F. ) ;
#27487 = CARTESIAN_POINT ( 'NONE',  ( 31.45873412499998523, 208.8750000013656347, 171.4326545832175839 ) ) ;
#27488 = VECTOR ( 'NONE', #42057, 1000.000000000000000 ) ;
#27489 = CARTESIAN_POINT ( 'NONE',  ( 7.188101187500000044, 20.34374999795161543, 0.000000000000000000 ) ) ;
#27490 = CARTESIAN_POINT ( 'NONE',  ( 11.35316468749999785, 170.8854166632526983, 3.042071309553174174 ) ) ;
#27491 = DIRECTION ( 'NONE',  ( -0.000000000000000000, 1.000000000000000000, -0.000000000000000000 ) ) ;
#27492 = CARTESIAN_POINT ( 'NONE',  ( -7.188101187500000044, 102.0312500020483810, 0.000000000000000000 ) ) ;
#27494 = DIRECTION ( 'NONE',  ( -0.000000000000000000, 1.000000000000000000, -0.000000000000000000 ) ) ;
#27493 = CARTESIAN_POINT ( 'NONE',  ( 1.656854249492381248, 17.93749999726881583, -4.000000000000001776 ) ) ;
#27495 = CARTESIAN_POINT ( 'NONE',  ( 25.55430564589115505, 208.5625000013656063, 172.4456943541086957 ) ) ;
#27496 = CARTESIAN_POINT ( 'NONE',  ( -7.188101187499992051, 0.000000000000000000, 16.86155278187175810 ) ) ;
#27497 = CARTESIAN_POINT ( 'NONE',  ( -4.000000000000015987, 207.5625000027312126, 140.3431457505076594 ) ) ;
#27498 = CARTESIAN_POINT ( 'NONE',  ( 5.676582343750001591, 56.61458332991934839, -9.832129032723420536 ) ) ;
#27499 = EDGE_CURVE ( 'NONE', #60229, #49815, #12786, .T. ) ;
#27500 = CYLINDRICAL_SURFACE ( 'NONE', #58119, 9.999999999999998224 ) ;
#27501 = CARTESIAN_POINT ( 'NONE',  ( 7.320508075688774596, 27.49999999317203248, -7.320508075688774596 ) ) ;
#27502 = CARTESIAN_POINT ( 'NONE',  ( 31.99999999999997868, 199.1875000000000284, 171.6568542494923122 ) ) ;
#27503 = EDGE_LOOP ( 'NONE', ( #16421, #52903, #48927, #22639, #43043, #25318, #58936, #4415, #10484 ) ) ;
#27504 = FACE_OUTER_BOUND ( 'NONE', #23253, .T. ) ;
#27505 = CARTESIAN_POINT ( 'NONE',  ( -10.00000000000000000, 169.1666666598387394, -2.679491924311229845 ) ) ;
#27506 = CARTESIAN_POINT ( 'NONE',  ( -8.311093377946841443, 48.90624999658600558, 8.311093377946830785 ) ) ;
#27507 = AXIS2_PLACEMENT_3D ( 'NONE', #33879, #68927, #63259 ) ;
#27508 = CARTESIAN_POINT ( 'NONE',  ( 4.556349186104051263, -10.99999999999999822, 72.15625000409677625 ) ) ;
#27509 = CARTESIAN_POINT ( 'NONE',  ( -2.754378923186476579E-14, 201.4375000013656063, 145.4587341250000350 ) ) ;
#27510 = CARTESIAN_POINT ( 'NONE',  ( 1.877992804784251124, 10.12031740952137859, 70.21778636471140089 ) ) ;
#27511 = CARTESIAN_POINT ( 'NONE',  ( -7.320508075688771932, 244.3750000000000000, -7.320508075688771932 ) ) ;
#27513 = CARTESIAN_POINT ( 'NONE',  ( -8.311093377946836114, 52.65624999658601268, -8.311093377946837890 ) ) ;
#27512 = CARTESIAN_POINT ( 'NONE',  ( 7.188101187500000933, 99.50000000204838102, -2.977408999572651371 ) ) ;
#27514 = CARTESIAN_POINT ( 'NONE',  ( -3.313708498984757167, 7.999999999999991118, 2.049052779823364645 ) ) ;
#27515 = CARTESIAN_POINT ( 'NONE',  ( 7.320508075688769267, 204.3750000000000284, 7.320508075688773708 ) ) ;
#27516 = CARTESIAN_POINT ( 'NONE',  ( -9.832129032723420536, 178.6979166632526983, 5.676582343749997150 ) ) ;
#27517 = AXIS2_PLACEMENT_3D ( 'NONE', #26839, #26075, #31759 ) ;
#27518 = CARTESIAN_POINT ( 'NONE',  ( 4.999999999999993783, 141.0416666598387110, 8.660254037844390851 ) ) ;
#27519 = CARTESIAN_POINT ( 'NONE',  ( -2.977408999572650927, 100.2500000020483952, -7.188101187500001821 ) ) ;
#27520 = CARTESIAN_POINT ( 'NONE',  ( -0.9674272439343540864, -47.84645297308037470, 139.0145720722314877 ) ) ;
#27521 = CARTESIAN_POINT ( 'NONE',  ( -9.832129032723420536, 39.01041666325268409, 5.676582343749997150 ) ) ;
#27522 = CARTESIAN_POINT ( 'NONE',  ( -10.18810118749999916, 0.000000000000000000, 117.5312500020483810 ) ) ;
#27523 = ORIENTED_EDGE ( 'NONE', *, *, #58852, .T. ) ;
#27524 = CARTESIAN_POINT ( 'NONE',  ( -29.65685424949236548, 204.0624999999999716, 166.0000000000003695 ) ) ;
#27525 = CARTESIAN_POINT ( 'NONE',  ( -4.220049686691935698, 10.18810118749999916, 70.37500000204838102 ) ) ;
#27526 = DIRECTION ( 'NONE',  ( 0.000000000000000000, 0.000000000000000000, -1.000000000000000000 ) ) ;
#27527 = CARTESIAN_POINT ( 'NONE',  ( 30.99999999999999645, 49.38786852594409993, 65.00000000000000000 ) ) ;
#27529 = CARTESIAN_POINT ( 'NONE',  ( -8.311093377946836114, 162.6562499965860127, -8.311093377946837890 ) ) ;
#27528 = CARTESIAN_POINT ( 'NONE',  ( -5.000000000000000000, -11.14555136602165675, -27.84144949604441166 ) ) ;
#27530 = CARTESIAN_POINT ( 'NONE',  ( 1.469576158976822172E-15, -7.999999999999991118, 13.26155278432982421 ) ) ;
#27531 = CARTESIAN_POINT ( 'NONE',  ( 2.020667218593132706E-15, -11.00000000000000000, 79.56250000409677625 ) ) ;
#27532 = CARTESIAN_POINT ( 'NONE',  ( -2.679491924311222295, 259.1666666734946602, 10.00000000000000178 ) ) ;
#27533 = FACE_OUTER_BOUND ( 'NONE', #48961, .T. ) ;
#27534 = CARTESIAN_POINT ( 'NONE',  ( 7.204075437095968759, -7.204075437095966983, 79.09375000204838102 ) ) ;
#27535 = EDGE_LOOP ( 'NONE', ( #24529, #51542, #48707, #56524, #14594, #51216, #60615, #11918, #33097, #66246, #59483, #12073, #58825, #45180, #27327, #28470, #59441, #50835, #42455, #28627, #16982, #8484, #55706, #5459, #29048, #52637, #7582, #9626, #27934, #64494, #72413, #35375, #68948, #59943, #61743, #40746, #39086, #45081, #11232, #40907, #59820 ) ) ;
#27536 = ADVANCED_FACE ( 'NONE', ( #73613 ), #3847, .F. ) ;
#27537 = CARTESIAN_POINT ( 'NONE',  ( -1.656854249492280440, 203.8125000000000568, 194.0000000000000284 ) ) ;
#27538 = CARTESIAN_POINT ( 'NONE',  ( 6.951808397369818766E-16, 122.3437499965860269, -11.35316468750000141 ) ) ;
#27539 = ADVANCED_FACE ( 'NONE', ( #21180 ), #67592, .T. ) ;
#27540 = FACE_OUTER_BOUND ( 'NONE', #10572, .T. ) ;
#27541 = VERTEX_POINT ( 'NONE', #16624 ) ;
#27542 = ORIENTED_EDGE ( 'NONE', *, *, #59567, .T. ) ;
#27543 = CARTESIAN_POINT ( 'NONE',  ( -4.541265875000003227, 8.999999998634406140, 1.881053915767121110 ) ) ;
#27544 = CARTESIAN_POINT ( 'NONE',  ( -2.977408999572654480, 5.999999997951610098, 7.188101187499999156 ) ) ;
#27545 = CARTESIAN_POINT ( 'NONE',  ( -7.999999999999998224, 108.7812500040967763, 3.313708498984766493 ) ) ;
#27546 = CARTESIAN_POINT ( 'NONE',  ( -4.220049686691935698, 10.18810118749999916, 90.25000000204838102 ) ) ;
#27547 = CARTESIAN_POINT ( 'NONE',  ( -29.43265458321766559, 202.7500000013655779, 166.5412658750003629 ) ) ;
#27548 = VECTOR ( 'NONE', #12395, 1000.000000000000000 ) ;
#27549 = EDGE_CURVE ( 'NONE', #41579, #42385, #20492, .T. ) ;
#27550 = CARTESIAN_POINT ( 'NONE',  ( -4.000000000000001776, 8.437500000000000000, -1.656854249492381470 ) ) ;
#27551 = CARTESIAN_POINT ( 'NONE',  ( 4.000000000000001776, 21.74999999726881583, 0.000000000000000000 ) ) ;
#27552 = CARTESIAN_POINT ( 'NONE',  ( 3.211159895383561835, 7.437499998634407028, -3.211159895383561835 ) ) ;
#27553 = CARTESIAN_POINT ( 'NONE',  ( -2.828427124746209831, 198.3750000000000284, 139.1715728752538723 ) ) ;
#27554 = VECTOR ( 'NONE', #59207, 1000.000000000000000 ) ;
#27555 = ORIENTED_EDGE ( 'NONE', *, *, #22758, .T. ) ;
#27556 = SURFACE_STYLE_USAGE ( .BOTH. , #73955 ) ;
#27557 = CARTESIAN_POINT ( 'NONE',  ( 7.188101187500000044, 109.9062500020483810, -8.802885111219163269E-16 ) ) ;
#27559 = CARTESIAN_POINT ( 'NONE',  ( 27.99999999999999645, 210.0000000000000284, 169.9999999999999147 ) ) ;
#27558 = CARTESIAN_POINT ( 'NONE',  ( -31.45873412499999233, 198.6875000013655779, 170.0000000000004547 ) ) ;
#27560 = AXIS2_PLACEMENT_3D ( 'NONE', #67691, #9225, #61657 ) ;
#27561 = CARTESIAN_POINT ( 'NONE',  ( -11.00000000000000533, 11.00000000000000000, 41.99999999999999289 ) ) ;
#27562 = CARTESIAN_POINT ( 'NONE',  ( 7.188101187499993827, -2.977408999572645598, 2.142802781871750550 ) ) ;
#27563 = VERTEX_POINT ( 'NONE', #34394 ) ;
#27564 =( BOUNDED_CURVE ( )  B_SPLINE_CURVE ( 2, ( #25292, #49432, #48679, #26031, #55113, #8702, #31334, #49052, #47935 ),
 .UNSPECIFIED., .F., .F. ) 
 B_SPLINE_CURVE_WITH_KNOTS ( ( 3, 2, 2, 2, 3 ),
 ( 0.5624999999999981126, 0.5729166666666647423, 0.5833333333333314830, 0.5937499999999982236, 0.6041666666666648533 ),
 .UNSPECIFIED. ) 
 CURVE ( )  GEOMETRIC_REPRESENTATION_ITEM ( )  RATIONAL_B_SPLINE_CURVE ( ( 1.000000000000013767, 0.9238795325112729717, 1.000000000000000000, 0.9238795325112867385, 1.000000000000000000, 0.9238795325112867385, 1.000000000000000000, 0.9238795325112997281, 0.9999999999999870104 ) ) 
 REPRESENTATION_ITEM ( '' )  );
#27565 =( BOUNDED_CURVE ( )  B_SPLINE_CURVE ( 2, ( #44785, #21016, #68532, #73449, #9714, #55370, #33120, #56114, #50435 ),
 .UNSPECIFIED., .F., .F. ) 
 B_SPLINE_CURVE_WITH_KNOTS ( ( 3, 2, 2, 2, 3 ),
 ( 0.8000000000000007105, 0.8083333333333340143, 0.8166666666666673180, 0.8250000000000006217, 0.8333333333333340365 ),
 .UNSPECIFIED. ) 
 CURVE ( )  GEOMETRIC_REPRESENTATION_ITEM ( )  RATIONAL_B_SPLINE_CURVE ( ( 0.9999999999999938938, 0.9238795325112928447, 1.000000000000000000, 0.9238795325112867385, 1.000000000000000000, 0.9238795325112867385, 1.000000000000000000, 0.9238795325112806323, 1.000000000000005995 ) ) 
 REPRESENTATION_ITEM ( '' )  );
#27566 = ORIENTED_EDGE ( 'NONE', *, *, #73700, .F. ) ;
#27567 = CARTESIAN_POINT ( 'NONE',  ( 7.204075437095966983, 7.204075437095967871, 94.09375000204838102 ) ) ;
#27568 = CARTESIAN_POINT ( 'NONE',  ( 28.00000000000002132, 204.1250000027312126, 173.9999999999999147 ) ) ;
#27569 = CARTESIAN_POINT ( 'NONE',  ( -24.54126587499999346, 201.4375000013656063, 170.0000000000003411 ) ) ;
#27570 = CARTESIAN_POINT ( 'NONE',  ( 7.778174593052023411, -7.778174593052021635, 109.5625000000000000 ) ) ;
#27571 = CARTESIAN_POINT ( 'NONE',  ( -1.432654583217608080, 205.8750000013656063, 201.4587341250000350 ) ) ;
#27572 = DIRECTION ( 'NONE',  ( 1.000000000000000000, 0.000000000000000000, 0.000000000000000000 ) ) ;
#27573 = CARTESIAN_POINT ( 'NONE',  ( -7.320508075688778149, 123.1250000000000000, 7.320508075688769267 ) ) ;
#27574 = CARTESIAN_POINT ( 'NONE',  ( 8.000000000000001776, 104.6562500000000000, 3.313708498984759387 ) ) ;
#27575 = CARTESIAN_POINT ( 'NONE',  ( -4.088227598258586603E-16, 291.3593750017070079, -6.676582343750001591 ) ) ;
#27576 = CARTESIAN_POINT ( 'NONE',  ( 2.977408999572650927, -7.188101187499990274, 8.330302781871752771 ) ) ;
#27577 = CARTESIAN_POINT ( 'NONE',  ( 8.000000000000000000, 19.59375000000000711, -3.313708498984761164 ) ) ;
#27578 = CARTESIAN_POINT ( 'NONE',  ( 26.56734541678238415, 208.0000000013656347, 166.5412658749999650 ) ) ;
#27579 = CARTESIAN_POINT ( 'NONE',  ( 3.313708498984762496, 26.53124999590322375, 7.999999999999998224 ) ) ;
#27580 = CARTESIAN_POINT ( 'NONE',  ( -1.432654583217662481, 200.1250000013656063, 145.4587341250000634 ) ) ;
#27581 = CARTESIAN_POINT ( 'NONE',  ( 2.977408999572654480, 123.5000000020483810, 7.188101187499999156 ) ) ;
#27583 = CARTESIAN_POINT ( 'NONE',  ( 2.445694354108783219, 203.8125000013656063, 139.5543056458912190 ) ) ;
#27582 = DIRECTION ( 'NONE',  ( 0.000000000000000000, 6.938893903907228378E-16, -1.000000000000000000 ) ) ;
#27584 = CARTESIAN_POINT ( 'NONE',  ( -5.676582343750000703, 248.3854166700806445, -9.832129032723418760 ) ) ;
#27585 = CARTESIAN_POINT ( 'NONE',  ( -5.447323953993864265, -4.689931814214729044, 0.5319290643893268555 ) ) ;
#27586 = CARTESIAN_POINT ( 'NONE',  ( -4.999999999999998224, 213.5416666598387110, -8.660254037844389075 ) ) ;
#27587 = CARTESIAN_POINT ( 'NONE',  ( -11.35316468750000141, 13.48958332991935016, 3.042071309553159963 ) ) ;
#27588 = CARTESIAN_POINT ( 'NONE',  ( 8.000000000000001776, 122.6562500000000000, 3.313708498984759387 ) ) ;
#27589 = CARTESIAN_POINT ( 'NONE',  ( -3.042071309553173730, 204.6354166632526699, 11.35316468749999785 ) ) ;
#27590 = CARTESIAN_POINT ( 'NONE',  ( 38.00000000000000000, -53.00000000000000711, -5.204170427930421283E-15 ) ) ;
#27591 = CARTESIAN_POINT ( 'NONE',  ( -11.01847871666547185, 7.494884807424044837, -0.7446230086126799375 ) ) ;
#27593 = CARTESIAN_POINT ( 'NONE',  ( 0.000000000000000000, 300.0000000000000000, 0.000000000000000000 ) ) ;
#27592 = CARTESIAN_POINT ( 'NONE',  ( 4.000000000000015987, 208.5000000000000284, 198.0000000000000284 ) ) ;
#27594 = ORIENTED_EDGE ( 'NONE', *, *, #33607, .F. ) ;
#27595 = CARTESIAN_POINT ( 'NONE',  ( -1.432654583217662481, 200.3750000013656063, 145.4587341250000634 ) ) ;
#27596 = CARTESIAN_POINT ( 'NONE',  ( 8.311093377946834337, 5.156249996586015349, 8.311093377946839666 ) ) ;
#27597 = CARTESIAN_POINT ( 'NONE',  ( 2.020667218593132706E-15, -11.00000000000000000, 93.06250000409677625 ) ) ;
#27598 = CARTESIAN_POINT ( 'NONE',  ( 7.320508075688776373, 226.8750000000000000, 7.320508075688767491 ) ) ;
#27599 = CARTESIAN_POINT ( 'NONE',  ( -31.45873412499999233, 196.6875000013655779, 170.0000000000004547 ) ) ;
#27600 = DIRECTION ( 'NONE',  ( -0.000000000000000000, 1.000000000000000000, -0.000000000000000000 ) ) ;
#27602 = CARTESIAN_POINT ( 'NONE',  ( -9.832129032723418760, 12.86458332991935194, -5.676582343750004256 ) ) ;
#27601 = CARTESIAN_POINT ( 'NONE',  ( -4.401442555609581635E-16, 114.7812500020483952, -7.188101187500000044 ) ) ;
#27603 = CARTESIAN_POINT ( 'NONE',  ( 7.999999999999991118, 3.313708498984757611, 27.17405277982336997 ) ) ;
#27604 = CARTESIAN_POINT ( 'NONE',  ( 9.832129032723420536, 131.1979166632526983, -5.676582343749999815 ) ) ;
#27605 = EDGE_CURVE ( 'NONE', #25744, #27119, #43651, .T. ) ;
#27606 = AXIS2_PLACEMENT_3D ( 'NONE', #55800, #24049, #703 ) ;
#27607 = CARTESIAN_POINT ( 'NONE',  ( 7.320508075688774596, 102.4999999931720112, -7.320508075688774596 ) ) ;
#27608 = CARTESIAN_POINT ( 'NONE',  ( -7.188101187499999156, 121.6250000020483810, 2.977408999572654924 ) ) ;
#27609 = CARTESIAN_POINT ( 'NONE',  ( -10.00000000000000355, 4.583333326505365513, 2.679491924311223183 ) ) ;
#27610 = CARTESIAN_POINT ( 'NONE',  ( -30.44569435410883784, 207.8125000013656063, 167.5543056458915885 ) ) ;
#27611 = CARTESIAN_POINT ( 'NONE',  ( -35.99999999999995026, -2.949029909160572061E-14, -21.50000000000000000 ) ) ;
#27612 = EDGE_LOOP ( 'NONE', ( #25459, #61523, #32456, #73197 ) ) ;
#27613 = CARTESIAN_POINT ( 'NONE',  ( 11.35316468750000141, 1.093749996586016682, 0.000000000000000000 ) ) ;
#27614 = B_SPLINE_CURVE_WITH_KNOTS ( 'NONE', 3,
 ( #25937, #9355, #9733, #55389, #14993, #32755, #48954, #14621, #21035, #55016, #13865, #32374 ),
 .UNSPECIFIED., .F., .F.,
 ( 4, 2, 2, 2, 2, 4 ),
 ( 2.602085213965210642E-18, 0.002547658444427999564, 0.005095316888855995659, 0.006369146111069992622, 0.007642975333283990452, 0.01019063377771198264 ),
 .UNSPECIFIED. ) ;
#27615 = CARTESIAN_POINT ( 'NONE',  ( 6.676582343750001591, 288.1093750017069510, -8.176455196517173205E-16 ) ) ;
#27616 = DIRECTION ( 'NONE',  ( 0.000000000000000000, 0.000000000000000000, 1.000000000000000000 ) ) ;
#27617 = CARTESIAN_POINT ( 'NONE',  ( -5.656854249492375253, 5.656854249492375253, 2.330302783920143561 ) ) ;
#27618 = CARTESIAN_POINT ( 'NONE',  ( -8.000000000000000000, 18.75000000000000355, -9.797174393178825657E-16 ) ) ;
#27619 = AXIS2_PLACEMENT_3D ( 'NONE', #41096, #17703, #69766 ) ;
#27620 = CARTESIAN_POINT ( 'NONE',  ( 9.832129032723416984, 261.8229166700807014, -5.676582343750003368 ) ) ;
#27621 = CARTESIAN_POINT ( 'NONE',  ( -4.220049686691935698, 10.18810118749999916, 97.75000000204838102 ) ) ;
#27622 = VERTEX_POINT ( 'NONE', #17381 ) ;
#27623 = ADVANCED_FACE ( 'NONE', ( #28702 ), #51370, .F. ) ;
#27624 = CARTESIAN_POINT ( 'NONE',  ( 10.00000000000000000, 216.6666666598387110, 2.679491924311235618 ) ) ;
#27625 = CARTESIAN_POINT ( 'NONE',  ( -11.35316468750000141, 168.8020833299193271, 3.042071309553159963 ) ) ;
#27626 = CARTESIAN_POINT ( 'NONE',  ( 4.556349186104045934, 11.00000000000000000, 98.03124999999997158 ) ) ;
#27627 = CARTESIAN_POINT ( 'NONE',  ( -2.445694354108784108, 202.5625000013656063, 195.5543056458912190 ) ) ;
#27628 = CARTESIAN_POINT ( 'NONE',  ( 30.99999999999998579, 50.00000000000000711, 65.00000000000000000 ) ) ;
#27629 = CARTESIAN_POINT ( 'NONE',  ( 6.951808397369818766E-16, 77.34374999658601268, -11.35316468750000141 ) ) ;
#27630 = ORIENTED_EDGE ( 'NONE', *, *, #36615, .F. ) ;
#27631 = CARTESIAN_POINT ( 'NONE',  ( -4.220049686691937474, -10.18810118749999738, 111.4375000020483810 ) ) ;
#27632 = EDGE_CURVE ( 'NONE', #3802, #55604, #43601, .T. ) ;
#27633 = CARTESIAN_POINT ( 'NONE',  ( 3.211159895383561835, 11.56249999863440614, -3.211159895383561835 ) ) ;
#27634 = EDGE_LOOP ( 'NONE', ( #68752, #70524, #37461, #6479 ) ) ;
#27635 = CARTESIAN_POINT ( 'NONE',  ( -3.313708498984765161, 2.531250000000000888, 7.999999999999998224 ) ) ;
#27636 = CARTESIAN_POINT ( 'NONE',  ( 0.000000000000000000, -2.500000000000000000, 0.000000000000000000 ) ) ;
#27637 = CARTESIAN_POINT ( 'NONE',  ( -26.34314575050759544, 198.0625000027312126, 166.0000000000004263 ) ) ;
#27638 = CARTESIAN_POINT ( 'NONE',  ( -7.188101187500001821, 20.99999999795161898, -2.977408999572651371 ) ) ;
#27639 = CARTESIAN_POINT ( 'NONE',  ( -11.00000000000000000, 0.000000000000000000, 103.1875000040967763 ) ) ;
#27640 = CARTESIAN_POINT ( 'NONE',  ( 4.220049686691934809, 10.18810118749999916, 112.5625000020483810 ) ) ;
#27641 = PRODUCT_DEFINITION_SHAPE ( 'NONE', 'NONE',  #74668 ) ;
#27642 = CARTESIAN_POINT ( 'NONE',  ( -3.469446951953614189E-15, -13.85640646055106728, -14.00000000000000178 ) ) ;
#27643 = CARTESIAN_POINT ( 'NONE',  ( -1.656854249492383691, 9.437499997268815832, 4.000000000000000888 ) ) ;
#27644 = CARTESIAN_POINT ( 'NONE',  ( 7.999999999836578723, -5.113295603412193572E-05, 3.267801294049292871 ) ) ;
#27645 = EDGE_LOOP ( 'NONE', ( #25756, #48810, #64505, #43197 ) ) ;
#27646 = CARTESIAN_POINT ( 'NONE',  ( -1.432654583217607858, 201.6250000013656063, 201.4587341250000065 ) ) ;
#27647 = CARTESIAN_POINT ( 'NONE',  ( -25.17157287525385456, 195.0000000027312126, 167.1715728752541281 ) ) ;
#27648 = DIRECTION ( 'NONE',  ( -0.000000000000000000, -0.000000000000000000, -1.000000000000000000 ) ) ;
#27649 = CARTESIAN_POINT ( 'NONE',  ( -3.211159895383562723, 9.937499998634406140, 3.211159895383561391 ) ) ;
#27650 = AXIS2_PLACEMENT_3D ( 'NONE', #45042, #27679, #62376 ) ;
#27651 = CARTESIAN_POINT ( 'NONE',  ( 27.99999999999999645, 210.0000000000000284, 173.9999999999998863 ) ) ;
#27652 = CARTESIAN_POINT ( 'NONE',  ( 2.977408999572650927, -7.188101187499990274, 19.95530278187175810 ) ) ;
#27653 = ORIENTED_EDGE ( 'NONE', *, *, #67296, .F. ) ;
#27654 = CARTESIAN_POINT ( 'NONE',  ( 5.082755093536324154, 27.28124999795161543, 5.082755093536326818 ) ) ;
#27655 = ORIENTED_EDGE ( 'NONE', *, *, #11068, .T. ) ;
#27656 = CARTESIAN_POINT ( 'NONE',  ( 10.18810118749999916, 4.220049686691935698, 110.5000000020483810 ) ) ;
#27657 = CARTESIAN_POINT ( 'NONE',  ( -1.656854249492383468, 18.68750000000000000, 4.000000000000000888 ) ) ;
#27658 = CARTESIAN_POINT ( 'NONE',  ( -2.445694354108782775, 205.5625000013656063, 200.4456943541088663 ) ) ;
#27660 =( BOUNDED_CURVE ( )  B_SPLINE_CURVE ( 2, ( #4079, #25567, #71590, #19912, #31618, #27073, #2948, #50451, #56505 ),
 .UNSPECIFIED., .F., .F. ) 
 B_SPLINE_CURVE_WITH_KNOTS ( ( 3, 2, 2, 2, 3 ),
 ( 0.3666666666666669738, 0.3750000000000003331, 0.3833333333333336923, 0.3916666666666669960, 0.4000000000000003553 ),
 .UNSPECIFIED. ) 
 CURVE ( )  GEOMETRIC_REPRESENTATION_ITEM ( )  RATIONAL_B_SPLINE_CURVE ( ( 0.9999999999999970024, 0.9238795325112897361, 1.000000000000000000, 0.9238795325112867385, 1.000000000000000000, 0.9238795325112867385, 1.000000000000000000, 0.9238795325112837409, 1.000000000000003109 ) ) 
 REPRESENTATION_ITEM ( '' )  );
#27659 = CARTESIAN_POINT ( 'NONE',  ( 24.54126587499998280, 199.1250000013656347, 168.5673454167822740 ) ) ;
#27661 = CARTESIAN_POINT ( 'NONE',  ( -4.999999999999998224, 81.66666666666667140, -8.660254037844389075 ) ) ;
#27662 = EDGE_CURVE ( 'NONE', #62682, #39861, #64636, .T. ) ;
#27663 = AXIS2_PLACEMENT_3D ( 'NONE', #73089, #61020, #73458 ) ;
#27664 = CARTESIAN_POINT ( 'NONE',  ( -3.313708498984762052, 123.2187500000000000, -8.000000000000000000 ) ) ;
#27665 = CARTESIAN_POINT ( 'NONE',  ( -4.242640687119285658, 294.1249999999999432, 4.242640687119287435 ) ) ;
#27666 = CARTESIAN_POINT ( 'NONE',  ( 30.82842712474620939, 203.2500000027312126, 172.8284271247460424 ) ) ;
#27667 = VERTEX_POINT ( 'NONE', #20353 ) ;
#27668 = CARTESIAN_POINT ( 'NONE',  ( 0.000000000000000000, 300.0000000000000000, 10.00000000000000178 ) ) ;
#27669 = CARTESIAN_POINT ( 'NONE',  ( 4.336811714529327233, -16.30209246797837608, 69.46462972173030437 ) ) ;
#27670 = CARTESIAN_POINT ( 'NONE',  ( -4.000000000000015987, 194.5625000027311842, 140.3431457505076594 ) ) ;
#27671 = CARTESIAN_POINT ( 'NONE',  ( -5.000000000000000000, 68.60357193678683529, 20.85024232999420946 ) ) ;
#27672 = CARTESIAN_POINT ( 'NONE',  ( 3.313708498984762496, -7.999999999999989342, 22.29905277982336287 ) ) ;
#27673 = CARTESIAN_POINT ( 'NONE',  ( -6.123233995736766282E-16, 253.7500000000000284, -10.00000000000000000 ) ) ;
#27674 = CARTESIAN_POINT ( 'NONE',  ( -27.99999999999999645, 210.0000000000000284, 170.0000000000003695 ) ) ;
#27675 = CARTESIAN_POINT ( 'NONE',  ( 5.000000000000001776, 200.8333333333333428, -8.660254037844389075 ) ) ;
#27676 = DIRECTION ( 'NONE',  ( 0.000000000000000000, -1.000000000000000000, 0.000000000000000000 ) ) ;
#27677 = CARTESIAN_POINT ( 'NONE',  ( 1.320432766682872962E-15, -7.188101187499992051, 14.23655278187175455 ) ) ;
#27678 = CARTESIAN_POINT ( 'NONE',  ( 11.35316468750000141, 166.0937499965860127, 0.000000000000000000 ) ) ;
#27679 = DIRECTION ( 'NONE',  ( -0.000000000000000000, 1.000000000000000000, 0.000000000000000000 ) ) ;
#27680 = CARTESIAN_POINT ( 'NONE',  ( -32.22967180057197822, 42.54924275222214902, 64.99999999999998579 ) ) ;
#27681 = CARTESIAN_POINT ( 'NONE',  ( -10.99999999999978684, -4.556349186104264426, 82.28125000409677625 ) ) ;
#27683 = CARTESIAN_POINT ( 'NONE',  ( 11.27292232226671054, 225.9999999999999432, 1.347431162485829281 ) ) ;
#27682 =( NAMED_UNIT ( * ) PLANE_ANGLE_UNIT ( ) SI_UNIT ( $, .RADIAN. ) );
#27684 = VERTEX_POINT ( 'NONE', #12573 ) ;
#27685 = CARTESIAN_POINT ( 'NONE',  ( -3.042071309553164404, 27.55208332991935194, -11.35316468749999963 ) ) ;
#27686 = CARTESIAN_POINT ( 'NONE',  ( -0.4320110153365275818, 10.28109898471437766, -63.57214792341211762 ) ) ;
#27687 = CARTESIAN_POINT ( 'NONE',  ( -16.43645510912099184, -45.73726923468687033, 196.2927731230203960 ) ) ;
#27688 = CARTESIAN_POINT ( 'NONE',  ( 2.445694354108783664, 204.3125000013656063, 144.4456943541088663 ) ) ;
#27689 =( BOUNDED_CURVE ( )  B_SPLINE_CURVE ( 2, ( #254, #22858, #40593, #7005, #34953, #57968, #40968, #34582, #52288, #12649, #57587, #62846, #35323 ),
 .UNSPECIFIED., .F., .F. ) 
 B_SPLINE_CURVE_WITH_KNOTS ( ( 3, 2, 2, 2, 2, 2, 3 ),
 ( 2.433485766383421289, 2.438719635847170775, 2.443953505310920260, 2.449187374774670189, 2.454421244238419675, 2.459655113702169160, 2.464888983165918646 ),
 .UNSPECIFIED. ) 
 CURVE ( )  GEOMETRIC_REPRESENTATION_ITEM ( )  RATIONAL_B_SPLINE_CURVE ( ( 1.000000000000001998, 0.9659258262890662028, 1.000000000000000000, 0.9659258262890683122, 1.000000000000000000, 0.9659258262890683122, 1.000000000000000000, 0.9659258262890683122, 1.000000000000000000, 0.9659258262890683122, 1.000000000000000000, 0.9659258262891685654, 0.9999999999998997469 ) ) 
 REPRESENTATION_ITEM ( '' )  );
#27690 = CARTESIAN_POINT ( 'NONE',  ( -8.660254037844390851, 59.79166665983870388, 4.999999999999998224 ) ) ;
#27691 = CARTESIAN_POINT ( 'NONE',  ( 7.188101187500002709, 102.3125000020483810, 2.977408999572649151 ) ) ;
#27692 = CARTESIAN_POINT ( 'NONE',  ( 2.780723358947928197E-16, 8.687499998634407916, -4.541265875000002339 ) ) ;
#27693 = CARTESIAN_POINT ( 'NONE',  ( 27.99999999999999645, 210.0000000000000284, 169.9999999999999147 ) ) ;
#27694 = CARTESIAN_POINT ( 'NONE',  ( 3.313708498984762496, -7.999999999999989342, 5.799052779823364645 ) ) ;
#27695 = CARTESIAN_POINT ( 'NONE',  ( 10.00000000000000000, 165.2083333333333712, -2.679491924311226736 ) ) ;
#27696 = ORIENTED_EDGE ( 'NONE', *, *, #11971, .F. ) ;
#27697 = ORIENTED_EDGE ( 'NONE', *, *, #13700, .F. ) ;
#27698 = CARTESIAN_POINT ( 'NONE',  ( -10.00000000000011013, 197.5000000000000568, -1.224646799147366470E-15 ) ) ;
#27699 = CARTESIAN_POINT ( 'NONE',  ( -3.458734124999959469, 194.7500000013656063, 199.4326545832176976 ) ) ;
#27700 = CARTESIAN_POINT ( 'NONE',  ( 1.502314598737163567E-15, -20.78460969082658494, -20.69999999999999929 ) ) ;
#27701 = CARTESIAN_POINT ( 'NONE',  ( -5.676582343749992710, 220.0520833367473301, 9.832129032723422313 ) ) ;
#27702 = CARTESIAN_POINT ( 'NONE',  ( 9.832129032723420536, 141.1979166632526699, -5.676582343749999815 ) ) ;
#27703 = ORIENTED_EDGE ( 'NONE', *, *, #28909, .F. ) ;
#27704 = CARTESIAN_POINT ( 'NONE',  ( 3.313708498984762496, -7.999999999999989342, 10.48655278392014800 ) ) ;
#27705 = ADVANCED_FACE ( 'NONE', ( #41981 ), #45716, .F. ) ;
#27706 = CARTESIAN_POINT ( 'NONE',  ( 4.220049686691934809, 10.18810118749999916, 91.18750000204836681 ) ) ;
#27707 = LINE ( 'NONE', #57892, #6790 ) ;
#27708 = CARTESIAN_POINT ( 'NONE',  ( -1.656854249492348607, 208.1875000000000853, 202.0000000000000284 ) ) ;
#27709 = CARTESIAN_POINT ( 'NONE',  ( -3.999999999999960032, 204.9375000000000284, 196.3431457505076594 ) ) ;
#27710 = CARTESIAN_POINT ( 'NONE',  ( -31.99999999999995737, 197.4375000027312126, 171.6568542494928522 ) ) ;
#27711 = DIRECTION ( 'NONE',  ( -1.000000000000000000, -0.000000000000000000, -0.000000000000000000 ) ) ;
#27712 = EDGE_LOOP ( 'NONE', ( #35560, #74414, #74635, #36185 ) ) ;
#27713 = VECTOR ( 'NONE', #50662, 1000.000000000000000 ) ;
#27714 = DIRECTION ( 'NONE',  ( -0.000000000000000000, -0.000000000000000000, -1.000000000000000000 ) ) ;
#27715 = DIRECTION ( 'NONE',  ( 0.000000000000000000, 0.000000000000000000, 1.000000000000000000 ) ) ;
#27716 = CARTESIAN_POINT ( 'NONE',  ( -11.35316468750000141, 118.5937499965860269, -1.390361679473963753E-15 ) ) ;
#27717 = CARTESIAN_POINT ( 'NONE',  ( 2.445694354108838731, 204.0625000013656063, 195.5543056458912190 ) ) ;
#27718 = CARTESIAN_POINT ( 'NONE',  ( 7.188101187500000044, 21.84374999795161543, 0.000000000000000000 ) ) ;
#27719 = CARTESIAN_POINT ( 'NONE',  ( 7.204075437095968759, -7.204075437095966983, 85.09375000204836681 ) ) ;
#27720 = CARTESIAN_POINT ( 'NONE',  ( 9.832129032723416984, 40.67708332991935549, 5.676582343750006032 ) ) ;
#27721 = VERTEX_POINT ( 'NONE', #40884 ) ;
#27722 = DIRECTION ( 'NONE',  ( -0.000000000000000000, -1.000000000000000000, -0.000000000000000000 ) ) ;
#27723 = CARTESIAN_POINT ( 'NONE',  ( -5.662595241051933570, -5.662595241051936235, 20.70061528394062833 ) ) ;
#27724 = CARTESIAN_POINT ( 'NONE',  ( 9.999999999999998224, 237.7083333333333144, -2.679491924311229401 ) ) ;
#27725 = VECTOR ( 'NONE', #32654, 999.9999999999998863 ) ;
#27726 = CARTESIAN_POINT ( 'NONE',  ( 3.999999999999960032, 200.9375000000000284, 143.6568542494924259 ) ) ;
#27727 = CARTESIAN_POINT ( 'NONE',  ( 7.188101187500000044, 10.96874999795161187, 0.000000000000000000 ) ) ;
#27728 = CARTESIAN_POINT ( 'NONE',  ( -2.485281374238572649, 297.2500000034140157, 6.000000000000002665 ) ) ;
#27729 = EDGE_CURVE ( 'NONE', #1549, #49847, #32068, .T. ) ;
#27730 = CARTESIAN_POINT ( 'NONE',  ( 4.999999999999993783, 111.0416666598387110, 8.660254037844390851 ) ) ;
#27731 = CYLINDRICAL_SURFACE ( 'NONE', #20504, 3.999999999999988010 ) ;
#27732 = CARTESIAN_POINT ( 'NONE',  ( 8.311093377946837890, 156.7187499965860127, -8.311093377946837890 ) ) ;
#27733 = CARTESIAN_POINT ( 'NONE',  ( -10.18810118749999916, 0.000000000000000000, 79.65625000204836681 ) ) ;
#27734 = CARTESIAN_POINT ( 'NONE',  ( -24.54126587499998635, 208.3750000013656063, 171.4326545832179818 ) ) ;
#27735 = CARTESIAN_POINT ( 'NONE',  ( 1.656854249492381914, 2.812500000000000000, 4.000000000000000888 ) ) ;
#27736 = CARTESIAN_POINT ( 'NONE',  ( 4.541265875000002339, 15.49999999863440792, -1.881053915767121554 ) ) ;
#27737 = ORIENTED_EDGE ( 'NONE', *, *, #7928, .T. ) ;
#27738 = CARTESIAN_POINT ( 'NONE',  ( -3.999999999999960032, 198.0625000027312410, 196.3431457505076594 ) ) ;
#27739 = AXIS2_PLACEMENT_3D ( 'NONE', #11934, #57981, #6286 ) ;
#27740 = CARTESIAN_POINT ( 'NONE',  ( 1.432654583217608080, 195.8750000013655779, 138.5412658750000503 ) ) ;
#27741 = CARTESIAN_POINT ( 'NONE',  ( -28.00000000000007816, 205.1250000027312126, 166.0000000000003695 ) ) ;
#27742 = CARTESIAN_POINT ( 'NONE',  ( 7.999999999999991118, 9.797174393178815797E-16, 13.58030277982336465 ) ) ;
#27743 = VERTEX_POINT ( 'NONE', #12201 ) ;
#27744 = CARTESIAN_POINT ( 'NONE',  ( -5.082755093536326818, 8.906249997951610098, 5.082755093536325042 ) ) ;
#27745 = DIRECTION ( 'NONE',  ( 0.000000000000000000, 0.000000000000000000, -1.000000000000000000 ) ) ;
#27746 = DIRECTION ( 'NONE',  ( -0.000000000000000000, -0.000000000000000000, -1.000000000000000000 ) ) ;
#27747 = CARTESIAN_POINT ( 'NONE',  ( 10.00000000000000178, 35.00000000000000000, 0.000000000000000000 ) ) ;
#27748 = CARTESIAN_POINT ( 'NONE',  ( -7.188101187500000044, 108.0312500020483810, 0.000000000000000000 ) ) ;
#27749 = DIRECTION ( 'NONE',  ( 0.000000000000000000, 0.000000000000000000, -1.000000000000000000 ) ) ;
#27750 = CARTESIAN_POINT ( 'NONE',  ( -6.676582343750002480, 288.3906250017070079, -2.765530957081996810 ) ) ;
#27752 = CARTESIAN_POINT ( 'NONE',  ( 0.000000000000000000, 0.000000000000000000, 0.000000000000000000 ) ) ;
#27751 = CARTESIAN_POINT ( 'NONE',  ( 7.320508075688772820, 35.62500000000000711, -7.320508075688772820 ) ) ;
#27753 = ORIENTED_EDGE ( 'NONE', *, *, #60386, .F. ) ;
#27755 = CARTESIAN_POINT ( 'NONE',  ( -11.35316468749999608, 254.1145833367473585, 3.042071309553173730 ) ) ;
#27754 = AXIS2_PLACEMENT_3D ( 'NONE', #52805, #42205, #65595 ) ;
#27756 = CARTESIAN_POINT ( 'NONE',  ( -7.188101187499991163, 2.977408999572646930, 24.26780278187175455 ) ) ;
#27757 = CARTESIAN_POINT ( 'NONE',  ( -0.8997857291014387249, 51.17549659652912908, 48.53090770943328636 ) ) ;
#27758 = CARTESIAN_POINT ( 'NONE',  ( -18.89444362769112473, -70.00000000000001421, 167.9999999999997442 ) ) ;
#27759 = CARTESIAN_POINT ( 'NONE',  ( 3.496982156820216403, -68.06496700477795514, -20.41687962716770599 ) ) ;
#27760 = CARTESIAN_POINT ( 'NONE',  ( -4.081160451454018734, 22.00000000000000000, 2.014106693209854804 ) ) ;
#27761 = CARTESIAN_POINT ( 'NONE',  ( -10.00000000000000355, 152.7083333333333428, 2.679491924311223183 ) ) ;
#27762 = DIRECTION ( 'NONE',  ( -0.000000000000000000, -0.000000000000000000, -1.000000000000000000 ) ) ;
#27763 = CARTESIAN_POINT ( 'NONE',  ( 16.53139458858881738, 11.24020457502483872, -1.118160017449573385 ) ) ;
#27764 = FACE_OUTER_BOUND ( 'NONE', #28862, .T. ) ;
#27765 = CARTESIAN_POINT ( 'NONE',  ( -8.311093377946836114, 127.9687499965860269, -8.311093377946837890 ) ) ;
#27766 = CARTESIAN_POINT ( 'NONE',  ( 2.679491924311228956, 212.9166666598386826, -10.00000000000000000 ) ) ;
#27767 = CARTESIAN_POINT ( 'NONE',  ( -4.556349186104047710, -10.99999999999999822, 71.78125000000000000 ) ) ;
#27768 = AXIS2_PLACEMENT_3D ( 'NONE', #3012, #72028, #47906 ) ;
#27771 = CARTESIAN_POINT ( 'NONE',  ( -38.00000000000000000, 52.99999999999992895, -6.791607979884335933E-15 ) ) ;
#27770 = CARTESIAN_POINT ( 'NONE',  ( 28.00000000000001421, 196.4375000013655779, 173.4587341249998929 ) ) ;
#27769 = CARTESIAN_POINT ( 'NONE',  ( 24.54126587499998990, 195.4375000013655779, 169.9999999999998863 ) ) ;
#27772 = ORIENTED_EDGE ( 'NONE', *, *, #68963, .F. ) ;
#27773 = EDGE_CURVE ( 'NONE', #57934, #55774, #9510, .T. ) ;
#27774 = AXIS2_PLACEMENT_3D ( 'NONE', #67410, #21000, #8947 ) ;
#27775 = CARTESIAN_POINT ( 'NONE',  ( 5.563815795553805899, 224.2175593924927739, 8.329924368427569448 ) ) ;
#27776 = CARTESIAN_POINT ( 'NONE',  ( -38.00000000000002132, 50.00000000000000711, 69.99999999999998579 ) ) ;
#27777 = CARTESIAN_POINT ( 'NONE',  ( 24.54126587499997925, 197.5000000013656063, 171.4326545832175555 ) ) ;
#27778 = CARTESIAN_POINT ( 'NONE',  ( 8.311093377946837890, 201.7187499965860411, -8.311093377946837890 ) ) ;
#27779 = CARTESIAN_POINT ( 'NONE',  ( 7.188101187500002709, 118.8125000020483810, 2.977408999572649151 ) ) ;
#27780 = CARTESIAN_POINT ( 'NONE',  ( -4.541265875000002339, 17.74999999863440792, -1.881053915767121998 ) ) ;
#27781 = CARTESIAN_POINT ( 'NONE',  ( 2.216418498311605312, -51.36626494304428547, 48.60390812669808724 ) ) ;
#27782 = CARTESIAN_POINT ( 'NONE',  ( -3.313708498984757167, 7.999999999999991118, 18.54905277982336287 ) ) ;
#27784 = CARTESIAN_POINT ( 'NONE',  ( 2.449293598294707893E-16, 20.25000000000000000, -4.000000000000001776 ) ) ;
#27783 = DIRECTION ( 'NONE',  ( 1.000000000000000000, 0.000000000000000000, 0.000000000000000000 ) ) ;
#27785 = CARTESIAN_POINT ( 'NONE',  ( 5.676582343749993598, 99.94791666325268409, 9.832129032723422313 ) ) ;
#27786 = ORIENTED_EDGE ( 'NONE', *, *, #44122, .F. ) ;
#27787 =( BOUNDED_SURFACE ( )  B_SPLINE_SURFACE ( 1, 2, ( 
 ( #17578, #4786, #51535, #17202, #16076, #57212, #45137, #5161, #21742, #74175, #11551, #39482, #40221, #27405, #34210, #50420, #33468, #33103, #62114, #39110, #23240, #5901, #57591, #63224, #16446, #5526, #16820, #62478, #28527, #51919, #22479, #22113, #10808, #62849, #28155, #74552, #45500, #68518, #45878, #40596, #73805, #22864, #10438, #34585, #28901, #257, #39848, #10068, #4409, #67784, #68149, #56100, #44770, #11185, #33842, #73434, #56470, #27779, #46248, #69267, #50792, #56840, #51166, #68892, #25074, #629, #70384, #1729, #47721, #69640, #41706, #30387, #17954, #64720, #53406, #57971, #70742, #63597, #13016, #18325, #1364, #29283, #24709, #47358, #6277, #19060, #42062, #52293, #58699, #65070, #997, #40972, #11924, #18699, #34956, #23610, #63979, #12292, #36054, #30752, #13383, #36421, #53773, #52661, #29646, #46620, #59435, #23978, #19420, #59071, #7747, #35327, #7380, #58339, #2082, #30019, #6643, #48091, #53033, #71100, #46986, #70019, #41340, #64350, #12653, #35684, #7010, #24349, #72607, #66943, #8860, #36789, #37157, #65816, #9230, #60159, #8478, #49210, #13746, #71467, #54519, #65449, #72979, #59799, #3575, #49591, #19793, #20158, #37910, #37534, #72219, #14495, #66562, #43548, #25447, #15247, #26946, #20913, #43175, #9613, #61286, #3957, #54145, #20534, #55270, #26567, #48462, #14871, #32252, #42800, #60907, #43934, #8112, #38281, #42433, #32633, #71841, #54891, #31117, #55642, #26190, #2454, #49965, #14123, #31498, #60534, #2825, #25816, #48835, #66191, #31870, #3202, #38660, #21656, #44681, #45411, #63141, #74460, #5439, #11469, #10352, #62028, #67323, #34124, #33376, #51827, #74092, #62758, #67697, #16730, #73352, #34503, #62391, #15994, #57124, #10718, #28809, #68801, #15620, #51078, #33012, #73718, #50330, #57508, #68065, #51447, #45791, #33750, #61662, #39024, #56377, #11101, #4698, #27691, #28067, #9981, #50700, #22028, #44308, #21285, #56013, #28441, #22768, #45054, #16354, #39756, #39392, #22391, #56753, #68427, #17113, #40135, #5073, #5814, #4325, #27314, #12198, #29561, #52947, #18238, #47270, #64262, #35599, #35967, #30668, #63887, #64634, #52206, #30300, #53319, #18974, #58614, #173, #69179, #57878, #58254, #23149, #11837, #1280, #6555, #46162, #34872, #35236, #59351, #24624, #1643, #12931, #52572, #46535, #40509, #12570, #6920, #539, #29931, #7662, #47635, #17490, #58987, #23895, #24257, #909, #46904, #6185, #13298, #69928, #36336, #7292, #41253, #29194, #70657, #17864, #41978, #63513, #70296, #69553, #18611, #23521, #40881, #41622, #64989, #59716, #26102, #14033, #48748, #65365, #43087, #55184, #8392, #9146, #71019, #3117, #19336, #2366, #1999, #31032, #8024, #66860, #49503, #26478, #60823, #60073, #49122, #31406, #54057, #20447, #24989, #61201, #9532, #43464, #54433, #60444, #31786, #72522, #19705, #8774, #20071, #53688, #48006, #25361, #15168, #42718, #66104, #2741, #72134, #42348, #25727, #66478, #54806, #14414, #48378, #38198, #65731, #37070, #13664, #71381 ),
 ( #36704, #14786, #71757, #37446, #37826, #32163, #20830, #3490, #43847, #10270, #74375, #51364, #68717, #44230, #39316, #45334, #16646, #38578, #10639, #74007, #61578, #33668, #22309, #26866, #68351, #56295, #16273, #21574, #4611, #67241, #45704, #27608, #17028, #39679, #33297, #15537, #57043, #50248, #62678, #40054, #56673, #27232, #21944, #63057, #73270, #11015, #34048, #9897, #4989, #67613, #50618, #32927, #44973, #5355, #61942, #28357, #49880, #27990, #72895, #55933, #55557, #4244, #44600, #32547, #22686, #3870, #21203, #38941, #50995, #73637, #15910, #67978, #62313, #18891, #41897, #1191, #63798, #18154, #64180, #30212, #52125, #41169, #52488, #11381, #57419, #57793, #24542, #457, #826, #12116, #35514, #34416, #35154, #52859, #12484, #23814, #6101, #47550, #23436, #46451, #5725, #11752, #28724, #69469, #17402, #70574, #51740, #29106, #53232, #40425, #24173, #58527, #89, #6834, #58170, #34789, #1563, #18524, #35882, #29848, #23067, #17779, #46076, #69095, #47183, #63424, #40792, #70215, #46816, #41532, #64548, #6475, #29479, #69842, #12844, #58899, #7210, #25273, #49409, #14698, #20357, #54719, #48291, #36616, #30580, #2654, #25644, #42261, #19988, #72430, #43374, #36250, #13579, #71298, #20739, #37737, #66390, #3026, #19618, #59625, #53602, #48659, #71668, #65273, #42996, #64906, #60736, #59265, #26009, #13942, #66016, #53967, #36984, #1914, #3400, #59989, #26384, #49033, #42633, #47918, #9058, #7940, #72040, #13212, #14323, #30945, #54343, #7577, #2278, #31697, #32072, #70937, #37356, #65646, #8306, #24901, #60355, #55094, #31316, #19250, #8682, #67889, #61108, #67152, #66770, #21117, #72809, #56956, #39595, #16558, #50906, #50164, #16181, #21489, #49794, #10550, #15074, #51279, #74288, #33582, #44510, #50530, #21853, #62591, #9810, #73546, #10179, #43756, #38108, #15447, #5271, #32833, #33213, #67521, #39223, #9438, #15819, #56586, #44885, #56210, #38483, #28272, #55842, #4159, #32455, #44140, #55465, #27147, #61486, #3774, #26777, #73181, #10922, #38855, #4899, #62223, #61859, #27895, #4524, #27519, #33957, #73919, #68262, #22223, #45250, #17314, #7122, #62972, #23724, #51655, #41452, #46728, #63710, #740, #29397, #68633, #35796, #23351, #16942, #57705, #5640, #47093, #40334, #35435, #58811, #69753, #63337, #12034, #30130, #11662, #64092, #29756, #28640, #18066, #6012, #17689, #34328, #35068, #24085, #52032, #52771, #39966, #41082, #11296, #45992, #45619, #4460, #22986, #53145, #18439, #70132, #1109, #29015, #12401, #370, #69008, #58444, #57329, #22598, #34697, #6753, #46363, #52405, #64465, #12764, #69379, #40706, #58080, #6391, #47469, #47834, #14613, #65183, #42549, #2194, #25558, #1478, #25190, #42911, #31234, #13856, #70856, #37651, #13494, #36533, #31985, #1833, #18810, #59543, #7492, #60650, #8972, #19168, #43292, #30496, #14236, #48572, #41814, #71582, #48204, #24821, #66307, #8595, #25928, #8223, #54631, #53883, #24461, #20269, #70492, #13127, #54259, #37275, #60269, #53516 ) ),
 .UNSPECIFIED., .F., .F., .F. ) 
 B_SPLINE_SURFACE_WITH_KNOTS ( ( 2, 2 ),
 ( 3, 2, 2, 2, 2, 2, 2, 2, 2, 2, 2, 2, 2, 2, 2, 2, 2, 2, 2, 2, 2, 2, 2, 2, 2, 2, 2, 2, 2, 2, 2, 2, 2, 2, 2, 2, 2, 2, 2, 2, 2, 2, 2, 2, 2, 2, 2, 2, 2, 2, 2, 2, 2, 2, 2, 2, 2, 2, 2, 2, 2, 2, 2, 2, 2, 2, 2, 2, 2, 2, 2, 2, 2, 2, 2, 2, 2, 2, 2, 2, 2, 2, 2, 2, 2, 2, 2, 2, 2, 2, 2, 2, 2, 2, 2, 2, 2, 2, 2, 2, 2, 2, 2, 2, 2, 2, 2, 2, 2, 2, 2, 2, 2, 2, 2, 2, 2, 2, 2, 2, 2, 2, 2, 2, 2, 2, 2, 2, 2, 2, 2, 2, 2, 2, 2, 2, 2, 2, 2, 2, 2, 2, 2, 2, 2, 2, 2, 2, 2, 2, 2, 2, 2, 2, 2, 2, 2, 2, 2, 2, 2, 2, 2, 2, 2, 2, 2, 2, 2, 2, 2, 2, 2, 2, 2, 2, 2, 2, 2, 2, 2, 2, 2, 2, 2, 2, 2, 3 ),
 ( 0.000000000000000000, 1.000000000000000000 ),
 ( 0.000000000000000000, 0.005208333333333333044, 0.01041666666666666609, 0.01562500000000000000, 0.02083333333333333218, 0.02604166666666666782, 0.03125000000000000000, 0.03645833333333333565, 0.04166666666666666435, 0.04687500000000000000, 0.05208333333333333565, 0.05729166666666666435, 0.06250000000000000000, 0.06770833333333332871, 0.07291666666666667129, 0.07812500000000000000, 0.08333333333333332871, 0.08854166666666667129, 0.09375000000000000000, 0.09895833333333332871, 0.1041666666666666713, 0.1093750000000000000, 0.1145833333333333287, 0.1197916666666666713, 0.1250000000000000000, 0.1302083333333333426, 0.1354166666666666574, 0.1406250000000000000, 0.1458333333333333426, 0.1510416666666666574, 0.1562500000000000000, 0.1614583333333333426, 0.1666666666666666574, 0.1718750000000000000, 0.1770833333333333426, 0.1822916666666666574, 0.1875000000000000000, 0.1927083333333333426, 0.1979166666666666574, 0.2031250000000000000, 0.2083333333333333426, 0.2135416666666666574, 0.2187500000000000000, 0.2239583333333333426, 0.2291666666666666574, 0.2343750000000000000, 0.2395833333333333426, 0.2447916666666666574, 0.2500000000000000000, 0.2552083333333333148, 0.2604166666666666852, 0.2656250000000000000, 0.2708333333333333148, 0.2760416666666666852, 0.2812500000000000000, 0.2864583333333333148, 0.2916666666666666852, 0.2968750000000000000, 0.3020833333333333148, 0.3072916666666666852, 0.3125000000000000000, 0.3177083333333333148, 0.3229166666666666852, 0.3281250000000000000, 0.3333333333333333148, 0.3385416666666666852, 0.3437500000000000000, 0.3489583333333333148, 0.3541666666666666852, 0.3593750000000000000, 0.3645833333333333148, 0.3697916666666666852, 0.3750000000000000000, 0.3802083333333333148, 0.3854166666666666852, 0.3906250000000000000, 0.3958333333333333148, 0.4010416666666666852, 0.4062500000000000000, 0.4114583333333333148, 0.4166666666666666852, 0.4218750000000000000, 0.4270833333333333148, 0.4322916666666666852, 0.4375000000000000000, 0.4427083333333333148, 0.4479166666666666852, 0.4531250000000000000, 0.4583333333333333148, 0.4635416666666666852, 0.4687500000000000000, 0.4739583333333333148, 0.4791666666666666852, 0.4843750000000000000, 0.4895833333333333148, 0.4947916666666666852, 0.5000000000000000000, 0.5052083333333333703, 0.5104166666666666297, 0.5156250000000000000, 0.5208333333333333703, 0.5260416666666666297, 0.5312500000000000000, 0.5364583333333333703, 0.5416666666666666297, 0.5468750000000000000, 0.5520833333333333703, 0.5572916666666666297, 0.5625000000000000000, 0.5677083333333333703, 0.5729166666666666297, 0.5781250000000000000, 0.5833333333333333703, 0.5885416666666666297, 0.5937500000000000000, 0.5989583333333333703, 0.6041666666666666297, 0.6093750000000000000, 0.6145833333333333703, 0.6197916666666666297, 0.6250000000000000000, 0.6302083333333333703, 0.6354166666666666297, 0.6406250000000000000, 0.6458333333333333703, 0.6510416666666666297, 0.6562500000000000000, 0.6614583333333333703, 0.6666666666666666297, 0.6718750000000000000, 0.6770833333333333703, 0.6822916666666666297, 0.6875000000000000000, 0.6927083333333333703, 0.6979166666666666297, 0.7031250000000000000, 0.7083333333333333703, 0.7135416666666666297, 0.7187500000000000000, 0.7239583333333333703, 0.7291666666666666297, 0.7343750000000000000, 0.7395833333333333703, 0.7447916666666666297, 0.7500000000000000000, 0.7552083333333333703, 0.7604166666666666297, 0.7656250000000000000, 0.7708333333333333703, 0.7760416666666666297, 0.7812500000000000000, 0.7864583333333333703, 0.7916666666666666297, 0.7968750000000000000, 0.8020833333333333703, 0.8072916666666666297, 0.8125000000000000000, 0.8177083333333333703, 0.8229166666666666297, 0.8281250000000000000, 0.8333333333333333703, 0.8385416666666666297, 0.8437500000000000000, 0.8489583333333333703, 0.8541666666666666297, 0.8593750000000000000, 0.8645833333333333703, 0.8697916666666666297, 0.8750000000000000000, 0.8802083333333333703, 0.8854166666666666297, 0.8906250000000000000, 0.8958333333333333703, 0.9010416666666666297, 0.9062500000000000000, 0.9114583333333333703, 0.9166666666666666297, 0.9218750000000000000, 0.9270833333333333703, 0.9322916666666666297, 0.9375000000000000000, 0.9427083333333333703, 0.9479166666666666297, 0.9531250000000000000, 0.9583333333333333703, 0.9635416666666666297, 0.9687500000000000000, 0.9722122636433919718 ),
 .UNSPECIFIED. ) 
 GEOMETRIC_REPRESENTATION_ITEM ( )  RATIONAL_B_SPLINE_SURFACE ( (
 ( 1.000000000000000000, 0.9238795325112867385, 1.000000000000000000, 0.9238795325112867385, 1.000000000000000000, 0.9238795325112867385, 1.000000000000000000, 0.9238795325112867385, 1.000000000000000000, 0.9238795325112867385, 1.000000000000000000, 0.9238795325112867385, 1.000000000000000000, 0.9238795325112867385, 1.000000000000000000, 0.9238795325112867385, 1.000000000000000000, 0.9238795325112867385, 1.000000000000000000, 0.9238795325112867385, 1.000000000000000000, 0.9238795325112867385, 1.000000000000000000, 0.9238795325112867385, 1.000000000000000000, 0.9238795325112867385, 1.000000000000000000, 0.9238795325112867385, 1.000000000000000000, 0.9238795325112867385, 1.000000000000000000, 0.9238795325112867385, 1.000000000000000000, 0.9238795325112867385, 1.000000000000000000, 0.9238795325112867385, 1.000000000000000000, 0.9238795325112867385, 1.000000000000000000, 0.9238795325112867385, 1.000000000000000000, 0.9238795325112867385, 1.000000000000000000, 0.9238795325112867385, 1.000000000000000000, 0.9238795325112867385, 1.000000000000000000, 0.9238795325112867385, 1.000000000000000000, 0.9238795325112867385, 1.000000000000000000, 0.9238795325112867385, 1.000000000000000000, 0.9238795325112867385, 1.000000000000000000, 0.9238795325112867385, 1.000000000000000000, 0.9238795325112867385, 1.000000000000000000, 0.9238795325112867385, 1.000000000000000000, 0.9238795325112867385, 1.000000000000000000, 0.9238795325112867385, 1.000000000000000000, 0.9238795325112867385, 1.000000000000000000, 0.9238795325112867385, 1.000000000000000000, 0.9238795325112867385, 1.000000000000000000, 0.9238795325112867385, 1.000000000000000000, 0.9238795325112867385, 1.000000000000000000, 0.9238795325112867385, 1.000000000000000000, 0.9238795325112867385, 1.000000000000000000, 0.9238795325112867385, 1.000000000000000000, 0.9238795325112867385, 1.000000000000000000, 0.9238795325112867385, 1.000000000000000000, 0.9238795325112867385, 1.000000000000000000, 0.9238795325112867385, 1.000000000000000000, 0.9238795325112867385, 1.000000000000000000, 0.9238795325112867385, 1.000000000000000000, 0.9238795325112867385, 1.000000000000000000, 0.9238795325112867385, 1.000000000000000000, 0.9238795325112867385, 1.000000000000000000, 0.9238795325112867385, 1.000000000000000000, 0.9238795325112867385, 1.000000000000000000, 0.9238795325112867385, 1.000000000000000000, 0.9238795325112867385, 1.000000000000000000, 0.9238795325112867385, 1.000000000000000000, 0.9238795325112867385, 1.000000000000000000, 0.9238795325112867385, 1.000000000000000000, 0.9238795325112867385, 1.000000000000000000, 0.9238795325112867385, 1.000000000000000000, 0.9238795325112867385, 1.000000000000000000, 0.9238795325112867385, 1.000000000000000000, 0.9238795325112867385, 1.000000000000000000, 0.9238795325112867385, 1.000000000000000000, 0.9238795325112867385, 1.000000000000000000, 0.9238795325112867385, 1.000000000000000000, 0.9238795325112867385, 1.000000000000000000, 0.9238795325112867385, 1.000000000000000000, 0.9238795325112867385, 1.000000000000000000, 0.9238795325112867385, 1.000000000000000000, 0.9238795325112867385, 1.000000000000000000, 0.9238795325112867385, 1.000000000000000000, 0.9238795325112867385, 1.000000000000000000, 0.9238795325112867385, 1.000000000000000000, 0.9238795325112867385, 1.000000000000000000, 0.9238795325112867385, 1.000000000000000000, 0.9238795325112867385, 1.000000000000000000, 0.9238795325112867385, 1.000000000000000000, 0.9238795325112867385, 1.000000000000000000, 0.9238795325112867385, 1.000000000000000000, 0.9238795325112867385, 1.000000000000000000, 0.9238795325112867385, 1.000000000000000000, 0.9238795325112867385, 1.000000000000000000, 0.9238795325112867385, 1.000000000000000000, 0.9238795325112867385, 1.000000000000000000, 0.9238795325112867385, 1.000000000000000000, 0.9238795325112867385, 1.000000000000000000, 0.9238795325112867385, 1.000000000000000000, 0.9238795325112867385, 1.000000000000000000, 0.9238795325112867385, 1.000000000000000000, 0.9238795325112867385, 1.000000000000000000, 0.9238795325112867385, 1.000000000000000000, 0.9238795325112867385, 1.000000000000000000, 0.9238795325112867385, 1.000000000000000000, 0.9238795325112867385, 1.000000000000000000, 0.9238795325112867385, 1.000000000000000000, 0.9238795325112867385, 1.000000000000000000, 0.9238795325112867385, 1.000000000000000000, 0.9238795325112867385, 1.000000000000000000, 0.9238795325112867385, 1.000000000000000000, 0.9238795325112867385, 1.000000000000000000, 0.9238795325112867385, 1.000000000000000000, 0.9238795325112867385, 1.000000000000000000, 0.9238795325112867385, 1.000000000000000000, 0.9238795325112867385, 1.000000000000000000, 0.9238795325112867385, 1.000000000000000000, 0.9238795325112867385, 1.000000000000000000, 0.9238795325112867385, 1.000000000000000000, 0.9238795325112867385, 1.000000000000000000, 0.9238795325112867385, 1.000000000000000000, 0.9238795325112867385, 1.000000000000000000, 0.9238795325112867385, 1.000000000000000000, 0.9238795325112867385, 1.000000000000000000, 0.9238795325112867385, 1.000000000000000000, 0.9238795325112867385, 1.000000000000000000, 0.9238795325112867385, 1.000000000000000000, 0.9238795325112867385, 1.000000000000000000, 0.9238795325112867385, 1.000000000000000000, 0.9238795325112867385, 1.000000000000000000, 0.9238795325112867385, 1.000000000000000000, 0.9238795325112867385, 1.000000000000000000, 0.9238795325112867385, 1.000000000000000000, 0.9238795325112867385, 1.000000000000000000, 0.9238795325112867385, 1.000000000000000000, 0.9238795325112867385, 1.000000000000000000, 0.9238795325112867385, 1.000000000000000000, 0.9238795325112867385, 1.000000000000000000, 0.9238795325112867385, 1.000000000000000000, 0.9238795325112867385, 1.000000000000000000, 0.9238795325112867385, 1.000000000000000000, 0.9238795325112867385, 1.000000000000000000, 0.9238795325112867385, 1.000000000000000000, 0.9238795325112867385, 1.000000000000000000, 0.9238795325112867385, 1.000000000000000000, 0.9238795325112867385, 1.000000000000000000, 0.9238795325112867385, 1.000000000000000000, 0.9238795325112867385, 1.000000000000000000, 0.9238795325112867385, 1.000000000000000000, 0.9238795325112867385, 1.000000000000000000, 0.9238795325112867385, 1.000000000000000000, 0.9238795325112867385, 1.000000000000000000, 0.9238795325112867385, 1.000000000000000000, 0.9238795325112867385, 1.000000000000000000, 0.9238795325112867385, 1.000000000000000000, 0.9238795325112867385, 1.000000000000000000, 0.9238795325112867385, 1.000000000000000000, 0.9238795325112867385, 1.000000000000000000, 0.9238795325112867385, 1.000000000000000000, 0.9238795325112867385, 1.000000000000000000, 0.9238795325112867385, 1.000000000000000000, 0.9238795325112867385, 1.000000000000000000, 0.9238795325112867385, 1.000000000000000000, 0.9238795325112867385, 1.000000000000000000, 0.9238795325112867385, 1.000000000000000000, 0.9238795325112867385, 1.000000000000000000, 0.9238795325112867385, 1.000000000000000000, 0.9238795325112867385, 1.000000000000000000, 0.9238795325112867385, 1.000000000000000000, 0.9238795325112867385, 1.000000000000000000, 0.9238795325112867385, 1.000000000000000000, 0.9238795325112867385, 1.000000000000000000, 0.9238795325112867385, 1.000000000000000000, 0.9238795325112867385, 1.000000000000000000, 0.9238795325112867385, 1.000000000000000000, 0.9238795325112867385, 1.000000000000000000, 0.9238795325112867385, 1.000000000000000000, 0.9238795325112867385, 1.000000000000000000, 0.9238795325112867385, 1.000000000000000000, 0.9238795325112867385, 1.000000000000000000, 0.9238795325112867385, 1.000000000000000000, 0.9238795325112867385, 1.000000000000000000, 0.9238795325112867385, 1.000000000000000000, 0.9238795325112867385, 1.000000000000000000, 0.9238795325112867385, 1.000000000000000000, 0.9238795325112867385, 1.000000000000000000, 0.9238795325112867385, 1.000000000000000000, 0.9238795325112867385, 1.000000000000000000, 0.9238795325112867385, 1.000000000000000000, 0.9238795325112867385, 1.000000000000000000, 0.9238795325112867385, 1.000000000000000000, 0.9238795325112867385, 1.000000000000000000, 0.9238795325112867385, 1.000000000000000000, 0.9238795325112867385, 1.000000000000000000, 0.9238795325112867385, 1.000000000000000000, 0.9238795325112867385, 1.000000000000000000, 0.9238795325112867385, 1.000000000000000000, 0.9238795325112867385, 1.000000000000000000, 0.9238795325112867385, 1.000000000000000000, 0.9493985675959992765, 0.9660722070829144137),
 ( 1.000000000000000000, 0.9238795325112867385, 1.000000000000000000, 0.9238795325112867385, 1.000000000000000000, 0.9238795325112867385, 1.000000000000000000, 0.9238795325112867385, 1.000000000000000000, 0.9238795325112867385, 1.000000000000000000, 0.9238795325112867385, 1.000000000000000000, 0.9238795325112867385, 1.000000000000000000, 0.9238795325112867385, 1.000000000000000000, 0.9238795325112867385, 1.000000000000000000, 0.9238795325112867385, 1.000000000000000000, 0.9238795325112867385, 1.000000000000000000, 0.9238795325112867385, 1.000000000000000000, 0.9238795325112867385, 1.000000000000000000, 0.9238795325112867385, 1.000000000000000000, 0.9238795325112867385, 1.000000000000000000, 0.9238795325112867385, 1.000000000000000000, 0.9238795325112867385, 1.000000000000000000, 0.9238795325112867385, 1.000000000000000000, 0.9238795325112867385, 1.000000000000000000, 0.9238795325112867385, 1.000000000000000000, 0.9238795325112867385, 1.000000000000000000, 0.9238795325112867385, 1.000000000000000000, 0.9238795325112867385, 1.000000000000000000, 0.9238795325112867385, 1.000000000000000000, 0.9238795325112867385, 1.000000000000000000, 0.9238795325112867385, 1.000000000000000000, 0.9238795325112867385, 1.000000000000000000, 0.9238795325112867385, 1.000000000000000000, 0.9238795325112867385, 1.000000000000000000, 0.9238795325112867385, 1.000000000000000000, 0.9238795325112867385, 1.000000000000000000, 0.9238795325112867385, 1.000000000000000000, 0.9238795325112867385, 1.000000000000000000, 0.9238795325112867385, 1.000000000000000000, 0.9238795325112867385, 1.000000000000000000, 0.9238795325112867385, 1.000000000000000000, 0.9238795325112867385, 1.000000000000000000, 0.9238795325112867385, 1.000000000000000000, 0.9238795325112867385, 1.000000000000000000, 0.9238795325112867385, 1.000000000000000000, 0.9238795325112867385, 1.000000000000000000, 0.9238795325112867385, 1.000000000000000000, 0.9238795325112867385, 1.000000000000000000, 0.9238795325112867385, 1.000000000000000000, 0.9238795325112867385, 1.000000000000000000, 0.9238795325112867385, 1.000000000000000000, 0.9238795325112867385, 1.000000000000000000, 0.9238795325112867385, 1.000000000000000000, 0.9238795325112867385, 1.000000000000000000, 0.9238795325112867385, 1.000000000000000000, 0.9238795325112867385, 1.000000000000000000, 0.9238795325112867385, 1.000000000000000000, 0.9238795325112867385, 1.000000000000000000, 0.9238795325112867385, 1.000000000000000000, 0.9238795325112867385, 1.000000000000000000, 0.9238795325112867385, 1.000000000000000000, 0.9238795325112867385, 1.000000000000000000, 0.9238795325112867385, 1.000000000000000000, 0.9238795325112867385, 1.000000000000000000, 0.9238795325112867385, 1.000000000000000000, 0.9238795325112867385, 1.000000000000000000, 0.9238795325112867385, 1.000000000000000000, 0.9238795325112867385, 1.000000000000000000, 0.9238795325112867385, 1.000000000000000000, 0.9238795325112867385, 1.000000000000000000, 0.9238795325112867385, 1.000000000000000000, 0.9238795325112867385, 1.000000000000000000, 0.9238795325112867385, 1.000000000000000000, 0.9238795325112867385, 1.000000000000000000, 0.9238795325112867385, 1.000000000000000000, 0.9238795325112867385, 1.000000000000000000, 0.9238795325112867385, 1.000000000000000000, 0.9238795325112867385, 1.000000000000000000, 0.9238795325112867385, 1.000000000000000000, 0.9238795325112867385, 1.000000000000000000, 0.9238795325112867385, 1.000000000000000000, 0.9238795325112867385, 1.000000000000000000, 0.9238795325112867385, 1.000000000000000000, 0.9238795325112867385, 1.000000000000000000, 0.9238795325112867385, 1.000000000000000000, 0.9238795325112867385, 1.000000000000000000, 0.9238795325112867385, 1.000000000000000000, 0.9238795325112867385, 1.000000000000000000, 0.9238795325112867385, 1.000000000000000000, 0.9238795325112867385, 1.000000000000000000, 0.9238795325112867385, 1.000000000000000000, 0.9238795325112867385, 1.000000000000000000, 0.9238795325112867385, 1.000000000000000000, 0.9238795325112867385, 1.000000000000000000, 0.9238795325112867385, 1.000000000000000000, 0.9238795325112867385, 1.000000000000000000, 0.9238795325112867385, 1.000000000000000000, 0.9238795325112867385, 1.000000000000000000, 0.9238795325112867385, 1.000000000000000000, 0.9238795325112867385, 1.000000000000000000, 0.9238795325112867385, 1.000000000000000000, 0.9238795325112867385, 1.000000000000000000, 0.9238795325112867385, 1.000000000000000000, 0.9238795325112867385, 1.000000000000000000, 0.9238795325112867385, 1.000000000000000000, 0.9238795325112867385, 1.000000000000000000, 0.9238795325112867385, 1.000000000000000000, 0.9238795325112867385, 1.000000000000000000, 0.9238795325112867385, 1.000000000000000000, 0.9238795325112867385, 1.000000000000000000, 0.9238795325112867385, 1.000000000000000000, 0.9238795325112867385, 1.000000000000000000, 0.9238795325112867385, 1.000000000000000000, 0.9238795325112867385, 1.000000000000000000, 0.9238795325112867385, 1.000000000000000000, 0.9238795325112867385, 1.000000000000000000, 0.9238795325112867385, 1.000000000000000000, 0.9238795325112867385, 1.000000000000000000, 0.9238795325112867385, 1.000000000000000000, 0.9238795325112867385, 1.000000000000000000, 0.9238795325112867385, 1.000000000000000000, 0.9238795325112867385, 1.000000000000000000, 0.9238795325112867385, 1.000000000000000000, 0.9238795325112867385, 1.000000000000000000, 0.9238795325112867385, 1.000000000000000000, 0.9238795325112867385, 1.000000000000000000, 0.9238795325112867385, 1.000000000000000000, 0.9238795325112867385, 1.000000000000000000, 0.9238795325112867385, 1.000000000000000000, 0.9238795325112867385, 1.000000000000000000, 0.9238795325112867385, 1.000000000000000000, 0.9238795325112867385, 1.000000000000000000, 0.9238795325112867385, 1.000000000000000000, 0.9238795325112867385, 1.000000000000000000, 0.9238795325112867385, 1.000000000000000000, 0.9238795325112867385, 1.000000000000000000, 0.9238795325112867385, 1.000000000000000000, 0.9238795325112867385, 1.000000000000000000, 0.9238795325112867385, 1.000000000000000000, 0.9238795325112867385, 1.000000000000000000, 0.9238795325112867385, 1.000000000000000000, 0.9238795325112867385, 1.000000000000000000, 0.9238795325112867385, 1.000000000000000000, 0.9238795325112867385, 1.000000000000000000, 0.9238795325112867385, 1.000000000000000000, 0.9238795325112867385, 1.000000000000000000, 0.9238795325112867385, 1.000000000000000000, 0.9238795325112867385, 1.000000000000000000, 0.9238795325112867385, 1.000000000000000000, 0.9238795325112867385, 1.000000000000000000, 0.9238795325112867385, 1.000000000000000000, 0.9238795325112867385, 1.000000000000000000, 0.9238795325112867385, 1.000000000000000000, 0.9238795325112867385, 1.000000000000000000, 0.9238795325112867385, 1.000000000000000000, 0.9238795325112867385, 1.000000000000000000, 0.9238795325112867385, 1.000000000000000000, 0.9238795325112867385, 1.000000000000000000, 0.9238795325112867385, 1.000000000000000000, 0.9238795325112867385, 1.000000000000000000, 0.9238795325112867385, 1.000000000000000000, 0.9238795325112867385, 1.000000000000000000, 0.9238795325112867385, 1.000000000000000000, 0.9238795325112867385, 1.000000000000000000, 0.9238795325112867385, 1.000000000000000000, 0.9238795325112867385, 1.000000000000000000, 0.9238795325112867385, 1.000000000000000000, 0.9238795325112867385, 1.000000000000000000, 0.9238795325112867385, 1.000000000000000000, 0.9238795325112867385, 1.000000000000000000, 0.9238795325112867385, 1.000000000000000000, 0.9238795325112867385, 1.000000000000000000, 0.9238795325112867385, 1.000000000000000000, 0.9238795325112867385, 1.000000000000000000, 0.9238795325112867385, 1.000000000000000000, 0.9238795325112867385, 1.000000000000000000, 0.9238795325112867385, 1.000000000000000000, 0.9238795325112867385, 1.000000000000000000, 0.9238795325112867385, 1.000000000000000000, 0.9238795325112867385, 1.000000000000000000, 0.9238795325112867385, 1.000000000000000000, 0.9238795325112867385, 1.000000000000000000, 0.9238795325112867385, 1.000000000000000000, 0.9238795325112867385, 1.000000000000000000, 0.9238795325112867385, 1.000000000000000000, 0.9238795325112867385, 1.000000000000000000, 0.9238795325112867385, 1.000000000000000000, 0.9238795325112867385, 1.000000000000000000, 0.9238795325112867385, 1.000000000000000000, 0.9238795325112867385, 1.000000000000000000, 0.9238795325112867385, 1.000000000000000000, 0.9493985675959992765, 0.9660722070829144137) ) ) 
 REPRESENTATION_ITEM ( '' )  SURFACE ( )  );
#27788 = LINE ( 'NONE', #55364, #13420 ) ;
#27789 = CARTESIAN_POINT ( 'NONE',  ( -1.320432766682874540E-15, 18.09374999795161187, 7.188101187500000044 ) ) ;
#27790 = CARTESIAN_POINT ( 'NONE',  ( 7.320508075688890059, 40.62500000000008527, -7.320508075688890059 ) ) ;
#27791 = CARTESIAN_POINT ( 'NONE',  ( 3.042071309553163516, 252.7604166700806445, -11.35316468749999785 ) ) ;
#27792 = CARTESIAN_POINT ( 'NONE',  ( -9.832129032723420536, 108.6979166632526983, 5.676582343749997150 ) ) ;
#27793 = EDGE_LOOP ( 'NONE', ( #5312, #71498, #19499, #12415 ) ) ;
#27794 = CARTESIAN_POINT ( 'NONE',  ( -19.99999999999993250, -31.99999999999978684, 193.6854385646540209 ) ) ;
#27795 = ADVANCED_FACE ( 'NONE', ( #29564 ), #1283, .T. ) ;
#27796 = CARTESIAN_POINT ( 'NONE',  ( -10.18810118749999738, -4.220049686691941915, 108.2500000020483810 ) ) ;
#27797 = LINE ( 'NONE', #43283, #9318 ) ;
#27798 = CARTESIAN_POINT ( 'NONE',  ( -2.445694354108784108, 204.5625000013656063, 195.5543056458912190 ) ) ;
#27799 = CARTESIAN_POINT ( 'NONE',  ( -75.00000000000001421, 272.0000000000000000, 20.00000000000003553 ) ) ;
#27801 = CARTESIAN_POINT ( 'NONE',  ( -11.35316468750000141, 83.28124999658602690, -1.390361679473963753E-15 ) ) ;
#27800 = CARTESIAN_POINT ( 'NONE',  ( 7.778174593052023411, -7.778174593052021635, 97.56250000000000000 ) ) ;
#27802 = CARTESIAN_POINT ( 'NONE',  ( -4.898587196589407898E-16, 7.999999999999991118, 14.14280278392014623 ) ) ;
#27803 = CARTESIAN_POINT ( 'NONE',  ( -29.43265458321766559, 202.7500000013655779, 166.5412658750003629 ) ) ;
#27804 = DIRECTION ( 'NONE',  ( 1.000000000000000000, 0.000000000000000000, 0.000000000000000000 ) ) ;
#27805 = VECTOR ( 'NONE', #14951, 1000.000000000000000 ) ;
#27806 = ORIENTED_EDGE ( 'NONE', *, *, #28356, .F. ) ;
#27807 = EDGE_CURVE ( 'NONE', #40460, #56676, #32482, .T. ) ;
#27808 = CARTESIAN_POINT ( 'NONE',  ( -5.000000000000005329, 185.2083333265053682, 8.660254037844387298 ) ) ;
#27809 = CARTESIAN_POINT ( 'NONE',  ( -2.751064625579944321E-14, 207.7500000000000284, 146.0000000000000284 ) ) ;
#27810 = CARTESIAN_POINT ( 'NONE',  ( 5.000000000000000000, -51.30314553820225854, 41.49361401976497632 ) ) ;
#27811 = CARTESIAN_POINT ( 'NONE',  ( -11.35316468749999785, 73.38541666325268409, -3.042071309553167957 ) ) ;
#27812 = CARTESIAN_POINT ( 'NONE',  ( 2.765530957082001251, 288.7656250017068942, 6.676582343750000703 ) ) ;
#27813 = FACE_OUTER_BOUND ( 'NONE', #51569, .T. ) ;
#27814 = CARTESIAN_POINT ( 'NONE',  ( -7.204075437095967871, 7.204075437095967871, 100.8437500020483668 ) ) ;
#27815 = CARTESIAN_POINT ( 'NONE',  ( -11.35316468750000141, 218.4895833299193271, 3.042071309553159963 ) ) ;
#27817 = VERTEX_POINT ( 'NONE', #7295 ) ;
#27816 =( BOUNDED_CURVE ( )  B_SPLINE_CURVE ( 2, ( #16825, #1369, #34961, #23615, #5531, #51924, #28532, #24354, #40601 ),
 .UNSPECIFIED., .F., .F. ) 
 B_SPLINE_CURVE_WITH_KNOTS ( ( 3, 2, 2, 2, 3 ),
 ( 0.8666666666666673624, 0.8750000000000006661, 0.8833333333333339699, 0.8916666666666674956, 0.9000000000000007994 ),
 .UNSPECIFIED. ) 
 CURVE ( )  GEOMETRIC_REPRESENTATION_ITEM ( )  RATIONAL_B_SPLINE_CURVE ( ( 0.9999999999999938938, 0.9238795325112928447, 1.000000000000000000, 0.9238795325112867385, 1.000000000000000000, 0.9238795325112867385, 1.000000000000000000, 0.9238795325112796331, 1.000000000000007105 ) ) 
 REPRESENTATION_ITEM ( '' )  );
#27818 = CARTESIAN_POINT ( 'NONE',  ( 4.898587196589412829E-16, 19.68749999590322020, -8.000000000000000000 ) ) ;
#27819 = DIRECTION ( 'NONE',  ( 0.000000000000000000, 0.000000000000000000, 1.000000000000000000 ) ) ;
#27820 = DIRECTION ( 'NONE',  ( 0.8660254037844505870, 0.4999999999999792388, 0.000000000000000000 ) ) ;
#27821 = CARTESIAN_POINT ( 'NONE',  ( -2.085542519210945728E-15, 204.5312499965860411, 11.35316468750000141 ) ) ;
#27822 = B_SPLINE_CURVE_WITH_KNOTS ( 'NONE', 3,
 ( #29322, #41380, #52332, #23653, #64392, #30058, #53070, #64754, #47757, #70781, #71504, #14530, #25849, #31533, #37570, #36458, #13421, #18736, #60194, #59472, #3236, #36824 ),
 .UNSPECIFIED., .F., .F.,
 ( 4, 2, 2, 2, 2, 2, 2, 2, 2, 2, 4 ),
 ( 8.588689904434031851E-20, 0.001045978366599488755, 0.001568967549899233024, 0.002091956733198977510, 0.003137935099798465181, 0.004183913466397953286, 0.005229891832997441391, 0.005752881016297185443, 0.006275870199596930363, 0.007321848566196421070, 0.008367826932795910042 ),
 .UNSPECIFIED. ) ;
#27823 = CARTESIAN_POINT ( 'NONE',  ( -4.999999999999992895, 223.9583333401612890, 8.660254037844390851 ) ) ;
#27824 = DIRECTION ( 'NONE',  ( -0.000000000000000000, 0.000000000000000000, 1.000000000000000000 ) ) ;
#27825 = CARTESIAN_POINT ( 'NONE',  ( 6.676582343750001591, 298.9531250017069510, -8.176455196517173205E-16 ) ) ;
#27826 = EDGE_CURVE ( 'NONE', #26800, #25744, #61048, .T. ) ;
#27827 = EDGE_LOOP ( 'NONE', ( #42686, #2404, #65276, #39882 ) ) ;
#27828 = CARTESIAN_POINT ( 'NONE',  ( 3.042071309553159519, 200.0520833299193555, 11.35316468750000141 ) ) ;
#27829 = CARTESIAN_POINT ( 'NONE',  ( -31.45873412499998523, 208.7500000013656063, 171.4326545832180386 ) ) ;
#27830 = CARTESIAN_POINT ( 'NONE',  ( 7.999999999999998224, 10.40625000000000178, 3.313708498984766493 ) ) ;
#27831 = ORIENTED_EDGE ( 'NONE', *, *, #74034, .F. ) ;
#27832 = VECTOR ( 'NONE', #30485, 1000.000000000000000 ) ;
#27833 = CARTESIAN_POINT ( 'NONE',  ( -3.313708498984762052, 94.90625000409677625, -8.000000000000000000 ) ) ;
#27834 = CARTESIAN_POINT ( 'NONE',  ( 2.679491924311222739, 13.95833333333333393, 10.00000000000000355 ) ) ;
#27835 = ADVANCED_FACE ( 'NONE', ( #26005 ), #55839, .F. ) ;
#27836 = AXIS2_PLACEMENT_3D ( 'NONE', #39694, #67259, #28005 ) ;
#27837 = CARTESIAN_POINT ( 'NONE',  ( 4.220049686691941027, -10.18810118749999738, 82.00000000204836681 ) ) ;
#27838 = ORIENTED_EDGE ( 'NONE', *, *, #2670, .F. ) ;
#27839 = CARTESIAN_POINT ( 'NONE',  ( 4.000000000000000888, 18.93749999999999645, 1.656854249492384135 ) ) ;
#27840 = CARTESIAN_POINT ( 'NONE',  ( -1.881053915767124440, 19.99999999863440436, 4.541265875000001451 ) ) ;
#27841 = AXIS2_PLACEMENT_3D ( 'NONE', #64248, #35586, #53307 ) ;
#27842 = CARTESIAN_POINT ( 'NONE',  ( 0.000000000000000000, 0.000000000000000000, 11.00000000000000000 ) ) ;
#27843 = EDGE_LOOP ( 'NONE', ( #27277, #65551, #5399, #36341 ) ) ;
#27844 = LINE ( 'NONE', #4471, #51145 ) ;
#27845 = CARTESIAN_POINT ( 'NONE',  ( -5.000000000000000000, -10.26105934116143281, 64.40045319026697257 ) ) ;
#27848 = CARTESIAN_POINT ( 'NONE',  ( 2.751064625579944321E-14, 197.7500000000000000, 194.0000000000000568 ) ) ;
#27847 = CARTESIAN_POINT ( 'NONE',  ( 9.832129032723416984, 241.8229166700806445, -5.676582343750003368 ) ) ;
#27846 = CARTESIAN_POINT ( 'NONE',  ( 28.00000000000002132, 206.4375000013656063, 173.4587341249998929 ) ) ;
#27849 = APPLICATION_PROTOCOL_DEFINITION ( 'draft international standard', 'automotive_design', 1998, #18274 ) ;
#27850 = VERTEX_POINT ( 'NONE', #55460 ) ;
#27851 = CARTESIAN_POINT ( 'NONE',  ( 3.042071309553163960, 247.7604166700806161, -11.35316468749999785 ) ) ;
#27852 = CARTESIAN_POINT ( 'NONE',  ( -7.188101187499992051, 0.000000000000000000, 11.98655278187175277 ) ) ;
#27853 = ORIENTED_EDGE ( 'NONE', *, *, #5374, .F. ) ;
#27854 = VERTEX_POINT ( 'NONE', #32829 ) ;
#27855 = CARTESIAN_POINT ( 'NONE',  ( 7.204075437095968759, -7.204075437095966983, 75.71875000204836681 ) ) ;
#27856 = CARTESIAN_POINT ( 'NONE',  ( 3.042071309553167069, 87.13541666325268409, -11.35316468749999785 ) ) ;
#27857 = DIRECTION ( 'NONE',  ( -0.000000000000000000, -0.000000000000000000, 1.000000000000000000 ) ) ;
#27858 = CARTESIAN_POINT ( 'NONE',  ( 7.778174593052023411, -7.778174593052021635, 87.06249999999998579 ) ) ;
#27861 = CARTESIAN_POINT ( 'NONE',  ( 1.226468279477575784E-15, 289.8593750017070079, 6.676582343750001591 ) ) ;
#27860 = CARTESIAN_POINT ( 'NONE',  ( 26.56734541678238060, 209.3750000013656063, 173.4587341249998929 ) ) ;
#27859 = CARTESIAN_POINT ( 'NONE',  ( 29.43265458321766559, 207.1250000013656347, 166.5412658749999650 ) ) ;
#27862 = CARTESIAN_POINT ( 'NONE',  ( -53.22044411043375334, 204.9003350349723007, 52.35350010398858700 ) ) ;
#27863 = CARTESIAN_POINT ( 'NONE',  ( -1.469576158976823947E-15, 2.437499995903220196, 8.000000000000000000 ) ) ;
#27864 = CARTESIAN_POINT ( 'NONE',  ( 9.832129032723420536, 196.1979166632526983, -5.676582343749999815 ) ) ;
#27865 = CARTESIAN_POINT ( 'NONE',  ( 5.656854249492378806, 7.124999995903221084, 5.656854249492381470 ) ) ;
#27866 = ORIENTED_EDGE ( 'NONE', *, *, #34122, .F. ) ;
#27867 = CARTESIAN_POINT ( 'NONE',  ( 31.45873412500001010, 209.0000000013655779, 168.5673454167822740 ) ) ;
#27868 = CARTESIAN_POINT ( 'NONE',  ( 2.977408999572650927, 17.62499999795161543, -7.188101187500001821 ) ) ;
#27869 = CARTESIAN_POINT ( 'NONE',  ( 9.832129032723420536, 171.5104166632526983, -5.676582343749999815 ) ) ;
#27870 = CARTESIAN_POINT ( 'NONE',  ( -4.898587196589412829E-16, 105.1250000000000000, -8.000000000000000000 ) ) ;
#27871 = CARTESIAN_POINT ( 'NONE',  ( 7.188101187500000044, 104.2812500020483810, -8.802885111219163269E-16 ) ) ;
#27873 = FACE_OUTER_BOUND ( 'NONE', #26141, .T. ) ;
#27872 = CARTESIAN_POINT ( 'NONE',  ( -2.664923566518097392E-11, 208.7499999999979252, 10.00000000000000178 ) ) ;
#27874 = CARTESIAN_POINT ( 'NONE',  ( 26.56734541678238415, 207.2500000013655779, 166.5412658749999650 ) ) ;
#27875 = CARTESIAN_POINT ( 'NONE',  ( -2.977408999572648707, -7.188101187499990274, 14.14280278187175455 ) ) ;
#27876 = CARTESIAN_POINT ( 'NONE',  ( 5.676582343750001591, 61.61458332991935549, -9.832129032723420536 ) ) ;
#27877 = CARTESIAN_POINT ( 'NONE',  ( -2.260181558736319207, -43.01762864706988410, 139.0821933904439334 ) ) ;
#27878 = CARTESIAN_POINT ( 'NONE',  ( 1.656854249492381248, 17.18750000000000000, -4.000000000000001776 ) ) ;
#27879 = ORIENTED_EDGE ( 'NONE', *, *, #32404, .F. ) ;
#27880 = CYLINDRICAL_SURFACE ( 'NONE', #42253, 3.999999999999976019 ) ;
#27881 = CARTESIAN_POINT ( 'NONE',  ( 2.449293598294707893E-16, 1.250000000000000222, -4.000000000000001776 ) ) ;
#27882 = CARTESIAN_POINT ( 'NONE',  ( 3.042071309553159519, 64.73958332991935549, 11.35316468750000141 ) ) ;
#27883 = CARTESIAN_POINT ( 'NONE',  ( 2.020667218593132706E-15, -11.00000000000000000, 76.56250000409677625 ) ) ;
#27884 = CARTESIAN_POINT ( 'NONE',  ( -2.445694354108839175, 201.3125000013656063, 144.4456943541088663 ) ) ;
#27886 = AXIS2_PLACEMENT_3D ( 'NONE', #29571, #58995, #12578 ) ;
#27885 = CARTESIAN_POINT ( 'NONE',  ( 4.471435261918252024, 10.26549131683129445, 64.21726486257941247 ) ) ;
#27887 = CARTESIAN_POINT ( 'NONE',  ( -8.660254037844390851, 12.91666666666666963, 4.999999999999998224 ) ) ;
#27889 = CARTESIAN_POINT ( 'NONE',  ( 8.311093377946837890, 51.40624999658601268, -8.311093377946837890 ) ) ;
#27888 = CARTESIAN_POINT ( 'NONE',  ( -2.977408999572652260, 94.43750000204838102, 7.188101187500000044 ) ) ;
#27890 = CARTESIAN_POINT ( 'NONE',  ( -5.656854249492375253, 5.656854249492375253, 3.642802779823362869 ) ) ;
#27891 = CARTESIAN_POINT ( 'NONE',  ( 7.999999999988127719, 1.377684776014802281E-05, 21.26780317368888618 ) ) ;
#27892 = CARTESIAN_POINT ( 'NONE',  ( -8.311093377946841443, 168.9062499965860411, 8.311093377946830785 ) ) ;
#27893 = EDGE_CURVE ( 'NONE', #70895, #58068, #48040, .T. ) ;
#27894 = CARTESIAN_POINT ( 'NONE',  ( 7.320508075688774596, 137.4999999931720254, -7.320508075688774596 ) ) ;
#27895 = CARTESIAN_POINT ( 'NONE',  ( -7.188101187500001821, 100.4375000020483668, -2.977408999572650483 ) ) ;
#27896 = VECTOR ( 'NONE', #56275, 1000.000000000000000 ) ;
#27897 = CARTESIAN_POINT ( 'NONE',  ( -3.000000000000002220, -45.19827753562250905, 139.1455027589170754 ) ) ;
#27898 = CARTESIAN_POINT ( 'NONE',  ( 9.832129032723420536, 31.51041666325268764, -5.676582343749999815 ) ) ;
#27899 = CARTESIAN_POINT ( 'NONE',  ( -10.18810118749999916, 4.220049686691934809, 117.4375000020483810 ) ) ;
#27900 = CARTESIAN_POINT ( 'NONE',  ( 8.311093377946837890, 181.4062499965860411, -8.311093377946837890 ) ) ;
#27901 = VERTEX_POINT ( 'NONE', #44506 ) ;
#27902 = CARTESIAN_POINT ( 'NONE',  ( 0.000000000000000000, 0.000000000000000000, -81.50000000000000000 ) ) ;
#27903 = CARTESIAN_POINT ( 'NONE',  ( 4.220049686691941027, -10.18810118749999738, 71.12500000204836681 ) ) ;
#27904 = CARTESIAN_POINT ( 'NONE',  ( -3.999999999999959144, 196.0625000000000284, 199.6568542494924259 ) ) ;
#27905 = LINE ( 'NONE', #28282, #73877 ) ;
#27907 = CARTESIAN_POINT ( 'NONE',  ( 11.35316468749999963, 160.9895833299193555, -3.042071309553165293 ) ) ;
#27906 = CARTESIAN_POINT ( 'NONE',  ( 4.231687259402287182, -68.27410168872741281, 20.58597903916479055 ) ) ;
#27908 = AXIS2_PLACEMENT_3D ( 'NONE', #1177, #41518, #49689 ) ;
#27909 = CARTESIAN_POINT ( 'NONE',  ( 7.999999999999991118, 9.797174393178815797E-16, 7.636552784329823318 ) ) ;
#27910 = CARTESIAN_POINT ( 'NONE',  ( 5.656854249492374365, 5.656854249492375253, 4.767802779823363757 ) ) ;
#27911 = CARTESIAN_POINT ( 'NONE',  ( -11.35316468749999608, 224.1145833367473301, 3.042071309553173730 ) ) ;
#27912 = CARTESIAN_POINT ( 'NONE',  ( -2.436599634633916711, 51.42120007173274132, -48.62500384162247968 ) ) ;
#27913 = CARTESIAN_POINT ( 'NONE',  ( -10.18810118749999916, 4.220049686691934809, 78.43750000204838102 ) ) ;
#27914 = VERTEX_POINT ( 'NONE', #21849 ) ;
#27915 =( BOUNDED_CURVE ( )  B_SPLINE_CURVE ( 2, ( #3535, #9943, #14458, #43509, #43895, #72180, #3921, #60868, #15957 ),
 .UNSPECIFIED., .F., .F. ) 
 B_SPLINE_CURVE_WITH_KNOTS ( ( 3, 2, 2, 2, 3 ),
 ( 0.02083333333333103887, 0.03124999999999771363, 0.04166666666666438146, 0.05208333333333105969, 0.06249999999999773792 ),
 .UNSPECIFIED. ) 
 CURVE ( )  GEOMETRIC_REPRESENTATION_ITEM ( )  RATIONAL_B_SPLINE_CURVE ( ( 1.000000000000016653, 0.9238795325112698631, 1.000000000000000000, 0.9238795325112867385, 1.000000000000000000, 0.9238795325112867385, 1.000000000000000000, 0.9238795325113032808, 0.9999999999999834577 ) ) 
 REPRESENTATION_ITEM ( '' )  );
#27916 = EDGE_CURVE ( 'NONE', #8888, #68267, #22812, .T. ) ;
#27917 = CARTESIAN_POINT ( 'NONE',  ( 49.70177871865296026, 146.0000000000000000, 69.99999999999998579 ) ) ;
#27918 = CARTESIAN_POINT ( 'NONE',  ( 9.832129032723416984, 120.6770833299193555, 5.676582343750006032 ) ) ;
#27919 = EDGE_CURVE ( 'NONE', #8618, #60482, #71170, .T. ) ;
#27920 = CARTESIAN_POINT ( 'NONE',  ( 27.99999999999996803, 199.0000000000000000, 173.9999999999999147 ) ) ;
#27921 = EDGE_LOOP ( 'NONE', ( #39612, #60180, #46406, #21749 ) ) ;
#27922 = ORIENTED_EDGE ( 'NONE', *, *, #67087, .F. ) ;
#27923 = AXIS2_PLACEMENT_3D ( 'NONE', #44378, #72293, #54962 ) ;
#27924 = CARTESIAN_POINT ( 'NONE',  ( 4.541265875000002339, 7.437499998634407028, 0.000000000000000000 ) ) ;
#27925 = CARTESIAN_POINT ( 'NONE',  ( -5.082755093536326818, 13.40624999795161187, 5.082755093536325042 ) ) ;
#27926 = CARTESIAN_POINT ( 'NONE',  ( 5.656854249492379694, 109.6250000040967763, -5.656854249492380582 ) ) ;
#27927 = CARTESIAN_POINT ( 'NONE',  ( -27.99999999999996447, 199.1875000013655779, 173.4587341250003760 ) ) ;
#27928 = EDGE_CURVE ( 'NONE', #9105, #40460, #37266, .T. ) ;
#27929 = EDGE_CURVE ( 'NONE', #19453, #16032, #45638, .T. ) ;
#27930 = CARTESIAN_POINT ( 'NONE',  ( -2.828427124746192067, 8.625000000000000000, 2.828427124746190735 ) ) ;
#27931 = CARTESIAN_POINT ( 'NONE',  ( 2.828427124746190291, 21.62499999726881583, 2.828427124746192067 ) ) ;
#27932 = CARTESIAN_POINT ( 'NONE',  ( -4.541265875000002339, 9.749999998634404363, -1.881053915767121998 ) ) ;
#27933 = CARTESIAN_POINT ( 'NONE',  ( 3.999999999999959144, 200.0625000000000568, 140.3431457505076594 ) ) ;
#27934 = ORIENTED_EDGE ( 'NONE', *, *, #57094, .T. ) ;
#27935 =( LENGTH_UNIT ( ) NAMED_UNIT ( * ) SI_UNIT ( .MILLI., .METRE. ) );
#27936 = CARTESIAN_POINT ( 'NONE',  ( 7.188101187500001821, 105.5000000020483810, -2.977408999572651371 ) ) ;
#27938 = CARTESIAN_POINT ( 'NONE',  ( -5.656854249492380582, 123.3125000000000000, -5.656854249492380582 ) ) ;
#27937 = CARTESIAN_POINT ( 'NONE',  ( 54.00000000000000711, 272.0000000000000000, 20.00000000000001776 ) ) ;
#27939 =( LENGTH_UNIT ( ) NAMED_UNIT ( * ) SI_UNIT ( .MILLI., .METRE. ) );
#27940 = CARTESIAN_POINT ( 'NONE',  ( -1.656854249492383468, 10.68750000000000000, 4.000000000000000888 ) ) ;
#27941 = AXIS2_PLACEMENT_3D ( 'NONE', #30926, #71279, #21099 ) ;
#27942 = DIRECTION ( 'NONE',  ( -0.000000000000000000, 1.000000000000000000, -0.000000000000000000 ) ) ;
#27943 = VERTEX_POINT ( 'NONE', #39591 ) ;
#27944 = VERTEX_POINT ( 'NONE', #50902 ) ;
#27945 = CARTESIAN_POINT ( 'NONE',  ( -10.18810118749999916, 0.000000000000000000, 93.15625000204836681 ) ) ;
#27946 = CARTESIAN_POINT ( 'NONE',  ( 1.102182119232618108E-15, 288.2500000000000000, 6.000000000000001776 ) ) ;
#27947 = CARTESIAN_POINT ( 'NONE',  ( -27.99999999999996447, 201.1875000013656063, 173.4587341250003760 ) ) ;
#27948 = CARTESIAN_POINT ( 'NONE',  ( -7.778174593052023411, 7.778174593052023411, 104.3124999999999858 ) ) ;
#27949 = CARTESIAN_POINT ( 'NONE',  ( 2.445694354108840063, 202.0625000013656063, 200.4456943541088663 ) ) ;
#27951 = CARTESIAN_POINT ( 'NONE',  ( -6.123233995736766282E-16, 253.7500000000000284, -10.00000000000000000 ) ) ;
#27950 = CARTESIAN_POINT ( 'NONE',  ( 2.849036369511732440E-14, 203.3750000027312126, 202.0000000000000000 ) ) ;
#27952 = EDGE_CURVE ( 'NONE', #59170, #71548, #17209, .T. ) ;
#27953 = CARTESIAN_POINT ( 'NONE',  ( -10.00000000000000355, 127.7083333333333570, 2.679491924311223183 ) ) ;
#27954 = CARTESIAN_POINT ( 'NONE',  ( -3.313708498984762496, 105.7812500000000000, 7.999999999999998224 ) ) ;
#27955 = CARTESIAN_POINT ( 'NONE',  ( -10.99999999999978684, -4.556349186104264426, 86.78125000409677625 ) ) ;
#27956 = CARTESIAN_POINT ( 'NONE',  ( 7.188101187499992051, 8.802885111219154394E-16, 8.611552781871752771 ) ) ;
#27957 = EDGE_CURVE ( 'NONE', #35571, #38454, #17646, .T. ) ;
#27958 = APPLICATION_CONTEXT ( 'automotive_design' ) ;
#27959 = CARTESIAN_POINT ( 'NONE',  ( -3.313708498984707429, 97.71875000000000000, -8.000000000000055067 ) ) ;
#27960 = CARTESIAN_POINT ( 'NONE',  ( 24.54126587500000412, 208.1250000013656063, 168.5673454167822172 ) ) ;
#27961 = CARTESIAN_POINT ( 'NONE',  ( 5.656854249492378806, 26.62499999590322375, 5.656854249492381470 ) ) ;
#27962 = CARTESIAN_POINT ( 'NONE',  ( 1.432654583217607192, 200.2500000013656631, 145.4587341250000634 ) ) ;
#27963 = CARTESIAN_POINT ( 'NONE',  ( -7.188101187500000044, 121.5312500020483810, 0.000000000000000000 ) ) ;
#27965 = CARTESIAN_POINT ( 'NONE',  ( -1.432654583217662481, 202.3750000013655779, 145.4587341250000634 ) ) ;
#27964 = CARTESIAN_POINT ( 'NONE',  ( -2.250000000000000000, 274.6666666666666288, 5.427076266392048431 ) ) ;
#27966 = CARTESIAN_POINT ( 'NONE',  ( -11.35316468749999608, 239.4270833367473301, 3.042071309553173730 ) ) ;
#27967 = CARTESIAN_POINT ( 'NONE',  ( -8.660254037844387298, 93.95833332650536818, -5.000000000000004441 ) ) ;
#27968 = CARTESIAN_POINT ( 'NONE',  ( 29.65685424949235482, 202.0625000000000284, 173.9999999999999147 ) ) ;
#27969 = CARTESIAN_POINT ( 'NONE',  ( 11.35316468750000141, 10.78124999658601624, 0.000000000000000000 ) ) ;
#27970 = EDGE_CURVE ( 'NONE', #25962, #7137, #14352, .T. ) ;
#27971 = CARTESIAN_POINT ( 'NONE',  ( 5.656854249492379694, 122.9375000000000000, -5.656854249492380582 ) ) ;
#27972 = CARTESIAN_POINT ( 'NONE',  ( 11.35316468749999785, 210.8854166632526983, 3.042071309553174174 ) ) ;
#27973 = CARTESIAN_POINT ( 'NONE',  ( 6.123233995736767268E-16, 133.1249999931720254, -10.00000000000000178 ) ) ;
#27974 = CARTESIAN_POINT ( 'NONE',  ( -10.00000000000000000, 219.1666666598387110, -2.679491924311229845 ) ) ;
#27976 = CARTESIAN_POINT ( 'NONE',  ( 1.469576158976823947E-15, 101.5625000040967763, 8.000000000000000000 ) ) ;
#27975 = CARTESIAN_POINT ( 'NONE',  ( -8.000000000000000000, 25.96874999590322375, -3.313708498984762496 ) ) ;
#27977 = ORIENTED_EDGE ( 'NONE', *, *, #51059, .F. ) ;
#27978 = CARTESIAN_POINT ( 'NONE',  ( -1.432654583217662481, 202.3750000013655779, 145.4587341250000634 ) ) ;
#27979 = CARTESIAN_POINT ( 'NONE',  ( -9.832129032723420536, 18.69791666325268409, 5.676582343749997150 ) ) ;
#27980 = CARTESIAN_POINT ( 'NONE',  ( 11.00000000000000000, 4.556349186104045934, 90.53125000409676204 ) ) ;
#27981 = CARTESIAN_POINT ( 'NONE',  ( 10.00000000000000000, 209.7916666666666856, 2.679491924311236062 ) ) ;
#27982 = CARTESIAN_POINT ( 'NONE',  ( -31.45873412500002075, 197.6250000013656063, 168.5673454167828140 ) ) ;
#27983 = DIRECTION ( 'NONE',  ( 0.000000000000000000, 0.000000000000000000, -1.000000000000000000 ) ) ;
#27985 = CARTESIAN_POINT ( 'NONE',  ( -9.832129032723420536, 3.697916663252683200, 5.676582343749997150 ) ) ;
#27984 = CARTESIAN_POINT ( 'NONE',  ( 5.082755093536325042, 110.0937500020483810, -5.082755093536325930 ) ) ;
#27986 = CARTESIAN_POINT ( 'NONE',  ( 7.999999999999992895, -3.313708498984756279, 23.98655277982336642 ) ) ;
#27987 = VECTOR ( 'NONE', #22763, 1000.000000000000000 ) ;
#27988 = CARTESIAN_POINT ( 'NONE',  ( -2.085542519210945728E-15, 134.5312499965860411, 11.35316468750000141 ) ) ;
#27989 = CARTESIAN_POINT ( 'NONE',  ( -2.679491924311225848, 98.33333332650538239, -10.00000000000000178 ) ) ;
#27990 = CARTESIAN_POINT ( 'NONE',  ( 7.188101187500002709, 119.1875000020483810, 2.977408999572649151 ) ) ;
#27991 = CARTESIAN_POINT ( 'NONE',  ( -29.43265458321761230, 208.1250000013656063, 173.4587341250003760 ) ) ;
#27992 = CARTESIAN_POINT ( 'NONE',  ( -5.000000000000000888, 53.57132521838762074, -46.19376297453450775 ) ) ;
#27993 = ORIENTED_EDGE ( 'NONE', *, *, #35372, .T. ) ;
#27994 = CARTESIAN_POINT ( 'NONE',  ( -0.7581620860326259148, -65.76154746681233121, 26.27794529687887604 ) ) ;
#27995 = CARTESIAN_POINT ( 'NONE',  ( 3.313708498984706985, 108.0312500000000000, -8.000000000000055067 ) ) ;
#27996 = CARTESIAN_POINT ( 'NONE',  ( 6.676582343750004256, 290.0468750017070079, 2.765530957081995478 ) ) ;
#27997 = CARTESIAN_POINT ( 'NONE',  ( 2.775557561562891351E-14, 210.0000000000000284, 198.0000000000000284 ) ) ;
#27998 = CARTESIAN_POINT ( 'NONE',  ( 1.469576158976822172E-15, -7.999999999999991118, 23.76155278432982598 ) ) ;
#27999 = LINE ( 'NONE', #33306, #4433 ) ;
#28000 = CARTESIAN_POINT ( 'NONE',  ( 8.000000000000000000, 103.2500000000000000, -9.797174393178825657E-16 ) ) ;
#28001 = CARTESIAN_POINT ( 'NONE',  ( 4.220049686691941027, -10.18810118749999738, 95.50000000204838102 ) ) ;
#28002 = EDGE_LOOP ( 'NONE', ( #622, #57631, #12203, #52962 ) ) ;
#28003 = VECTOR ( 'NONE', #4663, 1000.000000000000000 ) ;
#28004 = DIRECTION ( 'NONE',  ( -0.000000000000000000, -1.000000000000000000, -0.000000000000000000 ) ) ;
#28005 = DIRECTION ( 'NONE',  ( 0.000000000000000000, 0.000000000000000000, 1.000000000000000000 ) ) ;
#28006 = CARTESIAN_POINT ( 'NONE',  ( -2.445694354108784108, 200.5625000013656063, 195.5543056458912190 ) ) ;
#28007 = CARTESIAN_POINT ( 'NONE',  ( -11.35316468750000141, 73.80208332991935549, 3.042071309553159963 ) ) ;
#28008 = ORIENTED_EDGE ( 'NONE', *, *, #67405, .F. ) ;
#28009 = CARTESIAN_POINT ( 'NONE',  ( 7.204075437095968759, -7.204075437095966983, 111.7187500020483810 ) ) ;
#28010 = CARTESIAN_POINT ( 'NONE',  ( -1.881053915767121776, 11.74999999863440792, -4.541265875000002339 ) ) ;
#28011 = ORIENTED_EDGE ( 'NONE', *, *, #47224, .F. ) ;
#28012 = CARTESIAN_POINT ( 'NONE',  ( 5.082755093536324154, 24.28124999795161543, 5.082755093536326818 ) ) ;
#28013 = CARTESIAN_POINT ( 'NONE',  ( 7.999999999999991118, 9.797174393178815797E-16, 12.08030277982336642 ) ) ;
#28014 = CARTESIAN_POINT ( 'NONE',  ( -5.082755093536326818, 24.28124999795161543, 5.082755093536325042 ) ) ;
#28015 = DIRECTION ( 'NONE',  ( -0.000000000000000000, -1.000000000000000000, -4.283267841918042741E-17 ) ) ;
#28016 = CARTESIAN_POINT ( 'NONE',  ( 7.204075437095968759, -7.204075437095966983, 112.0937500020483810 ) ) ;
#28017 = VECTOR ( 'NONE', #51571, 1000.000000000000000 ) ;
#28018 =( BOUNDED_CURVE ( )  B_SPLINE_CURVE ( 2, ( #67331, #74100, #22398, #34132, #57132, #33759, #68073, #50710, #62036, #9989, #33021 ),
 .UNSPECIFIED., .F., .F. ) 
 B_SPLINE_CURVE_WITH_KNOTS ( ( 3, 2, 2, 2, 2, 3 ),
 ( 0.4500427433262104704, 0.4566610153275200701, 0.4632792909119768376, 0.4698975664964336607, 0.4765158420808904283, 0.4765158731794318925 ),
 .UNSPECIFIED. ) 
 CURVE ( )  GEOMETRIC_REPRESENTATION_ITEM ( )  RATIONAL_B_SPLINE_CURVE ( ( 1.000000000000000000, 0.9238795325112867385, 1.000000000000000000, 0.9238795325112867385, 1.000000000000000000, 0.9238795325112867385, 1.000000000000000000, 0.9238795325112867385, 1.000000000000000000, 0.9999996423183825645, 0.9999992846401264401 ) ) 
 REPRESENTATION_ITEM ( '' )  );
#28019 = DIRECTION ( 'NONE',  ( 0.000000000000000000, 0.000000000000000000, 1.000000000000000000 ) ) ;
#28020 = CARTESIAN_POINT ( 'NONE',  ( -7.347880794884122694E-16, 11.49999999726881406, 4.000000000000001776 ) ) ;
#28021 =( BOUNDED_CURVE ( )  B_SPLINE_CURVE ( 2, ( #50872, #11263, #28238, #68227, #16147, #12006, #40676, #34669, #45960 ),
 .UNSPECIFIED., .F., .F. ) 
 B_SPLINE_CURVE_WITH_KNOTS ( ( 3, 2, 2, 2, 3 ),
 ( 0.2812499999999997780, 0.2864583333333330928, 0.2916666666666665186, 0.2968749999999998335, 0.3020833333333331483 ),
 .UNSPECIFIED. ) 
 CURVE ( )  GEOMETRIC_REPRESENTATION_ITEM ( )  RATIONAL_B_SPLINE_CURVE ( ( 1.000000000000003331, 0.9238795325112835188, 1.000000000000000000, 0.9238795325112867385, 1.000000000000000000, 0.9238795325112867385, 1.000000000000000000, 0.9238795325112891810, 0.9999999999999975575 ) ) 
 REPRESENTATION_ITEM ( '' )  );
#28022 = CARTESIAN_POINT ( 'NONE',  ( 11.00000000000000000, 1.347111479062088405E-15, 112.7499999999999858 ) ) ;
#28023 = ORIENTED_EDGE ( 'NONE', *, *, #3084, .T. ) ;
#28024 = CARTESIAN_POINT ( 'NONE',  ( -1.432654583217607858, 202.6250000013656063, 201.4587341250000065 ) ) ;
#28025 = AXIS2_PLACEMENT_3D ( 'NONE', #32991, #4676, #37514 ) ;
#28026 = CARTESIAN_POINT ( 'NONE',  ( -25.55430564589111953, 206.0625000013656063, 172.4456943541091505 ) ) ;
#28027 = CARTESIAN_POINT ( 'NONE',  ( 3.999999999999960032, 207.0000000000000284, 142.0000000000000568 ) ) ;
#28028 = CARTESIAN_POINT ( 'NONE',  ( 3.211159895383561835, 11.43749999863440614, -3.211159895383561835 ) ) ;
#28029 = CARTESIAN_POINT ( 'NONE',  ( -1.656854249492381248, 18.06249999726881938, -4.000000000000001776 ) ) ;
#28030 = CARTESIAN_POINT ( 'NONE',  ( -4.401442555609577197E-16, 7.188101187499992051, 20.61155278187175455 ) ) ;
#28031 = ORIENTED_EDGE ( 'NONE', *, *, #43390, .F. ) ;
#28032 = CARTESIAN_POINT ( 'NONE',  ( 2.449293598294707893E-16, 20.99999999726881583, -4.000000000000001776 ) ) ;
#28033 = VERTEX_POINT ( 'NONE', #22982 ) ;
#28034 = CARTESIAN_POINT ( 'NONE',  ( -10.18810118749999916, 4.220049686691934809, 109.5625000020483810 ) ) ;
#28035 = CARTESIAN_POINT ( 'NONE',  ( 26.34314575050759188, 208.6875000027311842, 165.9999999999998295 ) ) ;
#28036 = CARTESIAN_POINT ( 'NONE',  ( 2.445694354108839619, 203.8125000013656063, 200.4456943541088663 ) ) ;
#28037 = CARTESIAN_POINT ( 'NONE',  ( 26.56734541678237704, 200.3750000013656063, 173.4587341249998929 ) ) ;
#28038 = CARTESIAN_POINT ( 'NONE',  ( 8.660254037844389075, 75.41666666666667140, -5.000000000000000000 ) ) ;
#28039 = CARTESIAN_POINT ( 'NONE',  ( 3.313708498984765161, 122.4687500000000000, 7.999999999999998224 ) ) ;
#28040 = CARTESIAN_POINT ( 'NONE',  ( -6.676582343750003368, 299.5468750017069510, -2.765530957081996810 ) ) ;
#28041 = ADVANCED_FACE ( 'NONE', ( #14065 ), #11292, .T. ) ;
#28042 = VERTEX_POINT ( 'NONE', #64463 ) ;
#28043 = DIRECTION ( 'NONE',  ( 1.000000000000000000, -0.000000000000000000, -0.000000000000000000 ) ) ;
#28044 = CARTESIAN_POINT ( 'NONE',  ( -4.104248244567244797, -66.38464254922357100, 26.65807398666778738 ) ) ;
#28045 = CARTESIAN_POINT ( 'NONE',  ( 1.656854249492347719, 197.9375000027312410, 146.0000000000000284 ) ) ;
#28046 = CARTESIAN_POINT ( 'NONE',  ( 11.00000000000000000, 1.347111479062088405E-15, 91.74999999999998579 ) ) ;
#28047 = CARTESIAN_POINT ( 'NONE',  ( 2.849036369511732440E-14, 203.3750000027312126, 202.0000000000000000 ) ) ;
#28048 = CARTESIAN_POINT ( 'NONE',  ( 8.660254037844389075, 232.0833333333333428, 4.999999999999997335 ) ) ;
#28049 = CARTESIAN_POINT ( 'NONE',  ( 30.82842712474617031, 204.1250000000000284, 172.8284271247460993 ) ) ;
#28050 = CARTESIAN_POINT ( 'NONE',  ( -8.660254037844387298, 202.0833333333333428, -5.000000000000004441 ) ) ;
#28051 = EDGE_CURVE ( 'NONE', #31217, #67743, #64976, .T. ) ;
#28052 = CARTESIAN_POINT ( 'NONE',  ( 7.188101187499993827, -2.977408999572645598, 14.51780278187175455 ) ) ;
#28053 = CARTESIAN_POINT ( 'NONE',  ( -5.676582343749998039, 172.7604166632526983, -9.832129032723420536 ) ) ;
#28054 = DIRECTION ( 'NONE',  ( -0.000000000000000000, -0.000000000000000000, -1.000000000000000000 ) ) ;
#28055 = DIRECTION ( 'NONE',  ( 0.000000000000000000, 0.000000000000000000, 1.000000000000000000 ) ) ;
#28057 = DIRECTION ( 'NONE',  ( 0.000000000000000000, 0.000000000000000000, 1.000000000000000000 ) ) ;
#28056 = FACE_OUTER_BOUND ( 'NONE', #18798, .T. ) ;
#28058 = ORIENTED_EDGE ( 'NONE', *, *, #35388, .F. ) ;
#28059 = CARTESIAN_POINT ( 'NONE',  ( 3.042071309553167069, 27.13541666325268409, -11.35316468749999785 ) ) ;
#28060 = CARTESIAN_POINT ( 'NONE',  ( 7.778174593052023411, -7.778174593052021635, 111.2500000040967763 ) ) ;
#28061 = CARTESIAN_POINT ( 'NONE',  ( -23.99999999999998934, 200.7500000000000000, 170.0000000000003411 ) ) ;
#28063 = CARTESIAN_POINT ( 'NONE',  ( -2.436599634634027289, -16.39988855009439561, -68.84456747601407756 ) ) ;
#28062 = CARTESIAN_POINT ( 'NONE',  ( -18.00000000000000355, 7.009507535100746978, -0.7186345456308798063 ) ) ;
#28064 = CARTESIAN_POINT ( 'NONE',  ( -11.35016239271863903, -35.84841446392682229, 198.8478103360236844 ) ) ;
#28065 = CARTESIAN_POINT ( 'NONE',  ( -2.445694354108838731, 197.0625000013656063, 144.4456943541088663 ) ) ;
#28066 = CARTESIAN_POINT ( 'NONE',  ( 6.123233995736767268E-16, 58.12499999317203248, -10.00000000000000178 ) ) ;
#28067 = CARTESIAN_POINT ( 'NONE',  ( 5.082755093536326818, 102.2187500020483810, 5.082755093536325042 ) ) ;
#28068 = CARTESIAN_POINT ( 'NONE',  ( -1.881053915767121554, 10.74999999863440969, -4.541265875000002339 ) ) ;
#28069 = CARTESIAN_POINT ( 'NONE',  ( 27.99999999999999645, 210.0000000000000284, 173.9999999999998863 ) ) ;
#28070 = CARTESIAN_POINT ( 'NONE',  ( 7.513779688745833241, 0.2176969057608504621, -1.780879344281421472 ) ) ;
#28071 = DIRECTION ( 'NONE',  ( 0.000000000000000000, 1.000000000000000000, 2.238352872228138170E-16 ) ) ;
#28072 = ORIENTED_EDGE ( 'NONE', *, *, #50100, .T. ) ;
#28073 = ORIENTED_EDGE ( 'NONE', *, *, #52180, .F. ) ;
#28074 = CARTESIAN_POINT ( 'NONE',  ( -3.458734124999959469, 195.7500000013656063, 199.4326545832176976 ) ) ;
#28075 = CARTESIAN_POINT ( 'NONE',  ( -2.679491924311961704, 86.45833333333341386, -9.999999999999579003 ) ) ;
#28076 = AXIS2_PLACEMENT_3D ( 'NONE', #25852, #20194, #8896 ) ;
#28077 = CARTESIAN_POINT ( 'NONE',  ( 5.676582343750001591, 146.6145833299193555, -9.832129032723420536 ) ) ;
#28078 = ORIENTED_EDGE ( 'NONE', *, *, #54865, .F. ) ;
#28079 = CARTESIAN_POINT ( 'NONE',  ( -5.000000000000000000, 10.38759426015435139, -65.74583990312709147 ) ) ;
#28080 = CARTESIAN_POINT ( 'NONE',  ( -7.204075437095965206, -7.204075437095968759, 88.84375000204838102 ) ) ;
#28081 = CARTESIAN_POINT ( 'NONE',  ( -1.469576158976823947E-15, 4.125000000000000888, 8.000000000000000000 ) ) ;
#28082 = CARTESIAN_POINT ( 'NONE',  ( 4.000000000000015099, 207.5625000000000284, 196.3431457505076594 ) ) ;
#28083 = CARTESIAN_POINT ( 'NONE',  ( 1.656854249492466735, 195.1875000000000000, 138.0000000000001705 ) ) ;
#28084 = CARTESIAN_POINT ( 'NONE',  ( -7.204075437095965206, -7.204075437095968759, 114.7187500020483810 ) ) ;
#28085 = ORIENTED_EDGE ( 'NONE', *, *, #57635, .T. ) ;
#28086 = CARTESIAN_POINT ( 'NONE',  ( -2.775557561562891351E-14, 210.0000000000000284, 146.0000000000000284 ) ) ;
#28087 = CARTESIAN_POINT ( 'NONE',  ( 29.34617108035431698, 180.6013230617538738, 159.7592319357839585 ) ) ;
#28088 = CARTESIAN_POINT ( 'NONE',  ( -5.676582343749998039, 132.7604166632526983, -9.832129032723420536 ) ) ;
#28089 = CARTESIAN_POINT ( 'NONE',  ( 2.445694354108838731, 202.0625000013656063, 195.5543056458912190 ) ) ;
#28090 = CARTESIAN_POINT ( 'NONE',  ( -5.082755093536325042, 25.40624999795161543, -5.082755093536325930 ) ) ;
#28091 = CARTESIAN_POINT ( 'NONE',  ( -10.18810118749999916, 4.220049686691934809, 81.43750000204836681 ) ) ;
#28092 = CARTESIAN_POINT ( 'NONE',  ( 6.951808397369818766E-16, 42.34374999658601979, -11.35316468750000141 ) ) ;
#28093 = VERTEX_POINT ( 'NONE', #28268 ) ;
#28094 = DIRECTION ( 'NONE',  ( 0.000000000000000000, 0.000000000000000000, 1.000000000000000000 ) ) ;
#28095 = CARTESIAN_POINT ( 'NONE',  ( -2.679491924311235174, 195.4166666598387394, 10.00000000000000000 ) ) ;
#28096 = CARTESIAN_POINT ( 'NONE',  ( -4.903558642999205574E-16, 8.008118988124991233, 20.13811528394062833 ) ) ;
#28097 = CARTESIAN_POINT ( 'NONE',  ( -2.445694354108839175, 206.3125000013656063, 144.4456943541088663 ) ) ;
#28098 = CARTESIAN_POINT ( 'NONE',  ( -7.188101187500000044, 11.71874999795161010, -8.802885111219163269E-16 ) ) ;
#28099 = CARTESIAN_POINT ( 'NONE',  ( 1.102182119232618108E-15, 295.3125000034140157, 6.000000000000001776 ) ) ;
#28100 = CARTESIAN_POINT ( 'NONE',  ( -23.97267925649051534, -13.27111351839745979, 137.7942046442823028 ) ) ;
#28101 = CARTESIAN_POINT ( 'NONE',  ( 4.401442555609581635E-16, 7.218749997951610986, -7.188101187500000044 ) ) ;
#28102 = CARTESIAN_POINT ( 'NONE',  ( -9.832129032723418760, 158.1770833299193555, -5.676582343750004256 ) ) ;
#28103 = B_SPLINE_CURVE_WITH_KNOTS ( 'NONE', 3,
 ( #59353, #30670, #55186, #21205, #26480, #54808, #15539, #20073 ),
 .UNSPECIFIED., .F., .F.,
 ( 4, 2, 2, 4 ),
 ( 0.005257893453559874149, 0.006567392922673220834, 0.007876892391786566652, 0.01049589133001326002 ),
 .UNSPECIFIED. ) ;
#28104 = CARTESIAN_POINT ( 'NONE',  ( 4.220049686691941027, -10.18810118749999738, 80.12500000204835260 ) ) ;
#28105 = AXIS2_PLACEMENT_3D ( 'NONE', #36805, #71859, #37174 ) ;
#28106 = CARTESIAN_POINT ( 'NONE',  ( -25.55430564589119058, 195.3125000013656063, 167.5543056458915316 ) ) ;
#28107 = DIRECTION ( 'NONE',  ( -0.000000000000000000, -1.000000000000000000, -0.000000000000000000 ) ) ;
#28108 = CARTESIAN_POINT ( 'NONE',  ( -3.211159895383562723, 19.06249999863440436, 3.211159895383561391 ) ) ;
#28109 = EDGE_LOOP ( 'NONE', ( #73237, #23122, #45724, #33603 ) ) ;
#28110 = CARTESIAN_POINT ( 'NONE',  ( 4.000000000000015987, 197.5625000027312126, 199.6568542494924259 ) ) ;
#28111 =( BOUNDED_CURVE ( )  B_SPLINE_CURVE ( 2, ( #43134, #60492, #8818, #31830, #54849, #14829, #57464, #6513, #68021 ),
 .UNSPECIFIED., .F., .F. ) 
 B_SPLINE_CURVE_WITH_KNOTS ( ( 3, 2, 2, 2, 3 ),
 ( 0.3333333333333336479, 0.3416666666666670071, 0.3500000000000003109, 0.3583333333333336701, 0.3666666666666669738 ),
 .UNSPECIFIED. ) 
 CURVE ( )  GEOMETRIC_REPRESENTATION_ITEM ( )  RATIONAL_B_SPLINE_CURVE ( ( 0.9999999999999970024, 0.9238795325112897361, 1.000000000000000000, 0.9238795325112867385, 1.000000000000000000, 0.9238795325112867385, 1.000000000000000000, 0.9238795325112837409, 1.000000000000003109 ) ) 
 REPRESENTATION_ITEM ( '' )  );
#28112 = CARTESIAN_POINT ( 'NONE',  ( 3.458734124999960358, 196.6250000013656063, 143.4326545832176976 ) ) ;
#28113 = CARTESIAN_POINT ( 'NONE',  ( -29.65685424949245785, 204.1875000027312126, 166.0000000000004263 ) ) ;
#28114 = EDGE_CURVE ( 'NONE', #51815, #60780, #57806, .T. ) ;
#28115 = EDGE_CURVE ( 'NONE', #69413, #73838, #66790, .T. ) ;
#28116 = CARTESIAN_POINT ( 'NONE',  ( -11.00000000000000000, 0.000000000000000000, 94.18750000409677625 ) ) ;
#28117 = EDGE_LOOP ( 'NONE', ( #22038, #71106, #2955, #27753 ) ) ;
#28118 = CARTESIAN_POINT ( 'NONE',  ( 2.977408999572652260, 16.68749999795161543, 7.188101187500000044 ) ) ;
#28119 = FACE_OUTER_BOUND ( 'NONE', #54302, .T. ) ;
#28120 = CARTESIAN_POINT ( 'NONE',  ( -1.982243585727051727, -47.26028742471972777, 151.1031732575197566 ) ) ;
#28121 = CARTESIAN_POINT ( 'NONE',  ( -7.320508075688778149, 43.12500000000000000, 7.320508075688769267 ) ) ;
#28122 = AXIS2_PLACEMENT_3D ( 'NONE', #6189, #69557, #17868 ) ;
#28123 = CARTESIAN_POINT ( 'NONE',  ( 7.188101187500001821, 104.3750000020483952, -2.977408999572651371 ) ) ;
#28124 = CARTESIAN_POINT ( 'NONE',  ( -25.55430564589115505, 207.3125000013656063, 172.4456943541091789 ) ) ;
#28125 = CARTESIAN_POINT ( 'NONE',  ( -4.088227598258586603E-16, 290.2031250017069510, -6.676582343750001591 ) ) ;
#28127 = CARTESIAN_POINT ( 'NONE',  ( -7.118986530994914297, -3.658836280118772599, 0.000000000000000000 ) ) ;
#28126 = CARTESIAN_POINT ( 'NONE',  ( 9.999999999999998224, 34.79166666666667140, 2.679491924311235174 ) ) ;
#28128 = EDGE_LOOP ( 'NONE', ( #39630, #24805, #5102, #6692, #34003, #52720 ) ) ;
#28129 =( BOUNDED_CURVE ( )  B_SPLINE_CURVE ( 2, ( #15354, #9341, #54626, #2935, #19898, #21393, #25921, #37647, #49704 ),
 .UNSPECIFIED., .F., .F. ) 
 B_SPLINE_CURVE_WITH_KNOTS ( ( 3, 2, 2, 2, 3 ),
 ( 0.05208333333333337034, 0.05729166666666669905, 0.06250000000000004163, 0.06770833333333337034, 0.07291666666666671293 ),
 .UNSPECIFIED. ) 
 CURVE ( )  GEOMETRIC_REPRESENTATION_ITEM ( )  RATIONAL_B_SPLINE_CURVE ( ( 0.9999999999999994449, 0.9238795325112872936, 1.000000000000000000, 0.9238795325112867385, 1.000000000000000000, 0.9238795325112867385, 1.000000000000000000, 0.9238795325112861834, 1.000000000000000666 ) ) 
 REPRESENTATION_ITEM ( '' )  );
#28130 = CARTESIAN_POINT ( 'NONE',  ( 11.35316468749999608, 261.6145833367473301, -3.042071309553167069 ) ) ;
#28131 = CARTESIAN_POINT ( 'NONE',  ( -7.188101187499990274, -2.977408999572651371, 21.45530278187175810 ) ) ;
#28132 = CARTESIAN_POINT ( 'NONE',  ( 6.123233995736767268E-16, 8.124999993172032475, -10.00000000000000178 ) ) ;
#28133 = CARTESIAN_POINT ( 'NONE',  ( -3.999999999999960032, 209.5625000013656063, 198.0000000000000284 ) ) ;
#28134 = FACE_OUTER_BOUND ( 'NONE', #49580, .T. ) ;
#28135 = CARTESIAN_POINT ( 'NONE',  ( 1.432654583217664701, 197.0000000013656347, 201.4587341250000065 ) ) ;
#28136 = CARTESIAN_POINT ( 'NONE',  ( 8.660254037844385522, 164.5833333333333428, 5.000000000000005329 ) ) ;
#28137 = CARTESIAN_POINT ( 'NONE',  ( -2.485281374238990093, 299.8124999999999432, -5.999999999999583444 ) ) ;
#28138 = CARTESIAN_POINT ( 'NONE',  ( -2.947441116742341105, 219.7440169426842544, 11.00000000000000355 ) ) ;
#28139 = CARTESIAN_POINT ( 'NONE',  ( 5.000000000000000888, -53.12474899268170248, -47.87640533067879289 ) ) ;
#28140 = CARTESIAN_POINT ( 'NONE',  ( -11.35316468749999785, 133.3854166632526699, -3.042071309553167513 ) ) ;
#28141 = DIRECTION ( 'NONE',  ( 1.000000000000000000, -0.000000000000000000, -0.000000000000000000 ) ) ;
#28142 = CARTESIAN_POINT ( 'NONE',  ( 1.736494649845409910, -16.42394793108440254, -68.69316892220882664 ) ) ;
#28145 = DIRECTION ( 'NONE',  ( -0.000000000000000000, 1.000000000000000000, -0.000000000000000000 ) ) ;
#28144 = CARTESIAN_POINT ( 'NONE',  ( 27.99999999999996447, 195.9375000013655779, 166.5412658749999082 ) ) ;
#28143 = CARTESIAN_POINT ( 'NONE',  ( 28.00000000000002132, 209.5000000000000284, 165.9999999999998863 ) ) ;
#28146 = ORIENTED_EDGE ( 'NONE', *, *, #5394, .F. ) ;
#28147 = CARTESIAN_POINT ( 'NONE',  ( 9.015042500306268636, 224.6398387169884074, 4.368317829918140660 ) ) ;
#28148 = EDGE_CURVE ( 'NONE', #44095, #48616, #2354, .T. ) ;
#28149 = CARTESIAN_POINT ( 'NONE',  ( 11.00000000000000000, 1.347111479062088405E-15, 88.93750000409677625 ) ) ;
#28150 = DIRECTION ( 'NONE',  ( 0.000000000000000000, 0.000000000000000000, 1.000000000000000000 ) ) ;
#28151 = CARTESIAN_POINT ( 'NONE',  ( -2.751064625579944321E-14, 198.7500000000000000, 146.0000000000000284 ) ) ;
#28152 = CARTESIAN_POINT ( 'NONE',  ( 11.35316468749999963, 211.3020833299193839, -3.042071309553165293 ) ) ;
#28153 =( BOUNDED_CURVE ( )  B_SPLINE_CURVE ( 2, ( #2388, #42004, #7318, #59740, #8048, #31053, #53711, #30324, #53342 ),
 .UNSPECIFIED., .F., .F. ) 
 B_SPLINE_CURVE_WITH_KNOTS ( ( 3, 2, 2, 2, 3 ),
 ( 0.5526315789473684736, 0.5592105263157894912, 0.5657894736842106198, 0.5723684210526316374, 0.5789473684210527660 ),
 .UNSPECIFIED. ) 
 CURVE ( )  GEOMETRIC_REPRESENTATION_ITEM ( )  RATIONAL_B_SPLINE_CURVE ( ( 1.000000000000000000, 0.9238795325112867385, 1.000000000000000000, 0.9238795325112867385, 1.000000000000000000, 0.9238795325112867385, 1.000000000000000000, 0.9238795325112854062, 1.000000000000001332 ) ) 
 REPRESENTATION_ITEM ( '' )  );
#28154 = AXIS2_PLACEMENT_3D ( 'NONE', #19369, #9564, #55218 ) ;
#28155 = CARTESIAN_POINT ( 'NONE',  ( -5.082755093536325930, 120.9687500020483952, -5.082755093536325930 ) ) ;
#28156 = CARTESIAN_POINT ( 'NONE',  ( -3.211159895383562723, 1.062499998634406806, 3.211159895383561391 ) ) ;
#28157 = CARTESIAN_POINT ( 'NONE',  ( -2.997005883571752349, -55.94527535363520343, 43.97975057405725607 ) ) ;
#28158 = CARTESIAN_POINT ( 'NONE',  ( -5.656854249492375253, 5.656854249492375253, 20.14280277982336642 ) ) ;
#28160 = DIRECTION ( 'NONE',  ( -0.000000000000000000, 1.000000000000000000, -0.000000000000000000 ) ) ;
#28159 = DIRECTION ( 'NONE',  ( 0.000000000000000000, -0.02418647091589873691, -0.9997074645238147594 ) ) ;
#28161 = CARTESIAN_POINT ( 'NONE',  ( 5.676582343749993598, 89.94791666325269830, 9.832129032723422313 ) ) ;
#28162 = ORIENTED_EDGE ( 'NONE', *, *, #21630, .F. ) ;
#28163 = CARTESIAN_POINT ( 'NONE',  ( -8.000000000000003553, 22.99999999999999645, 1.000000000000000000 ) ) ;
#28164 = CARTESIAN_POINT ( 'NONE',  ( 2.977408999572650927, 26.24999999795161898, -7.188101187500001821 ) ) ;
#28165 = DIRECTION ( 'NONE',  ( -0.000000000000000000, -1.000000000000000000, -0.000000000000000000 ) ) ;
#28166 = CARTESIAN_POINT ( 'NONE',  ( -11.35316468749999963, 259.2187500034140157, 0.000000000000000000 ) ) ;
#28167 = CARTESIAN_POINT ( 'NONE',  ( -8.311093377946836114, 102.6562499965860269, -8.311093377946837890 ) ) ;
#28168 = VERTEX_POINT ( 'NONE', #40330 ) ;
#28169 = CARTESIAN_POINT ( 'NONE',  ( 9.797174393178825657E-16, 125.0000000000000000, -8.000000000000000000 ) ) ;
#28170 = CARTESIAN_POINT ( 'NONE',  ( 10.18810118749999916, 4.220049686691935698, 104.5000000020483668 ) ) ;
#28171 = CARTESIAN_POINT ( 'NONE',  ( -10.00000000000000355, 224.5833333265053398, 2.679491924311223183 ) ) ;
#28172 = CARTESIAN_POINT ( 'NONE',  ( 1.432654583217664701, 206.0000000013656347, 201.4587341250000065 ) ) ;
#28173 = CARTESIAN_POINT ( 'NONE',  ( 18.00000000000000000, -6.968949133139053842, -0.7423331077269011979 ) ) ;
#28175 = CARTESIAN_POINT ( 'NONE',  ( 8.311093377946834337, 105.1562499965860269, 8.311093377946839666 ) ) ;
#28174 = CARTESIAN_POINT ( 'NONE',  ( -10.99999999999999822, -4.556349186104053040, 97.09375000000001421 ) ) ;
#28176 = CARTESIAN_POINT ( 'NONE',  ( 1.469576158976822172E-15, -7.999999999999991118, 11.89280278392014445 ) ) ;
#28177 = CARTESIAN_POINT ( 'NONE',  ( -27.99999999999996447, 201.1875000013656063, 173.4587341250003760 ) ) ;
#28178 = DIRECTION ( 'NONE',  ( -0.000000000000000000, 1.000000000000000000, -0.000000000000000000 ) ) ;
#28179 = ORIENTED_EDGE ( 'NONE', *, *, #39043, .T. ) ;
#28180 = CARTESIAN_POINT ( 'NONE',  ( -10.00000000000000178, 184.3749999931720538, -1.224646799147353454E-15 ) ) ;
#28181 = CARTESIAN_POINT ( 'NONE',  ( -2.849036369511732440E-14, 208.2500000000000284, 138.0000000000000568 ) ) ;
#28182 = DIRECTION ( 'NONE',  ( 0.000000000000000000, 0.000000000000000000, 1.000000000000000000 ) ) ;
#28183 = CARTESIAN_POINT ( 'NONE',  ( 9.832129032723416984, 90.67708332991934128, 5.676582343750006032 ) ) ;
#28184 = CARTESIAN_POINT ( 'NONE',  ( 6.676582343750004256, 288.8906250017070079, 2.765530957081995478 ) ) ;
#28185 = CARTESIAN_POINT ( 'NONE',  ( 7.188101187500000044, 3.843749997951610542, 0.000000000000000000 ) ) ;
#28186 = B_SPLINE_CURVE_WITH_KNOTS ( 'NONE', 3,
 ( #41385, #34255, #57257, #48133, #71880, #59112, #7420, #30427, #66231, #31910 ),
 .UNSPECIFIED., .F., .F.,
 ( 4, 2, 2, 2, 4 ),
 ( 0.000000000000000000, 0.001314083742615275224, 0.002628167485230550448, 0.003942251227845825455, 0.005256334970461100896 ),
 .UNSPECIFIED. ) ;
#28187 = CARTESIAN_POINT ( 'NONE',  ( 10.18810118749999916, 4.220049686691935698, 100.3750000020483952 ) ) ;
#28188 = CARTESIAN_POINT ( 'NONE',  ( 11.35316468750000141, 225.7812499965860127, 0.000000000000000000 ) ) ;
#28189 = ORIENTED_EDGE ( 'NONE', *, *, #29148, .T. ) ;
#28190 = CARTESIAN_POINT ( 'NONE',  ( -4.999999999999998224, 68.54166665983869677, -8.660254037844389075 ) ) ;
#28191 = CARTESIAN_POINT ( 'NONE',  ( -5.000000000000000000, -60.90295814858257017, 23.31388853594792820 ) ) ;
#28192 = CARTESIAN_POINT ( 'NONE',  ( -5.656854249492380582, 120.3125000000000000, -5.656854249492380582 ) ) ;
#28193 = CARTESIAN_POINT ( 'NONE',  ( -11.35316468750000141, 208.2812499965860411, -1.390361679473963753E-15 ) ) ;
#28194 = CARTESIAN_POINT ( 'NONE',  ( 8.660254037844389075, 230.2083333401612890, 4.999999999999997335 ) ) ;
#28195 = CARTESIAN_POINT ( 'NONE',  ( -10.00000000000000355, 99.58333332650536818, 2.679491924311223183 ) ) ;
#28196 = CARTESIAN_POINT ( 'NONE',  ( 1.226468279477575784E-15, 297.7031250017070079, 6.676582343750001591 ) ) ;
#28197 = VERTEX_POINT ( 'NONE', #52769 ) ;
#28198 = CARTESIAN_POINT ( 'NONE',  ( -8.311093377946841443, 189.2187499965860411, 8.311093377946834337 ) ) ;
#28199 = CARTESIAN_POINT ( 'NONE',  ( 7.204075437095966983, 7.204075437095967871, 94.09375000204838102 ) ) ;
#28200 = EDGE_CURVE ( 'NONE', #21048, #31338, #39963, .T. ) ;
#28201 = CARTESIAN_POINT ( 'NONE',  ( -24.54126587499999701, 206.1875000013656063, 170.0000000000003411 ) ) ;
#28202 = CARTESIAN_POINT ( 'NONE',  ( 8.000000000000000000, 19.50000000000000355, 0.000000000000000000 ) ) ;
#28203 = VERTEX_POINT ( 'NONE', #6010 ) ;
#28204 = PRODUCT_DEFINITION_CONTEXT ( 'detailed design', #27958, 'design' ) ;
#28205 = CARTESIAN_POINT ( 'NONE',  ( -3.313708498984762052, 90.40625000409676204, -8.000000000000000000 ) ) ;
#28206 = DIRECTION ( 'NONE',  ( 0.000000000000000000, -3.469446951953613400E-15, 1.000000000000000000 ) ) ;
#28207 = CARTESIAN_POINT ( 'NONE',  ( -10.00000000000000355, 12.70833333333333570, 2.679491924311223183 ) ) ;
#28208 = VECTOR ( 'NONE', #11700, 1000.000000000000000 ) ;
#28209 = CARTESIAN_POINT ( 'NONE',  ( 7.204075437095966983, 7.204075437095967871, 77.96875000204836681 ) ) ;
#28210 = ORIENTED_EDGE ( 'NONE', *, *, #13597, .T. ) ;
#28211 = CARTESIAN_POINT ( 'NONE',  ( -4.000000000000001776, 21.43750000000000000, -1.656854249492381470 ) ) ;
#28212 = CARTESIAN_POINT ( 'NONE',  ( 2.828427124746190291, 2.624999997268812724, 2.828427124746192067 ) ) ;
#28213 = DIRECTION ( 'NONE',  ( -1.000000000000000000, -0.000000000000000000, -0.000000000000000000 ) ) ;
#28214 = EDGE_CURVE ( 'NONE', #20187, #42638, #33674, .T. ) ;
#28215 = ADVANCED_FACE ( 'NONE', ( #14233 ), #8593, .F. ) ;
#28216 = CARTESIAN_POINT ( 'NONE',  ( -7.347880794884122694E-16, 4.499999997268813168, 4.000000000000001776 ) ) ;
#28217 = CARTESIAN_POINT ( 'NONE',  ( 1.320432766682874540E-15, 123.4062500020483810, 7.188101187500000044 ) ) ;
#28218 = CARTESIAN_POINT ( 'NONE',  ( -1.836970198721029983E-15, 150.6249999931720538, 10.00000000000000178 ) ) ;
#28221 = CARTESIAN_POINT ( 'NONE',  ( 4.000000000000015987, 206.5625000000000000, 196.3431457505076594 ) ) ;
#28220 = CARTESIAN_POINT ( 'NONE',  ( 5.676582343750005144, 250.5729166700807014, 9.832129032723416984 ) ) ;
#28219 = CARTESIAN_POINT ( 'NONE',  ( 24.54126587499998635, 209.1250000013656347, 168.5673454167822740 ) ) ;
#28222 = APPLICATION_PROTOCOL_DEFINITION ( 'draft international standard', 'automotive_design', 1998, #39985 ) ;
#28223 = ORIENTED_EDGE ( 'NONE', *, *, #48223, .T. ) ;
#28224 = ADVANCED_FACE ( 'NONE', ( #30127 ), #19166, .F. ) ;
#28225 = CARTESIAN_POINT ( 'NONE',  ( 9.832129032723416984, 247.1354166700806445, -5.676582343750003368 ) ) ;
#28226 = CARTESIAN_POINT ( 'NONE',  ( 7.188101187499992051, 8.802885111219154394E-16, 12.73655278187175277 ) ) ;
#28227 = ORIENTED_EDGE ( 'NONE', *, *, #55900, .T. ) ;
#28228 =( BOUNDED_CURVE ( )  B_SPLINE_CURVE ( 2, ( #2340, #43822, #38171, #14760, #7999, #8365, #60044, #55155, #43061, #37800, #60421, #60795, #49475 ),
 .UNSPECIFIED., .F., .F. ) 
 B_SPLINE_CURVE_WITH_KNOTS ( ( 3, 2, 2, 2, 2, 2, 3 ),
 ( 0.7880434782608697342, 0.7898550724637682929, 0.7916666666666668517, 0.7934782608695654105, 0.7952898550724638582, 0.7971014492753624170, 0.7989130434782609758 ),
 .UNSPECIFIED. ) 
 CURVE ( )  GEOMETRIC_REPRESENTATION_ITEM ( )  RATIONAL_B_SPLINE_CURVE ( ( 0.9999999999999957812, 0.9659258262890725311, 1.000000000000000000, 0.9659258262890683122, 1.000000000000000000, 0.9659258262890683122, 1.000000000000000000, 0.9659258262890683122, 1.000000000000000000, 0.9659258262890683122, 1.000000000000000000, 0.9659258262890662028, 1.000000000000001998 ) ) 
 REPRESENTATION_ITEM ( '' )  );
#28229 = ORIENTED_EDGE ( 'NONE', *, *, #41835, .T. ) ;
#28230 = CARTESIAN_POINT ( 'NONE',  ( -10.18810118749999916, 4.220049686691934809, 76.56250000204836681 ) ) ;
#28231 = CARTESIAN_POINT ( 'NONE',  ( -5.676582343749998039, 92.76041666325268409, -9.832129032723420536 ) ) ;
#28232 = CARTESIAN_POINT ( 'NONE',  ( -15.04468117448323028, 12.09855896486652505, -0.7126204852947278789 ) ) ;
#28233 = CARTESIAN_POINT ( 'NONE',  ( -10.99999999999999822, -4.556349186104052151, 83.59375000000000000 ) ) ;
#28236 = CARTESIAN_POINT ( 'NONE',  ( 2.765530957082001251, 290.9218750017070647, 6.676582343749999815 ) ) ;
#28235 = CARTESIAN_POINT ( 'NONE',  ( 24.54126587499998635, 207.1250000013656347, 168.5673454167822740 ) ) ;
#28234 = CARTESIAN_POINT ( 'NONE',  ( 28.00000000000002487, 206.1875000013656063, 166.5412658749999082 ) ) ;
#28237 = VECTOR ( 'NONE', #62739, 1000.000000000000227 ) ;
#28238 = CARTESIAN_POINT ( 'NONE',  ( -5.656854249492378806, 114.6875000000000000, 5.656854249492381470 ) ) ;
#28239 = CARTESIAN_POINT ( 'NONE',  ( 4.529167459315944555, 225.9997407208379911, 8.915528146188176351 ) ) ;
#28240 = EDGE_CURVE ( 'NONE', #23989, #46215, #53354, .T. ) ;
#28241 = CARTESIAN_POINT ( 'NONE',  ( 3.042071309553167069, 201.8229166632526415, -11.35316468749999785 ) ) ;
#28242 = CARTESIAN_POINT ( 'NONE',  ( 5.656854249492378806, 8.624999995903221972, 5.656854249492381470 ) ) ;
#28243 = ORIENTED_EDGE ( 'NONE', *, *, #32388, .F. ) ;
#28244 = CARTESIAN_POINT ( 'NONE',  ( 30.44569435410883074, 196.8125000013656063, 167.5543056458911053 ) ) ;
#28245 = CARTESIAN_POINT ( 'NONE',  ( -5.082755093536325042, 19.40624999795161543, -5.082755093536325930 ) ) ;
#28246 = CARTESIAN_POINT ( 'NONE',  ( 5.676582343749993598, 170.2604166632526983, 9.832129032723422313 ) ) ;
#28247 = CARTESIAN_POINT ( 'NONE',  ( 11.00000000000010836, -4.556349186103939353, 99.34375000409680467 ) ) ;
#28248 = CARTESIAN_POINT ( 'NONE',  ( 7.188101187500002709, 101.1875000020483810, 2.977408999572649151 ) ) ;
#28250 = CARTESIAN_POINT ( 'NONE',  ( -6.123233995736766282E-16, 233.7500000000000000, -10.00000000000000000 ) ) ;
#28249 = CARTESIAN_POINT ( 'NONE',  ( 2.751064625579944321E-14, 206.8750000027312126, 194.0000000000000568 ) ) ;
#28251 = CARTESIAN_POINT ( 'NONE',  ( 27.99999999999996447, 205.6875000013656063, 173.4587341249998929 ) ) ;
#28252 = CARTESIAN_POINT ( 'NONE',  ( -2.977408999572647819, 7.188101187499991163, 12.08030278187175099 ) ) ;
#28253 = CARTESIAN_POINT ( 'NONE',  ( 3.042071309553159519, 49.73958332991935549, 11.35316468750000141 ) ) ;
#28255 =( BOUNDED_CURVE ( )  B_SPLINE_CURVE ( 2, ( #17303, #52021, #68996, #35057, #29387, #12024, #1468, #24074, #46716 ),
 .UNSPECIFIED., .F., .F. ) 
 B_SPLINE_CURVE_WITH_KNOTS ( ( 3, 2, 2, 2, 3 ),
 ( 0.1666666666666668239, 0.1750000000000001554, 0.1833333333333334869, 0.1916666666666668462, 0.2000000000000001776 ),
 .UNSPECIFIED. ) 
 CURVE ( )  GEOMETRIC_REPRESENTATION_ITEM ( )  RATIONAL_B_SPLINE_CURVE ( ( 0.9999999999999984457, 0.9238795325112882928, 1.000000000000000000, 0.9238795325112867385, 1.000000000000000000, 0.9238795325112867385, 1.000000000000000000, 0.9238795325112851842, 1.000000000000001554 ) ) 
 REPRESENTATION_ITEM ( '' )  );
#28254 = CARTESIAN_POINT ( 'NONE',  ( 7.999999999752645863, -6.290875383172500320E-05, 1.767801038436179750 ) ) ;
#28256 = CARTESIAN_POINT ( 'NONE',  ( -9.121419926064122663, -1.666886344965055722, -0.5794300317457429239 ) ) ;
#28257 = EDGE_LOOP ( 'NONE', ( #4248, #66636, #35291, #30337, #66795, #36652, #27542, #55109, #49162, #11683, #68393, #62147, #66448, #71202, #32596, #54812, #11385, #60939, #14400, #57721, #52916, #71690, #53647, #23089, #32729, #57780, #70950, #10948, #17447, #13988, #62127, #46319, #39518 ) ) ;
#28258 = FACE_OUTER_BOUND ( 'NONE', #9866, .T. ) ;
#28259 = CARTESIAN_POINT ( 'NONE',  ( -10.00000000000000355, 169.5833333265053398, 2.679491924311223183 ) ) ;
#28260 = CARTESIAN_POINT ( 'NONE',  ( 11.35316468749999963, 65.98958332991936970, -3.042071309553165293 ) ) ;
#28261 = CARTESIAN_POINT ( 'NONE',  ( 4.556349186104045934, 11.00000000000000000, 74.21875000409677625 ) ) ;
#28262 = CARTESIAN_POINT ( 'NONE',  ( 2.445694354108784108, 199.5625000013656063, 144.4456943541088663 ) ) ;
#28263 = CYLINDRICAL_SURFACE ( 'NONE', #33609, 3.999999999999976019 ) ;
#28264 = CARTESIAN_POINT ( 'NONE',  ( -10.00000000000000355, 12.70833333333333570, 2.679491924311223183 ) ) ;
#28266 = CARTESIAN_POINT ( 'NONE',  ( -9.832129032723420536, 58.69791666325268409, 5.676582343749997150 ) ) ;
#28265 = CARTESIAN_POINT ( 'NONE',  ( -5.082755093536324154, 95.84375000204838102, 5.082755093536326818 ) ) ;
#28267 = CARTESIAN_POINT ( 'NONE',  ( 3.313708498984756279, 7.999999999999991118, 4.861552779823364645 ) ) ;
#28268 = CARTESIAN_POINT ( 'NONE',  ( -5.000000000000000000, 10.26105934116143281, -64.40045319026697257 ) ) ;
#28269 = CARTESIAN_POINT ( 'NONE',  ( 5.676582343750001591, 176.6145833299193555, -9.832129032723420536 ) ) ;
#28271 = CARTESIAN_POINT ( 'NONE',  ( 10.00000000000000000, 141.6666666598387110, 2.679491924311236062 ) ) ;
#28270 = PRODUCT_DEFINITION_SHAPE ( 'NONE', 'NONE',  #74660 ) ;
#28272 = CARTESIAN_POINT ( 'NONE',  ( -7.188101187500001821, 101.9375000020483810, -2.977408999572650483 ) ) ;
#28273=STYLED_ITEM('',(#74692),#66799);
#28274 = DIRECTION ( 'NONE',  ( 0.000000000000000000, 0.000000000000000000, 1.000000000000000000 ) ) ;
#28275 = CARTESIAN_POINT ( 'NONE',  ( 9.832129032723416984, 30.67708332991935194, 5.676582343750006032 ) ) ;
#28276 = CARTESIAN_POINT ( 'NONE',  ( 10.18810118749999916, 4.220049686691935698, 116.8750000020483952 ) ) ;
#28277 = CARTESIAN_POINT ( 'NONE',  ( -11.35316468750000141, 188.4895833299193555, 3.042071309553159963 ) ) ;
#28278 = ORIENTED_EDGE ( 'NONE', *, *, #43593, .F. ) ;
#28279 = CARTESIAN_POINT ( 'NONE',  ( 49.26241139540195491, 138.7648113368695419, 58.97004729982020876 ) ) ;
#28280 = CARTESIAN_POINT ( 'NONE',  ( -4.220049686691937474, -10.18810118749999738, 72.43750000204838102 ) ) ;
#28281 = CARTESIAN_POINT ( 'NONE',  ( 2.751064625579944321E-14, 197.7500000000000000, 194.0000000000000568 ) ) ;
#28282 = CARTESIAN_POINT ( 'NONE',  ( 2.775557561562891351E-14, 210.0000000000000284, 202.0000000000000000 ) ) ;
#28284 = CARTESIAN_POINT ( 'NONE',  ( -11.35316468750000141, 168.4895833299193555, 3.042071309553159963 ) ) ;
#28283 = CARTESIAN_POINT ( 'NONE',  ( -7.347880794884122694E-16, 18.49999999726881583, 4.000000000000001776 ) ) ;
#28285 = CARTESIAN_POINT ( 'NONE',  ( -7.999999999999991118, 3.313708498984756723, 6.792802784329821542 ) ) ;
#28286 = CARTESIAN_POINT ( 'NONE',  ( 0.000000000000000000, 101.0525588832578734, 7.949999999999993960 ) ) ;
#28287 = CARTESIAN_POINT ( 'NONE',  ( -8.660254037844387298, 262.7083333401612890, -4.999999999999999112 ) ) ;
#28288 = CARTESIAN_POINT ( 'NONE',  ( -2.751064625579944321E-14, 205.8750000027312126, 146.0000000000000284 ) ) ;
#28289 = ORIENTED_EDGE ( 'NONE', *, *, #58364, .T. ) ;
#28290 = CARTESIAN_POINT ( 'NONE',  ( -2.926785083138225622E-14, 16.44602605510714355, 68.55492853905353456 ) ) ;
#28291 = CARTESIAN_POINT ( 'NONE',  ( 11.35316468749999785, 115.8854166632526841, 3.042071309553174174 ) ) ;
#28292 = CARTESIAN_POINT ( 'NONE',  ( 10.00000000000000178, 11.87499999317203248, 0.000000000000000000 ) ) ;
#28293 = ORIENTED_EDGE ( 'NONE', *, *, #11345, .T. ) ;
#28294 = AXIS2_PLACEMENT_3D ( 'NONE', #42323, #19683, #42693 ) ;
#28295 = EDGE_CURVE ( 'NONE', #7053, #57749, #22941, .T. ) ;
#28296 = CARTESIAN_POINT ( 'NONE',  ( -1.881053915767121554, 7.749999998634407916, -4.541265875000002339 ) ) ;
#28297 = CARTESIAN_POINT ( 'NONE',  ( 5.082755093536324154, 15.28124999795161187, 5.082755093536326818 ) ) ;
#28298 = CARTESIAN_POINT ( 'NONE',  ( 8.000000000000000000, 110.9375000040967905, -9.797174393178825657E-16 ) ) ;
#28299 = CARTESIAN_POINT ( 'NONE',  ( -25.55430564589115150, 200.3125000013656063, 172.4456943541091789 ) ) ;
#28300 = CARTESIAN_POINT ( 'NONE',  ( -2.828427124746192067, 7.625000000000000000, 2.828427124746190735 ) ) ;
#28301 = CARTESIAN_POINT ( 'NONE',  ( 2.751064625579944321E-14, 197.7500000000000000, 194.0000000000000568 ) ) ;
#28302 = CARTESIAN_POINT ( 'NONE',  ( 2.780723358947928197E-16, 6.562499998634407028, -4.541265875000002339 ) ) ;
#28303 = CARTESIAN_POINT ( 'NONE',  ( -1.656854249492405451, 198.3125000000000284, 138.0000000000000568 ) ) ;
#28304 = ORIENTED_EDGE ( 'NONE', *, *, #4440, .T. ) ;
#28305 = CARTESIAN_POINT ( 'NONE',  ( 8.000000000000000000, 116.7499999999999858, -9.797174393178825657E-16 ) ) ;
#28306 = CARTESIAN_POINT ( 'NONE',  ( -7.188101187499999156, 104.7500000020483810, 2.977408999572654924 ) ) ;
#28307 = VECTOR ( 'NONE', #15348, 1000.000000000000000 ) ;
#28309 = CARTESIAN_POINT ( 'NONE',  ( 4.242640687119287435, 293.3750000000000000, 4.242640687119285658 ) ) ;
#28308 = CARTESIAN_POINT ( 'NONE',  ( 0.000000000000000000, 0.000000000000000000, 118.0000000000000000 ) ) ;
#28310 = CARTESIAN_POINT ( 'NONE',  ( -6.891449706540977438, 10.24244278380984774, -65.16993756079918398 ) ) ;
#28311 = VECTOR ( 'NONE', #48903, 1000.000000000000000 ) ;
#28312 = CARTESIAN_POINT ( 'NONE',  ( -2.977408999572647819, 7.188101187499991163, 2.705302781871750994 ) ) ;
#28313 = ORIENTED_EDGE ( 'NONE', *, *, #58467, .F. ) ;
#28314 = ORIENTED_EDGE ( 'NONE', *, *, #63393, .F. ) ;
#28315 = CARTESIAN_POINT ( 'NONE',  ( 7.204075437095966983, 7.204075437095967871, 91.09375000204838102 ) ) ;
#28316 = DIRECTION ( 'NONE',  ( -0.000000000000000000, -0.000000000000000000, 1.000000000000000000 ) ) ;
#28317 = CARTESIAN_POINT ( 'NONE',  ( -31.45873412499999944, 201.8750000013656063, 168.5673454167827572 ) ) ;
#28318 = CARTESIAN_POINT ( 'NONE',  ( 11.00000000000000000, 4.556349186104045934, 106.8437500000000000 ) ) ;
#28319 = CARTESIAN_POINT ( 'NONE',  ( 1.432654583217664701, 205.0000000013655779, 201.4587341250000065 ) ) ;
#28321 = CARTESIAN_POINT ( 'NONE',  ( -4.556349186104045934, 11.00000000000000000, 113.4062500040967620 ) ) ;
#28320 = CARTESIAN_POINT ( 'NONE',  ( 26.34314575050759188, 203.0625000027312126, 173.9999999999998863 ) ) ;
#28322 = CARTESIAN_POINT ( 'NONE',  ( -5.000000000000005329, 123.3333333333333428, 8.660254037844387298 ) ) ;
#28323 = CARTESIAN_POINT ( 'NONE',  ( 5.656854249492379694, 107.9374999999999858, -5.656854249492380582 ) ) ;
#28324 = CARTESIAN_POINT ( 'NONE',  ( 6.676582343750004256, 289.0468750017070079, 2.765530957081995478 ) ) ;
#28325 = CARTESIAN_POINT ( 'NONE',  ( 5.082755093536318824, 5.082755093536319713, 7.299052781871751883 ) ) ;
#28326 = EDGE_CURVE ( 'NONE', #51761, #65370, #71210, .T. ) ;
#28327 = DIRECTION ( 'NONE',  ( -0.000000000000000000, -1.000000000000000000, -0.000000000000000000 ) ) ;
#28328 = ADVANCED_FACE ( 'NONE', ( #48570 ), #71580, .T. ) ;
#28329 = CARTESIAN_POINT ( 'NONE',  ( 25.55430564589119768, 208.0625000013656063, 167.5543056458910485 ) ) ;
#28330 = CARTESIAN_POINT ( 'NONE',  ( -3.313708498984765161, 26.34374999590322375, 7.999999999999998224 ) ) ;
#28331 = CARTESIAN_POINT ( 'NONE',  ( 3.458734124999959025, 198.5000000013656347, 140.5673454167824161 ) ) ;
#28332 = CARTESIAN_POINT ( 'NONE',  ( -5.082755093536325930, 119.8437500020483810, -5.082755093536325930 ) ) ;
#28334 = CARTESIAN_POINT ( 'NONE',  ( 1.885018014105903861, 194.8695402653108033, 194.5852816951263833 ) ) ;
#28333 = CARTESIAN_POINT ( 'NONE',  ( 0.000000000000000000, -3.149999999999999911, 0.000000000000000000 ) ) ;
#28335 = CARTESIAN_POINT ( 'NONE',  ( -5.676582343749992710, 240.0520833367473301, 9.832129032723422313 ) ) ;
#28336 = CARTESIAN_POINT ( 'NONE',  ( 32.00000000000000000, 199.3125000000000853, 168.3431457505075741 ) ) ;
#28337 = CARTESIAN_POINT ( 'NONE',  ( 9.832129032723416984, 20.36458332991935194, 5.676582343750006032 ) ) ;
#28338 = CARTESIAN_POINT ( 'NONE',  ( -8.311093377946836114, 212.9687499965860411, -8.311093377946837890 ) ) ;
#28339 = CARTESIAN_POINT ( 'NONE',  ( -2.828427124746208943, 197.7500000027312126, 144.8284271247462129 ) ) ;
#28340 = CARTESIAN_POINT ( 'NONE',  ( -1.836970198721029983E-15, 220.6249999931720538, 10.00000000000000178 ) ) ;
#28342 = CARTESIAN_POINT ( 'NONE',  ( -4.898587196589407898E-16, 7.999999999999991118, 28.95530277982336642 ) ) ;
#28341 = DIRECTION ( 'NONE',  ( 1.000000000000000000, -0.000000000000000000, -0.000000000000000000 ) ) ;
#28343 = VERTEX_POINT ( 'NONE', #42168 ) ;
#28344 = EDGE_CURVE ( 'NONE', #71925, #30287, #9941, .T. ) ;
#28345 = CARTESIAN_POINT ( 'NONE',  ( -3.458734125000015425, 200.2500000013656631, 143.4326545832176976 ) ) ;
#28346 = CARTESIAN_POINT ( 'NONE',  ( -9.832129032723420536, 23.69791666325268409, 5.676582343749997150 ) ) ;
#28347 = CARTESIAN_POINT ( 'NONE',  ( 11.00000000000000355, -4.556349186104045046, 93.34375000409677625 ) ) ;
#28348 = CARTESIAN_POINT ( 'NONE',  ( -6.123233995736766282E-16, 228.7500000000000000, -10.00000000000000000 ) ) ;
#28349 = CARTESIAN_POINT ( 'NONE',  ( -27.99999999999991829, 198.9375000013655779, 173.4587341250003760 ) ) ;
#28351 = CARTESIAN_POINT ( 'NONE',  ( -8.311093377946836114, 7.656249996586015349, -8.311093377946837890 ) ) ;
#28350 = CARTESIAN_POINT ( 'NONE',  ( -7.188101187499999156, 113.7500000020483810, 2.977408999572654924 ) ) ;
#28352 = CARTESIAN_POINT ( 'NONE',  ( 5.656854249492376141, -5.656854249492374365, 20.89280277982336642 ) ) ;
#28353 =( BOUNDED_CURVE ( )  B_SPLINE_CURVE ( 2, ( #41119, #47498, #69787, #53548, #2227, #18840, #7156, #30160, #18103 ),
 .UNSPECIFIED., .F., .F. ) 
 B_SPLINE_CURVE_WITH_KNOTS ( ( 3, 2, 2, 2, 3 ),
 ( 0.8833333333333341919, 0.8916666666666676067, 0.9000000000000007994, 0.9083333333333341031, 0.9166666666666674068 ),
 .UNSPECIFIED. ) 
 CURVE ( )  GEOMETRIC_REPRESENTATION_ITEM ( )  RATIONAL_B_SPLINE_CURVE ( ( 0.9999999999999918954, 0.9238795325112948431, 1.000000000000000000, 0.9238795325112867385, 1.000000000000000000, 0.9238795325112867385, 1.000000000000000000, 0.9238795325112796331, 1.000000000000007105 ) ) 
 REPRESENTATION_ITEM ( '' )  );
#28354 = CARTESIAN_POINT ( 'NONE',  ( 3.042071309553167069, 131.8229166632526983, -11.35316468749999785 ) ) ;
#28355 = CARTESIAN_POINT ( 'NONE',  ( 2.679491924311228956, 107.9166666598386826, -10.00000000000000000 ) ) ;
#28356 = EDGE_CURVE ( 'NONE', #60340, #31431, #37936, .T. ) ;
#28357 = CARTESIAN_POINT ( 'NONE',  ( 7.188101187500001821, 119.3750000020483810, -2.977408999572651371 ) ) ;
#28358 = CARTESIAN_POINT ( 'NONE',  ( 11.00000000000000000, 11.00000000000000000, -6.938893903907228378E-15 ) ) ;
#28359 = CARTESIAN_POINT ( 'NONE',  ( 4.898587196589412829E-16, 16.87500000000000000, -8.000000000000000000 ) ) ;
#28360 = CARTESIAN_POINT ( 'NONE',  ( -5.000000000000000000, -53.17721328501337297, -43.91924822456289235 ) ) ;
#28361 = ORIENTED_EDGE ( 'NONE', *, *, #1506, .F. ) ;
#28362 = CARTESIAN_POINT ( 'NONE',  ( -10.00000000000000178, 154.3749999931720254, -1.224646799147353454E-15 ) ) ;
#28363 = CARTESIAN_POINT ( 'NONE',  ( -2.765530957081996810, 291.4218750017070079, -6.676582343750003368 ) ) ;
#28364 = CARTESIAN_POINT ( 'NONE',  ( 3.042071309553167513, 131.8229166632526983, -11.35316468749999785 ) ) ;
#28365 = CARTESIAN_POINT ( 'NONE',  ( -4.000000000000015987, 207.6250000027312126, 142.0000000000000568 ) ) ;
#28366 = CARTESIAN_POINT ( 'NONE',  ( -5.656854249492373476, -5.656854249492376141, 26.57405278432982243 ) ) ;
#28367 = DIRECTION ( 'NONE',  ( -0.000000000000000000, -0.000000000000000000, -1.000000000000000000 ) ) ;
#28368 = CARTESIAN_POINT ( 'NONE',  ( 8.000000000000001776, 103.1562499999999858, 3.313708498984759387 ) ) ;
#28369 = AXIS2_PLACEMENT_3D ( 'NONE', #58372, #13048, #17613 ) ;
#28370 = CARTESIAN_POINT ( 'NONE',  ( 4.220049686691941027, -10.18810118749999738, 98.50000000204838102 ) ) ;
#28371 = EDGE_LOOP ( 'NONE', ( #31702, #51160, #36195, #69310 ) ) ;
#28372 = AXIS2_PLACEMENT_3D ( 'NONE', #66544, #48076, #8094 ) ;
#28373 = CARTESIAN_POINT ( 'NONE',  ( 4.999999999999993783, 216.0416666598387110, 8.660254037844390851 ) ) ;
#28374 = CARTESIAN_POINT ( 'NONE',  ( -31.05507224581699788, -21.00013786233002833, 171.9999999999997726 ) ) ;
#28375 = CARTESIAN_POINT ( 'NONE',  ( -3.458734124999960358, 202.6875000013656063, 198.0000000000000284 ) ) ;
#28376 = CARTESIAN_POINT ( 'NONE',  ( -3.042071309553164404, 72.55208332991934128, -11.35316468749999963 ) ) ;
#28377 = ORIENTED_EDGE ( 'NONE', *, *, #53528, .T. ) ;
#28378 = CARTESIAN_POINT ( 'NONE',  ( -7.204075437095967871, 7.204075437095967871, 109.4687500020483810 ) ) ;
#28379 = CARTESIAN_POINT ( 'NONE',  ( 1.881053915767122664, 13.24999999863440969, 4.541265875000001451 ) ) ;
#28380 = ORIENTED_EDGE ( 'NONE', *, *, #16396, .T. ) ;
#28381 = CARTESIAN_POINT ( 'NONE',  ( 3.313708498984762052, 0.2812500000000000000, -8.000000000000000000 ) ) ;
#28382 = CARTESIAN_POINT ( 'NONE',  ( -10.00000000000000355, 109.5833333265053540, 2.679491924311223183 ) ) ;
#28383 = CARTESIAN_POINT ( 'NONE',  ( -12.00000000000000000, -6.928203230275527424, -14.80000000000000071 ) ) ;
#28384 = CARTESIAN_POINT ( 'NONE',  ( -5.082755093536325042, 23.90624999795161543, -5.082755093536325930 ) ) ;
#28385 = DIRECTION ( 'NONE',  ( -0.000000000000000000, -1.000000000000000000, -0.000000000000000000 ) ) ;
#28386 = EDGE_CURVE ( 'NONE', #53910, #20164, #50557, .T. ) ;
#28387 = CARTESIAN_POINT ( 'NONE',  ( 4.220049686691941027, -10.18810118749999738, 104.5000000020483668 ) ) ;
#28388 = ADVANCED_FACE ( 'NONE', ( #27427 ), #26685, .F. ) ;
#28389 = CARTESIAN_POINT ( 'NONE',  ( 4.999999999999991118, 109.1666666666666714, 8.660254037844387298 ) ) ;
#28390 = CARTESIAN_POINT ( 'NONE',  ( -4.000000000000001776, 11.18749999726881406, -1.656854249492381470 ) ) ;
#28391 = CARTESIAN_POINT ( 'NONE',  ( -3.458734124999959914, 209.5625000013656063, 198.0000000000000284 ) ) ;
#28392 = ORIENTED_EDGE ( 'NONE', *, *, #63054, .F. ) ;
#28393 = CARTESIAN_POINT ( 'NONE',  ( -11.00000000000000000, 0.000000000000000000, 97.18750000409677625 ) ) ;
#28394 = CARTESIAN_POINT ( 'NONE',  ( -3.458734124999959025, 204.5000000013656063, 199.4326545832176691 ) ) ;
#28395 = APPLICATION_CONTEXT ( 'automotive_design' ) ;
#28396 = CARTESIAN_POINT ( 'NONE',  ( -30.44569435410886982, 205.5625000013656063, 167.5543056458916169 ) ) ;
#28397 = CARTESIAN_POINT ( 'NONE',  ( -2.045563441603947318E-15, 16.70329308849007077, 0.000000000000000000 ) ) ;
#28398 = ADVANCED_FACE ( 'NONE', ( #38021 ), #32744, .F. ) ;
#28399 = CARTESIAN_POINT ( 'NONE',  ( -3.211159895383561391, 9.687499998634406140, -3.211159895383561835 ) ) ;
#28400 = CARTESIAN_POINT ( 'NONE',  ( 4.000000000000000888, 15.93750000000000000, 1.656854249492384135 ) ) ;
#28401 = CARTESIAN_POINT ( 'NONE',  ( -5.082755093536319713, 5.082755093536319713, 20.79905278187175455 ) ) ;
#28402 = ORIENTED_EDGE ( 'NONE', *, *, #21506, .T. ) ;
#28403 = CARTESIAN_POINT ( 'NONE',  ( -6.000000000000003553, 291.9374999999999432, -2.485281374238571317 ) ) ;
#28404 = ORIENTED_EDGE ( 'NONE', *, *, #45740, .T. ) ;
#28405 = CARTESIAN_POINT ( 'NONE',  ( 4.220049686691934809, 10.18810118749999916, 110.6875000020483810 ) ) ;
#28406 = CARTESIAN_POINT ( 'NONE',  ( -11.00000000000000000, 0.000000000000000000, 103.0000000000000000 ) ) ;
#28407 = CARTESIAN_POINT ( 'NONE',  ( 2.754378923186476579E-14, 199.1875000013655779, 194.5412658750000219 ) ) ;
#28408 = CARTESIAN_POINT ( 'NONE',  ( 24.54126587500000056, 197.2500000013656063, 171.4326545832176123 ) ) ;
#28409 = CARTESIAN_POINT ( 'NONE',  ( 8.660254037844385522, 79.58333333333334281, 5.000000000000005329 ) ) ;
#28410 = CARTESIAN_POINT ( 'NONE',  ( -8.000000000000000000, 122.0000000000000000, 0.000000000000000000 ) ) ;
#28411 = CARTESIAN_POINT ( 'NONE',  ( 2.485281374238575314, 288.3125000000000000, 6.000000000000000888 ) ) ;
#28412 = AXIS2_PLACEMENT_3D ( 'NONE', #25753, #12955, #48774 ) ;
#28413 = ORIENTED_EDGE ( 'NONE', *, *, #55686, .F. ) ;
#28414 = CARTESIAN_POINT ( 'NONE',  ( 1.102182119232618108E-15, 294.2500000000000000, 6.000000000000001776 ) ) ;
#28415 = EDGE_CURVE ( 'NONE', #26128, #46167, #73615, .T. ) ;
#28416 = AXIS2_PLACEMENT_3D ( 'NONE', #18197, #41211, #7248 ) ;
#28417 = CARTESIAN_POINT ( 'NONE',  ( 0.000000000000000000, 284.0000000000000000, 6.000000000000001776 ) ) ;
#28418 = CARTESIAN_POINT ( 'NONE',  ( 3.999999999999960032, 194.1250000027311842, 142.0000000000000568 ) ) ;
#28419 = CARTESIAN_POINT ( 'NONE',  ( 7.320508075688771044, 56.24999999317203248, 7.320508075688775484 ) ) ;
#28420 = CARTESIAN_POINT ( 'NONE',  ( 3.313708498984762496, 13.03124999590322197, 7.999999999999998224 ) ) ;
#28421 = CARTESIAN_POINT ( 'NONE',  ( 10.00000000000000178, 242.2916666666666288, 2.679491924311222739 ) ) ;
#28422 = CARTESIAN_POINT ( 'NONE',  ( 30.82842712474620939, 203.2500000027312126, 172.8284271247460424 ) ) ;
#28423 = CARTESIAN_POINT ( 'NONE',  ( -2.679491924311225848, 206.4583333333333712, -10.00000000000000178 ) ) ;
#28424 = CARTESIAN_POINT ( 'NONE',  ( 2.977408999572646486, 7.188101187499992051, 16.39280278187175455 ) ) ;
#28425 = CARTESIAN_POINT ( 'NONE',  ( -3.042071309553173730, 164.6354166632526983, 11.35316468749999785 ) ) ;
#28426 = CARTESIAN_POINT ( 'NONE',  ( -2.775557561562891351E-14, 210.0000000000000284, 142.0000000000000568 ) ) ;
#28427 = CARTESIAN_POINT ( 'NONE',  ( -7.347880794884122694E-16, 1.499999997268813168, 4.000000000000001776 ) ) ;
#28428 = LINE ( 'NONE', #17851, #44714 ) ;
#28429 = EDGE_LOOP ( 'NONE', ( #32914, #28608, #39539, #67195 ) ) ;
#28430 = CARTESIAN_POINT ( 'NONE',  ( -2.754378923186476579E-14, 196.1875000013655779, 145.4587341250000350 ) ) ;
#28431 = CARTESIAN_POINT ( 'NONE',  ( 11.35316468749999963, 31.30208332991934839, -3.042071309553165293 ) ) ;
#28432 = CARTESIAN_POINT ( 'NONE',  ( -7.778174593052020747, -7.778174593052023411, 109.3750000040967763 ) ) ;
#28433 = CARTESIAN_POINT ( 'NONE',  ( -23.99999999999997513, 200.6875000000000284, 171.6568542494927385 ) ) ;
#28434 = DIRECTION ( 'NONE',  ( -0.000000000000000000, 1.000000000000000000, -0.000000000000000000 ) ) ;
#28436 = CARTESIAN_POINT ( 'NONE',  ( 4.193030820682222881, 10.26769724739507872, -64.12608639927633192 ) ) ;
#28435 = DIRECTION ( 'NONE',  ( 0.000000000000000000, 0.000000000000000000, 1.000000000000000000 ) ) ;
#28437 = CARTESIAN_POINT ( 'NONE',  ( -13.69492884422165879, -42.06953881359651604, 197.8167139002727311 ) ) ;
#28438 = CARTESIAN_POINT ( 'NONE',  ( -3.458734125000016313, 200.8750000013656063, 140.5673454167823593 ) ) ;
#28439 = VECTOR ( 'NONE', #23536, 1000.000000000000000 ) ;
#28440 = CARTESIAN_POINT ( 'NONE',  ( 6.123233995736767268E-16, 68.12499999317203958, -10.00000000000000178 ) ) ;
#28441 = CARTESIAN_POINT ( 'NONE',  ( -7.188101187500001821, 101.5625000020483810, -2.977408999572650483 ) ) ;
#28442 = CARTESIAN_POINT ( 'NONE',  ( 1.881053915767122664, 14.24999999863440969, 4.541265875000001451 ) ) ;
#28443 = CARTESIAN_POINT ( 'NONE',  ( -1.173938163346586453E-11, 213.7499999999991189, 10.00000000000000178 ) ) ;
#28444 = CARTESIAN_POINT ( 'NONE',  ( 7.231266549477588512, 0.2382077480156526428, -2.766445194245858996 ) ) ;
#28445 = CARTESIAN_POINT ( 'NONE',  ( 7.320508075688774596, 102.4999999931720254, -7.320508075688774596 ) ) ;
#28446 = B_SPLINE_CURVE_WITH_KNOTS ( 'NONE', 3,
 ( #32356, #72712, #44040, #34598, #51549, #12666, #51934, #64364, #34970, #28917, #74567, #69654, #39863, #57987, #57605, #46263, #6657, #24363, #63238, #11939 ),
 .UNSPECIFIED., .F., .F.,
 ( 4, 2, 2, 2, 2, 2, 2, 2, 2, 4 ),
 ( 0.000000000000000000, 0.001156441540183998683, 0.001734662310276000301, 0.002312883080368001703, 0.003469324620552004506, 0.004625766160736007743, 0.005782207700920009678, 0.006938649241104013349, 0.008095090781288016152, 0.009251532321472018955 ),
 .UNSPECIFIED. ) ;
#28447 = ORIENTED_EDGE ( 'NONE', *, *, #60201, .F. ) ;
#28448 = ORIENTED_EDGE ( 'NONE', *, *, #24572, .F. ) ;
#28449 = CARTESIAN_POINT ( 'NONE',  ( -1.704527592502770306, -49.99193291617143586, -40.73198448289709717 ) ) ;
#28450 = FACE_OUTER_BOUND ( 'NONE', #41918, .T. ) ;
#28451 =( LENGTH_UNIT ( ) NAMED_UNIT ( * ) SI_UNIT ( .MILLI., .METRE. ) );
#28452 = CARTESIAN_POINT ( 'NONE',  ( -10.00000000000000000, 87.29166666666667140, -2.679491924311229401 ) ) ;
#28453 = CARTESIAN_POINT ( 'NONE',  ( 3.042071309553167069, 136.8229166632526699, -11.35316468749999785 ) ) ;
#28454 = CARTESIAN_POINT ( 'NONE',  ( -8.000000000000001776, 6.656249995903221084, 3.313708498984759387 ) ) ;
#28455 = CARTESIAN_POINT ( 'NONE',  ( -6.238412754330611322E-16, 10.18810118749999916, 88.28125000204836681 ) ) ;
#28456 = CARTESIAN_POINT ( 'NONE',  ( -30.10854392850805539, 194.7007961766996118, 173.0496692959133895 ) ) ;
#28457 = CARTESIAN_POINT ( 'NONE',  ( 4.000000000000015987, 204.4375000000000853, 199.6568542494924259 ) ) ;
#28458 = DIRECTION ( 'NONE',  ( -0.000000000000000000, -1.000000000000000000, -0.000000000000000000 ) ) ;
#28459 = CARTESIAN_POINT ( 'NONE',  ( 7.152797884309432419, -3.603458643537627459, -0.000000000000000000 ) ) ;
#28460 = CARTESIAN_POINT ( 'NONE',  ( 10.18810118749999916, 4.220049686691935698, 116.8750000020483668 ) ) ;
#28461 = ORIENTED_EDGE ( 'NONE', *, *, #12788, .F. ) ;
#28462 = LINE ( 'NONE', #28086, #11780 ) ;
#28463 = CARTESIAN_POINT ( 'NONE',  ( 20.64146325552921368, 182.5281491049150873, 146.7620766355258013 ) ) ;
#28464 = CARTESIAN_POINT ( 'NONE',  ( 3.042071309553167513, 122.1354166632526841, -11.35316468749999785 ) ) ;
#28465 = CARTESIAN_POINT ( 'NONE',  ( 1.432654583217662259, 203.1250000013656347, 194.5412658750000219 ) ) ;
#28466 = CARTESIAN_POINT ( 'NONE',  ( 2.977408999572650927, 23.62499999795161543, -7.188101187500000933 ) ) ;
#28467 = CARTESIAN_POINT ( 'NONE',  ( 10.18810118749999916, 1.247682550866122264E-15, 76.28125000204836681 ) ) ;
#28468 = CARTESIAN_POINT ( 'NONE',  ( 11.35316468749999785, 40.88541666325268409, 3.042071309553174174 ) ) ;
#28470 = ORIENTED_EDGE ( 'NONE', *, *, #19444, .T. ) ;
#28469 =( BOUNDED_CURVE ( )  B_SPLINE_CURVE ( 2, ( #59644, #44156, #61877, #72826, #43776, #5290, #39242, #44528, #16202 ),
 .UNSPECIFIED., .F., .F. ) 
 B_SPLINE_CURVE_WITH_KNOTS ( ( 3, 2, 2, 2, 3 ),
 ( 0.6833333333333340143, 0.6916666666666673180, 0.7000000000000005107, 0.7083333333333339255, 0.7166666666666671182 ),
 .UNSPECIFIED. ) 
 CURVE ( )  GEOMETRIC_REPRESENTATION_ITEM ( )  RATIONAL_B_SPLINE_CURVE ( ( 0.9999999999999938938, 0.9238795325112928447, 1.000000000000000000, 0.9238795325112867385, 1.000000000000000000, 0.9238795325112867385, 1.000000000000000000, 0.9238795325112826307, 1.000000000000003997 ) ) 
 REPRESENTATION_ITEM ( '' )  );
#28471 = DIRECTION ( 'NONE',  ( 0.000000000000000000, 0.000000000000000000, 1.000000000000000000 ) ) ;
#28472 = CARTESIAN_POINT ( 'NONE',  ( 7.999999999999920064, -1.061780717098090627E-06, 7.767802753882760314 ) ) ;
#28473 = CARTESIAN_POINT ( 'NONE',  ( 5.662595241051934458, 5.662595241051935346, 21.45061528394063188 ) ) ;
#28474 = CARTESIAN_POINT ( 'NONE',  ( -2.445694354108839175, 208.3125000013656063, 144.4456943541088663 ) ) ;
#28475 = CARTESIAN_POINT ( 'NONE',  ( -7.188101187500002709, 10.31249999795161010, 2.977408999572649151 ) ) ;
#28476 = CARTESIAN_POINT ( 'NONE',  ( -6.000000000000003553, 297.0000000034139589, -2.485281374238571317 ) ) ;
#28477 = CARTESIAN_POINT ( 'NONE',  ( -15.61960406851433625, -19.18890331593440379, 137.5897893581104654 ) ) ;
#28478 = CARTESIAN_POINT ( 'NONE',  ( 5.082755093536324154, 8.156249997951611874, 5.082755093536326818 ) ) ;
#28479 = ADVANCED_FACE ( 'NONE', ( #15731 ), #10763, .F. ) ;
#28480 = CARTESIAN_POINT ( 'NONE',  ( 11.35316468749999785, 150.8854166632527267, 3.042071309553174174 ) ) ;
#28481 = CARTESIAN_POINT ( 'NONE',  ( 4.220049686691941027, -10.18810118749999738, 75.62500000204838102 ) ) ;
#28482 = CARTESIAN_POINT ( 'NONE',  ( -25.55430564589114795, 196.0625000013656063, 172.4456943541091789 ) ) ;
#28483 = ADVANCED_FACE ( 'NONE', ( #21025 ), #8969, .F. ) ;
#28484 = CARTESIAN_POINT ( 'NONE',  ( 7.778174593052021635, 7.778174593052023411, 109.9375000000000000 ) ) ;
#28485 = CARTESIAN_POINT ( 'NONE',  ( -1.881053915767124440, 19.12499999863441147, 4.541265875000001451 ) ) ;
#28486 = ORIENTED_EDGE ( 'NONE', *, *, #9662, .T. ) ;
#28487 = CARTESIAN_POINT ( 'NONE',  ( 2.828427124746209831, 198.5000000027312126, 200.8284271247462129 ) ) ;
#28488 = CARTESIAN_POINT ( 'NONE',  ( -1.656854249492405451, 206.3125000000000284, 138.0000000000000568 ) ) ;
#28489 = CARTESIAN_POINT ( 'NONE',  ( -24.00000000000002487, 202.9375000027312410, 168.3431457505079152 ) ) ;
#28490 = CIRCLE ( 'NONE', #30862, 3.999999999999976019 ) ;
#28491 = CARTESIAN_POINT ( 'NONE',  ( 4.556349186104052151, -10.99999999999999822, 75.15625000409677625 ) ) ;
#28492 = CARTESIAN_POINT ( 'NONE',  ( 7.999999999999991118, 3.313708498984757611, 10.86155278392014800 ) ) ;
#28493 = ORIENTED_EDGE ( 'NONE', *, *, #60214, .T. ) ;
#28494 = CARTESIAN_POINT ( 'NONE',  ( 7.188101187500000044, 19.96874999795161543, 0.000000000000000000 ) ) ;
#28495 = FACE_OUTER_BOUND ( 'NONE', #68078, .T. ) ;
#28496 = CARTESIAN_POINT ( 'NONE',  ( 2.124081043562863869, -10.27770035960974759, -63.71262442773669221 ) ) ;
#28497 = CARTESIAN_POINT ( 'NONE',  ( 10.00000000000000178, 45.00000000000000711, 0.000000000000000000 ) ) ;
#28498 = CARTESIAN_POINT ( 'NONE',  ( -5.082755093536325930, 103.3437500020483668, -5.082755093536325930 ) ) ;
#28499 = CARTESIAN_POINT ( 'NONE',  ( -29.43265458321766914, 207.7500000013656063, 166.5412658750003629 ) ) ;
#28500 = CARTESIAN_POINT ( 'NONE',  ( 6.000000000000001776, 298.5000000000000000, -7.347880794884121708E-16 ) ) ;
#28502 = CARTESIAN_POINT ( 'NONE',  ( -11.00000000000000000, 0.000000000000000000, 118.0000000000000000 ) ) ;
#28501 = CARTESIAN_POINT ( 'NONE',  ( -23.99999999999997513, 201.6875000000000284, 171.6568542494927385 ) ) ;
#28503 = ORIENTED_EDGE ( 'NONE', *, *, #38047, .F. ) ;
#28504 = CARTESIAN_POINT ( 'NONE',  ( 9.832129032723420536, 245.9895833367473301, 5.676582343749996262 ) ) ;
#28505 = CARTESIAN_POINT ( 'NONE',  ( -5.082755093536317936, -5.082755093536320601, 18.54905278187175455 ) ) ;
#28506 = CARTESIAN_POINT ( 'NONE',  ( -3.074111742570588834, 51.58078258920524206, 48.68628732315647767 ) ) ;
#28507 = CARTESIAN_POINT ( 'NONE',  ( -28.00000000000007461, 195.1250000027311842, 166.0000000000003695 ) ) ;
#28508 = CARTESIAN_POINT ( 'NONE',  ( 24.22789396521254801, 194.9514163098568531, 171.1920755165970718 ) ) ;
#28509 = CARTESIAN_POINT ( 'NONE',  ( -1.432654583217608080, 196.8750000013656063, 201.4587341250000350 ) ) ;
#28510 = CARTESIAN_POINT ( 'NONE',  ( -10.00000000000000355, 157.7083333333333712, 2.679491924311223183 ) ) ;
#28511 = CARTESIAN_POINT ( 'NONE',  ( 0.000000000000000000, 300.0000000000000000, 0.000000000000000000 ) ) ;
#28512 =( NAMED_UNIT ( * ) PLANE_ANGLE_UNIT ( ) SI_UNIT ( $, .RADIAN. ) );
#28513 = CARTESIAN_POINT ( 'NONE',  ( 7.000000000000000000, 0.000000000000000000, -0.7002075382097148193 ) ) ;
#28514 = CARTESIAN_POINT ( 'NONE',  ( -8.311093377946836114, 122.9687499965860127, -8.311093377946837890 ) ) ;
#28515 = PLANE ( 'NONE',  #31207 ) ;
#28516 = CARTESIAN_POINT ( 'NONE',  ( 4.556349186104045934, 11.00000000000000000, 107.0312500000000000 ) ) ;
#28519 = CARTESIAN_POINT ( 'NONE',  ( 3.999999999999959144, 202.0625000000000284, 140.3431457505076594 ) ) ;
#28518 = CARTESIAN_POINT ( 'NONE',  ( 25.55430564589118703, 196.3125000013656063, 172.4456943541087526 ) ) ;
#28517 = CARTESIAN_POINT ( 'NONE',  ( 28.00000000000001776, 195.1875000013655779, 166.5412658749999082 ) ) ;
#28520 = EDGE_LOOP ( 'NONE', ( #49894, #11144, #65412, #30820 ) ) ;
#28521 = CARTESIAN_POINT ( 'NONE',  ( 4.012887317181695224, 224.0794175527780965, 9.164256819418794109 ) ) ;
#28522 = CARTESIAN_POINT ( 'NONE',  ( -2.997005883563423012, 10.11494357241938147, 70.43990496500997267 ) ) ;
#28523 = CYLINDRICAL_SURFACE ( 'NONE', #48225, 4.000000000000001776 ) ;
#28524 = CARTESIAN_POINT ( 'NONE',  ( 28.00000000000001776, 196.1250000027311842, 173.9999999999999147 ) ) ;
#28525 = CARTESIAN_POINT ( 'NONE',  ( 31.45873412499999233, 195.9375000013655779, 169.9999999999999432 ) ) ;
#28526 = CARTESIAN_POINT ( 'NONE',  ( -3.042071309553173730, 219.6354166632526699, 11.35316468749999785 ) ) ;
#28527 = CARTESIAN_POINT ( 'NONE',  ( 1.320432766682874540E-15, 121.5312500020483810, 7.188101187500000044 ) ) ;
#28528 = CARTESIAN_POINT ( 'NONE',  ( -1.881053915767124440, 21.99999999863440792, 4.541265875000001451 ) ) ;
#28529 = CARTESIAN_POINT ( 'NONE',  ( -2.216418498321459207, 67.77535163244979799, -20.18253627484908463 ) ) ;
#28530 = CARTESIAN_POINT ( 'NONE',  ( -3.313708498984758943, -7.999999999999989342, 23.61155277982336997 ) ) ;
#28532 = CARTESIAN_POINT ( 'NONE',  ( 25.17157287525381193, 196.6250000000000284, 167.1715728752537018 ) ) ;
#28531 = LINE ( 'NONE', #34214, #19057 ) ;
#28533 = CARTESIAN_POINT ( 'NONE',  ( 8.311093377946834337, 100.1562499965860127, 8.311093377946839666 ) ) ;
#28534 = ORIENTED_EDGE ( 'NONE', *, *, #757, .T. ) ;
#28535 = CARTESIAN_POINT ( 'NONE',  ( -1.656854249492381248, 19.06249999726881228, -4.000000000000001776 ) ) ;
#28536 = CARTESIAN_POINT ( 'NONE',  ( 4.401442555609581635E-16, 24.84374999795161543, -7.188101187500000044 ) ) ;
#28537 = CARTESIAN_POINT ( 'NONE',  ( 7.999999999999950262, -3.313708498984798467, 8.986552779823366421 ) ) ;
#28538 = CARTESIAN_POINT ( 'NONE',  ( -5.676582343750000703, 238.3854166700806445, -9.832129032723418760 ) ) ;
#28539 = CARTESIAN_POINT ( 'NONE',  ( -5.676582343749998039, 102.4479166632526841, -9.832129032723420536 ) ) ;
#28540 = ORIENTED_EDGE ( 'NONE', *, *, #10463, .F. ) ;
#28541 = CARTESIAN_POINT ( 'NONE',  ( -0.9087844426713385104, 10.88091015416974550, 117.5913480126766473 ) ) ;
#28542 = CARTESIAN_POINT ( 'NONE',  ( -10.18810118749999916, 4.220049686691934809, 106.5625000020483668 ) ) ;
#28543 = CARTESIAN_POINT ( 'NONE',  ( 7.320508075688774596, 222.4999999931719969, -7.320508075688774596 ) ) ;
#28544 = CARTESIAN_POINT ( 'NONE',  ( 2.754378923186476579E-14, 203.4375000013656063, 194.5412658750000219 ) ) ;
#28545 = DIRECTION ( 'NONE',  ( -0.000000000000000000, 1.000000000000000000, -4.476705744456276341E-16 ) ) ;
#28547 = CARTESIAN_POINT ( 'NONE',  ( 3.042071309553159519, 99.73958332991935549, 11.35316468750000141 ) ) ;
#28546 = DIRECTION ( 'NONE',  ( -0.1513591288559071046, 0.000000000000000000, -0.9884788384745426537 ) ) ;
#28548 = CARTESIAN_POINT ( 'NONE',  ( -7.999999999999991118, 0.000000000000000000, 11.51780278392014445 ) ) ;
#28549 = CARTESIAN_POINT ( 'NONE',  ( -26.56734541678232375, 195.2500000013656063, 173.4587341250003760 ) ) ;
#28550 = CARTESIAN_POINT ( 'NONE',  ( -8.000000000000001776, 27.65624999590322730, 3.313708498984759387 ) ) ;
#28551 = VERTEX_POINT ( 'NONE', #44794 ) ;
#28552 = EDGE_CURVE ( 'NONE', #60791, #67709, #12005, .T. ) ;
#28553 = AXIS2_PLACEMENT_3D ( 'NONE', #46829, #1575, #69854 ) ;
#28554 = CARTESIAN_POINT ( 'NONE',  ( -2.679491924311235618, 200.4166666598386826, 10.00000000000000000 ) ) ;
#28555 = DIRECTION ( 'NONE',  ( -0.000000000000000000, 1.000000000000000000, -0.000000000000000000 ) ) ;
#28556 = CARTESIAN_POINT ( 'NONE',  ( 2.449293598294707893E-16, 9.999999997268814056, -4.000000000000001776 ) ) ;
#28557 = CARTESIAN_POINT ( 'NONE',  ( 9.832129032723416984, 85.67708332991935549, 5.676582343750006032 ) ) ;
#28558 = CARTESIAN_POINT ( 'NONE',  ( 1.226468279477575784E-15, 289.7031250017069510, 6.676582343750001591 ) ) ;
#28559 = CARTESIAN_POINT ( 'NONE',  ( 5.082755093536324154, 3.656249997951610542, 5.082755093536326818 ) ) ;
#28560 = CARTESIAN_POINT ( 'NONE',  ( -7.204075437095967871, 7.204075437095967871, 102.3437500020483668 ) ) ;
#28561 = CARTESIAN_POINT ( 'NONE',  ( 5.676582343750001591, 216.6145833299193555, -9.832129032723420536 ) ) ;
#28562 = ORIENTED_EDGE ( 'NONE', *, *, #20706, .T. ) ;
#28563 = CARTESIAN_POINT ( 'NONE',  ( -4.000000000000001776, 2.500000000000000000, -4.898587196589415787E-16 ) ) ;
#28564 = LINE ( 'NONE', #50829, #15941 ) ;
#28565 = CARTESIAN_POINT ( 'NONE',  ( 11.35316468749999963, 215.9895833299193271, -3.042071309553165293 ) ) ;
#28566 = CARTESIAN_POINT ( 'NONE',  ( -3.018451720292563716E-14, -16.44602605510714355, -68.55492853905353456 ) ) ;
#28567 = CARTESIAN_POINT ( 'NONE',  ( -2.765530957081996810, 297.2656250017069510, -6.676582343750003368 ) ) ;
#28568 = ORIENTED_EDGE ( 'NONE', *, *, #29708, .F. ) ;
#28569 = CARTESIAN_POINT ( 'NONE',  ( -5.000000000000005329, 120.2083333265053824, 8.660254037844387298 ) ) ;
#28570 = CARTESIAN_POINT ( 'NONE',  ( 11.35316468749999785, 210.8854166632526983, 3.042071309553174174 ) ) ;
#28571 = ADVANCED_FACE ( 'NONE', ( #67059 ), #38394, .F. ) ;
#28572 =( BOUNDED_CURVE ( )  B_SPLINE_CURVE ( 2, ( #51499, #34172, #35287, #28491, #68478, #57932, #22822, #45838, #11887 ),
 .UNSPECIFIED., .F., .F. ) 
 B_SPLINE_CURVE_WITH_KNOTS ( ( 3, 2, 2, 2, 3 ),
 ( 0.8088235294117646079, 0.8124999999999998890, 0.8161764705882351700, 0.8198529411764704511, 0.8235294117647057321 ),
 .UNSPECIFIED. ) 
 CURVE ( )  GEOMETRIC_REPRESENTATION_ITEM ( )  RATIONAL_B_SPLINE_CURVE ( ( 1.000000000000002220, 0.9238795325112844070, 1.000000000000000000, 0.9238795325112867385, 1.000000000000000000, 0.9238795325112867385, 1.000000000000000000, 0.9238795325112890700, 0.9999999999999976685 ) ) 
 REPRESENTATION_ITEM ( '' )  );
#28573 = CARTESIAN_POINT ( 'NONE',  ( -10.18810118749999916, 0.000000000000000000, 96.15625000204838102 ) ) ;
#28574 = EDGE_CURVE ( 'NONE', #74182, #7001, #7079, .T. ) ;
#28575 = CARTESIAN_POINT ( 'NONE',  ( -29.43265458321761230, 206.8750000013656347, 173.4587341250003760 ) ) ;
#28576 = CARTESIAN_POINT ( 'NONE',  ( -8.000000000000001776, 20.34375000000000355, 3.313708498984759387 ) ) ;
#28577 = ORIENTED_EDGE ( 'NONE', *, *, #70513, .T. ) ;
#28578 = CARTESIAN_POINT ( 'NONE',  ( -7.188101187500000044, 121.1562500020483810, 0.000000000000000000 ) ) ;
#28579 = CARTESIAN_POINT ( 'NONE',  ( -1.472282454178774014, -19.93458701958330082, -1.116934336526977711 ) ) ;
#28580 = CARTESIAN_POINT ( 'NONE',  ( 4.999999999999993783, 24.16666666666667140, 8.660254037844390851 ) ) ;
#28581 =( BOUNDED_CURVE ( )  B_SPLINE_CURVE ( 2, ( #62870, #21761, #22885, #56489, #4806, #46268, #45157, #63243, #62498 ),
 .UNSPECIFIED., .F., .F. ) 
 B_SPLINE_CURVE_WITH_KNOTS ( ( 3, 2, 2, 2, 3 ),
 ( 0.2105263157894737558, 0.2171052631578948011, 0.2236842105263158187, 0.2302631578947368085, 0.2368421052631578261 ),
 .UNSPECIFIED. ) 
 CURVE ( )  GEOMETRIC_REPRESENTATION_ITEM ( )  RATIONAL_B_SPLINE_CURVE ( ( 0.9999999999999990008, 0.9238795325112877377, 1.000000000000000000, 0.9238795325112867385, 1.000000000000000000, 0.9238795325112867385, 1.000000000000000000, 0.9238795325112874046, 0.9999999999999993339 ) ) 
 REPRESENTATION_ITEM ( '' )  );
#28582 = DIRECTION ( 'NONE',  ( -1.000000000000000000, 0.000000000000000000, 0.000000000000000000 ) ) ;
#28583 = CARTESIAN_POINT ( 'NONE',  ( 10.18810118750000093, -4.220049686691933921, 80.68750000204836681 ) ) ;
#28584 = ORIENTED_EDGE ( 'NONE', *, *, #27105, .T. ) ;
#28585 = CARTESIAN_POINT ( 'NONE',  ( 4.000000000000001776, 20.06250000000000355, -1.656854249492381248 ) ) ;
#28586 = CARTESIAN_POINT ( 'NONE',  ( 4.000000000000001776, 2.812499997268813612, -1.656854249492381248 ) ) ;
#28587 = CARTESIAN_POINT ( 'NONE',  ( 25.17157287525381903, 199.0000000027312126, 172.8284271247460993 ) ) ;
#28588 = CARTESIAN_POINT ( 'NONE',  ( -4.999999999999999112, -13.57248045702108818, 69.64920683919132216 ) ) ;
#28589 = CARTESIAN_POINT ( 'NONE',  ( 4.999999999999998224, -62.69792629052213329, 24.03557775816873487 ) ) ;
#28590 = CARTESIAN_POINT ( 'NONE',  ( -4.721056650415999201, 296.3281250017069510, -4.721056650415999201 ) ) ;
#28593 = CARTESIAN_POINT ( 'NONE',  ( 7.999999999732929190, -6.536825277765295045E-05, 6.267800880277100362 ) ) ;
#28592 = CARTESIAN_POINT ( 'NONE',  ( -3.042071309553166625, 242.8645833367473301, -11.35316468749999608 ) ) ;
#28591 = CARTESIAN_POINT ( 'NONE',  ( 25.55430564589115860, 209.0625000013656063, 167.5543056458911053 ) ) ;
#28594 = PRODUCT_CONTEXT ( 'NONE', #20675, 'mechanical' ) ;
#28595 = ORIENTED_EDGE ( 'NONE', *, *, #74467, .T. ) ;
#28596 = VECTOR ( 'NONE', #35466, 1000.000000000000000 ) ;
#28597 = CARTESIAN_POINT ( 'NONE',  ( -9.832129032723418760, 233.8020833367473301, -5.676582343749998927 ) ) ;
#28598 = CARTESIAN_POINT ( 'NONE',  ( 2.977408999572646486, 7.188101187499991163, 8.517802781871754547 ) ) ;
#28599 = ORIENTED_EDGE ( 'NONE', *, *, #29834, .F. ) ;
#28600 = VERTEX_POINT ( 'NONE', #34981 ) ;
#28601 = CARTESIAN_POINT ( 'NONE',  ( 10.18810118749999916, 4.220049686691935698, 76.00000000204835260 ) ) ;
#28602 = CARTESIAN_POINT ( 'NONE',  ( -3.042071309553173730, 89.63541666325268409, 11.35316468749999785 ) ) ;
#28603 = CARTESIAN_POINT ( 'NONE',  ( -12.04760458715721505, 13.82892193934112690, -0.1532218116813564290 ) ) ;
#28604 = CARTESIAN_POINT ( 'NONE',  ( -7.778174593052020747, -7.778174593052023411, 82.18750000000000000 ) ) ;
#28607 = CARTESIAN_POINT ( 'NONE',  ( 7.778174593052023411, -7.778174593052021635, 114.0625000000000000 ) ) ;
#28606 = CARTESIAN_POINT ( 'NONE',  ( 26.56734541678233086, 209.0000000013655779, 166.5412658749999650 ) ) ;
#28605 = CARTESIAN_POINT ( 'NONE',  ( 29.43265458321766559, 208.1250000013656063, 166.5412658749999650 ) ) ;
#28608 = ORIENTED_EDGE ( 'NONE', *, *, #67155, .T. ) ;
#28609 = DIRECTION ( 'NONE',  ( 0.000000000000000000, 0.000000000000000000, -1.000000000000000000 ) ) ;
#28610 = CARTESIAN_POINT ( 'NONE',  ( -30.99999999999992895, -31.99999999999978684, 135.0000000000000000 ) ) ;
#28611 = CARTESIAN_POINT ( 'NONE',  ( -11.35316468750000141, 203.4895833299193271, 3.042071309553159963 ) ) ;
#28612 = CARTESIAN_POINT ( 'NONE',  ( -1.432654583217664479, 204.7500000013656063, 138.5412658750000787 ) ) ;
#28613 = CARTESIAN_POINT ( 'NONE',  ( 29.43265458321766559, 208.1250000013656063, 166.5412658749999650 ) ) ;
#28614 = EDGE_CURVE ( 'NONE', #65370, #2593, #15671, .T. ) ;
#28615 = CARTESIAN_POINT ( 'NONE',  ( 4.401442555609581635E-16, 17.71874999795161187, -7.188101187500000044 ) ) ;
#28616 = CARTESIAN_POINT ( 'NONE',  ( 3.042071309553167069, 177.1354166632527267, -11.35316468749999785 ) ) ;
#28617 = CARTESIAN_POINT ( 'NONE',  ( -5.656854249492381470, 8.249999995903221972, 5.656854249492379694 ) ) ;
#28618 = CARTESIAN_POINT ( 'NONE',  ( 7.188101187500000933, 95.37500000204839523, -2.977408999572651371 ) ) ;
#28620 = CARTESIAN_POINT ( 'NONE',  ( -2.679491924311228512, 233.9583333333333428, -9.999999999999998224 ) ) ;
#28619 = CARTESIAN_POINT ( 'NONE',  ( 0.000000000000000000, 125.0000000000000000, 0.000000000000000000 ) ) ;
#28621 = CARTESIAN_POINT ( 'NONE',  ( 1.881053915767122664, 12.12499999863440969, 4.541265875000001451 ) ) ;
#28622 = CARTESIAN_POINT ( 'NONE',  ( 24.54126587500000412, 201.3750000013656347, 168.5673454167822172 ) ) ;
#28623 = CARTESIAN_POINT ( 'NONE',  ( 1.320432766682872962E-15, -7.188101187499992051, 8.236552781871752771 ) ) ;
#28624 = CARTESIAN_POINT ( 'NONE',  ( -11.35316468749999785, 58.07291666325269119, -3.042071309553167513 ) ) ;
#28625 = FACE_OUTER_BOUND ( 'NONE', #45096, .T. ) ;
#28626 = CARTESIAN_POINT ( 'NONE',  ( -5.656854249492380582, 119.0000000040967905, -5.656854249492380582 ) ) ;
#28627 = ORIENTED_EDGE ( 'NONE', *, *, #8106, .T. ) ;
#28628 = VECTOR ( 'NONE', #5718, 1000.000000000000000 ) ;
#28629 = CARTESIAN_POINT ( 'NONE',  ( 8.535034553343558983, 8.928701963635351291, -0.1959795092987683951 ) ) ;
#28630 = CARTESIAN_POINT ( 'NONE',  ( 11.35316468749999963, 60.98958332991934839, -3.042071309553165293 ) ) ;
#28631 = CARTESIAN_POINT ( 'NONE',  ( 11.00000000000000355, -4.556349186104045046, 75.34375000409676204 ) ) ;
#28632 = CARTESIAN_POINT ( 'NONE',  ( 1.432654583217608080, 200.8750000013656063, 138.5412658750000503 ) ) ;
#28633 = CARTESIAN_POINT ( 'NONE',  ( -1.317228840344603968, 10.12208498181967364, 70.14472670972865842 ) ) ;
#28635 = CARTESIAN_POINT ( 'NONE',  ( -11.35316468749999785, 53.07291666325266988, -3.042071309553167957 ) ) ;
#28634 = CARTESIAN_POINT ( 'NONE',  ( 5.082755093536325042, 92.09375000204838102, -5.082755093536325930 ) ) ;
#28636 = CARTESIAN_POINT ( 'NONE',  ( 1.469576158976822172E-15, -7.999999999999991118, 2.705302779823365533 ) ) ;
#28637 = DIRECTION ( 'NONE',  ( -0.000000000000000000, -1.000000000000000000, -0.000000000000000000 ) ) ;
#28638 = CARTESIAN_POINT ( 'NONE',  ( -8.311093377946836114, 172.6562499965860411, -8.311093377946837890 ) ) ;
#28639 = CARTESIAN_POINT ( 'NONE',  ( 7.320508075688771044, 141.2499999931720538, 7.320508075688775484 ) ) ;
#28640 = CARTESIAN_POINT ( 'NONE',  ( -4.401442555609581635E-16, 97.15625000204839523, -7.188101187500000044 ) ) ;
#28641 = CARTESIAN_POINT ( 'NONE',  ( 8.660254037844392627, 20.41666666666667140, -5.000000000000004441 ) ) ;
#28642 = CARTESIAN_POINT ( 'NONE',  ( 11.35316468749999785, 50.88541666325269119, 3.042071309553174174 ) ) ;
#28643 = CARTESIAN_POINT ( 'NONE',  ( -10.00000000000000000, 79.16666665983871098, -2.679491924311229845 ) ) ;
#28644 = CARTESIAN_POINT ( 'NONE',  ( 11.35316468750000141, 175.7812499965860411, 0.000000000000000000 ) ) ;
#28645 = VERTEX_POINT ( 'NONE', #70040 ) ;
#28646 = LINE ( 'NONE', #39972, #9087 ) ;
#28647 = CARTESIAN_POINT ( 'NONE',  ( 10.18810118749999916, 1.247682550866122264E-15, 71.40625000204836681 ) ) ;
#28648 = CARTESIAN_POINT ( 'NONE',  ( -2.828427124746152987, 195.1250000000000284, 200.8284271247462129 ) ) ;
#28650 = CARTESIAN_POINT ( 'NONE',  ( 3.042071309553167513, 181.8229166632526983, -11.35316468749999785 ) ) ;
#28649 = DIRECTION ( 'NONE',  ( 1.000000000000000000, -0.000000000000000000, -0.000000000000000000 ) ) ;
#28651 = CARTESIAN_POINT ( 'NONE',  ( -7.999999999999991118, 0.000000000000000000, 3.886552784329822874 ) ) ;
#28652 = EDGE_CURVE ( 'NONE', #53531, #71925, #62502, .T. ) ;
#28653 = CARTESIAN_POINT ( 'NONE',  ( 8.660254037844385522, 256.0416666734946602, -5.000000000000003553 ) ) ;
#28654 = FACE_BOUND ( 'NONE', #29870, .T. ) ;
#28655 = ORIENTED_EDGE ( 'NONE', *, *, #25141, .F. ) ;
#28656 = AXIS2_PLACEMENT_3D ( 'NONE', #26463, #49487, #20815 ) ;
#28657 = CARTESIAN_POINT ( 'NONE',  ( -5.082755093536319713, 5.082755093536319713, 28.29905278187175810 ) ) ;
#28658 = CARTESIAN_POINT ( 'NONE',  ( 5.676582343749993598, 125.2604166632526841, 9.832129032723422313 ) ) ;
#28659 = ORIENTED_EDGE ( 'NONE', *, *, #53389, .F. ) ;
#28660 = CARTESIAN_POINT ( 'NONE',  ( 3.211159895383561835, 8.562499998634407916, -3.211159895383561835 ) ) ;
#28661 = CARTESIAN_POINT ( 'NONE',  ( -2.977408999572654480, 14.99999999795161187, 7.188101187499999156 ) ) ;
#28662 = EDGE_CURVE ( 'NONE', #52532, #33382, #68763, .T. ) ;
#28663 = CARTESIAN_POINT ( 'NONE',  ( -8.000000000000000000, 102.5937500040967763, -3.313708498984761608 ) ) ;
#28664 = CARTESIAN_POINT ( 'NONE',  ( -29.43265458321766559, 197.7500000013656063, 166.5412658750003629 ) ) ;
#28665 =( BOUNDED_SURFACE ( )  B_SPLINE_SURFACE ( 1, 2, ( 
 ( #55395, #26702, #49722, #9738, #4827, #72738, #44807, #10477, #27825, #50834, #43306, #58015, #64022, #62892, #16863, #23655, #51962, #39888, #29687, #33883, #6684, #57254, #69307, #51207, #12334, #40262, #62522, #46289, #28196, #56883, #35367, #29324, #34624, #45179, #68192, #28567, #11224, #39525, #52334, #63636, #5567, #45542, #10849, #34253, #51575, #46662, #74594, #73845, #671, #16488, #34998, #11967, #22152, #57630, #5199, #74218, #58379, #22907, #22523, #6320, #45919, #68561, #69681, #68931, #17242, #63263, #11589, #5944, #17618, #28943, #299, #40636, #17994, #23278, #41012, #36093, #53811, #18368, #48132, #12691, #70060, #25486, #47024, #36460, #70782, #53446, #30060, #53072, #7051, #65853, #48500, #71506, #59836, #59111, #25114, #13055, #24391, #52703, #19830, #30791, #47399, #31155, #42834, #59474, #2120, #14163, #18738, #7787, #19095, #8518, #24017, #70422, #37196, #41746, #42100, #64756, #13423, #35725, #1037, #41382, #8150, #71138, #54187, #19461, #2493, #65111, #60196, #1407, #64394, #7419, #58741, #30426, #1767, #24748, #47759, #42473, #65490, #13782, #36826, #66230, #21691, #49630, #49998, #32670, #48871, #15655, #3610, #26224, #16028, #71879, #55680, #60571, #50368, #3995, #72645, #9650, #38318, #2863, #44717, #32288, #25851, #66602, #54929, #26984, #20193, #67732, #39061, #9266, #73385, #62062, #31535, #43212, #61324, #44346, #38696, #37572, #73015, #21325, #8895, #67356, #61697, #14532, #60946, #10019, #33051, #31908, #43970, #3238, #56050, #15281, #43587, #49244, #55302 ),
 ( #4359, #54556, #66979, #72260, #20573, #14908, #26606, #37947, #27351, #20948, #68101, #34906, #5474, #16765, #16390, #69587, #68836, #5850, #51484, #74495, #51866, #17523, #39429, #57541, #68465, #11502, #50739, #28843, #45086, #27728, #57914, #4734, #17149, #28476, #11135, #62428, #10754, #33791, #23554, #6223, #29226, #40539, #39792, #207, #45448, #56788, #10387, #52239, #63176, #5109, #63545, #573, #40171, #34535, #46566, #51114, #23185, #22804, #40913, #56413, #28099, #17900, #74126, #45825, #22428, #46196, #62796, #33413, #73753, #11870, #69211, #22059, #34158, #57158, #1673, #31057, #64295, #6587, #47303, #69962, #2395, #25392, #6950, #54085, #18270, #2029, #13326, #29594, #23925, #48407, #7324, #7690, #65017, #52605, #48035, #35999, #58644, #41285, #41651, #59379, #59016, #70685, #30329, #36363, #30697, #19003, #70328, #12602, #943, #35271, #47663, #58284, #19737, #18643, #42009, #46934, #53715, #24653, #35629, #52975, #25015, #29962, #19363, #42377, #8054, #71044, #63924, #1309, #24292, #64661, #12234, #12961, #53348, #65394, #13691, #36733, #59744, #71413, #9173, #21231, #20471, #9921, #61601, #4269, #54465, #49530, #55582, #26891, #48779, #20856, #9559, #71786, #43874, #32574, #37100, #72161, #66890, #61230, #20104, #55211, #8422, #3897, #26506, #54837, #43116, #43491, #32953, #37856, #49907, #3147, #66135, #2772, #60853, #55959, #8805, #14440, #37474, #15196, #27259, #44257, #72921, #50277, #31816, #60475, #67268, #38225, #26131, #73297, #25758, #42746, #49150, #15563, #66503 ) ),
 .UNSPECIFIED., .F., .F., .F. ) 
 B_SPLINE_SURFACE_WITH_KNOTS ( ( 2, 2 ),
 ( 3, 2, 2, 2, 2, 2, 2, 2, 2, 2, 2, 2, 2, 2, 2, 2, 2, 2, 2, 2, 2, 2, 2, 2, 2, 2, 2, 2, 2, 2, 2, 2, 2, 2, 2, 2, 2, 2, 2, 2, 2, 2, 2, 2, 2, 2, 2, 2, 2, 2, 2, 2, 2, 2, 2, 2, 2, 2, 2, 2, 2, 2, 2, 2, 2, 2, 2, 2, 2, 2, 2, 2, 2, 2, 2, 2, 2, 2, 2, 2, 2, 2, 2, 2, 2, 2, 2, 2, 2, 2, 2, 2, 2, 2, 2, 2, 3 ),
 ( 0.000000000000000000, 1.000000000000000000 ),
 ( 0.000000000000000000, 0.01041666666666666609, 0.02083333333333333218, 0.03125000000000000000, 0.04166666666666666435, 0.05208333333333333565, 0.06250000000000000000, 0.07291666666666667129, 0.08333333333333332871, 0.09375000000000000000, 0.1041666666666666713, 0.1145833333333333287, 0.1250000000000000000, 0.1354166666666666574, 0.1458333333333333426, 0.1562500000000000000, 0.1666666666666666574, 0.1770833333333333426, 0.1875000000000000000, 0.1979166666666666574, 0.2083333333333333426, 0.2187500000000000000, 0.2291666666666666574, 0.2395833333333333426, 0.2500000000000000000, 0.2604166666666666852, 0.2708333333333333148, 0.2812500000000000000, 0.2916666666666666852, 0.3020833333333333148, 0.3125000000000000000, 0.3229166666666666852, 0.3333333333333333148, 0.3437500000000000000, 0.3541666666666666852, 0.3645833333333333148, 0.3750000000000000000, 0.3854166666666666852, 0.3958333333333333148, 0.4062500000000000000, 0.4166666666666666852, 0.4270833333333333148, 0.4375000000000000000, 0.4479166666666666852, 0.4583333333333333148, 0.4687500000000000000, 0.4791666666666666852, 0.4895833333333333148, 0.5000000000000000000, 0.5104166666666666297, 0.5208333333333333703, 0.5312500000000000000, 0.5416666666666666297, 0.5520833333333333703, 0.5625000000000000000, 0.5729166666666666297, 0.5833333333333333703, 0.5937500000000000000, 0.6041666666666666297, 0.6145833333333333703, 0.6250000000000000000, 0.6354166666666666297, 0.6458333333333333703, 0.6562500000000000000, 0.6666666666666666297, 0.6770833333333333703, 0.6875000000000000000, 0.6979166666666666297, 0.7083333333333333703, 0.7187500000000000000, 0.7291666666666666297, 0.7395833333333333703, 0.7500000000000000000, 0.7604166666666666297, 0.7708333333333333703, 0.7812500000000000000, 0.7916666666666666297, 0.8020833333333333703, 0.8125000000000000000, 0.8229166666666666297, 0.8333333333333333703, 0.8437500000000000000, 0.8541666666666666297, 0.8645833333333333703, 0.8750000000000000000, 0.8854166666666666297, 0.8958333333333333703, 0.9062500000000000000, 0.9166666666666666297, 0.9270833333333333703, 0.9375000000000000000, 0.9479166666666666297, 0.9583333333333333703, 0.9687500000000000000, 0.9791666666666666297, 0.9895833333333333703, 1.000000000000000000 ),
 .UNSPECIFIED. ) 
 GEOMETRIC_REPRESENTATION_ITEM ( )  RATIONAL_B_SPLINE_SURFACE ( (
 ( 1.000000000000000000, 0.9238795325112867385, 1.000000000000000000, 0.9238795325112867385, 1.000000000000000000, 0.9238795325112867385, 1.000000000000000000, 0.9238795325112867385, 1.000000000000000000, 0.9238795325112867385, 1.000000000000000000, 0.9238795325112867385, 1.000000000000000000, 0.9238795325112867385, 1.000000000000000000, 0.9238795325112867385, 1.000000000000000000, 0.9238795325112867385, 1.000000000000000000, 0.9238795325112867385, 1.000000000000000000, 0.9238795325112867385, 1.000000000000000000, 0.9238795325112867385, 1.000000000000000000, 0.9238795325112867385, 1.000000000000000000, 0.9238795325112867385, 1.000000000000000000, 0.9238795325112867385, 1.000000000000000000, 0.9238795325112867385, 1.000000000000000000, 0.9238795325112867385, 1.000000000000000000, 0.9238795325112867385, 1.000000000000000000, 0.9238795325112867385, 1.000000000000000000, 0.9238795325112867385, 1.000000000000000000, 0.9238795325112867385, 1.000000000000000000, 0.9238795325112867385, 1.000000000000000000, 0.9238795325112867385, 1.000000000000000000, 0.9238795325112867385, 1.000000000000000000, 0.9238795325112867385, 1.000000000000000000, 0.9238795325112867385, 1.000000000000000000, 0.9238795325112867385, 1.000000000000000000, 0.9238795325112867385, 1.000000000000000000, 0.9238795325112867385, 1.000000000000000000, 0.9238795325112867385, 1.000000000000000000, 0.9238795325112867385, 1.000000000000000000, 0.9238795325112867385, 1.000000000000000000, 0.9238795325112867385, 1.000000000000000000, 0.9238795325112867385, 1.000000000000000000, 0.9238795325112867385, 1.000000000000000000, 0.9238795325112867385, 1.000000000000000000, 0.9238795325112867385, 1.000000000000000000, 0.9238795325112867385, 1.000000000000000000, 0.9238795325112867385, 1.000000000000000000, 0.9238795325112867385, 1.000000000000000000, 0.9238795325112867385, 1.000000000000000000, 0.9238795325112867385, 1.000000000000000000, 0.9238795325112867385, 1.000000000000000000, 0.9238795325112867385, 1.000000000000000000, 0.9238795325112867385, 1.000000000000000000, 0.9238795325112867385, 1.000000000000000000, 0.9238795325112867385, 1.000000000000000000, 0.9238795325112867385, 1.000000000000000000, 0.9238795325112867385, 1.000000000000000000, 0.9238795325112867385, 1.000000000000000000, 0.9238795325112867385, 1.000000000000000000, 0.9238795325112867385, 1.000000000000000000, 0.9238795325112867385, 1.000000000000000000, 0.9238795325112867385, 1.000000000000000000, 0.9238795325112867385, 1.000000000000000000, 0.9238795325112867385, 1.000000000000000000, 0.9238795325112867385, 1.000000000000000000, 0.9238795325112867385, 1.000000000000000000, 0.9238795325112867385, 1.000000000000000000, 0.9238795325112867385, 1.000000000000000000, 0.9238795325112867385, 1.000000000000000000, 0.9238795325112867385, 1.000000000000000000, 0.9238795325112867385, 1.000000000000000000, 0.9238795325112867385, 1.000000000000000000, 0.9238795325112867385, 1.000000000000000000, 0.9238795325112867385, 1.000000000000000000, 0.9238795325112867385, 1.000000000000000000, 0.9238795325112867385, 1.000000000000000000, 0.9238795325112867385, 1.000000000000000000, 0.9238795325112867385, 1.000000000000000000, 0.9238795325112867385, 1.000000000000000000, 0.9238795325112867385, 1.000000000000000000, 0.9238795325112867385, 1.000000000000000000, 0.9238795325112867385, 1.000000000000000000, 0.9238795325112867385, 1.000000000000000000, 0.9238795325112867385, 1.000000000000000000, 0.9238795325112867385, 1.000000000000000000, 0.9238795325112867385, 1.000000000000000000, 0.9238795325112867385, 1.000000000000000000, 0.9238795325112867385, 1.000000000000000000, 0.9238795325112867385, 1.000000000000000000, 0.9238795325112867385, 1.000000000000000000, 0.9238795325112867385, 1.000000000000000000, 0.9238795325112867385, 1.000000000000000000, 0.9238795325112867385, 1.000000000000000000, 0.9238795325112867385, 1.000000000000000000, 0.9238795325112867385, 1.000000000000000000, 0.9238795325112867385, 1.000000000000000000, 0.9238795325112867385, 1.000000000000000000, 0.9238795325112867385, 1.000000000000000000, 0.9238795325112867385, 1.000000000000000000, 0.9238795325112867385, 1.000000000000000000, 0.9238795325112867385, 1.000000000000000000, 0.9238795325112867385, 1.000000000000000000, 0.9238795325112867385, 1.000000000000000000, 0.9238795325112867385, 1.000000000000000000),
 ( 1.000000000000000000, 0.9238795325112867385, 1.000000000000000000, 0.9238795325112867385, 1.000000000000000000, 0.9238795325112867385, 1.000000000000000000, 0.9238795325112867385, 1.000000000000000000, 0.9238795325112867385, 1.000000000000000000, 0.9238795325112867385, 1.000000000000000000, 0.9238795325112867385, 1.000000000000000000, 0.9238795325112867385, 1.000000000000000000, 0.9238795325112867385, 1.000000000000000000, 0.9238795325112867385, 1.000000000000000000, 0.9238795325112867385, 1.000000000000000000, 0.9238795325112867385, 1.000000000000000000, 0.9238795325112867385, 1.000000000000000000, 0.9238795325112867385, 1.000000000000000000, 0.9238795325112867385, 1.000000000000000000, 0.9238795325112867385, 1.000000000000000000, 0.9238795325112867385, 1.000000000000000000, 0.9238795325112867385, 1.000000000000000000, 0.9238795325112867385, 1.000000000000000000, 0.9238795325112867385, 1.000000000000000000, 0.9238795325112867385, 1.000000000000000000, 0.9238795325112867385, 1.000000000000000000, 0.9238795325112867385, 1.000000000000000000, 0.9238795325112867385, 1.000000000000000000, 0.9238795325112867385, 1.000000000000000000, 0.9238795325112867385, 1.000000000000000000, 0.9238795325112867385, 1.000000000000000000, 0.9238795325112867385, 1.000000000000000000, 0.9238795325112867385, 1.000000000000000000, 0.9238795325112867385, 1.000000000000000000, 0.9238795325112867385, 1.000000000000000000, 0.9238795325112867385, 1.000000000000000000, 0.9238795325112867385, 1.000000000000000000, 0.9238795325112867385, 1.000000000000000000, 0.9238795325112867385, 1.000000000000000000, 0.9238795325112867385, 1.000000000000000000, 0.9238795325112867385, 1.000000000000000000, 0.9238795325112867385, 1.000000000000000000, 0.9238795325112867385, 1.000000000000000000, 0.9238795325112867385, 1.000000000000000000, 0.9238795325112867385, 1.000000000000000000, 0.9238795325112867385, 1.000000000000000000, 0.9238795325112867385, 1.000000000000000000, 0.9238795325112867385, 1.000000000000000000, 0.9238795325112867385, 1.000000000000000000, 0.9238795325112867385, 1.000000000000000000, 0.9238795325112867385, 1.000000000000000000, 0.9238795325112867385, 1.000000000000000000, 0.9238795325112867385, 1.000000000000000000, 0.9238795325112867385, 1.000000000000000000, 0.9238795325112867385, 1.000000000000000000, 0.9238795325112867385, 1.000000000000000000, 0.9238795325112867385, 1.000000000000000000, 0.9238795325112867385, 1.000000000000000000, 0.9238795325112867385, 1.000000000000000000, 0.9238795325112867385, 1.000000000000000000, 0.9238795325112867385, 1.000000000000000000, 0.9238795325112867385, 1.000000000000000000, 0.9238795325112867385, 1.000000000000000000, 0.9238795325112867385, 1.000000000000000000, 0.9238795325112867385, 1.000000000000000000, 0.9238795325112867385, 1.000000000000000000, 0.9238795325112867385, 1.000000000000000000, 0.9238795325112867385, 1.000000000000000000, 0.9238795325112867385, 1.000000000000000000, 0.9238795325112867385, 1.000000000000000000, 0.9238795325112867385, 1.000000000000000000, 0.9238795325112867385, 1.000000000000000000, 0.9238795325112867385, 1.000000000000000000, 0.9238795325112867385, 1.000000000000000000, 0.9238795325112867385, 1.000000000000000000, 0.9238795325112867385, 1.000000000000000000, 0.9238795325112867385, 1.000000000000000000, 0.9238795325112867385, 1.000000000000000000, 0.9238795325112867385, 1.000000000000000000, 0.9238795325112867385, 1.000000000000000000, 0.9238795325112867385, 1.000000000000000000, 0.9238795325112867385, 1.000000000000000000, 0.9238795325112867385, 1.000000000000000000, 0.9238795325112867385, 1.000000000000000000, 0.9238795325112867385, 1.000000000000000000, 0.9238795325112867385, 1.000000000000000000, 0.9238795325112867385, 1.000000000000000000, 0.9238795325112867385, 1.000000000000000000, 0.9238795325112867385, 1.000000000000000000, 0.9238795325112867385, 1.000000000000000000, 0.9238795325112867385, 1.000000000000000000, 0.9238795325112867385, 1.000000000000000000, 0.9238795325112867385, 1.000000000000000000, 0.9238795325112867385, 1.000000000000000000, 0.9238795325112867385, 1.000000000000000000, 0.9238795325112867385, 1.000000000000000000, 0.9238795325112867385, 1.000000000000000000, 0.9238795325112867385, 1.000000000000000000, 0.9238795325112867385, 1.000000000000000000, 0.9238795325112867385, 1.000000000000000000) ) ) 
 REPRESENTATION_ITEM ( '' )  SURFACE ( )  );
#28666 = CARTESIAN_POINT ( 'NONE',  ( 1.656854249492381248, 8.187500000000000000, -4.000000000000001776 ) ) ;
#28667 = DIRECTION ( 'NONE',  ( 0.000000000000000000, 0.000000000000000000, -1.000000000000000000 ) ) ;
#28668 = CARTESIAN_POINT ( 'NONE',  ( -4.541265875000002339, 13.74999999863440969, -1.881053915767121998 ) ) ;
#28669 = CARTESIAN_POINT ( 'NONE',  ( -5.656854249492375253, 5.656854249492375253, 21.83030278392014623 ) ) ;
#28670 = CARTESIAN_POINT ( 'NONE',  ( 1.656854249492348607, 197.1875000000000284, 138.0000000000000568 ) ) ;
#28671 = ORIENTED_EDGE ( 'NONE', *, *, #23566, .F. ) ;
#28672 = CARTESIAN_POINT ( 'NONE',  ( -5.656854249492375253, 5.656854249492375253, 9.830302783920146226 ) ) ;
#28673 = CARTESIAN_POINT ( 'NONE',  ( -7.188101187500001821, 103.0625000020483810, -2.977408999572650483 ) ) ;
#28674 = VECTOR ( 'NONE', #14314, 1000.000000000000000 ) ;
#28676 = DIRECTION ( 'NONE',  ( -0.000000000000000000, -0.000000000000000000, -1.000000000000000000 ) ) ;
#28675 = FACE_OUTER_BOUND ( 'NONE', #52543, .T. ) ;
#28677 = CARTESIAN_POINT ( 'NONE',  ( -4.541265875000002339, 21.81249999863440792, -5.561446717895856393E-16 ) ) ;
#28678 = AXIS2_PLACEMENT_3D ( 'NONE', #69070, #35127, #58142 ) ;
#28679 = CARTESIAN_POINT ( 'NONE',  ( 1.320432766682872962E-15, -7.188101187499992051, 0.3615527818717524378 ) ) ;
#28680 = VERTEX_POINT ( 'NONE', #40619 ) ;
#28681 = B_SPLINE_CURVE_WITH_KNOTS ( 'NONE', 3,
 ( #42543, #70850, #19163, #59538, #7850, #13850, #32740, #48939 ),
 .UNSPECIFIED., .F., .F.,
 ( 4, 2, 2, 4 ),
 ( 0.005256334970490776810, 0.006570121696662009278, 0.007883908422833242613, 0.01051148187517571622 ),
 .UNSPECIFIED. ) ;
#28682 = ORIENTED_EDGE ( 'NONE', *, *, #39801, .T. ) ;
#28683 = CARTESIAN_POINT ( 'NONE',  ( -10.18810118749999916, 0.000000000000000000, 90.15625000204838102 ) ) ;
#28684 = CARTESIAN_POINT ( 'NONE',  ( 0.000000000000000000, 0.000000000000000000, 118.0000000000000000 ) ) ;
#28685 = CARTESIAN_POINT ( 'NONE',  ( -4.556349186104045934, 11.00000000000000000, 99.71875000000000000 ) ) ;
#28686 = CARTESIAN_POINT ( 'NONE',  ( 2.445694354108840063, 203.0625000013656063, 200.4456943541088663 ) ) ;
#28688 = CARTESIAN_POINT ( 'NONE',  ( 2.765530957082001251, 298.9218750017070647, 6.676582343749999815 ) ) ;
#28687 = CARTESIAN_POINT ( 'NONE',  ( 7.778174593052023411, -7.778174593052021635, 87.06249999999998579 ) ) ;
#28689 = CARTESIAN_POINT ( 'NONE',  ( 10.00000000000000178, 120.0000000000000142, 0.000000000000000000 ) ) ;
#28690 = CARTESIAN_POINT ( 'NONE',  ( -8.000000000000000000, 103.9062500000000000, -3.313708498984761608 ) ) ;
#28691 = VECTOR ( 'NONE', #21194, 999.9999999999998863 ) ;
#28692 = CARTESIAN_POINT ( 'NONE',  ( -4.721056650415999201, 288.4843750017070079, -4.721056650415999201 ) ) ;
#28693 = CARTESIAN_POINT ( 'NONE',  ( -2.977408999572648707, -7.188101187499990274, 8.142802781871750994 ) ) ;
#28694 = AXIS2_PLACEMENT_3D ( 'NONE', #7561, #67788, #71282 ) ;
#28695 = CARTESIAN_POINT ( 'NONE',  ( 28.00000000000002132, 201.9375000013656063, 166.5412658749999082 ) ) ;
#28696 = CARTESIAN_POINT ( 'NONE',  ( -3.313708498984760720, 25.78124999590322375, -8.000000000000000000 ) ) ;
#28697 = CARTESIAN_POINT ( 'NONE',  ( -2.445694354108838731, 197.0625000013656063, 144.4456943541088663 ) ) ;
#28698 = CARTESIAN_POINT ( 'NONE',  ( -5.082755093536324154, 121.7187500020483952, 5.082755093536326818 ) ) ;
#28700 = CARTESIAN_POINT ( 'NONE',  ( 1.209040393344284148, 194.8891453581537121, 194.2954438887121569 ) ) ;
#28699 = DIRECTION ( 'NONE',  ( -0.000000000000000000, 1.000000000000000000, 4.689100369878284071E-30 ) ) ;
#28701 = CARTESIAN_POINT ( 'NONE',  ( 8.311093377946839666, 246.0937500034139873, 8.311093377946829008 ) ) ;
#28702 = FACE_OUTER_BOUND ( 'NONE', #7619, .T. ) ;
#28703 = CARTESIAN_POINT ( 'NONE',  ( 27.99999999999996447, 198.0000000000000000, 173.9999999999999147 ) ) ;
#28704 = CARTESIAN_POINT ( 'NONE',  ( -8.311093377946841443, 18.90624999658601624, 8.311093377946830785 ) ) ;
#28705 = CARTESIAN_POINT ( 'NONE',  ( 3.313708498984815343, 100.7187500040967763, -7.999999999999944933 ) ) ;
#28706 = CARTESIAN_POINT ( 'NONE',  ( 5.676582343749993598, 215.2604166632526983, 9.832129032723422313 ) ) ;
#28707 = CARTESIAN_POINT ( 'NONE',  ( -26.34314575050758123, 198.5625000000000000, 174.0000000000003411 ) ) ;
#28708 = CARTESIAN_POINT ( 'NONE',  ( -5.000000000000005329, 220.2083333265053966, 8.660254037844387298 ) ) ;
#28710 = CYLINDRICAL_SURFACE ( 'NONE', #18268, 10.00000000000000178 ) ;
#28709 = CARTESIAN_POINT ( 'NONE',  ( 2.849036369511732440E-14, 208.2500000000000284, 202.0000000000000000 ) ) ;
#28711 = VERTEX_POINT ( 'NONE', #11948 ) ;
#28712 = EDGE_CURVE ( 'NONE', #50841, #66964, #63472, .T. ) ;
#28713 = CARTESIAN_POINT ( 'NONE',  ( -2.445694354108840063, 202.0625000013656063, 139.5543056458912190 ) ) ;
#28714 = CARTESIAN_POINT ( 'NONE',  ( 6.951808397369818766E-16, 22.03124999658601624, -11.35316468750000141 ) ) ;
#28715 = CARTESIAN_POINT ( 'NONE',  ( 11.00000000000000000, 4.556349186104045934, 93.53125000409676204 ) ) ;
#28716 = CARTESIAN_POINT ( 'NONE',  ( 7.999999999999991118, 9.797174393178815797E-16, 18.08030277982336642 ) ) ;
#28717 = CARTESIAN_POINT ( 'NONE',  ( -26.56734541678243033, 198.3750000013656063, 166.5412658750003345 ) ) ;
#28718 = CARTESIAN_POINT ( 'NONE',  ( 0.000000000000000000, 300.0000000000000000, 0.000000000000000000 ) ) ;
#28720 = CARTESIAN_POINT ( 'NONE',  ( -3.042071309553163960, 22.23958332991935194, -11.35316468749999963 ) ) ;
#28719 = CARTESIAN_POINT ( 'NONE',  ( 2.977408999572650039, 110.1875000020483810, -7.188101187500000933 ) ) ;
#28721 = CARTESIAN_POINT ( 'NONE',  ( -3.313708498984757167, 7.999999999999991118, 21.54905277982336287 ) ) ;
#28722 = CARTESIAN_POINT ( 'NONE',  ( -9.832129032723418760, 132.8645833299193555, -5.676582343750004256 ) ) ;
#28723 = CARTESIAN_POINT ( 'NONE',  ( 10.00000000000000000, 106.6666666598387110, 2.679491924311236062 ) ) ;
#28724 = CARTESIAN_POINT ( 'NONE',  ( 5.082755093536325042, 114.9687500020483810, -5.082755093536325930 ) ) ;
#28725 = CARTESIAN_POINT ( 'NONE',  ( -7.320508075688773708, 3.749999993172032475, -7.320508075688774596 ) ) ;
#28726 = CARTESIAN_POINT ( 'NONE',  ( -30.44569435410879521, 207.0625000013656063, 172.4456943541092357 ) ) ;
#28727 = CARTESIAN_POINT ( 'NONE',  ( -4.999999999999999112, -51.74377041917529851, -41.86884046506285273 ) ) ;
#28728 = ORIENTED_EDGE ( 'NONE', *, *, #3917, .T. ) ;
#28729 = CARTESIAN_POINT ( 'NONE',  ( 11.35316468750000141, 11.09374999658601624, 0.000000000000000000 ) ) ;
#28730 = CARTESIAN_POINT ( 'NONE',  ( -4.000000000000001776, 20.24999999726881228, -4.898587196589415787E-16 ) ) ;
#28731 = CARTESIAN_POINT ( 'NONE',  ( -6.676582343750000703, 296.5156250017069510, 2.765530957082001251 ) ) ;
#28732 = CARTESIAN_POINT ( 'NONE',  ( 9.832129032723416984, 145.3645833299193555, 5.676582343750006032 ) ) ;
#28733 = CARTESIAN_POINT ( 'NONE',  ( 7.999999999999991118, 3.313708498984757611, 21.23030278432982954 ) ) ;
#28734 = CARTESIAN_POINT ( 'NONE',  ( -24.00000000000000711, 198.8125000000000284, 168.3431457505080289 ) ) ;
#28735 = EDGE_CURVE ( 'NONE', #28855, #47954, #30646, .T. ) ;
#28736 = CARTESIAN_POINT ( 'NONE',  ( -3.042071309553166181, 262.8645833367473301, -11.35316468749999608 ) ) ;
#28737 = CARTESIAN_POINT ( 'NONE',  ( -4.220049686691937474, -10.18810118749999738, 98.31250000204836681 ) ) ;
#28738 = VERTEX_POINT ( 'NONE', #56865 ) ;
#28739 = EDGE_CURVE ( 'NONE', #47641, #23624, #6666, .T. ) ;
#28740 = VECTOR ( 'NONE', #35701, 1000.000000000000000 ) ;
#28741 = FACE_OUTER_BOUND ( 'NONE', #63696, .T. ) ;
#28742 = DIRECTION ( 'NONE',  ( 0.000000000000000000, 0.000000000000000000, 1.000000000000000000 ) ) ;
#28743 = CARTESIAN_POINT ( 'NONE',  ( -2.445694354108784108, 201.5625000013656063, 195.5543056458912190 ) ) ;
#28744 = CARTESIAN_POINT ( 'NONE',  ( 5.676582343750001591, 71.92708332991934128, -9.832129032723420536 ) ) ;
#28745 = VERTEX_POINT ( 'NONE', #34235 ) ;
#28746 = CARTESIAN_POINT ( 'NONE',  ( 1.871523826299183495E-15, -10.18810118749999916, 110.0312500020483668 ) ) ;
#28747 = CARTESIAN_POINT ( 'NONE',  ( 4.541265875000002339, 11.49999999863440969, -1.881053915767121776 ) ) ;
#28748 = VERTEX_POINT ( 'NONE', #57236 ) ;
#28749 = ORIENTED_EDGE ( 'NONE', *, *, #19874, .F. ) ;
#28750 = CARTESIAN_POINT ( 'NONE',  ( -2.977408999572650039, 26.43749999795162253, -7.188101187500001821 ) ) ;
#28751 = CARTESIAN_POINT ( 'NONE',  ( -10.00000000000000178, 109.3749999931720396, -1.224646799147353454E-15 ) ) ;
#28752 = AXIS2_PLACEMENT_3D ( 'NONE', #20239, #3282, #25158 ) ;
#28753 = DIRECTION ( 'NONE',  ( -0.000000000000000000, -1.000000000000000000, -0.000000000000000000 ) ) ;
#28754 = CARTESIAN_POINT ( 'NONE',  ( -5.082755093536326818, 25.78124999795161543, 5.082755093536325042 ) ) ;
#28755 = ADVANCED_FACE ( 'NONE', ( #51190 ), #69291, .F. ) ;
#28756 = CARTESIAN_POINT ( 'NONE',  ( 2.828427124746152987, 200.1250000000000284, 139.1715728752538723 ) ) ;
#28757 = VECTOR ( 'NONE', #45596, 1000.000000000000000 ) ;
#28758 = CARTESIAN_POINT ( 'NONE',  ( 1.871523826299183495E-15, -10.18810118749999916, 105.9062500020483810 ) ) ;
#28759 = CARTESIAN_POINT ( 'NONE',  ( -7.778174593052023411, 7.778174593052023411, 75.81249999999997158 ) ) ;
#28760 = CARTESIAN_POINT ( 'NONE',  ( -1.656854249492381248, 9.062499997268815832, -4.000000000000001776 ) ) ;
#28761 = ORIENTED_EDGE ( 'NONE', *, *, #71459, .F. ) ;
#28762 = DIRECTION ( 'NONE',  ( -0.000000000000000000, -1.000000000000000000, -0.000000000000000000 ) ) ;
#28763 = CARTESIAN_POINT ( 'NONE',  ( 2.754378923186476579E-14, 201.1875000013656063, 194.5412658750000219 ) ) ;
#28764 = CARTESIAN_POINT ( 'NONE',  ( -29.43265458321756256, 205.8750000013656063, 173.4587341250004044 ) ) ;
#28765 = CARTESIAN_POINT ( 'NONE',  ( 1.881053915767121776, 10.49999999863440792, -4.541265875000002339 ) ) ;
#28766 = EDGE_CURVE ( 'NONE', #65516, #45475, #46082, .T. ) ;
#28767 = CARTESIAN_POINT ( 'NONE',  ( -2.751064625579944321E-14, 206.8750000027312126, 146.0000000000000284 ) ) ;
#28768 = CARTESIAN_POINT ( 'NONE',  ( -7.188101187499992051, 0.000000000000000000, 16.48655278187175810 ) ) ;
#28769 = VERTEX_POINT ( 'NONE', #1388 ) ;
#28770 = DIRECTION ( 'NONE',  ( -0.000000000000000000, -1.000000000000000000, -0.000000000000000000 ) ) ;
#28771 = ORIENTED_EDGE ( 'NONE', *, *, #71979, .F. ) ;
#28772 = CARTESIAN_POINT ( 'NONE',  ( -4.220049686691937474, -10.18810118749999738, 108.4375000020483952 ) ) ;
#28773 = DIRECTION ( 'NONE',  ( -0.8660254037844389297, -0.4999999999999994449, 0.000000000000000000 ) ) ;
#28774 = CARTESIAN_POINT ( 'NONE',  ( -23.99999999999997513, 205.6875000000000284, 171.6568542494927385 ) ) ;
#28775 = CARTESIAN_POINT ( 'NONE',  ( 2.839093476692135984E-14, 201.6875000013656063, 201.4587341250000350 ) ) ;
#28776 = DIRECTION ( 'NONE',  ( 1.000000000000000000, 0.000000000000000000, 0.000000000000000000 ) ) ;
#28777 = CARTESIAN_POINT ( 'NONE',  ( -8.660254037844390851, 77.91666666666667140, 4.999999999999998224 ) ) ;
#28778 = CARTESIAN_POINT ( 'NONE',  ( 5.656854249492379694, 121.4375000000000000, -5.656854249492380582 ) ) ;
#28779 = CARTESIAN_POINT ( 'NONE',  ( -9.832129032723418760, 58.17708332991936260, -5.676582343750004256 ) ) ;
#28780 = CARTESIAN_POINT ( 'NONE',  ( 4.242640687119287435, 290.3750000000000000, 4.242640687119285658 ) ) ;
#28781 = ORIENTED_EDGE ( 'NONE', *, *, #28614, .T. ) ;
#28782 =( BOUNDED_CURVE ( )  B_SPLINE_CURVE ( 2, ( #45211, #32792, #68222, #3358, #49369, #72386, #20699, #3734, #49753 ),
 .UNSPECIFIED., .F., .F. ) 
 B_SPLINE_CURVE_WITH_KNOTS ( ( 3, 2, 2, 2, 3 ),
 ( 0.4895833333333333148, 0.4947916666666666852, 0.5000000000000000000, 0.5052083333333333703, 0.5104166666666666297 ),
 .UNSPECIFIED. ) 
 CURVE ( )  GEOMETRIC_REPRESENTATION_ITEM ( )  RATIONAL_B_SPLINE_CURVE ( ( 1.000000000000000000, 0.9238795325112867385, 1.000000000000000000, 0.9238795325112867385, 1.000000000000000000, 0.9238795325112867385, 1.000000000000000000, 0.9238795325112867385, 1.000000000000000000 ) ) 
 REPRESENTATION_ITEM ( '' )  );
#28783 = CARTESIAN_POINT ( 'NONE',  ( 8.660254037844385522, 252.9166666666666856, -5.000000000000003553 ) ) ;
#28784 = AXIS2_PLACEMENT_3D ( 'NONE', #37697, #36207, #30542 ) ;
#28785 = CARTESIAN_POINT ( 'NONE',  ( 2.589639417659363563, -10.27590863719301062, 63.78668228762852976 ) ) ;
#28786 = CARTESIAN_POINT ( 'NONE',  ( 3.999999999999959144, 195.1875000027312410, 140.3431457505076594 ) ) ;
#28787 = CARTESIAN_POINT ( 'NONE',  ( -5.000000000000000888, 65.75515815785517759, 23.82162496270711216 ) ) ;
#28788 = CARTESIAN_POINT ( 'NONE',  ( -10.99999999999999645, -11.00000000000000000, -6.938893903907228378E-15 ) ) ;
#28789 = CARTESIAN_POINT ( 'NONE',  ( 8.660254037844385522, 242.9166666666666572, -5.000000000000003553 ) ) ;
#28790 = CARTESIAN_POINT ( 'NONE',  ( 0.000000000000000000, 0.000000000000000000, 0.000000000000000000 ) ) ;
#28791 = CARTESIAN_POINT ( 'NONE',  ( -10.18810118749999738, -4.220049686691941915, 69.62500000204838102 ) ) ;
#28792 = CARTESIAN_POINT ( 'NONE',  ( -10.00000000000000000, 202.2916666666666572, -2.679491924311229845 ) ) ;
#28793 = CARTESIAN_POINT ( 'NONE',  ( -2.977408999572647819, 7.188101187499992051, 18.08030278187175455 ) ) ;
#28794 = CARTESIAN_POINT ( 'NONE',  ( -5.676582343749998039, 162.7604166632526983, -9.832129032723420536 ) ) ;
#28795 = CARTESIAN_POINT ( 'NONE',  ( 27.99999999999996447, 197.6250000027312126, 165.9999999999998863 ) ) ;
#28797 = CARTESIAN_POINT ( 'NONE',  ( 2.775557561562891351E-14, 210.0000000000000284, 198.0000000000000284 ) ) ;
#28796 = DIRECTION ( 'NONE',  ( -0.000000000000000000, 1.000000000000000000, -0.000000000000000000 ) ) ;
#28798 = ORIENTED_EDGE ( 'NONE', *, *, #35904, .T. ) ;
#28799 = CARTESIAN_POINT ( 'NONE',  ( -3.458734125000015425, 196.0000000013656347, 143.4326545832176976 ) ) ;
#28800 = CARTESIAN_POINT ( 'NONE',  ( 11.35316468749999785, 35.88541666325268409, 3.042071309553174174 ) ) ;
#28801 = CARTESIAN_POINT ( 'NONE',  ( -10.99999999999999822, -4.556349186104052151, 110.7812500040967905 ) ) ;
#28802 = CARTESIAN_POINT ( 'NONE',  ( -31.45873412499996391, 208.7500000013656063, 171.4326545832181239 ) ) ;
#28803 = CARTESIAN_POINT ( 'NONE',  ( 12.00000000000000000, 0.000000000000000000, 28.00000000000000000 ) ) ;
#28805 = DIRECTION ( 'NONE',  ( -0.000000000000000000, 1.000000000000000000, -0.000000000000000000 ) ) ;
#28804 = CARTESIAN_POINT ( 'NONE',  ( -18.00000000000000355, 0.000000000000000000, 0.000000000000000000 ) ) ;
#28806 = CARTESIAN_POINT ( 'NONE',  ( 25.17157287525377996, 201.7500000027312126, 167.1715728752537586 ) ) ;
#28807 = CARTESIAN_POINT ( 'NONE',  ( -1.432654583217662259, 199.1250000013656347, 145.4587341250000350 ) ) ;
#28808 = CARTESIAN_POINT ( 'NONE',  ( -2.679491924311225848, 58.33333332650537528, -10.00000000000000178 ) ) ;
#28809 = CARTESIAN_POINT ( 'NONE',  ( 7.188101187500000044, 103.9062500020483810, -8.802885111219163269E-16 ) ) ;
#28810 = CARTESIAN_POINT ( 'NONE',  ( -3.211159895383561391, 11.81249999863440614, -3.211159895383561835 ) ) ;
#28811 = CARTESIAN_POINT ( 'NONE',  ( 2.966170491840901068E-11, 66.24999999999768363, -9.999999999999998224 ) ) ;
#28812 = CARTESIAN_POINT ( 'NONE',  ( -3.313708498984758943, -7.999999999999989342, 5.611552779823364645 ) ) ;
#28813 = CARTESIAN_POINT ( 'NONE',  ( 4.000000000000001776, 7.812499997268812280, -1.656854249492381248 ) ) ;
#28814 = ORIENTED_EDGE ( 'NONE', *, *, #123, .F. ) ;
#28815 = ORIENTED_EDGE ( 'NONE', *, *, #55588, .T. ) ;
#28816 = ADVANCED_FACE ( 'NONE', ( #7401 ), #53056, .T. ) ;
#28817 = CARTESIAN_POINT ( 'NONE',  ( -1.656854249492297093, 204.9375000027312126, 194.0000000000000568 ) ) ;
#28818 = CARTESIAN_POINT ( 'NONE',  ( 4.721056650415999201, 298.2343750017069510, -4.721056650415999201 ) ) ;
#28819 = CARTESIAN_POINT ( 'NONE',  ( 10.99999999999994849, 4.556349186104097448, 103.8437500000000000 ) ) ;
#28820 = CARTESIAN_POINT ( 'NONE',  ( -11.00000000000000000, 0.000000000000000000, 117.4999999999999716 ) ) ;
#28821 = CARTESIAN_POINT ( 'NONE',  ( 9.832129032723420536, 136.1979166632526983, -5.676582343749999815 ) ) ;
#28822 = CARTESIAN_POINT ( 'NONE',  ( -5.656854249492379694, 6.374999995903221084, -5.656854249492380582 ) ) ;
#28823 = CARTESIAN_POINT ( 'NONE',  ( -10.18810118749999738, -4.220049686691941915, 82.75000000204838102 ) ) ;
#28824 = CARTESIAN_POINT ( 'NONE',  ( 0.000000000000000000, 125.0000000000000000, 0.000000000000000000 ) ) ;
#28825 = CARTESIAN_POINT ( 'NONE',  ( -2.828427124746153876, 203.8750000000000284, 195.1715728752538439 ) ) ;
#28826 = CARTESIAN_POINT ( 'NONE',  ( 2.449293598294707893E-16, 15.25000000000000000, -4.000000000000001776 ) ) ;
#28827 = CARTESIAN_POINT ( 'NONE',  ( 10.18810118749999916, 4.220049686691935698, 115.3750000020483810 ) ) ;
#28828 = EDGE_LOOP ( 'NONE', ( #12919, #11756, #71429, #7233 ) ) ;
#28829 = EDGE_CURVE ( 'NONE', #38870, #31834, #24906, .T. ) ;
#28830 = DIRECTION ( 'NONE',  ( -0.000000000000000000, 1.000000000000000000, -4.476705744456276341E-16 ) ) ;
#28831 = CARTESIAN_POINT ( 'NONE',  ( 17.56925112071948902, 178.1485276299210341, 137.8365335656187085 ) ) ;
#28832 = CARTESIAN_POINT ( 'NONE',  ( -5.676582343750006032, 134.4270833299193555, 9.832129032723418760 ) ) ;
#28833 = CARTESIAN_POINT ( 'NONE',  ( 3.458734125000016313, 200.8750000013656063, 199.4326545832176976 ) ) ;
#28834 = CARTESIAN_POINT ( 'NONE',  ( 7.188101187499999156, 24.74999999795161543, 2.977408999572654924 ) ) ;
#28835 = CARTESIAN_POINT ( 'NONE',  ( -7.204075437095967871, 7.204075437095967871, 79.84375000204838102 ) ) ;
#28836 = CARTESIAN_POINT ( 'NONE',  ( 5.676582343750001591, 31.92708332991935194, -9.832129032723420536 ) ) ;
#28837 = ORIENTED_EDGE ( 'NONE', *, *, #25641, .F. ) ;
#28838 = FACE_OUTER_BOUND ( 'NONE', #68193, .T. ) ;
#28839 = CARTESIAN_POINT ( 'NONE',  ( -4.898587196589407898E-16, 7.999999999999991118, 8.142802783920144449 ) ) ;
#28840 = CARTESIAN_POINT ( 'NONE',  ( -8.008118988124989457, -3.317071493978883900, 14.60686528394063011 ) ) ;
#28841 = CARTESIAN_POINT ( 'NONE',  ( -3.458734125000016757, 205.1250000013656347, 140.5673454167824161 ) ) ;
#28842 = CARTESIAN_POINT ( 'NONE',  ( -7.188101187500001821, 10.12499999795161187, -2.977408999572651371 ) ) ;
#28843 = CARTESIAN_POINT ( 'NONE',  ( 2.485281374238575314, 297.3750000034139589, 6.000000000000000888 ) ) ;
#28844 = CARTESIAN_POINT ( 'NONE',  ( -34.31181274103728640, -12.27221881832708483, 147.4792081091980833 ) ) ;
#28845 = CARTESIAN_POINT ( 'NONE',  ( 5.082755093536325930, 4.031249997951610986, -5.082755093536325930 ) ) ;
#28846 = CARTESIAN_POINT ( 'NONE',  ( 7.188101187499992051, 2.977408999572647819, 14.33030278187175277 ) ) ;
#28847 = CARTESIAN_POINT ( 'NONE',  ( -3.042071309553164404, 157.5520833299193555, -11.35316468749999963 ) ) ;
#28848 = CARTESIAN_POINT ( 'NONE',  ( 7.204075437095966983, 7.204075437095967871, 68.59375000204836681 ) ) ;
#28849 = EDGE_CURVE ( 'NONE', #8118, #5410, #1791, .T. ) ;
#28850 = AXIS2_PLACEMENT_3D ( 'NONE', #73671, #45366, #44633 ) ;
#28851 = CARTESIAN_POINT ( 'NONE',  ( -28.00000000000002487, 207.6875000013656063, 166.5412658750003629 ) ) ;
#28852 = EDGE_CURVE ( 'NONE', #3504, #4422, #7515, .T. ) ;
#28853 = CARTESIAN_POINT ( 'NONE',  ( 2.449293598294707893E-16, 3.250000000000000444, -4.000000000000001776 ) ) ;
#28854 = CARTESIAN_POINT ( 'NONE',  ( -8.342170076843785083E-16, 18.18749999863440792, 4.541265875000002339 ) ) ;
#28855 = VERTEX_POINT ( 'NONE', #13038 ) ;
#28856 = AXIS2_PLACEMENT_3D ( 'NONE', #45988, #6389, #69750 ) ;
#28857 = CARTESIAN_POINT ( 'NONE',  ( -3.999999999999959144, 199.1875000027312694, 199.6568542494924259 ) ) ;
#28858 = CARTESIAN_POINT ( 'NONE',  ( -4.000000000000015987, 205.5000000000000284, 142.0000000000000568 ) ) ;
#28859 = CARTESIAN_POINT ( 'NONE',  ( -29.65685424949245785, 200.1875000027312126, 166.0000000000004263 ) ) ;
#28860 = CARTESIAN_POINT ( 'NONE',  ( -8.660254037844454800, 57.08333333333337833, -5.000000000000044409 ) ) ;
#28861 = CARTESIAN_POINT ( 'NONE',  ( -5.656854249492375253, 5.656854249492375253, 9.830302783920146226 ) ) ;
#28862 = EDGE_LOOP ( 'NONE', ( #40899, #52787, #19933, #14901 ) ) ;
#28863 = EDGE_CURVE ( 'NONE', #39259, #61133, #35707, .T. ) ;
#28864 = CARTESIAN_POINT ( 'NONE',  ( 2.977408999572650927, 14.24999999795161187, -7.188101187500000933 ) ) ;
#28865 = CARTESIAN_POINT ( 'NONE',  ( -4.242640687119285658, 298.1875000034139589, 4.242640687119287435 ) ) ;
#28866 = CARTESIAN_POINT ( 'NONE',  ( -5.000000000000005329, 45.20833332650536818, 8.660254037844387298 ) ) ;
#28867 = CARTESIAN_POINT ( 'NONE',  ( -8.660254037844390851, 42.91666666666667140, 4.999999999999998224 ) ) ;
#28868 = CARTESIAN_POINT ( 'NONE',  ( 7.188101187500000044, 105.7812500020483810, -8.802885111219163269E-16 ) ) ;
#28869 = CARTESIAN_POINT ( 'NONE',  ( -31.45873412500001010, 206.8750000013656347, 168.5673454167827572 ) ) ;
#28870 = CARTESIAN_POINT ( 'NONE',  ( 4.193030820682221993, -10.26769724739507872, 64.12608639927633192 ) ) ;
#28872 = CARTESIAN_POINT ( 'NONE',  ( 2.679491924311222739, 195.8333333265053682, 10.00000000000000355 ) ) ;
#28871 = CARTESIAN_POINT ( 'NONE',  ( -7.999999999999998224, 111.7812500040967763, 3.313708498984766049 ) ) ;
#28873 = EDGE_LOOP ( 'NONE', ( #50206, #33899, #61893, #15009 ) ) ;
#28874 = CARTESIAN_POINT ( 'NONE',  ( 3.042071309553163960, 242.4479166700806729, -11.35316468749999785 ) ) ;
#28875 = PRODUCT_DEFINITION_SHAPE ( 'NONE', 'NONE',  #74671 ) ;
#28876 = CARTESIAN_POINT ( 'NONE',  ( 7.188101187499991163, 2.977408999572648707, 19.20530278187175810 ) ) ;
#28877 = CARTESIAN_POINT ( 'NONE',  ( 1.882291019709844582, 55.75505015263103559, 43.87597576789043785 ) ) ;
#28878 = CARTESIAN_POINT ( 'NONE',  ( -9.036584110083673238, 219.9999999999999716, 5.919388431620439484 ) ) ;
#28879 = CARTESIAN_POINT ( 'NONE',  ( 2.828427124746209831, 198.5000000027312126, 200.8284271247462129 ) ) ;
#28880 =( BOUNDED_CURVE ( )  B_SPLINE_CURVE ( 2, ( #21934, #15901, #38932, #10261, #11005, #62303, #33287, #44964, #16265 ),
 .UNSPECIFIED., .F., .F. ) 
 B_SPLINE_CURVE_WITH_KNOTS ( ( 3, 2, 2, 2, 3 ),
 ( 0.6041666666666648533, 0.6145833333333315940, 0.6249999999999982236, 0.6354166666666647423, 0.6458333333333314830 ),
 .UNSPECIFIED. ) 
 CURVE ( )  GEOMETRIC_REPRESENTATION_ITEM ( )  RATIONAL_B_SPLINE_CURVE ( ( 1.000000000000012879, 0.9238795325112737489, 1.000000000000000000, 0.9238795325112867385, 1.000000000000000000, 0.9238795325112867385, 1.000000000000000000, 0.9238795325113005052, 0.9999999999999862332 ) ) 
 REPRESENTATION_ITEM ( '' )  );
#28881 = CARTESIAN_POINT ( 'NONE',  ( -10.00000000000000355, 139.5833333265053682, 2.679491924311223183 ) ) ;
#28882 = CARTESIAN_POINT ( 'NONE',  ( -4.999999999999998224, 156.6666666666666856, -8.660254037844389075 ) ) ;
#28883 = CARTESIAN_POINT ( 'NONE',  ( 16.00000000000000711, -16.00000000000000000, 20.00000000000000000 ) ) ;
#28884 = DIRECTION ( 'NONE',  ( -0.000000000000000000, 1.000000000000000000, -4.476705744456276341E-16 ) ) ;
#28885 = CARTESIAN_POINT ( 'NONE',  ( 7.999999999999992895, -3.313708498984756279, 4.486552779823363757 ) ) ;
#28886 = CARTESIAN_POINT ( 'NONE',  ( -2.085542519210945728E-15, 129.8437499965860127, 11.35316468750000141 ) ) ;
#28887 = CARTESIAN_POINT ( 'NONE',  ( -5.999999999999999112, 294.1250000034140157, 2.485281374238575314 ) ) ;
#28888 = CARTESIAN_POINT ( 'NONE',  ( 5.656854249492374365, 5.656854249492375253, 27.45530278392014978 ) ) ;
#28891 = CARTESIAN_POINT ( 'NONE',  ( 2.485281374238974994, 298.3124999999999432, 5.999999999999600320 ) ) ;
#28890 = CARTESIAN_POINT ( 'NONE',  ( 26.56734541678237349, 196.3750000013656063, 173.4587341249998929 ) ) ;
#28889 = CARTESIAN_POINT ( 'NONE',  ( 29.43265458321766204, 196.1250000013655779, 166.5412658749999650 ) ) ;
#28892 = EDGE_CURVE ( 'NONE', #48188, #13863, #11932, .T. ) ;
#28893 = ORIENTED_EDGE ( 'NONE', *, *, #60070, .T. ) ;
#28894 = DIRECTION ( 'NONE',  ( -0.000000000000000000, -0.000000000000000000, -1.000000000000000000 ) ) ;
#28895 = ADVANCED_FACE ( 'NONE', ( #55289 ), #20556, .T. ) ;
#28896 = CARTESIAN_POINT ( 'NONE',  ( 0.000000000000000000, 0.000000000000000000, 0.000000000000000000 ) ) ;
#28897 = CARTESIAN_POINT ( 'NONE',  ( 25.17157287525381548, 196.0000000027312126, 172.8284271247460993 ) ) ;
#28898 = CARTESIAN_POINT ( 'NONE',  ( 31.45873412499997812, 194.8750000013656063, 171.4326545832175839 ) ) ;
#28899 = CIRCLE ( 'NONE', #8427, 12.00000000000000000 ) ;
#28900 = CARTESIAN_POINT ( 'NONE',  ( 4.999999999999993783, 21.04166665983870033, 8.660254037844390851 ) ) ;
#28901 = CARTESIAN_POINT ( 'NONE',  ( 1.320432766682874540E-15, 120.0312500020483810, 7.188101187500000044 ) ) ;
#28902 = CARTESIAN_POINT ( 'NONE',  ( 3.211159895383560947, 22.18749999863440792, 3.211159895383562723 ) ) ;
#28903 = CARTESIAN_POINT ( 'NONE',  ( -6.298842414731080197, 61.32333038069598530, -23.57034304878899533 ) ) ;
#28904 = CARTESIAN_POINT ( 'NONE',  ( -7.999999999999991118, 3.313708498984756723, 18.73655277982336642 ) ) ;
#28906 = CARTESIAN_POINT ( 'NONE',  ( -2.679491924311171225, 223.9583333333333144, -10.00000000000003197 ) ) ;
#28905 = CARTESIAN_POINT ( 'NONE',  ( 3.459103461385761413, -7.213501455148458419, -0.0001169852011744028255 ) ) ;
#28907 = CARTESIAN_POINT ( 'NONE',  ( -3.042071309553173730, 114.3229166632526841, 11.35316468749999785 ) ) ;
#28908 = ORIENTED_EDGE ( 'NONE', *, *, #55900, .F. ) ;
#28909 = EDGE_CURVE ( 'NONE', #19, #3350, #12862, .T. ) ;
#28910 =( BOUNDED_CURVE ( )  B_SPLINE_CURVE ( 2, ( #24033, #30075, #17262, #64040, #53464, #689, #58396, #35743, #11984 ),
 .UNSPECIFIED., .F., .F. ) 
 B_SPLINE_CURVE_WITH_KNOTS ( ( 3, 2, 2, 2, 3 ),
 ( 0.1029411764705883137, 0.1066176470588236086, 0.1102941176470589035, 0.1139705882352941985, 0.1176470588235294934 ),
 .UNSPECIFIED. ) 
 CURVE ( )  GEOMETRIC_REPRESENTATION_ITEM ( )  RATIONAL_B_SPLINE_CURVE ( ( 0.9999999999999982236, 0.9238795325112885148, 1.000000000000000000, 0.9238795325112867385, 1.000000000000000000, 0.9238795325112867385, 1.000000000000000000, 0.9238795325112849621, 1.000000000000001776 ) ) 
 REPRESENTATION_ITEM ( '' )  );
#28911 = DIRECTION ( 'NONE',  ( -0.000000000000000000, 1.000000000000000000, -0.000000000000000000 ) ) ;
#28912 = CARTESIAN_POINT ( 'NONE',  ( -7.188101187500002709, 23.81249999795161543, 2.977408999572649151 ) ) ;
#28913 = CARTESIAN_POINT ( 'NONE',  ( 0.000000000000000000, 0.000000000000000000, -4.000000000000001776 ) ) ;
#28914 = CARTESIAN_POINT ( 'NONE',  ( -8.311093377946834337, 244.8437500034139873, 8.311093377946837890 ) ) ;
#28915 = CARTESIAN_POINT ( 'NONE',  ( 5.676582343749993598, 104.9479166632526841, 9.832129032723422313 ) ) ;
#28916 = ORIENTED_EDGE ( 'NONE', *, *, #32420, .F. ) ;
#28917 = CARTESIAN_POINT ( 'NONE',  ( 5.000000000000000888, -12.55543720214775760, 69.09376167622102116 ) ) ;
#28918 = CIRCLE ( 'NONE', #54227, 18.99999999999998934 ) ;
#28919 = CARTESIAN_POINT ( 'NONE',  ( -10.18810118749999916, 4.220049686691934809, 102.0625000020483810 ) ) ;
#28920 = CARTESIAN_POINT ( 'NONE',  ( 4.999999999999993783, 221.0416666598387110, 8.660254037844390851 ) ) ;
#28921 = CARTESIAN_POINT ( 'NONE',  ( 2.445694354108840063, 202.0625000013656063, 200.4456943541088663 ) ) ;
#28922 = CARTESIAN_POINT ( 'NONE',  ( -7.347880794884122694E-16, 8.750000000000000000, 4.000000000000001776 ) ) ;
#28924 = CARTESIAN_POINT ( 'NONE',  ( 8.311093377946837890, 101.4062499965860127, -8.311093377946837890 ) ) ;
#28923 = LINE ( 'NONE', #17221, #68961 ) ;
#28925 = CARTESIAN_POINT ( 'NONE',  ( 5.656854249492374365, 5.656854249492375253, 13.95530278392014623 ) ) ;
#28926 = CARTESIAN_POINT ( 'NONE',  ( -27.99999999999996092, 197.1875000013655779, 173.4587341250003760 ) ) ;
#28927 = CARTESIAN_POINT ( 'NONE',  ( 2.679491924311081963, 171.0416666666666572, -10.00000000000008349 ) ) ;
#28928 = VERTEX_POINT ( 'NONE', #54913 ) ;
#28929 = CARTESIAN_POINT ( 'NONE',  ( -1.836970198721029983E-15, 200.6249999931720538, 10.00000000000000178 ) ) ;
#28930 = CARTESIAN_POINT ( 'NONE',  ( 1.656854249492346609, 208.1875000000000853, 138.0000000000000568 ) ) ;
#28931 = CARTESIAN_POINT ( 'NONE',  ( 1.656854249492394349, 9.562499997268814056, 3.999999999999988898 ) ) ;
#28932 = CARTESIAN_POINT ( 'NONE',  ( -9.832129032723420536, 89.01041666325268409, 5.676582343749997150 ) ) ;
#28933 = CARTESIAN_POINT ( 'NONE',  ( 2.765530957082001251, 289.7656250017069510, 6.676582343750000703 ) ) ;
#28934 = CARTESIAN_POINT ( 'NONE',  ( -5.082755093536326818, 4.781249997951610986, 5.082755093536325042 ) ) ;
#28935 = CARTESIAN_POINT ( 'NONE',  ( -10.18810118749999916, 4.220049686691934809, 94.93750000204836681 ) ) ;
#28936 = CARTESIAN_POINT ( 'NONE',  ( 11.35316468750000141, 1.093749996586016682, 0.000000000000000000 ) ) ;
#28937 = VERTEX_POINT ( 'NONE', #66211 ) ;
#28938 = FACE_OUTER_BOUND ( 'NONE', #61624, .T. ) ;
#28939 = CARTESIAN_POINT ( 'NONE',  ( -5.000000000000000000, 0.000000000000000000, 0.000000000000000000 ) ) ;
#28940 = CARTESIAN_POINT ( 'NONE',  ( -8.311093377946841443, 213.9062499965860411, 8.311093377946834337 ) ) ;
#28941 = CARTESIAN_POINT ( 'NONE',  ( -5.656854249492375253, 5.656854249492375253, 11.33030278392014445 ) ) ;
#28942 = CARTESIAN_POINT ( 'NONE',  ( -1.739508062077476325, -16.42388987907938613, -68.69353258878828683 ) ) ;
#28943 = CARTESIAN_POINT ( 'NONE',  ( 2.765530957081996366, 295.1406250017069510, -6.676582343750003368 ) ) ;
#28944 = EDGE_LOOP ( 'NONE', ( #36940, #36751, #67688, #38054 ) ) ;
#28945 = CARTESIAN_POINT ( 'NONE',  ( -11.00000000000031619, 4.556349186103730631, 89.59375000409677625 ) ) ;
#28946 = CARTESIAN_POINT ( 'NONE',  ( 5.676582343750001591, 201.9270833299193555, -9.832129032723420536 ) ) ;
#28947 = CARTESIAN_POINT ( 'NONE',  ( -4.220049686691937474, -10.18810118749999738, 88.93750000204839523 ) ) ;
#28948 = CARTESIAN_POINT ( 'NONE',  ( -31.45873412499999944, 201.6250000013656063, 168.5673454167827572 ) ) ;
#28949 = CARTESIAN_POINT ( 'NONE',  ( -1.469576158976823947E-15, 17.62500000000000000, 8.000000000000000000 ) ) ;
#28950 = ORIENTED_EDGE ( 'NONE', *, *, #18768, .T. ) ;
#28951 = CARTESIAN_POINT ( 'NONE',  ( -4.401442555609581635E-16, 120.7812500020483810, -7.188101187500000044 ) ) ;
#28952 = CARTESIAN_POINT ( 'NONE',  ( -27.99999999999991118, 199.6250000027312126, 174.0000000000003695 ) ) ;
#28953 = CARTESIAN_POINT ( 'NONE',  ( -10.00000000000000178, 22.50000000000000355, -1.224646799147353454E-15 ) ) ;
#28954 = CIRCLE ( 'NONE', #21717, 10.99999999999999645 ) ;
#28955 = CARTESIAN_POINT ( 'NONE',  ( -27.99999999999995381, 197.5000000000000000, 174.0000000000003695 ) ) ;
#28956 = CARTESIAN_POINT ( 'NONE',  ( -4.220049686691935698, 10.18810118749999916, 76.75000000204838102 ) ) ;
#28957 = EDGE_LOOP ( 'NONE', ( #70437, #11840 ) ) ;
#28958 = CYLINDRICAL_SURFACE ( 'NONE', #18083, 3.999999999999976019 ) ;
#28959 = AXIS2_PLACEMENT_3D ( 'NONE', #27776, #23235, #50417 ) ;
#28960 = DIRECTION ( 'NONE',  ( 0.000000000000000000, 0.000000000000000000, -1.000000000000000000 ) ) ;
#28961 = VECTOR ( 'NONE', #49133, 1000.000000000000000 ) ;
#28962 = CARTESIAN_POINT ( 'NONE',  ( 0.000000000000000000, 300.0000000000000000, 0.000000000000000000 ) ) ;
#28963 = CARTESIAN_POINT ( 'NONE',  ( -5.082755093536324154, 121.7187500020483952, 5.082755093536326818 ) ) ;
#28964 = CARTESIAN_POINT ( 'NONE',  ( 5.000000000000000000, -63.46149047932930642, 24.14127879314051839 ) ) ;
#28965 = CARTESIAN_POINT ( 'NONE',  ( -4.721056650415999201, 297.3281250017069510, -4.721056650415999201 ) ) ;
#28967 = CARTESIAN_POINT ( 'NONE',  ( 2.020667218593132706E-15, -11.00000000000000000, 88.56250000409676204 ) ) ;
#28966 = CARTESIAN_POINT ( 'NONE',  ( 9.832129032723420536, 245.9895833367473301, 5.676582343749996262 ) ) ;
#28968 = CONTEXT_DEPENDENT_SHAPE_REPRESENTATION ( #35680, #67384 ) ;
#28969 = ORIENTED_EDGE ( 'NONE', *, *, #18760, .T. ) ;
#28970 = CARTESIAN_POINT ( 'NONE',  ( -11.35316468749999608, 244.4270833367473017, 3.042071309553173730 ) ) ;
#28971 = CARTESIAN_POINT ( 'NONE',  ( 5.082755093536320601, -5.082755093536318824, 6.549052781871754547 ) ) ;
#28972 = B_SPLINE_CURVE_WITH_KNOTS ( 'NONE', 3,
 ( #63672, #57291, #28232, #28603, #52367, #64054 ),
 .UNSPECIFIED., .F., .F.,
 ( 4, 2, 4 ),
 ( 2.380728322768173715E-07, 0.005257893135091030838, 0.01051554819734978365 ),
 .UNSPECIFIED. ) ;
#28973 = VERTEX_POINT ( 'NONE', #67716 ) ;
#28974 = DIRECTION ( 'NONE',  ( -0.000000000000000000, 1.000000000000000000, -0.000000000000000000 ) ) ;
#28975 = CARTESIAN_POINT ( 'NONE',  ( 6.951808397369818766E-16, 82.34374999658601268, -11.35316468750000141 ) ) ;
#28976 = CARTESIAN_POINT ( 'NONE',  ( 2.124081043562908722, 60.31560147600158217, 22.95556260996253783 ) ) ;
#28977 = CARTESIAN_POINT ( 'NONE',  ( 2.020667218593132706E-15, -11.00000000000000000, 85.37499999999997158 ) ) ;
#28980 = DIRECTION ( 'NONE',  ( -0.000000000000000000, 1.000000000000000000, -0.000000000000000000 ) ) ;
#28979 = CARTESIAN_POINT ( 'NONE',  ( 30.44569435410883429, 207.5625000013656063, 172.4456943541086957 ) ) ;
#28978 = CARTESIAN_POINT ( 'NONE',  ( 26.56734541678238415, 208.2500000013656063, 166.5412658749999650 ) ) ;
#28981 = VERTEX_POINT ( 'NONE', #66586 ) ;
#28982 = DIRECTION ( 'NONE',  ( 0.000000000000000000, 0.000000000000000000, 1.000000000000000000 ) ) ;
#28983 = FACE_OUTER_BOUND ( 'NONE', #62617, .T. ) ;
#28984 = EDGE_CURVE ( 'NONE', #18528, #26793, #4659, .T. ) ;
#28985 = VECTOR ( 'NONE', #11989, 1000.000000000000000 ) ;
#28986 = CARTESIAN_POINT ( 'NONE',  ( 3.042071309553159519, 194.7395833299193555, 11.35316468750000141 ) ) ;
#28987 = CARTESIAN_POINT ( 'NONE',  ( -2.839093476692135984E-14, 206.6875000013656063, 138.5412658750000503 ) ) ;
#28988 = CARTESIAN_POINT ( 'NONE',  ( 27.99999999999996447, 205.6875000013656063, 173.4587341249998929 ) ) ;
#28989 = CARTESIAN_POINT ( 'NONE',  ( 5.082755093536325930, 22.03124999795161543, -5.082755093536325930 ) ) ;
#28990 = CARTESIAN_POINT ( 'NONE',  ( 8.311093377946834337, 185.4687499965860127, 8.311093377946839666 ) ) ;
#28991 = DIRECTION ( 'NONE',  ( -0.000000000000000000, -1.000000000000000000, -0.000000000000000000 ) ) ;
#28992 = CARTESIAN_POINT ( 'NONE',  ( 7.188101187500000933, 96.87500000204838102, -2.977408999572651371 ) ) ;
#28994 = CARTESIAN_POINT ( 'NONE',  ( 1.592277918221149080E-13, 106.2500000000000142, -10.00000000000000178 ) ) ;
#28993 = CARTESIAN_POINT ( 'NONE',  ( 4.000000000000001776, 16.74999999726881583, 0.000000000000000000 ) ) ;
#28995 = CARTESIAN_POINT ( 'NONE',  ( 4.541265875000002339, 8.374999998634406140, -1.881053915767121554 ) ) ;
#28996 = CARTESIAN_POINT ( 'NONE',  ( 26.56734541678232731, 204.6250000013656063, 173.4587341249998929 ) ) ;
#28997 = CARTESIAN_POINT ( 'NONE',  ( -7.188101187499990274, -2.977408999572651371, 7.955302781871752771 ) ) ;
#28998 = CARTESIAN_POINT ( 'NONE',  ( -9.832129032723420536, 63.69791666325269830, 5.676582343749997150 ) ) ;
#28999 = EDGE_CURVE ( 'NONE', #40278, #56693, #14516, .T. ) ;
#29000 = CARTESIAN_POINT ( 'NONE',  ( -4.898587196589407898E-16, 7.999999999999991118, 0.5115527843298234290 ) ) ;
#29001 = ORIENTED_EDGE ( 'NONE', *, *, #58712, .F. ) ;
#29002 = CARTESIAN_POINT ( 'NONE',  ( -7.778174593052020747, -7.778174593052023411, 74.68749999999998579 ) ) ;
#29003 = CARTESIAN_POINT ( 'NONE',  ( 10.99999999999999467, -4.556349186104054816, 117.1562499999999858 ) ) ;
#29004 = CARTESIAN_POINT ( 'NONE',  ( 3.042071309553167069, 66.82291666325266988, -11.35316468749999785 ) ) ;
#29005 = CARTESIAN_POINT ( 'NONE',  ( -11.00000000000000000, 0.000000000000000000, 70.18750000409676204 ) ) ;
#29006 = CARTESIAN_POINT ( 'NONE',  ( -1.432654583217664701, 195.0000000013656063, 138.5412658750000787 ) ) ;
#29007 = CARTESIAN_POINT ( 'NONE',  ( 0.000000000000000000, 125.0000000000000000, 0.000000000000000000 ) ) ;
#29009 = CARTESIAN_POINT ( 'NONE',  ( -2.085542519210945728E-15, 64.53124999658602690, 11.35316468750000141 ) ) ;
#29008 = CARTESIAN_POINT ( 'NONE',  ( -2.977408999572652260, 95.93750000204839523, 7.188101187500000044 ) ) ;
#29010 = CARTESIAN_POINT ( 'NONE',  ( 7.999999999999991118, 3.313708498984757611, 6.174052779823364645 ) ) ;
#29012 = CARTESIAN_POINT ( 'NONE',  ( -2.751549872419339698E-14, 194.9207531772045741, 145.9207531772046025 ) ) ;
#29011 = B_SPLINE_CURVE_WITH_KNOTS ( 'NONE', 3,
 ( #60389, #37770, #59657, #2308, #8714, #43027, #42291, #15107 ),
 .UNSPECIFIED., .F., .F.,
 ( 4, 2, 2, 4 ),
 ( 0.007010445034807201957, 0.008756443665256739492, 0.01050244229570627269, 0.01399443955660533909 ),
 .UNSPECIFIED. ) ;
#29013 =( BOUNDED_CURVE ( )  B_SPLINE_CURVE ( 2, ( #23666, #11978, #39534, #16873, #74228, #69319, #17252, #3810, #28952 ),
 .UNSPECIFIED., .F., .F. ) 
 B_SPLINE_CURVE_WITH_KNOTS ( ( 3, 2, 2, 2, 3 ),
 ( 0.6000000000000004219, 0.6083333333333338366, 0.6166666666666672514, 0.6250000000000006661, 0.6333333333333339699 ),
 .UNSPECIFIED. ) 
 CURVE ( )  GEOMETRIC_REPRESENTATION_ITEM ( )  RATIONAL_B_SPLINE_CURVE ( ( 0.9999999999999958922, 0.9238795325112908463, 1.000000000000000000, 0.9238795325112867385, 1.000000000000000000, 0.9238795325112867385, 1.000000000000000000, 0.9238795325112806323, 1.000000000000005995 ) ) 
 REPRESENTATION_ITEM ( '' )  );
#29014 = CARTESIAN_POINT ( 'NONE',  ( -8.660254037844390851, 154.7916666598387110, 4.999999999999998224 ) ) ;
#29015 = CARTESIAN_POINT ( 'NONE',  ( 7.188101187500000044, 95.28125000204836681, -8.802885111219163269E-16 ) ) ;
#29016 = CARTESIAN_POINT ( 'NONE',  ( 8.660254037844390851, 19.58333333333333925, 5.000000000000009770 ) ) ;
#29017 = CARTESIAN_POINT ( 'NONE',  ( 3.042071309553159519, 45.05208332991934839, 11.35316468750000141 ) ) ;
#29018 = CARTESIAN_POINT ( 'NONE',  ( 7.204075437095966983, 7.204075437095967871, 110.9687500020483810 ) ) ;
#29019 = CARTESIAN_POINT ( 'NONE',  ( -9.832129032723420536, 178.6979166632526983, 5.676582343749997150 ) ) ;
#29020 = EDGE_LOOP ( 'NONE', ( #61340, #26591, #9389, #12204 ) ) ;
#29021 = CARTESIAN_POINT ( 'NONE',  ( 2.990854866095820075, 66.07503719301756462, 26.46919450145244568 ) ) ;
#29022 = CARTESIAN_POINT ( 'NONE',  ( -4.220049686691937474, -10.18810118749999738, 70.93750000204838102 ) ) ;
#29023 = CARTESIAN_POINT ( 'NONE',  ( 4.000000000000015099, 197.5625000000000853, 196.3431457505076594 ) ) ;
#29025 = CARTESIAN_POINT ( 'NONE',  ( -3.042071309553163960, 177.2395833299193555, -11.35316468749999963 ) ) ;
#29024 = CARTESIAN_POINT ( 'NONE',  ( 29.65685424949229798, 203.0625000000000568, 174.0000000000000000 ) ) ;
#29026 = CARTESIAN_POINT ( 'NONE',  ( 3.313708498984756279, 7.999999999999991118, 7.917802784329823318 ) ) ;
#29027 = CARTESIAN_POINT ( 'NONE',  ( 0.000000000000000000, 0.000000000000000000, 0.000000000000000000 ) ) ;
#29028 = CARTESIAN_POINT ( 'NONE',  ( 7.320508075688776373, 250.0000000068279746, 7.320508075688767491 ) ) ;
#29029 = FACE_OUTER_BOUND ( 'NONE', #18530, .T. ) ;
#29030 = CIRCLE ( 'NONE', #72363, 3.999999999999986233 ) ;
#29031 = EDGE_LOOP ( 'NONE', ( #71763, #70166, #19675, #40469, #45009, #27071 ) ) ;
#29032 = CARTESIAN_POINT ( 'NONE',  ( -5.676582343749998039, 167.7604166632526983, -9.832129032723420536 ) ) ;
#29033 =( BOUNDED_CURVE ( )  B_SPLINE_CURVE ( 2, ( #51292, #38866, #68646, #34343, #27531, #73932, #57342, #62236, #50543 ),
 .UNSPECIFIED., .F., .F. ) 
 B_SPLINE_CURVE_WITH_KNOTS ( ( 3, 2, 2, 2, 3 ),
 ( 0.7205882352941175295, 0.7242647058823528106, 0.7279411764705880916, 0.7316176470588233727, 0.7352941176470587648 ),
 .UNSPECIFIED. ) 
 CURVE ( )  GEOMETRIC_REPRESENTATION_ITEM ( )  RATIONAL_B_SPLINE_CURVE ( ( 1.000000000000002220, 0.9238795325112844070, 1.000000000000000000, 0.9238795325112867385, 1.000000000000000000, 0.9238795325112867385, 1.000000000000000000, 0.9238795325112890700, 0.9999999999999976685 ) ) 
 REPRESENTATION_ITEM ( '' )  );
#29034 = CARTESIAN_POINT ( 'NONE',  ( 2.977408999572650927, -7.188101187499990274, 24.45530278187175810 ) ) ;
#29035 = CARTESIAN_POINT ( 'NONE',  ( 9.832129032723416984, 135.6770833299193555, 5.676582343750006032 ) ) ;
#29036 = CARTESIAN_POINT ( 'NONE',  ( 31.99999999999999289, 195.2500000000000000, 169.9999999999999432 ) ) ;
#29037 = VECTOR ( 'NONE', #14113, 999.9999999999998863 ) ;
#29038 = ORIENTED_EDGE ( 'NONE', *, *, #73766, .F. ) ;
#29039 = CARTESIAN_POINT ( 'NONE',  ( 4.541265875000002339, 11.49999999863440792, -1.881053915767121554 ) ) ;
#29040 = CARTESIAN_POINT ( 'NONE',  ( -7.188101187500002709, 14.81249999795161543, 2.977408999572649151 ) ) ;
#29041 = CARTESIAN_POINT ( 'NONE',  ( -4.898587196589412829E-16, 106.8125000040967763, -8.000000000000000000 ) ) ;
#29042 = CARTESIAN_POINT ( 'NONE',  ( -31.45873412499999944, 198.8750000013656347, 168.5673454167827572 ) ) ;
#29043 = CARTESIAN_POINT ( 'NONE',  ( -7.347880794884122694E-16, 13.75000000000000000, 4.000000000000001776 ) ) ;
#29044 = CARTESIAN_POINT ( 'NONE',  ( -4.000000000000002665, 21.31249999726881228, 1.656854249492380804 ) ) ;
#29045 = CARTESIAN_POINT ( 'NONE',  ( -1.881053915767124440, 12.99999999863440969, 4.541265875000001451 ) ) ;
#29046 = CARTESIAN_POINT ( 'NONE',  ( 7.999999999999991118, 3.313708498984757611, 18.36155278392014623 ) ) ;
#29047 = CARTESIAN_POINT ( 'NONE',  ( 1.656854249492195619, 195.8125000000000568, 146.0000000000001990 ) ) ;
#29048 = ORIENTED_EDGE ( 'NONE', *, *, #62975, .T. ) ;
#29049 = DIRECTION ( 'NONE',  ( -0.000000000000000000, 1.000000000000000000, -0.000000000000000000 ) ) ;
#29050 = CARTESIAN_POINT ( 'NONE',  ( 7.188101187500002709, 106.8125000020484094, 2.977408999572649151 ) ) ;
#29052 = CARTESIAN_POINT ( 'NONE',  ( 12.00000000000000178, 0.000000000000000000, 28.00000000000000000 ) ) ;
#29051 = LINE ( 'NONE', #52071, #31360 ) ;
#29053 = SHAPE_REPRESENTATION_RELATIONSHIP ( 'NONE' , 'NONE' ,  #66708, #24546 ) ;
#29055 = ADVANCED_FACE ( 'NONE', ( #73370 ), #38680, .F. ) ;
#29054 = VERTEX_POINT ( 'NONE', #50349 ) ;
#29056 = EDGE_CURVE ( 'NONE', #24907, #25826, #39044, .T. ) ;
#29057 = CARTESIAN_POINT ( 'NONE',  ( 3.211159895383560947, 21.18749999863440792, 3.211159895383562723 ) ) ;
#29058 = CARTESIAN_POINT ( 'NONE',  ( 7.188101187499991163, 2.977408999572648707, 21.83030278187175810 ) ) ;
#29059 = EDGE_LOOP ( 'NONE', ( #56389, #60586, #56570, #46822 ) ) ;
#29060 = EDGE_LOOP ( 'NONE', ( #24926, #56113, #68899, #44461 ) ) ;
#29061 = CARTESIAN_POINT ( 'NONE',  ( 4.220049686691941027, -10.18810118749999738, 84.62500000204836681 ) ) ;
#29062 = CARTESIAN_POINT ( 'NONE',  ( 11.00000000000000000, 1.347111479062088405E-15, 106.9375000040967763 ) ) ;
#29063 = CARTESIAN_POINT ( 'NONE',  ( -27.99999999999996447, 198.1875000013655779, 173.4587341250003760 ) ) ;
#29064 = CARTESIAN_POINT ( 'NONE',  ( 4.556349186104045934, 11.00000000000000000, 101.0312499999999858 ) ) ;
#29067 = CARTESIAN_POINT ( 'NONE',  ( -6.676582343750001591, 297.6093750017069510, 0.000000000000000000 ) ) ;
#29066 = CARTESIAN_POINT ( 'NONE',  ( 32.00000000000000000, 204.3750000027312126, 169.9999999999998863 ) ) ;
#29065 = CARTESIAN_POINT ( 'NONE',  ( 0.000000000000000000, 0.000000000000000000, 118.0000000000000000 ) ) ;
#29068 = CARTESIAN_POINT ( 'NONE',  ( 2.679491924311228956, 136.0416666666666572, -10.00000000000000000 ) ) ;
#29069 = EDGE_CURVE ( 'NONE', #13964, #42156, #72628, .T. ) ;
#29070 = CARTESIAN_POINT ( 'NONE',  ( 8.000000000000000000, 101.7500000000000000, -9.797174393178825657E-16 ) ) ;
#29071 = CARTESIAN_POINT ( 'NONE',  ( 2.765530957082001251, 287.9218750017069510, 6.676582343750000703 ) ) ;
#29072 = PRESENTATION_LAYER_ASSIGNMENT (  '', '', ( #31491 ) ) ;
#29073 = CARTESIAN_POINT ( 'NONE',  ( -2.977408999572648707, -7.188101187499990274, 0.6428027818717528818 ) ) ;
#29074 = LINE ( 'NONE', #57012, #30182 ) ;
#29075 = CARTESIAN_POINT ( 'NONE',  ( 25.55430564589115150, 204.3125000013656063, 172.4456943541086957 ) ) ;
#29076 = CARTESIAN_POINT ( 'NONE',  ( -1.320432766682874540E-15, 6.468749997951610098, 7.188101187500000044 ) ) ;
#29077 = CARTESIAN_POINT ( 'NONE',  ( -4.903558642999205574E-16, 8.008118988124991233, 5.138115283940630107 ) ) ;
#29078 = CARTESIAN_POINT ( 'NONE',  ( 5.000000000000000000, 0.000000000000000000, 0.000000000000000000 ) ) ;
#29079 = CARTESIAN_POINT ( 'NONE',  ( -2.977408999572652260, 115.8125000020483952, 7.188101187500000044 ) ) ;
#29081 = DIRECTION ( 'NONE',  ( 0.000000000000000000, 0.4789076340208558435, -0.8778652960884979484 ) ) ;
#29080 = CARTESIAN_POINT ( 'NONE',  ( 27.99999999999996092, 195.6250000027311842, 165.9999999999998863 ) ) ;
#29082 = CARTESIAN_POINT ( 'NONE',  ( 2.085542519210945334E-15, 245.4687500034140157, 11.35316468749999963 ) ) ;
#29083 = CARTESIAN_POINT ( 'NONE',  ( -38.00000000000002132, 39.09128788536428800, 65.00000000000000000 ) ) ;
#29084 = CARTESIAN_POINT ( 'NONE',  ( 2.977408999572646486, 7.188101187499991163, 25.39280278187176165 ) ) ;
#29085 = CARTESIAN_POINT ( 'NONE',  ( 32.00000000000000000, 200.3125000000000284, 168.3431457505075741 ) ) ;
#29086 = CARTESIAN_POINT ( 'NONE',  ( -11.35316468749999785, 18.07291666325267698, -3.042071309553167513 ) ) ;
#29087 = LINE ( 'NONE', #30195, #72475 ) ;
#29088 = CARTESIAN_POINT ( 'NONE',  ( 3.042071309553159519, 225.0520833299193555, 11.35316468750000141 ) ) ;
#29089 = CARTESIAN_POINT ( 'NONE',  ( 2.265596578422603396E-15, 0.000000000000000000, -18.50000000000000000 ) ) ;
#29091 = CARTESIAN_POINT ( 'NONE',  ( -3.447890238427822496, 194.4587341249999781, 198.3162544498398177 ) ) ;
#29090 = CARTESIAN_POINT ( 'NONE',  ( 2.775557561562891351E-14, 210.0000000000000284, 202.0000000000000000 ) ) ;
#29092 = AXIS2_PLACEMENT_3D ( 'NONE', #46149, #74447, #6172 ) ;
#29093 = ORIENTED_EDGE ( 'NONE', *, *, #72837, .T. ) ;
#29094 = CARTESIAN_POINT ( 'NONE',  ( 3.458734124999959469, 197.7500000013656063, 140.5673454167824161 ) ) ;
#29095 = CARTESIAN_POINT ( 'NONE',  ( 8.311093377946834337, 25.15624999658601268, 8.311093377946839666 ) ) ;
#29096 = CARTESIAN_POINT ( 'NONE',  ( -7.778174593052023411, 7.778174593052023411, 95.50000000409677625 ) ) ;
#29097 = CARTESIAN_POINT ( 'NONE',  ( 1.432654583217607414, 209.5000000013656063, 145.4587341250000350 ) ) ;
#29098 = ADVANCED_FACE ( 'NONE', ( #26966 ), #49613, .F. ) ;
#29099 = CARTESIAN_POINT ( 'NONE',  ( 10.99999999999993605, -4.556349186104108995, 111.3437500040967620 ) ) ;
#29100 = CARTESIAN_POINT ( 'NONE',  ( -38.00000000000000000, 63.00000000000000000, 15.00000000000000178 ) ) ;
#29102 = CARTESIAN_POINT ( 'NONE',  ( 8.311093377946837890, 16.40624999658601624, -8.311093377946837890 ) ) ;
#29101 = CARTESIAN_POINT ( 'NONE',  ( 2.977408999572650039, 108.6875000020483810, -7.188101187500000933 ) ) ;
#29103 = CARTESIAN_POINT ( 'NONE',  ( -7.999999999999991118, 3.313708498984756723, 21.73655277982336287 ) ) ;
#29104 = CARTESIAN_POINT ( 'NONE',  ( -3.042071309553173730, 139.3229166632526699, 11.35316468749999785 ) ) ;
#29105 = CARTESIAN_POINT ( 'NONE',  ( -2.679491924311235618, 120.4166666598386826, 10.00000000000000000 ) ) ;
#29106 = CARTESIAN_POINT ( 'NONE',  ( 2.977408999572654480, 114.5000000020483810, 7.188101187499999156 ) ) ;
#29107 = CARTESIAN_POINT ( 'NONE',  ( 0.000000000000000000, 300.0000000000000000, 0.000000000000000000 ) ) ;
#29108 = CARTESIAN_POINT ( 'NONE',  ( -26.56734541678238415, 208.6250000013655779, 166.5412658750003629 ) ) ;
#29109 = CARTESIAN_POINT ( 'NONE',  ( -4.999999999999999112, -52.62657404299689290, -48.70092614269891129 ) ) ;
#29110 = VERTEX_POINT ( 'NONE', #20932 ) ;
#29111 = CARTESIAN_POINT ( 'NONE',  ( -11.35316468750000141, 8.802083329919348387, 3.042071309553159963 ) ) ;
#29112 = CARTESIAN_POINT ( 'NONE',  ( -8.660254037844390851, 154.7916666598387110, 4.999999999999998224 ) ) ;
#29113 = CARTESIAN_POINT ( 'NONE',  ( -6.676582343750001591, 299.4531250017069510, 0.000000000000000000 ) ) ;
#29114 = CARTESIAN_POINT ( 'NONE',  ( -11.35316468750000141, 143.2812499965860411, -1.390361679473963753E-15 ) ) ;
#29115 = CARTESIAN_POINT ( 'NONE',  ( -7.347880794884122694E-16, 16.49999999726881228, 4.000000000000001776 ) ) ;
#29116 = CARTESIAN_POINT ( 'NONE',  ( -7.999999999999989342, -3.313708498984762496, 24.98030278432982598 ) ) ;
#29117 = AXIS2_PLACEMENT_3D ( 'NONE', #26753, #43733, #42973 ) ;
#29118 = CARTESIAN_POINT ( 'NONE',  ( -5.656854249492379694, 18.56250000000000355, -5.656854249492380582 ) ) ;
#29119 = CARTESIAN_POINT ( 'NONE',  ( -11.35316468749999963, 253.9062500034139873, 0.000000000000000000 ) ) ;
#29120 = CARTESIAN_POINT ( 'NONE',  ( 7.204075437095966983, 7.204075437095967871, 95.96875000204838102 ) ) ;
#29121 = VERTEX_POINT ( 'NONE', #43196 ) ;
#29122 = EDGE_CURVE ( 'NONE', #30116, #61426, #21674, .T. ) ;
#29123 = LINE ( 'NONE', #34805, #15947 ) ;
#29124 = CARTESIAN_POINT ( 'NONE',  ( 5.000000000000000000, 60.90295814858271939, -23.31388853594749833 ) ) ;
#29125 = CARTESIAN_POINT ( 'NONE',  ( 5.676582343749993598, 95.26041666325268409, 9.832129032723422313 ) ) ;
#29127 = ORIENTED_EDGE ( 'NONE', *, *, #63112, .F. ) ;
#29126 =( BOUNDED_CURVE ( )  B_SPLINE_CURVE ( 2, ( #41827, #53159, #47850, #70505, #48960, #71971, #59195, #31624, #18824, #54274, #65574, #1493, #13140 ),
 .UNSPECIFIED., .F., .F. ) 
 B_SPLINE_CURVE_WITH_KNOTS ( ( 3, 2, 2, 2, 2, 2, 3 ),
 ( 0.8097826086956521063, 0.8115942028985506651, 0.8134057971014491129, 0.8152173913043476716, 0.8170289855072463414, 0.8188405797101449002, 0.8206521739130434590 ),
 .UNSPECIFIED. ) 
 CURVE ( )  GEOMETRIC_REPRESENTATION_ITEM ( )  RATIONAL_B_SPLINE_CURVE ( ( 1.000000000000001998, 0.9659258262890662028, 1.000000000000000000, 0.9659258262890683122, 1.000000000000000000, 0.9659258262890683122, 1.000000000000000000, 0.9659258262890683122, 1.000000000000000000, 0.9659258262890683122, 1.000000000000000000, 0.9659258262890683122, 1.000000000000000000 ) ) 
 REPRESENTATION_ITEM ( '' )  );
#29128 = CARTESIAN_POINT ( 'NONE',  ( -10.18810118749999738, -4.220049686691941915, 106.7500000020483668 ) ) ;
#29129 = CARTESIAN_POINT ( 'NONE',  ( 1.881053915767121998, 12.62499999863441147, -4.541265875000002339 ) ) ;
#29130 = VERTEX_POINT ( 'NONE', #55663 ) ;
#29131 = ORIENTED_EDGE ( 'NONE', *, *, #57299, .F. ) ;
#29132 = CARTESIAN_POINT ( 'NONE',  ( 8.000000000000000000, 4.593750000000000888, -3.313708498984761608 ) ) ;
#29133 = CARTESIAN_POINT ( 'NONE',  ( -4.898587196589412829E-16, 109.8125000040967905, -8.000000000000000000 ) ) ;
#29134 = PLANE ( 'NONE',  #67876 ) ;
#29135 = CARTESIAN_POINT ( 'NONE',  ( 7.188101187500001821, 26.43749999795162253, -2.977408999572650483 ) ) ;
#29136 = CARTESIAN_POINT ( 'NONE',  ( 8.000000000000000000, 121.5312500040968047, -3.313708498984762496 ) ) ;
#29137 = CARTESIAN_POINT ( 'NONE',  ( -10.18810118749999738, -4.220049686691941915, 102.6250000020483810 ) ) ;
#29138 = VECTOR ( 'NONE', #31716, 1000.000000000000000 ) ;
#29139 = CARTESIAN_POINT ( 'NONE',  ( 11.00000000000000000, 1.347111479062088405E-15, 75.24999999999998579 ) ) ;
#29140 = CARTESIAN_POINT ( 'NONE',  ( 4.000000000000001776, 9.812499997268812280, -1.656854249492381248 ) ) ;
#29141 = CARTESIAN_POINT ( 'NONE',  ( 7.999991080290834056, 3.313717418693915562, 12.36155314080052214 ) ) ;
#29142 = ORIENTED_EDGE ( 'NONE', *, *, #18006, .T. ) ;
#29143 = ADVANCED_FACE ( 'NONE', ( #33032 ), #16013, .F. ) ;
#29144 = CARTESIAN_POINT ( 'NONE',  ( -8.660254037844387298, 262.7083333401612890, -4.999999999999999112 ) ) ;
#29145 = CARTESIAN_POINT ( 'NONE',  ( -2.445694354108783664, 198.3125000013656063, 195.5543056458912190 ) ) ;
#29146 = CARTESIAN_POINT ( 'NONE',  ( -26.56734541678227757, 206.0000000013656347, 173.4587341250003476 ) ) ;
#29147 = CARTESIAN_POINT ( 'NONE',  ( 4.541265875000002339, 9.312499998634407916, 0.000000000000000000 ) ) ;
#29148 = EDGE_CURVE ( 'NONE', #50014, #48435, #32661, .T. ) ;
#29149 = FACE_BOUND ( 'NONE', #71406, .T. ) ;
#29150 = CARTESIAN_POINT ( 'NONE',  ( -5.082755093536317936, -5.082755093536320601, 15.17405278187175455 ) ) ;
#29151 = VERTEX_POINT ( 'NONE', #63530 ) ;
#29152 = ORIENTED_EDGE ( 'NONE', *, *, #14822, .F. ) ;
#29153 = CARTESIAN_POINT ( 'NONE',  ( 1.871523826299183495E-15, -10.18810118749999916, 111.5312500020483668 ) ) ;
#29154 = CARTESIAN_POINT ( 'NONE',  ( -41.99999999999992895, -31.99999999999978684, 205.0000000000000284 ) ) ;
#29155 = CARTESIAN_POINT ( 'NONE',  ( -30.82842712474615965, 203.3750000000000284, 172.8284271247465824 ) ) ;
#29156 = CARTESIAN_POINT ( 'NONE',  ( 3.458734125000015425, 198.9375000013655779, 198.0000000000000284 ) ) ;
#29157 = CARTESIAN_POINT ( 'NONE',  ( 24.54126587499998990, 196.1875000013655779, 169.9999999999999432 ) ) ;
#29158 = CARTESIAN_POINT ( 'NONE',  ( 4.999999999999993783, 99.16666666666667140, 8.660254037844390851 ) ) ;
#29159 = AXIS2_PLACEMENT_3D ( 'NONE', #62592, #33583, #28274 ) ;
#29160 = ADVANCED_FACE ( 'NONE', ( #17882 ), #12361, .T. ) ;
#29161 = EDGE_CURVE ( 'NONE', #5036, #15595, #68139, .T. ) ;
#29162 = CARTESIAN_POINT ( 'NONE',  ( -8.000000000000000000, 115.9999999999999858, 0.000000000000000000 ) ) ;
#29163 = CARTESIAN_POINT ( 'NONE',  ( 9.832129032723420536, 66.51041666325268409, -5.676582343749999815 ) ) ;
#29164 = CARTESIAN_POINT ( 'NONE',  ( -2.765530957081996810, 299.4218750017070079, -6.676582343750003368 ) ) ;
#29165 = ORIENTED_EDGE ( 'NONE', *, *, #42912, .T. ) ;
#29166 = EDGE_CURVE ( 'NONE', #43538, #56060, #2218, .T. ) ;
#29167 = CARTESIAN_POINT ( 'NONE',  ( 0.000000000000000000, 0.000000000000000000, 0.000000000000000000 ) ) ;
#29168 = CARTESIAN_POINT ( 'NONE',  ( -0.8997857290927073759, -16.44125064681654891, 68.58473395859566324 ) ) ;
#29169 = CARTESIAN_POINT ( 'NONE',  ( 3.458734124999959025, 207.5000000013655779, 140.5673454167824161 ) ) ;
#29170 = CARTESIAN_POINT ( 'NONE',  ( 4.999999999999999112, 84.16666666666668561, 8.660254037844399733 ) ) ;
#29171 = CARTESIAN_POINT ( 'NONE',  ( 4.531193156845210737E-15, 201.0000000000000284, 133.0000000000000000 ) ) ;
#29172 = CARTESIAN_POINT ( 'NONE',  ( 7.320508075688776373, 241.8749999999999716, 7.320508075688767491 ) ) ;
#29173 = CARTESIAN_POINT ( 'NONE',  ( 2.249999999999999112, -2.249999999999999556, 28.00000000000000000 ) ) ;
#29174 = CARTESIAN_POINT ( 'NONE',  ( 10.18810118749999916, 4.220049686691935698, 68.87500000204838102 ) ) ;
#29175 = CARTESIAN_POINT ( 'NONE',  ( -10.00000000000000355, 207.7083333333333712, 2.679491924311223183 ) ) ;
#29176 = CARTESIAN_POINT ( 'NONE',  ( -2.977408999572647819, -7.188101187499990274, 14.14280278187175455 ) ) ;
#29177 = CARTESIAN_POINT ( 'NONE',  ( 5.676582343750001591, 181.9270833299193555, -9.832129032723420536 ) ) ;
#29178 = DIRECTION ( 'NONE',  ( 0.000000000000000000, 0.000000000000000000, 1.000000000000000000 ) ) ;
#29179 = FACE_OUTER_BOUND ( 'NONE', #66433, .T. ) ;
#29181 = DIRECTION ( 'NONE',  ( 9.064933076349553851E-15, -0.7071067811865469066, 0.7071067811865482389 ) ) ;
#29180 = CARTESIAN_POINT ( 'NONE',  ( -2.679491924311228512, 227.0833333401612890, -9.999999999999998224 ) ) ;
#29182 = ORIENTED_EDGE ( 'NONE', *, *, #45905, .T. ) ;
#29183 = CARTESIAN_POINT ( 'NONE',  ( -2.839093476692135984E-14, 208.9375000013656063, 138.5412658750000503 ) ) ;
#29184 = CARTESIAN_POINT ( 'NONE',  ( -5.676582343750006032, 39.42708332991935549, 9.832129032723418760 ) ) ;
#29185 = CARTESIAN_POINT ( 'NONE',  ( 2.020667218593132706E-15, -11.00000000000000000, 108.0625000040967905 ) ) ;
#29186 = EDGE_CURVE ( 'NONE', #55947, #31825, #14327, .T. ) ;
#29187 = CARTESIAN_POINT ( 'NONE',  ( -30.44569435410876324, 205.8125000013656063, 172.4456943541092642 ) ) ;
#29188 = CYLINDRICAL_SURFACE ( 'NONE', #50274, 8.000000000000000000 ) ;
#29190 = CARTESIAN_POINT ( 'NONE',  ( 0.000000000000000000, 0.000000000000000000, 118.0000000000000000 ) ) ;
#29189 = CARTESIAN_POINT ( 'NONE',  ( 5.000000000000001776, 222.7083333265053966, -8.660254037844389075 ) ) ;
#29191 = CARTESIAN_POINT ( 'NONE',  ( 1.432654583217607858, 197.6250000013656063, 138.5412658750000787 ) ) ;
#29192 = CARTESIAN_POINT ( 'NONE',  ( 4.999999999999993783, 61.04166665983870388, 8.660254037844390851 ) ) ;
#29193 = AXIS2_PLACEMENT_3D ( 'NONE', #22079, #45105, #56806 ) ;
#29194 = CARTESIAN_POINT ( 'NONE',  ( -4.401442555609581635E-16, 95.28125000204836681, -7.188101187500000044 ) ) ;
#29195 = CARTESIAN_POINT ( 'NONE',  ( 3.211159895383561835, 12.56249999863440792, -3.211159895383561835 ) ) ;
#29196 = DIRECTION ( 'NONE',  ( -3.469446951953619612E-16, 0.000000000000000000, -1.000000000000000000 ) ) ;
#29197 = CARTESIAN_POINT ( 'NONE',  ( 7.999999999999991118, 3.313708498984757611, 1.674052779823364423 ) ) ;
#29198 = CARTESIAN_POINT ( 'NONE',  ( 11.00000000000000000, 1.347111479062088405E-15, 115.7499999999999858 ) ) ;
#29199 = VERTEX_POINT ( 'NONE', #34574 ) ;
#29200 = EDGE_LOOP ( 'NONE', ( #43110, #58662, #25384, #32318 ) ) ;
#29201 = CARTESIAN_POINT ( 'NONE',  ( -8.660254037844477892, 197.0833333333333997, -5.000000000000058620 ) ) ;
#29202 = FACE_OUTER_BOUND ( 'NONE', #57086, .T. ) ;
#29203 = CARTESIAN_POINT ( 'NONE',  ( -11.00000000000010658, 4.556349186103942017, 104.4062500000000142 ) ) ;
#29204 = CARTESIAN_POINT ( 'NONE',  ( 8.660254037844385522, 41.45833332650536818, 5.000000000000005329 ) ) ;
#29205 = CARTESIAN_POINT ( 'NONE',  ( 11.35316468750000141, 150.7812499965860411, 0.000000000000000000 ) ) ;
#29206 = CYLINDRICAL_SURFACE ( 'NONE', #30723, 3.999999999999976019 ) ;
#29207 = CARTESIAN_POINT ( 'NONE',  ( 7.204075437095966983, 7.204075437095967871, 83.59375000204836681 ) ) ;
#29208 = CARTESIAN_POINT ( 'NONE',  ( -30.94238183655258823, 194.5434106550122806, 168.0128564637870170 ) ) ;
#29209 = CARTESIAN_POINT ( 'NONE',  ( 2.751064625579944321E-14, 202.7500000000000000, 194.0000000000000568 ) ) ;
#29210 = DIRECTION ( 'NONE',  ( -1.000000000000000000, 0.000000000000000000, -0.000000000000000000 ) ) ;
#29211 = CARTESIAN_POINT ( 'NONE',  ( -10.18810118749999738, -4.220049686691941915, 114.6250000020483810 ) ) ;
#29212 = VERTEX_POINT ( 'NONE', #74540 ) ;
#29213 = CARTESIAN_POINT ( 'NONE',  ( -2.828427124746153876, 202.0000000027312126, 195.1715728752538439 ) ) ;
#29214 = CARTESIAN_POINT ( 'NONE',  ( -10.80039871840854637, 177.7629128266401324, 140.8571828581494856 ) ) ;
#29215 = CARTESIAN_POINT ( 'NONE',  ( -3.042071309553173730, 124.6354166632526699, 11.35316468749999785 ) ) ;
#29216 = CARTESIAN_POINT ( 'NONE',  ( 1.432654583217662259, 198.1250000013656063, 194.5412658750000219 ) ) ;
#29217 = CARTESIAN_POINT ( 'NONE',  ( -7.188101187500002709, 22.68749999795161187, 2.977408999572649151 ) ) ;
#29218 = CARTESIAN_POINT ( 'NONE',  ( 1.871523826299183495E-15, -10.18810118749999916, 75.90625000204836681 ) ) ;
#29219 = CARTESIAN_POINT ( 'NONE',  ( -11.35316468749999785, 43.38541666325269119, -3.042071309553167513 ) ) ;
#29220 = ORIENTED_EDGE ( 'NONE', *, *, #69293, .T. ) ;
#29221 = CARTESIAN_POINT ( 'NONE',  ( 3.211159895383561835, 0.5624999986344069169, -3.211159895383561835 ) ) ;
#29222 = CARTESIAN_POINT ( 'NONE',  ( -8.008118988124989457, -3.317071493978883900, 11.60686528394062833 ) ) ;
#29223 = CARTESIAN_POINT ( 'NONE',  ( -2.445694354108839175, 205.3125000013656063, 144.4456943541088663 ) ) ;
#29224 = VECTOR ( 'NONE', #71774, 1000.000000000000114 ) ;
#29225 = CARTESIAN_POINT ( 'NONE',  ( -2.977408999572650039, 8.437499997951611874, -7.188101187500001821 ) ) ;
#29226 = CARTESIAN_POINT ( 'NONE',  ( 6.000000000000001776, 296.5625000034140157, -7.347880794884121708E-16 ) ) ;
#29227 = CARTESIAN_POINT ( 'NONE',  ( -12.98006904901808944, -23.31385468863603450, 138.6286961562448710 ) ) ;
#29228 = CARTESIAN_POINT ( 'NONE',  ( -5.082755093536325042, 8.906249997951611874, -5.082755093536325930 ) ) ;
#29229 = CARTESIAN_POINT ( 'NONE',  ( 7.188101187499992051, 2.977408999572647819, 11.33030278187175455 ) ) ;
#29230 = AXIS2_PLACEMENT_3D ( 'NONE', #41617, #35960, #19329 ) ;
#29231 = CARTESIAN_POINT ( 'NONE',  ( -4.220049686691935698, 10.18810118749999916, 70.37500000204838102 ) ) ;
#29232 = CARTESIAN_POINT ( 'NONE',  ( -31.45873412499999944, 205.9375000013656063, 170.0000000000003979 ) ) ;
#29233 = DIRECTION ( 'NONE',  ( 0.000000000000000000, 0.000000000000000000, -1.000000000000000000 ) ) ;
#29234 = CARTESIAN_POINT ( 'NONE',  ( 1.881053915767122664, 20.24999999863440436, 4.541265875000001451 ) ) ;
#29235 = UNCERTAINTY_MEASURE_WITH_UNIT (LENGTH_MEASURE( 1.000000000000000082E-05 ), #30986, 'distance_accuracy_value', 'NONE');
#29236 = ORIENTED_EDGE ( 'NONE', *, *, #37866, .F. ) ;
#29237 = EDGE_CURVE ( 'NONE', #34061, #59630, #28918, .T. ) ;
#29238 = CARTESIAN_POINT ( 'NONE',  ( -3.999999999999959144, 201.1875000027312694, 199.6568542494924259 ) ) ;
#29239 = CARTESIAN_POINT ( 'NONE',  ( -2.828427124746209831, 204.3750000000000284, 139.1715728752538723 ) ) ;
#29241 =( BOUNDED_CURVE ( )  B_SPLINE_CURVE ( 2, ( #51768, #16674, #46477, #33696, #40080, #5017, #56701, #57445, #45360 ),
 .UNSPECIFIED., .F., .F. ) 
 B_SPLINE_CURVE_WITH_KNOTS ( ( 3, 2, 2, 2, 3 ),
 ( 0.7833333333333338810, 0.7916666666666671848, 0.8000000000000007105, 0.8083333333333340143, 0.8166666666666674290 ),
 .UNSPECIFIED. ) 
 CURVE ( )  GEOMETRIC_REPRESENTATION_ITEM ( )  RATIONAL_B_SPLINE_CURVE ( ( 0.9999999999999948930, 0.9238795325112918455, 1.000000000000000000, 0.9238795325112867385, 1.000000000000000000, 0.9238795325112867385, 1.000000000000000000, 0.9238795325112796331, 1.000000000000007105 ) ) 
 REPRESENTATION_ITEM ( '' )  );
#29240 = CARTESIAN_POINT ( 'NONE',  ( -24.00000000000002487, 201.9375000027311842, 168.3431457505079152 ) ) ;
#29242 = CARTESIAN_POINT ( 'NONE',  ( 2.977408999572654480, 115.6250000020483810, 7.188101187499999156 ) ) ;
#29243 = CARTESIAN_POINT ( 'NONE',  ( 11.00000000000000000, 1.347111479062088405E-15, 78.43750000409677625 ) ) ;
#29244 = CARTESIAN_POINT ( 'NONE',  ( -5.656854249492375253, 5.656854249492375253, 8.330302783920144449 ) ) ;
#29245 = EDGE_LOOP ( 'NONE', ( #59928, #4175, #63786, #67134 ) ) ;
#29246 = CARTESIAN_POINT ( 'NONE',  ( -2.977408999572650039, 17.43749999795161187, -7.188101187500000933 ) ) ;
#29247 = VERTEX_POINT ( 'NONE', #52282 ) ;
#29248 = CARTESIAN_POINT ( 'NONE',  ( -2.849036369511732440E-14, 208.3750000027312126, 138.0000000000000568 ) ) ;
#29249 = CARTESIAN_POINT ( 'NONE',  ( -10.00000000000000000, 44.16666665983870388, -2.679491924311229845 ) ) ;
#29250 = CARTESIAN_POINT ( 'NONE',  ( -7.320508075688778149, 38.12499999999999289, 7.320508075688769267 ) ) ;
#29251 = CARTESIAN_POINT ( 'NONE',  ( -7.188101187499999156, 102.1250000020483810, 2.977408999572654924 ) ) ;
#29252 = CARTESIAN_POINT ( 'NONE',  ( -30.44569435410883784, 206.8125000013656063, 167.5543056458915885 ) ) ;
#29254 = CARTESIAN_POINT ( 'NONE',  ( -5.656854249492380582, 95.00000000409677625, -5.656854249492380582 ) ) ;
#29253 = CARTESIAN_POINT ( 'NONE',  ( -4.999999999999998224, 33.54166665983870388, -8.660254037844389075 ) ) ;
#29255 = ORIENTED_EDGE ( 'NONE', *, *, #43779, .T. ) ;
#29256 = EDGE_CURVE ( 'NONE', #65370, #9404, #25339, .T. ) ;
#29257 = CARTESIAN_POINT ( 'NONE',  ( 2.085542519210945334E-15, 245.1562500034140157, 11.35316468749999963 ) ) ;
#29258 = CIRCLE ( 'NONE', #30440, 9.000000000000001776 ) ;
#29259 = CARTESIAN_POINT ( 'NONE',  ( -7.188101187499990274, -2.977408999572651371, 15.45530278187175455 ) ) ;
#29260 = CARTESIAN_POINT ( 'NONE',  ( 6.308070865150001261, 51.03903544634584222, 41.30321721932931922 ) ) ;
#29261 = CARTESIAN_POINT ( 'NONE',  ( 32.00000000000000711, 206.3124999999999716, 168.3431457505075457 ) ) ;
#29262 = CYLINDRICAL_SURFACE ( 'NONE', #73687, 8.000000000000000000 ) ;
#29263 = CARTESIAN_POINT ( 'NONE',  ( -10.00000000000000178, 139.3749999931720538, -1.224646799147353454E-15 ) ) ;
#29264 = CARTESIAN_POINT ( 'NONE',  ( 8.660254037844389075, 160.4166666666666856, -5.000000000000000000 ) ) ;
#29265 = DIRECTION ( 'NONE',  ( 0.000000000000000000, 0.000000000000000000, 1.000000000000000000 ) ) ;
#29266 = CARTESIAN_POINT ( 'NONE',  ( -32.28715334068198928, 176.0068012088921421, 163.9536661001924358 ) ) ;
#29267 = CARTESIAN_POINT ( 'NONE',  ( 5.000000000000000000, -53.57132521838697414, -46.19376297453524671 ) ) ;
#29268 = CARTESIAN_POINT ( 'NONE',  ( 5.676582343749993598, 135.2604166632526983, 9.832129032723422313 ) ) ;
#29269 = CARTESIAN_POINT ( 'NONE',  ( 28.00000000000001776, 198.5000000000000000, 165.9999999999998863 ) ) ;
#29270 = CARTESIAN_POINT ( 'NONE',  ( 2.947433605447500327, 11.00000000000000000, 68.06435453820057546 ) ) ;
#29273 = CARTESIAN_POINT ( 'NONE',  ( 0.000000000000000000, 125.0000000000000000, 8.000000000000000000 ) ) ;
#29272 = DIRECTION ( 'NONE',  ( -1.577021341797097560E-16, 1.000000000000000000, -0.000000000000000000 ) ) ;
#29271 = CARTESIAN_POINT ( 'NONE',  ( 31.45873412499997812, 196.8750000013656063, 171.4326545832175839 ) ) ;
#29274 = ORIENTED_EDGE ( 'NONE', *, *, #48033, .F. ) ;
#29275 = AXIS2_PLACEMENT_3D ( 'NONE', #9077, #60374, #38126 ) ;
#29276 = CARTESIAN_POINT ( 'NONE',  ( 5.656854249492380582, 10.68750000000000178, -5.656854249492380582 ) ) ;
#29277 = EDGE_CURVE ( 'NONE', #37240, #72436, #41750, .T. ) ;
#29278 = CARTESIAN_POINT ( 'NONE',  ( 0.000000000000000000, 0.000000000000000000, 0.000000000000000000 ) ) ;
#29279 = DIRECTION ( 'NONE',  ( -0.000000000000000000, -0.000000000000000000, 1.000000000000000000 ) ) ;
#29280 = CARTESIAN_POINT ( 'NONE',  ( 31.45873412499999944, 195.0000000013656063, 168.5673454167822740 ) ) ;
#29281 = ADVANCED_FACE ( 'NONE', ( #11541 ), #57201, .F. ) ;
#29282 = CARTESIAN_POINT ( 'NONE',  ( 6.123233995736767268E-16, 28.12499999317203603, -10.00000000000000178 ) ) ;
#29283 = CARTESIAN_POINT ( 'NONE',  ( -7.188101187500001821, 116.5625000020483810, -2.977408999572650483 ) ) ;
#29284 = CARTESIAN_POINT ( 'NONE',  ( 4.541265875000002339, 1.499999998634407028, -1.881053915767121554 ) ) ;
#29285 = CARTESIAN_POINT ( 'NONE',  ( -4.330454160167791500, 68.33163558029933426, -20.63184982502332687 ) ) ;
#29286 = CARTESIAN_POINT ( 'NONE',  ( 7.999999999999991118, 9.797174393178815797E-16, 22.58030277982336997 ) ) ;
#29288 = FACE_OUTER_BOUND ( 'NONE', #55696, .T. ) ;
#29287 = PLANE ( 'NONE',  #21424 ) ;
#29289 = CARTESIAN_POINT ( 'NONE',  ( 11.35316468749999785, 105.5729166632526983, 3.042071309553174174 ) ) ;
#29290 = ORIENTED_EDGE ( 'NONE', *, *, #23291, .F. ) ;
#29291 = LINE ( 'NONE', #11933, #62915 ) ;
#29292 = CARTESIAN_POINT ( 'NONE',  ( 7.188101187500001821, 24.56249999795161543, -2.977408999572650483 ) ) ;
#29293 = CARTESIAN_POINT ( 'NONE',  ( 37.94562015984923420, 38.00000000000001421, 127.0000000000000000 ) ) ;
#29294 = CARTESIAN_POINT ( 'NONE',  ( -11.35316468749999608, 249.4270833367473017, 3.042071309553173730 ) ) ;
#29295 = CARTESIAN_POINT ( 'NONE',  ( -9.832129032723418760, 117.8645833299193697, -5.676582343750004256 ) ) ;
#29296 = EDGE_LOOP ( 'NONE', ( #60919, #67935, #69054, #36795 ) ) ;
#29297 = CARTESIAN_POINT ( 'NONE',  ( 5.656854249492378806, 25.31250000000000355, 5.656854249492381470 ) ) ;
#29298 = CARTESIAN_POINT ( 'NONE',  ( -7.204075437095967871, 7.204075437095967871, 98.96875000204838102 ) ) ;
#29299 = CARTESIAN_POINT ( 'NONE',  ( 5.000000000000001776, 222.7083333265053966, -8.660254037844389075 ) ) ;
#29300 = CARTESIAN_POINT ( 'NONE',  ( -2.445694354108784108, 201.5625000013656063, 195.5543056458912190 ) ) ;
#29301 = DIRECTION ( 'NONE',  ( -0.000000000000000000, -1.000000000000000000, -0.000000000000000000 ) ) ;
#29303 = CARTESIAN_POINT ( 'NONE',  ( 9.832129032723416984, 95.36458332991935549, 5.676582343750006032 ) ) ;
#29302 = CARTESIAN_POINT ( 'NONE',  ( -7.320508075688776373, 183.1250000000000000, 7.320508075688768379 ) ) ;
#29304 = CARTESIAN_POINT ( 'NONE',  ( -3.313708498984757167, 7.999999999999991118, 8.236552783920144449 ) ) ;
#29305 = CARTESIAN_POINT ( 'NONE',  ( -26.56734541678232375, 196.2500000013656631, 173.4587341250003760 ) ) ;
#29306 = CARTESIAN_POINT ( 'NONE',  ( -2.222453528114265639E-12, 168.7499999999998295, 10.00000000000000178 ) ) ;
#29307 = VERTEX_POINT ( 'NONE', #63213 ) ;
#29308 = B_SPLINE_CURVE_WITH_KNOTS ( 'NONE', 3,
 ( #49400, #32063, #25999, #72420, #36608, #20348, #49024, #72032 ),
 .UNSPECIFIED., .F., .F.,
 ( 4, 2, 2, 4 ),
 ( 0.005256334970490779412, 0.006570121696662016217, 0.007883908422833253021, 0.01051148187517571969 ),
 .UNSPECIFIED. ) ;
#29309 = CARTESIAN_POINT ( 'NONE',  ( -4.999999999999998224, 193.5416666598387110, -8.660254037844389075 ) ) ;
#29310 = EDGE_CURVE ( 'NONE', #28343, #62422, #4222, .T. ) ;
#29311 = CARTESIAN_POINT ( 'NONE',  ( -7.347880794884122694E-16, 9.499999997268814056, 4.000000000000001776 ) ) ;
#29312 = CARTESIAN_POINT ( 'NONE',  ( -11.35316468750000141, 88.59374999658602690, -1.390361679473963753E-15 ) ) ;
#29313 = CARTESIAN_POINT ( 'NONE',  ( 2.249999999999999112, 2.250000000000000000, 28.00000000000000000 ) ) ;
#29314 = CARTESIAN_POINT ( 'NONE',  ( -5.082755093536325042, 5.906249997951610986, -5.082755093536325930 ) ) ;
#29315 = CARTESIAN_POINT ( 'NONE',  ( 10.18810118749999916, 1.247682550866122264E-15, 97.28125000204838102 ) ) ;
#29316 = CARTESIAN_POINT ( 'NONE',  ( -3.042071309553173730, 219.3229166632526699, 11.35316468749999785 ) ) ;
#29317 = ORIENTED_EDGE ( 'NONE', *, *, #38391, .F. ) ;
#29318 = DIRECTION ( 'NONE',  ( 0.000000000000000000, 0.000000000000000000, -1.000000000000000000 ) ) ;
#29319 = CARTESIAN_POINT ( 'NONE',  ( -1.512640440460914449E-15, 7.999999999999991118, 29.33030277982336642 ) ) ;
#29320 = CARTESIAN_POINT ( 'NONE',  ( -2.085542519210945728E-15, 224.5312499965860127, 11.35316468750000141 ) ) ;
#29321 = CARTESIAN_POINT ( 'NONE',  ( 1.871523826299183495E-15, -10.18810118749999916, 77.40625000204836681 ) ) ;
#29322 = CARTESIAN_POINT ( 'NONE',  ( 4.000000000000002665, 22.00000000000000000, 0.000000000000000000 ) ) ;
#29323 = CARTESIAN_POINT ( 'NONE',  ( 3.153939666463620179E-13, 158.7500000000000284, 9.999999999999998224 ) ) ;
#29324 = CARTESIAN_POINT ( 'NONE',  ( -6.676582343750000703, 297.5156250017070079, 2.765530957082001251 ) ) ;
#29325 = ORIENTED_EDGE ( 'NONE', *, *, #39433, .F. ) ;
#29326 = CARTESIAN_POINT ( 'NONE',  ( 1.656854249492504705, 199.6875000000000284, 194.0000000000001990 ) ) ;
#29327 = CARTESIAN_POINT ( 'NONE',  ( -5.676582343750006032, 214.4270833299193555, 9.832129032723418760 ) ) ;
#29328 = CARTESIAN_POINT ( 'NONE',  ( 1.871523826299183495E-15, -10.18810118749999916, 92.03125000204836681 ) ) ;
#29329 = CARTESIAN_POINT ( 'NONE',  ( -31.45873412499999944, 203.6875000013656063, 170.0000000000003979 ) ) ;
#29330 = CARTESIAN_POINT ( 'NONE',  ( 8.000000000000000000, 18.00000000000000355, 0.000000000000000000 ) ) ;
#29331 = ORIENTED_EDGE ( 'NONE', *, *, #14426, .F. ) ;
#29332 = VECTOR ( 'NONE', #28753, 1000.000000000000000 ) ;
#29333 = CARTESIAN_POINT ( 'NONE',  ( -7.188101187500001821, 124.0625000020483810, -2.977408999572650483 ) ) ;
#29334 =( NAMED_UNIT ( * ) SI_UNIT ( $, .STERADIAN. ) SOLID_ANGLE_UNIT ( ) );
#29335 = ADVANCED_FACE ( 'NONE', ( #2070 ), #37142, .T. ) ;
#29336 = CARTESIAN_POINT ( 'NONE',  ( -2.679491924311225848, 31.45833333333333925, -10.00000000000000178 ) ) ;
#29337 = CARTESIAN_POINT ( 'NONE',  ( -2.828427124746153876, 209.8750000000000284, 195.1715728752538439 ) ) ;
#29338 = CARTESIAN_POINT ( 'NONE',  ( 7.204075437095968759, -7.204075437095966983, 74.59375000204838102 ) ) ;
#29340 = EDGE_LOOP ( 'NONE', ( #65378, #63294, #1583, #65423 ) ) ;
#29339 =( BOUNDED_CURVE ( )  B_SPLINE_CURVE ( 2, ( #62939, #16148, #11264, #34295, #67489, #5611, #62190, #56552, #33549 ),
 .UNSPECIFIED., .F., .F. ) 
 B_SPLINE_CURVE_WITH_KNOTS ( ( 3, 2, 2, 2, 3 ),
 ( 0.6354166666666667407, 0.6406250000000001110, 0.6458333333333334814, 0.6510416666666666297, 0.6562500000000000000 ),
 .UNSPECIFIED. ) 
 CURVE ( )  GEOMETRIC_REPRESENTATION_ITEM ( )  RATIONAL_B_SPLINE_CURVE ( ( 0.9999999999999983347, 0.9238795325112884038, 1.000000000000000000, 0.9238795325112867385, 1.000000000000000000, 0.9238795325112867385, 1.000000000000000000, 0.9238795325112867385, 1.000000000000000000 ) ) 
 REPRESENTATION_ITEM ( '' )  );
#29341 = AXIS2_PLACEMENT_3D ( 'NONE', #31941, #20608, #37982 ) ;
#29342 = EDGE_CURVE ( 'NONE', #57841, #35174, #65058, .T. ) ;
#29343 = CARTESIAN_POINT ( 'NONE',  ( 3.313708498984679895, 114.0312500000000000, -8.000000000000081712 ) ) ;
#29344 = LINE ( 'NONE', #18386, #66735 ) ;
#29345 = FACE_OUTER_BOUND ( 'NONE', #67525, .T. ) ;
#29346 = CARTESIAN_POINT ( 'NONE',  ( -7.188101187499999156, 123.1250000020484094, 2.977408999572654924 ) ) ;
#29347 = DIRECTION ( 'NONE',  ( 0.000000000000000000, -0.000000000000000000, -1.000000000000000000 ) ) ;
#29348 = CARTESIAN_POINT ( 'NONE',  ( -6.676582343750001591, 298.4531250017069510, 0.000000000000000000 ) ) ;
#29350 = FACE_OUTER_BOUND ( 'NONE', #54662, .T. ) ;
#29349 = CARTESIAN_POINT ( 'NONE',  ( 2.085542519210945334E-15, 230.1562500034139873, 11.35316468749999963 ) ) ;
#29351 = CONTEXT_DEPENDENT_SHAPE_REPRESENTATION ( #6273, #28270 ) ;
#29352 = VERTEX_POINT ( 'NONE', #1352 ) ;
#29353 = ADVANCED_FACE ( 'NONE', ( #53759 ), #64707, .T. ) ;
#29354 = CARTESIAN_POINT ( 'NONE',  ( -5.676582343749992710, 245.0520833367473301, 9.832129032723422313 ) ) ;
#29355 = CARTESIAN_POINT ( 'NONE',  ( 2.977408999572650927, -7.188101187499990274, 6.455302781871754547 ) ) ;
#29356 = AXIS2_PLACEMENT_3D ( 'NONE', #67160, #14332, #71675 ) ;
#29357 =( BOUNDED_CURVE ( )  B_SPLINE_CURVE ( 2, ( #36700, #48372, #71376, #42713, #37066, #60066, #8388, #31401, #71751, #56668, #32542, #61573, #9893 ),
 .UNSPECIFIED., .F., .F. ) 
 B_SPLINE_CURVE_WITH_KNOTS ( ( 3, 2, 2, 2, 2, 2, 3 ),
 ( 0.7500000000000000000, 0.7592592592592593004, 0.7685185185185184897, 0.7777777777777777901, 0.7870370370370370905, 0.7962962962962962798, 0.8055555555555555802 ),
 .UNSPECIFIED. ) 
 CURVE ( )  GEOMETRIC_REPRESENTATION_ITEM ( )  RATIONAL_B_SPLINE_CURVE ( ( 1.000000000000000000, 0.9659258262890683122, 1.000000000000000000, 0.9659258262890683122, 1.000000000000000000, 0.9659258262890683122, 1.000000000000000000, 0.9659258262890683122, 1.000000000000000000, 0.9659258262890683122, 1.000000000000000000, 0.9659258262890683122, 1.000000000000000000 ) ) 
 REPRESENTATION_ITEM ( '' )  );
#29358 = ORIENTED_EDGE ( 'NONE', *, *, #13130, .T. ) ;
#29359 = CARTESIAN_POINT ( 'NONE',  ( -10.18810118749999916, 0.000000000000000000, 70.65625000204836681 ) ) ;
#29360 = CARTESIAN_POINT ( 'NONE',  ( 9.832129032723420536, 81.51041666325268409, -5.676582343749999815 ) ) ;
#29361 = DIRECTION ( 'NONE',  ( 0.5000000000000019984, 0.8660254037844375974, -0.000000000000000000 ) ) ;
#29362 = CARTESIAN_POINT ( 'NONE',  ( -11.00000000000000000, 4.556349186104045934, 84.90624999999998579 ) ) ;
#29365 = CYLINDRICAL_SURFACE ( 'NONE', #24189, 11.00000000000000000 ) ;
#29364 = CARTESIAN_POINT ( 'NONE',  ( 25.55430564589115860, 209.0625000013656063, 167.5543056458911053 ) ) ;
#29363 = CARTESIAN_POINT ( 'NONE',  ( 31.45873412500001010, 207.0000000013656063, 168.5673454167822740 ) ) ;
#29366 = ORIENTED_EDGE ( 'NONE', *, *, #25573, .F. ) ;
#29367 = CARTESIAN_POINT ( 'NONE',  ( 0.000000000000000000, 0.000000000000000000, 30.00000000000000000 ) ) ;
#29368 = FACE_OUTER_BOUND ( 'NONE', #20757, .T. ) ;
#29369 = CARTESIAN_POINT ( 'NONE',  ( 11.35316468749999785, 205.5729166632526699, 3.042071309553174174 ) ) ;
#29370 = CARTESIAN_POINT ( 'NONE',  ( -2.754378923186476579E-14, 204.1875000013656063, 145.4587341250000350 ) ) ;
#29371 = CARTESIAN_POINT ( 'NONE',  ( 28.00000000000002487, 207.1875000013656063, 166.5412658749999082 ) ) ;
#29372 = EDGE_CURVE ( 'NONE', #35319, #47640, #18688, .T. ) ;
#29373 = CARTESIAN_POINT ( 'NONE',  ( -7.188101187500000044, 25.59374999795161543, -8.802885111219163269E-16 ) ) ;
#29374 = CARTESIAN_POINT ( 'NONE',  ( 5.676582343749993598, 185.2604166632526983, 9.832129032723422313 ) ) ;
#29375 = CARTESIAN_POINT ( 'NONE',  ( -5.082755093536324154, 99.21875000204838102, 5.082755093536326818 ) ) ;
#29377 = CARTESIAN_POINT ( 'NONE',  ( 1.469576158976823947E-15, 106.0625000040967763, 8.000000000000000000 ) ) ;
#29376 = CARTESIAN_POINT ( 'NONE',  ( 2.828427124746153876, 196.0000000027312126, 144.8284271247462129 ) ) ;
#29378 = CARTESIAN_POINT ( 'NONE',  ( 3.211159895383561835, 10.43749999863440792, -3.211159895383561835 ) ) ;
#29379 = CARTESIAN_POINT ( 'NONE',  ( 25.55430564589119413, 201.3125000013656063, 167.5543056458910485 ) ) ;
#29380 = CARTESIAN_POINT ( 'NONE',  ( 7.188101187499992051, 8.802885111219154394E-16, 7.111552781871754547 ) ) ;
#29381 = CARTESIAN_POINT ( 'NONE',  ( 11.35316468750000141, 65.78124999658602690, 0.000000000000000000 ) ) ;
#29382 = CARTESIAN_POINT ( 'NONE',  ( -4.999999999999999112, -53.39837237779295265, 47.14918772354921828 ) ) ;
#29383 = CARTESIAN_POINT ( 'NONE',  ( -1.656854249492487607, 201.6875000000000284, 145.9999999999999716 ) ) ;
#29384 = ORIENTED_EDGE ( 'NONE', *, *, #24789, .T. ) ;
#29385 = CARTESIAN_POINT ( 'NONE',  ( 5.656854249492376141, -5.656854249492374365, 7.580302783920144449 ) ) ;
#29387 = CARTESIAN_POINT ( 'NONE',  ( 32.00000000000000000, 206.3750000027312126, 169.9999999999998863 ) ) ;
#29386 = VECTOR ( 'NONE', #63891, 1000.000000000000000 ) ;
#29388 = CARTESIAN_POINT ( 'NONE',  ( -11.35316468749999785, 58.07291666325268409, -3.042071309553167513 ) ) ;
#29389 = CARTESIAN_POINT ( 'NONE',  ( -7.778174593052020747, -7.778174593052023411, 67.37500000409676204 ) ) ;
#29390 = CARTESIAN_POINT ( 'NONE',  ( -1.432654583217662481, 196.3750000013656063, 145.4587341250000350 ) ) ;
#29391 = DIRECTION ( 'NONE',  ( -0.000000000000000000, -0.000000000000000000, 1.000000000000000000 ) ) ;
#29393 = CARTESIAN_POINT ( 'NONE',  ( 11.35316468749999785, 55.57291666325267698, 3.042071309553174174 ) ) ;
#29392 = CARTESIAN_POINT ( 'NONE',  ( 5.082755093536325042, 90.59375000204838102, -5.082755093536325930 ) ) ;
#29394 = CARTESIAN_POINT ( 'NONE',  ( -3.313708498984758943, -7.999999999999989342, 23.79905278392014978 ) ) ;
#29395 = CARTESIAN_POINT ( 'NONE',  ( -0.9718321562519303125, 194.8957299692297340, 145.7806464578187047 ) ) ;
#29396 = CARTESIAN_POINT ( 'NONE',  ( -7.320508075688778149, 159.9999999931720254, 7.320508075688769267 ) ) ;
#29397 = CARTESIAN_POINT ( 'NONE',  ( -5.082755093536325930, 98.84375000204838102, -5.082755093536325930 ) ) ;
#29398 = CARTESIAN_POINT ( 'NONE',  ( 38.00000000000000000, 242.0000000000000284, 20.00000000000002132 ) ) ;
#29399 = CARTESIAN_POINT ( 'NONE',  ( -2.085542519210945728E-15, 44.84374999658602690, 11.35316468750000141 ) ) ;
#29400 = CARTESIAN_POINT ( 'NONE',  ( -10.18810118749999916, 0.000000000000000000, 116.0312500020483810 ) ) ;
#29401 = CARTESIAN_POINT ( 'NONE',  ( 9.832129032723420536, 186.1979166632526983, -5.676582343749999815 ) ) ;
#29402 = ORIENTED_EDGE ( 'NONE', *, *, #47295, .F. ) ;
#29403 = CARTESIAN_POINT ( 'NONE',  ( 4.000000000000015987, 205.6250000027312126, 198.0000000000000284 ) ) ;
#29404 = CARTESIAN_POINT ( 'NONE',  ( -15.99999999999999645, 0.000000000000000000, 38.34805510287551300 ) ) ;
#29405 = CARTESIAN_POINT ( 'NONE',  ( 2.679491924311228956, 162.9166666598387110, -10.00000000000000000 ) ) ;
#29407 = CARTESIAN_POINT ( 'NONE',  ( -8.311093377946841443, 173.9062499965860127, 8.311093377946834337 ) ) ;
#29406 = CARTESIAN_POINT ( 'NONE',  ( 28.00000000000001776, 203.5000000000000000, 165.9999999999998863 ) ) ;
#29408 = DIRECTION ( 'NONE',  ( -0.000000000000000000, 1.000000000000000000, -0.000000000000000000 ) ) ;
#29409 = CARTESIAN_POINT ( 'NONE',  ( 7.320508075688776373, 255.0000000068279746, 7.320508075688767491 ) ) ;
#29410 = CARTESIAN_POINT ( 'NONE',  ( 27.99999999999996447, 196.0000000000000000, 173.9999999999999147 ) ) ;
#29411 = VERTEX_POINT ( 'NONE', #53394 ) ;
#29412 = CARTESIAN_POINT ( 'NONE',  ( -5.676582343749998039, 162.7604166632526983, -9.832129032723420536 ) ) ;
#29413 = AXIS2_PLACEMENT_3D ( 'NONE', #72269, #14541, #38325 ) ;
#29414 = CARTESIAN_POINT ( 'NONE',  ( 8.311093377946834337, 130.4687499965860127, 8.311093377946839666 ) ) ;
#29415 = CARTESIAN_POINT ( 'NONE',  ( 4.898587196589412829E-16, 3.187499995903220640, -8.000000000000000000 ) ) ;
#29416 = ORIENTED_EDGE ( 'NONE', *, *, #54476, .T. ) ;
#29417 = CARTESIAN_POINT ( 'NONE',  ( -5.656854249492378806, 102.8750000040967763, 5.656854249492381470 ) ) ;
#29418 = EDGE_CURVE ( 'NONE', #25275, #62362, #40355, .T. ) ;
#29419 = EDGE_CURVE ( 'NONE', #45526, #41123, #13369, .T. ) ;
#29420 = CARTESIAN_POINT ( 'NONE',  ( -4.000000000000001776, 10.43750000000000000, -1.656854249492381470 ) ) ;
#29421 = CARTESIAN_POINT ( 'NONE',  ( 5.265513565426386933, 7.352259170992713422, -0.01899995639453637419 ) ) ;
#29422 = CARTESIAN_POINT ( 'NONE',  ( 1.881053915767121998, 11.49999999863440969, -4.541265875000002339 ) ) ;
#29423 = CARTESIAN_POINT ( 'NONE',  ( -7.999999999999989342, -3.313708498984762496, 22.11155278392014623 ) ) ;
#29424 = CARTESIAN_POINT ( 'NONE',  ( 3.999999999999959144, 195.0625000000000284, 140.3431457505076594 ) ) ;
#29425 = ORIENTED_EDGE ( 'NONE', *, *, #54136, .F. ) ;
#29426 = CARTESIAN_POINT ( 'NONE',  ( -10.00000000000005684, 177.7083333333333712, 2.679491924311237838 ) ) ;
#29427 = CARTESIAN_POINT ( 'NONE',  ( -5.082755093536324154, 104.8437500020483810, 5.082755093536326818 ) ) ;
#29429 = CARTESIAN_POINT ( 'NONE',  ( -7.999999999999998224, 123.5937500000000000, 3.313708498984766049 ) ) ;
#29428 = CARTESIAN_POINT ( 'NONE',  ( -3.729367062499960195, 209.8437500006828031, 198.0000000000000284 ) ) ;
#29430 = ORIENTED_EDGE ( 'NONE', *, *, #56516, .T. ) ;
#29431 = CARTESIAN_POINT ( 'NONE',  ( 3.228176881614038596, 10.27295505383825791, -63.90876373295822788 ) ) ;
#29432 = CARTESIAN_POINT ( 'NONE',  ( 2.977408999572650927, -7.188101187499990274, 24.45530278187175455 ) ) ;
#29433 = ORIENTED_EDGE ( 'NONE', *, *, #68834, .T. ) ;
#29434 = ORIENTED_EDGE ( 'NONE', *, *, #28574, .T. ) ;
#29435 = CARTESIAN_POINT ( 'NONE',  ( -4.220049686691937474, -10.18810118749999738, 84.43750000204838102 ) ) ;
#29436 = CARTESIAN_POINT ( 'NONE',  ( 11.00000000000000000, 1.347111479062088405E-15, 91.74999999999998579 ) ) ;
#29437 = CARTESIAN_POINT ( 'NONE',  ( -26.56734541678237704, 197.6250000013656063, 166.5412658750003629 ) ) ;
#29438 = CARTESIAN_POINT ( 'NONE',  ( -4.556349186104045934, 11.00000000000000000, 102.7187499999999858 ) ) ;
#29441 = CARTESIAN_POINT ( 'NONE',  ( 6.676582343750002480, 297.1718750017071216, -2.765530957081997254 ) ) ;
#29440 = CARTESIAN_POINT ( 'NONE',  ( 26.34314575050758833, 204.6875000027312126, 165.9999999999998863 ) ) ;
#29439 = CYLINDRICAL_SURFACE ( 'NONE', #41080, 8.000000000000000000 ) ;
#29442 = CARTESIAN_POINT ( 'NONE',  ( 7.320508075688771044, 139.3750000000000000, 7.320508075688775484 ) ) ;
#29443 = CARTESIAN_POINT ( 'NONE',  ( -8.000000000000000000, 99.40625000000000000, -3.313708498984761608 ) ) ;
#29444 = CARTESIAN_POINT ( 'NONE',  ( 6.676582343750004256, 290.0468750017070079, 2.765530957081995478 ) ) ;
#29445 = CARTESIAN_POINT ( 'NONE',  ( 5.082755093536318824, 5.082755093536319713, 1.299052781871753215 ) ) ;
#29446 =( BOUNDED_CURVE ( )  B_SPLINE_CURVE ( 2, ( #53011, #7356, #24685, #53383, #70717, #46597, #63959 ),
 .UNSPECIFIED., .F., .F. ) 
 B_SPLINE_CURVE_WITH_KNOTS ( ( 3, 2, 2, 3 ),
 ( 0.9166666666666674068, 0.9250000000000005995, 0.9333333333333335702, 0.9416666668637480031 ),
 .UNSPECIFIED. ) 
 CURVE ( )  GEOMETRIC_REPRESENTATION_ITEM ( )  RATIONAL_B_SPLINE_CURVE ( ( 0.9999999999999928946, 0.9238795325112938439, 1.000000000000000000, 0.9238795325112867385, 1.000000000000000000, 0.9238795325112867385, 1.000000000000000000 ) ) 
 REPRESENTATION_ITEM ( '' )  );
#29447 = CARTESIAN_POINT ( 'NONE',  ( -26.34314575050759899, 208.5624999999999716, 174.0000000000003695 ) ) ;
#29448 = CARTESIAN_POINT ( 'NONE',  ( 30.44569435410879166, 202.5625000013656063, 172.4456943541087526 ) ) ;
#29449 = CARTESIAN_POINT ( 'NONE',  ( -5.082755093536325042, 5.906249997951610986, -5.082755093536325930 ) ) ;
#29450 = AXIS2_PLACEMENT_3D ( 'NONE', #7154, #35827, #64121 ) ;
#29451 = CARTESIAN_POINT ( 'NONE',  ( -4.903558642999205574E-16, 8.008118988124991233, 2.138115283940627442 ) ) ;
#29452 = CARTESIAN_POINT ( 'NONE',  ( 3.458734124999959914, 197.3750000013656063, 143.4326545832176976 ) ) ;
#29453 = CARTESIAN_POINT ( 'NONE',  ( 2.977408999572654480, 116.0000000020483810, 7.188101187499999156 ) ) ;
#29455 = FACE_OUTER_BOUND ( 'NONE', #44057, .T. ) ;
#29454 = DIRECTION ( 'NONE',  ( 0.000000000000000000, 0.000000000000000000, -1.000000000000000000 ) ) ;
#29456 = CARTESIAN_POINT ( 'NONE',  ( 8.311093377946834337, 222.3437500034139589, -8.311093377946836114 ) ) ;
#29457 = DIRECTION ( 'NONE',  ( 0.000000000000000000, 0.000000000000000000, -1.000000000000000000 ) ) ;
#29458 = CARTESIAN_POINT ( 'NONE',  ( 2.977408999572650927, -7.188101187499990274, 27.83030278187176165 ) ) ;
#29459 = CARTESIAN_POINT ( 'NONE',  ( 23.99999999999998934, 198.7500000000000000, 169.9999999999998863 ) ) ;
#29460 = CARTESIAN_POINT ( 'NONE',  ( -3.042071309553173730, 29.32291666325268764, 11.35316468749999785 ) ) ;
#29461 = CARTESIAN_POINT ( 'NONE',  ( -2.828427124746153876, 202.8750000000000284, 195.1715728752538439 ) ) ;
#29462 = CARTESIAN_POINT ( 'NONE',  ( 8.311093377946837890, 226.7187499965860411, -8.311093377946837890 ) ) ;
#29463 = CARTESIAN_POINT ( 'NONE',  ( -8.660254037844387298, 239.5833333333333428, -4.999999999999999112 ) ) ;
#29465 = LINE ( 'NONE', #52475, #24289 ) ;
#29464 = DIRECTION ( 'NONE',  ( -0.000000000000000000, -0.000000000000000000, -1.000000000000000000 ) ) ;
#29466 = ORIENTED_EDGE ( 'NONE', *, *, #38502, .T. ) ;
#29467 = CARTESIAN_POINT ( 'NONE',  ( -3.458734125000015869, 197.1875000013655779, 142.0000000000000568 ) ) ;
#29468 = CARTESIAN_POINT ( 'NONE',  ( -9.832129032723418760, 17.86458332991935194, -5.676582343750004256 ) ) ;
#29469 = CARTESIAN_POINT ( 'NONE',  ( -6.735557395310442023E-16, 11.00000000000000000, 87.81250000409676204 ) ) ;
#29470 = CARTESIAN_POINT ( 'NONE',  ( -3.458734125000015869, 209.1875000013656063, 142.0000000000000568 ) ) ;
#29471 = CARTESIAN_POINT ( 'NONE',  ( -4.242640687119285658, 295.1875000034139589, 4.242640687119287435 ) ) ;
#29472 = CARTESIAN_POINT ( 'NONE',  ( 0.000000000000000000, 300.0000000000000000, 10.00000000000000178 ) ) ;
#29474 = CARTESIAN_POINT ( 'NONE',  ( 8.311093377946837890, 21.40624999658601268, -8.311093377946837890 ) ) ;
#29473 = CARTESIAN_POINT ( 'NONE',  ( 2.977408999572654480, 109.6250000020483952, 7.188101187499999156 ) ) ;
#29475 = CARTESIAN_POINT ( 'NONE',  ( 1.469576158976822172E-15, -7.999999999999991118, 22.20530277982336997 ) ) ;
#29476 = CARTESIAN_POINT ( 'NONE',  ( 5.676582343750001591, 151.6145833299193555, -9.832129032723420536 ) ) ;
#29477 =( BOUNDED_CURVE ( )  B_SPLINE_CURVE ( 2, ( #19189, #42190, #65204, #13511, #21046, #71231, #9744, #43690, #20671 ),
 .UNSPECIFIED., .F., .F. ) 
 B_SPLINE_CURVE_WITH_KNOTS ( ( 3, 2, 2, 2, 3 ),
 ( 0.6527777777777777901, 0.6597222222222222099, 0.6666666666666665186, 0.6736111111111110494, 0.6805555555555554692 ),
 .UNSPECIFIED. ) 
 CURVE ( )  GEOMETRIC_REPRESENTATION_ITEM ( )  RATIONAL_B_SPLINE_CURVE ( ( 1.000000000000000000, 0.9238795325112867385, 1.000000000000000000, 0.9238795325112867385, 1.000000000000000000, 0.9238795325112867385, 1.000000000000000000, 0.9238795325112879597, 0.9999999999999987788 ) ) 
 REPRESENTATION_ITEM ( '' )  );
#29478 = CARTESIAN_POINT ( 'NONE',  ( 10.00000000000000178, 122.0833333265053540, -2.679491924311226736 ) ) ;
#29479 = CARTESIAN_POINT ( 'NONE',  ( -4.401442555609581635E-16, 112.1562500020483952, -7.188101187500000044 ) ) ;
#29480 = CYLINDRICAL_SURFACE ( 'NONE', #48116, 9.000000000000001776 ) ;
#29481 = CARTESIAN_POINT ( 'NONE',  ( -28.00000000000002132, 205.6875000013656063, 166.5412658750003629 ) ) ;
#29482 = ORIENTED_EDGE ( 'NONE', *, *, #10147, .T. ) ;
#29483 = CARTESIAN_POINT ( 'NONE',  ( -8.311093377946841443, 14.21874999658601801, 8.311093377946834337 ) ) ;
#29484 = ORIENTED_EDGE ( 'NONE', *, *, #43452, .T. ) ;
#29485 = PLANE ( 'NONE',  #57046 ) ;
#29486 = CARTESIAN_POINT ( 'NONE',  ( 4.721056650416000089, 297.8281250017069510, 4.721056650415999201 ) ) ;
#29487 = CARTESIAN_POINT ( 'NONE',  ( 8.311093377946834337, 135.1562499965860695, 8.311093377946839666 ) ) ;
#29488 =( NAMED_UNIT ( * ) PLANE_ANGLE_UNIT ( ) SI_UNIT ( $, .RADIAN. ) );
#29489 = CARTESIAN_POINT ( 'NONE',  ( 3.313708498984762496, -7.999999999999989342, 25.35530278432982598 ) ) ;
#29490 = CIRCLE ( 'NONE', #583, 11.49999999999999112 ) ;
#29491 = CARTESIAN_POINT ( 'NONE',  ( 5.656854249492380582, 15.18750000000000355, -5.656854249492380582 ) ) ;
#29492 = CARTESIAN_POINT ( 'NONE',  ( -11.35316468749999785, 253.6979166700807014, -3.042071309553164848 ) ) ;
#29493 = CARTESIAN_POINT ( 'NONE',  ( 10.18810118749999916, 4.220049686691935698, 94.37500000204839523 ) ) ;
#29494 = ORIENTED_EDGE ( 'NONE', *, *, #13304, .T. ) ;
#29495 = EDGE_CURVE ( 'NONE', #69396, #23177, #24337, .T. ) ;
#29496 = CARTESIAN_POINT ( 'NONE',  ( 10.00000000000000533, 120.0000000000000142, 0.000000000000000000 ) ) ;
#29497 = CARTESIAN_POINT ( 'NONE',  ( 5.000000000000000000, 68.60357193678729004, -20.85024232999272087 ) ) ;
#29498 = UNCERTAINTY_MEASURE_WITH_UNIT (LENGTH_MEASURE( 1.000000000000000082E-05 ), #16824, 'distance_accuracy_value', 'NONE');
#29499 = CARTESIAN_POINT ( 'NONE',  ( -11.35316468750000141, 93.59374999658602690, -1.390361679473963753E-15 ) ) ;
#29500 = ORIENTED_EDGE ( 'NONE', *, *, #63422, .T. ) ;
#29501 = CARTESIAN_POINT ( 'NONE',  ( 10.18810118749999916, 4.220049686691935698, 107.5000000020483668 ) ) ;
#29502 = CARTESIAN_POINT ( 'NONE',  ( 3.211159895383560947, 16.31249999863440436, 3.211159895383562723 ) ) ;
#29503 = ORIENTED_EDGE ( 'NONE', *, *, #60676, .F. ) ;
#29504 = ORIENTED_EDGE ( 'NONE', *, *, #25141, .T. ) ;
#29505 = CARTESIAN_POINT ( 'NONE',  ( -8.000000000000001776, 8.343750000000001776, 3.313708498984759387 ) ) ;
#29506 = CARTESIAN_POINT ( 'NONE',  ( 38.00000000000000000, -53.00000000000000000, 15.00000000000000178 ) ) ;
#29507 = CARTESIAN_POINT ( 'NONE',  ( 7.188101187500000044, 26.34374999795161543, 0.000000000000000000 ) ) ;
#29508 = AXIS2_PLACEMENT_3D ( 'NONE', #61926, #39296, #50601 ) ;
#29509 = EDGE_CURVE ( 'NONE', #48426, #9276, #19406, .T. ) ;
#29510 = CARTESIAN_POINT ( 'NONE',  ( 7.204075437095966983, 7.204075437095967871, 101.9687500020483668 ) ) ;
#29511 = PRODUCT_DEFINITION_SHAPE ( 'NONE', 'NONE',  #74657 ) ;
#29512 = CARTESIAN_POINT ( 'NONE',  ( 4.000000000000001776, 12.74999999726881406, 0.000000000000000000 ) ) ;
#29513 = CARTESIAN_POINT ( 'NONE',  ( 27.99999999999996803, 206.6250000027312126, 165.9999999999998863 ) ) ;
#29514 = ORIENTED_EDGE ( 'NONE', *, *, #48312, .F. ) ;
#29515 = CYLINDRICAL_SURFACE ( 'NONE', #722, 4.000000000000001776 ) ;
#29516 = CARTESIAN_POINT ( 'NONE',  ( -2.445694354108782775, 199.5625000013656063, 200.4456943541088663 ) ) ;
#29517 = CARTESIAN_POINT ( 'NONE',  ( -25.55430564589111953, 207.0625000013656063, 172.4456943541091505 ) ) ;
#29518 =( NAMED_UNIT ( * ) PLANE_ANGLE_UNIT ( ) SI_UNIT ( $, .RADIAN. ) );
#29519 = CARTESIAN_POINT ( 'NONE',  ( -3.211159895383562723, 12.93749999863440792, 3.211159895383561391 ) ) ;
#29520 = PLANE ( 'NONE',  #6729 ) ;
#29521 = CARTESIAN_POINT ( 'NONE',  ( -2.977408999572647819, 7.188101187499991163, 10.20530278187175455 ) ) ;
#29522 = ORIENTED_EDGE ( 'NONE', *, *, #33498, .F. ) ;
#29523 = VERTEX_POINT ( 'NONE', #36777 ) ;
#29524 = CARTESIAN_POINT ( 'NONE',  ( -6.238412754330611322E-16, 10.18810118749999916, 103.2812500020483810 ) ) ;
#29525 = CARTESIAN_POINT ( 'NONE',  ( -7.320508075688770155, 220.6250000000000284, 7.320508075688774596 ) ) ;
#29526 = CARTESIAN_POINT ( 'NONE',  ( -26.34314575050764518, 202.9375000000000000, 166.0000000000003695 ) ) ;
#29527 = CARTESIAN_POINT ( 'NONE',  ( 3.458734125000015425, 200.0000000013656347, 196.5673454167823877 ) ) ;
#29528 = CARTESIAN_POINT ( 'NONE',  ( 31.45873412499997812, 195.7500000013656063, 168.5673454167822172 ) ) ;
#29529 = CARTESIAN_POINT ( 'NONE',  ( 10.00000000000000178, 95.00000000000000000, 0.000000000000000000 ) ) ;
#29530 = CARTESIAN_POINT ( 'NONE',  ( 3.313708498984760720, 117.0312500000000000, -8.000000000000000000 ) ) ;
#29531 = CARTESIAN_POINT ( 'NONE',  ( -8.311093377946841443, 59.21874999658601979, 8.311093377946830785 ) ) ;
#29532 = CARTESIAN_POINT ( 'NONE',  ( -2.765530957081996810, 298.4218750017069510, -6.676582343750003368 ) ) ;
#29533 = ORIENTED_EDGE ( 'NONE', *, *, #31063, .T. ) ;
#29534 = DIRECTION ( 'NONE',  ( 1.000000000000000000, 0.000000000000000000, 0.000000000000000000 ) ) ;
#29535 = CARTESIAN_POINT ( 'NONE',  ( -1.469576158976823947E-15, 15.93749999590322197, 8.000000000000000000 ) ) ;
#29536 = CARTESIAN_POINT ( 'NONE',  ( -2.445694354108839619, 208.8125000013656063, 139.5543056458912190 ) ) ;
#29537 = CARTESIAN_POINT ( 'NONE',  ( -1.469576158976823947E-15, 11.43749999590322197, 8.000000000000000000 ) ) ;
#29538 = CARTESIAN_POINT ( 'NONE',  ( 5.656854249492374365, 5.656854249492375253, 25.95530278392014623 ) ) ;
#29539 = CARTESIAN_POINT ( 'NONE',  ( -7.320508075688771932, 239.3749999999999716, -7.320508075688771932 ) ) ;
#29540 = DIRECTION ( 'NONE',  ( 0.000000000000000000, 0.000000000000000000, 1.000000000000000000 ) ) ;
#29541 = CARTESIAN_POINT ( 'NONE',  ( -4.556349186104047710, -10.99999999999999822, 116.7812499999999858 ) ) ;
#29542 = CARTESIAN_POINT ( 'NONE',  ( -10.00000000000000000, 217.2916666666667140, -2.679491924311229845 ) ) ;
#29543 = CARTESIAN_POINT ( 'NONE',  ( 7.188101187499993827, -2.977408999572645598, 11.51780278187175632 ) ) ;
#29544 = CARTESIAN_POINT ( 'NONE',  ( 6.951808397369818766E-16, 182.3437499965860411, -11.35316468750000141 ) ) ;
#29545 = CARTESIAN_POINT ( 'NONE',  ( -4.541265875000002339, 1.749999998634406584, -1.881053915767121998 ) ) ;
#29546 = CARTESIAN_POINT ( 'NONE',  ( 2.828427124746191623, 1.874999997268813390, -2.828427124746191623 ) ) ;
#29548 = CARTESIAN_POINT ( 'NONE',  ( 0.000000000000000000, 237.9999999999999716, 0.000000000000000000 ) ) ;
#29547 = CYLINDRICAL_SURFACE ( 'NONE', #12965, 6.000000000000001776 ) ;
#29549 = ORIENTED_EDGE ( 'NONE', *, *, #71893, .T. ) ;
#29550 = B_SPLINE_CURVE_WITH_KNOTS ( 'NONE', 3,
 ( #53891, #8233, #61031, #38406, #42921, #32375, #31619, #21036, #72732, #15369, #36909, #3323, #9356, #26311, #72350, #55390, #61408, #54640, #14248, #3699, #2579, #59917 ),
 .UNSPECIFIED., .F., .F.,
 ( 4, 2, 2, 2, 2, 2, 2, 2, 2, 2, 4 ),
 ( 0.000000000000000000, 0.001156727053362440957, 0.001735090580043662954, 0.002313454106724884950, 0.003470181160087330678, 0.004048544686768553759, 0.004626908213449776840, 0.005783635266812262032, 0.006940362320174748960, 0.008097089373537234153, 0.009253816426899720213 ),
 .UNSPECIFIED. ) ;
#29551 = CARTESIAN_POINT ( 'NONE',  ( -3.458734125000015425, 195.0000000013656063, 143.4326545832176976 ) ) ;
#29552 = CARTESIAN_POINT ( 'NONE',  ( -9.832129032723420536, 34.01041666325269119, 5.676582343749997150 ) ) ;
#29553 = CARTESIAN_POINT ( 'NONE',  ( -7.778174593052020747, -7.778174593052023411, 101.8750000040967763 ) ) ;
#29554 = CARTESIAN_POINT ( 'NONE',  ( -24.54126587499999346, 204.1875000013656063, 170.0000000000002842 ) ) ;
#29555 = CARTESIAN_POINT ( 'NONE',  ( 0.000000000000000000, 0.000000000000000000, -4.000000000000001776 ) ) ;
#29557 = CARTESIAN_POINT ( 'NONE',  ( 6.123233995736767268E-16, 58.12499999317203248, -10.00000000000000178 ) ) ;
#29556 = DIRECTION ( 'NONE',  ( -0.000000000000000000, 1.000000000000000000, -0.000000000000000000 ) ) ;
#29558 = CARTESIAN_POINT ( 'NONE',  ( -2.445694354108839619, 198.8125000013656063, 139.5543056458912190 ) ) ;
#29559 = EDGE_CURVE ( 'NONE', #70980, #65791, #12642, .T. ) ;
#29560 = CARTESIAN_POINT ( 'NONE',  ( 7.320508075688774596, 77.49999999317205379, -7.320508075688774596 ) ) ;
#29561 = CARTESIAN_POINT ( 'NONE',  ( -7.188101187500001821, 100.0625000020483952, -2.977408999572650483 ) ) ;
#29562 = CARTESIAN_POINT ( 'NONE',  ( 4.541265875000002339, 13.49999999863440969, -1.881053915767121554 ) ) ;
#29563 = CARTESIAN_POINT ( 'NONE',  ( 9.999999999999996447, 55.00000000000000000, 0.000000000000000000 ) ) ;
#29564 = FACE_OUTER_BOUND ( 'NONE', #35397, .T. ) ;
#29565 = CARTESIAN_POINT ( 'NONE',  ( 0.000000000000000000, 300.0000000000000000, 10.00000000000000178 ) ) ;
#29566 = ORIENTED_EDGE ( 'NONE', *, *, #52876, .T. ) ;
#29567 = ORIENTED_EDGE ( 'NONE', *, *, #37754, .T. ) ;
#29568 =( BOUNDED_CURVE ( )  B_SPLINE_CURVE ( 2, ( #8552, #60226, #49661, #31566, #21721, #72292, #20981, #54961, #71914 ),
 .UNSPECIFIED., .F., .F. ) 
 B_SPLINE_CURVE_WITH_KNOTS ( ( 3, 2, 2, 2, 3 ),
 ( 0.4235696451107979765, 0.4301879129896927778, 0.4368061885741496009, 0.4434244641586063684, 0.4500427433262104704 ),
 .UNSPECIFIED. ) 
 CURVE ( )  GEOMETRIC_REPRESENTATION_ITEM ( )  RATIONAL_B_SPLINE_CURVE ( ( 1.000000000000000000, 0.9238795325112867385, 1.000000000000000000, 0.9238795325112867385, 1.000000000000000000, 0.9238795325112867385, 1.000000000000000000, 0.9238795325112867385, 1.000000000000000000 ) ) 
 REPRESENTATION_ITEM ( '' )  );
#29569 = FACE_OUTER_BOUND ( 'NONE', #31918, .T. ) ;
#29570 = CARTESIAN_POINT ( 'NONE',  ( 2.765530957082001251, 297.9218750017069510, 6.676582343750000703 ) ) ;
#29571 = CARTESIAN_POINT ( 'NONE',  ( 0.000000000000000000, 0.000000000000000000, 118.0000000000000000 ) ) ;
#29572 = CARTESIAN_POINT ( 'NONE',  ( -54.00000000000000711, 0.000000000000000000, 0.000000000000000000 ) ) ;
#29573 = CARTESIAN_POINT ( 'NONE',  ( -5.676582343750006032, 149.1145833299193555, 9.832129032723418760 ) ) ;
#29574 = CARTESIAN_POINT ( 'NONE',  ( -10.18810118749999916, 0.000000000000000000, 85.65625000204838102 ) ) ;
#29575 = FACE_OUTER_BOUND ( 'NONE', #40098, .T. ) ;
#29576 = CARTESIAN_POINT ( 'NONE',  ( -3.999999999999960032, 205.9375000000000284, 196.3431457505076594 ) ) ;
#29577 = CARTESIAN_POINT ( 'NONE',  ( 0.000000000000000000, 101.0525588832578734, 0.000000000000000000 ) ) ;
#29578 = CARTESIAN_POINT ( 'NONE',  ( -10.18810118749999916, 0.000000000000000000, 110.0312500020483668 ) ) ;
#29579 = ORIENTED_EDGE ( 'NONE', *, *, #19333, .T. ) ;
#29580 = FACE_OUTER_BOUND ( 'NONE', #18731, .T. ) ;
#29581 = CARTESIAN_POINT ( 'NONE',  ( 4.396006015781283693, 177.9701120841904469, 139.2341220073807904 ) ) ;
#29582 = CARTESIAN_POINT ( 'NONE',  ( -11.35316468750000141, 128.8020833299193555, 3.042071309553159963 ) ) ;
#29583 = CARTESIAN_POINT ( 'NONE',  ( 3.458734125000015425, 196.9375000013655779, 198.0000000000000284 ) ) ;
#29584 = CARTESIAN_POINT ( 'NONE',  ( -5.999999999999999112, 291.0625000000000000, 2.485281374238575314 ) ) ;
#29585 = CARTESIAN_POINT ( 'NONE',  ( -6.238412754330611322E-16, 10.18810118749999916, 79.65625000204836681 ) ) ;
#29586 = CARTESIAN_POINT ( 'NONE',  ( -3.042071309553164404, 47.55208332991935549, -11.35316468749999963 ) ) ;
#29587 = ORIENTED_EDGE ( 'NONE', *, *, #63145, .F. ) ;
#29588 = CARTESIAN_POINT ( 'NONE',  ( 38.00000000000000000, -63.00000000000000000, 15.00000000000000178 ) ) ;
#29589 = CARTESIAN_POINT ( 'NONE',  ( 4.541265875000002339, 1.437499998634406806, 0.000000000000000000 ) ) ;
#29590 = CARTESIAN_POINT ( 'NONE',  ( -4.903558642999205574E-16, 8.008118988124991233, 17.13811528394063544 ) ) ;
#29591 = EDGE_CURVE ( 'NONE', #282, #59211, #14110, .T. ) ;
#29592 = EDGE_CURVE ( 'NONE', #39207, #1937, #55779, .T. ) ;
#29593 = CARTESIAN_POINT ( 'NONE',  ( -2.977408999572650039, 14.43749999795161365, -7.188101187500001821 ) ) ;
#29594 = CARTESIAN_POINT ( 'NONE',  ( 6.000000000000003553, 293.6250000034140157, -2.485281374238571761 ) ) ;
#29595 = CARTESIAN_POINT ( 'NONE',  ( -47.41040786394007256, 145.0102112535165304, 65.18845003359888324 ) ) ;
#29596 = CARTESIAN_POINT ( 'NONE',  ( -7.188101187500000044, 6.093749997951610986, -8.802885111219163269E-16 ) ) ;
#29597 = CARTESIAN_POINT ( 'NONE',  ( -4.401442555609577197E-16, 7.188101187499992051, 7.111552781871751883 ) ) ;
#29598 = CARTESIAN_POINT ( 'NONE',  ( 4.220049686691934809, 10.18810118749999916, 70.18750000204838102 ) ) ;
#29599 = CARTESIAN_POINT ( 'NONE',  ( -29.43265458321761230, 208.1250000013656063, 173.4587341250003760 ) ) ;
#29600 = DIRECTION ( 'NONE',  ( -1.000000000000000000, -3.154042683594195121E-16, 0.000000000000000000 ) ) ;
#29601 = CARTESIAN_POINT ( 'NONE',  ( 3.211159895383561835, 21.56249999863440792, -3.211159895383561835 ) ) ;
#29602 = VERTEX_POINT ( 'NONE', #59421 ) ;
#29603 = CARTESIAN_POINT ( 'NONE',  ( -3.999999999999959144, 196.1875000027312126, 199.6568542494924259 ) ) ;
#29604 = VECTOR ( 'NONE', #50169, 1000.000000000000000 ) ;
#29605 = EDGE_CURVE ( 'NONE', #2210, #40213, #48174, .T. ) ;
#29606 = CARTESIAN_POINT ( 'NONE',  ( 3.999999999999960032, 206.0000000000000284, 142.0000000000000568 ) ) ;
#29607 = CARTESIAN_POINT ( 'NONE',  ( -29.65685424949229088, 203.5625000027312126, 174.0000000000004547 ) ) ;
#29608 = CARTESIAN_POINT ( 'NONE',  ( -4.401442555609581635E-16, 119.2812500020483810, -7.188101187500000044 ) ) ;
#29609 = VECTOR ( 'NONE', #26906, 1000.000000000000000 ) ;
#29610 = CARTESIAN_POINT ( 'NONE',  ( 7.778174593052021635, 7.778174593052023411, 93.62500000409677625 ) ) ;
#29611 = CARTESIAN_POINT ( 'NONE',  ( 3.313708498984756279, 7.999999999999991118, 3.549052783920144893 ) ) ;
#29612 = VECTOR ( 'NONE', #1229, 1000.000000000000000 ) ;
#29613 = ORIENTED_EDGE ( 'NONE', *, *, #21242, .T. ) ;
#29614 = CARTESIAN_POINT ( 'NONE',  ( 2.977408999572650927, 17.24999999795162253, -7.188101187500000933 ) ) ;
#29615 = ORIENTED_EDGE ( 'NONE', *, *, #43204, .T. ) ;
#29616 = LINE ( 'NONE', #70705, #12339 ) ;
#29617 = CARTESIAN_POINT ( 'NONE',  ( 1.704527592502717459, -10.27896685065643290, -63.66027613114049188 ) ) ;
#29618 = CARTESIAN_POINT ( 'NONE',  ( -10.00000000000000355, 57.70833333333332149, 2.679491924311223183 ) ) ;
#29619 = CARTESIAN_POINT ( 'NONE',  ( 7.188101187500001821, 101.3750000020483952, -2.977408999572651371 ) ) ;
#29620 = CARTESIAN_POINT ( 'NONE',  ( -30.44569435410883429, 203.8125000013656063, 167.5543056458915885 ) ) ;
#29621 = CARTESIAN_POINT ( 'NONE',  ( 54.00000000000000711, 0.000000000000000000, 20.00000000000001776 ) ) ;
#29623 = CARTESIAN_POINT ( 'NONE',  ( 105.0000000000000000, 205.0000000000000284, 20.00000000000000000 ) ) ;
#29622 = CARTESIAN_POINT ( 'NONE',  ( -6.000000000000001776, 288.0625000034140157, 0.000000000000000000 ) ) ;
#29624 = VERTEX_POINT ( 'NONE', #60521 ) ;
#29625 = CARTESIAN_POINT ( 'NONE',  ( -8.311093377946836114, 248.2812500034139873, -8.311093377946836114 ) ) ;
#29626 = CARTESIAN_POINT ( 'NONE',  ( -5.082755093536319713, 5.082755093536319713, 19.67405278187175455 ) ) ;
#29627 = CARTESIAN_POINT ( 'NONE',  ( 38.00000000000000000, -63.00000000000000000, 10.00000000000006217 ) ) ;
#29628 = LINE ( 'NONE', #12634, #35807 ) ;
#29629 = DIRECTION ( 'NONE',  ( -1.000000000000000000, -0.000000000000000000, -0.000000000000000000 ) ) ;
#29630 = CARTESIAN_POINT ( 'NONE',  ( 7.999999999999991118, -2.975320552349488356E-08, 19.76780278304987348 ) ) ;
#29631 = CARTESIAN_POINT ( 'NONE',  ( -7.320508075688778149, 168.1250000000000284, 7.320508075688769267 ) ) ;
#29632 = CARTESIAN_POINT ( 'NONE',  ( 11.00000000000000000, 1.347111479062088405E-15, 79.74999999999998579 ) ) ;
#29633 = CARTESIAN_POINT ( 'NONE',  ( 1.469576158976823947E-15, 119.3750000000000000, 8.000000000000000000 ) ) ;
#29634 = CARTESIAN_POINT ( 'NONE',  ( 1.469576158976822172E-15, -7.999999999999991118, 4.205302779823362869 ) ) ;
#29635 = CARTESIAN_POINT ( 'NONE',  ( -11.35316468750000141, 143.5937499965860411, -1.390361679473963753E-15 ) ) ;
#29636 = CARTESIAN_POINT ( 'NONE',  ( 12.00000000000000000, 6.928203230275491009, -14.80000000000000071 ) ) ;
#29637 = CARTESIAN_POINT ( 'NONE',  ( 7.778174593052021635, 7.778174593052023411, 106.9374999999999858 ) ) ;
#29640 = DIRECTION ( 'NONE',  ( 0.000000000000000000, 1.000000000000000000, 0.000000000000000000 ) ) ;
#29639 = CARTESIAN_POINT ( 'NONE',  ( -3.428378827827393227, -51.66489094708095564, 48.71857030467474914 ) ) ;
#29638 = CARTESIAN_POINT ( 'NONE',  ( 32.00000000000000711, 208.3125000000000000, 168.3431457505075741 ) ) ;
#29641 = ORIENTED_EDGE ( 'NONE', *, *, #23954, .T. ) ;
#29642 = CARTESIAN_POINT ( 'NONE',  ( 5.239869872917444660, 225.8121258658414092, -8.537502151162962960 ) ) ;
#29643 = CARTESIAN_POINT ( 'NONE',  ( -3.458734125000015425, 209.0000000013656063, 143.4326545832176976 ) ) ;
#29644 = CARTESIAN_POINT ( 'NONE',  ( 31.45873412499999233, 194.9375000013655779, 169.9999999999999432 ) ) ;
#29645 = CARTESIAN_POINT ( 'NONE',  ( 8.660254037844385522, 41.45833332650536818, 5.000000000000005329 ) ) ;
#29646 = CARTESIAN_POINT ( 'NONE',  ( 7.188101187500000044, 114.4062500020483810, -8.802885111219163269E-16 ) ) ;
#29647 = CARTESIAN_POINT ( 'NONE',  ( 4.541265875000002339, 21.31249999863440792, 0.000000000000000000 ) ) ;
#29648 = CARTESIAN_POINT ( 'NONE',  ( -1.877992804783608305, 65.87054549412373206, -26.34444121135337369 ) ) ;
#29649 = CARTESIAN_POINT ( 'NONE',  ( 7.999999999999991118, 9.797174393178815797E-16, 18.08030277982336642 ) ) ;
#29651 = CYLINDRICAL_SURFACE ( 'NONE', #64273, 14.00000000000000000 ) ;
#29650 = DIRECTION ( 'NONE',  ( -0.000000000000000000, 1.000000000000000000, -0.000000000000000000 ) ) ;
#29652 = ORIENTED_EDGE ( 'NONE', *, *, #26990, .T. ) ;
#29653 = CARTESIAN_POINT ( 'NONE',  ( 4.999999999999999112, 0.000000000000000000, 0.000000000000000000 ) ) ;
#29654 = CARTESIAN_POINT ( 'NONE',  ( 5.082755093536325930, 23.15624999795161543, -5.082755093536325930 ) ) ;
#29655 = CARTESIAN_POINT ( 'NONE',  ( -8.660254037844435260, 62.91666666666670693, 5.000000000000023981 ) ) ;
#29656 = CARTESIAN_POINT ( 'NONE',  ( -5.676582343749992710, 240.0520833367473301, 9.832129032723422313 ) ) ;
#29657 = CARTESIAN_POINT ( 'NONE',  ( -3.042071309553164404, 117.2395833299193555, -11.35316468749999963 ) ) ;
#29658 = ORIENTED_EDGE ( 'NONE', *, *, #21735, .T. ) ;
#29659 = EDGE_CURVE ( 'NONE', #3175, #5966, #65026, .T. ) ;
#29660 = CARTESIAN_POINT ( 'NONE',  ( 8.000000000000000000, 25.59375000000000711, -3.313708498984761164 ) ) ;
#29661 = CARTESIAN_POINT ( 'NONE',  ( 1.871523826299183495E-15, -10.18810118749999916, 99.53125000204838102 ) ) ;
#29662 = CARTESIAN_POINT ( 'NONE',  ( 8.660254037844389075, 217.2916666598387110, -5.000000000000000000 ) ) ;
#29663 = CARTESIAN_POINT ( 'NONE',  ( 1.432654583217664701, 201.0000000013655779, 201.4587341250000065 ) ) ;
#29664 = CARTESIAN_POINT ( 'NONE',  ( -1.656854249492383468, 6.437499997268813168, 4.000000000000000888 ) ) ;
#29666 = CARTESIAN_POINT ( 'NONE',  ( -11.35316468749999785, 98.07291666325269830, -3.042071309553167957 ) ) ;
#29665 = DIRECTION ( 'NONE',  ( -0.000000000000000000, -0.000000000000000000, -1.000000000000000000 ) ) ;
#29667 = CARTESIAN_POINT ( 'NONE',  ( -7.999999999999989342, -3.313708498984762496, 8.611552783920146226 ) ) ;
#29668 = CARTESIAN_POINT ( 'NONE',  ( -30.44569435410883074, 196.8125000013656063, 167.5543056458915885 ) ) ;
#29669 = CARTESIAN_POINT ( 'NONE',  ( 2.679491924295794192, 176.0416666666681635, -10.00000000000901323 ) ) ;
#29670 = ORIENTED_EDGE ( 'NONE', *, *, #71439, .F. ) ;
#29671 = CARTESIAN_POINT ( 'NONE',  ( 10.00000000000000000, 191.6666666598387394, 2.679491924311236062 ) ) ;
#29672 = FACE_OUTER_BOUND ( 'NONE', #53921, .T. ) ;
#29673 = AXIS2_PLACEMENT_3D ( 'NONE', #8649, #44475, #3363 ) ;
#29674 = CARTESIAN_POINT ( 'NONE',  ( 1.656854249492381248, 9.937499997268814056, -4.000000000000001776 ) ) ;
#29675 = CARTESIAN_POINT ( 'NONE',  ( 11.35316468749999785, 85.88541666325268409, 3.042071309553174174 ) ) ;
#29676 = CARTESIAN_POINT ( 'NONE',  ( -1.432654583217607192, 209.2500000013656063, 194.5412658750000219 ) ) ;
#29677 = CARTESIAN_POINT ( 'NONE',  ( 2.977408999572652260, 8.062499997951611874, 7.188101187500000044 ) ) ;
#29678 = CARTESIAN_POINT ( 'NONE',  ( -7.204075437095967871, 7.204075437095967871, 96.34375000204836681 ) ) ;
#29679 = CARTESIAN_POINT ( 'NONE',  ( 3.042071309553159519, 15.05208332991935194, 11.35316468750000141 ) ) ;
#29680 = ORIENTED_EDGE ( 'NONE', *, *, #21579, .F. ) ;
#29681 = CARTESIAN_POINT ( 'NONE',  ( -10.00000000000001066, 137.2916666666666856, -2.679491924311232953 ) ) ;
#29682 = CARTESIAN_POINT ( 'NONE',  ( -11.35316468749999785, 213.0729166632526983, -3.042071309553167957 ) ) ;
#29683 = CARTESIAN_POINT ( 'NONE',  ( -4.220049686691937474, -10.18810118749999738, 78.81250000204838102 ) ) ;
#29684 = EDGE_CURVE ( 'NONE', #42285, #3856, #68732, .T. ) ;
#29685 = CARTESIAN_POINT ( 'NONE',  ( 10.00000000000000178, 47.08333332650536107, -2.679491924311226736 ) ) ;
#29686 = CARTESIAN_POINT ( 'NONE',  ( -7.320508075688778149, 149.9999999931720254, 7.320508075688769267 ) ) ;
#29687 = CARTESIAN_POINT ( 'NONE',  ( -4.721056650415999201, 298.3281250017069510, -4.721056650415999201 ) ) ;
#29688 = VERTEX_POINT ( 'NONE', #38647 ) ;
#29689 = CARTESIAN_POINT ( 'NONE',  ( 3.999999999999960032, 202.1250000027312126, 142.0000000000000568 ) ) ;
#29690 = CARTESIAN_POINT ( 'NONE',  ( -5.676582343749998039, 207.7604166632526983, -9.832129032723420536 ) ) ;
#29691 =( BOUNDED_CURVE ( )  B_SPLINE_CURVE ( 2, ( #3181, #49187, #72197, #27672, #32229, #15228, #60513, #14849, #26926 ),
 .UNSPECIFIED., .F., .F. ) 
 B_SPLINE_CURVE_WITH_KNOTS ( ( 3, 2, 2, 2, 3 ),
 ( 0.2368421052631578261, 0.2434210526315789269, 0.2499999999999999722, 0.2565789473684210731, 0.2631578947368420907 ),
 .UNSPECIFIED. ) 
 CURVE ( )  GEOMETRIC_REPRESENTATION_ITEM ( )  RATIONAL_B_SPLINE_CURVE ( ( 1.000000000000000666, 0.9238795325112860723, 1.000000000000000000, 0.9238795325112867385, 1.000000000000000000, 0.9238795325112867385, 1.000000000000000000, 0.9238795325112867385, 1.000000000000000000 ) ) 
 REPRESENTATION_ITEM ( '' )  );
#29692 = VECTOR ( 'NONE', #65374, 1000.000000000000000 ) ;
#29693 = CARTESIAN_POINT ( 'NONE',  ( 10.18810118750000093, -4.220049686691933921, 92.31250000204838102 ) ) ;
#29694 = CARTESIAN_POINT ( 'NONE',  ( -29.43265458321760519, 202.8750000013656347, 173.4587341250003760 ) ) ;
#29695 = B_SPLINE_CURVE_WITH_KNOTS ( 'NONE', 3,
 ( #10786, #62830, #51146, #45854, #28878, #45479, #51898, #16058, #69247, #239, #23220, #73784, #68497, #40201, #39826, #68871 ),
 .UNSPECIFIED., .F., .F.,
 ( 4, 2, 2, 2, 2, 2, 2, 4 ),
 ( 0.002858817767436716648, 0.003816970720266378483, 0.004775123673096039884, 0.005733276625925702585, 0.006691429578755363553, 0.008607735484414683752, 0.009565888437244344719, 0.01052404139007400395 ),
 .UNSPECIFIED. ) ;
#29696 = CARTESIAN_POINT ( 'NONE',  ( 3.313708498984762052, 16.78125000000000355, -8.000000000000000000 ) ) ;
#29697 = VERTEX_POINT ( 'NONE', #43533 ) ;
#29698 = CARTESIAN_POINT ( 'NONE',  ( -7.188101187499999156, 119.7500000020483810, 2.977408999572654924 ) ) ;
#29699 = CARTESIAN_POINT ( 'NONE',  ( -3.999999999999960032, 207.1250000027312126, 198.0000000000000284 ) ) ;
#29700 = ADVANCED_FACE ( 'NONE', ( #32620 ), #26552, .F. ) ;
#29701 = CARTESIAN_POINT ( 'NONE',  ( 10.00000000000000178, 25.20833333333333570, -2.679491924311226736 ) ) ;
#29702 = DIRECTION ( 'NONE',  ( -0.000000000000000000, 1.000000000000000000, -0.000000000000000000 ) ) ;
#29703 = CARTESIAN_POINT ( 'NONE',  ( -7.204075437095967871, 7.204075437095967871, 76.84375000204838102 ) ) ;
#29704 = VERTEX_POINT ( 'NONE', #15608 ) ;
#29705 = CARTESIAN_POINT ( 'NONE',  ( 5.082755093536325930, 0.6562499979516100979, -5.082755093536325930 ) ) ;
#29706 = EDGE_CURVE ( 'NONE', #29523, #5036, #19623, .T. ) ;
#29707 = DIRECTION ( 'NONE',  ( -0.000000000000000000, 1.000000000000000000, -0.000000000000000000 ) ) ;
#29708 = EDGE_CURVE ( 'NONE', #25175, #36433, #27341, .T. ) ;
#29709 = DIRECTION ( 'NONE',  ( 0.000000000000000000, 0.000000000000000000, -1.000000000000000000 ) ) ;
#29710 = CARTESIAN_POINT ( 'NONE',  ( 7.188101187500001821, 117.8750000020483810, -2.977408999572651371 ) ) ;
#29711 = AXIS2_PLACEMENT_3D ( 'NONE', #19204, #42208, #13527 ) ;
#29712 = CARTESIAN_POINT ( 'NONE',  ( 5.000000000000000000, -60.90295814858255596, 23.31388853594792110 ) ) ;
#29713 = CARTESIAN_POINT ( 'NONE',  ( 4.721056650415999201, 298.0781250017069510, -4.721056650415999201 ) ) ;
#29715 = CARTESIAN_POINT ( 'NONE',  ( -2.485281374238268004, 289.2500000034140726, 6.000000000000304645 ) ) ;
#29714 = CARTESIAN_POINT ( 'NONE',  ( 3.042071309553173286, 235.3645833367473017, 11.35316468749999608 ) ) ;
#29716 = VERTEX_POINT ( 'NONE', #38268 ) ;
#29717 = CARTESIAN_POINT ( 'NONE',  ( -11.35316468749999785, 239.0104166700806161, -3.042071309553164848 ) ) ;
#29718 = EDGE_CURVE ( 'NONE', #37264, #61963, #60576, .T. ) ;
#29719 = CARTESIAN_POINT ( 'NONE',  ( 2.977408999572646486, 7.188101187499991163, 7.017802781871751883 ) ) ;
#29720 = ORIENTED_EDGE ( 'NONE', *, *, #70130, .F. ) ;
#29721 = CARTESIAN_POINT ( 'NONE',  ( 4.220049686691941027, -10.18810118749999738, 68.12500000204838102 ) ) ;
#29722 = CARTESIAN_POINT ( 'NONE',  ( 3.042071309553159519, 105.0520833299193271, 11.35316468750000141 ) ) ;
#29723 = DIRECTION ( 'NONE',  ( -0.000000000000000000, 1.000000000000000000, 0.000000000000000000 ) ) ;
#29724 = CARTESIAN_POINT ( 'NONE',  ( 11.00000000000000000, 4.556349186104045934, 82.84375000000000000 ) ) ;
#29727 = DIRECTION ( 'NONE',  ( -0.000000000000000000, -1.000000000000000000, -0.000000000000000000 ) ) ;
#29726 = CARTESIAN_POINT ( 'NONE',  ( 25.55430564589119058, 205.3125000013656063, 172.4456943541087526 ) ) ;
#29725 = CARTESIAN_POINT ( 'NONE',  ( 24.54126587499999346, 203.4375000013656063, 169.9999999999998863 ) ) ;
#29728 = ORIENTED_EDGE ( 'NONE', *, *, #10946, .T. ) ;
#29729 = CARTESIAN_POINT ( 'NONE',  ( -23.99999999999995026, 195.8125000027312410, 171.6568542494926817 ) ) ;
#29730 = CARTESIAN_POINT ( 'NONE',  ( -7.320508075688778149, 179.9999999931720254, 7.320508075688769267 ) ) ;
#29731 = CARTESIAN_POINT ( 'NONE',  ( -2.085542519210945728E-15, 219.5312499965860411, 11.35316468750000141 ) ) ;
#29732 = CARTESIAN_POINT ( 'NONE',  ( 1.432654583217607858, 205.6250000013656063, 138.5412658750000787 ) ) ;
#29733 = CARTESIAN_POINT ( 'NONE',  ( 25.55430564589119768, 207.3125000013656063, 167.5543056458910485 ) ) ;
#29734 = CARTESIAN_POINT ( 'NONE',  ( -7.188101187500001821, 25.49999999795161898, -2.977408999572651371 ) ) ;
#29735 = CARTESIAN_POINT ( 'NONE',  ( -5.676582343749998039, 182.7604166632526699, -9.832129032723420536 ) ) ;
#29736 = CARTESIAN_POINT ( 'NONE',  ( -5.082755093536325930, 98.84375000204838102, -5.082755093536325930 ) ) ;
#29737 = PLANE ( 'NONE',  #10716 ) ;
#29738 = CARTESIAN_POINT ( 'NONE',  ( -4.541265875000002339, 8.812499998634407916, -5.561446717895856393E-16 ) ) ;
#29739 = CARTESIAN_POINT ( 'NONE',  ( 31.45873412499999944, 202.9375000013656063, 169.9999999999999432 ) ) ;
#29740 = CARTESIAN_POINT ( 'NONE',  ( -5.082755093536317936, -5.082755093536320601, 11.04905278187175455 ) ) ;
#29741 = CARTESIAN_POINT ( 'NONE',  ( -3.042071309553173730, 64.32291666325269830, 11.35316468749999785 ) ) ;
#29742 = CYLINDRICAL_SURFACE ( 'NONE', #6325, 11.00000000000000000 ) ;
#29743 = CARTESIAN_POINT ( 'NONE',  ( 7.999999999999992895, -3.313708498984756279, 3.042802784329822430 ) ) ;
#29744 = ORIENTED_EDGE ( 'NONE', *, *, #34635, .T. ) ;
#29745 = CARTESIAN_POINT ( 'NONE',  ( -7.999999999999991118, 0.000000000000000000, 7.017802783920144449 ) ) ;
#29746 = CARTESIAN_POINT ( 'NONE',  ( -2.849036369511732440E-14, 203.3750000027312126, 138.0000000000000568 ) ) ;
#29747 = CARTESIAN_POINT ( 'NONE',  ( -8.311093377946836114, 72.65624999658604111, -8.311093377946837890 ) ) ;
#29748 = CARTESIAN_POINT ( 'NONE',  ( -7.778174593052020747, -7.778174593052023411, 70.37500000409677625 ) ) ;
#29749 = CARTESIAN_POINT ( 'NONE',  ( -1.432654583217662481, 195.3750000013656063, 145.4587341250000350 ) ) ;
#29750 = CARTESIAN_POINT ( 'NONE',  ( -5.126144196591292612, 16.23426282122703057, 69.90718656545274712 ) ) ;
#29752 = CARTESIAN_POINT ( 'NONE',  ( -8.311093377946836114, 57.65624999658601268, -8.311093377946837890 ) ) ;
#29751 = CARTESIAN_POINT ( 'NONE',  ( 8.000000000000001776, 103.3437500040967763, 3.313708498984759387 ) ) ;
#29753 = CARTESIAN_POINT ( 'NONE',  ( -4.898587196589407898E-16, 7.999999999999991118, 23.14280278392014978 ) ) ;
#29754 = CARTESIAN_POINT ( 'NONE',  ( -8.660254037844387298, 13.95833332650536818, -5.000000000000004441 ) ) ;
#29755 = CARTESIAN_POINT ( 'NONE',  ( 10.00000000000000000, 151.6666666598387110, 2.679491924311236062 ) ) ;
#29756 = CARTESIAN_POINT ( 'NONE',  ( -2.977408999572650927, 97.25000000204839523, -7.188101187500001821 ) ) ;
#29757 = DIRECTION ( 'NONE',  ( 0.000000000000000000, 0.02418647091589873691, -0.9997074645238147594 ) ) ;
#29758 = CARTESIAN_POINT ( 'NONE',  ( -8.311093377946841443, 44.21874999658602690, 8.311093377946834337 ) ) ;
#29759 = ADVANCED_FACE ( 'NONE', ( #35493 ), #12824, .F. ) ;
#29760 = CARTESIAN_POINT ( 'NONE',  ( -10.18810118749999738, -4.220049686691941915, 116.1250000020483810 ) ) ;
#29761 = CARTESIAN_POINT ( 'NONE',  ( 9.832129032723420536, 191.1979166632526983, -5.676582343749999815 ) ) ;
#29762 = ORIENTED_EDGE ( 'NONE', *, *, #11313, .T. ) ;
#29763 = CARTESIAN_POINT ( 'NONE',  ( 4.465349678524218824, 66.51625814178468943, 26.73836809291932326 ) ) ;
#29764 = CARTESIAN_POINT ( 'NONE',  ( 7.204075437095968759, -7.204075437095966983, 68.21875000204836681 ) ) ;
#29765 = CARTESIAN_POINT ( 'NONE',  ( -6.062591786044946751, -5.219672483564715471, -0.3118205092643556720 ) ) ;
#29767 = CARTESIAN_POINT ( 'NONE',  ( 9.832129032723416984, 180.3645833299193555, 5.676582343750006032 ) ) ;
#29766 = CARTESIAN_POINT ( 'NONE',  ( 1.656854249492555331, 195.6875000000000284, 194.0000000000002842 ) ) ;
#29768 = TOROIDAL_SURFACE ( 'NONE', #69684, 37.00000000000003553, 6.000000000000005329 ) ;
#29769 = DIRECTION ( 'NONE',  ( -1.000000000000000000, -0.000000000000000000, -0.000000000000000000 ) ) ;
#29770 = CARTESIAN_POINT ( 'NONE',  ( 9.999999999999998224, 250.8333333401613459, -2.679491924311229401 ) ) ;
#29771 = CARTESIAN_POINT ( 'NONE',  ( 0.000000000000000000, 0.000000000000000000, 0.000000000000000000 ) ) ;
#29772 =( GEOMETRIC_REPRESENTATION_CONTEXT ( 3 ) GLOBAL_UNCERTAINTY_ASSIGNED_CONTEXT ( ( #24504 ) ) GLOBAL_UNIT_ASSIGNED_CONTEXT ( ( #32402, #48980, #20689 ) ) REPRESENTATION_CONTEXT ( 'NONE', 'WORKASPACE' ) );
#29773 = ORIENTED_EDGE ( 'NONE', *, *, #2401, .F. ) ;
#29774 = CARTESIAN_POINT ( 'NONE',  ( -9.832129032723418760, 173.1770833299193555, -5.676582343750004256 ) ) ;
#29775 = EDGE_CURVE ( 'NONE', #31077, #25259, #35087, .T. ) ;
#29776 = CARTESIAN_POINT ( 'NONE',  ( -2.977408999572647819, 7.188101187499992051, 26.70530278187175455 ) ) ;
#29777 = CARTESIAN_POINT ( 'NONE',  ( 3.042071309553159519, 130.0520833299193555, 11.35316468750000141 ) ) ;
#29778 =( BOUNDED_CURVE ( )  B_SPLINE_CURVE ( 2, ( #46906, #10720, #62760, #911, #5441, #57510, #63143, #63515, #39394, #11471, #57880, #69181, #28811 ),
 .UNSPECIFIED., .F., .F. ) 
 B_SPLINE_CURVE_WITH_KNOTS ( ( 3, 2, 2, 2, 2, 2, 3 ),
 ( 0.8006953296466258196, 0.8059278359778203615, 0.8111603423090147924, 0.8163928486402091123, 0.8216253549714036541, 0.8268578613025980850, 0.8320903676337926269 ),
 .UNSPECIFIED. ) 
 CURVE ( )  GEOMETRIC_REPRESENTATION_ITEM ( )  RATIONAL_B_SPLINE_CURVE ( ( 1.000000000000000000, 0.9659258262890684232, 1.000000000000000000, 0.9659258262890684232, 1.000000000000000000, 0.9659258262890684232, 1.000000000000000000, 0.9659258262890684232, 1.000000000000000000, 0.9659258262890684232, 1.000000000000000000, 0.9659258262894588887, 0.9999999999996095346 ) ) 
 REPRESENTATION_ITEM ( '' )  );
#29779 = CARTESIAN_POINT ( 'NONE',  ( 10.58424618561840092, 225.9999999999999147, -3.898667594295466277 ) ) ;
#29780 = PRODUCT_DEFINITION ( 'UNKNOWN', '', #17704, #38522 ) ;
#29781 = ORIENTED_EDGE ( 'NONE', *, *, #11877, .T. ) ;
#29782 = CARTESIAN_POINT ( 'NONE',  ( -7.999999999999998224, 102.7812500040967905, 3.313708498984766493 ) ) ;
#29783 = CIRCLE ( 'NONE', #20117, 27.99999999999999645 ) ;
#29784 = EDGE_CURVE ( 'NONE', #31074, #67076, #42751, .T. ) ;
#29785 = EDGE_CURVE ( 'NONE', #5866, #8328, #64887, .T. ) ;
#29786 = CARTESIAN_POINT ( 'NONE',  ( 2.449293598294707893E-16, 10.25000000000000000, -4.000000000000001776 ) ) ;
#29787 =( BOUNDED_CURVE ( )  B_SPLINE_CURVE ( 2, ( #601, #28872, #45474, #74525, #22834, #11528, #57945, #40569, #10780, #11899, #16791, #51892, #17930 ),
 .UNSPECIFIED., .F., .F. ) 
 B_SPLINE_CURVE_WITH_KNOTS ( ( 3, 2, 2, 2, 2, 2, 3 ),
 ( 0.8423913043478260532, 0.8442028985507246119, 0.8460144927536231707, 0.8478260869565217295, 0.8496376811594202882, 0.8514492753623188470, 0.8532608695652174058 ),
 .UNSPECIFIED. ) 
 CURVE ( )  GEOMETRIC_REPRESENTATION_ITEM ( )  RATIONAL_B_SPLINE_CURVE ( ( 1.000000000000000000, 0.9659258262890683122, 1.000000000000000000, 0.9659258262890683122, 1.000000000000000000, 0.9659258262890683122, 1.000000000000000000, 0.9659258262890683122, 1.000000000000000000, 0.9659258262890683122, 1.000000000000000000, 0.9659258262890683122, 1.000000000000000000 ) ) 
 REPRESENTATION_ITEM ( '' )  );
#29788 = CARTESIAN_POINT ( 'NONE',  ( 0.000000000000000000, 300.0000000000000000, 0.000000000000000000 ) ) ;
#29789 = CARTESIAN_POINT ( 'NONE',  ( -8.342170076843785083E-16, 10.06249999863440614, 4.541265875000002339 ) ) ;
#29790 = CARTESIAN_POINT ( 'NONE',  ( -5.656854249492373476, -5.656854249492376141, 19.20530278392014978 ) ) ;
#29791 = CARTESIAN_POINT ( 'NONE',  ( 1.269536070779894168E-12, 186.2499999999999147, -10.00000000000000178 ) ) ;
#29792 = ORIENTED_EDGE ( 'NONE', *, *, #37258, .T. ) ;
#29793 = CARTESIAN_POINT ( 'NONE',  ( -2.751064625579944321E-14, 204.7500000000000284, 146.0000000000000284 ) ) ;
#29794 = CARTESIAN_POINT ( 'NONE',  ( -7.188101187500001821, 97.06250000204838102, -2.977408999572650483 ) ) ;
#29796 = CYLINDRICAL_SURFACE ( 'NONE', #3286, 4.000000000000001776 ) ;
#29795 = CARTESIAN_POINT ( 'NONE',  ( -6.338495502905945601E-13, 181.2500000000000853, -10.00000000000000533 ) ) ;
#29797 = VERTEX_POINT ( 'NONE', #46430 ) ;
#29798 = CARTESIAN_POINT ( 'NONE',  ( -0.4501631047671846297, 16.44600848780500257, -68.55503832938671849 ) ) ;
#29799 = CARTESIAN_POINT ( 'NONE',  ( 7.188101187499993827, -2.977408999572645598, 27.64280278187175810 ) ) ;
#29800 = VERTEX_POINT ( 'NONE', #6075 ) ;
#29801 = ADVANCED_FACE ( 'NONE', ( #23415 ), #24522, .F. ) ;
#29802 = EDGE_LOOP ( 'NONE', ( #26979, #67400, #29892, #34720 ) ) ;
#29803 = CARTESIAN_POINT ( 'NONE',  ( 10.18810118749999916, 1.247682550866122264E-15, 89.40625000204838102 ) ) ;
#29804 = UNCERTAINTY_MEASURE_WITH_UNIT (LENGTH_MEASURE( 1.000000000000000082E-05 ), #17354, 'distance_accuracy_value', 'NONE');
#29805 = CARTESIAN_POINT ( 'NONE',  ( -29.43265458321760164, 195.1250000013656063, 173.4587341250003760 ) ) ;
#29806 = CARTESIAN_POINT ( 'NONE',  ( 7.778174593052021635, 7.778174593052023411, 99.43749999999998579 ) ) ;
#29807 = AXIS2_PLACEMENT_3D ( 'NONE', #47999, #58250, #30662 ) ;
#29810 = CARTESIAN_POINT ( 'NONE',  ( -4.088227598258586603E-16, 296.3593750017070079, -6.676582343750001591 ) ) ;
#29809 = CARTESIAN_POINT ( 'NONE',  ( 26.34314575050758833, 201.6875000027312126, 165.9999999999998863 ) ) ;
#29808 = CARTESIAN_POINT ( 'NONE',  ( 0.000000000000000000, 300.0000000000000000, 0.000000000000000000 ) ) ;
#29811 = CARTESIAN_POINT ( 'NONE',  ( 6.123233995736767268E-16, 141.2500000000000284, -10.00000000000000178 ) ) ;
#29812 = CARTESIAN_POINT ( 'NONE',  ( 3.313708498984760720, 102.0312499999999858, -8.000000000000000000 ) ) ;
#29813 = DIRECTION ( 'NONE',  ( 0.000000000000000000, -1.000000000000000000, 0.000000000000000000 ) ) ;
#29814 = CARTESIAN_POINT ( 'NONE',  ( -5.272366635369878374, -4.893143551702760163, 0.5406094755204297053 ) ) ;
#29815 = CARTESIAN_POINT ( 'NONE',  ( 4.898587196589415787E-16, 0.000000000000000000, 4.000000000000001776 ) ) ;
#29816 = CARTESIAN_POINT ( 'NONE',  ( 26.56734541678232375, 202.3750000013655779, 173.4587341249998929 ) ) ;
#29817 = CARTESIAN_POINT ( 'NONE',  ( 5.082755093536325930, 2.531249997951610542, -5.082755093536325930 ) ) ;
#29818 = CARTESIAN_POINT ( 'NONE',  ( 8.008118988124991233, 3.317071493978879015, 3.356865283940628331 ) ) ;
#29819 = CARTESIAN_POINT ( 'NONE',  ( 12.00000000000000000, 0.000000000000000000, 0.000000000000000000 ) ) ;
#29820 = CARTESIAN_POINT ( 'NONE',  ( 1.320432766682874540E-15, 118.9062500020483810, 7.188101187500000044 ) ) ;
#29822 = CARTESIAN_POINT ( 'NONE',  ( 1.216591630144955749, 194.6379550352074830, 201.4372753964553624 ) ) ;
#29821 = DIRECTION ( 'NONE',  ( 0.000000000000000000, 0.8778652960885012790, 0.4789076340208496818 ) ) ;
#29823 = CARTESIAN_POINT ( 'NONE',  ( -5.676582343750000703, 233.3854166700806729, -9.832129032723418760 ) ) ;
#29824 = CARTESIAN_POINT ( 'NONE',  ( -5.656854249492381470, 3.937500000000000888, 5.656854249492379694 ) ) ;
#29825 = CARTESIAN_POINT ( 'NONE',  ( 11.00000000000000000, 1.347111479062088405E-15, 85.75000000000000000 ) ) ;
#29826 = CARTESIAN_POINT ( 'NONE',  ( 31.99999999999997868, 199.1875000000000000, 171.6568542494923122 ) ) ;
#29827 = CARTESIAN_POINT ( 'NONE',  ( -2.085542519210945728E-15, 24.53124999658601624, 11.35316468750000141 ) ) ;
#29828 = CARTESIAN_POINT ( 'NONE',  ( 5.490800045006650976, -10.68629157650006256, -1.191902411728888722E-14 ) ) ;
#29829 = CARTESIAN_POINT ( 'NONE',  ( -9.832129032723418760, 223.1770833299193555, -5.676582343750004256 ) ) ;
#29830 = CARTESIAN_POINT ( 'NONE',  ( 30.82842712474620939, 201.2500000027312126, 172.8284271247460424 ) ) ;
#29832 = DIRECTION ( 'NONE',  ( -1.000000000000000000, 0.000000000000000000, 0.000000000000000000 ) ) ;
#29831 = CARTESIAN_POINT ( 'NONE',  ( -30.64284399271078740, 271.9999999999999432, 174.6921329945331536 ) ) ;
#29833 = ORIENTED_EDGE ( 'NONE', *, *, #7216, .F. ) ;
#29834 = EDGE_CURVE ( 'NONE', #66256, #10305, #63777, .T. ) ;
#29835 = CARTESIAN_POINT ( 'NONE',  ( -2.839093476692135984E-14, 194.9375000013655779, 138.5412658750000503 ) ) ;
#29836 = CARTESIAN_POINT ( 'NONE',  ( 6.951808397369818766E-16, 37.03124999658601979, -11.35316468750000141 ) ) ;
#29837 = CARTESIAN_POINT ( 'NONE',  ( -4.556349186104047710, -10.99999999999999822, 83.96875000409676204 ) ) ;
#29838 = CARTESIAN_POINT ( 'NONE',  ( 3.458734124999960358, 209.6875000013656063, 142.0000000000000568 ) ) ;
#29839 = CARTESIAN_POINT ( 'NONE',  ( -28.00000000000003197, 210.0000000000000284, 166.0000000000003695 ) ) ;
#29840 = FACE_OUTER_BOUND ( 'NONE', #102, .T. ) ;
#29842 = CARTESIAN_POINT ( 'NONE',  ( 8.311093377946834337, 20.15624999658601268, 8.311093377946839666 ) ) ;
#29841 = CARTESIAN_POINT ( 'NONE',  ( 5.082755093536326818, 108.2187500020483810, 5.082755093536325042 ) ) ;
#29844 = ADVANCED_FACE ( 'NONE', ( #58147 ), #72257, .T. ) ;
#29843 = CARTESIAN_POINT ( 'NONE',  ( -5.656854249492373476, -5.656854249492376141, 17.51780277982336287 ) ) ;
#29845 = CARTESIAN_POINT ( 'NONE',  ( 8.311093377946837890, 146.4062499965860127, -8.311093377946837890 ) ) ;
#29846 = VECTOR ( 'NONE', #37432, 1000.000000000000000 ) ;
#29847 = CARTESIAN_POINT ( 'NONE',  ( 8.660254037844385522, 121.4583333265053824, 5.000000000000005329 ) ) ;
#29848 = CARTESIAN_POINT ( 'NONE',  ( 7.188101187500001821, 113.3750000020483810, -2.977408999572651371 ) ) ;
#29849 = CARTESIAN_POINT ( 'NONE',  ( -18.00000000000000000, 10.39230484541324628, -20.69999999999999929 ) ) ;
#29850 = CARTESIAN_POINT ( 'NONE',  ( -30.44569435410883429, 203.8125000013656063, 167.5543056458915885 ) ) ;
#29851 = EDGE_LOOP ( 'NONE', ( #46438, #5908, #15740, #11418 ) ) ;
#29852 = CARTESIAN_POINT ( 'NONE',  ( -9.832129032723420536, 9.010416663252684089, 5.676582343749997150 ) ) ;
#29853 = EDGE_CURVE ( 'NONE', #11891, #10738, #14765, .T. ) ;
#29854 = EDGE_LOOP ( 'NONE', ( #30262, #26667, #26431, #10445 ) ) ;
#29855 = CARTESIAN_POINT ( 'NONE',  ( -7.778174593052020747, -7.778174593052023411, 100.1874999999999858 ) ) ;
#29856 = CARTESIAN_POINT ( 'NONE',  ( -2.765530957081996810, 297.2656250017069510, -6.676582343750003368 ) ) ;
#29857 = CARTESIAN_POINT ( 'NONE',  ( 8.311093377946837890, 136.4062499965859843, -8.311093377946837890 ) ) ;
#29858 = CARTESIAN_POINT ( 'NONE',  ( -32.00000000000003553, 207.3125000027312126, 168.3431457505080857 ) ) ;
#29859 = CARTESIAN_POINT ( 'NONE',  ( 5.656854249492374365, 5.656854249492375253, 18.32405278432982243 ) ) ;
#29860 = CARTESIAN_POINT ( 'NONE',  ( 8.000000000000000000, 15.09375000000000711, -3.313708498984761164 ) ) ;
#29861 = CARTESIAN_POINT ( 'NONE',  ( -11.35316468749999963, 248.9062500034139873, 0.000000000000000000 ) ) ;
#29862 = CARTESIAN_POINT ( 'NONE',  ( -10.18810118749999738, -4.220049686691941915, 90.62500000204836681 ) ) ;
#29863 = ORIENTED_EDGE ( 'NONE', *, *, #58835, .F. ) ;
#29864 = DIRECTION ( 'NONE',  ( 0.000000000000000000, 0.000000000000000000, 1.000000000000000000 ) ) ;
#29865 = CARTESIAN_POINT ( 'NONE',  ( -4.000000000000001776, 8.500000000000000000, -4.898587196589415787E-16 ) ) ;
#29866 = CARTESIAN_POINT ( 'NONE',  ( -2.085542519210945728E-15, 94.84374999658601268, 11.35316468750000141 ) ) ;
#29867 = ADVANCED_FACE ( 'NONE', ( #36226 ), #55069, .F. ) ;
#29868 = CARTESIAN_POINT ( 'NONE',  ( -7.204075437095965206, -7.204075437095968759, 106.8437500020483810 ) ) ;
#29869 = CARTESIAN_POINT ( 'NONE',  ( 4.541265875000002339, 15.49999999863440614, -1.881053915767121776 ) ) ;
#29870 = EDGE_LOOP ( 'NONE', ( #23081, #6144 ) ) ;
#29871 = EDGE_LOOP ( 'NONE', ( #59456, #17215, #29290 ) ) ;
#29872 = CARTESIAN_POINT ( 'NONE',  ( -3.313708498984760720, 4.968750000000000888, -8.000000000000000000 ) ) ;
#29873 = PLANE ( 'NONE',  #26353 ) ;
#29874 = CARTESIAN_POINT ( 'NONE',  ( 7.188101187500000044, 3.468749997951610542, 0.000000000000000000 ) ) ;
#29875 = CARTESIAN_POINT ( 'NONE',  ( 3.313708498984765161, 119.6562500040968047, 7.999999999999998224 ) ) ;
#29876 = VECTOR ( 'NONE', #56869, 1000.000000000000000 ) ;
#29877 = CARTESIAN_POINT ( 'NONE',  ( 7.204075437095968759, -7.204075437095966983, 101.5937500020483668 ) ) ;
#29878 = CARTESIAN_POINT ( 'NONE',  ( 4.898587196589412829E-16, 6.375000000000000888, -8.000000000000000000 ) ) ;
#29879 = CARTESIAN_POINT ( 'NONE',  ( -4.000000000000001776, 15.18749999726881406, -1.656854249492381470 ) ) ;
#29880 = CARTESIAN_POINT ( 'NONE',  ( 11.00000000000000000, 1.347111479062088405E-15, 118.0000000000000000 ) ) ;
#29881 = ORIENTED_EDGE ( 'NONE', *, *, #52927, .F. ) ;
#29882 = CARTESIAN_POINT ( 'NONE',  ( -11.00000000000000000, 0.000000000000000000, 77.68750000409677625 ) ) ;
#29883 = CARTESIAN_POINT ( 'NONE',  ( 2.445694354108838731, 200.0625000013656063, 195.5543056458912190 ) ) ;
#29886 = CARTESIAN_POINT ( 'NONE',  ( -7.320508075688778149, 224.9999999931720254, 7.320508075688769267 ) ) ;
#29885 = CARTESIAN_POINT ( 'NONE',  ( -30.44569435410875968, 202.8125000013656063, 172.4456943541092642 ) ) ;
#29884 =( BOUNDED_CURVE ( )  B_SPLINE_CURVE ( 2, ( #14313, #37348, #2271, #60346, #31689, #59618, #42252, #25265, #8674 ),
 .UNSPECIFIED., .F., .F. ) 
 B_SPLINE_CURVE_WITH_KNOTS ( ( 3, 2, 2, 2, 3 ),
 ( 0.4666666666666670626, 0.4750000000000003664, 0.4833333333333337256, 0.4916666666666670849, 0.5000000000000004441 ),
 .UNSPECIFIED. ) 
 CURVE ( )  GEOMETRIC_REPRESENTATION_ITEM ( )  RATIONAL_B_SPLINE_CURVE ( ( 0.9999999999999964473, 0.9238795325112902912, 1.000000000000000000, 0.9238795325112867385, 1.000000000000000000, 0.9238795325112867385, 1.000000000000000000, 0.9238795325112826307, 1.000000000000003997 ) ) 
 REPRESENTATION_ITEM ( '' )  );
#29887 =( LENGTH_UNIT ( ) NAMED_UNIT ( * ) SI_UNIT ( .MILLI., .METRE. ) );
#29888 = CARTESIAN_POINT ( 'NONE',  ( -4.541265875000002339, 14.74999999863440969, -1.881053915767121998 ) ) ;
#29889 = CARTESIAN_POINT ( 'NONE',  ( -1.836970198721029983E-15, 200.6249999931720538, 10.00000000000000178 ) ) ;
#29890 = CARTESIAN_POINT ( 'NONE',  ( 7.188101187499991163, 2.977408999572648707, 12.83030278187175277 ) ) ;
#29891 = VERTEX_POINT ( 'NONE', #48637 ) ;
#29892 = ORIENTED_EDGE ( 'NONE', *, *, #570, .T. ) ;
#29893 = CARTESIAN_POINT ( 'NONE',  ( 4.220049686691934809, 10.18810118749999916, 103.1875000020483810 ) ) ;
#29894 = CARTESIAN_POINT ( 'NONE',  ( -4.999999999999999112, 98.33333333333332860, 8.660254037844376640 ) ) ;
#29895 = CARTESIAN_POINT ( 'NONE',  ( -27.99999999999995737, 204.5000000000000284, 174.0000000000003695 ) ) ;
#29896 = CARTESIAN_POINT ( 'NONE',  ( -1.432654583217607858, 201.6250000013656063, 201.4587341250000065 ) ) ;
#29897 = CARTESIAN_POINT ( 'NONE',  ( 31.45873412499999944, 194.6250000013656063, 171.4326545832175555 ) ) ;
#29898 = CARTESIAN_POINT ( 'NONE',  ( -5.000000000000005329, 98.33333333333334281, 8.660254037844387298 ) ) ;
#29899 = CARTESIAN_POINT ( 'NONE',  ( -3.313708498984762052, 117.2187500000000000, -8.000000000000000000 ) ) ;
#29900 = CARTESIAN_POINT ( 'NONE',  ( -11.35316468749999785, 63.38541666325269119, -3.042071309553167513 ) ) ;
#29901 = CARTESIAN_POINT ( 'NONE',  ( 2.765530957081996366, 296.2968750017070079, -6.676582343750003368 ) ) ;
#29902 = ORIENTED_EDGE ( 'NONE', *, *, #23555, .T. ) ;
#29903 = EDGE_CURVE ( 'NONE', #46734, #37508, #30097, .T. ) ;
#29904 = CARTESIAN_POINT ( 'NONE',  ( 7.320508075688803018, 190.6250000000000568, -7.320508075688803018 ) ) ;
#29905 = CARTESIAN_POINT ( 'NONE',  ( 3.313708498984762052, 13.59374999590322375, -8.000000000000000000 ) ) ;
#29906 = CARTESIAN_POINT ( 'NONE',  ( 3.458734124999959914, 208.4375000013656063, 142.0000000000000568 ) ) ;
#29907 = DIRECTION ( 'NONE',  ( -0.000000000000000000, 1.000000000000000000, -0.000000000000000000 ) ) ;
#29908 = CARTESIAN_POINT ( 'NONE',  ( 7.320508075688776373, 226.8749999999999716, 7.320508075688767491 ) ) ;
#29909 = CARTESIAN_POINT ( 'NONE',  ( -5.999999999999999112, 293.0624999999999432, 2.485281374238575314 ) ) ;
#29910 = CARTESIAN_POINT ( 'NONE',  ( -11.00000000000000000, 0.000000000000000000, 116.4999999999999858 ) ) ;
#29911 = CARTESIAN_POINT ( 'NONE',  ( 10.00000000000000000, 214.7916666666666572, 2.679491924311236062 ) ) ;
#29912 = CARTESIAN_POINT ( 'NONE',  ( 5.082755093536318824, 5.082755093536319713, 8.799052781871752771 ) ) ;
#29913 = CARTESIAN_POINT ( 'NONE',  ( -8.311093377946841443, 179.2187499965859843, 8.311093377946830785 ) ) ;
#29914 = CARTESIAN_POINT ( 'NONE',  ( 4.541265875000001451, 4.249999998634406140, 1.881053915767124440 ) ) ;
#29915 = CARTESIAN_POINT ( 'NONE',  ( 0.000000000000000000, 0.000000000000000000, 0.000000000000000000 ) ) ;
#29917 = CARTESIAN_POINT ( 'NONE',  ( 4.000000000000001776, 5.062500000000000888, -1.656854249492381248 ) ) ;
#29916 = CARTESIAN_POINT ( 'NONE',  ( -7.320508075688770155, 228.7500000068279746, 7.320508075688774596 ) ) ;
#29918 = VERTEX_POINT ( 'NONE', #13921 ) ;
#29919 = CARTESIAN_POINT ( 'NONE',  ( -3.458734125000016757, 208.1250000013656063, 140.5673454167824161 ) ) ;
#29920 = CARTESIAN_POINT ( 'NONE',  ( 8.311093377946837890, 41.71874999658601979, -8.311093377946837890 ) ) ;
#29921 = CARTESIAN_POINT ( 'NONE',  ( 7.778174593052021635, 7.778174593052023411, 107.1250000040967763 ) ) ;
#29922 = CARTESIAN_POINT ( 'NONE',  ( -2.085542519210945728E-15, 214.8437499965860411, 11.35316468750000141 ) ) ;
#29923 = CARTESIAN_POINT ( 'NONE',  ( -25.55430564589123321, 207.3125000013656063, 167.5543056458915032 ) ) ;
#29924 = CARTESIAN_POINT ( 'NONE',  ( -2.679491924311235174, 125.4166666598386968, 10.00000000000000000 ) ) ;
#29926 = CARTESIAN_POINT ( 'NONE',  ( -7.320508075688762162, 103.1249999999999858, 7.320508075688755056 ) ) ;
#29925 = CARTESIAN_POINT ( 'NONE',  ( 7.188101187500000044, 123.4062500020483810, -8.802885111219163269E-16 ) ) ;
#29928 = ADVANCED_FACE ( 'NONE', ( #26365 ), #53577, .F. ) ;
#29927 = DIRECTION ( 'NONE',  ( 0.000000000000000000, 1.000000000000000000, 0.000000000000000000 ) ) ;
#29929 = AXIS2_PLACEMENT_3D ( 'NONE', #42239, #30193, #53210 ) ;
#29930 = CARTESIAN_POINT ( 'NONE',  ( 10.00000000000000178, 81.87499999317203958, 0.000000000000000000 ) ) ;
#29931 = CARTESIAN_POINT ( 'NONE',  ( 2.977408999572650039, 96.68750000204836681, -7.188101187500001821 ) ) ;
#29932 = CARTESIAN_POINT ( 'NONE',  ( 1.881053915767122664, 18.24999999863440792, 4.541265875000001451 ) ) ;
#29933 = FACE_OUTER_BOUND ( 'NONE', #58972, .T. ) ;
#29934 = FACE_OUTER_BOUND ( 'NONE', #18211, .T. ) ;
#29935 = VERTEX_POINT ( 'NONE', #42237 ) ;
#29936 = EDGE_LOOP ( 'NONE', ( #64930, #64306, #61763, #72507 ) ) ;
#29937 = EDGE_CURVE ( 'NONE', #271, #29212, #50469, .T. ) ;
#29938 = CARTESIAN_POINT ( 'NONE',  ( -6.676582343750003368, 296.5468750017069510, -2.765530957081996810 ) ) ;
#29939 = DIRECTION ( 'NONE',  ( -1.000000000000000000, 0.000000000000000000, 0.000000000000000000 ) ) ;
#29940 = CARTESIAN_POINT ( 'NONE',  ( -9.000000000000000000, -5.196152422706648899, -0.8038475772933779684 ) ) ;
#29941 = CARTESIAN_POINT ( 'NONE',  ( 3.042071309553159519, 154.7395833299193555, 11.35316468750000141 ) ) ;
#29942 = CARTESIAN_POINT ( 'NONE',  ( -7.204075437095967871, 7.204075437095967871, 80.96875000204836681 ) ) ;
#29943 = CARTESIAN_POINT ( 'NONE',  ( 10.00000000000000355, 5.000000000000000888, 0.000000000000000000 ) ) ;
#29944 = VECTOR ( 'NONE', #3364, 1000.000000000000000 ) ;
#29945 = CARTESIAN_POINT ( 'NONE',  ( -3.999999999999959144, 203.0625000000000284, 199.6568542494924259 ) ) ;
#29946 = LINE ( 'NONE', #6201, #73559 ) ;
#29947 = CARTESIAN_POINT ( 'NONE',  ( 10.18810118750000093, -4.220049686691933921, 110.6875000020483952 ) ) ;
#29948 = ORIENTED_EDGE ( 'NONE', *, *, #50287, .T. ) ;
#29949 = AXIS2_PLACEMENT_3D ( 'NONE', #73155, #43731, #50140 ) ;
#29950 = LINE ( 'NONE', #69947, #26238 ) ;
#29951 = CARTESIAN_POINT ( 'NONE',  ( 0.000000000000000000, 125.0000000000000000, 0.000000000000000000 ) ) ;
#29952 = CARTESIAN_POINT ( 'NONE',  ( -9.832129032723420536, 144.0104166632526699, 5.676582343749997150 ) ) ;
#29953 = CARTESIAN_POINT ( 'NONE',  ( -3.458734124999959914, 197.4375000013655779, 198.0000000000000284 ) ) ;
#29954 = CARTESIAN_POINT ( 'NONE',  ( 1.469576158976823947E-15, 113.3750000000000000, 8.000000000000000000 ) ) ;
#29955 = CARTESIAN_POINT ( 'NONE',  ( 4.220049686691934809, 10.18810118749999916, 79.56250000204836681 ) ) ;
#29956 = CARTESIAN_POINT ( 'NONE',  ( 3.042071309553159519, 50.05208332991935549, 11.35316468750000141 ) ) ;
#29957 = EDGE_LOOP ( 'NONE', ( #9845, #45492, #28447, #68674 ) ) ;
#29958 = CARTESIAN_POINT ( 'NONE',  ( -8.660254037844394404, 27.91666666666667140, 5.000000000000001776 ) ) ;
#29959 = CARTESIAN_POINT ( 'NONE',  ( -1.881053915767121776, 3.749999998634407028, -4.541265875000002339 ) ) ;
#29960 = CARTESIAN_POINT ( 'NONE',  ( -5.662595241051933570, -5.662595241051936235, 13.20061528394063011 ) ) ;
#29961 = CARTESIAN_POINT ( 'NONE',  ( -2.977408999572654480, 17.99999999795161898, 7.188101187499999156 ) ) ;
#29962 = CARTESIAN_POINT ( 'NONE',  ( 6.000000000000003553, 291.5000000034140157, 2.485281374238571317 ) ) ;
#29963 = LINE ( 'NONE', #42747, #69062 ) ;
#29964 = CARTESIAN_POINT ( 'NONE',  ( -2.977408999572650039, 10.31249999795161010, -7.188101187500001821 ) ) ;
#29965 = CARTESIAN_POINT ( 'NONE',  ( 7.188101187499993827, -2.977408999572645598, 8.142802781871752771 ) ) ;
#29966 = CARTESIAN_POINT ( 'NONE',  ( -10.18810118749999738, -4.220049686691941915, 69.25000000204836681 ) ) ;
#29967 = CARTESIAN_POINT ( 'NONE',  ( -27.99999999999996447, 205.1875000013656063, 173.4587341250003760 ) ) ;
#29968 = CARTESIAN_POINT ( 'NONE',  ( 4.000000000000001776, 0.8124999972688135008, -1.656854249492381248 ) ) ;
#29969 = VERTEX_POINT ( 'NONE', #20717 ) ;
#29970 = EDGE_CURVE ( 'NONE', #13268, #22395, #43734, .T. ) ;
#29971 = CARTESIAN_POINT ( 'NONE',  ( 3.458734125000015425, 209.0000000013655779, 196.5673454167823877 ) ) ;
#29972 = CARTESIAN_POINT ( 'NONE',  ( -4.000000000000015987, 204.5000000000000284, 142.0000000000000568 ) ) ;
#29973 = CARTESIAN_POINT ( 'NONE',  ( -27.99999999999991118, 202.6250000027312126, 174.0000000000003695 ) ) ;
#29974 = CARTESIAN_POINT ( 'NONE',  ( -3.211159895383561391, 3.687499998634407028, -3.211159895383561835 ) ) ;
#29975 = CARTESIAN_POINT ( 'NONE',  ( -2.977408999572650927, 117.8750000020483810, -7.188101187500001821 ) ) ;
#29976 = DIRECTION ( 'NONE',  ( 0.000000000000000000, 0.000000000000000000, 1.000000000000000000 ) ) ;
#29977 = CARTESIAN_POINT ( 'NONE',  ( 5.656854249492374365, 5.656854249492375253, 3.455302783920144449 ) ) ;
#29978 = ORIENTED_EDGE ( 'NONE', *, *, #70378, .F. ) ;
#29979 = CARTESIAN_POINT ( 'NONE',  ( 7.188101187499999156, 25.87499999795161543, 2.977408999572654924 ) ) ;
#29980 = VERTEX_POINT ( 'NONE', #66748 ) ;
#29981 = DIRECTION ( 'NONE',  ( 0.000000000000000000, 0.000000000000000000, -1.000000000000000000 ) ) ;
#29982 = CARTESIAN_POINT ( 'NONE',  ( 7.999999999999998224, 13.40625000000000178, 3.313708498984766049 ) ) ;
#29983 = CARTESIAN_POINT ( 'NONE',  ( 31.45873412499999944, 207.6875000013656063, 169.9999999999998863 ) ) ;
#29984 = CARTESIAN_POINT ( 'NONE',  ( -10.00000000000000178, 52.50000000000000711, -1.224646799147353454E-15 ) ) ;
#29985 = AXIS2_PLACEMENT_3D ( 'NONE', #385, #69026, #68648 ) ;
#29986 = CARTESIAN_POINT ( 'NONE',  ( 7.188101187500001821, 98.37500000204840944, -2.977408999572651371 ) ) ;
#29987 = CARTESIAN_POINT ( 'NONE',  ( 3.999999999999959144, 205.1875000027312126, 140.3431457505076594 ) ) ;
#29989 = CARTESIAN_POINT ( 'NONE',  ( -20.06865579516544784, -33.26774268797971246, 193.6273222312369739 ) ) ;
#29988 = DIRECTION ( 'NONE',  ( 0.000000000000000000, 0.1266318867579376284, -0.9919497796038491133 ) ) ;
#29990 = VERTEX_POINT ( 'NONE', #49011 ) ;
#29991 = ORIENTED_EDGE ( 'NONE', *, *, #11324, .F. ) ;
#29992 = EDGE_CURVE ( 'NONE', #2415, #7053, #58214, .T. ) ;
#29993 = EDGE_CURVE ( 'NONE', #39701, #14809, #38377, .T. ) ;
#29994 = CARTESIAN_POINT ( 'NONE',  ( 8.311093377946839666, 250.7812500034139873, 8.311093377946829008 ) ) ;
#29995 = CARTESIAN_POINT ( 'NONE',  ( -7.188101187499990274, -2.977408999572651371, 16.95530278187175455 ) ) ;
#29996 = CARTESIAN_POINT ( 'NONE',  ( -8.000000000000000000, 14.15625000000000178, -3.313708498984762496 ) ) ;
#29997 = CARTESIAN_POINT ( 'NONE',  ( 0.000000000000000000, 201.0000000000000284, 170.0000000000000284 ) ) ;
#29998 = CARTESIAN_POINT ( 'NONE',  ( 1.656854249492229592, 196.9375000027311842, 146.0000000000001421 ) ) ;
#29999 = CARTESIAN_POINT ( 'NONE',  ( 7.320508075688771044, 258.1250000000000000, -7.320508075688771932 ) ) ;
#30000 = CARTESIAN_POINT ( 'NONE',  ( 2.679491924311228956, 202.9166666598387110, -10.00000000000000000 ) ) ;
#30001 =( BOUNDED_CURVE ( )  B_SPLINE_CURVE ( 2, ( #11905, #34938, #6257, #29261, #52273, #22093, #609, #44750, #67764 ),
 .UNSPECIFIED., .F., .F. ) 
 B_SPLINE_CURVE_WITH_KNOTS ( ( 3, 2, 2, 2, 3 ),
 ( 0.2333333333333335313, 0.2416666666666668628, 0.2500000000000002220, 0.2583333333333335813, 0.2666666666666668850 ),
 .UNSPECIFIED. ) 
 CURVE ( )  GEOMETRIC_REPRESENTATION_ITEM ( )  RATIONAL_B_SPLINE_CURVE ( ( 0.9999999999999982236, 0.9238795325112885148, 1.000000000000000000, 0.9238795325112867385, 1.000000000000000000, 0.9238795325112867385, 1.000000000000000000, 0.9238795325112847401, 1.000000000000001998 ) ) 
 REPRESENTATION_ITEM ( '' )  );
#30002 = CARTESIAN_POINT ( 'NONE',  ( 10.00000000000000178, 175.0000000000000284, 0.000000000000000000 ) ) ;
#30003 = CARTESIAN_POINT ( 'NONE',  ( 5.656854249492376141, -5.656854249492374365, 5.892802779823364645 ) ) ;
#30004 = CARTESIAN_POINT ( 'NONE',  ( -4.898587196589412829E-16, 91.62499999999998579, -8.000000000000000000 ) ) ;
#30005 = CARTESIAN_POINT ( 'NONE',  ( -2.977408999572647819, 7.188101187499992051, 27.08030278187175810 ) ) ;
#30006 = CARTESIAN_POINT ( 'NONE',  ( 11.35316468750000141, 146.0937499965860411, 0.000000000000000000 ) ) ;
#30007 = CARTESIAN_POINT ( 'NONE',  ( -4.556349186104045934, 11.00000000000000000, 75.90625000409677625 ) ) ;
#30008 = CARTESIAN_POINT ( 'NONE',  ( 5.000000000000001776, 27.70833332650536818, -8.660254037844389075 ) ) ;
#30011 = CARTESIAN_POINT ( 'NONE',  ( -10.00000000000000533, 167.7083333333333428, 2.679491924311223627 ) ) ;
#30010 = CARTESIAN_POINT ( 'NONE',  ( 8.000000000000000000, 110.8437500000000000, -3.313708498984762496 ) ) ;
#30009 = CARTESIAN_POINT ( 'NONE',  ( 32.00000000000000000, 205.2500000000000284, 169.9999999999999432 ) ) ;
#30012 = EDGE_LOOP ( 'NONE', ( #4925, #50931, #19190, #21438, #58781, #22158 ) ) ;
#30013 = ADVANCED_FACE ( 'NONE', ( #9325 ), #33111, .F. ) ;
#30014 = CARTESIAN_POINT ( 'NONE',  ( 4.193030820682221105, -60.66866849074666135, 23.17095654502632840 ) ) ;
#30015 = CARTESIAN_POINT ( 'NONE',  ( -26.34314575050758478, 209.5625000000000000, 174.0000000000003411 ) ) ;
#30016 = CARTESIAN_POINT ( 'NONE',  ( -3.295887129531270165, -7.292874925529289065, -0.000000000000000000 ) ) ;
#30017 = DIRECTION ( 'NONE',  ( 1.000000000000000000, 0.000000000000000000, 0.000000000000000000 ) ) ;
#30018 = CARTESIAN_POINT ( 'NONE',  ( 8.660254037844389075, 37.29166665983869677, -5.000000000000000000 ) ) ;
#30019 = CARTESIAN_POINT ( 'NONE',  ( -2.977408999572650927, 113.3750000020483810, -7.188101187500001821 ) ) ;
#30020 = CARTESIAN_POINT ( 'NONE',  ( -4.541265875000003227, 5.999999998634407028, 1.881053915767121110 ) ) ;
#30021 = CARTESIAN_POINT ( 'NONE',  ( 6.308070865130366300, 61.28915309316995774, -23.54949267154435688 ) ) ;
#30022 = CARTESIAN_POINT ( 'NONE',  ( 7.999999999999992895, -3.313708498984756279, 17.98655277982336642 ) ) ;
#30023 = CARTESIAN_POINT ( 'NONE',  ( -5.656854249492381470, 24.74999999590322375, 5.656854249492379694 ) ) ;
#30024 = VERTEX_POINT ( 'NONE', #11553 ) ;
#30025 = CARTESIAN_POINT ( 'NONE',  ( -6.123233995736766282E-16, 221.8750000068279746, -10.00000000000000000 ) ) ;
#30026 = CARTESIAN_POINT ( 'NONE',  ( -10.00003937256114028, 225.9999999999999716, 0.6562093533521827782 ) ) ;
#30027 = DIRECTION ( 'NONE',  ( 0.000000000000000000, 0.000000000000000000, -1.000000000000000000 ) ) ;
#30028 = CARTESIAN_POINT ( 'NONE',  ( -11.35316468749999785, 239.0104166700806445, -3.042071309553164848 ) ) ;
#30029 = CARTESIAN_POINT ( 'NONE',  ( -8.311093377946836114, 117.6562499965860269, -8.311093377946837890 ) ) ;
#30030 = ORIENTED_EDGE ( 'NONE', *, *, #41924, .T. ) ;
#30031 = CARTESIAN_POINT ( 'NONE',  ( -4.951871933616136978, 9.664417241377410761, 117.6512260359776150 ) ) ;
#30032 = CARTESIAN_POINT ( 'NONE',  ( 10.18810118749999916, 4.220049686691935698, 98.50000000204838102 ) ) ;
#30033 = CARTESIAN_POINT ( 'NONE',  ( 5.000000000000001776, 227.7083333265053966, -8.660254037844389075 ) ) ;
#30034 = CARTESIAN_POINT ( 'NONE',  ( -3.458734124999959469, 201.7500000013655779, 199.4326545832176691 ) ) ;
#30035 = CARTESIAN_POINT ( 'NONE',  ( 1.224646799147353256E-15, 0.000000000000000000, 10.00000000000000000 ) ) ;
#30037 = CARTESIAN_POINT ( 'NONE',  ( 5.676582343750001591, 116.6145833299193697, -9.832129032723420536 ) ) ;
#30036 = FACE_OUTER_BOUND ( 'NONE', #64565, .T. ) ;
#30038 = ADVANCED_FACE ( 'NONE', ( #17204 ), #64352, .F. ) ;
#30039 = CARTESIAN_POINT ( 'NONE',  ( 3.313708498984756279, 7.999999999999991118, 8.049052783920146226 ) ) ;
#30040 = CARTESIAN_POINT ( 'NONE',  ( -25.55430564589119058, 195.5625000013656063, 167.5543056458915316 ) ) ;
#30041 = CARTESIAN_POINT ( 'NONE',  ( 5.000000000000001776, 82.70833332650536818, -8.660254037844389075 ) ) ;
#30042 = VERTEX_POINT ( 'NONE', #12655 ) ;
#30043 = CARTESIAN_POINT ( 'NONE',  ( -8.660254037844390851, 189.7916666598387110, 4.999999999999998224 ) ) ;
#30044 = AXIS2_PLACEMENT_3D ( 'NONE', #46975, #59058, #54129 ) ;
#30045 = CARTESIAN_POINT ( 'NONE',  ( -7.778174593052020747, -7.778174593052023411, 73.18749999999998579 ) ) ;
#30046 = CARTESIAN_POINT ( 'NONE',  ( -11.00000000000021139, 4.556349186103834548, 83.59375000409677625 ) ) ;
#30047 = CARTESIAN_POINT ( 'NONE',  ( 8.311093377946834337, 95.46874999658601268, 8.311093377946839666 ) ) ;
#30048 = CARTESIAN_POINT ( 'NONE',  ( -4.721056650415998313, 287.5781250017069510, 4.721056650416000089 ) ) ;
#30049 = CARTESIAN_POINT ( 'NONE',  ( 2.977408999572650927, 13.12499999795161187, -7.188101187500000933 ) ) ;
#30050 = CARTESIAN_POINT ( 'NONE',  ( 7.204075437095968759, -7.204075437095966983, 95.59375000204838102 ) ) ;
#30051 = CARTESIAN_POINT ( 'NONE',  ( 3.042071309553159519, 10.05208332991935016, 11.35316468750000141 ) ) ;
#30052 = ORIENTED_EDGE ( 'NONE', *, *, #45656, .T. ) ;
#30053 = PLANE ( 'NONE',  #71746 ) ;
#30054 = CARTESIAN_POINT ( 'NONE',  ( 2.828427124746208943, 196.7500000027312126, 195.1715728752538439 ) ) ;
#30055 = CYLINDRICAL_SURFACE ( 'NONE', #39071, 8.000000000000000000 ) ;
#30056 = CARTESIAN_POINT ( 'NONE',  ( -10.18810118749999916, 0.000000000000000000, 80.03125000204836681 ) ) ;
#30057 = VECTOR ( 'NONE', #63248, 1000.000000000000000 ) ;
#30058 = CARTESIAN_POINT ( 'NONE',  ( 3.746198271157959336, 21.99999999999999289, 1.721400972335161761 ) ) ;
#30059 = CARTESIAN_POINT ( 'NONE',  ( -6.123233995736766282E-16, 263.7500000000000568, -10.00000000000000178 ) ) ;
#30060 = CARTESIAN_POINT ( 'NONE',  ( 4.721056650415999201, 294.0781250017069510, -4.721056650415999201 ) ) ;
#30061 = ORIENTED_EDGE ( 'NONE', *, *, #63840, .F. ) ;
#30062 = CARTESIAN_POINT ( 'NONE',  ( -1.836970198721029983E-15, 120.6249999931720396, 10.00000000000000178 ) ) ;
#30063 = CARTESIAN_POINT ( 'NONE',  ( 3.042071309553167513, 202.1354166632526983, -11.35316468749999785 ) ) ;
#30064 = CARTESIAN_POINT ( 'NONE',  ( 10.18810118749999916, 4.220049686691935698, 88.00000000204836681 ) ) ;
#30065 = CARTESIAN_POINT ( 'NONE',  ( -29.43265458321760519, 201.8750000013656063, 173.4587341250003760 ) ) ;
#30066 = CARTESIAN_POINT ( 'NONE',  ( -5.656854249492379694, 21.56250000000000355, -5.656854249492380582 ) ) ;
#30067 = EDGE_LOOP ( 'NONE', ( #55150, #9747, #69140, #47964 ) ) ;
#30068 = CARTESIAN_POINT ( 'NONE',  ( -23.99999999999996447, 207.8125000027312410, 171.6568542494926817 ) ) ;
#30069 = CARTESIAN_POINT ( 'NONE',  ( 2.751064625579944321E-14, 206.8750000027312126, 194.0000000000000568 ) ) ;
#30070 = CARTESIAN_POINT ( 'NONE',  ( 10.00000000000000178, 30.20833333333333570, -2.679491924311226736 ) ) ;
#30071 = CARTESIAN_POINT ( 'NONE',  ( -5.000000000000000000, 14.13320814749880583, 69.81894086168458102 ) ) ;
#30072 = CARTESIAN_POINT ( 'NONE',  ( -4.220049686691937474, -10.18810118749999738, 77.31250000204836681 ) ) ;
#30073 = ORIENTED_EDGE ( 'NONE', *, *, #59311, .F. ) ;
#30074 = CARTESIAN_POINT ( 'NONE',  ( -7.188101187500000933, 7.124999997951611874, -2.977408999572651371 ) ) ;
#30075 = CARTESIAN_POINT ( 'NONE',  ( 10.99999999999992006, -4.556349186104122317, 112.6562499999999716 ) ) ;
#30076 =( NAMED_UNIT ( * ) SI_UNIT ( $, .STERADIAN. ) SOLID_ANGLE_UNIT ( ) );
#30077 = CARTESIAN_POINT ( 'NONE',  ( 7.188101187500000044, 120.7812500020483810, -8.802885111219163269E-16 ) ) ;
#30078 = CARTESIAN_POINT ( 'NONE',  ( -2.295000000000000373, 272.8559999999997672, 5.415577408909600265 ) ) ;
#30079 = CARTESIAN_POINT ( 'NONE',  ( -2.765530957081996810, 295.2656250017070079, -6.676582343750002480 ) ) ;
#30081 = CARTESIAN_POINT ( 'NONE',  ( 2.679491924311222739, 135.8333333265053682, 10.00000000000000355 ) ) ;
#30080 = CARTESIAN_POINT ( 'NONE',  ( -3.042071309553159075, 234.9479166700806445, 11.35316468749999963 ) ) ;
#30082 = ORIENTED_EDGE ( 'NONE', *, *, #62191, .T. ) ;
#30084 = VECTOR ( 'NONE', #12485, 1000.000000000000000 ) ;
#30083 = CARTESIAN_POINT ( 'NONE',  ( -8.311093377946834337, 234.8437500034139305, 8.311093377946837890 ) ) ;
#30085 = CARTESIAN_POINT ( 'NONE',  ( -5.082755093536319713, 5.082755093536319713, 4.299052781871752771 ) ) ;
#30086 = CARTESIAN_POINT ( 'NONE',  ( 1.432654583217662481, 205.3750000013656063, 194.5412658750000219 ) ) ;
#30087 = ORIENTED_EDGE ( 'NONE', *, *, #73944, .T. ) ;
#30088 = CARTESIAN_POINT ( 'NONE',  ( 5.656854249492381470, 104.7500000040967905, 5.656854249492379694 ) ) ;
#30089 = CARTESIAN_POINT ( 'NONE',  ( 11.35316468749999963, 96.30208332991934128, -3.042071309553165293 ) ) ;
#30090 = CARTESIAN_POINT ( 'NONE',  ( -10.00000000000000000, 122.5000000000000284, -1.224646799147353059E-15 ) ) ;
#30091 = CARTESIAN_POINT ( 'NONE',  ( -4.556349186104047710, -10.99999999999999822, 79.28124999999998579 ) ) ;
#30094 = CARTESIAN_POINT ( 'NONE',  ( -8.000000000000000000, 2.250000000000000444, -9.797174393178825657E-16 ) ) ;
#30093 = CARTESIAN_POINT ( 'NONE',  ( 29.43265458321761230, 203.8750000013656063, 166.5412658749999650 ) ) ;
#30092 = CARTESIAN_POINT ( 'NONE',  ( 24.54126587499998280, 204.5000000013656063, 171.4326545832175555 ) ) ;
#30095 =( BOUNDED_CURVE ( )  B_SPLINE_CURVE ( 2, ( #15807, #50151, #62958, #34314, #50516, #44128, #67138, #51266, #44871 ),
 .UNSPECIFIED., .F., .F. ) 
 B_SPLINE_CURVE_WITH_KNOTS ( ( 3, 2, 2, 2, 3 ),
 ( 0.7916666666666667407, 0.7986111111111111605, 0.8055555555555555802, 0.8124999999999998890, 0.8194444444444443088 ),
 .UNSPECIFIED. ) 
 CURVE ( )  GEOMETRIC_REPRESENTATION_ITEM ( )  RATIONAL_B_SPLINE_CURVE ( ( 0.9999999999999987788, 0.9238795325112879597, 1.000000000000000000, 0.9238795325112867385, 1.000000000000000000, 0.9238795325112867385, 1.000000000000000000, 0.9238795325112879597, 0.9999999999999987788 ) ) 
 REPRESENTATION_ITEM ( '' )  );
#30096 = ORIENTED_EDGE ( 'NONE', *, *, #48158, .F. ) ;
#30097 = CIRCLE ( 'NONE', #9647, 8.000000000000000000 ) ;
#30098 = ADVANCED_FACE ( 'NONE', ( #39850 ), #40798, .F. ) ;
#30099 = CARTESIAN_POINT ( 'NONE',  ( -25.17157287525385456, 196.0000000027312126, 167.1715728752541281 ) ) ;
#30100 = CARTESIAN_POINT ( 'NONE',  ( -2.775557561562891351E-14, 210.0000000000000284, 142.0000000000000568 ) ) ;
#30101 = CARTESIAN_POINT ( 'NONE',  ( -5.676582343749998039, 212.4479166632526983, -9.832129032723420536 ) ) ;
#30103 = ADVANCED_FACE ( 'NONE', ( #42064 ), #42435, .T. ) ;
#30102 = CARTESIAN_POINT ( 'NONE',  ( 2.445694354108783664, 204.3125000013656063, 144.4456943541088663 ) ) ;
#30104 = CARTESIAN_POINT ( 'NONE',  ( 25.55430564589115505, 207.5625000013656063, 172.4456943541086957 ) ) ;
#30105 = CARTESIAN_POINT ( 'NONE',  ( 2.977408999572651815, 23.06249999795161187, 7.188101187500000933 ) ) ;
#30106 = CARTESIAN_POINT ( 'NONE',  ( -5.676582343750006032, 184.4270833299193555, 9.832129032723418760 ) ) ;
#30107 = CARTESIAN_POINT ( 'NONE',  ( 2.977408999572650039, 95.56250000204838102, -7.188101187500000933 ) ) ;
#30108 = DIRECTION ( 'NONE',  ( -0.000000000000000000, 1.000000000000000000, -4.476705744456276341E-16 ) ) ;
#30109 = CARTESIAN_POINT ( 'NONE',  ( -25.17157287525381903, 197.8750000000000284, 167.1715728752541565 ) ) ;
#30110 = CARTESIAN_POINT ( 'NONE',  ( -4.541265875000002339, 9.749999998634406140, -1.881053915767121998 ) ) ;
#30111 = CARTESIAN_POINT ( 'NONE',  ( 27.99999999999996447, 201.6875000013656063, 173.4587341249998929 ) ) ;
#30112 = CARTESIAN_POINT ( 'NONE',  ( -7.188101187499991163, 2.977408999572646930, 3.267802781871751439 ) ) ;
#30113 = CARTESIAN_POINT ( 'NONE',  ( 5.676582343750001591, 66.61458332991935549, -9.832129032723420536 ) ) ;
#30114 = LINE ( 'NONE', #6377, #37585 ) ;
#30115 = DIRECTION ( 'NONE',  ( 0.000000000000000000, 0.000000000000000000, 1.000000000000000000 ) ) ;
#30116 = VERTEX_POINT ( 'NONE', #18701 ) ;
#30117 = CARTESIAN_POINT ( 'NONE',  ( -10.00000000000002842, 47.50000000000001421, -1.224646799147356412E-15 ) ) ;
#30118 = CARTESIAN_POINT ( 'NONE',  ( -7.778174593052023411, 7.778174593052023411, 67.00000000409676204 ) ) ;
#30119 = CARTESIAN_POINT ( 'NONE',  ( 11.35316468750000141, 75.78124999658602690, 0.000000000000000000 ) ) ;
#30120 = CARTESIAN_POINT ( 'NONE',  ( -7.778174593052023411, 7.778174593052023411, 71.50000000409677625 ) ) ;
#30121 = CARTESIAN_POINT ( 'NONE',  ( 2.445694354108783219, 195.8125000013656063, 139.5543056458912190 ) ) ;
#30122 = CARTESIAN_POINT ( 'NONE',  ( -31.05906957182392958, -34.87773535871937014, 167.9999999999998010 ) ) ;
#30124 = CARTESIAN_POINT ( 'NONE',  ( -5.676582343749998039, 77.44791666325269830, -9.832129032723420536 ) ) ;
#30123 = DIRECTION ( 'NONE',  ( 0.000000000000000000, 0.000000000000000000, 1.000000000000000000 ) ) ;
#30125 = EDGE_CURVE ( 'NONE', #71597, #70510, #6650, .T. ) ;
#30126 = CARTESIAN_POINT ( 'NONE',  ( 1.469576158976822172E-15, -7.999999999999991118, 23.89280278392014978 ) ) ;
#30127 = FACE_OUTER_BOUND ( 'NONE', #29020, .T. ) ;
#30128 =( BOUNDED_CURVE ( )  B_SPLINE_CURVE ( 2, ( #888, #28420, #23873, #68043, #16334, #39372, #62368, #10698, #33731 ),
 .UNSPECIFIED., .F., .F. ) 
 B_SPLINE_CURVE_WITH_KNOTS ( ( 3, 2, 2, 2, 3 ),
 ( 0.4305555555555555802, 0.4375000000000000000, 0.4444444444444444753, 0.4513888888888889506, 0.4583333333333334259 ),
 .UNSPECIFIED. ) 
 CURVE ( )  GEOMETRIC_REPRESENTATION_ITEM ( )  RATIONAL_B_SPLINE_CURVE ( ( 1.000000000000000000, 0.9238795325112867385, 1.000000000000000000, 0.9238795325112867385, 1.000000000000000000, 0.9238795325112867385, 1.000000000000000000, 0.9238795325112855172, 1.000000000000001110 ) ) 
 REPRESENTATION_ITEM ( '' )  );
#30129 = CARTESIAN_POINT ( 'NONE',  ( -10.00000000000000000, 159.1666666598386541, -2.679491924311229845 ) ) ;
#30130 = CARTESIAN_POINT ( 'NONE',  ( -7.188101187500000044, 97.53125000204838102, 0.000000000000000000 ) ) ;
#30131 = CARTESIAN_POINT ( 'NONE',  ( 6.123233995736767268E-16, 53.12499999317203958, -10.00000000000000178 ) ) ;
#30132 = CARTESIAN_POINT ( 'NONE',  ( 5.676582343750001591, 46.92708332991934839, -9.832129032723420536 ) ) ;
#30133 = CARTESIAN_POINT ( 'NONE',  ( -7.204075437095965206, -7.204075437095968759, 114.7187500020483810 ) ) ;
#30134 = CARTESIAN_POINT ( 'NONE',  ( -3.042071309553164404, 197.2395833299193555, -11.35316468749999963 ) ) ;
#30135 = VERTEX_POINT ( 'NONE', #13385 ) ;
#30136 = CARTESIAN_POINT ( 'NONE',  ( 28.00000000000002132, 207.5000000000000284, 165.9999999999998863 ) ) ;
#30137 = CARTESIAN_POINT ( 'NONE',  ( -24.00000000000002487, 198.9375000027312126, 168.3431457505079152 ) ) ;
#30138 = CARTESIAN_POINT ( 'NONE',  ( 7.320508075688771044, 161.2499999931720538, 7.320508075688775484 ) ) ;
#30140 = CARTESIAN_POINT ( 'NONE',  ( 6.951808397369818766E-16, 177.0312499965860411, -11.35316468750000141 ) ) ;
#30139 = CARTESIAN_POINT ( 'NONE',  ( 0.000000000000000000, 125.0000000000000000, 8.000000000000000000 ) ) ;
#30141 = CARTESIAN_POINT ( 'NONE',  ( 4.000000000000001776, 21.81249999726881583, -1.656854249492381248 ) ) ;
#30142 = CARTESIAN_POINT ( 'NONE',  ( -9.999999999999998224, 253.3333333401613174, 2.679491924311235618 ) ) ;
#30143 = CARTESIAN_POINT ( 'NONE',  ( -3.313708498984759387, -7.999999999999989342, 11.79905278392014623 ) ) ;
#30144 = ORIENTED_EDGE ( 'NONE', *, *, #27268, .T. ) ;
#30145 = CARTESIAN_POINT ( 'NONE',  ( -9.832129032723420536, 174.0104166632526983, 5.676582343749997150 ) ) ;
#30146 = AXIS2_PLACEMENT_3D ( 'NONE', #8744, #37796, #60792 ) ;
#30147 = SHAPE_REPRESENTATION ( 'screw', ( #57354 ), #58583 ) ;
#30148 = CARTESIAN_POINT ( 'NONE',  ( 5.082755093536320601, -5.082755093536318824, 24.54905278187175810 ) ) ;
#30149 = VECTOR ( 'NONE', #72875, 1000.000000000000000 ) ;
#30150 = VERTEX_POINT ( 'NONE', #47360 ) ;
#30151 = CARTESIAN_POINT ( 'NONE',  ( 3.313708498984765161, 101.6562500040968047, 7.999999999999998224 ) ) ;
#30152 = CARTESIAN_POINT ( 'NONE',  ( -4.000000000000001776, 12.50000000000000000, -4.898587196589415787E-16 ) ) ;
#30153 = DIRECTION ( 'NONE',  ( -1.000000000000000000, -0.000000000000000000, -0.000000000000000000 ) ) ;
#30154 = CARTESIAN_POINT ( 'NONE',  ( -3.211159895383561391, 11.68749999863440614, -3.211159895383561835 ) ) ;
#30155 = CARTESIAN_POINT ( 'NONE',  ( 5.656854249492374365, 5.656854249492375253, 18.45530278392014623 ) ) ;
#30156 = CARTESIAN_POINT ( 'NONE',  ( -2.828427124746208943, 195.6250000000000284, 144.8284271247462129 ) ) ;
#30157 = ORIENTED_EDGE ( 'NONE', *, *, #20328, .T. ) ;
#30158 = CARTESIAN_POINT ( 'NONE',  ( 3.999999999999959144, 205.0625000000000568, 140.3431457505076594 ) ) ;
#30159 = CARTESIAN_POINT ( 'NONE',  ( 7.188101187500000044, 97.90625000204838102, -8.802885111219163269E-16 ) ) ;
#30162 = AXIS2_PLACEMENT_3D ( 'NONE', #50957, #5319, #37507 ) ;
#30161 = CARTESIAN_POINT ( 'NONE',  ( -26.34314575050765939, 205.0625000027312126, 166.0000000000003695 ) ) ;
#30160 = CARTESIAN_POINT ( 'NONE',  ( 1.656854249492287101, 196.3125000000000000, 202.0000000000001137 ) ) ;
#30163 =( NAMED_UNIT ( * ) PLANE_ANGLE_UNIT ( ) SI_UNIT ( $, .RADIAN. ) );
#30164 = ORIENTED_EDGE ( 'NONE', *, *, #59906, .F. ) ;
#30165 = CARTESIAN_POINT ( 'NONE',  ( 2.219371606097434224, 16.40787039054625041, -68.79427927095591144 ) ) ;
#30166 = LINE ( 'NONE', #74052, #27713 ) ;
#30167 = CARTESIAN_POINT ( 'NONE',  ( -5.082755093536319713, 5.082755093536319713, 26.79905278187175455 ) ) ;
#30168 = ORIENTED_EDGE ( 'NONE', *, *, #26613, .F. ) ;
#30169 = B_SPLINE_CURVE_WITH_KNOTS ( 'NONE', 3,
 ( #42254, #6828, #36609, #65266, #23806, #46809, #70568, #69833 ),
 .UNSPECIFIED., .F., .F.,
 ( 4, 2, 2, 4 ),
 ( 0.01936970057594189498, 0.02112296051615078496, 0.02287622045635967841, 0.02638274033677746183 ),
 .UNSPECIFIED. ) ;
#30170 = VERTEX_POINT ( 'NONE', #41708 ) ;
#30171 = CARTESIAN_POINT ( 'NONE',  ( 1.871523826299183495E-15, -10.18810118749999916, 89.03125000204836681 ) ) ;
#30172 = CARTESIAN_POINT ( 'NONE',  ( -27.99999999999996092, 197.1875000013655779, 173.4587341250003760 ) ) ;
#30173 = CARTESIAN_POINT ( 'NONE',  ( -4.556349186104047710, -10.99999999999999822, 101.7812499999999858 ) ) ;
#30176 = CARTESIAN_POINT ( 'NONE',  ( -6.676582343750001591, 298.6093750017069510, 0.000000000000000000 ) ) ;
#30175 = CARTESIAN_POINT ( 'NONE',  ( 26.34314575050763807, 203.0625000027311842, 173.9999999999999147 ) ) ;
#30174 = LINE ( 'NONE', #70900, #19350 ) ;
#30177 = CARTESIAN_POINT ( 'NONE',  ( 5.000000000000001776, 130.8333333333333428, -8.660254037844389075 ) ) ;
#30178 = DIRECTION ( 'NONE',  ( 0.000000000000000000, -0.000000000000000000, -1.000000000000000000 ) ) ;
#30179 = DIRECTION ( 'NONE',  ( 0.000000000000000000, 0.000000000000000000, 1.000000000000000000 ) ) ;
#30180 = CARTESIAN_POINT ( 'NONE',  ( -7.999999999999991118, 0.000000000000000000, 15.83030277982336642 ) ) ;
#30181 = EDGE_CURVE ( 'NONE', #7590, #38509, #40808, .T. ) ;
#30182 = VECTOR ( 'NONE', #28327, 1000.000000000000000 ) ;
#30183 = CARTESIAN_POINT ( 'NONE',  ( 25.55430564589119413, 202.0625000013656063, 167.5543056458910485 ) ) ;
#30184 = CARTESIAN_POINT ( 'NONE',  ( 4.401442555609581635E-16, 7.218749997951610986, -7.188101187500000044 ) ) ;
#30185 = CARTESIAN_POINT ( 'NONE',  ( 1.471067592899761672E-15, -8.008118988124991233, 1.388115283940630107 ) ) ;
#30186 = CARTESIAN_POINT ( 'NONE',  ( 3.458734124999959914, 195.3750000013656063, 143.4326545832176976 ) ) ;
#30187 = CARTESIAN_POINT ( 'NONE',  ( 1.320432766682874540E-15, 117.4062500020483810, 7.188101187500000044 ) ) ;
#30189 = CARTESIAN_POINT ( 'NONE',  ( -9.999999999999998224, 132.2916666666666572, -2.679491924311230289 ) ) ;
#30188 = CARTESIAN_POINT ( 'NONE',  ( -30.99999999999992895, -31.99999999999978684, 205.0000000000000284 ) ) ;
#30190 = CARTESIAN_POINT ( 'NONE',  ( -8.311093377946834337, 229.8437500034140157, 8.311093377946837890 ) ) ;
#30191 = DIRECTION ( 'NONE',  ( -0.000000000000000000, -1.000000000000000000, -0.000000000000000000 ) ) ;
#30192 = CARTESIAN_POINT ( 'NONE',  ( -5.082755093536319713, 5.082755093536319713, 22.67405278187175455 ) ) ;
#30193 = DIRECTION ( 'NONE',  ( -0.000000000000000000, 1.000000000000000000, -0.000000000000000000 ) ) ;
#30194 = CARTESIAN_POINT ( 'NONE',  ( -11.35316468750000141, 33.48958332991934128, 3.042071309553159963 ) ) ;
#30195 = CARTESIAN_POINT ( 'NONE',  ( -47.32259252271279593, 272.0000000000000000, 65.76194439203463560 ) ) ;
#30196 = CARTESIAN_POINT ( 'NONE',  ( 3.042071309553159519, 215.0520833299193555, 11.35316468750000141 ) ) ;
#30197 = DIRECTION ( 'NONE',  ( 0.000000000000000000, -0.000000000000000000, -1.000000000000000000 ) ) ;
#30198 = ORIENTED_EDGE ( 'NONE', *, *, #40727, .F. ) ;
#30199 = CARTESIAN_POINT ( 'NONE',  ( -2.445694354108839175, 195.3125000013656063, 144.4456943541088663 ) ) ;
#30200 = CARTESIAN_POINT ( 'NONE',  ( 5.676582343750001591, 36.61458332991934839, -9.832129032723420536 ) ) ;
#30201 = CARTESIAN_POINT ( 'NONE',  ( -4.556349186104047710, -10.99999999999999822, 85.46875000409677625 ) ) ;
#30202 = CARTESIAN_POINT ( 'NONE',  ( -3.458734125000015425, 207.2500000013655779, 143.4326545832176976 ) ) ;
#30204 = CIRCLE ( 'NONE', #71160, 20.00000000000001066 ) ;
#30203 = CARTESIAN_POINT ( 'NONE',  ( -29.62416036582309431, 194.5118150472866034, 166.7327716576058663 ) ) ;
#30205 = CARTESIAN_POINT ( 'NONE',  ( -11.00000000000005151, 4.556349186103993532, 101.4062500000000000 ) ) ;
#30207 = CARTESIAN_POINT ( 'NONE',  ( 5.676582343749993598, 19.94791666325268409, 9.832129032723422313 ) ) ;
#30206 = CARTESIAN_POINT ( 'NONE',  ( -4.401442555609581635E-16, 102.7812500020483810, -7.188101187500000044 ) ) ;
#30208 = CARTESIAN_POINT ( 'NONE',  ( -5.656854249492375253, 5.656854249492375253, 14.14280277982336465 ) ) ;
#30209 = CARTESIAN_POINT ( 'NONE',  ( 3.042071309553167069, 146.8229166632527267, -11.35316468749999785 ) ) ;
#30210 = EDGE_CURVE ( 'NONE', #42385, #69514, #65886, .T. ) ;
#30211 = CARTESIAN_POINT ( 'NONE',  ( -8.660254037844387298, 113.9583333265053682, -5.000000000000004441 ) ) ;
#30212 = CARTESIAN_POINT ( 'NONE',  ( -7.188101187499999156, 117.1250000020483952, 2.977408999572654924 ) ) ;
#30213 = DIRECTION ( 'NONE',  ( -1.000000000000000000, 1.776356839400250465E-15, 0.000000000000000000 ) ) ;
#30214 = CARTESIAN_POINT ( 'NONE',  ( -27.99999999999996803, 206.1875000013656063, 173.4587341250003760 ) ) ;
#30215 = ORIENTED_EDGE ( 'NONE', *, *, #64194, .F. ) ;
#30216 = CARTESIAN_POINT ( 'NONE',  ( -8.311093377946841443, 9.218749996586016238, 8.311093377946834337 ) ) ;
#30217 =( BOUNDED_CURVE ( )  B_SPLINE_CURVE ( 2, ( #73354, #26948, #21287, #15249, #72981, #56379, #29563, #40137, #52574, #6187, #68803, #74094, #40883 ),
 .UNSPECIFIED., .F., .F. ) 
 B_SPLINE_CURVE_WITH_KNOTS ( ( 3, 2, 2, 2, 2, 2, 3 ),
 ( 0.6750949594983258750, 0.6803281766356090721, 0.6855613937728922691, 0.6907946109101755772, 0.6960278280474587742, 0.7012610451847419712, 0.7064942623220252793 ),
 .UNSPECIFIED. ) 
 CURVE ( )  GEOMETRIC_REPRESENTATION_ITEM ( )  RATIONAL_B_SPLINE_CURVE ( ( 1.000000000000013545, 0.9659258262890547675, 1.000000000000000000, 0.9659258262890683122, 1.000000000000000000, 0.9659258262890683122, 1.000000000000000000, 0.9659258262890683122, 1.000000000000000000, 0.9659258262890683122, 1.000000000000000000, 0.9659258262890683122, 1.000000000000000000 ) ) 
 REPRESENTATION_ITEM ( '' )  );
#30218 = EDGE_CURVE ( 'NONE', #30602, #26622, #59801, .T. ) ;
#30219 = VERTEX_POINT ( 'NONE', #67699 ) ;
#30220 = CARTESIAN_POINT ( 'NONE',  ( 2.485281374238858643, 289.3125000000000000, 5.999999999999716671 ) ) ;
#30222 = CARTESIAN_POINT ( 'NONE',  ( -9.832129032723418760, 137.8645833299193555, -5.676582343750004256 ) ) ;
#30221 = CARTESIAN_POINT ( 'NONE',  ( -3.313708498984815343, 108.2187499999999858, -7.999999999999944933 ) ) ;
#30223 = CYLINDRICAL_SURFACE ( 'NONE', #15820, 10.00000000000000178 ) ;
#30224 = CARTESIAN_POINT ( 'NONE',  ( 3.313708498984756279, 7.999999999999991118, 16.91780278432982243 ) ) ;
#30225 = CARTESIAN_POINT ( 'NONE',  ( 61.41514572949041195, 222.7647159382047448, 45.51486146420612044 ) ) ;
#30226 = CARTESIAN_POINT ( 'NONE',  ( -3.042071309553159075, 249.9479166700806729, 11.35316468749999963 ) ) ;
#30227 = CARTESIAN_POINT ( 'NONE',  ( 4.220049686691934809, 10.18810118749999916, 93.06250000204839523 ) ) ;
#30228 = ORIENTED_EDGE ( 'NONE', *, *, #53092, .T. ) ;
#30229 = EDGE_CURVE ( 'NONE', #53439, #40870, #46943, .T. ) ;
#30230 = CYLINDRICAL_SURFACE ( 'NONE', #59426, 10.00000000000000178 ) ;
#30231 = CARTESIAN_POINT ( 'NONE',  ( -1.656854249492381248, 8.312500000000000000, -4.000000000000001776 ) ) ;
#30232 = CARTESIAN_POINT ( 'NONE',  ( 9.832129032723420536, 86.51041666325268409, -5.676582343749999815 ) ) ;
#30233 = CARTESIAN_POINT ( 'NONE',  ( -4.220049686691937474, -10.18810118749999738, 102.4375000020483810 ) ) ;
#30234 =( BOUNDED_CURVE ( )  B_SPLINE_CURVE ( 2, ( #44371, #34183, #35298, #51140, #57185, #6251, #29254, #46225, #5876 ),
 .UNSPECIFIED., .F., .F. ) 
 B_SPLINE_CURVE_WITH_KNOTS ( ( 3, 2, 2, 2, 3 ),
 ( 0.7812500000000001110, 0.7864583333333334814, 0.7916666666666667407, 0.7968750000000001110, 0.8020833333333334814 ),
 .UNSPECIFIED. ) 
 CURVE ( )  GEOMETRIC_REPRESENTATION_ITEM ( )  RATIONAL_B_SPLINE_CURVE ( ( 0.9999999999999983347, 0.9238795325112884038, 1.000000000000000000, 0.9238795325112867385, 1.000000000000000000, 0.9238795325112867385, 1.000000000000000000, 0.9238795325112850731, 1.000000000000001554 ) ) 
 REPRESENTATION_ITEM ( '' )  );
#30235 = CARTESIAN_POINT ( 'NONE',  ( -8.342170076843785083E-16, 16.18749999863440436, 4.541265875000002339 ) ) ;
#30236 = ORIENTED_EDGE ( 'NONE', *, *, #10370, .T. ) ;
#30237 = ORIENTED_EDGE ( 'NONE', *, *, #47632, .F. ) ;
#30238 = CARTESIAN_POINT ( 'NONE',  ( 8.000000000000000000, 6.000000000000000888, 0.000000000000000000 ) ) ;
#30239 = CARTESIAN_POINT ( 'NONE',  ( -27.99999999999995737, 203.5000000000000000, 174.0000000000003695 ) ) ;
#30240 = CARTESIAN_POINT ( 'NONE',  ( -7.188101187500001821, 1.124999997951610098, -2.977408999572651371 ) ) ;
#30241 = CARTESIAN_POINT ( 'NONE',  ( -5.656854249492380582, 123.5000000040967905, -5.656854249492380582 ) ) ;
#30242 = CARTESIAN_POINT ( 'NONE',  ( 10.18810118749999916, 4.220049686691935698, 95.87500000204838102 ) ) ;
#30243 = CYLINDRICAL_SURFACE ( 'NONE', #10180, 8.000000000000000000 ) ;
#30244 = CARTESIAN_POINT ( 'NONE',  ( -2.828427124746190735, 16.12499999726881228, -2.828427124746191623 ) ) ;
#30245 = CARTESIAN_POINT ( 'NONE',  ( 27.99999999999999289, 191.0000000000000284, 169.9999999999999147 ) ) ;
#30246 = ORIENTED_EDGE ( 'NONE', *, *, #47975, .T. ) ;
#30247 = ADVANCED_FACE ( 'NONE', ( #38662 ), #8862, .T. ) ;
#30248 = B_SPLINE_CURVE_WITH_KNOTS ( 'NONE', 3,
 ( #39085, #73411, #4760, #43615, #62090, #49655, #8921, #15306 ),
 .UNSPECIFIED., .F., .F.,
 ( 4, 2, 2, 4 ),
 ( 0.01854123755286043312, 0.02116956588062352679, 0.02379789420838662392, 0.02905455086391281472 ),
 .UNSPECIFIED. ) ;
#30249 = CARTESIAN_POINT ( 'NONE',  ( 3.458734124999959914, 208.4375000013656063, 142.0000000000000568 ) ) ;
#30250 = CARTESIAN_POINT ( 'NONE',  ( -1.432654583217607858, 200.6250000013655779, 201.4587341250000065 ) ) ;
#30251 = VECTOR ( 'NONE', #37166, 1000.000000000000000 ) ;
#30252 = EDGE_CURVE ( 'NONE', #36674, #33382, #61288, .T. ) ;
#30254 = CYLINDRICAL_SURFACE ( 'NONE', #23750, 8.000000000000000000 ) ;
#30253 = CARTESIAN_POINT ( 'NONE',  ( -24.54126587499999346, 200.1875000013656063, 170.0000000000002842 ) ) ;
#30255 = SHAPE_REPRESENTATION_RELATIONSHIP ( 'NONE' , 'NONE' ,  #5031, #54364 ) ;
#30256 = CARTESIAN_POINT ( 'NONE',  ( -1.881053915767121554, 13.62499999863440792, -4.541265875000002339 ) ) ;
#30257 = CARTESIAN_POINT ( 'NONE',  ( 1.656854249492356157, 12.18749999999999645, -4.000000000000026645 ) ) ;
#30258 = CIRCLE ( 'NONE', #41141, 5.099999999999999645 ) ;
#30259 = CARTESIAN_POINT ( 'NONE',  ( 7.188101187499993827, -2.977408999572645598, 12.64280278187175277 ) ) ;
#30260 = ORIENTED_EDGE ( 'NONE', *, *, #13052, .T. ) ;
#30261 = EDGE_CURVE ( 'NONE', #28748, #46215, #9615, .T. ) ;
#30262 = ORIENTED_EDGE ( 'NONE', *, *, #6641, .T. ) ;
#30263 = CARTESIAN_POINT ( 'NONE',  ( 10.18810118750000093, -4.220049686691933033, 104.3125000020483810 ) ) ;
#30264 = LINE ( 'NONE', #64224, #11148 ) ;
#30265 = AXIS2_PLACEMENT_3D ( 'NONE', #31393, #52934, #47257 ) ;
#30266 = CARTESIAN_POINT ( 'NONE',  ( -23.99999999999997513, 204.6875000000000284, 171.6568542494927385 ) ) ;
#30267 = CARTESIAN_POINT ( 'NONE',  ( -1.432654583217607858, 194.6250000013655779, 201.4587341250000065 ) ) ;
#30268 = CARTESIAN_POINT ( 'NONE',  ( 5.000000000000000888, -52.35862550122958936, 48.98731492261398301 ) ) ;
#30269 = CARTESIAN_POINT ( 'NONE',  ( 2.679491924311228956, 96.04166666666665719, -10.00000000000000000 ) ) ;
#30270 = CARTESIAN_POINT ( 'NONE',  ( -3.313708498984762496, 119.2812499999999858, 7.999999999999998224 ) ) ;
#30271 = CARTESIAN_POINT ( 'NONE',  ( -4.088227598258586603E-16, 297.3593750017070079, -6.676582343750001591 ) ) ;
#30272 = ORIENTED_EDGE ( 'NONE', *, *, #18919, .F. ) ;
#30273 = CARTESIAN_POINT ( 'NONE',  ( 0.000000000000000000, 300.0000000000000000, 0.000000000000000000 ) ) ;
#30274 = CARTESIAN_POINT ( 'NONE',  ( -8.000000000000000000, 17.06249999590322375, -9.797174393178825657E-16 ) ) ;
#30275 = CARTESIAN_POINT ( 'NONE',  ( -3.458734125000016313, 205.8750000013656063, 140.5673454167824161 ) ) ;
#30276 = CARTESIAN_POINT ( 'NONE',  ( 7.320508075688779037, 84.37500000000000000, 7.320508075688782590 ) ) ;
#30277 = CARTESIAN_POINT ( 'NONE',  ( -10.00000000000000000, 225.0000000000000000, 0.000000000000000000 ) ) ;
#30278 = FACE_OUTER_BOUND ( 'NONE', #58544, .T. ) ;
#30279 = CARTESIAN_POINT ( 'NONE',  ( -4.220049686691937474, -10.18810118749999738, 68.31250000204838102 ) ) ;
#30280 = CARTESIAN_POINT ( 'NONE',  ( 2.679491924311222739, 213.9583333333332860, 10.00000000000000355 ) ) ;
#30281 = CARTESIAN_POINT ( 'NONE',  ( 7.188101187499993827, -2.977408999572645598, 10.01780278187175632 ) ) ;
#30282 = CARTESIAN_POINT ( 'NONE',  ( -9.832129032723420536, 179.0104166632526699, 5.676582343749997150 ) ) ;
#30283 = CARTESIAN_POINT ( 'NONE',  ( -4.541265875000003227, 1.874999998634406806, 1.881053915767121110 ) ) ;
#30284 = FACE_OUTER_BOUND ( 'NONE', #72986, .T. ) ;
#30286 = CARTESIAN_POINT ( 'NONE',  ( -7.999999999999989342, -1.759397900368767025E-05, 4.017803281681348260 ) ) ;
#30285 = CARTESIAN_POINT ( 'NONE',  ( -1.347111479062088207E-15, 0.000000000000000000, 0.000000000000000000 ) ) ;
#30287 = VERTEX_POINT ( 'NONE', #67325 ) ;
#30288 = VECTOR ( 'NONE', #70719, 1000.000000000000000 ) ;
#30289 = CARTESIAN_POINT ( 'NONE',  ( -2.445694354108839175, 207.3125000013656063, 144.4456943541088663 ) ) ;
#30290 = CARTESIAN_POINT ( 'NONE',  ( 9.832129032723416984, 45.67708332991934839, 5.676582343750006032 ) ) ;
#30291 = CARTESIAN_POINT ( 'NONE',  ( 7.778174593052023411, -7.778174593052021635, 105.2500000040967763 ) ) ;
#30292 = CARTESIAN_POINT ( 'NONE',  ( 9.832129032723420536, 226.5104166632526983, -5.676582343749999815 ) ) ;
#30293 = CARTESIAN_POINT ( 'NONE',  ( -25.55430564589111953, 205.0625000013656063, 172.4456943541091505 ) ) ;
#30294 = CARTESIAN_POINT ( 'NONE',  ( -7.778174593052023411, 7.778174593052023411, 95.50000000409677625 ) ) ;
#30296 = DIRECTION ( 'NONE',  ( 0.000000000000000000, 0.000000000000000000, 1.000000000000000000 ) ) ;
#30295 = CARTESIAN_POINT ( 'NONE',  ( -5.082755093536325930, 123.9687500020483952, -5.082755093536325930 ) ) ;
#30297 = CARTESIAN_POINT ( 'NONE',  ( -2.445694354108838731, 196.0625000013656063, 144.4456943541088663 ) ) ;
#30298 = ADVANCED_FACE ( 'NONE', ( #43936 ), #22030, .F. ) ;
#30299 = CARTESIAN_POINT ( 'NONE',  ( 2.679491924311222739, 75.83333332650533976, 10.00000000000000355 ) ) ;
#30300 = CARTESIAN_POINT ( 'NONE',  ( 1.320432766682874540E-15, 99.03125000204838102, 7.188101187500000044 ) ) ;
#30301 = CARTESIAN_POINT ( 'NONE',  ( 2.780723358947928197E-16, 16.68749999863440436, -4.541265875000002339 ) ) ;
#30302 = CARTESIAN_POINT ( 'NONE',  ( -7.320508075688778149, 49.99999999317202537, 7.320508075688769267 ) ) ;
#30303 = DIRECTION ( 'NONE',  ( -0.000000000000000000, -0.000000000000000000, 1.000000000000000000 ) ) ;
#30304 = VERTEX_POINT ( 'NONE', #32635 ) ;
#30305 = VERTEX_POINT ( 'NONE', #68067 ) ;
#30306 = CARTESIAN_POINT ( 'NONE',  ( -1.836970198721029983E-15, 143.7500000000000284, 10.00000000000000178 ) ) ;
#30307 = CARTESIAN_POINT ( 'NONE',  ( -4.000000000000015987, 195.6250000027311842, 142.0000000000000568 ) ) ;
#30308 = CARTESIAN_POINT ( 'NONE',  ( -3.042071309553173730, 149.3229166632526699, 11.35316468749999785 ) ) ;
#30309 = FACE_OUTER_BOUND ( 'NONE', #63160, .T. ) ;
#30310 = CARTESIAN_POINT ( 'NONE',  ( -2.828427124746152987, 199.1250000000000284, 200.8284271247462129 ) ) ;
#30311 = CARTESIAN_POINT ( 'NONE',  ( -27.99999999999999645, 210.0000000000000284, 166.0000000000003979 ) ) ;
#30312 = CIRCLE ( 'NONE', #72470, 18.00000000000000355 ) ;
#30313 = CARTESIAN_POINT ( 'NONE',  ( 7.204075437095968759, -7.204075437095966983, 110.5937500020483810 ) ) ;
#30314 = VERTEX_POINT ( 'NONE', #9983 ) ;
#30315 = CARTESIAN_POINT ( 'NONE',  ( -1.656854249492390574, 202.3125000027312126, 201.9999999999999716 ) ) ;
#30316 = CIRCLE ( 'NONE', #47153, 7.999999999999991118 ) ;
#30317 = DIRECTION ( 'NONE',  ( 1.000000000000000000, -0.000000000000000000, -0.000000000000000000 ) ) ;
#30318 = CARTESIAN_POINT ( 'NONE',  ( 8.311093377946837890, 146.7187499965860127, -8.311093377946837890 ) ) ;
#30319 = CARTESIAN_POINT ( 'NONE',  ( -2.445694354108782775, 198.5625000013656063, 200.4456943541088663 ) ) ;
#30320 = CARTESIAN_POINT ( 'NONE',  ( 7.188101187500000044, 27.84374999795161543, 0.000000000000000000 ) ) ;
#30321 = CARTESIAN_POINT ( 'NONE',  ( -7.204075437095967871, 7.204075437095967871, 69.34375000204836681 ) ) ;
#30322 = CARTESIAN_POINT ( 'NONE',  ( -11.35316468749999785, 53.38541666325267698, -3.042071309553167513 ) ) ;
#30323 = ORIENTED_EDGE ( 'NONE', *, *, #26499, .F. ) ;
#30324 = CARTESIAN_POINT ( 'NONE',  ( -8.000000000000033751, -3.313708498984719864, 12.92405277982336465 ) ) ;
#30325 = CARTESIAN_POINT ( 'NONE',  ( 2.780723358947928197E-16, 4.687499998634407028, -4.541265875000002339 ) ) ;
#30326 = CARTESIAN_POINT ( 'NONE',  ( -3.317071493978880348, -8.008118988124989457, 13.29436528394063011 ) ) ;
#30327 = CARTESIAN_POINT ( 'NONE',  ( 5.082755093536325930, 14.15624999795161187, -5.082755093536325930 ) ) ;
#30328 = EDGE_CURVE ( 'NONE', #45065, #56250, #63930, .T. ) ;
#30329 = CARTESIAN_POINT ( 'NONE',  ( 4.242640687119285658, 292.6875000034139589, -4.242640687119286547 ) ) ;
#30330 = CARTESIAN_POINT ( 'NONE',  ( 0.000000000000000000, 300.0000000000000000, 0.000000000000000000 ) ) ;
#30331 = CARTESIAN_POINT ( 'NONE',  ( -7.188101187500001821, 13.49999999795161187, -2.977408999572651371 ) ) ;
#30332 = CARTESIAN_POINT ( 'NONE',  ( 7.188101187499992051, 8.802885111219154394E-16, 11.23655278187175455 ) ) ;
#30333 =( BOUNDED_CURVE ( )  B_SPLINE_CURVE ( 2, ( #15945, #38611, #34452, #61612, #50284, #21238, #38973, #68382, #63091 ),
 .UNSPECIFIED., .F., .F. ) 
 B_SPLINE_CURVE_WITH_KNOTS ( ( 3, 2, 2, 2, 3 ),
 ( 0.01666666666666679827, 0.02500000000000007772, 0.03333333333333335369, 0.04166666666666662966, 0.04999999999999991951 ),
 .UNSPECIFIED. ) 
 CURVE ( )  GEOMETRIC_REPRESENTATION_ITEM ( )  RATIONAL_B_SPLINE_CURVE ( ( 0.9999999999999988898, 0.9238795325112879597, 1.000000000000000000, 0.9238795325112867385, 1.000000000000000000, 0.9238795325112867385, 1.000000000000000000, 0.9238795325112875156, 0.9999999999999992228 ) ) 
 REPRESENTATION_ITEM ( '' )  );
#30334 = CARTESIAN_POINT ( 'NONE',  ( -10.18810118749999916, 4.220049686691934809, 72.06250000204836681 ) ) ;
#30335 = CARTESIAN_POINT ( 'NONE',  ( -6.000000000000021316, -10.39230484541325161, 0.000000000000000000 ) ) ;
#30336 = CARTESIAN_POINT ( 'NONE',  ( -8.342170076843785083E-16, 22.18749999863440792, 4.541265875000002339 ) ) ;
#30337 = ORIENTED_EDGE ( 'NONE', *, *, #17110, .T. ) ;
#30338 = VECTOR ( 'NONE', #56107, 1000.000000000000000 ) ;
#30339 = CARTESIAN_POINT ( 'NONE',  ( 2.828427124746208943, 196.7500000027312126, 195.1715728752538439 ) ) ;
#30340 = EDGE_CURVE ( 'NONE', #46864, #12752, #72221, .T. ) ;
#30341 = CARTESIAN_POINT ( 'NONE',  ( 3.999999999999959144, 203.0625000000000284, 140.3431457505076594 ) ) ;
#30342 = CARTESIAN_POINT ( 'NONE',  ( -26.34314575050752794, 196.6875000027312126, 174.0000000000003411 ) ) ;
#30343 = CARTESIAN_POINT ( 'NONE',  ( 4.541265875000001451, 4.249999998634406140, 1.881053915767124440 ) ) ;
#30344 = CARTESIAN_POINT ( 'NONE',  ( 7.188101187500000044, 115.9062500020483810, -8.802885111219163269E-16 ) ) ;
#30345 = CARTESIAN_POINT ( 'NONE',  ( 9.000000000000001776, -5.196152422706648899, -0.8038475772933779684 ) ) ;
#30346 = CARTESIAN_POINT ( 'NONE',  ( 5.656854249492374365, 5.656854249492375253, 0.4553027839201452265 ) ) ;
#30347 = ORIENTED_EDGE ( 'NONE', *, *, #59669, .T. ) ;
#30348 = EDGE_CURVE ( 'NONE', #52317, #3422, #22487, .T. ) ;
#30349 = CARTESIAN_POINT ( 'NONE',  ( 7.188101187499999156, 21.37499999795161543, 2.977408999572654924 ) ) ;
#30350 = ORIENTED_EDGE ( 'NONE', *, *, #41105, .F. ) ;
#30351 = CARTESIAN_POINT ( 'NONE',  ( -10.18810118749999916, 0.000000000000000000, 117.5312500020483810 ) ) ;
#30352 = CARTESIAN_POINT ( 'NONE',  ( 2.445694354108838731, 209.0625000013656063, 195.5543056458912190 ) ) ;
#30353 = CARTESIAN_POINT ( 'NONE',  ( 25.55430564589119058, 205.3125000013656063, 172.4456943541087526 ) ) ;
#30354 = CARTESIAN_POINT ( 'NONE',  ( -8.660254037844390851, 57.91666666666667140, 4.999999999999998224 ) ) ;
#30355 = CARTESIAN_POINT ( 'NONE',  ( 7.188101187500001821, 99.87500000204838102, -2.977408999572651371 ) ) ;
#30356 = CARTESIAN_POINT ( 'NONE',  ( 4.242640687119287435, 298.3750000000000000, 4.242640687119285658 ) ) ;
#30358 = CARTESIAN_POINT ( 'NONE',  ( -30.93541659651595666, -51.99989572432781415, 167.9999999999997726 ) ) ;
#30357 = CARTESIAN_POINT ( 'NONE',  ( -3.313708498984708317, 89.46875000409679046, 8.000000000000053291 ) ) ;
#30359 = ORIENTED_EDGE ( 'NONE', *, *, #51117, .F. ) ;
#30360 = B_SPLINE_CURVE_WITH_KNOTS ( 'NONE', 3,
 ( #69248, #68498, #62831, #5508, #17558, #28508, #51517, #74532, #22842, #25051, #48815, #53385, #48072, #25426, #64699, #14101, #24688, #53751, #42044, #7726, #70720, #1345, #13361, #37137, #7359, #12635 ),
 .UNSPECIFIED., .F., .F.,
 ( 4, 2, 2, 2, 2, 2, 2, 2, 2, 2, 2, 2, 4 ),
 ( 8.415322201872837476E-16, 0.001138349480798921381, 0.001707524221197996746, 0.002276698961597071677, 0.002845873701996146608, 0.003415048442395222407, 0.004553397923193374004, 0.005122572663592448068, 0.005691747403991522132, 0.006260922144390596196, 0.006830096884789671127, 0.007968446365587819255, 0.009106795846385969118 ),
 .UNSPECIFIED. ) ;
#30361 = CARTESIAN_POINT ( 'NONE',  ( 11.35316468749999963, 236.1979166700806445, 3.042071309553159519 ) ) ;
#30362 = CARTESIAN_POINT ( 'NONE',  ( -2.977408999572648707, -7.188101187499990274, 14.14280278187175455 ) ) ;
#30363 = VECTOR ( 'NONE', #13478, 1000.000000000000000 ) ;
#30364 = CARTESIAN_POINT ( 'NONE',  ( 6.123233995736767268E-16, 91.25000000000001421, -10.00000000000000178 ) ) ;
#30365 = CARTESIAN_POINT ( 'NONE',  ( -3.313708498984757611, 7.999999999999991118, 3.549052779823362425 ) ) ;
#30366 = CARTESIAN_POINT ( 'NONE',  ( 3.999999999999960032, 197.1250000027312126, 142.0000000000000568 ) ) ;
#30367 = CARTESIAN_POINT ( 'NONE',  ( -2.679491924311222295, 261.0416666666666856, 10.00000000000000178 ) ) ;
#30368 = CARTESIAN_POINT ( 'NONE',  ( 4.898587196589412829E-16, 24.18749999590322375, -8.000000000000000000 ) ) ;
#30369 = CARTESIAN_POINT ( 'NONE',  ( -1.836970198721029983E-15, 168.7500000000000000, 10.00000000000000178 ) ) ;
#30370 = CARTESIAN_POINT ( 'NONE',  ( 4.242640687119285658, 297.6875000034139589, -4.242640687119286547 ) ) ;
#30371 = FACE_OUTER_BOUND ( 'NONE', #2527, .T. ) ;
#30372 = CARTESIAN_POINT ( 'NONE',  ( 7.778174593052023411, -7.778174593052021635, 69.25000000409677625 ) ) ;
#30373 = CARTESIAN_POINT ( 'NONE',  ( -8.311093377946841443, 139.2187499965860127, 8.311093377946830785 ) ) ;
#30374 = CARTESIAN_POINT ( 'NONE',  ( 2.775557561562891351E-14, 271.9999999999999432, 170.0000000000000284 ) ) ;
#30375 = CARTESIAN_POINT ( 'NONE',  ( 7.320508075688774596, 27.49999999317203248, -7.320508075688774596 ) ) ;
#30378 = CARTESIAN_POINT ( 'NONE',  ( 18.00000000000000355, 0.8785859941773086490, 1.951563910473907981E-15 ) ) ;
#30377 = CARTESIAN_POINT ( 'NONE',  ( 8.660254037844389075, 107.2916666598387110, -5.000000000000000000 ) ) ;
#30376 = CARTESIAN_POINT ( 'NONE',  ( 30.82842712474617031, 206.1250000000000284, 172.8284271247460993 ) ) ;
#30379 = ORIENTED_EDGE ( 'NONE', *, *, #67678, .T. ) ;
#30380 = CARTESIAN_POINT ( 'NONE',  ( -8.311093377946836114, 12.96874999658601446, -8.311093377946837890 ) ) ;
#30381 = CARTESIAN_POINT ( 'NONE',  ( 0.000000000000000000, 125.0000000000000000, 8.000000000000000000 ) ) ;
#30382 = DIRECTION ( 'NONE',  ( -1.000000000000000000, -0.000000000000000000, -0.000000000000000000 ) ) ;
#30383 = CARTESIAN_POINT ( 'NONE',  ( -3.458734125000016313, 206.8750000013656347, 140.5673454167823593 ) ) ;
#30384 = FACE_OUTER_BOUND ( 'NONE', #62257, .T. ) ;
#30385 = CIRCLE ( 'NONE', #72556, 17.50000000000000000 ) ;
#30386 = CARTESIAN_POINT ( 'NONE',  ( -7.320508075688773708, 38.74999999317203958, -7.320508075688774596 ) ) ;
#30387 = CARTESIAN_POINT ( 'NONE',  ( 7.188101187500001821, 117.5000000020483810, -2.977408999572651371 ) ) ;
#30388 = CARTESIAN_POINT ( 'NONE',  ( 4.541265875000002339, 3.499999998634407028, -1.881053915767121554 ) ) ;
#30389 = CARTESIAN_POINT ( 'NONE',  ( 3.313708498984762496, -7.999999999999989342, 13.48655278392014623 ) ) ;
#30390 = CARTESIAN_POINT ( 'NONE',  ( -7.999999999999991118, 0.000000000000000000, 12.83030277982336465 ) ) ;
#30392 = CARTESIAN_POINT ( 'NONE',  ( -3.313708498984719864, 25.96875000000000355, -8.000000000000040856 ) ) ;
#30391 = CYLINDRICAL_SURFACE ( 'NONE', #17821, 6.000000000000001776 ) ;
#30393 = ORIENTED_EDGE ( 'NONE', *, *, #24474, .T. ) ;
#30394 = LINE ( 'NONE', #60167, #25529 ) ;
#30395 = CARTESIAN_POINT ( 'NONE',  ( -2.679491924311249385, 63.54166666666669983, 10.00000000000005329 ) ) ;
#30396 = CARTESIAN_POINT ( 'NONE',  ( -3.042071309553166625, 228.1770833367473301, -11.35316468749999608 ) ) ;
#30397 = CIRCLE ( 'NONE', #66511, 8.000000000000000000 ) ;
#30398 = CARTESIAN_POINT ( 'NONE',  ( 9.832129032723416984, 110.3645833299193555, 5.676582343750006032 ) ) ;
#30399 = ORIENTED_EDGE ( 'NONE', *, *, #22844, .F. ) ;
#30400 = CARTESIAN_POINT ( 'NONE',  ( 4.999999999999999112, 0.000000000000000000, -17.50000000000000000 ) ) ;
#30401 = CARTESIAN_POINT ( 'NONE',  ( -7.204075437095965206, -7.204075437095968759, 100.8437500020483668 ) ) ;
#30402 = CARTESIAN_POINT ( 'NONE',  ( -4.195582579073398932, 22.00000000000000355, 1.737867247408543925 ) ) ;
#30403 = CARTESIAN_POINT ( 'NONE',  ( 3.458734125000015425, 197.2500000013656063, 196.5673454167823877 ) ) ;
#30404 = DIRECTION ( 'NONE',  ( 0.000000000000000000, -0.9996144206527183274, -0.02776706724035331308 ) ) ;
#30406 = CARTESIAN_POINT ( 'NONE',  ( 3.042071309553167513, 116.8229166632526841, -11.35316468749999785 ) ) ;
#30405 = CARTESIAN_POINT ( 'NONE',  ( 33.48318503342264307, 175.8115626168855385, 156.1427595010632956 ) ) ;
#30407 = CARTESIAN_POINT ( 'NONE',  ( -23.99999999999997868, 207.6875000000000000, 171.6568542494927385 ) ) ;
#30408 = CARTESIAN_POINT ( 'NONE',  ( 7.320508075688775484, 49.37500000000000000, 7.320508075688779037 ) ) ;
#30409 = ORIENTED_EDGE ( 'NONE', *, *, #35372, .F. ) ;
#30410 = CARTESIAN_POINT ( 'NONE',  ( 2.679491924311222739, 205.8333333265053966, 10.00000000000000355 ) ) ;
#30411 = CARTESIAN_POINT ( 'NONE',  ( 2.679491924311096174, 258.5416666666666856, -10.00000000000007283 ) ) ;
#30412 = CARTESIAN_POINT ( 'NONE',  ( 37.99999999999999289, 50.00000000000000711, 69.99999999999998579 ) ) ;
#30413 = CARTESIAN_POINT ( 'NONE',  ( -3.042071309553173730, 99.63541666325268409, 11.35316468749999785 ) ) ;
#30414 = CARTESIAN_POINT ( 'NONE',  ( -1.432654583217607858, 208.6250000013656063, 201.4587341250000065 ) ) ;
#30415 = CARTESIAN_POINT ( 'NONE',  ( 5.082755093536325930, 10.03124999795161187, -5.082755093536325930 ) ) ;
#30416 = CARTESIAN_POINT ( 'NONE',  ( -10.18810118749999916, 0.000000000000000000, 90.53125000204836681 ) ) ;
#30417 = CARTESIAN_POINT ( 'NONE',  ( 11.35316468749999963, 6.302083329919350163, -3.042071309553165293 ) ) ;
#30418 = ORIENTED_EDGE ( 'NONE', *, *, #69616, .T. ) ;
#30419 = EDGE_CURVE ( 'NONE', #54290, #5538, #30217, .T. ) ;
#30420 = CARTESIAN_POINT ( 'NONE',  ( -7.320508075688779925, 136.8750000000000000, -7.320508075688781702 ) ) ;
#30421 = CARTESIAN_POINT ( 'NONE',  ( 2.849036369511732440E-14, 196.3750000027311842, 202.0000000000000000 ) ) ;
#30422 = LINE ( 'NONE', #53807, #47457 ) ;
#30423 = CARTESIAN_POINT ( 'NONE',  ( -10.18810118749999916, 0.000000000000000000, 75.53125000204836681 ) ) ;
#30424 = CARTESIAN_POINT ( 'NONE',  ( -4.898587196589412829E-16, 97.81250000409677625, -8.000000000000000000 ) ) ;
#30425 = LINE ( 'NONE', #1766, #34264 ) ;
#30426 = CARTESIAN_POINT ( 'NONE',  ( -2.765530957081996810, 291.2656250017070079, -6.676582343750003368 ) ) ;
#30427 = CARTESIAN_POINT ( 'NONE',  ( 0.8761883848947588094, 51.17400877215430199, -48.53033992007421915 ) ) ;
#30428 = CARTESIAN_POINT ( 'NONE',  ( 8.311093377946834337, 225.4687499965860411, 8.311093377946839666 ) ) ;
#30429 = EDGE_CURVE ( 'NONE', #73073, #3534, #22051, .T. ) ;
#30430 = EDGE_CURVE ( 'NONE', #27563, #47025, #56755, .T. ) ;
#30431 = CARTESIAN_POINT ( 'NONE',  ( 7.204075437095968759, -7.204075437095966983, 90.71875000204838102 ) ) ;
#30432 = CARTESIAN_POINT ( 'NONE',  ( -24.54126587499999346, 202.1875000013656063, 170.0000000000003411 ) ) ;
#30433 = CARTESIAN_POINT ( 'NONE',  ( 8.000000000000000000, 25.50000000000000355, 0.000000000000000000 ) ) ;
#30434 = CARTESIAN_POINT ( 'NONE',  ( -3.211159895383561391, 11.81249999863440614, -3.211159895383561835 ) ) ;
#30435 = EDGE_LOOP ( 'NONE', ( #54762, #21661, #6686, #36781, #66611, #43940, #27079, #24846, #6214, #386, #54675, #37694, #21042, #31924, #71815, #19722, #42403, #33941, #55297, #65217 ) ) ;
#30436 = CARTESIAN_POINT ( 'NONE',  ( -30.93541659651595666, -51.99989572432781415, 167.9999999999997726 ) ) ;
#30437 = CARTESIAN_POINT ( 'NONE',  ( 2.828427124746208943, 207.7500000027312126, 195.1715728752538439 ) ) ;
#30438 = CARTESIAN_POINT ( 'NONE',  ( -2.754378923186476579E-14, 198.4375000013655779, 145.4587341250000350 ) ) ;
#30439 = CARTESIAN_POINT ( 'NONE',  ( 2.828427124746153876, 206.0000000027312126, 144.8284271247462129 ) ) ;
#30440 = AXIS2_PLACEMENT_3D ( 'NONE', #58263, #34514, #39766 ) ;
#30441 = CARTESIAN_POINT ( 'NONE',  ( 32.00000000000000711, 208.3125000027312126, 171.6568542494922553 ) ) ;
#30442 = CARTESIAN_POINT ( 'NONE',  ( 4.220049686691934809, 10.18810118749999916, 73.56250000204835260 ) ) ;
#30443 = ORIENTED_EDGE ( 'NONE', *, *, #69176, .F. ) ;
#30444 =( BOUNDED_CURVE ( )  B_SPLINE_CURVE ( 2, ( #42440, #59807, #36429, #35693, #58708, #7757, #53042, #65459, #8121 ),
 .UNSPECIFIED., .F., .F. ) 
 B_SPLINE_CURVE_WITH_KNOTS ( ( 3, 2, 2, 2, 3 ),
 ( 0.04411764705882356002, 0.04779411764705884802, 0.05147058823529414989, 0.05514705882352945177, 0.05882352941176474670 ),
 .UNSPECIFIED. ) 
 CURVE ( )  GEOMETRIC_REPRESENTATION_ITEM ( )  RATIONAL_B_SPLINE_CURVE ( ( 0.9999999999999994449, 0.9238795325112872936, 1.000000000000000000, 0.9238795325112867385, 1.000000000000000000, 0.9238795325112867385, 1.000000000000000000, 0.9238795325112858503, 1.000000000000000888 ) ) 
 REPRESENTATION_ITEM ( '' )  );
#30445 = CARTESIAN_POINT ( 'NONE',  ( -7.188101187500002709, 7.312499997951610986, 2.977408999572649151 ) ) ;
#30446 =( BOUNDED_CURVE ( )  B_SPLINE_CURVE ( 2, ( #41863, #2245, #8270, #25238, #18856, #64875, #41499, #53195, #13540 ),
 .UNSPECIFIED., .F., .F. ) 
 B_SPLINE_CURVE_WITH_KNOTS ( ( 3, 2, 2, 2, 3 ),
 ( 0.2058823529411765996, 0.2095588235294118529, 0.2132352941176470507, 0.2169117647058823040, 0.2205882352941175018 ),
 .UNSPECIFIED. ) 
 CURVE ( )  GEOMETRIC_REPRESENTATION_ITEM ( )  RATIONAL_B_SPLINE_CURVE ( ( 0.9999999999999971134, 0.9238795325112896251, 1.000000000000000000, 0.9238795325112867385, 1.000000000000000000, 0.9238795325112867385, 1.000000000000000000, 0.9238795325112896251, 0.9999999999999971134 ) ) 
 REPRESENTATION_ITEM ( '' )  );
#30447 = CARTESIAN_POINT ( 'NONE',  ( 0.000000000000000000, 30.78460969082653875, -20.69999999999999929 ) ) ;
#30448 = AXIS2_PLACEMENT_3D ( 'NONE', #36720, #31425, #70315 ) ;
#30449 = CARTESIAN_POINT ( 'NONE',  ( 7.188101187500002709, 120.6875000020483952, 2.977408999572649151 ) ) ;
#30450 = CARTESIAN_POINT ( 'NONE',  ( 1.377000000000000002, 284.2799999999998590, 5.684444333912814784 ) ) ;
#30451 = CARTESIAN_POINT ( 'NONE',  ( -4.721056650415998313, 290.5781250017069510, 4.721056650416000089 ) ) ;
#30453 = DIRECTION ( 'NONE',  ( -0.000000000000000000, 1.000000000000000000, 4.689100369878284071E-30 ) ) ;
#30452 = CARTESIAN_POINT ( 'NONE',  ( -11.35316468749999963, 228.9062500034139873, 0.000000000000000000 ) ) ;
#30454 = ITEM_DEFINED_TRANSFORMATION ( 'NONE', 'NONE', #74238,  #57354 ) ;
#30455 = EDGE_LOOP ( 'NONE', ( #60930, #15032, #39762, #58330 ) ) ;
#30456 = CARTESIAN_POINT ( 'NONE',  ( -11.35316468749999785, 224.0104166700806161, -3.042071309553164848 ) ) ;
#30457 = CARTESIAN_POINT ( 'NONE',  ( 2.977408999572650927, -7.188101187499990274, 3.455302781871751439 ) ) ;
#30458 = CARTESIAN_POINT ( 'NONE',  ( -2.445694354108784108, 202.5625000013656063, 195.5543056458912190 ) ) ;
#30459 = ORIENTED_EDGE ( 'NONE', *, *, #35277, .T. ) ;
#30460 = CARTESIAN_POINT ( 'NONE',  ( 10.18810118750000093, -4.220049686691933033, 69.81250000204835260 ) ) ;
#30461 = CARTESIAN_POINT ( 'NONE',  ( 11.35316468749999785, 105.8854166632526983, 3.042071309553174174 ) ) ;
#30462 = CARTESIAN_POINT ( 'NONE',  ( -2.828427124746153876, 208.8750000000000284, 195.1715728752538439 ) ) ;
#30463 = CARTESIAN_POINT ( 'NONE',  ( -7.778174593052023411, 7.778174593052023411, 78.81249999999998579 ) ) ;
#30466 = CARTESIAN_POINT ( 'NONE',  ( -11.00000000000004796, -4.556349186104000637, 113.5937499999999858 ) ) ;
#30465 = CARTESIAN_POINT ( 'NONE',  ( 31.45873412499998523, 203.7500000013656063, 168.5673454167822172 ) ) ;
#30464 = CARTESIAN_POINT ( 'NONE',  ( 28.00000000000002132, 203.1875000013656063, 166.5412658749999082 ) ) ;
#30467 = ORIENTED_EDGE ( 'NONE', *, *, #5772, .F. ) ;
#30468 = CARTESIAN_POINT ( 'NONE',  ( -38.00000000000000000, -63.00000000000000000, 10.00000000000006217 ) ) ;
#30469 = CARTESIAN_POINT ( 'NONE',  ( -10.00000000000000000, 179.1666666598387110, -2.679491924311229845 ) ) ;
#30470 = CARTESIAN_POINT ( 'NONE',  ( -8.311093377946836114, 217.6562499965860127, -8.311093377946837890 ) ) ;
#30471 = CARTESIAN_POINT ( 'NONE',  ( -3.458734125000015425, 200.9375000013656063, 142.0000000000000568 ) ) ;
#30472 = CARTESIAN_POINT ( 'NONE',  ( 27.99999999999996447, 201.6875000013656063, 173.4587341249998929 ) ) ;
#30473 = CARTESIAN_POINT ( 'NONE',  ( -7.188101187500001821, 22.49999999795161543, -2.977408999572651371 ) ) ;
#30474 = CARTESIAN_POINT ( 'NONE',  ( -11.35316468749999785, 188.3854166632526983, -3.042071309553167513 ) ) ;
#30475 = CARTESIAN_POINT ( 'NONE',  ( 1.320432766682874540E-15, 93.40625000204838102, 7.188101187500000044 ) ) ;
#30476 = CARTESIAN_POINT ( 'NONE',  ( -4.999999999999999112, 68.48952624890550567, -21.22548696402827773 ) ) ;
#30477 = CARTESIAN_POINT ( 'NONE',  ( -24.00000000000001066, 198.8125000000000284, 168.3431457505080004 ) ) ;
#30478 = CARTESIAN_POINT ( 'NONE',  ( -1.881053915767121554, 15.62499999863440614, -4.541265875000002339 ) ) ;
#30479 = CARTESIAN_POINT ( 'NONE',  ( 24.54126587499999346, 200.4375000013656063, 169.9999999999998863 ) ) ;
#30480 = CARTESIAN_POINT ( 'NONE',  ( -5.082755093536317936, -5.082755093536320601, 6.549052781871754547 ) ) ;
#30481 = CARTESIAN_POINT ( 'NONE',  ( -3.042071309553164404, 72.23958332991935549, -11.35316468749999963 ) ) ;
#30482 = CARTESIAN_POINT ( 'NONE',  ( -5.000000000000000000, -52.62579568235233296, 48.70175807017984937 ) ) ;
#30483 = DIRECTION ( 'NONE',  ( -0.000000000000000000, -0.000000000000000000, 1.000000000000000000 ) ) ;
#30484 = VERTEX_POINT ( 'NONE', #74462 ) ;
#30485 = DIRECTION ( 'NONE',  ( -0.000000000000000000, -1.000000000000000000, -0.000000000000000000 ) ) ;
#30486 = CARTESIAN_POINT ( 'NONE',  ( 2.679491924311234730, 231.4583333333333428, 9.999999999999998224 ) ) ;
#30487 = CARTESIAN_POINT ( 'NONE',  ( -5.676582343750006032, 74.11458332991935549, 9.832129032723418760 ) ) ;
#30488 = CARTESIAN_POINT ( 'NONE',  ( 4.220049686691934809, 10.18810118749999916, 85.56250000204838102 ) ) ;
#30489 = CARTESIAN_POINT ( 'NONE',  ( 7.778174593052023411, -7.778174593052021635, 70.75000000409677625 ) ) ;
#30490 = CARTESIAN_POINT ( 'NONE',  ( -2.754378923186476579E-14, 196.4375000013655779, 145.4587341250000350 ) ) ;
#30491 = CARTESIAN_POINT ( 'NONE',  ( 1.567784982238203817E-13, 73.75000000000002842, 10.00000000000000533 ) ) ;
#30493 = CARTESIAN_POINT ( 'NONE',  ( 9.832129032723420536, 71.19791666325268409, -5.676582343749999815 ) ) ;
#30492 = FACE_OUTER_BOUND ( 'NONE', #56914, .T. ) ;
#30494 = CARTESIAN_POINT ( 'NONE',  ( 7.999999999999992895, -3.313708498984756279, 22.67405278392015333 ) ) ;
#30495 = CARTESIAN_POINT ( 'NONE',  ( 2.679491924311222739, 160.8333333265053682, 10.00000000000000355 ) ) ;
#30496 = CARTESIAN_POINT ( 'NONE',  ( -5.082755093536325930, 91.34375000204838102, -5.082755093536325930 ) ) ;
#30497 = EDGE_CURVE ( 'NONE', #28711, #46242, #29778, .T. ) ;
#30498 = CARTESIAN_POINT ( 'NONE',  ( 37.94562015984924130, 146.0000000000000000, 126.9999999999999716 ) ) ;
#30499 = CARTESIAN_POINT ( 'NONE',  ( -5.676582343750006032, 64.42708332991935549, 9.832129032723418760 ) ) ;
#30500 = CARTESIAN_POINT ( 'NONE',  ( 10.18810118750000093, -4.220049686691933033, 113.6875000020483810 ) ) ;
#30501 = CARTESIAN_POINT ( 'NONE',  ( 5.676582343749993598, 194.9479166632526983, 9.832129032723422313 ) ) ;
#30502 = VERTEX_POINT ( 'NONE', #23523 ) ;
#30503 = CARTESIAN_POINT ( 'NONE',  ( 4.000000000000015987, 205.6875000027312126, 196.3431457505076594 ) ) ;
#30504 = CARTESIAN_POINT ( 'NONE',  ( -7.204075437095967871, 7.204075437095967871, 67.46875000204836681 ) ) ;
#30505 = LINE ( 'NONE', #64475, #68602 ) ;
#30506 = AXIS2_PLACEMENT_3D ( 'NONE', #54125, #25429, #2436 ) ;
#30508 = CARTESIAN_POINT ( 'NONE',  ( 8.311093377946837890, 191.4062499965860127, -8.311093377946837890 ) ) ;
#30507 = PLANE ( 'NONE',  #60556 ) ;
#30509 = VECTOR ( 'NONE', #1310, 1000.000000000000000 ) ;
#30510 = CARTESIAN_POINT ( 'NONE',  ( -2.679491924311228512, 242.0833333401612606, -9.999999999999998224 ) ) ;
#30511 = LINE ( 'NONE', #65948, #13117 ) ;
#30512 = VERTEX_POINT ( 'NONE', #52208 ) ;
#30513 = CARTESIAN_POINT ( 'NONE',  ( -9.832129032723420536, 179.0104166632526699, 5.676582343749997150 ) ) ;
#30514 = CARTESIAN_POINT ( 'NONE',  ( -7.188101187499990274, -2.977408999572651815, 21.08030278187175810 ) ) ;
#30515 = CARTESIAN_POINT ( 'NONE',  ( 3.527950947924078040, 225.9999999999998295, -9.433590150150084952 ) ) ;
#30516 = ORIENTED_EDGE ( 'NONE', *, *, #23626, .T. ) ;
#30517 = EDGE_CURVE ( 'NONE', #69231, #35453, #11103, .T. ) ;
#30518 = EDGE_CURVE ( 'NONE', #24126, #7225, #23897, .T. ) ;
#30519 = CARTESIAN_POINT ( 'NONE',  ( -3.313708498984762052, 100.9062500040967905, -8.000000000000000000 ) ) ;
#30520 = ADVANCED_FACE ( 'NONE', ( #22770 ), #5075, .T. ) ;
#30521 = VECTOR ( 'NONE', #30404, 1000.000000000000000 ) ;
#30522 = CARTESIAN_POINT ( 'NONE',  ( -4.000000000000001776, 13.43749999999999822, -1.656854249492381470 ) ) ;
#30523 = CARTESIAN_POINT ( 'NONE',  ( -37.63829155267674764, -2.416132644680692554, 129.0070664184191003 ) ) ;
#30524 = CARTESIAN_POINT ( 'NONE',  ( -8.342170076843785083E-16, 17.06249999863440792, 4.541265875000002339 ) ) ;
#30525 = CARTESIAN_POINT ( 'NONE',  ( -5.656854249492375253, 5.656854249492375253, 15.83030278392014800 ) ) ;
#30526 = CARTESIAN_POINT ( 'NONE',  ( -5.000000000000000000, 186.6666666666666856, -8.660254037844390851 ) ) ;
#30527 = ORIENTED_EDGE ( 'NONE', *, *, #55921, .T. ) ;
#30528 = DIRECTION ( 'NONE',  ( -0.000000000000000000, 1.000000000000000000, -0.000000000000000000 ) ) ;
#30529 = CARTESIAN_POINT ( 'NONE',  ( 1.320432766682874540E-15, 100.5312500020483810, 7.188101187500000044 ) ) ;
#30530 = EDGE_CURVE ( 'NONE', #68303, #62350, #12104, .T. ) ;
#30533 = CARTESIAN_POINT ( 'NONE',  ( 2.020667218593132706E-15, -11.00000000000000000, 98.87499999999998579 ) ) ;
#30532 = CARTESIAN_POINT ( 'NONE',  ( -3.313708498984599515, 91.90625000409679046, -8.000000000000163425 ) ) ;
#30531 =( BOUNDED_CURVE ( )  B_SPLINE_CURVE ( 2, ( #8345, #52901, #31361, #64219, #70255, #12526, #18566, #30257, #53276 ),
 .UNSPECIFIED., .F., .F. ) 
 B_SPLINE_CURVE_WITH_KNOTS ( ( 3, 2, 2, 2, 3 ),
 ( 0.5340909090909090606, 0.5397727272727272929, 0.5454545454545454142, 0.5511363636363637575, 0.5568181818181818787 ),
 .UNSPECIFIED. ) 
 CURVE ( )  GEOMETRIC_REPRESENTATION_ITEM ( )  RATIONAL_B_SPLINE_CURVE ( ( 1.000000000000000000, 0.9238795325112867385, 1.000000000000000000, 0.9238795325112867385, 1.000000000000000000, 0.9238795325112867385, 1.000000000000000000, 0.9238795325112852952, 1.000000000000001554 ) ) 
 REPRESENTATION_ITEM ( '' )  );
#30534 = CARTESIAN_POINT ( 'NONE',  ( 1424.688200795887496, 828.9677537767817057, 1025.842160456058764 ) ) ;
#30535 = ORIENTED_EDGE ( 'NONE', *, *, #11317, .F. ) ;
#30536 = CARTESIAN_POINT ( 'NONE',  ( 7.456209740496399618, 10.23501300384517876, -65.47703513267221354 ) ) ;
#30537 = CARTESIAN_POINT ( 'NONE',  ( 3.042071309553163960, 262.7604166700806445, -11.35316468749999785 ) ) ;
#30538 = CARTESIAN_POINT ( 'NONE',  ( -7.188101187499991163, 2.977408999572646930, 25.39280278187176165 ) ) ;
#30539 = ORIENTED_EDGE ( 'NONE', *, *, #65856, .F. ) ;
#30540 = EDGE_LOOP ( 'NONE', ( #49723, #46296, #62844, #61310 ) ) ;
#30541 = CARTESIAN_POINT ( 'NONE',  ( 10.18810118749999916, 4.220049686691935698, 86.50000000204836681 ) ) ;
#30542 = DIRECTION ( 'NONE',  ( 1.000000000000000000, 0.000000000000000000, 0.000000000000000000 ) ) ;
#30543 = CARTESIAN_POINT ( 'NONE',  ( -7.778174593052020747, -7.778174593052023411, 92.68749999999998579 ) ) ;
#30546 = CARTESIAN_POINT ( 'NONE',  ( 4.721056650416000089, 293.9843750017070079, 4.721056650415999201 ) ) ;
#30545 = CARTESIAN_POINT ( 'NONE',  ( 29.65685424949240456, 202.1875000027311842, 173.9999999999999147 ) ) ;
#30544 = CARTESIAN_POINT ( 'NONE',  ( 27.99999999999996092, 196.6250000027312126, 165.9999999999998863 ) ) ;
#30547 = CARTESIAN_POINT ( 'NONE',  ( -5.000000000000005329, 128.3333333333333428, 8.660254037844387298 ) ) ;
#30548 = VECTOR ( 'NONE', #60153, 1000.000000000000000 ) ;
#30549 = CARTESIAN_POINT ( 'NONE',  ( -23.99999999999997513, 203.6875000000000284, 171.6568542494927385 ) ) ;
#30550 = CARTESIAN_POINT ( 'NONE',  ( -41.99999999999992895, -31.99999999999978684, 205.0000000000000284 ) ) ;
#30552 =( BOUNDED_CURVE ( )  B_SPLINE_CURVE ( 2, ( #59710, #64629, #2734, #25722, #71375, #48743, #36331, #31026, #48000 ),
 .UNSPECIFIED., .F., .F. ) 
 B_SPLINE_CURVE_WITH_KNOTS ( ( 3, 2, 2, 2, 3 ),
 ( 0.1911764705882354198, 0.1948529411764707286, 0.1985294117647060097, 0.2022058823529413463, 0.2058823529411766273 ),
 .UNSPECIFIED. ) 
 CURVE ( )  GEOMETRIC_REPRESENTATION_ITEM ( )  RATIONAL_B_SPLINE_CURVE ( ( 0.9999999999999971134, 0.9238795325112896251, 1.000000000000000000, 0.9238795325112867385, 1.000000000000000000, 0.9238795325112867385, 1.000000000000000000, 0.9238795325112832968, 1.000000000000003553 ) ) 
 REPRESENTATION_ITEM ( '' )  );
#30551 = CARTESIAN_POINT ( 'NONE',  ( 2.485281374238247132, 290.7500000034139020, -6.000000000000325961 ) ) ;
#30553 = CARTESIAN_POINT ( 'NONE',  ( 0.000000000000000000, 20.39230484541327471, -10.20000000000000284 ) ) ;
#30554 = CARTESIAN_POINT ( 'NONE',  ( 24.54126587499999346, 198.1875000013655779, 169.9999999999998863 ) ) ;
#30555 = CARTESIAN_POINT ( 'NONE',  ( 2.977408999572650927, 2.624999997951610986, -7.188101187500001821 ) ) ;
#30556 = CARTESIAN_POINT ( 'NONE',  ( -8.008118988124989457, -3.317071493978883900, 4.106865283940629219 ) ) ;
#30557 = DIRECTION ( 'NONE',  ( 0.000000000000000000, 0.000000000000000000, 1.000000000000000000 ) ) ;
#30558 = CARTESIAN_POINT ( 'NONE',  ( 5.082755093536326818, 114.5937500020483810, 5.082755093536325042 ) ) ;
#30559 = CARTESIAN_POINT ( 'NONE',  ( -5.711993833409989278E-12, 133.7499999999995737, 9.999999999999998224 ) ) ;
#30560 = CARTESIAN_POINT ( 'NONE',  ( -6.951808397369817780E-16, 222.9687500034139873, -11.35316468749999963 ) ) ;
#30561 = CARTESIAN_POINT ( 'NONE',  ( -4.000000000000001776, 12.50000000000000000, -4.898587196589415787E-16 ) ) ;
#30562 = CARTESIAN_POINT ( 'NONE',  ( 7.188101187499992051, 8.802885111219154394E-16, 20.61155278187175455 ) ) ;
#30563 = CARTESIAN_POINT ( 'NONE',  ( 32.00000000000000000, 195.3125000000000853, 168.3431457505075741 ) ) ;
#30564 = CARTESIAN_POINT ( 'NONE',  ( -11.35316468750000141, 23.28124999658601979, -1.390361679473963753E-15 ) ) ;
#30565 = CARTESIAN_POINT ( 'NONE',  ( -8.660254037844387298, 13.95833332650536818, -5.000000000000004441 ) ) ;
#30566 =( NAMED_UNIT ( * ) SI_UNIT ( $, .STERADIAN. ) SOLID_ANGLE_UNIT ( ) );
#30567 = ORIENTED_EDGE ( 'NONE', *, *, #21519, .F. ) ;
#30568 = FACE_OUTER_BOUND ( 'NONE', #2961, .T. ) ;
#30569 = CARTESIAN_POINT ( 'NONE',  ( -3.458734125000015869, 195.1875000013655779, 142.0000000000000568 ) ) ;
#30570 = CARTESIAN_POINT ( 'NONE',  ( 11.35316468750000141, 30.78124999658601979, 0.000000000000000000 ) ) ;
#30571 = CARTESIAN_POINT ( 'NONE',  ( -7.778174593052023411, 7.778174593052023411, 89.50000000409677625 ) ) ;
#30572 = CARTESIAN_POINT ( 'NONE',  ( 2.445694354108784108, 209.5625000013656063, 144.4456943541088663 ) ) ;
#30573 = CARTESIAN_POINT ( 'NONE',  ( -31.45873412500002075, 194.6250000013656063, 168.5673454167828140 ) ) ;
#30574 = FACE_OUTER_BOUND ( 'NONE', #36028, .T. ) ;
#30576 = CARTESIAN_POINT ( 'NONE',  ( -11.35316468750000141, 33.48958332991934839, 3.042071309553159963 ) ) ;
#30575 = CARTESIAN_POINT ( 'NONE',  ( 2.977408999572654480, 106.6250000020483810, 7.188101187499999156 ) ) ;
#30577 = CARTESIAN_POINT ( 'NONE',  ( 5.656854249492376141, -5.656854249492374365, 13.39280277982336465 ) ) ;
#30578 = CARTESIAN_POINT ( 'NONE',  ( -3.042071309553173730, 149.3229166632526699, 11.35316468749999785 ) ) ;
#30579 = CARTESIAN_POINT ( 'NONE',  ( 5.000000000000001776, 112.7083333265053682, -8.660254037844389075 ) ) ;
#30580 = CARTESIAN_POINT ( 'NONE',  ( -7.188101187500000044, 111.0312500020483810, 0.000000000000000000 ) ) ;
#30581 = CARTESIAN_POINT ( 'NONE',  ( 1.102182119232618108E-15, 296.2500000000000000, 6.000000000000001776 ) ) ;
#30582 = CARTESIAN_POINT ( 'NONE',  ( -25.55430564589115505, 206.3125000013656063, 172.4456943541091789 ) ) ;
#30583 =( BOUNDED_CURVE ( )  B_SPLINE_CURVE ( 2, ( #40631, #11584, #18732, #11962, #24385, #74587, #34993, #34619, #22901 ),
 .UNSPECIFIED., .F., .F. ) 
 B_SPLINE_CURVE_WITH_KNOTS ( ( 3, 2, 2, 2, 3 ),
 ( 0.01041666666666667303, 0.01562500000000001041, 0.02083333333333334605, 0.02604166666666668517, 0.03125000000000002082 ),
 .UNSPECIFIED. ) 
 CURVE ( )  GEOMETRIC_REPRESENTATION_ITEM ( )  RATIONAL_B_SPLINE_CURVE ( ( 0.9999999999999998890, 0.9238795325112868495, 1.000000000000000000, 0.9238795325112867385, 1.000000000000000000, 0.9238795325112867385, 1.000000000000000000, 0.9238795325112864054, 1.000000000000000222 ) ) 
 REPRESENTATION_ITEM ( '' )  );
#30584 = VECTOR ( 'NONE', #57074, 1000.000000000000000 ) ;
#30585 = ORIENTED_EDGE ( 'NONE', *, *, #18477, .F. ) ;
#30586 = CARTESIAN_POINT ( 'NONE',  ( 11.35316468750000141, 26.09374999658601624, 0.000000000000000000 ) ) ;
#30587 = VERTEX_POINT ( 'NONE', #34126 ) ;
#30588 = CARTESIAN_POINT ( 'NONE',  ( 5.000000000000000000, 0.000000000000000000, 0.000000000000000000 ) ) ;
#30590 = CARTESIAN_POINT ( 'NONE',  ( -5.676582343750006032, 154.1145833299193555, 9.832129032723418760 ) ) ;
#30589 = CARTESIAN_POINT ( 'NONE',  ( -22.54460849151098145, -24.94403623018969895, 145.4749499906720018 ) ) ;
#30591 = SURFACE_SIDE_STYLE ('',( #63809 ) ) ;
#30592 = CARTESIAN_POINT ( 'NONE',  ( 1.469576158976822172E-15, -7.999999999999991118, 17.76155278432982243 ) ) ;
#30593 = EDGE_CURVE ( 'NONE', #3133, #59034, #74501, .T. ) ;
#30594 = CARTESIAN_POINT ( 'NONE',  ( 10.00000000000000178, 225.4166666734946602, 2.679491924311222739 ) ) ;
#30595 = CARTESIAN_POINT ( 'NONE',  ( 8.311093377946834337, 252.0312500034139589, -8.311093377946836114 ) ) ;
#30596 = CARTESIAN_POINT ( 'NONE',  ( 10.18810118749999916, 1.247682550866122264E-15, 89.78125000204836681 ) ) ;
#30597 = VERTEX_POINT ( 'NONE', #8394 ) ;
#30598 = LINE ( 'NONE', #60006, #29138 ) ;
#30599 = CARTESIAN_POINT ( 'NONE',  ( -9.832129032723418760, 93.17708332991935549, -5.676582343750004256 ) ) ;
#30600 = CARTESIAN_POINT ( 'NONE',  ( -4.220049686691935698, 10.18810118749999916, 103.3750000020484094 ) ) ;
#30601 = CARTESIAN_POINT ( 'NONE',  ( 2.780723358947928197E-16, 15.68749999863440436, -4.541265875000002339 ) ) ;
#30602 = VERTEX_POINT ( 'NONE', #6922 ) ;
#30603 = ORIENTED_EDGE ( 'NONE', *, *, #11437, .F. ) ;
#30604 = VECTOR ( 'NONE', #21320, 1000.000000000000000 ) ;
#30605 = CARTESIAN_POINT ( 'NONE',  ( 8.000000000000000000, 7.500000000000001776, 0.000000000000000000 ) ) ;
#30606 = CARTESIAN_POINT ( 'NONE',  ( -8.342170076843785083E-16, 1.187499998634406806, 4.541265875000002339 ) ) ;
#30607 = EDGE_CURVE ( 'NONE', #34733, #22556, #15211, .T. ) ;
#30608 = CARTESIAN_POINT ( 'NONE',  ( 2.977408999572651815, 4.687499997951610986, 7.188101187500000933 ) ) ;
#30609 = CARTESIAN_POINT ( 'NONE',  ( 1.469576158976823947E-15, 122.5625000040967763, 8.000000000000000000 ) ) ;
#30610 = CARTESIAN_POINT ( 'NONE',  ( -6.238412754330611322E-16, 10.18810118749999916, 100.6562500020483810 ) ) ;
#30611 = CARTESIAN_POINT ( 'NONE',  ( 0.000000000000000000, 125.0000000000000000, 8.000000000000000000 ) ) ;
#30612 = CARTESIAN_POINT ( 'NONE',  ( 31.99999999999998579, 208.1875000000000853, 171.6568542494923122 ) ) ;
#30613 = CARTESIAN_POINT ( 'NONE',  ( -4.000000000000001776, 16.18749999726881228, -1.656854249492381470 ) ) ;
#30614 = CARTESIAN_POINT ( 'NONE',  ( 3.211159895383560947, 2.187499998634407028, 3.211159895383562723 ) ) ;
#30615 = ORIENTED_EDGE ( 'NONE', *, *, #66706, .T. ) ;
#30616 = CARTESIAN_POINT ( 'NONE',  ( 2.445694354108782775, 208.5625000013656063, 139.5543056458912190 ) ) ;
#30617 = CARTESIAN_POINT ( 'NONE',  ( 1.432654583217662481, 198.1250000013656063, 194.5412658750000219 ) ) ;
#30618 = EDGE_CURVE ( 'NONE', #31653, #10862, #24991, .T. ) ;
#30620 = CARTESIAN_POINT ( 'NONE',  ( -74.99999999999998579, 242.0000000000000284, 70.00000000000002842 ) ) ;
#30619 = CARTESIAN_POINT ( 'NONE',  ( -30.44569435410886982, 201.5625000013656063, 167.5543056458916169 ) ) ;
#30621 = ADVANCED_FACE ( 'NONE', ( #36706 ), #59718, .F. ) ;
#30622 = CARTESIAN_POINT ( 'NONE',  ( -1.881053915767124440, 13.99999999863440792, 4.541265875000001451 ) ) ;
#30623 = CARTESIAN_POINT ( 'NONE',  ( 27.99999999999996803, 206.6250000027312126, 165.9999999999998863 ) ) ;
#30624 = CARTESIAN_POINT ( 'NONE',  ( 7.188101187499992051, 8.802885111219154394E-16, 14.23655278187175455 ) ) ;
#30625 = ORIENTED_EDGE ( 'NONE', *, *, #65422, .T. ) ;
#30626 = ORIENTED_EDGE ( 'NONE', *, *, #68581, .F. ) ;
#30627 = CARTESIAN_POINT ( 'NONE',  ( -4.220049686691935698, 10.18810118749999916, 103.3750000020483952 ) ) ;
#30628 = CARTESIAN_POINT ( 'NONE',  ( 8.000000000000001776, 95.84375000409679046, 3.313708498984759387 ) ) ;
#30629 = CARTESIAN_POINT ( 'NONE',  ( -30.82842712474615965, 202.3750000000000284, 172.8284271247465824 ) ) ;
#30630 = CARTESIAN_POINT ( 'NONE',  ( 3.458734125000015425, 198.0000000013656063, 196.5673454167823877 ) ) ;
#30631 = CARTESIAN_POINT ( 'NONE',  ( -7.320508075688770155, 31.87500000000000000, -7.320508075688771044 ) ) ;
#30632 = CARTESIAN_POINT ( 'NONE',  ( -2.679491924311225848, 91.45833333333332860, -10.00000000000000178 ) ) ;
#30633 = EDGE_CURVE ( 'NONE', #64059, #18479, #71605, .T. ) ;
#30634 = EDGE_CURVE ( 'NONE', #21170, #39246, #53801, .T. ) ;
#30635 = CARTESIAN_POINT ( 'NONE',  ( 8.000000000000000000, 116.8437500000000000, -3.313708498984762496 ) ) ;
#30636 = CARTESIAN_POINT ( 'NONE',  ( -2.765530957081998586, 295.7968750017070079, 6.676582343750001591 ) ) ;
#30637 = ORIENTED_EDGE ( 'NONE', *, *, #51034, .F. ) ;
#30638 = CARTESIAN_POINT ( 'NONE',  ( 7.778174593052021635, 7.778174593052023411, 73.93749999999998579 ) ) ;
#30639 = ADVANCED_FACE ( 'NONE', ( #24259 ), #3653, .F. ) ;
#30640 = CARTESIAN_POINT ( 'NONE',  ( 7.999999999999998224, 16.21874999590322020, 3.313708498984766493 ) ) ;
#30641 = CARTESIAN_POINT ( 'NONE',  ( 2.445694354108782775, 207.5625000013656063, 139.5543056458912190 ) ) ;
#30642 = CARTESIAN_POINT ( 'NONE',  ( -5.000000000000006217, 53.33333333333333570, 8.660254037844390851 ) ) ;
#30643 = LINE ( 'NONE', #24233, #7006 ) ;
#30644 = CARTESIAN_POINT ( 'NONE',  ( 3.042071309553163960, 262.7604166700806445, -11.35316468749999785 ) ) ;
#30645 = CARTESIAN_POINT ( 'NONE',  ( 4.556349186104045934, 11.00000000000000000, 114.5312500000000142 ) ) ;
#30646 =( BOUNDED_CURVE ( )  B_SPLINE_CURVE ( 2, ( #57614, #11574, #16845, #39872, #62874, #1020, #35349, #12317, #46644, #68915, #23637, #29669, #40995 ),
 .UNSPECIFIED., .F., .F. ) 
 B_SPLINE_CURVE_WITH_KNOTS ( ( 3, 2, 2, 2, 2, 2, 3 ),
 ( 2.182283889826081236, 2.187517731460320913, 2.192751573094560591, 2.197985414728800269, 2.203219256363039502, 2.208453097997279180, 2.213686939631518857 ),
 .UNSPECIFIED. ) 
 CURVE ( )  GEOMETRIC_REPRESENTATION_ITEM ( )  RATIONAL_B_SPLINE_CURVE ( ( 1.000000000000085709, 0.9659258262889827140, 1.000000000000000000, 0.9659258262890683122, 1.000000000000000000, 0.9659258262890683122, 1.000000000000000000, 0.9659258262890683122, 1.000000000000000000, 0.9659258262890683122, 1.000000000000000000, 0.9659258262888490432, 1.000000000000219158 ) ) 
 REPRESENTATION_ITEM ( '' )  );
#30647 = CARTESIAN_POINT ( 'NONE',  ( -7.320508075688773708, 211.8749999999999432, -7.320508075688774596 ) ) ;
#30648 = CARTESIAN_POINT ( 'NONE',  ( 7.188101187499992051, 2.977408999572647819, 13.20530278187175277 ) ) ;
#30649 = CARTESIAN_POINT ( 'NONE',  ( 9.832129032723420536, 176.5104166632526699, -5.676582343749999815 ) ) ;
#30650 = DIRECTION ( 'NONE',  ( -0.000000000000000000, -0.000000000000000000, 1.000000000000000000 ) ) ;
#30651 = CARTESIAN_POINT ( 'NONE',  ( 1.881053915767121776, 3.499999998634407028, -4.541265875000002339 ) ) ;
#30652 = DIRECTION ( 'NONE',  ( -0.000000000000000000, -0.000000000000000000, 1.000000000000000000 ) ) ;
#30654 = CARTESIAN_POINT ( 'NONE',  ( 5.000000000000000000, 0.000000000000000000, 0.000000000000000000 ) ) ;
#30653 = DIRECTION ( 'NONE',  ( 0.000000000000000000, 0.000000000000000000, -1.000000000000000000 ) ) ;
#30655 = ORIENTED_EDGE ( 'NONE', *, *, #2405, .F. ) ;
#30656 = VECTOR ( 'NONE', #58305, 1000.000000000000000 ) ;
#30657 = CARTESIAN_POINT ( 'NONE',  ( -1.432654583217664701, 209.0000000013655779, 138.5412658750000787 ) ) ;
#30658 = CARTESIAN_POINT ( 'NONE',  ( -5.676582343749998039, 47.76041666325269119, -9.832129032723420536 ) ) ;
#30659 = CARTESIAN_POINT ( 'NONE',  ( 11.00000000000000000, 4.556349186104045934, 102.5312500040967905 ) ) ;
#30660 = CARTESIAN_POINT ( 'NONE',  ( 3.042071309553167069, 217.1354166632526983, -11.35316468749999785 ) ) ;
#30661 = CARTESIAN_POINT ( 'NONE',  ( -27.99999999999991829, 203.9375000013656063, 173.4587341250003760 ) ) ;
#30662 = DIRECTION ( 'NONE',  ( 0.000000000000000000, 0.000000000000000000, -1.000000000000000000 ) ) ;
#30664 = CARTESIAN_POINT ( 'NONE',  ( 5.656854249492379694, 119.9375000000000000, -5.656854249492380582 ) ) ;
#30663 = CARTESIAN_POINT ( 'NONE',  ( -2.977408999572650927, 120.8750000020483810, -7.188101187500000933 ) ) ;
#30665 = CARTESIAN_POINT ( 'NONE',  ( 1.432654583217607192, 196.2500000013656347, 145.4587341250000350 ) ) ;
#30666 = CARTESIAN_POINT ( 'NONE',  ( -11.35316468750000141, 103.4895833299193697, 3.042071309553159963 ) ) ;
#30667 = CARTESIAN_POINT ( 'NONE',  ( -1.836970198721029983E-15, 80.62499999317203958, 10.00000000000000178 ) ) ;
#30668 = CARTESIAN_POINT ( 'NONE',  ( 7.188101187500000044, 99.40625000204838102, -8.802885111219163269E-16 ) ) ;
#30669 = CARTESIAN_POINT ( 'NONE',  ( 4.541265875000002339, 16.43749999863440436, 0.000000000000000000 ) ) ;
#30670 = CARTESIAN_POINT ( 'NONE',  ( 4.118099735505524883, -8.014718854569444773, -6.906706651911562598E-15 ) ) ;
#30671 = CARTESIAN_POINT ( 'NONE',  ( 11.00000000000000355, -4.556349186104044158, 67.84375000409677625 ) ) ;
#30672 = ORIENTED_EDGE ( 'NONE', *, *, #46309, .F. ) ;
#30673 = EDGE_LOOP ( 'NONE', ( #40934, #9986, #11226, #73364 ) ) ;
#30674 =( BOUNDED_CURVE ( )  B_SPLINE_CURVE ( 2, ( #43559, #14880, #37920, #67333, #45063, #32644, #16365, #60917, #9240 ),
 .UNSPECIFIED., .F., .F. ) 
 B_SPLINE_CURVE_WITH_KNOTS ( ( 3, 2, 2, 2, 3 ),
 ( 0.6979166666666667407, 0.7031250000000001110, 0.7083333333333334814, 0.7135416666666667407, 0.7187500000000001110 ),
 .UNSPECIFIED. ) 
 CURVE ( )  GEOMETRIC_REPRESENTATION_ITEM ( )  RATIONAL_B_SPLINE_CURVE ( ( 0.9999999999999983347, 0.9238795325112884038, 1.000000000000000000, 0.9238795325112867385, 1.000000000000000000, 0.9238795325112867385, 1.000000000000000000, 0.9238795325112850731, 1.000000000000001554 ) ) 
 REPRESENTATION_ITEM ( '' )  );
#30675 = CARTESIAN_POINT ( 'NONE',  ( -4.721056650415998313, 293.7343750017069510, 4.721056650416000089 ) ) ;
#30676 = DIRECTION ( 'NONE',  ( -0.000000000000000000, 1.000000000000000000, -4.476705744456276341E-16 ) ) ;
#30677 = CARTESIAN_POINT ( 'NONE',  ( -11.35316468750000141, 153.2812499965860127, -1.390361679473963753E-15 ) ) ;
#30678 = CYLINDRICAL_SURFACE ( 'NONE', #23660, 8.000000000000000000 ) ;
#30679 = CARTESIAN_POINT ( 'NONE',  ( -3.999999999999959144, 199.0625000000000284, 199.6568542494924259 ) ) ;
#30680 = CARTESIAN_POINT ( 'NONE',  ( -30.82842712474621294, 201.1250000000000284, 167.1715728752542134 ) ) ;
#30681 = ADVANCED_FACE ( 'NONE', ( #13666 ), #58616, .T. ) ;
#30682 = CARTESIAN_POINT ( 'NONE',  ( -4.220049686691937474, -10.18810118749999738, 111.8125000020484094 ) ) ;
#30683 = ORIENTED_EDGE ( 'NONE', *, *, #18411, .F. ) ;
#30684 = CARTESIAN_POINT ( 'NONE',  ( 0.000000000000000000, 0.000000000000000000, 30.00000000000000000 ) ) ;
#30685 = CARTESIAN_POINT ( 'NONE',  ( -4.000000000000001776, 17.43750000000000000, -1.656854249492381470 ) ) ;
#30686 = CARTESIAN_POINT ( 'NONE',  ( -9.832129032723418760, 148.1770833299193555, -5.676582343750004256 ) ) ;
#30687 = CARTESIAN_POINT ( 'NONE',  ( -2.445694354108783664, 198.3125000013656063, 195.5543056458912190 ) ) ;
#30688 = CARTESIAN_POINT ( 'NONE',  ( 1.432654583217662481, 209.3750000013656063, 194.5412658750000219 ) ) ;
#30690 = ADVANCED_FACE ( 'NONE', ( #29933, #52949 ), #1645, .T. ) ;
#30689 = CARTESIAN_POINT ( 'NONE',  ( 10.18810118749999916, 1.247682550866122264E-15, 68.78125000204838102 ) ) ;
#30691 = CARTESIAN_POINT ( 'NONE',  ( -9.832129032723418760, 43.17708332991934839, -5.676582343750004256 ) ) ;
#30692 = VERTEX_POINT ( 'NONE', #36338 ) ;
#30693 = CARTESIAN_POINT ( 'NONE',  ( 0.000000000000000000, 23.85640646055104241, -14.00000000000000178 ) ) ;
#30694 = CARTESIAN_POINT ( 'NONE',  ( 4.541265875000002339, 4.499999998634407028, -1.881053915767121776 ) ) ;
#30695 = CARTESIAN_POINT ( 'NONE',  ( 5.662595241051936235, -5.662595241051934458, 10.57561528394063188 ) ) ;
#30696 = CARTESIAN_POINT ( 'NONE',  ( -1.320432766682874540E-15, 13.59374999795161187, 7.188101187500000044 ) ) ;
#30697 = CARTESIAN_POINT ( 'NONE',  ( 6.000000000000001776, 292.5625000034140157, -7.347880794884121708E-16 ) ) ;
#30698 = DIRECTION ( 'NONE',  ( -1.000000000000000000, 0.000000000000000000, 1.826024711554534406E-16 ) ) ;
#30699 = CARTESIAN_POINT ( 'NONE',  ( 2.977408999572650927, 10.12499999795161187, -7.188101187500001821 ) ) ;
#30700 = CARTESIAN_POINT ( 'NONE',  ( 2.977408999572650927, -7.188101187499990274, 6.455302781871754547 ) ) ;
#30701 = CARTESIAN_POINT ( 'NONE',  ( -6.238412754330611322E-16, 10.18810118749999916, 67.28125000204838102 ) ) ;
#30702 = EDGE_CURVE ( 'NONE', #4091, #61956, #28103, .T. ) ;
#30703 = CARTESIAN_POINT ( 'NONE',  ( -10.00000000000000178, 64.37499999317203958, -1.224646799147353454E-15 ) ) ;
#30704 = CARTESIAN_POINT ( 'NONE',  ( -1.881053915767124440, 22.12499999863441502, 4.541265875000001451 ) ) ;
#30705 = VERTEX_POINT ( 'NONE', #15170 ) ;
#30706 = CARTESIAN_POINT ( 'NONE',  ( -2.828427124746152987, 197.2500000027312126, 200.8284271247462129 ) ) ;
#30707 = CARTESIAN_POINT ( 'NONE',  ( -2.751064625579944321E-14, 203.7500000000000284, 146.0000000000000284 ) ) ;
#30708 = CARTESIAN_POINT ( 'NONE',  ( -31.99999999999999289, 198.3750000027312126, 170.0000000000004547 ) ) ;
#30709 = EDGE_CURVE ( 'NONE', #35470, #46714, #61506, .T. ) ;
#30710 = CARTESIAN_POINT ( 'NONE',  ( 4.541265875000002339, 0.3749999986344066949, -1.881053915767121554 ) ) ;
#30711 = CARTESIAN_POINT ( 'NONE',  ( 7.188101187500000044, 117.4062500020483810, -8.802885111219163269E-16 ) ) ;
#30712 = PLANE ( 'NONE',  #72954 ) ;
#30713 = CARTESIAN_POINT ( 'NONE',  ( 7.999999999999991118, 9.797174393178815797E-16, 1.767802783920142895 ) ) ;
#30714 = VERTEX_POINT ( 'NONE', #66106 ) ;
#30715 = CARTESIAN_POINT ( 'NONE',  ( 4.401442555609581635E-16, 24.84374999795161543, -7.188101187500000044 ) ) ;
#30716 = ORIENTED_EDGE ( 'NONE', *, *, #45655, .F. ) ;
#30717 = CYLINDRICAL_SURFACE ( 'NONE', #65306, 37.00000000000000711 ) ;
#30718 = CARTESIAN_POINT ( 'NONE',  ( -1.432654583217607192, 209.2500000013655779, 194.5412658750000219 ) ) ;
#30719 = CARTESIAN_POINT ( 'NONE',  ( 26.56734541678233086, 205.0000000013655779, 166.5412658749999650 ) ) ;
#30720 = CARTESIAN_POINT ( 'NONE',  ( -2.679491924311225848, 51.45833333333332860, -10.00000000000000178 ) ) ;
#30721 = CARTESIAN_POINT ( 'NONE',  ( 5.082755093536325042, 101.4687500020483810, -5.082755093536325930 ) ) ;
#30722 = CARTESIAN_POINT ( 'NONE',  ( 4.242640687119285658, 296.6250000000000000, -4.242640687119286547 ) ) ;
#30723 = AXIS2_PLACEMENT_3D ( 'NONE', #69190, #23161, #42269 ) ;
#30725 = CARTESIAN_POINT ( 'NONE',  ( -20.01361425935840543, -32.63307661884115873, 193.6739634518839637 ) ) ;
#30724 = LINE ( 'NONE', #58311, #47858 ) ;
#30726 = EDGE_LOOP ( 'NONE', ( #39990, #64097, #58584, #40450 ) ) ;
#30727 = CARTESIAN_POINT ( 'NONE',  ( 11.35316468749999963, 226.4062500034139873, -1.390361679473963556E-15 ) ) ;
#30728 = VECTOR ( 'NONE', #57955, 1000.000000000000000 ) ;
#30729 = CARTESIAN_POINT ( 'NONE',  ( -5.656854249492381470, 14.43750000000000178, 5.656854249492379694 ) ) ;
#30730 = CARTESIAN_POINT ( 'NONE',  ( -18.00000000000000000, 10.39230484541324628, -21.50000000000000000 ) ) ;
#30731 = CARTESIAN_POINT ( 'NONE',  ( 25.17157287525381903, 206.6250000000000284, 167.1715728752537018 ) ) ;
#30732 = CARTESIAN_POINT ( 'NONE',  ( 8.660254037844385522, 262.9166666666666856, -5.000000000000003553 ) ) ;
#30733 = EDGE_CURVE ( 'NONE', #60122, #27721, #69218, .T. ) ;
#30734 = DIRECTION ( 'NONE',  ( -0.000000000000000000, -0.000000000000000000, -1.000000000000000000 ) ) ;
#30735 = CARTESIAN_POINT ( 'NONE',  ( -8.660254037844390851, 172.9166666666666856, 4.999999999999998224 ) ) ;
#30736 = CARTESIAN_POINT ( 'NONE',  ( 28.00000000000002487, 208.9375000013656063, 166.5412658749999082 ) ) ;
#30737 = CARTESIAN_POINT ( 'NONE',  ( 1.347111479062088405E-15, 0.000000000000000000, 11.00000000000000000 ) ) ;
#30738 = CARTESIAN_POINT ( 'NONE',  ( -7.188101187499992051, 2.977408999572646930, 28.76780278187175810 ) ) ;
#30739 = CARTESIAN_POINT ( 'NONE',  ( 8.311093377946834337, 145.4687499965860411, 8.311093377946839666 ) ) ;
#30740 = CARTESIAN_POINT ( 'NONE',  ( 2.485281374238939911, 294.3750000034140157, 5.999999999999634959 ) ) ;
#30741 = DIRECTION ( 'NONE',  ( -0.000000000000000000, 1.000000000000000000, -1.563033456626094573E-30 ) ) ;
#30743 = CARTESIAN_POINT ( 'NONE',  ( -1.040834085586084257E-14, 82.00000000000001421, 20.00000000000000355 ) ) ;
#30742 = CARTESIAN_POINT ( 'NONE',  ( 32.00000000000000711, 207.3125000000000284, 168.3431457505075741 ) ) ;
#30744 = ORIENTED_EDGE ( 'NONE', *, *, #45264, .F. ) ;
#30745 = CARTESIAN_POINT ( 'NONE',  ( -8.311093377946841443, 4.218749996586018014, 8.311093377946830785 ) ) ;
#30746 = CARTESIAN_POINT ( 'NONE',  ( 3.999985685286083115, 88.68677412680156635, -6.928211494859723985 ) ) ;
#30747 = CARTESIAN_POINT ( 'NONE',  ( -9.999999999999994671, 112.4999999999999858, -1.224646799147352665E-15 ) ) ;
#30748 = CARTESIAN_POINT ( 'NONE',  ( -26.34314575050765583, 209.9375000000000000, 166.0000000000003126 ) ) ;
#30749 = CARTESIAN_POINT ( 'NONE',  ( 2.445694354108783664, 206.3125000013656063, 144.4456943541088663 ) ) ;
#30750 = CARTESIAN_POINT ( 'NONE',  ( -6.159719417591432489, 124.7163422235197885, -4.786194028158367253 ) ) ;
#30751 = CARTESIAN_POINT ( 'NONE',  ( -7.320508075688778149, 34.99999999317203958, 7.320508075688769267 ) ) ;
#30752 = CARTESIAN_POINT ( 'NONE',  ( -2.977408999572650927, 114.8750000020483810, -7.188101187500001821 ) ) ;
#30753 = CARTESIAN_POINT ( 'NONE',  ( 1.881053915767122664, 5.249999998634406140, 4.541265875000001451 ) ) ;
#30754 = CARTESIAN_POINT ( 'NONE',  ( 3.228176881614462701, 60.48309044411729474, -23.05774181791798227 ) ) ;
#30755 = CARTESIAN_POINT ( 'NONE',  ( 1.469576158976822172E-15, -7.999999999999991118, 14.70530277982336642 ) ) ;
#30757 = CARTESIAN_POINT ( 'NONE',  ( -4.556349186104048599, -10.99999999999999822, 104.9687500040967620 ) ) ;
#30756 = CARTESIAN_POINT ( 'NONE',  ( -4.500000000000022204, -7.794228634059960470, -10.20000000000000462 ) ) ;
#30758 = EDGE_LOOP ( 'NONE', ( #15684, #65279, #59203, #13900 ) ) ;
#30759 = LINE ( 'NONE', #48098, #19500 ) ;
#30760 = CARTESIAN_POINT ( 'NONE',  ( 3.313708498984819339, 108.9687500000000000, 7.999999999999943157 ) ) ;
#30761 = CARTESIAN_POINT ( 'NONE',  ( -5.676582343749992710, 225.0520833367473017, 9.832129032723422313 ) ) ;
#30762 = CARTESIAN_POINT ( 'NONE',  ( 11.35316468750000141, 120.7812499965860269, 0.000000000000000000 ) ) ;
#30763 = ORIENTED_EDGE ( 'NONE', *, *, #63112, .T. ) ;
#30764 = FACE_OUTER_BOUND ( 'NONE', #25171, .T. ) ;
#30765 = CARTESIAN_POINT ( 'NONE',  ( 7.204075437095968759, -7.204075437095966983, 93.71875000204838102 ) ) ;
#30766 = CARTESIAN_POINT ( 'NONE',  ( 2.754378923186476579E-14, 195.4375000013655779, 194.5412658750000219 ) ) ;
#30767 = PLANE ( 'NONE',  #4046 ) ;
#30769 = CARTESIAN_POINT ( 'NONE',  ( -11.35316468750000141, 118.4895833299193697, 3.042071309553159963 ) ) ;
#30768 = LINE ( 'NONE', #23632, #44834 ) ;
#30770 = CARTESIAN_POINT ( 'NONE',  ( -28.00000000000001776, 194.6875000013655779, 166.5412658750003629 ) ) ;
#30771 = EDGE_CURVE ( 'NONE', #42176, #68967, #48492, .T. ) ;
#30772 = CARTESIAN_POINT ( 'NONE',  ( 5.000000000000004441, 50.83333333333333570, -8.660254037844390851 ) ) ;
#30773 = ORIENTED_EDGE ( 'NONE', *, *, #1211, .T. ) ;
#30774 =( BOUNDED_CURVE ( )  B_SPLINE_CURVE ( 2, ( #33669, #11753, #5726, #16274, #73638, #57044, #58171, #11382, #34790 ),
 .UNSPECIFIED., .F., .F. ) 
 B_SPLINE_CURVE_WITH_KNOTS ( ( 3, 2, 2, 2, 3 ),
 ( 0.4583333333333334259, 0.4652777777777779011, 0.4722222222222222654, 0.4791666666666667407, 0.4861111111111111605 ),
 .UNSPECIFIED. ) 
 CURVE ( )  GEOMETRIC_REPRESENTATION_ITEM ( )  RATIONAL_B_SPLINE_CURVE ( ( 0.9999999999999987788, 0.9238795325112879597, 1.000000000000000000, 0.9238795325112867385, 1.000000000000000000, 0.9238795325112867385, 1.000000000000000000, 0.9238795325112861834, 1.000000000000000666 ) ) 
 REPRESENTATION_ITEM ( '' )  );
#30775 = CARTESIAN_POINT ( 'NONE',  ( -4.999999999999998224, 208.5416666598387394, -8.660254037844389075 ) ) ;
#30776 = DIRECTION ( 'NONE',  ( 0.000000000000000000, 1.000000000000000000, 0.000000000000000000 ) ) ;
#30777 = CARTESIAN_POINT ( 'NONE',  ( 11.00000000000000000, 1.347111479062088405E-15, 82.93750000409677625 ) ) ;
#30778 = CARTESIAN_POINT ( 'NONE',  ( -5.676582343750006032, 104.4270833299193555, 9.832129032723418760 ) ) ;
#30779 = FACE_OUTER_BOUND ( 'NONE', #70322, .T. ) ;
#30780 = CARTESIAN_POINT ( 'NONE',  ( 2.977408999572650927, 10.12499999795161187, -7.188101187500000933 ) ) ;
#30782 = EDGE_CURVE ( 'NONE', #27089, #55503, #49882, .T. ) ;
#30781 = CARTESIAN_POINT ( 'NONE',  ( 10.18810118750000093, -4.220049686691933033, 89.68750000204838102 ) ) ;
#30783 = CARTESIAN_POINT ( 'NONE',  ( -8.311093377946836114, 7.968749996586014461, -8.311093377946837890 ) ) ;
#30784 = ORIENTED_EDGE ( 'NONE', *, *, #5070, .T. ) ;
#30785 = CARTESIAN_POINT ( 'NONE',  ( 4.999999999999993783, 181.0416666598387110, 8.660254037844390851 ) ) ;
#30786 = CARTESIAN_POINT ( 'NONE',  ( -5.662595241051935346, 5.662595241051935346, 24.82561528394063544 ) ) ;
#30787 = CARTESIAN_POINT ( 'NONE',  ( 10.00000000000000178, 117.0833333265053824, -2.679491924311226736 ) ) ;
#30788 = CARTESIAN_POINT ( 'NONE',  ( 4.220049686691941027, -10.18810118749999738, 76.00000000204838102 ) ) ;
#30789 = FACE_OUTER_BOUND ( 'NONE', #8535, .T. ) ;
#30790 = CARTESIAN_POINT ( 'NONE',  ( 1.469576158976823947E-15, 123.8750000000000000, 8.000000000000000000 ) ) ;
#30791 = CARTESIAN_POINT ( 'NONE',  ( -2.765530957081996810, 293.2656250017068942, -6.676582343750003368 ) ) ;
#30792 = CIRCLE ( 'NONE', #3055, 12.00000000000000178 ) ;
#30793 = CARTESIAN_POINT ( 'NONE',  ( 6.951808397369818766E-16, 222.3437499965860127, -11.35316468750000141 ) ) ;
#30794 = CARTESIAN_POINT ( 'NONE',  ( 10.18810118749999916, 1.247682550866122264E-15, 83.40625000204838102 ) ) ;
#30795 = VECTOR ( 'NONE', #34921, 1000.000000000000000 ) ;
#30796 = CARTESIAN_POINT ( 'NONE',  ( -30.44569435410883074, 197.5625000013656063, 167.5543056458915885 ) ) ;
#30797 = CARTESIAN_POINT ( 'NONE',  ( -3.313708498984765161, 23.53125000000000355, 7.999999999999998224 ) ) ;
#30798 = CARTESIAN_POINT ( 'NONE',  ( 3.211159895383560947, 12.31249999863440792, 3.211159895383562723 ) ) ;
#30799 = EDGE_LOOP ( 'NONE', ( #17764, #55229, #43398, #63375 ) ) ;
#30800 = CARTESIAN_POINT ( 'NONE',  ( -11.92121597166104863, -37.99999999999992184, 141.3838400592076709 ) ) ;
#30801 = CARTESIAN_POINT ( 'NONE',  ( 4.000000000000015099, 207.6875000027311842, 196.3431457505076594 ) ) ;
#30802 = CARTESIAN_POINT ( 'NONE',  ( -2.445694354108839175, 197.3125000013656063, 144.4456943541088663 ) ) ;
#30803 = CARTESIAN_POINT ( 'NONE',  ( -1.656854249492405451, 204.4375000027311842, 138.0000000000000568 ) ) ;
#30804 = DIRECTION ( 'NONE',  ( 0.000000000000000000, 0.2588190451025145777, -0.9659258262890699775 ) ) ;
#30805 = CARTESIAN_POINT ( 'NONE',  ( -7.204075437095967871, 7.204075437095967871, 70.84375000204836681 ) ) ;
#30806 = EDGE_LOOP ( 'NONE', ( #963, #43019, #36253, #19021 ) ) ;
#30807 = CARTESIAN_POINT ( 'NONE',  ( 4.401442555609581635E-16, 2.343749997951610098, -7.188101187500000044 ) ) ;
#30808 = CARTESIAN_POINT ( 'NONE',  ( -8.660254037844390851, 29.79166665983870388, 4.999999999999998224 ) ) ;
#30809 = CARTESIAN_POINT ( 'NONE',  ( -4.401442555609581635E-16, 119.6562500020483810, -7.188101187500000044 ) ) ;
#30810 = CARTESIAN_POINT ( 'NONE',  ( -1.377000000000000002, 284.2799999999998590, 5.684453117602865646 ) ) ;
#30811 = CARTESIAN_POINT ( 'NONE',  ( -6.676582343749999815, 293.5156250017070079, 2.765530957082001251 ) ) ;
#30813 = LINE ( 'NONE', #54583, #14469 ) ;
#30812 = CARTESIAN_POINT ( 'NONE',  ( 5.676582343749997150, 227.2395833367473301, -9.832129032723418760 ) ) ;
#30814 =( REPRESENTATION_RELATIONSHIP ('NONE','NONE', #46008, #64301 ) REPRESENTATION_RELATIONSHIP_WITH_TRANSFORMATION ( #71909 )SHAPE_REPRESENTATION_RELATIONSHIP( ) );
#30815 = ORIENTED_EDGE ( 'NONE', *, *, #16817, .F. ) ;
#30816 = CARTESIAN_POINT ( 'NONE',  ( 11.35316468749999963, 221.5104166700805877, 3.042071309553159519 ) ) ;
#30817 = CARTESIAN_POINT ( 'NONE',  ( -2.977408999572648707, -7.188101187499990274, 0.2678027818717523822 ) ) ;
#30818 = CARTESIAN_POINT ( 'NONE',  ( 3.313708498984761608, 3.281250000000001332, -8.000000000000000000 ) ) ;
#30819 = CARTESIAN_POINT ( 'NONE',  ( 2.445694354108840063, 199.0625000013656063, 200.4456943541088663 ) ) ;
#30820 = ORIENTED_EDGE ( 'NONE', *, *, #30210, .F. ) ;
#30821 = CARTESIAN_POINT ( 'NONE',  ( -1.469576158976823947E-15, 11.43749999590322197, 8.000000000000000000 ) ) ;
#30822 = CARTESIAN_POINT ( 'NONE',  ( 8.311093377946834337, 105.4687499965860127, 8.311093377946839666 ) ) ;
#30823 = CARTESIAN_POINT ( 'NONE',  ( 27.99999999999996447, 200.6250000027312126, 165.9999999999998863 ) ) ;
#30824 = CARTESIAN_POINT ( 'NONE',  ( 7.778174593052023411, -7.778174593052021635, 78.06249999999998579 ) ) ;
#30827 = CARTESIAN_POINT ( 'NONE',  ( -3.999999999999960032, 202.0000000000000000, 198.0000000000000284 ) ) ;
#30826 = CARTESIAN_POINT ( 'NONE',  ( 26.56734541678232731, 203.0000000013655779, 166.5412658749999650 ) ) ;
#30825 = CARTESIAN_POINT ( 'NONE',  ( 30.44569435410883429, 203.0625000013656063, 167.5543056458911053 ) ) ;
#30828 = VERTEX_POINT ( 'NONE', #37828 ) ;
#30829 = CARTESIAN_POINT ( 'NONE',  ( 1.656854249492363040, 202.4375000027311557, 202.0000000000000284 ) ) ;
#30830 = CARTESIAN_POINT ( 'NONE',  ( 5.676582343750001591, 206.6145833299193555, -9.832129032723420536 ) ) ;
#30831 = CARTESIAN_POINT ( 'NONE',  ( -3.458734125000015425, 202.9375000013656063, 142.0000000000000568 ) ) ;
#30832 = ADVANCED_FACE ( 'NONE', ( #60825 ), #8493, .F. ) ;
#30833 = CARTESIAN_POINT ( 'NONE',  ( 25.55430564589119413, 201.3125000013656063, 167.5543056458910485 ) ) ;
#30834 = CARTESIAN_POINT ( 'NONE',  ( 4.556349186104051263, -10.99999999999999822, 115.6562500040967905 ) ) ;
#30835 = VECTOR ( 'NONE', #32239, 1000.000000000000000 ) ;
#30836 = CARTESIAN_POINT ( 'NONE',  ( 8.311093377946834337, 195.4687499965859843, 8.311093377946839666 ) ) ;
#30837 = CARTESIAN_POINT ( 'NONE',  ( 7.188101187500000933, 92.37500000204838102, -2.977408999572651371 ) ) ;
#30838 = DIRECTION ( 'NONE',  ( -0.000000000000000000, -0.000000000000000000, -1.000000000000000000 ) ) ;
#30839 = CARTESIAN_POINT ( 'NONE',  ( -29.65685424949240812, 196.0625000000000284, 166.0000000000004263 ) ) ;
#30840 = CARTESIAN_POINT ( 'NONE',  ( -4.541265875000003227, 12.87499999863440969, 1.881053915767121110 ) ) ;
#30841 = CARTESIAN_POINT ( 'NONE',  ( 27.99999999999996092, 197.6875000013655779, 173.4587341249998929 ) ) ;
#30842 = CARTESIAN_POINT ( 'NONE',  ( -7.188101187499991163, 2.977408999572646930, 1.767802781871753881 ) ) ;
#30843 = CARTESIAN_POINT ( 'NONE',  ( 5.676582343750001591, 81.61458332991935549, -9.832129032723420536 ) ) ;
#30844 = ORIENTED_EDGE ( 'NONE', *, *, #52704, .T. ) ;
#30845 = B_SPLINE_CURVE_WITH_KNOTS ( 'NONE', 3,
 ( #46314, #40658, #45567, #52354, #63662, #62541, #16505, #51600 ),
 .UNSPECIFIED., .F., .F.,
 ( 4, 2, 2, 4 ),
 ( 0.005256334970461813000, 0.006570121696640287938, 0.007883908422818762876, 0.01051148187517571102 ),
 .UNSPECIFIED. ) ;
#30846 = CARTESIAN_POINT ( 'NONE',  ( 8.660254037844396180, 140.4166666666666572, -5.000000000000004441 ) ) ;
#30847 = DIRECTION ( 'NONE',  ( -0.000000000000000000, -1.000000000000000000, -0.000000000000000000 ) ) ;
#30848 = VERTEX_POINT ( 'NONE', #9148 ) ;
#30849 = CYLINDRICAL_SURFACE ( 'NONE', #14557, 8.000000000000000000 ) ;
#30850 = CARTESIAN_POINT ( 'NONE',  ( 7.320508075688771044, 233.1250000000000284, -7.320508075688771932 ) ) ;
#30851 = CARTESIAN_POINT ( 'NONE',  ( -11.35316468750000141, 73.28124999658602690, -1.390361679473963753E-15 ) ) ;
#30852 = VERTEX_POINT ( 'NONE', #55559 ) ;
#30853 = CARTESIAN_POINT ( 'NONE',  ( 1.871523826299183495E-15, -10.18810118749999916, 87.90625000204838102 ) ) ;
#30854 = CARTESIAN_POINT ( 'NONE',  ( -7.204075437095967871, 7.204075437095967871, 115.4687500020483810 ) ) ;
#30855 = CARTESIAN_POINT ( 'NONE',  ( 1.432654583217664701, 209.0000000013655779, 201.4587341250000065 ) ) ;
#30856 = CARTESIAN_POINT ( 'NONE',  ( 0.000000000000000000, 0.000000000000000000, 0.000000000000000000 ) ) ;
#30858 = CARTESIAN_POINT ( 'NONE',  ( 9.832129032723416984, 75.36458332991935549, 5.676582343750006032 ) ) ;
#30857 = CARTESIAN_POINT ( 'NONE',  ( -4.000000000000001776, 13.18749999726881583, -1.656854249492381470 ) ) ;
#30859 = CARTESIAN_POINT ( 'NONE',  ( -5.656854249492375253, 5.656854249492375253, 24.83030278392014978 ) ) ;
#30860 = ADVANCED_FACE ( 'NONE', ( #33299 ), #67615, .T. ) ;
#30861 = CARTESIAN_POINT ( 'NONE',  ( -30.82842712474612057, 196.5000000027312126, 172.8284271247466108 ) ) ;
#30862 = AXIS2_PLACEMENT_3D ( 'NONE', #71551, #48175, #60616 ) ;
#30863 = CARTESIAN_POINT ( 'NONE',  ( 5.000000000000001776, 162.7083333265053966, -8.660254037844389075 ) ) ;
#30864 = CARTESIAN_POINT ( 'NONE',  ( 2.828427124746153876, 200.0000000027312126, 144.8284271247462129 ) ) ;
#30865 = CARTESIAN_POINT ( 'NONE',  ( -27.61630405986317882, 194.7720153983104012, 173.7720153983105718 ) ) ;
#30866 = CARTESIAN_POINT ( 'NONE',  ( -5.676582343749998039, 57.76041666325268409, -9.832129032723420536 ) ) ;
#30867 = EDGE_CURVE ( 'NONE', #59993, #63061, #22927, .T. ) ;
#30868 = CARTESIAN_POINT ( 'NONE',  ( -6.238412754330611322E-16, 10.18810118749999916, 108.1562500020483668 ) ) ;
#30869 = CARTESIAN_POINT ( 'NONE',  ( 8.311093377946837890, 201.4062499965860127, -8.311093377946837890 ) ) ;
#30870 = EDGE_LOOP ( 'NONE', ( #49255, #41638, #73358, #44251, #32077 ) ) ;
#30871 = DIRECTION ( 'NONE',  ( -0.000000000000000000, 1.000000000000000000, -0.000000000000000000 ) ) ;
#30872 = CARTESIAN_POINT ( 'NONE',  ( -4.220049686691935698, 10.18810118749999916, 67.37500000204838102 ) ) ;
#30873 = CARTESIAN_POINT ( 'NONE',  ( 2.679491924311149464, 60.83333332650535397, 10.00000000000004619 ) ) ;
#30875 = CARTESIAN_POINT ( 'NONE',  ( -8.311093377946836114, 187.6562499965860411, -8.311093377946837890 ) ) ;
#30874 = CARTESIAN_POINT ( 'NONE',  ( 2.249999999999999112, -2.249999999999999556, 28.00000000000000000 ) ) ;
#30876 = CARTESIAN_POINT ( 'NONE',  ( -2.849036369511732440E-14, 203.2500000000000000, 138.0000000000000568 ) ) ;
#30877 = CARTESIAN_POINT ( 'NONE',  ( 5.000000000000004441, 244.7916666734946318, 8.660254037844385522 ) ) ;
#30878 = CARTESIAN_POINT ( 'NONE',  ( -29.65685424949244364, 200.4375000000000568, 174.0000000000003126 ) ) ;
#30879 = ORIENTED_EDGE ( 'NONE', *, *, #59688, .F. ) ;
#30880 = CARTESIAN_POINT ( 'NONE',  ( -3.042071309553173730, 184.6354166632526983, 11.35316468749999785 ) ) ;
#30881 = CARTESIAN_POINT ( 'NONE',  ( -7.188101187499992051, 2.977408999572646930, 19.39280278187176165 ) ) ;
#30882 =( BOUNDED_CURVE ( )  B_SPLINE_CURVE ( 2, ( #21875, #61127, #45270, #68281, #9827, #74310, #3796, #10944, #55861 ),
 .UNSPECIFIED., .F., .F. ) 
 B_SPLINE_CURVE_WITH_KNOTS ( ( 3, 2, 2, 2, 3 ),
 ( 0.3166666666666668184, 0.3250000000000002331, 0.3333333333333335924, 0.3416666666666670626, 0.3500000000000004219 ),
 .UNSPECIFIED. ) 
 CURVE ( )  GEOMETRIC_REPRESENTATION_ITEM ( )  RATIONAL_B_SPLINE_CURVE ( ( 0.9999999999999984457, 0.9238795325112882928, 1.000000000000000000, 0.9238795325112867385, 1.000000000000000000, 0.9238795325112867385, 1.000000000000000000, 0.9238795325112826307, 1.000000000000003997 ) ) 
 REPRESENTATION_ITEM ( '' )  );
#30883 = CARTESIAN_POINT ( 'NONE',  ( 7.999999999842164478, 5.025161467855852442E-05, 22.76780420562571905 ) ) ;
#30884 =( BOUNDED_CURVE ( )  B_SPLINE_CURVE ( 2, ( #17967, #62865, #29297, #5915, #69281, #29660, #70396, #272, #52307 ),
 .UNSPECIFIED., .F., .F. ) 
 B_SPLINE_CURVE_WITH_KNOTS ( ( 3, 2, 2, 2, 3 ),
 ( 0.9305555555555554692, 0.9374999999999998890, 0.9444444444444443088, 0.9513888888888887285, 0.9583333333333332593 ),
 .UNSPECIFIED. ) 
 CURVE ( )  GEOMETRIC_REPRESENTATION_ITEM ( )  RATIONAL_B_SPLINE_CURVE ( ( 1.000000000000001110, 0.9238795325112855172, 1.000000000000000000, 0.9238795325112867385, 1.000000000000000000, 0.9238795325112867385, 1.000000000000000000, 0.9238795325112879597, 0.9999999999999987788 ) ) 
 REPRESENTATION_ITEM ( '' )  );
#30885 = VERTEX_POINT ( 'NONE', #15912 ) ;
#30886 = CARTESIAN_POINT ( 'NONE',  ( 8.000000000000000000, 96.03125000409677625, -3.313708498984762496 ) ) ;
#30887 = CARTESIAN_POINT ( 'NONE',  ( 2.679491924311228956, 6.041666666666666075, -10.00000000000000000 ) ) ;
#30888 = CARTESIAN_POINT ( 'NONE',  ( -7.347880794884122694E-16, 16.75000000000000000, 4.000000000000001776 ) ) ;
#30889 = CARTESIAN_POINT ( 'NONE',  ( -8.342170076843785083E-16, 14.06249999863440614, 4.541265875000002339 ) ) ;
#30890 = CARTESIAN_POINT ( 'NONE',  ( -7.999999999999989342, -3.313708498984762496, 11.61155278392014445 ) ) ;
#30891 = CARTESIAN_POINT ( 'NONE',  ( -25.17157287525377285, 195.6250000000000284, 172.8284271247465256 ) ) ;
#30892 = B_SPLINE_CURVE_WITH_KNOTS ( 'NONE', 3,
 ( #8650, #32037, #7906, #31664 ),
 .UNSPECIFIED., .F., .F.,
 ( 4, 4 ),
 ( 1.001577211601604482E-15, 0.0004743803571056590031 ),
 .UNSPECIFIED. ) ;
#30893 = VERTEX_POINT ( 'NONE', #4613 ) ;
#30894 = CARTESIAN_POINT ( 'NONE',  ( 11.00000000000010658, 4.556349186103942017, 72.34374999999997158 ) ) ;
#30895 = CARTESIAN_POINT ( 'NONE',  ( -7.188101187500000044, 100.1562500020483810, 0.000000000000000000 ) ) ;
#30897 = CARTESIAN_POINT ( 'NONE',  ( 8.000000000000001776, 119.8437500040967620, 3.313708498984759387 ) ) ;
#30896 = CARTESIAN_POINT ( 'NONE',  ( 5.000000000000028422, 180.8333333333333997, -8.660254037844435260 ) ) ;
#30898 = DIRECTION ( 'NONE',  ( 1.000000000000000000, 0.000000000000000000, 0.000000000000000000 ) ) ;
#30899 = VERTEX_POINT ( 'NONE', #12118 ) ;
#30900 = CARTESIAN_POINT ( 'NONE',  ( 9.832129032723416984, 262.1354166700806445, -5.676582343750003368 ) ) ;
#30901 = CARTESIAN_POINT ( 'NONE',  ( -2.977408999572648707, -7.188101187499990274, 21.26780278187175810 ) ) ;
#30902 = ORIENTED_EDGE ( 'NONE', *, *, #49917, .F. ) ;
#30903 = EDGE_LOOP ( 'NONE', ( #23827, #72379, #51180 ) ) ;
#30904 = CARTESIAN_POINT ( 'NONE',  ( -7.204075437095965206, -7.204075437095968759, 78.34375000204838102 ) ) ;
#30905 = FACE_OUTER_BOUND ( 'NONE', #6489, .T. ) ;
#30906 = CARTESIAN_POINT ( 'NONE',  ( -10.99999999999999822, -4.556349186104052151, 94.09375000000001421 ) ) ;
#30909 = CARTESIAN_POINT ( 'NONE',  ( -2.765530957081998142, 293.7968750017070079, 6.676582343750000703 ) ) ;
#30908 = CARTESIAN_POINT ( 'NONE',  ( 25.17157287525377996, 200.7500000027312126, 167.1715728752537586 ) ) ;
#30907 = DIRECTION ( 'NONE',  ( -0.000000000000000000, 1.000000000000000000, -1.563033456626094573E-30 ) ) ;
#30910 = CARTESIAN_POINT ( 'NONE',  ( -2.679491924311235618, 153.5416666666666856, 10.00000000000000000 ) ) ;
#30911 = FACE_OUTER_BOUND ( 'NONE', #55593, .T. ) ;
#30912 = CARTESIAN_POINT ( 'NONE',  ( -2.751064625579944321E-14, 208.8750000027312126, 146.0000000000000284 ) ) ;
#30913 = CARTESIAN_POINT ( 'NONE',  ( -7.999999999999968914, 3.313708498984778039, 15.73655277982336287 ) ) ;
#30914 = DIRECTION ( 'NONE',  ( -1.000000000000000000, 0.000000000000000000, -0.000000000000000000 ) ) ;
#30915 = CARTESIAN_POINT ( 'NONE',  ( 31.45873412499999944, 200.7500000013656347, 168.5673454167822740 ) ) ;
#30916 = CARTESIAN_POINT ( 'NONE',  ( 7.188101187500001821, 11.43749999795161010, -2.977408999572650483 ) ) ;
#30917 = CARTESIAN_POINT ( 'NONE',  ( 7.999999999999991118, 9.797174393178815797E-16, 25.76780278392014978 ) ) ;
#30918 = DIRECTION ( 'NONE',  ( 0.000000000000000000, 1.000000000000000000, 0.000000000000000000 ) ) ;
#30919 = CARTESIAN_POINT ( 'NONE',  ( -7.188101187500000933, 112.4375000020483810, -2.977408999572650483 ) ) ;
#30920 = PLANE ( 'NONE',  #59484 ) ;
#30921 = CARTESIAN_POINT ( 'NONE',  ( -8.311093377946836114, 233.5937500034139305, -8.311093377946836114 ) ) ;
#30922 = CARTESIAN_POINT ( 'NONE',  ( -1.656854249492383468, 12.68750000000000178, 4.000000000000000888 ) ) ;
#30923 = CARTESIAN_POINT ( 'NONE',  ( 2.977408999572650927, -7.188101187499990274, 20.33030278187175455 ) ) ;
#30924 = CARTESIAN_POINT ( 'NONE',  ( 29.65685424949235482, 195.0625000000000284, 173.9999999999999147 ) ) ;
#30925 = CARTESIAN_POINT ( 'NONE',  ( 9.832129032723420536, 36.19791666325268409, -5.676582343749999815 ) ) ;
#30926 = CARTESIAN_POINT ( 'NONE',  ( 27.99999999999999645, 210.0000000000000284, 169.9999999999999147 ) ) ;
#30927 = CARTESIAN_POINT ( 'NONE',  ( -10.00000000000000178, 4.374999993172032475, -1.224646799147353454E-15 ) ) ;
#30928 = DIRECTION ( 'NONE',  ( 0.000000000000000000, 0.000000000000000000, 1.000000000000000000 ) ) ;
#30929 = CARTESIAN_POINT ( 'NONE',  ( 2.775557561562891351E-14, 210.0000000000000284, 198.0000000000000284 ) ) ;
#30930 = ORIENTED_EDGE ( 'NONE', *, *, #3515, .F. ) ;
#30931 = CARTESIAN_POINT ( 'NONE',  ( -7.320508075688778149, 129.9999999931719969, 7.320508075688769267 ) ) ;
#30932 = CARTESIAN_POINT ( 'NONE',  ( 3.313708498984756279, 7.999999999999991118, 18.36155277982337353 ) ) ;
#30933 = EDGE_CURVE ( 'NONE', #35109, #53701, #48227, .T. ) ;
#30934 = CARTESIAN_POINT ( 'NONE',  ( 11.35316468749999785, 40.57291666325268409, 3.042071309553174174 ) ) ;
#30935 = CARTESIAN_POINT ( 'NONE',  ( 11.00000000000000355, -4.556349186104045046, 85.84375000409676204 ) ) ;
#30936 = CARTESIAN_POINT ( 'NONE',  ( -3.458734125000015425, 199.2500000013656063, 143.4326545832176976 ) ) ;
#30937 = CARTESIAN_POINT ( 'NONE',  ( 1.432654583217608080, 205.8750000013656063, 138.5412658750000503 ) ) ;
#30938 = DIRECTION ( 'NONE',  ( -0.8660254037844391517, 0.4999999999999990563, -0.000000000000000000 ) ) ;
#30939 = CARTESIAN_POINT ( 'NONE',  ( -2.849036369511732440E-14, 195.2500000000000000, 138.0000000000000568 ) ) ;
#30941 = CARTESIAN_POINT ( 'NONE',  ( -8.311093377946836114, 27.65624999658601979, -8.311093377946837890 ) ) ;
#30940 = CARTESIAN_POINT ( 'NONE',  ( -7.188101187499999156, 104.7500000020483810, 2.977408999572654924 ) ) ;
#30942 = CARTESIAN_POINT ( 'NONE',  ( 7.999999999999992895, -3.313708498984756279, 17.98655277982336642 ) ) ;
#30943 = CARTESIAN_POINT ( 'NONE',  ( -8.311093377946841443, 153.9062499965860127, 8.311093377946830785 ) ) ;
#30944 = CARTESIAN_POINT ( 'NONE',  ( -2.679491924311225848, 128.3333333265053682, -10.00000000000000178 ) ) ;
#30945 = CARTESIAN_POINT ( 'NONE',  ( 7.188101187500002709, 107.1875000020483810, 2.977408999572649151 ) ) ;
#30946 = FACE_OUTER_BOUND ( 'NONE', #15381, .T. ) ;
#30947 = CARTESIAN_POINT ( 'NONE',  ( -31.45873412499998523, 203.0000000013655779, 171.4326545832180386 ) ) ;
#30948 = ORIENTED_EDGE ( 'NONE', *, *, #69039, .T. ) ;
#30949 = CARTESIAN_POINT ( 'NONE',  ( -5.999999999999999112, 289.0625000000000000, 2.485281374238575314 ) ) ;
#30950 = CARTESIAN_POINT ( 'NONE',  ( 3.042071309553159519, 25.05208332991934839, 11.35316468750000141 ) ) ;
#30951 = EDGE_LOOP ( 'NONE', ( #412, #29434, #56299, #74247, #66041, #15020, #35648, #23167, #46090, #9940, #4689, #58244, #50296, #74401, #55241, #38826, #8438, #42869, #16000, #3320, #5492, #23311, #38487, #52985, #41628, #55206, #74294, #17118, #7712, #54853, #46877, #14095, #46504, #48754 ) ) ;
#30952 = FACE_OUTER_BOUND ( 'NONE', #37146, .T. ) ;
#30953 = CARTESIAN_POINT ( 'NONE',  ( 1.959434878635763554E-15, 237.9999999999999716, -15.99999999999998579 ) ) ;
#30955 = CARTESIAN_POINT ( 'NONE',  ( 8.311093377946834337, 155.1562499965860127, 8.311093377946839666 ) ) ;
#30954 = DIRECTION ( 'NONE',  ( -0.000000000000000000, 1.000000000000000000, 4.476705744456276341E-16 ) ) ;
#30956 = LINE ( 'NONE', #9449, #31497 ) ;
#30957 = CARTESIAN_POINT ( 'NONE',  ( 5.656854249492374365, 5.656854249492375253, 15.32405278432982421 ) ) ;
#30958 = CARTESIAN_POINT ( 'NONE',  ( 5.000000000000004441, 224.7916666734946602, 8.660254037844385522 ) ) ;
#30959 = CARTESIAN_POINT ( 'NONE',  ( -5.676582343750000703, 228.0729166700806729, -9.832129032723418760 ) ) ;
#30960 = EDGE_CURVE ( 'NONE', #71006, #32560, #56229, .T. ) ;
#30961 = CARTESIAN_POINT ( 'NONE',  ( 4.220049686691934809, 10.18810118749999916, 94.56250000204838102 ) ) ;
#30962 = EDGE_LOOP ( 'NONE', ( #9739, #19477, #46770, #2180 ) ) ;
#30963 = AXIS2_PLACEMENT_3D ( 'NONE', #53005, #59405, #12989 ) ;
#30964 = CARTESIAN_POINT ( 'NONE',  ( -1.469576158976823947E-15, 20.43749999590322375, 8.000000000000000000 ) ) ;
#30965 = CARTESIAN_POINT ( 'NONE',  ( 31.99999999999998579, 205.1875000000000000, 171.6568542494923122 ) ) ;
#30966 = CARTESIAN_POINT ( 'NONE',  ( -11.35316468749999785, 103.3854166632526699, -3.042071309553167513 ) ) ;
#30967 = CARTESIAN_POINT ( 'NONE',  ( -10.18810118749999738, -4.220049686691941915, 102.2500000020483952 ) ) ;
#30968 = CARTESIAN_POINT ( 'NONE',  ( -4.541265875000002339, 18.87499999863441147, -1.881053915767121998 ) ) ;
#30969 = VERTEX_POINT ( 'NONE', #28359 ) ;
#30970 = VERTEX_POINT ( 'NONE', #17030 ) ;
#30971 = CARTESIAN_POINT ( 'NONE',  ( -8.000000000000000000, 9.750000000000001776, -9.797174393178825657E-16 ) ) ;
#30972 = CARTESIAN_POINT ( 'NONE',  ( -8.000000000000000000, 106.9062500000000000, -3.313708498984761164 ) ) ;
#30973 = CARTESIAN_POINT ( 'NONE',  ( 2.977408999572651815, 27.56249999795161187, 7.188101187500000933 ) ) ;
#30974 = CARTESIAN_POINT ( 'NONE',  ( -8.000000000000000000, 116.1875000040967763, 0.000000000000000000 ) ) ;
#30975 =( BOUNDED_CURVE ( )  B_SPLINE_CURVE ( 2, ( #69220, #27735, #46572, #57549, #50746, #4742, #34541, #5856, #28853 ),
 .UNSPECIFIED., .F., .F. ) 
 B_SPLINE_CURVE_WITH_KNOTS ( ( 3, 2, 2, 2, 3 ),
 ( 0.1250000000000000000, 0.1306818181818181768, 0.1363636363636363535, 0.1420454545454545581, 0.1477272727272727348 ),
 .UNSPECIFIED. ) 
 CURVE ( )  GEOMETRIC_REPRESENTATION_ITEM ( )  RATIONAL_B_SPLINE_CURVE ( ( 1.000000000000000000, 0.9238795325112867385, 1.000000000000000000, 0.9238795325112867385, 1.000000000000000000, 0.9238795325112867385, 1.000000000000000000, 0.9238795325112867385, 1.000000000000000000 ) ) 
 REPRESENTATION_ITEM ( '' )  );
#30976 = CARTESIAN_POINT ( 'NONE',  ( -10.18810118749999916, 0.000000000000000000, 98.03125000204838102 ) ) ;
#30977 = CARTESIAN_POINT ( 'NONE',  ( -4.000000000000001776, 0.4375000000000002220, -1.656854249492381470 ) ) ;
#30978 = CARTESIAN_POINT ( 'NONE',  ( 2.449293598294707893E-16, 14.99999999726881406, -4.000000000000001776 ) ) ;
#30979 = CARTESIAN_POINT ( 'NONE',  ( 1.881053915767122664, 2.124999998634406584, 4.541265875000001451 ) ) ;
#30980 = ORIENTED_EDGE ( 'NONE', *, *, #63303, .T. ) ;
#30981 = AXIS2_PLACEMENT_3D ( 'NONE', #65796, #55618, #49943 ) ;
#30982 = DIRECTION ( 'NONE',  ( -0.000000000000000000, -1.000000000000000000, -0.000000000000000000 ) ) ;
#30983 = CARTESIAN_POINT ( 'NONE',  ( 26.34314575050766649, 207.5625000000000284, 165.9999999999998579 ) ) ;
#30985 = LINE ( 'NONE', #60025, #51489 ) ;
#30984 = CARTESIAN_POINT ( 'NONE',  ( -24.54126587499996148, 200.1250000013656063, 171.4326545832179534 ) ) ;
#30986 =( LENGTH_UNIT ( ) NAMED_UNIT ( * ) SI_UNIT ( .MILLI., .METRE. ) );
#30987 =( BOUNDED_SURFACE ( )  B_SPLINE_SURFACE ( 1, 2, ( 
 ( #19389, #13717, #54493, #31085, #59774, #2425, #60878, #25419, #43147, #20884, #65789, #42774, #9200, #37128, #61255, #32221, #2798, #55239, #3545, #60131, #26536, #8449, #31470, #9587, #25786, #49561, #66164, #60505, #72579, #43906, #15221, #48065, #10324, #44652, #62361, #23399, #3930, #21257, #12445, #46414, #10692, #419, #26921, #6438, #49936, #72951, #38995, #63761, #33725, #22002, #46776, #52087, #15593, #44282, #64137, #67668, #61634, #6060, #73690, #52451, #16328, #69428, #41130, #35477, #789, #35115, #17737, #57755, #39364, #50304, #45028, #29440, #67293, #38632, #62000, #12079, #29066, #68035, #69800, #40752, #9952, #32985, #55986, #15966, #4297, #58129, #23773, #18116, #27288, #73325, #21628, #33349, #56351, #4669, #27666, #50671, #70901, #30175, #53561, #19216, #7170, #42221, #58858, #1154, #41860, #64512, #19951, #65233, #71629, #25235, #1877, #30545, #24863, #7539, #47882, #13537, #12811, #36576, #6797, #29809, #36210, #52819, #58491, #31280, #24132, #71259, #53192, #47145, #59589, #18486, #1528, #7902, #18853, #13174, #30908, #65608, #53928, #35844, #24508, #70177, #59951, #41496, #59227, #2241, #47512, #70538, #64871, #48252, #54308, #19578, #42593, #13907, #36946, #25609, #8266, #2619, #48622, #42960, #65979, #14283, #50493, #26351, #9020, #9395, #44846, #3737, #55054, #50127, #73506, #61449, #61073, #25971, #3361, #72004, #56175, #32034, #49372, #32415, #9776, #67853, #61821, #72389, #4119, #27479, #4488, #21813, #54681, #49756, #43720, #20702, #21079, #55803, #37321, #2987, #60318, #27112, #44103, #32795, #8646, #73143, #48994, #37700, #66733, #66355, #33177, #21449, #60700, #15038, #14659, #31660, #55428, #67111, #38074, #26736, #72773, #20319, #43335, #15406, #38446, #44472, #67485, #15783, #38820, #10139, #52370, #40299, #39930, #4864, #56921, #50869, #35034, #62556, #10887, #62936, #63300, #23689, #40672, #5234, #57669, #6360, #58046 ),
 ( #56547, #27860, #74254, #46695, #706, #51243, #29364, #28606, #23317, #73885, #63675, #11261, #34290, #68973, #22189, #33546, #12002, #39183, #16144, #11628, #34666, #45214, #17653, #17282, #68225, #62187, #10514, #5976, #16522, #45583, #28979, #57294, #51999, #336, #22949, #39562, #68597, #28235, #46329, #33921, #69343, #5608, #22562, #16904, #51617, #74633, #45956, #47798, #41781, #71180, #53482, #64792, #1799, #47061, #70458, #59510, #64431, #54224, #2534, #58779, #24783, #1446, #42513, #35762, #70098, #24427, #29726, #35403, #18776, #70821, #13093, #18404, #7823, #25526, #36128, #59149, #52740, #69719, #19133, #64057, #18033, #7458, #41049, #42137, #58413, #6719, #53112, #12368, #1074, #30093, #13823, #30465, #2161, #24052, #65530, #65150, #13459, #36497, #41419, #12730, #36867, #7087, #31199, #30826, #53848, #47434, #19497, #25155, #48171, #59875, #8188, #38357, #15700, #3280, #26650, #66643, #20990, #44014, #55346, #10058, #26267, #37614, #61365, #25890, #4036, #72304, #8561, #2905, #60987, #71546, #48538, #49671, #20616, #50041, #32333, #43633, #3650, #48909, #49287, #9692, #43255, #33095, #56092, #60613, #72688, #54971, #21363, #14579, #71923, #14950, #31575, #14201, #37989, #67024, #9309, #20236, #32713, #4401, #15321, #55721, #54599, #19870, #27030, #42876, #73055, #44387, #65895, #67398, #66271, #38743, #61741, #37238, #8937, #60236, #31948, #73427, #44762, #56831, #10429, #67775, #4777, #45867, #62106, #74166, #23230, #68141, #21731, #40211, #39472, #40587, #63215, #5151, #74542, #5518, #16069, #11543, #50782, #73795, #63587, #62469, #5892, #33459, #56460, #22104, #39103, #16809, #57960, #22853, #27770, #28890, #28518, #45129, #249, #46240, #17192, #69258, #28144, #51526, #45490, #68882, #34576, #34199, #11916, #51158, #16436, #57582, #10797, #51909, #22470, #33833, #68509, #39837, #50413, #27393, #17568, #62842, #34949, #11177, #57203, #64709, #58328 ) ),
 .UNSPECIFIED., .F., .F., .F. ) 
 B_SPLINE_SURFACE_WITH_KNOTS ( ( 2, 2 ),
 ( 3, 2, 2, 2, 2, 2, 2, 2, 2, 2, 2, 2, 2, 2, 2, 2, 2, 2, 2, 2, 2, 2, 2, 2, 2, 2, 2, 2, 2, 2, 2, 2, 2, 2, 2, 2, 2, 2, 2, 2, 2, 2, 2, 2, 2, 2, 2, 2, 2, 2, 2, 2, 2, 2, 2, 2, 2, 2, 2, 2, 2, 2, 2, 2, 2, 2, 2, 2, 2, 2, 2, 2, 2, 2, 2, 2, 2, 2, 2, 2, 2, 2, 2, 2, 2, 2, 2, 2, 2, 2, 2, 2, 2, 2, 2, 2, 2, 2, 2, 2, 2, 2, 2, 2, 2, 2, 2, 2, 2, 2, 2, 2, 2, 2, 2, 2, 2, 2, 2, 2, 3 ),
 ( 0.000000000000000000, 1.000000000000000000 ),
 ( 0.000000000000000000, 0.008333333333333333218, 0.01666666666666666644, 0.02500000000000000139, 0.03333333333333333287, 0.04166666666666666435, 0.05000000000000000278, 0.05833333333333333426, 0.06666666666666666574, 0.07499999999999999722, 0.08333333333333332871, 0.09166666666666666019, 0.1000000000000000056, 0.1083333333333333370, 0.1166666666666666685, 0.1250000000000000000, 0.1333333333333333315, 0.1416666666666666630, 0.1499999999999999944, 0.1583333333333333259, 0.1666666666666666574, 0.1749999999999999889, 0.1833333333333333204, 0.1916666666666666796, 0.2000000000000000111, 0.2083333333333333426, 0.2166666666666666741, 0.2250000000000000056, 0.2333333333333333370, 0.2416666666666666685, 0.2500000000000000000, 0.2583333333333333592, 0.2666666666666666630, 0.2750000000000000222, 0.2833333333333333259, 0.2916666666666666852, 0.2999999999999999889, 0.3083333333333333481, 0.3166666666666666519, 0.3250000000000000111, 0.3333333333333333148, 0.3416666666666666741, 0.3499999999999999778, 0.3583333333333333370, 0.3666666666666666408, 0.3750000000000000000, 0.3833333333333333592, 0.3916666666666666630, 0.4000000000000000222, 0.4083333333333333259, 0.4166666666666666852, 0.4249999999999999889, 0.4333333333333333481, 0.4416666666666666519, 0.4500000000000000111, 0.4583333333333333148, 0.4666666666666666741, 0.4749999999999999778, 0.4833333333333333370, 0.4916666666666666408, 0.5000000000000000000, 0.5083333333333333037, 0.5166666666666667185, 0.5250000000000000222, 0.5333333333333333259, 0.5416666666666666297, 0.5500000000000000444, 0.5583333333333333481, 0.5666666666666666519, 0.5749999999999999556, 0.5833333333333333703, 0.5916666666666666741, 0.5999999999999999778, 0.6083333333333332815, 0.6166666666666666963, 0.6250000000000000000, 0.6333333333333333037, 0.6416666666666667185, 0.6500000000000000222, 0.6583333333333333259, 0.6666666666666666297, 0.6750000000000000444, 0.6833333333333333481, 0.6916666666666666519, 0.6999999999999999556, 0.7083333333333333703, 0.7166666666666666741, 0.7249999999999999778, 0.7333333333333332815, 0.7416666666666666963, 0.7500000000000000000, 0.7583333333333333037, 0.7666666666666667185, 0.7750000000000000222, 0.7833333333333333259, 0.7916666666666666297, 0.8000000000000000444, 0.8083333333333333481, 0.8166666666666666519, 0.8249999999999999556, 0.8333333333333333703, 0.8416666666666666741, 0.8499999999999999778, 0.8583333333333332815, 0.8666666666666666963, 0.8750000000000000000, 0.8833333333333333037, 0.8916666666666667185, 0.9000000000000000222, 0.9083333333333333259, 0.9166666666666666297, 0.9250000000000000444, 0.9333333333333333481, 0.9416666666666666519, 0.9499999999999999556, 0.9583333333333333703, 0.9666666666666666741, 0.9749999999999999778, 0.9833333333333332815, 0.9916666666666666963, 1.000000000000000000 ),
 .UNSPECIFIED. ) 
 GEOMETRIC_REPRESENTATION_ITEM ( )  RATIONAL_B_SPLINE_SURFACE ( (
 ( 1.000000000000000000, 0.9238795325112867385, 1.000000000000000000, 0.9238795325112867385, 1.000000000000000000, 0.9238795325112867385, 1.000000000000000000, 0.9238795325112867385, 1.000000000000000000, 0.9238795325112867385, 1.000000000000000000, 0.9238795325112867385, 1.000000000000000000, 0.9238795325112867385, 1.000000000000000000, 0.9238795325112867385, 1.000000000000000000, 0.9238795325112867385, 1.000000000000000000, 0.9238795325112867385, 1.000000000000000000, 0.9238795325112867385, 1.000000000000000000, 0.9238795325112867385, 1.000000000000000000, 0.9238795325112867385, 1.000000000000000000, 0.9238795325112867385, 1.000000000000000000, 0.9238795325112867385, 1.000000000000000000, 0.9238795325112867385, 1.000000000000000000, 0.9238795325112867385, 1.000000000000000000, 0.9238795325112867385, 1.000000000000000000, 0.9238795325112867385, 1.000000000000000000, 0.9238795325112867385, 1.000000000000000000, 0.9238795325112867385, 1.000000000000000000, 0.9238795325112867385, 1.000000000000000000, 0.9238795325112867385, 1.000000000000000000, 0.9238795325112867385, 1.000000000000000000, 0.9238795325112867385, 1.000000000000000000, 0.9238795325112867385, 1.000000000000000000, 0.9238795325112867385, 1.000000000000000000, 0.9238795325112867385, 1.000000000000000000, 0.9238795325112867385, 1.000000000000000000, 0.9238795325112867385, 1.000000000000000000, 0.9238795325112867385, 1.000000000000000000, 0.9238795325112867385, 1.000000000000000000, 0.9238795325112867385, 1.000000000000000000, 0.9238795325112867385, 1.000000000000000000, 0.9238795325112867385, 1.000000000000000000, 0.9238795325112867385, 1.000000000000000000, 0.9238795325112867385, 1.000000000000000000, 0.9238795325112867385, 1.000000000000000000, 0.9238795325112867385, 1.000000000000000000, 0.9238795325112867385, 1.000000000000000000, 0.9238795325112867385, 1.000000000000000000, 0.9238795325112867385, 1.000000000000000000, 0.9238795325112867385, 1.000000000000000000, 0.9238795325112867385, 1.000000000000000000, 0.9238795325112867385, 1.000000000000000000, 0.9238795325112867385, 1.000000000000000000, 0.9238795325112867385, 1.000000000000000000, 0.9238795325112867385, 1.000000000000000000, 0.9238795325112867385, 1.000000000000000000, 0.9238795325112867385, 1.000000000000000000, 0.9238795325112867385, 1.000000000000000000, 0.9238795325112867385, 1.000000000000000000, 0.9238795325112867385, 1.000000000000000000, 0.9238795325112867385, 1.000000000000000000, 0.9238795325112867385, 1.000000000000000000, 0.9238795325112867385, 1.000000000000000000, 0.9238795325112867385, 1.000000000000000000, 0.9238795325112867385, 1.000000000000000000, 0.9238795325112867385, 1.000000000000000000, 0.9238795325112867385, 1.000000000000000000, 0.9238795325112867385, 1.000000000000000000, 0.9238795325112867385, 1.000000000000000000, 0.9238795325112867385, 1.000000000000000000, 0.9238795325112867385, 1.000000000000000000, 0.9238795325112867385, 1.000000000000000000, 0.9238795325112867385, 1.000000000000000000, 0.9238795325112867385, 1.000000000000000000, 0.9238795325112867385, 1.000000000000000000, 0.9238795325112867385, 1.000000000000000000, 0.9238795325112867385, 1.000000000000000000, 0.9238795325112867385, 1.000000000000000000, 0.9238795325112867385, 1.000000000000000000, 0.9238795325112867385, 1.000000000000000000, 0.9238795325112867385, 1.000000000000000000, 0.9238795325112867385, 1.000000000000000000, 0.9238795325112867385, 1.000000000000000000, 0.9238795325112867385, 1.000000000000000000, 0.9238795325112867385, 1.000000000000000000, 0.9238795325112867385, 1.000000000000000000, 0.9238795325112867385, 1.000000000000000000, 0.9238795325112867385, 1.000000000000000000, 0.9238795325112867385, 1.000000000000000000, 0.9238795325112867385, 1.000000000000000000, 0.9238795325112867385, 1.000000000000000000, 0.9238795325112867385, 1.000000000000000000, 0.9238795325112867385, 1.000000000000000000, 0.9238795325112867385, 1.000000000000000000, 0.9238795325112867385, 1.000000000000000000, 0.9238795325112867385, 1.000000000000000000, 0.9238795325112867385, 1.000000000000000000, 0.9238795325112867385, 1.000000000000000000, 0.9238795325112867385, 1.000000000000000000, 0.9238795325112867385, 1.000000000000000000, 0.9238795325112867385, 1.000000000000000000, 0.9238795325112867385, 1.000000000000000000, 0.9238795325112867385, 1.000000000000000000, 0.9238795325112867385, 1.000000000000000000, 0.9238795325112867385, 1.000000000000000000, 0.9238795325112867385, 1.000000000000000000, 0.9238795325112867385, 1.000000000000000000, 0.9238795325112867385, 1.000000000000000000, 0.9238795325112867385, 1.000000000000000000, 0.9238795325112867385, 1.000000000000000000, 0.9238795325112867385, 1.000000000000000000, 0.9238795325112867385, 1.000000000000000000, 0.9238795325112867385, 1.000000000000000000, 0.9238795325112867385, 1.000000000000000000, 0.9238795325112867385, 1.000000000000000000, 0.9238795325112867385, 1.000000000000000000, 0.9238795325112867385, 1.000000000000000000, 0.9238795325112867385, 1.000000000000000000, 0.9238795325112867385, 1.000000000000000000, 0.9238795325112867385, 1.000000000000000000, 0.9238795325112867385, 1.000000000000000000, 0.9238795325112867385, 1.000000000000000000, 0.9238795325112867385, 1.000000000000000000, 0.9238795325112867385, 1.000000000000000000, 0.9238795325112867385, 1.000000000000000000, 0.9238795325112867385, 1.000000000000000000, 0.9238795325112867385, 1.000000000000000000),
 ( 1.000000000000000000, 0.9238795325112867385, 1.000000000000000000, 0.9238795325112867385, 1.000000000000000000, 0.9238795325112867385, 1.000000000000000000, 0.9238795325112867385, 1.000000000000000000, 0.9238795325112867385, 1.000000000000000000, 0.9238795325112867385, 1.000000000000000000, 0.9238795325112867385, 1.000000000000000000, 0.9238795325112867385, 1.000000000000000000, 0.9238795325112867385, 1.000000000000000000, 0.9238795325112867385, 1.000000000000000000, 0.9238795325112867385, 1.000000000000000000, 0.9238795325112867385, 1.000000000000000000, 0.9238795325112867385, 1.000000000000000000, 0.9238795325112867385, 1.000000000000000000, 0.9238795325112867385, 1.000000000000000000, 0.9238795325112867385, 1.000000000000000000, 0.9238795325112867385, 1.000000000000000000, 0.9238795325112867385, 1.000000000000000000, 0.9238795325112867385, 1.000000000000000000, 0.9238795325112867385, 1.000000000000000000, 0.9238795325112867385, 1.000000000000000000, 0.9238795325112867385, 1.000000000000000000, 0.9238795325112867385, 1.000000000000000000, 0.9238795325112867385, 1.000000000000000000, 0.9238795325112867385, 1.000000000000000000, 0.9238795325112867385, 1.000000000000000000, 0.9238795325112867385, 1.000000000000000000, 0.9238795325112867385, 1.000000000000000000, 0.9238795325112867385, 1.000000000000000000, 0.9238795325112867385, 1.000000000000000000, 0.9238795325112867385, 1.000000000000000000, 0.9238795325112867385, 1.000000000000000000, 0.9238795325112867385, 1.000000000000000000, 0.9238795325112867385, 1.000000000000000000, 0.9238795325112867385, 1.000000000000000000, 0.9238795325112867385, 1.000000000000000000, 0.9238795325112867385, 1.000000000000000000, 0.9238795325112867385, 1.000000000000000000, 0.9238795325112867385, 1.000000000000000000, 0.9238795325112867385, 1.000000000000000000, 0.9238795325112867385, 1.000000000000000000, 0.9238795325112867385, 1.000000000000000000, 0.9238795325112867385, 1.000000000000000000, 0.9238795325112867385, 1.000000000000000000, 0.9238795325112867385, 1.000000000000000000, 0.9238795325112867385, 1.000000000000000000, 0.9238795325112867385, 1.000000000000000000, 0.9238795325112867385, 1.000000000000000000, 0.9238795325112867385, 1.000000000000000000, 0.9238795325112867385, 1.000000000000000000, 0.9238795325112867385, 1.000000000000000000, 0.9238795325112867385, 1.000000000000000000, 0.9238795325112867385, 1.000000000000000000, 0.9238795325112867385, 1.000000000000000000, 0.9238795325112867385, 1.000000000000000000, 0.9238795325112867385, 1.000000000000000000, 0.9238795325112867385, 1.000000000000000000, 0.9238795325112867385, 1.000000000000000000, 0.9238795325112867385, 1.000000000000000000, 0.9238795325112867385, 1.000000000000000000, 0.9238795325112867385, 1.000000000000000000, 0.9238795325112867385, 1.000000000000000000, 0.9238795325112867385, 1.000000000000000000, 0.9238795325112867385, 1.000000000000000000, 0.9238795325112867385, 1.000000000000000000, 0.9238795325112867385, 1.000000000000000000, 0.9238795325112867385, 1.000000000000000000, 0.9238795325112867385, 1.000000000000000000, 0.9238795325112867385, 1.000000000000000000, 0.9238795325112867385, 1.000000000000000000, 0.9238795325112867385, 1.000000000000000000, 0.9238795325112867385, 1.000000000000000000, 0.9238795325112867385, 1.000000000000000000, 0.9238795325112867385, 1.000000000000000000, 0.9238795325112867385, 1.000000000000000000, 0.9238795325112867385, 1.000000000000000000, 0.9238795325112867385, 1.000000000000000000, 0.9238795325112867385, 1.000000000000000000, 0.9238795325112867385, 1.000000000000000000, 0.9238795325112867385, 1.000000000000000000, 0.9238795325112867385, 1.000000000000000000, 0.9238795325112867385, 1.000000000000000000, 0.9238795325112867385, 1.000000000000000000, 0.9238795325112867385, 1.000000000000000000, 0.9238795325112867385, 1.000000000000000000, 0.9238795325112867385, 1.000000000000000000, 0.9238795325112867385, 1.000000000000000000, 0.9238795325112867385, 1.000000000000000000, 0.9238795325112867385, 1.000000000000000000, 0.9238795325112867385, 1.000000000000000000, 0.9238795325112867385, 1.000000000000000000, 0.9238795325112867385, 1.000000000000000000, 0.9238795325112867385, 1.000000000000000000, 0.9238795325112867385, 1.000000000000000000, 0.9238795325112867385, 1.000000000000000000, 0.9238795325112867385, 1.000000000000000000, 0.9238795325112867385, 1.000000000000000000, 0.9238795325112867385, 1.000000000000000000, 0.9238795325112867385, 1.000000000000000000, 0.9238795325112867385, 1.000000000000000000, 0.9238795325112867385, 1.000000000000000000, 0.9238795325112867385, 1.000000000000000000, 0.9238795325112867385, 1.000000000000000000, 0.9238795325112867385, 1.000000000000000000, 0.9238795325112867385, 1.000000000000000000, 0.9238795325112867385, 1.000000000000000000, 0.9238795325112867385, 1.000000000000000000, 0.9238795325112867385, 1.000000000000000000, 0.9238795325112867385, 1.000000000000000000, 0.9238795325112867385, 1.000000000000000000, 0.9238795325112867385, 1.000000000000000000, 0.9238795325112867385, 1.000000000000000000, 0.9238795325112867385, 1.000000000000000000, 0.9238795325112867385, 1.000000000000000000, 0.9238795325112867385, 1.000000000000000000, 0.9238795325112867385, 1.000000000000000000, 0.9238795325112867385, 1.000000000000000000, 0.9238795325112867385, 1.000000000000000000, 0.9238795325112867385, 1.000000000000000000, 0.9238795325112867385, 1.000000000000000000) ) ) 
 REPRESENTATION_ITEM ( '' )  SURFACE ( )  );
#30988 = CARTESIAN_POINT ( 'NONE',  ( -3.211159895383561391, 14.68749999863440792, -3.211159895383561835 ) ) ;
#30989 = CARTESIAN_POINT ( 'NONE',  ( 5.082755093536318824, 5.082755093536319713, 6.924052781871750994 ) ) ;
#30990 = ORIENTED_EDGE ( 'NONE', *, *, #23939, .F. ) ;
#30991 = VERTEX_POINT ( 'NONE', #16648 ) ;
#30992 = CARTESIAN_POINT ( 'NONE',  ( -6.238412754330611322E-16, 10.18810118749999916, 101.7812500020483810 ) ) ;
#30993 = DIRECTION ( 'NONE',  ( -1.577021341797097560E-16, 1.000000000000000000, -0.000000000000000000 ) ) ;
#30994 = CARTESIAN_POINT ( 'NONE',  ( -30.44569435410879166, 203.0625000013656063, 172.4456943541092357 ) ) ;
#30995 = CARTESIAN_POINT ( 'NONE',  ( -29.65685424949234061, 200.4375000000000568, 174.0000000000004547 ) ) ;
#30996 = CARTESIAN_POINT ( 'NONE',  ( -1.432654583217607192, 196.2500000013656631, 194.5412658750000219 ) ) ;
#30997 = CARTESIAN_POINT ( 'NONE',  ( -10.00000000000000000, 112.2916666666666714, -2.679491924311229845 ) ) ;
#30998 = ADVANCED_FACE ( 'NONE', ( #62680 ), #20048, .F. ) ;
#30999 = CARTESIAN_POINT ( 'NONE',  ( -3.313708498984762052, 109.7187500000000000, -8.000000000000000000 ) ) ;
#31000 = CARTESIAN_POINT ( 'NONE',  ( -6.676582343750003368, 296.5468750017069510, -2.765530957081996810 ) ) ;
#31001 = ORIENTED_EDGE ( 'NONE', *, *, #49985, .F. ) ;
#31002 = CARTESIAN_POINT ( 'NONE',  ( 0.000000000000000000, 2.348141146763140925E-15, 0.000000000000000000 ) ) ;
#31003 = CARTESIAN_POINT ( 'NONE',  ( 8.000000000000000000, 13.31249999590322375, 0.000000000000000000 ) ) ;
#31004 = CARTESIAN_POINT ( 'NONE',  ( -1.432654583217664479, 201.7500000013655779, 138.5412658750000787 ) ) ;
#31005 = CARTESIAN_POINT ( 'NONE',  ( -1.836970198721029983E-15, 40.62499999317203248, 10.00000000000000178 ) ) ;
#31006 = DIRECTION ( 'NONE',  ( -0.000000000000000000, -0.000000000000000000, 1.000000000000000000 ) ) ;
#31007 = CARTESIAN_POINT ( 'NONE',  ( 4.999999999999997335, 228.3333333333333428, -8.660254037844387298 ) ) ;
#31008 = CARTESIAN_POINT ( 'NONE',  ( 4.556349186104052151, -10.99999999999999822, 91.65625000409680467 ) ) ;
#31009 = CARTESIAN_POINT ( 'NONE',  ( -6.735557395310442023E-16, 11.00000000000000000, 114.6249999999999858 ) ) ;
#31010 = CARTESIAN_POINT ( 'NONE',  ( -7.320508075688778149, 213.1249999999999716, 7.320508075688769267 ) ) ;
#31011 = CARTESIAN_POINT ( 'NONE',  ( 5.082755093536318824, 5.082755093536319713, 13.29905278187175277 ) ) ;
#31012 = CARTESIAN_POINT ( 'NONE',  ( 5.676582343750001591, 196.9270833299193839, -9.832129032723420536 ) ) ;
#31013 = CARTESIAN_POINT ( 'NONE',  ( -10.99999999999994671, -4.556349186104105442, 101.5937500000000000 ) ) ;
#31014 = CARTESIAN_POINT ( 'NONE',  ( 4.541265875000001451, 1.249999998634407028, 1.881053915767124440 ) ) ;
#31015 = CARTESIAN_POINT ( 'NONE',  ( 8.660254037844385522, 242.9166666666666572, -5.000000000000003553 ) ) ;
#31017 = CARTESIAN_POINT ( 'NONE',  ( -38.00000000000000000, 205.0000000000000284, 20.00000000000003553 ) ) ;
#31016 = CYLINDRICAL_SURFACE ( 'NONE', #62346, 8.000000000000000000 ) ;
#31018 = VERTEX_POINT ( 'NONE', #53494 ) ;
#31020 = ADVANCED_FACE ( 'NONE', ( #31211 ), #26277, .T. ) ;
#31019 = CARTESIAN_POINT ( 'NONE',  ( -1.432654583217664701, 205.0000000013655779, 138.5412658750000787 ) ) ;
#31021 = CARTESIAN_POINT ( 'NONE',  ( -9.832129032723420536, 44.01041666325268409, 5.676582343749997150 ) ) ;
#31022 = CARTESIAN_POINT ( 'NONE',  ( 11.00000000000000355, -4.556349186104045046, 102.3437500040967905 ) ) ;
#31023 = CARTESIAN_POINT ( 'NONE',  ( 9.832129032723416984, 220.6770833299193555, 5.676582343750006032 ) ) ;
#31024 = CARTESIAN_POINT ( 'NONE',  ( -31.45873412499999944, 202.6875000013656063, 170.0000000000004547 ) ) ;
#31025 = CARTESIAN_POINT ( 'NONE',  ( -5.000000000000005329, 125.2083333265053540, 8.660254037844387298 ) ) ;
#31027 = CARTESIAN_POINT ( 'NONE',  ( -7.320508075688778149, 59.99999999317203248, 7.320508075688769267 ) ) ;
#31026 = CARTESIAN_POINT ( 'NONE',  ( -11.00000000000015632, -4.556349186103894944, 107.5937499999999716 ) ) ;
#31028 = CARTESIAN_POINT ( 'NONE',  ( 2.445694354108783664, 195.3125000013656063, 144.4456943541088663 ) ) ;
#31029 = CARTESIAN_POINT ( 'NONE',  ( 3.042071309553167069, 111.8229166632526983, -11.35316468749999785 ) ) ;
#31030 = ADVANCED_FACE ( 'NONE', ( #73066 ), #54984, .T. ) ;
#31031 = CARTESIAN_POINT ( 'NONE',  ( -8.660254037844390851, 89.79166665983869677, 4.999999999999998224 ) ) ;
#31032 = CARTESIAN_POINT ( 'NONE',  ( -5.082755093536324154, 92.84375000204838102, 5.082755093536326818 ) ) ;
#31033 = CARTESIAN_POINT ( 'NONE',  ( 4.541265875000002339, 14.43749999863440792, 0.000000000000000000 ) ) ;
#31034 = CARTESIAN_POINT ( 'NONE',  ( -28.00000000000007816, 204.1250000027312126, 166.0000000000003695 ) ) ;
#31035 = CARTESIAN_POINT ( 'NONE',  ( 7.999999999999983125, -3.313708498984766493, 23.98655277982336287 ) ) ;
#31036 = ORIENTED_EDGE ( 'NONE', *, *, #16971, .T. ) ;
#31037 = ORIENTED_EDGE ( 'NONE', *, *, #32009, .F. ) ;
#31038 = CARTESIAN_POINT ( 'NONE',  ( 4.721056650416000089, 294.9843750017070079, 4.721056650415999201 ) ) ;
#31039 = DIRECTION ( 'NONE',  ( 0.000000000000000000, -0.8536788251725986321, -0.5207998305029790664 ) ) ;
#31040 = CARTESIAN_POINT ( 'NONE',  ( -11.35316468750000141, 168.2812499965860411, -1.390361679473963753E-15 ) ) ;
#31041 = LINE ( 'NONE', #3129, #17622 ) ;
#31042 = CARTESIAN_POINT ( 'NONE',  ( -1.656854249492347719, 199.8125000000000284, 194.0000000000000853 ) ) ;
#31043 = EDGE_CURVE ( 'NONE', #70823, #7225, #43388, .T. ) ;
#31044 = CARTESIAN_POINT ( 'NONE',  ( -7.204075437095967871, 7.204075437095967871, 108.3437500020483810 ) ) ;
#31045 = ORIENTED_EDGE ( 'NONE', *, *, #7668, .T. ) ;
#31046 = CARTESIAN_POINT ( 'NONE',  ( -1.558072418987822783, 51.25713184919987953, -48.56213741370757475 ) ) ;
#31047 = CARTESIAN_POINT ( 'NONE',  ( -11.35316468749999785, 143.3854166632526983, -3.042071309553167957 ) ) ;
#31048 = CARTESIAN_POINT ( 'NONE',  ( 3.458734125000015425, 194.9375000013655779, 198.0000000000000284 ) ) ;
#31049 = CYLINDRICAL_SURFACE ( 'NONE', #12220, 11.00000000000000000 ) ;
#31050 = CARTESIAN_POINT ( 'NONE',  ( -4.220049686691935698, 10.18810118749999916, 69.25000000204836681 ) ) ;
#31051 = CARTESIAN_POINT ( 'NONE',  ( 11.35316468749999963, 61.30208332991934839, -3.042071309553165293 ) ) ;
#31052 = ORIENTED_EDGE ( 'NONE', *, *, #61987, .F. ) ;
#31053 = CARTESIAN_POINT ( 'NONE',  ( -3.313708498984759387, -7.999999999999989342, 13.11155277982336465 ) ) ;
#31054 = CARTESIAN_POINT ( 'NONE',  ( -4.541265875000002339, 2.937499998634407028, -5.561446717895856393E-16 ) ) ;
#31055 = CARTESIAN_POINT ( 'NONE',  ( -3.317071493978878571, 8.008118988124991233, 9.731865283940631883 ) ) ;
#31056 = CARTESIAN_POINT ( 'NONE',  ( 5.082755093536325930, 17.15624999795161543, -5.082755093536325930 ) ) ;
#31057 = CARTESIAN_POINT ( 'NONE',  ( 2.485281374238575314, 294.3750000034139589, 6.000000000000000888 ) ) ;
#31058 = CARTESIAN_POINT ( 'NONE',  ( 2.828427124746209831, 202.3750000000000284, 200.8284271247462129 ) ) ;
#31059 = CARTESIAN_POINT ( 'NONE',  ( -1.320432766682874540E-15, 10.96874999795161187, 7.188101187500000044 ) ) ;
#31060 = CARTESIAN_POINT ( 'NONE',  ( -2.977408999572647819, -7.188101187499990274, 1.767802781871753437 ) ) ;
#31061 = VECTOR ( 'NONE', #28159, 1000.000000000000000 ) ;
#31062 = CARTESIAN_POINT ( 'NONE',  ( -10.18810118749999738, -4.220049686691941915, 116.1250000020483810 ) ) ;
#31063 = EDGE_CURVE ( 'NONE', #34861, #6677, #46134, .T. ) ;
#31064 = CARTESIAN_POINT ( 'NONE',  ( -10.00000000000000355, 64.58333332650536818, 2.679491924311223183 ) ) ;
#31065 = CARTESIAN_POINT ( 'NONE',  ( 4.000000000000001776, 3.812499997268813168, -1.656854249492381248 ) ) ;
#31066 = VERTEX_POINT ( 'NONE', #44026 ) ;
#31067 = CARTESIAN_POINT ( 'NONE',  ( -1.432654583217607192, 208.2500000013656063, 194.5412658750000219 ) ) ;
#31068 = CARTESIAN_POINT ( 'NONE',  ( -1.656854249492405451, 201.3125000000000568, 138.0000000000000568 ) ) ;
#31069 = CARTESIAN_POINT ( 'NONE',  ( -25.17157287525385811, 198.0000000027312126, 167.1715728752541281 ) ) ;
#31070 = CARTESIAN_POINT ( 'NONE',  ( -3.211159895383562723, 2.937499998634407028, 3.211159895383561391 ) ) ;
#31071 = CARTESIAN_POINT ( 'NONE',  ( -4.401442555609581635E-16, 113.2812500020483952, -7.188101187500000044 ) ) ;
#31072 = CARTESIAN_POINT ( 'NONE',  ( 2.849036369511732440E-14, 195.2500000000000000, 202.0000000000000000 ) ) ;
#31073 = CARTESIAN_POINT ( 'NONE',  ( -5.656854249492373476, -5.656854249492376141, 2.705302783920143561 ) ) ;
#31074 = VERTEX_POINT ( 'NONE', #21372 ) ;
#31075 =( BOUNDED_CURVE ( )  B_SPLINE_CURVE ( 2, ( #72127, #54427, #55927, #55177, #43841 ),
 .UNSPECIFIED., .F., .F. ) 
 B_SPLINE_CURVE_WITH_KNOTS ( ( 3, 2, 3 ),
 ( 0.009783017809147894275, 0.01102941176470588480, 0.01470588235294118667 ),
 .UNSPECIFIED. ) 
 CURVE ( )  GEOMETRIC_REPRESENTATION_ITEM ( )  RATIONAL_B_SPLINE_CURVE ( ( 0.9658850645339760455, 0.9741937033643668364, 1.000000000000000000, 0.9238795325112865164, 1.000000000000000222 ) ) 
 REPRESENTATION_ITEM ( '' )  );
#31076 = CARTESIAN_POINT ( 'NONE',  ( 5.082755093536324154, 21.28124999795161543, 5.082755093536326818 ) ) ;
#31077 = VERTEX_POINT ( 'NONE', #55730 ) ;
#31078 = CARTESIAN_POINT ( 'NONE',  ( -5.000000000000005329, 203.3333333333333428, 8.660254037844387298 ) ) ;
#31079 = CARTESIAN_POINT ( 'NONE',  ( 2.445694354108839619, 206.8125000013656063, 200.4456943541088663 ) ) ;
#31080 = CARTESIAN_POINT ( 'NONE',  ( 30.44569435410879521, 203.8125000013656063, 167.5543056458910485 ) ) ;
#31081 = CARTESIAN_POINT ( 'NONE',  ( 6.123233995736767268E-16, 56.25000000000000000, -10.00000000000000178 ) ) ;
#31082 = CARTESIAN_POINT ( 'NONE',  ( -7.188101187500001821, 94.43750000204838102, -2.977408999572650483 ) ) ;
#31083 = CARTESIAN_POINT ( 'NONE',  ( -4.242640687119286547, 296.8750000000000000, -4.242640687119286547 ) ) ;
#31084 = VECTOR ( 'NONE', #73228, 1000.000000000000000 ) ;
#31086 = CARTESIAN_POINT ( 'NONE',  ( -26.09554935459949121, -41.85248577121735281, 186.7451459553997211 ) ) ;
#31085 = CARTESIAN_POINT ( 'NONE',  ( 24.00000000000001066, 208.9375000027312410, 171.6568542494923122 ) ) ;
#31087 = VERTEX_POINT ( 'NONE', #66281 ) ;
#31088 = CARTESIAN_POINT ( 'NONE',  ( 3.042071309553163960, 227.4479166700806729, -11.35316468749999785 ) ) ;
#31089 = AXIS2_PLACEMENT_3D ( 'NONE', #59240, #65990, #31672 ) ;
#31090 = CARTESIAN_POINT ( 'NONE',  ( -4.000000000000015987, 200.6250000027312126, 142.0000000000000568 ) ) ;
#31091 = CARTESIAN_POINT ( 'NONE',  ( 0.000000000000000000, 237.9999999999999716, 0.000000000000000000 ) ) ;
#31092 = CARTESIAN_POINT ( 'NONE',  ( -7.999999999999991118, 3.313708498984757167, 2.424052783920144005 ) ) ;
#31093 = CARTESIAN_POINT ( 'NONE',  ( -10.00000000000000000, 259.7916666666666288, -2.679491924311226292 ) ) ;
#31094 = CARTESIAN_POINT ( 'NONE',  ( 11.00000000000000000, 1.347111479062088405E-15, 115.9375000040967763 ) ) ;
#31095 = CARTESIAN_POINT ( 'NONE',  ( 6.123233995736767268E-16, 171.2500000000000000, -10.00000000000000178 ) ) ;
#31096 = CARTESIAN_POINT ( 'NONE',  ( -5.656854249492373476, -5.656854249492376141, 5.517802779823364645 ) ) ;
#31097 = FILL_AREA_STYLE_COLOUR ( '', #13858 ) ;
#31098 = CARTESIAN_POINT ( 'NONE',  ( -4.615726161709600817, -68.43878643976945853, 20.71807028113862970 ) ) ;
#31099 = CARTESIAN_POINT ( 'NONE',  ( -11.35316468749999785, 153.3854166632526699, -3.042071309553167513 ) ) ;
#31100 = CARTESIAN_POINT ( 'NONE',  ( 0.000000000000000000, 0.000000000000000000, 30.00000000000000000 ) ) ;
#31101 = CARTESIAN_POINT ( 'NONE',  ( 0.000000000000000000, 0.000000000000000000, -4.000000000000001776 ) ) ;
#31104 = CARTESIAN_POINT ( 'NONE',  ( -7.320508075688775484, 166.8750000000000284, -7.320508075688776373 ) ) ;
#31103 = LINE ( 'NONE', #49578, #2041 ) ;
#31102 = CARTESIAN_POINT ( 'NONE',  ( 26.34314575050758833, 203.9375000000000000, 173.9999999999999147 ) ) ;
#31105 = EDGE_LOOP ( 'NONE', ( #32851, #7076, #30443, #29833 ) ) ;
#31106 = VECTOR ( 'NONE', #8766, 1000.000000000000000 ) ;
#31107 = CARTESIAN_POINT ( 'NONE',  ( 11.35316468749999963, 11.30208332991934839, -3.042071309553165293 ) ) ;
#31108 = ADVANCED_FACE ( 'NONE', ( #61750 ), #2545, .T. ) ;
#31109 = CARTESIAN_POINT ( 'NONE',  ( 6.123233995736767268E-16, 93.12499999317203958, -10.00000000000000178 ) ) ;
#31110 = FACE_OUTER_BOUND ( 'NONE', #5568, .T. ) ;
#31111 = CARTESIAN_POINT ( 'NONE',  ( -31.99999999999999289, 196.2500000000000000, 170.0000000000003979 ) ) ;
#31112 = CARTESIAN_POINT ( 'NONE',  ( -3.458734125000016313, 205.8750000013656063, 140.5673454167823593 ) ) ;
#31113 = MECHANICAL_DESIGN_GEOMETRIC_PRESENTATION_REPRESENTATION (  '', ( #72086 ), #70906 ) ;
#31114 = CARTESIAN_POINT ( 'NONE',  ( -2.849036369511732440E-14, 202.2500000000000000, 138.0000000000000568 ) ) ;
#31115 = ADVANCED_FACE ( 'NONE', ( #26661 ), #14212, .T. ) ;
#31116 = CARTESIAN_POINT ( 'NONE',  ( -2.679491924311235618, 40.41666665983869677, 10.00000000000000000 ) ) ;
#31117 = CARTESIAN_POINT ( 'NONE',  ( -5.082755093536325930, 107.4687500020483810, -5.082755093536325930 ) ) ;
#31118 = CARTESIAN_POINT ( 'NONE',  ( 1.881053915767121776, 2.624999998634407028, -4.541265875000002339 ) ) ;
#31119 = CARTESIAN_POINT ( 'NONE',  ( 5.107860025163145856, 60.88642786445311827, -23.30380398316370716 ) ) ;
#31120 = CARTESIAN_POINT ( 'NONE',  ( -3.313708498984757167, 7.999999999999991118, 12.54905277982336287 ) ) ;
#31122 = FACE_OUTER_BOUND ( 'NONE', #16230, .T. ) ;
#31121 = CARTESIAN_POINT ( 'NONE',  ( 6.000000000000003553, 291.5000000034140157, 2.485281374238571317 ) ) ;
#31123 = EDGE_LOOP ( 'NONE', ( #46403, #11396, #66465, #14831, #7142 ) ) ;
#31124 = DIRECTION ( 'NONE',  ( 0.000000000000000000, -1.000000000000000000, 0.000000000000000000 ) ) ;
#31125 = CARTESIAN_POINT ( 'NONE',  ( -8.311093377946834337, 224.8437500034139589, 8.311093377946837890 ) ) ;
#31126 = CARTESIAN_POINT ( 'NONE',  ( 9.832129032723420536, 126.1979166632526983, -5.676582343749999815 ) ) ;
#31127 = ORIENTED_EDGE ( 'NONE', *, *, #52585, .T. ) ;
#31128 = CARTESIAN_POINT ( 'NONE',  ( 0.000000000000000000, 0.000000000000000000, 118.0000000000000000 ) ) ;
#31129 = CARTESIAN_POINT ( 'NONE',  ( 10.18810118749999916, 1.247682550866122264E-15, 92.40625000204836681 ) ) ;
#31130 = LINE ( 'NONE', #42447, #56181 ) ;
#31131 = CARTESIAN_POINT ( 'NONE',  ( -3.458734124999959469, 198.7500000013656063, 199.4326545832176691 ) ) ;
#31132 = CARTESIAN_POINT ( 'NONE',  ( 11.00000000000000000, 1.347111479062088405E-15, 118.0000000000000000 ) ) ;
#31134 = CARTESIAN_POINT ( 'NONE',  ( -3.042071309553163960, 112.2395833299193555, -11.35316468749999963 ) ) ;
#31133 = CARTESIAN_POINT ( 'NONE',  ( 26.34314575050773755, 197.5625000000000568, 165.9999999999998010 ) ) ;
#31135 = CARTESIAN_POINT ( 'NONE',  ( -25.17157287525382614, 208.8750000000000284, 167.1715728752541565 ) ) ;
#31136 = CARTESIAN_POINT ( 'NONE',  ( 4.999999999999993783, 146.0416666598387110, 8.660254037844390851 ) ) ;
#31137 = VERTEX_POINT ( 'NONE', #38750 ) ;
#31138 = CARTESIAN_POINT ( 'NONE',  ( -10.00000000000000178, 204.3749999931720538, -1.224646799147353454E-15 ) ) ;
#31139 = EDGE_CURVE ( 'NONE', #36860, #62341, #65906, .T. ) ;
#31140 = DIRECTION ( 'NONE',  ( 0.000000000000000000, 0.000000000000000000, 1.000000000000000000 ) ) ;
#31141 = CARTESIAN_POINT ( 'NONE',  ( 30.82842712474617031, 202.1250000000000284, 172.8284271247460993 ) ) ;
#31142 = CARTESIAN_POINT ( 'NONE',  ( 9.832129032723420536, 106.5104166632526841, -5.676582343749999815 ) ) ;
#31143 = CARTESIAN_POINT ( 'NONE',  ( 1.432654583217664479, 207.7500000013656063, 201.4587341250000065 ) ) ;
#31144 = CARTESIAN_POINT ( 'NONE',  ( 5.082755093536324154, 12.65624999795161187, 5.082755093536326818 ) ) ;
#31145 = CARTESIAN_POINT ( 'NONE',  ( 1.871523826299183495E-15, -10.18810118749999916, 89.40625000204838102 ) ) ;
#31146 = EDGE_CURVE ( 'NONE', #38422, #39639, #10867, .T. ) ;
#31147 = CARTESIAN_POINT ( 'NONE',  ( 9.832129032723416984, 15.67708332991935016, 5.676582343750006032 ) ) ;
#31148 = ORIENTED_EDGE ( 'NONE', *, *, #15464, .T. ) ;
#31149 = CARTESIAN_POINT ( 'NONE',  ( 10.00000000000000000, 181.6666666598387110, 2.679491924311235618 ) ) ;
#31150 = CARTESIAN_POINT ( 'NONE',  ( -5.662595241051933570, -5.662595241051936235, 26.70061528394063188 ) ) ;
#31151 = CARTESIAN_POINT ( 'NONE',  ( 8.660254037844389075, 117.2916666598386968, -5.000000000000000000 ) ) ;
#31152 = CARTESIAN_POINT ( 'NONE',  ( 7.204075437095968759, -7.204075437095966983, 73.09375000204838102 ) ) ;
#31153 = CARTESIAN_POINT ( 'NONE',  ( -46.89594099591774068, 38.00000000000000711, 68.54827124808609540 ) ) ;
#31154 = CARTESIAN_POINT ( 'NONE',  ( -5.656854249492378806, 93.87500000409677625, 5.656854249492381470 ) ) ;
#31155 = CARTESIAN_POINT ( 'NONE',  ( 2.765530957081996366, 293.1406250017069510, -6.676582343750003368 ) ) ;
#31156 = DIRECTION ( 'NONE',  ( -0.000000000000000000, -0.000000000000000000, 1.000000000000000000 ) ) ;
#31157 = FACE_OUTER_BOUND ( 'NONE', #68492, .T. ) ;
#31158 = B_SPLINE_CURVE_WITH_KNOTS ( 'NONE', 3,
 ( #67890, #26778, #61860, #33959, #56587, #22225, #21855, #50531, #44141, #67153 ),
 .UNSPECIFIED., .F., .F.,
 ( 4, 2, 2, 2, 4 ),
 ( 0.01226735695020646048, 0.01330218961086247764, 0.01433702227151849307, 0.01537185493217450849, 0.01640668759283052391 ),
 .UNSPECIFIED. ) ;
#31159 = CARTESIAN_POINT ( 'NONE',  ( 11.35316468749999963, 131.3020833299193555, -3.042071309553165293 ) ) ;
#31160 = CARTESIAN_POINT ( 'NONE',  ( -7.204075437095967871, 7.204075437095967871, 82.46875000204836681 ) ) ;
#31161 = AXIS2_PLACEMENT_3D ( 'NONE', #16917, #51630, #68983 ) ;
#31162 = ADVANCED_FACE ( 'NONE', ( #20246 ), #31959, .F. ) ;
#31163 = ADVANCED_FACE ( 'NONE', ( #72315 ), #49684, .T. ) ;
#31164 = CARTESIAN_POINT ( 'NONE',  ( -31.45873412499999233, 198.6875000013655779, 170.0000000000003979 ) ) ;
#31165 = CARTESIAN_POINT ( 'NONE',  ( -8.000000000000000000, 23.25000000000000355, -9.797174393178825657E-16 ) ) ;
#31166 = CARTESIAN_POINT ( 'NONE',  ( 4.541265875000001451, 12.37499999863440969, 1.881053915767124440 ) ) ;
#31167 = ORIENTED_EDGE ( 'NONE', *, *, #36266, .F. ) ;
#31168 = CIRCLE ( 'NONE', #28752, 9.999999999999996447 ) ;
#31169 = CARTESIAN_POINT ( 'NONE',  ( -1.656854249492348607, 207.3125000027312126, 202.0000000000000284 ) ) ;
#31170 = CARTESIAN_POINT ( 'NONE',  ( -2.839093476692135984E-14, 199.9375000013656063, 138.5412658750000503 ) ) ;
#31171 = AXIS2_PLACEMENT_3D ( 'NONE', #66556, #38654, #5066 ) ;
#31172 = CARTESIAN_POINT ( 'NONE',  ( 1.656854249492347719, 204.9375000027312410, 146.0000000000000284 ) ) ;
#31173 = CARTESIAN_POINT ( 'NONE',  ( 5.000000000000000000, 14.13320814749867615, -69.81894086168455260 ) ) ;
#31174 = CARTESIAN_POINT ( 'NONE',  ( 1.871523826299183495E-15, -10.18810118749999916, 71.40625000204836681 ) ) ;
#31175 = ORIENTED_EDGE ( 'NONE', *, *, #2505, .F. ) ;
#31176 = CARTESIAN_POINT ( 'NONE',  ( 2.977408999572652260, 4.687499997951610986, 7.188101187500000044 ) ) ;
#31177 = CARTESIAN_POINT ( 'NONE',  ( -21.26492961553635297, -14.52577668104750863, 192.5606694468046101 ) ) ;
#31178 = ADVANCED_FACE ( 'NONE', ( #9323 ), #27787, .T. ) ;
#31179 = FACE_OUTER_BOUND ( 'NONE', #45869, .T. ) ;
#31180 = CARTESIAN_POINT ( 'NONE',  ( -2.977408999572651815, 115.8125000020484094, 7.188101187500000933 ) ) ;
#31181 = CARTESIAN_POINT ( 'NONE',  ( 1.377000000000000002, 261.4319999999996753, 5.673913216232851831 ) ) ;
#31182 = CARTESIAN_POINT ( 'NONE',  ( 6.676582343750001591, 293.9531250017069510, -8.176455196517173205E-16 ) ) ;
#31183 = EDGE_CURVE ( 'NONE', #22730, #71803, #35519, .T. ) ;
#31185 = CARTESIAN_POINT ( 'NONE',  ( -3.967492730755044494, 11.56577346444171717, -0.1233701403699368204 ) ) ;
#31184 = CARTESIAN_POINT ( 'NONE',  ( 11.35316468749999963, 221.1979166700806161, 3.042071309553159519 ) ) ;
#31186 = VERTEX_POINT ( 'NONE', #19531 ) ;
#31187 = CARTESIAN_POINT ( 'NONE',  ( -5.676582343749992710, 225.0520833367473017, 9.832129032723422313 ) ) ;
#31188 = CARTESIAN_POINT ( 'NONE',  ( -7.188101187499991163, 2.977408999572646930, 1.392802781871753437 ) ) ;
#31189 = CARTESIAN_POINT ( 'NONE',  ( -30.82842712474624136, 195.2500000027312126, 167.1715728752542418 ) ) ;
#31191 = EDGE_CURVE ( 'NONE', #54742, #65546, #43202, .T. ) ;
#31190 = CARTESIAN_POINT ( 'NONE',  ( -3.458734124999959469, 197.7500000013656063, 199.4326545832176691 ) ) ;
#31192 = ORIENTED_EDGE ( 'NONE', *, *, #18755, .F. ) ;
#31193 = CARTESIAN_POINT ( 'NONE',  ( 7.999999999999998224, 23.90625000000000000, 3.313708498984766049 ) ) ;
#31194 = CARTESIAN_POINT ( 'NONE',  ( -7.999999999999998224, 102.5937499999999858, 3.313708498984766493 ) ) ;
#31195 = CARTESIAN_POINT ( 'NONE',  ( -5.676582343749998039, 107.7604166632526841, -9.832129032723420536 ) ) ;
#31196 = CARTESIAN_POINT ( 'NONE',  ( -2.828427124746152987, 209.1250000000000284, 200.8284271247462129 ) ) ;
#31197 = CARTESIAN_POINT ( 'NONE',  ( 4.556349186104051263, -10.99999999999999822, 77.96874999999998579 ) ) ;
#31200 = DIRECTION ( 'NONE',  ( 0.000000000000000000, -0.000000000000000000, 1.000000000000000000 ) ) ;
#31199 = CARTESIAN_POINT ( 'NONE',  ( 25.55430564589115505, 203.0625000013656063, 167.5543056458911053 ) ) ;
#31198 = CARTESIAN_POINT ( 'NONE',  ( 31.45873412500001010, 202.0000000013656063, 168.5673454167822740 ) ) ;
#31201 = VERTEX_POINT ( 'NONE', #39411 ) ;
#31202 = DIRECTION ( 'NONE',  ( -0.000000000000000000, 1.000000000000000000, -0.000000000000000000 ) ) ;
#31203 = CARTESIAN_POINT ( 'NONE',  ( -8.311093377946841443, 208.9062499965860411, 8.311093377946830785 ) ) ;
#31204 =( BOUNDED_CURVE ( )  B_SPLINE_CURVE ( 2, ( #43630, #32709, #22101, #3277, #61362, #56457, #73424, #61738, #4774 ),
 .UNSPECIFIED., .F., .F. ) 
 B_SPLINE_CURVE_WITH_KNOTS ( ( 3, 2, 2, 2, 3 ),
 ( 0.3124999999999979461, 0.3229166666666646313, 0.3333333333333312609, 0.3437499999999979461, 0.3541666666666646313 ),
 .UNSPECIFIED. ) 
 CURVE ( )  GEOMETRIC_REPRESENTATION_ITEM ( )  RATIONAL_B_SPLINE_CURVE ( ( 1.000000000000015099, 0.9238795325112717505, 1.000000000000000000, 0.9238795325112867385, 1.000000000000000000, 0.9238795325112867385, 1.000000000000000000, 0.9238795325113017265, 0.9999999999999850120 ) ) 
 REPRESENTATION_ITEM ( '' )  );
#31205 = CARTESIAN_POINT ( 'NONE',  ( 1.432654583217607192, 199.2500000013656063, 145.4587341250000634 ) ) ;
#31206 = CARTESIAN_POINT ( 'NONE',  ( 28.00000000000002132, 203.1875000013656063, 166.5412658749999082 ) ) ;
#31207 = AXIS2_PLACEMENT_3D ( 'NONE', #29636, #16806, #69629 ) ;
#31208 = LINE ( 'NONE', #37624, #71338 ) ;
#31209 = CARTESIAN_POINT ( 'NONE',  ( -8.311093377946836114, 192.9687499965859843, -8.311093377946837890 ) ) ;
#31210 = CARTESIAN_POINT ( 'NONE',  ( 5.082755093536326818, 90.59375000204839523, 5.082755093536325042 ) ) ;
#31211 = FACE_OUTER_BOUND ( 'NONE', #42068, .T. ) ;
#31212 = CARTESIAN_POINT ( 'NONE',  ( -3.211159895383562723, 14.93749999863440792, 3.211159895383561391 ) ) ;
#31213 = CARTESIAN_POINT ( 'NONE',  ( 31.45873412499997812, 198.8750000013656063, 171.4326545832176123 ) ) ;
#31214 = CARTESIAN_POINT ( 'NONE',  ( -5.082755093536317936, -5.082755093536320601, 5.049052781871752771 ) ) ;
#31215 = CARTESIAN_POINT ( 'NONE',  ( 0.000000000000000000, 0.000000000000000000, 0.000000000000000000 ) ) ;
#31216 = CARTESIAN_POINT ( 'NONE',  ( 11.35316468750000141, 85.78124999658602690, 0.000000000000000000 ) ) ;
#31217 = VERTEX_POINT ( 'NONE', #16748 ) ;
#31218 = CARTESIAN_POINT ( 'NONE',  ( -5.000000000000000000, -50.98458432551155539, 41.27351214092421827 ) ) ;
#31219 = DIRECTION ( 'NONE',  ( -0.000000000000000000, -1.000000000000000000, -0.000000000000000000 ) ) ;
#31220 = CARTESIAN_POINT ( 'NONE',  ( 1.224646799147353256E-15, 0.000000000000000000, 10.00000000000000000 ) ) ;
#31221 = CARTESIAN_POINT ( 'NONE',  ( 6.123233995736767268E-16, 108.1249999931720396, -10.00000000000000178 ) ) ;
#31222 = CARTESIAN_POINT ( 'NONE',  ( 11.35316468749999963, 85.98958332991936970, -3.042071309553165293 ) ) ;
#31223 = VERTEX_POINT ( 'NONE', #23165 ) ;
#31224 = CARTESIAN_POINT ( 'NONE',  ( -4.220049686691937474, -10.18810118749999738, 89.31250000204838102 ) ) ;
#31225 = VECTOR ( 'NONE', #52887, 999.9999999999997726 ) ;
#31226 = CARTESIAN_POINT ( 'NONE',  ( -10.18810118749999738, -4.220049686691941915, 111.2500000020483952 ) ) ;
#31227 = CARTESIAN_POINT ( 'NONE',  ( 2.839093476692135984E-14, 207.9375000013656063, 201.4587341250000350 ) ) ;
#31228 = CARTESIAN_POINT ( 'NONE',  ( 7.320508075688794136, 74.37500000000004263, 7.320508075688798577 ) ) ;
#31230 = CARTESIAN_POINT ( 'NONE',  ( 11.35316468749999963, 75.98958332991935549, -3.042071309553165293 ) ) ;
#31229 = DIRECTION ( 'NONE',  ( 0.000000000000000000, 0.000000000000000000, -1.000000000000000000 ) ) ;
#31231 = CARTESIAN_POINT ( 'NONE',  ( 3.313708498984756279, 7.999999999999991118, 20.04905278392014978 ) ) ;
#31232 = CARTESIAN_POINT ( 'NONE',  ( -2.845451689122913574, 194.6919015541251099, 139.6347610879342369 ) ) ;
#31233 = CARTESIAN_POINT ( 'NONE',  ( 2.679491924311222739, 165.8333333265053682, 10.00000000000000355 ) ) ;
#31234 = CARTESIAN_POINT ( 'NONE',  ( -2.977408999572650927, 92.75000000204839523, -7.188101187500001821 ) ) ;
#31235 = CARTESIAN_POINT ( 'NONE',  ( -24.22789396521246275, 194.9514163098568815, 168.8079244834036388 ) ) ;
#31236 = CARTESIAN_POINT ( 'NONE',  ( 3.042071309553167513, 67.13541666325268409, -11.35316468749999785 ) ) ;
#31237 = CARTESIAN_POINT ( 'NONE',  ( 6.676582343750004256, 291.8906250017069510, 2.765530957081995478 ) ) ;
#31238 = CARTESIAN_POINT ( 'NONE',  ( -10.18810118749999916, 0.000000000000000000, 107.0312500020483810 ) ) ;
#31239 = CARTESIAN_POINT ( 'NONE',  ( 8.311093377946834337, 200.1562499965860695, 8.311093377946839666 ) ) ;
#31240 = EDGE_LOOP ( 'NONE', ( #7081, #22244, #36265, #64680, #45797, #57433 ) ) ;
#31241 = CYLINDRICAL_SURFACE ( 'NONE', #18739, 3.999999999999976019 ) ;
#31242 = CARTESIAN_POINT ( 'NONE',  ( 3.999999999999960032, 206.0625000027312410, 143.6568542494924259 ) ) ;
#31243 = CARTESIAN_POINT ( 'NONE',  ( -2.124081043562906501, 50.03790111639161609, 40.75706181777542270 ) ) ;
#31245 = CARTESIAN_POINT ( 'NONE',  ( -11.35316468750000141, 193.2812499965860127, -1.390361679473963753E-15 ) ) ;
#31244 = DIRECTION ( 'NONE',  ( 0.000000000000000000, 0.000000000000000000, -1.000000000000000000 ) ) ;
#31246 = DIRECTION ( 'NONE',  ( -1.000000000000000000, 0.000000000000000000, 0.000000000000000000 ) ) ;
#31247 = CARTESIAN_POINT ( 'NONE',  ( -6.123233995736766282E-16, 236.8750000068279746, -10.00000000000000000 ) ) ;
#31248 = CARTESIAN_POINT ( 'NONE',  ( -7.999999999999015010, 2.678670460604446806E-06, 11.51770387648012317 ) ) ;
#31249 = VERTEX_POINT ( 'NONE', #62045 ) ;
#31250 = CARTESIAN_POINT ( 'NONE',  ( -11.35316468749999785, 183.3854166632526699, -3.042071309553167957 ) ) ;
#31251 = CARTESIAN_POINT ( 'NONE',  ( 2.977408999572650927, -7.188101187499990274, 18.45530278187175455 ) ) ;
#31252 = CARTESIAN_POINT ( 'NONE',  ( -3.373128826976388162, 60.49298623944847719, -23.06377889928770486 ) ) ;
#31253 = ORIENTED_EDGE ( 'NONE', *, *, #3024, .F. ) ;
#31254 = CARTESIAN_POINT ( 'NONE',  ( -8.000000000000000000, 99.68750000409677625, 0.000000000000000000 ) ) ;
#31255 = AXIS2_PLACEMENT_3D ( 'NONE', #4684, #28054, #57493 ) ;
#31256 = CARTESIAN_POINT ( 'NONE',  ( 4.000000000000000888, 14.93750000000000178, 1.656854249492384135 ) ) ;
#31257 = CIRCLE ( 'NONE', #28678, 8.000000000000000000 ) ;
#31258 = CARTESIAN_POINT ( 'NONE',  ( -4.541265875000002339, 14.74999999863440969, -1.881053915767121998 ) ) ;
#31259 = CARTESIAN_POINT ( 'NONE',  ( -7.999999999999991118, 0.000000000000000000, 14.51780278392014800 ) ) ;
#31260 = CARTESIAN_POINT ( 'NONE',  ( -25.17157287525381903, 195.8750000000000284, 167.1715728752541565 ) ) ;
#31261 = AXIS2_PLACEMENT_3D ( 'NONE', #69663, #17976, #74198 ) ;
#31262 = ORIENTED_EDGE ( 'NONE', *, *, #58223, .F. ) ;
#31263 = CARTESIAN_POINT ( 'NONE',  ( 5.000000000000000888, -10.54112798502250570, -66.30787999718575065 ) ) ;
#31264 = CARTESIAN_POINT ( 'NONE',  ( 5.082755093536326818, 100.7187500020483810, 5.082755093536325042 ) ) ;
#31265 = EDGE_CURVE ( 'NONE', #30042, #19911, #50929, .T. ) ;
#31267 = CARTESIAN_POINT ( 'NONE',  ( 1.656854249492381914, 6.562499997268813168, 4.000000000000000888 ) ) ;
#31266 = CARTESIAN_POINT ( 'NONE',  ( 3.999999999999960032, 204.0625000027312410, 143.6568542494924259 ) ) ;
#31268 = DIRECTION ( 'NONE',  ( 0.000000000000000000, 0.000000000000000000, 1.000000000000000000 ) ) ;
#31269 = ORIENTED_EDGE ( 'NONE', *, *, #1574, .T. ) ;
#31270 = CARTESIAN_POINT ( 'NONE',  ( -11.00000000000010658, 4.556349186103942017, 83.40624999999998579 ) ) ;
#31271 = CARTESIAN_POINT ( 'NONE',  ( 7.188101187499991163, 2.977408999572648707, 17.33030278187175455 ) ) ;
#31272 = EDGE_LOOP ( 'NONE', ( #65291, #6649, #7779, #48278, #26821, #21151 ) ) ;
#31273 = EDGE_CURVE ( 'NONE', #32512, #47954, #57141, .T. ) ;
#31274 = ORIENTED_EDGE ( 'NONE', *, *, #28326, .F. ) ;
#31275 = CARTESIAN_POINT ( 'NONE',  ( -6.238412754330611322E-16, 10.18810118749999916, 82.28125000204838102 ) ) ;
#31276 = CARTESIAN_POINT ( 'NONE',  ( 11.35316468749999785, 60.88541666325269119, 3.042071309553174174 ) ) ;
#31277 = CARTESIAN_POINT ( 'NONE',  ( 1.469576158976822172E-15, -7.999999999999991118, 5.892802783920146226 ) ) ;
#31278 = CARTESIAN_POINT ( 'NONE',  ( 4.556349186104051263, -10.99999999999999822, 92.96875000000000000 ) ) ;
#31281 = CARTESIAN_POINT ( 'NONE',  ( -6.676582343750001591, 292.6093750017069510, 0.000000000000000000 ) ) ;
#31280 = CARTESIAN_POINT ( 'NONE',  ( 31.99999999999998579, 201.4375000027311842, 168.3431457505075173 ) ) ;
#31279 = CARTESIAN_POINT ( 'NONE',  ( -74.99999999999998579, 0.000000000000000000, 70.00000000000001421 ) ) ;
#31282 = CARTESIAN_POINT ( 'NONE',  ( -4.999999999999998224, 146.6666666666666572, -8.660254037844389075 ) ) ;
#31283 = DIRECTION ( 'NONE',  ( 0.000000000000000000, 0.000000000000000000, 1.000000000000000000 ) ) ;
#31284 = CARTESIAN_POINT ( 'NONE',  ( -8.660254037844385522, 233.5416666734946318, 5.000000000000004441 ) ) ;
#31285 = CARTESIAN_POINT ( 'NONE',  ( -8.000000000000000000, 4.968749995903220196, -3.313708498984762496 ) ) ;
#31286 = CARTESIAN_POINT ( 'NONE',  ( 28.00000000000001776, 196.9375000013655779, 166.5412658749999082 ) ) ;
#31287 = CARTESIAN_POINT ( 'NONE',  ( 7.188101187499999156, 9.749999997951611874, 2.977408999572654924 ) ) ;
#31288 = CARTESIAN_POINT ( 'NONE',  ( 5.656854249492376141, -5.656854249492374365, 24.08030278392014978 ) ) ;
#31289 = DIRECTION ( 'NONE',  ( 1.000000000000000000, 0.000000000000000000, 0.000000000000000000 ) ) ;
#31290 = CARTESIAN_POINT ( 'NONE',  ( 2.977408999572650039, 110.5625000020483810, -7.188101187500000933 ) ) ;
#31291 = LINE ( 'NONE', #66367, #9481 ) ;
#31292 = CARTESIAN_POINT ( 'NONE',  ( 10.00000000000000533, 135.2083333333333144, -2.679491924311227624 ) ) ;
#31293 = CARTESIAN_POINT ( 'NONE',  ( 30.44569435410883784, 209.0625000013656063, 167.5543056458911053 ) ) ;
#31294 = CARTESIAN_POINT ( 'NONE',  ( 2.977408999572646486, 7.188101187499991163, 23.89280278187176165 ) ) ;
#31296 =( BOUNDED_CURVE ( )  B_SPLINE_CURVE ( 2, ( #46764, #23761, #58845, #7892, #30533, #36199, #65596, #70888, #58478 ),
 .UNSPECIFIED., .F., .F. ) 
 B_SPLINE_CURVE_WITH_KNOTS ( ( 3, 2, 2, 2, 3 ),
 ( 0.3676470588235293824, 0.3713235294117646634, 0.3750000000000000000, 0.3786764705882352811, 0.3823529411764705621 ),
 .UNSPECIFIED. ) 
 CURVE ( )  GEOMETRIC_REPRESENTATION_ITEM ( )  RATIONAL_B_SPLINE_CURVE ( ( 1.000000000000001110, 0.9238795325112856283, 1.000000000000000000, 0.9238795325112867385, 1.000000000000000000, 0.9238795325112867385, 1.000000000000000000, 0.9238795325112867385, 1.000000000000000000 ) ) 
 REPRESENTATION_ITEM ( '' )  );
#31295 = CARTESIAN_POINT ( 'NONE',  ( 32.00000000000000000, 200.3125000027312126, 171.6568542494922553 ) ) ;
#31297 = CARTESIAN_POINT ( 'NONE',  ( -8.311093377946836114, 42.65624999658600558, -8.311093377946837890 ) ) ;
#31298 = CARTESIAN_POINT ( 'NONE',  ( 2.679491924312849882, 151.0416666666665151, -9.999999999999067413 ) ) ;
#31299 = CARTESIAN_POINT ( 'NONE',  ( -7.320508075688773708, 8.749999993172030699, -7.320508075688774596 ) ) ;
#31300 = CARTESIAN_POINT ( 'NONE',  ( 29.65685424949241167, 201.5625000027311557, 165.9999999999999716 ) ) ;
#31301 = DIRECTION ( 'NONE',  ( -1.000000000000000000, 0.000000000000000000, 0.000000000000000000 ) ) ;
#31302 = EDGE_LOOP ( 'NONE', ( #7608, #29466, #55864, #12732 ) ) ;
#31303 = CARTESIAN_POINT ( 'NONE',  ( -7.320508075688773708, 128.7499999931720538, -7.320508075688774596 ) ) ;
#31304 = CARTESIAN_POINT ( 'NONE',  ( -7.347880794884122694E-16, 8.499999997268814056, 4.000000000000001776 ) ) ;
#31305 = CARTESIAN_POINT ( 'NONE',  ( 8.311093377946834337, 35.15624999658601979, 8.311093377946839666 ) ) ;
#31306 = CARTESIAN_POINT ( 'NONE',  ( 11.00000000000000000, 1.347111479062088405E-15, 79.93750000409677625 ) ) ;
#31307 = CARTESIAN_POINT ( 'NONE',  ( -2.445694354108839175, 204.3125000013656063, 144.4456943541088663 ) ) ;
#31308 = CARTESIAN_POINT ( 'NONE',  ( -6.000000000000003553, 298.9374999999999432, -2.485281374238571317 ) ) ;
#31309 = DIRECTION ( 'NONE',  ( 1.000000000000000000, -0.000000000000000000, -0.000000000000000000 ) ) ;
#31311 = CARTESIAN_POINT ( 'NONE',  ( -5.676582343749998039, 27.44791666325268409, -9.832129032723420536 ) ) ;
#31310 = CARTESIAN_POINT ( 'NONE',  ( 7.188101187500000933, 105.5000000020483810, -2.977408999572651371 ) ) ;
#31312 = CARTESIAN_POINT ( 'NONE',  ( -5.656854249492373476, -5.656854249492376141, 16.01780277982336642 ) ) ;
#31313 = CARTESIAN_POINT ( 'NONE',  ( -11.35316468749999785, 158.0729166632526699, -3.042071309553167513 ) ) ;
#31314 = VECTOR ( 'NONE', #26910, 1000.000000000000000 ) ;
#31315 = CARTESIAN_POINT ( 'NONE',  ( -10.00000000000000355, 124.5833333265053682, 2.679491924311223183 ) ) ;
#31316 = CARTESIAN_POINT ( 'NONE',  ( 5.082755093536325042, 105.9687500020483952, -5.082755093536325930 ) ) ;
#31317 = ORIENTED_EDGE ( 'NONE', *, *, #22614, .T. ) ;
#31318 = CARTESIAN_POINT ( 'NONE',  ( 4.217983994790212243, -68.29231466825473262, -20.60018752343863824 ) ) ;
#31319 = CARTESIAN_POINT ( 'NONE',  ( -5.676582343749998039, 17.76041666325268409, -9.832129032723420536 ) ) ;
#31320 =( BOUNDED_CURVE ( )  B_SPLINE_CURVE ( 2, ( #41322, #34567, #46232, #63962, #11535, #12273, #6626, #70366, #34940, #23962, #5883, #30000, #40576 ),
 .UNSPECIFIED., .F., .F. ) 
 B_SPLINE_CURVE_WITH_KNOTS ( ( 3, 2, 2, 2, 2, 2, 3 ),
 ( 0.8641304347826086474, 0.8659420289855072062, 0.8677536231884057649, 0.8695652173913043237, 0.8713768115942028825, 0.8731884057971014412, 0.8750000000000000000 ),
 .UNSPECIFIED. ) 
 CURVE ( )  GEOMETRIC_REPRESENTATION_ITEM ( )  RATIONAL_B_SPLINE_CURVE ( ( 1.000000000000000000, 0.9659258262890683122, 1.000000000000000000, 0.9659258262890683122, 1.000000000000000000, 0.9659258262890683122, 1.000000000000000000, 0.9659258262890683122, 1.000000000000000000, 0.9659258262890683122, 1.000000000000000000, 0.9659258262890683122, 1.000000000000000000 ) ) 
 REPRESENTATION_ITEM ( '' )  );
#31321 = ORIENTED_EDGE ( 'NONE', *, *, #54673, .F. ) ;
#31322 = CARTESIAN_POINT ( 'NONE',  ( -5.000000000000000000, 8.780967503833453037E-15, 71.70204102886728492 ) ) ;
#31323 = CARTESIAN_POINT ( 'NONE',  ( -10.18810118749999916, 0.000000000000000000, 76.65625000204836681 ) ) ;
#31324 = CARTESIAN_POINT ( 'NONE',  ( -31.99999999999997868, 197.3125000000000568, 171.6568542494928238 ) ) ;
#31325 = CARTESIAN_POINT ( 'NONE',  ( -3.042071309553163960, 157.2395833299193555, -11.35316468749999963 ) ) ;
#31326 = CYLINDRICAL_SURFACE ( 'NONE', #68821, 3.999999999999976019 ) ;
#31327 = CARTESIAN_POINT ( 'NONE',  ( -7.999999999999991118, 0.000000000000000000, 20.38655278432982243 ) ) ;
#31328 = CARTESIAN_POINT ( 'NONE',  ( 4.999999999999995559, -16.24494643555759410, -69.83755725260751035 ) ) ;
#31329 = VECTOR ( 'NONE', #65436, 1000.000000000000000 ) ;
#31330 = CARTESIAN_POINT ( 'NONE',  ( 9.832129032723416984, 231.8229166700806445, -5.676582343750003368 ) ) ;
#31331 = CARTESIAN_POINT ( 'NONE',  ( -6.238412754330611322E-16, 10.18810118749999916, 87.15625000204838102 ) ) ;
#31332 = VERTEX_POINT ( 'NONE', #45071 ) ;
#31333 = CARTESIAN_POINT ( 'NONE',  ( 8.000000000000000000, 1.312499995903220196, 0.000000000000000000 ) ) ;
#31334 = CARTESIAN_POINT ( 'NONE',  ( -4.242640687119286547, 291.9375000034140157, -4.242640687119286547 ) ) ;
#31335 = CARTESIAN_POINT ( 'NONE',  ( 5.676582343749993598, 100.2604166632526841, 9.832129032723422313 ) ) ;
#31336 = CARTESIAN_POINT ( 'NONE',  ( 1.871523826299183495E-15, -10.18810118749999916, 102.5312500020483810 ) ) ;
#31337 = CARTESIAN_POINT ( 'NONE',  ( 2.780723358947928197E-16, 21.68749999863440792, -4.541265875000002339 ) ) ;
#31338 = VERTEX_POINT ( 'NONE', #20653 ) ;
#31339 = ORIENTED_EDGE ( 'NONE', *, *, #59157, .T. ) ;
#31340 = CARTESIAN_POINT ( 'NONE',  ( -4.541265875000002339, 3.937499998634406584, -5.561446717895856393E-16 ) ) ;
#31341 = CARTESIAN_POINT ( 'NONE',  ( -5.082755093536325042, 4.031249997951610986, -5.082755093536325930 ) ) ;
#31342 = CARTESIAN_POINT ( 'NONE',  ( -4.898587196589412829E-16, 117.3125000040967763, -8.000000000000000000 ) ) ;
#31343 = CIRCLE ( 'NONE', #61515, 8.000000000000005329 ) ;
#31345 = EDGE_CURVE ( 'NONE', #6572, #28033, #58649, .T. ) ;
#31344 = CARTESIAN_POINT ( 'NONE',  ( -4.220049686691937474, -10.18810118749999738, 96.81250000204839523 ) ) ;
#31346 = EDGE_CURVE ( 'NONE', #3963, #60631, #42522, .T. ) ;
#31347 = CARTESIAN_POINT ( 'NONE',  ( -25.55430564589119413, 204.5625000013656063, 167.5543056458915316 ) ) ;
#31348 = LINE ( 'NONE', #30611, #16288 ) ;
#31349 = CARTESIAN_POINT ( 'NONE',  ( -4.000000000000001776, 4.500000000000000888, -4.898587196589415787E-16 ) ) ;
#31350 = CARTESIAN_POINT ( 'NONE',  ( 4.000000000000001776, 16.74999999726881583, 0.000000000000000000 ) ) ;
#31351 = CARTESIAN_POINT ( 'NONE',  ( -4.541265875000003227, 1.874999998634406806, 1.881053915767121110 ) ) ;
#31352 = EDGE_CURVE ( 'NONE', #56611, #55577, #66331, .T. ) ;
#31353 = EDGE_CURVE ( 'NONE', #2699, #70596, #10736, .T. ) ;
#31354 = CARTESIAN_POINT ( 'NONE',  ( -2.445694354108838731, 208.0625000013656063, 144.4456943541088663 ) ) ;
#31355 = CARTESIAN_POINT ( 'NONE',  ( 0.000000000000000000, 0.000000000000000000, 30.00000000000000000 ) ) ;
#31357 = DIRECTION ( 'NONE',  ( 0.000000000000000000, 0.000000000000000000, 1.000000000000000000 ) ) ;
#31356 = CARTESIAN_POINT ( 'NONE',  ( -24.54126587499996148, 201.1250000013656347, 171.4326545832179534 ) ) ;
#31358 =( NAMED_UNIT ( * ) SI_UNIT ( $, .STERADIAN. ) SOLID_ANGLE_UNIT ( ) );
#31359 = CARTESIAN_POINT ( 'NONE',  ( -8.342170076843785083E-16, 20.06249999863440436, 4.541265875000002339 ) ) ;
#31360 = VECTOR ( 'NONE', #407, 1000.000000000000000 ) ;
#31361 = CARTESIAN_POINT ( 'NONE',  ( 2.828427124746190291, 11.87500000000000000, 2.828427124746192067 ) ) ;
#31362 = CARTESIAN_POINT ( 'NONE',  ( -5.082755093536317936, -5.082755093536320601, 6.174052781871754547 ) ) ;
#31363 = ORIENTED_EDGE ( 'NONE', *, *, #69600, .F. ) ;
#31364 = ORIENTED_EDGE ( 'NONE', *, *, #52180, .T. ) ;
#31365 = CARTESIAN_POINT ( 'NONE',  ( 4.220049686691934809, 10.18810118749999916, 97.18750000204836681 ) ) ;
#31366 = CYLINDRICAL_SURFACE ( 'NONE', #24887, 3.999999999999986233 ) ;
#31367 = CIRCLE ( 'NONE', #17057, 7.999999999999991118 ) ;
#31368 = CARTESIAN_POINT ( 'NONE',  ( -31.45873412499999944, 205.9375000013656063, 170.0000000000003979 ) ) ;
#31369 = CARTESIAN_POINT ( 'NONE',  ( -30.82842712474615965, 201.3750000000000284, 172.8284271247465824 ) ) ;
#31370 = CARTESIAN_POINT ( 'NONE',  ( -1.432654583217607858, 196.6250000013656063, 201.4587341250000065 ) ) ;
#31371 = CARTESIAN_POINT ( 'NONE',  ( -2.679491924311123263, 33.54166666666668561, 10.00000000000006040 ) ) ;
#31372 = CARTESIAN_POINT ( 'NONE',  ( 7.320508075688771044, 114.3750000000000142, 7.320508075688775484 ) ) ;
#31373 = AXIS2_PLACEMENT_3D ( 'NONE', #12213, #63903, #48018 ) ;
#31374 = CARTESIAN_POINT ( 'NONE',  ( 5.656854249492381470, 110.5625000000000000, 5.656854249492379694 ) ) ;
#31375 = CARTESIAN_POINT ( 'NONE',  ( 4.721056650415999201, 294.2343750017069510, -4.721056650415999201 ) ) ;
#31376 = EDGE_CURVE ( 'NONE', #43835, #6290, #74051, .T. ) ;
#31377 = EDGE_LOOP ( 'NONE', ( #74248, #22773, #34508, #66884 ) ) ;
#31378 = CYLINDRICAL_SURFACE ( 'NONE', #33773, 6.000000000000001776 ) ;
#31379 = CARTESIAN_POINT ( 'NONE',  ( -8.000000000000001776, 18.65624999590322020, 3.313708498984759387 ) ) ;
#31380 = CARTESIAN_POINT ( 'NONE',  ( 1.432654583217607858, 201.6250000013656063, 138.5412658750000787 ) ) ;
#31381 = CARTESIAN_POINT ( 'NONE',  ( -21.78045554270713424, -37.99999999999992184, 147.9407217626652198 ) ) ;
#31382 = SURFACE_STYLE_USAGE ( .BOTH. , #64238 ) ;
#31383 = CARTESIAN_POINT ( 'NONE',  ( -6.951808397369817780E-16, 257.9687500034140157, -11.35316468749999963 ) ) ;
#31384 = CARTESIAN_POINT ( 'NONE',  ( -2.828427124746208943, 207.6250000000000284, 144.8284271247462129 ) ) ;
#31385 = CARTESIAN_POINT ( 'NONE',  ( 11.00000000000000000, 4.556349186104045934, 114.3437499999999858 ) ) ;
#31386 = CARTESIAN_POINT ( 'NONE',  ( 11.35316468750000141, 0.7812499965860163487, 0.000000000000000000 ) ) ;
#31387 = CARTESIAN_POINT ( 'NONE',  ( 5.082755093536320601, -5.082755093536318824, 5.424052781871753659 ) ) ;
#31388 = CARTESIAN_POINT ( 'NONE',  ( -9.832129032723420536, 194.0104166632526983, 5.676582343749997150 ) ) ;
#31389 = LINE ( 'NONE', #31767, #15434 ) ;
#31390 = CARTESIAN_POINT ( 'NONE',  ( -3.211159895383562723, 7.937499998634407028, 3.211159895383561391 ) ) ;
#31391 = CARTESIAN_POINT ( 'NONE',  ( 2.679491924311292905, 241.4583333333333712, 9.999999999999968026 ) ) ;
#31393 = CARTESIAN_POINT ( 'NONE',  ( -11.00000000000000000, 11.00000000000000000, -6.938893903907228378E-15 ) ) ;
#31392 = CYLINDRICAL_SURFACE ( 'NONE', #28656, 10.00000000000000178 ) ;
#31394 = ORIENTED_EDGE ( 'NONE', *, *, #47466, .T. ) ;
#31395 = CARTESIAN_POINT ( 'NONE',  ( 3.458734124999959469, 203.7500000013656063, 140.5673454167824161 ) ) ;
#31396 = CARTESIAN_POINT ( 'NONE',  ( -9.832129032723418760, 48.17708332991934839, -5.676582343750004256 ) ) ;
#31397 = CARTESIAN_POINT ( 'NONE',  ( -7.778174593052023411, 7.778174593052023411, 98.50000000409677625 ) ) ;
#31398 = LINE ( 'NONE', #49113, #28691 ) ;
#31399 = CARTESIAN_POINT ( 'NONE',  ( -30.44569435410875968, 200.8125000013656063, 172.4456943541092642 ) ) ;
#31400 = FACE_OUTER_BOUND ( 'NONE', #63103, .T. ) ;
#31401 = CARTESIAN_POINT ( 'NONE',  ( -10.00000000000000000, 229.7916666666666572, -2.679491924311226292 ) ) ;
#31402 = CARTESIAN_POINT ( 'NONE',  ( -2.445694354108839619, 196.8125000013656063, 139.5543056458912190 ) ) ;
#31403 = AXIS2_PLACEMENT_3D ( 'NONE', #5977, #28980, #45584 ) ;
#31404 = CARTESIAN_POINT ( 'NONE',  ( 11.35316468750000141, 105.7812499965860269, 0.000000000000000000 ) ) ;
#31405 = CARTESIAN_POINT ( 'NONE',  ( 2.679491924311228956, 92.91666665983871098, -10.00000000000000000 ) ) ;
#31406 = CARTESIAN_POINT ( 'NONE',  ( 5.082755093536325042, 92.09375000204838102, -5.082755093536325930 ) ) ;
#31407 = CARTESIAN_POINT ( 'NONE',  ( -3.211159895383561391, 14.81249999863440792, -3.211159895383561835 ) ) ;
#31408 = DIRECTION ( 'NONE',  ( -0.000000000000000000, -0.000000000000000000, 1.000000000000000000 ) ) ;
#31409 = FACE_OUTER_BOUND ( 'NONE', #2155, .T. ) ;
#31410 = ORIENTED_EDGE ( 'NONE', *, *, #19987, .F. ) ;
#31411 = CARTESIAN_POINT ( 'NONE',  ( -8.679299243466303437, 226.0000000000000000, -5.010106067796166407 ) ) ;
#31412 = EDGE_LOOP ( 'NONE', ( #55987, #65523, #7676, #64639 ) ) ;
#31413 = CARTESIAN_POINT ( 'NONE',  ( 1.226468279477575784E-15, 292.8593750017070079, 6.676582343750001591 ) ) ;
#31414 = CARTESIAN_POINT ( 'NONE',  ( 2.449293598294707893E-16, 11.99999999726881406, -4.000000000000001776 ) ) ;
#31415 = CARTESIAN_POINT ( 'NONE',  ( 5.656854249492374365, 5.656854249492375253, 7.955302783920145338 ) ) ;
#31416 = CARTESIAN_POINT ( 'NONE',  ( 11.35316468749999785, 170.5729166632526983, 3.042071309553174174 ) ) ;
#31417 = CARTESIAN_POINT ( 'NONE',  ( 9.000000000000000000, 1.769118300197576321, -0.07756262466202530625 ) ) ;
#31418 = CARTESIAN_POINT ( 'NONE',  ( -1.656854249492348607, 201.1875000000000284, 202.0000000000000284 ) ) ;
#31419 = CARTESIAN_POINT ( 'NONE',  ( 27.99999999999999645, 195.0000000000000000, 169.9999999999999147 ) ) ;
#31420 = CARTESIAN_POINT ( 'NONE',  ( 1.871523826299183495E-15, -10.18810118749999916, 105.9062500020483810 ) ) ;
#31421 = ORIENTED_EDGE ( 'NONE', *, *, #38912, .F. ) ;
#31422 =( BOUNDED_CURVE ( )  B_SPLINE_CURVE ( 2, ( #46110, #67645, #28389, #15943, #39709, #34078, #57827, #34450, #51397, #56326, #11784, #34821, #74039 ),
 .UNSPECIFIED., .F., .F. ) 
 B_SPLINE_CURVE_WITH_KNOTS ( ( 3, 2, 2, 2, 2, 2, 3 ),
 ( 1.365892743354367500, 1.371125127663376464, 1.376357511972385650, 1.381589896281394614, 1.386822280590403800, 1.392054664899412764, 1.397287049208421728 ),
 .UNSPECIFIED. ) 
 CURVE ( )  GEOMETRIC_REPRESENTATION_ITEM ( )  RATIONAL_B_SPLINE_CURVE ( ( 1.000000000000000000, 0.9659258262890684232, 1.000000000000000000, 0.9659258262890684232, 1.000000000000000000, 0.9659258262890684232, 1.000000000000000000, 0.9659258262890684232, 1.000000000000000000, 0.9659258262890684232, 1.000000000000000000, 0.9659258262893064551, 0.9999999999997619682 ) ) 
 REPRESENTATION_ITEM ( '' )  );
#31423 = VECTOR ( 'NONE', #65607, 1000.000000000000000 ) ;
#31424 = CARTESIAN_POINT ( 'NONE',  ( 3.223881452091114763, 50.20043732028305783, -40.84573126306947444 ) ) ;
#31425 = DIRECTION ( 'NONE',  ( 0.000000000000000000, 0.000000000000000000, -1.000000000000000000 ) ) ;
#31426 = CARTESIAN_POINT ( 'NONE',  ( 11.35316468749999963, 141.3020833299193271, -3.042071309553165293 ) ) ;
#31427 = LINE ( 'NONE', #31806, #60356 ) ;
#31428 = CARTESIAN_POINT ( 'NONE',  ( 3.458734125000016757, 206.1250000013656063, 199.4326545832176976 ) ) ;
#31429 = CARTESIAN_POINT ( 'NONE',  ( 10.18810118749999916, 4.220049686691935698, 73.37500000204838102 ) ) ;
#31430 = CARTESIAN_POINT ( 'NONE',  ( -8.311093377946841443, 64.21874999658601268, 8.311093377946830785 ) ) ;
#31431 = VERTEX_POINT ( 'NONE', #28826 ) ;
#31432 = CARTESIAN_POINT ( 'NONE',  ( -26.34314575050753504, 208.6875000027311842, 174.0000000000003411 ) ) ;
#31433 = CARTESIAN_POINT ( 'NONE',  ( -3.211159895383561391, 4.812499998634407028, -3.211159895383561835 ) ) ;
#31434 = CARTESIAN_POINT ( 'NONE',  ( 3.317071493978883456, -8.008118988124989457, 7.481865283940628331 ) ) ;
#31435 = ORIENTED_EDGE ( 'NONE', *, *, #56462, .T. ) ;
#31436 = ADVANCED_FACE ( 'NONE', ( #74110 ), #51843, .T. ) ;
#31437 = CARTESIAN_POINT ( 'NONE',  ( 7.188101187499999156, 19.87499999795161543, 2.977408999572654924 ) ) ;
#31438 = CYLINDRICAL_SURFACE ( 'NONE', #48061, 4.000000000000001776 ) ;
#31439 = AXIS2_PLACEMENT_3D ( 'NONE', #53953, #21838, #26372 ) ;
#31440 = CARTESIAN_POINT ( 'NONE',  ( 1.469576158976823947E-15, 118.0625000040967763, 8.000000000000000000 ) ) ;
#31441 = CARTESIAN_POINT ( 'NONE',  ( -7.188101187500001821, 10.49999999795161010, -2.977408999572651371 ) ) ;
#31442 = CARTESIAN_POINT ( 'NONE',  ( 5.082755093536320601, -5.082755093536318824, 5.049052781871752771 ) ) ;
#31443 =( BOUNDED_CURVE ( )  B_SPLINE_CURVE ( 2, ( #4195, #8724, #27184, #21893, #50201, #31736, #49071, #49453, #14364 ),
 .UNSPECIFIED., .F., .F. ) 
 B_SPLINE_CURVE_WITH_KNOTS ( ( 3, 2, 2, 2, 3 ),
 ( 0.3970588235294116863, 0.4007352941176470229, 0.4044117647058823040, 0.4080882352941175850, 0.4117647058823528661 ),
 .UNSPECIFIED. ) 
 CURVE ( )  GEOMETRIC_REPRESENTATION_ITEM ( )  RATIONAL_B_SPLINE_CURVE ( ( 1.000000000000001110, 0.9238795325112856283, 1.000000000000000000, 0.9238795325112867385, 1.000000000000000000, 0.9238795325112867385, 1.000000000000000000, 0.9238795325112878487, 0.9999999999999988898 ) ) 
 REPRESENTATION_ITEM ( '' )  );
#31444 = CARTESIAN_POINT ( 'NONE',  ( 10.18810118749999916, 1.247682550866122264E-15, 68.40625000204836681 ) ) ;
#31445 = DIRECTION ( 'NONE',  ( -0.000000000000000000, 1.000000000000000000, -0.000000000000000000 ) ) ;
#31446 = CARTESIAN_POINT ( 'NONE',  ( 1.656854249492381914, 2.562499997268814056, 4.000000000000000888 ) ) ;
#31447 = CIRCLE ( 'NONE', #19428, 3.999999999999976019 ) ;
#31448 = ORIENTED_EDGE ( 'NONE', *, *, #48477, .F. ) ;
#31449 = ADVANCED_FACE ( 'NONE', ( #23909 ), #57894, .T. ) ;
#31450 = ADVANCED_FACE ( 'NONE', ( #1656 ), #40897, .F. ) ;
#31451 = CARTESIAN_POINT ( 'NONE',  ( -3.458734124999959025, 208.5000000013656063, 199.4326545832176691 ) ) ;
#31452 = CARTESIAN_POINT ( 'NONE',  ( -32.00000000000002842, 199.3125000027311842, 168.3431457505080573 ) ) ;
#31453 = ADVANCED_FACE ( 'NONE', ( #58269 ), #41268, .T. ) ;
#31454 = CARTESIAN_POINT ( 'NONE',  ( -4.541265875000002339, 0.8124999986344066949, -5.561446717895856393E-16 ) ) ;
#31455 = CARTESIAN_POINT ( 'NONE',  ( 7.188101187500000044, 112.9062500020483952, -8.802885111219163269E-16 ) ) ;
#31456 = CARTESIAN_POINT ( 'NONE',  ( -5.999999999999999112, 295.0625000000000000, 2.485281374238575314 ) ) ;
#31457 = CARTESIAN_POINT ( 'NONE',  ( 7.188101187499991163, 2.977408999572648707, 24.83030278187175455 ) ) ;
#31458 = EDGE_LOOP ( 'NONE', ( #55232, #11667, #1682, #21969 ) ) ;
#31459 = CARTESIAN_POINT ( 'NONE',  ( 5.082755093536325930, 21.65624999795161543, -5.082755093536325930 ) ) ;
#31460 = ORIENTED_EDGE ( 'NONE', *, *, #32578, .T. ) ;
#31461 = CARTESIAN_POINT ( 'NONE',  ( 10.18810118749999916, 1.247682550866122264E-15, 116.4062500020483810 ) ) ;
#31462 = CARTESIAN_POINT ( 'NONE',  ( -10.00000000000000000, 202.2916666666666572, -2.679491924311229845 ) ) ;
#31463 = CARTESIAN_POINT ( 'NONE',  ( 1.432654583217662481, 209.1250000013656631, 194.5412658750000219 ) ) ;
#31464 = CARTESIAN_POINT ( 'NONE',  ( 26.56734541678237704, 202.3750000013656063, 173.4587341249998929 ) ) ;
#31465 = CARTESIAN_POINT ( 'NONE',  ( -7.320508075688778149, 73.12500000000001421, 7.320508075688769267 ) ) ;
#31466 = AXIS2_PLACEMENT_3D ( 'NONE', #31849, #10331, #50678 ) ;
#31467 = CARTESIAN_POINT ( 'NONE',  ( -5.082755093536324154, 91.71875000204838102, 5.082755093536326818 ) ) ;
#31468 = CARTESIAN_POINT ( 'NONE',  ( -2.485281374238571761, 296.8125000000000000, -6.000000000000003553 ) ) ;
#31469 = EDGE_CURVE ( 'NONE', #62108, #24834, #42360, .T. ) ;
#31471 = CARTESIAN_POINT ( 'NONE',  ( -24.72185337047553588, -41.03491067804711179, 188.7060743403438892 ) ) ;
#31470 = CARTESIAN_POINT ( 'NONE',  ( 25.17157287525378351, 207.7500000027312126, 167.1715728752537586 ) ) ;
#31472 = ORIENTED_EDGE ( 'NONE', *, *, #9250, .F. ) ;
#31473 = CARTESIAN_POINT ( 'NONE',  ( -3.042071309553166181, 232.8645833367473017, -11.35316468749999608 ) ) ;
#31474 = CARTESIAN_POINT ( 'NONE',  ( 4.556349186104045934, 11.00000000000000000, 87.71875000409677625 ) ) ;
#31475 = CARTESIAN_POINT ( 'NONE',  ( 3.999999999999959144, 198.1875000027312126, 140.3431457505076594 ) ) ;
#31476 = CARTESIAN_POINT ( 'NONE',  ( 7.999999999999992895, -2.501763238865420012E-05, 24.26780207613217399 ) ) ;
#31477 = CARTESIAN_POINT ( 'NONE',  ( -4.000000000000001776, 17.24999999726881583, -4.898587196589415787E-16 ) ) ;
#31478 = CARTESIAN_POINT ( 'NONE',  ( 5.000000000000004441, 261.6666666666666856, 8.660254037844385522 ) ) ;
#31479 = CARTESIAN_POINT ( 'NONE',  ( 1.334622868157815783E-15, 10.39230484541327293, -10.20000000000000284 ) ) ;
#31480 = CARTESIAN_POINT ( 'NONE',  ( 8.660254037844385522, 194.5833333333333712, 5.000000000000005329 ) ) ;
#31481 = CARTESIAN_POINT ( 'NONE',  ( -7.778174593052020747, -7.778174593052023411, 89.68749999999998579 ) ) ;
#31482 = CARTESIAN_POINT ( 'NONE',  ( -7.188101187499992051, 2.977408999572646930, 22.76780278187175455 ) ) ;
#31483 = CARTESIAN_POINT ( 'NONE',  ( -11.35316468750000141, 153.5937499965860127, -1.390361679473963753E-15 ) ) ;
#31484 = CARTESIAN_POINT ( 'NONE',  ( 26.34314575050770557, 201.5625000000000853, 165.9999999999998579 ) ) ;
#31485 = CARTESIAN_POINT ( 'NONE',  ( 1.469576158976823947E-15, 117.8750000000000000, 8.000000000000000000 ) ) ;
#31488 = CARTESIAN_POINT ( 'NONE',  ( -5.999999999999999112, 294.0625000000000000, 2.485281374238575314 ) ) ;
#31487 = CARTESIAN_POINT ( 'NONE',  ( -5.000000000000005329, 85.20833332650538239, 8.660254037844387298 ) ) ;
#31486 = CARTESIAN_POINT ( 'NONE',  ( 27.99999999999996803, 201.0000000000000000, 173.9999999999999147 ) ) ;
#31489 = ORIENTED_EDGE ( 'NONE', *, *, #64560, .T. ) ;
#31490 = CARTESIAN_POINT ( 'NONE',  ( 3.042071309553159519, 10.05208332991935016, 11.35316468750000141 ) ) ;
#31491=STYLED_ITEM('',(#74706),#16403);
#31492 = CARTESIAN_POINT ( 'NONE',  ( 12.00000000000000178, 0.000000000000000000, -28.00000000000000000 ) ) ;
#31493 = CARTESIAN_POINT ( 'NONE',  ( -2.828427124746153876, 207.8750000000000284, 195.1715728752538439 ) ) ;
#31494 = CARTESIAN_POINT ( 'NONE',  ( 1.469576158976823947E-15, 116.3750000000000000, 8.000000000000000000 ) ) ;
#31495 = CARTESIAN_POINT ( 'NONE',  ( 3.458734124999958581, 205.5000000013655779, 140.5673454167823593 ) ) ;
#31496 = CARTESIAN_POINT ( 'NONE',  ( 2.679491924311228956, 47.91666665983869677, -10.00000000000000000 ) ) ;
#31497 = VECTOR ( 'NONE', #19629, 1000.000000000000000 ) ;
#31498 = CARTESIAN_POINT ( 'NONE',  ( 7.188101187500000044, 106.9062500020483810, -8.802885111219163269E-16 ) ) ;
#31499 = CARTESIAN_POINT ( 'NONE',  ( 1.881053915767122664, 4.249999998634406140, 4.541265875000001451 ) ) ;
#31500 = CARTESIAN_POINT ( 'NONE',  ( 7.456209740496425376, 61.82228229130313224, -23.87473629694153132 ) ) ;
#31501 = CARTESIAN_POINT ( 'NONE',  ( -3.313708498984758943, -7.999999999999989342, 11.61155277982336820 ) ) ;
#31503 = CARTESIAN_POINT ( 'NONE',  ( -7.999999999970034636, -1.442163225726577833E-05, 17.51834960462420909 ) ) ;
#31502 = LINE ( 'NONE', #49214, #67273 ) ;
#31504 = VERTEX_POINT ( 'NONE', #7674 ) ;
#31505 = CARTESIAN_POINT ( 'NONE',  ( 6.000000000000003553, 292.6250000034139589, -2.485281374238571761 ) ) ;
#31506 = CARTESIAN_POINT ( 'NONE',  ( -2.679491924311229401, 161.4583333333333712, -10.00000000000001421 ) ) ;
#31507 = CARTESIAN_POINT ( 'NONE',  ( 5.676582343749997150, 232.5520833367473301, -9.832129032723418760 ) ) ;
#31508 = CARTESIAN_POINT ( 'NONE',  ( -9.832129032723418760, 132.8645833299193555, -5.676582343750004256 ) ) ;
#31509 = ORIENTED_EDGE ( 'NONE', *, *, #22420, .T. ) ;
#31510 = CARTESIAN_POINT ( 'NONE',  ( 0.000000000000000000, 1.806524977843537691E-16, 0.000000000000000000 ) ) ;
#31511 = CARTESIAN_POINT ( 'NONE',  ( 4.220049686691941027, -10.18810118749999738, 96.62500000204838102 ) ) ;
#31512 = DIRECTION ( 'NONE',  ( -0.000000000000000000, 1.000000000000000000, -0.000000000000000000 ) ) ;
#31513 = CARTESIAN_POINT ( 'NONE',  ( 3.458734125000016757, 198.1250000013656063, 199.4326545832176691 ) ) ;
#31514 = CARTESIAN_POINT ( 'NONE',  ( 30.82842712474619873, 197.3750000000000284, 167.1715728752537586 ) ) ;
#31516 = CARTESIAN_POINT ( 'NONE',  ( 3.042071309553159519, 109.7395833299193555, 11.35316468750000141 ) ) ;
#31515 = CARTESIAN_POINT ( 'NONE',  ( 6.123233995736767268E-16, 46.25000000000000711, -10.00000000000000178 ) ) ;
#31517 = CARTESIAN_POINT ( 'NONE',  ( -31.45873412499999944, 194.8750000013656063, 168.5673454167827572 ) ) ;
#31518 = CARTESIAN_POINT ( 'NONE',  ( -4.898587196589412829E-16, 91.62499999999998579, -8.000000000000000000 ) ) ;
#31519 = EDGE_LOOP ( 'NONE', ( #54210, #63837, #20030, #43561, #22538, #22126 ) ) ;
#31520 = CARTESIAN_POINT ( 'NONE',  ( -2.679491924311235174, 25.41666665983869677, 10.00000000000000000 ) ) ;
#31521 = CARTESIAN_POINT ( 'NONE',  ( 47.32259252271278882, 191.7059220763548524, 65.76194439203457875 ) ) ;
#31522 = CARTESIAN_POINT ( 'NONE',  ( -3.042071309553173730, 104.6354166632526699, 11.35316468749999785 ) ) ;
#31523 = CARTESIAN_POINT ( 'NONE',  ( -3.458734124999958581, 204.5000000013655779, 199.4326545832176976 ) ) ;
#31524 = CARTESIAN_POINT ( 'NONE',  ( 7.188101187500000933, 14.43749999795161365, -2.977408999572650483 ) ) ;
#31525 = CARTESIAN_POINT ( 'NONE',  ( 7.204075437095966983, 7.204075437095967871, 86.96875000204836681 ) ) ;
#31526 = CARTESIAN_POINT ( 'NONE',  ( 11.35316468749999963, 16.30208332991935194, -3.042071309553165293 ) ) ;
#31527 = EDGE_LOOP ( 'NONE', ( #74490, #39761, #50574, #54200 ) ) ;
#31528 = CARTESIAN_POINT ( 'NONE',  ( 5.000000000000001776, 182.7083333265053682, -8.660254037844389075 ) ) ;
#31529 = CARTESIAN_POINT ( 'NONE',  ( 8.660254037844389075, 245.2083333401613174, 4.999999999999997335 ) ) ;
#31530 = CARTESIAN_POINT ( 'NONE',  ( 6.123233995736767268E-16, 118.1249999931720396, -10.00000000000000178 ) ) ;
#31531 = CARTESIAN_POINT ( 'NONE',  ( 10.18810118749999916, 4.220049686691935698, 71.87500000204836681 ) ) ;
#31532 = EDGE_CURVE ( 'NONE', #32586, #19432, #69944, .T. ) ;
#31533 = CARTESIAN_POINT ( 'NONE',  ( 1.184329452913352121, 21.99999999999999289, 4.197665287320669236 ) ) ;
#31534 = CARTESIAN_POINT ( 'NONE',  ( -1.320432766682874540E-15, 6.093749997951610986, 7.188101187500000044 ) ) ;
#31535 = CARTESIAN_POINT ( 'NONE',  ( 4.721056650416000089, 288.8281250017069510, 4.721056650415999201 ) ) ;
#31536 = PLANE ( 'NONE',  #28076 ) ;
#31537 = CARTESIAN_POINT ( 'NONE',  ( 11.35316468750000141, 221.0937499965860127, 0.000000000000000000 ) ) ;
#31538 = CARTESIAN_POINT ( 'NONE',  ( -9.832129032723418760, 138.1770833299193555, -5.676582343750004256 ) ) ;
#31539 = CARTESIAN_POINT ( 'NONE',  ( 1.871523826299183495E-15, -10.18810118749999916, 84.53125000204836681 ) ) ;
#31540 =( BOUNDED_CURVE ( )  B_SPLINE_CURVE ( 2, ( #43437, #49095, #54030, #26450, #72108, #48722, #19680, #14387, #44200 ),
 .UNSPECIFIED., .F., .F. ) 
 B_SPLINE_CURVE_WITH_KNOTS ( ( 3, 2, 2, 2, 3 ),
 ( 0.2386363636363636465, 0.2443181818181818232, 0.2500000000000000000, 0.2556818181818181768, 0.2613636363636363535 ),
 .UNSPECIFIED. ) 
 CURVE ( )  GEOMETRIC_REPRESENTATION_ITEM ( )  RATIONAL_B_SPLINE_CURVE ( ( 1.000000000000000000, 0.9238795325112867385, 1.000000000000000000, 0.9238795325112867385, 1.000000000000000000, 0.9238795325112867385, 1.000000000000000000, 0.9238795325112867385, 1.000000000000000000 ) ) 
 REPRESENTATION_ITEM ( '' )  );
#31541 = CARTESIAN_POINT ( 'NONE',  ( -31.45873412499999233, 199.6875000013656063, 170.0000000000003979 ) ) ;
#31542 = CARTESIAN_POINT ( 'NONE',  ( 5.656854249492378806, 20.81250000000000355, 5.656854249492381470 ) ) ;
#31543 = CARTESIAN_POINT ( 'NONE',  ( -3.211159895383562723, 10.06249999863440614, 3.211159895383561391 ) ) ;
#31544 = ORIENTED_EDGE ( 'NONE', *, *, #54813, .F. ) ;
#31545 = CARTESIAN_POINT ( 'NONE',  ( 2.828427124746208943, 203.7500000027312126, 195.1715728752538439 ) ) ;
#31546 = CARTESIAN_POINT ( 'NONE',  ( 3.458734124999960358, 200.6250000013655779, 143.4326545832176976 ) ) ;
#31547 = CARTESIAN_POINT ( 'NONE',  ( -4.000000000000015099, 202.6875000027311842, 143.6568542494924543 ) ) ;
#31548 = EDGE_CURVE ( 'NONE', #39105, #62930, #11013, .T. ) ;
#31549 = CARTESIAN_POINT ( 'NONE',  ( -2.679491924317297435, 173.5416666666662024, 9.999999999996612488 ) ) ;
#31550 = VERTEX_POINT ( 'NONE', #34888 ) ;
#31551 = CARTESIAN_POINT ( 'NONE',  ( 7.188101187500000044, 3.468749997951610542, 0.000000000000000000 ) ) ;
#31552 = CARTESIAN_POINT ( 'NONE',  ( -11.61006277764976602, -27.07698728651038778, 198.7441070070757689 ) ) ;
#31553 = DIRECTION ( 'NONE',  ( -0.000000000000000000, 1.000000000000000000, -4.476705744456276341E-16 ) ) ;
#31554 = CARTESIAN_POINT ( 'NONE',  ( -11.35316468750000141, 183.4895833299193839, 3.042071309553159963 ) ) ;
#31555 = CARTESIAN_POINT ( 'NONE',  ( -5.082755093536325930, 113.8437500020483810, -5.082755093536325930 ) ) ;
#31556 = CARTESIAN_POINT ( 'NONE',  ( 6.000000000000003553, 295.5625000000000000, -2.485281374238571761 ) ) ;
#31557 = CARTESIAN_POINT ( 'NONE',  ( 2.765530957081996366, 291.1406250017069510, -6.676582343750002480 ) ) ;
#31558 = EDGE_CURVE ( 'NONE', #1239, #22615, #29946, .T. ) ;
#31559 = CARTESIAN_POINT ( 'NONE',  ( -30.82842712474616320, 209.3750000000000284, 172.8284271247465824 ) ) ;
#31560 = CONTEXT_DEPENDENT_SHAPE_REPRESENTATION ( #47221, #6620 ) ;
#31561 = ORIENTED_EDGE ( 'NONE', *, *, #68733, .T. ) ;
#31562 = ADVANCED_FACE ( 'NONE', ( #58627, #24273 ), #6935, .F. ) ;
#31563 = CARTESIAN_POINT ( 'NONE',  ( -3.042071309553159075, 220.2604166700806161, 11.35316468749999963 ) ) ;
#31564 = CARTESIAN_POINT ( 'NONE',  ( -4.401442555609577197E-16, 7.188101187499992051, 28.48655278187175810 ) ) ;
#31565 = CARTESIAN_POINT ( 'NONE',  ( -5.099999999999999645, 6.245698675651499853E-16, -10.14441321561125520 ) ) ;
#31566 = CARTESIAN_POINT ( 'NONE',  ( -3.313708498984757611, 7.999999999999991118, 15.73655278392014623 ) ) ;
#31567 = CARTESIAN_POINT ( 'NONE',  ( -3.458734124999960358, 198.6250000013655779, 196.5673454167823877 ) ) ;
#31568 = ORIENTED_EDGE ( 'NONE', *, *, #15876, .F. ) ;
#31569 = CARTESIAN_POINT ( 'NONE',  ( -6.000000000000003553, 299.0000000034139589, -2.485281374238571317 ) ) ;
#31570 = CARTESIAN_POINT ( 'NONE',  ( 3.313708498984760720, 96.03125000000000000, -8.000000000000000000 ) ) ;
#31571 = CARTESIAN_POINT ( 'NONE',  ( -8.311093377946841443, 119.2187499965860127, 8.311093377946830785 ) ) ;
#31572 = FACE_OUTER_BOUND ( 'NONE', #30726, .T. ) ;
#31573 = CARTESIAN_POINT ( 'NONE',  ( 4.556349186104045934, 11.00000000000000000, 77.03125000000000000 ) ) ;
#31576 = CARTESIAN_POINT ( 'NONE',  ( -1.656854249492399234, 202.1875000000000568, 201.9999999999999432 ) ) ;
#31575 = CARTESIAN_POINT ( 'NONE',  ( 25.55430564589115505, 200.0625000013656063, 167.5543056458911053 ) ) ;
#31574 = CARTESIAN_POINT ( 'NONE',  ( 26.56734541678232375, 197.6250000013656063, 173.4587341249998929 ) ) ;
#31577 = ORIENTED_EDGE ( 'NONE', *, *, #3806, .T. ) ;
#31578 = VECTOR ( 'NONE', #28911, 1000.000000000000000 ) ;
#31579 = DIRECTION ( 'NONE',  ( 0.8660254037844380415, -0.5000000000000009992, 0.000000000000000000 ) ) ;
#31580 = CARTESIAN_POINT ( 'NONE',  ( 9.832129032723420536, 226.1979166632526983, -5.676582343749999815 ) ) ;
#31581 = AXIS2_PLACEMENT_3D ( 'NONE', #71207, #18432, #47088 ) ;
#31582 = CARTESIAN_POINT ( 'NONE',  ( 1.432654583217607858, 201.6250000013656063, 138.5412658750000787 ) ) ;
#31583 = CARTESIAN_POINT ( 'NONE',  ( 31.45873412499997812, 200.8750000013656063, 171.4326545832175839 ) ) ;
#31584 = CARTESIAN_POINT ( 'NONE',  ( 11.00000000000000355, -4.556349186104045046, 114.3437500040967763 ) ) ;
#31585 = ADVANCED_FACE ( 'NONE', ( #70310 ), #41636, .F. ) ;
#31586 = CARTESIAN_POINT ( 'NONE',  ( -11.35316468749999785, 198.3854166632526699, -3.042071309553167513 ) ) ;
#31587 = CARTESIAN_POINT ( 'NONE',  ( 7.188101187500000044, 93.78125000204836681, -8.802885111219163269E-16 ) ) ;
#31588 = CARTESIAN_POINT ( 'NONE',  ( 9.420701371451851713, 225.9999999999999716, 5.314304958673083057 ) ) ;
#31589 = CARTESIAN_POINT ( 'NONE',  ( -3.211159895383561391, 12.68749999863440792, -3.211159895383561835 ) ) ;
#31590 = CARTESIAN_POINT ( 'NONE',  ( 29.43265458321761230, 199.7500000013656063, 173.4587341249998929 ) ) ;
#31591 = CARTESIAN_POINT ( 'NONE',  ( -7.188101187499991163, 2.977408999572646930, 4.767802781871753659 ) ) ;
#31592 = CYLINDRICAL_SURFACE ( 'NONE', #58030, 7.999999999999991118 ) ;
#31593 = CARTESIAN_POINT ( 'NONE',  ( -11.35316468750000141, 88.28124999658602690, -1.390361679473963753E-15 ) ) ;
#31594 = ORIENTED_EDGE ( 'NONE', *, *, #70792, .F. ) ;
#31595 = CARTESIAN_POINT ( 'NONE',  ( -1.001543065824775909E-15, -10.39230484541329247, -10.20000000000000284 ) ) ;
#31596 = CARTESIAN_POINT ( 'NONE',  ( 2.828427124746208943, 209.6250000000000284, 195.1715728752538439 ) ) ;
#31597 = CARTESIAN_POINT ( 'NONE',  ( 2.679491924311891093, 38.95833333333347781, 9.999999999999802824 ) ) ;
#31598 = LINE ( 'NONE', #24807, #43688 ) ;
#31599 = CARTESIAN_POINT ( 'NONE',  ( -8.311093377946841443, 88.90624999658602690, 8.311093377946830785 ) ) ;
#31600 = ORIENTED_EDGE ( 'NONE', *, *, #73577, .T. ) ;
#31601 = CARTESIAN_POINT ( 'NONE',  ( -7.204075437095965206, -7.204075437095968759, 86.21875000204836681 ) ) ;
#31602 = CARTESIAN_POINT ( 'NONE',  ( 4.220049686691934809, 10.18810118749999916, 113.6875000020483952 ) ) ;
#31603 = CARTESIAN_POINT ( 'NONE',  ( -2.445694354108784108, 208.5625000013656063, 195.5543056458912190 ) ) ;
#31604 = CARTESIAN_POINT ( 'NONE',  ( 31.99999999999998579, 207.1875000000000284, 171.6568542494923122 ) ) ;
#31605 = CARTESIAN_POINT ( 'NONE',  ( 5.676582343750001591, 71.61458332991935549, -9.832129032723420536 ) ) ;
#31606 = CARTESIAN_POINT ( 'NONE',  ( -7.999999999999989342, -3.313708498984762496, 17.61155278392014623 ) ) ;
#31607 = CARTESIAN_POINT ( 'NONE',  ( 0.000000000000000000, 0.000000000000000000, 30.00000000000000000 ) ) ;
#31608 = CARTESIAN_POINT ( 'NONE',  ( 4.999999999999993783, 171.0416666598387110, 8.660254037844390851 ) ) ;
#31609 = CARTESIAN_POINT ( 'NONE',  ( 3.999999999999960032, 200.0625000027312410, 143.6568542494924259 ) ) ;
#31610 = VECTOR ( 'NONE', #45022, 1000.000000000000000 ) ;
#31611 = DIRECTION ( 'NONE',  ( 0.000000000000000000, 0.000000000000000000, -1.000000000000000000 ) ) ;
#31612 = CARTESIAN_POINT ( 'NONE',  ( 9.832129032723416984, 55.67708332991935549, 5.676582343750006032 ) ) ;
#31613 = CARTESIAN_POINT ( 'NONE',  ( 4.721056650415999201, 294.0781250017069510, -4.721056650415999201 ) ) ;
#31614 = CARTESIAN_POINT ( 'NONE',  ( 10.18810118749999916, 1.247682550866122264E-15, 104.7812500020483810 ) ) ;
#31615 = CARTESIAN_POINT ( 'NONE',  ( -9.832129032723418760, 207.8645833299193555, -5.676582343750004256 ) ) ;
#31616 = VERTEX_POINT ( 'NONE', #7305 ) ;
#31617 = CARTESIAN_POINT ( 'NONE',  ( 7.999999999999992895, -7.224685084787812073E-14, 27.26780278391845513 ) ) ;
#31618 = CARTESIAN_POINT ( 'NONE',  ( -32.00000000000000000, 203.3750000027312126, 170.0000000000004547 ) ) ;
#31619 = CARTESIAN_POINT ( 'NONE',  ( 5.000000000000000000, 62.88740100213628637, 24.06179116403814078 ) ) ;
#31621 = CARTESIAN_POINT ( 'NONE',  ( -9.832129032723418760, 197.8645833299193555, -5.676582343750004256 ) ) ;
#31620 = DIRECTION ( 'NONE',  ( 0.000000000000000000, 0.000000000000000000, 1.000000000000000000 ) ) ;
#31622 = DIRECTION ( 'NONE',  ( -0.000000000000000000, 1.000000000000000000, -0.000000000000000000 ) ) ;
#31623 = CARTESIAN_POINT ( 'NONE',  ( -2.679491924311222295, 239.1666666734946034, 10.00000000000000178 ) ) ;
#31624 = CARTESIAN_POINT ( 'NONE',  ( -10.00000000000000355, 189.5833333265053682, 2.679491924311223183 ) ) ;
#31625 = ORIENTED_EDGE ( 'NONE', *, *, #38104, .F. ) ;
#31626 = ADVANCED_FACE ( 'NONE', ( #24637 ), #52223, .T. ) ;
#31627 = CARTESIAN_POINT ( 'NONE',  ( 6.951808397369818766E-16, 187.3437499965860127, -11.35316468750000141 ) ) ;
#31628 = AXIS2_PLACEMENT_3D ( 'NONE', #48580, #60658, #26696 ) ;
#31629 = CARTESIAN_POINT ( 'NONE',  ( -2.977408999572647819, 7.188101187499992051, 23.70530278187175455 ) ) ;
#31630 = EDGE_CURVE ( 'NONE', #33654, #53057, #45191, .T. ) ;
#31631 = CARTESIAN_POINT ( 'NONE',  ( 3.369429374625368734, 60.49191766694088557, -23.06312700027788765 ) ) ;
#31632 = VERTEX_POINT ( 'NONE', #49516 ) ;
#31633 = AXIS2_PLACEMENT_3D ( 'NONE', #33870, #16474, #73832 ) ;
#31634 = CARTESIAN_POINT ( 'NONE',  ( 5.656854249492381470, 95.75000000409677625, 5.656854249492379694 ) ) ;
#31635 = CARTESIAN_POINT ( 'NONE',  ( 7.320508075688774596, 0.6250000000000000000, -7.320508075688774596 ) ) ;
#31636 = EDGE_CURVE ( 'NONE', #36130, #70797, #34641, .T. ) ;
#31637 = CARTESIAN_POINT ( 'NONE',  ( -4.000000000000002665, 14.56250000000000000, 1.656854249492380804 ) ) ;
#31638 = CARTESIAN_POINT ( 'NONE',  ( 4.541265875000001451, 16.24999999863440436, 1.881053915767124440 ) ) ;
#31639 = CARTESIAN_POINT ( 'NONE',  ( 5.656854249492376141, -5.656854249492374365, 15.08030278392014623 ) ) ;
#31640 = PRODUCT_RELATED_PRODUCT_CATEGORY ( 'part', '', ( #8304 ) ) ;
#31641 = CARTESIAN_POINT ( 'NONE',  ( 27.99999999999996092, 194.7622595281506790, 166.2377404718492357 ) ) ;
#31642 = ORIENTED_EDGE ( 'NONE', *, *, #27729, .F. ) ;
#31643 = CARTESIAN_POINT ( 'NONE',  ( 4.999999999999998224, -11.32881245867858944, -67.85521288293395514 ) ) ;
#31644 = CARTESIAN_POINT ( 'NONE',  ( 1.320432766682874540E-15, 91.53125000204836681, 7.188101187500000044 ) ) ;
#31646 = CARTESIAN_POINT ( 'NONE',  ( -3.042071309553159075, 259.9479166700806445, 11.35316468749999963 ) ) ;
#31645 = CARTESIAN_POINT ( 'NONE',  ( -5.656854249492375253, 5.656854249492375253, 12.64280277982336287 ) ) ;
#31647 = DIRECTION ( 'NONE',  ( -0.6583937118378737630, -0.7526737143094255345, 0.000000000000000000 ) ) ;
#31648 =( BOUNDED_CURVE ( )  B_SPLINE_CURVE ( 2, ( #10136, #44469, #44843, #21076, #56172, #4485, #61446, #55051, #26733 ),
 .UNSPECIFIED., .F., .F. ) 
 B_SPLINE_CURVE_WITH_KNOTS ( ( 3, 2, 2, 2, 3 ),
 ( 0.3947368421052632192, 0.4013157894736842923, 0.4078947368421053654, 0.4144736842105264385, 0.4210526315789475116 ),
 .UNSPECIFIED. ) 
 CURVE ( )  GEOMETRIC_REPRESENTATION_ITEM ( )  RATIONAL_B_SPLINE_CURVE ( ( 0.9999999999999993339, 0.9238795325112874046, 1.000000000000000000, 0.9238795325112867385, 1.000000000000000000, 0.9238795325112867385, 1.000000000000000000, 0.9238795325112848511, 1.000000000000001998 ) ) 
 REPRESENTATION_ITEM ( '' )  );
#31649 = ORIENTED_EDGE ( 'NONE', *, *, #69523, .F. ) ;
#31650 = EDGE_CURVE ( 'NONE', #40937, #11029, #31742, .T. ) ;
#31651 = CARTESIAN_POINT ( 'NONE',  ( -8.000000000000000000, 101.1875000040967763, 0.000000000000000000 ) ) ;
#31652 = CARTESIAN_POINT ( 'NONE',  ( -7.188101187499991163, 2.977408999572646930, 19.39280278187176165 ) ) ;
#31653 = VERTEX_POINT ( 'NONE', #66871 ) ;
#31654 = ORIENTED_EDGE ( 'NONE', *, *, #39451, .T. ) ;
#31655 = CARTESIAN_POINT ( 'NONE',  ( 10.18810118750000093, -4.220049686691933033, 81.81250000204838102 ) ) ;
#31656 = CARTESIAN_POINT ( 'NONE',  ( -11.35316468750000141, 78.59374999658601268, -1.390361679473963753E-15 ) ) ;
#31657 = CARTESIAN_POINT ( 'NONE',  ( -2.679491924311226292, 113.3333333265053540, -10.00000000000000178 ) ) ;
#31658 = CARTESIAN_POINT ( 'NONE',  ( 4.556349186104051263, -10.99999999999999822, 94.46874999999998579 ) ) ;
#31661 = CARTESIAN_POINT ( 'NONE',  ( 2.765530957081996366, 292.2968750017070079, -6.676582343750002480 ) ) ;
#31660 = CARTESIAN_POINT ( 'NONE',  ( 26.34314575050763452, 196.0625000027312694, 173.9999999999999147 ) ) ;
#31659 = DIRECTION ( 'NONE',  ( 0.000000000000000000, 0.000000000000000000, 1.000000000000000000 ) ) ;
#31662 = CARTESIAN_POINT ( 'NONE',  ( -2.679491924311235618, 148.5416666666666288, 10.00000000000000000 ) ) ;
#31663 = CARTESIAN_POINT ( 'NONE',  ( -24.00000000000002487, 203.9375000027311842, 168.3431457505079152 ) ) ;
#31664 = CARTESIAN_POINT ( 'NONE',  ( 3.458734124999959914, 194.4587341250000065, 142.0000000000000568 ) ) ;
#31665 = B_SPLINE_CURVE_WITH_KNOTS ( 'NONE', 1,
 ( #49572, #38264 ),
 .UNSPECIFIED., .F., .F.,
 ( 2, 2 ),
 ( 0.000000000000000000, 1.000000000000000000 ),
 .UNSPECIFIED. ) ;
#31666 = CARTESIAN_POINT ( 'NONE',  ( 3.458734125000015425, 199.2500000013656063, 196.5673454167823877 ) ) ;
#31667 = CARTESIAN_POINT ( 'NONE',  ( -2.849036369511732440E-14, 199.2500000000000000, 138.0000000000000568 ) ) ;
#31668 = CARTESIAN_POINT ( 'NONE',  ( 8.000000000000000000, 2.812499995903220640, 0.000000000000000000 ) ) ;
#31669 = CARTESIAN_POINT ( 'NONE',  ( 24.54126587499999346, 199.1875000013655779, 169.9999999999998863 ) ) ;
#31670 = CARTESIAN_POINT ( 'NONE',  ( -5.082755093536326818, 12.28124999795161187, 5.082755093536325042 ) ) ;
#31671 = CARTESIAN_POINT ( 'NONE',  ( 3.317071493978883456, -8.008118988124989457, -0.01813471605937123921 ) ) ;
#31672 = DIRECTION ( 'NONE',  ( 0.000000000000000000, 0.000000000000000000, -1.000000000000000000 ) ) ;
#31673 = CARTESIAN_POINT ( 'NONE',  ( 7.188101187500000044, 110.2812500020483810, -8.802885111219163269E-16 ) ) ;
#31675 = CARTESIAN_POINT ( 'NONE',  ( -1.836970198721029983E-15, 170.6249999931720538, 10.00000000000000178 ) ) ;
#31674 = CARTESIAN_POINT ( 'NONE',  ( 2.849036369511732440E-14, 201.2500000000000000, 202.0000000000000000 ) ) ;
#31676 = CARTESIAN_POINT ( 'NONE',  ( 2.679491924311377282, 136.0416666666666572, -9.999999999999918288 ) ) ;
#31677 = CARTESIAN_POINT ( 'NONE',  ( 2.485281374238266672, 288.7500000034140726, -6.000000000000306422 ) ) ;
#31678 = CARTESIAN_POINT ( 'NONE',  ( 5.082755093536320601, -5.082755093536318824, 21.92405278187175455 ) ) ;
#31679 = CARTESIAN_POINT ( 'NONE',  ( 30.82842712474619873, 195.3750000000000284, 167.1715728752537586 ) ) ;
#31680 = CARTESIAN_POINT ( 'NONE',  ( 5.676582343749993598, 44.94791666325267698, 9.832129032723422313 ) ) ;
#31681 = CARTESIAN_POINT ( 'NONE',  ( 10.00000000000000533, 150.0000000000000000, 0.000000000000000000 ) ) ;
#31682 = CARTESIAN_POINT ( 'NONE',  ( -4.999999999999998224, 3.541666659838699438, -8.660254037844389075 ) ) ;
#31683 = ORIENTED_EDGE ( 'NONE', *, *, #5787, .T. ) ;
#31684 = LINE ( 'NONE', #66002, #37405 ) ;
#31685 = CARTESIAN_POINT ( 'NONE',  ( -11.00000000000000000, 0.000000000000000000, 80.68750000409677625 ) ) ;
#31686 = CARTESIAN_POINT ( 'NONE',  ( 8.311093377946837890, 46.40624999658601268, -8.311093377946837890 ) ) ;
#31687 = CARTESIAN_POINT ( 'NONE',  ( 7.778174593052021635, 7.778174593052023411, 78.62500000409677625 ) ) ;
#31688 = CARTESIAN_POINT ( 'NONE',  ( -2.839093476692135984E-14, 202.9375000013656063, 138.5412658750000503 ) ) ;
#31689 = CARTESIAN_POINT ( 'NONE',  ( 23.99999999999998934, 202.7500000000000000, 169.9999999999998863 ) ) ;
#31690 = CARTESIAN_POINT ( 'NONE',  ( -1.040834085586084257E-14, 82.00000000000001421, 97.52691193458117880 ) ) ;
#31692 = CARTESIAN_POINT ( 'NONE',  ( 3.042071309553167513, 26.82291666325268054, -11.35316468749999785 ) ) ;
#31691 = CARTESIAN_POINT ( 'NONE',  ( 1.320432766682874540E-15, 100.5312500020483810, 7.188101187500000044 ) ) ;
#31693 = CARTESIAN_POINT ( 'NONE',  ( -7.999999999999991118, 0.000000000000000000, 9.830302779823364645 ) ) ;
#31694 = CARTESIAN_POINT ( 'NONE',  ( -10.00000000000000000, 49.16666665983869677, -2.679491924311229845 ) ) ;
#31695 = CARTESIAN_POINT ( 'NONE',  ( 3.042071309553159519, 164.7395833299193271, 11.35316468750000141 ) ) ;
#31696 = CARTESIAN_POINT ( 'NONE',  ( 5.000000000000001776, 127.7083333265053824, -8.660254037844389075 ) ) ;
#31697 = CARTESIAN_POINT ( 'NONE',  ( -2.977408999572651815, 106.8125000020484094, 7.188101187500000933 ) ) ;
#31698 = VERTEX_POINT ( 'NONE', #3131 ) ;
#31699 = CARTESIAN_POINT ( 'NONE',  ( 4.999999999999993783, 21.04166665983870033, 8.660254037844390851 ) ) ;
#31700 = CARTESIAN_POINT ( 'NONE',  ( 6.951808397369818766E-16, 22.34374999658601979, -11.35316468750000141 ) ) ;
#31701 = CARTESIAN_POINT ( 'NONE',  ( 2.449293598294707893E-16, 12.25000000000000000, -4.000000000000001776 ) ) ;
#31702 = ORIENTED_EDGE ( 'NONE', *, *, #57172, .F. ) ;
#31703 = CARTESIAN_POINT ( 'NONE',  ( -31.99999999999998579, 204.3125000000000000, 171.6568542494928238 ) ) ;
#31704 = CARTESIAN_POINT ( 'NONE',  ( 7.204075437095966983, 7.204075437095967871, 74.59375000204838102 ) ) ;
#31705 = LINE ( 'NONE', #49041, #11253 ) ;
#31707 = CARTESIAN_POINT ( 'NONE',  ( -9.832129032723420536, 153.6979166632526983, 5.676582343749997150 ) ) ;
#31706 = DIRECTION ( 'NONE',  ( -0.000000000000000000, -0.000000000000000000, -1.000000000000000000 ) ) ;
#31708 = DIRECTION ( 'NONE',  ( -0.000000000000000000, 1.000000000000000000, 4.689100369878284071E-30 ) ) ;
#31709 = CARTESIAN_POINT ( 'NONE',  ( 5.656854249492376141, -5.656854249492374365, 11.94905278432982243 ) ) ;
#31710 = CARTESIAN_POINT ( 'NONE',  ( -20.71009187733394086, -28.10211377453205372, 193.0675474620159093 ) ) ;
#31711 = CARTESIAN_POINT ( 'NONE',  ( 5.676582343750005144, 235.5729166700806729, 9.832129032723416984 ) ) ;
#31712 = CARTESIAN_POINT ( 'NONE',  ( 10.18810118749999916, 4.220049686691935698, 85.37500000204839523 ) ) ;
#31713 = ORIENTED_EDGE ( 'NONE', *, *, #14518, .F. ) ;
#31714 = EDGE_CURVE ( 'NONE', #30991, #27901, #34190, .T. ) ;
#31715 = PLANE ( 'NONE',  #34135 ) ;
#31716 = DIRECTION ( 'NONE',  ( -0.000000000000000000, 1.000000000000000000, -4.476705744456276341E-16 ) ) ;
#31717 = CARTESIAN_POINT ( 'NONE',  ( 8.311093377946837890, 96.71874999658599847, -8.311093377946837890 ) ) ;
#31718 = CARTESIAN_POINT ( 'NONE',  ( 10.18810118749999916, 1.247682550866122264E-15, 102.9062500020483810 ) ) ;
#31719 = EDGE_CURVE ( 'NONE', #59533, #40040, #31800, .T. ) ;
#31720 = CARTESIAN_POINT ( 'NONE',  ( -1.881053915767121776, 21.74999999863440792, -4.541265875000002339 ) ) ;
#31721 = ORIENTED_EDGE ( 'NONE', *, *, #34454, .F. ) ;
#31722 = VERTEX_POINT ( 'NONE', #14047 ) ;
#31723 = CARTESIAN_POINT ( 'NONE',  ( -3.211159895383561391, 5.812499998634407028, -3.211159895383561835 ) ) ;
#31724 = CARTESIAN_POINT ( 'NONE',  ( 7.188101187499999156, 6.374999997951610986, 2.977408999572654924 ) ) ;
#31725 = CARTESIAN_POINT ( 'NONE',  ( -3.313708498984762052, 117.4062500040967905, -8.000000000000000000 ) ) ;
#31726 = CARTESIAN_POINT ( 'NONE',  ( 7.204075437095968759, -7.204075437095966983, 95.59375000204838102 ) ) ;
#31727 = CARTESIAN_POINT ( 'NONE',  ( -28.00000000000002132, 201.6875000013656063, 166.5412658750003629 ) ) ;
#31728 = CARTESIAN_POINT ( 'NONE',  ( -7.320508075688773708, 158.7499999931720254, -7.320508075688774596 ) ) ;
#31729 = CARTESIAN_POINT ( 'NONE',  ( -2.828427124746192067, 2.625000000000000000, 2.828427124746190735 ) ) ;
#31730 = CARTESIAN_POINT ( 'NONE',  ( -1.656854249492381248, 20.06249999726881228, -4.000000000000001776 ) ) ;
#31731 = CARTESIAN_POINT ( 'NONE',  ( -4.541265875000003227, 4.874999998634406140, 1.881053915767121110 ) ) ;
#31732 = CONICAL_SURFACE ( 'NONE', #37775, 10.00000000000000000, 0.02777063659342106361 ) ;
#31733 = CARTESIAN_POINT ( 'NONE',  ( -1.432654583217664479, 208.7500000013656063, 138.5412658750000787 ) ) ;
#31734 = DIRECTION ( 'NONE',  ( -1.224646799147353207E-16, 1.000000000000000000, 0.000000000000000000 ) ) ;
#31736 = CARTESIAN_POINT ( 'NONE',  ( -4.556349186104048599, -10.99999999999999822, 95.96875000409676204 ) ) ;
#31735 = CARTESIAN_POINT ( 'NONE',  ( -25.55430564589111953, 199.0625000013656063, 172.4456943541091505 ) ) ;
#31737 =( NAMED_UNIT ( * ) PLANE_ANGLE_UNIT ( ) SI_UNIT ( $, .RADIAN. ) );
#31738 = CARTESIAN_POINT ( 'NONE',  ( 4.541265875000002339, 18.37499999863441147, -1.881053915767121554 ) ) ;
#31739 = DIRECTION ( 'NONE',  ( -0.000000000000000000, -0.000000000000000000, -1.000000000000000000 ) ) ;
#31740 = CARTESIAN_POINT ( 'NONE',  ( -7.188101187499992051, 0.000000000000000000, 7.486552781871751883 ) ) ;
#31741 = EDGE_LOOP ( 'NONE', ( #50034, #71031, #73326, #19294 ) ) ;
#31742 =( BOUNDED_CURVE ( )  B_SPLINE_CURVE ( 2, ( #8406, #44241, #54068, #14799, #65745, #32558, #37838, #54820, #60835 ),
 .UNSPECIFIED., .F., .F. ) 
 B_SPLINE_CURVE_WITH_KNOTS ( ( 3, 2, 2, 2, 3 ),
 ( 0.8970588235294117974, 0.9007352941176470784, 0.9044117647058823595, 0.9080882352941176405, 0.9117647058823529216 ),
 .UNSPECIFIED. ) 
 CURVE ( )  GEOMETRIC_REPRESENTATION_ITEM ( )  RATIONAL_B_SPLINE_CURVE ( ( 1.000000000000000000, 0.9238795325112867385, 1.000000000000000000, 0.9238795325112867385, 1.000000000000000000, 0.9238795325112867385, 1.000000000000000000, 0.9238795325112867385, 1.000000000000000000 ) ) 
 REPRESENTATION_ITEM ( '' )  );
#31743 = ORIENTED_EDGE ( 'NONE', *, *, #69031, .T. ) ;
#31744 = CARTESIAN_POINT ( 'NONE',  ( 10.18810118750000093, -4.220049686691933033, 98.31250000204836681 ) ) ;
#31745 = CARTESIAN_POINT ( 'NONE',  ( -1.469576158976823947E-15, 26.43749999590322375, 8.000000000000000000 ) ) ;
#31746 = CARTESIAN_POINT ( 'NONE',  ( -27.99999999999996803, 206.1875000013656063, 173.4587341250003760 ) ) ;
#31747 = CARTESIAN_POINT ( 'NONE',  ( -26.34314575050764518, 198.9375000000000000, 166.0000000000003695 ) ) ;
#31748 = CARTESIAN_POINT ( 'NONE',  ( -3.458734124999959914, 197.3750000013656063, 196.5673454167823877 ) ) ;
#31749 = CARTESIAN_POINT ( 'NONE',  ( 8.000000000000000000, 104.8437500000000000, -3.313708498984762496 ) ) ;
#31750 = CARTESIAN_POINT ( 'NONE',  ( -1.836970198721029983E-15, 103.7500000000000142, 10.00000000000000178 ) ) ;
#31751 = CARTESIAN_POINT ( 'NONE',  ( -5.656854249492380582, 109.8125000000000000, -5.656854249492380582 ) ) ;
#31752 = CARTESIAN_POINT ( 'NONE',  ( -2.765530957081998586, 291.7968750017070079, 6.676582343750001591 ) ) ;
#31753 = CARTESIAN_POINT ( 'NONE',  ( 1.320432766682872962E-15, -7.188101187499992051, 14.23655278187175455 ) ) ;
#31754 = ORIENTED_EDGE ( 'NONE', *, *, #25040, .T. ) ;
#31755 = CARTESIAN_POINT ( 'NONE',  ( 7.999999999999998224, 19.21874999590322375, 3.313708498984766493 ) ) ;
#31756 = AXIS2_PLACEMENT_3D ( 'NONE', #3218, #19075, #65089 ) ;
#31757 = CARTESIAN_POINT ( 'NONE',  ( -1.432654583217664479, 204.7500000013656063, 138.5412658750000787 ) ) ;
#31758 = CARTESIAN_POINT ( 'NONE',  ( -20.20205423947337664, -34.16752681039474027, 146.2363330641790071 ) ) ;
#31759 = DIRECTION ( 'NONE',  ( 0.000000000000000000, 0.000000000000000000, 1.000000000000000000 ) ) ;
#31760 = CARTESIAN_POINT ( 'NONE',  ( -11.35316468749999785, 249.0104166700806445, -3.042071309553164848 ) ) ;
#31761 = CARTESIAN_POINT ( 'NONE',  ( 2.849036369511732440E-14, 207.3750000027312126, 202.0000000000000000 ) ) ;
#31762 = CARTESIAN_POINT ( 'NONE',  ( 2.020667218593132706E-15, -11.00000000000000000, 113.8749999999999858 ) ) ;
#31763 = CARTESIAN_POINT ( 'NONE',  ( 5.676582343750001591, 6.614583329919350163, -9.832129032723420536 ) ) ;
#31764 =( BOUNDED_CURVE ( )  B_SPLINE_CURVE ( 2, ( #53442, #2117, #59107, #7414, #1402, #24387, #70417, #25110, #47395 ),
 .UNSPECIFIED., .F., .F. ) 
 B_SPLINE_CURVE_WITH_KNOTS ( ( 3, 2, 2, 2, 3 ),
 ( 0.2941176470588234837, 0.2977941176470587648, 0.3014705882352940458, 0.3051470588235293824, 0.3088235294117646634 ),
 .UNSPECIFIED. ) 
 CURVE ( )  GEOMETRIC_REPRESENTATION_ITEM ( )  RATIONAL_B_SPLINE_CURVE ( ( 1.000000000000001110, 0.9238795325112856283, 1.000000000000000000, 0.9238795325112867385, 1.000000000000000000, 0.9238795325112867385, 1.000000000000000000, 0.9238795325112878487, 0.9999999999999988898 ) ) 
 REPRESENTATION_ITEM ( '' )  );
#31765 = CARTESIAN_POINT ( 'NONE',  ( -7.188101187499990274, -2.977408999572651815, 6.455302781871754547 ) ) ;
#31766 = CARTESIAN_POINT ( 'NONE',  ( -11.35316468749999785, 188.3854166632526983, -3.042071309553167513 ) ) ;
#31767 = CARTESIAN_POINT ( 'NONE',  ( 7.347880794884121708E-16, 300.0000000000000000, -6.000000000000001776 ) ) ;
#31768 = CARTESIAN_POINT ( 'NONE',  ( -1.881053915767124440, 6.999999998634407916, 4.541265875000001451 ) ) ;
#31769 = CARTESIAN_POINT ( 'NONE',  ( -5.000000000000002665, 0.000000000000000000, 0.000000000000000000 ) ) ;
#31771 = CARTESIAN_POINT ( 'NONE',  ( 6.000000000000003553, 297.5625000000001137, -2.485281374238571761 ) ) ;
#31770 = FACE_OUTER_BOUND ( 'NONE', #19846, .T. ) ;
#31772 = EDGE_LOOP ( 'NONE', ( #17729, #25453, #72027, #28671, #56094, #37930 ) ) ;
#31773 = CARTESIAN_POINT ( 'NONE',  ( -2.754378923186476579E-14, 205.4375000013656063, 145.4587341250000350 ) ) ;
#31774 = CARTESIAN_POINT ( 'NONE',  ( -8.311093377946836114, 7.656249996586014461, -8.311093377946837890 ) ) ;
#31775 = CARTESIAN_POINT ( 'NONE',  ( -10.99999999999999822, -4.556349186104052151, 98.78125000409679046 ) ) ;
#31776 = CARTESIAN_POINT ( 'NONE',  ( 2.449293598294707893E-16, 19.99999999726881228, -4.000000000000001776 ) ) ;
#31777 = CARTESIAN_POINT ( 'NONE',  ( -24.54126587499999346, 203.1875000013656063, 170.0000000000002842 ) ) ;
#31778 = DIRECTION ( 'NONE',  ( -1.836970198721037823E-16, -4.283267841918042125E-17, 1.000000000000000000 ) ) ;
#31780 = CARTESIAN_POINT ( 'NONE',  ( -27.99999999999996092, 209.5000000000000284, 174.0000000000003695 ) ) ;
#31779 = CARTESIAN_POINT ( 'NONE',  ( -7.188101187499999156, 119.7500000020483810, 2.977408999572654924 ) ) ;
#31781 = CARTESIAN_POINT ( 'NONE',  ( -4.898587196589407898E-16, 7.999999999999991118, 25.95530277982336997 ) ) ;
#31782 = CARTESIAN_POINT ( 'NONE',  ( -11.35316468749999785, 118.0729166632526983, -3.042071309553167513 ) ) ;
#31783 = EDGE_CURVE ( 'NONE', #18300, #1549, #67535, .T. ) ;
#31784 = ADVANCED_FACE ( 'NONE', ( #49892 ), #25742, .T. ) ;
#31785 = CARTESIAN_POINT ( 'NONE',  ( 6.123233995736767268E-16, 88.12499999317203958, -10.00000000000000178 ) ) ;
#31786 = CARTESIAN_POINT ( 'NONE',  ( -7.188101187499999156, 91.25000000204838102, 2.977408999572654924 ) ) ;
#31787 = CARTESIAN_POINT ( 'NONE',  ( 2.780723358947928197E-16, 19.68749999863440436, -4.541265875000002339 ) ) ;
#31788 = CARTESIAN_POINT ( 'NONE',  ( -26.34314575050759899, 204.9375000000000284, 166.0000000000004263 ) ) ;
#31789 = CARTESIAN_POINT ( 'NONE',  ( 8.660254037844390851, 144.5833333333333428, 5.000000000000008882 ) ) ;
#31790 = ORIENTED_EDGE ( 'NONE', *, *, #26612, .F. ) ;
#31791 = CARTESIAN_POINT ( 'NONE',  ( -2.849036369511732440E-14, 209.2500000000000284, 138.0000000000000568 ) ) ;
#31792 = ORIENTED_EDGE ( 'NONE', *, *, #10257, .T. ) ;
#31793 = CARTESIAN_POINT ( 'NONE',  ( 4.721056650416000089, 293.9843750017070079, 4.721056650415999201 ) ) ;
#31794 = FILL_AREA_STYLE_COLOUR ( '', #54384 ) ;
#31795 = CARTESIAN_POINT ( 'NONE',  ( -7.999999999999991118, 0.000000000000000000, 5.517802783920146226 ) ) ;
#31796 = CARTESIAN_POINT ( 'NONE',  ( 3.042071309553159519, 164.7395833299193271, 11.35316468750000141 ) ) ;
#31797 = VECTOR ( 'NONE', #13520, 1000.000000000000000 ) ;
#31798 = CARTESIAN_POINT ( 'NONE',  ( -11.00000000000000000, 0.000000000000000000, 73.18750000409676204 ) ) ;
#31799 = CARTESIAN_POINT ( 'NONE',  ( -1.656854249492347719, 201.8125000000000000, 194.0000000000000853 ) ) ;
#31800 = LINE ( 'NONE', #26114, #28961 ) ;
#31801 = CARTESIAN_POINT ( 'NONE',  ( -4.220049686691935698, 10.18810118749999916, 102.2500000020483952 ) ) ;
#31802 = VERTEX_POINT ( 'NONE', #60087 ) ;
#31803 = ADVANCED_FACE ( 'NONE', ( #72534 ), #43859, .F. ) ;
#31804 = DIRECTION ( 'NONE',  ( 0.000000000000000000, 0.000000000000000000, -1.000000000000000000 ) ) ;
#31805 = CARTESIAN_POINT ( 'NONE',  ( -9.832129032723420536, 154.0104166632526983, 5.676582343749997150 ) ) ;
#31806 = CARTESIAN_POINT ( 'NONE',  ( -75.00000000000001421, 0.000000000000000000, 20.00000000000003553 ) ) ;
#31807 = CARTESIAN_POINT ( 'NONE',  ( 2.754378923186476579E-14, 206.4375000013656063, 194.5412658750000219 ) ) ;
#31808 = CARTESIAN_POINT ( 'NONE',  ( -7.204075437095967871, 7.204075437095967871, 72.34375000204836681 ) ) ;
#31809 = CARTESIAN_POINT ( 'NONE',  ( -8.311093377946836114, 57.96874999658602690, -8.311093377946837890 ) ) ;
#31810 = ORIENTED_EDGE ( 'NONE', *, *, #66443, .F. ) ;
#31811 = CARTESIAN_POINT ( 'NONE',  ( 10.18810118749999916, 4.220049686691935698, 116.5000000020483810 ) ) ;
#31812 = CARTESIAN_POINT ( 'NONE',  ( 4.541265875000001451, 7.374999998634407916, 1.881053915767124440 ) ) ;
#31813 = CARTESIAN_POINT ( 'NONE',  ( 3.317071493978877683, 8.008118988124991233, 8.044365283940630107 ) ) ;
#31814 = ORIENTED_EDGE ( 'NONE', *, *, #30517, .F. ) ;
#31815 = CARTESIAN_POINT ( 'NONE',  ( -2.977408999572654480, 19.49999999795161898, 7.188101187499999156 ) ) ;
#31816 = CARTESIAN_POINT ( 'NONE',  ( 4.242640687119285658, 287.6875000034139589, -4.242640687119286547 ) ) ;
#31817 = CARTESIAN_POINT ( 'NONE',  ( -27.99999999999991118, 197.6250000027312126, 174.0000000000003695 ) ) ;
#31818 = CARTESIAN_POINT ( 'NONE',  ( 4.401442555609581635E-16, 16.21874999795161543, -7.188101187500000044 ) ) ;
#31819 = CARTESIAN_POINT ( 'NONE',  ( -7.188101187499990274, -2.977408999572651815, 6.080302781871753659 ) ) ;
#31820 = APPLICATION_CONTEXT ( 'automotive_design' ) ;
#31821 = CARTESIAN_POINT ( 'NONE',  ( -4.220049686691937474, -10.18810118749999738, 116.3125000020483668 ) ) ;
#31822 = CIRCLE ( 'NONE', #71535, 71.70204102886728492 ) ;
#31823 = CARTESIAN_POINT ( 'NONE',  ( 2.326828918379973337E-15, 0.000000000000000000, 19.00000000000001776 ) ) ;
#31824 = CARTESIAN_POINT ( 'NONE',  ( -4.000000000000001776, 5.249999997268813168, -4.898587196589415787E-16 ) ) ;
#31825 = VERTEX_POINT ( 'NONE', #9545 ) ;
#31826 = CARTESIAN_POINT ( 'NONE',  ( 2.445694354108838731, 205.0625000013656063, 195.5543056458912190 ) ) ;
#31827 = CARTESIAN_POINT ( 'NONE',  ( -32.00000000000002842, 196.3125000027312126, 168.3431457505080573 ) ) ;
#31828 = CARTESIAN_POINT ( 'NONE',  ( -1.881053915767124440, 7.999999998634407028, 4.541265875000001451 ) ) ;
#31829 = CARTESIAN_POINT ( 'NONE',  ( 7.188101187500001821, 110.0000000020483668, -2.977408999572651371 ) ) ;
#31830 = CARTESIAN_POINT ( 'NONE',  ( 23.99999999999997868, 204.8125000000000000, 171.6568542494922553 ) ) ;
#31831 = CARTESIAN_POINT ( 'NONE',  ( 2.977408999572646486, 7.188101187499991163, 22.01780278187175455 ) ) ;
#31832 = ORIENTED_EDGE ( 'NONE', *, *, #47295, .T. ) ;
#31833 = DIRECTION ( 'NONE',  ( -1.281975129857798973E-14, 0.000000000000000000, -1.000000000000000000 ) ) ;
#31834 = VERTEX_POINT ( 'NONE', #54446 ) ;
#31835 = CARTESIAN_POINT ( 'NONE',  ( -6.238412754330611322E-16, 10.18810118749999916, 115.2812500020483810 ) ) ;
#31836 = DIRECTION ( 'NONE',  ( -0.000000000000000000, 1.000000000000000000, -0.000000000000000000 ) ) ;
#31837 = CARTESIAN_POINT ( 'NONE',  ( 2.754378923186476579E-14, 208.1875000013656063, 194.5412658750000219 ) ) ;
#31838 = CARTESIAN_POINT ( 'NONE',  ( 30.44569435410883074, 204.5625000013656063, 172.4456943541086957 ) ) ;
#31839 = CARTESIAN_POINT ( 'NONE',  ( -7.320508075688778149, 63.12500000000000000, 7.320508075688769267 ) ) ;
#31840 = CARTESIAN_POINT ( 'NONE',  ( 2.977408999572650039, 95.56250000204838102, -7.188101187500001821 ) ) ;
#31841 = CARTESIAN_POINT ( 'NONE',  ( -2.485281374238572649, 296.1875000000000000, 6.000000000000002665 ) ) ;
#31843 = CARTESIAN_POINT ( 'NONE',  ( -10.00000000000000000, 255.0000000000000000, 0.000000000000000000 ) ) ;
#31842 = CARTESIAN_POINT ( 'NONE',  ( 30.70075241164968105, 178.2885270399156923, 174.3139513339800146 ) ) ;
#31844 = ORIENTED_EDGE ( 'NONE', *, *, #53630, .T. ) ;
#31845 = CARTESIAN_POINT ( 'NONE',  ( -1.469576158976823947E-15, 8.437499995903221972, 8.000000000000000000 ) ) ;
#31846 = EDGE_CURVE ( 'NONE', #45576, #24477, #16304, .T. ) ;
#31847 = CARTESIAN_POINT ( 'NONE',  ( -2.828427124746208943, 199.7500000027312126, 144.8284271247462129 ) ) ;
#31848 = FACE_OUTER_BOUND ( 'NONE', #23885, .T. ) ;
#31849 = CARTESIAN_POINT ( 'NONE',  ( -30.99999999999992895, -31.99999999999978684, 171.9999999999997726 ) ) ;
#31850 = CARTESIAN_POINT ( 'NONE',  ( -6.123233995736766282E-16, 248.7500000000000284, -10.00000000000000000 ) ) ;
#31851 = CARTESIAN_POINT ( 'NONE',  ( -11.00000000000000000, 0.000000000000000000, 110.4999999999999858 ) ) ;
#31852 = CARTESIAN_POINT ( 'NONE',  ( 2.679491924311228956, 186.0416666666666572, -10.00000000000000000 ) ) ;
#31853 = FACE_OUTER_BOUND ( 'NONE', #51989, .T. ) ;
#31854 = CARTESIAN_POINT ( 'NONE',  ( -4.401442555609577197E-16, 7.188101187499992051, 20.98655278187175455 ) ) ;
#31855 = CARTESIAN_POINT ( 'NONE',  ( 11.35316468750000141, 151.0937499965860411, 0.000000000000000000 ) ) ;
#31856 = CARTESIAN_POINT ( 'NONE',  ( 0.000000000000000000, 0.000000000000000000, 0.000000000000000000 ) ) ;
#31857 = CARTESIAN_POINT ( 'NONE',  ( -5.000000000000000000, 53.55895565990245899, 45.41404144516120311 ) ) ;
#31860 = CARTESIAN_POINT ( 'NONE',  ( 1.102182119232618108E-15, 297.3125000034140157, 6.000000000000001776 ) ) ;
#31859 = CARTESIAN_POINT ( 'NONE',  ( 4.000000000000016875, 199.5625000027312126, 199.6568542494924259 ) ) ;
#31858 = CARTESIAN_POINT ( 'NONE',  ( 28.00000000000001776, 202.5000000000000000, 165.9999999999998863 ) ) ;
#31861 = VERTEX_POINT ( 'NONE', #21585 ) ;
#31862 = CARTESIAN_POINT ( 'NONE',  ( -11.35316468749999785, 8.385416663252684089, -3.042071309553167513 ) ) ;
#31863 = CARTESIAN_POINT ( 'NONE',  ( -3.999999999999959144, 199.0625000000000000, 199.6568542494924259 ) ) ;
#31864 = CARTESIAN_POINT ( 'NONE',  ( 2.620431783921701285, -10.11675809139960691, -70.36490484706366999 ) ) ;
#31865 = CARTESIAN_POINT ( 'NONE',  ( -3.673940397442060854E-16, 296.7500000000000000, -6.000000000000001776 ) ) ;
#31866 = CARTESIAN_POINT ( 'NONE',  ( -1.432654583217662259, 205.1250000013656347, 145.4587341250000350 ) ) ;
#31867 =( BOUNDED_CURVE ( )  B_SPLINE_CURVE ( 2, ( #59428, #7740, #42425, #65443, #36783, #34676, #28617, #8105, #5989 ),
 .UNSPECIFIED., .F., .F. ) 
 B_SPLINE_CURVE_WITH_KNOTS ( ( 3, 2, 2, 2, 3 ),
 ( 0.2361111111111111049, 0.2430555555555555802, 0.2500000000000000000, 0.2569444444444444753, 0.2638888888888889506 ),
 .UNSPECIFIED. ) 
 CURVE ( )  GEOMETRIC_REPRESENTATION_ITEM ( )  RATIONAL_B_SPLINE_CURVE ( ( 1.000000000000000000, 0.9238795325112867385, 1.000000000000000000, 0.9238795325112867385, 1.000000000000000000, 0.9238795325112867385, 1.000000000000000000, 0.9238795325112861834, 1.000000000000000666 ) ) 
 REPRESENTATION_ITEM ( '' )  );
#31868 = CARTESIAN_POINT ( 'NONE',  ( -4.999999999999998224, 53.54166665983870388, -8.660254037844389075 ) ) ;
#31869 = AXIS2_PLACEMENT_3D ( 'NONE', #8149, #59835, #42099 ) ;
#31870 = CARTESIAN_POINT ( 'NONE',  ( -5.082755093536324154, 106.3437500020483810, 5.082755093536326818 ) ) ;
#31871 = CARTESIAN_POINT ( 'NONE',  ( 3.211159895383560947, 8.312499998634407916, 3.211159895383562723 ) ) ;
#31872 = DIRECTION ( 'NONE',  ( 0.000000000000000000, 0.000000000000000000, 1.000000000000000000 ) ) ;
#31873 = CARTESIAN_POINT ( 'NONE',  ( -5.656854249492373476, -5.656854249492376141, 11.51780277982336642 ) ) ;
#31875 = CARTESIAN_POINT ( 'NONE',  ( 7.778174593052023411, -7.778174593052021635, 105.2500000040967763 ) ) ;
#31874 = CARTESIAN_POINT ( 'NONE',  ( 0.2097676960538606694, 194.5981977461298982, 138.4018022538700734 ) ) ;
#31876 = VERTEX_POINT ( 'NONE', #74018 ) ;
#31877 = CARTESIAN_POINT ( 'NONE',  ( -4.999999999999999112, -63.84827628760526608, 24.15557308422303961 ) ) ;
#31878 = CARTESIAN_POINT ( 'NONE',  ( -1.656854249492287101, 196.3125000000000000, 137.9999999999998863 ) ) ;
#31879 = CARTESIAN_POINT ( 'NONE',  ( 9.832129032723416984, 237.1354166700806445, -5.676582343750003368 ) ) ;
#31880 = CARTESIAN_POINT ( 'NONE',  ( 11.35316468749999785, 135.5729166632526983, 3.042071309553174174 ) ) ;
#31881 = ORIENTED_EDGE ( 'NONE', *, *, #68591, .T. ) ;
#31882 = CARTESIAN_POINT ( 'NONE',  ( 7.999999999999991118, 3.313708498984758055, 4.861552783920145338 ) ) ;
#31883 = ADVANCED_FACE ( 'NONE', ( #45346, #61587 ), #57431, .F. ) ;
#31884 = EDGE_CURVE ( 'NONE', #35453, #57840, #44983, .T. ) ;
#31885 = CARTESIAN_POINT ( 'NONE',  ( 10.18810118749999916, 4.220049686691935698, 94.00000000204838102 ) ) ;
#31886 = PLANE ( 'NONE',  #34501 ) ;
#31887 = CARTESIAN_POINT ( 'NONE',  ( 2.445694354108840063, 197.0625000013656063, 200.4456943541088663 ) ) ;
#31888 = CARTESIAN_POINT ( 'NONE',  ( 27.99999999999996447, 197.0000000000000000, 173.9999999999999147 ) ) ;
#31890 = CARTESIAN_POINT ( 'NONE',  ( 11.35316468749999963, 125.9895833299193271, -3.042071309553165293 ) ) ;
#31889 = CARTESIAN_POINT ( 'NONE',  ( 27.99999999999996447, 198.0000000000000000, 173.9999999999999147 ) ) ;
#31891 = CARTESIAN_POINT ( 'NONE',  ( 6.123233995736767268E-16, 148.1249999931720538, -10.00000000000000178 ) ) ;
#31892 = ORIENTED_EDGE ( 'NONE', *, *, #73203, .T. ) ;
#31893 =( BOUNDED_CURVE ( )  B_SPLINE_CURVE ( 2, ( #17724, #16225, #10590, #12067, #35103, #33620, #58112, #775, #44923 ),
 .UNSPECIFIED., .F., .F. ) 
 B_SPLINE_CURVE_WITH_KNOTS ( ( 3, 2, 2, 2, 3 ),
 ( 0.01666666666666679827, 0.02500000000000007772, 0.03333333333333335369, 0.04166666666666662966, 0.04999999999999991951 ),
 .UNSPECIFIED. ) 
 CURVE ( )  GEOMETRIC_REPRESENTATION_ITEM ( )  RATIONAL_B_SPLINE_CURVE ( ( 0.9999999999999988898, 0.9238795325112879597, 1.000000000000000000, 0.9238795325112867385, 1.000000000000000000, 0.9238795325112867385, 1.000000000000000000, 0.9238795325112875156, 0.9999999999999992228 ) ) 
 REPRESENTATION_ITEM ( '' )  );
#31894 = CARTESIAN_POINT ( 'NONE',  ( 5.000000000000004441, 256.6666666666666288, 8.660254037844385522 ) ) ;
#31895 = CARTESIAN_POINT ( 'NONE',  ( -33.12275679046507548, 175.9544041245378594, 155.0238343577867397 ) ) ;
#31896 = CARTESIAN_POINT ( 'NONE',  ( 3.042071309553167513, 117.1354166632526699, -11.35316468749999785 ) ) ;
#31897 = CARTESIAN_POINT ( 'NONE',  ( -3.458734124999959914, 206.3750000013656063, 196.5673454167823877 ) ) ;
#31898 = CARTESIAN_POINT ( 'NONE',  ( 7.188101187500000044, 18.84374999795161187, 0.000000000000000000 ) ) ;
#31899 = CARTESIAN_POINT ( 'NONE',  ( -4.220049686691937474, -10.18810118749999738, 90.81250000204838102 ) ) ;
#31900 = CARTESIAN_POINT ( 'NONE',  ( -11.35316468750000141, 23.59374999658601979, -1.390361679473963753E-15 ) ) ;
#31901 = VERTEX_POINT ( 'NONE', #62323 ) ;
#31902 = DIRECTION ( 'NONE',  ( 0.000000000000000000, 1.000000000000000000, -0.000000000000000000 ) ) ;
#31903 = CARTESIAN_POINT ( 'NONE',  ( 4.999999999999997335, 246.4583333401613174, -8.660254037844387298 ) ) ;
#31904 = CARTESIAN_POINT ( 'NONE',  ( 1.432654583217607414, 208.5000000013656063, 145.4587341250000634 ) ) ;
#31905 = VECTOR ( 'NONE', #26546, 1000.000000000000000 ) ;
#31906 = CARTESIAN_POINT ( 'NONE',  ( -5.656854249492380582, 98.00000000409677625, -5.656854249492380582 ) ) ;
#31907 = CARTESIAN_POINT ( 'NONE',  ( -1.320432766682874540E-15, 4.593749997951610986, 7.188101187500000044 ) ) ;
#31908 = CARTESIAN_POINT ( 'NONE',  ( 6.676582343750004256, 287.8906250017069510, 2.765530957081995478 ) ) ;
#31909 = ADVANCED_FACE ( 'NONE', ( #22319 ), #55337, .T. ) ;
#31910 = CARTESIAN_POINT ( 'NONE',  ( 2.957351242930898602E-11, 51.14729664189404446, -48.52014062454985321 ) ) ;
#31911 = CARTESIAN_POINT ( 'NONE',  ( 9.832129032723420536, 216.5104166632526983, -5.676582343749999815 ) ) ;
#31912 = ORIENTED_EDGE ( 'NONE', *, *, #26151, .T. ) ;
#31913 = CARTESIAN_POINT ( 'NONE',  ( 6.951808397369818766E-16, 142.3437499965860411, -11.35316468750000141 ) ) ;
#31914 = CARTESIAN_POINT ( 'NONE',  ( 10.18810118750000093, -4.220049686691933921, 86.31250000204838102 ) ) ;
#31915 = CARTESIAN_POINT ( 'NONE',  ( -31.45873412499999233, 200.6875000013656063, 170.0000000000003979 ) ) ;
#31916 = CARTESIAN_POINT ( 'NONE',  ( -5.656854249492375253, 5.656854249492375253, 21.64280277982336997 ) ) ;
#31917 = CARTESIAN_POINT ( 'NONE',  ( -4.541265875000002339, 15.93749999863440436, -5.561446717895856393E-16 ) ) ;
#31918 = EDGE_LOOP ( 'NONE', ( #63755, #3405, #24858 ) ) ;
#31919 = CARTESIAN_POINT ( 'NONE',  ( -1.656854249492347719, 202.9375000027312410, 194.0000000000000853 ) ) ;
#31920 = VECTOR ( 'NONE', #69822, 1000.000000000000000 ) ;
#31921 = CARTESIAN_POINT ( 'NONE',  ( 3.458734124999960358, 198.6875000013655779, 142.0000000000000568 ) ) ;
#31922 = CARTESIAN_POINT ( 'NONE',  ( -2.828427124746209831, 204.5000000027312126, 139.1715728752538723 ) ) ;
#31923 = CIRCLE ( 'NONE', #607, 31.00000000000000000 ) ;
#31924 = ORIENTED_EDGE ( 'NONE', *, *, #36186, .F. ) ;
#31925 = CARTESIAN_POINT ( 'NONE',  ( -7.188101187500002709, 13.31249999795161187, 2.977408999572649151 ) ) ;
#31926 = CARTESIAN_POINT ( 'NONE',  ( 4.556349186104052151, -10.99999999999999822, 76.46874999999998579 ) ) ;
#31927 = DIRECTION ( 'NONE',  ( -0.000000000000000000, 1.000000000000000000, -0.000000000000000000 ) ) ;
#31928 = CARTESIAN_POINT ( 'NONE',  ( 9.832129032723420536, 186.1979166632526983, -5.676582343749999815 ) ) ;
#31929 = CARTESIAN_POINT ( 'NONE',  ( -5.082755093536324154, 112.7187500020483810, 5.082755093536326818 ) ) ;
#31930 = DIRECTION ( 'NONE',  ( -7.885106708985487801E-17, 1.000000000000000000, -0.000000000000000000 ) ) ;
#31931 = CARTESIAN_POINT ( 'NONE',  ( -4.088227598258586603E-16, 292.2031250017069510, -6.676582343750001591 ) ) ;
#31933 = CARTESIAN_POINT ( 'NONE',  ( 5.000000000000000000, -11.14555136602165675, -27.84144949604441166 ) ) ;
#31932 = CARTESIAN_POINT ( 'NONE',  ( 9.832129032723416984, 221.8229166700806729, -5.676582343750003368 ) ) ;
#31934 = ORIENTED_EDGE ( 'NONE', *, *, #33706, .F. ) ;
#31935 = CARTESIAN_POINT ( 'NONE',  ( -9.832129032723418760, 228.8020833367473301, -5.676582343749998927 ) ) ;
#31936 = CARTESIAN_POINT ( 'NONE',  ( 5.082755093536320601, -5.082755093536318824, 2.049052781871754103 ) ) ;
#31937 = CARTESIAN_POINT ( 'NONE',  ( 7.778174593052023411, -7.778174593052021635, 93.06249999999998579 ) ) ;
#31938 = CYLINDRICAL_SURFACE ( 'NONE', #8220, 10.00000000000000178 ) ;
#31939 = CARTESIAN_POINT ( 'NONE',  ( -0.6474643998351045093, -60.19533971085457580, -22.88219507985856538 ) ) ;
#31940 = CARTESIAN_POINT ( 'NONE',  ( 2.839093476692135984E-14, 199.9375000013656063, 201.4587341250000350 ) ) ;
#31941 = CARTESIAN_POINT ( 'NONE',  ( 0.000000000000000000, 300.0000000000000000, 0.000000000000000000 ) ) ;
#31942 = DIRECTION ( 'NONE',  ( -0.000000000000000000, 1.000000000000000000, -0.000000000000000000 ) ) ;
#31943 = CARTESIAN_POINT ( 'NONE',  ( 3.313708498984765161, 93.96874999999998579, 7.999999999999998224 ) ) ;
#31944 = CARTESIAN_POINT ( 'NONE',  ( 6.951808397369818766E-16, 117.3437499965860127, -11.35316468750000141 ) ) ;
#31945 = CARTESIAN_POINT ( 'NONE',  ( 27.99999999999996803, 206.0000000000000284, 173.9999999999999147 ) ) ;
#31946 = CARTESIAN_POINT ( 'NONE',  ( -7.778174593052023411, 7.778174593052023411, 69.81249999999998579 ) ) ;
#31949 = DIRECTION ( 'NONE',  ( -0.000000000000000000, -0.000000000000000000, 1.000000000000000000 ) ) ;
#31948 = CARTESIAN_POINT ( 'NONE',  ( 30.44569435410883074, 198.5625000013656063, 172.4456943541086957 ) ) ;
#31947 = CARTESIAN_POINT ( 'NONE',  ( 30.44569435410883429, 200.0625000013656063, 167.5543056458911053 ) ) ;
#31950 = ORIENTED_EDGE ( 'NONE', *, *, #989, .T. ) ;
#31951 = EDGE_CURVE ( 'NONE', #73165, #18628, #58739, .T. ) ;
#31952 = PLANE ( 'NONE',  #50454 ) ;
#31953 = CARTESIAN_POINT ( 'NONE',  ( 3.508290994201011870, 226.7807916744830550, -10.79751095028410290 ) ) ;
#31954 = CARTESIAN_POINT ( 'NONE',  ( 3.458734124999959025, 200.5000000013655779, 140.5673454167824161 ) ) ;
#31955 = CARTESIAN_POINT ( 'NONE',  ( 26.56734541678232375, 200.6250000013655779, 173.4587341249998929 ) ) ;
#31956 = CARTESIAN_POINT ( 'NONE',  ( -6.735557395310442023E-16, 11.00000000000000000, 114.8125000040967763 ) ) ;
#31957 = CARTESIAN_POINT ( 'NONE',  ( 9.832129032723420536, 191.5104166632526983, -5.676582343749999815 ) ) ;
#31958 = CARTESIAN_POINT ( 'NONE',  ( -4.401442555609581635E-16, 92.65625000204838102, -7.188101187500000044 ) ) ;
#31959 = PLANE ( 'NONE',  #56660 ) ;
#31960 = CARTESIAN_POINT ( 'NONE',  ( 4.541265875000001451, 14.24999999863440969, 1.881053915767124440 ) ) ;
#31961 = CARTESIAN_POINT ( 'NONE',  ( 25.55430564589119413, 200.3125000013656063, 167.5543056458910485 ) ) ;
#31962 = CARTESIAN_POINT ( 'NONE',  ( -5.082755093536317936, -5.082755093536320601, 0.5490527818717526598 ) ) ;
#31963 = CARTESIAN_POINT ( 'NONE',  ( -10.67658234375000070, 263.5156250051209668, 0.000000000000000000 ) ) ;
#31964 = CARTESIAN_POINT ( 'NONE',  ( -5.676582343750006032, 84.11458332991935549, 9.832129032723418760 ) ) ;
#31965 = ORIENTED_EDGE ( 'NONE', *, *, #17341, .T. ) ;
#31966 = CARTESIAN_POINT ( 'NONE',  ( 2.679491924311084627, 141.0416666666667425, -10.00000000000009592 ) ) ;
#31967 = CARTESIAN_POINT ( 'NONE',  ( 1.268984979720182487E-11, 76.24999999999903366, -10.00000000000000178 ) ) ;
#31968 = CARTESIAN_POINT ( 'NONE',  ( 2.977408999572650927, 17.24999999795162253, -7.188101187500001821 ) ) ;
#31969 = CARTESIAN_POINT ( 'NONE',  ( 5.656854249492376141, -5.656854249492374365, 14.89280277982336642 ) ) ;
#31970 = FACE_OUTER_BOUND ( 'NONE', #21991, .T. ) ;
#31971 = CARTESIAN_POINT ( 'NONE',  ( -2.085542519210945728E-15, 84.53124999658602690, 11.35316468750000141 ) ) ;
#31972 = VERTEX_POINT ( 'NONE', #39886 ) ;
#31973 = CARTESIAN_POINT ( 'NONE',  ( 1.871523826299183495E-15, -10.18810118749999916, 84.90625000204838102 ) ) ;
#31974 = ADVANCED_FACE ( 'NONE', ( #68929 ), #1405, .F. ) ;
#31975 = CARTESIAN_POINT ( 'NONE',  ( 4.220049686691941027, -10.18810118749999738, 113.1250000020483810 ) ) ;
#31976 = CARTESIAN_POINT ( 'NONE',  ( -24.54126587499997925, 195.3750000013656063, 171.4326545832179818 ) ) ;
#31977 = CARTESIAN_POINT ( 'NONE',  ( 2.839093476692135984E-14, 206.9375000013656063, 201.4587341250000350 ) ) ;
#31978 = CARTESIAN_POINT ( 'NONE',  ( -3.428378827827395892, 16.35907404636618878, 69.10239319626211341 ) ) ;
#31980 = CARTESIAN_POINT ( 'NONE',  ( 9.832129032723416984, 80.36458332991935549, 5.676582343750006032 ) ) ;
#31979 = CARTESIAN_POINT ( 'NONE',  ( -11.00000000000000000, 0.000000000000000000, 118.0000000000000000 ) ) ;
#31981 = CARTESIAN_POINT ( 'NONE',  ( -5.656854249492375253, 5.656854249492375253, 20.33030278392014623 ) ) ;
#31982 = CARTESIAN_POINT ( 'NONE',  ( -31.99999999999995737, 196.4375000027312410, 171.6568542494928522 ) ) ;
#31983 = ADVANCED_FACE ( 'NONE', ( #62890 ), #5565, .F. ) ;
#31984 = CARTESIAN_POINT ( 'NONE',  ( 2.679491924311228956, 172.9166666598386826, -10.00000000000000000 ) ) ;
#31985 = CARTESIAN_POINT ( 'NONE',  ( 7.188101187500002709, 92.18750000204838102, 2.977408999572649151 ) ) ;
#31986 = AXIS2_PLACEMENT_3D ( 'NONE', #24693, #13728, #36773 ) ;
#31987 = DIRECTION ( 'NONE',  ( 0.000000000000000000, 0.000000000000000000, -1.000000000000000000 ) ) ;
#31988 = CARTESIAN_POINT ( 'NONE',  ( -8.311093377946841443, 64.21874999658601268, 8.311093377946834337 ) ) ;
#31989 = CARTESIAN_POINT ( 'NONE',  ( 2.765530957082001251, 294.7656250017070079, 6.676582343750000703 ) ) ;
#31990 =( BOUNDED_CURVE ( )  B_SPLINE_CURVE ( 2, ( #26824, #38533, #38899, #55515, #21534, #56253, #4570, #4947, #27946 ),
 .UNSPECIFIED., .F., .F. ) 
 B_SPLINE_CURVE_WITH_KNOTS ( ( 3, 2, 2, 2, 3 ),
 ( 0.9374999999999984457, 0.9479166666666650753, 0.9583333333333319271, 0.9687499999999985567, 0.9791666666666651864 ),
 .UNSPECIFIED. ) 
 CURVE ( )  GEOMETRIC_REPRESENTATION_ITEM ( )  RATIONAL_B_SPLINE_CURVE ( ( 1.000000000000011324, 0.9238795325112754142, 1.000000000000000000, 0.9238795325112867385, 1.000000000000000000, 0.9238795325112867385, 1.000000000000000000, 0.9238795325112972856, 0.9999999999999894529 ) ) 
 REPRESENTATION_ITEM ( '' )  );
#31991 = CARTESIAN_POINT ( 'NONE',  ( -7.204075437095965206, -7.204075437095968759, 104.2187500020483810 ) ) ;
#31992 = CARTESIAN_POINT ( 'NONE',  ( 3.042071309553159519, 209.7395833299193839, 11.35316468750000141 ) ) ;
#31993 = ORIENTED_EDGE ( 'NONE', *, *, #56605, .T. ) ;
#31994 = CARTESIAN_POINT ( 'NONE',  ( 2.828427124746153876, 202.8750000000000284, 144.8284271247462129 ) ) ;
#31995 = FACE_OUTER_BOUND ( 'NONE', #15204, .T. ) ;
#31996 = CARTESIAN_POINT ( 'NONE',  ( -5.999999999999999112, 288.0625000000000000, 2.485281374238575314 ) ) ;
#31998 = CARTESIAN_POINT ( 'NONE',  ( -9.832129032723418760, 187.8645833299193839, -5.676582343750004256 ) ) ;
#31997 = CYLINDRICAL_SURFACE ( 'NONE', #73646, 3.999999999999976019 ) ;
#31999 = B_SPLINE_CURVE_WITH_KNOTS ( 'NONE', 3,
 ( #33096, #55347, #73428, #27394, #4778, #62107 ),
 .UNSPECIFIED., .F., .F.,
 ( 4, 2, 4 ),
 ( 2.380728322738124163E-07, 0.005257893135091018695, 0.01051554819734976456 ),
 .UNSPECIFIED. ) ;
#32000 = CARTESIAN_POINT ( 'NONE',  ( 28.00000000000001421, 195.5000000000000000, 165.9999999999998863 ) ) ;
#32001 = CARTESIAN_POINT ( 'NONE',  ( -7.320508075688770155, 233.7500000068279462, 7.320508075688774596 ) ) ;
#32002 = CARTESIAN_POINT ( 'NONE',  ( -1.656854249492405895, 20.31250000000000000, -3.999999999999976463 ) ) ;
#32003 = EDGE_CURVE ( 'NONE', #18299, #26800, #63036, .T. ) ;
#32004 = ORIENTED_EDGE ( 'NONE', *, *, #66875, .F. ) ;
#32005 = CARTESIAN_POINT ( 'NONE',  ( 11.35316468750000141, 181.0937499965860411, 0.000000000000000000 ) ) ;
#32006 = CARTESIAN_POINT ( 'NONE',  ( -5.082755093536319713, 5.082755093536319713, 23.79905278187175455 ) ) ;
#32007 = CARTESIAN_POINT ( 'NONE',  ( -25.55430564589119768, 209.3125000013656063, 167.5543056458915316 ) ) ;
#32008 = ORIENTED_EDGE ( 'NONE', *, *, #55983, .F. ) ;
#32009 = EDGE_CURVE ( 'NONE', #26389, #12072, #11048, .T. ) ;
#32010 = CARTESIAN_POINT ( 'NONE',  ( -8.000000000000000000, 95.18750000409679046, 0.000000000000000000 ) ) ;
#32011 = CARTESIAN_POINT ( 'NONE',  ( 6.123233995736767268E-16, 1.250000000000000000, -10.00000000000000178 ) ) ;
#32012 = EDGE_CURVE ( 'NONE', #34174, #6758, #39841, .T. ) ;
#32013 = CARTESIAN_POINT ( 'NONE',  ( -4.000000000000001776, 15.50000000000000000, -4.898587196589415787E-16 ) ) ;
#32014 = CARTESIAN_POINT ( 'NONE',  ( -4.541265875000003227, 16.87499999863440436, 1.881053915767121110 ) ) ;
#32015 = CARTESIAN_POINT ( 'NONE',  ( 3.313708498984762496, -7.999999999999989342, 13.48655278392014445 ) ) ;
#32016 = CARTESIAN_POINT ( 'NONE',  ( -4.556349186104048599, -10.99999999999999822, 77.96875000409677625 ) ) ;
#32017 = ORIENTED_EDGE ( 'NONE', *, *, #29992, .F. ) ;
#32018 = CARTESIAN_POINT ( 'NONE',  ( 4.242640687119285658, 293.6875000034139589, -4.242640687119286547 ) ) ;
#32019 = CARTESIAN_POINT ( 'NONE',  ( -4.401442555609581635E-16, 90.78125000204836681, -7.188101187500000044 ) ) ;
#32022 = DIRECTION ( 'NONE',  ( 0.000000000000000000, 0.000000000000000000, 1.000000000000000000 ) ) ;
#32021 = CARTESIAN_POINT ( 'NONE',  ( -9.832129032723415207, 254.3229166700806729, 5.676582343750005144 ) ) ;
#32020 = CARTESIAN_POINT ( 'NONE',  ( -7.320508075688771932, 257.5000000068279746, -7.320508075688771932 ) ) ;
#32023 = DIRECTION ( 'NONE',  ( 0.000000000000000000, 0.000000000000000000, 1.000000000000000000 ) ) ;
#32024 = ORIENTED_EDGE ( 'NONE', *, *, #31558, .F. ) ;
#32025 = CARTESIAN_POINT ( 'NONE',  ( 9.832129032723420536, 261.3020833367473301, 5.676582343749996262 ) ) ;
#32026 = CARTESIAN_POINT ( 'NONE',  ( 7.188101187499992051, 8.802885111219154394E-16, 18.73655278187175455 ) ) ;
#32027 = ORIENTED_EDGE ( 'NONE', *, *, #45931, .F. ) ;
#32028 = ORIENTED_EDGE ( 'NONE', *, *, #69346, .T. ) ;
#32029 = CARTESIAN_POINT ( 'NONE',  ( 10.18810118749999916, 1.247682550866122264E-15, 81.90625000204838102 ) ) ;
#32030 = CARTESIAN_POINT ( 'NONE',  ( 6.951808397369818766E-16, 77.34374999658601268, -11.35316468750000141 ) ) ;
#32031 = CARTESIAN_POINT ( 'NONE',  ( -7.999985423429806453, -3.313723075554945385, 5.611553367133312875 ) ) ;
#32032 = CARTESIAN_POINT ( 'NONE',  ( -7.778174593052020747, -7.778174593052023411, 95.68750000000000000 ) ) ;
#32035 = CARTESIAN_POINT ( 'NONE',  ( 1.226468279477575784E-15, 293.8593750017070079, 6.676582343750001591 ) ) ;
#32034 = CARTESIAN_POINT ( 'NONE',  ( 29.65685424949240456, 198.1875000027312126, 173.9999999999999147 ) ) ;
#32033 = CARTESIAN_POINT ( 'NONE',  ( 0.000000000000000000, 125.0000000000000000, 8.000000000000000000 ) ) ;
#32036 = CARTESIAN_POINT ( 'NONE',  ( -4.556349186104048599, -10.99999999999999822, 83.78124999999998579 ) ) ;
#32037 = CARTESIAN_POINT ( 'NONE',  ( 3.447890238427801179, 194.4587341250000350, 141.6837455501598413 ) ) ;
#32038 = CARTESIAN_POINT ( 'NONE',  ( -1.432654583217607414, 199.5000000013656063, 194.5412658750000219 ) ) ;
#32039 = CARTESIAN_POINT ( 'NONE',  ( 3.999999999999960032, 199.0000000000000000, 142.0000000000000568 ) ) ;
#32040 = CARTESIAN_POINT ( 'NONE',  ( 8.000000000000000000, 4.312499995903220196, 0.000000000000000000 ) ) ;
#32041 = CARTESIAN_POINT ( 'NONE',  ( 29.43265458321766559, 199.8750000013655779, 166.5412658749999650 ) ) ;
#32042 = CARTESIAN_POINT ( 'NONE',  ( 2.977408999572651815, 9.562499997951608322, 7.188101187500000933 ) ) ;
#32043 = CARTESIAN_POINT ( 'NONE',  ( -4.898587196589407898E-16, 7.999999999999991118, 27.64280278392014978 ) ) ;
#32044 = LINE ( 'NONE', #53572, #2346 ) ;
#32045 = CARTESIAN_POINT ( 'NONE',  ( -2.977408999572652260, 109.8125000020483952, 7.188101187500000044 ) ) ;
#32047 = CARTESIAN_POINT ( 'NONE',  ( -2.591411123065558986, -50.09422832877655907, -40.78779037275307928 ) ) ;
#32046 = CARTESIAN_POINT ( 'NONE',  ( 4.242640687119287435, 289.4375000034140157, 4.242640687119285658 ) ) ;
#32048 = CARTESIAN_POINT ( 'NONE',  ( 9.797174393178825657E-16, 125.0000000000000000, -8.000000000000000000 ) ) ;
#32049 = CARTESIAN_POINT ( 'NONE',  ( -23.99999999999997868, 207.6875000000000284, 171.6568542494927385 ) ) ;
#32050 = CARTESIAN_POINT ( 'NONE',  ( -7.188101187499991163, 2.977408999572646930, 15.26780278187175455 ) ) ;
#32051 = CARTESIAN_POINT ( 'NONE',  ( -2.828427124746208943, 206.7500000027312126, 144.8284271247462129 ) ) ;
#32052 = CARTESIAN_POINT ( 'NONE',  ( -11.35316468749999785, 43.07291666325269119, -3.042071309553167513 ) ) ;
#32053 = EDGE_CURVE ( 'NONE', #8699, #31338, #489, .T. ) ;
#32054 = CARTESIAN_POINT ( 'NONE',  ( -3.000000000000001332, -44.80191526431281090, 139.1455027589170754 ) ) ;
#32055 = CARTESIAN_POINT ( 'NONE',  ( 10.00000000000000000, 11.66666665983870033, 2.679491924311236062 ) ) ;
#32056 = CARTESIAN_POINT ( 'NONE',  ( -30.82842712474612412, 200.5000000027312126, 172.8284271247466108 ) ) ;
#32057 = ORIENTED_EDGE ( 'NONE', *, *, #51227, .F. ) ;
#32058 = CARTESIAN_POINT ( 'NONE',  ( -1.836970198721029983E-15, 140.6249999931720538, 10.00000000000000178 ) ) ;
#32059 = CARTESIAN_POINT ( 'NONE',  ( -4.898587196589407898E-16, 7.999999999999991118, 18.45530277982336642 ) ) ;
#32060 = CARTESIAN_POINT ( 'NONE',  ( -9.832129032723418760, 47.86458332991934839, -5.676582343750004256 ) ) ;
#32061 = CARTESIAN_POINT ( 'NONE',  ( -7.778174593052023411, 7.778174593052023411, 82.00000000409676204 ) ) ;
#32062 = CARTESIAN_POINT ( 'NONE',  ( 2.445694354108784108, 203.5625000013656063, 144.4456943541088663 ) ) ;
#32063 = CARTESIAN_POINT ( 'NONE',  ( -0.4368895104720016409, -67.59332269700065865, -20.03478791450352858 ) ) ;
#32064 = CARTESIAN_POINT ( 'NONE',  ( -4.000000000000015987, 195.5000000000000000, 142.0000000000000568 ) ) ;
#32066 = CARTESIAN_POINT ( 'NONE',  ( 11.35316468749999785, 35.57291666325267698, 3.042071309553174174 ) ) ;
#32065 = CARTESIAN_POINT ( 'NONE',  ( -2.977408999572650927, 98.37500000204839523, -7.188101187500000933 ) ) ;
#32067 = CARTESIAN_POINT ( 'NONE',  ( -3.313708498984757167, 7.999999999999991118, 9.549052779823362869 ) ) ;
#32068 = LINE ( 'NONE', #14694, #9584 ) ;
#32069 = CARTESIAN_POINT ( 'NONE',  ( -11.35316468750000141, 163.2812499965860127, -1.390361679473963753E-15 ) ) ;
#32070 = ADVANCED_FACE ( 'NONE', ( #70058 ), #18366, .T. ) ;
#32071 = CARTESIAN_POINT ( 'NONE',  ( -1.836970198721029983E-15, 135.6249999931720538, 10.00000000000000178 ) ) ;
#32072 = CARTESIAN_POINT ( 'NONE',  ( -5.082755093536324154, 106.7187500020483952, 5.082755093536326818 ) ) ;
#32073 = ORIENTED_EDGE ( 'NONE', *, *, #70064, .T. ) ;
#32074 = CARTESIAN_POINT ( 'NONE',  ( 2.679491924311228956, 22.91666665983870033, -10.00000000000000000 ) ) ;
#32075 = CARTESIAN_POINT ( 'NONE',  ( 11.35316468749999963, 26.30208332991934839, -3.042071309553165293 ) ) ;
#32076 = CARTESIAN_POINT ( 'NONE',  ( -5.265513565426391374, -7.352259170992729409, -0.01899995639454697682 ) ) ;
#32077 = ORIENTED_EDGE ( 'NONE', *, *, #28739, .F. ) ;
#32078 = CYLINDRICAL_SURFACE ( 'NONE', #24749, 10.00000000000000178 ) ;
#32079 = CARTESIAN_POINT ( 'NONE',  ( -4.220049686691937474, -10.18810118749999738, 79.93750000204839523 ) ) ;
#32080 = CARTESIAN_POINT ( 'NONE',  ( 0.000000000000000000, 0.000000000000000000, 0.000000000000000000 ) ) ;
#32082 = CARTESIAN_POINT ( 'NONE',  ( -2.085542519210945728E-15, 149.5312499965860411, 11.35316468750000141 ) ) ;
#32081 = FACE_OUTER_BOUND ( 'NONE', #11196, .T. ) ;
#32083 = LINE ( 'NONE', #72051, #26637 ) ;
#32084 = CARTESIAN_POINT ( 'NONE',  ( -7.999999999999989342, -3.313708498984762496, 11.48030278432982243 ) ) ;
#32085 = CARTESIAN_POINT ( 'NONE',  ( 0.000000000000000000, 125.0000000000000000, 0.000000000000000000 ) ) ;
#32086 = CARTESIAN_POINT ( 'NONE',  ( -11.35316468749999963, 233.9062500034139873, 0.000000000000000000 ) ) ;
#32087 = AXIS2_PLACEMENT_3D ( 'NONE', #61060, #32023, #71617 ) ;
#32088 = CARTESIAN_POINT ( 'NONE',  ( -4.220049686691935698, 10.18810118749999916, 85.75000000204838102 ) ) ;
#32089 = VERTEX_POINT ( 'NONE', #6318 ) ;
#32090 = EDGE_CURVE ( 'NONE', #47792, #56773, #27822, .T. ) ;
#32091 = DIRECTION ( 'NONE',  ( -0.000000000000000000, -0.000000000000000000, 1.000000000000000000 ) ) ;
#32092 = CARTESIAN_POINT ( 'NONE',  ( -5.656854249492378806, 122.3750000040967905, 5.656854249492381470 ) ) ;
#32093 = CARTESIAN_POINT ( 'NONE',  ( -2.085542519210945728E-15, 104.8437499965860269, 11.35316468750000141 ) ) ;
#32094 = CARTESIAN_POINT ( 'NONE',  ( 10.18810118750000093, -4.220049686691933921, 95.31250000204838102 ) ) ;
#32095 = EDGE_CURVE ( 'NONE', #33244, #49884, #18752, .T. ) ;
#32096 = CARTESIAN_POINT ( 'NONE',  ( 4.541265875000001451, 21.37499999863441147, 1.881053915767124440 ) ) ;
#32097 = EDGE_LOOP ( 'NONE', ( #43908, #63876, #36383, #31394, #58673, #74028 ) ) ;
#32098 = ORIENTED_EDGE ( 'NONE', *, *, #33351, .F. ) ;
#32099 = CARTESIAN_POINT ( 'NONE',  ( -8.342170076843785083E-16, 4.187499998634407028, 4.541265875000002339 ) ) ;
#32100 = CARTESIAN_POINT ( 'NONE',  ( 7.188101187500000044, 10.96874999795161187, 0.000000000000000000 ) ) ;
#32101 = CARTESIAN_POINT ( 'NONE',  ( 5.656854249492381470, 118.2500000040967905, 5.656854249492379694 ) ) ;
#32102 =( BOUNDED_CURVE ( )  B_SPLINE_CURVE ( 2, ( #64698, #12996, #25794, #48814, #30366, #6988, #42409, #29998, #65428 ),
 .UNSPECIFIED., .F., .F. ) 
 B_SPLINE_CURVE_WITH_KNOTS ( ( 3, 2, 2, 2, 3 ),
 ( 0.7833333333333338810, 0.7916666666666671848, 0.8000000000000007105, 0.8083333333333340143, 0.8166666666666674290 ),
 .UNSPECIFIED. ) 
 CURVE ( )  GEOMETRIC_REPRESENTATION_ITEM ( )  RATIONAL_B_SPLINE_CURVE ( ( 0.9999999999999948930, 0.9238795325112918455, 1.000000000000000000, 0.9238795325112867385, 1.000000000000000000, 0.9238795325112867385, 1.000000000000000000, 0.9238795325112796331, 1.000000000000007105 ) ) 
 REPRESENTATION_ITEM ( '' )  );
#32103 = CARTESIAN_POINT ( 'NONE',  ( 1.871523826299183495E-15, -10.18810118749999916, 92.40625000204836681 ) ) ;
#32104 = VECTOR ( 'NONE', #35699, 1000.000000000000000 ) ;
#32105 = CARTESIAN_POINT ( 'NONE',  ( -29.43265458321760519, 201.1250000013656347, 173.4587341250003760 ) ) ;
#32106 = FACE_OUTER_BOUND ( 'NONE', #69772, .T. ) ;
#32107 = EDGE_CURVE ( 'NONE', #39701, #53439, #20191, .T. ) ;
#32108 = CARTESIAN_POINT ( 'NONE',  ( 2.828427124746191623, 4.125000000000000000, -2.828427124746191623 ) ) ;
#32109 = CARTESIAN_POINT ( 'NONE',  ( -4.000000000000001776, 20.24999999726881228, -4.898587196589415787E-16 ) ) ;
#32110 = CARTESIAN_POINT ( 'NONE',  ( -8.342170076843785083E-16, 3.062499998634406584, 4.541265875000002339 ) ) ;
#32111 = ORIENTED_EDGE ( 'NONE', *, *, #39480, .F. ) ;
#32112 = DIRECTION ( 'NONE',  ( -0.000000000000000000, -0.000000000000000000, 1.000000000000000000 ) ) ;
#32114 = CARTESIAN_POINT ( 'NONE',  ( -26.34314575050768070, 199.5625000000000284, 174.0000000000004547 ) ) ;
#32113 = CARTESIAN_POINT ( 'NONE',  ( -27.99999999999991473, 195.9375000013655779, 173.4587341250003760 ) ) ;
#32115 = CARTESIAN_POINT ( 'NONE',  ( -4.541265875000002339, 16.74999999863440792, -1.881053915767121998 ) ) ;
#32116 = CARTESIAN_POINT ( 'NONE',  ( 2.602273132848076820, -46.50542310266120438, 151.1787311068359827 ) ) ;
#32117 = CARTESIAN_POINT ( 'NONE',  ( 5.082755093536320601, -5.082755093536318824, 5.049052781871752771 ) ) ;
#32118 = ORIENTED_EDGE ( 'NONE', *, *, #61208, .T. ) ;
#32119 = ORIENTED_EDGE ( 'NONE', *, *, #13355, .F. ) ;
#32120 = CARTESIAN_POINT ( 'NONE',  ( 10.18810118749999916, 1.247682550866122264E-15, 96.90625000204838102 ) ) ;
#32121 = CARTESIAN_POINT ( 'NONE',  ( 8.660254037844390851, 125.4166666666666714, -5.000000000000000888 ) ) ;
#32122 = CARTESIAN_POINT ( 'NONE',  ( -31.45873412499998523, 204.0000000013656063, 171.4326545832180386 ) ) ;
#32123 = CARTESIAN_POINT ( 'NONE',  ( -25.17157287525377640, 202.6250000000000284, 172.8284271247465256 ) ) ;
#32124 = CARTESIAN_POINT ( 'NONE',  ( 2.754378923186476579E-14, 209.4375000013656063, 194.5412658750000219 ) ) ;
#32125 = CARTESIAN_POINT ( 'NONE',  ( 8.660254037844451247, 59.58333333333337833, 5.000000000000044409 ) ) ;
#32126 = EDGE_CURVE ( 'NONE', #47640, #67456, #8148, .T. ) ;
#32127 = CARTESIAN_POINT ( 'NONE',  ( 6.123233995736767268E-16, 111.2500000000000000, -10.00000000000000178 ) ) ;
#32128 = CARTESIAN_POINT ( 'NONE',  ( -8.000000000000000000, 112.9062500000000000, -3.313708498984761608 ) ) ;
#32129 = CARTESIAN_POINT ( 'NONE',  ( -2.765530957081996810, 293.4218750017070079, -6.676582343750003368 ) ) ;
#32130 = PRODUCT_DEFINITION_FORMATION_WITH_SPECIFIED_SOURCE ( 'ANY', '', #39708, .NOT_KNOWN. ) ;
#32131 = CARTESIAN_POINT ( 'NONE',  ( -7.188101187499990274, -2.977408999572651371, 9.455302781871754547 ) ) ;
#32132 = EDGE_CURVE ( 'NONE', #26283, #25826, #16956, .T. ) ;
#32133 = ORIENTED_EDGE ( 'NONE', *, *, #72520, .F. ) ;
#32134 = CARTESIAN_POINT ( 'NONE',  ( -5.000000000000005329, 175.2083333265053682, 8.660254037844387298 ) ) ;
#32135 = CARTESIAN_POINT ( 'NONE',  ( 3.313708498984762052, 21.09374999590322375, -8.000000000000000000 ) ) ;
#32136 = CARTESIAN_POINT ( 'NONE',  ( -2.754378923186476579E-14, 203.1875000013656063, 145.4587341250000350 ) ) ;
#32137 = CARTESIAN_POINT ( 'NONE',  ( 0.000000000000000000, 0.000000000000000000, -4.000000000000001776 ) ) ;
#32138 = CARTESIAN_POINT ( 'NONE',  ( 3.042071309553163960, 252.7604166700806445, -11.35316468749999785 ) ) ;
#32139 = LINE ( 'NONE', #9123, #70461 ) ;
#32140 = CARTESIAN_POINT ( 'NONE',  ( -4.556349186104045934, 11.00000000000000000, 116.2187500000000000 ) ) ;
#32141 = CARTESIAN_POINT ( 'NONE',  ( -5.676582343749998039, 7.447916663252683200, -9.832129032723420536 ) ) ;
#32142 = EDGE_CURVE ( 'NONE', #73206, #34267, #2491, .T. ) ;
#32143 = CARTESIAN_POINT ( 'NONE',  ( 7.188101187499992051, 2.977408999572647819, 5.705302781871753659 ) ) ;
#32144 = CARTESIAN_POINT ( 'NONE',  ( -5.676582343750006032, 194.4270833299193839, 9.832129032723418760 ) ) ;
#32145 = CARTESIAN_POINT ( 'NONE',  ( 6.123233995736767268E-16, 173.1249999931720538, -10.00000000000000178 ) ) ;
#32146 = CARTESIAN_POINT ( 'NONE',  ( 4.541265875000002339, 5.312499998634407028, 0.000000000000000000 ) ) ;
#32147 = CARTESIAN_POINT ( 'NONE',  ( 2.775557561562891351E-14, 210.0000000000000284, 198.0000000000000284 ) ) ;
#32149 = DIRECTION ( 'NONE',  ( -0.000000000000000000, 1.000000000000000000, -0.000000000000000000 ) ) ;
#32148 = CARTESIAN_POINT ( 'NONE',  ( -3.313708498984815343, 106.9062500040967763, -7.999999999999944933 ) ) ;
#32150 = ORIENTED_EDGE ( 'NONE', *, *, #54285, .F. ) ;
#32151 = CARTESIAN_POINT ( 'NONE',  ( 3.458734124999960358, 205.6875000013656063, 142.0000000000000568 ) ) ;
#32152 = CARTESIAN_POINT ( 'NONE',  ( 11.35316468749999785, 15.57291666325268409, 3.042071309553174174 ) ) ;
#32153 = CARTESIAN_POINT ( 'NONE',  ( -4.556349186104047710, -10.99999999999999822, 97.46875000409677625 ) ) ;
#32154 = CARTESIAN_POINT ( 'NONE',  ( -27.99999999999999645, 210.0000000000000284, 170.0000000000003695 ) ) ;
#32155 = CARTESIAN_POINT ( 'NONE',  ( -24.54126587499999346, 201.1875000013656063, 170.0000000000002842 ) ) ;
#32156 = DIRECTION ( 'NONE',  ( -0.000000000000000000, 1.000000000000000000, -4.476705744456276341E-16 ) ) ;
#32158 = CARTESIAN_POINT ( 'NONE',  ( -4.898587196589412829E-16, 120.1250000000000000, -8.000000000000000000 ) ) ;
#32157 = CARTESIAN_POINT ( 'NONE',  ( -4.401442555609581635E-16, 116.2812500020483810, -7.188101187500000044 ) ) ;
#32159 = CARTESIAN_POINT ( 'NONE',  ( -5.656854249492373476, -5.656854249492376141, 25.01780277982336642 ) ) ;
#32160 = CARTESIAN_POINT ( 'NONE',  ( 5.676582343750001591, 126.6145833299193697, -9.832129032723420536 ) ) ;
#32161 = CIRCLE ( 'NONE', #57434, 11.00000000000000000 ) ;
#32162 = CARTESIAN_POINT ( 'NONE',  ( -8.660254037844387298, 93.95833332650536818, -5.000000000000004441 ) ) ;
#32163 = CARTESIAN_POINT ( 'NONE',  ( 2.977408999572650039, 124.0625000020483810, -7.188101187500001821 ) ) ;
#32164 = CARTESIAN_POINT ( 'NONE',  ( 4.541265875000002339, 19.43749999863440436, 0.000000000000000000 ) ) ;
#32165 = CARTESIAN_POINT ( 'NONE',  ( -25.17157287525382259, 204.8750000000000284, 167.1715728752541565 ) ) ;
#32166 = CARTESIAN_POINT ( 'NONE',  ( -1.836970198721029983E-15, 40.62499999317203248, 10.00000000000000178 ) ) ;
#32167 = ORIENTED_EDGE ( 'NONE', *, *, #41757, .T. ) ;
#32168 = CARTESIAN_POINT ( 'NONE',  ( -2.828427124746208943, 200.7500000027312126, 144.8284271247462129 ) ) ;
#32169 = ADVANCED_FACE ( 'NONE', ( #30789 ), #53444, .T. ) ;
#32170 = CARTESIAN_POINT ( 'NONE',  ( 4.721056650416000089, 292.9843750017070079, 4.721056650415999201 ) ) ;
#32171 = CARTESIAN_POINT ( 'NONE',  ( 10.00000000000000178, 186.8749999931720538, 0.000000000000000000 ) ) ;
#32172 = CARTESIAN_POINT ( 'NONE',  ( 1.469576158976822172E-15, -7.999999999999991118, 2.892802783920144005 ) ) ;
#32173 = CARTESIAN_POINT ( 'NONE',  ( 8.311093377946837890, 171.4062499965860127, -8.311093377946837890 ) ) ;
#32174 = CARTESIAN_POINT ( 'NONE',  ( -3.999999999999959144, 201.1875000027312694, 199.6568542494924259 ) ) ;
#32175 = CARTESIAN_POINT ( 'NONE',  ( 2.828427124746209831, 195.3750000000000284, 200.8284271247462129 ) ) ;
#32176 = DIRECTION ( 'NONE',  ( -0.000000000000000000, -0.000000000000000000, -1.000000000000000000 ) ) ;
#32177 = CARTESIAN_POINT ( 'NONE',  ( 10.18810118749999916, 1.247682550866122264E-15, 101.7812500020483810 ) ) ;
#32178 = ORIENTED_EDGE ( 'NONE', *, *, #72229, .F. ) ;
#32179 = CARTESIAN_POINT ( 'NONE',  ( -27.99999999999991118, 199.6250000027312126, 174.0000000000003695 ) ) ;
#32180 = CARTESIAN_POINT ( 'NONE',  ( 6.951808397369818766E-16, 152.3437499965860411, -11.35316468750000141 ) ) ;
#32181 = CARTESIAN_POINT ( 'NONE',  ( -3.426202465283580523, 194.4587341250000350, 198.4732635780662235 ) ) ;
#32182 = CARTESIAN_POINT ( 'NONE',  ( -3.458734124999959469, 204.7500000013655779, 199.4326545832176976 ) ) ;
#32183 = CARTESIAN_POINT ( 'NONE',  ( -6.238412754330611322E-16, 10.18810118749999916, 67.65625000204836681 ) ) ;
#32184 = CARTESIAN_POINT ( 'NONE',  ( 6.951808397369818766E-16, 67.34374999658601268, -11.35316468750000141 ) ) ;
#32185 = ORIENTED_EDGE ( 'NONE', *, *, #10764, .F. ) ;
#32186 = CARTESIAN_POINT ( 'NONE',  ( -7.204075437095965206, -7.204075437095968759, 112.8437500020483810 ) ) ;
#32187 = EDGE_CURVE ( 'NONE', #43392, #71847, #2119, .T. ) ;
#32188 = CARTESIAN_POINT ( 'NONE',  ( 3.211159895383561835, 7.562499998634407028, -3.211159895383561835 ) ) ;
#32189 = ORIENTED_EDGE ( 'NONE', *, *, #17826, .T. ) ;
#32190 = AXIS2_PLACEMENT_3D ( 'NONE', #60438, #38191, #26094 ) ;
#32191 = CARTESIAN_POINT ( 'NONE',  ( -7.188101187500002709, 23.81249999795161543, 2.977408999572649151 ) ) ;
#32192 = CARTESIAN_POINT ( 'NONE',  ( -2.679491924311300011, 108.3333333265053682, -9.999999999999959144 ) ) ;
#32193 = CARTESIAN_POINT ( 'NONE',  ( -7.320508075688771932, 247.5000000068279746, -7.320508075688771932 ) ) ;
#32194 = CARTESIAN_POINT ( 'NONE',  ( 7.188101187499999156, 20.24999999795161898, 2.977408999572654924 ) ) ;
#32195 = CARTESIAN_POINT ( 'NONE',  ( -5.082755093536317936, -5.082755093536320601, 1.674052781871753659 ) ) ;
#32196 = CARTESIAN_POINT ( 'NONE',  ( -10.18810118749999916, 0.000000000000000000, 67.65625000204836681 ) ) ;
#32197 =( BOUNDED_CURVE ( )  B_SPLINE_CURVE ( 2, ( #39040, #4339, #9998, #56030, #54533, #15263, #38675, #66959, #38296, #54907, #9629 ),
 .UNSPECIFIED., .F., .F. ) 
 B_SPLINE_CURVE_WITH_KNOTS ( ( 3, 2, 2, 2, 2, 3 ),
 ( 0.2647310102845484292, 0.2647310233782620981, 0.2713492989627193097, 0.2779675745471765214, 0.2845858501316336775, 0.2912041257482609335 ),
 .UNSPECIFIED. ) 
 CURVE ( )  GEOMETRIC_REPRESENTATION_ITEM ( )  RATIONAL_B_SPLINE_CURVE ( ( 0.9999996988044332902, 0.9999998494019186612, 1.000000000000000000, 0.9238795325112867385, 1.000000000000000000, 0.9238795325112867385, 1.000000000000000000, 0.9238795325112867385, 1.000000000000000000, 0.9238795325112867385, 1.000000000000000000 ) ) 
 REPRESENTATION_ITEM ( '' )  );
#32198 = CARTESIAN_POINT ( 'NONE',  ( 2.260304885651728934, -43.01775818952310004, 151.1344127914718172 ) ) ;
#32199 = CARTESIAN_POINT ( 'NONE',  ( -7.347880794884122694E-16, 6.499999997268813168, 4.000000000000001776 ) ) ;
#32200 = CARTESIAN_POINT ( 'NONE',  ( -32.00000000000000000, 208.3750000027312126, 170.0000000000004547 ) ) ;
#32201 = VERTEX_POINT ( 'NONE', #59109 ) ;
#32202 = CARTESIAN_POINT ( 'NONE',  ( -3.458734124999959914, 208.4375000013656063, 198.0000000000000284 ) ) ;
#32203 = CARTESIAN_POINT ( 'NONE',  ( -30.82842712474612057, 195.5000000027312126, 172.8284271247466108 ) ) ;
#32204 = EDGE_CURVE ( 'NONE', #71916, #4761, #65488, .T. ) ;
#32205 = AXIS2_PLACEMENT_3D ( 'NONE', #7736, #69632, #46977 ) ;
#32206 = CARTESIAN_POINT ( 'NONE',  ( -1.881053915767121554, 6.624999998634407916, -4.541265875000002339 ) ) ;
#32207 = CARTESIAN_POINT ( 'NONE',  ( -2.977408999572650927, 111.8750000020483668, -7.188101187500001821 ) ) ;
#32208 = CARTESIAN_POINT ( 'NONE',  ( -7.347880794884122694E-16, 13.75000000000000000, 4.000000000000001776 ) ) ;
#32209 = CARTESIAN_POINT ( 'NONE',  ( -5.082755093536319713, 5.082755093536319713, 26.79905278187175455 ) ) ;
#32210 = ORIENTED_EDGE ( 'NONE', *, *, #58904, .T. ) ;
#32212 =( BOUNDED_CURVE ( )  B_SPLINE_CURVE ( 2, ( #56475, #26665, #33108, #55735, #61001, #45505, #51170, #4051, #4791 ),
 .UNSPECIFIED., .F., .F. ) 
 B_SPLINE_CURVE_WITH_KNOTS ( ( 3, 2, 2, 2, 3 ),
 ( 0.03333333333333336063, 0.04166666666666669905, 0.05000000000000004441, 0.05833333333333338283, 0.06666666666666672125 ),
 .UNSPECIFIED. ) 
 CURVE ( )  GEOMETRIC_REPRESENTATION_ITEM ( )  RATIONAL_B_SPLINE_CURVE ( ( 0.9999999999999997780, 0.9238795325112869605, 1.000000000000000000, 0.9238795325112867385, 1.000000000000000000, 0.9238795325112867385, 1.000000000000000000, 0.9238795325112861834, 1.000000000000000444 ) ) 
 REPRESENTATION_ITEM ( '' )  );
#32211 = CARTESIAN_POINT ( 'NONE',  ( 4.401442555609581635E-16, 26.34374999795161543, -7.188101187500000044 ) ) ;
#32213 = ORIENTED_EDGE ( 'NONE', *, *, #17273, .T. ) ;
#32214 = DIRECTION ( 'NONE',  ( -0.000000000000000000, 1.000000000000000000, -0.000000000000000000 ) ) ;
#32215 = FACE_OUTER_BOUND ( 'NONE', #10799, .T. ) ;
#32216 = CARTESIAN_POINT ( 'NONE',  ( 1.432654583217662481, 206.1250000013655779, 194.5412658750000219 ) ) ;
#32217 = CARTESIAN_POINT ( 'NONE',  ( 25.55430564589119058, 201.3125000013656063, 172.4456943541087526 ) ) ;
#32218 = CARTESIAN_POINT ( 'NONE',  ( -10.00000000000000178, 62.50000000000000000, -1.224646799147353454E-15 ) ) ;
#32219 = CARTESIAN_POINT ( 'NONE',  ( 7.188101187500002709, 93.68750000204838102, 2.977408999572649151 ) ) ;
#32220 = CARTESIAN_POINT ( 'NONE',  ( -4.242640687119285658, 293.1249999999999432, 4.242640687119287435 ) ) ;
#32222 = CARTESIAN_POINT ( 'NONE',  ( 1.469576158976823947E-15, 111.8750000000000000, 8.000000000000000000 ) ) ;
#32221 = CARTESIAN_POINT ( 'NONE',  ( 29.65685424949240812, 208.1875000027311842, 173.9999999999999147 ) ) ;
#32223 = EDGE_CURVE ( 'NONE', #64185, #39207, #3333, .T. ) ;
#32224 = VERTEX_POINT ( 'NONE', #2861 ) ;
#32225 = CARTESIAN_POINT ( 'NONE',  ( -9.832129032723415207, 224.3229166700806729, 5.676582343750005144 ) ) ;
#32226 = CARTESIAN_POINT ( 'NONE',  ( -3.496982156811836440, -16.35094707925444624, 69.15443034746803619 ) ) ;
#32227 = CARTESIAN_POINT ( 'NONE',  ( -1.656854249492405451, 198.4375000027312126, 138.0000000000000568 ) ) ;
#32228 = CARTESIAN_POINT ( 'NONE',  ( -7.347880794884122694E-16, 17.49999999726881583, 4.000000000000001776 ) ) ;
#32229 = CARTESIAN_POINT ( 'NONE',  ( 1.469576158976822172E-15, -7.999999999999991118, 22.20530277982336997 ) ) ;
#32230 = CARTESIAN_POINT ( 'NONE',  ( 2.679491924311235174, 256.4583333333333712, 9.999999999999998224 ) ) ;
#32231 = CARTESIAN_POINT ( 'NONE',  ( -4.898587196589412829E-16, 108.3125000040967905, -8.000000000000000000 ) ) ;
#32232 = CARTESIAN_POINT ( 'NONE',  ( -5.000000000000005329, 183.3333333333333428, 8.660254037844387298 ) ) ;
#32233 = EDGE_CURVE ( 'NONE', #74331, #60459, #49466, .T. ) ;
#32234 = DIRECTION ( 'NONE',  ( -1.000000000000000000, -0.000000000000000000, -0.000000000000000000 ) ) ;
#32235 = CARTESIAN_POINT ( 'NONE',  ( -2.977408999572647819, -7.188101187499990274, 20.14280278187176165 ) ) ;
#32236 = CARTESIAN_POINT ( 'NONE',  ( 11.35316468750000141, 156.0937499965860127, 0.000000000000000000 ) ) ;
#32237 = CYLINDRICAL_SURFACE ( 'NONE', #55405, 11.00000000000000000 ) ;
#32238 = CARTESIAN_POINT ( 'NONE',  ( -5.000000000000000000, 51.74377041917500009, 41.86884046506322932 ) ) ;
#32239 = DIRECTION ( 'NONE',  ( 1.000000000000000000, -0.000000000000000000, -0.000000000000000000 ) ) ;
#32242 = CARTESIAN_POINT ( 'NONE',  ( -4.000000000000002665, 7.312499997268813168, 1.656854249492380582 ) ) ;
#32241 = CARTESIAN_POINT ( 'NONE',  ( 2.751064625579944321E-14, 199.8750000027312126, 194.0000000000000568 ) ) ;
#32240 = CARTESIAN_POINT ( 'NONE',  ( 28.00000000000001776, 201.5000000000000000, 165.9999999999998863 ) ) ;
#32243 = AXIS2_PLACEMENT_3D ( 'NONE', #55551, #3864, #26859 ) ;
#32244 = ORIENTED_EDGE ( 'NONE', *, *, #15678, .T. ) ;
#32245 = CARTESIAN_POINT ( 'NONE',  ( -8.311093377946841443, 19.21874999658601979, 8.311093377946830785 ) ) ;
#32246 = CARTESIAN_POINT ( 'NONE',  ( -1.836970198721029983E-15, 95.62499999317203958, 10.00000000000000178 ) ) ;
#32248 = CARTESIAN_POINT ( 'NONE',  ( 2.679491924311222739, 30.83333332650536462, 10.00000000000000355 ) ) ;
#32247 = DIRECTION ( 'NONE',  ( -0.000000000000000000, 1.000000000000000000, -0.000000000000000000 ) ) ;
#32249 = CARTESIAN_POINT ( 'NONE',  ( -1.656854249492433206, 196.3125000027312126, 201.9999999999999432 ) ) ;
#32250 = CARTESIAN_POINT ( 'NONE',  ( -3.458734125000015425, 204.9375000013656063, 142.0000000000000568 ) ) ;
#32251 = CARTESIAN_POINT ( 'NONE',  ( -2.679491924311235618, 50.41666665983868967, 10.00000000000000000 ) ) ;
#32252 = CARTESIAN_POINT ( 'NONE',  ( 7.188101187500000044, 108.4062500020483810, -8.802885111219163269E-16 ) ) ;
#32253 = CARTESIAN_POINT ( 'NONE',  ( -4.541265875000002339, 9.937499998634406140, -5.561446717895856393E-16 ) ) ;
#32254 = CARTESIAN_POINT ( 'NONE',  ( 8.660254037844376640, 100.4166666666666856, -4.999999999999992006 ) ) ;
#32255 = CARTESIAN_POINT ( 'NONE',  ( -7.999999999999989342, -3.313708498984762496, 9.924052779823364645 ) ) ;
#32257 = CARTESIAN_POINT ( 'NONE',  ( -7.347880794884122694E-16, 5.499999997268813168, 4.000000000000001776 ) ) ;
#32256 = FACE_OUTER_BOUND ( 'NONE', #3401, .T. ) ;
#32258 = ORIENTED_EDGE ( 'NONE', *, *, #36836, .T. ) ;
#32259 = ORIENTED_EDGE ( 'NONE', *, *, #21950, .F. ) ;
#32260 = CARTESIAN_POINT ( 'NONE',  ( 0.000000000000000000, 0.000000000000000000, 14.00000000000000000 ) ) ;
#32261 = CARTESIAN_POINT ( 'NONE',  ( -4.000000000000016875, 196.4375000000000568, 140.3431457505076594 ) ) ;
#32262 = CARTESIAN_POINT ( 'NONE',  ( 2.085542519210945334E-15, 220.4687500034139873, 11.35316468749999963 ) ) ;
#32263 = CARTESIAN_POINT ( 'NONE',  ( -8.311093377946836114, 132.6562499965860411, -8.311093377946837890 ) ) ;
#32264 = ORIENTED_EDGE ( 'NONE', *, *, #22173, .F. ) ;
#32265 = CARTESIAN_POINT ( 'NONE',  ( -5.999999999999999112, 298.0625000000000000, 2.485281374238575314 ) ) ;
#32266 = CARTESIAN_POINT ( 'NONE',  ( 1.871523826299183495E-15, -10.18810118749999916, 96.53125000204838102 ) ) ;
#32267 = CARTESIAN_POINT ( 'NONE',  ( -3.313708498984870410, 93.78125000000000000, 7.999999999999890754 ) ) ;
#32268 = CARTESIAN_POINT ( 'NONE',  ( 4.000000000000015099, 209.5625000000000000, 196.3431457505076594 ) ) ;
#32269 = DIRECTION ( 'NONE',  ( 0.000000000000000000, -0.8778652960884978373, -0.4789076340208558435 ) ) ;
#32271 = CARTESIAN_POINT ( 'NONE',  ( -5.676582343749998039, 127.4479166632526983, -9.832129032723420536 ) ) ;
#32270 = CARTESIAN_POINT ( 'NONE',  ( 2.679491924311309337, 46.04166666666667851, -9.999999999999980460 ) ) ;
#32272 = CARTESIAN_POINT ( 'NONE',  ( -7.778174593052020747, -7.778174593052023411, 95.68750000000000000 ) ) ;
#32273 = EDGE_LOOP ( 'NONE', ( #18157, #26290, #38435, #38974 ) ) ;
#32274 = APPLICATION_CONTEXT ( 'automotive_design' ) ;
#32275 = VECTOR ( 'NONE', #49865, 1000.000000000000000 ) ;
#32276 = CARTESIAN_POINT ( 'NONE',  ( -4.999999999999998224, 23.54166665983870033, -8.660254037844389075 ) ) ;
#32277 = CARTESIAN_POINT ( 'NONE',  ( -29.23829287408424804, 176.8253085577700290, 148.2017496308014017 ) ) ;
#32278 = CARTESIAN_POINT ( 'NONE',  ( -8.311093377946836114, 117.9687499965860127, -8.311093377946837890 ) ) ;
#32279 = CARTESIAN_POINT ( 'NONE',  ( 3.458734125000015425, 207.9375000013656063, 198.0000000000000284 ) ) ;
#32280 = CARTESIAN_POINT ( 'NONE',  ( -7.188101187500002709, 21.18749999795161543, 2.977408999572649151 ) ) ;
#32281 = CARTESIAN_POINT ( 'NONE',  ( 4.220049686691941027, -10.18810118749999738, 83.50000000204839523 ) ) ;
#32282 = CARTESIAN_POINT ( 'NONE',  ( 9.832129032723420536, 21.51041666325268409, -5.676582343749999815 ) ) ;
#32283 = EDGE_LOOP ( 'NONE', ( #4329, #60468, #33540 ) ) ;
#32284 = CARTESIAN_POINT ( 'NONE',  ( -3.968262987731734359, -11.56532875636891156, -0.1021479564361298803 ) ) ;
#32285 = CARTESIAN_POINT ( 'NONE',  ( 8.008118988124991233, 9.807117285998411148E-16, 24.26311528394063188 ) ) ;
#32286 = CARTESIAN_POINT ( 'NONE',  ( -2.445694354108839175, 209.3125000013656063, 144.4456943541088663 ) ) ;
#32287 = CARTESIAN_POINT ( 'NONE',  ( 4.401442555609581635E-16, 2.343749997951610098, -7.188101187500000044 ) ) ;
#32288 = CARTESIAN_POINT ( 'NONE',  ( -6.676582343750000703, 289.5156250017070647, 2.765530957082001251 ) ) ;
#32289 = CARTESIAN_POINT ( 'NONE',  ( 7.320508075688774596, 112.4999999931720396, -7.320508075688774596 ) ) ;
#32290 = CARTESIAN_POINT ( 'NONE',  ( -7.188101187500000044, 1.593749997951610098, -8.802885111219163269E-16 ) ) ;
#32291 = ORIENTED_EDGE ( 'NONE', *, *, #43131, .F. ) ;
#32292 = CARTESIAN_POINT ( 'NONE',  ( -2.085542519210945728E-15, 144.8437499965860411, 11.35316468750000141 ) ) ;
#32293 = CARTESIAN_POINT ( 'NONE',  ( -10.18810118749999916, 4.220049686691934809, 81.06250000204836681 ) ) ;
#32294 = CARTESIAN_POINT ( 'NONE',  ( -30.44569435410879166, 198.8125000013656063, 172.4456943541092357 ) ) ;
#32295 = CARTESIAN_POINT ( 'NONE',  ( -4.898587196589407898E-16, 7.999999999999991118, 21.45530277982336642 ) ) ;
#32296 = CARTESIAN_POINT ( 'NONE',  ( 2.780723358947928197E-16, 14.68749999863440792, -4.541265875000002339 ) ) ;
#32297 = ORIENTED_EDGE ( 'NONE', *, *, #13247, .T. ) ;
#32298 = CARTESIAN_POINT ( 'NONE',  ( 4.000000000000015987, 203.6250000027312126, 198.0000000000000284 ) ) ;
#32299 = AXIS2_PLACEMENT_3D ( 'NONE', #58363, #30776, #1753 ) ;
#32300 = CARTESIAN_POINT ( 'NONE',  ( 2.828427124746153876, 209.8750000000000284, 144.8284271247462129 ) ) ;
#32301 = CARTESIAN_POINT ( 'NONE',  ( -25.17157287525385811, 204.0000000027312126, 167.1715728752541281 ) ) ;
#32302 = EDGE_CURVE ( 'NONE', #27023, #37342, #71877, .T. ) ;
#32303 = ADVANCED_FACE ( 'NONE', ( #42832, #65851 ), #43210, .F. ) ;
#32304 = CARTESIAN_POINT ( 'NONE',  ( 3.313708498984752726, 5.718750000000000000, 8.000000000000008882 ) ) ;
#32305 = EDGE_LOOP ( 'NONE', ( #70871, #48173, #66972, #54946 ) ) ;
#32306 = B_SPLINE_CURVE_WITH_KNOTS ( 'NONE', 1,
 ( #3952, #15615 ),
 .UNSPECIFIED., .F., .F.,
 ( 2, 2 ),
 ( 0.000000000000000000, 1.000000000000000000 ),
 .UNSPECIFIED. ) ;
#32307 = CARTESIAN_POINT ( 'NONE',  ( 4.401442555609581635E-16, 12.84374999795161187, -7.188101187500000044 ) ) ;
#32308 = CARTESIAN_POINT ( 'NONE',  ( -20.95783343414908018, -14.70016487423047202, 192.8459963085001618 ) ) ;
#32309 = DIRECTION ( 'NONE',  ( 1.000000000000000000, 0.000000000000000000, -6.409875649288994867E-15 ) ) ;
#32310 = CARTESIAN_POINT ( 'NONE',  ( 9.832129032723416984, 190.3645833299193839, 5.676582343750006032 ) ) ;
#32311 = EDGE_CURVE ( 'NONE', #72648, #68675, #26982, .T. ) ;
#32312 = CARTESIAN_POINT ( 'NONE',  ( -5.082755093536324154, 111.2187500020483810, 5.082755093536326818 ) ) ;
#32313 = LINE ( 'NONE', #26250, #58264 ) ;
#32314 = CARTESIAN_POINT ( 'NONE',  ( 0.000000000000000000, 0.000000000000000000, 0.000000000000000000 ) ) ;
#32316 = DIRECTION ( 'NONE',  ( 0.000000000000000000, 0.000000000000000000, 1.000000000000000000 ) ) ;
#32315 = CARTESIAN_POINT ( 'NONE',  ( 3.042071309553173286, 220.3645833367473017, 11.35316468749999608 ) ) ;
#32317 =( BOUNDED_CURVE ( )  B_SPLINE_CURVE ( 2, ( #68058, #73711, #51820, #22022, #16348, #57502, #57117, #5805, #39386, #27308, #62384, #28802, #23142, #50324, #22384, #16723, #11828, #46154, #62750, #39018, #69171, #44675, #33743, #56746, #5065, #62021, #11091, #5430, #51441, #74452, #22761, #45784, #35592, #6912, #29923, #12192, #42340, #36697, #18232, #52941, #47263, #41615, #23512, #23889, #58606, #41971, #1271, #65357, #35230, #46898, #70290, #24982, #35958, #47998, #13657, #58249, #59343, #6179, #29187, #40875, #7655, #64628, #7285, #24251, #1637, #47627, #18604, #12924, #6548, #58978, #30293, #69546, #52201, #532, #41247, #53313, #24618, #70649, #18968, #46527, #63880, #64981, #13289, #17856, #29554, #69922, #36329, #71012, #30661, #19327, #52563, #902, #53679, #64255, #12565, #1991, #61194, #19698, #3863, #54426, #31777, #26471, #54797, #3109, #65722, #26093, #20440, #48369, #31024, #14025, #49114, #38190, #3481, #54049, #55176, #60814, #2359, #59709, #25720, #72126, #9138, #8385, #72888, #25353, #43456, #71373, #42710, #66471, #37063, #14779, #37819, #43840, #32155, #49495, #20062, #72514, #20823, #55550, #31399, #66854, #15159, #26858, #9524, #32539, #2732, #49873, #43080, #21195, #44220, #67233, #15529, #8017, #60063, #48741, #71748, #66096, #14406, #37439, #60437, #8767, #32920, #4604, #15902, #63049, #67605, #21566, #74367, #45327, #28349, #56286, #46068, #44593, #5348, #51357, #69088, #10632, #56665, #28717, #22678, #50987, #4237, #11374, #50610, #34408, #33659, #68710, #82, #17021, #4981, #27982, #33289, #44965, #45696, #23059, #61935, #74000, #38933, #34039, #39672, #9890, #38570, #10262, #39307, #62671, #27599, #51732, #55926, #22302, #27224, #50240, #68343, #73630, #16639, #11006, #40045, #57036, #57411, #21935, #5717, #61570, #73262, #67971, #16266, #62305, #13203, #70567, #1556, #40785, #64899, #818, #24535, #36241, #59257, #70208, #52851, #7569, #450, #30573, #35147, #30203, #53595 ),
 .UNSPECIFIED., .F., .F. ) 
 B_SPLINE_CURVE_WITH_KNOTS ( ( 3, 2, 2, 2, 2, 2, 2, 2, 2, 2, 2, 2, 2, 2, 2, 2, 2, 2, 2, 2, 2, 2, 2, 2, 2, 2, 2, 2, 2, 2, 2, 2, 2, 2, 2, 2, 2, 2, 2, 2, 2, 2, 2, 2, 2, 2, 2, 2, 2, 2, 2, 2, 2, 2, 2, 2, 2, 2, 2, 2, 2, 2, 2, 2, 2, 2, 2, 2, 2, 2, 2, 2, 2, 2, 2, 2, 2, 2, 2, 2, 2, 2, 2, 2, 2, 2, 2, 2, 2, 2, 2, 2, 2, 2, 2, 2, 2, 2, 2, 2, 2, 2, 2, 2, 2, 2, 2, 2, 2, 2, 2, 2, 2, 2, 2, 2, 2, 2, 2, 2, 3 ),
 ( 0.000000000000000000, 0.008333333333333333218, 0.01666666666666666644, 0.02500000000000000139, 0.03333333333333333287, 0.04166666666666666435, 0.05000000000000000278, 0.05833333333333333426, 0.06666666666666666574, 0.07499999999999999722, 0.08333333333333332871, 0.09166666666666666019, 0.1000000000000000056, 0.1083333333333333370, 0.1166666666666666685, 0.1250000000000000000, 0.1333333333333333315, 0.1416666666666666630, 0.1499999999999999944, 0.1583333333333333259, 0.1666666666666666574, 0.1749999999999999889, 0.1833333333333333204, 0.1916666666666666796, 0.2000000000000000111, 0.2083333333333333426, 0.2166666666666666741, 0.2250000000000000056, 0.2333333333333333370, 0.2416666666666666685, 0.2500000000000000000, 0.2583333333333333592, 0.2666666666666666630, 0.2750000000000000222, 0.2833333333333333259, 0.2916666666666666852, 0.2999999999999999889, 0.3083333333333333481, 0.3166666666666666519, 0.3250000000000000111, 0.3333333333333333148, 0.3416666666666666741, 0.3499999999999999778, 0.3583333333333333370, 0.3666666666666666408, 0.3750000000000000000, 0.3833333333333333592, 0.3916666666666666630, 0.4000000000000000222, 0.4083333333333333259, 0.4166666666666666852, 0.4249999999999999889, 0.4333333333333333481, 0.4416666666666666519, 0.4500000000000000111, 0.4583333333333333148, 0.4666666666666666741, 0.4749999999999999778, 0.4833333333333333370, 0.4916666666666666408, 0.5000000000000000000, 0.5083333333333333037, 0.5166666666666667185, 0.5250000000000000222, 0.5333333333333333259, 0.5416666666666666297, 0.5500000000000000444, 0.5583333333333333481, 0.5666666666666666519, 0.5749999999999999556, 0.5833333333333333703, 0.5916666666666666741, 0.5999999999999999778, 0.6083333333333332815, 0.6166666666666666963, 0.6250000000000000000, 0.6333333333333333037, 0.6416666666666667185, 0.6500000000000000222, 0.6583333333333333259, 0.6666666666666666297, 0.6750000000000000444, 0.6833333333333333481, 0.6916666666666666519, 0.6999999999999999556, 0.7083333333333333703, 0.7166666666666666741, 0.7249999999999999778, 0.7333333333333332815, 0.7416666666666666963, 0.7500000000000000000, 0.7583333333333333037, 0.7666666666666667185, 0.7750000000000000222, 0.7833333333333333259, 0.7916666666666666297, 0.8000000000000000444, 0.8083333333333333481, 0.8166666666666666519, 0.8249999999999999556, 0.8333333333333333703, 0.8416666666666666741, 0.8499999999999999778, 0.8583333333333332815, 0.8666666666666666963, 0.8750000000000000000, 0.8833333333333333037, 0.8916666666666667185, 0.9000000000000000222, 0.9083333333333333259, 0.9166666666666666297, 0.9250000000000000444, 0.9333333333333333481, 0.9416666666666666519, 0.9499999999999999556, 0.9583333333333333703, 0.9666666666666666741, 0.9749999999999999778, 0.9833333333333332815, 0.9916666666666666963, 0.9985233269883817542 ),
 .UNSPECIFIED. ) 
 CURVE ( )  GEOMETRIC_REPRESENTATION_ITEM ( )  RATIONAL_B_SPLINE_CURVE ( ( 1.000000000000000000, 0.9238795325112867385, 1.000000000000000000, 0.9238795325112867385, 1.000000000000000000, 0.9238795325112867385, 1.000000000000000000, 0.9238795325112867385, 1.000000000000000000, 0.9238795325112867385, 1.000000000000000000, 0.9238795325112867385, 1.000000000000000000, 0.9238795325112867385, 1.000000000000000000, 0.9238795325112867385, 1.000000000000000000, 0.9238795325112867385, 1.000000000000000000, 0.9238795325112867385, 1.000000000000000000, 0.9238795325112867385, 1.000000000000000000, 0.9238795325112867385, 1.000000000000000000, 0.9238795325112867385, 1.000000000000000000, 0.9238795325112867385, 1.000000000000000000, 0.9238795325112867385, 1.000000000000000000, 0.9238795325112867385, 1.000000000000000000, 0.9238795325112867385, 1.000000000000000000, 0.9238795325112867385, 1.000000000000000000, 0.9238795325112867385, 1.000000000000000000, 0.9238795325112867385, 1.000000000000000000, 0.9238795325112867385, 1.000000000000000000, 0.9238795325112867385, 1.000000000000000000, 0.9238795325112867385, 1.000000000000000000, 0.9238795325112867385, 1.000000000000000000, 0.9238795325112867385, 1.000000000000000000, 0.9238795325112867385, 1.000000000000000000, 0.9238795325112867385, 1.000000000000000000, 0.9238795325112867385, 1.000000000000000000, 0.9238795325112867385, 1.000000000000000000, 0.9238795325112867385, 1.000000000000000000, 0.9238795325112867385, 1.000000000000000000, 0.9238795325112867385, 1.000000000000000000, 0.9238795325112867385, 1.000000000000000000, 0.9238795325112867385, 1.000000000000000000, 0.9238795325112867385, 1.000000000000000000, 0.9238795325112867385, 1.000000000000000000, 0.9238795325112867385, 1.000000000000000000, 0.9238795325112867385, 1.000000000000000000, 0.9238795325112867385, 1.000000000000000000, 0.9238795325112867385, 1.000000000000000000, 0.9238795325112867385, 1.000000000000000000, 0.9238795325112867385, 1.000000000000000000, 0.9238795325112867385, 1.000000000000000000, 0.9238795325112867385, 1.000000000000000000, 0.9238795325112867385, 1.000000000000000000, 0.9238795325112867385, 1.000000000000000000, 0.9238795325112867385, 1.000000000000000000, 0.9238795325112867385, 1.000000000000000000, 0.9238795325112867385, 1.000000000000000000, 0.9238795325112867385, 1.000000000000000000, 0.9238795325112867385, 1.000000000000000000, 0.9238795325112867385, 1.000000000000000000, 0.9238795325112867385, 1.000000000000000000, 0.9238795325112867385, 1.000000000000000000, 0.9238795325112867385, 1.000000000000000000, 0.9238795325112867385, 1.000000000000000000, 0.9238795325112867385, 1.000000000000000000, 0.9238795325112867385, 1.000000000000000000, 0.9238795325112867385, 1.000000000000000000, 0.9238795325112867385, 1.000000000000000000, 0.9238795325112867385, 1.000000000000000000, 0.9238795325112867385, 1.000000000000000000, 0.9238795325112867385, 1.000000000000000000, 0.9238795325112867385, 1.000000000000000000, 0.9238795325112867385, 1.000000000000000000, 0.9238795325112867385, 1.000000000000000000, 0.9238795325112867385, 1.000000000000000000, 0.9238795325112867385, 1.000000000000000000, 0.9238795325112867385, 1.000000000000000000, 0.9238795325112867385, 1.000000000000000000, 0.9238795325112867385, 1.000000000000000000, 0.9238795325112867385, 1.000000000000000000, 0.9238795325112867385, 1.000000000000000000, 0.9238795325112867385, 1.000000000000000000, 0.9238795325112867385, 1.000000000000000000, 0.9238795325112867385, 1.000000000000000000, 0.9238795325112867385, 1.000000000000000000, 0.9238795325112867385, 1.000000000000000000, 0.9238795325112867385, 1.000000000000000000, 0.9238795325112867385, 1.000000000000000000, 0.9238795325112867385, 1.000000000000000000, 0.9238795325112867385, 1.000000000000000000, 0.9238795325112867385, 1.000000000000000000, 0.9238795325112867385, 1.000000000000000000, 0.9238795325112867385, 1.000000000000000000, 0.9238795325112867385, 1.000000000000000000, 0.9238795325112867385, 1.000000000000000000, 0.9238795325112867385, 1.000000000000000000, 0.9238795325112867385, 1.000000000000000000, 0.9238795325112867385, 1.000000000000000000, 0.9238795325112867385, 1.000000000000000000, 0.9238795325112867385, 1.000000000000000000, 0.9238795325112867385, 1.000000000000000000, 0.9238795325112867385, 1.000000000000000000, 0.9238795325112867385, 1.000000000000000000, 0.9238795325112867385, 1.000000000000000000, 0.9238795325112867385, 1.000000000000000000, 0.9238795325112867385, 1.000000000000000000, 0.9238795325112867385, 1.000000000000000000, 0.9238795325112867385, 1.000000000000000000, 0.9238795325112867385, 1.000000000000000000, 0.9238795325112867385, 1.000000000000000000, 0.9238795325112867385, 1.000000000000000000, 0.9238795325112867385, 1.000000000000000000, 0.9238795325112867385, 1.000000000000000000, 0.9238795325112867385, 1.000000000000000000, 0.9238795325112867385, 1.000000000000000000, 0.9238795325112867385, 1.000000000000000000, 0.9238795325112867385, 1.000000000000000000, 0.9238795325112867385, 1.000000000000000000, 0.9238795325112867385, 1.000000000000000000, 0.9238795325112867385, 1.000000000000000000, 0.9238795325112867385, 1.000000000000000000, 0.9238795325112867385, 1.000000000000000000, 0.9238795325112867385, 1.000000000000000000, 0.9238795325112867385, 1.000000000000000000, 0.9238795325112867385, 1.000000000000000000, 0.9238795325112867385, 1.000000000000000000, 0.9238795325112867385, 1.000000000000000000, 0.9373681373079684187, 0.9778031724868712082 ) ) 
 REPRESENTATION_ITEM ( '' )  );
#32318 = ORIENTED_EDGE ( 'NONE', *, *, #35254, .F. ) ;
#32319 = CIRCLE ( 'NONE', #66014, 3.999999999999976019 ) ;
#32320 = CARTESIAN_POINT ( 'NONE',  ( 9.832129032723416984, 251.8229166700806729, -5.676582343750003368 ) ) ;
#32321 = CARTESIAN_POINT ( 'NONE',  ( 7.188101187499992051, 8.802885111219154394E-16, 26.61155278187175810 ) ) ;
#32322 = DIRECTION ( 'NONE',  ( 0.000000000000000000, 0.000000000000000000, -1.000000000000000000 ) ) ;
#32323 = DIRECTION ( 'NONE',  ( -0.000000000000000000, 1.000000000000000000, -0.000000000000000000 ) ) ;
#32324 = CARTESIAN_POINT ( 'NONE',  ( 1.506680654954019039, -65.82403019918146470, -26.31606384388913611 ) ) ;
#32325 = CARTESIAN_POINT ( 'NONE',  ( 3.458734125000015425, 199.2500000013656063, 196.5673454167823877 ) ) ;
#32326 = CARTESIAN_POINT ( 'NONE',  ( 38.00000000000000000, 272.0000000000000000, 20.00000000000002132 ) ) ;
#32327 = CARTESIAN_POINT ( 'NONE',  ( -2.485281374238990093, 298.8750000034140726, -5.999999999999583444 ) ) ;
#32328 = CARTESIAN_POINT ( 'NONE',  ( 5.656854249492379694, 92.93749999999998579, -5.656854249492380582 ) ) ;
#32329 = CARTESIAN_POINT ( 'NONE',  ( 11.35316468749999963, 121.3020833299193697, -3.042071309553165293 ) ) ;
#32330 = CARTESIAN_POINT ( 'NONE',  ( 25.17157287525378351, 205.8750000000000284, 172.8284271247460424 ) ) ;
#32331 = CARTESIAN_POINT ( 'NONE',  ( -7.778174593052020747, -7.778174593052023411, 71.68749999999998579 ) ) ;
#32334 = LINE ( 'NONE', #66644, #27805 ) ;
#32333 = CARTESIAN_POINT ( 'NONE',  ( 25.55430564589115505, 201.0625000013656063, 167.5543056458911053 ) ) ;
#32332 = CARTESIAN_POINT ( 'NONE',  ( 26.56734541678238060, 198.2500000013656347, 166.5412658749999650 ) ) ;
#32335 = ORIENTED_EDGE ( 'NONE', *, *, #58896, .F. ) ;
#32336 = CARTESIAN_POINT ( 'NONE',  ( 2.775557561562891351E-14, 271.9999999999999432, 170.0000000000000284 ) ) ;
#32337 = EDGE_CURVE ( 'NONE', #64267, #9770, #60166, .T. ) ;
#32338 = CARTESIAN_POINT ( 'NONE',  ( 5.676582343750001591, 226.6145833299193839, -9.832129032723420536 ) ) ;
#32339 = CARTESIAN_POINT ( 'NONE',  ( -2.839093476692135984E-14, 198.6875000013655779, 138.5412658750000503 ) ) ;
#32340 = CARTESIAN_POINT ( 'NONE',  ( 25.55430564589119413, 198.3125000013656063, 167.5543056458910485 ) ) ;
#32341 = DIRECTION ( 'NONE',  ( 1.000000000000000000, 0.000000000000000000, 0.000000000000000000 ) ) ;
#32342 = CARTESIAN_POINT ( 'NONE',  ( -5.676582343750006032, 209.4270833299193555, 9.832129032723418760 ) ) ;
#32343 = FACE_OUTER_BOUND ( 'NONE', #1668, .T. ) ;
#32344 = CARTESIAN_POINT ( 'NONE',  ( 4.541265875000002339, 20.31249999863440436, 0.000000000000000000 ) ) ;
#32345 = CARTESIAN_POINT ( 'NONE',  ( 4.330454160156406829, -52.03352386568032983, 48.86100738216652672 ) ) ;
#32346 = CARTESIAN_POINT ( 'NONE',  ( -2.977408999572648707, -7.188101187499990274, 0.6428027818717528818 ) ) ;
#32347 = CARTESIAN_POINT ( 'NONE',  ( 11.00000000000000000, 1.347111479062088405E-15, 111.2499999999999858 ) ) ;
#32348 = CARTESIAN_POINT ( 'NONE',  ( -8.311093377946836114, 82.65624999658602690, -8.311093377946837890 ) ) ;
#32349 = ORIENTED_EDGE ( 'NONE', *, *, #61345, .T. ) ;
#32350 = CARTESIAN_POINT ( 'NONE',  ( 25.17157287525377996, 204.7500000027312126, 167.1715728752537586 ) ) ;
#32351 = CARTESIAN_POINT ( 'NONE',  ( -7.188101187500000044, 19.21874999795161543, -8.802885111219163269E-16 ) ) ;
#32352 = CARTESIAN_POINT ( 'NONE',  ( 0.000000000000000000, 0.000000000000000000, 0.000000000000000000 ) ) ;
#32353 = CARTESIAN_POINT ( 'NONE',  ( 9.832129032723420536, 251.3020833367473017, 5.676582343749996262 ) ) ;
#32354 = CARTESIAN_POINT ( 'NONE',  ( -11.35316468750000141, 88.28124999658602690, -1.390361679473963753E-15 ) ) ;
#32355 = EDGE_LOOP ( 'NONE', ( #70010, #17995, #25752, #44673, #48777, #45891, #23837 ) ) ;
#32356 = CARTESIAN_POINT ( 'NONE',  ( 5.000000000000000000, -16.24494643555759410, 69.83755725260752456 ) ) ;
#32357 = CARTESIAN_POINT ( 'NONE',  ( 4.220049686691934809, 10.18810118749999916, 115.1875000020483668 ) ) ;
#32358 = CARTESIAN_POINT ( 'NONE',  ( -25.55430564589114795, 196.3125000013656063, 172.4456943541091789 ) ) ;
#32359 = CARTESIAN_POINT ( 'NONE',  ( 2.449293598294707893E-16, 8.999999997268814056, -4.000000000000001776 ) ) ;
#32360 = CARTESIAN_POINT ( 'NONE',  ( 18.00000000000000355, -9.547192751170710423, -1.363732307033565405 ) ) ;
#32362 = CARTESIAN_POINT ( 'NONE',  ( 11.35316468749999785, 85.57291666325268409, 3.042071309553174174 ) ) ;
#32361 = CARTESIAN_POINT ( 'NONE',  ( 4.556349186104052151, -10.99999999999999822, 106.4687499999999716 ) ) ;
#32363 = CARTESIAN_POINT ( 'NONE',  ( -7.999999999999991118, 0.000000000000000000, 19.01780278392014623 ) ) ;
#32364 = CARTESIAN_POINT ( 'NONE',  ( -24.54126587500000056, 201.5000000013655779, 168.5673454167827003 ) ) ;
#32365 = CARTESIAN_POINT ( 'NONE',  ( -27.99999999999999645, 210.0000000000000284, 170.0000000000003695 ) ) ;
#32366 = CARTESIAN_POINT ( 'NONE',  ( 7.320508075688771044, 176.2499999931720254, 7.320508075688775484 ) ) ;
#32367 = CARTESIAN_POINT ( 'NONE',  ( 5.000000000000000888, -52.35862550122958936, 48.98731492261398301 ) ) ;
#32368 = CARTESIAN_POINT ( 'NONE',  ( -9.832129032723418760, 73.17708332991934128, -5.676582343750004256 ) ) ;
#32369 = CARTESIAN_POINT ( 'NONE',  ( -6.676582343750003368, 293.3906250017069510, -2.765530957081996810 ) ) ;
#32370 = CARTESIAN_POINT ( 'NONE',  ( -4.220049686691937474, -10.18810118749999738, 108.8125000020483952 ) ) ;
#32371 = CARTESIAN_POINT ( 'NONE',  ( -9.832129032723418760, 202.8645833299193555, -5.676582343750004256 ) ) ;
#32372 = ORIENTED_EDGE ( 'NONE', *, *, #66274, .T. ) ;
#32373 = CYLINDRICAL_SURFACE ( 'NONE', #45218, 6.000000000000001776 ) ;
#32374 = CARTESIAN_POINT ( 'NONE',  ( 5.000000000000000000, -60.90295814858238543, -23.31388853594834032 ) ) ;
#32375 = CARTESIAN_POINT ( 'NONE',  ( 5.000000000000000888, 62.69487254116386055, 24.02505537902103683 ) ) ;
#32377 = CARTESIAN_POINT ( 'NONE',  ( -9.832129032723420536, 208.6979166632526983, 5.676582343749997150 ) ) ;
#32376 = DIRECTION ( 'NONE',  ( -0.000000000000000000, 1.000000000000000000, 4.689100369878284071E-30 ) ) ;
#32378 = VECTOR ( 'NONE', #55806, 1000.000000000000000 ) ;
#32379 = CARTESIAN_POINT ( 'NONE',  ( 2.679491924311225848, 231.6666666734946318, -10.00000000000000000 ) ) ;
#32380 = CARTESIAN_POINT ( 'NONE',  ( 2.020667218593132706E-15, -11.00000000000000000, 72.06250000409677625 ) ) ;
#32381 = ORIENTED_EDGE ( 'NONE', *, *, #52290, .F. ) ;
#32382 = CARTESIAN_POINT ( 'NONE',  ( 11.35316468750000141, 201.0937499965860127, 0.000000000000000000 ) ) ;
#32383 = AXIS2_PLACEMENT_3D ( 'NONE', #70914, #19228, #46791 ) ;
#32384 = CARTESIAN_POINT ( 'NONE',  ( 2.977408999572650927, -7.188101187499990274, 15.45530278187175632 ) ) ;
#32385 = CARTESIAN_POINT ( 'NONE',  ( 1.469576158976822172E-15, -7.999999999999991118, 16.39280278392014978 ) ) ;
#32386 = CARTESIAN_POINT ( 'NONE',  ( 8.000000000000000000, 12.09375000000000178, -3.313708498984761608 ) ) ;
#32387 = ORIENTED_EDGE ( 'NONE', *, *, #40394, .T. ) ;
#32388 = EDGE_CURVE ( 'NONE', #25993, #30848, #57773, .T. ) ;
#32389 = CARTESIAN_POINT ( 'NONE',  ( 8.000000000000000000, 91.53125000409679046, -3.313708498984762496 ) ) ;
#32390 = CARTESIAN_POINT ( 'NONE',  ( 10.00000000000000178, 0.000000000000000000, 0.000000000000000000 ) ) ;
#32391 = ORIENTED_EDGE ( 'NONE', *, *, #65738, .T. ) ;
#32392 = CARTESIAN_POINT ( 'NONE',  ( 2.449293598294707893E-16, 17.25000000000000000, -4.000000000000001776 ) ) ;
#32393 = CARTESIAN_POINT ( 'NONE',  ( 1.881053915767122664, 19.12499999863441147, 4.541265875000001451 ) ) ;
#32394 = CARTESIAN_POINT ( 'NONE',  ( 7.999999999999991118, 3.313708498984757611, 7.861552783920145338 ) ) ;
#32395 = CARTESIAN_POINT ( 'NONE',  ( -3.313708498984757611, 7.999999999999991118, 18.73655278392014623 ) ) ;
#32397 = ORIENTED_EDGE ( 'NONE', *, *, #68852, .T. ) ;
#32396 = EDGE_CURVE ( 'NONE', #1774, #37163, #3778, .T. ) ;
#32398 = CYLINDRICAL_SURFACE ( 'NONE', #27017, 3.999999999999976019 ) ;
#32399 = CARTESIAN_POINT ( 'NONE',  ( -5.082755093536324154, 89.84375000204839523, 5.082755093536326818 ) ) ;
#32401 = CARTESIAN_POINT ( 'NONE',  ( 3.407298021510795749, -51.68473891413731991, 48.72627478609596352 ) ) ;
#32400 = CARTESIAN_POINT ( 'NONE',  ( -3.042071309553166625, 257.8645833367473301, -11.35316468749999608 ) ) ;
#32402 =( LENGTH_UNIT ( ) NAMED_UNIT ( * ) SI_UNIT ( .MILLI., .METRE. ) );
#32403 = EDGE_LOOP ( 'NONE', ( #1614, #73207, #37118, #3922 ) ) ;
#32404 = EDGE_CURVE ( 'NONE', #37163, #18829, #43585, .T. ) ;
#32406 = AXIS2_PLACEMENT_3D ( 'NONE', #71905, #43237, #66252 ) ;
#32405 = CARTESIAN_POINT ( 'NONE',  ( -5.676582343749992710, 255.0520833367473301, 9.832129032723422313 ) ) ;
#32407 = CARTESIAN_POINT ( 'NONE',  ( 2.977408999572650927, -7.188101187499990274, 21.45530278187175810 ) ) ;
#32408 = VERTEX_POINT ( 'NONE', #66600 ) ;
#32409 = ORIENTED_EDGE ( 'NONE', *, *, #10238, .T. ) ;
#32410 = CARTESIAN_POINT ( 'NONE',  ( 4.220049686691941027, -10.18810118749999738, 81.62500000204836681 ) ) ;
#32411 = CARTESIAN_POINT ( 'NONE',  ( 11.35316468750000141, 71.09374999658601268, 0.000000000000000000 ) ) ;
#32412 = CYLINDRICAL_SURFACE ( 'NONE', #26402, 3.999999999999976019 ) ;
#32413 = CARTESIAN_POINT ( 'NONE',  ( 2.020667218593132706E-15, -11.00000000000000000, 89.87499999999998579 ) ) ;
#32416 = CARTESIAN_POINT ( 'NONE',  ( -6.676582343750002480, 289.5468750017070079, -2.765530957081996810 ) ) ;
#32415 = CARTESIAN_POINT ( 'NONE',  ( 26.34314575050763807, 198.0625000027312410, 173.9999999999999147 ) ) ;
#32414 = PLANE ( 'NONE',  #1042 ) ;
#32417 = VECTOR ( 'NONE', #17428, 1000.000000000000000 ) ;
#32418 = CYLINDRICAL_SURFACE ( 'NONE', #33296, 3.000000000000001332 ) ;
#32419 = CARTESIAN_POINT ( 'NONE',  ( 30.99999999999998934, 82.00000000000001421, 65.00000000000000000 ) ) ;
#32420 = EDGE_CURVE ( 'NONE', #22788, #32460, #16026, .T. ) ;
#32421 = CARTESIAN_POINT ( 'NONE',  ( 3.458734125000016757, 197.1250000013656347, 199.4326545832176976 ) ) ;
#32422 = CARTESIAN_POINT ( 'NONE',  ( 7.999999999999998224, 8.718749995903221972, 3.313708498984766493 ) ) ;
#32423 = EDGE_LOOP ( 'NONE', ( #40197, #44687, #54462, #3580 ) ) ;
#32424 = CARTESIAN_POINT ( 'NONE',  ( 25.55430564589119768, 208.3125000013656063, 167.5543056458910485 ) ) ;
#32425 = CARTESIAN_POINT ( 'NONE',  ( 5.082755093536324154, 14.15624999795161187, 5.082755093536326818 ) ) ;
#32426 = CARTESIAN_POINT ( 'NONE',  ( 5.656854249492374365, 5.656854249492375253, 24.45530278392014978 ) ) ;
#32427 = CARTESIAN_POINT ( 'NONE',  ( -11.00000000000000000, 0.000000000000000000, 98.68750000409677625 ) ) ;
#32428 = CARTESIAN_POINT ( 'NONE',  ( 7.188101187500000044, 107.2812500020483810, -8.802885111219163269E-16 ) ) ;
#32430 = CARTESIAN_POINT ( 'NONE',  ( 2.266287154879883303, -50.05783744175294459, -40.76793781259145533 ) ) ;
#32429 = CARTESIAN_POINT ( 'NONE',  ( -7.320508075688773708, 18.74999999317203248, -7.320508075688774596 ) ) ;
#32431 = CARTESIAN_POINT ( 'NONE',  ( 10.00000000000000533, 135.0000000000000284, 0.000000000000000000 ) ) ;
#32432 = CARTESIAN_POINT ( 'NONE',  ( 31.45873412499999944, 207.9375000013656063, 169.9999999999999432 ) ) ;
#32433 = CARTESIAN_POINT ( 'NONE',  ( 5.082755093536318824, 5.082755093536319713, 13.29905278187175277 ) ) ;
#32434 = CARTESIAN_POINT ( 'NONE',  ( 2.828427124746153876, 209.0000000027312126, 144.8284271247462129 ) ) ;
#32435 = CARTESIAN_POINT ( 'NONE',  ( -5.676582343749998039, 47.44791666325268409, -9.832129032723420536 ) ) ;
#32436 =( BOUNDED_CURVE ( )  B_SPLINE_CURVE ( 2, ( #16425, #11533, #74155, #34188, #57192 ),
 .UNSPECIFIED., .F., .F. ) 
 B_SPLINE_CURVE_WITH_KNOTS ( ( 3, 2, 3 ),
 ( 0.9791666666666651864, 0.9895833333333325932, 1.000000000000000000 ),
 .UNSPECIFIED. ) 
 CURVE ( )  GEOMETRIC_REPRESENTATION_ITEM ( )  RATIONAL_B_SPLINE_CURVE ( ( 1.000000000000010436, 0.9238795325112761914, 1.000000000000000000, 0.9238795325112867385, 1.000000000000000000 ) ) 
 REPRESENTATION_ITEM ( '' )  );
#32437 = CARTESIAN_POINT ( 'NONE',  ( 2.775557561562891351E-14, 210.0000000000000284, 198.0000000000000284 ) ) ;
#32438 = CARTESIAN_POINT ( 'NONE',  ( 8.660254037844385522, 16.45833332650536818, 5.000000000000005329 ) ) ;
#32439 = CARTESIAN_POINT ( 'NONE',  ( 2.020667218593132706E-15, -11.00000000000000000, 71.87500000000000000 ) ) ;
#32440 = VERTEX_POINT ( 'NONE', #38694 ) ;
#32441 = CYLINDRICAL_SURFACE ( 'NONE', #44700, 14.00000000000000000 ) ;
#32442 = DIRECTION ( 'NONE',  ( 0.000000000000000000, 0.000000000000000000, 1.000000000000000000 ) ) ;
#32443 = CARTESIAN_POINT ( 'NONE',  ( 11.35316468749999785, 55.57291666325266988, 3.042071309553174174 ) ) ;
#32444 = CARTESIAN_POINT ( 'NONE',  ( 7.778174593052021635, 7.778174593052023411, 81.62500000409677625 ) ) ;
#32445 = CARTESIAN_POINT ( 'NONE',  ( 1.432654583217607414, 202.5000000013656063, 145.4587341250000350 ) ) ;
#32446 = PLANE ( 'NONE',  #68545 ) ;
#32447 = PLANE ( 'NONE',  #33510 ) ;
#32449 = CARTESIAN_POINT ( 'NONE',  ( -8.311093377946841443, 43.90624999658601979, 8.311093377946834337 ) ) ;
#32448 = CARTESIAN_POINT ( 'NONE',  ( 2.977408999572654480, 97.62500000204836681, 7.188101187499999156 ) ) ;
#32450 = CARTESIAN_POINT ( 'NONE',  ( -7.999999999999991118, 0.000000000000000000, 6.830302779823365533 ) ) ;
#32451 = CARTESIAN_POINT ( 'NONE',  ( 3.313708498984756279, 7.999999999999991118, 21.54905278392014623 ) ) ;
#32452 = CARTESIAN_POINT ( 'NONE',  ( 3.042071309553167069, 161.8229166632526983, -11.35316468749999785 ) ) ;
#32454 = CARTESIAN_POINT ( 'NONE',  ( -10.00000000000000178, 124.3749999931720396, -1.224646799147353454E-15 ) ) ;
#32453 = PRODUCT ( 'plain washer (type a)_is_IS 2016 A- 22', 'plain washer (type a)_is_IS 2016 A- 22', '', ( #61810 ) ) ;
#32455 = CARTESIAN_POINT ( 'NONE',  ( -4.401442555609581635E-16, 101.6562500020483810, -7.188101187500000044 ) ) ;
#32456 = ORIENTED_EDGE ( 'NONE', *, *, #7927, .F. ) ;
#32457 = CYLINDRICAL_SURFACE ( 'NONE', #59320, 10.00000000000000000 ) ;
#32458 = CARTESIAN_POINT ( 'NONE',  ( 8.311093377946834337, 40.46874999658601979, 8.311093377946839666 ) ) ;
#32459 = CARTESIAN_POINT ( 'NONE',  ( -8.265697409064609147, -5.620102221249831942, -0.5590800469813734797 ) ) ;
#32460 = VERTEX_POINT ( 'NONE', #27349 ) ;
#32461 = DIRECTION ( 'NONE',  ( -0.000000000000000000, 1.000000000000000000, -0.000000000000000000 ) ) ;
#32462 = CARTESIAN_POINT ( 'NONE',  ( -10.18810118749999738, -4.220049686691941915, 75.25000000204836681 ) ) ;
#32463 = CARTESIAN_POINT ( 'NONE',  ( -30.78011882844933211, -36.99586229965066053, 173.7956342421400677 ) ) ;
#32465 = CARTESIAN_POINT ( 'NONE',  ( -5.676582343750006032, 169.1145833299193555, 9.832129032723418760 ) ) ;
#32464 = FACE_OUTER_BOUND ( 'NONE', #46962, .T. ) ;
#32466 = CARTESIAN_POINT ( 'NONE',  ( -5.082755093536326818, 3.281249997951610542, 5.082755093536325042 ) ) ;
#32467 = CARTESIAN_POINT ( 'NONE',  ( -3.313708498984758943, -7.999999999999989342, 13.16780278432982421 ) ) ;
#32468 = CARTESIAN_POINT ( 'NONE',  ( -20.22612057219620141, -29.70682742716073577, 193.4929402770383433 ) ) ;
#32469 = CARTESIAN_POINT ( 'NONE',  ( -9.832129032723415207, 239.3229166700806445, 5.676582343750005144 ) ) ;
#32470 = CARTESIAN_POINT ( 'NONE',  ( -4.220049686691937474, -10.18810118749999738, 87.81250000204838102 ) ) ;
#32471 = ORIENTED_EDGE ( 'NONE', *, *, #25598, .F. ) ;
#32472 = AXIS2_PLACEMENT_3D ( 'NONE', #52126, #458, #23437 ) ;
#32473 = LINE ( 'NONE', #71685, #17250 ) ;
#32474 = CARTESIAN_POINT ( 'NONE',  ( 0.000000000000000000, 22.99999999999999645, 0.000000000000000000 ) ) ;
#32475 = CARTESIAN_POINT ( 'NONE',  ( 6.951808397369818766E-16, 102.3437499965860127, -11.35316468750000141 ) ) ;
#32476 = CARTESIAN_POINT ( 'NONE',  ( -7.204075437095967871, 7.204075437095967871, 94.46875000204838102 ) ) ;
#32477 = CARTESIAN_POINT ( 'NONE',  ( 4.541265875000002339, 19.49999999863440436, -1.881053915767121776 ) ) ;
#32478 = ORIENTED_EDGE ( 'NONE', *, *, #31650, .F. ) ;
#32479 = VERTEX_POINT ( 'NONE', #49996 ) ;
#32480 = ADVANCED_FACE ( 'NONE', ( #37945 ), #990, .F. ) ;
#32481 = CARTESIAN_POINT ( 'NONE',  ( 1.881053915767122664, 2.249999998634407028, 4.541265875000001451 ) ) ;
#32482 = CIRCLE ( 'NONE', #5979, 71.70204102886728492 ) ;
#32483 = CARTESIAN_POINT ( 'NONE',  ( 5.082755093536325930, 11.15624999795161187, -5.082755093536325930 ) ) ;
#32484 = CARTESIAN_POINT ( 'NONE',  ( 8.000000000000000000, 113.9375000040967763, -9.797174393178825657E-16 ) ) ;
#32485 = CARTESIAN_POINT ( 'NONE',  ( 10.18810118749999916, 1.247682550866122264E-15, 92.78125000204836681 ) ) ;
#32486 = CARTESIAN_POINT ( 'NONE',  ( -24.54126587499998280, 203.3750000013656063, 171.4326545832179818 ) ) ;
#32487 = DIRECTION ( 'NONE',  ( 0.000000000000000000, 1.000000000000000000, 4.283267841918042741E-17 ) ) ;
#32488 = CARTESIAN_POINT ( 'NONE',  ( 2.449293598294707893E-16, 3.250000000000000444, -4.000000000000001776 ) ) ;
#32489 = CARTESIAN_POINT ( 'NONE',  ( -1.656854249492383691, 18.43749999726881583, 4.000000000000000888 ) ) ;
#32490 = CARTESIAN_POINT ( 'NONE',  ( -8.342170076843785083E-16, 7.062499998634407028, 4.541265875000002339 ) ) ;
#32491 = CARTESIAN_POINT ( 'NONE',  ( -2.751064625579944321E-14, 200.7500000000000000, 146.0000000000000284 ) ) ;
#32492 = VERTEX_POINT ( 'NONE', #55300 ) ;
#32493 = CARTESIAN_POINT ( 'NONE',  ( 2.445694354108838731, 195.0625000013656063, 195.5543056458912190 ) ) ;
#32495 = FACE_OUTER_BOUND ( 'NONE', #61844, .T. ) ;
#32494 = CARTESIAN_POINT ( 'NONE',  ( -27.99999999999991473, 196.9375000013655779, 173.4587341250003760 ) ) ;
#32496 = ADVANCED_FACE ( 'NONE', ( #72643 ), #39059, .T. ) ;
#32497 = CARTESIAN_POINT ( 'NONE',  ( 1.881053915767122664, 19.12499999863441147, 4.541265875000001451 ) ) ;
#32498 = CARTESIAN_POINT ( 'NONE',  ( 6.676582343750001591, 298.9531250017069510, -8.176455196517173205E-16 ) ) ;
#32499 = CARTESIAN_POINT ( 'NONE',  ( 2.977408999572650927, -7.188101187499990274, 9.455302781871754547 ) ) ;
#32500 = ORIENTED_EDGE ( 'NONE', *, *, #13879, .F. ) ;
#32501 = EDGE_LOOP ( 'NONE', ( #32119, #67966, #27162, #10470, #56604, #41519 ) ) ;
#32502 = CARTESIAN_POINT ( 'NONE',  ( -7.204075437095965206, -7.204075437095968759, 99.34375000204836681 ) ) ;
#32503 = LINE ( 'NONE', #3827, #46762 ) ;
#32504 = CARTESIAN_POINT ( 'NONE',  ( -24.54126587499999346, 199.4375000013655779, 170.0000000000003411 ) ) ;
#32505 = CARTESIAN_POINT ( 'NONE',  ( 11.00000000000000000, 4.556349186104045934, 105.3437499999999858 ) ) ;
#32506 = CARTESIAN_POINT ( 'NONE',  ( -2.445694354108784108, 208.5625000013656063, 195.5543056458912190 ) ) ;
#32507 = LINE ( 'NONE', #27195, #6067 ) ;
#32508 = CARTESIAN_POINT ( 'NONE',  ( 8.660254037844385522, 104.5833333333333286, 5.000000000000005329 ) ) ;
#32509 = CARTESIAN_POINT ( 'NONE',  ( 1.469576158976823947E-15, 110.3750000000000000, 8.000000000000000000 ) ) ;
#32510 = CARTESIAN_POINT ( 'NONE',  ( 1.226468279477575784E-15, 293.8593750017070079, 6.676582343750001591 ) ) ;
#32511 = CARTESIAN_POINT ( 'NONE',  ( -7.188101187499990274, -2.977408999572651371, 13.95530278187175277 ) ) ;
#32512 = VERTEX_POINT ( 'NONE', #32145 ) ;
#32513 = CARTESIAN_POINT ( 'NONE',  ( 3.313708498984721640, 19.21875000000000000, 8.000000000000039080 ) ) ;
#32514 = EDGE_CURVE ( 'NONE', #26713, #65546, #48731, .T. ) ;
#32515 = AXIS2_PLACEMENT_3D ( 'NONE', #26152, #49170, #21249 ) ;
#32516 = DIRECTION ( 'NONE',  ( -0.000000000000000000, 1.000000000000000000, 4.689100369878284071E-30 ) ) ;
#32517 = CARTESIAN_POINT ( 'NONE',  ( 8.000000000000000000, 20.90624999590322375, -3.313708498984761608 ) ) ;
#32518 = CARTESIAN_POINT ( 'NONE',  ( -2.754378923186476579E-14, 204.1875000013656063, 145.4587341250000350 ) ) ;
#32519 = LINE ( 'NONE', #59691, #39445 ) ;
#32521 = CARTESIAN_POINT ( 'NONE',  ( -2.445694354108839175, 204.3125000013656063, 144.4456943541088663 ) ) ;
#32520 = CARTESIAN_POINT ( 'NONE',  ( 2.249999999999997335, 255.9999999999998295, 5.427273999917215264 ) ) ;
#32522 = CARTESIAN_POINT ( 'NONE',  ( 9.832129032723420536, 256.3020833367473301, 5.676582343749996262 ) ) ;
#32523 = CARTESIAN_POINT ( 'NONE',  ( 7.999999999999991118, 0.000000000000000000, 30.00000000000000000 ) ) ;
#32524 = CARTESIAN_POINT ( 'NONE',  ( -27.99999999999999645, 210.0000000000000284, 166.0000000000003979 ) ) ;
#32525 = CARTESIAN_POINT ( 'NONE',  ( 10.00000000000000178, 225.0000000000000000, 0.000000000000000000 ) ) ;
#32526 = ADVANCED_FACE ( 'NONE', ( #54415 ), #71737, .F. ) ;
#32527 = CARTESIAN_POINT ( 'NONE',  ( -7.188101187499992051, 2.977408999572646930, 6.267802781871754547 ) ) ;
#32528 = CARTESIAN_POINT ( 'NONE',  ( 11.35316468750000141, 201.0937499965860127, 0.000000000000000000 ) ) ;
#32529 = CARTESIAN_POINT ( 'NONE',  ( -27.99999999999991118, 202.6250000027312126, 174.0000000000003695 ) ) ;
#32530 = CARTESIAN_POINT ( 'NONE',  ( 3.211159895383561835, 7.437499998634407028, -3.211159895383561835 ) ) ;
#32531 = CARTESIAN_POINT ( 'NONE',  ( 6.000000000000003553, 290.5625000000000000, -2.485281374238571761 ) ) ;
#32532 = CARTESIAN_POINT ( 'NONE',  ( 9.000000000000040856, -15.58845726811991739, -20.69999999999999929 ) ) ;
#32533 = ORIENTED_EDGE ( 'NONE', *, *, #41485, .F. ) ;
#32534 = AXIS2_PLACEMENT_3D ( 'NONE', #71452, #25059, #13005 ) ;
#32535 = CARTESIAN_POINT ( 'NONE',  ( -3.458734125000015869, 204.1875000013656063, 142.0000000000000568 ) ) ;
#32536 = CARTESIAN_POINT ( 'NONE',  ( -3.042071309553164404, 7.239583329919349275, -11.35316468749999963 ) ) ;
#32537 = CARTESIAN_POINT ( 'NONE',  ( 11.00000000000000000, 4.556349186104045934, 96.53125000409677625 ) ) ;
#32538 = CARTESIAN_POINT ( 'NONE',  ( -2.726571689596997292E-14, 210.0000000000000284, 138.0000000000000568 ) ) ;
#32539 = CARTESIAN_POINT ( 'NONE',  ( -29.43265458321770822, 200.5000000013655779, 166.5412658750003914 ) ) ;
#32540 = CARTESIAN_POINT ( 'NONE',  ( 38.00000000000000000, 52.99999999999992895, -6.791607979884335933E-15 ) ) ;
#32542 = CARTESIAN_POINT ( 'NONE',  ( -5.000000000000000888, 229.1666666666666856, -8.660254037844387298 ) ) ;
#32541 = CARTESIAN_POINT ( 'NONE',  ( -2.977408999572652260, 118.4375000020483952, 7.188101187500000044 ) ) ;
#32543 = CARTESIAN_POINT ( 'NONE',  ( -7.999999999999991118, 0.000000000000000000, 26.33030277982336997 ) ) ;
#32544 = CARTESIAN_POINT ( 'NONE',  ( 5.676582343750001591, 116.6145833299193697, -9.832129032723420536 ) ) ;
#32545 = CARTESIAN_POINT ( 'NONE',  ( -8.660254037844387298, 88.95833332650536818, -5.000000000000004441 ) ) ;
#32546 = EDGE_CURVE ( 'NONE', #28645, #43835, #11493, .T. ) ;
#32547 = CARTESIAN_POINT ( 'NONE',  ( -7.188101187499999156, 118.6250000020483810, 2.977408999572654924 ) ) ;
#32548 = CARTESIAN_POINT ( 'NONE',  ( 4.541265875000001451, 20.37499999863441147, 1.881053915767124440 ) ) ;
#32549 = DIRECTION ( 'NONE',  ( 1.000000000000000000, 0.000000000000000000, 0.000000000000000000 ) ) ;
#32550 = CARTESIAN_POINT ( 'NONE',  ( 2.775557561562891351E-14, 271.9999999999999432, 170.0000000000000284 ) ) ;
#32551 = ORIENTED_EDGE ( 'NONE', *, *, #73767, .F. ) ;
#32552 = CARTESIAN_POINT ( 'NONE',  ( -9.679871326005349275, 225.9999999999998863, 2.594511375997681668 ) ) ;
#32553 = CARTESIAN_POINT ( 'NONE',  ( 1.226468279477575784E-15, 289.8593750017070079, 6.676582343750001591 ) ) ;
#32554 = CARTESIAN_POINT ( 'NONE',  ( 2.395154805519954641E-11, 111.2499999999981242, -9.999999999999998224 ) ) ;
#32555 = CARTESIAN_POINT ( 'NONE',  ( 7.999999999999991118, 3.313708498984757611, 27.23030278432983309 ) ) ;
#32556 = DIRECTION ( 'NONE',  ( -0.000000000000000000, 1.000000000000000000, 4.689100369878284071E-30 ) ) ;
#32557 = CARTESIAN_POINT ( 'NONE',  ( 10.00000000000000000, 206.6666666598387110, 2.679491924311236062 ) ) ;
#32558 = CARTESIAN_POINT ( 'NONE',  ( -4.556349186104048599, -10.99999999999999822, 70.46875000409677625 ) ) ;
#32559 = CARTESIAN_POINT ( 'NONE',  ( -10.18810118749999738, -4.220049686691941915, 104.1250000020483810 ) ) ;
#32560 = VERTEX_POINT ( 'NONE', #26460 ) ;
#32561 =( BOUNDED_CURVE ( )  B_SPLINE_CURVE ( 2, ( #11077, #23497, #17089, #58233, #34105, #6532, #29538, #57100, #52549 ),
 .UNSPECIFIED., .F., .F. ) 
 B_SPLINE_CURVE_WITH_KNOTS ( ( 3, 2, 2, 2, 3 ),
 ( 0.05294620388485415940, 0.05956448026011130353, 0.06618275584456811966, 0.07280103142902494273, 0.07941930701348173804 ),
 .UNSPECIFIED. ) 
 CURVE ( )  GEOMETRIC_REPRESENTATION_ITEM ( )  RATIONAL_B_SPLINE_CURVE ( ( 1.000000000000000000, 0.9238795325112867385, 1.000000000000000000, 0.9238795325112867385, 1.000000000000000000, 0.9238795325112867385, 1.000000000000000000, 0.9238795325112867385, 1.000000000000000000 ) ) 
 REPRESENTATION_ITEM ( '' )  );
#32562 = CARTESIAN_POINT ( 'NONE',  ( 2.679491924311222739, 155.8333333265053682, 10.00000000000000355 ) ) ;
#32563 = CARTESIAN_POINT ( 'NONE',  ( -11.35316468750000141, 148.5937499965860411, -1.390361679473963753E-15 ) ) ;
#32564 = CARTESIAN_POINT ( 'NONE',  ( 7.778174593052021635, 7.778174593052023411, 97.93749999999998579 ) ) ;
#32565 = CARTESIAN_POINT ( 'NONE',  ( -3.458734124999959469, 205.7500000013656063, 199.4326545832176976 ) ) ;
#32566 = CARTESIAN_POINT ( 'NONE',  ( 0.000000000000000000, 0.000000000000000000, 0.000000000000000000 ) ) ;
#32567 = CARTESIAN_POINT ( 'NONE',  ( 11.35316468750000141, 66.09374999658601268, 0.000000000000000000 ) ) ;
#32568 = EDGE_LOOP ( 'NONE', ( #7411, #30082, #10967, #45902 ) ) ;
#32569 = CARTESIAN_POINT ( 'NONE',  ( -10.18810118749999916, 4.220049686691934809, 115.5625000020483810 ) ) ;
#32570 = CARTESIAN_POINT ( 'NONE',  ( 3.211159895383560947, 9.312499998634407916, 3.211159895383562723 ) ) ;
#32571 = EDGE_LOOP ( 'NONE', ( #69234, #60639 ) ) ;
#32572 = EDGE_CURVE ( 'NONE', #7760, #55468, #31389, .T. ) ;
#32573 = CARTESIAN_POINT ( 'NONE',  ( 7.188101187500000044, 18.46874999795161187, 0.000000000000000000 ) ) ;
#32574 = CARTESIAN_POINT ( 'NONE',  ( 6.000000000000003553, 289.5000000034139589, 2.485281374238571317 ) ) ;
#32575 = DIRECTION ( 'NONE',  ( -1.000000000000000000, 0.000000000000000000, 0.000000000000000000 ) ) ;
#32576 = CARTESIAN_POINT ( 'NONE',  ( 5.082755093536324154, 15.65624999795161365, 5.082755093536326818 ) ) ;
#32577 = CARTESIAN_POINT ( 'NONE',  ( -4.401442555609577197E-16, 7.188101187499992051, 2.611552781871750994 ) ) ;
#32578 = EDGE_CURVE ( 'NONE', #33233, #51609, #54038, .T. ) ;
#32579 = CARTESIAN_POINT ( 'NONE',  ( 10.18810118749999916, 4.220049686691935698, 110.8750000020483810 ) ) ;
#32580 = VECTOR ( 'NONE', #39651, 1000.000000000000000 ) ;
#32581 = EDGE_CURVE ( 'NONE', #15471, #9634, #24031, .T. ) ;
#32582 = LINE ( 'NONE', #4274, #64349 ) ;
#32583 = CARTESIAN_POINT ( 'NONE',  ( 1.656854249492381248, 6.937499997268813168, -4.000000000000001776 ) ) ;
#32584 = CARTESIAN_POINT ( 'NONE',  ( -24.00000000000002842, 207.9375000027312126, 168.3431457505079152 ) ) ;
#32585 = VECTOR ( 'NONE', #66940, 1000.000000000000000 ) ;
#32586 = VERTEX_POINT ( 'NONE', #60803 ) ;
#32587 = AXIS2_PLACEMENT_3D ( 'NONE', #18613, #41624, #25729 ) ;
#32588 = CARTESIAN_POINT ( 'NONE',  ( -1.432654583217607192, 207.2500000013655779, 194.5412658750000219 ) ) ;
#32589 = CARTESIAN_POINT ( 'NONE',  ( -31.45873412499996746, 208.7500000013656063, 171.4326545832181239 ) ) ;
#32590 = CARTESIAN_POINT ( 'NONE',  ( -10.18810118749999916, 0.000000000000000000, 69.53125000204838102 ) ) ;
#32591 = CARTESIAN_POINT ( 'NONE',  ( 3.211159895383560947, 7.187499998634407028, 3.211159895383562723 ) ) ;
#32592 = CARTESIAN_POINT ( 'NONE',  ( -6.000000000000001776, 290.0000000000000000, 0.000000000000000000 ) ) ;
#32593 = CARTESIAN_POINT ( 'NONE',  ( 2.977408999572646486, 7.188101187499991163, 25.01780278187175455 ) ) ;
#32594 = ORIENTED_EDGE ( 'NONE', *, *, #18926, .F. ) ;
#32595 = CARTESIAN_POINT ( 'NONE',  ( 0.000000000000000000, 300.0000000000000000, 10.00000000000000178 ) ) ;
#32596 = ORIENTED_EDGE ( 'NONE', *, *, #58655, .T. ) ;
#32597 = CARTESIAN_POINT ( 'NONE',  ( -2.679491924311234285, 3.541666666666664742, 9.999999999999996447 ) ) ;
#32598 = CARTESIAN_POINT ( 'NONE',  ( -4.999999999999952927, -68.60357193678709109, 20.85024232999324667 ) ) ;
#32599 = CARTESIAN_POINT ( 'NONE',  ( -3.458734124999959914, 205.4375000013656063, 198.0000000000000284 ) ) ;
#32600 = CARTESIAN_POINT ( 'NONE',  ( 31.45873412499997812, 198.7500000013656063, 168.5673454167822172 ) ) ;
#32601 = CARTESIAN_POINT ( 'NONE',  ( 10.00000000000000178, 70.20833333333331439, -2.679491924311226736 ) ) ;
#32602 = CARTESIAN_POINT ( 'NONE',  ( 7.188101187500000044, 92.28125000204836681, -8.802885111219163269E-16 ) ) ;
#32603 = CARTESIAN_POINT ( 'NONE',  ( -2.485281374238572649, 293.1875000000000000, 6.000000000000002665 ) ) ;
#32604 = CARTESIAN_POINT ( 'NONE',  ( 30.87580095862601226, 177.9909331892631315, 173.1707643607214209 ) ) ;
#32605 = CIRCLE ( 'NONE', #7290, 8.000000000000003553 ) ;
#32606 = VERTEX_POINT ( 'NONE', #64970 ) ;
#32607 = CARTESIAN_POINT ( 'NONE',  ( -4.898587196589412829E-16, 94.62499999999998579, -8.000000000000000000 ) ) ;
#32608 = EDGE_CURVE ( 'NONE', #8159, #21431, #37429, .T. ) ;
#32609 = DIRECTION ( 'NONE',  ( 0.000000000000000000, 0.000000000000000000, -1.000000000000000000 ) ) ;
#32610 = CARTESIAN_POINT ( 'NONE',  ( 3.999999999999959144, 199.1875000027312694, 140.3431457505076594 ) ) ;
#32611 = DIRECTION ( 'NONE',  ( -0.000000000000000000, -1.000000000000000000, -0.000000000000000000 ) ) ;
#32612 = LINE ( 'NONE', #37889, #35275 ) ;
#32613 = CARTESIAN_POINT ( 'NONE',  ( -2.679491924311228512, 253.9583333333333428, -9.999999999999998224 ) ) ;
#32614 = CYLINDRICAL_SURFACE ( 'NONE', #70419, 10.00000000000000178 ) ;
#32615 = CARTESIAN_POINT ( 'NONE',  ( -7.320508075688773708, 191.8750000000000284, -7.320508075688774596 ) ) ;
#32616 = CARTESIAN_POINT ( 'NONE',  ( 0.000000000000000000, 300.0000000000000000, 10.00000000000000178 ) ) ;
#32617 = CARTESIAN_POINT ( 'NONE',  ( 7.188101187499992051, 8.802885111219154394E-16, 23.61155278187175455 ) ) ;
#32618 = CARTESIAN_POINT ( 'NONE',  ( -3.042071309553173730, 149.6354166632526983, 11.35316468749999785 ) ) ;
#32619 = CARTESIAN_POINT ( 'NONE',  ( -1.836970198721029983E-15, 38.75000000000000000, 10.00000000000000178 ) ) ;
#32620 = FACE_OUTER_BOUND ( 'NONE', #65666, .T. ) ;
#32621 = CARTESIAN_POINT ( 'NONE',  ( 8.660254037844541841, 154.5833333333334565, 5.000000000000096811 ) ) ;
#32623 = CARTESIAN_POINT ( 'NONE',  ( 0.000000000000000000, 0.000000000000000000, 118.0000000000000000 ) ) ;
#32622 = CARTESIAN_POINT ( 'NONE',  ( -10.00000000000000000, 84.16666665983869677, -2.679491924311229845 ) ) ;
#32624 = ORIENTED_EDGE ( 'NONE', *, *, #1429, .F. ) ;
#32625 = CARTESIAN_POINT ( 'NONE',  ( -9.832129032723418760, 18.17708332991935194, -5.676582343750004256 ) ) ;
#32626 = FACE_OUTER_BOUND ( 'NONE', #41770, .T. ) ;
#32628 = CARTESIAN_POINT ( 'NONE',  ( 10.00000000000000178, 31.87499999317203248, 0.000000000000000000 ) ) ;
#32627 = CARTESIAN_POINT ( 'NONE',  ( 0.000000000000000000, 125.0000000000000000, 0.000000000000000000 ) ) ;
#32629 = CARTESIAN_POINT ( 'NONE',  ( -1.656854249492212938, 195.9375000027312126, 193.9999999999999432 ) ) ;
#32630 = CARTESIAN_POINT ( 'NONE',  ( 2.445694354108782775, 202.5625000013656063, 139.5543056458912190 ) ) ;
#32631 = CIRCLE ( 'NONE', #119, 36.00000000000000000 ) ;
#32632 = CARTESIAN_POINT ( 'NONE',  ( 6.123233995736767268E-16, 43.12499999317203248, -10.00000000000000178 ) ) ;
#32633 = CARTESIAN_POINT ( 'NONE',  ( -7.188101187499999156, 107.7500000020483810, 2.977408999572654924 ) ) ;
#32634 = CARTESIAN_POINT ( 'NONE',  ( 4.541265875000002339, 8.437499998634407916, 0.000000000000000000 ) ) ;
#32635 = CARTESIAN_POINT ( 'NONE',  ( 2.775557561562891351E-14, 210.0000000000000284, 202.0000000000000000 ) ) ;
#32636 = CARTESIAN_POINT ( 'NONE',  ( -5.656854249492373476, -5.656854249492376141, 10.01780277982336465 ) ) ;
#32638 = CARTESIAN_POINT ( 'NONE',  ( 7.999999999999992895, 6.888416461457931717E-06, 21.26780297880423021 ) ) ;
#32637 = DIRECTION ( 'NONE',  ( -0.000000000000000000, 1.000000000000000000, -0.000000000000000000 ) ) ;
#32639 = ORIENTED_EDGE ( 'NONE', *, *, #73288, .T. ) ;
#32640 = VERTEX_POINT ( 'NONE', #13648 ) ;
#32641 = CARTESIAN_POINT ( 'NONE',  ( -5.000000000000000888, -68.32828612846157057, 21.58087353894127247 ) ) ;
#32642 = CARTESIAN_POINT ( 'NONE',  ( 3.458734125000015425, 196.2500000013656347, 196.5673454167823877 ) ) ;
#32643 = CARTESIAN_POINT ( 'NONE',  ( 5.656854249492374365, 5.656854249492375253, 13.95530278392014623 ) ) ;
#32644 = CARTESIAN_POINT ( 'NONE',  ( -8.000000000000000000, 99.40625000000000000, -3.313708498984761164 ) ) ;
#32645 = CARTESIAN_POINT ( 'NONE',  ( 3.042071309553159519, 124.7395833299193555, 11.35316468750000141 ) ) ;
#32646 = ORIENTED_EDGE ( 'NONE', *, *, #55574, .F. ) ;
#32647 = CARTESIAN_POINT ( 'NONE',  ( -6.000000000000003553, 297.9375000000000000, -2.485281374238571317 ) ) ;
#32648 = CARTESIAN_POINT ( 'NONE',  ( 10.18810118749999916, 1.247682550866122264E-15, 90.90625000204836681 ) ) ;
#32649 = PLANE ( 'NONE',  #50133 ) ;
#32650 = CARTESIAN_POINT ( 'NONE',  ( 2.849036369511732440E-14, 209.2500000000000284, 202.0000000000000000 ) ) ;
#32652 = CARTESIAN_POINT ( 'NONE',  ( -11.35316468750000141, 128.4895833299193555, 3.042071309553159963 ) ) ;
#32651 = CARTESIAN_POINT ( 'NONE',  ( 0.000000000000000000, 125.0000000000000000, 8.000000000000000000 ) ) ;
#32653 = AXIS2_PLACEMENT_3D ( 'NONE', #52020, #11651, #5628 ) ;
#32654 = DIRECTION ( 'NONE',  ( -0.8660254037844379305, 0.5000000000000014433, 0.000000000000000000 ) ) ;
#32655 = ORIENTED_EDGE ( 'NONE', *, *, #52267, .F. ) ;
#32656 = CARTESIAN_POINT ( 'NONE',  ( -11.00000000000000000, 4.556349186104045934, 77.40624999999998579 ) ) ;
#32657 = CARTESIAN_POINT ( 'NONE',  ( 47.41040786394009388, 38.98978874648344828, 65.18845003359885482 ) ) ;
#32658 = CARTESIAN_POINT ( 'NONE',  ( -5.676582343750006032, 119.4270833299193555, 9.832129032723418760 ) ) ;
#32659 = CARTESIAN_POINT ( 'NONE',  ( -2.445694354108782775, 207.5625000013656063, 200.4456943541088663 ) ) ;
#32660 = CARTESIAN_POINT ( 'NONE',  ( 5.082755093536325930, 16.03124999795161543, -5.082755093536325930 ) ) ;
#32661 =( BOUNDED_CURVE ( )  B_SPLINE_CURVE ( 2, ( #22411, #63905, #39774, #17130, #62777, #11486, #33771, #73737, #50722 ),
 .UNSPECIFIED., .F., .F. ) 
 B_SPLINE_CURVE_WITH_KNOTS ( ( 3, 2, 2, 2, 3 ),
 ( 0.6562500000000000000, 0.6614583333333333703, 0.6666666666666667407, 0.6718750000000001110, 0.6770833333333334814 ),
 .UNSPECIFIED. ) 
 CURVE ( )  GEOMETRIC_REPRESENTATION_ITEM ( )  RATIONAL_B_SPLINE_CURVE ( ( 1.000000000000000000, 0.9238795325112867385, 1.000000000000000000, 0.9238795325112867385, 1.000000000000000000, 0.9238795325112867385, 1.000000000000000000, 0.9238795325112850731, 1.000000000000001554 ) ) 
 REPRESENTATION_ITEM ( '' )  );
#32662 = CARTESIAN_POINT ( 'NONE',  ( 4.220049686691934809, 10.18810118749999916, 84.06250000204838102 ) ) ;
#32663 = CARTESIAN_POINT ( 'NONE',  ( 5.676582343750001591, 16.92708332991935194, -9.832129032723420536 ) ) ;
#32664 = EDGE_LOOP ( 'NONE', ( #40320, #40590, #15079, #71074 ) ) ;
#32665 = CARTESIAN_POINT ( 'NONE',  ( -2.828427124746192067, 4.625000000000000000, 2.828427124746190735 ) ) ;
#32666 = CARTESIAN_POINT ( 'NONE',  ( 8.008118988124991233, 9.807117285998411148E-16, 22.76311528394063188 ) ) ;
#32667 = CARTESIAN_POINT ( 'NONE',  ( 7.320508075688771044, 238.1249999999999716, -7.320508075688771932 ) ) ;
#32668 = CARTESIAN_POINT ( 'NONE',  ( -4.000000000000001776, 7.500000000000000000, -4.898587196589415787E-16 ) ) ;
#32669 = CARTESIAN_POINT ( 'NONE',  ( -7.188101187500001821, 4.124999997951610986, -2.977408999572651371 ) ) ;
#32670 = CARTESIAN_POINT ( 'NONE',  ( -6.676582343750000703, 290.5156250017070079, 2.765530957082001251 ) ) ;
#32671 = CARTESIAN_POINT ( 'NONE',  ( 2.679491924311228956, 112.9166666598387110, -10.00000000000000000 ) ) ;
#32672 = CARTESIAN_POINT ( 'NONE',  ( 0.000000000000000000, 0.000000000000000000, -14.77459999999999951 ) ) ;
#32673 = EDGE_CURVE ( 'NONE', #34420, #21248, #71363, .T. ) ;
#32674 = VERTEX_POINT ( 'NONE', #19317 ) ;
#32675 = CARTESIAN_POINT ( 'NONE',  ( -5.676582343749998039, 147.7604166632526699, -9.832129032723420536 ) ) ;
#32676 = CARTESIAN_POINT ( 'NONE',  ( 10.18810118749999916, 4.220049686691935698, 74.50000000204838102 ) ) ;
#32677 = CARTESIAN_POINT ( 'NONE',  ( -27.99999999999996092, 194.9375000013655779, 173.4587341250003760 ) ) ;
#32678 = EDGE_CURVE ( 'NONE', #20933, #19911, #48357, .T. ) ;
#32679 =( BOUNDED_CURVE ( )  B_SPLINE_CURVE ( 2, ( #49125, #26869, #20833, #4247, #31789, #44976, #73273, #44233, #3873, #61204, #37829, #67244, #49883 ),
 .UNSPECIFIED., .F., .F. ) 
 B_SPLINE_CURVE_WITH_KNOTS ( ( 3, 2, 2, 2, 2, 2, 3 ),
 ( 1.805491404681675016, 1.810723803553510036, 1.815956202425345056, 1.821188601297179854, 1.826421000169014874, 1.831653399040849894, 1.836885797912684914 ),
 .UNSPECIFIED. ) 
 CURVE ( )  GEOMETRIC_REPRESENTATION_ITEM ( )  RATIONAL_B_SPLINE_CURVE ( ( 1.000000000000000000, 0.9659258262890683122, 1.000000000000000000, 0.9659258262890683122, 1.000000000000000000, 0.9659258262890683122, 1.000000000000000000, 0.9659258262890683122, 1.000000000000000000, 0.9659258262890683122, 1.000000000000000000, 0.9659258262891664559, 0.9999999999999018563 ) ) 
 REPRESENTATION_ITEM ( '' )  );
#32680 = CARTESIAN_POINT ( 'NONE',  ( -11.00000000000000000, 0.000000000000000000, 110.4999999999999858 ) ) ;
#32681 = CARTESIAN_POINT ( 'NONE',  ( -8.342170076843785083E-16, 15.18749999863440792, 4.541265875000002339 ) ) ;
#32682 = ORIENTED_EDGE ( 'NONE', *, *, #6344, .F. ) ;
#32683 = CARTESIAN_POINT ( 'NONE',  ( 2.751064625579944321E-14, 201.8750000027312126, 194.0000000000000568 ) ) ;
#32684 = CARTESIAN_POINT ( 'NONE',  ( -2.849036369511732440E-14, 209.2500000000000284, 138.0000000000000568 ) ) ;
#32685 = CARTESIAN_POINT ( 'NONE',  ( -32.00000000000000000, 205.3750000027312126, 170.0000000000004547 ) ) ;
#32686 = DIRECTION ( 'NONE',  ( 0.000000000000000000, 0.02418647091589873691, 0.9997074645238147594 ) ) ;
#32687 = ORIENTED_EDGE ( 'NONE', *, *, #14412, .F. ) ;
#32688 = CARTESIAN_POINT ( 'NONE',  ( 2.977408999572650927, 9.749999997951610098, -7.188101187500000933 ) ) ;
#32689 = CARTESIAN_POINT ( 'NONE',  ( -7.778174593052020747, -7.778174593052023411, 76.18749999999998579 ) ) ;
#32690 = CARTESIAN_POINT ( 'NONE',  ( 2.020667218593132706E-15, -11.00000000000000000, 73.56250000409676204 ) ) ;
#32691 = CARTESIAN_POINT ( 'NONE',  ( 11.35316468749999963, 180.9895833299193555, -3.042071309553165293 ) ) ;
#32692 = CARTESIAN_POINT ( 'NONE',  ( -7.188101187500001821, 109.4375000020483810, -2.977408999572650483 ) ) ;
#32693 = AXIS2_PLACEMENT_3D ( 'NONE', #41986, #7670, #63896 ) ;
#32694 = CARTESIAN_POINT ( 'NONE',  ( 10.99999999999999467, 11.00000000000000355, 41.99999999999999289 ) ) ;
#32695 = CARTESIAN_POINT ( 'NONE',  ( 1.226468279477575784E-15, 288.7031250017069510, 6.676582343750001591 ) ) ;
#32697 = CARTESIAN_POINT ( 'NONE',  ( 0.000000000000000000, 101.0525588832578734, 10.99999999999998934 ) ) ;
#32696 = CARTESIAN_POINT ( 'NONE',  ( -11.35316468749999963, 218.9062500034139873, 0.000000000000000000 ) ) ;
#32698 = ORIENTED_EDGE ( 'NONE', *, *, #63063, .F. ) ;
#32699 = CARTESIAN_POINT ( 'NONE',  ( -3.042071309553159075, 254.9479166700806729, 11.35316468749999963 ) ) ;
#32700 = CARTESIAN_POINT ( 'NONE',  ( 2.977408999572650927, -7.188101187499990274, 21.83030278187175810 ) ) ;
#32701 = CIRCLE ( 'NONE', #62780, 37.00000000000000711 ) ;
#32702 = CARTESIAN_POINT ( 'NONE',  ( 5.656854249492378806, 19.12499999590322020, 5.656854249492381470 ) ) ;
#32703 = CARTESIAN_POINT ( 'NONE',  ( 0.8997857291013038328, -67.61674724335156839, -20.05382624916256518 ) ) ;
#32704 = CARTESIAN_POINT ( 'NONE',  ( -10.00000000000000000, 139.1666666598387110, -2.679491924311229845 ) ) ;
#32705 = CYLINDRICAL_SURFACE ( 'NONE', #40162, 6.000000000000001776 ) ;
#32706 = CARTESIAN_POINT ( 'NONE',  ( 2.020667218593132706E-15, 219.9523502760175973, 11.00000000000000000 ) ) ;
#32707 = CARTESIAN_POINT ( 'NONE',  ( -4.898587196589412829E-16, 93.12499999999998579, -8.000000000000000000 ) ) ;
#32708 = CARTESIAN_POINT ( 'NONE',  ( -3.042071309553164404, 117.5520833299193413, -11.35316468749999963 ) ) ;
#32709 = CARTESIAN_POINT ( 'NONE',  ( -2.485281374238197394, 296.1875000000000000, 6.000000000000376588 ) ) ;
#32710 = CARTESIAN_POINT ( 'NONE',  ( 7.778174593052021635, 7.778174593052023411, 72.43749999999998579 ) ) ;
#32711 = VECTOR ( 'NONE', #29181, 999.9999999999998863 ) ;
#32714 = CARTESIAN_POINT ( 'NONE',  ( 8.000000000000000000, 118.4375000040967763, -9.797174393178825657E-16 ) ) ;
#32713 = CARTESIAN_POINT ( 'NONE',  ( 31.45873412499999233, 199.6875000013656063, 169.9999999999998863 ) ) ;
#32712 = CARTESIAN_POINT ( 'NONE',  ( 29.43265458321766204, 197.1250000013656347, 166.5412658749999650 ) ) ;
#32715 = VERTEX_POINT ( 'NONE', #26083 ) ;
#32716 = CARTESIAN_POINT ( 'NONE',  ( 9.692727098607901937, 225.2031118130280731, -2.530001495371571707 ) ) ;
#32717 = CARTESIAN_POINT ( 'NONE',  ( -7.778174593052020747, -7.778174593052023411, 113.8750000040967763 ) ) ;
#32718 = CARTESIAN_POINT ( 'NONE',  ( -2.445694354108838731, 196.0625000013656063, 144.4456943541088663 ) ) ;
#32719 = CARTESIAN_POINT ( 'NONE',  ( 31.45873412499999233, 198.9375000013655779, 169.9999999999999432 ) ) ;
#32720 = CARTESIAN_POINT ( 'NONE',  ( -11.35316468750000141, 213.5937499965860411, -1.390361679473963753E-15 ) ) ;
#32721 = DIRECTION ( 'NONE',  ( -1.000000000000000000, -0.000000000000000000, -0.000000000000000000 ) ) ;
#32722 = CARTESIAN_POINT ( 'NONE',  ( 5.355978476798539667, 225.9999999999999716, 8.594851559336273539 ) ) ;
#32723 = CARTESIAN_POINT ( 'NONE',  ( -1.881053915767124440, 16.99999999863440792, 4.541265875000001451 ) ) ;
#32724 = CARTESIAN_POINT ( 'NONE',  ( 6.298842414714818538, -51.07418104650420787, 41.32239042994850564 ) ) ;
#32725 = CARTESIAN_POINT ( 'NONE',  ( 5.656854249492374365, 5.656854249492375253, 25.76780277982336997 ) ) ;
#32727 = DIRECTION ( 'NONE',  ( 0.000000000000000000, -0.4789076340208496818, 0.8778652960885012790 ) ) ;
#32726 = CARTESIAN_POINT ( 'NONE',  ( -5.447323953993864265, -4.689931814214729044, 0.5319290643893268555 ) ) ;
#32728 = CARTESIAN_POINT ( 'NONE',  ( 6.951808397369818766E-16, 97.03124999658602690, -11.35316468750000141 ) ) ;
#32729 = ORIENTED_EDGE ( 'NONE', *, *, #20482, .T. ) ;
#32730 = CARTESIAN_POINT ( 'NONE',  ( 28.00000000000002132, 205.1250000027312126, 173.9999999999999147 ) ) ;
#32731 = CARTESIAN_POINT ( 'NONE',  ( 7.188101187500001821, 20.06249999795161543, -2.977408999572650483 ) ) ;
#32732 = CARTESIAN_POINT ( 'NONE',  ( -4.999999999999992895, 223.9583333401612890, 8.660254037844390851 ) ) ;
#32733 = CARTESIAN_POINT ( 'NONE',  ( -3.042071309553166625, 258.1770833367473301, -11.35316468749999608 ) ) ;
#32734 = CARTESIAN_POINT ( 'NONE',  ( -11.35316468750000141, 93.28124999658602690, -1.390361679473963753E-15 ) ) ;
#32735 = ORIENTED_EDGE ( 'NONE', *, *, #48044, .F. ) ;
#32736 = CARTESIAN_POINT ( 'NONE',  ( 1.871523826299183495E-15, -10.18810118749999916, 107.0312500020483810 ) ) ;
#32737 = CARTESIAN_POINT ( 'NONE',  ( -27.99999999999996092, 196.1875000013655779, 173.4587341250003760 ) ) ;
#32738 = CARTESIAN_POINT ( 'NONE',  ( -3.458734124999960358, 204.6250000013655779, 196.5673454167823877 ) ) ;
#32739 = CARTESIAN_POINT ( 'NONE',  ( -5.656854249492373476, -5.656854249492376141, 11.51780277982336642 ) ) ;
#32741 = CARTESIAN_POINT ( 'NONE',  ( -8.311093377946841443, 88.90624999658602690, 8.311093377946834337 ) ) ;
#32740 = CARTESIAN_POINT ( 'NONE',  ( -4.231687259407060253, 68.27410168872913232, 20.58597903916736627 ) ) ;
#32742 = CARTESIAN_POINT ( 'NONE',  ( 7.999999999999992895, -3.313708498984756279, 21.17405278392015333 ) ) ;
#32743 = CARTESIAN_POINT ( 'NONE',  ( -24.54126587499999346, 200.4375000013656063, 170.0000000000003411 ) ) ;
#32744 = CYLINDRICAL_SURFACE ( 'NONE', #66160, 7.999999999999991118 ) ;
#32745 = EDGE_CURVE ( 'NONE', #11774, #22621, #43117, .T. ) ;
#32746 = EDGE_CURVE ( 'NONE', #72571, #5227, #52904, .T. ) ;
#32747 = CARTESIAN_POINT ( 'NONE',  ( 4.999999999999993783, 186.0416666598387110, 8.660254037844390851 ) ) ;
#32748 = CARTESIAN_POINT ( 'NONE',  ( 13.99999999999999822, 0.000000000000000000, -8.000000000000000000 ) ) ;
#32749 = CARTESIAN_POINT ( 'NONE',  ( -8.311093377946841443, 74.21874999658602690, 8.311093377946834337 ) ) ;
#32750 = CARTESIAN_POINT ( 'NONE',  ( 6.676582343750003368, 295.0156250017069510, -2.765530957081997254 ) ) ;
#32751 = CARTESIAN_POINT ( 'NONE',  ( -6.238412754330611322E-16, 10.18810118749999916, 102.1562500020483810 ) ) ;
#32752 = CARTESIAN_POINT ( 'NONE',  ( -8.311093377946841443, 203.9062499965859843, 8.311093377946830785 ) ) ;
#32753 = ORIENTED_EDGE ( 'NONE', *, *, #66444, .F. ) ;
#32754 = CARTESIAN_POINT ( 'NONE',  ( 38.00000000000000000, -53.00000000000000711, 9.999999999999991118 ) ) ;
#32755 = CARTESIAN_POINT ( 'NONE',  ( 0.4320110153365262495, -60.19564456717412071, -22.88238106212127576 ) ) ;
#32756 = CARTESIAN_POINT ( 'NONE',  ( 6.000000000000003553, 291.5625000000000000, -2.485281374238571761 ) ) ;
#32758 = CARTESIAN_POINT ( 'NONE',  ( -5.676582343750006032, 209.1145833299193555, 9.832129032723418760 ) ) ;
#32757 = LINE ( 'NONE', #66692, #37502 ) ;
#32759 = CARTESIAN_POINT ( 'NONE',  ( 1.836970198721029589E-15, 219.3750000068279746, 10.00000000000000000 ) ) ;
#32760 = CARTESIAN_POINT ( 'NONE',  ( -4.999999999999992895, 253.9583333401613174, 8.660254037844390851 ) ) ;
#32761 = VERTEX_POINT ( 'NONE', #14769 ) ;
#32762 = CARTESIAN_POINT ( 'NONE',  ( 8.311093377946837890, 196.7187499965860127, -8.311093377946837890 ) ) ;
#32763 = AXIS2_PLACEMENT_3D ( 'NONE', #10299, #4272, #17060 ) ;
#32764 = CARTESIAN_POINT ( 'NONE',  ( -5.082755093536317936, -5.082755093536320601, 12.17405278187175277 ) ) ;
#32765 = CARTESIAN_POINT ( 'NONE',  ( 0.8419854211626177642, 60.19512794652395371, -22.88206588978716383 ) ) ;
#32766 = CARTESIAN_POINT ( 'NONE',  ( 8.000000000000000000, 10.59375000000000178, -3.313708498984761608 ) ) ;
#32767 = ORIENTED_EDGE ( 'NONE', *, *, #8700, .T. ) ;
#32768 = CARTESIAN_POINT ( 'NONE',  ( 1.469576158976823947E-15, 92.56250000409677625, 8.000000000000000000 ) ) ;
#32769 =( BOUNDED_CURVE ( )  B_SPLINE_CURVE ( 2, ( #31667, #3368, #43341, #66360, #32039, #14664, #37705, #25613, #60706 ),
 .UNSPECIFIED., .F., .F. ) 
 B_SPLINE_CURVE_WITH_KNOTS ( ( 3, 2, 2, 2, 3 ),
 ( 0.7166666666666671182, 0.7250000000000005329, 0.7333333333333338366, 0.7416666666666673624, 0.7500000000000006661 ),
 .UNSPECIFIED. ) 
 CURVE ( )  GEOMETRIC_REPRESENTATION_ITEM ( )  RATIONAL_B_SPLINE_CURVE ( ( 0.9999999999999958922, 0.9238795325112908463, 1.000000000000000000, 0.9238795325112867385, 1.000000000000000000, 0.9238795325112867385, 1.000000000000000000, 0.9238795325112806323, 1.000000000000005995 ) ) 
 REPRESENTATION_ITEM ( '' )  );
#32770 = CARTESIAN_POINT ( 'NONE',  ( 6.123233995736767268E-16, 16.25000000000000000, -10.00000000000000178 ) ) ;
#32771 = CARTESIAN_POINT ( 'NONE',  ( -10.18810118749999916, 0.000000000000000000, 78.53125000204836681 ) ) ;
#32772 = EDGE_LOOP ( 'NONE', ( #70808, #74232, #13461 ) ) ;
#32773 = CARTESIAN_POINT ( 'NONE',  ( 2.828427124746191623, 21.12500000000000000, -2.828427124746191623 ) ) ;
#32774 = CARTESIAN_POINT ( 'NONE',  ( -1.881053915767124440, 18.99999999863440436, 4.541265875000001451 ) ) ;
#32775 = CARTESIAN_POINT ( 'NONE',  ( 1.469576158976822172E-15, -7.999999999999991118, 10.39280278392014800 ) ) ;
#32776 = CARTESIAN_POINT ( 'NONE',  ( 31.03434905890983231, 194.6645454233662065, 167.9330682077203960 ) ) ;
#32777 = AXIS2_PLACEMENT_3D ( 'NONE', #52301, #10815, #51173 ) ;
#32778 = ORIENTED_EDGE ( 'NONE', *, *, #28214, .T. ) ;
#32779 =( LENGTH_UNIT ( ) NAMED_UNIT ( * ) SI_UNIT ( .MILLI., .METRE. ) );
#32780 = CARTESIAN_POINT ( 'NONE',  ( -2.977408999572650927, 93.87500000204836681, -7.188101187500001821 ) ) ;
#32783 = CARTESIAN_POINT ( 'NONE',  ( 2.828427124746209831, 197.3750000000000284, 200.8284271247462129 ) ) ;
#32782 = CARTESIAN_POINT ( 'NONE',  ( -11.35316468749999608, 254.1145833367473585, 3.042071309553173730 ) ) ;
#32781 = CARTESIAN_POINT ( 'NONE',  ( -1.836970198721029983E-15, 83.75000000000000000, 10.00000000000000178 ) ) ;
#32784 = CARTESIAN_POINT ( 'NONE',  ( 1424.688200795887951, 892.2677537767814329, 997.8421604560580818 ) ) ;
#32785 = ORIENTED_EDGE ( 'NONE', *, *, #65085, .F. ) ;
#32786 = CARTESIAN_POINT ( 'NONE',  ( -5.676582343750000703, 253.3854166700806445, -9.832129032723418760 ) ) ;
#32787 = CARTESIAN_POINT ( 'NONE',  ( -7.188101187499992051, 0.000000000000000000, 10.48655278187175455 ) ) ;
#32788 = ORIENTED_EDGE ( 'NONE', *, *, #17317, .T. ) ;
#32789 = ORIENTED_EDGE ( 'NONE', *, *, #72053, .T. ) ;
#32790 = CARTESIAN_POINT ( 'NONE',  ( -10.18810118749999916, 0.000000000000000000, 76.65625000204836681 ) ) ;
#32791 = CARTESIAN_POINT ( 'NONE',  ( 9.832129032723420536, 76.51041666325268409, -5.676582343749999815 ) ) ;
#32792 = CARTESIAN_POINT ( 'NONE',  ( -3.313708498984762496, 105.9687500040967620, 7.999999999999998224 ) ) ;
#32793 = CARTESIAN_POINT ( 'NONE',  ( 4.556349186104045934, 11.00000000000000000, 92.03124999999998579 ) ) ;
#32796 = CARTESIAN_POINT ( 'NONE',  ( -2.765530957081996810, 291.4218750017069510, -6.676582343750002480 ) ) ;
#32795 = CARTESIAN_POINT ( 'NONE',  ( 23.99999999999997513, 196.8125000027311842, 168.3431457505075741 ) ) ;
#32794 = CARTESIAN_POINT ( 'NONE',  ( 7.999999999971009856, 2.153409470846384379E-05, 12.26780339315719814 ) ) ;
#32797 = CARTESIAN_POINT ( 'NONE',  ( -49.56159862150887108, 197.7137834522780793, 58.21195810585798114 ) ) ;
#32798 = CARTESIAN_POINT ( 'NONE',  ( -1.656854249492246467, 199.8125000000000284, 193.9999999999999716 ) ) ;
#32799 = CARTESIAN_POINT ( 'NONE',  ( -1.432654583217607414, 197.5000000013656063, 194.5412658750000219 ) ) ;
#32800 = CARTESIAN_POINT ( 'NONE',  ( 3.313708498984762496, 7.031249995903221084, 7.999999999999998224 ) ) ;
#32801 = EDGE_LOOP ( 'NONE', ( #12285, #60964, #35423, #61432 ) ) ;
#32802 = CARTESIAN_POINT ( 'NONE',  ( 25.55430564589114795, 195.3125000013656063, 172.4456943541086957 ) ) ;
#32803 = EDGE_CURVE ( 'NONE', #34844, #19664, #9128, .T. ) ;
#32804 = CARTESIAN_POINT ( 'NONE',  ( -5.082755093536326818, 18.28124999795161187, 5.082755093536325042 ) ) ;
#32805 = VECTOR ( 'NONE', #31836, 1000.000000000000000 ) ;
#32806 = CARTESIAN_POINT ( 'NONE',  ( -9.832129032723420536, 174.0104166632526983, 5.676582343749997150 ) ) ;
#32807 = PLANE ( 'NONE',  #8224 ) ;
#32808 = CARTESIAN_POINT ( 'NONE',  ( 2.977408999572654480, 102.5000000020483810, 7.188101187499999156 ) ) ;
#32810 = CARTESIAN_POINT ( 'NONE',  ( 1.836970198721029589E-15, 236.2500000000000284, 10.00000000000000000 ) ) ;
#32809 = CARTESIAN_POINT ( 'NONE',  ( 1.102182119232618108E-15, 289.3125000034140157, 6.000000000000001776 ) ) ;
#32811 = CARTESIAN_POINT ( 'NONE',  ( 31.45873412499998523, 205.8750000013656063, 171.4326545832176123 ) ) ;
#32812 = CARTESIAN_POINT ( 'NONE',  ( 7.188101187499992051, 8.802885111219154394E-16, 13.11155278187175277 ) ) ;
#32813 = CARTESIAN_POINT ( 'NONE',  ( -4.000000000000015987, 207.6250000027312126, 142.0000000000000568 ) ) ;
#32814 = CARTESIAN_POINT ( 'NONE',  ( -2.085542519210945728E-15, 54.53124999658602690, 11.35316468750000141 ) ) ;
#32815 = CARTESIAN_POINT ( 'NONE',  ( 8.000000000000000000, 21.09375000000000355, -3.313708498984761164 ) ) ;
#32816 = CARTESIAN_POINT ( 'NONE',  ( 7.320508075688771044, 26.24999999317203603, 7.320508075688775484 ) ) ;
#32817 = CARTESIAN_POINT ( 'NONE',  ( 28.00000000000001776, 199.5000000000000000, 165.9999999999998863 ) ) ;
#32818 = ORIENTED_EDGE ( 'NONE', *, *, #21217, .F. ) ;
#32819 = CARTESIAN_POINT ( 'NONE',  ( 3.999999999999960032, 199.1250000027312126, 142.0000000000000568 ) ) ;
#32820 = CARTESIAN_POINT ( 'NONE',  ( -3.313708498984719864, 19.78124999590321664, -8.000000000000040856 ) ) ;
#32821 = CARTESIAN_POINT ( 'NONE',  ( -5.676582343749998039, 47.44791666325268409, -9.832129032723420536 ) ) ;
#32822 = CARTESIAN_POINT ( 'NONE',  ( 11.00000000000000355, -4.556349186104045046, 82.84375000409676204 ) ) ;
#32823 = CARTESIAN_POINT ( 'NONE',  ( -3.458734125000015869, 201.1875000013656063, 142.0000000000000568 ) ) ;
#32824 = CARTESIAN_POINT ( 'NONE',  ( 2.591411123065536781, 10.27614846265000637, 63.77676950207272455 ) ) ;
#32825 = CARTESIAN_POINT ( 'NONE',  ( 1.836970198721029589E-15, 246.2500000000000284, 10.00000000000000000 ) ) ;
#32827 = CARTESIAN_POINT ( 'NONE',  ( 11.35316468749999963, 40.98958332991934839, -3.042071309553165293 ) ) ;
#32826 = CARTESIAN_POINT ( 'NONE',  ( -4.401442555609581635E-16, 101.2812500020483810, -7.188101187500000044 ) ) ;
#32828 = CARTESIAN_POINT ( 'NONE',  ( 7.999999999999992895, -3.313708498984756279, 7.486552779823366421 ) ) ;
#32829 = CARTESIAN_POINT ( 'NONE',  ( 2.449293598294707893E-16, 17.99999999726881583, -4.000000000000001776 ) ) ;
#32830 = CARTESIAN_POINT ( 'NONE',  ( -9.832129032723418760, 167.8645833299193555, -5.676582343750004256 ) ) ;
#32831 = CARTESIAN_POINT ( 'NONE',  ( -1.836970198721029983E-15, 140.6249999931720538, 10.00000000000000178 ) ) ;
#32832 = VECTOR ( 'NONE', #42920, 999.9999999999998863 ) ;
#32833 = CARTESIAN_POINT ( 'NONE',  ( 7.188101187500001821, 102.8750000020483810, -2.977408999572651371 ) ) ;
#32834 = DIRECTION ( 'NONE',  ( -0.000000000000000000, 1.000000000000000000, -0.000000000000000000 ) ) ;
#32835 = CARTESIAN_POINT ( 'NONE',  ( -2.085542519210945728E-15, 39.84374999658601979, 11.35316468750000141 ) ) ;
#32836 = CARTESIAN_POINT ( 'NONE',  ( -7.204075437095967871, 7.204075437095967871, 117.3437500020483810 ) ) ;
#32837 = ORIENTED_EDGE ( 'NONE', *, *, #51131, .T. ) ;
#32838 = CARTESIAN_POINT ( 'NONE',  ( 49.04048506803781038, 139.8460563971956105, 59.50300479923077290 ) ) ;
#32839 = CARTESIAN_POINT ( 'NONE',  ( 4.220049686691941027, -10.18810118749999738, 77.12500000204838102 ) ) ;
#32840 = CARTESIAN_POINT ( 'NONE',  ( 7.999999999999998224, 16.40625000000000355, 3.313708498984766049 ) ) ;
#32842 = CARTESIAN_POINT ( 'NONE',  ( 11.35316468750000141, 170.7812499965860411, 0.000000000000000000 ) ) ;
#32841 = CYLINDRICAL_SURFACE ( 'NONE', #64177, 11.00000000000000000 ) ;
#32843 = CARTESIAN_POINT ( 'NONE',  ( -5.656854249492375253, 5.656854249492375253, 12.69905278432982421 ) ) ;
#32844 = AXIS2_PLACEMENT_3D ( 'NONE', #286, #57618, #56870 ) ;
#32845 = CARTESIAN_POINT ( 'NONE',  ( 5.656854249492376141, -5.656854249492374365, 16.39280277982336287 ) ) ;
#32846 = EDGE_CURVE ( 'NONE', #37372, #32761, #37481, .T. ) ;
#32847 = EDGE_CURVE ( 'NONE', #27119, #5538, #73252, .T. ) ;
#32848 = CARTESIAN_POINT ( 'NONE',  ( 9.832129032723416984, 226.8229166700806729, -5.676582343750003368 ) ) ;
#32849 = CARTESIAN_POINT ( 'NONE',  ( -2.266287154886474919, 50.05783744175423777, -40.76793781259114979 ) ) ;
#32850 = CARTESIAN_POINT ( 'NONE',  ( -7.204075437095967871, 7.204075437095967871, 84.34375000204836681 ) ) ;
#32851 = ORIENTED_EDGE ( 'NONE', *, *, #53996, .T. ) ;
#32852 = AXIS2_PLACEMENT_3D ( 'NONE', #16747, #24551, #7219 ) ;
#32853 = EDGE_CURVE ( 'NONE', #46305, #26674, #66845, .T. ) ;
#32854 = CARTESIAN_POINT ( 'NONE',  ( -7.778174593052020747, -7.778174593052023411, 89.87500000409677625 ) ) ;
#32855 = LINE ( 'NONE', #27917, #68869 ) ;
#32856 = CARTESIAN_POINT ( 'NONE',  ( 3.042071309553159519, 115.0520833299193555, 11.35316468750000141 ) ) ;
#32857 = CARTESIAN_POINT ( 'NONE',  ( -7.204075437095965206, -7.204075437095968759, 96.34375000204836681 ) ) ;
#32858 = CARTESIAN_POINT ( 'NONE',  ( 4.999999999999998224, 14.16666666666667318, 8.660254037844397956 ) ) ;
#32859 = EDGE_LOOP ( 'NONE', ( #51528, #69793, #20078, #7597 ) ) ;
#32860 = EDGE_LOOP ( 'NONE', ( #3731, #52577, #73770, #59425 ) ) ;
#32861 = CARTESIAN_POINT ( 'NONE',  ( -1.881053915767121554, 6.749999998634407916, -4.541265875000002339 ) ) ;
#32862 = CARTESIAN_POINT ( 'NONE',  ( -2.977408999572654480, 8.999999997951610098, 7.188101187499999156 ) ) ;
#32863 = ADVANCED_FACE ( 'NONE', ( #15519 ), #22293, .T. ) ;
#32864 = CARTESIAN_POINT ( 'NONE',  ( 8.000000000000000000, 111.0312500040967763, -3.313708498984762496 ) ) ;
#32865 = CARTESIAN_POINT ( 'NONE',  ( -4.220049686691937474, -10.18810118749999738, 92.31250000204838102 ) ) ;
#32866 = CARTESIAN_POINT ( 'NONE',  ( -27.99999999999996447, 201.1875000013656063, 173.4587341250003760 ) ) ;
#32867 = CARTESIAN_POINT ( 'NONE',  ( 1.656854249492381914, 5.812500000000000000, 4.000000000000000888 ) ) ;
#32868 = CARTESIAN_POINT ( 'NONE',  ( 4.000000000000001776, 17.74999999726881583, 0.000000000000000000 ) ) ;
#32869 = CARTESIAN_POINT ( 'NONE',  ( 4.541265875000002339, 8.312499998634407916, 0.000000000000000000 ) ) ;
#32870 = CARTESIAN_POINT ( 'NONE',  ( -4.000000000000015099, 202.5625000000000000, 143.6568542494924543 ) ) ;
#32871 = ORIENTED_EDGE ( 'NONE', *, *, #48982, .F. ) ;
#32872 = CARTESIAN_POINT ( 'NONE',  ( -7.999999999999991118, 0.000000000000000000, 28.01780278392014978 ) ) ;
#32874 = CARTESIAN_POINT ( 'NONE',  ( 7.999999999999991118, 9.797174393178815797E-16, 16.58030277982336287 ) ) ;
#32873 = CARTESIAN_POINT ( 'NONE',  ( -26.56734541678227757, 196.0000000013656347, 173.4587341250003476 ) ) ;
#32875 =( LENGTH_UNIT ( ) NAMED_UNIT ( * ) SI_UNIT ( .MILLI., .METRE. ) );
#32876 = CARTESIAN_POINT ( 'NONE',  ( -3.211159895383562723, 19.93749999863440436, 3.211159895383561391 ) ) ;
#32877 = VECTOR ( 'NONE', #49782, 999.9999999999998863 ) ;
#32878 = CARTESIAN_POINT ( 'NONE',  ( 7.320508075688774596, 72.49999999317203958, -7.320508075688774596 ) ) ;
#32879 = CARTESIAN_POINT ( 'NONE',  ( 2.977408999572646486, 7.188101187499991163, 1.017802781871753215 ) ) ;
#32880 = VERTEX_POINT ( 'NONE', #21557 ) ;
#32881 =( BOUNDED_CURVE ( )  B_SPLINE_CURVE ( 2, ( #43558, #31506, #66573, #39033, #68074, #46170, #34513, #16364, #57517, #11845, #62037, #67706, #51088 ),
 .UNSPECIFIED., .F., .F. ) 
 B_SPLINE_CURVE_WITH_KNOTS ( ( 3, 2, 2, 2, 2, 2, 3 ),
 ( 2.025290649010746513, 2.030523086516430098, 2.035755524022114127, 2.040987961527798156, 2.046220399033481741, 2.051452836539165325, 2.056685274044849354 ),
 .UNSPECIFIED. ) 
 CURVE ( )  GEOMETRIC_REPRESENTATION_ITEM ( )  RATIONAL_B_SPLINE_CURVE ( ( 1.000000000000000000, 0.9659258262890682012, 1.000000000000000000, 0.9659258262890682012, 1.000000000000000000, 0.9659258262890682012, 1.000000000000000000, 0.9659258262890682012, 1.000000000000000000, 0.9659258262890682012, 1.000000000000000000, 0.9659258262890577651, 1.000000000000010436 ) ) 
 REPRESENTATION_ITEM ( '' )  );
#32882 =( BOUNDED_CURVE ( )  B_SPLINE_CURVE ( 2, ( #51890, #57183, #53004, #29987, #46960, #12262, #35655, #58670, #52266 ),
 .UNSPECIFIED., .F., .F. ) 
 B_SPLINE_CURVE_WITH_KNOTS ( ( 3, 2, 2, 2, 3 ),
 ( 0.2500000000000001110, 0.2583333333333335258, 0.2666666666666668850, 0.2750000000000002998, 0.2833333333333336590 ),
 .UNSPECIFIED. ) 
 CURVE ( )  GEOMETRIC_REPRESENTATION_ITEM ( )  RATIONAL_B_SPLINE_CURVE ( ( 0.9999999999999990008, 0.9238795325112877377, 1.000000000000000000, 0.9238795325112867385, 1.000000000000000000, 0.9238795325112867385, 1.000000000000000000, 0.9238795325112837409, 1.000000000000003109 ) ) 
 REPRESENTATION_ITEM ( '' )  );
#32883 = ORIENTED_EDGE ( 'NONE', *, *, #45089, .F. ) ;
#32884 = CARTESIAN_POINT ( 'NONE',  ( -4.220049686691937474, -10.18810118749999738, 97.93750000204836681 ) ) ;
#32885 = CARTESIAN_POINT ( 'NONE',  ( -10.99999999999999822, 219.4226497308103774, 0.000000000000000000 ) ) ;
#32886 = CARTESIAN_POINT ( 'NONE',  ( -26.56734541678232731, 200.2500000013656063, 173.4587341250003760 ) ) ;
#32887 = CARTESIAN_POINT ( 'NONE',  ( 11.00000000000000000, 1.347111479062088405E-15, 106.7500000000000000 ) ) ;
#32888 = CARTESIAN_POINT ( 'NONE',  ( 2.445694354108840063, 208.0625000013656063, 200.4456943541088663 ) ) ;
#32889 = CARTESIAN_POINT ( 'NONE',  ( 1.656854249492470732, 203.8125000027311842, 194.0000000000001421 ) ) ;
#32890 = CARTESIAN_POINT ( 'NONE',  ( -5.000000000000005329, 118.3333333333333428, 8.660254037844387298 ) ) ;
#32891 = AXIS2_PLACEMENT_3D ( 'NONE', #73200, #26403, #20758 ) ;
#32892 = CARTESIAN_POINT ( 'NONE',  ( 8.000000000000000000, 103.3437500000000000, -3.313708498984762496 ) ) ;
#32893 = CARTESIAN_POINT ( 'NONE',  ( -6.676582343750001591, 290.6093750017069510, 0.000000000000000000 ) ) ;
#32894 = CARTESIAN_POINT ( 'NONE',  ( 7.188101187499992051, 8.802885111219154394E-16, 11.61155278187175632 ) ) ;
#32895 = EDGE_LOOP ( 'NONE', ( #4871, #61701, #70340 ) ) ;
#32896 = FACE_OUTER_BOUND ( 'NONE', #52139, .T. ) ;
#32897 = CARTESIAN_POINT ( 'NONE',  ( 31.45873412499998523, 207.6250000013656347, 171.4326545832175839 ) ) ;
#32898 = CARTESIAN_POINT ( 'NONE',  ( -8.000000000000000000, 18.56249999590322020, -9.797174393178825657E-16 ) ) ;
#32899 = CARTESIAN_POINT ( 'NONE',  ( -2.754378923186476579E-14, 201.1875000013656063, 145.4587341250000350 ) ) ;
#32900 = CARTESIAN_POINT ( 'NONE',  ( -4.401442555609581635E-16, 122.6562500020483810, -7.188101187500000044 ) ) ;
#32902 = CARTESIAN_POINT ( 'NONE',  ( 3.458734124999960358, 202.6875000013656063, 142.0000000000000568 ) ) ;
#32901 = DIRECTION ( 'NONE',  ( -0.000000000000000000, -1.000000000000000000, -0.000000000000000000 ) ) ;
#32903 = CARTESIAN_POINT ( 'NONE',  ( -3.042071309553159075, 250.2604166700806445, 11.35316468749999963 ) ) ;
#32904 = CARTESIAN_POINT ( 'NONE',  ( -27.99999999999999645, 210.0000000000000284, 166.0000000000003979 ) ) ;
#32905 = CARTESIAN_POINT ( 'NONE',  ( 5.000000000000000000, -60.11723469343116477, 46.25570701698070764 ) ) ;
#32906 = CARTESIAN_POINT ( 'NONE',  ( -10.00000000000000178, 222.5000000000000000, -1.224646799147353454E-15 ) ) ;
#32907 = CARTESIAN_POINT ( 'NONE',  ( -28.00000000000007816, 200.1250000027312126, 166.0000000000003695 ) ) ;
#32908 = CARTESIAN_POINT ( 'NONE',  ( 11.35316468750000141, 211.0937499965860411, 0.000000000000000000 ) ) ;
#32909 = DIRECTION ( 'NONE',  ( 0.000000000000000000, 0.000000000000000000, 1.000000000000000000 ) ) ;
#32910 = CARTESIAN_POINT ( 'NONE',  ( 2.780723358947928197E-16, 4.562499998634407028, -4.541265875000002339 ) ) ;
#32911 = CARTESIAN_POINT ( 'NONE',  ( -6.000000000000012434, 10.39230484541325694, 0.000000000000000000 ) ) ;
#32913 = DIRECTION ( 'NONE',  ( -0.000000000000000000, 1.000000000000000000, -4.476705744456276341E-16 ) ) ;
#32912 = CARTESIAN_POINT ( 'NONE',  ( -8.000000000000000000, 26.06249999590322375, -9.797174393178825657E-16 ) ) ;
#32914 = ORIENTED_EDGE ( 'NONE', *, *, #73132, .T. ) ;
#32915 = EDGE_CURVE ( 'NONE', #60693, #13964, #67892, .T. ) ;
#32916 = CARTESIAN_POINT ( 'NONE',  ( 3.458734124999960358, 198.6875000013655779, 142.0000000000000568 ) ) ;
#32917 = CARTESIAN_POINT ( 'NONE',  ( -5.676582343749998039, 7.447916663252683200, -9.832129032723420536 ) ) ;
#32918 = CARTESIAN_POINT ( 'NONE',  ( 7.778174593052023411, -7.778174593052021635, 96.25000000409677625 ) ) ;
#32919 = CARTESIAN_POINT ( 'NONE',  ( -2.751064625579944321E-14, 205.7500000000000284, 146.0000000000000284 ) ) ;
#32920 = CARTESIAN_POINT ( 'NONE',  ( -28.00000000000007105, 199.4375000013655779, 166.5412658750003629 ) ) ;
#32921 = CARTESIAN_POINT ( 'NONE',  ( -7.347880794884122694E-16, 18.75000000000000000, 4.000000000000001776 ) ) ;
#32923 = CARTESIAN_POINT ( 'NONE',  ( 11.35316468750000141, 0.7812499965860163487, 0.000000000000000000 ) ) ;
#32922 = CARTESIAN_POINT ( 'NONE',  ( 5.082755093536326818, 117.2187500020483810, 5.082755093536325042 ) ) ;
#32924 = CARTESIAN_POINT ( 'NONE',  ( -7.999999999999991118, 3.313708498984756723, 24.73655277982336997 ) ) ;
#32925 = CARTESIAN_POINT ( 'NONE',  ( -8.311093377946836114, 117.6562499965860269, -8.311093377946837890 ) ) ;
#32926 = CARTESIAN_POINT ( 'NONE',  ( -10.00000000000000000, 99.16666665983871098, -2.679491924311229845 ) ) ;
#32927 = CARTESIAN_POINT ( 'NONE',  ( -2.977408999572650927, 119.7500000020483810, -7.188101187500001821 ) ) ;
#32928 = CARTESIAN_POINT ( 'NONE',  ( -3.211159895383562723, 22.06249999863440792, 3.211159895383561391 ) ) ;
#32929 = DIRECTION ( 'NONE',  ( -0.000000000000000000, -0.000000000000000000, 1.000000000000000000 ) ) ;
#32930 = CARTESIAN_POINT ( 'NONE',  ( -7.320508075688773708, 38.74999999317203958, -7.320508075688774596 ) ) ;
#32931 = EDGE_LOOP ( 'NONE', ( #55188, #63752, #23462, #30087 ) ) ;
#32932 = CARTESIAN_POINT ( 'NONE',  ( 1.558072418983288632, -67.68461058694124688, 20.10890959968006797 ) ) ;
#32933 = CARTESIAN_POINT ( 'NONE',  ( -4.721056650415998313, 291.7343750017069510, 4.721056650416000089 ) ) ;
#32934 = CARTESIAN_POINT ( 'NONE',  ( 5.000000000000000000, 53.50771145605643397, 45.03482491321383918 ) ) ;
#32935 = CARTESIAN_POINT ( 'NONE',  ( -5.867873826482948196, -5.445834672501801421, -0.3031401758652553791 ) ) ;
#32936 = CARTESIAN_POINT ( 'NONE',  ( 54.00000000000000711, 0.000000000000000000, 20.00000000000000711 ) ) ;
#32937 = EDGE_CURVE ( 'NONE', #51172, #60780, #10606, .T. ) ;
#32938 = CARTESIAN_POINT ( 'NONE',  ( -11.35316468749999963, 258.9062500034140157, 0.000000000000000000 ) ) ;
#32939 = CARTESIAN_POINT ( 'NONE',  ( -10.18810118749999916, 4.220049686691934809, 100.9375000020483810 ) ) ;
#32940 = ORIENTED_EDGE ( 'NONE', *, *, #30181, .F. ) ;
#32941 = FACE_OUTER_BOUND ( 'NONE', #72468, .T. ) ;
#32942 = CARTESIAN_POINT ( 'NONE',  ( 8.311093377946837890, 156.7187499965860127, -8.311093377946837890 ) ) ;
#32943 = DIRECTION ( 'NONE',  ( 0.000000000000000000, 0.000000000000000000, 1.000000000000000000 ) ) ;
#32944 = CARTESIAN_POINT ( 'NONE',  ( 3.458734125000016757, 204.1250000013656063, 199.4326545832176976 ) ) ;
#32945 = DIRECTION ( 'NONE',  ( 0.000000000000000000, 2.238352872228138170E-16, -1.000000000000000000 ) ) ;
#32946 = CARTESIAN_POINT ( 'NONE',  ( -9.832129032723418760, 78.17708332991935549, -5.676582343750004256 ) ) ;
#32947 = ORIENTED_EDGE ( 'NONE', *, *, #1077, .T. ) ;
#32948 = CARTESIAN_POINT ( 'NONE',  ( 7.204075437095968759, -7.204075437095966983, 113.2187500020483810 ) ) ;
#32949 = CARTESIAN_POINT ( 'NONE',  ( 4.541265875000002339, 8.499999998634407916, -1.881053915767121776 ) ) ;
#32950 = ORIENTED_EDGE ( 'NONE', *, *, #29706, .T. ) ;
#32951 = AXIS2_PLACEMENT_3D ( 'NONE', #9560, #26507, #60854 ) ;
#32952 = CARTESIAN_POINT ( 'NONE',  ( -3.313708498984760720, 1.968750000000000444, -8.000000000000000000 ) ) ;
#32953 = CARTESIAN_POINT ( 'NONE',  ( 4.242640687119285658, 288.6875000034139589, -4.242640687119286547 ) ) ;
#32954 = DIRECTION ( 'NONE',  ( 0.000000000000000000, 0.000000000000000000, 1.000000000000000000 ) ) ;
#32955 = CARTESIAN_POINT ( 'NONE',  ( -5.082755093536326818, 15.28124999795161187, 5.082755093536325042 ) ) ;
#32956 = EDGE_CURVE ( 'NONE', #27817, #68115, #60604, .T. ) ;
#32957 = DIRECTION ( 'NONE',  ( -0.000000000000000000, 1.000000000000000000, -0.000000000000000000 ) ) ;
#32958 = CARTESIAN_POINT ( 'NONE',  ( -10.18810118749999738, -4.220049686691941915, 110.1250000020483810 ) ) ;
#32959 = EDGE_CURVE ( 'NONE', #33017, #8939, #39295, .T. ) ;
#32960 = AXIS2_PLACEMENT_3D ( 'NONE', #46234, #52277, #29265 ) ;
#32961 = CYLINDRICAL_SURFACE ( 'NONE', #12527, 8.000000000000000000 ) ;
#32962 = CARTESIAN_POINT ( 'NONE',  ( 2.828427124746190291, 6.624999997268813168, 2.828427124746192067 ) ) ;
#32963 = DIRECTION ( 'NONE',  ( -0.000000000000000000, 1.000000000000000000, -0.000000000000000000 ) ) ;
#32964 = ORIENTED_EDGE ( 'NONE', *, *, #35325, .F. ) ;
#32965 = ADVANCED_FACE ( 'NONE', ( #10624 ), #70749, .F. ) ;
#32966 = ADVANCED_FACE ( 'NONE', ( #20061 ), #19052, .F. ) ;
#32967 = CARTESIAN_POINT ( 'NONE',  ( -2.445694354108782775, 203.5625000013656063, 200.4456943541088663 ) ) ;
#32968 = CARTESIAN_POINT ( 'NONE',  ( -32.00000000000002842, 194.3125000027312126, 168.3431457505080573 ) ) ;
#32969 = CARTESIAN_POINT ( 'NONE',  ( -1.881053915767124440, 5.999999998634407028, 4.541265875000001451 ) ) ;
#32970 = EDGE_CURVE ( 'NONE', #32640, #29624, #42709, .T. ) ;
#32971 = CARTESIAN_POINT ( 'NONE',  ( 1.102182119232618108E-15, 290.2500000000000000, 6.000000000000001776 ) ) ;
#32972 = VECTOR ( 'NONE', #72625, 1000.000000000000000 ) ;
#32973 = CARTESIAN_POINT ( 'NONE',  ( -2.977408999572648707, -7.188101187499990274, 27.26780278187175099 ) ) ;
#32974 = VERTEX_POINT ( 'NONE', #26857 ) ;
#32975 = DIRECTION ( 'NONE',  ( -0.000000000000000000, 1.000000000000000000, -0.000000000000000000 ) ) ;
#32976 = ORIENTED_EDGE ( 'NONE', *, *, #69212, .F. ) ;
#32977 = CARTESIAN_POINT ( 'NONE',  ( -2.679491924317381812, 1.458333333333883930, -9.999999999996445510 ) ) ;
#32978 = LINE ( 'NONE', #57471, #34062 ) ;
#32979 = CARTESIAN_POINT ( 'NONE',  ( 2.445694354108838731, 204.0625000013656063, 195.5543056458912190 ) ) ;
#32981 =( BOUNDED_CURVE ( )  B_SPLINE_CURVE ( 2, ( #51282, #56213, #16561, #5643, #39969, #67893, #21493, #62976, #73549 ),
 .UNSPECIFIED., .F., .F. ) 
 B_SPLINE_CURVE_WITH_KNOTS ( ( 3, 2, 2, 2, 3 ),
 ( 0.2708333333333312609, 0.2812499999999979461, 0.2916666666666646313, 0.3020833333333312609, 0.3124999999999979461 ),
 .UNSPECIFIED. ) 
 CURVE ( )  GEOMETRIC_REPRESENTATION_ITEM ( )  RATIONAL_B_SPLINE_CURVE ( ( 1.000000000000015099, 0.9238795325112717505, 1.000000000000000000, 0.9238795325112867385, 1.000000000000000000, 0.9238795325112867385, 1.000000000000000000, 0.9238795325113017265, 0.9999999999999850120 ) ) 
 REPRESENTATION_ITEM ( '' )  );
#32980 = CARTESIAN_POINT ( 'NONE',  ( 30.44569435410879521, 200.8125000013656063, 167.5543056458910485 ) ) ;
#32982 = CARTESIAN_POINT ( 'NONE',  ( 8.660254037844389075, 70.41666666666667140, -5.000000000000000000 ) ) ;
#32983 = CARTESIAN_POINT ( 'NONE',  ( -3.313708498984762496, 123.7812500000000000, 7.999999999999998224 ) ) ;
#32984 = CARTESIAN_POINT ( 'NONE',  ( -2.485281374238571761, 293.8124999999999432, -6.000000000000003553 ) ) ;
#32985 = CARTESIAN_POINT ( 'NONE',  ( 26.34314575050763807, 204.0625000027312410, 173.9999999999999147 ) ) ;
#32986 = ORIENTED_EDGE ( 'NONE', *, *, #23212, .T. ) ;
#32987 = CARTESIAN_POINT ( 'NONE',  ( 0.000000000000000000, 0.000000000000000000, 0.000000000000000000 ) ) ;
#32988 = CARTESIAN_POINT ( 'NONE',  ( -2.591411123055096688, -10.27614846265026038, 63.77676950206216588 ) ) ;
#32989 = CARTESIAN_POINT ( 'NONE',  ( 1.656854249492347719, 195.9375000027312126, 146.0000000000000284 ) ) ;
#32990 = CARTESIAN_POINT ( 'NONE',  ( 0.000000000000000000, 0.000000000000000000, 0.000000000000000000 ) ) ;
#32991 = CARTESIAN_POINT ( 'NONE',  ( 27.99999999999999645, 210.0000000000000284, 169.9999999999999147 ) ) ;
#32992 = CARTESIAN_POINT ( 'NONE',  ( 2.679491924311225848, 253.5416666666666572, -10.00000000000000000 ) ) ;
#32993 = DIRECTION ( 'NONE',  ( 0.000000000000000000, 0.000000000000000000, 1.000000000000000000 ) ) ;
#32994 = CARTESIAN_POINT ( 'NONE',  ( 8.660254037844385522, 189.5833333333333428, 5.000000000000005329 ) ) ;
#32995 = LINE ( 'NONE', #15233, #69314 ) ;
#32996 = CARTESIAN_POINT ( 'NONE',  ( -4.401442555609577197E-16, 7.188101187499992051, 25.48655278187175810 ) ) ;
#32997 = CARTESIAN_POINT ( 'NONE',  ( -8.311093377946836114, 167.9687499965859843, -8.311093377946837890 ) ) ;
#32998 = FACE_OUTER_BOUND ( 'NONE', #40165, .T. ) ;
#32999 = CARTESIAN_POINT ( 'NONE',  ( -5.000000000000000000, 53.21762015693831671, 47.70201125340263104 ) ) ;
#33000 = CARTESIAN_POINT ( 'NONE',  ( 2.679491924329232777, 153.9583333333350197, 9.999999999989814370 ) ) ;
#33001 = CARTESIAN_POINT ( 'NONE',  ( 26.34314575050751728, 195.0625000027311557, 173.9999999999998010 ) ) ;
#33002 = ORIENTED_EDGE ( 'NONE', *, *, #67401, .T. ) ;
#33003 = VECTOR ( 'NONE', #35129, 1000.000000000000000 ) ;
#33004 = CARTESIAN_POINT ( 'NONE',  ( -11.35316468749999785, 18.38541666325267698, -3.042071309553167513 ) ) ;
#33005 = CARTESIAN_POINT ( 'NONE',  ( 4.000000000000016875, 200.5625000027312126, 199.6568542494924259 ) ) ;
#33007 = CARTESIAN_POINT ( 'NONE',  ( -3.511653767258354986, -16.35475815726549342, -69.12977678000822834 ) ) ;
#33006 = LINE ( 'NONE', #4320, #40825 ) ;
#33008 = CARTESIAN_POINT ( 'NONE',  ( -20.30555188694492230, -48.91983502101248149, 193.4397630911809927 ) ) ;
#33009 = CARTESIAN_POINT ( 'NONE',  ( -2.445694354108838731, 201.0625000013656063, 144.4456943541088663 ) ) ;
#33010 =( BOUNDED_CURVE ( )  B_SPLINE_CURVE ( 2, ( #17586, #34592, #46628, #17210, #22120, #40229, #57599, #12301, #63606 ),
 .UNSPECIFIED., .F., .F. ) 
 B_SPLINE_CURVE_WITH_KNOTS ( ( 3, 2, 2, 2, 3 ),
 ( 0.6704545454545455252, 0.6761363636363637575, 0.6818181818181817677, 0.6875000000000000000, 0.6931818181818182323 ),
 .UNSPECIFIED. ) 
 CURVE ( )  GEOMETRIC_REPRESENTATION_ITEM ( )  RATIONAL_B_SPLINE_CURVE ( ( 0.9999999999999985567, 0.9238795325112881818, 1.000000000000000000, 0.9238795325112867385, 1.000000000000000000, 0.9238795325112867385, 1.000000000000000000, 0.9238795325112867385, 1.000000000000000000 ) ) 
 REPRESENTATION_ITEM ( '' )  );
#33011 = CARTESIAN_POINT ( 'NONE',  ( 5.000000000000001776, 47.70833332650536818, -8.660254037844389075 ) ) ;
#33012 = CARTESIAN_POINT ( 'NONE',  ( 1.320432766682874540E-15, 103.5312500020483810, 7.188101187500000044 ) ) ;
#33013 = CARTESIAN_POINT ( 'NONE',  ( 3.211159895383560947, 9.312499998634407916, 3.211159895383562723 ) ) ;
#33014 = DIRECTION ( 'NONE',  ( 0.000000000000000000, 0.000000000000000000, 1.000000000000000000 ) ) ;
#33015 = CARTESIAN_POINT ( 'NONE',  ( 5.656854249492374365, 5.656854249492375253, 7.767802779823362869 ) ) ;
#33016 = CARTESIAN_POINT ( 'NONE',  ( 2.449293598294707893E-16, 4.999999997268813168, -4.000000000000001776 ) ) ;
#33017 = VERTEX_POINT ( 'NONE', #4235 ) ;
#33018 = ORIENTED_EDGE ( 'NONE', *, *, #32746, .T. ) ;
#33019 = EDGE_CURVE ( 'NONE', #2280, #2612, #72125, .T. ) ;
#33020 = CARTESIAN_POINT ( 'NONE',  ( -10.00000000000000000, 222.2916666666666856, -2.679491924311229845 ) ) ;
#33021 = CARTESIAN_POINT ( 'NONE',  ( -7.999999999974042098, 1.357258486152048259E-05, 14.51729352187485311 ) ) ;
#33022 = CARTESIAN_POINT ( 'NONE',  ( -3.313708498984757611, 7.999999999999991118, 2.049052779823364645 ) ) ;
#33023 = CARTESIAN_POINT ( 'NONE',  ( 3.042071309553163516, 222.7604166700806445, -11.35316468749999785 ) ) ;
#33024 = CARTESIAN_POINT ( 'NONE',  ( -9.832129032723418760, 137.8645833299193555, -5.676582343750004256 ) ) ;
#33025 = ORIENTED_EDGE ( 'NONE', *, *, #10258, .F. ) ;
#33026 = CARTESIAN_POINT ( 'NONE',  ( -4.999999999999999112, 14.70234347858786528, -69.93881661156081009 ) ) ;
#33027 = CARTESIAN_POINT ( 'NONE',  ( 1.871523826299183495E-15, -10.18810118749999916, 89.03125000204836681 ) ) ;
#33028 = FACE_OUTER_BOUND ( 'NONE', #11106, .T. ) ;
#33029 = CARTESIAN_POINT ( 'NONE',  ( -3.999999999999960032, 207.9375000000000000, 196.3431457505076594 ) ) ;
#33031 = CARTESIAN_POINT ( 'NONE',  ( 5.676582343750001591, 131.6145833299193555, -9.832129032723420536 ) ) ;
#33030 = CARTESIAN_POINT ( 'NONE',  ( -11.00000000000000000, 0.000000000000000000, 106.0000000000000000 ) ) ;
#33032 = FACE_OUTER_BOUND ( 'NONE', #28109, .T. ) ;
#33033 = VERTEX_POINT ( 'NONE', #61569 ) ;
#33034 = ADVANCED_FACE ( 'NONE', ( #26470 ), #49494, .F. ) ;
#33035 = CARTESIAN_POINT ( 'NONE',  ( 1.469576158976823947E-15, 110.3750000000000000, 8.000000000000000000 ) ) ;
#33036 =( BOUNDED_CURVE ( )  B_SPLINE_CURVE ( 2, ( #35193, #17820, #51404, #33709, #28027, #51037, #58209, #45371, #68017 ),
 .UNSPECIFIED., .F., .F. ) 
 B_SPLINE_CURVE_WITH_KNOTS ( ( 3, 2, 2, 2, 3 ),
 ( 0.1833333333333333481, 0.1916666666666667629, 0.2000000000000001776, 0.2083333333333335646, 0.2166666666666669516 ),
 .UNSPECIFIED. ) 
 CURVE ( )  GEOMETRIC_REPRESENTATION_ITEM ( )  RATIONAL_B_SPLINE_CURVE ( ( 0.9999999999999997780, 0.9238795325112869605, 1.000000000000000000, 0.9238795325112867385, 1.000000000000000000, 0.9238795325112867385, 1.000000000000000000, 0.9238795325112841850, 1.000000000000002442 ) ) 
 REPRESENTATION_ITEM ( '' )  );
#33037 = AXIS2_PLACEMENT_3D ( 'NONE', #57923, #39798, #52246 ) ;
#33038 = CARTESIAN_POINT ( 'NONE',  ( -29.34617108035451949, 180.6013230617538738, 159.7592319357849249 ) ) ;
#33039 = CARTESIAN_POINT ( 'NONE',  ( 9.832129032723416984, 120.6770833299193555, 5.676582343750006032 ) ) ;
#33040 = CARTESIAN_POINT ( 'NONE',  ( 2.839093476692135984E-14, 203.6875000013656063, 201.4587341250000350 ) ) ;
#33041 = CARTESIAN_POINT ( 'NONE',  ( -5.082755093536326818, 18.28124999795161187, 5.082755093536325042 ) ) ;
#33042 = CARTESIAN_POINT ( 'NONE',  ( 7.204075437095968759, -7.204075437095966983, 80.59375000204838102 ) ) ;
#33043 = CARTESIAN_POINT ( 'NONE',  ( -2.085542519210945728E-15, 19.84374999658601979, 11.35316468750000141 ) ) ;
#33044 = ORIENTED_EDGE ( 'NONE', *, *, #46505, .F. ) ;
#33045 = CARTESIAN_POINT ( 'NONE',  ( 3.313708498984869077, 90.21875000409677625, -7.999999999999892530 ) ) ;
#33046 = CARTESIAN_POINT ( 'NONE',  ( 8.008118988124991233, 3.317071493978879015, 19.85686528394063188 ) ) ;
#33047 = DIRECTION ( 'NONE',  ( -1.000000000000000000, -0.000000000000000000, -0.000000000000000000 ) ) ;
#33048 = PRODUCT_DEFINITION ( 'UNKNOWN', '', #50215, #28204 ) ;
#33049 = DIRECTION ( 'NONE',  ( 0.000000000000000000, 0.000000000000000000, -1.000000000000000000 ) ) ;
#33050 = CARTESIAN_POINT ( 'NONE',  ( 7.188101187500001821, 3.562499997951610542, -2.977408999572650483 ) ) ;
#33051 = CARTESIAN_POINT ( 'NONE',  ( 6.676582343750001591, 287.9531250017069510, -8.176455196517173205E-16 ) ) ;
#33052 = CARTESIAN_POINT ( 'NONE',  ( -4.242640687119286547, 296.8750000000000000, -4.242640687119286547 ) ) ;
#33053 = CARTESIAN_POINT ( 'NONE',  ( -2.977408999572654480, 1.874999997951610098, 7.188101187499999156 ) ) ;
#33054 = ORIENTED_EDGE ( 'NONE', *, *, #6221, .F. ) ;
#33055 = CARTESIAN_POINT ( 'NONE',  ( -8.311093377946836114, 137.9687499965860411, -8.311093377946837890 ) ) ;
#33056 = CARTESIAN_POINT ( 'NONE',  ( -10.18810118749999916, 0.000000000000000000, 78.15625000204836681 ) ) ;
#33057 = EDGE_CURVE ( 'NONE', #23491, #5483, #59735, .T. ) ;
#33058 = CARTESIAN_POINT ( 'NONE',  ( -29.43265458321766559, 196.5000000013656063, 166.5412658750003629 ) ) ;
#33059 = EDGE_CURVE ( 'NONE', #28928, #8230, #26432, .T. ) ;
#33060 = CARTESIAN_POINT ( 'NONE',  ( 5.656854249492374365, 5.656854249492375253, 21.26780277982336642 ) ) ;
#33061 = CARTESIAN_POINT ( 'NONE',  ( 4.541265875000001451, 16.37499999863440436, 1.881053915767124440 ) ) ;
#33062 = ORIENTED_EDGE ( 'NONE', *, *, #37326, .F. ) ;
#33063 = VECTOR ( 'NONE', #15019, 1000.000000000000000 ) ;
#33064 = CARTESIAN_POINT ( 'NONE',  ( -3.999999999999959144, 205.1875000027311842, 199.6568542494924259 ) ) ;
#33065 = CARTESIAN_POINT ( 'NONE',  ( -2.828427124746209831, 209.3750000000000284, 139.1715728752538723 ) ) ;
#33066 = CARTESIAN_POINT ( 'NONE',  ( -26.34314575050770202, 207.0625000027311842, 166.0000000000003695 ) ) ;
#33067 = CARTESIAN_POINT ( 'NONE',  ( -7.999999999999998224, 104.0937500000000142, 3.313708498984766049 ) ) ;
#33068 = ORIENTED_EDGE ( 'NONE', *, *, #34800, .T. ) ;
#33069 = ADVANCED_FACE ( 'NONE', ( #60062 ), #8383, .F. ) ;
#33070 = CARTESIAN_POINT ( 'NONE',  ( 5.082755093536324154, 12.28124999795161187, 5.082755093536326818 ) ) ;
#33071 = CARTESIAN_POINT ( 'NONE',  ( -24.00000000000002132, 196.9375000027312126, 168.3431457505079152 ) ) ;
#33072 = CARTESIAN_POINT ( 'NONE',  ( 4.999999999999999112, 52.84347807771189309, -43.21644271080158717 ) ) ;
#33073 = CARTESIAN_POINT ( 'NONE',  ( -8.311093377946836114, 187.6562499965860411, -8.311093377946837890 ) ) ;
#33074 = CARTESIAN_POINT ( 'NONE',  ( 7.188101187500001821, 110.3750000020484094, -2.977408999572651371 ) ) ;
#33075 = CARTESIAN_POINT ( 'NONE',  ( -3.673940397442060854E-16, 295.7500000000000000, -6.000000000000001776 ) ) ;
#33076 = CARTESIAN_POINT ( 'NONE',  ( 6.676582343750002480, 290.0156250017069510, -2.765530957081997254 ) ) ;
#33078 = CARTESIAN_POINT ( 'NONE',  ( 6.123233995736767268E-16, 96.25000000000000000, -10.00000000000000178 ) ) ;
#33077 = CARTESIAN_POINT ( 'NONE',  ( 2.679491924318032403, 81.04166666666614560, -9.999999999996202149 ) ) ;
#33079 = ORIENTED_EDGE ( 'NONE', *, *, #46018, .T. ) ;
#33080 = CARTESIAN_POINT ( 'NONE',  ( 3.042071309553163960, 257.4479166700806445, -11.35316468749999785 ) ) ;
#33081 = CARTESIAN_POINT ( 'NONE',  ( 2.977408999572646486, 7.188101187499991163, 20.89280278187176521 ) ) ;
#33082 = AXIS2_PLACEMENT_3D ( 'NONE', #63262, #63635, #39524 ) ;
#33083 = CARTESIAN_POINT ( 'NONE',  ( 10.00000000000000178, 166.8749999931720538, 0.000000000000000000 ) ) ;
#33084 = CARTESIAN_POINT ( 'NONE',  ( 11.00000000000000000, 1.347111479062088405E-15, 109.7499999999999858 ) ) ;
#33085 = DIRECTION ( 'NONE',  ( 0.000000000000000000, 0.000000000000000000, -1.000000000000000000 ) ) ;
#33086 = CARTESIAN_POINT ( 'NONE',  ( 1.432654583217664701, 196.0000000013656347, 201.4587341250000065 ) ) ;
#33087 = CARTESIAN_POINT ( 'NONE',  ( -8.660254037844387298, 142.0833333333333428, -5.000000000000004441 ) ) ;
#33088 = VERTEX_POINT ( 'NONE', #66469 ) ;
#33089 = CARTESIAN_POINT ( 'NONE',  ( 5.204170427930421283E-15, 10.39230484541327293, -0.8038475772933779684 ) ) ;
#33090 = CARTESIAN_POINT ( 'NONE',  ( -8.000000000000000000, 96.50000000000000000, 0.000000000000000000 ) ) ;
#33091 = CARTESIAN_POINT ( 'NONE',  ( 5.676582343750001591, 116.9270833299193555, -9.832129032723420536 ) ) ;
#33092 = CARTESIAN_POINT ( 'NONE',  ( -4.898587196589412829E-16, 99.12499999999998579, -8.000000000000000000 ) ) ;
#33093 = CARTESIAN_POINT ( 'NONE',  ( -10.99999999999999822, -4.556349186104052151, 68.59374999999997158 ) ) ;
#33096 = CARTESIAN_POINT ( 'NONE',  ( 18.00000000000000355, -10.39230484541328892, -1.607695154586745501 ) ) ;
#33095 = CARTESIAN_POINT ( 'NONE',  ( 31.45873412499999944, 200.6250000013655779, 171.4326545832175555 ) ) ;
#33094 = CARTESIAN_POINT ( 'NONE',  ( 30.44569435410879166, 200.8125000013656063, 172.4456943541087526 ) ) ;
#33097 = ORIENTED_EDGE ( 'NONE', *, *, #36266, .T. ) ;
#33098 = DIRECTION ( 'NONE',  ( -0.000000000000000000, 1.000000000000000000, -0.000000000000000000 ) ) ;
#33099 = EDGE_CURVE ( 'NONE', #2971, #3802, #31398, .T. ) ;
#33100 = CARTESIAN_POINT ( 'NONE',  ( 8.311093377946834337, 225.1562499965860411, 8.311093377946839666 ) ) ;
#33101 = CARTESIAN_POINT ( 'NONE',  ( 25.55430564589119058, 197.3125000013656063, 167.5543056458910485 ) ) ;
#33102 = CARTESIAN_POINT ( 'NONE',  ( -11.35316468750000141, 203.8020833299193839, 3.042071309553159963 ) ) ;
#33103 = CARTESIAN_POINT ( 'NONE',  ( -7.188101187500001821, 122.5625000020483952, -2.977408999572650483 ) ) ;
#33104 = CARTESIAN_POINT ( 'NONE',  ( -1.881053915767121554, 18.62499999863440792, -4.541265875000002339 ) ) ;
#33105 = CARTESIAN_POINT ( 'NONE',  ( 24.54126587499997569, 196.5000000013656063, 171.4326545832175555 ) ) ;
#33106 = CARTESIAN_POINT ( 'NONE',  ( -3.313708498984757167, 7.999999999999991118, 24.54905277982336287 ) ) ;
#33108 = CARTESIAN_POINT ( 'NONE',  ( -30.82842712474612767, 208.5000000027312126, 172.8284271247466108 ) ) ;
#33107 = CARTESIAN_POINT ( 'NONE',  ( -47.73049838254535615, 39.79673206543596820, 63.57013892992242887 ) ) ;
#33109 = CARTESIAN_POINT ( 'NONE',  ( 8.311093377946834337, 95.15624999658601268, 8.311093377946839666 ) ) ;
#33110 = VERTEX_POINT ( 'NONE', #20439 ) ;
#33111 =( BOUNDED_SURFACE ( )  B_SPLINE_SURFACE ( 3, 2, ( 
 ( #21002, #21744, #16448 ),
 ( #56472, #62480, #15336 ),
 ( #32345, #4788, #32724 ),
 ( #49300, #33844, #44028 ),
 ( #67037, #56842, #15710 ),
 ( #27781, #61752, #55358 ),
 ( #55732, #44772, #4049 ),
 ( #50052, #73068, #44398 ),
 ( #73807, #67786, #16078 ),
 ( #22115, #45139, #74554 ),
 ( #11926, #51168, #34212 ),
 ( #22866, #58341, #52663 ),
 ( #57973, #23980, #45880 ),
 ( #6645, #63981, #70021 ),
 ( #68894, #74177, #17956 ),
 ( #259, #28157, #18327 ),
 ( #631, #57214, #41342 ),
 ( #5528, #40974, #69269 ) ),
 .UNSPECIFIED., .F., .F., .F. ) 
 B_SPLINE_SURFACE_WITH_KNOTS ( ( 4, 2, 2, 2, 2, 2, 2, 2, 4 ),
 ( 3, 3 ),
 ( 0.04202945594034800114, 0.04396162471218434398, 0.04589379348402068681, 0.04782596225585702965, 0.04975813102769337248, 0.05169029979952971532, 0.05265638418544788674, 0.05362246857136605815, 0.05748680611503874383 ),
 ( 0.000000000000000000, 1.000000000000000000 ),
 .UNSPECIFIED. ) 
 GEOMETRIC_REPRESENTATION_ITEM ( )  RATIONAL_B_SPLINE_SURFACE ( (
 ( 1.000000000000000000, 0.6241276099607500072, 1.000000000000000000),
 ( 1.000000000000000000, 0.6218761496802208688, 1.000000000000000000),
 ( 1.000000000000000000, 0.6198047272360279747, 1.000000000000000000),
 ( 1.000000000000000000, 0.6161935119827212093, 1.000000000000000000),
 ( 1.000000000000000000, 0.6146642324083134712, 1.000000000000000000),
 ( 1.000000000000000000, 0.6121850116868342573, 1.000000000000000000),
 ( 1.000000000000000000, 0.6112350889398914244, 1.000000000000000000),
 ( 1.000000000000000000, 0.6099522725973434145, 1.000000000000000000),
 ( 1.000000000000000000, 0.6096208180309086178, 1.000000000000000000),
 ( 1.000000000000000000, 0.6096183796348277895, 1.000000000000000000),
 ( 1.000000000000000000, 0.6099422200098292279, 1.000000000000000000),
 ( 1.000000000000000000, 0.6109087447825207740, 1.000000000000000000),
 ( 1.000000000000000000, 0.6113123981689779773, 1.000000000000000000),
 ( 1.000000000000000000, 0.6122677719807979591, 1.000000000000000000),
 ( 1.000000000000000000, 0.6128199619019198963, 1.000000000000000000),
 ( 1.000000000000000000, 0.6159350830273242483, 1.000000000000000000),
 ( 1.000000000000000000, 0.6195556778510084017, 1.000000000000000000),
 ( 1.000000000000000000, 0.6241278272307887454, 1.000000000000000000) ) ) 
 REPRESENTATION_ITEM ( '' )  SURFACE ( )  );
#33112 = ADVANCED_FACE ( 'NONE', ( #60436 ), #54425, .F. ) ;
#33113 = CARTESIAN_POINT ( 'NONE',  ( -5.000000000000000000, 0.000000000000000000, 0.000000000000000000 ) ) ;
#33114 = CARTESIAN_POINT ( 'NONE',  ( -5.082755093536326818, 22.40624999795161187, 5.082755093536325042 ) ) ;
#33115 = CARTESIAN_POINT ( 'NONE',  ( -6.123233995736766282E-16, 221.8750000068279746, -10.00000000000000000 ) ) ;
#33117 = CARTESIAN_POINT ( 'NONE',  ( -5.676582343750000703, 253.3854166700806445, -9.832129032723418760 ) ) ;
#33116 = AXIS2_PLACEMENT_3D ( 'NONE', #36020, #18664, #5496 ) ;
#33118 = CARTESIAN_POINT ( 'NONE',  ( -11.35316468750000141, 98.28124999658602690, -1.390361679473963753E-15 ) ) ;
#33119 = ORIENTED_EDGE ( 'NONE', *, *, #68348, .T. ) ;
#33120 = CARTESIAN_POINT ( 'NONE',  ( 25.17157287525377640, 196.7500000027312126, 167.1715728752537586 ) ) ;
#33121 = CARTESIAN_POINT ( 'NONE',  ( -10.18810118749999916, 0.000000000000000000, 105.1562500020483810 ) ) ;
#33122 = CARTESIAN_POINT ( 'NONE',  ( 2.775557561822899905E-14, -42.00000000000000711, 151.0000000000000284 ) ) ;
#33123 = CARTESIAN_POINT ( 'NONE',  ( 1.432654583217664701, 205.0000000013655779, 201.4587341250000065 ) ) ;
#33124 = DIRECTION ( 'NONE',  ( -0.000000000000000000, 1.000000000000000000, -0.000000000000000000 ) ) ;
#33126 = CARTESIAN_POINT ( 'NONE',  ( -3.042071309553173730, 89.32291666325268409, 11.35316468749999785 ) ) ;
#33125 = DIRECTION ( 'NONE',  ( 0.000000000000000000, 0.000000000000000000, -1.000000000000000000 ) ) ;
#33127 = CARTESIAN_POINT ( 'NONE',  ( 7.999999999999991118, 3.313708498984757611, 10.86155278392014800 ) ) ;
#33128 = CARTESIAN_POINT ( 'NONE',  ( -24.54126587499999346, 199.4375000013655779, 170.0000000000003411 ) ) ;
#33129 = CARTESIAN_POINT ( 'NONE',  ( 1.656854249492406783, 14.81250000000000355, 3.999999999999976019 ) ) ;
#33130 = CARTESIAN_POINT ( 'NONE',  ( 5.000000000000001776, 187.7083333265053966, -8.660254037844389075 ) ) ;
#33131 = CARTESIAN_POINT ( 'NONE',  ( 5.000000000000000888, -52.63864145287922014, 42.88977517748058688 ) ) ;
#33132 = CARTESIAN_POINT ( 'NONE',  ( -3.042071309553163960, 72.55208332991934128, -11.35316468749999963 ) ) ;
#33133 = CARTESIAN_POINT ( 'NONE',  ( 6.676582343750004256, 287.8906250017069510, 2.765530957081995478 ) ) ;
#33134 = EDGE_CURVE ( 'NONE', #21890, #33983, #41877, .T. ) ;
#33135 = CARTESIAN_POINT ( 'NONE',  ( -10.18810118749999916, 0.000000000000000000, 102.5312500020483810 ) ) ;
#33136 = CARTESIAN_POINT ( 'NONE',  ( 6.951808397369818766E-16, 207.0312499965860411, -11.35316468750000141 ) ) ;
#33138 = VERTEX_POINT ( 'NONE', #55175 ) ;
#33137 =( BOUNDED_CURVE ( )  B_SPLINE_CURVE ( 2, ( #73694, #15970, #16704, #22005, #45388, #45032, #68040, #39369, #63114 ),
 .UNSPECIFIED., .F., .F. ) 
 B_SPLINE_CURVE_WITH_KNOTS ( ( 3, 2, 2, 2, 3 ),
 ( 0.7368421052631579649, 0.7434210526315789824, 0.7500000000000000000, 0.7565789473684210176, 0.7631578947368420351 ),
 .UNSPECIFIED. ) 
 CURVE ( )  GEOMETRIC_REPRESENTATION_ITEM ( )  RATIONAL_B_SPLINE_CURVE ( ( 0.9999999999999986677, 0.9238795325112880708, 1.000000000000000000, 0.9238795325112867385, 1.000000000000000000, 0.9238795325112867385, 1.000000000000000000, 0.9238795325112880708, 0.9999999999999986677 ) ) 
 REPRESENTATION_ITEM ( '' )  );
#33139 = CARTESIAN_POINT ( 'NONE',  ( -1.656854249492381248, 2.312500000000000888, -4.000000000000001776 ) ) ;
#33140 = CARTESIAN_POINT ( 'NONE',  ( -3.313708498984762496, 1.781249995903220640, -8.000000000000000000 ) ) ;
#33141 = CARTESIAN_POINT ( 'NONE',  ( 13.99999999999999822, 0.000000000000000000, -17.50000000000000000 ) ) ;
#33142 = CARTESIAN_POINT ( 'NONE',  ( 11.35316468750000141, 210.7812499965860411, 0.000000000000000000 ) ) ;
#33143 = CARTESIAN_POINT ( 'NONE',  ( -10.00000000000000000, 222.9166666734946602, -2.679491924311226292 ) ) ;
#33144 = CARTESIAN_POINT ( 'NONE',  ( -2.726571689596997292E-14, 210.0000000000000284, 138.0000000000000568 ) ) ;
#33145 = AXIS2_PLACEMENT_3D ( 'NONE', #39380, #3563, #73341 ) ;
#33146 = ORIENTED_EDGE ( 'NONE', *, *, #45573, .F. ) ;
#33147 = CARTESIAN_POINT ( 'NONE',  ( -5.676582343749998039, 192.7604166632526983, -9.832129032723420536 ) ) ;
#33148 = AXIS2_PLACEMENT_3D ( 'NONE', #45196, #3721, #33160 ) ;
#33149 = CARTESIAN_POINT ( 'NONE',  ( 5.082755093536318824, 5.082755093536319713, 17.42405278187175810 ) ) ;
#33150 = CARTESIAN_POINT ( 'NONE',  ( -29.43265458321761230, 208.8750000013656347, 173.4587341250003760 ) ) ;
#33151 = CARTESIAN_POINT ( 'NONE',  ( 8.000000000000000000, 9.000000000000001776, 0.000000000000000000 ) ) ;
#33152 = ORIENTED_EDGE ( 'NONE', *, *, #9142, .T. ) ;
#33153 = CARTESIAN_POINT ( 'NONE',  ( -4.898587196589412829E-16, 90.31250000409676204, -8.000000000000000000 ) ) ;
#33154 = CARTESIAN_POINT ( 'NONE',  ( -7.320508075688773708, 16.87500000000000355, -7.320508075688774596 ) ) ;
#33155 = CARTESIAN_POINT ( 'NONE',  ( 10.18810118749999916, 1.247682550866122264E-15, 83.78125000204838102 ) ) ;
#33156 = ORIENTED_EDGE ( 'NONE', *, *, #43034, .F. ) ;
#33157 = CARTESIAN_POINT ( 'NONE',  ( -4.000000000000001776, 19.50000000000000000, -4.898587196589415787E-16 ) ) ;
#33158 = CARTESIAN_POINT ( 'NONE',  ( 4.541265875000002339, 18.37499999863441147, -1.881053915767121776 ) ) ;
#33159 = EDGE_LOOP ( 'NONE', ( #66090, #15181, #73274, #48010 ) ) ;
#33160 = DIRECTION ( 'NONE',  ( -1.000000000000000000, 0.000000000000000000, 0.000000000000000000 ) ) ;
#33161 = CARTESIAN_POINT ( 'NONE',  ( 2.977408999572654480, 90.12500000204836681, 7.188101187499999156 ) ) ;
#33164 = CARTESIAN_POINT ( 'NONE',  ( 2.249999999999999112, -2.249999999999999556, 28.00000000000000000 ) ) ;
#33163 = CARTESIAN_POINT ( 'NONE',  ( 5.676582343750005144, 260.5729166700806445, 9.832129032723416984 ) ) ;
#33162 = CARTESIAN_POINT ( 'NONE',  ( 1.836970198721029589E-15, 259.3750000068280315, 10.00000000000000000 ) ) ;
#33165 = APPLICATION_PROTOCOL_DEFINITION ( 'draft international standard', 'automotive_design', 1998, #27400 ) ;
#33166 = ORIENTED_EDGE ( 'NONE', *, *, #71458, .F. ) ;
#33167 = EDGE_CURVE ( 'NONE', #3255, #72883, #61934, .T. ) ;
#33168 = CARTESIAN_POINT ( 'NONE',  ( -11.35316468749999608, 254.4270833367473585, 3.042071309553173730 ) ) ;
#33169 = CARTESIAN_POINT ( 'NONE',  ( -7.188101187499991163, 2.977408999572646930, 10.39280278187175810 ) ) ;
#33170 = ORIENTED_EDGE ( 'NONE', *, *, #65929, .T. ) ;
#33171 = EDGE_LOOP ( 'NONE', ( #67343, #65168, #61332, #62033 ) ) ;
#33172 = CARTESIAN_POINT ( 'NONE',  ( 7.204075437095966983, 7.204075437095967871, 73.09375000204838102 ) ) ;
#33173 = CARTESIAN_POINT ( 'NONE',  ( 5.676582343749993598, 80.26041666325268409, 9.832129032723422313 ) ) ;
#33174 = CARTESIAN_POINT ( 'NONE',  ( 7.999999999843520726, -5.003525229023116430E-05, 24.26780136833107093 ) ) ;
#33175 = CARTESIAN_POINT ( 'NONE',  ( 4.556349186104045934, 11.00000000000000000, 90.53125000000000000 ) ) ;
#33178 = CARTESIAN_POINT ( 'NONE',  ( 6.676582343750001591, 290.1093750017069510, -8.176455196517173205E-16 ) ) ;
#33177 = CARTESIAN_POINT ( 'NONE',  ( 31.99999999999999289, 196.3750000027311842, 169.9999999999998863 ) ) ;
#33176 = CARTESIAN_POINT ( 'NONE',  ( -27.99999999999991473, 205.6250000027312126, 174.0000000000003695 ) ) ;
#33179 = CARTESIAN_POINT ( 'NONE',  ( 4.000000000000000888, 13.93750000000000000, 1.656854249492384135 ) ) ;
#33180 = CYLINDRICAL_SURFACE ( 'NONE', #69692, 11.00000000000000000 ) ;
#33181 = AXIS2_PLACEMENT_3D ( 'NONE', #50978, #22294, #10997 ) ;
#33182 = EDGE_CURVE ( 'NONE', #30219, #17320, #1371, .T. ) ;
#33183 = CARTESIAN_POINT ( 'NONE',  ( -1.432654583217607414, 200.5000000013656063, 194.5412658750000219 ) ) ;
#33184 = CARTESIAN_POINT ( 'NONE',  ( -5.656854249492381470, 8.249999995903221972, 5.656854249492379694 ) ) ;
#33185 = EDGE_LOOP ( 'NONE', ( #1899, #642, #16591, #19426 ) ) ;
#33186 = CARTESIAN_POINT ( 'NONE',  ( 29.43265458321766559, 209.1250000013656631, 166.5412658749999650 ) ) ;
#33187 = CARTESIAN_POINT ( 'NONE',  ( 7.188101187499999156, 20.24999999795161898, 2.977408999572654924 ) ) ;
#33188 = CARTESIAN_POINT ( 'NONE',  ( -3.042071309553164404, 172.5520833299193555, -11.35316468749999963 ) ) ;
#33189 = CARTESIAN_POINT ( 'NONE',  ( 3.313708498984782036, 7.781250000000001776, -7.999999999999981348 ) ) ;
#33190 = CARTESIAN_POINT ( 'NONE',  ( 1.320432766682874540E-15, 103.9062500020483810, 7.188101187500000044 ) ) ;
#33192 = CARTESIAN_POINT ( 'NONE',  ( -4.471435261918684567, -50.48103707412959551, -40.99880869399324723 ) ) ;
#33191 = CARTESIAN_POINT ( 'NONE',  ( -9.999999999999996447, 207.7083333333333428, 2.679491924311221851 ) ) ;
#33193 = CARTESIAN_POINT ( 'NONE',  ( 25.55430564589115505, 206.5625000013656063, 172.4456943541086957 ) ) ;
#33194 = CARTESIAN_POINT ( 'NONE',  ( -4.401442555609577197E-16, 7.188101187499992051, 14.98655278187175455 ) ) ;
#33195 = CARTESIAN_POINT ( 'NONE',  ( 3.999999999999960032, 206.1250000027312126, 142.0000000000000568 ) ) ;
#33196 = CARTESIAN_POINT ( 'NONE',  ( 5.676582343749993598, 59.94791666325269119, 9.832129032723422313 ) ) ;
#33197 = CARTESIAN_POINT ( 'NONE',  ( 0.000000000000000000, 192.0000000000000284, 170.0000000000000284 ) ) ;
#33198 = CARTESIAN_POINT ( 'NONE',  ( 7.320508075688774596, 17.49999999317202892, -7.320508075688774596 ) ) ;
#33199 = CARTESIAN_POINT ( 'NONE',  ( -4.556349186104048599, -10.99999999999999822, 71.78125000000000000 ) ) ;
#33200 = ORIENTED_EDGE ( 'NONE', *, *, #32187, .F. ) ;
#33201 = CARTESIAN_POINT ( 'NONE',  ( -5.000000000000000000, -10.00000000000000000, -75.19090595827292134 ) ) ;
#33202 = DIRECTION ( 'NONE',  ( -0.000000000000000000, -0.000000000000000000, 1.000000000000000000 ) ) ;
#33203 = CARTESIAN_POINT ( 'NONE',  ( 9.832129032723420536, 51.19791666325268409, -5.676582343749999815 ) ) ;
#33204 = CARTESIAN_POINT ( 'NONE',  ( 11.00000000000000000, 4.556349186104045934, 74.03125000409677625 ) ) ;
#33205 = CARTESIAN_POINT ( 'NONE',  ( -1.432654583217662481, 198.3750000013656063, 145.4587341250000350 ) ) ;
#33206 = CARTESIAN_POINT ( 'NONE',  ( 3.496982156820435783, 16.35094707925456348, 69.15443034747086415 ) ) ;
#33207 = CARTESIAN_POINT ( 'NONE',  ( -10.00000000000000000, 12.29166666666666963, -2.679491924311229845 ) ) ;
#33209 = CARTESIAN_POINT ( 'NONE',  ( 5.676582343750001591, 51.61458332991934839, -9.832129032723420536 ) ) ;
#33208 = CARTESIAN_POINT ( 'NONE',  ( 7.188101187500002709, 97.81250000204840944, 2.977408999572649151 ) ) ;
#33210 = CARTESIAN_POINT ( 'NONE',  ( -3.313708498984758943, -7.999999999999989342, 7.111552779823365533 ) ) ;
#33211 = CARTESIAN_POINT ( 'NONE',  ( -11.35316468750000141, 178.4895833299193555, 3.042071309553159963 ) ) ;
#33212 = CARTESIAN_POINT ( 'NONE',  ( 7.320508075688771044, 136.2499999931720538, 7.320508075688775484 ) ) ;
#33213 = CARTESIAN_POINT ( 'NONE',  ( 7.188101187500000044, 102.7812500020483810, -8.802885111219163269E-16 ) ) ;
#33214 = CARTESIAN_POINT ( 'NONE',  ( -2.904230799389556861, -45.77698594726980730, 139.1363172591317152 ) ) ;
#33215 = CARTESIAN_POINT ( 'NONE',  ( 9.832129032723416984, 35.67708332991935549, 5.676582343750006032 ) ) ;
#33216 = CARTESIAN_POINT ( 'NONE',  ( 2.775557561562891351E-14, 271.9999999999999432, 139.0000000000000568 ) ) ;
#33217 = VERTEX_POINT ( 'NONE', #68709 ) ;
#33218 = DIRECTION ( 'NONE',  ( -0.7071067811865482389, -0.7071067811865469066, -0.000000000000000000 ) ) ;
#33219 = CARTESIAN_POINT ( 'NONE',  ( 10.18810118750000093, -4.220049686691933921, 69.81250000204835260 ) ) ;
#33220 = DIRECTION ( 'NONE',  ( -0.000000000000000000, 1.000000000000000000, 4.476705744456276341E-16 ) ) ;
#33222 = CARTESIAN_POINT ( 'NONE',  ( -3.042071309553163960, 172.2395833299193839, -11.35316468749999963 ) ) ;
#33221 = CARTESIAN_POINT ( 'NONE',  ( 0.000000000000000000, 125.0000000000000000, 0.000000000000000000 ) ) ;
#33223 = CARTESIAN_POINT ( 'NONE',  ( -7.999999999999991118, 0.000000000000000000, 9.886552784329824206 ) ) ;
#33224 = CARTESIAN_POINT ( 'NONE',  ( 3.042071309553163960, 222.4479166700806729, -11.35316468749999785 ) ) ;
#33225 = CARTESIAN_POINT ( 'NONE',  ( 4.471435261904963987, 50.48103707412082031, -40.99880869398744210 ) ) ;
#33226 = CARTESIAN_POINT ( 'NONE',  ( -10.18810118749999916, 4.220049686691934809, 79.93750000204839523 ) ) ;
#33227 = ORIENTED_EDGE ( 'NONE', *, *, #64067, .T. ) ;
#33228 =( BOUNDED_CURVE ( )  B_SPLINE_CURVE ( 2, ( #20518, #25802, #48822, #71829, #3189, #66178, #37521, #43532, #66547, #9216, #50685 ),
 .UNSPECIFIED., .F., .F. ) 
 B_SPLINE_CURVE_WITH_KNOTS ( ( 3, 2, 2, 2, 2, 3 ),
 ( 0.1853116620478932886, 0.1853117163647907406, 0.1919299919492475637, 0.1985482675337043590, 0.2051665431181611821, 0.2117847674899544508 ),
 .UNSPECIFIED. ) 
 CURVE ( )  GEOMETRIC_REPRESENTATION_ITEM ( )  RATIONAL_B_SPLINE_CURVE ( ( 0.9999987505525751441, 0.9999993752711603401, 1.000000000000000000, 0.9238795325112867385, 1.000000000000000000, 0.9238795325112867385, 1.000000000000000000, 0.9238795325112867385, 1.000000000000000000, 0.9238801215366059250, 0.9999988219584774463 ) ) 
 REPRESENTATION_ITEM ( '' )  );
#33229 = FACE_OUTER_BOUND ( 'NONE', #14911, .T. ) ;
#33230 = CARTESIAN_POINT ( 'NONE',  ( 3.042071309553167069, 122.1354166632526841, -11.35316468749999785 ) ) ;
#33231 = CARTESIAN_POINT ( 'NONE',  ( -4.076600168545496672E-14, -10.39230484541327471, -0.8038475772933779684 ) ) ;
#33232 = ORIENTED_EDGE ( 'NONE', *, *, #9835, .F. ) ;
#33233 = VERTEX_POINT ( 'NONE', #28716 ) ;
#33234 = CARTESIAN_POINT ( 'NONE',  ( -4.541265875000002339, 8.874999998634407916, -1.881053915767121998 ) ) ;
#33235 = CARTESIAN_POINT ( 'NONE',  ( 2.977408999572651815, 6.187499997951610986, 7.188101187500000933 ) ) ;
#33236 = CIRCLE ( 'NONE', #36827, 6.000000000000000000 ) ;
#33237 = CARTESIAN_POINT ( 'NONE',  ( 3.313708498984760720, 112.7187500040967763, -8.000000000000000000 ) ) ;
#33238 = CARTESIAN_POINT ( 'NONE',  ( -10.18810118749999916, 4.220049686691934809, 90.43750000204836681 ) ) ;
#33239 = CARTESIAN_POINT ( 'NONE',  ( -29.43265458321766559, 203.7500000013656063, 166.5412658750003629 ) ) ;
#33240 = CARTESIAN_POINT ( 'NONE',  ( -4.000000000000002665, 9.562500000000000000, 1.656854249492380804 ) ) ;
#33241 = CARTESIAN_POINT ( 'NONE',  ( -1.656854249492433206, 198.1875000000000568, 201.9999999999999432 ) ) ;
#33242 = CARTESIAN_POINT ( 'NONE',  ( 3.211159895383560947, 7.187499998634407028, 3.211159895383562723 ) ) ;
#33243 = CARTESIAN_POINT ( 'NONE',  ( 2.828427124746153876, 198.8750000000000284, 144.8284271247462129 ) ) ;
#33244 = VERTEX_POINT ( 'NONE', #11743 ) ;
#33245 = CARTESIAN_POINT ( 'NONE',  ( -4.898587196589412829E-16, 117.1250000000000000, -8.000000000000000000 ) ) ;
#33246 = PRODUCT_DEFINITION_CONTEXT ( 'detailed design', #13939, 'design' ) ;
#33248 = PLANE ( 'NONE',  #44228 ) ;
#33247 = CARTESIAN_POINT ( 'NONE',  ( -26.56734541678242678, 198.3750000013655779, 166.5412658750003345 ) ) ;
#33249 = CARTESIAN_POINT ( 'NONE',  ( -1.881053915767121554, 21.62499999863441502, -4.541265875000002339 ) ) ;
#33250 = CARTESIAN_POINT ( 'NONE',  ( -5.082755093536319713, 5.082755093536319713, 2.799052781871750994 ) ) ;
#33251 = VERTEX_POINT ( 'NONE', #34038 ) ;
#33252 = ORIENTED_EDGE ( 'NONE', *, *, #31469, .F. ) ;
#33253 = CARTESIAN_POINT ( 'NONE',  ( 7.204075437095966983, 7.204075437095967871, 89.59375000204838102 ) ) ;
#33254 = CARTESIAN_POINT ( 'NONE',  ( 32.00000000000000711, 204.3125000027312126, 171.6568542494922553 ) ) ;
#33255 = CARTESIAN_POINT ( 'NONE',  ( -28.00000000000002132, 200.6875000013656063, 166.5412658750003629 ) ) ;
#33256 = CARTESIAN_POINT ( 'NONE',  ( 4.556349186104045934, 11.00000000000000000, 110.0312500000000000 ) ) ;
#33257 = CARTESIAN_POINT ( 'NONE',  ( 3.458734125000015425, 206.2500000013656063, 196.5673454167823877 ) ) ;
#33258 = DIRECTION ( 'NONE',  ( -0.000000000000000000, 1.000000000000000000, -0.000000000000000000 ) ) ;
#33259 = CARTESIAN_POINT ( 'NONE',  ( 2.679491924311228956, 121.0416666666666714, -10.00000000000000000 ) ) ;
#33260 = EDGE_CURVE ( 'NONE', #24629, #52326, #39461, .T. ) ;
#33261 = CARTESIAN_POINT ( 'NONE',  ( -7.999999999999998224, 107.0937500000000142, 3.313708498984766493 ) ) ;
#33262 = CARTESIAN_POINT ( 'NONE',  ( 1.226468279477575784E-15, 292.8593750017070079, 6.676582343750001591 ) ) ;
#33263 = CARTESIAN_POINT ( 'NONE',  ( -5.082755093536319713, 5.082755093536319713, 7.674052781871751883 ) ) ;
#33264 = ORIENTED_EDGE ( 'NONE', *, *, #59152, .F. ) ;
#33265 = DIRECTION ( 'NONE',  ( 1.000000000000000000, 0.000000000000000000, -0.000000000000000000 ) ) ;
#33266 = CARTESIAN_POINT ( 'NONE',  ( 24.54126587499998635, 207.2500000013655779, 171.4326545832175555 ) ) ;
#33267 = CARTESIAN_POINT ( 'NONE',  ( -5.656854249492379694, 25.87499999590322375, -5.656854249492380582 ) ) ;
#33268 = CARTESIAN_POINT ( 'NONE',  ( -1.432654583217664479, 197.7500000013656063, 138.5412658750000787 ) ) ;
#33269 = CARTESIAN_POINT ( 'NONE',  ( -7.188101187499999156, 121.6250000020483810, 2.977408999572654924 ) ) ;
#33271 = CARTESIAN_POINT ( 'NONE',  ( 2.445694354108783219, 201.8125000013656063, 139.5543056458912190 ) ) ;
#33270 = CARTESIAN_POINT ( 'NONE',  ( 0.000000000000000000, 300.0000000000000000, 10.00000000000000178 ) ) ;
#33272 = CARTESIAN_POINT ( 'NONE',  ( 8.311093377946834337, 237.3437500034139589, -8.311093377946836114 ) ) ;
#33273 = DIRECTION ( 'NONE',  ( -1.110223029476700175E-14, 0.5000000000000113243, -0.8660254037844320463 ) ) ;
#33274 = CARTESIAN_POINT ( 'NONE',  ( 37.99999999999999289, 242.0000000000000284, 0.000000000000000000 ) ) ;
#33275 = CARTESIAN_POINT ( 'NONE',  ( 3.042071309553159519, 19.73958332991934483, 11.35316468750000141 ) ) ;
#33276 = CARTESIAN_POINT ( 'NONE',  ( -4.898587196589412829E-16, 123.1250000000000000, -8.000000000000000000 ) ) ;
#33277 = CARTESIAN_POINT ( 'NONE',  ( -11.35316468749999785, 213.3854166632526983, -3.042071309553167513 ) ) ;
#33278 = CARTESIAN_POINT ( 'NONE',  ( -7.320508075688773708, 133.7499999931720538, -7.320508075688774596 ) ) ;
#33279 = CARTESIAN_POINT ( 'NONE',  ( -3.673940397442060854E-16, 290.7500000000000000, -6.000000000000001776 ) ) ;
#33281 = CARTESIAN_POINT ( 'NONE',  ( -1.656854249492444975, 206.6875000000000284, 146.0000000000000000 ) ) ;
#33280 = CARTESIAN_POINT ( 'NONE',  ( 1.656854249492432318, 208.6875000000000000, 194.0000000000000568 ) ) ;
#33282 = ORIENTED_EDGE ( 'NONE', *, *, #15774, .T. ) ;
#33283 = CARTESIAN_POINT ( 'NONE',  ( 1.432654583217608080, 201.8750000013656063, 138.5412658750000503 ) ) ;
#33284 = CARTESIAN_POINT ( 'NONE',  ( 5.676582343749993598, 14.94791666325268409, 9.832129032723422313 ) ) ;
#33285 = CARTESIAN_POINT ( 'NONE',  ( 7.778174593052023411, -7.778174593052021635, 94.75000000409677625 ) ) ;
#33286 =( GEOMETRIC_REPRESENTATION_CONTEXT ( 3 ) GLOBAL_UNCERTAINTY_ASSIGNED_CONTEXT ( ( #11880 ) ) GLOBAL_UNIT_ASSIGNED_CONTEXT ( ( #57835, #52164, #46488 ) ) REPRESENTATION_CONTEXT ( 'NONE', 'WORKASPACE' ) );
#33287 = CARTESIAN_POINT ( 'NONE',  ( 4.242640687119287435, 292.3750000000000000, 4.242640687119285658 ) ) ;
#33288 = EDGE_CURVE ( 'NONE', #22076, #21755, #8033, .T. ) ;
#33289 = CARTESIAN_POINT ( 'NONE',  ( -30.44569435410886626, 197.5625000013656063, 167.5543056458916169 ) ) ;
#33290 = DIRECTION ( 'NONE',  ( -0.000000000000000000, -1.000000000000000000, -0.000000000000000000 ) ) ;
#33292 = CARTESIAN_POINT ( 'NONE',  ( -5.676582343749998039, 12.44791666325268409, -9.832129032723420536 ) ) ;
#33291 = CARTESIAN_POINT ( 'NONE',  ( -4.401442555609581635E-16, 119.2812500020483810, -7.188101187500000044 ) ) ;
#33293 = CARTESIAN_POINT ( 'NONE',  ( 7.999999999999992895, -3.313708498984756279, 28.48655277982336642 ) ) ;
#33294 = CARTESIAN_POINT ( 'NONE',  ( -5.676582343749998039, 137.4479166632526983, -9.832129032723420536 ) ) ;
#33295 = CARTESIAN_POINT ( 'NONE',  ( -4.999999999999998224, 103.5416666598386968, -8.660254037844389075 ) ) ;
#33296 = AXIS2_PLACEMENT_3D ( 'NONE', #3739, #21081, #10142 ) ;
#33297 = CARTESIAN_POINT ( 'NONE',  ( -5.082755093536325930, 121.3437500020483952, -5.082755093536325930 ) ) ;
#33298 = CARTESIAN_POINT ( 'NONE',  ( 3.211159895383560947, 20.31249999863440436, 3.211159895383562723 ) ) ;
#33299 = FACE_OUTER_BOUND ( 'NONE', #25035, .T. ) ;
#33300 = FACE_BOUND ( 'NONE', #48676, .T. ) ;
#33301 = ORIENTED_EDGE ( 'NONE', *, *, #19598, .T. ) ;
#33302 = CARTESIAN_POINT ( 'NONE',  ( -54.00000000000000711, 0.000000000000000000, 20.00000000000002132 ) ) ;
#33303 = CARTESIAN_POINT ( 'NONE',  ( 4.721056650415999201, 288.2343750017069510, -4.721056650415999201 ) ) ;
#33304 = CARTESIAN_POINT ( 'NONE',  ( 5.000000000000000888, 53.57132521838664729, 46.19376297453561619 ) ) ;
#33305 = CARTESIAN_POINT ( 'NONE',  ( -4.898587196589407898E-16, 7.999999999999991118, 3.642802783920144449 ) ) ;
#33306 = CARTESIAN_POINT ( 'NONE',  ( -41.99999999999992895, -31.99999999999978684, 205.0000000000000284 ) ) ;
#33307 = DIRECTION ( 'NONE',  ( 0.000000000000000000, -1.000000000000000000, -0.000000000000000000 ) ) ;
#33308 = CARTESIAN_POINT ( 'NONE',  ( 10.18810118749999916, 4.220049686691935698, 100.3750000020484094 ) ) ;
#33309 = ORIENTED_EDGE ( 'NONE', *, *, #32012, .T. ) ;
#33310 = CIRCLE ( 'NONE', #779, 12.50000000000000711 ) ;
#33311 = CARTESIAN_POINT ( 'NONE',  ( -29.65685424949239390, 199.5625000027312126, 174.0000000000003126 ) ) ;
#33312 = CARTESIAN_POINT ( 'NONE',  ( 5.676582343749993598, 150.2604166632526699, 9.832129032723422313 ) ) ;
#33313 = CARTESIAN_POINT ( 'NONE',  ( -7.999999999999991118, 0.000000000000000000, 24.83030277982336642 ) ) ;
#33314 = CARTESIAN_POINT ( 'NONE',  ( 3.458734125000015869, 203.1875000013656063, 198.0000000000000284 ) ) ;
#33315 = CYLINDRICAL_SURFACE ( 'NONE', #70183, 8.000000000000000000 ) ;
#33316 = CARTESIAN_POINT ( 'NONE',  ( 5.676582343749993598, 80.26041666325268409, 9.832129032723422313 ) ) ;
#33317 = ORIENTED_EDGE ( 'NONE', *, *, #52249, .F. ) ;
#33318 = CARTESIAN_POINT ( 'NONE',  ( 10.18810118749999916, 1.247682550866122264E-15, 111.9062500020483810 ) ) ;
#33319 = CARTESIAN_POINT ( 'NONE',  ( 1.881053915767122664, 8.249999998634406140, 4.541265875000001451 ) ) ;
#33320 = ORIENTED_EDGE ( 'NONE', *, *, #47975, .F. ) ;
#33321 = CARTESIAN_POINT ( 'NONE',  ( -8.000000000000000000, 2.250000000000000444, -9.797174393178825657E-16 ) ) ;
#33322 = DIRECTION ( 'NONE',  ( 0.000000000000000000, 0.000000000000000000, 1.000000000000000000 ) ) ;
#33323 = CARTESIAN_POINT ( 'NONE',  ( -7.320508075688770155, 248.7500000068279746, 7.320508075688774596 ) ) ;
#33324 = CARTESIAN_POINT ( 'NONE',  ( -5.082755093536325042, 16.40624999795161543, -5.082755093536325930 ) ) ;
#33325 = CARTESIAN_POINT ( 'NONE',  ( -7.778174593052020747, -7.778174593052023411, 103.3750000040967763 ) ) ;
#33326 = CARTESIAN_POINT ( 'NONE',  ( -6.238412754330611322E-16, 10.18810118749999916, 112.6562500020483810 ) ) ;
#33327 =( BOUNDED_CURVE ( )  B_SPLINE_CURVE ( 2, ( #21581, #16280, #34057, #73277, #28365, #68725, #45713, #74384, #5365 ),
 .UNSPECIFIED., .F., .F. ) 
 B_SPLINE_CURVE_WITH_KNOTS ( ( 3, 2, 2, 2, 3 ),
 ( 0.08333333333333352300, 0.09166666666666679897, 0.1000000000000000888, 0.1083333333333333787, 0.1166666666666666546 ),
 .UNSPECIFIED. ) 
 CURVE ( )  GEOMETRIC_REPRESENTATION_ITEM ( )  RATIONAL_B_SPLINE_CURVE ( ( 0.9999999999999982236, 0.9238795325112885148, 1.000000000000000000, 0.9238795325112867385, 1.000000000000000000, 0.9238795325112867385, 1.000000000000000000, 0.9238795325112868495, 0.9999999999999998890 ) ) 
 REPRESENTATION_ITEM ( '' )  );
#33328 = CARTESIAN_POINT ( 'NONE',  ( -11.00000000000000000, 4.556349186104045934, 75.90624999999998579 ) ) ;
#33329 = CARTESIAN_POINT ( 'NONE',  ( -1.656854249492381248, 8.062499997268812280, -4.000000000000001776 ) ) ;
#33330 =( BOUNDED_CURVE ( )  B_SPLINE_CURVE ( 2, ( #55430, #49758, #20323, #60321, #73145, #32036, #50129, #20704, #55805 ),
 .UNSPECIFIED., .F., .F. ) 
 B_SPLINE_CURVE_WITH_KNOTS ( ( 3, 2, 2, 2, 3 ),
 ( 0.6617647058823528106, 0.6654411764705880916, 0.6691176470588233727, 0.6727941176470587648, 0.6764705882352940458 ),
 .UNSPECIFIED. ) 
 CURVE ( )  GEOMETRIC_REPRESENTATION_ITEM ( )  RATIONAL_B_SPLINE_CURVE ( ( 1.000000000000002220, 0.9238795325112844070, 1.000000000000000000, 0.9238795325112867385, 1.000000000000000000, 0.9238795325112867385, 1.000000000000000000, 0.9238795325112890700, 0.9999999999999976685 ) ) 
 REPRESENTATION_ITEM ( '' )  );
#33331 = CARTESIAN_POINT ( 'NONE',  ( 4.000000000000000888, 17.93750000000000355, 1.656854249492384135 ) ) ;
#33332 = ORIENTED_EDGE ( 'NONE', *, *, #40133, .T. ) ;
#33333 = CARTESIAN_POINT ( 'NONE',  ( -1.432654583217607192, 203.2500000013656063, 194.5412658750000219 ) ) ;
#33334 = CARTESIAN_POINT ( 'NONE',  ( -31.45873412499999944, 207.6875000013656063, 170.0000000000004547 ) ) ;
#33335 = CARTESIAN_POINT ( 'NONE',  ( -10.18810118749999916, 4.220049686691934809, 69.43750000204838102 ) ) ;
#33336 = CARTESIAN_POINT ( 'NONE',  ( -8.342170076843785083E-16, 6.062499998634407028, 4.541265875000002339 ) ) ;
#33337 = CARTESIAN_POINT ( 'NONE',  ( 2.977408999572646486, 7.188101187499991163, 19.01780278187175810 ) ) ;
#33338 = ORIENTED_EDGE ( 'NONE', *, *, #65271, .T. ) ;
#33339 = CARTESIAN_POINT ( 'NONE',  ( -5.082755093536326818, 26.90624999795161543, 5.082755093536325042 ) ) ;
#33340 = ORIENTED_EDGE ( 'NONE', *, *, #63422, .F. ) ;
#33341 = CARTESIAN_POINT ( 'NONE',  ( 4.220049686691941027, -10.18810118749999738, 108.6250000020483668 ) ) ;
#33342 = CARTESIAN_POINT ( 'NONE',  ( -1.656854249492381248, 18.31250000000000000, -4.000000000000001776 ) ) ;
#33343 = CARTESIAN_POINT ( 'NONE',  ( 2.839093476692135984E-14, 205.6875000013656063, 201.4587341250000350 ) ) ;
#33344 = CARTESIAN_POINT ( 'NONE',  ( 25.55430564589119058, 198.3125000013656063, 172.4456943541087526 ) ) ;
#33345 = CARTESIAN_POINT ( 'NONE',  ( 8.660254037844389075, 85.41666666666667140, -5.000000000000000000 ) ) ;
#33346 = EDGE_CURVE ( 'NONE', #70231, #6481, #28880, .T. ) ;
#33347 = CARTESIAN_POINT ( 'NONE',  ( 3.313708498984760720, 124.5312500000000142, -8.000000000000000000 ) ) ;
#33348 = CARTESIAN_POINT ( 'NONE',  ( 6.000000000000001776, 293.5000000000000000, -7.347880794884121708E-16 ) ) ;
#33349 = CARTESIAN_POINT ( 'NONE',  ( 31.99999999999998579, 203.4375000027312126, 168.3431457505075173 ) ) ;
#33350 = ORIENTED_EDGE ( 'NONE', *, *, #44827, .F. ) ;
#33351 = EDGE_CURVE ( 'NONE', #60808, #37692, #10631, .T. ) ;
#33352 = CARTESIAN_POINT ( 'NONE',  ( 2.085542519210945334E-15, 220.1562500034139873, 11.35316468749999963 ) ) ;
#33353 = CARTESIAN_POINT ( 'NONE',  ( 2.069125466541355873, -10.11940336925128214, 70.25556669588236502 ) ) ;
#33354 = CARTESIAN_POINT ( 'NONE',  ( 3.999999999999959144, 197.1875000027312694, 140.3431457505076594 ) ) ;
#33355 = CARTESIAN_POINT ( 'NONE',  ( -5.000000000000000000, 60.90295814858222201, 23.31388853594875599 ) ) ;
#33356 = PLANE ( 'NONE',  #15949 ) ;
#33357 = CARTESIAN_POINT ( 'NONE',  ( -9.999999999999998224, 245.2083333333333428, 2.679491924311235618 ) ) ;
#33358 = DIRECTION ( 'NONE',  ( 0.000000000000000000, 0.000000000000000000, 1.000000000000000000 ) ) ;
#33359 = CARTESIAN_POINT ( 'NONE',  ( 6.123233995736767268E-16, 201.2500000000000000, -10.00000000000000178 ) ) ;
#33360 = DIRECTION ( 'NONE',  ( -0.000000000000000000, 1.000000000000000000, -0.000000000000000000 ) ) ;
#33361 = CARTESIAN_POINT ( 'NONE',  ( 7.188101187499992051, 8.802885111219154394E-16, 14.61155278187175455 ) ) ;
#33362 = CARTESIAN_POINT ( 'NONE',  ( 3.042071309553159519, 170.0520833299193271, 11.35316468750000141 ) ) ;
#33363 = CARTESIAN_POINT ( 'NONE',  ( -1.656854249492379916, 204.4375000027312410, 138.0000000000000284 ) ) ;
#33364 = CARTESIAN_POINT ( 'NONE',  ( 5.094045771088254959, 8.823157229062946527, 67.15552375567561683 ) ) ;
#33366 = CARTESIAN_POINT ( 'NONE',  ( -2.828427124746190735, 7.124999997268813168, -2.828427124746191623 ) ) ;
#33365 = CARTESIAN_POINT ( 'NONE',  ( -1.836970198721029983E-15, 85.62499999317203958, 10.00000000000000178 ) ) ;
#33367 = EDGE_LOOP ( 'NONE', ( #57143, #72629, #66569, #8260 ) ) ;
#33368 = CARTESIAN_POINT ( 'NONE',  ( -5.676582343750006032, 19.42708332991934839, 9.832129032723418760 ) ) ;
#33369 = EDGE_CURVE ( 'NONE', #1466, #64770, #49151, .T. ) ;
#33370 = CARTESIAN_POINT ( 'NONE',  ( 2.751064625579944321E-14, 198.7500000000000000, 194.0000000000000568 ) ) ;
#33372 = CARTESIAN_POINT ( 'NONE',  ( -3.544144923088220711, -10.27124247550359826, -63.97955030412420996 ) ) ;
#33371 = CARTESIAN_POINT ( 'NONE',  ( 0.000000000000000000, 300.0000000000000000, 0.000000000000000000 ) ) ;
#33373 = CARTESIAN_POINT ( 'NONE',  ( 11.00000000000000000, 1.347111479062088405E-15, 118.0000000000000000 ) ) ;
#33374 = CARTESIAN_POINT ( 'NONE',  ( 1.432654583217607192, 204.2500000013655779, 145.4587341250000350 ) ) ;
#33375 = CARTESIAN_POINT ( 'NONE',  ( 10.00000000000000178, 62.08333332650536818, -2.679491924311226736 ) ) ;
#33376 = CARTESIAN_POINT ( 'NONE',  ( 1.320432766682874540E-15, 105.0312500020483810, 7.188101187500000044 ) ) ;
#33377 = CARTESIAN_POINT ( 'NONE',  ( -3.211159895383561391, 7.812499998634407028, -3.211159895383561835 ) ) ;
#33378 = DIRECTION ( 'NONE',  ( -0.000000000000000000, -0.000000000000000000, -1.000000000000000000 ) ) ;
#33379 = CARTESIAN_POINT ( 'NONE',  ( 7.999999999999991118, 3.313708498984757611, 3.174052779823361981 ) ) ;
#33380 = CARTESIAN_POINT ( 'NONE',  ( 8.660254037844403285, 160.4166666666666856, -5.000000000000008882 ) ) ;
#33381 = ORIENTED_EDGE ( 'NONE', *, *, #47224, .T. ) ;
#33382 = VERTEX_POINT ( 'NONE', #62670 ) ;
#33383 = CARTESIAN_POINT ( 'NONE',  ( -1.656854249492365705, 205.3125000027312126, 202.0000000000000000 ) ) ;
#33384 = CARTESIAN_POINT ( 'NONE',  ( 2.754378923186476579E-14, 195.4375000013655779, 194.5412658750000219 ) ) ;
#33385 = CARTESIAN_POINT ( 'NONE',  ( 4.556349186104045934, 11.00000000000000000, 104.0312499999999858 ) ) ;
#33386 = VECTOR ( 'NONE', #30993, 1000.000000000000000 ) ;
#33387 = CARTESIAN_POINT ( 'NONE',  ( -3.042071309553166625, 223.1770833367473017, -11.35316468749999608 ) ) ;
#33388 = CARTESIAN_POINT ( 'NONE',  ( 8.311093377946837890, 146.4062499965860127, -8.311093377946837890 ) ) ;
#33389 = ORIENTED_EDGE ( 'NONE', *, *, #62565, .F. ) ;
#33390 = CARTESIAN_POINT ( 'NONE',  ( 7.999999999999992895, -3.313708498984756279, 10.67405278392014623 ) ) ;
#33391 = CARTESIAN_POINT ( 'NONE',  ( -10.18810118749999916, 0.000000000000000000, 87.15625000204838102 ) ) ;
#33392 = CARTESIAN_POINT ( 'NONE',  ( -28.70021146449832727, 194.4653435848668721, 166.5984737776517761 ) ) ;
#33393 = CARTESIAN_POINT ( 'NONE',  ( -3.999999999999959144, 208.0625000000000000, 199.6568542494924259 ) ) ;
#33394 = DIRECTION ( 'NONE',  ( -0.000000000000000000, 1.000000000000000000, 4.689100369878284071E-30 ) ) ;
#33395 = CARTESIAN_POINT ( 'NONE',  ( 2.020667218593132706E-15, -11.00000000000000000, 73.56250000409676204 ) ) ;
#33396 = CARTESIAN_POINT ( 'NONE',  ( 1.469576158976823947E-15, 116.5625000040967763, 8.000000000000000000 ) ) ;
#33397 = DIRECTION ( 'NONE',  ( 0.000000000000000000, 0.000000000000000000, 1.000000000000000000 ) ) ;
#33398 = EDGE_LOOP ( 'NONE', ( #22119, #33252, #57264, #52617 ) ) ;
#33399 = CARTESIAN_POINT ( 'NONE',  ( 8.000000000000000000, 106.4375000040967763, -9.797174393178825657E-16 ) ) ;
#33400 = EDGE_CURVE ( 'NONE', #34152, #27667, #35146, .T. ) ;
#33401 = CARTESIAN_POINT ( 'NONE',  ( 49.26344083597084733, 45.24085890704858315, 58.96767091637842384 ) ) ;
#33402 = CARTESIAN_POINT ( 'NONE',  ( 9.832129032723420536, 121.5104166632526841, -5.676582343749999815 ) ) ;
#33403 = CARTESIAN_POINT ( 'NONE',  ( 2.839093476692135984E-14, 202.6875000013656063, 201.4587341250000350 ) ) ;
#33404 = CARTESIAN_POINT ( 'NONE',  ( 4.401442555609581635E-16, 19.21874999795161543, -7.188101187500000044 ) ) ;
#33405 = CARTESIAN_POINT ( 'NONE',  ( -10.18810118749999916, 0.000000000000000000, 86.03125000204836681 ) ) ;
#33406 = CARTESIAN_POINT ( 'NONE',  ( 11.35316468749999785, 35.88541666325268409, 3.042071309553174174 ) ) ;
#33407 = VERTEX_POINT ( 'NONE', #58160 ) ;
#33408 = CARTESIAN_POINT ( 'NONE',  ( -1.836970198721029983E-15, 100.6249999931720396, 10.00000000000000178 ) ) ;
#33409 = CARTESIAN_POINT ( 'NONE',  ( -8.008118988124991233, 0.000000000000000000, 17.51311528394063188 ) ) ;
#33410 = CARTESIAN_POINT ( 'NONE',  ( -2.754378923186476579E-14, 209.4375000013656063, 145.4587341250000350 ) ) ;
#33411 = CARTESIAN_POINT ( 'NONE',  ( -4.000000000000002665, 7.562500000000000000, 1.656854249492380582 ) ) ;
#33412 = CARTESIAN_POINT ( 'NONE',  ( -2.977408999572654480, 10.49999999795161010, 7.188101187499999156 ) ) ;
#33413 = CARTESIAN_POINT ( 'NONE',  ( -2.485281374238571761, 294.8750000034140157, -6.000000000000003553 ) ) ;
#33414 = CARTESIAN_POINT ( 'NONE',  ( 2.679491924311296014, 110.8333333265053682, 9.999999999999959144 ) ) ;
#33415 = CARTESIAN_POINT ( 'NONE',  ( -28.00000000000008171, 208.1250000027312126, 166.0000000000003695 ) ) ;
#33416 = ORIENTED_EDGE ( 'NONE', *, *, #5400, .F. ) ;
#33417 = CARTESIAN_POINT ( 'NONE',  ( 11.35316468750000141, 151.0937499965860411, 0.000000000000000000 ) ) ;
#33418 = VECTOR ( 'NONE', #20972, 1000.000000000000114 ) ;
#33419 = CARTESIAN_POINT ( 'NONE',  ( 10.18810118749999916, 1.247682550866122264E-15, 78.90625000204836681 ) ) ;
#33420 = CARTESIAN_POINT ( 'NONE',  ( -27.99999999999996803, 209.1875000013656063, 173.4587341250003760 ) ) ;
#33421 = CARTESIAN_POINT ( 'NONE',  ( 7.999999999999998224, 26.90625000000000355, 3.313708498984766493 ) ) ;
#33422 = CARTESIAN_POINT ( 'NONE',  ( -8.342170076843785083E-16, 14.18749999863440792, 4.541265875000002339 ) ) ;
#33423 = ORIENTED_EDGE ( 'NONE', *, *, #16036, .F. ) ;
#33424 =( BOUNDED_CURVE ( )  B_SPLINE_CURVE ( 2, ( #33826, #56823, #5144, #28137, #53388 ),
 .UNSPECIFIED., .F., .F. ) 
 B_SPLINE_CURVE_WITH_KNOTS ( ( 3, 2, 3 ),
 ( 0.000000000000000000, 0.01041666666666551944, 0.02083333333333103887 ),
 .UNSPECIFIED. ) 
 CURVE ( )  GEOMETRIC_REPRESENTATION_ITEM ( )  RATIONAL_B_SPLINE_CURVE ( ( 1.000000000000000000, 0.9238795325112867385, 1.000000000000000000, 0.9238795325113035029, 0.9999999999999832356 ) ) 
 REPRESENTATION_ITEM ( '' )  );
#33425 = CARTESIAN_POINT ( 'NONE',  ( -2.828427124746152987, 198.2500000027312126, 200.8284271247462129 ) ) ;
#33426 =( BOUNDED_CURVE ( )  B_SPLINE_CURVE ( 2, ( #47704, #66175, #8843, #37893, #3940, #73336, #44666, #44292, #67306 ),
 .UNSPECIFIED., .F., .F. ) 
 B_SPLINE_CURVE_WITH_KNOTS ( ( 3, 2, 2, 2, 3 ),
 ( 0.7000000000000006217, 0.7083333333333340365, 0.7166666666666673402, 0.7250000000000006439, 0.7333333333333339477 ),
 .UNSPECIFIED. ) 
 CURVE ( )  GEOMETRIC_REPRESENTATION_ITEM ( )  RATIONAL_B_SPLINE_CURVE ( ( 0.9999999999999938938, 0.9238795325112928447, 1.000000000000000000, 0.9238795325112867385, 1.000000000000000000, 0.9238795325112867385, 1.000000000000000000, 0.9238795325112806323, 1.000000000000005995 ) ) 
 REPRESENTATION_ITEM ( '' )  );
#33427 = CARTESIAN_POINT ( 'NONE',  ( -2.445694354108840063, 196.0625000013656063, 139.5543056458912190 ) ) ;
#33428 = CARTESIAN_POINT ( 'NONE',  ( -29.65685424949229088, 204.5625000027312126, 174.0000000000004547 ) ) ;
#33429 = CARTESIAN_POINT ( 'NONE',  ( -1.469576158976823947E-15, 22.12500000000000355, 8.000000000000000000 ) ) ;
#33430 = VERTEX_POINT ( 'NONE', #6826 ) ;
#33431 = CARTESIAN_POINT ( 'NONE',  ( 2.977408999572650927, 8.249999997951611874, -7.188101187500000933 ) ) ;
#33432 = CARTESIAN_POINT ( 'NONE',  ( 0.000000000000000000, 0.000000000000000000, 0.000000000000000000 ) ) ;
#33433 = CIRCLE ( 'NONE', #55129, 18.00000000000000000 ) ;
#33434 = CARTESIAN_POINT ( 'NONE',  ( 5.000000000000000000, 50.64189880742144823, -41.08656465431842975 ) ) ;
#33435 = CARTESIAN_POINT ( 'NONE',  ( -4.999999999999998224, 41.66666666666667140, -8.660254037844389075 ) ) ;
#33436 = CARTESIAN_POINT ( 'NONE',  ( 2.977408999572650039, 107.5625000020483810, -7.188101187500001821 ) ) ;
#33437 = CARTESIAN_POINT ( 'NONE',  ( -30.44569435410879521, 209.0625000013656063, 172.4456943541092357 ) ) ;
#33438 = CARTESIAN_POINT ( 'NONE',  ( 2.765530957082001251, 289.7656250017069510, 6.676582343749999815 ) ) ;
#33440 = DIRECTION ( 'NONE',  ( -3.469446951953619612E-16, 0.000000000000000000, -1.000000000000000000 ) ) ;
#33439 = CARTESIAN_POINT ( 'NONE',  ( 9.999999999999998224, 35.20833333333333570, -2.679491924311226292 ) ) ;
#33441 = VERTEX_POINT ( 'NONE', #59617 ) ;
#33442 =( BOUNDED_CURVE ( )  B_SPLINE_CURVE ( 2, ( #12186, #58599, #52557, #46892, #6905, #47618, #18595, #46521, #69540 ),
 .UNSPECIFIED., .F., .F. ) 
 B_SPLINE_CURVE_WITH_KNOTS ( ( 3, 2, 2, 2, 3 ),
 ( 0.2894736842105262720, 0.2960526315789473450, 0.3026315789473684181, 0.3092105263157894912, 0.3157894736842105643 ),
 .UNSPECIFIED. ) 
 CURVE ( )  GEOMETRIC_REPRESENTATION_ITEM ( )  RATIONAL_B_SPLINE_CURVE ( ( 1.000000000000000666, 0.9238795325112860723, 1.000000000000000000, 0.9238795325112867385, 1.000000000000000000, 0.9238795325112867385, 1.000000000000000000, 0.9238795325112860723, 1.000000000000000666 ) ) 
 REPRESENTATION_ITEM ( '' )  );
#33443 = EDGE_CURVE ( 'NONE', #40449, #53476, #47592, .T. ) ;
#33444 = CARTESIAN_POINT ( 'NONE',  ( 8.311093377946839666, 260.7812500034140157, 8.311093377946829008 ) ) ;
#33445 = CLOSED_SHELL ( 'NONE', ( #8476, #11695, #74305, #73855, #55223, #58205, #32169, #72535, #234, #73042, #25489, #28041, #56953, #22338, #72680, #10145, #50815, #72630, #62508, #18435, #13577, #7440, #40641, #41771, #34889, #68339, #43980, #26425, #13662, #62246, #23740, #7793, #35963, #8335, #45321, #39731, #20070, #55131, #5663, #57058, #52253, #71525, #56158, #3351, #40827, #19267, #3910, #72637, #3981, #36375, #61167, #12863, #74006, #47118, #36502, #146, #24202, #17147, #30247, #70526, #21992, #13787, #11738, #49158, #20558, #27348, #42097, #46702, #51844, #36913, #64840, #37767, #57935, #26441, #7543, #62358, #40863, #62034, #32070, #24716, #51003, #49155, #8989, #11684, #31030, #60181, #60088, #49544, #38878, #14232, #31163, #43862, #38805, #59478, #40678, #7576, #59282, #8803, #18577, #18193, #53449, #9577, #71042, #12958, #40441, #39555, #9280, #16957, #55088, #37655, #54670, #2064, #26656, #27795, #40389, #29335, #34101, #14570, #66213, #62363, #72179, #55505, #71253, #36066, #53703, #17911, #24332, #59063, #11716, #12250, #54559, #32965, #13585, #35736, #4236, #64331, #17635, #69309, #26741, #48219, #688, #16031, #52990 ) ) ;
#33446 = CARTESIAN_POINT ( 'NONE',  ( -2.977408999572647819, 7.188101187499991163, 25.58030278187175810 ) ) ;
#33447 = CARTESIAN_POINT ( 'NONE',  ( -6.891449706549017229, 51.31760009878102835, 41.45518442798194059 ) ) ;
#33448 = CARTESIAN_POINT ( 'NONE',  ( 7.188101187500000044, 0.8437499979516100979, 0.000000000000000000 ) ) ;
#33449 = CARTESIAN_POINT ( 'NONE',  ( 13.99999999999999822, 0.000000000000000000, 0.000000000000000000 ) ) ;
#33450 = CARTESIAN_POINT ( 'NONE',  ( 2.445694354108840063, 195.0625000013656063, 200.4456943541088663 ) ) ;
#33451 = CARTESIAN_POINT ( 'NONE',  ( -10.00000000000000355, 147.7083333333333144, 2.679491924311223183 ) ) ;
#33452 = CARTESIAN_POINT ( 'NONE',  ( 11.00000000000000000, 1.347111479062088405E-15, 118.0000000000000000 ) ) ;
#33453 = CARTESIAN_POINT ( 'NONE',  ( 9.765709903158406036, 15.14637444941022792, -0.009429105422156979638 ) ) ;
#33454 = CARTESIAN_POINT ( 'NONE',  ( -5.656854249492378806, 90.68750000000000000, 5.656854249492381470 ) ) ;
#33455 = CARTESIAN_POINT ( 'NONE',  ( -11.35316468749999785, 123.3854166632526699, -3.042071309553167513 ) ) ;
#33456 = CARTESIAN_POINT ( 'NONE',  ( 8.660254037844389075, 212.2916666598387110, -5.000000000000000000 ) ) ;
#33457 = CARTESIAN_POINT ( 'NONE',  ( 7.778174593052023411, -7.778174593052021635, 72.06249999999998579 ) ) ;
#33460 = CARTESIAN_POINT ( 'NONE',  ( -6.123233995736766282E-16, 241.8750000068280031, -10.00000000000000000 ) ) ;
#33459 = CARTESIAN_POINT ( 'NONE',  ( 29.43265458321760519, 196.8750000013656063, 166.5412658749999650 ) ) ;
#33458 = CARTESIAN_POINT ( 'NONE',  ( 24.00000000000001066, 208.6875000000000284, 168.3431457505075173 ) ) ;
#33461 = ORIENTED_EDGE ( 'NONE', *, *, #23238, .T. ) ;
#33462 = CARTESIAN_POINT ( 'NONE',  ( 9.992507110355417055, 225.0379066577874880, -0.4855310866818578486 ) ) ;
#33463 = FACE_OUTER_BOUND ( 'NONE', #40570, .T. ) ;
#33464 = VECTOR ( 'NONE', #65350, 1000.000000000000000 ) ;
#33465 = CARTESIAN_POINT ( 'NONE',  ( 31.45873412499999944, 198.0000000013656063, 168.5673454167822740 ) ) ;
#33466 = EDGE_CURVE ( 'NONE', #11029, #30991, #1825, .T. ) ;
#33467 = CARTESIAN_POINT ( 'NONE',  ( -11.35316468750000141, 203.5937499965860127, -1.390361679473963753E-15 ) ) ;
#33468 = CARTESIAN_POINT ( 'NONE',  ( -7.188101187500000044, 122.6562500020483810, 0.000000000000000000 ) ) ;
#33469 = CARTESIAN_POINT ( 'NONE',  ( 3.211159895383560947, 17.18749999863440792, 3.211159895383562723 ) ) ;
#33470 = CARTESIAN_POINT ( 'NONE',  ( 24.54126587499997569, 195.5000000013656347, 171.4326545832175555 ) ) ;
#33471 = CARTESIAN_POINT ( 'NONE',  ( -5.656854249492373476, -5.656854249492376141, 26.51780277982336997 ) ) ;
#33473 = CARTESIAN_POINT ( 'NONE',  ( -27.99999999999995737, 202.5000000000000000, 174.0000000000003695 ) ) ;
#33472 = DIRECTION ( 'NONE',  ( -1.000000000000000000, 0.000000000000000000, -0.000000000000000000 ) ) ;
#33474 = CARTESIAN_POINT ( 'NONE',  ( -5.676582343749998039, 97.44791666325269830, -9.832129032723420536 ) ) ;
#33475 = ORIENTED_EDGE ( 'NONE', *, *, #27549, .F. ) ;
#33476 = EDGE_CURVE ( 'NONE', #46180, #37342, #58803, .T. ) ;
#33477 = CARTESIAN_POINT ( 'NONE',  ( -7.188101187500001821, 22.12499999795161187, -2.977408999572651371 ) ) ;
#33478 = DIRECTION ( 'NONE',  ( -1.000000000000000000, 0.000000000000000000, 0.000000000000000000 ) ) ;
#33479 = CARTESIAN_POINT ( 'NONE',  ( 5.676582343750005144, 255.8854166700806445, 9.832129032723416984 ) ) ;
#33480 = CARTESIAN_POINT ( 'NONE',  ( -3.042071309553164404, 107.2395833299193413, -11.35316468749999963 ) ) ;
#33481 = ORIENTED_EDGE ( 'NONE', *, *, #49345, .F. ) ;
#33482 = CARTESIAN_POINT ( 'NONE',  ( 7.320508075688774596, 207.4999999931720254, -7.320508075688774596 ) ) ;
#33483 = CARTESIAN_POINT ( 'NONE',  ( 4.220049686691934809, 10.18810118749999916, 106.1875000020483810 ) ) ;
#33484 = LINE ( 'NONE', #60642, #12903 ) ;
#33485 = CARTESIAN_POINT ( 'NONE',  ( -2.445694354108783219, 205.8125000013656063, 200.4456943541088663 ) ) ;
#33486 = CARTESIAN_POINT ( 'NONE',  ( -29.65685424949239746, 201.1875000027312694, 166.0000000000003126 ) ) ;
#33488 = CARTESIAN_POINT ( 'NONE',  ( 8.311093377946837890, 86.40624999658599847, -8.311093377946837890 ) ) ;
#33487 = CARTESIAN_POINT ( 'NONE',  ( -31.99999999999998579, 202.3125000000000000, 171.6568542494928238 ) ) ;
#33489 = CARTESIAN_POINT ( 'NONE',  ( 5.656854249492376141, -5.656854249492374365, 10.58030278392014800 ) ) ;
#33490 = CARTESIAN_POINT ( 'NONE',  ( -30.44569435410879166, 199.0625000013656063, 172.4456943541092357 ) ) ;
#33491 = CARTESIAN_POINT ( 'NONE',  ( -5.656854249492379694, 21.37499999590322375, -5.656854249492380582 ) ) ;
#33492 = CARTESIAN_POINT ( 'NONE',  ( -10.00000000000000000, 184.1666666598386826, -2.679491924311229845 ) ) ;
#33493 = LINE ( 'NONE', #45904, #29876 ) ;
#33494 = ADVANCED_FACE ( 'NONE', ( #12394 ), #6746, .F. ) ;
#33495 = CARTESIAN_POINT ( 'NONE',  ( 6.000000000000003553, 296.5000000034139589, 2.485281374238571317 ) ) ;
#33496 = CARTESIAN_POINT ( 'NONE',  ( -3.042071309553163960, 77.55208332991934128, -11.35316468749999963 ) ) ;
#33497 = CARTESIAN_POINT ( 'NONE',  ( -6.676582343750001591, 289.4531250017069510, 0.000000000000000000 ) ) ;
#33498 = EDGE_CURVE ( 'NONE', #24477, #60299, #70319, .T. ) ;
#33499 = CARTESIAN_POINT ( 'NONE',  ( 1.871523826299183495E-15, -10.18810118749999916, 101.4062500020483810 ) ) ;
#33500 = CARTESIAN_POINT ( 'NONE',  ( 8.311093377946834337, 225.1562499965860411, 8.311093377946839666 ) ) ;
#33501 = ORIENTED_EDGE ( 'NONE', *, *, #66030, .F. ) ;
#33502 = CARTESIAN_POINT ( 'NONE',  ( -4.000000000000002665, 2.562500000000000444, 1.656854249492380582 ) ) ;
#33503 = LINE ( 'NONE', #5194, #28017 ) ;
#33504 = CARTESIAN_POINT ( 'NONE',  ( -4.898587196589412829E-16, 90.31250000409676204, -8.000000000000000000 ) ) ;
#33505 = CARTESIAN_POINT ( 'NONE',  ( 11.35316468749999785, 205.5729166632526699, 3.042071309553174174 ) ) ;
#33506 = CARTESIAN_POINT ( 'NONE',  ( -10.00000000000000000, 223.1250000068279746, 0.000000000000000000 ) ) ;
#33507 = CARTESIAN_POINT ( 'NONE',  ( -7.320508075688778149, 99.99999999317203958, 7.320508075688769267 ) ) ;
#33508 = CARTESIAN_POINT ( 'NONE',  ( -6.000000000000001776, 300.0000000000000000, 0.000000000000000000 ) ) ;
#33509 = VERTEX_POINT ( 'NONE', #20260 ) ;
#33510 = AXIS2_PLACEMENT_3D ( 'NONE', #66763, #60348, #54710 ) ;
#33511 = CARTESIAN_POINT ( 'NONE',  ( -8.311093377946836114, 197.9687499965860411, -8.311093377946837890 ) ) ;
#33512 = CARTESIAN_POINT ( 'NONE',  ( -7.188101187499992051, 0.000000000000000000, 17.98655278187175455 ) ) ;
#33513 = CARTESIAN_POINT ( 'NONE',  ( -31.45873412499999944, 208.6875000013656063, 170.0000000000003979 ) ) ;
#33514 = CARTESIAN_POINT ( 'NONE',  ( -3.313708498984765161, 13.03125000000000355, 7.999999999999998224 ) ) ;
#33515 = VERTEX_POINT ( 'NONE', #32359 ) ;
#33516 = ADVANCED_FACE ( 'NONE', ( #26678 ), #47163, .F. ) ;
#33517 = VECTOR ( 'NONE', #64171, 1000.000000000000000 ) ;
#33518 = CARTESIAN_POINT ( 'NONE',  ( 3.313708498984760720, 90.21875000409679046, -8.000000000000000000 ) ) ;
#33519 = ADVANCED_FACE ( 'NONE', ( #21862 ), #57713, .T. ) ;
#33520 = CARTESIAN_POINT ( 'NONE',  ( 10.00000000000000178, 10.20833333333333393, -2.679491924311226736 ) ) ;
#33521 = VECTOR ( 'NONE', #35500, 1000.000000000000000 ) ;
#33522 = CARTESIAN_POINT ( 'NONE',  ( 10.18810118749999916, 4.220049686691935698, 79.37500000204838102 ) ) ;
#33523 = ORIENTED_EDGE ( 'NONE', *, *, #15952, .T. ) ;
#33524 = EDGE_CURVE ( 'NONE', #4164, #57226, #36596, .T. ) ;
#33525 = CARTESIAN_POINT ( 'NONE',  ( -1.656854249492383691, 20.68750000000000000, 4.000000000000000888 ) ) ;
#33526 = CARTESIAN_POINT ( 'NONE',  ( -4.541265875000002339, 18.81249999863440436, -5.561446717895856393E-16 ) ) ;
#33527 = CARTESIAN_POINT ( 'NONE',  ( 30.61924198572770450, 194.6825674383569833, 167.4014549884537075 ) ) ;
#33528 = ORIENTED_EDGE ( 'NONE', *, *, #53779, .T. ) ;
#33529 = CYLINDRICAL_SURFACE ( 'NONE', #33148, 11.00000000000000000 ) ;
#33530 = CARTESIAN_POINT ( 'NONE',  ( -5.082755093536325930, 89.46875000204838102, -5.082755093536325930 ) ) ;
#33533 = DIRECTION ( 'NONE',  ( -0.000000000000000000, 1.000000000000000000, -0.000000000000000000 ) ) ;
#33532 = CARTESIAN_POINT ( 'NONE',  ( -8.311093377946834337, 249.5312500034139873, 8.311093377946837890 ) ) ;
#33531 = CARTESIAN_POINT ( 'NONE',  ( 30.44569435410883429, 208.5625000013656063, 172.4456943541086957 ) ) ;
#33534 = APPLICATION_PROTOCOL_DEFINITION ( 'draft international standard', 'automotive_design', 1998, #19676 ) ;
#33535 = VERTEX_POINT ( 'NONE', #23732 ) ;
#33536 = CARTESIAN_POINT ( 'NONE',  ( -8.311093377946834337, 254.8437500034139873, 8.311093377946837890 ) ) ;
#33537 = CARTESIAN_POINT ( 'NONE',  ( 7.188101187499992051, 8.802885111219154394E-16, 14.23655278187175455 ) ) ;
#33538 = VERTEX_POINT ( 'NONE', #52413 ) ;
#33539 =( BOUNDED_CURVE ( )  B_SPLINE_CURVE ( 2, ( #40900, #36719, #52963, #59730, #18990, #6938, #12219, #53704, #24277 ),
 .UNSPECIFIED., .F., .F. ) 
 B_SPLINE_CURVE_WITH_KNOTS ( ( 3, 2, 2, 2, 3 ),
 ( 0.3229166666666665186, 0.3281249999999998335, 0.3333333333333331483, 0.3385416666666665186, 0.3437499999999998335 ),
 .UNSPECIFIED. ) 
 CURVE ( )  GEOMETRIC_REPRESENTATION_ITEM ( )  RATIONAL_B_SPLINE_CURVE ( ( 1.000000000000002442, 0.9238795325112842960, 1.000000000000000000, 0.9238795325112867385, 1.000000000000000000, 0.9238795325112867385, 1.000000000000000000, 0.9238795325112891810, 0.9999999999999975575 ) ) 
 REPRESENTATION_ITEM ( '' )  );
#33540 = ORIENTED_EDGE ( 'NONE', *, *, #35808, .F. ) ;
#33541 = CARTESIAN_POINT ( 'NONE',  ( 10.18810118750000093, -4.220049686691933033, 77.31250000204836681 ) ) ;
#33542 = CARTESIAN_POINT ( 'NONE',  ( -5.676582343750006032, 84.42708332991935549, 9.832129032723418760 ) ) ;
#33543 = DIRECTION ( 'NONE',  ( 0.000000000000000000, 0.000000000000000000, -1.000000000000000000 ) ) ;
#33544 = CARTESIAN_POINT ( 'NONE',  ( -7.778174593052020747, -7.778174593052023411, 89.68749999999998579 ) ) ;
#33547 = CARTESIAN_POINT ( 'NONE',  ( -4.088227598258586603E-16, 288.3593750017070079, -6.676582343750001591 ) ) ;
#33546 = CARTESIAN_POINT ( 'NONE',  ( 29.43265458321766559, 208.5000000013656063, 173.4587341249998929 ) ) ;
#33545 = CARTESIAN_POINT ( 'NONE',  ( 30.44569435410879521, 207.8125000013656063, 172.4456943541087526 ) ) ;
#33548 = CARTESIAN_POINT ( 'NONE',  ( 5.000000000000001776, 77.70833332650536818, -8.660254037844389075 ) ) ;
#33549 = CARTESIAN_POINT ( 'NONE',  ( 1.469576158976823947E-15, 101.3750000000000000, 8.000000000000000000 ) ) ;
#33550 = CARTESIAN_POINT ( 'NONE',  ( 8.311093377946837890, 206.4062499965860127, -8.311093377946837890 ) ) ;
#33551 = CARTESIAN_POINT ( 'NONE',  ( -8.000000000000001776, 6.656249995903221084, 3.313708498984759387 ) ) ;
#33552 = VERTEX_POINT ( 'NONE', #18074 ) ;
#33553 = CARTESIAN_POINT ( 'NONE',  ( 24.54126587500000412, 209.3750000013656063, 168.5673454167822172 ) ) ;
#33554 = CARTESIAN_POINT ( 'NONE',  ( -5.082755093536326818, 19.78124999795161543, 5.082755093536325042 ) ) ;
#33555 = CARTESIAN_POINT ( 'NONE',  ( -11.35316468750000141, 168.8020833299193271, 3.042071309553159963 ) ) ;
#33556 = CARTESIAN_POINT ( 'NONE',  ( 0.000000000000000000, 22.00000000000000000, 8.000000000000003553 ) ) ;
#33557 = CARTESIAN_POINT ( 'NONE',  ( -7.188101187499999156, 106.6250000020483810, 2.977408999572654924 ) ) ;
#33559 = CARTESIAN_POINT ( 'NONE',  ( -0.4501631047669842345, -51.14740050675992222, -48.52018030598949139 ) ) ;
#33558 = CARTESIAN_POINT ( 'NONE',  ( 0.000000000000000000, 300.0000000000000000, 0.000000000000000000 ) ) ;
#33560 = CARTESIAN_POINT ( 'NONE',  ( 29.43265458321766914, 206.1250000013656063, 166.5412658749999650 ) ) ;
#33561 = CARTESIAN_POINT ( 'NONE',  ( -2.977408999572647819, 7.188101187499991163, 18.08030278187175455 ) ) ;
#33562 = CARTESIAN_POINT ( 'NONE',  ( -5.676582343750006032, 49.11458332991935549, 9.832129032723418760 ) ) ;
#33564 =( BOUNDED_CURVE ( )  B_SPLINE_CURVE ( 2, ( #14472, #73329, #21633, #9590, #37511, #48812, #44658, #71817, #72194 ),
 .UNSPECIFIED., .F., .F. ) 
 B_SPLINE_CURVE_WITH_KNOTS ( ( 3, 2, 2, 2, 3 ),
 ( 0.4305555555555555247, 0.4374999999999999445, 0.4444444444444444198, 0.4513888888888888951, 0.4583333333333333148 ),
 .UNSPECIFIED. ) 
 CURVE ( )  GEOMETRIC_REPRESENTATION_ITEM ( )  RATIONAL_B_SPLINE_CURVE ( ( 1.000000000000000666, 0.9238795325112861834, 1.000000000000000000, 0.9238795325112867385, 1.000000000000000000, 0.9238795325112867385, 1.000000000000000000, 0.9238795325112867385, 1.000000000000000000 ) ) 
 REPRESENTATION_ITEM ( '' )  );
#33563 = DIRECTION ( 'NONE',  ( 0.000000000000000000, 0.000000000000000000, 1.000000000000000000 ) ) ;
#33565 = CARTESIAN_POINT ( 'NONE',  ( 2.828427124746208943, 195.7500000027312126, 195.1715728752538439 ) ) ;
#33566 = ORIENTED_EDGE ( 'NONE', *, *, #73576, .T. ) ;
#33567 = CARTESIAN_POINT ( 'NONE',  ( 10.00000000000000178, 142.0833333265053966, -2.679491924311226736 ) ) ;
#33568 = CARTESIAN_POINT ( 'NONE',  ( -4.999999999999998224, 168.5416666598387110, -8.660254037844389075 ) ) ;
#33569 = CARTESIAN_POINT ( 'NONE',  ( 6.951808397369818766E-16, 67.03124999658602690, -11.35316468750000141 ) ) ;
#33570 = CIRCLE ( 'NONE', #56435, 18.00000000000000355 ) ;
#33571 = CARTESIAN_POINT ( 'NONE',  ( 7.778174593052021635, 7.778174593052023411, 77.12500000409677625 ) ) ;
#33572 = CARTESIAN_POINT ( 'NONE',  ( -3.458734125000015869, 198.1875000013655779, 142.0000000000000568 ) ) ;
#33573 = DIRECTION ( 'NONE',  ( -0.000000000000000000, 1.000000000000000000, -0.000000000000000000 ) ) ;
#33574 = CARTESIAN_POINT ( 'NONE',  ( 2.751064625579944321E-14, 207.7500000000000284, 194.0000000000000568 ) ) ;
#33576 = CARTESIAN_POINT ( 'NONE',  ( 9.832129032723416984, 50.36458332991934839, 5.676582343750006032 ) ) ;
#33575 = CARTESIAN_POINT ( 'NONE',  ( 7.188101187500000044, 93.40625000204838102, -8.802885111219163269E-16 ) ) ;
#33577 = CARTESIAN_POINT ( 'NONE',  ( 7.999999999999991118, 9.797174393178815797E-16, 4.580302779823363757 ) ) ;
#33578 = CARTESIAN_POINT ( 'NONE',  ( 2.679491924311074857, 203.9583333333333428, 10.00000000000008349 ) ) ;
#33579 = CARTESIAN_POINT ( 'NONE',  ( -3.042071309553164404, 177.2395833299193555, -11.35316468749999963 ) ) ;
#33580 = AXIS2_PLACEMENT_3D ( 'NONE', #50506, #56188, #39574 ) ;
#33581 = CARTESIAN_POINT ( 'NONE',  ( 2.679491924311228956, 142.9166666598386826, -10.00000000000000000 ) ) ;
#33582 = CARTESIAN_POINT ( 'NONE',  ( 2.977408999572654480, 104.0000000020483810, 7.188101187499999156 ) ) ;
#33583 = DIRECTION ( 'NONE',  ( -0.000000000000000000, 1.000000000000000000, -1.563033456626094573E-30 ) ) ;
#33584 = CARTESIAN_POINT ( 'NONE',  ( 11.35316468749999963, 31.30208332991934839, -3.042071309553165293 ) ) ;
#33585 = CARTESIAN_POINT ( 'NONE',  ( 9.832129032723420536, 181.1979166632526983, -5.676582343749999815 ) ) ;
#33586 = ORIENTED_EDGE ( 'NONE', *, *, #311, .T. ) ;
#33587 = CARTESIAN_POINT ( 'NONE',  ( -2.775557561562891351E-14, 191.0000000000000284, 142.0000000000000568 ) ) ;
#33588 = CARTESIAN_POINT ( 'NONE',  ( -10.18810118749999916, 0.000000000000000000, 69.15625000204836681 ) ) ;
#33589 = CARTESIAN_POINT ( 'NONE',  ( -3.999999999999960032, 195.0000000000000000, 198.0000000000000284 ) ) ;
#33590 = CARTESIAN_POINT ( 'NONE',  ( 8.000000000000000000, 16.59375000000000355, -3.313708498984761164 ) ) ;
#33592 = CARTESIAN_POINT ( 'NONE',  ( 5.676582343749993598, 159.9479166632526983, 9.832129032723422313 ) ) ;
#33591 = DIRECTION ( 'NONE',  ( -0.000000000000000000, 1.000000000000000000, -0.000000000000000000 ) ) ;
#33593 = CARTESIAN_POINT ( 'NONE',  ( 1.469576158976822172E-15, -7.999999999999991118, 8.761552784329824206 ) ) ;
#33594 = CARTESIAN_POINT ( 'NONE',  ( -2.775557561562891351E-14, 210.0000000000000284, 142.0000000000000568 ) ) ;
#33595 = CARTESIAN_POINT ( 'NONE',  ( -8.311093377946834337, 224.5312500034140157, 8.311093377946837890 ) ) ;
#33596 = CARTESIAN_POINT ( 'NONE',  ( -3.511653767258854586, 51.69076377080494922, -48.72852442694383512 ) ) ;
#33597 = CARTESIAN_POINT ( 'NONE',  ( -7.204075437095965206, -7.204075437095968759, 81.71875000204836681 ) ) ;
#33598 = ORIENTED_EDGE ( 'NONE', *, *, #59152, .T. ) ;
#33599 = CARTESIAN_POINT ( 'NONE',  ( -2.828427124746153876, 203.8750000000000284, 195.1715728752538439 ) ) ;
#33600 = CARTESIAN_POINT ( 'NONE',  ( -5.676582343750006032, 114.4270833299193555, 9.832129032723418760 ) ) ;
#33601 = CARTESIAN_POINT ( 'NONE',  ( 0.000000000000000000, 0.000000000000000000, 30.00000000000000000 ) ) ;
#33602 = ORIENTED_EDGE ( 'NONE', *, *, #68936, .F. ) ;
#33603 = ORIENTED_EDGE ( 'NONE', *, *, #35269, .T. ) ;
#33604 = CARTESIAN_POINT ( 'NONE',  ( -3.211159895383561391, 8.812499998634407916, -3.211159895383561835 ) ) ;
#33605 = CARTESIAN_POINT ( 'NONE',  ( 5.082755093536325930, 12.65624999795161187, -5.082755093536325930 ) ) ;
#33606 = CARTESIAN_POINT ( 'NONE',  ( -8.000000000000000000, 107.0937500040967905, -3.313708498984761608 ) ) ;
#33607 = EDGE_CURVE ( 'NONE', #61626, #66396, #19187, .T. ) ;
#33608 = CARTESIAN_POINT ( 'NONE',  ( -27.99999999999996447, 200.1875000013656063, 173.4587341250003760 ) ) ;
#33609 = AXIS2_PLACEMENT_3D ( 'NONE', #4515, #50520, #73535 ) ;
#33610 = EDGE_CURVE ( 'NONE', #10215, #37742, #18447, .T. ) ;
#33611 = CARTESIAN_POINT ( 'NONE',  ( 4.000000000000000888, 9.937499999999998224, 1.656854249492384135 ) ) ;
#33612 = CARTESIAN_POINT ( 'NONE',  ( 2.828427124746191623, 20.87499999726881583, -2.828427124746191623 ) ) ;
#33613 = CARTESIAN_POINT ( 'NONE',  ( -3.211159895383562723, 8.937499998634407916, 3.211159895383561391 ) ) ;
#33614 = CARTESIAN_POINT ( 'NONE',  ( 1.656854249492347719, 199.8125000000000284, 146.0000000000000284 ) ) ;
#33615 = VECTOR ( 'NONE', #42926, 1000.000000000000000 ) ;
#33616 = ORIENTED_EDGE ( 'NONE', *, *, #69028, .T. ) ;
#33617 = CARTESIAN_POINT ( 'NONE',  ( 3.313708498984887285, 116.4687500000000142, 7.999999999999878320 ) ) ;
#33618 = CARTESIAN_POINT ( 'NONE',  ( -5.082755093536325930, 110.4687500020483810, -5.082755093536325930 ) ) ;
#33620 = CARTESIAN_POINT ( 'NONE',  ( -4.000000000000016875, 209.4375000000000284, 140.3431457505076594 ) ) ;
#33619 = CARTESIAN_POINT ( 'NONE',  ( 3.178432602446558121E-13, 206.2500000000000000, -10.00000000000000533 ) ) ;
#33621 = CARTESIAN_POINT ( 'NONE',  ( -4.541265875000002339, 20.74999999863440436, -1.881053915767121998 ) ) ;
#33622 = CARTESIAN_POINT ( 'NONE',  ( -2.977408999572648707, -7.188101187499990274, 3.267802781871751439 ) ) ;
#33623 = ORIENTED_EDGE ( 'NONE', *, *, #23010, .T. ) ;
#33624 = ORIENTED_EDGE ( 'NONE', *, *, #53368, .T. ) ;
#33625 = CARTESIAN_POINT ( 'NONE',  ( 4.220049686691934809, 10.18810118749999916, 91.18750000204836681 ) ) ;
#33626 = CARTESIAN_POINT ( 'NONE',  ( 30.82842712474616675, 204.5000000027312126, 167.1715728752537018 ) ) ;
#33627 = CARTESIAN_POINT ( 'NONE',  ( -28.00000000000002132, 198.6875000013655779, 166.5412658750003629 ) ) ;
#33628 = CARTESIAN_POINT ( 'NONE',  ( -11.00000000000000000, 0.000000000000000000, 104.5000000000000000 ) ) ;
#33629 = CARTESIAN_POINT ( 'NONE',  ( -3.458734124999960358, 205.6875000013656063, 198.0000000000000284 ) ) ;
#33631 = CARTESIAN_POINT ( 'NONE',  ( -2.679491924311106832, 256.0416666666666856, 10.00000000000006928 ) ) ;
#33630 = CARTESIAN_POINT ( 'NONE',  ( 7.320508075688830552, 60.62500000000004974, -7.320508075688830552 ) ) ;
#33632 = CARTESIAN_POINT ( 'NONE',  ( -1.836970198721029983E-15, 123.7500000000000142, 10.00000000000000178 ) ) ;
#33633 = CARTESIAN_POINT ( 'NONE',  ( -3.313708498984762052, 103.7187500000000000, -8.000000000000000000 ) ) ;
#33634 = CARTESIAN_POINT ( 'NONE',  ( 0.000000000000000000, 210.0000000000000284, 170.0000000000000284 ) ) ;
#33635 = CARTESIAN_POINT ( 'NONE',  ( -2.977408999572647819, 7.188101187499991163, 7.580302781871751883 ) ) ;
#33636 = CARTESIAN_POINT ( 'NONE',  ( 0.000000000000000000, 300.0000000000000000, 6.000000000000001776 ) ) ;
#33637 = CARTESIAN_POINT ( 'NONE',  ( 30.44569435410883784, 207.8125000013656063, 167.5543056458911053 ) ) ;
#33638 = CARTESIAN_POINT ( 'NONE',  ( -8.000000000000000000, 24.56249999590322375, -9.797174393178825657E-16 ) ) ;
#33639 = CARTESIAN_POINT ( 'NONE',  ( 3.458734124999959914, 201.3750000013656347, 143.4326545832176976 ) ) ;
#33640 = CARTESIAN_POINT ( 'NONE',  ( -4.401442555609581635E-16, 124.1562500020483810, -7.188101187500000044 ) ) ;
#33642 = CARTESIAN_POINT ( 'NONE',  ( 1.432654583217608080, 204.8750000013656063, 138.5412658750000503 ) ) ;
#33641 = DIRECTION ( 'NONE',  ( 0.000000000000000000, 0.000000000000000000, 1.000000000000000000 ) ) ;
#33643 = CARTESIAN_POINT ( 'NONE',  ( 11.35316468749999963, 241.7187500034139873, -1.390361679473963556E-15 ) ) ;
#33644 = CARTESIAN_POINT ( 'NONE',  ( 0.000000000000000000, 0.000000000000000000, 30.00000000000000000 ) ) ;
#33645 = CARTESIAN_POINT ( 'NONE',  ( -7.999999999999991118, 0.000000000000000000, 18.83030277982336642 ) ) ;
#33646 = CARTESIAN_POINT ( 'NONE',  ( 25.17157287525378351, 202.8750000000000284, 172.8284271247460424 ) ) ;
#33647 = CARTESIAN_POINT ( 'NONE',  ( -3.042071309553164404, 17.23958332991935194, -11.35316468749999963 ) ) ;
#33648 = CARTESIAN_POINT ( 'NONE',  ( 10.00000000000000178, 0.000000000000000000, 0.000000000000000000 ) ) ;
#33649 = CARTESIAN_POINT ( 'NONE',  ( -5.676582343750006032, 214.4270833299193555, 9.832129032723418760 ) ) ;
#33650 = CARTESIAN_POINT ( 'NONE',  ( -26.34314575050758123, 202.6875000027312126, 174.0000000000003979 ) ) ;
#33651 = CARTESIAN_POINT ( 'NONE',  ( -3.190679070438223991E-13, 203.7500000000000000, 10.00000000000000533 ) ) ;
#33653 = CARTESIAN_POINT ( 'NONE',  ( 1.656854249492381248, 11.93749999726881406, -4.000000000000001776 ) ) ;
#33652 = CARTESIAN_POINT ( 'NONE',  ( 7.778174593052023411, -7.778174593052021635, 88.56249999999998579 ) ) ;
#33654 = VERTEX_POINT ( 'NONE', #63720 ) ;
#33655 = CARTESIAN_POINT ( 'NONE',  ( -3.458734125000016757, 202.1250000013656063, 140.5673454167824161 ) ) ;
#33656 = CARTESIAN_POINT ( 'NONE',  ( -8.311093377946836114, 22.65624999658601979, -8.311093377946837890 ) ) ;
#33657 = CARTESIAN_POINT ( 'NONE',  ( -7.778174593052020747, -7.778174593052023411, 92.87500000409677625 ) ) ;
#33658 = CARTESIAN_POINT ( 'NONE',  ( -1.688721909672441956, 10.27943647337372468, 63.64086505882563216 ) ) ;
#33659 = CARTESIAN_POINT ( 'NONE',  ( -27.99999999999991829, 197.9375000013655779, 173.4587341250003760 ) ) ;
#33660 = CARTESIAN_POINT ( 'NONE',  ( 1.349999999999999201, 283.9999999999998863, 5.686520093750307758 ) ) ;
#33662 = CARTESIAN_POINT ( 'NONE',  ( 8.311093377946837890, 11.40624999658601624, -8.311093377946837890 ) ) ;
#33661 = CARTESIAN_POINT ( 'NONE',  ( -7.188101187500000933, 113.5625000020483810, -2.977408999572650483 ) ) ;
#33663 = CARTESIAN_POINT ( 'NONE',  ( 7.999999999999991118, 9.797174393178815797E-16, 19.58030277982336642 ) ) ;
#33664 =( BOUNDED_CURVE ( )  B_SPLINE_CURVE ( 2, ( #31945, #54968, #32330, #55343, #3646, #26646, #45126, #69255, #17189 ),
 .UNSPECIFIED., .F., .F. ) 
 B_SPLINE_CURVE_WITH_KNOTS ( ( 3, 2, 2, 2, 3 ),
 ( 0.2666666666666668850, 0.2750000000000002442, 0.2833333333333335480, 0.2916666666666669072, 0.3000000000000002109 ),
 .UNSPECIFIED. ) 
 CURVE ( )  GEOMETRIC_REPRESENTATION_ITEM ( )  RATIONAL_B_SPLINE_CURVE ( ( 0.9999999999999980016, 0.9238795325112887369, 1.000000000000000000, 0.9238795325112867385, 1.000000000000000000, 0.9238795325112867385, 1.000000000000000000, 0.9238795325112847401, 1.000000000000001998 ) ) 
 REPRESENTATION_ITEM ( '' )  );
#33665 = CARTESIAN_POINT ( 'NONE',  ( 5.676582343750001591, 141.6145833299193555, -9.832129032723420536 ) ) ;
#33666 = VECTOR ( 'NONE', #28141, 1000.000000000000000 ) ;
#33667 = CARTESIAN_POINT ( 'NONE',  ( 7.320508075688774596, 107.4999999931720254, -7.320508075688774596 ) ) ;
#33668 = CARTESIAN_POINT ( 'NONE',  ( 2.977408999572650039, 122.5625000020483952, -7.188101187500001821 ) ) ;
#33669 = CARTESIAN_POINT ( 'NONE',  ( 4.898587196589412829E-16, 13.68749999590322375, -8.000000000000000000 ) ) ;
#33670 = CARTESIAN_POINT ( 'NONE',  ( -31.45873412499998523, 209.0000000013655779, 171.4326545832180386 ) ) ;
#33671 = CARTESIAN_POINT ( 'NONE',  ( -5.000000000000000000, -53.55895565990277163, -45.41404144516085495 ) ) ;
#33672 = ORIENTED_EDGE ( 'NONE', *, *, #16309, .F. ) ;
#33673 = CARTESIAN_POINT ( 'NONE',  ( 4.336811714534362316, -68.30918023750064094, 20.61428864871788846 ) ) ;
#33674 = B_SPLINE_CURVE_WITH_KNOTS ( 'NONE', 3,
 ( #29012, #52030, #367, #29395, #69376, #58809, #17687, #64090, #40703, #12399, #35432, #1106, #24082, #12762, #35794, #37273, #60266, #25926, #42547, #7120, #1476, #19902, #31232, #47467, #41812, #71952, #25188, #25556, #8221, #24457, #65927, #53881 ),
 .UNSPECIFIED., .F., .F.,
 ( 4, 2, 2, 2, 2, 2, 2, 2, 2, 2, 2, 2, 2, 2, 2, 4 ),
 ( 0.003096835164517084023, 0.003832390200800732134, 0.004567945237084380244, 0.006039055309651706824, 0.006774610345935370113, 0.007510165382219033403, 0.008245720418502697560, 0.008981275454786361717, 0.009716830491070024139, 0.01045238552735368830, 0.01118794056363735245, 0.01192349559992101488, 0.01265905063620468077, 0.01339460567248834319, 0.01413016070877200561, 0.01486571574505567150 ),
 .UNSPECIFIED. ) ;
#33675 = CARTESIAN_POINT ( 'NONE',  ( -1.656854249492381248, 20.06249999726881228, -4.000000000000001776 ) ) ;
#33676 = CARTESIAN_POINT ( 'NONE',  ( 6.676582343750003368, 291.1718750017069510, -2.765530957081997254 ) ) ;
#33677 = FILL_AREA_STYLE_COLOUR ( '', #61602 ) ;
#33678 = CARTESIAN_POINT ( 'NONE',  ( -7.999999999999991118, -4.672035931492118266, 28.01873199342790244 ) ) ;
#33679 = CARTESIAN_POINT ( 'NONE',  ( -8.000000000000000000, 18.65625000000000355, -3.313708498984762496 ) ) ;
#33680 = AXIS2_PLACEMENT_3D ( 'NONE', #15888, #39289, #62290 ) ;
#33681 = CARTESIAN_POINT ( 'NONE',  ( 8.311093377946834337, 257.0312500034139020, -8.311093377946836114 ) ) ;
#33682 = CARTESIAN_POINT ( 'NONE',  ( -7.204075437095967871, 7.204075437095967871, 96.34375000204836681 ) ) ;
#33683 = VERTEX_POINT ( 'NONE', #24469 ) ;
#33684 = EDGE_CURVE ( 'NONE', #47672, #33138, #36170, .T. ) ;
#33685 = EDGE_CURVE ( 'NONE', #1178, #45978, #11851, .T. ) ;
#33686 = FACE_OUTER_BOUND ( 'NONE', #68855, .T. ) ;
#33687 = FILL_AREA_STYLE_COLOUR ( '', #37480 ) ;
#33688 = CARTESIAN_POINT ( 'NONE',  ( 2.445694354108840063, 202.0625000013656063, 200.4456943541088663 ) ) ;
#33689 = CARTESIAN_POINT ( 'NONE',  ( 3.042071309553167069, 82.13541666325269830, -11.35316468749999785 ) ) ;
#33690 = ORIENTED_EDGE ( 'NONE', *, *, #44530, .T. ) ;
#33691 = CARTESIAN_POINT ( 'NONE',  ( 7.204075437095968759, -7.204075437095966983, 116.2187500020483810 ) ) ;
#33692 = CARTESIAN_POINT ( 'NONE',  ( 4.541265875000002339, 12.49999999863440969, -1.881053915767121776 ) ) ;
#33693 = VERTEX_POINT ( 'NONE', #41090 ) ;
#33694 = CARTESIAN_POINT ( 'NONE',  ( -1.469576158976823947E-15, 1.125000000000000222, 8.000000000000000000 ) ) ;
#33695 = CARTESIAN_POINT ( 'NONE',  ( -5.656854249492378806, 110.3750000040967763, 5.656854249492381470 ) ) ;
#33696 = CARTESIAN_POINT ( 'NONE',  ( -3.999999999999959144, 197.1875000027312410, 199.6568542494924259 ) ) ;
#33697 = CARTESIAN_POINT ( 'NONE',  ( 2.977408999572651815, 23.06249999795161187, 7.188101187500000933 ) ) ;
#33698 = DIRECTION ( 'NONE',  ( -1.000000000000000000, -0.000000000000000000, -0.000000000000000000 ) ) ;
#33699 = CARTESIAN_POINT ( 'NONE',  ( 1.871523826299183495E-15, -10.18810118749999916, 108.9062500020483668 ) ) ;
#33700 = PRODUCT_DEFINITION_SHAPE ( 'NONE', 'NONE',  #74670 ) ;
#33701 = CARTESIAN_POINT ( 'NONE',  ( 1.656854249492470732, 204.6875000000000284, 194.0000000000001421 ) ) ;
#33702 = CARTESIAN_POINT ( 'NONE',  ( 4.000000000000001776, 8.812499997268815832, -1.656854249492381248 ) ) ;
#33703 = DIRECTION ( 'NONE',  ( -0.000000000000000000, 1.000000000000000000, -0.000000000000000000 ) ) ;
#33704 = EDGE_LOOP ( 'NONE', ( #44839, #70351, #7532, #45358 ) ) ;
#33705 = CARTESIAN_POINT ( 'NONE',  ( -3.458734124999959914, 204.3750000013656063, 196.5673454167823877 ) ) ;
#33706 = EDGE_CURVE ( 'NONE', #20204, #74274, #64099, .T. ) ;
#33707 = APPLICATION_CONTEXT ( 'automotive_design' ) ;
#33708 = CARTESIAN_POINT ( 'NONE',  ( -24.54126587500002543, 207.2500000013655779, 168.5673454167826435 ) ) ;
#33709 = CARTESIAN_POINT ( 'NONE',  ( 3.999999999999959144, 207.0625000000000568, 140.3431457505076594 ) ) ;
#33710 = CARTESIAN_POINT ( 'NONE',  ( -4.541265875000002339, 9.812499998634406140, -5.561446717895856393E-16 ) ) ;
#33711 = AXIS2_PLACEMENT_3D ( 'NONE', #64907, #65274, #58528 ) ;
#33712 = CARTESIAN_POINT ( 'NONE',  ( 2.449293598294707893E-16, 16.25000000000000000, -4.000000000000001776 ) ) ;
#33713 = CARTESIAN_POINT ( 'NONE',  ( -2.977408999572647819, 7.188101187499991163, 16.20530278187175455 ) ) ;
#33714 = ORIENTED_EDGE ( 'NONE', *, *, #51947, .F. ) ;
#33715 = CARTESIAN_POINT ( 'NONE',  ( -3.313708498984762496, 104.4687500040967763, 7.999999999999998224 ) ) ;
#33716 = ORIENTED_EDGE ( 'NONE', *, *, #8192, .F. ) ;
#33717 = CARTESIAN_POINT ( 'NONE',  ( -7.204075437095965206, -7.204075437095968759, 108.3437500020483810 ) ) ;
#33718 = DIRECTION ( 'NONE',  ( 0.000000000000000000, 0.000000000000000000, -1.000000000000000000 ) ) ;
#33719 = CARTESIAN_POINT ( 'NONE',  ( 3.458734125000015425, 204.9375000013656063, 198.0000000000000284 ) ) ;
#33720 = CARTESIAN_POINT ( 'NONE',  ( 31.45873412499997812, 199.7500000013656063, 168.5673454167822172 ) ) ;
#33721 = CARTESIAN_POINT ( 'NONE',  ( -7.320508075688773708, 86.87500000000001421, -7.320508075688774596 ) ) ;
#33722 = AXIS2_PLACEMENT_3D ( 'NONE', #61681, #14890, #9633 ) ;
#33723 = CARTESIAN_POINT ( 'NONE',  ( -5.082755093536325930, 89.84375000204839523, -5.082755093536325930 ) ) ;
#33724 = CARTESIAN_POINT ( 'NONE',  ( 6.000000000000003553, 290.5625000000000568, -2.485281374238571761 ) ) ;
#33725 = CARTESIAN_POINT ( 'NONE',  ( 28.00000000000002487, 206.1250000027312126, 173.9999999999999147 ) ) ;
#33726 = ORIENTED_EDGE ( 'NONE', *, *, #33981, .F. ) ;
#33727 = CARTESIAN_POINT ( 'NONE',  ( 1.836970198721029589E-15, 251.2500000000000284, 10.00000000000000000 ) ) ;
#33728 = CARTESIAN_POINT ( 'NONE',  ( -7.456155213548125715, -61.82225697226411398, 23.87472085067487271 ) ) ;
#33729 = CARTESIAN_POINT ( 'NONE',  ( 3.999999999999960032, 197.1250000027312126, 142.0000000000000568 ) ) ;
#33730 = CARTESIAN_POINT ( 'NONE',  ( -5.000000000000000000, 68.33088307291085073, 21.57589723056566910 ) ) ;
#33731 = CARTESIAN_POINT ( 'NONE',  ( 4.898587196589412829E-16, 13.68749999590322375, -8.000000000000000000 ) ) ;
#33732 = CARTESIAN_POINT ( 'NONE',  ( -10.00000000000000000, 234.7916666666666856, -2.679491924311226292 ) ) ;
#33733 = CARTESIAN_POINT ( 'NONE',  ( 4.556349186104045934, 11.00000000000000000, 107.2187500040967905 ) ) ;
#33734 = CARTESIAN_POINT ( 'NONE',  ( -4.999999999999998224, 196.6666666666666856, -8.660254037844389075 ) ) ;
#33735 = CARTESIAN_POINT ( 'NONE',  ( 2.977408999572646486, 7.188101187499992051, 17.89280278187175455 ) ) ;
#33736 = CARTESIAN_POINT ( 'NONE',  ( 8.311093377946837890, 166.7187499965859843, -8.311093377946837890 ) ) ;
#33737 = CARTESIAN_POINT ( 'NONE',  ( -27.99999999999991473, 208.6250000027312126, 174.0000000000003695 ) ) ;
#33738 = CARTESIAN_POINT ( 'NONE',  ( -2.602489044093041493, -43.49466919167058165, 151.1787532638200560 ) ) ;
#33739 = FACE_OUTER_BOUND ( 'NONE', #69604, .T. ) ;
#33740 = ORIENTED_EDGE ( 'NONE', *, *, #67182, .T. ) ;
#33741 = CARTESIAN_POINT ( 'NONE',  ( -8.311093377946841443, 24.21874999658601979, 8.311093377946830785 ) ) ;
#33742 = CARTESIAN_POINT ( 'NONE',  ( -4.556349186104045934, 11.00000000000000000, 113.4062500040967763 ) ) ;
#33743 = CARTESIAN_POINT ( 'NONE',  ( -25.55430564589111953, 208.0625000013656063, 172.4456943541091505 ) ) ;
#33745 = CARTESIAN_POINT ( 'NONE',  ( -1.558072418987778152, -16.42747873774261080, -68.67104701338908512 ) ) ;
#33744 = CARTESIAN_POINT ( 'NONE',  ( -5.867873826487101319, -5.445834672497646523, -0.3031401758654214129 ) ) ;
#33746 = CARTESIAN_POINT ( 'NONE',  ( -11.08833711610816053, -33.93952974122410637, 198.9490969008575405 ) ) ;
#33747 = CARTESIAN_POINT ( 'NONE',  ( -2.839093476692135984E-14, 197.6875000013655779, 138.5412658750000503 ) ) ;
#33748 = ADVANCED_FACE ( 'NONE', ( #70865, #35443 ), #58454, .F. ) ;
#33749 = CARTESIAN_POINT ( 'NONE',  ( 10.00000000000000178, 57.08333332650536107, -2.679491924311226736 ) ) ;
#33750 = CARTESIAN_POINT ( 'NONE',  ( -2.977408999572650927, 102.8750000020483810, -7.188101187500001821 ) ) ;
#33751 = CARTESIAN_POINT ( 'NONE',  ( -1.881053915767124440, 11.12499999863440792, 4.541265875000001451 ) ) ;
#33752 = CARTESIAN_POINT ( 'NONE',  ( 10.00000000000022204, 214.7916666666668277, 2.679491924311295570 ) ) ;
#33753 = CARTESIAN_POINT ( 'NONE',  ( 7.651181638696392895, 0.2025150128294917473, -1.024910111847489924 ) ) ;
#33754 = CARTESIAN_POINT ( 'NONE',  ( 2.828427124746191623, 1.125000000000000444, -2.828427124746191623 ) ) ;
#33755 = VERTEX_POINT ( 'NONE', #378 ) ;
#33756 =( BOUNDED_CURVE ( )  B_SPLINE_CURVE ( 2, ( #16979, #46028, #17353, #40376, #63373, #408, #11698, #34739, #46402 ),
 .UNSPECIFIED., .F., .F. ) 
 B_SPLINE_CURVE_WITH_KNOTS ( ( 3, 2, 2, 2, 3 ),
 ( 0.5138888888888888395, 0.5208333333333333703, 0.5277777777777777901, 0.5347222222222222099, 0.5416666666666666297 ),
 .UNSPECIFIED. ) 
 CURVE ( )  GEOMETRIC_REPRESENTATION_ITEM ( )  RATIONAL_B_SPLINE_CURVE ( ( 1.000000000000000000, 0.9238795325112867385, 1.000000000000000000, 0.9238795325112867385, 1.000000000000000000, 0.9238795325112867385, 1.000000000000000000, 0.9238795325112867385, 1.000000000000000000 ) ) 
 REPRESENTATION_ITEM ( '' )  );
#33757 = ORIENTED_EDGE ( 'NONE', *, *, #12284, .T. ) ;
#33758 = CARTESIAN_POINT ( 'NONE',  ( -0.8588954341815023819, -49.93020820668186133, -40.69831139579137869 ) ) ;
#33759 = CARTESIAN_POINT ( 'NONE',  ( -3.313708498984759387, -7.999999999999989342, 14.79905278392014978 ) ) ;
#33760 = CARTESIAN_POINT ( 'NONE',  ( 11.00000000000000000, 1.347111479062088405E-15, 103.7500000000000000 ) ) ;
#33761 = CARTESIAN_POINT ( 'NONE',  ( -11.35316468749999785, 224.0104166700806161, -3.042071309553164848 ) ) ;
#33762 = CARTESIAN_POINT ( 'NONE',  ( -11.35316468749999785, 138.0729166632526699, -3.042071309553167513 ) ) ;
#33763 = VERTEX_POINT ( 'NONE', #24093 ) ;
#33764 = EDGE_CURVE ( 'NONE', #5549, #60564, #5236, .T. ) ;
#33765 = CARTESIAN_POINT ( 'NONE',  ( 28.00000000000001776, 201.5000000000000000, 165.9999999999998863 ) ) ;
#33766 = CARTESIAN_POINT ( 'NONE',  ( 1.871523826299183495E-15, -10.18810118749999916, 92.03125000204836681 ) ) ;
#33767 = CARTESIAN_POINT ( 'NONE',  ( -30.49788809810225843, 194.5246287112378809, 167.5029336707353309 ) ) ;
#33768 = CARTESIAN_POINT ( 'NONE',  ( 2.828427124746208943, 206.6250000000000284, 195.1715728752538439 ) ) ;
#33769 = CARTESIAN_POINT ( 'NONE',  ( -27.99999999999999645, 210.0000000000000284, 174.0000000000003411 ) ) ;
#33770 = CARTESIAN_POINT ( 'NONE',  ( -3.313708498984842432, 112.9062500040967763, -7.999999999999920064 ) ) ;
#33771 = CARTESIAN_POINT ( 'NONE',  ( -5.656854249492380582, 100.8125000000000000, -5.656854249492380582 ) ) ;
#33772 = VERTEX_POINT ( 'NONE', #18819 ) ;
#33773 = AXIS2_PLACEMENT_3D ( 'NONE', #30273, #24598, #12904 ) ;
#33774 = LINE ( 'NONE', #39777, #44302 ) ;
#33775 = CARTESIAN_POINT ( 'NONE',  ( 26.12704298118493895, 176.1929651070205978, 153.1551066619960011 ) ) ;
#33776 = CARTESIAN_POINT ( 'NONE',  ( -11.35316468749999785, 128.3854166632526699, -3.042071309553167957 ) ) ;
#33777 = CARTESIAN_POINT ( 'NONE',  ( 2.754378923186476579E-14, 203.1875000013656063, 194.5412658750000219 ) ) ;
#33778 = CARTESIAN_POINT ( 'NONE',  ( -7.188101187500000044, 24.09374999795161543, -8.802885111219163269E-16 ) ) ;
#33779 = CARTESIAN_POINT ( 'NONE',  ( 10.18810118749999916, 4.220049686691935698, 83.87500000204836681 ) ) ;
#33780 = CARTESIAN_POINT ( 'NONE',  ( -3.042071309553173730, 29.63541666325268054, 11.35316468749999785 ) ) ;
#33782 = ORIENTED_EDGE ( 'NONE', *, *, #35551, .F. ) ;
#33781 =( BOUNDED_CURVE ( )  B_SPLINE_CURVE ( 2, ( #20424, #19312, #31384, #36681, #2343, #14390, #64964, #7639, #41957 ),
 .UNSPECIFIED., .F., .F. ) 
 B_SPLINE_CURVE_WITH_KNOTS ( ( 3, 2, 2, 2, 3 ),
 ( 0.1500000000000002442, 0.1583333333333335202, 0.1666666666666667962, 0.1750000000000000722, 0.1833333333333333481 ),
 .UNSPECIFIED. ) 
 CURVE ( )  GEOMETRIC_REPRESENTATION_ITEM ( )  RATIONAL_B_SPLINE_CURVE ( ( 0.9999999999999976685, 0.9238795325112890700, 1.000000000000000000, 0.9238795325112867385, 1.000000000000000000, 0.9238795325112867385, 1.000000000000000000, 0.9238795325112865164, 1.000000000000000222 ) ) 
 REPRESENTATION_ITEM ( '' )  );
#33783 = CARTESIAN_POINT ( 'NONE',  ( 1.224646799147353454E-15, 300.0000000000000000, -10.00000000000000178 ) ) ;
#33784 = CARTESIAN_POINT ( 'NONE',  ( -1.836970198721029983E-15, 195.6249999931720254, 10.00000000000000178 ) ) ;
#33785 = CARTESIAN_POINT ( 'NONE',  ( -3.317071493978880348, -8.008118988124989457, 19.29436528394063544 ) ) ;
#33786 = CARTESIAN_POINT ( 'NONE',  ( -1.432654583217664701, 207.0000000013656063, 138.5412658750000787 ) ) ;
#33787 = VECTOR ( 'NONE', #70659, 1000.000000000000000 ) ;
#33788 = EDGE_CURVE ( 'NONE', #24215, #71882, #44315, .T. ) ;
#33789 = EDGE_CURVE ( 'NONE', #55561, #62160, #30505, .T. ) ;
#33790 = CARTESIAN_POINT ( 'NONE',  ( -2.977408999572650039, 6.937499997951610986, -7.188101187500001821 ) ) ;
#33791 = CARTESIAN_POINT ( 'NONE',  ( 2.485281374238571317, 296.7500000034140157, -6.000000000000003553 ) ) ;
#33792 = CARTESIAN_POINT ( 'NONE',  ( -49.70177871865297448, 135.2396306966484190, 57.99999999999998579 ) ) ;
#33793 = CARTESIAN_POINT ( 'NONE',  ( -8.000000000000001776, 17.15624999590322375, 3.313708498984759387 ) ) ;
#33794 = EDGE_CURVE ( 'NONE', #15999, #69396, #9734, .T. ) ;
#33795 = CARTESIAN_POINT ( 'NONE',  ( -5.676582343749998039, 157.7604166632526983, -9.832129032723420536 ) ) ;
#33796 = CARTESIAN_POINT ( 'NONE',  ( -10.18810118749999738, -4.220049686691941915, 75.25000000204836681 ) ) ;
#33797 = CARTESIAN_POINT ( 'NONE',  ( -24.54126587499998990, 195.1875000013655779, 170.0000000000003411 ) ) ;
#33798 = CARTESIAN_POINT ( 'NONE',  ( -4.000000000000002665, 15.56249999999999822, 1.656854249492380582 ) ) ;
#33799 = CARTESIAN_POINT ( 'NONE',  ( 4.541265875000002339, 20.43749999863440436, 0.000000000000000000 ) ) ;
#33800 = ORIENTED_EDGE ( 'NONE', *, *, #34510, .T. ) ;
#33801 = CARTESIAN_POINT ( 'NONE',  ( 2.828427124746208943, 197.7500000027312126, 195.1715728752538439 ) ) ;
#33802 = EDGE_CURVE ( 'NONE', #23110, #25788, #37028, .T. ) ;
#33803 = VECTOR ( 'NONE', #38725, 1000.000000000000000 ) ;
#33804 = CARTESIAN_POINT ( 'NONE',  ( -1.656854249492403008, 209.6875000000000284, 146.0000000000000284 ) ) ;
#33805 = CARTESIAN_POINT ( 'NONE',  ( -32.00000000000003553, 205.3125000027312126, 168.3431457505080573 ) ) ;
#33806 = CARTESIAN_POINT ( 'NONE',  ( 11.00000000000000000, 1.347111479062088405E-15, 93.43750000409677625 ) ) ;
#33807 = VERTEX_POINT ( 'NONE', #55017 ) ;
#33808 = CARTESIAN_POINT ( 'NONE',  ( 2.977408999572652260, 18.18749999795161187, 7.188101187500000044 ) ) ;
#33809 = PLANE ( 'NONE',  #29193 ) ;
#33810 = CARTESIAN_POINT ( 'NONE',  ( -3.000000000000001776, -45.19859959603262212, 151.2383369607062775 ) ) ;
#33811 = CARTESIAN_POINT ( 'NONE',  ( -7.320508075688773708, 41.87499999999999289, -7.320508075688774596 ) ) ;
#33812 = CARTESIAN_POINT ( 'NONE',  ( -2.977408999572650927, 106.2500000020484094, -7.188101187500001821 ) ) ;
#33813 = CARTESIAN_POINT ( 'NONE',  ( -29.43265458321766914, 208.7500000013656063, 166.5412658750003629 ) ) ;
#33814 = CARTESIAN_POINT ( 'NONE',  ( 6.676582343750002480, 289.0156250017070079, -2.765530957081997254 ) ) ;
#33816 = DIRECTION ( 'NONE',  ( -0.000000000000000000, 0.5207998305029671871, 0.8536788251726059595 ) ) ;
#33815 = CARTESIAN_POINT ( 'NONE',  ( 2.679491924311179218, 78.95833333333339965, 10.00000000000015810 ) ) ;
#33817 = ORIENTED_EDGE ( 'NONE', *, *, #24034, .F. ) ;
#33819 = CARTESIAN_POINT ( 'NONE',  ( -8.311093377946836114, 253.2812500034139873, -8.311093377946836114 ) ) ;
#33818 = CIRCLE ( 'NONE', #1297, 11.00000000000000000 ) ;
#33820 = CARTESIAN_POINT ( 'NONE',  ( 1.320432766682872962E-15, -7.188101187499992051, 21.73655278187175455 ) ) ;
#33821 = CARTESIAN_POINT ( 'NONE',  ( 0.3752463838824043885, 55.62178951997592691, 43.80327721769204885 ) ) ;
#33822 = CARTESIAN_POINT ( 'NONE',  ( 2.849036369511732440E-14, 200.3750000027312126, 202.0000000000000000 ) ) ;
#33823 = CARTESIAN_POINT ( 'NONE',  ( -2.679491924324927776, 148.5416666666654351, 9.999999999992095212 ) ) ;
#33824 = CARTESIAN_POINT ( 'NONE',  ( 2.445694354108839175, 195.3125000013656063, 195.5543056458912190 ) ) ;
#33825 = CARTESIAN_POINT ( 'NONE',  ( -10.00000000000000178, 162.5000000000000000, -1.224646799147353454E-15 ) ) ;
#33826 = CARTESIAN_POINT ( 'NONE',  ( -6.000000000000001776, 300.0000000000000000, 0.000000000000000000 ) ) ;
#33827 = FILL_AREA_STYLE ('',( #68135 ) ) ;
#33828 = CARTESIAN_POINT ( 'NONE',  ( 5.000000000000000888, -51.89737250574506078, -42.00009673807131350 ) ) ;
#33829 = CARTESIAN_POINT ( 'NONE',  ( 11.35316468749999963, 131.3020833299193555, -3.042071309553165293 ) ) ;
#33830 = CARTESIAN_POINT ( 'NONE',  ( -4.898587196589412829E-16, 105.3125000040967763, -8.000000000000000000 ) ) ;
#33831 = CARTESIAN_POINT ( 'NONE',  ( -4.898587196589407898E-16, 7.999999999999991118, 27.64280278392014978 ) ) ;
#33834 = CARTESIAN_POINT ( 'NONE',  ( 5.656854249492381470, 118.2500000040967905, 5.656854249492379694 ) ) ;
#33833 = CARTESIAN_POINT ( 'NONE',  ( 24.54126587499997925, 195.1250000013656063, 168.5673454167822740 ) ) ;
#33832 = CARTESIAN_POINT ( 'NONE',  ( 26.34314575050763807, 209.5625000000000000, 165.9999999999998863 ) ) ;
#33835 = VERTEX_POINT ( 'NONE', #60659 ) ;
#33836 = VECTOR ( 'NONE', #5738, 1000.000000000000000 ) ;
#33837 = LINE ( 'NONE', #44391, #3176 ) ;
#33838 = CARTESIAN_POINT ( 'NONE',  ( 29.65685424949234772, 202.1875000027311842, 174.0000000000000000 ) ) ;
#33839 = CARTESIAN_POINT ( 'NONE',  ( 2.085542519210945334E-15, 220.4687500034139873, 11.35316468749999963 ) ) ;
#33840 = CARTESIAN_POINT ( 'NONE',  ( 30.44569435410883074, 197.0625000013656063, 167.5543056458911053 ) ) ;
#33841 = CARTESIAN_POINT ( 'NONE',  ( 8.311093377946834337, 210.4687499965859843, 8.311093377946839666 ) ) ;
#33842 = CARTESIAN_POINT ( 'NONE',  ( 5.082755093536325042, 119.0937500020483810, -5.082755093536325930 ) ) ;
#33843 = CARTESIAN_POINT ( 'NONE',  ( -4.541265875000002339, 19.81249999863440436, -5.561446717895856393E-16 ) ) ;
#33844 = CARTESIAN_POINT ( 'NONE',  ( 2.990854866091075870, -55.96051345247121134, 43.98806351442848950 ) ) ;
#33845 = CARTESIAN_POINT ( 'NONE',  ( -3.313708498984757167, 7.999999999999991118, 21.54905277982336287 ) ) ;
#33847 = CARTESIAN_POINT ( 'NONE',  ( -25.17157287525377640, 202.6250000000000284, 172.8284271247465256 ) ) ;
#33846 =( NAMED_UNIT ( * ) PLANE_ANGLE_UNIT ( ) SI_UNIT ( $, .RADIAN. ) );
#33848 = CARTESIAN_POINT ( 'NONE',  ( 11.35316468749999785, 95.57291666325269830, 3.042071309553174174 ) ) ;
#33849 = ORIENTED_EDGE ( 'NONE', *, *, #2034, .F. ) ;
#33850 = FACE_OUTER_BOUND ( 'NONE', #35170, .T. ) ;
#33851 = CARTESIAN_POINT ( 'NONE',  ( 2.977408999572651815, 25.68749999795162253, 7.188101187500000933 ) ) ;
#33852 = PLANE ( 'NONE',  #33890 ) ;
#33853 = CARTESIAN_POINT ( 'NONE',  ( 9.832129032723416984, 257.1354166700806445, -5.676582343750003368 ) ) ;
#33854 = CARTESIAN_POINT ( 'NONE',  ( 11.35316468749999963, 105.9895833299193555, -3.042071309553165293 ) ) ;
#33855 = ORIENTED_EDGE ( 'NONE', *, *, #67295, .T. ) ;
#33856 = EDGE_CURVE ( 'NONE', #72830, #42285, #70056, .T. ) ;
#33857 = CARTESIAN_POINT ( 'NONE',  ( -5.000000000000000000, 0.000000000000000000, 0.000000000000000000 ) ) ;
#33858 = CARTESIAN_POINT ( 'NONE',  ( -7.204075437095965206, -7.204075437095968759, 106.8437500020483810 ) ) ;
#33859 = CARTESIAN_POINT ( 'NONE',  ( 6.123233995736767268E-16, 218.1249999931720538, -10.00000000000000178 ) ) ;
#33860 = CARTESIAN_POINT ( 'NONE',  ( -1.432654583217607414, 204.5000000013656063, 194.5412658750000219 ) ) ;
#33861 = CARTESIAN_POINT ( 'NONE',  ( 1.469576158976823947E-15, 117.8750000000000000, 8.000000000000000000 ) ) ;
#33863 = CARTESIAN_POINT ( 'NONE',  ( -8.311093377946841443, 103.9062499965860269, 8.311093377946834337 ) ) ;
#33862 = CARTESIAN_POINT ( 'NONE',  ( 38.00000000000000000, -63.00000000000000000, 15.00000000000000178 ) ) ;
#33864 = CARTESIAN_POINT ( 'NONE',  ( -7.999999999999989342, -3.313708498984762496, 13.11155278392014623 ) ) ;
#33865 = CARTESIAN_POINT ( 'NONE',  ( -30.44569435410879166, 200.0625000013656063, 172.4456943541092357 ) ) ;
#33866 = VECTOR ( 'NONE', #70459, 1000.000000000000000 ) ;
#33867 = ORIENTED_EDGE ( 'NONE', *, *, #69282, .F. ) ;
#33868 = CARTESIAN_POINT ( 'NONE',  ( 4.999999999999993783, 176.0416666598387110, 8.660254037844390851 ) ) ;
#33869 = CARTESIAN_POINT ( 'NONE',  ( 1.469576158976823947E-15, 117.8750000000000000, 8.000000000000000000 ) ) ;
#33870 = CARTESIAN_POINT ( 'NONE',  ( 0.000000000000000000, 125.0000000000000000, 0.000000000000000000 ) ) ;
#33871 = CARTESIAN_POINT ( 'NONE',  ( 6.951808397369818766E-16, 72.34374999658602690, -11.35316468750000141 ) ) ;
#33872 = CARTESIAN_POINT ( 'NONE',  ( -6.676582343750003368, 291.3906250017070079, -2.765530957081996810 ) ) ;
#33873 = CARTESIAN_POINT ( 'NONE',  ( 7.188101187500000933, 6.937499997951610986, -2.977408999572650483 ) ) ;
#33874 = CARTESIAN_POINT ( 'NONE',  ( -10.18810118749999916, 0.000000000000000000, 101.0312500020483810 ) ) ;
#33875 = CARTESIAN_POINT ( 'NONE',  ( 3.042071309553167069, 216.8229166632526699, -11.35316468749999785 ) ) ;
#33876 = ORIENTED_EDGE ( 'NONE', *, *, #29186, .F. ) ;
#33877 = CARTESIAN_POINT ( 'NONE',  ( -4.000000000000001776, 2.437500000000000444, -1.656854249492381470 ) ) ;
#33878 = CARTESIAN_POINT ( 'NONE',  ( 3.313708498984828221, 115.7187500040967905, -7.999999999999932498 ) ) ;
#33879 = CARTESIAN_POINT ( 'NONE',  ( 0.000000000000000000, 300.0000000000000000, 0.000000000000000000 ) ) ;
#33880 = CARTESIAN_POINT ( 'NONE',  ( 5.676582343750001591, 201.6145833299193555, -9.832129032723420536 ) ) ;
#33881 = CARTESIAN_POINT ( 'NONE',  ( -6.123233995736766282E-16, 226.8750000068279746, -10.00000000000000000 ) ) ;
#33882 = DIRECTION ( 'NONE',  ( 0.000000000000000000, 0.000000000000000000, 1.000000000000000000 ) ) ;
#33883 = CARTESIAN_POINT ( 'NONE',  ( -2.765530957081996810, 298.2656250017068942, -6.676582343750003368 ) ) ;
#33884 = ORIENTED_EDGE ( 'NONE', *, *, #73450, .T. ) ;
#33885 = CARTESIAN_POINT ( 'NONE',  ( 3.042071309553167513, 197.1354166632526415, -11.35316468749999785 ) ) ;
#33886 =( BOUNDED_CURVE ( )  B_SPLINE_CURVE ( 2, ( #9213, #61268, #38643, #72963, #22013, #43917, #3558, #55251, #9964 ),
 .UNSPECIFIED., .F., .F. ) 
 B_SPLINE_CURVE_WITH_KNOTS ( ( 3, 2, 2, 2, 3 ),
 ( 0.1323529411764707009, 0.1360294117647059819, 0.1397058823529412908, 0.1433823529411765718, 0.1470588235294118806 ),
 .UNSPECIFIED. ) 
 CURVE ( )  GEOMETRIC_REPRESENTATION_ITEM ( )  RATIONAL_B_SPLINE_CURVE ( ( 0.9999999999999976685, 0.9238795325112890700, 1.000000000000000000, 0.9238795325112867385, 1.000000000000000000, 0.9238795325112867385, 1.000000000000000000, 0.9238795325112844070, 1.000000000000002220 ) ) 
 REPRESENTATION_ITEM ( '' )  );
#33887 = CARTESIAN_POINT ( 'NONE',  ( -29.43265458321766559, 208.5000000013656063, 166.5412658750003629 ) ) ;
#33888 = CARTESIAN_POINT ( 'NONE',  ( -8.000000000000000000, 20.15625000000000355, -3.313708498984762496 ) ) ;
#33889 = ORIENTED_EDGE ( 'NONE', *, *, #55182, .T. ) ;
#33890 = AXIS2_PLACEMENT_3D ( 'NONE', #22490, #63234, #267 ) ;
#33891 = CARTESIAN_POINT ( 'NONE',  ( -7.999999999999998224, 93.78125000409679046, 3.313708498984766493 ) ) ;
#33892 = DIRECTION ( 'NONE',  ( 1.000000000000000000, 0.000000000000000000, 0.000000000000000000 ) ) ;
#33893 = EDGE_CURVE ( 'NONE', #44073, #74219, #29550, .T. ) ;
#33894 = CARTESIAN_POINT ( 'NONE',  ( -1.836970198721029983E-15, 8.750000000000000000, 10.00000000000000178 ) ) ;
#33895 =( BOUNDED_CURVE ( )  B_SPLINE_CURVE ( 2, ( #12296, #1368, #25078, #47725, #59075, #8116, #13387, #52665, #35331 ),
 .UNSPECIFIED., .F., .F. ) 
 B_SPLINE_CURVE_WITH_KNOTS ( ( 3, 2, 2, 2, 3 ),
 ( 0.2941176470588234282, 0.2977941176470587092, 0.3014705882352939903, 0.3051470588235293269, 0.3088235294117646079 ),
 .UNSPECIFIED. ) 
 CURVE ( )  GEOMETRIC_REPRESENTATION_ITEM ( )  RATIONAL_B_SPLINE_CURVE ( ( 1.000000000000002220, 0.9238795325112844070, 1.000000000000000000, 0.9238795325112867385, 1.000000000000000000, 0.9238795325112867385, 1.000000000000000000, 0.9238795325112890700, 0.9999999999999976685 ) ) 
 REPRESENTATION_ITEM ( '' )  );
#33896 = ADVANCED_FACE ( 'NONE', ( #37285 ), #2203, .F. ) ;
#33897 = CIRCLE ( 'NONE', #67644, 10.99999999999999112 ) ;
#33898 = CARTESIAN_POINT ( 'NONE',  ( -7.204075437095967871, 7.204075437095967871, 78.34375000204838102 ) ) ;
#33899 = ORIENTED_EDGE ( 'NONE', *, *, #50364, .T. ) ;
#33900 = CARTESIAN_POINT ( 'NONE',  ( -7.347880794884122694E-16, 18.75000000000000000, 4.000000000000001776 ) ) ;
#33901 = CARTESIAN_POINT ( 'NONE',  ( 1.881053915767122664, 18.12499999863441147, 4.541265875000001451 ) ) ;
#33902 = VECTOR ( 'NONE', #61652, 1000.000000000000000 ) ;
#33903 = CARTESIAN_POINT ( 'NONE',  ( 29.35489318557348781, 194.4854955639154639, 173.2193748936120414 ) ) ;
#33904 = CARTESIAN_POINT ( 'NONE',  ( 7.320508075688771044, 16.24999999317203248, 7.320508075688775484 ) ) ;
#33905 = CARTESIAN_POINT ( 'NONE',  ( -2.977408999572650927, 124.2500000020484094, -7.188101187500001821 ) ) ;
#33906 = CARTESIAN_POINT ( 'NONE',  ( 0.000000000000000000, 265.0000000000000000, 0.000000000000000000 ) ) ;
#33908 = CARTESIAN_POINT ( 'NONE',  ( 11.35316468749999608, 246.6145833367473017, -3.042071309553167513 ) ) ;
#33907 = CARTESIAN_POINT ( 'NONE',  ( 28.00000000000002132, 207.4375000013656063, 173.4587341249998929 ) ) ;
#33909 = APPLICATION_PROTOCOL_DEFINITION ( 'draft international standard', 'automotive_design', 1998, #71235 ) ;
#33910 = ORIENTED_EDGE ( 'NONE', *, *, #54111, .F. ) ;
#33911 = CARTESIAN_POINT ( 'NONE',  ( -5.676582343750000703, 258.3854166700806445, -9.832129032723418760 ) ) ;
#33912 = EDGE_CURVE ( 'NONE', #7386, #7343, #21605, .T. ) ;
#33913 = CARTESIAN_POINT ( 'NONE',  ( -7.188101187499992051, 0.000000000000000000, 13.48655278187175455 ) ) ;
#33914 = VERTEX_POINT ( 'NONE', #48955 ) ;
#33915 = VERTEX_POINT ( 'NONE', #71965 ) ;
#33916 = CARTESIAN_POINT ( 'NONE',  ( -7.204075437095965206, -7.204075437095968759, 76.84375000204838102 ) ) ;
#33917 = CARTESIAN_POINT ( 'NONE',  ( 8.311093377946837890, 81.71874999658601268, -8.311093377946837890 ) ) ;
#33918 = CARTESIAN_POINT ( 'NONE',  ( 1.656854249492381248, 21.18750000000000000, -4.000000000000001776 ) ) ;
#33919 = CARTESIAN_POINT ( 'NONE',  ( 7.778174593052023411, -7.778174593052021635, 81.06249999999998579 ) ) ;
#33922 = CARTESIAN_POINT ( 'NONE',  ( -6.676582343749999815, 289.6718750017070079, 2.765530957082001251 ) ) ;
#33921 = CARTESIAN_POINT ( 'NONE',  ( 26.56734541678233086, 207.0000000013656063, 166.5412658749999650 ) ) ;
#33920 = CARTESIAN_POINT ( 'NONE',  ( 29.43265458321761585, 206.7500000013655779, 173.4587341249998929 ) ) ;
#33923 = VECTOR ( 'NONE', #71221, 1000.000000000000000 ) ;
#33924 = CARTESIAN_POINT ( 'NONE',  ( 10.00000000000000000, 76.66666665983871098, 2.679491924311235618 ) ) ;
#33925 = DIRECTION ( 'NONE',  ( 0.000000000000000000, 0.000000000000000000, -1.000000000000000000 ) ) ;
#33926 = CARTESIAN_POINT ( 'NONE',  ( 8.311093377946837890, 196.4062499965860411, -8.311093377946837890 ) ) ;
#33927 = CARTESIAN_POINT ( 'NONE',  ( -5.656854249492379694, 7.874999995903221972, -5.656854249492380582 ) ) ;
#33928 = ORIENTED_EDGE ( 'NONE', *, *, #37843, .F. ) ;
#33929 = CARTESIAN_POINT ( 'NONE',  ( 24.54126587499998635, 208.5000000013656063, 171.4326545832175555 ) ) ;
#33930 = CARTESIAN_POINT ( 'NONE',  ( -5.082755093536326818, 16.78124999795161543, 5.082755093536325042 ) ) ;
#33931 = CARTESIAN_POINT ( 'NONE',  ( -9.832129032723418760, 168.1770833299193555, -5.676582343750004256 ) ) ;
#33932 = DIRECTION ( 'NONE',  ( -0.000000000000000000, 1.000000000000000000, -0.000000000000000000 ) ) ;
#33933 = CARTESIAN_POINT ( 'NONE',  ( 2.977408999572650039, 104.5625000020483810, -7.188101187500000933 ) ) ;
#33935 = CARTESIAN_POINT ( 'NONE',  ( -2.679491924311233397, 113.5416666666666714, 9.999999999999992895 ) ) ;
#33934 = CARTESIAN_POINT ( 'NONE',  ( 4.000000000000001776, 17.74999999726881583, 0.000000000000000000 ) ) ;
#33936 = CARTESIAN_POINT ( 'NONE',  ( 31.45873412499999944, 204.9375000013656063, 169.9999999999999432 ) ) ;
#33937 = CARTESIAN_POINT ( 'NONE',  ( -2.977408999572648707, -7.188101187499990274, 8.142802781871750994 ) ) ;
#33938 = CARTESIAN_POINT ( 'NONE',  ( -5.676582343749998039, 57.44791666325269119, -9.832129032723420536 ) ) ;
#33939 = CARTESIAN_POINT ( 'NONE',  ( 11.00000000000000000, 1.347111479062088405E-15, 118.0000000000000000 ) ) ;
#33940 = CARTESIAN_POINT ( 'NONE',  ( -3.313708498984757167, 7.999999999999991118, 3.605302784329822874 ) ) ;
#33941 = ORIENTED_EDGE ( 'NONE', *, *, #42215, .F. ) ;
#33942 = CARTESIAN_POINT ( 'NONE',  ( 11.00000000000000000, 1.347111479062088405E-15, 75.24999999999998579 ) ) ;
#33943 = CARTESIAN_POINT ( 'NONE',  ( -3.729367062499960195, 209.8437500006828031, 198.0000000000000284 ) ) ;
#33944 = CARTESIAN_POINT ( 'NONE',  ( -11.35316468749999785, 63.07291666325268409, -3.042071309553167513 ) ) ;
#33945 = CARTESIAN_POINT ( 'NONE',  ( 4.556349186104045934, 11.00000000000000000, 77.21875000409679046 ) ) ;
#33946 = CARTESIAN_POINT ( 'NONE',  ( 1.432654583217607414, 200.5000000013656063, 145.4587341250000350 ) ) ;
#33948 = VECTOR ( 'NONE', #52215, 1000.000000000000000 ) ;
#33947 = CARTESIAN_POINT ( 'NONE',  ( -6.123233995736766282E-16, 258.7500000000000568, -10.00000000000000000 ) ) ;
#33949 = LINE ( 'NONE', #73536, #17809 ) ;
#33951 = CARTESIAN_POINT ( 'NONE',  ( 11.35316468749999785, 45.57291666325266988, 3.042071309553174174 ) ) ;
#33950 = CARTESIAN_POINT ( 'NONE',  ( -5.082755093536325930, 93.96875000204838102, -5.082755093536325930 ) ) ;
#33953 = EDGE_CURVE ( 'NONE', #62160, #13147, #49598, .T. ) ;
#33952 = CARTESIAN_POINT ( 'NONE',  ( -7.999999999999991118, -4.672035931492118266, 28.14998199301822623 ) ) ;
#33954 = CARTESIAN_POINT ( 'NONE',  ( -4.556349186104045934, 11.00000000000000000, 98.40625000409677625 ) ) ;
#33955 = CARTESIAN_POINT ( 'NONE',  ( 8.311093377946834337, 170.1562499965860127, 8.311093377946839666 ) ) ;
#33956 = CARTESIAN_POINT ( 'NONE',  ( 10.00000000000000178, 146.8749999931720538, 0.000000000000000000 ) ) ;
#33957 = CARTESIAN_POINT ( 'NONE',  ( -4.401442555609581635E-16, 100.1562500020483810, -7.188101187500000044 ) ) ;
#33958 = AXIS2_PLACEMENT_3D ( 'NONE', #62992, #41101, #58462 ) ;
#33959 = CARTESIAN_POINT ( 'NONE',  ( -1.377103048673273156, 0.4464676475659328236, -7.833776318515849546 ) ) ;
#33960 = CARTESIAN_POINT ( 'NONE',  ( -9.832129032723418760, 33.17708332991934839, -5.676582343750004256 ) ) ;
#33961 = ADVANCED_FACE ( 'NONE', ( #73101 ), #56506, .F. ) ;
#33962 = CARTESIAN_POINT ( 'NONE',  ( -1.656854249492399234, 201.1875000000000284, 201.9999999999999432 ) ) ;
#33963 = CARTESIAN_POINT ( 'NONE',  ( -8.311093377946836114, 187.6562499965860411, -8.311093377946837890 ) ) ;
#33964 = ORIENTED_EDGE ( 'NONE', *, *, #15384, .T. ) ;
#33965 = LINE ( 'NONE', #22992, #53677 ) ;
#33966 = CARTESIAN_POINT ( 'NONE',  ( -7.204075437095965206, -7.204075437095968759, 73.84375000204838102 ) ) ;
#33967 = CARTESIAN_POINT ( 'NONE',  ( -1.656854249492347719, 196.8125000000000284, 194.0000000000000853 ) ) ;
#33968 = CARTESIAN_POINT ( 'NONE',  ( 3.313708498984802020, 16.78125000000000000, -7.999999999999958256 ) ) ;
#33970 = CARTESIAN_POINT ( 'NONE',  ( -9.832129032723418760, 162.8645833299193839, -5.676582343750004256 ) ) ;
#33969 = CARTESIAN_POINT ( 'NONE',  ( -0.5213318599190973623, 194.9337052864028692, 194.0924152123214981 ) ) ;
#33971 = AXIS2_PLACEMENT_3D ( 'NONE', #38374, #73810, #62483 ) ;
#33972 = CARTESIAN_POINT ( 'NONE',  ( 1.469576158976822172E-15, -7.999999999999991118, 5.761552784329825094 ) ) ;
#33973 = FACE_OUTER_BOUND ( 'NONE', #7153, .T. ) ;
#33974 = CARTESIAN_POINT ( 'NONE',  ( 2.085542519210945334E-15, 220.1562500034139873, 11.35316468749999963 ) ) ;
#33975 = FACE_OUTER_BOUND ( 'NONE', #22797, .T. ) ;
#33976 = CARTESIAN_POINT ( 'NONE',  ( -7.204075437095965206, -7.204075437095968759, 78.71875000204836681 ) ) ;
#33977 = ORIENTED_EDGE ( 'NONE', *, *, #23102, .T. ) ;
#33978 = EDGE_CURVE ( 'NONE', #12256, #68975, #50088, .T. ) ;
#33979 = CARTESIAN_POINT ( 'NONE',  ( 9.832129032723416984, 115.6770833299193555, 5.676582343750006032 ) ) ;
#33980 = CARTESIAN_POINT ( 'NONE',  ( 1.349999999999996092, 255.9999999999997726, 5.686528119825783989 ) ) ;
#33981 = EDGE_CURVE ( 'NONE', #25179, #53910, #57498, .T. ) ;
#33982 = PRODUCT_DEFINITION ( 'UNKNOWN', '', #27333, #69796 ) ;
#33983 = VERTEX_POINT ( 'NONE', #4823 ) ;
#33984 = VECTOR ( 'NONE', #30115, 1000.000000000000000 ) ;
#33985 = CARTESIAN_POINT ( 'NONE',  ( 1.881053915767122664, 8.249999998634406140, 4.541265875000001451 ) ) ;
#33986 = CARTESIAN_POINT ( 'NONE',  ( 4.401442555609581635E-16, 14.34374999795161187, -7.188101187500000044 ) ) ;
#33987 = CARTESIAN_POINT ( 'NONE',  ( 5.656854249492381470, 112.2500000040967763, 5.656854249492379694 ) ) ;
#33988 = CARTESIAN_POINT ( 'NONE',  ( -29.43265458321766559, 199.7500000013656063, 166.5412658750003629 ) ) ;
#33989 = EDGE_CURVE ( 'NONE', #29411, #65897, #21158, .T. ) ;
#33990 =( BOUNDED_CURVE ( )  B_SPLINE_CURVE ( 2, ( #48117, #12321, #42458, #7772, #40999, #53430, #30045, #47383, #18723 ),
 .UNSPECIFIED., .F., .T. ) 
 B_SPLINE_CURVE_WITH_KNOTS ( ( 3, 2, 2, 2, 3 ),
 ( 0.8676470588235295489, 0.8713235294117648300, 0.8750000000000001110, 0.8786764705882353921, 0.8823529411764706731 ),
 .UNSPECIFIED. ) 
 CURVE ( )  GEOMETRIC_REPRESENTATION_ITEM ( )  RATIONAL_B_SPLINE_CURVE ( ( 0.9999999999999976685, 0.9238795325112890700, 1.000000000000000000, 0.9238795325112867385, 1.000000000000000000, 0.9238795325112867385, 1.000000000000000000, 0.9238795325112844070, 1.000000000000002220 ) ) 
 REPRESENTATION_ITEM ( '' )  );
#33991 = CARTESIAN_POINT ( 'NONE',  ( 2.828427124746190291, 9.875000000000000000, 2.828427124746192067 ) ) ;
#33992 = CARTESIAN_POINT ( 'NONE',  ( -4.000000000000002665, 22.31249999726881583, 1.656854249492380804 ) ) ;
#33993 = CARTESIAN_POINT ( 'NONE',  ( 4.541265875000001451, 6.249999998634407916, 1.881053915767124440 ) ) ;
#33994 = CARTESIAN_POINT ( 'NONE',  ( -4.000000000000015987, 198.5000000000000000, 142.0000000000000568 ) ) ;
#33995 = VERTEX_POINT ( 'NONE', #33504 ) ;
#33996 = CARTESIAN_POINT ( 'NONE',  ( 1.836970198721029589E-15, 221.2500000000000000, 10.00000000000000000 ) ) ;
#33997 = CARTESIAN_POINT ( 'NONE',  ( -2.977408999572651815, 101.9375000020483810, 7.188101187500000933 ) ) ;
#33999 = CARTESIAN_POINT ( 'NONE',  ( 6.000000000000001776, 293.5000000000000000, -7.347880794884121708E-16 ) ) ;
#33998 = FACE_OUTER_BOUND ( 'NONE', #68590, .T. ) ;
#34000 = CARTESIAN_POINT ( 'NONE',  ( -4.541265875000003227, 21.87499999863441147, 1.881053915767121110 ) ) ;
#34001 = VECTOR ( 'NONE', #40938, 1000.000000000000000 ) ;
#34002 = CARTESIAN_POINT ( 'NONE',  ( 5.082755093536318824, 5.082755093536319713, 0.9240527818717529929 ) ) ;
#34003 = ORIENTED_EDGE ( 'NONE', *, *, #16454, .T. ) ;
#34004 = VERTEX_POINT ( 'NONE', #38782 ) ;
#34005 = CARTESIAN_POINT ( 'NONE',  ( -10.18810118749999916, 0.000000000000000000, 91.65625000204836681 ) ) ;
#34006 = CARTESIAN_POINT ( 'NONE',  ( 1.469576158976823947E-15, 91.06250000409676204, 8.000000000000000000 ) ) ;
#34007 = CARTESIAN_POINT ( 'NONE',  ( -26.56734541678238060, 198.6250000013656063, 166.5412658750003629 ) ) ;
#34008 = CARTESIAN_POINT ( 'NONE',  ( 7.778174593052021635, 7.778174593052023411, 108.4374999999999858 ) ) ;
#34009 = CARTESIAN_POINT ( 'NONE',  ( -1.432654583217608080, 204.8750000013656063, 201.4587341250000350 ) ) ;
#34011 = DIRECTION ( 'NONE',  ( -0.000000000000000000, 1.000000000000000000, -0.000000000000000000 ) ) ;
#34010 = DIRECTION ( 'NONE',  ( 1.000000000000000000, 0.000000000000000000, 0.000000000000000000 ) ) ;
#34012 = CARTESIAN_POINT ( 'NONE',  ( 5.000000000000001776, 115.8333333333333428, -8.660254037844389075 ) ) ;
#34013 = CARTESIAN_POINT ( 'NONE',  ( 3.313708498984760720, 106.5312500000000142, -8.000000000000000000 ) ) ;
#34014 = CARTESIAN_POINT ( 'NONE',  ( 11.00000000000000000, 1.347111479062088405E-15, 87.43750000409677625 ) ) ;
#34015 = CARTESIAN_POINT ( 'NONE',  ( -2.977408999572647819, 7.188101187499991163, 4.580302781871752771 ) ) ;
#34016 = CARTESIAN_POINT ( 'NONE',  ( -24.00000000000001421, 208.8125000000000000, 168.3431457505080289 ) ) ;
#34017 = CARTESIAN_POINT ( 'NONE',  ( 24.54126587500000412, 207.1250000013656347, 168.5673454167822172 ) ) ;
#34018 = CARTESIAN_POINT ( 'NONE',  ( 7.999999999999998224, 25.21874999590322020, 3.313708498984766493 ) ) ;
#34019 = CARTESIAN_POINT ( 'NONE',  ( -2.445694354108838731, 198.0625000013656063, 144.4456943541088663 ) ) ;
#34020 = CARTESIAN_POINT ( 'NONE',  ( -7.188101187500000044, 120.0312500020483810, 0.000000000000000000 ) ) ;
#34022 = CARTESIAN_POINT ( 'NONE',  ( 27.99999999999996803, 202.0000000000000000, 173.9999999999999147 ) ) ;
#34021 = CARTESIAN_POINT ( 'NONE',  ( -2.250000000000000000, 265.3333333333333144, 5.427076266392048431 ) ) ;
#34023 = CARTESIAN_POINT ( 'NONE',  ( 2.085542519210945334E-15, 240.4687500034139873, 11.35316468749999963 ) ) ;
#34024 = CARTESIAN_POINT ( 'NONE',  ( -4.556349186104045934, 11.00000000000000000, 86.21874999999998579 ) ) ;
#34025 = CARTESIAN_POINT ( 'NONE',  ( 29.65685424949235482, 197.0625000000000000, 173.9999999999999147 ) ) ;
#34026 = CARTESIAN_POINT ( 'NONE',  ( 11.35316468750000141, 20.78124999658601624, 0.000000000000000000 ) ) ;
#34027 = CARTESIAN_POINT ( 'NONE',  ( 2.977408999572646486, 7.188101187499992051, 1.392802781871753437 ) ) ;
#34028 = CARTESIAN_POINT ( 'NONE',  ( -11.35316468750000141, 208.8020833299193555, 3.042071309553159963 ) ) ;
#34029 = DIRECTION ( 'NONE',  ( -0.000000000000000000, 1.000000000000000000, -0.000000000000000000 ) ) ;
#34030 = LINE ( 'NONE', #29089, #43982 ) ;
#34032 = CARTESIAN_POINT ( 'NONE',  ( 3.313708498984765161, 101.6562500040967905, 7.999999999999998224 ) ) ;
#34031 = CARTESIAN_POINT ( 'NONE',  ( -27.99999999999999645, 210.0000000000000284, 166.0000000000003979 ) ) ;
#34033 = ORIENTED_EDGE ( 'NONE', *, *, #64585, .T. ) ;
#34034 = CIRCLE ( 'NONE', #50849, 20.00000000000000355 ) ;
#34035 = CARTESIAN_POINT ( 'NONE',  ( 2.445694354108784108, 200.5625000013656063, 144.4456943541088663 ) ) ;
#34036 = CARTESIAN_POINT ( 'NONE',  ( -3.042071309553173730, 19.32291666325268409, 11.35316468749999785 ) ) ;
#34037 = CARTESIAN_POINT ( 'NONE',  ( 7.778174593052021635, 7.778174593052023411, 95.12500000409676204 ) ) ;
#34038 = CARTESIAN_POINT ( 'NONE',  ( 7.999999999999991118, 9.797174393178815797E-16, 1.580302779823364201 ) ) ;
#34039 = CARTESIAN_POINT ( 'NONE',  ( -24.54126587499995793, 197.1250000013656347, 171.4326545832179534 ) ) ;
#34040 = CYLINDRICAL_SURFACE ( 'NONE', #64762, 4.000000000000001776 ) ;
#34042 = CARTESIAN_POINT ( 'NONE',  ( 5.676582343750001591, 6.614583329919350163, -9.832129032723420536 ) ) ;
#34041 = CARTESIAN_POINT ( 'NONE',  ( 2.977408999572650039, 113.1875000020483810, -7.188101187500000933 ) ) ;
#34044 = EDGE_CURVE ( 'NONE', #4744, #49471, #62150, .T. ) ;
#34043 = CARTESIAN_POINT ( 'NONE',  ( -3.313708498984757167, 7.999999999999991118, 20.04905277982336642 ) ) ;
#34045 = VECTOR ( 'NONE', #66675, 1000.000000000000000 ) ;
#34046 = CARTESIAN_POINT ( 'NONE',  ( 9.832129032723416984, 140.3645833299193555, 5.676582343750006032 ) ) ;
#34047 = CARTESIAN_POINT ( 'NONE',  ( -4.999999999999998224, 108.5416666598387110, -8.660254037844389075 ) ) ;
#34048 = CARTESIAN_POINT ( 'NONE',  ( -5.082755093536324154, 120.2187500020483952, 5.082755093536326818 ) ) ;
#34049 = CARTESIAN_POINT ( 'NONE',  ( -8.000000000000000000, 120.6875000040967763, 0.000000000000000000 ) ) ;
#34050 = CARTESIAN_POINT ( 'NONE',  ( -29.43265458321766559, 207.7500000013656063, 166.5412658750003629 ) ) ;
#34051 = CARTESIAN_POINT ( 'NONE',  ( 7.999999999999992895, -3.313708498984756279, 0.1740527839201450044 ) ) ;
#34052 = VERTEX_POINT ( 'NONE', #50830 ) ;
#34053 = CARTESIAN_POINT ( 'NONE',  ( -0.3794862803196089041, -65.74576272852164038, 26.26831557574494624 ) ) ;
#34054 = ADVANCED_FACE ( 'NONE', ( #57250 ), #73841, .T. ) ;
#34055 = DIRECTION ( 'NONE',  ( -0.000000000000000000, 1.000000000000000000, -0.000000000000000000 ) ) ;
#34056 = CARTESIAN_POINT ( 'NONE',  ( -2.765530957081998586, 289.7968750017070079, 6.676582343750001591 ) ) ;
#34057 = CARTESIAN_POINT ( 'NONE',  ( -2.828427124746208943, 207.7500000027312126, 144.8284271247462129 ) ) ;
#34058 = CARTESIAN_POINT ( 'NONE',  ( 5.656854249492376141, -5.656854249492374365, 20.94905278432982243 ) ) ;
#34059 = CARTESIAN_POINT ( 'NONE',  ( 11.35316468749999608, 261.6145833367473301, -3.042071309553167069 ) ) ;
#34060 = CARTESIAN_POINT ( 'NONE',  ( 1.871523826299183495E-15, -10.18810118749999916, 99.90625000204838102 ) ) ;
#34061 = VERTEX_POINT ( 'NONE', #62517 ) ;
#34062 = VECTOR ( 'NONE', #5777, 1000.000000000000000 ) ;
#34063 = DIRECTION ( 'NONE',  ( 0.000000000000000000, 0.000000000000000000, 1.000000000000000000 ) ) ;
#34064 = CARTESIAN_POINT ( 'NONE',  ( -6.123233995736766282E-16, 253.7500000000000284, -10.00000000000000000 ) ) ;
#34065 = CARTESIAN_POINT ( 'NONE',  ( 3.458734125000015425, 202.2500000013655779, 196.5673454167823877 ) ) ;
#34066 = CARTESIAN_POINT ( 'NONE',  ( -11.35316468749999785, 73.38541666325268409, -3.042071309553167513 ) ) ;
#34067 = VERTEX_POINT ( 'NONE', #33141 ) ;
#34068 = CARTESIAN_POINT ( 'NONE',  ( -7.204075437095965206, -7.204075437095968759, 105.3437500020483810 ) ) ;
#34069 = CARTESIAN_POINT ( 'NONE',  ( -8.342170076843785083E-16, 12.18749999863440614, 4.541265875000002339 ) ) ;
#34070 = ORIENTED_EDGE ( 'NONE', *, *, #44390, .T. ) ;
#34071 = CARTESIAN_POINT ( 'NONE',  ( 7.188101187500000044, 24.46874999795161543, 0.000000000000000000 ) ) ;
#34072 = CARTESIAN_POINT ( 'NONE',  ( -7.320508075688778149, 109.9999999931720396, 7.320508075688769267 ) ) ;
#34073 = CARTESIAN_POINT ( 'NONE',  ( -5.000000000000000000, -63.46149047932912879, -24.14127879314093761 ) ) ;
#34074 = CARTESIAN_POINT ( 'NONE',  ( 7.188101187499999156, 21.74999999795162253, 2.977408999572654924 ) ) ;
#34075 = CARTESIAN_POINT ( 'NONE',  ( 0.000000000000000000, 54.99999999999999289, 0.000000000000000000 ) ) ;
#34076 = CARTESIAN_POINT ( 'NONE',  ( 10.18810118749999916, 4.220049686691935698, 107.8750000020483668 ) ) ;
#34077 = AXIS2_PLACEMENT_3D ( 'NONE', #71655, #9423, #25261 ) ;
#34078 = CARTESIAN_POINT ( 'NONE',  ( 9.999999999999994671, 109.7916666666666572, 2.679491924311234730 ) ) ;
#34079 = CARTESIAN_POINT ( 'NONE',  ( 1.656854249492381248, 10.93749999726881406, -4.000000000000001776 ) ) ;
#34080 = CARTESIAN_POINT ( 'NONE',  ( 1.836970198721029589E-15, 246.2500000000000284, 10.00000000000000000 ) ) ;
#34081 = ORIENTED_EDGE ( 'NONE', *, *, #7352, .T. ) ;
#34082 = VECTOR ( 'NONE', #40443, 1000.000000000000000 ) ;
#34083 = CARTESIAN_POINT ( 'NONE',  ( 3.458734125000015425, 201.0000000013655779, 196.5673454167823877 ) ) ;
#34084 = CARTESIAN_POINT ( 'NONE',  ( -31.45873412499999944, 203.6875000013656063, 170.0000000000004547 ) ) ;
#34085 = CARTESIAN_POINT ( 'NONE',  ( -1.881053915767124440, 9.999999998634407916, 4.541265875000001451 ) ) ;
#34086 = DIRECTION ( 'NONE',  ( -0.000000000000000000, 1.000000000000000000, -0.000000000000000000 ) ) ;
#34087 = CARTESIAN_POINT ( 'NONE',  ( 5.082755093536318824, 5.082755093536319713, 20.42405278187175455 ) ) ;
#34088 = VERTEX_POINT ( 'NONE', #56136 ) ;
#34089 = DIRECTION ( 'NONE',  ( 0.8660254037844380415, -0.5000000000000009992, 0.000000000000000000 ) ) ;
#34090 = ORIENTED_EDGE ( 'NONE', *, *, #22932, .T. ) ;
#34091 = CARTESIAN_POINT ( 'NONE',  ( 10.18810118750000093, -4.220049686691933033, 113.3125000020483668 ) ) ;
#34092 = CARTESIAN_POINT ( 'NONE',  ( 0.000000000000000000, 0.000000000000000000, 0.000000000000000000 ) ) ;
#34093 = CARTESIAN_POINT ( 'NONE',  ( 3.458734125000015425, 201.9375000013656063, 198.0000000000000284 ) ) ;
#34094 = CARTESIAN_POINT ( 'NONE',  ( 29.43265458321760519, 196.8750000013656347, 166.5412658749999650 ) ) ;
#34095 = CARTESIAN_POINT ( 'NONE',  ( 4.999999999999993783, 79.16666666666667140, 8.660254037844390851 ) ) ;
#34096 = CARTESIAN_POINT ( 'NONE',  ( 3.594034666126828981, 89.53052424436678791, -6.225087429138448591 ) ) ;
#34097 = CARTESIAN_POINT ( 'NONE',  ( -3.673940397442060854E-16, 289.7500000000000000, -6.000000000000001776 ) ) ;
#34098 = ORIENTED_EDGE ( 'NONE', *, *, #11198, .T. ) ;
#34099 =( BOUNDED_CURVE ( )  B_SPLINE_CURVE ( 2, ( #61969, #4643, #10297, #38226, #50644, #73664, #21972, #43493, #45000, #20472, #16299, #37857, #4270 ),
 .UNSPECIFIED., .F., .F. ) 
 B_SPLINE_CURVE_WITH_KNOTS ( ( 3, 2, 2, 2, 2, 2, 3 ),
 ( 0.2771739130434782705, 0.2789855072463768293, 0.2807971014492753881, 0.2826086956521738913, 0.2844202898550724501, 0.2862318840579710089, 0.2880434782608695676 ),
 .UNSPECIFIED. ) 
 CURVE ( )  GEOMETRIC_REPRESENTATION_ITEM ( )  RATIONAL_B_SPLINE_CURVE ( ( 1.000000000000000000, 0.9659258262890683122, 1.000000000000000000, 0.9659258262890683122, 1.000000000000000000, 0.9659258262890683122, 1.000000000000000000, 0.9659258262890683122, 1.000000000000000000, 0.9659258262890683122, 1.000000000000000000, 0.9659258262890683122, 1.000000000000000000 ) ) 
 REPRESENTATION_ITEM ( '' )  );
#34100 = EDGE_CURVE ( 'NONE', #74424, #66034, #8615, .T. ) ;
#34101 = ADVANCED_FACE ( 'NONE', ( #40257 ), #45915, .T. ) ;
#34102 = CARTESIAN_POINT ( 'NONE',  ( -2.990854866096253950, -66.07503719301790568, 26.46919450145037445 ) ) ;
#34103 = CARTESIAN_POINT ( 'NONE',  ( -4.000000000000015987, 194.6250000027311842, 142.0000000000000568 ) ) ;
#34104 = LINE ( 'NONE', #62005, #12940 ) ;
#34105 = CARTESIAN_POINT ( 'NONE',  ( -4.898587196589407898E-16, 7.999999999999991118, 26.14280278392014623 ) ) ;
#34106 = CARTESIAN_POINT ( 'NONE',  ( 2.679491924311235174, 231.4583333333333428, 9.999999999999998224 ) ) ;
#34107 = CARTESIAN_POINT ( 'NONE',  ( 6.123233995736767268E-16, 206.2500000000000284, -10.00000000000000178 ) ) ;
#34108 = CARTESIAN_POINT ( 'NONE',  ( 5.082755093536318824, 5.082755093536319713, 17.79905278187175810 ) ) ;
#34109 = CARTESIAN_POINT ( 'NONE',  ( 3.042071309553167069, 172.1354166632526983, -11.35316468749999785 ) ) ;
#34110 = CARTESIAN_POINT ( 'NONE',  ( -10.00000000000022382, 212.5000000000001705, -1.224646799147380669E-15 ) ) ;
#34111 = DIRECTION ( 'NONE',  ( -1.000000000000000000, 0.000000000000000000, 0.000000000000000000 ) ) ;
#34112 = CARTESIAN_POINT ( 'NONE',  ( 5.656854249492378806, 10.12499999590322020, 5.656854249492381470 ) ) ;
#34113 = ORIENTED_EDGE ( 'NONE', *, *, #40263, .T. ) ;
#34114 = CARTESIAN_POINT ( 'NONE',  ( 1.432654583217607858, 197.6250000013656063, 138.5412658750000787 ) ) ;
#34115 = CARTESIAN_POINT ( 'NONE',  ( -8.311093377946841443, 34.21874999658601979, 8.311093377946830785 ) ) ;
#34116 = CARTESIAN_POINT ( 'NONE',  ( 4.556349186104051263, -10.99999999999999822, 112.6562500040968047 ) ) ;
#34117 = CARTESIAN_POINT ( 'NONE',  ( -0.4207882399904094850, 194.5923675076498682, 201.5739307914007270 ) ) ;
#34118 = CARTESIAN_POINT ( 'NONE',  ( 27.99999999999996803, 207.6250000027312126, 165.9999999999998863 ) ) ;
#34119 = CARTESIAN_POINT ( 'NONE',  ( -0.7509181236822947136, -10.12341933770111879, -70.08957333326543448 ) ) ;
#34120 = CARTESIAN_POINT ( 'NONE',  ( -18.97632743905945674, -48.00260402960699224, 194.5282883244980496 ) ) ;
#34122 = EDGE_CURVE ( 'NONE', #15778, #4458, #36757, .T. ) ;
#34121 = CARTESIAN_POINT ( 'NONE',  ( -1.432654583217662259, 200.1250000013656063, 145.4587341250000350 ) ) ;
#34123 = CARTESIAN_POINT ( 'NONE',  ( 10.00000000000000178, 66.87499999317203958, 0.000000000000000000 ) ) ;
#34124 = CARTESIAN_POINT ( 'NONE',  ( 2.977408999572654480, 105.1250000020483668, 7.188101187499999156 ) ) ;
#34125 = CARTESIAN_POINT ( 'NONE',  ( 1.881053915767121776, 13.62499999863440792, -4.541265875000002339 ) ) ;
#34126 = CARTESIAN_POINT ( 'NONE',  ( 5.000000000000000000, -11.14555136602166208, 27.84144949604419494 ) ) ;
#34127 = CARTESIAN_POINT ( 'NONE',  ( -6.062601303906716588, -5.219661428662635494, 1.000679062340938064 ) ) ;
#34128 = CARTESIAN_POINT ( 'NONE',  ( -4.000000000000001776, 4.187499997268813168, -1.656854249492381470 ) ) ;
#34129 = ORIENTED_EDGE ( 'NONE', *, *, #62692, .F. ) ;
#34130 = ORIENTED_EDGE ( 'NONE', *, *, #4137, .F. ) ;
#34131 = CARTESIAN_POINT ( 'NONE',  ( 11.00000000000000000, 1.347111479062088405E-15, 118.0000000000000000 ) ) ;
#34132 = CARTESIAN_POINT ( 'NONE',  ( 3.313708498984762496, -7.999999999999989342, 14.98655278392014623 ) ) ;
#34133 = DIRECTION ( 'NONE',  ( -1.000000000000000000, -0.000000000000000000, -0.000000000000000000 ) ) ;
#34134 = CARTESIAN_POINT ( 'NONE',  ( -8.660254037844385522, 87.08333333333332860, -5.000000000000004441 ) ) ;
#34135 = AXIS2_PLACEMENT_3D ( 'NONE', #14717, #49809, #37002 ) ;
#34136 = CARTESIAN_POINT ( 'NONE',  ( 11.35316468750000141, 145.7812499965860411, 0.000000000000000000 ) ) ;
#34137 = CARTESIAN_POINT ( 'NONE',  ( 9.999999999999982236, 104.7916666666666572, 2.679491924311231621 ) ) ;
#34138 = CARTESIAN_POINT ( 'NONE',  ( -10.18810118749999916, 4.220049686691934809, 87.06250000204838102 ) ) ;
#34139 = LINE ( 'NONE', #39770, #28439 ) ;
#34140 = CARTESIAN_POINT ( 'NONE',  ( 4.000000000000015987, 204.5000000000000284, 198.0000000000000284 ) ) ;
#34141 = CARTESIAN_POINT ( 'NONE',  ( -3.999999999999960032, 205.0000000000000284, 198.0000000000000284 ) ) ;
#34142 = CARTESIAN_POINT ( 'NONE',  ( 5.656854249492381470, 116.7500000040967905, 5.656854249492379694 ) ) ;
#34143 = CARTESIAN_POINT ( 'NONE',  ( 1.871523826299183495E-15, -10.18810118749999916, 114.9062500020483810 ) ) ;
#34144 = ORIENTED_EDGE ( 'NONE', *, *, #72310, .T. ) ;
#34145 = CARTESIAN_POINT ( 'NONE',  ( -11.00000000000000000, 0.000000000000000000, 109.1875000040967763 ) ) ;
#34146 = CARTESIAN_POINT ( 'NONE',  ( 30.92609751907032489, 178.6226547575664938, 173.1060824877058053 ) ) ;
#34147 = CARTESIAN_POINT ( 'NONE',  ( 9.832129032723416984, 125.6770833299193697, 5.676582343750006032 ) ) ;
#34148 = CARTESIAN_POINT ( 'NONE',  ( -2.445694354108783664, 204.3125000013656063, 195.5543056458912190 ) ) ;
#34149 = CARTESIAN_POINT ( 'NONE',  ( -1.320432766682874540E-15, 22.96874999795161543, 7.188101187500000044 ) ) ;
#34150 = CARTESIAN_POINT ( 'NONE',  ( -10.18810118749999738, -4.220049686691941915, 80.12500000204836681 ) ) ;
#34151 = CARTESIAN_POINT ( 'NONE',  ( 9.832129032723420536, 31.51041666325268764, -5.676582343749999815 ) ) ;
#34152 = VERTEX_POINT ( 'NONE', #41377 ) ;
#34153 = FACE_OUTER_BOUND ( 'NONE', #31458, .T. ) ;
#34154 = CARTESIAN_POINT ( 'NONE',  ( -8.660254037844390851, 194.7916666598387110, 4.999999999999998224 ) ) ;
#34155 = CARTESIAN_POINT ( 'NONE',  ( 8.008118988124993010, -3.317071493978877239, 18.16936528394062833 ) ) ;
#34156 = CARTESIAN_POINT ( 'NONE',  ( -3.458734125000015869, 207.1875000013656063, 142.0000000000000568 ) ) ;
#34157 = CARTESIAN_POINT ( 'NONE',  ( 7.188101187500001821, 6.562499997951610986, -2.977408999572650483 ) ) ;
#34158 = CARTESIAN_POINT ( 'NONE',  ( 6.000000000000001776, 294.5625000034140157, -7.347880794884121708E-16 ) ) ;
#34159 = CARTESIAN_POINT ( 'NONE',  ( -23.59917512397327499, -13.41521301004928191, 137.6719463071689233 ) ) ;
#34160 = CARTESIAN_POINT ( 'NONE',  ( -7.188101187500000044, 7.593749997951610986, -8.802885111219163269E-16 ) ) ;
#34161 = CARTESIAN_POINT ( 'NONE',  ( -2.085542519210945728E-15, 159.8437499965860127, 11.35316468750000141 ) ) ;
#34162 = CARTESIAN_POINT ( 'NONE',  ( 1.871523826299183495E-15, -10.18810118749999916, 77.03125000204836681 ) ) ;
#34163 = VECTOR ( 'NONE', #22314, 1000.000000000000000 ) ;
#34164 = CARTESIAN_POINT ( 'NONE',  ( -29.43265458321761230, 209.1250000013656631, 173.4587341250003760 ) ) ;
#34165 = CARTESIAN_POINT ( 'NONE',  ( -1.656854249492381248, 15.31249999999999822, -4.000000000000001776 ) ) ;
#34166 = CARTESIAN_POINT ( 'NONE',  ( 4.541265875000002339, 18.49999999863440436, -1.881053915767121554 ) ) ;
#34167 = VERTEX_POINT ( 'NONE', #34994 ) ;
#34168 = CARTESIAN_POINT ( 'NONE',  ( 2.828427124746208943, 198.7500000027312126, 195.1715728752538439 ) ) ;
#34169 = CARTESIAN_POINT ( 'NONE',  ( 2.828427124746153876, 207.8750000000000284, 144.8284271247462129 ) ) ;
#34170 = CARTESIAN_POINT ( 'NONE',  ( -25.17157287525385811, 202.0000000027312126, 167.1715728752541281 ) ) ;
#34171 = ADVANCED_FACE ( 'NONE', ( #70053 ), #12686, .T. ) ;
#34172 = CARTESIAN_POINT ( 'NONE',  ( 11.00000000000010836, -4.556349186103939353, 75.34375000409674783 ) ) ;
#34173 = CARTESIAN_POINT ( 'NONE',  ( 7.999999999999991118, 3.313708498984757611, 9.361552783920146226 ) ) ;
#34174 = VERTEX_POINT ( 'NONE', #29319 ) ;
#34175 = CARTESIAN_POINT ( 'NONE',  ( -7.188101187500002709, 14.81249999795161365, 2.977408999572649151 ) ) ;
#34176 = CARTESIAN_POINT ( 'NONE',  ( 0.000000000000000000, 30.78460969082653875, -20.69999999999999929 ) ) ;
#34177 = CARTESIAN_POINT ( 'NONE',  ( -0.9680369701234169399, -47.84624114664195105, 151.0238146273429720 ) ) ;
#34178 = CARTESIAN_POINT ( 'NONE',  ( -8.660254037844387298, 37.08333333333333570, -5.000000000000004441 ) ) ;
#34179 = CARTESIAN_POINT ( 'NONE',  ( 7.188101187500002709, 108.6875000020483952, 2.977408999572649151 ) ) ;
#34180 = CARTESIAN_POINT ( 'NONE',  ( -26.56734541678233086, 209.2500000013656063, 173.4587341250003760 ) ) ;
#34181 = CARTESIAN_POINT ( 'NONE',  ( -4.242640687119286547, 298.8750000000000000, -4.242640687119286547 ) ) ;
#34183 = CARTESIAN_POINT ( 'NONE',  ( -3.313708498984816231, 95.46875000409679046, 7.999999999999943157 ) ) ;
#34182 = CARTESIAN_POINT ( 'NONE',  ( -26.34314575050765228, 201.5625000000000853, 174.0000000000004547 ) ) ;
#34184 = VERTEX_POINT ( 'NONE', #58009 ) ;
#34185 = CARTESIAN_POINT ( 'NONE',  ( -11.35316468749999963, 238.9062500034140157, 0.000000000000000000 ) ) ;
#34186 = CARTESIAN_POINT ( 'NONE',  ( -7.188101187499992051, 0.000000000000000000, 19.86155278187175455 ) ) ;
#34187 = CARTESIAN_POINT ( 'NONE',  ( -1.308779242312746893, 49.95118570763212773, 40.70975538998155940 ) ) ;
#34188 = CARTESIAN_POINT ( 'NONE',  ( -5.999999999999999112, 287.1250000034140157, 2.485281374238575314 ) ) ;
#34189 = CYLINDRICAL_SURFACE ( 'NONE', #14641, 8.000000000000000000 ) ;
#34190 =( BOUNDED_CURVE ( )  B_SPLINE_CURVE ( 2, ( #3882, #20841, #2377, #9159, #43100, #55196, #8787, #72146, #19720 ),
 .UNSPECIFIED., .F., .F. ) 
 B_SPLINE_CURVE_WITH_KNOTS ( ( 3, 2, 2, 2, 3 ),
 ( 0.9411764705882355031, 0.9448529411764707842, 0.9485294117647060652, 0.9522058823529412352, 0.9558823529411766273 ),
 .UNSPECIFIED. ) 
 CURVE ( )  GEOMETRIC_REPRESENTATION_ITEM ( )  RATIONAL_B_SPLINE_CURVE ( ( 0.9999999999999954481, 0.9238795325112912904, 1.000000000000000000, 0.9238795325112867385, 1.000000000000000000, 0.9238795325112867385, 1.000000000000000000, 0.9238795325112844070, 1.000000000000002220 ) ) 
 REPRESENTATION_ITEM ( '' )  );
#34191 = CARTESIAN_POINT ( 'NONE',  ( -3.458734124999960358, 195.6875000013655779, 198.0000000000000284 ) ) ;
#34192 = CARTESIAN_POINT ( 'NONE',  ( -10.00000000000000355, 162.7083333333333428, 2.679491924311223183 ) ) ;
#34193 = DIRECTION ( 'NONE',  ( -0.000000000000000000, -1.000000000000000000, -0.000000000000000000 ) ) ;
#34194 = CARTESIAN_POINT ( 'NONE',  ( -8.000000000000000000, 90.50000000000000000, 0.000000000000000000 ) ) ;
#34195 = CARTESIAN_POINT ( 'NONE',  ( 6.951808397369818766E-16, 122.3437499965860269, -11.35316468750000141 ) ) ;
#34196 = FACE_OUTER_BOUND ( 'NONE', #9768, .T. ) ;
#34197 = CARTESIAN_POINT ( 'NONE',  ( 0.4369882809721241101, -16.44602605510714710, -68.55492853905353456 ) ) ;
#34200 = CARTESIAN_POINT ( 'NONE',  ( 1.656854249492399234, 202.1875000000000568, 138.0000000000000853 ) ) ;
#34199 = CARTESIAN_POINT ( 'NONE',  ( 31.45873412499999944, 195.6250000013656063, 171.4326545832175555 ) ) ;
#34198 = CARTESIAN_POINT ( 'NONE',  ( 31.45873412499997812, 195.8750000013655779, 171.4326545832175839 ) ) ;
#34201 = ORIENTED_EDGE ( 'NONE', *, *, #62121, .T. ) ;
#34202 = ADVANCED_FACE ( 'NONE', ( #47394 ), #35720, .T. ) ;
#34203 = EDGE_CURVE ( 'NONE', #38109, #38945, #33570, .T. ) ;
#34204 = CARTESIAN_POINT ( 'NONE',  ( -8.000000000000001776, 20.34375000000000355, 3.313708498984759387 ) ) ;
#34205 = FACE_OUTER_BOUND ( 'NONE', #8452, .T. ) ;
#34206 = CARTESIAN_POINT ( 'NONE',  ( -3.689217076869665934, -7.102672987750866085, -0.000000000000000000 ) ) ;
#34207 = CARTESIAN_POINT ( 'NONE',  ( 5.000000000000000000, -66.79212039439826754, -23.29662735513450400 ) ) ;
#34208 = CARTESIAN_POINT ( 'NONE',  ( 8.311093377946837890, 216.7187499965860411, -8.311093377946837890 ) ) ;
#34209 = AXIS2_PLACEMENT_3D ( 'NONE', #12994, #36032, #59050 ) ;
#34210 = CARTESIAN_POINT ( 'NONE',  ( -5.082755093536324154, 122.8437500020483952, 5.082755093536326818 ) ) ;
#34211 = CARTESIAN_POINT ( 'NONE',  ( 1.881053915767122664, 22.12499999863441502, 4.541265875000001451 ) ) ;
#34212 = CARTESIAN_POINT ( 'NONE',  ( -1.296342370391162069, -49.95006747299220251, 40.70914535207602825 ) ) ;
#34213 = CARTESIAN_POINT ( 'NONE',  ( 7.999999999999991118, 3.313708498984757611, 19.67405277982336642 ) ) ;
#34215 = CARTESIAN_POINT ( 'NONE',  ( -7.285838599102589797E-14, -20.78460969082654231, -1.607695154586745501 ) ) ;
#34214 = CARTESIAN_POINT ( 'NONE',  ( -12.00000000000000000, 6.928203230275504332, -14.80000000000000071 ) ) ;
#34216 = CARTESIAN_POINT ( 'NONE',  ( -11.35316468749999785, 98.07291666325269830, -3.042071309553167513 ) ) ;
#34217 = EDGE_LOOP ( 'NONE', ( #2445, #4634, #63647, #56196 ) ) ;
#34218 =( BOUNDED_CURVE ( )  B_SPLINE_CURVE ( 2, ( #45106, #9670, #73033, #4377, #32690, #55699, #39446, #50757, #67001 ),
 .UNSPECIFIED., .F., .F. ) 
 B_SPLINE_CURVE_WITH_KNOTS ( ( 3, 2, 2, 2, 3 ),
 ( 0.8382352941176470784, 0.8419117647058823595, 0.8455882352941176405, 0.8492647058823529216, 0.8529411764705882026 ),
 .UNSPECIFIED. ) 
 CURVE ( )  GEOMETRIC_REPRESENTATION_ITEM ( )  RATIONAL_B_SPLINE_CURVE ( ( 1.000000000000000000, 0.9238795325112867385, 1.000000000000000000, 0.9238795325112867385, 1.000000000000000000, 0.9238795325112867385, 1.000000000000000000, 0.9238795325112867385, 1.000000000000000000 ) ) 
 REPRESENTATION_ITEM ( '' )  );
#34219 = CARTESIAN_POINT ( 'NONE',  ( 10.49999999999998224, 1.316495309083403434E-15, 118.0000000000000000 ) ) ;
#34220 = CARTESIAN_POINT ( 'NONE',  ( 7.188101187499999156, 22.87499999795161187, 2.977408999572654924 ) ) ;
#34221 = CARTESIAN_POINT ( 'NONE',  ( 0.000000000000000000, 124.5000000000000284, 0.000000000000000000 ) ) ;
#34222 = CARTESIAN_POINT ( 'NONE',  ( -5.676582343750000703, 248.3854166700806445, -9.832129032723418760 ) ) ;
#34223 = CARTESIAN_POINT ( 'NONE',  ( 11.35316468749999785, 100.5729166632526699, 3.042071309553174174 ) ) ;
#34224 = ORIENTED_EDGE ( 'NONE', *, *, #14754, .T. ) ;
#34225 = CARTESIAN_POINT ( 'NONE',  ( -10.68301270189220098, 0.000000000000000000, 117.8169872981077617 ) ) ;
#34226 = CARTESIAN_POINT ( 'NONE',  ( 10.18810118749999916, 4.220049686691935698, 107.5000000020483668 ) ) ;
#34227 = CARTESIAN_POINT ( 'NONE',  ( -8.660254037844390851, 214.7916666598387110, 4.999999999999998224 ) ) ;
#34228 = CARTESIAN_POINT ( 'NONE',  ( 2.445694354108839175, 206.3125000013656063, 195.5543056458912190 ) ) ;
#34229 = LINE ( 'NONE', #69658, #57678 ) ;
#34231 = CARTESIAN_POINT ( 'NONE',  ( -3.042071309553173730, 94.32291666325268409, 11.35316468749999785 ) ) ;
#34230 = CARTESIAN_POINT ( 'NONE',  ( -49.70177871865297448, 50.00000000000007105, 57.99999999999998579 ) ) ;
#34232 = EDGE_CURVE ( 'NONE', #3989, #72569, #67315, .T. ) ;
#34233 = CARTESIAN_POINT ( 'NONE',  ( 3.313708498984762496, -7.999999999999989342, 14.98655278392014623 ) ) ;
#34234 = CARTESIAN_POINT ( 'NONE',  ( -26.56734541678238060, 198.6250000013655779, 166.5412658750003629 ) ) ;
#34235 = CARTESIAN_POINT ( 'NONE',  ( 6.123233995736767268E-16, 213.1249999931720538, -10.00000000000000178 ) ) ;
#34236 = VERTEX_POINT ( 'NONE', #24743 ) ;
#34237 = CARTESIAN_POINT ( 'NONE',  ( 10.00000000000000178, 196.8749999931720254, 0.000000000000000000 ) ) ;
#34238 = CARTESIAN_POINT ( 'NONE',  ( 1.656854249492381248, 6.187500000000000000, -4.000000000000001776 ) ) ;
#34239 = CARTESIAN_POINT ( 'NONE',  ( -2.775557561562891351E-14, 195.0000000000000000, 142.0000000000000568 ) ) ;
#34240 = CARTESIAN_POINT ( 'NONE',  ( -9.832129032723418760, 83.17708332991935549, -5.676582343750004256 ) ) ;
#34241 = CARTESIAN_POINT ( 'NONE',  ( 2.765530957081996366, 291.1406250017069510, -6.676582343750003368 ) ) ;
#34242 = CARTESIAN_POINT ( 'NONE',  ( 7.188101187500000044, 6.843749997951610986, 0.000000000000000000 ) ) ;
#34243 = CARTESIAN_POINT ( 'NONE',  ( 10.18810118749999916, 1.247682550866122264E-15, 103.2812500020483810 ) ) ;
#34244 = CARTESIAN_POINT ( 'NONE',  ( 5.676582343749993598, 219.9479166632526983, 9.832129032723422313 ) ) ;
#34245 = VERTEX_POINT ( 'NONE', #7046 ) ;
#34246 = CARTESIAN_POINT ( 'NONE',  ( -8.660254037844390851, 69.79166665983869677, 4.999999999999998224 ) ) ;
#34247 = CARTESIAN_POINT ( 'NONE',  ( -1.469576158976823947E-15, 2.437499995903220196, 8.000000000000000000 ) ) ;
#34248 = CARTESIAN_POINT ( 'NONE',  ( 27.99999999999999645, 210.0000000000000284, 169.9999999999999147 ) ) ;
#34249 = CARTESIAN_POINT ( 'NONE',  ( -11.35316468750000141, 213.4895833299193839, 3.042071309553159963 ) ) ;
#34250 = VECTOR ( 'NONE', #29707, 1000.000000000000000 ) ;
#34251 = CARTESIAN_POINT ( 'NONE',  ( 10.00000000000000000, 46.66666665983868967, 2.679491924311235618 ) ) ;
#34252 = CARTESIAN_POINT ( 'NONE',  ( -23.99999999999999289, 207.8750000027312126, 170.0000000000002842 ) ) ;
#34253 = CARTESIAN_POINT ( 'NONE',  ( 2.765530957082001251, 296.7656250017069510, 6.676582343750000703 ) ) ;
#34254 = EDGE_LOOP ( 'NONE', ( #73859, #72844, #42878, #66628, #18081, #35708 ) ) ;
#34255 = CARTESIAN_POINT ( 'NONE',  ( 4.615726161709589270, 52.16176840074273002, -48.91069252044838578 ) ) ;
#34256 = CARTESIAN_POINT ( 'NONE',  ( 6.951808397369818766E-16, 212.3437499965860411, -11.35316468750000141 ) ) ;
#34257 = CARTESIAN_POINT ( 'NONE',  ( -7.204075437095965206, -7.204075437095968759, 97.84375000204836681 ) ) ;
#34258 = CARTESIAN_POINT ( 'NONE',  ( -24.54126587499999701, 207.1875000013656063, 170.0000000000003411 ) ) ;
#34259 = CARTESIAN_POINT ( 'NONE',  ( 7.999999999999998224, 14.90625000000000178, 3.313708498984766493 ) ) ;
#34260 = EDGE_LOOP ( 'NONE', ( #39723, #28815, #13284, #34793 ) ) ;
#34261 = PRODUCT_DEFINITION_CONTEXT ( 'detailed design', #65515, 'design' ) ;
#34262 = CARTESIAN_POINT ( 'NONE',  ( 7.188101187500000044, 123.4062500020483810, -8.802885111219163269E-16 ) ) ;
#34263 = CARTESIAN_POINT ( 'NONE',  ( -2.679491924311225848, 26.45833333333333215, -10.00000000000000178 ) ) ;
#34264 = VECTOR ( 'NONE', #24747, 1000.000000000000000 ) ;
#34265 = CYLINDRICAL_SURFACE ( 'NONE', #17480, 11.00000000000000000 ) ;
#34266 = CARTESIAN_POINT ( 'NONE',  ( 10.18810118749999916, 4.220049686691935698, 83.87500000204835260 ) ) ;
#34267 = VERTEX_POINT ( 'NONE', #46657 ) ;
#34268 = CARTESIAN_POINT ( 'NONE',  ( 2.828427124746190291, 19.87500000000000000, 2.828427124746192067 ) ) ;
#34269 = CARTESIAN_POINT ( 'NONE',  ( -2.775557561562891351E-14, 210.0000000000000284, 142.0000000000000568 ) ) ;
#34270 = CARTESIAN_POINT ( 'NONE',  ( -2.967813307894019431E-11, 16.44602605510714355, -68.55492853905352035 ) ) ;
#34271 = EDGE_CURVE ( 'NONE', #30714, #10291, #26896, .T. ) ;
#34272 =( LENGTH_UNIT ( ) NAMED_UNIT ( * ) SI_UNIT ( .MILLI., .METRE. ) );
#34273 = CARTESIAN_POINT ( 'NONE',  ( 7.188101187500002709, 122.1875000020483668, 2.977408999572649151 ) ) ;
#34274 = DIRECTION ( 'NONE',  ( 0.000000000000000000, 0.8778652960885012790, 0.4789076340208496818 ) ) ;
#34275 = CARTESIAN_POINT ( 'NONE',  ( 2.765530957081996366, 297.1406250017069510, -6.676582343750002480 ) ) ;
#34278 = CARTESIAN_POINT ( 'NONE',  ( 4.000000000000016875, 206.4375000000000568, 199.6568542494924259 ) ) ;
#34277 = CARTESIAN_POINT ( 'NONE',  ( 8.311093377946839666, 250.7812500034140157, 8.311093377946830785 ) ) ;
#34276 = CARTESIAN_POINT ( 'NONE',  ( 30.44569435410879876, 205.8125000013656063, 167.5543056458910485 ) ) ;
#34279 = PRODUCT_CONTEXT ( 'NONE', #73674, 'mechanical' ) ;
#34280 = ORIENTED_EDGE ( 'NONE', *, *, #25302, .F. ) ;
#34281 = CARTESIAN_POINT ( 'NONE',  ( -11.35316468749999963, 244.2187500034140157, 0.000000000000000000 ) ) ;
#34282 = CARTESIAN_POINT ( 'NONE',  ( 7.188101187499992051, 8.802885111219154394E-16, 9.736552781871754547 ) ) ;
#34283 = ORIENTED_EDGE ( 'NONE', *, *, #31884, .F. ) ;
#34284 = EDGE_LOOP ( 'NONE', ( #1296, #68070, #36988, #2800 ) ) ;
#34285 = CARTESIAN_POINT ( 'NONE',  ( 10.18810118749999916, 1.247682550866122264E-15, 72.90625000204836681 ) ) ;
#34286 = CARTESIAN_POINT ( 'NONE',  ( -5.676582343750006032, 94.42708332991935549, 9.832129032723418760 ) ) ;
#34287 = CARTESIAN_POINT ( 'NONE',  ( -1.836970198721029983E-15, 220.6249999931720538, 10.00000000000000178 ) ) ;
#34288 = CARTESIAN_POINT ( 'NONE',  ( -4.556349186104045934, 11.00000000000000000, 83.21874999999998579 ) ) ;
#34291 = CARTESIAN_POINT ( 'NONE',  ( -2.765530957081998142, 287.7968750017070079, 6.676582343750000703 ) ) ;
#34290 = CARTESIAN_POINT ( 'NONE',  ( 31.45873412499999944, 208.6875000013656063, 169.9999999999998863 ) ) ;
#34289 = CARTESIAN_POINT ( 'NONE',  ( 30.44569435410883429, 205.0625000013656063, 167.5543056458911053 ) ) ;
#34292 = AXIS2_PLACEMENT_3D ( 'NONE', #59414, #65799, #59782 ) ;
#34293 = EDGE_CURVE ( 'NONE', #56998, #45708, #73344, .T. ) ;
#34294 = CARTESIAN_POINT ( 'NONE',  ( 7.320508075688771044, 76.24999999317203958, 7.320508075688775484 ) ) ;
#34295 = CARTESIAN_POINT ( 'NONE',  ( 8.000000000000000000, 101.8437500000000000, -3.313708498984762496 ) ) ;
#34296 = CARTESIAN_POINT ( 'NONE',  ( -11.35316468749999785, 203.0729166632526415, -3.042071309553167513 ) ) ;
#34298 = EDGE_CURVE ( 'NONE', #65440, #64185, #57332, .T. ) ;
#34297 = CARTESIAN_POINT ( 'NONE',  ( -2.839093476692135984E-14, 205.6875000013656063, 138.5412658750000503 ) ) ;
#34299 = CARTESIAN_POINT ( 'NONE',  ( 24.54126587499999346, 205.4375000013656063, 169.9999999999998863 ) ) ;
#34300 = CARTESIAN_POINT ( 'NONE',  ( 2.977408999572650927, 19.12499999795161187, -7.188101187500001821 ) ) ;
#34301 = CARTESIAN_POINT ( 'NONE',  ( 3.042071309553159519, 165.0520833299193839, 11.35316468750000141 ) ) ;
#34302 = CARTESIAN_POINT ( 'NONE',  ( -4.898587196589412829E-16, 102.1250000000000000, -8.000000000000000000 ) ) ;
#34303 = CARTESIAN_POINT ( 'NONE',  ( -7.188101187500000933, 106.4375000020483810, -2.977408999572650483 ) ) ;
#34305 = CARTESIAN_POINT ( 'NONE',  ( -9.999999999999998224, 107.5000000000000142, -1.224646799147352862E-15 ) ) ;
#34304 = CARTESIAN_POINT ( 'NONE',  ( 4.898587196589415787E-16, 0.000000000000000000, 4.000000000000001776 ) ) ;
#34306 = CARTESIAN_POINT ( 'NONE',  ( 4.541265875000001451, 11.24999999863440792, 1.881053915767124440 ) ) ;
#34307 = CARTESIAN_POINT ( 'NONE',  ( 30.44569435410883429, 204.0625000013656063, 167.5543056458911053 ) ) ;
#34308 = CARTESIAN_POINT ( 'NONE',  ( -7.188101187499991163, 2.977408999572646930, 12.26780278187175455 ) ) ;
#34309 = CARTESIAN_POINT ( 'NONE',  ( 6.951808397369818766E-16, 52.03124999658602690, -11.35316468750000141 ) ) ;
#34310 = CARTESIAN_POINT ( 'NONE',  ( 7.999999999999991118, 9.797174393178815797E-16, 3.136552784329822430 ) ) ;
#34311 = ORIENTED_EDGE ( 'NONE', *, *, #51085, .F. ) ;
#34312 = CARTESIAN_POINT ( 'NONE',  ( 0.000000000000000000, 0.5000000000000004441, 0.000000000000000000 ) ) ;
#34313 = B_SPLINE_CURVE_WITH_KNOTS ( 'NONE', 3,
 ( #56740, #72595, #20900, #43922, #38269, #45043, #15238, #73706, #22017, #68052, #10704, #33738, #45398, #12185, #52194, #1263, #62743, #22753 ),
 .UNSPECIFIED., .F., .F.,
 ( 4, 2, 2, 2, 2, 2, 2, 2, 4 ),
 ( 0.01409179046407141832, 0.01467854081050602028, 0.01526529115694062050, 0.01585204150337522072, 0.01643879184980982441, 0.01702554219624442464, 0.01761229254267902833, 0.01819904288911362855, 0.01878579323554823224 ),
 .UNSPECIFIED. ) ;
#34314 = CARTESIAN_POINT ( 'NONE',  ( -8.000000000000000000, 22.96874999590322020, -3.313708498984762496 ) ) ;
#34315 = CARTESIAN_POINT ( 'NONE',  ( -5.676582343749998039, 62.44791666325268409, -9.832129032723420536 ) ) ;
#34316 = CARTESIAN_POINT ( 'NONE',  ( -7.778174593052023411, 7.778174593052023411, 77.50000000409676204 ) ) ;
#34317 = CARTESIAN_POINT ( 'NONE',  ( -2.445694354108840063, 201.0625000013656063, 139.5543056458912190 ) ) ;
#34318 = CARTESIAN_POINT ( 'NONE',  ( 6.298842414732200190, 10.24914933418224194, 64.89273347874026854 ) ) ;
#34320 = CARTESIAN_POINT ( 'NONE',  ( 8.311093377946834337, 55.15624999658601268, 8.311093377946839666 ) ) ;
#34319 = CARTESIAN_POINT ( 'NONE',  ( 7.188101187500002709, 91.81250000204838102, 2.977408999572649151 ) ) ;
#34321 = EDGE_CURVE ( 'NONE', #46305, #32440, #65009, .T. ) ;
#34322 = CARTESIAN_POINT ( 'NONE',  ( 5.656854249492376141, -5.656854249492374365, 1.392802779823364201 ) ) ;
#34323 = CARTESIAN_POINT ( 'NONE',  ( -7.320508075688778149, 14.99999999317203425, 7.320508075688769267 ) ) ;
#34324 =( BOUNDED_CURVE ( )  B_SPLINE_CURVE ( 2, ( #72784, #28247, #50138, #4498, #22200, #16532, #21825, #39572, #32427 ),
 .UNSPECIFIED., .F., .F. ) 
 B_SPLINE_CURVE_WITH_KNOTS ( ( 3, 2, 2, 2, 3 ),
 ( 0.3382352941176469674, 0.3419117647058822484, 0.3455882352941175295, 0.3492647058823528661, 0.3529411764705882026 ),
 .UNSPECIFIED. ) 
 CURVE ( )  GEOMETRIC_REPRESENTATION_ITEM ( )  RATIONAL_B_SPLINE_CURVE ( ( 1.000000000000002220, 0.9238795325112844070, 1.000000000000000000, 0.9238795325112867385, 1.000000000000000000, 0.9238795325112867385, 1.000000000000000000, 0.9238795325112878487, 0.9999999999999988898 ) ) 
 REPRESENTATION_ITEM ( '' )  );
#34325 = CARTESIAN_POINT ( 'NONE',  ( 3.042071309553159519, 169.7395833299193839, 11.35316468750000141 ) ) ;
#34327 = CARTESIAN_POINT ( 'NONE',  ( -5.000000000000005329, 145.2083333265053682, 8.660254037844387298 ) ) ;
#34326 = PRODUCT_DEFINITION_SHAPE ( 'NONE', 'NONE',  #74652 ) ;
#34328 = CARTESIAN_POINT ( 'NONE',  ( 7.188101187500000044, 96.78125000204838102, -8.802885111219163269E-16 ) ) ;
#34329 = AXIS2_PLACEMENT_3D ( 'NONE', #21726, #38351, #16430 ) ;
#34330 = DIRECTION ( 'NONE',  ( 0.000000000000000000, 0.000000000000000000, -1.000000000000000000 ) ) ;
#34331 = CARTESIAN_POINT ( 'NONE',  ( 9.832129032723420536, 51.51041666325269119, -5.676582343749999815 ) ) ;
#34332 = CARTESIAN_POINT ( 'NONE',  ( -7.320508075688778149, 79.99999999317203958, 7.320508075688769267 ) ) ;
#34333 = CARTESIAN_POINT ( 'NONE',  ( -8.311093377946836114, 182.6562499965860411, -8.311093377946837890 ) ) ;
#34334 = ORIENTED_EDGE ( 'NONE', *, *, #28148, .T. ) ;
#34335 = CARTESIAN_POINT ( 'NONE',  ( 48.12154660295335162, 143.0822719893220096, 62.15125942254319114 ) ) ;
#34336 = CARTESIAN_POINT ( 'NONE',  ( 10.18810118750000093, -4.220049686691933921, 72.81250000204836681 ) ) ;
#34337 = CARTESIAN_POINT ( 'NONE',  ( -2.828427124746153876, 196.8750000000000284, 195.1715728752538439 ) ) ;
#34338 = CARTESIAN_POINT ( 'NONE',  ( 31.16562362098048311, 45.73052608861913626, 65.00000000000000000 ) ) ;
#34340 = CARTESIAN_POINT ( 'NONE',  ( -2.085542519210945728E-15, 184.5312499965860411, 11.35316468750000141 ) ) ;
#34339 = CARTESIAN_POINT ( 'NONE',  ( 4.000000000000001776, 18.74999999726881583, 0.000000000000000000 ) ) ;
#34341 = CARTESIAN_POINT ( 'NONE',  ( 1.469576158976822172E-15, -7.999999999999991118, 4.261552784329823318 ) ) ;
#34342 = AXIS2_PLACEMENT_3D ( 'NONE', #12155, #63093, #5763 ) ;
#34343 = CARTESIAN_POINT ( 'NONE',  ( 4.556349186104052151, -10.99999999999999822, 79.65625000409676204 ) ) ;
#34344 = CARTESIAN_POINT ( 'NONE',  ( 11.35316468749999963, 226.1979166700806729, 3.042071309553159519 ) ) ;
#34345 = FACE_BOUND ( 'NONE', #8563, .T. ) ;
#34346 = ORIENTED_EDGE ( 'NONE', *, *, #54022, .F. ) ;
#34347 =( BOUNDED_CURVE ( )  B_SPLINE_CURVE ( 2, ( #60221, #8545, #31559, #25875, #67006, #54582, #20220, #43239, #14561 ),
 .UNSPECIFIED., .F., .F. ) 
 B_SPLINE_CURVE_WITH_KNOTS ( ( 3, 2, 2, 2, 3 ),
 ( 0.03333333333333336063, 0.04166666666666669905, 0.05000000000000004441, 0.05833333333333338283, 0.06666666666666672125 ),
 .UNSPECIFIED. ) 
 CURVE ( )  GEOMETRIC_REPRESENTATION_ITEM ( )  RATIONAL_B_SPLINE_CURVE ( ( 0.9999999999999997780, 0.9238795325112869605, 1.000000000000000000, 0.9238795325112867385, 1.000000000000000000, 0.9238795325112867385, 1.000000000000000000, 0.9238795325112861834, 1.000000000000000444 ) ) 
 REPRESENTATION_ITEM ( '' )  );
#34348 = ADVANCED_FACE ( 'NONE', ( #8890 ), #65456, .F. ) ;
#34349 = CARTESIAN_POINT ( 'NONE',  ( 7.188101187499993827, -2.977408999572645598, 26.14280278187175455 ) ) ;
#34350 = CARTESIAN_POINT ( 'NONE',  ( 9.832129032723420536, 111.5104166632526841, -5.676582343749999815 ) ) ;
#34351 = CARTESIAN_POINT ( 'NONE',  ( -1.477658550686901773, -9.539178283403858316, -0.3563104543936471691 ) ) ;
#34352 = EDGE_LOOP ( 'NONE', ( #3511, #12701 ) ) ;
#34353 = CARTESIAN_POINT ( 'NONE',  ( -3.211159895383561391, 9.812499998634406140, -3.211159895383561835 ) ) ;
#34354 = CARTESIAN_POINT ( 'NONE',  ( -5.082755093536326818, 16.40624999795161543, 5.082755093536325042 ) ) ;
#34355 = CARTESIAN_POINT ( 'NONE',  ( 8.000000000000001776, 112.3437500040967905, 3.313708498984759387 ) ) ;
#34356 = CARTESIAN_POINT ( 'NONE',  ( -26.56734541678232375, 198.2500000013656347, 173.4587341250003760 ) ) ;
#34357 = CARTESIAN_POINT ( 'NONE',  ( 2.828427124746191623, 8.125000000000000000, -2.828427124746191623 ) ) ;
#34358 = CARTESIAN_POINT ( 'NONE',  ( -1.656854249492383691, 22.43749999726881583, 4.000000000000000888 ) ) ;
#34359 = CARTESIAN_POINT ( 'NONE',  ( -1.881053915767121776, 11.62499999863440792, -4.541265875000002339 ) ) ;
#34360 = CARTESIAN_POINT ( 'NONE',  ( 7.999999999999991118, 9.797174393178815797E-16, 22.76780278392014623 ) ) ;
#34361 = CARTESIAN_POINT ( 'NONE',  ( -2.828427124746209831, 197.3750000000000284, 139.1715728752538723 ) ) ;
#34362 = ORIENTED_EDGE ( 'NONE', *, *, #14265, .T. ) ;
#34363 = CARTESIAN_POINT ( 'NONE',  ( 3.313708498984756279, 7.999999999999991118, 9.549052783920144449 ) ) ;
#34364 = CARTESIAN_POINT ( 'NONE',  ( -5.082755093536324154, 103.3437500020483668, 5.082755093536326818 ) ) ;
#34365 = AXIS2_PLACEMENT_3D ( 'NONE', #25088, #71113, #20170 ) ;
#34367 = CYLINDRICAL_SURFACE ( 'NONE', #10503, 17.50000000000000000 ) ;
#34366 = CARTESIAN_POINT ( 'NONE',  ( 5.841566664369303132E-15, 13.85640646055103531, -14.00000000000000178 ) ) ;
#34368 = CARTESIAN_POINT ( 'NONE',  ( 1.881053915767122664, 21.12499999863441147, 4.541265875000001451 ) ) ;
#34369 = CIRCLE ( 'NONE', #50012, 7.999999999999991118 ) ;
#34370 = CARTESIAN_POINT ( 'NONE',  ( -5.082755093536319713, 5.082755093536319713, 28.29905278187175810 ) ) ;
#34371 = ORIENTED_EDGE ( 'NONE', *, *, #58885, .F. ) ;
#34372 = EDGE_CURVE ( 'NONE', #31698, #15376, #21896, .T. ) ;
#34373 = ORIENTED_EDGE ( 'NONE', *, *, #39302, .F. ) ;
#34374 = CARTESIAN_POINT ( 'NONE',  ( 10.18810118749999916, 4.220049686691935698, 94.00000000204838102 ) ) ;
#34375 = FACE_OUTER_BOUND ( 'NONE', #13250, .T. ) ;
#34376 = CARTESIAN_POINT ( 'NONE',  ( -31.45873412499997812, 197.0000000013656063, 171.4326545832180386 ) ) ;
#34377 = CARTESIAN_POINT ( 'NONE',  ( -11.00000000000000000, 4.556349186104045934, 101.4062500000000000 ) ) ;
#34378 = CARTESIAN_POINT ( 'NONE',  ( 1.432654583217664701, 204.0000000013656347, 201.4587341250000065 ) ) ;
#34380 = CARTESIAN_POINT ( 'NONE',  ( 1.681385197618709730E-11, 51.24999999999869971, -10.00000000000000178 ) ) ;
#34379 = CARTESIAN_POINT ( 'NONE',  ( 4.556349186104052151, -10.99999999999999822, 86.96875000000000000 ) ) ;
#34381 = CARTESIAN_POINT ( 'NONE',  ( -10.00000000000000178, 122.5000000000000142, -1.224646799147353454E-15 ) ) ;
#34382 = CARTESIAN_POINT ( 'NONE',  ( 3.313708498984765161, 105.9687500000000142, 7.999999999999998224 ) ) ;
#34383 = CARTESIAN_POINT ( 'NONE',  ( 6.676582343750003368, 289.1718750017070647, -2.765530957081997254 ) ) ;
#34384 = CARTESIAN_POINT ( 'NONE',  ( 2.977408999572646486, 7.188101187499991163, 5.892802781871754547 ) ) ;
#34385 = CARTESIAN_POINT ( 'NONE',  ( 105.0000000000000000, 38.00000000000000711, 57.99999999999999289 ) ) ;
#34386 = EDGE_CURVE ( 'NONE', #9236, #32674, #1046, .T. ) ;
#34387 = CARTESIAN_POINT ( 'NONE',  ( 27.99999999999996447, 203.4375000013656063, 173.4587341249998929 ) ) ;
#34388 = CARTESIAN_POINT ( 'NONE',  ( -8.000000000000000000, 24.46874999590322375, -3.313708498984762496 ) ) ;
#34389 = CARTESIAN_POINT ( 'NONE',  ( -3.458734125000015425, 199.9375000013656063, 142.0000000000000568 ) ) ;
#34390 = CARTESIAN_POINT ( 'NONE',  ( 7.188101187500000933, 122.3750000020483952, -2.977408999572651371 ) ) ;
#34392 = CARTESIAN_POINT ( 'NONE',  ( -7.999999999999991118, 0.000000000000000000, 6.830302779823365533 ) ) ;
#34391 = SURFACE_SIDE_STYLE ('',( #34765 ) ) ;
#34393 = CARTESIAN_POINT ( 'NONE',  ( -9.832129032723418760, 238.8020833367473301, -5.676582343749998927 ) ) ;
#34394 = CARTESIAN_POINT ( 'NONE',  ( 27.99999999999996447, 197.0000000000000000, 173.9999999999999147 ) ) ;
#34395 = CARTESIAN_POINT ( 'NONE',  ( 26.34314575050758833, 198.9375000000000000, 173.9999999999999147 ) ) ;
#34396 = CARTESIAN_POINT ( 'NONE',  ( 5.676582343749993598, 9.947916663252682312, 9.832129032723422313 ) ) ;
#34397 = CARTESIAN_POINT ( 'NONE',  ( -5.447323953993864265, -4.689931814214729044, 0.5319290643893268555 ) ) ;
#34398 = CARTESIAN_POINT ( 'NONE',  ( -2.085542519210945728E-15, 209.8437499965860411, 11.35316468750000141 ) ) ;
#34399 = CARTESIAN_POINT ( 'NONE',  ( -31.99999999999997868, 197.3125000000000568, 171.6568542494928238 ) ) ;
#34400 = CARTESIAN_POINT ( 'NONE',  ( -4.999999999999998224, 218.5416666598387110, -8.660254037844389075 ) ) ;
#34402 = CARTESIAN_POINT ( 'NONE',  ( 1.656854249492381914, 11.56249999726881406, 4.000000000000000888 ) ) ;
#34401 = CARTESIAN_POINT ( 'NONE',  ( 1.656854249492382358, 203.3125000027312126, 138.0000000000001137 ) ) ;
#34403 = ORIENTED_EDGE ( 'NONE', *, *, #72395, .F. ) ;
#34404 = CARTESIAN_POINT ( 'NONE',  ( -3.458734125000016757, 200.1250000013656063, 140.5673454167824161 ) ) ;
#34405 = CARTESIAN_POINT ( 'NONE',  ( -9.832129032723418760, 27.86458332991935194, -5.676582343750004256 ) ) ;
#34406 = CARTESIAN_POINT ( 'NONE',  ( 4.556349186104045934, 11.00000000000000000, 95.21875000409679046 ) ) ;
#34407 = CARTESIAN_POINT ( 'NONE',  ( -5.000000000000000000, 10.26105934116142215, 64.40045319026754100 ) ) ;
#34408 = CARTESIAN_POINT ( 'NONE',  ( -26.56734541678228112, 198.0000000013656063, 173.4587341250003476 ) ) ;
#34409 = CARTESIAN_POINT ( 'NONE',  ( -9.000000000000000000, 5.196152422706624918, -0.8038475772933814101 ) ) ;
#34411 = CARTESIAN_POINT ( 'NONE',  ( -8.311093377946841443, 13.90624999658601801, 8.311093377946834337 ) ) ;
#34410 = CARTESIAN_POINT ( 'NONE',  ( -4.401442555609581635E-16, 113.2812500020483952, -7.188101187500000044 ) ) ;
#34412 = CARTESIAN_POINT ( 'NONE',  ( -5.656854249492375253, 5.656854249492375253, 20.14280277982336642 ) ) ;
#34413 = CARTESIAN_POINT ( 'NONE',  ( 8.311093377946837890, 131.4062499965860411, -8.311093377946837890 ) ) ;
#34414 = EDGE_CURVE ( 'NONE', #38802, #32408, #61530, .T. ) ;
#34415 = CARTESIAN_POINT ( 'NONE',  ( 6.123233995736767268E-16, 103.1249999931720396, -10.00000000000000178 ) ) ;
#34416 = CARTESIAN_POINT ( 'NONE',  ( 2.977408999572654480, 116.0000000020483810, 7.188101187499999156 ) ) ;
#34417 = CARTESIAN_POINT ( 'NONE',  ( -8.660254037844390851, 4.791666659838699438, 4.999999999999998224 ) ) ;
#34418 = CARTESIAN_POINT ( 'NONE',  ( -29.43265458321761230, 207.1250000013656347, 173.4587341250003760 ) ) ;
#34419 = FACE_OUTER_BOUND ( 'NONE', #64386, .T. ) ;
#34420 = VERTEX_POINT ( 'NONE', #45290 ) ;
#34421 = CARTESIAN_POINT ( 'NONE',  ( 3.042071309553159519, 5.052083329919350163, 11.35316468750000141 ) ) ;
#34422 = ADVANCED_FACE ( 'NONE', ( #68302 ), #42304, .F. ) ;
#34423 = CARTESIAN_POINT ( 'NONE',  ( 8.000000000000000000, 107.7500000000000000, -9.797174393178825657E-16 ) ) ;
#34424 = CARTESIAN_POINT ( 'NONE',  ( -6.676582343750000703, 287.6718750017070079, 2.765530957082001251 ) ) ;
#34425 = CARTESIAN_POINT ( 'NONE',  ( -11.35316468749999785, 128.0729166632526699, -3.042071309553167957 ) ) ;
#34426 =( NAMED_UNIT ( * ) PLANE_ANGLE_UNIT ( ) SI_UNIT ( $, .RADIAN. ) );
#34427 = CARTESIAN_POINT ( 'NONE',  ( -5.656854249492373476, -5.656854249492376141, 22.07405278432982243 ) ) ;
#34428 = CARTESIAN_POINT ( 'NONE',  ( -8.000000000000001776, 18.84375000000000355, 3.313708498984759387 ) ) ;
#34429 = CARTESIAN_POINT ( 'NONE',  ( 2.085542519210945334E-15, 255.1562500034140157, 11.35316468749999963 ) ) ;
#34430 = VECTOR ( 'NONE', #11302, 1000.000000000000000 ) ;
#34431 = CARTESIAN_POINT ( 'NONE',  ( -10.18810118749999916, 0.000000000000000000, 98.03125000204838102 ) ) ;
#34432 = ORIENTED_EDGE ( 'NONE', *, *, #32126, .T. ) ;
#34433 = CIRCLE ( 'NONE', #48877, 5.000000000000000888 ) ;
#34434 = DIRECTION ( 'NONE',  ( -0.000000000000000000, 1.000000000000000000, -0.000000000000000000 ) ) ;
#34435 = CARTESIAN_POINT ( 'NONE',  ( 5.000000000000000000, 67.10993666412761627, -23.06595724273550374 ) ) ;
#34436 = CARTESIAN_POINT ( 'NONE',  ( -3.458734124999960358, 201.6875000013656063, 198.0000000000000284 ) ) ;
#34437 = ADVANCED_FACE ( 'NONE', ( #18491, #17742 ), #23404, .F. ) ;
#34438 = CARTESIAN_POINT ( 'NONE',  ( 9.832129032723420536, 71.51041666325268409, -5.676582343749999815 ) ) ;
#34440 = ORIENTED_EDGE ( 'NONE', *, *, #24555, .T. ) ;
#34439 =( BOUNDED_CURVE ( )  B_SPLINE_CURVE ( 2, ( #31745, #20407, #7987, #54765, #43423, #47967, #19666, #24950, #3446 ),
 .UNSPECIFIED., .F., .F. ) 
 B_SPLINE_CURVE_WITH_KNOTS ( ( 3, 2, 2, 2, 3 ),
 ( 0.9305555555555554692, 0.9374999999999998890, 0.9444444444444443088, 0.9513888888888887285, 0.9583333333333332593 ),
 .UNSPECIFIED. ) 
 CURVE ( )  GEOMETRIC_REPRESENTATION_ITEM ( )  RATIONAL_B_SPLINE_CURVE ( ( 1.000000000000001110, 0.9238795325112855172, 1.000000000000000000, 0.9238795325112867385, 1.000000000000000000, 0.9238795325112867385, 1.000000000000000000, 0.9238795325112879597, 0.9999999999999987788 ) ) 
 REPRESENTATION_ITEM ( '' )  );
#34441 = CARTESIAN_POINT ( 'NONE',  ( 7.204075437095968759, -7.204075437095966983, 107.2187500020483810 ) ) ;
#34442 = CARTESIAN_POINT ( 'NONE',  ( 4.541265875000002339, 13.49999999863440792, -1.881053915767121776 ) ) ;
#34443 = ORIENTED_EDGE ( 'NONE', *, *, #2738, .T. ) ;
#34444 = CARTESIAN_POINT ( 'NONE',  ( -7.188101187500000044, 26.71874999795161543, -8.802885111219163269E-16 ) ) ;
#34445 = CARTESIAN_POINT ( 'NONE',  ( 10.00000000000000178, 115.2083333333333428, -2.679491924311227180 ) ) ;
#34446 = CARTESIAN_POINT ( 'NONE',  ( 0.000000000000000000, 4.408728476930470856E-15, -36.00000000000000000 ) ) ;
#34447 = CARTESIAN_POINT ( 'NONE',  ( -2.977408999572650039, 25.31249999795161543, -7.188101187500001821 ) ) ;
#34448 = CARTESIAN_POINT ( 'NONE',  ( 0.000000000000000000, 125.0000000000000000, 8.000000000000000000 ) ) ;
#34449 = CARTESIAN_POINT ( 'NONE',  ( -4.220049686691935698, 10.18810118749999916, 103.7500000020483668 ) ) ;
#34450 = CARTESIAN_POINT ( 'NONE',  ( 9.999999999999996447, 110.2083333333333286, -2.679491924311225848 ) ) ;
#34451 = CARTESIAN_POINT ( 'NONE',  ( -2.828427124746192067, 8.374999997268814056, 2.828427124746190735 ) ) ;
#34452 = CARTESIAN_POINT ( 'NONE',  ( -2.828427124746208943, 208.7500000027312126, 144.8284271247462129 ) ) ;
#34453 = EDGE_LOOP ( 'NONE', ( #67539, #20618 ) ) ;
#34454 = EDGE_CURVE ( 'NONE', #21379, #1593, #1881, .T. ) ;
#34455 = CARTESIAN_POINT ( 'NONE',  ( -27.99999999999999645, 195.0000000000000000, 170.0000000000003695 ) ) ;
#34456 = CARTESIAN_POINT ( 'NONE',  ( 2.445694354108839619, 202.8125000013656063, 200.4456943541088663 ) ) ;
#34457 = EDGE_CURVE ( 'NONE', #50622, #34951, #50032, .T. ) ;
#34458 = CARTESIAN_POINT ( 'NONE',  ( -26.56734541678227757, 207.0000000013656063, 173.4587341250003476 ) ) ;
#34459 = DIRECTION ( 'NONE',  ( 1.000000000000000000, 0.000000000000000000, 0.000000000000000000 ) ) ;
#34460 = CARTESIAN_POINT ( 'NONE',  ( 2.780723358947928197E-16, 10.56249999863440792, -4.541265875000002339 ) ) ;
#34461 = CARTESIAN_POINT ( 'NONE',  ( -4.000000000000015987, 206.6250000027312126, 142.0000000000000568 ) ) ;
#34462 = CARTESIAN_POINT ( 'NONE',  ( 7.188101187499993827, -2.977408999572645598, 17.14280278187175455 ) ) ;
#34463 = ORIENTED_EDGE ( 'NONE', *, *, #62342, .F. ) ;
#34464 = EDGE_CURVE ( 'NONE', #63265, #22556, #23778, .T. ) ;
#34465 = EDGE_LOOP ( 'NONE', ( #69721, #65716, #74188, #24042 ) ) ;
#34466 = CARTESIAN_POINT ( 'NONE',  ( 4.220049686691941027, -10.18810118749999738, 111.6250000020483810 ) ) ;
#34467 = CARTESIAN_POINT ( 'NONE',  ( 24.00000000000000711, 208.9375000027312410, 171.6568542494923122 ) ) ;
#34468 = CARTESIAN_POINT ( 'NONE',  ( -23.99999999999997513, 203.6875000000000000, 171.6568542494927385 ) ) ;
#34469 = CARTESIAN_POINT ( 'NONE',  ( -2.445694354108783664, 198.3125000013656063, 195.5543056458912190 ) ) ;
#34470 = CARTESIAN_POINT ( 'NONE',  ( 27.99999999999996447, 194.9375000013655779, 166.5412658749999082 ) ) ;
#34471 = CARTESIAN_POINT ( 'NONE',  ( 2.679491924311222739, 78.95833333333334281, 10.00000000000000355 ) ) ;
#34472 = CARTESIAN_POINT ( 'NONE',  ( -4.898587196589412829E-16, 121.6250000000000000, -8.000000000000000000 ) ) ;
#34473 = CARTESIAN_POINT ( 'NONE',  ( -6.676582343750001591, 298.6093750017069510, 0.000000000000000000 ) ) ;
#34474 = AXIS2_PLACEMENT_3D ( 'NONE', #54832, #36727, #19359 ) ;
#34475 = ORIENTED_EDGE ( 'NONE', *, *, #32126, .F. ) ;
#34476 = CARTESIAN_POINT ( 'NONE',  ( -5.126106709314337095, -68.65851429197823563, 20.89429596904591691 ) ) ;
#34477 = CARTESIAN_POINT ( 'NONE',  ( -1.656854249492405451, 195.4375000027312410, 138.0000000000000568 ) ) ;
#34478 = CARTESIAN_POINT ( 'NONE',  ( -8.000000000000001776, 23.34375000000000355, 3.313708498984759387 ) ) ;
#34479 = CARTESIAN_POINT ( 'NONE',  ( 8.660254037844385522, 237.9166666666666572, -5.000000000000003553 ) ) ;
#34480 = ADVANCED_FACE ( 'NONE', ( #13541 ), #74520, .F. ) ;
#34481 = DIRECTION ( 'NONE',  ( 1.000000000000000000, -0.000000000000000000, 0.000000000000000000 ) ) ;
#34482 = CARTESIAN_POINT ( 'NONE',  ( -11.00000000000000000, 4.556349186104045934, 117.9062499999999858 ) ) ;
#34483 = ADVANCED_FACE ( 'NONE', ( #64142 ), #53565, .F. ) ;
#34484 = CARTESIAN_POINT ( 'NONE',  ( 10.00000000000000000, 194.7916666666666856, 2.679491924311236062 ) ) ;
#34485 = CARTESIAN_POINT ( 'NONE',  ( 7.188101187499993827, -2.977408999572645598, 16.01780278187175099 ) ) ;
#34486 = CARTESIAN_POINT ( 'NONE',  ( 6.951808397369818766E-16, 162.3437499965860127, -11.35316468750000141 ) ) ;
#34487 = DIRECTION ( 'NONE',  ( -0.000000000000000000, 1.000000000000000000, -4.476705744456276341E-16 ) ) ;
#34488 = CARTESIAN_POINT ( 'NONE',  ( 32.00000000000000000, 197.3125000027312126, 171.6568542494922553 ) ) ;
#34490 = CARTESIAN_POINT ( 'NONE',  ( -4.242640687119286547, 296.9375000034140157, -4.242640687119286547 ) ) ;
#34489 = FILL_AREA_STYLE ('',( #39381 ) ) ;
#34491 = ORIENTED_EDGE ( 'NONE', *, *, #74046, .T. ) ;
#34492 = CARTESIAN_POINT ( 'NONE',  ( 3.458734124999959914, 198.4375000013655779, 142.0000000000000568 ) ) ;
#34493 = CARTESIAN_POINT ( 'NONE',  ( -8.311093377946841443, 39.21874999658600558, 8.311093377946830785 ) ) ;
#34494 = CARTESIAN_POINT ( 'NONE',  ( 11.00000000000000355, -4.556349186104045046, 108.3437500040967763 ) ) ;
#34495 = CARTESIAN_POINT ( 'NONE',  ( -3.403184810911366487, 194.4648993367464698, 198.6849573932121018 ) ) ;
#34496 = DIRECTION ( 'NONE',  ( -0.000000000000000000, 1.000000000000000000, -0.000000000000000000 ) ) ;
#34498 = CARTESIAN_POINT ( 'NONE',  ( 0.3794862803135433671, -10.12385276104027199, -70.07165850195889334 ) ) ;
#34497 = DIRECTION ( 'NONE',  ( -0.000000000000000000, 1.000000000000000000, 4.476705744456276341E-16 ) ) ;
#34499 = CARTESIAN_POINT ( 'NONE',  ( -30.51145194585395259, -51.99965134929454535, 175.8069438503486595 ) ) ;
#34500 = CARTESIAN_POINT ( 'NONE',  ( 1.432654583217607192, 200.2500000013656063, 145.4587341250000350 ) ) ;
#34501 = AXIS2_PLACEMENT_3D ( 'NONE', #67338, #3975, #20172 ) ;
#34502 = CARTESIAN_POINT ( 'NONE',  ( -4.999999999999998224, 68.54166665983869677, -8.660254037844389075 ) ) ;
#34503 = CARTESIAN_POINT ( 'NONE',  ( -2.977408999572650927, 104.3750000020483952, -7.188101187500001821 ) ) ;
#34504 = CARTESIAN_POINT ( 'NONE',  ( 3.211159895383560947, 11.31249999863440792, 3.211159895383562723 ) ) ;
#34505 = CARTESIAN_POINT ( 'NONE',  ( 0.000000000000000000, 125.0000000000000000, 0.000000000000000000 ) ) ;
#34506 = CARTESIAN_POINT ( 'NONE',  ( -3.313708498984757167, 7.999999999999991118, 3.549052779823362425 ) ) ;
#34507 = CARTESIAN_POINT ( 'NONE',  ( 1.656854249492381914, 7.562499997268812280, 4.000000000000000888 ) ) ;
#34508 = ORIENTED_EDGE ( 'NONE', *, *, #55476, .T. ) ;
#34509 = ORIENTED_EDGE ( 'NONE', *, *, #9451, .F. ) ;
#34510 = EDGE_CURVE ( 'NONE', #72569, #9105, #52823, .T. ) ;
#34511 = CARTESIAN_POINT ( 'NONE',  ( -2.828427124746153876, 205.0000000027312126, 195.1715728752538439 ) ) ;
#34512 = CARTESIAN_POINT ( 'NONE',  ( 2.765530957082001251, 296.9218750017069510, 6.676582343750000703 ) ) ;
#34513 = CARTESIAN_POINT ( 'NONE',  ( -10.00000000000001243, 162.5000000000000000, -1.224646799147354637E-15 ) ) ;
#34514 = DIRECTION ( 'NONE',  ( -0.000000000000000000, -0.000000000000000000, 1.000000000000000000 ) ) ;
#34515 = CARTESIAN_POINT ( 'NONE',  ( 9.832129032723416984, 140.3645833299193555, 5.676582343750006032 ) ) ;
#34516 = FACE_OUTER_BOUND ( 'NONE', #39698, .T. ) ;
#34517 = CARTESIAN_POINT ( 'NONE',  ( -7.204075437095967871, 7.204075437095967871, 85.46875000204836681 ) ) ;
#34518 = CARTESIAN_POINT ( 'NONE',  ( -29.73028433449594132, 194.7132116749263275, 173.2931147924143147 ) ) ;
#34519 = CARTESIAN_POINT ( 'NONE',  ( 2.828427124746209831, 202.3750000000000284, 200.8284271247462129 ) ) ;
#34520 = CARTESIAN_POINT ( 'NONE',  ( 5.886648204683470276, -5.430392733765462054, 0.000000000000000000 ) ) ;
#34521 = CARTESIAN_POINT ( 'NONE',  ( -4.220049686691935698, 10.18810118749999916, 115.7500000020483668 ) ) ;
#34522 = ORIENTED_EDGE ( 'NONE', *, *, #62991, .F. ) ;
#34523 = DIRECTION ( 'NONE',  ( 0.000000000000000000, 0.000000000000000000, -1.000000000000000000 ) ) ;
#34524 = CARTESIAN_POINT ( 'NONE',  ( -2.199244671006176599, 177.9999999999999716, 139.0000000000001137 ) ) ;
#34525 = CARTESIAN_POINT ( 'NONE',  ( -9.832129032723418760, 128.1770833299193555, -5.676582343750004256 ) ) ;
#34526 = CARTESIAN_POINT ( 'NONE',  ( -3.458734124999959914, 203.4375000013656063, 198.0000000000000284 ) ) ;
#34527 = CARTESIAN_POINT ( 'NONE',  ( -1.320432766682874540E-15, 21.46874999795161543, 7.188101187500000044 ) ) ;
#34528 = CARTESIAN_POINT ( 'NONE',  ( 1.871523826299183495E-15, -10.18810118749999916, 74.40625000204836681 ) ) ;
#34529 = CARTESIAN_POINT ( 'NONE',  ( 8.311093377946834337, 35.46874999658600558, 8.311093377946839666 ) ) ;
#34530 = VERTEX_POINT ( 'NONE', #47516 ) ;
#34531 = CARTESIAN_POINT ( 'NONE',  ( 2.780723358947928197E-16, 1.687499998634406806, -4.541265875000002339 ) ) ;
#34532 = CARTESIAN_POINT ( 'NONE',  ( -3.317071493978878571, 8.008118988124991233, 12.73186528394062833 ) ) ;
#34533 = CARTESIAN_POINT ( 'NONE',  ( -2.754378923186476579E-14, 205.4375000013656063, 145.4587341250000350 ) ) ;
#34534 = CARTESIAN_POINT ( 'NONE',  ( 2.977408999572651815, 10.68749999795161187, 7.188101187500000933 ) ) ;
#34535 = CARTESIAN_POINT ( 'NONE',  ( 2.485281374238571317, 295.7500000034140157, -6.000000000000003553 ) ) ;
#34536 = CARTESIAN_POINT ( 'NONE',  ( -20.64452614720341828, -14.86907989394238783, 137.0888134331518984 ) ) ;
#34537 = CARTESIAN_POINT ( 'NONE',  ( 7.188101187499999156, 8.249999997951611874, 2.977408999572654924 ) ) ;
#34538 = CARTESIAN_POINT ( 'NONE',  ( 5.676582343749993598, 160.2604166632526983, 9.832129032723422313 ) ) ;
#34539 = CARTESIAN_POINT ( 'NONE',  ( 4.220049686691934809, 10.18810118749999916, 68.68750000204836681 ) ) ;
#34540 = CARTESIAN_POINT ( 'NONE',  ( -24.54126587499998635, 207.3750000013656063, 171.4326545832179818 ) ) ;
#34541 = CARTESIAN_POINT ( 'NONE',  ( 2.828427124746191623, 3.125000000000000000, -2.828427124746191623 ) ) ;
#34542 = CARTESIAN_POINT ( 'NONE',  ( 1.881053915767121776, 20.62499999863441147, -4.541265875000002339 ) ) ;
#34543 = ORIENTED_EDGE ( 'NONE', *, *, #45936, .T. ) ;
#34544 = B_SPLINE_CURVE_WITH_KNOTS ( 'NONE', 3,
 ( #41334, #23604, #58331, #70011, #22856, #17572 ),
 .UNSPECIFIED., .F., .F.,
 ( 4, 2, 4 ),
 ( 2.380730968220572225E-07, 0.002629065763328352658, 0.005257893453559882822 ),
 .UNSPECIFIED. ) ;
#34545 = CARTESIAN_POINT ( 'NONE',  ( 4.000000000000015987, 199.5625000027311842, 199.6568542494924259 ) ) ;
#34546 = EDGE_CURVE ( 'NONE', #42073, #38454, #13178, .T. ) ;
#34547 = CARTESIAN_POINT ( 'NONE',  ( -1.656854249492403008, 206.6875000000000284, 146.0000000000000284 ) ) ;
#34549 =( BOUNDED_CURVE ( )  B_SPLINE_CURVE ( 2, ( #26225, #36461, #48873, #25487, #59475, #2121, #37197, #54931, #7788 ),
 .UNSPECIFIED., .F., .F. ) 
 B_SPLINE_CURVE_WITH_KNOTS ( ( 3, 2, 2, 2, 3 ),
 ( 0.6833333333333340143, 0.6916666666666673180, 0.7000000000000005107, 0.7083333333333339255, 0.7166666666666671182 ),
 .UNSPECIFIED. ) 
 CURVE ( )  GEOMETRIC_REPRESENTATION_ITEM ( )  RATIONAL_B_SPLINE_CURVE ( ( 0.9999999999999938938, 0.9238795325112928447, 1.000000000000000000, 0.9238795325112867385, 1.000000000000000000, 0.9238795325112867385, 1.000000000000000000, 0.9238795325112826307, 1.000000000000003997 ) ) 
 REPRESENTATION_ITEM ( '' )  );
#34548 = CARTESIAN_POINT ( 'NONE',  ( -29.65685424949229088, 200.5625000027312126, 174.0000000000004547 ) ) ;
#34550 = CARTESIAN_POINT ( 'NONE',  ( 2.679491924311117934, 251.6666666734946887, -10.00000000000006217 ) ) ;
#34551 = CARTESIAN_POINT ( 'NONE',  ( -7.999999999999991118, 3.313708498984756723, 9.924052783920146226 ) ) ;
#34552 = ORIENTED_EDGE ( 'NONE', *, *, #48243, .F. ) ;
#34553 = EDGE_CURVE ( 'NONE', #68525, #26153, #2244, .T. ) ;
#34554 = CARTESIAN_POINT ( 'NONE',  ( 7.188101187500000044, 15.46874999795161187, 0.000000000000000000 ) ) ;
#34555 = CARTESIAN_POINT ( 'NONE',  ( -2.679491924311226292, 208.3333333265054250, -10.00000000000000178 ) ) ;
#34556 = CARTESIAN_POINT ( 'NONE',  ( 27.99999999999996803, 204.0000000000000284, 173.9999999999999147 ) ) ;
#34557 = CARTESIAN_POINT ( 'NONE',  ( 8.660254037844385522, 39.58333333333333570, 5.000000000000005329 ) ) ;
#34558 = CARTESIAN_POINT ( 'NONE',  ( -5.082755093536325930, 106.3437500020483810, -5.082755093536325930 ) ) ;
#34559 = CARTESIAN_POINT ( 'NONE',  ( 0.000000000000000000, 0.000000000000000000, 0.000000000000000000 ) ) ;
#34560 = CARTESIAN_POINT ( 'NONE',  ( 5.000000000000000000, -10.26105934116143459, 64.40045319026695836 ) ) ;
#34561 = CARTESIAN_POINT ( 'NONE',  ( -27.99999999999999645, 210.0000000000000284, 170.0000000000003695 ) ) ;
#34562 = VERTEX_POINT ( 'NONE', #59955 ) ;
#34563 = CARTESIAN_POINT ( 'NONE',  ( -5.676582343750000703, 243.0729166700806445, -9.832129032723418760 ) ) ;
#34564 = CARTESIAN_POINT ( 'NONE',  ( 5.082755093536320601, -5.082755093536318824, 15.92405278187175632 ) ) ;
#34565 = CARTESIAN_POINT ( 'NONE',  ( -0.3794862803192503020, 55.62190996747682448, 43.80334292620992187 ) ) ;
#34566 = CARTESIAN_POINT ( 'NONE',  ( 28.00000000000001776, 197.1250000027312126, 173.9999999999999147 ) ) ;
#34567 = CARTESIAN_POINT ( 'NONE',  ( 2.679491924311222739, 200.8333333265053398, 10.00000000000000355 ) ) ;
#34568 = CARTESIAN_POINT ( 'NONE',  ( 2.679491924311222739, 163.9583333333333712, 10.00000000000000355 ) ) ;
#34569 = CARTESIAN_POINT ( 'NONE',  ( -11.00000000000010658, 4.556349186103942017, 80.40624999999998579 ) ) ;
#34570 = CARTESIAN_POINT ( 'NONE',  ( 1.334622868157815783E-15, 10.39230484541327293, -10.20000000000000284 ) ) ;
#34571 = DIRECTION ( 'NONE',  ( 0.000000000000000000, 0.000000000000000000, 1.000000000000000000 ) ) ;
#34572 = CARTESIAN_POINT ( 'NONE',  ( -2.085542519210945728E-15, 124.8437499965860269, 11.35316468750000141 ) ) ;
#34573 = CARTESIAN_POINT ( 'NONE',  ( 23.99999999999999645, 198.6875000000000284, 168.3431457505074889 ) ) ;
#34574 = CARTESIAN_POINT ( 'NONE',  ( -11.35316468749999963, 263.9062500034140157, 0.000000000000000000 ) ) ;
#34577 = CARTESIAN_POINT ( 'NONE',  ( 3.999999999999960032, 196.9375000000000284, 143.6568542494924259 ) ) ;
#34576 = CARTESIAN_POINT ( 'NONE',  ( 31.45873412499999233, 195.6875000013655779, 169.9999999999998863 ) ) ;
#34575 = CARTESIAN_POINT ( 'NONE',  ( 24.54126587499998990, 196.4375000013655779, 169.9999999999998863 ) ) ;
#34578 = ORIENTED_EDGE ( 'NONE', *, *, #46299, .F. ) ;
#34579 = CARTESIAN_POINT ( 'NONE',  ( -1.704527592502768307, -60.27089976682808015, 22.92829164824352262 ) ) ;
#34580 = PRODUCT_DEFINITION_FORMATION_WITH_SPECIFIED_SOURCE ( 'ANY', '', #61975, .NOT_KNOWN. ) ;
#34581 = CARTESIAN_POINT ( 'NONE',  ( 31.99999999999998579, 202.4375000027311842, 168.3431457505074889 ) ) ;
#34582 = CARTESIAN_POINT ( 'NONE',  ( 10.00000000000010836, 195.2083333333334281, -2.679491924311255602 ) ) ;
#34583 = CARTESIAN_POINT ( 'NONE',  ( 29.43265458321766204, 196.1250000013655779, 166.5412658749999650 ) ) ;
#34584 = CARTESIAN_POINT ( 'NONE',  ( 10.00000000000000000, 21.66666665983870388, 2.679491924311236062 ) ) ;
#34585 = CARTESIAN_POINT ( 'NONE',  ( 2.977408999572654480, 120.1250000020483952, 7.188101187499999156 ) ) ;
#34586 = CARTESIAN_POINT ( 'NONE',  ( 3.211159895383561835, 20.43749999863440436, -3.211159895383561835 ) ) ;
#34587 = CARTESIAN_POINT ( 'NONE',  ( -0.4501631047670816010, 67.59340899456853435, -20.03485802339563193 ) ) ;
#34588 = CARTESIAN_POINT ( 'NONE',  ( -3.313708498984758943, -7.999999999999989342, 20.61155277982337353 ) ) ;
#34589 = CARTESIAN_POINT ( 'NONE',  ( -29.65685424949238325, 207.0625000000000284, 166.0000000000003979 ) ) ;
#34590 = CARTESIAN_POINT ( 'NONE',  ( -11.35316468750000141, 113.2812499965860269, -1.390361679473963753E-15 ) ) ;
#34591 = ORIENTED_EDGE ( 'NONE', *, *, #1238, .F. ) ;
#34592 = CARTESIAN_POINT ( 'NONE',  ( 1.656854249492406783, 15.56249999726881406, 3.999999999999976019 ) ) ;
#34593 = CARTESIAN_POINT ( 'NONE',  ( -7.188101187500002709, 26.81249999795161543, 2.977408999572649151 ) ) ;
#34594 = DIRECTION ( 'NONE',  ( 1.000000000000000000, -0.000000000000000000, -0.000000000000000000 ) ) ;
#34595 = CARTESIAN_POINT ( 'NONE',  ( 11.35316468749999963, 241.7187500034139873, -1.390361679473963556E-15 ) ) ;
#34596 = CARTESIAN_POINT ( 'NONE',  ( 11.35316468750000141, 95.78124999658602690, 0.000000000000000000 ) ) ;
#34597 = VERTEX_POINT ( 'NONE', #2246 ) ;
#34598 = CARTESIAN_POINT ( 'NONE',  ( 5.000000000000000000, -14.89980876190738179, 69.94558486267358433 ) ) ;
#34599 = CARTESIAN_POINT ( 'NONE',  ( 10.18810118750000093, -4.220049686691933921, 102.8125000020483952 ) ) ;
#34600 = CARTESIAN_POINT ( 'NONE',  ( -10.00000000000000355, 219.5833333265053966, 2.679491924311223183 ) ) ;
#34601 = CARTESIAN_POINT ( 'NONE',  ( -1.432654583217607414, 199.5000000013656063, 194.5412658750000219 ) ) ;
#34602 = CYLINDRICAL_SURFACE ( 'NONE', #54055, 3.999999999999976019 ) ;
#34604 = CARTESIAN_POINT ( 'NONE',  ( -11.35316468750000141, 98.28124999658602690, -1.390361679473963753E-15 ) ) ;
#34603 = CARTESIAN_POINT ( 'NONE',  ( -2.828427124746152987, 206.2500000027312126, 200.8284271247462129 ) ) ;
#34605 = CARTESIAN_POINT ( 'NONE',  ( 3.313708498984762496, -7.999999999999989342, 10.48655278392014800 ) ) ;
#34606 = CARTESIAN_POINT ( 'NONE',  ( -31.45873412499999944, 198.8750000013656347, 168.5673454167827572 ) ) ;
#34607 = CARTESIAN_POINT ( 'NONE',  ( 8.660254037844385522, 169.5833333333333428, 5.000000000000005329 ) ) ;
#34608 = ORIENTED_EDGE ( 'NONE', *, *, #16283, .T. ) ;
#34609 = VECTOR ( 'NONE', #67312, 1000.000000000000000 ) ;
#34610 = CARTESIAN_POINT ( 'NONE',  ( -8.660254037844387298, 193.9583333265053966, -5.000000000000004441 ) ) ;
#34611 = DIRECTION ( 'NONE',  ( -0.000000000000000000, 1.000000000000000000, 4.476705744456276341E-16 ) ) ;
#34612 = CARTESIAN_POINT ( 'NONE',  ( 28.00000000000001776, 202.5000000000000000, 165.9999999999998863 ) ) ;
#34613 = CARTESIAN_POINT ( 'NONE',  ( 3.042071309553167513, 87.13541666325268409, -11.35316468749999785 ) ) ;
#34614 = CARTESIAN_POINT ( 'NONE',  ( -6.676582343750000703, 290.5156250017070079, 2.765530957082001251 ) ) ;
#34615 = CARTESIAN_POINT ( 'NONE',  ( -5.082755093536325042, 7.406249997951610986, -5.082755093536325930 ) ) ;
#34616 = CARTESIAN_POINT ( 'NONE',  ( 7.204075437095966983, 7.204075437095967871, 97.46875000204838102 ) ) ;
#34617 = CARTESIAN_POINT ( 'NONE',  ( -11.35316468749999785, 218.0729166632526699, -3.042071309553167513 ) ) ;
#34618 = ORIENTED_EDGE ( 'NONE', *, *, #39546, .T. ) ;
#34619 = CARTESIAN_POINT ( 'NONE',  ( 3.313708498984755391, 122.6562500040968189, 8.000000000000008882 ) ) ;
#34620 = CARTESIAN_POINT ( 'NONE',  ( 2.384540947862909377, -43.16890813840797847, 139.0916505681292676 ) ) ;
#34621 = CARTESIAN_POINT ( 'NONE',  ( 6.951808397369818766E-16, 217.0312499965860411, -11.35316468750000141 ) ) ;
#34622 = CARTESIAN_POINT ( 'NONE',  ( 6.123233995736767268E-16, 48.12499999317203958, -10.00000000000000178 ) ) ;
#34623 = CARTESIAN_POINT ( 'NONE',  ( -10.00000000000018829, 157.5000000000001137, -1.224646799147375936E-15 ) ) ;
#34624 = CARTESIAN_POINT ( 'NONE',  ( -6.676582343750001591, 297.4531250017069510, 0.000000000000000000 ) ) ;
#34625 = VERTEX_POINT ( 'NONE', #32419 ) ;
#34626 = CARTESIAN_POINT ( 'NONE',  ( -3.407298021510761998, -51.68473891413697174, -48.72627478609629037 ) ) ;
#34627 = CARTESIAN_POINT ( 'NONE',  ( 9.832129032723420536, 206.5104166632526983, -5.676582343749999815 ) ) ;
#34628 = EDGE_CURVE ( 'NONE', #13563, #17389, #30892, .T. ) ;
#34629 = EDGE_CURVE ( 'NONE', #65897, #71712, #9023, .T. ) ;
#34630 = CARTESIAN_POINT ( 'NONE',  ( 1.871523826299183495E-15, -10.18810118749999916, 87.53125000204836681 ) ) ;
#34631 = CARTESIAN_POINT ( 'NONE',  ( -29.43265458321761230, 205.8750000013656063, 173.4587341250003760 ) ) ;
#34632 = CARTESIAN_POINT ( 'NONE',  ( -3.313708498984760720, 16.96875000000000000, -8.000000000000000000 ) ) ;
#34633 = AXIS2_PLACEMENT_3D ( 'NONE', #63134, #28434, #51442 ) ;
#34634 = EDGE_LOOP ( 'NONE', ( #34403, #4144, #56226, #18720 ) ) ;
#34635 = EDGE_CURVE ( 'NONE', #71834, #27023, #20705, .T. ) ;
#34636 = CARTESIAN_POINT ( 'NONE',  ( -4.401442555609581635E-16, 122.2812500020483810, -7.188101187500000044 ) ) ;
#34637 = CARTESIAN_POINT ( 'NONE',  ( -38.00000000000000000, 52.99999999999992895, -6.791607979884335933E-15 ) ) ;
#34638 = CARTESIAN_POINT ( 'NONE',  ( 8.660254037844389075, 25.41666666666666785, -5.000000000000000000 ) ) ;
#34639 = CARTESIAN_POINT ( 'NONE',  ( -3.999999999999960032, 210.0000000000000284, 198.0000000000000284 ) ) ;
#34640 = CARTESIAN_POINT ( 'NONE',  ( 7.204075437095966983, 7.204075437095967871, 71.96875000204836681 ) ) ;
#34642 = ORIENTED_EDGE ( 'NONE', *, *, #72950, .T. ) ;
#34641 =( BOUNDED_CURVE ( )  B_SPLINE_CURVE ( 2, ( #13676, #8036, #71394, #71770, #36715, #48390, #66489, #20086, #59727, #42731, #26490, #72906, #2754 ),
 .UNSPECIFIED., .F., .F. ) 
 B_SPLINE_CURVE_WITH_KNOTS ( ( 3, 2, 2, 2, 2, 2, 3 ),
 ( 2.402083059725570013, 2.407316844168545078, 2.412550628611520587, 2.417784413054495651, 2.423018197497470716, 2.428251981940446225, 2.433485766383421289 ),
 .UNSPECIFIED. ) 
 CURVE ( )  GEOMETRIC_REPRESENTATION_ITEM ( )  RATIONAL_B_SPLINE_CURVE ( ( 1.000000000000087708, 0.9659258262889806046, 1.000000000000000000, 0.9659258262890683122, 1.000000000000000000, 0.9659258262890683122, 1.000000000000000000, 0.9659258262890683122, 1.000000000000000000, 0.9659258262890683122, 1.000000000000000000, 0.9659258262890704216, 0.9999999999999978906 ) ) 
 REPRESENTATION_ITEM ( '' )  );
#34643 = CARTESIAN_POINT ( 'NONE',  ( 3.211159895383561835, 3.437499998634407028, -3.211159895383561835 ) ) ;
#34644 = CARTESIAN_POINT ( 'NONE',  ( -7.347880794884122694E-16, 2.499999997268813168, 4.000000000000001776 ) ) ;
#34645 = DIRECTION ( 'NONE',  ( -1.000000000000000000, -0.000000000000000000, -0.000000000000000000 ) ) ;
#34646 =( NAMED_UNIT ( * ) SI_UNIT ( $, .STERADIAN. ) SOLID_ANGLE_UNIT ( ) );
#34647 = CARTESIAN_POINT ( 'NONE',  ( -4.999999999999992006, -10.25159769123454900, 64.79153472057838314 ) ) ;
#34648 = EDGE_CURVE ( 'NONE', #47940, #71597, #38451, .T. ) ;
#34649 = CARTESIAN_POINT ( 'NONE',  ( 4.999999999999999112, -63.85408791058082301, 24.15552328276479699 ) ) ;
#34650 = CARTESIAN_POINT ( 'NONE',  ( -4.721056650415998313, 294.5781250017069510, 4.721056650416000089 ) ) ;
#34653 = CARTESIAN_POINT ( 'NONE',  ( 2.751064625579944321E-14, 206.7500000000000284, 194.0000000000000568 ) ) ;
#34652 = CARTESIAN_POINT ( 'NONE',  ( 5.676582343750005144, 240.5729166700806445, 9.832129032723416984 ) ) ;
#34651 = CARTESIAN_POINT ( 'NONE',  ( 26.56734541678238060, 207.3750000013656063, 173.4587341249998929 ) ) ;
#34654 = SHAPE_DEFINITION_REPRESENTATION ( #22838, #22414 ) ;
#34655 = ORIENTED_EDGE ( 'NONE', *, *, #74388, .F. ) ;
#34656 = VECTOR ( 'NONE', #51435, 1000.000000000000000 ) ;
#34657 = CARTESIAN_POINT ( 'NONE',  ( 8.311093377946834337, 237.3437500034139589, -8.311093377946836114 ) ) ;
#34658 = CARTESIAN_POINT ( 'NONE',  ( 5.082755093536320601, -5.082755093536318824, 8.049052781871752771 ) ) ;
#34659 =( BOUNDED_CURVE ( )  B_SPLINE_CURVE ( 2, ( #71981, #60675, #66707, #65584, #2964, #59930, #48600, #8995, #36554 ),
 .UNSPECIFIED., .F., .F. ) 
 B_SPLINE_CURVE_WITH_KNOTS ( ( 3, 2, 2, 2, 3 ),
 ( 0.06666666666666672125, 0.07500000000000006661, 0.08333333333333339810, 0.09166666666666672958, 0.1000000000000000888 ),
 .UNSPECIFIED. ) 
 CURVE ( )  GEOMETRIC_REPRESENTATION_ITEM ( )  RATIONAL_B_SPLINE_CURVE ( ( 0.9999999999999994449, 0.9238795325112872936, 1.000000000000000000, 0.9238795325112867385, 1.000000000000000000, 0.9238795325112867385, 1.000000000000000000, 0.9238795325112859613, 1.000000000000000666 ) ) 
 REPRESENTATION_ITEM ( '' )  );
#34660 = ORIENTED_EDGE ( 'NONE', *, *, #46613, .T. ) ;
#34661 = CARTESIAN_POINT ( 'NONE',  ( -4.220049686691935698, 10.18810118749999916, 67.37500000204838102 ) ) ;
#34662 = CARTESIAN_POINT ( 'NONE',  ( 3.042071309553159519, 85.05208332991934128, 11.35316468750000141 ) ) ;
#34663 = CARTESIAN_POINT ( 'NONE',  ( 3.373128826976390826, 60.49298623944800823, 23.06377889928895186 ) ) ;
#34664 = CARTESIAN_POINT ( 'NONE',  ( -7.778174593052023411, 7.778174593052023411, 83.31249999999998579 ) ) ;
#34667 = CARTESIAN_POINT ( 'NONE',  ( 0.000000000000000000, 0.000000000000000000, 118.0000000000000000 ) ) ;
#34666 = CARTESIAN_POINT ( 'NONE',  ( 24.54126587499999701, 208.1875000013656063, 169.9999999999999432 ) ) ;
#34665 = CARTESIAN_POINT ( 'NONE',  ( 30.44569435410883784, 207.0625000013656063, 167.5543056458911053 ) ) ;
#34668 = VERTEX_POINT ( 'NONE', #15041 ) ;
#34669 = CARTESIAN_POINT ( 'NONE',  ( -3.313708498984842432, 114.2187500000000000, -7.999999999999920064 ) ) ;
#34670 = CARTESIAN_POINT ( 'NONE',  ( -4.999999999999998224, 178.5416666598387110, -8.660254037844389075 ) ) ;
#34671 = CARTESIAN_POINT ( 'NONE',  ( -11.35316468750000141, 193.2812499965860127, -1.390361679473963753E-15 ) ) ;
#34672 = CARTESIAN_POINT ( 'NONE',  ( 3.458734124999959914, 204.4375000013656063, 142.0000000000000568 ) ) ;
#34673 = CARTESIAN_POINT ( 'NONE',  ( 30.44569435410883429, 205.0625000013656063, 167.5543056458911053 ) ) ;
#34674 = CARTESIAN_POINT ( 'NONE',  ( 7.188101187500001821, 24.93749999795161543, -2.977408999572650483 ) ) ;
#34675 = CARTESIAN_POINT ( 'NONE',  ( -9.832129032723418760, 178.1770833299193555, -5.676582343750004256 ) ) ;
#34676 = CARTESIAN_POINT ( 'NONE',  ( -8.000000000000001776, 8.156249995903221972, 3.313708498984759387 ) ) ;
#34677 = CARTESIAN_POINT ( 'NONE',  ( -2.977408999572652260, 100.8125000020484094, 7.188101187500000044 ) ) ;
#34678 = CARTESIAN_POINT ( 'NONE',  ( -1.836970198721029983E-15, 90.62499999317203958, 10.00000000000000178 ) ) ;
#34679 = CARTESIAN_POINT ( 'NONE',  ( 3.211159895383560947, 12.18749999863440614, 3.211159895383562723 ) ) ;
#34680 = CARTESIAN_POINT ( 'NONE',  ( 31.45873412499999233, 200.9375000013656063, 169.9999999999999432 ) ) ;
#34681 = CARTESIAN_POINT ( 'NONE',  ( 7.188101187499993827, -2.977408999572645598, 11.51780278187175810 ) ) ;
#34682 = CARTESIAN_POINT ( 'NONE',  ( -5.676582343749998039, 62.44791666325268409, -9.832129032723420536 ) ) ;
#34683 = CARTESIAN_POINT ( 'NONE',  ( -5.000000000000001776, -53.53067326687894933, 46.58593137613084423 ) ) ;
#34684 = CARTESIAN_POINT ( 'NONE',  ( -5.656854249492375253, 5.656854249492375253, 2.199052784329821542 ) ) ;
#34685 = ORIENTED_EDGE ( 'NONE', *, *, #35781, .T. ) ;
#34686 = CARTESIAN_POINT ( 'NONE',  ( -4.556349186104045934, 11.00000000000000000, 66.90625000409677625 ) ) ;
#34687 = CARTESIAN_POINT ( 'NONE',  ( 5.676582343749993598, 59.94791666325268409, 9.832129032723422313 ) ) ;
#34688 = CARTESIAN_POINT ( 'NONE',  ( -4.556349186104047710, -10.99999999999999822, 74.96875000409677625 ) ) ;
#34689 = CARTESIAN_POINT ( 'NONE',  ( -3.458734125000015425, 196.2500000013656347, 143.4326545832176976 ) ) ;
#34690 = CARTESIAN_POINT ( 'NONE',  ( -2.069125466538952907, 10.11940336925101924, 70.25556669587955128 ) ) ;
#34692 = CARTESIAN_POINT ( 'NONE',  ( 3.042071309553167513, 61.82291666325267698, -11.35316468749999785 ) ) ;
#34691 = CARTESIAN_POINT ( 'NONE',  ( -2.977408999572650927, 93.87500000204838102, -7.188101187500000933 ) ) ;
#34694 = CIRCLE ( 'NONE', #25043, 11.00000000000000000 ) ;
#34693 = CARTESIAN_POINT ( 'NONE',  ( -5.656854249492373476, -5.656854249492376141, 5.517802779823364645 ) ) ;
#34695 = CARTESIAN_POINT ( 'NONE',  ( 7.999999999999991118, 0.000000000000000000, 30.00000000000000000 ) ) ;
#34696 = CARTESIAN_POINT ( 'NONE',  ( -4.999999999999998224, 158.5416666598387110, -8.660254037844389075 ) ) ;
#34697 = CARTESIAN_POINT ( 'NONE',  ( -7.188101187499999156, 94.62500000204838102, 2.977408999572654924 ) ) ;
#34698 = DIRECTION ( 'NONE',  ( 1.000000000000000000, 0.000000000000000000, 0.000000000000000000 ) ) ;
#34699 = CARTESIAN_POINT ( 'NONE',  ( -5.676582343749998039, 52.76041666325269119, -9.832129032723420536 ) ) ;
#34700 = CARTESIAN_POINT ( 'NONE',  ( 10.18810118749999916, 1.247682550866122264E-15, 112.2812500020483810 ) ) ;
#34701 = CARTESIAN_POINT ( 'NONE',  ( 5.676582343750001591, 176.6145833299193555, -9.832129032723420536 ) ) ;
#34702 = ORIENTED_EDGE ( 'NONE', *, *, #39790, .F. ) ;
#34703 = CARTESIAN_POINT ( 'NONE',  ( -7.204075437095967871, 7.204075437095967871, 73.46875000204838102 ) ) ;
#34704 = CARTESIAN_POINT ( 'NONE',  ( 2.828427124746208943, 197.6250000000000284, 195.1715728752538439 ) ) ;
#34706 = CARTESIAN_POINT ( 'NONE',  ( -8.311093377946841443, 178.9062499965859843, 8.311093377946834337 ) ) ;
#34705 = CARTESIAN_POINT ( 'NONE',  ( 4.000000000000000888, 18.68749999726881583, 1.656854249492384135 ) ) ;
#34707 = CARTESIAN_POINT ( 'NONE',  ( -3.313708498984757167, 7.999999999999991118, 8.105302784329824206 ) ) ;
#34708 = EDGE_CURVE ( 'NONE', #66396, #34804, #54898, .T. ) ;
#34709 = EDGE_CURVE ( 'NONE', #71916, #445, #73184, .T. ) ;
#34710 = CARTESIAN_POINT ( 'NONE',  ( -8.000000000000000000, 11.06249999590322020, -9.797174393178825657E-16 ) ) ;
#34711 = CARTESIAN_POINT ( 'NONE',  ( -6.123233995736766282E-16, 256.8750000068279746, -10.00000000000000000 ) ) ;
#34712 = CARTESIAN_POINT ( 'NONE',  ( -28.00000000000002842, 206.0000000000000284, 166.0000000000003695 ) ) ;
#34713 = ORIENTED_EDGE ( 'NONE', *, *, #32803, .T. ) ;
#34714 = CARTESIAN_POINT ( 'NONE',  ( 9.832129032723420536, 166.5104166632526983, -5.676582343749999815 ) ) ;
#34715 =( REPRESENTATION_RELATIONSHIP ('NONE','NONE', #46008, #66259 ) REPRESENTATION_RELATIONSHIP_WITH_TRANSFORMATION ( #53100 )SHAPE_REPRESENTATION_RELATIONSHIP( ) );
#34716 = VECTOR ( 'NONE', #9234, 1000.000000000000000 ) ;
#34717 = CARTESIAN_POINT ( 'NONE',  ( 7.188101187499992051, 2.977408999572647819, 27.83030278187176165 ) ) ;
#34718 = CARTESIAN_POINT ( 'NONE',  ( -11.35316468750000141, 128.5937499965860127, -1.390361679473963753E-15 ) ) ;
#34719 = DIRECTION ( 'NONE',  ( 0.000000000000000000, 0.000000000000000000, -1.000000000000000000 ) ) ;
#34720 = ORIENTED_EDGE ( 'NONE', *, *, #66288, .F. ) ;
#34721 = CARTESIAN_POINT ( 'NONE',  ( -4.541265875000002339, 10.87499999863440792, -1.881053915767121998 ) ) ;
#34722 = EDGE_CURVE ( 'NONE', #2215, #64126, #6211, .T. ) ;
#34723 = EDGE_CURVE ( 'NONE', #4353, #33995, #72742, .T. ) ;
#34724 = CARTESIAN_POINT ( 'NONE',  ( 2.977408999572651815, 13.68749999795161365, 7.188101187500000933 ) ) ;
#34725 = CARTESIAN_POINT ( 'NONE',  ( -3.313708498984762496, 101.4687500040967763, 7.999999999999998224 ) ) ;
#34726 = EDGE_CURVE ( 'NONE', #52578, #1735, #13875, .T. ) ;
#34727 = CARTESIAN_POINT ( 'NONE',  ( -30.44569435410883429, 199.8125000013656063, 167.5543056458915885 ) ) ;
#34728 = CARTESIAN_POINT ( 'NONE',  ( 2.828427124746191623, 9.125000000000000000, -2.828427124746191623 ) ) ;
#34729 = CARTESIAN_POINT ( 'NONE',  ( -2.828427124746192067, 20.37499999726881228, 2.828427124746190735 ) ) ;
#34730 = CARTESIAN_POINT ( 'NONE',  ( -1.881053915767124440, 9.999999998634407916, 4.541265875000001451 ) ) ;
#34731 = CARTESIAN_POINT ( 'NONE',  ( -7.999999999999989342, -3.313708498984762496, 19.11155278392014623 ) ) ;
#34732 = CARTESIAN_POINT ( 'NONE',  ( -2.751064625579944321E-14, 196.7500000000000000, 146.0000000000000284 ) ) ;
#34733 = VERTEX_POINT ( 'NONE', #10143 ) ;
#34734 = FACE_OUTER_BOUND ( 'NONE', #50306, .T. ) ;
#34735 = CARTESIAN_POINT ( 'NONE',  ( -7.188101187499999156, 103.2500000020483810, 2.977408999572654924 ) ) ;
#34736 = EDGE_CURVE ( 'NONE', #53073, #53710, #10890, .T. ) ;
#34737 = AXIS2_PLACEMENT_3D ( 'NONE', #41731, #65474, #13768 ) ;
#34739 = CARTESIAN_POINT ( 'NONE',  ( -3.313708498984765161, 15.84374999590322197, 7.999999999999998224 ) ) ;
#34738 = CARTESIAN_POINT ( 'NONE',  ( 7.778174593052021635, 7.778174593052023411, 78.62500000409677625 ) ) ;
#34740 =( NAMED_UNIT ( * ) SI_UNIT ( $, .STERADIAN. ) SOLID_ANGLE_UNIT ( ) );
#34741 = EDGE_LOOP ( 'NONE', ( #67475, #66017, #56477, #1448 ) ) ;
#34742 = FACE_OUTER_BOUND ( 'NONE', #5682, .T. ) ;
#34743 = CARTESIAN_POINT ( 'NONE',  ( -4.401442555609577197E-16, 7.188101187499992051, 23.61155278187175455 ) ) ;
#34744 = ORIENTED_EDGE ( 'NONE', *, *, #73567, .F. ) ;
#34745 = ORIENTED_EDGE ( 'NONE', *, *, #30419, .F. ) ;
#34746 = CARTESIAN_POINT ( 'NONE',  ( 10.18810118750000093, -4.220049686691933033, 84.81250000204838102 ) ) ;
#34747 = CYLINDRICAL_SURFACE ( 'NONE', #67082, 11.00000000000000000 ) ;
#34748 = CARTESIAN_POINT ( 'NONE',  ( -31.66756539373098178, -12.01114419369879016, 167.9999999999997726 ) ) ;
#34749 = CARTESIAN_POINT ( 'NONE',  ( -7.778174593052023411, 7.778174593052023411, 101.3124999999999858 ) ) ;
#34751 = CARTESIAN_POINT ( 'NONE',  ( -2.765530957081998142, 297.7968750017069510, 6.676582343750000703 ) ) ;
#34750 = CARTESIAN_POINT ( 'NONE',  ( 0.000000000000000000, 0.000000000000000000, 0.000000000000000000 ) ) ;
#34752 = CARTESIAN_POINT ( 'NONE',  ( -5.000000000000005329, 138.3333333333333428, 8.660254037844387298 ) ) ;
#34753 = CARTESIAN_POINT ( 'NONE',  ( -5.656854249492380582, 100.8125000000000000, -5.656854249492380582 ) ) ;
#34754 = AXIS2_PLACEMENT_3D ( 'NONE', #36541, #12042, #47477 ) ;
#34755 = CARTESIAN_POINT ( 'NONE',  ( -6.676582343750000703, 289.6718750017070079, 2.765530957082001251 ) ) ;
#34756 = CARTESIAN_POINT ( 'NONE',  ( 2.977408999572650927, -7.188101187499990274, 6.830302781871755435 ) ) ;
#34757 =( BOUNDED_CURVE ( )  B_SPLINE_CURVE ( 2, ( #39684, #6107, #26586, #38298, #62684, #17409, #28362, #40431, #29112, #49610, #95, #72237, #20553 ),
 .UNSPECIFIED., .F., .F. ) 
 B_SPLINE_CURVE_WITH_KNOTS ( ( 3, 2, 2, 2, 2, 2, 3 ),
 ( 0.6576086956521739468, 0.6594202898550725056, 0.6612318840579710644, 0.6630434782608695121, 0.6648550724637680709, 0.6666666666666666297, 0.6684782608695651884 ),
 .UNSPECIFIED. ) 
 CURVE ( )  GEOMETRIC_REPRESENTATION_ITEM ( )  RATIONAL_B_SPLINE_CURVE ( ( 1.000000000000000000, 0.9659258262890683122, 1.000000000000000000, 0.9659258262890683122, 1.000000000000000000, 0.9659258262890683122, 1.000000000000000000, 0.9659258262890683122, 1.000000000000000000, 0.9659258262890683122, 1.000000000000000000, 0.9659258262890683122, 1.000000000000000000 ) ) 
 REPRESENTATION_ITEM ( '' )  );
#34758 = VECTOR ( 'NONE', #12548, 1000.000000000000000 ) ;
#34759 = FACE_OUTER_BOUND ( 'NONE', #61061, .T. ) ;
#34760 = CARTESIAN_POINT ( 'NONE',  ( 25.55430564589119413, 204.0625000013656063, 167.5543056458910485 ) ) ;
#34761 = CARTESIAN_POINT ( 'NONE',  ( -5.656854249492379694, 27.37499999590322375, -5.656854249492380582 ) ) ;
#34762 = CARTESIAN_POINT ( 'NONE',  ( -8.008118988124991233, 0.000000000000000000, 2.513115283940627886 ) ) ;
#34763 = CARTESIAN_POINT ( 'NONE',  ( 1.432654583217607858, 196.6250000013656063, 138.5412658750000787 ) ) ;
#34764 = CARTESIAN_POINT ( 'NONE',  ( 5.082755093536325042, 116.4687500020483810, -5.082755093536325930 ) ) ;
#34766 = CARTESIAN_POINT ( 'NONE',  ( 3.765320639486768428, 194.7591455152330013, 198.1202362305605504 ) ) ;
#34765 = SURFACE_STYLE_FILL_AREA ( #52100 ) ;
#34767 = CARTESIAN_POINT ( 'NONE',  ( 11.35316468749999963, 236.5104166700806161, 3.042071309553159519 ) ) ;
#34768 = CARTESIAN_POINT ( 'NONE',  ( -34.77571750417828866, 39.95510246977180202, 65.00000000000001421 ) ) ;
#34769 = CARTESIAN_POINT ( 'NONE',  ( -5.082755093536319713, 5.082755093536319713, 28.67405278187175810 ) ) ;
#34770 = CARTESIAN_POINT ( 'NONE',  ( 29.65685424949240101, 196.4375000000000568, 165.9999999999998863 ) ) ;
#34771 = CARTESIAN_POINT ( 'NONE',  ( 3.042071309553159519, 14.73958332991935016, 11.35316468750000141 ) ) ;
#34772 = CARTESIAN_POINT ( 'NONE',  ( -3.999999999999960032, 203.0000000000000000, 198.0000000000000284 ) ) ;
#34773 = CARTESIAN_POINT ( 'NONE',  ( 3.042071309553167069, 222.1354166632526699, -11.35316468749999785 ) ) ;
#34774 = CARTESIAN_POINT ( 'NONE',  ( -10.00000000000000355, 219.5833333265053682, 2.679491924311223183 ) ) ;
#34776 = LINE ( 'NONE', #4598, #37542 ) ;
#34775 = CARTESIAN_POINT ( 'NONE',  ( 1.224646799147353256E-15, 0.000000000000000000, 10.00000000000000000 ) ) ;
#34777 = VERTEX_POINT ( 'NONE', #21818 ) ;
#34778 = CARTESIAN_POINT ( 'NONE',  ( 3.458734124999959469, 195.7500000013656063, 140.5673454167824161 ) ) ;
#34779 = CARTESIAN_POINT ( 'NONE',  ( 3.042071309553167069, 21.82291666325268054, -11.35316468749999785 ) ) ;
#34780 = CARTESIAN_POINT ( 'NONE',  ( -11.00000000000000000, 0.000000000000000000, 92.68750000409677625 ) ) ;
#34781 = CARTESIAN_POINT ( 'NONE',  ( 9.999999999999998224, 227.7083333333333144, -2.679491924311229401 ) ) ;
#34782 = FACE_OUTER_BOUND ( 'NONE', #40073, .T. ) ;
#34783 = DIRECTION ( 'NONE',  ( -0.000000000000000000, -1.000000000000000000, -4.283267841918042741E-17 ) ) ;
#34785 = CARTESIAN_POINT ( 'NONE',  ( 9.832129032723416984, 25.36458332991935194, 5.676582343750006032 ) ) ;
#34784 = CARTESIAN_POINT ( 'NONE',  ( -7.188101187500000933, 109.0625000020483810, -2.977408999572650483 ) ) ;
#34786 = CARTESIAN_POINT ( 'NONE',  ( 3.313708498984762496, -7.999999999999989342, 19.29905277982336642 ) ) ;
#34787 = CARTESIAN_POINT ( 'NONE',  ( -8.311093377946836114, 137.6562499965859558, -8.311093377946837890 ) ) ;
#34788 = CARTESIAN_POINT ( 'NONE',  ( -8.660254037844390851, 109.7916666598387110, 4.999999999999998224 ) ) ;
#34789 = CARTESIAN_POINT ( 'NONE',  ( -2.977408999572650927, 113.7500000020483668, -7.188101187500001821 ) ) ;
#34790 = CARTESIAN_POINT ( 'NONE',  ( -1.469576158976823947E-15, 14.43749999590322375, 8.000000000000000000 ) ) ;
#34791 = CARTESIAN_POINT ( 'NONE',  ( -30.44569435410879521, 209.0625000013656063, 172.4456943541092357 ) ) ;
#34792 = CARTESIAN_POINT ( 'NONE',  ( -5.000000000000000000, -53.35645474066778604, -47.33026262608771617 ) ) ;
#34793 = ORIENTED_EDGE ( 'NONE', *, *, #50379, .F. ) ;
#34794 = CARTESIAN_POINT ( 'NONE',  ( 9.832129032723420536, 11.51041666325268409, -5.676582343749999815 ) ) ;
#34795 = CARTESIAN_POINT ( 'NONE',  ( -4.000000000000002665, 20.31249999726881228, 1.656854249492380582 ) ) ;
#34796 = CARTESIAN_POINT ( 'NONE',  ( 6.676582343750004256, 298.8906250017069510, 2.765530957081995478 ) ) ;
#34797 = CARTESIAN_POINT ( 'NONE',  ( -5.676582343750006032, 139.1145833299193555, 9.832129032723418760 ) ) ;
#34798 = CARTESIAN_POINT ( 'NONE',  ( -4.000000000000001776, 3.437500000000000000, -1.656854249492381470 ) ) ;
#34799 = CARTESIAN_POINT ( 'NONE',  ( -3.313708498984757167, 7.999999999999991118, 24.60530278432982598 ) ) ;
#34800 = EDGE_CURVE ( 'NONE', #27473, #29054, #61452, .T. ) ;
#34801 = DIRECTION ( 'NONE',  ( 0.000000000000000000, 0.000000000000000000, 1.000000000000000000 ) ) ;
#34802 = CARTESIAN_POINT ( 'NONE',  ( 11.35316468749999608, 246.6145833367472733, -3.042071309553167069 ) ) ;
#34803 = CARTESIAN_POINT ( 'NONE',  ( 10.18810118749999916, 4.220049686691935698, 97.37500000204839523 ) ) ;
#34804 = VERTEX_POINT ( 'NONE', #38823 ) ;
#34805 = CARTESIAN_POINT ( 'NONE',  ( -11.00000000000000000, 11.00000000000000000, -6.938893903907228378E-15 ) ) ;
#34806 = DIRECTION ( 'NONE',  ( -1.000000000000000000, -0.000000000000000000, -0.000000000000000000 ) ) ;
#34807 = CARTESIAN_POINT ( 'NONE',  ( -11.35316468749999785, 88.38541666325268409, -3.042071309553167513 ) ) ;
#34808 = VERTEX_POINT ( 'NONE', #44849 ) ;
#34809 = CARTESIAN_POINT ( 'NONE',  ( -4.220049686691935698, 10.18810118749999916, 109.3750000020483810 ) ) ;
#34810 = CARTESIAN_POINT ( 'NONE',  ( 3.211159895383561835, 14.56249999863440792, -3.211159895383561835 ) ) ;
#34811 = ORIENTED_EDGE ( 'NONE', *, *, #36176, .F. ) ;
#34812 = ORIENTED_EDGE ( 'NONE', *, *, #54723, .T. ) ;
#34813 = CARTESIAN_POINT ( 'NONE',  ( 4.898587196589412829E-16, 7.875000000000001776, -8.000000000000000000 ) ) ;
#34814 = CARTESIAN_POINT ( 'NONE',  ( 6.123233995736767268E-16, 48.12499999317203958, -10.00000000000000178 ) ) ;
#34815 = VECTOR ( 'NONE', #49375, 1000.000000000000000 ) ;
#34816 = DIRECTION ( 'NONE',  ( -1.000000000000000000, 0.000000000000000000, 0.000000000000000000 ) ) ;
#34817 = CARTESIAN_POINT ( 'NONE',  ( 2.977408999572651815, 24.56249999795161543, 7.188101187500000933 ) ) ;
#34818 = CARTESIAN_POINT ( 'NONE',  ( -4.556349186104045934, 11.00000000000000000, 96.71874999999998579 ) ) ;
#34819 = CARTESIAN_POINT ( 'NONE',  ( 10.18810118749999916, 1.247682550866122264E-15, 103.2812500020483810 ) ) ;
#34820 = EDGE_CURVE ( 'NONE', #68303, #18980, #39186, .T. ) ;
#34821 = CARTESIAN_POINT ( 'NONE',  ( 2.679491924328011532, 111.0416666666651651, -9.999999999990302868 ) ) ;
#34822 = CARTESIAN_POINT ( 'NONE',  ( 4.000000000000001776, 9.749999997268814056, 0.000000000000000000 ) ) ;
#34823 = CARTESIAN_POINT ( 'NONE',  ( -1.881053915767121776, 1.624999998634407028, -4.541265875000002339 ) ) ;
#34824 = VERTEX_POINT ( 'NONE', #61824 ) ;
#34825 = FACE_OUTER_BOUND ( 'NONE', #14114, .T. ) ;
#34826 = CARTESIAN_POINT ( 'NONE',  ( 2.754378923186476579E-14, 200.1875000013656063, 194.5412658750000219 ) ) ;
#34827 = ADVANCED_FACE ( 'NONE', ( #57297, #21452 ), #4123, .T. ) ;
#34828 = CARTESIAN_POINT ( 'NONE',  ( -29.43265458321755901, 203.8750000013656063, 173.4587341250004044 ) ) ;
#34829 = ADVANCED_FACE ( 'NONE', ( #74257 ), #33180, .T. ) ;
#34830 = CARTESIAN_POINT ( 'NONE',  ( 2.780723358947928197E-16, 8.562499998634407916, -4.541265875000002339 ) ) ;
#34831 = CARTESIAN_POINT ( 'NONE',  ( 2.449293598294707893E-16, 0.2500000000000001665, -4.000000000000001776 ) ) ;
#34832 = CARTESIAN_POINT ( 'NONE',  ( 1.320432766682872962E-15, -7.188101187499992051, 16.86155278187175810 ) ) ;
#34833 = ORIENTED_EDGE ( 'NONE', *, *, #51847, .T. ) ;
#34834 = ORIENTED_EDGE ( 'NONE', *, *, #8119, .F. ) ;
#34835 = CARTESIAN_POINT ( 'NONE',  ( 7.204075437095966983, 7.204075437095967871, 107.5937500020483810 ) ) ;
#34836 = CARTESIAN_POINT ( 'NONE',  ( -9.381899668004583859, -15.36796739199406225, -2.007213975108514882E-14 ) ) ;
#34837 = CARTESIAN_POINT ( 'NONE',  ( -30.82842712474621294, 203.1250000000000284, 167.1715728752542134 ) ) ;
#34838 = CARTESIAN_POINT ( 'NONE',  ( 2.839093476692135984E-14, 200.6875000013656063, 201.4587341250000350 ) ) ;
#34839 = CARTESIAN_POINT ( 'NONE',  ( 25.55430564589115150, 197.0625000013656063, 167.5543056458911053 ) ) ;
#34840 = CARTESIAN_POINT ( 'NONE',  ( -10.00000000000000355, 87.70833333333334281, 2.679491924311223183 ) ) ;
#34841 = CARTESIAN_POINT ( 'NONE',  ( -8.000000000000000000, 118.9062500000000000, -3.313708498984761608 ) ) ;
#34842 = CARTESIAN_POINT ( 'NONE',  ( 6.951808397369818766E-16, 57.34374999658601979, -11.35316468750000141 ) ) ;
#34843 = CARTESIAN_POINT ( 'NONE',  ( -2.485281374238572649, 288.1875000000000000, 6.000000000000002665 ) ) ;
#34844 = VERTEX_POINT ( 'NONE', #27482 ) ;
#34845 = CARTESIAN_POINT ( 'NONE',  ( -3.673940397442060854E-16, 294.7500000000000000, -6.000000000000001776 ) ) ;
#34846 = VECTOR ( 'NONE', #68678, 1000.000000000000000 ) ;
#34847 = ADVANCED_FACE ( 'NONE', ( #44476 ), #51621, .T. ) ;
#34848 = CARTESIAN_POINT ( 'NONE',  ( -1.877992804784410330, -65.87054549411909932, 26.34444121134937333 ) ) ;
#34849 = CARTESIAN_POINT ( 'NONE',  ( 2.445694354108783664, 207.3125000013656063, 144.4456943541088663 ) ) ;
#34850 = DIRECTION ( 'NONE',  ( 0.000000000000000000, -0.8778652960885044987, 0.4789076340208435756 ) ) ;
#34851 = CARTESIAN_POINT ( 'NONE',  ( 4.898587196589412829E-16, 6.187499995903221084, -8.000000000000000000 ) ) ;
#34852 = CARTESIAN_POINT ( 'NONE',  ( -10.00000000000000000, 240.0000000000000284, 0.000000000000000000 ) ) ;
#34853 = CARTESIAN_POINT ( 'NONE',  ( 4.220049686691941027, -10.18810118749999738, 70.00000000204836681 ) ) ;
#34854 = CARTESIAN_POINT ( 'NONE',  ( 10.00000000000000178, 200.2083333333333144, -2.679491924311226736 ) ) ;
#34855 = CARTESIAN_POINT ( 'NONE',  ( 7.188101187499993827, -2.977408999572645598, 19.01780278187175099 ) ) ;
#34856 = CARTESIAN_POINT ( 'NONE',  ( 3.042071309553167069, 177.1354166632527267, -11.35316468749999785 ) ) ;
#34857 = DIRECTION ( 'NONE',  ( 0.000000000000000000, -0.000000000000000000, -1.000000000000000000 ) ) ;
#34858 = CARTESIAN_POINT ( 'NONE',  ( 2.449293598294707893E-16, 1.999999997268813168, -4.000000000000001776 ) ) ;
#34860 = CARTESIAN_POINT ( 'NONE',  ( -2.849036369511732440E-14, 206.3750000027312126, 138.0000000000000568 ) ) ;
#34859 = CARTESIAN_POINT ( 'NONE',  ( 11.00000000000000000, 1.347111479062088405E-15, 111.4375000040967763 ) ) ;
#34861 = VERTEX_POINT ( 'NONE', #28239 ) ;
#34862 = AXIS2_PLACEMENT_3D ( 'NONE', #25745, #16573, #39610 ) ;
#34863 = CARTESIAN_POINT ( 'NONE',  ( -3.458734125000015425, 198.9375000013655779, 142.0000000000000568 ) ) ;
#34864 = CARTESIAN_POINT ( 'NONE',  ( -5.676582343749998039, 37.76041666325267698, -9.832129032723420536 ) ) ;
#34865 = CARTESIAN_POINT ( 'NONE',  ( -11.00000000000000000, 4.556349186104045934, 110.5937500040967905 ) ) ;
#34866 = CARTESIAN_POINT ( 'NONE',  ( -1.426884777062336740, 194.5622161278626265, 201.2706892433777170 ) ) ;
#34867 = CARTESIAN_POINT ( 'NONE',  ( 6.123233995736767268E-16, 123.1249999931720396, -10.00000000000000178 ) ) ;
#34869 = FACE_OUTER_BOUND ( 'NONE', #47436, .T. ) ;
#34868 = CARTESIAN_POINT ( 'NONE',  ( 8.660254037844389075, 222.2916666598387110, -5.000000000000000000 ) ) ;
#34870 = CARTESIAN_POINT ( 'NONE',  ( -2.445694354108838731, 198.0625000013656063, 144.4456943541088663 ) ) ;
#34871 = CARTESIAN_POINT ( 'NONE',  ( -10.00000000000000355, 64.58333332650536818, 2.679491924311223183 ) ) ;
#34872 = CARTESIAN_POINT ( 'NONE',  ( 7.188101187500002709, 97.81250000204840944, 2.977408999572649151 ) ) ;
#34873 = CARTESIAN_POINT ( 'NONE',  ( 3.211159895383561835, 13.56249999863440614, -3.211159895383561835 ) ) ;
#34874 = CARTESIAN_POINT ( 'NONE',  ( 0.000000000000000000, 0.000000000000000000, -14.07439246179028203 ) ) ;
#34875 = CARTESIAN_POINT ( 'NONE',  ( 7.999999999999992895, -3.313708498984756279, 5.986552779823365533 ) ) ;
#34876 = CARTESIAN_POINT ( 'NONE',  ( 1.656854249492381248, 7.937499997268813168, -4.000000000000001776 ) ) ;
#34877 = ORIENTED_EDGE ( 'NONE', *, *, #39412, .T. ) ;
#34878 = VERTEX_POINT ( 'NONE', #67856 ) ;
#34879 =( BOUNDED_CURVE ( )  B_SPLINE_CURVE ( 2, ( #45315, #28705, #46059, #44954, #4594, #44582, #69078, #40409, #63406 ),
 .UNSPECIFIED., .F., .F. ) 
 B_SPLINE_CURVE_WITH_KNOTS ( ( 3, 2, 2, 2, 3 ),
 ( 0.6354166666666667407, 0.6406250000000001110, 0.6458333333333334814, 0.6510416666666666297, 0.6562500000000000000 ),
 .UNSPECIFIED. ) 
 CURVE ( )  GEOMETRIC_REPRESENTATION_ITEM ( )  RATIONAL_B_SPLINE_CURVE ( ( 0.9999999999999983347, 0.9238795325112884038, 1.000000000000000000, 0.9238795325112867385, 1.000000000000000000, 0.9238795325112867385, 1.000000000000000000, 0.9238795325112867385, 1.000000000000000000 ) ) 
 REPRESENTATION_ITEM ( '' )  );
#34880 = CARTESIAN_POINT ( 'NONE',  ( -3.373128826976394823, -50.22031155377506195, -40.85657338450078413 ) ) ;
#34881 = CARTESIAN_POINT ( 'NONE',  ( -4.088227598258586603E-16, 298.3593750017070079, -6.676582343750001591 ) ) ;
#34882 = CARTESIAN_POINT ( 'NONE',  ( 11.00000000000000000, 1.347111479062088405E-15, 118.0000000000000000 ) ) ;
#34883 = CARTESIAN_POINT ( 'NONE',  ( -5.000000000000005329, 88.33333333333332860, 8.660254037844385522 ) ) ;
#34884 = CARTESIAN_POINT ( 'NONE',  ( -5.676582343750006032, 159.1145833299193839, 9.832129032723418760 ) ) ;
#34885 = CARTESIAN_POINT ( 'NONE',  ( 4.898587196589412829E-16, 6.187499995903221084, -8.000000000000000000 ) ) ;
#34886 = CARTESIAN_POINT ( 'NONE',  ( 7.204075437095968759, -7.204075437095966983, 86.21875000204836681 ) ) ;
#34887 = CARTESIAN_POINT ( 'NONE',  ( 2.849036369511732440E-14, 202.2500000000000000, 202.0000000000000000 ) ) ;
#34888 = CARTESIAN_POINT ( 'NONE',  ( -7.999999999995399236, -5.826008446853342637E-06, 20.51801720710344767 ) ) ;
#34889 = ADVANCED_FACE ( 'NONE', ( #22565 ), #45585, .T. ) ;
#34890 = CARTESIAN_POINT ( 'NONE',  ( -7.204075437095967871, 7.204075437095967871, 117.3437500020483810 ) ) ;
#34891 = ORIENTED_EDGE ( 'NONE', *, *, #1077, .F. ) ;
#34892 = CARTESIAN_POINT ( 'NONE',  ( 35.50560533077673142, -8.753322590441932505, 142.9349689862337982 ) ) ;
#34893 = CARTESIAN_POINT ( 'NONE',  ( -12.82798793381759950, 178.4304155043994342, 135.6284118822045741 ) ) ;
#34894 = CARTESIAN_POINT ( 'NONE',  ( -2.085542519210945728E-15, 134.8437499965860127, 11.35316468750000141 ) ) ;
#34895 = CARTESIAN_POINT ( 'NONE',  ( 2.839093476692135984E-14, 197.6875000013655779, 201.4587341250000350 ) ) ;
#34896 = CARTESIAN_POINT ( 'NONE',  ( -7.188101187500002709, 24.18749999795161543, 2.977408999572649151 ) ) ;
#34898 = EDGE_CURVE ( 'NONE', #27106, #44162, #4491, .T. ) ;
#34897 = CARTESIAN_POINT ( 'NONE',  ( 10.18810118749999916, 4.220049686691935698, 77.87500000204838102 ) ) ;
#34899 = CARTESIAN_POINT ( 'NONE',  ( 3.042071309553167069, 47.13541666325268409, -11.35316468749999785 ) ) ;
#34900 = ORIENTED_EDGE ( 'NONE', *, *, #29277, .F. ) ;
#34901 = CARTESIAN_POINT ( 'NONE',  ( 10.00000000000000000, 36.66666665983869677, 2.679491924311235618 ) ) ;
#34902 = CARTESIAN_POINT ( 'NONE',  ( 4.541265875000002339, 0.4999999986344068059, -1.881053915767121776 ) ) ;
#34903 = CARTESIAN_POINT ( 'NONE',  ( -8.008118988124991233, 3.317071493978878127, 12.91936528394062833 ) ) ;
#34904 = CARTESIAN_POINT ( 'NONE',  ( 2.445694354108784108, 206.5625000013656063, 144.4456943541088663 ) ) ;
#34905 = CARTESIAN_POINT ( 'NONE',  ( 4.401442555609581635E-16, 9.843749997951610098, -7.188101187500000044 ) ) ;
#34906 = CARTESIAN_POINT ( 'NONE',  ( 2.485281374238575314, 298.3750000034140157, 6.000000000000000888 ) ) ;
#34907 = CARTESIAN_POINT ( 'NONE',  ( -18.58325885507763431, -16.31562058779092794, 137.0903562646631428 ) ) ;
#34908 = CARTESIAN_POINT ( 'NONE',  ( -2.977408999572654480, 7.874999997951610986, 7.188101187499999156 ) ) ;
#34909 = CARTESIAN_POINT ( 'NONE',  ( -2.977408999572647819, 7.188101187499992051, 10.20530278187175455 ) ) ;
#34910 = CARTESIAN_POINT ( 'NONE',  ( 10.18810118750000093, -4.220049686691933921, 72.81250000204836681 ) ) ;
#34911 = EDGE_CURVE ( 'NONE', #60299, #50014, #29339, .T. ) ;
#34912 = CARTESIAN_POINT ( 'NONE',  ( -24.54126587500000412, 206.5000000013655779, 168.5673454167827003 ) ) ;
#34913 = DIRECTION ( 'NONE',  ( -1.000000000000000000, 0.000000000000000000, 0.000000000000000000 ) ) ;
#34914 = CARTESIAN_POINT ( 'NONE',  ( 3.211159895383561835, 18.56249999863440436, -3.211159895383561835 ) ) ;
#34915 = ORIENTED_EDGE ( 'NONE', *, *, #14243, .T. ) ;
#34916 = CARTESIAN_POINT ( 'NONE',  ( -1.656854249492347719, 197.9375000027312410, 194.0000000000000853 ) ) ;
#34917 = CARTESIAN_POINT ( 'NONE',  ( -1.656854249492403008, 204.6875000000000284, 146.0000000000000284 ) ) ;
#34918 = CARTESIAN_POINT ( 'NONE',  ( -30.82842712474612412, 202.5000000027312126, 172.8284271247466108 ) ) ;
#34919 = EDGE_CURVE ( 'NONE', #8347, #8993, #3432, .T. ) ;
#34920 = CARTESIAN_POINT ( 'NONE',  ( 5.082755093536326818, 115.7187500020483810, 5.082755093536325042 ) ) ;
#34921 = DIRECTION ( 'NONE',  ( -0.000000000000000000, 1.000000000000000000, -0.000000000000000000 ) ) ;
#34922 = CARTESIAN_POINT ( 'NONE',  ( -7.999999999999991118, 0.000000000000000000, 5.517802783920146226 ) ) ;
#34923 = VERTEX_POINT ( 'NONE', #27863 ) ;
#34924 = CARTESIAN_POINT ( 'NONE',  ( 7.188101187500000933, 18.56249999795161187, -2.977408999572650483 ) ) ;
#34925 = ORIENTED_EDGE ( 'NONE', *, *, #51992, .T. ) ;
#34926 = CARTESIAN_POINT ( 'NONE',  ( 28.00000000000001776, 198.5000000000000000, 165.9999999999998863 ) ) ;
#34927 = CARTESIAN_POINT ( 'NONE',  ( -2.775557561562891351E-14, 210.0000000000000284, 146.0000000000000284 ) ) ;
#34928 = CARTESIAN_POINT ( 'NONE',  ( -7.320508075688773708, 46.87500000000000000, -7.320508075688774596 ) ) ;
#34929 = CARTESIAN_POINT ( 'NONE',  ( 5.082755093536326818, 107.0937500020483810, 5.082755093536325042 ) ) ;
#34930 = CARTESIAN_POINT ( 'NONE',  ( -26.56734541678233086, 207.2500000013655779, 173.4587341250003760 ) ) ;
#34931 = LINE ( 'NONE', #969, #35646 ) ;
#34933 = DIRECTION ( 'NONE',  ( 0.000000000000000000, -0.8536788251726059595, 0.5207998305029671871 ) ) ;
#34932 = CARTESIAN_POINT ( 'NONE',  ( -3.313708498984842432, 111.4062500040967763, -7.999999999999920064 ) ) ;
#34934 = VERTEX_POINT ( 'NONE', #50873 ) ;
#34935 = CARTESIAN_POINT ( 'NONE',  ( 3.042071309553163960, 247.4479166700806445, -11.35316468749999785 ) ) ;
#34936 = CARTESIAN_POINT ( 'NONE',  ( 2.977408999572646486, 7.188101187499991163, 19.39280278187176165 ) ) ;
#34937 = CARTESIAN_POINT ( 'NONE',  ( 7.456209740496436034, 51.58726928745726070, 41.60229883573070708 ) ) ;
#34938 = CARTESIAN_POINT ( 'NONE',  ( 29.65685424949242588, 206.4375000000000000, 165.9999999999998863 ) ) ;
#34939 = CYLINDRICAL_SURFACE ( 'NONE', #64060, 7.999999999999991118 ) ;
#34940 = CARTESIAN_POINT ( 'NONE',  ( 8.660254037844389075, 202.2916666598387110, -5.000000000000000000 ) ) ;
#34941 = CARTESIAN_POINT ( 'NONE',  ( -10.00000000000000178, 157.5000000000000000, -1.224646799147353454E-15 ) ) ;
#34942 = CARTESIAN_POINT ( 'NONE',  ( -7.778174593052023411, 7.778174593052023411, 80.31249999999998579 ) ) ;
#34943 = CARTESIAN_POINT ( 'NONE',  ( 3.313708498984819339, 90.96875000000000000, 7.999999999999943157 ) ) ;
#34944 = CARTESIAN_POINT ( 'NONE',  ( 8.572527594031473190E-16, -2.500000000000000000, -7.000000000000000000 ) ) ;
#34945 = CARTESIAN_POINT ( 'NONE',  ( -3.042071309553164404, 122.5520833299193413, -11.35316468749999963 ) ) ;
#34946 = CARTESIAN_POINT ( 'NONE',  ( 9.000000000000000000, 5.196152422706622254, -10.80000000000000071 ) ) ;
#34947 = CARTESIAN_POINT ( 'NONE',  ( 2.160335347077970702, -16.41093803200690715, -68.77481055341485217 ) ) ;
#34950 = LINE ( 'NONE', #12645, #48460 ) ;
#34949 = CARTESIAN_POINT ( 'NONE',  ( 31.45873412499999233, 194.6875000013655779, 169.9999999999998863 ) ) ;
#34948 = CARTESIAN_POINT ( 'NONE',  ( 30.44569435410883074, 196.0625000013656063, 167.5543056458911053 ) ) ;
#34951 = VERTEX_POINT ( 'NONE', #73888 ) ;
#34952 = CARTESIAN_POINT ( 'NONE',  ( -2.124081043562907833, -60.31560147600191613, 22.95556260996172782 ) ) ;
#34953 = CARTESIAN_POINT ( 'NONE',  ( 8.660254037844477892, 194.5833333333334281, 5.000000000000059508 ) ) ;
#34954 = CARTESIAN_POINT ( 'NONE',  ( 27.99999999999996092, 194.6875000013655779, 173.4587341249998929 ) ) ;
#34955 = CARTESIAN_POINT ( 'NONE',  ( 6.123233995736767268E-16, 23.12499999317203603, -10.00000000000000178 ) ) ;
#34956 = CARTESIAN_POINT ( 'NONE',  ( -5.082755093536324154, 115.3437500020483810, 5.082755093536326818 ) ) ;
#34957 = CARTESIAN_POINT ( 'NONE',  ( 2.780723358947928197E-16, 0.6874999986344068059, -4.541265875000002339 ) ) ;
#34958 = DIRECTION ( 'NONE',  ( -0.000000000000000000, -0.000000000000000000, 1.000000000000000000 ) ) ;
#34959 = CARTESIAN_POINT ( 'NONE',  ( 5.656854249492376141, -5.656854249492374365, 23.89280277982336642 ) ) ;
#34961 = CARTESIAN_POINT ( 'NONE',  ( 25.17157287525377996, 196.8750000000000284, 172.8284271247460424 ) ) ;
#34960 = CARTESIAN_POINT ( 'NONE',  ( -49.26241139540196201, 45.23518866313047226, 58.97004729982017324 ) ) ;
#34962 = CARTESIAN_POINT ( 'NONE',  ( 6.951808397369818766E-16, 102.0312499965860269, -11.35316468750000141 ) ) ;
#34963 = ORIENTED_EDGE ( 'NONE', *, *, #21142, .F. ) ;
#34964 = CARTESIAN_POINT ( 'NONE',  ( -4.000000000000002665, 19.31249999726881228, 1.656854249492380582 ) ) ;
#34965 = CYLINDRICAL_SURFACE ( 'NONE', #27739, 10.00000000000000178 ) ;
#34966 = CARTESIAN_POINT ( 'NONE',  ( 2.679491924333024855, 41.04166666666481689, -9.999999999987601029 ) ) ;
#34967 = CARTESIAN_POINT ( 'NONE',  ( -9.832129032723418760, 248.8020833367473301, -5.676582343749998927 ) ) ;
#34968 = CARTESIAN_POINT ( 'NONE',  ( 11.35316468749999785, 115.5729166632526841, 3.042071309553174174 ) ) ;
#34969 = ORIENTED_EDGE ( 'NONE', *, *, #15733, .F. ) ;
#34970 = CARTESIAN_POINT ( 'NONE',  ( 5.000000000000000000, -13.21930962315071767, 69.49101004078875121 ) ) ;
#34971 = VECTOR ( 'NONE', #56035, 1000.000000000000000 ) ;
#34972 = CARTESIAN_POINT ( 'NONE',  ( 4.220049686691941027, -10.18810118749999738, 104.1250000020483810 ) ) ;
#34973 = CARTESIAN_POINT ( 'NONE',  ( -10.00000000000000355, 214.5833333265053682, 2.679491924311223183 ) ) ;
#34974 = CARTESIAN_POINT ( 'NONE',  ( 2.754378923186476579E-14, 199.4375000013655779, 194.5412658750000219 ) ) ;
#34975 = FACE_OUTER_BOUND ( 'NONE', #13751, .T. ) ;
#34977 = CARTESIAN_POINT ( 'NONE',  ( -9.832129032723418760, 97.86458332991935549, -5.676582343750004256 ) ) ;
#34976 = CARTESIAN_POINT ( 'NONE',  ( -7.320508075688771932, 181.8750000000000000, -7.320508075688772820 ) ) ;
#34978 = CARTESIAN_POINT ( 'NONE',  ( 5.656854249492374365, 5.656854249492375253, 9.455302783920146226 ) ) ;
#34979 = CARTESIAN_POINT ( 'NONE',  ( -30.44569435410879166, 198.0625000013656063, 172.4456943541092357 ) ) ;
#34980 = EDGE_CURVE ( 'NONE', #45507, #19485, #22193, .T. ) ;
#34981 = CARTESIAN_POINT ( 'NONE',  ( 3.999982273345623174, 89.99927424231840689, -6.928213464733948612 ) ) ;
#34982 = ORIENTED_EDGE ( 'NONE', *, *, #13058, .F. ) ;
#34983 = CARTESIAN_POINT ( 'NONE',  ( 7.320508075688774596, 192.4999999931720538, -7.320508075688774596 ) ) ;
#34984 = LINE ( 'NONE', #5929, #46725 ) ;
#34985 = DIRECTION ( 'NONE',  ( -0.000000000000000000, 1.000000000000000000, -1.563033456626094573E-30 ) ) ;
#34986 = CARTESIAN_POINT ( 'NONE',  ( -3.042071309553163960, 82.55208332991935549, -11.35316468749999963 ) ) ;
#34987 = FACE_OUTER_BOUND ( 'NONE', #65104, .T. ) ;
#34988 = CARTESIAN_POINT ( 'NONE',  ( 2.977408999572650927, 8.624999997951611874, -7.188101187500000933 ) ) ;
#34990 = ADVANCED_FACE ( 'NONE', ( #63679 ), #64062, .F. ) ;
#34989 = CARTESIAN_POINT ( 'NONE',  ( -4.220049686691937474, -10.18810118749999738, 95.31250000204838102 ) ) ;
#34991 = CARTESIAN_POINT ( 'NONE',  ( 5.676582343750001591, 221.6145833299193839, -9.832129032723420536 ) ) ;
#34992 = ORIENTED_EDGE ( 'NONE', *, *, #52416, .T. ) ;
#34993 = CARTESIAN_POINT ( 'NONE',  ( 5.656854249492381470, 122.7500000040967905, 5.656854249492379694 ) ) ;
#34994 = CARTESIAN_POINT ( 'NONE',  ( -4.898587196589412829E-16, 94.81250000409677625, -8.000000000000000000 ) ) ;
#34995 = CARTESIAN_POINT ( 'NONE',  ( -8.311093377946836114, 217.6562499965860127, -8.311093377946837890 ) ) ;
#34996 = DIRECTION ( 'NONE',  ( 0.000000000000000000, 0.000000000000000000, 1.000000000000000000 ) ) ;
#34997 = PLANE ( 'NONE',  #39090 ) ;
#34998 = CARTESIAN_POINT ( 'NONE',  ( -4.721056650415999201, 296.3281250017069510, -4.721056650415999201 ) ) ;
#34999 = ORIENTED_EDGE ( 'NONE', *, *, #21072, .F. ) ;
#35000 = CARTESIAN_POINT ( 'NONE',  ( 2.828427124746208943, 199.6250000000000284, 195.1715728752538439 ) ) ;
#35001 = CARTESIAN_POINT ( 'NONE',  ( -9.832129032723420536, 214.0104166632526699, 5.676582343749997150 ) ) ;
#35002 = CIRCLE ( 'NONE', #50632, 3.999999999999976019 ) ;
#35003 =( BOUNDED_CURVE ( )  B_SPLINE_CURVE ( 2, ( #37746, #10190, #26785, #26393, #38118, #73190, #16192, #3409, #3784 ),
 .UNSPECIFIED., .F., .F. ) 
 B_SPLINE_CURVE_WITH_KNOTS ( ( 3, 2, 2, 2, 3 ),
 ( 0.8736124324192364732, 0.8802306527327560248, 0.8868489283172127369, 0.8934672039016696710, 0.9000854414465758735 ),
 .UNSPECIFIED. ) 
 CURVE ( )  GEOMETRIC_REPRESENTATION_ITEM ( )  RATIONAL_B_SPLINE_CURVE ( ( 0.9999987286070540771, 0.9238801682130686199, 1.000000000000000000, 0.9238795325112867385, 1.000000000000000000, 0.9238795325112867385, 1.000000000000000000, 0.9238799700253094160, 0.9999991249769839552 ) ) 
 REPRESENTATION_ITEM ( '' )  );
#35004 = CARTESIAN_POINT ( 'NONE',  ( 1.871523826299183495E-15, -10.18810118749999916, 89.03125000204836681 ) ) ;
#35005 = CARTESIAN_POINT ( 'NONE',  ( -27.99999999999996447, 202.9375000013656063, 173.4587341250003760 ) ) ;
#35006 = B_SPLINE_CURVE_WITH_KNOTS ( 'NONE', 3,
 ( #73640, #60447, #8777, #17782, #62681, #92, #56675, #4992, #27992, #57047, #51743, #461, #62316, #50999, #40057, #5358, #46079, #10642, #40795, #40428 ),
 .UNSPECIFIED., .F., .F.,
 ( 4, 2, 2, 2, 2, 2, 2, 2, 2, 4 ),
 ( 0.000000000000000000, 0.001156441540183978300, 0.001734662310275972546, 0.002312883080367967008, 0.003469324620551975016, 0.004625766160735983457, 0.005782207700919991464, 0.006938649241103999471, 0.008095090781288007478, 0.009251532321472015485 ),
 .UNSPECIFIED. ) ;
#35007 = CARTESIAN_POINT ( 'NONE',  ( 5.656854249492380582, 16.68750000000000355, -5.656854249492380582 ) ) ;
#35008 = ORIENTED_EDGE ( 'NONE', *, *, #23238, .F. ) ;
#35009 = CARTESIAN_POINT ( 'NONE',  ( -3.313708498984762052, 88.90625000409677625, -8.000000000000000000 ) ) ;
#35010 = CARTESIAN_POINT ( 'NONE',  ( 7.320508075688774596, 25.62499999999999645, -7.320508075688774596 ) ) ;
#35011 = CIRCLE ( 'NONE', #22984, 10.00000000000000000 ) ;
#35012 = CARTESIAN_POINT ( 'NONE',  ( -23.99999999999997158, 197.6875000000000284, 171.6568542494927385 ) ) ;
#35013 = CARTESIAN_POINT ( 'NONE',  ( -7.204075437095967871, 7.204075437095967871, 75.34375000204838102 ) ) ;
#35014 = ORIENTED_EDGE ( 'NONE', *, *, #38793, .F. ) ;
#35015 = CARTESIAN_POINT ( 'NONE',  ( 2.828427124746191623, 2.874999997268813168, -2.828427124746191623 ) ) ;
#35016 = VECTOR ( 'NONE', #69174, 1000.000000000000000 ) ;
#35017 = DIRECTION ( 'NONE',  ( -0.000000000000000000, -0.000000000000000000, -1.000000000000000000 ) ) ;
#35018 = AXIS2_PLACEMENT_3D ( 'NONE', #31419, #43476, #37083 ) ;
#35019 = CARTESIAN_POINT ( 'NONE',  ( -4.556349186104048599, -10.99999999999999822, 92.96875000409676204 ) ) ;
#35020 = CARTESIAN_POINT ( 'NONE',  ( -4.999999999999999112, -12.24343743989404310, 68.85270403949348861 ) ) ;
#35021 = CARTESIAN_POINT ( 'NONE',  ( 4.999999999999692690, -68.48985753891565764, 21.22439692019619883 ) ) ;
#35022 = CARTESIAN_POINT ( 'NONE',  ( 6.676582343750003368, 297.8906250017069510, 2.765530957081995478 ) ) ;
#35023 = CARTESIAN_POINT ( 'NONE',  ( 11.35316468749999963, 231.1979166700806445, 3.042071309553159519 ) ) ;
#35024 = ITEM_DEFINED_TRANSFORMATION ( 'NONE', 'NONE', #816,  #57354 ) ;
#35025 = ORIENTED_EDGE ( 'NONE', *, *, #27916, .T. ) ;
#35026 = CARTESIAN_POINT ( 'NONE',  ( -3.042071309553159075, 245.2604166700806729, 11.35316468749999963 ) ) ;
#35027 = CARTESIAN_POINT ( 'NONE',  ( -7.188101187499990274, -2.977408999572651371, 7.580302781871751883 ) ) ;
#35028 = ORIENTED_EDGE ( 'NONE', *, *, #10806, .T. ) ;
#35029 = CARTESIAN_POINT ( 'NONE',  ( 10.18810118750000093, -4.220049686691933033, 68.31250000204836681 ) ) ;
#35030 = CARTESIAN_POINT ( 'NONE',  ( -11.35316468750000141, 93.59374999658602690, -1.390361679473963753E-15 ) ) ;
#35031 = CARTESIAN_POINT ( 'NONE',  ( -4.898587196589412829E-16, 120.3125000040967763, -8.000000000000000000 ) ) ;
#35032 = CARTESIAN_POINT ( 'NONE',  ( -6.735557395310442023E-16, 11.00000000000000000, 81.62499999999998579 ) ) ;
#35035 = CARTESIAN_POINT ( 'NONE',  ( 4.721056650416000089, 287.9843750017070079, 4.721056650415999201 ) ) ;
#35034 = CARTESIAN_POINT ( 'NONE',  ( 25.17157287525377640, 194.7500000027312126, 167.1715728752537586 ) ) ;
#35033 = CARTESIAN_POINT ( 'NONE',  ( 24.54126587499999701, 208.4375000013656063, 169.9999999999998863 ) ) ;
#35036 = EDGE_LOOP ( 'NONE', ( #38132, #21617, #27053, #58902 ) ) ;
#35037 = DIRECTION ( 'NONE',  ( 1.000000000000000000, -0.000000000000000000, -0.000000000000000000 ) ) ;
#35038 = FACE_OUTER_BOUND ( 'NONE', #50217, .T. ) ;
#35039 = CARTESIAN_POINT ( 'NONE',  ( 9.832129032723420536, 201.1979166632526983, -5.676582343749999815 ) ) ;
#35040 = EDGE_CURVE ( 'NONE', #1694, #15967, #52036, .T. ) ;
#35041 = CARTESIAN_POINT ( 'NONE',  ( -3.458734125000016313, 205.8750000013656063, 140.5673454167824161 ) ) ;
#35042 = ADVANCED_FACE ( 'NONE', ( #63305 ), #18408, .T. ) ;
#35043 = CARTESIAN_POINT ( 'NONE',  ( 26.56734541678238060, 205.2500000013655779, 166.5412658749999650 ) ) ;
#35044 = CARTESIAN_POINT ( 'NONE',  ( 7.188101187500000044, 24.84374999795161543, 0.000000000000000000 ) ) ;
#35045 = CARTESIAN_POINT ( 'NONE',  ( -8.311093377946836114, 182.9687499965859843, -8.311093377946837890 ) ) ;
#35046 = CARTESIAN_POINT ( 'NONE',  ( 7.188101187500002709, 95.18750000204838102, 2.977408999572649151 ) ) ;
#35048 = CARTESIAN_POINT ( 'NONE',  ( -7.320508075688770155, 235.6250000000000000, 7.320508075688774596 ) ) ;
#35047 = CARTESIAN_POINT ( 'NONE',  ( -5.000000000000000888, 63.84827628760543661, -24.15557308422260263 ) ) ;
#35049 = CARTESIAN_POINT ( 'NONE',  ( 1.881053915767122664, 9.124999998634407916, 4.541265875000001451 ) ) ;
#35050 = CARTESIAN_POINT ( 'NONE',  ( 27.99999999999996447, 204.6875000013656063, 173.4587341249998929 ) ) ;
#35051 = CARTESIAN_POINT ( 'NONE',  ( -7.188101187499991163, 2.977408999572646930, 7.767802781871751883 ) ) ;
#35052 = CARTESIAN_POINT ( 'NONE',  ( 8.311093377946834337, 75.15624999658602690, 8.311093377946839666 ) ) ;
#35053 = FACE_OUTER_BOUND ( 'NONE', #29296, .T. ) ;
#35054 = CARTESIAN_POINT ( 'NONE',  ( -3.313708498984796691, 119.4687500040968047, 7.999999999999965361 ) ) ;
#35055 = ORIENTED_EDGE ( 'NONE', *, *, #14492, .F. ) ;
#35056 = DIRECTION ( 'NONE',  ( 0.000000000000000000, -2.238352872228138170E-16, 1.000000000000000000 ) ) ;
#35057 = CARTESIAN_POINT ( 'NONE',  ( 31.99999999999998579, 206.4375000027312126, 168.3431457505074889 ) ) ;
#35058 = CARTESIAN_POINT ( 'NONE',  ( -8.311093377946841443, 63.90624999658601979, 8.311093377946830785 ) ) ;
#35059 = CARTESIAN_POINT ( 'NONE',  ( 2.020667218593132706E-15, -11.00000000000000000, 69.06250000409677625 ) ) ;
#35060 = CARTESIAN_POINT ( 'NONE',  ( -2.445694354108840063, 198.0625000013656063, 139.5543056458912190 ) ) ;
#35061 = DIRECTION ( 'NONE',  ( -1.000000000000000000, 0.000000000000000000, -0.000000000000000000 ) ) ;
#35063 = CARTESIAN_POINT ( 'NONE',  ( 8.311093377946834337, 65.15624999658602690, 8.311093377946839666 ) ) ;
#35062 = CARTESIAN_POINT ( 'NONE',  ( 5.082755093536326818, 93.21875000204838102, 5.082755093536325042 ) ) ;
#35064 = CARTESIAN_POINT ( 'NONE',  ( -7.999999999999989342, -3.313708498984762496, 25.11155278392014623 ) ) ;
#35065 = DIRECTION ( 'NONE',  ( 1.000000000000000000, 0.000000000000000000, 0.000000000000000000 ) ) ;
#35066 = CIRCLE ( 'NONE', #48259, 18.00000000000000355 ) ;
#35067 = CARTESIAN_POINT ( 'NONE',  ( -5.000000000000005329, 160.2083333265053966, 8.660254037844387298 ) ) ;
#35068 = CARTESIAN_POINT ( 'NONE',  ( 7.188101187500002709, 96.68750000204836681, 2.977408999572649151 ) ) ;
#35069 = CARTESIAN_POINT ( 'NONE',  ( -5.394762896564973355E-12, 18.74999999999958433, 10.00000000000000178 ) ) ;
#35070 = CARTESIAN_POINT ( 'NONE',  ( -8.311093377946836114, 52.96874999658601268, -8.311093377946837890 ) ) ;
#35071 = CARTESIAN_POINT ( 'NONE',  ( -4.220049686691935698, 10.18810118749999916, 114.2500000020483952 ) ) ;
#35072 = CARTESIAN_POINT ( 'NONE',  ( -8.311093377946841443, 183.9062499965860411, 8.311093377946830785 ) ) ;
#35073 = ORIENTED_EDGE ( 'NONE', *, *, #74388, .T. ) ;
#35074 = CARTESIAN_POINT ( 'NONE',  ( 2.216418498320175345, 67.77535163244897376, 20.18253627485079349 ) ) ;
#35075 = DIRECTION ( 'NONE',  ( -0.000000000000000000, 1.000000000000000000, -0.000000000000000000 ) ) ;
#35076 = CARTESIAN_POINT ( 'NONE',  ( 4.999999999999993783, 61.04166665983870388, 8.660254037844390851 ) ) ;
#35078 = CARTESIAN_POINT ( 'NONE',  ( -11.35316468750000141, 173.2812499965860411, -1.390361679473963753E-15 ) ) ;
#35077 = CARTESIAN_POINT ( 'NONE',  ( 1.739508062057428139, -67.70228923712181768, 20.12326043015085730 ) ) ;
#35079 = CARTESIAN_POINT ( 'NONE',  ( -8.000000000000000000, 10.96874999590322020, -3.313708498984762496 ) ) ;
#35080 = CARTESIAN_POINT ( 'NONE',  ( -7.320508075688770155, 253.7500000068279462, 7.320508075688774596 ) ) ;
#35081 = CARTESIAN_POINT ( 'NONE',  ( -7.999999999999991118, 0.000000000000000000, 27.83030277982336642 ) ) ;
#35082 = CIRCLE ( 'NONE', #8542, 8.000000000000000000 ) ;
#35083 = ORIENTED_EDGE ( 'NONE', *, *, #20371, .T. ) ;
#35084 = CARTESIAN_POINT ( 'NONE',  ( -3.042071309553173730, 164.6354166632526699, 11.35316468749999785 ) ) ;
#35085 = CARTESIAN_POINT ( 'NONE',  ( 7.188101187499993827, -2.977408999572645598, 24.64280278187176165 ) ) ;
#35086 = CARTESIAN_POINT ( 'NONE',  ( 8.311093377946837890, 131.7187499965860127, -8.311093377946837890 ) ) ;
#35087 =( BOUNDED_CURVE ( )  B_SPLINE_CURVE ( 2, ( #7185, #6811, #69074, #435, #41874, #23044, #29824, #57770, #1542 ),
 .UNSPECIFIED., .F., .F. ) 
 B_SPLINE_CURVE_WITH_KNOTS ( ( 3, 2, 2, 2, 3 ),
 ( 0.1250000000000000000, 0.1319444444444444475, 0.1388888888888888951, 0.1458333333333333426, 0.1527777777777777901 ),
 .UNSPECIFIED. ) 
 CURVE ( )  GEOMETRIC_REPRESENTATION_ITEM ( )  RATIONAL_B_SPLINE_CURVE ( ( 1.000000000000000000, 0.9238795325112867385, 1.000000000000000000, 0.9238795325112867385, 1.000000000000000000, 0.9238795325112867385, 1.000000000000000000, 0.9238795325112867385, 1.000000000000000000 ) ) 
 REPRESENTATION_ITEM ( '' )  );
#35088 = CARTESIAN_POINT ( 'NONE',  ( -3.313708498984760276, 3.281249995903220640, -8.000000000000000000 ) ) ;
#35089 = VECTOR ( 'NONE', #14773, 1000.000000000000000 ) ;
#35090 = EDGE_LOOP ( 'NONE', ( #25935, #59408, #56340, #68364 ) ) ;
#35091 = CARTESIAN_POINT ( 'NONE',  ( 3.313708498984760720, 102.2187500040967905, -8.000000000000000000 ) ) ;
#35092 = CARTESIAN_POINT ( 'NONE',  ( 4.000000000000001776, 12.06250000000000000, -1.656854249492381248 ) ) ;
#35093 =( BOUNDED_CURVE ( )  B_SPLINE_CURVE ( 2, ( #18704, #3207, #8865, #13388, #14128, #36426, #7752, #64724, #19425, #59076, #42067, #8117, #65821 ),
 .UNSPECIFIED., .F., .F. ) 
 B_SPLINE_CURVE_WITH_KNOTS ( ( 3, 2, 2, 2, 2, 2, 3 ),
 ( 0.01630434782608695607, 0.01811594202898550790, 0.01992753623188405626, 0.02173913043478260809, 0.02355072463768115992, 0.02536231884057971175, 0.02717391304347826012 ),
 .UNSPECIFIED. ) 
 CURVE ( )  GEOMETRIC_REPRESENTATION_ITEM ( )  RATIONAL_B_SPLINE_CURVE ( ( 1.000000000000000000, 0.9659258262890683122, 1.000000000000000000, 0.9659258262890683122, 1.000000000000000000, 0.9659258262890683122, 1.000000000000000000, 0.9659258262890683122, 1.000000000000000000, 0.9659258262890683122, 1.000000000000000000, 0.9659258262890683122, 1.000000000000000000 ) ) 
 REPRESENTATION_ITEM ( '' )  );
#35094 = CARTESIAN_POINT ( 'NONE',  ( -36.73900432967512586, -4.539912797669342304, 134.8800282699232866 ) ) ;
#35095 = CARTESIAN_POINT ( 'NONE',  ( -8.342170076843785083E-16, 11.06249999863440792, 4.541265875000002339 ) ) ;
#35096 = CARTESIAN_POINT ( 'NONE',  ( -5.656854249492375253, 5.656854249492375253, 17.33030278392014623 ) ) ;
#35097 = CARTESIAN_POINT ( 'NONE',  ( -4.000000000000015987, 195.4375000000000000, 140.3431457505076594 ) ) ;
#35098 = VECTOR ( 'NONE', #63346, 1000.000000000000000 ) ;
#35099 = ORIENTED_EDGE ( 'NONE', *, *, #61775, .F. ) ;
#35100 = CARTESIAN_POINT ( 'NONE',  ( -10.00000000000005507, 177.5000000000000853, -1.224646799147360159E-15 ) ) ;
#35101 = CARTESIAN_POINT ( 'NONE',  ( 5.082755093536326818, 105.2187500020483952, 5.082755093536325042 ) ) ;
#35103 = CARTESIAN_POINT ( 'NONE',  ( -4.000000000000015987, 209.5000000000000284, 142.0000000000000568 ) ) ;
#35102 = CYLINDRICAL_SURFACE ( 'NONE', #2452, 3.999999999999986233 ) ;
#35104 = DIRECTION ( 'NONE',  ( 1.000000000000000000, 0.000000000000000000, 0.000000000000000000 ) ) ;
#35105 = EDGE_LOOP ( 'NONE', ( #12709, #32687, #3354, #35826, #12575, #48974 ) ) ;
#35106 = CARTESIAN_POINT ( 'NONE',  ( 1.780377099648907224, 16.42166210098345758, -68.70754022607248146 ) ) ;
#35107 = ADVANCED_FACE ( 'NONE', ( #28983 ), #54066, .T. ) ;
#35108 = CARTESIAN_POINT ( 'NONE',  ( -2.977408999572647819, 7.188101187499991163, 25.20530278187175810 ) ) ;
#35109 = VERTEX_POINT ( 'NONE', #47438 ) ;
#35110 = ORIENTED_EDGE ( 'NONE', *, *, #1965, .T. ) ;
#35111 = CARTESIAN_POINT ( 'NONE',  ( -10.18810118749999916, 0.000000000000000000, 85.65625000204838102 ) ) ;
#35112 = CARTESIAN_POINT ( 'NONE',  ( -28.00000000000001776, 196.6875000013655779, 166.5412658750003629 ) ) ;
#35113 = CARTESIAN_POINT ( 'NONE',  ( -11.00000000000000000, 4.556349186104045934, 98.40625000000000000 ) ) ;
#35116 = CARTESIAN_POINT ( 'NONE',  ( 2.765530957082001251, 296.9218750017069510, 6.676582343749999815 ) ) ;
#35115 = CARTESIAN_POINT ( 'NONE',  ( 26.34314575050763807, 205.0625000027312126, 173.9999999999999147 ) ) ;
#35114 = DIRECTION ( 'NONE',  ( -0.000000000000000000, -0.000000000000000000, -1.000000000000000000 ) ) ;
#35117 = CARTESIAN_POINT ( 'NONE',  ( -7.320508075688778149, 138.1250000000000000, 7.320508075688769267 ) ) ;
#35118 = CARTESIAN_POINT ( 'NONE',  ( 8.000000000000001776, 100.1562500000000000, 3.313708498984759387 ) ) ;
#35119 = CARTESIAN_POINT ( 'NONE',  ( 3.819983998516707224, 225.9999999999999716, 9.249899904189801347 ) ) ;
#35120 = CIRCLE ( 'NONE', #19412, 12.00000000000000178 ) ;
#35121 = CARTESIAN_POINT ( 'NONE',  ( 7.188101187499993827, -2.977408999572645598, 1.017802781871753215 ) ) ;
#35122 = CARTESIAN_POINT ( 'NONE',  ( -23.99999999999999289, 208.7500000000000284, 170.0000000000003411 ) ) ;
#35123 = CARTESIAN_POINT ( 'NONE',  ( 31.45873412500001010, 203.7500000013656063, 168.5673454167822740 ) ) ;
#35124 = CARTESIAN_POINT ( 'NONE',  ( 2.977408999572651815, 3.562499997951610542, 7.188101187500000933 ) ) ;
#35125 = MECHANICAL_DESIGN_GEOMETRIC_PRESENTATION_REPRESENTATION (  '', ( #71226 ), #61608 ) ;
#35126 = CARTESIAN_POINT ( 'NONE',  ( 5.662595241051934458, 5.662595241051935346, 0.4506152839406291633 ) ) ;
#35127 = DIRECTION ( 'NONE',  ( -0.000000000000000000, 1.000000000000000000, -0.000000000000000000 ) ) ;
#35128 = CARTESIAN_POINT ( 'NONE',  ( 7.188101187500000044, 117.7812500020483810, -8.802885111219163269E-16 ) ) ;
#35129 = DIRECTION ( 'NONE',  ( -0.000000000000000000, 1.000000000000000000, -4.476705744456276341E-16 ) ) ;
#35130 = CARTESIAN_POINT ( 'NONE',  ( -11.35316468749999963, 229.2187500034139873, 0.000000000000000000 ) ) ;
#35131 = CARTESIAN_POINT ( 'NONE',  ( -35.04272297593036711, 39.80858140855857386, 65.00000000000001421 ) ) ;
#35132 = CARTESIAN_POINT ( 'NONE',  ( 4.556349186104045934, 11.00000000000000000, 86.03124999999998579 ) ) ;
#35133 = CARTESIAN_POINT ( 'NONE',  ( 29.65685424949240101, 199.4375000000000284, 165.9999999999998863 ) ) ;
#35134 = CARTESIAN_POINT ( 'NONE',  ( 3.042071309553159519, 24.73958332991934483, 11.35316468750000141 ) ) ;
#35135 = CARTESIAN_POINT ( 'NONE',  ( 10.00000000000000178, 1.874999993172032697, 0.000000000000000000 ) ) ;
#35136 = LINE ( 'NONE', #64161, #31920 ) ;
#35138 = CARTESIAN_POINT ( 'NONE',  ( -1.836970198721029983E-15, 43.75000000000000711, 10.00000000000000178 ) ) ;
#35137 = CARTESIAN_POINT ( 'NONE',  ( 4.556349186104045934, 11.00000000000000000, 99.53125000000000000 ) ) ;
#35139 = AXIS2_PLACEMENT_3D ( 'NONE', #27593, #11368, #74360 ) ;
#35140 = ORIENTED_EDGE ( 'NONE', *, *, #4386, .F. ) ;
#35142 = EDGE_CURVE ( 'NONE', #64126, #65735, #70463, .T. ) ;
#35141 = CARTESIAN_POINT ( 'NONE',  ( -1.432654583217662481, 197.3750000013656063, 145.4587341250000634 ) ) ;
#35143 = EDGE_CURVE ( 'NONE', #5256, #49691, #58783, .T. ) ;
#35144 = CARTESIAN_POINT ( 'NONE',  ( -5.676582343749998039, 27.44791666325268409, -9.832129032723420536 ) ) ;
#35145 = CARTESIAN_POINT ( 'NONE',  ( 4.556349186104051263, -10.99999999999999822, 84.15625000409676204 ) ) ;
#35146 = LINE ( 'NONE', #70207, #33517 ) ;
#35147 = CARTESIAN_POINT ( 'NONE',  ( -30.44569435410886626, 194.5625000013656063, 167.5543056458916169 ) ) ;
#35148 = DIRECTION ( 'NONE',  ( -0.000000000000000000, 1.000000000000000000, -0.000000000000000000 ) ) ;
#35150 = CARTESIAN_POINT ( 'NONE',  ( -2.085542519210945728E-15, 14.53124999658601624, 11.35316468750000141 ) ) ;
#35149 = CARTESIAN_POINT ( 'NONE',  ( 7.188101187500002709, 112.8125000020483952, 2.977408999572649151 ) ) ;
#35151 = CARTESIAN_POINT ( 'NONE',  ( -5.656854249492373476, -5.656854249492376141, 23.51780277982336642 ) ) ;
#35152 = CARTESIAN_POINT ( 'NONE',  ( 5.676582343749993598, 154.9479166632526983, 9.832129032723422313 ) ) ;
#35153 = CARTESIAN_POINT ( 'NONE',  ( 4.999999999999993783, 121.0416666598386968, 8.660254037844390851 ) ) ;
#35154 = CARTESIAN_POINT ( 'NONE',  ( 1.320432766682874540E-15, 115.9062500020483810, 7.188101187500000044 ) ) ;
#35155 = CARTESIAN_POINT ( 'NONE',  ( 1.469576158976823947E-15, 121.0625000040967763, 8.000000000000000000 ) ) ;
#35156 = CARTESIAN_POINT ( 'NONE',  ( -27.99999999999996803, 209.1875000013656063, 173.4587341250003760 ) ) ;
#35157 = EDGE_LOOP ( 'NONE', ( #12529, #42918, #5661, #46493 ) ) ;
#35158 = CARTESIAN_POINT ( 'NONE',  ( -11.35316468750000141, 13.80208332991934839, 3.042071309553159963 ) ) ;
#35159 = VERTEX_POINT ( 'NONE', #41784 ) ;
#35160 = CARTESIAN_POINT ( 'NONE',  ( 3.313708498984765161, 107.4687500000000000, 7.999999999999998224 ) ) ;
#35161 = CARTESIAN_POINT ( 'NONE',  ( -4.088227598258586603E-16, 297.2031250017070079, -6.676582343750001591 ) ) ;
#35162 = CARTESIAN_POINT ( 'NONE',  ( 3.042071309553167513, 141.8229166632526983, -11.35316468749999785 ) ) ;
#35163 = SURFACE_STYLE_USAGE ( .BOTH. , #30591 ) ;
#35164 = CARTESIAN_POINT ( 'NONE',  ( 7.999999999999991118, 9.797174393178815797E-16, 24.13655278432982598 ) ) ;
#35165 = AXIS2_PLACEMENT_3D ( 'NONE', #62857, #57220, #68526 ) ;
#35166 = CARTESIAN_POINT ( 'NONE',  ( -11.00000000000000000, 4.556349186104045934, 91.09375000409676204 ) ) ;
#35167 = CARTESIAN_POINT ( 'NONE',  ( 9.832129032723416984, 251.8229166700806729, -5.676582343750003368 ) ) ;
#35168 = EDGE_CURVE ( 'NONE', #38241, #37485, #24480, .T. ) ;
#35169 = CARTESIAN_POINT ( 'NONE',  ( -10.18810118749999738, -4.220049686691941915, 93.62500000204838102 ) ) ;
#35170 = EDGE_LOOP ( 'NONE', ( #51017, #30359, #13312, #61863, #42733 ) ) ;
#35171 = CARTESIAN_POINT ( 'NONE',  ( 5.000000000000000000, 10.28295106684163684, 65.17663434001590872 ) ) ;
#35172 = CARTESIAN_POINT ( 'NONE',  ( 0.000000000000000000, 300.0000000000000000, 0.000000000000000000 ) ) ;
#35173 = CARTESIAN_POINT ( 'NONE',  ( 11.35316468749999963, 86.30208332991936970, -3.042071309553165293 ) ) ;
#35174 = VERTEX_POINT ( 'NONE', #59154 ) ;
#35175 = CARTESIAN_POINT ( 'NONE',  ( -7.204075437095967871, 7.204075437095967871, 104.9687500020483810 ) ) ;
#35176 = CARTESIAN_POINT ( 'NONE',  ( -4.541265875000002339, 14.87499999863440969, -1.881053915767121998 ) ) ;
#35177 = ORIENTED_EDGE ( 'NONE', *, *, #58738, .F. ) ;
#35178 = ORIENTED_EDGE ( 'NONE', *, *, #46834, .F. ) ;
#35179 = CARTESIAN_POINT ( 'NONE',  ( -1.469576158976823947E-15, 4.125000000000000888, 8.000000000000000000 ) ) ;
#35180 = CARTESIAN_POINT ( 'NONE',  ( -5.656854249492380582, 106.8125000000000000, -5.656854249492380582 ) ) ;
#35181 = CARTESIAN_POINT ( 'NONE',  ( 5.082755093536324154, 24.65624999795161543, 5.082755093536326818 ) ) ;
#35182 = CARTESIAN_POINT ( 'NONE',  ( -8.000000000000000000, 122.1875000040967763, 0.000000000000000000 ) ) ;
#35183 = CARTESIAN_POINT ( 'NONE',  ( 10.18810118749999916, 4.220049686691935698, 103.3750000020484094 ) ) ;
#35184 = AXIS2_PLACEMENT_3D ( 'NONE', #38504, #61504, #51297 ) ;
#35185 = FACE_OUTER_BOUND ( 'NONE', #70663, .T. ) ;
#35186 = CARTESIAN_POINT ( 'NONE',  ( 4.000000000000000888, 12.68749999726881406, 1.656854249492384135 ) ) ;
#35187 = CARTESIAN_POINT ( 'NONE',  ( 25.17157287525378351, 206.7500000027312126, 167.1715728752537586 ) ) ;
#35188 = ORIENTED_EDGE ( 'NONE', *, *, #47390, .F. ) ;
#35189 = CARTESIAN_POINT ( 'NONE',  ( 2.824543433528785410E-14, 210.0000000000000284, 194.0000000000000568 ) ) ;
#35190 = CARTESIAN_POINT ( 'NONE',  ( -1.432654583217607858, 197.6250000013656063, 201.4587341250000065 ) ) ;
#35192 = CARTESIAN_POINT ( 'NONE',  ( -30.44569435410875968, 203.8125000013656063, 172.4456943541092642 ) ) ;
#35191 =( BOUNDED_CURVE ( )  B_SPLINE_CURVE ( 2, ( #10898, #15795, #67863, #16156, #39197, #62199, #53401, #40311, #25440 ),
 .UNSPECIFIED., .F., .F. ) 
 B_SPLINE_CURVE_WITH_KNOTS ( ( 3, 2, 2, 2, 3 ),
 ( 0.7333333333333339477, 0.7416666666666673624, 0.7500000000000006661, 0.7583333333333339699, 0.7666666666666673846 ),
 .UNSPECIFIED. ) 
 CURVE ( )  GEOMETRIC_REPRESENTATION_ITEM ( )  RATIONAL_B_SPLINE_CURVE ( ( 0.9999999999999938938, 0.9238795325112928447, 1.000000000000000000, 0.9238795325112867385, 1.000000000000000000, 0.9238795325112867385, 1.000000000000000000, 0.9238795325112806323, 1.000000000000005995 ) ) 
 REPRESENTATION_ITEM ( '' )  );
#35193 = CARTESIAN_POINT ( 'NONE',  ( -2.849036369511732440E-14, 207.2500000000000284, 138.0000000000000568 ) ) ;
#35194 = CARTESIAN_POINT ( 'NONE',  ( 4.541265875000001451, 12.24999999863440969, 1.881053915767124440 ) ) ;
#35195 = CARTESIAN_POINT ( 'NONE',  ( -7.347880794884122694E-16, 18.49999999726881583, 4.000000000000001776 ) ) ;
#35196 = CARTESIAN_POINT ( 'NONE',  ( -5.082755093536317936, -5.082755093536320601, 13.67405278187175455 ) ) ;
#35197 = ORIENTED_EDGE ( 'NONE', *, *, #56468, .F. ) ;
#35198 = ORIENTED_EDGE ( 'NONE', *, *, #1189, .F. ) ;
#35199 = CARTESIAN_POINT ( 'NONE',  ( 7.204075437095966983, 7.204075437095967871, 104.5937500020483810 ) ) ;
#35200 = CARTESIAN_POINT ( 'NONE',  ( -11.00000000000000000, 0.000000000000000000, 103.0000000000000000 ) ) ;
#35201 = CARTESIAN_POINT ( 'NONE',  ( -25.17157287525377640, 203.6250000000000284, 172.8284271247465256 ) ) ;
#35202 = CARTESIAN_POINT ( 'NONE',  ( 3.458734125000016313, 199.8750000013655779, 199.4326545832176691 ) ) ;
#35203 = DIRECTION ( 'NONE',  ( 0.000000000000000000, 0.000000000000000000, 1.000000000000000000 ) ) ;
#35204 = CARTESIAN_POINT ( 'NONE',  ( 7.320508075688774596, 95.62499999999998579, -7.320508075688774596 ) ) ;
#35205 = AXIS2_PLACEMENT_3D ( 'NONE', #19427, #1372, #36428 ) ;
#35206 = ADVANCED_FACE ( 'NONE', ( #35038 ), #41423, .F. ) ;
#35207 = CARTESIAN_POINT ( 'NONE',  ( 3.313708498984760720, 115.5312500000000142, -8.000000000000000000 ) ) ;
#35208 = CARTESIAN_POINT ( 'NONE',  ( 8.311093377946834337, 60.46874999658602690, 8.311093377946839666 ) ) ;
#35209 = CARTESIAN_POINT ( 'NONE',  ( -4.088227598258586603E-16, 299.3593750017070079, -6.676582343750001591 ) ) ;
#35210 = EDGE_LOOP ( 'NONE', ( #1840, #49049, #30716, #2048, #57423, #21562, #35538 ) ) ;
#35211 = AXIS2_PLACEMENT_3D ( 'NONE', #55749, #31229, #44416 ) ;
#35212 = CARTESIAN_POINT ( 'NONE',  ( 6.000000000000003553, 294.5625000000000000, -2.485281374238571761 ) ) ;
#35213 = CARTESIAN_POINT ( 'NONE',  ( -8.000000000000000000, 14.06249999590322375, -9.797174393178825657E-16 ) ) ;
#35214 = CARTESIAN_POINT ( 'NONE',  ( 3.458734124999959025, 205.5000000013655779, 140.5673454167824161 ) ) ;
#35215 = CARTESIAN_POINT ( 'NONE',  ( -4.999999999999992895, 235.8333333333333428, 8.660254037844390851 ) ) ;
#35216 = CARTESIAN_POINT ( 'NONE',  ( -30.82842712474624491, 202.2500000027312126, 167.1715728752542418 ) ) ;
#35217 = CARTESIAN_POINT ( 'NONE',  ( 1.871523826299183495E-15, -10.18810118749999916, 69.90625000204836681 ) ) ;
#35218 = CARTESIAN_POINT ( 'NONE',  ( -7.320508075688778149, 208.1250000000000000, 7.320508075688769267 ) ) ;
#35219 = CARTESIAN_POINT ( 'NONE',  ( -5.082755093536317936, -5.082755093536320601, 12.54905278187175277 ) ) ;
#35220 = CARTESIAN_POINT ( 'NONE',  ( -11.35316468749999785, 183.3854166632526699, -3.042071309553167513 ) ) ;
#35221 = CARTESIAN_POINT ( 'NONE',  ( -8.342170076843785083E-16, 2.062499998634406584, 4.541265875000002339 ) ) ;
#35222 = CARTESIAN_POINT ( 'NONE',  ( -10.99999999999999822, -4.556349186104053040, 97.28125000409677625 ) ) ;
#35224 = CARTESIAN_POINT ( 'NONE',  ( 8.660254037844389075, 87.29166665983869677, -5.000000000000000000 ) ) ;
#35223 = CARTESIAN_POINT ( 'NONE',  ( -2.679491924311222295, 229.1666666734946034, 10.00000000000000178 ) ) ;
#35225 = ORIENTED_EDGE ( 'NONE', *, *, #39480, .T. ) ;
#35227 = EDGE_CURVE ( 'NONE', #62350, #68303, #15484, .T. ) ;
#35226 = CARTESIAN_POINT ( 'NONE',  ( 1.432654583217607414, 207.5000000013655779, 145.4587341250000634 ) ) ;
#35228 = CARTESIAN_POINT ( 'NONE',  ( -8.311093377946836114, 37.96874999658601979, -8.311093377946837890 ) ) ;
#35229 = CARTESIAN_POINT ( 'NONE',  ( -7.778174593052023411, 7.778174593052023411, 112.0000000040967763 ) ) ;
#35230 = CARTESIAN_POINT ( 'NONE',  ( -28.00000000000007461, 206.4375000013656063, 166.5412658750003629 ) ) ;
#35231 = CARTESIAN_POINT ( 'NONE',  ( -8.660254037844390851, 124.7916666598387110, 4.999999999999998224 ) ) ;
#35232 = DIRECTION ( 'NONE',  ( -0.000000000000000000, -1.000000000000000000, -4.283267841918042741E-17 ) ) ;
#35233 = CARTESIAN_POINT ( 'NONE',  ( 2.445694354108782775, 198.5625000013656063, 139.5543056458912190 ) ) ;
#35234 = CARTESIAN_POINT ( 'NONE',  ( -10.00000000000000000, 79.16666665983872520, -2.679491924311229845 ) ) ;
#35235 = VECTOR ( 'NONE', #41438, 1000.000000000000000 ) ;
#35236 = CARTESIAN_POINT ( 'NONE',  ( 5.082755093536326818, 97.71875000204838102, 5.082755093536325042 ) ) ;
#35237 = CARTESIAN_POINT ( 'NONE',  ( 1.881053915767122664, 11.24999999863440792, 4.541265875000001451 ) ) ;
#35238 = CARTESIAN_POINT ( 'NONE',  ( -32.00000000000000000, 206.3750000027312126, 170.0000000000004547 ) ) ;
#35239 = CARTESIAN_POINT ( 'NONE',  ( 4.850062511589654031E-16, 0.4207531754730554074, -7.920753175473053354 ) ) ;
#35240 = CARTESIAN_POINT ( 'NONE',  ( -1.836970198721029983E-15, 100.6249999931720396, 10.00000000000000178 ) ) ;
#35241 = ORIENTED_EDGE ( 'NONE', *, *, #65946, .T. ) ;
#35242 = ORIENTED_EDGE ( 'NONE', *, *, #5446, .F. ) ;
#35243 = CARTESIAN_POINT ( 'NONE',  ( -6.000000000000003553, 288.9375000000000000, -2.485281374238571317 ) ) ;
#35244 = CARTESIAN_POINT ( 'NONE',  ( 1.226468279477575784E-15, 297.8593750017070079, 6.676582343750001591 ) ) ;
#35245 = FACE_OUTER_BOUND ( 'NONE', #58693, .T. ) ;
#35246 = CARTESIAN_POINT ( 'NONE',  ( 4.999999999999993783, 41.04166665983870388, 8.660254037844390851 ) ) ;
#35247 = CARTESIAN_POINT ( 'NONE',  ( -2.085542519210945728E-15, 159.5312499965860127, 11.35316468750000141 ) ) ;
#35248 = CARTESIAN_POINT ( 'NONE',  ( 10.18810118749999916, 1.247682550866122264E-15, 84.90625000204838102 ) ) ;
#35249 = CARTESIAN_POINT ( 'NONE',  ( -31.05507224581699788, -21.00013786233002833, 171.9999999999997726 ) ) ;
#35250 = CARTESIAN_POINT ( 'NONE',  ( -1.656854249492348607, 204.1875000000000568, 202.0000000000000284 ) ) ;
#35251 = ADVANCED_FACE ( 'NONE', ( #29368 ), #58051, .T. ) ;
#35252 = CARTESIAN_POINT ( 'NONE',  ( -7.204075437095967871, 7.204075437095967871, 112.8437500020483810 ) ) ;
#35253 = ORIENTED_EDGE ( 'NONE', *, *, #59396, .T. ) ;
#35254 = EDGE_CURVE ( 'NONE', #53455, #3727, #68328, .T. ) ;
#35255 = LINE ( 'NONE', #6573, #43225 ) ;
#35256 = VECTOR ( 'NONE', #26165, 1000.000000000000000 ) ;
#35257 = CARTESIAN_POINT ( 'NONE',  ( 11.04632294301736906, 183.3901644024232382, 140.9474641888003532 ) ) ;
#35258 = CARTESIAN_POINT ( 'NONE',  ( 9.832129032723416984, 130.6770833299193555, 5.676582343750006032 ) ) ;
#35259 = CARTESIAN_POINT ( 'NONE',  ( 3.458734125000015425, 197.0000000013656063, 196.5673454167823877 ) ) ;
#35260 = CARTESIAN_POINT ( 'NONE',  ( 4.898587196589412829E-16, 9.187499995903221972, -8.000000000000000000 ) ) ;
#35261 = AXIS2_PLACEMENT_3D ( 'NONE', #45498, #16816, #63222 ) ;
#35262 = CARTESIAN_POINT ( 'NONE',  ( 10.18810118749999916, 4.220049686691935698, 79.37500000204838102 ) ) ;
#35263 = CARTESIAN_POINT ( 'NONE',  ( 11.35316468749999785, 50.88541666325269119, 3.042071309553174174 ) ) ;
#35264 = ORIENTED_EDGE ( 'NONE', *, *, #9748, .F. ) ;
#35265 = CARTESIAN_POINT ( 'NONE',  ( 54.00000000000000711, 272.0000000000000000, 20.00000000000001776 ) ) ;
#35266 = CARTESIAN_POINT ( 'NONE',  ( 2.780723358947928197E-16, 2.687499998634407028, -4.541265875000002339 ) ) ;
#35267 = CARTESIAN_POINT ( 'NONE',  ( -5.662595241051933570, -5.662595241051936235, 16.20061528394063188 ) ) ;
#35268 = EDGE_CURVE ( 'NONE', #64829, #61351, #60990, .T. ) ;
#35269 = EDGE_CURVE ( 'NONE', #24263, #36324, #31168, .T. ) ;
#35270 = CARTESIAN_POINT ( 'NONE',  ( -7.188101187500002709, 17.81249999795161543, 2.977408999572649151 ) ) ;
#35271 = CARTESIAN_POINT ( 'NONE',  ( -2.485281374238572649, 292.2500000034140726, 6.000000000000002665 ) ) ;
#35272 = CARTESIAN_POINT ( 'NONE',  ( -13.73527132085065539, -21.87124688732590982, 138.2595740764830339 ) ) ;
#35273 = CARTESIAN_POINT ( 'NONE',  ( -5.082755093536326818, 4.781249997951610986, 5.082755093536325042 ) ) ;
#35274 = CARTESIAN_POINT ( 'NONE',  ( -2.977408999572647819, 7.188101187499992051, 11.70530278187175277 ) ) ;
#35275 = VECTOR ( 'NONE', #14475, 1000.000000000000000 ) ;
#35276 = CARTESIAN_POINT ( 'NONE',  ( 10.18810118749999916, 1.247682550866122264E-15, 71.40625000204836681 ) ) ;
#35277 = EDGE_CURVE ( 'NONE', #7596, #58094, #8269, .T. ) ;
#35278 = CARTESIAN_POINT ( 'NONE',  ( -29.43265458321761230, 207.1250000013656347, 173.4587341250003760 ) ) ;
#35279 = DIRECTION ( 'NONE',  ( 0.000000000000000000, -0.000000000000000000, 1.000000000000000000 ) ) ;
#35280 = CARTESIAN_POINT ( 'NONE',  ( -4.541265875000002339, 19.93749999863440436, -5.561446717895856393E-16 ) ) ;
#35281 = UNCERTAINTY_MEASURE_WITH_UNIT (LENGTH_MEASURE( 1.000000000000000082E-05 ), #55498, 'distance_accuracy_value', 'NONE');
#35282 = ORIENTED_EDGE ( 'NONE', *, *, #67657, .F. ) ;
#35283 = CARTESIAN_POINT ( 'NONE',  ( 2.751064625579944321E-14, 194.8750000027311842, 194.0000000000000568 ) ) ;
#35284 = CARTESIAN_POINT ( 'NONE',  ( -2.828427124746209831, 206.3750000000000284, 139.1715728752538723 ) ) ;
#35285 = CARTESIAN_POINT ( 'NONE',  ( -26.34314575050753149, 202.6875000027311842, 174.0000000000003411 ) ) ;
#35286 = CARTESIAN_POINT ( 'NONE',  ( -4.401442555609581635E-16, 116.2812500020483810, -7.188101187500000044 ) ) ;
#35287 = CARTESIAN_POINT ( 'NONE',  ( 7.778174593052023411, -7.778174593052021635, 75.25000000409676204 ) ) ;
#35288 = CARTESIAN_POINT ( 'NONE',  ( 7.999999999999991118, 3.313708498984757611, 0.3615527839201451710 ) ) ;
#35289 = VERTEX_POINT ( 'NONE', #59877 ) ;
#35290 = CARTESIAN_POINT ( 'NONE',  ( -7.188101187500000933, 19.12499999795161898, -2.977408999572651371 ) ) ;
#35291 = ORIENTED_EDGE ( 'NONE', *, *, #64921, .T. ) ;
#35292 = CARTESIAN_POINT ( 'NONE',  ( 30.82842712474616675, 198.1250000000000284, 172.8284271247460993 ) ) ;
#35293 = CARTESIAN_POINT ( 'NONE',  ( 2.679491924311222739, 48.95833333333333570, 10.00000000000000355 ) ) ;
#35294 = CARTESIAN_POINT ( 'NONE',  ( 5.082755093536326818, 101.0937500020483810, 5.082755093536325042 ) ) ;
#35295 = CARTESIAN_POINT ( 'NONE',  ( -30.44569435410883429, 205.8125000013656063, 167.5543056458915885 ) ) ;
#35296 = CARTESIAN_POINT ( 'NONE',  ( -4.242640687119286547, 299.8750000000000000, -4.242640687119286547 ) ) ;
#35298 = CARTESIAN_POINT ( 'NONE',  ( -5.656854249492378806, 95.37500000409677625, 5.656854249492381470 ) ) ;
#35297 = CARTESIAN_POINT ( 'NONE',  ( -7.320508075688778149, 34.99999999317203248, 7.320508075688769267 ) ) ;
#35299 = ORIENTED_EDGE ( 'NONE', *, *, #5392, .T. ) ;
#35300 = CARTESIAN_POINT ( 'NONE',  ( -9.832129032723415207, 249.3229166700806729, 5.676582343750005144 ) ) ;
#35301 = CARTESIAN_POINT ( 'NONE',  ( -2.977408999572647819, 7.188101187499991163, 15.08030278187175455 ) ) ;
#35302 = CARTESIAN_POINT ( 'NONE',  ( 1.469576158976823947E-15, 107.5625000040967905, 8.000000000000000000 ) ) ;
#35303 = DIRECTION ( 'NONE',  ( -0.000000000000000000, -0.000000000000000000, 1.000000000000000000 ) ) ;
#35304 = CARTESIAN_POINT ( 'NONE',  ( -5.126144196591281954, -68.65853088339370913, -20.89430926783084885 ) ) ;
#35306 = ADVANCED_FACE ( 'NONE', ( #19873 ), #31952, .T. ) ;
#35305 = CARTESIAN_POINT ( 'NONE',  ( -1.836970198721029983E-15, 140.6249999931720538, 10.00000000000000178 ) ) ;
#35307 =( BOUNDED_CURVE ( )  B_SPLINE_CURVE ( 2, ( #43015, #59284, #19269, #71317, #36268, #30965, #37003, #8324, #20006 ),
 .UNSPECIFIED., .F., .F. ) 
 B_SPLINE_CURVE_WITH_KNOTS ( ( 3, 2, 2, 2, 3 ),
 ( 0.3000000000000002109, 0.3083333333333335702, 0.3166666666666669294, 0.3250000000000002887, 0.3333333333333336479 ),
 .UNSPECIFIED. ) 
 CURVE ( )  GEOMETRIC_REPRESENTATION_ITEM ( )  RATIONAL_B_SPLINE_CURVE ( ( 0.9999999999999980016, 0.9238795325112887369, 1.000000000000000000, 0.9238795325112867385, 1.000000000000000000, 0.9238795325112867385, 1.000000000000000000, 0.9238795325112837409, 1.000000000000003109 ) ) 
 REPRESENTATION_ITEM ( '' )  );
#35308 = CARTESIAN_POINT ( 'NONE',  ( 10.00000000000000178, 165.0000000000000000, 0.000000000000000000 ) ) ;
#35309 = CARTESIAN_POINT ( 'NONE',  ( -6.735557395310442023E-16, 11.00000000000000000, 80.12499999999998579 ) ) ;
#35310 = CARTESIAN_POINT ( 'NONE',  ( -33.48318503342263597, 175.8115626168855101, 156.1427595010634377 ) ) ;
#35311 =( BOUNDED_CURVE ( )  B_SPLINE_CURVE ( 2, ( #60920, #9243, #9627, #32265, #49606, #32647, #72993, #46546, #17503 ),
 .UNSPECIFIED., .F., .F. ) 
 B_SPLINE_CURVE_WITH_KNOTS ( ( 3, 2, 2, 2, 3 ),
 ( 0.1458333333333311499, 0.1562499999999978073, 0.1666666666666644647, 0.1770833333333311777, 0.1874999999999978351 ),
 .UNSPECIFIED. ) 
 CURVE ( )  GEOMETRIC_REPRESENTATION_ITEM ( )  RATIONAL_B_SPLINE_CURVE ( ( 1.000000000000015987, 0.9238795325112707513, 1.000000000000000000, 0.9238795325112867385, 1.000000000000000000, 0.9238795325112867385, 1.000000000000000000, 0.9238795325113025037, 0.9999999999999842348 ) ) 
 REPRESENTATION_ITEM ( '' )  );
#35312 = CARTESIAN_POINT ( 'NONE',  ( -7.188101187499990274, -2.977408999572651815, 27.45530278187175455 ) ) ;
#35313 = CARTESIAN_POINT ( 'NONE',  ( 11.35316468749999963, 136.3020833299193555, -3.042071309553165293 ) ) ;
#35314 = DIRECTION ( 'NONE',  ( -6.558680509637768569E-18, 1.000000000000000000, 0.000000000000000000 ) ) ;
#35315 = CARTESIAN_POINT ( 'NONE',  ( 7.320508075688771044, 26.24999999317203248, 7.320508075688775484 ) ) ;
#35318 = DIRECTION ( 'NONE',  ( 0.000000000000000000, 0.000000000000000000, 1.000000000000000000 ) ) ;
#35317 = CARTESIAN_POINT ( 'NONE',  ( -0.4368895104720019740, -51.14729664189371761, 48.52014062455020138 ) ) ;
#35316 = CARTESIAN_POINT ( 'NONE',  ( 25.17157287525381903, 206.6250000000000284, 167.1715728752537018 ) ) ;
#35319 = VERTEX_POINT ( 'NONE', #65154 ) ;
#35320 = CIRCLE ( 'NONE', #54577, 8.000000000000000000 ) ;
#35321 = CARTESIAN_POINT ( 'NONE',  ( 0.8419854211626226492, -60.19512794652378318, 22.88206588978759015 ) ) ;
#35322 = CARTESIAN_POINT ( 'NONE',  ( -10.99999999999989342, 4.556349186104152515, 68.59375000409677625 ) ) ;
#35323 = CARTESIAN_POINT ( 'NONE',  ( 1.522769729196201526E-11, 196.2499999999988063, -10.00000000000000178 ) ) ;
#35324 = CARTESIAN_POINT ( 'NONE',  ( 4.999999999999999112, -64.42874436516109427, -24.11656705754197816 ) ) ;
#35325 = EDGE_CURVE ( 'NONE', #9770, #69514, #54602, .T. ) ;
#35326 = CARTESIAN_POINT ( 'NONE',  ( -1.836970198721029983E-15, 40.62499999317203248, 10.00000000000000178 ) ) ;
#35327 = CARTESIAN_POINT ( 'NONE',  ( -7.188101187499999156, 113.7500000020483668, 2.977408999572654924 ) ) ;
#35328 = CARTESIAN_POINT ( 'NONE',  ( 3.211159895383561835, 21.43749999863440792, -3.211159895383561835 ) ) ;
#35329 = CARTESIAN_POINT ( 'NONE',  ( -3.074111742569602956, 67.95395293240338219, -20.32712440775815210 ) ) ;
#35330 = CARTESIAN_POINT ( 'NONE',  ( -3.313708498984757167, 7.999999999999991118, 20.04905277982336642 ) ) ;
#35332 = CARTESIAN_POINT ( 'NONE',  ( -27.99999999999996092, 207.5000000000000284, 174.0000000000003695 ) ) ;
#35331 = CARTESIAN_POINT ( 'NONE',  ( 11.00000000000000000, 1.347111479062088405E-15, 100.9375000040967763 ) ) ;
#35333 = ORIENTED_EDGE ( 'NONE', *, *, #67657, .T. ) ;
#35334 = DIRECTION ( 'NONE',  ( 1.000000000000000000, -0.000000000000000000, -0.000000000000000000 ) ) ;
#35335 = CARTESIAN_POINT ( 'NONE',  ( -2.977408999572654480, 23.99999999795161543, 7.188101187499999156 ) ) ;
#35336 = CARTESIAN_POINT ( 'NONE',  ( -1.836970198721029983E-15, 180.6249999931720538, 10.00000000000000178 ) ) ;
#35337 = CARTESIAN_POINT ( 'NONE',  ( 11.35316468749999963, 246.7187500034139873, -1.390361679473963556E-15 ) ) ;
#35338 = CARTESIAN_POINT ( 'NONE',  ( -11.35316468750000141, 118.2812499965860269, -1.390361679473963753E-15 ) ) ;
#35339 = VERTEX_POINT ( 'NONE', #36870 ) ;
#35340 = CARTESIAN_POINT ( 'NONE',  ( 1.224646799147353454E-15, 300.0000000000000000, -10.00000000000000178 ) ) ;
#35341 = CARTESIAN_POINT ( 'NONE',  ( 4.220049686691934809, 10.18810118749999916, 100.1875000020483668 ) ) ;
#35342 = CARTESIAN_POINT ( 'NONE',  ( -7.320508075688773708, 218.7499999931720538, -7.320508075688774596 ) ) ;
#35343 = CARTESIAN_POINT ( 'NONE',  ( -2.445694354108783219, 199.8125000013656063, 200.4456943541088663 ) ) ;
#35344 = CARTESIAN_POINT ( 'NONE',  ( 0.000000000000000000, 300.0000000000000000, 10.00000000000000178 ) ) ;
#35346 = CARTESIAN_POINT ( 'NONE',  ( -9.832129032723420536, 98.69791666325269830, 5.676582343749997150 ) ) ;
#35345 = LINE ( 'NONE', #59452, #50858 ) ;
#35347 = CARTESIAN_POINT ( 'NONE',  ( -3.313708498984758943, -7.999999999999989342, 4.299052783920145338 ) ) ;
#35348 = CARTESIAN_POINT ( 'NONE',  ( -29.43265458321760519, 198.1250000013656063, 173.4587341250003760 ) ) ;
#35349 = CARTESIAN_POINT ( 'NONE',  ( 10.00000000000009059, 175.0000000000000568, 0.000000000000000000 ) ) ;
#35350 = ORIENTED_EDGE ( 'NONE', *, *, #64002, .T. ) ;
#35351 = CARTESIAN_POINT ( 'NONE',  ( 10.00000000000000178, 192.0833333265053682, -2.679491924311226736 ) ) ;
#35352 = ADVANCED_FACE ( 'NONE', ( #2537 ), #65533, .T. ) ;
#35353 = CYLINDRICAL_SURFACE ( 'NONE', #69613, 3.999999999999976019 ) ;
#35354 = FACE_OUTER_BOUND ( 'NONE', #63848, .T. ) ;
#35355 = CARTESIAN_POINT ( 'NONE',  ( -3.042071309553163960, 92.55208332991935549, -11.35316468749999963 ) ) ;
#35356 = CARTESIAN_POINT ( 'NONE',  ( -7.188101187500000933, 8.999999997951611874, -2.977408999572651371 ) ) ;
#35357 = CARTESIAN_POINT ( 'NONE',  ( -10.18810118749999916, 0.000000000000000000, 96.53125000204838102 ) ) ;
#35358 = EDGE_CURVE ( 'NONE', #74465, #4004, #28490, .T. ) ;
#35359 = CARTESIAN_POINT ( 'NONE',  ( -11.35316468749999785, 3.385416663252682756, -3.042071309553167513 ) ) ;
#35360 = VERTEX_POINT ( 'NONE', #42879 ) ;
#35361 = CARTESIAN_POINT ( 'NONE',  ( -7.999999999999991118, 0.000000000000000000, 26.33030277982336997 ) ) ;
#35362 = DIRECTION ( 'NONE',  ( 0.000000000000000000, 0.000000000000000000, -1.000000000000000000 ) ) ;
#35363 = CARTESIAN_POINT ( 'NONE',  ( -5.676582343749998039, 222.4479166632526983, -9.832129032723420536 ) ) ;
#35364 = CARTESIAN_POINT ( 'NONE',  ( -10.18810118749999916, 4.220049686691934809, 76.93750000204839523 ) ) ;
#35365 = CARTESIAN_POINT ( 'NONE',  ( 7.320508075688771044, 46.24999999317203248, 7.320508075688775484 ) ) ;
#35366 = CARTESIAN_POINT ( 'NONE',  ( -8.000000000000000000, 93.68750000409679046, 0.000000000000000000 ) ) ;
#35367 = CARTESIAN_POINT ( 'NONE',  ( -4.721056650415998313, 297.5781250017069510, 4.721056650416000089 ) ) ;
#35368 = ORIENTED_EDGE ( 'NONE', *, *, #21630, .T. ) ;
#35369 = CARTESIAN_POINT ( 'NONE',  ( 3.153939666463620179E-13, 118.7500000000000426, 9.999999999999998224 ) ) ;
#35370 = CARTESIAN_POINT ( 'NONE',  ( 8.311093377946834337, 210.4687499965859843, 8.311093377946839666 ) ) ;
#35371 = CARTESIAN_POINT ( 'NONE',  ( -7.204075437095965206, -7.204075437095968759, 87.34375000204836681 ) ) ;
#35372 = EDGE_CURVE ( 'NONE', #48435, #59499, #67453, .T. ) ;
#35373 = CARTESIAN_POINT ( 'NONE',  ( -29.43265458321760519, 204.8750000013656063, 173.4587341250003760 ) ) ;
#35374 = CARTESIAN_POINT ( 'NONE',  ( 5.656854249492380582, 15.18750000000000355, -5.656854249492380582 ) ) ;
#35375 = ORIENTED_EDGE ( 'NONE', *, *, #68008, .T. ) ;
#35376 = VECTOR ( 'NONE', #74031, 1000.000000000000000 ) ;
#35377 = CARTESIAN_POINT ( 'NONE',  ( -7.188101187500000044, 119.6562500020483810, 0.000000000000000000 ) ) ;
#35378 = CARTESIAN_POINT ( 'NONE',  ( 4.000000000000015987, 206.5625000027312126, 199.6568542494924259 ) ) ;
#35379 = CARTESIAN_POINT ( 'NONE',  ( -7.320508075688778149, 23.12500000000000355, 7.320508075688769267 ) ) ;
#35380 = CARTESIAN_POINT ( 'NONE',  ( -8.000000000000000000, 8.250000000000001776, -9.797174393178825657E-16 ) ) ;
#35381 = CARTESIAN_POINT ( 'NONE',  ( 7.204075437095968759, -7.204075437095966983, 76.09375000204838102 ) ) ;
#35382 = ORIENTED_EDGE ( 'NONE', *, *, #42494, .F. ) ;
#35383 = CARTESIAN_POINT ( 'NONE',  ( 3.313708498984846429, 113.4687500000000000, 7.999999999999918288 ) ) ;
#35384 = LINE ( 'NONE', #6701, #34250 ) ;
#35385 = CARTESIAN_POINT ( 'NONE',  ( 1.320432766682874540E-15, 120.4062500020483810, 7.188101187500000044 ) ) ;
#35386 = DIRECTION ( 'NONE',  ( 0.000000000000000000, 0.000000000000000000, -1.000000000000000000 ) ) ;
#35387 = CARTESIAN_POINT ( 'NONE',  ( 4.721056650415999201, 297.0781250017069510, -4.721056650415999201 ) ) ;
#35388 = EDGE_CURVE ( 'NONE', #31834, #12265, #48542, .T. ) ;
#35390 = LINE ( 'NONE', #40661, #28985 ) ;
#35389 = CARTESIAN_POINT ( 'NONE',  ( -9.832129032723418760, 228.4895833367473585, -5.676582343749998927 ) ) ;
#35391 = ITEM_DEFINED_TRANSFORMATION ( 'NONE', 'NONE', #52606,  #57354 ) ;
#35392 = ORIENTED_EDGE ( 'NONE', *, *, #73132, .F. ) ;
#35393 = CARTESIAN_POINT ( 'NONE',  ( -6.951808397369817780E-16, 237.9687500034139873, -11.35316468749999963 ) ) ;
#35394 = CARTESIAN_POINT ( 'NONE',  ( -5.082755093536319713, 5.082755093536319713, 7.299052781871751883 ) ) ;
#35395 = CIRCLE ( 'NONE', #31756, 9.999999999999996447 ) ;
#35396 = EDGE_CURVE ( 'NONE', #58407, #44702, #62594, .T. ) ;
#35397 = EDGE_LOOP ( 'NONE', ( #20951, #2334, #68738, #41548 ) ) ;
#35398 = CARTESIAN_POINT ( 'NONE',  ( -10.18810118749999916, 0.000000000000000000, 69.15625000204836681 ) ) ;
#35399 = CARTESIAN_POINT ( 'NONE',  ( -9.832129032723418760, 98.17708332991935549, -5.676582343750004256 ) ) ;
#35400 = CARTESIAN_POINT ( 'NONE',  ( -2.849036369511732440E-14, 204.3750000027312126, 138.0000000000000568 ) ) ;
#35401 = CARTESIAN_POINT ( 'NONE',  ( -4.556349186104047710, -10.99999999999999822, 82.28124999999998579 ) ) ;
#35404 = CARTESIAN_POINT ( 'NONE',  ( -4.721056650415998313, 287.7343750017069510, 4.721056650416000089 ) ) ;
#35403 = CARTESIAN_POINT ( 'NONE',  ( 24.54126587500000056, 205.2500000013655779, 171.4326545832175839 ) ) ;
#35402 = CARTESIAN_POINT ( 'NONE',  ( 28.00000000000002132, 204.1875000013656063, 166.5412658749999082 ) ) ;
#35405 =( BOUNDED_CURVE ( )  B_SPLINE_CURVE ( 2, ( #44496, #32820, #73907, #15432, #38470, #61846, #45238, #61473, #55829 ),
 .UNSPECIFIED., .F., .T. ) 
 B_SPLINE_CURVE_WITH_KNOTS ( ( 3, 2, 2, 2, 3 ),
 ( 0.6805555555555554692, 0.6874999999999998890, 0.6944444444444443088, 0.7013888888888887285, 0.7083333333333332593 ),
 .UNSPECIFIED. ) 
 CURVE ( )  GEOMETRIC_REPRESENTATION_ITEM ( )  RATIONAL_B_SPLINE_CURVE ( ( 1.000000000000001110, 0.9238795325112855172, 1.000000000000000000, 0.9238795325112867385, 1.000000000000000000, 0.9238795325112867385, 1.000000000000000000, 0.9238795325112879597, 0.9999999999999987788 ) ) 
 REPRESENTATION_ITEM ( '' )  );
#35406 = EDGE_LOOP ( 'NONE', ( #31790, #69984, #29165, #4481 ) ) ;
#35407 = CARTESIAN_POINT ( 'NONE',  ( -28.00000000000007461, 196.1250000027311842, 166.0000000000003695 ) ) ;
#35408 = CARTESIAN_POINT ( 'NONE',  ( 4.000000000000016875, 202.5625000027312126, 199.6568542494924259 ) ) ;
#35409 = CARTESIAN_POINT ( 'NONE',  ( -5.676582343749998039, 207.4479166632527267, -9.832129032723420536 ) ) ;
#35410 = CARTESIAN_POINT ( 'NONE',  ( -3.458734125000015425, 206.0000000013656347, 143.4326545832176976 ) ) ;
#35411 = CARTESIAN_POINT ( 'NONE',  ( 27.99999999999996803, 207.6875000013656063, 173.4587341249998929 ) ) ;
#35412 = CARTESIAN_POINT ( 'NONE',  ( 5.082755093536324154, 23.15624999795161543, 5.082755093536326818 ) ) ;
#35413 = CARTESIAN_POINT ( 'NONE',  ( 5.676582343749993598, 180.2604166632526699, 9.832129032723422313 ) ) ;
#35414 = CARTESIAN_POINT ( 'NONE',  ( 7.188101187500000933, 98.37500000204839523, -2.977408999572651371 ) ) ;
#35415 = FACE_OUTER_BOUND ( 'NONE', #1207, .T. ) ;
#35416 = CARTESIAN_POINT ( 'NONE',  ( -3.211159895383561391, 9.687499998634406140, -3.211159895383561835 ) ) ;
#35417 = CARTESIAN_POINT ( 'NONE',  ( 24.54126587500000412, 202.3750000013656063, 168.5673454167822172 ) ) ;
#35418 = CARTESIAN_POINT ( 'NONE',  ( 7.188101187499993827, -2.977408999572645598, 13.01780278187175277 ) ) ;
#35419 = CARTESIAN_POINT ( 'NONE',  ( 11.35316468749999963, 65.98958332991936970, -3.042071309553165293 ) ) ;
#35420 = EDGE_CURVE ( 'NONE', #10908, #71473, #42141, .T. ) ;
#35421 = CARTESIAN_POINT ( 'NONE',  ( -4.999999999999999112, -52.85071664756715393, 48.38833198888253406 ) ) ;
#35422 = CARTESIAN_POINT ( 'NONE',  ( 3.313708498984762496, -7.999999999999989342, -0.1446972156701771817 ) ) ;
#35423 = ORIENTED_EDGE ( 'NONE', *, *, #48230, .T. ) ;
#35424 = CARTESIAN_POINT ( 'NONE',  ( -7.594050593750000466, 124.7656250010242047, 0.000000000000000000 ) ) ;
#35426 = CARTESIAN_POINT ( 'NONE',  ( -49.70177871865298869, 133.9999999999999716, 57.99999999999999289 ) ) ;
#35425 = VECTOR ( 'NONE', #2448, 1000.000000000000000 ) ;
#35427 = CARTESIAN_POINT ( 'NONE',  ( 11.35316468749999963, 75.98958332991935549, -3.042071309553165293 ) ) ;
#35428 = CARTESIAN_POINT ( 'NONE',  ( -4.556349186104047710, -10.99999999999999822, 70.46875000409679046 ) ) ;
#35429 = CARTESIAN_POINT ( 'NONE',  ( 1.432654583217607414, 195.5000000013656347, 145.4587341250000350 ) ) ;
#35430 = CARTESIAN_POINT ( 'NONE',  ( -3.042071309553173730, 54.32291666325268409, 11.35316468749999785 ) ) ;
#35431 = CARTESIAN_POINT ( 'NONE',  ( -7.999999999999991118, 0.000000000000000000, 22.01780278392014623 ) ) ;
#35432 = CARTESIAN_POINT ( 'NONE',  ( -3.373160349817548198, 194.8118071516788916, 143.7921994470694358 ) ) ;
#35433 =( BOUNDED_CURVE ( )  B_SPLINE_CURVE ( 2, ( #16442, #43351, #74171, #37714, #60714, #56837, #2634, #60333, #14299 ),
 .UNSPECIFIED., .F., .F. ) 
 B_SPLINE_CURVE_WITH_KNOTS ( ( 3, 2, 2, 2, 3 ),
 ( 0.07352941176470592644, 0.07720588235294122137, 0.08088235294117651630, 0.08455882352941181124, 0.08823529411764710617 ),
 .UNSPECIFIED. ) 
 CURVE ( )  GEOMETRIC_REPRESENTATION_ITEM ( )  RATIONAL_B_SPLINE_CURVE ( ( 0.9999999999999991118, 0.9238795325112876267, 1.000000000000000000, 0.9238795325112867385, 1.000000000000000000, 0.9238795325112867385, 1.000000000000000000, 0.9238795325112858503, 1.000000000000000888 ) ) 
 REPRESENTATION_ITEM ( '' )  );
#35434 = CARTESIAN_POINT ( 'NONE',  ( 10.00000000000000178, 151.8749999931720538, 0.000000000000000000 ) ) ;
#35435 = CARTESIAN_POINT ( 'NONE',  ( 2.977408999572654480, 98.00000000204838102, 7.188101187499999156 ) ) ;
#35436 = CARTESIAN_POINT ( 'NONE',  ( 2.679491924305151596, 18.95833333333278858, 10.00000000000351896 ) ) ;
#35437 = CARTESIAN_POINT ( 'NONE',  ( 3.042071309553159519, 55.05208332991934128, 11.35316468750000141 ) ) ;
#35438 = CARTESIAN_POINT ( 'NONE',  ( 10.18810118749999916, 4.220049686691935698, 110.8750000020483810 ) ) ;
#35439 = CARTESIAN_POINT ( 'NONE',  ( 6.951808397369818766E-16, 197.0312499965860411, -11.35316468750000141 ) ) ;
#35440 = ORIENTED_EDGE ( 'NONE', *, *, #71439, .T. ) ;
#35441 = CARTESIAN_POINT ( 'NONE',  ( -32.14014598159626246, -21.04900802997393683, 164.9137248997816982 ) ) ;
#35442 = CYLINDRICAL_SURFACE ( 'NONE', #36419, 8.000000000000000000 ) ;
#35443 = FACE_BOUND ( 'NONE', #1327, .T. ) ;
#35445 = CARTESIAN_POINT ( 'NONE',  ( -5.676582343750006032, 174.1145833299193555, 9.832129032723418760 ) ) ;
#35444 = CARTESIAN_POINT ( 'NONE',  ( -26.34314575050763096, 201.0625000027311842, 166.0000000000004263 ) ) ;
#35446 = DIRECTION ( 'NONE',  ( 0.000000000000000000, 0.000000000000000000, -1.000000000000000000 ) ) ;
#35447 = CARTESIAN_POINT ( 'NONE',  ( 2.679491924311225848, 246.6666666734946602, -10.00000000000000000 ) ) ;
#35448 = VERTEX_POINT ( 'NONE', #14954 ) ;
#35449 = CARTESIAN_POINT ( 'NONE',  ( 5.676582343750001591, 171.9270833299193555, -9.832129032723420536 ) ) ;
#35450 = CARTESIAN_POINT ( 'NONE',  ( -4.401442555609577197E-16, 7.188101187499992051, 28.11155278187175455 ) ) ;
#35451 = CARTESIAN_POINT ( 'NONE',  ( -2.085542519210945728E-15, 124.8437499965860269, 11.35316468750000141 ) ) ;
#35452 = CARTESIAN_POINT ( 'NONE',  ( 27.99999999999996447, 203.6250000027312126, 165.9999999999998863 ) ) ;
#35453 = VERTEX_POINT ( 'NONE', #37992 ) ;
#35454 = CARTESIAN_POINT ( 'NONE',  ( -3.313708498984762052, 105.4062500040967763, -8.000000000000000000 ) ) ;
#35455 = EDGE_CURVE ( 'NONE', #23710, #58094, #60239, .T. ) ;
#35456 = CARTESIAN_POINT ( 'NONE',  ( 4.000000000000000888, 12.93750000000000000, 1.656854249492384135 ) ) ;
#35457 = CARTESIAN_POINT ( 'NONE',  ( -35.48203846897828839, -8.846376413071666889, 143.0888767442469316 ) ) ;
#35458 = CARTESIAN_POINT ( 'NONE',  ( 1.881053915767122664, 13.12499999863440969, 4.541265875000001451 ) ) ;
#35459 = CARTESIAN_POINT ( 'NONE',  ( 1.469576158976822172E-15, -7.999999999999991118, 22.39280278392014623 ) ) ;
#35460 = CARTESIAN_POINT ( 'NONE',  ( 3.999999999999959144, 196.0625000000000284, 140.3431457505076594 ) ) ;
#35461 = EDGE_LOOP ( 'NONE', ( #23338, #14628, #29587, #43999 ) ) ;
#35462 = CARTESIAN_POINT ( 'NONE',  ( -8.000000000000000000, 24.65625000000000355, -3.313708498984762496 ) ) ;
#35463 = CARTESIAN_POINT ( 'NONE',  ( -4.401442555609581635E-16, 104.2812500020483810, -7.188101187500000044 ) ) ;
#35464 = EDGE_CURVE ( 'NONE', #34267, #69918, #44752, .T. ) ;
#35466 = DIRECTION ( 'NONE',  ( -0.000000000000000000, 1.000000000000000000, 4.689100369878284071E-30 ) ) ;
#35465 = LINE ( 'NONE', #42581, #63907 ) ;
#35467 = ORIENTED_EDGE ( 'NONE', *, *, #63393, .T. ) ;
#35468 = CARTESIAN_POINT ( 'NONE',  ( -2.620431783929222824, 10.11675809140012561, -70.36490484707876192 ) ) ;
#35469 = CARTESIAN_POINT ( 'NONE',  ( 2.977408999572650927, -7.188101187499990274, 22.95530278187175455 ) ) ;
#35470 = VERTEX_POINT ( 'NONE', #67403 ) ;
#35471 = EDGE_CURVE ( 'NONE', #58564, #56214, #52469, .T. ) ;
#35472 = ORIENTED_EDGE ( 'NONE', *, *, #55381, .T. ) ;
#35473 = CARTESIAN_POINT ( 'NONE',  ( 10.18810118749999916, 4.220049686691935698, 83.50000000204839523 ) ) ;
#35474 = CARTESIAN_POINT ( 'NONE',  ( -26.56734541678232731, 195.2500000013656063, 173.4587341250003760 ) ) ;
#35475 = CARTESIAN_POINT ( 'NONE',  ( 2.020667218593132706E-15, -11.00000000000000000, 100.3749999999999858 ) ) ;
#35478 = CARTESIAN_POINT ( 'NONE',  ( 2.765530957081996366, 298.2968750017070079, -6.676582343750002480 ) ) ;
#35477 = CARTESIAN_POINT ( 'NONE',  ( 29.65685424949240456, 205.1875000027311842, 173.9999999999999147 ) ) ;
#35476 = DIRECTION ( 'NONE',  ( 0.000000000000000000, 0.000000000000000000, 1.000000000000000000 ) ) ;
#35479 = CARTESIAN_POINT ( 'NONE',  ( 2.679491924311228956, 141.0416666666666572, -10.00000000000000000 ) ) ;
#35480 = CARTESIAN_POINT ( 'NONE',  ( -8.000000000000000000, 98.00000000000000000, 0.000000000000000000 ) ) ;
#35481 = CARTESIAN_POINT ( 'NONE',  ( -26.34314575050759899, 203.9375000000000568, 166.0000000000004263 ) ) ;
#35482 = DIRECTION ( 'NONE',  ( -0.000000000000000000, 1.000000000000000000, 0.000000000000000000 ) ) ;
#35483 = CARTESIAN_POINT ( 'NONE',  ( -8.660254037844387298, 232.7083333401613174, -4.999999999999999112 ) ) ;
#35484 = CARTESIAN_POINT ( 'NONE',  ( 29.43265458321766559, 201.8750000013656063, 166.5412658749999650 ) ) ;
#35485 = CARTESIAN_POINT ( 'NONE',  ( 5.082755093536325930, 4.031249997951610986, -5.082755093536325930 ) ) ;
#35486 = CIRCLE ( 'NONE', #41503, 11.00000000000000000 ) ;
#35487 = CARTESIAN_POINT ( 'NONE',  ( 8.008118988124991233, 3.317071493978879015, 0.3568652839406291077 ) ) ;
#35488 = CARTESIAN_POINT ( 'NONE',  ( 3.458734124999959025, 194.5000000013656063, 140.5673454167824161 ) ) ;
#35489 = CARTESIAN_POINT ( 'NONE',  ( -4.401442555609581635E-16, 116.6562500020483810, -7.188101187500000044 ) ) ;
#35491 = CARTESIAN_POINT ( 'NONE',  ( 8.000000000000037303, -3.313708498984713202, 7.486552779823369086 ) ) ;
#35490 = FACE_OUTER_BOUND ( 'NONE', #10573, .T. ) ;
#35492 = CARTESIAN_POINT ( 'NONE',  ( -11.35316468749999785, 229.0104166700806445, -3.042071309553164848 ) ) ;
#35493 = FACE_OUTER_BOUND ( 'NONE', #29200, .T. ) ;
#35494 = CARTESIAN_POINT ( 'NONE',  ( 10.99999999999989342, 4.556349186104152515, 85.84375000000000000 ) ) ;
#35495 = CARTESIAN_POINT ( 'NONE',  ( 26.34314575050758833, 197.9375000000000000, 173.9999999999999147 ) ) ;
#35496 = CARTESIAN_POINT ( 'NONE',  ( -11.35316468750000141, 28.28124999658601624, -1.390361679473963753E-15 ) ) ;
#35497 = CARTESIAN_POINT ( 'NONE',  ( -27.99999999999995737, 199.5000000000000000, 174.0000000000003695 ) ) ;
#35498 = CARTESIAN_POINT ( 'NONE',  ( -5.676582343749998039, 217.7604166632526983, -9.832129032723420536 ) ) ;
#35499 = DIRECTION ( 'NONE',  ( 0.000000000000000000, 0.000000000000000000, 1.000000000000000000 ) ) ;
#35501 = DIRECTION ( 'NONE',  ( -0.000000000000000000, 1.000000000000000000, -0.000000000000000000 ) ) ;
#35500 = DIRECTION ( 'NONE',  ( -0.000000000000000000, 1.000000000000000000, 4.476705744456276341E-16 ) ) ;
#35502 = VERTEX_POINT ( 'NONE', #16440 ) ;
#35503 = CARTESIAN_POINT ( 'NONE',  ( 3.458734124999960358, 195.6875000013655779, 142.0000000000000568 ) ) ;
#35504 = CARTESIAN_POINT ( 'NONE',  ( 9.832129032723420536, 36.19791666325267698, -5.676582343749999815 ) ) ;
#35505 = CARTESIAN_POINT ( 'NONE',  ( 7.778174593052021635, 7.778174593052023411, 84.62500000409677625 ) ) ;
#35506 = CARTESIAN_POINT ( 'NONE',  ( -2.839093476692135984E-14, 207.9375000013656063, 138.5412658750000503 ) ) ;
#35507 = CARTESIAN_POINT ( 'NONE',  ( -2.250000000000000888, -2.250000000000000000, 28.00000000000000000 ) ) ;
#35508 = DIRECTION ( 'NONE',  ( 0.000000000000000000, 0.000000000000000000, 1.000000000000000000 ) ) ;
#35510 = CARTESIAN_POINT ( 'NONE',  ( -9.832129032723420536, 18.69791666325268409, 5.676582343749997150 ) ) ;
#35509 = CARTESIAN_POINT ( 'NONE',  ( 2.977408999572654480, 108.1250000020483810, 7.188101187499999156 ) ) ;
#35511 = CARTESIAN_POINT ( 'NONE',  ( -7.999999999999989342, -3.313708498984762496, 15.92405277982336465 ) ) ;
#35512 = CARTESIAN_POINT ( 'NONE',  ( -8.311093377946836114, 147.6562499965860411, -8.311093377946837890 ) ) ;
#35513 = CARTESIAN_POINT ( 'NONE',  ( -4.999999999999998224, 118.5416666598386968, -8.660254037844389075 ) ) ;
#35514 = CARTESIAN_POINT ( 'NONE',  ( 5.082755093536326818, 116.0937500020483810, 5.082755093536325042 ) ) ;
#35515 = CARTESIAN_POINT ( 'NONE',  ( 5.000000000000001776, 172.7083333265053682, -8.660254037844389075 ) ) ;
#35516 = CARTESIAN_POINT ( 'NONE',  ( -31.45873412500001010, 203.8750000013656063, 168.5673454167827572 ) ) ;
#35517 = EDGE_LOOP ( 'NONE', ( #18616, #13889, #40271, #48296 ) ) ;
#35518 = CARTESIAN_POINT ( 'NONE',  ( -11.35316468750000141, 3.802083329919350163, 3.042071309553159963 ) ) ;
#35519 =( BOUNDED_CURVE ( )  B_SPLINE_CURVE ( 2, ( #42170, #7859, #36162, #71955, #48945, #31609, #30864, #19904, #71212 ),
 .UNSPECIFIED., .F., .F. ) 
 B_SPLINE_CURVE_WITH_KNOTS ( ( 3, 2, 2, 2, 3 ),
 ( 0.5833333333333337034, 0.5916666666666670071, 0.6000000000000004219, 0.6083333333333338366, 0.6166666666666672514 ),
 .UNSPECIFIED. ) 
 CURVE ( )  GEOMETRIC_REPRESENTATION_ITEM ( )  RATIONAL_B_SPLINE_CURVE ( ( 0.9999999999999970024, 0.9238795325112897361, 1.000000000000000000, 0.9238795325112867385, 1.000000000000000000, 0.9238795325112867385, 1.000000000000000000, 0.9238795325112816315, 1.000000000000005107 ) ) 
 REPRESENTATION_ITEM ( '' )  );
#35520 = EDGE_LOOP ( 'NONE', ( #35241, #51236, #47298, #13793 ) ) ;
#35521 = CARTESIAN_POINT ( 'NONE',  ( -4.556349186104048599, -10.99999999999999822, 100.2812499999999858 ) ) ;
#35522 = CARTESIAN_POINT ( 'NONE',  ( 4.721056650415999201, 298.0781250017069510, -4.721056650415999201 ) ) ;
#35524 = CARTESIAN_POINT ( 'NONE',  ( -11.35316468750000141, 138.4895833299193555, 3.042071309553159963 ) ) ;
#35523 = CARTESIAN_POINT ( 'NONE',  ( 4.898587196589412829E-16, 18.18749999590322020, -8.000000000000000000 ) ) ;
#35525 = FILL_AREA_STYLE ('',( #40802 ) ) ;
#35526 = CARTESIAN_POINT ( 'NONE',  ( 3.313708498984756279, 7.999999999999991118, 25.91780278432982598 ) ) ;
#35527 = EDGE_CURVE ( 'NONE', #4846, #54330, #33837, .T. ) ;
#35528 = DIRECTION ( 'NONE',  ( -0.000000000000000000, 1.000000000000000000, -0.000000000000000000 ) ) ;
#35529 = CARTESIAN_POINT ( 'NONE',  ( 9.832129032723416984, 241.8229166700806445, -5.676582343750003368 ) ) ;
#35530 = CARTESIAN_POINT ( 'NONE',  ( 10.18810118749999916, 4.220049686691935698, 92.87500000204838102 ) ) ;
#35531 = ORIENTED_EDGE ( 'NONE', *, *, #6153, .T. ) ;
#35532 = CARTESIAN_POINT ( 'NONE',  ( 4.999999999999999112, 13.57248045702108818, 69.64920683919132216 ) ) ;
#35533 = CARTESIAN_POINT ( 'NONE',  ( -2.828427124746190735, 8.375000000000000000, -2.828427124746191623 ) ) ;
#35534 = CARTESIAN_POINT ( 'NONE',  ( -9.832129032723418760, 83.17708332991935549, -5.676582343750004256 ) ) ;
#35535 = CARTESIAN_POINT ( 'NONE',  ( -6.238412754330611322E-16, 10.18810118749999916, 107.7812500020483810 ) ) ;
#35536 =( BOUNDED_CURVE ( )  B_SPLINE_CURVE ( 2, ( #72984, #32638, #5077, #56757, #15998, #16358, #10356, #21660, #39396, #55647, #21290 ),
 .UNSPECIFIED., .F., .F. ) 
 B_SPLINE_CURVE_WITH_KNOTS ( ( 3, 2, 2, 2, 2, 3 ),
 ( 0.2382579061490637251, 0.2382579210404291437, 0.2448761966248874100, 0.2514944722093456209, 0.2581127477938038872, 0.2647310102845484292 ),
 .UNSPECIFIED. ) 
 CURVE ( )  GEOMETRIC_REPRESENTATION_ITEM ( )  RATIONAL_B_SPLINE_CURVE ( ( 0.9999996574530229942, 0.9999998287261261387, 1.000000000000000000, 0.9238795325112867385, 1.000000000000000000, 0.9238795325112867385, 1.000000000000000000, 0.9238795325112867385, 1.000000000000000000, 0.9238796831093680773, 0.9999996988044332902 ) ) 
 REPRESENTATION_ITEM ( '' )  );
#35537 = CARTESIAN_POINT ( 'NONE',  ( -4.541265875000002339, 15.87499999863440436, -1.881053915767121998 ) ) ;
#35538 = ORIENTED_EDGE ( 'NONE', *, *, #60680, .F. ) ;
#35539 = ORIENTED_EDGE ( 'NONE', *, *, #8071, .T. ) ;
#35540 = CARTESIAN_POINT ( 'NONE',  ( -8.000000000000000000, 3.656250000000000888, -3.313708498984762496 ) ) ;
#35541 = DIRECTION ( 'NONE',  ( -0.5000000000000011102, 0.8660254037844380415, 0.000000000000000000 ) ) ;
#35542 = CARTESIAN_POINT ( 'NONE',  ( -7.188101187500002709, 2.812499997951610098, 2.977408999572649151 ) ) ;
#35543 = CIRCLE ( 'NONE', #2992, 9.949874371066211864 ) ;
#35544 = CARTESIAN_POINT ( 'NONE',  ( 8.000000000000001776, 122.8437500040967763, 3.313708498984759387 ) ) ;
#35545 = CARTESIAN_POINT ( 'NONE',  ( 4.220049686691941027, -10.18810118749999738, 101.5000000020483810 ) ) ;
#35546 = VECTOR ( 'NONE', #28974, 1000.000000000000000 ) ;
#35547 = DIRECTION ( 'NONE',  ( 0.000000000000000000, 2.238352872228138170E-16, -1.000000000000000000 ) ) ;
#35548 = CARTESIAN_POINT ( 'NONE',  ( -2.828427124746190735, 15.12499999726881406, -2.828427124746191623 ) ) ;
#35549 = CARTESIAN_POINT ( 'NONE',  ( 25.17157287525381903, 209.6250000000000284, 167.1715728752537018 ) ) ;
#35550 = ORIENTED_EDGE ( 'NONE', *, *, #42627, .T. ) ;
#35551 = EDGE_CURVE ( 'NONE', #3815, #72057, #71368, .T. ) ;
#35552 = DIRECTION ( 'NONE',  ( 0.000000000000000000, 0.000000000000000000, 1.000000000000000000 ) ) ;
#35553 = CARTESIAN_POINT ( 'NONE',  ( 2.754378923186476579E-14, 199.1875000013655779, 194.5412658750000219 ) ) ;
#35555 = CARTESIAN_POINT ( 'NONE',  ( -1.836970198721029983E-15, 80.62499999317203958, 10.00000000000000178 ) ) ;
#35554 = CARTESIAN_POINT ( 'NONE',  ( -24.54126587499996148, 203.1250000013656347, 171.4326545832179534 ) ) ;
#35556 = SHAPE_REPRESENTATION_RELATIONSHIP ( 'NONE' , 'NONE' ,  #22414, #8525 ) ;
#35557 = CARTESIAN_POINT ( 'NONE',  ( 2.780723358947928197E-16, 13.56249999863440614, -4.541265875000002339 ) ) ;
#35558 = CARTESIAN_POINT ( 'NONE',  ( -3.999999999999960032, 200.0625000027312410, 196.3431457505076594 ) ) ;
#35559 = CARTESIAN_POINT ( 'NONE',  ( -2.977408999572648707, -7.188101187499990274, 12.26780278187175455 ) ) ;
#35560 = ORIENTED_EDGE ( 'NONE', *, *, #13144, .F. ) ;
#35561 = ORIENTED_EDGE ( 'NONE', *, *, #70877, .T. ) ;
#35562 = CARTESIAN_POINT ( 'NONE',  ( 10.18810118749999916, 1.247682550866122264E-15, 107.4062500020483668 ) ) ;
#35563 = CARTESIAN_POINT ( 'NONE',  ( -29.65685424949241167, 206.0625000000000000, 166.0000000000004263 ) ) ;
#35564 = CARTESIAN_POINT ( 'NONE',  ( 3.458734125000016313, 198.8750000013656347, 199.4326545832176691 ) ) ;
#35565 = CARTESIAN_POINT ( 'NONE',  ( 24.54126587499997569, 195.1250000013656063, 168.5673454167822740 ) ) ;
#35566 = CARTESIAN_POINT ( 'NONE',  ( -8.660254037844390851, 92.91666666666667140, 4.999999999999998224 ) ) ;
#35567 = CARTESIAN_POINT ( 'NONE',  ( -5.656854249492378806, 117.6875000000000000, 5.656854249492381470 ) ) ;
#35568 = CARTESIAN_POINT ( 'NONE',  ( 3.042071309553167069, 62.13541666325267698, -11.35316468749999785 ) ) ;
#35569 = CARTESIAN_POINT ( 'NONE',  ( 6.676582343750003368, 297.1718750017071216, -2.765530957081997254 ) ) ;
#35570 = ADVANCED_FACE ( 'NONE', ( #17196 ), #63973, .T. ) ;
#35571 = VERTEX_POINT ( 'NONE', #991 ) ;
#35572 = CARTESIAN_POINT ( 'NONE',  ( -2.679491924311226292, 173.3333333265053682, -10.00000000000000178 ) ) ;
#35573 = CARTESIAN_POINT ( 'NONE',  ( 3.313708498984762052, 16.59374999590322020, -8.000000000000000000 ) ) ;
#35574 = CARTESIAN_POINT ( 'NONE',  ( -1.432654583217664479, 207.7500000013656063, 138.5412658750000787 ) ) ;
#35575 = CARTESIAN_POINT ( 'NONE',  ( -10.00000000000000355, 104.5833333265053824, 2.679491924311223183 ) ) ;
#35576 = CARTESIAN_POINT ( 'NONE',  ( -15.99999999999999645, -16.00000000000000355, 20.00000000000000000 ) ) ;
#35577 = CARTESIAN_POINT ( 'NONE',  ( 10.00000000000000000, 222.5000000000000000, -1.224646799147353256E-15 ) ) ;
#35578 = CARTESIAN_POINT ( 'NONE',  ( 7.778174593052021635, 7.778174593052023411, 72.62500000409677625 ) ) ;
#35579 = CARTESIAN_POINT ( 'NONE',  ( 4.556349186104051263, -10.99999999999999822, 116.9687500000000142 ) ) ;
#35580 = CARTESIAN_POINT ( 'NONE',  ( -1.836970198721029983E-15, 218.7500000000000284, 10.00000000000000178 ) ) ;
#35581 = CARTESIAN_POINT ( 'NONE',  ( -2.977408999572647819, -7.188101187499990274, 9.642802781871756324 ) ) ;
#35582 = CARTESIAN_POINT ( 'NONE',  ( -5.676582343749998039, 187.7604166632526983, -9.832129032723420536 ) ) ;
#35583 = CARTESIAN_POINT ( 'NONE',  ( 3.211159895383560947, 4.187499998634407028, 3.211159895383562723 ) ) ;
#35584 = CARTESIAN_POINT ( 'NONE',  ( 7.320508075688771044, 176.2499999931720254, 7.320508075688775484 ) ) ;
#35586 = DIRECTION ( 'NONE',  ( -1.000000000000000000, -7.885106708985487801E-17, 0.000000000000000000 ) ) ;
#35585 =( NAMED_UNIT ( * ) SI_UNIT ( $, .STERADIAN. ) SOLID_ANGLE_UNIT ( ) );
#35587 = ORIENTED_EDGE ( 'NONE', *, *, #57922, .T. ) ;
#35588 = CARTESIAN_POINT ( 'NONE',  ( -2.754378923186476579E-14, 195.1875000013655779, 145.4587341250000350 ) ) ;
#35589 = CARTESIAN_POINT ( 'NONE',  ( 3.042071309553167069, 37.13541666325268409, -11.35316468749999785 ) ) ;
#35590 = CARTESIAN_POINT ( 'NONE',  ( -10.99999999999999822, -4.556349186104052151, 103.2812500040967763 ) ) ;
#35591 = CARTESIAN_POINT ( 'NONE',  ( 8.311093377946837890, 226.7187499965860411, -8.311093377946837890 ) ) ;
#35592 = CARTESIAN_POINT ( 'NONE',  ( -28.00000000000007461, 207.4375000013656063, 166.5412658750003629 ) ) ;
#35593 = CARTESIAN_POINT ( 'NONE',  ( -4.556349186104045934, 11.00000000000000000, 95.40625000409677625 ) ) ;
#35595 = DIRECTION ( 'NONE',  ( 0.000000000000000000, 0.000000000000000000, -1.000000000000000000 ) ) ;
#35594 = CARTESIAN_POINT ( 'NONE',  ( -18.00000000000000000, 10.39230484541324628, -1.607695154586745501 ) ) ;
#35596 = CARTESIAN_POINT ( 'NONE',  ( 3.458734124999959914, 195.4375000013655779, 142.0000000000000568 ) ) ;
#35597 = CARTESIAN_POINT ( 'NONE',  ( 2.679491924311228956, 72.91666665983871098, -10.00000000000000000 ) ) ;
#35598=STYLED_ITEM('',(#74706),#67548);
#35599 = CARTESIAN_POINT ( 'NONE',  ( 5.082755093536325042, 99.59375000204838102, -5.082755093536325930 ) ) ;
#35600 = CARTESIAN_POINT ( 'NONE',  ( -1.881053915767124440, 18.12499999863440792, 4.541265875000001451 ) ) ;
#35601 = CARTESIAN_POINT ( 'NONE',  ( -32.00000000000000000, 204.3750000027312126, 170.0000000000004547 ) ) ;
#35602 = CARTESIAN_POINT ( 'NONE',  ( 5.303777043537039049, 0.3075051904528932623, -5.735125114186721440 ) ) ;
#35603 = CYLINDRICAL_SURFACE ( 'NONE', #12508, 3.999999999999976019 ) ;
#35604 = ORIENTED_EDGE ( 'NONE', *, *, #27395, .T. ) ;
#35605 = ORIENTED_EDGE ( 'NONE', *, *, #7880, .F. ) ;
#35606 = CARTESIAN_POINT ( 'NONE',  ( 4.721056650416000089, 297.9843750017070079, 4.721056650415999201 ) ) ;
#35607 = CARTESIAN_POINT ( 'NONE',  ( -3.166186134455097228E-13, 141.2500000000000284, -9.999999999999998224 ) ) ;
#35608 = CARTESIAN_POINT ( 'NONE',  ( 8.660254037844389075, 42.29166665983870388, -5.000000000000000000 ) ) ;
#35609 = CARTESIAN_POINT ( 'NONE',  ( -11.35316468750000141, 158.2812499965860127, -1.390361679473963753E-15 ) ) ;
#35610 = CARTESIAN_POINT ( 'NONE',  ( 10.18810118750000093, -4.220049686691933921, 84.81250000204838102 ) ) ;
#35611 = FACE_OUTER_BOUND ( 'NONE', #65650, .T. ) ;
#35612 = CARTESIAN_POINT ( 'NONE',  ( -2.828427124746153876, 205.8750000000000284, 195.1715728752538439 ) ) ;
#35613 = CARTESIAN_POINT ( 'NONE',  ( -7.089540251308589447, 16.69146171830283265, -0.07476367467994493587 ) ) ;
#35614 = CARTESIAN_POINT ( 'NONE',  ( 10.18810118750000093, -4.220049686691933921, 112.1875000020483810 ) ) ;
#35615 = EDGE_LOOP ( 'NONE', ( #4077, #20491, #17355 ) ) ;
#35616 = CARTESIAN_POINT ( 'NONE',  ( 5.656854249492378806, 17.62499999590322375, 5.656854249492381470 ) ) ;
#35617 = DIRECTION ( 'NONE',  ( -0.000000000000000000, 1.000000000000000000, -0.000000000000000000 ) ) ;
#35618 = CARTESIAN_POINT ( 'NONE',  ( 5.676582343750001591, 146.9270833299193555, -9.832129032723420536 ) ) ;
#35619 = CARTESIAN_POINT ( 'NONE',  ( -3.458734124999958581, 196.5000000013656063, 199.4326545832176976 ) ) ;
#35620 = CARTESIAN_POINT ( 'NONE',  ( -2.485281374238875962, 290.8125000000000568, -5.999999999999697131 ) ) ;
#35621 = CARTESIAN_POINT ( 'NONE',  ( 4.220049686691934809, 10.18810118749999916, 75.06250000204836681 ) ) ;
#35622 = CARTESIAN_POINT ( 'NONE',  ( 9.832129032723416984, 45.67708332991934839, 5.676582343750006032 ) ) ;
#35623 = ORIENTED_EDGE ( 'NONE', *, *, #54022, .T. ) ;
#35624 = DIRECTION ( 'NONE',  ( 0.000000000000000000, 0.000000000000000000, 1.000000000000000000 ) ) ;
#35625 = CARTESIAN_POINT ( 'NONE',  ( 2.780723358947928197E-16, 5.687499998634407028, -4.541265875000002339 ) ) ;
#35626 = CARTESIAN_POINT ( 'NONE',  ( 3.317071493978877683, 8.008118988124991233, 14.04436528394063011 ) ) ;
#35627 = EDGE_CURVE ( 'NONE', #10862, #73500, #9062, .T. ) ;
#35628 = CARTESIAN_POINT ( 'NONE',  ( -7.188101187500002709, 13.31249999795161187, 2.977408999572649151 ) ) ;
#35629 = CARTESIAN_POINT ( 'NONE',  ( 4.242640687119285658, 291.6875000034139589, -4.242640687119286547 ) ) ;
#35630 = CARTESIAN_POINT ( 'NONE',  ( -12.48113115107485882, -24.43575951774235477, 138.9105880183523425 ) ) ;
#35631 = CARTESIAN_POINT ( 'NONE',  ( 7.188101187500000044, 5.343749997951610098, 0.000000000000000000 ) ) ;
#35632 = CARTESIAN_POINT ( 'NONE',  ( 7.188101187499992051, 8.802885111219154394E-16, 8.236552781871752771 ) ) ;
#35633 =( BOUNDED_CURVE ( )  B_SPLINE_CURVE ( 2, ( #10682, #33715, #57467, #24124, #18476, #47503, #41852, #13165, #5035 ),
 .UNSPECIFIED., .F., .F. ) 
 B_SPLINE_CURVE_WITH_KNOTS ( ( 3, 2, 2, 2, 3 ),
 ( 0.5312500000000000000, 0.5364583333333333703, 0.5416666666666665186, 0.5468749999999998890, 0.5520833333333332593 ),
 .UNSPECIFIED. ) 
 CURVE ( )  GEOMETRIC_REPRESENTATION_ITEM ( )  RATIONAL_B_SPLINE_CURVE ( ( 1.000000000000000000, 0.9238795325112867385, 1.000000000000000000, 0.9238795325112867385, 1.000000000000000000, 0.9238795325112867385, 1.000000000000000000, 0.9238795325112884038, 0.9999999999999983347 ) ) 
 REPRESENTATION_ITEM ( '' )  );
#35634 = CARTESIAN_POINT ( 'NONE',  ( 7.204075437095968759, -7.204075437095966983, 74.21875000204836681 ) ) ;
#35635 = CARTESIAN_POINT ( 'NONE',  ( -24.54126587499999701, 206.4375000013656063, 170.0000000000003411 ) ) ;
#35636 = DIRECTION ( 'NONE',  ( 0.000000000000000000, -1.000000000000000000, 0.000000000000000000 ) ) ;
#35637 = CARTESIAN_POINT ( 'NONE',  ( 2.449293598294707893E-16, 1.999999997268813168, -4.000000000000001776 ) ) ;
#35638 = ORIENTED_EDGE ( 'NONE', *, *, #56056, .T. ) ;
#35639 = EDGE_CURVE ( 'NONE', #4298, #3455, #39862, .T. ) ;
#35640 = CARTESIAN_POINT ( 'NONE',  ( -2.828427124746153876, 197.0000000027312126, 195.1715728752538439 ) ) ;
#35641 = CIRCLE ( 'NONE', #3107, 10.99999999999999112 ) ;
#35642 = CARTESIAN_POINT ( 'NONE',  ( 3.999999999999960032, 206.9375000000000284, 143.6568542494924543 ) ) ;
#35643 = CARTESIAN_POINT ( 'NONE',  ( -23.99999999999998934, 199.8750000027312126, 170.0000000000002842 ) ) ;
#35644 = EDGE_CURVE ( 'NONE', #59533, #51478, #935, .T. ) ;
#35645 = CARTESIAN_POINT ( 'NONE',  ( 7.188101187500001821, 117.5000000020483810, -2.977408999572651371 ) ) ;
#35646 = VECTOR ( 'NONE', #6249, 999.9999999999998863 ) ;
#35647 = CARTESIAN_POINT ( 'NONE',  ( 1.469576158976822172E-15, -7.999999999999991118, 4.392802783920145338 ) ) ;
#35648 = ORIENTED_EDGE ( 'NONE', *, *, #44731, .T. ) ;
#35649 = CARTESIAN_POINT ( 'NONE',  ( -7.188101187500000933, 23.62499999795161543, -2.977408999572651371 ) ) ;
#35650 = EDGE_LOOP ( 'NONE', ( #25024, #71571, #14723, #26035 ) ) ;
#35651 = CARTESIAN_POINT ( 'NONE',  ( 2.679491924311096174, 256.6666666734946602, -10.00000000000007283 ) ) ;
#35652 = CARTESIAN_POINT ( 'NONE',  ( -1.469576158976823947E-15, 13.12500000000000355, 8.000000000000000000 ) ) ;
#35653 = CARTESIAN_POINT ( 'NONE',  ( 2.679491924311228956, 51.04166666666665719, -10.00000000000000000 ) ) ;
#35654 = CARTESIAN_POINT ( 'NONE',  ( 2.977408999572654480, 98.00000000204838102, 7.188101187499999156 ) ) ;
#35655 = CARTESIAN_POINT ( 'NONE',  ( 2.828427124746153876, 205.0000000027312126, 144.8284271247462129 ) ) ;
#35656 = EDGE_CURVE ( 'NONE', #23177, #63081, #34544, .T. ) ;
#35658 = CARTESIAN_POINT ( 'NONE',  ( -21.09460362812031420, -36.79295498084548655, 192.7166349764662527 ) ) ;
#35657 = FACE_OUTER_BOUND ( 'NONE', #2655, .T. ) ;
#35659 = ORIENTED_EDGE ( 'NONE', *, *, #16441, .F. ) ;
#35660 = ORIENTED_EDGE ( 'NONE', *, *, #69434, .T. ) ;
#35661 = CARTESIAN_POINT ( 'NONE',  ( -5.676582343750000703, 248.0729166700806729, -9.832129032723418760 ) ) ;
#35662 = CARTESIAN_POINT ( 'NONE',  ( -2.977408999572648707, -7.188101187499990274, 15.64280278187175632 ) ) ;
#35663 = FACE_OUTER_BOUND ( 'NONE', #26726, .T. ) ;
#35664 = DIRECTION ( 'NONE',  ( -1.000000000000000000, 0.000000000000000000, 0.000000000000000000 ) ) ;
#35665 = FACE_OUTER_BOUND ( 'NONE', #43979, .T. ) ;
#35666 = CARTESIAN_POINT ( 'NONE',  ( -8.660254037844387298, 259.5833333333333144, -4.999999999999999112 ) ) ;
#35667 = CARTESIAN_POINT ( 'NONE',  ( -1.744157829248402118E-12, 86.25000000000015632, -10.00000000000000533 ) ) ;
#35668 = CARTESIAN_POINT ( 'NONE',  ( -1.836970198721029983E-15, 178.7500000000000284, 10.00000000000000178 ) ) ;
#35669 = FACE_OUTER_BOUND ( 'NONE', #4884, .T. ) ;
#35670 = CARTESIAN_POINT ( 'NONE',  ( -4.556349186104048599, -10.99999999999999822, 68.96875000409677625 ) ) ;
#35671 = CARTESIAN_POINT ( 'NONE',  ( 11.35316468750000141, 141.0937499965860127, 0.000000000000000000 ) ) ;
#35672 = DIRECTION ( 'NONE',  ( -0.000000000000000000, -1.000000000000000000, -4.283267841918042741E-17 ) ) ;
#35673 = CARTESIAN_POINT ( 'NONE',  ( -8.000000000000000000, 117.5000000000000000, 0.000000000000000000 ) ) ;
#35676 = CARTESIAN_POINT ( 'NONE',  ( -8.660254037844389075, 167.0833333333333428, -5.000000000000006217 ) ) ;
#35675 = CARTESIAN_POINT ( 'NONE',  ( -3.107148544787702027E-14, -51.14729664189371761, 48.52014062455021559 ) ) ;
#35674 = CARTESIAN_POINT ( 'NONE',  ( 32.00000000000000000, 207.2500000000000284, 169.9999999999999432 ) ) ;
#35677 = ORIENTED_EDGE ( 'NONE', *, *, #16099, .F. ) ;
#35678 = CARTESIAN_POINT ( 'NONE',  ( 5.676582343750001591, 1.927083329919350163, -9.832129032723420536 ) ) ;
#35679 = CARTESIAN_POINT ( 'NONE',  ( -2.828427124746153876, 209.0000000027312126, 195.1715728752538439 ) ) ;
#35681 = CARTESIAN_POINT ( 'NONE',  ( -3.093166311732832963, -7.380995655184879212, 0.000000000000000000 ) ) ;
#35680 =( REPRESENTATION_RELATIONSHIP ('NONE','NONE', #46008, #30147 ) REPRESENTATION_RELATIONSHIP_WITH_TRANSFORMATION ( #35024 )SHAPE_REPRESENTATION_RELATIONSHIP( ) );
#35682 = CARTESIAN_POINT ( 'NONE',  ( 0.000000000000000000, 0.000000000000000000, 30.00000000000000000 ) ) ;
#35683 = CARTESIAN_POINT ( 'NONE',  ( -5.000000000000005329, 40.20833332650536818, 8.660254037844387298 ) ) ;
#35684 = CARTESIAN_POINT ( 'NONE',  ( -2.977408999572651815, 112.4375000020483810, 7.188101187500000933 ) ) ;
#35685 = CARTESIAN_POINT ( 'NONE',  ( -3.211159895383561391, 20.68749999863440436, -3.211159895383561835 ) ) ;
#35686 = CARTESIAN_POINT ( 'NONE',  ( -4.465349678524273003, 66.51625814178524365, -26.73836809291795191 ) ) ;
#35687 = CARTESIAN_POINT ( 'NONE',  ( 3.313708498984756279, 7.999999999999991118, 15.36155277982336642 ) ) ;
#35689 = CARTESIAN_POINT ( 'NONE',  ( -8.000000000000000000, 24.56249999590322375, -9.797174393178825657E-16 ) ) ;
#35688 = CARTESIAN_POINT ( 'NONE',  ( -5.000000000000000888, 237.2916666734946318, -8.660254037844387298 ) ) ;
#35690 = ORIENTED_EDGE ( 'NONE', *, *, #1479, .F. ) ;
#35691 = CARTESIAN_POINT ( 'NONE',  ( 8.000000000000000000, 92.93750000409679046, -9.797174393178825657E-16 ) ) ;
#35692 = CARTESIAN_POINT ( 'NONE',  ( -2.594694132007996146, 225.9999999999999432, 9.679754673387174435 ) ) ;
#35693 = CARTESIAN_POINT ( 'NONE',  ( 4.556349186104052151, -10.99999999999999822, 115.4687500000000000 ) ) ;
#35694 = CARTESIAN_POINT ( 'NONE',  ( -11.35316468749999963, 239.2187500034139873, 0.000000000000000000 ) ) ;
#35695 = CARTESIAN_POINT ( 'NONE',  ( 3.042071309553159519, 119.7395833299193413, 11.35316468750000141 ) ) ;
#35696 = ORIENTED_EDGE ( 'NONE', *, *, #55182, .F. ) ;
#35697 = CARTESIAN_POINT ( 'NONE',  ( -30.82842712474621649, 208.1250000000000284, 167.1715728752542134 ) ) ;
#35698 = CARTESIAN_POINT ( 'NONE',  ( -10.18810118749999738, -4.220049686691941915, 100.7500000020483526 ) ) ;
#35699 = DIRECTION ( 'NONE',  ( -0.000000000000000000, -0.000000000000000000, -1.000000000000000000 ) ) ;
#35700 = CARTESIAN_POINT ( 'NONE',  ( 1.432654583217664701, 199.0000000013656063, 201.4587341250000065 ) ) ;
#35701 = DIRECTION ( 'NONE',  ( -0.000000000000000000, -1.000000000000000000, -0.000000000000000000 ) ) ;
#35703 = CARTESIAN_POINT ( 'NONE',  ( -8.311093377946841443, 108.9062499965860127, 8.311093377946834337 ) ) ;
#35702 = FACE_OUTER_BOUND ( 'NONE', #69366, .T. ) ;
#35704 = VECTOR ( 'NONE', #45012, 1000.000000000000227 ) ;
#35705 = CARTESIAN_POINT ( 'NONE',  ( 5.656854249492376141, -5.656854249492374365, 9.080302783920146226 ) ) ;
#35706 = CARTESIAN_POINT ( 'NONE',  ( -31.45873412499997812, 196.0000000013656347, 171.4326545832180386 ) ) ;
#35707 = LINE ( 'NONE', #65093, #40927 ) ;
#35708 = ORIENTED_EDGE ( 'NONE', *, *, #55402, .T. ) ;
#35709 = CARTESIAN_POINT ( 'NONE',  ( -10.00000000000000178, 199.3749999931720538, -1.224646799147353454E-15 ) ) ;
#35710 = CARTESIAN_POINT ( 'NONE',  ( 0.000000000000000000, 300.0000000000000000, 0.000000000000000000 ) ) ;
#35711 = VECTOR ( 'NONE', #65349, 1000.000000000000000 ) ;
#35712 = CARTESIAN_POINT ( 'NONE',  ( 49.70177871865296026, 50.00000000000007105, 57.99999999999998579 ) ) ;
#35713 = CARTESIAN_POINT ( 'NONE',  ( -3.042071309553163960, 102.5520833299193697, -11.35316468749999963 ) ) ;
#35714 = CARTESIAN_POINT ( 'NONE',  ( 2.754378923186476579E-14, 209.1875000013656063, 194.5412658750000219 ) ) ;
#35715 = CARTESIAN_POINT ( 'NONE',  ( 7.188101187500000044, 9.843749997951610098, 0.000000000000000000 ) ) ;
#35716 = CARTESIAN_POINT ( 'NONE',  ( -10.18810118749999916, 0.000000000000000000, 93.53125000204836681 ) ) ;
#35717 = CARTESIAN_POINT ( 'NONE',  ( 5.676582343750001591, 6.927083329919350163, -9.832129032723420536 ) ) ;
#35718 = ORIENTED_EDGE ( 'NONE', *, *, #57482, .T. ) ;
#35719 = FACE_OUTER_BOUND ( 'NONE', #17045, .T. ) ;
#35720 = CYLINDRICAL_SURFACE ( 'NONE', #17925, 11.00000000000000000 ) ;
#35721 = CARTESIAN_POINT ( 'NONE',  ( 8.311093377946834337, 220.1562499965860127, 8.311093377946839666 ) ) ;
#35722 = CARTESIAN_POINT ( 'NONE',  ( 7.204075437095966983, 7.204075437095967871, 79.46875000204836681 ) ) ;
#35723 = CARTESIAN_POINT ( 'NONE',  ( -7.999999999999991118, 3.313708498984757167, 11.42405278392014623 ) ) ;
#35724 = CARTESIAN_POINT ( 'NONE',  ( -2.679491924311383499, 263.9583333333334281, -9.999999999999909406 ) ) ;
#35725 = CARTESIAN_POINT ( 'NONE',  ( 2.765530957081996366, 292.1406250017070079, -6.676582343750003368 ) ) ;
#35726 = EDGE_LOOP ( 'NONE', ( #51501, #46765, #10314, #2745 ) ) ;
#35727 = CARTESIAN_POINT ( 'NONE',  ( 10.99999999999989342, 4.556349186104152515, 89.03125000409679046 ) ) ;
#35728 = CARTESIAN_POINT ( 'NONE',  ( 5.676582343749993598, 210.2604166632526699, 9.832129032723422313 ) ) ;
#35729 = CARTESIAN_POINT ( 'NONE',  ( -10.18810118749999916, 0.000000000000000000, 91.65625000204836681 ) ) ;
#35730 = CARTESIAN_POINT ( 'NONE',  ( -25.55430564589115150, 201.0625000013656063, 172.4456943541091789 ) ) ;
#35731 = CARTESIAN_POINT ( 'NONE',  ( 3.313708498984762496, 20.71875000000000355, 7.999999999999998224 ) ) ;
#35732 = ORIENTED_EDGE ( 'NONE', *, *, #45005, .F. ) ;
#35733 = CARTESIAN_POINT ( 'NONE',  ( -28.07539850426995187, -51.79510720262685908, 156.7510221886425938 ) ) ;
#35734 = CARTESIAN_POINT ( 'NONE',  ( 2.849036369511732440E-14, 208.3750000027312126, 202.0000000000000000 ) ) ;
#35735 = CARTESIAN_POINT ( 'NONE',  ( 2.679491924311228956, 26.04166666666666430, -10.00000000000000000 ) ) ;
#35736 = ADVANCED_FACE ( 'NONE', ( #40591 ), #5758, .F. ) ;
#35737 = CARTESIAN_POINT ( 'NONE',  ( -5.000000000000000888, 14.70421557449314953, 69.92631206022693391 ) ) ;
#35738 = CARTESIAN_POINT ( 'NONE',  ( -10.18810118749999916, 0.000000000000000000, 72.53125000204838102 ) ) ;
#35739 = VERTEX_POINT ( 'NONE', #64366 ) ;
#35740 =( BOUNDED_CURVE ( )  B_SPLINE_CURVE ( 2, ( #41002, #64009, #12324, #2109, #7775, #58729, #19449, #7040, #70771 ),
 .UNSPECIFIED., .F., .F. ) 
 B_SPLINE_CURVE_WITH_KNOTS ( ( 3, 2, 2, 2, 3 ),
 ( 0.2833333333333336590, 0.2916666666666669627, 0.3000000000000002665, 0.3083333333333335702, 0.3166666666666668184 ),
 .UNSPECIFIED. ) 
 CURVE ( )  GEOMETRIC_REPRESENTATION_ITEM ( )  RATIONAL_B_SPLINE_CURVE ( ( 0.9999999999999970024, 0.9238795325112897361, 1.000000000000000000, 0.9238795325112867385, 1.000000000000000000, 0.9238795325112867385, 1.000000000000000000, 0.9238795325112851842, 1.000000000000001554 ) ) 
 REPRESENTATION_ITEM ( '' )  );
#35741 = LINE ( 'NONE', #12349, #69884 ) ;
#35742 =( BOUNDED_SURFACE ( )  B_SPLINE_SURFACE ( 1, 2, ( 
 ( #45472, #16790, #35296, #598, #11157, #69988, #18296, #23211, #41312, #23581, #64320, #68488, #12624, #46591, #69612, #40194, #17928, #58310, #34181, #63196, #63952, #74523, #5500, #22831, #28500, #11526, #30356, #59404, #13716, #65788, #71070, #48063, #14466, #24679, #36025, #12987, #65419, #36760, #59773, #13351, #7719, #36389, #19388, #8448, #18668, #60130, #47689, #70711, #8082, #42401, #31083, #31468, #54492, #54113, #30722, #53743, #19029, #2423, #25418, #2054, #59042, #31841, #60503, #2797, #14092, #37505, #8830, #48432, #7349, #53377, #42036, #71435, #19765, #54860, #65042, #42772, #25042, #37127, #25785, #48804, #24319, #71813, #1701, #20131, #43146, #66163, #47330, #70357, #41679, #64688, #38631, #61633, #61254, #39363, #27665, #60876, #9586, #15220, #61999, #32984, #26160, #21627, #3171, #9951, #33348, #44651, #72189, #67292, #9199, #32603, #32220, #26920, #68034, #55238, #55985, #38251, #55612, #27286, #20883, #3544, #38994, #4295, #49178, #43904, #3929, #22001, #66915, #26535, #50670, #49560, #72578, #50303, #49935, #72948, #73324, #10322, #67667, #20501, #44281, #16327, #21256, #62360, #43516, #15965, #15592, #66530, #56349, #73689, #4668, #45027, #10690, #33724, #14840, #37881, #28780, #51797, #51419, #63110, #23490, #41224, #5409, #144, #11071, #18210, #34097, #52179, #23120, #62731, #17083, #46132, #46502, #69150, #5784, #46876, #57093, #68401, #45385, #17457, #40478, #63483, #45761, #40105, #68772, #11805, #40850, #51051, #17836, #28411, #74433, #34843, #57850, #6156, #63858 ),
 ( #64232, #28040, #22740, #29164, #35209, #511, #74062, #69522, #12173, #22361, #56726, #11436, #58226, #5044, #16699, #23866, #34473, #57478, #6525, #29532, #52542, #880, #39730, #69899, #12541, #13999, #64957, #36304, #59322, #41591, #71722, #66071, #47602, #7627, #1967, #13267, #30271, #7994, #58582, #35569, #36673, #42315, #2708, #53288, #1613, #47974, #12900, #54024, #58953, #31000, #25696, #54401, #6890, #29901, #47240, #35936, #42685, #52914, #18943, #2332, #25329, #30636, #53656, #24959, #48344, #70989, #20038, #1249, #64604, #19305, #37038, #71351, #24226, #19673, #59685, #70267, #18580, #24596, #65331, #7261, #65697, #60039, #13635, #41949, #8359, #70625, #31375, #48716, #43054, #20414, #26831, #67205, #32510, #61165, #4578, #38163, #50214, #73601, #49845, #32129, #44565, #10234, #67577, #73235, #37793, #61909, #72488, #21541, #33262, #56261, #15503, #15874, #43431, #9114, #38540, #72863, #49087, #21908, #21168, #66446, #8740, #9496, #55523, #3835, #60789, #31752, #3082, #20797, #44192, #55148, #61541, #3453, #27575, #26066, #44939, #14379, #26443, #49468, #60414, #9864, #43814, #66829, #50583, #54772, #32893, #55895, #15131, #72101, #37415, #4209, #38907, #27198, #14753, #29444, #23403, #40021, #63024, #62646, #74342, #34755, #52455, #16614, #11348, #22279, #793, #45301, #63390, #34383, #73974, #28324, #57383, #57759, #5693, #16994, #58135, #68316, #4955, #56640, #28692, #51705, #52, #57009, #51334, #5322, #23035, #52091, #62279, #29071, #39649, #10979, #46044, #69064, #17368 ) ),
 .UNSPECIFIED., .F., .F., .F. ) 
 B_SPLINE_SURFACE_WITH_KNOTS ( ( 2, 2 ),
 ( 3, 2, 2, 2, 2, 2, 2, 2, 2, 2, 2, 2, 2, 2, 2, 2, 2, 2, 2, 2, 2, 2, 2, 2, 2, 2, 2, 2, 2, 2, 2, 2, 2, 2, 2, 2, 2, 2, 2, 2, 2, 2, 2, 2, 2, 2, 2, 2, 2, 2, 2, 2, 2, 2, 2, 2, 2, 2, 2, 2, 2, 2, 2, 2, 2, 2, 2, 2, 2, 2, 2, 2, 2, 2, 2, 2, 2, 2, 2, 2, 2, 2, 2, 2, 2, 2, 2, 2, 2, 2, 2, 2, 2, 2, 2, 2, 3 ),
 ( 0.000000000000000000, 1.000000000000000000 ),
 ( 0.000000000000000000, 0.01041666666666666609, 0.02083333333333333218, 0.03125000000000000000, 0.04166666666666666435, 0.05208333333333333565, 0.06250000000000000000, 0.07291666666666667129, 0.08333333333333332871, 0.09375000000000000000, 0.1041666666666666713, 0.1145833333333333287, 0.1250000000000000000, 0.1354166666666666574, 0.1458333333333333426, 0.1562500000000000000, 0.1666666666666666574, 0.1770833333333333426, 0.1875000000000000000, 0.1979166666666666574, 0.2083333333333333426, 0.2187500000000000000, 0.2291666666666666574, 0.2395833333333333426, 0.2500000000000000000, 0.2604166666666666852, 0.2708333333333333148, 0.2812500000000000000, 0.2916666666666666852, 0.3020833333333333148, 0.3125000000000000000, 0.3229166666666666852, 0.3333333333333333148, 0.3437500000000000000, 0.3541666666666666852, 0.3645833333333333148, 0.3750000000000000000, 0.3854166666666666852, 0.3958333333333333148, 0.4062500000000000000, 0.4166666666666666852, 0.4270833333333333148, 0.4375000000000000000, 0.4479166666666666852, 0.4583333333333333148, 0.4687500000000000000, 0.4791666666666666852, 0.4895833333333333148, 0.5000000000000000000, 0.5104166666666666297, 0.5208333333333333703, 0.5312500000000000000, 0.5416666666666666297, 0.5520833333333333703, 0.5625000000000000000, 0.5729166666666666297, 0.5833333333333333703, 0.5937500000000000000, 0.6041666666666666297, 0.6145833333333333703, 0.6250000000000000000, 0.6354166666666666297, 0.6458333333333333703, 0.6562500000000000000, 0.6666666666666666297, 0.6770833333333333703, 0.6875000000000000000, 0.6979166666666666297, 0.7083333333333333703, 0.7187500000000000000, 0.7291666666666666297, 0.7395833333333333703, 0.7500000000000000000, 0.7604166666666666297, 0.7708333333333333703, 0.7812500000000000000, 0.7916666666666666297, 0.8020833333333333703, 0.8125000000000000000, 0.8229166666666666297, 0.8333333333333333703, 0.8437500000000000000, 0.8541666666666666297, 0.8645833333333333703, 0.8750000000000000000, 0.8854166666666666297, 0.8958333333333333703, 0.9062500000000000000, 0.9166666666666666297, 0.9270833333333333703, 0.9375000000000000000, 0.9479166666666666297, 0.9583333333333333703, 0.9687500000000000000, 0.9791666666666666297, 0.9895833333333333703, 1.000000000000000000 ),
 .UNSPECIFIED. ) 
 GEOMETRIC_REPRESENTATION_ITEM ( )  RATIONAL_B_SPLINE_SURFACE ( (
 ( 1.000000000000000000, 0.9238795325112867385, 1.000000000000000000, 0.9238795325112867385, 1.000000000000000000, 0.9238795325112867385, 1.000000000000000000, 0.9238795325112867385, 1.000000000000000000, 0.9238795325112867385, 1.000000000000000000, 0.9238795325112867385, 1.000000000000000000, 0.9238795325112867385, 1.000000000000000000, 0.9238795325112867385, 1.000000000000000000, 0.9238795325112867385, 1.000000000000000000, 0.9238795325112867385, 1.000000000000000000, 0.9238795325112867385, 1.000000000000000000, 0.9238795325112867385, 1.000000000000000000, 0.9238795325112867385, 1.000000000000000000, 0.9238795325112867385, 1.000000000000000000, 0.9238795325112867385, 1.000000000000000000, 0.9238795325112867385, 1.000000000000000000, 0.9238795325112867385, 1.000000000000000000, 0.9238795325112867385, 1.000000000000000000, 0.9238795325112867385, 1.000000000000000000, 0.9238795325112867385, 1.000000000000000000, 0.9238795325112867385, 1.000000000000000000, 0.9238795325112867385, 1.000000000000000000, 0.9238795325112867385, 1.000000000000000000, 0.9238795325112867385, 1.000000000000000000, 0.9238795325112867385, 1.000000000000000000, 0.9238795325112867385, 1.000000000000000000, 0.9238795325112867385, 1.000000000000000000, 0.9238795325112867385, 1.000000000000000000, 0.9238795325112867385, 1.000000000000000000, 0.9238795325112867385, 1.000000000000000000, 0.9238795325112867385, 1.000000000000000000, 0.9238795325112867385, 1.000000000000000000, 0.9238795325112867385, 1.000000000000000000, 0.9238795325112867385, 1.000000000000000000, 0.9238795325112867385, 1.000000000000000000, 0.9238795325112867385, 1.000000000000000000, 0.9238795325112867385, 1.000000000000000000, 0.9238795325112867385, 1.000000000000000000, 0.9238795325112867385, 1.000000000000000000, 0.9238795325112867385, 1.000000000000000000, 0.9238795325112867385, 1.000000000000000000, 0.9238795325112867385, 1.000000000000000000, 0.9238795325112867385, 1.000000000000000000, 0.9238795325112867385, 1.000000000000000000, 0.9238795325112867385, 1.000000000000000000, 0.9238795325112867385, 1.000000000000000000, 0.9238795325112867385, 1.000000000000000000, 0.9238795325112867385, 1.000000000000000000, 0.9238795325112867385, 1.000000000000000000, 0.9238795325112867385, 1.000000000000000000, 0.9238795325112867385, 1.000000000000000000, 0.9238795325112867385, 1.000000000000000000, 0.9238795325112867385, 1.000000000000000000, 0.9238795325112867385, 1.000000000000000000, 0.9238795325112867385, 1.000000000000000000, 0.9238795325112867385, 1.000000000000000000, 0.9238795325112867385, 1.000000000000000000, 0.9238795325112867385, 1.000000000000000000, 0.9238795325112867385, 1.000000000000000000, 0.9238795325112867385, 1.000000000000000000, 0.9238795325112867385, 1.000000000000000000, 0.9238795325112867385, 1.000000000000000000, 0.9238795325112867385, 1.000000000000000000, 0.9238795325112867385, 1.000000000000000000, 0.9238795325112867385, 1.000000000000000000, 0.9238795325112867385, 1.000000000000000000, 0.9238795325112867385, 1.000000000000000000, 0.9238795325112867385, 1.000000000000000000, 0.9238795325112867385, 1.000000000000000000, 0.9238795325112867385, 1.000000000000000000, 0.9238795325112867385, 1.000000000000000000, 0.9238795325112867385, 1.000000000000000000, 0.9238795325112867385, 1.000000000000000000, 0.9238795325112867385, 1.000000000000000000, 0.9238795325112867385, 1.000000000000000000, 0.9238795325112867385, 1.000000000000000000, 0.9238795325112867385, 1.000000000000000000, 0.9238795325112867385, 1.000000000000000000, 0.9238795325112867385, 1.000000000000000000, 0.9238795325112867385, 1.000000000000000000, 0.9238795325112867385, 1.000000000000000000, 0.9238795325112867385, 1.000000000000000000, 0.9238795325112867385, 1.000000000000000000, 0.9238795325112867385, 1.000000000000000000, 0.9238795325112867385, 1.000000000000000000, 0.9238795325112867385, 1.000000000000000000, 0.9238795325112867385, 1.000000000000000000, 0.9238795325112867385, 1.000000000000000000, 0.9238795325112867385, 1.000000000000000000, 0.9238795325112867385, 1.000000000000000000, 0.9238795325112867385, 1.000000000000000000, 0.9238795325112867385, 1.000000000000000000, 0.9238795325112867385, 1.000000000000000000, 0.9238795325112867385, 1.000000000000000000, 0.9238795325112867385, 1.000000000000000000, 0.9238795325112867385, 1.000000000000000000),
 ( 1.000000000000000000, 0.9238795325112867385, 1.000000000000000000, 0.9238795325112867385, 1.000000000000000000, 0.9238795325112867385, 1.000000000000000000, 0.9238795325112867385, 1.000000000000000000, 0.9238795325112867385, 1.000000000000000000, 0.9238795325112867385, 1.000000000000000000, 0.9238795325112867385, 1.000000000000000000, 0.9238795325112867385, 1.000000000000000000, 0.9238795325112867385, 1.000000000000000000, 0.9238795325112867385, 1.000000000000000000, 0.9238795325112867385, 1.000000000000000000, 0.9238795325112867385, 1.000000000000000000, 0.9238795325112867385, 1.000000000000000000, 0.9238795325112867385, 1.000000000000000000, 0.9238795325112867385, 1.000000000000000000, 0.9238795325112867385, 1.000000000000000000, 0.9238795325112867385, 1.000000000000000000, 0.9238795325112867385, 1.000000000000000000, 0.9238795325112867385, 1.000000000000000000, 0.9238795325112867385, 1.000000000000000000, 0.9238795325112867385, 1.000000000000000000, 0.9238795325112867385, 1.000000000000000000, 0.9238795325112867385, 1.000000000000000000, 0.9238795325112867385, 1.000000000000000000, 0.9238795325112867385, 1.000000000000000000, 0.9238795325112867385, 1.000000000000000000, 0.9238795325112867385, 1.000000000000000000, 0.9238795325112867385, 1.000000000000000000, 0.9238795325112867385, 1.000000000000000000, 0.9238795325112867385, 1.000000000000000000, 0.9238795325112867385, 1.000000000000000000, 0.9238795325112867385, 1.000000000000000000, 0.9238795325112867385, 1.000000000000000000, 0.9238795325112867385, 1.000000000000000000, 0.9238795325112867385, 1.000000000000000000, 0.9238795325112867385, 1.000000000000000000, 0.9238795325112867385, 1.000000000000000000, 0.9238795325112867385, 1.000000000000000000, 0.9238795325112867385, 1.000000000000000000, 0.9238795325112867385, 1.000000000000000000, 0.9238795325112867385, 1.000000000000000000, 0.9238795325112867385, 1.000000000000000000, 0.9238795325112867385, 1.000000000000000000, 0.9238795325112867385, 1.000000000000000000, 0.9238795325112867385, 1.000000000000000000, 0.9238795325112867385, 1.000000000000000000, 0.9238795325112867385, 1.000000000000000000, 0.9238795325112867385, 1.000000000000000000, 0.9238795325112867385, 1.000000000000000000, 0.9238795325112867385, 1.000000000000000000, 0.9238795325112867385, 1.000000000000000000, 0.9238795325112867385, 1.000000000000000000, 0.9238795325112867385, 1.000000000000000000, 0.9238795325112867385, 1.000000000000000000, 0.9238795325112867385, 1.000000000000000000, 0.9238795325112867385, 1.000000000000000000, 0.9238795325112867385, 1.000000000000000000, 0.9238795325112867385, 1.000000000000000000, 0.9238795325112867385, 1.000000000000000000, 0.9238795325112867385, 1.000000000000000000, 0.9238795325112867385, 1.000000000000000000, 0.9238795325112867385, 1.000000000000000000, 0.9238795325112867385, 1.000000000000000000, 0.9238795325112867385, 1.000000000000000000, 0.9238795325112867385, 1.000000000000000000, 0.9238795325112867385, 1.000000000000000000, 0.9238795325112867385, 1.000000000000000000, 0.9238795325112867385, 1.000000000000000000, 0.9238795325112867385, 1.000000000000000000, 0.9238795325112867385, 1.000000000000000000, 0.9238795325112867385, 1.000000000000000000, 0.9238795325112867385, 1.000000000000000000, 0.9238795325112867385, 1.000000000000000000, 0.9238795325112867385, 1.000000000000000000, 0.9238795325112867385, 1.000000000000000000, 0.9238795325112867385, 1.000000000000000000, 0.9238795325112867385, 1.000000000000000000, 0.9238795325112867385, 1.000000000000000000, 0.9238795325112867385, 1.000000000000000000, 0.9238795325112867385, 1.000000000000000000, 0.9238795325112867385, 1.000000000000000000, 0.9238795325112867385, 1.000000000000000000, 0.9238795325112867385, 1.000000000000000000, 0.9238795325112867385, 1.000000000000000000, 0.9238795325112867385, 1.000000000000000000, 0.9238795325112867385, 1.000000000000000000, 0.9238795325112867385, 1.000000000000000000, 0.9238795325112867385, 1.000000000000000000, 0.9238795325112867385, 1.000000000000000000, 0.9238795325112867385, 1.000000000000000000, 0.9238795325112867385, 1.000000000000000000, 0.9238795325112867385, 1.000000000000000000, 0.9238795325112867385, 1.000000000000000000, 0.9238795325112867385, 1.000000000000000000, 0.9238795325112867385, 1.000000000000000000, 0.9238795325112867385, 1.000000000000000000) ) ) 
 REPRESENTATION_ITEM ( '' )  SURFACE ( )  );
#35743 = CARTESIAN_POINT ( 'NONE',  ( -11.00000000000007816, -4.556349186103974880, 112.0937499999999858 ) ) ;
#35744 = CARTESIAN_POINT ( 'NONE',  ( -7.188101187500000044, 120.0312500020483810, 0.000000000000000000 ) ) ;
#35745 = CARTESIAN_POINT ( 'NONE',  ( -2.349324367397504609, 21.99999999999999645, -3.445024555465882266 ) ) ;
#35746 = CARTESIAN_POINT ( 'NONE',  ( 6.676582343750002480, 298.0156250017069510, -2.765530957081997254 ) ) ;
#35748 = DIRECTION ( 'NONE',  ( 0.000000000000000000, 0.000000000000000000, 1.000000000000000000 ) ) ;
#35747 = CARTESIAN_POINT ( 'NONE',  ( -5.676582343750000703, 228.0729166700806729, -9.832129032723418760 ) ) ;
#35749 = CONTEXT_DEPENDENT_SHAPE_REPRESENTATION ( #47667, #5386 ) ;
#35750 = VERTEX_POINT ( 'NONE', #2096 ) ;
#35751 = EDGE_CURVE ( 'NONE', #30305, #31550, #31130, .T. ) ;
#35752 = CARTESIAN_POINT ( 'NONE',  ( -11.35316468749999608, 234.4270833367473017, 3.042071309553173730 ) ) ;
#35753 = CARTESIAN_POINT ( 'NONE',  ( -5.082755093536317936, -5.082755093536320601, 6.174052781871754547 ) ) ;
#35754 = CARTESIAN_POINT ( 'NONE',  ( -1.432654583217608080, 201.8750000013656063, 201.4587341250000350 ) ) ;
#35755 = EDGE_CURVE ( 'NONE', #28680, #33915, #25462, .T. ) ;
#35756 = ORIENTED_EDGE ( 'NONE', *, *, #38494, .F. ) ;
#35757 = CARTESIAN_POINT ( 'NONE',  ( -10.18810118749999916, 4.220049686691934809, 69.06250000204838102 ) ) ;
#35758 = CARTESIAN_POINT ( 'NONE',  ( -5.676582343749998039, 102.7604166632526841, -9.832129032723420536 ) ) ;
#35759 = CARTESIAN_POINT ( 'NONE',  ( -9.999999999999996447, 122.2916666666666856, -2.679491924311229401 ) ) ;
#35760 = CARTESIAN_POINT ( 'NONE',  ( -4.556349186104045934, 11.00000000000000000, 80.21874999999997158 ) ) ;
#35763 = CARTESIAN_POINT ( 'NONE',  ( 0.000000000000000000, 265.0000000000000000, 0.000000000000000000 ) ) ;
#35762 = CARTESIAN_POINT ( 'NONE',  ( 29.43265458321766559, 205.5000000013655779, 173.4587341249998929 ) ) ;
#35761 = CARTESIAN_POINT ( 'NONE',  ( 26.56734541678232375, 202.6250000013656063, 173.4587341249998929 ) ) ;
#35764 = ORIENTED_EDGE ( 'NONE', *, *, #16376, .F. ) ;
#35765 = DIRECTION ( 'NONE',  ( -3.469446951953617147E-16, 0.000000000000000000, 1.000000000000000000 ) ) ;
#35766 = CARTESIAN_POINT ( 'NONE',  ( -7.320508075688773708, 178.7499999931720254, -7.320508075688774596 ) ) ;
#35767 = CARTESIAN_POINT ( 'NONE',  ( -11.35316468750000141, 213.4895833299193839, 3.042071309553159963 ) ) ;
#35768 = CARTESIAN_POINT ( 'NONE',  ( 3.458734124999959914, 206.3750000013656063, 143.4326545832176976 ) ) ;
#35769 = AXIS2_PLACEMENT_3D ( 'NONE', #11682, #10571, #34719 ) ;
#35770 = CARTESIAN_POINT ( 'NONE',  ( 25.55430564589119768, 206.3125000013656063, 167.5543056458910485 ) ) ;
#35771 = CARTESIAN_POINT ( 'NONE',  ( 7.188101187499999156, 26.24999999795161898, 2.977408999572654924 ) ) ;
#35772 = EDGE_CURVE ( 'NONE', #1216, #64267, #13438, .T. ) ;
#35773 = CARTESIAN_POINT ( 'NONE',  ( -9.832129032723418760, 183.1770833299193555, -5.676582343750004256 ) ) ;
#35774 = CARTESIAN_POINT ( 'NONE',  ( -7.188101187499999156, 100.6250000020483810, 2.977408999572654924 ) ) ;
#35775 = CARTESIAN_POINT ( 'NONE',  ( -2.485281374238947016, 295.8750000034140726, -5.999999999999626965 ) ) ;
#35776 = CARTESIAN_POINT ( 'NONE',  ( -30.82842712474620939, 195.1250000000000284, 167.1715728752542134 ) ) ;
#35777 = CARTESIAN_POINT ( 'NONE',  ( -3.211159895383562723, 10.93749999863440792, 3.211159895383561391 ) ) ;
#35778 = CARTESIAN_POINT ( 'NONE',  ( 29.43265458321761230, 201.7500000013655779, 173.4587341249998929 ) ) ;
#35779 = CARTESIAN_POINT ( 'NONE',  ( -2.977408999572648707, -7.188101187499990274, 5.142802781871752771 ) ) ;
#35780 = CARTESIAN_POINT ( 'NONE',  ( -8.311093377946836114, 62.65624999658601268, -8.311093377946837890 ) ) ;
#35781 = EDGE_CURVE ( 'NONE', #54369, #70088, #16756, .T. ) ;
#35782 = DIRECTION ( 'NONE',  ( -1.000000000000000000, 0.000000000000000000, 0.000000000000000000 ) ) ;
#35783 = CARTESIAN_POINT ( 'NONE',  ( -2.775557561562891351E-14, 210.0000000000000284, 142.0000000000000568 ) ) ;
#35784 = ORIENTED_EDGE ( 'NONE', *, *, #31352, .F. ) ;
#35785 = LINE ( 'NONE', #65548, #60347 ) ;
#35786 = LINE ( 'NONE', #58070, #38894 ) ;
#35787 = CARTESIAN_POINT ( 'NONE',  ( -8.311093377946841443, 78.90624999658602690, 8.311093377946830785 ) ) ;
#35788 = CARTESIAN_POINT ( 'NONE',  ( 2.947434672556987323, 11.00000000000000000, 66.75185452034084221 ) ) ;
#35789 = CARTESIAN_POINT ( 'NONE',  ( -2.445694354108840063, 195.0625000013656063, 139.5543056458912190 ) ) ;
#35790 = CARTESIAN_POINT ( 'NONE',  ( -30.93541659651596021, -37.99999999999992184, 167.9999999999998295 ) ) ;
#35792 = CARTESIAN_POINT ( 'NONE',  ( 11.35316468749999963, 60.98958332991934839, -3.042071309553165293 ) ) ;
#35791 = CYLINDRICAL_SURFACE ( 'NONE', #31581, 3.999999999999976019 ) ;
#35793 = CARTESIAN_POINT ( 'NONE',  ( -5.656854249492373476, -5.656854249492376141, 26.70530278392014623 ) ) ;
#35794 = CARTESIAN_POINT ( 'NONE',  ( -3.761416977589127519, 194.7718537773880030, 142.3735565596915933 ) ) ;
#35795 = CARTESIAN_POINT ( 'NONE',  ( 5.000000000000001776, 157.7083333265053966, -8.660254037844389075 ) ) ;
#35796 = CARTESIAN_POINT ( 'NONE',  ( -4.401442555609581635E-16, 98.65625000204838102, -7.188101187500000044 ) ) ;
#35797 = CARTESIAN_POINT ( 'NONE',  ( 4.556349186104045934, 11.00000000000000000, 108.5312500000000142 ) ) ;
#35798 = CARTESIAN_POINT ( 'NONE',  ( 5.676582343749993598, 45.26041666325268409, 9.832129032723422313 ) ) ;
#35799 = CARTESIAN_POINT ( 'NONE',  ( -7.204075437095967871, 7.204075437095967871, 114.3437500020483810 ) ) ;
#35800 = CARTESIAN_POINT ( 'NONE',  ( 5.676582343750001591, 191.6145833299193839, -9.832129032723420536 ) ) ;
#35801 = ORIENTED_EDGE ( 'NONE', *, *, #27807, .T. ) ;
#35802 = CARTESIAN_POINT ( 'NONE',  ( 0.8997857291008781733, 67.61674724335057363, 20.05382624916572709 ) ) ;
#35803 = CARTESIAN_POINT ( 'NONE',  ( 8.000000000000000000, 0.5000000000000004441, 0.000000000000000000 ) ) ;
#35804 = DIRECTION ( 'NONE',  ( 0.000000000000000000, -1.000000000000000000, -0.000000000000000000 ) ) ;
#35806 = CARTESIAN_POINT ( 'NONE',  ( 11.35316468749999963, 180.9895833299193555, -3.042071309553165293 ) ) ;
#35805 = CARTESIAN_POINT ( 'NONE',  ( 2.849036369511732440E-14, 195.2500000000000000, 202.0000000000000000 ) ) ;
#35807 = VECTOR ( 'NONE', #70364, 1000.000000000000000 ) ;
#35808 = EDGE_CURVE ( 'NONE', #57937, #72372, #70398, .T. ) ;
#35809 = CARTESIAN_POINT ( 'NONE',  ( -1.469576158976823947E-15, 11.43749999590322197, 8.000000000000000000 ) ) ;
#35810 = CARTESIAN_POINT ( 'NONE',  ( 7.320508075688771044, 256.2500000068279746, -7.320508075688771932 ) ) ;
#35811 = DIRECTION ( 'NONE',  ( 0.000000000000000000, 0.000000000000000000, 1.000000000000000000 ) ) ;
#35812 = ORIENTED_EDGE ( 'NONE', *, *, #32223, .F. ) ;
#35813 = EDGE_CURVE ( 'NONE', #61945, #31223, #18713, .T. ) ;
#35814 = CARTESIAN_POINT ( 'NONE',  ( -8.311093377946841443, 169.2187499965860127, 8.311093377946834337 ) ) ;
#35815 = CARTESIAN_POINT ( 'NONE',  ( -5.082755093536319713, 5.082755093536319713, 25.29905278187175810 ) ) ;
#35816 = EDGE_CURVE ( 'NONE', #11598, #27411, #70757, .T. ) ;
#35817 = CARTESIAN_POINT ( 'NONE',  ( 8.482974764195253314, 225.9999999999999432, -6.716101469744629959 ) ) ;
#35818 = ORIENTED_EDGE ( 'NONE', *, *, #71979, .T. ) ;
#35819 = CARTESIAN_POINT ( 'NONE',  ( -5.656854249492380582, 105.5000000040967905, -5.656854249492380582 ) ) ;
#35820 = VECTOR ( 'NONE', #3334, 1000.000000000000000 ) ;
#35821 = CARTESIAN_POINT ( 'NONE',  ( 2.828427124746190291, 11.87500000000000000, 2.828427124746192067 ) ) ;
#35822 = CARTESIAN_POINT ( 'NONE',  ( 8.265697409064602041, 5.620102221249814178, -0.5590800469813634876 ) ) ;
#35823 = CARTESIAN_POINT ( 'NONE',  ( -3.211159895383561391, 13.68749999863440614, -3.211159895383561835 ) ) ;
#35824 = CARTESIAN_POINT ( 'NONE',  ( -3.313708498984757167, 7.999999999999991118, 20.23655278392014978 ) ) ;
#35825 = CARTESIAN_POINT ( 'NONE',  ( 7.778174593052023411, -7.778174593052021635, 78.25000000409676204 ) ) ;
#35826 = ORIENTED_EDGE ( 'NONE', *, *, #11448, .F. ) ;
#35827 = DIRECTION ( 'NONE',  ( -0.000000000000000000, -0.000000000000000000, 1.000000000000000000 ) ) ;
#35828 = CARTESIAN_POINT ( 'NONE',  ( -5.082755093536325930, 101.4687500020483810, -5.082755093536325930 ) ) ;
#35830 = CARTESIAN_POINT ( 'NONE',  ( -7.999999999999998224, 92.28125000409679046, 3.313708498984766049 ) ) ;
#35829 =( BOUNDED_CURVE ( )  B_SPLINE_CURVE ( 2, ( #5397, #5032, #69138, #28400, #51407, #63469, #52167, #11793, #33712 ),
 .UNSPECIFIED., .F., .F. ) 
 B_SPLINE_CURVE_WITH_KNOTS ( ( 3, 2, 2, 2, 3 ),
 ( 0.7159090909090909394, 0.7215909090909090606, 0.7272727272727272929, 0.7329545454545454142, 0.7386363636363636465 ),
 .UNSPECIFIED. ) 
 CURVE ( )  GEOMETRIC_REPRESENTATION_ITEM ( )  RATIONAL_B_SPLINE_CURVE ( ( 1.000000000000000000, 0.9238795325112867385, 1.000000000000000000, 0.9238795325112867385, 1.000000000000000000, 0.9238795325112867385, 1.000000000000000000, 0.9238795325112867385, 1.000000000000000000 ) ) 
 REPRESENTATION_ITEM ( '' )  );
#35831 = EDGE_LOOP ( 'NONE', ( #20843, #15254, #29615, #18281 ) ) ;
#35832 = CARTESIAN_POINT ( 'NONE',  ( 0.3752463838827005405, 10.12385607954436573, -70.07152133708838448 ) ) ;
#35833 = EDGE_CURVE ( 'NONE', #62884, #61146, #13032, .T. ) ;
#35834 = LINE ( 'NONE', #45019, #13256 ) ;
#35835 = CARTESIAN_POINT ( 'NONE',  ( 2.977408999572646486, 7.188101187499991163, 25.01780278187175455 ) ) ;
#35836 = EDGE_LOOP ( 'NONE', ( #71304, #55037, #10850 ) ) ;
#35837 = VERTEX_POINT ( 'NONE', #25090 ) ;
#35838 = CARTESIAN_POINT ( 'NONE',  ( -4.220049686691935698, 10.18810118749999916, 83.87500000204836681 ) ) ;
#35839 = UNCERTAINTY_MEASURE_WITH_UNIT (LENGTH_MEASURE( 1.000000000000000082E-05 ), #53915, 'distance_accuracy_value', 'NONE');
#35840 = LINE ( 'NONE', #45663, #34846 ) ;
#35841 = CARTESIAN_POINT ( 'NONE',  ( 4.556349186104045934, 11.00000000000000000, 102.5312500000000142 ) ) ;
#35842 = AXIS2_PLACEMENT_3D ( 'NONE', #72697, #11829, #22762 ) ;
#35845 = CARTESIAN_POINT ( 'NONE',  ( 6.676582343750002480, 298.1718750017070079, -2.765530957081997254 ) ) ;
#35844 = CARTESIAN_POINT ( 'NONE',  ( 29.65685424949235127, 200.5625000027312126, 165.9999999999998863 ) ) ;
#35843 = CARTESIAN_POINT ( 'NONE',  ( -4.556349186104048599, -10.99999999999999822, 86.78124999999998579 ) ) ;
#35846 = CARTESIAN_POINT ( 'NONE',  ( -7.320508075688773708, 136.8750000000000000, -7.320508075688774596 ) ) ;
#35847 = CARTESIAN_POINT ( 'NONE',  ( -7.347880794884122694E-16, 0.7500000000000002220, 4.000000000000001776 ) ) ;
#35848 = CARTESIAN_POINT ( 'NONE',  ( -5.447323953993864265, -4.689931814214729933, 0.5319290643893268555 ) ) ;
#35850 =( BOUNDED_CURVE ( )  B_SPLINE_CURVE ( 2, ( #525, #35223, #57865, #29916, #17474, #11822, #1983, #41241, #63500, #41606, #6171, #29180, #896 ),
 .UNSPECIFIED., .F., .F. ) 
 B_SPLINE_CURVE_WITH_KNOTS ( ( 3, 2, 2, 2, 2, 2, 3 ),
 ( 0.7500000000000000000, 0.7592592592592593004, 0.7685185185185184897, 0.7777777777777777901, 0.7870370370370370905, 0.7962962962962962798, 0.8055555555555555802 ),
 .UNSPECIFIED. ) 
 CURVE ( )  GEOMETRIC_REPRESENTATION_ITEM ( )  RATIONAL_B_SPLINE_CURVE ( ( 1.000000000000000000, 0.9659258262890683122, 1.000000000000000000, 0.9659258262890683122, 1.000000000000000000, 0.9659258262890683122, 1.000000000000000000, 0.9659258262890683122, 1.000000000000000000, 0.9659258262890683122, 1.000000000000000000, 0.9659258262890683122, 1.000000000000000000 ) ) 
 REPRESENTATION_ITEM ( '' )  );
#35849 = CARTESIAN_POINT ( 'NONE',  ( 7.071067811865484387, 22.99999999999999645, -1.000000000000000000 ) ) ;
#35851 = CARTESIAN_POINT ( 'NONE',  ( 24.54126587500000056, 203.1250000013656347, 168.5673454167822172 ) ) ;
#35852 = CARTESIAN_POINT ( 'NONE',  ( -2.977408999572654480, 7.874999997951610986, 7.188101187499999156 ) ) ;
#35853 = CARTESIAN_POINT ( 'NONE',  ( -5.662595241051933570, -5.662595241051936235, 5.700615283940630995 ) ) ;
#35854 = CARTESIAN_POINT ( 'NONE',  ( -1.432654583217662481, 195.1250000013656063, 145.4587341250000634 ) ) ;
#35855 = CARTESIAN_POINT ( 'NONE',  ( -7.188101187500000044, 114.0312500020483952, 0.000000000000000000 ) ) ;
#35857 = CARTESIAN_POINT ( 'NONE',  ( 11.00000000000000000, 1.347111479062088405E-15, 118.0000000000000000 ) ) ;
#35856 = CARTESIAN_POINT ( 'NONE',  ( 27.99999999999999645, 210.0000000000000284, 165.9999999999999147 ) ) ;
#35858 = CARTESIAN_POINT ( 'NONE',  ( 5.676582343750005144, 230.8854166700806729, 9.832129032723416984 ) ) ;
#35859 = DIRECTION ( 'NONE',  ( 0.000000000000000000, 0.000000000000000000, 1.000000000000000000 ) ) ;
#35860 = CARTESIAN_POINT ( 'NONE',  ( 7.188101187499991163, 2.977408999572648707, 20.70530278187175455 ) ) ;
#35861 = FACE_OUTER_BOUND ( 'NONE', #73225, .T. ) ;
#35862 = CARTESIAN_POINT ( 'NONE',  ( -9.832129032723420536, 23.69791666325268409, 5.676582343749997150 ) ) ;
#35863 = CARTESIAN_POINT ( 'NONE',  ( -31.99999999999999289, 199.2500000000000000, 170.0000000000003979 ) ) ;
#35864 = CARTESIAN_POINT ( 'NONE',  ( 11.35316468749999785, 220.8854166632526699, 3.042071309553174174 ) ) ;
#35865 = CARTESIAN_POINT ( 'NONE',  ( 5.656854249492379694, 112.4375000000000000, -5.656854249492380582 ) ) ;
#35866 = LINE ( 'NONE', #59250, #59987 ) ;
#35867 = ORIENTED_EDGE ( 'NONE', *, *, #45465, .T. ) ;
#35868 = DIRECTION ( 'NONE',  ( 0.000000000000000000, 0.000000000000000000, 1.000000000000000000 ) ) ;
#35869 = CARTESIAN_POINT ( 'NONE',  ( 3.458734124999960358, 194.6875000013655779, 142.0000000000000568 ) ) ;
#35870 = CARTESIAN_POINT ( 'NONE',  ( 11.35316468749999785, 30.57291666325268409, 3.042071309553174174 ) ) ;
#35871 = EDGE_CURVE ( 'NONE', #59993, #44162, #48105, .T. ) ;
#35872 = CARTESIAN_POINT ( 'NONE',  ( -7.778174593052020747, -7.778174593052023411, 86.87500000409677625 ) ) ;
#35873 = CARTESIAN_POINT ( 'NONE',  ( 3.458734124999959469, 208.7500000013656063, 140.5673454167823593 ) ) ;
#35874 = CARTESIAN_POINT ( 'NONE',  ( -5.999999999999999112, 295.1250000034140157, 2.485281374238575314 ) ) ;
#35875 = CARTESIAN_POINT ( 'NONE',  ( 2.775557561562891351E-14, -37.99999999999992184, 170.0000000000000284 ) ) ;
#35877 = CARTESIAN_POINT ( 'NONE',  ( 9.832129032723420536, 21.19791666325268409, -5.676582343749999815 ) ) ;
#35876 = CARTESIAN_POINT ( 'NONE',  ( -2.977408999572650927, 102.8750000020483810, -7.188101187500000933 ) ) ;
#35878 = CARTESIAN_POINT ( 'NONE',  ( 5.656854249492376141, -5.656854249492374365, 14.89280277982336642 ) ) ;
#35879 = CARTESIAN_POINT ( 'NONE',  ( 6.951808397369818766E-16, 147.0312499965860411, -11.35316468750000141 ) ) ;
#35880 = AXIS2_PLACEMENT_3D ( 'NONE', #22018, #28796, #45399 ) ;
#35881 = CARTESIAN_POINT ( 'NONE',  ( 8.660254037844385522, 111.4583333265053682, 5.000000000000005329 ) ) ;
#35882 = CARTESIAN_POINT ( 'NONE',  ( 5.082755093536325042, 113.4687500020483810, -5.082755093536325930 ) ) ;
#35883 = FACE_OUTER_BOUND ( 'NONE', #15253, .T. ) ;
#35884 = CARTESIAN_POINT ( 'NONE',  ( -24.54126587499998280, 205.3750000013656063, 171.4326545832179818 ) ) ;
#35885 =( BOUNDED_CURVE ( )  B_SPLINE_CURVE ( 2, ( #17894, #58280, #1304, #57907, #40534, #11497, #46189, #5845, #18638 ),
 .UNSPECIFIED., .F., .F. ) 
 B_SPLINE_CURVE_WITH_KNOTS ( ( 3, 2, 2, 2, 3 ),
 ( 0.4264705882352941013, 0.4301470588235294379, 0.4338235294117647189, 0.4375000000000000000, 0.4411764705882352811 ),
 .UNSPECIFIED. ) 
 CURVE ( )  GEOMETRIC_REPRESENTATION_ITEM ( )  RATIONAL_B_SPLINE_CURVE ( ( 1.000000000000000000, 0.9238795325112867385, 1.000000000000000000, 0.9238795325112867385, 1.000000000000000000, 0.9238795325112867385, 1.000000000000000000, 0.9238795325112867385, 1.000000000000000000 ) ) 
 REPRESENTATION_ITEM ( '' )  );
#35886 = ORIENTED_EDGE ( 'NONE', *, *, #5578, .F. ) ;
#35887 = CARTESIAN_POINT ( 'NONE',  ( -5.676582343750006032, 9.427083329919350163, 9.832129032723418760 ) ) ;
#35888 = ORIENTED_EDGE ( 'NONE', *, *, #30252, .F. ) ;
#35889 = CARTESIAN_POINT ( 'NONE',  ( 0.000000000000000000, 300.0000000000000000, 0.000000000000000000 ) ) ;
#35890 = CARTESIAN_POINT ( 'NONE',  ( -6.676582343750001591, 298.4531250017069510, 0.000000000000000000 ) ) ;
#35892 = CARTESIAN_POINT ( 'NONE',  ( 8.311093377946834337, 140.1562499965860127, 8.311093377946839666 ) ) ;
#35891 = CARTESIAN_POINT ( 'NONE',  ( -8.000000000000000000, 108.4062500000000000, -3.313708498984761164 ) ) ;
#35893 = CARTESIAN_POINT ( 'NONE',  ( -2.828427124746192067, 16.37499999726881228, 2.828427124746190735 ) ) ;
#35894 = CARTESIAN_POINT ( 'NONE',  ( -7.999999999999991118, 0.000000000000000000, 17.38655278432982243 ) ) ;
#35895 = CARTESIAN_POINT ( 'NONE',  ( 0.000000000000000000, 0.000000000000000000, 0.000000000000000000 ) ) ;
#35896 = CARTESIAN_POINT ( 'NONE',  ( 3.042071309553163960, 247.4479166700806445, -11.35316468749999785 ) ) ;
#35897 = CARTESIAN_POINT ( 'NONE',  ( 10.18810118749999916, 1.247682550866122264E-15, 91.28125000204836681 ) ) ;
#35898 = ORIENTED_EDGE ( 'NONE', *, *, #17815, .F. ) ;
#35899 = EDGE_CURVE ( 'NONE', #74219, #45651, #41749, .T. ) ;
#35900 = CARTESIAN_POINT ( 'NONE',  ( -4.000000000000016875, 197.4375000000000284, 140.3431457505076594 ) ) ;
#35901 = CARTESIAN_POINT ( 'NONE',  ( 5.000000000000000000, 66.11467145570921389, -23.67355326542971383 ) ) ;
#35902 = CARTESIAN_POINT ( 'NONE',  ( -3.042071309553164404, 92.55208332991934128, -11.35316468749999963 ) ) ;
#35903 = CARTESIAN_POINT ( 'NONE',  ( 7.204075437095966983, 7.204075437095967871, 98.59375000204836681 ) ) ;
#35904 = EDGE_CURVE ( 'NONE', #25046, #7770, #68234, .T. ) ;
#35905 = CARTESIAN_POINT ( 'NONE',  ( -3.211159895383562723, 17.06249999863440792, 3.211159895383561391 ) ) ;
#35906 = ORIENTED_EDGE ( 'NONE', *, *, #73117, .T. ) ;
#35907 = ORIENTED_EDGE ( 'NONE', *, *, #62809, .T. ) ;
#35908 = CARTESIAN_POINT ( 'NONE',  ( -8.000000000000000000, 5.156250000000000888, -3.313708498984762496 ) ) ;
#35909 = LINE ( 'NONE', #18181, #60128 ) ;
#35910 = CARTESIAN_POINT ( 'NONE',  ( -2.977408999572654480, 2.999999997951610542, 7.188101187499999156 ) ) ;
#35911 = CARTESIAN_POINT ( 'NONE',  ( -8.000000000000000000, 123.6875000040967905, 0.000000000000000000 ) ) ;
#35912 = CARTESIAN_POINT ( 'NONE',  ( -10.18810118749999916, 4.220049686691934809, 97.93750000204836681 ) ) ;
#35913 = DIRECTION ( 'NONE',  ( -0.000000000000000000, 1.000000000000000000, -0.000000000000000000 ) ) ;
#35914 = CARTESIAN_POINT ( 'NONE',  ( -1.656854249492381248, 16.06249999726881228, -4.000000000000001776 ) ) ;
#35915 = CARTESIAN_POINT ( 'NONE',  ( 4.541265875000001451, 1.249999998634407028, 1.881053915767124440 ) ) ;
#35916 = VERTEX_POINT ( 'NONE', #30402 ) ;
#35917 = VECTOR ( 'NONE', #34029, 1000.000000000000000 ) ;
#35918 = CARTESIAN_POINT ( 'NONE',  ( 4.556349186104052151, -10.99999999999999822, 80.96874999999995737 ) ) ;
#35919 = CARTESIAN_POINT ( 'NONE',  ( -3.458734124999959914, 200.4375000013656063, 198.0000000000000284 ) ) ;
#35921 = CARTESIAN_POINT ( 'NONE',  ( -5.000000000000000000, 18.53862685874501537, 23.57305537018163477 ) ) ;
#35920 = CARTESIAN_POINT ( 'NONE',  ( -26.56734541678242678, 202.3750000013655779, 166.5412658750003345 ) ) ;
#35922 =( NAMED_UNIT ( * ) PLANE_ANGLE_UNIT ( ) SI_UNIT ( $, .RADIAN. ) );
#35923 = MECHANICAL_DESIGN_GEOMETRIC_PRESENTATION_REPRESENTATION (  '', ( #64842 ), #67208 ) ;
#35924 = CARTESIAN_POINT ( 'NONE',  ( -3.211159895383562723, 13.93749999863440614, 3.211159895383561391 ) ) ;
#35925 = CARTESIAN_POINT ( 'NONE',  ( -4.556349186104045934, 11.00000000000000000, 84.71874999999998579 ) ) ;
#35926 = CARTESIAN_POINT ( 'NONE',  ( 1.320432766682872962E-15, -7.188101187499992051, 15.36155278187175277 ) ) ;
#35927 = ORIENTED_EDGE ( 'NONE', *, *, #23020, .F. ) ;
#35928 = ORIENTED_EDGE ( 'NONE', *, *, #64300, .T. ) ;
#35929 = CARTESIAN_POINT ( 'NONE',  ( 10.18810118749999916, 1.247682550866122264E-15, 104.4062500020483810 ) ) ;
#35930 = LINE ( 'NONE', #57843, #2027 ) ;
#35931 = CARTESIAN_POINT ( 'NONE',  ( -32.00000000000000000, 205.2500000000000284, 170.0000000000003979 ) ) ;
#35932 = CARTESIAN_POINT ( 'NONE',  ( 3.458734125000016313, 194.8750000013656063, 199.4326545832176691 ) ) ;
#35933 = DIRECTION ( 'NONE',  ( 0.000000000000000000, 0.8536788251726059595, -0.5207998305029671871 ) ) ;
#35934 = CARTESIAN_POINT ( 'NONE',  ( 10.00000000000000178, 90.00000000000001421, 0.000000000000000000 ) ) ;
#35935 = CARTESIAN_POINT ( 'NONE',  ( 5.656854249492381470, 121.0625000000000000, 5.656854249492379694 ) ) ;
#35936 = CARTESIAN_POINT ( 'NONE',  ( 6.676582343750003368, 296.1718750017069510, -2.765530957081997254 ) ) ;
#35937 = VERTEX_POINT ( 'NONE', #13759 ) ;
#35938 = FACE_OUTER_BOUND ( 'NONE', #59373, .T. ) ;
#35939 = CARTESIAN_POINT ( 'NONE',  ( -8.000000000000000000, 16.96874999590322730, -3.313708498984762496 ) ) ;
#35940 = CARTESIAN_POINT ( 'NONE',  ( -2.445694354108838731, 206.0625000013656063, 144.4456943541088663 ) ) ;
#35941 = CARTESIAN_POINT ( 'NONE',  ( 5.656854249492380582, 11.99999999590322197, -5.656854249492380582 ) ) ;
#35942 = CARTESIAN_POINT ( 'NONE',  ( 8.000000000000000000, 0.000000000000000000, 3.577867169202164632E-15 ) ) ;
#35943 = CARTESIAN_POINT ( 'NONE',  ( 2.679491924311235174, 226.4583333333333144, 9.999999999999998224 ) ) ;
#35944 = CARTESIAN_POINT ( 'NONE',  ( 5.094039351226809842, 8.823160935565649510, 67.53052393240218976 ) ) ;
#35945 =( BOUNDED_CURVE ( )  B_SPLINE_CURVE ( 2, ( #25266, #60728, #13935, #3768, #32064, #26000, #37730, #66383, #30939 ),
 .UNSPECIFIED., .F., .F. ) 
 B_SPLINE_CURVE_WITH_KNOTS ( ( 3, 2, 2, 2, 3 ),
 ( 0.9500000000000009548, 0.9583333333333343695, 0.9666666666666675622, 0.9750000000000007550, 0.9833333333333340587 ),
 .UNSPECIFIED. ) 
 CURVE ( )  GEOMETRIC_REPRESENTATION_ITEM ( )  RATIONAL_B_SPLINE_CURVE ( ( 0.9999999999999908962, 0.9238795325112958423, 1.000000000000000000, 0.9238795325112867385, 1.000000000000000000, 0.9238795325112867385, 1.000000000000000000, 0.9238795325112796331, 1.000000000000007105 ) ) 
 REPRESENTATION_ITEM ( '' )  );
#35946 = CARTESIAN_POINT ( 'NONE',  ( -10.00000000000000355, 212.7083333333333144, 2.679491924311223183 ) ) ;
#35947 = EDGE_CURVE ( 'NONE', #545, #50184, #24724, .T. ) ;
#35948 = CARTESIAN_POINT ( 'NONE',  ( 1.320432766682872962E-15, -7.188101187499992051, 12.73655278187175277 ) ) ;
#35949 = CARTESIAN_POINT ( 'NONE',  ( 9.832129032723420536, 186.5104166632526983, -5.676582343749999815 ) ) ;
#35950 = CARTESIAN_POINT ( 'NONE',  ( -1.881053915767124440, 0.9999999986344065839, 4.541265875000001451 ) ) ;
#35951 = CARTESIAN_POINT ( 'NONE',  ( -3.313708498984707429, 99.40625000409677625, -8.000000000000055067 ) ) ;
#35952 = CARTESIAN_POINT ( 'NONE',  ( 1.347111479062088405E-15, 45.00000000000000000, 11.00000000000000000 ) ) ;
#35953 = VERTEX_POINT ( 'NONE', #42077 ) ;
#35954 = CARTESIAN_POINT ( 'NONE',  ( 1.432654583217607414, 208.5000000013656063, 145.4587341250000634 ) ) ;
#35955 = CARTESIAN_POINT ( 'NONE',  ( -8.311093377946841443, 44.21874999658602690, 8.311093377946830785 ) ) ;
#35956 = CARTESIAN_POINT ( 'NONE',  ( 11.00000000000000355, -4.556349186104045046, 105.3437500040967763 ) ) ;
#35957 = CARTESIAN_POINT ( 'NONE',  ( -5.676582343749998039, 217.7604166632526983, -9.832129032723420536 ) ) ;
#35958 = CARTESIAN_POINT ( 'NONE',  ( -24.54126587499999701, 206.1875000013656063, 170.0000000000002842 ) ) ;
#35959 = CARTESIAN_POINT ( 'NONE',  ( -6.735557395310442023E-16, 11.00000000000000000, 71.12500000000000000 ) ) ;
#35961 = CYLINDRICAL_SURFACE ( 'NONE', #53502, 6.000000000000001776 ) ;
#35960 = DIRECTION ( 'NONE',  ( 1.000000000000000000, 0.000000000000000000, 0.000000000000000000 ) ) ;
#35962 = CARTESIAN_POINT ( 'NONE',  ( -11.00000000000000000, 0.000000000000000000, 88.00000000000000000 ) ) ;
#35963 = ADVANCED_FACE ( 'NONE', ( #65087 ), #36436, .T. ) ;
#35964 = ADVANCED_FACE ( 'NONE', ( #7026 ), #65830, .T. ) ;
#35965 = AXIS2_PLACEMENT_3D ( 'NONE', #72023, #21097, #50510 ) ;
#35966 = CARTESIAN_POINT ( 'NONE',  ( 10.00000000000000178, 71.87499999317203958, 0.000000000000000000 ) ) ;
#35967 = CARTESIAN_POINT ( 'NONE',  ( 7.188101187500001821, 99.50000000204838102, -2.977408999572651371 ) ) ;
#35968 = CARTESIAN_POINT ( 'NONE',  ( -4.541265875000002339, 15.87499999863440436, -1.881053915767121998 ) ) ;
#35969 = CARTESIAN_POINT ( 'NONE',  ( -10.00000000000000888, 72.70833333333332860, 2.679491924311224516 ) ) ;
#35970 = CARTESIAN_POINT ( 'NONE',  ( 2.012362677162108593, 0.3822906927398848076, -7.638045755507497425 ) ) ;
#35971 = CARTESIAN_POINT ( 'NONE',  ( 7.999999999999991118, 9.797174393178815797E-16, 1.580302779823364201 ) ) ;
#35972 = ORIENTED_EDGE ( 'NONE', *, *, #26071, .T. ) ;
#35973 = ORIENTED_EDGE ( 'NONE', *, *, #63303, .F. ) ;
#35974 =( BOUNDED_CURVE ( )  B_SPLINE_CURVE ( 2, ( #27522, #27899, #32836, #22227, #68265, #62595, #1, #28276, #56959, #50534, #44888, #22989, #22601, #45995, #27150, #29760, #29400, #63714, #1838, #24824, #23727, #6394, #70135, #23354, #40709, #18069, #46368, #70495, #1112, #47097, #30133, #12037, #47838, #70860, #35799, #35071, #24464, #1483, #24088, #18442, #40338, #30500, #58083, #18813, #6756, #52409, #46732, #63340, #11665, #47472, #12404, #41456, #64469, #17692, #53149, #69756, #34700, #58815, #7125, #64827, #12767, #744, #41817, #13131, #36165, #59185, #57708, #7495, #53519, #6014, #29018, #35438, #52037, #69382, #41085, #64095, #373, #58448, #52774, #65935, #25933, #49329, #26306, #65186, #26691, #20274, #72344, #48576, #20657, #37280, #71960, #25563, #19909, #32370, #19171, #3694, #14242, #66686, #2574, #43674, #30868, #55012, #37656, #7863, #8976, #13861, #48949, #14989, #59547, #53886, #38027, #55385, #31238, #13498, #42916, #2198, #66311, #60273, #25194, #61027, #14617, #9351, #48207, #49713, #42174, #3318, #43296, #36536, #71586, #36904, #71215, #65564, #19535, #8600, #42553, #59912, #31614, #8228, #54635, #54264, #2944, #60654, #31991, #39516, #39880, #62145, #4441, #21772, #16104, #5558, #15364, #56874, #34243, #38400, #57245, #16479, #27069, #73096, #10097, #67440, #33135, #56131, #28560, #45171, #32751, #51198, #10468, #61780, #21403, #72727, #21031, #27432, #33499, #44799, #4075, #38777, #33874, #9729, #27814, #44055, #50825, #50447, #5190, #28187, #22142, #56501, #73464, #62882, #68182, #67065, #50083, #44425, #67812, #61403, #39140, #4818, #73836, #68551, #62514, #10840, #74209, #22512, #45534, #16854, #55759, #15738, #11215, #1396, #5934, #41737, #63256, #51566, #17610, #6674, #34616, #51953, #29315, #57622, #7042, #12326, #58369, #47017, #70049, #24382, #35357, #46280, #29678, #7409, #74584, #22898, #52694, #64011, #64747, #291, #30050, #17985, #69299, #34989, #1028, #24008, #40254, #28935, #13045, #23646, #18358, #41373, #46653, #52324, #45910, #53063, #68923, #40628, #58005, #64383, #18728, #12682, #35716, #36083, #6310, #661, #47389, #70412, #69672, #59102, #11581, #17233, #41004, #23271, #58731, #63628, #11958, #7777, #25842, #36817, #25105, #66219, #59826, #59464, #48122, #36451, #37187, #42090, #42464, #60186, #14899, #31899, #65102, #54920, #30416, #14524, #54547, #24739, #8142, #71128, #70773, #2111, #3229, #30781, #53802, #48862, #31145, #26216, #43578, #65480, #47749, #54177, #19087, #2854, #2483, #13413, #49236, #71871, #19451, #13773, #25475, #66594, #72250, #60562, #42826, #14152, #48493, #71496, #19820, #20564, #65844, #8509, #31525, #20185, #53437, #43203, #37563, #37937, #8886, #60936, #1758, #68093, #33405, #67723, #44337, #74118, #56405, #26598, #16382, #45441, #49620, #68456, #27719, #38310, #9641, #21315, #3987, #67348, #61316, #39051, #15646, #39421, #9258, #32662, #22052, #33779, #55670, #16757, #38687, #32281, #39782, #62420, #56042, #16021, #62054, #26976, #73745, #61689, #55295, #4724, #50730, #56779, #10379, #49990, #44708, #3601, #72636, #45079, #20940, #10745, #5100, #28091, #51106, #4351, #43961, #15274, #10010, #73006, #66970, #22419, #33042, #27342, #50358, #73377, #21682, #34150, #70320, #57150, #28835, #46186, #29585, #29955, #936, #35262, #52968, #69204, #11862, #41277, #563, #5466, #52598, #69579, #52231, #23918, #6579, #51475, #46927, #69952, #23546, #34897, #68826, #51854, #18261, #74488, #17890, #11127, #40905, #17138, #17515, #64287, #1301, #46558, #40531, #57904, #6212, #18635, #28467, #40163, #63537, #62785, #29218, #63913, #12225, #58635, #12593, #58277, #198, #23174, #24283, #35621, #22795, #6943, #47294, #45815, #11494, #63168, #34528, #57533, #5841, #71403, #24646, #42001, #19356, #47657, #71778, #2385, #48399, #31429, #65010, #26122, #49142, #37092, #36356, #25750, #2763, #25382, #19728, #54077, #31808, #13318, #20094, #8045, #59371, #42738, #72153, #65385, #54829, #41644, #43107, #66125, #3138, #65753, #14432, #48771, #12952, #64654, #14055, #7682, #25008, #8414, #8795, #54456, #60096, #35992, #48027, #13683, #37465, #60466, #59009, #7314, #30321, #31050, #53339, #1665, #70678, #18995, #30689, #53708, #2019, #71037, #42370, #36724, #59736, #3509, #20849, #55204, #61594, #20464, #32183, #61222, #9913 ),
 .UNSPECIFIED., .F., .F. ) 
 B_SPLINE_CURVE_WITH_KNOTS ( ( 3, 2, 2, 2, 2, 2, 2, 2, 2, 2, 2, 2, 2, 2, 2, 2, 2, 2, 2, 2, 2, 2, 2, 2, 2, 2, 2, 2, 2, 2, 2, 2, 2, 2, 2, 2, 2, 2, 2, 2, 2, 2, 2, 2, 2, 2, 2, 2, 2, 2, 2, 2, 2, 2, 2, 2, 2, 2, 2, 2, 2, 2, 2, 2, 2, 2, 2, 2, 2, 2, 2, 2, 2, 2, 2, 2, 2, 2, 2, 2, 2, 2, 2, 2, 2, 2, 2, 2, 2, 2, 2, 2, 2, 2, 2, 2, 2, 2, 2, 2, 2, 2, 2, 2, 2, 2, 2, 2, 2, 2, 2, 2, 2, 2, 2, 2, 2, 2, 2, 2, 2, 2, 2, 2, 2, 2, 2, 2, 2, 2, 2, 2, 2, 2, 2, 2, 2, 2, 2, 2, 2, 2, 2, 2, 2, 2, 2, 2, 2, 2, 2, 2, 2, 2, 2, 2, 2, 2, 2, 2, 2, 2, 2, 2, 2, 2, 2, 2, 2, 2, 2, 2, 2, 2, 2, 2, 2, 2, 2, 2, 2, 2, 2, 2, 2, 2, 2, 2, 2, 2, 2, 2, 2, 2, 2, 2, 2, 2, 2, 2, 2, 2, 2, 2, 2, 2, 2, 2, 2, 2, 2, 2, 2, 2, 2, 2, 2, 2, 2, 2, 2, 2, 2, 2, 2, 2, 2, 2, 2, 2, 2, 2, 2, 2, 2, 2, 2, 2, 2, 2, 2, 2, 2, 2, 2, 2, 2, 2, 2, 2, 2, 2, 2, 2, 2, 2, 2, 2, 2, 2, 2, 2, 2, 2, 2, 2, 2, 3 ),
 ( 0.000000000000000000, 0.003750026888355633900, 0.007500053776711267800, 0.01125008066506690170, 0.01500010755342253560, 0.01875013444177817123, 0.02250016133013380340, 0.02625018821848943557, 0.03000021510684507120, 0.03375024199520070683, 0.03750026888355634247, 0.04125029577191197117, 0.04500032266026760680, 0.04875034954862323550, 0.05250037643697887113, 0.05625040332533450677, 0.06000043021369014240, 0.06375045710204577110, 0.06750048399040141367, 0.07125051087875704237, 0.07500053776711268494, 0.07875056465546831364, 0.08250059154382394233, 0.08625061843217958490, 0.09000064532053521360, 0.09375067220889085617, 0.09750069909724647099, 0.1012507259856021136, 0.1050007528739577423, 0.1087507797623133710, 0.1125008066506690135, 0.1162508335390246422, 0.1200008604273802848, 0.1237508873157359135, 0.1275009142040915422, 0.1312509410924471709, 0.1350009679808028273, 0.1387509948691584283, 0.1425010217575140847, 0.1462510486458697134, 0.1500010755342253699, 0.1537511024225809708, 0.1575011293109366273, 0.1612511561992922560, 0.1650011830876478847, 0.1687512099760035134, 0.1725012368643591698, 0.1762512637527147985, 0.1800012906410704272, 0.1837513175294260559, 0.1875013444177817123, 0.1912513713061373133, 0.1950013981944929420, 0.1987514250828485984, 0.2025014519712042271, 0.2062514788595598558, 0.2100015057479154845, 0.2137515326362711410, 0.2175015595246267419, 0.2212515864129823984, 0.2250016133013380271, 0.2287516401896936835, 0.2325016670780492845, 0.2362516939664049409, 0.2400017208547605696, 0.2437517477431161983, 0.2475017746314718270, 0.2512518015198274557, 0.2550018284081830844, 0.2587518552965387131, 0.2625018821848943418, 0.2662519090732500260, 0.2700019359616056547, 0.2737519628499612834, 0.2775019897383168566, 0.2812520166266725408, 0.2850020435150281695, 0.2887520704033837982, 0.2925020972917394269, 0.2962521241800951111, 0.3000021510684507398, 0.3037521779568063129, 0.3075022048451619416, 0.3112522317335176258, 0.3150022586218732545, 0.3187522855102288832, 0.3225023123985845119, 0.3262523392869401406, 0.3300023661752957693, 0.3337523930636513980, 0.3375024199520070267, 0.3412524468403626554, 0.3450024737287183396, 0.3487525006170739683, 0.3525025275054295970, 0.3562525543937851702, 0.3600025812821408544, 0.3637526081704964831, 0.3675026350588521118, 0.3712526619472077405, 0.3750026888355634247, 0.3787527157239190534, 0.3825027426122746266, 0.3862527695006302553, 0.3900027963889858840, 0.3937528232773415682, 0.3975028501656971969, 0.4012528770540528256, 0.4050029039424084543, 0.4087529308307640830, 0.4125029577191197117, 0.4162529846074753404, 0.4200030114958309690, 0.4237530383841866533, 0.4275030652725422819, 0.4312530921608979106, 0.4350031190492534838, 0.4387531459376091680, 0.4425031728259647967, 0.4462531997143204254, 0.4500032266026760541, 0.4537532534910316828, 0.4575032803793873670, 0.4612533072677429402, 0.4650033341560985689, 0.4687533610444541976, 0.4725033879328098818, 0.4762534148211655105, 0.4800034417095211392, 0.4837534685978767679, 0.4875034954862323966, 0.4912535223745880253, 0.4950035492629436540, 0.4987535761512992827, 0.5025036030396549114, 0.5062536299280105956, 0.5100036568163661688, 0.5137536837047218530, 0.5175037105930774262, 0.5212537374814331104, 0.5250037643697886836, 0.5287537912581443678, 0.5325038181465000520, 0.5362538450348556252, 0.5400038719232113094, 0.5437538988115668825, 0.5475039256999225667, 0.5512539525882781399, 0.5550039794766337131, 0.5587540063649895083, 0.5625040332533450815, 0.5662540601417007657, 0.5700040870300563389, 0.5737541139184120231, 0.5775041408067675963, 0.5812541676951231695, 0.5850041945834788537, 0.5887542214718344269, 0.5925042483601902221, 0.5962542752485457953, 0.6000043021369014795, 0.6037543290252570527, 0.6075043559136126259, 0.6112543828019683101, 0.6150044096903238833, 0.6187544365786795675, 0.6225044634670352517, 0.6262544903553909359, 0.6300045172437465091, 0.6337545441321020823, 0.6375045710204577665, 0.6412545979088133397, 0.6450046247971690239, 0.6487546516855245970, 0.6525046785738802813, 0.6562547054622359655, 0.6600047323505915386, 0.6637547592389472229, 0.6675047861273027960, 0.6712548130156584802, 0.6750048399040140534, 0.6787548667923697376, 0.6825048936807253108, 0.6862549205690809950, 0.6900049474574366792, 0.6937549743457922524, 0.6975050012341479366, 0.7012550281225035098, 0.7050050550108591940, 0.7087550818992147672, 0.7125051087875703404, 0.7162551356759260246, 0.7200051625642817088, 0.7237551894526373930, 0.7275052163409929662, 0.7312552432293486504, 0.7350052701177042236, 0.7387552970060597968, 0.7425053238944154810, 0.7462553507827710542, 0.7500053776711268494, 0.7537554045594824226, 0.7575054314478381068, 0.7612554583361936800, 0.7650054852245492532, 0.7687555121129049374, 0.7725055390012605105, 0.7762555658896161948, 0.7800055927779717679, 0.7837556196663275632, 0.7875056465546831364, 0.7912556734430387095, 0.7950057003313943937, 0.7987557272197499669, 0.8025057541081056511, 0.8062557809964612243, 0.8100058078848169085, 0.8137558347731725927, 0.8175058616615281659, 0.8212558885498838501, 0.8250059154382394233, 0.8287559423265951075, 0.8325059692149506807, 0.8362559961033063649, 0.8400060229916619381, 0.8437560498800175113, 0.8475060767683733065, 0.8512561036567288797, 0.8550061305450845639, 0.8587561574334401371, 0.8625061843217958213, 0.8662562112101513945, 0.8700062380985069677, 0.8737562649868626519, 0.8775062918752183361, 0.8812563187635740203, 0.8850063456519295935, 0.8887563725402852777, 0.8925063994286408509, 0.8962564263169964240, 0.9000064532053521082, 0.9037564800937076814, 0.9075065069820633656, 0.9112565338704190498, 0.9150065607587747341, 0.9187565876471303072, 0.9225066145354858804, 0.9262566414238415646, 0.9300066683121971378, 0.9337566952005528220, 0.9375067220889083952, 0.9412567489772641904, 0.9450067758656197636, 0.9487568027539753368, 0.9525068296423310210, 0.9562568565306865942, 0.9600068834190422784, 0.9637569103073978516, 0.9675069371957535358, 0.9712569640841091090, 0.9750069909724647932, 0.9787570178608204774, 0.9825070447491760506, 0.9862570716375317348, 0.9900070985258873080, 0.9937571254142429922, 0.9975071523025985654, 1.000000000000000000 ),
 .UNSPECIFIED. ) 
 CURVE ( )  GEOMETRIC_REPRESENTATION_ITEM ( )  RATIONAL_B_SPLINE_CURVE ( ( 1.000000000000000000, 0.9238795325112867385, 1.000000000000000000, 0.9238795325112867385, 1.000000000000000000, 0.9238795325112867385, 1.000000000000000000, 0.9238795325112867385, 1.000000000000000000, 0.9238795325112867385, 1.000000000000000000, 0.9238795325112867385, 1.000000000000000000, 0.9238795325112867385, 1.000000000000000000, 0.9238795325112867385, 1.000000000000000000, 0.9238795325112867385, 1.000000000000000000, 0.9238795325112867385, 1.000000000000000000, 0.9238795325112867385, 1.000000000000000000, 0.9238795325112867385, 1.000000000000000000, 0.9238795325112867385, 1.000000000000000000, 0.9238795325112867385, 1.000000000000000000, 0.9238795325112867385, 1.000000000000000000, 0.9238795325112867385, 1.000000000000000000, 0.9238795325112867385, 1.000000000000000000, 0.9238795325112867385, 1.000000000000000000, 0.9238795325112867385, 1.000000000000000000, 0.9238795325112867385, 1.000000000000000000, 0.9238795325112867385, 1.000000000000000000, 0.9238795325112867385, 1.000000000000000000, 0.9238795325112867385, 1.000000000000000000, 0.9238795325112867385, 1.000000000000000000, 0.9238795325112867385, 1.000000000000000000, 0.9238795325112867385, 1.000000000000000000, 0.9238795325112867385, 1.000000000000000000, 0.9238795325112867385, 1.000000000000000000, 0.9238795325112867385, 1.000000000000000000, 0.9238795325112867385, 1.000000000000000000, 0.9238795325112867385, 1.000000000000000000, 0.9238795325112867385, 1.000000000000000000, 0.9238795325112867385, 1.000000000000000000, 0.9238795325112867385, 1.000000000000000000, 0.9238795325112867385, 1.000000000000000000, 0.9238795325112867385, 1.000000000000000000, 0.9238795325112867385, 1.000000000000000000, 0.9238795325112867385, 1.000000000000000000, 0.9238795325112867385, 1.000000000000000000, 0.9238795325112867385, 1.000000000000000000, 0.9238795325112867385, 1.000000000000000000, 0.9238795325112867385, 1.000000000000000000, 0.9238795325112867385, 1.000000000000000000, 0.9238795325112867385, 1.000000000000000000, 0.9238795325112867385, 1.000000000000000000, 0.9238795325112867385, 1.000000000000000000, 0.9238795325112867385, 1.000000000000000000, 0.9238795325112867385, 1.000000000000000000, 0.9238795325112867385, 1.000000000000000000, 0.9238795325112867385, 1.000000000000000000, 0.9238795325112867385, 1.000000000000000000, 0.9238795325112867385, 1.000000000000000000, 0.9238795325112867385, 1.000000000000000000, 0.9238795325112867385, 1.000000000000000000, 0.9238795325112867385, 1.000000000000000000, 0.9238795325112867385, 1.000000000000000000, 0.9238795325112867385, 1.000000000000000000, 0.9238795325112867385, 1.000000000000000000, 0.9238795325112867385, 1.000000000000000000, 0.9238795325112867385, 1.000000000000000000, 0.9238795325112867385, 1.000000000000000000, 0.9238795325112867385, 1.000000000000000000, 0.9238795325112867385, 1.000000000000000000, 0.9238795325112867385, 1.000000000000000000, 0.9238795325112867385, 1.000000000000000000, 0.9238795325112867385, 1.000000000000000000, 0.9238795325112867385, 1.000000000000000000, 0.9238795325112867385, 1.000000000000000000, 0.9238795325112867385, 1.000000000000000000, 0.9238795325112867385, 1.000000000000000000, 0.9238795325112867385, 1.000000000000000000, 0.9238795325112867385, 1.000000000000000000, 0.9238795325112867385, 1.000000000000000000, 0.9238795325112867385, 1.000000000000000000, 0.9238795325112867385, 1.000000000000000000, 0.9238795325112867385, 1.000000000000000000, 0.9238795325112867385, 1.000000000000000000, 0.9238795325112867385, 1.000000000000000000, 0.9238795325112867385, 1.000000000000000000, 0.9238795325112867385, 1.000000000000000000, 0.9238795325112867385, 1.000000000000000000, 0.9238795325112867385, 1.000000000000000000, 0.9238795325112867385, 1.000000000000000000, 0.9238795325112867385, 1.000000000000000000, 0.9238795325112867385, 1.000000000000000000, 0.9238795325112867385, 1.000000000000000000, 0.9238795325112867385, 1.000000000000000000, 0.9238795325112867385, 1.000000000000000000, 0.9238795325112867385, 1.000000000000000000, 0.9238795325112867385, 1.000000000000000000, 0.9238795325112867385, 1.000000000000000000, 0.9238795325112867385, 1.000000000000000000, 0.9238795325112867385, 1.000000000000000000, 0.9238795325112867385, 1.000000000000000000, 0.9238795325112867385, 1.000000000000000000, 0.9238795325112867385, 1.000000000000000000, 0.9238795325112867385, 1.000000000000000000, 0.9238795325112867385, 1.000000000000000000, 0.9238795325112867385, 1.000000000000000000, 0.9238795325112867385, 1.000000000000000000, 0.9238795325112867385, 1.000000000000000000, 0.9238795325112867385, 1.000000000000000000, 0.9238795325112867385, 1.000000000000000000, 0.9238795325112867385, 1.000000000000000000, 0.9238795325112867385, 1.000000000000000000, 0.9238795325112867385, 1.000000000000000000, 0.9238795325112867385, 1.000000000000000000, 0.9238795325112867385, 1.000000000000000000, 0.9238795325112867385, 1.000000000000000000, 0.9238795325112867385, 1.000000000000000000, 0.9238795325112867385, 1.000000000000000000, 0.9238795325112867385, 1.000000000000000000, 0.9238795325112867385, 1.000000000000000000, 0.9238795325112867385, 1.000000000000000000, 0.9238795325112867385, 1.000000000000000000, 0.9238795325112867385, 1.000000000000000000, 0.9238795325112867385, 1.000000000000000000, 0.9238795325112867385, 1.000000000000000000, 0.9238795325112867385, 1.000000000000000000, 0.9238795325112867385, 1.000000000000000000, 0.9238795325112867385, 1.000000000000000000, 0.9238795325112867385, 1.000000000000000000, 0.9238795325112867385, 1.000000000000000000, 0.9238795325112867385, 1.000000000000000000, 0.9238795325112867385, 1.000000000000000000, 0.9238795325112867385, 1.000000000000000000, 0.9238795325112867385, 1.000000000000000000, 0.9238795325112867385, 1.000000000000000000, 0.9238795325112867385, 1.000000000000000000, 0.9238795325112867385, 1.000000000000000000, 0.9238795325112867385, 1.000000000000000000, 0.9238795325112867385, 1.000000000000000000, 0.9238795325112867385, 1.000000000000000000, 0.9238795325112867385, 1.000000000000000000, 0.9238795325112867385, 1.000000000000000000, 0.9238795325112867385, 1.000000000000000000, 0.9238795325112867385, 1.000000000000000000, 0.9238795325112867385, 1.000000000000000000, 0.9238795325112867385, 1.000000000000000000, 0.9238795325112867385, 1.000000000000000000, 0.9238795325112867385, 1.000000000000000000, 0.9238795325112867385, 1.000000000000000000, 0.9238795325112867385, 1.000000000000000000, 0.9238795325112867385, 1.000000000000000000, 0.9238795325112867385, 1.000000000000000000, 0.9238795325112867385, 1.000000000000000000, 0.9238795325112867385, 1.000000000000000000, 0.9238795325112867385, 1.000000000000000000, 0.9238795325112867385, 1.000000000000000000, 0.9238795325112867385, 1.000000000000000000, 0.9238795325112867385, 1.000000000000000000, 0.9238795325112867385, 1.000000000000000000, 0.9238795325112867385, 1.000000000000000000, 0.9238795325112867385, 1.000000000000000000, 0.9238795325112867385, 1.000000000000000000, 0.9238795325112867385, 1.000000000000000000, 0.9238795325112867385, 1.000000000000000000, 0.9238795325112867385, 1.000000000000000000, 0.9238795325112867385, 1.000000000000000000, 0.9238795325112867385, 1.000000000000000000, 0.9238795325112867385, 1.000000000000000000, 0.9238795325112867385, 1.000000000000000000, 0.9238795325112867385, 1.000000000000000000, 0.9238795325112867385, 1.000000000000000000, 0.9238795325112867385, 1.000000000000000000, 0.9238795325112867385, 1.000000000000000000, 0.9238795325112867385, 1.000000000000000000, 0.9238795325112867385, 1.000000000000000000, 0.9238795325112867385, 1.000000000000000000, 0.9238795325112867385, 1.000000000000000000, 0.9238795325112867385, 1.000000000000000000, 0.9238795325112867385, 1.000000000000000000, 0.9238795325112867385, 1.000000000000000000, 0.9238795325112867385, 1.000000000000000000, 0.9238795325112867385, 1.000000000000000000, 0.9238795325112867385, 1.000000000000000000, 0.9238795325112867385, 1.000000000000000000, 0.9238795325112867385, 1.000000000000000000, 0.9238795325112867385, 1.000000000000000000, 0.9238795325112867385, 1.000000000000000000, 0.9238795325112867385, 1.000000000000000000, 0.9238795325112867385, 1.000000000000000000, 0.9238795325112867385, 1.000000000000000000, 0.9238795325112867385, 1.000000000000000000, 0.9238795325112867385, 1.000000000000000000, 0.9238795325112867385, 1.000000000000000000, 0.9238795325112867385, 1.000000000000000000, 0.9238795325112867385, 1.000000000000000000, 0.9238795325112867385, 1.000000000000000000, 0.9238795325112867385, 1.000000000000000000, 0.9238795325112867385, 1.000000000000000000, 0.9238795325112867385, 1.000000000000000000, 0.9238795325112867385, 1.000000000000000000, 0.9238795325112867385, 1.000000000000000000, 0.9238795325112867385, 1.000000000000000000, 0.9238795325112867385, 1.000000000000000000, 0.9238795325112867385, 1.000000000000000000, 0.9238795325112867385, 1.000000000000000000, 0.9238795325112867385, 1.000000000000000000, 0.9238795325112867385, 1.000000000000000000, 0.9238795325112867385, 1.000000000000000000, 0.9238795325112867385, 1.000000000000000000, 0.9238795325112867385, 1.000000000000000000, 0.9238795325112867385, 1.000000000000000000, 0.9238795325112867385, 1.000000000000000000, 0.9238795325112867385, 1.000000000000000000, 0.9238795325112867385, 1.000000000000000000, 0.9238795325112867385, 1.000000000000000000, 0.9238795325112867385, 1.000000000000000000, 0.9238795325112867385, 1.000000000000000000, 0.9238795325112867385, 1.000000000000000000, 0.9238795325112867385, 1.000000000000000000, 0.9238795325112867385, 1.000000000000000000, 0.9238795325112867385, 1.000000000000000000, 0.9238795325112867385, 1.000000000000000000, 0.9238795325112867385, 1.000000000000000000, 0.9238795325112867385, 1.000000000000000000, 0.9238795325112867385, 1.000000000000000000, 0.9238795325112867385, 1.000000000000000000, 0.9238795325112867385, 1.000000000000000000, 0.9238795325112867385, 1.000000000000000000, 0.9238795325112867385, 1.000000000000000000, 0.9238795325112867385, 1.000000000000000000, 0.9238795325112867385, 1.000000000000000000, 0.9238795325112867385, 1.000000000000000000, 0.9238795325112867385, 1.000000000000000000, 0.9238795325112867385, 1.000000000000000000, 0.9238795325112867385, 1.000000000000000000, 0.9238795325112867385, 1.000000000000000000, 0.9238795325112867385, 1.000000000000000000, 0.9238795325112867385, 1.000000000000000000, 0.9238795325112867385, 1.000000000000000000, 0.9238795325112867385, 1.000000000000000000, 0.9238795325112867385, 1.000000000000000000, 0.9238795325112867385, 1.000000000000000000, 0.9238795325112867385, 1.000000000000000000, 0.9238795325112867385, 1.000000000000000000, 0.9238795325112867385, 1.000000000000000000, 0.9238795325112867385, 1.000000000000000000, 0.9238795325112867385, 1.000000000000000000, 0.9238795325112867385, 1.000000000000000000, 0.9238795325112867385, 1.000000000000000000, 0.9238795325112867385, 1.000000000000000000, 0.9238795325112867385, 1.000000000000000000, 0.9238795325112867385, 1.000000000000000000, 0.9238795325112867385, 1.000000000000000000, 0.9238795325112867385, 1.000000000000000000, 0.9238795325112867385, 1.000000000000000000, 0.9238795325112867385, 1.000000000000000000, 0.9238795325112867385, 1.000000000000000000, 0.9238795325112867385, 1.000000000000000000, 0.9238795325112867385, 1.000000000000000000, 0.9238795325112867385, 1.000000000000000000, 0.9238795325112867385, 1.000000000000000000, 0.9238795325112867385, 1.000000000000000000, 0.9238795325112867385, 1.000000000000000000, 0.9238795325112867385, 1.000000000000000000, 0.9238795325112867385, 1.000000000000000000, 0.9238795325112867385, 1.000000000000000000, 0.9238795325112867385, 1.000000000000000000, 0.9238795325112867385, 1.000000000000000000, 0.9238795325112867385, 1.000000000000000000, 0.9238795325112867385, 1.000000000000000000, 0.9238795325112867385, 1.000000000000000000, 0.9238795325112867385, 1.000000000000000000, 0.9238795325112867385, 1.000000000000000000, 0.9493985675959865089, 0.9660722070829228514 ) ) 
 REPRESENTATION_ITEM ( '' )  );
#35975 = CARTESIAN_POINT ( 'NONE',  ( 2.765530957082001251, 295.9218750017070079, 6.676582343750000703 ) ) ;
#35976 = CARTESIAN_POINT ( 'NONE',  ( -2.679491924311238282, 143.5416666666667140, 10.00000000000001243 ) ) ;
#35977 = CARTESIAN_POINT ( 'NONE',  ( -10.00000000000000888, 17.29166666666666430, -2.679491924311232953 ) ) ;
#35978 = CARTESIAN_POINT ( 'NONE',  ( 11.35316468750000141, 160.7812499965860127, 0.000000000000000000 ) ) ;
#35979 = CARTESIAN_POINT ( 'NONE',  ( -4.220049686691935698, 10.18810118749999916, 83.87500000204835260 ) ) ;
#35980 = CARTESIAN_POINT ( 'NONE',  ( 1.881637226502129035E-11, 6.249999999998538058, -10.00000000000000178 ) ) ;
#35981 = AXIS2_PLACEMENT_3D ( 'NONE', #16524, #73146, #39564 ) ;
#35982 = CARTESIAN_POINT ( 'NONE',  ( 2.828427124746208943, 200.6250000000000284, 195.1715728752538439 ) ) ;
#35983 = CARTESIAN_POINT ( 'NONE',  ( 37.99999999999999289, 38.00000000000000711, 65.00000000000000000 ) ) ;
#35984 = CARTESIAN_POINT ( 'NONE',  ( -4.220049686691935698, 10.18810118749999916, 108.2500000020483810 ) ) ;
#35985 = EDGE_LOOP ( 'NONE', ( #8212, #5223, #62380, #38288 ) ) ;
#35986 = PRESENTATION_LAYER_ASSIGNMENT (  '', '', ( #72086 ) ) ;
#35987 = CARTESIAN_POINT ( 'NONE',  ( 39.02743293177866235, -0.3100107776955418060, 119.9350212284735875 ) ) ;
#35988 = CYLINDRICAL_SURFACE ( 'NONE', #19553, 11.00000000000000000 ) ;
#35989 = CARTESIAN_POINT ( 'NONE',  ( 11.35316468749999785, 140.8854166632526699, 3.042071309553174174 ) ) ;
#35990 = CARTESIAN_POINT ( 'NONE',  ( 2.839093476692135984E-14, 199.6875000013656063, 201.4587341250000350 ) ) ;
#35991 = CARTESIAN_POINT ( 'NONE',  ( 2.445694354108839175, 209.3125000013656063, 195.5543056458912190 ) ) ;
#35992 = CARTESIAN_POINT ( 'NONE',  ( 4.220049686691941027, -10.18810118749999738, 70.00000000204836681 ) ) ;
#35993 = CARTESIAN_POINT ( 'NONE',  ( -5.676582343750006032, 49.42708332991935549, 9.832129032723418760 ) ) ;
#35994 = ORIENTED_EDGE ( 'NONE', *, *, #31273, .F. ) ;
#35995 = FACE_OUTER_BOUND ( 'NONE', #41844, .T. ) ;
#35996 = CARTESIAN_POINT ( 'NONE',  ( 1.881053915767122664, 6.249999998634407916, 4.541265875000001451 ) ) ;
#35997 = CARTESIAN_POINT ( 'NONE',  ( -8.008118988124991233, 0.000000000000000000, 14.51311528394063188 ) ) ;
#35998 = CARTESIAN_POINT ( 'NONE',  ( 5.082755093536325930, 12.65624999795161187, -5.082755093536325930 ) ) ;
#35999 = CARTESIAN_POINT ( 'NONE',  ( -6.000000000000000888, 293.1250000034141294, 2.485281374238575758 ) ) ;
#36000 = ADVANCED_FACE ( 'NONE', ( #8873 ), #31886, .F. ) ;
#36001 = CARTESIAN_POINT ( 'NONE',  ( -2.977408999572654480, 12.37499999795161010, 7.188101187499999156 ) ) ;
#36002 = CARTESIAN_POINT ( 'NONE',  ( -5.082755093536319713, 5.082755093536319713, 10.29905278187175455 ) ) ;
#36003 = CARTESIAN_POINT ( 'NONE',  ( -4.220049686691937474, -10.18810118749999738, 73.93750000204838102 ) ) ;
#36004 = CARTESIAN_POINT ( 'NONE',  ( -28.00000000000002132, 204.6875000013656063, 166.5412658750003629 ) ) ;
#36005 = CARTESIAN_POINT ( 'NONE',  ( -7.320508075688778149, 64.99999999317203958, 7.320508075688769267 ) ) ;
#36006 = CARTESIAN_POINT ( 'NONE',  ( -2.828427124746192067, 3.374999997268813612, 2.828427124746190735 ) ) ;
#36007 = ORIENTED_EDGE ( 'NONE', *, *, #62110, .T. ) ;
#36008 = CARTESIAN_POINT ( 'NONE',  ( 1.656854249492405451, 196.4375000027311842, 202.0000000000000284 ) ) ;
#36009 = CARTESIAN_POINT ( 'NONE',  ( -2.828427124746209831, 202.3750000000000284, 139.1715728752538723 ) ) ;
#36010 = CARTESIAN_POINT ( 'NONE',  ( -29.65685424949229088, 199.5625000027311842, 174.0000000000004547 ) ) ;
#36011 = CARTESIAN_POINT ( 'NONE',  ( -4.541265875000002339, 3.749999998634407028, -1.881053915767121998 ) ) ;
#36013 = CARTESIAN_POINT ( 'NONE',  ( 7.188101187500002709, 114.3125000020483952, 2.977408999572649151 ) ) ;
#36012 = CIRCLE ( 'NONE', #48004, 3.999999999999986233 ) ;
#36014 = CARTESIAN_POINT ( 'NONE',  ( 9.797174393178825657E-16, 125.0000000000000000, -8.000000000000000000 ) ) ;
#36015 = CARTESIAN_POINT ( 'NONE',  ( -7.999999999999991118, 0.000000000000000000, 2.517802783920143561 ) ) ;
#36016 = ORIENTED_EDGE ( 'NONE', *, *, #33346, .F. ) ;
#36017 = CARTESIAN_POINT ( 'NONE',  ( 5.082755093536325930, 26.15624999795161543, -5.082755093536325930 ) ) ;
#36018 = ORIENTED_EDGE ( 'NONE', *, *, #31558, .T. ) ;
#36019 = CARTESIAN_POINT ( 'NONE',  ( 9.999999999999998224, 255.8333333401613459, -2.679491924311229401 ) ) ;
#36020 = CARTESIAN_POINT ( 'NONE',  ( 0.000000000000000000, 255.9999999999999432, 0.000000000000000000 ) ) ;
#36021 = CARTESIAN_POINT ( 'NONE',  ( 27.99999999999997158, 206.9375000013656063, 166.5412658749999082 ) ) ;
#36022 = CARTESIAN_POINT ( 'NONE',  ( 8.660254037844385522, 49.58333333333333570, 5.000000000000005329 ) ) ;
#36023 = CIRCLE ( 'NONE', #46846, 10.99999999999998934 ) ;
#36024 = CARTESIAN_POINT ( 'NONE',  ( -5.082755093536324154, 100.7187500020483810, 5.082755093536326818 ) ) ;
#36025 = CARTESIAN_POINT ( 'NONE',  ( -4.242640687119286547, 297.8750000000000000, -4.242640687119286547 ) ) ;
#36027 = LINE ( 'NONE', #47332, #38590 ) ;
#36026 = CARTESIAN_POINT ( 'NONE',  ( 1.102182119232618108E-15, 288.3125000034140157, 6.000000000000001776 ) ) ;
#36028 = EDGE_LOOP ( 'NONE', ( #17099, #69050, #71052, #14350 ) ) ;
#36029 = CARTESIAN_POINT ( 'NONE',  ( 8.311093377946834337, 232.0312500034139873, -8.311093377946836114 ) ) ;
#36030 = EDGE_CURVE ( 'NONE', #31550, #63012, #32197, .T. ) ;
#36031 = CARTESIAN_POINT ( 'NONE',  ( -4.401442555609577197E-16, 7.188101187499992051, 11.98655278187175632 ) ) ;
#36032 = DIRECTION ( 'NONE',  ( -0.000000000000000000, 1.000000000000000000, 4.689100369878284071E-30 ) ) ;
#36033 = CARTESIAN_POINT ( 'NONE',  ( -27.99999999999999645, 195.0000000000000000, 166.0000000000003979 ) ) ;
#36034 = CARTESIAN_POINT ( 'NONE',  ( 2.775557561562891351E-14, -70.00000000000000000, 170.0000000000000000 ) ) ;
#36035 = CARTESIAN_POINT ( 'NONE',  ( 4.999999999999997335, 263.3333333333333712, -8.660254037844387298 ) ) ;
#36036 = CARTESIAN_POINT ( 'NONE',  ( -11.00000000000000000, 4.556349186104045934, 116.5937500040967763 ) ) ;
#36037 = CARTESIAN_POINT ( 'NONE',  ( 10.00000000000000178, 180.2083333333333144, -2.679491924311226736 ) ) ;
#36038 = CARTESIAN_POINT ( 'NONE',  ( 9.000000000000000000, 5.196152422706622254, -10.20000000000000284 ) ) ;
#36039 = DIRECTION ( 'NONE',  ( 0.000000000000000000, 0.000000000000000000, -1.000000000000000000 ) ) ;
#36040 = CARTESIAN_POINT ( 'NONE',  ( -5.082755093536319713, 5.082755093536319713, 28.67405278187175810 ) ) ;
#36041 = CARTESIAN_POINT ( 'NONE',  ( -9.832129032723420536, 144.0104166632526699, 5.676582343749997150 ) ) ;
#36042 = DIRECTION ( 'NONE',  ( 1.000000000000000000, 0.000000000000000000, 0.000000000000000000 ) ) ;
#36043 = CARTESIAN_POINT ( 'NONE',  ( 2.250000000000000000, 284.0000000000000000, 7.677076266392047543 ) ) ;
#36046 = CARTESIAN_POINT ( 'NONE',  ( 23.99999999999999645, 203.6875000000000284, 168.3431457505074889 ) ) ;
#36045 = LINE ( 'NONE', #18690, #56293 ) ;
#36044 = CARTESIAN_POINT ( 'NONE',  ( 26.34314575050758833, 206.9375000000000284, 173.9999999999999147 ) ) ;
#36047 = ORIENTED_EDGE ( 'NONE', *, *, #43022, .F. ) ;
#36048 = CARTESIAN_POINT ( 'NONE',  ( -3.999999999999960032, 206.0000000000000284, 198.0000000000000284 ) ) ;
#36049 = CYLINDRICAL_SURFACE ( 'NONE', #16661, 11.00000000000000000 ) ;
#36050 = DIRECTION ( 'NONE',  ( -0.000000000000000000, 1.000000000000000000, 4.689100369878284071E-30 ) ) ;
#36051 = CARTESIAN_POINT ( 'NONE',  ( -3.458734125000015425, 208.0000000013656063, 143.4326545832176976 ) ) ;
#36052 = CARTESIAN_POINT ( 'NONE',  ( -7.232528283688802517, 124.7618676830046098, -2.762902653109465145 ) ) ;
#36053 = CARTESIAN_POINT ( 'NONE',  ( -10.00000000000000178, 29.37499999317203248, -1.224646799147353454E-15 ) ) ;
#36054 = CARTESIAN_POINT ( 'NONE',  ( -5.082755093536325930, 114.9687500020483810, -5.082755093536325930 ) ) ;
#36055 = CARTESIAN_POINT ( 'NONE',  ( -1.881053915767121554, 2.749999998634406584, -4.541265875000002339 ) ) ;
#36056 = CARTESIAN_POINT ( 'NONE',  ( 2.436599634630261413, 67.82108862182671771, -20.21956363439073101 ) ) ;
#36057 = CARTESIAN_POINT ( 'NONE',  ( 7.999999999999992895, -3.313708498984756279, 13.48655277982336465 ) ) ;
#36059 = CARTESIAN_POINT ( 'NONE',  ( -5.656854249492373476, -5.656854249492376141, 17.70530278392014623 ) ) ;
#36058 = DIRECTION ( 'NONE',  ( -0.000000000000000000, 1.000000000000000000, -0.000000000000000000 ) ) ;
#36060 = VERTEX_POINT ( 'NONE', #44696 ) ;
#36061 = CARTESIAN_POINT ( 'NONE',  ( 4.898587196589412829E-16, 4.687499995903220196, -8.000000000000000000 ) ) ;
#36062 = DIRECTION ( 'NONE',  ( 1.000000000000000000, 0.000000000000000000, 0.000000000000000000 ) ) ;
#36063 = CARTESIAN_POINT ( 'NONE',  ( 9.832129032723416984, 227.1354166700806729, -5.676582343750003368 ) ) ;
#36064 = CARTESIAN_POINT ( 'NONE',  ( -5.676582343749998039, 117.4479166632526841, -9.832129032723420536 ) ) ;
#36065 = VERTEX_POINT ( 'NONE', #16010 ) ;
#36066 = ADVANCED_FACE ( 'NONE', ( #43949 ), #32649, .T. ) ;
#36067 = EDGE_CURVE ( 'NONE', #55362, #6054, #27330, .T. ) ;
#36068 = CARTESIAN_POINT ( 'NONE',  ( -10.18810118749999916, 4.220049686691934809, 100.5625000020483668 ) ) ;
#36069 = DIRECTION ( 'NONE',  ( -0.000000000000000000, -1.000000000000000000, -0.000000000000000000 ) ) ;
#36070 = CARTESIAN_POINT ( 'NONE',  ( 3.458734125000015425, 199.2500000013656063, 196.5673454167823877 ) ) ;
#36071 = FACE_OUTER_BOUND ( 'NONE', #7722, .T. ) ;
#36072 = CARTESIAN_POINT ( 'NONE',  ( -11.35316468749999785, 113.0729166632526841, -3.042071309553167957 ) ) ;
#36073 = CARTESIAN_POINT ( 'NONE',  ( -32.00000000000000000, 207.2500000000000284, 170.0000000000003979 ) ) ;
#36074 = ORIENTED_EDGE ( 'NONE', *, *, #56687, .T. ) ;
#36075 =( BOUNDED_CURVE ( )  B_SPLINE_CURVE ( 2, ( #62728, #41946, #65327, #47598, #25325, #70620, #37409, #54019, #36670 ),
 .UNSPECIFIED., .F., .F. ) 
 B_SPLINE_CURVE_WITH_KNOTS ( ( 3, 2, 2, 2, 3 ),
 ( 0.4027777777777777901, 0.4097222222222222099, 0.4166666666666666852, 0.4236111111111111049, 0.4305555555555555802 ),
 .UNSPECIFIED. ) 
 CURVE ( )  GEOMETRIC_REPRESENTATION_ITEM ( )  RATIONAL_B_SPLINE_CURVE ( ( 1.000000000000000000, 0.9238795325112867385, 1.000000000000000000, 0.9238795325112867385, 1.000000000000000000, 0.9238795325112867385, 1.000000000000000000, 0.9238795325112867385, 1.000000000000000000 ) ) 
 REPRESENTATION_ITEM ( '' )  );
#36076 = ADVANCED_FACE ( 'NONE', ( #33028 ), #3216, .T. ) ;
#36077 = CARTESIAN_POINT ( 'NONE',  ( 8.660254037844389075, 207.2916666598387110, -5.000000000000000000 ) ) ;
#36078 = VECTOR ( 'NONE', #25232, 1000.000000000000227 ) ;
#36079 = DIRECTION ( 'NONE',  ( -0.000000000000000000, 1.000000000000000000, -4.476705744456276341E-16 ) ) ;
#36080 = CARTESIAN_POINT ( 'NONE',  ( 3.042071309553167513, 97.13541666325268409, -11.35316468749999785 ) ) ;
#36081 = CARTESIAN_POINT ( 'NONE',  ( 3.458734125000016313, 208.8750000013656063, 199.4326545832176976 ) ) ;
#36082 = CARTESIAN_POINT ( 'NONE',  ( -2.977408999572650039, 13.31249999795161187, -7.188101187500000933 ) ) ;
#36083 = CARTESIAN_POINT ( 'NONE',  ( -10.18810118749999916, 4.220049686691934809, 93.43750000204836681 ) ) ;
#36084 = CARTESIAN_POINT ( 'NONE',  ( 9.832129032723420536, 11.51041666325268409, -5.676582343749999815 ) ) ;
#36085 = EDGE_LOOP ( 'NONE', ( #34999, #20992, #34522 ) ) ;
#36086 = CARTESIAN_POINT ( 'NONE',  ( 3.178432602446558121E-13, 136.2499999999999716, -10.00000000000000533 ) ) ;
#36087 = CARTESIAN_POINT ( 'NONE',  ( 1.503440688489920962, -42.39651873420264394, 139.0360479356116628 ) ) ;
#36088 = CARTESIAN_POINT ( 'NONE',  ( 2.020667218593132706E-15, -11.00000000000000000, 102.0625000040967763 ) ) ;
#36089 = CARTESIAN_POINT ( 'NONE',  ( 7.204075437095966983, 7.204075437095967871, 76.46875000204836681 ) ) ;
#36090 = AXIS2_PLACEMENT_3D ( 'NONE', #23720, #23349, #35065 ) ;
#36091 = DIRECTION ( 'NONE',  ( -0.000000000000000000, 1.000000000000000000, -0.000000000000000000 ) ) ;
#36092 = CARTESIAN_POINT ( 'NONE',  ( -8.660254037844387298, 264.5833333333333144, -4.999999999999999112 ) ) ;
#36093 = CARTESIAN_POINT ( 'NONE',  ( 2.765530957082001251, 294.7656250017070079, 6.676582343750000703 ) ) ;
#36094 = EDGE_CURVE ( 'NONE', #56146, #11062, #39903, .T. ) ;
#36095 = DIRECTION ( 'NONE',  ( -0.000000000000000000, 1.000000000000000000, -0.000000000000000000 ) ) ;
#36096 = CARTESIAN_POINT ( 'NONE',  ( -5.676582343750006032, 224.4270833299193555, 9.832129032723418760 ) ) ;
#36097 = AXIS2_PLACEMENT_3D ( 'NONE', #42902, #20646, #2933 ) ;
#36098 = CARTESIAN_POINT ( 'NONE',  ( -6.238412754330611322E-16, 10.18810118749999916, 89.78125000204836681 ) ) ;
#36099 = CARTESIAN_POINT ( 'NONE',  ( -24.54126587499998280, 203.1250000013656347, 171.4326545832179818 ) ) ;
#36100 = CARTESIAN_POINT ( 'NONE',  ( -5.656854249492381470, 26.43750000000000355, 5.656854249492379694 ) ) ;
#36101 = CARTESIAN_POINT ( 'NONE',  ( -4.541265875000002339, 12.93749999863440792, -5.561446717895856393E-16 ) ) ;
#36102 = ORIENTED_EDGE ( 'NONE', *, *, #57637, .F. ) ;
#36103 = CARTESIAN_POINT ( 'NONE',  ( -19.10415431754897142, -48.09380208991064620, 145.5760750361723979 ) ) ;
#36104 = CARTESIAN_POINT ( 'NONE',  ( 2.828427124746208943, 208.7500000027312126, 195.1715728752538439 ) ) ;
#36105 = CARTESIAN_POINT ( 'NONE',  ( -3.458734125000015425, 198.2500000013656347, 143.4326545832176976 ) ) ;
#36106 = CARTESIAN_POINT ( 'NONE',  ( 3.999999999999959144, 202.1875000027311842, 140.3431457505076594 ) ) ;
#36107 = CARTESIAN_POINT ( 'NONE',  ( 10.18810118749999916, 4.220049686691935698, 76.37500000204838102 ) ) ;
#36108 = ORIENTED_EDGE ( 'NONE', *, *, #19750, .T. ) ;
#36109 = CARTESIAN_POINT ( 'NONE',  ( 7.188101187500000044, 6.468749997951610986, 0.000000000000000000 ) ) ;
#36110 = FACE_OUTER_BOUND ( 'NONE', #134, .T. ) ;
#36111 = CARTESIAN_POINT ( 'NONE',  ( -5.082755093536325930, 115.3437500020483810, -5.082755093536325930 ) ) ;
#36112 = CARTESIAN_POINT ( 'NONE',  ( -1.377000000000000002, 278.5679999999998699, 5.673913216228727130 ) ) ;
#36113 = CARTESIAN_POINT ( 'NONE',  ( -6.676582343750002480, 292.3906250017069510, -2.765530957081996810 ) ) ;
#36115 = DIRECTION ( 'NONE',  ( 1.000000000000000000, -0.000000000000000000, -0.000000000000000000 ) ) ;
#36114 = CARTESIAN_POINT ( 'NONE',  ( 8.311093377946834337, 232.0312500034139873, -8.311093377946836114 ) ) ;
#36116 = APPLICATION_CONTEXT ( 'automotive_design' ) ;
#36117 = ORIENTED_EDGE ( 'NONE', *, *, #71796, .F. ) ;
#36119 = AXIS2_PLACEMENT_3D ( 'NONE', #68013, #32963, #16306 ) ;
#36118 = CARTESIAN_POINT ( 'NONE',  ( 11.35316468749999963, 226.5104166700806445, 3.042071309553159519 ) ) ;
#36120 = CARTESIAN_POINT ( 'NONE',  ( 1.320432766682872962E-15, -7.188101187499992051, 7.861552781871751883 ) ) ;
#36121 = CARTESIAN_POINT ( 'NONE',  ( 3.458734125000015425, 203.2500000013656063, 196.5673454167823877 ) ) ;
#36122 = EDGE_LOOP ( 'NONE', ( #38321, #61239, #33301, #67914 ) ) ;
#36123 = CARTESIAN_POINT ( 'NONE',  ( 10.18810118749999916, 4.220049686691935698, 68.50000000204838102 ) ) ;
#36124 = CARTESIAN_POINT ( 'NONE',  ( 5.676582343749993598, 105.2604166632526841, 9.832129032723422313 ) ) ;
#36125 = CARTESIAN_POINT ( 'NONE',  ( -5.000000000000004441, 123.3333333333333712, 8.660254037844383745 ) ) ;
#36126 = CARTESIAN_POINT ( 'NONE',  ( -11.00000000000000000, 4.556349186104045934, 75.90624999999998579 ) ) ;
#36129 = CARTESIAN_POINT ( 'NONE',  ( 0.000000000000000000, 0.000000000000000000, -4.000000000000001776 ) ) ;
#36128 = CARTESIAN_POINT ( 'NONE',  ( 30.44569435410879521, 204.8125000013656063, 167.5543056458910485 ) ) ;
#36127 = CARTESIAN_POINT ( 'NONE',  ( 31.45873412499998523, 203.8750000013656063, 171.4326545832175839 ) ) ;
#36130 = VERTEX_POINT ( 'NONE', #44325 ) ;
#36131 = EDGE_CURVE ( 'NONE', #9782, #27854, #10366, .T. ) ;
#36132 = VECTOR ( 'NONE', #59787, 1000.000000000000000 ) ;
#36133 = CARTESIAN_POINT ( 'NONE',  ( -11.00000000000000000, 0.000000000000000000, 82.18750000409677625 ) ) ;
#36134 = CARTESIAN_POINT ( 'NONE',  ( -36.86924962228700764, 146.0000000000000000, 134.0294372515228645 ) ) ;
#36135 = CARTESIAN_POINT ( 'NONE',  ( 9.832129032723420536, 216.1979166632526983, -5.676582343749999815 ) ) ;
#36136 = CARTESIAN_POINT ( 'NONE',  ( 3.458734124999959914, 201.3750000013656347, 143.4326545832176976 ) ) ;
#36137 = CARTESIAN_POINT ( 'NONE',  ( 27.99999999999996447, 203.6875000013656063, 173.4587341249998929 ) ) ;
#36138 = CARTESIAN_POINT ( 'NONE',  ( -1.320432766682874540E-15, 25.96874999795161543, 7.188101187500000044 ) ) ;
#36139 = CARTESIAN_POINT ( 'NONE',  ( 11.35316468749999785, 185.8854166632526983, 3.042071309553174174 ) ) ;
#36140 = CARTESIAN_POINT ( 'NONE',  ( 11.00000000000000355, -4.556349186104044158, 70.65625000000000000 ) ) ;
#36141 = CYLINDRICAL_SURFACE ( 'NONE', #56514, 3.999999999999976019 ) ;
#36142 = CARTESIAN_POINT ( 'NONE',  ( -31.99999999999999289, 196.2500000000000000, 170.0000000000003979 ) ) ;
#36143 = CARTESIAN_POINT ( 'NONE',  ( -4.541265875000002339, 14.81249999863440792, -5.561446717895856393E-16 ) ) ;
#36144 = CARTESIAN_POINT ( 'NONE',  ( 26.56734541678232731, 198.6250000013656063, 173.4587341249998929 ) ) ;
#36145 = CARTESIAN_POINT ( 'NONE',  ( 7.188101187499993827, -2.977408999572645598, 7.017802781871755435 ) ) ;
#36146 = CARTESIAN_POINT ( 'NONE',  ( 3.042071309553167069, 66.82291666325266988, -11.35316468749999785 ) ) ;
#36147 = DIRECTION ( 'NONE',  ( -1.000000000000000000, -1.224646799147353207E-16, 0.000000000000000000 ) ) ;
#36148 = CARTESIAN_POINT ( 'NONE',  ( 2.849036369511732440E-14, 205.2500000000000284, 202.0000000000000000 ) ) ;
#36149 = ORIENTED_EDGE ( 'NONE', *, *, #40779, .T. ) ;
#36150 = CARTESIAN_POINT ( 'NONE',  ( -5.000000000000011546, 46.66666666666668561, -8.660254037844410391 ) ) ;
#36151 = LINE ( 'NONE', #58800, #56955 ) ;
#36152 = CARTESIAN_POINT ( 'NONE',  ( -5.676582343749998039, 72.44791666325268409, -9.832129032723420536 ) ) ;
#36153 = ADVANCED_FACE ( 'NONE', ( #14885 ), #59776, .T. ) ;
#36154 = CARTESIAN_POINT ( 'NONE',  ( -6.735557395310442023E-16, 11.00000000000000000, 71.31250000409677625 ) ) ;
#36155 = CARTESIAN_POINT ( 'NONE',  ( 3.458734124999959469, 195.7500000013656063, 140.5673454167823593 ) ) ;
#36156 = DIRECTION ( 'NONE',  ( -0.000000000000000000, -0.000000000000000000, 1.000000000000000000 ) ) ;
#36158 = CARTESIAN_POINT ( 'NONE',  ( -5.676582343750006032, 69.11458332991936970, 9.832129032723418760 ) ) ;
#36157 = CARTESIAN_POINT ( 'NONE',  ( 1.320432766682874540E-15, 90.03125000204838102, 7.188101187500000044 ) ) ;
#36159 = CARTESIAN_POINT ( 'NONE',  ( -7.999999999999989342, -3.313708498984762496, 23.61155278392014978 ) ) ;
#36160 = CARTESIAN_POINT ( 'NONE',  ( 10.00000000000000000, 130.2083333333333428, -2.679491924311226736 ) ) ;
#36161 = CARTESIAN_POINT ( 'NONE',  ( -10.00000000000000000, 154.1666666598387394, -2.679491924311229845 ) ) ;
#36162 = CARTESIAN_POINT ( 'NONE',  ( 2.828427124746152987, 200.2500000027312126, 139.1715728752538723 ) ) ;
#36163 = CARTESIAN_POINT ( 'NONE',  ( 0.000000000000000000, 0.000000000000000000, 117.4999999999999716 ) ) ;
#36164 = CARTESIAN_POINT ( 'NONE',  ( 11.35316468750000141, 61.09374999658602690, 0.000000000000000000 ) ) ;
#36165 = CARTESIAN_POINT ( 'NONE',  ( -10.18810118749999916, 0.000000000000000000, 111.5312500020483668 ) ) ;
#36166 = CARTESIAN_POINT ( 'NONE',  ( 5.676582343749993598, 199.9479166632526983, 9.832129032723422313 ) ) ;
#36167 = ORIENTED_EDGE ( 'NONE', *, *, #70525, .F. ) ;
#36168 = CARTESIAN_POINT ( 'NONE',  ( -0.3752463838826867737, 65.74564559951204501, 26.26824411940225446 ) ) ;
#36169 = CARTESIAN_POINT ( 'NONE',  ( -8.000000000000000000, 122.0000000000000000, 0.000000000000000000 ) ) ;
#36170 = LINE ( 'NONE', #7130, #67269 ) ;
#36172 = CARTESIAN_POINT ( 'NONE',  ( 3.042071309553167513, 186.8229166632526983, -11.35316468749999785 ) ) ;
#36171 = LINE ( 'NONE', #52780, #58167 ) ;
#36173 = CARTESIAN_POINT ( 'NONE',  ( -7.240284387734133737E-08, 22.00000000000001066, -4.000000000000000888 ) ) ;
#36174 = CARTESIAN_POINT ( 'NONE',  ( 7.320508075688771044, 241.2500000068279178, -7.320508075688771932 ) ) ;
#36175 = CARTESIAN_POINT ( 'NONE',  ( 3.458734124999959914, 194.5625000013656063, 142.0000000000000568 ) ) ;
#36176 = EDGE_CURVE ( 'NONE', #6116, #47241, #11593, .T. ) ;
#36177 = EDGE_LOOP ( 'NONE', ( #70579, #45660, #12675, #43307 ) ) ;
#36178 = CARTESIAN_POINT ( 'NONE',  ( 6.951808397369818766E-16, 167.3437499965860127, -11.35316468750000141 ) ) ;
#36179 = EDGE_CURVE ( 'NONE', #68569, #10908, #70448, .T. ) ;
#36180 = VECTOR ( 'NONE', #4582, 1000.000000000000000 ) ;
#36181 = CARTESIAN_POINT ( 'NONE',  ( -7.188101187499992051, 2.977408999572646930, 23.89280278187175810 ) ) ;
#36182 =( BOUNDED_CURVE ( )  B_SPLINE_CURVE ( 2, ( #35607, #58622, #6928, #71025, #52954, #47278, #70304, #64641, #12939, #19343, #47643, #35976, #30306 ),
 .UNSPECIFIED., .F., .F. ) 
 B_SPLINE_CURVE_WITH_KNOTS ( ( 3, 2, 2, 2, 2, 2, 3 ),
 ( 1.774089285059882615, 1.779322971663514608, 1.784556658267146823, 1.789790344870778815, 1.795024031474410808, 1.800257718078043023, 1.805491404681675016 ),
 .UNSPECIFIED. ) 
 CURVE ( )  GEOMETRIC_REPRESENTATION_ITEM ( )  RATIONAL_B_SPLINE_CURVE ( ( 0.9999999999999978906, 0.9659258262890704216, 1.000000000000000000, 0.9659258262890683122, 1.000000000000000000, 0.9659258262890683122, 1.000000000000000000, 0.9659258262890683122, 1.000000000000000000, 0.9659258262890683122, 1.000000000000000000, 0.9659258262890683122, 1.000000000000000000 ) ) 
 REPRESENTATION_ITEM ( '' )  );
#36183 = CARTESIAN_POINT ( 'NONE',  ( 5.202883259092580204, 225.9999999999999432, -8.895588268986850622 ) ) ;
#36184 = AXIS2_PLACEMENT_3D ( 'NONE', #29278, #65445, #24705 ) ;
#36185 = ORIENTED_EDGE ( 'NONE', *, *, #23608, .F. ) ;
#36186 = EDGE_CURVE ( 'NONE', #60310, #6969, #27707, .T. ) ;
#36187 = AXIS2_PLACEMENT_3D ( 'NONE', #52960, #69569, #29210 ) ;
#36188 = CARTESIAN_POINT ( 'NONE',  ( -8.000000000000000000, 96.59375000409677625, -3.313708498984761608 ) ) ;
#36189 = ADVANCED_FACE ( 'NONE', ( #10733 ), #69567, .T. ) ;
#36190 = CARTESIAN_POINT ( 'NONE',  ( -2.828427124746190735, 13.37500000000000000, -2.828427124746191623 ) ) ;
#36191 = CARTESIAN_POINT ( 'NONE',  ( -2.726571689596997292E-14, 210.0000000000000284, 138.0000000000000568 ) ) ;
#36192 = CARTESIAN_POINT ( 'NONE',  ( 4.541265875000001451, 15.24999999863440969, 1.881053915767124440 ) ) ;
#36193 = CARTESIAN_POINT ( 'NONE',  ( 3.313708498984762496, -7.999999999999989342, 16.48655278392014623 ) ) ;
#36194 = CARTESIAN_POINT ( 'NONE',  ( -1.656854249492405451, 196.3125000000000284, 138.0000000000000568 ) ) ;
#36195 = ORIENTED_EDGE ( 'NONE', *, *, #38576, .T. ) ;
#36196 = CARTESIAN_POINT ( 'NONE',  ( 7.999999999999991118, 0.000000000000000000, 30.00000000000000000 ) ) ;
#36197 = CARTESIAN_POINT ( 'NONE',  ( -4.401442555609581635E-16, 101.2812500020483810, -7.188101187500000044 ) ) ;
#36199 = CARTESIAN_POINT ( 'NONE',  ( -4.556349186104048599, -10.99999999999999822, 98.78124999999998579 ) ) ;
#36198 = CARTESIAN_POINT ( 'NONE',  ( 8.660254037844435260, 180.4166666666666856, -5.000000000000026645 ) ) ;
#36200 = ORIENTED_EDGE ( 'NONE', *, *, #6849, .T. ) ;
#36201 = CARTESIAN_POINT ( 'NONE',  ( -1.506680654954751120, 10.12163528317106120, -70.16331425390788468 ) ) ;
#36202 = CARTESIAN_POINT ( 'NONE',  ( 0.000000000000000000, -2.500000000000000000, 0.000000000000000000 ) ) ;
#36203 = CARTESIAN_POINT ( 'NONE',  ( -7.188101187499991163, 2.977408999572646930, 22.39280278187175810 ) ) ;
#36204 = ORIENTED_EDGE ( 'NONE', *, *, #13968, .T. ) ;
#36205 = VERTEX_POINT ( 'NONE', #50717 ) ;
#36206 = CARTESIAN_POINT ( 'NONE',  ( 10.18810118749999916, 4.220049686691935698, 88.00000000204836681 ) ) ;
#36207 = DIRECTION ( 'NONE',  ( -0.000000000000000000, -0.000000000000000000, 1.000000000000000000 ) ) ;
#36208 = CARTESIAN_POINT ( 'NONE',  ( -10.99999999999999822, -4.556349186104052151, 95.59374999999998579 ) ) ;
#36211 = CARTESIAN_POINT ( 'NONE',  ( -6.676582343750002480, 294.5468750017069510, -2.765530957081996810 ) ) ;
#36210 = CARTESIAN_POINT ( 'NONE',  ( 27.99999999999996447, 201.6250000027312126, 165.9999999999998863 ) ) ;
#36209 = DIRECTION ( 'NONE',  ( 0.000000000000000000, 0.000000000000000000, 1.000000000000000000 ) ) ;
#36212 = CARTESIAN_POINT ( 'NONE',  ( -2.679491924311235618, 138.5416666666666572, 10.00000000000000000 ) ) ;
#36213 = DIRECTION ( 'NONE',  ( 0.000000000000000000, 0.000000000000000000, 1.000000000000000000 ) ) ;
#36214 = CARTESIAN_POINT ( 'NONE',  ( 0.000000000000000000, 125.0000000000000000, 8.000000000000000000 ) ) ;
#36215 = EDGE_CURVE ( 'NONE', #15967, #4343, #34139, .T. ) ;
#36216 = CARTESIAN_POINT ( 'NONE',  ( -7.347880794884122694E-16, 2.499999997268813168, 4.000000000000001776 ) ) ;
#36217 = CARTESIAN_POINT ( 'NONE',  ( -62.39047978708158126, 242.0000000000000284, 45.00000000000000000 ) ) ;
#36218 = CIRCLE ( 'NONE', #45850, 34.85072926314708042 ) ;
#36219 = CARTESIAN_POINT ( 'NONE',  ( 25.55430564589119413, 200.0625000013656063, 167.5543056458910485 ) ) ;
#36220 = CARTESIAN_POINT ( 'NONE',  ( 7.188101187500000044, 6.843749997951610986, 0.000000000000000000 ) ) ;
#36221 = CARTESIAN_POINT ( 'NONE',  ( 5.662595241051934458, 5.662595241051935346, 4.950615283940630107 ) ) ;
#36222 = CARTESIAN_POINT ( 'NONE',  ( 7.999999999999991118, 0.000000000000000000, 30.00000000000000000 ) ) ;
#36223 = CARTESIAN_POINT ( 'NONE',  ( -7.188101187500000933, 113.9375000020483952, -2.977408999572650483 ) ) ;
#36224 = CARTESIAN_POINT ( 'NONE',  ( -3.734423912265953938, -56.16062404875297887, -44.09723116535785437 ) ) ;
#36225 = CARTESIAN_POINT ( 'NONE',  ( -11.35316468749999963, 224.2187500034139873, 0.000000000000000000 ) ) ;
#36226 = FACE_OUTER_BOUND ( 'NONE', #19256, .T. ) ;
#36227 = CARTESIAN_POINT ( 'NONE',  ( 5.082755093536318824, 5.082755093536319713, 22.29905278187175455 ) ) ;
#36228 = CARTESIAN_POINT ( 'NONE',  ( 26.34314575050758833, 195.9375000000000000, 173.9999999999999147 ) ) ;
#36229 = CARTESIAN_POINT ( 'NONE',  ( 11.35316468749999963, 30.98958332991935194, -3.042071309553165293 ) ) ;
#36230 = EDGE_CURVE ( 'NONE', #53923, #54226, #48787, .T. ) ;
#36231 = CARTESIAN_POINT ( 'NONE',  ( 1.966308894373107963, -12.72115749107479310, -0.4760262082327907929 ) ) ;
#36232 = CARTESIAN_POINT ( 'NONE',  ( 8.311093377946837890, 216.7187499965860411, -8.311093377946837890 ) ) ;
#36233 = DIRECTION ( 'NONE',  ( 1.000000000000000000, 0.000000000000000000, 0.000000000000000000 ) ) ;
#36234 = CARTESIAN_POINT ( 'NONE',  ( -5.000000000000002665, 2.143131898507868248E-15, 17.50000000000000000 ) ) ;
#36235 = ORIENTED_EDGE ( 'NONE', *, *, #42516, .T. ) ;
#36236 = CARTESIAN_POINT ( 'NONE',  ( 7.999999999999991118, 9.797174393178815797E-16, 15.08030277982336642 ) ) ;
#36237 = AXIS2_PLACEMENT_3D ( 'NONE', #69679, #23277, #16861 ) ;
#36238 = CARTESIAN_POINT ( 'NONE',  ( -5.676582343749998039, 32.44791666325268409, -9.832129032723420536 ) ) ;
#36239 = CARTESIAN_POINT ( 'NONE',  ( -4.556349186104047710, -10.99999999999999822, 86.96875000409677625 ) ) ;
#36240 = CARTESIAN_POINT ( 'NONE',  ( -2.445694354108839175, 208.3125000013656063, 144.4456943541088663 ) ) ;
#36242 = CIRCLE ( 'NONE', #55524, 37.00000000000000711 ) ;
#36241 = CARTESIAN_POINT ( 'NONE',  ( -26.56734541678228112, 195.0000000013656063, 173.4587341250003476 ) ) ;
#36243 = CARTESIAN_POINT ( 'NONE',  ( -15.99999999999999645, -16.00000000000000355, 20.00000000000000000 ) ) ;
#36245 = CARTESIAN_POINT ( 'NONE',  ( -11.35316468750000141, 38.28124999658601979, -1.390361679473963753E-15 ) ) ;
#36244 = CARTESIAN_POINT ( 'NONE',  ( 7.188101187500000044, 108.4062500020483810, -8.802885111219163269E-16 ) ) ;
#36246 = CARTESIAN_POINT ( 'NONE',  ( 3.313708498984756279, 7.999999999999991118, 13.86155277982336465 ) ) ;
#36247 = CARTESIAN_POINT ( 'NONE',  ( 8.311093377946834337, 145.1562499965860127, 8.311093377946839666 ) ) ;
#36248 = EDGE_CURVE ( 'NONE', #66203, #69053, #16745, .T. ) ;
#36249 = CARTESIAN_POINT ( 'NONE',  ( -8.660254037844387298, 118.9583333265053824, -5.000000000000004441 ) ) ;
#36250 = CARTESIAN_POINT ( 'NONE',  ( 7.188101187500001821, 110.3750000020484094, -2.977408999572651371 ) ) ;
#36251 = DIRECTION ( 'NONE',  ( -1.000000000000000000, -0.000000000000000000, -0.000000000000000000 ) ) ;
#36252 = CARTESIAN_POINT ( 'NONE',  ( -31.45873412500001010, 206.8750000013656347, 168.5673454167827572 ) ) ;
#36253 = ORIENTED_EDGE ( 'NONE', *, *, #54530, .T. ) ;
#36254 = CARTESIAN_POINT ( 'NONE',  ( -5.676582343749998039, 22.76041666325268409, -9.832129032723420536 ) ) ;
#36255 = ORIENTED_EDGE ( 'NONE', *, *, #285, .T. ) ;
#36256 = FACE_OUTER_BOUND ( 'NONE', #20416, .T. ) ;
#36257 = DIRECTION ( 'NONE',  ( 0.000000000000000000, 0.000000000000000000, -1.000000000000000000 ) ) ;
#36258 = PRODUCT_RELATED_PRODUCT_CATEGORY ( 'part', '', ( #11413 ) ) ;
#36260 = CARTESIAN_POINT ( 'NONE',  ( -11.35316468749999785, 133.0729166632526983, -3.042071309553167957 ) ) ;
#36259 = CARTESIAN_POINT ( 'NONE',  ( -7.778174593052023411, 7.778174593052023411, 92.50000000409677625 ) ) ;
#36261 = CARTESIAN_POINT ( 'NONE',  ( 7.999999999999992895, -3.313708498984756279, 16.54280278432982598 ) ) ;
#36262 = CARTESIAN_POINT ( 'NONE',  ( 53.23568937185515892, 204.9218605378435427, 52.37283670179199646 ) ) ;
#36263 = CARTESIAN_POINT ( 'NONE',  ( -9.832129032723418760, 248.4895833367473301, -5.676582343749998927 ) ) ;
#36264 = CARTESIAN_POINT ( 'NONE',  ( 10.18810118749999916, 4.220049686691935698, 91.37500000204838102 ) ) ;
#36265 = ORIENTED_EDGE ( 'NONE', *, *, #4625, .T. ) ;
#36266 = EDGE_CURVE ( 'NONE', #25259, #55947, #25989, .T. ) ;
#36267 = CARTESIAN_POINT ( 'NONE',  ( -2.828427124746208943, 197.6250000000000284, 144.8284271247462129 ) ) ;
#36268 = CARTESIAN_POINT ( 'NONE',  ( 32.00000000000000000, 205.2500000000000284, 169.9999999999999432 ) ) ;
#36269 = CARTESIAN_POINT ( 'NONE',  ( -2.085542519210945728E-15, 84.84374999658601268, 11.35316468750000141 ) ) ;
#36270 = CARTESIAN_POINT ( 'NONE',  ( 7.204075437095968759, -7.204075437095966983, 104.2187500020483810 ) ) ;
#36271 = CARTESIAN_POINT ( 'NONE',  ( -8.342170076843785083E-16, 17.18749999863440792, 4.541265875000002339 ) ) ;
#36272 = VERTEX_POINT ( 'NONE', #40152 ) ;
#36273 = ORIENTED_EDGE ( 'NONE', *, *, #74560, .F. ) ;
#36274 = CARTESIAN_POINT ( 'NONE',  ( 5.656854249492378806, 7.312500000000000888, 5.656854249492381470 ) ) ;
#36275 = CARTESIAN_POINT ( 'NONE',  ( -8.000000000000001776, 11.34375000000000178, 3.313708498984759387 ) ) ;
#36276 = CARTESIAN_POINT ( 'NONE',  ( -2.977408999572650039, 3.937499997951610986, -7.188101187500001821 ) ) ;
#36277 = CARTESIAN_POINT ( 'NONE',  ( -7.999999999999998224, 122.2812500040967763, 3.313708498984766493 ) ) ;
#36278 =( BOUNDED_CURVE ( )  B_SPLINE_CURVE ( 2, ( #12690, #53810, #31154, #54186, #35366, #58378, #1036, #64393, #42472 ),
 .UNSPECIFIED., .F., .F. ) 
 B_SPLINE_CURVE_WITH_KNOTS ( ( 3, 2, 2, 2, 3 ),
 ( 0.8229166666666667407, 0.8281250000000001110, 0.8333333333333334814, 0.8385416666666668517, 0.8437500000000002220 ),
 .UNSPECIFIED. ) 
 CURVE ( )  GEOMETRIC_REPRESENTATION_ITEM ( )  RATIONAL_B_SPLINE_CURVE ( ( 0.9999999999999983347, 0.9238795325112884038, 1.000000000000000000, 0.9238795325112867385, 1.000000000000000000, 0.9238795325112867385, 1.000000000000000000, 0.9238795325112835188, 1.000000000000003331 ) ) 
 REPRESENTATION_ITEM ( '' )  );
#36279 = CARTESIAN_POINT ( 'NONE',  ( -10.18810118749999916, 4.220049686691934809, 100.9375000020483810 ) ) ;
#36280 = CARTESIAN_POINT ( 'NONE',  ( -4.000000000000001776, 1.500000000000000222, -4.898587196589415787E-16 ) ) ;
#36281 = CARTESIAN_POINT ( 'NONE',  ( -4.000000000000001776, 13.24999999726881406, -4.898587196589415787E-16 ) ) ;
#36282 = CARTESIAN_POINT ( 'NONE',  ( 26.34314575050759188, 209.9375000000000000, 173.9999999999999147 ) ) ;
#36283 = ORIENTED_EDGE ( 'NONE', *, *, #55653, .T. ) ;
#36284 = CARTESIAN_POINT ( 'NONE',  ( 1.432654583217607858, 207.6250000013656347, 138.5412658750000787 ) ) ;
#36285 = CARTESIAN_POINT ( 'NONE',  ( -3.458734124999959914, 198.3750000013655779, 196.5673454167823877 ) ) ;
#36287 = CARTESIAN_POINT ( 'NONE',  ( -1.836970198721029983E-15, 123.7500000000000142, 10.00000000000000178 ) ) ;
#36286 = CARTESIAN_POINT ( 'NONE',  ( -29.43265458321771177, 200.5000000013655779, 166.5412658750003914 ) ) ;
#36288 =( NAMED_UNIT ( * ) PLANE_ANGLE_UNIT ( ) SI_UNIT ( $, .RADIAN. ) );
#36289 =( BOUNDED_CURVE ( )  B_SPLINE_CURVE ( 2, ( #36528, #64086, #25185, #65178, #24079, #29751, #64459, #48198, #64819 ),
 .UNSPECIFIED., .F., .F. ) 
 B_SPLINE_CURVE_WITH_KNOTS ( ( 3, 2, 2, 2, 3 ),
 ( 0.5520833333333332593, 0.5572916666666665186, 0.5625000000000000000, 0.5677083333333333703, 0.5729166666666666297 ),
 .UNSPECIFIED. ) 
 CURVE ( )  GEOMETRIC_REPRESENTATION_ITEM ( )  RATIONAL_B_SPLINE_CURVE ( ( 1.000000000000001554, 0.9238795325112850731, 1.000000000000000000, 0.9238795325112867385, 1.000000000000000000, 0.9238795325112867385, 1.000000000000000000, 0.9238795325112867385, 1.000000000000000000 ) ) 
 REPRESENTATION_ITEM ( '' )  );
#36290 = CARTESIAN_POINT ( 'NONE',  ( -4.541265875000003227, 12.87499999863440969, 1.881053915767121110 ) ) ;
#36291 = CARTESIAN_POINT ( 'NONE',  ( 10.00000000000000178, 121.8749999931720396, 0.000000000000000000 ) ) ;
#36292 = VECTOR ( 'NONE', #6672, 1000.000000000000000 ) ;
#36293 = CARTESIAN_POINT ( 'NONE',  ( -7.188101187499991163, 2.977408999572646930, 13.39280278187175455 ) ) ;
#36294 = ORIENTED_EDGE ( 'NONE', *, *, #63641, .F. ) ;
#36295 = VERTEX_POINT ( 'NONE', #63156 ) ;
#36296 = CARTESIAN_POINT ( 'NONE',  ( 10.18810118749999916, 4.220049686691935698, 103.0000000020483668 ) ) ;
#36297 = CARTESIAN_POINT ( 'NONE',  ( -9.999999999999989342, 97.50000000000000000, -1.224646799147351876E-15 ) ) ;
#36298 = CIRCLE ( 'NONE', #15761, 71.70204102886728492 ) ;
#36299 = CARTESIAN_POINT ( 'NONE',  ( -32.00000000000000711, 201.1875000000000284, 168.3431457505080004 ) ) ;
#36300 = CARTESIAN_POINT ( 'NONE',  ( -3.458734124999959914, 195.4375000013655779, 198.0000000000000284 ) ) ;
#36301 = LINE ( 'NONE', #24954, #39822 ) ;
#36302 = CARTESIAN_POINT ( 'NONE',  ( -5.000000000000005329, 93.33333333333334281, 8.660254037844387298 ) ) ;
#36303 = CARTESIAN_POINT ( 'NONE',  ( -7.999999999999998224, 117.5937499999999858, 3.313708498984766493 ) ) ;
#36304 = CARTESIAN_POINT ( 'NONE',  ( 2.765530957082001251, 297.9218750017069510, 6.676582343750000703 ) ) ;
#36305 = EDGE_CURVE ( 'NONE', #8103, #14923, #52165, .T. ) ;
#36306 = EDGE_LOOP ( 'NONE', ( #25010, #51108, #64711, #18672 ) ) ;
#36307 = CARTESIAN_POINT ( 'NONE',  ( 0.000000000000000000, 0.000000000000000000, 41.99999999999999289 ) ) ;
#36308 = CARTESIAN_POINT ( 'NONE',  ( 3.313708498984762496, 17.53124999590322375, 7.999999999999998224 ) ) ;
#36309 = CARTESIAN_POINT ( 'NONE',  ( 2.445694354108782775, 206.5625000013656063, 139.5543056458912190 ) ) ;
#36310 = CARTESIAN_POINT ( 'NONE',  ( -10.00000000000000711, 52.70833333333334281, 2.679491924311223627 ) ) ;
#36311 = CARTESIAN_POINT ( 'NONE',  ( 2.449293598294707893E-16, 8.250000000000000000, -4.000000000000001776 ) ) ;
#36312 = CARTESIAN_POINT ( 'NONE',  ( 5.000000000000004441, 221.6666666666666856, 8.660254037844385522 ) ) ;
#36313 = DIRECTION ( 'NONE',  ( -0.9884788384745426537, 6.483116892092366181E-18, -0.1513591288559072434 ) ) ;
#36314 = CARTESIAN_POINT ( 'NONE',  ( 4.556349186104051263, -10.99999999999999822, 115.4687500000000000 ) ) ;
#36315 = CARTESIAN_POINT ( 'NONE',  ( 8.660254037844389075, 210.4166666666666572, -5.000000000000000000 ) ) ;
#36316 = EDGE_CURVE ( 'NONE', #16317, #61723, #36738, .T. ) ;
#36317 = CARTESIAN_POINT ( 'NONE',  ( 7.188101187499993827, -2.977408999572645598, 13.01780278187175277 ) ) ;
#36318 = CARTESIAN_POINT ( 'NONE',  ( -11.35316468750000141, 183.5937499965860411, -1.390361679473963753E-15 ) ) ;
#36319 = DIRECTION ( 'NONE',  ( -0.000000000000000000, -0.000000000000000000, -1.000000000000000000 ) ) ;
#36320 = CARTESIAN_POINT ( 'NONE',  ( -4.541265875000002339, 2.749999998634406584, -1.881053915767121998 ) ) ;
#36321 = CARTESIAN_POINT ( 'NONE',  ( 2.824543433528785410E-14, 210.0000000000000284, 194.0000000000000568 ) ) ;
#36323 = CARTESIAN_POINT ( 'NONE',  ( 7.999999999999991118, 3.313708498984758055, 3.361552783920144893 ) ) ;
#36322 = CARTESIAN_POINT ( 'NONE',  ( 3.008240453400889395E-14, 210.0000000000000284, 189.0000000000000284 ) ) ;
#36324 = VERTEX_POINT ( 'NONE', #48388 ) ;
#36325 = CARTESIAN_POINT ( 'NONE',  ( -2.445694354108839175, 209.3125000013656063, 144.4456943541088663 ) ) ;
#36326 = CARTESIAN_POINT ( 'NONE',  ( -5.676582343749998039, 52.76041666325269119, -9.832129032723420536 ) ) ;
#36327 = CARTESIAN_POINT ( 'NONE',  ( -10.99999999999999822, -4.556349186104052151, 104.7812500040967763 ) ) ;
#36328 = CARTESIAN_POINT ( 'NONE',  ( -2.085542519210945728E-15, 224.8437499965860127, 11.35316468750000141 ) ) ;
#36329 = CARTESIAN_POINT ( 'NONE',  ( -25.55430564589111953, 204.0625000013656063, 172.4456943541091505 ) ) ;
#36330 = CARTESIAN_POINT ( 'NONE',  ( 7.778174593052021635, 7.778174593052023411, 70.93749999999998579 ) ) ;
#36332 = CARTESIAN_POINT ( 'NONE',  ( -10.00000000000000178, 59.37499999317203248, -1.224646799147353454E-15 ) ) ;
#36331 = CARTESIAN_POINT ( 'NONE',  ( -7.778174593052020747, -7.778174593052023411, 107.6874999999999858 ) ) ;
#36333 = CARTESIAN_POINT ( 'NONE',  ( -1.432654583217662259, 195.1250000013656063, 145.4587341250000350 ) ) ;
#36334 = CARTESIAN_POINT ( 'NONE',  ( -5.676582343750006032, 114.1145833299193555, 9.832129032723418760 ) ) ;
#36335 = CARTESIAN_POINT ( 'NONE',  ( -2.679491924311225848, 78.33333332650536818, -10.00000000000000178 ) ) ;
#36336 = CARTESIAN_POINT ( 'NONE',  ( -7.188101187500001821, 95.56250000204838102, -2.977408999572650483 ) ) ;
#36337 = CARTESIAN_POINT ( 'NONE',  ( 4.541265875000001451, 15.37499999863440969, 1.881053915767124440 ) ) ;
#36338 = CARTESIAN_POINT ( 'NONE',  ( 11.00000000000000000, 1.347111479062088405E-15, 87.25000000000000000 ) ) ;
#36339 = CARTESIAN_POINT ( 'NONE',  ( -5.656854249492373476, -5.656854249492376141, 23.51780277982336642 ) ) ;
#36340 = ORIENTED_EDGE ( 'NONE', *, *, #36658, .T. ) ;
#36341 = ORIENTED_EDGE ( 'NONE', *, *, #29069, .F. ) ;
#36342 = CARTESIAN_POINT ( 'NONE',  ( 1.226468279477575784E-15, 291.8593750017070079, 6.676582343750001591 ) ) ;
#36343 = FACE_OUTER_BOUND ( 'NONE', #27335, .T. ) ;
#36344 = CARTESIAN_POINT ( 'NONE',  ( 11.35316468750000141, 155.7812499965860127, 0.000000000000000000 ) ) ;
#36345 = CARTESIAN_POINT ( 'NONE',  ( -3.458734124999959914, 194.4587341250000065, 198.0000000000000284 ) ) ;
#36346 = CARTESIAN_POINT ( 'NONE',  ( 2.828427124746209831, 199.3750000000000284, 200.8284271247462129 ) ) ;
#36347 = CARTESIAN_POINT ( 'NONE',  ( -31.99999999999997868, 201.3125000000000284, 171.6568542494928238 ) ) ;
#36348 = CARTESIAN_POINT ( 'NONE',  ( 7.204075437095966983, 7.204075437095967871, 112.4687500020483810 ) ) ;
#36349 = ORIENTED_EDGE ( 'NONE', *, *, #64128, .T. ) ;
#36350 = DIRECTION ( 'NONE',  ( -0.000000000000000000, -0.000000000000000000, 1.000000000000000000 ) ) ;
#36351 = AXIS2_PLACEMENT_3D ( 'NONE', #6772, #46748, #46383 ) ;
#36352 = CARTESIAN_POINT ( 'NONE',  ( -1.656854249492358155, 17.68750000000000355, 4.000000000000024869 ) ) ;
#36353 = CARTESIAN_POINT ( 'NONE',  ( 11.35316468749999963, 136.3020833299193555, -3.042071309553165293 ) ) ;
#36354 = CARTESIAN_POINT ( 'NONE',  ( 1.432654583217664479, 198.7500000013656063, 201.4587341250000065 ) ) ;
#36355 = CARTESIAN_POINT ( 'NONE',  ( -2.977408999572654480, 27.37499999795161543, 7.188101187499999156 ) ) ;
#36356 = CARTESIAN_POINT ( 'NONE',  ( 1.871523826299183495E-15, -10.18810118749999916, 72.90625000204836681 ) ) ;
#36357 = CARTESIAN_POINT ( 'NONE',  ( 9.832129032723416984, 55.67708332991935549, 5.676582343750006032 ) ) ;
#36358 = ORIENTED_EDGE ( 'NONE', *, *, #38112, .T. ) ;
#36359 = FACE_OUTER_BOUND ( 'NONE', #53380, .T. ) ;
#36360 = CARTESIAN_POINT ( 'NONE',  ( -4.541265875000002339, 3.937499998634406584, -5.561446717895856393E-16 ) ) ;
#36361 = CARTESIAN_POINT ( 'NONE',  ( -8.008118988124991233, 3.317071493978878127, 6.919365283940628331 ) ) ;
#36362 = CARTESIAN_POINT ( 'NONE',  ( -5.082755093536326818, 16.40624999795161543, 5.082755093536325042 ) ) ;
#36363 = CARTESIAN_POINT ( 'NONE',  ( 6.000000000000003553, 292.6250000034140157, -2.485281374238571761 ) ) ;
#36364 = DIRECTION ( 'NONE',  ( 0.000000000000000000, 0.000000000000000000, 1.000000000000000000 ) ) ;
#36365 = CARTESIAN_POINT ( 'NONE',  ( 5.082755093536324154, 9.656249997951610098, 5.082755093536326818 ) ) ;
#36366 = CARTESIAN_POINT ( 'NONE',  ( 5.082755093536318824, 5.082755093536319713, 9.924052781871754547 ) ) ;
#36367 = CARTESIAN_POINT ( 'NONE',  ( 2.729893485599593106, 10.18810118750000093, 67.22060438569887708 ) ) ;
#36368 = CARTESIAN_POINT ( 'NONE',  ( 38.00000000000000000, 63.00000000000000000, 15.00000000000000178 ) ) ;
#36369 = CARTESIAN_POINT ( 'NONE',  ( -1.656854249492381248, 4.062499997268813168, -4.000000000000001776 ) ) ;
#36370 = ORIENTED_EDGE ( 'NONE', *, *, #41210, .T. ) ;
#36371 = VECTOR ( 'NONE', #25646, 1000.000000000000000 ) ;
#36372 = CARTESIAN_POINT ( 'NONE',  ( -3.999999999999959144, 197.1875000027312694, 199.6568542494924259 ) ) ;
#36373 = CARTESIAN_POINT ( 'NONE',  ( 3.999999999999960032, 202.9375000000000000, 143.6568542494924543 ) ) ;
#36374 = CARTESIAN_POINT ( 'NONE',  ( -28.00000000000007461, 196.1250000027311842, 166.0000000000003695 ) ) ;
#36375 = ADVANCED_FACE ( 'NONE', ( #30309 ), #2375, .T. ) ;
#36376 = CARTESIAN_POINT ( 'NONE',  ( -8.342170076843785083E-16, 1.062499998634406584, 4.541265875000002339 ) ) ;
#36377 = CARTESIAN_POINT ( 'NONE',  ( 7.188101187500000044, 118.9062500020483810, -8.802885111219163269E-16 ) ) ;
#36378 = CYLINDRICAL_SURFACE ( 'NONE', #47634, 7.999999999999991118 ) ;
#36379 = CARTESIAN_POINT ( 'NONE',  ( -3.313708498984758943, -7.999999999999989342, 4.299052783920145338 ) ) ;
#36380 = ORIENTED_EDGE ( 'NONE', *, *, #53537, .F. ) ;
#36381 =( BOUNDED_CURVE ( )  B_SPLINE_CURVE ( 2, ( #8018, #52564, #69923, #70291, #18605, #41248, #69547, #17858, #14780 ),
 .UNSPECIFIED., .F., .F. ) 
 B_SPLINE_CURVE_WITH_KNOTS ( ( 3, 2, 2, 2, 3 ),
 ( 0.09722222222222220989, 0.1041666666666666574, 0.1111111111111111049, 0.1180555555555555525, 0.1250000000000000000 ),
 .UNSPECIFIED. ) 
 CURVE ( )  GEOMETRIC_REPRESENTATION_ITEM ( )  RATIONAL_B_SPLINE_CURVE ( ( 1.000000000000000222, 0.9238795325112866275, 1.000000000000000000, 0.9238795325112867385, 1.000000000000000000, 0.9238795325112867385, 1.000000000000000000, 0.9238795325112867385, 1.000000000000000000 ) ) 
 REPRESENTATION_ITEM ( '' )  );
#36382 = CARTESIAN_POINT ( 'NONE',  ( 5.082755093536324154, 22.78124999795161187, 5.082755093536326818 ) ) ;
#36383 = ORIENTED_EDGE ( 'NONE', *, *, #57811, .T. ) ;
#36384 = CARTESIAN_POINT ( 'NONE',  ( 1.836970198721029589E-15, 254.3750000068280031, 10.00000000000000000 ) ) ;
#36385 = CARTESIAN_POINT ( 'NONE',  ( 1.102182119232618108E-15, 296.2500000000000000, 6.000000000000001776 ) ) ;
#36386 = CARTESIAN_POINT ( 'NONE',  ( 29.43265458321766914, 201.5000000013655779, 173.4587341249998929 ) ) ;
#36387 = CARTESIAN_POINT ( 'NONE',  ( -7.320508075688773708, 51.87499999999999289, -7.320508075688774596 ) ) ;
#36388 = CARTESIAN_POINT ( 'NONE',  ( -5.082755093536325930, 101.8437500020483810, -5.082755093536325930 ) ) ;
#36389 = CARTESIAN_POINT ( 'NONE',  ( 6.000000000000003553, 297.4374999999999432, 2.485281374238571317 ) ) ;
#36391 = CARTESIAN_POINT ( 'NONE',  ( -21.64212435450982142, -37.81041767653802310, 192.1983126227046625 ) ) ;
#36390 = CARTESIAN_POINT ( 'NONE',  ( 105.0000000000000000, 189.9999999999999432, 44.99999999999999289 ) ) ;
#36392 = ADVANCED_FACE ( 'NONE', ( #29575 ), #30678, .T. ) ;
#36393 = VERTEX_POINT ( 'NONE', #54065 ) ;
#36394 = CARTESIAN_POINT ( 'NONE',  ( -6.951808397369817780E-16, 232.6562500034139873, -11.35316468749999963 ) ) ;
#36395 = VECTOR ( 'NONE', #74143, 1000.000000000000000 ) ;
#36396 = CARTESIAN_POINT ( 'NONE',  ( 9.999999999999985789, 90.20833333333331439, -2.679491924311223183 ) ) ;
#36398 = ADVANCED_FACE ( 'NONE', ( #41266, #23907 ), #2008, .T. ) ;
#36397 = CARTESIAN_POINT ( 'NONE',  ( -7.999999999999976019, -3.611371706259009353E-07, 26.51781575558936055 ) ) ;
#36399 = FACE_OUTER_BOUND ( 'NONE', #14527, .T. ) ;
#36400 = FACE_OUTER_BOUND ( 'NONE', #6243, .T. ) ;
#36401 = FACE_OUTER_BOUND ( 'NONE', #14277, .T. ) ;
#36402 = CARTESIAN_POINT ( 'NONE',  ( -10.00000000000000178, 172.5000000000000284, -1.224646799147353454E-15 ) ) ;
#36403 = FACE_OUTER_BOUND ( 'NONE', #10118, .T. ) ;
#36404 = CARTESIAN_POINT ( 'NONE',  ( -1.040834085586084257E-14, 82.00000000000001421, 97.52691193458117880 ) ) ;
#36405 = CARTESIAN_POINT ( 'NONE',  ( -4.217983994794788138, -68.29231466825659425, 20.60018752343953707 ) ) ;
#36406 = CARTESIAN_POINT ( 'NONE',  ( 6.951808397369818766E-16, 142.3437499965860411, -11.35316468750000141 ) ) ;
#36407 = CARTESIAN_POINT ( 'NONE',  ( 28.00000000000001776, 201.5000000000000000, 165.9999999999998863 ) ) ;
#36408 = CARTESIAN_POINT ( 'NONE',  ( -3.313708498984693218, 117.2187499999999858, -8.000000000000065725 ) ) ;
#36411 = CARTESIAN_POINT ( 'NONE',  ( 1.836970198721029589E-15, 261.2500000000000568, 10.00000000000000000 ) ) ;
#36410 = CARTESIAN_POINT ( 'NONE',  ( -38.00000000000000000, 53.00000000000000000, 15.00000000000000178 ) ) ;
#36409 = CARTESIAN_POINT ( 'NONE',  ( 29.65685424949235482, 205.0625000000000568, 173.9999999999999147 ) ) ;
#36412 = VERTEX_POINT ( 'NONE', #35249 ) ;
#36413 = CARTESIAN_POINT ( 'NONE',  ( -11.35316468750000141, 13.80208332991934661, 3.042071309553159963 ) ) ;
#36414 = CARTESIAN_POINT ( 'NONE',  ( 2.775557561562891351E-14, 210.0000000000000284, 198.0000000000000284 ) ) ;
#36415 = CARTESIAN_POINT ( 'NONE',  ( -2.679491924294440608, 111.4583333333318222, -10.00000000000968470 ) ) ;
#36416 = CARTESIAN_POINT ( 'NONE',  ( -27.99999999999999645, 210.0000000000000284, 174.0000000000003411 ) ) ;
#36417 = CARTESIAN_POINT ( 'NONE',  ( 1.432654583217607858, 207.6250000013656063, 138.5412658750000787 ) ) ;
#36418 = CARTESIAN_POINT ( 'NONE',  ( -8.000000000000000000, 4.968749995903221084, -3.313708498984762496 ) ) ;
#36419 = AXIS2_PLACEMENT_3D ( 'NONE', #58453, #52778, #6760 ) ;
#36420 = CARTESIAN_POINT ( 'NONE',  ( 5.000000000000001776, 37.70833332650536818, -8.660254037844389075 ) ) ;
#36421 = CARTESIAN_POINT ( 'NONE',  ( 2.977408999572650039, 114.6875000020484094, -7.188101187500001821 ) ) ;
#36422 = CARTESIAN_POINT ( 'NONE',  ( 3.211159895383560947, 6.312499998634407028, 3.211159895383562723 ) ) ;
#36423 = CARTESIAN_POINT ( 'NONE',  ( -10.99999999999916866, -33.01269182176501715, 140.6807770096220338 ) ) ;
#36424 = CARTESIAN_POINT ( 'NONE',  ( -4.898587196589407898E-16, 7.999999999999991118, 13.95530277982336465 ) ) ;
#36426 = CARTESIAN_POINT ( 'NONE',  ( 10.00000000000000000, 6.666666659838699438, 2.679491924311235618 ) ) ;
#36425 = CARTESIAN_POINT ( 'NONE',  ( -11.00000000000000000, 0.000000000000000000, 111.9999999999999858 ) ) ;
#36427 = ORIENTED_EDGE ( 'NONE', *, *, #56751, .F. ) ;
#36428 = DIRECTION ( 'NONE',  ( 0.000000000000000000, 0.000000000000000000, 1.000000000000000000 ) ) ;
#36429 = CARTESIAN_POINT ( 'NONE',  ( 7.778174593052023411, -7.778174593052021635, 115.5625000000000000 ) ) ;
#36430 = CARTESIAN_POINT ( 'NONE',  ( 9.832129032723420536, 226.3020833367473301, 5.676582343749996262 ) ) ;
#36431 = AXIS2_PLACEMENT_3D ( 'NONE', #55843, #38110, #61110 ) ;
#36432 = CARTESIAN_POINT ( 'NONE',  ( 11.35316468749999785, 110.5729166632526983, 3.042071309553174174 ) ) ;
#36433 = VERTEX_POINT ( 'NONE', #47646 ) ;
#36434 = CARTESIAN_POINT ( 'NONE',  ( 4.000000000000015987, 198.5000000000000000, 198.0000000000000284 ) ) ;
#36435 = CARTESIAN_POINT ( 'NONE',  ( 1.871523826299183495E-15, -10.18810118749999916, 95.03125000204836681 ) ) ;
#36436 = CYLINDRICAL_SURFACE ( 'NONE', #64632, 10.00000000000000178 ) ;
#36437 = CARTESIAN_POINT ( 'NONE',  ( 3.458734125000016757, 195.1250000013656063, 199.4326545832176691 ) ) ;
#36438 = CARTESIAN_POINT ( 'NONE',  ( 1.469576158976823947E-15, 94.06250000409677625, 8.000000000000000000 ) ) ;
#36440 = CARTESIAN_POINT ( 'NONE',  ( -9.832129032723418760, 117.8645833299193697, -5.676582343750004256 ) ) ;
#36439 = CARTESIAN_POINT ( 'NONE',  ( 0.000000000000000000, 19.05255888325788050, 0.000000000000000000 ) ) ;
#36441 = CARTESIAN_POINT ( 'NONE',  ( -28.00000000000003197, 210.0000000000000284, 166.0000000000003695 ) ) ;
#36442 = DIRECTION ( 'NONE',  ( -0.000000000000000000, 1.000000000000000000, -0.000000000000000000 ) ) ;
#36443 = ORIENTED_EDGE ( 'NONE', *, *, #70336, .F. ) ;
#36444 = AXIS2_PLACEMENT_3D ( 'NONE', #69659, #46639, #52312 ) ;
#36445 = CARTESIAN_POINT ( 'NONE',  ( 7.320508075688771044, 211.2499999931719969, 7.320508075688775484 ) ) ;
#36446 = CYLINDRICAL_SURFACE ( 'NONE', #8162, 6.000000000000001776 ) ;
#36447 = CARTESIAN_POINT ( 'NONE',  ( -5.000000000000002665, 0.000000000000000000, 0.000000000000000000 ) ) ;
#36448 = CARTESIAN_POINT ( 'NONE',  ( 5.676582343749993598, 100.2604166632526841, 9.832129032723422313 ) ) ;
#36449 = LINE ( 'NONE', #63626, #8613 ) ;
#36450 = CARTESIAN_POINT ( 'NONE',  ( -7.188101187500000044, 12.09374999795161187, -8.802885111219163269E-16 ) ) ;
#36451 = CARTESIAN_POINT ( 'NONE',  ( 10.18810118749999916, 4.220049686691935698, 91.37500000204838102 ) ) ;
#36452 = CARTESIAN_POINT ( 'NONE',  ( 5.676582343750001591, 11.92708332991935016, -9.832129032723420536 ) ) ;
#36453 = ORIENTED_EDGE ( 'NONE', *, *, #34298, .T. ) ;
#36454 = CARTESIAN_POINT ( 'NONE',  ( 2.775557561562891351E-14, 191.0000000000000284, 198.0000000000000284 ) ) ;
#36455 = CARTESIAN_POINT ( 'NONE',  ( -3.317071493978878571, 8.008118988124991233, 27.73186528394063544 ) ) ;
#36456 = CARTESIAN_POINT ( 'NONE',  ( 7.778174593052023411, -7.778174593052021635, 102.2500000040967763 ) ) ;
#36457 = CARTESIAN_POINT ( 'NONE',  ( 10.18810118749999916, 1.247682550866122264E-15, 73.28125000204838102 ) ) ;
#36458 = CARTESIAN_POINT ( 'NONE',  ( 0.6771042881593288820, 22.00000000000000355, 4.342542294227817123 ) ) ;
#36459 = CARTESIAN_POINT ( 'NONE',  ( 0.000000000000000000, 210.0000000000000284, 207.0000000000000568 ) ) ;
#36460 = CARTESIAN_POINT ( 'NONE',  ( -2.765530957081996810, 294.2656250017069510, -6.676582343750003368 ) ) ;
#36461 = CARTESIAN_POINT ( 'NONE',  ( -1.656854249492504705, 199.6875000000000284, 145.9999999999999716 ) ) ;
#36462 = CARTESIAN_POINT ( 'NONE',  ( 13.99999999999999822, 0.000000000000000000, 0.000000000000000000 ) ) ;
#36463 = CARTESIAN_POINT ( 'NONE',  ( 4.220049686691934809, 10.18810118749999916, 80.68750000204836681 ) ) ;
#36464 = CARTESIAN_POINT ( 'NONE',  ( -30.44569435410879166, 202.8125000013656063, 172.4456943541092357 ) ) ;
#36465 = CARTESIAN_POINT ( 'NONE',  ( -3.313708498984760720, 22.96875000000000355, -8.000000000000000000 ) ) ;
#36466 = CARTESIAN_POINT ( 'NONE',  ( -1.881053915767121554, 13.74999999863440969, -4.541265875000002339 ) ) ;
#36467 = ORIENTED_EDGE ( 'NONE', *, *, #67432, .F. ) ;
#36468 = DIRECTION ( 'NONE',  ( 0.000000000000000000, 0.000000000000000000, 1.000000000000000000 ) ) ;
#36469 = CARTESIAN_POINT ( 'NONE',  ( 1.656854249492403008, 207.8125000027312410, 194.0000000000000853 ) ) ;
#36470 = CARTESIAN_POINT ( 'NONE',  ( 3.458734124999959469, 197.7500000013656063, 140.5673454167824161 ) ) ;
#36471 = CARTESIAN_POINT ( 'NONE',  ( -2.828427124746208943, 203.7500000027312126, 144.8284271247462129 ) ) ;
#36472 = AXIS2_PLACEMENT_3D ( 'NONE', #54995, #26288, #59896 ) ;
#36473 = CARTESIAN_POINT ( 'NONE',  ( -5.000000000000000000, 10.42446448370097656, 65.94449134867544160 ) ) ;
#36474 = CARTESIAN_POINT ( 'NONE',  ( 4.220049686691934809, 10.18810118749999916, 69.06250000204839523 ) ) ;
#36475 = ORIENTED_EDGE ( 'NONE', *, *, #50193, .T. ) ;
#36476 = CARTESIAN_POINT ( 'NONE',  ( -5.082755093536326818, 2.906249997951610098, 5.082755093536325042 ) ) ;
#36477 = CARTESIAN_POINT ( 'NONE',  ( -7.320508075688773708, 28.74999999317203248, -7.320508075688774596 ) ) ;
#36478 = AXIS2_PLACEMENT_3D ( 'NONE', #36447, #37183, #24378 ) ;
#36479 = EDGE_CURVE ( 'NONE', #22362, #53235, #13674, .T. ) ;
#36480 = CARTESIAN_POINT ( 'NONE',  ( 7.188101187500002709, 116.1875000020483952, 2.977408999572649151 ) ) ;
#36481 = CARTESIAN_POINT ( 'NONE',  ( 0.4589999999999999636, 272.8559999999997672, 5.793770692573254166 ) ) ;
#36482 = CARTESIAN_POINT ( 'NONE',  ( -6.676582343750002480, 294.3906250017070079, -2.765530957081996810 ) ) ;
#36484 = CARTESIAN_POINT ( 'NONE',  ( -1.966308894373119287, 12.72115749107475402, -0.4760262082327688105 ) ) ;
#36483 = CARTESIAN_POINT ( 'NONE',  ( 8.311093377946839666, 225.7812500034140157, 8.311093377946830785 ) ) ;
#36485 = ITEM_DEFINED_TRANSFORMATION ( 'NONE', 'NONE', #65835,  #57354 ) ;
#36486 = ORIENTED_EDGE ( 'NONE', *, *, #62144, .T. ) ;
#36487 = CARTESIAN_POINT ( 'NONE',  ( 11.35316468749999963, 221.7187500034139873, -1.390361679473963556E-15 ) ) ;
#36488 = CARTESIAN_POINT ( 'NONE',  ( -2.977408999572647819, 7.188101187499991163, 2.705302781871750994 ) ) ;
#36489 = CARTESIAN_POINT ( 'NONE',  ( -29.65685424949233351, 195.1875000027312126, 166.0000000000002558 ) ) ;
#36490 = CARTESIAN_POINT ( 'NONE',  ( -1.432654583217607414, 203.5000000013655779, 194.5412658750000219 ) ) ;
#36491 = ORIENTED_EDGE ( 'NONE', *, *, #53181, .T. ) ;
#36492 = CARTESIAN_POINT ( 'NONE',  ( 0.000000000000000000, 0.000000000000000000, 0.000000000000000000 ) ) ;
#36493 = CARTESIAN_POINT ( 'NONE',  ( 8.311093377946834337, 95.46874999658601268, 8.311093377946839666 ) ) ;
#36494 = CARTESIAN_POINT ( 'NONE',  ( -4.999999999999997335, 121.6666666666666856, -8.660254037844385522 ) ) ;
#36495 = CARTESIAN_POINT ( 'NONE',  ( 7.778174593052023411, -7.778174593052021635, 76.56249999999997158 ) ) ;
#36498 = CARTESIAN_POINT ( 'NONE',  ( -27.99999999999995737, 205.5000000000000284, 174.0000000000003695 ) ) ;
#36497 = CARTESIAN_POINT ( 'NONE',  ( 26.56734541678237704, 203.3750000013656063, 173.4587341249998929 ) ) ;
#36496 = CARTESIAN_POINT ( 'NONE',  ( 29.43265458321761230, 201.7500000013655779, 173.4587341249998929 ) ) ;
#36499 = ORIENTED_EDGE ( 'NONE', *, *, #20050, .F. ) ;
#36500 = FACE_OUTER_BOUND ( 'NONE', #133, .T. ) ;
#36501 = CARTESIAN_POINT ( 'NONE',  ( -11.00000000000000000, 0.000000000000000000, 118.0000000000000000 ) ) ;
#36502 = ADVANCED_FACE ( 'NONE', ( #35611 ), #58267, .T. ) ;
#36503 = CARTESIAN_POINT ( 'NONE',  ( 6.951808397369818766E-16, 212.0312499965860411, -11.35316468750000141 ) ) ;
#36504 =( BOUNDED_CURVE ( )  B_SPLINE_CURVE ( 2, ( #8701, #54737, #9457, #44155, #67170, #15465, #38503, #6322, #11969, #5946, #28569, #24392, #30062 ),
 .UNSPECIFIED., .F., .F. ) 
 B_SPLINE_CURVE_WITH_KNOTS ( ( 3, 2, 2, 2, 2, 2, 3 ),
 ( 0.5054347826086956763, 0.5072463768115942351, 0.5090579710144927938, 0.5108695652173913526, 0.5126811594202898004, 0.5144927536231883591, 0.5163043478260869179 ),
 .UNSPECIFIED. ) 
 CURVE ( )  GEOMETRIC_REPRESENTATION_ITEM ( )  RATIONAL_B_SPLINE_CURVE ( ( 1.000000000000000000, 0.9659258262890683122, 1.000000000000000000, 0.9659258262890683122, 1.000000000000000000, 0.9659258262890683122, 1.000000000000000000, 0.9659258262890683122, 1.000000000000000000, 0.9659258262890683122, 1.000000000000000000, 0.9659258262890683122, 1.000000000000000000 ) ) 
 REPRESENTATION_ITEM ( '' )  );
#36505 = B_SPLINE_CURVE_WITH_KNOTS ( 'NONE', 3,
 ( #10725, #39399, #51454, #68807, #22035, #50709, #33758, #28449, #11843, #34880, #17498, #16362 ),
 .UNSPECIFIED., .F., .F.,
 ( 4, 2, 2, 2, 2, 4 ),
 ( 3.469446951953614189E-18, 0.002547658444427999130, 0.005095316888855994791, 0.006369146111069992622, 0.007642975333283991320, 0.01019063377771198438 ),
 .UNSPECIFIED. ) ;
#36506 = CARTESIAN_POINT ( 'NONE',  ( -2.754378923186476579E-14, 202.1875000013656063, 145.4587341250000350 ) ) ;
#36507 = CARTESIAN_POINT ( 'NONE',  ( 29.43265458321766559, 201.1250000013656347, 166.5412658749999650 ) ) ;
#36508 = CARTESIAN_POINT ( 'NONE',  ( 11.00000000000000000, 1.347111479062088405E-15, 115.9375000040967763 ) ) ;
#36509 = CARTESIAN_POINT ( 'NONE',  ( 3.042071309553159519, 190.0520833299193839, 11.35316468750000141 ) ) ;
#36510 = CARTESIAN_POINT ( 'NONE',  ( -7.188101187500000933, 92.93750000204839523, -2.977408999572650483 ) ) ;
#36511 = LINE ( 'NONE', #24439, #54071 ) ;
#36512 = CARTESIAN_POINT ( 'NONE',  ( -31.99999999999999289, 195.2500000000000000, 170.0000000000003979 ) ) ;
#36513 = CARTESIAN_POINT ( 'NONE',  ( -4.541265875000002339, 13.74999999863440969, -1.881053915767121998 ) ) ;
#36514 = CARTESIAN_POINT ( 'NONE',  ( 25.55430564589119413, 198.3125000013656063, 167.5543056458910485 ) ) ;
#36515 = CARTESIAN_POINT ( 'NONE',  ( -5.082755093536317936, -5.082755093536320601, 2.049052781871754103 ) ) ;
#36516 = CARTESIAN_POINT ( 'NONE',  ( 3.042071309553159519, 79.73958332991934128, 11.35316468750000141 ) ) ;
#36517 = CARTESIAN_POINT ( 'NONE',  ( -11.32023332186857800, -28.40672683819000000, 198.8593480330762873 ) ) ;
#36518 = CYLINDRICAL_SURFACE ( 'NONE', #61631, 3.999999999999976019 ) ;
#36519 = ORIENTED_EDGE ( 'NONE', *, *, #11198, .F. ) ;
#36520 = CARTESIAN_POINT ( 'NONE',  ( -2.679491924310542394, 48.54166666666674246, 10.00000000000043165 ) ) ;
#36521 = CARTESIAN_POINT ( 'NONE',  ( 2.849036369511732440E-14, 197.3750000027312126, 202.0000000000000000 ) ) ;
#36522 = CARTESIAN_POINT ( 'NONE',  ( 5.676582343750001591, 76.61458332991935549, -9.832129032723420536 ) ) ;
#36523 = ORIENTED_EDGE ( 'NONE', *, *, #52060, .F. ) ;
#36524 = CARTESIAN_POINT ( 'NONE',  ( 4.220049686691934809, 10.18810118749999916, 84.06250000204838102 ) ) ;
#36525 = CARTESIAN_POINT ( 'NONE',  ( 7.778174593052021635, 7.778174593052023411, 71.12500000409677625 ) ) ;
#36526 = CARTESIAN_POINT ( 'NONE',  ( -5.656854249492380582, 102.3125000000000000, -5.656854249492380582 ) ) ;
#36527 = CARTESIAN_POINT ( 'NONE',  ( 5.656854249492378806, 23.62499999590322020, 5.656854249492381470 ) ) ;
#36529 = CARTESIAN_POINT ( 'NONE',  ( 11.35316468750000141, 75.78124999658602690, 0.000000000000000000 ) ) ;
#36528 = CARTESIAN_POINT ( 'NONE',  ( -4.898587196589412829E-16, 103.8125000040967763, -8.000000000000000000 ) ) ;
#36530 = CARTESIAN_POINT ( 'NONE',  ( 7.999999999999991118, 3.313708498984757611, 22.86155278392014623 ) ) ;
#36531 = CARTESIAN_POINT ( 'NONE',  ( -27.99999999999990763, 196.6250000027312126, 174.0000000000003695 ) ) ;
#36532 = CARTESIAN_POINT ( 'NONE',  ( 4.999999999999993783, 166.0416666598387110, 8.660254037844390851 ) ) ;
#36533 = CARTESIAN_POINT ( 'NONE',  ( 7.188101187500000044, 92.28125000204836681, -8.802885111219163269E-16 ) ) ;
#36534 = CARTESIAN_POINT ( 'NONE',  ( -26.50088068719052004, 194.8029862363522966, 173.5160492912119423 ) ) ;
#36535 = CARTESIAN_POINT ( 'NONE',  ( 5.676582343749993598, 55.26041666325268409, 9.832129032723422313 ) ) ;
#36536 = CARTESIAN_POINT ( 'NONE',  ( -10.18810118749999738, -4.220049686691941915, 105.6250000020483668 ) ) ;
#36537 = CARTESIAN_POINT ( 'NONE',  ( 3.042071309553167069, 191.8229166632526415, -11.35316468749999785 ) ) ;
#36538 = VERTEX_POINT ( 'NONE', #36345 ) ;
#36539 = CARTESIAN_POINT ( 'NONE',  ( -2.069125466537580227, 65.90280720053385721, 26.36412295902896830 ) ) ;
#36540 = DIRECTION ( 'NONE',  ( 0.000000000000000000, 0.000000000000000000, 1.000000000000000000 ) ) ;
#36541 = CARTESIAN_POINT ( 'NONE',  ( 11.99999999999999822, 0.000000000000000000, 0.000000000000000000 ) ) ;
#36543 = CARTESIAN_POINT ( 'NONE',  ( -9.832129032723420536, 198.6979166632526983, 5.676582343749997150 ) ) ;
#36542 = CARTESIAN_POINT ( 'NONE',  ( -24.00000000000002487, 200.9375000027312126, 168.3431457505079152 ) ) ;
#36544 = CYLINDRICAL_SURFACE ( 'NONE', #14031, 10.00000000000000178 ) ;
#36545 = CARTESIAN_POINT ( 'NONE',  ( 8.660254037844389075, 235.2083333401613174, 4.999999999999997335 ) ) ;
#36546 = LINE ( 'NONE', #7505, #74591 ) ;
#36547 = ORIENTED_EDGE ( 'NONE', *, *, #13997, .F. ) ;
#36548 = CARTESIAN_POINT ( 'NONE',  ( 5.676582343749993598, 180.2604166632526699, 9.832129032723422313 ) ) ;
#36549 = CARTESIAN_POINT ( 'NONE',  ( -4.401442555609577197E-16, 7.188101187499992051, 22.11155278187175455 ) ) ;
#36550 = CARTESIAN_POINT ( 'NONE',  ( 9.371230106042952812, 225.9999999999998863, -5.731621267630282013 ) ) ;
#36551 = ORIENTED_EDGE ( 'NONE', *, *, #19462, .F. ) ;
#36552 = EDGE_CURVE ( 'NONE', #67207, #47217, #19718, .T. ) ;
#36553 = CARTESIAN_POINT ( 'NONE',  ( 3.313708498984760720, 97.71875000409676204, -8.000000000000000000 ) ) ;
#36554 = CARTESIAN_POINT ( 'NONE',  ( 28.00000000000002132, 208.5000000000000284, 165.9999999999998863 ) ) ;
#36555 = CARTESIAN_POINT ( 'NONE',  ( -2.828427124746192067, 17.62500000000000000, 2.828427124746190735 ) ) ;
#36556 = CARTESIAN_POINT ( 'NONE',  ( -3.211159895383561391, 17.68749999863440792, -3.211159895383561835 ) ) ;
#36557 = CARTESIAN_POINT ( 'NONE',  ( 3.313708498984756279, 7.999999999999991118, 12.54905278392014800 ) ) ;
#36558 = FACE_OUTER_BOUND ( 'NONE', #33159, .T. ) ;
#36560 = EDGE_LOOP ( 'NONE', ( #58123, #18764, #32118, #51695 ) ) ;
#36559 = EDGE_CURVE ( 'NONE', #55260, #48752, #16015, .T. ) ;
#36561 = PLANE ( 'NONE',  #60737 ) ;
#36562 = CARTESIAN_POINT ( 'NONE',  ( 2.977408999572650039, 96.68750000204836681, -7.188101187500001821 ) ) ;
#36564 = CARTESIAN_POINT ( 'NONE',  ( 4.000000000000001776, 13.81249999726881406, -1.656854249492381248 ) ) ;
#36563 = CARTESIAN_POINT ( 'NONE',  ( -8.000000000000000000, 92.18750000409679046, 0.000000000000000000 ) ) ;
#36565 = DIRECTION ( 'NONE',  ( 0.000000000000000000, -1.000000000000000000, -3.491481338843133355E-15 ) ) ;
#36566 = ORIENTED_EDGE ( 'NONE', *, *, #15261, .T. ) ;
#36567 = EDGE_CURVE ( 'NONE', #67450, #50481, #31041, .T. ) ;
#36568 = CARTESIAN_POINT ( 'NONE',  ( 0.8588954341814997173, 49.93020820668242266, -40.69831139579068235 ) ) ;
#36569 = CARTESIAN_POINT ( 'NONE',  ( 5.082755093536318824, 5.082755093536319713, 18.92405278187175455 ) ) ;
#36570 = ORIENTED_EDGE ( 'NONE', *, *, #32142, .T. ) ;
#36571 = ORIENTED_EDGE ( 'NONE', *, *, #36737, .F. ) ;
#36572 = CARTESIAN_POINT ( 'NONE',  ( -4.220049686691935698, 10.18810118749999916, 79.37500000204838102 ) ) ;
#36573 = CARTESIAN_POINT ( 'NONE',  ( -1.836970198721029983E-15, 115.6249999931720396, 10.00000000000000178 ) ) ;
#36574 = CARTESIAN_POINT ( 'NONE',  ( 2.020667218593132706E-15, -11.00000000000000000, 97.37499999999998579 ) ) ;
#36577 = CARTESIAN_POINT ( 'NONE',  ( -2.765530957081998142, 295.7968750017070647, 6.676582343750000703 ) ) ;
#36576 = CARTESIAN_POINT ( 'NONE',  ( 23.99999999999997868, 201.8125000027312126, 168.3431457505075741 ) ) ;
#36575 = CARTESIAN_POINT ( 'NONE',  ( 30.82842712474620583, 196.2500000027312126, 172.8284271247460424 ) ) ;
#36578 = CARTESIAN_POINT ( 'NONE',  ( -5.000000000000005329, 148.3333333333333428, 8.660254037844387298 ) ) ;
#36579 = AXIS2_PLACEMENT_3D ( 'NONE', #8282, #19229, #13553 ) ;
#36580 = CARTESIAN_POINT ( 'NONE',  ( 27.99999999999996447, 199.6250000027312126, 165.9999999999998863 ) ) ;
#36581 = CARTESIAN_POINT ( 'NONE',  ( 7.188101187499991163, 2.977408999572648707, 1.205302781871753215 ) ) ;
#36582 = EDGE_CURVE ( 'NONE', #58121, #36130, #14045, .T. ) ;
#36583 = CARTESIAN_POINT ( 'NONE',  ( 5.398500733969330945, 9.350505071208255359, 67.88208643086591110 ) ) ;
#36584 = CARTESIAN_POINT ( 'NONE',  ( 3.313708498984762496, 5.531249995903220196, 7.999999999999998224 ) ) ;
#36585 = CARTESIAN_POINT ( 'NONE',  ( 25.55430564589114795, 197.3125000013656063, 172.4456943541086957 ) ) ;
#36586 = CARTESIAN_POINT ( 'NONE',  ( -5.082755093536325042, 10.40624999795161187, -5.082755093536325930 ) ) ;
#36587 = CARTESIAN_POINT ( 'NONE',  ( -6.068751001326191385, -5.224962297650614040, -0.3165082965516815006 ) ) ;
#36588 = DIRECTION ( 'NONE',  ( -0.000000000000000000, 1.000000000000000000, -0.000000000000000000 ) ) ;
#36589 = CARTESIAN_POINT ( 'NONE',  ( 7.188101187500000044, 111.7812500020483810, -8.802885111219163269E-16 ) ) ;
#36591 = FACE_OUTER_BOUND ( 'NONE', #11575, .T. ) ;
#36590 = CARTESIAN_POINT ( 'NONE',  ( 2.775557561562891351E-14, -70.00000000000000000, 170.0000000000000000 ) ) ;
#36592 = CARTESIAN_POINT ( 'NONE',  ( -8.311093377946834337, 224.8437500034139589, 8.311093377946837890 ) ) ;
#36593 = CARTESIAN_POINT ( 'NONE',  ( 27.99999999999999645, 210.0000000000000284, 169.9999999999999147 ) ) ;
#36594 = CARTESIAN_POINT ( 'NONE',  ( 2.977408999572646486, 7.188101187499991163, 22.39280278187175810 ) ) ;
#36596 =( BOUNDED_CURVE ( )  B_SPLINE_CURVE ( 2, ( #67898, #39231, #62231, #27904, #50913, #22232, #16566, #12409, #47844 ),
 .UNSPECIFIED., .F., .F. ) 
 B_SPLINE_CURVE_WITH_KNOTS ( ( 3, 2, 2, 2, 3 ),
 ( 0.9166666666666674068, 0.9250000000000009326, 0.9333333333333342363, 0.9416666666666675400, 0.9500000000000009548 ),
 .UNSPECIFIED. ) 
 CURVE ( )  GEOMETRIC_REPRESENTATION_ITEM ( )  RATIONAL_B_SPLINE_CURVE ( ( 0.9999999999999928946, 0.9238795325112938439, 1.000000000000000000, 0.9238795325112867385, 1.000000000000000000, 0.9238795325112867385, 1.000000000000000000, 0.9238795325112776347, 1.000000000000009104 ) ) 
 REPRESENTATION_ITEM ( '' )  );
#36595 = DIRECTION ( 'NONE',  ( -0.000000000000000000, -0.000000000000000000, -1.000000000000000000 ) ) ;
#36597 = CARTESIAN_POINT ( 'NONE',  ( -9.832129032723418760, 27.86458332991935194, -5.676582343750004256 ) ) ;
#36598 = CARTESIAN_POINT ( 'NONE',  ( 23.99999999999999645, 200.6875000000000284, 168.3431457505074889 ) ) ;
#36599 = CARTESIAN_POINT ( 'NONE',  ( 6.123233995736767268E-16, 3.124999993172032919, -10.00000000000000178 ) ) ;
#36600 = FACE_OUTER_BOUND ( 'NONE', #63128, .T. ) ;
#36601 = CARTESIAN_POINT ( 'NONE',  ( 0.000000000000000000, 300.0000000000000000, 6.000000000000001776 ) ) ;
#36602 = ORIENTED_EDGE ( 'NONE', *, *, #47285, .T. ) ;
#36603 = CARTESIAN_POINT ( 'NONE',  ( -2.775557561562891351E-14, 210.0000000000000284, 142.0000000000000568 ) ) ;
#36604 = CARTESIAN_POINT ( 'NONE',  ( -1.656854249492371034, 8.437499997268815832, 4.000000000000013323 ) ) ;
#36605 = CARTESIAN_POINT ( 'NONE',  ( -8.311093377946841443, 33.90624999658601979, 8.311093377946830785 ) ) ;
#36606 = CARTESIAN_POINT ( 'NONE',  ( 11.00000000000000000, 4.556349186104045934, 84.53125000409677625 ) ) ;
#36607 = CARTESIAN_POINT ( 'NONE',  ( -2.445694354108840063, 209.0625000013656063, 139.5543056458912190 ) ) ;
#36608 = CARTESIAN_POINT ( 'NONE',  ( -2.170320029210516921, -67.76782500014672905, -20.17643218080532108 ) ) ;
#36609 = CARTESIAN_POINT ( 'NONE',  ( 12.00000000000000178, 1.173324140324976783, -0.02489140746004406615 ) ) ;
#36611 = CARTESIAN_POINT ( 'NONE',  ( 11.35316468750000141, 30.78124999658601979, 0.000000000000000000 ) ) ;
#36610 = CARTESIAN_POINT ( 'NONE',  ( 5.082755093536326818, 105.2187500020483952, 5.082755093536325042 ) ) ;
#36612 = CARTESIAN_POINT ( 'NONE',  ( 3.313708498984762496, -7.999999999999989342, 13.29905277982336465 ) ) ;
#36613 = CARTESIAN_POINT ( 'NONE',  ( -3.042071309553164404, 142.2395833299193839, -11.35316468749999963 ) ) ;
#36614 = CARTESIAN_POINT ( 'NONE',  ( -7.320508075688778149, 124.9999999931720538, 7.320508075688769267 ) ) ;
#36615 = EDGE_CURVE ( 'NONE', #20600, #33407, #10595, .T. ) ;
#36616 = CARTESIAN_POINT ( 'NONE',  ( -7.188101187499999156, 111.1250000020483810, 2.977408999572654924 ) ) ;
#36617 = CARTESIAN_POINT ( 'NONE',  ( 0.000000000000000000, 300.0000000000000000, 10.00000000000000178 ) ) ;
#36618 = CARTESIAN_POINT ( 'NONE',  ( -28.00000000000002132, 204.6875000013656063, 166.5412658750003629 ) ) ;
#36619 = AXIS2_PLACEMENT_3D ( 'NONE', #66238, #26992, #26615 ) ;
#36620 = VERTEX_POINT ( 'NONE', #38208 ) ;
#36621 = DIRECTION ( 'NONE',  ( -0.000000000000000000, -1.000000000000000000, -0.000000000000000000 ) ) ;
#36622 = CARTESIAN_POINT ( 'NONE',  ( -11.35316468750000141, 18.59374999658601979, -1.390361679473963753E-15 ) ) ;
#36623 =( BOUNDED_CURVE ( )  B_SPLINE_CURVE ( 2, ( #52384, #719, #17295, #52012, #23330, #39575, #39943, #74648, #62570 ),
 .UNSPECIFIED., .F., .F. ) 
 B_SPLINE_CURVE_WITH_KNOTS ( ( 3, 2, 2, 2, 3 ),
 ( 0.4431818181818181768, 0.4488636363636363535, 0.4545454545454545858, 0.4602272727272727626, 0.4659090909090909394 ),
 .UNSPECIFIED. ) 
 CURVE ( )  GEOMETRIC_REPRESENTATION_ITEM ( )  RATIONAL_B_SPLINE_CURVE ( ( 1.000000000000000000, 0.9238795325112867385, 1.000000000000000000, 0.9238795325112867385, 1.000000000000000000, 0.9238795325112867385, 1.000000000000000000, 0.9238795325112859613, 1.000000000000000666 ) ) 
 REPRESENTATION_ITEM ( '' )  );
#36624 = ORIENTED_EDGE ( 'NONE', *, *, #27468, .F. ) ;
#36625 = CARTESIAN_POINT ( 'NONE',  ( 4.500000000000017764, -7.794228634059961358, -10.20000000000000462 ) ) ;
#36626 = CARTESIAN_POINT ( 'NONE',  ( -1.736494649864694706, 16.42394793108385898, -68.69316892221223725 ) ) ;
#36628 = CARTESIAN_POINT ( 'NONE',  ( -11.35316468750000141, 153.2812499965860127, -1.390361679473963753E-15 ) ) ;
#36627 = LINE ( 'NONE', #70223, #61747 ) ;
#36629 = CARTESIAN_POINT ( 'NONE',  ( 7.188101187500000044, 0.8437499979516100979, 0.000000000000000000 ) ) ;
#36630 = CARTESIAN_POINT ( 'NONE',  ( 3.313708498984756279, 7.999999999999991118, 15.41780278432982598 ) ) ;
#36631 = CARTESIAN_POINT ( 'NONE',  ( 59.97427153372161257, 218.5830059962467260, 46.37215406069778112 ) ) ;
#36632 = CARTESIAN_POINT ( 'NONE',  ( -9.832129032723418760, 238.4895833367473301, -5.676582343749998927 ) ) ;
#36633 = CARTESIAN_POINT ( 'NONE',  ( -4.220049686691937474, -10.18810118749999738, 89.31250000204838102 ) ) ;
#36634 = ORIENTED_EDGE ( 'NONE', *, *, #33167, .T. ) ;
#36635 = CARTESIAN_POINT ( 'NONE',  ( 7.320508075688777261, 120.6250000000000284, -7.320508075688777261 ) ) ;
#36636 = CARTESIAN_POINT ( 'NONE',  ( -54.00000000000000000, 272.0000000000000000, 4.085831468968145267E-14 ) ) ;
#36637 = CARTESIAN_POINT ( 'NONE',  ( -2.085542519210945728E-15, 99.84374999658601268, 11.35316468750000141 ) ) ;
#36638 = CARTESIAN_POINT ( 'NONE',  ( -10.18810118749999916, 0.000000000000000000, 103.6562500020483810 ) ) ;
#36639 = CARTESIAN_POINT ( 'NONE',  ( 1.881053915767121998, 17.62499999863440436, -4.541265875000002339 ) ) ;
#36640 = ORIENTED_EDGE ( 'NONE', *, *, #14377, .T. ) ;
#36641 = ORIENTED_EDGE ( 'NONE', *, *, #45834, .F. ) ;
#36642 = AXIS2_PLACEMENT_3D ( 'NONE', #59855, #60967, #25134 ) ;
#36643 = CARTESIAN_POINT ( 'NONE',  ( -1.469576158976823947E-15, 13.12500000000000355, 8.000000000000000000 ) ) ;
#36644 = CARTESIAN_POINT ( 'NONE',  ( -5.656854249492379694, 11.06250000000000178, -5.656854249492380582 ) ) ;
#36645 = CARTESIAN_POINT ( 'NONE',  ( 7.188101187499999156, 4.874999997951610098, 2.977408999572654924 ) ) ;
#36646 = CARTESIAN_POINT ( 'NONE',  ( 5.656854249492381470, 113.7500000040967763, 5.656854249492379694 ) ) ;
#36647 = CARTESIAN_POINT ( 'NONE',  ( -10.18810118749999738, -4.220049686691941915, 98.12500000204836681 ) ) ;
#36648 = CARTESIAN_POINT ( 'NONE',  ( -54.00000000000000711, 205.0000000000000284, 0.000000000000000000 ) ) ;
#36649 = CARTESIAN_POINT ( 'NONE',  ( -1.469576158976823947E-15, 7.125000000000000888, 8.000000000000000000 ) ) ;
#36650 = CARTESIAN_POINT ( 'NONE',  ( -7.347880794884122694E-16, 13.49999999726881406, 4.000000000000001776 ) ) ;
#36651 = CARTESIAN_POINT ( 'NONE',  ( 4.541265875000001451, 4.249999998634407028, 1.881053915767124440 ) ) ;
#36652 = ORIENTED_EDGE ( 'NONE', *, *, #30593, .T. ) ;
#36653 = LINE ( 'NONE', #25678, #66518 ) ;
#36654 = CARTESIAN_POINT ( 'NONE',  ( 26.34314575050758123, 207.9375000000000568, 173.9999999999999147 ) ) ;
#36656 = CARTESIAN_POINT ( 'NONE',  ( -8.000000000000000000, 15.65625000000000355, -3.313708498984762496 ) ) ;
#36655 = CARTESIAN_POINT ( 'NONE',  ( -24.54126587500002188, 200.2500000013656631, 168.5673454167826435 ) ) ;
#36657 =( LENGTH_UNIT ( ) NAMED_UNIT ( * ) SI_UNIT ( .MILLI., .METRE. ) );
#36658 = EDGE_CURVE ( 'NONE', #62350, #34052, #20839, .T. ) ;
#36659 = CARTESIAN_POINT ( 'NONE',  ( 3.211159895383560947, 13.18749999863440792, 3.211159895383562723 ) ) ;
#36660 = CARTESIAN_POINT ( 'NONE',  ( -11.00000000000000000, 0.000000000000000000, 84.99999999999998579 ) ) ;
#36661 = CIRCLE ( 'NONE', #13745, 38.34805510287551300 ) ;
#36662 = CARTESIAN_POINT ( 'NONE',  ( 2.977408999572646486, 7.188101187499991163, 8.517802781871754547 ) ) ;
#36663 = ORIENTED_EDGE ( 'NONE', *, *, #12476, .F. ) ;
#36664 = EDGE_LOOP ( 'NONE', ( #8205, #22136, #60753, #39617 ) ) ;
#36665 = CARTESIAN_POINT ( 'NONE',  ( -4.220049686691937474, -10.18810118749999738, 103.9375000020483810 ) ) ;
#36666 = DIRECTION ( 'NONE',  ( -4.532466538174778503E-15, -0.7071067811865465735, -0.7071067811865484609 ) ) ;
#36667 = CARTESIAN_POINT ( 'NONE',  ( -31.45873412499999944, 203.9375000013656063, 170.0000000000003979 ) ) ;
#36668 = CARTESIAN_POINT ( 'NONE',  ( -25.17157287525382259, 200.8750000000000284, 167.1715728752541565 ) ) ;
#36669 = CARTESIAN_POINT ( 'NONE',  ( 3.458734125000015425, 195.0000000013656063, 196.5673454167823877 ) ) ;
#36670 = CARTESIAN_POINT ( 'NONE',  ( -1.469576158976823947E-15, 12.93749999590322197, 8.000000000000000000 ) ) ;
#36671 = CARTESIAN_POINT ( 'NONE',  ( 7.320508075688771044, 89.37499999999998579, 7.320508075688775484 ) ) ;
#36672 = CARTESIAN_POINT ( 'NONE',  ( 8.000000000000001776, 113.6562500000000000, 3.313708498984759387 ) ) ;
#36673 = CARTESIAN_POINT ( 'NONE',  ( 6.676582343750001591, 297.1093750017069510, -8.176455196517173205E-16 ) ) ;
#36674 = VERTEX_POINT ( 'NONE', #20084 ) ;
#36675 = CARTESIAN_POINT ( 'NONE',  ( 10.00000000000004263, 190.2083333333333428, -2.679491924311237394 ) ) ;
#36676 = EDGE_CURVE ( 'NONE', #41098, #30287, #60084, .T. ) ;
#36677 = CARTESIAN_POINT ( 'NONE',  ( -8.000000000000000000, 12.46874999590322197, -3.313708498984762496 ) ) ;
#36678 = CARTESIAN_POINT ( 'NONE',  ( -3.458734125000015425, 202.0000000013656063, 143.4326545832176976 ) ) ;
#36679 = LINE ( 'NONE', #32137, #37019 ) ;
#36680 = CARTESIAN_POINT ( 'NONE',  ( -4.999999999999992895, 220.8333333333333428, 8.660254037844390851 ) ) ;
#36681 = CARTESIAN_POINT ( 'NONE',  ( -4.000000000000015987, 207.5625000000000000, 143.6568542494924259 ) ) ;
#36682 = CARTESIAN_POINT ( 'NONE',  ( 4.556349186104045934, 11.00000000000000000, 111.5312500000000142 ) ) ;
#36683 = CARTESIAN_POINT ( 'NONE',  ( -2.679491924311225848, 216.4583333333333144, -10.00000000000000178 ) ) ;
#36684 = EDGE_CURVE ( 'NONE', #8398, #31722, #62299, .T. ) ;
#36685 = CARTESIAN_POINT ( 'NONE',  ( -7.188101187499990274, -2.977408999572651815, 7.955302781871751883 ) ) ;
#36686 = CARTESIAN_POINT ( 'NONE',  ( 11.35316468750000141, 196.0937499965860127, 0.000000000000000000 ) ) ;
#36687 = DIRECTION ( 'NONE',  ( 0.000000000000000000, 0.000000000000000000, 1.000000000000000000 ) ) ;
#36688 = CARTESIAN_POINT ( 'NONE',  ( 2.780723358947928197E-16, 3.562499998634407028, -4.541265875000002339 ) ) ;
#36689 = CARTESIAN_POINT ( 'NONE',  ( 4.999999999999997335, 243.3333333333333428, -8.660254037844387298 ) ) ;
#36690 = CARTESIAN_POINT ( 'NONE',  ( -3.313708498984708317, 107.4687500040968047, 8.000000000000053291 ) ) ;
#36691 = ORIENTED_EDGE ( 'NONE', *, *, #15091, .T. ) ;
#36692 = AXIS2_PLACEMENT_3D ( 'NONE', #49570, #14103, #3555 ) ;
#36693 = CARTESIAN_POINT ( 'NONE',  ( -3.458734125000016757, 205.1250000013656347, 140.5673454167824161 ) ) ;
#36694 = CARTESIAN_POINT ( 'NONE',  ( -3.042071309553164404, 47.55208332991935549, -11.35316468749999963 ) ) ;
#36695 = CARTESIAN_POINT ( 'NONE',  ( -4.556349186104045934, 11.00000000000000000, 102.9062500040967905 ) ) ;
#36696 = CARTESIAN_POINT ( 'NONE',  ( -5.676582343750006032, 224.4270833299193555, 9.832129032723418760 ) ) ;
#36697 = CARTESIAN_POINT ( 'NONE',  ( -24.54126587499996504, 207.1250000013656347, 171.4326545832179534 ) ) ;
#36698 = DIRECTION ( 'NONE',  ( -0.000000000000000000, -1.000000000000000000, -0.000000000000000000 ) ) ;
#36700 = CARTESIAN_POINT ( 'NONE',  ( 1.836970198721029589E-15, 231.2500000000000000, 10.00000000000000000 ) ) ;
#36699 = CARTESIAN_POINT ( 'NONE',  ( 7.778174593052021635, 7.778174593052023411, 71.12500000409677625 ) ) ;
#36701 = CARTESIAN_POINT ( 'NONE',  ( -3.458734125000015425, 195.9375000013655779, 142.0000000000000568 ) ) ;
#36702 = CARTESIAN_POINT ( 'NONE',  ( -3.042071309553164404, 102.2395833299193697, -11.35316468749999963 ) ) ;
#36703 = CARTESIAN_POINT ( 'NONE',  ( -8.660254037844387298, 78.95833332650536818, -5.000000000000004441 ) ) ;
#36704 = CARTESIAN_POINT ( 'NONE',  ( -7.188101187500000044, 124.5312500020483810, 0.000000000000000000 ) ) ;
#36705 = CARTESIAN_POINT ( 'NONE',  ( -8.342170076843785083E-16, 15.18749999863440792, 4.541265875000002339 ) ) ;
#36706 = FACE_OUTER_BOUND ( 'NONE', #32355, .T. ) ;
#36707 = ORIENTED_EDGE ( 'NONE', *, *, #43713, .F. ) ;
#36709 = EDGE_CURVE ( 'NONE', #68975, #43686, #59863, .T. ) ;
#36708 = ORIENTED_EDGE ( 'NONE', *, *, #33059, .T. ) ;
#36710 = CARTESIAN_POINT ( 'NONE',  ( -4.088227598258586603E-16, 294.3593750017070079, -6.676582343750001591 ) ) ;
#36711 = DIRECTION ( 'NONE',  ( 2.168404344971008868E-16, -1.000000000000000000, 0.000000000000000000 ) ) ;
#36712 = CARTESIAN_POINT ( 'NONE',  ( 6.951808397369818766E-16, 172.0312499965860411, -11.35316468750000141 ) ) ;
#36713 = CARTESIAN_POINT ( 'NONE',  ( -5.656854249492375253, 5.656854249492375253, 9.642802779823364645 ) ) ;
#36714 = CARTESIAN_POINT ( 'NONE',  ( 4.000000000000015099, 200.5625000000000284, 196.3431457505076594 ) ) ;
#36715 = CARTESIAN_POINT ( 'NONE',  ( -8.660254037844424602, 192.0833333333333428, -5.000000000000025757 ) ) ;
#36716 = CARTESIAN_POINT ( 'NONE',  ( -4.220049686691937474, -10.18810118749999738, 110.3125000020483810 ) ) ;
#36717 = ORIENTED_EDGE ( 'NONE', *, *, #65730, .F. ) ;
#36718 =( BOUNDED_CURVE ( )  B_SPLINE_CURVE ( 2, ( #16221, #39260, #68295, #10961, #39631, #16592, #67188, #27182, #62258, #74325, #62630, #15486, #33996 ),
 .UNSPECIFIED., .F., .F. ) 
 B_SPLINE_CURVE_WITH_KNOTS ( ( 3, 2, 2, 2, 2, 2, 3 ),
 ( 0.9166666666666668517, 0.9259259259259261521, 0.9351851851851854525, 0.9444444444444445308, 0.9537037037037038312, 0.9629629629629630205, 0.9722222222222223209 ),
 .UNSPECIFIED. ) 
 CURVE ( )  GEOMETRIC_REPRESENTATION_ITEM ( )  RATIONAL_B_SPLINE_CURVE ( ( 0.9999999999999992228, 0.9659258262890690894, 1.000000000000000000, 0.9659258262890683122, 1.000000000000000000, 0.9659258262890683122, 1.000000000000000000, 0.9659258262890683122, 1.000000000000000000, 0.9659258262890683122, 1.000000000000000000, 0.9659258262890678681, 1.000000000000000444 ) ) 
 REPRESENTATION_ITEM ( '' )  );
#36719 = CARTESIAN_POINT ( 'NONE',  ( -3.313708498984681672, 113.2812500000000142, 8.000000000000078160 ) ) ;
#36720 = CARTESIAN_POINT ( 'NONE',  ( 0.000000000000000000, 30.78460969082653875, -20.69999999999999929 ) ) ;
#36721 = CARTESIAN_POINT ( 'NONE',  ( 11.35316468749999785, 135.8854166632526699, 3.042071309553174174 ) ) ;
#36722 = CARTESIAN_POINT ( 'NONE',  ( -3.458734124999959914, 196.4375000013655779, 198.0000000000000284 ) ) ;
#36723 = CARTESIAN_POINT ( 'NONE',  ( 4.242640687119285658, 298.6875000034139589, -4.242640687119286547 ) ) ;
#36724 = CARTESIAN_POINT ( 'NONE',  ( -4.220049686691937474, -10.18810118749999738, 68.31250000204836681 ) ) ;
#36725 = CARTESIAN_POINT ( 'NONE',  ( -3.042071309553173730, 64.63541666325269830, 11.35316468749999785 ) ) ;
#36726 = ORIENTED_EDGE ( 'NONE', *, *, #42517, .F. ) ;
#36727 = DIRECTION ( 'NONE',  ( -0.000000000000000000, 1.000000000000000000, -4.476705744456276341E-16 ) ) ;
#36728 = CARTESIAN_POINT ( 'NONE',  ( -8.342170076843785083E-16, 5.187499998634407028, 4.541265875000002339 ) ) ;
#36729 = CARTESIAN_POINT ( 'NONE',  ( -3.317071493978880348, -8.008118988124989457, 7.294365283940629219 ) ) ;
#36730 = UNCERTAINTY_MEASURE_WITH_UNIT (LENGTH_MEASURE( 1.000000000000000082E-05 ), #1255, 'distance_accuracy_value', 'NONE');
#36731 = EDGE_CURVE ( 'NONE', #16346, #68294, #66996, .T. ) ;
#36732 = CARTESIAN_POINT ( 'NONE',  ( 2.977408999572650927, 17.24999999795162253, -7.188101187500001821 ) ) ;
#36733 = CARTESIAN_POINT ( 'NONE',  ( 6.000000000000003553, 290.6250000034140157, -2.485281374238571761 ) ) ;
#36734 = CARTESIAN_POINT ( 'NONE',  ( -4.850062511589670794E-16, 124.5792468245269475, -7.920753175473082663 ) ) ;
#36735 = CARTESIAN_POINT ( 'NONE',  ( 7.188101187500000044, 9.843749997951610098, 0.000000000000000000 ) ) ;
#36736 = CARTESIAN_POINT ( 'NONE',  ( -2.977408999572647819, 7.188101187499992051, 1.205302781871753215 ) ) ;
#36737 = EDGE_CURVE ( 'NONE', #38597, #4709, #27246, .T. ) ;
#36738 =( BOUNDED_CURVE ( )  B_SPLINE_CURVE ( 2, ( #48015, #19345, #12211, #13308, #41634, #53697, #7303 ),
 .UNSPECIFIED., .F., .F. ) 
 B_SPLINE_CURVE_WITH_KNOTS ( ( 3, 2, 2, 3 ),
 ( 0.000000000000000000, 0.001811594202898550747, 0.003623188405797101493, 0.005434782608695652023 ),
 .UNSPECIFIED. ) 
 CURVE ( )  GEOMETRIC_REPRESENTATION_ITEM ( )  RATIONAL_B_SPLINE_CURVE ( ( 1.000000000000000000, 0.9659258262890683122, 1.000000000000000000, 0.9659258262890683122, 1.000000000000000000, 0.9659258262890683122, 1.000000000000000000 ) ) 
 REPRESENTATION_ITEM ( '' )  );
#36739 = CARTESIAN_POINT ( 'NONE',  ( -10.18810118749999916, 4.220049686691934809, 114.4375000020483668 ) ) ;
#36740 = ADVANCED_FACE ( 'NONE', ( #61586 ), #8785, .F. ) ;
#36741 = CARTESIAN_POINT ( 'NONE',  ( 2.449293598294707893E-16, 9.250000000000000000, -4.000000000000001776 ) ) ;
#36742 = CARTESIAN_POINT ( 'NONE',  ( -4.000000000000001776, 1.187499997268813390, -1.656854249492381470 ) ) ;
#36743 = VERTEX_POINT ( 'NONE', #55194 ) ;
#36744 = CARTESIAN_POINT ( 'NONE',  ( 1.656854249492403008, 194.8125000027312126, 194.0000000000000853 ) ) ;
#36745 = CARTESIAN_POINT ( 'NONE',  ( -2.849036369511732440E-14, 201.2500000000000000, 138.0000000000000568 ) ) ;
#36746 = CARTESIAN_POINT ( 'NONE',  ( -30.82842712474612412, 199.5000000027312126, 172.8284271247466108 ) ) ;
#36747 = CARTESIAN_POINT ( 'NONE',  ( -1.881053915767124440, 1.999999998634406806, 4.541265875000001451 ) ) ;
#36748 = CARTESIAN_POINT ( 'NONE',  ( 2.977408999572650039, 110.1875000020483810, -7.188101187500001821 ) ) ;
#36749 = CARTESIAN_POINT ( 'NONE',  ( 1.102182119232618108E-15, 295.2500000000000000, 6.000000000000001776 ) ) ;
#36750 = CARTESIAN_POINT ( 'NONE',  ( 5.656854249492374365, 5.656854249492375253, 1.955302783920143117 ) ) ;
#36751 = ORIENTED_EDGE ( 'NONE', *, *, #21008, .T. ) ;
#36752 = CARTESIAN_POINT ( 'NONE',  ( -7.188101187500000933, 25.12499999795161543, -2.977408999572651371 ) ) ;
#36753 = EDGE_LOOP ( 'NONE', ( #72941, #68000 ) ) ;
#36754 = CARTESIAN_POINT ( 'NONE',  ( 2.020667218593132706E-15, -11.00000000000000000, 84.06250000409676204 ) ) ;
#36755 = CARTESIAN_POINT ( 'NONE',  ( -1.432654583217607192, 207.2500000013655779, 194.5412658750000219 ) ) ;
#36756 = CARTESIAN_POINT ( 'NONE',  ( 29.43265458321766914, 204.5000000013655779, 173.4587341249998929 ) ) ;
#36757 = B_SPLINE_CURVE_WITH_KNOTS ( 'NONE', 3,
 ( #51203, #55764, #40632, #1763, #58373, #41741, #36087, #52698, #5939, #64388, #34620, #59106, #63632, #6315, #18363, #57626, #11963, #23650 ),
 .UNSPECIFIED., .F., .F.,
 ( 4, 2, 2, 2, 2, 2, 2, 2, 4 ),
 ( 1.087004710699503354E-17, 0.0005866892120924655993, 0.001173378424184919923, 0.001760067636277374246, 0.002346756848369828570, 0.002933446060462282894, 0.003520135272554736783, 0.004106824484647191541, 0.004693513696739645864 ),
 .UNSPECIFIED. ) ;
#36758 = CARTESIAN_POINT ( 'NONE',  ( -5.000000000000005329, 58.33333333333333570, 8.660254037844387298 ) ) ;
#36759 = CARTESIAN_POINT ( 'NONE',  ( -4.401442555609581635E-16, 100.1562500020483810, -7.188101187500000044 ) ) ;
#36760 = CARTESIAN_POINT ( 'NONE',  ( 2.485281374238571317, 297.6875000000000000, -6.000000000000003553 ) ) ;
#36761 = VECTOR ( 'NONE', #13947, 1000.000000000000000 ) ;
#36763 = CARTESIAN_POINT ( 'NONE',  ( -25.24771445596618236, -41.37820964980527805, 187.9900717105972774 ) ) ;
#36762 = LINE ( 'NONE', #55613, #16512 ) ;
#36764 = EDGE_LOOP ( 'NONE', ( #67507, #56622, #10075, #24838 ) ) ;
#36765 = CARTESIAN_POINT ( 'NONE',  ( 2.085542519210945334E-15, 230.1562500034139873, 11.35316468749999963 ) ) ;
#36766 = CARTESIAN_POINT ( 'NONE',  ( -2.828427124746208943, 201.7500000027312126, 144.8284271247462129 ) ) ;
#36767 = CARTESIAN_POINT ( 'NONE',  ( 3.313708498984756279, 7.999999999999991118, 3.361552779823362425 ) ) ;
#36768 = CARTESIAN_POINT ( 'NONE',  ( 7.778174593052023411, -7.778174593052021635, 94.56250000000000000 ) ) ;
#36769 = CARTESIAN_POINT ( 'NONE',  ( 7.320508075688771044, 263.1249999999999432, -7.320508075688771932 ) ) ;
#36770 = DIRECTION ( 'NONE',  ( 0.000000000000000000, -0.000000000000000000, 1.000000000000000000 ) ) ;
#36771 = CARTESIAN_POINT ( 'NONE',  ( -10.00000000000000000, 172.2916666666666288, -2.679491924311229845 ) ) ;
#36772 = CARTESIAN_POINT ( 'NONE',  ( 1.102182119232618108E-15, 297.3125000034140157, 6.000000000000001776 ) ) ;
#36773 = DIRECTION ( 'NONE',  ( 0.000000000000000000, 0.000000000000000000, 1.000000000000000000 ) ) ;
#36774 = CARTESIAN_POINT ( 'NONE',  ( 7.188101187499993827, -2.977408999572645598, 26.51780278187175455 ) ) ;
#36775 = CARTESIAN_POINT ( 'NONE',  ( -8.311093377946836114, 147.9687499965860411, -8.311093377946837890 ) ) ;
#36776 = CARTESIAN_POINT ( 'NONE',  ( 10.99999999999989342, 4.556349186104152515, 75.53125000409677625 ) ) ;
#36777 = CARTESIAN_POINT ( 'NONE',  ( -6.123233995736766282E-16, 261.8750000068280315, -10.00000000000000000 ) ) ;
#36780 = DIRECTION ( 'NONE',  ( 1.000000000000000000, 0.000000000000000000, 0.000000000000000000 ) ) ;
#36779 = CARTESIAN_POINT ( 'NONE',  ( 10.00000000000000000, 106.6666666598387252, 2.679491924311235618 ) ) ;
#36778 = CARTESIAN_POINT ( 'NONE',  ( 31.99999999999998579, 205.1875000000000000, 171.6568542494923122 ) ) ;
#36781 = ORIENTED_EDGE ( 'NONE', *, *, #31469, .T. ) ;
#36782 = CARTESIAN_POINT ( 'NONE',  ( -11.35316468750000141, 13.59374999658601801, -1.390361679473963753E-15 ) ) ;
#36783 = CARTESIAN_POINT ( 'NONE',  ( -8.000000000000000000, 8.062499995903221972, -9.797174393178825657E-16 ) ) ;
#36784 = CARTESIAN_POINT ( 'NONE',  ( 6.891449706524926277, -10.24244278381002005, -65.16993756079213540 ) ) ;
#36785 = CARTESIAN_POINT ( 'NONE',  ( -30.82842712474615610, 196.3750000000000284, 172.8284271247465824 ) ) ;
#36786 = CARTESIAN_POINT ( 'NONE',  ( -2.754378923186476579E-14, 206.1875000013656063, 145.4587341250000350 ) ) ;
#36787 = CARTESIAN_POINT ( 'NONE',  ( -6.719196256674477397, 124.7364742007443965, -3.922907429097691967 ) ) ;
#36788 = CARTESIAN_POINT ( 'NONE',  ( 6.123233995736767268E-16, 38.12499999317203958, -10.00000000000000178 ) ) ;
#36789 = CARTESIAN_POINT ( 'NONE',  ( -2.977408999572650927, 111.8750000020483668, -7.188101187500001821 ) ) ;
#36790 = CARTESIAN_POINT ( 'NONE',  ( -3.211159895383562723, 4.062499998634407028, 3.211159895383561391 ) ) ;
#36791 = CARTESIAN_POINT ( 'NONE',  ( -11.92121597166104863, -37.99999999999992184, 141.3838400592076709 ) ) ;
#36792 = CARTESIAN_POINT ( 'NONE',  ( -5.656854249492373476, -5.656854249492376141, 14.51780277982336465 ) ) ;
#36794 = CARTESIAN_POINT ( 'NONE',  ( 3.313708498984762496, -7.999999999999989342, 17.98655278392014623 ) ) ;
#36793 = CARTESIAN_POINT ( 'NONE',  ( 6.000000000000003553, 291.6250000034140157, -2.485281374238571761 ) ) ;
#36795 = ORIENTED_EDGE ( 'NONE', *, *, #44530, .F. ) ;
#36796 = CARTESIAN_POINT ( 'NONE',  ( -5.711993833409989278E-12, 133.7499999999995737, 9.999999999999998224 ) ) ;
#36797 = CARTESIAN_POINT ( 'NONE',  ( -5.000000000000031086, 63.33333333333336412, 8.660254037844431707 ) ) ;
#36798 = CARTESIAN_POINT ( 'NONE',  ( 2.085542519210945334E-15, 225.4687500034139873, 11.35316468749999963 ) ) ;
#36799 = CARTESIAN_POINT ( 'NONE',  ( -11.35316468750000141, 128.4895833299193555, 3.042071309553159963 ) ) ;
#36800 = ORIENTED_EDGE ( 'NONE', *, *, #65344, .T. ) ;
#36801 = CARTESIAN_POINT ( 'NONE',  ( 4.627539443576518252, 9.975780150077198982, 117.5133370941326945 ) ) ;
#36802 = CARTESIAN_POINT ( 'NONE',  ( -6.238412754330611322E-16, 10.18810118749999916, 92.78125000204836681 ) ) ;
#36803 = CARTESIAN_POINT ( 'NONE',  ( -1.001543065824775909E-15, -10.39230484541329247, -10.20000000000000284 ) ) ;
#36804 = CARTESIAN_POINT ( 'NONE',  ( 2.839093476692135984E-14, 194.9375000013655779, 201.4587341250000350 ) ) ;
#36805 = CARTESIAN_POINT ( 'NONE',  ( 0.000000000000000000, 300.0000000000000000, 0.000000000000000000 ) ) ;
#36807 = CARTESIAN_POINT ( 'NONE',  ( 5.676582343750001591, 111.6145833299193555, -9.832129032723420536 ) ) ;
#36806 = CARTESIAN_POINT ( 'NONE',  ( 28.00000000000001421, 197.5000000000000000, 165.9999999999998863 ) ) ;
#36808 = CARTESIAN_POINT ( 'NONE',  ( -26.34314575050758478, 209.5625000000000000, 174.0000000000003411 ) ) ;
#36809 = DIRECTION ( 'NONE',  ( 0.000000000000000000, 0.000000000000000000, 1.000000000000000000 ) ) ;
#36810 = VERTEX_POINT ( 'NONE', #9905 ) ;
#36811 = CARTESIAN_POINT ( 'NONE',  ( 2.679491924311228956, 212.9166666598386826, -10.00000000000000000 ) ) ;
#36812 = CARTESIAN_POINT ( 'NONE',  ( 5.656854249492379694, 112.6250000040967763, -5.656854249492380582 ) ) ;
#36813 = CYLINDRICAL_SURFACE ( 'NONE', #50918, 7.999999999999991118 ) ;
#36814 = CARTESIAN_POINT ( 'NONE',  ( 11.35316468749999963, 101.3020833299193555, -3.042071309553165293 ) ) ;
#36815 = CARTESIAN_POINT ( 'NONE',  ( -3.458734124999958581, 207.5000000013656063, 199.4326545832176976 ) ) ;
#36816 = CARTESIAN_POINT ( 'NONE',  ( -2.977408999572654480, 10.87499999795161187, 7.188101187499999156 ) ) ;
#36817 = CARTESIAN_POINT ( 'NONE',  ( -10.18810118749999916, 4.220049686691934809, 91.93750000204836681 ) ) ;
#36818 = CARTESIAN_POINT ( 'NONE',  ( 8.311093377946834337, 15.46874999658601624, 8.311093377946839666 ) ) ;
#36819 = EDGE_LOOP ( 'NONE', ( #62333, #36255, #37830, #65003 ) ) ;
#36820 = CARTESIAN_POINT ( 'NONE',  ( 11.00000000000000000, 1.347111479062088405E-15, 115.9375000040967763 ) ) ;
#36821 = CARTESIAN_POINT ( 'NONE',  ( 1.471067592899761672E-15, -8.008118988124991233, 25.38811528394063544 ) ) ;
#36822 = CARTESIAN_POINT ( 'NONE',  ( 4.999999999999993783, 116.0416666598387110, 8.660254037844390851 ) ) ;
#36823 = CARTESIAN_POINT ( 'NONE',  ( 10.18810118750000093, -4.220049686691933921, 74.68750000204836681 ) ) ;
#36824 = CARTESIAN_POINT ( 'NONE',  ( -1.737867177246331662, 21.99999999999999645, 4.195582608135537406 ) ) ;
#36825 = CARTESIAN_POINT ( 'NONE',  ( -10.00000000000000000, 149.1666666598387110, -2.679491924311229845 ) ) ;
#36826 = CARTESIAN_POINT ( 'NONE',  ( 4.721056650416000089, 290.8281250017069510, 4.721056650415999201 ) ) ;
#36827 = AXIS2_PLACEMENT_3D ( 'NONE', #37940, #25108, #25478 ) ;
#36828 = CARTESIAN_POINT ( 'NONE',  ( 10.00000000000000178, 126.8749999931720396, 0.000000000000000000 ) ) ;
#36829 = DIRECTION ( 'NONE',  ( 0.000000000000000000, -1.000000000000000000, 0.000000000000000000 ) ) ;
#36830 = EDGE_CURVE ( 'NONE', #7497, #69231, #60833, .T. ) ;
#36831 = CARTESIAN_POINT ( 'NONE',  ( -8.311093377946841443, 129.2187499965860127, 8.311093377946830785 ) ) ;
#36832 = CARTESIAN_POINT ( 'NONE',  ( -4.220049686691937474, -10.18810118749999738, 85.93750000204839523 ) ) ;
#36833 = AXIS2_PLACEMENT_3D ( 'NONE', #21615, #72176, #26523 ) ;
#36834 =( BOUNDED_CURVE ( )  B_SPLINE_CURVE ( 2, ( #47246, #1620, #70273, #70631, #18950, #41954, #13271, #36310, #59327, #7636, #30642, #42320, #65338 ),
 .UNSPECIFIED., .F., .F. ) 
 B_SPLINE_CURVE_WITH_KNOTS ( ( 3, 2, 2, 2, 2, 2, 3 ),
 ( 0.6436908981619412495, 0.6489249083846719834, 0.6541589186074028284, 0.6593929288301335623, 0.6646269390528642962, 0.6698609492755951411, 0.6750949594983258750 ),
 .UNSPECIFIED. ) 
 CURVE ( )  GEOMETRIC_REPRESENTATION_ITEM ( )  RATIONAL_B_SPLINE_CURVE ( ( 1.000000000000161871, 0.9659258262889065527, 1.000000000000000000, 0.9659258262890684232, 1.000000000000000000, 0.9659258262890684232, 1.000000000000000000, 0.9659258262890684232, 1.000000000000000000, 0.9659258262890684232, 1.000000000000000000, 0.9659258262890819680, 0.9999999999999864553 ) ) 
 REPRESENTATION_ITEM ( '' )  );
#36835 = CARTESIAN_POINT ( 'NONE',  ( -24.54126587500000056, 200.2500000013656631, 168.5673454167827003 ) ) ;
#36836 = EDGE_CURVE ( 'NONE', #4709, #38597, #33310, .T. ) ;
#36837 = CARTESIAN_POINT ( 'NONE',  ( -3.313708498984765161, 25.03125000000000355, 7.999999999999998224 ) ) ;
#36838 = CARTESIAN_POINT ( 'NONE',  ( -3.211159895383562723, 12.06249999863440614, 3.211159895383561391 ) ) ;
#36839 = ORIENTED_EDGE ( 'NONE', *, *, #39692, .T. ) ;
#36840 = CARTESIAN_POINT ( 'NONE',  ( -31.99999999999996447, 208.4375000027311842, 171.6568542494928522 ) ) ;
#36841 = CARTESIAN_POINT ( 'NONE',  ( 1.656854249492403008, 208.8125000027312126, 194.0000000000000853 ) ) ;
#36842 = CARTESIAN_POINT ( 'NONE',  ( 2.445694354108784108, 197.5625000013656063, 144.4456943541088663 ) ) ;
#36843 = CARTESIAN_POINT ( 'NONE',  ( -4.000000000000015987, 205.6250000027312126, 142.0000000000000568 ) ) ;
#36844 = CARTESIAN_POINT ( 'NONE',  ( 5.000000000000000000, 10.42446448370085577, -65.94449134867498685 ) ) ;
#36845 = CARTESIAN_POINT ( 'NONE',  ( -7.204075437095967871, 7.204075437095967871, 69.34375000204836681 ) ) ;
#36846 = ORIENTED_EDGE ( 'NONE', *, *, #39818, .F. ) ;
#36847 = B_SPLINE_CURVE_WITH_KNOTS ( 'NONE', 3,
 ( #1548, #24528, #18508, #70559, #58153, #6819, #46801, #1176 ),
 .UNSPECIFIED., .F., .F.,
 ( 4, 2, 2, 4 ),
 ( 0.005256334970490775943, 0.006570121696662012747, 0.007883908422833249552, 0.01051148187517572316 ),
 .UNSPECIFIED. ) ;
#36848 = CARTESIAN_POINT ( 'NONE',  ( 7.188101187500000933, 6.562499997951610986, -2.977408999572650483 ) ) ;
#36849 = CARTESIAN_POINT ( 'NONE',  ( -10.00000000000000000, 29.16666665983869677, -2.679491924311229845 ) ) ;
#36850 = CARTESIAN_POINT ( 'NONE',  ( 2.977408999572650039, 118.0625000020483952, -7.188101187500001821 ) ) ;
#36851 = CARTESIAN_POINT ( 'NONE',  ( 2.949463562550349138, -19.08173610902314721, -0.7140392532422756844 ) ) ;
#36852 = CARTESIAN_POINT ( 'NONE',  ( 2.765530957082001251, 293.7656250017069510, 6.676582343749999815 ) ) ;
#36854 = DIRECTION ( 'NONE',  ( 0.000000000000000000, 0.000000000000000000, 1.000000000000000000 ) ) ;
#36853 = CARTESIAN_POINT ( 'NONE',  ( -6.951808397369817780E-16, 222.6562500034139873, -11.35316468749999963 ) ) ;
#36855 = ORIENTED_EDGE ( 'NONE', *, *, #32132, .T. ) ;
#36856 = CARTESIAN_POINT ( 'NONE',  ( 8.311093377946839666, 226.0937500034140157, 8.311093377946829008 ) ) ;
#36857 = CARTESIAN_POINT ( 'NONE',  ( -5.082755093536317936, -5.082755093536320601, 1.674052781871753659 ) ) ;
#36858 = CARTESIAN_POINT ( 'NONE',  ( -1.656854249492381248, 9.062499997268812280, -4.000000000000001776 ) ) ;
#36859 = CARTESIAN_POINT ( 'NONE',  ( -3.458734124999959469, 198.7500000013656063, 199.4326545832176691 ) ) ;
#36860 = VERTEX_POINT ( 'NONE', #31798 ) ;
#36861 = CARTESIAN_POINT ( 'NONE',  ( -6.000000000000001776, 299.0625000034140157, 0.000000000000000000 ) ) ;
#36862 = CARTESIAN_POINT ( 'NONE',  ( -8.000000000000000000, 102.5000000000000000, 0.000000000000000000 ) ) ;
#36863 = CARTESIAN_POINT ( 'NONE',  ( 6.951808397369818766E-16, 107.3437499965860269, -11.35316468750000141 ) ) ;
#36864 = CYLINDRICAL_SURFACE ( 'NONE', #14342, 4.000000000000001776 ) ;
#36865 = CARTESIAN_POINT ( 'NONE',  ( 7.778174593052021635, 7.778174593052023411, 78.43750000000000000 ) ) ;
#36868 = DIRECTION ( 'NONE',  ( 0.000000000000000000, 0.000000000000000000, -1.000000000000000000 ) ) ;
#36867 = CARTESIAN_POINT ( 'NONE',  ( 24.54126587499999346, 203.1875000013656063, 169.9999999999999432 ) ) ;
#36866 = CARTESIAN_POINT ( 'NONE',  ( 31.45873412500001010, 203.0000000013655779, 168.5673454167822740 ) ) ;
#36869 = EDGE_LOOP ( 'NONE', ( #35253, #62039, #8529 ) ) ;
#36870 = CARTESIAN_POINT ( 'NONE',  ( -28.00000000000007816, 205.1250000027312126, 166.0000000000003695 ) ) ;
#36871 = CARTESIAN_POINT ( 'NONE',  ( -9.832129032723420536, 218.6979166632526983, 5.676582343749997150 ) ) ;
#36872 = CARTESIAN_POINT ( 'NONE',  ( 1.432654583217607858, 202.6250000013656063, 138.5412658750000787 ) ) ;
#36873 = CARTESIAN_POINT ( 'NONE',  ( 29.43265458321766559, 202.1250000013656063, 166.5412658749999650 ) ) ;
#36874 = CARTESIAN_POINT ( 'NONE',  ( 4.898587196589415787E-16, 0.000000000000000000, 4.000000000000001776 ) ) ;
#36875 = AXIS2_PLACEMENT_3D ( 'NONE', #21273, #49953, #61650 ) ;
#36876 = CARTESIAN_POINT ( 'NONE',  ( 6.951808397369818766E-16, 192.3437499965860127, -11.35316468750000141 ) ) ;
#36877 = CARTESIAN_POINT ( 'NONE',  ( -7.188101187499999156, 93.12500000204838102, 2.977408999572654924 ) ) ;
#36878 = CARTESIAN_POINT ( 'NONE',  ( -26.34314575050757412, 195.5625000000000568, 174.0000000000003411 ) ) ;
#36879 = CARTESIAN_POINT ( 'NONE',  ( -1.881053915767121554, 13.62499999863440792, -4.541265875000002339 ) ) ;
#36880 = CARTESIAN_POINT ( 'NONE',  ( 31.45873412499999233, 196.9375000013655779, 169.9999999999999432 ) ) ;
#36881 = CARTESIAN_POINT ( 'NONE',  ( -4.401442555609577197E-16, 7.188101187499992051, 2.986552781871751439 ) ) ;
#36882 = DIRECTION ( 'NONE',  ( -0.000000000000000000, -0.000000000000000000, 1.000000000000000000 ) ) ;
#36883 = CARTESIAN_POINT ( 'NONE',  ( 9.832129032723416984, 75.36458332991935549, 5.676582343750006032 ) ) ;
#36884 = ORIENTED_EDGE ( 'NONE', *, *, #8536, .F. ) ;
#36885 = LINE ( 'NONE', #31595, #30363 ) ;
#36886 = DIRECTION ( 'NONE',  ( 0.000000000000000000, 0.000000000000000000, 1.000000000000000000 ) ) ;
#36887 = CARTESIAN_POINT ( 'NONE',  ( 11.35316468750000141, 70.78124999658602690, 0.000000000000000000 ) ) ;
#36888 = EDGE_LOOP ( 'NONE', ( #39064, #4277, #5970, #58450, #60496, #12253 ) ) ;
#36889 = CARTESIAN_POINT ( 'NONE',  ( 4.220049686691941027, -10.18810118749999738, 89.50000000204836681 ) ) ;
#36890 = CARTESIAN_POINT ( 'NONE',  ( 1.871523826299183495E-15, -10.18810118749999916, 111.5312500020483668 ) ) ;
#36891 = CARTESIAN_POINT ( 'NONE',  ( 3.458734125000015869, 208.1875000013656063, 198.0000000000000284 ) ) ;
#36892 = CARTESIAN_POINT ( 'NONE',  ( 29.65685424949232996, 207.0625000000000284, 173.9999999999999716 ) ) ;
#36894 = CARTESIAN_POINT ( 'NONE',  ( -11.35316468749999785, 73.07291666325266988, -3.042071309553167957 ) ) ;
#36893 = CARTESIAN_POINT ( 'NONE',  ( -18.00000000000000000, -10.39230484541329425, -21.50000000000000000 ) ) ;
#36895 = CARTESIAN_POINT ( 'NONE',  ( -3.313708498984758943, -7.999999999999989342, 17.79905278392014623 ) ) ;
#36896 = DIRECTION ( 'NONE',  ( -0.000000000000000000, -1.000000000000000000, -0.000000000000000000 ) ) ;
#36897 = EDGE_CURVE ( 'NONE', #32640, #51123, #73311, .T. ) ;
#36898 = EDGE_CURVE ( 'NONE', #7590, #8993, #61952, .T. ) ;
#36899 = VECTOR ( 'NONE', #32556, 1000.000000000000000 ) ;
#36900 = CARTESIAN_POINT ( 'NONE',  ( 6.123233995736767268E-16, 168.1249999931720538, -10.00000000000000178 ) ) ;
#36901 = CARTESIAN_POINT ( 'NONE',  ( -3.313708498984654138, 113.4687500040968047, 8.000000000000106581 ) ) ;
#36902 = DIRECTION ( 'NONE',  ( 0.000000000000000000, 0.000000000000000000, 1.000000000000000000 ) ) ;
#36903 = CARTESIAN_POINT ( 'NONE',  ( -3.042071309553173730, 64.63541666325268409, 11.35316468749999785 ) ) ;
#36904 = CARTESIAN_POINT ( 'NONE',  ( -10.18810118749999916, 4.220049686691934809, 105.4375000020483810 ) ) ;
#36905 = CARTESIAN_POINT ( 'NONE',  ( 11.35316468749999963, 195.9895833299193555, -3.042071309553165293 ) ) ;
#36906 = EDGE_LOOP ( 'NONE', ( #34130, #66183 ) ) ;
#36907 = CARTESIAN_POINT ( 'NONE',  ( -2.589639417653282649, 60.37884160280883350, 22.99414321703751440 ) ) ;
#36908 = DIRECTION ( 'NONE',  ( 0.000000000000000000, 0.000000000000000000, 1.000000000000000000 ) ) ;
#36909 = CARTESIAN_POINT ( 'NONE',  ( 5.000000000000001776, 64.62379132009235150, 24.09319349500452034 ) ) ;
#36911 = CARTESIAN_POINT ( 'NONE',  ( -2.085542519210945728E-15, 189.5312499965860127, 11.35316468750000141 ) ) ;
#36910 = CARTESIAN_POINT ( 'NONE',  ( 7.320508075688776373, 261.8750000000000000, 7.320508075688767491 ) ) ;
#36912 = CARTESIAN_POINT ( 'NONE',  ( -10.00000000000000000, 194.1666666598387110, -2.679491924311229845 ) ) ;
#36913 = ADVANCED_FACE ( 'NONE', ( #15919 ), #57805, .T. ) ;
#36914 = CARTESIAN_POINT ( 'NONE',  ( -7.320508075688771932, 232.5000000068279462, -7.320508075688771932 ) ) ;
#36915 = CARTESIAN_POINT ( 'NONE',  ( -28.00000000000002842, 200.0000000000000000, 166.0000000000003695 ) ) ;
#36916 = ORIENTED_EDGE ( 'NONE', *, *, #66420, .T. ) ;
#36917 = CARTESIAN_POINT ( 'NONE',  ( 9.832129032723416984, 175.6770833299193555, 5.676582343750006032 ) ) ;
#36918 = CARTESIAN_POINT ( 'NONE',  ( 7.188101187499992051, 8.802885111219154394E-16, 23.23655278187175455 ) ) ;
#36919 = DIRECTION ( 'NONE',  ( 1.000000000000000000, 3.169619151431689753E-17, -1.182917971378671814E-16 ) ) ;
#36920 = ORIENTED_EDGE ( 'NONE', *, *, #51862, .T. ) ;
#36921 = EDGE_CURVE ( 'NONE', #74219, #14457, #60412, .T. ) ;
#36922 = CARTESIAN_POINT ( 'NONE',  ( 3.313708498984765161, 97.15625000409677625, 7.999999999999998224 ) ) ;
#36923 = CARTESIAN_POINT ( 'NONE',  ( 2.449293598294707893E-16, 6.999999997268813168, -4.000000000000001776 ) ) ;
#36924 = CARTESIAN_POINT ( 'NONE',  ( 4.000000000000001776, 16.06250000000000000, -1.656854249492381248 ) ) ;
#36925 = CARTESIAN_POINT ( 'NONE',  ( -3.211159895383562723, 13.93749999863440614, 3.211159895383561391 ) ) ;
#36926 = CARTESIAN_POINT ( 'NONE',  ( 7.999999999999992895, -3.313708498984756279, 12.17405278392014800 ) ) ;
#36927 = CARTESIAN_POINT ( 'NONE',  ( 5.656854249492374365, 5.656854249492375253, 18.45530278392014623 ) ) ;
#36928 = ORIENTED_EDGE ( 'NONE', *, *, #52915, .T. ) ;
#36929 = DIRECTION ( 'NONE',  ( -0.000000000000000000, -0.000000000000000000, -1.000000000000000000 ) ) ;
#36930 = CARTESIAN_POINT ( 'NONE',  ( 2.977408999572650039, 101.1875000020483810, -7.188101187500001821 ) ) ;
#36931 = CARTESIAN_POINT ( 'NONE',  ( -2.849036369511732440E-14, 204.3750000027312126, 138.0000000000000568 ) ) ;
#36932 = EDGE_CURVE ( 'NONE', #40831, #17794, #18307, .T. ) ;
#36933 = PRODUCT_CONTEXT ( 'NONE', #64545, 'mechanical' ) ;
#36934 =( BOUNDED_CURVE ( )  B_SPLINE_CURVE ( 2, ( #61719, #50021, #43994, #39082, #62087, #54952, #8918, #38340, #61347 ),
 .UNSPECIFIED., .F., .F. ) 
 B_SPLINE_CURVE_WITH_KNOTS ( ( 3, 2, 2, 2, 3 ),
 ( 0.08333333333333352300, 0.09166666666666679897, 0.1000000000000000888, 0.1083333333333333787, 0.1166666666666666546 ),
 .UNSPECIFIED. ) 
 CURVE ( )  GEOMETRIC_REPRESENTATION_ITEM ( )  RATIONAL_B_SPLINE_CURVE ( ( 0.9999999999999982236, 0.9238795325112885148, 1.000000000000000000, 0.9238795325112867385, 1.000000000000000000, 0.9238795325112867385, 1.000000000000000000, 0.9238795325112868495, 0.9999999999999998890 ) ) 
 REPRESENTATION_ITEM ( '' )  );
#36935 = ORIENTED_EDGE ( 'NONE', *, *, #31191, .F. ) ;
#36936 = CIRCLE ( 'NONE', #9271, 10.49999999999998224 ) ;
#36937 = DIRECTION ( 'NONE',  ( -0.000000000000000000, -1.000000000000000000, -0.000000000000000000 ) ) ;
#36938 = CARTESIAN_POINT ( 'NONE',  ( 1.320432766682872962E-15, -7.188101187499992051, 21.36155278187175455 ) ) ;
#36939 = ORIENTED_EDGE ( 'NONE', *, *, #47841, .F. ) ;
#36940 = ORIENTED_EDGE ( 'NONE', *, *, #55808, .F. ) ;
#36941 = CARTESIAN_POINT ( 'NONE',  ( -4.220049686691937474, -10.18810118749999738, 79.93750000204838102 ) ) ;
#36942 = CARTESIAN_POINT ( 'NONE',  ( -8.311093377946836114, 57.96874999658602690, -8.311093377946837890 ) ) ;
#36943 = LINE ( 'NONE', #19575, #36078 ) ;
#36944 = CARTESIAN_POINT ( 'NONE',  ( 2.020667218593132706E-15, -11.00000000000000000, 94.37499999999998579 ) ) ;
#36947 = CARTESIAN_POINT ( 'NONE',  ( -4.721056650415998313, 292.7343750017069510, 4.721056650416000089 ) ) ;
#36946 = CARTESIAN_POINT ( 'NONE',  ( 27.99999999999996447, 199.6250000027312126, 165.9999999999998863 ) ) ;
#36945 = CARTESIAN_POINT ( 'NONE',  ( -29.65685424949239390, 198.5625000027312694, 174.0000000000003126 ) ) ;
#36948 = CARTESIAN_POINT ( 'NONE',  ( 4.999999999999993783, 154.1666666666666856, 8.660254037844390851 ) ) ;
#36949 = CARTESIAN_POINT ( 'NONE',  ( -5.000000000000005329, 165.2083333265053682, 8.660254037844387298 ) ) ;
#36950 = CARTESIAN_POINT ( 'NONE',  ( 5.656854249492374365, 5.656854249492375253, 15.26780277982336642 ) ) ;
#36951 = CARTESIAN_POINT ( 'NONE',  ( 3.313708498984762052, 3.093749995903220196, -8.000000000000000000 ) ) ;
#36952 = CARTESIAN_POINT ( 'NONE',  ( 26.56734541678237704, 197.0000000013656347, 166.5412658749999650 ) ) ;
#36953 = CARTESIAN_POINT ( 'NONE',  ( 4.401442555609581635E-16, 10.21874999795161187, -7.188101187500000044 ) ) ;
#36954 = CARTESIAN_POINT ( 'NONE',  ( 5.656854249492374365, 5.656854249492375253, 27.45530278392014978 ) ) ;
#36955 = CARTESIAN_POINT ( 'NONE',  ( -28.00000000000002842, 205.0000000000000284, 166.0000000000003695 ) ) ;
#36956 = CARTESIAN_POINT ( 'NONE',  ( -7.188101187500000044, 112.5312500020483952, 0.000000000000000000 ) ) ;
#36958 = LINE ( 'NONE', #35857, #20904 ) ;
#36957 = CARTESIAN_POINT ( 'NONE',  ( -10.00000000000000355, 19.58333332650536462, 2.679491924311223183 ) ) ;
#36959 = CARTESIAN_POINT ( 'NONE',  ( 7.320508075688774596, 134.3750000000000000, 7.320508075688778149 ) ) ;
#36960 = CARTESIAN_POINT ( 'NONE',  ( 4.242640687119285658, 288.6875000034139589, -4.242640687119286547 ) ) ;
#36961 = CARTESIAN_POINT ( 'NONE',  ( -2.977408999572647819, 7.188101187499991163, 21.08030278187175810 ) ) ;
#36962 = CARTESIAN_POINT ( 'NONE',  ( 29.65685424949241167, 200.5625000027311842, 165.9999999999999716 ) ) ;
#36963 = CARTESIAN_POINT ( 'NONE',  ( -2.085542519210945728E-15, 39.53124999658601268, 11.35316468750000141 ) ) ;
#36964 = CARTESIAN_POINT ( 'NONE',  ( -2.828427124746190735, 6.375000000000000888, -2.828427124746191623 ) ) ;
#36965 = CARTESIAN_POINT ( 'NONE',  ( 2.679491924311228956, 12.91666665983869677, -10.00000000000000000 ) ) ;
#36966 = CARTESIAN_POINT ( 'NONE',  ( 32.00000000000000000, 201.3125000027312126, 171.6568542494922553 ) ) ;
#36967 = ORIENTED_EDGE ( 'NONE', *, *, #53007, .T. ) ;
#36968 = AXIS2_PLACEMENT_3D ( 'NONE', #15311, #32323, #44005 ) ;
#36969 = DIRECTION ( 'NONE',  ( 0.000000000000000000, 0.000000000000000000, 1.000000000000000000 ) ) ;
#36970 = EDGE_CURVE ( 'NONE', #72478, #51619, #13576, .T. ) ;
#36971 = DIRECTION ( 'NONE',  ( -0.000000000000000000, -0.000000000000000000, 1.000000000000000000 ) ) ;
#36972 = CARTESIAN_POINT ( 'NONE',  ( -5.676582343750006032, 39.11458332991934839, 9.832129032723418760 ) ) ;
#36973 = CARTESIAN_POINT ( 'NONE',  ( 4.556349186104045934, 11.00000000000000000, 78.71875000409677625 ) ) ;
#36974 = CARTESIAN_POINT ( 'NONE',  ( 5.676582343750001591, 61.61458332991934839, -9.832129032723420536 ) ) ;
#36975 = CARTESIAN_POINT ( 'NONE',  ( 2.445694354108784108, 205.5625000013656063, 144.4456943541088663 ) ) ;
#36976 = CARTESIAN_POINT ( 'NONE',  ( 6.123233995736767268E-16, 33.12499999317203248, -10.00000000000000178 ) ) ;
#36977 = DIRECTION ( 'NONE',  ( 0.000000000000000000, 0.000000000000000000, 1.000000000000000000 ) ) ;
#36979 = CARTESIAN_POINT ( 'NONE',  ( -9.832129032723420536, 38.69791666325268409, 5.676582343749997150 ) ) ;
#36978 = CARTESIAN_POINT ( 'NONE',  ( 7.188101187500000933, 107.0000000020483810, -2.977408999572651371 ) ) ;
#36980 = CARTESIAN_POINT ( 'NONE',  ( -7.999999999999989342, -3.313708498984762496, 12.92405277982336287 ) ) ;
#36981 = CARTESIAN_POINT ( 'NONE',  ( 9.832129032723416984, 165.3645833299193555, 5.676582343750006032 ) ) ;
#36982 = EDGE_CURVE ( 'NONE', #14878, #32201, #10279, .T. ) ;
#36983 = CARTESIAN_POINT ( 'NONE',  ( 2.679491924311222739, 130.8333333265053398, 10.00000000000000355 ) ) ;
#36984 = CARTESIAN_POINT ( 'NONE',  ( 1.320432766682874540E-15, 108.4062500020483810, 7.188101187500000044 ) ) ;
#36985 = VERTEX_POINT ( 'NONE', #99 ) ;
#36986 = CARTESIAN_POINT ( 'NONE',  ( 4.615726161707419450, -68.43878643976833587, -20.71807028113835614 ) ) ;
#36987 = CARTESIAN_POINT ( 'NONE',  ( -3.042071309553163960, 17.55208332991935194, -11.35316468749999963 ) ) ;
#36988 = ORIENTED_EDGE ( 'NONE', *, *, #58759, .F. ) ;
#36989 = CARTESIAN_POINT ( 'NONE',  ( -28.00000000000007816, 205.1250000027312126, 166.0000000000003695 ) ) ;
#36991 = CARTESIAN_POINT ( 'NONE',  ( 11.35316468750000141, 155.7812499965860127, 0.000000000000000000 ) ) ;
#36990 = CARTESIAN_POINT ( 'NONE',  ( -23.64658221358208223, -23.81493467166859546, 145.9231949188717579 ) ) ;
#36992 = CARTESIAN_POINT ( 'NONE',  ( -5.000000000000000000, -16.14408868864072844, 22.96238185062368586 ) ) ;
#36993 = CARTESIAN_POINT ( 'NONE',  ( 7.999999999999992895, -3.313708498984756279, 18.04280278432982598 ) ) ;
#36994 = CARTESIAN_POINT ( 'NONE',  ( 2.828427124746152987, 208.2500000027312126, 139.1715728752538723 ) ) ;
#36995 = EDGE_CURVE ( 'NONE', #55487, #44869, #27999, .T. ) ;
#36996 = EDGE_CURVE ( 'NONE', #20696, #54079, #39029, .T. ) ;
#36997 = CARTESIAN_POINT ( 'NONE',  ( -3.042071309553159075, 234.9479166700806445, 11.35316468749999963 ) ) ;
#36998 = CARTESIAN_POINT ( 'NONE',  ( -7.204075437095965206, -7.204075437095968759, 83.21875000204836681 ) ) ;
#36999 = ORIENTED_EDGE ( 'NONE', *, *, #50098, .T. ) ;
#37000 = EDGE_CURVE ( 'NONE', #23729, #46331, #6350, .T. ) ;
#37001 = CIRCLE ( 'NONE', #61125, 3.999999999999989786 ) ;
#37002 = DIRECTION ( 'NONE',  ( 0.000000000000000000, -0.000000000000000000, -1.000000000000000000 ) ) ;
#37003 = CARTESIAN_POINT ( 'NONE',  ( 30.82842712474617031, 205.1250000000000284, 172.8284271247460993 ) ) ;
#37004 = CARTESIAN_POINT ( 'NONE',  ( 11.35316468749999963, 101.3020833299193555, -3.042071309553165293 ) ) ;
#37005 = CARTESIAN_POINT ( 'NONE',  ( 10.18810118750000093, -4.220049686691933921, 99.81250000204838102 ) ) ;
#37006 = CARTESIAN_POINT ( 'NONE',  ( -1.903569318090136080E-11, 13.74999999999851852, 10.00000000000000178 ) ) ;
#37007 = ORIENTED_EDGE ( 'NONE', *, *, #34820, .T. ) ;
#37008 = ORIENTED_EDGE ( 'NONE', *, *, #60690, .F. ) ;
#37009 = CARTESIAN_POINT ( 'NONE',  ( 3.313708498984762496, 13.21875000000000178, 7.999999999999998224 ) ) ;
#37010 = CARTESIAN_POINT ( 'NONE',  ( 4.541265875000002339, 4.499999998634407028, -1.881053915767121554 ) ) ;
#37011 = CARTESIAN_POINT ( 'NONE',  ( -5.082755093536325042, 5.531249997951610986, -5.082755093536325930 ) ) ;
#37012 = EDGE_CURVE ( 'NONE', #45576, #35289, #65288, .T. ) ;
#37013 = CARTESIAN_POINT ( 'NONE',  ( -8.000000000000000000, 116.0937500040968189, -3.313708498984761608 ) ) ;
#37014 = CARTESIAN_POINT ( 'NONE',  ( 4.220049686691941027, -10.18810118749999738, 97.00000000204836681 ) ) ;
#37015 = CARTESIAN_POINT ( 'NONE',  ( 0.000000000000000000, 125.0000000000000000, 0.000000000000000000 ) ) ;
#37016 = CARTESIAN_POINT ( 'NONE',  ( 2.828427124746191623, 5.125000000000000000, -2.828427124746191623 ) ) ;
#37017 = CARTESIAN_POINT ( 'NONE',  ( 2.828427124746191623, 17.87499999726881583, -2.828427124746191623 ) ) ;
#37018 = CARTESIAN_POINT ( 'NONE',  ( 2.780723358947928197E-16, 2.562499998634407028, -4.541265875000002339 ) ) ;
#37019 = VECTOR ( 'NONE', #20803, 1000.000000000000000 ) ;
#37020 = CARTESIAN_POINT ( 'NONE',  ( -2.839093476692135984E-14, 208.6875000013656063, 138.5412658750000503 ) ) ;
#37021 = CARTESIAN_POINT ( 'NONE',  ( -3.458734124999959025, 195.5000000013655779, 199.4326545832176691 ) ) ;
#37023 = CARTESIAN_POINT ( 'NONE',  ( -8.000000000000001776, 15.84375000000000355, 3.313708498984759387 ) ) ;
#37022 = CARTESIAN_POINT ( 'NONE',  ( -31.45873412499995680, 200.7500000013656347, 171.4326545832181239 ) ) ;
#37024 =( NAMED_UNIT ( * ) PLANE_ANGLE_UNIT ( ) SI_UNIT ( $, .RADIAN. ) );
#37025 = CARTESIAN_POINT ( 'NONE',  ( 4.541265875000002339, 15.37499999863440614, -1.881053915767121554 ) ) ;
#37026 = CARTESIAN_POINT ( 'NONE',  ( -5.082755093536317936, -5.082755093536320601, 9.174052781871752771 ) ) ;
#37027 = ORIENTED_EDGE ( 'NONE', *, *, #14426, .T. ) ;
#37028 =( BOUNDED_CURVE ( )  B_SPLINE_CURVE ( 2, ( #71220, #8981, #65569, #31996, #14622 ),
 .UNSPECIFIED., .F., .F. ) 
 B_SPLINE_CURVE_WITH_KNOTS ( ( 3, 2, 3 ),
 ( 0.9791666666666651864, 0.9895833333333325932, 1.000000000000000000 ),
 .UNSPECIFIED. ) 
 CURVE ( )  GEOMETRIC_REPRESENTATION_ITEM ( )  RATIONAL_B_SPLINE_CURVE ( ( 1.000000000000010436, 0.9238795325112761914, 1.000000000000000000, 0.9238795325112867385, 1.000000000000000000 ) ) 
 REPRESENTATION_ITEM ( '' )  );
#37029 = EDGE_LOOP ( 'NONE', ( #21308, #42109, #16137, #12559 ) ) ;
#37030 = CARTESIAN_POINT ( 'NONE',  ( 10.18810118750000093, -4.220049686691933033, 96.81250000204838102 ) ) ;
#37031 = LINE ( 'NONE', #14371, #33386 ) ;
#37032 = CARTESIAN_POINT ( 'NONE',  ( -24.54126587499998280, 205.3750000013656063, 171.4326545832179818 ) ) ;
#37033 = CARTESIAN_POINT ( 'NONE',  ( -24.00000000000001066, 199.8125000000000284, 168.3431457505080004 ) ) ;
#37034 = CARTESIAN_POINT ( 'NONE',  ( -2.445694354108783664, 197.3125000013656063, 195.5543056458912190 ) ) ;
#37035 = CARTESIAN_POINT ( 'NONE',  ( -8.660254037844383745, 32.08333333333333570, -5.000000000000002665 ) ) ;
#37036 = CARTESIAN_POINT ( 'NONE',  ( 2.679491924311222739, 113.9583333333333428, 10.00000000000000355 ) ) ;
#37037 = CARTESIAN_POINT ( 'NONE',  ( -4.898587196589412829E-16, 114.1250000000000000, -8.000000000000000000 ) ) ;
#37038 = CARTESIAN_POINT ( 'NONE',  ( 4.721056650415999201, 295.2343750017069510, -4.721056650415999201 ) ) ;
#37039 = EDGE_LOOP ( 'NONE', ( #9378, #17517, #10404, #71998 ) ) ;
#37040 = AXIS2_PLACEMENT_3D ( 'NONE', #72119, #54041, #65714 ) ;
#37041 = CARTESIAN_POINT ( 'NONE',  ( -2.679491924311373729, 143.3333333265053966, -9.999999999999916511 ) ) ;
#37042 = CARTESIAN_POINT ( 'NONE',  ( -5.656854249492381470, 23.24999999590322020, 5.656854249492379694 ) ) ;
#37043 = CARTESIAN_POINT ( 'NONE',  ( -2.839093476692135984E-14, 202.6875000013656063, 138.5412658750000503 ) ) ;
#37044 =( NAMED_UNIT ( * ) PLANE_ANGLE_UNIT ( ) SI_UNIT ( $, .RADIAN. ) );
#37045 = CARTESIAN_POINT ( 'NONE',  ( 8.660254037844389075, 222.0833333333333428, 4.999999999999997335 ) ) ;
#37046 = CARTESIAN_POINT ( 'NONE',  ( -3.313708498984640816, 114.9687500040968047, 8.000000000000119016 ) ) ;
#37047 = CARTESIAN_POINT ( 'NONE',  ( 11.00000000000000000, 1.347111479062088405E-15, 112.7499999999999858 ) ) ;
#37048 = CARTESIAN_POINT ( 'NONE',  ( -3.042071309553164404, 7.239583329919349275, -11.35316468749999963 ) ) ;
#37049 =( BOUNDED_CURVE ( )  B_SPLINE_CURVE ( 2, ( #4041, #27034, #14205, #43258, #67404, #50045, #60617, #15705, #61746 ),
 .UNSPECIFIED., .F., .F. ) 
 B_SPLINE_CURVE_WITH_KNOTS ( ( 3, 2, 2, 2, 3 ),
 ( 0.9374999999999984457, 0.9479166666666650753, 0.9583333333333319271, 0.9687499999999985567, 0.9791666666666651864 ),
 .UNSPECIFIED. ) 
 CURVE ( )  GEOMETRIC_REPRESENTATION_ITEM ( )  RATIONAL_B_SPLINE_CURVE ( ( 1.000000000000011324, 0.9238795325112754142, 1.000000000000000000, 0.9238795325112867385, 1.000000000000000000, 0.9238795325112867385, 1.000000000000000000, 0.9238795325112972856, 0.9999999999999894529 ) ) 
 REPRESENTATION_ITEM ( '' )  );
#37050 = CARTESIAN_POINT ( 'NONE',  ( 7.188101187499993827, -2.977408999572645598, 5.517802781871753659 ) ) ;
#37051 = CARTESIAN_POINT ( 'NONE',  ( -9.832129032723420536, 199.0104166632526983, 5.676582343749997150 ) ) ;
#37052 = DIRECTION ( 'NONE',  ( -0.000000000000000000, 1.000000000000000000, -4.476705744456276341E-16 ) ) ;
#37053 = CARTESIAN_POINT ( 'NONE',  ( -4.541265875000002339, 4.749999998634407028, -1.881053915767121998 ) ) ;
#37054 = CARTESIAN_POINT ( 'NONE',  ( -2.751064625579944321E-14, 209.7500000000000284, 146.0000000000000284 ) ) ;
#37056 = CARTESIAN_POINT ( 'NONE',  ( 4.898587196589412829E-16, 9.375000000000001776, -8.000000000000000000 ) ) ;
#37055 = DIRECTION ( 'NONE',  ( 0.000000000000000000, 0.000000000000000000, 1.000000000000000000 ) ) ;
#37057 = ORIENTED_EDGE ( 'NONE', *, *, #59544, .F. ) ;
#37058 = EDGE_CURVE ( 'NONE', #61881, #70764, #10061, .T. ) ;
#37059 = CARTESIAN_POINT ( 'NONE',  ( -2.839093476692135984E-14, 202.9375000013656063, 138.5412658750000503 ) ) ;
#37060 = CARTESIAN_POINT ( 'NONE',  ( -11.35316468749999785, 48.38541666325268409, -3.042071309553167513 ) ) ;
#37061 = CARTESIAN_POINT ( 'NONE',  ( -10.99999999999999822, -4.556349186104052151, 106.2812500040967620 ) ) ;
#37062 = CARTESIAN_POINT ( 'NONE',  ( -2.849036369511732440E-14, 205.2500000000000284, 138.0000000000000568 ) ) ;
#37063 = CARTESIAN_POINT ( 'NONE',  ( -28.00000000000007105, 201.4375000013656063, 166.5412658750003629 ) ) ;
#37064 = LINE ( 'NONE', #67234, #55077 ) ;
#37066 = CARTESIAN_POINT ( 'NONE',  ( -8.660254037844385522, 230.4166666666666856, 5.000000000000004441 ) ) ;
#37065 = CARTESIAN_POINT ( 'NONE',  ( -2.977408999572652260, 122.9375000020483810, 7.188101187500000044 ) ) ;
#37067 = CARTESIAN_POINT ( 'NONE',  ( -1.432654583217664479, 195.7500000013656063, 138.5412658750000787 ) ) ;
#37068 = CARTESIAN_POINT ( 'NONE',  ( 6.951808397369818766E-16, 107.0312499965860269, -11.35316468750000141 ) ) ;
#37069 = CARTESIAN_POINT ( 'NONE',  ( -5.000000000000005329, 90.20833332650536818, 8.660254037844387298 ) ) ;
#37070 = CARTESIAN_POINT ( 'NONE',  ( -4.401442555609581635E-16, 89.28125000204838102, -7.188101187500000044 ) ) ;
#37071 = CARTESIAN_POINT ( 'NONE',  ( 2.780723358947928197E-16, 17.68749999863440792, -4.541265875000002339 ) ) ;
#37072 = CARTESIAN_POINT ( 'NONE',  ( -5.000000000000000888, 71.66666666666667140, -8.660254037844390851 ) ) ;
#37073 = DIRECTION ( 'NONE',  ( 0.000000000000000000, 0.000000000000000000, 1.000000000000000000 ) ) ;
#37074 = ORIENTED_EDGE ( 'NONE', *, *, #4932, .F. ) ;
#37075 = CARTESIAN_POINT ( 'NONE',  ( -4.000000000000015987, 200.6250000027312126, 142.0000000000000568 ) ) ;
#37076 = ORIENTED_EDGE ( 'NONE', *, *, #20474, .F. ) ;
#37077 = CARTESIAN_POINT ( 'NONE',  ( -6.676582343750001591, 294.6093750017069510, 0.000000000000000000 ) ) ;
#37078 = CARTESIAN_POINT ( 'NONE',  ( 8.660254037844389075, 187.2916666598387110, -5.000000000000000000 ) ) ;
#37079 = CARTESIAN_POINT ( 'NONE',  ( -7.999999999999991118, 3.313708498984756723, 8.424052783920146226 ) ) ;
#37080 = CARTESIAN_POINT ( 'NONE',  ( -9.832129032723420536, 173.6979166632526983, 5.676582343749997150 ) ) ;
#37081 = DIRECTION ( 'NONE',  ( -0.000000000000000000, 1.000000000000000000, -0.000000000000000000 ) ) ;
#37082 = CARTESIAN_POINT ( 'NONE',  ( -3.999999999999960032, 198.9375000000000000, 196.3431457505076594 ) ) ;
#37083 = DIRECTION ( 'NONE',  ( 0.000000000000000000, 0.000000000000000000, 1.000000000000000000 ) ) ;
#37084 = VECTOR ( 'NONE', #38934, 1000.000000000000000 ) ;
#37085 = CARTESIAN_POINT ( 'NONE',  ( 4.220049686691934809, 10.18810118749999916, 108.0625000020483810 ) ) ;
#37086 = ORIENTED_EDGE ( 'NONE', *, *, #2590, .T. ) ;
#37087 = ADVANCED_FACE ( 'NONE', ( #23448 ), #58912, .T. ) ;
#37088 = CARTESIAN_POINT ( 'NONE',  ( 3.496982156811288434, 51.71401992552112148, -48.73755072030355251 ) ) ;
#37089 = CARTESIAN_POINT ( 'NONE',  ( -4.556349186104048599, -10.99999999999999822, 109.4687500040967763 ) ) ;
#37090 = CARTESIAN_POINT ( 'NONE',  ( 11.35316468749999963, 146.3020833299193555, -3.042071309553165293 ) ) ;
#37091 = CARTESIAN_POINT ( 'NONE',  ( 1.432654583217664701, 204.0000000013656063, 201.4587341250000065 ) ) ;
#37092 = CARTESIAN_POINT ( 'NONE',  ( 4.220049686691941027, -10.18810118749999738, 73.00000000204836681 ) ) ;
#37093 = CARTESIAN_POINT ( 'NONE',  ( -11.35316468750000141, 68.80208332991935549, 3.042071309553159963 ) ) ;
#37094 = ORIENTED_EDGE ( 'NONE', *, *, #63063, .T. ) ;
#37095 = CYLINDRICAL_SURFACE ( 'NONE', #34474, 3.999999999999976019 ) ;
#37096 = CARTESIAN_POINT ( 'NONE',  ( 1.881053915767121998, 6.624999998634407916, -4.541265875000002339 ) ) ;
#37097 = CARTESIAN_POINT ( 'NONE',  ( -8.008118988124989457, -3.317071493978883900, 8.606865283940630107 ) ) ;
#37098 = ORIENTED_EDGE ( 'NONE', *, *, #43890, .F. ) ;
#37099 = CARTESIAN_POINT ( 'NONE',  ( -1.320432766682874540E-15, 21.09374999795161543, 7.188101187500000044 ) ) ;
#37100 = CARTESIAN_POINT ( 'NONE',  ( 4.242640687119287435, 289.4375000034140157, 4.242640687119285658 ) ) ;
#37101 = FACE_OUTER_BOUND ( 'NONE', #23071, .T. ) ;
#37102 = CARTESIAN_POINT ( 'NONE',  ( -5.082755093536325042, 10.40624999795161187, -5.082755093536325930 ) ) ;
#37103 = EDGE_CURVE ( 'NONE', #47406, #38757, #68018, .T. ) ;
#37104 = CARTESIAN_POINT ( 'NONE',  ( -2.977408999572647819, -7.188101187499990274, 0.2678027818717523822 ) ) ;
#37105 =( REPRESENTATION_RELATIONSHIP ('NONE','NONE', #46008, #30147 ) REPRESENTATION_RELATIONSHIP_WITH_TRANSFORMATION ( #52729 )SHAPE_REPRESENTATION_RELATIONSHIP( ) );
#37106 = CARTESIAN_POINT ( 'NONE',  ( -10.18810118749999916, 0.000000000000000000, 114.5312500020483810 ) ) ;
#37107 = EDGE_CURVE ( 'NONE', #3972, #2312, #39160, .T. ) ;
#37108 = CARTESIAN_POINT ( 'NONE',  ( 0.000000000000000000, 125.0000000000000000, 0.000000000000000000 ) ) ;
#37109 = CARTESIAN_POINT ( 'NONE',  ( 2.828427124746191623, 0.8749999972688131678, -2.828427124746191623 ) ) ;
#37110 = ORIENTED_EDGE ( 'NONE', *, *, #50786, .F. ) ;
#37111 = CARTESIAN_POINT ( 'NONE',  ( 2.445694354108839619, 204.8125000013656063, 200.4456943541088663 ) ) ;
#37112 = CARTESIAN_POINT ( 'NONE',  ( -26.34314575050769136, 196.0625000027312694, 166.0000000000003695 ) ) ;
#37113 = CARTESIAN_POINT ( 'NONE',  ( 2.780723358947928197E-16, 1.562499998634406584, -4.541265875000002339 ) ) ;
#37114 = CARTESIAN_POINT ( 'NONE',  ( 5.082755093536325042, 108.5937500020483810, -5.082755093536325930 ) ) ;
#37115 = ADVANCED_FACE ( 'NONE', ( #18537 ), #41545, .T. ) ;
#37116 = CARTESIAN_POINT ( 'NONE',  ( -2.485281374238208052, 295.1875000000000568, 6.000000000000366818 ) ) ;
#37117 = CARTESIAN_POINT ( 'NONE',  ( 2.977408999572650927, -7.188101187499990274, 24.45530278187175455 ) ) ;
#37118 = ORIENTED_EDGE ( 'NONE', *, *, #4902, .F. ) ;
#37119 = CARTESIAN_POINT ( 'NONE',  ( -5.082755093536325042, 20.53124999795161543, -5.082755093536325930 ) ) ;
#37120 = ORIENTED_EDGE ( 'NONE', *, *, #3049, .F. ) ;
#37121 = CARTESIAN_POINT ( 'NONE',  ( -8.660254037844383745, 2.083333333333331261, -5.000000000000001776 ) ) ;
#37122 = DIRECTION ( 'NONE',  ( -0.000000000000000000, -1.000000000000000000, -0.000000000000000000 ) ) ;
#37123 = CARTESIAN_POINT ( 'NONE',  ( 3.458734125000015425, 208.9375000013656063, 198.0000000000000284 ) ) ;
#37124 = CARTESIAN_POINT ( 'NONE',  ( 30.44569435410879521, 202.8125000013656063, 167.5543056458910485 ) ) ;
#37125 = CARTESIAN_POINT ( 'NONE',  ( -8.660254037844390851, 72.91666666666667140, 4.999999999999998224 ) ) ;
#37126 = CARTESIAN_POINT ( 'NONE',  ( 7.188101187500000044, 95.28125000204836681, -8.802885111219163269E-16 ) ) ;
#37127 = CARTESIAN_POINT ( 'NONE',  ( -2.485281374238572649, 295.1875000000000000, 6.000000000000002665 ) ) ;
#37129 = CARTESIAN_POINT ( 'NONE',  ( -30.69786616161692550, -42.99835545478840260, 174.4992099361770954 ) ) ;
#37128 = CARTESIAN_POINT ( 'NONE',  ( 32.00000000000000711, 208.3125000027312126, 171.6568542494922553 ) ) ;
#37130 = VERTEX_POINT ( 'NONE', #43010 ) ;
#37131 = CARTESIAN_POINT ( 'NONE',  ( 2.085542519210945334E-15, 225.1562500034139873, 11.35316468749999963 ) ) ;
#37132 = CIRCLE ( 'NONE', #69687, 9.000000000000001776 ) ;
#37133 = DIRECTION ( 'NONE',  ( -1.000000000000000000, 0.000000000000000000, -0.000000000000000000 ) ) ;
#37134 = CARTESIAN_POINT ( 'NONE',  ( -2.751064625579944321E-14, 200.8750000027312126, 146.0000000000000284 ) ) ;
#37135 = CARTESIAN_POINT ( 'NONE',  ( 11.00000000000000000, 1.347111479062088405E-15, 118.0000000000000000 ) ) ;
#37136 = DIRECTION ( 'NONE',  ( -0.000000000000000000, -1.000000000000000000, -0.000000000000000000 ) ) ;
#37137 = CARTESIAN_POINT ( 'NONE',  ( 27.23973938214588131, 194.7821183710414914, 166.2752610582897432 ) ) ;
#37138 = CARTESIAN_POINT ( 'NONE',  ( 10.00000000000000000, 179.7916666666666856, 2.679491924311236062 ) ) ;
#37139 = CARTESIAN_POINT ( 'NONE',  ( 7.188101187499993827, -2.977408999572645598, 23.51780278187175455 ) ) ;
#37140 = CARTESIAN_POINT ( 'NONE',  ( -9.832129032723418760, 148.1770833299193555, -5.676582343750004256 ) ) ;
#37141 = CARTESIAN_POINT ( 'NONE',  ( -50.99999999999994316, -31.99999999999978684, 167.9999999999997726 ) ) ;
#37142 = CYLINDRICAL_SURFACE ( 'NONE', #19263, 10.00000000000000178 ) ;
#37145 = CARTESIAN_POINT ( 'NONE',  ( -10.00000000000000533, 167.5000000000000000, -1.224646799147353848E-15 ) ) ;
#37144 = CARTESIAN_POINT ( 'NONE',  ( -2.849036369511732440E-14, 202.3750000027312126, 138.0000000000000568 ) ) ;
#37143 = CARTESIAN_POINT ( 'NONE',  ( 29.65685424949235482, 204.0625000000000000, 173.9999999999999147 ) ) ;
#37146 = EDGE_LOOP ( 'NONE', ( #69280, #16880, #6667, #13825 ) ) ;
#37147 = CARTESIAN_POINT ( 'NONE',  ( 3.042071309553159519, 5.052083329919351051, 11.35316468750000141 ) ) ;
#37148 = FACE_BOUND ( 'NONE', #51409, .T. ) ;
#37149 = ADVANCED_FACE ( 'NONE', ( #60001 ), #67164, .T. ) ;
#37150 = LINE ( 'NONE', #20529, #35425 ) ;
#37151 = DIRECTION ( 'NONE',  ( 0.000000000000000000, 0.000000000000000000, 1.000000000000000000 ) ) ;
#37152 = CARTESIAN_POINT ( 'NONE',  ( -3.458734125000016313, 208.8750000013656063, 140.5673454167823593 ) ) ;
#37153 =( BOUNDED_CURVE ( )  B_SPLINE_CURVE ( 2, ( #60152, #19786, #25810, #9224, #21278, #44301, #42794, #67317, #49583 ),
 .UNSPECIFIED., .F., .F. ) 
 B_SPLINE_CURVE_WITH_KNOTS ( ( 3, 2, 2, 2, 3 ),
 ( 0.7647058823529411242, 0.7683823529411765163, 0.7720588235294116863, 0.7757352941176469674, 0.7794117647058822484 ),
 .UNSPECIFIED. ) 
 CURVE ( )  GEOMETRIC_REPRESENTATION_ITEM ( )  RATIONAL_B_SPLINE_CURVE ( ( 1.000000000000000000, 0.9238795325112867385, 1.000000000000000000, 0.9238795325112867385, 1.000000000000000000, 0.9238795325112867385, 1.000000000000000000, 0.9238795325112890700, 0.9999999999999976685 ) ) 
 REPRESENTATION_ITEM ( '' )  );
#37154 = VECTOR ( 'NONE', #28699, 1000.000000000000000 ) ;
#37155 = CARTESIAN_POINT ( 'NONE',  ( -7.455611905271029904, 124.7772109312973328, -2.029970500747677598 ) ) ;
#37156 = CARTESIAN_POINT ( 'NONE',  ( -5.000000000000005329, 45.20833332650536818, 8.660254037844387298 ) ) ;
#37157 = CARTESIAN_POINT ( 'NONE',  ( -4.401442555609581635E-16, 111.7812500020483810, -7.188101187500000044 ) ) ;
#37158 = CARTESIAN_POINT ( 'NONE',  ( 4.541265875000001451, 5.374999998634406140, 1.881053915767124440 ) ) ;
#37159 = CARTESIAN_POINT ( 'NONE',  ( 4.465384415997327494, 66.51627080308891493, -26.73837581714001033 ) ) ;
#37160 = CARTESIAN_POINT ( 'NONE',  ( -7.999999999999991118, 3.313708498984756723, 8.236552779823362869 ) ) ;
#37162 = CARTESIAN_POINT ( 'NONE',  ( 4.556349186104052151, -10.99999999999999822, 105.1562500040967763 ) ) ;
#37161 = CARTESIAN_POINT ( 'NONE',  ( 2.856636953006502999, 194.5084785699607721, 139.9521677304649074 ) ) ;
#37163 = VERTEX_POINT ( 'NONE', #3413 ) ;
#37164 = EDGE_CURVE ( 'NONE', #71806, #69504, #19924, .T. ) ;
#37165 = CARTESIAN_POINT ( 'NONE',  ( 8.001991528333338266, 220.1059721264024347, 6.140144111190926957 ) ) ;
#37166 = DIRECTION ( 'NONE',  ( -0.000000000000000000, 1.000000000000000000, -0.000000000000000000 ) ) ;
#37167 = CARTESIAN_POINT ( 'NONE',  ( 8.311093377946834337, 227.3437500034140157, -8.311093377946836114 ) ) ;
#37168 = CARTESIAN_POINT ( 'NONE',  ( 11.35316468750000141, 125.7812499965860127, 0.000000000000000000 ) ) ;
#37169 = ORIENTED_EDGE ( 'NONE', *, *, #64424, .T. ) ;
#37170 = DIRECTION ( 'NONE',  ( -0.000000000000000000, -0.000000000000000000, -1.000000000000000000 ) ) ;
#37171 = CARTESIAN_POINT ( 'NONE',  ( 7.204075437095966983, 7.204075437095967871, 94.09375000204838102 ) ) ;
#37172 = CARTESIAN_POINT ( 'NONE',  ( -7.778174593052023411, 7.778174593052023411, 86.50000000409677625 ) ) ;
#37173 = CARTESIAN_POINT ( 'NONE',  ( -3.458734124999959469, 197.7500000013656063, 199.4326545832176691 ) ) ;
#37174 = DIRECTION ( 'NONE',  ( 0.000000000000000000, 0.000000000000000000, 1.000000000000000000 ) ) ;
#37176 = CARTESIAN_POINT ( 'NONE',  ( -3.042071309553173730, 119.3229166632526557, 11.35316468749999785 ) ) ;
#37175 = CARTESIAN_POINT ( 'NONE',  ( 1.901548650871797615E-12, 218.7500000000001990, 10.00000000000000533 ) ) ;
#37177 = CARTESIAN_POINT ( 'NONE',  ( -32.00000000000000000, 208.2500000000000284, 170.0000000000003979 ) ) ;
#37178 = CARTESIAN_POINT ( 'NONE',  ( 2.679491924322640273, 51.04166666666564112, -9.999999999993418598 ) ) ;
#37179 = ORIENTED_EDGE ( 'NONE', *, *, #61620, .T. ) ;
#37180 =( BOUNDED_CURVE ( )  B_SPLINE_CURVE ( 2, ( #6047, #68298, #39635, #29429, #56993, #23388, #27938, #22261, #62633 ),
 .UNSPECIFIED., .F., .F. ) 
 B_SPLINE_CURVE_WITH_KNOTS ( ( 3, 2, 2, 2, 3 ),
 ( 0.03125000000000002082, 0.03645833333333335646, 0.04166666666666669211, 0.04687500000000002776, 0.05208333333333337034 ),
 .UNSPECIFIED. ) 
 CURVE ( )  GEOMETRIC_REPRESENTATION_ITEM ( )  RATIONAL_B_SPLINE_CURVE ( ( 0.9999999999999996669, 0.9238795325112870716, 1.000000000000000000, 0.9238795325112867385, 1.000000000000000000, 0.9238795325112867385, 1.000000000000000000, 0.9238795325112861834, 1.000000000000000444 ) ) 
 REPRESENTATION_ITEM ( '' )  );
#37181 = EDGE_CURVE ( 'NONE', #73315, #41375, #70326, .T. ) ;
#37182 = CARTESIAN_POINT ( 'NONE',  ( 10.00000000000000000, 257.5000000000000000, -1.224646799147353256E-15 ) ) ;
#37183 = DIRECTION ( 'NONE',  ( 1.000000000000000000, -0.000000000000000000, -0.000000000000000000 ) ) ;
#37184 = CARTESIAN_POINT ( 'NONE',  ( -11.35316468749999785, 108.3854166632526841, -3.042071309553167957 ) ) ;
#37185 = CARTESIAN_POINT ( 'NONE',  ( 1.432654583217664479, 204.7500000013655779, 201.4587341250000065 ) ) ;
#37186 = CARTESIAN_POINT ( 'NONE',  ( 4.401442555609581635E-16, 11.71874999795161010, -7.188101187500000044 ) ) ;
#37187 = CARTESIAN_POINT ( 'NONE',  ( 10.18810118749999916, 1.247682550866122264E-15, 91.28125000204836681 ) ) ;
#37188 = CARTESIAN_POINT ( 'NONE',  ( -5.676582343749998039, 27.76041666325268409, -9.832129032723420536 ) ) ;
#37189 = ORIENTED_EDGE ( 'NONE', *, *, #12739, .F. ) ;
#37190 = CARTESIAN_POINT ( 'NONE',  ( -4.999999999999944045, 68.60357193678724741, -20.85024232999276350 ) ) ;
#37191 = CARTESIAN_POINT ( 'NONE',  ( 8.008118988124991233, 9.807117285998411148E-16, 25.76311528394063544 ) ) ;
#37192 = CARTESIAN_POINT ( 'NONE',  ( 5.000000000000001776, 117.7083333265053824, -8.660254037844389075 ) ) ;
#37193 = CARTESIAN_POINT ( 'NONE',  ( -10.18810118749999916, 4.220049686691934809, 73.93750000204838102 ) ) ;
#37194 = CARTESIAN_POINT ( 'NONE',  ( 0.000000000000000000, 300.0000000000000000, 0.000000000000000000 ) ) ;
#37195 = CARTESIAN_POINT ( 'NONE',  ( -2.977408999572654480, 1.499999997951610542, 7.188101187499999156 ) ) ;
#37196 = CARTESIAN_POINT ( 'NONE',  ( -6.676582343750001591, 292.4531250017069510, 0.000000000000000000 ) ) ;
#37197 = CARTESIAN_POINT ( 'NONE',  ( -2.828427124746209831, 199.3750000000000284, 139.1715728752538723 ) ) ;
#37198 = CARTESIAN_POINT ( 'NONE',  ( -11.35316468749999785, 218.3854166632526415, -3.042071309553167957 ) ) ;
#37199 = CARTESIAN_POINT ( 'NONE',  ( 5.676582343750001591, 141.9270833299193555, -9.832129032723420536 ) ) ;
#37200 = CARTESIAN_POINT ( 'NONE',  ( 4.220049686691941027, -10.18810118749999738, 84.62500000204838102 ) ) ;
#37201 = EDGE_CURVE ( 'NONE', #413, #34861, #16443, .T. ) ;
#37202 = VECTOR ( 'NONE', #42989, 1000.000000000000000 ) ;
#37203 = CARTESIAN_POINT ( 'NONE',  ( -28.00000000000002132, 200.4375000013656063, 166.5412658750003629 ) ) ;
#37204 = CARTESIAN_POINT ( 'NONE',  ( 3.313708498984762052, 21.28125000000000711, -8.000000000000000000 ) ) ;
#37205 = CARTESIAN_POINT ( 'NONE',  ( -3.211159895383561391, 13.81249999863440614, -3.211159895383561835 ) ) ;
#37206 = ORIENTED_EDGE ( 'NONE', *, *, #11971, .T. ) ;
#37207 = AXIS2_PLACEMENT_3D ( 'NONE', #20089, #67166, #73195 ) ;
#37208 = CARTESIAN_POINT ( 'NONE',  ( 1.656854249492403008, 203.8125000027312410, 194.0000000000000853 ) ) ;
#37209 = CARTESIAN_POINT ( 'NONE',  ( -2.754378923186476579E-14, 199.4375000013655779, 145.4587341250000350 ) ) ;
#37210 = AXIS2_PLACEMENT_3D ( 'NONE', #21827, #11642, #16158 ) ;
#37211 = CARTESIAN_POINT ( 'NONE',  ( -4.000000000000015987, 205.5625000027311842, 140.3431457505076594 ) ) ;
#37212 = CARTESIAN_POINT ( 'NONE',  ( 4.999999999999999112, 10.82378452496227261, -67.02990231369372509 ) ) ;
#37213 = LINE ( 'NONE', #67652, #65773 ) ;
#37214 = ORIENTED_EDGE ( 'NONE', *, *, #62081, .T. ) ;
#37215 = CARTESIAN_POINT ( 'NONE',  ( 7.188101187500000933, 8.062499997951611874, -2.977408999572650483 ) ) ;
#37216 = CARTESIAN_POINT ( 'NONE',  ( -12.97459525119566948, -23.28945777676194595, 198.1568323241545500 ) ) ;
#37217 = CARTESIAN_POINT ( 'NONE',  ( -10.00000000000000355, 29.58333332650536818, 2.679491924311223183 ) ) ;
#37218 = CARTESIAN_POINT ( 'NONE',  ( -3.042071309553164404, 182.2395833299193555, -11.35316468749999963 ) ) ;
#37219 = CARTESIAN_POINT ( 'NONE',  ( 2.977408999572650039, 112.0625000020483810, -7.188101187500001821 ) ) ;
#37220 = CARTESIAN_POINT ( 'NONE',  ( -0.4590000000000000746, 267.1439999999997212, 5.793770692572753234 ) ) ;
#37221 = CARTESIAN_POINT ( 'NONE',  ( 1.226468279477575784E-15, 292.7031250017069510, 6.676582343750001591 ) ) ;
#37223 = DIRECTION ( 'NONE',  ( -0.000000000000000000, -0.000000000000000000, 1.000000000000000000 ) ) ;
#37222 = LINE ( 'NONE', #54954, #33418 ) ;
#37224 = ITEM_DEFINED_TRANSFORMATION ( 'NONE', 'NONE', #18881,  #57354 ) ;
#37225 = VERTEX_POINT ( 'NONE', #49046 ) ;
#37226 = CARTESIAN_POINT ( 'NONE',  ( -6.951808397369817780E-16, 232.9687500034139873, -11.35316468749999963 ) ) ;
#37227 = CARTESIAN_POINT ( 'NONE',  ( -5.082755093536319713, 5.082755093536319713, 28.67405278187175810 ) ) ;
#37228 = CARTESIAN_POINT ( 'NONE',  ( -4.000000000000001776, 2.187499997268813168, -1.656854249492381470 ) ) ;
#37229 = CARTESIAN_POINT ( 'NONE',  ( 28.00000000000002132, 198.1250000027312126, 173.9999999999999147 ) ) ;
#37230 = CARTESIAN_POINT ( 'NONE',  ( -2.445694354108783219, 199.8125000013656063, 200.4456943541088663 ) ) ;
#37231 = ORIENTED_EDGE ( 'NONE', *, *, #53613, .T. ) ;
#37232 = DIRECTION ( 'NONE',  ( 0.000000000000000000, -0.000000000000000000, 1.000000000000000000 ) ) ;
#37233 = CARTESIAN_POINT ( 'NONE',  ( -5.656854249492378806, 102.6875000000000000, 5.656854249492381470 ) ) ;
#37234 = CARTESIAN_POINT ( 'NONE',  ( -9.832129032723420536, 119.0104166632526841, 5.676582343749997150 ) ) ;
#37235 = CARTESIAN_POINT ( 'NONE',  ( 7.320508075688771044, 211.2499999931719969, 7.320508075688775484 ) ) ;
#37236 = CARTESIAN_POINT ( 'NONE',  ( -7.778174593052023411, 7.778174593052023411, 75.81249999999997158 ) ) ;
#37239 = DIRECTION ( 'NONE',  ( 0.000000000000000000, 0.000000000000000000, 1.000000000000000000 ) ) ;
#37238 = CARTESIAN_POINT ( 'NONE',  ( 31.45873412499997812, 198.7500000013656063, 168.5673454167822172 ) ) ;
#37237 = CARTESIAN_POINT ( 'NONE',  ( 24.54126587500000056, 199.3750000013656063, 168.5673454167822172 ) ) ;
#37240 = VERTEX_POINT ( 'NONE', #31328 ) ;
#37241 = CARTESIAN_POINT ( 'NONE',  ( 29.65685424949236548, 205.1875000027311842, 173.9999999999999147 ) ) ;
#37242 = EDGE_CURVE ( 'NONE', #6596, #60098, #23590, .T. ) ;
#37243 = CARTESIAN_POINT ( 'NONE',  ( 9.832129032723416984, 220.3645833299193839, 5.676582343750006032 ) ) ;
#37244 = CARTESIAN_POINT ( 'NONE',  ( -2.445694354108838731, 202.0625000013656063, 144.4456943541088663 ) ) ;
#37245 = CARTESIAN_POINT ( 'NONE',  ( 31.45873412500001010, 202.0000000013656063, 168.5673454167822740 ) ) ;
#37246 = AXIS2_PLACEMENT_3D ( 'NONE', #19130, #7820, #8185 ) ;
#37247 = CARTESIAN_POINT ( 'NONE',  ( -11.00000000000000000, 4.556349186104045934, 115.0937500040967905 ) ) ;
#37248 = CARTESIAN_POINT ( 'NONE',  ( -8.311093377946841443, 189.2187499965860411, 8.311093377946830785 ) ) ;
#37249 = CARTESIAN_POINT ( 'NONE',  ( 5.082755093536325042, 93.96875000204838102, -5.082755093536325930 ) ) ;
#37250 = CARTESIAN_POINT ( 'NONE',  ( -11.00000000000000000, 0.000000000000000000, 118.0000000000000000 ) ) ;
#37251 = CARTESIAN_POINT ( 'NONE',  ( 3.211159895383560947, 15.18749999863440792, 3.211159895383562723 ) ) ;
#37252 = CARTESIAN_POINT ( 'NONE',  ( 24.54126587499999346, 199.4375000013655779, 169.9999999999998863 ) ) ;
#37253 = ADVANCED_BREP_SHAPE_REPRESENTATION ( '', ( #66162, #57354 ), #18781 ) ;
#37254 = CARTESIAN_POINT ( 'NONE',  ( 7.188101187499993827, -2.977408999572645598, 5.517802781871753659 ) ) ;
#37255 = CARTESIAN_POINT ( 'NONE',  ( -9.797174393178831574E-16, 22.00000000000000355, -8.000000000000003553 ) ) ;
#37256 = CARTESIAN_POINT ( 'NONE',  ( 8.311093377946837890, 86.40624999658601268, -8.311093377946837890 ) ) ;
#37257 = EDGE_LOOP ( 'NONE', ( #25437, #69385, #27254, #11406 ) ) ;
#37258 = EDGE_CURVE ( 'NONE', #20745, #44182, #21309, .T. ) ;
#37259 = CARTESIAN_POINT ( 'NONE',  ( -30.82842712474615610, 195.3750000000000284, 172.8284271247465824 ) ) ;
#37260 = CARTESIAN_POINT ( 'NONE',  ( 4.000000000000015987, 209.5000000000000284, 198.0000000000000284 ) ) ;
#37261 = CARTESIAN_POINT ( 'NONE',  ( -3.313708498984786033, 9.843749995903220196, 7.999999999999979572 ) ) ;
#37262 = CARTESIAN_POINT ( 'NONE',  ( 0.000000000000000000, 23.85640646055104241, -14.00000000000000178 ) ) ;
#37263 = CARTESIAN_POINT ( 'NONE',  ( -11.35316468750000141, 83.28124999658602690, -1.390361679473963753E-15 ) ) ;
#37264 = VERTEX_POINT ( 'NONE', #4536 ) ;
#37265 = CARTESIAN_POINT ( 'NONE',  ( 10.18810118749999916, 4.220049686691935698, 86.87500000204836681 ) ) ;
#37266 = CIRCLE ( 'NONE', #22817, 10.99999999999999645 ) ;
#37267 = CARTESIAN_POINT ( 'NONE',  ( -7.204075437095967871, 7.204075437095967871, 112.4687500020483810 ) ) ;
#37268 = CARTESIAN_POINT ( 'NONE',  ( 1.432654583217662481, 207.3750000013656063, 194.5412658750000219 ) ) ;
#37269 = FACE_OUTER_BOUND ( 'NONE', #39228, .T. ) ;
#37271 = CARTESIAN_POINT ( 'NONE',  ( -5.676582343750006032, 74.11458332991935549, 9.832129032723418760 ) ) ;
#37270 = CARTESIAN_POINT ( 'NONE',  ( -11.00000000000000000, 0.000000000000000000, 118.0000000000000000 ) ) ;
#37272 = CARTESIAN_POINT ( 'NONE',  ( -7.999999999999991118, 3.313708498984756723, 18.92405278392014978 ) ) ;
#37273 = CARTESIAN_POINT ( 'NONE',  ( -3.765320639486814169, 194.7591455152330582, 141.8797637694395917 ) ) ;
#37274 = CARTESIAN_POINT ( 'NONE',  ( -10.00000000000000000, 164.1666666598387110, -2.679491924311229845 ) ) ;
#37275 = CARTESIAN_POINT ( 'NONE',  ( -4.401442555609581635E-16, 89.65625000204838102, -7.188101187500000044 ) ) ;
#37276 = DIRECTION ( 'NONE',  ( 0.000000000000000000, 0.000000000000000000, 1.000000000000000000 ) ) ;
#37277 = CARTESIAN_POINT ( 'NONE',  ( -8.311093377946836114, 57.96874999658601979, -8.311093377946837890 ) ) ;
#37278 = CARTESIAN_POINT ( 'NONE',  ( 2.765530957081996366, 294.1406250017069510, -6.676582343750003368 ) ) ;
#37279 =( BOUNDED_CURVE ( )  B_SPLINE_CURVE ( 2, ( #2511, #49648, #25505, #71899, #3257, #45842, #74517, #10035, #45467 ),
 .UNSPECIFIED., .F., .F. ) 
 B_SPLINE_CURVE_WITH_KNOTS ( ( 3, 2, 2, 2, 3 ),
 ( 0.6618275503331610965, 0.6684458340301022705, 0.6750641096145244546, 0.6816823851989468608, 0.6883006607833690449 ),
 .UNSPECIFIED. ) 
 CURVE ( )  GEOMETRIC_REPRESENTATION_ITEM ( )  RATIONAL_B_SPLINE_CURVE ( ( 1.000000000000000000, 0.9238795325112867385, 1.000000000000000000, 0.9238795325112867385, 1.000000000000000000, 0.9238795325112867385, 1.000000000000000000, 0.9238795325128899005, 0.9999999999983968380 ) ) 
 REPRESENTATION_ITEM ( '' )  );
#37280 = CARTESIAN_POINT ( 'NONE',  ( 10.18810118750000093, -4.220049686691933033, 109.1875000020483810 ) ) ;
#37281 = CARTESIAN_POINT ( 'NONE',  ( 3.042071309553167069, 211.8229166632527267, -11.35316468749999785 ) ) ;
#37282 = ORIENTED_EDGE ( 'NONE', *, *, #32853, .F. ) ;
#37283 = CARTESIAN_POINT ( 'NONE',  ( -3.728321214213454748, 66.24762070553359194, 26.57448171416459459 ) ) ;
#37284 = CARTESIAN_POINT ( 'NONE',  ( 1.656854249492381248, 3.937499997268813168, -4.000000000000001776 ) ) ;
#37285 = FACE_OUTER_BOUND ( 'NONE', #55526, .T. ) ;
#37287 = CARTESIAN_POINT ( 'NONE',  ( -8.311093377946836114, 197.6562499965860411, -8.311093377946837890 ) ) ;
#37286 = DIRECTION ( 'NONE',  ( 0.000000000000000000, 0.000000000000000000, -1.000000000000000000 ) ) ;
#37288 = CARTESIAN_POINT ( 'NONE',  ( 5.656854249492378806, 2.624999995903220196, 5.656854249492381470 ) ) ;
#37289 = CARTESIAN_POINT ( 'NONE',  ( -2.679491924311222295, 244.1666666734946318, 10.00000000000000178 ) ) ;
#37290 = CARTESIAN_POINT ( 'NONE',  ( -31.99999999999999289, 200.2500000000000000, 170.0000000000003979 ) ) ;
#37291 = VERTEX_POINT ( 'NONE', #11309 ) ;
#37292 = CARTESIAN_POINT ( 'NONE',  ( 5.676582343750001591, 186.9270833299193555, -9.832129032723420536 ) ) ;
#37293 = CARTESIAN_POINT ( 'NONE',  ( 2.977408999572646486, 7.188101187499992051, 23.51780278187175455 ) ) ;
#37294 = DIRECTION ( 'NONE',  ( -1.182917971378671814E-16, 0.000000000000000000, -1.000000000000000000 ) ) ;
#37295 = ORIENTED_EDGE ( 'NONE', *, *, #65929, .F. ) ;
#37296 = CARTESIAN_POINT ( 'NONE',  ( 1.469576158976823947E-15, 100.0625000040967763, 8.000000000000000000 ) ) ;
#37297 = CARTESIAN_POINT ( 'NONE',  ( -8.660254037844387298, 7.083333333333333925, -5.000000000000004441 ) ) ;
#37298 = AXIS2_PLACEMENT_3D ( 'NONE', #14856, #61648, #43920 ) ;
#37299 = CARTESIAN_POINT ( 'NONE',  ( 4.000000000000001776, 18.06250000000000000, -1.656854249492381248 ) ) ;
#37300 = CARTESIAN_POINT ( 'NONE',  ( 3.211159895383561835, 14.43749999863440792, -3.211159895383561835 ) ) ;
#37301 = CARTESIAN_POINT ( 'NONE',  ( -3.313708498984757167, 7.999999999999991118, 12.73655278392014623 ) ) ;
#37302 = CARTESIAN_POINT ( 'NONE',  ( -11.00000000000000000, 0.000000000000000000, 77.68750000409677625 ) ) ;
#37303 = ORIENTED_EDGE ( 'NONE', *, *, #50900, .T. ) ;
#37304 = DIRECTION ( 'NONE',  ( 0.000000000000000000, -0.8536788251726096233, 0.5207998305029611918 ) ) ;
#37305 = CARTESIAN_POINT ( 'NONE',  ( -7.188101187499999156, 98.75000000204838102, 2.977408999572654924 ) ) ;
#37307 = CARTESIAN_POINT ( 'NONE',  ( 3.042071309553163516, 262.4479166700805877, -11.35316468749999785 ) ) ;
#37306 = CARTESIAN_POINT ( 'NONE',  ( -8.660254037844490327, 82.91666666666674246, 5.000000000000055955 ) ) ;
#37308 = PRODUCT_CONTEXT ( 'NONE', #37556, 'mechanical' ) ;
#37309 = ORIENTED_EDGE ( 'NONE', *, *, #55597, .T. ) ;
#37310 = ADVANCED_FACE ( 'NONE', ( #33973 ), #63349, .F. ) ;
#37311 = DIRECTION ( 'NONE',  ( -0.000000000000000000, -0.000000000000000000, -1.000000000000000000 ) ) ;
#37312 = EDGE_CURVE ( 'NONE', #66661, #7158, #46731, .T. ) ;
#37313 = CARTESIAN_POINT ( 'NONE',  ( -5.082755093536319713, 5.082755093536319713, 16.29905278187175455 ) ) ;
#37314 = ORIENTED_EDGE ( 'NONE', *, *, #40052, .F. ) ;
#37315 = ORIENTED_EDGE ( 'NONE', *, *, #21571, .T. ) ;
#37316 = CARTESIAN_POINT ( 'NONE',  ( -10.18810118749999916, 4.220049686691934809, 82.56250000204836681 ) ) ;
#37317 = CARTESIAN_POINT ( 'NONE',  ( 6.951808397369818766E-16, 72.34374999658602690, -11.35316468750000141 ) ) ;
#37318 = DIRECTION ( 'NONE',  ( 1.000000000000000000, -0.000000000000000000, -0.000000000000000000 ) ) ;
#37319 = CARTESIAN_POINT ( 'NONE',  ( 11.00000000000000000, 4.556349186104045934, 94.84374999999998579 ) ) ;
#37322 = CARTESIAN_POINT ( 'NONE',  ( -2.765530957081996810, 293.4218750017070079, -6.676582343750002480 ) ) ;
#37321 = CARTESIAN_POINT ( 'NONE',  ( 28.00000000000001776, 197.1250000027312126, 173.9999999999999147 ) ) ;
#37320 = DIRECTION ( 'NONE',  ( 0.000000000000000000, 0.000000000000000000, -1.000000000000000000 ) ) ;
#37323 = CARTESIAN_POINT ( 'NONE',  ( 4.999999999999993783, 149.1666666666666572, 8.660254037844390851 ) ) ;
#37324 = CARTESIAN_POINT ( 'NONE',  ( 2.828427124746190291, 13.87500000000000000, 2.828427124746192067 ) ) ;
#37325 = CARTESIAN_POINT ( 'NONE',  ( -2.828427124746152987, 200.1250000000000284, 200.8284271247462129 ) ) ;
#37326 = EDGE_CURVE ( 'NONE', #46484, #53923, #17326, .T. ) ;
#37327 = CARTESIAN_POINT ( 'NONE',  ( -2.679491924311228512, 232.0833333401613174, -9.999999999999998224 ) ) ;
#37328 = CARTESIAN_POINT ( 'NONE',  ( 7.999972022862700705, 3.313736476122048025, 0.3615539032942260977 ) ) ;
#37329 = CARTESIAN_POINT ( 'NONE',  ( 26.56734541678232375, 199.3750000013656063, 173.4587341249998929 ) ) ;
#37330 = CARTESIAN_POINT ( 'NONE',  ( 5.082755093536325930, 11.53124999795161187, -5.082755093536325930 ) ) ;
#37331 = CARTESIAN_POINT ( 'NONE',  ( 3.313708498984756279, 7.999999999999991118, 26.04905278392014623 ) ) ;
#37332 = CARTESIAN_POINT ( 'NONE',  ( -7.188101187500000044, 124.1562500020483810, 0.000000000000000000 ) ) ;
#37333 = CARTESIAN_POINT ( 'NONE',  ( 1.320432766682874540E-15, 112.9062500020483952, 7.188101187500000044 ) ) ;
#37334 = CARTESIAN_POINT ( 'NONE',  ( -14.00000000000000178, -2.250000000005106138, 7.677076266390546522 ) ) ;
#37335 = CARTESIAN_POINT ( 'NONE',  ( 8.660254037844390851, 135.4166666666667140, -5.000000000000001776 ) ) ;
#37336 = CARTESIAN_POINT ( 'NONE',  ( 25.55430564589115505, 209.5625000013656063, 172.4456943541086957 ) ) ;
#37337 = CARTESIAN_POINT ( 'NONE',  ( -7.188101187499992051, 0.000000000000000000, 21.36155278187175455 ) ) ;
#37338 = CARTESIAN_POINT ( 'NONE',  ( 3.458734124999959914, 209.5625000013656063, 142.0000000000000568 ) ) ;
#37339 = CARTESIAN_POINT ( 'NONE',  ( -5.676582343750006032, 39.11458332991934839, 9.832129032723418760 ) ) ;
#37340 = CARTESIAN_POINT ( 'NONE',  ( 4.615726161707415898, 16.27701803902727917, 69.62876280158647546 ) ) ;
#37341 = CARTESIAN_POINT ( 'NONE',  ( -8.660254037844390851, 4.791666659838699438, 4.999999999999998224 ) ) ;
#37342 = VERTEX_POINT ( 'NONE', #21501 ) ;
#37343 = CARTESIAN_POINT ( 'NONE',  ( -2.679491924311226292, 128.3333333265053682, -10.00000000000000178 ) ) ;
#37344 = CARTESIAN_POINT ( 'NONE',  ( -11.00000000000000000, 0.000000000000000000, 70.18750000409676204 ) ) ;
#37345 = CARTESIAN_POINT ( 'NONE',  ( 5.676582343750001591, 51.61458332991934839, -9.832129032723420536 ) ) ;
#37346 = CARTESIAN_POINT ( 'NONE',  ( 11.00000000000000000, 1.347111479062088405E-15, 82.93750000409677625 ) ) ;
#37347 = CARTESIAN_POINT ( 'NONE',  ( 3.458734124999960358, 204.6875000013656063, 142.0000000000000568 ) ) ;
#37348 = CARTESIAN_POINT ( 'NONE',  ( 26.34314575050753149, 202.9375000000000284, 173.9999999999998295 ) ) ;
#37349 = FACE_OUTER_BOUND ( 'NONE', #3586, .T. ) ;
#37351 = CARTESIAN_POINT ( 'NONE',  ( -8.311093377946841443, 28.90624999658601624, 8.311093377946834337 ) ) ;
#37350 = CARTESIAN_POINT ( 'NONE',  ( 7.188101187500002709, 100.8125000020484094, 2.977408999572649151 ) ) ;
#37352 = CARTESIAN_POINT ( 'NONE',  ( 7.999999999999991118, 9.797174393178815797E-16, 9.080302779823364645 ) ) ;
#37353 = CARTESIAN_POINT ( 'NONE',  ( 9.832129032723416984, 160.3645833299193839, 5.676582343750006032 ) ) ;
#37354 = VECTOR ( 'NONE', #34089, 1000.000000000000000 ) ;
#37355 = CARTESIAN_POINT ( 'NONE',  ( -4.999999999999998224, 133.5416666598387110, -8.660254037844389075 ) ) ;
#37356 = CARTESIAN_POINT ( 'NONE',  ( -7.188101187500000044, 106.5312500020483810, 0.000000000000000000 ) ) ;
#37357 = EDGE_LOOP ( 'NONE', ( #14369, #45640, #52794, #67843 ) ) ;
#37358 = CARTESIAN_POINT ( 'NONE',  ( 4.500000000000010658, 7.794228634059937377, 0.000000000000000000 ) ) ;
#37359 = CARTESIAN_POINT ( 'NONE',  ( -11.35316468750000141, 23.59374999658601979, -1.390361679473963753E-15 ) ) ;
#37360 = LINE ( 'NONE', #3404, #46109 ) ;
#37361 = VERTEX_POINT ( 'NONE', #5653 ) ;
#37362 = DIRECTION ( 'NONE',  ( 0.000000000000000000, 0.000000000000000000, 1.000000000000000000 ) ) ;
#37363 = CARTESIAN_POINT ( 'NONE',  ( 4.220049686691941027, -10.18810118749999738, 75.62500000204838102 ) ) ;
#37364 = CARTESIAN_POINT ( 'NONE',  ( -31.99999999999999289, 197.2500000000000000, 170.0000000000003979 ) ) ;
#37366 = CARTESIAN_POINT ( 'NONE',  ( -3.042071309553173730, 149.3229166632526699, 11.35316468749999785 ) ) ;
#37365 = CARTESIAN_POINT ( 'NONE',  ( -4.556349186104045934, 11.00000000000000000, 92.40625000409677625 ) ) ;
#37367 = DIRECTION ( 'NONE',  ( -0.000000000000000000, 1.000000000000000000, -0.000000000000000000 ) ) ;
#37368 = CARTESIAN_POINT ( 'NONE',  ( -7.999999999999989342, -3.313708498984762496, 14.48030278432982598 ) ) ;
#37369 = CARTESIAN_POINT ( 'NONE',  ( 3.313708498984762496, -7.999999999999989342, 16.29905277982336642 ) ) ;
#37370 = CARTESIAN_POINT ( 'NONE',  ( 8.311093377946834337, 237.0312500034140157, -8.311093377946836114 ) ) ;
#37371 = CARTESIAN_POINT ( 'NONE',  ( -10.18810118749999916, 4.220049686691934809, 82.93750000204838102 ) ) ;
#37372 = VERTEX_POINT ( 'NONE', #69024 ) ;
#37373 = CARTESIAN_POINT ( 'NONE',  ( -2.751064625579944321E-14, 197.7500000000000000, 146.0000000000000284 ) ) ;
#37374 = CARTESIAN_POINT ( 'NONE',  ( -33.07484552657816579, -21.19745326134420083, 158.8094963175336432 ) ) ;
#37375 = CARTESIAN_POINT ( 'NONE',  ( -5.676582343750006032, 109.4270833299193555, 9.832129032723418760 ) ) ;
#37376 = CARTESIAN_POINT ( 'NONE',  ( 10.18810118749999916, 4.220049686691935698, 103.0000000020483668 ) ) ;
#37377 = CARTESIAN_POINT ( 'NONE',  ( 1.881053915767121998, 20.62499999863441147, -4.541265875000002339 ) ) ;
#37378 = EDGE_LOOP ( 'NONE', ( #25410, #56940 ) ) ;
#37379 = EDGE_LOOP ( 'NONE', ( #19211, #64693, #38681, #37303 ) ) ;
#37380 = CARTESIAN_POINT ( 'NONE',  ( 3.211159895383561835, 2.562499998634407028, -3.211159895383561835 ) ) ;
#37381 = CARTESIAN_POINT ( 'NONE',  ( -5.082755093536325042, 10.03124999795161187, -5.082755093536325930 ) ) ;
#37382 = CARTESIAN_POINT ( 'NONE',  ( -8.000000000000000000, 113.1875000040967763, 0.000000000000000000 ) ) ;
#37383 = AXIS2_PLACEMENT_3D ( 'NONE', #67473, #39549, #55790 ) ;
#37384 =( BOUNDED_CURVE ( )  B_SPLINE_CURVE ( 2, ( #22488, #28535, #23248, #51543, #74561, #34964, #6284, #24356, #47727 ),
 .UNSPECIFIED., .F., .F. ) 
 B_SPLINE_CURVE_WITH_KNOTS ( ( 3, 2, 2, 2, 3 ),
 ( 0.8295454545454545858, 0.8352272727272727071, 0.8409090909090909394, 0.8465909090909090606, 0.8522727272727272929 ),
 .UNSPECIFIED. ) 
 CURVE ( )  GEOMETRIC_REPRESENTATION_ITEM ( )  RATIONAL_B_SPLINE_CURVE ( ( 1.000000000000000000, 0.9238795325112867385, 1.000000000000000000, 0.9238795325112867385, 1.000000000000000000, 0.9238795325112867385, 1.000000000000000000, 0.9238795325112867385, 1.000000000000000000 ) ) 
 REPRESENTATION_ITEM ( '' )  );
#37385 = CARTESIAN_POINT ( 'NONE',  ( -4.220049686691935698, 10.18810118749999916, 99.25000000204838102 ) ) ;
#37386 = CARTESIAN_POINT ( 'NONE',  ( -24.54126587499999346, 201.4375000013656063, 170.0000000000003411 ) ) ;
#37387 = ADVANCED_FACE ( 'NONE', ( #51667 ), #67534, .F. ) ;
#37388 = DIRECTION ( 'NONE',  ( -1.000000000000000000, 0.000000000000000000, 0.000000000000000000 ) ) ;
#37389 = B_SPLINE_CURVE_WITH_KNOTS ( 'NONE', 3,
 ( #68268, #16564, #67896, #45998, #34335, #15825, #16188, #62229, #68639, #39601, #32838, #28279, #55848, #62598, #62979, #51285, #4165, #73925, #38860, #10556 ),
 .UNSPECIFIED., .F., .F.,
 ( 4, 2, 2, 2, 2, 2, 2, 2, 2, 4 ),
 ( 3.986091072867590107E-17, 0.003663249189234787061, 0.004579061486543473634, 0.005494873783852158473, 0.007326498378469529886, 0.009158122973086902166, 0.01098974756770427358, 0.01190555986501299832, 0.01282137216232172305, 0.01465299675693917773 ),
 .UNSPECIFIED. ) ;
#37390 = CARTESIAN_POINT ( 'NONE',  ( -2.828427124746190735, 3.375000000000000000, -2.828427124746191623 ) ) ;
#37391 = CARTESIAN_POINT ( 'NONE',  ( 4.000000000000000888, 16.68749999726881583, 1.656854249492384135 ) ) ;
#37392 = CARTESIAN_POINT ( 'NONE',  ( -3.211159895383561391, 4.687499998634407028, -3.211159895383561835 ) ) ;
#37393 = CARTESIAN_POINT ( 'NONE',  ( 5.656854249492381470, 95.56250000000000000, 5.656854249492379694 ) ) ;
#37394 = CARTESIAN_POINT ( 'NONE',  ( 1.432654583217662481, 195.1250000013656063, 194.5412658750000219 ) ) ;
#37396 = CARTESIAN_POINT ( 'NONE',  ( 18.00000000000000000, 10.39230484541325161, -20.69999999999999929 ) ) ;
#37395 = CARTESIAN_POINT ( 'NONE',  ( -28.00000000000006750, 195.4375000013655779, 166.5412658750003629 ) ) ;
#37397 = SHAPE_REPRESENTATION_RELATIONSHIP ( 'NONE' , 'NONE' ,  #66259, #50744 ) ;
#37398 = CARTESIAN_POINT ( 'NONE',  ( -3.211159895383562723, 16.93749999863440436, 3.211159895383561391 ) ) ;
#37399 = AXIS2_PLACEMENT_3D ( 'NONE', #41865, #7907, #795 ) ;
#37400 = CARTESIAN_POINT ( 'NONE',  ( 7.188101187499991163, 2.977408999572648707, 8.330302781871752771 ) ) ;
#37401 = ORIENTED_EDGE ( 'NONE', *, *, #67136, .T. ) ;
#37402 = EDGE_LOOP ( 'NONE', ( #13484, #46370, #29504, #28413 ) ) ;
#37403 = CARTESIAN_POINT ( 'NONE',  ( -7.204075437095967871, 7.204075437095967871, 95.96875000204838102 ) ) ;
#37404 = DIRECTION ( 'NONE',  ( -0.000000000000000000, -1.000000000000000000, -0.000000000000000000 ) ) ;
#37405 = VECTOR ( 'NONE', #19604, 1000.000000000000000 ) ;
#37406 = CARTESIAN_POINT ( 'NONE',  ( -30.44569435410879166, 205.0625000013656063, 172.4456943541092357 ) ) ;
#37407 = CARTESIAN_POINT ( 'NONE',  ( -29.65685424949234061, 201.4375000000000000, 174.0000000000004547 ) ) ;
#37408 = CARTESIAN_POINT ( 'NONE',  ( -3.458734124999959025, 195.5000000013655779, 199.4326545832176691 ) ) ;
#37409 = CARTESIAN_POINT ( 'NONE',  ( -5.656854249492381470, 12.74999999590322197, 5.656854249492379694 ) ) ;
#37410 = CARTESIAN_POINT ( 'NONE',  ( 8.660254037844389075, 105.4166666666666714, -5.000000000000000000 ) ) ;
#37411 = AXIS2_PLACEMENT_3D ( 'NONE', #66117, #32176, #3502 ) ;
#37412 = EDGE_CURVE ( 'NONE', #23833, #24773, #29033, .T. ) ;
#37413 = EDGE_CURVE ( 'NONE', #11426, #28973, #44903, .T. ) ;
#37414 = CARTESIAN_POINT ( 'NONE',  ( -5.656854249492378806, 113.1875000000000000, 5.656854249492381470 ) ) ;
#37415 = CARTESIAN_POINT ( 'NONE',  ( -4.088227598258586603E-16, 290.3593750017070079, -6.676582343750001591 ) ) ;
#37416 = CARTESIAN_POINT ( 'NONE',  ( -2.977408999572647819, 7.188101187499991163, 10.58030278187175455 ) ) ;
#37417 = ORIENTED_EDGE ( 'NONE', *, *, #32053, .T. ) ;
#37418 = DIRECTION ( 'NONE',  ( 0.000000000000000000, 0.000000000000000000, 1.000000000000000000 ) ) ;
#37419 = CARTESIAN_POINT ( 'NONE',  ( 5.656854249492380582, 23.99999999590322375, -5.656854249492380582 ) ) ;
#37420 = CARTESIAN_POINT ( 'NONE',  ( 1.432654583217607192, 204.2500000013655779, 145.4587341250000634 ) ) ;
#37421 = LINE ( 'NONE', #26074, #9286 ) ;
#37422 = CARTESIAN_POINT ( 'NONE',  ( 3.313708498984794915, 121.5312500000000000, -7.999999999999967137 ) ) ;
#37423 = CARTESIAN_POINT ( 'NONE',  ( 5.676582343750005144, 250.8854166700806729, 9.832129032723416984 ) ) ;
#37424 = CARTESIAN_POINT ( 'NONE',  ( -2.828427124746190735, 3.124999997268813168, -2.828427124746191623 ) ) ;
#37425 = CARTESIAN_POINT ( 'NONE',  ( 11.00000000000000000, 1.347111479062088405E-15, 111.2499999999999858 ) ) ;
#37426 = CARTESIAN_POINT ( 'NONE',  ( -5.676582343749998039, 2.447916663252683200, -9.832129032723420536 ) ) ;
#37427 = CARTESIAN_POINT ( 'NONE',  ( 1.320432766682872962E-15, -7.188101187499992051, 2.236552781871754103 ) ) ;
#37428 = CARTESIAN_POINT ( 'NONE',  ( -5.676582343750006032, 199.4270833299193555, 9.832129032723418760 ) ) ;
#37429 = LINE ( 'NONE', #59334, #16780 ) ;
#37430 = CARTESIAN_POINT ( 'NONE',  ( -4.541265875000002339, 6.749999998634407916, -1.881053915767121998 ) ) ;
#37431 = DIRECTION ( 'NONE',  ( -0.000000000000000000, -0.000000000000000000, -1.000000000000000000 ) ) ;
#37433 = CARTESIAN_POINT ( 'NONE',  ( 1.102182119232618108E-15, 297.2500000000000000, 6.000000000000001776 ) ) ;
#37432 = DIRECTION ( 'NONE',  ( 0.000000000000000000, 0.02418647091589873691, -0.9997074645238147594 ) ) ;
#37434 = ORIENTED_EDGE ( 'NONE', *, *, #45182, .F. ) ;
#37435 = CARTESIAN_POINT ( 'NONE',  ( 2.445694354108784108, 202.5625000013656063, 144.4456943541088663 ) ) ;
#37436 = CARTESIAN_POINT ( 'NONE',  ( 11.00000000000000000, 4.556349186104045934, 99.53125000409679046 ) ) ;
#37437 = DIRECTION ( 'NONE',  ( -0.000000000000000000, 1.000000000000000000, 4.476705744456276341E-16 ) ) ;
#37438 = ADVANCED_FACE ( 'NONE', ( #45263 ), #68275, .T. ) ;
#37439 = CARTESIAN_POINT ( 'NONE',  ( -31.45873412500002075, 199.6250000013656063, 168.5673454167828140 ) ) ;
#37441 = CARTESIAN_POINT ( 'NONE',  ( -10.00000000000000000, 59.16666665983869677, -2.679491924311229845 ) ) ;
#37440 = CARTESIAN_POINT ( 'NONE',  ( 5.082755093536326818, 121.7187500020483952, 5.082755093536325042 ) ) ;
#37442 = CARTESIAN_POINT ( 'NONE',  ( -4.898587196589407898E-16, 7.999999999999991118, 27.45530277982336642 ) ) ;
#37443 = CONICAL_SURFACE ( 'NONE', #60305, 18.00000000000000355, 1.047197551196596965 ) ;
#37444 = CARTESIAN_POINT ( 'NONE',  ( -11.35316468750000141, 123.2812499965860269, -1.390361679473963753E-15 ) ) ;
#37445 = CARTESIAN_POINT ( 'NONE',  ( 7.320508075688771044, 91.24999999317205379, 7.320508075688775484 ) ) ;
#37446 = CARTESIAN_POINT ( 'NONE',  ( -2.977408999572650927, 124.2500000020484094, -7.188101187500001821 ) ) ;
#37447 = CARTESIAN_POINT ( 'NONE',  ( -4.541265875000002339, 18.87499999863441147, -1.881053915767121998 ) ) ;
#37448 = CARTESIAN_POINT ( 'NONE',  ( -7.320508075688778149, 199.9999999931720254, 7.320508075688769267 ) ) ;
#37449 = CARTESIAN_POINT ( 'NONE',  ( 0.000000000000000000, 300.0000000000000000, 0.000000000000000000 ) ) ;
#37450 = ORIENTED_EDGE ( 'NONE', *, *, #18413, .F. ) ;
#37451 = CARTESIAN_POINT ( 'NONE',  ( 1.656854249492336173, 209.1875000000000568, 138.0000000000000853 ) ) ;
#37452 = ORIENTED_EDGE ( 'NONE', *, *, #25497, .T. ) ;
#37453 = CARTESIAN_POINT ( 'NONE',  ( -6.676582343750000703, 293.6718750017070079, 2.765530957082001251 ) ) ;
#37454 = CARTESIAN_POINT ( 'NONE',  ( -10.99999999999992006, -31.99999999999978684, 205.0000000000000284 ) ) ;
#37455 = CARTESIAN_POINT ( 'NONE',  ( -7.999999999999989342, -3.313708498984762496, 5.611552783920146226 ) ) ;
#37456 = CARTESIAN_POINT ( 'NONE',  ( -3.042071309553173730, 169.3229166632526699, 11.35316468749999785 ) ) ;
#37457 = DIRECTION ( 'NONE',  ( 0.000000000000000000, 0.000000000000000000, -1.000000000000000000 ) ) ;
#37458 = CARTESIAN_POINT ( 'NONE',  ( -2.828427124746153876, 201.8750000000000284, 195.1715728752538439 ) ) ;
#37459 = CARTESIAN_POINT ( 'NONE',  ( 5.656854249492379694, 103.4374999999999858, -5.656854249492380582 ) ) ;
#37460 = CARTESIAN_POINT ( 'NONE',  ( -4.220049686691937474, -10.18810118749999738, 104.3125000020483810 ) ) ;
#37461 = ORIENTED_EDGE ( 'NONE', *, *, #38615, .T. ) ;
#37462 = CARTESIAN_POINT ( 'NONE',  ( -5.676582343749998039, 152.7604166632526983, -9.832129032723420536 ) ) ;
#37463 = DIRECTION ( 'NONE',  ( 0.8660254037844389297, 0.4999999999999994449, -0.000000000000000000 ) ) ;
#37464 = CARTESIAN_POINT ( 'NONE',  ( -3.458734124999960358, 206.6250000013656063, 196.5673454167823877 ) ) ;
#37465 = CARTESIAN_POINT ( 'NONE',  ( -7.204075437095965206, -7.204075437095968759, 69.71875000204836681 ) ) ;
#37466 = CARTESIAN_POINT ( 'NONE',  ( 8.311093377946837890, 61.71874999658601979, -8.311093377946837890 ) ) ;
#37467 = ORIENTED_EDGE ( 'NONE', *, *, #29903, .F. ) ;
#37468 = CARTESIAN_POINT ( 'NONE',  ( -6.238412754330611322E-16, 10.18810118749999916, 116.7812500020483810 ) ) ;
#37469 = CARTESIAN_POINT ( 'NONE',  ( -3.211159895383562723, 8.062499998634406140, 3.211159895383561391 ) ) ;
#37470 = CARTESIAN_POINT ( 'NONE',  ( 3.317071493978883456, -8.008118988124989457, 8.981865283940631883 ) ) ;
#37471 = ORIENTED_EDGE ( 'NONE', *, *, #8997, .T. ) ;
#37472 = B_SPLINE_CURVE_WITH_KNOTS ( 'NONE', 3,
 ( #68212, #16508, #38060, #32401, #9383, #4106, #22177, #55042, #62174, #4851 ),
 .UNSPECIFIED., .F., .F.,
 ( 4, 2, 2, 2, 4 ),
 ( 0.000000000000000000, 0.001314083742622695287, 0.002628167485245389273, 0.003942251227868082825, 0.005256334970490777678 ),
 .UNSPECIFIED. ) ;
#37473 = CARTESIAN_POINT ( 'NONE',  ( -5.082755093536325042, 23.53124999795161543, -5.082755093536325930 ) ) ;
#37474 = CARTESIAN_POINT ( 'NONE',  ( -6.000000000000001776, 288.0625000034140157, 0.000000000000000000 ) ) ;
#37475 = AXIS2_PLACEMENT_3D ( 'NONE', #36603, #41884, #35868 ) ;
#37476 = LINE ( 'NONE', #59017, #30509 ) ;
#37477 = CARTESIAN_POINT ( 'NONE',  ( -7.188101187500002709, 9.187499997951611874, 2.977408999572649151 ) ) ;
#37478 = CARTESIAN_POINT ( 'NONE',  ( -7.188101187499990274, -2.977408999572651815, 4.580302781871752771 ) ) ;
#37479 = CARTESIAN_POINT ( 'NONE',  ( -7.204075437095967871, 7.204075437095967871, 114.3437500020483810 ) ) ;
#37480 = COLOUR_RGB ( '',0.7921568627450980005, 0.8196078431372548767, 0.9333333333333333481 ) ;
#37481 =( BOUNDED_CURVE ( )  B_SPLINE_CURVE ( 2, ( #43830, #5340, #28339, #62295, #50231, #50600, #73620, #16629, #38559 ),
 .UNSPECIFIED., .F., .F. ) 
 B_SPLINE_CURVE_WITH_KNOTS ( ( 3, 2, 2, 2, 3 ),
 ( 0.7500000000000006661, 0.7583333333333339699, 0.7666666666666672736, 0.7750000000000005773, 0.7833333333333338810 ),
 .UNSPECIFIED. ) 
 CURVE ( )  GEOMETRIC_REPRESENTATION_ITEM ( )  RATIONAL_B_SPLINE_CURVE ( ( 0.9999999999999938938, 0.9238795325112928447, 1.000000000000000000, 0.9238795325112867385, 1.000000000000000000, 0.9238795325112867385, 1.000000000000000000, 0.9238795325112816315, 1.000000000000005107 ) ) 
 REPRESENTATION_ITEM ( '' )  );
#37482 = CARTESIAN_POINT ( 'NONE',  ( 1.983773374183288363, -42.74103918334439811, 151.1033335718026080 ) ) ;
#37483 = CARTESIAN_POINT ( 'NONE',  ( 2.828427124746190291, 5.624999997268813168, 2.828427124746192067 ) ) ;
#37484 = CIRCLE ( 'NONE', #68833, 10.00000000000000178 ) ;
#37485 = VERTEX_POINT ( 'NONE', #16571 ) ;
#37486 = EDGE_CURVE ( 'NONE', #42303, #48426, #54159, .T. ) ;
#37487 = CARTESIAN_POINT ( 'NONE',  ( 3.458734125000015425, 207.0000000013656063, 196.5673454167823877 ) ) ;
#37488 = CARTESIAN_POINT ( 'NONE',  ( -31.99999999999995737, 196.4375000027311842, 171.6568542494928522 ) ) ;
#37489 = CARTESIAN_POINT ( 'NONE',  ( -4.541265875000002339, 7.812499998634407028, -5.561446717895856393E-16 ) ) ;
#37490 = CARTESIAN_POINT ( 'NONE',  ( 2.977408999572650039, 108.6875000020483952, -7.188101187500001821 ) ) ;
#37491 = CARTESIAN_POINT ( 'NONE',  ( 3.313708498984711426, 94.15625000409679046, 8.000000000000053291 ) ) ;
#37492 = CARTESIAN_POINT ( 'NONE',  ( -4.401442555609577197E-16, 7.188101187499992051, 25.11155278187175810 ) ) ;
#37493 = ORIENTED_EDGE ( 'NONE', *, *, #74639, .F. ) ;
#37495 =( BOUNDED_CURVE ( )  B_SPLINE_CURVE ( 2, ( #57583, #68510, #51910, #250, #69259, #57961, #6269, #56832, #5152 ),
 .UNSPECIFIED., .F., .F. ) 
 B_SPLINE_CURVE_WITH_KNOTS ( ( 3, 2, 2, 2, 3 ),
 ( 0.6176470588235292158, 0.6213235294117644969, 0.6249999999999997780, 0.6286764705882351700, 0.6323529411764704511 ),
 .UNSPECIFIED. ) 
 CURVE ( )  GEOMETRIC_REPRESENTATION_ITEM ( )  RATIONAL_B_SPLINE_CURVE ( ( 1.000000000000004663, 0.9238795325112821866, 1.000000000000000000, 0.9238795325112867385, 1.000000000000000000, 0.9238795325112867385, 1.000000000000000000, 0.9238795325112890700, 0.9999999999999976685 ) ) 
 REPRESENTATION_ITEM ( '' )  );
#37494 = LINE ( 'NONE', #32595, #71049 ) ;
#37496 = ORIENTED_EDGE ( 'NONE', *, *, #1189, .T. ) ;
#37497 = CARTESIAN_POINT ( 'NONE',  ( -7.204075437095965206, -7.204075437095968759, 114.3437500020483810 ) ) ;
#37498 = CARTESIAN_POINT ( 'NONE',  ( -4.041240684891906021, 6.985286989850277628, -0.000000000000000000 ) ) ;
#37499 = CARTESIAN_POINT ( 'NONE',  ( -3.458734124999959914, 209.3750000013656063, 196.5673454167823877 ) ) ;
#37500 = CARTESIAN_POINT ( 'NONE',  ( 24.54126587499999346, 204.1875000013656063, 169.9999999999999432 ) ) ;
#37501 = CARTESIAN_POINT ( 'NONE',  ( 7.320508075688774596, 70.62500000000000000, -7.320508075688774596 ) ) ;
#37502 = VECTOR ( 'NONE', #9357, 1000.000000000000000 ) ;
#37503 = EDGE_CURVE ( 'NONE', #53794, #36060, #70868, .T. ) ;
#37504 = CARTESIAN_POINT ( 'NONE',  ( -2.977408999572650927, 97.25000000204839523, -7.188101187500001821 ) ) ;
#37505 = CARTESIAN_POINT ( 'NONE',  ( -6.000000000000003553, 295.9374999999999432, -2.485281374238571317 ) ) ;
#37507 = DIRECTION ( 'NONE',  ( 0.000000000000000000, -2.238352872228138170E-16, 1.000000000000000000 ) ) ;
#37506 = CARTESIAN_POINT ( 'NONE',  ( 32.28714208167072997, 176.0068115675577474, 163.9537396292517997 ) ) ;
#37508 = VERTEX_POINT ( 'NONE', #41093 ) ;
#37509 = ADVANCED_FACE ( 'NONE', ( #53157 ), #23697, .T. ) ;
#37510 = CARTESIAN_POINT ( 'NONE',  ( -11.35316468749999785, 228.6979166700806729, -3.042071309553164848 ) ) ;
#37511 = CARTESIAN_POINT ( 'NONE',  ( 8.000000000000000000, 12.00000000000000178, 0.000000000000000000 ) ) ;
#37512 = CARTESIAN_POINT ( 'NONE',  ( -2.849036369511732440E-14, 201.3750000027312126, 138.0000000000000568 ) ) ;
#37513 = CARTESIAN_POINT ( 'NONE',  ( 3.313708498984756279, 7.999999999999991118, 24.54905278392014978 ) ) ;
#37514 = DIRECTION ( 'NONE',  ( 0.000000000000000000, 0.000000000000000000, 1.000000000000000000 ) ) ;
#37515 = CARTESIAN_POINT ( 'NONE',  ( -10.00000000000000000, 244.7916666666666856, -2.679491924311226292 ) ) ;
#37516 = DIRECTION ( 'NONE',  ( 0.000000000000000000, 0.000000000000000000, 1.000000000000000000 ) ) ;
#37517 = CARTESIAN_POINT ( 'NONE',  ( 2.679491924311222739, 183.9583333333333428, 10.00000000000000355 ) ) ;
#37518 = SURFACE_SIDE_STYLE ('',( #14106 ) ) ;
#37519 = CARTESIAN_POINT ( 'NONE',  ( 7.188101187499993827, -2.977408999572645598, 20.51780278187175810 ) ) ;
#37520 = CARTESIAN_POINT ( 'NONE',  ( 8.311093377946834337, 150.4687499965860127, 8.311093377946839666 ) ) ;
#37521 = CARTESIAN_POINT ( 'NONE',  ( 1.469576158976822172E-15, -7.999999999999991118, 22.39280278392014623 ) ) ;
#37522 = CARTESIAN_POINT ( 'NONE',  ( -5.000000000000000000, 52.15374455614115590, 42.28282461816605320 ) ) ;
#37524 = CARTESIAN_POINT ( 'NONE',  ( 4.000000000000015987, 199.6875000027312126, 196.3431457505076594 ) ) ;
#37523 = CARTESIAN_POINT ( 'NONE',  ( 32.00000000000000000, 201.3125000000000568, 168.3431457505075741 ) ) ;
#37525 = ORIENTED_EDGE ( 'NONE', *, *, #3489, .F. ) ;
#37526 = CARTESIAN_POINT ( 'NONE',  ( 8.311093377946837890, 6.718749996586016238, -8.311093377946837890 ) ) ;
#37527 = ADVANCED_FACE ( 'NONE', ( #69392 ), #64102, .F. ) ;
#37528 = CARTESIAN_POINT ( 'NONE',  ( -2.828427124746152987, 199.1250000000000284, 200.8284271247462129 ) ) ;
#37529 = CARTESIAN_POINT ( 'NONE',  ( 8.660254037844389075, 32.29166665983870388, -5.000000000000000000 ) ) ;
#37530 = DIRECTION ( 'NONE',  ( -0.000000000000000000, 1.000000000000000000, -0.000000000000000000 ) ) ;
#37531 = CARTESIAN_POINT ( 'NONE',  ( 2.445694354108783664, 205.3125000013656063, 144.4456943541088663 ) ) ;
#37532 = CARTESIAN_POINT ( 'NONE',  ( 7.320508075688774596, 42.49999999317203248, -7.320508075688774596 ) ) ;
#37533 = CIRCLE ( 'NONE', #55641, 7.141428428542858420 ) ;
#37534 = CARTESIAN_POINT ( 'NONE',  ( 2.977408999572650039, 110.1875000020483810, -7.188101187500001821 ) ) ;
#37535 = CARTESIAN_POINT ( 'NONE',  ( 1.881053915767121776, 8.624999998634406140, -4.541265875000002339 ) ) ;
#37536 = CARTESIAN_POINT ( 'NONE',  ( 1.901548650871797615E-12, 218.7500000000001990, 10.00000000000000533 ) ) ;
#37537 = CARTESIAN_POINT ( 'NONE',  ( -3.313708498984757167, 7.999999999999991118, 6.549052779823365533 ) ) ;
#37539 = CARTESIAN_POINT ( 'NONE',  ( -5.656854249492379694, 26.06250000000000711, -5.656854249492380582 ) ) ;
#37538 = FACE_OUTER_BOUND ( 'NONE', #43581, .T. ) ;
#37540 = ORIENTED_EDGE ( 'NONE', *, *, #66150, .F. ) ;
#37541 = CARTESIAN_POINT ( 'NONE',  ( -4.999999999999999112, -64.62379132009267835, 24.09319349500363217 ) ) ;
#37542 = VECTOR ( 'NONE', #23423, 1000.000000000000000 ) ;
#37543 = CARTESIAN_POINT ( 'NONE',  ( 8.000000000000000000, 27.00000000000000355, 0.000000000000000000 ) ) ;
#37544 = CARTESIAN_POINT ( 'NONE',  ( 8.311093377946839666, 231.0937500034139873, 8.311093377946830785 ) ) ;
#37545 = CARTESIAN_POINT ( 'NONE',  ( -9.832129032723420536, 133.6979166632526983, 5.676582343749997150 ) ) ;
#37546 = ORIENTED_EDGE ( 'NONE', *, *, #10238, .F. ) ;
#37547 = EDGE_CURVE ( 'NONE', #45848, #65881, #44447, .T. ) ;
#37548 = CARTESIAN_POINT ( 'NONE',  ( -3.313708498984757611, 7.999999999999991118, 5.236552783920146226 ) ) ;
#37549 = CARTESIAN_POINT ( 'NONE',  ( -7.204075437095967871, 7.204075437095967871, 97.46875000204838102 ) ) ;
#37550 = CARTESIAN_POINT ( 'NONE',  ( -3.458734124999960358, 195.6250000013656063, 196.5673454167823877 ) ) ;
#37551 = CARTESIAN_POINT ( 'NONE',  ( -7.347880794884122694E-16, 6.499999997268813168, 4.000000000000001776 ) ) ;
#37553 = CARTESIAN_POINT ( 'NONE',  ( -5.676582343750006032, 124.1145833299193555, 9.832129032723418760 ) ) ;
#37552 = CARTESIAN_POINT ( 'NONE',  ( 23.99999999999999645, 197.6875000000000284, 168.3431457505074889 ) ) ;
#37554 = CARTESIAN_POINT ( 'NONE',  ( 7.778174593052023411, -7.778174593052021635, 96.06250000000000000 ) ) ;
#37555 = VERTEX_POINT ( 'NONE', #42182 ) ;
#37556 = APPLICATION_CONTEXT ( 'automotive_design' ) ;
#37557 = CARTESIAN_POINT ( 'NONE',  ( -11.00000000000000000, 0.000000000000000000, 118.0000000000000000 ) ) ;
#37558 = EDGE_CURVE ( 'NONE', #31201, #832, #63724, .T. ) ;
#37559 = CARTESIAN_POINT ( 'NONE',  ( 48.72590952693010280, 42.90176518940880612, 60.31981441777210051 ) ) ;
#37560 = CARTESIAN_POINT ( 'NONE',  ( 9.832129032723416984, 115.6770833299193555, 5.676582343750006032 ) ) ;
#37561 = CARTESIAN_POINT ( 'NONE',  ( -2.445694354108783664, 207.3125000013656063, 195.5543056458912190 ) ) ;
#37562 = CARTESIAN_POINT ( 'NONE',  ( -2.977408999572654480, 16.87499999795161543, 7.188101187499999156 ) ) ;
#37563 = CARTESIAN_POINT ( 'NONE',  ( 7.204075437095968759, -7.204075437095966983, 86.59375000204836681 ) ) ;
#37564 = CARTESIAN_POINT ( 'NONE',  ( -11.35316468749999785, 23.38541666325268054, -3.042071309553167513 ) ) ;
#37565 = ORIENTED_EDGE ( 'NONE', *, *, #36932, .T. ) ;
#37566 = DIRECTION ( 'NONE',  ( -0.000000000000000000, -1.000000000000000000, -0.000000000000000000 ) ) ;
#37567 = CARTESIAN_POINT ( 'NONE',  ( 3.317071493978883456, -8.008118988124989457, 23.98186528394063899 ) ) ;
#37568 = DIRECTION ( 'NONE',  ( 3.469446951953617147E-16, 0.000000000000000000, -1.000000000000000000 ) ) ;
#37569 = VECTOR ( 'NONE', #31219, 1000.000000000000000 ) ;
#37570 = CARTESIAN_POINT ( 'NONE',  ( 1.015769982161393470, 21.99999999999999645, 4.253290409823233809 ) ) ;
#37571 = CARTESIAN_POINT ( 'NONE',  ( -1.320432766682874540E-15, 1.593749997951610098, 7.188101187500000044 ) ) ;
#37572 = CARTESIAN_POINT ( 'NONE',  ( -6.676582343750000703, 288.5156250017069510, 2.765530957082001251 ) ) ;
#37573 = CARTESIAN_POINT ( 'NONE',  ( -2.849036369511732440E-14, 199.2500000000000000, 138.0000000000000568 ) ) ;
#37574 = CARTESIAN_POINT ( 'NONE',  ( -11.35316468750000141, 218.5937499965860411, -1.390361679473963753E-15 ) ) ;
#37575 = VERTEX_POINT ( 'NONE', #52782 ) ;
#37576 = CARTESIAN_POINT ( 'NONE',  ( 9.832129032723416984, 145.6770833299193555, 5.676582343750006032 ) ) ;
#37577 = CARTESIAN_POINT ( 'NONE',  ( -6.238412754330611322E-16, 10.18810118749999916, 83.78125000204836681 ) ) ;
#37578 = CARTESIAN_POINT ( 'NONE',  ( -30.44569435410879166, 200.8125000013656063, 172.4456943541092357 ) ) ;
#37579 = DIRECTION ( 'NONE',  ( 0.000000000000000000, 0.000000000000000000, -1.000000000000000000 ) ) ;
#37580 = CARTESIAN_POINT ( 'NONE',  ( 2.780723358947928197E-16, 15.68749999863440436, -4.541265875000002339 ) ) ;
#37581 = ORIENTED_EDGE ( 'NONE', *, *, #39922, .T. ) ;
#37582 = CARTESIAN_POINT ( 'NONE',  ( 2.828427124746209831, 202.5000000027312126, 200.8284271247462129 ) ) ;
#37583 = CARTESIAN_POINT ( 'NONE',  ( -2.839093476692135984E-14, 198.9375000013655779, 138.5412658750000503 ) ) ;
#37584 = CARTESIAN_POINT ( 'NONE',  ( 1.656854249492348607, 202.3125000027312410, 138.0000000000000568 ) ) ;
#37585 = VECTOR ( 'NONE', #63322, 1000.000000000000000 ) ;
#37586 = CARTESIAN_POINT ( 'NONE',  ( 5.000000000000000000, 10.53354221205055907, -66.31578581128081851 ) ) ;
#37587 = VERTEX_POINT ( 'NONE', #52417 ) ;
#37588 = EDGE_CURVE ( 'NONE', #17422, #20975, #63440, .T. ) ;
#37589 = CARTESIAN_POINT ( 'NONE',  ( 2.977408999572650927, 3.749999997951610542, -7.188101187500000933 ) ) ;
#37590 = CARTESIAN_POINT ( 'NONE',  ( 7.778174593052023411, -7.778174593052021635, 76.56249999999997158 ) ) ;
#37591 = CARTESIAN_POINT ( 'NONE',  ( 0.000000000000000000, 300.0000000000000000, 0.000000000000000000 ) ) ;
#37592 = CARTESIAN_POINT ( 'NONE',  ( 9.832129032723420536, 181.1979166632526983, -5.676582343749999815 ) ) ;
#37593 = CARTESIAN_POINT ( 'NONE',  ( 2.977408999572650039, 115.0625000020483952, -7.188101187500001821 ) ) ;
#37594 = DIRECTION ( 'NONE',  ( -0.000000000000000000, 1.000000000000000000, -0.000000000000000000 ) ) ;
#37595 = CARTESIAN_POINT ( 'NONE',  ( 6.676582343750002480, 292.0156250017069510, -2.765530957081997254 ) ) ;
#37597 = CARTESIAN_POINT ( 'NONE',  ( 2.966170491840901068E-11, 66.24999999999768363, -9.999999999999998224 ) ) ;
#37596 = CARTESIAN_POINT ( 'NONE',  ( -9.832129032723418760, 223.4895833367473301, -5.676582343749998927 ) ) ;
#37598 =( BOUNDED_CURVE ( )  B_SPLINE_CURVE ( 2, ( #10455, #50438, #44415, #73823, #4427, #56860, #9718, #33486, #39502 ),
 .UNSPECIFIED., .F., .F. ) 
 B_SPLINE_CURVE_WITH_KNOTS ( ( 3, 2, 2, 2, 3 ),
 ( 0.5000000000000004441, 0.5083333333333337478, 0.5166666666666671626, 0.5250000000000004663, 0.5333333333333337700 ),
 .UNSPECIFIED. ) 
 CURVE ( )  GEOMETRIC_REPRESENTATION_ITEM ( )  RATIONAL_B_SPLINE_CURVE ( ( 0.9999999999999958922, 0.9238795325112908463, 1.000000000000000000, 0.9238795325112867385, 1.000000000000000000, 0.9238795325112867385, 1.000000000000000000, 0.9238795325112826307, 1.000000000000003997 ) ) 
 REPRESENTATION_ITEM ( '' )  );
#37599 = ORIENTED_EDGE ( 'NONE', *, *, #2962, .F. ) ;
#37600 = EDGE_CURVE ( 'NONE', #1389, #66596, #15864, .T. ) ;
#37601 = CARTESIAN_POINT ( 'NONE',  ( 2.085542519210945334E-15, 230.4687500034139873, 11.35316468749999963 ) ) ;
#37602 = CARTESIAN_POINT ( 'NONE',  ( -7.188101187499991163, 2.977408999572646930, 27.26780278187175099 ) ) ;
#37603 = CARTESIAN_POINT ( 'NONE',  ( 2.679491924311228956, 167.9166666598387110, -10.00000000000000000 ) ) ;
#37604 = LINE ( 'NONE', #44377, #27324 ) ;
#37605 = CARTESIAN_POINT ( 'NONE',  ( -3.458734124999960358, 200.6875000013656063, 198.0000000000000284 ) ) ;
#37606 = FACE_OUTER_BOUND ( 'NONE', #27843, .T. ) ;
#37607 = CARTESIAN_POINT ( 'NONE',  ( 4.898587196589412829E-16, 24.37500000000000355, -8.000000000000000000 ) ) ;
#37608 = CARTESIAN_POINT ( 'NONE',  ( -5.656854249492380582, 91.81249999999998579, -5.656854249492380582 ) ) ;
#37609 = CARTESIAN_POINT ( 'NONE',  ( -2.085542519210945728E-15, 109.8437499965860269, 11.35316468750000141 ) ) ;
#37610 = CARTESIAN_POINT ( 'NONE',  ( 1.224646799147353454E-15, 300.0000000000000000, -10.00000000000000178 ) ) ;
#37611 = PRODUCT_DEFINITION ( 'UNKNOWN', '', #34580, #5579 ) ;
#37612 = CARTESIAN_POINT ( 'NONE',  ( -7.778174593052023411, 7.778174593052023411, 71.31249999999998579 ) ) ;
#37615 = CARTESIAN_POINT ( 'NONE',  ( -2.828427124746153876, 201.8750000000000284, 195.1715728752538439 ) ) ;
#37614 = CARTESIAN_POINT ( 'NONE',  ( 29.43265458321761230, 201.8750000013656063, 166.5412658749999650 ) ) ;
#37613 = CARTESIAN_POINT ( 'NONE',  ( 25.55430564589114795, 197.5625000013656063, 172.4456943541086957 ) ) ;
#37616 = ORIENTED_EDGE ( 'NONE', *, *, #26003, .F. ) ;
#37617 = CIRCLE ( 'NONE', #6288, 9.949874371066211864 ) ;
#37618 = CARTESIAN_POINT ( 'NONE',  ( -4.898587196589412829E-16, 100.6249999999999858, -8.000000000000000000 ) ) ;
#37619 = CARTESIAN_POINT ( 'NONE',  ( 11.00000000000000000, 1.347111479062088405E-15, 114.4375000040967763 ) ) ;
#37620 = VECTOR ( 'NONE', #71949, 1000.000000000000000 ) ;
#37621 = CARTESIAN_POINT ( 'NONE',  ( 3.458734124999959914, 201.4375000013656063, 142.0000000000000568 ) ) ;
#37622 = CARTESIAN_POINT ( 'NONE',  ( 24.54126587500000056, 202.3750000013655779, 168.5673454167822172 ) ) ;
#37623 = ADVANCED_FACE ( 'NONE', ( #53527 ), #12412, .F. ) ;
#37624 = CARTESIAN_POINT ( 'NONE',  ( 9.797174393178825657E-16, 125.0000000000000000, -8.000000000000000000 ) ) ;
#37625 = CARTESIAN_POINT ( 'NONE',  ( 9.832129032723420536, 196.5104166632526983, -5.676582343749999815 ) ) ;
#37626 = CARTESIAN_POINT ( 'NONE',  ( -7.188101187499999156, 90.12500000204836681, 2.977408999572654924 ) ) ;
#37627 = CARTESIAN_POINT ( 'NONE',  ( 11.16751265488280787, 226.0000000000000000, 1.778318385449065842 ) ) ;
#37628 = CARTESIAN_POINT ( 'NONE',  ( -4.541265875000002339, 15.81249999863440436, -5.561446717895856393E-16 ) ) ;
#37629 = CARTESIAN_POINT ( 'NONE',  ( 26.56734541678238060, 198.2500000013656347, 166.5412658749999650 ) ) ;
#37630 = CARTESIAN_POINT ( 'NONE',  ( -4.898587196589407898E-16, 7.999999999999991118, 27.45530277982336642 ) ) ;
#37631 = CARTESIAN_POINT ( 'NONE',  ( -7.999999999999998224, 96.59374999999998579, 3.313708498984766049 ) ) ;
#37632 = CARTESIAN_POINT ( 'NONE',  ( -11.35316468749999785, 78.07291666325269830, -3.042071309553167513 ) ) ;
#37633 = ORIENTED_EDGE ( 'NONE', *, *, #57173, .F. ) ;
#37634 = EDGE_CURVE ( 'NONE', #65516, #3567, #70143, .T. ) ;
#37635 = CARTESIAN_POINT ( 'NONE',  ( -3.166186134455097228E-13, 141.2500000000000284, -9.999999999999998224 ) ) ;
#37636 = DIRECTION ( 'NONE',  ( 1.000000000000000000, -0.000000000000000000, 0.000000000000000000 ) ) ;
#37637 = CARTESIAN_POINT ( 'NONE',  ( 7.188101187500001821, 17.06249999795161543, -2.977408999572650483 ) ) ;
#37638 = DIRECTION ( 'NONE',  ( -0.000000000000000000, 1.000000000000000000, -0.000000000000000000 ) ) ;
#37639 = CARTESIAN_POINT ( 'NONE',  ( 1.836970198721029589E-15, 231.2500000000000000, 10.00000000000000000 ) ) ;
#37640 = CARTESIAN_POINT ( 'NONE',  ( -8.311093377946836114, 82.65624999658602690, -8.311093377946837890 ) ) ;
#37641 = VERTEX_POINT ( 'NONE', #23363 ) ;
#37642 = CARTESIAN_POINT ( 'NONE',  ( 10.18810118749999916, 1.247682550866122264E-15, 88.28125000204836681 ) ) ;
#37643 = CARTESIAN_POINT ( 'NONE',  ( 1.871523826299183495E-15, -10.18810118749999916, 114.5312500020483810 ) ) ;
#37644 = DIRECTION ( 'NONE',  ( -0.000000000000000000, 1.000000000000000000, -0.000000000000000000 ) ) ;
#37645 = CARTESIAN_POINT ( 'NONE',  ( 2.754378923186476579E-14, 207.4375000013656063, 194.5412658750000219 ) ) ;
#37646 = DIRECTION ( 'NONE',  ( -0.000000000000000000, -0.000000000000000000, 1.000000000000000000 ) ) ;
#37648 = CARTESIAN_POINT ( 'NONE',  ( -5.676582343749998039, 92.44791666325269830, -9.832129032723420536 ) ) ;
#37647 = CARTESIAN_POINT ( 'NONE',  ( 3.313708498984744732, 121.1562500040967905, 8.000000000000019540 ) ) ;
#37649 = CARTESIAN_POINT ( 'NONE',  ( 5.656854249492376141, -5.656854249492374365, 21.08030278392014623 ) ) ;
#37650 = CARTESIAN_POINT ( 'NONE',  ( -10.00000000000000355, 169.5833333265053398, 2.679491924311223183 ) ) ;
#37651 = CARTESIAN_POINT ( 'NONE',  ( 5.082755093536325042, 92.46875000204838102, -5.082755093536325930 ) ) ;
#37652 = DIRECTION ( 'NONE',  ( 1.000000000000000000, 0.000000000000000000, 0.000000000000000000 ) ) ;
#37653 = CARTESIAN_POINT ( 'NONE',  ( 6.951808397369818766E-16, 62.34374999658602690, -11.35316468750000141 ) ) ;
#37654 = CARTESIAN_POINT ( 'NONE',  ( -4.721056650415998313, 293.5781250017069510, 4.721056650416000089 ) ) ;
#37655 = ADVANCED_FACE ( 'NONE', ( #58822 ), #69764, .T. ) ;
#37656 = CARTESIAN_POINT ( 'NONE',  ( 7.204075437095966983, 7.204075437095967871, 107.9687500020483810 ) ) ;
#37657 = CARTESIAN_POINT ( 'NONE',  ( -2.085542519210945728E-15, 204.5312499965860411, 11.35316468750000141 ) ) ;
#37658 = VERTEX_POINT ( 'NONE', #41825 ) ;
#37659 = CARTESIAN_POINT ( 'NONE',  ( 1.469576158976822172E-15, -7.999999999999991118, 26.89280278392014623 ) ) ;
#37660 = CARTESIAN_POINT ( 'NONE',  ( 4.000000000000001776, 3.812499997268813168, -1.656854249492381248 ) ) ;
#37661 = CARTESIAN_POINT ( 'NONE',  ( 3.313708498984782924, 14.53124999590322197, 7.999999999999979572 ) ) ;
#37663 = CARTESIAN_POINT ( 'NONE',  ( -11.35316468750000141, 198.2812499965860411, -1.390361679473963753E-15 ) ) ;
#37662 = CARTESIAN_POINT ( 'NONE',  ( 23.99999999999999289, 206.7500000000000284, 169.9999999999998863 ) ) ;
#37664 = CARTESIAN_POINT ( 'NONE',  ( 25.17157287525377996, 195.8750000000000284, 172.8284271247460424 ) ) ;
#37665 = CARTESIAN_POINT ( 'NONE',  ( 10.00000000000000000, 240.6250000068279746, -1.224646799147353256E-15 ) ) ;
#37666 = LINE ( 'NONE', #33144, #22756 ) ;
#37667 = ORIENTED_EDGE ( 'NONE', *, *, #32578, .F. ) ;
#37668 = CARTESIAN_POINT ( 'NONE',  ( 3.042071309553167513, 187.1354166632526983, -11.35316468749999785 ) ) ;
#37669 = CIRCLE ( 'NONE', #43619, 8.000000000000000000 ) ;
#37670 = CARTESIAN_POINT ( 'NONE',  ( 2.977408999572646486, 7.188101187499992051, 19.01780278187175099 ) ) ;
#37671 = CARTESIAN_POINT ( 'NONE',  ( -26.56734541678238415, 209.3750000013656063, 166.5412658750003629 ) ) ;
#37672 = ORIENTED_EDGE ( 'NONE', *, *, #537, .F. ) ;
#37673 = EDGE_CURVE ( 'NONE', #48525, #16897, #47848, .T. ) ;
#37674 = CONICAL_SURFACE ( 'NONE', #61744, 8.999999999999998224, 1.047197551196595855 ) ;
#37675 = CARTESIAN_POINT ( 'NONE',  ( -7.999999999999998224, 95.28125000409677625, 3.313708498984766493 ) ) ;
#37676 = EDGE_CURVE ( 'NONE', #34923, #9455, #2878, .T. ) ;
#37677 = CARTESIAN_POINT ( 'NONE',  ( -10.00000000000000355, 2.708333333333333481, 2.679491924311223183 ) ) ;
#37678 = ADVANCED_FACE ( 'NONE', ( #60281 ), #54644, .F. ) ;
#37679 = CARTESIAN_POINT ( 'NONE',  ( -2.828427124746192067, 16.62500000000000000, 2.828427124746190735 ) ) ;
#37680 = CARTESIAN_POINT ( 'NONE',  ( 2.780723358947928197E-16, 16.56249999863440436, -4.541265875000002339 ) ) ;
#37681 = CARTESIAN_POINT ( 'NONE',  ( -5.656854249492373476, -5.656854249492376141, 11.70530278392014445 ) ) ;
#37682 = CARTESIAN_POINT ( 'NONE',  ( 4.556349186104052151, -10.99999999999999822, 78.15625000409677625 ) ) ;
#37683 = ORIENTED_EDGE ( 'NONE', *, *, #56789, .F. ) ;
#37684 = CARTESIAN_POINT ( 'NONE',  ( 0.000000000000000000, 125.0000000000000000, 0.000000000000000000 ) ) ;
#37685 = CARTESIAN_POINT ( 'NONE',  ( 2.977408999572654480, 94.62500000204838102, 7.188101187499999156 ) ) ;
#37687 = CARTESIAN_POINT ( 'NONE',  ( -8.311093377946836114, 258.2812500034140157, -8.311093377946836114 ) ) ;
#37686 = CARTESIAN_POINT ( 'NONE',  ( -10.00000000000000000, 257.9166666734946602, -2.679491924311226292 ) ) ;
#37688 = DIRECTION ( 'NONE',  ( 0.000000000000000000, 0.000000000000000000, 1.000000000000000000 ) ) ;
#37689 = ORIENTED_EDGE ( 'NONE', *, *, #29992, .T. ) ;
#37690 = CARTESIAN_POINT ( 'NONE',  ( 11.35316468749999963, 261.7187500034140157, -1.390361679473963556E-15 ) ) ;
#37691 = CARTESIAN_POINT ( 'NONE',  ( -7.188101187499990274, -2.977408999572651371, 19.58030278187175455 ) ) ;
#37692 = VERTEX_POINT ( 'NONE', #21039 ) ;
#37693 = EDGE_CURVE ( 'NONE', #15758, #40533, #65858, .T. ) ;
#37694 = ORIENTED_EDGE ( 'NONE', *, *, #23656, .T. ) ;
#37695 = CARTESIAN_POINT ( 'NONE',  ( -10.18810118749999916, 0.000000000000000000, 81.15625000204838102 ) ) ;
#37696 = CARTESIAN_POINT ( 'NONE',  ( -5.676582343750006032, 74.42708332991934128, 9.832129032723418760 ) ) ;
#37697 = CARTESIAN_POINT ( 'NONE',  ( 0.000000000000000000, 0.000000000000000000, 30.00000000000000000 ) ) ;
#37698 = CARTESIAN_POINT ( 'NONE',  ( -6.735557395310442023E-16, 11.00000000000000000, 95.12499999999998579 ) ) ;
#37701 = CARTESIAN_POINT ( 'NONE',  ( -2.765530957081998142, 294.7968750017070079, 6.676582343750000703 ) ) ;
#37700 = CARTESIAN_POINT ( 'NONE',  ( 29.65685424949234772, 196.5625000027312126, 165.9999999999998863 ) ) ;
#37699 = CARTESIAN_POINT ( 'NONE',  ( 0.000000000000000000, 300.0000000000000000, 0.000000000000000000 ) ) ;
#37702 = CARTESIAN_POINT ( 'NONE',  ( 4.000000000000001776, 14.06250000000000178, -1.656854249492381248 ) ) ;
#37703 = CARTESIAN_POINT ( 'NONE',  ( -10.00000000000000355, 164.5833333265053682, 2.679491924311223183 ) ) ;
#37704 = CARTESIAN_POINT ( 'NONE',  ( 2.839093476692135984E-14, 197.9375000013655779, 201.4587341250000350 ) ) ;
#37705 = CARTESIAN_POINT ( 'NONE',  ( 2.828427124746153876, 198.8750000000000284, 144.8284271247462129 ) ) ;
#37706 = CARTESIAN_POINT ( 'NONE',  ( 4.898587196589412829E-16, 3.187499995903220640, -8.000000000000000000 ) ) ;
#37707 = CARTESIAN_POINT ( 'NONE',  ( 25.55430564589115150, 199.3125000013656063, 172.4456943541086957 ) ) ;
#37708 = CARTESIAN_POINT ( 'NONE',  ( -2.977408999572654480, 13.87499999795161365, 7.188101187499999156 ) ) ;
#37709 = CARTESIAN_POINT ( 'NONE',  ( 1.469576158976822172E-15, -7.999999999999991118, 26.89280278392014623 ) ) ;
#37710 = CYLINDRICAL_SURFACE ( 'NONE', #31089, 10.00000000000000000 ) ;
#37711 = CARTESIAN_POINT ( 'NONE',  ( -5.082755093536324154, 112.7187500020483810, 5.082755093536326818 ) ) ;
#37713 = CARTESIAN_POINT ( 'NONE',  ( 1.567784982238203817E-13, 113.7500000000000284, 10.00000000000000533 ) ) ;
#37712 = DIRECTION ( 'NONE',  ( -0.000000000000000000, -0.000000000000000000, -1.000000000000000000 ) ) ;
#37714 = CARTESIAN_POINT ( 'NONE',  ( 4.556349186104052151, -10.99999999999999822, 112.6562500040967905 ) ) ;
#37715 = CARTESIAN_POINT ( 'NONE',  ( 6.000000000000003553, 288.5000000034140157, 2.485281374238571317 ) ) ;
#37716 = CARTESIAN_POINT ( 'NONE',  ( 7.188101187499993827, -2.977408999572645598, 17.51780278187175455 ) ) ;
#37717 = CARTESIAN_POINT ( 'NONE',  ( 2.828427124746152987, 208.2500000027312126, 139.1715728752538723 ) ) ;
#37718 = CARTESIAN_POINT ( 'NONE',  ( 9.832129032723416984, 45.36458332991935549, 5.676582343750006032 ) ) ;
#37719 =( BOUNDED_CURVE ( )  B_SPLINE_CURVE ( 2, ( #73319, #44646, #67661, #34467, #17078, #5038, #5404, #28035, #67287 ),
 .UNSPECIFIED., .F., .F. ) 
 B_SPLINE_CURVE_WITH_KNOTS ( ( 3, 2, 2, 2, 3 ),
 ( 0.000000000000000000, 0.008333333333333340157, 0.01666666666666668031, 0.02500000000000002220, 0.03333333333333336063 ),
 .UNSPECIFIED. ) 
 CURVE ( )  GEOMETRIC_REPRESENTATION_ITEM ( )  RATIONAL_B_SPLINE_CURVE ( ( 1.000000000000000000, 0.9238795325112867385, 1.000000000000000000, 0.9238795325112867385, 1.000000000000000000, 0.9238795325112867385, 1.000000000000000000, 0.9238795325112865164, 1.000000000000000222 ) ) 
 REPRESENTATION_ITEM ( '' )  );
#37720 = CARTESIAN_POINT ( 'NONE',  ( 0.8761883848702608502, 16.44150283900216181, 68.58316157020807680 ) ) ;
#37721 = ADVANCED_FACE ( 'NONE', ( #60662 ), #66319, .T. ) ;
#37722 = CARTESIAN_POINT ( 'NONE',  ( -1.836970198721029983E-15, 10.62499999317203425, 10.00000000000000178 ) ) ;
#37723 = VERTEX_POINT ( 'NONE', #42924 ) ;
#37724 = CARTESIAN_POINT ( 'NONE',  ( 7.806255641895631925E-15, 13.85640646055103709, -1.071796769724504550 ) ) ;
#37725 = CARTESIAN_POINT ( 'NONE',  ( 4.898587196589412829E-16, 10.68749999590322020, -8.000000000000000000 ) ) ;
#37726 = CARTESIAN_POINT ( 'NONE',  ( 3.042071309553159519, 54.73958332991934839, 11.35316468750000141 ) ) ;
#37727 = CARTESIAN_POINT ( 'NONE',  ( -7.778174593052023411, 7.778174593052023411, 80.50000000409676204 ) ) ;
#37728 = CARTESIAN_POINT ( 'NONE',  ( 3.458734124999960358, 204.6250000013656063, 143.4326545832176976 ) ) ;
#37729 = CARTESIAN_POINT ( 'NONE',  ( -10.00000000000000000, 260.0000000000000000, 0.000000000000000000 ) ) ;
#37730 = CARTESIAN_POINT ( 'NONE',  ( -2.828427124746209831, 195.3750000000000284, 139.1715728752538723 ) ) ;
#37732 = CARTESIAN_POINT ( 'NONE',  ( -9.832129032723418760, 27.86458332991935194, -5.676582343750004256 ) ) ;
#37731 = CARTESIAN_POINT ( 'NONE',  ( -7.188101187499999156, 100.2500000020483810, 2.977408999572654924 ) ) ;
#37733 = CARTESIAN_POINT ( 'NONE',  ( -4.898587196589407898E-16, 7.999999999999991118, 6.455302779823365533 ) ) ;
#37734 = CARTESIAN_POINT ( 'NONE',  ( 4.000000000000001776, 10.74999999726881406, 0.000000000000000000 ) ) ;
#37735 = CARTESIAN_POINT ( 'NONE',  ( -3.042071309553164404, 162.2395833299193271, -11.35316468749999963 ) ) ;
#37736 = CARTESIAN_POINT ( 'NONE',  ( 8.660254037844385522, 126.4583333265053540, 5.000000000000005329 ) ) ;
#37737 = CARTESIAN_POINT ( 'NONE',  ( 2.977408999572654480, 110.0000000020483668, 7.188101187499999156 ) ) ;
#37738 = ORIENTED_EDGE ( 'NONE', *, *, #68314, .F. ) ;
#37739 = CARTESIAN_POINT ( 'NONE',  ( 8.660254037844389075, 22.29166665983870033, -5.000000000000000000 ) ) ;
#37740 = CARTESIAN_POINT ( 'NONE',  ( 9.832129032723416984, 25.67708332991935194, 5.676582343750006032 ) ) ;
#37741 = CARTESIAN_POINT ( 'NONE',  ( -2.679491924317311202, 18.54166666666612073, 9.999999999996500577 ) ) ;
#37742 = VERTEX_POINT ( 'NONE', #48585 ) ;
#37743 = CARTESIAN_POINT ( 'NONE',  ( -32.00000000000000000, 204.2500000000000284, 170.0000000000003979 ) ) ;
#37744 = CARTESIAN_POINT ( 'NONE',  ( -7.204075437095967871, 7.204075437095967871, 77.96875000204836681 ) ) ;
#37745 = LINE ( 'NONE', #19626, #1618 ) ;
#37747 = CARTESIAN_POINT ( 'NONE',  ( -5.676582343749998039, 147.4479166632526983, -9.832129032723420536 ) ) ;
#37746 = CARTESIAN_POINT ( 'NONE',  ( 7.999999999836578723, -5.113295603412193572E-05, 3.267801294049292871 ) ) ;
#37748 = CARTESIAN_POINT ( 'NONE',  ( -2.977408999572650039, 2.812499997951610542, -7.188101187500000933 ) ) ;
#37749 = CARTESIAN_POINT ( 'NONE',  ( 7.999999999999991118, 3.313708498984757611, 13.73030278432982421 ) ) ;
#37750 = CARTESIAN_POINT ( 'NONE',  ( -25.08918728582654722, -22.71483774816627133, 188.2158713168095119 ) ) ;
#37751 = CARTESIAN_POINT ( 'NONE',  ( 11.35316468749999608, 231.6145833367473017, -3.042071309553167069 ) ) ;
#37752 = CARTESIAN_POINT ( 'NONE',  ( -10.18810118749999916, 4.220049686691934809, 84.43750000204838102 ) ) ;
#37753 = ORIENTED_EDGE ( 'NONE', *, *, #66003, .T. ) ;
#37754 = EDGE_CURVE ( 'NONE', #26409, #47201, #18889, .T. ) ;
#37755 = CARTESIAN_POINT ( 'NONE',  ( 6.123233995736767268E-16, 208.1249999931720538, -10.00000000000000178 ) ) ;
#37756 = VECTOR ( 'NONE', #12122, 1000.000000000000000 ) ;
#37757 = CARTESIAN_POINT ( 'NONE',  ( -1.656854249492246467, 198.9375000027312126, 193.9999999999999716 ) ) ;
#37758 = CARTESIAN_POINT ( 'NONE',  ( 11.35316468749999785, 100.8854166632526841, 3.042071309553174174 ) ) ;
#37759 = CARTESIAN_POINT ( 'NONE',  ( 10.18810118749999916, 1.247682550866122264E-15, 95.40625000204836681 ) ) ;
#37760 = CARTESIAN_POINT ( 'NONE',  ( 7.320508075688779925, 15.62500000000000355, -7.320508075688779925 ) ) ;
#37761 = AXIS2_PLACEMENT_3D ( 'NONE', #35682, #42798, #30017 ) ;
#37762 = ORIENTED_EDGE ( 'NONE', *, *, #16793, .T. ) ;
#37763 = ORIENTED_EDGE ( 'NONE', *, *, #19184, .T. ) ;
#37764 = CARTESIAN_POINT ( 'NONE',  ( -4.541265875000003227, 5.999999998634407028, 1.881053915767121110 ) ) ;
#37765 = CARTESIAN_POINT ( 'NONE',  ( -7.188101187500002709, 5.812499997951610986, 2.977408999572649151 ) ) ;
#37766 = CARTESIAN_POINT ( 'NONE',  ( -4.898587196589412829E-16, 118.8125000040967763, -8.000000000000000000 ) ) ;
#37767 = ADVANCED_FACE ( 'NONE', ( #3327 ), #36544, .T. ) ;
#37768 = CARTESIAN_POINT ( 'NONE',  ( -4.220049686691935698, 10.18810118749999916, 94.75000000204838102 ) ) ;
#37769 = CARTESIAN_POINT ( 'NONE',  ( -27.99999999999996447, 204.1875000013656063, 173.4587341250003760 ) ) ;
#37770 = CARTESIAN_POINT ( 'NONE',  ( -6.509199954993407644, -10.09831811432650817, -1.016439536705163562E-14 ) ) ;
#37771 = ADVANCED_FACE ( 'NONE', ( #48215 ), #27290, .T. ) ;
#37772 = CARTESIAN_POINT ( 'NONE',  ( -1.656854249492381248, 2.312500000000000888, -4.000000000000001776 ) ) ;
#37773 = CARTESIAN_POINT ( 'NONE',  ( -4.000000000000001776, 18.24999999726881583, -4.898587196589415787E-16 ) ) ;
#37774 = CARTESIAN_POINT ( 'NONE',  ( -4.541265875000003227, 3.874999998634407028, 1.881053915767121110 ) ) ;
#37775 = AXIS2_PLACEMENT_3D ( 'NONE', #1647, #47274, #59719 ) ;
#37776 = CARTESIAN_POINT ( 'NONE',  ( 3.458734124999959025, 208.5000000013656063, 140.5673454167824161 ) ) ;
#37777 = CARTESIAN_POINT ( 'NONE',  ( 3.458734125000015425, 196.0000000013656347, 196.5673454167823877 ) ) ;
#37779 = CARTESIAN_POINT ( 'NONE',  ( 7.320508075688776373, 235.0000000068279746, 7.320508075688767491 ) ) ;
#37778 = CARTESIAN_POINT ( 'NONE',  ( -31.45873412500001720, 197.6250000013656063, 168.5673454167828140 ) ) ;
#37780 = CARTESIAN_POINT ( 'NONE',  ( -1.881053915767124440, 19.99999999863440436, 4.541265875000001451 ) ) ;
#37781 = CARTESIAN_POINT ( 'NONE',  ( 1.982007808036869267, -47.26068138099743265, 151.1031377668321056 ) ) ;
#37782 = CARTESIAN_POINT ( 'NONE',  ( -7.188101187499990274, -2.977408999572651371, 7.580302781871751883 ) ) ;
#37783 = ORIENTED_EDGE ( 'NONE', *, *, #11610, .T. ) ;
#37784 = ORIENTED_EDGE ( 'NONE', *, *, #13491, .F. ) ;
#37785 = CARTESIAN_POINT ( 'NONE',  ( 1.871523826299183495E-15, -10.18810118749999916, 99.53125000204838102 ) ) ;
#37786 = CARTESIAN_POINT ( 'NONE',  ( 7.320508075688776373, 125.6250000000000142, -7.320508075688776373 ) ) ;
#37787 = CARTESIAN_POINT ( 'NONE',  ( -25.55430564589115150, 204.3125000013656063, 172.4456943541091789 ) ) ;
#37788 = CARTESIAN_POINT ( 'NONE',  ( -23.99999999999997513, 200.6875000000000284, 171.6568542494927385 ) ) ;
#37789 = CARTESIAN_POINT ( 'NONE',  ( 3.458734125000016757, 209.1250000013656631, 199.4326545832176691 ) ) ;
#37790 = CARTESIAN_POINT ( 'NONE',  ( -2.828427124746190735, 21.12499999726881583, -2.828427124746191623 ) ) ;
#37791 = CARTESIAN_POINT ( 'NONE',  ( 2.679491924311228956, 106.0416666666666856, -10.00000000000000000 ) ) ;
#37792 = CARTESIAN_POINT ( 'NONE',  ( -4.898587196589412829E-16, 109.6250000000000000, -8.000000000000000000 ) ) ;
#37793 = CARTESIAN_POINT ( 'NONE',  ( 6.676582343750001591, 293.1093750017069510, -8.176455196517173205E-16 ) ) ;
#37794 = CARTESIAN_POINT ( 'NONE',  ( -4.401442555609577197E-16, 7.188101187499992051, 13.48655278187175455 ) ) ;
#37795 = ORIENTED_EDGE ( 'NONE', *, *, #59637, .F. ) ;
#37796 = DIRECTION ( 'NONE',  ( -0.000000000000000000, -0.000000000000000000, -1.000000000000000000 ) ) ;
#37797 = CARTESIAN_POINT ( 'NONE',  ( 3.313708498984762052, 22.59374999590322375, -8.000000000000000000 ) ) ;
#37798 = AXIS2_PLACEMENT_3D ( 'NONE', #63181, #23561, #214 ) ;
#37799 = CARTESIAN_POINT ( 'NONE',  ( 1.432654583217607858, 202.6250000013656063, 138.5412658750000787 ) ) ;
#37800 = CARTESIAN_POINT ( 'NONE',  ( -7.320508075688778149, 184.9999999931720254, 7.320508075688769267 ) ) ;
#37801 = CARTESIAN_POINT ( 'NONE',  ( 1.764475369138093885, 194.9673491673438832, 145.5628433100874304 ) ) ;
#37802 = CARTESIAN_POINT ( 'NONE',  ( 9.832129032723416984, 257.1354166700806445, -5.676582343750003368 ) ) ;
#37803 = CARTESIAN_POINT ( 'NONE',  ( 2.020667218593132706E-15, -11.00000000000000000, 115.3749999999999858 ) ) ;
#37804 = CARTESIAN_POINT ( 'NONE',  ( -9.832129032723418760, 2.864583329919349719, -5.676582343750004256 ) ) ;
#37805 = CARTESIAN_POINT ( 'NONE',  ( 7.188101187499993827, -2.977408999572645598, 4.017802781871751883 ) ) ;
#37806 = CARTESIAN_POINT ( 'NONE',  ( -11.35316468750000141, 193.5937499965860127, -1.390361679473963753E-15 ) ) ;
#37807 = CARTESIAN_POINT ( 'NONE',  ( 3.594042629939374400, 89.53052393364181683, -6.225082831242716885 ) ) ;
#37808 = CARTESIAN_POINT ( 'NONE',  ( -3.211159895383562723, 6.937499998634407028, 3.211159895383561391 ) ) ;
#37809 = DIRECTION ( 'NONE',  ( 1.577021341797097560E-16, -1.000000000000000000, 0.000000000000000000 ) ) ;
#37811 = FACE_OUTER_BOUND ( 'NONE', #3948, .T. ) ;
#37810 = CARTESIAN_POINT ( 'NONE',  ( -1.656854249492383468, 14.43749999726881406, 4.000000000000000888 ) ) ;
#37812 = ORIENTED_EDGE ( 'NONE', *, *, #19598, .F. ) ;
#37813 =( BOUNDED_CURVE ( )  B_SPLINE_CURVE ( 2, ( #73168, #4146, #67877, #16168, #39209, #62578, #12754, #52394, #12391 ),
 .UNSPECIFIED., .F., .F. ) 
 B_SPLINE_CURVE_WITH_KNOTS ( ( 3, 2, 2, 2, 3 ),
 ( 0.6911764705882351700, 0.6948529411764704511, 0.6985294117647057321, 0.7022058823529410132, 0.7058823529411764053 ),
 .UNSPECIFIED. ) 
 CURVE ( )  GEOMETRIC_REPRESENTATION_ITEM ( )  RATIONAL_B_SPLINE_CURVE ( ( 1.000000000000002220, 0.9238795325112844070, 1.000000000000000000, 0.9238795325112867385, 1.000000000000000000, 0.9238795325112867385, 1.000000000000000000, 0.9238795325112890700, 0.9999999999999976685 ) ) 
 REPRESENTATION_ITEM ( '' )  );
#37814 = EDGE_CURVE ( 'NONE', #62787, #13943, #54455, .T. ) ;
#37815 = CARTESIAN_POINT ( 'NONE',  ( 3.458734124999959469, 205.7500000013656063, 140.5673454167824161 ) ) ;
#37816 = CARTESIAN_POINT ( 'NONE',  ( -11.35316468750000141, 8.281249996586016238, -1.390361679473963753E-15 ) ) ;
#37817 = CARTESIAN_POINT ( 'NONE',  ( 11.00000000000000355, -4.556349186104045046, 99.34375000409677625 ) ) ;
#37818 = CARTESIAN_POINT ( 'NONE',  ( -2.828427124746208943, 205.6250000000000284, 144.8284271247462129 ) ) ;
#37819 = CARTESIAN_POINT ( 'NONE',  ( -25.55430564589122966, 201.3125000013656063, 167.5543056458915032 ) ) ;
#37820 = LINE ( 'NONE', #61571, #68373 ) ;
#37822 = CARTESIAN_POINT ( 'NONE',  ( -2.751064625579944321E-14, 203.7500000000000284, 146.0000000000000284 ) ) ;
#37821 = CARTESIAN_POINT ( 'NONE',  ( -2.977408999572652260, 116.9375000020483952, 7.188101187500000044 ) ) ;
#37823 = CARTESIAN_POINT ( 'NONE',  ( 3.313708498984756279, 7.999999999999991118, 27.36155277982336642 ) ) ;
#37824 = CARTESIAN_POINT ( 'NONE',  ( 9.832129032723416984, 120.3645833299193697, 5.676582343750006032 ) ) ;
#37825 = CARTESIAN_POINT ( 'NONE',  ( 10.00000000000000178, 86.87499999317203958, 0.000000000000000000 ) ) ;
#37826 = CARTESIAN_POINT ( 'NONE',  ( -4.401442555609581635E-16, 124.1562500020483810, -7.188101187500000044 ) ) ;
#37827 = CARTESIAN_POINT ( 'NONE',  ( -4.541265875000003227, 20.99999999863440792, 1.881053915767121110 ) ) ;
#37828 = CARTESIAN_POINT ( 'NONE',  ( 11.00000000000000000, 1.347111479062088405E-15, 91.93750000409677625 ) ) ;
#37829 = CARTESIAN_POINT ( 'NONE',  ( 5.000000000000005329, 145.8333333333333428, -8.660254037844392627 ) ) ;
#37830 = ORIENTED_EDGE ( 'NONE', *, *, #53513, .F. ) ;
#37831 = CARTESIAN_POINT ( 'NONE',  ( 3.999999999999960032, 208.9375000000000284, 143.6568542494924259 ) ) ;
#37832 = CARTESIAN_POINT ( 'NONE',  ( -6.676582343750000703, 292.6718750017069510, 2.765530957082001251 ) ) ;
#37833 = CARTESIAN_POINT ( 'NONE',  ( -5.656854249492373476, -5.656854249492376141, 2.705302783920143561 ) ) ;
#37834 = CARTESIAN_POINT ( 'NONE',  ( -8.311093377946836114, 172.6562499965860411, -8.311093377946837890 ) ) ;
#37835 = VECTOR ( 'NONE', #20826, 1000.000000000000000 ) ;
#37836 = CARTESIAN_POINT ( 'NONE',  ( 2.849036369511732440E-14, 201.3750000027312126, 202.0000000000000000 ) ) ;
#37837 = CARTESIAN_POINT ( 'NONE',  ( 4.000000000000015987, 196.4375000000000568, 199.6568542494924259 ) ) ;
#37838 = CARTESIAN_POINT ( 'NONE',  ( -7.778174593052020747, -7.778174593052023411, 70.37500000409677625 ) ) ;
#37839 = CARTESIAN_POINT ( 'NONE',  ( 7.204075437095966983, 7.204075437095967871, 101.9687500020483668 ) ) ;
#37840 = ORIENTED_EDGE ( 'NONE', *, *, #13068, .T. ) ;
#37841 =( BOUNDED_CURVE ( )  B_SPLINE_CURVE ( 2, ( #32730, #55738, #61758, #26285, #4055, #10446, #32350, #50428, #27047 ),
 .UNSPECIFIED., .F., .F. ) 
 B_SPLINE_CURVE_WITH_KNOTS ( ( 3, 2, 2, 2, 3 ),
 ( 0.2666666666666668850, 0.2750000000000002442, 0.2833333333333335480, 0.2916666666666669072, 0.3000000000000002109 ),
 .UNSPECIFIED. ) 
 CURVE ( )  GEOMETRIC_REPRESENTATION_ITEM ( )  RATIONAL_B_SPLINE_CURVE ( ( 0.9999999999999980016, 0.9238795325112887369, 1.000000000000000000, 0.9238795325112867385, 1.000000000000000000, 0.9238795325112867385, 1.000000000000000000, 0.9238795325112847401, 1.000000000000001998 ) ) 
 REPRESENTATION_ITEM ( '' )  );
#37842 = ADVANCED_FACE ( 'NONE', ( #49720 ), #25571, .T. ) ;
#37843 = EDGE_CURVE ( 'NONE', #9634, #5468, #11182, .T. ) ;
#37844 = CARTESIAN_POINT ( 'NONE',  ( 8.000000000000000000, 22.31249999590322375, 0.000000000000000000 ) ) ;
#37845 = CARTESIAN_POINT ( 'NONE',  ( -2.085542519210945728E-15, 154.8437499965860127, 11.35316468750000141 ) ) ;
#37846 = CARTESIAN_POINT ( 'NONE',  ( -2.445694354108782775, 194.5625000013656063, 200.4456943541088663 ) ) ;
#37847 = CARTESIAN_POINT ( 'NONE',  ( 2.754378923186476579E-14, 205.4375000013656063, 194.5412658750000219 ) ) ;
#37848 = CARTESIAN_POINT ( 'NONE',  ( 8.660254037844389075, 230.2083333401612890, 4.999999999999997335 ) ) ;
#37849 = CARTESIAN_POINT ( 'NONE',  ( 11.35316468749999963, 56.30208332991934839, -3.042071309553165293 ) ) ;
#37850 = ORIENTED_EDGE ( 'NONE', *, *, #6344, .T. ) ;
#37851 = CARTESIAN_POINT ( 'NONE',  ( -6.238412754330611322E-16, 10.18810118749999916, 110.7812500020483668 ) ) ;
#37852 = CARTESIAN_POINT ( 'NONE',  ( -4.541265875000002339, 10.87499999863440969, -1.881053915767121998 ) ) ;
#37853 = EDGE_LOOP ( 'NONE', ( #21629, #72939, #31045, #53692 ) ) ;
#37854 = ADVANCED_FACE ( 'NONE', ( #51110 ), #6850, .F. ) ;
#37855 = CARTESIAN_POINT ( 'NONE',  ( 7.188101187500000044, 22.96874999795161543, 0.000000000000000000 ) ) ;
#37856 = CARTESIAN_POINT ( 'NONE',  ( 6.000000000000003553, 288.6250000034139589, -2.485281374238571761 ) ) ;
#37857 = CARTESIAN_POINT ( 'NONE',  ( 2.679491924311228956, 67.91666665983868256, -10.00000000000000000 ) ) ;
#37858 = CARTESIAN_POINT ( 'NONE',  ( 7.188101187500001821, 18.93749999795161187, -2.977408999572650483 ) ) ;
#37859 = CARTESIAN_POINT ( 'NONE',  ( -2.977408999572647819, 7.188101187499992051, 4.205302781871752771 ) ) ;
#37860 = CARTESIAN_POINT ( 'NONE',  ( -10.18810118749999916, 4.220049686691934809, 67.56250000204836681 ) ) ;
#37861 = VECTOR ( 'NONE', #4847, 1000.000000000000000 ) ;
#37862 = CARTESIAN_POINT ( 'NONE',  ( -6.676582343750001591, 287.5312500017070079, 0.000000000000000000 ) ) ;
#37863 = CARTESIAN_POINT ( 'NONE',  ( -2.828427124746192067, 7.374999997268813168, 2.828427124746190735 ) ) ;
#37864 = ORIENTED_EDGE ( 'NONE', *, *, #44247, .F. ) ;
#37865 = CARTESIAN_POINT ( 'NONE',  ( -3.458734124999959914, 206.4375000013656063, 198.0000000000000284 ) ) ;
#37866 = EDGE_CURVE ( 'NONE', #72561, #54725, #62718, .T. ) ;
#37867 = CARTESIAN_POINT ( 'NONE',  ( -27.99999999999990763, 194.6250000027311842, 174.0000000000003695 ) ) ;
#37868 = CARTESIAN_POINT ( 'NONE',  ( -4.541265875000002339, 7.749999998634407916, -1.881053915767121998 ) ) ;
#37869 = CARTESIAN_POINT ( 'NONE',  ( 7.188101187500001821, 113.0000000020483668, -2.977408999572651371 ) ) ;
#37870 = CARTESIAN_POINT ( 'NONE',  ( 7.188101187499993827, -2.977408999572645598, 27.64280278187175810 ) ) ;
#37871 = ORIENTED_EDGE ( 'NONE', *, *, #11437, .T. ) ;
#37872 = CARTESIAN_POINT ( 'NONE',  ( 4.270632937500002058, 0.1562499993172034307, 0.000000000000000000 ) ) ;
#37873 = ORIENTED_EDGE ( 'NONE', *, *, #285, .F. ) ;
#37874 = CARTESIAN_POINT ( 'NONE',  ( -19.99999999999993250, -31.99999999999978684, 135.0000000000000000 ) ) ;
#37875 = CARTESIAN_POINT ( 'NONE',  ( -7.999920465054277230, 1.060465953394919891, -0.000000000000000000 ) ) ;
#37876 = CARTESIAN_POINT ( 'NONE',  ( -2.445694354108783664, 202.3125000013656063, 195.5543056458912190 ) ) ;
#37877 = CARTESIAN_POINT ( 'NONE',  ( 31.45873412499998523, 201.7500000013655779, 168.5673454167822172 ) ) ;
#37878 = CARTESIAN_POINT ( 'NONE',  ( 7.320508075688771044, 74.37500000000001421, 7.320508075688775484 ) ) ;
#37879 = AXIS2_PLACEMENT_3D ( 'NONE', #42856, #54576, #71901 ) ;
#37880 = CARTESIAN_POINT ( 'NONE',  ( 1.320432766682874540E-15, 93.40625000204838102, 7.188101187500000044 ) ) ;
#37881 = CARTESIAN_POINT ( 'NONE',  ( 6.000000000000003553, 290.4375000000000000, 2.485281374238571317 ) ) ;
#37883 = CARTESIAN_POINT ( 'NONE',  ( -5.000000000000001776, 126.6666666666666714, -8.660254037844392627 ) ) ;
#37882 = CARTESIAN_POINT ( 'NONE',  ( 27.99999999999999645, 210.0000000000000284, 165.9999999999999147 ) ) ;
#37884 = ORIENTED_EDGE ( 'NONE', *, *, #70375, .T. ) ;
#37885 = CARTESIAN_POINT ( 'NONE',  ( 9.832129032723416984, 221.8229166700806729, -5.676582343750003368 ) ) ;
#37886 = CARTESIAN_POINT ( 'NONE',  ( -6.891449706524621632, -10.24244278381001472, 65.16993756079229172 ) ) ;
#37887 = CARTESIAN_POINT ( 'NONE',  ( -2.849036369511732440E-14, 199.3750000027312126, 138.0000000000000568 ) ) ;
#37888 = CARTESIAN_POINT ( 'NONE',  ( 7.999999999843520726, -5.003525229023116430E-05, 24.26780136833107093 ) ) ;
#37889 = CARTESIAN_POINT ( 'NONE',  ( 2.775557561562891351E-14, 210.0000000000000284, 202.0000000000000000 ) ) ;
#37890 = CARTESIAN_POINT ( 'NONE',  ( -8.660254037844385522, 250.4166666666666856, 5.000000000000004441 ) ) ;
#37891 = CARTESIAN_POINT ( 'NONE',  ( 8.000000000000000000, 107.9375000040967905, -9.797174393178825657E-16 ) ) ;
#37892 = CARTESIAN_POINT ( 'NONE',  ( 2.679491924311228956, 191.0416666666666572, -10.00000000000000000 ) ) ;
#37893 = CARTESIAN_POINT ( 'NONE',  ( 31.99999999999997868, 198.4375000027312126, 168.3431457505074889 ) ) ;
#37894 = CARTESIAN_POINT ( 'NONE',  ( 1.320432766682872962E-15, -7.188101187499992051, 20.23655278187175455 ) ) ;
#37895 = CARTESIAN_POINT ( 'NONE',  ( 8.311093377946837890, 156.7187499965860127, -8.311093377946837890 ) ) ;
#37896 = CARTESIAN_POINT ( 'NONE',  ( -2.849036369511732440E-14, 204.3750000027312126, 138.0000000000000568 ) ) ;
#37897 = DIRECTION ( 'NONE',  ( 0.000000000000000000, 0.000000000000000000, 1.000000000000000000 ) ) ;
#37898 = CARTESIAN_POINT ( 'NONE',  ( 10.00000000000018296, 155.2083333333334565, -2.679491924311276030 ) ) ;
#37901 = CARTESIAN_POINT ( 'NONE',  ( 4.898587196589412829E-16, 16.87500000000000000, -8.000000000000000000 ) ) ;
#37900 = FACE_OUTER_BOUND ( 'NONE', #17677, .T. ) ;
#37899 = CARTESIAN_POINT ( 'NONE',  ( 23.99999999999998934, 202.7500000000000000, 169.9999999999998863 ) ) ;
#37902 = ORIENTED_EDGE ( 'NONE', *, *, #59567, .F. ) ;
#37903 = CARTESIAN_POINT ( 'NONE',  ( 5.676582343749993598, 15.26041666325268409, 9.832129032723422313 ) ) ;
#37904 = CARTESIAN_POINT ( 'NONE',  ( 1.656854249492354825, 200.4375000027311842, 202.0000000000000853 ) ) ;
#37906 = CARTESIAN_POINT ( 'NONE',  ( 0.000000000000000000, 0.000000000000000000, 0.000000000000000000 ) ) ;
#37905 = CARTESIAN_POINT ( 'NONE',  ( 1.818965066830242394, -7.999999999999990230, -0.05573584732409991860 ) ) ;
#37907 = CARTESIAN_POINT ( 'NONE',  ( -5.656854249492380582, 115.8125000000000000, -5.656854249492380582 ) ) ;
#37908 = CARTESIAN_POINT ( 'NONE',  ( -3.458734125000015425, 203.9375000013656063, 142.0000000000000568 ) ) ;
#37909 = CARTESIAN_POINT ( 'NONE',  ( -2.679491924311235618, 55.41666665983870388, 10.00000000000000000 ) ) ;
#37910 = CARTESIAN_POINT ( 'NONE',  ( -4.401442555609581635E-16, 110.2812500020483810, -7.188101187500000044 ) ) ;
#37911 = CARTESIAN_POINT ( 'NONE',  ( 3.211159895383560947, 10.31249999863440792, 3.211159895383562723 ) ) ;
#37912 = DIRECTION ( 'NONE',  ( -0.000000000000000000, 1.000000000000000000, -1.563033456626094573E-30 ) ) ;
#37913 = CARTESIAN_POINT ( 'NONE',  ( 1.469576158976822172E-15, -7.999999999999991118, 8.705302779823362869 ) ) ;
#37915 = LINE ( 'NONE', #15252, #52263 ) ;
#37914 = CARTESIAN_POINT ( 'NONE',  ( 75.00000000000000000, 242.0000000000000284, 42.00000000000000000 ) ) ;
#37916 = ORIENTED_EDGE ( 'NONE', *, *, #63354, .T. ) ;
#37917 = VERTEX_POINT ( 'NONE', #22424 ) ;
#37918 = CYLINDRICAL_SURFACE ( 'NONE', #72562, 8.000000000000000000 ) ;
#37919 = CARTESIAN_POINT ( 'NONE',  ( -2.828427124746209831, 196.3750000000000284, 139.1715728752538723 ) ) ;
#37920 = CARTESIAN_POINT ( 'NONE',  ( -5.656854249492378806, 99.68750000000000000, 5.656854249492381470 ) ) ;
#37921 = CARTESIAN_POINT ( 'NONE',  ( -5.676582343750006032, 124.1145833299193555, 9.832129032723418760 ) ) ;
#37922 = VERTEX_POINT ( 'NONE', #11131 ) ;
#37923 = CARTESIAN_POINT ( 'NONE',  ( 4.220049686691934809, 10.18810118749999916, 94.18750000204836681 ) ) ;
#37924 = DIRECTION ( 'NONE',  ( 0.000000000000000000, 0.000000000000000000, -1.000000000000000000 ) ) ;
#37925 = CARTESIAN_POINT ( 'NONE',  ( -1.432654583217607414, 198.5000000013656347, 194.5412658750000219 ) ) ;
#37926 = CYLINDRICAL_SURFACE ( 'NONE', #47384, 8.000000000000003553 ) ;
#37928 = CARTESIAN_POINT ( 'NONE',  ( 9.832129032723416984, 130.3645833299193555, 5.676582343750006032 ) ) ;
#37927 = CARTESIAN_POINT ( 'NONE',  ( -8.000000000000000000, 94.90624999999998579, -3.313708498984761164 ) ) ;
#37929 = CARTESIAN_POINT ( 'NONE',  ( 0.000000000000000000, 300.0000000000000000, 10.00000000000000178 ) ) ;
#37930 = ORIENTED_EDGE ( 'NONE', *, *, #51872, .F. ) ;
#37931 = CARTESIAN_POINT ( 'NONE',  ( -5.000000000000005329, 25.20833332650536818, 8.660254037844387298 ) ) ;
#37932 = CARTESIAN_POINT ( 'NONE',  ( -36.08150342469651406, 173.9980443334521851, 170.3486527212912449 ) ) ;
#37933 = CARTESIAN_POINT ( 'NONE',  ( 6.951808397369818766E-16, 117.3437499965860127, -11.35316468750000141 ) ) ;
#37934 = CARTESIAN_POINT ( 'NONE',  ( 2.445694354108839619, 207.8125000013656063, 200.4456943541088663 ) ) ;
#37935 = CARTESIAN_POINT ( 'NONE',  ( -7.188101187500000933, 20.99999999795161898, -2.977408999572651371 ) ) ;
#37936 =( BOUNDED_CURVE ( )  B_SPLINE_CURVE ( 2, ( #49320, #33129, #14984, #20651, #73828, #39134, #21397, #3312, #72337 ),
 .UNSPECIFIED., .F., .F. ) 
 B_SPLINE_CURVE_WITH_KNOTS ( ( 3, 2, 2, 2, 3 ),
 ( 0.6704545454545455252, 0.6761363636363637575, 0.6818181818181817677, 0.6875000000000000000, 0.6931818181818182323 ),
 .UNSPECIFIED. ) 
 CURVE ( )  GEOMETRIC_REPRESENTATION_ITEM ( )  RATIONAL_B_SPLINE_CURVE ( ( 0.9999999999999985567, 0.9238795325112881818, 1.000000000000000000, 0.9238795325112867385, 1.000000000000000000, 0.9238795325112867385, 1.000000000000000000, 0.9238795325112867385, 1.000000000000000000 ) ) 
 REPRESENTATION_ITEM ( '' )  );
#37937 = CARTESIAN_POINT ( 'NONE',  ( 4.220049686691941027, -10.18810118749999738, 86.50000000204836681 ) ) ;
#37938 = CARTESIAN_POINT ( 'NONE',  ( 9.832129032723420536, 26.51041666325268409, -5.676582343749999815 ) ) ;
#37939 = ORIENTED_EDGE ( 'NONE', *, *, #823, .F. ) ;
#37940 = CARTESIAN_POINT ( 'NONE',  ( 0.000000000000000000, 0.000000000000000000, 0.000000000000000000 ) ) ;
#37941 = CARTESIAN_POINT ( 'NONE',  ( -5.662595241051935346, 5.662595241051935346, 26.32561528394063188 ) ) ;
#37942 = CARTESIAN_POINT ( 'NONE',  ( -3.458734125000015869, 209.1875000013656063, 142.0000000000000568 ) ) ;
#37943 = VECTOR ( 'NONE', #64614, 1000.000000000000000 ) ;
#37944 = EDGE_CURVE ( 'NONE', #55561, #35916, #14003, .T. ) ;
#37945 = FACE_OUTER_BOUND ( 'NONE', #44908, .T. ) ;
#37946 = CARTESIAN_POINT ( 'NONE',  ( -7.188101187500002709, 5.812499997951610986, 2.977408999572649151 ) ) ;
#37947 = CARTESIAN_POINT ( 'NONE',  ( 6.000000000000003553, 298.6250000034140157, -2.485281374238571761 ) ) ;
#37948 = CARTESIAN_POINT ( 'NONE',  ( -5.652405255243663440, -4.866521301246740983, 0.0006792023777823770567 ) ) ;
#37949 = CARTESIAN_POINT ( 'NONE',  ( -24.00000000000001421, 206.8125000000000000, 168.3431457505080289 ) ) ;
#37950 = ORIENTED_EDGE ( 'NONE', *, *, #17798, .T. ) ;
#37951 = EDGE_CURVE ( 'NONE', #32224, #10358, #8745, .T. ) ;
#37952 = CARTESIAN_POINT ( 'NONE',  ( 8.311093377946834337, 140.4687499965859843, 8.311093377946839666 ) ) ;
#37953 = CARTESIAN_POINT ( 'NONE',  ( -10.18810118749999916, 0.000000000000000000, 81.15625000204838102 ) ) ;
#37954 = CARTESIAN_POINT ( 'NONE',  ( -26.56734541678232375, 198.0000000013656063, 173.4587341250003760 ) ) ;
#37955 =( BOUNDED_CURVE ( )  B_SPLINE_CURVE ( 2, ( #13750, #30392, #37539, #25821, #42438, #59804, #70389, #70747, #71846 ),
 .UNSPECIFIED., .F., .F. ) 
 B_SPLINE_CURVE_WITH_KNOTS ( ( 3, 2, 2, 2, 3 ),
 ( 0.9583333333333332593, 0.9652777777777776791, 0.9722222222222220989, 0.9791666666666665186, 0.9861111111111110494 ),
 .UNSPECIFIED. ) 
 CURVE ( )  GEOMETRIC_REPRESENTATION_ITEM ( )  RATIONAL_B_SPLINE_CURVE ( ( 1.000000000000001110, 0.9238795325112855172, 1.000000000000000000, 0.9238795325112867385, 1.000000000000000000, 0.9238795325112867385, 1.000000000000000000, 0.9238795325112879597, 0.9999999999999987788 ) ) 
 REPRESENTATION_ITEM ( '' )  );
#37956 = CARTESIAN_POINT ( 'NONE',  ( 11.00000000000000000, 1.347111479062088405E-15, 100.9375000040967763 ) ) ;
#37957 = CARTESIAN_POINT ( 'NONE',  ( -1.881053915767124440, 17.12499999863440436, 4.541265875000001451 ) ) ;
#37958 = ORIENTED_EDGE ( 'NONE', *, *, #67087, .T. ) ;
#37959 = CARTESIAN_POINT ( 'NONE',  ( 4.000000000000015987, 204.6250000027312126, 198.0000000000000284 ) ) ;
#37960 = AXIS2_PLACEMENT_3D ( 'NONE', #31510, #13030, #59811 ) ;
#37961 = EDGE_CURVE ( 'NONE', #67735, #42303, #63898, .T. ) ;
#37962 = CARTESIAN_POINT ( 'NONE',  ( -2.828427124746208943, 208.6250000000000284, 144.8284271247462129 ) ) ;
#37963 = CARTESIAN_POINT ( 'NONE',  ( -28.00000000000007816, 204.1250000027312126, 166.0000000000003695 ) ) ;
#37964 =( GEOMETRIC_REPRESENTATION_CONTEXT ( 3 ) GLOBAL_UNCERTAINTY_ASSIGNED_CONTEXT ( ( #52616 ) ) GLOBAL_UNIT_ASSIGNED_CONTEXT ( ( #19402, #59055, #53755 ) ) REPRESENTATION_CONTEXT ( 'NONE', 'WORKASPACE' ) );
#37965 = ORIENTED_EDGE ( 'NONE', *, *, #73800, .T. ) ;
#37966 = CARTESIAN_POINT ( 'NONE',  ( -5.082755093536325042, 10.03124999795161187, -5.082755093536325930 ) ) ;
#37967 = CARTESIAN_POINT ( 'NONE',  ( -14.79008266047737585, -20.27703233285068052, 197.2457678486681800 ) ) ;
#37968 = CARTESIAN_POINT ( 'NONE',  ( 0.000000000000000000, 300.0000000000000000, 0.000000000000000000 ) ) ;
#37969 = CARTESIAN_POINT ( 'NONE',  ( -11.35316468750000141, 183.2812499965860411, -1.390361679473963753E-15 ) ) ;
#37970 = CARTESIAN_POINT ( 'NONE',  ( 2.977408999572650039, 113.5625000020483668, -7.188101187500001821 ) ) ;
#37971 = CARTESIAN_POINT ( 'NONE',  ( 2.775557561562891351E-14, 210.0000000000000284, 198.0000000000000284 ) ) ;
#37972 = CARTESIAN_POINT ( 'NONE',  ( 4.721056650416000089, 288.8281250017069510, 4.721056650415999201 ) ) ;
#37974 = CARTESIAN_POINT ( 'NONE',  ( 9.999999999999996447, 95.00000000000000000, 0.000000000000000000 ) ) ;
#37973 = CARTESIAN_POINT ( 'NONE',  ( -8.311093377946834337, 219.5312500034139873, 8.311093377946837890 ) ) ;
#37975 = ORIENTED_EDGE ( 'NONE', *, *, #63738, .T. ) ;
#37976 = CARTESIAN_POINT ( 'NONE',  ( -5.676582343749992710, 254.7395833367473301, 9.832129032723422313 ) ) ;
#37977 = CARTESIAN_POINT ( 'NONE',  ( 1.320432766682872962E-15, -7.188101187499992051, 23.23655278187175455 ) ) ;
#37978 = CARTESIAN_POINT ( 'NONE',  ( 10.00000000000000178, 167.0833333265053682, -2.679491924311226736 ) ) ;
#37979 = CARTESIAN_POINT ( 'NONE',  ( 3.313708498984762496, 19.03124999590322375, 7.999999999999998224 ) ) ;
#37980 = CARTESIAN_POINT ( 'NONE',  ( 4.330454160168685895, -68.33163558029976059, -20.63184982502311371 ) ) ;
#37981 = CARTESIAN_POINT ( 'NONE',  ( 1.432654583217664701, 201.0000000013655779, 201.4587341250000065 ) ) ;
#37982 = DIRECTION ( 'NONE',  ( 0.000000000000000000, 0.000000000000000000, 1.000000000000000000 ) ) ;
#37983 = CARTESIAN_POINT ( 'NONE',  ( -10.99999999999999822, 0.000000000000000000, 114.9999999999999858 ) ) ;
#37984 = CARTESIAN_POINT ( 'NONE',  ( -3.313708498984762496, 96.78125000000000000, 7.999999999999998224 ) ) ;
#37985 = CARTESIAN_POINT ( 'NONE',  ( 5.676582343749993598, 115.2604166632526983, 9.832129032723422313 ) ) ;
#37986 = LINE ( 'NONE', #37610, #7145 ) ;
#37987 = CARTESIAN_POINT ( 'NONE',  ( -4.556349186104045934, 11.00000000000000000, 71.21875000000000000 ) ) ;
#37990 = DIRECTION ( 'NONE',  ( -0.000000000000000000, 1.000000000000000000, -0.000000000000000000 ) ) ;
#37989 = CARTESIAN_POINT ( 'NONE',  ( 27.99999999999996803, 199.9375000013656063, 166.5412658749999082 ) ) ;
#37988 = CARTESIAN_POINT ( 'NONE',  ( 24.54126587500000056, 198.3750000013655779, 168.5673454167822172 ) ) ;
#37991 = ORIENTED_EDGE ( 'NONE', *, *, #20706, .F. ) ;
#37992 = CARTESIAN_POINT ( 'NONE',  ( 54.00000000000000000, 0.000000000000000000, 0.000000000000000000 ) ) ;
#37993 = CARTESIAN_POINT ( 'NONE',  ( -9.832129032723418760, 222.8645833299193839, -5.676582343750004256 ) ) ;
#37994 = CARTESIAN_POINT ( 'NONE',  ( 2.445694354108782775, 195.5625000013656063, 139.5543056458912190 ) ) ;
#37995 = CARTESIAN_POINT ( 'NONE',  ( 27.99999999999996092, 196.6875000013655779, 173.4587341249998929 ) ) ;
#37996 = CARTESIAN_POINT ( 'NONE',  ( 2.977408999572650927, 26.62499999795161543, -7.188101187500001821 ) ) ;
#37997 = CARTESIAN_POINT ( 'NONE',  ( -8.311093377946841443, 209.2187499965859843, 8.311093377946830785 ) ) ;
#37998 = CARTESIAN_POINT ( 'NONE',  ( 0.000000000000000000, 0.000000000000000000, 118.0000000000000000 ) ) ;
#37999 = DIRECTION ( 'NONE',  ( -0.000000000000000000, 1.000000000000000000, -0.000000000000000000 ) ) ;
#38000 = CARTESIAN_POINT ( 'NONE',  ( 1.881053915767122664, 20.12499999863441147, 4.541265875000001451 ) ) ;
#38001 = CARTESIAN_POINT ( 'NONE',  ( 31.45873412499999944, 195.0000000013656063, 168.5673454167822740 ) ) ;
#38002 = CARTESIAN_POINT ( 'NONE',  ( -7.999999999999991118, 3.313708498984756723, 26.23655277982336642 ) ) ;
#38003 = PLANE ( 'NONE',  #33971 ) ;
#38004 = CARTESIAN_POINT ( 'NONE',  ( -11.35316468750000141, 83.48958332991935549, 3.042071309553159963 ) ) ;
#38005 = EDGE_LOOP ( 'NONE', ( #32639, #66133, #31274, #18468, #28008, #67991 ) ) ;
#38006 = CARTESIAN_POINT ( 'NONE',  ( 11.00000000000000000, 1.347111479062088405E-15, 87.43750000409677625 ) ) ;
#38007 = CARTESIAN_POINT ( 'NONE',  ( 5.082755093536324154, 21.28124999795161543, 5.082755093536326818 ) ) ;
#38008 = CARTESIAN_POINT ( 'NONE',  ( -8.000000000000000000, 108.5937500040967763, -3.313708498984761164 ) ) ;
#38009 = CARTESIAN_POINT ( 'NONE',  ( 3.042071309553173286, 255.6770833367473301, 11.35316468749999608 ) ) ;
#38010 = CARTESIAN_POINT ( 'NONE',  ( 3.042071309553159519, 84.73958332991936970, 11.35316468750000141 ) ) ;
#38011 = ORIENTED_EDGE ( 'NONE', *, *, #49148, .T. ) ;
#38012 = CARTESIAN_POINT ( 'NONE',  ( -4.220049686691935698, 10.18810118749999916, 87.25000000204838102 ) ) ;
#38013 = CARTESIAN_POINT ( 'NONE',  ( -10.18810118749999916, 0.000000000000000000, 114.1562500020483810 ) ) ;
#38014 = CARTESIAN_POINT ( 'NONE',  ( -29.43265458321760164, 195.1250000013656063, 173.4587341250003760 ) ) ;
#38015 = CARTESIAN_POINT ( 'NONE',  ( -2.445694354108783219, 206.8125000013656063, 200.4456943541088663 ) ) ;
#38016 = CARTESIAN_POINT ( 'NONE',  ( 32.00000000000000711, 207.3125000000000284, 168.3431457505075457 ) ) ;
#38017 = CARTESIAN_POINT ( 'NONE',  ( 5.676582343749993598, 79.94791666325269830, 9.832129032723422313 ) ) ;
#38018 = CIRCLE ( 'NONE', #59707, 9.999999999999996447 ) ;
#38019 = CARTESIAN_POINT ( 'NONE',  ( 1.469576158976822172E-15, -7.999999999999991118, 16.39280278392014978 ) ) ;
#38020 = CARTESIAN_POINT ( 'NONE',  ( -29.43265458321766559, 206.7500000013655779, 166.5412658750003629 ) ) ;
#38021 = FACE_OUTER_BOUND ( 'NONE', #66819, .T. ) ;
#38022 = CARTESIAN_POINT ( 'NONE',  ( -4.999999999999998224, 168.5416666598387110, -8.660254037844389075 ) ) ;
#38023 = VECTOR ( 'NONE', #17628, 1000.000000000000000 ) ;
#38024 = CYLINDRICAL_SURFACE ( 'NONE', #31633, 8.000000000000000000 ) ;
#38025 = CARTESIAN_POINT ( 'NONE',  ( 3.042071309553167513, 72.13541666325268409, -11.35316468749999785 ) ) ;
#38026 = CARTESIAN_POINT ( 'NONE',  ( -6.676582343750003368, 292.3906250017068942, -2.765530957081996810 ) ) ;
#38027 = CARTESIAN_POINT ( 'NONE',  ( -7.204075437095965206, -7.204075437095968759, 107.2187500020483810 ) ) ;
#38028 = CARTESIAN_POINT ( 'NONE',  ( -11.35316468750000141, 208.2812499965860411, -1.390361679473963753E-15 ) ) ;
#38029 = ORIENTED_EDGE ( 'NONE', *, *, #19109, .T. ) ;
#38030 = CARTESIAN_POINT ( 'NONE',  ( -4.465384415997326606, 66.51627080308836071, 26.73837581714138878 ) ) ;
#38031 = CARTESIAN_POINT ( 'NONE',  ( 4.000000000000000888, 3.687499997268813168, 1.656854249492384135 ) ) ;
#38032 = CARTESIAN_POINT ( 'NONE',  ( -0.4320110153365296912, 49.91454558245937534, 40.68976686129168741 ) ) ;
#38034 = CARTESIAN_POINT ( 'NONE',  ( 11.35316468750000141, 200.7812499965860411, 0.000000000000000000 ) ) ;
#38033 = FACE_OUTER_BOUND ( 'NONE', #43709, .T. ) ;
#38035 = CARTESIAN_POINT ( 'NONE',  ( 23.99999999999998579, 195.7500000000000000, 169.9999999999998863 ) ) ;
#38036 = CARTESIAN_POINT ( 'NONE',  ( 9.999999999999998224, 230.8333333401612890, -2.679491924311229401 ) ) ;
#38037 = CARTESIAN_POINT ( 'NONE',  ( -4.556349186104048599, -10.99999999999999822, 71.96875000409677625 ) ) ;
#38038 = ORIENTED_EDGE ( 'NONE', *, *, #21051, .F. ) ;
#38039 = CARTESIAN_POINT ( 'NONE',  ( -9.832129032723420536, 194.0104166632526983, 5.676582343749997150 ) ) ;
#38040 = EDGE_CURVE ( 'NONE', #61956, #41819, #17124, .T. ) ;
#38041 = CARTESIAN_POINT ( 'NONE',  ( 1.320432766682872962E-15, -7.188101187499992051, 12.36155278187175277 ) ) ;
#38042 = CARTESIAN_POINT ( 'NONE',  ( -7.320508075688771932, 93.12500000000000000, 7.320508075688763938 ) ) ;
#38043 = ORIENTED_EDGE ( 'NONE', *, *, #26854, .F. ) ;
#38044 = CARTESIAN_POINT ( 'NONE',  ( -7.999999999999998224, 89.28125000409677625, 3.313708498984766493 ) ) ;
#38045 =( BOUNDED_CURVE ( )  B_SPLINE_CURVE ( 2, ( #59324, #42687, #65699, #25698, #1970, #47242, #48719, #36675, #70269, #29904, #59687, #8361, #41594 ),
 .UNSPECIFIED., .F., .F. ) 
 B_SPLINE_CURVE_WITH_KNOTS ( ( 3, 2, 2, 2, 2, 2, 3 ),
 ( 2.370688293668704372, 2.375920754678181979, 2.381153215687659586, 2.386385676697137193, 2.391618137706614799, 2.396850598716092406, 2.402083059725570013 ),
 .UNSPECIFIED. ) 
 CURVE ( )  GEOMETRIC_REPRESENTATION_ITEM ( )  RATIONAL_B_SPLINE_CURVE ( ( 0.9999999999999978906, 0.9659258262890704216, 1.000000000000000000, 0.9659258262890683122, 1.000000000000000000, 0.9659258262890683122, 1.000000000000000000, 0.9659258262890683122, 1.000000000000000000, 0.9659258262890683122, 1.000000000000000000, 0.9659258262891560198, 0.9999999999999122924 ) ) 
 REPRESENTATION_ITEM ( '' )  );
#38046 = FACE_OUTER_BOUND ( 'NONE', #29245, .T. ) ;
#38047 = EDGE_CURVE ( 'NONE', #47201, #1549, #49141, .T. ) ;
#38048 = ORIENTED_EDGE ( 'NONE', *, *, #33099, .F. ) ;
#38049 = ADVANCED_FACE ( 'NONE', ( #44906 ), #17335, .F. ) ;
#38050 = CARTESIAN_POINT ( 'NONE',  ( 1.656854249492381248, 17.18750000000000000, -4.000000000000001776 ) ) ;
#38051 = CARTESIAN_POINT ( 'NONE',  ( 2.780723358947928197E-16, 20.56249999863440436, -4.541265875000002339 ) ) ;
#38052 = CARTESIAN_POINT ( 'NONE',  ( -3.313708498984758943, -7.999999999999989342, 10.29905278392014623 ) ) ;
#38053 = CARTESIAN_POINT ( 'NONE',  ( 7.999999999999991118, 0.000000000000000000, 30.00000000000000000 ) ) ;
#38054 = ORIENTED_EDGE ( 'NONE', *, *, #69616, .F. ) ;
#38055 = CARTESIAN_POINT ( 'NONE',  ( 5.000000000000000000, -11.00479820989369983, -67.37201579502529114 ) ) ;
#38056 = CARTESIAN_POINT ( 'NONE',  ( 5.082755093536325042, 90.59375000204838102, -5.082755093536325930 ) ) ;
#38057 = CONICAL_SURFACE ( 'NONE', #66980, 3.999999999999976019, 0.7853981633974496113 ) ;
#38060 = CARTESIAN_POINT ( 'NONE',  ( 4.217983994790209579, -51.98644305214834560, 48.84278562423003933 ) ) ;
#38059 = CARTESIAN_POINT ( 'NONE',  ( 5.676582343749997150, 252.2395833367473301, -9.832129032723418760 ) ) ;
#38058 = CARTESIAN_POINT ( 'NONE',  ( -7.320508075688863414, 83.12500000000005684, 7.320508075688855421 ) ) ;
#38061 = CARTESIAN_POINT ( 'NONE',  ( 1424.688200795887496, 710.9677537767815920, 822.8421604560587639 ) ) ;
#38062 = EDGE_LOOP ( 'NONE', ( #28404, #39143, #23109, #16481 ) ) ;
#38063 = CARTESIAN_POINT ( 'NONE',  ( -8.000000000000000000, 101.0937500040968047, -3.313708498984761164 ) ) ;
#38065 = EDGE_CURVE ( 'NONE', #15485, #64014, #67912, .T. ) ;
#38064 = AXIS2_PLACEMENT_3D ( 'NONE', #7706, #47680, #24308 ) ;
#38066 = CARTESIAN_POINT ( 'NONE',  ( 2.977408999572646486, 7.188101187499991163, 17.51780278187175455 ) ) ;
#38067 = ORIENTED_EDGE ( 'NONE', *, *, #26612, .T. ) ;
#38068 = ORIENTED_EDGE ( 'NONE', *, *, #63245, .F. ) ;
#38069 = CARTESIAN_POINT ( 'NONE',  ( 4.220049686691941027, -10.18810118749999738, 80.12500000204836681 ) ) ;
#38070 = CARTESIAN_POINT ( 'NONE',  ( 5.676582343750001591, 71.92708332991934128, -9.832129032723420536 ) ) ;
#38071 = DIRECTION ( 'NONE',  ( -0.000000000000000000, 1.000000000000000000, -0.000000000000000000 ) ) ;
#38072 = CARTESIAN_POINT ( 'NONE',  ( -4.556349186104045934, 11.00000000000000000, 89.21874999999998579 ) ) ;
#38075 = CARTESIAN_POINT ( 'NONE',  ( -4.088227598258586603E-16, 291.3593750017070079, -6.676582343750001591 ) ) ;
#38074 = CARTESIAN_POINT ( 'NONE',  ( 23.99999999999998579, 195.8750000027311842, 169.9999999999999432 ) ) ;
#38073 = CARTESIAN_POINT ( 'NONE',  ( 105.0000000000000000, 242.0000000000000284, 45.00000000000000000 ) ) ;
#38076 = CARTESIAN_POINT ( 'NONE',  ( 11.00000000000000000, 1.347111479062088405E-15, 88.75000000000000000 ) ) ;
#38077 = CARTESIAN_POINT ( 'NONE',  ( -4.999999999999998224, 163.5416666598387110, -8.660254037844389075 ) ) ;
#38078 = CARTESIAN_POINT ( 'NONE',  ( -1.432654583217607414, 198.5000000013656063, 194.5412658750000219 ) ) ;
#38079 = CARTESIAN_POINT ( 'NONE',  ( 5.656854249492380582, 10.49999999590322020, -5.656854249492380582 ) ) ;
#38080 = VECTOR ( 'NONE', #36069, 1000.000000000000000 ) ;
#38081 = CARTESIAN_POINT ( 'NONE',  ( 30.44569435410878810, 194.5625000013656063, 172.4456943541087526 ) ) ;
#38082 = CARTESIAN_POINT ( 'NONE',  ( -2.977408999572654480, 10.87499999795161187, 7.188101187499999156 ) ) ;
#38083 = CARTESIAN_POINT ( 'NONE',  ( 3.313708498984756279, 7.999999999999991118, 27.54905278392014623 ) ) ;
#38084 = CARTESIAN_POINT ( 'NONE',  ( 5.656854249492378806, 7.312500000000000888, 5.656854249492381470 ) ) ;
#38085 = CARTESIAN_POINT ( 'NONE',  ( 5.082755093536326818, 111.5937500020483810, 5.082755093536325042 ) ) ;
#38086 = CARTESIAN_POINT ( 'NONE',  ( -2.216418498320683828, -51.36626494304695711, -48.60390812669793803 ) ) ;
#38087 = LINE ( 'NONE', #73802, #7461 ) ;
#38088 = CARTESIAN_POINT ( 'NONE',  ( 30.44569435410879166, 204.8125000013656063, 172.4456943541087526 ) ) ;
#38089 = CARTESIAN_POINT ( 'NONE',  ( 2.977408999572650927, -7.188101187499990274, 14.33030278187175277 ) ) ;
#38090 = CARTESIAN_POINT ( 'NONE',  ( -1.656854249492405451, 207.4375000027311842, 138.0000000000000568 ) ) ;
#38091 = CARTESIAN_POINT ( 'NONE',  ( 6.951808397369818766E-16, 47.03124999658601979, -11.35316468750000141 ) ) ;
#38092 = CARTESIAN_POINT ( 'NONE',  ( -2.846702928120025788, -44.03308537396124933, 139.1308893626236625 ) ) ;
#38093 = CARTESIAN_POINT ( 'NONE',  ( -10.00000000000000355, 9.583333326505362848, 2.679491924311223183 ) ) ;
#38094 = CARTESIAN_POINT ( 'NONE',  ( 1.656854249492287101, 195.4375000027312126, 202.0000000000001137 ) ) ;
#38095 = VERTEX_POINT ( 'NONE', #61879 ) ;
#38096 = EDGE_CURVE ( 'NONE', #49230, #69413, #21739, .T. ) ;
#38097 = CARTESIAN_POINT ( 'NONE',  ( 6.000000000000023093, 10.39230484541324984, 0.000000000000000000 ) ) ;
#38098 = CARTESIAN_POINT ( 'NONE',  ( -8.311093377946836114, 42.65624999658600558, -8.311093377946837890 ) ) ;
#38099 = CARTESIAN_POINT ( 'NONE',  ( -11.00000000000000000, 4.556349186104045934, 82.09375000409676204 ) ) ;
#38100 = CARTESIAN_POINT ( 'NONE',  ( 2.445694354108784108, 202.5625000013656063, 144.4456943541088663 ) ) ;
#38102 = CARTESIAN_POINT ( 'NONE',  ( -9.832129032723418760, 47.86458332991934839, -5.676582343750004256 ) ) ;
#38101 = CARTESIAN_POINT ( 'NONE',  ( 2.977408999572654480, 99.12500000204838102, 7.188101187499999156 ) ) ;
#38104 = EDGE_CURVE ( 'NONE', #53358, #14457, #26099, .T. ) ;
#38103 = CARTESIAN_POINT ( 'NONE',  ( -7.999999999999989342, -3.313708498984762496, 11.42405277982336465 ) ) ;
#38105 = DIRECTION ( 'NONE',  ( 0.000000000000000000, 1.224646799147353700E-16, 1.000000000000000000 ) ) ;
#38106 = CARTESIAN_POINT ( 'NONE',  ( -11.35316468750000141, 158.4895833299193839, 3.042071309553159963 ) ) ;
#38107 = CARTESIAN_POINT ( 'NONE',  ( -7.320508075688778149, 129.9999999931719969, 7.320508075688769267 ) ) ;
#38108 = CARTESIAN_POINT ( 'NONE',  ( -4.401442555609581635E-16, 103.1562500020483810, -7.188101187500000044 ) ) ;
#38109 = VERTEX_POINT ( 'NONE', #6031 ) ;
#38110 = DIRECTION ( 'NONE',  ( -0.000000000000000000, 1.000000000000000000, -0.000000000000000000 ) ) ;
#38111 = CARTESIAN_POINT ( 'NONE',  ( 11.35316468749999963, 36.30208332991935549, -3.042071309553165293 ) ) ;
#38112 = EDGE_CURVE ( 'NONE', #17726, #19443, #46385, .T. ) ;
#38113 = CARTESIAN_POINT ( 'NONE',  ( -1.656854249492212938, 196.8125000000000284, 193.9999999999999432 ) ) ;
#38114 = ORIENTED_EDGE ( 'NONE', *, *, #3024, .T. ) ;
#38115 = CYLINDRICAL_SURFACE ( 'NONE', #63306, 11.00000000000000000 ) ;
#38116 = CARTESIAN_POINT ( 'NONE',  ( 7.204075437095966983, 7.204075437095967871, 76.09375000204838102 ) ) ;
#38117 = CARTESIAN_POINT ( 'NONE',  ( 12.00000000000000000, -28.00000000000000000, -3.999999999999988010 ) ) ;
#38119 = CARTESIAN_POINT ( 'NONE',  ( -5.676582343750006032, 159.1145833299193839, 9.832129032723418760 ) ) ;
#38118 = CARTESIAN_POINT ( 'NONE',  ( 1.469576158976822172E-15, -7.999999999999991118, 2.892802783920144005 ) ) ;
#38120 = CYLINDRICAL_SURFACE ( 'NONE', #2588, 3.999999999999976019 ) ;
#38121 = CARTESIAN_POINT ( 'NONE',  ( 3.313708498984756279, 7.999999999999991118, 9.417802784329825982 ) ) ;
#38122 = CARTESIAN_POINT ( 'NONE',  ( -24.44677210787030930, -23.15651939682537375, 189.0693633873734143 ) ) ;
#38123 = CARTESIAN_POINT ( 'NONE',  ( -3.042071309553166181, 237.8645833367473301, -11.35316468749999608 ) ) ;
#38124 = CARTESIAN_POINT ( 'NONE',  ( -10.18810118749999916, 4.220049686691934809, 85.93750000204839523 ) ) ;
#38125 = ORIENTED_EDGE ( 'NONE', *, *, #10764, .T. ) ;
#38126 = DIRECTION ( 'NONE',  ( 0.000000000000000000, 0.000000000000000000, 1.000000000000000000 ) ) ;
#38127 = CARTESIAN_POINT ( 'NONE',  ( -7.778174593052023411, 7.778174593052023411, 105.8124999999999858 ) ) ;
#38128 = CARTESIAN_POINT ( 'NONE',  ( -3.042071309553173730, 104.6354166632526699, 11.35316468749999785 ) ) ;
#38129 = CARTESIAN_POINT ( 'NONE',  ( -7.204075437095967871, 7.204075437095967871, 95.96875000204838102 ) ) ;
#38130 = CARTESIAN_POINT ( 'NONE',  ( -8.342170076843785083E-16, 20.18749999863440436, 4.541265875000002339 ) ) ;
#38131 = ORIENTED_EDGE ( 'NONE', *, *, #25894, .T. ) ;
#38132 = ORIENTED_EDGE ( 'NONE', *, *, #7614, .T. ) ;
#38133 = CARTESIAN_POINT ( 'NONE',  ( 3.211159895383561835, 3.562499998634407028, -3.211159895383561835 ) ) ;
#38134 = CARTESIAN_POINT ( 'NONE',  ( -1.320432766682874540E-15, 10.59374999795161187, 7.188101187500000044 ) ) ;
#38135 = CARTESIAN_POINT ( 'NONE',  ( -5.656854249492380582, 114.5000000040967763, -5.656854249492380582 ) ) ;
#38136 = CARTESIAN_POINT ( 'NONE',  ( 10.18810118750000093, -4.220049686691933921, 94.18750000204836681 ) ) ;
#38137 = VECTOR ( 'NONE', #35528, 1000.000000000000000 ) ;
#38138 = CARTESIAN_POINT ( 'NONE',  ( -24.54126587500000056, 202.5000000013656063, 168.5673454167827003 ) ) ;
#38139 = ADVANCED_FACE ( 'NONE', ( #27540 ), #73568, .F. ) ;
#38140 = CARTESIAN_POINT ( 'NONE',  ( -10.00000000000000355, 159.5833333265053398, 2.679491924311223183 ) ) ;
#38141 = CARTESIAN_POINT ( 'NONE',  ( -4.000000000000001776, 5.437500000000001776, -1.656854249492381470 ) ) ;
#38142 = CARTESIAN_POINT ( 'NONE',  ( -1.656854249492383691, 16.43749999726881228, 4.000000000000000888 ) ) ;
#38143 = CARTESIAN_POINT ( 'NONE',  ( -4.541265875000002339, 8.749999998634407916, -1.881053915767121998 ) ) ;
#38144 = CARTESIAN_POINT ( 'NONE',  ( -1.656854249492405451, 204.3125000000000000, 138.0000000000000568 ) ) ;
#38145 = ORIENTED_EDGE ( 'NONE', *, *, #33099, .T. ) ;
#38146 = CARTESIAN_POINT ( 'NONE',  ( -1.432654583217607858, 194.6250000013655779, 201.4587341250000065 ) ) ;
#38147 = CARTESIAN_POINT ( 'NONE',  ( -25.55430564589111597, 197.0625000013656063, 172.4456943541091505 ) ) ;
#38148 = CARTESIAN_POINT ( 'NONE',  ( 2.780723358947928197E-16, 18.56249999863440436, -4.541265875000002339 ) ) ;
#38149 = CARTESIAN_POINT ( 'NONE',  ( 2.775557558920088989E-14, -48.00000000000001421, 151.0000000000000284 ) ) ;
#38150 = CARTESIAN_POINT ( 'NONE',  ( -7.188101187499991163, 2.977408999572646930, 4.392802781871752771 ) ) ;
#38151 = EDGE_LOOP ( 'NONE', ( #35368, #49975, #31810, #2780 ) ) ;
#38152 =( BOUNDED_CURVE ( )  B_SPLINE_CURVE ( 2, ( #40130, #5810, #21652, #67693, #74088, #15990, #28806, #51824, #39021 ),
 .UNSPECIFIED., .F., .F. ) 
 B_SPLINE_CURVE_WITH_KNOTS ( ( 3, 2, 2, 2, 3 ),
 ( 0.4666666666666670626, 0.4750000000000003664, 0.4833333333333337256, 0.4916666666666670849, 0.5000000000000004441 ),
 .UNSPECIFIED. ) 
 CURVE ( )  GEOMETRIC_REPRESENTATION_ITEM ( )  RATIONAL_B_SPLINE_CURVE ( ( 0.9999999999999964473, 0.9238795325112902912, 1.000000000000000000, 0.9238795325112867385, 1.000000000000000000, 0.9238795325112867385, 1.000000000000000000, 0.9238795325112826307, 1.000000000000003997 ) ) 
 REPRESENTATION_ITEM ( '' )  );
#38153 =( BOUNDED_CURVE ( )  B_SPLINE_CURVE ( 2, ( #58242, #24242, #40119, #63499, #45776, #52932, #68788, #35222, #57864 ),
 .UNSPECIFIED., .F., .F. ) 
 B_SPLINE_CURVE_WITH_KNOTS ( ( 3, 2, 2, 2, 3 ),
 ( 0.3676470588235293824, 0.3713235294117646634, 0.3750000000000000000, 0.3786764705882352811, 0.3823529411764705621 ),
 .UNSPECIFIED. ) 
 CURVE ( )  GEOMETRIC_REPRESENTATION_ITEM ( )  RATIONAL_B_SPLINE_CURVE ( ( 1.000000000000001110, 0.9238795325112856283, 1.000000000000000000, 0.9238795325112867385, 1.000000000000000000, 0.9238795325112867385, 1.000000000000000000, 0.9238795325112867385, 1.000000000000000000 ) ) 
 REPRESENTATION_ITEM ( '' )  );
#38154 = VERTEX_POINT ( 'NONE', #27920 ) ;
#38155 = CARTESIAN_POINT ( 'NONE',  ( 7.204075437095968759, -7.204075437095966983, 99.71875000204838102 ) ) ;
#38156 = CARTESIAN_POINT ( 'NONE',  ( 10.00000000000000355, 125.2083333333333428, -2.679491924311227180 ) ) ;
#38157 = CARTESIAN_POINT ( 'NONE',  ( -24.54126587499998280, 199.3750000013656063, 171.4326545832179818 ) ) ;
#38158 = CARTESIAN_POINT ( 'NONE',  ( 11.00000000000000355, -4.556349186104045046, 109.6562500000000000 ) ) ;
#38159 = CARTESIAN_POINT ( 'NONE',  ( -2.445694354108784108, 206.5625000013656063, 195.5543056458912190 ) ) ;
#38160 = CARTESIAN_POINT ( 'NONE',  ( 4.000000000000015987, 203.6250000027312126, 198.0000000000000284 ) ) ;
#38161 = CARTESIAN_POINT ( 'NONE',  ( 7.320508075688774596, 105.6250000000000142, -7.320508075688774596 ) ) ;
#38162 = CARTESIAN_POINT ( 'NONE',  ( -3.313708498984762496, 111.7812500000000000, 7.999999999999998224 ) ) ;
#38163 = CARTESIAN_POINT ( 'NONE',  ( -6.676582343750000703, 293.6718750017070079, 2.765530957082001251 ) ) ;
#38164 = CARTESIAN_POINT ( 'NONE',  ( -2.849036369511732440E-14, 201.2500000000000000, 138.0000000000000568 ) ) ;
#38165 = CARTESIAN_POINT ( 'NONE',  ( -5.082755093536317936, -5.082755093536320601, 14.04905278187175455 ) ) ;
#38166 = ORIENTED_EDGE ( 'NONE', *, *, #68863, .T. ) ;
#38167 = FACE_OUTER_BOUND ( 'NONE', #63302, .T. ) ;
#38168 = CARTESIAN_POINT ( 'NONE',  ( 1.469576158976822172E-15, -7.999999999999991118, 5.705302779823364645 ) ) ;
#38169 = CARTESIAN_POINT ( 'NONE',  ( -5.656854249492381470, 21.74999999590322375, 5.656854249492379694 ) ) ;
#38170 = CARTESIAN_POINT ( 'NONE',  ( -2.445694354108838731, 203.0625000013656063, 144.4456943541088663 ) ) ;
#38171 = CARTESIAN_POINT ( 'NONE',  ( -4.999999999999998224, 183.5416666598387110, -8.660254037844389075 ) ) ;
#38173 = CARTESIAN_POINT ( 'NONE',  ( 3.458734124999960358, 203.6875000013656063, 142.0000000000000568 ) ) ;
#38172 = CARTESIAN_POINT ( 'NONE',  ( -10.99999999999991829, 4.556349186104124982, 111.9062499999999858 ) ) ;
#38174 = CARTESIAN_POINT ( 'NONE',  ( 9.832129032723416984, 262.1354166700806445, -5.676582343750003368 ) ) ;
#38175 = CARTESIAN_POINT ( 'NONE',  ( -8.000000000000000000, 114.6875000040967763, 0.000000000000000000 ) ) ;
#38176 = CARTESIAN_POINT ( 'NONE',  ( -8.660254037844390851, 94.79166665983871098, 4.999999999999998224 ) ) ;
#38177 = CARTESIAN_POINT ( 'NONE',  ( -2.679491924311235618, 223.5416666666666856, 10.00000000000000000 ) ) ;
#38178 = CARTESIAN_POINT ( 'NONE',  ( -5.082755093536319713, 5.082755093536319713, 6.174052781871754547 ) ) ;
#38179 = CARTESIAN_POINT ( 'NONE',  ( 11.35316468749999785, 200.8854166632526699, 3.042071309553174174 ) ) ;
#38180 = CARTESIAN_POINT ( 'NONE',  ( -10.00000000000000000, 134.1666666598387110, -2.679491924311229845 ) ) ;
#38181 = CARTESIAN_POINT ( 'NONE',  ( 3.211159895383560947, 7.187499998634407028, 3.211159895383562723 ) ) ;
#38182 = CARTESIAN_POINT ( 'NONE',  ( 1.102182119232618108E-15, 290.2500000000000000, 6.000000000000001776 ) ) ;
#38184 = CARTESIAN_POINT ( 'NONE',  ( 1.734723475976807489E-15, -16.00000000000000355, 38.34805510287551300 ) ) ;
#38183 = CARTESIAN_POINT ( 'NONE',  ( 0.000000000000000000, 0.000000000000000000, 118.0000000000000000 ) ) ;
#38185 = ORIENTED_EDGE ( 'NONE', *, *, #8384, .F. ) ;
#38186 = CARTESIAN_POINT ( 'NONE',  ( -2.445694354108840063, 205.0625000013656063, 139.5543056458912190 ) ) ;
#38187 = CARTESIAN_POINT ( 'NONE',  ( -3.042071309553173730, 9.322916663252685865, 11.35316468749999785 ) ) ;
#38188 = CARTESIAN_POINT ( 'NONE',  ( 11.00000000000000000, 1.347111479062088405E-15, 99.43750000409677625 ) ) ;
#38189 = CARTESIAN_POINT ( 'NONE',  ( 2.828427124746190291, 19.62499999726881228, 2.828427124746192067 ) ) ;
#38190 = CARTESIAN_POINT ( 'NONE',  ( -29.43265458321770822, 202.5000000013656063, 166.5412658750003914 ) ) ;
#38191 = DIRECTION ( 'NONE',  ( 1.000000000000000000, 0.000000000000000000, 0.000000000000000000 ) ) ;
#38193 = CARTESIAN_POINT ( 'NONE',  ( 8.311093377946837890, 1.406249996586016238, -8.311093377946837890 ) ) ;
#38192 = CARTESIAN_POINT ( 'NONE',  ( -7.188101187500000933, 119.5625000020483810, -2.977408999572650483 ) ) ;
#38195 = ADVANCED_FACE ( 'NONE', ( #56978 ), #62615, .T. ) ;
#38194 = DIRECTION ( 'NONE',  ( -0.000000000000000000, -0.000000000000000000, 1.000000000000000000 ) ) ;
#38196 = CARTESIAN_POINT ( 'NONE',  ( -11.35316468750000141, 118.2812499965860269, -1.390361679473963753E-15 ) ) ;
#38197 = CARTESIAN_POINT ( 'NONE',  ( 10.00000000000000000, 86.66666665983869677, 2.679491924311236062 ) ) ;
#38198 = CARTESIAN_POINT ( 'NONE',  ( -5.082755093536325930, 89.46875000204838102, -5.082755093536325930 ) ) ;
#38199 = CARTESIAN_POINT ( 'NONE',  ( -1.881053915767124440, 19.12499999863441147, 4.541265875000001451 ) ) ;
#38200 = CARTESIAN_POINT ( 'NONE',  ( -7.999999999999989342, -3.313708498984762496, 25.11155278392014978 ) ) ;
#38201 = CARTESIAN_POINT ( 'NONE',  ( -2.679491924311235174, 40.41666665983869677, 10.00000000000000000 ) ) ;
#38202 = ORIENTED_EDGE ( 'NONE', *, *, #23518, .F. ) ;
#38203 = CARTESIAN_POINT ( 'NONE',  ( -8.987638501917114553, 226.0000000000000000, -4.433077647033027091 ) ) ;
#38204 = EDGE_CURVE ( 'NONE', #9455, #4200, #67582, .T. ) ;
#38205 = CARTESIAN_POINT ( 'NONE',  ( 2.765530957082001251, 289.9218750017069510, 6.676582343750000703 ) ) ;
#38206 = PRESENTATION_STYLE_ASSIGNMENT (( #67250 ) ) ;
#38207 = CARTESIAN_POINT ( 'NONE',  ( -5.656854249492375253, 5.656854249492375253, 27.69905278432982598 ) ) ;
#38208 = CARTESIAN_POINT ( 'NONE',  ( 9.797174393178825657E-16, 75.00000000000000000, -8.000000000000000000 ) ) ;
#38209 = CARTESIAN_POINT ( 'NONE',  ( -8.660254037844390851, 209.7916666598387110, 4.999999999999998224 ) ) ;
#38210 = DIRECTION ( 'NONE',  ( -0.000000000000000000, -0.000000000000000000, 1.000000000000000000 ) ) ;
#38211 = CARTESIAN_POINT ( 'NONE',  ( -10.18810118749999738, -4.220049686691941915, 105.6250000020483668 ) ) ;
#38212 = ORIENTED_EDGE ( 'NONE', *, *, #25808, .F. ) ;
#38213 = CARTESIAN_POINT ( 'NONE',  ( -2.828427124746153876, 198.0000000027312126, 195.1715728752538439 ) ) ;
#38214 = CARTESIAN_POINT ( 'NONE',  ( -11.35316468749999785, 158.3854166632526699, -3.042071309553167957 ) ) ;
#38215 = CARTESIAN_POINT ( 'NONE',  ( 1.432654583217662259, 196.1250000013656063, 194.5412658750000219 ) ) ;
#38216 = CARTESIAN_POINT ( 'NONE',  ( 2.754378923186476579E-14, 204.4375000013656063, 194.5412658750000219 ) ) ;
#38217 = CARTESIAN_POINT ( 'NONE',  ( -7.188101187500000044, 124.5312500020483810, 0.000000000000000000 ) ) ;
#38218 = CARTESIAN_POINT ( 'NONE',  ( -11.35316468750000141, 58.80208332991933418, 3.042071309553159963 ) ) ;
#38219 = EDGE_LOOP ( 'NONE', ( #65226, #37916, #54524, #45659 ) ) ;
#38220 = CARTESIAN_POINT ( 'NONE',  ( -7.204075437095965206, -7.204075437095968759, 115.8437500020483810 ) ) ;
#38221 = CARTESIAN_POINT ( 'NONE',  ( 3.211159895383560947, 7.312499998634407028, 3.211159895383562723 ) ) ;
#38222 = ORIENTED_EDGE ( 'NONE', *, *, #65095, .F. ) ;
#38223 = VECTOR ( 'NONE', #21196, 1000.000000000000000 ) ;
#38224 = CARTESIAN_POINT ( 'NONE',  ( 7.188101187500000044, 21.46874999795161543, 0.000000000000000000 ) ) ;
#38225 = CARTESIAN_POINT ( 'NONE',  ( 6.000000000000003553, 287.5000000034140157, 2.485281374238571317 ) ) ;
#38226 = CARTESIAN_POINT ( 'NONE',  ( 7.320508075688771044, 66.24999999317203958, 7.320508075688775484 ) ) ;
#38227 = CARTESIAN_POINT ( 'NONE',  ( 2.977408999572651815, 20.06249999795161543, 7.188101187500000933 ) ) ;
#38228 = CARTESIAN_POINT ( 'NONE',  ( -5.082755093536319713, 5.082755093536319713, 5.799052781871753659 ) ) ;
#38229 = CARTESIAN_POINT ( 'NONE',  ( -4.220049686691937474, -10.18810118749999738, 111.8125000020484094 ) ) ;
#38230 = CLOSED_SHELL ( 'NONE', ( #36740, #41700, #66186, #4319, #17487, #34483 ) ) ;
#38231 = CARTESIAN_POINT ( 'NONE',  ( 3.000000000000001332, -45.00000000000001421, 151.2383369607063344 ) ) ;
#38232 = CARTESIAN_POINT ( 'NONE',  ( -4.000000000000001776, 7.249999997268813168, -4.898587196589415787E-16 ) ) ;
#38233 = CARTESIAN_POINT ( 'NONE',  ( -29.65685424949246496, 208.1875000027311842, 166.0000000000004263 ) ) ;
#38234 = ORIENTED_EDGE ( 'NONE', *, *, #26499, .T. ) ;
#38235 = CARTESIAN_POINT ( 'NONE',  ( -1.432654583217607858, 205.6250000013656063, 201.4587341250000065 ) ) ;
#38236 = CARTESIAN_POINT ( 'NONE',  ( -27.99999999999992184, 207.9375000013656063, 173.4587341250003760 ) ) ;
#38237 = AXIS2_PLACEMENT_3D ( 'NONE', #26427, #28676, #45288 ) ;
#38238 = CARTESIAN_POINT ( 'NONE',  ( -4.541265875000003227, 5.874999998634406140, 1.881053915767121110 ) ) ;
#38239 = CARTESIAN_POINT ( 'NONE',  ( -5.656854249492373476, -5.656854249492376141, 10.01780277982336465 ) ) ;
#38240 = CARTESIAN_POINT ( 'NONE',  ( 7.188101187499992051, 8.802885111219154394E-16, 27.73655278187175455 ) ) ;
#38241 = VERTEX_POINT ( 'NONE', #41103 ) ;
#38242 = EDGE_CURVE ( 'NONE', #10672, #3255, #32161, .T. ) ;
#38243 = VERTEX_POINT ( 'NONE', #30883 ) ;
#38244 = CARTESIAN_POINT ( 'NONE',  ( 4.220049686691941027, -10.18810118749999738, 114.6250000020483810 ) ) ;
#38245 = CARTESIAN_POINT ( 'NONE',  ( -4.999999999999998224, 201.6666666666666856, -8.660254037844389075 ) ) ;
#38246 = CARTESIAN_POINT ( 'NONE',  ( 1.432654583217662481, 205.1250000013656347, 194.5412658750000219 ) ) ;
#38248 =( BOUNDED_CURVE ( )  B_SPLINE_CURVE ( 2, ( #46115, #69133, #29144, #494, #40461, #18560, #862 ),
 .UNSPECIFIED., .F., .F. ) 
 B_SPLINE_CURVE_WITH_KNOTS ( ( 3, 2, 2, 3 ),
 ( 0.000000000000000000, 0.009259259259259060987, 0.01851851851851812197, 0.02777777777777718296 ),
 .UNSPECIFIED. ) 
 CURVE ( )  GEOMETRIC_REPRESENTATION_ITEM ( )  RATIONAL_B_SPLINE_CURVE ( ( 1.000000000000000000, 0.9659258262890683122, 1.000000000000000000, 0.9659258262890683122, 1.000000000000000000, 0.9659258262890705327, 0.9999999999999977796 ) ) 
 REPRESENTATION_ITEM ( '' )  );
#38247 = CARTESIAN_POINT ( 'NONE',  ( 26.56734541678237704, 199.3750000013656063, 173.4587341249998929 ) ) ;
#38249 = CARTESIAN_POINT ( 'NONE',  ( 10.00000000000000000, 69.79166666666664298, 2.679491924311236062 ) ) ;
#38250 = CARTESIAN_POINT ( 'NONE',  ( 7.188101187500000044, 96.78125000204838102, -8.802885111219163269E-16 ) ) ;
#38251 = CARTESIAN_POINT ( 'NONE',  ( -2.485281374238571761, 292.8125000000000000, -6.000000000000003553 ) ) ;
#38252 = CARTESIAN_POINT ( 'NONE',  ( 5.000000000000000000, -52.35862550122924830, -48.98731492261435250 ) ) ;
#38253 =( BOUNDED_CURVE ( )  B_SPLINE_CURVE ( 2, ( #3532, #61243, #3160, #55973, #73313, #43892, #38239, #21246, #44640 ),
 .UNSPECIFIED., .F., .F. ) 
 B_SPLINE_CURVE_WITH_KNOTS ( ( 3, 2, 2, 2, 3 ),
 ( 0.6578947368421053099, 0.6644736842105263275, 0.6710526315789473450, 0.6776315789473684736, 0.6842105263157894912 ),
 .UNSPECIFIED. ) 
 CURVE ( )  GEOMETRIC_REPRESENTATION_ITEM ( )  RATIONAL_B_SPLINE_CURVE ( ( 1.000000000000000000, 0.9238795325112867385, 1.000000000000000000, 0.9238795325112867385, 1.000000000000000000, 0.9238795325112867385, 1.000000000000000000, 0.9238795325112867385, 1.000000000000000000 ) ) 
 REPRESENTATION_ITEM ( '' )  );
#38254 = ORIENTED_EDGE ( 'NONE', *, *, #69377, .F. ) ;
#38255 = EDGE_CURVE ( 'NONE', #20942, #48097, #36936, .T. ) ;
#38256 = EDGE_CURVE ( 'NONE', #28600, #28645, #39613, .T. ) ;
#38257 = CARTESIAN_POINT ( 'NONE',  ( 1.469576158976823947E-15, 115.0625000040967905, 8.000000000000000000 ) ) ;
#38258 = CARTESIAN_POINT ( 'NONE',  ( -1.656854249492403008, 201.8125000027312126, 146.0000000000000284 ) ) ;
#38259 = CARTESIAN_POINT ( 'NONE',  ( -4.556349186104048599, -10.99999999999999822, 77.78125000000001421 ) ) ;
#38260 = CARTESIAN_POINT ( 'NONE',  ( 2.020667218593132706E-15, -11.00000000000000000, 94.37499999999998579 ) ) ;
#38261 = CARTESIAN_POINT ( 'NONE',  ( -5.000000000000000888, 254.1666666666666572, -8.660254037844387298 ) ) ;
#38262 = LINE ( 'NONE', #5416, #11392 ) ;
#38263 = CARTESIAN_POINT ( 'NONE',  ( 10.00000000000000178, 185.2083333333332860, -2.679491924311226736 ) ) ;
#38264 = CARTESIAN_POINT ( 'NONE',  ( 10.00000000000000178, 1.874999993172032697, 0.000000000000000000 ) ) ;
#38265 = CARTESIAN_POINT ( 'NONE',  ( -7.188101187499992051, 0.000000000000000000, 21.36155278187175455 ) ) ;
#38266 = CARTESIAN_POINT ( 'NONE',  ( 8.311093377946834337, 160.4687499965860127, 8.311093377946839666 ) ) ;
#38267 = DIRECTION ( 'NONE',  ( -1.000000000000000000, -0.000000000000000000, -0.000000000000000000 ) ) ;
#38268 = CARTESIAN_POINT ( 'NONE',  ( 1.102182119232618108E-15, 294.2500000000000000, 6.000000000000001776 ) ) ;
#38269 = CARTESIAN_POINT ( 'NONE',  ( -0.9677553211737895955, -42.15360157663097596, 151.0237924948687862 ) ) ;
#38271 = CARTESIAN_POINT ( 'NONE',  ( -15.99999999999999645, 15.99999999999999645, 20.00000000000000000 ) ) ;
#38270 = CARTESIAN_POINT ( 'NONE',  ( 6.123233995736767268E-16, 83.12499999317203958, -10.00000000000000178 ) ) ;
#38272 = AXIS2_PLACEMENT_3D ( 'NONE', #28718, #57037, #51733 ) ;
#38273 = ORIENTED_EDGE ( 'NONE', *, *, #53263, .F. ) ;
#38274 = CARTESIAN_POINT ( 'NONE',  ( -9.832129032723418760, 28.17708332991935194, -5.676582343750004256 ) ) ;
#38275 = PLANE ( 'NONE',  #73328 ) ;
#38276 = CARTESIAN_POINT ( 'NONE',  ( 8.660254037844385522, 31.45833332650536818, 5.000000000000005329 ) ) ;
#38277 = DIRECTION ( 'NONE',  ( 0.000000000000000000, 0.000000000000000000, 1.000000000000000000 ) ) ;
#38278 = CARTESIAN_POINT ( 'NONE',  ( -2.754378923186476579E-14, 204.1875000013656063, 145.4587341250000350 ) ) ;
#38279 =( BOUNDED_CURVE ( )  B_SPLINE_CURVE ( 2, ( #41882, #47534, #64893, #443, #58513, #35137, #69454, #70200, #12831 ),
 .UNSPECIFIED., .F., .F. ) 
 B_SPLINE_CURVE_WITH_KNOTS ( ( 3, 2, 2, 2, 3 ),
 ( 0.3529411764705882026, 0.3566176470588234837, 0.3602941176470587648, 0.3639705882352940458, 0.3676470588235293824 ),
 .UNSPECIFIED. ) 
 CURVE ( )  GEOMETRIC_REPRESENTATION_ITEM ( )  RATIONAL_B_SPLINE_CURVE ( ( 1.000000000000001110, 0.9238795325112856283, 1.000000000000000000, 0.9238795325112867385, 1.000000000000000000, 0.9238795325112867385, 1.000000000000000000, 0.9238795325112878487, 0.9999999999999988898 ) ) 
 REPRESENTATION_ITEM ( '' )  );
#38280 = CARTESIAN_POINT ( 'NONE',  ( 2.679491924311222739, 45.83333332650537528, 10.00000000000000355 ) ) ;
#38281 = CARTESIAN_POINT ( 'NONE',  ( -2.977408999572651815, 107.9375000020483810, 7.188101187500000933 ) ) ;
#38282 = CARTESIAN_POINT ( 'NONE',  ( 3.211159895383561835, 7.562499998634407028, -3.211159895383561835 ) ) ;
#38283 = DIRECTION ( 'NONE',  ( -0.000000000000000000, 1.000000000000000000, -0.000000000000000000 ) ) ;
#38284 = CARTESIAN_POINT ( 'NONE',  ( 7.999999999999991118, 3.313708498984757611, 10.67405277982336465 ) ) ;
#38286 = CARTESIAN_POINT ( 'NONE',  ( 2.449293598294707893E-16, 3.999999997268813168, -4.000000000000001776 ) ) ;
#38285 = CARTESIAN_POINT ( 'NONE',  ( 3.426202465283471721, 194.4587341250000350, 141.5267364219330943 ) ) ;
#38287 = EDGE_LOOP ( 'NONE', ( #28814, #70137, #34070, #57884 ) ) ;
#38288 = ORIENTED_EDGE ( 'NONE', *, *, #51817, .F. ) ;
#38289 = CARTESIAN_POINT ( 'NONE',  ( -5.000000000000000888, -66.79212039439843807, 23.29662735513404925 ) ) ;
#38290 = CARTESIAN_POINT ( 'NONE',  ( -7.778174593052020747, -7.778174593052023411, 82.18750000000000000 ) ) ;
#38291 = CARTESIAN_POINT ( 'NONE',  ( -23.89971782876810380, -40.43634890630519862, 150.2388575686201762 ) ) ;
#38292 = CARTESIAN_POINT ( 'NONE',  ( 8.311093377946834337, 135.1562499965860411, 8.311093377946839666 ) ) ;
#38293 = EDGE_LOOP ( 'NONE', ( #28908, #40246, #8490, #24407, #40609, #1957 ) ) ;
#38294 = CARTESIAN_POINT ( 'NONE',  ( 7.999999999999991118, -3.647060904601942273E-05, 4.767801752109533275 ) ) ;
#38295 = CARTESIAN_POINT ( 'NONE',  ( -10.18810118749999916, 0.000000000000000000, 90.15625000204838102 ) ) ;
#38296 = CARTESIAN_POINT ( 'NONE',  ( 5.656854249492374365, 5.656854249492375253, 19.95530278392014623 ) ) ;
#38297 = CARTESIAN_POINT ( 'NONE',  ( -3.458734124999960358, 194.6875000013655779, 198.0000000000000284 ) ) ;
#38298 = CARTESIAN_POINT ( 'NONE',  ( -7.320508075688773708, 153.7499999931720538, -7.320508075688774596 ) ) ;
#38300 = CARTESIAN_POINT ( 'NONE',  ( -11.35316468749999785, 123.0729166632526983, -3.042071309553167957 ) ) ;
#38299 = CARTESIAN_POINT ( 'NONE',  ( 0.6686838642329748783, 220.0000000000000284, 10.97965672913483814 ) ) ;
#38301 = CARTESIAN_POINT ( 'NONE',  ( 8.660254037844389075, 147.2916666598387110, -5.000000000000000000 ) ) ;
#38302 = ORIENTED_EDGE ( 'NONE', *, *, #17408, .F. ) ;
#38303 = CIRCLE ( 'NONE', #51532, 20.00000000000000355 ) ;
#38304 = LINE ( 'NONE', #37557, #65984 ) ;
#38305 =( BOUNDED_CURVE ( )  B_SPLINE_CURVE ( 2, ( #294, #6314, #52327, #19454, #13776, #2115, #71131, #60191, #3232 ),
 .UNSPECIFIED., .F., .F. ) 
 B_SPLINE_CURVE_WITH_KNOTS ( ( 3, 2, 2, 2, 3 ),
 ( 0.8977272727272727071, 0.9034090909090909394, 0.9090909090909091717, 0.9147727272727274039, 0.9204545454545455252 ),
 .UNSPECIFIED. ) 
 CURVE ( )  GEOMETRIC_REPRESENTATION_ITEM ( )  RATIONAL_B_SPLINE_CURVE ( ( 1.000000000000000000, 0.9238795325112867385, 1.000000000000000000, 0.9238795325112867385, 1.000000000000000000, 0.9238795325112867385, 1.000000000000000000, 0.9238795325112852952, 1.000000000000001554 ) ) 
 REPRESENTATION_ITEM ( '' )  );
#38306 = CARTESIAN_POINT ( 'NONE',  ( -17.06637649525482914, 182.9342320177846375, 144.0228969870641151 ) ) ;
#38307 = CARTESIAN_POINT ( 'NONE',  ( 6.951808397369818766E-16, 112.3437499965860127, -11.35316468750000141 ) ) ;
#38308 = CARTESIAN_POINT ( 'NONE',  ( 3.458734125000016313, 204.8750000013656063, 199.4326545832176976 ) ) ;
#38309 = CARTESIAN_POINT ( 'NONE',  ( 5.082755093536324154, 20.15624999795161543, 5.082755093536326818 ) ) ;
#38310 = CARTESIAN_POINT ( 'NONE',  ( 4.220049686691941027, -10.18810118749999738, 85.00000000204838102 ) ) ;
#38311 = CARTESIAN_POINT ( 'NONE',  ( -9.832129032723418760, 18.17708332991935194, -5.676582343750004256 ) ) ;
#38312 = VERTEX_POINT ( 'NONE', #24104 ) ;
#38313 = CARTESIAN_POINT ( 'NONE',  ( 8.000000000000000000, 90.03125000409679046, -3.313708498984762496 ) ) ;
#38314 = CARTESIAN_POINT ( 'NONE',  ( -8.008118988124989457, -3.317071493978883900, 22.10686528394063188 ) ) ;
#38315 = CARTESIAN_POINT ( 'NONE',  ( -11.00000000000000533, 11.00000000000000000, 41.99999999999999289 ) ) ;
#38316 = CARTESIAN_POINT ( 'NONE',  ( 1.656854249492263564, 200.8125000000000284, 146.0000000000001421 ) ) ;
#38317 = CARTESIAN_POINT ( 'NONE',  ( 7.188101187499999156, 1.874999997951610098, 2.977408999572654924 ) ) ;
#38318 = CARTESIAN_POINT ( 'NONE',  ( 1.226468279477575784E-15, 289.7031250017069510, 6.676582343750001591 ) ) ;
#38319 = LINE ( 'NONE', #49631, #50959 ) ;
#38320 = CARTESIAN_POINT ( 'NONE',  ( -5.082755093536325042, 1.406249997951610098, -5.082755093536325930 ) ) ;
#38321 = ORIENTED_EDGE ( 'NONE', *, *, #141, .F. ) ;
#38322 = CARTESIAN_POINT ( 'NONE',  ( -8.311093377946841443, 144.2187499965860127, 8.311093377946830785 ) ) ;
#38323 = CARTESIAN_POINT ( 'NONE',  ( 10.18810118749999916, 4.220049686691935698, 77.50000000204839523 ) ) ;
#38324 = CARTESIAN_POINT ( 'NONE',  ( -29.43265458321766559, 195.5000000013655779, 166.5412658750003629 ) ) ;
#38325 = DIRECTION ( 'NONE',  ( 0.000000000000000000, 0.000000000000000000, 1.000000000000000000 ) ) ;
#38326 = CARTESIAN_POINT ( 'NONE',  ( 4.541265875000002339, 17.43749999863440792, 0.000000000000000000 ) ) ;
#38327 = ORIENTED_EDGE ( 'NONE', *, *, #34464, .F. ) ;
#38328 = CARTESIAN_POINT ( 'NONE',  ( 4.000000000000015099, 204.6875000027312126, 196.3431457505076594 ) ) ;
#38329 = CARTESIAN_POINT ( 'NONE',  ( 2.445694354108783219, 196.8125000013656063, 139.5543056458912190 ) ) ;
#38330 = CARTESIAN_POINT ( 'NONE',  ( -27.99999999999991473, 205.6250000027312126, 174.0000000000003695 ) ) ;
#38331 = AXIS2_PLACEMENT_3D ( 'NONE', #14671, #54691, #30557 ) ;
#38332 = EDGE_CURVE ( 'NONE', #49983, #66273, #18828, .T. ) ;
#38333 = CARTESIAN_POINT ( 'NONE',  ( -3.313708498984757611, 7.999999999999991118, 14.04905277982336465 ) ) ;
#38334 = ORIENTED_EDGE ( 'NONE', *, *, #73848, .F. ) ;
#38335 = CARTESIAN_POINT ( 'NONE',  ( 7.188101187500000933, 14.06249999795161365, -2.977408999572650483 ) ) ;
#38336 = CARTESIAN_POINT ( 'NONE',  ( -29.64466390338454715, -12.04383764958612701, 179.1111867292734985 ) ) ;
#38337 = CARTESIAN_POINT ( 'NONE',  ( 0.000000000000000000, 0.000000000000000000, 0.000000000000000000 ) ) ;
#38338 = CARTESIAN_POINT ( 'NONE',  ( 5.676582343750001591, 186.6145833299193839, -9.832129032723420536 ) ) ;
#38339 = CARTESIAN_POINT ( 'NONE',  ( 2.977408999572654480, 111.5000000020483810, 7.188101187499999156 ) ) ;
#38340 = CARTESIAN_POINT ( 'NONE',  ( 1.656854249492407449, 207.4375000027312126, 202.0000000000000000 ) ) ;
#38341 = CARTESIAN_POINT ( 'NONE',  ( -2.765530957081996810, 289.2656250017069510, -6.676582343750002480 ) ) ;
#38343 = DIRECTION ( 'NONE',  ( 0.000000000000000000, 0.000000000000000000, 1.000000000000000000 ) ) ;
#38342 = LINE ( 'NONE', #27011, #63485 ) ;
#38344 = ORIENTED_EDGE ( 'NONE', *, *, #58222, .T. ) ;
#38345 = CARTESIAN_POINT ( 'NONE',  ( 2.085542519210945334E-15, 260.1562500034140157, 11.35316468749999963 ) ) ;
#38346 = CARTESIAN_POINT ( 'NONE',  ( -7.188101187499991163, 2.977408999572646930, 22.76780278187175455 ) ) ;
#38347 = DIRECTION ( 'NONE',  ( -0.000000000000000000, -0.000000000000000000, 1.000000000000000000 ) ) ;
#38348 = CARTESIAN_POINT ( 'NONE',  ( -2.219371606097689131, -67.78152867896241673, -20.18750705526169043 ) ) ;
#38349 = CARTESIAN_POINT ( 'NONE',  ( -2.445694354108784108, 200.5625000013656063, 195.5543056458912190 ) ) ;
#38350 = DIRECTION ( 'NONE',  ( -0.000000000000000000, 1.000000000000000000, -0.000000000000000000 ) ) ;
#38351 = DIRECTION ( 'NONE',  ( -0.000000000000000000, -0.000000000000000000, 1.000000000000000000 ) ) ;
#38352 = CARTESIAN_POINT ( 'NONE',  ( 3.313708498984760720, 93.03124999999998579, -8.000000000000000000 ) ) ;
#38353 = CARTESIAN_POINT ( 'NONE',  ( 11.35316468749999963, 116.3020833299193413, -3.042071309553165293 ) ) ;
#38354 = CARTESIAN_POINT ( 'NONE',  ( -5.000000000000000000, -14.32120916179462711, -69.86289779849464310 ) ) ;
#38355 = CARTESIAN_POINT ( 'NONE',  ( 7.778174593052023411, -7.778174593052021635, 69.06249999999998579 ) ) ;
#38358 = LINE ( 'NONE', #50042, #53118 ) ;
#38357 = CARTESIAN_POINT ( 'NONE',  ( 29.43265458321766559, 202.5000000013656063, 173.4587341249998929 ) ) ;
#38356 = CARTESIAN_POINT ( 'NONE',  ( 25.55430564589119058, 197.3125000013656063, 167.5543056458910485 ) ) ;
#38359 = EDGE_LOOP ( 'NONE', ( #47230, #69132, #22890, #37189, #41467, #4976 ) ) ;
#38360 = EDGE_CURVE ( 'NONE', #24671, #39497, #58831, .T. ) ;
#38361 = EDGE_CURVE ( 'NONE', #1524, #33755, #65139, .T. ) ;
#38362 = CARTESIAN_POINT ( 'NONE',  ( 10.00943074283379097, 224.9691878336754769, 0.3937656040914069289 ) ) ;
#38363 = CARTESIAN_POINT ( 'NONE',  ( 10.99999999999998046, -4.556349186104063698, 114.3437500040967763 ) ) ;
#38365 = EDGE_CURVE ( 'NONE', #65401, #72057, #48646, .T. ) ;
#38364 = CARTESIAN_POINT ( 'NONE',  ( 3.458734124999959914, 196.3750000013656063, 143.4326545832176976 ) ) ;
#38366 = CARTESIAN_POINT ( 'NONE',  ( 24.54126587499998990, 196.4375000013655779, 169.9999999999998863 ) ) ;
#38367 = CARTESIAN_POINT ( 'NONE',  ( -9.832129032723418760, 208.1770833299193555, -5.676582343750004256 ) ) ;
#38368 = CARTESIAN_POINT ( 'NONE',  ( -54.00000000000000711, 242.0000000000000284, 20.00000000000003197 ) ) ;
#38369 = CARTESIAN_POINT ( 'NONE',  ( 11.03609750322952898, 225.9999999999999716, 2.202692091203484637 ) ) ;
#38370 = CARTESIAN_POINT ( 'NONE',  ( -4.541265875000003227, 16.87499999863440436, 1.881053915767121110 ) ) ;
#38371 = CARTESIAN_POINT ( 'NONE',  ( 26.56734541678237704, 195.2500000013656063, 166.5412658749999650 ) ) ;
#38372 = CARTESIAN_POINT ( 'NONE',  ( -5.656854249492373476, -5.656854249492376141, 25.01780277982336642 ) ) ;
#38374 = CARTESIAN_POINT ( 'NONE',  ( 105.0000000000000000, 242.0000000000000284, 45.00000000000000000 ) ) ;
#38373 = CARTESIAN_POINT ( 'NONE',  ( -47.32259252271279593, 38.77329591270029141, 65.76194439203462139 ) ) ;
#38375 = CARTESIAN_POINT ( 'NONE',  ( 5.676582343750001591, 91.61458332991935549, -9.832129032723420536 ) ) ;
#38376 = ORIENTED_EDGE ( 'NONE', *, *, #56977, .T. ) ;
#38377 =( BOUNDED_CURVE ( )  B_SPLINE_CURVE ( 2, ( #54696, #25623, #37336, #3005, #25251, #48268, #59966, #71275, #65624, #8284, #31293, #54324, #71647, #19968, #25986, #20335, #61464, #55443, #27495, #50508, #67127, #10156, #73899, #27127, #15422, #15054, #21829, #61085, #32432, #38461, #9789, #39201, #56935, #68243, #22204, #5251, #4136, #55819, #9414, #27874, #50142, #73522, #10528, #56190, #4502, #56564, #45231, #21095, #62203, #73157, #33193, #26754, #44862, #16535, #44487, #39576, #3753, #33560, #38834, #67867, #21465, #32811, #67500, #4879, #28251, #62571, #10902, #51259, #15799, #61837, #49771, #50885, #16160, #45598, #72788, #22578, #33936, #74269, #38088, #44118, #35050, #28996, #63690, #5622, #58062, #70114, #23332, #24067, #11275, #18049, #34307, #17297, #16922, #45973, #22965, #7103, #64446, #41434, #1090, #352, #41064, #721, #39945, #68988, #62950, #69734, #52754, #52014, #29739, #47077, #40315, #46344, #64074, #12017, #23705, #40688, #12382, #35417, #46709, #69361, #58427, #6735, #68613, #17671, #57311, #18420, #12747, #35778, #30111, #57686, #6373, #24442, #63319, #28622, #29379, #69508, #53128, #1461, #11645, #58793, #34680, #52386, #51635, #5994, #25538, #53862, #47450, #7474, #30479, #20248, #31961, #25906, #25168, #14590, #66283, #8949, #59165, #54238, #60248, #31590, #53496, #14214, #1813, #48551, #37252, #41797, #54611, #70474, #71561, #2174, #59888, #13108, #8574, #31213, #64806, #2918, #48923, #36144, #42529, #71936, #59523, #43268, #36514, #37629, #24799, #60627, #54986, #3293, #8201, #18792, #47813, #70836, #30841, #19148, #42151, #19883, #48185, #65164, #13475, #7836, #71192, #19511, #65543, #13834, #36880, #42889, #2547, #65908, #50422, #67412, #4411, #33105, #72317, #39484, #27041, #20630, #61376, #49686, #9703, #10810, #50794, #38752, #66657, #39112, #10070, #43646, #62116, #33470, #14964, #21374, #10440, #38371, #3663, #26279, #56102, #38001, #60999, #26663, #72701, #73436, #68151 ),
 .UNSPECIFIED., .F., .F. ) 
 B_SPLINE_CURVE_WITH_KNOTS ( ( 3, 2, 2, 2, 2, 2, 2, 2, 2, 2, 2, 2, 2, 2, 2, 2, 2, 2, 2, 2, 2, 2, 2, 2, 2, 2, 2, 2, 2, 2, 2, 2, 2, 2, 2, 2, 2, 2, 2, 2, 2, 2, 2, 2, 2, 2, 2, 2, 2, 2, 2, 2, 2, 2, 2, 2, 2, 2, 2, 2, 2, 2, 2, 2, 2, 2, 2, 2, 2, 2, 2, 2, 2, 2, 2, 2, 2, 2, 2, 2, 2, 2, 2, 2, 2, 2, 2, 2, 2, 2, 2, 2, 2, 2, 2, 2, 2, 2, 2, 2, 2, 2, 2, 2, 2, 2, 2, 2, 2, 2, 2, 2, 2, 2, 2, 2, 2, 2, 2, 2, 3 ),
 ( 0.000000000000000000, 0.008333333333333333218, 0.01666666666666666644, 0.02500000000000000139, 0.03333333333333333287, 0.04166666666666666435, 0.05000000000000000278, 0.05833333333333333426, 0.06666666666666666574, 0.07499999999999999722, 0.08333333333333332871, 0.09166666666666666019, 0.1000000000000000056, 0.1083333333333333370, 0.1166666666666666685, 0.1250000000000000000, 0.1333333333333333315, 0.1416666666666666630, 0.1499999999999999944, 0.1583333333333333259, 0.1666666666666666574, 0.1749999999999999889, 0.1833333333333333204, 0.1916666666666666796, 0.2000000000000000111, 0.2083333333333333426, 0.2166666666666666741, 0.2250000000000000056, 0.2333333333333333370, 0.2416666666666666685, 0.2500000000000000000, 0.2583333333333333592, 0.2666666666666666630, 0.2750000000000000222, 0.2833333333333333259, 0.2916666666666666852, 0.2999999999999999889, 0.3083333333333333481, 0.3166666666666666519, 0.3250000000000000111, 0.3333333333333333148, 0.3416666666666666741, 0.3499999999999999778, 0.3583333333333333370, 0.3666666666666666408, 0.3750000000000000000, 0.3833333333333333592, 0.3916666666666666630, 0.4000000000000000222, 0.4083333333333333259, 0.4166666666666666852, 0.4249999999999999889, 0.4333333333333333481, 0.4416666666666666519, 0.4500000000000000111, 0.4583333333333333148, 0.4666666666666666741, 0.4749999999999999778, 0.4833333333333333370, 0.4916666666666666408, 0.5000000000000000000, 0.5083333333333333037, 0.5166666666666667185, 0.5250000000000000222, 0.5333333333333333259, 0.5416666666666666297, 0.5500000000000000444, 0.5583333333333333481, 0.5666666666666666519, 0.5749999999999999556, 0.5833333333333333703, 0.5916666666666666741, 0.5999999999999999778, 0.6083333333333332815, 0.6166666666666666963, 0.6250000000000000000, 0.6333333333333333037, 0.6416666666666667185, 0.6500000000000000222, 0.6583333333333333259, 0.6666666666666666297, 0.6750000000000000444, 0.6833333333333333481, 0.6916666666666666519, 0.6999999999999999556, 0.7083333333333333703, 0.7166666666666666741, 0.7249999999999999778, 0.7333333333333332815, 0.7416666666666666963, 0.7500000000000000000, 0.7583333333333333037, 0.7666666666666667185, 0.7750000000000000222, 0.7833333333333333259, 0.7916666666666666297, 0.8000000000000000444, 0.8083333333333333481, 0.8166666666666666519, 0.8249999999999999556, 0.8333333333333333703, 0.8416666666666666741, 0.8499999999999999778, 0.8583333333333332815, 0.8666666666666666963, 0.8750000000000000000, 0.8833333333333333037, 0.8916666666666667185, 0.9000000000000000222, 0.9083333333333333259, 0.9166666666666666297, 0.9250000000000000444, 0.9333333333333333481, 0.9416666666666666519, 0.9499999999999999556, 0.9583333333333333703, 0.9666666666666666741, 0.9749999999999999778, 0.9833333333333332815, 0.9916666666666666963, 1.000000000000000000 ),
 .UNSPECIFIED. ) 
 CURVE ( )  GEOMETRIC_REPRESENTATION_ITEM ( )  RATIONAL_B_SPLINE_CURVE ( ( 1.000000000000000000, 0.9238795325112867385, 1.000000000000000000, 0.9238795325112867385, 1.000000000000000000, 0.9238795325112867385, 1.000000000000000000, 0.9238795325112867385, 1.000000000000000000, 0.9238795325112867385, 1.000000000000000000, 0.9238795325112867385, 1.000000000000000000, 0.9238795325112867385, 1.000000000000000000, 0.9238795325112867385, 1.000000000000000000, 0.9238795325112867385, 1.000000000000000000, 0.9238795325112867385, 1.000000000000000000, 0.9238795325112867385, 1.000000000000000000, 0.9238795325112867385, 1.000000000000000000, 0.9238795325112867385, 1.000000000000000000, 0.9238795325112867385, 1.000000000000000000, 0.9238795325112867385, 1.000000000000000000, 0.9238795325112867385, 1.000000000000000000, 0.9238795325112867385, 1.000000000000000000, 0.9238795325112867385, 1.000000000000000000, 0.9238795325112867385, 1.000000000000000000, 0.9238795325112867385, 1.000000000000000000, 0.9238795325112867385, 1.000000000000000000, 0.9238795325112867385, 1.000000000000000000, 0.9238795325112867385, 1.000000000000000000, 0.9238795325112867385, 1.000000000000000000, 0.9238795325112867385, 1.000000000000000000, 0.9238795325112867385, 1.000000000000000000, 0.9238795325112867385, 1.000000000000000000, 0.9238795325112867385, 1.000000000000000000, 0.9238795325112867385, 1.000000000000000000, 0.9238795325112867385, 1.000000000000000000, 0.9238795325112867385, 1.000000000000000000, 0.9238795325112867385, 1.000000000000000000, 0.9238795325112867385, 1.000000000000000000, 0.9238795325112867385, 1.000000000000000000, 0.9238795325112867385, 1.000000000000000000, 0.9238795325112867385, 1.000000000000000000, 0.9238795325112867385, 1.000000000000000000, 0.9238795325112867385, 1.000000000000000000, 0.9238795325112867385, 1.000000000000000000, 0.9238795325112867385, 1.000000000000000000, 0.9238795325112867385, 1.000000000000000000, 0.9238795325112867385, 1.000000000000000000, 0.9238795325112867385, 1.000000000000000000, 0.9238795325112867385, 1.000000000000000000, 0.9238795325112867385, 1.000000000000000000, 0.9238795325112867385, 1.000000000000000000, 0.9238795325112867385, 1.000000000000000000, 0.9238795325112867385, 1.000000000000000000, 0.9238795325112867385, 1.000000000000000000, 0.9238795325112867385, 1.000000000000000000, 0.9238795325112867385, 1.000000000000000000, 0.9238795325112867385, 1.000000000000000000, 0.9238795325112867385, 1.000000000000000000, 0.9238795325112867385, 1.000000000000000000, 0.9238795325112867385, 1.000000000000000000, 0.9238795325112867385, 1.000000000000000000, 0.9238795325112867385, 1.000000000000000000, 0.9238795325112867385, 1.000000000000000000, 0.9238795325112867385, 1.000000000000000000, 0.9238795325112867385, 1.000000000000000000, 0.9238795325112867385, 1.000000000000000000, 0.9238795325112867385, 1.000000000000000000, 0.9238795325112867385, 1.000000000000000000, 0.9238795325112867385, 1.000000000000000000, 0.9238795325112867385, 1.000000000000000000, 0.9238795325112867385, 1.000000000000000000, 0.9238795325112867385, 1.000000000000000000, 0.9238795325112867385, 1.000000000000000000, 0.9238795325112867385, 1.000000000000000000, 0.9238795325112867385, 1.000000000000000000, 0.9238795325112867385, 1.000000000000000000, 0.9238795325112867385, 1.000000000000000000, 0.9238795325112867385, 1.000000000000000000, 0.9238795325112867385, 1.000000000000000000, 0.9238795325112867385, 1.000000000000000000, 0.9238795325112867385, 1.000000000000000000, 0.9238795325112867385, 1.000000000000000000, 0.9238795325112867385, 1.000000000000000000, 0.9238795325112867385, 1.000000000000000000, 0.9238795325112867385, 1.000000000000000000, 0.9238795325112867385, 1.000000000000000000, 0.9238795325112867385, 1.000000000000000000, 0.9238795325112867385, 1.000000000000000000, 0.9238795325112867385, 1.000000000000000000, 0.9238795325112867385, 1.000000000000000000, 0.9238795325112867385, 1.000000000000000000, 0.9238795325112867385, 1.000000000000000000, 0.9238795325112867385, 1.000000000000000000, 0.9238795325112867385, 1.000000000000000000, 0.9238795325112867385, 1.000000000000000000, 0.9238795325112867385, 1.000000000000000000, 0.9238795325112867385, 1.000000000000000000, 0.9238795325112867385, 1.000000000000000000, 0.9238795325112867385, 1.000000000000000000, 0.9238795325112867385, 1.000000000000000000, 0.9238795325112867385, 1.000000000000000000, 0.9238795325112867385, 1.000000000000000000, 0.9238795325112867385, 1.000000000000000000, 0.9238795325112867385, 1.000000000000000000, 0.9238795325112867385, 1.000000000000000000, 0.9238795325112867385, 1.000000000000000000, 0.9238795325112867385, 1.000000000000000000, 0.9238795325112867385, 1.000000000000000000, 0.9238795325112867385, 1.000000000000000000, 0.9238795325112867385, 1.000000000000000000, 0.9238795325112867385, 1.000000000000000000, 0.9238795325112867385, 1.000000000000000000, 0.9238795325112867385, 1.000000000000000000, 0.9238795325112867385, 1.000000000000000000, 0.9238795325112867385, 1.000000000000000000, 0.9238795325112867385, 1.000000000000000000, 0.9238795325112867385, 1.000000000000000000, 0.9238795325112867385, 1.000000000000000000, 0.9238795325112867385, 1.000000000000000000, 0.9238795325112867385, 1.000000000000000000, 0.9238795325112867385, 1.000000000000000000, 0.9238795325112867385, 1.000000000000000000, 0.9238795325112867385, 1.000000000000000000, 0.9238795325112867385, 1.000000000000000000, 0.9238795325112867385, 1.000000000000000000 ) ) 
 REPRESENTATION_ITEM ( '' )  );
#38378 = LINE ( 'NONE', #4417, #67665 ) ;
#38379 = CARTESIAN_POINT ( 'NONE',  ( -5.082755093536326818, 20.90624999795161543, 5.082755093536325042 ) ) ;
#38380 = CARTESIAN_POINT ( 'NONE',  ( -3.313708498984708317, 108.9687500040967905, 8.000000000000053291 ) ) ;
#38381 = CARTESIAN_POINT ( 'NONE',  ( 2.085542519210945334E-15, 255.4687500034140157, 11.35316468749999963 ) ) ;
#38382 = CARTESIAN_POINT ( 'NONE',  ( 3.042071309553167069, 91.82291666325269830, -11.35316468749999785 ) ) ;
#38383 = ORIENTED_EDGE ( 'NONE', *, *, #71804, .F. ) ;
#38384 = LINE ( 'NONE', #27418, #28307 ) ;
#38385 = CARTESIAN_POINT ( 'NONE',  ( -6.238412754330611322E-16, 10.18810118749999916, 113.7812500020483810 ) ) ;
#38386 = CARTESIAN_POINT ( 'NONE',  ( -24.54126587499998990, 195.4375000013655779, 170.0000000000003411 ) ) ;
#38387 = CARTESIAN_POINT ( 'NONE',  ( 1.432654583217662481, 203.3750000013656063, 194.5412658750000219 ) ) ;
#38388 = LINE ( 'NONE', #27422, #38396 ) ;
#38390 = CARTESIAN_POINT ( 'NONE',  ( 11.35316468750000141, 80.78124999658602690, 0.000000000000000000 ) ) ;
#38389 = CARTESIAN_POINT ( 'NONE',  ( -24.00000000000002842, 206.9375000027312410, 168.3431457505079152 ) ) ;
#38391 = EDGE_CURVE ( 'NONE', #40603, #58773, #1851, .T. ) ;
#38392 = CARTESIAN_POINT ( 'NONE',  ( 5.656854249492374365, 5.656854249492375253, 16.95530278392014978 ) ) ;
#38393 = CARTESIAN_POINT ( 'NONE',  ( -28.00000000000002132, 201.6875000013656063, 166.5412658750003629 ) ) ;
#38394 = CYLINDRICAL_SURFACE ( 'NONE', #18036, 11.99999999999999645 ) ;
#38395 = CARTESIAN_POINT ( 'NONE',  ( 6.123233995736767268E-16, 183.1249999931720538, -10.00000000000000178 ) ) ;
#38396 = VECTOR ( 'NONE', #15353, 1000.000000000000000 ) ;
#38397 = CARTESIAN_POINT ( 'NONE',  ( 38.00000000000000000, -63.00000000000000000, 15.00000000000000178 ) ) ;
#38398 = CARTESIAN_POINT ( 'NONE',  ( 3.042071309553159519, 80.05208332991935549, 11.35316468750000141 ) ) ;
#38399 = CARTESIAN_POINT ( 'NONE',  ( 2.765530957082001251, 293.7656250017068942, 6.676582343750000703 ) ) ;
#38400 = CARTESIAN_POINT ( 'NONE',  ( 10.18810118750000093, -4.220049686691933033, 103.1875000020483810 ) ) ;
#38401 = CARTESIAN_POINT ( 'NONE',  ( -8.311093377946836114, 207.6562499965860411, -8.311093377946837890 ) ) ;
#38403 = VERTEX_POINT ( 'NONE', #24837 ) ;
#38402 =( BOUNDED_CURVE ( )  B_SPLINE_CURVE ( 2, ( #55467, #54724, #26780, #49797, #30307, #72813, #3030, #53327, #21120 ),
 .UNSPECIFIED., .F., .F. ) 
 B_SPLINE_CURVE_WITH_KNOTS ( ( 3, 2, 2, 2, 3 ),
 ( 0.8833333333333341919, 0.8916666666666676067, 0.9000000000000007994, 0.9083333333333341031, 0.9166666666666674068 ),
 .UNSPECIFIED. ) 
 CURVE ( )  GEOMETRIC_REPRESENTATION_ITEM ( )  RATIONAL_B_SPLINE_CURVE ( ( 0.9999999999999918954, 0.9238795325112948431, 1.000000000000000000, 0.9238795325112867385, 1.000000000000000000, 0.9238795325112867385, 1.000000000000000000, 0.9238795325112796331, 1.000000000000007105 ) ) 
 REPRESENTATION_ITEM ( '' )  );
#38404 = CARTESIAN_POINT ( 'NONE',  ( -2.679491924311235174, 70.41666665983869677, 10.00000000000000000 ) ) ;
#38405 = CARTESIAN_POINT ( 'NONE',  ( 4.000000000000001776, 3.749999997268813168, 0.000000000000000000 ) ) ;
#38406 = CARTESIAN_POINT ( 'NONE',  ( 5.000000000000001776, 62.13136467932960016, 23.87699943806516245 ) ) ;
#38408 = CARTESIAN_POINT ( 'NONE',  ( 9.832129032723416984, 205.3645833299193555, 5.676582343750006032 ) ) ;
#38407 = CARTESIAN_POINT ( 'NONE',  ( 27.99999999999999645, 210.0000000000000284, 169.9999999999999147 ) ) ;
#38409 = AXIS2_PLACEMENT_3D ( 'NONE', #28610, #4867, #50130 ) ;
#38410 = CARTESIAN_POINT ( 'NONE',  ( 8.660254037844385522, 231.0416666734946318, -5.000000000000003553 ) ) ;
#38411 = CARTESIAN_POINT ( 'NONE',  ( -4.000000000000002665, 20.56249999999999645, 1.656854249492380582 ) ) ;
#38412 = ORIENTED_EDGE ( 'NONE', *, *, #44070, .T. ) ;
#38413 = CARTESIAN_POINT ( 'NONE',  ( 5.676582343749993598, 195.2604166632526983, 9.832129032723422313 ) ) ;
#38414 = AXIS2_PLACEMENT_3D ( 'NONE', #22659, #18865, #18129 ) ;
#38415 = CARTESIAN_POINT ( 'NONE',  ( -7.188101187499992051, 0.000000000000000000, 16.48655278187175810 ) ) ;
#38416 = CARTESIAN_POINT ( 'NONE',  ( 11.00000000000000000, 1.347111479062088405E-15, 118.0000000000000000 ) ) ;
#38417 = CARTESIAN_POINT ( 'NONE',  ( 3.313708498984762052, 9.281250000000001776, -8.000000000000000000 ) ) ;
#38418 = ORIENTED_EDGE ( 'NONE', *, *, #48641, .T. ) ;
#38419 = CARTESIAN_POINT ( 'NONE',  ( 5.656854249492379694, 91.62500000409677625, -5.656854249492380582 ) ) ;
#38420 = CARTESIAN_POINT ( 'NONE',  ( -2.679491924311235618, 8.541666666666667851, 10.00000000000000000 ) ) ;
#38421 = CARTESIAN_POINT ( 'NONE',  ( -4.220049686691937474, -10.18810118749999738, 78.81250000204838102 ) ) ;
#38422 = VERTEX_POINT ( 'NONE', #63732 ) ;
#38423 = CARTESIAN_POINT ( 'NONE',  ( -2.828427124746192067, 21.62500000000000355, 2.828427124746190735 ) ) ;
#38424 = CARTESIAN_POINT ( 'NONE',  ( -4.541265875000002339, 19.74999999863440081, -1.881053915767121998 ) ) ;
#38425 = CARTESIAN_POINT ( 'NONE',  ( -7.999999999999989342, -3.313708498984762496, 7.111552783920144449 ) ) ;
#38426 = CARTESIAN_POINT ( 'NONE',  ( 3.428378827818292951, 16.35907404636675366, -69.10239319625853227 ) ) ;
#38427 = EDGE_CURVE ( 'NONE', #38665, #72478, #29477, .T. ) ;
#38428 = ORIENTED_EDGE ( 'NONE', *, *, #21851, .T. ) ;
#38429 = SURFACE_STYLE_USAGE ( .BOTH. , #67095 ) ;
#38430 = CARTESIAN_POINT ( 'NONE',  ( -4.401442555609581635E-16, 95.28125000204836681, -7.188101187500000044 ) ) ;
#38433 = CARTESIAN_POINT ( 'NONE',  ( 32.00000000000000711, 207.3125000027312126, 171.6568542494922553 ) ) ;
#38432 = CARTESIAN_POINT ( 'NONE',  ( 11.35316468749999608, 261.6145833367473301, -3.042071309553167513 ) ) ;
#38431 = DIRECTION ( 'NONE',  ( -0.000000000000000000, -0.000000000000000000, 1.000000000000000000 ) ) ;
#38434 = CARTESIAN_POINT ( 'NONE',  ( 1424.688200795887269, 478.5363650752479430, 997.8421604560587639 ) ) ;
#38435 = ORIENTED_EDGE ( 'NONE', *, *, #65708, .T. ) ;
#38437 = VECTOR ( 'NONE', #617, 1000.000000000000000 ) ;
#38436 = CARTESIAN_POINT ( 'NONE',  ( -3.042071309553166181, 248.1770833367472733, -11.35316468749999608 ) ) ;
#38438 = CARTESIAN_POINT ( 'NONE',  ( 5.082755093536320601, -5.082755093536318824, 15.54905278187175455 ) ) ;
#38439 = EDGE_LOOP ( 'NONE', ( #33461, #16007, #60771, #56891 ) ) ;
#38440 = ORIENTED_EDGE ( 'NONE', *, *, #49584, .F. ) ;
#38441 = CARTESIAN_POINT ( 'NONE',  ( 10.18810118750000093, -4.220049686691933033, 75.81250000204838102 ) ) ;
#38442 = CARTESIAN_POINT ( 'NONE',  ( 11.35316468749999785, 70.88541666325265567, 3.042071309553174174 ) ) ;
#38443 = FACE_OUTER_BOUND ( 'NONE', #59583, .T. ) ;
#38444 = CARTESIAN_POINT ( 'NONE',  ( -6.735557395310442023E-16, 11.00000000000000000, 89.12499999999998579 ) ) ;
#38447 = CARTESIAN_POINT ( 'NONE',  ( 2.765530957081996366, 289.2968750017069510, -6.676582343750002480 ) ) ;
#38446 = CARTESIAN_POINT ( 'NONE',  ( 30.82842712474616320, 195.5000000027312126, 167.1715728752537018 ) ) ;
#38445 = DIRECTION ( 'NONE',  ( -0.000000000000000000, 1.000000000000000000, -0.000000000000000000 ) ) ;
#38448 = VECTOR ( 'NONE', #12777, 1000.000000000000000 ) ;
#38449 = EDGE_CURVE ( 'NONE', #46612, #33535, #14258, .T. ) ;
#38450 = CARTESIAN_POINT ( 'NONE',  ( -48.96653803850838216, 196.4080344070507351, 59.57636250011221080 ) ) ;
#38451 = LINE ( 'NONE', #43723, #58861 ) ;
#38452 = CARTESIAN_POINT ( 'NONE',  ( 2.445694354108840063, 200.0625000013656063, 200.4456943541088663 ) ) ;
#38453 = CARTESIAN_POINT ( 'NONE',  ( -8.000000000000000000, 9.468749995903223748, -3.313708498984762496 ) ) ;
#38454 = VERTEX_POINT ( 'NONE', #54278 ) ;
#38455 = CARTESIAN_POINT ( 'NONE',  ( 31.45873412499997812, 194.6250000013655779, 171.4326545832175839 ) ) ;
#38456 = CARTESIAN_POINT ( 'NONE',  ( 7.188101187500000044, 17.34374999795161543, 0.000000000000000000 ) ) ;
#38457 = CARTESIAN_POINT ( 'NONE',  ( 11.35316468749999785, 165.8854166632526415, 3.042071309553174174 ) ) ;
#38458 = CARTESIAN_POINT ( 'NONE',  ( 1.269536070779894168E-12, 186.2499999999999147, -10.00000000000000178 ) ) ;
#38459 = CARTESIAN_POINT ( 'NONE',  ( -5.082755093536324154, 103.7187500020483810, 5.082755093536326818 ) ) ;
#38460 = CARTESIAN_POINT ( 'NONE',  ( -10.00000000000000000, 19.16666665983869322, -2.679491924311229845 ) ) ;
#38461 = CARTESIAN_POINT ( 'NONE',  ( 31.45873412499998523, 207.8750000013656063, 171.4326545832176123 ) ) ;
#38462 = CARTESIAN_POINT ( 'NONE',  ( 2.977408999572650927, -7.188101187499990274, 17.33030278187175455 ) ) ;
#38463 = CARTESIAN_POINT ( 'NONE',  ( 1.656854249492348607, 208.3125000027312126, 138.0000000000000568 ) ) ;
#38464 = CARTESIAN_POINT ( 'NONE',  ( 9.832129032723420536, 41.19791666325269119, -5.676582343749999815 ) ) ;
#38465 = CARTESIAN_POINT ( 'NONE',  ( 8.000000000000000000, 21.00000000000000355, 0.000000000000000000 ) ) ;
#38466 = CARTESIAN_POINT ( 'NONE',  ( -10.00000000000000178, 24.37499999317203603, -1.224646799147353454E-15 ) ) ;
#38467 = CARTESIAN_POINT ( 'NONE',  ( 4.000000000000015987, 195.6875000027312126, 196.3431457505076594 ) ) ;
#38468 = VERTEX_POINT ( 'NONE', #25579 ) ;
#38469 = CARTESIAN_POINT ( 'NONE',  ( 4.999999999999993783, 141.0416666598387110, 8.660254037844390851 ) ) ;
#38470 = CARTESIAN_POINT ( 'NONE',  ( -8.000000000000000000, 20.06249999590322375, -9.797174393178825657E-16 ) ) ;
#38471 = CARTESIAN_POINT ( 'NONE',  ( 3.042071309553167069, 51.82291666325266988, -11.35316468749999785 ) ) ;
#38472 = CARTESIAN_POINT ( 'NONE',  ( 7.778174593052023411, -7.778174593052021635, 82.75000000409676204 ) ) ;
#38473 = CARTESIAN_POINT ( 'NONE',  ( 2.445694354108783219, 205.8125000013656063, 139.5543056458912190 ) ) ;
#38474 = DIRECTION ( 'NONE',  ( -1.000000000000000000, 0.000000000000000000, 0.000000000000000000 ) ) ;
#38475 = CARTESIAN_POINT ( 'NONE',  ( 2.828427124746208943, 207.6250000000000284, 195.1715728752538439 ) ) ;
#38477 = CARTESIAN_POINT ( 'NONE',  ( -3.042071309553173730, 44.32291666325267698, 11.35316468749999785 ) ) ;
#38476 = CARTESIAN_POINT ( 'NONE',  ( 2.977408999572654480, 100.6250000020483810, 7.188101187499999156 ) ) ;
#38478 = EDGE_CURVE ( 'NONE', #51172, #51815, #67060, .T. ) ;
#38479 = CARTESIAN_POINT ( 'NONE',  ( 5.656854249492374365, 5.656854249492375253, 12.26780277982336642 ) ) ;
#38480 = CARTESIAN_POINT ( 'NONE',  ( 8.311093377946837890, 156.4062499965860411, -8.311093377946837890 ) ) ;
#38481 = EDGE_CURVE ( 'NONE', #4443, #3266, #52611, .T. ) ;
#38482 = CARTESIAN_POINT ( 'NONE',  ( -7.320508075688773708, 143.7499999931719969, -7.320508075688774596 ) ) ;
#38483 = CARTESIAN_POINT ( 'NONE',  ( -7.188101187500000044, 102.0312500020483810, 0.000000000000000000 ) ) ;
#38484 = CYLINDRICAL_SURFACE ( 'NONE', #24360, 10.00000000000000178 ) ;
#38485 = CARTESIAN_POINT ( 'NONE',  ( 3.042071309553167513, 37.13541666325267698, -11.35316468749999785 ) ) ;
#38486 = CARTESIAN_POINT ( 'NONE',  ( 2.220677790255211837E-11, 201.2499999999982663, -9.999999999999998224 ) ) ;
#38487 = ORIENTED_EDGE ( 'NONE', *, *, #50562, .T. ) ;
#38488 = CARTESIAN_POINT ( 'NONE',  ( 11.00000000000000000, 1.347111479062088405E-15, 102.2500000000000000 ) ) ;
#38489 = CARTESIAN_POINT ( 'NONE',  ( 4.220049686691934809, 10.18810118749999916, 79.18750000204836681 ) ) ;
#38490 = DIRECTION ( 'NONE',  ( -0.000000000000000000, 1.000000000000000000, -4.476705744456276341E-16 ) ) ;
#38492 = CARTESIAN_POINT ( 'NONE',  ( 9.832129032723420536, 166.1979166632526983, -5.676582343749999815 ) ) ;
#38491 = LINE ( 'NONE', #49418, #14716 ) ;
#38493 = CARTESIAN_POINT ( 'NONE',  ( 5.656854249492374365, 5.656854249492375253, 9.324052784329824206 ) ) ;
#38494 = EDGE_CURVE ( 'NONE', #6205, #22530, #51332, .T. ) ;
#38495 = EDGE_CURVE ( 'NONE', #52730, #19485, #60294, .T. ) ;
#38496 = CARTESIAN_POINT ( 'NONE',  ( -26.90181813323773241, -21.77641390633945662, 185.4466768143425952 ) ) ;
#38497 = CARTESIAN_POINT ( 'NONE',  ( 8.660254037844389075, 260.2083333401612890, 4.999999999999997335 ) ) ;
#38498 = CARTESIAN_POINT ( 'NONE',  ( 0.8997857290934923036, 51.17549659653047200, -48.53090770943093446 ) ) ;
#38499 = CARTESIAN_POINT ( 'NONE',  ( -7.204075437095967871, 7.204075437095967871, 87.34375000204836681 ) ) ;
#38500 = EDGE_LOOP ( 'NONE', ( #43804, #60238, #55512, #15090 ) ) ;
#38501 =( BOUNDED_CURVE ( )  B_SPLINE_CURVE ( 2, ( #63280, #29343, #22541, #57650, #52721, #51978, #41030, #35383, #69324 ),
 .UNSPECIFIED., .F., .F. ) 
 B_SPLINE_CURVE_WITH_KNOTS ( ( 3, 2, 2, 2, 3 ),
 ( 0.3020833333333331483, 0.3072916666666665186, 0.3124999999999998335, 0.3177083333333331483, 0.3229166666666665186 ),
 .UNSPECIFIED. ) 
 CURVE ( )  GEOMETRIC_REPRESENTATION_ITEM ( )  RATIONAL_B_SPLINE_CURVE ( ( 1.000000000000002442, 0.9238795325112842960, 1.000000000000000000, 0.9238795325112867385, 1.000000000000000000, 0.9238795325112867385, 1.000000000000000000, 0.9238795325112891810, 0.9999999999999975575 ) ) 
 REPRESENTATION_ITEM ( '' )  );
#38502 = EDGE_CURVE ( 'NONE', #23833, #9171, #72360, .T. ) ;
#38503 = CARTESIAN_POINT ( 'NONE',  ( -10.00000000000000178, 119.3749999931720396, -1.224646799147353454E-15 ) ) ;
#38504 = CARTESIAN_POINT ( 'NONE',  ( 0.000000000000000000, 300.0000000000000000, 0.000000000000000000 ) ) ;
#38505 = CARTESIAN_POINT ( 'NONE',  ( -3.042071309553173730, 114.6354166632526983, 11.35316468749999785 ) ) ;
#38506 = CARTESIAN_POINT ( 'NONE',  ( 4.220049686691941027, -10.18810118749999738, 95.12500000204836681 ) ) ;
#38507 = CARTESIAN_POINT ( 'NONE',  ( 2.780723358947928197E-16, 19.68749999863440436, -4.541265875000002339 ) ) ;
#38508 = EDGE_LOOP ( 'NONE', ( #57283, #50427, #47965, #22671 ) ) ;
#38509 = VERTEX_POINT ( 'NONE', #3709 ) ;
#38510 = CARTESIAN_POINT ( 'NONE',  ( 1.881053915767122664, 3.249999998634406584, 4.541265875000001451 ) ) ;
#38511 = AXIS2_PLACEMENT_3D ( 'NONE', #4070, #4432, #61773 ) ;
#38512 = CARTESIAN_POINT ( 'NONE',  ( 7.188101187499999156, 7.874999997951610986, 2.977408999572654924 ) ) ;
#38513 = CARTESIAN_POINT ( 'NONE',  ( 8.000000000000000000, 112.4375000040967905, -9.797174393178825657E-16 ) ) ;
#38514 = CARTESIAN_POINT ( 'NONE',  ( 10.18810118750000093, -4.220049686691933921, 91.18750000204836681 ) ) ;
#38515 = CARTESIAN_POINT ( 'NONE',  ( -24.54126587500000056, 203.5000000013655779, 168.5673454167827003 ) ) ;
#38516 = CARTESIAN_POINT ( 'NONE',  ( -1.656854249492381248, 5.312500000000001776, -4.000000000000001776 ) ) ;
#38517 = CARTESIAN_POINT ( 'NONE',  ( -4.000000000000002665, 19.31249999726881583, 1.656854249492380804 ) ) ;
#38518 = CARTESIAN_POINT ( 'NONE',  ( 3.211159895383560947, 8.187499998634406140, 3.211159895383562723 ) ) ;
#38519 = CARTESIAN_POINT ( 'NONE',  ( -4.000000000000015987, 203.4375000000000284, 140.3431457505076594 ) ) ;
#38520 = ORIENTED_EDGE ( 'NONE', *, *, #72240, .T. ) ;
#38521 = DIRECTION ( 'NONE',  ( -0.000000000000000000, -1.000000000000000000, -0.000000000000000000 ) ) ;
#38522 = PRODUCT_DEFINITION_CONTEXT ( 'detailed design', #31820, 'design' ) ;
#38524 = CARTESIAN_POINT ( 'NONE',  ( 5.000000000000000000, -10.00000000000000000, -75.19090595827292134 ) ) ;
#38523 = CARTESIAN_POINT ( 'NONE',  ( -25.55430564589122966, 198.3125000013656063, 167.5543056458915032 ) ) ;
#38525 = B_SPLINE_CURVE_WITH_KNOTS ( 'NONE', 1,
 ( #9006, #15394 ),
 .UNSPECIFIED., .F., .F.,
 ( 2, 2 ),
 ( 0.000000000000000000, 0.6095729009237784712 ),
 .UNSPECIFIED. ) ;
#38526 = CARTESIAN_POINT ( 'NONE',  ( 3.211159895383561835, 19.43749999863440436, -3.211159895383561835 ) ) ;
#38527 = CARTESIAN_POINT ( 'NONE',  ( 5.000000000000001776, 72.70833332650536818, -8.660254037844389075 ) ) ;
#38528 = CARTESIAN_POINT ( 'NONE',  ( 7.188101187499993827, -2.977408999572645598, 0.6428027818717528818 ) ) ;
#38529 = ORIENTED_EDGE ( 'NONE', *, *, #70810, .F. ) ;
#38530 = ADVANCED_FACE ( 'NONE', ( #48224 ), #626, .F. ) ;
#38531 = ORIENTED_EDGE ( 'NONE', *, *, #27970, .T. ) ;
#38532 = CARTESIAN_POINT ( 'NONE',  ( -4.220049686691935698, 10.18810118749999916, 100.3750000020483952 ) ) ;
#38533 = CARTESIAN_POINT ( 'NONE',  ( 2.485281374238286656, 288.6875000000000568, -6.000000000000285105 ) ) ;
#38534 = CARTESIAN_POINT ( 'NONE',  ( -25.55430564589119413, 198.5625000013656063, 167.5543056458915316 ) ) ;
#38535 = CARTESIAN_POINT ( 'NONE',  ( 4.556349186104051263, -10.99999999999999822, 107.9687500000000142 ) ) ;
#38536 = CARTESIAN_POINT ( 'NONE',  ( 2.839093476692135984E-14, 206.9375000013656063, 201.4587341250000350 ) ) ;
#38537 = CARTESIAN_POINT ( 'NONE',  ( 2.828427124746208943, 203.7500000027312126, 195.1715728752538439 ) ) ;
#38538 = CARTESIAN_POINT ( 'NONE',  ( -8.660254037844387298, 117.0833333333333428, -5.000000000000004441 ) ) ;
#38539 = CARTESIAN_POINT ( 'NONE',  ( 5.656854249492379694, 104.9374999999999858, -5.656854249492380582 ) ) ;
#38540 = CARTESIAN_POINT ( 'NONE',  ( -4.721056650415999201, 292.4843750017070079, -4.721056650415999201 ) ) ;
#38541 = CARTESIAN_POINT ( 'NONE',  ( -5.082755093536317936, -5.082755093536320601, 9.549052781871754547 ) ) ;
#38542 = ORIENTED_EDGE ( 'NONE', *, *, #46785, .T. ) ;
#38543 =( REPRESENTATION_RELATIONSHIP ('NONE','NONE', #46008, #69137 ) REPRESENTATION_RELATIONSHIP_WITH_TRANSFORMATION ( #37224 )SHAPE_REPRESENTATION_RELATIONSHIP( ) );
#38544 = CARTESIAN_POINT ( 'NONE',  ( 1.469576158976823947E-15, 103.0625000040967763, 8.000000000000000000 ) ) ;
#38545 = ADVANCED_FACE ( 'NONE', ( #61766 ), #21018, .F. ) ;
#38546 = AXIS2_PLACEMENT_3D ( 'NONE', #65969, #37311, #25227 ) ;
#38547 = CARTESIAN_POINT ( 'NONE',  ( 24.54126587499999701, 208.1875000013656063, 169.9999999999998863 ) ) ;
#38548 = CARTESIAN_POINT ( 'NONE',  ( 7.999999999999998224, 22.21874999590322375, 3.313708498984766493 ) ) ;
#38549 = CARTESIAN_POINT ( 'NONE',  ( -3.458734125000015425, 200.9375000013656063, 142.0000000000000568 ) ) ;
#38550 = CARTESIAN_POINT ( 'NONE',  ( 7.188101187500000933, 123.8750000020483952, -2.977408999572651371 ) ) ;
#38552 = CARTESIAN_POINT ( 'NONE',  ( 2.445694354108784108, 204.5625000013656063, 144.4456943541088663 ) ) ;
#38551 = LINE ( 'NONE', #33270, #45617 ) ;
#38553 = CARTESIAN_POINT ( 'NONE',  ( 11.35316468749999963, 261.7187500034140157, -1.390361679473963556E-15 ) ) ;
#38554 = FACE_OUTER_BOUND ( 'NONE', #12800, .T. ) ;
#38555 = CARTESIAN_POINT ( 'NONE',  ( 6.123233995736767268E-16, 93.12499999317203958, -10.00000000000000178 ) ) ;
#38556 = CARTESIAN_POINT ( 'NONE',  ( 6.951808397369818766E-16, 7.031249996586016238, -11.35316468750000141 ) ) ;
#38557 = CARTESIAN_POINT ( 'NONE',  ( -5.082755093536317936, -5.082755093536320601, 2.049052781871754103 ) ) ;
#38558 = CARTESIAN_POINT ( 'NONE',  ( -3.042071309553173730, 209.6354166632526415, 11.35316468749999785 ) ) ;
#38559 = CARTESIAN_POINT ( 'NONE',  ( -2.849036369511732440E-14, 197.3750000027312126, 138.0000000000000568 ) ) ;
#38560 = CARTESIAN_POINT ( 'NONE',  ( -8.342170076843785083E-16, 6.062499998634407028, 4.541265875000002339 ) ) ;
#38561 = CARTESIAN_POINT ( 'NONE',  ( 47.32259252271278882, 191.7059220763548524, 65.76194439203457875 ) ) ;
#38562 = PRODUCT_RELATED_PRODUCT_CATEGORY ( 'part', '', ( #51143 ) ) ;
#38564 = CARTESIAN_POINT ( 'NONE',  ( 6.000000000000003553, 297.4374999999999432, 2.485281374238571317 ) ) ;
#38563 = CARTESIAN_POINT ( 'NONE',  ( -25.17157287525382259, 205.8750000000000284, 167.1715728752541565 ) ) ;
#38565 = EDGE_LOOP ( 'NONE', ( #37315, #56065, #47820, #11900 ) ) ;
#38566 = CARTESIAN_POINT ( 'NONE',  ( -1.432654583217664701, 201.0000000013655779, 138.5412658750000787 ) ) ;
#38567 = CARTESIAN_POINT ( 'NONE',  ( 11.35316468749999785, 5.572916663252682312, 3.042071309553174174 ) ) ;
#38568 = CARTESIAN_POINT ( 'NONE',  ( 2.020667218593132706E-15, -11.00000000000000000, 96.06250000409677625 ) ) ;
#38569 = CARTESIAN_POINT ( 'NONE',  ( 0.000000000000000000, 0.000000000000000000, 128.5000000000001990 ) ) ;
#38570 = CARTESIAN_POINT ( 'NONE',  ( -27.99999999999991473, 196.9375000013655779, 173.4587341250003760 ) ) ;
#38571 = CARTESIAN_POINT ( 'NONE',  ( -1.836970198721029983E-15, 60.62499999317203958, 10.00000000000000178 ) ) ;
#38573 = CARTESIAN_POINT ( 'NONE',  ( 11.35316468750000141, 10.78124999658601624, 0.000000000000000000 ) ) ;
#38572 = CARTESIAN_POINT ( 'NONE',  ( -4.401442555609581635E-16, 117.7812500020483810, -7.188101187500000044 ) ) ;
#38574 = CARTESIAN_POINT ( 'NONE',  ( 1.469576158976822172E-15, -7.999999999999991118, 25.20530277982336642 ) ) ;
#38575 = CARTESIAN_POINT ( 'NONE',  ( -2.085542519210945728E-15, 119.5312499965860269, 11.35316468750000141 ) ) ;
#38576 = EDGE_CURVE ( 'NONE', #5834, #51512, #33484, .T. ) ;
#38577 = CARTESIAN_POINT ( 'NONE',  ( 7.320508075688774596, 82.49999999317202537, -7.320508075688774596 ) ) ;
#38578 = CARTESIAN_POINT ( 'NONE',  ( -7.188101187500001821, 122.9375000020483810, -2.977408999572650483 ) ) ;
#38579 = CARTESIAN_POINT ( 'NONE',  ( 3.211159895383561835, 19.56249999863440436, -3.211159895383561835 ) ) ;
#38580 = DIRECTION ( 'NONE',  ( -0.000000000000000000, -0.000000000000000000, 1.000000000000000000 ) ) ;
#38581 = CARTESIAN_POINT ( 'NONE',  ( -12.00000000000000000, 2.937369556047691788, -0.1973350489338370206 ) ) ;
#38582 = ORIENTED_EDGE ( 'NONE', *, *, #48129, .F. ) ;
#38583 = CARTESIAN_POINT ( 'NONE',  ( 6.676582343750001591, 289.1093750017069510, -8.176455196517173205E-16 ) ) ;
#38584 = FILL_AREA_STYLE ('',( #31794 ) ) ;
#38585 = CARTESIAN_POINT ( 'NONE',  ( -7.999999999999991118, 0.000000000000000000, 1.017802783920145782 ) ) ;
#38586 = CARTESIAN_POINT ( 'NONE',  ( -2.828427124746152987, 201.2500000027312126, 200.8284271247462129 ) ) ;
#38587 = DIRECTION ( 'NONE',  ( 0.000000000000000000, 0.000000000000000000, -1.000000000000000000 ) ) ;
#38588 = CARTESIAN_POINT ( 'NONE',  ( -7.204075437095965206, -7.204075437095968759, 105.7187500020483810 ) ) ;
#38589 = EDGE_LOOP ( 'NONE', ( #69083, #71564 ) ) ;
#38590 = VECTOR ( 'NONE', #65421, 1000.000000000000000 ) ;
#38591 = CARTESIAN_POINT ( 'NONE',  ( 10.00000000000000000, 156.6666666598386826, 2.679491924311235618 ) ) ;
#38592 = CARTESIAN_POINT ( 'NONE',  ( 11.35316468749999785, 150.8854166632526983, 3.042071309553174174 ) ) ;
#38593 = CARTESIAN_POINT ( 'NONE',  ( -2.445694354108783219, 207.8125000013656063, 200.4456943541088663 ) ) ;
#38594 = EDGE_CURVE ( 'NONE', #49230, #32224, #27797, .T. ) ;
#38595 = CARTESIAN_POINT ( 'NONE',  ( 5.499989586027935751, 9.526285454130809072, 66.68677389048282578 ) ) ;
#38596 = CARTESIAN_POINT ( 'NONE',  ( -5.676582343749998039, 77.76041666325268409, -9.832129032723420536 ) ) ;
#38597 = VERTEX_POINT ( 'NONE', #44787 ) ;
#38598 = CARTESIAN_POINT ( 'NONE',  ( 4.220049686691941027, -10.18810118749999738, 114.6250000020483810 ) ) ;
#38599 = CARTESIAN_POINT ( 'NONE',  ( 4.541265875000002339, 9.499999998634404363, -1.881053915767121776 ) ) ;
#38600 = ORIENTED_EDGE ( 'NONE', *, *, #57024, .T. ) ;
#38601 = CARTESIAN_POINT ( 'NONE',  ( -5.082755093536325042, 19.03124999795161543, -5.082755093536325930 ) ) ;
#38602 = FACE_OUTER_BOUND ( 'NONE', #22182, .T. ) ;
#38603 = CARTESIAN_POINT ( 'NONE',  ( 0.000000000000000000, 0.000000000000000000, 118.0000000000000000 ) ) ;
#38604 = CARTESIAN_POINT ( 'NONE',  ( 7.188101187500000044, 15.84374999795161365, 0.000000000000000000 ) ) ;
#38605 = CARTESIAN_POINT ( 'NONE',  ( -7.204075437095965206, -7.204075437095968759, 110.2187500020483810 ) ) ;
#38606 = VECTOR ( 'NONE', #55145, 1000.000000000000000 ) ;
#38607 =( BOUNDED_CURVE ( )  B_SPLINE_CURVE ( 2, ( #4177, #15093, #38127, #49810, #27164, #50181, #73201, #21508, #18084 ),
 .UNSPECIFIED., .F., .F. ) 
 B_SPLINE_CURVE_WITH_KNOTS ( ( 3, 2, 2, 2, 3 ),
 ( 0.2352941176470587092, 0.2389705882352940181, 0.2426470588235292991, 0.2463235294117646079, 0.2499999999999998890 ),
 .UNSPECIFIED. ) 
 CURVE ( )  GEOMETRIC_REPRESENTATION_ITEM ( )  RATIONAL_B_SPLINE_CURVE ( ( 1.000000000000002220, 0.9238795325112844070, 1.000000000000000000, 0.9238795325112867385, 1.000000000000000000, 0.9238795325112867385, 1.000000000000000000, 0.9238795325112890700, 0.9999999999999976685 ) ) 
 REPRESENTATION_ITEM ( '' )  );
#38608 = FACE_OUTER_BOUND ( 'NONE', #43657, .T. ) ;
#38609 = CARTESIAN_POINT ( 'NONE',  ( -2.828427124746192067, 6.374999997268813168, 2.828427124746190735 ) ) ;
#38610 =( BOUNDED_CURVE ( )  B_SPLINE_CURVE ( 2, ( #16630, #69453, #51722, #71, #23050, #46061, #63783, #6460, #29463, #70199, #71281, #1547, #48276 ),
 .UNSPECIFIED., .F., .F. ) 
 B_SPLINE_CURVE_WITH_KNOTS ( ( 3, 2, 2, 2, 2, 2, 3 ),
 ( 0.5277777777777775681, 0.5370370370370368684, 0.5462962962962960578, 0.5555555555555553582, 0.5648148148148145475, 0.5740740740740738479, 0.5833333333333331483 ),
 .UNSPECIFIED. ) 
 CURVE ( )  GEOMETRIC_REPRESENTATION_ITEM ( )  RATIONAL_B_SPLINE_CURVE ( ( 1.000000000000000888, 0.9659258262890675351, 1.000000000000000000, 0.9659258262890683122, 1.000000000000000000, 0.9659258262890683122, 1.000000000000000000, 0.9659258262890683122, 1.000000000000000000, 0.9659258262890683122, 1.000000000000000000, 0.9659258262890690894, 0.9999999999999992228 ) ) 
 REPRESENTATION_ITEM ( '' )  );
#38611 = CARTESIAN_POINT ( 'NONE',  ( -1.656854249492422992, 208.8125000027311842, 146.0000000000000284 ) ) ;
#38612 = CONICAL_SURFACE ( 'NONE', #3817, 3.999999999999976019, 0.7853981633974491672 ) ;
#38613 = ORIENTED_EDGE ( 'NONE', *, *, #67533, .F. ) ;
#38614 = CARTESIAN_POINT ( 'NONE',  ( -1.432654583217607858, 206.6250000013656063, 201.4587341250000065 ) ) ;
#38615 = EDGE_CURVE ( 'NONE', #5468, #21228, #49701, .T. ) ;
#38616 = CARTESIAN_POINT ( 'NONE',  ( -23.99999999999998579, 194.8750000027311842, 170.0000000000002842 ) ) ;
#38617 = CARTESIAN_POINT ( 'NONE',  ( -6.238412754330611322E-16, 10.18810118749999916, 70.65625000204836681 ) ) ;
#38618 = CARTESIAN_POINT ( 'NONE',  ( 2.780723358947928197E-16, 5.562499998634407028, -4.541265875000002339 ) ) ;
#38619 = CARTESIAN_POINT ( 'NONE',  ( 8.000000000000001776, 94.34375000409677625, 3.313708498984759387 ) ) ;
#38620 = CARTESIAN_POINT ( 'NONE',  ( 7.188101187499991163, 2.977408999572648707, 23.33030278187175455 ) ) ;
#38621 = ORIENTED_EDGE ( 'NONE', *, *, #63929, .F. ) ;
#38622 = EDGE_CURVE ( 'NONE', #47573, #6721, #44042, .T. ) ;
#38623 = CARTESIAN_POINT ( 'NONE',  ( 2.977408999572652260, 27.18749999795161898, 7.188101187500000044 ) ) ;
#38624 = ORIENTED_EDGE ( 'NONE', *, *, #34709, .F. ) ;
#38625 = CARTESIAN_POINT ( 'NONE',  ( -7.204075437095967871, 7.204075437095967871, 113.9687500020483810 ) ) ;
#38626 = CARTESIAN_POINT ( 'NONE',  ( -4.000000000000002665, 18.56250000000000000, 1.656854249492380582 ) ) ;
#38627 = CARTESIAN_POINT ( 'NONE',  ( -3.458734124999959025, 205.5000000013655779, 199.4326545832176691 ) ) ;
#38628 = CARTESIAN_POINT ( 'NONE',  ( 31.45873412499999233, 199.6875000013656063, 169.9999999999998863 ) ) ;
#38629 = CARTESIAN_POINT ( 'NONE',  ( -10.00000000000000178, 67.50000000000000000, -1.224646799147353454E-15 ) ) ;
#38630 = CARTESIAN_POINT ( 'NONE',  ( 7.188101187500001821, 96.87500000204836681, -2.977408999572651371 ) ) ;
#38631 = CARTESIAN_POINT ( 'NONE',  ( 4.242640687119287435, 294.3750000000000000, 4.242640687119285658 ) ) ;
#38632 = CARTESIAN_POINT ( 'NONE',  ( 29.65685424949235127, 204.5625000027312126, 165.9999999999998863 ) ) ;
#38633 = CONICAL_SURFACE ( 'NONE', #55493, 3.999999999999976019, 0.7853981633974491672 ) ;
#38634 = VERTEX_POINT ( 'NONE', #73082 ) ;
#38635 = CARTESIAN_POINT ( 'NONE',  ( -27.99999999999995737, 205.5000000000000284, 174.0000000000003695 ) ) ;
#38636 = CARTESIAN_POINT ( 'NONE',  ( -6.735557395310442023E-16, 11.00000000000000000, 87.81250000409676204 ) ) ;
#38637 = CARTESIAN_POINT ( 'NONE',  ( -1.656854249492403008, 197.8125000027312126, 146.0000000000000284 ) ) ;
#38638 = CARTESIAN_POINT ( 'NONE',  ( -11.00000000000000000, 0.000000000000000000, 92.68750000409677625 ) ) ;
#38639 = CARTESIAN_POINT ( 'NONE',  ( 1.836970198721029589E-15, 224.3750000068279746, 10.00000000000000000 ) ) ;
#38640 = CARTESIAN_POINT ( 'NONE',  ( 7.320508075688776373, 246.8750000000000284, 7.320508075688767491 ) ) ;
#38641 = CARTESIAN_POINT ( 'NONE',  ( -1.604524386212670052E-13, 78.75000000000000000, 10.00000000000000178 ) ) ;
#38642 = CARTESIAN_POINT ( 'NONE',  ( 10.00000000000000000, 189.7916666666666856, 2.679491924311236062 ) ) ;
#38643 = CARTESIAN_POINT ( 'NONE',  ( 7.778174593052023411, -7.778174593052021635, 111.0625000000000000 ) ) ;
#38644 = CARTESIAN_POINT ( 'NONE',  ( -5.082755093536319713, 5.082755093536319713, 21.17405278187175455 ) ) ;
#38645 = CARTESIAN_POINT ( 'NONE',  ( -5.676582343750006032, 164.4270833299193555, 9.832129032723418760 ) ) ;
#38646 = CARTESIAN_POINT ( 'NONE',  ( -1.656854249492318409, 207.9375000027311842, 194.0000000000000284 ) ) ;
#38647 = CARTESIAN_POINT ( 'NONE',  ( -4.898587196589412829E-16, 108.1250000000000000, -8.000000000000000000 ) ) ;
#38648 = CARTESIAN_POINT ( 'NONE',  ( 4.556349186104052151, -10.99999999999999822, 82.65625000409676204 ) ) ;
#38650 = CARTESIAN_POINT ( 'NONE',  ( -1.469576158976823947E-15, 17.62500000000000000, 8.000000000000000000 ) ) ;
#38649 = LINE ( 'NONE', #4687, #10568 ) ;
#38651 = ORIENTED_EDGE ( 'NONE', *, *, #36479, .F. ) ;
#38652 = CARTESIAN_POINT ( 'NONE',  ( -3.042071309553173730, 19.63541666325268764, 11.35316468749999785 ) ) ;
#38653 = CARTESIAN_POINT ( 'NONE',  ( 2.679491924311302675, 97.91666665983869677, -9.999999999999957367 ) ) ;
#38655 = FACE_OUTER_BOUND ( 'NONE', #25317, .T. ) ;
#38654 = DIRECTION ( 'NONE',  ( -0.000000000000000000, -0.000000000000000000, -1.000000000000000000 ) ) ;
#38656 = CARTESIAN_POINT ( 'NONE',  ( -7.778174593052020747, -7.778174593052023411, 79.18750000000000000 ) ) ;
#38657 = CARTESIAN_POINT ( 'NONE',  ( -1.432654583217662259, 201.1250000013656347, 145.4587341250000350 ) ) ;
#38658 = VECTOR ( 'NONE', #43427, 1000.000000000000000 ) ;
#38659 = CARTESIAN_POINT ( 'NONE',  ( -10.00000000000000178, 54.37499999317203958, -1.224646799147353454E-15 ) ) ;
#38660 = CARTESIAN_POINT ( 'NONE',  ( -7.188101187500000044, 106.1562500020483810, 0.000000000000000000 ) ) ;
#38661 = CARTESIAN_POINT ( 'NONE',  ( -3.211159895383561391, 8.812499998634407916, -3.211159895383561835 ) ) ;
#38662 = FACE_OUTER_BOUND ( 'NONE', #66349, .T. ) ;
#38663 = CARTESIAN_POINT ( 'NONE',  ( -7.999999999999991118, 0.000000000000000000, 8.330302779823362869 ) ) ;
#38664 = CARTESIAN_POINT ( 'NONE',  ( 2.679491924330074770, 166.0416666666649803, -9.999999999989118038 ) ) ;
#38665 = VERTEX_POINT ( 'NONE', #21390 ) ;
#38666 = VERTEX_POINT ( 'NONE', #33122 ) ;
#38667 = CARTESIAN_POINT ( 'NONE',  ( -5.000000000000000000, -62.13136467932989859, 23.87699943806431335 ) ) ;
#38668 = CARTESIAN_POINT ( 'NONE',  ( -6.123233995736766282E-16, 223.7500000000000000, -10.00000000000000000 ) ) ;
#38669 = CARTESIAN_POINT ( 'NONE',  ( -1.604524386212670052E-13, 78.75000000000000000, 10.00000000000000178 ) ) ;
#38670 = CARTESIAN_POINT ( 'NONE',  ( -27.07824451268698951, -42.29133078361556386, 154.8773963665347537 ) ) ;
#38671 = CARTESIAN_POINT ( 'NONE',  ( -8.311093377946841443, 138.9062499965859843, 8.311093377946830785 ) ) ;
#38672 = EDGE_LOOP ( 'NONE', ( #46012, #36999 ) ) ;
#38673 = CARTESIAN_POINT ( 'NONE',  ( -7.999999999999991118, 1.918013197678222425E-05, 10.01780224128419405 ) ) ;
#38674 = CARTESIAN_POINT ( 'NONE',  ( -10.18810118749999738, -4.220049686691941915, 90.25000000204838102 ) ) ;
#38675 = CARTESIAN_POINT ( 'NONE',  ( -4.898587196589407898E-16, 7.999999999999991118, 20.14280278392014623 ) ) ;
#38676 = CARTESIAN_POINT ( 'NONE',  ( 2.828427124746209831, 208.3750000000000284, 200.8284271247462129 ) ) ;
#38678 = CARTESIAN_POINT ( 'NONE',  ( -8.311093377946836114, 122.6562499965860269, -8.311093377946837890 ) ) ;
#38677 = CARTESIAN_POINT ( 'NONE',  ( 2.828427124746152987, 195.1250000000000284, 139.1715728752538723 ) ) ;
#38679 = AXIS2_PLACEMENT_3D ( 'NONE', #42896, #70120, #47083 ) ;
#38680 = CYLINDRICAL_SURFACE ( 'NONE', #33722, 10.00000000000000000 ) ;
#38681 = ORIENTED_EDGE ( 'NONE', *, *, #3439, .F. ) ;
#38682 = CARTESIAN_POINT ( 'NONE',  ( -4.556349186104045934, 11.00000000000000000, 77.21875000000000000 ) ) ;
#38683 = CARTESIAN_POINT ( 'NONE',  ( -9.000000000000000000, -5.196152422706648899, -0.8038475772933779684 ) ) ;
#38684 = CARTESIAN_POINT ( 'NONE',  ( -3.042071309553163960, 117.5520833299193413, -11.35316468749999963 ) ) ;
#38685 = CARTESIAN_POINT ( 'NONE',  ( -1.432654583217607858, 200.6250000013656063, 201.4587341250000065 ) ) ;
#38686 = CARTESIAN_POINT ( 'NONE',  ( -7.188101187500000933, 17.99999999795161543, -2.977408999572651371 ) ) ;
#38687 = CARTESIAN_POINT ( 'NONE',  ( 7.204075437095968759, -7.204075437095966983, 83.59375000204838102 ) ) ;
#38688 = CARTESIAN_POINT ( 'NONE',  ( -5.676582343749998039, 17.76041666325268409, -9.832129032723420536 ) ) ;
#38689 = ORIENTED_EDGE ( 'NONE', *, *, #11739, .F. ) ;
#38690 = CARTESIAN_POINT ( 'NONE',  ( 1.224646799147353454E-15, 300.0000000000000000, -10.00000000000000178 ) ) ;
#38691 = CARTESIAN_POINT ( 'NONE',  ( -4.903558642999205574E-16, 8.008118988124991233, 21.63811528394063188 ) ) ;
#38692 = CARTESIAN_POINT ( 'NONE',  ( -4.898587196589407898E-16, 7.999999999999991118, 23.14280278392014978 ) ) ;
#38693 = VECTOR ( 'NONE', #22019, 1000.000000000000000 ) ;
#38694 = CARTESIAN_POINT ( 'NONE',  ( 1.836970198721029589E-15, 244.3750000068280031, 10.00000000000000000 ) ) ;
#38695 = CARTESIAN_POINT ( 'NONE',  ( -5.082755093536325042, 4.031249997951610986, -5.082755093536325930 ) ) ;
#38696 = CARTESIAN_POINT ( 'NONE',  ( -4.721056650415998313, 288.5781250017069510, 4.721056650416000089 ) ) ;
#38697 = CARTESIAN_POINT ( 'NONE',  ( -1.269107444400135093E-11, 58.74999999999901945, 10.00000000000000178 ) ) ;
#38698 = CARTESIAN_POINT ( 'NONE',  ( -7.188101187500001821, 1.499999997951610098, -2.977408999572651371 ) ) ;
#38699 = VERTEX_POINT ( 'NONE', #27420 ) ;
#38700 = EDGE_CURVE ( 'NONE', #42029, #4267, #8303, .T. ) ;
#38701 = CARTESIAN_POINT ( 'NONE',  ( -9.832129032723420536, 149.0104166632526699, 5.676582343749997150 ) ) ;
#38702 = CARTESIAN_POINT ( 'NONE',  ( 10.18810118750000093, -4.220049686691933921, 78.81250000204838102 ) ) ;
#38703 = CARTESIAN_POINT ( 'NONE',  ( -31.45873412499999944, 208.9375000013656063, 170.0000000000003979 ) ) ;
#38704 = FACE_OUTER_BOUND ( 'NONE', #25966, .T. ) ;
#38705 = CARTESIAN_POINT ( 'NONE',  ( 3.211159895383560947, 15.31249999863440792, 3.211159895383562723 ) ) ;
#38706 = VERTEX_POINT ( 'NONE', #36287 ) ;
#38707 = VECTOR ( 'NONE', #43681, 1000.000000000000000 ) ;
#38708 = CARTESIAN_POINT ( 'NONE',  ( 2.828427124746209831, 204.5000000027312126, 200.8284271247462129 ) ) ;
#38709 = EDGE_CURVE ( 'NONE', #2312, #38953, #23743, .T. ) ;
#38710 =( BOUNDED_CURVE ( )  B_SPLINE_CURVE ( 3, ( #52983, #951, #41657, #1315 ),
 .UNSPECIFIED., .F., .F. ) 
 B_SPLINE_CURVE_WITH_KNOTS ( ( 4, 4 ),
 ( 4.351430296279056975, 4.712388980384687898 ),
 .UNSPECIFIED. ) 
 CURVE ( )  GEOMETRIC_REPRESENTATION_ITEM ( )  RATIONAL_B_SPLINE_CURVE ( ( 1.000000000000000000, 0.9891718422399167210, 0.9891718422399167210, 1.000000000000000000 ) ) 
 REPRESENTATION_ITEM ( '' )  );
#38711 = CARTESIAN_POINT ( 'NONE',  ( -2.445694354108839175, 195.3125000013656063, 144.4456943541088663 ) ) ;
#38712 = CARTESIAN_POINT ( 'NONE',  ( -24.00000000000002487, 204.9375000027312410, 168.3431457505079152 ) ) ;
#38713 = CARTESIAN_POINT ( 'NONE',  ( -8.000000000000000000, 104.0000000000000000, 0.000000000000000000 ) ) ;
#38714 = EDGE_CURVE ( 'NONE', #48595, #62682, #30985, .T. ) ;
#38715 = ORIENTED_EDGE ( 'NONE', *, *, #42007, .F. ) ;
#38716 = CARTESIAN_POINT ( 'NONE',  ( -7.188101187500000044, 8.718749997951611874, -8.802885111219163269E-16 ) ) ;
#38717 = CARTESIAN_POINT ( 'NONE',  ( -2.751064625579944321E-14, 208.7500000000000284, 146.0000000000000284 ) ) ;
#38718 = CARTESIAN_POINT ( 'NONE',  ( -2.695368319209359154, -46.33178872148012317, 151.1920017723726630 ) ) ;
#38719 = CARTESIAN_POINT ( 'NONE',  ( 3.042071309553167069, 181.8229166632526983, -11.35316468749999785 ) ) ;
#38720 = CARTESIAN_POINT ( 'NONE',  ( 7.188101187500001821, 114.8750000020483810, -2.977408999572651371 ) ) ;
#38721 = VECTOR ( 'NONE', #48099, 999.9999999999998863 ) ;
#38722 = DIRECTION ( 'NONE',  ( -0.000000000000000000, -1.000000000000000000, -0.000000000000000000 ) ) ;
#38723 = CARTESIAN_POINT ( 'NONE',  ( -4.721056650415999201, 290.3281250017069510, -4.721056650415999201 ) ) ;
#38725 = DIRECTION ( 'NONE',  ( -0.000000000000000000, 1.000000000000000000, -0.000000000000000000 ) ) ;
#38724 = DIRECTION ( 'NONE',  ( -0.000000000000000000, 1.000000000000000000, -0.000000000000000000 ) ) ;
#38726 = ORIENTED_EDGE ( 'NONE', *, *, #48999, .F. ) ;
#38727 =( BOUNDED_CURVE ( )  B_SPLINE_CURVE ( 2, ( #42321, #47247, #48350, #70274, #18586, #7268, #54031, #53661, #36311 ),
 .UNSPECIFIED., .F., .F. ) 
 B_SPLINE_CURVE_WITH_KNOTS ( ( 3, 2, 2, 2, 3 ),
 ( 0.3522727272727272929, 0.3579545454545454697, 0.3636363636363636465, 0.3693181818181818232, 0.3750000000000000000 ),
 .UNSPECIFIED. ) 
 CURVE ( )  GEOMETRIC_REPRESENTATION_ITEM ( )  RATIONAL_B_SPLINE_CURVE ( ( 1.000000000000000000, 0.9238795325112867385, 1.000000000000000000, 0.9238795325112867385, 1.000000000000000000, 0.9238795325112867385, 1.000000000000000000, 0.9238795325112867385, 1.000000000000000000 ) ) 
 REPRESENTATION_ITEM ( '' )  );
#38728 = CARTESIAN_POINT ( 'NONE',  ( -11.35316468749999963, 263.9062500034140157, 0.000000000000000000 ) ) ;
#38729 = CARTESIAN_POINT ( 'NONE',  ( -4.401442555609577197E-16, 7.188101187499992051, 23.98655278187175455 ) ) ;
#38730 = CARTESIAN_POINT ( 'NONE',  ( 5.656854249492379694, 106.4374999999999858, -5.656854249492380582 ) ) ;
#38731 = DIRECTION ( 'NONE',  ( -0.000000000000000000, -0.02418647091589873691, 0.9997074645238147594 ) ) ;
#38732 = CARTESIAN_POINT ( 'NONE',  ( 5.126106709314299792, -68.65851429197805089, -20.89429596904636099 ) ) ;
#38733 = CARTESIAN_POINT ( 'NONE',  ( 3.458734125000015869, 195.1875000013655779, 198.0000000000000284 ) ) ;
#38734 = CARTESIAN_POINT ( 'NONE',  ( -10.00000000000000178, 142.5000000000000284, -1.224646799147353454E-15 ) ) ;
#38735 = FACE_OUTER_BOUND ( 'NONE', #27793, .T. ) ;
#38736 = CARTESIAN_POINT ( 'NONE',  ( -0.7343025909353899650, 9.968355046870078340, -0.5590800469813719253 ) ) ;
#38737 = CARTESIAN_POINT ( 'NONE',  ( 1.469576158976823947E-15, 93.87499999999998579, 8.000000000000000000 ) ) ;
#38738 = CARTESIAN_POINT ( 'NONE',  ( -11.35316468750000141, 108.5937499965860269, -1.390361679473963753E-15 ) ) ;
#38739 = CARTESIAN_POINT ( 'NONE',  ( -5.000000000000000888, -10.25161785469022035, -64.79070129774558495 ) ) ;
#38740 = CARTESIAN_POINT ( 'NONE',  ( -7.778174593052023411, 7.778174593052023411, 72.81249999999998579 ) ) ;
#38741 = VECTOR ( 'NONE', #47363, 1000.000000000000000 ) ;
#38744 = DIRECTION ( 'NONE',  ( -0.000000000000000000, 1.000000000000000000, -0.000000000000000000 ) ) ;
#38743 = CARTESIAN_POINT ( 'NONE',  ( 29.43265458321761230, 198.8750000013656347, 166.5412658749999650 ) ) ;
#38742 = CARTESIAN_POINT ( 'NONE',  ( 26.56734541678232375, 198.6250000013655779, 173.4587341249998929 ) ) ;
#38745 = VERTEX_POINT ( 'NONE', #7613 ) ;
#38746 = CARTESIAN_POINT ( 'NONE',  ( 2.338768297991025147, 223.9372515351016659, 9.740328430350823297 ) ) ;
#38747 = DIRECTION ( 'NONE',  ( -0.000000000000000000, -0.000000000000000000, -1.000000000000000000 ) ) ;
#38748 = CARTESIAN_POINT ( 'NONE',  ( 26.56734541678232375, 198.6250000013655779, 173.4587341249998929 ) ) ;
#38749 = CARTESIAN_POINT ( 'NONE',  ( -11.35316468749999785, 203.3854166632526983, -3.042071309553167513 ) ) ;
#38750 = CARTESIAN_POINT ( 'NONE',  ( -11.00000000000000000, 0.000000000000000000, 116.4999999999999858 ) ) ;
#38751 = CARTESIAN_POINT ( 'NONE',  ( -8.342170076843785083E-16, 18.06249999863440792, 4.541265875000002339 ) ) ;
#38752 = CARTESIAN_POINT ( 'NONE',  ( 31.45873412499997812, 195.8750000013655779, 171.4326545832176123 ) ) ;
#38753 = CARTESIAN_POINT ( 'NONE',  ( -5.656854249492375253, 5.656854249492375253, 27.64280277982336642 ) ) ;
#38755 = DIRECTION ( 'NONE',  ( -0.000000000000000000, 1.000000000000000000, 4.689100369878284071E-30 ) ) ;
#38754 = CARTESIAN_POINT ( 'NONE',  ( 4.541265875000002339, 0.3749999986344067504, 0.000000000000000000 ) ) ;
#38756 = CARTESIAN_POINT ( 'NONE',  ( 11.35316468749999785, 90.57291666325268409, 3.042071309553174174 ) ) ;
#38757 = VERTEX_POINT ( 'NONE', #70974 ) ;
#38758 = CARTESIAN_POINT ( 'NONE',  ( 3.313708498984922812, 93.03124999999998579, -7.999999999999837463 ) ) ;
#38759 = CARTESIAN_POINT ( 'NONE',  ( 5.082755093536324154, 19.78124999795161543, 5.082755093536326818 ) ) ;
#38760 = CARTESIAN_POINT ( 'NONE',  ( 11.00000000000000000, 1.347111479062088405E-15, 72.43750000409676204 ) ) ;
#38761 = CARTESIAN_POINT ( 'NONE',  ( -6.951808397369817780E-16, 262.9687500034140157, -11.35316468749999963 ) ) ;
#38762 = AXIS2_PLACEMENT_3D ( 'NONE', #23619, #22872, #52668 ) ;
#38763 = CARTESIAN_POINT ( 'NONE',  ( -8.311093377946841443, 83.90624999658602690, 8.311093377946830785 ) ) ;
#38764 = EDGE_LOOP ( 'NONE', ( #51674, #55406 ) ) ;
#38765 = CARTESIAN_POINT ( 'NONE',  ( 10.00000000000000000, 206.6666666598387110, 2.679491924311235618 ) ) ;
#38766 = CARTESIAN_POINT ( 'NONE',  ( 1.871523826299183495E-15, -10.18810118749999916, 105.5312500020483810 ) ) ;
#38767 = CARTESIAN_POINT ( 'NONE',  ( -31.45873412499999233, 194.9375000013655779, 170.0000000000003979 ) ) ;
#38768 = CARTESIAN_POINT ( 'NONE',  ( 2.445694354108839175, 203.3125000013656063, 195.5543056458912190 ) ) ;
#38769 = CARTESIAN_POINT ( 'NONE',  ( 6.951808397369818766E-16, 87.03124999658602690, -11.35316468750000141 ) ) ;
#38770 = CARTESIAN_POINT ( 'NONE',  ( -7.999999999999991118, 3.313708498984756723, 11.42405278392014623 ) ) ;
#38771 = CARTESIAN_POINT ( 'NONE',  ( -26.56734541678238060, 199.6250000013656063, 166.5412658750003629 ) ) ;
#38772 = DIRECTION ( 'NONE',  ( -0.000000000000000000, -1.000000000000000000, -0.000000000000000000 ) ) ;
#38773 = CARTESIAN_POINT ( 'NONE',  ( -4.999999999999998224, 188.5416666598387110, -8.660254037844389075 ) ) ;
#38774 = LINE ( 'NONE', #38397, #55677 ) ;
#38775 = CARTESIAN_POINT ( 'NONE',  ( 5.676582343749993598, 80.26041666325268409, 9.832129032723422313 ) ) ;
#38776 = CARTESIAN_POINT ( 'NONE',  ( -2.765530957081998586, 295.6406250017069510, 6.676582343750001591 ) ) ;
#38777 = CARTESIAN_POINT ( 'NONE',  ( -10.18810118749999738, -4.220049686691941915, 101.1250000020483810 ) ) ;
#38778 = CARTESIAN_POINT ( 'NONE',  ( 5.676582343749993598, 214.9479166632526983, 9.832129032723422313 ) ) ;
#38779 = VERTEX_POINT ( 'NONE', #41574 ) ;
#38780 = FACE_OUTER_BOUND ( 'NONE', #40228, .T. ) ;
#38781 = DIRECTION ( 'NONE',  ( 0.8660254037844696828, -0.4999999999999462097, 0.000000000000000000 ) ) ;
#38782 = CARTESIAN_POINT ( 'NONE',  ( -1.836970198721029983E-15, 143.7500000000000284, 10.00000000000000178 ) ) ;
#38783 = CARTESIAN_POINT ( 'NONE',  ( 5.676582343749993598, 204.9479166632526983, 9.832129032723422313 ) ) ;
#38784 = CARTESIAN_POINT ( 'NONE',  ( 5.000000000000004441, 224.7916666734946602, 8.660254037844385522 ) ) ;
#38785 = CARTESIAN_POINT ( 'NONE',  ( 4.556349186104052151, -10.99999999999999822, 72.15625000409677625 ) ) ;
#38786 = EDGE_LOOP ( 'NONE', ( #45543, #63955, #60694, #9294 ) ) ;
#38787 = CARTESIAN_POINT ( 'NONE',  ( -11.35316468750000141, 188.8020833299193555, 3.042071309553159963 ) ) ;
#38788 = VECTOR ( 'NONE', #16431, 1000.000000000000000 ) ;
#38789 = CARTESIAN_POINT ( 'NONE',  ( 7.188101187499992051, 8.802885111219154394E-16, 15.73655278187175632 ) ) ;
#38790 = CARTESIAN_POINT ( 'NONE',  ( -31.45873412500001010, 206.6250000013656063, 168.5673454167827572 ) ) ;
#38791 = CARTESIAN_POINT ( 'NONE',  ( -8.000000000000001776, 14.34375000000000355, 3.313708498984759387 ) ) ;
#38792 = ORIENTED_EDGE ( 'NONE', *, *, #72838, .F. ) ;
#38793 = EDGE_CURVE ( 'NONE', #2846, #63656, #29783, .T. ) ;
#38794 = CARTESIAN_POINT ( 'NONE',  ( 5.656854249492379694, 94.62500000409677625, -5.656854249492380582 ) ) ;
#38795 = CARTESIAN_POINT ( 'NONE',  ( 2.679491924311222739, 8.958333333333333925, 10.00000000000000355 ) ) ;
#38796 = CARTESIAN_POINT ( 'NONE',  ( -4.220049686691937474, -10.18810118749999738, 83.31250000204836681 ) ) ;
#38797 = VERTEX_POINT ( 'NONE', #42299 ) ;
#38798 = CARTESIAN_POINT ( 'NONE',  ( 1.656854249492381914, 19.81250000000000000, 4.000000000000000888 ) ) ;
#38799 = CARTESIAN_POINT ( 'NONE',  ( 4.541265875000002339, 21.31249999863440792, 0.000000000000000000 ) ) ;
#38800 = CARTESIAN_POINT ( 'NONE',  ( 28.00000000000002132, 199.1250000027312126, 173.9999999999999147 ) ) ;
#38801 = VECTOR ( 'NONE', #22987, 1000.000000000000000 ) ;
#38802 = VERTEX_POINT ( 'NONE', #12886 ) ;
#38803 = CARTESIAN_POINT ( 'NONE',  ( 10.00000000000000178, 16.87499999317203248, 0.000000000000000000 ) ) ;
#38804 = CARTESIAN_POINT ( 'NONE',  ( 5.082755093536326818, 91.71875000204838102, 5.082755093536325042 ) ) ;
#38805 = ADVANCED_FACE ( 'NONE', ( #18563 ), #1233, .T. ) ;
#38808 = PLANE ( 'NONE',  #16909 ) ;
#38807 = CARTESIAN_POINT ( 'NONE',  ( -5.676582343750000703, 263.0729166700806445, -9.832129032723418760 ) ) ;
#38806 = CARTESIAN_POINT ( 'NONE',  ( 11.00000000000000355, -11.00000000000000000, -6.938893903907228378E-15 ) ) ;
#38809 = APPLICATION_PROTOCOL_DEFINITION ( 'draft international standard', 'automotive_design', 1998, #51531 ) ;
#38810 = AXIS2_PLACEMENT_3D ( 'NONE', #41540, #30954, #53975 ) ;
#38811 = ORIENTED_EDGE ( 'NONE', *, *, #20434, .F. ) ;
#38812 = CARTESIAN_POINT ( 'NONE',  ( -8.311093377946836114, 258.5937500034140157, -8.311093377946836114 ) ) ;
#38813 = CARTESIAN_POINT ( 'NONE',  ( 2.977408999572650927, -7.188101187499990274, 13.95530278187175277 ) ) ;
#38814 = ORIENTED_EDGE ( 'NONE', *, *, #40236, .F. ) ;
#38815 =( BOUNDED_CURVE ( )  B_SPLINE_CURVE ( 2, ( #47809, #36140, #59161, #55355, #46155, #40502, #57118, #9322, #9700 ),
 .UNSPECIFIED., .F., .F. ) 
 B_SPLINE_CURVE_WITH_KNOTS ( ( 3, 2, 2, 2, 3 ),
 ( 0.9264705882352941568, 0.9301470588235294379, 0.9338235294117648300, 0.9375000000000002220, 0.9411764705882355031 ),
 .UNSPECIFIED. ) 
 CURVE ( )  GEOMETRIC_REPRESENTATION_ITEM ( )  RATIONAL_B_SPLINE_CURVE ( ( 1.000000000000000000, 0.9238795325112867385, 1.000000000000000000, 0.9238795325112867385, 1.000000000000000000, 0.9238795325112867385, 1.000000000000000000, 0.9238795325112821866, 1.000000000000004663 ) ) 
 REPRESENTATION_ITEM ( '' )  );
#38816 = VERTEX_POINT ( 'NONE', #12524 ) ;
#38817 = CARTESIAN_POINT ( 'NONE',  ( -4.220049686691937474, -10.18810118749999738, 72.43750000204838102 ) ) ;
#38818 = CARTESIAN_POINT ( 'NONE',  ( -3.042071309553173730, 79.63541666325268409, 11.35316468749999785 ) ) ;
#38819 = CARTESIAN_POINT ( 'NONE',  ( -11.00000000000000000, 4.556349186104045934, 90.90625000000000000 ) ) ;
#38821 = CARTESIAN_POINT ( 'NONE',  ( 4.721056650416000089, 290.9843750017070079, 4.721056650415999201 ) ) ;
#38820 = CARTESIAN_POINT ( 'NONE',  ( 30.82842712474620583, 195.2500000027312126, 172.8284271247460424 ) ) ;
#38822 = CARTESIAN_POINT ( 'NONE',  ( -6.735557395310442023E-16, 11.00000000000000000, 89.12499999999998579 ) ) ;
#38823 = CARTESIAN_POINT ( 'NONE',  ( -1.836970198721029983E-15, 165.6249999931720254, 10.00000000000000178 ) ) ;
#38824 = CARTESIAN_POINT ( 'NONE',  ( 2.445694354108839175, 197.3125000013656063, 195.5543056458912190 ) ) ;
#38825 = CARTESIAN_POINT ( 'NONE',  ( -3.313708498984765161, 6.843749995903221084, 7.999999999999998224 ) ) ;
#38826 = ORIENTED_EDGE ( 'NONE', *, *, #64449, .T. ) ;
#38827 = CARTESIAN_POINT ( 'NONE',  ( 24.54126587499998990, 195.1875000013655779, 169.9999999999998863 ) ) ;
#38828 = CARTESIAN_POINT ( 'NONE',  ( -2.977408999572654480, 15.37499999795161187, 7.188101187499999156 ) ) ;
#38829 = CARTESIAN_POINT ( 'NONE',  ( -3.042071309553164404, 162.5520833299193555, -11.35316468749999963 ) ) ;
#38830 = CYLINDRICAL_SURFACE ( 'NONE', #15415, 8.000000000000000000 ) ;
#38831 = CARTESIAN_POINT ( 'NONE',  ( -7.188101187500000933, 104.9375000020483810, -2.977408999572650483 ) ) ;
#38833 = CARTESIAN_POINT ( 'NONE',  ( 5.107860025164819184, -50.62490018645517154, -41.07729128472065838 ) ) ;
#38832 = DIRECTION ( 'NONE',  ( 0.000000000000000000, 0.000000000000000000, -1.000000000000000000 ) ) ;
#38834 = CARTESIAN_POINT ( 'NONE',  ( 30.44569435410883784, 206.0625000013656063, 167.5543056458911053 ) ) ;
#38835 = CARTESIAN_POINT ( 'NONE',  ( 1.320432766682872962E-15, -7.188101187499992051, 15.73655278187175632 ) ) ;
#38836 = CARTESIAN_POINT ( 'NONE',  ( 3.999999999999959144, 206.1875000027311842, 140.3431457505076594 ) ) ;
#38837 = CARTESIAN_POINT ( 'NONE',  ( 9.832129032723420536, 61.19791666325267698, -5.676582343749999815 ) ) ;
#38838 = DIRECTION ( 'NONE',  ( 0.000000000000000000, 0.000000000000000000, 1.000000000000000000 ) ) ;
#38839 = CARTESIAN_POINT ( 'NONE',  ( -7.320508075688773708, 18.74999999317203248, -7.320508075688774596 ) ) ;
#38840 = CARTESIAN_POINT ( 'NONE',  ( 32.00000000000000000, 199.3125000000000568, 168.3431457505075457 ) ) ;
#38841 = ORIENTED_EDGE ( 'NONE', *, *, #29591, .F. ) ;
#38842 = CARTESIAN_POINT ( 'NONE',  ( -2.775557561562891351E-14, 210.0000000000000284, 146.0000000000000284 ) ) ;
#38843 = CARTESIAN_POINT ( 'NONE',  ( -41.99999999999992895, -31.99999999999978684, 171.9999999999997726 ) ) ;
#38844 = CARTESIAN_POINT ( 'NONE',  ( 5.676582343749993598, 44.94791666325267698, 9.832129032723422313 ) ) ;
#38845 = CARTESIAN_POINT ( 'NONE',  ( -7.778174593052023411, 7.778174593052023411, 73.00000000409677625 ) ) ;
#38846 = CARTESIAN_POINT ( 'NONE',  ( -2.445694354108840063, 200.0625000013656063, 139.5543056458912190 ) ) ;
#38847 = DIRECTION ( 'NONE',  ( 0.000000000000000000, -0.000000000000000000, -1.000000000000000000 ) ) ;
#38849 = CARTESIAN_POINT ( 'NONE',  ( -9.832129032723420536, 48.69791666325268409, 5.676582343749997150 ) ) ;
#38848 = CARTESIAN_POINT ( 'NONE',  ( -4.401442555609581635E-16, 96.78125000204838102, -7.188101187500000044 ) ) ;
#38850 = CARTESIAN_POINT ( 'NONE',  ( -5.656854249492373476, -5.656854249492376141, 10.01780277982336465 ) ) ;
#38851 = CARTESIAN_POINT ( 'NONE',  ( -7.999985424683830004, -3.313723074300923610, 4.111553367083139676 ) ) ;
#38852 = CARTESIAN_POINT ( 'NONE',  ( -9.832129032723418760, 172.8645833299193555, -5.676582343750004256 ) ) ;
#38853 = CARTESIAN_POINT ( 'NONE',  ( 8.660254037844389075, 147.2916666598387110, -5.000000000000000000 ) ) ;
#38854 = AXIS2_PLACEMENT_3D ( 'NONE', #58087, #71219, #42178 ) ;
#38855 = CARTESIAN_POINT ( 'NONE',  ( -2.977408999572651815, 100.8125000020484094, 7.188101187500000933 ) ) ;
#38856 = DIRECTION ( 'NONE',  ( 0.000000000000000000, 0.000000000000000000, 1.000000000000000000 ) ) ;
#38857 = CARTESIAN_POINT ( 'NONE',  ( -8.311093377946841443, 29.21874999658601624, 8.311093377946834337 ) ) ;
#38858 = LINE ( 'NONE', #57333, #21976 ) ;
#38859 = ORIENTED_EDGE ( 'NONE', *, *, #6951, .T. ) ;
#38860 = CARTESIAN_POINT ( 'NONE',  ( 49.70177871865297448, 134.6202577753208516, 58.00000000000000711 ) ) ;
#38861 = CARTESIAN_POINT ( 'NONE',  ( -10.18810118749999916, 4.220049686691934809, 79.56250000204836681 ) ) ;
#38862 = CARTESIAN_POINT ( 'NONE',  ( 5.000000000000000000, -16.14408868864072844, 27.96238185062368586 ) ) ;
#38864 = CARTESIAN_POINT ( 'NONE',  ( -11.35316468750000141, 163.2812499965860127, -1.390361679473963753E-15 ) ) ;
#38863 = CARTESIAN_POINT ( 'NONE',  ( -8.660254037844394404, 7.916666666666672292, 5.000000000000001776 ) ) ;
#38865 = CARTESIAN_POINT ( 'NONE',  ( -4.898587196589407898E-16, 7.999999999999991118, 9.511552784329824206 ) ) ;
#38866 = CARTESIAN_POINT ( 'NONE',  ( 11.00000000000010836, -4.556349186103939353, 79.84375000409677625 ) ) ;
#38867 = CARTESIAN_POINT ( 'NONE',  ( -6.951808397369817780E-16, 222.6562500034139873, -11.35316468749999963 ) ) ;
#38868 = CARTESIAN_POINT ( 'NONE',  ( 2.216418498311663487, 51.36626494304667290, -48.60390812669556482 ) ) ;
#38869 = CARTESIAN_POINT ( 'NONE',  ( 4.220049686691934809, 10.18810118749999916, 82.56250000204836681 ) ) ;
#38870 = VERTEX_POINT ( 'NONE', #35555 ) ;
#38871 = AXIS2_PLACEMENT_3D ( 'NONE', #26964, #55287, #49980 ) ;
#38872 = DIRECTION ( 'NONE',  ( 0.000000000000000000, 0.000000000000000000, 1.000000000000000000 ) ) ;
#38873 = CARTESIAN_POINT ( 'NONE',  ( 8.311093377946837890, 116.7187499965859985, -8.311093377946837890 ) ) ;
#38874 = CARTESIAN_POINT ( 'NONE',  ( -4.500000000000010658, -7.794228634059939154, 0.000000000000000000 ) ) ;
#38875 = ORIENTED_EDGE ( 'NONE', *, *, #8908, .F. ) ;
#38876 = ORIENTED_EDGE ( 'NONE', *, *, #37258, .F. ) ;
#38877 = CARTESIAN_POINT ( 'NONE',  ( -4.541265875000002339, 6.874999998634407916, -1.881053915767121998 ) ) ;
#38878 = ADVANCED_FACE ( 'NONE', ( #24211 ), #70610, .T. ) ;
#38879 = CARTESIAN_POINT ( 'NONE',  ( 7.188101187500001821, 8.062499997951611874, -2.977408999572650483 ) ) ;
#38880 = CARTESIAN_POINT ( 'NONE',  ( 8.000000000000001776, 107.8437500040967620, 3.313708498984759387 ) ) ;
#38881 = CARTESIAN_POINT ( 'NONE',  ( -10.18810118749999916, 0.000000000000000000, 93.53125000204836681 ) ) ;
#38882 = EDGE_CURVE ( 'NONE', #11598, #502, #24942, .T. ) ;
#38883 = CARTESIAN_POINT ( 'NONE',  ( -24.54126587500000056, 200.5000000013656063, 168.5673454167827003 ) ) ;
#38884 = CARTESIAN_POINT ( 'NONE',  ( -4.000000000000001776, 9.437500000000000000, -1.656854249492381470 ) ) ;
#38885 = CARTESIAN_POINT ( 'NONE',  ( -31.05507224581699788, -12.00007582394998984, 171.9999999999997726 ) ) ;
#38886 = CARTESIAN_POINT ( 'NONE',  ( 1.881053915767121998, 9.499999998634404363, -4.541265875000002339 ) ) ;
#38887 = CARTESIAN_POINT ( 'NONE',  ( -1.656854249492405451, 197.3125000000000568, 138.0000000000000568 ) ) ;
#38888 = VERTEX_POINT ( 'NONE', #35921 ) ;
#38889 = DIRECTION ( 'NONE',  ( 0.000000000000000000, 0.000000000000000000, -1.000000000000000000 ) ) ;
#38890 = ADVANCED_FACE ( 'NONE', ( #13620 ), #30254, .T. ) ;
#38892 = CARTESIAN_POINT ( 'NONE',  ( -24.00000000000000711, 199.8125000000000284, 168.3431457505080289 ) ) ;
#38891 = CARTESIAN_POINT ( 'NONE',  ( -24.54126587499998990, 197.1875000013655779, 170.0000000000002842 ) ) ;
#38893 = CARTESIAN_POINT ( 'NONE',  ( -2.828427124746190735, 10.37500000000000000, -2.828427124746191623 ) ) ;
#38894 = VECTOR ( 'NONE', #13115, 1000.000000000000000 ) ;
#38895 = CARTESIAN_POINT ( 'NONE',  ( 7.188101187499992051, 8.802885111219154394E-16, 0.7365527818717527708 ) ) ;
#38896 = ORIENTED_EDGE ( 'NONE', *, *, #21631, .T. ) ;
#38897 = ORIENTED_EDGE ( 'NONE', *, *, #3343, .F. ) ;
#38898 = CARTESIAN_POINT ( 'NONE',  ( 10.18810118750000093, -4.220049686691933033, 90.81250000204838102 ) ) ;
#38899 = CARTESIAN_POINT ( 'NONE',  ( 4.242640687119285658, 288.6249999999999432, -4.242640687119286547 ) ) ;
#38900 = CARTESIAN_POINT ( 'NONE',  ( -31.45873412499999944, 200.8750000013656063, 168.5673454167827572 ) ) ;
#38901 = CARTESIAN_POINT ( 'NONE',  ( -4.556349186104045934, 11.00000000000000000, 110.2187499999999858 ) ) ;
#38902 = CARTESIAN_POINT ( 'NONE',  ( 3.458734125000015425, 208.2500000013656063, 196.5673454167823877 ) ) ;
#38903 = CARTESIAN_POINT ( 'NONE',  ( 8.660254037844454800, 60.41666666666670693, -5.000000000000039080 ) ) ;
#38904 = CARTESIAN_POINT ( 'NONE',  ( 2.679491924311228956, 116.0416666666666430, -10.00000000000000000 ) ) ;
#38905 = VECTOR ( 'NONE', #68933, 1000.000000000000000 ) ;
#38906 = CARTESIAN_POINT ( 'NONE',  ( 5.656854249492381470, 109.0624999999999858, 5.656854249492379694 ) ) ;
#38907 = CARTESIAN_POINT ( 'NONE',  ( 4.721056650415999201, 290.2343750017069510, -4.721056650415999201 ) ) ;
#38908 = CARTESIAN_POINT ( 'NONE',  ( -4.401442555609577197E-16, 7.188101187499992051, 4.486552781871752771 ) ) ;
#38909 = ORIENTED_EDGE ( 'NONE', *, *, #40479, .T. ) ;
#38910 = DIRECTION ( 'NONE',  ( 1.836970198721037823E-16, -4.283267841918042125E-17, 1.000000000000000000 ) ) ;
#38912 = EDGE_CURVE ( 'NONE', #11319, #413, #62157, .T. ) ;
#38911 = CARTESIAN_POINT ( 'NONE',  ( 28.00000000000002487, 206.9375000013656063, 166.5412658749999082 ) ) ;
#38913 = CARTESIAN_POINT ( 'NONE',  ( -8.000000000000001776, 27.65624999590323085, 3.313708498984759387 ) ) ;
#38914 = CARTESIAN_POINT ( 'NONE',  ( -3.458734125000015425, 197.9375000013655779, 142.0000000000000568 ) ) ;
#38915 = CARTESIAN_POINT ( 'NONE',  ( -2.977408999572652260, 123.3125000020483810, 7.188101187500000044 ) ) ;
#38917 = CARTESIAN_POINT ( 'NONE',  ( -3.458734125000015869, 202.1875000013656063, 142.0000000000000568 ) ) ;
#38916 = DIRECTION ( 'NONE',  ( -0.000000000000000000, 1.000000000000000000, -0.000000000000000000 ) ) ;
#38918 = CARTESIAN_POINT ( 'NONE',  ( -11.35316468749999963, 259.2187500034140157, 0.000000000000000000 ) ) ;
#38919 = CARTESIAN_POINT ( 'NONE',  ( -28.00000000000002487, 195.0000000000000000, 166.0000000000003695 ) ) ;
#38920 = CARTESIAN_POINT ( 'NONE',  ( -10.00000000000000178, 94.37499999317203958, -1.224646799147353454E-15 ) ) ;
#38921 = CARTESIAN_POINT ( 'NONE',  ( 9.832129032723416984, 10.36458332991935016, 5.676582343750006032 ) ) ;
#38922 = DIRECTION ( 'NONE',  ( 5.505339259226019480E-18, -0.9989890351440378069, 0.04495450658148170825 ) ) ;
#38923 = CARTESIAN_POINT ( 'NONE',  ( 11.35316468749999963, 206.3020833299193271, -3.042071309553165293 ) ) ;
#38924 = CARTESIAN_POINT ( 'NONE',  ( 0.000000000000000000, 0.000000000000000000, 118.0000000000000000 ) ) ;
#38925 = CYLINDRICAL_SURFACE ( 'NONE', #29508, 11.00000000000000000 ) ;
#38927 = CARTESIAN_POINT ( 'NONE',  ( 4.898587196589412829E-16, 15.18749999590322197, -8.000000000000000000 ) ) ;
#38926 = CARTESIAN_POINT ( 'NONE',  ( 4.556349186104052151, -10.99999999999999822, 88.46874999999998579 ) ) ;
#38928 = VERTEX_POINT ( 'NONE', #14739 ) ;
#38929 = CARTESIAN_POINT ( 'NONE',  ( 1.432654583217608080, 199.8750000013655779, 138.5412658750000503 ) ) ;
#38930 = CARTESIAN_POINT ( 'NONE',  ( -5.676582343749998039, 2.447916663252682756, -9.832129032723420536 ) ) ;
#38931 = CARTESIAN_POINT ( 'NONE',  ( -4.556349186104045934, 11.00000000000000000, 90.90625000409677625 ) ) ;
#38932 = CARTESIAN_POINT ( 'NONE',  ( 4.242640687119285658, 292.6249999999999432, -4.242640687119286547 ) ) ;
#38933 = CARTESIAN_POINT ( 'NONE',  ( -24.54126587499998990, 197.1875000013655779, 170.0000000000002842 ) ) ;
#38934 = DIRECTION ( 'NONE',  ( -0.000000000000000000, 1.000000000000000000, -1.563033456626094573E-30 ) ) ;
#38936 = CARTESIAN_POINT ( 'NONE',  ( 3.042071309553167513, 11.82291666325268231, -11.35316468749999785 ) ) ;
#38935 = CARTESIAN_POINT ( 'NONE',  ( -2.977408999572652260, 115.4375000020483810, 7.188101187500000044 ) ) ;
#38937 = DIRECTION ( 'NONE',  ( 0.000000000000000000, 0.000000000000000000, -1.000000000000000000 ) ) ;
#38938 =( BOUNDED_CURVE ( )  B_SPLINE_CURVE ( 2, ( #44258, #15936, #9174, #33323, #43875, #72922, #61232, #26892, #15197, #32193, #55584, #68003, #21232 ),
 .UNSPECIFIED., .F., .F. ) 
 B_SPLINE_CURVE_WITH_KNOTS ( ( 3, 2, 2, 2, 2, 2, 3 ),
 ( 0.3055555555555558023, 0.3148148148148149361, 0.3240740740740741255, 0.3333333333333332593, 0.3425925925925924487, 0.3518518518518516380, 0.3611111111111107719 ),
 .UNSPECIFIED. ) 
 CURVE ( )  GEOMETRIC_REPRESENTATION_ITEM ( )  RATIONAL_B_SPLINE_CURVE ( ( 0.9999999999999992228, 0.9659258262890690894, 1.000000000000000000, 0.9659258262890683122, 1.000000000000000000, 0.9659258262890683122, 1.000000000000000000, 0.9659258262890683122, 1.000000000000000000, 0.9659258262890683122, 1.000000000000000000, 0.9659258262890695335, 0.9999999999999987788 ) ) 
 REPRESENTATION_ITEM ( '' )  );
#38939 = CARTESIAN_POINT ( 'NONE',  ( -8.311093377946836114, 127.6562499965860411, -8.311093377946837890 ) ) ;
#38940 = CARTESIAN_POINT ( 'NONE',  ( -1.836970198721029983E-15, 105.6249999931720396, 10.00000000000000178 ) ) ;
#38941 = CARTESIAN_POINT ( 'NONE',  ( -2.977408999572650927, 118.2500000020483952, -7.188101187500001821 ) ) ;
#38942 = CARTESIAN_POINT ( 'NONE',  ( -1.881053915767124440, 21.12499999863441147, 4.541265875000001451 ) ) ;
#38943 = CARTESIAN_POINT ( 'NONE',  ( 3.313708498984762496, -7.999999999999989342, 25.48655278392014623 ) ) ;
#38944 = CARTESIAN_POINT ( 'NONE',  ( -5.000000000000005329, 40.20833332650536818, 8.660254037844387298 ) ) ;
#38945 = VERTEX_POINT ( 'NONE', #20779 ) ;
#38946 = CARTESIAN_POINT ( 'NONE',  ( -1.781595147096710186, -67.70776641946466157, 20.12770457511388855 ) ) ;
#38947 = CARTESIAN_POINT ( 'NONE',  ( -4.721056650415999201, 290.4843750017070079, -4.721056650415999201 ) ) ;
#38948 = CARTESIAN_POINT ( 'NONE',  ( 4.999999999999999112, 52.85071664756648602, 48.38833198888325882 ) ) ;
#38949 = CARTESIAN_POINT ( 'NONE',  ( 1.469576158976822172E-15, -7.999999999999991118, -0.1071972160798552454 ) ) ;
#38950 = CARTESIAN_POINT ( 'NONE',  ( -2.751064625579944321E-14, 206.8750000027312126, 146.0000000000000284 ) ) ;
#38951 = CARTESIAN_POINT ( 'NONE',  ( 3.042071309553173286, 255.3645833367473301, 11.35316468749999608 ) ) ;
#38952 = CARTESIAN_POINT ( 'NONE',  ( -6.238412754330611322E-16, 10.18810118749999916, 105.1562500020483810 ) ) ;
#38953 = VERTEX_POINT ( 'NONE', #9479 ) ;
#38954 = CARTESIAN_POINT ( 'NONE',  ( 2.751064625579944321E-14, 197.8750000027312126, 194.0000000000000568 ) ) ;
#38955 = CARTESIAN_POINT ( 'NONE',  ( 11.35316468749999963, 151.3020833299193555, -3.042071309553165293 ) ) ;
#38956 = DIRECTION ( 'NONE',  ( -0.000000000000000000, 1.000000000000000000, -0.000000000000000000 ) ) ;
#38957 = CARTESIAN_POINT ( 'NONE',  ( -3.458734124999960358, 200.6875000013656063, 198.0000000000000284 ) ) ;
#38958 = CARTESIAN_POINT ( 'NONE',  ( -7.999999999999991118, -1.759867635265925965E-05, 1.017803281814245064 ) ) ;
#38959 = CARTESIAN_POINT ( 'NONE',  ( 8.311093377946834337, 80.46874999658601268, 8.311093377946839666 ) ) ;
#38960 = VERTEX_POINT ( 'NONE', #66814 ) ;
#38961 = CARTESIAN_POINT ( 'NONE',  ( 4.220049686691934809, 10.18810118749999916, 112.1875000020483810 ) ) ;
#38962 = CARTESIAN_POINT ( 'NONE',  ( 4.541265875000002339, 10.43749999863440792, 0.000000000000000000 ) ) ;
#38963 = ORIENTED_EDGE ( 'NONE', *, *, #16210, .F. ) ;
#38964 = CARTESIAN_POINT ( 'NONE',  ( 5.082755093536324154, 25.78124999795161543, 5.082755093536326818 ) ) ;
#38965 = CARTESIAN_POINT ( 'NONE',  ( 27.99999999999999645, 210.0000000000000284, 169.9999999999999147 ) ) ;
#38966 = CARTESIAN_POINT ( 'NONE',  ( -2.977408999572650039, 19.31249999795161543, -7.188101187500001821 ) ) ;
#38967 = ADVANCED_FACE ( 'NONE', ( #32495 ), #21153, .F. ) ;
#38968 = CARTESIAN_POINT ( 'NONE',  ( -4.556349186104048599, -10.99999999999999822, 103.4687500040967763 ) ) ;
#38969 = CARTESIAN_POINT ( 'NONE',  ( 10.18810118749999916, 1.247682550866122264E-15, 109.2812500020483668 ) ) ;
#38970 = EDGE_CURVE ( 'NONE', #23384, #41296, #69872, .T. ) ;
#38971 = CARTESIAN_POINT ( 'NONE',  ( 2.828427124746209831, 204.3750000000000284, 200.8284271247462129 ) ) ;
#38972 = CARTESIAN_POINT ( 'NONE',  ( -4.000000000000002665, 4.312499997268814056, 1.656854249492380804 ) ) ;
#38973 = CARTESIAN_POINT ( 'NONE',  ( -2.828427124746209831, 208.5000000027312126, 139.1715728752538723 ) ) ;
#38974 = ORIENTED_EDGE ( 'NONE', *, *, #41524, .F. ) ;
#38975 = CARTESIAN_POINT ( 'NONE',  ( 1.432654583217662481, 201.1250000013656347, 194.5412658750000219 ) ) ;
#38976 = CARTESIAN_POINT ( 'NONE',  ( -24.54126587499999701, 208.1875000013656063, 170.0000000000002842 ) ) ;
#38977 = CARTESIAN_POINT ( 'NONE',  ( -10.18810118749999916, 4.220049686691934809, 70.93750000204838102 ) ) ;
#38978 = ADVANCED_FACE ( 'NONE', ( #9100 ), #33248, .F. ) ;
#38979 = CARTESIAN_POINT ( 'NONE',  ( 2.780723358947928197E-16, 6.562499998634407028, -4.541265875000002339 ) ) ;
#38980 = LINE ( 'NONE', #10310, #40442 ) ;
#38981 = AXIS2_PLACEMENT_3D ( 'NONE', #30588, #52495, #36257 ) ;
#38982 = CARTESIAN_POINT ( 'NONE',  ( 7.188101187499991163, 2.977408999572648707, 17.33030278187175455 ) ) ;
#38983 = ADVANCED_BREP_SHAPE_REPRESENTATION ( '', ( #40499, #57354 ), #1968 ) ;
#38984 = ORIENTED_EDGE ( 'NONE', *, *, #9313, .T. ) ;
#38985 = EDGE_CURVE ( 'NONE', #49310, #6596, #24170, .T. ) ;
#38986 = CARTESIAN_POINT ( 'NONE',  ( 1.469576158976823947E-15, 95.56250000409677625, 8.000000000000000000 ) ) ;
#38987 = ORIENTED_EDGE ( 'NONE', *, *, #70951, .T. ) ;
#38988 = CARTESIAN_POINT ( 'NONE',  ( 4.220049686691934809, 10.18810118749999916, 109.1875000020483810 ) ) ;
#38989 = CARTESIAN_POINT ( 'NONE',  ( 11.00000000000000000, 1.347111479062088405E-15, 103.7500000000000000 ) ) ;
#38990 = CARTESIAN_POINT ( 'NONE',  ( 2.445694354108839619, 205.8125000013656063, 200.4456943541088663 ) ) ;
#38991 = CARTESIAN_POINT ( 'NONE',  ( 31.45873412499999944, 198.6250000013656063, 171.4326545832175555 ) ) ;
#38992 = CARTESIAN_POINT ( 'NONE',  ( -7.320508075688773708, 81.87500000000000000, -7.320508075688774596 ) ) ;
#38993 = CARTESIAN_POINT ( 'NONE',  ( 8.197002254987593162, 89.35092984469676480, -3.567578555610324997 ) ) ;
#38994 = CARTESIAN_POINT ( 'NONE',  ( 6.000000000000001776, 292.5000000000000000, -7.347880794884121708E-16 ) ) ;
#38995 = CARTESIAN_POINT ( 'NONE',  ( 30.82842712474621294, 206.2500000027312126, 172.8284271247460424 ) ) ;
#38996 = ORIENTED_EDGE ( 'NONE', *, *, #29418, .T. ) ;
#38997 = CARTESIAN_POINT ( 'NONE',  ( 1.469576158976823947E-15, 93.87499999999998579, 8.000000000000000000 ) ) ;
#38998 = EDGE_CURVE ( 'NONE', #39166, #72729, #31443, .T. ) ;
#38999 = CARTESIAN_POINT ( 'NONE',  ( -0.4501631047602908664, -16.44600848780494218, 68.55503832938644848 ) ) ;
#39000 = CARTESIAN_POINT ( 'NONE',  ( 3.999999999999959144, 196.1875000027312126, 140.3431457505076594 ) ) ;
#39001 = CARTESIAN_POINT ( 'NONE',  ( -5.000000000000003553, 68.48985753891551553, 21.22439692019726820 ) ) ;
#39002 = DIRECTION ( 'NONE',  ( -0.000000000000000000, 1.000000000000000000, -0.000000000000000000 ) ) ;
#39003 = CARTESIAN_POINT ( 'NONE',  ( 4.999999999999997335, 248.3333333333333428, -8.660254037844387298 ) ) ;
#39004 = EDGE_CURVE ( 'NONE', #32586, #69889, #1065, .T. ) ;
#39005 = CARTESIAN_POINT ( 'NONE',  ( -6.735557395310442023E-16, 11.00000000000000000, 107.3125000040967905 ) ) ;
#39006 = CARTESIAN_POINT ( 'NONE',  ( -10.00000000000000178, 187.5000000000000000, -1.224646799147353454E-15 ) ) ;
#39007 = DIRECTION ( 'NONE',  ( -0.000000000000000000, 1.000000000000000000, -0.000000000000000000 ) ) ;
#39008 = CARTESIAN_POINT ( 'NONE',  ( -7.188101187499990274, -2.977408999572651815, 16.95530278187175455 ) ) ;
#39009 = CARTESIAN_POINT ( 'NONE',  ( -8.311093377946836114, 162.9687499965860411, -8.311093377946837890 ) ) ;
#39010 = CYLINDRICAL_SURFACE ( 'NONE', #37298, 10.00000000000000178 ) ;
#39011 = CARTESIAN_POINT ( 'NONE',  ( 5.000000000000004441, 259.7916666734946034, 8.660254037844385522 ) ) ;
#39012 = CARTESIAN_POINT ( 'NONE',  ( 9.498558403365325509E-13, 68.75000000000008527, 10.00000000000000178 ) ) ;
#39014 = CARTESIAN_POINT ( 'NONE',  ( 25.17157282405715435, 195.0000000000000284, 172.8284270735494772 ) ) ;
#39013 = DIRECTION ( 'NONE',  ( -0.000000000000000000, 1.000000000000000000, -0.000000000000000000 ) ) ;
#39015 = VERTEX_POINT ( 'NONE', #37396 ) ;
#39016 = VECTOR ( 'NONE', #27235, 1000.000000000000000 ) ;
#39017 = CARTESIAN_POINT ( 'NONE',  ( -9.832129032723418760, 23.17708332991934839, -5.676582343750004256 ) ) ;
#39018 = CARTESIAN_POINT ( 'NONE',  ( -24.54126587500002543, 208.2500000013656063, 168.5673454167826435 ) ) ;
#39020 = CARTESIAN_POINT ( 'NONE',  ( -0.4451317748925319173, -16.44604352396231661, -68.55481936398555831 ) ) ;
#39019 = LINE ( 'NONE', #22023, #73350 ) ;
#39021 = CARTESIAN_POINT ( 'NONE',  ( 27.99999999999996447, 201.6250000027312126, 165.9999999999998863 ) ) ;
#39022 = CARTESIAN_POINT ( 'NONE',  ( -2.445694354108838731, 202.0625000013656063, 144.4456943541088663 ) ) ;
#39023 = CARTESIAN_POINT ( 'NONE',  ( -8.660254037844387298, 58.95833332650537528, -5.000000000000004441 ) ) ;
#39024 = CARTESIAN_POINT ( 'NONE',  ( 2.977408999572650039, 102.6875000020483810, -7.188101187500001821 ) ) ;
#39025 = CARTESIAN_POINT ( 'NONE',  ( -4.541265875000003227, 9.999999998634407916, 1.881053915767121110 ) ) ;
#39026 = CARTESIAN_POINT ( 'NONE',  ( 7.999999999999992895, -3.313708498984756279, 1.486552779823364201 ) ) ;
#39027 = CARTESIAN_POINT ( 'NONE',  ( 1.584317714026805320E-12, 163.7500000000001137, 9.999999999999998224 ) ) ;
#39028 = ORIENTED_EDGE ( 'NONE', *, *, #62277, .F. ) ;
#39029 =( BOUNDED_CURVE ( )  B_SPLINE_CURVE ( 2, ( #52136, #468, #16656, #28734, #50628, #73647, #67624, #21954, #67988 ),
 .UNSPECIFIED., .F., .F. ) 
 B_SPLINE_CURVE_WITH_KNOTS ( ( 3, 2, 2, 2, 3 ),
 ( 0.7333333333333339477, 0.7416666666666673624, 0.7500000000000006661, 0.7583333333333339699, 0.7666666666666673846 ),
 .UNSPECIFIED. ) 
 CURVE ( )  GEOMETRIC_REPRESENTATION_ITEM ( )  RATIONAL_B_SPLINE_CURVE ( ( 0.9999999999999938938, 0.9238795325112928447, 1.000000000000000000, 0.9238795325112867385, 1.000000000000000000, 0.9238795325112867385, 1.000000000000000000, 0.9238795325112806323, 1.000000000000005995 ) ) 
 REPRESENTATION_ITEM ( '' )  );
#39030 = ORIENTED_EDGE ( 'NONE', *, *, #9204, .T. ) ;
#39031 = CARTESIAN_POINT ( 'NONE',  ( 2.449293598294707893E-16, 5.250000000000000000, -4.000000000000001776 ) ) ;
#39032 = CARTESIAN_POINT ( 'NONE',  ( -3.458734124999960358, 195.6250000013656063, 196.5673454167823877 ) ) ;
#39033 = CARTESIAN_POINT ( 'NONE',  ( -7.320508075688783478, 161.8750000000000284, -7.320508075688784366 ) ) ;
#39034 = ADVANCED_FACE ( 'NONE', ( #3437 ), #54757, .T. ) ;
#39035 = CARTESIAN_POINT ( 'NONE',  ( -28.76409496788549092, -42.77215576984802681, 158.4297396669575164 ) ) ;
#39036 = CARTESIAN_POINT ( 'NONE',  ( 8.311093377946837890, 136.4062499965859558, -8.311093377946837890 ) ) ;
#39037 = EDGE_LOOP ( 'NONE', ( #45386, #462, #25375, #22991 ) ) ;
#39038 = CARTESIAN_POINT ( 'NONE',  ( -5.000000000000001776, 11.69579520003552098, -68.31051037013783400 ) ) ;
#39039 = CARTESIAN_POINT ( 'NONE',  ( 7.204075437095968759, -7.204075437095966983, 87.71875000204836681 ) ) ;
#39040 = CARTESIAN_POINT ( 'NONE',  ( -7.999999999995399236, -5.826008446853342637E-06, 20.51801720710344767 ) ) ;
#39041 = CARTESIAN_POINT ( 'NONE',  ( -3.999999999999960032, 209.0000000000000284, 198.0000000000000284 ) ) ;
#39042 = CARTESIAN_POINT ( 'NONE',  ( -4.898587196589412829E-16, 112.8125000040967905, -8.000000000000000000 ) ) ;
#39043 = EDGE_CURVE ( 'NONE', #26371, #53710, #46860, .T. ) ;
#39044 = LINE ( 'NONE', #56397, #34971 ) ;
#39045 = ORIENTED_EDGE ( 'NONE', *, *, #37012, .T. ) ;
#39046 = CARTESIAN_POINT ( 'NONE',  ( -2.775557561562891351E-14, 210.0000000000000284, 142.0000000000000568 ) ) ;
#39047 = CARTESIAN_POINT ( 'NONE',  ( -30.39335777026762386, 174.8762529804568260, 163.4693516532521755 ) ) ;
#39048 = CARTESIAN_POINT ( 'NONE',  ( -9.832129032723420536, 109.0104166632526841, 5.676582343749997150 ) ) ;
#39049 = CARTESIAN_POINT ( 'NONE',  ( -2.445694354108782775, 203.5625000013656063, 200.4456943541088663 ) ) ;
#39050 = CARTESIAN_POINT ( 'NONE',  ( -5.082755093536326818, 19.78124999795161543, 5.082755093536325042 ) ) ;
#39052 = EDGE_CURVE ( 'NONE', #64014, #66240, #37001, .T. ) ;
#39051 = CARTESIAN_POINT ( 'NONE',  ( -10.18810118749999916, 4.220049686691934809, 84.43750000204838102 ) ) ;
#39053 = CARTESIAN_POINT ( 'NONE',  ( -9.832129032723418760, 38.17708332991935549, -5.676582343750004256 ) ) ;
#39055 = ORIENTED_EDGE ( 'NONE', *, *, #8471, .F. ) ;
#39054 =( BOUNDED_CURVE ( )  B_SPLINE_CURVE ( 2, ( #32810, #10155, #4135, #35048, #46342, #5250, #22577, #56934, #11643, #68611, #68242, #28620, #28250 ),
 .UNSPECIFIED., .F., .T. ) 
 B_SPLINE_CURVE_WITH_KNOTS ( ( 3, 2, 2, 2, 2, 2, 3 ),
 ( 0.6388888888888887285, 0.6481481481481480289, 0.6574074074074073293, 0.6666666666666665186, 0.6759259259259259300, 0.6851851851851852304, 0.6944444444444444198 ),
 .UNSPECIFIED. ) 
 CURVE ( )  GEOMETRIC_REPRESENTATION_ITEM ( )  RATIONAL_B_SPLINE_CURVE ( ( 1.000000000000000444, 0.9659258262890678681, 1.000000000000000000, 0.9659258262890683122, 1.000000000000000000, 0.9659258262890683122, 1.000000000000000000, 0.9659258262890683122, 1.000000000000000000, 0.9659258262890683122, 1.000000000000000000, 0.9659258262890683122, 1.000000000000000000 ) ) 
 REPRESENTATION_ITEM ( '' )  );
#39056 = CARTESIAN_POINT ( 'NONE',  ( -7.347880794884122694E-16, 4.750000000000000000, 4.000000000000001776 ) ) ;
#39057 = CARTESIAN_POINT ( 'NONE',  ( -5.662595241051933570, -5.662595241051936235, 17.70061528394063188 ) ) ;
#39058 = CARTESIAN_POINT ( 'NONE',  ( 3.458734124999960358, 209.6250000013656063, 143.4326545832176976 ) ) ;
#39059 = CYLINDRICAL_SURFACE ( 'NONE', #7159, 11.00000000000000000 ) ;
#39060 = CARTESIAN_POINT ( 'NONE',  ( 7.188101187500000044, 7.968749997951610986, 0.000000000000000000 ) ) ;
#39061 = CARTESIAN_POINT ( 'NONE',  ( 4.721056650415999201, 289.0781250017069510, -4.721056650415999201 ) ) ;
#39062 = CARTESIAN_POINT ( 'NONE',  ( -5.999999999999999112, 297.0624999999999432, 2.485281374238575314 ) ) ;
#39063 = CARTESIAN_POINT ( 'NONE',  ( 7.188101187499999156, 2.249999997951610098, 2.977408999572654924 ) ) ;
#39064 = ORIENTED_EDGE ( 'NONE', *, *, #38332, .F. ) ;
#39065 = CARTESIAN_POINT ( 'NONE',  ( 3.042071309553159519, 155.0520833299192986, 11.35316468750000141 ) ) ;
#39066 = CARTESIAN_POINT ( 'NONE',  ( 7.204075437095966983, 7.204075437095967871, 79.09375000204838102 ) ) ;
#39067 = CARTESIAN_POINT ( 'NONE',  ( -24.54126587500000412, 208.5000000013656063, 168.5673454167827003 ) ) ;
#39068 = FACE_OUTER_BOUND ( 'NONE', #60149, .T. ) ;
#39069 = CARTESIAN_POINT ( 'NONE',  ( -3.211159895383562723, 16.06249999863440436, 3.211159895383561391 ) ) ;
#39070 = ORIENTED_EDGE ( 'NONE', *, *, #54530, .F. ) ;
#39071 = AXIS2_PLACEMENT_3D ( 'NONE', #18734, #70779, #25847 ) ;
#39072 = CARTESIAN_POINT ( 'NONE',  ( -3.999999999999960032, 199.1250000027312126, 198.0000000000000284 ) ) ;
#39073 = CARTESIAN_POINT ( 'NONE',  ( -2.751064625579944321E-14, 208.7500000000000284, 146.0000000000000284 ) ) ;
#39074 = CARTESIAN_POINT ( 'NONE',  ( -30.82842712474624491, 205.2500000027312126, 167.1715728752542418 ) ) ;
#39075 = CARTESIAN_POINT ( 'NONE',  ( 5.656854249492378806, 5.812500000000000888, 5.656854249492381470 ) ) ;
#39076 = EDGE_LOOP ( 'NONE', ( #46979, #45355, #64280, #51611 ) ) ;
#39077 = CARTESIAN_POINT ( 'NONE',  ( 2.977408999572652260, 12.18749999795161365, 7.188101187500000044 ) ) ;
#39078 = CARTESIAN_POINT ( 'NONE',  ( -3.673940397442060854E-16, 297.8125000034140157, -6.000000000000001776 ) ) ;
#39079 = CARTESIAN_POINT ( 'NONE',  ( -1.831327383322115310, -47.38435823436159211, 151.0877460353534047 ) ) ;
#39080 = CARTESIAN_POINT ( 'NONE',  ( -8.660254037844390851, 47.91666666666667140, 4.999999999999998224 ) ) ;
#39081 = CARTESIAN_POINT ( 'NONE',  ( -5.082755093536324154, 106.7187500020483952, 5.082755093536326818 ) ) ;
#39082 = CARTESIAN_POINT ( 'NONE',  ( 4.000000000000015987, 207.6875000027312126, 196.3431457505076594 ) ) ;
#39083 = CARTESIAN_POINT ( 'NONE',  ( -3.313708498984759387, -7.999999999999989342, 2.611552779823365533 ) ) ;
#39085 = CARTESIAN_POINT ( 'NONE',  ( -18.00000000000000000, -10.39230484541329247, -1.607695154586745501 ) ) ;
#39084 = CARTESIAN_POINT ( 'NONE',  ( 6.900000000000001243, 0.000000000000000000, -0.7702282920306856573 ) ) ;
#39086 = ORIENTED_EDGE ( 'NONE', *, *, #71956, .T. ) ;
#39087 = CARTESIAN_POINT ( 'NONE',  ( -9.832129032723418760, 258.4895833367473301, -5.676582343749998927 ) ) ;
#39088 = PRODUCT_DEFINITION_SHAPE ( 'NONE', 'NONE',  #74651 ) ;
#39089 = CARTESIAN_POINT ( 'NONE',  ( -5.082755093536317936, -5.082755093536320601, 24.54905278187175810 ) ) ;
#39090 = AXIS2_PLACEMENT_3D ( 'NONE', #58014, #6319, #27824 ) ;
#39091 = CARTESIAN_POINT ( 'NONE',  ( -3.496982156821625498, 51.71401992552586080, 48.73755072030351698 ) ) ;
#39092 = LINE ( 'NONE', #10417, #46611 ) ;
#39093 = CARTESIAN_POINT ( 'NONE',  ( -4.336811714530219852, -68.30918023749046597, -20.61428864874384104 ) ) ;
#39094 = CARTESIAN_POINT ( 'NONE',  ( -2.445694354108783219, 195.8125000013656063, 200.4456943541088663 ) ) ;
#39095 = CARTESIAN_POINT ( 'NONE',  ( -7.320508075688773708, 151.8750000000000000, -7.320508075688774596 ) ) ;
#39096 = CARTESIAN_POINT ( 'NONE',  ( -1.469576158976823947E-15, 8.437499995903221972, 8.000000000000000000 ) ) ;
#39097 = DIRECTION ( 'NONE',  ( 0.000000000000000000, 0.000000000000000000, -1.000000000000000000 ) ) ;
#39098 = CARTESIAN_POINT ( 'NONE',  ( -4.898587196589412829E-16, 96.12499999999998579, -8.000000000000000000 ) ) ;
#39099 = CARTESIAN_POINT ( 'NONE',  ( -5.676582343750006032, 129.4270833299193555, 9.832129032723418760 ) ) ;
#39100 = CARTESIAN_POINT ( 'NONE',  ( 10.00000000000000178, 211.8749999931720538, 0.000000000000000000 ) ) ;
#39101 = CARTESIAN_POINT ( 'NONE',  ( 4.556349186104045934, 11.00000000000000000, 74.03125000000000000 ) ) ;
#39104 = DIRECTION ( 'NONE',  ( 0.000000000000000000, 0.000000000000000000, 1.000000000000000000 ) ) ;
#39103 = CARTESIAN_POINT ( 'NONE',  ( 31.45873412499999233, 196.6875000013655779, 169.9999999999998863 ) ) ;
#39102 = CARTESIAN_POINT ( 'NONE',  ( 24.54126587499997925, 196.5000000013656063, 171.4326545832175555 ) ) ;
#39105 = VERTEX_POINT ( 'NONE', #50946 ) ;
#39106 = CARTESIAN_POINT ( 'NONE',  ( 1.472960921100393561, 223.8667061704458092, 9.895268813711334488 ) ) ;
#39107 = CARTESIAN_POINT ( 'NONE',  ( -7.999999999999991118, 0.000000000000000000, 12.83030277982336465 ) ) ;
#39108 = CARTESIAN_POINT ( 'NONE',  ( 29.43265458321761230, 198.7500000013656063, 173.4587341249998929 ) ) ;
#39109 = CARTESIAN_POINT ( 'NONE',  ( -3.042071309553173730, 204.6354166632526699, 11.35316468749999785 ) ) ;
#39110 = CARTESIAN_POINT ( 'NONE',  ( -2.977408999572650927, 122.3750000020483952, -7.188101187500001821 ) ) ;
#39111 = CARTESIAN_POINT ( 'NONE',  ( -4.541265875000002339, 16.81249999863440436, -5.561446717895856393E-16 ) ) ;
#39112 = CARTESIAN_POINT ( 'NONE',  ( 29.43265458321760519, 195.7500000013656063, 173.4587341249998929 ) ) ;
#39113 = CARTESIAN_POINT ( 'NONE',  ( -3.313708498984758943, -7.999999999999989342, 28.11155277982336642 ) ) ;
#39115 = CARTESIAN_POINT ( 'NONE',  ( -23.99999999999998934, 202.7500000000000000, 170.0000000000003411 ) ) ;
#39114 =( LENGTH_UNIT ( ) NAMED_UNIT ( * ) SI_UNIT ( .MILLI., .METRE. ) );
#39116 = CARTESIAN_POINT ( 'NONE',  ( 11.35316468749999963, 95.98958332991935549, -3.042071309553165293 ) ) ;
#39117 = ORIENTED_EDGE ( 'NONE', *, *, #48476, .T. ) ;
#39118 = CARTESIAN_POINT ( 'NONE',  ( 0.000000000000000000, 125.0000000000000000, 0.000000000000000000 ) ) ;
#39119 = CARTESIAN_POINT ( 'NONE',  ( 5.082755093536325930, 21.65624999795161543, -5.082755093536325930 ) ) ;
#39120 = CARTESIAN_POINT ( 'NONE',  ( -7.999999999999991118, 0.000000000000000000, 14.33030277982336465 ) ) ;
#39121 = CARTESIAN_POINT ( 'NONE',  ( -6.951808397369817780E-16, 252.9687500034140157, -11.35316468749999963 ) ) ;
#39122 = CARTESIAN_POINT ( 'NONE',  ( -9.832129032723418760, 97.86458332991935549, -5.676582343750004256 ) ) ;
#39123 = ORIENTED_EDGE ( 'NONE', *, *, #34203, .F. ) ;
#39124 = CARTESIAN_POINT ( 'NONE',  ( -2.751064625579944321E-14, 199.8750000027312126, 146.0000000000000284 ) ) ;
#39125 = CARTESIAN_POINT ( 'NONE',  ( 1.871523826299183495E-15, -10.18810118749999916, 108.5312500020483810 ) ) ;
#39126 = CARTESIAN_POINT ( 'NONE',  ( -30.44569435410883074, 196.8125000013656063, 167.5543056458915885 ) ) ;
#39127 = CARTESIAN_POINT ( 'NONE',  ( 2.839093476692135984E-14, 202.9375000013656063, 201.4587341250000350 ) ) ;
#39128 = CARTESIAN_POINT ( 'NONE',  ( -7.999999999999991118, 0.000000000000000000, 11.33030277982336642 ) ) ;
#39130 = CARTESIAN_POINT ( 'NONE',  ( -11.35316468750000141, 88.28124999658602690, -1.390361679473963753E-15 ) ) ;
#39129 = DIRECTION ( 'NONE',  ( 0.000000000000000000, 0.000000000000000000, -1.000000000000000000 ) ) ;
#39131 = CARTESIAN_POINT ( 'NONE',  ( 3.313708498984762496, -7.999999999999989342, 13.48655278392014445 ) ) ;
#39132 = CARTESIAN_POINT ( 'NONE',  ( -30.44569435410883429, 202.8125000013656063, 167.5543056458915885 ) ) ;
#39133 = ADVANCED_FACE ( 'NONE', ( #11333 ), #34367, .T. ) ;
#39134 = CARTESIAN_POINT ( 'NONE',  ( 4.000000000000001776, 15.06249999999999822, -1.656854249492381248 ) ) ;
#39135 = CARTESIAN_POINT ( 'NONE',  ( -7.320508075688773708, 178.7499999931720254, -7.320508075688774596 ) ) ;
#39136 = CARTESIAN_POINT ( 'NONE',  ( 1.656854249492309972, 207.8124999999999716, 146.0000000000001137 ) ) ;
#39137 = CARTESIAN_POINT ( 'NONE',  ( 6.000000000000001776, 296.5625000034140157, -7.347880794884121708E-16 ) ) ;
#39138 = CARTESIAN_POINT ( 'NONE',  ( 11.35316468750000141, 81.09374999658601268, 0.000000000000000000 ) ) ;
#39139 = CARTESIAN_POINT ( 'NONE',  ( -4.721056650415999201, 289.3281250017069510, -4.721056650415999201 ) ) ;
#39141 = EDGE_CURVE ( 'NONE', #65034, #21298, #37180, .T. ) ;
#39140 = CARTESIAN_POINT ( 'NONE',  ( -7.204075437095967871, 7.204075437095967871, 99.34375000204836681 ) ) ;
#39142 = CARTESIAN_POINT ( 'NONE',  ( 3.042071309553159519, 224.7395833299193555, 11.35316468750000141 ) ) ;
#39143 = ORIENTED_EDGE ( 'NONE', *, *, #65928, .T. ) ;
#39144 = DIRECTION ( 'NONE',  ( 0.000000000000000000, 0.000000000000000000, -1.000000000000000000 ) ) ;
#39145 = DIRECTION ( 'NONE',  ( 1.000000000000000000, 0.000000000000000000, -0.000000000000000000 ) ) ;
#39146 = CARTESIAN_POINT ( 'NONE',  ( 4.242640687119285658, 291.6249999999999432, -4.242640687119286547 ) ) ;
#39147 = CARTESIAN_POINT ( 'NONE',  ( -11.35316468750000141, 203.4895833299193555, 3.042071309553159963 ) ) ;
#39148 = CARTESIAN_POINT ( 'NONE',  ( 4.999999999999997335, 231.4583333401613174, -8.660254037844387298 ) ) ;
#39149 = CARTESIAN_POINT ( 'NONE',  ( -7.320508075688771932, 252.5000000068279178, -7.320508075688771932 ) ) ;
#39150 = CIRCLE ( 'NONE', #16223, 71.70204102886728492 ) ;
#39151 = ORIENTED_EDGE ( 'NONE', *, *, #14729, .T. ) ;
#39152 = CARTESIAN_POINT ( 'NONE',  ( -3.042071309553173730, 199.6354166632526983, 11.35316468749999785 ) ) ;
#39153 =( BOUNDED_CURVE ( )  B_SPLINE_CURVE ( 2, ( #29878, #53635, #65309, #13610, #24575, #53264, #19281, #858, #36649 ),
 .UNSPECIFIED., .F., .F. ) 
 B_SPLINE_CURVE_WITH_KNOTS ( ( 3, 2, 2, 2, 3 ),
 ( 0.2361111111111111049, 0.2430555555555555525, 0.2500000000000000000, 0.2569444444444444198, 0.2638888888888888951 ),
 .UNSPECIFIED. ) 
 CURVE ( )  GEOMETRIC_REPRESENTATION_ITEM ( )  RATIONAL_B_SPLINE_CURVE ( ( 1.000000000000000000, 0.9238795325112867385, 1.000000000000000000, 0.9238795325112867385, 1.000000000000000000, 0.9238795325112867385, 1.000000000000000000, 0.9238795325112867385, 1.000000000000000000 ) ) 
 REPRESENTATION_ITEM ( '' )  );
#39154 = CARTESIAN_POINT ( 'NONE',  ( -7.188101187499992051, 2.977408999572646930, 17.89280278187175455 ) ) ;
#39155 = CARTESIAN_POINT ( 'NONE',  ( -31.45873412500001010, 207.6250000013656347, 168.5673454167827572 ) ) ;
#39156 = CARTESIAN_POINT ( 'NONE',  ( -5.656854249492381470, 9.937500000000001776, 5.656854249492379694 ) ) ;
#39157 = ORIENTED_EDGE ( 'NONE', *, *, #53175, .F. ) ;
#39158 = CARTESIAN_POINT ( 'NONE',  ( 5.656854249492381470, 94.25000000409677625, 5.656854249492379694 ) ) ;
#39159 = CARTESIAN_POINT ( 'NONE',  ( -2.679491924311225848, 16.45833333333333570, -10.00000000000000178 ) ) ;
#39160 =( BOUNDED_CURVE ( )  B_SPLINE_CURVE ( 2, ( #47930, #24185, #70947, #19262, #7953, #29860, #29491, #52872, #18167 ),
 .UNSPECIFIED., .F., .F. ) 
 B_SPLINE_CURVE_WITH_KNOTS ( ( 3, 2, 2, 2, 3 ),
 ( 0.5416666666666666297, 0.5486111111111111605, 0.5555555555555555802, 0.5625000000000000000, 0.5694444444444444198 ),
 .UNSPECIFIED. ) 
 CURVE ( )  GEOMETRIC_REPRESENTATION_ITEM ( )  RATIONAL_B_SPLINE_CURVE ( ( 1.000000000000000000, 0.9238795325112867385, 1.000000000000000000, 0.9238795325112867385, 1.000000000000000000, 0.9238795325112867385, 1.000000000000000000, 0.9238795325112867385, 1.000000000000000000 ) ) 
 REPRESENTATION_ITEM ( '' )  );
#39161 = CARTESIAN_POINT ( 'NONE',  ( 7.204075437095966983, 7.204075437095967871, 79.46875000204836681 ) ) ;
#39162 = ORIENTED_EDGE ( 'NONE', *, *, #12239, .F. ) ;
#39163 = CARTESIAN_POINT ( 'NONE',  ( 1.656854249492381248, 18.18750000000000000, -4.000000000000001776 ) ) ;
#39164 = CARTESIAN_POINT ( 'NONE',  ( -1.881053915767121776, 21.62499999863441147, -4.541265875000002339 ) ) ;
#39165 = CARTESIAN_POINT ( 'NONE',  ( 30.28816258356557967, 194.6946065536776587, 167.0903623255752848 ) ) ;
#39166 = VERTEX_POINT ( 'NONE', #52072 ) ;
#39167 = CARTESIAN_POINT ( 'NONE',  ( 10.00000000000000000, 16.66666665983870033, 2.679491924311235618 ) ) ;
#39168 = CARTESIAN_POINT ( 'NONE',  ( -5.000000000000000000, -15.86295220590816513, 69.92641310672760824 ) ) ;
#39171 = CARTESIAN_POINT ( 'NONE',  ( 30.82842712474617031, 207.5000000027312126, 167.1715728752537018 ) ) ;
#39170 = CARTESIAN_POINT ( 'NONE',  ( -5.676582343749992710, 244.7395833367473301, 9.832129032723422313 ) ) ;
#39169 = CARTESIAN_POINT ( 'NONE',  ( 29.43265458321761585, 206.8750000013656347, 166.5412658749999650 ) ) ;
#39172 = APPLICATION_PROTOCOL_DEFINITION ( 'draft international standard', 'automotive_design', 1998, #1435 ) ;
#39173 = VERTEX_POINT ( 'NONE', #56626 ) ;
#39174 = CARTESIAN_POINT ( 'NONE',  ( -9.832129032723415207, 249.6354166700806445, 5.676582343750005144 ) ) ;
#39175 = CARTESIAN_POINT ( 'NONE',  ( 5.082755093536318824, 5.082755093536319713, 9.924052781871754547 ) ) ;
#39176 = ORIENTED_EDGE ( 'NONE', *, *, #6353, .F. ) ;
#39177 = ORIENTED_EDGE ( 'NONE', *, *, #13521, .F. ) ;
#39178 = CARTESIAN_POINT ( 'NONE',  ( -10.18810118749999738, -4.220049686691941915, 75.25000000204836681 ) ) ;
#39179 = CARTESIAN_POINT ( 'NONE',  ( -3.042071309553164404, 92.55208332991934128, -11.35316468749999963 ) ) ;
#39180 = FACE_OUTER_BOUND ( 'NONE', #3603, .T. ) ;
#39181 = CARTESIAN_POINT ( 'NONE',  ( 4.556349186104051263, -10.99999999999999822, 86.96874999999998579 ) ) ;
#39184 = CARTESIAN_POINT ( 'NONE',  ( -2.765530957081998142, 289.7968750017068942, 6.676582343750000703 ) ) ;
#39183 = CARTESIAN_POINT ( 'NONE',  ( 26.56734541678238060, 208.3750000013656063, 173.4587341249998929 ) ) ;
#39182 = CARTESIAN_POINT ( 'NONE',  ( 29.43265458321766559, 209.1250000013656631, 166.5412658749999650 ) ) ;
#39185 = DIRECTION ( 'NONE',  ( -0.000000000000000000, -0.000000000000000000, -1.000000000000000000 ) ) ;
#39186 = LINE ( 'NONE', #45217, #39584 ) ;
#39187 = AXIS2_PLACEMENT_3D ( 'NONE', #42488, #2877, #59851 ) ;
#39188 = CARTESIAN_POINT ( 'NONE',  ( 11.35316468749999963, 195.9895833299193555, -3.042071309553165293 ) ) ;
#39189 = EDGE_CURVE ( 'NONE', #7760, #57671, #8166, .T. ) ;
#39190 = CARTESIAN_POINT ( 'NONE',  ( -8.000000000000000000, 11.06249999590322020, -9.797174393178825657E-16 ) ) ;
#39191 = EDGE_CURVE ( 'NONE', #852, #6758, #51318, .T. ) ;
#39192 = ORIENTED_EDGE ( 'NONE', *, *, #42019, .T. ) ;
#39193 = CARTESIAN_POINT ( 'NONE',  ( 27.99999999999996092, 195.4375000013655779, 173.4587341249998929 ) ) ;
#39194 = CARTESIAN_POINT ( 'NONE',  ( -2.977408999572654480, 18.37499999795161187, 7.188101187499999156 ) ) ;
#39195 =( GEOMETRIC_REPRESENTATION_CONTEXT ( 3 ) GLOBAL_UNCERTAINTY_ASSIGNED_CONTEXT ( ( #17908 ) ) GLOBAL_UNIT_ASSIGNED_CONTEXT ( ( #14731, #49063, #42663 ) ) REPRESENTATION_CONTEXT ( 'NONE', 'WORKASPACE' ) );
#39196 = CARTESIAN_POINT ( 'NONE',  ( 6.951808397369818766E-16, 167.3437499965860127, -11.35316468750000141 ) ) ;
#39197 = CARTESIAN_POINT ( 'NONE',  ( 23.99999999999998934, 197.8750000027312126, 169.9999999999999432 ) ) ;
#39198 = CARTESIAN_POINT ( 'NONE',  ( 7.188101187500000044, 105.7812500020483810, -8.802885111219163269E-16 ) ) ;
#39200 = CARTESIAN_POINT ( 'NONE',  ( 1.506524674528859187, -55.70638416847143048, -43.84942669317729980 ) ) ;
#39199 = CARTESIAN_POINT ( 'NONE',  ( -10.00000000000000000, 263.1250000068279746, 0.000000000000000000 ) ) ;
#39201 = CARTESIAN_POINT ( 'NONE',  ( 29.43265458321761585, 207.7500000013656063, 173.4587341249998929 ) ) ;
#39202 = CARTESIAN_POINT ( 'NONE',  ( -7.188101187499992051, 0.000000000000000000, 15.36155278187175455 ) ) ;
#39203 = CARTESIAN_POINT ( 'NONE',  ( -11.35316468750000141, 53.48958332991935549, 3.042071309553159963 ) ) ;
#39204 = CARTESIAN_POINT ( 'NONE',  ( -12.00000000000000000, -6.928203230275542523, -1.071796769724504550 ) ) ;
#39205 = CARTESIAN_POINT ( 'NONE',  ( 5.000000000000001776, 27.70833332650536818, -8.660254037844389075 ) ) ;
#39206 = CARTESIAN_POINT ( 'NONE',  ( 11.00000000000000000, 1.347111479062088405E-15, 72.24999999999998579 ) ) ;
#39207 = VERTEX_POINT ( 'NONE', #22635 ) ;
#39208 = LINE ( 'NONE', #62210, #12157 ) ;
#39209 = CARTESIAN_POINT ( 'NONE',  ( 2.020667218593132706E-15, -11.00000000000000000, 81.06250000409677625 ) ) ;
#39210 = EDGE_CURVE ( 'NONE', #7343, #21929, #33756, .T. ) ;
#39211 = CARTESIAN_POINT ( 'NONE',  ( 9.832129032723416984, 65.36458332991935549, 5.676582343750006032 ) ) ;
#39212 = EDGE_CURVE ( 'NONE', #48495, #34420, #31893, .T. ) ;
#39213 = CARTESIAN_POINT ( 'NONE',  ( 4.556349186104051263, -10.99999999999999822, 75.15625000409677625 ) ) ;
#39214 = CARTESIAN_POINT ( 'NONE',  ( 3.458734124999960358, 201.6875000013656063, 142.0000000000000568 ) ) ;
#39215 = CARTESIAN_POINT ( 'NONE',  ( 0.000000000000000000, 300.0000000000000000, 0.000000000000000000 ) ) ;
#39216 = DIRECTION ( 'NONE',  ( 6.123233995736705639E-17, 0.8660254037844414832, -0.4999999999999950595 ) ) ;
#39218 = CARTESIAN_POINT ( 'NONE',  ( 8.311093377946837890, 41.40624999658601268, -8.311093377946837890 ) ) ;
#39217 = CARTESIAN_POINT ( 'NONE',  ( 2.977408999572650039, 90.68750000204838102, -7.188101187500000933 ) ) ;
#39219 = CARTESIAN_POINT ( 'NONE',  ( 7.999999999999992895, -3.313708498984756279, 1.486552779823364201 ) ) ;
#39220 = CARTESIAN_POINT ( 'NONE',  ( 9.999999999999998224, 205.2083333333333712, -2.679491924311226292 ) ) ;
#39221 = CARTESIAN_POINT ( 'NONE',  ( -3.042071309553173730, 174.3229166632526983, 11.35316468749999785 ) ) ;
#39222 = CARTESIAN_POINT ( 'NONE',  ( 10.00000000000000178, 136.8749999931720538, 0.000000000000000000 ) ) ;
#39223 = CARTESIAN_POINT ( 'NONE',  ( 5.082755093536326818, 102.5937500020483810, 5.082755093536325042 ) ) ;
#39224 = DIRECTION ( 'NONE',  ( 0.000000000000000000, -0.9997074645238147594, -0.02418647091589873691 ) ) ;
#39225 = CARTESIAN_POINT ( 'NONE',  ( -11.35316468750000141, 33.59374999658601268, -1.390361679473963753E-15 ) ) ;
#39226 = CARTESIAN_POINT ( 'NONE',  ( -3.999999999999960032, 200.9375000000000284, 196.3431457505076594 ) ) ;
#39227 = CARTESIAN_POINT ( 'NONE',  ( -11.35316468750000141, 163.2812499965860127, -1.390361679473963753E-15 ) ) ;
#39228 = EDGE_LOOP ( 'NONE', ( #1038, #32789, #66197, #56759 ) ) ;
#39229 = CARTESIAN_POINT ( 'NONE',  ( 16.00000000000000711, 16.00000000000000355, 7.387219678533750056 ) ) ;
#39230 = CARTESIAN_POINT ( 'NONE',  ( 1.871523826299183495E-15, -10.18810118749999916, 69.53125000204838102 ) ) ;
#39231 = CARTESIAN_POINT ( 'NONE',  ( -1.656854249492466735, 196.1875000000000284, 201.9999999999999147 ) ) ;
#39232 = LINE ( 'NONE', #62232, #42572 ) ;
#39234 = CARTESIAN_POINT ( 'NONE',  ( 11.35316468749999785, 160.5729166632526983, 3.042071309553174174 ) ) ;
#39233 = CARTESIAN_POINT ( 'NONE',  ( -8.660254037844390851, 7.083333333333338366, -5.000000000000007994 ) ) ;
#39235 = CARTESIAN_POINT ( 'NONE',  ( -5.656854249492375253, 5.656854249492375253, 5.199052784329824206 ) ) ;
#39236 = DIRECTION ( 'NONE',  ( 1.000000000000000000, 0.000000000000000000, 0.000000000000000000 ) ) ;
#39237 = CARTESIAN_POINT ( 'NONE',  ( 11.35316468749999963, 221.4062500034139873, -1.390361679473963556E-15 ) ) ;
#39238 = CARTESIAN_POINT ( 'NONE',  ( -0.3752463838875753632, 55.62178951997461240, -43.80327721769091198 ) ) ;
#39239 = EDGE_CURVE ( 'NONE', #60077, #50120, #9919, .T. ) ;
#39240 = CARTESIAN_POINT ( 'NONE',  ( -10.18810118749999738, -4.220049686691941915, 80.12500000204835260 ) ) ;
#39241 = ORIENTED_EDGE ( 'NONE', *, *, #47105, .T. ) ;
#39242 = CARTESIAN_POINT ( 'NONE',  ( -2.828427124746209831, 198.5000000027312126, 139.1715728752538723 ) ) ;
#39243 = CARTESIAN_POINT ( 'NONE',  ( 5.676582343750001591, 121.9270833299193413, -9.832129032723420536 ) ) ;
#39244 = CARTESIAN_POINT ( 'NONE',  ( 5.000000000000001776, 12.70833332650536640, -8.660254037844389075 ) ) ;
#39245 = EDGE_LOOP ( 'NONE', ( #2765, #13586, #66616, #33389, #10060, #38726, #29566, #70732, #57287, #31625, #14062, #73008, #58301, #52864, #10413, #49597 ) ) ;
#39246 = VERTEX_POINT ( 'NONE', #6786 ) ;
#39247 = CARTESIAN_POINT ( 'NONE',  ( 4.541265875000002339, 7.499999998634408804, -1.881053915767121554 ) ) ;
#39248 = CARTESIAN_POINT ( 'NONE',  ( -7.188101187500000044, 11.71874999795161010, -8.802885111219163269E-16 ) ) ;
#39249 = VECTOR ( 'NONE', #42093, 1000.000000000000000 ) ;
#39250 = CARTESIAN_POINT ( 'NONE',  ( -7.999999999999998224, 111.7812500040967763, 3.313708498984766493 ) ) ;
#39251 = CARTESIAN_POINT ( 'NONE',  ( -10.18810118749999916, 0.000000000000000000, 92.03125000204836681 ) ) ;
#39252 = CARTESIAN_POINT ( 'NONE',  ( -25.55430564589114795, 197.3125000013656063, 172.4456943541091789 ) ) ;
#39253 = CIRCLE ( 'NONE', #36833, 9.000000000000001776 ) ;
#39254 =( BOUNDED_CURVE ( )  B_SPLINE_CURVE ( 2, ( #72033, #22591, #56947, #62583, #45611, #33207, #61851, #28264, #27887, #10171, #62963, #50156, #39959 ),
 .UNSPECIFIED., .F., .F. ) 
 B_SPLINE_CURVE_WITH_KNOTS ( ( 3, 2, 2, 2, 2, 2, 3 ),
 ( 0.1412976416564819815, 0.1465300236806699186, 0.1517624057048578279, 0.1569947877290457372, 0.1622271697532336743, 0.1674595517774215836, 0.1726919338016095207 ),
 .UNSPECIFIED. ) 
 CURVE ( )  GEOMETRIC_REPRESENTATION_ITEM ( )  RATIONAL_B_SPLINE_CURVE ( ( 0.9999999999999994449, 0.9659258262890690894, 1.000000000000000000, 0.9659258262890684232, 1.000000000000000000, 0.9659258262890684232, 1.000000000000000000, 0.9659258262890684232, 1.000000000000000000, 0.9659258262890684232, 1.000000000000000000, 0.9659258262892563840, 0.9999999999998120392 ) ) 
 REPRESENTATION_ITEM ( '' )  );
#39255 = CARTESIAN_POINT ( 'NONE',  ( 1.656854249492381914, 9.812500000000000000, 4.000000000000000888 ) ) ;
#39256 = CARTESIAN_POINT ( 'NONE',  ( 2.449293598294707893E-16, 21.99999999726881583, -4.000000000000001776 ) ) ;
#39257 = CARTESIAN_POINT ( 'NONE',  ( 3.211159895383560947, 9.187499998634407916, 3.211159895383562723 ) ) ;
#39258 = CARTESIAN_POINT ( 'NONE',  ( -4.000000000000015099, 197.5625000000000853, 143.6568542494924543 ) ) ;
#39259 = VERTEX_POINT ( 'NONE', #24850 ) ;
#39260 = CARTESIAN_POINT ( 'NONE',  ( 2.679491924311283579, 223.5416666666666856, -9.999999999999969802 ) ) ;
#39261 = CARTESIAN_POINT ( 'NONE',  ( 1.320432766682874540E-15, 108.0312500020483810, 7.188101187500000044 ) ) ;
#39263 = CARTESIAN_POINT ( 'NONE',  ( -7.188101187500000044, 124.5312500020483810, 0.000000000000000000 ) ) ;
#39262 = DIRECTION ( 'NONE',  ( -0.000000000000000000, 1.000000000000000000, -0.000000000000000000 ) ) ;
#39264 = CARTESIAN_POINT ( 'NONE',  ( 1.881053915767121776, 21.49999999863440792, -4.541265875000002339 ) ) ;
#39265 = CARTESIAN_POINT ( 'NONE',  ( 5.082755093536318824, 5.082755093536319713, 3.924052781871752327 ) ) ;
#39266 = ORIENTED_EDGE ( 'NONE', *, *, #5361, .T. ) ;
#39267 = ORIENTED_EDGE ( 'NONE', *, *, #68301, .T. ) ;
#39268 = CARTESIAN_POINT ( 'NONE',  ( -6.238412754330611322E-16, 10.18810118749999916, 92.78125000204836681 ) ) ;
#39269 = CARTESIAN_POINT ( 'NONE',  ( 1.347111479062087419E-15, 51.05255888325788050, -10.99999999999999112 ) ) ;
#39270 = CARTESIAN_POINT ( 'NONE',  ( -30.44569435410879166, 202.0625000013656063, 172.4456943541092357 ) ) ;
#39271 = CARTESIAN_POINT ( 'NONE',  ( -11.00000000000000000, 0.000000000000000000, 106.0000000000000000 ) ) ;
#39272 = CARTESIAN_POINT ( 'NONE',  ( -2.445694354108783219, 205.8125000013656063, 200.4456943541088663 ) ) ;
#39274 = CARTESIAN_POINT ( 'NONE',  ( -8.660254037844394404, 127.9166666666666856, 5.000000000000001776 ) ) ;
#39273 = CARTESIAN_POINT ( 'NONE',  ( 0.000000000000000000, 0.000000000000000000, 11.00000000000000000 ) ) ;
#39275 = CARTESIAN_POINT ( 'NONE',  ( -7.320508075688778149, 118.1250000000000000, 7.320508075688769267 ) ) ;
#39276 = EDGE_CURVE ( 'NONE', #65259, #67450, #41848, .T. ) ;
#39277 = CARTESIAN_POINT ( 'NONE',  ( 5.656854249492381470, 107.5625000000000000, 5.656854249492379694 ) ) ;
#39278 = CARTESIAN_POINT ( 'NONE',  ( 4.556349186104052151, -10.99999999999999822, 87.15625000409676204 ) ) ;
#39279 = CARTESIAN_POINT ( 'NONE',  ( 7.188101187499993827, -2.977408999572645598, 8.517802781871754547 ) ) ;
#39280 = CARTESIAN_POINT ( 'NONE',  ( 4.000000000000015987, 200.5000000000000000, 198.0000000000000284 ) ) ;
#39281 = CARTESIAN_POINT ( 'NONE',  ( 27.99999999999996803, 208.4375000013656063, 173.4587341249998929 ) ) ;
#39282 = CARTESIAN_POINT ( 'NONE',  ( 7.188101187499999156, 2.249999997951610098, 2.977408999572654924 ) ) ;
#39283 = CARTESIAN_POINT ( 'NONE',  ( -3.458734125000016313, 198.8750000013656347, 140.5673454167824161 ) ) ;
#39284 = CARTESIAN_POINT ( 'NONE',  ( -7.188101187499999156, 123.1250000020484094, 2.977408999572654924 ) ) ;
#39286 = CARTESIAN_POINT ( 'NONE',  ( 2.445694354108783219, 204.8125000013656063, 139.5543056458912190 ) ) ;
#39285 = DIRECTION ( 'NONE',  ( -0.000000000000000000, 1.000000000000000000, -0.000000000000000000 ) ) ;
#39287 = CARTESIAN_POINT ( 'NONE',  ( 9.832129032723416984, 247.1354166700806445, -5.676582343750003368 ) ) ;
#39288 = LINE ( 'NONE', #27209, #57911 ) ;
#39289 = DIRECTION ( 'NONE',  ( -1.000000000000000000, -0.000000000000000000, -0.000000000000000000 ) ) ;
#39290 = CARTESIAN_POINT ( 'NONE',  ( 25.17157287525381548, 203.6250000000000284, 167.1715728752537018 ) ) ;
#39291 = CARTESIAN_POINT ( 'NONE',  ( 8.311093377946837890, 16.40624999658601268, -8.311093377946837890 ) ) ;
#39292 = B_SPLINE_CURVE_WITH_KNOTS ( 'NONE', 3,
 ( #1895, #29828, #1173, #13192, #11732, #36231, #12828, #59247 ),
 .UNSPECIFIED., .F., .F.,
 ( 4, 2, 2, 4 ),
 ( 0.007010445034807124762, 0.008756443665256687450, 0.01050244229570624840, 0.01399443955660537552 ),
 .UNSPECIFIED. ) ;
#39293 = CARTESIAN_POINT ( 'NONE',  ( 7.188101187499992051, 2.977408999572647819, 1.205302781871753215 ) ) ;
#39294 = CARTESIAN_POINT ( 'NONE',  ( -11.35316468749999785, 203.3854166632526983, -3.042071309553167513 ) ) ;
#39295 = LINE ( 'NONE', #3851, #35917 ) ;
#39296 = DIRECTION ( 'NONE',  ( -0.000000000000000000, -0.000000000000000000, -1.000000000000000000 ) ) ;
#39298 = CYLINDRICAL_SURFACE ( 'NONE', #35139, 10.00000000000000178 ) ;
#39297 = CARTESIAN_POINT ( 'NONE',  ( -5.656854249492379694, 25.87499999590322375, -5.656854249492380582 ) ) ;
#39299 = VERTEX_POINT ( 'NONE', #13162 ) ;
#39301 = EDGE_CURVE ( 'NONE', #28981, #74545, #31296, .T. ) ;
#39300 = CARTESIAN_POINT ( 'NONE',  ( -2.839093476692135984E-14, 198.9375000013655779, 138.5412658750000503 ) ) ;
#39302 = EDGE_CURVE ( 'NONE', #49926, #13507, #72867, .T. ) ;
#39303 = CARTESIAN_POINT ( 'NONE',  ( -5.676582343750006032, 4.114583329919349275, 9.832129032723418760 ) ) ;
#39304 = CARTESIAN_POINT ( 'NONE',  ( 4.556349186104051263, -10.99999999999999822, 91.65625000409679046 ) ) ;
#39305 = AXIS2_PLACEMENT_3D ( 'NONE', #49993, #72640, #20943 ) ;
#39306 = CARTESIAN_POINT ( 'NONE',  ( 10.00000000000000178, 227.2916666666666288, 2.679491924311222739 ) ) ;
#39307 = CARTESIAN_POINT ( 'NONE',  ( -30.44569435410875613, 196.8125000013656063, 172.4456943541092642 ) ) ;
#39308 = CARTESIAN_POINT ( 'NONE',  ( 0.000000000000000000, 0.000000000000000000, 0.000000000000000000 ) ) ;
#39310 = CARTESIAN_POINT ( 'NONE',  ( -11.35316468749999785, 3.072916663252683200, -3.042071309553167957 ) ) ;
#39309 = CARTESIAN_POINT ( 'NONE',  ( -7.188101187500000044, 112.1562500020483952, 0.000000000000000000 ) ) ;
#39311 = CARTESIAN_POINT ( 'NONE',  ( 3.313708498984756279, 7.999999999999991118, 22.86155277982337353 ) ) ;
#39312 = CARTESIAN_POINT ( 'NONE',  ( 11.35316468750000141, 135.7812499965860411, 0.000000000000000000 ) ) ;
#39313 = ADVANCED_FACE ( 'NONE', ( #47133 ), #29796, .T. ) ;
#39314 = CARTESIAN_POINT ( 'NONE',  ( 8.660254037844385522, 96.45833332650536818, 5.000000000000005329 ) ) ;
#39315 = AXIS2_PLACEMENT_3D ( 'NONE', #29915, #5422, #51434 ) ;
#39316 = CARTESIAN_POINT ( 'NONE',  ( -5.082755093536324154, 123.2187500020483952, 5.082755093536326818 ) ) ;
#39317 = CARTESIAN_POINT ( 'NONE',  ( -8.660254037844387298, 3.958333326505365957, -5.000000000000004441 ) ) ;
#39318 = DIRECTION ( 'NONE',  ( -0.000000000000000000, -0.000000000000000000, -1.000000000000000000 ) ) ;
#39319 = ORIENTED_EDGE ( 'NONE', *, *, #73848, .T. ) ;
#39320 = CARTESIAN_POINT ( 'NONE',  ( 1.882291019709147140, -65.87523470714363327, 26.34730193751357419 ) ) ;
#39321 = CARTESIAN_POINT ( 'NONE',  ( -6.676582343750000703, 289.6718750017070079, 2.765530957082001251 ) ) ;
#39322 = CARTESIAN_POINT ( 'NONE',  ( 0.000000000000000000, 116.0729912458811839, 42.10166426739785095 ) ) ;
#39323 = CARTESIAN_POINT ( 'NONE',  ( 5.656854249492376141, -5.656854249492374365, 0.08030278392014492117 ) ) ;
#39324 = CARTESIAN_POINT ( 'NONE',  ( 8.311093377946839666, 255.7812500034139589, 8.311093377946829008 ) ) ;
#39325 = EDGE_CURVE ( 'NONE', #33915, #55673, #41455, .T. ) ;
#39326 = CARTESIAN_POINT ( 'NONE',  ( 1.871523826299183495E-15, -10.18810118749999916, 96.90625000204838102 ) ) ;
#39327 = VERTEX_POINT ( 'NONE', #42582 ) ;
#39328 = VECTOR ( 'NONE', #66581, 1000.000000000000000 ) ;
#39329 = CARTESIAN_POINT ( 'NONE',  ( 5.000000000000000000, 11.00479820989369806, 67.37201579502529114 ) ) ;
#39330 = DIRECTION ( 'NONE',  ( 0.000000000000000000, 0.000000000000000000, 1.000000000000000000 ) ) ;
#39331 = CARTESIAN_POINT ( 'NONE',  ( 2.445694354108839175, 201.3125000013656063, 195.5543056458912190 ) ) ;
#39332 = CARTESIAN_POINT ( 'NONE',  ( 8.311093377946837890, 81.71874999658601268, -8.311093377946837890 ) ) ;
#39333 = ORIENTED_EDGE ( 'NONE', *, *, #9760, .F. ) ;
#39334 = CARTESIAN_POINT ( 'NONE',  ( -10.18810118749999916, 0.000000000000000000, 111.1562500020483668 ) ) ;
#39335 = CARTESIAN_POINT ( 'NONE',  ( -4.541265875000002339, 11.93749999863440614, -5.561446717895856393E-16 ) ) ;
#39336 = EDGE_LOOP ( 'NONE', ( #69558, #1194, #61443, #48056 ) ) ;
#39337 = CARTESIAN_POINT ( 'NONE',  ( -1.320432766682874540E-15, 27.09374999795161543, 7.188101187500000044 ) ) ;
#39338 = CARTESIAN_POINT ( 'NONE',  ( 7.320508075688771044, 114.3750000000000142, 7.320508075688774596 ) ) ;
#39339 = CARTESIAN_POINT ( 'NONE',  ( -4.556349186104048599, -10.99999999999999822, 76.46875000409677625 ) ) ;
#39340 = CARTESIAN_POINT ( 'NONE',  ( -5.082755093536326818, 22.78124999795161187, 5.082755093536325042 ) ) ;
#39341 = CARTESIAN_POINT ( 'NONE',  ( -6.238412754330611322E-16, 10.18810118749999916, 108.1562500020483668 ) ) ;
#39342 = FACE_OUTER_BOUND ( 'NONE', #38508, .T. ) ;
#39343 = CARTESIAN_POINT ( 'NONE',  ( -4.000000000000001776, 9.187499997268814056, -1.656854249492381470 ) ) ;
#39344 = CARTESIAN_POINT ( 'NONE',  ( -11.00000000000000000, 0.000000000000000000, 117.3437500020483810 ) ) ;
#39345 = ORIENTED_EDGE ( 'NONE', *, *, #3689, .F. ) ;
#39346 = CARTESIAN_POINT ( 'NONE',  ( 1.432654583217664479, 202.7500000013655779, 201.4587341250000065 ) ) ;
#39347 = AXIS2_PLACEMENT_3D ( 'NONE', #776, #66722, #31647 ) ;
#39348 = CARTESIAN_POINT ( 'NONE',  ( -25.17157287525373732, 194.7500000027312126, 172.8284271247464972 ) ) ;
#39349 = LINE ( 'NONE', #68759, #68208 ) ;
#39350 = CARTESIAN_POINT ( 'NONE',  ( 4.541265875000002339, 11.37499999863440969, -1.881053915767121554 ) ) ;
#39351 = CARTESIAN_POINT ( 'NONE',  ( -1.656854249492383468, 10.43749999726881228, 4.000000000000000888 ) ) ;
#39352 = CARTESIAN_POINT ( 'NONE',  ( -5.082755093536317936, -5.082755093536320601, 16.67405278187175810 ) ) ;
#39353 = ORIENTED_EDGE ( 'NONE', *, *, #70739, .F. ) ;
#39354 = DIRECTION ( 'NONE',  ( -0.000000000000000000, -1.000000000000000000, -0.000000000000000000 ) ) ;
#39355 = ORIENTED_EDGE ( 'NONE', *, *, #23534, .T. ) ;
#39356 = CARTESIAN_POINT ( 'NONE',  ( 10.18810118750000093, -4.220049686691933033, 111.8125000020483810 ) ) ;
#39357 = CARTESIAN_POINT ( 'NONE',  ( -7.778174593052023411, 7.778174593052023411, 97.00000000409677625 ) ) ;
#39358 = CARTESIAN_POINT ( 'NONE',  ( 3.458734125000015425, 203.0000000013655779, 196.5673454167823877 ) ) ;
#39359 = CARTESIAN_POINT ( 'NONE',  ( 24.54126587499998280, 200.1250000013656063, 168.5673454167822740 ) ) ;
#39360 = CARTESIAN_POINT ( 'NONE',  ( 10.00000000000000178, 85.20833333333334281, -2.679491924311226736 ) ) ;
#39361 = EDGE_CURVE ( 'NONE', #53657, #2559, #3457, .T. ) ;
#39362 = CARTESIAN_POINT ( 'NONE',  ( -8.000000000000000000, 124.9062499999999858, -3.313708498984761608 ) ) ;
#39363 = CARTESIAN_POINT ( 'NONE',  ( -2.485281374238572649, 294.1875000000000000, 6.000000000000002665 ) ) ;
#39364 = CARTESIAN_POINT ( 'NONE',  ( 23.99999999999998934, 204.8750000027312126, 169.9999999999999432 ) ) ;
#39365 = EDGE_LOOP ( 'NONE', ( #50350, #21668, #48516, #23765 ) ) ;
#39366 =( BOUNDED_CURVE ( )  B_SPLINE_CURVE ( 2, ( #13090, #59146, #31196, #2531, #25523, #7455, #30462, #1796, #48535 ),
 .UNSPECIFIED., .F., .F. ) 
 B_SPLINE_CURVE_WITH_KNOTS ( ( 3, 2, 2, 2, 3 ),
 ( 0.04999999999999991951, 0.05833333333333332038, 0.06666666666666672125, 0.07500000000000012212, 0.08333333333333352300 ),
 .UNSPECIFIED. ) 
 CURVE ( )  GEOMETRIC_REPRESENTATION_ITEM ( )  RATIONAL_B_SPLINE_CURVE ( ( 1.000000000000000666, 0.9238795325112859613, 1.000000000000000000, 0.9238795325112867385, 1.000000000000000000, 0.9238795325112867385, 1.000000000000000000, 0.9238795325112849621, 1.000000000000001776 ) ) 
 REPRESENTATION_ITEM ( '' )  );
#39367 = AXIS2_PLACEMENT_3D ( 'NONE', #14251, #31622, #71969 ) ;
#39368 = CARTESIAN_POINT ( 'NONE',  ( 8.000000000000000000, 94.34374999999998579, -3.313708498984762496 ) ) ;
#39369 = CARTESIAN_POINT ( 'NONE',  ( 7.999999999999948486, 3.313708498984800244, 7.674052779823369086 ) ) ;
#39370 = CARTESIAN_POINT ( 'NONE',  ( -1.656854249492405451, 194.4375000027312126, 138.0000000000000568 ) ) ;
#39371 = CARTESIAN_POINT ( 'NONE',  ( -5.000000000000000888, 67.66364885638930105, 22.52891795222361893 ) ) ;
#39372 = CARTESIAN_POINT ( 'NONE',  ( 8.000000000000000000, 13.40624999590322375, -3.313708498984761164 ) ) ;
#39373 = CARTESIAN_POINT ( 'NONE',  ( 10.00000000000000178, 232.2916666666666856, 2.679491924311222739 ) ) ;
#39374 = CARTESIAN_POINT ( 'NONE',  ( 11.00000000000000000, 1.347111479062088405E-15, 73.93750000409676204 ) ) ;
#39375 = CARTESIAN_POINT ( 'NONE',  ( -7.320508075688773708, 201.8749999999999716, -7.320508075688774596 ) ) ;
#39376 = SURFACE_STYLE_FILL_AREA ( #50315 ) ;
#39377 = CARTESIAN_POINT ( 'NONE',  ( -7.188101187499992051, 0.000000000000000000, 13.86155278187175455 ) ) ;
#39378 = CARTESIAN_POINT ( 'NONE',  ( -2.085542519210945728E-15, 164.8437499965860127, 11.35316468750000141 ) ) ;
#39379 = DIRECTION ( 'NONE',  ( -1.000000000000000000, 0.000000000000000000, -0.000000000000000000 ) ) ;
#39380 = CARTESIAN_POINT ( 'NONE',  ( 0.000000000000000000, 0.000000000000000000, 0.000000000000000000 ) ) ;
#39382 = CARTESIAN_POINT ( 'NONE',  ( -3.673940397442060854E-16, 296.8125000034140157, -6.000000000000001776 ) ) ;
#39381 = FILL_AREA_STYLE_COLOUR ( '', #65957 ) ;
#39383 = VERTEX_POINT ( 'NONE', #2228 ) ;
#39384 = CARTESIAN_POINT ( 'NONE',  ( 11.35316468750000141, 21.09374999658601624, 0.000000000000000000 ) ) ;
#39385 = CARTESIAN_POINT ( 'NONE',  ( 7.778174593052021635, 7.778174593052023411, 113.1250000040967763 ) ) ;
#39386 = CARTESIAN_POINT ( 'NONE',  ( -27.99999999999992184, 208.9375000013656063, 173.4587341250003760 ) ) ;
#39388 = CARTESIAN_POINT ( 'NONE',  ( -5.126144196591213564, -16.23426282122703768, -69.90718656545267606 ) ) ;
#39387 = CARTESIAN_POINT ( 'NONE',  ( -7.999999999999991118, 3.313708498984757167, 17.42405278392013912 ) ) ;
#39389 = CARTESIAN_POINT ( 'NONE',  ( 0.000000000000000000, 54.99999999999999289, 0.000000000000000000 ) ) ;
#39390 = CARTESIAN_POINT ( 'NONE',  ( 2.445694354108783664, 203.3125000013656063, 144.4456943541088663 ) ) ;
#39391 = CARTESIAN_POINT ( 'NONE',  ( -10.00000000000000178, 64.37499999317203958, -1.224646799147353454E-15 ) ) ;
#39392 = CARTESIAN_POINT ( 'NONE',  ( 5.082755093536325042, 101.0937500020483810, -5.082755093536325930 ) ) ;
#39393 = CARTESIAN_POINT ( 'NONE',  ( -4.541265875000003227, 13.99999999863440792, 1.881053915767121110 ) ) ;
#39394 = CARTESIAN_POINT ( 'NONE',  ( 8.660254037844433483, 65.41666666666669983, -5.000000000000025757 ) ) ;
#39395 = CARTESIAN_POINT ( 'NONE',  ( 5.656854249492374365, 5.656854249492375253, 3.267802779823362425 ) ) ;
#39396 = CARTESIAN_POINT ( 'NONE',  ( -5.656854249492373476, -5.656854249492376141, 20.70530278392014623 ) ) ;
#39397 = VERTEX_POINT ( 'NONE', #48239 ) ;
#39398 = ORIENTED_EDGE ( 'NONE', *, *, #3689, .T. ) ;
#39399 = CARTESIAN_POINT ( 'NONE',  ( 4.193030820682224658, -50.40097124335133572, -40.95512985425011010 ) ) ;
#39400 = CARTESIAN_POINT ( 'NONE',  ( 3.458734125000015869, 196.1875000013655779, 198.0000000000000284 ) ) ;
#39401 = CARTESIAN_POINT ( 'NONE',  ( 18.00000000000000355, 0.000000000000000000, 0.000000000000000000 ) ) ;
#39402 = CARTESIAN_POINT ( 'NONE',  ( 9.832129032723416984, 222.1354166700806729, -5.676582343750003368 ) ) ;
#39403 = CARTESIAN_POINT ( 'NONE',  ( -3.042071309553173730, 144.3229166632527267, 11.35316468749999785 ) ) ;
#39404 = ORIENTED_EDGE ( 'NONE', *, *, #5787, .F. ) ;
#39405 = CARTESIAN_POINT ( 'NONE',  ( -4.999999999999999112, 10.60557809245594463, -66.49298242784793445 ) ) ;
#39406 = CARTESIAN_POINT ( 'NONE',  ( -7.204075437095967871, 7.204075437095967871, 86.96875000204836681 ) ) ;
#39407 = CARTESIAN_POINT ( 'NONE',  ( -31.57880696627669792, 194.6197631453349288, 170.5879734657860922 ) ) ;
#39408 = CARTESIAN_POINT ( 'NONE',  ( 1.656854249492403008, 207.6875000000000000, 194.0000000000000853 ) ) ;
#39409 = CARTESIAN_POINT ( 'NONE',  ( 4.999999999999997335, 248.3333333333333428, -8.660254037844387298 ) ) ;
#39410 = DIRECTION ( 'NONE',  ( 1.000000000000000000, 0.000000000000000000, -0.000000000000000000 ) ) ;
#39411 = CARTESIAN_POINT ( 'NONE',  ( 0.000000000000000000, 0.000000000000000000, 7.499999999999992895 ) ) ;
#39412 = EDGE_CURVE ( 'NONE', #22196, #59151, #55110, .T. ) ;
#39413 = CARTESIAN_POINT ( 'NONE',  ( -6.238412754330611322E-16, 10.18810118749999916, 115.6562500020483810 ) ) ;
#39414 = ORIENTED_EDGE ( 'NONE', *, *, #8491, .F. ) ;
#39415 = EDGE_CURVE ( 'NONE', #29697, #41900, #41482, .T. ) ;
#39416 = CARTESIAN_POINT ( 'NONE',  ( -4.898587196589412829E-16, 106.8125000040967763, -8.000000000000000000 ) ) ;
#39417 = CARTESIAN_POINT ( 'NONE',  ( 25.87252272011448540, 177.3363770347625064, 144.1983798943604143 ) ) ;
#39418 = CARTESIAN_POINT ( 'NONE',  ( -11.35316468750000141, 128.5937499965860127, -1.390361679473963753E-15 ) ) ;
#39419 = CARTESIAN_POINT ( 'NONE',  ( -3.458734124999959914, 204.4375000013656063, 198.0000000000000284 ) ) ;
#39420 = CARTESIAN_POINT ( 'NONE',  ( -5.082755093536326818, 22.78124999795161187, 5.082755093536325042 ) ) ;
#39421 = CARTESIAN_POINT ( 'NONE',  ( -4.220049686691935698, 10.18810118749999916, 84.25000000204838102 ) ) ;
#39422 = CARTESIAN_POINT ( 'NONE',  ( 11.35316468750000141, 41.09374999658601979, 0.000000000000000000 ) ) ;
#39423 = ORIENTED_EDGE ( 'NONE', *, *, #31548, .T. ) ;
#39424 = DIRECTION ( 'NONE',  ( 0.7071067811865482389, -0.7071067811865469066, -0.000000000000000000 ) ) ;
#39425 = CARTESIAN_POINT ( 'NONE',  ( -3.313708498984757611, 7.999999999999991118, 8.236552783920144449 ) ) ;
#39426 = CARTESIAN_POINT ( 'NONE',  ( -4.903558642999205574E-16, 8.008118988124991233, 18.63811528394063188 ) ) ;
#39427 = CARTESIAN_POINT ( 'NONE',  ( 3.458734124999960358, 208.6875000013656063, 142.0000000000000568 ) ) ;
#39428 = CARTESIAN_POINT ( 'NONE',  ( 7.188101187500001821, 8.062499997951611874, -2.977408999572650483 ) ) ;
#39429 = CARTESIAN_POINT ( 'NONE',  ( 4.242640687119285658, 297.6875000034139589, -4.242640687119286547 ) ) ;
#39430 = CARTESIAN_POINT ( 'NONE',  ( 38.00000000000000000, -52.99999999999999289, 25.00000000000000000 ) ) ;
#39431 = CARTESIAN_POINT ( 'NONE',  ( 3.042071309553159519, 150.0520833299193555, 11.35316468750000141 ) ) ;
#39432 = CARTESIAN_POINT ( 'NONE',  ( -4.220049686691937474, -10.18810118749999738, 75.43750000204836681 ) ) ;
#39433 = EDGE_CURVE ( 'NONE', #35339, #34733, #26592, .T. ) ;
#39434 = CARTESIAN_POINT ( 'NONE',  ( -29.43265458321760164, 195.8750000013655779, 173.4587341250003760 ) ) ;
#39435 = LINE ( 'NONE', #56420, #23369 ) ;
#39436 = CARTESIAN_POINT ( 'NONE',  ( -4.541265875000003227, 18.99999999863440436, 1.881053915767121110 ) ) ;
#39437 = ORIENTED_EDGE ( 'NONE', *, *, #2105, .F. ) ;
#39438 = CARTESIAN_POINT ( 'NONE',  ( 1.656854249492403008, 198.8125000027312126, 194.0000000000000853 ) ) ;
#39439 = CARTESIAN_POINT ( 'NONE',  ( -3.458734125000016757, 195.1250000013656063, 140.5673454167824161 ) ) ;
#39440 = CARTESIAN_POINT ( 'NONE',  ( -27.99999999999991473, 207.6250000027312126, 174.0000000000003695 ) ) ;
#39441 = DIRECTION ( 'NONE',  ( -0.000000000000000000, 1.000000000000000000, 4.689100369878284071E-30 ) ) ;
#39442 = ORIENTED_EDGE ( 'NONE', *, *, #45695, .F. ) ;
#39443 = CARTESIAN_POINT ( 'NONE',  ( -7.188101187500000933, 16.12499999795161543, -2.977408999572651371 ) ) ;
#39444 = CARTESIAN_POINT ( 'NONE',  ( -2.679491924311382611, 210.4166666598386541, 9.999999999999914735 ) ) ;
#39445 = VECTOR ( 'NONE', #48349, 1000.000000000000000 ) ;
#39446 = CARTESIAN_POINT ( 'NONE',  ( -7.778174593052020747, -7.778174593052023411, 73.37500000409677625 ) ) ;
#39447 = CARTESIAN_POINT ( 'NONE',  ( 10.00000000000000178, 40.00000000000000000, 0.000000000000000000 ) ) ;
#39448 = CARTESIAN_POINT ( 'NONE',  ( -2.977408999572650927, 109.2500000020483952, -7.188101187500001821 ) ) ;
#39449 = CARTESIAN_POINT ( 'NONE',  ( 0.000000000000000000, 0.000000000000000000, 14.00000000000000000 ) ) ;
#39450 = CARTESIAN_POINT ( 'NONE',  ( -8.000000000000033751, -3.313708498984719864, 2.424052779823363757 ) ) ;
#39451 = EDGE_CURVE ( 'NONE', #29199, #53500, #57918, .T. ) ;
#39453 = CARTESIAN_POINT ( 'NONE',  ( -7.833566452622682696, -1.888151595330326726, -0.000000000000000000 ) ) ;
#39452 = CARTESIAN_POINT ( 'NONE',  ( -26.34314575050757767, 201.9375000000000000, 166.0000000000004263 ) ) ;
#39454 = ORIENTED_EDGE ( 'NONE', *, *, #65308, .T. ) ;
#39455 = CARTESIAN_POINT ( 'NONE',  ( -11.35316468749999785, 253.6979166700807014, -3.042071309553164848 ) ) ;
#39456 = VECTOR ( 'NONE', #27762, 1000.000000000000000 ) ;
#39457 = CARTESIAN_POINT ( 'NONE',  ( 5.082755093536318824, 5.082755093536319713, 25.29905278187175810 ) ) ;
#39458 = CARTESIAN_POINT ( 'NONE',  ( 1.317228840344865981, 55.68607278122992454, 43.83834608838541413 ) ) ;
#39459 = CYLINDRICAL_SURFACE ( 'NONE', #4622, 6.000000000000001776 ) ;
#39460 = CARTESIAN_POINT ( 'NONE',  ( 4.104248244554821845, -66.38464254924988950, -26.65807398668032491 ) ) ;
#39461 =( BOUNDED_CURVE ( )  B_SPLINE_CURVE ( 2, ( #28348, #68342, #22677, #17020, #40044, #34781, #50986, #39306, #63048, #27598, #5716, #80, #69087 ),
 .UNSPECIFIED., .F., .F. ) 
 B_SPLINE_CURVE_WITH_KNOTS ( ( 3, 2, 2, 2, 2, 2, 3 ),
 ( 0.8055555555555555802, 0.8148148148148147696, 0.8240740740740740700, 0.8333333333333333703, 0.8425925925925925597, 0.8518518518518518601, 0.8611111111111111605 ),
 .UNSPECIFIED. ) 
 CURVE ( )  GEOMETRIC_REPRESENTATION_ITEM ( )  RATIONAL_B_SPLINE_CURVE ( ( 1.000000000000000000, 0.9659258262890683122, 1.000000000000000000, 0.9659258262890683122, 1.000000000000000000, 0.9659258262890683122, 1.000000000000000000, 0.9659258262890683122, 1.000000000000000000, 0.9659258262890683122, 1.000000000000000000, 0.9659258262890683122, 1.000000000000000000 ) ) 
 REPRESENTATION_ITEM ( '' )  );
#39463 = EDGE_CURVE ( 'NONE', #61990, #60693, #65585, .T. ) ;
#39462 = CARTESIAN_POINT ( 'NONE',  ( 3.458734125000015869, 197.1875000013655779, 198.0000000000000284 ) ) ;
#39464 = CARTESIAN_POINT ( 'NONE',  ( 8.660254037844389075, 165.4166666666666856, -5.000000000000000000 ) ) ;
#39465 = CARTESIAN_POINT ( 'NONE',  ( -1.224646799147353454E-15, 225.9999999999999432, 10.00000000000000178 ) ) ;
#39466 = CARTESIAN_POINT ( 'NONE',  ( 9.000000000000014211, 15.58845726811988719, 0.000000000000000000 ) ) ;
#39467 = CARTESIAN_POINT ( 'NONE',  ( 4.999999999999999112, -53.39837237779262580, -47.14918772354958065 ) ) ;
#39468 = CARTESIAN_POINT ( 'NONE',  ( -5.676582343749998039, 127.7604166632526841, -9.832129032723420536 ) ) ;
#39469 = FACE_OUTER_BOUND ( 'NONE', #30012, .T. ) ;
#39470 = CARTESIAN_POINT ( 'NONE',  ( -7.778174593052023411, 7.778174593052023411, 107.3124999999999858 ) ) ;
#39473 = CARTESIAN_POINT ( 'NONE',  ( -5.000000000000000000, 68.60357193678683529, 20.85024232999420946 ) ) ;
#39472 = CARTESIAN_POINT ( 'NONE',  ( 31.45873412499999233, 197.6875000013655779, 169.9999999999998863 ) ) ;
#39471 = CARTESIAN_POINT ( 'NONE',  ( 31.45873412499999944, 195.0000000013656063, 168.5673454167822740 ) ) ;
#39474 = ORIENTED_EDGE ( 'NONE', *, *, #9847, .F. ) ;
#39475 = CARTESIAN_POINT ( 'NONE',  ( 9.910777348998651703, 225.1079956670950821, -1.365085748358755735 ) ) ;
#39476 = CARTESIAN_POINT ( 'NONE',  ( 32.00000000000000711, 202.3125000027312410, 171.6568542494922553 ) ) ;
#39477 = CARTESIAN_POINT ( 'NONE',  ( 4.898587196589412829E-16, 22.87500000000000355, -8.000000000000000000 ) ) ;
#39478 = VECTOR ( 'NONE', #2443, 1000.000000000000000 ) ;
#39479 = CARTESIAN_POINT ( 'NONE',  ( 31.45873412499999233, 197.9375000013655779, 169.9999999999999432 ) ) ;
#39480 = EDGE_CURVE ( 'NONE', #60780, #38597, #37222, .T. ) ;
#39481 = CARTESIAN_POINT ( 'NONE',  ( -8.311093377946836114, 207.9687499965859843, -8.311093377946837890 ) ) ;
#39482 = CARTESIAN_POINT ( 'NONE',  ( 2.977408999572654480, 123.1250000020484094, 7.188101187499999156 ) ) ;
#39483 = CARTESIAN_POINT ( 'NONE',  ( -4.541265875000002339, 19.74999999863440792, -1.881053915767121998 ) ) ;
#39484 = CARTESIAN_POINT ( 'NONE',  ( 24.54126587500000056, 196.3750000013656063, 168.5673454167822172 ) ) ;
#39485 = CARTESIAN_POINT ( 'NONE',  ( 7.999999999999992895, -3.313708498984756279, 20.98655277982336642 ) ) ;
#39487 = CARTESIAN_POINT ( 'NONE',  ( -24.00000000000000711, 202.8125000000000000, 168.3431457505080289 ) ) ;
#39486 = CARTESIAN_POINT ( 'NONE',  ( -5.000000000000000000, -10.00000000000000000, 75.19090595827292134 ) ) ;
#39488 = CARTESIAN_POINT ( 'NONE',  ( -11.35316468750000141, 93.48958332991934128, 3.042071309553159963 ) ) ;
#39489 = ORIENTED_EDGE ( 'NONE', *, *, #33400, .T. ) ;
#39490 =( BOUNDED_CURVE ( )  B_SPLINE_CURVE ( 2, ( #22475, #63220, #69263, #34581, #40592, #39476, #11547, #33838, #17573 ),
 .UNSPECIFIED., .F., .F. ) 
 B_SPLINE_CURVE_WITH_KNOTS ( ( 3, 2, 2, 2, 3 ),
 ( 0.4333333333333336812, 0.4416666666666669849, 0.4500000000000003997, 0.4583333333333337034, 0.4666666666666670626 ),
 .UNSPECIFIED. ) 
 CURVE ( )  GEOMETRIC_REPRESENTATION_ITEM ( )  RATIONAL_B_SPLINE_CURVE ( ( 0.9999999999999970024, 0.9238795325112897361, 1.000000000000000000, 0.9238795325112867385, 1.000000000000000000, 0.9238795325112867385, 1.000000000000000000, 0.9238795325112831858, 1.000000000000003553 ) ) 
 REPRESENTATION_ITEM ( '' )  );
#39491 = EDGE_CURVE ( 'NONE', #10325, #65259, #34347, .T. ) ;
#39492 = CARTESIAN_POINT ( 'NONE',  ( -2.751064625579944321E-14, 205.8750000027312126, 146.0000000000000284 ) ) ;
#39493 = CARTESIAN_POINT ( 'NONE',  ( 5.082755093536324154, 25.78124999795161543, 5.082755093536326818 ) ) ;
#39494 = CARTESIAN_POINT ( 'NONE',  ( 1.469576158976822172E-15, -7.999999999999991118, 8.705302779823362869 ) ) ;
#39495 = CARTESIAN_POINT ( 'NONE',  ( 11.35316468749999608, 251.9270833367473585, -3.042071309553167513 ) ) ;
#39496 = CARTESIAN_POINT ( 'NONE',  ( -3.042071309553164404, 102.2395833299193697, -11.35316468749999963 ) ) ;
#39497 = VERTEX_POINT ( 'NONE', #3264 ) ;
#39498 = CARTESIAN_POINT ( 'NONE',  ( -10.00000000000000000, 265.0000000000000000, 0.000000000000000000 ) ) ;
#39499 = CARTESIAN_POINT ( 'NONE',  ( -4.220049686691935698, 10.18810118749999916, 106.3750000020483668 ) ) ;
#39500 = CARTESIAN_POINT ( 'NONE',  ( -8.660254037844390851, 219.7916666598387110, 4.999999999999998224 ) ) ;
#39501 = CARTESIAN_POINT ( 'NONE',  ( 3.458734125000015425, 204.2500000013655779, 196.5673454167823877 ) ) ;
#39502 = CARTESIAN_POINT ( 'NONE',  ( -28.00000000000007816, 201.1250000027312126, 166.0000000000003695 ) ) ;
#39504 = CARTESIAN_POINT ( 'NONE',  ( -11.35316468749999785, 93.07291666325268409, -3.042071309553167957 ) ) ;
#39503 = CARTESIAN_POINT ( 'NONE',  ( -29.65685424949234772, 202.0625000000000568, 166.0000000000003126 ) ) ;
#39505 = CARTESIAN_POINT ( 'NONE',  ( -5.656854249492373476, -5.656854249492376141, 14.70530278392014800 ) ) ;
#39506 = CARTESIAN_POINT ( 'NONE',  ( -29.43265458321760519, 201.1250000013656347, 173.4587341250003760 ) ) ;
#39507 = CARTESIAN_POINT ( 'NONE',  ( -3.313708498984719864, 27.28124999590322020, -8.000000000000040856 ) ) ;
#39508 = ORIENTED_EDGE ( 'NONE', *, *, #10691, .F. ) ;
#39509 = CARTESIAN_POINT ( 'NONE',  ( 10.00000000000000178, 181.8749999931720538, 0.000000000000000000 ) ) ;
#39510 = EDGE_CURVE ( 'NONE', #9276, #41900, #38342, .T. ) ;
#39511 = CARTESIAN_POINT ( 'NONE',  ( 25.17157287525377996, 200.7500000027312126, 167.1715728752537586 ) ) ;
#39512 = CARTESIAN_POINT ( 'NONE',  ( 5.000000000000000000, -52.84347807771159466, 43.21644271080197086 ) ) ;
#39513 = CARTESIAN_POINT ( 'NONE',  ( -9.832129032723420536, 74.01041666325268409, 5.676582343749997150 ) ) ;
#39514 = CARTESIAN_POINT ( 'NONE',  ( 4.721056650415999201, 290.0781250017069510, -4.721056650415999201 ) ) ;
#39515 = CARTESIAN_POINT ( 'NONE',  ( 2.977408999572652260, 3.562499997951610542, 7.188101187500000044 ) ) ;
#39516 = CARTESIAN_POINT ( 'NONE',  ( -10.18810118749999738, -4.220049686691941915, 104.1250000020483810 ) ) ;
#39517 = CARTESIAN_POINT ( 'NONE',  ( 3.042071309553159519, 219.7395833299193271, 11.35316468750000141 ) ) ;
#39518 = ORIENTED_EDGE ( 'NONE', *, *, #36567, .F. ) ;
#39519 = CARTESIAN_POINT ( 'NONE',  ( -5.656854249492373476, -5.656854249492376141, 28.01780277982336642 ) ) ;
#39520 = CARTESIAN_POINT ( 'NONE',  ( -8.000000000000000000, 2.062499995903220196, -9.797174393178825657E-16 ) ) ;
#39521 = DIRECTION ( 'NONE',  ( -0.000000000000000000, 1.000000000000000000, -1.563033456626094573E-30 ) ) ;
#39522 = CARTESIAN_POINT ( 'NONE',  ( -3.042071309553163960, 207.2395833299193839, -11.35316468749999963 ) ) ;
#39523 = CARTESIAN_POINT ( 'NONE',  ( 8.660254037844385522, 221.0416666734946602, -5.000000000000003553 ) ) ;
#39524 = DIRECTION ( 'NONE',  ( 0.000000000000000000, 0.000000000000000000, 1.000000000000000000 ) ) ;
#39525 = CARTESIAN_POINT ( 'NONE',  ( 2.765530957081996366, 297.1406250017070079, -6.676582343750003368 ) ) ;
#39526 = ORIENTED_EDGE ( 'NONE', *, *, #66091, .F. ) ;
#39527 = AXIS2_PLACEMENT_3D ( 'NONE', #24536, #18518, #9050 ) ;
#39528 = CARTESIAN_POINT ( 'NONE',  ( 8.311093377946834337, 200.4687499965860411, 8.311093377946839666 ) ) ;
#39529 = CARTESIAN_POINT ( 'NONE',  ( -30.44569435410883429, 205.5625000013656063, 167.5543056458915885 ) ) ;
#39530 = CARTESIAN_POINT ( 'NONE',  ( -3.313708498984760720, 19.96875000000000355, -8.000000000000000000 ) ) ;
#39531 = ORIENTED_EDGE ( 'NONE', *, *, #12704, .F. ) ;
#39532 = VECTOR ( 'NONE', #46373, 1000.000000000000000 ) ;
#39533 = CARTESIAN_POINT ( 'NONE',  ( -4.898587196589412829E-16, 94.81250000409677625, -8.000000000000000000 ) ) ;
#39534 = CARTESIAN_POINT ( 'NONE',  ( -25.17157287525385811, 200.0000000027312126, 167.1715728752541281 ) ) ;
#39535 =( REPRESENTATION_RELATIONSHIP ('NONE','NONE', #46008, #68567 ) REPRESENTATION_RELATIONSHIP_WITH_TRANSFORMATION ( #58766 )SHAPE_REPRESENTATION_RELATIONSHIP( ) );
#39536 = CARTESIAN_POINT ( 'NONE',  ( 10.00000000000000178, 20.00000000000000000, 0.000000000000000000 ) ) ;
#39537 =( GEOMETRIC_REPRESENTATION_CONTEXT ( 3 ) GLOBAL_UNCERTAINTY_ASSIGNED_CONTEXT ( ( #36730 ) ) GLOBAL_UNIT_ASSIGNED_CONTEXT ( ( #1255, #37044, #7637 ) ) REPRESENTATION_CONTEXT ( 'NONE', 'WORKASPACE' ) );
#39538 = CARTESIAN_POINT ( 'NONE',  ( 4.220049686691941027, -10.18810118749999738, 79.00000000204838102 ) ) ;
#39539 = ORIENTED_EDGE ( 'NONE', *, *, #5394, .T. ) ;
#39540 = CARTESIAN_POINT ( 'NONE',  ( 1.656854249492381248, 20.18749999999999645, -4.000000000000001776 ) ) ;
#39541 = CARTESIAN_POINT ( 'NONE',  ( 4.541265875000001451, 21.24999999863440792, 1.881053915767124440 ) ) ;
#39542 = CARTESIAN_POINT ( 'NONE',  ( 31.06932850344420771, 194.5499615265470652, 171.7980732949242508 ) ) ;
#39543 = CARTESIAN_POINT ( 'NONE',  ( 2.828427124746191623, 4.874999997268813168, -2.828427124746191623 ) ) ;
#39544 = CARTESIAN_POINT ( 'NONE',  ( -5.000000000000000888, -11.44657803507906024, 68.01244171956641082 ) ) ;
#39545 = DIRECTION ( 'NONE',  ( -0.000000000000000000, -1.000000000000000000, -0.000000000000000000 ) ) ;
#39546 = EDGE_CURVE ( 'NONE', #18980, #42139, #43614, .T. ) ;
#39549 = DIRECTION ( 'NONE',  ( 0.5000000000000008882, 0.8660254037844381525, -0.000000000000000000 ) ) ;
#39548 = CARTESIAN_POINT ( 'NONE',  ( -3.042071309553159075, 239.9479166700806729, 11.35316468749999963 ) ) ;
#39547 = CARTESIAN_POINT ( 'NONE',  ( 31.45873412499998523, 206.7500000013655779, 168.5673454167822172 ) ) ;
#39550 = PRODUCT_CONTEXT ( 'NONE', #19676, 'mechanical' ) ;
#39551 = ORIENTED_EDGE ( 'NONE', *, *, #13953, .F. ) ;
#39552 = CARTESIAN_POINT ( 'NONE',  ( 5.676582343749997150, 247.5520833367473301, -9.832129032723418760 ) ) ;
#39553 = CARTESIAN_POINT ( 'NONE',  ( -2.977408999572647819, 7.188101187499991163, 11.70530278187175099 ) ) ;
#39554 = EDGE_LOOP ( 'NONE', ( #54458, #22054, #47555, #28503, #42500, #71252, #20724, #62990, #63170, #55130, #41124, #73529, #17931, #61155, #23279, #47042, #41698, #7479, #678, #33146, #23911, #62763, #71623, #15673, #70518, #4779, #64004, #49038, #26813, #56018, #39177, #25129, #3223 ) ) ;
#39555 = ADVANCED_FACE ( 'NONE', ( #62089 ), #67381, .T. ) ;
#39556 = ORIENTED_EDGE ( 'NONE', *, *, #45418, .T. ) ;
#39557 = CARTESIAN_POINT ( 'NONE',  ( -6.238412754330611322E-16, 10.18810118749999916, 73.28125000204838102 ) ) ;
#39558 = CARTESIAN_POINT ( 'NONE',  ( -11.35316468749999785, 83.38541666325265567, -3.042071309553167513 ) ) ;
#39559 = DIRECTION ( 'NONE',  ( 0.000000000000000000, 0.000000000000000000, 1.000000000000000000 ) ) ;
#39560 = CARTESIAN_POINT ( 'NONE',  ( -4.556349186104045934, 11.00000000000000000, 87.71874999999997158 ) ) ;
#39563 = CARTESIAN_POINT ( 'NONE',  ( 4.721056650415999201, 290.2343750017069510, -4.721056650415999201 ) ) ;
#39562 = CARTESIAN_POINT ( 'NONE',  ( 24.54126587500000412, 207.2500000013655779, 171.4326545832175839 ) ) ;
#39561 = CARTESIAN_POINT ( 'NONE',  ( 28.00000000000002487, 207.1875000013656063, 166.5412658749999082 ) ) ;
#39564 = DIRECTION ( 'NONE',  ( 1.000000000000000000, 0.000000000000000000, -0.000000000000000000 ) ) ;
#39565 = CARTESIAN_POINT ( 'NONE',  ( 9.832129032723416984, 200.3645833299193555, 5.676582343750006032 ) ) ;
#39566 = CARTESIAN_POINT ( 'NONE',  ( -1.469576158976823947E-15, 11.43749999590322197, 8.000000000000000000 ) ) ;
#39567 = ORIENTED_EDGE ( 'NONE', *, *, #5842, .T. ) ;
#39568 = CARTESIAN_POINT ( 'NONE',  ( 31.45873412499999233, 194.6875000013655779, 169.9999999999999432 ) ) ;
#39569 = VECTOR ( 'NONE', #36595, 1000.000000000000000 ) ;
#39570 = CARTESIAN_POINT ( 'NONE',  ( -7.188101187500002709, 18.18749999795161187, 2.977408999572649151 ) ) ;
#39571 = CARTESIAN_POINT ( 'NONE',  ( 6.951808397369818766E-16, 162.3437499965860127, -11.35316468750000141 ) ) ;
#39572 = CARTESIAN_POINT ( 'NONE',  ( -10.99999999999994671, -4.556349186104105442, 98.78125000409679046 ) ) ;
#39573 = CARTESIAN_POINT ( 'NONE',  ( -5.082755093536325930, 101.8437500020483810, -5.082755093536325930 ) ) ;
#39575 = CARTESIAN_POINT ( 'NONE',  ( 4.000000000000001776, 10.06250000000000000, -1.656854249492381248 ) ) ;
#39574 = DIRECTION ( 'NONE',  ( 0.000000000000000000, 0.000000000000000000, -1.000000000000000000 ) ) ;
#39576 = CARTESIAN_POINT ( 'NONE',  ( 26.56734541678238415, 206.2500000013655779, 166.5412658749999650 ) ) ;
#39577 = CARTESIAN_POINT ( 'NONE',  ( 5.082755093536318824, 5.082755093536319713, 8.799052781871752771 ) ) ;
#39578 = CARTESIAN_POINT ( 'NONE',  ( 11.35316468749999785, 50.57291666325268409, 3.042071309553174174 ) ) ;
#39579 = CARTESIAN_POINT ( 'NONE',  ( -1.970469249063935269E-15, 20.78460969082654231, -21.50000000000000000 ) ) ;
#39580 = ORIENTED_EDGE ( 'NONE', *, *, #31183, .T. ) ;
#39581 = LINE ( 'NONE', #12390, #18192 ) ;
#39582 = CARTESIAN_POINT ( 'NONE',  ( 4.556349186104045934, 11.00000000000000000, 80.21875000409680467 ) ) ;
#39583 = CARTESIAN_POINT ( 'NONE',  ( -3.042071309553164404, 57.23958332991934839, -11.35316468749999963 ) ) ;
#39584 = VECTOR ( 'NONE', #51246, 1000.000000000000000 ) ;
#39585 = CARTESIAN_POINT ( 'NONE',  ( 7.778174593052023411, -7.778174593052021635, 75.25000000409676204 ) ) ;
#39586 = CARTESIAN_POINT ( 'NONE',  ( 2.445694354108784108, 201.5625000013656063, 144.4456943541088663 ) ) ;
#39587 = CARTESIAN_POINT ( 'NONE',  ( -0.3752463838827032050, 10.12385607954549371, 70.07152133708838448 ) ) ;
#39589 = CARTESIAN_POINT ( 'NONE',  ( -8.311093377946836114, 42.65624999658600558, -8.311093377946837890 ) ) ;
#39588 = CARTESIAN_POINT ( 'NONE',  ( -7.188101187500000044, 95.65625000204838102, 0.000000000000000000 ) ) ;
#39590 = CARTESIAN_POINT ( 'NONE',  ( -7.999999999999991118, 0.000000000000000000, 3.830302779823362869 ) ) ;
#39591 = CARTESIAN_POINT ( 'NONE',  ( 2.997893585525398702E-11, 31.24999999999767653, -10.00000000000000178 ) ) ;
#39592 =( BOUNDED_CURVE ( )  B_SPLINE_CURVE ( 2, ( #42623, #26768, #54709, #26376, #19980, #31308, #54336, #19242, #13570 ),
 .UNSPECIFIED., .F., .F. ) 
 B_SPLINE_CURVE_WITH_KNOTS ( ( 3, 2, 2, 2, 3 ),
 ( 0.06249999999999773792, 0.07291666666666440921, 0.08333333333333108051, 0.09374999999999775180, 0.1041666666666644370 ),
 .UNSPECIFIED. ) 
 CURVE ( )  GEOMETRIC_REPRESENTATION_ITEM ( )  RATIONAL_B_SPLINE_CURVE ( ( 1.000000000000016431, 0.9238795325112701962, 1.000000000000000000, 0.9238795325112867385, 1.000000000000000000, 0.9238795325112867385, 1.000000000000000000, 0.9238795325113030588, 0.9999999999999836797 ) ) 
 REPRESENTATION_ITEM ( '' )  );
#39593 = CARTESIAN_POINT ( 'NONE',  ( 11.35316468749999785, 175.5729166632526415, 3.042071309553174174 ) ) ;
#39594 = CARTESIAN_POINT ( 'NONE',  ( 10.00000000000000178, 142.0833333265053966, -2.679491924311226736 ) ) ;
#39595 = CARTESIAN_POINT ( 'NONE',  ( -7.188101187500000044, 105.0312500020483810, 0.000000000000000000 ) ) ;
#39596 = CARTESIAN_POINT ( 'NONE',  ( 9.000000000000000000, 5.196152422706622254, -10.20000000000000284 ) ) ;
#39597 = CARTESIAN_POINT ( 'NONE',  ( -3.042071309553173730, 34.63541666325269119, 11.35316468749999785 ) ) ;
#39598 = CARTESIAN_POINT ( 'NONE',  ( -8.660254037844387298, 78.95833332650536818, -5.000000000000004441 ) ) ;
#39599 = CARTESIAN_POINT ( 'NONE',  ( 11.35316468750000141, 185.7812499965860411, 0.000000000000000000 ) ) ;
#39600 = ORIENTED_EDGE ( 'NONE', *, *, #53355, .F. ) ;
#39601 = CARTESIAN_POINT ( 'NONE',  ( 48.91597330207462591, 140.3719646824568201, 59.81383913423206877 ) ) ;
#39602 = CARTESIAN_POINT ( 'NONE',  ( 4.220049686691941027, -10.18810118749999738, 72.62500000204836681 ) ) ;
#39603 = CARTESIAN_POINT ( 'NONE',  ( 4.000000000000015987, 197.4375000000000000, 199.6568542494924259 ) ) ;
#39604 = DIRECTION ( 'NONE',  ( 1.000000000000000000, -0.000000000000000000, -0.000000000000000000 ) ) ;
#39606 = CARTESIAN_POINT ( 'NONE',  ( 3.042071309553159519, 164.7395833299193271, 11.35316468750000141 ) ) ;
#39605 = CARTESIAN_POINT ( 'NONE',  ( 5.000000000000000000, 52.35862550122891435, 48.98731492261470777 ) ) ;
#39607 = CARTESIAN_POINT ( 'NONE',  ( 3.313708498984756279, 7.999999999999991118, 4.917802784329824206 ) ) ;
#39608 = CARTESIAN_POINT ( 'NONE',  ( 2.249999999999997335, 255.9999999999998295, 5.427273999917215264 ) ) ;
#39609 = CARTESIAN_POINT ( 'NONE',  ( 8.311093377946839666, 225.7812500034140157, 8.311093377946829008 ) ) ;
#39610 = DIRECTION ( 'NONE',  ( 0.000000000000000000, 0.000000000000000000, 1.000000000000000000 ) ) ;
#39611 = CARTESIAN_POINT ( 'NONE',  ( 10.18810118749999916, 4.220049686691935698, 79.37500000204838102 ) ) ;
#39612 = ORIENTED_EDGE ( 'NONE', *, *, #23362, .T. ) ;
#39613 =( BOUNDED_CURVE ( )  B_SPLINE_CURVE ( 1, ( #64484, #53164 ),
 .UNSPECIFIED., .F., .F. ) 
 B_SPLINE_CURVE_WITH_KNOTS ( ( 2, 2 ),
 ( 0.000000000000000000, 1.000000000000000000 ),
 .UNSPECIFIED. ) 
 CURVE ( )  GEOMETRIC_REPRESENTATION_ITEM ( )  RATIONAL_B_SPLINE_CURVE ( ( 0.9660720450733824016, 0.9660720450733824016 ) ) 
 REPRESENTATION_ITEM ( '' )  );
#39614 = DIRECTION ( 'NONE',  ( -0.000000000000000000, 1.000000000000000000, -0.000000000000000000 ) ) ;
#39615 = CARTESIAN_POINT ( 'NONE',  ( -11.35316468749999785, 113.3854166632526841, -3.042071309553167513 ) ) ;
#39616 = CARTESIAN_POINT ( 'NONE',  ( 7.320508075688771044, 11.24999999317203248, 7.320508075688775484 ) ) ;
#39617 = ORIENTED_EDGE ( 'NONE', *, *, #36248, .F. ) ;
#39618 = EDGE_LOOP ( 'NONE', ( #62154, #52713, #57535, #8348 ) ) ;
#39619 = CARTESIAN_POINT ( 'NONE',  ( 2.780723358947928197E-16, 8.687499998634407916, -4.541265875000002339 ) ) ;
#39620 = CARTESIAN_POINT ( 'NONE',  ( -7.188101187500002709, 13.31249999795161187, 2.977408999572649151 ) ) ;
#39621 = CARTESIAN_POINT ( 'NONE',  ( 1.469576158976823947E-15, 112.0625000040967905, 8.000000000000000000 ) ) ;
#39622 = EDGE_CURVE ( 'NONE', #16277, #49691, #47307, .T. ) ;
#39623 = CARTESIAN_POINT ( 'NONE',  ( -24.54126587499998280, 198.3750000013655779, 171.4326545832179818 ) ) ;
#39624 = CIRCLE ( 'NONE', #7096, 18.00000000000000000 ) ;
#39625 = EDGE_CURVE ( 'NONE', #1761, #44090, #55031, .T. ) ;
#39626 = CARTESIAN_POINT ( 'NONE',  ( -4.000000000000002665, 8.562500000000001776, 1.656854249492380804 ) ) ;
#39627 = FACE_OUTER_BOUND ( 'NONE', #4920, .T. ) ;
#39628 = CARTESIAN_POINT ( 'NONE',  ( 4.541265875000002339, 7.312499998634407028, 0.000000000000000000 ) ) ;
#39629 = CARTESIAN_POINT ( 'NONE',  ( 3.999999999999960032, 197.9375000000000000, 143.6568542494924543 ) ) ;
#39630 = ORIENTED_EDGE ( 'NONE', *, *, #51227, .T. ) ;
#39631 = CARTESIAN_POINT ( 'NONE',  ( 8.660254037844385522, 222.9166666666666856, -5.000000000000003553 ) ) ;
#39632 = CARTESIAN_POINT ( 'NONE',  ( 1.320432766682874540E-15, 103.5312500020483810, 7.188101187500000044 ) ) ;
#39633 = ADVANCED_FACE ( 'NONE', ( #56440 ), #57184, .T. ) ;
#39635 = CARTESIAN_POINT ( 'NONE',  ( -5.656854249492378806, 123.6875000000000000, 5.656854249492381470 ) ) ;
#39634 = FACE_OUTER_BOUND ( 'NONE', #21292, .T. ) ;
#39636 = CARTESIAN_POINT ( 'NONE',  ( 6.123233995736767268E-16, 113.1249999931720396, -10.00000000000000178 ) ) ;
#39637 = CARTESIAN_POINT ( 'NONE',  ( 2.977408999572646486, 7.188101187499991163, 2.517802781871750550 ) ) ;
#39638 = ORIENTED_EDGE ( 'NONE', *, *, #47764, .T. ) ;
#39639 = VERTEX_POINT ( 'NONE', #50763 ) ;
#39640 = CARTESIAN_POINT ( 'NONE',  ( 4.220049686691941027, -10.18810118749999738, 93.62500000204838102 ) ) ;
#39641 = CARTESIAN_POINT ( 'NONE',  ( 8.000000000000000000, 91.43750000409679046, -9.797174393178825657E-16 ) ) ;
#39642 = CARTESIAN_POINT ( 'NONE',  ( -26.56734541678238060, 200.6250000013656063, 166.5412658750003629 ) ) ;
#39643 = CARTESIAN_POINT ( 'NONE',  ( -11.00000000000000000, 4.556349186104045934, 108.9062500000000000 ) ) ;
#39644 = CARTESIAN_POINT ( 'NONE',  ( -3.458734124999960358, 201.6875000013656063, 198.0000000000000284 ) ) ;
#39646 = CARTESIAN_POINT ( 'NONE',  ( -2.679491924311337314, 253.9583333333333997, -9.999999999999936051 ) ) ;
#39645 = DIRECTION ( 'NONE',  ( -0.000000000000000000, -0.000000000000000000, -1.000000000000000000 ) ) ;
#39647 = CARTESIAN_POINT ( 'NONE',  ( -2.679491924311225848, 121.4583333333333428, -10.00000000000000178 ) ) ;
#39648 = CARTESIAN_POINT ( 'NONE',  ( -5.656854249492380582, 105.3125000000000000, -5.656854249492380582 ) ) ;
#39649 = CARTESIAN_POINT ( 'NONE',  ( 1.226468279477575784E-15, 287.8593750017070079, 6.676582343750001591 ) ) ;
#39650 = CARTESIAN_POINT ( 'NONE',  ( -2.977408999572648707, -7.188101187499990274, 6.642802781871754547 ) ) ;
#39651 = DIRECTION ( 'NONE',  ( -0.000000000000000000, 1.000000000000000000, -0.000000000000000000 ) ) ;
#39652 = CARTESIAN_POINT ( 'NONE',  ( 30.44569435410879521, 208.5625000013656063, 172.4456943541087526 ) ) ;
#39653 = CARTESIAN_POINT ( 'NONE',  ( 8.000000000000000000, 26.90624999590322730, -3.313708498984761608 ) ) ;
#39654 = CARTESIAN_POINT ( 'NONE',  ( 3.458734124999959025, 200.5000000013655779, 140.5673454167824161 ) ) ;
#39655 = CARTESIAN_POINT ( 'NONE',  ( -5.082755093536324154, 120.2187500020483952, 5.082755093536326818 ) ) ;
#39657 = CARTESIAN_POINT ( 'NONE',  ( -2.754378923186476579E-14, 201.4375000013656063, 145.4587341250000350 ) ) ;
#39656 = CARTESIAN_POINT ( 'NONE',  ( -4.000000000000015987, 204.5000000000000284, 142.0000000000000568 ) ) ;
#39658 = CARTESIAN_POINT ( 'NONE',  ( 11.35316468749999608, 246.9270833367472733, -3.042071309553167069 ) ) ;
#39659 = CARTESIAN_POINT ( 'NONE',  ( -5.000000000000005329, 215.2083333265053682, 8.660254037844387298 ) ) ;
#39660 = CARTESIAN_POINT ( 'NONE',  ( 25.17157287525381548, 200.6250000000000284, 167.1715728752537018 ) ) ;
#39661 = CARTESIAN_POINT ( 'NONE',  ( -2.085542519210945728E-15, 19.53124999658601979, 11.35316468750000141 ) ) ;
#39662 = CARTESIAN_POINT ( 'NONE',  ( 5.082755093536318824, 5.082755093536319713, 1.299052781871753215 ) ) ;
#39663 = CARTESIAN_POINT ( 'NONE',  ( 11.35316468749999963, 211.3020833299193839, -3.042071309553165293 ) ) ;
#39664 = CARTESIAN_POINT ( 'NONE',  ( -4.999999999999998224, 133.5416666598387110, -8.660254037844389075 ) ) ;
#39666 = CARTESIAN_POINT ( 'NONE',  ( -10.99999999999992184, -31.99999999998497202, 140.5079502042485728 ) ) ;
#39665 = CARTESIAN_POINT ( 'NONE',  ( -25.17157287525377640, 205.6250000000000284, 172.8284271247465256 ) ) ;
#39667 = VERTEX_POINT ( 'NONE', #231 ) ;
#39668 = CARTESIAN_POINT ( 'NONE',  ( -3.458734125000015869, 200.1875000013656063, 142.0000000000000568 ) ) ;
#39669 = CARTESIAN_POINT ( 'NONE',  ( 8.311093377946837890, 21.40624999658601268, -8.311093377946837890 ) ) ;
#39670 = CARTESIAN_POINT ( 'NONE',  ( 4.556349186104051263, -10.99999999999999822, 90.15625000409677625 ) ) ;
#39671 = DIRECTION ( 'NONE',  ( 0.000000000000000000, 0.000000000000000000, 1.000000000000000000 ) ) ;
#39672 = CARTESIAN_POINT ( 'NONE',  ( -25.55430564589111597, 197.0625000013656063, 172.4456943541091505 ) ) ;
#39673 = LINE ( 'NONE', #45697, #28628 ) ;
#39675 = CARTESIAN_POINT ( 'NONE',  ( 8.311093377946837890, 6.406249996586016238, -8.311093377946837890 ) ) ;
#39674 = CARTESIAN_POINT ( 'NONE',  ( -5.082755093536325930, 108.9687500020483810, -5.082755093536325930 ) ) ;
#39676 = CARTESIAN_POINT ( 'NONE',  ( 5.656854249492374365, 5.656854249492375253, 22.76780277982336642 ) ) ;
#39677 = CARTESIAN_POINT ( 'NONE',  ( 3.042071309553167069, 136.8229166632526699, -11.35316468749999785 ) ) ;
#39678 = CARTESIAN_POINT ( 'NONE',  ( -2.679491924311235618, 105.4166666598387110, 10.00000000000000000 ) ) ;
#39679 = CARTESIAN_POINT ( 'NONE',  ( -7.188101187500001821, 121.4375000020483668, -2.977408999572650483 ) ) ;
#39680 = CARTESIAN_POINT ( 'NONE',  ( -2.679491924311235174, 5.416666659838698550, 10.00000000000000000 ) ) ;
#39681 = CARTESIAN_POINT ( 'NONE',  ( 7.999999999999991118, 3.377145119393935320E-05, 0.2678037393673578515 ) ) ;
#39682 = VERTEX_POINT ( 'NONE', #73778 ) ;
#39683 = CARTESIAN_POINT ( 'NONE',  ( 1.780377099648655870, -67.71330631781141562, 20.13219356122130677 ) ) ;
#39684 = CARTESIAN_POINT ( 'NONE',  ( 6.123233995736767268E-16, 153.1249999931720538, -10.00000000000000178 ) ) ;
#39685 = CARTESIAN_POINT ( 'NONE',  ( 6.676582343750004256, 289.0468750017070079, 2.765530957081995478 ) ) ;
#39686 = CARTESIAN_POINT ( 'NONE',  ( -5.656854249492375253, 5.656854249492375253, 23.19905278432982598 ) ) ;
#39687 = CARTESIAN_POINT ( 'NONE',  ( -2.751064625579944321E-14, 197.7500000000000000, 146.0000000000000284 ) ) ;
#39688 = VECTOR ( 'NONE', #4221, 1000.000000000000227 ) ;
#39689 = CARTESIAN_POINT ( 'NONE',  ( -6.951808397369817780E-16, 262.6562500034140157, -11.35316468749999963 ) ) ;
#39690 = CARTESIAN_POINT ( 'NONE',  ( -7.204075437095967871, 7.204075437095967871, 99.34375000204836681 ) ) ;
#39691 = ORIENTED_EDGE ( 'NONE', *, *, #26336, .F. ) ;
#39692 = EDGE_CURVE ( 'NONE', #41682, #33654, #42013, .T. ) ;
#39693 = CARTESIAN_POINT ( 'NONE',  ( 8.660254037844385522, 216.4583333265053682, 5.000000000000005329 ) ) ;
#39694 = CARTESIAN_POINT ( 'NONE',  ( -15.99999999999998579, 237.9999999999999716, 0.000000000000000000 ) ) ;
#39695 = CARTESIAN_POINT ( 'NONE',  ( 3.458734125000015869, 202.1875000013656063, 198.0000000000000284 ) ) ;
#39696 = CARTESIAN_POINT ( 'NONE',  ( 11.35316468749999963, 81.30208332991935549, -3.042071309553165293 ) ) ;
#39698 = EDGE_LOOP ( 'NONE', ( #12981, #71988, #8801, #12439 ) ) ;
#39697 =( BOUNDED_CURVE ( )  B_SPLINE_CURVE ( 2, ( #7357, #12995, #47337, #23960, #46967, #52641, #54120, #19395, #71078, #25049, #12271, #70718, #69997 ),
 .UNSPECIFIED., .F., .F. ) 
 B_SPLINE_CURVE_WITH_KNOTS ( ( 3, 2, 2, 2, 2, 2, 3 ),
 ( 0.3097826086956522174, 0.3115942028985507761, 0.3134057971014493349, 0.3152173913043478937, 0.3170289855072464524, 0.3188405797101449557, 0.3206521739130435145 ),
 .UNSPECIFIED. ) 
 CURVE ( )  GEOMETRIC_REPRESENTATION_ITEM ( )  RATIONAL_B_SPLINE_CURVE ( ( 0.9999999999999990008, 0.9659258262890693114, 1.000000000000000000, 0.9659258262890683122, 1.000000000000000000, 0.9659258262890683122, 1.000000000000000000, 0.9659258262890683122, 1.000000000000000000, 0.9659258262890683122, 1.000000000000000000, 0.9659258262890673130, 1.000000000000001110 ) ) 
 REPRESENTATION_ITEM ( '' )  );
#39699 = CARTESIAN_POINT ( 'NONE',  ( 7.204075437095966983, 7.204075437095967871, 106.0937500020483810 ) ) ;
#39700 = CARTESIAN_POINT ( 'NONE',  ( -1.881053915767124440, 12.12499999863440792, 4.541265875000001451 ) ) ;
#39701 = VERTEX_POINT ( 'NONE', #39819 ) ;
#39702 = CARTESIAN_POINT ( 'NONE',  ( 5.082755093536325930, 26.15624999795161543, -5.082755093536325930 ) ) ;
#39703 = CARTESIAN_POINT ( 'NONE',  ( 8.660254037844385522, 114.5833333333333712, 5.000000000000005329 ) ) ;
#39704 = CARTESIAN_POINT ( 'NONE',  ( -5.000000000000000000, -68.60357193678697740, -20.85024232999374050 ) ) ;
#39705 = CARTESIAN_POINT ( 'NONE',  ( 4.401442555609581635E-16, 22.21874999795161543, -7.188101187500000044 ) ) ;
#39706 = CARTESIAN_POINT ( 'NONE',  ( 0.000000000000000000, 125.0000000000000000, 0.000000000000000000 ) ) ;
#39707 = CARTESIAN_POINT ( 'NONE',  ( 10.18810118749999916, 1.247682550866122264E-15, 110.7812500020483668 ) ) ;
#39708 = PRODUCT ( 'body', 'body', '', ( #10128 ) ) ;
#39709 = CARTESIAN_POINT ( 'NONE',  ( 8.660254037844380193, 109.5833333333333428, 5.000000000000002665 ) ) ;
#39710 = CARTESIAN_POINT ( 'NONE',  ( 4.000000000000000888, 8.687499997268814056, 1.656854249492384135 ) ) ;
#39711 = DIRECTION ( 'NONE',  ( -0.000000000000000000, 1.000000000000000000, -1.563033456626094573E-30 ) ) ;
#39712 = ORIENTED_EDGE ( 'NONE', *, *, #27010, .T. ) ;
#39713 = EDGE_CURVE ( 'NONE', #48764, #45738, #62824, .T. ) ;
#39714 = EDGE_CURVE ( 'NONE', #49924, #35571, #49733, .T. ) ;
#39715 = CARTESIAN_POINT ( 'NONE',  ( 2.445694354108839619, 201.8125000013656063, 200.4456943541088663 ) ) ;
#39716 = CARTESIAN_POINT ( 'NONE',  ( -31.45873412500002431, 205.6250000013656063, 168.5673454167828140 ) ) ;
#39717 = CARTESIAN_POINT ( 'NONE',  ( -3.211159895383561391, 8.687499998634407916, -3.211159895383561835 ) ) ;
#39718 = AXIS2_PLACEMENT_3D ( 'NONE', #29107, #50619, #63058 ) ;
#39719 = CARTESIAN_POINT ( 'NONE',  ( -4.000000000000015987, 206.6875000027312694, 143.6568542494924259 ) ) ;
#39720 = CARTESIAN_POINT ( 'NONE',  ( 7.188101187499991163, 2.977408999572648707, 20.33030278187175455 ) ) ;
#39721 = ORIENTED_EDGE ( 'NONE', *, *, #6712, .T. ) ;
#39722 = LINE ( 'NONE', #1521, #37354 ) ;
#39723 = ORIENTED_EDGE ( 'NONE', *, *, #21735, .F. ) ;
#39724 = CARTESIAN_POINT ( 'NONE',  ( -4.220049686691935698, 10.18810118749999916, 112.3750000020483810 ) ) ;
#39725 = CARTESIAN_POINT ( 'NONE',  ( -4.000000000000001776, 18.43750000000000000, -1.656854249492381470 ) ) ;
#39726 = CARTESIAN_POINT ( 'NONE',  ( 2.445694354108839619, 201.8125000013656063, 200.4456943541088663 ) ) ;
#39727 = CARTESIAN_POINT ( 'NONE',  ( -10.00000000000000178, 87.50000000000001421, -1.224646799147353454E-15 ) ) ;
#39728 = AXIS2_PLACEMENT_3D ( 'NONE', #3944, #9601, #9217 ) ;
#39729 = CARTESIAN_POINT ( 'NONE',  ( 8.000000000000000000, 121.3437500000000000, -3.313708498984762496 ) ) ;
#39730 = CARTESIAN_POINT ( 'NONE',  ( 4.721056650415999201, 298.2343750017069510, -4.721056650415999201 ) ) ;
#39731 = ADVANCED_FACE ( 'NONE', ( #46224 ), #7720, .T. ) ;
#39732 = ORIENTED_EDGE ( 'NONE', *, *, #63680, .T. ) ;
#39733 = CARTESIAN_POINT ( 'NONE',  ( 1.656854249492470732, 203.6875000000000000, 194.0000000000001421 ) ) ;
#39734 = CARTESIAN_POINT ( 'NONE',  ( -3.734423912265183887, -66.26963445013821286, 26.58791153593155343 ) ) ;
#39735 = CARTESIAN_POINT ( 'NONE',  ( 3.999999999999960032, 195.0625000027312126, 143.6568542494924543 ) ) ;
#39736 = CARTESIAN_POINT ( 'NONE',  ( -5.000000000000000888, 61.23620218020138140, 23.51718915682135957 ) ) ;
#39737 = CARTESIAN_POINT ( 'NONE',  ( -3.313708498984765161, 23.53125000000000355, 7.999999999999998224 ) ) ;
#39738 = CARTESIAN_POINT ( 'NONE',  ( -10.00000000000000000, 235.0000000000000284, 0.000000000000000000 ) ) ;
#39739 = CARTESIAN_POINT ( 'NONE',  ( 5.000000000000000000, -70.11723469343094450, -28.93519894129240910 ) ) ;
#39740 = CARTESIAN_POINT ( 'NONE',  ( 7.320508075688771044, 204.3750000000000000, 7.320508075688775484 ) ) ;
#39741 = CARTESIAN_POINT ( 'NONE',  ( -2.977408999572647819, -7.188101187499990274, 18.64280278187176521 ) ) ;
#39742 = CARTESIAN_POINT ( 'NONE',  ( 9.832129032723420536, 166.5104166632526983, -5.676582343749999815 ) ) ;
#39743 = FACE_OUTER_BOUND ( 'NONE', #71249, .T. ) ;
#39744 = CARTESIAN_POINT ( 'NONE',  ( -1.836970198721029983E-15, 175.6249999931720538, 10.00000000000000178 ) ) ;
#39745 = ORIENTED_EDGE ( 'NONE', *, *, #13151, .F. ) ;
#39746 = CARTESIAN_POINT ( 'NONE',  ( -2.754378923186476579E-14, 197.1875000013655779, 145.4587341250000350 ) ) ;
#39747 = CARTESIAN_POINT ( 'NONE',  ( -11.35316468749999785, 28.38541666325268054, -3.042071309553167513 ) ) ;
#39748 = CARTESIAN_POINT ( 'NONE',  ( 4.556349186104051263, -10.99999999999999822, 111.1562500040967620 ) ) ;
#39749 = CARTESIAN_POINT ( 'NONE',  ( -3.240027456986786625, 194.4836769270507091, 199.2972688138627575 ) ) ;
#39750 = DIRECTION ( 'NONE',  ( -1.000000000000000000, 0.000000000000000000, 0.000000000000000000 ) ) ;
#39752 = CARTESIAN_POINT ( 'NONE',  ( -1.317228840348697361, -10.12208498181994543, -70.14472670972902790 ) ) ;
#39751 = CARTESIAN_POINT ( 'NONE',  ( 0.000000000000000000, 300.0000000000000000, 0.000000000000000000 ) ) ;
#39753 = CARTESIAN_POINT ( 'NONE',  ( -15.55551651078417663, -44.71496288649983342, 196.8168351944428878 ) ) ;
#39754 = CARTESIAN_POINT ( 'NONE',  ( 1.432654583217607192, 199.2500000013656063, 145.4587341250000350 ) ) ;
#39755 = CARTESIAN_POINT ( 'NONE',  ( 10.00000000000000000, 66.66666665983871098, 2.679491924311236062 ) ) ;
#39756 = CARTESIAN_POINT ( 'NONE',  ( 2.977408999572650039, 101.1875000020483810, -7.188101187500001821 ) ) ;
#39757 = CARTESIAN_POINT ( 'NONE',  ( -4.541265875000002339, 12.93749999863440792, -5.561446717895856393E-16 ) ) ;
#39758 = CARTESIAN_POINT ( 'NONE',  ( 10.00000000000022204, 215.2083333333334849, -2.679491924311286688 ) ) ;
#39759 = CARTESIAN_POINT ( 'NONE',  ( -5.867882488397293095, -5.445826010587458299, 1.009359473472040802 ) ) ;
#39760 = CARTESIAN_POINT ( 'NONE',  ( 2.124081043562912718, -50.03790111639220584, 40.75706181777475479 ) ) ;
#39761 = ORIENTED_EDGE ( 'NONE', *, *, #36552, .T. ) ;
#39762 = ORIENTED_EDGE ( 'NONE', *, *, #38622, .T. ) ;
#39763 = CARTESIAN_POINT ( 'NONE',  ( 2.849036369511732440E-14, 205.3750000027312126, 202.0000000000000000 ) ) ;
#39764 = CARTESIAN_POINT ( 'NONE',  ( 2.445694354108839175, 195.3125000013656063, 195.5543056458912190 ) ) ;
#39765 = FILL_AREA_STYLE_COLOUR ( '', #5016 ) ;
#39766 = DIRECTION ( 'NONE',  ( 1.000000000000000000, 0.000000000000000000, 0.000000000000000000 ) ) ;
#39767 = CARTESIAN_POINT ( 'NONE',  ( -9.832129032723418760, 147.8645833299193555, -5.676582343750004256 ) ) ;
#39768 = CARTESIAN_POINT ( 'NONE',  ( -8.000000000000001776, 0.8437500000000000000, 3.313708498984759387 ) ) ;
#39769 = CARTESIAN_POINT ( 'NONE',  ( 1.871523826299183495E-15, -10.18810118749999916, 87.53125000204836681 ) ) ;
#39770 = CARTESIAN_POINT ( 'NONE',  ( 0.000000000000000000, 300.0000000000000000, 10.00000000000000178 ) ) ;
#39771 = CARTESIAN_POINT ( 'NONE',  ( 4.000000000000015987, 209.5000000000000284, 198.0000000000000284 ) ) ;
#39772 = DIRECTION ( 'NONE',  ( 0.000000000000000000, 0.000000000000000000, -1.000000000000000000 ) ) ;
#39773 = CARTESIAN_POINT ( 'NONE',  ( -30.82842712474624136, 197.2500000027312126, 167.1715728752542418 ) ) ;
#39774 = CARTESIAN_POINT ( 'NONE',  ( -5.656854249492378806, 101.1875000000000000, 5.656854249492381470 ) ) ;
#39775 = EDGE_LOOP ( 'NONE', ( #52411, #57810, #41259, #57048 ) ) ;
#39776 = VECTOR ( 'NONE', #53183, 1000.000000000000000 ) ;
#39777 = CARTESIAN_POINT ( 'NONE',  ( 11.00000000000000000, 1.347111479062088405E-15, 118.0000000000000000 ) ) ;
#39778 = CARTESIAN_POINT ( 'NONE',  ( -5.230138811818777711, 178.6826066192510609, 133.6529148158666942 ) ) ;
#39779 = CARTESIAN_POINT ( 'NONE',  ( -8.311093377946841443, 129.2187499965860127, 8.311093377946834337 ) ) ;
#39780 = CARTESIAN_POINT ( 'NONE',  ( -1.432654583217607192, 203.2500000013655495, 194.5412658750000219 ) ) ;
#39781 = CARTESIAN_POINT ( 'NONE',  ( -7.188101187500000044, 22.59374999795161187, -8.802885111219163269E-16 ) ) ;
#39782 = CARTESIAN_POINT ( 'NONE',  ( 1.871523826299183495E-15, -10.18810118749999916, 83.40625000204838102 ) ) ;
#39783 = CARTESIAN_POINT ( 'NONE',  ( -9.832129032723420536, 34.01041666325269119, 5.676582343749997150 ) ) ;
#39784 = ORIENTED_EDGE ( 'NONE', *, *, #48591, .F. ) ;
#39785 = CARTESIAN_POINT ( 'NONE',  ( 1.469576158976823947E-15, 97.06250000409677625, 8.000000000000000000 ) ) ;
#39786 = CARTESIAN_POINT ( 'NONE',  ( -7.999999999999991118, -1.288204405367768053E-10, 8.517802783929960597 ) ) ;
#39787 = CARTESIAN_POINT ( 'NONE',  ( 8.008118988124993010, -3.317071493978877239, 19.66936528394063544 ) ) ;
#39788 = CARTESIAN_POINT ( 'NONE',  ( -2.754378923186476579E-14, 206.4375000013656063, 145.4587341250000350 ) ) ;
#39789 = AXIS2_PLACEMENT_3D ( 'NONE', #22857, #74170, #50788 ) ;
#39790 = EDGE_CURVE ( 'NONE', #26710, #3422, #30724, .T. ) ;
#39791 = CARTESIAN_POINT ( 'NONE',  ( 5.082755093536324154, 6.281249997951610986, 5.082755093536326818 ) ) ;
#39792 = CARTESIAN_POINT ( 'NONE',  ( 4.242640687119287435, 296.4375000034140157, 4.242640687119285658 ) ) ;
#39793 = CARTESIAN_POINT ( 'NONE',  ( -16.72710596938094341, -17.96556829620605455, 137.3278482264859690 ) ) ;
#39794 = CARTESIAN_POINT ( 'NONE',  ( -1.320432766682874540E-15, 6.468749997951610098, 7.188101187500000044 ) ) ;
#39795 = CARTESIAN_POINT ( 'NONE',  ( -5.676582343750006032, 159.4270833299193555, 9.832129032723418760 ) ) ;
#39796 = CARTESIAN_POINT ( 'NONE',  ( -7.204075437095967871, 7.204075437095967871, 76.46875000204836681 ) ) ;
#39797 = CARTESIAN_POINT ( 'NONE',  ( -25.55430564589114795, 195.0625000013656063, 172.4456943541091789 ) ) ;
#39798 = DIRECTION ( 'NONE',  ( 0.000000000000000000, -1.000000000000000000, -4.476705744456276341E-16 ) ) ;
#39799 = CARTESIAN_POINT ( 'NONE',  ( -1.881053915767121554, 20.74999999863440436, -4.541265875000002339 ) ) ;
#39800 = ORIENTED_EDGE ( 'NONE', *, *, #12218, .T. ) ;
#39801 = EDGE_CURVE ( 'NONE', #61049, #64051, #57461, .T. ) ;
#39802 = CARTESIAN_POINT ( 'NONE',  ( 2.828427124746208943, 199.7500000027312126, 195.1715728752538439 ) ) ;
#39803 = AXIS2_PLACEMENT_3D ( 'NONE', #51330, #10976, #11344 ) ;
#39804 = CARTESIAN_POINT ( 'NONE',  ( 1.656854249492347719, 204.8124999999999716, 146.0000000000000284 ) ) ;
#39806 =( BOUNDED_CURVE ( )  B_SPLINE_CURVE ( 2, ( #24470, #35444, #19541, #36542, #65570, #59553, #7868, #13867, #58455 ),
 .UNSPECIFIED., .F., .F. ) 
 B_SPLINE_CURVE_WITH_KNOTS ( ( 3, 2, 2, 2, 3 ),
 ( 0.5333333333333337700, 0.5416666666666670737, 0.5500000000000004885, 0.5583333333333337922, 0.5666666666666670960 ),
 .UNSPECIFIED. ) 
 CURVE ( )  GEOMETRIC_REPRESENTATION_ITEM ( )  RATIONAL_B_SPLINE_CURVE ( ( 0.9999999999999958922, 0.9238795325112908463, 1.000000000000000000, 0.9238795325112867385, 1.000000000000000000, 0.9238795325112867385, 1.000000000000000000, 0.9238795325112826307, 1.000000000000003997 ) ) 
 REPRESENTATION_ITEM ( '' )  );
#39805 = CARTESIAN_POINT ( 'NONE',  ( -28.00000000000007816, 200.1250000027312126, 166.0000000000003695 ) ) ;
#39807 = EDGE_CURVE ( 'NONE', #29212, #28203, #5898, .T. ) ;
#39808 = CARTESIAN_POINT ( 'NONE',  ( -2.679491924311247164, 56.45833333333338544, -10.00000000000007994 ) ) ;
#39809 = CARTESIAN_POINT ( 'NONE',  ( -3.313708498984757167, 7.999999999999991118, 8.236552783920144449 ) ) ;
#39810 = ORIENTED_EDGE ( 'NONE', *, *, #35871, .T. ) ;
#39811 = CARTESIAN_POINT ( 'NONE',  ( 5.082755093536325930, 18.65624999795161187, -5.082755093536325930 ) ) ;
#39812 = CARTESIAN_POINT ( 'NONE',  ( -13.99999999999999822, 2.249999999994893862, 7.677076266393539683 ) ) ;
#39813 = DIRECTION ( 'NONE',  ( -0.000000000000000000, -0.000000000000000000, 1.000000000000000000 ) ) ;
#39814 = CARTESIAN_POINT ( 'NONE',  ( -10.00000000000000000, 37.29166666666667140, -2.679491924311229845 ) ) ;
#39815 = CARTESIAN_POINT ( 'NONE',  ( 2.977408999572650039, 104.5625000020483668, -7.188101187500001821 ) ) ;
#39816 = CARTESIAN_POINT ( 'NONE',  ( -24.54126587500000767, 209.5000000013656063, 168.5673454167827003 ) ) ;
#39817 = CARTESIAN_POINT ( 'NONE',  ( -0.4320110153365241401, -10.28109898471437589, 63.57214792341211762 ) ) ;
#39818 = EDGE_CURVE ( 'NONE', #61963, #71315, #40621, .T. ) ;
#39820 = CARTESIAN_POINT ( 'NONE',  ( 1.836970198721029589E-15, 259.3750000068280315, 10.00000000000000000 ) ) ;
#39819 = CARTESIAN_POINT ( 'NONE',  ( 27.99999999999996803, 209.6875000013656063, 173.4587341249998929 ) ) ;
#39821 = ORIENTED_EDGE ( 'NONE', *, *, #3252, .F. ) ;
#39823 = CARTESIAN_POINT ( 'NONE',  ( -8.311093377946834337, 249.5312500034139873, 8.311093377946837890 ) ) ;
#39822 = VECTOR ( 'NONE', #47971, 1000.000000000000000 ) ;
#39824 = CARTESIAN_POINT ( 'NONE',  ( 7.188101187499993827, -2.977408999572645598, 19.01780278187175810 ) ) ;
#39825 = CARTESIAN_POINT ( 'NONE',  ( -2.990854866100027820, 55.96051345247528985, 43.98806351443512597 ) ) ;
#39826 = CARTESIAN_POINT ( 'NONE',  ( -10.04313107478231260, 220.0000000000000284, 0.3202752235055294494 ) ) ;
#39827 = CARTESIAN_POINT ( 'NONE',  ( -1.967015505459129087E-11, 148.7499999999984936, 10.00000000000000533 ) ) ;
#39828 = DIRECTION ( 'NONE',  ( -0.000000000000000000, 1.000000000000000000, -0.000000000000000000 ) ) ;
#39829 = CARTESIAN_POINT ( 'NONE',  ( 10.00000000000000000, 159.7916666666666288, 2.679491924311236062 ) ) ;
#39830 = CARTESIAN_POINT ( 'NONE',  ( -7.999999999999991118, 9.797174393178815797E-16, 30.00000000000000000 ) ) ;
#39831 = DIRECTION ( 'NONE',  ( 0.000000000000000000, 0.2588190451025145777, -0.9659258262890699775 ) ) ;
#39832 = CARTESIAN_POINT ( 'NONE',  ( 4.999999999999999112, -51.30401030464736323, -41.49390406302068612 ) ) ;
#39833 = CARTESIAN_POINT ( 'NONE',  ( -9.832129032723420536, 134.0104166632526983, 5.676582343749997150 ) ) ;
#39834 = DIRECTION ( 'NONE',  ( -0.8660254037844379305, 0.5000000000000014433, 0.000000000000000000 ) ) ;
#39835 = CARTESIAN_POINT ( 'NONE',  ( 4.999999999999995559, -16.24494643555759410, -69.83755725260751035 ) ) ;
#39838 = CARTESIAN_POINT ( 'NONE',  ( 3.999999999999959144, 197.0625000000000000, 140.3431457505076594 ) ) ;
#39837 = CARTESIAN_POINT ( 'NONE',  ( 26.56734541678232375, 195.0000000013656063, 166.5412658749999650 ) ) ;
#39836 = CARTESIAN_POINT ( 'NONE',  ( 28.00000000000001776, 196.1875000013655779, 166.5412658749999082 ) ) ;
#39839 = ORIENTED_EDGE ( 'NONE', *, *, #1502, .T. ) ;
#39840 = EDGE_CURVE ( 'NONE', #4108, #46386, #59003, .T. ) ;
#39841 = CIRCLE ( 'NONE', #62714, 7.999999999999991118 ) ;
#39842 = CARTESIAN_POINT ( 'NONE',  ( 8.218888959140699058, 225.4831672038039585, -5.726997447258057150 ) ) ;
#39843 = DIRECTION ( 'NONE',  ( 1.000000000000000000, 0.000000000000000000, 0.000000000000000000 ) ) ;
#39844 = CARTESIAN_POINT ( 'NONE',  ( 23.99999999999998579, 195.8750000027311842, 169.9999999999999432 ) ) ;
#39845 = CARTESIAN_POINT ( 'NONE',  ( 30.44569435410883074, 195.0625000013656063, 167.5543056458911053 ) ) ;
#39846 = ADVANCED_FACE ( 'NONE', ( #35657 ), #58671, .F. ) ;
#39847 = CARTESIAN_POINT ( 'NONE',  ( -11.35316468750000141, 218.5937499965860411, -1.390361679473963753E-15 ) ) ;
#39848 = CARTESIAN_POINT ( 'NONE',  ( -5.082755093536324154, 119.8437500020483810, 5.082755093536326818 ) ) ;
#39849 = CARTESIAN_POINT ( 'NONE',  ( 4.541265875000002339, 0.4999999986344068614, -1.881053915767121554 ) ) ;
#39850 = FACE_OUTER_BOUND ( 'NONE', #56629, .T. ) ;
#39851 = CARTESIAN_POINT ( 'NONE',  ( 7.999999999999991118, 3.313708498984757611, 18.17405277982336642 ) ) ;
#39853 = CARTESIAN_POINT ( 'NONE',  ( -9.000000000000001776, 1.102182119232617911E-15, -10.80000000000000071 ) ) ;
#39852 = DIRECTION ( 'NONE',  ( -1.000000000000000000, 0.000000000000000000, 0.000000000000000000 ) ) ;
#39854 = CARTESIAN_POINT ( 'NONE',  ( -9.832129032723420536, 98.69791666325269830, 5.676582343749997150 ) ) ;
#39855 = ORIENTED_EDGE ( 'NONE', *, *, #27970, .F. ) ;
#39856 = CARTESIAN_POINT ( 'NONE',  ( -1.656854249492388576, 205.4375000027311842, 138.0000000000000000 ) ) ;
#39857 = CARTESIAN_POINT ( 'NONE',  ( 7.188101187499999156, 27.37499999795161187, 2.977408999572654924 ) ) ;
#39858 = DIRECTION ( 'NONE',  ( 0.000000000000000000, -0.4789076340208436311, -0.8778652960885046097 ) ) ;
#39859 = CARTESIAN_POINT ( 'NONE',  ( -8.311093377946836114, 243.5937500034139873, -8.311093377946836114 ) ) ;
#39860 = CARTESIAN_POINT ( 'NONE',  ( 8.311093377946834337, 100.1562499965860127, 8.311093377946839666 ) ) ;
#39861 = VERTEX_POINT ( 'NONE', #2055 ) ;
#39862 = B_SPLINE_CURVE_WITH_KNOTS ( 'NONE', 3,
 ( #51912, #30014, #1357, #70377, #35321, #51529, #45871, #34579, #34952, #74546, #63219, #46980 ),
 .UNSPECIFIED., .F., .F.,
 ( 4, 2, 2, 2, 2, 4 ),
 ( 0.000000000000000000, 0.002547658444427998263, 0.005095316888855995659, 0.006369146111069994357, 0.007642975333283993054, 0.01019063377771198611 ),
 .UNSPECIFIED. ) ;
#39863 = CARTESIAN_POINT ( 'NONE',  ( 5.000000000000000000, -11.43937387734352029, 68.01947305042915559 ) ) ;
#39864 = CARTESIAN_POINT ( 'NONE',  ( 7.204075437095966983, 7.204075437095967871, 107.5937500020483810 ) ) ;
#39865 = CARTESIAN_POINT ( 'NONE',  ( -7.320508075688778149, 214.9999999931720254, 7.320508075688769267 ) ) ;
#39866 = CARTESIAN_POINT ( 'NONE',  ( -2.445694354108783219, 204.8125000013656063, 200.4456943541088663 ) ) ;
#39867 = CYLINDRICAL_SURFACE ( 'NONE', #52877, 3.999999999999976019 ) ;
#39869 = CARTESIAN_POINT ( 'NONE',  ( 3.042071309553167513, 101.8229166632526699, -11.35316468749999785 ) ) ;
#39868 = DIRECTION ( 'NONE',  ( -0.000000000000000000, -1.000000000000000000, -0.000000000000000000 ) ) ;
#39870 = CARTESIAN_POINT ( 'NONE',  ( -3.313708498984758943, -7.999999999999989342, 13.29905278392014800 ) ) ;
#39871 = CARTESIAN_POINT ( 'NONE',  ( -25.55430564589114795, 195.3125000013656063, 172.4456943541091789 ) ) ;
#39872 = CARTESIAN_POINT ( 'NONE',  ( 7.320508075688834992, 174.3750000000000284, 7.320508075688839433 ) ) ;
#39873 = VERTEX_POINT ( 'NONE', #1338 ) ;
#39874 = CARTESIAN_POINT ( 'NONE',  ( 5.000000000000001776, 177.7083333265053682, -8.660254037844389075 ) ) ;
#39875 = CARTESIAN_POINT ( 'NONE',  ( 4.000000000000001776, 6.062500000000000000, -1.656854249492381248 ) ) ;
#39876 = CARTESIAN_POINT ( 'NONE',  ( 4.000000000000001776, 9.749999997268814056, 0.000000000000000000 ) ) ;
#39877 = CARTESIAN_POINT ( 'NONE',  ( 8.311093377946837890, 91.71874999658601268, -8.311093377946837890 ) ) ;
#39878 = CARTESIAN_POINT ( 'NONE',  ( 6.676582343750001591, 290.9531250017069510, -8.176455196517173205E-16 ) ) ;
#39879 = CARTESIAN_POINT ( 'NONE',  ( -2.977408999572650039, 7.312499997951610986, -7.188101187500000933 ) ) ;
#39880 = CARTESIAN_POINT ( 'NONE',  ( -10.18810118749999916, 0.000000000000000000, 104.0312500020483810 ) ) ;
#39881 = CARTESIAN_POINT ( 'NONE',  ( -8.311093377946836114, 217.6562499965860127, -8.311093377946837890 ) ) ;
#39882 = ORIENTED_EDGE ( 'NONE', *, *, #1902, .T. ) ;
#39883 = CARTESIAN_POINT ( 'NONE',  ( -2.828427124746190735, 1.124999997268813390, -2.828427124746191623 ) ) ;
#39884 = CARTESIAN_POINT ( 'NONE',  ( 8.000000000000000000, 115.4375000040967763, -9.797174393178825657E-16 ) ) ;
#39885 = CARTESIAN_POINT ( 'NONE',  ( 11.35316468750000141, 225.7812499965860127, 0.000000000000000000 ) ) ;
#39886 = CARTESIAN_POINT ( 'NONE',  ( 6.123233995736767268E-16, 123.1249999931720396, -10.00000000000000178 ) ) ;
#39887 = CARTESIAN_POINT ( 'NONE',  ( 2.679491924302094485, 198.9583333333325186, 10.00000000000527400 ) ) ;
#39888 = CARTESIAN_POINT ( 'NONE',  ( -6.676582343750003368, 298.3906250017070079, -2.765530957081996810 ) ) ;
#39889 = ORIENTED_EDGE ( 'NONE', *, *, #57548, .F. ) ;
#39890 = CARTESIAN_POINT ( 'NONE',  ( -8.311093377946841443, 209.2187499965859843, 8.311093377946834337 ) ) ;
#39891 = CARTESIAN_POINT ( 'NONE',  ( 1.871523826299183495E-15, -10.18810118749999916, 93.53125000204836681 ) ) ;
#39892 = EDGE_CURVE ( 'NONE', #17643, #66510, #24320, .T. ) ;
#39893 = CARTESIAN_POINT ( 'NONE',  ( -31.45873412499999944, 207.6875000013656063, 170.0000000000003979 ) ) ;
#39894 = CARTESIAN_POINT ( 'NONE',  ( 8.000000000000000000, 16.50000000000000355, 0.000000000000000000 ) ) ;
#39895 = ORIENTED_EDGE ( 'NONE', *, *, #16914, .T. ) ;
#39896 = CIRCLE ( 'NONE', #59196, 11.00000000000000000 ) ;
#39897 = CARTESIAN_POINT ( 'NONE',  ( -5.082755093536325930, 122.4687500020483952, -5.082755093536325930 ) ) ;
#39898 = LINE ( 'NONE', #69694, #46465 ) ;
#39899 = CARTESIAN_POINT ( 'NONE',  ( 6.123233995736767268E-16, 21.25000000000000000, -10.00000000000000178 ) ) ;
#39900 = EDGE_CURVE ( 'NONE', #63985, #26525, #2777, .T. ) ;
#39901 = CARTESIAN_POINT ( 'NONE',  ( -5.000000000000000000, 13.21930962315089353, 69.49101004078882227 ) ) ;
#39902 = CARTESIAN_POINT ( 'NONE',  ( -10.18810118749999916, 4.220049686691934809, 82.93750000204838102 ) ) ;
#39904 = VERTEX_POINT ( 'NONE', #49179 ) ;
#39903 =( BOUNDED_CURVE ( )  B_SPLINE_CURVE ( 2, ( #43564, #72995, #43190, #26204, #61677, #14511, #50346, #26962, #21302 ),
 .UNSPECIFIED., .F., .F. ) 
 B_SPLINE_CURVE_WITH_KNOTS ( ( 3, 2, 2, 2, 3 ),
 ( 0.4705882352941177516, 0.4742647058823530326, 0.4779411764705883692, 0.4816176470588236502, 0.4852941176470589313 ),
 .UNSPECIFIED. ) 
 CURVE ( )  GEOMETRIC_REPRESENTATION_ITEM ( )  RATIONAL_B_SPLINE_CURVE ( ( 0.9999999999999976685, 0.9238795325112890700, 1.000000000000000000, 0.9238795325112867385, 1.000000000000000000, 0.9238795325112867385, 1.000000000000000000, 0.9238795325112844070, 1.000000000000002220 ) ) 
 REPRESENTATION_ITEM ( '' )  );
#39905 = CARTESIAN_POINT ( 'NONE',  ( -1.656854249492383691, 19.68749999999999645, 4.000000000000000888 ) ) ;
#39906 = CARTESIAN_POINT ( 'NONE',  ( 7.188101187500000933, 0.5624999979516099868, -2.977408999572650483 ) ) ;
#39907 = AXIS2_PLACEMENT_3D ( 'NONE', #4316, #9604, #60525 ) ;
#39908 = CARTESIAN_POINT ( 'NONE',  ( 31.50809115661295223, 194.5826323124041153, 170.7610556930222003 ) ) ;
#39909 = LINE ( 'NONE', #21432, #47484 ) ;
#39910 = CARTESIAN_POINT ( 'NONE',  ( -5.000000000000000000, -11.00479820989369806, 67.37201579502529114 ) ) ;
#39911 = CARTESIAN_POINT ( 'NONE',  ( 4.999999999999998224, -68.02455775458935250, 22.06917953199485183 ) ) ;
#39912 = CARTESIAN_POINT ( 'NONE',  ( 8.660254037844385522, 71.45833332650538239, 5.000000000000005329 ) ) ;
#39915 = CARTESIAN_POINT ( 'NONE',  ( -2.828427124746209831, 199.5000000027312126, 139.1715728752538723 ) ) ;
#39914 = CARTESIAN_POINT ( 'NONE',  ( 2.085542519210945334E-15, 250.1562500034140157, 11.35316468749999963 ) ) ;
#39913 = CARTESIAN_POINT ( 'NONE',  ( 25.55430564589115860, 208.0625000013656063, 167.5543056458911053 ) ) ;
#39916 = APPLICATION_PROTOCOL_DEFINITION ( 'draft international standard', 'automotive_design', 1998, #72242 ) ;
#39917 = ORIENTED_EDGE ( 'NONE', *, *, #5392, .F. ) ;
#39918 = EDGE_CURVE ( 'NONE', #10343, #29247, #44206, .T. ) ;
#39919 = CARTESIAN_POINT ( 'NONE',  ( -9.832129032723418760, 253.8020833367473017, -5.676582343749998927 ) ) ;
#39920 = CARTESIAN_POINT ( 'NONE',  ( 5.082755093536318824, 5.082755093536319713, 14.42405278187175455 ) ) ;
#39921 = ORIENTED_EDGE ( 'NONE', *, *, #73117, .F. ) ;
#39922 = EDGE_CURVE ( 'NONE', #9475, #28855, #36762, .T. ) ;
#39923 =( BOUNDED_CURVE ( )  B_SPLINE_CURVE ( 2, ( #22296, #44959, #12102, #17763, #28342, #23052, #51350, #68704, #16259 ),
 .UNSPECIFIED., .F., .F. ) 
 B_SPLINE_CURVE_WITH_KNOTS ( ( 3, 2, 2, 2, 3 ),
 ( 0.000000000000000000, 0.006578947368421057471, 0.01315789473684211494, 0.01973684210526317415, 0.02631578947368422988 ),
 .UNSPECIFIED. ) 
 CURVE ( )  GEOMETRIC_REPRESENTATION_ITEM ( )  RATIONAL_B_SPLINE_CURVE ( ( 1.000000000000000000, 0.9238795325112867385, 1.000000000000000000, 0.9238795325112867385, 1.000000000000000000, 0.9238795325112867385, 1.000000000000000000, 0.9238795325112865164, 1.000000000000000222 ) ) 
 REPRESENTATION_ITEM ( '' )  );
#39924 = ORIENTED_EDGE ( 'NONE', *, *, #41210, .F. ) ;
#39925 = CARTESIAN_POINT ( 'NONE',  ( -7.204075437095967871, 7.204075437095967871, 76.46875000204836681 ) ) ;
#39926 = CARTESIAN_POINT ( 'NONE',  ( 11.35316468749999963, 91.30208332991934128, -3.042071309553165293 ) ) ;
#39927 = CARTESIAN_POINT ( 'NONE',  ( 46.67364751762348618, 38.00000000000001421, 69.99999999999997158 ) ) ;
#39928 = CARTESIAN_POINT ( 'NONE',  ( -7.778174593052020747, -7.778174593052023411, 85.18749999999998579 ) ) ;
#39931 = CARTESIAN_POINT ( 'NONE',  ( 10.00000000000000178, 69.79166666666665719, 2.679491924311236062 ) ) ;
#39930 = CARTESIAN_POINT ( 'NONE',  ( 25.17157287525381548, 195.0000000027312126, 172.8284271247460993 ) ) ;
#39929 = CARTESIAN_POINT ( 'NONE',  ( 26.56734541678238060, 205.2500000013655779, 166.5412658749999650 ) ) ;
#39932 = CIRCLE ( 'NONE', #8743, 17.50000000000000000 ) ;
#39933 = CARTESIAN_POINT ( 'NONE',  ( 4.531193156845207581E-15, 210.0000000000000284, 133.0000000000000284 ) ) ;
#39934 = CARTESIAN_POINT ( 'NONE',  ( -3.042071309553173730, 199.3229166632526983, 11.35316468749999785 ) ) ;
#39935 = CARTESIAN_POINT ( 'NONE',  ( -2.445694354108839619, 206.8125000013656063, 139.5543056458912190 ) ) ;
#39936 = ORIENTED_EDGE ( 'NONE', *, *, #45586, .T. ) ;
#39937 = CARTESIAN_POINT ( 'NONE',  ( 29.43265458321766559, 207.1250000013656347, 166.5412658749999650 ) ) ;
#39938 = CARTESIAN_POINT ( 'NONE',  ( -2.977408999572654480, 16.87499999795161543, 7.188101187499999156 ) ) ;
#39939 = CARTESIAN_POINT ( 'NONE',  ( -9.832129032723420536, 164.0104166632526983, 5.676582343749997150 ) ) ;
#39940 = FACE_OUTER_BOUND ( 'NONE', #63411, .T. ) ;
#39941 = CARTESIAN_POINT ( 'NONE',  ( -7.188101187500000044, 105.0312500020483810, 0.000000000000000000 ) ) ;
#39943 = CARTESIAN_POINT ( 'NONE',  ( 2.828427124746191623, 10.12500000000000000, -2.828427124746191623 ) ) ;
#39942 = CARTESIAN_POINT ( 'NONE',  ( -7.320508075688773708, 208.1250000000000000, 7.320508075688764826 ) ) ;
#39944 = CARTESIAN_POINT ( 'NONE',  ( -8.342170076843785083E-16, 12.06249999863440614, 4.541265875000002339 ) ) ;
#39945 = CARTESIAN_POINT ( 'NONE',  ( 25.55430564589119413, 203.3125000013656063, 167.5543056458910485 ) ) ;
#39946 = CARTESIAN_POINT ( 'NONE',  ( 2.977408999572646486, 7.188101187499991163, 10.39280278187175810 ) ) ;
#39947 = CARTESIAN_POINT ( 'NONE',  ( 11.35316468750000141, 55.78124999658601268, 0.000000000000000000 ) ) ;
#39948 = EDGE_CURVE ( 'NONE', #55769, #48531, #65420, .T. ) ;
#39949 = DIRECTION ( 'NONE',  ( -0.8660254037844380415, -0.5000000000000012212, 0.000000000000000000 ) ) ;
#39950 = CARTESIAN_POINT ( 'NONE',  ( -5.656854249492375253, 5.656854249492375253, 0.6990527843298235400 ) ) ;
#39951 = ORIENTED_EDGE ( 'NONE', *, *, #63723, .T. ) ;
#39952 = CARTESIAN_POINT ( 'NONE',  ( 2.020667218593132706E-15, -11.00000000000000000, 74.87499999999998579 ) ) ;
#39953 = CARTESIAN_POINT ( 'NONE',  ( 6.123233995736767268E-16, 168.1249999931720538, -10.00000000000000178 ) ) ;
#39954 = CARTESIAN_POINT ( 'NONE',  ( -2.085542519210945728E-15, 59.53124999658601979, 11.35316468750000141 ) ) ;
#39955 = CARTESIAN_POINT ( 'NONE',  ( 4.556349186104051263, -10.99999999999999822, 73.65625000409676204 ) ) ;
#39956 = CARTESIAN_POINT ( 'NONE',  ( -1.432654583217664701, 200.0000000013656063, 138.5412658750000787 ) ) ;
#39958 = CIRCLE ( 'NONE', #65237, 8.000000000000000000 ) ;
#39957 = CYLINDRICAL_SURFACE ( 'NONE', #4672, 10.99999999999999645 ) ;
#39959 = CARTESIAN_POINT ( 'NONE',  ( -1.903569318090136080E-11, 13.74999999999851852, 10.00000000000000178 ) ) ;
#39961 = CARTESIAN_POINT ( 'NONE',  ( 9.832129032723420536, 66.19791666325268409, -5.676582343749999815 ) ) ;
#39960 = CARTESIAN_POINT ( 'NONE',  ( 7.188101187500000933, 92.00000000204838102, -2.977408999572651371 ) ) ;
#39962 = CARTESIAN_POINT ( 'NONE',  ( -7.999999999999991118, 3.313708498984756723, 2.236552779823365533 ) ) ;
#39963 = LINE ( 'NONE', #34695, #71007 ) ;
#39964 = CARTESIAN_POINT ( 'NONE',  ( 11.35316468750000141, 170.7812499965860411, 0.000000000000000000 ) ) ;
#39965 = CARTESIAN_POINT ( 'NONE',  ( -10.00000000000000000, 139.1666666598387110, -2.679491924311229845 ) ) ;
#39966 = CARTESIAN_POINT ( 'NONE',  ( -2.977408999572651815, 96.31250000204838102, 7.188101187500000933 ) ) ;
#39967 =( GEOMETRIC_REPRESENTATION_CONTEXT ( 3 ) GLOBAL_UNCERTAINTY_ASSIGNED_CONTEXT ( ( #6853 ) ) GLOBAL_UNIT_ASSIGNED_CONTEXT ( ( #3888, #27250, #61592 ) ) REPRESENTATION_CONTEXT ( 'NONE', 'WORKASPACE' ) );
#39968 = CARTESIAN_POINT ( 'NONE',  ( 8.311093377946834337, 50.46874999658601979, 8.311093377946839666 ) ) ;
#39969 = CARTESIAN_POINT ( 'NONE',  ( 6.000000000000001776, 295.5625000034140157, -7.347880794884121708E-16 ) ) ;
#39970 = CARTESIAN_POINT ( 'NONE',  ( 6.951808397369818766E-16, 177.0312499965860411, -11.35316468750000141 ) ) ;
#39971 = ORIENTED_EDGE ( 'NONE', *, *, #26864, .F. ) ;
#39972 = CARTESIAN_POINT ( 'NONE',  ( -27.99999999999999645, 210.0000000000000284, 166.0000000000003979 ) ) ;
#39973 = CARTESIAN_POINT ( 'NONE',  ( 1.871523826299183495E-15, -10.18810118749999916, 71.03125000204838102 ) ) ;
#39974 = CARTESIAN_POINT ( 'NONE',  ( 4.000000000000015987, 195.4375000000000000, 199.6568542494924259 ) ) ;
#39975 = CARTESIAN_POINT ( 'NONE',  ( 32.22790813659745623, 42.55246065645124531, 65.00000000000001421 ) ) ;
#39977 = CARTESIAN_POINT ( 'NONE',  ( 8.311093377946837890, 181.4062499965860411, -8.311093377946837890 ) ) ;
#39976 = CARTESIAN_POINT ( 'NONE',  ( 30.82842712474617031, 203.1250000000000284, 172.8284271247460993 ) ) ;
#39978 = CARTESIAN_POINT ( 'NONE',  ( -7.999999999999989342, -3.313708498984762496, 8.480302784329822430 ) ) ;
#39979 = EDGE_CURVE ( 'NONE', #61067, #70268, #8083, .T. ) ;
#39980 = DIRECTION ( 'NONE',  ( -0.000000000000000000, -0.000000000000000000, 1.000000000000000000 ) ) ;
#39981 = CARTESIAN_POINT ( 'NONE',  ( 10.00000000000000178, 260.4166666734946034, 2.679491924311222739 ) ) ;
#39982 = CARTESIAN_POINT ( 'NONE',  ( 0.000000000000000000, 19.05255888325788050, 0.000000000000000000 ) ) ;
#39983 = ORIENTED_EDGE ( 'NONE', *, *, #30218, .T. ) ;
#39984 = ADVANCED_FACE ( 'NONE', ( #54114 ), #30987, .F. ) ;
#39985 = APPLICATION_CONTEXT ( 'automotive_design' ) ;
#39986 = CARTESIAN_POINT ( 'NONE',  ( 7.188101187499992051, 8.802885111219154394E-16, 27.73655278187175455 ) ) ;
#39987 = CARTESIAN_POINT ( 'NONE',  ( 5.676582343749993598, 115.2604166632526983, 9.832129032723422313 ) ) ;
#39988 = ADVANCED_FACE ( 'NONE', ( #6268 ), #47710, .T. ) ;
#39989 = CARTESIAN_POINT ( 'NONE',  ( -2.775557561562891351E-14, 210.0000000000000284, 142.0000000000000568 ) ) ;
#39990 = ORIENTED_EDGE ( 'NONE', *, *, #59665, .F. ) ;
#39991 = CIRCLE ( 'NONE', #35165, 6.000000000000001776 ) ;
#39992 = CARTESIAN_POINT ( 'NONE',  ( -4.541265875000003227, 7.999999998634407028, 1.881053915767121110 ) ) ;
#39993 = CARTESIAN_POINT ( 'NONE',  ( 2.977408999572650927, 14.24999999795161010, -7.188101187500001821 ) ) ;
#39994 = CARTESIAN_POINT ( 'NONE',  ( 1.469576158976823947E-15, 107.5625000040967905, 8.000000000000000000 ) ) ;
#39995 = CARTESIAN_POINT ( 'NONE',  ( -28.00000000000001776, 197.6875000013655779, 166.5412658750003629 ) ) ;
#39996 = EDGE_CURVE ( 'NONE', #60275, #45526, #23600, .T. ) ;
#39997 = EDGE_CURVE ( 'NONE', #47712, #2022, #41575, .T. ) ;
#39998 = CARTESIAN_POINT ( 'NONE',  ( 2.828427124746191623, 7.125000000000000000, -2.828427124746191623 ) ) ;
#39999 = CARTESIAN_POINT ( 'NONE',  ( 2.828427124746190291, 22.62499999726881583, 2.828427124746192067 ) ) ;
#40000 = CARTESIAN_POINT ( 'NONE',  ( 1.881053915767121998, 10.49999999863440969, -4.541265875000002339 ) ) ;
#40001 = CARTESIAN_POINT ( 'NONE',  ( -2.828427124746208943, 198.6250000000000284, 144.8284271247462129 ) ) ;
#40002 = ORIENTED_EDGE ( 'NONE', *, *, #49379, .T. ) ;
#40003 = CARTESIAN_POINT ( 'NONE',  ( 1.320432766682874540E-15, 105.0312500020483810, 7.188101187500000044 ) ) ;
#40005 = CARTESIAN_POINT ( 'NONE',  ( -3.673940397442060854E-16, 293.7500000000000000, -6.000000000000001776 ) ) ;
#40004 = CARTESIAN_POINT ( 'NONE',  ( -26.56734541678227757, 195.0000000013656063, 173.4587341250003476 ) ) ;
#40006 = CARTESIAN_POINT ( 'NONE',  ( 2.780723358947928197E-16, 20.56249999863440436, -4.541265875000002339 ) ) ;
#40007 = VECTOR ( 'NONE', #54487, 1000.000000000000000 ) ;
#40008 = CARTESIAN_POINT ( 'NONE',  ( -7.188101187499991163, 2.977408999572646930, 2.892802781871751439 ) ) ;
#40009 = ORIENTED_EDGE ( 'NONE', *, *, #74420, .T. ) ;
#40010 = EDGE_CURVE ( 'NONE', #30828, #70626, #40962, .T. ) ;
#40011 = ORIENTED_EDGE ( 'NONE', *, *, #45165, .T. ) ;
#40012 = CARTESIAN_POINT ( 'NONE',  ( 10.18810118749999916, 4.220049686691935698, 91.00000000204836681 ) ) ;
#40013 = DIRECTION ( 'NONE',  ( -1.000000000000000000, -0.000000000000000000, -0.000000000000000000 ) ) ;
#40014 = CARTESIAN_POINT ( 'NONE',  ( -11.00000000000000000, 0.000000000000000000, 71.68750000409676204 ) ) ;
#40015 = CARTESIAN_POINT ( 'NONE',  ( 11.00000000000000000, 4.556349186104045934, 103.8437499999999858 ) ) ;
#40016 = CARTESIAN_POINT ( 'NONE',  ( 3.458734125000015425, 204.2500000013655779, 196.5673454167823877 ) ) ;
#40018 = CARTESIAN_POINT ( 'NONE',  ( -7.320508075688770155, 255.6250000000000000, 7.320508075688774596 ) ) ;
#40017 = CARTESIAN_POINT ( 'NONE',  ( 0.000000000000000000, 0.000000000000000000, -21.50000000000000000 ) ) ;
#40019 = CARTESIAN_POINT ( 'NONE',  ( -4.999999999999998224, 116.6666666666666714, -8.660254037844389075 ) ) ;
#40020 = CARTESIAN_POINT ( 'NONE',  ( 8.000000000000001776, 106.1562499999999858, 3.313708498984759387 ) ) ;
#40021 = CARTESIAN_POINT ( 'NONE',  ( 2.765530957082001251, 289.9218750017069510, 6.676582343750000703 ) ) ;
#40022 = CARTESIAN_POINT ( 'NONE',  ( 5.082755093536320601, -5.082755093536318824, 8.424052781871752771 ) ) ;
#40023 =( BOUNDED_CURVE ( )  B_SPLINE_CURVE ( 2, ( #1014, #58356, #40240, #69287, #17596, #6661, #40614, #29664, #37551 ),
 .UNSPECIFIED., .F., .F. ) 
 B_SPLINE_CURVE_WITH_KNOTS ( ( 3, 2, 2, 2, 3 ),
 ( 0.2386363636363636465, 0.2443181818181818232, 0.2500000000000000000, 0.2556818181818181768, 0.2613636363636363535 ),
 .UNSPECIFIED. ) 
 CURVE ( )  GEOMETRIC_REPRESENTATION_ITEM ( )  RATIONAL_B_SPLINE_CURVE ( ( 1.000000000000000000, 0.9238795325112867385, 1.000000000000000000, 0.9238795325112867385, 1.000000000000000000, 0.9238795325112867385, 1.000000000000000000, 0.9238795325112867385, 1.000000000000000000 ) ) 
 REPRESENTATION_ITEM ( '' )  );
#40024 = CARTESIAN_POINT ( 'NONE',  ( -4.898587196589412829E-16, 102.3125000040967763, -8.000000000000000000 ) ) ;
#40025 = CARTESIAN_POINT ( 'NONE',  ( 30.44569435410883784, 208.8125000013656063, 167.5543056458911053 ) ) ;
#40026 = CARTESIAN_POINT ( 'NONE',  ( 5.082755093536325930, 1.031249997951610098, -5.082755093536325930 ) ) ;
#40027 = CARTESIAN_POINT ( 'NONE',  ( -2.445694354108838731, 201.0625000013656063, 144.4456943541088663 ) ) ;
#40028 = CARTESIAN_POINT ( 'NONE',  ( 2.977408999572650039, 119.5625000020483810, -7.188101187500000933 ) ) ;
#40030 = CARTESIAN_POINT ( 'NONE',  ( 0.000000000000000000, 125.0000000000000000, 8.000000000000000000 ) ) ;
#40029 = CYLINDRICAL_SURFACE ( 'NONE', #17884, 3.999999999999976019 ) ;
#40031 = CARTESIAN_POINT ( 'NONE',  ( -9.832129032723415207, 239.6354166700806445, 5.676582343750005144 ) ) ;
#40032 = CARTESIAN_POINT ( 'NONE',  ( -4.401442555609577197E-16, 7.188101187499992051, 25.48655278187175810 ) ) ;
#40033 = CARTESIAN_POINT ( 'NONE',  ( 26.34314575050758833, 199.9375000000000000, 173.9999999999999147 ) ) ;
#40034 = CARTESIAN_POINT ( 'NONE',  ( -9.832129032723420536, 8.697916663252684089, 5.676582343749997150 ) ) ;
#40035 = CARTESIAN_POINT ( 'NONE',  ( 5.656854249492381470, 122.5625000000000000, 5.656854249492379694 ) ) ;
#40036 = CARTESIAN_POINT ( 'NONE',  ( -3.042071309553164404, 202.5520833299193839, -11.35316468749999963 ) ) ;
#40037 = CARTESIAN_POINT ( 'NONE',  ( -25.17157287525381903, 195.8750000000000284, 167.1715728752541565 ) ) ;
#40038 = CARTESIAN_POINT ( 'NONE',  ( 7.999999999996472155, 7.505344305739403062E-06, 9.267802996260090964 ) ) ;
#40039 = CARTESIAN_POINT ( 'NONE',  ( 4.000000000000001776, 11.81249999726881228, -1.656854249492381248 ) ) ;
#40040 = VERTEX_POINT ( 'NONE', #70730 ) ;
#40041 = CARTESIAN_POINT ( 'NONE',  ( 2.445694354108783219, 199.8125000013656063, 139.5543056458912190 ) ) ;
#40042 = CARTESIAN_POINT ( 'NONE',  ( -11.35316468750000141, 28.28124999658601624, -1.390361679473963753E-15 ) ) ;
#40043 = CARTESIAN_POINT ( 'NONE',  ( -11.00000000000000000, 0.000000000000000000, 91.18750000409677625 ) ) ;
#40044 = CARTESIAN_POINT ( 'NONE',  ( 8.660254037844385522, 227.9166666666666856, -5.000000000000003553 ) ) ;
#40045 = CARTESIAN_POINT ( 'NONE',  ( -25.55430564589111597, 196.0625000013656063, 172.4456943541091505 ) ) ;
#40046 = CARTESIAN_POINT ( 'NONE',  ( 0.000000000000000000, 0.000000000000000000, 9.999999999999996447 ) ) ;
#40048 = CARTESIAN_POINT ( 'NONE',  ( 6.951808397369818766E-16, 22.03124999658601624, -11.35316468750000141 ) ) ;
#40047 = CARTESIAN_POINT ( 'NONE',  ( -2.977408999572650927, 113.3750000020483810, -7.188101187500000933 ) ) ;
#40049 = CARTESIAN_POINT ( 'NONE',  ( -7.999999999999991118, 0.000000000000000000, 20.33030277982336642 ) ) ;
#40050 = AXIS2_PLACEMENT_3D ( 'NONE', #39751, #29556, #46529 ) ;
#40051 = CARTESIAN_POINT ( 'NONE',  ( 11.35316468749999963, 140.9895833299193555, -3.042071309553165293 ) ) ;
#40052 = EDGE_CURVE ( 'NONE', #66964, #3547, #36045, .T. ) ;
#40053 = CARTESIAN_POINT ( 'NONE',  ( 2.679491924311228956, 97.91666665983871098, -10.00000000000000000 ) ) ;
#40054 = CARTESIAN_POINT ( 'NONE',  ( 7.188101187500001821, 120.8750000020483810, -2.977408999572651371 ) ) ;
#40055 = CARTESIAN_POINT ( 'NONE',  ( 5.000000000000000000, 68.60357193678729004, -20.85024232999272087 ) ) ;
#40056 = CARTESIAN_POINT ( 'NONE',  ( -28.00000000000002487, 208.6875000013656063, 166.5412658750003629 ) ) ;
#40057 = CARTESIAN_POINT ( 'NONE',  ( -5.000000000000000000, 52.63770595436734823, -42.88862352055258498 ) ) ;
#40058 = ORIENTED_EDGE ( 'NONE', *, *, #33351, .T. ) ;
#40059 = CARTESIAN_POINT ( 'NONE',  ( 3.544144923084093790, -60.54353712382357600, 23.09461823984349849 ) ) ;
#40060 = CARTESIAN_POINT ( 'NONE',  ( 8.000000000000000000, 107.8437500000000000, -3.313708498984762496 ) ) ;
#40061 = CARTESIAN_POINT ( 'NONE',  ( 6.676582343750003368, 296.0156250017069510, -2.765530957081997254 ) ) ;
#40062 = CARTESIAN_POINT ( 'NONE',  ( -5.676582343749998039, 132.4479166632526983, -9.832129032723420536 ) ) ;
#40063 = FACE_OUTER_BOUND ( 'NONE', #57176, .T. ) ;
#40064 = CARTESIAN_POINT ( 'NONE',  ( 3.313708498984756279, 7.999999999999991118, 22.91780278432982598 ) ) ;
#40065 = CARTESIAN_POINT ( 'NONE',  ( 4.615726161707420339, 68.43878643976823639, 20.71807028113882510 ) ) ;
#40066 = CARTESIAN_POINT ( 'NONE',  ( 11.35316468749999963, 256.4062500034140157, -1.390361679473963556E-15 ) ) ;
#40067 = CARTESIAN_POINT ( 'NONE',  ( -10.18810118749999916, 0.000000000000000000, 96.53125000204838102 ) ) ;
#40068 = ORIENTED_EDGE ( 'NONE', *, *, #26624, .F. ) ;
#40069 = EDGE_CURVE ( 'NONE', #20164, #57466, #46865, .T. ) ;
#40070 = CARTESIAN_POINT ( 'NONE',  ( 0.000000000000000000, 300.0000000000000000, 0.000000000000000000 ) ) ;
#40071 = CARTESIAN_POINT ( 'NONE',  ( -1.432654583217608080, 203.8750000013656063, 201.4587341250000350 ) ) ;
#40072 = CARTESIAN_POINT ( 'NONE',  ( -11.35316468750000141, 73.59374999658602690, -1.390361679473963753E-15 ) ) ;
#40073 = EDGE_LOOP ( 'NONE', ( #44450, #24054, #50942, #39055 ) ) ;
#40074 = CARTESIAN_POINT ( 'NONE',  ( 1.871523826299183495E-15, -10.18810118749999916, 108.5312500020483810 ) ) ;
#40075 = EDGE_CURVE ( 'NONE', #50397, #42073, #10739, .T. ) ;
#40076 = CARTESIAN_POINT ( 'NONE',  ( -4.541265875000002339, 11.87499999863440792, -1.881053915767121998 ) ) ;
#40077 = ORIENTED_EDGE ( 'NONE', *, *, #38576, .F. ) ;
#40078 = CARTESIAN_POINT ( 'NONE',  ( 4.401442555609581635E-16, 24.84374999795161543, -7.188101187500000044 ) ) ;
#40079 = DIRECTION ( 'NONE',  ( 0.000000000000000000, 0.7071067811865472397, 0.7071067811865479058 ) ) ;
#40080 = CARTESIAN_POINT ( 'NONE',  ( -3.999999999999960032, 197.1250000027312126, 198.0000000000000284 ) ) ;
#40081 = CARTESIAN_POINT ( 'NONE',  ( -2.977408999572650039, 23.81249999795161543, -7.188101187500001821 ) ) ;
#40082 = FACE_OUTER_BOUND ( 'NONE', #68531, .T. ) ;
#40083 = CARTESIAN_POINT ( 'NONE',  ( -6.238412754330611322E-16, 10.18810118749999916, 105.1562500020483810 ) ) ;
#40084 = AXIS2_PLACEMENT_3D ( 'NONE', #51642, #22974, #46351 ) ;
#40085 = CARTESIAN_POINT ( 'NONE',  ( 4.000000000000015987, 201.6250000027312126, 198.0000000000000284 ) ) ;
#40086 = CARTESIAN_POINT ( 'NONE',  ( 4.000000000000000888, 11.68749999726881406, 1.656854249492384135 ) ) ;
#40087 = ORIENTED_EDGE ( 'NONE', *, *, #31783, .T. ) ;
#40088 = AXIS2_PLACEMENT_3D ( 'NONE', #8410, #10286, #49137 ) ;
#40089 = DIRECTION ( 'NONE',  ( -0.000000000000000000, -1.000000000000000000, -0.000000000000000000 ) ) ;
#40090 = CARTESIAN_POINT ( 'NONE',  ( 2.445694354108838731, 204.0625000013656063, 195.5543056458912190 ) ) ;
#40091 = CARTESIAN_POINT ( 'NONE',  ( -30.44569435410886982, 203.5625000013656063, 167.5543056458916169 ) ) ;
#40092 =( NAMED_UNIT ( * ) SI_UNIT ( $, .STERADIAN. ) SOLID_ANGLE_UNIT ( ) );
#40093 = CARTESIAN_POINT ( 'NONE',  ( -4.541265875000002339, 10.81249999863440792, -5.561446717895856393E-16 ) ) ;
#40094 = DIRECTION ( 'NONE',  ( 0.000000000000000000, 0.000000000000000000, 1.000000000000000000 ) ) ;
#40095 = CARTESIAN_POINT ( 'NONE',  ( -7.188101187499990274, -2.977408999572651371, 18.08030278187175455 ) ) ;
#40096 = VERTEX_POINT ( 'NONE', #36410 ) ;
#40097 = CARTESIAN_POINT ( 'NONE',  ( -3.673940397442060854E-16, 291.7500000000000000, -6.000000000000001776 ) ) ;
#40098 = EDGE_LOOP ( 'NONE', ( #21015, #57986, #49017, #16575 ) ) ;
#40099 = CARTESIAN_POINT ( 'NONE',  ( 10.18810118749999916, 1.247682550866122264E-15, 108.9062500020483668 ) ) ;
#40100 = CARTESIAN_POINT ( 'NONE',  ( 4.556349186104045934, 11.00000000000000000, 96.71875000409677625 ) ) ;
#40101 = CARTESIAN_POINT ( 'NONE',  ( -3.458734124999959914, 198.3750000013655779, 196.5673454167823877 ) ) ;
#40102 = CARTESIAN_POINT ( 'NONE',  ( 5.000000000000000000, -10.00000000000000000, 75.19090595827292134 ) ) ;
#40103 = CARTESIAN_POINT ( 'NONE',  ( -4.999999999999998224, 76.66666666666667140, -8.660254037844389075 ) ) ;
#40104 = CARTESIAN_POINT ( 'NONE',  ( -7.999999999999998224, 123.5937500000000000, 3.313708498984766493 ) ) ;
#40105 = CARTESIAN_POINT ( 'NONE',  ( 2.485281374238571317, 288.6875000000000568, -6.000000000000003553 ) ) ;
#40106 = VERTEX_POINT ( 'NONE', #48082 ) ;
#40107 = CARTESIAN_POINT ( 'NONE',  ( 4.242640687119285658, 294.6249999999999432, -4.242640687119286547 ) ) ;
#40108 = CARTESIAN_POINT ( 'NONE',  ( 2.849036369511732440E-14, 202.3750000027312126, 202.0000000000000000 ) ) ;
#40109 = CARTESIAN_POINT ( 'NONE',  ( -4.000000000000015987, 195.6250000027311842, 142.0000000000000568 ) ) ;
#40110 = CARTESIAN_POINT ( 'NONE',  ( 8.660254037844389075, 57.29166665983870388, -5.000000000000000000 ) ) ;
#40111 = CARTESIAN_POINT ( 'NONE',  ( -1.469576158976823947E-15, 23.62500000000000355, 8.000000000000000000 ) ) ;
#40112 = CARTESIAN_POINT ( 'NONE',  ( 10.00000000000000000, 237.5000000000000284, -1.224646799147353256E-15 ) ) ;
#40113 = DIRECTION ( 'NONE',  ( -0.000000000000000000, 1.000000000000000000, -0.000000000000000000 ) ) ;
#40114 = CARTESIAN_POINT ( 'NONE',  ( 10.18810118749999916, 1.247682550866122264E-15, 68.78125000204838102 ) ) ;
#40115 = CARTESIAN_POINT ( 'NONE',  ( -10.00000000000000355, 197.7083333333332860, 2.679491924311223183 ) ) ;
#40116 = CARTESIAN_POINT ( 'NONE',  ( 5.082755093536320601, -5.082755093536318824, 15.92405278187175632 ) ) ;
#40117 = CARTESIAN_POINT ( 'NONE',  ( -5.676582343750006032, 174.4270833299193555, 9.832129032723418760 ) ) ;
#40118 = CARTESIAN_POINT ( 'NONE',  ( -7.320508075688776373, 38.12499999999999289, 7.320508075688768379 ) ) ;
#40119 = CARTESIAN_POINT ( 'NONE',  ( 7.778174593052023411, -7.778174593052021635, 97.75000000409677625 ) ) ;
#40121 = CARTESIAN_POINT ( 'NONE',  ( 7.999999999999998224, 10.21874999590321842, 3.313708498984766049 ) ) ;
#40120 = FILL_AREA_STYLE ('',( #57495 ) ) ;
#40122 = ORIENTED_EDGE ( 'NONE', *, *, #54211, .F. ) ;
#40123 = CARTESIAN_POINT ( 'NONE',  ( -1.432654583217664479, 197.7500000013656063, 138.5412658750000787 ) ) ;
#40124 = CARTESIAN_POINT ( 'NONE',  ( 5.676582343750001591, 31.92708332991935194, -9.832129032723420536 ) ) ;
#40125 = CARTESIAN_POINT ( 'NONE',  ( -6.735557395310442023E-16, 11.00000000000000000, 108.8125000040967763 ) ) ;
#40126 = CARTESIAN_POINT ( 'NONE',  ( -2.143195687316029385, 194.5378148448417335, 200.8225804235214582 ) ) ;
#40127 = CARTESIAN_POINT ( 'NONE',  ( 0.000000000000000000, 0.000000000000000000, -10.80000000000000071 ) ) ;
#40129 = CARTESIAN_POINT ( 'NONE',  ( 23.99999999999999645, 199.6875000000000000, 168.3431457505074889 ) ) ;
#40128 = FACE_OUTER_BOUND ( 'NONE', #16329, .T. ) ;
#40130 = CARTESIAN_POINT ( 'NONE',  ( 28.00000000000002132, 202.1250000027312126, 173.9999999999999147 ) ) ;
#40131 = CARTESIAN_POINT ( 'NONE',  ( 1.432654583217607858, 200.6250000013656063, 138.5412658750000787 ) ) ;
#40132 = ADVANCED_FACE ( 'NONE', ( #59423 ), #23970, .F. ) ;
#40133 = EDGE_CURVE ( 'NONE', #1239, #34597, #12706, .T. ) ;
#40134 = CARTESIAN_POINT ( 'NONE',  ( 7.320508075688771044, 56.24999999317203248, 7.320508075688775484 ) ) ;
#40135 = CARTESIAN_POINT ( 'NONE',  ( 2.977408999572654480, 100.6250000020483810, 7.188101187499999156 ) ) ;
#40136 = CARTESIAN_POINT ( 'NONE',  ( 3.211159895383561835, 10.56249999863440792, -3.211159895383561835 ) ) ;
#40137 = CARTESIAN_POINT ( 'NONE',  ( 9.999999999999996447, 55.20833333333332860, -2.679491924311226292 ) ) ;
#40138 = CARTESIAN_POINT ( 'NONE',  ( 7.999999999999991118, 3.313708498984757611, 4.674052779823363757 ) ) ;
#40139 = CARTESIAN_POINT ( 'NONE',  ( 4.999999999999993783, 101.0416666598386968, 8.660254037844390851 ) ) ;
#40140 = ORIENTED_EDGE ( 'NONE', *, *, #65085, .T. ) ;
#40141 = ORIENTED_EDGE ( 'NONE', *, *, #45885, .T. ) ;
#40142 =( BOUNDED_CURVE ( )  B_SPLINE_CURVE ( 2, ( #3628, #20591, #37590, #31926, #54948, #26245, #32689, #43233, #25868 ),
 .UNSPECIFIED., .F., .F. ) 
 B_SPLINE_CURVE_WITH_KNOTS ( ( 3, 2, 2, 2, 3 ),
 ( 0.8088235294117647189, 0.8125000000000000000, 0.8161764705882352811, 0.8198529411764705621, 0.8235294117647058432 ),
 .UNSPECIFIED. ) 
 CURVE ( )  GEOMETRIC_REPRESENTATION_ITEM ( )  RATIONAL_B_SPLINE_CURVE ( ( 1.000000000000000000, 0.9238795325112867385, 1.000000000000000000, 0.9238795325112867385, 1.000000000000000000, 0.9238795325112867385, 1.000000000000000000, 0.9238795325112867385, 1.000000000000000000 ) ) 
 REPRESENTATION_ITEM ( '' )  );
#40143 = CIRCLE ( 'NONE', #30506, 27.99999999999998224 ) ;
#40144 = CARTESIAN_POINT ( 'NONE',  ( 7.999999999999991118, 3.313708498984758055, 10.67405277982336465 ) ) ;
#40145 = CARTESIAN_POINT ( 'NONE',  ( 1.226468279477575784E-15, 295.8593750017070079, 6.676582343750001591 ) ) ;
#40146 = CARTESIAN_POINT ( 'NONE',  ( 28.00000000000002487, 207.1250000027312126, 173.9999999999999147 ) ) ;
#40147 = CARTESIAN_POINT ( 'NONE',  ( -5.000000000000000000, 52.35862550122993042, -48.98731492261362064 ) ) ;
#40148 = CARTESIAN_POINT ( 'NONE',  ( -5.676582343749998039, 147.4479166632526983, -9.832129032723420536 ) ) ;
#40149 = CARTESIAN_POINT ( 'NONE',  ( -30.99999999999992895, -31.99999999999978684, 205.0000000000000284 ) ) ;
#40150 = EDGE_CURVE ( 'NONE', #56997, #7251, #15567, .T. ) ;
#40151 = CARTESIAN_POINT ( 'NONE',  ( 4.220049686691941027, -10.18810118749999738, 83.12500000204835260 ) ) ;
#40152 = CARTESIAN_POINT ( 'NONE',  ( 39.97324732667616587, 0.000000000000000000, 113.7582050592233429 ) ) ;
#40153 = CARTESIAN_POINT ( 'NONE',  ( 1.656854249492403008, 204.6875000000000284, 194.0000000000000853 ) ) ;
#40154 = CARTESIAN_POINT ( 'NONE',  ( 8.000000000000000000, 116.9375000040967763, -9.797174393178825657E-16 ) ) ;
#40155 = CARTESIAN_POINT ( 'NONE',  ( 10.18810118749999916, 1.247682550866122264E-15, 115.2812500020483810 ) ) ;
#40156 = EDGE_LOOP ( 'NONE', ( #45515, #33119, #47117, #57624, #61811, #73441 ) ) ;
#40157 = CARTESIAN_POINT ( 'NONE',  ( 9.000000000000000000, -5.196152422706648011, -10.80000000000000071 ) ) ;
#40158 = CARTESIAN_POINT ( 'NONE',  ( 2.615118447421970860, 178.7191267362284464, 133.3668405662103851 ) ) ;
#40159 = CARTESIAN_POINT ( 'NONE',  ( -8.311093377946836114, 132.9687499965860411, -8.311093377946837890 ) ) ;
#40160 = CARTESIAN_POINT ( 'NONE',  ( -2.445694354108783664, 201.3125000013656063, 195.5543056458912190 ) ) ;
#40161 = CARTESIAN_POINT ( 'NONE',  ( 4.401442555609581635E-16, 22.21874999795161543, -7.188101187500000044 ) ) ;
#40162 = AXIS2_PLACEMENT_3D ( 'NONE', #28511, #6262, #22097 ) ;
#40163 = CARTESIAN_POINT ( 'NONE',  ( 10.18810118750000093, -4.220049686691933033, 76.18750000204838102 ) ) ;
#40164 = CARTESIAN_POINT ( 'NONE',  ( 11.35316468750000141, 31.09374999658601979, 0.000000000000000000 ) ) ;
#40165 = EDGE_LOOP ( 'NONE', ( #41646, #48139, #24341, #29991 ) ) ;
#40166 = CARTESIAN_POINT ( 'NONE',  ( 0.000000000000000000, 125.0000000000000000, 0.000000000000000000 ) ) ;
#40167 = CARTESIAN_POINT ( 'NONE',  ( 4.541265875000002339, 1.499999998634407028, -1.881053915767121776 ) ) ;
#40168 = CARTESIAN_POINT ( 'NONE',  ( -3.317071493978880348, -8.008118988124989457, 14.79436528394063011 ) ) ;
#40169 = CARTESIAN_POINT ( 'NONE',  ( -2.445694354108840063, 206.0625000013656063, 139.5543056458912190 ) ) ;
#40170 = CARTESIAN_POINT ( 'NONE',  ( -1.320432766682874540E-15, 10.59374999795161187, 7.188101187500000044 ) ) ;
#40171 = CARTESIAN_POINT ( 'NONE',  ( -3.673940397442060854E-16, 295.8125000034140157, -6.000000000000001776 ) ) ;
#40172 = ADVANCED_FACE ( 'NONE', ( #37900 ), #25805, .F. ) ;
#40173 = CARTESIAN_POINT ( 'NONE',  ( -27.23562031587983867, -12.35442697173115079, 139.4057307757919375 ) ) ;
#40174 = CARTESIAN_POINT ( 'NONE',  ( -2.977408999572650039, 4.312499997951610098, -7.188101187500001821 ) ) ;
#40175 = CARTESIAN_POINT ( 'NONE',  ( 11.35316468749999785, 155.8854166632526699, 3.042071309553174174 ) ) ;
#40176 = CARTESIAN_POINT ( 'NONE',  ( -4.220049686691935698, 10.18810118749999916, 68.87500000204838102 ) ) ;
#40177 = CARTESIAN_POINT ( 'NONE',  ( -31.45873412499999944, 207.9375000013656063, 170.0000000000003979 ) ) ;
#40178 = CYLINDRICAL_SURFACE ( 'NONE', #37798, 3.999999999999976019 ) ;
#40179 = CARTESIAN_POINT ( 'NONE',  ( -3.211159895383561391, 21.81249999863440792, -3.211159895383561835 ) ) ;
#40180 = VERTEX_POINT ( 'NONE', #71454 ) ;
#40181 = CARTESIAN_POINT ( 'NONE',  ( -1.656854249492347719, 199.9375000027312126, 194.0000000000000853 ) ) ;
#40182 = CARTESIAN_POINT ( 'NONE',  ( 1.656854249492348607, 207.1875000000000284, 138.0000000000000568 ) ) ;
#40183 = CARTESIAN_POINT ( 'NONE',  ( -32.00000000000003553, 202.3125000027312410, 168.3431457505080573 ) ) ;
#40184 = PLANE ( 'NONE',  #19942 ) ;
#40185 = CARTESIAN_POINT ( 'NONE',  ( 3.313708498984762496, -7.999999999999989342, 5.986552783920146226 ) ) ;
#40186 = ORIENTED_EDGE ( 'NONE', *, *, #24158, .F. ) ;
#40187 = CARTESIAN_POINT ( 'NONE',  ( -7.188101187500002709, 17.81249999795161187, 2.977408999572649151 ) ) ;
#40188 = CARTESIAN_POINT ( 'NONE',  ( -4.242640687119286547, 297.9375000034140157, -4.242640687119286547 ) ) ;
#40189 = CARTESIAN_POINT ( 'NONE',  ( -2.679491924311226292, 43.33333332650536107, -10.00000000000000178 ) ) ;
#40190 = CARTESIAN_POINT ( 'NONE',  ( 7.320508075688774596, 45.62500000000000000, -7.320508075688774596 ) ) ;
#40191 = AXIS2_PLACEMENT_3D ( 'NONE', #27611, #49506, #50621 ) ;
#40192 = CARTESIAN_POINT ( 'NONE',  ( -7.188101187499999156, 108.1250000020483810, 2.977408999572654924 ) ) ;
#40193 = CARTESIAN_POINT ( 'NONE',  ( -30.44569435410883784, 207.8125000013656063, 167.5543056458915885 ) ) ;
#40194 = CARTESIAN_POINT ( 'NONE',  ( -6.000000000000000888, 299.0625000000000000, 2.485281374238575758 ) ) ;
#40196 = CARTESIAN_POINT ( 'NONE',  ( -6.735557395310442023E-16, 11.00000000000000000, 74.31250000409676204 ) ) ;
#40195 = CARTESIAN_POINT ( 'NONE',  ( 3.153939666463669656E-13, 33.75000000000002842, 9.999999999999998224 ) ) ;
#40197 = ORIENTED_EDGE ( 'NONE', *, *, #63218, .F. ) ;
#40198 = CARTESIAN_POINT ( 'NONE',  ( -8.311093377946834337, 244.5312500034139589, 8.311093377946837890 ) ) ;
#40199 = CARTESIAN_POINT ( 'NONE',  ( -7.188101187499991163, 2.977408999572646930, 16.76780278187175099 ) ) ;
#40200 = CARTESIAN_POINT ( 'NONE',  ( -4.471435261918103699, 50.48103707413024210, 40.99880869399409988 ) ) ;
#40201 = CARTESIAN_POINT ( 'NONE',  ( -10.07107371533886386, 220.0000000000001705, 0.6428371030747326298 ) ) ;
#40202 = DIRECTION ( 'NONE',  ( 0.000000000000000000, 0.2588190451025143557, -0.9659258262890699775 ) ) ;
#40203 = FACE_OUTER_BOUND ( 'NONE', #12141, .T. ) ;
#40204 = CARTESIAN_POINT ( 'NONE',  ( 6.123233995736767268E-16, 161.2500000000000000, -10.00000000000000178 ) ) ;
#40205 = CARTESIAN_POINT ( 'NONE',  ( -30.87565027077453905, 177.9895344370344503, 173.1717484556583315 ) ) ;
#40206 = CARTESIAN_POINT ( 'NONE',  ( 4.999999999999999112, -52.63770595436673716, -42.88862352055331684 ) ) ;
#40207 = CARTESIAN_POINT ( 'NONE',  ( 8.311093377946837890, 126.7187499965860269, -8.311093377946837890 ) ) ;
#40208 = CARTESIAN_POINT ( 'NONE',  ( 27.99999999999996803, 199.0000000000000000, 173.9999999999999147 ) ) ;
#40209 = DIRECTION ( 'NONE',  ( 0.000000000000000000, -0.000000000000000000, 1.000000000000000000 ) ) ;
#40212 = DIRECTION ( 'NONE',  ( -0.000000000000000000, -0.000000000000000000, 1.000000000000000000 ) ) ;
#40211 = CARTESIAN_POINT ( 'NONE',  ( 31.45873412499997812, 197.7500000013656063, 168.5673454167822172 ) ) ;
#40210 = CARTESIAN_POINT ( 'NONE',  ( 31.45873412499999944, 197.0000000013656347, 168.5673454167822740 ) ) ;
#40213 = VERTEX_POINT ( 'NONE', #65806 ) ;
#40214 = EDGE_CURVE ( 'NONE', #61038, #35937, #41837, .T. ) ;
#40215 = EDGE_CURVE ( 'NONE', #1694, #14172, #43165, .T. ) ;
#40216 = CARTESIAN_POINT ( 'NONE',  ( 11.35316468749999963, 1.302083329919349941, -3.042071309553165293 ) ) ;
#40217 = CARTESIAN_POINT ( 'NONE',  ( 9.797174393178825657E-16, 125.0000000000000000, -8.000000000000000000 ) ) ;
#40218 = DIRECTION ( 'NONE',  ( 0.000000000000000000, 0.000000000000000000, 1.000000000000000000 ) ) ;
#40219 = CARTESIAN_POINT ( 'NONE',  ( 5.000000000000000000, -62.88740100213644268, -24.06179116403768958 ) ) ;
#40220 = CARTESIAN_POINT ( 'NONE',  ( -8.311093377946836114, 222.9687499965860127, -8.311093377946837890 ) ) ;
#40221 = CARTESIAN_POINT ( 'NONE',  ( 1.320432766682874540E-15, 123.0312500020483810, 7.188101187500000044 ) ) ;
#40222 = CARTESIAN_POINT ( 'NONE',  ( 1.881053915767122664, 2.249999998634407028, 4.541265875000001451 ) ) ;
#40223 = CARTESIAN_POINT ( 'NONE',  ( -4.104248244544275614, 66.38464254927804120, -26.65807398668060912 ) ) ;
#40224 = CARTESIAN_POINT ( 'NONE',  ( 1.469576158976822172E-15, -7.999999999999991118, 19.20530277982336642 ) ) ;
#40226 = CARTESIAN_POINT ( 'NONE',  ( -30.82842712474616320, 207.3750000000000284, 172.8284271247465824 ) ) ;
#40225 = CARTESIAN_POINT ( 'NONE',  ( -49.52045638478375622, 46.95127057776231538, 58.38971101614413328 ) ) ;
#40227 = CARTESIAN_POINT ( 'NONE',  ( -5.676582343750006032, 109.1145833299193555, 9.832129032723418760 ) ) ;
#40228 = EDGE_LOOP ( 'NONE', ( #26269, #58386, #25807 ) ) ;
#40229 = CARTESIAN_POINT ( 'NONE',  ( 4.000000000000001776, 15.81249999726881406, -1.656854249492381248 ) ) ;
#40230 = CARTESIAN_POINT ( 'NONE',  ( 5.082755093536325930, 24.65624999795161543, -5.082755093536325930 ) ) ;
#40231 = DIRECTION ( 'NONE',  ( 0.000000000000000000, 0.000000000000000000, 1.000000000000000000 ) ) ;
#40232 = CARTESIAN_POINT ( 'NONE',  ( -9.832129032723415207, 244.6354166700806445, 5.676582343750005144 ) ) ;
#40233 = CARTESIAN_POINT ( 'NONE',  ( -5.676582343750006032, 104.1145833299193697, 9.832129032723418760 ) ) ;
#40234 = ORIENTED_EDGE ( 'NONE', *, *, #14243, .F. ) ;
#40235 = CARTESIAN_POINT ( 'NONE',  ( -3.205257545844395928, 10.40344923676435052, 117.6241125671348868 ) ) ;
#40236 = EDGE_CURVE ( 'NONE', #40180, #41775, #31103, .T. ) ;
#40237 = CARTESIAN_POINT ( 'NONE',  ( -7.204075437095965206, -7.204075437095968759, 103.8437500020483810 ) ) ;
#40238 = CARTESIAN_POINT ( 'NONE',  ( 8.660254037844385522, 226.4583333265053966, 5.000000000000005329 ) ) ;
#40239 = CARTESIAN_POINT ( 'NONE',  ( -3.458734124999960358, 200.6250000013655779, 196.5673454167823877 ) ) ;
#40240 = CARTESIAN_POINT ( 'NONE',  ( -2.828427124746190735, 6.124999997268813168, -2.828427124746191623 ) ) ;
#40242 = CARTESIAN_POINT ( 'NONE',  ( 5.676582343750001591, 101.6145833299193697, -9.832129032723420536 ) ) ;
#40241 = CARTESIAN_POINT ( 'NONE',  ( -30.82842712474621294, 202.1250000000000284, 167.1715728752542134 ) ) ;
#40243 = CARTESIAN_POINT ( 'NONE',  ( 1.469576158976822172E-15, -7.999999999999991118, 13.39280278392014623 ) ) ;
#40244 = CARTESIAN_POINT ( 'NONE',  ( -28.00000000000001776, 195.6875000013655779, 166.5412658750003629 ) ) ;
#40245 = CARTESIAN_POINT ( 'NONE',  ( 2.679491924310192008, 168.9583333333332291, 10.00000000000059863 ) ) ;
#40246 = ORIENTED_EDGE ( 'NONE', *, *, #25870, .F. ) ;
#40247 = EDGE_CURVE ( 'NONE', #74244, #72648, #59789, .T. ) ;
#40248 = CARTESIAN_POINT ( 'NONE',  ( 8.660254037844389075, 197.2916666598387110, -5.000000000000000000 ) ) ;
#40249 = CARTESIAN_POINT ( 'NONE',  ( -4.898587196589412829E-16, 115.6250000000000000, -8.000000000000000000 ) ) ;
#40250 = CARTESIAN_POINT ( 'NONE',  ( 7.778174593052021635, 7.778174593052023411, 99.62500000409677625 ) ) ;
#40251 = CARTESIAN_POINT ( 'NONE',  ( -9.832129032723418760, 93.17708332991935549, -5.676582343750004256 ) ) ;
#40252 = CARTESIAN_POINT ( 'NONE',  ( -4.088227598258586603E-16, 289.2031250017069510, -6.676582343750001591 ) ) ;
#40253 = CARTESIAN_POINT ( 'NONE',  ( -2.977408999572654480, 6.374999997951610098, 7.188101187499999156 ) ) ;
#40254 = CARTESIAN_POINT ( 'NONE',  ( -10.18810118749999916, 0.000000000000000000, 95.03125000204836681 ) ) ;
#40255 = CARTESIAN_POINT ( 'NONE',  ( -8.311093377946841443, 223.9062499965860411, 8.311093377946830785 ) ) ;
#40256 = ORIENTED_EDGE ( 'NONE', *, *, #52512, .T. ) ;
#40257 = FACE_OUTER_BOUND ( 'NONE', #36122, .T. ) ;
#40258 = CARTESIAN_POINT ( 'NONE',  ( 3.042071309553159519, 219.7395833299193271, 11.35316468750000141 ) ) ;
#40259 = AXIS2_PLACEMENT_3D ( 'NONE', #20190, #2488, #37568 ) ;
#40260 = CARTESIAN_POINT ( 'NONE',  ( 4.999999999999993783, 46.04166665983869677, 8.660254037844390851 ) ) ;
#40261 = CARTESIAN_POINT ( 'NONE',  ( -7.320508075688773708, 98.74999999317202537, -7.320508075688774596 ) ) ;
#40262 = CARTESIAN_POINT ( 'NONE',  ( 6.676582343750004256, 297.8906250017069510, 2.765530957081995478 ) ) ;
#40263 = EDGE_CURVE ( 'NONE', #9014, #13929, #72969, .T. ) ;
#40264 = EDGE_LOOP ( 'NONE', ( #52862, #30164, #33501, #19662 ) ) ;
#40265 = LINE ( 'NONE', #6687, #13565 ) ;
#40266 = CARTESIAN_POINT ( 'NONE',  ( -2.085542519210945728E-15, 204.8437499965860411, 11.35316468750000141 ) ) ;
#40267 =( BOUNDED_CURVE ( )  B_SPLINE_CURVE ( 2, ( #56032, #28083, #38677, #72997, #69850 ),
 .UNSPECIFIED., .F., .F. ) 
 B_SPLINE_CURVE_WITH_KNOTS ( ( 3, 2, 3 ),
 ( 0.9833333333333340587, 0.9916666666666671404, 1.000000000000000000 ),
 .UNSPECIFIED. ) 
 CURVE ( )  GEOMETRIC_REPRESENTATION_ITEM ( )  RATIONAL_B_SPLINE_CURVE ( ( 0.9999999999999928946, 0.9238795325112938439, 1.000000000000000000, 0.9238795325112867385, 1.000000000000000000 ) ) 
 REPRESENTATION_ITEM ( '' )  );
#40268 = CARTESIAN_POINT ( 'NONE',  ( 7.204075437095968759, -7.204075437095966983, 96.71875000204838102 ) ) ;
#40269 = CARTESIAN_POINT ( 'NONE',  ( -30.44569435410883784, 207.5625000013656063, 167.5543056458915885 ) ) ;
#40270 = CARTESIAN_POINT ( 'NONE',  ( -5.656854249492381470, 15.93750000000000355, 5.656854249492379694 ) ) ;
#40271 = ORIENTED_EDGE ( 'NONE', *, *, #45277, .T. ) ;
#40272 = PRODUCT_DEFINITION_CONTEXT ( 'detailed design', #70807, 'design' ) ;
#40273 = CARTESIAN_POINT ( 'NONE',  ( 2.977408999572654480, 123.1250000020484094, 7.188101187499999156 ) ) ;
#40274 = CARTESIAN_POINT ( 'NONE',  ( -2.679491924311235618, 33.54166666666667140, 10.00000000000000000 ) ) ;
#40275 = VECTOR ( 'NONE', #36929, 1000.000000000000000 ) ;
#40276 = CARTESIAN_POINT ( 'NONE',  ( -5.656854249492379694, 8.062500000000001776, -5.656854249492380582 ) ) ;
#40277 = CARTESIAN_POINT ( 'NONE',  ( 10.18810118750000093, -4.220049686691933921, 74.68750000204836681 ) ) ;
#40278 = VERTEX_POINT ( 'NONE', #26179 ) ;
#40279 = CARTESIAN_POINT ( 'NONE',  ( 4.541265875000001451, 2.249999998634407028, 1.881053915767124440 ) ) ;
#40280 = CARTESIAN_POINT ( 'NONE',  ( -2.977408999572654480, 1.499999997951610098, 7.188101187499999156 ) ) ;
#40281 = CARTESIAN_POINT ( 'NONE',  ( 3.313708498984756279, 7.999999999999991118, 6.361552779823365533 ) ) ;
#40282 = DIRECTION ( 'NONE',  ( 1.000000000000000000, 0.000000000000000000, 0.000000000000000000 ) ) ;
#40283 = CARTESIAN_POINT ( 'NONE',  ( 2.977408999572650039, 122.5625000020483952, -7.188101187500001821 ) ) ;
#40284 = CARTESIAN_POINT ( 'NONE',  ( 30.82842712474617031, 199.1250000000000284, 172.8284271247460993 ) ) ;
#40285 = CARTESIAN_POINT ( 'NONE',  ( 2.765530957082001251, 297.7656250017069510, 6.676582343749999815 ) ) ;
#40288 = CARTESIAN_POINT ( 'NONE',  ( 4.000000000000015987, 206.5000000000000284, 198.0000000000000284 ) ) ;
#40287 = CARTESIAN_POINT ( 'NONE',  ( 9.832129032723420536, 240.9895833367473301, 5.676582343749996262 ) ) ;
#40286 = CARTESIAN_POINT ( 'NONE',  ( 30.44569435410879876, 206.8125000013656063, 167.5543056458910485 ) ) ;
#40289 = SHAPE_DEFINITION_REPRESENTATION ( #72807, #61424 ) ;
#40290 = ORIENTED_EDGE ( 'NONE', *, *, #14729, .F. ) ;
#40291 = CARTESIAN_POINT ( 'NONE',  ( 9.832129032723416984, 242.1354166700806445, -5.676582343750003368 ) ) ;
#40292 = CARTESIAN_POINT ( 'NONE',  ( 7.188101187499993827, -2.977408999572645598, 5.142802781871752771 ) ) ;
#40293 = VERTEX_POINT ( 'NONE', #8100 ) ;
#40294 = CARTESIAN_POINT ( 'NONE',  ( -4.220049686691937474, -10.18810118749999738, 70.93750000204838102 ) ) ;
#40295 = CARTESIAN_POINT ( 'NONE',  ( -3.042071309553164404, 82.55208332991936970, -11.35316468749999963 ) ) ;
#40296 = DIRECTION ( 'NONE',  ( 0.000000000000000000, 0.000000000000000000, 1.000000000000000000 ) ) ;
#40297 = CARTESIAN_POINT ( 'NONE',  ( -4.556349186104047710, -10.99999999999999822, 85.28124999999998579 ) ) ;
#40300 = CARTESIAN_POINT ( 'NONE',  ( -6.676582343749999815, 287.6718750017070079, 2.765530957082001251 ) ) ;
#40299 = CARTESIAN_POINT ( 'NONE',  ( 26.34314575050763452, 195.0625000027312126, 173.9999999999999147 ) ) ;
#40298 = CARTESIAN_POINT ( 'NONE',  ( 24.54126587500000412, 206.3750000013656063, 168.5673454167822172 ) ) ;
#40301 = VERTEX_POINT ( 'NONE', #71832 ) ;
#40302 = AXIS2_PLACEMENT_3D ( 'NONE', #49174, #48058, #8443 ) ;
#40303 = EDGE_CURVE ( 'NONE', #65410, #41950, #66551, .T. ) ;
#40304 = CARTESIAN_POINT ( 'NONE',  ( 0.000000000000000000, 201.0000000000000284, 207.0000000000000853 ) ) ;
#40305 = DIRECTION ( 'NONE',  ( -0.000000000000000000, -0.000000000000000000, -1.000000000000000000 ) ) ;
#40306 = CARTESIAN_POINT ( 'NONE',  ( -5.676582343749998039, 197.4479166632526983, -9.832129032723420536 ) ) ;
#40307 = CARTESIAN_POINT ( 'NONE',  ( 2.445694354108782775, 205.5625000013656063, 139.5543056458912190 ) ) ;
#40308 = CARTESIAN_POINT ( 'NONE',  ( 24.54126587500000412, 207.3750000013656063, 168.5673454167822172 ) ) ;
#40309 = CARTESIAN_POINT ( 'NONE',  ( -2.977408999572654480, 24.37499999795161543, 7.188101187499999156 ) ) ;
#40310 = CARTESIAN_POINT ( 'NONE',  ( 3.042071309553159519, 180.0520833299193271, 11.35316468750000141 ) ) ;
#40311 = CARTESIAN_POINT ( 'NONE',  ( 26.34314575050768426, 197.6875000027312126, 165.9999999999998010 ) ) ;
#40312 = CARTESIAN_POINT ( 'NONE',  ( -4.401442555609581635E-16, 100.1562500020483810, -7.188101187500000044 ) ) ;
#40313 = CARTESIAN_POINT ( 'NONE',  ( -8.660254037844381969, 112.0833333333333286, -5.000000000000000888 ) ) ;
#40314 = CARTESIAN_POINT ( 'NONE',  ( -8.342170076843785083E-16, 10.06249999863440614, 4.541265875000002339 ) ) ;
#40315 = CARTESIAN_POINT ( 'NONE',  ( 30.44569435410879166, 202.8125000013656063, 172.4456943541087526 ) ) ;
#40316 = CARTESIAN_POINT ( 'NONE',  ( -4.401442555609577197E-16, 7.188101187499992051, 7.486552781871751883 ) ) ;
#40317 = CARTESIAN_POINT ( 'NONE',  ( 5.676582343749993598, 49.94791666325268409, 9.832129032723422313 ) ) ;
#40318 = CARTESIAN_POINT ( 'NONE',  ( 25.17157287525382259, 206.0000000027312126, 172.8284271247460993 ) ) ;
#40319 = CARTESIAN_POINT ( 'NONE',  ( -7.999999999999991118, 0.000000000000000000, 2.386552784329821542 ) ) ;
#40320 = ORIENTED_EDGE ( 'NONE', *, *, #66198, .F. ) ;
#40321 = DIRECTION ( 'NONE',  ( -0.000000000000000000, 1.000000000000000000, -0.000000000000000000 ) ) ;
#40322 = CARTESIAN_POINT ( 'NONE',  ( 2.947432525776574330, 11.00000000000000178, 66.75185456451232824 ) ) ;
#40323 = CARTESIAN_POINT ( 'NONE',  ( -11.35316468750000141, 58.48958332991933418, 3.042071309553159963 ) ) ;
#40324 = CARTESIAN_POINT ( 'NONE',  ( 11.00000000000000000, 4.556349186104045934, 77.03125000409677625 ) ) ;
#40325 = CARTESIAN_POINT ( 'NONE',  ( 3.458734124999960358, 197.6875000013655779, 142.0000000000000568 ) ) ;
#40326 = CARTESIAN_POINT ( 'NONE',  ( 2.828427124746190291, 8.624999997268814056, 2.828427124746192067 ) ) ;
#40328 = CARTESIAN_POINT ( 'NONE',  ( 5.676582343749993598, 59.94791666325268409, 9.832129032723422313 ) ) ;
#40327 = CARTESIAN_POINT ( 'NONE',  ( -5.082755093536324154, 91.34375000204838102, 5.082755093536326818 ) ) ;
#40329 = CARTESIAN_POINT ( 'NONE',  ( 7.999999999999991118, 9.797174393178815797E-16, 1.580302779823364201 ) ) ;
#40330 = CARTESIAN_POINT ( 'NONE',  ( 9.797174393178825657E-16, 54.99999999999999289, -8.000000000000000000 ) ) ;
#40331 = EDGE_CURVE ( 'NONE', #1603, #61509, #49273, .T. ) ;
#40333 = CARTESIAN_POINT ( 'NONE',  ( -2.679491924311235618, 155.4166666598387394, 10.00000000000000000 ) ) ;
#40332 = PRODUCT_DEFINITION_SHAPE ( 'NONE', 'NONE',  #74666 ) ;
#40334 = CARTESIAN_POINT ( 'NONE',  ( 5.082755093536326818, 98.09375000204838102, 5.082755093536325042 ) ) ;
#40335 = PRESENTATION_LAYER_ASSIGNMENT (  '', '', ( #70434 ) ) ;
#40336 = CARTESIAN_POINT ( 'NONE',  ( -10.00000000000000355, 54.58333332650536818, 2.679491924311223183 ) ) ;
#40337 = CARTESIAN_POINT ( 'NONE',  ( 8.311093377946837890, 51.71874999658602690, -8.311093377946837890 ) ) ;
#40338 = CARTESIAN_POINT ( 'NONE',  ( 10.18810118749999916, 1.247682550866122264E-15, 113.7812500020483810 ) ) ;
#40339 = CARTESIAN_POINT ( 'NONE',  ( 11.35316468749999963, 175.9895833299193555, -3.042071309553165293 ) ) ;
#40340 = VERTEX_POINT ( 'NONE', #42790 ) ;
#40341 = CARTESIAN_POINT ( 'NONE',  ( -30.82842712474621294, 204.1250000000000284, 167.1715728752542134 ) ) ;
#40342 = CARTESIAN_POINT ( 'NONE',  ( -10.18810118749999916, 4.220049686691934809, 73.56250000204835260 ) ) ;
#40343 = CARTESIAN_POINT ( 'NONE',  ( -3.999999999999960032, 198.0000000000000000, 198.0000000000000284 ) ) ;
#40345 = CARTESIAN_POINT ( 'NONE',  ( 5.676582343749993598, 184.9479166632526983, 9.832129032723422313 ) ) ;
#40344 = CARTESIAN_POINT ( 'NONE',  ( 32.00000000000000711, 203.3125000000000284, 168.3431457505075457 ) ) ;
#40346 = CARTESIAN_POINT ( 'NONE',  ( -5.656854249492373476, -5.656854249492376141, 5.574052784329824206 ) ) ;
#40347 = CARTESIAN_POINT ( 'NONE',  ( 2.250000000000000888, 272.7999999999997272, 5.427799975595259063 ) ) ;
#40348 = CARTESIAN_POINT ( 'NONE',  ( -8.660254037844385522, 253.5416666734946602, 5.000000000000004441 ) ) ;
#40349 = CARTESIAN_POINT ( 'NONE',  ( -44.48374486120346205, 184.9827789239285494, 84.30156509589276936 ) ) ;
#40350 = ORIENTED_EDGE ( 'NONE', *, *, #15012, .F. ) ;
#40351 = CARTESIAN_POINT ( 'NONE',  ( 8.311093377946837890, 171.7187499965860127, -8.311093377946837890 ) ) ;
#40352 = EDGE_CURVE ( 'NONE', #31834, #57818, #25682, .T. ) ;
#40353 = CARTESIAN_POINT ( 'NONE',  ( 7.188101187499992051, 2.977408999572647819, 24.83030278187175455 ) ) ;
#40354 = CARTESIAN_POINT ( 'NONE',  ( 5.676582343750001591, 131.9270833299193555, -9.832129032723420536 ) ) ;
#40355 =( BOUNDED_CURVE ( )  B_SPLINE_CURVE ( 2, ( #31485, #42788, #18315, #48080, #35673, #41328, #24697, #36408, #64338 ),
 .UNSPECIFIED., .F., .F. ) 
 B_SPLINE_CURVE_WITH_KNOTS ( ( 3, 2, 2, 2, 3 ),
 ( 0.1979166666666667962, 0.2031250000000001388, 0.2083333333333334814, 0.2135416666666667962, 0.2187500000000001388 ),
 .UNSPECIFIED. ) 
 CURVE ( )  GEOMETRIC_REPRESENTATION_ITEM ( )  RATIONAL_B_SPLINE_CURVE ( ( 0.9999999999999980016, 0.9238795325112887369, 1.000000000000000000, 0.9238795325112867385, 1.000000000000000000, 0.9238795325112867385, 1.000000000000000000, 0.9238795325112847401, 1.000000000000001998 ) ) 
 REPRESENTATION_ITEM ( '' )  );
#40356 = ADVANCED_FACE ( 'NONE', ( #28056 ), #56366, .F. ) ;
#40357 = DIRECTION ( 'NONE',  ( 1.000000000000000000, -0.000000000000000000, -0.000000000000000000 ) ) ;
#40358 = ORIENTED_EDGE ( 'NONE', *, *, #74582, .F. ) ;
#40359 = CARTESIAN_POINT ( 'NONE',  ( 4.541265875000002339, 6.437499998634407028, 0.000000000000000000 ) ) ;
#40360 = CARTESIAN_POINT ( 'NONE',  ( 2.977408999572650927, 12.74999999795161187, -7.188101187500001821 ) ) ;
#40361 = CARTESIAN_POINT ( 'NONE',  ( 8.000000000000001776, 103.3437500040967763, 3.313708498984759387 ) ) ;
#40362 = CARTESIAN_POINT ( 'NONE',  ( -29.43265458321760519, 198.1250000013656063, 173.4587341250003760 ) ) ;
#40363 = EDGE_CURVE ( 'NONE', #38241, #30899, #38649, .T. ) ;
#40364 = CARTESIAN_POINT ( 'NONE',  ( 4.000000000000001776, 9.000000000000001776, 0.000000000000000000 ) ) ;
#40365 =( BOUNDED_CURVE ( )  B_SPLINE_CURVE ( 2, ( #9900, #26105, #55187, #32930, #67981, #55936, #43467, #72524, #61581, #66481, #38944, #38201, #32166 ),
 .UNSPECIFIED., .F., .F. ) 
 B_SPLINE_CURVE_WITH_KNOTS ( ( 3, 2, 2, 2, 2, 2, 3 ),
 ( 0.1576086956521739191, 0.1594202898550724501, 0.1612318840579710089, 0.1630434782608695676, 0.1648550724637681264, 0.1666666666666666574, 0.1684782608695652162 ),
 .UNSPECIFIED. ) 
 CURVE ( )  GEOMETRIC_REPRESENTATION_ITEM ( )  RATIONAL_B_SPLINE_CURVE ( ( 1.000000000000000000, 0.9659258262890683122, 1.000000000000000000, 0.9659258262890683122, 1.000000000000000000, 0.9659258262890683122, 1.000000000000000000, 0.9659258262890683122, 1.000000000000000000, 0.9659258262890683122, 1.000000000000000000, 0.9659258262890683122, 1.000000000000000000 ) ) 
 REPRESENTATION_ITEM ( '' )  );
#40366 = CARTESIAN_POINT ( 'NONE',  ( -30.78024028171753557, -12.00073527780299543, 173.7948410690662797 ) ) ;
#40367 = CARTESIAN_POINT ( 'NONE',  ( -3.211159895383561391, 10.68749999863440792, -3.211159895383561835 ) ) ;
#40368 = CARTESIAN_POINT ( 'NONE',  ( 5.656854249492376141, -5.656854249492374365, 19.58030278392014978 ) ) ;
#40369 = CARTESIAN_POINT ( 'NONE',  ( 3.999999999999960032, 196.9375000000000284, 143.6568542494924543 ) ) ;
#40370 = ORIENTED_EDGE ( 'NONE', *, *, #65766, .F. ) ;
#40371 = CYLINDRICAL_SURFACE ( 'NONE', #74037, 8.000000000000000000 ) ;
#40372 = CARTESIAN_POINT ( 'NONE',  ( -2.977408999572651815, 104.9375000020483810, 7.188101187500000933 ) ) ;
#40373 = MANIFOLD_SOLID_BREP ( 'EndChamfer', #10549 ) ;
#40374 = AXIS2_PLACEMENT_3D ( 'NONE', #809, #22668, #6081 ) ;
#40376 = CARTESIAN_POINT ( 'NONE',  ( -8.000000000000000000, 15.46874999590322197, -3.313708498984762496 ) ) ;
#40375 = CARTESIAN_POINT ( 'NONE',  ( 0.000000000000000000, -10.39230484541329247, -10.20000000000000284 ) ) ;
#40377 = EDGE_LOOP ( 'NONE', ( #9104, #15648 ) ) ;
#40378 = PLANE ( 'NONE',  #8990 ) ;
#40379 = AXIS2_PLACEMENT_3D ( 'NONE', #36404, #36039, #60141 ) ;
#40380 = CARTESIAN_POINT ( 'NONE',  ( -7.188101187499991163, 2.977408999572646930, 26.89280278187175455 ) ) ;
#40381 = ORIENTED_EDGE ( 'NONE', *, *, #36479, .T. ) ;
#40382 = EDGE_LOOP ( 'NONE', ( #22256, #65575, #50360, #38302, #32646 ) ) ;
#40383 = CARTESIAN_POINT ( 'NONE',  ( -6.238412754330611322E-16, 10.18810118749999916, 89.78125000204836681 ) ) ;
#40384 = CARTESIAN_POINT ( 'NONE',  ( -32.00000000000002842, 195.3125000027312126, 168.3431457505080857 ) ) ;
#40385 = CARTESIAN_POINT ( 'NONE',  ( -25.55430564589114795, 195.3125000013656063, 172.4456943541091789 ) ) ;
#40386 = CARTESIAN_POINT ( 'NONE',  ( 2.020667218593132706E-15, -11.00000000000000000, 98.87499999999998579 ) ) ;
#40388 = CARTESIAN_POINT ( 'NONE',  ( 4.721056650415999201, 298.2343750017069510, -4.721056650415999201 ) ) ;
#40387 = CARTESIAN_POINT ( 'NONE',  ( -2.485281374238268004, 290.2500000034139589, 6.000000000000304645 ) ) ;
#40389 = ADVANCED_FACE ( 'NONE', ( #56741 ), #57110, .T. ) ;
#40390 = CARTESIAN_POINT ( 'NONE',  ( 10.00000000000000000, 129.7916666666666856, 2.679491924311236062 ) ) ;
#40391 = CARTESIAN_POINT ( 'NONE',  ( -7.999999999999998224, 101.0937500000000142, 3.313708498984766493 ) ) ;
#40392 = CARTESIAN_POINT ( 'NONE',  ( 7.778174593052023411, -7.778174593052021635, 87.25000000409677625 ) ) ;
#40393 = CARTESIAN_POINT ( 'NONE',  ( -2.977408999572647819, 7.188101187499991163, 6.080302781871753659 ) ) ;
#40394 = EDGE_CURVE ( 'NONE', #36412, #8888, #5060, .T. ) ;
#40395 = CARTESIAN_POINT ( 'NONE',  ( 7.999999999999998224, 1.406250000000000000, 3.313708498984766049 ) ) ;
#40396 = CARTESIAN_POINT ( 'NONE',  ( 24.54126587500000056, 204.1250000013656063, 168.5673454167822172 ) ) ;
#40397 = CARTESIAN_POINT ( 'NONE',  ( 7.188101187500001821, 0.9374999979516102089, -2.977408999572650483 ) ) ;
#40398 = CARTESIAN_POINT ( 'NONE',  ( -8.008118988124989457, -3.317071493978883900, 5.606865283940630995 ) ) ;
#40399 = CARTESIAN_POINT ( 'NONE',  ( 3.458734124999959914, 196.4375000013655779, 142.0000000000000568 ) ) ;
#40400 = CARTESIAN_POINT ( 'NONE',  ( 2.977408999572654480, 119.0000000020483810, 7.188101187499999156 ) ) ;
#40402 = CARTESIAN_POINT ( 'NONE',  ( 2.303252245372744866, 194.8562092600117523, 194.8685895655538332 ) ) ;
#40401 = FACE_OUTER_BOUND ( 'NONE', #15639, .T. ) ;
#40403 = CARTESIAN_POINT ( 'NONE',  ( 11.35316468749999608, 241.9270833367473301, -3.042071309553167069 ) ) ;
#40404 = CARTESIAN_POINT ( 'NONE',  ( -3.313708498984761608, 90.21874999999998579, -8.000000000000000000 ) ) ;
#40405 = CARTESIAN_POINT ( 'NONE',  ( 5.082755093536320601, -5.082755093536318824, 26.42405278187175810 ) ) ;
#40406 = CARTESIAN_POINT ( 'NONE',  ( 31.99999999999999289, 198.2500000000000000, 169.9999999999999432 ) ) ;
#40407 = CARTESIAN_POINT ( 'NONE',  ( 5.676582343750001591, 21.61458332991935194, -9.832129032723420536 ) ) ;
#40408 = ADVANCED_FACE ( 'NONE', ( #4315 ), #23136, .F. ) ;
#40409 = CARTESIAN_POINT ( 'NONE',  ( 3.313708498984765161, 100.1562500040967763, 7.999999999999998224 ) ) ;
#40410 = CARTESIAN_POINT ( 'NONE',  ( -8.311093377946836114, 222.9687499965860127, -8.311093377946837890 ) ) ;
#40411 = FACE_OUTER_BOUND ( 'NONE', #11250, .T. ) ;
#40413 = CARTESIAN_POINT ( 'NONE',  ( -7.320508075688892724, 41.87500000000009237, -7.320508075688893612 ) ) ;
#40412 = DIRECTION ( 'NONE',  ( 0.9884788384745426537, 6.483116892092363099E-18, -0.1513591288559071046 ) ) ;
#40414 = EDGE_LOOP ( 'NONE', ( #5293, #41190, #19520 ) ) ;
#40415 = CARTESIAN_POINT ( 'NONE',  ( 2.445694354108783219, 196.8125000013656063, 139.5543056458912190 ) ) ;
#40416 = CARTESIAN_POINT ( 'NONE',  ( 8.311093377946834337, 20.15624999658600913, 8.311093377946839666 ) ) ;
#40417 = CARTESIAN_POINT ( 'NONE',  ( -6.735557395310442023E-16, 11.00000000000000000, 93.81250000409677625 ) ) ;
#40418 = CARTESIAN_POINT ( 'NONE',  ( -5.000000000000008882, 153.3333333333333428, 8.660254037844392627 ) ) ;
#40419 = CARTESIAN_POINT ( 'NONE',  ( 4.898587196589412829E-16, 7.687499995903221084, -8.000000000000000000 ) ) ;
#40421 = CARTESIAN_POINT ( 'NONE',  ( 3.042071309553159519, 24.73958332991934839, 11.35316468750000141 ) ) ;
#40420 = CARTESIAN_POINT ( 'NONE',  ( 5.082755093536326818, 109.7187500020483810, 5.082755093536325042 ) ) ;
#40422 = CARTESIAN_POINT ( 'NONE',  ( 7.999999999999992895, -3.313708498984756279, 22.48655277982336287 ) ) ;
#40423 = CARTESIAN_POINT ( 'NONE',  ( -11.35316468750000141, 133.4895833299193839, 3.042071309553159963 ) ) ;
#40424 = CARTESIAN_POINT ( 'NONE',  ( 6.123233995736767268E-16, 108.1249999931720396, -10.00000000000000178 ) ) ;
#40425 = CARTESIAN_POINT ( 'NONE',  ( -2.977408999572651815, 114.3125000020483952, 7.188101187500000933 ) ) ;
#40426 = CARTESIAN_POINT ( 'NONE',  ( 13.99999999999999822, -2.250000000005106138, 7.677076266390546522 ) ) ;
#40427 = CARTESIAN_POINT ( 'NONE',  ( -25.55430564589119768, 209.5625000013656063, 167.5543056458915316 ) ) ;
#40428 = CARTESIAN_POINT ( 'NONE',  ( -5.000000000000000000, 50.64189880742145533, -41.08656465431843685 ) ) ;
#40429 = ORIENTED_EDGE ( 'NONE', *, *, #58829, .F. ) ;
#40430 = CARTESIAN_POINT ( 'NONE',  ( 9.832129032723416984, 10.67708332991935016, 5.676582343750006032 ) ) ;
#40431 = CARTESIAN_POINT ( 'NONE',  ( -10.00000000000000355, 154.5833333265053682, 2.679491924311223183 ) ) ;
#40432 = CARTESIAN_POINT ( 'NONE',  ( 4.721056650416000089, 296.8281250017069510, 4.721056650415999201 ) ) ;
#40433 = CARTESIAN_POINT ( 'NONE',  ( -8.311093377946841443, 143.9062499965860127, 8.311093377946834337 ) ) ;
#40434 = DIRECTION ( 'NONE',  ( 0.000000000000000000, 0.000000000000000000, 1.000000000000000000 ) ) ;
#40435 = CARTESIAN_POINT ( 'NONE',  ( 3.313708498984762496, -7.999999999999989342, 22.35530278432982598 ) ) ;
#40436 = CARTESIAN_POINT ( 'NONE',  ( 0.000000000000000000, 300.0000000000000000, 0.000000000000000000 ) ) ;
#40437 = CARTESIAN_POINT ( 'NONE',  ( -11.35316468749999608, 254.1145833367473585, 3.042071309553173730 ) ) ;
#40438 = CIRCLE ( 'NONE', #47625, 11.00000000000000000 ) ;
#40439 = CARTESIAN_POINT ( 'NONE',  ( 10.18810118749999916, 4.220049686691935698, 95.87500000204838102 ) ) ;
#40440 = ORIENTED_EDGE ( 'NONE', *, *, #32053, .F. ) ;
#40441 = ADVANCED_FACE ( 'NONE', ( #22378 ), #27304, .T. ) ;
#40442 = VECTOR ( 'NONE', #56338, 1000.000000000000000 ) ;
#40443 = DIRECTION ( 'NONE',  ( -0.000000000000000000, 1.000000000000000000, -0.000000000000000000 ) ) ;
#40444 = CARTESIAN_POINT ( 'NONE',  ( 2.449293598294707893E-16, 8.250000000000000000, -4.000000000000001776 ) ) ;
#40445 = CARTESIAN_POINT ( 'NONE',  ( -11.35316468750000141, 83.80208332991934128, 3.042071309553159963 ) ) ;
#40446 = ORIENTED_EDGE ( 'NONE', *, *, #2931, .F. ) ;
#40447 = CARTESIAN_POINT ( 'NONE',  ( 4.220049686691934809, 10.18810118749999916, 109.1875000020483810 ) ) ;
#40448 = CARTESIAN_POINT ( 'NONE',  ( -1.881053915767124440, 14.12499999863440792, 4.541265875000001451 ) ) ;
#40449 = VERTEX_POINT ( 'NONE', #45044 ) ;
#40450 = ORIENTED_EDGE ( 'NONE', *, *, #13168, .T. ) ;
#40451 = CARTESIAN_POINT ( 'NONE',  ( 4.898587196589412829E-16, 1.875000000000000444, -8.000000000000000000 ) ) ;
#40452 = CARTESIAN_POINT ( 'NONE',  ( -3.673940397442060854E-16, 292.8125000034140157, -6.000000000000001776 ) ) ;
#40453 = CARTESIAN_POINT ( 'NONE',  ( -5.000000000000000000, -62.32183698944596983, -23.94439461060419916 ) ) ;
#40454 = CARTESIAN_POINT ( 'NONE',  ( 5.082755093536324154, 26.15624999795161543, 5.082755093536326818 ) ) ;
#40455 = CARTESIAN_POINT ( 'NONE',  ( 3.313708498984760720, 120.2187500040967763, -8.000000000000000000 ) ) ;
#40456 = CARTESIAN_POINT ( 'NONE',  ( -10.18810118749999916, 4.220049686691934809, 105.4375000020483668 ) ) ;
#40457 = CARTESIAN_POINT ( 'NONE',  ( -4.556349186104045934, 11.00000000000000000, 75.71874999999998579 ) ) ;
#40458 = CARTESIAN_POINT ( 'NONE',  ( 2.828427124746190291, 10.62499999726881406, 2.828427124746192067 ) ) ;
#40459 = CARTESIAN_POINT ( 'NONE',  ( 36.10814071610729314, 49.99999999999998579, 139.0000000000000000 ) ) ;
#40460 = VERTEX_POINT ( 'NONE', #11454 ) ;
#40461 = CARTESIAN_POINT ( 'NONE',  ( -5.000000000000000888, 262.2916666734946034, -8.660254037844387298 ) ) ;
#40462 = CARTESIAN_POINT ( 'NONE',  ( 2.754378923186476579E-14, 204.1875000013656063, 194.5412658750000219 ) ) ;
#40464 =( BOUNDED_SURFACE ( )  B_SPLINE_SURFACE ( 1, 2, ( 
 ( #47769, #72560, #42110, #8160, #65121, #49541, #64764, #47035, #59485, #42483, #41755, #36840, #32200, #20864, #15203, #38233, #61238, #7060, #9566, #32584, #18747, #30068, #55591, #66995, #39440, #43985, #72659, #15294, #16042, #50382, #44729, #44360, #16406, #33066, #15668, #45461, #61710, #56064, #5121, #56427, #27365, #55318, #50751, #62439, #26998, #10767, #10031, #45100, #51128, #68112, #4371, #73399, #9664, #21339, #4749, #74139, #38330, #21703, #61336, #67747, #32685, #33805, #39074, #62078, #27741, #55693, #10401, #38712, #73028, #22440, #4007, #60961, #50011, #33428, #14921, #67371, #56802, #73765, #22074, #28113, #37963, #9279, #32301, #3624, #26620, #49643, #20962, #40553, #52620, #29607, #63558, #957, #68477, #17913, #11884, #17536, #57554, #5488, #1322, #28489, #17164, #62811, #5861, #35285, #29973, #45837, #34918, #69227, #69599, #40183, #6964, #11147, #57930, #57171, #34170, #29240, #74509, #6237, #52252, #58297, #41299, #46947, #51880, #16779, #68851, #51497, #63939, #587, #23937, #12248, #22821, #23568, #63186, #220, #11515, #46578, #58657, #34548, #40930, #6601, #69976, #64309, #18284, #28859, #39805, #12614, #23199, #46212, #35643, #52989, #24305, #19015, #41664, #36010, #36746, #65404, #53361, #31452, #25405, #59029, #18654, #2040, #3155, #8067, #54478, #71057, #59390, #7703, #70343, #64673, #14452, #13337, #30708, #70696, #25769, #13702, #48789, #12974, #31069, #42757, #71797, #25028, #48047, #19375, #1686, #8815, #24665, #2782, #54097, #20116, #42389, #59757, #7335, #2409, #66146, #48419, #71422, #43130, #19749, #30342, #65774, #53729, #14075, #37488, #42021, #31827, #47676, #65029, #36374, #37112, #60114, #8433, #60488, #54846, #47316, #67651, #21243, #44267, #32203, #67279, #61616, #14825, #72171, #55224, #15575, #4654, #27647, #16311, #38616, #60862, #39348, #50288, #37867, #43503, #73309, #45011, #3529, #32968, #55970, #49546, #20485 ),
 ( #9570, #26144, #26520, #9184, #21611, #9934, #56333, #44637, #66514, #4280, #72565, #32589, #20868, #49919, #62344, #43889, #27272, #72933, #15950, #21986, #38976, #66901, #15206, #61984, #38236, #61241, #10307, #55595, #33334, #50656, #3914, #10676, #26903, #73675, #68016, #33708, #56711, #49164, #29517, #34458, #17819, #45743, #58208, #22726, #5028, #51779, #57459, #74417, #63096, #128, #63841, #40834, #23105, #12158, #28026, #29146, #46117, #28764, #68758, #16685, #12523, #39716, #28396, #74044, #17069, #46487, #41208, #57080, #69135, #5765, #6140, #51403, #18194, #22344, #17442, #68385, #45370, #40463, #11055, #63466, #11790, #69509, #52527, #6511, #11421, #51035, #5395, #62717, #496, #34828, #35192, #23476, #34084, #57834, #40091, #52163, #865, #23850, #69880, #46859, #64217, #35554, #24941, #54385, #59666, #24582, #29885, #71335, #70609, #47586, #64942, #2693, #18929, #35920, #8342, #12885, #41573, #58939, #7980, #19288, #13619, #13253, #60024, #1951, #59304, #14363, #30619, #47959, #48699, #25311, #70973, #24210, #19656, #31356, #41934, #25680, #53641, #13981, #20022, #37022, #42298, #65315, #53270, #36286, #48328, #43035, #7244, #36655, #30253, #30984, #1597, #71706, #54004, #2317, #42670, #65681, #66055, #58567, #7612, #6875, #52898, #64588, #1232, #47222, #70253, #18562, #31735, #26815, #20398, #20778, #43412, #61148, #27558, #66427, #21152, #9478, #3818, #33247, #38523, #3436, #8723, #50200, #49452, #26426, #43798, #56246, #72471, #14738, #61895, #37778, #60773, #9099, #61525, #72847, #67189, #66813, #38891, #55506, #38147, #67931, #32494, #49829, #50568, #4194, #44175, #3066, #73220, #10218, #15115, #4562, #15487, #67560, #73585, #15855, #9848, #32873, #32113, #55879, #27183, #21892, #55132, #21527, #44549, #44922, #37395, #60397, #54756, #26050, #49070, #72083, #63008, #40004, #74327, #774, #62632, #62262, #51317, #17352, #23760, #45654, #40740 ) ),
 .UNSPECIFIED., .F., .F., .F. ) 
 B_SPLINE_SURFACE_WITH_KNOTS ( ( 2, 2 ),
 ( 3, 2, 2, 2, 2, 2, 2, 2, 2, 2, 2, 2, 2, 2, 2, 2, 2, 2, 2, 2, 2, 2, 2, 2, 2, 2, 2, 2, 2, 2, 2, 2, 2, 2, 2, 2, 2, 2, 2, 2, 2, 2, 2, 2, 2, 2, 2, 2, 2, 2, 2, 2, 2, 2, 2, 2, 2, 2, 2, 2, 2, 2, 2, 2, 2, 2, 2, 2, 2, 2, 2, 2, 2, 2, 2, 2, 2, 2, 2, 2, 2, 2, 2, 2, 2, 2, 2, 2, 2, 2, 2, 2, 2, 2, 2, 2, 2, 2, 2, 2, 2, 2, 2, 2, 2, 2, 2, 2, 2, 2, 2, 2, 2, 2, 2, 2, 2, 2, 2, 2, 3 ),
 ( 0.000000000000000000, 1.000000000000000000 ),
 ( 0.000000000000000000, 0.008333333333333333218, 0.01666666666666666644, 0.02500000000000000139, 0.03333333333333333287, 0.04166666666666666435, 0.05000000000000000278, 0.05833333333333333426, 0.06666666666666666574, 0.07499999999999999722, 0.08333333333333332871, 0.09166666666666666019, 0.1000000000000000056, 0.1083333333333333370, 0.1166666666666666685, 0.1250000000000000000, 0.1333333333333333315, 0.1416666666666666630, 0.1499999999999999944, 0.1583333333333333259, 0.1666666666666666574, 0.1749999999999999889, 0.1833333333333333204, 0.1916666666666666796, 0.2000000000000000111, 0.2083333333333333426, 0.2166666666666666741, 0.2250000000000000056, 0.2333333333333333370, 0.2416666666666666685, 0.2500000000000000000, 0.2583333333333333592, 0.2666666666666666630, 0.2750000000000000222, 0.2833333333333333259, 0.2916666666666666852, 0.2999999999999999889, 0.3083333333333333481, 0.3166666666666666519, 0.3250000000000000111, 0.3333333333333333148, 0.3416666666666666741, 0.3499999999999999778, 0.3583333333333333370, 0.3666666666666666408, 0.3750000000000000000, 0.3833333333333333592, 0.3916666666666666630, 0.4000000000000000222, 0.4083333333333333259, 0.4166666666666666852, 0.4249999999999999889, 0.4333333333333333481, 0.4416666666666666519, 0.4500000000000000111, 0.4583333333333333148, 0.4666666666666666741, 0.4749999999999999778, 0.4833333333333333370, 0.4916666666666666408, 0.5000000000000000000, 0.5083333333333333037, 0.5166666666666667185, 0.5250000000000000222, 0.5333333333333333259, 0.5416666666666666297, 0.5500000000000000444, 0.5583333333333333481, 0.5666666666666666519, 0.5749999999999999556, 0.5833333333333333703, 0.5916666666666666741, 0.5999999999999999778, 0.6083333333333332815, 0.6166666666666666963, 0.6250000000000000000, 0.6333333333333333037, 0.6416666666666667185, 0.6500000000000000222, 0.6583333333333333259, 0.6666666666666666297, 0.6750000000000000444, 0.6833333333333333481, 0.6916666666666666519, 0.6999999999999999556, 0.7083333333333333703, 0.7166666666666666741, 0.7249999999999999778, 0.7333333333333332815, 0.7416666666666666963, 0.7500000000000000000, 0.7583333333333333037, 0.7666666666666667185, 0.7750000000000000222, 0.7833333333333333259, 0.7916666666666666297, 0.8000000000000000444, 0.8083333333333333481, 0.8166666666666666519, 0.8249999999999999556, 0.8333333333333333703, 0.8416666666666666741, 0.8499999999999999778, 0.8583333333333332815, 0.8666666666666666963, 0.8750000000000000000, 0.8833333333333333037, 0.8916666666666667185, 0.9000000000000000222, 0.9083333333333333259, 0.9166666666666666297, 0.9250000000000000444, 0.9333333333333333481, 0.9416666666666666519, 0.9499999999999999556, 0.9583333333333333703, 0.9666666666666666741, 0.9749999999999999778, 0.9833333333333332815, 0.9916666666666666963, 1.000000000000000000 ),
 .UNSPECIFIED. ) 
 GEOMETRIC_REPRESENTATION_ITEM ( )  RATIONAL_B_SPLINE_SURFACE ( (
 ( 1.000000000000000000, 0.9238795325112867385, 1.000000000000000000, 0.9238795325112867385, 1.000000000000000000, 0.9238795325112867385, 1.000000000000000000, 0.9238795325112867385, 1.000000000000000000, 0.9238795325112867385, 1.000000000000000000, 0.9238795325112867385, 1.000000000000000000, 0.9238795325112867385, 1.000000000000000000, 0.9238795325112867385, 1.000000000000000000, 0.9238795325112867385, 1.000000000000000000, 0.9238795325112867385, 1.000000000000000000, 0.9238795325112867385, 1.000000000000000000, 0.9238795325112867385, 1.000000000000000000, 0.9238795325112867385, 1.000000000000000000, 0.9238795325112867385, 1.000000000000000000, 0.9238795325112867385, 1.000000000000000000, 0.9238795325112867385, 1.000000000000000000, 0.9238795325112867385, 1.000000000000000000, 0.9238795325112867385, 1.000000000000000000, 0.9238795325112867385, 1.000000000000000000, 0.9238795325112867385, 1.000000000000000000, 0.9238795325112867385, 1.000000000000000000, 0.9238795325112867385, 1.000000000000000000, 0.9238795325112867385, 1.000000000000000000, 0.9238795325112867385, 1.000000000000000000, 0.9238795325112867385, 1.000000000000000000, 0.9238795325112867385, 1.000000000000000000, 0.9238795325112867385, 1.000000000000000000, 0.9238795325112867385, 1.000000000000000000, 0.9238795325112867385, 1.000000000000000000, 0.9238795325112867385, 1.000000000000000000, 0.9238795325112867385, 1.000000000000000000, 0.9238795325112867385, 1.000000000000000000, 0.9238795325112867385, 1.000000000000000000, 0.9238795325112867385, 1.000000000000000000, 0.9238795325112867385, 1.000000000000000000, 0.9238795325112867385, 1.000000000000000000, 0.9238795325112867385, 1.000000000000000000, 0.9238795325112867385, 1.000000000000000000, 0.9238795325112867385, 1.000000000000000000, 0.9238795325112867385, 1.000000000000000000, 0.9238795325112867385, 1.000000000000000000, 0.9238795325112867385, 1.000000000000000000, 0.9238795325112867385, 1.000000000000000000, 0.9238795325112867385, 1.000000000000000000, 0.9238795325112867385, 1.000000000000000000, 0.9238795325112867385, 1.000000000000000000, 0.9238795325112867385, 1.000000000000000000, 0.9238795325112867385, 1.000000000000000000, 0.9238795325112867385, 1.000000000000000000, 0.9238795325112867385, 1.000000000000000000, 0.9238795325112867385, 1.000000000000000000, 0.9238795325112867385, 1.000000000000000000, 0.9238795325112867385, 1.000000000000000000, 0.9238795325112867385, 1.000000000000000000, 0.9238795325112867385, 1.000000000000000000, 0.9238795325112867385, 1.000000000000000000, 0.9238795325112867385, 1.000000000000000000, 0.9238795325112867385, 1.000000000000000000, 0.9238795325112867385, 1.000000000000000000, 0.9238795325112867385, 1.000000000000000000, 0.9238795325112867385, 1.000000000000000000, 0.9238795325112867385, 1.000000000000000000, 0.9238795325112867385, 1.000000000000000000, 0.9238795325112867385, 1.000000000000000000, 0.9238795325112867385, 1.000000000000000000, 0.9238795325112867385, 1.000000000000000000, 0.9238795325112867385, 1.000000000000000000, 0.9238795325112867385, 1.000000000000000000, 0.9238795325112867385, 1.000000000000000000, 0.9238795325112867385, 1.000000000000000000, 0.9238795325112867385, 1.000000000000000000, 0.9238795325112867385, 1.000000000000000000, 0.9238795325112867385, 1.000000000000000000, 0.9238795325112867385, 1.000000000000000000, 0.9238795325112867385, 1.000000000000000000, 0.9238795325112867385, 1.000000000000000000, 0.9238795325112867385, 1.000000000000000000, 0.9238795325112867385, 1.000000000000000000, 0.9238795325112867385, 1.000000000000000000, 0.9238795325112867385, 1.000000000000000000, 0.9238795325112867385, 1.000000000000000000, 0.9238795325112867385, 1.000000000000000000, 0.9238795325112867385, 1.000000000000000000, 0.9238795325112867385, 1.000000000000000000, 0.9238795325112867385, 1.000000000000000000, 0.9238795325112867385, 1.000000000000000000, 0.9238795325112867385, 1.000000000000000000, 0.9238795325112867385, 1.000000000000000000, 0.9238795325112867385, 1.000000000000000000, 0.9238795325112867385, 1.000000000000000000, 0.9238795325112867385, 1.000000000000000000, 0.9238795325112867385, 1.000000000000000000, 0.9238795325112867385, 1.000000000000000000, 0.9238795325112867385, 1.000000000000000000, 0.9238795325112867385, 1.000000000000000000, 0.9238795325112867385, 1.000000000000000000, 0.9238795325112867385, 1.000000000000000000, 0.9238795325112867385, 1.000000000000000000, 0.9238795325112867385, 1.000000000000000000, 0.9238795325112867385, 1.000000000000000000, 0.9238795325112867385, 1.000000000000000000, 0.9238795325112867385, 1.000000000000000000, 0.9238795325112867385, 1.000000000000000000, 0.9238795325112867385, 1.000000000000000000, 0.9238795325112867385, 1.000000000000000000, 0.9238795325112867385, 1.000000000000000000, 0.9238795325112867385, 1.000000000000000000, 0.9238795325112867385, 1.000000000000000000, 0.9238795325112867385, 1.000000000000000000, 0.9238795325112867385, 1.000000000000000000, 0.9238795325112867385, 1.000000000000000000, 0.9238795325112867385, 1.000000000000000000, 0.9238795325112867385, 1.000000000000000000, 0.9238795325112867385, 1.000000000000000000, 0.9238795325112867385, 1.000000000000000000, 0.9238795325112867385, 1.000000000000000000, 0.9238795325112867385, 1.000000000000000000, 0.9238795325112867385, 1.000000000000000000, 0.9238795325112867385, 1.000000000000000000, 0.9238795325112867385, 1.000000000000000000),
 ( 1.000000000000000000, 0.9238795325112867385, 1.000000000000000000, 0.9238795325112867385, 1.000000000000000000, 0.9238795325112867385, 1.000000000000000000, 0.9238795325112867385, 1.000000000000000000, 0.9238795325112867385, 1.000000000000000000, 0.9238795325112867385, 1.000000000000000000, 0.9238795325112867385, 1.000000000000000000, 0.9238795325112867385, 1.000000000000000000, 0.9238795325112867385, 1.000000000000000000, 0.9238795325112867385, 1.000000000000000000, 0.9238795325112867385, 1.000000000000000000, 0.9238795325112867385, 1.000000000000000000, 0.9238795325112867385, 1.000000000000000000, 0.9238795325112867385, 1.000000000000000000, 0.9238795325112867385, 1.000000000000000000, 0.9238795325112867385, 1.000000000000000000, 0.9238795325112867385, 1.000000000000000000, 0.9238795325112867385, 1.000000000000000000, 0.9238795325112867385, 1.000000000000000000, 0.9238795325112867385, 1.000000000000000000, 0.9238795325112867385, 1.000000000000000000, 0.9238795325112867385, 1.000000000000000000, 0.9238795325112867385, 1.000000000000000000, 0.9238795325112867385, 1.000000000000000000, 0.9238795325112867385, 1.000000000000000000, 0.9238795325112867385, 1.000000000000000000, 0.9238795325112867385, 1.000000000000000000, 0.9238795325112867385, 1.000000000000000000, 0.9238795325112867385, 1.000000000000000000, 0.9238795325112867385, 1.000000000000000000, 0.9238795325112867385, 1.000000000000000000, 0.9238795325112867385, 1.000000000000000000, 0.9238795325112867385, 1.000000000000000000, 0.9238795325112867385, 1.000000000000000000, 0.9238795325112867385, 1.000000000000000000, 0.9238795325112867385, 1.000000000000000000, 0.9238795325112867385, 1.000000000000000000, 0.9238795325112867385, 1.000000000000000000, 0.9238795325112867385, 1.000000000000000000, 0.9238795325112867385, 1.000000000000000000, 0.9238795325112867385, 1.000000000000000000, 0.9238795325112867385, 1.000000000000000000, 0.9238795325112867385, 1.000000000000000000, 0.9238795325112867385, 1.000000000000000000, 0.9238795325112867385, 1.000000000000000000, 0.9238795325112867385, 1.000000000000000000, 0.9238795325112867385, 1.000000000000000000, 0.9238795325112867385, 1.000000000000000000, 0.9238795325112867385, 1.000000000000000000, 0.9238795325112867385, 1.000000000000000000, 0.9238795325112867385, 1.000000000000000000, 0.9238795325112867385, 1.000000000000000000, 0.9238795325112867385, 1.000000000000000000, 0.9238795325112867385, 1.000000000000000000, 0.9238795325112867385, 1.000000000000000000, 0.9238795325112867385, 1.000000000000000000, 0.9238795325112867385, 1.000000000000000000, 0.9238795325112867385, 1.000000000000000000, 0.9238795325112867385, 1.000000000000000000, 0.9238795325112867385, 1.000000000000000000, 0.9238795325112867385, 1.000000000000000000, 0.9238795325112867385, 1.000000000000000000, 0.9238795325112867385, 1.000000000000000000, 0.9238795325112867385, 1.000000000000000000, 0.9238795325112867385, 1.000000000000000000, 0.9238795325112867385, 1.000000000000000000, 0.9238795325112867385, 1.000000000000000000, 0.9238795325112867385, 1.000000000000000000, 0.9238795325112867385, 1.000000000000000000, 0.9238795325112867385, 1.000000000000000000, 0.9238795325112867385, 1.000000000000000000, 0.9238795325112867385, 1.000000000000000000, 0.9238795325112867385, 1.000000000000000000, 0.9238795325112867385, 1.000000000000000000, 0.9238795325112867385, 1.000000000000000000, 0.9238795325112867385, 1.000000000000000000, 0.9238795325112867385, 1.000000000000000000, 0.9238795325112867385, 1.000000000000000000, 0.9238795325112867385, 1.000000000000000000, 0.9238795325112867385, 1.000000000000000000, 0.9238795325112867385, 1.000000000000000000, 0.9238795325112867385, 1.000000000000000000, 0.9238795325112867385, 1.000000000000000000, 0.9238795325112867385, 1.000000000000000000, 0.9238795325112867385, 1.000000000000000000, 0.9238795325112867385, 1.000000000000000000, 0.9238795325112867385, 1.000000000000000000, 0.9238795325112867385, 1.000000000000000000, 0.9238795325112867385, 1.000000000000000000, 0.9238795325112867385, 1.000000000000000000, 0.9238795325112867385, 1.000000000000000000, 0.9238795325112867385, 1.000000000000000000, 0.9238795325112867385, 1.000000000000000000, 0.9238795325112867385, 1.000000000000000000, 0.9238795325112867385, 1.000000000000000000, 0.9238795325112867385, 1.000000000000000000, 0.9238795325112867385, 1.000000000000000000, 0.9238795325112867385, 1.000000000000000000, 0.9238795325112867385, 1.000000000000000000, 0.9238795325112867385, 1.000000000000000000, 0.9238795325112867385, 1.000000000000000000, 0.9238795325112867385, 1.000000000000000000, 0.9238795325112867385, 1.000000000000000000, 0.9238795325112867385, 1.000000000000000000, 0.9238795325112867385, 1.000000000000000000, 0.9238795325112867385, 1.000000000000000000, 0.9238795325112867385, 1.000000000000000000, 0.9238795325112867385, 1.000000000000000000, 0.9238795325112867385, 1.000000000000000000, 0.9238795325112867385, 1.000000000000000000, 0.9238795325112867385, 1.000000000000000000, 0.9238795325112867385, 1.000000000000000000, 0.9238795325112867385, 1.000000000000000000, 0.9238795325112867385, 1.000000000000000000, 0.9238795325112867385, 1.000000000000000000, 0.9238795325112867385, 1.000000000000000000, 0.9238795325112867385, 1.000000000000000000, 0.9238795325112867385, 1.000000000000000000, 0.9238795325112867385, 1.000000000000000000, 0.9238795325112867385, 1.000000000000000000) ) ) 
 REPRESENTATION_ITEM ( '' )  SURFACE ( )  );
#40463 = CARTESIAN_POINT ( 'NONE',  ( -31.45873412500002431, 204.6250000013655779, 168.5673454167828140 ) ) ;
#40465 = CARTESIAN_POINT ( 'NONE',  ( -4.541265875000002339, 11.74999999863440792, -1.881053915767121998 ) ) ;
#40466 = CARTESIAN_POINT ( 'NONE',  ( -2.828427124746209831, 206.5000000027312126, 139.1715728752538723 ) ) ;
#40467 = CARTESIAN_POINT ( 'NONE',  ( -5.082755093536319713, 5.082755093536319713, 19.29905278187175455 ) ) ;
#40468 = ORIENTED_EDGE ( 'NONE', *, *, #63735, .T. ) ;
#40469 = ORIENTED_EDGE ( 'NONE', *, *, #27173, .T. ) ;
#40470 = CARTESIAN_POINT ( 'NONE',  ( -10.18810118749999916, 4.220049686691934809, 108.0625000020483810 ) ) ;
#40471 = CARTESIAN_POINT ( 'NONE',  ( -10.91045974869146029, -14.48545281793697548, -0.07476367467996689053 ) ) ;
#40472 = CARTESIAN_POINT ( 'NONE',  ( -29.65685424949234772, 206.4375000000000568, 174.0000000000004547 ) ) ;
#40473 = CARTESIAN_POINT ( 'NONE',  ( 2.445694354108838731, 199.0625000013656063, 195.5543056458912190 ) ) ;
#40474 = CARTESIAN_POINT ( 'NONE',  ( 29.43265458321766204, 196.5000000013656063, 173.4587341249998929 ) ) ;
#40475 = CARTESIAN_POINT ( 'NONE',  ( 10.00000000000000178, 80.20833333333334281, -2.679491924311226736 ) ) ;
#40476 = CARTESIAN_POINT ( 'NONE',  ( 5.656854249492381470, 116.5625000000000000, 5.656854249492379694 ) ) ;
#40477 = CARTESIAN_POINT ( 'NONE',  ( 9.832129032723416984, 60.67708332991934839, 5.676582343750006032 ) ) ;
#40478 = CARTESIAN_POINT ( 'NONE',  ( -4.242640687119286547, 288.8750000000000000, -4.242640687119286547 ) ) ;
#40479 = EDGE_CURVE ( 'NONE', #26525, #30150, #67686, .T. ) ;
#40480 = ORIENTED_EDGE ( 'NONE', *, *, #58228, .T. ) ;
#40481 = CARTESIAN_POINT ( 'NONE',  ( 1.656854249492363040, 203.3125000000000000, 202.0000000000000284 ) ) ;
#40482 = CARTESIAN_POINT ( 'NONE',  ( -4.330454160168802247, -68.33163558030018692, 20.63184982502184184 ) ) ;
#40483 = CARTESIAN_POINT ( 'NONE',  ( -3.458734125000015425, 209.0000000013655779, 143.4326545832176976 ) ) ;
#40484 = DIRECTION ( 'NONE',  ( -0.8660254037844380415, -0.5000000000000011102, 0.000000000000000000 ) ) ;
#40485 = CARTESIAN_POINT ( 'NONE',  ( 5.656854249492379694, 97.43750000000000000, -5.656854249492380582 ) ) ;
#40486 = CARTESIAN_POINT ( 'NONE',  ( -9.999999999999998224, 240.2083333333333144, 2.679491924311235618 ) ) ;
#40487 = CARTESIAN_POINT ( 'NONE',  ( 1.102182119232618108E-15, 293.2500000000000000, 6.000000000000001776 ) ) ;
#40488 = CARTESIAN_POINT ( 'NONE',  ( -7.204075437095965206, -7.204075437095968759, 71.21875000204836681 ) ) ;
#40489 = CARTESIAN_POINT ( 'NONE',  ( 6.123233995736767268E-16, 196.2500000000000000, -10.00000000000000178 ) ) ;
#40490 = EDGE_CURVE ( 'NONE', #41883, #63044, #15983, .T. ) ;
#40491 = CARTESIAN_POINT ( 'NONE',  ( -7.188101187499992051, 0.000000000000000000, 15.36155278187175455 ) ) ;
#40492 = CARTESIAN_POINT ( 'NONE',  ( -2.085542519210945728E-15, 184.8437499965860411, 11.35316468750000141 ) ) ;
#40493 = CARTESIAN_POINT ( 'NONE',  ( -8.660254037844579145, 212.0833333333334565, -5.000000000000115463 ) ) ;
#40494 = CARTESIAN_POINT ( 'NONE',  ( 29.65685424949245075, 197.5625000027312126, 165.9999999999999716 ) ) ;
#40495 = CARTESIAN_POINT ( 'NONE',  ( -1.836970198721029983E-15, 85.62499999317203958, 10.00000000000000178 ) ) ;
#40496 = ORIENTED_EDGE ( 'NONE', *, *, #45264, .T. ) ;
#40497 = CARTESIAN_POINT ( 'NONE',  ( 2.445694354108782775, 198.5625000013656063, 139.5543056458912190 ) ) ;
#40498 = CARTESIAN_POINT ( 'NONE',  ( -11.35316468750000141, 33.59374999658601268, -1.390361679473963753E-15 ) ) ;
#40499 = MANIFOLD_SOLID_BREP ( 'BaseBody', #53899 ) ;
#40500 = CARTESIAN_POINT ( 'NONE',  ( -6.735557395310442023E-16, 11.00000000000000000, 110.3125000040967763 ) ) ;
#40501 = CARTESIAN_POINT ( 'NONE',  ( -28.00000000000002842, 201.0000000000000000, 166.0000000000003695 ) ) ;
#40502 = CARTESIAN_POINT ( 'NONE',  ( -4.556349186104048599, -10.99999999999999822, 70.28124999999998579 ) ) ;
#40504 = CARTESIAN_POINT ( 'NONE',  ( -2.726571689596997292E-14, 210.0000000000000284, 138.0000000000000568 ) ) ;
#40503 = CARTESIAN_POINT ( 'NONE',  ( -18.00000000000000000, 4.406054334071535905, -0.2960025734007523113 ) ) ;
#40505 = FACE_OUTER_BOUND ( 'NONE', #12869, .T. ) ;
#40506 = CARTESIAN_POINT ( 'NONE',  ( -2.445694354108838731, 200.0625000013656063, 144.4456943541088663 ) ) ;
#40507 = AXIS2_PLACEMENT_3D ( 'NONE', #28824, #5828, #45068 ) ;
#40508 = CARTESIAN_POINT ( 'NONE',  ( 2.679491924311228956, 67.91666665983868256, -10.00000000000000000 ) ) ;
#40509 = CARTESIAN_POINT ( 'NONE',  ( -7.188101187500001821, 97.06250000204838102, -2.977408999572650483 ) ) ;
#40510 = CARTESIAN_POINT ( 'NONE',  ( -1.881053915767124440, 13.12499999863440969, 4.541265875000001451 ) ) ;
#40511 = CARTESIAN_POINT ( 'NONE',  ( 8.660254037844579145, 215.4166666666667993, -5.000000000000111022 ) ) ;
#40512 = CARTESIAN_POINT ( 'NONE',  ( -7.999999999999991118, 0.000000000000000000, 2.330302779823365089 ) ) ;
#40513 = CARTESIAN_POINT ( 'NONE',  ( -0.8419854211626197626, -49.91401432488752477, 40.68947704085019978 ) ) ;
#40514 = ORIENTED_EDGE ( 'NONE', *, *, #11317, .T. ) ;
#40515 = ORIENTED_EDGE ( 'NONE', *, *, #27929, .F. ) ;
#40516 = CARTESIAN_POINT ( 'NONE',  ( -3.999999999999960032, 205.0625000027312126, 196.3431457505076594 ) ) ;
#40517 = CARTESIAN_POINT ( 'NONE',  ( 2.765530957081996366, 299.2968750017070079, -6.676582343750003368 ) ) ;
#40518 = CARTESIAN_POINT ( 'NONE',  ( 7.320508075688774596, 42.49999999317203248, -7.320508075688774596 ) ) ;
#40519 = CARTESIAN_POINT ( 'NONE',  ( 5.676582343749993598, 149.9479166632526983, 9.832129032723422313 ) ) ;
#40520 = CYLINDRICAL_SURFACE ( 'NONE', #69308, 20.00000000000001066 ) ;
#40521 = CARTESIAN_POINT ( 'NONE',  ( -10.18810118749999916, 4.220049686691934809, 81.06250000204836681 ) ) ;
#40522 = DIRECTION ( 'NONE',  ( -0.000000000000000000, -0.000000000000000000, -1.000000000000000000 ) ) ;
#40523 = CARTESIAN_POINT ( 'NONE',  ( -2.828427124746152987, 203.1250000000000284, 200.8284271247462129 ) ) ;
#40524 = CARTESIAN_POINT ( 'NONE',  ( -4.220049686691937474, -10.18810118749999738, 114.8125000020483668 ) ) ;
#40525 = ORIENTED_EDGE ( 'NONE', *, *, #38494, .T. ) ;
#40526 = CARTESIAN_POINT ( 'NONE',  ( 34.53143086303403919, -13.12057785534301324, 149.2969958664399428 ) ) ;
#40527 = CARTESIAN_POINT ( 'NONE',  ( 28.27213368403181804, 175.6923493049426384, 157.0765971109610746 ) ) ;
#40528 = CARTESIAN_POINT ( 'NONE',  ( -11.35316468750000141, 123.5937499965860269, -1.390361679473963753E-15 ) ) ;
#40529 = CARTESIAN_POINT ( 'NONE',  ( -1.432654583217607192, 197.2500000013656063, 194.5412658750000219 ) ) ;
#40530 = CARTESIAN_POINT ( 'NONE',  ( 7.188101187499999156, 23.24999999795161543, 2.977408999572654924 ) ) ;
#40531 = CARTESIAN_POINT ( 'NONE',  ( -6.238412754330611322E-16, 10.18810118749999916, 76.65625000204836681 ) ) ;
#40532 = CARTESIAN_POINT ( 'NONE',  ( -11.35316468750000141, 38.80208332991934839, 3.042071309553159963 ) ) ;
#40533 = VERTEX_POINT ( 'NONE', #16344 ) ;
#40534 = CARTESIAN_POINT ( 'NONE',  ( 2.020667218593132706E-15, -11.00000000000000000, 94.56250000409677625 ) ) ;
#40535 = CARTESIAN_POINT ( 'NONE',  ( -3.211159895383562723, 1.062499998634406806, 3.211159895383561391 ) ) ;
#40536 = CARTESIAN_POINT ( 'NONE',  ( -5.662595241051935346, 5.662595241051935346, 14.32561528394063188 ) ) ;
#40537 = CARTESIAN_POINT ( 'NONE',  ( -1.432654583217664701, 208.0000000013656347, 138.5412658750000787 ) ) ;
#40538 = CARTESIAN_POINT ( 'NONE',  ( -7.188101187500002709, 8.812499997951611874, 2.977408999572649151 ) ) ;
#40539 = CARTESIAN_POINT ( 'NONE',  ( 6.000000000000003553, 296.5000000034139589, 2.485281374238571317 ) ) ;
#40540 =( GEOMETRIC_REPRESENTATION_CONTEXT ( 3 ) GLOBAL_UNCERTAINTY_ASSIGNED_CONTEXT ( ( #18482 ) ) GLOBAL_UNIT_ASSIGNED_CONTEXT ( ( #3438, #61150, #31358 ) ) REPRESENTATION_CONTEXT ( 'NONE', 'WORKASPACE' ) );
#40541 = CARTESIAN_POINT ( 'NONE',  ( -29.82468019811799564, -12.02611497903660087, 141.4727170242123577 ) ) ;
#40542 = CARTESIAN_POINT ( 'NONE',  ( 7.188101187500001821, 8.437499997951611874, -2.977408999572650483 ) ) ;
#40543 = CARTESIAN_POINT ( 'NONE',  ( -4.401442555609577197E-16, 7.188101187499992051, 13.11155278187175277 ) ) ;
#40544 = CARTESIAN_POINT ( 'NONE',  ( -9.832129032723418760, 153.1770833299193555, -5.676582343750004256 ) ) ;
#40545 = CARTESIAN_POINT ( 'NONE',  ( -4.220049686691935698, 10.18810118749999916, 73.37500000204838102 ) ) ;
#40546 = CARTESIAN_POINT ( 'NONE',  ( -24.54126587499999701, 207.4375000013656063, 170.0000000000003411 ) ) ;
#40547 = DIRECTION ( 'NONE',  ( -0.000000000000000000, -0.000000000000000000, 1.000000000000000000 ) ) ;
#40548 = CARTESIAN_POINT ( 'NONE',  ( 3.211159895383560947, 21.31249999863440792, 3.211159895383562723 ) ) ;
#40549 = UNCERTAINTY_MEASURE_WITH_UNIT (LENGTH_MEASURE( 1.000000000000000082E-05 ), #52528, 'distance_accuracy_value', 'NONE');
#40550 = VERTEX_POINT ( 'NONE', #36322 ) ;
#40551 = CARTESIAN_POINT ( 'NONE',  ( -2.828427124746153876, 201.0000000027312126, 195.1715728752538439 ) ) ;
#40552 = CARTESIAN_POINT ( 'NONE',  ( 1.656854249492348607, 205.1875000000000000, 138.0000000000000568 ) ) ;
#40553 = CARTESIAN_POINT ( 'NONE',  ( -26.34314575050753149, 203.6875000027311842, 174.0000000000003411 ) ) ;
#40554 = EDGE_CURVE ( 'NONE', #43701, #30305, #33442, .T. ) ;
#40555 = ADVANCED_FACE ( 'NONE', ( #6541 ), #47991, .F. ) ;
#40556 = AXIS2_PLACEMENT_3D ( 'NONE', #33594, #61870, #22611 ) ;
#40557 = CARTESIAN_POINT ( 'NONE',  ( -2.977408999572650927, 119.3750000020483810, -7.188101187500001821 ) ) ;
#40558 = CARTESIAN_POINT ( 'NONE',  ( -8.000000000000003553, 22.99999999999999645, 1.000000000000000000 ) ) ;
#40559 = CARTESIAN_POINT ( 'NONE',  ( 1.469576158976822172E-15, -7.999999999999991118, 8.892802783920146226 ) ) ;
#40560 = VERTEX_POINT ( 'NONE', #34859 ) ;
#40561 = CARTESIAN_POINT ( 'NONE',  ( -5.082755093536326818, 17.90624999795161187, 5.082755093536325042 ) ) ;
#40562 = ORIENTED_EDGE ( 'NONE', *, *, #21322, .F. ) ;
#40563 = CARTESIAN_POINT ( 'NONE',  ( -1.836970198721029983E-15, 210.6249999931720538, 10.00000000000000178 ) ) ;
#40564 = CARTESIAN_POINT ( 'NONE',  ( 3.313708498984762496, 13.21875000000000355, 7.999999999999998224 ) ) ;
#40565 = CARTESIAN_POINT ( 'NONE',  ( -2.679491924311235618, 43.54166666666667140, 10.00000000000000000 ) ) ;
#40566 = CARTESIAN_POINT ( 'NONE',  ( -4.401442555609581635E-16, 104.6562500020483810, -7.188101187500000044 ) ) ;
#40567 = CARTESIAN_POINT ( 'NONE',  ( -24.54126587499999701, 206.4375000013656063, 170.0000000000003411 ) ) ;
#40568 = CARTESIAN_POINT ( 'NONE',  ( -5.000000000000000000, -10.26105934116143281, 64.40045319026697257 ) ) ;
#40569 = CARTESIAN_POINT ( 'NONE',  ( 10.00000000000000178, 197.0833333265053398, -2.679491924311226736 ) ) ;
#40570 = EDGE_LOOP ( 'NONE', ( #43635, #11583, #25844, #18924 ) ) ;
#40571 = CARTESIAN_POINT ( 'NONE',  ( 3.042071309553173286, 250.3645833367473301, 11.35316468749999608 ) ) ;
#40572 = CARTESIAN_POINT ( 'NONE',  ( 2.977408999572646486, 7.188101187499991163, 14.89280278187175455 ) ) ;
#40573 = CARTESIAN_POINT ( 'NONE',  ( -10.00000000000000178, 9.374999993172032475, -1.224646799147353454E-15 ) ) ;
#40574 = CARTESIAN_POINT ( 'NONE',  ( -30.64284399271075188, 178.3875230420588878, 174.6921329945331536 ) ) ;
#40575 = DIRECTION ( 'NONE',  ( -0.000000000000000000, 1.000000000000000000, -0.000000000000000000 ) ) ;
#40576 = CARTESIAN_POINT ( 'NONE',  ( 6.123233995736767268E-16, 203.1249999931720538, -10.00000000000000178 ) ) ;
#40577 =( BOUNDED_SURFACE ( )  B_SPLINE_SURFACE ( 1, 2, ( 
 ( #58994, #58621, #6563, #24266, #23157, #40517, #17872, #46169, #69187, #52953, #64269, #5822, #181, #53326, #58261, #6927, #17499, #52214, #41261, #63521, #34881, #24631, #28818, #12577, #11844, #7299, #35606, #29570, #35244, #547, #47642, #57516, #18618, #57886, #51835, #52580, #1287, #23529, #6193, #12938, #46543, #69561, #1650, #34512, #11477, #18245, #40889, #63895, #12206, #29938, #70664, #918, #23903, #47277, #46912, #41629, #69937, #70303, #64640, #35975, #40145, #63150, #2005, #43470, #14041, #25368, #24995, #3496, #13671, #66111, #60080, #20452, #48012, #2748, #31038, #48385, #8781, #71388, #71024, #66484, #37077, #19713, #19342, #26484, #36710, #14420, #59357, #7669, #54440, #54814, #31793, #3125, #2372, #20081, #30675, #37453, #26108, #49129, #60451, #72140, #25735, #8400, #42725, #42355, #65371, #59722, #32170, #14793, #31413, #49509, #48756, #37832, #53694, #60829, #9153, #8030, #54063, #71764, #65739, #43094, #55190, #18982, #41985, #64996, #36342, #13305, #32933, #72901, #56301, #44606, #72528, #28363, #22315, #10645, #44236, #33676, #62685, #15174, #43853, #27238, #9903, #11022, #4617, #56680, #16653, #16279, #38947, #4997, #55563, #21209, #50254, #3876, #26872, #27996, #21951, #38205, #32553, #34056, #15916, #39321, #49886, #55939, #73644, #67249, #15543, #57051, #61209, #44979, #38583, #39685, #67984, #61948, #67620, #61584, #5363, #9539, #51005, #4251, #73276, #10276, #74014, #21580, #33303, #45341, #27615, #50625, #20836, #66866, #62319, #68359, #63066, #34424, #69103 ),
 ( #29113, #18532, #70222, #12851, #11388, #58177, #64187, #46824, #51747, #34796, #8227, #46458, #96, #69476, #5733, #51372, #35890, #69849, #52132, #23821, #47191, #57426, #35522, #17410, #12492, #6483, #29486, #41539, #58534, #6841, #52867, #17036, #18161, #41177, #465, #29856, #35161, #23443, #52496, #1199, #24180, #64555, #40432, #63432, #58907, #834, #11759, #28731, #23074, #46084, #17787, #57801, #74382, #40800, #63807, #40061, #22693, #6108, #12123, #45711, #68723, #38776, #54634, #25562, #60653, #48948, #71585, #61402, #55758, #72343, #48575, #32750, #67064, #20273, #9728, #31989, #71959, #55011, #15363, #49712, #72726, #4074, #26689, #3317, #19908, #37278, #31613, #43295, #9350, #21029, #44054, #38399, #42915, #27068, #37654, #21401, #65934, #32369, #26305, #49328, #66310, #44424, #50081, #20656, #43673, #8975, #2943, #67439, #73095, #66684, #14616, #15737, #14988, #38026, #55384, #14240, #60272, #61025, #54262, #3693, #61779, #31237, #2573, #8598, #25932, #11213, #62143, #73463, #16852, #33872, #16102, #11579, #51196, #34241, #23269, #27431, #39878, #45169, #10467, #68549, #56872, #10096, #40626, #34614, #22896, #56500, #45908, #288, #50446, #56130, #39514, #22141, #46278, #62880, #68921, #28933, #28558, #74207, #17231, #67811, #33497, #62511, #39139, #4816, #40252, #57243, #21771, #44798, #69297, #28184, #51564, #27812, #68180, #5555, #50823, #73834, #17608, #16476, #74580, #10837, #51951, #63254, #22510, #5188, #45531, #33133, #57620, #5932, #4439, #6308, #30048, #1756, #52692 ) ),
 .UNSPECIFIED., .F., .F., .F. ) 
 B_SPLINE_SURFACE_WITH_KNOTS ( ( 2, 2 ),
 ( 3, 2, 2, 2, 2, 2, 2, 2, 2, 2, 2, 2, 2, 2, 2, 2, 2, 2, 2, 2, 2, 2, 2, 2, 2, 2, 2, 2, 2, 2, 2, 2, 2, 2, 2, 2, 2, 2, 2, 2, 2, 2, 2, 2, 2, 2, 2, 2, 2, 2, 2, 2, 2, 2, 2, 2, 2, 2, 2, 2, 2, 2, 2, 2, 2, 2, 2, 2, 2, 2, 2, 2, 2, 2, 2, 2, 2, 2, 2, 2, 2, 2, 2, 2, 2, 2, 2, 2, 2, 2, 2, 2, 2, 2, 2, 2, 3 ),
 ( 0.000000000000000000, 1.000000000000000000 ),
 ( 0.000000000000000000, 0.01041666666666666609, 0.02083333333333333218, 0.03125000000000000000, 0.04166666666666666435, 0.05208333333333333565, 0.06250000000000000000, 0.07291666666666667129, 0.08333333333333332871, 0.09375000000000000000, 0.1041666666666666713, 0.1145833333333333287, 0.1250000000000000000, 0.1354166666666666574, 0.1458333333333333426, 0.1562500000000000000, 0.1666666666666666574, 0.1770833333333333426, 0.1875000000000000000, 0.1979166666666666574, 0.2083333333333333426, 0.2187500000000000000, 0.2291666666666666574, 0.2395833333333333426, 0.2500000000000000000, 0.2604166666666666852, 0.2708333333333333148, 0.2812500000000000000, 0.2916666666666666852, 0.3020833333333333148, 0.3125000000000000000, 0.3229166666666666852, 0.3333333333333333148, 0.3437500000000000000, 0.3541666666666666852, 0.3645833333333333148, 0.3750000000000000000, 0.3854166666666666852, 0.3958333333333333148, 0.4062500000000000000, 0.4166666666666666852, 0.4270833333333333148, 0.4375000000000000000, 0.4479166666666666852, 0.4583333333333333148, 0.4687500000000000000, 0.4791666666666666852, 0.4895833333333333148, 0.5000000000000000000, 0.5104166666666666297, 0.5208333333333333703, 0.5312500000000000000, 0.5416666666666666297, 0.5520833333333333703, 0.5625000000000000000, 0.5729166666666666297, 0.5833333333333333703, 0.5937500000000000000, 0.6041666666666666297, 0.6145833333333333703, 0.6250000000000000000, 0.6354166666666666297, 0.6458333333333333703, 0.6562500000000000000, 0.6666666666666666297, 0.6770833333333333703, 0.6875000000000000000, 0.6979166666666666297, 0.7083333333333333703, 0.7187500000000000000, 0.7291666666666666297, 0.7395833333333333703, 0.7500000000000000000, 0.7604166666666666297, 0.7708333333333333703, 0.7812500000000000000, 0.7916666666666666297, 0.8020833333333333703, 0.8125000000000000000, 0.8229166666666666297, 0.8333333333333333703, 0.8437500000000000000, 0.8541666666666666297, 0.8645833333333333703, 0.8750000000000000000, 0.8854166666666666297, 0.8958333333333333703, 0.9062500000000000000, 0.9166666666666666297, 0.9270833333333333703, 0.9375000000000000000, 0.9479166666666666297, 0.9583333333333333703, 0.9687500000000000000, 0.9791666666666666297, 0.9895833333333333703, 1.000000000000000000 ),
 .UNSPECIFIED. ) 
 GEOMETRIC_REPRESENTATION_ITEM ( )  RATIONAL_B_SPLINE_SURFACE ( (
 ( 1.000000000000000000, 0.9238795325112867385, 1.000000000000000000, 0.9238795325112867385, 1.000000000000000000, 0.9238795325112867385, 1.000000000000000000, 0.9238795325112867385, 1.000000000000000000, 0.9238795325112867385, 1.000000000000000000, 0.9238795325112867385, 1.000000000000000000, 0.9238795325112867385, 1.000000000000000000, 0.9238795325112867385, 1.000000000000000000, 0.9238795325112867385, 1.000000000000000000, 0.9238795325112867385, 1.000000000000000000, 0.9238795325112867385, 1.000000000000000000, 0.9238795325112867385, 1.000000000000000000, 0.9238795325112867385, 1.000000000000000000, 0.9238795325112867385, 1.000000000000000000, 0.9238795325112867385, 1.000000000000000000, 0.9238795325112867385, 1.000000000000000000, 0.9238795325112867385, 1.000000000000000000, 0.9238795325112867385, 1.000000000000000000, 0.9238795325112867385, 1.000000000000000000, 0.9238795325112867385, 1.000000000000000000, 0.9238795325112867385, 1.000000000000000000, 0.9238795325112867385, 1.000000000000000000, 0.9238795325112867385, 1.000000000000000000, 0.9238795325112867385, 1.000000000000000000, 0.9238795325112867385, 1.000000000000000000, 0.9238795325112867385, 1.000000000000000000, 0.9238795325112867385, 1.000000000000000000, 0.9238795325112867385, 1.000000000000000000, 0.9238795325112867385, 1.000000000000000000, 0.9238795325112867385, 1.000000000000000000, 0.9238795325112867385, 1.000000000000000000, 0.9238795325112867385, 1.000000000000000000, 0.9238795325112867385, 1.000000000000000000, 0.9238795325112867385, 1.000000000000000000, 0.9238795325112867385, 1.000000000000000000, 0.9238795325112867385, 1.000000000000000000, 0.9238795325112867385, 1.000000000000000000, 0.9238795325112867385, 1.000000000000000000, 0.9238795325112867385, 1.000000000000000000, 0.9238795325112867385, 1.000000000000000000, 0.9238795325112867385, 1.000000000000000000, 0.9238795325112867385, 1.000000000000000000, 0.9238795325112867385, 1.000000000000000000, 0.9238795325112867385, 1.000000000000000000, 0.9238795325112867385, 1.000000000000000000, 0.9238795325112867385, 1.000000000000000000, 0.9238795325112867385, 1.000000000000000000, 0.9238795325112867385, 1.000000000000000000, 0.9238795325112867385, 1.000000000000000000, 0.9238795325112867385, 1.000000000000000000, 0.9238795325112867385, 1.000000000000000000, 0.9238795325112867385, 1.000000000000000000, 0.9238795325112867385, 1.000000000000000000, 0.9238795325112867385, 1.000000000000000000, 0.9238795325112867385, 1.000000000000000000, 0.9238795325112867385, 1.000000000000000000, 0.9238795325112867385, 1.000000000000000000, 0.9238795325112867385, 1.000000000000000000, 0.9238795325112867385, 1.000000000000000000, 0.9238795325112867385, 1.000000000000000000, 0.9238795325112867385, 1.000000000000000000, 0.9238795325112867385, 1.000000000000000000, 0.9238795325112867385, 1.000000000000000000, 0.9238795325112867385, 1.000000000000000000, 0.9238795325112867385, 1.000000000000000000, 0.9238795325112867385, 1.000000000000000000, 0.9238795325112867385, 1.000000000000000000, 0.9238795325112867385, 1.000000000000000000, 0.9238795325112867385, 1.000000000000000000, 0.9238795325112867385, 1.000000000000000000, 0.9238795325112867385, 1.000000000000000000, 0.9238795325112867385, 1.000000000000000000, 0.9238795325112867385, 1.000000000000000000, 0.9238795325112867385, 1.000000000000000000, 0.9238795325112867385, 1.000000000000000000, 0.9238795325112867385, 1.000000000000000000, 0.9238795325112867385, 1.000000000000000000, 0.9238795325112867385, 1.000000000000000000, 0.9238795325112867385, 1.000000000000000000, 0.9238795325112867385, 1.000000000000000000, 0.9238795325112867385, 1.000000000000000000, 0.9238795325112867385, 1.000000000000000000, 0.9238795325112867385, 1.000000000000000000, 0.9238795325112867385, 1.000000000000000000, 0.9238795325112867385, 1.000000000000000000, 0.9238795325112867385, 1.000000000000000000, 0.9238795325112867385, 1.000000000000000000, 0.9238795325112867385, 1.000000000000000000, 0.9238795325112867385, 1.000000000000000000, 0.9238795325112867385, 1.000000000000000000, 0.9238795325112867385, 1.000000000000000000, 0.9238795325112867385, 1.000000000000000000, 0.9238795325112867385, 1.000000000000000000, 0.9238795325112867385, 1.000000000000000000, 0.9238795325112867385, 1.000000000000000000, 0.9238795325112867385, 1.000000000000000000),
 ( 1.000000000000000000, 0.9238795325112867385, 1.000000000000000000, 0.9238795325112867385, 1.000000000000000000, 0.9238795325112867385, 1.000000000000000000, 0.9238795325112867385, 1.000000000000000000, 0.9238795325112867385, 1.000000000000000000, 0.9238795325112867385, 1.000000000000000000, 0.9238795325112867385, 1.000000000000000000, 0.9238795325112867385, 1.000000000000000000, 0.9238795325112867385, 1.000000000000000000, 0.9238795325112867385, 1.000000000000000000, 0.9238795325112867385, 1.000000000000000000, 0.9238795325112867385, 1.000000000000000000, 0.9238795325112867385, 1.000000000000000000, 0.9238795325112867385, 1.000000000000000000, 0.9238795325112867385, 1.000000000000000000, 0.9238795325112867385, 1.000000000000000000, 0.9238795325112867385, 1.000000000000000000, 0.9238795325112867385, 1.000000000000000000, 0.9238795325112867385, 1.000000000000000000, 0.9238795325112867385, 1.000000000000000000, 0.9238795325112867385, 1.000000000000000000, 0.9238795325112867385, 1.000000000000000000, 0.9238795325112867385, 1.000000000000000000, 0.9238795325112867385, 1.000000000000000000, 0.9238795325112867385, 1.000000000000000000, 0.9238795325112867385, 1.000000000000000000, 0.9238795325112867385, 1.000000000000000000, 0.9238795325112867385, 1.000000000000000000, 0.9238795325112867385, 1.000000000000000000, 0.9238795325112867385, 1.000000000000000000, 0.9238795325112867385, 1.000000000000000000, 0.9238795325112867385, 1.000000000000000000, 0.9238795325112867385, 1.000000000000000000, 0.9238795325112867385, 1.000000000000000000, 0.9238795325112867385, 1.000000000000000000, 0.9238795325112867385, 1.000000000000000000, 0.9238795325112867385, 1.000000000000000000, 0.9238795325112867385, 1.000000000000000000, 0.9238795325112867385, 1.000000000000000000, 0.9238795325112867385, 1.000000000000000000, 0.9238795325112867385, 1.000000000000000000, 0.9238795325112867385, 1.000000000000000000, 0.9238795325112867385, 1.000000000000000000, 0.9238795325112867385, 1.000000000000000000, 0.9238795325112867385, 1.000000000000000000, 0.9238795325112867385, 1.000000000000000000, 0.9238795325112867385, 1.000000000000000000, 0.9238795325112867385, 1.000000000000000000, 0.9238795325112867385, 1.000000000000000000, 0.9238795325112867385, 1.000000000000000000, 0.9238795325112867385, 1.000000000000000000, 0.9238795325112867385, 1.000000000000000000, 0.9238795325112867385, 1.000000000000000000, 0.9238795325112867385, 1.000000000000000000, 0.9238795325112867385, 1.000000000000000000, 0.9238795325112867385, 1.000000000000000000, 0.9238795325112867385, 1.000000000000000000, 0.9238795325112867385, 1.000000000000000000, 0.9238795325112867385, 1.000000000000000000, 0.9238795325112867385, 1.000000000000000000, 0.9238795325112867385, 1.000000000000000000, 0.9238795325112867385, 1.000000000000000000, 0.9238795325112867385, 1.000000000000000000, 0.9238795325112867385, 1.000000000000000000, 0.9238795325112867385, 1.000000000000000000, 0.9238795325112867385, 1.000000000000000000, 0.9238795325112867385, 1.000000000000000000, 0.9238795325112867385, 1.000000000000000000, 0.9238795325112867385, 1.000000000000000000, 0.9238795325112867385, 1.000000000000000000, 0.9238795325112867385, 1.000000000000000000, 0.9238795325112867385, 1.000000000000000000, 0.9238795325112867385, 1.000000000000000000, 0.9238795325112867385, 1.000000000000000000, 0.9238795325112867385, 1.000000000000000000, 0.9238795325112867385, 1.000000000000000000, 0.9238795325112867385, 1.000000000000000000, 0.9238795325112867385, 1.000000000000000000, 0.9238795325112867385, 1.000000000000000000, 0.9238795325112867385, 1.000000000000000000, 0.9238795325112867385, 1.000000000000000000, 0.9238795325112867385, 1.000000000000000000, 0.9238795325112867385, 1.000000000000000000, 0.9238795325112867385, 1.000000000000000000, 0.9238795325112867385, 1.000000000000000000, 0.9238795325112867385, 1.000000000000000000, 0.9238795325112867385, 1.000000000000000000, 0.9238795325112867385, 1.000000000000000000, 0.9238795325112867385, 1.000000000000000000, 0.9238795325112867385, 1.000000000000000000, 0.9238795325112867385, 1.000000000000000000, 0.9238795325112867385, 1.000000000000000000, 0.9238795325112867385, 1.000000000000000000, 0.9238795325112867385, 1.000000000000000000, 0.9238795325112867385, 1.000000000000000000, 0.9238795325112867385, 1.000000000000000000) ) ) 
 REPRESENTATION_ITEM ( '' )  SURFACE ( )  );
#40578 = CARTESIAN_POINT ( 'NONE',  ( -7.320508075688773708, 156.8750000000000284, -7.320508075688774596 ) ) ;
#40579 = DIRECTION ( 'NONE',  ( 0.000000000000000000, 0.000000000000000000, 1.000000000000000000 ) ) ;
#40580 = CARTESIAN_POINT ( 'NONE',  ( -33.00328001739791262, 175.6261367261117812, 159.2768681366241026 ) ) ;
#40581 =( BOUNDED_CURVE ( )  B_SPLINE_CURVE ( 2, ( #7192, #70558, #35865, #53214, #41881, #7560, #13194, #1897, #70922 ),
 .UNSPECIFIED., .F., .F. ) 
 B_SPLINE_CURVE_WITH_KNOTS ( ( 3, 2, 2, 2, 3 ),
 ( 0.3437499999999998335, 0.3489583333333331483, 0.3541666666666665186, 0.3593749999999998335, 0.3645833333333331483 ),
 .UNSPECIFIED. ) 
 CURVE ( )  GEOMETRIC_REPRESENTATION_ITEM ( )  RATIONAL_B_SPLINE_CURVE ( ( 1.000000000000002442, 0.9238795325112842960, 1.000000000000000000, 0.9238795325112867385, 1.000000000000000000, 0.9238795325112867385, 1.000000000000000000, 0.9238795325112891810, 0.9999999999999975575 ) ) 
 REPRESENTATION_ITEM ( '' )  );
#40582 = CARTESIAN_POINT ( 'NONE',  ( 0.000000000000000000, 0.000000000000000000, 118.0000000000000000 ) ) ;
#40583 = CARTESIAN_POINT ( 'NONE',  ( 5.676582343749993598, 130.2604166632526983, 9.832129032723422313 ) ) ;
#40584 = CARTESIAN_POINT ( 'NONE',  ( -2.485281374238208052, 294.2500000034139589, 6.000000000000366818 ) ) ;
#40585 = CARTESIAN_POINT ( 'NONE',  ( 105.0000000000000000, 205.0000000000000284, 20.00000000000000000 ) ) ;
#40588 = CARTESIAN_POINT ( 'NONE',  ( 2.449293598294707893E-16, 6.250000000000000000, -4.000000000000001776 ) ) ;
#40587 = CARTESIAN_POINT ( 'NONE',  ( 31.45873412499999944, 197.6250000013656063, 171.4326545832175555 ) ) ;
#40586 = CARTESIAN_POINT ( 'NONE',  ( 32.00000000000000711, 209.3125000000000568, 168.3431457505075741 ) ) ;
#40589 = AXIS2_PLACEMENT_3D ( 'NONE', #67387, #4390, #27383 ) ;
#40590 = ORIENTED_EDGE ( 'NONE', *, *, #17656, .T. ) ;
#40591 = FACE_OUTER_BOUND ( 'NONE', #8430, .T. ) ;
#40592 = CARTESIAN_POINT ( 'NONE',  ( 32.00000000000000000, 202.3750000027312126, 169.9999999999998863 ) ) ;
#40593 = CARTESIAN_POINT ( 'NONE',  ( 5.000000000000047962, 194.1666666666667709, 8.660254037844484998 ) ) ;
#40594 = CARTESIAN_POINT ( 'NONE',  ( 25.55430564589119058, 195.3125000013656063, 167.5543056458910485 ) ) ;
#40595 = CARTESIAN_POINT ( 'NONE',  ( 7.320508075688771044, 21.24999999317203248, 7.320508075688775484 ) ) ;
#40596 = CARTESIAN_POINT ( 'NONE',  ( 7.188101187500001821, 120.5000000020483810, -2.977408999572651371 ) ) ;
#40597 = CARTESIAN_POINT ( 'NONE',  ( -1.881053915767121554, 21.62499999863441502, -4.541265875000002339 ) ) ;
#40598 = CARTESIAN_POINT ( 'NONE',  ( -5.086519500889289169, 60.91611154180230869, -23.32191296475761533 ) ) ;
#40599 = CARTESIAN_POINT ( 'NONE',  ( 1.469576158976822172E-15, -7.999999999999991118, 23.70530277982336642 ) ) ;
#40601 = CARTESIAN_POINT ( 'NONE',  ( 28.00000000000001421, 196.5000000000000000, 165.9999999999998863 ) ) ;
#40600 =( NAMED_UNIT ( * ) SI_UNIT ( $, .STERADIAN. ) SOLID_ANGLE_UNIT ( ) );
#40602 = CARTESIAN_POINT ( 'NONE',  ( 3.042071309553159519, 114.7395833299193555, 11.35316468750000141 ) ) ;
#40603 = VERTEX_POINT ( 'NONE', #7278 ) ;
#40604 = CARTESIAN_POINT ( 'NONE',  ( 28.00000000000002132, 209.4375000013656063, 173.4587341249998929 ) ) ;
#40605 = CARTESIAN_POINT ( 'NONE',  ( -1.320432766682874540E-15, 25.59374999795161543, 7.188101187500000044 ) ) ;
#40606 = CARTESIAN_POINT ( 'NONE',  ( 0.000000000000000000, 0.000000000000000000, 0.000000000000000000 ) ) ;
#40607 = CARTESIAN_POINT ( 'NONE',  ( -11.35316468749999785, 249.0104166700806445, -3.042071309553164848 ) ) ;
#40608 = CARTESIAN_POINT ( 'NONE',  ( -11.35316468750000141, 98.48958332991936970, 3.042071309553159963 ) ) ;
#40609 = ORIENTED_EDGE ( 'NONE', *, *, #73161, .T. ) ;
#40610 = CARTESIAN_POINT ( 'NONE',  ( -29.65685424949235838, 208.4375000000000284, 174.0000000000003979 ) ) ;
#40611 = CARTESIAN_POINT ( 'NONE',  ( -6.238412754330611322E-16, 10.18810118749999916, 98.78125000204838102 ) ) ;
#40612 = CARTESIAN_POINT ( 'NONE',  ( -7.320508075688773708, 213.7499999931719969, -7.320508075688774596 ) ) ;
#40613 = CARTESIAN_POINT ( 'NONE',  ( 1.432654583217662481, 199.3750000013656063, 194.5412658750000219 ) ) ;
#40614 = CARTESIAN_POINT ( 'NONE',  ( -2.828427124746192067, 6.374999997268813168, 2.828427124746190735 ) ) ;
#40616 = CARTESIAN_POINT ( 'NONE',  ( -11.35316468750000141, 98.48958332991935549, 3.042071309553159963 ) ) ;
#40615 = FACE_OUTER_BOUND ( 'NONE', #54823, .T. ) ;
#40617 = CARTESIAN_POINT ( 'NONE',  ( -4.898587196589407898E-16, 7.999999999999991118, 9.642802783920146226 ) ) ;
#40618 = CARTESIAN_POINT ( 'NONE',  ( -29.43265458321766559, 196.7500000013656063, 166.5412658750003629 ) ) ;
#40619 = CARTESIAN_POINT ( 'NONE',  ( -7.347880794884122694E-16, 13.75000000000000000, 4.000000000000001776 ) ) ;
#40620 = ORIENTED_EDGE ( 'NONE', *, *, #4001, .T. ) ;
#40621 = CIRCLE ( 'NONE', #58724, 11.99999999999999645 ) ;
#40622 = CARTESIAN_POINT ( 'NONE',  ( 8.660254037844389075, 202.2916666598387110, -5.000000000000000000 ) ) ;
#40623 = CARTESIAN_POINT ( 'NONE',  ( 3.999999999999960032, 208.0000000000000284, 142.0000000000000568 ) ) ;
#40624 = CARTESIAN_POINT ( 'NONE',  ( -7.778174593052023411, 7.778174593052023411, 100.0000000040967763 ) ) ;
#40625 = CARTESIAN_POINT ( 'NONE',  ( -11.35316468750000141, 93.59374999658602690, -1.390361679473963753E-15 ) ) ;
#40626 = CARTESIAN_POINT ( 'NONE',  ( -4.721056650415998313, 290.5781250017069510, 4.721056650416000089 ) ) ;
#40627 = CARTESIAN_POINT ( 'NONE',  ( -7.188101187500000933, 5.999999997951610986, -2.977408999572651371 ) ) ;
#40628 = CARTESIAN_POINT ( 'NONE',  ( 4.220049686691941027, -10.18810118749999738, 94.00000000204838102 ) ) ;
#40629 = CARTESIAN_POINT ( 'NONE',  ( 3.042071309553167069, 2.135416663252682756, -11.35316468749999785 ) ) ;
#40630 = ORIENTED_EDGE ( 'NONE', *, *, #35142, .F. ) ;
#40631 = CARTESIAN_POINT ( 'NONE',  ( -4.898587196589412829E-16, 123.3125000040967905, -8.000000000000000000 ) ) ;
#40632 = CARTESIAN_POINT ( 'NONE',  ( 0.3934360395497230045, -42.01948486950624329, 139.0019028451173142 ) ) ;
#40633 = CARTESIAN_POINT ( 'NONE',  ( -11.35316468750000141, 223.4895833299193555, 3.042071309553159963 ) ) ;
#40634 = CARTESIAN_POINT ( 'NONE',  ( 7.999999999999991118, 3.313708498984758055, 10.86155278392014800 ) ) ;
#40635 = FACE_OUTER_BOUND ( 'NONE', #3514, .T. ) ;
#40636 = CARTESIAN_POINT ( 'NONE',  ( 6.676582343750003368, 295.0156250017069510, -2.765530957081997254 ) ) ;
#40637 = ORIENTED_EDGE ( 'NONE', *, *, #39141, .T. ) ;
#40638 = CARTESIAN_POINT ( 'NONE',  ( -11.00000000000000000, 0.000000000000000000, 89.68750000409677625 ) ) ;
#40639 = CARTESIAN_POINT ( 'NONE',  ( -8.311093377946836114, 212.9687499965860127, -8.311093377946837890 ) ) ;
#40640 = CARTESIAN_POINT ( 'NONE',  ( -7.204075437095965206, -7.204075437095968759, 91.84375000204838102 ) ) ;
#40641 = ADVANCED_FACE ( 'NONE', ( #40868 ), #29547, .T. ) ;
#40642 = CARTESIAN_POINT ( 'NONE',  ( -26.56734541678238060, 203.3750000013656063, 166.5412658750003629 ) ) ;
#40643 = CARTESIAN_POINT ( 'NONE',  ( -8.000000000000001776, 17.34375000000000000, 3.313708498984759387 ) ) ;
#40644 = CIRCLE ( 'NONE', #35842, 30.99999999999994316 ) ;
#40645 = ORIENTED_EDGE ( 'NONE', *, *, #56011, .T. ) ;
#40646 = CARTESIAN_POINT ( 'NONE',  ( -5.082755093536324154, 121.3437500020483952, 5.082755093536326818 ) ) ;
#40647 = CARTESIAN_POINT ( 'NONE',  ( -27.99999999999999645, 210.0000000000000284, 174.0000000000003411 ) ) ;
#40648 = CARTESIAN_POINT ( 'NONE',  ( 2.679491924311222739, 23.95833333333332860, 10.00000000000000355 ) ) ;
#40649 = CARTESIAN_POINT ( 'NONE',  ( -62.39047978708158126, 184.9827789239285494, 84.30156509589279779 ) ) ;
#40650 = CARTESIAN_POINT ( 'NONE',  ( 4.220049686691941027, -10.18810118749999738, 76.00000000204838102 ) ) ;
#40651 = ORIENTED_EDGE ( 'NONE', *, *, #38970, .F. ) ;
#40652 = CARTESIAN_POINT ( 'NONE',  ( 4.401442555609581635E-16, 0.8437499979516099868, -7.188101187500000044 ) ) ;
#40653 = LINE ( 'NONE', #1055, #18550 ) ;
#40654 = EDGE_CURVE ( 'NONE', #16856, #23729, #35850, .T. ) ;
#40655 = EDGE_CURVE ( 'NONE', #10343, #72436, #69591, .T. ) ;
#40656 =( NAMED_UNIT ( * ) PLANE_ANGLE_UNIT ( ) SI_UNIT ( $, .RADIAN. ) );
#40657 = CARTESIAN_POINT ( 'NONE',  ( 7.188101187500001821, 122.3750000020483952, -2.977408999572651371 ) ) ;
#40658 = CARTESIAN_POINT ( 'NONE',  ( 0.4368895104455872702, 51.14729664189188441, 48.52014062455049270 ) ) ;
#40659 = CARTESIAN_POINT ( 'NONE',  ( 1.226468279477575784E-15, 295.7031250017069510, 6.676582343750001591 ) ) ;
#40661 = CARTESIAN_POINT ( 'NONE',  ( 12.00000000000000000, 0.000000000000000000, 24.00000000000001421 ) ) ;
#40660 = CARTESIAN_POINT ( 'NONE',  ( -11.35316468749999785, 248.6979166700806445, -3.042071309553164848 ) ) ;
#40662 = ORIENTED_EDGE ( 'NONE', *, *, #50624, .T. ) ;
#40663 = EDGE_CURVE ( 'NONE', #66327, #6848, #64621, .T. ) ;
#40664 = CARTESIAN_POINT ( 'NONE',  ( -8.311093377946836114, 233.5937500034139305, -8.311093377946836114 ) ) ;
#40665 = CARTESIAN_POINT ( 'NONE',  ( -2.977408999572648707, -7.188101187499990274, 7.767802781871751883 ) ) ;
#40666 = ORIENTED_EDGE ( 'NONE', *, *, #72766, .F. ) ;
#40667 = CARTESIAN_POINT ( 'NONE',  ( 7.204075437095966983, 7.204075437095967871, 70.09375000204836681 ) ) ;
#40668 = CARTESIAN_POINT ( 'NONE',  ( -11.35316468749999785, 88.38541666325268409, -3.042071309553167513 ) ) ;
#40669 = CARTESIAN_POINT ( 'NONE',  ( -7.347880794884122694E-16, 20.75000000000000000, 4.000000000000001776 ) ) ;
#40670 = CARTESIAN_POINT ( 'NONE',  ( -11.00000000000000000, 0.000000000000000000, 83.49999999999998579 ) ) ;
#40673 = CARTESIAN_POINT ( 'NONE',  ( 7.320508075688776373, 70.62500000000000000, -7.320508075688776373 ) ) ;
#40672 = CARTESIAN_POINT ( 'NONE',  ( 31.99999999999999289, 194.3750000027311842, 169.9999999999998863 ) ) ;
#40671 = CARTESIAN_POINT ( 'NONE',  ( 26.56734541678232731, 207.6250000013656347, 173.4587341249998929 ) ) ;
#40674 =( BOUNDED_CURVE ( )  B_SPLINE_CURVE ( 2, ( #31685, #14684, #10910, #50892, #10537, #39582, #57318, #11284, #16929 ),
 .UNSPECIFIED., .F., .F. ) 
 B_SPLINE_CURVE_WITH_KNOTS ( ( 3, 2, 2, 2, 3 ),
 ( 0.7058823529411764053, 0.7095588235294116863, 0.7132352941176469674, 0.7169117647058822484, 0.7205882352941175295 ),
 .UNSPECIFIED. ) 
 CURVE ( )  GEOMETRIC_REPRESENTATION_ITEM ( )  RATIONAL_B_SPLINE_CURVE ( ( 1.000000000000002220, 0.9238795325112844070, 1.000000000000000000, 0.9238795325112867385, 1.000000000000000000, 0.9238795325112867385, 1.000000000000000000, 0.9238795325112890700, 0.9999999999999976685 ) ) 
 REPRESENTATION_ITEM ( '' )  );
#40675 = ORIENTED_EDGE ( 'NONE', *, *, #56073, .T. ) ;
#40676 = CARTESIAN_POINT ( 'NONE',  ( -5.656854249492380582, 114.3125000000000000, -5.656854249492380582 ) ) ;
#40677 = CARTESIAN_POINT ( 'NONE',  ( -10.00000000000000355, 179.5833333265053966, 2.679491924311223183 ) ) ;
#40678 = ADVANCED_FACE ( 'NONE', ( #52933 ), #23883, .T. ) ;
#40679 = CARTESIAN_POINT ( 'NONE',  ( -9.832129032723420536, 193.6979166632526983, 5.676582343749997150 ) ) ;
#40680 = CARTESIAN_POINT ( 'NONE',  ( -2.445694354108839619, 204.8125000013656063, 139.5543056458912190 ) ) ;
#40681 = CARTESIAN_POINT ( 'NONE',  ( 26.56734541678238415, 206.2500000013656063, 166.5412658749999650 ) ) ;
#40682 = CARTESIAN_POINT ( 'NONE',  ( 5.082755093536325930, 25.03124999795161543, -5.082755093536325930 ) ) ;
#40683 = CARTESIAN_POINT ( 'NONE',  ( 5.676582343750001591, 181.9270833299193555, -9.832129032723420536 ) ) ;
#40684 = CARTESIAN_POINT ( 'NONE',  ( 7.999999999999991118, 9.797174393178815797E-16, 22.58030277982336997 ) ) ;
#40685 = CARTESIAN_POINT ( 'NONE',  ( -7.188101187500000044, 96.03125000204838102, 0.000000000000000000 ) ) ;
#40686 = CARTESIAN_POINT ( 'NONE',  ( -4.999999999999998224, 88.54166665983869677, -8.660254037844389075 ) ) ;
#40687 = CARTESIAN_POINT ( 'NONE',  ( 3.211159895383561835, 8.437499998634407916, -3.211159895383561835 ) ) ;
#40688 = CARTESIAN_POINT ( 'NONE',  ( 24.54126587499998280, 202.5000000013656063, 171.4326545832175555 ) ) ;
#40689 = CARTESIAN_POINT ( 'NONE',  ( 2.977408999572650927, -7.188101187499990274, 11.33030278187175632 ) ) ;
#40690 = CARTESIAN_POINT ( 'NONE',  ( -2.085542519210945728E-15, 74.53124999658602690, 11.35316468750000141 ) ) ;
#40691 = DIRECTION ( 'NONE',  ( 1.000000000000000000, -0.000000000000000000, -0.000000000000000000 ) ) ;
#40692 = CARTESIAN_POINT ( 'NONE',  ( -7.999999999999991118, 0.000000000000000000, 0.8865527843298237620 ) ) ;
#40693 = ORIENTED_EDGE ( 'NONE', *, *, #24114, .T. ) ;
#40694 = CARTESIAN_POINT ( 'NONE',  ( -30.99999999999992895, -31.99999999999978684, 171.9999999999997726 ) ) ;
#40695 = CARTESIAN_POINT ( 'NONE',  ( -1.656854249492470732, 203.8125000027311842, 145.9999999999999716 ) ) ;
#40696 = CARTESIAN_POINT ( 'NONE',  ( 9.832129032723420536, 56.19791666325268409, -5.676582343749999815 ) ) ;
#40697 = CARTESIAN_POINT ( 'NONE',  ( 7.778174593052021635, 7.778174593052023411, 69.62500000409677625 ) ) ;
#40698 = CARTESIAN_POINT ( 'NONE',  ( -3.458734125000016757, 197.1250000013656347, 140.5673454167823593 ) ) ;
#40699 = CARTESIAN_POINT ( 'NONE',  ( -31.42542129632872872, -31.79855065832677852, 167.9999999999997726 ) ) ;
#40701 = CARTESIAN_POINT ( 'NONE',  ( 11.35316468749999963, 65.98958332991935549, -3.042071309553165293 ) ) ;
#40700 = CARTESIAN_POINT ( 'NONE',  ( 5.082755093536325042, 93.59375000204838102, -5.082755093536325930 ) ) ;
#40702 = CARTESIAN_POINT ( 'NONE',  ( -3.313708498984757167, 7.999999999999991118, 5.049052779823364645 ) ) ;
#40703 = CARTESIAN_POINT ( 'NONE',  ( -2.981778917433090204, 194.8314443964916336, 144.4186737426478260 ) ) ;
#40704 =( BOUNDED_CURVE ( )  B_SPLINE_CURVE ( 2, ( #63323, #29383, #52391, #69738, #25912, #7840, #2179, #60254, #53868 ),
 .UNSPECIFIED., .F., .F. ) 
 B_SPLINE_CURVE_WITH_KNOTS ( ( 3, 2, 2, 2, 3 ),
 ( 0.5500000000000005995, 0.5583333333333337922, 0.5666666666666670960, 0.5750000000000003997, 0.5833333333333337034 ),
 .UNSPECIFIED. ) 
 CURVE ( )  GEOMETRIC_REPRESENTATION_ITEM ( )  RATIONAL_B_SPLINE_CURVE ( ( 0.9999999999999948930, 0.9238795325112918455, 1.000000000000000000, 0.9238795325112867385, 1.000000000000000000, 0.9238795325112867385, 1.000000000000000000, 0.9238795325112837409, 1.000000000000003109 ) ) 
 REPRESENTATION_ITEM ( '' )  );
#40705 = CARTESIAN_POINT ( 'NONE',  ( -10.00000000000000000, 149.1666666598387110, -2.679491924311229845 ) ) ;
#40706 = CARTESIAN_POINT ( 'NONE',  ( 5.082755093536325042, 93.96875000204838102, -5.082755093536325930 ) ) ;
#40707 = CARTESIAN_POINT ( 'NONE',  ( 5.471491410962281421, 9.542682104092435225, 117.5000000000000568 ) ) ;
#40708 = CARTESIAN_POINT ( 'NONE',  ( -11.35316468750000141, 53.59374999658601979, -1.390361679473963753E-15 ) ) ;
#40709 = CARTESIAN_POINT ( 'NONE',  ( 10.18810118749999916, 1.247682550866122264E-15, 115.2812500020483810 ) ) ;
#40710 = CARTESIAN_POINT ( 'NONE',  ( 9.832129032723416984, 185.3645833299193555, 5.676582343750006032 ) ) ;
#40711 = ORIENTED_EDGE ( 'NONE', *, *, #51754, .T. ) ;
#40712 = FACE_OUTER_BOUND ( 'NONE', #46759, .T. ) ;
#40713 = CARTESIAN_POINT ( 'NONE',  ( -10.18810118749999916, 0.000000000000000000, 73.65625000204836681 ) ) ;
#40714 = CARTESIAN_POINT ( 'NONE',  ( 7.320508075688774596, 162.4999999931720538, -7.320508075688774596 ) ) ;
#40716 = CARTESIAN_POINT ( 'NONE',  ( 11.35316468749999785, 180.5729166632526983, 3.042071309553174174 ) ) ;
#40715 = CARTESIAN_POINT ( 'NONE',  ( 27.99999999999996803, 203.0000000000000000, 173.9999999999999147 ) ) ;
#40717 = CARTESIAN_POINT ( 'NONE',  ( 5.656854249492374365, 5.656854249492375253, 4.824052784329824206 ) ) ;
#40718 = CARTESIAN_POINT ( 'NONE',  ( 1.656854249492381248, 21.93749999726881583, -4.000000000000001776 ) ) ;
#40719 = CARTESIAN_POINT ( 'NONE',  ( 10.00000000000000000, 250.6250000068279746, -1.224646799147353256E-15 ) ) ;
#40720 = DIRECTION ( 'NONE',  ( 0.000000000000000000, 0.000000000000000000, -1.000000000000000000 ) ) ;
#40721 = EDGE_LOOP ( 'NONE', ( #31410, #33309, #72919, #70258, #35197, #13239, #23457 ) ) ;
#40722 = CARTESIAN_POINT ( 'NONE',  ( 8.311093377946834337, 165.4687499965859843, 8.311093377946839666 ) ) ;
#40723 = CARTESIAN_POINT ( 'NONE',  ( 5.082755093536318824, 5.082755093536319713, 26.42405278187175455 ) ) ;
#40724 = CARTESIAN_POINT ( 'NONE',  ( -11.35316468750000141, 133.8020833299193555, 3.042071309553159963 ) ) ;
#40725 = DIRECTION ( 'NONE',  ( -0.000000000000000000, -1.000000000000000000, -0.000000000000000000 ) ) ;
#40726 = ORIENTED_EDGE ( 'NONE', *, *, #38112, .F. ) ;
#40727 = EDGE_CURVE ( 'NONE', #46655, #53455, #10300, .T. ) ;
#40728 = CARTESIAN_POINT ( 'NONE',  ( -4.541265875000002339, 11.93749999863440614, -5.561446717895856393E-16 ) ) ;
#40729 = CARTESIAN_POINT ( 'NONE',  ( 3.313708498984765161, 104.6562500040968047, 7.999999999999998224 ) ) ;
#40730 = CARTESIAN_POINT ( 'NONE',  ( 4.000000000000000888, 11.93750000000000000, 1.656854249492384135 ) ) ;
#40731 = DIRECTION ( 'NONE',  ( -1.000000000000000000, -1.486057055854350565E-32, 3.469446951953619612E-16 ) ) ;
#40732 = CARTESIAN_POINT ( 'NONE',  ( 3.211159895383561835, 12.43749999863440792, -3.211159895383561835 ) ) ;
#40733 = CARTESIAN_POINT ( 'NONE',  ( -7.999999999999991118, 3.313708498984756723, 17.42405278392014623 ) ) ;
#40734 = CARTESIAN_POINT ( 'NONE',  ( 1.656854249492348607, 196.1875000000000568, 138.0000000000000568 ) ) ;
#40736 = ADVANCED_FACE ( 'NONE', ( #25713 ), #31016, .T. ) ;
#40735 = ORIENTED_EDGE ( 'NONE', *, *, #35755, .T. ) ;
#40737 = CARTESIAN_POINT ( 'NONE',  ( -7.320508075688818117, 178.1250000000000568, 7.320508075688810123 ) ) ;
#40738 = CARTESIAN_POINT ( 'NONE',  ( 2.977408999572654480, 106.6250000020483952, 7.188101187499999156 ) ) ;
#40739 = VECTOR ( 'NONE', #54500, 1000.000000000000000 ) ;
#40740 = CARTESIAN_POINT ( 'NONE',  ( -28.00000000000006750, 194.4375000013656063, 166.5412658750003629 ) ) ;
#40741 = SHAPE_REPRESENTATION_RELATIONSHIP ( 'NONE' , 'NONE' ,  #15137, #11994 ) ;
#40742 = ORIENTED_EDGE ( 'NONE', *, *, #74503, .F. ) ;
#40743 = CARTESIAN_POINT ( 'NONE',  ( -0.8997857291008479752, 16.44125064681836790, -68.58473395859590482 ) ) ;
#40744 = CARTESIAN_POINT ( 'NONE',  ( -2.977408999572648707, -7.188101187499990274, 22.76780278187175455 ) ) ;
#40745 = VERTEX_POINT ( 'NONE', #66088 ) ;
#40746 = ORIENTED_EDGE ( 'NONE', *, *, #65509, .T. ) ;
#40747 = CARTESIAN_POINT ( 'NONE',  ( -10.18810118749999916, 0.000000000000000000, 88.65625000204838102 ) ) ;
#40748 = CARTESIAN_POINT ( 'NONE',  ( -7.778174593052023411, 7.778174593052023411, 92.31249999999998579 ) ) ;
#40749 = CARTESIAN_POINT ( 'NONE',  ( -25.55430564589119058, 197.5625000013656063, 167.5543056458915316 ) ) ;
#40750 = CARTESIAN_POINT ( 'NONE',  ( -6.735557395310442023E-16, 11.00000000000000000, 104.1250000000000000 ) ) ;
#40753 = CARTESIAN_POINT ( 'NONE',  ( 3.170472398252169882E-12, 128.7500000000002558, 10.00000000000000178 ) ) ;
#40752 = CARTESIAN_POINT ( 'NONE',  ( 29.65685424949240456, 204.1875000027312126, 173.9999999999999147 ) ) ;
#40751 = CARTESIAN_POINT ( 'NONE',  ( -2.250000000000000888, -2.250000000000000000, 28.00000000000000000 ) ) ;
#40754 = CARTESIAN_POINT ( 'NONE',  ( 10.00000000000000178, 140.0000000000000000, 0.000000000000000000 ) ) ;
#40755 = CARTESIAN_POINT ( 'NONE',  ( -5.656854249492380582, 102.3125000000000000, -5.656854249492380582 ) ) ;
#40756 = AXIS2_PLACEMENT_3D ( 'NONE', #43475, #56217, #27526 ) ;
#40757 = CARTESIAN_POINT ( 'NONE',  ( -11.00000000000000000, 0.000000000000000000, 86.68750000409677625 ) ) ;
#40758 = DIRECTION ( 'NONE',  ( 0.000000000000000000, 0.000000000000000000, 1.000000000000000000 ) ) ;
#40759 = ADVANCED_FACE ( 'NONE', ( #60055 ), #9131, .T. ) ;
#40760 = CARTESIAN_POINT ( 'NONE',  ( 2.828427124746209831, 200.3750000000000284, 200.8284271247462129 ) ) ;
#40761 = EDGE_CURVE ( 'NONE', #4853, #21807, #72506, .T. ) ;
#40762 = CARTESIAN_POINT ( 'NONE',  ( 29.43265458321761230, 202.5000000013656063, 173.4587341249998929 ) ) ;
#40763 = CARTESIAN_POINT ( 'NONE',  ( 2.977408999572651815, 5.062499997951609210, 7.188101187500000933 ) ) ;
#40764 = CARTESIAN_POINT ( 'NONE',  ( -5.662595241051933570, -5.662595241051936235, 1.200615283940629885 ) ) ;
#40765 = CARTESIAN_POINT ( 'NONE',  ( 2.445694354108783664, 195.3125000013656063, 144.4456943541088663 ) ) ;
#40766 = CARTESIAN_POINT ( 'NONE',  ( -2.977408999572650927, 118.2500000020483952, -7.188101187500000933 ) ) ;
#40768 = CARTESIAN_POINT ( 'NONE',  ( 1.469576158976822172E-15, -7.999999999999991118, 7.205302779823365533 ) ) ;
#40767 = DIRECTION ( 'NONE',  ( -0.000000000000000000, 1.000000000000000000, 4.476705744456276341E-16 ) ) ;
#40769 = CARTESIAN_POINT ( 'NONE',  ( -8.311093377946834337, 239.8437500034139873, 8.311093377946837890 ) ) ;
#40770 = CARTESIAN_POINT ( 'NONE',  ( 7.188101187499992051, 8.802885111219154394E-16, 26.61155278187175810 ) ) ;
#40771 = CARTESIAN_POINT ( 'NONE',  ( 27.99999999999996803, 199.0000000000000000, 173.9999999999999147 ) ) ;
#40772 = CARTESIAN_POINT ( 'NONE',  ( 11.35316468750000141, 25.78124999658601624, 0.000000000000000000 ) ) ;
#40773 = CARTESIAN_POINT ( 'NONE',  ( -1.469576158976823947E-15, 10.12500000000000178, 8.000000000000000000 ) ) ;
#40774 = CARTESIAN_POINT ( 'NONE',  ( -9.832129032723420536, 219.0104166632526983, 5.676582343749997150 ) ) ;
#40775 = CARTESIAN_POINT ( 'NONE',  ( 12.00000000000000000, 6.928203230275491009, -14.00000000000000178 ) ) ;
#40777 = CARTESIAN_POINT ( 'NONE',  ( -5.000000000000080824, 41.66666666666677088, -8.660254037844531183 ) ) ;
#40776 = DIRECTION ( 'NONE',  ( 3.400485001760801611E-18, -0.9996144206527183274, 0.02776706724035331308 ) ) ;
#40778 = ORIENTED_EDGE ( 'NONE', *, *, #36970, .F. ) ;
#40779 = EDGE_CURVE ( 'NONE', #55673, #8511, #44000, .T. ) ;
#40780 = EDGE_CURVE ( 'NONE', #49272, #31332, #23811, .T. ) ;
#40781 = CARTESIAN_POINT ( 'NONE',  ( 2.445694354108783219, 195.8125000013656063, 139.5543056458912190 ) ) ;
#40782 = CARTESIAN_POINT ( 'NONE',  ( 5.676582343750001591, 26.61458332991935194, -9.832129032723420536 ) ) ;
#40783 = CARTESIAN_POINT ( 'NONE',  ( -11.00000000000000000, 0.000000000000000000, 86.68750000409677625 ) ) ;
#40784 = CARTESIAN_POINT ( 'NONE',  ( 3.458734124999960358, 206.6875000013656063, 142.0000000000000568 ) ) ;
#40785 = CARTESIAN_POINT ( 'NONE',  ( -24.54126587500001833, 195.2500000013656063, 168.5673454167826435 ) ) ;
#40787 = CARTESIAN_POINT ( 'NONE',  ( 11.35316468749999963, 20.98958332991935194, -3.042071309553165293 ) ) ;
#40786 = CARTESIAN_POINT ( 'NONE',  ( -5.082755093536324154, 112.3437500020483810, 5.082755093536326818 ) ) ;
#40788 = CARTESIAN_POINT ( 'NONE',  ( 7.999999999999992895, -3.313708498984756279, 20.98655277982336642 ) ) ;
#40789 = CARTESIAN_POINT ( 'NONE',  ( 9.832129032723416984, 135.3645833299193555, 5.676582343750006032 ) ) ;
#40790 = CARTESIAN_POINT ( 'NONE',  ( -8.660254037844390851, 114.7916666598387110, 4.999999999999998224 ) ) ;
#40791 = EDGE_CURVE ( 'NONE', #63531, #47572, #41138, .T. ) ;
#40792 = CARTESIAN_POINT ( 'NONE',  ( -5.082755093536324154, 112.7187500020483810, 5.082755093536326818 ) ) ;
#40793 = CARTESIAN_POINT ( 'NONE',  ( 4.999999999999993783, 171.0416666598387110, 8.660254037844390851 ) ) ;
#40794 = CARTESIAN_POINT ( 'NONE',  ( -31.45873412499998523, 208.0000000013656347, 171.4326545832180386 ) ) ;
#40795 = CARTESIAN_POINT ( 'NONE',  ( -5.000000000000000888, 50.98458432551188224, -41.27351214092388432 ) ) ;
#40796 = ORIENTED_EDGE ( 'NONE', *, *, #43669, .F. ) ;
#40797 = CARTESIAN_POINT ( 'NONE',  ( 11.35316468749999963, 6.302083329919350163, -3.042071309553165293 ) ) ;
#40798 =( BOUNDED_SURFACE ( )  B_SPLINE_SURFACE ( 3, 2, ( 
 ( #46250, #35686, #22481 ),
 ( #5163, #40223, #17580 ),
 ( #29285, #45502, #28903 ),
 ( #23242, #52295, #40598 ),
 ( #35329, #68520, #63226 ),
 ( #28529, #29648, #999 ),
 ( #63599, #62851, #11187 ),
 ( #69642, #57593, #51537 ),
 ( #34587, #46988, #5903 ),
 ( #51921, #23612, #46622 ),
 ( #25449, #65818, #64722 ),
 ( #19795, #48093, #66193 ),
 ( #53035, #13748, #70386 ),
 ( #13018, #48837, #30754 ),
 ( #36056, #71843, #54521 ),
 ( #14125, #65072, #31119 ),
 ( #59073, #48464, #30021 ),
 ( #53408, #37159, #31500 ) ),
 .UNSPECIFIED., .F., .F., .F. ) 
 B_SPLINE_SURFACE_WITH_KNOTS ( ( 4, 2, 2, 2, 2, 2, 2, 2, 4 ),
 ( 3, 3 ),
 ( 0.04202945594032907878, 0.04396162471216779472, 0.04589379348400651065, 0.04782596225584522659, 0.04975813102768394253, 0.05169029979952265846, 0.05265638418544201643, 0.05362246857136137440, 0.05748680611503880628 ),
 ( 0.000000000000000000, 1.000000000000000000 ),
 .UNSPECIFIED. ) 
 GEOMETRIC_REPRESENTATION_ITEM ( )  RATIONAL_B_SPLINE_SURFACE ( (
 ( 1.000000000000000000, 0.6241276099608162875, 1.000000000000000000),
 ( 1.000000000000000000, 0.6218761496799840582, 1.000000000000000000),
 ( 1.000000000000000000, 0.6198047272364743954, 1.000000000000000000),
 ( 1.000000000000000000, 0.6161935119823676033, 1.000000000000000000),
 ( 1.000000000000000000, 0.6146642324081269537, 1.000000000000000000),
 ( 1.000000000000000000, 0.6121850116870736214, 1.000000000000000000),
 ( 1.000000000000000000, 0.6112350889400831599, 1.000000000000000000),
 ( 1.000000000000000000, 0.6099522725971745496, 1.000000000000000000),
 ( 1.000000000000000000, 0.6096208180306917912, 1.000000000000000000),
 ( 1.000000000000000000, 0.6096183796350446160, 1.000000000000000000),
 ( 1.000000000000000000, 0.6099422200101833891, 1.000000000000000000),
 ( 1.000000000000000000, 0.6109087447823334793, 1.000000000000000000),
 ( 1.000000000000000000, 0.6113123981688253217, 1.000000000000000000),
 ( 1.000000000000000000, 0.6122677719809350716, 1.000000000000000000),
 ( 1.000000000000000000, 0.6128199619021440503, 1.000000000000000000),
 ( 1.000000000000000000, 0.6159350830263871091, 1.000000000000000000),
 ( 1.000000000000000000, 0.6195556778517007368, 1.000000000000000000),
 ( 1.000000000000000000, 0.6241278272307889674, 1.000000000000000000) ) ) 
 REPRESENTATION_ITEM ( '' )  SURFACE ( )  );
#40799 = EDGE_LOOP ( 'NONE', ( #61599, #22951, #57797, #10842 ) ) ;
#40800 = CARTESIAN_POINT ( 'NONE',  ( 2.765530957081996366, 296.1406250017070647, -6.676582343750003368 ) ) ;
#40801 = CARTESIAN_POINT ( 'NONE',  ( -11.35316468750000141, 133.2812499965860127, -1.390361679473963753E-15 ) ) ;
#40802 = FILL_AREA_STYLE_COLOUR ( '', #3775 ) ;
#40803 = CARTESIAN_POINT ( 'NONE',  ( -5.656854249492375253, 5.656854249492375253, 26.19905278432982243 ) ) ;
#40804 = CARTESIAN_POINT ( 'NONE',  ( 60.15263178277086809, 219.0366716794782747, 46.25981138231621514 ) ) ;
#40805 = CARTESIAN_POINT ( 'NONE',  ( -9.832129032723415207, 244.3229166700806445, 5.676582343750005144 ) ) ;
#40806 = CARTESIAN_POINT ( 'NONE',  ( 7.204075437095968759, -7.204075437095966983, 89.59375000204838102 ) ) ;
#40807 = ORIENTED_EDGE ( 'NONE', *, *, #40010, .T. ) ;
#40808 = B_SPLINE_CURVE_WITH_KNOTS ( 'NONE', 3,
 ( #65451, #36423, #2456, #14497, #71102, #70744, #7749, #36791 ),
 .UNSPECIFIED., .F., .F.,
 ( 4, 2, 2, 4 ),
 ( 0.06671927442655799234, 0.06976857645812635511, 0.07129322747391053650, 0.07281787848969473176 ),
 .UNSPECIFIED. ) ;
#40809 = AXIS2_PLACEMENT_3D ( 'NONE', #64540, #7200, #53224 ) ;
#40810 = DIRECTION ( 'NONE',  ( -0.000000000000000000, -0.000000000000000000, -1.000000000000000000 ) ) ;
#40811 = CARTESIAN_POINT ( 'NONE',  ( -7.778174593052020747, -7.778174593052023411, 100.3750000040967763 ) ) ;
#40812 = UNCERTAINTY_MEASURE_WITH_UNIT (LENGTH_MEASURE( 1.000000000000000082E-05 ), #11085, 'distance_accuracy_value', 'NONE');
#40813 = CARTESIAN_POINT ( 'NONE',  ( 5.676582343750001591, 86.92708332991935549, -9.832129032723420536 ) ) ;
#40814 = VERTEX_POINT ( 'NONE', #19320 ) ;
#40815 = CARTESIAN_POINT ( 'NONE',  ( 1.871523826299183495E-15, -10.18810118749999916, 105.5312500020483810 ) ) ;
#40816 =( BOUNDED_CURVE ( )  B_SPLINE_CURVE ( 2, ( #27613, #15915, #50623, #21949, #41901, #58174, #24548, #64910, #64552, #58903, #70578, #41174, #12489, #35518, #47554, #58531, #11757, #46455, #463, #34421, #41536, #1567, #47187, #6838, #18895, #40797, #6480, #12848, #46820, #5731, #24177, #64184, #23818, #70219, #52863, #23072, #18529, #29111, #29852, #30216, #35887, #69474, #57424, #63803, #63429, #52130, #40430, #1195, #28729, #51745, #34794, #7214, #94, #53236, #69101, #46081, #17407, #57798, #6106, #23441, #12120, #35158, #17784, #29483, #69846, #52492, #830, #18158, #49036, #24905, #42999, #66019, #42266, #14326, #54722, #3029, #55097, #2656, #19622, #36987, #31319, #20742, #60740, #42637, #36622, #72043, #8685, #72434, #65649, #14702, #53971, #26012, #43759, #47922, #49412, #60359, #70941, #66394, #25647, #2282, #59629, #26387, #31700, #13216, #36254, #20360, #59992, #19991, #37359, #7581, #19255, #71302, #59269, #1918, #9061, #30950, #54346, #43377, #37740, #3403, #30586, #32075, #65278, #13584, #53606, #7945, #25277, #48295, #13945, #8309, #48663, #71671, #67523, #44142, #56958, #38857, #73548, #10552, #74290, #15822, #5273, #67154, #28275, #61861, #21856, #33584, #27898, #50908, #44887, #21491, #50166, #22600, #66773, #56588, #33960, #4901, #39225, #51281, #73183, #10182, #45252, #39597, #44512, #22226, #3777, #15077, #33215, #55466, #56212, #38111, #72812, #15449, #27149, #38485, #4162, #61111, #4526, #21119, #61488, #9812, #67891, #16184, #27521, #73921, #62225, #49796, #32835, #55844, #9441, #32458, #68264, #50532, #16560, #62593, #10924, #26779, #12403, #6393, #17691, #51657, #11664, #68635, #372, #57707, #58813, #74650, #6013, #29758, #52773, #69755, #29399, #29017, #35798, #18068, #53147, #18441, #23353, #69010, #6755, #41084, #30132, #7124, #52035, #47096, #1482, #63339, #41454, #46366, #1111, #45621, #45994, #58446, #70134, #22988, #16944, #12036, #11298, #39968, #62974, #28642, #17316, #23726, #34331, #40337, #69381, #57331, #5642, #64468, #34699, #35070, #24087, #46730, #40708, #63712, #58082, #52408, #742, #12766, #64094, #35437, #36535, #53885, #31612, #60652, #24823, #43294, #59546, #18812, #48206, #13129, #71958, #2572, #30866, #37277, #71584, #7494, #53518, #65185, #8974, #66309, #54633, #41816, #2197, #42172, #64826, #70859, #48947, #71214, #36164, #59184, #25192, #47471, #19534, #7862, #37653, #1836, #42551, #8597, #2942, #48574, #8226, #65563, #13860, #31988, #30499, #36903, #47836, #20272, #60271, #55010, #25931, #14615, #59911, #24463, #70494, #13497, #19170, #31236, #54261, #25561, #19907, #42914, #65933, #14239, #16475, #50445, #3316, #26304, #10466, #50080, #10095, #56129, #72342, #61024, #61401, #49327, #66683, #50822, #21028, #44423, #62142, #38025, #33871, #33132, #44797, #9349, #32368, #27811, #55383, #67063, #39513, #32749, #72725, #9727, #26688, #4073, #3692, #68179, #73094, #4438, #21770, #62510, #27430, #49711, #15362, #44053, #20655, #33496, #21400, #73462, #55757, #27067, #10836, #43672, #14987, #67438, #73833, #15736, #56499, #38398, #38775, #67810, #61778, #16101, #39138, #4815, #22140, #45168, #11212, #51563, #62879, #34986, #18356, #41370, #34240, #63625, #64379, #58366, #16851, #6671, #56871, #6307, #51195, #11578, #74579, #22509, #28557, #29675, #5931, #74206, #45530, #57619, #5187, #34613, #68920, #70046, #57242, #17230, #41001, #64008, #29312, #63253, #28932, #287, #12679, #68548, #51950, #5554, #52691, #69668, #28183, #12323, #47014, #23268, #1025, #39877, #22895, #24005, #46277, #35355, #45907, #69296, #40251, #17607, #40625, #11955, #52321, #58001, #657, #23643, #46650, #17982, #13770, #30047, #18725, #19084, #58728, #24379, #8506, #53433, #2108, #36080, #70409, #66216, #42460, #2480, #41734, #64744, #60183, #13042, #24736, #71868, #65099, #30413, #42087, #59098, #36448, #7406, #25839, #7774, #65477, #36814, #48859, #59823, #1755, #47746, #70770, #35713, #42823, #53798, #8139, #13410, #59461, #20182, #7039, #43199, #30778, #31522, #25102, #65841, #47386, #71493, #54174, #48119, #25472, #71125, #31142, #54544, #14149, #53060, #19448, #2851, #48489, #1393, #19817, #37184, #45076, #44705, #39048, #50727, #21312, #50355, #73374, #44334, #43958, #72633, #14521, #22048, #56039, #56402, #27338, #61686, #4721, #20937, #38307, #67720, #26973, #60559, #4348, #67345, #3984, #61313, #3226, #66967, #73742, #20561, #66591, #49617, #60933, #26595, #37560, #15271, #43575, #9255, #14896, #15643, #8883, #31896, #37933, #38684, #54917, #32278, #55292, #26213, #27716, #16018, #49987, #73003, #32658, #9638, #3598, #21679, #10007, #55667, #33039, #62051, #10376, #49233, #33402, #72246, #22416, #28464, #52228, #560, #17512, #51851, #51472, #58274, #40528, #932, #40902, #22792, #16753, #29215, #63534, #52595, #45812, #69576, #34147, #6208, #23915, #63910, #74485, #23543, #68090, #68453, #46555, #17887, #45438, #6576, #34525, #33776, #39418, #29582, #51103, #39779, #68823, #74115, #62782, #12222, #11859, #56776, #35258, #11124, #57530, #16379, #69201, #62417, #10742, #5097, #57147, #195, #28088, #40159, #17135, #5463, #23171, #63165, #11490, #5838, #28832, #46183, #34894, #57901, #1298, #25005, #13680, #36721, #14052, #36353, #53336, #70675, #65006, #54452, #64284, #1662, #70316, #19725, #59732, #2760, #2382, #48396, #12949, #8042, #46924, #58632, #8411, #19353, #6940, #25379, #59368, #35989, #18632, #31426, #60093, #42367, #69949, #18258, #54074, #18992, #53706, #52965, #24279, #31047, #71034, #12590, #29952, #71400, #65382, #42736, #47291, #41641, #41274, #2016, #65750, #64652, #59006, #37090, #7311, #30318, #35618, #24643, #47654, #41998, #13315, #7679, #30686, #48024, #32563, #44246, #61591, #9911, #55572, #55201, #9163, #56310, #33312, #67258, #67629, #38592, #72912, #38955, #25747, #10287, #72540, #73286, #32180, #55949, #37462, #48768, #49520, #14429, #3506, #61958, #31805, #3135, #60842, #72150, #37845, #71775, #26495, #20091, #20846, #60463, #21589, #3887, #43864, #32942, #21219, #8792, #54826, #66493, #43105, #15925, #4259, #38214, #9549, #66879, #15184, #26119, #15554, #26881, #27249, #50264, #44615, #49897, #61219, #66122, #49138, #20461, #43481, #14804, #18455, #52788, #70507, #12050, #29412, #58826, #18082, #50634, #70148, #17330, #13142, #52422, #67993, #35084, #41829, #11679, #57722, #40722, #52050, #17706, #64841, #58095, #34714, #387, #6027, #58461, #36178, #4629, #29032, #1124, #63353, #23368, #46381, #27625, #47483, #35814, #41099, #64106, #23742, #6407, #69397, #47111, #12416, #756, #63728, #46745, #41468, #40351, #35449, #18826, #69768, #6770, #64482, #12779, #29774, #24100, #7138, #73652, #30145, #21961, #53161, #1495, #24478, #44987, #54648, #43687, #36917, #60668, #25206, #66699, #2211, #55023, #65576, #43308, #59198, #59559, #71973, #8988, #13508, #49340, #25575, #24835, #30513, #72357, #42186, #7875, #59925, #65200, #36548, #42565, #7507, #47852, #32005, #48220, #48590, #66323, #60285, #20669, #15002, #53532, #53898, #65950, #20287, #31250, #13873, #71228, #14256, #19920, #1849, #30880, #8239, #19548, #70872, #54276, #14629, #8612, #19185, #2586, #71598, #42928, #37292, #37668, #31627, #2956, #25945, #48962, #3331, #26319, #61790, #38787, #15377, #28198, #10109, #44809, #56513, #73847, #22154, #67822, #67451, #21415, #68563, #45545, #4829, #5201, #50836, #10479, #51209, #44438, #33147, #56141, #10851, #15747, #68194, #49724, #38039, #4451, #26705, #27443, #74220, #44068, #38413, #73107, #9740, #50093, #22525, #50458, #67077, #32762, #61414, #33885, #16114, #73474, #45181, #33511, #21043, #55770, #4087, #61039, #9363, #16490, #21781, #39152, #62155, #27828, #27080, #39528, #62524, #56886, #32382, #55397, #3706, #72740, #28946, #30063, #45922, #51965, #1040, #24020, #41015, #674, #302, #7054, #64025, #24393, #64397, #46292, #40266, #52707, #12337, #47027, #53075, #23281, #18371, #47401, #34627, #12695, #69312, #70063, #16865, #17245, #29690, #41386, #68934, #1409, #58018, #57258, #62895, #39890, #74597, #17621, #22910, #63267, #35728, #35370, #5570, #28570, #58744, #58382, #6688, #51578, #11592, #11228, #34256, #57634, #5947, #40639, #63640, #23659, #11970, #46665, #35001, #6323, #29327, #52336, #69685, #17997, #3240, #19464, #60573, #26226, #25853, #20195, #31911, #2495, #48503, #8897, #71508, #47761, #7789, #70424, #18741, #37198, #37574, #8520, #42837, #54932, #2122, #42475, #48874, #8152, #41748, #60197, #25488, #59838, #31537, #14165, #59113, #54558, #65114, #70784, #30793, #42102, #53813, #64758, #25116, #24751, #13425, #1769, #19832, #13057, #36096, #19097, #65855, #7421, #71881, #30428, #43214, #53448, #2866 ),
 .UNSPECIFIED., .F., .F. ) 
 B_SPLINE_CURVE_WITH_KNOTS ( ( 3, 2, 2, 2, 2, 2, 2, 2, 2, 2, 2, 2, 2, 2, 2, 2, 2, 2, 2, 2, 2, 2, 2, 2, 2, 2, 2, 2, 2, 2, 2, 2, 2, 2, 2, 2, 2, 2, 2, 2, 2, 2, 2, 2, 2, 2, 2, 2, 2, 2, 2, 2, 2, 2, 2, 2, 2, 2, 2, 2, 2, 2, 2, 2, 2, 2, 2, 2, 2, 2, 2, 2, 2, 2, 2, 2, 2, 2, 2, 2, 2, 2, 2, 2, 2, 2, 2, 2, 2, 2, 2, 2, 2, 2, 2, 2, 2, 2, 2, 2, 2, 2, 2, 2, 2, 2, 2, 2, 2, 2, 2, 2, 2, 2, 2, 2, 2, 2, 2, 2, 2, 2, 2, 2, 2, 2, 2, 2, 2, 2, 2, 2, 2, 2, 2, 2, 2, 2, 2, 2, 2, 2, 2, 2, 2, 2, 2, 2, 2, 2, 2, 2, 2, 2, 2, 2, 2, 2, 2, 2, 2, 2, 2, 2, 2, 2, 2, 2, 2, 2, 2, 2, 2, 2, 2, 2, 2, 2, 2, 2, 2, 2, 2, 2, 2, 2, 2, 2, 2, 2, 2, 2, 2, 2, 2, 2, 2, 2, 2, 2, 2, 2, 2, 2, 2, 2, 2, 2, 2, 2, 2, 2, 2, 2, 2, 2, 2, 2, 2, 2, 2, 2, 2, 2, 2, 2, 2, 2, 2, 2, 2, 2, 2, 2, 2, 2, 2, 2, 2, 2, 2, 2, 2, 2, 2, 2, 2, 2, 2, 2, 2, 2, 2, 2, 2, 2, 2, 2, 2, 2, 2, 2, 2, 2, 2, 2, 2, 2, 2, 2, 2, 2, 2, 2, 2, 2, 2, 2, 2, 2, 2, 2, 2, 2, 2, 2, 2, 2, 2, 2, 2, 2, 2, 2, 2, 2, 2, 2, 2, 2, 2, 2, 2, 2, 2, 2, 2, 2, 2, 2, 2, 2, 2, 2, 2, 2, 2, 2, 2, 2, 2, 2, 2, 2, 2, 2, 2, 2, 2, 2, 2, 2, 2, 2, 2, 2, 2, 2, 2, 2, 2, 2, 2, 2, 2, 2, 2, 2, 2, 2, 2, 2, 2, 2, 2, 2, 2, 2, 2, 2, 2, 2, 2, 2, 2, 2, 2, 2, 2, 2, 2, 2, 2, 2, 2, 2, 2, 2, 2, 2, 2, 2, 2, 2, 2, 2, 2, 2, 2, 2, 2, 2, 2, 2, 2, 2, 2, 2, 2, 2, 2, 2, 2, 2, 2, 2, 2, 2, 2, 2, 2, 2, 2, 2, 2, 2, 2, 2, 2, 2, 2, 2, 2, 2, 2, 2, 2, 2, 2, 2, 2, 2, 2, 2, 2, 2, 2, 2, 2, 2, 2, 2, 2, 2, 2, 2, 2, 2, 2, 2, 2, 2, 2, 2, 2, 2, 2, 2, 2, 2, 2, 2, 2, 2, 2, 2, 2, 2, 2, 2, 2, 2, 2, 2, 2, 2, 2, 2, 2, 2, 2, 2, 2, 2, 2, 2, 2, 2, 2, 2, 2, 2, 2, 2, 2, 2, 2, 2, 2, 2, 2, 2, 2, 2, 2, 2, 2, 2, 2, 2, 2, 2, 2, 2, 2, 2, 2, 2, 2, 2, 2, 2, 2, 2, 2, 2, 2, 2, 2, 2, 2, 2, 2, 2, 2, 2, 2, 2, 2, 2, 3 ),
 ( 0.000000000000000000, 0.001843655950715879319, 0.003687311901431758639, 0.005530967852147637524, 0.007374623802863517277, 0.009218279753579396163, 0.01106193570429527505, 0.01290559165501115740, 0.01474924760572703455, 0.01659290355644291518, 0.01843655950715879233, 0.02028021545787467295, 0.02212387140859055010, 0.02396752735930643072, 0.02581118331002231481, 0.02765483926073818849, 0.02949849521145406911, 0.03134215116216994973, 0.03318580711288583035, 0.03502946306360170403, 0.03687311901431758465, 0.03871677496503347221, 0.04056043091574934589, 0.04240408686646522651, 0.04424774281718110019, 0.04609139876789698081, 0.04793505471861286144, 0.04977871066932874899, 0.05162236662004462961, 0.05346602257076050330, 0.05530967852147637698, 0.05715333447219225760, 0.05899699042290813822, 0.06084064637362402578, 0.06268430232433989946, 0.06452795827505578008, 0.06637161422577166070, 0.06821527017648754132, 0.07005892612720340806, 0.07190258207791928868, 0.07374623802863516930, 0.07558989397935104992, 0.07743354993006694442, 0.07927720588078281116, 0.08112086183149869179, 0.08296451778221457241, 0.08480817373293045303, 0.08665182968364633365, 0.08849548563436220039, 0.09033914158507809489, 0.09218279753579396163, 0.09402645348650984225, 0.09587010943722572287, 0.09771376538794160349, 0.09955742133865749799, 0.1014010772893733647, 0.1032447332400892592, 0.1050883891908051260, 0.1069320451415210066, 0.1087757010922368872, 0.1106193570429527540, 0.1124630129936686485, 0.1143066689443845152, 0.1161503248951003958, 0.1179939808458162764, 0.1198376367965321432, 0.1216812927472480516, 0.1235249486979639183, 0.1253686046486797989, 0.1272122605993956657, 0.1290559165501115602, 0.1308995725008273991, 0.1327432284515433214, 0.1345868844022592159, 0.1364305403529750826, 0.1382741963036909494, 0.1401178522544068161, 0.1419615082051227384, 0.1438051641558385774, 0.1456488201065544719, 0.1474924760572703386, 0.1493361320079862331, 0.1511797879587020998, 0.1530234439094179943, 0.1548670998601338888, 0.1567107558108497278, 0.1585544117615656223, 0.1603980677122815168, 0.1622417236629973836, 0.1640853796137132503, 0.1659290355644291448, 0.1677726915151450116, 0.1696163474658609061, 0.1714600034165767728, 0.1733036593672926673, 0.1751473153180085063, 0.1769909712687244008, 0.1788346272194403230, 0.1806782831701561898, 0.1825219391208720565, 0.1843655950715879233, 0.1862092510223038178, 0.1880529069730196845, 0.1898965629237355790, 0.1917402188744514457, 0.1935838748251673402, 0.1954275307758832070, 0.1972711867265991015, 0.1991148426773149960, 0.2009584986280308350, 0.2028021545787467295, 0.2046458105294626240, 0.2064894664801785185, 0.2083331224308943574, 0.2101767783816102519, 0.2120204343323261187, 0.2138640902830420132, 0.2157077462337578799, 0.2175514021844737744, 0.2193950581351896689, 0.2212387140859055079, 0.2230823700366214302, 0.2249260259873372969, 0.2267696819380531637, 0.2286133378887690304, 0.2304569938394849249, 0.2323006497902007916, 0.2341443057409166861, 0.2359879616916325529, 0.2378316176423484474, 0.2396752735930642864, 0.2415189295437802086, 0.2433625854944961031, 0.2452062414452119421, 0.2470498973959278366, 0.2488935533466437033, 0.2507372092973595978, 0.2525808652480754923, 0.2544245211987913313, 0.2562681771495072258, 0.2581118331002231203, 0.2599554890509390148, 0.2617991450016547983, 0.2636428009523707483, 0.2654864569030866428, 0.2673301128538025373, 0.2691737688045184318, 0.2710174247552342708, 0.2728610807059501653, 0.2747047366566660043, 0.2765483926073818988, 0.2783920485580977378, 0.2802357045088136323, 0.2820793604595295823, 0.2839230164102454768, 0.2857666723609613713, 0.2876103283116771547, 0.2894539842623930492, 0.2912976402131089437, 0.2931412961638248382, 0.2949849521145406772, 0.2968286080652565717, 0.2986722640159724662, 0.3005159199666883607, 0.3023595759174041997, 0.3042032318681200942, 0.3060468878188359887, 0.3078905437695518832, 0.3097341997202677777, 0.3115778556709836167, 0.3134215116216994557, 0.3152651675724153502, 0.3171088235231312447, 0.3189524794738471392, 0.3207961354245630337, 0.3226397913752789282, 0.3244834473259947671, 0.3263271032767106061, 0.3281707592274265006, 0.3300144151781423951, 0.3318580711288582896, 0.3337017270795741841, 0.3355453830302900231, 0.3373890389810059176, 0.3392326949317218121, 0.3410763508824377066, 0.3429200068331535456, 0.3447636627838694401, 0.3466073187345853346, 0.3484509746853012291, 0.3502946306360170126, 0.3521382865867329071, 0.3539819425374488016, 0.3558255984881647516, 0.3576692544388806461, 0.3595129103895964851, 0.3613565663403123795, 0.3632002222910282185, 0.3650438782417441130, 0.3668875341924599520, 0.3687311901431758465, 0.3705748460938917410, 0.3724185020446076355, 0.3742621579953235855, 0.3761058139460393690, 0.3779494698967552635, 0.3797931258474711580, 0.3816367817981870525, 0.3834804377489028915, 0.3853240936996187860, 0.3871677496503346805, 0.3890114056010505195, 0.3908550615517664140, 0.3926987175024823085, 0.3945423734531982030, 0.3963860294039140975, 0.3982296853546299920, 0.4000733413053458309, 0.4019169972560616699, 0.4037606532067775644, 0.4056043091574934589, 0.4074479651082092979, 0.4092916210589252479, 0.4111352770096411424, 0.4129789329603570369, 0.4148225889110728204, 0.4166662448617887149, 0.4185099008125046094, 0.4203535567632205039, 0.4221972127139363984, 0.4240408686646522374, 0.4258845246153681319, 0.4277281805660840264, 0.4295718365167999209, 0.4314154924675157599, 0.4332591484182316544, 0.4351028043689475489, 0.4369464603196634434, 0.4387901162703793378, 0.4406337722210951213, 0.4424774281718110158, 0.4443210841225269103, 0.4461647400732428603, 0.4480083960239586993, 0.4498520519746745938, 0.4516957079253904328, 0.4535393638761063273, 0.4553830198268221663, 0.4572266757775380608, 0.4590703317282539553, 0.4609139876789698498, 0.4627576436296857443, 0.4646012995804015833, 0.4664449555311174778, 0.4682886114818333723, 0.4701322674325492668, 0.4719759233832651057, 0.4738195793339810002, 0.4756632352846968947, 0.4775068912354127337, 0.4793505471861285727, 0.4811942031368444672, 0.4830378590875604172, 0.4848815150382763117, 0.4867251709889922062, 0.4885688269397080452, 0.4904124828904238842, 0.4922561388411397787, 0.4940997947918556732, 0.4959434507425715122, 0.4977871066932874067, 0.4996307626440033012, 0.5014744185947191957, 0.5033180745454350902, 0.5051617304961509847, 0.5070053864468668792, 0.5088490423975826626, 0.5106926983482985571, 0.5125363542990144516, 0.5143800102497303461, 0.5162236662004462406, 0.5180673221511621351, 0.5199109781018780296, 0.5217546340525938131, 0.5235982900033095966, 0.5254419459540254911, 0.5272856019047414966, 0.5291292578554573911, 0.5309729138061732856, 0.5328165697568891801, 0.5346602257076050746, 0.5365038816583209691, 0.5383475376090368636, 0.5401911935597526471, 0.5420348495104685416, 0.5438785054611844361, 0.5457221614119003306, 0.5475658173626161140, 0.5494094733133320085, 0.5512531292640479030, 0.5530967852147637975, 0.5549404411654796920, 0.5567840971161954755, 0.5586277530669113700, 0.5604714090176272645, 0.5623150649683431590, 0.5641587209190591645, 0.5660023768697750590, 0.5678460328204909535, 0.5696896887712068480, 0.5715333447219227425, 0.5733770006726384150, 0.5752206566233543095, 0.5770643125740702040, 0.5789079685247860985, 0.5807516244755019930, 0.5825952804262178875, 0.5844389363769337820, 0.5862825923276496765, 0.5881262482783654599, 0.5899699042290813544, 0.5918135601797972489, 0.5936572161305131434, 0.5955008720812290379, 0.5973445280319449324, 0.5991881839826607159, 0.6010318399333767214, 0.6028754958840926159, 0.6047191518348083994, 0.6065628077855242939, 0.6084064637362401884, 0.6102501196869560829, 0.6120937756376719774, 0.6139374315883878719, 0.6157810875391037664, 0.6176247434898196609, 0.6194683994405355554, 0.6213120553912513389, 0.6231557113419672334, 0.6249993672926830168, 0.6268430232433989113, 0.6286866791941148058, 0.6305303351448307003, 0.6323739910955465948, 0.6342176470462624893, 0.6360613029969782728, 0.6379049589476942783, 0.6397486148984101728, 0.6415922708491260673, 0.6434359267998419618, 0.6452795827505578563, 0.6471232387012737508, 0.6489668946519895343, 0.6508105506027054288, 0.6526542065534212123, 0.6544978625041371068, 0.6563415184548530013, 0.6581851744055688958, 0.6600288303562847902, 0.6618724863070006847, 0.6637161422577165792, 0.6655597982084324737, 0.6674034541591483682, 0.6692471101098641517, 0.6710907660605800462, 0.6729344220112960517, 0.6747780779620118352, 0.6766217339127277297, 0.6784653898634436242, 0.6803090458141595187, 0.6821527017648754132, 0.6839963577155913077, 0.6858400136663070912, 0.6876836696170229857, 0.6895273255677388802, 0.6913709815184547747, 0.6932146374691706692, 0.6950582934198865637, 0.6969019493706024582, 0.6987456053213183527, 0.7005892612720340251, 0.7024329172227499196, 0.7042765731734658141, 0.7061202291241817086, 0.7079638850748976031, 0.7098075410256136086, 0.7116511969763295031, 0.7134948529270453976, 0.7153385088777612921, 0.7171821648284770756, 0.7190258207791929701, 0.7208694767299088646, 0.7227131326806247591, 0.7245567886313406536, 0.7264004445820564371, 0.7282441005327723316, 0.7300877564834882261, 0.7319314124342041206, 0.7337750683849199040, 0.7356187243356357985, 0.7374623802863516930, 0.7393060362370675875, 0.7411496921877834820, 0.7429933481384993765, 0.7448370040892152710, 0.7466806600399312766, 0.7485243159906471710, 0.7503679719413629545, 0.7522116278920787380, 0.7540552838427946325, 0.7558989397935105270, 0.7577425957442264215, 0.7595862516949423160, 0.7614299076456582105, 0.7632735635963741050, 0.7651172195470898885, 0.7669608754978057830, 0.7688045314485216775, 0.7706481873992375720, 0.7724918433499534665, 0.7743354993006693610, 0.7761791552513851444, 0.7780228112021010389, 0.7798664671528169334, 0.7817101231035328279, 0.7835537790542487224, 0.7853974350049646169, 0.7872410909556805114, 0.7890847469063964059, 0.7909284028571123004, 0.7927720588078281949, 0.7946157147585440894, 0.7964593707092599839, 0.7983030266599757674, 0.8001466826106916619, 0.8019903385614074454, 0.8038339945121233399, 0.8056776504628392344, 0.8075213064135551289, 0.8093649623642710234, 0.8112086183149869179, 0.8130522742657027013, 0.8148959302164185958, 0.8167395861671344903, 0.8185832421178504958, 0.8204268980685663903, 0.8222705540192822848, 0.8241142099699981793, 0.8259578659207140738, 0.8278015218714298573, 0.8296451778221456408, 0.8314888337728615353, 0.8333324897235774298, 0.8351761456742933243, 0.8370198016250092188, 0.8388634575757251133, 0.8407071135264410078, 0.8425507694771569023, 0.8443944254278727968, 0.8462380813785885803, 0.8480817373293044747, 0.8499253932800203692, 0.8517690492307362637, 0.8536127051814520472, 0.8554563611321680527, 0.8573000170828839472, 0.8591436730335998417, 0.8609873289843157362, 0.8628309849350315197, 0.8646746408857474142, 0.8665182968364633087, 0.8683619527871792032, 0.8702056087378950977, 0.8720492646886109922, 0.8738929206393268867, 0.8757365765900427812, 0.8775802325407586757, 0.8794238884914743482, 0.8812675444421902426, 0.8831112003929061371, 0.8849548563436220316, 0.8867985122943379261, 0.8886421682450538206, 0.8904858241957698262, 0.8923294801464857207, 0.8941731360972015041, 0.8960167920479173986, 0.8978604479986332931, 0.8997041039493491876, 0.9015477599000650821, 0.9033914158507808656, 0.9052350718014967601, 0.9070787277522126546, 0.9089223837029285491, 0.9107660396536443326, 0.9126096956043602271, 0.9144533515550761216, 0.9162970075057920161, 0.9181406634565079106, 0.9199843194072238051, 0.9218279753579396996, 0.9236716313086555941, 0.9255152872593714886, 0.9273589432100873831, 0.9292025991608031665, 0.9310462551115190610, 0.9328899110622349555, 0.9347335670129508500, 0.9365772229636667445, 0.9384208789143826390, 0.9402645348650985335, 0.9421081908158143170, 0.9439518467665302115, 0.9457955027172461060, 0.9476391586679620005, 0.9494828146186778950, 0.9513264705693937895, 0.9531701265201096840, 0.9550137824708254675, 0.9568574384215413620, 0.9587010943722571454, 0.9605447503229730399, 0.9623884062736889344, 0.9642320622244049400, 0.9660757181751208345, 0.9679193741258367290, 0.9697630300765526234, 0.9716066860272685179, 0.9734503419779844124, 0.9752939979287001959, 0.9771376538794160904, 0.9789813098301319849, 0.9808249657808477684, 0.9826686217315636629, 0.9845122776822795574, 0.9863559336329954519, 0.9881995895837113464, 0.9900432455344272409, 0.9918869014851430244, 0.9937305574358589189, 0.9951533035133235394 ),
 .UNSPECIFIED. ) 
 CURVE ( )  GEOMETRIC_REPRESENTATION_ITEM ( )  RATIONAL_B_SPLINE_CURVE ( ( 1.000000000000000000, 0.9659258262890683122, 1.000000000000000000, 0.9659258262890683122, 1.000000000000000000, 0.9659258262890683122, 1.000000000000000000, 0.9659258262890683122, 1.000000000000000000, 0.9659258262890683122, 1.000000000000000000, 0.9659258262890683122, 1.000000000000000000, 0.9659258262890683122, 1.000000000000000000, 0.9659258262890683122, 1.000000000000000000, 0.9659258262890683122, 1.000000000000000000, 0.9659258262890683122, 1.000000000000000000, 0.9659258262890683122, 1.000000000000000000, 0.9659258262890683122, 1.000000000000000000, 0.9659258262890683122, 1.000000000000000000, 0.9659258262890683122, 1.000000000000000000, 0.9659258262890683122, 1.000000000000000000, 0.9659258262890683122, 1.000000000000000000, 0.9659258262890683122, 1.000000000000000000, 0.9659258262890683122, 1.000000000000000000, 0.9659258262890683122, 1.000000000000000000, 0.9659258262890683122, 1.000000000000000000, 0.9659258262890683122, 1.000000000000000000, 0.9659258262890683122, 1.000000000000000000, 0.9659258262890683122, 1.000000000000000000, 0.9659258262890683122, 1.000000000000000000, 0.9659258262890683122, 1.000000000000000000, 0.9659258262890683122, 1.000000000000000000, 0.9659258262890683122, 1.000000000000000000, 0.9659258262890683122, 1.000000000000000000, 0.9659258262890683122, 1.000000000000000000, 0.9659258262890683122, 1.000000000000000000, 0.9659258262890683122, 1.000000000000000000, 0.9659258262890683122, 1.000000000000000000, 0.9659258262890683122, 1.000000000000000000, 0.9659258262890683122, 1.000000000000000000, 0.9659258262890683122, 1.000000000000000000, 0.9659258262890683122, 1.000000000000000000, 0.9659258262890683122, 1.000000000000000000, 0.9659258262890683122, 1.000000000000000000, 0.9659258262890683122, 1.000000000000000000, 0.9659258262890683122, 1.000000000000000000, 0.9659258262890683122, 1.000000000000000000, 0.9659258262890683122, 1.000000000000000000, 0.9659258262890683122, 1.000000000000000000, 0.9659258262890683122, 1.000000000000000000, 0.9659258262890683122, 1.000000000000000000, 0.9659258262890683122, 1.000000000000000000, 0.9659258262890683122, 1.000000000000000000, 0.9659258262890683122, 1.000000000000000000, 0.9659258262890683122, 1.000000000000000000, 0.9659258262890683122, 1.000000000000000000, 0.9659258262890683122, 1.000000000000000000, 0.9659258262890683122, 1.000000000000000000, 0.9659258262890683122, 1.000000000000000000, 0.9659258262890683122, 1.000000000000000000, 0.9659258262890683122, 1.000000000000000000, 0.9659258262890683122, 1.000000000000000000, 0.9659258262890683122, 1.000000000000000000, 0.9659258262890683122, 1.000000000000000000, 0.9659258262890683122, 1.000000000000000000, 0.9659258262890683122, 1.000000000000000000, 0.9659258262890683122, 1.000000000000000000, 0.9659258262890683122, 1.000000000000000000, 0.9659258262890683122, 1.000000000000000000, 0.9659258262890683122, 1.000000000000000000, 0.9659258262890683122, 1.000000000000000000, 0.9659258262890683122, 1.000000000000000000, 0.9659258262890683122, 1.000000000000000000, 0.9659258262890683122, 1.000000000000000000, 0.9659258262890683122, 1.000000000000000000, 0.9659258262890683122, 1.000000000000000000, 0.9659258262890683122, 1.000000000000000000, 0.9659258262890683122, 1.000000000000000000, 0.9659258262890683122, 1.000000000000000000, 0.9659258262890683122, 1.000000000000000000, 0.9659258262890683122, 1.000000000000000000, 0.9659258262890683122, 1.000000000000000000, 0.9659258262890683122, 1.000000000000000000, 0.9659258262890683122, 1.000000000000000000, 0.9659258262890683122, 1.000000000000000000, 0.9659258262890683122, 1.000000000000000000, 0.9659258262890683122, 1.000000000000000000, 0.9659258262890683122, 1.000000000000000000, 0.9659258262890683122, 1.000000000000000000, 0.9659258262890683122, 1.000000000000000000, 0.9659258262890683122, 1.000000000000000000, 0.9659258262890683122, 1.000000000000000000, 0.9659258262890683122, 1.000000000000000000, 0.9659258262890683122, 1.000000000000000000, 0.9659258262890683122, 1.000000000000000000, 0.9659258262890683122, 1.000000000000000000, 0.9659258262890683122, 1.000000000000000000, 0.9659258262890683122, 1.000000000000000000, 0.9659258262890683122, 1.000000000000000000, 0.9659258262890683122, 1.000000000000000000, 0.9659258262890683122, 1.000000000000000000, 0.9659258262890683122, 1.000000000000000000, 0.9659258262890683122, 1.000000000000000000, 0.9659258262890683122, 1.000000000000000000, 0.9659258262890683122, 1.000000000000000000, 0.9659258262890683122, 1.000000000000000000, 0.9659258262890683122, 1.000000000000000000, 0.9659258262890683122, 1.000000000000000000, 0.9659258262890683122, 1.000000000000000000, 0.9659258262890683122, 1.000000000000000000, 0.9659258262890683122, 1.000000000000000000, 0.9659258262890683122, 1.000000000000000000, 0.9659258262890683122, 1.000000000000000000, 0.9659258262890683122, 1.000000000000000000, 0.9659258262890683122, 1.000000000000000000, 0.9659258262890683122, 1.000000000000000000, 0.9659258262890683122, 1.000000000000000000, 0.9659258262890683122, 1.000000000000000000, 0.9659258262890683122, 1.000000000000000000, 0.9659258262890683122, 1.000000000000000000, 0.9659258262890683122, 1.000000000000000000, 0.9659258262890683122, 1.000000000000000000, 0.9659258262890683122, 1.000000000000000000, 0.9659258262890683122, 1.000000000000000000, 0.9659258262890683122, 1.000000000000000000, 0.9659258262890683122, 1.000000000000000000, 0.9659258262890683122, 1.000000000000000000, 0.9659258262890683122, 1.000000000000000000, 0.9659258262890683122, 1.000000000000000000, 0.9659258262890683122, 1.000000000000000000, 0.9659258262890683122, 1.000000000000000000, 0.9659258262890683122, 1.000000000000000000, 0.9659258262890683122, 1.000000000000000000, 0.9659258262890683122, 1.000000000000000000, 0.9659258262890683122, 1.000000000000000000, 0.9659258262890683122, 1.000000000000000000, 0.9659258262890683122, 1.000000000000000000, 0.9659258262890683122, 1.000000000000000000, 0.9659258262890683122, 1.000000000000000000, 0.9659258262890683122, 1.000000000000000000, 0.9659258262890683122, 1.000000000000000000, 0.9659258262890683122, 1.000000000000000000, 0.9659258262890683122, 1.000000000000000000, 0.9659258262890683122, 1.000000000000000000, 0.9659258262890683122, 1.000000000000000000, 0.9659258262890683122, 1.000000000000000000, 0.9659258262890683122, 1.000000000000000000, 0.9659258262890683122, 1.000000000000000000, 0.9659258262890683122, 1.000000000000000000, 0.9659258262890683122, 1.000000000000000000, 0.9659258262890683122, 1.000000000000000000, 0.9659258262890683122, 1.000000000000000000, 0.9659258262890683122, 1.000000000000000000, 0.9659258262890683122, 1.000000000000000000, 0.9659258262890683122, 1.000000000000000000, 0.9659258262890683122, 1.000000000000000000, 0.9659258262890683122, 1.000000000000000000, 0.9659258262890683122, 1.000000000000000000, 0.9659258262890683122, 1.000000000000000000, 0.9659258262890683122, 1.000000000000000000, 0.9659258262890683122, 1.000000000000000000, 0.9659258262890683122, 1.000000000000000000, 0.9659258262890683122, 1.000000000000000000, 0.9659258262890683122, 1.000000000000000000, 0.9659258262890683122, 1.000000000000000000, 0.9659258262890683122, 1.000000000000000000, 0.9659258262890683122, 1.000000000000000000, 0.9659258262890683122, 1.000000000000000000, 0.9659258262890683122, 1.000000000000000000, 0.9659258262890683122, 1.000000000000000000, 0.9659258262890683122, 1.000000000000000000, 0.9659258262890683122, 1.000000000000000000, 0.9659258262890683122, 1.000000000000000000, 0.9659258262890683122, 1.000000000000000000, 0.9659258262890683122, 1.000000000000000000, 0.9659258262890683122, 1.000000000000000000, 0.9659258262890683122, 1.000000000000000000, 0.9659258262890683122, 1.000000000000000000, 0.9659258262890683122, 1.000000000000000000, 0.9659258262890683122, 1.000000000000000000, 0.9659258262890683122, 1.000000000000000000, 0.9659258262890683122, 1.000000000000000000, 0.9659258262890683122, 1.000000000000000000, 0.9659258262890683122, 1.000000000000000000, 0.9659258262890683122, 1.000000000000000000, 0.9659258262890683122, 1.000000000000000000, 0.9659258262890683122, 1.000000000000000000, 0.9659258262890683122, 1.000000000000000000, 0.9659258262890683122, 1.000000000000000000, 0.9659258262890683122, 1.000000000000000000, 0.9659258262890683122, 1.000000000000000000, 0.9659258262890683122, 1.000000000000000000, 0.9659258262890683122, 1.000000000000000000, 0.9659258262890683122, 1.000000000000000000, 0.9659258262890683122, 1.000000000000000000, 0.9659258262890683122, 1.000000000000000000, 0.9659258262890683122, 1.000000000000000000, 0.9659258262890683122, 1.000000000000000000, 0.9659258262890683122, 1.000000000000000000, 0.9659258262890683122, 1.000000000000000000, 0.9659258262890683122, 1.000000000000000000, 0.9659258262890683122, 1.000000000000000000, 0.9659258262890683122, 1.000000000000000000, 0.9659258262890683122, 1.000000000000000000, 0.9659258262890683122, 1.000000000000000000, 0.9659258262890683122, 1.000000000000000000, 0.9659258262890683122, 1.000000000000000000, 0.9659258262890683122, 1.000000000000000000, 0.9659258262890683122, 1.000000000000000000, 0.9659258262890683122, 1.000000000000000000, 0.9659258262890683122, 1.000000000000000000, 0.9659258262890683122, 1.000000000000000000, 0.9659258262890683122, 1.000000000000000000, 0.9659258262890683122, 1.000000000000000000, 0.9659258262890683122, 1.000000000000000000, 0.9659258262890683122, 1.000000000000000000, 0.9659258262890683122, 1.000000000000000000, 0.9659258262890683122, 1.000000000000000000, 0.9659258262890683122, 1.000000000000000000, 0.9659258262890683122, 1.000000000000000000, 0.9659258262890683122, 1.000000000000000000, 0.9659258262890683122, 1.000000000000000000, 0.9659258262890683122, 1.000000000000000000, 0.9659258262890683122, 1.000000000000000000, 0.9659258262890683122, 1.000000000000000000, 0.9659258262890683122, 1.000000000000000000, 0.9659258262890683122, 1.000000000000000000, 0.9659258262890683122, 1.000000000000000000, 0.9659258262890683122, 1.000000000000000000, 0.9659258262890683122, 1.000000000000000000, 0.9659258262890683122, 1.000000000000000000, 0.9659258262890683122, 1.000000000000000000, 0.9659258262890683122, 1.000000000000000000, 0.9659258262890683122, 1.000000000000000000, 0.9659258262890683122, 1.000000000000000000, 0.9659258262890683122, 1.000000000000000000, 0.9659258262890683122, 1.000000000000000000, 0.9659258262890683122, 1.000000000000000000, 0.9659258262890683122, 1.000000000000000000, 0.9659258262890683122, 1.000000000000000000, 0.9659258262890683122, 1.000000000000000000, 0.9659258262890683122, 1.000000000000000000, 0.9659258262890683122, 1.000000000000000000, 0.9659258262890683122, 1.000000000000000000, 0.9659258262890683122, 1.000000000000000000, 0.9659258262890683122, 1.000000000000000000, 0.9659258262890683122, 1.000000000000000000, 0.9659258262890683122, 1.000000000000000000, 0.9659258262890683122, 1.000000000000000000, 0.9659258262890683122, 1.000000000000000000, 0.9659258262890683122, 1.000000000000000000, 0.9659258262890683122, 1.000000000000000000, 0.9659258262890683122, 1.000000000000000000, 0.9659258262890683122, 1.000000000000000000, 0.9659258262890683122, 1.000000000000000000, 0.9659258262890683122, 1.000000000000000000, 0.9659258262890683122, 1.000000000000000000, 0.9659258262890683122, 1.000000000000000000, 0.9659258262890683122, 1.000000000000000000, 0.9659258262890683122, 1.000000000000000000, 0.9659258262890683122, 1.000000000000000000, 0.9659258262890683122, 1.000000000000000000, 0.9659258262890683122, 1.000000000000000000, 0.9659258262890683122, 1.000000000000000000, 0.9659258262890683122, 1.000000000000000000, 0.9659258262890683122, 1.000000000000000000, 0.9659258262890683122, 1.000000000000000000, 0.9659258262890683122, 1.000000000000000000, 0.9659258262890683122, 1.000000000000000000, 0.9659258262890683122, 1.000000000000000000, 0.9659258262890683122, 1.000000000000000000, 0.9659258262890683122, 1.000000000000000000, 0.9659258262890683122, 1.000000000000000000, 0.9659258262890683122, 1.000000000000000000, 0.9659258262890683122, 1.000000000000000000, 0.9659258262890683122, 1.000000000000000000, 0.9659258262890683122, 1.000000000000000000, 0.9659258262890683122, 1.000000000000000000, 0.9659258262890683122, 1.000000000000000000, 0.9659258262890683122, 1.000000000000000000, 0.9659258262890683122, 1.000000000000000000, 0.9659258262890683122, 1.000000000000000000, 0.9659258262890683122, 1.000000000000000000, 0.9659258262890683122, 1.000000000000000000, 0.9659258262890683122, 1.000000000000000000, 0.9659258262890683122, 1.000000000000000000, 0.9659258262890683122, 1.000000000000000000, 0.9659258262890683122, 1.000000000000000000, 0.9659258262890683122, 1.000000000000000000, 0.9659258262890683122, 1.000000000000000000, 0.9659258262890683122, 1.000000000000000000, 0.9659258262890683122, 1.000000000000000000, 0.9659258262890683122, 1.000000000000000000, 0.9659258262890683122, 1.000000000000000000, 0.9659258262890683122, 1.000000000000000000, 0.9659258262890683122, 1.000000000000000000, 0.9659258262890683122, 1.000000000000000000, 0.9659258262890683122, 1.000000000000000000, 0.9659258262890683122, 1.000000000000000000, 0.9659258262890683122, 1.000000000000000000, 0.9659258262890683122, 1.000000000000000000, 0.9659258262890683122, 1.000000000000000000, 0.9659258262890683122, 1.000000000000000000, 0.9659258262890683122, 1.000000000000000000, 0.9659258262890683122, 1.000000000000000000, 0.9659258262890683122, 1.000000000000000000, 0.9659258262890683122, 1.000000000000000000, 0.9659258262890683122, 1.000000000000000000, 0.9659258262890683122, 1.000000000000000000, 0.9659258262890683122, 1.000000000000000000, 0.9659258262890683122, 1.000000000000000000, 0.9659258262890683122, 1.000000000000000000, 0.9659258262890683122, 1.000000000000000000, 0.9659258262890683122, 1.000000000000000000, 0.9659258262890683122, 1.000000000000000000, 0.9659258262890683122, 1.000000000000000000, 0.9659258262890683122, 1.000000000000000000, 0.9659258262890683122, 1.000000000000000000, 0.9659258262890683122, 1.000000000000000000, 0.9659258262890683122, 1.000000000000000000, 0.9659258262890683122, 1.000000000000000000, 0.9659258262890683122, 1.000000000000000000, 0.9659258262890683122, 1.000000000000000000, 0.9659258262890683122, 1.000000000000000000, 0.9659258262890683122, 1.000000000000000000, 0.9659258262890683122, 1.000000000000000000, 0.9659258262890683122, 1.000000000000000000, 0.9659258262890683122, 1.000000000000000000, 0.9659258262890683122, 1.000000000000000000, 0.9659258262890683122, 1.000000000000000000, 0.9659258262890683122, 1.000000000000000000, 0.9659258262890683122, 1.000000000000000000, 0.9659258262890683122, 1.000000000000000000, 0.9659258262890683122, 1.000000000000000000, 0.9659258262890683122, 1.000000000000000000, 0.9659258262890683122, 1.000000000000000000, 0.9659258262890683122, 1.000000000000000000, 0.9659258262890683122, 1.000000000000000000, 0.9659258262890683122, 1.000000000000000000, 0.9659258262890683122, 1.000000000000000000, 0.9659258262890683122, 1.000000000000000000, 0.9659258262890683122, 1.000000000000000000, 0.9659258262890683122, 1.000000000000000000, 0.9659258262890683122, 1.000000000000000000, 0.9659258262890683122, 1.000000000000000000, 0.9659258262890683122, 1.000000000000000000, 0.9659258262890683122, 1.000000000000000000, 0.9659258262890683122, 1.000000000000000000, 0.9659258262890683122, 1.000000000000000000, 0.9659258262890683122, 1.000000000000000000, 0.9659258262890683122, 1.000000000000000000, 0.9659258262890683122, 1.000000000000000000, 0.9659258262890683122, 1.000000000000000000, 0.9659258262890683122, 1.000000000000000000, 0.9659258262890683122, 1.000000000000000000, 0.9659258262890683122, 1.000000000000000000, 0.9659258262890683122, 1.000000000000000000, 0.9659258262890683122, 1.000000000000000000, 0.9659258262890683122, 1.000000000000000000, 0.9659258262890683122, 1.000000000000000000, 0.9659258262890683122, 1.000000000000000000, 0.9659258262890683122, 1.000000000000000000, 0.9659258262890683122, 1.000000000000000000, 0.9659258262890683122, 1.000000000000000000, 0.9659258262890683122, 1.000000000000000000, 0.9659258262890683122, 1.000000000000000000, 0.9659258262890683122, 1.000000000000000000, 0.9659258262890683122, 1.000000000000000000, 0.9659258262890683122, 1.000000000000000000, 0.9659258262890683122, 1.000000000000000000, 0.9659258262890683122, 1.000000000000000000, 0.9659258262890683122, 1.000000000000000000, 0.9659258262890683122, 1.000000000000000000, 0.9659258262890683122, 1.000000000000000000, 0.9659258262890683122, 1.000000000000000000, 0.9659258262890683122, 1.000000000000000000, 0.9659258262890683122, 1.000000000000000000, 0.9659258262890683122, 1.000000000000000000, 0.9659258262890683122, 1.000000000000000000, 0.9659258262890683122, 1.000000000000000000, 0.9659258262890683122, 1.000000000000000000, 0.9659258262890683122, 1.000000000000000000, 0.9659258262890683122, 1.000000000000000000, 0.9659258262890683122, 1.000000000000000000, 0.9659258262890683122, 1.000000000000000000, 0.9659258262890683122, 1.000000000000000000, 0.9659258262890683122, 1.000000000000000000, 0.9659258262890683122, 1.000000000000000000, 0.9659258262890683122, 1.000000000000000000, 0.9659258262890683122, 1.000000000000000000, 0.9659258262890683122, 1.000000000000000000, 0.9659258262890683122, 1.000000000000000000, 0.9659258262890683122, 1.000000000000000000, 0.9659258262890683122, 1.000000000000000000, 0.9659258262890683122, 1.000000000000000000, 0.9659258262890683122, 1.000000000000000000, 0.9659258262890683122, 1.000000000000000000, 0.9659258262890683122, 1.000000000000000000, 0.9659258262890683122, 1.000000000000000000, 0.9659258262890683122, 1.000000000000000000, 0.9659258262890683122, 1.000000000000000000, 0.9659258262890683122, 1.000000000000000000, 0.9659258262890683122, 1.000000000000000000, 0.9659258262890683122, 1.000000000000000000, 0.9659258262890683122, 1.000000000000000000, 0.9659258262890683122, 1.000000000000000000, 0.9659258262890683122, 1.000000000000000000, 0.9659258262890683122, 1.000000000000000000, 0.9659258262890683122, 1.000000000000000000, 0.9659258262890683122, 1.000000000000000000, 0.9659258262890683122, 1.000000000000000000, 0.9659258262890683122, 1.000000000000000000, 0.9659258262890683122, 1.000000000000000000, 0.9659258262890683122, 1.000000000000000000, 0.9659258262890683122, 1.000000000000000000, 0.9659258262890683122, 1.000000000000000000, 0.9659258262890683122, 1.000000000000000000, 0.9659258262890683122, 1.000000000000000000, 0.9659258262890683122, 1.000000000000000000, 0.9659258262890683122, 1.000000000000000000, 0.9659258262890683122, 1.000000000000000000, 0.9659258262890683122, 1.000000000000000000, 0.9659258262890683122, 1.000000000000000000, 0.9659258262890683122, 1.000000000000000000, 0.9659258262890683122, 1.000000000000000000, 0.9659258262890683122, 1.000000000000000000, 0.9659258262890683122, 1.000000000000000000, 0.9659258262890683122, 1.000000000000000000, 0.9659258262890683122, 1.000000000000000000, 0.9659258262890683122, 1.000000000000000000, 0.9659258262890683122, 1.000000000000000000, 0.9659258262890683122, 1.000000000000000000, 0.9659258262890683122, 1.000000000000000000, 0.9659258262890683122, 1.000000000000000000, 0.9659258262890683122, 1.000000000000000000, 0.9659258262890683122, 1.000000000000000000, 0.9659258262890683122, 1.000000000000000000, 0.9659258262890683122, 1.000000000000000000, 0.9659258262890683122, 1.000000000000000000, 0.9659258262890683122, 1.000000000000000000, 0.9659258262890683122, 1.000000000000000000, 0.9659258262890683122, 1.000000000000000000, 0.9659258262890683122, 1.000000000000000000, 0.9659258262890683122, 1.000000000000000000, 0.9659258262890683122, 1.000000000000000000, 0.9659258262890683122, 1.000000000000000000, 0.9659258262890683122, 1.000000000000000000, 0.9659258262890683122, 1.000000000000000000, 0.9659258262890683122, 1.000000000000000000, 0.9659258262890683122, 1.000000000000000000, 0.9659258262890683122, 1.000000000000000000, 0.9659258262890683122, 1.000000000000000000, 0.9659258262890683122, 1.000000000000000000, 0.9659258262890683122, 1.000000000000000000, 0.9659258262890683122, 1.000000000000000000, 0.9659258262890683122, 1.000000000000000000, 0.9659258262890683122, 1.000000000000000000, 0.9659258262890683122, 1.000000000000000000, 0.9659258262890683122, 1.000000000000000000, 0.9659258262890683122, 1.000000000000000000, 0.9659258262890683122, 1.000000000000000000, 0.9659258262890683122, 1.000000000000000000, 0.9659258262890683122, 1.000000000000000000, 0.9659258262890683122, 1.000000000000000000, 0.9659258262890683122, 1.000000000000000000, 0.9659258262890683122, 1.000000000000000000, 0.9659258262890683122, 1.000000000000000000, 0.9659258262890683122, 1.000000000000000000, 0.9659258262890683122, 1.000000000000000000, 0.9659258262890683122, 1.000000000000000000, 0.9659258262890683122, 1.000000000000000000, 0.9659258262890683122, 1.000000000000000000, 0.9659258262890683122, 1.000000000000000000, 0.9659258262890683122, 1.000000000000000000, 0.9659258262890683122, 1.000000000000000000, 0.9659258262890683122, 1.000000000000000000, 0.9659258262890683122, 1.000000000000000000, 0.9659258262890683122, 1.000000000000000000, 0.9659258262890683122, 1.000000000000000000, 0.9659258262890683122, 1.000000000000000000, 0.9659258262890683122, 1.000000000000000000, 0.9659258262890683122, 1.000000000000000000, 0.9659258262890683122, 1.000000000000000000, 0.9659258262890683122, 1.000000000000000000, 0.9659258262890683122, 1.000000000000000000, 0.9659258262890683122, 1.000000000000000000, 0.9659258262890683122, 1.000000000000000000, 0.9659258262890683122, 1.000000000000000000, 0.9659258262890683122, 1.000000000000000000, 0.9659258262890683122, 1.000000000000000000, 0.9659258262890683122, 1.000000000000000000, 0.9659258262890683122, 1.000000000000000000, 0.9659258262890683122, 1.000000000000000000, 0.9659258262890683122, 1.000000000000000000, 0.9659258262890683122, 1.000000000000000000, 0.9659258262890683122, 1.000000000000000000, 0.9659258262890683122, 1.000000000000000000, 0.9659258262890683122, 1.000000000000000000, 0.9659258262890683122, 1.000000000000000000, 0.9659258262890683122, 1.000000000000000000, 0.9659258262890683122, 1.000000000000000000, 0.9659258262890683122, 1.000000000000000000, 0.9659258262890683122, 1.000000000000000000, 0.9659258262890683122, 1.000000000000000000, 0.9659258262890683122, 1.000000000000000000, 0.9659258262890683122, 1.000000000000000000, 0.9659258262890683122, 1.000000000000000000, 0.9659258262890683122, 1.000000000000000000, 0.9659258262890683122, 1.000000000000000000, 0.9659258262890683122, 1.000000000000000000, 0.9659258262890683122, 1.000000000000000000, 0.9659258262890683122, 1.000000000000000000, 0.9659258262890683122, 1.000000000000000000, 0.9659258262890683122, 1.000000000000000000, 0.9659258262890683122, 1.000000000000000000, 0.9659258262890683122, 1.000000000000000000, 0.9659258262890683122, 1.000000000000000000, 0.9659258262890683122, 1.000000000000000000, 0.9659258262890683122, 1.000000000000000000, 0.9659258262890683122, 1.000000000000000000, 0.9659258262890683122, 1.000000000000000000, 0.9659258262890683122, 1.000000000000000000, 0.9659258262890683122, 1.000000000000000000, 0.9659258262890683122, 1.000000000000000000, 0.9659258262890683122, 1.000000000000000000, 0.9659258262890683122, 1.000000000000000000, 0.9659258262890683122, 1.000000000000000000, 0.9659258262890683122, 1.000000000000000000, 0.9659258262890683122, 1.000000000000000000, 0.9659258262890683122, 1.000000000000000000, 0.9659258262890683122, 1.000000000000000000, 0.9659258262890683122, 1.000000000000000000, 0.9659258262890683122, 1.000000000000000000, 0.9659258262890683122, 1.000000000000000000, 0.9659258262890683122, 1.000000000000000000, 0.9659258262890683122, 1.000000000000000000, 0.9659258262890683122, 1.000000000000000000, 0.9659258262890683122, 1.000000000000000000, 0.9659258262890683122, 1.000000000000000000, 0.9659258262890683122, 1.000000000000000000, 0.9659258262890683122, 1.000000000000000000, 0.9659258262890683122, 1.000000000000000000, 0.9659258262890683122, 1.000000000000000000, 0.9659258262890683122, 1.000000000000000000, 0.9659258262890683122, 1.000000000000000000, 0.9737050196533417745, 0.9879936201322587763 ) ) 
 REPRESENTATION_ITEM ( '' )  );
#40817 = CARTESIAN_POINT ( 'NONE',  ( 3.211159895383560947, 14.31249999863440792, 3.211159895383562723 ) ) ;
#40818 = ORIENTED_EDGE ( 'NONE', *, *, #64560, .F. ) ;
#40819 = ORIENTED_EDGE ( 'NONE', *, *, #73691, .T. ) ;
#40820 = CARTESIAN_POINT ( 'NONE',  ( 3.313708498984762052, 4.781250000000000888, -8.000000000000000000 ) ) ;
#40821 = CARTESIAN_POINT ( 'NONE',  ( -3.211159895383562723, 1.062499998634406806, 3.211159895383561391 ) ) ;
#40822 = CARTESIAN_POINT ( 'NONE',  ( 2.020667218593132706E-15, -11.00000000000000000, 76.56250000409677625 ) ) ;
#40823 = CARTESIAN_POINT ( 'NONE',  ( -7.188101187500001821, 22.49999999795161543, -2.977408999572651371 ) ) ;
#40824 = CARTESIAN_POINT ( 'NONE',  ( -4.898587196589412829E-16, 120.3125000040967763, -8.000000000000000000 ) ) ;
#40825 = VECTOR ( 'NONE', #44303, 1000.000000000000000 ) ;
#40826 = CARTESIAN_POINT ( 'NONE',  ( -10.18810118749999916, 0.000000000000000000, 105.5312500020483810 ) ) ;
#40827 = ADVANCED_FACE ( 'NONE', ( #31770 ), #42332, .T. ) ;
#40828 = CARTESIAN_POINT ( 'NONE',  ( -2.828427124746190735, 0.3750000000000001665, -2.828427124746191623 ) ) ;
#40829 = CARTESIAN_POINT ( 'NONE',  ( -4.000000000000001776, 12.24999999726881406, -4.898587196589415787E-16 ) ) ;
#40830 = CARTESIAN_POINT ( 'NONE',  ( 9.797174393178825657E-16, 125.0000000000000000, -8.000000000000000000 ) ) ;
#40831 = VERTEX_POINT ( 'NONE', #20431 ) ;
#40832 = CARTESIAN_POINT ( 'NONE',  ( 2.775557561562891351E-14, 210.0000000000000284, 198.0000000000000284 ) ) ;
#40833 = CARTESIAN_POINT ( 'NONE',  ( -2.445694354108783664, 199.3125000013656063, 195.5543056458912190 ) ) ;
#40834 = CARTESIAN_POINT ( 'NONE',  ( -24.54126587500002543, 206.2500000013656063, 168.5673454167826435 ) ) ;
#40835 = EDGE_CURVE ( 'NONE', #55027, #11019, #43448, .T. ) ;
#40836 = CARTESIAN_POINT ( 'NONE',  ( 1.881053915767122664, 11.12499999863440792, 4.541265875000001451 ) ) ;
#40837 = CARTESIAN_POINT ( 'NONE',  ( -1.656854249492358155, 18.43749999726881228, 4.000000000000024869 ) ) ;
#40838 = CARTESIAN_POINT ( 'NONE',  ( -5.082755093536317936, -5.082755093536320601, 12.17405278187175277 ) ) ;
#40839 = ORIENTED_EDGE ( 'NONE', *, *, #585, .F. ) ;
#40840 = ORIENTED_EDGE ( 'NONE', *, *, #65201, .F. ) ;
#40841 = CARTESIAN_POINT ( 'NONE',  ( -10.18810118749999916, 0.000000000000000000, 105.1562500020483810 ) ) ;
#40842 = PRODUCT_RELATED_PRODUCT_CATEGORY ( 'part', '', ( #62589 ) ) ;
#40843 = CARTESIAN_POINT ( 'NONE',  ( 8.000000000000000000, 95.93750000409679046, -9.797174393178825657E-16 ) ) ;
#40844 = CARTESIAN_POINT ( 'NONE',  ( -28.00000000000002842, 206.0000000000000284, 166.0000000000003695 ) ) ;
#40845 = CARTESIAN_POINT ( 'NONE',  ( -2.445694354108783664, 201.3125000013656063, 195.5543056458912190 ) ) ;
#40846 = CARTESIAN_POINT ( 'NONE',  ( 28.00000000000001421, 196.4375000013655779, 173.4587341249998929 ) ) ;
#40847 = CARTESIAN_POINT ( 'NONE',  ( 10.00000000000000000, 99.79166666666667140, 2.679491924311236062 ) ) ;
#40848 = CARTESIAN_POINT ( 'NONE',  ( -8.000000000000000000, 117.4062500000000000, -3.313708498984761608 ) ) ;
#40849 = CARTESIAN_POINT ( 'NONE',  ( -11.35316468750000141, 63.59374999658601268, -1.390361679473963753E-15 ) ) ;
#40850 = CARTESIAN_POINT ( 'NONE',  ( 6.000000000000001776, 288.5000000000000000, -7.347880794884121708E-16 ) ) ;
#40851 = ORIENTED_EDGE ( 'NONE', *, *, #56695, .T. ) ;
#40852 = CARTESIAN_POINT ( 'NONE',  ( 5.000000000000000000, -16.24494643555759410, 69.83755725260752456 ) ) ;
#40853 = EDGE_CURVE ( 'NONE', #22710, #38109, #59701, .T. ) ;
#40854 = AXIS2_PLACEMENT_3D ( 'NONE', #67482, #62553, #39559 ) ;
#40855 = CARTESIAN_POINT ( 'NONE',  ( -5.656854249492379694, 15.37499999590322197, -5.656854249492380582 ) ) ;
#40856 = CARTESIAN_POINT ( 'NONE',  ( -2.839093476692135984E-14, 205.6875000013656063, 138.5412658750000503 ) ) ;
#40857 = CARTESIAN_POINT ( 'NONE',  ( 6.123233995736767268E-16, 58.12499999317203248, -10.00000000000000178 ) ) ;
#40858 = CARTESIAN_POINT ( 'NONE',  ( 8.000000000000001776, 97.15625000000000000, 3.313708498984759387 ) ) ;
#40859 = CARTESIAN_POINT ( 'NONE',  ( -2.679491924311228512, 233.9583333333333712, -9.999999999999998224 ) ) ;
#40860 = CARTESIAN_POINT ( 'NONE',  ( -4.242640687119285658, 293.1249999999999432, 4.242640687119287435 ) ) ;
#40861 = CARTESIAN_POINT ( 'NONE',  ( 7.778174593052023411, -7.778174593052021635, 117.0625000000000000 ) ) ;
#40862 = CARTESIAN_POINT ( 'NONE',  ( 10.00000000000000178, 220.0000000000000000, 0.000000000000000000 ) ) ;
#40863 = ADVANCED_FACE ( 'NONE', ( #3474 ), #31392, .T. ) ;
#40864 = CARTESIAN_POINT ( 'NONE',  ( 7.188101187499993827, -2.977408999572645598, 8.517802781871756324 ) ) ;
#40865 = CARTESIAN_POINT ( 'NONE',  ( 11.35316468749999963, 186.3020833299193555, -3.042071309553165293 ) ) ;
#40866 = CARTESIAN_POINT ( 'NONE',  ( -4.999999999999996447, 36.66666666666665719, -8.660254037844387298 ) ) ;
#40867 = CARTESIAN_POINT ( 'NONE',  ( 8.660254037844389075, 177.2916666598387110, -5.000000000000000000 ) ) ;
#40869 = CARTESIAN_POINT ( 'NONE',  ( -6.000000000000001776, 297.0625000034140157, 0.000000000000000000 ) ) ;
#40868 = FACE_OUTER_BOUND ( 'NONE', #43489, .T. ) ;
#40870 = VERTEX_POINT ( 'NONE', #43833 ) ;
#40871 = AXIS2_PLACEMENT_3D ( 'NONE', #64104, #58459, #52785 ) ;
#40872 = CARTESIAN_POINT ( 'NONE',  ( -2.754378923186476579E-14, 209.4375000013656063, 145.4587341250000350 ) ) ;
#40873 = CARTESIAN_POINT ( 'NONE',  ( 8.311093377946834337, 35.46874999658600558, 8.311093377946839666 ) ) ;
#40874 = CARTESIAN_POINT ( 'NONE',  ( -11.00000000000000000, 0.000000000000000000, 107.6875000040967763 ) ) ;
#40875 = CARTESIAN_POINT ( 'NONE',  ( -31.45873412499996391, 205.7500000013656063, 171.4326545832181239 ) ) ;
#40876 = CARTESIAN_POINT ( 'NONE',  ( -8.660254037844387298, 123.9583333265053682, -5.000000000000004441 ) ) ;
#40878 = CARTESIAN_POINT ( 'NONE',  ( -9.999999999999982236, 102.7083333333333286, 2.679491924311216966 ) ) ;
#40877 = CARTESIAN_POINT ( 'NONE',  ( -7.999999999999998224, 116.2812500040967905, 3.313708498984766049 ) ) ;
#40879 = CARTESIAN_POINT ( 'NONE',  ( -2.445694354108839619, 200.8125000013656063, 139.5543056458912190 ) ) ;
#40880 = CARTESIAN_POINT ( 'NONE',  ( 8.660254037844385522, 76.45833332650536818, 5.000000000000005329 ) ) ;
#40881 = CARTESIAN_POINT ( 'NONE',  ( -2.977408999572651815, 94.43750000204838102, 7.188101187500000933 ) ) ;
#40882 = CARTESIAN_POINT ( 'NONE',  ( -4.541265875000003227, 11.99999999863440969, 1.881053915767121110 ) ) ;
#40883 = CARTESIAN_POINT ( 'NONE',  ( 6.123233995736767268E-16, 56.25000000000000000, -10.00000000000000178 ) ) ;
#40884 = CARTESIAN_POINT ( 'NONE',  ( -27.99999999999995737, 204.5000000000000284, 174.0000000000003695 ) ) ;
#40885 = CARTESIAN_POINT ( 'NONE',  ( -1.656854249492377029, 4.437499997268814056, 4.000000000000007994 ) ) ;
#40886 = VERTEX_POINT ( 'NONE', #15151 ) ;
#40888 = EDGE_CURVE ( 'NONE', #32560, #72571, #8009, .T. ) ;
#40887 = ORIENTED_EDGE ( 'NONE', *, *, #68094, .T. ) ;
#40889 = CARTESIAN_POINT ( 'NONE',  ( -4.721056650415998313, 296.7343750017069510, 4.721056650416000089 ) ) ;
#40890 = FACE_OUTER_BOUND ( 'NONE', #42444, .T. ) ;
#40891 = CARTESIAN_POINT ( 'NONE',  ( -4.231687259402721502, 51.96503165405514579, -48.83411696341705266 ) ) ;
#40892 = CARTESIAN_POINT ( 'NONE',  ( -2.085542519210945728E-15, 154.5312499965860127, 11.35316468750000141 ) ) ;
#40893 = CARTESIAN_POINT ( 'NONE',  ( 9.999999999999985789, 105.2083333333333286, -2.679491924311223183 ) ) ;
#40894 = CARTESIAN_POINT ( 'NONE',  ( -6.238412754330611322E-16, 10.18810118749999916, 82.28125000204838102 ) ) ;
#40895 = CARTESIAN_POINT ( 'NONE',  ( -31.61180006176079260, 194.6073834165950416, 170.1378488237272961 ) ) ;
#40896 = CARTESIAN_POINT ( 'NONE',  ( -3.999999999999960032, 206.0000000000000284, 198.0000000000000284 ) ) ;
#40897 = CYLINDRICAL_SURFACE ( 'NONE', #41034, 7.999999999999991118 ) ;
#40898 = CARTESIAN_POINT ( 'NONE',  ( -10.18810118749999916, 0.000000000000000000, 113.0312500020483810 ) ) ;
#40899 = ORIENTED_EDGE ( 'NONE', *, *, #37676, .T. ) ;
#40900 = CARTESIAN_POINT ( 'NONE',  ( 1.469576158976823947E-15, 113.3750000000000000, 8.000000000000000000 ) ) ;
#40901 = CARTESIAN_POINT ( 'NONE',  ( -15.12907735396284892, 183.1082765279311673, 142.8489023050566971 ) ) ;
#40902 = CARTESIAN_POINT ( 'NONE',  ( -9.832129032723420536, 124.0104166632526841, 5.676582343749997150 ) ) ;
#40903 = CARTESIAN_POINT ( 'NONE',  ( -2.445694354108782775, 197.5625000013656063, 200.4456943541088663 ) ) ;
#40904 = CARTESIAN_POINT ( 'NONE',  ( 2.977408999572652260, 24.56249999795161543, 7.188101187500000044 ) ) ;
#40905 = CARTESIAN_POINT ( 'NONE',  ( -7.204075437095965206, -7.204075437095968759, 77.21875000204836681 ) ) ;
#40906 = CARTESIAN_POINT ( 'NONE',  ( -5.676582343750006032, 44.42708332991934839, 9.832129032723418760 ) ) ;
#40907 = ORIENTED_EDGE ( 'NONE', *, *, #61021, .T. ) ;
#40908 = DIRECTION ( 'NONE',  ( -0.000000000000000000, 1.000000000000000000, -1.563033456626094573E-30 ) ) ;
#40909 = CARTESIAN_POINT ( 'NONE',  ( -10.00000000000000355, 194.5833333265053682, 2.679491924311223183 ) ) ;
#40910 = CARTESIAN_POINT ( 'NONE',  ( 8.008118988124991233, 9.807117285998411148E-16, 15.26311528394063011 ) ) ;
#40911 = CARTESIAN_POINT ( 'NONE',  ( 3.458734124999960358, 207.6875000013656063, 142.0000000000000568 ) ) ;
#40912 = CARTESIAN_POINT ( 'NONE',  ( 7.188101187500001821, 14.06249999795161365, -2.977408999572650483 ) ) ;
#40913 = CARTESIAN_POINT ( 'NONE',  ( 4.242640687119287435, 295.4375000034140157, 4.242640687119285658 ) ) ;
#40914 = CARTESIAN_POINT ( 'NONE',  ( -30.98599175293504970, -11.99157019563063997, 142.6895678882109735 ) ) ;
#40915 = CARTESIAN_POINT ( 'NONE',  ( -5.082755093536326818, 6.281249997951610098, 5.082755093536325042 ) ) ;
#40916 = CARTESIAN_POINT ( 'NONE',  ( 7.188101187499992051, 2.977408999572647819, 8.330302781871752771 ) ) ;
#40917 = EDGE_CURVE ( 'NONE', #851, #44182, #42701, .T. ) ;
#40918 =( BOUNDED_CURVE ( )  B_SPLINE_CURVE ( 2, ( #45705, #50996, #57794, #28725, #39317, #21945, #74376, #27609, #34417, #6102, #57420, #39680, #62679 ),
 .UNSPECIFIED., .F., .F. ) 
 B_SPLINE_CURVE_WITH_KNOTS ( ( 3, 2, 2, 2, 2, 2, 3 ),
 ( 0.005434782608695652023, 0.007246376811594202987, 0.009057971014492753950, 0.01086956521739130405, 0.01268115942028985588, 0.01449275362318840597, 0.01630434782608695607 ),
 .UNSPECIFIED. ) 
 CURVE ( )  GEOMETRIC_REPRESENTATION_ITEM ( )  RATIONAL_B_SPLINE_CURVE ( ( 1.000000000000000000, 0.9659258262890683122, 1.000000000000000000, 0.9659258262890683122, 1.000000000000000000, 0.9659258262890683122, 1.000000000000000000, 0.9659258262890683122, 1.000000000000000000, 0.9659258262890683122, 1.000000000000000000, 0.9659258262890683122, 1.000000000000000000 ) ) 
 REPRESENTATION_ITEM ( '' )  );
#40919 = CARTESIAN_POINT ( 'NONE',  ( 10.18810118749999916, 1.247682550866122264E-15, 72.90625000204836681 ) ) ;
#40920 = AXIS2_PLACEMENT_3D ( 'NONE', #62314, #74008, #90 ) ;
#40921 = CARTESIAN_POINT ( 'NONE',  ( -26.56734541678232731, 208.2500000013656063, 173.4587341250003760 ) ) ;
#40922 = EDGE_CURVE ( 'NONE', #4559, #40293, #16258, .T. ) ;
#40923 = AXIS2_PLACEMENT_3D ( 'NONE', #37699, #38445, #9019 ) ;
#40924 = CARTESIAN_POINT ( 'NONE',  ( -6.735557395310442023E-16, 11.00000000000000000, 110.1249999999999858 ) ) ;
#40925 = CARTESIAN_POINT ( 'NONE',  ( 4.541265875000001451, 21.37499999863441147, 1.881053915767124440 ) ) ;
#40926 = EDGE_LOOP ( 'NONE', ( #56854, #59703, #52169, #58202 ) ) ;
#40927 = VECTOR ( 'NONE', #42454, 999.9999999999998863 ) ;
#40928 = CARTESIAN_POINT ( 'NONE',  ( -3.999999999999960032, 194.1250000027311842, 198.0000000000000284 ) ) ;
#40929 = CARTESIAN_POINT ( 'NONE',  ( -2.751064625579944321E-14, 206.7500000000000284, 146.0000000000000284 ) ) ;
#40930 = CARTESIAN_POINT ( 'NONE',  ( -30.82842712474612412, 200.5000000027312126, 172.8284271247466108 ) ) ;
#40931 = CARTESIAN_POINT ( 'NONE',  ( 2.977408999572650039, 119.1875000020483810, -7.188101187500001821 ) ) ;
#40932 = CARTESIAN_POINT ( 'NONE',  ( 10.00000000000000000, 250.6250000068279746, -1.224646799147353256E-15 ) ) ;
#40933 = CARTESIAN_POINT ( 'NONE',  ( -4.898587196589407898E-16, 7.999999999999991118, 3.642802783920144449 ) ) ;
#40934 = ORIENTED_EDGE ( 'NONE', *, *, #65292, .F. ) ;
#40935 = ADVANCED_FACE ( 'NONE', ( #67226 ), #67965, .T. ) ;
#40936 = CARTESIAN_POINT ( 'NONE',  ( -2.977408999572654480, 14.99999999795161187, 7.188101187499999156 ) ) ;
#40937 = VERTEX_POINT ( 'NONE', #9883 ) ;
#40938 = DIRECTION ( 'NONE',  ( -0.000000000000000000, 1.000000000000000000, 4.689100369878284071E-30 ) ) ;
#40939 = CARTESIAN_POINT ( 'NONE',  ( 7.999999999999991118, 0.000000000000000000, 30.00000000000000000 ) ) ;
#40940 = CARTESIAN_POINT ( 'NONE',  ( 10.00000000000000000, 59.79166666666667851, 2.679491924311236062 ) ) ;
#40941 = CARTESIAN_POINT ( 'NONE',  ( -2.977408999572651815, 99.31250000204839523, 7.188101187500000933 ) ) ;
#40942 = CARTESIAN_POINT ( 'NONE',  ( -24.54126587499999701, 209.4375000013656063, 170.0000000000003411 ) ) ;
#40943 = CARTESIAN_POINT ( 'NONE',  ( -28.00000000000002487, 197.0000000000000000, 166.0000000000003695 ) ) ;
#40945 = PLANE ( 'NONE',  #53076 ) ;
#40944 = CARTESIAN_POINT ( 'NONE',  ( -8.000000000000000000, 89.09375000409676204, -3.313708498984761164 ) ) ;
#40946 = ORIENTED_EDGE ( 'NONE', *, *, #17146, .T. ) ;
#40947 = CARTESIAN_POINT ( 'NONE',  ( -3.042071309553159075, 249.9479166700806729, 11.35316468749999963 ) ) ;
#40948 = PRODUCT_DEFINITION_SHAPE ( 'NONE', 'NONE',  #50979 ) ;
#40949 = CARTESIAN_POINT ( 'NONE',  ( 7.188101187499991163, 2.977408999572648707, 16.20530278187175455 ) ) ;
#40950 = DIRECTION ( 'NONE',  ( -1.000000000000000000, -0.000000000000000000, -0.000000000000000000 ) ) ;
#40951 = DIRECTION ( 'NONE',  ( -0.000000000000000000, 1.000000000000000000, -0.000000000000000000 ) ) ;
#40952 = CARTESIAN_POINT ( 'NONE',  ( -4.465384415997324830, -66.51627080308854545, -26.73837581714093403 ) ) ;
#40953 = CARTESIAN_POINT ( 'NONE',  ( 13.99999999999999822, -2.250000000005106138, 10.23492587299426404 ) ) ;
#40954 = CARTESIAN_POINT ( 'NONE',  ( -7.320508075688778149, 158.1249999999999716, 7.320508075688769267 ) ) ;
#40955 = FACE_OUTER_BOUND ( 'NONE', #20301, .T. ) ;
#40956 = CARTESIAN_POINT ( 'NONE',  ( 5.656854249492379694, 91.43749999999998579, -5.656854249492380582 ) ) ;
#40957 = CARTESIAN_POINT ( 'NONE',  ( 5.000000000000000000, -52.35862550122924830, -48.98731492261435250 ) ) ;
#40958 = CARTESIAN_POINT ( 'NONE',  ( -8.311093377946841443, 144.2187499965860127, 8.311093377946830785 ) ) ;
#40959 = DIRECTION ( 'NONE',  ( 0.000000000000000000, 0.000000000000000000, -1.000000000000000000 ) ) ;
#40960 = CARTESIAN_POINT ( 'NONE',  ( -1.836970198721029983E-15, 25.62499999317203248, 10.00000000000000178 ) ) ;
#40963 = CARTESIAN_POINT ( 'NONE',  ( 2.775557561562891351E-14, 195.0000000000000000, 198.0000000000000284 ) ) ;
#40962 = LINE ( 'NONE', #53396, #69525 ) ;
#40961 = CARTESIAN_POINT ( 'NONE',  ( 23.99999999999998224, 207.8125000000000284, 171.6568542494922553 ) ) ;
#40964 = ORIENTED_EDGE ( 'NONE', *, *, #30518, .T. ) ;
#40965 = CARTESIAN_POINT ( 'NONE',  ( 11.35316468750000141, 1.093749996586016682, 0.000000000000000000 ) ) ;
#40966 = CARTESIAN_POINT ( 'NONE',  ( -5.656854249492373476, -5.656854249492376141, 25.01780277982336642 ) ) ;
#40968 = CARTESIAN_POINT ( 'NONE',  ( 10.00000000000011013, 195.0000000000000568, 0.000000000000000000 ) ) ;
#40967 =( REPRESENTATION_RELATIONSHIP ('NONE','NONE', #46008, #63845 ) REPRESENTATION_RELATIONSHIP_WITH_TRANSFORMATION ( #1063 )SHAPE_REPRESENTATION_RELATIONSHIP( ) );
#40969 = CARTESIAN_POINT ( 'NONE',  ( 24.54126587499998990, 195.4375000013655779, 169.9999999999998863 ) ) ;
#40970 = VECTOR ( 'NONE', #28770, 1000.000000000000000 ) ;
#40971 = CARTESIAN_POINT ( 'NONE',  ( -1.836970198721029983E-15, 30.62499999317203248, 10.00000000000000178 ) ) ;
#40972 = CARTESIAN_POINT ( 'NONE',  ( 2.977408999572654480, 115.6250000020483810, 7.188101187499999156 ) ) ;
#40973 = CARTESIAN_POINT ( 'NONE',  ( 1.881053915767122664, 21.12499999863441147, 4.541265875000001451 ) ) ;
#40974 = CARTESIAN_POINT ( 'NONE',  ( -4.465384415997270651, -56.41424811512369786, 44.23559237190949034 ) ) ;
#40975 = CARTESIAN_POINT ( 'NONE',  ( -4.898587196589407898E-16, 7.999999999999991118, 22.95530277982336642 ) ) ;
#40977 = CARTESIAN_POINT ( 'NONE',  ( -8.660254037844385522, 225.4166666666666856, 5.000000000000004441 ) ) ;
#40976 = DIRECTION ( 'NONE',  ( -0.000000000000000000, 1.000000000000000000, -1.563033456626094573E-30 ) ) ;
#40978 = CARTESIAN_POINT ( 'NONE',  ( -5.676582343749998039, 112.4479166632526983, -9.832129032723420536 ) ) ;
#40979 = ORIENTED_EDGE ( 'NONE', *, *, #8568, .T. ) ;
#40980 = DIRECTION ( 'NONE',  ( -0.000000000000000000, -0.000000000000000000, 1.000000000000000000 ) ) ;
#40981 = CARTESIAN_POINT ( 'NONE',  ( 7.999999999999991118, 9.797174393178815797E-16, 9.080302779823364645 ) ) ;
#40982 = CARTESIAN_POINT ( 'NONE',  ( -3.042071309553159075, 240.2604166700806729, 11.35316468749999963 ) ) ;
#40983 = CARTESIAN_POINT ( 'NONE',  ( -2.085542519210945728E-15, 114.5312499965860269, 11.35316468750000141 ) ) ;
#40984 = ORIENTED_EDGE ( 'NONE', *, *, #28735, .F. ) ;
#40985 = CARTESIAN_POINT ( 'NONE',  ( -10.68940375632318052, 0.4758252052427544010, 117.8105962436767697 ) ) ;
#40986 = VECTOR ( 'NONE', #63402, 1000.000000000000000 ) ;
#40987 = CARTESIAN_POINT ( 'NONE',  ( -7.204075437095967871, 7.204075437095967871, 101.9687500020483668 ) ) ;
#40988 = CARTESIAN_POINT ( 'NONE',  ( 2.679491924311222739, 225.8333333265053398, 10.00000000000000355 ) ) ;
#40989 = CARTESIAN_POINT ( 'NONE',  ( -3.458734124999960358, 202.6250000013656063, 196.5673454167823877 ) ) ;
#40990 = CARTESIAN_POINT ( 'NONE',  ( 2.775557561562891351E-14, 210.0000000000000284, 198.0000000000000284 ) ) ;
#40992 = CARTESIAN_POINT ( 'NONE',  ( -3.042071309553163960, 102.2395833299193697, -11.35316468749999963 ) ) ;
#40991 = DIRECTION ( 'NONE',  ( -0.000000000000000000, 1.000000000000000000, -1.563033456626094573E-30 ) ) ;
#40993 = CARTESIAN_POINT ( 'NONE',  ( -5.656854249492373476, -5.656854249492376141, 7.205302783920144449 ) ) ;
#40994 = CARTESIAN_POINT ( 'NONE',  ( -25.55430564589119413, 198.5625000013656063, 167.5543056458915316 ) ) ;
#40995 = CARTESIAN_POINT ( 'NONE',  ( -2.220555325575947149E-11, 176.2500000000017621, -10.00000000000000533 ) ) ;
#40996 = ORIENTED_EDGE ( 'NONE', *, *, #67930, .F. ) ;
#40997 = EDGE_CURVE ( 'NONE', #61205, #28769, #17553, .T. ) ;
#40998 = CARTESIAN_POINT ( 'NONE',  ( 2.679491924311228956, 192.9166666598387110, -10.00000000000000000 ) ) ;
#40999 = CARTESIAN_POINT ( 'NONE',  ( 2.020667218593132706E-15, -11.00000000000000000, 73.37500000000000000 ) ) ;
#41000 = CARTESIAN_POINT ( 'NONE',  ( 32.00000000000000000, 202.2500000000000000, 169.9999999999999432 ) ) ;
#41001 = CARTESIAN_POINT ( 'NONE',  ( -9.832129032723418760, 88.17708332991934128, -5.676582343750004256 ) ) ;
#41002 = CARTESIAN_POINT ( 'NONE',  ( 2.751064625579944321E-14, 205.7500000000000284, 194.0000000000000568 ) ) ;
#41003 = CARTESIAN_POINT ( 'NONE',  ( 5.082755093536325930, 7.031249997951610986, -5.082755093536325930 ) ) ;
#41004 = CARTESIAN_POINT ( 'NONE',  ( 7.204075437095968759, -7.204075437095966983, 92.59375000204838102 ) ) ;
#41005 = CARTESIAN_POINT ( 'NONE',  ( 3.042071309553159519, 5.052083329919351051, 11.35316468750000141 ) ) ;
#41006 = ORIENTED_EDGE ( 'NONE', *, *, #18755, .T. ) ;
#41007 = DIRECTION ( 'NONE',  ( 1.000000000000000000, 0.000000000000000000, 0.000000000000000000 ) ) ;
#41008 = CARTESIAN_POINT ( 'NONE',  ( 3.042071309553167513, 221.8229166632526983, -11.35316468749999785 ) ) ;
#41009 = CARTESIAN_POINT ( 'NONE',  ( 7.204075437095968759, -7.204075437095966983, 77.59375000204838102 ) ) ;
#41010 = CARTESIAN_POINT ( 'NONE',  ( -1.836970198721029983E-15, 45.62499999317203958, 10.00000000000000178 ) ) ;
#41011 = CARTESIAN_POINT ( 'NONE',  ( -25.17157287525386167, 208.0000000027312126, 167.1715728752541281 ) ) ;
#41012 = CARTESIAN_POINT ( 'NONE',  ( 4.721056650416000089, 294.8281250017069510, 4.721056650415999201 ) ) ;
#41013 = ORIENTED_EDGE ( 'NONE', *, *, #55490, .F. ) ;
#41014 = CARTESIAN_POINT ( 'NONE',  ( -0.4369882809721231665, -51.14729664189338365, -48.52014062455058507 ) ) ;
#41015 = CARTESIAN_POINT ( 'NONE',  ( -9.832129032723418760, 203.1770833299193555, -5.676582343750004256 ) ) ;
#41016 = EDGE_CURVE ( 'NONE', #61247, #1603, #7434, .T. ) ;
#41017 = AXIS2_PLACEMENT_3D ( 'NONE', #59498, #36115, #2519 ) ;
#41018 = CARTESIAN_POINT ( 'NONE',  ( 10.18810118749999916, 1.247682550866122264E-15, 92.40625000204836681 ) ) ;
#41019 = CARTESIAN_POINT ( 'NONE',  ( -29.43265458321766559, 203.5000000013655779, 166.5412658750003629 ) ) ;
#41020 = EDGE_CURVE ( 'NONE', #40301, #56539, #62282, .T. ) ;
#41021 = CARTESIAN_POINT ( 'NONE',  ( 7.999999999999998224, 19.40625000000000000, 3.313708498984766493 ) ) ;
#41022 = ORIENTED_EDGE ( 'NONE', *, *, #62342, .T. ) ;
#41023 = CARTESIAN_POINT ( 'NONE',  ( 2.977408999572654480, 120.1250000020483952, 7.188101187499999156 ) ) ;
#41024 = CARTESIAN_POINT ( 'NONE',  ( 1.656854249492403008, 205.8125000027312126, 194.0000000000000853 ) ) ;
#41025 = CARTESIAN_POINT ( 'NONE',  ( 7.320508075688771044, 24.37499999999999645, 7.320508075688775484 ) ) ;
#41026 = DIRECTION ( 'NONE',  ( 0.000000000000000000, 0.000000000000000000, 1.000000000000000000 ) ) ;
#41027 = CARTESIAN_POINT ( 'NONE',  ( -10.18810118749999738, -4.220049686691941915, 75.62500000204838102 ) ) ;
#41028 = ORIENTED_EDGE ( 'NONE', *, *, #21100, .F. ) ;
#41029 =( BOUNDED_CURVE ( )  B_SPLINE_CURVE ( 2, ( #41701, #30748, #52657, #13012, #41336, #7004, #7742, #30015, #992 ),
 .UNSPECIFIED., .F., .F. ) 
 B_SPLINE_CURVE_WITH_KNOTS ( ( 3, 2, 2, 2, 3 ),
 ( 0.000000000000000000, 0.008333333333333340157, 0.01666666666666668031, 0.02500000000000002220, 0.03333333333333336063 ),
 .UNSPECIFIED. ) 
 CURVE ( )  GEOMETRIC_REPRESENTATION_ITEM ( )  RATIONAL_B_SPLINE_CURVE ( ( 1.000000000000000000, 0.9238795325112867385, 1.000000000000000000, 0.9238795325112867385, 1.000000000000000000, 0.9238795325112867385, 1.000000000000000000, 0.9238795325112865164, 1.000000000000000222 ) ) 
 REPRESENTATION_ITEM ( '' )  );
#41030 = CARTESIAN_POINT ( 'NONE',  ( 5.656854249492381470, 113.5625000000000000, 5.656854249492379694 ) ) ;
#41031 =( BOUNDED_CURVE ( )  B_SPLINE_CURVE ( 1, ( #3191, #26177 ),
 .UNSPECIFIED., .F., .F. ) 
 B_SPLINE_CURVE_WITH_KNOTS ( ( 2, 2 ),
 ( 0.000000000000000000, 1.000000000000000000 ),
 .UNSPECIFIED. ) 
 CURVE ( )  GEOMETRIC_REPRESENTATION_ITEM ( )  RATIONAL_B_SPLINE_CURVE ( ( 0.9660721378631347278, 0.9660721378631347278 ) ) 
 REPRESENTATION_ITEM ( '' )  );
#41032 = AXIS2_PLACEMENT_3D ( 'NONE', #70925, #42247, #59252 ) ;
#41033 = DIRECTION ( 'NONE',  ( 0.000000000000000000, -1.000000000000000000, 0.000000000000000000 ) ) ;
#41034 = AXIS2_PLACEMENT_3D ( 'NONE', #71029, #19347, #52589 ) ;
#41035 = CARTESIAN_POINT ( 'NONE',  ( 7.188101187500002709, 119.1875000020483810, 2.977408999572649151 ) ) ;
#41036 = CARTESIAN_POINT ( 'NONE',  ( 10.00000000000000178, 152.0833333265053682, -2.679491924311226736 ) ) ;
#41037 = CARTESIAN_POINT ( 'NONE',  ( 6.676582343750002480, 297.0156250017069510, -2.765530957081997254 ) ) ;
#41039 = CARTESIAN_POINT ( 'NONE',  ( 11.00000000000010836, -4.556349186103939353, 88.84375000409677625 ) ) ;
#41038 = CARTESIAN_POINT ( 'NONE',  ( -11.35316468749999963, 233.9062500034139873, 0.000000000000000000 ) ) ;
#41040 = ORIENTED_EDGE ( 'NONE', *, *, #22699, .F. ) ;
#41041 = CARTESIAN_POINT ( 'NONE',  ( -3.042071309553166181, 238.1770833367473301, -11.35316468749999608 ) ) ;
#41042 = CARTESIAN_POINT ( 'NONE',  ( 2.977408999572646486, 7.188101187499991163, 4.017802781871751883 ) ) ;
#41043 = ORIENTED_EDGE ( 'NONE', *, *, #28829, .T. ) ;
#41044 = CARTESIAN_POINT ( 'NONE',  ( 4.220049686691934809, 10.18810118749999916, 70.18750000204838102 ) ) ;
#41045 = CARTESIAN_POINT ( 'NONE',  ( 11.35316468750000141, 101.0937499965860127, 0.000000000000000000 ) ) ;
#41046 = CARTESIAN_POINT ( 'NONE',  ( 9.797174393178825657E-16, 125.0000000000000000, -8.000000000000000000 ) ) ;
#41047 = CARTESIAN_POINT ( 'NONE',  ( 4.556349186104045934, 11.00000000000000000, 84.53125000000000000 ) ) ;
#41050 = CARTESIAN_POINT ( 'NONE',  ( -5.656854249492381470, 2.437500000000000444, 5.656854249492379694 ) ) ;
#41049 = CARTESIAN_POINT ( 'NONE',  ( 25.55430564589119058, 204.3125000013656063, 172.4456943541087526 ) ) ;
#41048 = CARTESIAN_POINT ( 'NONE',  ( 29.43265458321761230, 204.7500000013656063, 173.4587341249998929 ) ) ;
#41051 = EDGE_CURVE ( 'NONE', #16043, #13039, #20860, .T. ) ;
#41052 = ORIENTED_EDGE ( 'NONE', *, *, #17261, .F. ) ;
#41053 = CARTESIAN_POINT ( 'NONE',  ( 2.775557561562891351E-14, 210.0000000000000284, 198.0000000000000284 ) ) ;
#41054 = CARTESIAN_POINT ( 'NONE',  ( 1.656854249492470732, 202.8125000027312126, 194.0000000000001421 ) ) ;
#41055 = CARTESIAN_POINT ( 'NONE',  ( 3.042071309553167069, 216.8229166632526699, -11.35316468749999785 ) ) ;
#41056 = CARTESIAN_POINT ( 'NONE',  ( 3.458734124999959914, 206.4375000013656063, 142.0000000000000568 ) ) ;
#41057 = CARTESIAN_POINT ( 'NONE',  ( 24.54126587499999701, 207.4375000013656063, 169.9999999999998863 ) ) ;
#41058 = CARTESIAN_POINT ( 'NONE',  ( 5.082755093536324154, 21.65624999795161543, 5.082755093536326818 ) ) ;
#41059 = CARTESIAN_POINT ( 'NONE',  ( 11.35316468750000141, 176.0937499965860411, 0.000000000000000000 ) ) ;
#41060 = CARTESIAN_POINT ( 'NONE',  ( 2.977408999572650039, 97.06250000204838102, -7.188101187500000933 ) ) ;
#41062 = CARTESIAN_POINT ( 'NONE',  ( 1.567784982238203817E-13, 108.7500000000000426, 10.00000000000000533 ) ) ;
#41061 = CARTESIAN_POINT ( 'NONE',  ( -6.000000000000001776, 296.0625000034140157, 0.000000000000000000 ) ) ;
#41063 = CARTESIAN_POINT ( 'NONE',  ( -4.541265875000002339, 11.81249999863440614, -5.561446717895856393E-16 ) ) ;
#41064 = CARTESIAN_POINT ( 'NONE',  ( 24.54126587499999346, 203.4375000013656063, 169.9999999999998863 ) ) ;
#41065 = CARTESIAN_POINT ( 'NONE',  ( 7.188101187499992051, 8.802885111219154394E-16, 10.11155278187175455 ) ) ;
#41066 = CARTESIAN_POINT ( 'NONE',  ( 9.832129032723416984, 65.36458332991935549, 5.676582343750006032 ) ) ;
#41067 = DIRECTION ( 'NONE',  ( 0.000000000000000000, 0.000000000000000000, -1.000000000000000000 ) ) ;
#41068 = CARTESIAN_POINT ( 'NONE',  ( -7.999999999999989342, -3.313708498984762496, 0.9803027843298238730 ) ) ;
#41069 = ORIENTED_EDGE ( 'NONE', *, *, #23954, .F. ) ;
#41070 = CARTESIAN_POINT ( 'NONE',  ( -5.656854249492373476, -5.656854249492376141, 7.205302783920144449 ) ) ;
#41071 = CARTESIAN_POINT ( 'NONE',  ( -4.000000000000016875, 203.5625000027312126, 140.3431457505076594 ) ) ;
#41072 = CARTESIAN_POINT ( 'NONE',  ( -8.311093377946836114, 77.65624999658602690, -8.311093377946837890 ) ) ;
#41073 = CARTESIAN_POINT ( 'NONE',  ( 7.204075437095966983, 7.204075437095967871, 116.5937500020483810 ) ) ;
#41074 = DIRECTION ( 'NONE',  ( -0.000000000000000000, -0.000000000000000000, -1.000000000000000000 ) ) ;
#41075 = LINE ( 'NONE', #18431, #27548 ) ;
#41077 = CARTESIAN_POINT ( 'NONE',  ( 9.832129032723420536, 61.19791666325267698, -5.676582343749999815 ) ) ;
#41076 = CARTESIAN_POINT ( 'NONE',  ( -2.849036369511732440E-14, 196.3750000027311842, 138.0000000000000568 ) ) ;
#41078 = CARTESIAN_POINT ( 'NONE',  ( -7.999999999999991118, 0.000000000000000000, 23.51780278392014978 ) ) ;
#41079 = CARTESIAN_POINT ( 'NONE',  ( 5.656854249492379694, 111.1250000040967763, -5.656854249492380582 ) ) ;
#41080 = AXIS2_PLACEMENT_3D ( 'NONE', #57754, #23772, #35476 ) ;
#41081 = CARTESIAN_POINT ( 'NONE',  ( 10.00000000000000178, 162.0833333265053682, -2.679491924311226736 ) ) ;
#41082 = CARTESIAN_POINT ( 'NONE',  ( -5.082755093536324154, 96.21875000204838102, 5.082755093536326818 ) ) ;
#41083 = CARTESIAN_POINT ( 'NONE',  ( -10.99999999999989342, 4.556349186104152515, 108.9062500000000000 ) ) ;
#41084 = CARTESIAN_POINT ( 'NONE',  ( 8.311093377946837890, 46.71874999658602690, -8.311093377946837890 ) ) ;
#41085 = CARTESIAN_POINT ( 'NONE',  ( 7.204075437095968759, -7.204075437095966983, 110.5937500020483810 ) ) ;
#41086 = CARTESIAN_POINT ( 'NONE',  ( 3.042071309553159519, 184.7395833299193839, 11.35316468750000141 ) ) ;
#41087 = ORIENTED_EDGE ( 'NONE', *, *, #60228, .F. ) ;
#41088 = CARTESIAN_POINT ( 'NONE',  ( 4.000000000000016875, 205.5625000027312126, 199.6568542494924259 ) ) ;
#41089 = FACE_OUTER_BOUND ( 'NONE', #11039, .T. ) ;
#41090 = CARTESIAN_POINT ( 'NONE',  ( 27.99999999999997158, 208.0000000000000284, 173.9999999999999147 ) ) ;
#41092 = CARTESIAN_POINT ( 'NONE',  ( -5.676582343749998039, 177.4479166632526983, -9.832129032723420536 ) ) ;
#41091 = CARTESIAN_POINT ( 'NONE',  ( 0.000000000000000000, 125.0000000000000000, 8.000000000000000000 ) ) ;
#41093 = CARTESIAN_POINT ( 'NONE',  ( -13.99999999999999822, 0.000000000000000000, -8.000000000000000000 ) ) ;
#41094 = EDGE_CURVE ( 'NONE', #40301, #59034, #4973, .T. ) ;
#41095 = CARTESIAN_POINT ( 'NONE',  ( -2.679491924311228512, 257.0833333401612890, -9.999999999999998224 ) ) ;
#41096 = CARTESIAN_POINT ( 'NONE',  ( 0.000000000000000000, 0.000000000000000000, 9.999999999999996447 ) ) ;
#41097 = VECTOR ( 'NONE', #50515, 1000.000000000000000 ) ;
#41098 = VERTEX_POINT ( 'NONE', #5341 ) ;
#41099 = CARTESIAN_POINT ( 'NONE',  ( -5.676582343750006032, 169.4270833299193555, 9.832129032723418760 ) ) ;
#41100 = VECTOR ( 'NONE', #26395, 1000.000000000000000 ) ;
#41101 = DIRECTION ( 'NONE',  ( -0.000000000000000000, 1.000000000000000000, -4.476705744456276341E-16 ) ) ;
#41102 = CARTESIAN_POINT ( 'NONE',  ( -11.35316468749999785, 128.3854166632526699, -3.042071309553167513 ) ) ;
#41103 = CARTESIAN_POINT ( 'NONE',  ( -37.94562015984925551, 146.0000000000000000, 127.0000000000000000 ) ) ;
#41104 = ORIENTED_EDGE ( 'NONE', *, *, #60489, .T. ) ;
#41105 = EDGE_CURVE ( 'NONE', #31632, #3, #57029, .T. ) ;
#41106 = CARTESIAN_POINT ( 'NONE',  ( 8.000000000000000000, 103.5312500040967905, -3.313708498984762496 ) ) ;
#41107 = B_SPLINE_CURVE_WITH_KNOTS ( 'NONE', 3,
 ( #34270, #51597, #56528, #74612, #45940, #38426, #61430, #18756 ),
 .UNSPECIFIED., .F., .F.,
 ( 4, 2, 2, 4 ),
 ( 0.005256334970460992476, 0.006570121696639674713, 0.007883908422818356951, 0.01051148187517570928 ),
 .UNSPECIFIED. ) ;
#41108 = CARTESIAN_POINT ( 'NONE',  ( 4.000000000000001776, 12.00000000000000000, 0.000000000000000000 ) ) ;
#41109 = CARTESIAN_POINT ( 'NONE',  ( -39.49343742811511504, -1.219727444046192094E-15, 116.8916925125617752 ) ) ;
#41110 = CARTESIAN_POINT ( 'NONE',  ( 3.211159895383560947, 10.18749999863440614, 3.211159895383562723 ) ) ;
#41111 = CARTESIAN_POINT ( 'NONE',  ( 3.313708498984762496, -7.999999999999989342, 20.98655278392014978 ) ) ;
#41112 =( BOUNDED_CURVE ( )  B_SPLINE_CURVE ( 2, ( #47342, #41324, #30370, #1714, #7362, #71448, #18683, #65054, #36772 ),
 .UNSPECIFIED., .F., .F. ) 
 B_SPLINE_CURVE_WITH_KNOTS ( ( 3, 2, 2, 2, 3 ),
 ( 0.1041666666666644370, 0.1145833333333311083, 0.1249999999999977796, 0.1354166666666644647, 0.1458333333333311499 ),
 .UNSPECIFIED. ) 
 CURVE ( )  GEOMETRIC_REPRESENTATION_ITEM ( )  RATIONAL_B_SPLINE_CURVE ( ( 1.000000000000016431, 0.9238795325112704182, 1.000000000000000000, 0.9238795325112867385, 1.000000000000000000, 0.9238795325112867385, 1.000000000000000000, 0.9238795325113027257, 0.9999999999999840128 ) ) 
 REPRESENTATION_ITEM ( '' )  );
#41113 = CARTESIAN_POINT ( 'NONE',  ( 2.828427124746152987, 195.1250000000000284, 139.1715728752538723 ) ) ;
#41114 = VECTOR ( 'NONE', #66634, 1000.000000000000000 ) ;
#41115 = ORIENTED_EDGE ( 'NONE', *, *, #24122, .F. ) ;
#41116 = CARTESIAN_POINT ( 'NONE',  ( -3.313708498984719864, 24.46875000000000355, -8.000000000000040856 ) ) ;
#41117 = CARTESIAN_POINT ( 'NONE',  ( -7.188101187500000044, 106.1562500020483810, 0.000000000000000000 ) ) ;
#41119 = CARTESIAN_POINT ( 'NONE',  ( 2.751064625579944321E-14, 196.7500000000000000, 194.0000000000000568 ) ) ;
#41118 =( BOUNDED_CURVE ( )  B_SPLINE_CURVE ( 2, ( #66615, #32304, #39075, #49261, #55695, #27366, #21705, #26999, #50013 ),
 .UNSPECIFIED., .F., .F. ) 
 B_SPLINE_CURVE_WITH_KNOTS ( ( 3, 2, 2, 2, 3 ),
 ( 0.2083333333333333148, 0.2152777777777777624, 0.2222222222222221821, 0.2291666666666666574, 0.2361111111111111049 ),
 .UNSPECIFIED. ) 
 CURVE ( )  GEOMETRIC_REPRESENTATION_ITEM ( )  RATIONAL_B_SPLINE_CURVE ( ( 1.000000000000000222, 0.9238795325112864054, 1.000000000000000000, 0.9238795325112867385, 1.000000000000000000, 0.9238795325112867385, 1.000000000000000000, 0.9238795325112867385, 1.000000000000000000 ) ) 
 REPRESENTATION_ITEM ( '' )  );
#41120 = ORIENTED_EDGE ( 'NONE', *, *, #11136, .F. ) ;
#41121 = CARTESIAN_POINT ( 'NONE',  ( -10.00000000000018296, 157.2916666666667709, -2.679491924311279583 ) ) ;
#41122 = CARTESIAN_POINT ( 'NONE',  ( 5.082755093536318824, 5.082755093536319713, 26.42405278187175455 ) ) ;
#41123 = VERTEX_POINT ( 'NONE', #74359 ) ;
#41124 = ORIENTED_EDGE ( 'NONE', *, *, #54201, .F. ) ;
#41125 = CARTESIAN_POINT ( 'NONE',  ( -7.204075437095965206, -7.204075437095968759, 87.34375000204836681 ) ) ;
#41126 = PRODUCT_DEFINITION_CONTEXT ( 'detailed design', #52979, 'design' ) ;
#41127 = CARTESIAN_POINT ( 'NONE',  ( -25.55430564589119058, 195.5625000013656063, 167.5543056458915316 ) ) ;
#41128 = CARTESIAN_POINT ( 'NONE',  ( 4.556349186104045934, 11.00000000000000000, 104.0312499999999858 ) ) ;
#41131 = CARTESIAN_POINT ( 'NONE',  ( 6.676582343750003368, 299.0468750017069510, 2.765530957081995478 ) ) ;
#41130 = CARTESIAN_POINT ( 'NONE',  ( 30.82842712474621294, 205.2500000027312126, 172.8284271247460424 ) ) ;
#41129 = CARTESIAN_POINT ( 'NONE',  ( 1.102182119232618108E-15, 290.3125000034140157, 6.000000000000001776 ) ) ;
#41132 = CARTESIAN_POINT ( 'NONE',  ( 5.000000000000001776, 140.8333333333333428, -8.660254037844389075 ) ) ;
#41133 = CARTESIAN_POINT ( 'NONE',  ( -3.313708498984762496, 99.78124999999998579, 7.999999999999998224 ) ) ;
#41134 = DIRECTION ( 'NONE',  ( 1.000000000000000000, 0.000000000000000000, 0.000000000000000000 ) ) ;
#41135 = AXIS2_PLACEMENT_3D ( 'NONE', #23904, #69562, #29939 ) ;
#41136 = CARTESIAN_POINT ( 'NONE',  ( -27.99999999999999645, 210.0000000000000284, 166.0000000000003979 ) ) ;
#41138 =( BOUNDED_CURVE ( )  B_SPLINE_CURVE ( 2, ( #71365, #36690, #54418, #2351, #55544, #26087, #9517, #32148, #8759 ),
 .UNSPECIFIED., .F., .F. ) 
 B_SPLINE_CURVE_WITH_KNOTS ( ( 3, 2, 2, 2, 3 ),
 ( 0.4479166666666665741, 0.4531249999999998890, 0.4583333333333332038, 0.4635416666666665741, 0.4687499999999998890 ),
 .UNSPECIFIED. ) 
 CURVE ( )  GEOMETRIC_REPRESENTATION_ITEM ( )  RATIONAL_B_SPLINE_CURVE ( ( 1.000000000000001554, 0.9238795325112850731, 1.000000000000000000, 0.9238795325112867385, 1.000000000000000000, 0.9238795325112867385, 1.000000000000000000, 0.9238795325112884038, 0.9999999999999983347 ) ) 
 REPRESENTATION_ITEM ( '' )  );
#41137 = PLANE ( 'NONE',  #9678 ) ;
#41139 = CARTESIAN_POINT ( 'NONE',  ( 29.43265458321766559, 203.8750000013656063, 166.5412658749999650 ) ) ;
#41140 = CARTESIAN_POINT ( 'NONE',  ( 4.401442555609581635E-16, 2.718749997951610542, -7.188101187500000044 ) ) ;
#41141 = AXIS2_PLACEMENT_3D ( 'NONE', #61297, #55651, #3967 ) ;
#41142 = CARTESIAN_POINT ( 'NONE',  ( 5.662595241051934458, 5.662595241051935346, 1.950615283940626998 ) ) ;
#41143 = CARTESIAN_POINT ( 'NONE',  ( 3.458734124999959914, 197.4375000013655779, 142.0000000000000568 ) ) ;
#41144 = CARTESIAN_POINT ( 'NONE',  ( 5.082755093536326818, 113.0937500020483810, 5.082755093536325042 ) ) ;
#41146 = LINE ( 'NONE', #40030, #69121 ) ;
#41145 = CARTESIAN_POINT ( 'NONE',  ( -4.999999999999992895, 250.8333333333333428, 8.660254037844390851 ) ) ;
#41147 = CARTESIAN_POINT ( 'NONE',  ( -5.676582343749992710, 230.0520833367473017, 9.832129032723422313 ) ) ;
#41148 = CARTESIAN_POINT ( 'NONE',  ( -5.656854249492380582, 90.31249999999998579, -5.656854249492380582 ) ) ;
#41149 = CARTESIAN_POINT ( 'NONE',  ( 8.660254037844385522, 51.45833332650536818, 5.000000000000005329 ) ) ;
#41150 = CARTESIAN_POINT ( 'NONE',  ( 24.00000000000000355, 198.6875000000000284, 168.3431457505075173 ) ) ;
#41151 = CARTESIAN_POINT ( 'NONE',  ( -5.676582343749998039, 27.44791666325268409, -9.832129032723420536 ) ) ;
#41152 = CARTESIAN_POINT ( 'NONE',  ( 7.320508075689011740, 24.37500000000018829, 7.320508075689014404 ) ) ;
#41153 = CARTESIAN_POINT ( 'NONE',  ( 11.35316468749999785, 215.8854166632526983, 3.042071309553174174 ) ) ;
#41154 = CARTESIAN_POINT ( 'NONE',  ( 4.903509839973584583, 124.4676415472669788, -6.410198659011175693 ) ) ;
#41156 = DIRECTION ( 'NONE',  ( -0.000000000000000000, -1.000000000000000000, -0.000000000000000000 ) ) ;
#41155 = CARTESIAN_POINT ( 'NONE',  ( -0.8761883848941678377, 51.17400877215322197, 48.53033992007524944 ) ) ;
#41157 = ORIENTED_EDGE ( 'NONE', *, *, #42267, .F. ) ;
#41158 = CARTESIAN_POINT ( 'NONE',  ( -3.458734125000015425, 197.2500000013656063, 143.4326545832176976 ) ) ;
#41159 = CARTESIAN_POINT ( 'NONE',  ( -3.042071309553164404, 42.23958332991933418, -11.35316468749999963 ) ) ;
#41160 = CARTESIAN_POINT ( 'NONE',  ( 11.00000000000000355, -4.556349186104045046, 88.84375000409677625 ) ) ;
#41161 = CARTESIAN_POINT ( 'NONE',  ( -3.458734125000015869, 208.1875000013656063, 142.0000000000000568 ) ) ;
#41162 = CARTESIAN_POINT ( 'NONE',  ( -11.00000000000006395, -4.556349186103986426, 110.7812500040967620 ) ) ;
#41163 = CARTESIAN_POINT ( 'NONE',  ( -2.828427124746209831, 201.5000000027312126, 139.1715728752538723 ) ) ;
#41165 = CARTESIAN_POINT ( 'NONE',  ( -8.311093377946841443, 23.90624999658601979, 8.311093377946834337 ) ) ;
#41164 = CARTESIAN_POINT ( 'NONE',  ( -2.977408999572652260, 107.9375000020483810, 7.188101187500000044 ) ) ;
#41166 = CARTESIAN_POINT ( 'NONE',  ( 7.999999999999991118, 3.313708498984757611, 15.17405277982336642 ) ) ;
#41167 = CARTESIAN_POINT ( 'NONE',  ( 11.35316468750000141, 145.7812499965860411, 0.000000000000000000 ) ) ;
#41168 = CARTESIAN_POINT ( 'NONE',  ( -1.836970198721029983E-15, 110.6249999931720396, 10.00000000000000178 ) ) ;
#41169 = CARTESIAN_POINT ( 'NONE',  ( -7.188101187500001821, 116.9375000020483952, -2.977408999572650483 ) ) ;
#41170 = FACE_OUTER_BOUND ( 'NONE', #12174, .T. ) ;
#41171 = CARTESIAN_POINT ( 'NONE',  ( -29.43265458321760519, 204.1250000013656063, 173.4587341250003760 ) ) ;
#41172 =( BOUNDED_CURVE ( )  B_SPLINE_CURVE ( 2, ( #4444, #33139, #51201, #33877, #28563, #33502, #44428, #67443, #56504 ),
 .UNSPECIFIED., .F., .F. ) 
 B_SPLINE_CURVE_WITH_KNOTS ( ( 3, 2, 2, 2, 3 ),
 ( 0.1022727272727272790, 0.1079545454545454558, 0.1136363636363636326, 0.1193181818181818232, 0.1250000000000000000 ),
 .UNSPECIFIED. ) 
 CURVE ( )  GEOMETRIC_REPRESENTATION_ITEM ( )  RATIONAL_B_SPLINE_CURVE ( ( 1.000000000000000000, 0.9238795325112867385, 1.000000000000000000, 0.9238795325112867385, 1.000000000000000000, 0.9238795325112867385, 1.000000000000000000, 0.9238795325112867385, 1.000000000000000000 ) ) 
 REPRESENTATION_ITEM ( '' )  );
#41173 = EDGE_LOOP ( 'NONE', ( #27853, #41022, #62032, #49355 ) ) ;
#41174 = CARTESIAN_POINT ( 'NONE',  ( -11.35316468749999785, 3.385416663252682756, -3.042071309553167957 ) ) ;
#41175 = ORIENTED_EDGE ( 'NONE', *, *, #54378, .T. ) ;
#41176 = CARTESIAN_POINT ( 'NONE',  ( 11.00000000000005329, -4.556349186103991755, 100.6562500000000000 ) ) ;
#41177 = CARTESIAN_POINT ( 'NONE',  ( -6.676582343750003368, 297.3906250017068942, -2.765530957081996810 ) ) ;
#41179 = CARTESIAN_POINT ( 'NONE',  ( 9.832129032723420536, 136.1979166632526983, -5.676582343749999815 ) ) ;
#41178 = CARTESIAN_POINT ( 'NONE',  ( 4.000000000000001776, 14.81249999726881406, -1.656854249492381248 ) ) ;
#41180 = CARTESIAN_POINT ( 'NONE',  ( 3.313708498984756279, 7.999999999999991118, 21.41780278432982598 ) ) ;
#41181 = CARTESIAN_POINT ( 'NONE',  ( 54.05599858428173832, 206.4623432447938853, 51.40562160871029818 ) ) ;
#41182 = EDGE_CURVE ( 'NONE', #16792, #6496, #48833, .T. ) ;
#41183 = CARTESIAN_POINT ( 'NONE',  ( 5.676582343749997150, 247.2395833367473301, -9.832129032723418760 ) ) ;
#41184 = CARTESIAN_POINT ( 'NONE',  ( 4.220049686691934809, 10.18810118749999916, 91.56250000204836681 ) ) ;
#41185 = ORIENTED_EDGE ( 'NONE', *, *, #40663, .F. ) ;
#41186 = EDGE_CURVE ( 'NONE', #53439, #65735, #810, .T. ) ;
#41187 = CARTESIAN_POINT ( 'NONE',  ( -3.171697045051319909E-12, 121.2500000000002558, -10.00000000000000178 ) ) ;
#41188 = CARTESIAN_POINT ( 'NONE',  ( -27.99999999999995381, 195.5000000000000000, 174.0000000000003695 ) ) ;
#41189 = CARTESIAN_POINT ( 'NONE',  ( -3.042071309553173730, 89.63541666325268409, 11.35316468749999785 ) ) ;
#41190 = ORIENTED_EDGE ( 'NONE', *, *, #32937, .T. ) ;
#41191 = CARTESIAN_POINT ( 'NONE',  ( -7.204075437095967871, 7.204075437095967871, 107.9687500020483810 ) ) ;
#41192 = CARTESIAN_POINT ( 'NONE',  ( 1.881053915767121998, 16.62499999863440436, -4.541265875000002339 ) ) ;
#41193 = VERTEX_POINT ( 'NONE', #46062 ) ;
#41194 = ORIENTED_EDGE ( 'NONE', *, *, #50993, .F. ) ;
#41195 = CARTESIAN_POINT ( 'NONE',  ( 5.656854249492378806, 2.812500000000000444, 5.656854249492381470 ) ) ;
#41196 = CARTESIAN_POINT ( 'NONE',  ( -1.881053915767121554, 0.7499999986344069169, -4.541265875000002339 ) ) ;
#41197 = CARTESIAN_POINT ( 'NONE',  ( 7.188101187499999156, 1.874999997951610098, 2.977408999572654924 ) ) ;
#41198 = EDGE_CURVE ( 'NONE', #53910, #56676, #36847, .T. ) ;
#41199 = CARTESIAN_POINT ( 'NONE',  ( -6.735557395310442023E-16, 11.00000000000000000, 96.62499999999998579 ) ) ;
#41200 = CARTESIAN_POINT ( 'NONE',  ( 10.18810118749999916, 4.220049686691935698, 104.8750000020483668 ) ) ;
#41201 = VECTOR ( 'NONE', #62612, 1000.000000000000227 ) ;
#41202 = CARTESIAN_POINT ( 'NONE',  ( 4.000000000000001776, 2.000000000000000000, 0.000000000000000000 ) ) ;
#41203 = CARTESIAN_POINT ( 'NONE',  ( 2.828427124746191623, 14.87499999726881406, -2.828427124746191623 ) ) ;
#41204 = LINE ( 'NONE', #52523, #5968 ) ;
#41205 = VERTEX_POINT ( 'NONE', #18139 ) ;
#41206 = CARTESIAN_POINT ( 'NONE',  ( 4.898587196589415787E-16, 0.000000000000000000, 4.000000000000001776 ) ) ;
#41207 = CARTESIAN_POINT ( 'NONE',  ( 3.458734125000015425, 196.9375000013655779, 198.0000000000000284 ) ) ;
#41208 = CARTESIAN_POINT ( 'NONE',  ( -25.55430564589122966, 205.3125000013656063, 167.5543056458915032 ) ) ;
#41209 = CARTESIAN_POINT ( 'NONE',  ( 4.541265875000002339, 16.31249999863440436, 0.000000000000000000 ) ) ;
#41210 = EDGE_CURVE ( 'NONE', #3856, #21239, #24282, .T. ) ;
#41211 = DIRECTION ( 'NONE',  ( -0.000000000000000000, 1.000000000000000000, -0.000000000000000000 ) ) ;
#41212 = CARTESIAN_POINT ( 'NONE',  ( -4.401442555609577197E-16, 7.188101187499992051, 14.61155278187175455 ) ) ;
#41213 = ORIENTED_EDGE ( 'NONE', *, *, #45849, .T. ) ;
#41214 = ORIENTED_EDGE ( 'NONE', *, *, #14102, .T. ) ;
#41215 = CARTESIAN_POINT ( 'NONE',  ( -10.18810118749999916, 4.220049686691934809, 105.0625000020483810 ) ) ;
#41216 = CARTESIAN_POINT ( 'NONE',  ( 11.00000000000005329, -4.556349186103991755, 103.6562499999999716 ) ) ;
#41217 = CARTESIAN_POINT ( 'NONE',  ( -26.34314575050758123, 204.5625000000000000, 174.0000000000003411 ) ) ;
#41218 = CARTESIAN_POINT ( 'NONE',  ( 1.432654583217662481, 202.1250000013656063, 194.5412658750000219 ) ) ;
#41219 = CARTESIAN_POINT ( 'NONE',  ( 27.99999999999996447, 196.9375000013655779, 166.5412658749999082 ) ) ;
#41220 = CARTESIAN_POINT ( 'NONE',  ( 2.679491924311222739, 88.95833333333332860, 10.00000000000000355 ) ) ;
#41221 = AXIS2_PLACEMENT_3D ( 'NONE', #57330, #51656, #12035 ) ;
#41222 = CARTESIAN_POINT ( 'NONE',  ( 8.000000000000000000, 115.3437500000000000, -3.313708498984762496 ) ) ;
#41223 = CARTESIAN_POINT ( 'NONE',  ( 3.042071309553167069, 57.13541666325268409, -11.35316468749999785 ) ) ;
#41224 = CARTESIAN_POINT ( 'NONE',  ( -6.000000000000000888, 290.0625000000000000, 2.485281374238575758 ) ) ;
#41225 = ORIENTED_EDGE ( 'NONE', *, *, #63723, .F. ) ;
#41226 = VECTOR ( 'NONE', #33394, 1000.000000000000000 ) ;
#41227 = LINE ( 'NONE', #5047, #66257 ) ;
#41228 = CARTESIAN_POINT ( 'NONE',  ( -3.313708498984765161, 12.84374999590322197, 7.999999999999998224 ) ) ;
#41229 = CARTESIAN_POINT ( 'NONE',  ( -2.445694354108839619, 207.8125000013656063, 139.5543056458912190 ) ) ;
#41230 = DIRECTION ( 'NONE',  ( -0.8660254037844374864, 0.5000000000000018874, 0.000000000000000000 ) ) ;
#41231 = SURFACE_STYLE_FILL_AREA ( #19681 ) ;
#41232 = CARTESIAN_POINT ( 'NONE',  ( -8.660254037844387298, 224.5833333333333712, -4.999999999999999112 ) ) ;
#41233 = CARTESIAN_POINT ( 'NONE',  ( -11.00000000000000000, 0.000000000000000000, 73.18750000409676204 ) ) ;
#41234 = CARTESIAN_POINT ( 'NONE',  ( -11.00000000000000000, 0.000000000000000000, 118.0000000000000000 ) ) ;
#41235 =( BOUNDED_CURVE ( )  B_SPLINE_CURVE ( 2, ( #55021, #32002, #67820, #3329, #4085, #38411, #21041, #43685, #14999 ),
 .UNSPECIFIED., .F., .F. ) 
 B_SPLINE_CURVE_WITH_KNOTS ( ( 3, 2, 2, 2, 3 ),
 ( 0.9204545454545455252, 0.9261363636363637575, 0.9318181818181817677, 0.9375000000000000000, 0.9431818181818182323 ),
 .UNSPECIFIED. ) 
 CURVE ( )  GEOMETRIC_REPRESENTATION_ITEM ( )  RATIONAL_B_SPLINE_CURVE ( ( 0.9999999999999985567, 0.9238795325112881818, 1.000000000000000000, 0.9238795325112867385, 1.000000000000000000, 0.9238795325112867385, 1.000000000000000000, 0.9238795325112867385, 1.000000000000000000 ) ) 
 REPRESENTATION_ITEM ( '' )  );
#41236 = CARTESIAN_POINT ( 'NONE',  ( 5.000000000000001776, 220.8333333333333428, -8.660254037844389075 ) ) ;
#41237 = CARTESIAN_POINT ( 'NONE',  ( 7.188101187499992051, 8.802885111219154394E-16, 11.61155278187175632 ) ) ;
#41238 = CARTESIAN_POINT ( 'NONE',  ( 11.35316468749999785, 180.8854166632526699, 3.042071309553174174 ) ) ;
#41239 = CARTESIAN_POINT ( 'NONE',  ( 4.541265875000002339, 2.312499998634407028, 0.000000000000000000 ) ) ;
#41240 = CARTESIAN_POINT ( 'NONE',  ( 10.00000000000000178, 176.8749999931720538, 0.000000000000000000 ) ) ;
#41242 = FACE_OUTER_BOUND ( 'NONE', #36819, .T. ) ;
#41241 = CARTESIAN_POINT ( 'NONE',  ( -10.00000000000000000, 227.9166666734946034, -2.679491924311226292 ) ) ;
#41243 = EDGE_LOOP ( 'NONE', ( #64656, #48246, #15000, #17619 ) ) ;
#41244 = CARTESIAN_POINT ( 'NONE',  ( -1.432654583217664701, 208.0000000013656347, 138.5412658750000787 ) ) ;
#41245 = CARTESIAN_POINT ( 'NONE',  ( -9.832129032723418760, 43.17708332991934839, -5.676582343750004256 ) ) ;
#41246 = CARTESIAN_POINT ( 'NONE',  ( 11.00000000000000000, 1.347111479062088405E-15, 103.9375000040967763 ) ) ;
#41247 = CARTESIAN_POINT ( 'NONE',  ( -30.44569435410875968, 204.8125000013656063, 172.4456943541092642 ) ) ;
#41248 = CARTESIAN_POINT ( 'NONE',  ( 8.000000000000000000, 4.406249995903220196, -3.313708498984761164 ) ) ;
#41250 = CARTESIAN_POINT ( 'NONE',  ( -9.999999999999980460, 102.5000000000000000, -1.224646799147350693E-15 ) ) ;
#41249 = CARTESIAN_POINT ( 'NONE',  ( 1.469576158976823947E-15, 116.5625000040967763, 8.000000000000000000 ) ) ;
#41251 = CARTESIAN_POINT ( 'NONE',  ( 3.458734124999959914, 198.3750000013656063, 143.4326545832176976 ) ) ;
#41252 = CARTESIAN_POINT ( 'NONE',  ( -10.00000000000000355, 79.58333332650536818, 2.679491924311223183 ) ) ;
#41253 = CARTESIAN_POINT ( 'NONE',  ( -2.977408999572650927, 95.37500000204839523, -7.188101187500001821 ) ) ;
#41254 = CARTESIAN_POINT ( 'NONE',  ( -4.541265875000003227, 17.99999999863440436, 1.881053915767121110 ) ) ;
#41255 = CARTESIAN_POINT ( 'NONE',  ( -8.660254037844392627, 72.91666666666667140, 5.000000000000000888 ) ) ;
#41256 = CARTESIAN_POINT ( 'NONE',  ( -10.00000000000000355, 49.58333332650536818, 2.679491924311223183 ) ) ;
#41257 = PLANE ( 'NONE',  #10105 ) ;
#41258 = ORIENTED_EDGE ( 'NONE', *, *, #46382, .F. ) ;
#41259 = ORIENTED_EDGE ( 'NONE', *, *, #53007, .F. ) ;
#41260 =( BOUNDED_CURVE ( )  B_SPLINE_CURVE ( 2, ( #66865, #14039, #32168, #49508, #37075, #8779, #54811, #60078, #3121 ),
 .UNSPECIFIED., .F., .F. ) 
 B_SPLINE_CURVE_WITH_KNOTS ( ( 3, 2, 2, 2, 3 ),
 ( 0.5500000000000005995, 0.5583333333333337922, 0.5666666666666670960, 0.5750000000000003997, 0.5833333333333337034 ),
 .UNSPECIFIED. ) 
 CURVE ( )  GEOMETRIC_REPRESENTATION_ITEM ( )  RATIONAL_B_SPLINE_CURVE ( ( 0.9999999999999948930, 0.9238795325112918455, 1.000000000000000000, 0.9238795325112867385, 1.000000000000000000, 0.9238795325112867385, 1.000000000000000000, 0.9238795325112837409, 1.000000000000003109 ) ) 
 REPRESENTATION_ITEM ( '' )  );
#41261 = CARTESIAN_POINT ( 'NONE',  ( -4.721056650415999201, 298.4843750017070079, -4.721056650415999201 ) ) ;
#41262 = DIRECTION ( 'NONE',  ( -0.000000000000000000, -0.000000000000000000, -1.000000000000000000 ) ) ;
#41263 = CARTESIAN_POINT ( 'NONE',  ( 1.224646799147353454E-15, 300.0000000000000000, -10.00000000000000178 ) ) ;
#41264 = CARTESIAN_POINT ( 'NONE',  ( 5.676582343749993598, 154.9479166632526983, 9.832129032723422313 ) ) ;
#41265 = CARTESIAN_POINT ( 'NONE',  ( -4.220049686691935698, 10.18810118749999916, 80.87500000204836681 ) ) ;
#41266 = FACE_BOUND ( 'NONE', #3443, .T. ) ;
#41267 = CARTESIAN_POINT ( 'NONE',  ( -1.656854249492347719, 204.8124999999999716, 194.0000000000000853 ) ) ;
#41268 = CYLINDRICAL_SURFACE ( 'NONE', #21734, 10.99999999999998934 ) ;
#41269 = CARTESIAN_POINT ( 'NONE',  ( 4.220049686691934809, 10.18810118749999916, 112.5625000020483810 ) ) ;
#41270 = ORIENTED_EDGE ( 'NONE', *, *, #67295, .F. ) ;
#41271 = ADVANCED_FACE ( 'NONE', ( #17387 ), #24155, .F. ) ;
#41272 = CARTESIAN_POINT ( 'NONE',  ( 0.000000000000000000, 0.000000000000000000, -10.00000000000000000 ) ) ;
#41273 = CARTESIAN_POINT ( 'NONE',  ( 30.53930338426084745, 178.2937657132232232, 175.3245609024663452 ) ) ;
#41274 = CARTESIAN_POINT ( 'NONE',  ( 5.676582343749993598, 145.2604166632526699, 9.832129032723422313 ) ) ;
#41275 = CARTESIAN_POINT ( 'NONE',  ( 2.839093476692135984E-14, 196.6875000013655779, 201.4587341250000350 ) ) ;
#41276 = CARTESIAN_POINT ( 'NONE',  ( 2.485281374238152097, 298.7500000034140157, -6.000000000000420997 ) ) ;
#41277 = CARTESIAN_POINT ( 'NONE',  ( 4.220049686691941027, -10.18810118749999738, 79.00000000204838102 ) ) ;
#41278 = CARTESIAN_POINT ( 'NONE',  ( -11.35316468750000141, 43.80208332991934839, 3.042071309553159963 ) ) ;
#41279 = ORIENTED_EDGE ( 'NONE', *, *, #44541, .T. ) ;
#41280 = CARTESIAN_POINT ( 'NONE',  ( -28.00000000000008171, 207.1250000027312126, 166.0000000000003695 ) ) ;
#41281 = CARTESIAN_POINT ( 'NONE',  ( 3.211159895383561835, 5.562499998634407028, -3.211159895383561835 ) ) ;
#41282 = CARTESIAN_POINT ( 'NONE',  ( -8.008118988124989457, -3.317071493978883900, 16.10686528394062833 ) ) ;
#41283 = CONICAL_SURFACE ( 'NONE', #7564, 3.999999999999976019, 0.7853981633974491672 ) ;
#41284 = CARTESIAN_POINT ( 'NONE',  ( 5.082755093536325930, 15.65624999795161365, -5.082755093536325930 ) ) ;
#41285 = CARTESIAN_POINT ( 'NONE',  ( -6.000000000000003553, 293.0000000034139589, -2.485281374238571317 ) ) ;
#41286 = CARTESIAN_POINT ( 'NONE',  ( -26.88519731024062409, -12.42443664836448036, 139.1822229315743868 ) ) ;
#41287 = CARTESIAN_POINT ( 'NONE',  ( -5.082755093536325042, 4.406249997951610098, -5.082755093536325930 ) ) ;
#41288 = CARTESIAN_POINT ( 'NONE',  ( 2.977408999572650927, -7.188101187499990274, 7.955302781871751883 ) ) ;
#41289 = AXIS2_PLACEMENT_3D ( 'NONE', #15973, #39002, #62006 ) ;
#41290 = CARTESIAN_POINT ( 'NONE',  ( 10.18810118749999916, 4.220049686691935698, 71.50000000204839523 ) ) ;
#41291 = EDGE_CURVE ( 'NONE', #38597, #74609, #38303, .T. ) ;
#41292 = CARTESIAN_POINT ( 'NONE',  ( -26.56734541678238060, 205.6250000013656063, 166.5412658750003629 ) ) ;
#41293 = EDGE_CURVE ( 'NONE', #1009, #56815, #18875, .T. ) ;
#41294 = CARTESIAN_POINT ( 'NONE',  ( -2.679491924311235174, 65.41666665983871098, 10.00000000000000000 ) ) ;
#41295 = CARTESIAN_POINT ( 'NONE',  ( 3.211159895383560947, 22.31249999863440792, 3.211159895383562723 ) ) ;
#41296 = VERTEX_POINT ( 'NONE', #11735 ) ;
#41297 = CARTESIAN_POINT ( 'NONE',  ( 2.828427124746209831, 194.5000000027312126, 200.8284271247462129 ) ) ;
#41298 = CARTESIAN_POINT ( 'NONE',  ( -1.656854249492405451, 205.3125000000000568, 138.0000000000000568 ) ) ;
#41299 = CARTESIAN_POINT ( 'NONE',  ( -27.99999999999991118, 201.6250000027312126, 174.0000000000003695 ) ) ;
#41300 = CARTESIAN_POINT ( 'NONE',  ( 7.188101187500002709, 118.8125000020483810, 2.977408999572649151 ) ) ;
#41301 = EDGE_CURVE ( 'NONE', #3433, #5951, #13195, .T. ) ;
#41302 = CARTESIAN_POINT ( 'NONE',  ( -1.269107444400135093E-11, 58.74999999999901945, 10.00000000000000178 ) ) ;
#41303 = CARTESIAN_POINT ( 'NONE',  ( 3.313708498984762496, -7.999999999999989342, -0.01344721607985516210 ) ) ;
#41304 = ORIENTED_EDGE ( 'NONE', *, *, #8431, .F. ) ;
#41305 = EDGE_CURVE ( 'NONE', #55418, #7251, #63784, .T. ) ;
#41306 = CARTESIAN_POINT ( 'NONE',  ( -2.977408999572650039, 21.93749999795161187, -7.188101187500000933 ) ) ;
#41307 = VERTEX_POINT ( 'NONE', #36234 ) ;
#41308 = CARTESIAN_POINT ( 'NONE',  ( 27.99999999999996447, 198.0000000000000000, 173.9999999999999147 ) ) ;
#41309 = CARTESIAN_POINT ( 'NONE',  ( -4.999999999999998224, 43.54166665983870388, -8.660254037844389075 ) ) ;
#41310 = CARTESIAN_POINT ( 'NONE',  ( 6.123233995736767268E-16, 61.25000000000000711, -10.00000000000000178 ) ) ;
#41311 = CARTESIAN_POINT ( 'NONE',  ( -4.401442555609581635E-16, 101.6562500020483810, -7.188101187500000044 ) ) ;
#41312 = CARTESIAN_POINT ( 'NONE',  ( 6.000000000000001776, 299.5000000000000000, -7.347880794884121708E-16 ) ) ;
#41314 = CARTESIAN_POINT ( 'NONE',  ( -22.61274548586519728, -39.12181092119032400, 191.2067776501123433 ) ) ;
#41313 = CARTESIAN_POINT ( 'NONE',  ( -10.00000000000000355, 34.58333332650536818, 2.679491924311223183 ) ) ;
#41315 = VERTEX_POINT ( 'NONE', #52110 ) ;
#41316 = ORIENTED_EDGE ( 'NONE', *, *, #58065, .T. ) ;
#41317 = CARTESIAN_POINT ( 'NONE',  ( 11.35316468749999963, 241.4062500034140157, -1.390361679473963556E-15 ) ) ;
#41318 = CARTESIAN_POINT ( 'NONE',  ( 2.977408999572650927, -7.188101187499990274, 17.33030278187175455 ) ) ;
#41319 = CARTESIAN_POINT ( 'NONE',  ( 2.997005883565903250, 55.94527535364343862, 43.97975057406247146 ) ) ;
#41320 = CARTESIAN_POINT ( 'NONE',  ( 7.347880794884121708E-16, 284.0000000000000000, -6.000000000000001776 ) ) ;
#41321 = DIRECTION ( 'NONE',  ( -0.000000000000000000, 1.000000000000000000, -0.000000000000000000 ) ) ;
#41322 = CARTESIAN_POINT ( 'NONE',  ( -1.836970198721029983E-15, 200.6249999931720538, 10.00000000000000178 ) ) ;
#41323 = CARTESIAN_POINT ( 'NONE',  ( 10.00000000000000178, 175.2083333333333144, -2.679491924311226736 ) ) ;
#41324 = CARTESIAN_POINT ( 'NONE',  ( 2.485281374238163199, 297.7500000034140726, -6.000000000000410338 ) ) ;
#41325 = DIRECTION ( 'NONE',  ( 1.000000000000000000, -0.000000000000000000, -0.000000000000000000 ) ) ;
#41326 = CARTESIAN_POINT ( 'NONE',  ( -2.085542519210945728E-15, 139.8437499965860127, 11.35316468750000141 ) ) ;
#41327 = CARTESIAN_POINT ( 'NONE',  ( 6.000000000000001776, 294.5625000034140157, -7.347880794884121708E-16 ) ) ;
#41328 = CARTESIAN_POINT ( 'NONE',  ( -8.000000000000000000, 117.4062500000000000, -3.313708498984761164 ) ) ;
#41330 = CARTESIAN_POINT ( 'NONE',  ( 3.313708498984756279, 7.999999999999991118, 25.86155277982337353 ) ) ;
#41329 = CARTESIAN_POINT ( 'NONE',  ( 24.00000000000000355, 205.6875000000000284, 168.3431457505075173 ) ) ;
#41331 = EDGE_CURVE ( 'NONE', #69053, #28981, #38279, .T. ) ;
#41332 = VERTEX_POINT ( 'NONE', #53215 ) ;
#41333 = AXIS2_PLACEMENT_3D ( 'NONE', #12133, #40810, #474 ) ;
#41334 = CARTESIAN_POINT ( 'NONE',  ( -9.000000000000000000, 5.196152422706624918, -0.8038475772933814101 ) ) ;
#41335 = EDGE_CURVE ( 'NONE', #7250, #68586, #35866, .T. ) ;
#41336 = CARTESIAN_POINT ( 'NONE',  ( -23.99999999999999289, 209.7500000000000284, 170.0000000000003411 ) ) ;
#41337 = FACE_OUTER_BOUND ( 'NONE', #51911, .T. ) ;
#41338 = CARTESIAN_POINT ( 'NONE',  ( 27.99999999999996092, 195.6875000013655779, 173.4587341249998929 ) ) ;
#41339 = CARTESIAN_POINT ( 'NONE',  ( 5.000000000000001776, 32.70833332650536107, -8.660254037844389075 ) ) ;
#41340 = CARTESIAN_POINT ( 'NONE',  ( 5.082755093536326818, 112.7187500020483810, 5.082755093536325042 ) ) ;
#41341 = CARTESIAN_POINT ( 'NONE',  ( 1.881053915767121776, 21.49999999863440792, -4.541265875000002339 ) ) ;
#41342 = CARTESIAN_POINT ( 'NONE',  ( -6.308070865134226324, -51.03903544637460499, 41.30321721934398482 ) ) ;
#41343 = CARTESIAN_POINT ( 'NONE',  ( -7.999999999999989342, -3.313708498984762496, 17.42405277982336997 ) ) ;
#41345 = CARTESIAN_POINT ( 'NONE',  ( -3.313708498984760276, 24.28124999590322375, -8.000000000000000000 ) ) ;
#41344 = CARTESIAN_POINT ( 'NONE',  ( -7.320508075688770155, 238.7500000068279462, 7.320508075688774596 ) ) ;
#41346 = ORIENTED_EDGE ( 'NONE', *, *, #5832, .F. ) ;
#41347 = ADVANCED_FACE ( 'NONE', ( #23422 ), #46436, .T. ) ;
#41348 = CARTESIAN_POINT ( 'NONE',  ( 2.679491924311224071, 28.95833333333333570, 10.00000000000000711 ) ) ;
#41349 = CARTESIAN_POINT ( 'NONE',  ( -6.607085568835331379, 225.9999999999999716, 7.535105736105112584 ) ) ;
#41350 = DIRECTION ( 'NONE',  ( -0.000000000000000000, 1.000000000000000000, 4.476705744456276341E-16 ) ) ;
#41351 = CARTESIAN_POINT ( 'NONE',  ( -9.832129032723415207, 239.6354166700806445, 5.676582343750005144 ) ) ;
#41352 = CARTESIAN_POINT ( 'NONE',  ( 5.676582343749993598, 114.9479166632526983, 9.832129032723422313 ) ) ;
#41353 = ORIENTED_EDGE ( 'NONE', *, *, #25211, .T. ) ;
#41354 = CARTESIAN_POINT ( 'NONE',  ( -6.164216839359130340, 8.915442299230837975, 117.6714253161478183 ) ) ;
#41355 = CARTESIAN_POINT ( 'NONE',  ( 7.204075437095966983, 7.204075437095967871, 98.59375000204836681 ) ) ;
#41356 = CARTESIAN_POINT ( 'NONE',  ( 0.000000000000000000, 0.000000000000000000, -4.000000000000001776 ) ) ;
#41357 = CARTESIAN_POINT ( 'NONE',  ( 3.458734125000015869, 201.1875000013656063, 198.0000000000000284 ) ) ;
#41358 = CARTESIAN_POINT ( 'NONE',  ( -11.00000000000020783, -4.556349186103842541, 68.59374999999997158 ) ) ;
#41360 = CARTESIAN_POINT ( 'NONE',  ( 11.35316468749999963, 110.9895833299193555, -3.042071309553165293 ) ) ;
#41359 = FACE_OUTER_BOUND ( 'NONE', #1648, .T. ) ;
#41361 = CARTESIAN_POINT ( 'NONE',  ( 3.313708498984762496, -7.999999999999989342, 8.986552783920146226 ) ) ;
#41362 = CARTESIAN_POINT ( 'NONE',  ( -25.55430564589114795, 196.3125000013656063, 172.4456943541091789 ) ) ;
#41363 = CARTESIAN_POINT ( 'NONE',  ( 8.660254037844390851, 50.41666666666667851, -5.000000000000002665 ) ) ;
#41364 = VERTEX_POINT ( 'NONE', #21376 ) ;
#41365 =( BOUNDED_CURVE ( )  B_SPLINE_CURVE ( 2, ( #72759, #2974, #42945, #20686, #43705, #15023, #20304, #65965, #37306, #38058, #66719, #54665, #32781 ),
 .UNSPECIFIED., .F., .F. ) 
 B_SPLINE_CURVE_WITH_KNOTS ( ( 3, 2, 2, 2, 2, 2, 3 ),
 ( 1.020494457342402184, 1.025727047095130073, 1.030959636847857963, 1.036192226600586075, 1.041424816353313965, 1.046657406106042076, 1.051889995858769966 ),
 .UNSPECIFIED. ) 
 CURVE ( )  GEOMETRIC_REPRESENTATION_ITEM ( )  RATIONAL_B_SPLINE_CURVE ( ( 1.000000000000096145, 0.9659258262889722779, 1.000000000000000000, 0.9659258262890683122, 1.000000000000000000, 0.9659258262890683122, 1.000000000000000000, 0.9659258262890683122, 1.000000000000000000, 0.9659258262890683122, 1.000000000000000000, 0.9659258262890683122, 1.000000000000000000 ) ) 
 REPRESENTATION_ITEM ( '' )  );
#41366 = CARTESIAN_POINT ( 'NONE',  ( -2.679491924311225848, 198.3333333265053398, -10.00000000000000178 ) ) ;
#41367 = CARTESIAN_POINT ( 'NONE',  ( -7.347880794884122694E-16, 21.75000000000000355, 4.000000000000001776 ) ) ;
#41368 = AXIS2_PLACEMENT_3D ( 'NONE', #72817, #21124, #44146 ) ;
#41369 = CARTESIAN_POINT ( 'NONE',  ( 11.00000000000000000, 1.347111479062088405E-15, 99.43750000409677625 ) ) ;
#41370 = CARTESIAN_POINT ( 'NONE',  ( -8.311093377946836114, 82.96874999658602690, -8.311093377946837890 ) ) ;
#41371 = LINE ( 'NONE', #64380, #8551 ) ;
#41372 = CARTESIAN_POINT ( 'NONE',  ( 5.082755093536325930, 13.03124999795161187, -5.082755093536325930 ) ) ;
#41373 = CARTESIAN_POINT ( 'NONE',  ( 4.220049686691934809, 10.18810118749999916, 94.56250000204838102 ) ) ;
#41374 = CARTESIAN_POINT ( 'NONE',  ( 11.35316468749999785, 15.88541666325268586, 3.042071309553174174 ) ) ;
#41375 = VERTEX_POINT ( 'NONE', #32726 ) ;
#41376 = CARTESIAN_POINT ( 'NONE',  ( -8.660254037844397956, 137.9166666666667140, 5.000000000000002665 ) ) ;
#41377 = CARTESIAN_POINT ( 'NONE',  ( -7.347880794884122694E-16, 5.750000000000000000, 4.000000000000001776 ) ) ;
#41378 = CARTESIAN_POINT ( 'NONE',  ( -3.042071309553163960, 222.2395833299193555, -11.35316468749999963 ) ) ;
#41379 = CARTESIAN_POINT ( 'NONE',  ( 4.220049686691941027, -10.18810118749999738, 82.00000000204836681 ) ) ;
#41380 = CARTESIAN_POINT ( 'NONE',  ( 4.023044438063403838, 21.99999999999999645, 0.3527035116121371994 ) ) ;
#41381 = CARTESIAN_POINT ( 'NONE',  ( -5.000000000000000888, 264.1666666666666856, -8.660254037844387298 ) ) ;
#41382 = CARTESIAN_POINT ( 'NONE',  ( 6.676582343750003368, 292.0156250017069510, -2.765530957081997254 ) ) ;
#41383 = MANIFOLD_SOLID_BREP ( 'Boss-Extrude1', #38230 ) ;
#41384 = ORIENTED_EDGE ( 'NONE', *, *, #26577, .F. ) ;
#41385 = CARTESIAN_POINT ( 'NONE',  ( 5.000000000000000000, 52.35862550122993042, -48.98731492261362064 ) ) ;
#41386 = CARTESIAN_POINT ( 'NONE',  ( -8.311093377946836114, 207.9687499965859843, -8.311093377946837890 ) ) ;
#41387 = CARTESIAN_POINT ( 'NONE',  ( 4.220049686691941027, -10.18810118749999738, 89.12500000204836681 ) ) ;
#41388 = CARTESIAN_POINT ( 'NONE',  ( -24.54126587500000056, 201.2500000013656063, 168.5673454167827003 ) ) ;
#41389 = CARTESIAN_POINT ( 'NONE',  ( 5.656854249492378806, 22.31250000000000355, 5.656854249492381470 ) ) ;
#41390 = ORIENTED_EDGE ( 'NONE', *, *, #6413, .F. ) ;
#41391 = VECTOR ( 'NONE', #45707, 1000.000000000000000 ) ;
#41392 = DIRECTION ( 'NONE',  ( -0.000000000000000000, 1.000000000000000000, -4.476705744456276341E-16 ) ) ;
#41393 = CARTESIAN_POINT ( 'NONE',  ( -2.828427124746152987, 207.2500000027312126, 200.8284271247462129 ) ) ;
#41394 = CARTESIAN_POINT ( 'NONE',  ( 2.679491924311228956, 31.04166666666666430, -10.00000000000000000 ) ) ;
#41395 = CARTESIAN_POINT ( 'NONE',  ( -4.898587196589412829E-16, 93.31250000409677625, -8.000000000000000000 ) ) ;
#41396 = CARTESIAN_POINT ( 'NONE',  ( 4.220049686691941027, -10.18810118749999738, 73.00000000204836681 ) ) ;
#41397 = ORIENTED_EDGE ( 'NONE', *, *, #60989, .T. ) ;
#41398 = CARTESIAN_POINT ( 'NONE',  ( 7.188101187500000933, 2.062499997951610542, -2.977408999572650483 ) ) ;
#41399 = CARTESIAN_POINT ( 'NONE',  ( 7.999999999999991118, 9.797174393178815797E-16, 6.080302779823364645 ) ) ;
#41400 = DIRECTION ( 'NONE',  ( 2.771571441169508074E-17, 1.000000000000000000, 2.238352872228138663E-16 ) ) ;
#41401 = CARTESIAN_POINT ( 'NONE',  ( -7.188101187499999156, 120.1250000020483952, 2.977408999572654924 ) ) ;
#41402 = CARTESIAN_POINT ( 'NONE',  ( 5.197448530777795561, -17.78386138248279025, -0.2939692054342382121 ) ) ;
#41403 = CARTESIAN_POINT ( 'NONE',  ( 6.676582343750003368, 295.8906250017069510, 2.765530957081995478 ) ) ;
#41405 = CARTESIAN_POINT ( 'NONE',  ( 2.849036369511732440E-14, 206.2500000000000284, 202.0000000000000000 ) ) ;
#41404 = CARTESIAN_POINT ( 'NONE',  ( 8.311093377946839666, 230.7812500034139589, 8.311093377946830785 ) ) ;
#41406 = CONTEXT_DEPENDENT_SHAPE_REPRESENTATION ( #37105, #52403 ) ;
#41407 = APPLICATION_CONTEXT ( 'automotive_design' ) ;
#41408 = ORIENTED_EDGE ( 'NONE', *, *, #71440, .F. ) ;
#41409 = CARTESIAN_POINT ( 'NONE',  ( 11.35316468749999608, 236.9270833367473017, -3.042071309553167069 ) ) ;
#41410 = CARTESIAN_POINT ( 'NONE',  ( 7.188101187499991163, 2.977408999572648707, 5.330302781871753659 ) ) ;
#41411 = AXIS2_PLACEMENT_3D ( 'NONE', #45094, #62434, #57165 ) ;
#41412 = CARTESIAN_POINT ( 'NONE',  ( 3.458734125000015869, 202.1875000013656063, 198.0000000000000284 ) ) ;
#41413 = ORIENTED_EDGE ( 'NONE', *, *, #50785, .T. ) ;
#41414 = CARTESIAN_POINT ( 'NONE',  ( -10.18810118749999738, -4.220049686691941915, 69.25000000204836681 ) ) ;
#41415 = CARTESIAN_POINT ( 'NONE',  ( 9.832129032723416984, 100.6770833299193555, 5.676582343750006032 ) ) ;
#41416 = CARTESIAN_POINT ( 'NONE',  ( -5.000000000000000000, 60.90295814858222201, 23.31388853594875599 ) ) ;
#41417 = CARTESIAN_POINT ( 'NONE',  ( 7.778174593052021635, 7.778174593052023411, 82.93750000000000000 ) ) ;
#41420 = CARTESIAN_POINT ( 'NONE',  ( 4.556349186104052151, -10.99999999999999822, 113.9687500000000142 ) ) ;
#41419 = CARTESIAN_POINT ( 'NONE',  ( 25.55430564589119058, 203.3125000013656063, 172.4456943541087526 ) ) ;
#41418 = CARTESIAN_POINT ( 'NONE',  ( 26.56734541678238060, 202.2500000013656063, 166.5412658749999650 ) ) ;
#41421 = ORIENTED_EDGE ( 'NONE', *, *, #65945, .T. ) ;
#41422 = CARTESIAN_POINT ( 'NONE',  ( 38.00000000000000000, 63.00000000000000000, 15.00000000000000178 ) ) ;
#41423 = PLANE ( 'NONE',  #25123 ) ;
#41424 = EDGE_CURVE ( 'NONE', #30024, #11179, #32319, .T. ) ;
#41425 = CARTESIAN_POINT ( 'NONE',  ( -9.832129032723418760, 212.8645833299193555, -5.676582343750004256 ) ) ;
#41426 = CARTESIAN_POINT ( 'NONE',  ( 3.458734124999959914, 205.4375000013656063, 142.0000000000000568 ) ) ;
#41427 = CARTESIAN_POINT ( 'NONE',  ( 31.45873412499998523, 204.8750000013656063, 171.4326545832175839 ) ) ;
#41428 = CARTESIAN_POINT ( 'NONE',  ( -2.977408999572654480, 25.87499999795161543, 7.188101187499999156 ) ) ;
#41429 = CARTESIAN_POINT ( 'NONE',  ( 8.311093377946834337, 180.4687499965859843, 8.311093377946839666 ) ) ;
#41430 = CARTESIAN_POINT ( 'NONE',  ( -2.977408999572652260, 99.31250000204838102, 7.188101187500000044 ) ) ;
#41431 = CARTESIAN_POINT ( 'NONE',  ( -6.000000000000003553, 296.0000000034139589, -2.485281374238571317 ) ) ;
#41432 = CARTESIAN_POINT ( 'NONE',  ( -23.99999999999997158, 195.6875000000000284, 171.6568542494927385 ) ) ;
#41433 = CARTESIAN_POINT ( 'NONE',  ( 1.881053915767121776, 9.499999998634406140, -4.541265875000002339 ) ) ;
#41434 = CARTESIAN_POINT ( 'NONE',  ( 26.56734541678232731, 203.6250000013656063, 173.4587341249998929 ) ) ;
#41435 = CARTESIAN_POINT ( 'NONE',  ( -2.977408999572648707, -7.188101187499990274, 3.642802781871751883 ) ) ;
#41436 = CARTESIAN_POINT ( 'NONE',  ( -11.35316468750000141, 68.28124999658602690, -1.390361679473963753E-15 ) ) ;
#41437 = EDGE_CURVE ( 'NONE', #57818, #20466, #65258, .T. ) ;
#41438 = DIRECTION ( 'NONE',  ( -0.000000000000000000, -1.000000000000000000, -0.000000000000000000 ) ) ;
#41439 = CARTESIAN_POINT ( 'NONE',  ( 1.469576158976822172E-15, -7.999999999999991118, 2.761552784329821986 ) ) ;
#41440 = ORIENTED_EDGE ( 'NONE', *, *, #6616, .T. ) ;
#41441 = CARTESIAN_POINT ( 'NONE',  ( -1.836970198721029983E-15, 190.6249999931720254, 10.00000000000000178 ) ) ;
#41442 = VECTOR ( 'NONE', #66099, 1000.000000000000000 ) ;
#41443 = CARTESIAN_POINT ( 'NONE',  ( -3.042071309553173730, 74.32291666325268409, 11.35316468749999785 ) ) ;
#41444 = CARTESIAN_POINT ( 'NONE',  ( 7.778174593052023411, -7.778174593052021635, 67.75000000409677625 ) ) ;
#41445 = CARTESIAN_POINT ( 'NONE',  ( 3.458734124999960358, 196.6875000013655779, 142.0000000000000568 ) ) ;
#41446 = CARTESIAN_POINT ( 'NONE',  ( 2.828427124746191623, 8.874999997268814056, -2.828427124746191623 ) ) ;
#41448 = CARTESIAN_POINT ( 'NONE',  ( -11.35316468750000141, 53.28124999658601979, -1.390361679473963753E-15 ) ) ;
#41447 = CARTESIAN_POINT ( 'NONE',  ( 0.000000000000000000, 0.000000000000000000, -31.99999999999998579 ) ) ;
#41449 = CARTESIAN_POINT ( 'NONE',  ( 5.656854249492374365, 5.656854249492375253, 22.95530278392014623 ) ) ;
#41450 = CARTESIAN_POINT ( 'NONE',  ( 0.000000000000000000, 300.0000000000000000, 0.000000000000000000 ) ) ;
#41451 = CARTESIAN_POINT ( 'NONE',  ( 8.660254037844385522, 151.4583333265053682, 5.000000000000005329 ) ) ;
#41452 = CARTESIAN_POINT ( 'NONE',  ( -5.082755093536324154, 99.21875000204838102, 5.082755093536326818 ) ) ;
#41453 = CARTESIAN_POINT ( 'NONE',  ( 10.00000000000000711, 19.79166666666667140, 2.679491924311237838 ) ) ;
#41454 = CARTESIAN_POINT ( 'NONE',  ( -9.832129032723418760, 48.17708332991934839, -5.676582343750004256 ) ) ;
#41455 =( BOUNDED_CURVE ( )  B_SPLINE_CURVE ( 2, ( #13894, #53179, #1864, #59215, #65221, #36564, #47869, #8252, #1517 ),
 .UNSPECIFIED., .F., .F. ) 
 B_SPLINE_CURVE_WITH_KNOTS ( ( 3, 2, 2, 2, 3 ),
 ( 0.5795454545454545858, 0.5852272727272727071, 0.5909090909090909394, 0.5965909090909090606, 0.6022727272727272929 ),
 .UNSPECIFIED. ) 
 CURVE ( )  GEOMETRIC_REPRESENTATION_ITEM ( )  RATIONAL_B_SPLINE_CURVE ( ( 1.000000000000000000, 0.9238795325112867385, 1.000000000000000000, 0.9238795325112867385, 1.000000000000000000, 0.9238795325112867385, 1.000000000000000000, 0.9238795325112867385, 1.000000000000000000 ) ) 
 REPRESENTATION_ITEM ( '' )  );
#41456 = CARTESIAN_POINT ( 'NONE',  ( -4.220049686691935698, 10.18810118749999916, 112.7500000020483810 ) ) ;
#41457 = CARTESIAN_POINT ( 'NONE',  ( -5.676582343749998039, 197.4479166632526983, -9.832129032723420536 ) ) ;
#41458 = ORIENTED_EDGE ( 'NONE', *, *, #9748, .T. ) ;
#41459 = CARTESIAN_POINT ( 'NONE',  ( 1.781595147095992537, 67.70776641946450525, 20.12770457511415501 ) ) ;
#41460 = CYLINDRICAL_SURFACE ( 'NONE', #38854, 11.00000000000000000 ) ;
#41461 = CARTESIAN_POINT ( 'NONE',  ( 2.679491924311228956, 62.91666665983869677, -10.00000000000000000 ) ) ;
#41463 = CARTESIAN_POINT ( 'NONE',  ( 5.676582343750001591, 176.6145833299193555, -9.832129032723420536 ) ) ;
#41462 = CARTESIAN_POINT ( 'NONE',  ( 2.828427124746209831, 195.3750000000000284, 200.8284271247462129 ) ) ;
#41464 = B_SPLINE_CURVE_WITH_KNOTS ( 'NONE', 3,
 ( #73773, #33810, #22448, #21709, #56807, #38718, #44736, #43991, #16046, #28120, #39079, #45468, #11153, #34177, #965, #6245, #57561, #63567 ),
 .UNSPECIFIED., .F., .F.,
 ( 4, 2, 2, 2, 2, 2, 2, 2, 4 ),
 ( 0.000000000000000000, 0.0005872692987803027629, 0.001174538597560605526, 0.001761807896340908180, 0.002349077195121211051, 0.002936346493901515007, 0.003523615792681818529, 0.004110885091462122484, 0.004698154390242427307 ),
 .UNSPECIFIED. ) ;
#41465 = CARTESIAN_POINT ( 'NONE',  ( -10.00000000000000000, 252.9166666734946602, -2.679491924311226292 ) ) ;
#41466 = DIRECTION ( 'NONE',  ( 0.000000000000000000, 0.000000000000000000, 1.000000000000000000 ) ) ;
#41467 = ORIENTED_EDGE ( 'NONE', *, *, #66888, .T. ) ;
#41468 = CARTESIAN_POINT ( 'NONE',  ( 9.832129032723420536, 171.5104166632526983, -5.676582343749999815 ) ) ;
#41469 = CARTESIAN_POINT ( 'NONE',  ( 1.320432766682872962E-15, -7.188101187499992051, 25.86155278187175810 ) ) ;
#41470 =( BOUNDED_CURVE ( )  B_SPLINE_CURVE ( 2, ( #8368, #43064, #37424, #48352, #60424, #25337, #60047, #66455, #18953 ),
 .UNSPECIFIED., .F., .F. ) 
 B_SPLINE_CURVE_WITH_KNOTS ( ( 3, 2, 2, 2, 3 ),
 ( 0.1022727272727272790, 0.1079545454545454558, 0.1136363636363636326, 0.1193181818181818232, 0.1250000000000000000 ),
 .UNSPECIFIED. ) 
 CURVE ( )  GEOMETRIC_REPRESENTATION_ITEM ( )  RATIONAL_B_SPLINE_CURVE ( ( 1.000000000000000000, 0.9238795325112867385, 1.000000000000000000, 0.9238795325112867385, 1.000000000000000000, 0.9238795325112867385, 1.000000000000000000, 0.9238795325112867385, 1.000000000000000000 ) ) 
 REPRESENTATION_ITEM ( '' )  );
#41471 = ORIENTED_EDGE ( 'NONE', *, *, #63812, .T. ) ;
#41472 = CARTESIAN_POINT ( 'NONE',  ( -5.656854249492380582, 102.5000000040967905, -5.656854249492380582 ) ) ;
#41473 = CARTESIAN_POINT ( 'NONE',  ( 2.449293598294707893E-16, 11.25000000000000000, -4.000000000000001776 ) ) ;
#41474 = CARTESIAN_POINT ( 'NONE',  ( -37.41137591332039136, -2.905788984246647999, 130.4889810496550808 ) ) ;
#41475 = CARTESIAN_POINT ( 'NONE',  ( -8.342170076843785083E-16, 12.06249999863440614, 4.541265875000002339 ) ) ;
#41476 = CARTESIAN_POINT ( 'NONE',  ( 5.656854249492376141, -5.656854249492374365, 22.58030278392014623 ) ) ;
#41478 = CARTESIAN_POINT ( 'NONE',  ( -2.849036369511732440E-14, 196.2500000000000000, 138.0000000000000568 ) ) ;
#41477 = AXIS2_PLACEMENT_3D ( 'NONE', #28790, #12179, #58592 ) ;
#41479 = ORIENTED_EDGE ( 'NONE', *, *, #24394, .F. ) ;
#41480 = CARTESIAN_POINT ( 'NONE',  ( -5.656854249492379694, 24.56250000000000355, -5.656854249492380582 ) ) ;
#41481 = CARTESIAN_POINT ( 'NONE',  ( -7.188101187500000044, 95.65625000204838102, 0.000000000000000000 ) ) ;
#41482 = LINE ( 'NONE', #24495, #22551 ) ;
#41483 = CARTESIAN_POINT ( 'NONE',  ( 1452.688200795887496, 828.9677537767817057, 997.8421604560586502 ) ) ;
#41485 = EDGE_CURVE ( 'NONE', #51815, #4709, #24885, .T. ) ;
#41484 = ORIENTED_EDGE ( 'NONE', *, *, #48437, .T. ) ;
#41486 = EDGE_CURVE ( 'NONE', #46633, #55561, #50424, .T. ) ;
#41487 = CARTESIAN_POINT ( 'NONE',  ( 0.4451317748865717405, 16.44604352396224911, -68.55481936398530252 ) ) ;
#41488 = CARTESIAN_POINT ( 'NONE',  ( -32.12260501294203863, -27.36043622692760380, 165.0282794459930642 ) ) ;
#41489 = CARTESIAN_POINT ( 'NONE',  ( -4.401442555609577197E-16, 7.188101187499992051, 25.11155278187175810 ) ) ;
#41490 = ORIENTED_EDGE ( 'NONE', *, *, #63641, .T. ) ;
#41491 = ORIENTED_EDGE ( 'NONE', *, *, #48563, .F. ) ;
#41492 = CARTESIAN_POINT ( 'NONE',  ( -4.220049686691935698, 10.18810118749999916, 85.37500000204838102 ) ) ;
#41493 = CARTESIAN_POINT ( 'NONE',  ( -26.56734541678237704, 196.6250000013656063, 166.5412658750003629 ) ) ;
#41494 = CARTESIAN_POINT ( 'NONE',  ( -10.99999999999999822, -4.556349186104052151, 103.0937500000000000 ) ) ;
#41497 = CARTESIAN_POINT ( 'NONE',  ( 6.676582343750002480, 299.1718750017070079, -2.765530957081997254 ) ) ;
#41496 = CARTESIAN_POINT ( 'NONE',  ( 32.00000000000000000, 200.3125000027312126, 171.6568542494922553 ) ) ;
#41495 = FACE_OUTER_BOUND ( 'NONE', #48392, .T. ) ;
#41498 = CARTESIAN_POINT ( 'NONE',  ( 10.00000000000000000, 134.7916666666666572, 2.679491924311236062 ) ) ;
#41499 = CARTESIAN_POINT ( 'NONE',  ( 7.778174593052021635, 7.778174593052023411, 105.6250000040967763 ) ) ;
#41500 = DIRECTION ( 'NONE',  ( 0.000000000000000000, 0.000000000000000000, -1.000000000000000000 ) ) ;
#41501 = CARTESIAN_POINT ( 'NONE',  ( 29.43265458321766559, 204.8750000013656063, 166.5412658749999650 ) ) ;
#41502 = CARTESIAN_POINT ( 'NONE',  ( -2.977408999572650039, 7.312499997951610986, -7.188101187500001821 ) ) ;
#41503 = AXIS2_PLACEMENT_3D ( 'NONE', #53071, #1406, #70421 ) ;
#41504 = CARTESIAN_POINT ( 'NONE',  ( 3.317071493978877683, 8.008118988124991233, 5.044365283940630107 ) ) ;
#41505 = CARTESIAN_POINT ( 'NONE',  ( -3.458734125000015425, 195.9375000013655779, 142.0000000000000568 ) ) ;
#41506 = CARTESIAN_POINT ( 'NONE',  ( 1.320432766682874540E-15, 114.4062500020483810, 7.188101187500000044 ) ) ;
#41508 = CARTESIAN_POINT ( 'NONE',  ( 3.313708498984762496, -7.999999999999989342, 7.299052779823365533 ) ) ;
#41507 = DIRECTION ( 'NONE',  ( -0.000000000000000000, 1.000000000000000000, 2.238352872228138170E-16 ) ) ;
#41509 = CARTESIAN_POINT ( 'NONE',  ( -3.042071309553166181, 228.1770833367473301, -11.35316468749999608 ) ) ;
#41510 = CARTESIAN_POINT ( 'NONE',  ( -33.32783395544173999, 41.08565813395399857, 65.00000000000001421 ) ) ;
#41511 = CARTESIAN_POINT ( 'NONE',  ( 2.977408999572646486, 7.188101187499991163, 28.39280278187175810 ) ) ;
#41512 = CARTESIAN_POINT ( 'NONE',  ( 30.82842712474619873, 197.3750000000000284, 167.1715728752537586 ) ) ;
#41513 = CARTESIAN_POINT ( 'NONE',  ( -9.832129032723420536, 33.69791666325268409, 5.676582343749997150 ) ) ;
#41514 = CARTESIAN_POINT ( 'NONE',  ( -3.673940397442060854E-16, 288.7500000000000000, -6.000000000000001776 ) ) ;
#41515 = CARTESIAN_POINT ( 'NONE',  ( 9.832129032723416984, 215.6770833299193555, 5.676582343750006032 ) ) ;
#41516 = CARTESIAN_POINT ( 'NONE',  ( -38.00000000000002132, 50.00000000000000711, 57.99999999999999289 ) ) ;
#41518 = DIRECTION ( 'NONE',  ( 1.000000000000000000, 0.000000000000000000, 0.000000000000000000 ) ) ;
#41517 = CARTESIAN_POINT ( 'NONE',  ( -4.615726161709537756, 52.16176840074169974, 48.91069252044945870 ) ) ;
#41519 = ORIENTED_EDGE ( 'NONE', *, *, #34122, .T. ) ;
#41520 = CARTESIAN_POINT ( 'NONE',  ( -2.445694354108840063, 197.0625000013656063, 139.5543056458912190 ) ) ;
#41521 = CARTESIAN_POINT ( 'NONE',  ( -9.832129032723418760, 37.86458332991934839, -5.676582343750004256 ) ) ;
#41522 = CARTESIAN_POINT ( 'NONE',  ( 4.556349186104051263, -10.99999999999999822, 85.65625000409679046 ) ) ;
#41523 = CARTESIAN_POINT ( 'NONE',  ( -2.445694354108839175, 209.3125000013656063, 144.4456943541088663 ) ) ;
#41524 = EDGE_CURVE ( 'NONE', #57671, #18660, #2264, .T. ) ;
#41525 = CARTESIAN_POINT ( 'NONE',  ( -4.242640687119286547, 294.9375000034140157, -4.242640687119286547 ) ) ;
#41526 = CYLINDRICAL_SURFACE ( 'NONE', #70853, 19.00000000000000355 ) ;
#41528 = CARTESIAN_POINT ( 'NONE',  ( 11.35316468749999785, 20.57291666325268409, 3.042071309553174174 ) ) ;
#41527 = CARTESIAN_POINT ( 'NONE',  ( 2.977408999572654480, 103.6250000020483810, 7.188101187499999156 ) ) ;
#41529 = CARTESIAN_POINT ( 'NONE',  ( -7.999999999999991118, 3.313708498984756723, 14.23655277982336642 ) ) ;
#41530 = CARTESIAN_POINT ( 'NONE',  ( 11.35316468749999785, 150.5729166632526699, 3.042071309553174174 ) ) ;
#41531 = CARTESIAN_POINT ( 'NONE',  ( 10.00000000000000178, 112.0833333265053824, -2.679491924311226736 ) ) ;
#41532 = CARTESIAN_POINT ( 'NONE',  ( -7.188101187500001821, 112.4375000020483810, -2.977408999572650483 ) ) ;
#41533 = CARTESIAN_POINT ( 'NONE',  ( -3.673940397442060854E-16, 293.8125000034140157, -6.000000000000001776 ) ) ;
#41534 = CARTESIAN_POINT ( 'NONE',  ( -29.43265458321766559, 205.7500000013656063, 166.5412658750003629 ) ) ;
#41535 = ORIENTED_EDGE ( 'NONE', *, *, #32673, .F. ) ;
#41536 = CARTESIAN_POINT ( 'NONE',  ( 5.676582343749993598, 5.260416663252683200, 9.832129032723422313 ) ) ;
#41537 = ORIENTED_EDGE ( 'NONE', *, *, #50275, .T. ) ;
#41538 = CYLINDRICAL_SURFACE ( 'NONE', #69098, 8.000000000000000000 ) ;
#41539 = CARTESIAN_POINT ( 'NONE',  ( 2.765530957082001251, 297.7656250017069510, 6.676582343750000703 ) ) ;
#41541 = CARTESIAN_POINT ( 'NONE',  ( -3.042071309553173730, 134.3229166632526983, 11.35316468749999785 ) ) ;
#41540 = CARTESIAN_POINT ( 'NONE',  ( 2.775557561562891351E-14, 210.0000000000000284, 198.0000000000000284 ) ) ;
#41542 = CARTESIAN_POINT ( 'NONE',  ( -4.000000000000002665, 16.31249999726881228, 1.656854249492380582 ) ) ;
#41543 = CARTESIAN_POINT ( 'NONE',  ( 1.469576158976822172E-15, -7.999999999999991118, 16.26155278432982954 ) ) ;
#41544 = VECTOR ( 'NONE', #70996, 1000.000000000000000 ) ;
#41545 = CYLINDRICAL_SURFACE ( 'NONE', #56238, 4.000000000000001776 ) ;
#41546 = CARTESIAN_POINT ( 'NONE',  ( -11.35316468749999785, 243.6979166700806445, -3.042071309553164848 ) ) ;
#41547 = CARTESIAN_POINT ( 'NONE',  ( -7.204075437095965206, -7.204075437095968759, 90.71875000204838102 ) ) ;
#41548 = ORIENTED_EDGE ( 'NONE', *, *, #21030, .F. ) ;
#41549 = CARTESIAN_POINT ( 'NONE',  ( 0.000000000000000000, 300.0000000000000000, 0.000000000000000000 ) ) ;
#41550 = CARTESIAN_POINT ( 'NONE',  ( -2.828427124746192067, 8.625000000000000000, 2.828427124746190735 ) ) ;
#41551 = CARTESIAN_POINT ( 'NONE',  ( -5.676582343750006032, 89.42708332991934128, 9.832129032723418760 ) ) ;
#41552 = CARTESIAN_POINT ( 'NONE',  ( -6.238412754330611322E-16, 10.18810118749999916, 98.78125000204838102 ) ) ;
#41553 = CARTESIAN_POINT ( 'NONE',  ( 3.211159895383561835, 17.56249999863440792, -3.211159895383561835 ) ) ;
#41554 = ORIENTED_EDGE ( 'NONE', *, *, #2144, .T. ) ;
#41556 = ORIENTED_EDGE ( 'NONE', *, *, #51034, .T. ) ;
#41555 =( BOUNDED_CURVE ( )  B_SPLINE_CURVE ( 2, ( #48075, #58683, #30003, #41690, #38168, #66833, #31096, #13364, #2066 ),
 .UNSPECIFIED., .F., .F. ) 
 B_SPLINE_CURVE_WITH_KNOTS ( ( 3, 2, 2, 2, 3 ),
 ( 0.8157894736842106198, 0.8223684210526316374, 0.8289473684210527660, 0.8355263157894737835, 0.8421052631578948011 ),
 .UNSPECIFIED. ) 
 CURVE ( )  GEOMETRIC_REPRESENTATION_ITEM ( )  RATIONAL_B_SPLINE_CURVE ( ( 0.9999999999999986677, 0.9238795325112880708, 1.000000000000000000, 0.9238795325112867385, 1.000000000000000000, 0.9238795325112867385, 1.000000000000000000, 0.9238795325112854062, 1.000000000000001332 ) ) 
 REPRESENTATION_ITEM ( '' )  );
#41557 = CARTESIAN_POINT ( 'NONE',  ( 5.656854249492378806, 5.812500000000000888, 5.656854249492381470 ) ) ;
#41558 = CARTESIAN_POINT ( 'NONE',  ( 7.999999999999991118, 9.797174393178815797E-16, 3.080302779823361981 ) ) ;
#41559 = CARTESIAN_POINT ( 'NONE',  ( 7.188101187500000044, 1.968749997951610320, 0.000000000000000000 ) ) ;
#41560 = VECTOR ( 'NONE', #30928, 1000.000000000000000 ) ;
#41561 = CARTESIAN_POINT ( 'NONE',  ( -5.656854249492378806, 120.8750000040967905, 5.656854249492381470 ) ) ;
#41562 = B_SPLINE_CURVE_WITH_KNOTS ( 'NONE', 3,
 ( #10052, #50035, #62100, #68503, #61359, #10423, #38736, #33089 ),
 .UNSPECIFIED., .F., .F.,
 ( 4, 2, 2, 4 ),
 ( 0.005257893453559882822, 0.006567392922673223436, 0.007876892391786564918, 0.01049589133001324268 ),
 .UNSPECIFIED. ) ;
#41563 =( BOUNDED_CURVE ( )  B_SPLINE_CURVE ( 2, ( #4373, #54945, #62441, #33067, #38713, #73769, #20963, #43987, #44361 ),
 .UNSPECIFIED., .F., .T. ) 
 B_SPLINE_CURVE_WITH_KNOTS ( ( 3, 2, 2, 2, 3 ),
 ( 0.5729166666666666297, 0.5781250000000000000, 0.5833333333333333703, 0.5885416666666666297, 0.5937500000000000000 ),
 .UNSPECIFIED. ) 
 CURVE ( )  GEOMETRIC_REPRESENTATION_ITEM ( )  RATIONAL_B_SPLINE_CURVE ( ( 1.000000000000000000, 0.9238795325112867385, 1.000000000000000000, 0.9238795325112867385, 1.000000000000000000, 0.9238795325112867385, 1.000000000000000000, 0.9238795325112867385, 1.000000000000000000 ) ) 
 REPRESENTATION_ITEM ( '' )  );
#41564 = CARTESIAN_POINT ( 'NONE',  ( -7.204075437095967871, 7.204075437095967871, 102.3437500020483668 ) ) ;
#41565 = ADVANCED_FACE ( 'NONE', ( #48277 ), #7924, .F. ) ;
#41566 = AXIS2_PLACEMENT_3D ( 'NONE', #51598, #45941, #29709 ) ;
#41567 = CARTESIAN_POINT ( 'NONE',  ( 0.000000000000000000, 125.0000000000000000, 0.000000000000000000 ) ) ;
#41568 = CARTESIAN_POINT ( 'NONE',  ( 2.449293598294707893E-16, 15.99999999726881406, -4.000000000000001776 ) ) ;
#41569 = CARTESIAN_POINT ( 'NONE',  ( 28.00000000000002132, 209.5000000000000284, 165.9999999999998863 ) ) ;
#41570 = ORIENTED_EDGE ( 'NONE', *, *, #48376, .F. ) ;
#41571 = CYLINDRICAL_SURFACE ( 'NONE', #43694, 10.99999999999998934 ) ;
#41572 = CARTESIAN_POINT ( 'NONE',  ( 1.432654583217662481, 199.1250000013656347, 194.5412658750000219 ) ) ;
#41574 = CARTESIAN_POINT ( 'NONE',  ( 4.898587196589412829E-16, 22.68749999590322375, -8.000000000000000000 ) ) ;
#41573 = CARTESIAN_POINT ( 'NONE',  ( -24.54126587499999346, 202.1875000013656063, 170.0000000000002842 ) ) ;
#41575 =( BOUNDED_CURVE ( )  B_SPLINE_CURVE ( 2, ( #19049, #13734, #24339, #6999, #63970, #36779, #59060, #52284, #30377, #47349, #65438, #70373, #12282 ),
 .UNSPECIFIED., .F., .F. ) 
 B_SPLINE_CURVE_WITH_KNOTS ( ( 3, 2, 2, 2, 2, 2, 3 ),
 ( 0.4510869565217391353, 0.4528985507246376940, 0.4547101449275362528, 0.4565217391304348116, 0.4583333333333333703, 0.4601449275362319291, 0.4619565217391304879 ),
 .UNSPECIFIED. ) 
 CURVE ( )  GEOMETRIC_REPRESENTATION_ITEM ( )  RATIONAL_B_SPLINE_CURVE ( ( 1.000000000000000000, 0.9659258262890683122, 1.000000000000000000, 0.9659258262890683122, 1.000000000000000000, 0.9659258262890683122, 1.000000000000000000, 0.9659258262890683122, 1.000000000000000000, 0.9659258262890683122, 1.000000000000000000, 0.9659258262890673130, 1.000000000000001110 ) ) 
 REPRESENTATION_ITEM ( '' )  );
#41576 = CARTESIAN_POINT ( 'NONE',  ( -4.541265875000002339, 12.81249999863440792, -5.561446717895856393E-16 ) ) ;
#41577 = CARTESIAN_POINT ( 'NONE',  ( -3.999999999999959144, 200.1875000027312126, 199.6568542494924259 ) ) ;
#41578 = CARTESIAN_POINT ( 'NONE',  ( 5.082755093536320601, -5.082755093536318824, 14.04905278187175455 ) ) ;
#41579 = VERTEX_POINT ( 'NONE', #50054 ) ;
#41580 = ORIENTED_EDGE ( 'NONE', *, *, #54301, .F. ) ;
#41581 = CARTESIAN_POINT ( 'NONE',  ( 10.18810118749999916, 1.247682550866122264E-15, 102.9062500020483810 ) ) ;
#41582 = CARTESIAN_POINT ( 'NONE',  ( -8.660254037844380193, 97.91666666666667140, 4.999999999999992006 ) ) ;
#41583 = CARTESIAN_POINT ( 'NONE',  ( -25.17157287525377640, 205.6250000000000284, 172.8284271247465256 ) ) ;
#41584 = CARTESIAN_POINT ( 'NONE',  ( 1.432654583217662481, 196.1250000013655779, 194.5412658750000219 ) ) ;
#41585 = CARTESIAN_POINT ( 'NONE',  ( -5.000000000000000000, -70.11723469343111503, 28.93519894129190817 ) ) ;
#41586 = CARTESIAN_POINT ( 'NONE',  ( 5.000000000000001776, 100.8333333333333428, -8.660254037844389075 ) ) ;
#41587 = EDGE_CURVE ( 'NONE', #4343, #60165, #43544, .T. ) ;
#41588 = EDGE_CURVE ( 'NONE', #49884, #44710, #48593, .T. ) ;
#41589 = CARTESIAN_POINT ( 'NONE',  ( -7.999999999999998224, 119.0937500000000000, 3.313708498984766493 ) ) ;
#41590 = CARTESIAN_POINT ( 'NONE',  ( 5.676582343749993598, 60.26041666325268409, 9.832129032723422313 ) ) ;
#41591 = CARTESIAN_POINT ( 'NONE',  ( -2.765530957081998586, 297.7968750017069510, 6.676582343750001591 ) ) ;
#41592 = ORIENTED_EDGE ( 'NONE', *, *, #15005, .F. ) ;
#41593 = EDGE_CURVE ( 'NONE', #62682, #21543, #28531, .T. ) ;
#41594 = CARTESIAN_POINT ( 'NONE',  ( 1.332431167089188095E-11, 191.2499999999989768, -10.00000000000000533 ) ) ;
#41595 = CARTESIAN_POINT ( 'NONE',  ( -8.000000000000000000, 13.96874999590322375, -3.313708498984762496 ) ) ;
#41596 = CARTESIAN_POINT ( 'NONE',  ( 3.458734124999959914, 208.3750000013656063, 143.4326545832176976 ) ) ;
#41597 = CARTESIAN_POINT ( 'NONE',  ( -8.660254037844387298, 103.9583333265053824, -5.000000000000004441 ) ) ;
#41598 = CARTESIAN_POINT ( 'NONE',  ( -10.00000000000000000, 220.0000000000000000, 0.000000000000000000 ) ) ;
#41599 = LINE ( 'NONE', #29173, #37943 ) ;
#41600 = CARTESIAN_POINT ( 'NONE',  ( -11.00000000000000000, 4.556349186104045934, 116.4062500000000142 ) ) ;
#41601 = CARTESIAN_POINT ( 'NONE',  ( -5.000000000000005329, 208.3333333333333428, 8.660254037844387298 ) ) ;
#41602 = CARTESIAN_POINT ( 'NONE',  ( 1.320432766682872962E-15, -7.188101187499992051, 11.23655278187175455 ) ) ;
#41603 = CARTESIAN_POINT ( 'NONE',  ( -9.832129032723420536, 184.0104166632526983, 5.676582343749997150 ) ) ;
#41604 = CARTESIAN_POINT ( 'NONE',  ( -1.881053915767124440, 2.999999998634407028, 4.541265875000001451 ) ) ;
#41605 = CARTESIAN_POINT ( 'NONE',  ( 3.999999999999960032, 209.9375000000000000, 143.6568542494924259 ) ) ;
#41607 = LINE ( 'NONE', #54042, #49542 ) ;
#41606 = CARTESIAN_POINT ( 'NONE',  ( -7.320508075688771932, 227.5000000068279462, -7.320508075688771932 ) ) ;
#41608 = VERTEX_POINT ( 'NONE', #56844 ) ;
#41609 = CARTESIAN_POINT ( 'NONE',  ( 3.458734124999959469, 206.7500000013655779, 140.5673454167824161 ) ) ;
#41610 = CARTESIAN_POINT ( 'NONE',  ( -11.35316468750000141, 48.80208332991934128, 3.042071309553159963 ) ) ;
#41611 = MANIFOLD_SOLID_BREP ( 'Thread1', #17747 ) ;
#41612 = CARTESIAN_POINT ( 'NONE',  ( -4.556349186104047710, -10.99999999999999822, 101.9687500040967620 ) ) ;
#41613 = CARTESIAN_POINT ( 'NONE',  ( 3.508320828368888034, 227.0932894534376487, -10.79750125662090632 ) ) ;
#41614 = ADVANCED_FACE ( 'NONE', ( #11555, #57595 ), #261, .F. ) ;
#41615 = CARTESIAN_POINT ( 'NONE',  ( -29.43265458321755901, 206.8750000013656347, 173.4587341250004044 ) ) ;
#41616 = CARTESIAN_POINT ( 'NONE',  ( 10.00000000000000355, 10.00000000000000178, 0.000000000000000000 ) ) ;
#41618 = CARTESIAN_POINT ( 'NONE',  ( -7.320508075688757721, 101.8750000000000000, -7.320508075688758609 ) ) ;
#41617 = CARTESIAN_POINT ( 'NONE',  ( -5.000000000000000000, 32.28817737728141424, 3.295974604355933479E-13 ) ) ;
#41619 = CARTESIAN_POINT ( 'NONE',  ( -2.445694354108839619, 194.8125000013656063, 139.5543056458912190 ) ) ;
#41620 = CARTESIAN_POINT ( 'NONE',  ( 8.660254037844389075, 82.29166665983871098, -5.000000000000000000 ) ) ;
#41621 = PRESENTATION_LAYER_ASSIGNMENT (  '', '', ( #23520 ) ) ;
#41622 = CARTESIAN_POINT ( 'NONE',  ( -5.082755093536324154, 94.34375000204838102, 5.082755093536326818 ) ) ;
#41623 = CARTESIAN_POINT ( 'NONE',  ( -8.342170076843785083E-16, 16.18749999863440436, 4.541265875000002339 ) ) ;
#41624 = DIRECTION ( 'NONE',  ( -0.000000000000000000, -0.000000000000000000, -1.000000000000000000 ) ) ;
#41625 = CARTESIAN_POINT ( 'NONE',  ( 4.725576163437660959, 0.3220367818099649226, -6.238486278272107555 ) ) ;
#41626 = DIRECTION ( 'NONE',  ( 0.000000000000000000, 0.000000000000000000, 1.000000000000000000 ) ) ;
#41627 = ORIENTED_EDGE ( 'NONE', *, *, #61620, .F. ) ;
#41628 = ORIENTED_EDGE ( 'NONE', *, *, #52584, .T. ) ;
#41629 = CARTESIAN_POINT ( 'NONE',  ( 6.676582343750003368, 296.1718750017069510, -2.765530957081997254 ) ) ;
#41630 = DIRECTION ( 'NONE',  ( -1.000000000000000000, 0.000000000000000000, 0.000000000000000000 ) ) ;
#41631 = CARTESIAN_POINT ( 'NONE',  ( -28.00000000000001776, 194.4587341250000350, 166.5412658750003629 ) ) ;
#41632 = CARTESIAN_POINT ( 'NONE',  ( -8.311093377946836114, 152.6562499965859843, -8.311093377946837890 ) ) ;
#41633 = CARTESIAN_POINT ( 'NONE',  ( 4.220049686691941027, -10.18810118749999738, 84.62500000204838102 ) ) ;
#41634 = CARTESIAN_POINT ( 'NONE',  ( 5.000000000000001776, 2.708333326505365957, -8.660254037844389075 ) ) ;
#41635 = CARTESIAN_POINT ( 'NONE',  ( 1.656854249492403008, 200.6875000000000284, 194.0000000000000853 ) ) ;
#41636 = CYLINDRICAL_SURFACE ( 'NONE', #69960, 7.000000000000006217 ) ;
#41637 = CARTESIAN_POINT ( 'NONE',  ( 10.18810118749999916, 1.247682550866122264E-15, 110.7812500020483668 ) ) ;
#41638 = ORIENTED_EDGE ( 'NONE', *, *, #42649, .T. ) ;
#41639 = CARTESIAN_POINT ( 'NONE',  ( 0.000000000000000000, 0.000000000000000000, 0.000000000000000000 ) ) ;
#41640 = CARTESIAN_POINT ( 'NONE',  ( -2.828427124746192067, 17.62500000000000000, 2.828427124746190735 ) ) ;
#41641 = CARTESIAN_POINT ( 'NONE',  ( 3.042071309553159519, 145.0520833299193555, 11.35316468750000141 ) ) ;
#41642 = CARTESIAN_POINT ( 'NONE',  ( -3.458734124999959914, 200.3750000013656063, 196.5673454167823877 ) ) ;
#41643 = CARTESIAN_POINT ( 'NONE',  ( 3.458734125000016757, 208.1250000013656063, 199.4326545832176976 ) ) ;
#41644 = CARTESIAN_POINT ( 'NONE',  ( 4.220049686691941027, -10.18810118749999738, 71.50000000204838102 ) ) ;
#41645 = CARTESIAN_POINT ( 'NONE',  ( 11.35316468749999785, 45.88541666325268409, 3.042071309553174174 ) ) ;
#41646 = ORIENTED_EDGE ( 'NONE', *, *, #25576, .T. ) ;
#41647 = DIRECTION ( 'NONE',  ( 0.000000000000000000, -1.000000000000000000, 0.000000000000000000 ) ) ;
#41648 = CARTESIAN_POINT ( 'NONE',  ( -4.541265875000002339, 5.874999998634407916, -1.881053915767121998 ) ) ;
#41649 = CARTESIAN_POINT ( 'NONE',  ( 5.662595241051934458, 5.662595241051935346, 16.95061528394063188 ) ) ;
#41650 = CARTESIAN_POINT ( 'NONE',  ( 7.188101187499999156, 12.37499999795161010, 2.977408999572654924 ) ) ;
#41651 = CARTESIAN_POINT ( 'NONE',  ( -4.242640687119286547, 292.9375000034140157, -4.242640687119286547 ) ) ;
#41652 = CARTESIAN_POINT ( 'NONE',  ( -5.656854249492378806, 117.8750000040967905, 5.656854249492381470 ) ) ;
#41653 = CARTESIAN_POINT ( 'NONE',  ( -5.082755093536326818, 13.78124999795161187, 5.082755093536325042 ) ) ;
#41654 = CARTESIAN_POINT ( 'NONE',  ( -7.188101187499990274, -2.977408999572651815, 9.080302781871752771 ) ) ;
#41655 = CARTESIAN_POINT ( 'NONE',  ( 10.18810118750000093, -4.220049686691933921, 71.31250000204836681 ) ) ;
#41656 = CARTESIAN_POINT ( 'NONE',  ( -31.45873412499999944, 204.9375000013656063, 170.0000000000003979 ) ) ;
#41657 = CARTESIAN_POINT ( 'NONE',  ( -46.89594099591774068, 145.9999999999999716, 68.54827124808610961 ) ) ;
#41658 = CARTESIAN_POINT ( 'NONE',  ( 2.449293598294707893E-16, 0.9999999972688131678, -4.000000000000001776 ) ) ;
#41659 = ORIENTED_EDGE ( 'NONE', *, *, #40247, .F. ) ;
#41660 = EDGE_CURVE ( 'NONE', #21067, #3963, #56630, .T. ) ;
#41661 = CARTESIAN_POINT ( 'NONE',  ( 2.445694354108839619, 208.8125000013656063, 200.4456943541088663 ) ) ;
#41662 = VECTOR ( 'NONE', #56782, 1000.000000000000000 ) ;
#41663 = CARTESIAN_POINT ( 'NONE',  ( -2.828427124746209831, 200.3750000000000284, 139.1715728752538723 ) ) ;
#41664 = CARTESIAN_POINT ( 'NONE',  ( -27.99999999999991118, 199.6250000027312126, 174.0000000000003695 ) ) ;
#41665 = CARTESIAN_POINT ( 'NONE',  ( -1.881053915767124440, 3.999999998634406140, 4.541265875000001451 ) ) ;
#41666 = CARTESIAN_POINT ( 'NONE',  ( -7.188101187499999156, 115.2500000020484094, 2.977408999572654924 ) ) ;
#41667 = AXIS2_PLACEMENT_3D ( 'NONE', #33634, #13177, #36213 ) ;
#41668 = LINE ( 'NONE', #65032, #7895 ) ;
#41669 = CARTESIAN_POINT ( 'NONE',  ( 3.313708498984756279, 7.999999999999991118, 0.5490527839201453375 ) ) ;
#41670 = ORIENTED_EDGE ( 'NONE', *, *, #66956, .T. ) ;
#41671 =( BOUNDED_CURVE ( )  B_SPLINE_CURVE ( 2, ( #39416, #16751, #62414, #11121, #33399, #56774, #73740, #67718, #21677 ),
 .UNSPECIFIED., .F., .F. ) 
 B_SPLINE_CURVE_WITH_KNOTS ( ( 3, 2, 2, 2, 3 ),
 ( 0.4687499999999998890, 0.4739583333333332593, 0.4791666666666666297, 0.4843750000000000000, 0.4895833333333333148 ),
 .UNSPECIFIED. ) 
 CURVE ( )  GEOMETRIC_REPRESENTATION_ITEM ( )  RATIONAL_B_SPLINE_CURVE ( ( 1.000000000000001554, 0.9238795325112850731, 1.000000000000000000, 0.9238795325112867385, 1.000000000000000000, 0.9238795325112867385, 1.000000000000000000, 0.9238795325112867385, 1.000000000000000000 ) ) 
 REPRESENTATION_ITEM ( '' )  );
#41672 = CARTESIAN_POINT ( 'NONE',  ( -2.977408999572654480, 23.99999999795161543, 7.188101187499999156 ) ) ;
#41673 = EDGE_LOOP ( 'NONE', ( #48952, #34811 ) ) ;
#41674 = CARTESIAN_POINT ( 'NONE',  ( -10.18810118749999916, 0.000000000000000000, 117.1562500020483810 ) ) ;
#41675 = CARTESIAN_POINT ( 'NONE',  ( 2.485281374238196062, 296.6875000000000000, -6.000000000000377476 ) ) ;
#41676 = CARTESIAN_POINT ( 'NONE',  ( 27.99999999999997158, 208.9375000013656063, 166.5412658749999082 ) ) ;
#41677 = CARTESIAN_POINT ( 'NONE',  ( 6.123233995736767268E-16, 51.25000000000000711, -10.00000000000000178 ) ) ;
#41678 = CARTESIAN_POINT ( 'NONE',  ( 2.977408999572650039, 101.5625000020483810, -7.188101187500001821 ) ) ;
#41679 = CARTESIAN_POINT ( 'NONE',  ( 6.000000000000001776, 294.5000000000000000, -7.347880794884121708E-16 ) ) ;
#41681 = LINE ( 'NONE', #64691, #68731 ) ;
#41680 = CARTESIAN_POINT ( 'NONE',  ( 33.48318503342264307, 175.8115626168855385, 156.1427595010632956 ) ) ;
#41682 = VERTEX_POINT ( 'NONE', #46252 ) ;
#41683 = CARTESIAN_POINT ( 'NONE',  ( -8.311093377946834337, 234.5312500034139589, 8.311093377946837890 ) ) ;
#41684 = CARTESIAN_POINT ( 'NONE',  ( 5.082755093536320601, -5.082755093536318824, 14.42405278187175455 ) ) ;
#41685 = CARTESIAN_POINT ( 'NONE',  ( -8.000000000000001776, 14.34375000000000178, 3.313708498984759387 ) ) ;
#41686 = PLANE ( 'NONE',  #45422 ) ;
#41687 = CARTESIAN_POINT ( 'NONE',  ( -7.347880794884122694E-16, 17.49999999726881583, 4.000000000000001776 ) ) ;
#41688 = CARTESIAN_POINT ( 'NONE',  ( 2.679491924311235174, 261.4583333333332575, 9.999999999999998224 ) ) ;
#41689 = CARTESIAN_POINT ( 'NONE',  ( -2.679491924311235618, 178.5416666666666856, 10.00000000000000000 ) ) ;
#41690 = CARTESIAN_POINT ( 'NONE',  ( 3.313708498984762496, -7.999999999999989342, 5.799052779823364645 ) ) ;
#41691 = CARTESIAN_POINT ( 'NONE',  ( 2.977408999572650927, -7.188101187499990274, 27.83030278187176165 ) ) ;
#41692 = CARTESIAN_POINT ( 'NONE',  ( 5.676582343750001591, 146.9270833299193555, -9.832129032723420536 ) ) ;
#41693 = DIRECTION ( 'NONE',  ( 0.000000000000000000, 0.000000000000000000, -1.000000000000000000 ) ) ;
#41694 = CARTESIAN_POINT ( 'NONE',  ( 0.000000000000000000, 300.0000000000000000, 0.000000000000000000 ) ) ;
#41697 = CARTESIAN_POINT ( 'NONE',  ( 27.99999999999996803, 204.0000000000000284, 173.9999999999999147 ) ) ;
#41696 = CARTESIAN_POINT ( 'NONE',  ( -4.898587196589412829E-16, 111.1250000000000000, -8.000000000000000000 ) ) ;
#41695 = CARTESIAN_POINT ( 'NONE',  ( 26.34314575050763807, 207.5625000000000284, 165.9999999999998863 ) ) ;
#41698 = ORIENTED_EDGE ( 'NONE', *, *, #54463, .F. ) ;
#41699 = CARTESIAN_POINT ( 'NONE',  ( 7.999999999999998224, 10.40625000000000178, 3.313708498984766049 ) ) ;
#41700 = ADVANCED_FACE ( 'NONE', ( #74179 ), #29287, .F. ) ;
#41701 = CARTESIAN_POINT ( 'NONE',  ( -28.00000000000003197, 210.0000000000000284, 166.0000000000003695 ) ) ;
#41702 = CARTESIAN_POINT ( 'NONE',  ( -2.445694354108838731, 205.0625000013656063, 144.4456943541088663 ) ) ;
#41703 = CARTESIAN_POINT ( 'NONE',  ( -11.00000000000000533, -11.00000000000000355, 41.99999999999999289 ) ) ;
#41704 = EDGE_CURVE ( 'NONE', #44017, #46951, #52297, .T. ) ;
#41705 = CARTESIAN_POINT ( 'NONE',  ( -5.000000000000005329, 30.20833332650536818, 8.660254037844387298 ) ) ;
#41706 = CARTESIAN_POINT ( 'NONE',  ( 5.082755093536325042, 117.5937500020483810, -5.082755093536325930 ) ) ;
#41707 = CARTESIAN_POINT ( 'NONE',  ( -1.881053915767121554, 4.749999998634407028, -4.541265875000002339 ) ) ;
#41708 = CARTESIAN_POINT ( 'NONE',  ( 1.567784982238203817E-13, 108.7500000000000426, 10.00000000000000533 ) ) ;
#41709 = CARTESIAN_POINT ( 'NONE',  ( -4.898587196589407898E-16, 7.999999999999991118, 15.45530277982336642 ) ) ;
#41711 = CARTESIAN_POINT ( 'NONE',  ( 7.999963770166947263, -3.313744728817803242, 18.17405133435311271 ) ) ;
#41710 = CARTESIAN_POINT ( 'NONE',  ( -32.00000000000001421, 203.1875000000000284, 168.3431457505080289 ) ) ;
#41712 = ORIENTED_EDGE ( 'NONE', *, *, #37242, .F. ) ;
#41713 = CARTESIAN_POINT ( 'NONE',  ( 2.485281374238919927, 292.3750000034140157, 5.999999999999654499 ) ) ;
#41714 = CARTESIAN_POINT ( 'NONE',  ( 0.000000000000000000, 207.0000000000000568, 170.0000000000000284 ) ) ;
#41715 = ADVANCED_FACE ( 'NONE', ( #11928 ), #46624, .F. ) ;
#41716 = CARTESIAN_POINT ( 'NONE',  ( 9.832129032723420536, 236.3020833367473301, 5.676582343749996262 ) ) ;
#41717 = CARTESIAN_POINT ( 'NONE',  ( 8.311093377946834337, 110.1562499965860269, 8.311093377946839666 ) ) ;
#41718 = ORIENTED_EDGE ( 'NONE', *, *, #64424, .F. ) ;
#41719 = CARTESIAN_POINT ( 'NONE',  ( 2.849036369511732440E-14, 198.2500000000000000, 202.0000000000000000 ) ) ;
#41720 = CARTESIAN_POINT ( 'NONE',  ( -4.220049686691935698, 10.18810118749999916, 103.3750000020484094 ) ) ;
#41721 = DIRECTION ( 'NONE',  ( 0.000000000000000000, 0.000000000000000000, -1.000000000000000000 ) ) ;
#41722 = CARTESIAN_POINT ( 'NONE',  ( -2.445694354108783219, 198.8125000013656063, 200.4456943541088663 ) ) ;
#41723 = DIRECTION ( 'NONE',  ( -0.000000000000000000, 1.000000000000000000, 0.000000000000000000 ) ) ;
#41725 = CARTESIAN_POINT ( 'NONE',  ( 3.042071309553167513, 106.8229166632526841, -11.35316468749999785 ) ) ;
#41724 = CARTESIAN_POINT ( 'NONE',  ( 1.046914569402248141, 225.9999999999998863, -9.958971312565205736 ) ) ;
#41726 = AXIS2_PLACEMENT_3D ( 'NONE', #9384, #72378, #49744 ) ;
#41727 = CARTESIAN_POINT ( 'NONE',  ( -27.99999999999996092, 207.5000000000000284, 174.0000000000003695 ) ) ;
#41728 = CARTESIAN_POINT ( 'NONE',  ( 3.313708498984756279, 7.999999999999991118, 6.549052783920143561 ) ) ;
#41729 = EDGE_LOOP ( 'NONE', ( #30459, #7280, #16460, #69120 ) ) ;
#41730 = CARTESIAN_POINT ( 'NONE',  ( -2.679491924311235618, 195.4166666598387394, 10.00000000000000000 ) ) ;
#41731 = CARTESIAN_POINT ( 'NONE',  ( 4.999999999999999112, 0.000000000000000000, 0.000000000000000000 ) ) ;
#41732 = EDGE_CURVE ( 'NONE', #1512, #58564, #18010, .T. ) ;
#41733 = CARTESIAN_POINT ( 'NONE',  ( 7.778174593052021635, 7.778174593052023411, 83.12500000409676204 ) ) ;
#41734 = CARTESIAN_POINT ( 'NONE',  ( -9.832129032723418760, 98.17708332991935549, -5.676582343750004256 ) ) ;
#41735 = CARTESIAN_POINT ( 'NONE',  ( 0.000000000000000000, 0.000000000000000000, -25.03750572909317285 ) ) ;
#41736 = CARTESIAN_POINT ( 'NONE',  ( 2.977408999572652260, 9.562499997951608322, 7.188101187500000044 ) ) ;
#41737 = CARTESIAN_POINT ( 'NONE',  ( -10.18810118749999916, 4.220049686691934809, 97.93750000204836681 ) ) ;
#41738 = CARTESIAN_POINT ( 'NONE',  ( -8.311093377946841443, 9.218749996586016238, 8.311093377946830785 ) ) ;
#41739 = ORIENTED_EDGE ( 'NONE', *, *, #1196, .T. ) ;
#41740 = CARTESIAN_POINT ( 'NONE',  ( 1.469576158976822172E-15, -7.999999999999991118, 26.70530277982336642 ) ) ;
#41741 = CARTESIAN_POINT ( 'NONE',  ( 1.331130781283735187, -42.30430424668328016, 139.0280587967137933 ) ) ;
#41742 = LINE ( 'NONE', #64752, #63129 ) ;
#41743 = CARTESIAN_POINT ( 'NONE',  ( 10.18810118749999916, 4.220049686691935698, 73.37500000204838102 ) ) ;
#41744 = DIRECTION ( 'NONE',  ( -0.000000000000000000, -1.000000000000000000, -4.283267841918042741E-17 ) ) ;
#41745 = DIRECTION ( 'NONE',  ( 0.000000000000000000, 0.000000000000000000, 1.000000000000000000 ) ) ;
#41746 = CARTESIAN_POINT ( 'NONE',  ( -6.676582343750003368, 292.3906250017068942, -2.765530957081996810 ) ) ;
#41747 = CARTESIAN_POINT ( 'NONE',  ( 1.656854249492379916, 204.4375000027312410, 202.0000000000000284 ) ) ;
#41748 = CARTESIAN_POINT ( 'NONE',  ( 5.676582343749993598, 220.2604166632526983, 9.832129032723422313 ) ) ;
#41750 = B_SPLINE_CURVE_WITH_KNOTS ( 'NONE', 3,
 ( #39835, #11914, #62839, #22851, #74164, #34947, #28142, #17566, #34197, #45488 ),
 .UNSPECIFIED., .F., .F.,
 ( 4, 2, 2, 2, 4 ),
 ( 0.000000000000000000, 0.001314083742622691817, 0.002628167485245383635, 0.003942251227868075886, 0.005256334970490767269 ),
 .UNSPECIFIED. ) ;
#41749 = CIRCLE ( 'NONE', #5573, 71.70204102886728492 ) ;
#41751 = CARTESIAN_POINT ( 'NONE',  ( -4.220049686691935698, 10.18810118749999916, 89.87500000204836681 ) ) ;
#41752 = CARTESIAN_POINT ( 'NONE',  ( -28.00000000000002132, 204.4375000013656063, 166.5412658750003629 ) ) ;
#41753 = CARTESIAN_POINT ( 'NONE',  ( -5.656854249492379694, 26.06250000000000711, -5.656854249492380582 ) ) ;
#41754 = VERTEX_POINT ( 'NONE', #53410 ) ;
#41755 = CARTESIAN_POINT ( 'NONE',  ( -30.82842712474612767, 208.5000000027312126, 172.8284271247466108 ) ) ;
#41756 = CARTESIAN_POINT ( 'NONE',  ( 1.656854249492405451, 205.4375000027312126, 202.0000000000000284 ) ) ;
#41757 = EDGE_CURVE ( 'NONE', #50134, #37291, #42437, .T. ) ;
#41758 = CARTESIAN_POINT ( 'NONE',  ( -8.660254037844387298, 32.08333333333333570, -5.000000000000004441 ) ) ;
#41759 = CARTESIAN_POINT ( 'NONE',  ( 31.99999999999998579, 208.4375000027312126, 168.3431457505074889 ) ) ;
#41760 = CARTESIAN_POINT ( 'NONE',  ( 10.18810118749999916, 1.247682550866122264E-15, 77.78125000204836681 ) ) ;
#41761 = EDGE_LOOP ( 'NONE', ( #53366, #477, #52884, #55305, #72138 ) ) ;
#41762 = EDGE_CURVE ( 'NONE', #39397, #63637, #33895, .T. ) ;
#41763 = CARTESIAN_POINT ( 'NONE',  ( -2.977408999572650039, 5.437499997951610986, -7.188101187500000933 ) ) ;
#41764 = CARTESIAN_POINT ( 'NONE',  ( -5.656854249492375253, 5.656854249492375253, 6.642802779823365533 ) ) ;
#41765 = CARTESIAN_POINT ( 'NONE',  ( 2.977408999572654480, 119.0000000020483810, 7.188101187499999156 ) ) ;
#41766 = CARTESIAN_POINT ( 'NONE',  ( -1.216988651335362936, 22.00000000000001066, -3.901072361666817034 ) ) ;
#41767 = CARTESIAN_POINT ( 'NONE',  ( -6.676582343749999815, 295.5156250017069510, 2.765530957082001251 ) ) ;
#41769 = CARTESIAN_POINT ( 'NONE',  ( -4.979315568031092099, 10.98159727696817889, -0.02533325329315395946 ) ) ;
#41768 = CARTESIAN_POINT ( 'NONE',  ( -8.311093377946834337, 229.5312500034139589, 8.311093377946837890 ) ) ;
#41770 = EDGE_LOOP ( 'NONE', ( #19514, #74225, #27703 ) ) ;
#41771 = ADVANCED_FACE ( 'NONE', ( #54149 ), #30391, .T. ) ;
#41772 = CARTESIAN_POINT ( 'NONE',  ( 2.085542519210945334E-15, 225.4687500034139873, 11.35316468749999963 ) ) ;
#41773 = CARTESIAN_POINT ( 'NONE',  ( 7.188101187499991163, 2.977408999572648707, 3.830302781871751883 ) ) ;
#41774 = CARTESIAN_POINT ( 'NONE',  ( -3.458734124999959469, 204.7500000013656063, 199.4326545832176691 ) ) ;
#41775 = VERTEX_POINT ( 'NONE', #36425 ) ;
#41776 = FACE_OUTER_BOUND ( 'NONE', #40926, .T. ) ;
#41777 = CARTESIAN_POINT ( 'NONE',  ( -3.042071309553173730, 104.6354166632526699, 11.35316468749999785 ) ) ;
#41778 = PRODUCT_DEFINITION ( 'UNKNOWN', '', #23739, #45553 ) ;
#41779 = CARTESIAN_POINT ( 'NONE',  ( -6.735557395310442023E-16, 11.00000000000000000, 78.62499999999998579 ) ) ;
#41782 = CARTESIAN_POINT ( 'NONE',  ( -54.00000000000000711, 272.0000000000000000, 20.00000000000003197 ) ) ;
#41781 = CARTESIAN_POINT ( 'NONE',  ( 28.00000000000002132, 206.4375000013656063, 173.4587341249998929 ) ) ;
#41780 = CARTESIAN_POINT ( 'NONE',  ( 30.44569435410879166, 203.8125000013656063, 172.4456943541087526 ) ) ;
#41783 = ORIENTED_EDGE ( 'NONE', *, *, #51466, .F. ) ;
#41784 = CARTESIAN_POINT ( 'NONE',  ( -2.751064625579944321E-14, 204.7500000000000284, 146.0000000000000284 ) ) ;
#41785 = CARTESIAN_POINT ( 'NONE',  ( 8.311093377946834337, 215.1562499965860127, 8.311093377946839666 ) ) ;
#41786 =( BOUNDED_CURVE ( )  B_SPLINE_CURVE ( 2, ( #15429, #4883, #21836, #56569, #15059, #10533, #49393, #27878, #16541 ),
 .UNSPECIFIED., .F., .F. ) 
 B_SPLINE_CURVE_WITH_KNOTS ( ( 3, 2, 2, 2, 3 ),
 ( 0.7613636363636363535, 0.7670454545454545858, 0.7727272727272727071, 0.7784090909090909394, 0.7840909090909090606 ),
 .UNSPECIFIED. ) 
 CURVE ( )  GEOMETRIC_REPRESENTATION_ITEM ( )  RATIONAL_B_SPLINE_CURVE ( ( 1.000000000000000000, 0.9238795325112867385, 1.000000000000000000, 0.9238795325112867385, 1.000000000000000000, 0.9238795325112867385, 1.000000000000000000, 0.9238795325112867385, 1.000000000000000000 ) ) 
 REPRESENTATION_ITEM ( '' )  );
#41787 = CARTESIAN_POINT ( 'NONE',  ( 2.445694354108782775, 199.5625000013656063, 139.5543056458912190 ) ) ;
#41788 = AXIS2_PLACEMENT_3D ( 'NONE', #39989, #50553, #62994 ) ;
#41789 = CARTESIAN_POINT ( 'NONE',  ( 30.44569435410879166, 202.8125000013656063, 172.4456943541087526 ) ) ;
#41790 = EDGE_CURVE ( 'NONE', #60299, #44316, #46990, .T. ) ;
#41791 = CARTESIAN_POINT ( 'NONE',  ( 5.082755093536325930, 20.53124999795161543, -5.082755093536325930 ) ) ;
#41792 = CARTESIAN_POINT ( 'NONE',  ( -2.085542519210945728E-15, 174.8437499965860411, 11.35316468750000141 ) ) ;
#41793 = CARTESIAN_POINT ( 'NONE',  ( -7.188101187500000044, 99.03125000204838102, 0.000000000000000000 ) ) ;
#41794 = CARTESIAN_POINT ( 'NONE',  ( -5.000000000000000000, 66.79212039439858017, -23.29662735513358385 ) ) ;
#41795 = CARTESIAN_POINT ( 'NONE',  ( -31.99999999999999289, 198.2500000000000000, 170.0000000000003979 ) ) ;
#41796 = CARTESIAN_POINT ( 'NONE',  ( -3.211159895383561391, 14.68749999863440792, -3.211159895383561835 ) ) ;
#41797 = CARTESIAN_POINT ( 'NONE',  ( 24.54126587500000412, 199.3750000013656063, 168.5673454167822172 ) ) ;
#41798 = CARTESIAN_POINT ( 'NONE',  ( -7.188101187499992051, 0.000000000000000000, 4.861552781871752771 ) ) ;
#41799 = CARTESIAN_POINT ( 'NONE',  ( -9.832129032723418760, 67.86458332991935549, -5.676582343750004256 ) ) ;
#41800 = CARTESIAN_POINT ( 'NONE',  ( 0.000000000000000000, 0.000000000000000000, -19.00000000000001776 ) ) ;
#41801 = DIRECTION ( 'NONE',  ( -0.000000000000000000, 1.000000000000000000, -0.000000000000000000 ) ) ;
#41802 = EDGE_LOOP ( 'NONE', ( #22900, #8683 ) ) ;
#41803 = DIRECTION ( 'NONE',  ( 0.000000000000000000, -1.000000000000000000, 0.000000000000000000 ) ) ;
#41804 = CARTESIAN_POINT ( 'NONE',  ( 3.153939666463669656E-13, 33.75000000000002842, 9.999999999999998224 ) ) ;
#41805 = CARTESIAN_POINT ( 'NONE',  ( -5.676582343749998039, 77.44791666325269830, -9.832129032723420536 ) ) ;
#41806 = CARTESIAN_POINT ( 'NONE',  ( 10.18810118750000093, -4.220049686691933921, 116.3125000020483668 ) ) ;
#41807 = CARTESIAN_POINT ( 'NONE',  ( 3.458734124999959469, 197.7500000013656063, 140.5673454167823593 ) ) ;
#41808 = DIRECTION ( 'NONE',  ( -0.000000000000000000, 1.000000000000000000, -0.000000000000000000 ) ) ;
#41810 = CARTESIAN_POINT ( 'NONE',  ( -8.311093377946841443, 68.90624999658602690, 8.311093377946834337 ) ) ;
#41809 = CARTESIAN_POINT ( 'NONE',  ( 5.082755093536326818, 90.21875000204838102, 5.082755093536325042 ) ) ;
#41811 = CARTESIAN_POINT ( 'NONE',  ( 7.999999999999991118, 9.797174393178815797E-16, 27.26780278392014978 ) ) ;
#41812 = CARTESIAN_POINT ( 'NONE',  ( -2.306210152021532345, 194.6725217480081653, 139.1313145796361823 ) ) ;
#41813 = CARTESIAN_POINT ( 'NONE',  ( -10.00000000000000355, 154.5833333265053682, 2.679491924311223183 ) ) ;
#41814 = CARTESIAN_POINT ( 'NONE',  ( 2.977408999572650039, 91.06250000204838102, -7.188101187500001821 ) ) ;
#41815 = DIRECTION ( 'NONE',  ( 1.000000000000000000, 0.000000000000000000, 0.000000000000000000 ) ) ;
#41816 = CARTESIAN_POINT ( 'NONE',  ( -3.042071309553173730, 59.63541666325267698, 11.35316468749999785 ) ) ;
#41817 = CARTESIAN_POINT ( 'NONE',  ( -7.204075437095965206, -7.204075437095968759, 111.7187500020483810 ) ) ;
#41818 = CARTESIAN_POINT ( 'NONE',  ( 11.35316468750000141, 195.7812499965860127, 0.000000000000000000 ) ) ;
#41819 = VERTEX_POINT ( 'NONE', #24713 ) ;
#41820 = CARTESIAN_POINT ( 'NONE',  ( 4.330454160169023403, 68.33163558030062745, 20.63184982502072984 ) ) ;
#41821 = CARTESIAN_POINT ( 'NONE',  ( -10.18810118749999738, -4.220049686691941915, 67.75000000204836681 ) ) ;
#41822 = CARTESIAN_POINT ( 'NONE',  ( 7.320508075688771044, 61.24999999317203958, 7.320508075688775484 ) ) ;
#41824 = CARTESIAN_POINT ( 'NONE',  ( -3.042071309553163960, 187.2395833299193555, -11.35316468749999963 ) ) ;
#41823 = FACE_OUTER_BOUND ( 'NONE', #31772, .T. ) ;
#41825 = CARTESIAN_POINT ( 'NONE',  ( 2.849036369511732440E-14, 207.2500000000000284, 202.0000000000000000 ) ) ;
#41826 = CARTESIAN_POINT ( 'NONE',  ( -7.320508075688770155, 258.7500000068279746, 7.320508075688774596 ) ) ;
#41827 = CARTESIAN_POINT ( 'NONE',  ( 6.123233995736767268E-16, 188.1249999931720254, -10.00000000000000178 ) ) ;
#41828 = ORIENTED_EDGE ( 'NONE', *, *, #13625, .F. ) ;
#41829 = CARTESIAN_POINT ( 'NONE',  ( -2.085542519210945728E-15, 164.8437499965860127, 11.35316468750000141 ) ) ;
#41830 = CLOSED_SHELL ( 'NONE', ( #61547, #14143, #60200, #30690, #5572, #61126 ) ) ;
#41831 = CARTESIAN_POINT ( 'NONE',  ( -5.082755093536317936, -5.082755093536320601, 18.17405278187175455 ) ) ;
#41832 = CARTESIAN_POINT ( 'NONE',  ( 10.15167889325737960, 225.9999999999999147, -4.663489317652536492 ) ) ;
#41833 = ORIENTED_EDGE ( 'NONE', *, *, #16454, .F. ) ;
#41834 = CARTESIAN_POINT ( 'NONE',  ( -7.999999999999998224, 104.2812500040967763, 3.313708498984766493 ) ) ;
#41835 = EDGE_CURVE ( 'NONE', #39173, #23384, #56583, .T. ) ;
#41836 = B_SPLINE_CURVE_WITH_KNOTS ( 'NONE', 3,
 ( #9348, #3691, #49710, #27066, #9726, #21027, #5186, #51194, #24004, #22894, #17229, #5553, #1024, #51562, #64007, #12678, #17606, #52320 ),
 .UNSPECIFIED., .F., .F.,
 ( 4, 2, 2, 2, 2, 2, 2, 2, 4 ),
 ( 0.004693513696739645864, 0.005279931483811504608, 0.005866349270883363352, 0.006452767057955222096, 0.007039184845027080840, 0.007625602632098937850, 0.008212020419170795726, 0.008798438206242653603, 0.009384855993314511480 ),
 .UNSPECIFIED. ) ;
#41837 = CIRCLE ( 'NONE', #24918, 18.50000000000000000 ) ;
#41838 = EDGE_CURVE ( 'NONE', #27085, #24886, #51277, .T. ) ;
#41839 = CARTESIAN_POINT ( 'NONE',  ( 2.828427124746191623, 11.12500000000000000, -2.828427124746191623 ) ) ;
#41840 = CARTESIAN_POINT ( 'NONE',  ( -38.09511457376476073, -1.549599291698573911, 126.0236990279832696 ) ) ;
#41841 = CARTESIAN_POINT ( 'NONE',  ( -1.881053915767121776, 16.62499999863440436, -4.541265875000002339 ) ) ;
#41842 = CARTESIAN_POINT ( 'NONE',  ( 3.313708498984756279, 7.999999999999991118, 18.54905278392014623 ) ) ;
#41843 = CARTESIAN_POINT ( 'NONE',  ( 2.828427124746152987, 196.1250000000000284, 139.1715728752538723 ) ) ;
#41844 = EDGE_LOOP ( 'NONE', ( #27101, #10627, #10081, #10051 ) ) ;
#41845 = DIRECTION ( 'NONE',  ( -0.000000000000000000, -0.000000000000000000, 1.000000000000000000 ) ) ;
#41846 = CARTESIAN_POINT ( 'NONE',  ( 5.082755093536326818, 97.71875000204838102, 5.082755093536325042 ) ) ;
#41848 = LINE ( 'NONE', #64857, #28596 ) ;
#41847 = CARTESIAN_POINT ( 'NONE',  ( 10.00000000000005151, 179.7916666666667425, 2.679491924311249829 ) ) ;
#41849 = SHAPE_REPRESENTATION_RELATIONSHIP ( 'NONE' , 'NONE' ,  #22863, #5729 ) ;
#41850 = ORIENTED_EDGE ( 'NONE', *, *, #74034, .T. ) ;
#41851 = CARTESIAN_POINT ( 'NONE',  ( 5.126144196591270408, 16.23426282122703057, -69.90718656545273291 ) ) ;
#41852 = CARTESIAN_POINT ( 'NONE',  ( -5.656854249492380582, 104.0000000040967905, -5.656854249492380582 ) ) ;
#41853 = CARTESIAN_POINT ( 'NONE',  ( -7.188101187499990274, -2.977408999572651371, 24.08030278187175455 ) ) ;
#41854 = ORIENTED_EDGE ( 'NONE', *, *, #48591, .T. ) ;
#41855 = EDGE_LOOP ( 'NONE', ( #63716, #28798, #35198, #3421, #43696, #22243 ) ) ;
#41856 = CARTESIAN_POINT ( 'NONE',  ( 10.18810118750000093, -4.220049686691933033, 86.31250000204838102 ) ) ;
#41857 = CARTESIAN_POINT ( 'NONE',  ( 12.00000000000000000, -28.00000000000000000, 0.000000000000000000 ) ) ;
#41858 = CARTESIAN_POINT ( 'NONE',  ( -4.556349186104045934, 11.00000000000000000, 98.21875000000000000 ) ) ;
#41861 = CARTESIAN_POINT ( 'NONE',  ( 4.721056650416000089, 297.9843750017070079, 4.721056650415999201 ) ) ;
#41860 = CARTESIAN_POINT ( 'NONE',  ( 27.99999999999996447, 202.6250000027312126, 165.9999999999998863 ) ) ;
#41859 = CARTESIAN_POINT ( 'NONE',  ( -7.778174593052020747, -7.778174593052023411, 104.6874999999999858 ) ) ;
#41862 = CARTESIAN_POINT ( 'NONE',  ( -8.660254037844387298, 132.0833333333333428, -5.000000000000004441 ) ) ;
#41863 = CARTESIAN_POINT ( 'NONE',  ( -11.00000000000000000, 0.000000000000000000, 106.1875000040967620 ) ) ;
#41864 = CARTESIAN_POINT ( 'NONE',  ( -6.735557395310442023E-16, 11.00000000000000000, 78.62499999999998579 ) ) ;
#41865 = CARTESIAN_POINT ( 'NONE',  ( -2.775557561562891351E-14, 210.0000000000000284, 142.0000000000000568 ) ) ;
#41866 = CARTESIAN_POINT ( 'NONE',  ( 24.54126587499998280, 202.2500000013656063, 171.4326545832175555 ) ) ;
#41867 = CARTESIAN_POINT ( 'NONE',  ( 7.188101187500000044, 5.343749997951610098, 0.000000000000000000 ) ) ;
#41868 = CARTESIAN_POINT ( 'NONE',  ( -8.008118988124991233, 3.317071493978878127, 0.9193652839406296629 ) ) ;
#41869 = CARTESIAN_POINT ( 'NONE',  ( 1.432654583217607858, 194.6250000013655779, 138.5412658750000787 ) ) ;
#41870 = CARTESIAN_POINT ( 'NONE',  ( 7.188101187500000933, 114.8750000020483810, -2.977408999572651371 ) ) ;
#41872 = CARTESIAN_POINT ( 'NONE',  ( -7.456155213548131933, -51.58724325107842645, -41.60228463193305970 ) ) ;
#41871 = DIRECTION ( 'NONE',  ( 1.000000000000000000, 0.000000000000000000, 0.000000000000000000 ) ) ;
#41873 = CARTESIAN_POINT ( 'NONE',  ( -5.676582343750000703, 223.3854166700806729, -9.832129032723418760 ) ) ;
#41874 = CARTESIAN_POINT ( 'NONE',  ( -8.000000000000000000, 3.750000000000000888, -9.797174393178825657E-16 ) ) ;
#41875 = CARTESIAN_POINT ( 'NONE',  ( 5.082755093536318824, 5.082755093536319713, 19.29905278187175455 ) ) ;
#41877 =( BOUNDED_CURVE ( )  B_SPLINE_CURVE ( 2, ( #44219, #48740, #67232, #71747, #14405, #43079, #54796, #14778, #9137 ),
 .UNSPECIFIED., .F., .F. ) 
 B_SPLINE_CURVE_WITH_KNOTS ( ( 3, 2, 2, 2, 3 ),
 ( 0.1911764705882353921, 0.1948529411764707009, 0.1985294117647060097, 0.2022058823529413185, 0.2058823529411765996 ),
 .UNSPECIFIED. ) 
 CURVE ( )  GEOMETRIC_REPRESENTATION_ITEM ( )  RATIONAL_B_SPLINE_CURVE ( ( 0.9999999999999976685, 0.9238795325112890700, 1.000000000000000000, 0.9238795325112867385, 1.000000000000000000, 0.9238795325112867385, 1.000000000000000000, 0.9238795325112838519, 1.000000000000002887 ) ) 
 REPRESENTATION_ITEM ( '' )  );
#41876 = LINE ( 'NONE', #3007, #44531 ) ;
#41878 = CARTESIAN_POINT ( 'NONE',  ( -3.042071309553173730, 24.32291666325268764, 11.35316468749999785 ) ) ;
#41879 = CARTESIAN_POINT ( 'NONE',  ( -31.99999999999997868, 199.3125000000000568, 171.6568542494928238 ) ) ;
#41880 = CARTESIAN_POINT ( 'NONE',  ( -11.35316468750000141, 218.8020833299193271, 3.042071309553159963 ) ) ;
#41881 = CARTESIAN_POINT ( 'NONE',  ( 8.000000000000000000, 112.2500000000000000, -9.797174393178825657E-16 ) ) ;
#41882 = CARTESIAN_POINT ( 'NONE',  ( -11.00000000000000000, 0.000000000000000000, 99.99999999999998579 ) ) ;
#41883 = VERTEX_POINT ( 'NONE', #19064 ) ;
#41884 = DIRECTION ( 'NONE',  ( -0.000000000000000000, 1.000000000000000000, -4.476705744456276341E-16 ) ) ;
#41885 = CARTESIAN_POINT ( 'NONE',  ( 2.445694354108784108, 196.5625000013656063, 144.4456943541088663 ) ) ;
#41886 = CARTESIAN_POINT ( 'NONE',  ( -2.085542519210945728E-15, 39.53124999658601268, 11.35316468750000141 ) ) ;
#41887 = CARTESIAN_POINT ( 'NONE',  ( -4.556349186104045934, 11.00000000000000000, 89.40625000409676204 ) ) ;
#41888 = CARTESIAN_POINT ( 'NONE',  ( -1.432654583217662481, 209.3750000013656063, 145.4587341250000350 ) ) ;
#41889 = CARTESIAN_POINT ( 'NONE',  ( 0.000000000000000000, 125.0000000000000000, 0.000000000000000000 ) ) ;
#41890 = CARTESIAN_POINT ( 'NONE',  ( -1.656854249492354825, 201.4375000027311842, 138.0000000000000284 ) ) ;
#41892 = CARTESIAN_POINT ( 'NONE',  ( -8.311093377946836114, 37.65624999658601979, -8.311093377946837890 ) ) ;
#41891 = CARTESIAN_POINT ( 'NONE',  ( -7.188101187499999156, 103.2500000020483810, 2.977408999572654924 ) ) ;
#41893 = CARTESIAN_POINT ( 'NONE',  ( 5.656854249492374365, 5.656854249492375253, 15.26780277982336642 ) ) ;
#41894 = CARTESIAN_POINT ( 'NONE',  ( -8.311093377946841443, 148.9062499965860127, 8.311093377946830785 ) ) ;
#41895 = VECTOR ( 'NONE', #28341, 1000.000000000000000 ) ;
#41896 = CARTESIAN_POINT ( 'NONE',  ( 2.679491924311228956, 117.9166666598387110, -10.00000000000000000 ) ) ;
#41897 = CARTESIAN_POINT ( 'NONE',  ( 5.082755093536326818, 117.5937500020483810, 5.082755093536325042 ) ) ;
#41898 = DIRECTION ( 'NONE',  ( -0.000000000000000000, -1.000000000000000000, -0.000000000000000000 ) ) ;
#41899 = CARTESIAN_POINT ( 'NONE',  ( -24.54126587500000056, 205.5000000013655779, 168.5673454167827003 ) ) ;
#41900 = VERTEX_POINT ( 'NONE', #65074 ) ;
#41901 = CARTESIAN_POINT ( 'NONE',  ( 5.676582343750001591, 1.927083329919350163, -9.832129032723420536 ) ) ;
#41902 =( BOUNDED_CURVE ( )  B_SPLINE_CURVE ( 2, ( #67303, #45037, #55993, #68046, #72960, #4307, #28422, #27297, #16336 ),
 .UNSPECIFIED., .F., .F. ) 
 B_SPLINE_CURVE_WITH_KNOTS ( ( 3, 2, 2, 2, 3 ),
 ( 0.3666666666666669738, 0.3750000000000003331, 0.3833333333333336923, 0.3916666666666669960, 0.4000000000000003553 ),
 .UNSPECIFIED. ) 
 CURVE ( )  GEOMETRIC_REPRESENTATION_ITEM ( )  RATIONAL_B_SPLINE_CURVE ( ( 0.9999999999999970024, 0.9238795325112897361, 1.000000000000000000, 0.9238795325112867385, 1.000000000000000000, 0.9238795325112867385, 1.000000000000000000, 0.9238795325112837409, 1.000000000000003109 ) ) 
 REPRESENTATION_ITEM ( '' )  );
#41903 = VERTEX_POINT ( 'NONE', #30756 ) ;
#41904 = DIRECTION ( 'NONE',  ( -0.000000000000000000, 1.000000000000000000, -0.000000000000000000 ) ) ;
#41906 = CARTESIAN_POINT ( 'NONE',  ( -5.676582343750006032, 144.1145833299193555, 9.832129032723418760 ) ) ;
#41905 = CARTESIAN_POINT ( 'NONE',  ( 1.469576158976823947E-15, 108.8750000000000000, 8.000000000000000000 ) ) ;
#41907 = CARTESIAN_POINT ( 'NONE',  ( -4.000000000000002665, 3.562500000000000000, 1.656854249492380582 ) ) ;
#41908 = CARTESIAN_POINT ( 'NONE',  ( -5.656854249492375253, 5.656854249492375253, 17.19905278432982243 ) ) ;
#41909 = CARTESIAN_POINT ( 'NONE',  ( 48.23240602106716324, 194.5818757194704745, 61.74679865267219725 ) ) ;
#41910 = CARTESIAN_POINT ( 'NONE',  ( -8.311093377946836114, 243.2812500034139589, -8.311093377946836114 ) ) ;
#41911 = CARTESIAN_POINT ( 'NONE',  ( -10.18810118749999916, 0.000000000000000000, 92.03125000204836681 ) ) ;
#41912 = ORIENTED_EDGE ( 'NONE', *, *, #72199, .T. ) ;
#41913 = EDGE_CURVE ( 'NONE', #27622, #71712, #64281, .T. ) ;
#41914 = CARTESIAN_POINT ( 'NONE',  ( 7.320508075688774596, 119.3750000000000142, 7.320508075688778149 ) ) ;
#41915 = CARTESIAN_POINT ( 'NONE',  ( -11.35316468750000141, 93.80208332991934128, 3.042071309553159963 ) ) ;
#41916 = CARTESIAN_POINT ( 'NONE',  ( 10.18810118750000093, -4.220049686691933921, 104.3125000020483810 ) ) ;
#41917 = CARTESIAN_POINT ( 'NONE',  ( -3.211159895383562723, 16.06249999863440436, 3.211159895383561391 ) ) ;
#41918 = EDGE_LOOP ( 'NONE', ( #73292, #1286, #29744, #44083, #32297, #592, #41983, #45997, #15194, #12335 ) ) ;
#41919 = ORIENTED_EDGE ( 'NONE', *, *, #4730, .T. ) ;
#41920 = CARTESIAN_POINT ( 'NONE',  ( 3.313708498984762052, 3.281250000000001332, -8.000000000000000000 ) ) ;
#41921 = CARTESIAN_POINT ( 'NONE',  ( -4.541265875000002339, 0.9374999986344068059, -5.561446717895856393E-16 ) ) ;
#41922 = CARTESIAN_POINT ( 'NONE',  ( 7.188101187499999156, 3.374999997951610098, 2.977408999572654924 ) ) ;
#41923 = CARTESIAN_POINT ( 'NONE',  ( -11.00000000000000000, 4.556349186104045934, 96.90624999999998579 ) ) ;
#41924 = EDGE_CURVE ( 'NONE', #39166, #18528, #66566, .T. ) ;
#41925 = CARTESIAN_POINT ( 'NONE',  ( 4.220049686691934809, 10.18810118749999916, 97.56250000204836681 ) ) ;
#41926 = ADVANCED_FACE ( 'NONE', ( #32256 ), #42803, .T. ) ;
#41927 = CARTESIAN_POINT ( 'NONE',  ( 4.000000000000001776, 1.000000000000000222, 0.000000000000000000 ) ) ;
#41928 = CARTESIAN_POINT ( 'NONE',  ( 2.828427124746191623, 13.87499999726881406, -2.828427124746191623 ) ) ;
#41929 = CARTESIAN_POINT ( 'NONE',  ( -5.656854249492375253, 5.656854249492375253, 12.83030278392014623 ) ) ;
#41930 = ORIENTED_EDGE ( 'NONE', *, *, #16309, .T. ) ;
#41931 = AXIS2_PLACEMENT_3D ( 'NONE', #8373, #7645, #36687 ) ;
#41932 = CARTESIAN_POINT ( 'NONE',  ( 54.00000000000000711, 272.0000000000000000, 20.00000000000001776 ) ) ;
#41933 = CARTESIAN_POINT ( 'NONE',  ( 3.458734125000015425, 200.0000000013656347, 196.5673454167823877 ) ) ;
#41935 = CARTESIAN_POINT ( 'NONE',  ( -2.679491924332892516, 23.54166666666491636, 9.999999999987878141 ) ) ;
#41934 = CARTESIAN_POINT ( 'NONE',  ( -25.55430564589111953, 201.0625000013656063, 172.4456943541091505 ) ) ;
#41936 = VECTOR ( 'NONE', #40976, 1000.000000000000000 ) ;
#41937 = CARTESIAN_POINT ( 'NONE',  ( 4.541265875000002339, 12.37499999863440969, -1.881053915767121554 ) ) ;
#41938 = CARTESIAN_POINT ( 'NONE',  ( 8.660254037844385522, 121.4583333265053824, 5.000000000000005329 ) ) ;
#41939 = CARTESIAN_POINT ( 'NONE',  ( -5.082755093536319713, 5.082755093536319713, 14.79905278187175455 ) ) ;
#41940 = ORIENTED_EDGE ( 'NONE', *, *, #23812, .F. ) ;
#41941 = ORIENTED_EDGE ( 'NONE', *, *, #26417, .F. ) ;
#41942 = CARTESIAN_POINT ( 'NONE',  ( 1.871523826299183495E-15, -10.18810118749999916, 105.5312500020483810 ) ) ;
#41943 = CARTESIAN_POINT ( 'NONE',  ( 1.836970198721029589E-15, 221.2500000000000000, 10.00000000000000178 ) ) ;
#41944 = CARTESIAN_POINT ( 'NONE',  ( -32.00000000000001421, 204.1875000000000568, 168.3431457505080004 ) ) ;
#41945 = CARTESIAN_POINT ( 'NONE',  ( -2.445694354108782775, 197.5625000013656063, 200.4456943541088663 ) ) ;
#41946 = CARTESIAN_POINT ( 'NONE',  ( -3.313708498984760276, 12.28124999590322197, -8.000000000000000000 ) ) ;
#41947 = CARTESIAN_POINT ( 'NONE',  ( -4.999999999999998224, 91.66666666666667140, -8.660254037844389075 ) ) ;
#41948 = CARTESIAN_POINT ( 'NONE',  ( 8.000000000000000000, 118.2500000000000000, -9.797174393178825657E-16 ) ) ;
#41949 = CARTESIAN_POINT ( 'NONE',  ( -2.765530957081996810, 294.4218750017069510, -6.676582343750003368 ) ) ;
#41950 = VERTEX_POINT ( 'NONE', #43552 ) ;
#41951 = CARTESIAN_POINT ( 'NONE',  ( -10.00000000000000000, 174.1666666598386826, -2.679491924311229845 ) ) ;
#41952 = CARTESIAN_POINT ( 'NONE',  ( 3.313708498984762496, 14.53124999590322375, 7.999999999999998224 ) ) ;
#41953 = CARTESIAN_POINT ( 'NONE',  ( 1.432654583217607858, 206.6250000013656063, 138.5412658750000787 ) ) ;
#41954 = CARTESIAN_POINT ( 'NONE',  ( -10.00000000000000355, 52.29166666666665719, -2.679491924311230733 ) ) ;
#41955 = CARTESIAN_POINT ( 'NONE',  ( -4.898587196589412829E-16, 114.3125000040967905, -8.000000000000000000 ) ) ;
#41956 = CARTESIAN_POINT ( 'NONE',  ( -3.042071309553166181, 263.1770833367473301, -11.35316468749999608 ) ) ;
#41957 = CARTESIAN_POINT ( 'NONE',  ( -2.849036369511732440E-14, 207.2500000000000284, 138.0000000000000568 ) ) ;
#41958 = CARTESIAN_POINT ( 'NONE',  ( -6.735557395310442023E-16, 11.00000000000000000, 113.1249999999999858 ) ) ;
#41959 = CARTESIAN_POINT ( 'NONE',  ( 7.320508075688774596, 210.6249999999999716, -7.320508075688774596 ) ) ;
#41960 = CARTESIAN_POINT ( 'NONE',  ( 2.977408999572646486, 7.188101187499992051, 8.892802781871754547 ) ) ;
#41961 = CARTESIAN_POINT ( 'NONE',  ( -8.311093377946836114, 177.9687499965860127, -8.311093377946837890 ) ) ;
#41962 = CARTESIAN_POINT ( 'NONE',  ( 6.123233995736767268E-16, 193.1249999931720254, -10.00000000000000178 ) ) ;
#41963 = CARTESIAN_POINT ( 'NONE',  ( -1.881053915767121554, 0.6249999986344065839, -4.541265875000002339 ) ) ;
#41964 = CARTESIAN_POINT ( 'NONE',  ( 27.99999999999999645, 210.0000000000000284, 173.9999999999998863 ) ) ;
#41965 = CARTESIAN_POINT ( 'NONE',  ( 5.656854249492374365, 5.656854249492375253, 3.455302783920144449 ) ) ;
#41966 = ORIENTED_EDGE ( 'NONE', *, *, #57811, .F. ) ;
#41967 = CARTESIAN_POINT ( 'NONE',  ( 3.458734124999959025, 194.5000000013656063, 140.5673454167824161 ) ) ;
#41968 = CARTESIAN_POINT ( 'NONE',  ( -3.042071309553164404, 52.55208332991934839, -11.35316468749999963 ) ) ;
#41969 = CARTESIAN_POINT ( 'NONE',  ( 7.778174593052023411, -7.778174593052021635, 103.7500000040967763 ) ) ;
#41970 = CARTESIAN_POINT ( 'NONE',  ( 3.042071309553159519, 220.0520833299193271, 11.35316468750000141 ) ) ;
#41971 = CARTESIAN_POINT ( 'NONE',  ( -31.45873412500002786, 206.6250000013656063, 168.5673454167828140 ) ) ;
#41972 = CARTESIAN_POINT ( 'NONE',  ( 7.320508075688775484, 10.62500000000000178, -7.320508075688775484 ) ) ;
#41973 = CARTESIAN_POINT ( 'NONE',  ( -5.082755093536325930, 120.9687500020483952, -5.082755093536325930 ) ) ;
#41974 = CARTESIAN_POINT ( 'NONE',  ( -2.754378923186476579E-14, 195.1875000013655779, 145.4587341250000350 ) ) ;
#41975 = VECTOR ( 'NONE', #30938, 1000.000000000000114 ) ;
#41976 = EDGE_CURVE ( 'NONE', #26852, #4267, #31502, .T. ) ;
#41977 = CARTESIAN_POINT ( 'NONE',  ( 10.00000000000000178, 77.08333332650536818, -2.679491924311226736 ) ) ;
#41978 = CARTESIAN_POINT ( 'NONE',  ( 7.188101187500001821, 95.00000000204836681, -2.977408999572651371 ) ) ;
#41979 = CARTESIAN_POINT ( 'NONE',  ( -4.541265875000002339, 14.93749999863440792, -5.561446717895856393E-16 ) ) ;
#41980 = DIRECTION ( 'NONE',  ( -0.000000000000000000, 1.000000000000000000, 0.000000000000000000 ) ) ;
#41981 = FACE_OUTER_BOUND ( 'NONE', #24597, .T. ) ;
#41982 = CARTESIAN_POINT ( 'NONE',  ( 1.469576158976822172E-15, -7.999999999999991118, 23.70530277982336642 ) ) ;
#41983 = ORIENTED_EDGE ( 'NONE', *, *, #26877, .T. ) ;
#41984 = ORIENTED_EDGE ( 'NONE', *, *, #72397, .F. ) ;
#41985 = CARTESIAN_POINT ( 'NONE',  ( 4.721056650416000089, 291.9843750017070079, 4.721056650415999201 ) ) ;
#41986 = CARTESIAN_POINT ( 'NONE',  ( 0.000000000000000000, 125.0000000000000000, 0.000000000000000000 ) ) ;
#41987 = CARTESIAN_POINT ( 'NONE',  ( 9.832129032723416984, 160.3645833299193839, 5.676582343750006032 ) ) ;
#41988 = CARTESIAN_POINT ( 'NONE',  ( 10.00000000000000178, 4.791666666666666963, 2.679491924311235618 ) ) ;
#41989 = VECTOR ( 'NONE', #1079, 1000.000000000000000 ) ;
#41990 = CARTESIAN_POINT ( 'NONE',  ( 4.000000000000015099, 199.5625000000000568, 196.3431457505076594 ) ) ;
#41991 = CARTESIAN_POINT ( 'NONE',  ( -27.99999999999995737, 201.5000000000000000, 174.0000000000003695 ) ) ;
#41992 = CARTESIAN_POINT ( 'NONE',  ( -6.238412754330611322E-16, 10.18810118749999916, 111.1562500020483668 ) ) ;
#41993 = VERTEX_POINT ( 'NONE', #3206 ) ;
#41994 =( BOUNDED_CURVE ( )  B_SPLINE_CURVE ( 2, ( #70537, #48621, #71628, #14282, #18852, #12810, #41859, #64870, #61072 ),
 .UNSPECIFIED., .F., .F. ) 
 B_SPLINE_CURVE_WITH_KNOTS ( ( 3, 2, 2, 2, 3 ),
 ( 0.2499999999999998890, 0.2536764705882351700, 0.2573529411764704511, 0.2610294117647057877, 0.2647058823529410687 ),
 .UNSPECIFIED. ) 
 CURVE ( )  GEOMETRIC_REPRESENTATION_ITEM ( )  RATIONAL_B_SPLINE_CURVE ( ( 1.000000000000002220, 0.9238795325112844070, 1.000000000000000000, 0.9238795325112867385, 1.000000000000000000, 0.9238795325112867385, 1.000000000000000000, 0.9238795325112890700, 0.9999999999999976685 ) ) 
 REPRESENTATION_ITEM ( '' )  );
#41995 = VECTOR ( 'NONE', #7182, 1000.000000000000000 ) ;
#41996 = CYLINDRICAL_SURFACE ( 'NONE', #1099, 8.000000000000000000 ) ;
#41997 = CARTESIAN_POINT ( 'NONE',  ( 4.556349186104052151, -10.99999999999999822, 109.6562500040967905 ) ) ;
#41998 = CARTESIAN_POINT ( 'NONE',  ( -3.042071309553163960, 147.5520833299193271, -11.35316468749999963 ) ) ;
#41999 = CARTESIAN_POINT ( 'NONE',  ( 3.458734125000016313, 198.8750000013656063, 199.4326545832176976 ) ) ;
#42000 = CARTESIAN_POINT ( 'NONE',  ( 1.432654583217662481, 208.3750000013656063, 194.5412658750000219 ) ) ;
#42001 = CARTESIAN_POINT ( 'NONE',  ( -10.18810118749999916, 4.220049686691934809, 73.93750000204838102 ) ) ;
#42002 = CARTESIAN_POINT ( 'NONE',  ( 5.676582343749993598, 55.26041666325268409, 9.832129032723422313 ) ) ;
#42003 = ORIENTED_EDGE ( 'NONE', *, *, #19546, .F. ) ;
#42004 = CARTESIAN_POINT ( 'NONE',  ( 7.999999999999992895, -3.313708498984756279, 13.48655277982336465 ) ) ;
#42005 = CARTESIAN_POINT ( 'NONE',  ( 3.211159895383560947, 4.312499998634407028, 3.211159895383562723 ) ) ;
#42006 = CARTESIAN_POINT ( 'NONE',  ( -3.317071493978878571, 8.008118988124991233, 6.731865283940627442 ) ) ;
#42007 = EDGE_CURVE ( 'NONE', #24549, #68202, #72223, .T. ) ;
#42008 = CARTESIAN_POINT ( 'NONE',  ( 7.188101187500000044, 15.46874999795161187, 0.000000000000000000 ) ) ;
#42009 = CARTESIAN_POINT ( 'NONE',  ( -4.242640687119286547, 291.9375000034140157, -4.242640687119286547 ) ) ;
#42010 = CARTESIAN_POINT ( 'NONE',  ( 2.712922267096159246, 124.5269308481492487, -7.505356363335171643 ) ) ;
#42011 = CARTESIAN_POINT ( 'NONE',  ( 5.082755093536324154, 11.15624999795161187, 5.082755093536326818 ) ) ;
#42012 = CARTESIAN_POINT ( 'NONE',  ( -5.082755093536319713, 5.082755093536319713, 7.299052781871751883 ) ) ;
#42013 =( BOUNDED_CURVE ( )  B_SPLINE_CURVE ( 2, ( #17174, #39452, #62451, #5133, #51139, #28501, #63197, #34182, #45473 ),
 .UNSPECIFIED., .F., .F. ) 
 B_SPLINE_CURVE_WITH_KNOTS ( ( 3, 2, 2, 2, 3 ),
 ( 0.5333333333333337700, 0.5416666666666670737, 0.5500000000000004885, 0.5583333333333337922, 0.5666666666666670960 ),
 .UNSPECIFIED. ) 
 CURVE ( )  GEOMETRIC_REPRESENTATION_ITEM ( )  RATIONAL_B_SPLINE_CURVE ( ( 0.9999999999999958922, 0.9238795325112908463, 1.000000000000000000, 0.9238795325112867385, 1.000000000000000000, 0.9238795325112867385, 1.000000000000000000, 0.9238795325112826307, 1.000000000000003997 ) ) 
 REPRESENTATION_ITEM ( '' )  );
#42014 = CARTESIAN_POINT ( 'NONE',  ( 7.204075437095966983, 7.204075437095967871, 115.4687500020483810 ) ) ;
#42015 = CARTESIAN_POINT ( 'NONE',  ( 9.797174393178825657E-16, -2.500000000000000444, -8.000000000000000000 ) ) ;
#42016 = CARTESIAN_POINT ( 'NONE',  ( -7.347880794884122694E-16, 1.499999997268813168, 4.000000000000001776 ) ) ;
#42017 = VERTEX_POINT ( 'NONE', #37914 ) ;
#42018 = CARTESIAN_POINT ( 'NONE',  ( -3.458734124999959914, 209.3750000013656063, 196.5673454167823877 ) ) ;
#42019 = EDGE_CURVE ( 'NONE', #32880, #17794, #26950, .T. ) ;
#42020 = CARTESIAN_POINT ( 'NONE',  ( -4.000000000000015099, 203.5625000000000000, 143.6568542494924543 ) ) ;
#42021 = CARTESIAN_POINT ( 'NONE',  ( -31.99999999999999289, 196.3750000027311842, 170.0000000000004547 ) ) ;
#42022 = CARTESIAN_POINT ( 'NONE',  ( -1.881053915767124440, 0.9999999986344065839, 4.541265875000001451 ) ) ;
#42024 = CARTESIAN_POINT ( 'NONE',  ( 2.977408999572654480, 118.6250000020483810, 7.188101187499999156 ) ) ;
#42023 = CIRCLE ( 'NONE', #15535, 30.99999999999997158 ) ;
#42025 = LINE ( 'NONE', #18658, #24754 ) ;
#42026 = CARTESIAN_POINT ( 'NONE',  ( 7.999999999999991118, 9.797174393178815797E-16, 4.767802783920145338 ) ) ;
#42027 = ORIENTED_EDGE ( 'NONE', *, *, #61369, .F. ) ;
#42028 = CARTESIAN_POINT ( 'NONE',  ( 2.977408999572650927, 23.24999999795161543, -7.188101187500000933 ) ) ;
#42029 = VERTEX_POINT ( 'NONE', #2828 ) ;
#42030 = DIRECTION ( 'NONE',  ( 0.000000000000000000, 0.000000000000000000, 1.000000000000000000 ) ) ;
#42031 = CARTESIAN_POINT ( 'NONE',  ( -3.458734124999959914, 209.4375000013656063, 198.0000000000000284 ) ) ;
#42032 = CARTESIAN_POINT ( 'NONE',  ( 31.45873412499999944, 201.6875000013656063, 169.9999999999998863 ) ) ;
#42033 = CARTESIAN_POINT ( 'NONE',  ( -8.660254037844390851, 52.91666666666666430, 4.999999999999998224 ) ) ;
#42034 = CIRCLE ( 'NONE', #34862, 5.000000000000000888 ) ;
#42035 = CARTESIAN_POINT ( 'NONE',  ( -2.977408999572650927, 103.2500000020483810, -7.188101187500001821 ) ) ;
#42036 = CARTESIAN_POINT ( 'NONE',  ( 4.242640687119285658, 295.6249999999999432, -4.242640687119286547 ) ) ;
#42038 = CARTESIAN_POINT ( 'NONE',  ( -23.12837847082111509, -39.68748998523349059, 190.6433630951527221 ) ) ;
#42037 = CARTESIAN_POINT ( 'NONE',  ( -8.660254037844390851, 34.79166665983870388, 4.999999999999998224 ) ) ;
#42039 = VERTEX_POINT ( 'NONE', #55274 ) ;
#42040 = CARTESIAN_POINT ( 'NONE',  ( -5.676582343750000703, 238.0729166700806445, -9.832129032723418760 ) ) ;
#42041 = CARTESIAN_POINT ( 'NONE',  ( 5.082755093536318824, 5.082755093536319713, 11.79905278187175632 ) ) ;
#42042 = LINE ( 'NONE', #63960, #49018 ) ;
#42043 = CARTESIAN_POINT ( 'NONE',  ( 11.00000000000000000, 1.347111479062088405E-15, 94.74999999999998579 ) ) ;
#42044 = CARTESIAN_POINT ( 'NONE',  ( 25.23489602139266808, 194.8431269806823707, 167.3241800383374880 ) ) ;
#42045 = CARTESIAN_POINT ( 'NONE',  ( 7.778174593052021635, 7.778174593052023411, 116.1250000040967905 ) ) ;
#42046 = CARTESIAN_POINT ( 'NONE',  ( 6.123233995736767268E-16, 181.2500000000000284, -10.00000000000000178 ) ) ;
#42047 = CARTESIAN_POINT ( 'NONE',  ( 25.55430564589119768, 209.0625000013656063, 167.5543056458910485 ) ) ;
#42048 = CARTESIAN_POINT ( 'NONE',  ( -2.977408999572647819, -7.188101187499990274, 27.64280278187175455 ) ) ;
#42049 = CARTESIAN_POINT ( 'NONE',  ( 5.676582343749993598, 140.2604166632526983, 9.832129032723422313 ) ) ;
#42050 = CARTESIAN_POINT ( 'NONE',  ( -6.735557395310442023E-16, 11.00000000000000000, 75.81250000409677625 ) ) ;
#42051 = CARTESIAN_POINT ( 'NONE',  ( 3.313708498984711426, 97.15625000409679046, 8.000000000000053291 ) ) ;
#42054 = CARTESIAN_POINT ( 'NONE',  ( 18.00000000000000355, 7.009507535100778952, -0.7186345456308858015 ) ) ;
#42053 = CARTESIAN_POINT ( 'NONE',  ( 8.000000000000000000, 110.7500000000000000, -9.797174393178825657E-16 ) ) ;
#42052 = CARTESIAN_POINT ( 'NONE',  ( 23.99999999999997868, 204.8124999999999716, 171.6568542494922553 ) ) ;
#42055 = ORIENTED_EDGE ( 'NONE', *, *, #43009, .T. ) ;
#42056 = CARTESIAN_POINT ( 'NONE',  ( -9.832129032723418760, 8.177083329919350163, -5.676582343750004256 ) ) ;
#42057 = DIRECTION ( 'NONE',  ( 1.000000000000000000, -0.000000000000000000, -0.000000000000000000 ) ) ;
#42058 = CARTESIAN_POINT ( 'NONE',  ( 4.556349186104045934, 11.00000000000000000, 68.21875000409676204 ) ) ;
#42059 = CARTESIAN_POINT ( 'NONE',  ( -2.445694354108839619, 207.8125000013656063, 139.5543056458912190 ) ) ;
#42060 = CARTESIAN_POINT ( 'NONE',  ( -8.000000000000000000, 5.062499995903221084, -9.797174393178825657E-16 ) ) ;
#42061 = CARTESIAN_POINT ( 'NONE',  ( -10.00000000000000000, 29.16666665983869677, -2.679491924311229845 ) ) ;
#42062 = CARTESIAN_POINT ( 'NONE',  ( 5.082755093536325042, 116.0937500020483810, -5.082755093536325930 ) ) ;
#42063 = CARTESIAN_POINT ( 'NONE',  ( 3.211159895383560947, 4.312499998634407028, 3.211159895383562723 ) ) ;
#42064 = FACE_OUTER_BOUND ( 'NONE', #73873, .T. ) ;
#42065 = CARTESIAN_POINT ( 'NONE',  ( -3.313708498984758943, -7.999999999999989342, 16.11155277982336642 ) ) ;
#42067 = CARTESIAN_POINT ( 'NONE',  ( 5.000000000000001776, 7.708333326505366401, -8.660254037844389075 ) ) ;
#42066 = CARTESIAN_POINT ( 'NONE',  ( -2.679491924311165008, 239.1666666734946602, 10.00000000000003553 ) ) ;
#42068 = EDGE_LOOP ( 'NONE', ( #48218, #73131, #25542, #72490, #36200 ) ) ;
#42069 = CARTESIAN_POINT ( 'NONE',  ( 2.485281374238225816, 292.7500000034140157, -6.000000000000346390 ) ) ;
#42070 = CARTESIAN_POINT ( 'NONE',  ( 3.729367062499960195, 209.8437500006828031, 142.0000000000000568 ) ) ;
#42071 = CARTESIAN_POINT ( 'NONE',  ( 3.042071309553173286, 225.6770833367473017, 11.35316468749999608 ) ) ;
#42072 = CARTESIAN_POINT ( 'NONE',  ( -5.676582343750006032, 114.1145833299193555, 9.832129032723418760 ) ) ;
#42073 = VERTEX_POINT ( 'NONE', #9617 ) ;
#42074 = EDGE_CURVE ( 'NONE', #42638, #13563, #58508, .T. ) ;
#42075 = CYLINDRICAL_SURFACE ( 'NONE', #57255, 11.00000000000000000 ) ;
#42076 = CARTESIAN_POINT ( 'NONE',  ( -10.18810118749999916, 0.000000000000000000, 97.65625000204838102 ) ) ;
#42077 = CARTESIAN_POINT ( 'NONE',  ( -4.898587196589412829E-16, 109.6250000000000000, -8.000000000000000000 ) ) ;
#42078 = CARTESIAN_POINT ( 'NONE',  ( 2.754378923186476579E-14, 196.4375000013655779, 194.5412658750000219 ) ) ;
#42079 = CARTESIAN_POINT ( 'NONE',  ( -11.00000000000000533, 11.00000000000000000, 41.99999999999999289 ) ) ;
#42081 = CARTESIAN_POINT ( 'NONE',  ( 6.951808397369818766E-16, 117.0312499965860269, -11.35316468750000141 ) ) ;
#42080 = CARTESIAN_POINT ( 'NONE',  ( 3.090148520752590944, 225.9998984954551418, -9.510618362637927703 ) ) ;
#42082 = CARTESIAN_POINT ( 'NONE',  ( -28.00000000000003197, 207.0000000000000284, 166.0000000000003695 ) ) ;
#42083 = ORIENTED_EDGE ( 'NONE', *, *, #46456, .F. ) ;
#42084 = CARTESIAN_POINT ( 'NONE',  ( -8.660254037844387298, 203.9583333265053682, -5.000000000000004441 ) ) ;
#42085 = CARTESIAN_POINT ( 'NONE',  ( 3.313708498984761608, 22.78125000000000355, -8.000000000000000000 ) ) ;
#42086 = CARTESIAN_POINT ( 'NONE',  ( -4.000000000000001776, 9.500000000000000000, -4.898587196589415787E-16 ) ) ;
#42087 = CARTESIAN_POINT ( 'NONE',  ( -2.085542519210945728E-15, 99.84374999658601268, 11.35316468750000141 ) ) ;
#42088 = DIRECTION ( 'NONE',  ( 0.000000000000000000, -0.000000000000000000, -1.000000000000000000 ) ) ;
#42089 = CARTESIAN_POINT ( 'NONE',  ( 4.401442555609581635E-16, 10.21874999795161187, -7.188101187500000044 ) ) ;
#42090 = CARTESIAN_POINT ( 'NONE',  ( 10.18810118750000093, -4.220049686691933033, 91.18750000204836681 ) ) ;
#42091 = CARTESIAN_POINT ( 'NONE',  ( 5.676582343749993598, 10.26041666325268409, 9.832129032723422313 ) ) ;
#42092 = ORIENTED_EDGE ( 'NONE', *, *, #13521, .T. ) ;
#42093 = DIRECTION ( 'NONE',  ( -0.000000000000000000, 1.000000000000000000, -0.000000000000000000 ) ) ;
#42094 = CARTESIAN_POINT ( 'NONE',  ( 3.313708498984815343, 99.21875000409676204, -7.999999999999944933 ) ) ;
#42095 = CARTESIAN_POINT ( 'NONE',  ( -7.778174593052020747, -7.778174593052023411, 101.8750000040967763 ) ) ;
#42096 = CARTESIAN_POINT ( 'NONE',  ( 7.204075437095966983, 7.204075437095967871, 74.96875000204836681 ) ) ;
#42097 = ADVANCED_FACE ( 'NONE', ( #54895 ), #71845, .T. ) ;
#42098 = CARTESIAN_POINT ( 'NONE',  ( 27.99999999999996803, 209.8437500006828031, 173.7293670624999038 ) ) ;
#42099 = DIRECTION ( 'NONE',  ( 0.000000000000000000, 0.000000000000000000, -1.000000000000000000 ) ) ;
#42100 = CARTESIAN_POINT ( 'NONE',  ( -4.721056650415999201, 292.3281250017069510, -4.721056650415999201 ) ) ;
#42101 = CARTESIAN_POINT ( 'NONE',  ( 2.679491924311222739, 125.8333333265053682, 10.00000000000000355 ) ) ;
#42102 = CARTESIAN_POINT ( 'NONE',  ( -3.042071309553163960, 222.5520833299193271, -11.35316468749999963 ) ) ;
#42103 = ADVANCED_FACE ( 'NONE', ( #37538 ), #3961, .F. ) ;
#42104 = CARTESIAN_POINT ( 'NONE',  ( 7.204075437095968759, -7.204075437095966983, 89.21875000204838102 ) ) ;
#42105 =( BOUNDED_CURVE ( )  B_SPLINE_CURVE ( 2, ( #52083, #36858, #65142, #415, #42867, #46036, #19861, #17732, #7815 ),
 .UNSPECIFIED., .F., .F. ) 
 B_SPLINE_CURVE_WITH_KNOTS ( ( 3, 2, 2, 2, 3 ),
 ( 0.3750000000000000000, 0.3806818181818181768, 0.3863636363636363535, 0.3920454545454545858, 0.3977272727272727626 ),
 .UNSPECIFIED. ) 
 CURVE ( )  GEOMETRIC_REPRESENTATION_ITEM ( )  RATIONAL_B_SPLINE_CURVE ( ( 1.000000000000000000, 0.9238795325112867385, 1.000000000000000000, 0.9238795325112867385, 1.000000000000000000, 0.9238795325112867385, 1.000000000000000000, 0.9238795325112859613, 1.000000000000000666 ) ) 
 REPRESENTATION_ITEM ( '' )  );
#42106 = CARTESIAN_POINT ( 'NONE',  ( -30.44569435410883429, 203.5625000013656063, 167.5543056458915885 ) ) ;
#42107 = CARTESIAN_POINT ( 'NONE',  ( 3.313708498984762052, 24.28125000000000711, -8.000000000000000000 ) ) ;
#42108 = CARTESIAN_POINT ( 'NONE',  ( -1.881053915767121554, 12.74999999863440969, -4.541265875000002339 ) ) ;
#42109 = ORIENTED_EDGE ( 'NONE', *, *, #54172, .T. ) ;
#42110 = CARTESIAN_POINT ( 'NONE',  ( -25.17157287525386167, 209.0000000027312126, 167.1715728752541281 ) ) ;
#42111 = CARTESIAN_POINT ( 'NONE',  ( -1.656854249492347719, 206.9375000027312410, 194.0000000000000853 ) ) ;
#42112 = EDGE_CURVE ( 'NONE', #6721, #19857, #22653, .T. ) ;
#42113 = CARTESIAN_POINT ( 'NONE',  ( -3.458734125000016757, 200.1250000013656063, 140.5673454167824161 ) ) ;
#42114 = CARTESIAN_POINT ( 'NONE',  ( -4.000000000000015099, 205.6875000027312126, 143.6568542494924543 ) ) ;
#42115 = CARTESIAN_POINT ( 'NONE',  ( -5.000000000000000000, 12.24744670179871164, 68.85644987591972210 ) ) ;
#42116 = CARTESIAN_POINT ( 'NONE',  ( 4.220049686691941027, -10.18810118749999738, 70.00000000204836681 ) ) ;
#42117 = ORIENTED_EDGE ( 'NONE', *, *, #7954, .F. ) ;
#42118 = CARTESIAN_POINT ( 'NONE',  ( -2.977408999572654480, 2.999999997951610542, 7.188101187499999156 ) ) ;
#42119 = CARTESIAN_POINT ( 'NONE',  ( 4.000000000000000888, 19.93750000000000000, 1.656854249492384135 ) ) ;
#42120 = CARTESIAN_POINT ( 'NONE',  ( 1.320432766682874540E-15, 117.4062500020483810, 7.188101187500000044 ) ) ;
#42121 = CARTESIAN_POINT ( 'NONE',  ( 8.618100331995490748, -15.80894714424577607, -2.004418766382574114E-14 ) ) ;
#42122 = CARTESIAN_POINT ( 'NONE',  ( 2.765530957081996366, 293.1406250017069510, -6.676582343750002480 ) ) ;
#42124 = FACE_OUTER_BOUND ( 'NONE', #68126, .T. ) ;
#42123 = CARTESIAN_POINT ( 'NONE',  ( 11.35316468749999963, 226.1979166700806445, 3.042071309553159519 ) ) ;
#42125 = VERTEX_POINT ( 'NONE', #46883 ) ;
#42127 = CARTESIAN_POINT ( 'NONE',  ( 11.35316468749999608, 221.9270833367473017, -3.042071309553167069 ) ) ;
#42126 = AXIS2_PLACEMENT_3D ( 'NONE', #29167, #28043, #46878 ) ;
#42128 = EDGE_CURVE ( 'NONE', #68303, #37361, #13272, .T. ) ;
#42129 = CARTESIAN_POINT ( 'NONE',  ( -7.188101187499992051, 0.000000000000000000, 28.86155278187175810 ) ) ;
#42130 = CARTESIAN_POINT ( 'NONE',  ( 5.656854249492380582, 3.187500000000000444, -5.656854249492380582 ) ) ;
#42131 = CARTESIAN_POINT ( 'NONE',  ( 2.445694354108839175, 205.3125000013656063, 195.5543056458912190 ) ) ;
#42132 = ORIENTED_EDGE ( 'NONE', *, *, #11950, .T. ) ;
#42133 = CARTESIAN_POINT ( 'NONE',  ( 3.313708498984802020, 24.28125000000000000, -7.999999999999958256 ) ) ;
#42134 = CARTESIAN_POINT ( 'NONE',  ( 11.35316468750000141, 96.09374999658601268, 0.000000000000000000 ) ) ;
#42135 = CARTESIAN_POINT ( 'NONE',  ( -4.556349186104047710, -10.99999999999999822, 74.78125000000001421 ) ) ;
#42138 = CARTESIAN_POINT ( 'NONE',  ( -29.65685424949236548, 205.0625000000000284, 166.0000000000003695 ) ) ;
#42137 = CARTESIAN_POINT ( 'NONE',  ( 24.54126587500000056, 204.2500000013655779, 171.4326545832175839 ) ) ;
#42136 = CARTESIAN_POINT ( 'NONE',  ( 29.43265458321761230, 203.7500000013656063, 173.4587341249998929 ) ) ;
#42139 = VERTEX_POINT ( 'NONE', #35942 ) ;
#42140 = CARTESIAN_POINT ( 'NONE',  ( 1.347111479062088405E-15, 54.99999999999999289, -11.00000000000000000 ) ) ;
#42141 = LINE ( 'NONE', #66646, #22441 ) ;
#42142 = CARTESIAN_POINT ( 'NONE',  ( 11.35316468749999963, 210.9895833299193839, -3.042071309553165293 ) ) ;
#42143 = CARTESIAN_POINT ( 'NONE',  ( -2.445694354108838731, 201.0625000013656063, 144.4456943541088663 ) ) ;
#42144 = CARTESIAN_POINT ( 'NONE',  ( 29.43265458321761230, 200.7500000013656347, 173.4587341249998929 ) ) ;
#42145 = LINE ( 'NONE', #36874, #44884 ) ;
#42146 = CARTESIAN_POINT ( 'NONE',  ( 8.311093377946834337, 200.4687499965860411, 8.311093377946839666 ) ) ;
#42147 = CARTESIAN_POINT ( 'NONE',  ( -2.977408999572650927, 94.25000000204838102, -7.188101187500000933 ) ) ;
#42148 = LINE ( 'NONE', #13472, #8274 ) ;
#42149 = CARTESIAN_POINT ( 'NONE',  ( -23.99999999999997158, 196.6875000000000000, 171.6568542494927385 ) ) ;
#42150 = CARTESIAN_POINT ( 'NONE',  ( -8.342170076843785083E-16, 13.06249999863440792, 4.541265875000002339 ) ) ;
#42151 = CARTESIAN_POINT ( 'NONE',  ( 25.55430564589114795, 197.5625000013656063, 172.4456943541086957 ) ) ;
#42152 = CARTESIAN_POINT ( 'NONE',  ( 1.320432766682872962E-15, -7.188101187499992051, 2.236552781871754103 ) ) ;
#42153 = CARTESIAN_POINT ( 'NONE',  ( -3.042071309553173730, 79.32291666325271251, 11.35316468749999785 ) ) ;
#42154 = CARTESIAN_POINT ( 'NONE',  ( -30.82842712474620939, 195.1250000000000284, 167.1715728752542134 ) ) ;
#42155 = DIRECTION ( 'NONE',  ( 0.000000000000000000, 0.000000000000000000, 1.000000000000000000 ) ) ;
#42156 = VERTEX_POINT ( 'NONE', #1621 ) ;
#42157 = DIRECTION ( 'NONE',  ( 0.000000000000000000, -1.000000000000000000, -4.476705744456276341E-16 ) ) ;
#42158 = CARTESIAN_POINT ( 'NONE',  ( 5.000000000000004441, 231.6666666666666856, 8.660254037844385522 ) ) ;
#42159 = CARTESIAN_POINT ( 'NONE',  ( 11.35316468749999785, 75.57291666325269830, 3.042071309553174174 ) ) ;
#42160 = ORIENTED_EDGE ( 'NONE', *, *, #1678, .T. ) ;
#42161 = CARTESIAN_POINT ( 'NONE',  ( -6.238412754330611322E-16, 10.18810118749999916, 84.15625000204838102 ) ) ;
#42162 = CARTESIAN_POINT ( 'NONE',  ( -10.99999999999999822, -4.556349186104052151, 70.28125000409677625 ) ) ;
#42163 = CARTESIAN_POINT ( 'NONE',  ( -1.432654583217608080, 207.8750000013656063, 201.4587341250000350 ) ) ;
#42164 = CARTESIAN_POINT ( 'NONE',  ( -0.8721677472748838866, 16.44158143986581777, 68.58266913489940464 ) ) ;
#42166 = CARTESIAN_POINT ( 'NONE',  ( -11.35316468750000141, 68.48958332991935549, 3.042071309553159963 ) ) ;
#42165 = CARTESIAN_POINT ( 'NONE',  ( -4.401442555609581635E-16, 89.28125000204838102, -7.188101187500000044 ) ) ;
#42167 = CARTESIAN_POINT ( 'NONE',  ( -7.999999999999991118, 3.313708498984756723, 27.92405278392015333 ) ) ;
#42168 = CARTESIAN_POINT ( 'NONE',  ( -1.836970198721029983E-15, 25.62499999317203248, 10.00000000000000178 ) ) ;
#42169 = CARTESIAN_POINT ( 'NONE',  ( -7.320508075688778149, 169.9999999931720254, 7.320508075688769267 ) ) ;
#42170 = CARTESIAN_POINT ( 'NONE',  ( -2.849036369511732440E-14, 200.3750000027312126, 138.0000000000000568 ) ) ;
#42171 = CARTESIAN_POINT ( 'NONE',  ( -25.67311473297852586, 194.8285023284833528, 173.0462180535952825 ) ) ;
#42172 = CARTESIAN_POINT ( 'NONE',  ( 3.042071309553159519, 60.05208332991934128, 11.35316468750000141 ) ) ;
#42173 = EDGE_CURVE ( 'NONE', #26371, #64551, #19310, .T. ) ;
#42174 = CARTESIAN_POINT ( 'NONE',  ( 1.871523826299183495E-15, -10.18810118749999916, 105.9062500020483810 ) ) ;
#42175 = CARTESIAN_POINT ( 'NONE',  ( 11.35316468749999785, 200.5729166632526983, 3.042071309553174174 ) ) ;
#42176 = VERTEX_POINT ( 'NONE', #2715 ) ;
#42177 = CARTESIAN_POINT ( 'NONE',  ( 2.775557561562891351E-14, 210.0000000000000284, 202.0000000000000000 ) ) ;
#42178 = DIRECTION ( 'NONE',  ( -1.000000000000000000, 0.000000000000000000, 0.000000000000000000 ) ) ;
#42179 = CARTESIAN_POINT ( 'NONE',  ( -1.836970198721029983E-15, 60.62499999317203958, 10.00000000000000178 ) ) ;
#42181 = CARTESIAN_POINT ( 'NONE',  ( -9.832129032723420536, 193.6979166632526983, 5.676582343749997150 ) ) ;
#42180 = FACE_BOUND ( 'NONE', #51368, .T. ) ;
#42182 = CARTESIAN_POINT ( 'NONE',  ( 7.999999999999304556, -3.314968910423997278E-06, 15.26780269013280034 ) ) ;
#42183 = CARTESIAN_POINT ( 'NONE',  ( 8.660254037844385522, 236.0416666734946318, -5.000000000000003553 ) ) ;
#42184 = CARTESIAN_POINT ( 'NONE',  ( 7.999999999999991118, 9.797174393178815797E-16, 12.26780278392014623 ) ) ;
#42185 = ORIENTED_EDGE ( 'NONE', *, *, #42577, .F. ) ;
#42186 = CARTESIAN_POINT ( 'NONE',  ( -5.676582343750006032, 179.4270833299193555, 9.832129032723418760 ) ) ;
#42187 = EDGE_CURVE ( 'NONE', #70240, #3720, #2148, .T. ) ;
#42188 = AXIS2_PLACEMENT_3D ( 'NONE', #44935, #61906, #67574 ) ;
#42189 = CARTESIAN_POINT ( 'NONE',  ( 1.320432766682872962E-15, -7.188101187499992051, 22.86155278187175455 ) ) ;
#42190 = CARTESIAN_POINT ( 'NONE',  ( 3.313708498984762496, 17.71875000000000355, 7.999999999999998224 ) ) ;
#42191 = ORIENTED_EDGE ( 'NONE', *, *, #23025, .F. ) ;
#42192 = AXIS2_PLACEMENT_3D ( 'NONE', #68719, #58172, #73639 ) ;
#42193 = CARTESIAN_POINT ( 'NONE',  ( -7.999999999999998224, 96.78125000409679046, 3.313708498984766493 ) ) ;
#42194 = CARTESIAN_POINT ( 'NONE',  ( 8.660254037844389075, 0.4166666666666666852, -5.000000000000000000 ) ) ;
#42195 = EDGE_CURVE ( 'NONE', #24126, #8242, #69906, .T. ) ;
#42196 = EDGE_CURVE ( 'NONE', #60229, #38928, #13641, .T. ) ;
#42197 = CARTESIAN_POINT ( 'NONE',  ( -2.828427124746192067, 13.62500000000000000, 2.828427124746190735 ) ) ;
#42198 = CARTESIAN_POINT ( 'NONE',  ( -4.541265875000002339, 15.74999999863440436, -1.881053915767121998 ) ) ;
#42199 = CARTESIAN_POINT ( 'NONE',  ( 7.999999999999992895, -3.313708498984756279, 16.67405278392014623 ) ) ;
#42200 = CARTESIAN_POINT ( 'NONE',  ( 3.153939666463620179E-13, 188.7500000000000284, 9.999999999999998224 ) ) ;
#42201 = ORIENTED_EDGE ( 'NONE', *, *, #28984, .F. ) ;
#42202 = DIRECTION ( 'NONE',  ( 1.000000000000000000, 0.000000000000000000, 0.000000000000000000 ) ) ;
#42203 = CARTESIAN_POINT ( 'NONE',  ( 1.320432766682874540E-15, 99.03125000204838102, 7.188101187500000044 ) ) ;
#42204 = MANIFOLD_SOLID_BREP ( 'CirPattern1', #14121 ) ;
#42207 = AXIS2_PLACEMENT_3D ( 'NONE', #47146, #64872, #64513 ) ;
#42206 = CARTESIAN_POINT ( 'NONE',  ( 2.828427124746190291, 6.624999997268813168, 2.828427124746192067 ) ) ;
#42205 = DIRECTION ( 'NONE',  ( -0.000000000000000000, 1.000000000000000000, -0.000000000000000000 ) ) ;
#42208 = DIRECTION ( 'NONE',  ( 0.000000000000000000, 0.000000000000000000, 1.000000000000000000 ) ) ;
#42209 =( BOUNDED_CURVE ( )  B_SPLINE_CURVE ( 2, ( #62509, #26687, #15735, #10465, #39137, #33495, #14986, #61777, #10835 ),
 .UNSPECIFIED., .F., .F. ) 
 B_SPLINE_CURVE_WITH_KNOTS ( ( 3, 2, 2, 2, 3 ),
 ( 0.1874999999999978351, 0.1979166666666645202, 0.2083333333333312054, 0.2187499999999978906, 0.2291666666666645480 ),
 .UNSPECIFIED. ) 
 CURVE ( )  GEOMETRIC_REPRESENTATION_ITEM ( )  RATIONAL_B_SPLINE_CURVE ( ( 1.000000000000015765, 0.9238795325112709733, 1.000000000000000000, 0.9238795325112867385, 1.000000000000000000, 0.9238795325112867385, 1.000000000000000000, 0.9238795325113021706, 0.9999999999999845679 ) ) 
 REPRESENTATION_ITEM ( '' )  );
#42210 = ORIENTED_EDGE ( 'NONE', *, *, #26231, .F. ) ;
#42211 = CARTESIAN_POINT ( 'NONE',  ( -2.990854866096085640, 10.11452374054098335, -70.45725801588044135 ) ) ;
#42212 = CARTESIAN_POINT ( 'NONE',  ( -3.042071309553159075, 260.2604166700805877, 11.35316468749999963 ) ) ;
#42213 = CARTESIAN_POINT ( 'NONE',  ( -2.977408999572647819, 7.188101187499991163, 19.20530278187175810 ) ) ;
#42214 = VERTEX_POINT ( 'NONE', #35576 ) ;
#42215 = EDGE_CURVE ( 'NONE', #29797, #502, #30643, .T. ) ;
#42216 = ORIENTED_EDGE ( 'NONE', *, *, #68890, .T. ) ;
#42217 = CARTESIAN_POINT ( 'NONE',  ( -10.18810118749999738, -4.220049686691941915, 85.75000000204838102 ) ) ;
#42218 = CARTESIAN_POINT ( 'NONE',  ( -5.000000000000005329, 115.2083333265053682, 8.660254037844387298 ) ) ;
#42219 = CARTESIAN_POINT ( 'NONE',  ( -4.556349186104047710, -10.99999999999999822, 95.78124999999998579 ) ) ;
#42222 = CARTESIAN_POINT ( 'NONE',  ( -4.721056650415998313, 294.7343750017069510, 4.721056650416000089 ) ) ;
#42221 = CARTESIAN_POINT ( 'NONE',  ( 23.99999999999997868, 202.8125000027312126, 168.3431457505075741 ) ) ;
#42220 = DIRECTION ( 'NONE',  ( 1.000000000000000000, -0.000000000000000000, -0.000000000000000000 ) ) ;
#42223 = CARTESIAN_POINT ( 'NONE',  ( -4.999999999999998224, 151.6666666666666856, -8.660254037844389075 ) ) ;
#42224 = CARTESIAN_POINT ( 'NONE',  ( 23.99999999999997868, 199.8125000027312126, 168.3431457505075457 ) ) ;
#42225 = CARTESIAN_POINT ( 'NONE',  ( -5.082755093536319713, 5.082755093536319713, 1.674052781871753659 ) ) ;
#42226 = CYLINDRICAL_SURFACE ( 'NONE', #7308, 7.999999999999991118 ) ;
#42227 = CARTESIAN_POINT ( 'NONE',  ( -3.313708498984765161, 5.343749995903221084, 7.999999999999998224 ) ) ;
#42228 = VECTOR ( 'NONE', #35933, 1000.000000000000000 ) ;
#42229 = CARTESIAN_POINT ( 'NONE',  ( 29.43265458321760519, 197.5000000013656063, 173.4587341249998929 ) ) ;
#42230 = CARTESIAN_POINT ( 'NONE',  ( -2.977408999572654480, 4.874999997951610098, 7.188101187499999156 ) ) ;
#42231 = CARTESIAN_POINT ( 'NONE',  ( -3.317071493978880348, -8.008118988124989457, -0.2056347160593713919 ) ) ;
#42232 = LINE ( 'NONE', #36222, #4627 ) ;
#42233 = CARTESIAN_POINT ( 'NONE',  ( -5.082755093536324154, 108.2187500020483810, 5.082755093536326818 ) ) ;
#42235 = CARTESIAN_POINT ( 'NONE',  ( -1.656854249492381248, 16.31250000000000000, -4.000000000000001776 ) ) ;
#42234 = CYLINDRICAL_SURFACE ( 'NONE', #4646, 4.000000000000001776 ) ;
#42236 = CARTESIAN_POINT ( 'NONE',  ( 11.35316468749999963, 231.5104166700806445, 3.042071309553159519 ) ) ;
#42237 = CARTESIAN_POINT ( 'NONE',  ( -6.123233995736766282E-16, 233.7500000000000000, -10.00000000000000000 ) ) ;
#42238 = CARTESIAN_POINT ( 'NONE',  ( -2.977408999572648707, -7.188101187499990274, 21.64280278187176165 ) ) ;
#42239 = CARTESIAN_POINT ( 'NONE',  ( 0.000000000000000000, 125.0000000000000000, 0.000000000000000000 ) ) ;
#42240 = CARTESIAN_POINT ( 'NONE',  ( 8.311093377946834337, 35.15624999658602690, 8.311093377946839666 ) ) ;
#42241 = CARTESIAN_POINT ( 'NONE',  ( -1.656854249492390574, 203.1875000000000284, 201.9999999999999716 ) ) ;
#42242 = CARTESIAN_POINT ( 'NONE',  ( 10.00000000000000178, 6.874999993172033363, 0.000000000000000000 ) ) ;
#42243 = DIRECTION ( 'NONE',  ( -0.000000000000000000, 1.000000000000000000, -1.563033456626094573E-30 ) ) ;
#42244 = FILL_AREA_STYLE ('',( #55734 ) ) ;
#42245 = EDGE_LOOP ( 'NONE', ( #19275, #31339, #64485, #54720, #15958, #20690, #46473, #53873, #57468, #3072 ) ) ;
#42246 = EDGE_CURVE ( 'NONE', #30848, #62884, #38727, .T. ) ;
#42247 = DIRECTION ( 'NONE',  ( -0.000000000000000000, -0.000000000000000000, 1.000000000000000000 ) ) ;
#42248 = CARTESIAN_POINT ( 'NONE',  ( -4.000000000000001776, 8.249999997268814056, -4.898587196589415787E-16 ) ) ;
#42249 = CARTESIAN_POINT ( 'NONE',  ( 11.35316468750000141, 40.78124999658601268, 0.000000000000000000 ) ) ;
#42250 = CARTESIAN_POINT ( 'NONE',  ( -4.556349186104045934, 11.00000000000000000, 84.90625000409676204 ) ) ;
#42251 = CARTESIAN_POINT ( 'NONE',  ( 1.432654583217607414, 207.5000000013656063, 145.4587341250000350 ) ) ;
#42253 = AXIS2_PLACEMENT_3D ( 'NONE', #3761, #26762, #61845 ) ;
#42252 = CARTESIAN_POINT ( 'NONE',  ( 25.17157287525381548, 202.6250000000000284, 167.1715728752537018 ) ) ;
#42254 = CARTESIAN_POINT ( 'NONE',  ( 12.00000000000000000, 0.000000000000000000, 0.000000000000000000 ) ) ;
#42256 = CARTESIAN_POINT ( 'NONE',  ( 8.311093377946834337, 30.15624999658601624, 8.311093377946839666 ) ) ;
#42255 = CARTESIAN_POINT ( 'NONE',  ( -5.082755093536324154, 106.3437500020483810, 5.082755093536326818 ) ) ;
#42258 = EDGE_CURVE ( 'NONE', #66522, #30024, #65339, .T. ) ;
#42257 = CARTESIAN_POINT ( 'NONE',  ( 3.313708498984756279, 7.999999999999991118, 15.36155277982336642 ) ) ;
#42259 = CARTESIAN_POINT ( 'NONE',  ( -11.35316468749999785, 153.0729166632527267, -3.042071309553167513 ) ) ;
#42260 = CARTESIAN_POINT ( 'NONE',  ( -10.00000000000000000, 134.1666666598386826, -2.679491924311229845 ) ) ;
#42261 = CARTESIAN_POINT ( 'NONE',  ( -2.977408999572650927, 110.7500000020483668, -7.188101187500001821 ) ) ;
#42262 = CARTESIAN_POINT ( 'NONE',  ( 44.48374486120344784, 184.9827789239285210, 84.30156509589276936 ) ) ;
#42263 = CARTESIAN_POINT ( 'NONE',  ( -31.45873412499998523, 205.0000000013655779, 171.4326545832180386 ) ) ;
#42264 = ORIENTED_EDGE ( 'NONE', *, *, #25576, .F. ) ;
#42265 = CARTESIAN_POINT ( 'NONE',  ( 3.407298021510797525, -68.04056125360885687, -20.39715949456126154 ) ) ;
#42266 = CARTESIAN_POINT ( 'NONE',  ( 11.35316468750000141, 16.09374999658601979, 0.000000000000000000 ) ) ;
#42267 = EDGE_CURVE ( 'NONE', #60988, #54742, #3023, .T. ) ;
#42268 = EDGE_LOOP ( 'NONE', ( #6907, #32837, #33170, #15626 ) ) ;
#42269 = DIRECTION ( 'NONE',  ( 0.000000000000000000, 0.000000000000000000, 1.000000000000000000 ) ) ;
#42270 = CARTESIAN_POINT ( 'NONE',  ( 0.000000000000000000, 23.85640646055104241, -14.00000000000000178 ) ) ;
#42272 = CARTESIAN_POINT ( 'NONE',  ( -3.042071309553163960, 152.2395833299193271, -11.35316468749999963 ) ) ;
#42271 = CARTESIAN_POINT ( 'NONE',  ( -21.31731128724105062, -26.75158917425308758, 145.2037643689419326 ) ) ;
#42273 = FACE_OUTER_BOUND ( 'NONE', #73657, .T. ) ;
#42274 = CARTESIAN_POINT ( 'NONE',  ( 7.999999999999991118, 3.313708498984757611, 18.23030278432982598 ) ) ;
#42275 = CARTESIAN_POINT ( 'NONE',  ( 11.00000000000010658, 4.556349186103942017, 90.53125000409677625 ) ) ;
#42276 = CARTESIAN_POINT ( 'NONE',  ( 9.832129032723416984, 236.8229166700806445, -5.676582343750003368 ) ) ;
#42277 = CARTESIAN_POINT ( 'NONE',  ( -6.238412754330611322E-16, 10.18810118749999916, 91.65625000204836681 ) ) ;
#42278 = VERTEX_POINT ( 'NONE', #54779 ) ;
#42279 = LINE ( 'NONE', #23829, #11233 ) ;
#42280 = DIRECTION ( 'NONE',  ( -0.000000000000000000, 1.000000000000000000, -0.000000000000000000 ) ) ;
#42281 = CARTESIAN_POINT ( 'NONE',  ( 3.042071309553159519, 105.0520833299193271, 11.35316468750000141 ) ) ;
#42282 = CARTESIAN_POINT ( 'NONE',  ( 4.220049686691941027, -10.18810118749999738, 102.6250000020483810 ) ) ;
#42283 = CARTESIAN_POINT ( 'NONE',  ( 3.211159895383560947, 17.31249999863440792, 3.211159895383562723 ) ) ;
#42284 = ORIENTED_EDGE ( 'NONE', *, *, #23941, .T. ) ;
#42285 = VERTEX_POINT ( 'NONE', #15511 ) ;
#42286 = CARTESIAN_POINT ( 'NONE',  ( 3.313708498984762496, 4.218750000000000000, 7.999999999999998224 ) ) ;
#42287 = CARTESIAN_POINT ( 'NONE',  ( 4.898587196589412829E-16, 10.87500000000000178, -8.000000000000000000 ) ) ;
#42288 = CARTESIAN_POINT ( 'NONE',  ( -7.188101187500000044, 2.718749997951610098, -8.802885111219163269E-16 ) ) ;
#42289 = CARTESIAN_POINT ( 'NONE',  ( 5.656854249492381470, 115.2500000040967905, 5.656854249492379694 ) ) ;
#42290 = CARTESIAN_POINT ( 'NONE',  ( 7.204075437095966983, 7.204075437095967871, 98.96875000204838102 ) ) ;
#42291 = CARTESIAN_POINT ( 'NONE',  ( -11.02092980224262142, -7.493469672506294366, -0.7454400371385534463 ) ) ;
#42292 = DIRECTION ( 'NONE',  ( 0.000000000000000000, 0.000000000000000000, 1.000000000000000000 ) ) ;
#42293 = CARTESIAN_POINT ( 'NONE',  ( 2.828427124746190291, 15.62499999726881406, 2.828427124746192067 ) ) ;
#42294 = CARTESIAN_POINT ( 'NONE',  ( 1.881053915767121998, 5.499999998634407028, -4.541265875000002339 ) ) ;
#42295 = ORIENTED_EDGE ( 'NONE', *, *, #21146, .T. ) ;
#42296 = CARTESIAN_POINT ( 'NONE',  ( 1.432654583217607192, 207.2500000013655779, 145.4587341250000634 ) ) ;
#42297 = CARTESIAN_POINT ( 'NONE',  ( 1.432654583217662481, 196.1250000013655779, 194.5412658750000219 ) ) ;
#42299 = CARTESIAN_POINT ( 'NONE',  ( 5.000000000000000000, 10.26105934116143459, -64.40045319026695836 ) ) ;
#42298 = CARTESIAN_POINT ( 'NONE',  ( -31.45873412499999233, 200.6875000013656063, 170.0000000000004547 ) ) ;
#42300 = CARTESIAN_POINT ( 'NONE',  ( -8.342170076843785083E-16, 15.06249999863440792, 4.541265875000002339 ) ) ;
#42301 = CARTESIAN_POINT ( 'NONE',  ( 2.679491924311222739, 120.8333333265053682, 10.00000000000000355 ) ) ;
#42302 = CARTESIAN_POINT ( 'NONE',  ( 2.977408999572646486, 7.188101187499991163, 14.51780278187175455 ) ) ;
#42303 = VERTEX_POINT ( 'NONE', #32520 ) ;
#42304 =( BOUNDED_SURFACE ( )  B_SPLINE_SURFACE ( 1, 2, ( 
 ( #16600, #68673, #34370, #57371, #23024, #46032, #9853, #50204, #10222, #29799, #7162, #6791, #52812, #46405, #24125, #1870, #24500, #40380, #30167, #18108, #1145, #58120, #41122, #70530, #47138, #52443, #12437, #58850, #46768, #52076, #18845, #12071, #53184, #30538, #18478, #35108, #41489, #35835, #6428, #1522, #47505, #411, #64504, #29432, #64130, #6052, #58483, #41853, #23764, #64864, #11701, #12803, #34743, #17728, #17356, #69420, #23391, #7531, #13166, #35469, #59220, #40744, #24856, #69792, #63754, #36203, #63378, #69052, #57747, #53554, #70170, #29058, #780, #66725, #13899, #32407, #36938, #30901, #48985, #42951, #20694, #60309, #66346, #48614, #53920, #25964, #14650, #71251, #71620, #47874, #19571, #55046, #70894, #71996, #2611, #37691, #65970, #31652, #65225, #42213, #60692, #3353, #36569, #14275, #32026, #59942, #25228, #19209, #54671, #13530, #59582, #2979, #7896, #20311, #8637, #26343, #49363, #38066, #8258, #31271, #2232, #9012, #54299, #48245, #72381, #43711, #42585, #43328, #65601, #61064, #37313, #25599, #15030, #9387, #55420, #3729, #19943, #56538, #38438, #4480, #55794, #16896, #73498, #56913, #51235, #67845, #21069, #15776, #27103, #22181, #39920, #21441, #33537, #72764, #4111, #38813, #49748, #57286, #44094, #62548, #33913, #50119, #27470, #67103, #62928, #45205, #73876, #61441, #28226, #4856, #9767, #68217, #68589, #16136, #61813, #56166, #27852, #44838, #16514, #39553, #50861, #11252, #50484, #10131, #10878, #73134, #5225, #74246, #45575, #62179, #26728, #15399, #32787, #33169, #44464, #67477, #22553, #21805, #39175, #10505, #34282, #64783, #69336, #69712, #17645, #57662, #1438, #12360, #13085, #70450, #6711, #64422, #63668, #28598, #17274, #58406, #11993, #5600, #34658, #18396, #36120, #40665, #18026, #35027, #5969, #24419, #35394, #51608, #18766, #29719, #12720, #11621, #52733, #47054, #28971, #29355, #74625, #51991, #35753, #22939, #1067, #58039, #70090, #699, #64050, #45949, #68965, #41410, #58771, #40292, #23682, #7078, #6352, #329, #63293, #24045, #23308, #46322, #30085, #52362, #53104, #41042, #47425, #41773, #46688, #48161, #25144, #30457, #71912, #71168, #19123, #25879, #20225, #53473, #54588, #36488, #49275, #25515, #59501, #43244, #48527, #66631, #31936, #1790, #14190, #70812, #36857, #13450, #72290, #31188, #14565, #8924, #71534, #24775, #19487, #7814, #2892, #20602, #53840, #65883, #47789, #30817, #42503, #7450, #14938 ),
 ( #42129, #60601, #37227, #65141, #31564, #26256, #19859, #65519, #13813, #60224, #2523, #48898, #66260, #8550, #43620, #59865, #8178, #37602, #2151, #54959, #3268, #59141, #42865, #54214, #32321, #20978, #60976, #68495, #9297, #73782, #45116, #67010, #15687, #55333, #74153, #33446, #10415, #49659, #39457, #16056, #72676, #56445, #5138, #27381, #50028, #67385, #39089, #56078, #4764, #27756, #44747, #22457, #38729, #27016, #50767, #15309, #68128, #16423, #56817, #73415, #37977, #3638, #44003, #21351, #26636, #38346, #62093, #44375, #61353, #9680, #22091, #45477, #73044, #50400, #61726, #32700, #33820, #67762, #55709, #28131, #62456, #10784, #4023, #51144, #10045, #33081, #4388, #21719, #63202, #23958, #16796, #17933, #46228, #58315, #11903, #606, #34186, #11164, #29626, #46965, #5505, #34936, #975, #28876, #68868, #39824, #23586, #62827, #57189, #46596, #28505, #69619, #52271, #69995, #18302, #6985, #5880, #57570, #51514, #52639, #51896, #74529, #6621, #41318, #22839, #12268, #17179, #29995, #57949, #40199, #64326, #6254, #24324, #12631, #45852, #40949, #11531, #69245, #34564, #53010, #63576, #35662, #58676, #29259, #236, #23218, #17555, #35301, #1342, #40572, #63958, #47335, #24684, #8741, #41684, #9497, #31753, #30362, #38165, #32511, #64695, #66830, #47695, #61543, #37794, #70716, #55525, #60790, #4210, #44194, #12993, #26444, #7355, #49088, #19036, #9865, #43432, #26832, #21169, #9115, #36031, #60416, #42041, #15132, #32894, #66072, #3454, #59049, #14380, #54773, #18674, #27199, #53382, #3836, #49846, #37416, #72102, #1707, #55896, #61166, #43816, #3083, #72864, #49470, #26068, #67206, #38541, #32131, #20415, #66447, #72489, #14755, #15504, #70362, #20798, #55149, #27956, #39279, #40022, #27576, #5694, #28693, #69065, #10981, #50216, #44566, #33263, #33635, #73236, #61910, #28325, #56641, #21542, #4579, #63025, #34756, #62280, #39650, #10608, #50584, #46045, #57010, #57760, #40393, #51335, #34384, #56262, #74343, #16996, #73602, #73975, #67579, #21909, #57384, #15875, #22652, #4956, #11349, #45302, #34015, #38908, #10235, #51706, #53, #44940, #68317, #23036, #50962, #67947, #16241, #5323, #22280, #16615, #45672, #62647, #68686, #17369, #63391, #11715, #6065, #18121, #69805, #59232, #46419, #53197, #69433, #52456, #52092, #6444, #58136, #42225, #24867, #52825, #19220, #29445, #36581, #6801, #35121, #70542, #425, #59593, #29073, #18857, #29814, #35848 ) ),
 .UNSPECIFIED., .F., .F., .F. ) 
 B_SPLINE_SURFACE_WITH_KNOTS ( ( 2, 2 ),
 ( 3, 2, 2, 2, 2, 2, 2, 2, 2, 2, 2, 2, 2, 2, 2, 2, 2, 2, 2, 2, 2, 2, 2, 2, 2, 2, 2, 2, 2, 2, 2, 2, 2, 2, 2, 2, 2, 2, 2, 2, 2, 2, 2, 2, 2, 2, 2, 2, 2, 2, 2, 2, 2, 2, 2, 2, 2, 2, 2, 2, 2, 2, 2, 2, 2, 2, 2, 2, 2, 2, 2, 2, 2, 2, 2, 2, 2, 2, 2, 2, 2, 2, 2, 2, 2, 2, 2, 2, 2, 2, 2, 2, 2, 2, 2, 2, 2, 2, 2, 2, 2, 2, 2, 2, 2, 2, 2, 2, 2, 2, 2, 2, 2, 2, 2, 2, 2, 2, 2, 2, 2, 2, 2, 2, 2, 2, 2, 2, 2, 2, 2, 2, 2, 2, 2, 2, 2, 2, 2, 2, 2, 2, 2, 2, 2, 2, 2, 2, 2, 2, 2, 2, 3 ),
 ( 0.000000000000000000, 1.000000000000000000 ),
 ( 0.000000000000000000, 0.006578947368421052266, 0.01315789473684210453, 0.01973684210526315680, 0.02631578947368420907, 0.03289473684210526133, 0.03947368421052631360, 0.04605263157894736586, 0.05263157894736841813, 0.05921052631578947040, 0.06578947368421052266, 0.07236842105263158187, 0.07894736842105262720, 0.08552631578947368640, 0.09210526315789473173, 0.09868421052631579093, 0.1052631578947368363, 0.1118421052631578955, 0.1184210526315789408, 0.1250000000000000000, 0.1315789473684210453, 0.1381578947368421184, 0.1447368421052631637, 0.1513157894736842091, 0.1578947368421052544, 0.1644736842105263275, 0.1710526315789473728, 0.1776315789473684181, 0.1842105263157894635, 0.1907894736842105365, 0.1973684210526315819, 0.2039473684210526272, 0.2105263157894736725, 0.2171052631578947456, 0.2236842105263157909, 0.2302631578947368363, 0.2368421052631578816, 0.2434210526315789547, 0.2500000000000000000, 0.2565789473684210731, 0.2631578947368420907, 0.2697368421052631637, 0.2763157894736842368, 0.2828947368421052544, 0.2894736842105263275, 0.2960526315789473450, 0.3026315789473684181, 0.3092105263157894912, 0.3157894736842105088, 0.3223684210526315819, 0.3289473684210526550, 0.3355263157894736725, 0.3421052631578947456, 0.3486842105263157632, 0.3552631578947368363, 0.3618421052631579093, 0.3684210526315789269, 0.3750000000000000000, 0.3815789473684210731, 0.3881578947368420907, 0.3947368421052631637, 0.4013157894736842368, 0.4078947368421052544, 0.4144736842105263275, 0.4210526315789473450, 0.4276315789473684181, 0.4342105263157894912, 0.4407894736842105088, 0.4473684210526315819, 0.4539473684210526550, 0.4605263157894736725, 0.4671052631578947456, 0.4736842105263157632, 0.4802631578947368363, 0.4868421052631579093, 0.4934210526315789269, 0.5000000000000000000, 0.5065789473684210176, 0.5131578947368421462, 0.5197368421052631637, 0.5263157894736841813, 0.5328947368421053099, 0.5394736842105263275, 0.5460526315789473450, 0.5526315789473684736, 0.5592105263157894912, 0.5657894736842105088, 0.5723684210526315264, 0.5789473684210526550, 0.5855263157894736725, 0.5921052631578946901, 0.5986842105263158187, 0.6052631578947368363, 0.6118421052631578538, 0.6184210526315789824, 0.6250000000000000000, 0.6315789473684210176, 0.6381578947368421462, 0.6447368421052631637, 0.6513157894736841813, 0.6578947368421053099, 0.6644736842105263275, 0.6710526315789473450, 0.6776315789473684736, 0.6842105263157894912, 0.6907894736842105088, 0.6973684210526315264, 0.7039473684210526550, 0.7105263157894736725, 0.7171052631578946901, 0.7236842105263158187, 0.7302631578947368363, 0.7368421052631578538, 0.7434210526315789824, 0.7500000000000000000, 0.7565789473684210176, 0.7631578947368421462, 0.7697368421052631637, 0.7763157894736841813, 0.7828947368421053099, 0.7894736842105263275, 0.7960526315789473450, 0.8026315789473684736, 0.8092105263157894912, 0.8157894736842105088, 0.8223684210526315264, 0.8289473684210526550, 0.8355263157894736725, 0.8421052631578946901, 0.8486842105263158187, 0.8552631578947368363, 0.8618421052631578538, 0.8684210526315789824, 0.8750000000000000000, 0.8815789473684210176, 0.8881578947368421462, 0.8947368421052631637, 0.9013157894736841813, 0.9078947368421053099, 0.9144736842105263275, 0.9210526315789473450, 0.9276315789473684736, 0.9342105263157894912, 0.9407894736842105088, 0.9473684210526315264, 0.9539473684210526550, 0.9605263157894736725, 0.9671052631578946901, 0.9736842105263158187, 0.9802631578947368363, 0.9868421052631578538, 0.9934210526315789824, 0.9940576599040155115 ),
 .UNSPECIFIED. ) 
 GEOMETRIC_REPRESENTATION_ITEM ( )  RATIONAL_B_SPLINE_SURFACE ( (
 ( 1.000000000000000000, 0.9238795325112867385, 1.000000000000000000, 0.9238795325112867385, 1.000000000000000000, 0.9238795325112867385, 1.000000000000000000, 0.9238795325112867385, 1.000000000000000000, 0.9238795325112867385, 1.000000000000000000, 0.9238795325112867385, 1.000000000000000000, 0.9238795325112867385, 1.000000000000000000, 0.9238795325112867385, 1.000000000000000000, 0.9238795325112867385, 1.000000000000000000, 0.9238795325112867385, 1.000000000000000000, 0.9238795325112867385, 1.000000000000000000, 0.9238795325112867385, 1.000000000000000000, 0.9238795325112867385, 1.000000000000000000, 0.9238795325112867385, 1.000000000000000000, 0.9238795325112867385, 1.000000000000000000, 0.9238795325112867385, 1.000000000000000000, 0.9238795325112867385, 1.000000000000000000, 0.9238795325112867385, 1.000000000000000000, 0.9238795325112867385, 1.000000000000000000, 0.9238795325112867385, 1.000000000000000000, 0.9238795325112867385, 1.000000000000000000, 0.9238795325112867385, 1.000000000000000000, 0.9238795325112867385, 1.000000000000000000, 0.9238795325112867385, 1.000000000000000000, 0.9238795325112867385, 1.000000000000000000, 0.9238795325112867385, 1.000000000000000000, 0.9238795325112867385, 1.000000000000000000, 0.9238795325112867385, 1.000000000000000000, 0.9238795325112867385, 1.000000000000000000, 0.9238795325112867385, 1.000000000000000000, 0.9238795325112867385, 1.000000000000000000, 0.9238795325112867385, 1.000000000000000000, 0.9238795325112867385, 1.000000000000000000, 0.9238795325112867385, 1.000000000000000000, 0.9238795325112867385, 1.000000000000000000, 0.9238795325112867385, 1.000000000000000000, 0.9238795325112867385, 1.000000000000000000, 0.9238795325112867385, 1.000000000000000000, 0.9238795325112867385, 1.000000000000000000, 0.9238795325112867385, 1.000000000000000000, 0.9238795325112867385, 1.000000000000000000, 0.9238795325112867385, 1.000000000000000000, 0.9238795325112867385, 1.000000000000000000, 0.9238795325112867385, 1.000000000000000000, 0.9238795325112867385, 1.000000000000000000, 0.9238795325112867385, 1.000000000000000000, 0.9238795325112867385, 1.000000000000000000, 0.9238795325112867385, 1.000000000000000000, 0.9238795325112867385, 1.000000000000000000, 0.9238795325112867385, 1.000000000000000000, 0.9238795325112867385, 1.000000000000000000, 0.9238795325112867385, 1.000000000000000000, 0.9238795325112867385, 1.000000000000000000, 0.9238795325112867385, 1.000000000000000000, 0.9238795325112867385, 1.000000000000000000, 0.9238795325112867385, 1.000000000000000000, 0.9238795325112867385, 1.000000000000000000, 0.9238795325112867385, 1.000000000000000000, 0.9238795325112867385, 1.000000000000000000, 0.9238795325112867385, 1.000000000000000000, 0.9238795325112867385, 1.000000000000000000, 0.9238795325112867385, 1.000000000000000000, 0.9238795325112867385, 1.000000000000000000, 0.9238795325112867385, 1.000000000000000000, 0.9238795325112867385, 1.000000000000000000, 0.9238795325112867385, 1.000000000000000000, 0.9238795325112867385, 1.000000000000000000, 0.9238795325112867385, 1.000000000000000000, 0.9238795325112867385, 1.000000000000000000, 0.9238795325112867385, 1.000000000000000000, 0.9238795325112867385, 1.000000000000000000, 0.9238795325112867385, 1.000000000000000000, 0.9238795325112867385, 1.000000000000000000, 0.9238795325112867385, 1.000000000000000000, 0.9238795325112867385, 1.000000000000000000, 0.9238795325112867385, 1.000000000000000000, 0.9238795325112867385, 1.000000000000000000, 0.9238795325112867385, 1.000000000000000000, 0.9238795325112867385, 1.000000000000000000, 0.9238795325112867385, 1.000000000000000000, 0.9238795325112867385, 1.000000000000000000, 0.9238795325112867385, 1.000000000000000000, 0.9238795325112867385, 1.000000000000000000, 0.9238795325112867385, 1.000000000000000000, 0.9238795325112867385, 1.000000000000000000, 0.9238795325112867385, 1.000000000000000000, 0.9238795325112867385, 1.000000000000000000, 0.9238795325112867385, 1.000000000000000000, 0.9238795325112867385, 1.000000000000000000, 0.9238795325112867385, 1.000000000000000000, 0.9238795325112867385, 1.000000000000000000, 0.9238795325112867385, 1.000000000000000000, 0.9238795325112867385, 1.000000000000000000, 0.9238795325112867385, 1.000000000000000000, 0.9238795325112867385, 1.000000000000000000, 0.9238795325112867385, 1.000000000000000000, 0.9238795325112867385, 1.000000000000000000, 0.9238795325112867385, 1.000000000000000000, 0.9238795325112867385, 1.000000000000000000, 0.9238795325112867385, 1.000000000000000000, 0.9238795325112867385, 1.000000000000000000, 0.9238795325112867385, 1.000000000000000000, 0.9238795325112867385, 1.000000000000000000, 0.9238795325112867385, 1.000000000000000000, 0.9238795325112867385, 1.000000000000000000, 0.9238795325112867385, 1.000000000000000000, 0.9238795325112867385, 1.000000000000000000, 0.9238795325112867385, 1.000000000000000000, 0.9238795325112867385, 1.000000000000000000, 0.9238795325112867385, 1.000000000000000000, 0.9238795325112867385, 1.000000000000000000, 0.9238795325112867385, 1.000000000000000000, 0.9238795325112867385, 1.000000000000000000, 0.9238795325112867385, 1.000000000000000000, 0.9238795325112867385, 1.000000000000000000, 0.9238795325112867385, 1.000000000000000000, 0.9238795325112867385, 1.000000000000000000, 0.9238795325112867385, 1.000000000000000000, 0.9238795325112867385, 1.000000000000000000, 0.9238795325112867385, 1.000000000000000000, 0.9238795325112867385, 1.000000000000000000, 0.9238795325112867385, 1.000000000000000000, 0.9238795325112867385, 1.000000000000000000, 0.9238795325112867385, 1.000000000000000000, 0.9238795325112867385, 1.000000000000000000, 0.9238795325112867385, 1.000000000000000000, 0.9238795325112867385, 1.000000000000000000, 0.9238795325112867385, 1.000000000000000000, 0.9238795325112867385, 1.000000000000000000, 0.9238795325112867385, 1.000000000000000000, 0.9238795325112867385, 1.000000000000000000, 0.9238795325112867385, 1.000000000000000000, 0.9238795325112867385, 1.000000000000000000, 0.9238795325112867385, 1.000000000000000000, 0.9238795325112867385, 1.000000000000000000, 0.9238795325112867385, 1.000000000000000000, 0.9238795325112867385, 1.000000000000000000, 0.9238795325112867385, 1.000000000000000000, 0.9238795325112867385, 1.000000000000000000, 0.9238795325112867385, 1.000000000000000000, 0.9238795325112867385, 1.000000000000000000, 0.9238795325112867385, 1.000000000000000000, 0.9238795325112867385, 1.000000000000000000, 0.9238795325112867385, 1.000000000000000000, 0.9238795325112867385, 1.000000000000000000, 0.9238795325112867385, 1.000000000000000000, 0.9238795325112867385, 1.000000000000000000, 0.9238795325112867385, 1.000000000000000000, 0.9238795325112867385, 1.000000000000000000, 0.9238795325112867385, 1.000000000000000000, 0.9238795325112867385, 1.000000000000000000, 0.9926342558359432244, 0.9866939939076171395),
 ( 1.000000000000000000, 0.9238795325112867385, 1.000000000000000000, 0.9238795325112867385, 1.000000000000000000, 0.9238795325112867385, 1.000000000000000000, 0.9238795325112867385, 1.000000000000000000, 0.9238795325112867385, 1.000000000000000000, 0.9238795325112867385, 1.000000000000000000, 0.9238795325112867385, 1.000000000000000000, 0.9238795325112867385, 1.000000000000000000, 0.9238795325112867385, 1.000000000000000000, 0.9238795325112867385, 1.000000000000000000, 0.9238795325112867385, 1.000000000000000000, 0.9238795325112867385, 1.000000000000000000, 0.9238795325112867385, 1.000000000000000000, 0.9238795325112867385, 1.000000000000000000, 0.9238795325112867385, 1.000000000000000000, 0.9238795325112867385, 1.000000000000000000, 0.9238795325112867385, 1.000000000000000000, 0.9238795325112867385, 1.000000000000000000, 0.9238795325112867385, 1.000000000000000000, 0.9238795325112867385, 1.000000000000000000, 0.9238795325112867385, 1.000000000000000000, 0.9238795325112867385, 1.000000000000000000, 0.9238795325112867385, 1.000000000000000000, 0.9238795325112867385, 1.000000000000000000, 0.9238795325112867385, 1.000000000000000000, 0.9238795325112867385, 1.000000000000000000, 0.9238795325112867385, 1.000000000000000000, 0.9238795325112867385, 1.000000000000000000, 0.9238795325112867385, 1.000000000000000000, 0.9238795325112867385, 1.000000000000000000, 0.9238795325112867385, 1.000000000000000000, 0.9238795325112867385, 1.000000000000000000, 0.9238795325112867385, 1.000000000000000000, 0.9238795325112867385, 1.000000000000000000, 0.9238795325112867385, 1.000000000000000000, 0.9238795325112867385, 1.000000000000000000, 0.9238795325112867385, 1.000000000000000000, 0.9238795325112867385, 1.000000000000000000, 0.9238795325112867385, 1.000000000000000000, 0.9238795325112867385, 1.000000000000000000, 0.9238795325112867385, 1.000000000000000000, 0.9238795325112867385, 1.000000000000000000, 0.9238795325112867385, 1.000000000000000000, 0.9238795325112867385, 1.000000000000000000, 0.9238795325112867385, 1.000000000000000000, 0.9238795325112867385, 1.000000000000000000, 0.9238795325112867385, 1.000000000000000000, 0.9238795325112867385, 1.000000000000000000, 0.9238795325112867385, 1.000000000000000000, 0.9238795325112867385, 1.000000000000000000, 0.9238795325112867385, 1.000000000000000000, 0.9238795325112867385, 1.000000000000000000, 0.9238795325112867385, 1.000000000000000000, 0.9238795325112867385, 1.000000000000000000, 0.9238795325112867385, 1.000000000000000000, 0.9238795325112867385, 1.000000000000000000, 0.9238795325112867385, 1.000000000000000000, 0.9238795325112867385, 1.000000000000000000, 0.9238795325112867385, 1.000000000000000000, 0.9238795325112867385, 1.000000000000000000, 0.9238795325112867385, 1.000000000000000000, 0.9238795325112867385, 1.000000000000000000, 0.9238795325112867385, 1.000000000000000000, 0.9238795325112867385, 1.000000000000000000, 0.9238795325112867385, 1.000000000000000000, 0.9238795325112867385, 1.000000000000000000, 0.9238795325112867385, 1.000000000000000000, 0.9238795325112867385, 1.000000000000000000, 0.9238795325112867385, 1.000000000000000000, 0.9238795325112867385, 1.000000000000000000, 0.9238795325112867385, 1.000000000000000000, 0.9238795325112867385, 1.000000000000000000, 0.9238795325112867385, 1.000000000000000000, 0.9238795325112867385, 1.000000000000000000, 0.9238795325112867385, 1.000000000000000000, 0.9238795325112867385, 1.000000000000000000, 0.9238795325112867385, 1.000000000000000000, 0.9238795325112867385, 1.000000000000000000, 0.9238795325112867385, 1.000000000000000000, 0.9238795325112867385, 1.000000000000000000, 0.9238795325112867385, 1.000000000000000000, 0.9238795325112867385, 1.000000000000000000, 0.9238795325112867385, 1.000000000000000000, 0.9238795325112867385, 1.000000000000000000, 0.9238795325112867385, 1.000000000000000000, 0.9238795325112867385, 1.000000000000000000, 0.9238795325112867385, 1.000000000000000000, 0.9238795325112867385, 1.000000000000000000, 0.9238795325112867385, 1.000000000000000000, 0.9238795325112867385, 1.000000000000000000, 0.9238795325112867385, 1.000000000000000000, 0.9238795325112867385, 1.000000000000000000, 0.9238795325112867385, 1.000000000000000000, 0.9238795325112867385, 1.000000000000000000, 0.9238795325112867385, 1.000000000000000000, 0.9238795325112867385, 1.000000000000000000, 0.9238795325112867385, 1.000000000000000000, 0.9238795325112867385, 1.000000000000000000, 0.9238795325112867385, 1.000000000000000000, 0.9238795325112867385, 1.000000000000000000, 0.9238795325112867385, 1.000000000000000000, 0.9238795325112867385, 1.000000000000000000, 0.9238795325112867385, 1.000000000000000000, 0.9238795325112867385, 1.000000000000000000, 0.9238795325112867385, 1.000000000000000000, 0.9238795325112867385, 1.000000000000000000, 0.9238795325112867385, 1.000000000000000000, 0.9238795325112867385, 1.000000000000000000, 0.9238795325112867385, 1.000000000000000000, 0.9238795325112867385, 1.000000000000000000, 0.9238795325112867385, 1.000000000000000000, 0.9238795325112867385, 1.000000000000000000, 0.9238795325112867385, 1.000000000000000000, 0.9238795325112867385, 1.000000000000000000, 0.9238795325112867385, 1.000000000000000000, 0.9238795325112867385, 1.000000000000000000, 0.9238795325112867385, 1.000000000000000000, 0.9238795325112867385, 1.000000000000000000, 0.9238795325112867385, 1.000000000000000000, 0.9238795325112867385, 1.000000000000000000, 0.9238795325112867385, 1.000000000000000000, 0.9238795325112867385, 1.000000000000000000, 0.9238795325112867385, 1.000000000000000000, 0.9238795325112867385, 1.000000000000000000, 0.9238795325112867385, 1.000000000000000000, 0.9238795325112867385, 1.000000000000000000, 0.9238795325112867385, 1.000000000000000000, 0.9238795325112867385, 1.000000000000000000, 0.9238795325112867385, 1.000000000000000000, 0.9238795325112867385, 1.000000000000000000, 0.9238795325112867385, 1.000000000000000000, 0.9238795325112867385, 1.000000000000000000, 0.9238795325112867385, 1.000000000000000000, 0.9238795325112867385, 1.000000000000000000, 0.9238795325112867385, 1.000000000000000000, 0.9238795325112867385, 1.000000000000000000, 0.9238795325112867385, 1.000000000000000000, 0.9238795325112867385, 1.000000000000000000, 0.9238795325112867385, 1.000000000000000000, 0.9238795325112867385, 1.000000000000000000, 0.9238795325112867385, 1.000000000000000000, 0.9238795325112867385, 1.000000000000000000, 0.9238795325112867385, 1.000000000000000000, 0.9238795325112867385, 1.000000000000000000, 0.9238795325112867385, 1.000000000000000000, 0.9238795325112867385, 1.000000000000000000, 0.9238795325112867385, 1.000000000000000000, 0.9238795325112867385, 1.000000000000000000, 0.9238795325112867385, 1.000000000000000000, 0.9238795325112867385, 1.000000000000000000, 0.9238795325112867385, 1.000000000000000000, 0.9926342558359432244, 0.9866939939076171395) ) ) 
 REPRESENTATION_ITEM ( '' )  SURFACE ( )  );
#42305 = ORIENTED_EDGE ( 'NONE', *, *, #64472, .T. ) ;
#42306 = CARTESIAN_POINT ( 'NONE',  ( -7.204075437095965206, -7.204075437095968759, 103.8437500020483810 ) ) ;
#42307 = CARTESIAN_POINT ( 'NONE',  ( 4.556349186104045934, 11.00000000000000000, 114.7187500040967763 ) ) ;
#42308 = CIRCLE ( 'NONE', #9818, 34.85072926314708752 ) ;
#42309 = CARTESIAN_POINT ( 'NONE',  ( -31.45873412499999944, 204.9375000013656063, 170.0000000000003979 ) ) ;
#42310 = CARTESIAN_POINT ( 'NONE',  ( -26.34314575050758123, 201.5625000000000853, 174.0000000000003411 ) ) ;
#42311 = CARTESIAN_POINT ( 'NONE',  ( 2.839093476692135984E-14, 195.6875000013655779, 201.4587341250000350 ) ) ;
#42312 = CARTESIAN_POINT ( 'NONE',  ( 5.656854249492379694, 104.9374999999999858, -5.656854249492380582 ) ) ;
#42313 = CARTESIAN_POINT ( 'NONE',  ( -7.320508075688773708, 96.87499999999998579, -7.320508075688774596 ) ) ;
#42314 = CARTESIAN_POINT ( 'NONE',  ( 8.000000000000001776, 109.1562499999999858, 3.313708498984759387 ) ) ;
#42315 = CARTESIAN_POINT ( 'NONE',  ( 6.676582343750004256, 297.0468750017068942, 2.765530957081995478 ) ) ;
#42316 = ORIENTED_EDGE ( 'NONE', *, *, #5266, .T. ) ;
#42317 = FACE_OUTER_BOUND ( 'NONE', #66950, .T. ) ;
#42318 = CARTESIAN_POINT ( 'NONE',  ( -5.656854249492379694, 16.87499999590322375, -5.656854249492380582 ) ) ;
#42319 = CARTESIAN_POINT ( 'NONE',  ( -2.445694354108839619, 203.8125000013656063, 139.5543056458912190 ) ) ;
#42320 = CARTESIAN_POINT ( 'NONE',  ( -2.679491924312192630, 53.54166666666657903, 9.999999999999451106 ) ) ;
#42321 = CARTESIAN_POINT ( 'NONE',  ( -7.347880794884122694E-16, 7.750000000000000000, 4.000000000000001776 ) ) ;
#42322 = CARTESIAN_POINT ( 'NONE',  ( 10.00000000000000178, 222.2916666666666856, 2.679491924311222739 ) ) ;
#42323 = CARTESIAN_POINT ( 'NONE',  ( -27.99999999999999645, 210.0000000000000284, 170.0000000000003695 ) ) ;
#42324 = CARTESIAN_POINT ( 'NONE',  ( 7.778174593052021635, 7.778174593052023411, 111.4375000000000000 ) ) ;
#42325 = CARTESIAN_POINT ( 'NONE',  ( 8.660254037844389075, 215.4166666666666856, -5.000000000000000000 ) ) ;
#42326 =( BOUNDED_CURVE ( )  B_SPLINE_CURVE ( 2, ( #9226, #32248, #8856, #8473, #38276, #3571, #32628, #54888, #37529, #65811, #26561, #66187, #49586 ),
 .UNSPECIFIED., .F., .F. ) 
 B_SPLINE_CURVE_WITH_KNOTS ( ( 3, 2, 2, 2, 2, 2, 3 ),
 ( 0.1250000000000000000, 0.1268115942028985588, 0.1286231884057970898, 0.1304347826086956486, 0.1322463768115942073, 0.1340579710144927661, 0.1358695652173912971 ),
 .UNSPECIFIED. ) 
 CURVE ( )  GEOMETRIC_REPRESENTATION_ITEM ( )  RATIONAL_B_SPLINE_CURVE ( ( 1.000000000000000000, 0.9659258262890683122, 1.000000000000000000, 0.9659258262890683122, 1.000000000000000000, 0.9659258262890683122, 1.000000000000000000, 0.9659258262890683122, 1.000000000000000000, 0.9659258262890683122, 1.000000000000000000, 0.9659258262890683122, 1.000000000000000000 ) ) 
 REPRESENTATION_ITEM ( '' )  );
#42327 = CARTESIAN_POINT ( 'NONE',  ( -2.977408999572647819, -7.188101187499990274, 8.142802781871752771 ) ) ;
#42328 = CARTESIAN_POINT ( 'NONE',  ( 5.676582343749993598, 190.2604166632526983, 9.832129032723422313 ) ) ;
#42329 = CARTESIAN_POINT ( 'NONE',  ( 0.000000000000000000, 125.0000000000000000, 8.000000000000000000 ) ) ;
#42330 = CARTESIAN_POINT ( 'NONE',  ( 4.541265875000002339, 2.374999998634407028, -1.881053915767121554 ) ) ;
#42331 = DIRECTION ( 'NONE',  ( 1.000000000000000000, -0.000000000000000000, -0.000000000000000000 ) ) ;
#42333 = CARTESIAN_POINT ( 'NONE',  ( 7.999999999999989342, -2.556712563705454310E-05, 3.267802060586142865 ) ) ;
#42332 = CYLINDRICAL_SURFACE ( 'NONE', #37040, 10.00000000000000178 ) ;
#42334 = VERTEX_POINT ( 'NONE', #9505 ) ;
#42335 = AXIS2_PLACEMENT_3D ( 'NONE', #2433, #41321, #65429 ) ;
#42336 = CARTESIAN_POINT ( 'NONE',  ( -1.432654583217664479, 194.7500000013656063, 138.5412658750000787 ) ) ;
#42337 = CARTESIAN_POINT ( 'NONE',  ( -8.311093377946841443, 54.21874999658601979, 8.311093377946830785 ) ) ;
#42338 = CARTESIAN_POINT ( 'NONE',  ( -11.00000000000000000, 4.556349186104045934, 104.5937500040967763 ) ) ;
#42339 = CARTESIAN_POINT ( 'NONE',  ( 6.951808397369818766E-16, 222.3437499965860127, -11.35316468750000141 ) ) ;
#42340 = CARTESIAN_POINT ( 'NONE',  ( -24.54126587499999701, 207.1875000013656063, 170.0000000000002842 ) ) ;
#42341 = CARTESIAN_POINT ( 'NONE',  ( 11.00000000000000000, 1.347111479062088405E-15, 94.93750000409677625 ) ) ;
#42343 = CARTESIAN_POINT ( 'NONE',  ( 9.797174393178825657E-16, 125.0000000000000000, -8.000000000000000000 ) ) ;
#42342 = CARTESIAN_POINT ( 'NONE',  ( 2.977408999572650039, 123.6875000020483952, -7.188101187500000933 ) ) ;
#42345 = ADVANCED_FACE ( 'NONE', ( #3090 ), #66837, .F. ) ;
#42344 = FACE_OUTER_BOUND ( 'NONE', #64363, .T. ) ;
#42346 = CARTESIAN_POINT ( 'NONE',  ( 8.311093377946834337, 110.1562499965860269, 8.311093377946839666 ) ) ;
#42347 = CARTESIAN_POINT ( 'NONE',  ( -1.836970198721029983E-15, 75.62499999317203958, 10.00000000000000178 ) ) ;
#42348 = CARTESIAN_POINT ( 'NONE',  ( 1.320432766682874540E-15, 90.03125000204838102, 7.188101187500000044 ) ) ;
#42349 = CARTESIAN_POINT ( 'NONE',  ( 3.211159895383560947, 16.31249999863440436, 3.211159895383562723 ) ) ;
#42350 = CARTESIAN_POINT ( 'NONE',  ( 2.449293598294707893E-16, 11.25000000000000000, -4.000000000000001776 ) ) ;
#42351 = DIRECTION ( 'NONE',  ( -0.000000000000000000, 1.000000000000000000, -1.563033456626094573E-30 ) ) ;
#42352 = EDGE_LOOP ( 'NONE', ( #42466, #10814, #65320, #58351 ) ) ;
#42353 = EDGE_LOOP ( 'NONE', ( #6085, #3335, #44153, #24010, #36294 ) ) ;
#42354 = EDGE_CURVE ( 'NONE', #14756, #37555, #60422, .T. ) ;
#42355 = CARTESIAN_POINT ( 'NONE',  ( 6.676582343750003368, 293.1718750017070647, -2.765530957081997254 ) ) ;
#42356 = CARTESIAN_POINT ( 'NONE',  ( -11.35316468749999963, 219.2187500034139873, 0.000000000000000000 ) ) ;
#42357 = CARTESIAN_POINT ( 'NONE',  ( -2.085542519210945728E-15, 169.5312499965860411, 11.35316468750000141 ) ) ;
#42358 = CARTESIAN_POINT ( 'NONE',  ( -7.999999999999991118, 3.313708498984757167, 9.736552779823366421 ) ) ;
#42359 = CARTESIAN_POINT ( 'NONE',  ( -2.828427124746152987, 201.1250000000000284, 200.8284271247462129 ) ) ;
#42360 = LINE ( 'NONE', #46919, #59084 ) ;
#42361 = VECTOR ( 'NONE', #56836, 1000.000000000000000 ) ;
#42362 = CARTESIAN_POINT ( 'NONE',  ( 10.18810118749999916, 4.220049686691935698, 112.3750000020483810 ) ) ;
#42363 = ORIENTED_EDGE ( 'NONE', *, *, #6311, .F. ) ;
#42364 = LINE ( 'NONE', #64650, #62385 ) ;
#42365 = VECTOR ( 'NONE', #5755, 1000.000000000000000 ) ;
#42366 = CARTESIAN_POINT ( 'NONE',  ( -2.828427124746190735, 17.37500000000000000, -2.828427124746191623 ) ) ;
#42367 = CARTESIAN_POINT ( 'NONE',  ( 8.311093377946837890, 141.7187499965859843, -8.311093377946837890 ) ) ;
#42368 = CARTESIAN_POINT ( 'NONE',  ( 3.458734125000016313, 195.8750000013655779, 199.4326545832176976 ) ) ;
#42369 = CARTESIAN_POINT ( 'NONE',  ( 3.458734125000015869, 208.1875000013656063, 198.0000000000000284 ) ) ;
#42370 = CARTESIAN_POINT ( 'NONE',  ( 1.871523826299183495E-15, -10.18810118749999916, 68.40625000204836681 ) ) ;
#42371 = CARTESIAN_POINT ( 'NONE',  ( 3.042071309553159519, 45.05208332991935549, 11.35316468750000141 ) ) ;
#42372 = ORIENTED_EDGE ( 'NONE', *, *, #55922, .T. ) ;
#42373 = CARTESIAN_POINT ( 'NONE',  ( -24.00000000000002842, 208.9375000027312410, 168.3431457505079152 ) ) ;
#42374 = CARTESIAN_POINT ( 'NONE',  ( 4.541265875000002339, 3.437499998634407028, 0.000000000000000000 ) ) ;
#42375 = CARTESIAN_POINT ( 'NONE',  ( -3.317071493978878571, 8.008118988124991233, 8.231865283940630107 ) ) ;
#42376 = CARTESIAN_POINT ( 'NONE',  ( 7.188101187500000044, 16.96874999795161543, 0.000000000000000000 ) ) ;
#42377 = CARTESIAN_POINT ( 'NONE',  ( 2.485281374238575314, 291.3750000034140157, 6.000000000000000888 ) ) ;
#42378 = CARTESIAN_POINT ( 'NONE',  ( 0.6686838642329748783, 220.0000000000000284, 10.97965672913483814 ) ) ;
#42379 = CARTESIAN_POINT ( 'NONE',  ( 7.188101187500001821, 9.937499997951610098, -2.977408999572650483 ) ) ;
#42380 = CARTESIAN_POINT ( 'NONE',  ( -2.977408999572647819, -7.188101187499990274, 6.267802781871754547 ) ) ;
#42381 =( REPRESENTATION_RELATIONSHIP ('NONE','NONE', #46008, #4585 ) REPRESENTATION_RELATIONSHIP_WITH_TRANSFORMATION ( #70087 )SHAPE_REPRESENTATION_RELATIONSHIP( ) );
#42382 = CARTESIAN_POINT ( 'NONE',  ( -7.204075437095967871, 7.204075437095967871, 115.8437500020483810 ) ) ;
#42383 = CARTESIAN_POINT ( 'NONE',  ( -1.836970198721029983E-15, 35.62499999317203248, 10.00000000000000178 ) ) ;
#42384 = CARTESIAN_POINT ( 'NONE',  ( 1.656854249492381914, 1.562499997268813612, 4.000000000000000888 ) ) ;
#42385 = VERTEX_POINT ( 'NONE', #71730 ) ;
#42386 = VECTOR ( 'NONE', #62398, 1000.000000000000000 ) ;
#42387 = CARTESIAN_POINT ( 'NONE',  ( 2.849036369511732440E-14, 196.3750000027311842, 202.0000000000000000 ) ) ;
#42388 = CARTESIAN_POINT ( 'NONE',  ( -2.828427124746209831, 203.3750000000000284, 139.1715728752538723 ) ) ;
#42389 = CARTESIAN_POINT ( 'NONE',  ( -30.82842712474624136, 197.2500000027312126, 167.1715728752542418 ) ) ;
#42390 = CARTESIAN_POINT ( 'NONE',  ( -4.541265875000003227, 2.874999998634407028, 1.881053915767121110 ) ) ;
#42391 = CARTESIAN_POINT ( 'NONE',  ( -5.082755093536324154, 107.8437500020483810, 5.082755093536326818 ) ) ;
#42392 = CARTESIAN_POINT ( 'NONE',  ( 8.263859302085865721, -5.621163452808815464, -0.5584673446549284215 ) ) ;
#42393 = CARTESIAN_POINT ( 'NONE',  ( -3.313708498984757167, 7.999999999999991118, 2.236552783920143561 ) ) ;
#42394 = ORIENTED_EDGE ( 'NONE', *, *, #28240, .T. ) ;
#42395 = CARTESIAN_POINT ( 'NONE',  ( 7.188101187500000044, 24.46874999795161543, 0.000000000000000000 ) ) ;
#42396 = ORIENTED_EDGE ( 'NONE', *, *, #41301, .T. ) ;
#42397 = CARTESIAN_POINT ( 'NONE',  ( 7.999999999999992895, -9.797174393178815797E-16, 0.000000000000000000 ) ) ;
#42398 = CARTESIAN_POINT ( 'NONE',  ( 25.55430564589115505, 205.0625000013656063, 167.5543056458911053 ) ) ;
#42399 = CARTESIAN_POINT ( 'NONE',  ( -8.660254037844387298, 52.08333333333333570, -5.000000000000004441 ) ) ;
#42400 = CARTESIAN_POINT ( 'NONE',  ( 7.188101187500000044, 102.7812500020483810, -8.802885111219163269E-16 ) ) ;
#42401 = CARTESIAN_POINT ( 'NONE',  ( -6.000000000000003553, 296.9374999999999432, -2.485281374238571317 ) ) ;
#42402 = CARTESIAN_POINT ( 'NONE',  ( 30.93407847438118097, 177.8926861767890557, 172.7901722450143893 ) ) ;
#42403 = ORIENTED_EDGE ( 'NONE', *, *, #38882, .T. ) ;
#42404 = EDGE_CURVE ( 'NONE', #57815, #38960, #51653, .T. ) ;
#42405 = EDGE_CURVE ( 'NONE', #48764, #74424, #45990, .T. ) ;
#42406 = CARTESIAN_POINT ( 'NONE',  ( -11.35316468749999785, 233.6979166700806161, -3.042071309553164848 ) ) ;
#42407 = CARTESIAN_POINT ( 'NONE',  ( -3.313708498984760276, 13.96875000000000355, -8.000000000000000000 ) ) ;
#42408 = CARTESIAN_POINT ( 'NONE',  ( 11.35316468750000141, 0.7812499965860163487, 0.000000000000000000 ) ) ;
#42409 = CARTESIAN_POINT ( 'NONE',  ( 2.828427124746153876, 197.0000000027312126, 144.8284271247462129 ) ) ;
#42410 = CYLINDRICAL_SURFACE ( 'NONE', #42335, 10.00000000000000178 ) ;
#42411 = CARTESIAN_POINT ( 'NONE',  ( 5.656854249492381470, 107.7500000040967763, 5.656854249492379694 ) ) ;
#42412 = CARTESIAN_POINT ( 'NONE',  ( 10.00000000000000178, 170.0000000000000000, 0.000000000000000000 ) ) ;
#42413 = DIRECTION ( 'NONE',  ( -0.000000000000000000, -0.000000000000000000, 1.000000000000000000 ) ) ;
#42414 = CARTESIAN_POINT ( 'NONE',  ( -11.00000000000000000, 0.000000000000000000, 118.0000000000000000 ) ) ;
#42415 = CARTESIAN_POINT ( 'NONE',  ( 2.977408999572646486, 7.188101187499992051, 28.39280278187175810 ) ) ;
#42416 = CARTESIAN_POINT ( 'NONE',  ( -5.676582343749998039, 147.7604166632526699, -9.832129032723420536 ) ) ;
#42417 = CARTESIAN_POINT ( 'NONE',  ( -4.898587196589412829E-16, 106.6250000000000000, -8.000000000000000000 ) ) ;
#42418 = CARTESIAN_POINT ( 'NONE',  ( 5.656854249492381470, 97.25000000409677625, 5.656854249492379694 ) ) ;
#42421 = CARTESIAN_POINT ( 'NONE',  ( 1.102182119232618108E-15, 294.2500000000000000, 6.000000000000001776 ) ) ;
#42420 = CARTESIAN_POINT ( 'NONE',  ( -8.000000000000001776, 3.313708498984746509, 26.23655277982336997 ) ) ;
#42419 = CARTESIAN_POINT ( 'NONE',  ( 30.82842712474620583, 206.3750000000000284, 167.1715728752537586 ) ) ;
#42422 = ORIENTED_EDGE ( 'NONE', *, *, #1308, .F. ) ;
#42423 = EDGE_CURVE ( 'NONE', #6283, #66955, #55156, .T. ) ;
#42424 = CARTESIAN_POINT ( 'NONE',  ( 9.832129032723416984, 5.677083329919350163, 5.676582343750006032 ) ) ;
#42425 = CARTESIAN_POINT ( 'NONE',  ( -5.656854249492379694, 7.874999995903221972, -5.656854249492380582 ) ) ;
#42426 = PLANE ( 'NONE',  #4083 ) ;
#42427 = CARTESIAN_POINT ( 'NONE',  ( -9.000000000000000000, -0.8780643052077380384, -9.046311876675927621E-16 ) ) ;
#42428 = CARTESIAN_POINT ( 'NONE',  ( -1.432654583217662259, 208.1250000013656063, 145.4587341250000350 ) ) ;
#42429 =( BOUNDED_CURVE ( )  B_SPLINE_CURVE ( 2, ( #55710, #10046, #19860, #37228, #4024, #60225, #67386, #66261, #49276 ),
 .UNSPECIFIED., .F., .F. ) 
 B_SPLINE_CURVE_WITH_KNOTS ( ( 3, 2, 2, 2, 3 ),
 ( 0.05681818181818182323, 0.06250000000000000000, 0.06818181818181817677, 0.07386363636363636742, 0.07954545454545454419 ),
 .UNSPECIFIED. ) 
 CURVE ( )  GEOMETRIC_REPRESENTATION_ITEM ( )  RATIONAL_B_SPLINE_CURVE ( ( 0.9999999999999998890, 0.9238795325112868495, 1.000000000000000000, 0.9238795325112867385, 1.000000000000000000, 0.9238795325112867385, 1.000000000000000000, 0.9238795325112867385, 1.000000000000000000 ) ) 
 REPRESENTATION_ITEM ( '' )  );
#42430 = CARTESIAN_POINT ( 'NONE',  ( -7.314694799365487832, 124.7669723012753167, -2.521986419001934099 ) ) ;
#42431 = VECTOR ( 'NONE', #14097, 1000.000000000000000 ) ;
#42432 = CARTESIAN_POINT ( 'NONE',  ( -8.660254037844390851, 39.79166665983870388, 4.999999999999998224 ) ) ;
#42433 = CARTESIAN_POINT ( 'NONE',  ( -5.082755093536324154, 107.8437500020483810, 5.082755093536326818 ) ) ;
#42434 = CARTESIAN_POINT ( 'NONE',  ( -4.541265875000002339, 3.874999998634407028, -1.881053915767121998 ) ) ;
#42435 = CYLINDRICAL_SURFACE ( 'NONE', #1204, 11.00000000000000000 ) ;
#42436 = CARTESIAN_POINT ( 'NONE',  ( -3.313708498984757167, 7.999999999999991118, 15.54905277982336465 ) ) ;
#42438 = CARTESIAN_POINT ( 'NONE',  ( -8.000000000000000000, 26.25000000000000711, -9.797174393178825657E-16 ) ) ;
#42437 = LINE ( 'NONE', #1733, #41936 ) ;
#42439 = ORIENTED_EDGE ( 'NONE', *, *, #24957, .T. ) ;
#42440 = CARTESIAN_POINT ( 'NONE',  ( 11.00000000000000000, 1.347111479062088405E-15, 115.7499999999999858 ) ) ;
#42441 = CARTESIAN_POINT ( 'NONE',  ( 2.085542519210945334E-15, 230.4687500034139873, 11.35316468749999963 ) ) ;
#42442 = TOROIDAL_SURFACE ( 'NONE', #1551, 81.50000000000000000, 10.99999999999999822 ) ;
#42443 = CARTESIAN_POINT ( 'NONE',  ( -11.35316468750000141, 128.2812499965860127, -1.390361679473963753E-15 ) ) ;
#42444 = EDGE_LOOP ( 'NONE', ( #13946, #52813, #4113, #42820 ) ) ;
#42445 = CARTESIAN_POINT ( 'NONE',  ( -7.999999999999991118, 0.000000000000000000, 5.517802783920146226 ) ) ;
#42446 = CARTESIAN_POINT ( 'NONE',  ( -10.18810118749999916, 4.220049686691934809, 96.06250000204836681 ) ) ;
#42447 = CARTESIAN_POINT ( 'NONE',  ( -7.999999999999991118, 9.797174393178815797E-16, 30.00000000000000000 ) ) ;
#42448 = CARTESIAN_POINT ( 'NONE',  ( 1.432654583217664701, 195.0000000013656063, 201.4587341250000065 ) ) ;
#42449 = DIRECTION ( 'NONE',  ( 0.000000000000000000, 0.000000000000000000, 1.000000000000000000 ) ) ;
#42451 = CARTESIAN_POINT ( 'NONE',  ( 8.311093377946837890, 116.4062499965860269, -8.311093377946837890 ) ) ;
#42450 = CARTESIAN_POINT ( 'NONE',  ( -5.656854249492378806, 95.18750000000000000, 5.656854249492381470 ) ) ;
#42452 = ADVANCED_FACE ( 'NONE', ( #66078 ), #56269, .F. ) ;
#42453 = CARTESIAN_POINT ( 'NONE',  ( -29.65685424949241877, 209.0625000000000568, 166.0000000000004263 ) ) ;
#42454 = DIRECTION ( 'NONE',  ( 0.000000000000000000, -0.7071067811865425767, -0.7071067811865525687 ) ) ;
#42455 = ORIENTED_EDGE ( 'NONE', *, *, #3521, .T. ) ;
#42456 = CIRCLE ( 'NONE', #12319, 18.99999999999998934 ) ;
#42457 = CARTESIAN_POINT ( 'NONE',  ( 7.320508075688774596, 212.4999999931719969, -7.320508075688774596 ) ) ;
#42458 = CARTESIAN_POINT ( 'NONE',  ( 7.778174593052023411, -7.778174593052021635, 73.56249999999998579 ) ) ;
#42459 = CARTESIAN_POINT ( 'NONE',  ( 0.000000000000000000, 19.05255888325788050, 0.000000000000000000 ) ) ;
#42460 = CARTESIAN_POINT ( 'NONE',  ( -5.676582343749998039, 97.76041666325269830, -9.832129032723420536 ) ) ;
#42461 = CARTESIAN_POINT ( 'NONE',  ( 2.445694354108839619, 204.8125000013656063, 200.4456943541088663 ) ) ;
#42462 = CARTESIAN_POINT ( 'NONE',  ( 2.977408999572652260, 12.56249999795161365, 7.188101187500000044 ) ) ;
#42463 = B_SPLINE_CURVE_WITH_KNOTS ( 'NONE', 3,
 ( #41416, #47058, #6716, #5605, #52737, #23686, #64428, #11258, #28976, #34663, #58043, #51614 ),
 .UNSPECIFIED., .F., .F.,
 ( 4, 2, 2, 2, 2, 4 ),
 ( 0.000000000000000000, 0.002547658444427995661, 0.005095316888855991322, 0.006369146111069989152, 0.007642975333283986983, 0.01019063377771198264 ),
 .UNSPECIFIED. ) ;
#42464 = CARTESIAN_POINT ( 'NONE',  ( 7.204075437095968759, -7.204075437095966983, 91.09375000204838102 ) ) ;
#42465 = CARTESIAN_POINT ( 'NONE',  ( -11.35316468750000141, 13.80208332991934661, 3.042071309553159963 ) ) ;
#42466 = ORIENTED_EDGE ( 'NONE', *, *, #47817, .F. ) ;
#42467 = FACE_BOUND ( 'NONE', #56329, .T. ) ;
#42468 = CARTESIAN_POINT ( 'NONE',  ( 10.00000000000000000, 245.6250000068279746, -1.224646799147353256E-15 ) ) ;
#42469 = CARTESIAN_POINT ( 'NONE',  ( -7.999999999994639843, -6.164467849698474977E-06, 23.51803407853789807 ) ) ;
#42470 = CARTESIAN_POINT ( 'NONE',  ( -4.220049686691937474, -10.18810118749999738, 75.81250000204838102 ) ) ;
#42471 = DIRECTION ( 'NONE',  ( -0.000000000000000000, 1.000000000000000000, -0.000000000000000000 ) ) ;
#42472 = CARTESIAN_POINT ( 'NONE',  ( -4.898587196589412829E-16, 93.31250000409677625, -8.000000000000000000 ) ) ;
#42473 = CARTESIAN_POINT ( 'NONE',  ( 6.676582343750003368, 291.0156250017069510, -2.765530957081997254 ) ) ;
#42474 = CARTESIAN_POINT ( 'NONE',  ( 7.320508075688774596, 127.4999999931720538, -7.320508075688774596 ) ) ;
#42475 = CARTESIAN_POINT ( 'NONE',  ( -3.042071309553173730, 219.6354166632526699, 11.35316468749999785 ) ) ;
#42476 = ADVANCED_FACE ( 'NONE', ( #20804 ), #16677, .F. ) ;
#42477 = CARTESIAN_POINT ( 'NONE',  ( 11.35316468750000141, 131.0937499965860127, 0.000000000000000000 ) ) ;
#42478 = CARTESIAN_POINT ( 'NONE',  ( 7.204075437095966983, 7.204075437095967871, 83.59375000204836681 ) ) ;
#42479 = CARTESIAN_POINT ( 'NONE',  ( -30.44569435410883429, 198.5625000013656063, 167.5543056458915885 ) ) ;
#42480 = CARTESIAN_POINT ( 'NONE',  ( 3.313708498984762496, 23.71875000000000355, 7.999999999999998224 ) ) ;
#42481 = CARTESIAN_POINT ( 'NONE',  ( -8.342170076843785083E-16, 10.18749999863440614, 4.541265875000002339 ) ) ;
#42482 = ORIENTED_EDGE ( 'NONE', *, *, #1965, .F. ) ;
#42483 = CARTESIAN_POINT ( 'NONE',  ( -29.65685424949229443, 208.5625000027312410, 174.0000000000004547 ) ) ;
#42484 = CARTESIAN_POINT ( 'NONE',  ( 2.828427124746209831, 206.5000000027312126, 200.8284271247462129 ) ) ;
#42485 = CARTESIAN_POINT ( 'NONE',  ( 2.445694354108783219, 199.8125000013656063, 139.5543056458912190 ) ) ;
#42486 = CARTESIAN_POINT ( 'NONE',  ( 2.828427124746153876, 204.0000000027312126, 144.8284271247462129 ) ) ;
#42487 = VECTOR ( 'NONE', #6381, 1000.000000000000000 ) ;
#42488 = CARTESIAN_POINT ( 'NONE',  ( 0.000000000000000000, 130.3999865490244190, 45.94057108883949070 ) ) ;
#42489 = CARTESIAN_POINT ( 'NONE',  ( -10.18810118749999916, 4.220049686691934809, 67.93750000204838102 ) ) ;
#42490 = ORIENTED_EDGE ( 'NONE', *, *, #34271, .F. ) ;
#42491 = CARTESIAN_POINT ( 'NONE',  ( 7.188101187500000044, 4.968749997951610986, 0.000000000000000000 ) ) ;
#42492 = CARTESIAN_POINT ( 'NONE',  ( -2.775557561562891351E-14, 210.0000000000000284, 142.0000000000000568 ) ) ;
#42493 = AXIS2_PLACEMENT_3D ( 'NONE', #21692, #44718, #61698 ) ;
#42494 = EDGE_CURVE ( 'NONE', #9076, #12154, #38551, .T. ) ;
#42495 = CARTESIAN_POINT ( 'NONE',  ( 5.082755093536326818, 117.5937500020483810, 5.082755093536325042 ) ) ;
#42496 = CARTESIAN_POINT ( 'NONE',  ( -1.377000000000000002, 261.4319999999996753, 5.673918265509175107 ) ) ;
#42497 = CARTESIAN_POINT ( 'NONE',  ( 2.765530957082001251, 292.7656250017069510, 6.676582343749999815 ) ) ;
#42499 = CARTESIAN_POINT ( 'NONE',  ( -2.828427124746192067, 15.37499999726881406, 2.828427124746190735 ) ) ;
#42498 = CARTESIAN_POINT ( 'NONE',  ( -6.951808397369817780E-16, 237.6562500034140157, -11.35316468749999963 ) ) ;
#42500 = ORIENTED_EDGE ( 'NONE', *, *, #37754, .F. ) ;
#42501 = CARTESIAN_POINT ( 'NONE',  ( 5.676582343750005144, 220.8854166700806445, 9.832129032723416984 ) ) ;
#42502 = EDGE_CURVE ( 'NONE', #64593, #20187, #10788, .T. ) ;
#42503 = CARTESIAN_POINT ( 'NONE',  ( -5.082755093536317936, -5.082755093536320601, 0.1740527818717522990 ) ) ;
#42504 = LINE ( 'NONE', #8179, #73113 ) ;
#42505 = CARTESIAN_POINT ( 'NONE',  ( -2.445694354108783219, 198.8125000013656063, 200.4456943541088663 ) ) ;
#42506 = EDGE_LOOP ( 'NONE', ( #18444, #29863, #35539, #26870 ) ) ;
#42507 = CARTESIAN_POINT ( 'NONE',  ( -14.00000000000000178, -2.250000000005106138, 10.23492587299426404 ) ) ;
#42508 = CARTESIAN_POINT ( 'NONE',  ( 5.656854249492379694, 97.43750000000000000, -5.656854249492380582 ) ) ;
#42509 = CARTESIAN_POINT ( 'NONE',  ( -9.832129032723420536, 104.0104166632526841, 5.676582343749997150 ) ) ;
#42510 = DIRECTION ( 'NONE',  ( -0.000000000000000000, -1.000000000000000000, -0.000000000000000000 ) ) ;
#42511 = CARTESIAN_POINT ( 'NONE',  ( 7.778174593052021635, 7.778174593052023411, 79.93750000000000000 ) ) ;
#42514 = CARTESIAN_POINT ( 'NONE',  ( -2.828427124746152987, 202.1250000000000284, 200.8284271247462129 ) ) ;
#42513 = CARTESIAN_POINT ( 'NONE',  ( 30.44569435410883429, 205.5625000013656063, 172.4456943541086957 ) ) ;
#42512 = CARTESIAN_POINT ( 'NONE',  ( 26.56734541678238060, 201.2500000013656063, 166.5412658749999650 ) ) ;
#42515 = ORIENTED_EDGE ( 'NONE', *, *, #27662, .T. ) ;
#42516 = EDGE_CURVE ( 'NONE', #68675, #17249, #15140, .T. ) ;
#42517 = EDGE_CURVE ( 'NONE', #41775, #8028, #46421, .T. ) ;
#42518 = CARTESIAN_POINT ( 'NONE',  ( 5.656854249492379694, 100.4375000000000000, -5.656854249492380582 ) ) ;
#42519 = CARTESIAN_POINT ( 'NONE',  ( 11.35316468750000141, 215.7812499965860411, 0.000000000000000000 ) ) ;
#42521 = ADVANCED_FACE ( 'NONE', ( #50969 ), #46427, .F. ) ;
#42520 = CARTESIAN_POINT ( 'NONE',  ( 2.445694354108783664, 199.3125000013656063, 144.4456943541088663 ) ) ;
#42522 = B_SPLINE_CURVE_WITH_KNOTS ( 'NONE', 3,
 ( #63158, #26301, #63529, #11853, #34520, #56770, #5457, #28459, #189, #22043, #51465, #22409, #3314 ),
 .UNSPECIFIED., .F., .F.,
 ( 4, 2, 2, 1, 2, 2, 4 ),
 ( 0.8219935333350478768, 0.8664951500012858521, 0.8887459583344048397, 0.9109967666675239384, 0.9332475750006429260, 0.9554983833337619137, 1.000000000000000000 ),
 .UNSPECIFIED. ) ;
#42523 = CARTESIAN_POINT ( 'NONE',  ( 30.44569435410883429, 203.0625000013656063, 167.5543056458911053 ) ) ;
#42524 = CARTESIAN_POINT ( 'NONE',  ( 4.556349186104045934, 11.00000000000000000, 116.2187500040967763 ) ) ;
#42525 = CARTESIAN_POINT ( 'NONE',  ( 9.832129032723416984, 195.6770833299193839, 5.676582343750006032 ) ) ;
#42526 = CARTESIAN_POINT ( 'NONE',  ( 2.977408999572650039, 94.06250000204838102, -7.188101187500000933 ) ) ;
#42527 = CARTESIAN_POINT ( 'NONE',  ( -27.99999999999995737, 198.5000000000000000, 174.0000000000003695 ) ) ;
#42528 = CARTESIAN_POINT ( 'NONE',  ( 3.211159895383560947, 13.18749999863440792, 3.211159895383562723 ) ) ;
#42529 = CARTESIAN_POINT ( 'NONE',  ( 25.55430564589115150, 198.5625000013656063, 172.4456943541086957 ) ) ;
#42530 = CARTESIAN_POINT ( 'NONE',  ( 5.082755093536318824, 5.082755093536319713, 4.299052781871752771 ) ) ;
#42531 = CARTESIAN_POINT ( 'NONE',  ( -11.35316468750000141, 78.28124999658601268, -1.390361679473963753E-15 ) ) ;
#42532 = EDGE_LOOP ( 'NONE', ( #55876, #59612, #29680 ) ) ;
#42533 = CARTESIAN_POINT ( 'NONE',  ( -5.000000000000000000, -52.84634075987140278, 43.22150062466516118 ) ) ;
#42534 = DIRECTION ( 'NONE',  ( -1.084202172485504434E-16, 1.000000000000000000, 0.000000000000000000 ) ) ;
#42535 = CARTESIAN_POINT ( 'NONE',  ( -7.594050593749991585, 0.000000000000000000, 29.09592778084756048 ) ) ;
#42536 = CARTESIAN_POINT ( 'NONE',  ( -3.999999999999959144, 195.0625000000000000, 199.6568542494924259 ) ) ;
#42537 = CARTESIAN_POINT ( 'NONE',  ( -3.042071309553164404, 82.23958332991935549, -11.35316468749999963 ) ) ;
#42538 = ORIENTED_EDGE ( 'NONE', *, *, #44850, .T. ) ;
#42539 = CARTESIAN_POINT ( 'NONE',  ( 7.204075437095968759, -7.204075437095966983, 89.59375000204838102 ) ) ;
#42540 = CARTESIAN_POINT ( 'NONE',  ( 10.18810118750000093, -4.220049686691933921, 111.8125000020483952 ) ) ;
#42541 = CARTESIAN_POINT ( 'NONE',  ( -7.999999999999998224, 102.5937500000000000, 3.313708498984766049 ) ) ;
#42542 = CARTESIAN_POINT ( 'NONE',  ( -7.347880794884122694E-16, 20.75000000000000000, 4.000000000000001776 ) ) ;
#42544 = CARTESIAN_POINT ( 'NONE',  ( -11.35316468749999785, 78.07291666325269830, -3.042071309553167957 ) ) ;
#42543 = CARTESIAN_POINT ( 'NONE',  ( -2.986204309486589110E-14, 67.59332269700053075, 20.03478791450399399 ) ) ;
#42545 = EDGE_CURVE ( 'NONE', #35750, #49847, #71974, .T. ) ;
#42546 = CARTESIAN_POINT ( 'NONE',  ( 5.656854249492374365, 5.656854249492375253, 27.45530278392014978 ) ) ;
#42547 = CARTESIAN_POINT ( 'NONE',  ( -3.579993502731768196, 194.7328194181653771, 140.9139922525571365 ) ) ;
#42548 = CARTESIAN_POINT ( 'NONE',  ( -10.00000000000000178, 164.3749999931720254, -1.224646799147353454E-15 ) ) ;
#42549 = CARTESIAN_POINT ( 'NONE',  ( -2.977408999572651815, 93.31250000204838102, 7.188101187500000933 ) ) ;
#42550 = CARTESIAN_POINT ( 'NONE',  ( 0.000000000000000000, 300.0000000000000000, 0.000000000000000000 ) ) ;
#42551 = CARTESIAN_POINT ( 'NONE',  ( -5.676582343749998039, 62.76041666325269119, -9.832129032723420536 ) ) ;
#42552 =( BOUNDED_CURVE ( )  B_SPLINE_CURVE ( 2, ( #8580, #48929, #2923, #54616, #60253, #42894, #48556, #8207, #30846, #53867, #7839, #31966, #37635 ),
 .UNSPECIFIED., .F., .F. ) 
 B_SPLINE_CURVE_WITH_KNOTS ( ( 3, 2, 2, 2, 2, 2, 3 ),
 ( 1.742685697302758463, 1.747919628595612451, 1.753153559888466662, 1.758387491181320650, 1.763621422474174860, 1.768855353767028848, 1.774089285059882615 ),
 .UNSPECIFIED. ) 
 CURVE ( )  GEOMETRIC_REPRESENTATION_ITEM ( )  RATIONAL_B_SPLINE_CURVE ( ( 1.000000000000271561, 0.9659258262887968627, 1.000000000000000000, 0.9659258262890683122, 1.000000000000000000, 0.9659258262890683122, 1.000000000000000000, 0.9659258262890683122, 1.000000000000000000, 0.9659258262890683122, 1.000000000000000000, 0.9659258262890662028, 1.000000000000001998 ) ) 
 REPRESENTATION_ITEM ( '' )  );
#42553 = CARTESIAN_POINT ( 'NONE',  ( 7.204075437095966983, 7.204075437095967871, 104.9687500020483810 ) ) ;
#42554 = CARTESIAN_POINT ( 'NONE',  ( -5.676582343749998039, 192.4479166632526983, -9.832129032723420536 ) ) ;
#42555 = EDGE_LOOP ( 'NONE', ( #64779, #68649, #46645, #7067 ) ) ;
#42556 = CARTESIAN_POINT ( 'NONE',  ( 7.999999999999932498, -3.313708498984815787, 27.17405278392014623 ) ) ;
#42557 = DIRECTION ( 'NONE',  ( 0.000000000000000000, 0.000000000000000000, 1.000000000000000000 ) ) ;
#42559 = CARTESIAN_POINT ( 'NONE',  ( -3.042071309553173730, 189.3229166632526699, 11.35316468749999785 ) ) ;
#42558 = LINE ( 'NONE', #30874, #7416 ) ;
#42560 = VECTOR ( 'NONE', #38722, 1000.000000000000000 ) ;
#42561 = CARTESIAN_POINT ( 'NONE',  ( -4.999999999999998224, 193.5416666598387110, -8.660254037844389075 ) ) ;
#42562 = CARTESIAN_POINT ( 'NONE',  ( -10.00000000000000000, 233.1250000068279746, 0.000000000000000000 ) ) ;
#42563 = CARTESIAN_POINT ( 'NONE',  ( -29.65685424949231219, 200.0625000000000284, 166.0000000000003411 ) ) ;
#42564 = ORIENTED_EDGE ( 'NONE', *, *, #9043, .F. ) ;
#42565 = CARTESIAN_POINT ( 'NONE',  ( 8.311093377946834337, 180.4687499965859843, 8.311093377946839666 ) ) ;
#42566 = CARTESIAN_POINT ( 'NONE',  ( 7.188101187499992051, 8.802885111219154394E-16, 21.73655278187175455 ) ) ;
#42567 = VECTOR ( 'NONE', #14943, 1000.000000000000000 ) ;
#42568 = CARTESIAN_POINT ( 'NONE',  ( 7.999999999999991118, 9.797174393178815797E-16, 16.76780278392014978 ) ) ;
#42569 = ORIENTED_EDGE ( 'NONE', *, *, #69448, .F. ) ;
#42570 = CARTESIAN_POINT ( 'NONE',  ( 8.000000000000000000, 97.43750000409677625, -9.797174393178825657E-16 ) ) ;
#42571 = CARTESIAN_POINT ( 'NONE',  ( -10.00000000000000178, 2.500000000000000000, -1.224646799147353454E-15 ) ) ;
#42572 = VECTOR ( 'NONE', #73189, 1000.000000000000114 ) ;
#42573 = CARTESIAN_POINT ( 'NONE',  ( 4.000000000000000888, 17.93750000000000000, 1.656854249492384135 ) ) ;
#42574 = CARTESIAN_POINT ( 'NONE',  ( 4.541265875000002339, 15.37499999863440614, -1.881053915767121776 ) ) ;
#42575 = CARTESIAN_POINT ( 'NONE',  ( -5.656854249492373476, -5.656854249492376141, 14.70530278392014800 ) ) ;
#42576 = CARTESIAN_POINT ( 'NONE',  ( -7.778174593052020747, -7.778174593052023411, 77.87500000409677625 ) ) ;
#42577 = EDGE_CURVE ( 'NONE', #69767, #33807, #61284, .T. ) ;
#42578 = ORIENTED_EDGE ( 'NONE', *, *, #72930, .T. ) ;
#42579 = CARTESIAN_POINT ( 'NONE',  ( 4.999999999999995559, -16.24494643555759410, -69.83755725260751035 ) ) ;
#42580 = CARTESIAN_POINT ( 'NONE',  ( 7.188101187500000044, 96.40625000204838102, -8.802885111219163269E-16 ) ) ;
#42582 = CARTESIAN_POINT ( 'NONE',  ( -7.999999999999991118, 0.000000000000000000, 21.83030277982336997 ) ) ;
#42581 = CARTESIAN_POINT ( 'NONE',  ( 1.224646799147353256E-15, 0.000000000000000000, 10.00000000000000000 ) ) ;
#42583 = SHAPE_DEFINITION_REPRESENTATION ( #65518, #22863 ) ;
#42584 = ORIENTED_EDGE ( 'NONE', *, *, #6353, .T. ) ;
#42585 = CARTESIAN_POINT ( 'NONE',  ( -5.082755093536317936, -5.082755093536320601, 16.67405278187175810 ) ) ;
#42586 = ORIENTED_EDGE ( 'NONE', *, *, #9926, .F. ) ;
#42587 = B_SPLINE_CURVE_WITH_KNOTS ( 'NONE', 3,
 ( #17620, #17244, #1408, #34626, #51964, #673, #301, #52706, #41014, #12336 ),
 .UNSPECIFIED., .F., .F.,
 ( 4, 2, 2, 2, 4 ),
 ( 0.000000000000000000, 0.001314083742622679674, 0.002628167485245360650, 0.003942251227868041191, 0.005256334970490722167 ),
 .UNSPECIFIED. ) ;
#42588 = EDGE_LOOP ( 'NONE', ( #63231, #18460, #30516, #18541, #67099, #61502, #47063, #13775, #30246, #38896, #56631, #22166, #53279, #3027, #64183, #16633, #20799, #61565, #48561, #47171, #67047, #37401, #16581, #68284, #54402, #2200, #25581, #48293, #39721, #39241, #27655, #13596, #32753 ) ) ;
#42589 = CARTESIAN_POINT ( 'NONE',  ( -7.204075437095965206, -7.204075437095968759, 81.34375000204838102 ) ) ;
#42590 = CARTESIAN_POINT ( 'NONE',  ( 3.313708498984762496, -7.999999999999989342, 5.986552783920146226 ) ) ;
#42591 = CARTESIAN_POINT ( 'NONE',  ( 4.556349186104045934, 11.00000000000000000, 95.03124999999998579 ) ) ;
#42594 = CARTESIAN_POINT ( 'NONE',  ( 6.676582343750001591, 295.1093750017069510, -8.176455196517173205E-16 ) ) ;
#42593 = CARTESIAN_POINT ( 'NONE',  ( 25.17157287525377996, 199.7500000027312126, 167.1715728752537586 ) ) ;
#42592 = DIRECTION ( 'NONE',  ( 0.000000000000000000, 0.000000000000000000, 1.000000000000000000 ) ) ;
#42595 = CARTESIAN_POINT ( 'NONE',  ( 8.660254037844385522, 154.5833333333333428, 5.000000000000005329 ) ) ;
#42596 = CIRCLE ( 'NONE', #25739, 14.00000000000000000 ) ;
#42597 = CARTESIAN_POINT ( 'NONE',  ( -26.34314575050763096, 203.5625000000000284, 174.0000000000003979 ) ) ;
#42598 = CARTESIAN_POINT ( 'NONE',  ( 32.00000000000000000, 209.2500000000000284, 169.9999999999999432 ) ) ;
#42599 = CARTESIAN_POINT ( 'NONE',  ( -5.656854249492375253, 5.656854249492375253, 15.64280277982336642 ) ) ;
#42600 = DIRECTION ( 'NONE',  ( 0.000000000000000000, 0.000000000000000000, -1.000000000000000000 ) ) ;
#42601 = EDGE_CURVE ( 'NONE', #64342, #16471, #68323, .T. ) ;
#42602 = CARTESIAN_POINT ( 'NONE',  ( 24.54126587499997925, 197.2500000013656063, 171.4326545832175555 ) ) ;
#42603 = CARTESIAN_POINT ( 'NONE',  ( -2.977408999572654480, 9.374999997951610098, 7.188101187499999156 ) ) ;
#42604 = CARTESIAN_POINT ( 'NONE',  ( 7.999999999999991118, 3.313708498984757611, 24.36155278392014623 ) ) ;
#42605 = DIRECTION ( 'NONE',  ( -0.000000000000000000, -1.000000000000000000, -0.000000000000000000 ) ) ;
#42606 = CARTESIAN_POINT ( 'NONE',  ( 7.188101187500002709, 108.6875000020483810, 2.977408999572649151 ) ) ;
#42608 = CARTESIAN_POINT ( 'NONE',  ( -2.828427124746190735, 16.37500000000000000, -2.828427124746191623 ) ) ;
#42607 = CARTESIAN_POINT ( 'NONE',  ( 28.00000000000002487, 208.1250000027312126, 173.9999999999999147 ) ) ;
#42609 = FACE_OUTER_BOUND ( 'NONE', #38293, .T. ) ;
#42610 = CARTESIAN_POINT ( 'NONE',  ( -27.99999999999996092, 207.5000000000000284, 174.0000000000003695 ) ) ;
#42611 = CARTESIAN_POINT ( 'NONE',  ( 1.320432766682872962E-15, -7.188101187499992051, 20.23655278187175455 ) ) ;
#42612 = CARTESIAN_POINT ( 'NONE',  ( 0.000000000000000000, 192.0000000000000284, 207.0000000000000568 ) ) ;
#42613 = CARTESIAN_POINT ( 'NONE',  ( -5.676582343749998039, 37.44791666325268409, -9.832129032723420536 ) ) ;
#42614 = CARTESIAN_POINT ( 'NONE',  ( 28.00000000000001776, 200.5000000000000000, 165.9999999999998863 ) ) ;
#42615 = CARTESIAN_POINT ( 'NONE',  ( 8.660254037844389075, 12.29166665983870033, -5.000000000000000000 ) ) ;
#42616 = CARTESIAN_POINT ( 'NONE',  ( 1.102182119232618108E-15, 295.2500000000000000, 6.000000000000001776 ) ) ;
#42617 = ORIENTED_EDGE ( 'NONE', *, *, #58204, .F. ) ;
#42618 = DIRECTION ( 'NONE',  ( 0.000000000000000000, 0.000000000000000000, -1.000000000000000000 ) ) ;
#42619 = CARTESIAN_POINT ( 'NONE',  ( -7.999999999999968914, 3.313708498984778039, 18.73655277982336287 ) ) ;
#42620 = CARTESIAN_POINT ( 'NONE',  ( -11.35316468749999785, 33.07291666325268409, -3.042071309553167513 ) ) ;
#42621 = CARTESIAN_POINT ( 'NONE',  ( -10.99999999999999822, -4.556349186104052151, 79.28125000409677625 ) ) ;
#42622 = CARTESIAN_POINT ( 'NONE',  ( -1.432654583217664701, 205.0000000013655779, 138.5412658750000787 ) ) ;
#42623 = CARTESIAN_POINT ( 'NONE',  ( 1.102182119232618108E-15, 299.2500000000000000, 6.000000000000001776 ) ) ;
#42624 = CARTESIAN_POINT ( 'NONE',  ( -1.469576158976823947E-15, 24.93749999590322375, 8.000000000000000000 ) ) ;
#42626 = CARTESIAN_POINT ( 'NONE',  ( -9.832129032723418760, 37.86458332991934839, -5.676582343750004256 ) ) ;
#42625 = CARTESIAN_POINT ( 'NONE',  ( 1.320432766682874540E-15, 105.0312500020483810, 7.188101187500000044 ) ) ;
#42627 = EDGE_CURVE ( 'NONE', #30484, #19919, #5700, .T. ) ;
#42628 = CARTESIAN_POINT ( 'NONE',  ( -3.313708498984757167, 7.999999999999991118, 17.04905277982336642 ) ) ;
#42629 = CARTESIAN_POINT ( 'NONE',  ( 9.832129032723420536, 151.1979166632526983, -5.676582343749999815 ) ) ;
#42630 = EDGE_CURVE ( 'NONE', #71723, #5819, #432, .T. ) ;
#42632 = CARTESIAN_POINT ( 'NONE',  ( 10.00000000000000000, 126.6666666598386826, 2.679491924311236062 ) ) ;
#42631 = PRODUCT ( 'hexagon nut style 1_is_IS 1364-3 - M16-W-N', 'hexagon nut style 1_is_IS 1364-3 - M16-W-N', '', ( #36933 ) ) ;
#42633 = CARTESIAN_POINT ( 'NONE',  ( -5.082755093536325930, 107.8437500020483810, -5.082755093536325930 ) ) ;
#42634 = VECTOR ( 'NONE', #71050, 1000.000000000000000 ) ;
#42635 = ORIENTED_EDGE ( 'NONE', *, *, #48153, .T. ) ;
#42636 = CARTESIAN_POINT ( 'NONE',  ( 0.000000000000000000, 20.39230484541327471, -10.20000000000000284 ) ) ;
#42637 = CARTESIAN_POINT ( 'NONE',  ( -11.35316468749999785, 18.38541666325268054, -3.042071309553167957 ) ) ;
#42638 = VERTEX_POINT ( 'NONE', #68693 ) ;
#42639 = CARTESIAN_POINT ( 'NONE',  ( -38.00000000000000000, 272.0000000000000000, 3.791916237172779019E-14 ) ) ;
#42640 = DIRECTION ( 'NONE',  ( 1.000000000000000000, 0.000000000000000000, 1.652117596168387509E-16 ) ) ;
#42642 = CARTESIAN_POINT ( 'NONE',  ( 3.042071309553159519, 154.7395833299193555, 11.35316468750000141 ) ) ;
#42641 = CARTESIAN_POINT ( 'NONE',  ( -26.24676564526887290, -22.07761781137391921, 147.6128217146538191 ) ) ;
#42643 = CARTESIAN_POINT ( 'NONE',  ( -6.900000000000001243, 8.450062914116738633E-16, -0.7702282920306856573 ) ) ;
#42644 = CARTESIAN_POINT ( 'NONE',  ( 3.313708498984762496, -7.999999999999989342, 14.85530278432982243 ) ) ;
#42645 = CARTESIAN_POINT ( 'NONE',  ( -1.836970198721029983E-15, 225.6249999931720254, 10.00000000000000178 ) ) ;
#42646 = CARTESIAN_POINT ( 'NONE',  ( 9.832129032723420536, 235.9895833367473301, 5.676582343749996262 ) ) ;
#42647 = CARTESIAN_POINT ( 'NONE',  ( 7.204075437095966983, 7.204075437095967871, 88.46875000204838102 ) ) ;
#42648 = EDGE_LOOP ( 'NONE', ( #43570, #61911, #24731 ) ) ;
#42649 = EDGE_CURVE ( 'NONE', #67735, #67846, #71822, .T. ) ;
#42650 = DIRECTION ( 'NONE',  ( -0.000000000000000000, 1.000000000000000000, -0.000000000000000000 ) ) ;
#42651 = DIRECTION ( 'NONE',  ( 0.000000000000000000, 0.000000000000000000, 1.000000000000000000 ) ) ;
#42652 = CARTESIAN_POINT ( 'NONE',  ( -11.35316468749999785, 108.3854166632526841, -3.042071309553167513 ) ) ;
#42653 = CARTESIAN_POINT ( 'NONE',  ( 10.18810118749999916, 1.247682550866122264E-15, 101.4062500020483810 ) ) ;
#42654 = CARTESIAN_POINT ( 'NONE',  ( 4.541265875000001451, 16.37499999863440436, 1.881053915767124440 ) ) ;
#42655 = ORIENTED_EDGE ( 'NONE', *, *, #44925, .F. ) ;
#42656 = VERTEX_POINT ( 'NONE', #67954 ) ;
#42657 = CARTESIAN_POINT ( 'NONE',  ( -3.313708498984765161, 11.53125000000000178, 7.999999999999998224 ) ) ;
#42658 = CARTESIAN_POINT ( 'NONE',  ( 4.541265875000002339, 3.499999998634407028, -1.881053915767121554 ) ) ;
#42659 = CARTESIAN_POINT ( 'NONE',  ( -2.977408999572650039, 2.437499997951610542, -7.188101187500001821 ) ) ;
#42660 = CARTESIAN_POINT ( 'NONE',  ( -3.313708498984762496, 116.4687500040967905, 7.999999999999998224 ) ) ;
#42661 =( BOUNDED_CURVE ( )  B_SPLINE_CURVE ( 2, ( #50172, #61867, #27155, #67161, #39233, #62233, #72440, #72818, #38863, #21498, #15828, #43383, #15456 ),
 .UNSPECIFIED., .F., .F. ) 
 B_SPLINE_CURVE_WITH_KNOTS ( ( 3, 2, 2, 2, 2, 2, 3 ),
 ( 0.07849216663199026778, 0.08372612650475230733, 0.08896008637751434689, 0.09419404625027635869, 0.09942800612303839825, 0.1046619659958004378, 0.1098959258685624774 ),
 .UNSPECIFIED. ) 
 CURVE ( )  GEOMETRIC_REPRESENTATION_ITEM ( )  RATIONAL_B_SPLINE_CURVE ( ( 1.000000000000247802, 0.9659258262888206215, 1.000000000000000000, 0.9659258262890683122, 1.000000000000000000, 0.9659258262890683122, 1.000000000000000000, 0.9659258262890683122, 1.000000000000000000, 0.9659258262890683122, 1.000000000000000000, 0.9659258262890684232, 0.9999999999999998890 ) ) 
 REPRESENTATION_ITEM ( '' )  );
#42662 = CARTESIAN_POINT ( 'NONE',  ( -6.238412754330611322E-16, 10.18810118749999916, 99.15625000204838102 ) ) ;
#42663 =( NAMED_UNIT ( * ) SI_UNIT ( $, .STERADIAN. ) SOLID_ANGLE_UNIT ( ) );
#42664 = CARTESIAN_POINT ( 'NONE',  ( -4.000000000000002665, 3.562500000000000444, 1.656854249492380804 ) ) ;
#42665 = CARTESIAN_POINT ( 'NONE',  ( 4.000000000000001776, 15.81249999726881228, -1.656854249492381248 ) ) ;
#42666 = CARTESIAN_POINT ( 'NONE',  ( -1.881053915767124440, 1.999999998634406584, 4.541265875000001451 ) ) ;
#42667 = CARTESIAN_POINT ( 'NONE',  ( 3.458734124999959914, 209.3750000013656063, 143.4326545832176976 ) ) ;
#42668 = CARTESIAN_POINT ( 'NONE',  ( -3.458734124999959914, 196.4375000013655779, 198.0000000000000284 ) ) ;
#42669 = ADVANCED_FACE ( 'NONE', ( #40401 ), #40029, .F. ) ;
#42671 = CARTESIAN_POINT ( 'NONE',  ( -10.00000000000000000, 224.1666666598387110, -2.679491924311229845 ) ) ;
#42670 = CARTESIAN_POINT ( 'NONE',  ( -30.44569435410875968, 199.8125000013656063, 172.4456943541092642 ) ) ;
#42672 = CARTESIAN_POINT ( 'NONE',  ( -4.541265875000002339, 15.81249999863440436, -5.561446717895856393E-16 ) ) ;
#42673 = CARTESIAN_POINT ( 'NONE',  ( -7.188101187499991163, 2.977408999572646930, 8.892802781871754547 ) ) ;
#42674 = EDGE_LOOP ( 'NONE', ( #67067, #19709, #42584, #18179 ) ) ;
#42675 = EDGE_CURVE ( 'NONE', #35159, #69421, #5020, .T. ) ;
#42676 = ORIENTED_EDGE ( 'NONE', *, *, #74503, .T. ) ;
#42677 = CARTESIAN_POINT ( 'NONE',  ( 7.204075437095968759, -7.204075437095966983, 96.71875000204838102 ) ) ;
#42678 = CARTESIAN_POINT ( 'NONE',  ( 7.320508075688773708, 124.3750000000000000, 7.320508075688777261 ) ) ;
#42679 = CARTESIAN_POINT ( 'NONE',  ( -25.55430564589115150, 202.3125000013656063, 172.4456943541091789 ) ) ;
#42680 = CARTESIAN_POINT ( 'NONE',  ( -31.99999999999999289, 199.2500000000000000, 170.0000000000003979 ) ) ;
#42681 = CARTESIAN_POINT ( 'NONE',  ( -2.445694354108784108, 209.5625000013656063, 195.5543056458912190 ) ) ;
#42682 = DIRECTION ( 'NONE',  ( 0.000000000000000000, 0.000000000000000000, -1.000000000000000000 ) ) ;
#42683 = CARTESIAN_POINT ( 'NONE',  ( -7.320508075688773708, 111.8750000000000000, -7.320508075688774596 ) ) ;
#42684 = CARTESIAN_POINT ( 'NONE',  ( -8.000000000000000000, 114.4062500000000142, -3.313708498984761608 ) ) ;
#42685 = CARTESIAN_POINT ( 'NONE',  ( 6.676582343750001591, 296.1093750017069510, -8.176455196517173205E-16 ) ) ;
#42686 = ORIENTED_EDGE ( 'NONE', *, *, #53198, .T. ) ;
#42687 = CARTESIAN_POINT ( 'NONE',  ( 2.679491924311379947, 188.9583333333333712, 9.999999999999959144 ) ) ;
#42688 = EDGE_CURVE ( 'NONE', #11891, #3964, #57018, .T. ) ;
#42689 = CARTESIAN_POINT ( 'NONE',  ( 8.000000000000000000, 22.31249999590322375, 0.000000000000000000 ) ) ;
#42690 = CARTESIAN_POINT ( 'NONE',  ( -2.839093476692135984E-14, 203.6875000013656063, 138.5412658750000503 ) ) ;
#42691 = CARTESIAN_POINT ( 'NONE',  ( -9.000000000000000000, 5.196152422706624918, -10.80000000000000071 ) ) ;
#42692 = CARTESIAN_POINT ( 'NONE',  ( -8.660254037844385522, 225.4166666666666856, 5.000000000000004441 ) ) ;
#42693 = DIRECTION ( 'NONE',  ( 0.000000000000000000, 0.000000000000000000, 1.000000000000000000 ) ) ;
#42694 = CARTESIAN_POINT ( 'NONE',  ( -4.556349186104045934, 11.00000000000000000, 114.7187500000000000 ) ) ;
#42695 = CARTESIAN_POINT ( 'NONE',  ( -7.320508075688778149, 223.1250000000000284, 7.320508075688769267 ) ) ;
#42696 = CARTESIAN_POINT ( 'NONE',  ( -7.188101187499992051, 2.977408999572646930, 4.767802781871752771 ) ) ;
#42697 = CARTESIAN_POINT ( 'NONE',  ( -8.311093377946836114, 197.9687499965860411, -8.311093377946837890 ) ) ;
#42698 = CARTESIAN_POINT ( 'NONE',  ( 8.660254037844385522, 191.4583333265053966, 5.000000000000005329 ) ) ;
#42699 = CARTESIAN_POINT ( 'NONE',  ( 1.881053915767121776, 0.4999999986344067504, -4.541265875000002339 ) ) ;
#42700 = CARTESIAN_POINT ( 'NONE',  ( -14.00000000000000178, -2.250000000005106138, 10.23492587299426404 ) ) ;
#42702 = CARTESIAN_POINT ( 'NONE',  ( -3.673940397442060854E-16, 297.7500000000000000, -6.000000000000001776 ) ) ;
#42701 = LINE ( 'NONE', #14018, #27401 ) ;
#42703 = ORIENTED_EDGE ( 'NONE', *, *, #17261, .T. ) ;
#42704 = AXIS2_PLACEMENT_3D ( 'NONE', #24689, #17559, #17937 ) ;
#42705 = CARTESIAN_POINT ( 'NONE',  ( -2.445694354108840063, 203.0625000013656063, 139.5543056458912190 ) ) ;
#42706 = CARTESIAN_POINT ( 'NONE',  ( 8.311093377946834337, 45.46874999658601268, 8.311093377946839666 ) ) ;
#42707 = MANIFOLD_SOLID_BREP ( '\X2\00d8\X0\8.0mm Dowel Hole1', #11720 ) ;
#42708 = CARTESIAN_POINT ( 'NONE',  ( -6.735557395310442023E-16, 11.00000000000000000, 104.3125000040967763 ) ) ;
#42709 = LINE ( 'NONE', #32538, #31106 ) ;
#42710 = CARTESIAN_POINT ( 'NONE',  ( -30.44569435410886982, 201.5625000013656063, 167.5543056458916169 ) ) ;
#42711 = CARTESIAN_POINT ( 'NONE',  ( -30.99999999999992895, -31.99999999999978684, 205.0000000000000284 ) ) ;
#42713 = CARTESIAN_POINT ( 'NONE',  ( -7.320508075688770155, 230.6250000000000284, 7.320508075688774596 ) ) ;
#42712 = CARTESIAN_POINT ( 'NONE',  ( 2.977408999572650039, 122.1875000020483810, -7.188101187500000933 ) ) ;
#42714 = CARTESIAN_POINT ( 'NONE',  ( 11.00000000000000000, 1.347111479062088405E-15, 118.0000000000000000 ) ) ;
#42715 = CARTESIAN_POINT ( 'NONE',  ( -8.311093377946836114, 112.6562499965860127, -8.311093377946837890 ) ) ;
#42716 = EDGE_CURVE ( 'NONE', #27344, #16846, #69696, .T. ) ;
#42717 = CARTESIAN_POINT ( 'NONE',  ( 2.679491924311222739, 90.83333332650536818, 10.00000000000000355 ) ) ;
#42718 = CARTESIAN_POINT ( 'NONE',  ( 7.188101187500000044, 90.40625000204838102, -8.802885111219163269E-16 ) ) ;
#42719 = CARTESIAN_POINT ( 'NONE',  ( 4.541265875000002339, 14.49999999863440969, -1.881053915767121554 ) ) ;
#42720 = CARTESIAN_POINT ( 'NONE',  ( 1.656854249492381914, 10.81250000000000178, 4.000000000000000888 ) ) ;
#42721 = CARTESIAN_POINT ( 'NONE',  ( -7.778174593052020747, -7.778174593052023411, 67.37500000409676204 ) ) ;
#42722 = ORIENTED_EDGE ( 'NONE', *, *, #2140, .T. ) ;
#42723 = CARTESIAN_POINT ( 'NONE',  ( -3.220560865819809937, 225.9999999999999432, -9.489879397300258645 ) ) ;
#42724 = VERTEX_POINT ( 'NONE', #53941 ) ;
#42725 = CARTESIAN_POINT ( 'NONE',  ( 4.721056650415999201, 293.2343750017069510, -4.721056650415999201 ) ) ;
#42726 = DIRECTION ( 'NONE',  ( -0.000000000000000000, -0.000000000000000000, -1.000000000000000000 ) ) ;
#42727 = CARTESIAN_POINT ( 'NONE',  ( -5.656854249492375253, 5.656854249492375253, 5.330302783920146226 ) ) ;
#42728 = CARTESIAN_POINT ( 'NONE',  ( -5.676582343749998039, 172.4479166632526983, -9.832129032723420536 ) ) ;
#42729 = CARTESIAN_POINT ( 'NONE',  ( 8.660254037844385522, 4.583333333333333925, 5.000000000000006217 ) ) ;
#42730 = CARTESIAN_POINT ( 'NONE',  ( -3.999999999999960032, 200.0000000000000000, 198.0000000000000284 ) ) ;
#42731 = CARTESIAN_POINT ( 'NONE',  ( -7.320508075688810123, 193.1250000000000568, 7.320508075688802130 ) ) ;
#42732 = CARTESIAN_POINT ( 'NONE',  ( 7.204075437095968759, -7.204075437095966983, 109.0937500020483810 ) ) ;
#42733 = ORIENTED_EDGE ( 'NONE', *, *, #16874, .F. ) ;
#42734 = CARTESIAN_POINT ( 'NONE',  ( -3.544144923088096366, 50.27229464832369388, -40.88493206427705928 ) ) ;
#42735 = CARTESIAN_POINT ( 'NONE',  ( 2.824543433528785410E-14, 210.0000000000000284, 194.0000000000000568 ) ) ;
#42736 = CARTESIAN_POINT ( 'NONE',  ( -3.042071309553173730, 144.6354166632526983, 11.35316468749999785 ) ) ;
#42737 = CARTESIAN_POINT ( 'NONE',  ( -3.267228342394547624, 194.5118150472865750, 199.6241603658230588 ) ) ;
#42738 = CARTESIAN_POINT ( 'NONE',  ( 10.18810118749999916, 4.220049686691935698, 71.87500000204836681 ) ) ;
#42739 = CARTESIAN_POINT ( 'NONE',  ( 11.35316468749999963, 66.30208332991935549, -3.042071309553165293 ) ) ;
#42740 = EDGE_LOOP ( 'NONE', ( #53521, #39810, #49937, #66482 ) ) ;
#42741 = DIRECTION ( 'NONE',  ( 0.000000000000000000, 0.000000000000000000, -1.000000000000000000 ) ) ;
#42742 = CARTESIAN_POINT ( 'NONE',  ( -3.211159895383561391, 6.812499998634407028, -3.211159895383561835 ) ) ;
#42743 = CARTESIAN_POINT ( 'NONE',  ( -8.008118988124991233, 3.317071493978878127, 9.919365283940628331 ) ) ;
#42744 = ORIENTED_EDGE ( 'NONE', *, *, #17571, .F. ) ;
#42745 = CARTESIAN_POINT ( 'NONE',  ( 7.188101187500001821, 23.06249999795161187, -2.977408999572650483 ) ) ;
#42746 = CARTESIAN_POINT ( 'NONE',  ( -2.485281374238572649, 287.2500000034139589, 6.000000000000002665 ) ) ;
#42747 = CARTESIAN_POINT ( 'NONE',  ( 5.000000000000000000, 18.53862685874501537, 23.57305537018163832 ) ) ;
#42748 = CARTESIAN_POINT ( 'NONE',  ( -7.188101187500000044, 13.59374999795161187, -8.802885111219163269E-16 ) ) ;
#42749 = CARTESIAN_POINT ( 'NONE',  ( -7.188101187499992051, 2.977408999572646930, 4.392802781871752771 ) ) ;
#42750 = CARTESIAN_POINT ( 'NONE',  ( -6.238412754330611322E-16, 10.18810118749999916, 114.1562500020483810 ) ) ;
#42751 =( BOUNDED_CURVE ( )  B_SPLINE_CURVE ( 2, ( #4685, #52836, #12094, #69816, #17380, #70192, #41148, #40404, #58874 ),
 .UNSPECIFIED., .F., .F. ) 
 B_SPLINE_CURVE_WITH_KNOTS ( ( 3, 2, 2, 2, 3 ),
 ( 0.9479166666666665186, 0.9531249999999998890, 0.9583333333333332593, 0.9635416666666666297, 0.9687500000000000000 ),
 .UNSPECIFIED. ) 
 CURVE ( )  GEOMETRIC_REPRESENTATION_ITEM ( )  RATIONAL_B_SPLINE_CURVE ( ( 1.000000000000001554, 0.9238795325112850731, 1.000000000000000000, 0.9238795325112867385, 1.000000000000000000, 0.9238795325112867385, 1.000000000000000000, 0.9238795325112867385, 1.000000000000000000 ) ) 
 REPRESENTATION_ITEM ( '' )  );
#42752 = CARTESIAN_POINT ( 'NONE',  ( 2.828427124746191623, 9.125000000000000000, -2.828427124746191623 ) ) ;
#42753 = CARTESIAN_POINT ( 'NONE',  ( -4.000000000000001776, 2.187499997268813168, -1.656854249492381470 ) ) ;
#42754 = VERTEX_POINT ( 'NONE', #42607 ) ;
#42755 = CARTESIAN_POINT ( 'NONE',  ( 3.458734125000016313, 205.8750000013656063, 199.4326545832176691 ) ) ;
#42756 = ADVANCED_FACE ( 'NONE', ( #24145 ), #12460, .F. ) ;
#42757 = CARTESIAN_POINT ( 'NONE',  ( -24.00000000000002487, 197.9375000027312410, 168.3431457505079152 ) ) ;
#42758 = CARTESIAN_POINT ( 'NONE',  ( 1.881053915767121776, 3.499999998634407028, -4.541265875000002339 ) ) ;
#42759 = CARTESIAN_POINT ( 'NONE',  ( 7.188101187500002709, 112.8125000020483952, 2.977408999572649151 ) ) ;
#42760 = CARTESIAN_POINT ( 'NONE',  ( -11.00000000000000000, 0.000000000000000000, 118.0000000000000000 ) ) ;
#42761 = CARTESIAN_POINT ( 'NONE',  ( -7.188101187499992051, 0.000000000000000000, 23.98655278187175455 ) ) ;
#42762 = ORIENTED_EDGE ( 'NONE', *, *, #1104, .F. ) ;
#42763 = EDGE_CURVE ( 'NONE', #17476, #7034, #69813, .T. ) ;
#42765 =( BOUNDED_CURVE ( )  B_SPLINE_CURVE ( 2, ( #48009, #30671, #47639, #13667, #19339, #64993, #42721, #70661, #14037 ),
 .UNSPECIFIED., .F., .F. ) 
 B_SPLINE_CURVE_WITH_KNOTS ( ( 3, 2, 2, 2, 3 ),
 ( 0.9558823529411765163, 0.9595588235294117974, 0.9632352941176471894, 0.9669117647058824705, 0.9705882352941177516 ),
 .UNSPECIFIED. ) 
 CURVE ( )  GEOMETRIC_REPRESENTATION_ITEM ( )  RATIONAL_B_SPLINE_CURVE ( ( 1.000000000000000000, 0.9238795325112867385, 1.000000000000000000, 0.9238795325112867385, 1.000000000000000000, 0.9238795325112867385, 1.000000000000000000, 0.9238795325112844070, 1.000000000000002220 ) ) 
 REPRESENTATION_ITEM ( '' )  );
#42764 = CARTESIAN_POINT ( 'NONE',  ( 5.082755093536324154, 24.28124999795161543, 5.082755093536326818 ) ) ;
#42766 = ORIENTED_EDGE ( 'NONE', *, *, #9662, .F. ) ;
#42767 = CARTESIAN_POINT ( 'NONE',  ( -1.060465953394920335, 8.000079534944177340, -0.000000000000000000 ) ) ;
#42768 = CARTESIAN_POINT ( 'NONE',  ( 6.000000000000003553, 296.4374999999999432, 2.485281374238571317 ) ) ;
#42769 = CARTESIAN_POINT ( 'NONE',  ( 31.45873412499999944, 204.6875000013656063, 169.9999999999998863 ) ) ;
#42770 = CARTESIAN_POINT ( 'NONE',  ( 5.000000000000001776, 65.83333333333334281, -8.660254037844389075 ) ) ;
#42771 = CARTESIAN_POINT ( 'NONE',  ( 5.082755093536325042, 96.96875000204838102, -5.082755093536325930 ) ) ;
#42772 = CARTESIAN_POINT ( 'NONE',  ( 2.485281374238575314, 295.3125000000000000, 6.000000000000000888 ) ) ;
#42773 = AXIS2_PLACEMENT_3D ( 'NONE', #51181, #10082, #22127 ) ;
#42775 = CARTESIAN_POINT ( 'NONE',  ( -27.91882077332312306, -42.56310774691892362, 183.4882049149678096 ) ) ;
#42774 = CARTESIAN_POINT ( 'NONE',  ( 31.99999999999998579, 208.4375000027311842, 168.3431457505075173 ) ) ;
#42776 = ORIENTED_EDGE ( 'NONE', *, *, #11950, .F. ) ;
#42777 = CARTESIAN_POINT ( 'NONE',  ( -8.311093377946836114, 233.2812500034139589, -8.311093377946836114 ) ) ;
#42778 = CARTESIAN_POINT ( 'NONE',  ( -2.828427124746209831, 199.5000000027312126, 139.1715728752538723 ) ) ;
#42779 = DIRECTION ( 'NONE',  ( -0.000000000000000000, 1.000000000000000000, 4.476705744456276341E-16 ) ) ;
#42780 = CARTESIAN_POINT ( 'NONE',  ( 7.999999999999991118, 3.313708498984758055, 1.861552783920143117 ) ) ;
#42781 = CARTESIAN_POINT ( 'NONE',  ( -5.000000000000000888, 259.1666666666666288, -8.660254037844387298 ) ) ;
#42782 = CARTESIAN_POINT ( 'NONE',  ( 3.153939666463620179E-13, 188.7500000000000284, 9.999999999999998224 ) ) ;
#42783 = CARTESIAN_POINT ( 'NONE',  ( -2.679491924311235618, 173.5416666666666288, 10.00000000000000000 ) ) ;
#42784 = DIRECTION ( 'NONE',  ( 1.000000000000000000, 0.000000000000000000, 0.000000000000000000 ) ) ;
#42785 = CARTESIAN_POINT ( 'NONE',  ( 2.977408999572650927, -7.188101187499990274, 21.83030278187175810 ) ) ;
#42786 = CARTESIAN_POINT ( 'NONE',  ( 5.676582343750001591, 156.9270833299193555, -9.832129032723420536 ) ) ;
#42787 = CARTESIAN_POINT ( 'NONE',  ( 6.000000000000003553, 294.6250000034140157, -2.485281374238571761 ) ) ;
#42788 = CARTESIAN_POINT ( 'NONE',  ( -3.313708498984830442, 117.7812500000000000, 7.999999999999930722 ) ) ;
#42791 = CARTESIAN_POINT ( 'NONE',  ( -7.320508075688779925, 168.1250000000000284, 7.320508075688771044 ) ) ;
#42790 = CARTESIAN_POINT ( 'NONE',  ( 0.000000000000000000, 237.9999999999999716, 10.00000000000000178 ) ) ;
#42789 = CARTESIAN_POINT ( 'NONE',  ( 29.65685424949240101, 201.4375000000000000, 165.9999999999998863 ) ) ;
#42792 = ORIENTED_EDGE ( 'NONE', *, *, #71684, .F. ) ;
#42793 = CARTESIAN_POINT ( 'NONE',  ( 9.832129032723416984, 15.67708332991935016, 5.676582343750006032 ) ) ;
#42794 = CARTESIAN_POINT ( 'NONE',  ( 7.778174593052021635, 7.778174593052023411, 77.12500000409677625 ) ) ;
#42795 = FACE_OUTER_BOUND ( 'NONE', #70041, .T. ) ;
#42796 = CARTESIAN_POINT ( 'NONE',  ( -3.313708498984640816, 116.2812499999999858, 8.000000000000119016 ) ) ;
#42797 = CARTESIAN_POINT ( 'NONE',  ( -3.458734125000015425, 208.9375000013656063, 142.0000000000000568 ) ) ;
#42798 = DIRECTION ( 'NONE',  ( -0.000000000000000000, -0.000000000000000000, 1.000000000000000000 ) ) ;
#42799 = CARTESIAN_POINT ( 'NONE',  ( -8.660254037844390851, 54.79166665983869677, 4.999999999999998224 ) ) ;
#42800 = CARTESIAN_POINT ( 'NONE',  ( 7.188101187500002709, 108.3125000020483810, 2.977408999572649151 ) ) ;
#42801 = CARTESIAN_POINT ( 'NONE',  ( -1.881053915767124440, 4.124999998634407028, 4.541265875000001451 ) ) ;
#42802 = CARTESIAN_POINT ( 'NONE',  ( -7.999999999999991118, 0.000000000000000000, 14.33030277982336465 ) ) ;
#42804 = CARTESIAN_POINT ( 'NONE',  ( 11.00000000000013323, -4.556349186103911819, 105.3437500040967905 ) ) ;
#42803 = CYLINDRICAL_SURFACE ( 'NONE', #4581, 11.00000000000000000 ) ;
#42805 = ORIENTED_EDGE ( 'NONE', *, *, #40853, .T. ) ;
#42806 = CARTESIAN_POINT ( 'NONE',  ( 8.660254037844389075, 220.2083333401613174, 4.999999999999997335 ) ) ;
#42807 = CARTESIAN_POINT ( 'NONE',  ( 7.778174593052023411, -7.778174593052021635, 82.56249999999998579 ) ) ;
#42808 = CARTESIAN_POINT ( 'NONE',  ( -9.832129032723415207, 234.6354166700806445, 5.676582343750005144 ) ) ;
#42809 = CARTESIAN_POINT ( 'NONE',  ( 9.832129032723420536, 131.1979166632526983, -5.676582343749999815 ) ) ;
#42810 = VERTEX_POINT ( 'NONE', #47157 ) ;
#42811 = CARTESIAN_POINT ( 'NONE',  ( 4.000000000000015987, 198.5625000000000568, 196.3431457505076594 ) ) ;
#42812 = CARTESIAN_POINT ( 'NONE',  ( 10.18810118749999916, 4.220049686691935698, 95.50000000204838102 ) ) ;
#42813 = DIRECTION ( 'NONE',  ( 0.000000000000000000, 0.000000000000000000, 1.000000000000000000 ) ) ;
#42814 = CARTESIAN_POINT ( 'NONE',  ( -2.445694354108783219, 196.8125000013656063, 200.4456943541088663 ) ) ;
#42815 = CARTESIAN_POINT ( 'NONE',  ( 7.999999999999991118, 9.797174393178815797E-16, 27.08030277982336642 ) ) ;
#42817 = CARTESIAN_POINT ( 'NONE',  ( -11.35316468750000141, 113.4895833299193413, 3.042071309553159963 ) ) ;
#42816 = CARTESIAN_POINT ( 'NONE',  ( -1.836970198721029983E-15, 43.75000000000000711, 10.00000000000000178 ) ) ;
#42818 = CARTESIAN_POINT ( 'NONE',  ( -26.34314575050758478, 208.5625000000000000, 174.0000000000003411 ) ) ;
#42819 = CARTESIAN_POINT ( 'NONE',  ( 10.00000000000000533, 49.79166666666667140, 2.679491924311236506 ) ) ;
#42820 = ORIENTED_EDGE ( 'NONE', *, *, #62904, .F. ) ;
#42821 = CARTESIAN_POINT ( 'NONE',  ( -7.320508075688773708, 23.74999999317202892, -7.320508075688774596 ) ) ;
#42822 = CARTESIAN_POINT ( 'NONE',  ( -1.656854249492383468, 9.687500000000000000, 4.000000000000000888 ) ) ;
#42823 = CARTESIAN_POINT ( 'NONE',  ( -5.676582343749998039, 102.7604166632526841, -9.832129032723420536 ) ) ;
#42824 = CARTESIAN_POINT ( 'NONE',  ( 1.432654583217662259, 208.1250000013656063, 194.5412658750000219 ) ) ;
#42825 = CARTESIAN_POINT ( 'NONE',  ( -7.188101187500002709, 13.68749999795161187, 2.977408999572649151 ) ) ;
#42826 = CARTESIAN_POINT ( 'NONE',  ( -7.204075437095965206, -7.204075437095968759, 87.71875000204836681 ) ) ;
#42827 = CARTESIAN_POINT ( 'NONE',  ( -11.35316468749999785, 18.38541666325267698, -3.042071309553167513 ) ) ;
#42828 = ORIENTED_EDGE ( 'NONE', *, *, #15670, .F. ) ;
#42829 = CARTESIAN_POINT ( 'NONE',  ( 10.00000000000000178, 181.8749999931720538, 0.000000000000000000 ) ) ;
#42830 = CARTESIAN_POINT ( 'NONE',  ( -14.00000000000000178, 0.000000000000000000, 0.000000000000000000 ) ) ;
#42831 = CARTESIAN_POINT ( 'NONE',  ( 4.220049686691941027, -10.18810118749999738, 73.00000000204836681 ) ) ;
#42832 = FACE_OUTER_BOUND ( 'NONE', #24857, .T. ) ;
#42833 = CARTESIAN_POINT ( 'NONE',  ( 5.082755093536325930, 0.6562499979516100979, -5.082755093536325930 ) ) ;
#42834 = CARTESIAN_POINT ( 'NONE',  ( 4.721056650415999201, 293.0781250017069510, -4.721056650415999201 ) ) ;
#42835 = AXIS2_PLACEMENT_3D ( 'NONE', #54924, #66597, #47753 ) ;
#42836 = FACE_OUTER_BOUND ( 'NONE', #74136, .T. ) ;
#42837 = CARTESIAN_POINT ( 'NONE',  ( -9.832129032723420536, 219.0104166632526983, 5.676582343749997150 ) ) ;
#42838 = EDGE_CURVE ( 'NONE', #21379, #26888, #22716, .T. ) ;
#42839 = CARTESIAN_POINT ( 'NONE',  ( -11.35316468749999785, 123.3854166632526699, -3.042071309553167513 ) ) ;
#42840 = CARTESIAN_POINT ( 'NONE',  ( -10.18810118749999916, 0.000000000000000000, 82.65625000204838102 ) ) ;
#42841 = AXIS2_PLACEMENT_3D ( 'NONE', #46672, #33892, #28206 ) ;
#42842 = CARTESIAN_POINT ( 'NONE',  ( -28.00000000000001776, 197.4375000013655779, 166.5412658750003629 ) ) ;
#42843 = AXIS2_PLACEMENT_3D ( 'NONE', #12520, #30982, #70607 ) ;
#42844 = CARTESIAN_POINT ( 'NONE',  ( 8.000000000000000000, 25.59375000000000355, -3.313708498984761608 ) ) ;
#42845 = CARTESIAN_POINT ( 'NONE',  ( -4.541265875000003227, 10.99999999863440969, 1.881053915767121110 ) ) ;
#42846 = ORIENTED_EDGE ( 'NONE', *, *, #25899, .T. ) ;
#42847 = CARTESIAN_POINT ( 'NONE',  ( 1.656854249492403008, 202.8125000027312126, 194.0000000000000853 ) ) ;
#42848 = EDGE_CURVE ( 'NONE', #27168, #42334, #801, .T. ) ;
#42849 = CARTESIAN_POINT ( 'NONE',  ( 3.458734124999959469, 199.7500000013656063, 140.5673454167824161 ) ) ;
#42850 = CARTESIAN_POINT ( 'NONE',  ( -4.000000000000015099, 203.6875000027311842, 143.6568542494924543 ) ) ;
#42851 = CARTESIAN_POINT ( 'NONE',  ( -8.660254037844472563, 172.9166666666667425, 5.000000000000047073 ) ) ;
#42852 = CARTESIAN_POINT ( 'NONE',  ( -4.220049686691935698, 10.18810118749999916, 67.75000000204836681 ) ) ;
#42853 = ORIENTED_EDGE ( 'NONE', *, *, #38700, .F. ) ;
#42854 = CARTESIAN_POINT ( 'NONE',  ( -7.188101187500002709, 4.312499997951610986, 2.977408999572649151 ) ) ;
#42855 = CARTESIAN_POINT ( 'NONE',  ( -26.75015280308076981, -12.45179362709517967, 185.6919162887197672 ) ) ;
#42856 = CARTESIAN_POINT ( 'NONE',  ( 0.000000000000000000, 300.0000000000000000, 0.000000000000000000 ) ) ;
#42857 = CARTESIAN_POINT ( 'NONE',  ( -2.977408999572651815, 109.8125000020483952, 7.188101187500000933 ) ) ;
#42858 = CARTESIAN_POINT ( 'NONE',  ( 7.470240680701174085, -16.47166422291245524, -0.04683108270950198104 ) ) ;
#42859 = CARTESIAN_POINT ( 'NONE',  ( -2.765530957081998142, 291.6406250017068942, 6.676582343750000703 ) ) ;
#42861 = CARTESIAN_POINT ( 'NONE',  ( 7.320508075688774596, 137.4999999931720254, -7.320508075688774596 ) ) ;
#42860 = CARTESIAN_POINT ( 'NONE',  ( -5.676582343750000703, 223.0729166700806729, -9.832129032723418760 ) ) ;
#42862 =( BOUNDED_CURVE ( )  B_SPLINE_CURVE ( 2, ( #1963, #24593, #42312, #31749, #1609, #2329, #13632, #59680, #14375 ),
 .UNSPECIFIED., .F., .F. ) 
 B_SPLINE_CURVE_WITH_KNOTS ( ( 3, 2, 2, 2, 3 ),
 ( 0.5520833333333332593, 0.5572916666666665186, 0.5625000000000000000, 0.5677083333333333703, 0.5729166666666666297 ),
 .UNSPECIFIED. ) 
 CURVE ( )  GEOMETRIC_REPRESENTATION_ITEM ( )  RATIONAL_B_SPLINE_CURVE ( ( 1.000000000000001554, 0.9238795325112850731, 1.000000000000000000, 0.9238795325112867385, 1.000000000000000000, 0.9238795325112867385, 1.000000000000000000, 0.9238795325112867385, 1.000000000000000000 ) ) 
 REPRESENTATION_ITEM ( '' )  );
#42863 = ORIENTED_EDGE ( 'NONE', *, *, #4626, .F. ) ;
#42864 = CARTESIAN_POINT ( 'NONE',  ( -11.35316468749999963, 224.2187500034139873, 0.000000000000000000 ) ) ;
#42865 = CARTESIAN_POINT ( 'NONE',  ( 5.082755093536318824, 5.082755093536319713, 26.79905278187175455 ) ) ;
#42866 = FACE_OUTER_BOUND ( 'NONE', #68762, .T. ) ;
#42867 = CARTESIAN_POINT ( 'NONE',  ( -4.000000000000001776, 9.249999997268814056, -4.898587196589415787E-16 ) ) ;
#42868 = CARTESIAN_POINT ( 'NONE',  ( -2.445694354108784108, 199.5625000013656063, 195.5543056458912190 ) ) ;
#42869 = ORIENTED_EDGE ( 'NONE', *, *, #60595, .T. ) ;
#42870 = DIRECTION ( 'NONE',  ( -0.000000000000000000, -1.000000000000000000, -0.000000000000000000 ) ) ;
#42871 = CARTESIAN_POINT ( 'NONE',  ( -8.000000000000000000, 102.4062499999999858, -3.313708498984761608 ) ) ;
#42872 = CARTESIAN_POINT ( 'NONE',  ( -3.042071309553173730, 109.6354166632526557, 11.35316468749999785 ) ) ;
#42873 = CARTESIAN_POINT ( 'NONE',  ( 2.679491924311075302, 210.8333333265053682, 10.00000000000008704 ) ) ;
#42874 = CARTESIAN_POINT ( 'NONE',  ( 4.556349186104045934, 11.00000000000000000, 80.03124999999998579 ) ) ;
#42877 = CYLINDRICAL_SURFACE ( 'NONE', #44654, 8.000000000000003553 ) ;
#42876 = CARTESIAN_POINT ( 'NONE',  ( 24.54126587500000056, 199.2500000013656063, 171.4326545832175839 ) ) ;
#42875 = CARTESIAN_POINT ( 'NONE',  ( 31.45873412499999233, 199.9375000013656063, 169.9999999999999432 ) ) ;
#42878 = ORIENTED_EDGE ( 'NONE', *, *, #2080, .T. ) ;
#42879 = CARTESIAN_POINT ( 'NONE',  ( 0.000000000000000000, -2.500000000000000444, 8.000000000000000000 ) ) ;
#42880 = CARTESIAN_POINT ( 'NONE',  ( 11.35316468750000141, 220.7812499965860127, 0.000000000000000000 ) ) ;
#42881 = CARTESIAN_POINT ( 'NONE',  ( 3.458734124999959914, 202.3750000013655779, 143.4326545832176976 ) ) ;
#42882 = CARTESIAN_POINT ( 'NONE',  ( 24.54126587499998280, 203.5000000013655779, 171.4326545832175555 ) ) ;
#42883 = CARTESIAN_POINT ( 'NONE',  ( -11.00000000000000000, 4.556349186104045934, 116.5937500040967620 ) ) ;
#42884 = AXIS2_PLACEMENT_3D ( 'NONE', #29367, #64061, #53115 ) ;
#42885 = CARTESIAN_POINT ( 'NONE',  ( 5.676582343749993598, 200.2604166632526983, 9.832129032723422313 ) ) ;
#42886 = CARTESIAN_POINT ( 'NONE',  ( -4.401442555609581635E-16, 89.65625000204838102, -7.188101187500000044 ) ) ;
#42887 = CARTESIAN_POINT ( 'NONE',  ( 4.529167459315944555, 225.9997407208379911, 8.915528146188176351 ) ) ;
#42888 = CARTESIAN_POINT ( 'NONE',  ( -8.342170076843785083E-16, 16.06249999863440436, 4.541265875000002339 ) ) ;
#42889 = CARTESIAN_POINT ( 'NONE',  ( 31.45873412499997812, 196.8750000013656347, 171.4326545832176123 ) ) ;
#42890 = CARTESIAN_POINT ( 'NONE',  ( 7.188101187499992051, 8.802885111219154394E-16, 1.111552781871753215 ) ) ;
#42891 = DIRECTION ( 'NONE',  ( 0.000000000000000000, 0.000000000000000000, -1.000000000000000000 ) ) ;
#42892 = CARTESIAN_POINT ( 'NONE',  ( 9.832129032723416984, 80.36458332991935549, 5.676582343750006032 ) ) ;
#42893 = ORIENTED_EDGE ( 'NONE', *, *, #41587, .F. ) ;
#42894 = CARTESIAN_POINT ( 'NONE',  ( 10.00000000000001066, 139.7916666666666856, 2.679491924311238282 ) ) ;
#42895 = CARTESIAN_POINT ( 'NONE',  ( 0.000000000000000000, 0.000000000000000000, -10.00000000000000000 ) ) ;
#42896 = CARTESIAN_POINT ( 'NONE',  ( -1.040834085586084257E-14, 82.00000000000001421, 65.00000000000000000 ) ) ;
#42897 = CARTESIAN_POINT ( 'NONE',  ( 2.849036369511732440E-14, 207.2500000000000284, 202.0000000000000000 ) ) ;
#42898 = CARTESIAN_POINT ( 'NONE',  ( 8.311093377946837890, 91.40624999658604111, -8.311093377946837890 ) ) ;
#42899 = ORIENTED_EDGE ( 'NONE', *, *, #24704, .F. ) ;
#42900 = CARTESIAN_POINT ( 'NONE',  ( 4.220049686691941027, -10.18810118749999738, 88.00000000204836681 ) ) ;
#42901 = CARTESIAN_POINT ( 'NONE',  ( 10.18810118750000093, -4.220049686691933921, 110.3125000020483810 ) ) ;
#42902 = CARTESIAN_POINT ( 'NONE',  ( -27.99999999999999645, 210.0000000000000284, 170.0000000000003695 ) ) ;
#42903 = CARTESIAN_POINT ( 'NONE',  ( 2.679491924311304452, 73.95833333333334281, 9.999999999999992895 ) ) ;
#42905 = CARTESIAN_POINT ( 'NONE',  ( 5.676582343749993598, 69.94791666325268409, 9.832129032723422313 ) ) ;
#42904 = CARTESIAN_POINT ( 'NONE',  ( -4.898587196589412829E-16, 102.3125000040967763, -8.000000000000000000 ) ) ;
#42906 = CARTESIAN_POINT ( 'NONE',  ( 7.999999999999991118, 9.797174393178815797E-16, 21.26780278392014623 ) ) ;
#42907 = CARTESIAN_POINT ( 'NONE',  ( 8.660254037844389075, 130.4166666666666856, -5.000000000000000000 ) ) ;
#42908 = B_SPLINE_CURVE_WITH_KNOTS ( 'NONE', 3,
 ( #11812, #52186, #62737, #517 ),
 .UNSPECIFIED., .F., .F.,
 ( 4, 4 ),
 ( 6.719003021479604444E-16, 0.0004743803571056244171 ),
 .UNSPECIFIED. ) ;
#42909 = VECTOR ( 'NONE', #5001, 1000.000000000000000 ) ;
#42910 = CARTESIAN_POINT ( 'NONE',  ( -8.660254037844390851, 164.7916666598387110, 4.999999999999998224 ) ) ;
#42911 = CARTESIAN_POINT ( 'NONE',  ( -5.082755093536325930, 92.84375000204838102, -5.082755093536325930 ) ) ;
#42912 = EDGE_CURVE ( 'NONE', #50547, #14535, #18456, .T. ) ;
#42913 = DIRECTION ( 'NONE',  ( -1.000000000000000000, 0.000000000000000000, 0.000000000000000000 ) ) ;
#42914 = CARTESIAN_POINT ( 'NONE',  ( -8.311093377946836114, 67.96874999658601268, -8.311093377946837890 ) ) ;
#42915 = CARTESIAN_POINT ( 'NONE',  ( 1.226468279477575784E-15, 293.7031250017069510, 6.676582343750001591 ) ) ;
#42916 = CARTESIAN_POINT ( 'NONE',  ( -7.204075437095967871, 7.204075437095967871, 106.8437500020483810 ) ) ;
#42917 = CARTESIAN_POINT ( 'NONE',  ( -8.311093377946841443, 193.9062499965860411, 8.311093377946830785 ) ) ;
#42918 = ORIENTED_EDGE ( 'NONE', *, *, #63833, .T. ) ;
#42919 = CARTESIAN_POINT ( 'NONE',  ( -7.999999999999976019, -3.611371706259009353E-07, 26.51781575558936055 ) ) ;
#42920 = DIRECTION ( 'NONE',  ( -0.8660254037844379305, 0.5000000000000014433, 0.000000000000000000 ) ) ;
#42921 = CARTESIAN_POINT ( 'NONE',  ( 5.000000000000000000, 62.31673578527522750, 23.93255728291440931 ) ) ;
#42923 = CARTESIAN_POINT ( 'NONE',  ( 5.676582343750001591, 196.6145833299193839, -9.832129032723420536 ) ) ;
#42922 = CARTESIAN_POINT ( 'NONE',  ( -4.000000000000001776, 19.50000000000000000, -4.898587196589415787E-16 ) ) ;
#42924 = CARTESIAN_POINT ( 'NONE',  ( -5.000000000000000000, -68.60357193678697740, -20.85024232999374050 ) ) ;
#42925 = CARTESIAN_POINT ( 'NONE',  ( -10.00000000000000000, 242.9166666734946318, -2.679491924311226292 ) ) ;
#42926 = DIRECTION ( 'NONE',  ( -0.000000000000000000, 1.000000000000000000, 4.689100369878284071E-30 ) ) ;
#42927 = ORIENTED_EDGE ( 'NONE', *, *, #68314, .T. ) ;
#42928 = CARTESIAN_POINT ( 'NONE',  ( 8.311093377946837890, 186.7187499965860127, -8.311093377946837890 ) ) ;
#42929 = CARTESIAN_POINT ( 'NONE',  ( 5.082755093536320601, -5.082755093536318824, 23.04905278187175455 ) ) ;
#42930 = CARTESIAN_POINT ( 'NONE',  ( -1.237384350715592869E-11, 93.74999999999903366, 9.999999999999998224 ) ) ;
#42931 = ORIENTED_EDGE ( 'NONE', *, *, #69039, .F. ) ;
#42932 = ADVANCED_FACE ( 'NONE', ( #23787 ), #2255, .T. ) ;
#42933 = ADVANCED_FACE ( 'NONE', ( #35490 ), #70189, .T. ) ;
#42934 = AXIS2_PLACEMENT_3D ( 'NONE', #30534, #53550, #65222 ) ;
#42935 = CARTESIAN_POINT ( 'NONE',  ( 8.000000000000001776, 97.34375000409679046, 3.313708498984759387 ) ) ;
#42936 = CARTESIAN_POINT ( 'NONE',  ( 10.00000000000000178, 5.000000000000000000, 0.000000000000000000 ) ) ;
#42937 = CARTESIAN_POINT ( 'NONE',  ( 4.000000000000001776, 15.00000000000000000, 0.000000000000000000 ) ) ;
#42938 = CARTESIAN_POINT ( 'NONE',  ( 4.541265875000002339, 16.31249999863440436, 0.000000000000000000 ) ) ;
#42939 = CARTESIAN_POINT ( 'NONE',  ( -3.313708498984757167, 7.999999999999991118, 14.23655278392014623 ) ) ;
#42940 = CARTESIAN_POINT ( 'NONE',  ( 11.00000000000000000, 1.347111479062088405E-15, 93.24999999999998579 ) ) ;
#42941 = EDGE_LOOP ( 'NONE', ( #37110, #48382, #52158 ) ) ;
#42942 = CARTESIAN_POINT ( 'NONE',  ( 4.999999999999999112, -15.86295220590816868, -69.92641310672759403 ) ) ;
#42943 = CARTESIAN_POINT ( 'NONE',  ( 5.082755093536326818, 96.21875000204838102, 5.082755093536325042 ) ) ;
#42944 = ADVANCED_FACE ( 'NONE', ( #48265 ), #42234, .T. ) ;
#42946 = CARTESIAN_POINT ( 'NONE',  ( -11.35316468749999963, 263.9062500034140157, 0.000000000000000000 ) ) ;
#42945 = CARTESIAN_POINT ( 'NONE',  ( -5.000000000000055955, 81.66666666666672825, -8.660254037844488550 ) ) ;
#42947 = CARTESIAN_POINT ( 'NONE',  ( 1393.688200795887269, 596.9677537767817057, 945.5421604560588094 ) ) ;
#42948 = EDGE_LOOP ( 'NONE', ( #24447, #63518, #66336, #52019 ) ) ;
#42949 = AXIS2_PLACEMENT_3D ( 'NONE', #17701, #383, #12045 ) ;
#42950 = CARTESIAN_POINT ( 'NONE',  ( 11.00000000000000000, 4.556349186104045934, 82.84375000000000000 ) ) ;
#42951 = CARTESIAN_POINT ( 'NONE',  ( -7.188101187499990274, -2.977408999572651371, 21.08030278187175810 ) ) ;
#42952 = ORIENTED_EDGE ( 'NONE', *, *, #10463, .T. ) ;
#42953 = B_SPLINE_CURVE_WITH_KNOTS ( 'NONE', 3,
 ( #22778, #183, #17122, #921, #11846, #6195, #40891, #40147 ),
 .UNSPECIFIED., .F., .F.,
 ( 4, 2, 2, 4 ),
 ( 0.005256334970461100896, 0.006570121696639755378, 0.007883908422818408993, 0.01051148187517571796 ),
 .UNSPECIFIED. ) ;
#42954 = ORIENTED_EDGE ( 'NONE', *, *, #73059, .T. ) ;
#42955 = CARTESIAN_POINT ( 'NONE',  ( 4.220049686691934809, 10.18810118749999916, 77.68750000204838102 ) ) ;
#42956 = CARTESIAN_POINT ( 'NONE',  ( 8.311093377946834337, 55.46874999658601268, 8.311093377946839666 ) ) ;
#42957 = CARTESIAN_POINT ( 'NONE',  ( -7.999999999961182162, -1.665870058181487338E-05, 5.518425684709454160 ) ) ;
#42958 = CARTESIAN_POINT ( 'NONE',  ( 11.00000000000000000, 1.347111479062088405E-15, 93.24999999999998579 ) ) ;
#42961 = CARTESIAN_POINT ( 'NONE',  ( -6.676582343749999815, 293.6718750017070079, 2.765530957082001251 ) ) ;
#42960 = CARTESIAN_POINT ( 'NONE',  ( 32.00000000000000000, 199.3125000027311842, 171.6568542494922553 ) ) ;
#42959 = CARTESIAN_POINT ( 'NONE',  ( 31.99999999999999289, 196.3750000027311842, 169.9999999999998863 ) ) ;
#42962 = CARTESIAN_POINT ( 'NONE',  ( 6.123233995736767268E-16, 146.2500000000000284, -10.00000000000000178 ) ) ;
#42963 = CARTESIAN_POINT ( 'NONE',  ( -47.58097657422527504, 192.7846596221113202, 64.07451946398457210 ) ) ;
#42964 = CARTESIAN_POINT ( 'NONE',  ( -2.775557561562891351E-14, 210.0000000000000284, 146.0000000000000284 ) ) ;
#42965 = FACE_OUTER_BOUND ( 'NONE', #55171, .T. ) ;
#42966 = CARTESIAN_POINT ( 'NONE',  ( 24.54126587499998280, 200.2500000013656631, 171.4326545832175555 ) ) ;
#42967 = CARTESIAN_POINT ( 'NONE',  ( 5.082755093536324154, 9.656249997951610098, 5.082755093536326818 ) ) ;
#42968 = CARTESIAN_POINT ( 'NONE',  ( 5.662595241051936235, -5.662595241051934458, 0.07561528394062884406 ) ) ;
#42969 = CYLINDRICAL_SURFACE ( 'NONE', #38331, 8.000000000000000000 ) ;
#42970 = CARTESIAN_POINT ( 'NONE',  ( 7.188101187500002709, 111.6875000020483810, 2.977408999572649151 ) ) ;
#42972 = CARTESIAN_POINT ( 'NONE',  ( -2.679491924311226292, 131.4583333333333428, -10.00000000000000178 ) ) ;
#42971 = CARTESIAN_POINT ( 'NONE',  ( 2.751064625579944321E-14, 201.7500000000000000, 194.0000000000000568 ) ) ;
#42973 = DIRECTION ( 'NONE',  ( 0.000000000000000000, 0.000000000000000000, 1.000000000000000000 ) ) ;
#42974 = CARTESIAN_POINT ( 'NONE',  ( 2.485281374238858643, 288.3750000034139589, 5.999999999999716671 ) ) ;
#42975 = CARTESIAN_POINT ( 'NONE',  ( 1.320432766682872962E-15, -7.188101187499992051, 21.73655278187175455 ) ) ;
#42976 = CARTESIAN_POINT ( 'NONE',  ( 30.82842712474616675, 195.1250000000000284, 172.8284271247460993 ) ) ;
#42977 = CARTESIAN_POINT ( 'NONE',  ( 5.676582343749993598, 39.94791666325269119, 9.832129032723422313 ) ) ;
#42978 =( BOUNDED_CURVE ( )  B_SPLINE_CURVE ( 2, ( #66408, #13599, #7592, #54363, #72059, #2673, #24920, #37757, #25662 ),
 .UNSPECIFIED., .F., .F. ) 
 B_SPLINE_CURVE_WITH_KNOTS ( ( 3, 2, 2, 2, 3 ),
 ( 0.6500000000000004663, 0.6583333333333338810, 0.6666666666666671848, 0.6750000000000007105, 0.6833333333333340143 ),
 .UNSPECIFIED. ) 
 CURVE ( )  GEOMETRIC_REPRESENTATION_ITEM ( )  RATIONAL_B_SPLINE_CURVE ( ( 0.9999999999999958922, 0.9238795325112908463, 1.000000000000000000, 0.9238795325112867385, 1.000000000000000000, 0.9238795325112867385, 1.000000000000000000, 0.9238795325112806323, 1.000000000000005995 ) ) 
 REPRESENTATION_ITEM ( '' )  );
#42979 = CYLINDRICAL_SURFACE ( 'NONE', #18373, 3.999999999999976019 ) ;
#42981 = CARTESIAN_POINT ( 'NONE',  ( -8.660254037844390851, 14.79166665983870210, 4.999999999999998224 ) ) ;
#42980 =( BOUNDED_CURVE ( )  B_SPLINE_CURVE ( 2, ( #34885, #5826, #28822, #551, #68812, #28454, #13219, #57890, #74105 ),
 .UNSPECIFIED., .F., .F. ) 
 B_SPLINE_CURVE_WITH_KNOTS ( ( 3, 2, 2, 2, 3 ),
 ( 0.1805555555555555525, 0.1875000000000000000, 0.1944444444444444198, 0.2013888888888888673, 0.2083333333333333148 ),
 .UNSPECIFIED. ) 
 CURVE ( )  GEOMETRIC_REPRESENTATION_ITEM ( )  RATIONAL_B_SPLINE_CURVE ( ( 1.000000000000000000, 0.9238795325112867385, 1.000000000000000000, 0.9238795325112867385, 1.000000000000000000, 0.9238795325112867385, 1.000000000000000000, 0.9238795325112870716, 0.9999999999999996669 ) ) 
 REPRESENTATION_ITEM ( '' )  );
#42982 = ORIENTED_EDGE ( 'NONE', *, *, #33182, .F. ) ;
#42983 = CYLINDRICAL_SURFACE ( 'NONE', #27768, 10.00000000000000178 ) ;
#42984 = CARTESIAN_POINT ( 'NONE',  ( 0.000000000000000000, 225.9999999999999432, 15.99999999999998579 ) ) ;
#42985 = CARTESIAN_POINT ( 'NONE',  ( 9.832129032723420536, 46.19791666325268409, -5.676582343749999815 ) ) ;
#42986 = CARTESIAN_POINT ( 'NONE',  ( -4.556349186104047710, -10.99999999999999822, 79.46875000409677625 ) ) ;
#42987 = PRODUCT_DEFINITION_FORMATION_WITH_SPECIFIED_SOURCE ( 'ANY', '', #25763, .NOT_KNOWN. ) ;
#42988 = CARTESIAN_POINT ( 'NONE',  ( -2.754378923186476579E-14, 202.4375000013656063, 145.4587341250000350 ) ) ;
#42989 = DIRECTION ( 'NONE',  ( 0.000000000000000000, -1.000000000000000000, 0.000000000000000000 ) ) ;
#42990 = CARTESIAN_POINT ( 'NONE',  ( 7.999999999999998224, 25.21874999590322020, 3.313708498984766049 ) ) ;
#42992 = CARTESIAN_POINT ( 'NONE',  ( -2.085542519210945728E-15, 34.53124999658601268, 11.35316468750000141 ) ) ;
#42991 = CARTESIAN_POINT ( 'NONE',  ( -7.188101187500000044, 100.1562500020483810, 0.000000000000000000 ) ) ;
#42993 = CARTESIAN_POINT ( 'NONE',  ( 1.469576158976822172E-15, -7.999999999999991118, 10.20530277982336465 ) ) ;
#42994 = CARTESIAN_POINT ( 'NONE',  ( -5.676582343750006032, 159.1145833299193839, 9.832129032723418760 ) ) ;
#42995 = CARTESIAN_POINT ( 'NONE',  ( 8.660254037844389075, 132.2916666598387110, -5.000000000000000000 ) ) ;
#42996 = CARTESIAN_POINT ( 'NONE',  ( -4.401442555609581635E-16, 109.1562500020483810, -7.188101187500000044 ) ) ;
#42997 = EDGE_LOOP ( 'NONE', ( #47824, #35467, #68391, #47501 ) ) ;
#42998 = CARTESIAN_POINT ( 'NONE',  ( -2.485281374238855090, 288.8125000000000000, -5.999999999999718447 ) ) ;
#42999 = CARTESIAN_POINT ( 'NONE',  ( 9.832129032723416984, 15.67708332991935016, 5.676582343750006032 ) ) ;
#43000 = CARTESIAN_POINT ( 'NONE',  ( -7.320508075688784366, 18.12500000000000711, 7.320508075688776373 ) ) ;
#43001 = VERTEX_POINT ( 'NONE', #18498 ) ;
#43002 = CARTESIAN_POINT ( 'NONE',  ( 0.000000000000000000, 300.0000000000000000, 0.000000000000000000 ) ) ;
#43003 = CARTESIAN_POINT ( 'NONE',  ( 10.18810118749999916, 1.247682550866122264E-15, 75.90625000204836681 ) ) ;
#43004 = CARTESIAN_POINT ( 'NONE',  ( -30.64284399271074832, -37.99999999999991473, 174.6921329945331536 ) ) ;
#43006 = CARTESIAN_POINT ( 'NONE',  ( -11.35316468750000141, 148.4895833299193555, 3.042071309553159963 ) ) ;
#43005 = CARTESIAN_POINT ( 'NONE',  ( -11.00000000000000000, 0.000000000000000000, 92.68750000409677625 ) ) ;
#43007 = CARTESIAN_POINT ( 'NONE',  ( -11.00000000000000000, 0.000000000000000000, 74.49999999999998579 ) ) ;
#43008 = CARTESIAN_POINT ( 'NONE',  ( 5.656854249492374365, 5.656854249492375253, 19.82405278432982243 ) ) ;
#43009 = EDGE_CURVE ( 'NONE', #32674, #59221, #11856, .T. ) ;
#43010 = CARTESIAN_POINT ( 'NONE',  ( -11.00000000000000000, 0.000000000000000000, 116.6875000040967763 ) ) ;
#43011 = CARTESIAN_POINT ( 'NONE',  ( -6.951808397369817780E-16, 232.6562500034139873, -11.35316468749999963 ) ) ;
#43012 = CARTESIAN_POINT ( 'NONE',  ( -7.204075437095965206, -7.204075437095968759, 84.71875000204836681 ) ) ;
#43013 = ORIENTED_EDGE ( 'NONE', *, *, #31146, .F. ) ;
#43014 = LINE ( 'NONE', #66036, #9993 ) ;
#43015 = CARTESIAN_POINT ( 'NONE',  ( 28.00000000000001776, 205.5000000000000284, 165.9999999999998863 ) ) ;
#43016 = CARTESIAN_POINT ( 'NONE',  ( 6.951808397369818766E-16, 107.3437499965860269, -11.35316468750000141 ) ) ;
#43017 = CARTESIAN_POINT ( 'NONE',  ( 10.18810118749999916, 1.247682550866122264E-15, 104.4062500020483810 ) ) ;
#43018 = CARTESIAN_POINT ( 'NONE',  ( -3.211159895383561391, 20.81249999863440436, -3.211159895383561835 ) ) ;
#43019 = ORIENTED_EDGE ( 'NONE', *, *, #65680, .T. ) ;
#43020 = EDGE_LOOP ( 'NONE', ( #1095, #15930 ) ) ;
#43021 = CARTESIAN_POINT ( 'NONE',  ( 4.541265875000001451, 5.374999998634406140, 1.881053915767124440 ) ) ;
#43022 = EDGE_CURVE ( 'NONE', #2215, #40870, #12821, .T. ) ;
#43023 = CARTESIAN_POINT ( 'NONE',  ( -1.320432766682874540E-15, 9.093749997951610098, 7.188101187500000044 ) ) ;
#43024 = CARTESIAN_POINT ( 'NONE',  ( 8.000000000000000000, 115.5312500040968047, -3.313708498984762496 ) ) ;
#43025 = CARTESIAN_POINT ( 'NONE',  ( -7.204075437095967871, 7.204075437095967871, 100.8437500020483668 ) ) ;
#43026 = CARTESIAN_POINT ( 'NONE',  ( -31.45873412499999944, 201.9375000013656063, 170.0000000000003979 ) ) ;
#43027 = CARTESIAN_POINT ( 'NONE',  ( -10.03369110562688959, -8.063452199751800720, -0.4760262082327739175 ) ) ;
#43028 = CARTESIAN_POINT ( 'NONE',  ( 2.449293598294707893E-16, 2.250000000000000444, -4.000000000000001776 ) ) ;
#43029 = CARTESIAN_POINT ( 'NONE',  ( -1.656854249492383691, 19.43749999726880873, 4.000000000000000888 ) ) ;
#43030 = CARTESIAN_POINT ( 'NONE',  ( -4.541265875000002339, 3.812499998634407028, -5.561446717895856393E-16 ) ) ;
#43031 = VECTOR ( 'NONE', #42779, 1000.000000000000000 ) ;
#43032 = CARTESIAN_POINT ( 'NONE',  ( -2.445694354108838731, 209.0625000013656063, 144.4456943541088663 ) ) ;
#43033 = DIRECTION ( 'NONE',  ( -0.000000000000000000, 1.000000000000000000, -0.000000000000000000 ) ) ;
#43034 = EDGE_CURVE ( 'NONE', #11931, #8408, #71272, .T. ) ;
#43036 = DIRECTION ( 'NONE',  ( -0.8660254037844380415, -0.5000000000000011102, 0.000000000000000000 ) ) ;
#43035 = CARTESIAN_POINT ( 'NONE',  ( -26.56734541678242678, 200.3750000013656063, 166.5412658750003345 ) ) ;
#43037 = SHAPE_REPRESENTATION_RELATIONSHIP ( 'NONE' , 'NONE' ,  #4585, #47122 ) ;
#43038 = CARTESIAN_POINT ( 'NONE',  ( 4.541265875000001451, 19.24999999863440436, 1.881053915767124440 ) ) ;
#43039 = CLOSED_SHELL ( 'NONE', ( #8206, #48657, #4921, #13462, #14952, #36398 ) ) ;
#43040 = CARTESIAN_POINT ( 'NONE',  ( 1.226468279477575784E-15, 298.7031250017070079, 6.676582343750001591 ) ) ;
#43041 = CARTESIAN_POINT ( 'NONE',  ( 7.188101187499992051, 8.802885111219154394E-16, 5.236552781871753659 ) ) ;
#43042 = EDGE_LOOP ( 'NONE', ( #26617, #70672, #68665, #31321 ) ) ;
#43043 = ORIENTED_EDGE ( 'NONE', *, *, #22371, .T. ) ;
#43044 = CARTESIAN_POINT ( 'NONE',  ( -4.220049686691937474, -10.18810118749999738, 99.43750000204836681 ) ) ;
#43045 = CARTESIAN_POINT ( 'NONE',  ( 2.679491924311223183, 123.9583333333333286, 10.00000000000000533 ) ) ;
#43046 = CARTESIAN_POINT ( 'NONE',  ( -28.00000000000002132, 203.6875000013656063, 166.5412658750003629 ) ) ;
#43047 = CARTESIAN_POINT ( 'NONE',  ( -31.99999999999997868, 201.3125000000000568, 171.6568542494928238 ) ) ;
#43048 = CARTESIAN_POINT ( 'NONE',  ( 2.445694354108838731, 198.0625000013656063, 195.5543056458912190 ) ) ;
#43049 = CARTESIAN_POINT ( 'NONE',  ( -9.999999999999996447, 32.29166666666667140, -2.679491924311229401 ) ) ;
#43050 = CARTESIAN_POINT ( 'NONE',  ( -8.660254037844387298, 112.0833333333333428, -5.000000000000004441 ) ) ;
#43051 = EDGE_CURVE ( 'NONE', #26730, #26852, #20400, .T. ) ;
#43052 = EDGE_CURVE ( 'NONE', #36412, #1593, #23912, .T. ) ;
#43053 = CARTESIAN_POINT ( 'NONE',  ( -4.898587196589412829E-16, 112.6250000000000000, -8.000000000000000000 ) ) ;
#43054 = CARTESIAN_POINT ( 'NONE',  ( 6.676582343750001591, 294.1093750017069510, -8.176455196517173205E-16 ) ) ;
#43055 = ORIENTED_EDGE ( 'NONE', *, *, #56439, .T. ) ;
#43056 = VECTOR ( 'NONE', #14860, 1000.000000000000000 ) ;
#43057 = CARTESIAN_POINT ( 'NONE',  ( -8.000000000000000000, 102.6875000040967763, 0.000000000000000000 ) ) ;
#43058 = EDGE_CURVE ( 'NONE', #11129, #57815, #31291, .T. ) ;
#43059 = CARTESIAN_POINT ( 'NONE',  ( 8.000000000000000000, 23.81249999590322020, 0.000000000000000000 ) ) ;
#43060 = CARTESIAN_POINT ( 'NONE',  ( -3.458734125000015425, 205.0000000013655779, 143.4326545832176976 ) ) ;
#43061 = CARTESIAN_POINT ( 'NONE',  ( -8.660254037844390851, 184.7916666598387110, 4.999999999999998224 ) ) ;
#43062 = CARTESIAN_POINT ( 'NONE',  ( 5.656854249492379694, 121.4375000000000000, -5.656854249492380582 ) ) ;
#43063 = CARTESIAN_POINT ( 'NONE',  ( -8.311093377946834337, 254.8437500034139873, 8.311093377946837890 ) ) ;
#43064 = CARTESIAN_POINT ( 'NONE',  ( -1.656854249492381248, 3.062499997268813612, -4.000000000000001776 ) ) ;
#43065 = CARTESIAN_POINT ( 'NONE',  ( -7.778174593052023411, 7.778174593052023411, 113.3125000000000000 ) ) ;
#43066 = CARTESIAN_POINT ( 'NONE',  ( -11.35316468750000141, 3.489583329919349719, 3.042071309553159963 ) ) ;
#43067 = CARTESIAN_POINT ( 'NONE',  ( -4.401442555609577197E-16, 7.188101187499992051, 5.986552781871753659 ) ) ;
#43068 = CARTESIAN_POINT ( 'NONE',  ( -8.311093377946841443, 194.2187499965859843, 8.311093377946830785 ) ) ;
#43069 = CARTESIAN_POINT ( 'NONE',  ( 4.999999999999993783, 191.0416666598387110, 8.660254037844390851 ) ) ;
#43070 = CARTESIAN_POINT ( 'NONE',  ( -4.541265875000002339, 4.812499998634407028, -5.561446717895856393E-16 ) ) ;
#43071 = CARTESIAN_POINT ( 'NONE',  ( -5.656854249492380582, 99.50000000409679046, -5.656854249492380582 ) ) ;
#43073 = LINE ( 'NONE', #14399, #35089 ) ;
#43072 = CARTESIAN_POINT ( 'NONE',  ( 0.000000000000000000, 125.0000000000000000, 0.000000000000000000 ) ) ;
#43074 = ORIENTED_EDGE ( 'NONE', *, *, #22473, .F. ) ;
#43075 =( BOUNDED_CURVE ( )  B_SPLINE_CURVE ( 2, ( #58887, #42619, #66758, #65261, #32059, #30932, #3762, #3387, #72415 ),
 .UNSPECIFIED., .F., .F. ) 
 B_SPLINE_CURVE_WITH_KNOTS ( ( 3, 2, 2, 2, 3 ),
 ( 0.3684210526315789824, 0.3750000000000000555, 0.3815789473684211286, 0.3881578947368421462, 0.3947368421052632192 ),
 .UNSPECIFIED. ) 
 CURVE ( )  GEOMETRIC_REPRESENTATION_ITEM ( )  RATIONAL_B_SPLINE_CURVE ( ( 0.9999999999999993339, 0.9238795325112874046, 1.000000000000000000, 0.9238795325112867385, 1.000000000000000000, 0.9238795325112867385, 1.000000000000000000, 0.9238795325112860723, 1.000000000000000666 ) ) 
 REPRESENTATION_ITEM ( '' )  );
#43076 = CARTESIAN_POINT ( 'NONE',  ( 1.432654583217607414, 204.5000000013656063, 145.4587341250000634 ) ) ;
#43077 = CARTESIAN_POINT ( 'NONE',  ( -11.35316468750000141, 43.80208332991934839, 3.042071309553159963 ) ) ;
#43078 = CARTESIAN_POINT ( 'NONE',  ( 4.556349186104045934, 11.00000000000000000, 98.21875000409679046 ) ) ;
#43079 = CARTESIAN_POINT ( 'NONE',  ( -4.556349186104048599, -10.99999999999999822, 106.4687500040967763 ) ) ;
#43080 = CARTESIAN_POINT ( 'NONE',  ( -25.55430564589122966, 200.3125000013656063, 167.5543056458915032 ) ) ;
#43081 = DIRECTION ( 'NONE',  ( -1.000000000000000000, 0.000000000000000000, 1.652117596168387509E-16 ) ) ;
#43083 = CARTESIAN_POINT ( 'NONE',  ( 6.123233995736767268E-16, 203.1249999931720538, -10.00000000000000178 ) ) ;
#43082 = CARTESIAN_POINT ( 'NONE',  ( -4.401442555609581635E-16, 122.2812500020483810, -7.188101187500000044 ) ) ;
#43084 = CARTESIAN_POINT ( 'NONE',  ( 3.458734124999959914, 196.3750000013656063, 143.4326545832176976 ) ) ;
#43085 = CARTESIAN_POINT ( 'NONE',  ( -8.311093377946836114, 122.6562499965860269, -8.311093377946837890 ) ) ;
#43086 = CARTESIAN_POINT ( 'NONE',  ( -8.660254037844390851, 84.79166665983869677, 4.999999999999998224 ) ) ;
#43087 = CARTESIAN_POINT ( 'NONE',  ( 2.977408999572650039, 93.68750000204838102, -7.188101187500001821 ) ) ;
#43088 = CARTESIAN_POINT ( 'NONE',  ( -1.881053915767121554, 18.74999999863440436, -4.541265875000002339 ) ) ;
#43089 = CARTESIAN_POINT ( 'NONE',  ( -7.999999999999991118, 0.000000000000000000, 25.01780278392014978 ) ) ;
#43090 = DIRECTION ( 'NONE',  ( -0.000000000000000000, 1.000000000000000000, -0.000000000000000000 ) ) ;
#43091 = ORIENTED_EDGE ( 'NONE', *, *, #24572, .T. ) ;
#43092 = CARTESIAN_POINT ( 'NONE',  ( 4.500000000000006217, -7.794228634059941818, 0.000000000000000000 ) ) ;
#43093 = ORIENTED_EDGE ( 'NONE', *, *, #2307, .F. ) ;
#43094 = CARTESIAN_POINT ( 'NONE',  ( 6.676582343750003368, 292.1718750017070079, -2.765530957081997254 ) ) ;
#43095 = CARTESIAN_POINT ( 'NONE',  ( -1.656854249492383468, 12.43749999726881406, 4.000000000000000888 ) ) ;
#43096 = CARTESIAN_POINT ( 'NONE',  ( -7.999999999999991118, 0.000000000000000000, 8.517802783920146226 ) ) ;
#43097 = CARTESIAN_POINT ( 'NONE',  ( -9.832129032723420536, 168.6979166632526983, 5.676582343749997150 ) ) ;
#43098 = CARTESIAN_POINT ( 'NONE',  ( 9.000000000000000000, 3.504753767550392585, -0.3593172728154473972 ) ) ;
#43099 = CARTESIAN_POINT ( 'NONE',  ( 2.849036369511732440E-14, 198.2500000000000000, 202.0000000000000000 ) ) ;
#43100 = CARTESIAN_POINT ( 'NONE',  ( -6.735557395310442023E-16, 11.00000000000000000, 69.62499999999998579 ) ) ;
#43101 = CARTESIAN_POINT ( 'NONE',  ( -10.18810118749999916, 4.220049686691934809, 103.9375000020483810 ) ) ;
#43102 = ORIENTED_EDGE ( 'NONE', *, *, #62304, .T. ) ;
#43103 =( BOUNDED_CURVE ( )  B_SPLINE_CURVE ( 2, ( #17936, #57951, #240, #69998, #18306, #11167, #28879, #69622, #610 ),
 .UNSPECIFIED., .F., .F. ) 
 B_SPLINE_CURVE_WITH_KNOTS ( ( 3, 2, 2, 2, 3 ),
 ( 0.6833333333333340143, 0.6916666666666673180, 0.7000000000000005107, 0.7083333333333339255, 0.7166666666666671182 ),
 .UNSPECIFIED. ) 
 CURVE ( )  GEOMETRIC_REPRESENTATION_ITEM ( )  RATIONAL_B_SPLINE_CURVE ( ( 0.9999999999999938938, 0.9238795325112928447, 1.000000000000000000, 0.9238795325112867385, 1.000000000000000000, 0.9238795325112867385, 1.000000000000000000, 0.9238795325112826307, 1.000000000000003997 ) ) 
 REPRESENTATION_ITEM ( '' )  );
#43104 = CARTESIAN_POINT ( 'NONE',  ( 3.313708498984762496, 22.03124999590322375, 7.999999999999998224 ) ) ;
#43105 = CARTESIAN_POINT ( 'NONE',  ( -5.676582343749998039, 157.7604166632526983, -9.832129032723420536 ) ) ;
#43106 = CARTESIAN_POINT ( 'NONE',  ( 2.839093476692135984E-14, 206.9375000013656063, 201.4587341250000350 ) ) ;
#43108 = EDGE_CURVE ( 'NONE', #69954, #55449, #21463, .T. ) ;
#43107 = CARTESIAN_POINT ( 'NONE',  ( 1.871523826299183495E-15, -10.18810118749999916, 71.40625000204836681 ) ) ;
#43109 = CARTESIAN_POINT ( 'NONE',  ( -5.676582343749998039, 67.76041666325268409, -9.832129032723420536 ) ) ;
#43110 = ORIENTED_EDGE ( 'NONE', *, *, #62177, .F. ) ;
#43111 = CARTESIAN_POINT ( 'NONE',  ( -7.204075437095967871, 7.204075437095967871, 116.9687500020483810 ) ) ;
#43112 = CARTESIAN_POINT ( 'NONE',  ( -4.541265875000002339, 8.937499998634407916, -5.561446717895856393E-16 ) ) ;
#43113 = CARTESIAN_POINT ( 'NONE',  ( -4.903558642999205574E-16, 8.008118988124991233, 11.13811528394063188 ) ) ;
#43114 = ORIENTED_EDGE ( 'NONE', *, *, #19940, .F. ) ;
#43115 = CARTESIAN_POINT ( 'NONE',  ( 5.082755093536324154, 21.28124999795161543, 5.082755093536326818 ) ) ;
#43116 = CARTESIAN_POINT ( 'NONE',  ( -3.673940397442060854E-16, 288.8125000034140157, -6.000000000000001776 ) ) ;
#43117 = CIRCLE ( 'NONE', #41931, 7.949999999999993960 ) ;
#43118 = CARTESIAN_POINT ( 'NONE',  ( -8.000000000000000000, 117.5937500040967905, -3.313708498984761164 ) ) ;
#43119 = CARTESIAN_POINT ( 'NONE',  ( -7.188101187500000044, 10.59374999795161187, -8.802885111219163269E-16 ) ) ;
#43120 = CARTESIAN_POINT ( 'NONE',  ( 7.188101187499992051, 2.977408999572647819, 3.830302781871751883 ) ) ;
#43121 = VECTOR ( 'NONE', #20162, 1000.000000000000000 ) ;
#43122 = CARTESIAN_POINT ( 'NONE',  ( -10.18810118749999916, 4.220049686691934809, 117.4375000020483810 ) ) ;
#43123 = ADVANCED_FACE ( 'NONE', ( #19965 ), #15051, .F. ) ;
#43124 = SHAPE_REPRESENTATION ( 'spindle', ( #57354 ), #69405 ) ;
#43125 = CARTESIAN_POINT ( 'NONE',  ( 3.898495371540924292, 89.88208674283050925, -6.752431955835072941 ) ) ;
#43126 = CARTESIAN_POINT ( 'NONE',  ( -7.347880794884122694E-16, 5.499999997268813168, 4.000000000000001776 ) ) ;
#43127 = PRODUCT_DEFINITION ( 'UNKNOWN', '', #71904, #12441 ) ;
#43128 = ORIENTED_EDGE ( 'NONE', *, *, #63054, .T. ) ;
#43129 = CARTESIAN_POINT ( 'NONE',  ( -2.445694354108782775, 207.5625000013656063, 200.4456943541088663 ) ) ;
#43130 = CARTESIAN_POINT ( 'NONE',  ( -23.99999999999995026, 196.8125000027311842, 171.6568542494926817 ) ) ;
#43131 = EDGE_CURVE ( 'NONE', #22362, #12256, #57013, .T. ) ;
#43132 = CARTESIAN_POINT ( 'NONE',  ( -3.211159895383561391, 4.687499998634407028, -3.211159895383561835 ) ) ;
#43133 = CARTESIAN_POINT ( 'NONE',  ( -7.188101187499999156, 110.7500000020483668, 2.977408999572654924 ) ) ;
#43134 = CARTESIAN_POINT ( 'NONE',  ( 27.99999999999996803, 205.0000000000000284, 173.9999999999999147 ) ) ;
#43135 = CARTESIAN_POINT ( 'NONE',  ( -2.977408999572648707, -7.188101187499990274, 25.76780278187175810 ) ) ;
#43136 = ORIENTED_EDGE ( 'NONE', *, *, #65198, .T. ) ;
#43137 = EDGE_CURVE ( 'NONE', #18660, #26901, #64717, .T. ) ;
#43138 = CARTESIAN_POINT ( 'NONE',  ( 2.977408999572650927, 26.24999999795161543, -7.188101187500000933 ) ) ;
#43139 = ORIENTED_EDGE ( 'NONE', *, *, #16525, .T. ) ;
#43140 = CARTESIAN_POINT ( 'NONE',  ( 10.18810118750000093, -4.220049686691933033, 114.8125000020483668 ) ) ;
#43141 = CARTESIAN_POINT ( 'NONE',  ( 6.406660676652354169, 4.906935342933127053, 0.000000000000000000 ) ) ;
#43142 = CARTESIAN_POINT ( 'NONE',  ( 2.445694354108838731, 208.0625000013656063, 195.5543056458912190 ) ) ;
#43143 = CARTESIAN_POINT ( 'NONE',  ( 28.00000000000001776, 202.4375000013656063, 173.4587341249998929 ) ) ;
#43144 = CARTESIAN_POINT ( 'NONE',  ( -2.679491924311235618, 68.54166666666667140, 10.00000000000000000 ) ) ;
#43145 = CARTESIAN_POINT ( 'NONE',  ( -7.188101187499999156, 94.62500000204838102, 2.977408999572654924 ) ) ;
#43146 = CARTESIAN_POINT ( 'NONE',  ( -3.673940397442060854E-16, 294.7500000000000000, -6.000000000000001776 ) ) ;
#43148 = CARTESIAN_POINT ( 'NONE',  ( 6.123233995736767268E-16, 126.2500000000000000, -10.00000000000000178 ) ) ;
#43147 = CARTESIAN_POINT ( 'NONE',  ( 27.99999999999996803, 208.6250000027312126, 165.9999999999998863 ) ) ;
#43149 = ORIENTED_EDGE ( 'NONE', *, *, #66554, .F. ) ;
#43150 = CARTESIAN_POINT ( 'NONE',  ( 9.832129032723416984, 226.8229166700806729, -5.676582343750003368 ) ) ;
#43151 = AXIS2_PLACEMENT_3D ( 'NONE', #73518, #61460, #45594 ) ;
#43152 = CARTESIAN_POINT ( 'NONE',  ( -4.556349186104045934, 11.00000000000000000, 87.90625000409677625 ) ) ;
#43153 = CARTESIAN_POINT ( 'NONE',  ( -2.849036369511732440E-14, 200.3750000027312126, 138.0000000000000568 ) ) ;
#43154 = CARTESIAN_POINT ( 'NONE',  ( 27.99999999999999645, 210.0000000000000284, 169.9999999999999147 ) ) ;
#43155 = CARTESIAN_POINT ( 'NONE',  ( -3.313708498984757611, 7.999999999999991118, 2.236552783920144005 ) ) ;
#43156 = CARTESIAN_POINT ( 'NONE',  ( -10.00000000000000000, 250.0000000000000000, 0.000000000000000000 ) ) ;
#43157 = EDGE_CURVE ( 'NONE', #1871, #73371, #5460, .T. ) ;
#43158 = DIRECTION ( 'NONE',  ( 0.000000000000000000, -1.000000000000000000, 0.000000000000000000 ) ) ;
#43159 = CARTESIAN_POINT ( 'NONE',  ( 8.660254037844389075, 185.4166666666666856, -5.000000000000000000 ) ) ;
#43160 = CARTESIAN_POINT ( 'NONE',  ( -2.977408999572647819, -7.188101187499990274, 21.64280278187176165 ) ) ;
#43161 = CARTESIAN_POINT ( 'NONE',  ( -3.042071309553173730, 159.6354166632526983, 11.35316468749999785 ) ) ;
#43162 = CARTESIAN_POINT ( 'NONE',  ( -4.000000000000016875, 204.5625000027312126, 140.3431457505076594 ) ) ;
#43163 = CARTESIAN_POINT ( 'NONE',  ( 7.320508075688771044, 261.2500000068279178, -7.320508075688771932 ) ) ;
#43165 = LINE ( 'NONE', #3565, #34609 ) ;
#43164 = CARTESIAN_POINT ( 'NONE',  ( 28.00000000000001776, 203.5000000000000000, 165.9999999999998863 ) ) ;
#43166 = ORIENTED_EDGE ( 'NONE', *, *, #58204, .T. ) ;
#43167 = AXIS2_PLACEMENT_3D ( 'NONE', #12453, #35482, #30179 ) ;
#43168 = CARTESIAN_POINT ( 'NONE',  ( 9.832129032723416984, 10.67708332991935016, 5.676582343750006032 ) ) ;
#43169 = CARTESIAN_POINT ( 'NONE',  ( 2.828427124746208943, 200.7500000027312126, 195.1715728752538439 ) ) ;
#43170 = CARTESIAN_POINT ( 'NONE',  ( 2.751064625579944321E-14, 207.7500000000000284, 194.0000000000000568 ) ) ;
#43171 = CARTESIAN_POINT ( 'NONE',  ( -30.82842712474620939, 196.1250000000000284, 167.1715728752542134 ) ) ;
#43172 = CARTESIAN_POINT ( 'NONE',  ( -2.445694354108838731, 207.0625000013656063, 144.4456943541088663 ) ) ;
#43173 = CIRCLE ( 'NONE', #33580, 18.99999999999998934 ) ;
#43174 = CARTESIAN_POINT ( 'NONE',  ( -10.00000000000000000, 44.16666665983871098, -2.679491924311229845 ) ) ;
#43175 = CARTESIAN_POINT ( 'NONE',  ( -5.082755093536324154, 109.3437500020483810, 5.082755093536326818 ) ) ;
#43176 = CARTESIAN_POINT ( 'NONE',  ( 4.541265875000002339, 3.437499998634407028, 0.000000000000000000 ) ) ;
#43177 = CARTESIAN_POINT ( 'NONE',  ( 7.999999999999991118, 9.797174393178815797E-16, 13.76780278392014623 ) ) ;
#43178 = CARTESIAN_POINT ( 'NONE',  ( -3.313708498984758943, -7.999999999999989342, 7.111552779823365533 ) ) ;
#43180 = CARTESIAN_POINT ( 'NONE',  ( 3.153939666463620179E-13, 158.7500000000000284, 9.999999999999998224 ) ) ;
#43179 = DIRECTION ( 'NONE',  ( -1.000000000000000000, 0.000000000000000000, 0.000000000000000000 ) ) ;
#43181 = ORIENTED_EDGE ( 'NONE', *, *, #4800, .T. ) ;
#43182 = CARTESIAN_POINT ( 'NONE',  ( -7.999999999999991118, 9.797174393178815797E-16, 30.00000000000000000 ) ) ;
#43183 = CARTESIAN_POINT ( 'NONE',  ( -10.99999999999989164, -4.556349186104158733, 82.09375000000000000 ) ) ;
#43184 = ADVANCED_FACE ( 'NONE', ( #55066, #55817 ), #4134, .F. ) ;
#43185 = CARTESIAN_POINT ( 'NONE',  ( -3.042071309553159075, 235.2604166700806161, 11.35316468749999963 ) ) ;
#43186 = CARTESIAN_POINT ( 'NONE',  ( -3.042071309553173730, 124.3229166632526983, 11.35316468749999785 ) ) ;
#43187 = ORIENTED_EDGE ( 'NONE', *, *, #26521, .F. ) ;
#43188 = CARTESIAN_POINT ( 'NONE',  ( -1.656854249492487607, 200.6875000000000284, 145.9999999999999716 ) ) ;
#43189 = CARTESIAN_POINT ( 'NONE',  ( -7.204075437095965206, -7.204075437095968759, 96.34375000204836681 ) ) ;
#43190 = CARTESIAN_POINT ( 'NONE',  ( -7.778174593052023411, 7.778174593052023411, 93.81250000000000000 ) ) ;
#43191 = CARTESIAN_POINT ( 'NONE',  ( -1.432654583217608080, 196.8750000013656063, 201.4587341250000350 ) ) ;
#43192 = CARTESIAN_POINT ( 'NONE',  ( 30.82842712474616675, 197.1250000000000284, 172.8284271247460993 ) ) ;
#43193 = CARTESIAN_POINT ( 'NONE',  ( 11.35316468750000141, 120.7812499965860269, 0.000000000000000000 ) ) ;
#43194 = CARTESIAN_POINT ( 'NONE',  ( -27.99999999999996092, 208.5000000000000284, 174.0000000000003695 ) ) ;
#43195 = EDGE_CURVE ( 'NONE', #52578, #22331, #45971, .T. ) ;
#43196 = CARTESIAN_POINT ( 'NONE',  ( 1.469576158976823947E-15, 119.3750000000000000, 8.000000000000000000 ) ) ;
#43197 = ORIENTED_EDGE ( 'NONE', *, *, #73539, .F. ) ;
#43198 = CARTESIAN_POINT ( 'NONE',  ( 9.999999999999998224, 257.7083333333333712, -2.679491924311229401 ) ) ;
#43199 = CARTESIAN_POINT ( 'NONE',  ( -8.311093377946841443, 104.2187499965860127, 8.311093377946834337 ) ) ;
#43200 = CARTESIAN_POINT ( 'NONE',  ( 1.432654583217662259, 206.1250000013656063, 194.5412658750000219 ) ) ;
#43201 = CARTESIAN_POINT ( 'NONE',  ( -1.320432766682874540E-15, 15.46874999795161187, 7.188101187500000044 ) ) ;
#43202 =( BOUNDED_CURVE ( )  B_SPLINE_CURVE ( 2, ( #65561, #36901, #59909, #2570, #65931, #2940, #45806, #33770, #39042 ),
 .UNSPECIFIED., .F., .F. ) 
 B_SPLINE_CURVE_WITH_KNOTS ( ( 3, 2, 2, 2, 3 ),
 ( 0.2812499999999997780, 0.2864583333333330928, 0.2916666666666665186, 0.2968749999999998335, 0.3020833333333331483 ),
 .UNSPECIFIED. ) 
 CURVE ( )  GEOMETRIC_REPRESENTATION_ITEM ( )  RATIONAL_B_SPLINE_CURVE ( ( 1.000000000000003331, 0.9238795325112835188, 1.000000000000000000, 0.9238795325112867385, 1.000000000000000000, 0.9238795325112867385, 1.000000000000000000, 0.9238795325112891810, 0.9999999999999975575 ) ) 
 REPRESENTATION_ITEM ( '' )  );
#43204 = EDGE_CURVE ( 'NONE', #38870, #37587, #56562, .T. ) ;
#43203 = CARTESIAN_POINT ( 'NONE',  ( 10.18810118750000093, -4.220049686691933033, 86.68750000204838102 ) ) ;
#43205 = CARTESIAN_POINT ( 'NONE',  ( -5.676582343750006032, 29.42708332991935194, 9.832129032723418760 ) ) ;
#43206 = ORIENTED_EDGE ( 'NONE', *, *, #36094, .F. ) ;
#43207 = DIRECTION ( 'NONE',  ( 0.000000000000000000, 0.000000000000000000, 1.000000000000000000 ) ) ;
#43208 = CARTESIAN_POINT ( 'NONE',  ( -8.008118988124991233, 0.000000000000000000, 25.01311528394063544 ) ) ;
#43209 = CARTESIAN_POINT ( 'NONE',  ( 8.660254037844385522, 116.4583333265053824, 5.000000000000005329 ) ) ;
#43210 = PLANE ( 'NONE',  #3712 ) ;
#43211 = CARTESIAN_POINT ( 'NONE',  ( 5.082755093536325930, 2.156249997951610098, -5.082755093536325930 ) ) ;
#43212 = CARTESIAN_POINT ( 'NONE',  ( 2.765530957082001251, 288.7656250017068942, 6.676582343750000703 ) ) ;
#43213 = CARTESIAN_POINT ( 'NONE',  ( 4.999999999999993783, 126.0416666598387110, 8.660254037844390851 ) ) ;
#43214 = CARTESIAN_POINT ( 'NONE',  ( 9.832129032723416984, 225.6770833299193839, 5.676582343750006032 ) ) ;
#43215 = ORIENTED_EDGE ( 'NONE', *, *, #59179, .F. ) ;
#43216 = CARTESIAN_POINT ( 'NONE',  ( -8.311093377946841443, 139.2187499965860127, 8.311093377946830785 ) ) ;
#43217 = CARTESIAN_POINT ( 'NONE',  ( 7.204075437095968759, -7.204075437095966983, 81.71875000204836681 ) ) ;
#43218 = CIRCLE ( 'NONE', #51627, 9.000000000000001776 ) ;
#43219 = EDGE_CURVE ( 'NONE', #1819, #60275, #23329, .T. ) ;
#43220 = CARTESIAN_POINT ( 'NONE',  ( -30.44569435410883429, 199.5625000013656063, 167.5543056458915885 ) ) ;
#43221 =( BOUNDED_CURVE ( )  B_SPLINE_CURVE ( 2, ( #72210, #10342, #33366, #9221, #45045, #32242, #56367, #4688, #73708 ),
 .UNSPECIFIED., .F., .F. ) 
 B_SPLINE_CURVE_WITH_KNOTS ( ( 3, 2, 2, 2, 3 ),
 ( 0.2840909090909091161, 0.2897727272727272929, 0.2954545454545454697, 0.3011363636363636465, 0.3068181818181818232 ),
 .UNSPECIFIED. ) 
 CURVE ( )  GEOMETRIC_REPRESENTATION_ITEM ( )  RATIONAL_B_SPLINE_CURVE ( ( 1.000000000000000000, 0.9238795325112867385, 1.000000000000000000, 0.9238795325112867385, 1.000000000000000000, 0.9238795325112867385, 1.000000000000000000, 0.9238795325112867385, 1.000000000000000000 ) ) 
 REPRESENTATION_ITEM ( '' )  );
#43222 = CARTESIAN_POINT ( 'NONE',  ( -2.849036369511732440E-14, 198.2500000000000000, 138.0000000000000568 ) ) ;
#43223 = CARTESIAN_POINT ( 'NONE',  ( 3.211159895383560947, 10.31249999863440792, 3.211159895383562723 ) ) ;
#43224 = ORIENTED_EDGE ( 'NONE', *, *, #9942, .T. ) ;
#43225 = VECTOR ( 'NONE', #58272, 1000.000000000000000 ) ;
#43226 = CARTESIAN_POINT ( 'NONE',  ( 1.656854249492403008, 204.8125000027312126, 194.0000000000000853 ) ) ;
#43227 = CARTESIAN_POINT ( 'NONE',  ( -1.432654583217664701, 199.0000000013656063, 138.5412658750000787 ) ) ;
#43228 = CIRCLE ( 'NONE', #11901, 6.000000000000001776 ) ;
#43229 = CARTESIAN_POINT ( 'NONE',  ( -1.656854249492405451, 202.4375000027311842, 138.0000000000000568 ) ) ;
#43230 = CARTESIAN_POINT ( 'NONE',  ( 5.000000000000000000, 11.43937387734352029, -68.01947305042915559 ) ) ;
#43231 = ORIENTED_EDGE ( 'NONE', *, *, #24753, .T. ) ;
#43232 = CARTESIAN_POINT ( 'NONE',  ( 7.188101187499999156, 3.374999997951610098, 2.977408999572654924 ) ) ;
#43233 = CARTESIAN_POINT ( 'NONE',  ( -10.99999999999999822, -4.556349186104053040, 76.09375000000000000 ) ) ;
#43234 = FACE_OUTER_BOUND ( 'NONE', #31123, .T. ) ;
#43235 = CARTESIAN_POINT ( 'NONE',  ( 9.832129032723420536, 191.1979166632526983, -5.676582343749999815 ) ) ;
#43236 = CARTESIAN_POINT ( 'NONE',  ( 5.082755093536325042, 110.4687500020483810, -5.082755093536325930 ) ) ;
#43237 = DIRECTION ( 'NONE',  ( 0.000000000000000000, 0.000000000000000000, 1.000000000000000000 ) ) ;
#43238 = CARTESIAN_POINT ( 'NONE',  ( -6.676582343750001591, 293.4531250017069510, 0.000000000000000000 ) ) ;
#43240 = CARTESIAN_POINT ( 'NONE',  ( -1.237384350715592869E-11, 93.74999999999903366, 9.999999999999998224 ) ) ;
#43239 = CARTESIAN_POINT ( 'NONE',  ( -29.65685424949240812, 209.0625000000000284, 166.0000000000004263 ) ) ;
#43241 = EDGE_LOOP ( 'NONE', ( #46955, #11255, #11889, #35587, #3895, #17800, #44604, #35801, #29549, #57066, #12507, #44380, #64995, #59505, #64572, #14020, #48384, #54485, #24227, #64203, #10520, #38029, #67245, #15582, #12131, #7978, #63379, #69292, #70257, #4180, #32349, #30052, #47851, #40468, #45443, #10113, #74361, #49410, #52846 ) ) ;
#43242 = CARTESIAN_POINT ( 'NONE',  ( -3.042071309553159075, 230.2604166700806445, 11.35316468749999963 ) ) ;
#43243 = PRODUCT_DEFINITION_SHAPE ( 'NONE', 'NONE',  #7218 ) ;
#43244 = CARTESIAN_POINT ( 'NONE',  ( 7.188101187499991163, 2.977408999572648707, 2.330302781871750550 ) ) ;
#43245 = CARTESIAN_POINT ( 'NONE',  ( 8.000000000000000000, 106.2500000000000000, -9.797174393178825657E-16 ) ) ;
#43246 = CARTESIAN_POINT ( 'NONE',  ( -56.00000000000004974, -70.00000000000001421, 171.9999999999997442 ) ) ;
#43247 = CARTESIAN_POINT ( 'NONE',  ( 2.445694354108840063, 201.0625000013656063, 200.4456943541088663 ) ) ;
#43248 = DIRECTION ( 'NONE',  ( -0.000000000000000000, 1.000000000000000000, -0.000000000000000000 ) ) ;
#43249 = LINE ( 'NONE', #66265, #16227 ) ;
#43250 = CARTESIAN_POINT ( 'NONE',  ( 5.656854249492379694, 91.43749999999998579, -5.656854249492380582 ) ) ;
#43251 = CARTESIAN_POINT ( 'NONE',  ( 9.832129032723416984, 110.6770833299193555, 5.676582343750006032 ) ) ;
#43252 = DIRECTION ( 'NONE',  ( 0.000000000000000000, 0.000000000000000000, 1.000000000000000000 ) ) ;
#43253 = CARTESIAN_POINT ( 'NONE',  ( 4.556349186104051263, -10.99999999999999822, 79.46874999999998579 ) ) ;
#43255 = CARTESIAN_POINT ( 'NONE',  ( 31.45873412499999233, 200.6875000013656063, 169.9999999999998863 ) ) ;
#43254 = CARTESIAN_POINT ( 'NONE',  ( 26.56734541678232375, 199.6250000013656063, 173.4587341249998929 ) ) ;
#43256 = VERTEX_POINT ( 'NONE', #57683 ) ;
#43257 = CARTESIAN_POINT ( 'NONE',  ( 7.188101187500000044, 27.65624999795161543, 0.000000000000000000 ) ) ;
#43258 = CARTESIAN_POINT ( 'NONE',  ( 6.000000000000003553, 287.6250000034140157, -2.485281374238571761 ) ) ;
#43259 = CARTESIAN_POINT ( 'NONE',  ( -3.458734125000015425, 201.9375000013656063, 142.0000000000000568 ) ) ;
#43260 = EDGE_CURVE ( 'NONE', #22922, #27854, #9850, .T. ) ;
#43261 = CARTESIAN_POINT ( 'NONE',  ( 24.54126587499999346, 201.4375000013656063, 169.9999999999998863 ) ) ;
#43262 = CIRCLE ( 'NONE', #20376, 38.34805510287551300 ) ;
#43263 = LINE ( 'NONE', #3288, #64144 ) ;
#43264 = CARTESIAN_POINT ( 'NONE',  ( -3.042071309553164404, 187.5520833299193555, -11.35316468749999963 ) ) ;
#43265 = CARTESIAN_POINT ( 'NONE',  ( -5.082755093536325930, 94.34375000204838102, -5.082755093536325930 ) ) ;
#43266 = DIRECTION ( 'NONE',  ( -0.000000000000000000, -1.000000000000000000, -4.283267841918042741E-17 ) ) ;
#43267 = CARTESIAN_POINT ( 'NONE',  ( 1.881053915767122664, 14.12499999863440969, 4.541265875000001451 ) ) ;
#43268 = CARTESIAN_POINT ( 'NONE',  ( 24.54126587500000412, 198.3750000013656063, 168.5673454167822172 ) ) ;
#43269 = CARTESIAN_POINT ( 'NONE',  ( -3.313708498984757167, 7.999999999999991118, 29.04905277982337353 ) ) ;
#43270 = CARTESIAN_POINT ( 'NONE',  ( 1.469576158976823947E-15, 96.87499999999998579, 8.000000000000000000 ) ) ;
#43271 = CARTESIAN_POINT ( 'NONE',  ( 11.35316468749999963, 75.98958332991935549, -3.042071309553165293 ) ) ;
#43272 = ORIENTED_EDGE ( 'NONE', *, *, #3669, .F. ) ;
#43273 = CARTESIAN_POINT ( 'NONE',  ( -12.00000000000000355, 1.469576158976824342E-15, -25.03750572909317285 ) ) ;
#43274 = FACE_OUTER_BOUND ( 'NONE', #26761, .T. ) ;
#43275 = CARTESIAN_POINT ( 'NONE',  ( 4.401442555609581635E-16, 20.34374999795161543, -7.188101187500000044 ) ) ;
#43276 = CARTESIAN_POINT ( 'NONE',  ( -8.000000000000000000, 108.6875000040967905, 0.000000000000000000 ) ) ;
#43277 = CARTESIAN_POINT ( 'NONE',  ( 7.320508075688776373, 231.8750000000000000, 7.320508075688767491 ) ) ;
#43278 = CARTESIAN_POINT ( 'NONE',  ( 9.832129032723416984, 90.36458332991935549, 5.676582343750006032 ) ) ;
#43279 = ORIENTED_EDGE ( 'NONE', *, *, #67372, .F. ) ;
#43280 = CARTESIAN_POINT ( 'NONE',  ( 10.18810118750000093, -4.220049686691933921, 85.18750000204838102 ) ) ;
#43281 = AXIS2_PLACEMENT_3D ( 'NONE', #31607, #48942, #65559 ) ;
#43282 = CARTESIAN_POINT ( 'NONE',  ( -4.220049686691935698, 10.18810118749999916, 113.8750000020483668 ) ) ;
#43283 = CARTESIAN_POINT ( 'NONE',  ( 0.000000000000000000, 300.0000000000000000, 10.00000000000000178 ) ) ;
#43284 = CARTESIAN_POINT ( 'NONE',  ( 3.458734125000016757, 208.1250000013656063, 199.4326545832176691 ) ) ;
#43285 = CARTESIAN_POINT ( 'NONE',  ( 2.775557561562891351E-14, 210.0000000000000284, 198.0000000000000284 ) ) ;
#43287 = CARTESIAN_POINT ( 'NONE',  ( -9.832129032723420536, 78.69791666325269830, 5.676582343749997150 ) ) ;
#43286 = CARTESIAN_POINT ( 'NONE',  ( -54.00000000000000000, 272.0000000000000000, 4.085831468968145267E-14 ) ) ;
#43288 = CARTESIAN_POINT ( 'NONE',  ( 1.469576158976822172E-15, -7.999999999999991118, 19.39280278392014978 ) ) ;
#43289 = EDGE_CURVE ( 'NONE', #58393, #40550, #43173, .T. ) ;
#43290 = CARTESIAN_POINT ( 'NONE',  ( 8.660254037844385522, 129.5833333333333144, 5.000000000000005329 ) ) ;
#43291 = CARTESIAN_POINT ( 'NONE',  ( -1.836970198721029983E-15, 165.6249999931720254, 10.00000000000000178 ) ) ;
#43292 = CARTESIAN_POINT ( 'NONE',  ( -7.188101187500001821, 91.43750000204838102, -2.977408999572650483 ) ) ;
#43293 = CARTESIAN_POINT ( 'NONE',  ( -24.46046022537927556, 194.8779416066605563, 171.5956376062985100 ) ) ;
#43294 = CARTESIAN_POINT ( 'NONE',  ( 11.35316468749999963, 56.30208332991934839, -3.042071309553165293 ) ) ;
#43295 = CARTESIAN_POINT ( 'NONE',  ( 6.676582343750003368, 294.0156250017070079, -2.765530957081997254 ) ) ;
#43297 = EDGE_CURVE ( 'NONE', #3011, #33914, #192, .T. ) ;
#43296 = CARTESIAN_POINT ( 'NONE',  ( -7.204075437095965206, -7.204075437095968759, 105.7187500020483810 ) ) ;
#43298 = CARTESIAN_POINT ( 'NONE',  ( 11.35316468749999785, 210.5729166632526983, 3.042071309553174174 ) ) ;
#43299 = ORIENTED_EDGE ( 'NONE', *, *, #43607, .T. ) ;
#43300 = CARTESIAN_POINT ( 'NONE',  ( 3.999999999999959144, 203.0625000000000000, 140.3431457505076594 ) ) ;
#43301 = CARTESIAN_POINT ( 'NONE',  ( 1.224646799147353454E-15, 300.0000000000000000, -10.00000000000000178 ) ) ;
#43303 = CARTESIAN_POINT ( 'NONE',  ( 3.042071309553159519, 194.7395833299193555, 11.35316468750000141 ) ) ;
#43302 = CARTESIAN_POINT ( 'NONE',  ( -2.828427124746190735, 19.37500000000000000, -2.828427124746191623 ) ) ;
#43304 = CARTESIAN_POINT ( 'NONE',  ( 8.000000000000000000, 2.812499995903220640, 0.000000000000000000 ) ) ;
#43305 = CARTESIAN_POINT ( 'NONE',  ( -4.999999999999992895, 233.9583333401613174, 8.660254037844390851 ) ) ;
#43306 = CARTESIAN_POINT ( 'NONE',  ( 4.721056650416000089, 298.8281250017069510, 4.721056650415999201 ) ) ;
#43307 = ORIENTED_EDGE ( 'NONE', *, *, #50098, .F. ) ;
#43308 = CARTESIAN_POINT ( 'NONE',  ( 3.042071309553167513, 177.1354166632526983, -11.35316468749999785 ) ) ;
#43309 = CARTESIAN_POINT ( 'NONE',  ( -4.401442555609577197E-16, 7.188101187499992051, 19.11155278187175455 ) ) ;
#43310 = CARTESIAN_POINT ( 'NONE',  ( -5.000000000000000000, 60.90295814858271939, -23.31388853594749833 ) ) ;
#43311 = EDGE_LOOP ( 'NONE', ( #70748, #47875, #63369, #9388, #67026 ) ) ;
#43312 = CARTESIAN_POINT ( 'NONE',  ( -3.313708498984762496, 98.46875000409676204, 7.999999999999998224 ) ) ;
#43313 =( BOUNDED_CURVE ( )  B_SPLINE_CURVE ( 2, ( #15029, #2231, #1868, #65600, #31651, #38063, #59941, #55045, #8257 ),
 .UNSPECIFIED., .F., .F. ) 
 B_SPLINE_CURVE_WITH_KNOTS ( ( 3, 2, 2, 2, 3 ),
 ( 0.6145833333333333703, 0.6197916666666666297, 0.6250000000000000000, 0.6302083333333334814, 0.6354166666666667407 ),
 .UNSPECIFIED. ) 
 CURVE ( )  GEOMETRIC_REPRESENTATION_ITEM ( )  RATIONAL_B_SPLINE_CURVE ( ( 1.000000000000000000, 0.9238795325112867385, 1.000000000000000000, 0.9238795325112867385, 1.000000000000000000, 0.9238795325112867385, 1.000000000000000000, 0.9238795325112850731, 1.000000000000001554 ) ) 
 REPRESENTATION_ITEM ( '' )  );
#43314 = CARTESIAN_POINT ( 'NONE',  ( -2.679491924311225848, 1.458333333333333259, -10.00000000000000178 ) ) ;
#43315 = CARTESIAN_POINT ( 'NONE',  ( 2.449293598294707893E-16, 16.25000000000000000, -4.000000000000001776 ) ) ;
#43316 = CARTESIAN_POINT ( 'NONE',  ( 4.541265875000001451, 14.24999999863440969, 1.881053915767124440 ) ) ;
#43317 = CARTESIAN_POINT ( 'NONE',  ( 7.999999999999992895, -3.313708498984756279, 13.67405278392014978 ) ) ;
#43318 = EDGE_CURVE ( 'NONE', #58068, #30219, #61415, .T. ) ;
#43319 = CARTESIAN_POINT ( 'NONE',  ( 29.53044679813751117, 194.7194814984362381, 166.6023135781559574 ) ) ;
#43320 = AXIS2_PLACEMENT_3D ( 'NONE', #44683, #10354, #61664 ) ;
#43321 = ORIENTED_EDGE ( 'NONE', *, *, #43890, .T. ) ;
#43322 = CARTESIAN_POINT ( 'NONE',  ( 4.999999999999997335, -12.24343743989403777, -68.85270403949347440 ) ) ;
#43323 = CARTESIAN_POINT ( 'NONE',  ( -5.082755093536325930, 90.96875000204838102, -5.082755093536325930 ) ) ;
#43324 = CARTESIAN_POINT ( 'NONE',  ( 11.35316468749999963, 256.4062500034140157, -1.390361679473963556E-15 ) ) ;
#43325 = CARTESIAN_POINT ( 'NONE',  ( 1393.688200795887496, 596.9677537767818194, 1062.842160456058991 ) ) ;
#43326 = ORIENTED_EDGE ( 'NONE', *, *, #71167, .F. ) ;
#43327 = CARTESIAN_POINT ( 'NONE',  ( 11.35316468749999608, 261.9270833367472733, -3.042071309553167069 ) ) ;
#43328 = CARTESIAN_POINT ( 'NONE',  ( -7.188101187499990274, -2.977408999572651371, 16.58030278187175455 ) ) ;
#43329 = VERTEX_POINT ( 'NONE', #28249 ) ;
#43330 = EDGE_LOOP ( 'NONE', ( #64939, #31950, #7506, #34982 ) ) ;
#43331 = CARTESIAN_POINT ( 'NONE',  ( 7.204075437095968759, -7.204075437095966983, 78.71875000204836681 ) ) ;
#43332 = CARTESIAN_POINT ( 'NONE',  ( 3.042071309553159519, 75.05208332991935549, 11.35316468750000141 ) ) ;
#43333 = CARTESIAN_POINT ( 'NONE',  ( 11.00000000000000355, -4.556349186104045046, 97.65624999999998579 ) ) ;
#43336 = CARTESIAN_POINT ( 'NONE',  ( -6.676582343750002480, 295.5468750017069510, -2.765530957081996810 ) ) ;
#43335 = CARTESIAN_POINT ( 'NONE',  ( 27.99999999999996092, 195.6250000027311842, 165.9999999999998863 ) ) ;
#43334 = DIRECTION ( 'NONE',  ( -0.000000000000000000, 1.000000000000000000, -1.563033456626094573E-30 ) ) ;
#43337 = CARTESIAN_POINT ( 'NONE',  ( 8.660254037844385522, 149.5833333333333428, 5.000000000000005329 ) ) ;
#43338 = CARTESIAN_POINT ( 'NONE',  ( -7.347880794884122694E-16, 13.75000000000000000, 4.000000000000001776 ) ) ;
#43339 = CARTESIAN_POINT ( 'NONE',  ( 1.469576158976823947E-15, 91.06250000409676204, 8.000000000000000000 ) ) ;
#43340 = CARTESIAN_POINT ( 'NONE',  ( -3.458734124999960358, 198.6250000013656063, 196.5673454167823877 ) ) ;
#43341 = CARTESIAN_POINT ( 'NONE',  ( 2.828427124746152987, 199.1250000000000284, 139.1715728752538723 ) ) ;
#43342 = CARTESIAN_POINT ( 'NONE',  ( -5.656854249492381470, 3.749999995903220640, 5.656854249492379694 ) ) ;
#43343 = EDGE_CURVE ( 'NONE', #23983, #62814, #52011, .T. ) ;
#43344 = CARTESIAN_POINT ( 'NONE',  ( 27.99999999999996447, 198.4375000013655779, 173.4587341249998929 ) ) ;
#43345 = CARTESIAN_POINT ( 'NONE',  ( -2.977408999572650039, 10.31249999795161010, -7.188101187500001821 ) ) ;
#43346 = CARTESIAN_POINT ( 'NONE',  ( -7.999999999999989342, -3.313708498984762496, 26.61155278392014978 ) ) ;
#43347 = FACE_OUTER_BOUND ( 'NONE', #35836, .T. ) ;
#43348 = CARTESIAN_POINT ( 'NONE',  ( -2.977408999572652260, 108.3125000020483810, 7.188101187500000044 ) ) ;
#43350 = CARTESIAN_POINT ( 'NONE',  ( -5.126106709314337984, -52.42424824937356220, -49.01286957842727077 ) ) ;
#43349 = CARTESIAN_POINT ( 'NONE',  ( 6.000000000000001776, 289.5625000034140157, -7.347880794884121708E-16 ) ) ;
#43351 = CARTESIAN_POINT ( 'NONE',  ( 10.99999999999996270, -4.556349186104084126, 112.8437500040967620 ) ) ;
#43352 = CARTESIAN_POINT ( 'NONE',  ( -26.34314575050760965, 207.5625000000000284, 174.0000000000003979 ) ) ;
#43353 = CARTESIAN_POINT ( 'NONE',  ( -2.977408999572647819, 7.188101187499991163, 24.08030278187175455 ) ) ;
#43354 = CARTESIAN_POINT ( 'NONE',  ( 1.656854249492348607, 207.3125000027312126, 138.0000000000000568 ) ) ;
#43355 = CARTESIAN_POINT ( 'NONE',  ( 9.832129032723420536, 46.19791666325268409, -5.676582343749999815 ) ) ;
#43356 = CARTESIAN_POINT ( 'NONE',  ( 2.449293598294707893E-16, 6.250000000000000000, -4.000000000000001776 ) ) ;
#43357 = CARTESIAN_POINT ( 'NONE',  ( 10.00000000000000000, 6.666666659838698550, 2.679491924311236062 ) ) ;
#43358 = ORIENTED_EDGE ( 'NONE', *, *, #42019, .F. ) ;
#43359 = CARTESIAN_POINT ( 'NONE',  ( 1.970211975628451295, 12.71890404606132030, -0.4750804646944193355 ) ) ;
#43360 = CARTESIAN_POINT ( 'NONE',  ( -4.000000000000002665, 8.312499997268814056, 1.656854249492380582 ) ) ;
#43361 = ADVANCED_FACE ( 'NONE', ( #4500 ), #44860, .T. ) ;
#43362 = CARTESIAN_POINT ( 'NONE',  ( -9.832129032723420536, 53.69791666325267698, 5.676582343749997150 ) ) ;
#43363 = CARTESIAN_POINT ( 'NONE',  ( -4.556349186104045934, 11.00000000000000000, 81.90625000409676204 ) ) ;
#43364 = CARTESIAN_POINT ( 'NONE',  ( -1.432654583217662481, 204.3750000013656063, 145.4587341250000350 ) ) ;
#43365 = CARTESIAN_POINT ( 'NONE',  ( 11.49999999999998046, 82.00000000000001421, 97.52691193458117880 ) ) ;
#43366 = CARTESIAN_POINT ( 'NONE',  ( -5.000000000000000000, 0.000000000000000000, 0.000000000000000000 ) ) ;
#43368 = CARTESIAN_POINT ( 'NONE',  ( 11.35316468749999963, 30.98958332991934839, -3.042071309553165293 ) ) ;
#43367 = CARTESIAN_POINT ( 'NONE',  ( 1.320432766682874540E-15, 102.0312500020483810, 7.188101187500000044 ) ) ;
#43369 = CARTESIAN_POINT ( 'NONE',  ( 3.313708498984762496, -7.999999999999989342, 8.799052779823364645 ) ) ;
#43370 =( REPRESENTATION_RELATIONSHIP ('NONE','NONE', #46008, #30147 ) REPRESENTATION_RELATIONSHIP_WITH_TRANSFORMATION ( #35391 )SHAPE_REPRESENTATION_RELATIONSHIP( ) );
#43371 = CARTESIAN_POINT ( 'NONE',  ( 1.656854249492381914, 10.56249999726881406, 4.000000000000000888 ) ) ;
#43372 = CARTESIAN_POINT ( 'NONE',  ( 6.951808397369818766E-16, 157.0312499965860127, -11.35316468750000141 ) ) ;
#43373 = CARTESIAN_POINT ( 'NONE',  ( -5.000000000000005329, 135.2083333265053682, 8.660254037844387298 ) ) ;
#43374 = CARTESIAN_POINT ( 'NONE',  ( 5.082755093536325042, 110.4687500020483810, -5.082755093536325930 ) ) ;
#43375 = EDGE_LOOP ( 'NONE', ( #20577, #66874, #2898, #33714, #71022, #40666 ) ) ;
#43376 = CARTESIAN_POINT ( 'NONE',  ( 10.00000000000000178, 21.87499999317203248, 0.000000000000000000 ) ) ;
#43377 = CARTESIAN_POINT ( 'NONE',  ( 8.311093377946834337, 25.46874999658601624, 8.311093377946839666 ) ) ;
#43378 = DIRECTION ( 'NONE',  ( -0.000000000000000000, 1.000000000000000000, -0.000000000000000000 ) ) ;
#43379 = ORIENTED_EDGE ( 'NONE', *, *, #1017, .T. ) ;
#43380 = CARTESIAN_POINT ( 'NONE',  ( 0.000000000000000000, 0.000000000000000000, 118.0000000000000000 ) ) ;
#43381 = CARTESIAN_POINT ( 'NONE',  ( 10.18810118750000093, -4.220049686691933921, 74.31250000204836681 ) ) ;
#43382 = CARTESIAN_POINT ( 'NONE',  ( -30.98624024472907124, -35.49075962374925552, 172.4495201379627929 ) ) ;
#43384 = CARTESIAN_POINT ( 'NONE',  ( -3.042071309553163960, 147.2395833299193555, -11.35316468749999963 ) ) ;
#43383 = CARTESIAN_POINT ( 'NONE',  ( -2.679491924311246276, 8.541666666666673180, 10.00000000000000355 ) ) ;
#43385 = CARTESIAN_POINT ( 'NONE',  ( 10.99999999999999467, 11.00000000000000355, 20.00000000000000000 ) ) ;
#43386 = CARTESIAN_POINT ( 'NONE',  ( 7.999999999999991118, 9.797174393178815797E-16, 9.136552784329824206 ) ) ;
#43387 = CARTESIAN_POINT ( 'NONE',  ( 1.656854249492336173, 208.3125000027312126, 138.0000000000000853 ) ) ;
#43388 = CIRCLE ( 'NONE', #18142, 18.00000000000000355 ) ;
#43389 = CARTESIAN_POINT ( 'NONE',  ( -8.311093377946836114, 233.2812500034139589, -8.311093377946836114 ) ) ;
#43390 = EDGE_CURVE ( 'NONE', #22486, #70240, #57703, .T. ) ;
#43391 = CARTESIAN_POINT ( 'NONE',  ( 10.18810118749999916, 1.247682550866122264E-15, 88.28125000204836681 ) ) ;
#43392 = VERTEX_POINT ( 'NONE', #39199 ) ;
#43393 = FACE_BOUND ( 'NONE', #19620, .T. ) ;
#43394 = CARTESIAN_POINT ( 'NONE',  ( 1.469576158976823947E-15, 122.5625000040967763, 8.000000000000000000 ) ) ;
#43395 = CARTESIAN_POINT ( 'NONE',  ( 11.35316468750000141, 106.0937499965860269, 0.000000000000000000 ) ) ;
#43396 = CARTESIAN_POINT ( 'NONE',  ( 4.220049686691941027, -10.18810118749999738, 93.62500000204838102 ) ) ;
#43397 = CARTESIAN_POINT ( 'NONE',  ( -4.195582579073398932, 22.00000000000000355, 1.737867247408543925 ) ) ;
#43398 = ORIENTED_EDGE ( 'NONE', *, *, #41293, .T. ) ;
#43399 = ORIENTED_EDGE ( 'NONE', *, *, #48230, .F. ) ;
#43400 = CARTESIAN_POINT ( 'NONE',  ( -1.881053915767124440, 5.124999998634406140, 4.541265875000001451 ) ) ;
#43401 = CARTESIAN_POINT ( 'NONE',  ( -7.188101187500002709, 8.812499997951611874, 2.977408999572649151 ) ) ;
#43402 = CARTESIAN_POINT ( 'NONE',  ( 8.000000000000000000, 115.4375000040967763, -9.797174393178825657E-16 ) ) ;
#43403 = TOROIDAL_SURFACE ( 'NONE', #3686, 81.50000000000000000, 10.99999999999999822 ) ;
#43404 = CARTESIAN_POINT ( 'NONE',  ( 1.871523826299183495E-15, -10.18810118749999916, 99.90625000204838102 ) ) ;
#43405 = CARTESIAN_POINT ( 'NONE',  ( -25.55430564589115150, 203.3125000013656063, 172.4456943541091789 ) ) ;
#43406 = CARTESIAN_POINT ( 'NONE',  ( -28.00000000000008171, 209.1250000027312126, 166.0000000000003695 ) ) ;
#43407 = CARTESIAN_POINT ( 'NONE',  ( -4.000000000000001776, 4.437500000000000888, -1.656854249492381470 ) ) ;
#43408 = CARTESIAN_POINT ( 'NONE',  ( -1.656854249492381248, 17.06249999726881938, -4.000000000000001776 ) ) ;
#43409 = CARTESIAN_POINT ( 'NONE',  ( -3.211159895383561391, 2.687499998634407028, -3.211159895383561835 ) ) ;
#43410 = CARTESIAN_POINT ( 'NONE',  ( -3.458734125000015425, 208.9375000013656063, 142.0000000000000568 ) ) ;
#43411 = CARTESIAN_POINT ( 'NONE',  ( -2.445694354108783664, 196.3125000013656063, 195.5543056458912190 ) ) ;
#43413 = CARTESIAN_POINT ( 'NONE',  ( 8.660254037844385522, 236.0416666734946318, -5.000000000000003553 ) ) ;
#43412 = CARTESIAN_POINT ( 'NONE',  ( -30.44569435410875968, 198.8125000013656063, 172.4456943541092642 ) ) ;
#43414 = CARTESIAN_POINT ( 'NONE',  ( -1.881053915767124440, 17.99999999863440436, 4.541265875000001451 ) ) ;
#43415 = CIRCLE ( 'NONE', #24139, 12.00000000000000178 ) ;
#43416 = DIRECTION ( 'NONE',  ( -1.000000000000000000, -0.000000000000000000, -0.000000000000000000 ) ) ;
#43417 = CARTESIAN_POINT ( 'NONE',  ( 7.188101187499992051, 8.802885111219154394E-16, 8.236552781871752771 ) ) ;
#43418 = VERTEX_POINT ( 'NONE', #62201 ) ;
#43419 =( BOUNDED_CURVE ( )  B_SPLINE_CURVE ( 2, ( #66123, #53707, #60464, #60843, #54075, #72151, #20462, #25380, #65751 ),
 .UNSPECIFIED., .F., .F. ) 
 B_SPLINE_CURVE_WITH_KNOTS ( ( 3, 2, 2, 2, 3 ),
 ( 0.1500000000000002442, 0.1583333333333335202, 0.1666666666666667962, 0.1750000000000000722, 0.1833333333333333481 ),
 .UNSPECIFIED. ) 
 CURVE ( )  GEOMETRIC_REPRESENTATION_ITEM ( )  RATIONAL_B_SPLINE_CURVE ( ( 0.9999999999999976685, 0.9238795325112890700, 1.000000000000000000, 0.9238795325112867385, 1.000000000000000000, 0.9238795325112867385, 1.000000000000000000, 0.9238795325112865164, 1.000000000000000222 ) ) 
 REPRESENTATION_ITEM ( '' )  );
#43420 =( BOUNDED_CURVE ( )  B_SPLINE_CURVE ( 2, ( #43722, #26354, #61075, #66736, #38822, #2990, #56177, #25612, #38076 ),
 .UNSPECIFIED., .F., .F. ) 
 B_SPLINE_CURVE_WITH_KNOTS ( ( 3, 2, 2, 2, 3 ),
 ( 0.5588235294117646079, 0.5624999999999998890, 0.5661764705882351700, 0.5698529411764704511, 0.5735294117647057321 ),
 .UNSPECIFIED. ) 
 CURVE ( )  GEOMETRIC_REPRESENTATION_ITEM ( )  RATIONAL_B_SPLINE_CURVE ( ( 1.000000000000002220, 0.9238795325112844070, 1.000000000000000000, 0.9238795325112867385, 1.000000000000000000, 0.9238795325112867385, 1.000000000000000000, 0.9238795325112890700, 0.9999999999999976685 ) ) 
 REPRESENTATION_ITEM ( '' )  );
#43421 = ORIENTED_EDGE ( 'NONE', *, *, #55810, .F. ) ;
#43422 = CARTESIAN_POINT ( 'NONE',  ( 7.204075437095966983, 7.204075437095967871, 100.0937500020483668 ) ) ;
#43423 = CARTESIAN_POINT ( 'NONE',  ( 8.000000000000000000, 26.81249999590322375, 0.000000000000000000 ) ) ;
#43424 = CARTESIAN_POINT ( 'NONE',  ( -26.56734541678238060, 205.6250000013656063, 166.5412658750003629 ) ) ;
#43425 = CARTESIAN_POINT ( 'NONE',  ( -28.00000000000002842, 200.0000000000000000, 166.0000000000003695 ) ) ;
#43426 = CARTESIAN_POINT ( 'NONE',  ( -2.445694354108783219, 208.8125000013656063, 200.4456943541088663 ) ) ;
#43427 = DIRECTION ( 'NONE',  ( -0.000000000000000000, -0.02418647091589873691, 0.9997074645238147594 ) ) ;
#43428 = CARTESIAN_POINT ( 'NONE',  ( 7.320508075688774596, 110.6249999999999858, -7.320508075688774596 ) ) ;
#43429 = VECTOR ( 'NONE', #41744, 1000.000000000000000 ) ;
#43430 = CARTESIAN_POINT ( 'NONE',  ( 8.000000000000000000, 112.2500000000000000, -9.797174393178825657E-16 ) ) ;
#43431 = CARTESIAN_POINT ( 'NONE',  ( -6.676582343750001591, 292.6093750017069510, 0.000000000000000000 ) ) ;
#43432 = CARTESIAN_POINT ( 'NONE',  ( -7.188101187499992051, 0.000000000000000000, 12.36155278187175277 ) ) ;
#43433 = ORIENTED_EDGE ( 'NONE', *, *, #46814, .F. ) ;
#43434 = LINE ( 'NONE', #44569, #44570 ) ;
#43435 = CARTESIAN_POINT ( 'NONE',  ( -3.313708498984765161, 23.34374999590322020, 7.999999999999998224 ) ) ;
#43436 = CARTESIAN_POINT ( 'NONE',  ( 3.458734124999959914, 204.4375000013656063, 142.0000000000000568 ) ) ;
#43437 = CARTESIAN_POINT ( 'NONE',  ( 2.449293598294707893E-16, 5.250000000000000000, -4.000000000000001776 ) ) ;
#43438 = DIRECTION ( 'NONE',  ( -0.000000000000000000, -1.000000000000000000, -0.000000000000000000 ) ) ;
#43439 = CARTESIAN_POINT ( 'NONE',  ( 11.35316468749999608, 261.9270833367472733, -3.042071309553167069 ) ) ;
#43440 = LINE ( 'NONE', #24603, #41544 ) ;
#43441 = CARTESIAN_POINT ( 'NONE',  ( -7.778174593052023411, 7.778174593052023411, 110.3125000000000000 ) ) ;
#43442 = CARTESIAN_POINT ( 'NONE',  ( -3.042071309553164404, 2.239583329919349719, -11.35316468749999963 ) ) ;
#43443 = CARTESIAN_POINT ( 'NONE',  ( 5.082755093536320601, -5.082755093536318824, 3.924052781871752327 ) ) ;
#43444 = CARTESIAN_POINT ( 'NONE',  ( 3.042071309553159519, 195.0520833299193271, 11.35316468750000141 ) ) ;
#43445 = CARTESIAN_POINT ( 'NONE',  ( -7.778174593052020747, -7.778174593052023411, 101.6874999999999858 ) ) ;
#43446 = CARTESIAN_POINT ( 'NONE',  ( 3.211159895383560947, 5.187499998634407028, 3.211159895383562723 ) ) ;
#43447 = DIRECTION ( 'NONE',  ( -0.000000000000000000, 1.000000000000000000, -1.563033456626094573E-30 ) ) ;
#43449 = LINE ( 'NONE', #26088, #25400 ) ;
#43448 = LINE ( 'NONE', #26850, #33464 ) ;
#43450 = ORIENTED_EDGE ( 'NONE', *, *, #20343, .T. ) ;
#43452 = EDGE_CURVE ( 'NONE', #3208, #26622, #43228, .T. ) ;
#43451 = CARTESIAN_POINT ( 'NONE',  ( -1.432654583217662481, 205.3750000013656063, 145.4587341250000634 ) ) ;
#43453 = CARTESIAN_POINT ( 'NONE',  ( -8.311093377946836114, 12.65624999658601801, -8.311093377946837890 ) ) ;
#43454 = CARTESIAN_POINT ( 'NONE',  ( 11.00000000000000355, -4.556349186104045046, 97.84375000409676204 ) ) ;
#43455 = CARTESIAN_POINT ( 'NONE',  ( -7.347880794884122694E-16, 19.49999999726881228, 4.000000000000001776 ) ) ;
#43456 = CARTESIAN_POINT ( 'NONE',  ( -31.45873412499999944, 201.6875000013656063, 170.0000000000004547 ) ) ;
#43457 = FACE_OUTER_BOUND ( 'NONE', #13839, .T. ) ;
#43459 = LINE ( 'NONE', #3112, #41442 ) ;
#43458 = CARTESIAN_POINT ( 'NONE',  ( 2.977408999572650039, 117.6875000020484237, -7.188101187500000933 ) ) ;
#43460 = CARTESIAN_POINT ( 'NONE',  ( 5.656854249492376141, -5.656854249492374365, 28.39280277982336642 ) ) ;
#43461 = CARTESIAN_POINT ( 'NONE',  ( 5.676582343749993598, 119.9479166632526841, 9.832129032723422313 ) ) ;
#43462 = EDGE_CURVE ( 'NONE', #47712, #30170, #36511, .T. ) ;
#43463 = CARTESIAN_POINT ( 'NONE',  ( 7.320508075688774596, 92.49999999317205379, -7.320508075688774596 ) ) ;
#43464 = CARTESIAN_POINT ( 'NONE',  ( 1.320432766682874540E-15, 91.53125000204836681, 7.188101187500000044 ) ) ;
#43465 = CARTESIAN_POINT ( 'NONE',  ( 4.541265875000002339, 21.49999999863440792, -1.881053915767121554 ) ) ;
#43466 = CARTESIAN_POINT ( 'NONE',  ( -7.999999999999991118, 6.760989533162280693E-06, 25.01780259264117134 ) ) ;
#43467 = CARTESIAN_POINT ( 'NONE',  ( -10.00000000000000178, 39.37499999317203958, -1.224646799147353454E-15 ) ) ;
#43468 = ORIENTED_EDGE ( 'NONE', *, *, #68489, .T. ) ;
#43469 = CARTESIAN_POINT ( 'NONE',  ( 3.999999999999960032, 209.0000000000000284, 142.0000000000000568 ) ) ;
#43470 = CARTESIAN_POINT ( 'NONE',  ( -6.676582343750000703, 295.6718750017070079, 2.765530957082001251 ) ) ;
#43471 = CARTESIAN_POINT ( 'NONE',  ( 4.999999999999993783, 186.0416666598387110, 8.660254037844390851 ) ) ;
#43472 = CARTESIAN_POINT ( 'NONE',  ( -7.999999999999991118, -9.344071862984236532, 28.15091120252598245 ) ) ;
#43473 = CARTESIAN_POINT ( 'NONE',  ( 11.35316468749999785, 175.5729166632526415, 3.042071309553174174 ) ) ;
#43474 = CARTESIAN_POINT ( 'NONE',  ( -3.999999999999959144, 195.1875000027312410, 199.6568542494924259 ) ) ;
#43475 = CARTESIAN_POINT ( 'NONE',  ( 0.000000000000000000, 0.000000000000000000, 0.000000000000000000 ) ) ;
#43476 = DIRECTION ( 'NONE',  ( -0.000000000000000000, 1.000000000000000000, -1.563033456626094573E-30 ) ) ;
#43477 = EDGE_CURVE ( 'NONE', #44110, #31802, #23290, .T. ) ;
#43478 = CARTESIAN_POINT ( 'NONE',  ( -7.204075437095967871, 7.204075437095967871, 105.3437500020483810 ) ) ;
#43479 = ORIENTED_EDGE ( 'NONE', *, *, #47105, .F. ) ;
#43480 = CARTESIAN_POINT ( 'NONE',  ( -32.00000000000002842, 199.3125000027312126, 168.3431457505080857 ) ) ;
#43481 = CARTESIAN_POINT ( 'NONE',  ( 9.832129032723420536, 161.5104166632526983, -5.676582343749999815 ) ) ;
#43482 = CARTESIAN_POINT ( 'NONE',  ( 2.839093476692135984E-14, 195.6875000013655779, 201.4587341250000350 ) ) ;
#43483 = CARTESIAN_POINT ( 'NONE',  ( -1.432654583217607414, 206.5000000013655779, 194.5412658750000219 ) ) ;
#43484 = CARTESIAN_POINT ( 'NONE',  ( 10.00000000000000000, 230.6250000068279746, -1.224646799147353256E-15 ) ) ;
#43485 = CARTESIAN_POINT ( 'NONE',  ( 9.832129032723416984, 60.67708332991934839, 5.676582343750006032 ) ) ;
#43486 = ORIENTED_EDGE ( 'NONE', *, *, #73472, .T. ) ;
#43487 = CARTESIAN_POINT ( 'NONE',  ( 4.220049686691941027, -10.18810118749999738, 113.1250000020483810 ) ) ;
#43488 = CARTESIAN_POINT ( 'NONE',  ( 1.881053915767121998, 10.62499999863440969, -4.541265875000002339 ) ) ;
#43489 = EDGE_LOOP ( 'NONE', ( #47553, #70030, #47423, #23286 ) ) ;
#43490 = CARTESIAN_POINT ( 'NONE',  ( 7.188101187500001821, 20.06249999795161543, -2.977408999572650483 ) ) ;
#43491 = CARTESIAN_POINT ( 'NONE',  ( 2.485281374238571317, 288.7500000034139589, -6.000000000000003553 ) ) ;
#43492 = AXIS2_PLACEMENT_3D ( 'NONE', #50891, #73530, #3386 ) ;
#43493 = CARTESIAN_POINT ( 'NONE',  ( 10.00000000000000178, 67.08333332650538239, -2.679491924311226736 ) ) ;
#43494 = CARTESIAN_POINT ( 'NONE',  ( 5.082755093536325930, 16.03124999795161543, -5.082755093536325930 ) ) ;
#43495 = CARTESIAN_POINT ( 'NONE',  ( 5.082755093536318824, 5.082755093536319713, 3.924052781871752327 ) ) ;
#43496 = CARTESIAN_POINT ( 'NONE',  ( 10.18810118750000093, -4.220049686691933921, 115.1875000020483668 ) ) ;
#43497 = CONICAL_SURFACE ( 'NONE', #10985, 8.000000000000000000, 0.7853981633974552734 ) ;
#43498 = CARTESIAN_POINT ( 'NONE',  ( -2.849036369511732440E-14, 202.2500000000000000, 138.0000000000000568 ) ) ;
#43499 = CARTESIAN_POINT ( 'NONE',  ( 4.000000000000000888, 7.687499997268812280, 1.656854249492384135 ) ) ;
#43500 = AXIS2_PLACEMENT_3D ( 'NONE', #8010, #13283, #2726 ) ;
#43501 = ORIENTED_EDGE ( 'NONE', *, *, #41913, .T. ) ;
#43502 = CARTESIAN_POINT ( 'NONE',  ( 2.754378923186476579E-14, 208.1875000013656063, 194.5412658750000219 ) ) ;
#43503 = CARTESIAN_POINT ( 'NONE',  ( -29.65685424949228732, 194.5625000027311842, 174.0000000000004547 ) ) ;
#43504 = CARTESIAN_POINT ( 'NONE',  ( -8.342170076843785083E-16, 7.062499998634407028, 4.541265875000002339 ) ) ;
#43505 = CARTESIAN_POINT ( 'NONE',  ( -5.082755093536324154, 109.3437500020483810, 5.082755093536326818 ) ) ;
#43506 = CARTESIAN_POINT ( 'NONE',  ( 5.656854249492381470, 94.25000000409677625, 5.656854249492379694 ) ) ;
#43507 = CARTESIAN_POINT ( 'NONE',  ( 7.188101187499992051, 8.802885111219154394E-16, 26.23655278187175810 ) ) ;
#43508 = ORIENTED_EDGE ( 'NONE', *, *, #7424, .F. ) ;
#43509 = CARTESIAN_POINT ( 'NONE',  ( 6.000000000000003553, 299.5625000000000000, -2.485281374238571761 ) ) ;
#43510 = ORIENTED_EDGE ( 'NONE', *, *, #55105, .F. ) ;
#43511 = DIRECTION ( 'NONE',  ( 0.000000000000000000, 0.000000000000000000, 1.000000000000000000 ) ) ;
#43512 = CARTESIAN_POINT ( 'NONE',  ( -1.836970198721029983E-15, 8.750000000000000000, 10.00000000000000178 ) ) ;
#43513 = CARTESIAN_POINT ( 'NONE',  ( 25.55430564589119058, 204.3125000013656063, 172.4456943541087526 ) ) ;
#43514 = CARTESIAN_POINT ( 'NONE',  ( 6.123233995736767268E-16, 71.25000000000001421, -10.00000000000000178 ) ) ;
#43515 = CARTESIAN_POINT ( 'NONE',  ( -2.977408999572651815, 96.31250000204838102, 7.188101187500000933 ) ) ;
#43516 = CARTESIAN_POINT ( 'NONE',  ( -4.242640687119285658, 291.1249999999999432, 4.242640687119287435 ) ) ;
#43518 = DIRECTION ( 'NONE',  ( 0.000000000000000000, -1.000000000000000000, -0.000000000000000000 ) ) ;
#43517 = CARTESIAN_POINT ( 'NONE',  ( 31.22578248903377940, 177.4107786577398542, 170.8851451233488206 ) ) ;
#43519 =( BOUNDED_CURVE ( )  B_SPLINE_CURVE ( 2, ( #32971, #14455, #9574, #55227, #32592, #15208, #66517, #9938, #55599 ),
 .UNSPECIFIED., .F., .F. ) 
 B_SPLINE_CURVE_WITH_KNOTS ( ( 3, 2, 2, 2, 3 ),
 ( 0.8124999999999983347, 0.8229166666666649643, 0.8333333333333317050, 0.8437499999999983347, 0.8541666666666649643 ),
 .UNSPECIFIED. ) 
 CURVE ( )  GEOMETRIC_REPRESENTATION_ITEM ( )  RATIONAL_B_SPLINE_CURVE ( ( 1.000000000000012212, 0.9238795325112745260, 1.000000000000000000, 0.9238795325112867385, 1.000000000000000000, 0.9238795325112867385, 1.000000000000000000, 0.9238795325112989509, 0.9999999999999877875 ) ) 
 REPRESENTATION_ITEM ( '' )  );
#43520 = ORIENTED_EDGE ( 'NONE', *, *, #61981, .F. ) ;
#43521 = CARTESIAN_POINT ( 'NONE',  ( -9.832129032723418760, 223.4895833367473301, -5.676582343749998927 ) ) ;
#43522 = CARTESIAN_POINT ( 'NONE',  ( -4.104248244541351731, -10.10575198619676129, 70.81982386214673397 ) ) ;
#43523 = CARTESIAN_POINT ( 'NONE',  ( -4.000000000000015987, 200.5625000027312126, 140.3431457505076594 ) ) ;
#43524 = FACE_OUTER_BOUND ( 'NONE', #15400, .T. ) ;
#43525 = LINE ( 'NONE', #72958, #54541 ) ;
#43526 = CARTESIAN_POINT ( 'NONE',  ( -10.00000000000000000, 249.7916666666666572, -2.679491924311226292 ) ) ;
#43527 = CARTESIAN_POINT ( 'NONE',  ( 3.313708498984733186, 108.2187500040967763, -8.000000000000026645 ) ) ;
#43528 = CARTESIAN_POINT ( 'NONE',  ( -5.000000000000005329, 188.3333333333333428, 8.660254037844387298 ) ) ;
#43529 = CYLINDRICAL_SURFACE ( 'NONE', #40379, 11.49999999999999112 ) ;
#43530 = CARTESIAN_POINT ( 'NONE',  ( -5.082755093536319713, 5.082755093536319713, 22.67405278187175455 ) ) ;
#43531 = CARTESIAN_POINT ( 'NONE',  ( -2.085542519210945728E-15, 159.8437499965860127, 11.35316468750000141 ) ) ;
#43532 = CARTESIAN_POINT ( 'NONE',  ( -3.313708498984759387, -7.999999999999989342, 22.29905278392014623 ) ) ;
#43533 = CARTESIAN_POINT ( 'NONE',  ( 2.249999999999997780, 255.9999999999999432, 7.677076266392047543 ) ) ;
#43534 = CYLINDRICAL_SURFACE ( 'NONE', #42884, 7.999999999999991118 ) ;
#43537 = CARTESIAN_POINT ( 'NONE',  ( 3.313708498984819339, 109.1562500040967905, 7.999999999999943157 ) ) ;
#43536 = CARTESIAN_POINT ( 'NONE',  ( 2.828427124746209831, 199.5000000027312126, 200.8284271247462129 ) ) ;
#43535 = CARTESIAN_POINT ( 'NONE',  ( 23.99999999999997868, 201.8125000000000000, 171.6568542494922553 ) ) ;
#43538 = VERTEX_POINT ( 'NONE', #1088 ) ;
#43539 = CARTESIAN_POINT ( 'NONE',  ( -3.042071309553173730, 4.635416663252684089, 11.35316468749999785 ) ) ;
#43540 = DIRECTION ( 'NONE',  ( 1.000000000000000000, -0.000000000000000000, -0.000000000000000000 ) ) ;
#43541 = CARTESIAN_POINT ( 'NONE',  ( -4.898587196589407898E-16, 7.999999999999991118, 17.14280278392014978 ) ) ;
#43542 = DIRECTION ( 'NONE',  ( -0.000000000000000000, -0.000000000000000000, -1.000000000000000000 ) ) ;
#43543 = CARTESIAN_POINT ( 'NONE',  ( 2.445694354108782775, 201.5625000013656063, 139.5543056458912190 ) ) ;
#43544 =( BOUNDED_CURVE ( )  B_SPLINE_CURVE ( 2, ( #59973, #3665, #49688, #15712, #73070, #25258, #19602, #72703, #10072, #21004, #15338, #44400, #70923 ),
 .UNSPECIFIED., .F., .F. ) 
 B_SPLINE_CURVE_WITH_KNOTS ( ( 3, 2, 2, 2, 2, 2, 3 ),
 ( 2.307884339682968911, 2.313118351314716659, 2.318352362946464851, 2.323586374578212599, 2.328820386209960347, 2.334054397841708539, 2.339288409473456287 ),
 .UNSPECIFIED. ) 
 CURVE ( )  GEOMETRIC_REPRESENTATION_ITEM ( )  RATIONAL_B_SPLINE_CURVE ( ( 0.9999999999999916733, 0.9659258262890766389, 1.000000000000000000, 0.9659258262890683122, 1.000000000000000000, 0.9659258262890683122, 1.000000000000000000, 0.9659258262890683122, 1.000000000000000000, 0.9659258262890683122, 1.000000000000000000, 0.9659258262890766389, 0.9999999999999916733 ) ) 
 REPRESENTATION_ITEM ( '' )  );
#43545 = ADVANCED_FACE ( 'NONE', ( #59520 ), #29737, .T. ) ;
#43546 = CARTESIAN_POINT ( 'NONE',  ( 10.00000000000000178, 52.08333332650537528, -2.679491924311226736 ) ) ;
#43547 = AXIS2_PLACEMENT_3D ( 'NONE', #615, #63210, #34571 ) ;
#43548 = CARTESIAN_POINT ( 'NONE',  ( 7.188101187500002709, 109.8125000020483952, 2.977408999572649151 ) ) ;
#43549 = CARTESIAN_POINT ( 'NONE',  ( -4.541265875000002339, 8.874999998634407916, -1.881053915767121998 ) ) ;
#43550 = CARTESIAN_POINT ( 'NONE',  ( 9.999999999999982236, 99.79166666666665719, 2.679491924311231621 ) ) ;
#43551 = CARTESIAN_POINT ( 'NONE',  ( 3.313708498984756279, 7.999999999999991118, 10.86155277982336820 ) ) ;
#43553 = CARTESIAN_POINT ( 'NONE',  ( 7.320508075688787919, 159.3750000000000284, 7.320508075688790584 ) ) ;
#43552 = CARTESIAN_POINT ( 'NONE',  ( -3.000000000000001332, -45.00000000000001421, 139.1455027589170470 ) ) ;
#43554 = ORIENTED_EDGE ( 'NONE', *, *, #56599, .T. ) ;
#43555 = ORIENTED_EDGE ( 'NONE', *, *, #60759, .T. ) ;
#43556 = DIRECTION ( 'NONE',  ( -0.000000000000000000, 1.000000000000000000, -0.000000000000000000 ) ) ;
#43557 = AXIS2_PLACEMENT_3D ( 'NONE', #2920, #35501, #18509 ) ;
#43558 = CARTESIAN_POINT ( 'NONE',  ( 6.123233995736767268E-16, 161.2500000000000000, -10.00000000000000178 ) ) ;
#43559 = CARTESIAN_POINT ( 'NONE',  ( 1.469576158976823947E-15, 99.87499999999998579, 8.000000000000000000 ) ) ;
#43560 = CARTESIAN_POINT ( 'NONE',  ( 8.311093377946837890, 126.4062499965860269, -8.311093377946837890 ) ) ;
#43561 = ORIENTED_EDGE ( 'NONE', *, *, #66046, .T. ) ;
#43562 = CARTESIAN_POINT ( 'NONE',  ( 1.469576158976822172E-15, -7.999999999999991118, 10.39280278392014800 ) ) ;
#43563 = CARTESIAN_POINT ( 'NONE',  ( -4.220049686691935698, 10.18810118749999916, 97.37500000204839523 ) ) ;
#43564 = CARTESIAN_POINT ( 'NONE',  ( -11.00000000000000000, 0.000000000000000000, 93.99999999999998579 ) ) ;
#43565 = CARTESIAN_POINT ( 'NONE',  ( -3.458734124999960358, 197.6250000013656063, 196.5673454167823877 ) ) ;
#43566 = CARTESIAN_POINT ( 'NONE',  ( -7.000000000000000000, 8.572527594031473190E-16, -14.07439246179028203 ) ) ;
#43568 = CARTESIAN_POINT ( 'NONE',  ( -3.042071309553173730, 129.3229166632526983, 11.35316468749999785 ) ) ;
#43567 = CARTESIAN_POINT ( 'NONE',  ( 7.320508075688789695, 44.37500000000001421, 7.320508075688792360 ) ) ;
#43569 = CARTESIAN_POINT ( 'NONE',  ( 10.99999999999995026, -4.556349186104096560, 96.15625000000000000 ) ) ;
#43570 = ORIENTED_EDGE ( 'NONE', *, *, #55760, .T. ) ;
#43571 = EDGE_CURVE ( 'NONE', #50470, #51437, #53702, .T. ) ;
#43572 = CARTESIAN_POINT ( 'NONE',  ( 9.000000000000000000, -5.196152422706648011, -10.20000000000000284 ) ) ;
#43573 =( BOUNDED_CURVE ( )  B_SPLINE_CURVE ( 2, ( #16312, #51780, #129, #56712, #62345, #73676, #50657, #68386, #45745 ),
 .UNSPECIFIED., .F., .F. ) 
 B_SPLINE_CURVE_WITH_KNOTS ( ( 3, 2, 2, 2, 3 ),
 ( 0.6333333333333339699, 0.6416666666666673846, 0.6500000000000006883, 0.6583333333333339921, 0.6666666666666672958 ),
 .UNSPECIFIED. ) 
 CURVE ( )  GEOMETRIC_REPRESENTATION_ITEM ( )  RATIONAL_B_SPLINE_CURVE ( ( 0.9999999999999938938, 0.9238795325112928447, 1.000000000000000000, 0.9238795325112867385, 1.000000000000000000, 0.9238795325112867385, 1.000000000000000000, 0.9238795325112806323, 1.000000000000005995 ) ) 
 REPRESENTATION_ITEM ( '' )  );
#43574 = CARTESIAN_POINT ( 'NONE',  ( 48.65938015714536391, 42.65983833830404848, 60.50199723131335361 ) ) ;
#43575 = CARTESIAN_POINT ( 'NONE',  ( 11.35316468750000141, 116.0937499965860127, 0.000000000000000000 ) ) ;
#43576 = CARTESIAN_POINT ( 'NONE',  ( -3.458734124999959914, 207.4375000013656063, 198.0000000000000284 ) ) ;
#43577 = CARTESIAN_POINT ( 'NONE',  ( -5.082755093536326818, 16.78124999795161543, 5.082755093536325042 ) ) ;
#43578 = CARTESIAN_POINT ( 'NONE',  ( -7.204075437095965206, -7.204075437095968759, 89.21875000204838102 ) ) ;
#43579 = ADVANCED_FACE ( 'NONE', ( #35415 ), #36141, .F. ) ;
#43580 = CARTESIAN_POINT ( 'NONE',  ( 6.951808397369818766E-16, 17.34374999658601624, -11.35316468750000141 ) ) ;
#43581 = EDGE_LOOP ( 'NONE', ( #56866, #30061, #44403, #73395 ) ) ;
#43582 = LINE ( 'NONE', #8889, #57298 ) ;
#43583 = CARTESIAN_POINT ( 'NONE',  ( 5.662595241051936235, -5.662595241051934458, 24.07561528394063188 ) ) ;
#43584 = AXIS2_PLACEMENT_3D ( 'NONE', #14596, #8955, #3670 ) ;
#43585 = LINE ( 'NONE', #67354, #22651 ) ;
#43586 = FACE_OUTER_BOUND ( 'NONE', #27535, .T. ) ;
#43587 = CARTESIAN_POINT ( 'NONE',  ( -4.721056650415998313, 287.5781250017069510, 4.721056650416000089 ) ) ;
#43588 = CARTESIAN_POINT ( 'NONE',  ( 5.000000000000001776, 112.7083333265053682, -8.660254037844389075 ) ) ;
#43589 = CARTESIAN_POINT ( 'NONE',  ( -26.34314575050762386, 206.9375000000000284, 166.0000000000003411 ) ) ;
#43590 = ORIENTED_EDGE ( 'NONE', *, *, #61700, .T. ) ;
#43591 = CARTESIAN_POINT ( 'NONE',  ( -11.35316468750000141, 138.5937499965860127, -1.390361679473963753E-15 ) ) ;
#43592 = CARTESIAN_POINT ( 'NONE',  ( 1.871523826299183495E-15, -10.18810118749999916, 81.53125000204838102 ) ) ;
#43593 = EDGE_CURVE ( 'NONE', #22530, #45708, #15188, .T. ) ;
#43594 = CARTESIAN_POINT ( 'NONE',  ( -25.55430564589115150, 198.0625000013656063, 172.4456943541091789 ) ) ;
#43595 = CARTESIAN_POINT ( 'NONE',  ( -38.00000000000002132, 38.00000000000000711, 65.00000000000000000 ) ) ;
#43596 = CARTESIAN_POINT ( 'NONE',  ( -3.211159895383562723, 15.06249999863440792, 3.211159895383561391 ) ) ;
#43597 = ORIENTED_EDGE ( 'NONE', *, *, #34372, .T. ) ;
#43598 = CARTESIAN_POINT ( 'NONE',  ( -3.999999999999960032, 205.1250000027312126, 198.0000000000000284 ) ) ;
#43599 = CARTESIAN_POINT ( 'NONE',  ( 2.445694354108783219, 197.8125000013656063, 139.5543056458912190 ) ) ;
#43600 = CARTESIAN_POINT ( 'NONE',  ( -2.849036369511732440E-14, 202.3750000027312126, 138.0000000000000568 ) ) ;
#43601 = B_SPLINE_CURVE_WITH_KNOTS ( 'NONE', 3,
 ( #23524, #10721, #33753, #28070, #16733, #57127, #28444, #63890, #52575, #52950, #17867, #35602, #18614, #41625, #53322, #70660, #69556, #8679, #35970, #49029, #47273, #35239 ),
 .UNSPECIFIED., .F., .F.,
 ( 4, 2, 2, 2, 2, 2, 2, 2, 2, 2, 4 ),
 ( 0.000000000000000000, 0.001533419618775805826, 0.002300129428163708630, 0.003066839237551611651, 0.004600258856327418995, 0.006133678475103227640, 0.006900388284491131528, 0.007667098093879036284, 0.009200517712654843194, 0.01073393733143065097, 0.01226735695020646048 ),
 .UNSPECIFIED. ) ;
#43602 = VECTOR ( 'NONE', #50512, 1000.000000000000000 ) ;
#43603 = LINE ( 'NONE', #66997, #50078 ) ;
#43604 = VERTEX_POINT ( 'NONE', #1810 ) ;
#43605 = CARTESIAN_POINT ( 'NONE',  ( -2.977408999572654480, 8.999999997951610098, 7.188101187499999156 ) ) ;
#43606 = CARTESIAN_POINT ( 'NONE',  ( -2.828427124746208943, 208.6250000000000284, 144.8284271247462129 ) ) ;
#43607 = EDGE_CURVE ( 'NONE', #38757, #50500, #42148, .T. ) ;
#43608 = CARTESIAN_POINT ( 'NONE',  ( 0.000000000000000000, 300.0000000000000000, 0.000000000000000000 ) ) ;
#43609 = CARTESIAN_POINT ( 'NONE',  ( -5.676582343749998039, 182.4479166632526983, -9.832129032723420536 ) ) ;
#43610 = CARTESIAN_POINT ( 'NONE',  ( 7.188101187500002709, 110.1875000020483810, 2.977408999572649151 ) ) ;
#43611 = CARTESIAN_POINT ( 'NONE',  ( 1.224646799147353454E-15, 300.0000000000000000, -10.00000000000000178 ) ) ;
#43612 = CARTESIAN_POINT ( 'NONE',  ( -4.721056650415999201, 291.3281250017069510, -4.721056650415999201 ) ) ;
#43613 = ADVANCED_FACE ( 'NONE', ( #53859 ), #26185, .T. ) ;
#43615 = CARTESIAN_POINT ( 'NONE',  ( -17.99999999999999645, -6.968949133139060947, -0.7423331077269027523 ) ) ;
#43614 = LINE ( 'NONE', #39084, #883 ) ;
#43616 = CONTEXT_DEPENDENT_SHAPE_REPRESENTATION ( #38543, #33700 ) ;
#43617 = VERTEX_POINT ( 'NONE', #44676 ) ;
#43618 = CARTESIAN_POINT ( 'NONE',  ( -5.676582343750000703, 253.0729166700807014, -9.832129032723418760 ) ) ;
#43619 = AXIS2_PLACEMENT_3D ( 'NONE', #71556, #47807, #32341 ) ;
#43620 = CARTESIAN_POINT ( 'NONE',  ( -5.082755093536317936, -5.082755093536320601, 27.54905278187175455 ) ) ;
#43621 = CARTESIAN_POINT ( 'NONE',  ( 3.313708498984760276, 106.5312500000000142, -8.000000000000000000 ) ) ;
#43622 = CARTESIAN_POINT ( 'NONE',  ( 0.000000000000000000, 0.000000000000000000, 30.00000000000000000 ) ) ;
#43623 = CARTESIAN_POINT ( 'NONE',  ( 7.456155213548071536, -61.82225697226390793, -23.87472085067526706 ) ) ;
#43625 = EDGE_CURVE ( 'NONE', #37130, #53484, #32306, .T. ) ;
#43624 = CARTESIAN_POINT ( 'NONE',  ( -3.458734124999960358, 200.6250000013655779, 196.5673454167823877 ) ) ;
#43626 = ORIENTED_EDGE ( 'NONE', *, *, #40780, .F. ) ;
#43627 = CARTESIAN_POINT ( 'NONE',  ( 8.000000000000000000, 24.09375000000000355, -3.313708498984761164 ) ) ;
#43628 = CARTESIAN_POINT ( 'NONE',  ( 8.000000000000000000, 92.75000000000000000, -9.797174393178825657E-16 ) ) ;
#43629 = CARTESIAN_POINT ( 'NONE',  ( 5.676582343749993598, 120.2604166632526841, 9.832129032723422313 ) ) ;
#43630 = CARTESIAN_POINT ( 'NONE',  ( 1.102182119232618108E-15, 296.2500000000000000, 6.000000000000001776 ) ) ;
#43631 = CARTESIAN_POINT ( 'NONE',  ( 7.778174593052023411, -7.778174593052021635, 73.56249999999998579 ) ) ;
#43634 = FACE_OUTER_BOUND ( 'NONE', #15366, .T. ) ;
#43633 = CARTESIAN_POINT ( 'NONE',  ( 26.56734541678232731, 201.0000000013655779, 166.5412658749999650 ) ) ;
#43632 = CARTESIAN_POINT ( 'NONE',  ( 29.43265458321766559, 200.1250000013656063, 166.5412658749999650 ) ) ;
#43635 = ORIENTED_EDGE ( 'NONE', *, *, #63139, .T. ) ;
#43636 = DIRECTION ( 'NONE',  ( -0.000000000000000000, -1.000000000000000000, -4.283267841918042741E-17 ) ) ;
#43637 = CARTESIAN_POINT ( 'NONE',  ( -11.00000000000000000, 0.000000000000000000, 107.6875000040967763 ) ) ;
#43638 = VECTOR ( 'NONE', #25553, 1000.000000000000000 ) ;
#43639 = CARTESIAN_POINT ( 'NONE',  ( -3.458734125000015425, 198.0000000013656063, 143.4326545832176976 ) ) ;
#43640 = CARTESIAN_POINT ( 'NONE',  ( 30.44569435410879166, 199.8125000013656063, 172.4456943541087526 ) ) ;
#43641 = CARTESIAN_POINT ( 'NONE',  ( 2.977408999572651815, 27.56249999795161187, 7.188101187500000933 ) ) ;
#43642 = CARTESIAN_POINT ( 'NONE',  ( -9.832129032723420536, 194.0104166632526983, 5.676582343749997150 ) ) ;
#43643 = CARTESIAN_POINT ( 'NONE',  ( -7.188101187499999156, 94.62500000204838102, 2.977408999572654924 ) ) ;
#43644 = DIRECTION ( 'NONE',  ( -0.000000000000000000, -0.000000000000000000, -1.000000000000000000 ) ) ;
#43645 = CARTESIAN_POINT ( 'NONE',  ( -1.881053915767124440, 19.99999999863440436, 4.541265875000001451 ) ) ;
#43646 = CARTESIAN_POINT ( 'NONE',  ( 26.56734541678232731, 195.6250000013656063, 173.4587341249998929 ) ) ;
#43647 = CARTESIAN_POINT ( 'NONE',  ( -7.999999999999989342, -3.313708498984762496, 27.92405277982336642 ) ) ;
#43648 = DIRECTION ( 'NONE',  ( -0.000000000000000000, -0.000000000000000000, 1.000000000000000000 ) ) ;
#43649 = CARTESIAN_POINT ( 'NONE',  ( -8.311093377946841443, 78.90624999658602690, 8.311093377946830785 ) ) ;
#43650 = ORIENTED_EDGE ( 'NONE', *, *, #58161, .F. ) ;
#43651 =( BOUNDED_CURVE ( )  B_SPLINE_CURVE ( 2, ( #57395, #6455, #24149, #58506, #41149, #47161, #46056, #63, #6812, #58148, #23045, #12825, #17006 ),
 .UNSPECIFIED., .F., .F. ) 
 B_SPLINE_CURVE_WITH_KNOTS ( ( 3, 2, 2, 2, 2, 2, 3 ),
 ( 0.2119565217391304324, 0.2137681159420289911, 0.2155797101449275499, 0.2173913043478260809, 0.2192028985507246397, 0.2210144927536231985, 0.2228260869565217295 ),
 .UNSPECIFIED. ) 
 CURVE ( )  GEOMETRIC_REPRESENTATION_ITEM ( )  RATIONAL_B_SPLINE_CURVE ( ( 1.000000000000000000, 0.9659258262890683122, 1.000000000000000000, 0.9659258262890683122, 1.000000000000000000, 0.9659258262890683122, 1.000000000000000000, 0.9659258262890683122, 1.000000000000000000, 0.9659258262890683122, 1.000000000000000000, 0.9659258262890683122, 1.000000000000000000 ) ) 
 REPRESENTATION_ITEM ( '' )  );
#43652 = CARTESIAN_POINT ( 'NONE',  ( 7.999999999999991118, 9.797174393178815797E-16, 13.58030277982336465 ) ) ;
#43653 = CARTESIAN_POINT ( 'NONE',  ( 5.082755093536324154, 16.78124999795161543, 5.082755093536326818 ) ) ;
#43654 = LINE ( 'NONE', #48931, #24209 ) ;
#43655 = CARTESIAN_POINT ( 'NONE',  ( -2.828427124746152987, 195.1250000000000284, 200.8284271247462129 ) ) ;
#43656 = CARTESIAN_POINT ( 'NONE',  ( -9.832129032723418760, 92.86458332991935549, -5.676582343750004256 ) ) ;
#43657 = EDGE_LOOP ( 'NONE', ( #58742, #43712, #51452, #46575 ) ) ;
#43658 = CARTESIAN_POINT ( 'NONE',  ( -10.18810118749999916, 0.000000000000000000, 86.03125000204836681 ) ) ;
#43659 = CARTESIAN_POINT ( 'NONE',  ( 10.18810118749999916, 1.247682550866122264E-15, 110.4062500020483668 ) ) ;
#43660 = CARTESIAN_POINT ( 'NONE',  ( -28.00000000000001776, 196.6875000013655779, 166.5412658750003629 ) ) ;
#43661 = CARTESIAN_POINT ( 'NONE',  ( -3.458734124999960358, 208.6250000013655779, 196.5673454167823877 ) ) ;
#43662 = CARTESIAN_POINT ( 'NONE',  ( 30.82842712474620583, 207.3750000000000284, 167.1715728752537586 ) ) ;
#43664 = CARTESIAN_POINT ( 'NONE',  ( -9.832129032723418760, 92.86458332991935549, -5.676582343750004256 ) ) ;
#43663 = CARTESIAN_POINT ( 'NONE',  ( 2.775557561562891351E-14, 192.0000000000000284, 139.0000000000000568 ) ) ;
#43665 = CARTESIAN_POINT ( 'NONE',  ( 7.999999999999992895, -3.313708498984756279, 16.67405278392014623 ) ) ;
#43666 = CARTESIAN_POINT ( 'NONE',  ( -31.45873412500001010, 205.8750000013656063, 168.5673454167827572 ) ) ;
#43667 = CARTESIAN_POINT ( 'NONE',  ( 4.898587196589412829E-16, 21.18749999590322375, -8.000000000000000000 ) ) ;
#43668 = CARTESIAN_POINT ( 'NONE',  ( 2.679491924311222739, 170.8333333265053398, 10.00000000000000355 ) ) ;
#43669 = EDGE_CURVE ( 'NONE', #20642, #44181, #23956, .T. ) ;
#43670 = CIRCLE ( 'NONE', #5123, 11.99999999999999645 ) ;
#43671 = CARTESIAN_POINT ( 'NONE',  ( 0.000000000000000000, 0.000000000000000000, 0.000000000000000000 ) ) ;
#43672 = CARTESIAN_POINT ( 'NONE',  ( -11.35316468750000141, 78.80208332991935549, 3.042071309553159963 ) ) ;
#43673 = CARTESIAN_POINT ( 'NONE',  ( 6.676582343750001591, 292.9531250017069510, -8.176455196517173205E-16 ) ) ;
#43674 = CARTESIAN_POINT ( 'NONE',  ( -4.220049686691935698, 10.18810118749999916, 108.2500000020483810 ) ) ;
#43675 = CARTESIAN_POINT ( 'NONE',  ( 11.35316468749999785, 215.5729166632526699, 3.042071309553174174 ) ) ;
#43677 = ORIENTED_EDGE ( 'NONE', *, *, #18816, .T. ) ;
#43676 =( BOUNDED_CURVE ( )  B_SPLINE_CURVE ( 2, ( #44059, #66690, #59916, #26310, #60277, #31242, #14247, #67069, #49333 ),
 .UNSPECIFIED., .F., .F. ) 
 B_SPLINE_CURVE_WITH_KNOTS ( ( 3, 2, 2, 2, 3 ),
 ( 0.1833333333333333481, 0.1916666666666667629, 0.2000000000000001776, 0.2083333333333335646, 0.2166666666666669516 ),
 .UNSPECIFIED. ) 
 CURVE ( )  GEOMETRIC_REPRESENTATION_ITEM ( )  RATIONAL_B_SPLINE_CURVE ( ( 0.9999999999999997780, 0.9238795325112869605, 1.000000000000000000, 0.9238795325112867385, 1.000000000000000000, 0.9238795325112867385, 1.000000000000000000, 0.9238795325112841850, 1.000000000000002442 ) ) 
 REPRESENTATION_ITEM ( '' )  );
#43678 = DIRECTION ( 'NONE',  ( -0.000000000000000000, 1.000000000000000000, -0.000000000000000000 ) ) ;
#43679 = LINE ( 'NONE', #72731, #32832 ) ;
#43680 = CARTESIAN_POINT ( 'NONE',  ( 1.334622868157815783E-15, 10.39230484541327293, -10.20000000000000284 ) ) ;
#43682 = CARTESIAN_POINT ( 'NONE',  ( -5.676582343749998039, 212.4479166632526983, -9.832129032723420536 ) ) ;
#43681 = DIRECTION ( 'NONE',  ( -0.000000000000000000, 1.000000000000000000, 4.689100369878284071E-30 ) ) ;
#43683 = CARTESIAN_POINT ( 'NONE',  ( 26.34314575050774820, 195.5625000000000284, 165.9999999999997442 ) ) ;
#43684 = CARTESIAN_POINT ( 'NONE',  ( 10.00000000000000178, 245.4166666734946318, 2.679491924311222739 ) ) ;
#43685 = CARTESIAN_POINT ( 'NONE',  ( -1.656854249492383468, 20.68750000000000000, 4.000000000000000888 ) ) ;
#43686 = VERTEX_POINT ( 'NONE', #56007 ) ;
#43687 = CARTESIAN_POINT ( 'NONE',  ( 8.311093377946834337, 175.4687499965860127, 8.311093377946839666 ) ) ;
#43688 = VECTOR ( 'NONE', #47822, 1000.000000000000114 ) ;
#43689 = CARTESIAN_POINT ( 'NONE',  ( 2.977408999572650927, -7.188101187499990274, 16.95530278187175455 ) ) ;
#43690 = CARTESIAN_POINT ( 'NONE',  ( 3.313708498984802020, 18.28125000000000355, -7.999999999999958256 ) ) ;
#43691 = ORIENTED_EDGE ( 'NONE', *, *, #74202, .T. ) ;
#43692 = EDGE_CURVE ( 'NONE', #33441, #7497, #39019, .T. ) ;
#43693 = CARTESIAN_POINT ( 'NONE',  ( 5.656854249492381470, 98.75000000409677625, 5.656854249492379694 ) ) ;
#43694 = AXIS2_PLACEMENT_3D ( 'NONE', #68755, #17067, #63462 ) ;
#43695 = CARTESIAN_POINT ( 'NONE',  ( -10.00000000000000000, 7.291666666666665186, -2.679491924311229845 ) ) ;
#43696 = ORIENTED_EDGE ( 'NONE', *, *, #12476, .T. ) ;
#43697 = CARTESIAN_POINT ( 'NONE',  ( 1.656854249492381914, 16.81250000000000355, 4.000000000000000888 ) ) ;
#43698 = CARTESIAN_POINT ( 'NONE',  ( -1.881053915767121776, 20.62499999863441147, -4.541265875000002339 ) ) ;
#43699 = CARTESIAN_POINT ( 'NONE',  ( 1.469576158976822172E-15, -7.999999999999991118, 16.39280278392014978 ) ) ;
#43700 = DIRECTION ( 'NONE',  ( -1.000000000000000000, -0.000000000000000000, -0.000000000000000000 ) ) ;
#43701 = VERTEX_POINT ( 'NONE', #21279 ) ;
#43702 = CARTESIAN_POINT ( 'NONE',  ( 1.102182119232618108E-15, 293.3125000034140157, 6.000000000000001776 ) ) ;
#43703 = CARTESIAN_POINT ( 'NONE',  ( -2.977408999572651815, 91.43750000204838102, 7.188101187500000933 ) ) ;
#43704 = ADVANCED_FACE ( 'NONE', ( #50693 ), #14866, .T. ) ;
#43707 = DIRECTION ( 'NONE',  ( -0.000000000000000000, -0.000000000000000000, 1.000000000000000000 ) ) ;
#43706 = CARTESIAN_POINT ( 'NONE',  ( -11.35316468749999963, 253.9062500034139873, 0.000000000000000000 ) ) ;
#43705 = CARTESIAN_POINT ( 'NONE',  ( -8.660254037844486774, 82.08333333333341386, -5.000000000000061284 ) ) ;
#43708 = B_SPLINE_CURVE_WITH_KNOTS ( 'NONE', 3,
 ( #26679, #32360, #27058, #28173, #22498, #45520, #68536, #50070 ),
 .UNSPECIFIED., .F., .F.,
 ( 4, 2, 2, 4 ),
 ( 0.01854123755286043312, 0.02116956588062352679, 0.02379789420838662045, 0.02905455086391281125 ),
 .UNSPECIFIED. ) ;
#43709 = EDGE_LOOP ( 'NONE', ( #6493, #10762, #22396 ) ) ;
#43710 = CARTESIAN_POINT ( 'NONE',  ( 2.124081043562907833, 50.03790111639249005, -40.75706181777439951 ) ) ;
#43711 = CARTESIAN_POINT ( 'NONE',  ( -2.977408999572648707, -7.188101187499990274, 16.76780278187175099 ) ) ;
#43712 = ORIENTED_EDGE ( 'NONE', *, *, #61207, .F. ) ;
#43713 = EDGE_CURVE ( 'NONE', #21067, #5549, #69127, .T. ) ;
#43714 = ORIENTED_EDGE ( 'NONE', *, *, #39239, .F. ) ;
#43715 = CARTESIAN_POINT ( 'NONE',  ( -4.220049686691937474, -10.18810118749999738, 82.93750000204838102 ) ) ;
#43716 = CARTESIAN_POINT ( 'NONE',  ( 8.311093377946834337, 80.46874999658601268, 8.311093377946839666 ) ) ;
#43717 = CARTESIAN_POINT ( 'NONE',  ( 7.999979274741570556, -3.313729224243177729, 24.17405195469602575 ) ) ;
#43718 = CARTESIAN_POINT ( 'NONE',  ( 4.556349186104045934, 11.00000000000000000, 89.03124999999998579 ) ) ;
#43721 = CARTESIAN_POINT ( 'NONE',  ( -6.676582343750001591, 295.6093750017069510, 0.000000000000000000 ) ) ;
#43720 = CARTESIAN_POINT ( 'NONE',  ( 31.99999999999999289, 197.3750000027312126, 169.9999999999998863 ) ) ;
#43719 = DIRECTION ( 'NONE',  ( -0.000000000000000000, 1.000000000000000000, -0.000000000000000000 ) ) ;
#43722 = CARTESIAN_POINT ( 'NONE',  ( -11.00000000000000000, 0.000000000000000000, 89.50000000000000000 ) ) ;
#43723 = CARTESIAN_POINT ( 'NONE',  ( 7.999999999999991118, 0.000000000000000000, 30.00000000000000000 ) ) ;
#43724 = CARTESIAN_POINT ( 'NONE',  ( -3.458734124999959469, 198.7500000013656063, 199.4326545832176976 ) ) ;
#43725 = CARTESIAN_POINT ( 'NONE',  ( -8.000000000000000000, 2.062499995903220196, -9.797174393178825657E-16 ) ) ;
#43726 = CARTESIAN_POINT ( 'NONE',  ( 29.43265458321766559, 198.8750000013656347, 166.5412658749999650 ) ) ;
#43727 = CARTESIAN_POINT ( 'NONE',  ( 7.188101187500001821, 12.93749999795161365, -2.977408999572650483 ) ) ;
#43728 = CARTESIAN_POINT ( 'NONE',  ( -7.999999999999991118, 0.000000000000000000, 25.01780278392014978 ) ) ;
#43729 = CARTESIAN_POINT ( 'NONE',  ( -2.679491924311287132, 242.0833333401613174, -9.999999999999968026 ) ) ;
#43730 = CARTESIAN_POINT ( 'NONE',  ( 5.082755093536325042, 107.4687500020483952, -5.082755093536325930 ) ) ;
#43732 = CARTESIAN_POINT ( 'NONE',  ( 0.000000000000000000, 300.0000000000000000, 0.000000000000000000 ) ) ;
#43731 = DIRECTION ( 'NONE',  ( 0.000000000000000000, -2.238352872228138170E-16, 1.000000000000000000 ) ) ;
#43733 = DIRECTION ( 'NONE',  ( -0.000000000000000000, 1.000000000000000000, -0.000000000000000000 ) ) ;
#43734 = LINE ( 'NONE', #65250, #18088 ) ;
#43735 = CARTESIAN_POINT ( 'NONE',  ( -5.082755093536317936, -5.082755093536320601, 15.54905278187175632 ) ) ;
#43736 = CARTESIAN_POINT ( 'NONE',  ( 3.999999999999960032, 209.0625000027312126, 143.6568542494924543 ) ) ;
#43737 = CARTESIAN_POINT ( 'NONE',  ( 9.832129032723416984, 35.36458332991934839, 5.676582343750006032 ) ) ;
#43738 = CARTESIAN_POINT ( 'NONE',  ( 4.999999999999995559, 149.1666666666666288, 8.660254037844394404 ) ) ;
#43739 = CARTESIAN_POINT ( 'NONE',  ( -10.00000000000000000, 9.166666659838700326, -2.679491924311229845 ) ) ;
#43740 = AXIS2_PLACEMENT_3D ( 'NONE', #59784, #61171, #8093 ) ;
#43741 = CARTESIAN_POINT ( 'NONE',  ( -28.00000000000007816, 200.1250000027312126, 166.0000000000003695 ) ) ;
#43742 = ORIENTED_EDGE ( 'NONE', *, *, #46821, .T. ) ;
#43743 = CARTESIAN_POINT ( 'NONE',  ( 1.656854249492246467, 198.9375000027312126, 146.0000000000001421 ) ) ;
#43744 = CARTESIAN_POINT ( 'NONE',  ( -7.999999999999991118, 0.000000000000000000, 26.33030277982336997 ) ) ;
#43745 = CARTESIAN_POINT ( 'NONE',  ( -3.042071309553173730, 54.32291666325268409, 11.35316468749999785 ) ) ;
#43746 = CARTESIAN_POINT ( 'NONE',  ( -11.00000000000000000, 4.556349186104045934, 83.59375000409677625 ) ) ;
#43747 = CARTESIAN_POINT ( 'NONE',  ( 3.458734124999960358, 205.6875000013656063, 142.0000000000000568 ) ) ;
#43748 = CARTESIAN_POINT ( 'NONE',  ( -7.320508075688770155, 260.6249999999999432, 7.320508075688774596 ) ) ;
#43749 = CARTESIAN_POINT ( 'NONE',  ( -5.000000000000000000, 29.68417822476661527, -4.268394125862720934 ) ) ;
#43751 = CARTESIAN_POINT ( 'NONE',  ( -3.042071309553173730, 49.32291666325267698, 11.35316468749999785 ) ) ;
#43750 = CARTESIAN_POINT ( 'NONE',  ( -2.977408999572652260, 100.4375000020483810, 7.188101187500000044 ) ) ;
#43752 = CARTESIAN_POINT ( 'NONE',  ( 1.469576158976822172E-15, -7.999999999999991118, 11.70530277982336642 ) ) ;
#43753 = CARTESIAN_POINT ( 'NONE',  ( 8.660254037844387298, 205.4166666666666856, -4.999999999999999112 ) ) ;
#43754 = CARTESIAN_POINT ( 'NONE',  ( -5.676582343750006032, 164.1145833299193555, 9.832129032723418760 ) ) ;
#43755 = CARTESIAN_POINT ( 'NONE',  ( -2.679491924311225848, 133.3333333265053398, -10.00000000000000178 ) ) ;
#43756 = CARTESIAN_POINT ( 'NONE',  ( -2.977408999572650927, 103.2500000020483810, -7.188101187500001821 ) ) ;
#43757 = VERTEX_POINT ( 'NONE', #49959 ) ;
#43758 = CARTESIAN_POINT ( 'NONE',  ( -2.485281374238288432, 289.1875000000000568, 6.000000000000285105 ) ) ;
#43759 = CARTESIAN_POINT ( 'NONE',  ( 5.676582343749993598, 20.26041666325268409, 9.832129032723422313 ) ) ;
#43760 = CARTESIAN_POINT ( 'NONE',  ( -2.751064625579944321E-14, 197.8750000027312126, 146.0000000000000284 ) ) ;
#43761 = VERTEX_POINT ( 'NONE', #62022 ) ;
#43762 = CARTESIAN_POINT ( 'NONE',  ( -14.00000000000000178, -2.250000000005106138, 7.677076266390546522 ) ) ;
#43763 = CARTESIAN_POINT ( 'NONE',  ( -10.18810118749999916, 4.220049686691934809, 76.56250000204836681 ) ) ;
#43764 = FACE_OUTER_BOUND ( 'NONE', #46113, .T. ) ;
#43766 = CARTESIAN_POINT ( 'NONE',  ( -11.35316468750000141, 158.2812499965860127, -1.390361679473963753E-15 ) ) ;
#43765 = DIRECTION ( 'NONE',  ( 0.000000000000000000, 0.000000000000000000, 1.000000000000000000 ) ) ;
#43767 = CARTESIAN_POINT ( 'NONE',  ( -7.188101187500000933, 2.999999997951610542, -2.977408999572651371 ) ) ;
#43768 = CARTESIAN_POINT ( 'NONE',  ( -7.999999999999991118, 0.000000000000000000, 11.38655278432982243 ) ) ;
#43769 = CARTESIAN_POINT ( 'NONE',  ( -22.22933947883602812, -25.35659445746813034, 191.6079683191152583 ) ) ;
#43770 = CARTESIAN_POINT ( 'NONE',  ( -11.35316468749999963, 228.9062500034139873, 0.000000000000000000 ) ) ;
#43771 = CARTESIAN_POINT ( 'NONE',  ( 1.871523826299183495E-15, -10.18810118749999916, 86.40625000204838102 ) ) ;
#43772 = VERTEX_POINT ( 'NONE', #72974 ) ;
#43773 =( BOUNDED_CURVE ( )  B_SPLINE_CURVE ( 2, ( #31845, #3548, #49564, #50307, #61636, #62002, #44657, #26164, #9954 ),
 .UNSPECIFIED., .F., .F. ) 
 B_SPLINE_CURVE_WITH_KNOTS ( ( 3, 2, 2, 2, 3 ),
 ( 0.2638888888888889506, 0.2708333333333333703, 0.2777777777777778456, 0.2847222222222222654, 0.2916666666666667407 ),
 .UNSPECIFIED. ) 
 CURVE ( )  GEOMETRIC_REPRESENTATION_ITEM ( )  RATIONAL_B_SPLINE_CURVE ( ( 0.9999999999999994449, 0.9238795325112872936, 1.000000000000000000, 0.9238795325112867385, 1.000000000000000000, 0.9238795325112867385, 1.000000000000000000, 0.9238795325112861834, 1.000000000000000666 ) ) 
 REPRESENTATION_ITEM ( '' )  );
#43774 = CARTESIAN_POINT ( 'NONE',  ( 8.000000000000000000, 1.406249995903220196, -3.313708498984761164 ) ) ;
#43775 = VECTOR ( 'NONE', #18160, 1000.000000000000000 ) ;
#43776 = CARTESIAN_POINT ( 'NONE',  ( -4.000000000000015987, 198.6250000027312126, 142.0000000000000568 ) ) ;
#43777 = CARTESIAN_POINT ( 'NONE',  ( -11.35316468749999785, 98.38541666325268409, -3.042071309553167513 ) ) ;
#43778 = CARTESIAN_POINT ( 'NONE',  ( 10.18810118749999916, 1.247682550866122264E-15, 93.90625000204836681 ) ) ;
#43779 = EDGE_CURVE ( 'NONE', #39327, #19453, #33006, .T. ) ;
#43780 = CARTESIAN_POINT ( 'NONE',  ( -3.211159895383562723, 19.06249999863440436, 3.211159895383561391 ) ) ;
#43781 = ORIENTED_EDGE ( 'NONE', *, *, #60214, .F. ) ;
#43782 = EDGE_LOOP ( 'NONE', ( #43450, #19642, #53114, #73582 ) ) ;
#43783 = CARTESIAN_POINT ( 'NONE',  ( 4.541265875000002339, 4.437499998634407028, 0.000000000000000000 ) ) ;
#43784 = CARTESIAN_POINT ( 'NONE',  ( -5.082755093536326818, 7.406249997951610986, 5.082755093536325042 ) ) ;
#43785 = CARTESIAN_POINT ( 'NONE',  ( -8.000000000000000000, 117.6875000040967763, 0.000000000000000000 ) ) ;
#43787 = ADVANCED_FACE ( 'NONE', ( #45049 ), #27309, .T. ) ;
#43786 = CARTESIAN_POINT ( 'NONE',  ( -7.204075437095967871, 7.204075437095967871, 94.84375000204838102 ) ) ;
#43788 = ADVANCED_FACE ( 'NONE', ( #61280 ), #49585, .F. ) ;
#43789 = CARTESIAN_POINT ( 'NONE',  ( -24.54126587499999346, 202.4375000013656063, 170.0000000000003411 ) ) ;
#43790 = CARTESIAN_POINT ( 'NONE',  ( -2.679491924311235174, 160.4166666598386826, 10.00000000000000000 ) ) ;
#43791 = CARTESIAN_POINT ( 'NONE',  ( -4.000000000000001776, 2.437500000000000444, -1.656854249492381470 ) ) ;
#43792 = CARTESIAN_POINT ( 'NONE',  ( 1.656854249492381914, 16.56249999726881228, 4.000000000000000888 ) ) ;
#43793 = CARTESIAN_POINT ( 'NONE',  ( -8.342170076843785083E-16, 2.062499998634406584, 4.541265875000002339 ) ) ;
#43795 = AXIS2_PLACEMENT_3D ( 'NONE', #46625, #69645, #6648 ) ;
#43794 = CARTESIAN_POINT ( 'NONE',  ( -4.000000000000015987, 203.5000000000000000, 142.0000000000000568 ) ) ;
#43796 = ORIENTED_EDGE ( 'NONE', *, *, #37866, .T. ) ;
#43797 = CARTESIAN_POINT ( 'NONE',  ( -1.432654583217607858, 195.6250000013656063, 201.4587341250000065 ) ) ;
#43799 = DIRECTION ( 'NONE',  ( -0.000000000000000000, 1.000000000000000000, -1.563033456626094573E-30 ) ) ;
#43798 = CARTESIAN_POINT ( 'NONE',  ( -27.99999999999991829, 197.9375000013655779, 173.4587341250003760 ) ) ;
#43800 =( NAMED_UNIT ( * ) PLANE_ANGLE_UNIT ( ) SI_UNIT ( $, .RADIAN. ) );
#43801 = CARTESIAN_POINT ( 'NONE',  ( -4.541265875000003227, 17.87499999863441147, 1.881053915767121110 ) ) ;
#43802 = DIRECTION ( 'NONE',  ( 0.000000000000000000, 0.000000000000000000, 1.000000000000000000 ) ) ;
#43803 = CARTESIAN_POINT ( 'NONE',  ( -2.977408999572648707, -7.188101187499990274, 4.767802781871753659 ) ) ;
#43804 = ORIENTED_EDGE ( 'NONE', *, *, #68544, .T. ) ;
#43805 = ORIENTED_EDGE ( 'NONE', *, *, #73386, .F. ) ;
#43806 = CARTESIAN_POINT ( 'NONE',  ( 10.18810118749999916, 4.220049686691935698, 97.00000000204838102 ) ) ;
#43807 = FACE_OUTER_BOUND ( 'NONE', #22972, .T. ) ;
#43808 = CARTESIAN_POINT ( 'NONE',  ( -26.56734541678232731, 199.2500000013656063, 173.4587341250003760 ) ) ;
#43809 = CARTESIAN_POINT ( 'NONE',  ( -7.778174593052020747, -7.778174593052023411, 106.1874999999999858 ) ) ;
#43810 = CARTESIAN_POINT ( 'NONE',  ( 2.445694354108840063, 209.0625000013656063, 200.4456943541088663 ) ) ;
#43811 = CARTESIAN_POINT ( 'NONE',  ( -1.656854249492383468, 21.43749999726881583, 4.000000000000000888 ) ) ;
#43812 = CARTESIAN_POINT ( 'NONE',  ( -7.320508075688773708, 106.8750000000000142, -7.320508075688774596 ) ) ;
#43813 = CARTESIAN_POINT ( 'NONE',  ( 8.000000000000000000, 113.8437500000000000, -3.313708498984762496 ) ) ;
#43814 = CARTESIAN_POINT ( 'NONE',  ( 1.226468279477575784E-15, 290.8593750017070079, 6.676582343750001591 ) ) ;
#43815 = EDGE_CURVE ( 'NONE', #69767, #61038, #73346, .T. ) ;
#43816 = CARTESIAN_POINT ( 'NONE',  ( 7.188101187499992051, 8.802885111219154394E-16, 10.11155278187175455 ) ) ;
#43817 = ORIENTED_EDGE ( 'NONE', *, *, #44653, .T. ) ;
#43818 = DIRECTION ( 'NONE',  ( 1.000000000000000000, 0.000000000000000000, -1.836970198721037823E-16 ) ) ;
#43819 = CARTESIAN_POINT ( 'NONE',  ( 8.000000000000000000, 19.40624999590322375, -3.313708498984761608 ) ) ;
#43820 = CIRCLE ( 'NONE', #498, 7.000000000000000000 ) ;
#43821 = CARTESIAN_POINT ( 'NONE',  ( -3.458734125000016313, 204.8750000013656063, 140.5673454167824161 ) ) ;
#43822 = CARTESIAN_POINT ( 'NONE',  ( -2.679491924311521167, 183.3333333265053966, -9.999999999999833022 ) ) ;
#43824 = CARTESIAN_POINT ( 'NONE',  ( 1.432654583217608080, 203.8750000013656063, 138.5412658750000503 ) ) ;
#43823 = CARTESIAN_POINT ( 'NONE',  ( 7.778174593052021635, 7.778174593052023411, 111.4375000000000000 ) ) ;
#43825 = CARTESIAN_POINT ( 'NONE',  ( -11.35316468749999608, 259.4270833367472164, 3.042071309553173730 ) ) ;
#43826 = DIRECTION ( 'NONE',  ( -0.000000000000000000, 1.000000000000000000, 4.689100369878284071E-30 ) ) ;
#43827 = CARTESIAN_POINT ( 'NONE',  ( 5.676582343749993598, 4.947916663252683200, 9.832129032723422313 ) ) ;
#43828 = CARTESIAN_POINT ( 'NONE',  ( 5.082755093536320601, -5.082755093536318824, 6.924052781871754547 ) ) ;
#43829 = CARTESIAN_POINT ( 'NONE',  ( -2.085542519210945728E-15, 199.8437499965860127, 11.35316468750000141 ) ) ;
#43830 = CARTESIAN_POINT ( 'NONE',  ( -2.751064625579944321E-14, 197.8750000027312126, 146.0000000000000284 ) ) ;
#43831 = CARTESIAN_POINT ( 'NONE',  ( 1.881053915767122664, 5.124999998634406140, 4.541265875000001451 ) ) ;
#43832 = CARTESIAN_POINT ( 'NONE',  ( 0.000000000000000000, 300.0000000000000000, 6.000000000000001776 ) ) ;
#43834 = CARTESIAN_POINT ( 'NONE',  ( 5.656854249492379694, 102.1250000040967763, -5.656854249492380582 ) ) ;
#43833 = CARTESIAN_POINT ( 'NONE',  ( 27.99999999999999645, 210.0000000000000284, 165.9999999999999147 ) ) ;
#43835 = VERTEX_POINT ( 'NONE', #21650 ) ;
#43836 = CARTESIAN_POINT ( 'NONE',  ( -3.458734125000016757, 206.1250000013655779, 140.5673454167824161 ) ) ;
#43837 = CARTESIAN_POINT ( 'NONE',  ( -11.35316468749999785, 13.07291666325268409, -3.042071309553167513 ) ) ;
#43838 = CARTESIAN_POINT ( 'NONE',  ( 4.556349186104051263, -10.99999999999999822, 96.15625000409677625 ) ) ;
#43839 = CARTESIAN_POINT ( 'NONE',  ( -4.000000000000015987, 205.5625000000000284, 143.6568542494924259 ) ) ;
#43840 = CARTESIAN_POINT ( 'NONE',  ( -24.54126587500001833, 201.2500000013656063, 168.5673454167826435 ) ) ;
#43841 = CARTESIAN_POINT ( 'NONE',  ( 11.00000000000000000, 1.347111479062088405E-15, 117.2500000000000000 ) ) ;
#43843 = CARTESIAN_POINT ( 'NONE',  ( 2.828427124746152987, 204.1250000000000284, 139.1715728752538723 ) ) ;
#43842 = CARTESIAN_POINT ( 'NONE',  ( -5.082755093536325930, 116.4687500020483810, -5.082755093536325930 ) ) ;
#43844 = CARTESIAN_POINT ( 'NONE',  ( 7.999999999999992895, -3.313708498984756279, 26.98655277982336997 ) ) ;
#43845 = CARTESIAN_POINT ( 'NONE',  ( 11.35316468749999785, 125.5729166632526983, 3.042071309553174174 ) ) ;
#43846 = CARTESIAN_POINT ( 'NONE',  ( 4.999999999999993783, 86.04166665983869677, 8.660254037844390851 ) ) ;
#43847 = CARTESIAN_POINT ( 'NONE',  ( 7.188101187500000044, 123.7812500020483810, -8.802885111219163269E-16 ) ) ;
#43848 = CARTESIAN_POINT ( 'NONE',  ( 4.541265875000002339, 18.43749999863440792, 0.000000000000000000 ) ) ;
#43849 = CARTESIAN_POINT ( 'NONE',  ( -1.836970198721029983E-15, 200.6249999931720538, 10.00000000000000178 ) ) ;
#43850 = CARTESIAN_POINT ( 'NONE',  ( -26.34314575050757412, 195.0625000027311557, 166.0000000000004832 ) ) ;
#43851 = ORIENTED_EDGE ( 'NONE', *, *, #40917, .T. ) ;
#43852 = CARTESIAN_POINT ( 'NONE',  ( -9.489879397300773789, 225.9999999999999716, 3.220560865818566931 ) ) ;
#43853 = CARTESIAN_POINT ( 'NONE',  ( 4.721056650416000089, 290.9843750017070079, 4.721056650415999201 ) ) ;
#43854 = CARTESIAN_POINT ( 'NONE',  ( 0.000000000000000000, 220.0000000000000284, -10.00000000000000000 ) ) ;
#43855 = CARTESIAN_POINT ( 'NONE',  ( -3.313708498984758943, -7.999999999999989342, -0.2009472160798553009 ) ) ;
#43856 = VECTOR ( 'NONE', #60440, 1000.000000000000000 ) ;
#43857 = CARTESIAN_POINT ( 'NONE',  ( 0.000000000000000000, 15.08051212944140218, 15.04081104653146994 ) ) ;
#43858 = CARTESIAN_POINT ( 'NONE',  ( 2.679491924311228956, 202.9166666598387110, -10.00000000000000000 ) ) ;
#43859 = CYLINDRICAL_SURFACE ( 'NONE', #66328, 7.999999999999991118 ) ;
#43860 = CARTESIAN_POINT ( 'NONE',  ( 7.204075437095968759, -7.204075437095966983, 106.0937500020483810 ) ) ;
#43861 = ORIENTED_EDGE ( 'NONE', *, *, #51423, .F. ) ;
#43862 = ADVANCED_FACE ( 'NONE', ( #15988 ), #9975, .T. ) ;
#43863 = CARTESIAN_POINT ( 'NONE',  ( -1.469576158976823947E-15, 21.93749999590322375, 8.000000000000000000 ) ) ;
#43864 = CARTESIAN_POINT ( 'NONE',  ( 9.832129032723420536, 156.5104166632526983, -5.676582343749999815 ) ) ;
#43865 = CARTESIAN_POINT ( 'NONE',  ( -7.320508075688781702, 218.1250000000000284, 7.320508075688773708 ) ) ;
#43866 = CARTESIAN_POINT ( 'NONE',  ( 1.432654583217664701, 205.0000000013655779, 201.4587341250000065 ) ) ;
#43867 = CARTESIAN_POINT ( 'NONE',  ( 8.660254037844385522, 231.0416666734946318, -5.000000000000003553 ) ) ;
#43868 = CARTESIAN_POINT ( 'NONE',  ( -9.832129032723420536, 59.01041666325268409, 5.676582343749997150 ) ) ;
#43869 = EDGE_LOOP ( 'NONE', ( #32259, #1356, #42578, #603 ) ) ;
#43870 = CARTESIAN_POINT ( 'NONE',  ( 4.220049686691941027, -10.18810118749999738, 116.1250000020483810 ) ) ;
#43871 = CARTESIAN_POINT ( 'NONE',  ( -1.881053915767121776, 8.749999998634407916, -4.541265875000002339 ) ) ;
#43872 = ORIENTED_EDGE ( 'NONE', *, *, #22699, .T. ) ;
#43873 = CARTESIAN_POINT ( 'NONE',  ( -5.082755093536325042, 22.03124999795161543, -5.082755093536325930 ) ) ;
#43874 = CARTESIAN_POINT ( 'NONE',  ( 6.000000000000001776, 289.5625000034140157, -7.347880794884121708E-16 ) ) ;
#43875 = CARTESIAN_POINT ( 'NONE',  ( -8.660254037844385522, 248.5416666734946318, 5.000000000000004441 ) ) ;
#43876 = CARTESIAN_POINT ( 'NONE',  ( 2.977408999572650927, 16.12499999795161187, -7.188101187500001821 ) ) ;
#43877 = CARTESIAN_POINT ( 'NONE',  ( -7.188101187499992051, 2.977408999572646930, 5.892802781871753659 ) ) ;
#43878 = CARTESIAN_POINT ( 'NONE',  ( -4.220049686691937474, -10.18810118749999738, 107.3125000020483668 ) ) ;
#43879 = PRODUCT_DEFINITION_SHAPE ( 'NONE', 'NONE',  #26086 ) ;
#43880 =( BOUNDED_CURVE ( )  B_SPLINE_CURVE ( 2, ( #18726, #12680, #58367, #29676, #35714, #25103, #48120, #64745, #11956, #36081, #19085, #69669, #7407, #30414, #53435, #47747, #49234, #66217, #48490, #43959, #8884, #42824, #54545, #20562, #32279, #9256, #37934, #31143, #66968, #48860, #32659, #36815, #43576, #14522, #37561, #2852, #55668, #55293, #60560, #54918, #25840, #13771, #71869, #20183, #3985, #26214, #3599, #61314, #60934, #31897, #26596, #25473, #65842, #43200, #71494, #19818, #49618, #66592, #8140, #2481, #26974, #72248, #14897, #65478, #72634, #14150, #20938, #3227, #9639, #49988, #73004, #54175, #15272, #38308, #42461, #37185, #59824, #60184, #8507, #31523, #39419, #62418, #34148, #10377, #10008, #68824, #27717, #50728, #63166, #15644, #67346, #74116, #33040, #4349, #39049, #16754, #34526, #10743, #16380, #39780, #33777, #28465, #5098, #68091, #51104, #74486, #5464, #11491, #33403, #62052, #45813, #22417, #56403, #56040, #73375, #27339, #56777, #73743, #28089, #45439, #22049, #4722, #68454, #61687, #62783, #57148, #51473, #11125, #22793, #17136, #40160, #45077, #21680, #44706, #50356, #57531, #5839, #28833, #51852, #21313, #44335, #38685, #67721, #16019, #18633, #41642, #47655, #70317, #23916, #17513, #6209, #561, #12223, #52966, #64653, #12950, #35990, #63535, #24644, #6577, #65007, #59007, #46556, #7312, #13316, #1299, #52229, #53337, #52596, #41999, #18993, #36354, #11860, #6941, #30319, #1663, #23544, #58275, #30687, #69950, #69577, #29216, #196, #59369, #70676, #933, #47292, #7680, #34895, #23172, #40903, #46184, #29953, #24280, #69202, #40529, #57902, #17888, #63911, #35259, #29583, #46925, #18259, #58633, #41275, #64285, #12591, #35619, #36722, #3507, #48769, #60094, #59733, #38215, #48397, #26120, #19354, #42368, #14430, #14805, #43482, #65383, #49139, #8043, #13681, #19726, #61220, #9550, #2383, #48025, #8412, #71401, #31048, #9164, #26496, #20092, #71035, #55202, #37846, #42737, #32181 ),
 .UNSPECIFIED., .F., .F. ) 
 B_SPLINE_CURVE_WITH_KNOTS ( ( 3, 2, 2, 2, 2, 2, 2, 2, 2, 2, 2, 2, 2, 2, 2, 2, 2, 2, 2, 2, 2, 2, 2, 2, 2, 2, 2, 2, 2, 2, 2, 2, 2, 2, 2, 2, 2, 2, 2, 2, 2, 2, 2, 2, 2, 2, 2, 2, 2, 2, 2, 2, 2, 2, 2, 2, 2, 2, 2, 2, 2, 2, 2, 2, 2, 2, 2, 2, 2, 2, 2, 2, 2, 2, 2, 2, 2, 2, 2, 2, 2, 2, 2, 2, 2, 2, 2, 2, 2, 2, 2, 2, 2, 2, 2, 2, 2, 2, 2, 2, 2, 2, 2, 2, 2, 2, 2, 2, 2, 2, 2, 2, 2, 2, 2, 2, 2, 2, 2, 2, 3 ),
 ( 0.000000000000000000, 0.008333333333333333218, 0.01666666666666666644, 0.02500000000000000139, 0.03333333333333333287, 0.04166666666666666435, 0.05000000000000000278, 0.05833333333333333426, 0.06666666666666666574, 0.07499999999999999722, 0.08333333333333332871, 0.09166666666666666019, 0.1000000000000000056, 0.1083333333333333370, 0.1166666666666666685, 0.1250000000000000000, 0.1333333333333333315, 0.1416666666666666630, 0.1499999999999999944, 0.1583333333333333259, 0.1666666666666666574, 0.1749999999999999889, 0.1833333333333333204, 0.1916666666666666796, 0.2000000000000000111, 0.2083333333333333426, 0.2166666666666666741, 0.2250000000000000056, 0.2333333333333333370, 0.2416666666666666685, 0.2500000000000000000, 0.2583333333333333592, 0.2666666666666666630, 0.2750000000000000222, 0.2833333333333333259, 0.2916666666666666852, 0.2999999999999999889, 0.3083333333333333481, 0.3166666666666666519, 0.3250000000000000111, 0.3333333333333333148, 0.3416666666666666741, 0.3499999999999999778, 0.3583333333333333370, 0.3666666666666666408, 0.3749999999999999445, 0.3833333333333333592, 0.3916666666666666630, 0.4000000000000000222, 0.4083333333333333259, 0.4166666666666666852, 0.4249999999999999889, 0.4333333333333333481, 0.4416666666666666519, 0.4500000000000000111, 0.4583333333333333148, 0.4666666666666666741, 0.4749999999999999778, 0.4833333333333333370, 0.4916666666666666408, 0.5000000000000000000, 0.5083333333333333037, 0.5166666666666667185, 0.5250000000000000222, 0.5333333333333333259, 0.5416666666666666297, 0.5500000000000000444, 0.5583333333333333481, 0.5666666666666666519, 0.5749999999999999556, 0.5833333333333333703, 0.5916666666666666741, 0.5999999999999999778, 0.6083333333333332815, 0.6166666666666666963, 0.6250000000000000000, 0.6333333333333333037, 0.6416666666666667185, 0.6500000000000000222, 0.6583333333333333259, 0.6666666666666666297, 0.6750000000000000444, 0.6833333333333333481, 0.6916666666666666519, 0.6999999999999999556, 0.7083333333333333703, 0.7166666666666666741, 0.7249999999999999778, 0.7333333333333332815, 0.7416666666666666963, 0.7499999999999998890, 0.7583333333333333037, 0.7666666666666667185, 0.7750000000000000222, 0.7833333333333333259, 0.7916666666666666297, 0.8000000000000000444, 0.8083333333333333481, 0.8166666666666666519, 0.8249999999999999556, 0.8333333333333333703, 0.8416666666666666741, 0.8499999999999999778, 0.8583333333333332815, 0.8666666666666666963, 0.8750000000000000000, 0.8833333333333333037, 0.8916666666666667185, 0.9000000000000000222, 0.9083333333333333259, 0.9166666666666666297, 0.9250000000000000444, 0.9333333333333333481, 0.9416666666666666519, 0.9499999999999999556, 0.9583333333333333703, 0.9666666666666666741, 0.9749999999999999778, 0.9833333333333332815, 0.9916666666666666963, 0.9985233269883815321 ),
 .UNSPECIFIED. ) 
 CURVE ( )  GEOMETRIC_REPRESENTATION_ITEM ( )  RATIONAL_B_SPLINE_CURVE ( ( 1.000000000000000000, 0.9238795325112867385, 1.000000000000000000, 0.9238795325112867385, 1.000000000000000000, 0.9238795325112867385, 1.000000000000000000, 0.9238795325112867385, 1.000000000000000000, 0.9238795325112867385, 1.000000000000000000, 0.9238795325112867385, 1.000000000000000000, 0.9238795325112867385, 1.000000000000000000, 0.9238795325112867385, 1.000000000000000000, 0.9238795325112867385, 1.000000000000000000, 0.9238795325112867385, 1.000000000000000000, 0.9238795325112867385, 1.000000000000000000, 0.9238795325112867385, 1.000000000000000000, 0.9238795325112867385, 1.000000000000000000, 0.9238795325112867385, 1.000000000000000000, 0.9238795325112867385, 1.000000000000000000, 0.9238795325112867385, 1.000000000000000000, 0.9238795325112867385, 1.000000000000000000, 0.9238795325112867385, 1.000000000000000000, 0.9238795325112867385, 1.000000000000000000, 0.9238795325112867385, 1.000000000000000000, 0.9238795325112867385, 1.000000000000000000, 0.9238795325112867385, 1.000000000000000000, 0.9238795325112867385, 1.000000000000000000, 0.9238795325112867385, 1.000000000000000000, 0.9238795325112867385, 1.000000000000000000, 0.9238795325112867385, 1.000000000000000000, 0.9238795325112867385, 1.000000000000000000, 0.9238795325112867385, 1.000000000000000000, 0.9238795325112867385, 1.000000000000000000, 0.9238795325112867385, 1.000000000000000000, 0.9238795325112867385, 1.000000000000000000, 0.9238795325112867385, 1.000000000000000000, 0.9238795325112867385, 1.000000000000000000, 0.9238795325112867385, 1.000000000000000000, 0.9238795325112867385, 1.000000000000000000, 0.9238795325112867385, 1.000000000000000000, 0.9238795325112867385, 1.000000000000000000, 0.9238795325112867385, 1.000000000000000000, 0.9238795325112867385, 1.000000000000000000, 0.9238795325112867385, 1.000000000000000000, 0.9238795325112867385, 1.000000000000000000, 0.9238795325112867385, 1.000000000000000000, 0.9238795325112867385, 1.000000000000000000, 0.9238795325112867385, 1.000000000000000000, 0.9238795325112867385, 1.000000000000000000, 0.9238795325112867385, 1.000000000000000000, 0.9238795325112867385, 1.000000000000000000, 0.9238795325112867385, 1.000000000000000000, 0.9238795325112867385, 1.000000000000000000, 0.9238795325112867385, 1.000000000000000000, 0.9238795325112867385, 1.000000000000000000, 0.9238795325112867385, 1.000000000000000000, 0.9238795325112867385, 1.000000000000000000, 0.9238795325112867385, 1.000000000000000000, 0.9238795325112867385, 1.000000000000000000, 0.9238795325112867385, 1.000000000000000000, 0.9238795325112867385, 1.000000000000000000, 0.9238795325112867385, 1.000000000000000000, 0.9238795325112867385, 1.000000000000000000, 0.9238795325112867385, 1.000000000000000000, 0.9238795325112867385, 1.000000000000000000, 0.9238795325112867385, 1.000000000000000000, 0.9238795325112867385, 1.000000000000000000, 0.9238795325112867385, 1.000000000000000000, 0.9238795325112867385, 1.000000000000000000, 0.9238795325112867385, 1.000000000000000000, 0.9238795325112867385, 1.000000000000000000, 0.9238795325112867385, 1.000000000000000000, 0.9238795325112867385, 1.000000000000000000, 0.9238795325112867385, 1.000000000000000000, 0.9238795325112867385, 1.000000000000000000, 0.9238795325112867385, 1.000000000000000000, 0.9238795325112867385, 1.000000000000000000, 0.9238795325112867385, 1.000000000000000000, 0.9238795325112867385, 1.000000000000000000, 0.9238795325112867385, 1.000000000000000000, 0.9238795325112867385, 1.000000000000000000, 0.9238795325112867385, 1.000000000000000000, 0.9238795325112867385, 1.000000000000000000, 0.9238795325112867385, 1.000000000000000000, 0.9238795325112867385, 1.000000000000000000, 0.9238795325112867385, 1.000000000000000000, 0.9238795325112867385, 1.000000000000000000, 0.9238795325112867385, 1.000000000000000000, 0.9238795325112867385, 1.000000000000000000, 0.9238795325112867385, 1.000000000000000000, 0.9238795325112867385, 1.000000000000000000, 0.9238795325112867385, 1.000000000000000000, 0.9238795325112867385, 1.000000000000000000, 0.9238795325112867385, 1.000000000000000000, 0.9238795325112867385, 1.000000000000000000, 0.9238795325112867385, 1.000000000000000000, 0.9238795325112867385, 1.000000000000000000, 0.9238795325112867385, 1.000000000000000000, 0.9238795325112867385, 1.000000000000000000, 0.9238795325112867385, 1.000000000000000000, 0.9238795325112867385, 1.000000000000000000, 0.9238795325112867385, 1.000000000000000000, 0.9238795325112867385, 1.000000000000000000, 0.9238795325112867385, 1.000000000000000000, 0.9238795325112867385, 1.000000000000000000, 0.9238795325112867385, 1.000000000000000000, 0.9238795325112867385, 1.000000000000000000, 0.9238795325112867385, 1.000000000000000000, 0.9238795325112867385, 1.000000000000000000, 0.9238795325112867385, 1.000000000000000000, 0.9238795325112867385, 1.000000000000000000, 0.9238795325112867385, 1.000000000000000000, 0.9238795325112867385, 1.000000000000000000, 0.9238795325112867385, 1.000000000000000000, 0.9238795325112867385, 1.000000000000000000, 0.9238795325112867385, 1.000000000000000000, 0.9238795325112867385, 1.000000000000000000, 0.9238795325112867385, 1.000000000000000000, 0.9238795325112867385, 1.000000000000000000, 0.9238795325112867385, 1.000000000000000000, 0.9238795325112867385, 1.000000000000000000, 0.9238795325112867385, 1.000000000000000000, 0.9238795325112867385, 1.000000000000000000, 0.9373681373079704171, 0.9778031724868687657 ) ) 
 REPRESENTATION_ITEM ( '' )  );
#43881 = CYLINDRICAL_SURFACE ( 'NONE', #1679, 8.000000000000000000 ) ;
#43882 = CARTESIAN_POINT ( 'NONE',  ( 2.449293598294707893E-16, 4.999999997268813168, -4.000000000000001776 ) ) ;
#43883 =( BOUNDED_CURVE ( )  B_SPLINE_CURVE ( 3, ( #57646, #5583, #23292, #64407 ),
 .UNSPECIFIED., .F., .F. ) 
 B_SPLINE_CURVE_WITH_KNOTS ( ( 4, 4 ),
 ( 1.113649638898689757E-15, 1.570796326794898556 ),
 .UNSPECIFIED. ) 
 CURVE ( )  GEOMETRIC_REPRESENTATION_ITEM ( )  RATIONAL_B_SPLINE_CURVE ( ( 1.000000000000000000, 0.8047378541243648264, 0.8047378541243648264, 1.000000000000000000 ) ) 
 REPRESENTATION_ITEM ( '' )  );
#43884 = CARTESIAN_POINT ( 'NONE',  ( -13.14448688981998359, -41.04708797519155894, 141.9222238507286704 ) ) ;
#43885 = ORIENTED_EDGE ( 'NONE', *, *, #12385, .F. ) ;
#43886 = EDGE_CURVE ( 'NONE', #44274, #4443, #22836, .T. ) ;
#43887 = ADVANCED_FACE ( 'NONE', ( #5808 ), #17483, .F. ) ;
#43888 = CARTESIAN_POINT ( 'NONE',  ( -3.458734124999959914, 206.3750000013656063, 196.5673454167823877 ) ) ;
#43889 = CARTESIAN_POINT ( 'NONE',  ( -29.43265458321771533, 208.5000000013656063, 166.5412658750003914 ) ) ;
#43890 = EDGE_CURVE ( 'NONE', #43896, #61876, #52079, .T. ) ;
#43891 = CARTESIAN_POINT ( 'NONE',  ( 2.780723358947928197E-16, 7.562499998634407028, -4.541265875000002339 ) ) ;
#43892 = CARTESIAN_POINT ( 'NONE',  ( -3.313708498984759387, -7.999999999999989342, 10.11155277982336642 ) ) ;
#43893 = CARTESIAN_POINT ( 'NONE',  ( -7.188101187499991163, 2.977408999572646930, 23.89280278187176165 ) ) ;
#43894 = VERTEX_POINT ( 'NONE', #46156 ) ;
#43895 = CARTESIAN_POINT ( 'NONE',  ( 6.000000000000001776, 299.5000000000000000, -7.347880794884121708E-16 ) ) ;
#43896 = VERTEX_POINT ( 'NONE', #69924 ) ;
#43897 = CARTESIAN_POINT ( 'NONE',  ( -10.18810118749999916, 0.000000000000000000, 115.6562500020483810 ) ) ;
#43898 = CARTESIAN_POINT ( 'NONE',  ( 2.220677790255211837E-11, 201.2499999999982663, -9.999999999999998224 ) ) ;
#43899 = CARTESIAN_POINT ( 'NONE',  ( -1.432654583217607858, 205.6250000013656063, 201.4587341250000065 ) ) ;
#43900 = CARTESIAN_POINT ( 'NONE',  ( 26.56734541678233086, 198.0000000013656063, 166.5412658749999650 ) ) ;
#43901 = CARTESIAN_POINT ( 'NONE',  ( -5.000000000000005329, 63.33333333333333570, 8.660254037844387298 ) ) ;
#43902 = VECTOR ( 'NONE', #153, 1000.000000000000000 ) ;
#43903 = CARTESIAN_POINT ( 'NONE',  ( 5.082755093536326818, 96.59375000204838102, 5.082755093536325042 ) ) ;
#43904 = CARTESIAN_POINT ( 'NONE',  ( 2.485281374238575314, 292.3125000000000000, 6.000000000000000888 ) ) ;
#43905 = ADVANCED_FACE ( 'NONE', ( #534 ), #26794, .F. ) ;
#43907 = DIRECTION ( 'NONE',  ( 0.000000000000000000, 0.000000000000000000, 1.000000000000000000 ) ) ;
#43906 = CARTESIAN_POINT ( 'NONE',  ( 32.00000000000000711, 207.3125000027312126, 171.6568542494922553 ) ) ;
#43908 = ORIENTED_EDGE ( 'NONE', *, *, #36898, .F. ) ;
#43909 = CARTESIAN_POINT ( 'NONE',  ( 8.000000000000000000, 94.25000000000000000, -9.797174393178825657E-16 ) ) ;
#43910 = DIRECTION ( 'NONE',  ( -0.000000000000000000, -0.000000000000000000, -1.000000000000000000 ) ) ;
#43911 = CARTESIAN_POINT ( 'NONE',  ( 2.828427124746153876, 199.0000000027312126, 144.8284271247462129 ) ) ;
#43912 = CARTESIAN_POINT ( 'NONE',  ( 7.778174593052023411, -7.778174593052021635, 78.06249999999998579 ) ) ;
#43913 = CYLINDRICAL_SURFACE ( 'NONE', #28025, 3.999999999999976019 ) ;
#43914 = CARTESIAN_POINT ( 'NONE',  ( -7.320508075688770155, 255.6250000000000000, 7.320508075688774596 ) ) ;
#43915 = CARTESIAN_POINT ( 'NONE',  ( 11.00000000000000000, 1.347111479062088405E-15, 106.9375000040967763 ) ) ;
#43916 = CARTESIAN_POINT ( 'NONE',  ( -7.320508075688778149, 193.1250000000000284, 7.320508075688769267 ) ) ;
#43917 = CARTESIAN_POINT ( 'NONE',  ( -4.556349186104048599, -10.99999999999999822, 110.7812500000000000 ) ) ;
#43918 = CARTESIAN_POINT ( 'NONE',  ( 7.188101187499992051, 2.977408999572647819, 25.20530278187175810 ) ) ;
#43919 = CARTESIAN_POINT ( 'NONE',  ( -3.042071309553173730, 154.6354166632526699, 11.35316468749999785 ) ) ;
#43920 = DIRECTION ( 'NONE',  ( 0.000000000000000000, 0.000000000000000000, 1.000000000000000000 ) ) ;
#43921 = CARTESIAN_POINT ( 'NONE',  ( -31.01733368473114538, 47.55693698974732087, 65.00000000000000000 ) ) ;
#43922 = CARTESIAN_POINT ( 'NONE',  ( -0.7768891076261665862, -42.09574026589720575, 151.0149189110310601 ) ) ;
#43924 = CARTESIAN_POINT ( 'NONE',  ( 1.224646799147353454E-15, 300.0000000000000000, -10.00000000000000178 ) ) ;
#43923 = CARTESIAN_POINT ( 'NONE',  ( -4.000000000000016875, 202.5625000027312126, 140.3431457505076594 ) ) ;
#43925 = ORIENTED_EDGE ( 'NONE', *, *, #24753, .F. ) ;
#43926 = CARTESIAN_POINT ( 'NONE',  ( -11.35316468749999785, 23.38541666325268054, -3.042071309553167513 ) ) ;
#43927 = FACE_BOUND ( 'NONE', #60546, .T. ) ;
#43929 = CARTESIAN_POINT ( 'NONE',  ( 4.465349678513698350, -10.10202304668585604, -70.97395336192410298 ) ) ;
#43928 = CARTESIAN_POINT ( 'NONE',  ( 7.999992860684751683, 3.313715638299997490, 16.86155306956639777 ) ) ;
#43930 = CARTESIAN_POINT ( 'NONE',  ( -29.65685424949228377, 196.0625000000000284, 166.0000000000002558 ) ) ;
#43931 = CARTESIAN_POINT ( 'NONE',  ( -3.458734125000015425, 202.0000000013656063, 143.4326545832176976 ) ) ;
#43932 = CARTESIAN_POINT ( 'NONE',  ( -2.679491924311225848, 43.33333332650535397, -10.00000000000000178 ) ) ;
#43933 = AXIS2_PLACEMENT_3D ( 'NONE', #61734, #62463, #22464 ) ;
#43934 = CARTESIAN_POINT ( 'NONE',  ( 2.977408999572654480, 108.1250000020483810, 7.188101187499999156 ) ) ;
#43935 = CARTESIAN_POINT ( 'NONE',  ( 3.211159895383561835, 9.562499998634406140, -3.211159895383561835 ) ) ;
#43936 = FACE_OUTER_BOUND ( 'NONE', #27921, .T. ) ;
#43937 = CARTESIAN_POINT ( 'NONE',  ( -7.999999999999991118, 0.000000000000000000, 9.830302779823364645 ) ) ;
#43939 = CARTESIAN_POINT ( 'NONE',  ( 4.000000000000001776, 1.062500000000000222, -1.656854249492381248 ) ) ;
#43938 = CARTESIAN_POINT ( 'NONE',  ( 2.599720908691045107, 194.5204010206058740, 139.6168834790646542 ) ) ;
#43940 = ORIENTED_EDGE ( 'NONE', *, *, #52346, .T. ) ;
#43941 = ORIENTED_EDGE ( 'NONE', *, *, #30429, .T. ) ;
#43942 = CARTESIAN_POINT ( 'NONE',  ( -8.660254037844387298, 222.0833333333333428, -5.000000000000004441 ) ) ;
#43943 = CARTESIAN_POINT ( 'NONE',  ( -1.656854249492538234, 196.6875000000000284, 145.9999999999998863 ) ) ;
#43944 = CARTESIAN_POINT ( 'NONE',  ( -5.676582343750000703, 223.3854166700806729, -9.832129032723418760 ) ) ;
#43945 = CARTESIAN_POINT ( 'NONE',  ( 5.676582343749993598, 129.9479166632526983, 9.832129032723422313 ) ) ;
#43946 = ORIENTED_EDGE ( 'NONE', *, *, #22123, .F. ) ;
#43947 = CARTESIAN_POINT ( 'NONE',  ( 5.656854249492376141, -5.656854249492374365, 10.58030278392014800 ) ) ;
#43948 = CARTESIAN_POINT ( 'NONE',  ( 10.18810118749999916, 4.220049686691935698, 89.50000000204836681 ) ) ;
#43949 = FACE_OUTER_BOUND ( 'NONE', #22003, .T. ) ;
#43950 = CARTESIAN_POINT ( 'NONE',  ( 1.656854249492403008, 208.6875000000000284, 194.0000000000000853 ) ) ;
#43951 = LINE ( 'NONE', #3591, #18462 ) ;
#43953 = CARTESIAN_POINT ( 'NONE',  ( 8.311093377946834337, 130.1562499965860411, 8.311093377946839666 ) ) ;
#43952 = CARTESIAN_POINT ( 'NONE',  ( -3.313708498984653250, 94.71874999999998579, -8.000000000000108358 ) ) ;
#43954 = CARTESIAN_POINT ( 'NONE',  ( 8.031737012268331810, -9.219280934457653842, -0.1021479564361314485 ) ) ;
#43955 = ORIENTED_EDGE ( 'NONE', *, *, #38332, .T. ) ;
#43956 = DIRECTION ( 'NONE',  ( -0.000000000000000000, 1.000000000000000000, -0.000000000000000000 ) ) ;
#43957 = CARTESIAN_POINT ( 'NONE',  ( 47.73904998337091854, 39.83956789545236177, 63.58670016157656590 ) ) ;
#43958 = CARTESIAN_POINT ( 'NONE',  ( 5.676582343749993598, 110.2604166632526841, 9.832129032723422313 ) ) ;
#43959 = CARTESIAN_POINT ( 'NONE',  ( -1.432654583217607192, 208.2500000013656063, 194.5412658750000219 ) ) ;
#43960 = CARTESIAN_POINT ( 'NONE',  ( 5.082755093536324154, 17.15624999795161543, 5.082755093536326818 ) ) ;
#43961 = CARTESIAN_POINT ( 'NONE',  ( -6.238412754330611322E-16, 10.18810118749999916, 81.15625000204838102 ) ) ;
#43962 = CARTESIAN_POINT ( 'NONE',  ( -8.311093377946841443, 24.21874999658601979, 8.311093377946830785 ) ) ;
#43963 = VERTEX_POINT ( 'NONE', #11093 ) ;
#43964 = CARTESIAN_POINT ( 'NONE',  ( -6.331740687315345895E-14, -13.85640646055103531, -1.071796769724504550 ) ) ;
#43965 = CARTESIAN_POINT ( 'NONE',  ( 5.662595241051936235, -5.662595241051934458, 21.07561528394063188 ) ) ;
#43966 = CARTESIAN_POINT ( 'NONE',  ( -3.313708498984757611, 7.999999999999991118, 23.23655278392014978 ) ) ;
#43967 = EDGE_CURVE ( 'NONE', #53778, #11319, #72428, .T. ) ;
#43968 = CARTESIAN_POINT ( 'NONE',  ( -2.828427124746190735, 7.375000000000000888, -2.828427124746191623 ) ) ;
#43969 = CARTESIAN_POINT ( 'NONE',  ( 7.188101187500000044, 0.4687499979516099868, 0.000000000000000000 ) ) ;
#43970 = CARTESIAN_POINT ( 'NONE',  ( 4.721056650416000089, 287.8281250017069510, 4.721056650415999201 ) ) ;
#43971 = DIRECTION ( 'NONE',  ( 0.000000000000000000, 0.000000000000000000, 1.000000000000000000 ) ) ;
#43972 = CARTESIAN_POINT ( 'NONE',  ( -5.656854249492379694, 16.87499999590322375, -5.656854249492380582 ) ) ;
#43973 = ORIENTED_EDGE ( 'NONE', *, *, #24961, .F. ) ;
#43974 = CARTESIAN_POINT ( 'NONE',  ( 9.832129032723416984, 140.6770833299193555, 5.676582343750006032 ) ) ;
#43975 = CARTESIAN_POINT ( 'NONE',  ( -6.238412754330611322E-16, 10.18810118749999916, 80.78125000204838102 ) ) ;
#43976 = CARTESIAN_POINT ( 'NONE',  ( -24.54126587499999701, 197.2500000013656063, 168.5673454167827003 ) ) ;
#43977 = CYLINDRICAL_SURFACE ( 'NONE', #24545, 4.000000000000001776 ) ;
#43978 = CARTESIAN_POINT ( 'NONE',  ( -4.541265875000002339, 16.93749999863440436, -5.561446717895856393E-16 ) ) ;
#43979 = EDGE_LOOP ( 'NONE', ( #28599, #45796, #26885, #67669 ) ) ;
#43980 = ADVANCED_FACE ( 'NONE', ( #40128 ), #23514, .T. ) ;
#43981 = CARTESIAN_POINT ( 'NONE',  ( 2.849036369511732440E-14, 202.3750000027312126, 202.0000000000000000 ) ) ;
#43982 = VECTOR ( 'NONE', #12100, 1000.000000000000000 ) ;
#43983 =( BOUNDED_CURVE ( )  B_SPLINE_CURVE ( 2, ( #28116, #52623, #23571, #17916, #12251, #58299, #29610, #69978, #33806 ),
 .UNSPECIFIED., .F., .F. ) 
 B_SPLINE_CURVE_WITH_KNOTS ( ( 3, 2, 2, 2, 3 ),
 ( 0.4411764705882352811, 0.4448529411764705621, 0.4485294117647058987, 0.4522058823529411797, 0.4558823529411764608 ),
 .UNSPECIFIED. ) 
 CURVE ( )  GEOMETRIC_REPRESENTATION_ITEM ( )  RATIONAL_B_SPLINE_CURVE ( ( 1.000000000000000000, 0.9238795325112867385, 1.000000000000000000, 0.9238795325112867385, 1.000000000000000000, 0.9238795325112867385, 1.000000000000000000, 0.9238795325112867385, 1.000000000000000000 ) ) 
 REPRESENTATION_ITEM ( '' )  );
#43984 = CARTESIAN_POINT ( 'NONE',  ( -2.754378923186476579E-14, 196.4375000013655779, 145.4587341250000350 ) ) ;
#43985 = CARTESIAN_POINT ( 'NONE',  ( -29.65685424949229443, 207.5625000027312126, 174.0000000000004547 ) ) ;
#43986 = VECTOR ( 'NONE', #45860, 999.9999999999998863 ) ;
#43987 = CARTESIAN_POINT ( 'NONE',  ( -3.313708498984761608, 103.7187500000000000, -8.000000000000000000 ) ) ;
#43988 = ORIENTED_EDGE ( 'NONE', *, *, #21242, .F. ) ;
#43989 = CARTESIAN_POINT ( 'NONE',  ( 4.401442555609581635E-16, 8.343749997951611874, -7.188101187500000044 ) ) ;
#43990 = CARTESIAN_POINT ( 'NONE',  ( -15.83859651216086206, -18.92875543596370846, 196.6553547708986684 ) ) ;
#43991 = CARTESIAN_POINT ( 'NONE',  ( -2.385299476377879646, -46.82996453250010660, 151.1500021679194390 ) ) ;
#43992 = CARTESIAN_POINT ( 'NONE',  ( 9.832129032723416984, 180.3645833299193555, 5.676582343750006032 ) ) ;
#43993 = CARTESIAN_POINT ( 'NONE',  ( 2.977408999572654480, 113.0000000020483668, 7.188101187499999156 ) ) ;
#43994 = CARTESIAN_POINT ( 'NONE',  ( 2.828427124746208943, 207.7500000027312126, 195.1715728752538439 ) ) ;
#43995 = CARTESIAN_POINT ( 'NONE',  ( 2.765530957081996366, 290.1406250017069510, -6.676582343750002480 ) ) ;
#43996 = ADVANCED_FACE ( 'NONE', ( #18234 ), #69548, .F. ) ;
#43998 = CARTESIAN_POINT ( 'NONE',  ( -2.679491924283695425, 66.45833333333087012, -10.00000000001589839 ) ) ;
#43997 = CARTESIAN_POINT ( 'NONE',  ( -11.35316468749999785, 223.6979166700806445, -3.042071309553164848 ) ) ;
#43999 = ORIENTED_EDGE ( 'NONE', *, *, #20196, .F. ) ;
#44000 =( BOUNDED_CURVE ( )  B_SPLINE_CURVE ( 2, ( #2725, #8376, #54789, #14772, #71004, #13650, #3854, #37810, #3101 ),
 .UNSPECIFIED., .F., .F. ) 
 B_SPLINE_CURVE_WITH_KNOTS ( ( 3, 2, 2, 2, 3 ),
 ( 0.6022727272727272929, 0.6079545454545454142, 0.6136363636363636465, 0.6193181818181817677, 0.6250000000000000000 ),
 .UNSPECIFIED. ) 
 CURVE ( )  GEOMETRIC_REPRESENTATION_ITEM ( )  RATIONAL_B_SPLINE_CURVE ( ( 1.000000000000000000, 0.9238795325112867385, 1.000000000000000000, 0.9238795325112867385, 1.000000000000000000, 0.9238795325112867385, 1.000000000000000000, 0.9238795325112867385, 1.000000000000000000 ) ) 
 REPRESENTATION_ITEM ( '' )  );
#44001 = EDGE_CURVE ( 'NONE', #19911, #67659, #26136, .T. ) ;
#44002 = CARTESIAN_POINT ( 'NONE',  ( -3.042071309553166181, 252.8645833367473301, -11.35316468749999608 ) ) ;
#44003 = CARTESIAN_POINT ( 'NONE',  ( -5.082755093536317936, -5.082755093536320601, 23.04905278187175455 ) ) ;
#44004 = CARTESIAN_POINT ( 'NONE',  ( 0.000000000000000000, 28.00000000000000000, 0.000000000000000000 ) ) ;
#44005 = DIRECTION ( 'NONE',  ( 0.000000000000000000, 0.000000000000000000, 1.000000000000000000 ) ) ;
#44006 = CARTESIAN_POINT ( 'NONE',  ( 0.4501631047672336461, -67.59340899456768170, -20.03485802339844568 ) ) ;
#44007 = CARTESIAN_POINT ( 'NONE',  ( 3.458734125000016757, 199.1250000013656347, 199.4326545832176691 ) ) ;
#44008 = ORIENTED_EDGE ( 'NONE', *, *, #29372, .T. ) ;
#44009 = CARTESIAN_POINT ( 'NONE',  ( -3.313708498984762052, 91.71874999999998579, -8.000000000000000000 ) ) ;
#44010 = CARTESIAN_POINT ( 'NONE',  ( 5.676582343749993598, 110.2604166632526841, 9.832129032723422313 ) ) ;
#44011 = CARTESIAN_POINT ( 'NONE',  ( -5.000000000000000888, -14.89980876190747061, -69.94558486267359854 ) ) ;
#44012 = CARTESIAN_POINT ( 'NONE',  ( 11.00000000000000000, 1.347111479062088405E-15, 69.24999999999997158 ) ) ;
#44015 = DIRECTION ( 'NONE',  ( -0.000000000000000000, 1.000000000000000000, -0.000000000000000000 ) ) ;
#44014 = CARTESIAN_POINT ( 'NONE',  ( 24.54126587499998280, 202.1250000013656063, 168.5673454167822740 ) ) ;
#44013 = CARTESIAN_POINT ( 'NONE',  ( 30.44569435410878810, 197.8125000013656063, 172.4456943541087526 ) ) ;
#44016 = EDGE_CURVE ( 'NONE', #62856, #19857, #904, .T. ) ;
#44017 = VERTEX_POINT ( 'NONE', #23891 ) ;
#44018 = CARTESIAN_POINT ( 'NONE',  ( 9.830368419987745909, 224.8520141495858127, 1.857876432389923282 ) ) ;
#44019 = CARTESIAN_POINT ( 'NONE',  ( 11.35316468749999963, 225.9895833299193839, -3.042071309553165293 ) ) ;
#44020 = CARTESIAN_POINT ( 'NONE',  ( 1.432654583217607858, 198.6250000013655779, 138.5412658750000787 ) ) ;
#44021 = CARTESIAN_POINT ( 'NONE',  ( 30.44569435410878810, 196.8125000013656063, 172.4456943541087526 ) ) ;
#44022 = CARTESIAN_POINT ( 'NONE',  ( -4.556349186104045934, 11.00000000000000000, 111.9062500040967763 ) ) ;
#44023 = ADVANCED_FACE ( 'NONE', ( #68796 ), #46900, .T. ) ;
#44024 = CARTESIAN_POINT ( 'NONE',  ( -9.832129032723418760, 213.1770833299193555, -5.676582343750004256 ) ) ;
#44025 = DIRECTION ( 'NONE',  ( 1.000000000000000000, 0.000000000000000000, -1.652117596168387509E-16 ) ) ;
#44026 = CARTESIAN_POINT ( 'NONE',  ( 7.188101187500000044, 0.4687499979516099868, 0.000000000000000000 ) ) ;
#44027 = CARTESIAN_POINT ( 'NONE',  ( 1.881053915767121776, 19.49999999863440436, -4.541265875000002339 ) ) ;
#44028 = CARTESIAN_POINT ( 'NONE',  ( 5.086519500874516986, -50.65542486323015225, 41.09394361258718220 ) ) ;
#44029 = CARTESIAN_POINT ( 'NONE',  ( 7.999999999999991118, 3.313708498984757611, 27.17405277982336997 ) ) ;
#44031 = DIRECTION ( 'NONE',  ( 0.000000000000000000, -0.8778652960885011680, -0.4789076340208496263 ) ) ;
#44030 = DIRECTION ( 'NONE',  ( 0.000000000000000000, 0.000000000000000000, 1.000000000000000000 ) ) ;
#44032 = CARTESIAN_POINT ( 'NONE',  ( -3.042071309553164404, 92.23958332991935549, -11.35316468749999963 ) ) ;
#44033 = ORIENTED_EDGE ( 'NONE', *, *, #26877, .F. ) ;
#44034 = CARTESIAN_POINT ( 'NONE',  ( 8.000000000000000000, 92.75000000000000000, -9.797174393178825657E-16 ) ) ;
#44035 = CARTESIAN_POINT ( 'NONE',  ( 5.082755093536325930, 18.65624999795161187, -5.082755093536325930 ) ) ;
#44036 = LINE ( 'NONE', #50430, #66382 ) ;
#44037 = CARTESIAN_POINT ( 'NONE',  ( -11.35316468749999608, 254.4270833367473585, 3.042071309553173730 ) ) ;
#44038 = CARTESIAN_POINT ( 'NONE',  ( -11.35316468749999785, 88.07291666325266988, -3.042071309553167513 ) ) ;
#44039 = ORIENTED_EDGE ( 'NONE', *, *, #48790, .T. ) ;
#44040 = CARTESIAN_POINT ( 'NONE',  ( 5.000000000000000000, -15.48016642534403253, 69.96422921944753170 ) ) ;
#44041 = CARTESIAN_POINT ( 'NONE',  ( 7.204075437095968759, -7.204075437095966983, 116.2187500020483810 ) ) ;
#44042 = LINE ( 'NONE', #50068, #53854 ) ;
#44043 = CARTESIAN_POINT ( 'NONE',  ( 3.458734125000015425, 205.2500000013655779, 196.5673454167823877 ) ) ;
#44044 = DIRECTION ( 'NONE',  ( -0.000000000000000000, -1.000000000000000000, -0.000000000000000000 ) ) ;
#44046 = CARTESIAN_POINT ( 'NONE',  ( -8.311093377946841443, 83.90624999658602690, 8.311093377946834337 ) ) ;
#44045 = CARTESIAN_POINT ( 'NONE',  ( -7.778174593052020747, -7.778174593052023411, 106.1874999999999858 ) ) ;
#44047 = AXIS2_PLACEMENT_3D ( 'NONE', #53066, #29318, #664 ) ;
#44048 = CARTESIAN_POINT ( 'NONE',  ( -7.999999999999989342, -3.313708498984762496, 16.11155278392014267 ) ) ;
#44049 = CARTESIAN_POINT ( 'NONE',  ( -25.55430564589119413, 200.5625000013656063, 167.5543056458915316 ) ) ;
#44050 = DIRECTION ( 'NONE',  ( 0.000000000000000000, 0.000000000000000000, 1.000000000000000000 ) ) ;
#44051 = CARTESIAN_POINT ( 'NONE',  ( -8.660254037844387298, 183.9583333265053682, -5.000000000000004441 ) ) ;
#44052 = CARTESIAN_POINT ( 'NONE',  ( -6.000000000000001776, 287.0625000034140157, 0.000000000000000000 ) ) ;
#44053 = CARTESIAN_POINT ( 'NONE',  ( 3.042071309553167513, 77.13541666325266988, -11.35316468749999785 ) ) ;
#44054 = CARTESIAN_POINT ( 'NONE',  ( 4.721056650416000089, 293.8281250017069510, 4.721056650415999201 ) ) ;
#44055 = CARTESIAN_POINT ( 'NONE',  ( -4.220049686691935698, 10.18810118749999916, 100.7500000020483810 ) ) ;
#44056 = CARTESIAN_POINT ( 'NONE',  ( -8.311093377946841443, 208.9062499965860411, 8.311093377946830785 ) ) ;
#44057 = EDGE_LOOP ( 'NONE', ( #36624, #69980, #25503, #32682 ) ) ;
#44058 = CARTESIAN_POINT ( 'NONE',  ( -7.320508075688773708, 68.74999999317202537, -7.320508075688774596 ) ) ;
#44059 = CARTESIAN_POINT ( 'NONE',  ( -2.849036369511732440E-14, 206.3750000027312126, 138.0000000000000568 ) ) ;
#44060 = CARTESIAN_POINT ( 'NONE',  ( -3.373128826976389938, 50.22031155377479195, 40.85657338450112519 ) ) ;
#44062 = CARTESIAN_POINT ( 'NONE',  ( 11.35316468749999963, 200.9895833299193839, -3.042071309553165293 ) ) ;
#44061 = CARTESIAN_POINT ( 'NONE',  ( -4.000000000000001776, 11.18749999726881406, -1.656854249492381470 ) ) ;
#44063 = CARTESIAN_POINT ( 'NONE',  ( 23.99999999999997513, 195.8125000000000284, 171.6568542494922553 ) ) ;
#44064 = CARTESIAN_POINT ( 'NONE',  ( 10.00000000000000178, 230.4166666734946034, 2.679491924311222739 ) ) ;
#44065 = CARTESIAN_POINT ( 'NONE',  ( -7.778174593052020747, -7.778174593052023411, 71.87500000409677625 ) ) ;
#44066 = ORIENTED_EDGE ( 'NONE', *, *, #38970, .T. ) ;
#44067 = EDGE_CURVE ( 'NONE', #17960, #24993, #56910, .T. ) ;
#44068 = CARTESIAN_POINT ( 'NONE',  ( 3.042071309553159519, 195.0520833299193271, 11.35316468750000141 ) ) ;
#44069 = CARTESIAN_POINT ( 'NONE',  ( -2.977408999572647819, 7.188101187499992051, 17.70530278187175455 ) ) ;
#44070 = EDGE_CURVE ( 'NONE', #53323, #40937, #2135, .T. ) ;
#44071 = CARTESIAN_POINT ( 'NONE',  ( -4.193070328474951758, 60.66867996115669825, -23.17096354272497649 ) ) ;
#44072 = CARTESIAN_POINT ( 'NONE',  ( 5.656854249492380582, 12.18750000000000178, -5.656854249492380582 ) ) ;
#44073 = VERTEX_POINT ( 'NONE', #54428 ) ;
#44074 = CARTESIAN_POINT ( 'NONE',  ( 8.000000000000000000, 94.43750000409679046, -9.797174393178825657E-16 ) ) ;
#44075 = CARTESIAN_POINT ( 'NONE',  ( -10.00000000000000178, 12.50000000000000000, -1.224646799147353454E-15 ) ) ;
#44076 = EDGE_CURVE ( 'NONE', #8408, #43538, #30552, .T. ) ;
#44077 = EDGE_LOOP ( 'NONE', ( #3668, #43955, #17349, #10875, #29331, #61531 ) ) ;
#44078 = CARTESIAN_POINT ( 'NONE',  ( -2.828427124746190735, 15.37500000000000000, -2.828427124746191623 ) ) ;
#44079 = CARTESIAN_POINT ( 'NONE',  ( 3.211159895383561835, 21.43749999863440792, -3.211159895383561835 ) ) ;
#44080 = CARTESIAN_POINT ( 'NONE',  ( 3.313708498984756279, 7.999999999999991118, 9.549052783920146226 ) ) ;
#44081 = PRODUCT_DEFINITION ( 'UNKNOWN', '', #22532, #62901 ) ;
#44082 = FACE_OUTER_BOUND ( 'NONE', #52049, .T. ) ;
#44083 = ORIENTED_EDGE ( 'NONE', *, *, #50533, .T. ) ;
#44084 = CARTESIAN_POINT ( 'NONE',  ( -38.00000000000000000, 272.0000000000000000, 3.791916237172779019E-14 ) ) ;
#44085 = CARTESIAN_POINT ( 'NONE',  ( -7.188101187500001821, 94.06250000204838102, -2.977408999572650483 ) ) ;
#44088 = CARTESIAN_POINT ( 'NONE',  ( 1.267086777181619559E-12, 183.7500000000001137, 10.00000000000000178 ) ) ;
#44087 = CARTESIAN_POINT ( 'NONE',  ( 11.35316468749999963, 261.1979166700807014, 3.042071309553159519 ) ) ;
#44086 = DIRECTION ( 'NONE',  ( 0.000000000000000000, 0.000000000000000000, -1.000000000000000000 ) ) ;
#44089 = DIRECTION ( 'NONE',  ( 0.000000000000000000, 0.000000000000000000, 1.000000000000000000 ) ) ;
#44090 = VERTEX_POINT ( 'NONE', #6914 ) ;
#44091 = EDGE_CURVE ( 'NONE', #60077, #43835, #66700, .T. ) ;
#44092 = CARTESIAN_POINT ( 'NONE',  ( -8.311093377946836114, 253.5937500034140157, -8.311093377946836114 ) ) ;
#44093 = VECTOR ( 'NONE', #24055, 1000.000000000000000 ) ;
#44094 = CARTESIAN_POINT ( 'NONE',  ( -5.082755093536317936, -5.082755093536320601, 13.67405278187175455 ) ) ;
#44095 = VERTEX_POINT ( 'NONE', #65556 ) ;
#44096 =( BOUNDED_CURVE ( )  B_SPLINE_CURVE ( 2, ( #45328, #58892, #18884, #52119, #7201, #64900, #41163, #41890, #13204 ),
 .UNSPECIFIED., .F., .F. ) 
 B_SPLINE_CURVE_WITH_KNOTS ( ( 3, 2, 2, 2, 3 ),
 ( 0.4833333333333338366, 0.4916666666666670849, 0.5000000000000004441, 0.5083333333333336368, 0.5166666666666670515 ),
 .UNSPECIFIED. ) 
 CURVE ( )  GEOMETRIC_REPRESENTATION_ITEM ( )  RATIONAL_B_SPLINE_CURVE ( ( 0.9999999999999954481, 0.9238795325112912904, 1.000000000000000000, 0.9238795325112867385, 1.000000000000000000, 0.9238795325112867385, 1.000000000000000000, 0.9238795325112837409, 1.000000000000003109 ) ) 
 REPRESENTATION_ITEM ( '' )  );
#44097 = ORIENTED_EDGE ( 'NONE', *, *, #1506, .T. ) ;
#44098 = CARTESIAN_POINT ( 'NONE',  ( -4.220049686691935698, 10.18810118749999916, 80.87500000204836681 ) ) ;
#44099 = CARTESIAN_POINT ( 'NONE',  ( -5.676582343750006032, 69.42708332991935549, 9.832129032723418760 ) ) ;
#44100 = PLANE ( 'NONE',  #27606 ) ;
#44101 = CARTESIAN_POINT ( 'NONE',  ( 7.778174593052023411, -7.778174593052021635, 90.06249999999998579 ) ) ;
#44104 = CARTESIAN_POINT ( 'NONE',  ( 6.676582343750003368, 289.0468750017070079, 2.765530957081995478 ) ) ;
#44103 = CARTESIAN_POINT ( 'NONE',  ( 23.99999999999998579, 196.8750000027312126, 169.9999999999999432 ) ) ;
#44102 = CARTESIAN_POINT ( 'NONE',  ( -26.34314575050767360, 206.0625000027312126, 166.0000000000003411 ) ) ;
#44105 = CARTESIAN_POINT ( 'NONE',  ( -47.32259252271279593, 191.7059220763548240, 65.76194439203463560 ) ) ;
#44106 = CARTESIAN_POINT ( 'NONE',  ( -5.656854249492380582, 90.50000000409677625, -5.656854249492380582 ) ) ;
#44107 = CARTESIAN_POINT ( 'NONE',  ( 1.432654583217664701, 199.0000000013656063, 201.4587341250000065 ) ) ;
#44108 = CARTESIAN_POINT ( 'NONE',  ( -8.000000000000000000, 6.562499995903221084, -9.797174393178825657E-16 ) ) ;
#44109 = AXIS2_PLACEMENT_3D ( 'NONE', #55566, #14797, #37457 ) ;
#44110 = VERTEX_POINT ( 'NONE', #41076 ) ;
#44111 = CARTESIAN_POINT ( 'NONE',  ( 31.45873412499999233, 196.6875000013655779, 169.9999999999999432 ) ) ;
#44112 = CARTESIAN_POINT ( 'NONE',  ( -5.082755093536325042, 8.906249997951611874, -5.082755093536325930 ) ) ;
#44113 = CARTESIAN_POINT ( 'NONE',  ( -3.042071309553164404, 167.5520833299193271, -11.35316468749999963 ) ) ;
#44114 = CARTESIAN_POINT ( 'NONE',  ( -1.469576158976823947E-15, 7.125000000000000888, 8.000000000000000000 ) ) ;
#44115 = CARTESIAN_POINT ( 'NONE',  ( -5.082755093536324154, 105.2187500020483952, 5.082755093536326818 ) ) ;
#44117 = CARTESIAN_POINT ( 'NONE',  ( 3.228176881613692206, -50.21013539028081851, -40.85102191503939650 ) ) ;
#44116 = CARTESIAN_POINT ( 'NONE',  ( -3.673940397442060854E-16, 289.8125000034140157, -6.000000000000001776 ) ) ;
#44118 = CARTESIAN_POINT ( 'NONE',  ( 29.43265458321761230, 204.7500000013655779, 173.4587341249998929 ) ) ;
#44119 = CARTESIAN_POINT ( 'NONE',  ( -5.082755093536319713, 5.082755093536319713, 15.17405278187175455 ) ) ;
#44120 = CARTESIAN_POINT ( 'NONE',  ( 9.000000000000000000, 0.000000000000000000, -10.20000000000000462 ) ) ;
#44121 = CARTESIAN_POINT ( 'NONE',  ( -11.35316468750000141, 38.28124999658602690, -1.390361679473963753E-15 ) ) ;
#44122 = EDGE_CURVE ( 'NONE', #72985, #21405, #13143, .T. ) ;
#44123 = CARTESIAN_POINT ( 'NONE',  ( -1.833012674220245497, -42.61695885891957403, 139.0538056711343984 ) ) ;
#44124 = CARTESIAN_POINT ( 'NONE',  ( -8.660254037844387298, 18.95833332650536818, -5.000000000000004441 ) ) ;
#44125 = CARTESIAN_POINT ( 'NONE',  ( 11.00000000000006573, 4.556349186103981097, 111.5312500040967620 ) ) ;
#44126 = ORIENTED_EDGE ( 'NONE', *, *, #17047, .F. ) ;
#44127 = CARTESIAN_POINT ( 'NONE',  ( 0.9815212833345395849, 13.28972488340248681, -0.7446230086126863768 ) ) ;
#44128 = CARTESIAN_POINT ( 'NONE',  ( -8.000000000000001776, 23.15624999590322375, 3.313708498984759387 ) ) ;
#44129 = CARTESIAN_POINT ( 'NONE',  ( 8.311093377946834337, 50.15624999658601268, 8.311093377946839666 ) ) ;
#44130 = CARTESIAN_POINT ( 'NONE',  ( -6.735557395310442023E-16, 11.00000000000000000, 83.31250000409676204 ) ) ;
#44131 = CARTESIAN_POINT ( 'NONE',  ( 1.432654583217608080, 203.8750000013656063, 138.5412658750000503 ) ) ;
#44132 = FACE_OUTER_BOUND ( 'NONE', #60005, .T. ) ;
#44133 = FACE_OUTER_BOUND ( 'NONE', #32895, .T. ) ;
#44135 = CARTESIAN_POINT ( 'NONE',  ( 9.832129032723420536, 51.19791666325268409, -5.676582343749999815 ) ) ;
#44134 = CARTESIAN_POINT ( 'NONE',  ( -7.188101187499999156, 101.7500000020483810, 2.977408999572654924 ) ) ;
#44136 = CARTESIAN_POINT ( 'NONE',  ( -3.313708498984757167, 7.999999999999991118, 11.04905277982336642 ) ) ;
#44137 = CARTESIAN_POINT ( 'NONE',  ( -11.00000000000005151, 4.556349186103993532, 98.59375000409677625 ) ) ;
#44138 = CARTESIAN_POINT ( 'NONE',  ( 5.676582343749993598, 159.9479166632526983, 9.832129032723422313 ) ) ;
#44139 = CARTESIAN_POINT ( 'NONE',  ( -2.679491924311235618, 140.4166666598387110, 10.00000000000000000 ) ) ;
#44140 = CARTESIAN_POINT ( 'NONE',  ( 2.977408999572650039, 101.5625000020483810, -7.188101187500001821 ) ) ;
#44141 = CARTESIAN_POINT ( 'NONE',  ( -3.674341569227068671, 0.4933058160190353925, -7.107250865053620359 ) ) ;
#44142 = CARTESIAN_POINT ( 'NONE',  ( -11.35316468750000141, 28.80208332991935194, 3.042071309553159963 ) ) ;
#44143 = CARTESIAN_POINT ( 'NONE',  ( -2.679491924311284468, 16.45833333333334636, -9.999999999999980460 ) ) ;
#44144 = ORIENTED_EDGE ( 'NONE', *, *, #14931, .T. ) ;
#44145 = CARTESIAN_POINT ( 'NONE',  ( -10.18810118749999916, 4.220049686691934809, 75.06250000204836681 ) ) ;
#44146 = DIRECTION ( 'NONE',  ( 0.000000000000000000, -0.000000000000000000, -1.000000000000000000 ) ) ;
#44147 = CARTESIAN_POINT ( 'NONE',  ( 9.832129032723416984, 165.3645833299193555, 5.676582343750006032 ) ) ;
#44148 = CARTESIAN_POINT ( 'NONE',  ( 7.999999999999991118, 9.797174393178815797E-16, 13.63655278432982421 ) ) ;
#44149 = CARTESIAN_POINT ( 'NONE',  ( -11.35316468749999608, 219.1145833367473017, 3.042071309553173730 ) ) ;
#44150 = CARTESIAN_POINT ( 'NONE',  ( 3.734423912254124733, 56.16062404875547287, -44.09723116535789700 ) ) ;
#44151 =( GEOMETRIC_REPRESENTATION_CONTEXT ( 3 ) GLOBAL_UNCERTAINTY_ASSIGNED_CONTEXT ( ( #58487 ) ) GLOBAL_UNIT_ASSIGNED_CONTEXT ( ( #51319, #57744, #57368 ) ) REPRESENTATION_CONTEXT ( 'NONE', 'WORKASPACE' ) );
#44152 = CARTESIAN_POINT ( 'NONE',  ( 10.18810118749999916, 4.220049686691935698, 83.87500000204835260 ) ) ;
#44153 = ORIENTED_EDGE ( 'NONE', *, *, #64497, .F. ) ;
#44154 = EDGE_CURVE ( 'NONE', #35289, #14040, #36289, .T. ) ;
#44155 = CARTESIAN_POINT ( 'NONE',  ( -7.320508075688773708, 118.7499999931720396, -7.320508075688774596 ) ) ;
#44156 = CARTESIAN_POINT ( 'NONE',  ( -1.656854249492504705, 198.8125000027312126, 145.9999999999999716 ) ) ;
#44157 = CARTESIAN_POINT ( 'NONE',  ( 3.042071309553167069, 117.1354166632526557, -11.35316468749999785 ) ) ;
#44158 = CARTESIAN_POINT ( 'NONE',  ( 10.18810118750000093, -4.220049686691933921, 93.81250000204839523 ) ) ;
#44159 = ADVANCED_FACE ( 'NONE', ( #30492 ), #35791, .F. ) ;
#44160 = CARTESIAN_POINT ( 'NONE',  ( 3.211159895383561835, 21.56249999863440792, -3.211159895383561835 ) ) ;
#44161 = ORIENTED_EDGE ( 'NONE', *, *, #2124, .T. ) ;
#44162 = VERTEX_POINT ( 'NONE', #58805 ) ;
#44163 = CARTESIAN_POINT ( 'NONE',  ( -4.541265875000002339, 2.874999998634407028, -1.881053915767121998 ) ) ;
#44164 = CARTESIAN_POINT ( 'NONE',  ( 5.082755093536324154, 6.281249997951610986, 5.082755093536326818 ) ) ;
#44165 = CARTESIAN_POINT ( 'NONE',  ( -4.898587196589412829E-16, 112.8125000040967905, -8.000000000000000000 ) ) ;
#44166 = CARTESIAN_POINT ( 'NONE',  ( -4.220049686691937474, -10.18810118749999738, 90.81250000204838102 ) ) ;
#44167 = AXIS2_PLACEMENT_3D ( 'NONE', #1845, #29769, #18451 ) ;
#44168 = CARTESIAN_POINT ( 'NONE',  ( -27.99999999999996447, 202.1875000013656063, 173.4587341250003760 ) ) ;
#44169 = CARTESIAN_POINT ( 'NONE',  ( 2.828427124746190291, 5.875000000000000000, 2.828427124746192067 ) ) ;
#44170 = CARTESIAN_POINT ( 'NONE',  ( 2.828427124746190291, 17.62499999726881583, 2.828427124746192067 ) ) ;
#44171 = CARTESIAN_POINT ( 'NONE',  ( -4.541265875000002339, 6.812499998634407028, -5.561446717895856393E-16 ) ) ;
#44172 = CARTESIAN_POINT ( 'NONE',  ( -2.849036369511732440E-14, 203.2500000000000000, 138.0000000000000568 ) ) ;
#44173 = VERTEX_POINT ( 'NONE', #12396 ) ;
#44174 = CARTESIAN_POINT ( 'NONE',  ( -1.967015505459129087E-11, 148.7499999999984936, 10.00000000000000533 ) ) ;
#44176 = CARTESIAN_POINT ( 'NONE',  ( 7.320508075688771044, 236.2500000068279746, -7.320508075688771932 ) ) ;
#44175 = CARTESIAN_POINT ( 'NONE',  ( -31.45873412499999233, 196.6875000013655779, 170.0000000000004547 ) ) ;
#44177 =( NAMED_UNIT ( * ) SI_UNIT ( $, .STERADIAN. ) SOLID_ANGLE_UNIT ( ) );
#44178 = CARTESIAN_POINT ( 'NONE',  ( 3.211159895383560947, 18.18749999863440792, 3.211159895383562723 ) ) ;
#44179 = DIRECTION ( 'NONE',  ( 0.000000000000000000, 0.000000000000000000, 1.000000000000000000 ) ) ;
#44180 = CARTESIAN_POINT ( 'NONE',  ( -7.188101187499990274, -2.977408999572651371, 9.080302781871752771 ) ) ;
#44181 = VERTEX_POINT ( 'NONE', #41447 ) ;
#44182 = VERTEX_POINT ( 'NONE', #12759 ) ;
#44183 = CARTESIAN_POINT ( 'NONE',  ( 7.204075437095966983, 7.204075437095967871, 98.59375000204836681 ) ) ;
#44184 = CARTESIAN_POINT ( 'NONE',  ( 7.999999999999991118, 3.313708498984758055, 19.67405277982336642 ) ) ;
#44185 = CARTESIAN_POINT ( 'NONE',  ( -29.43265458321766914, 199.7500000013656063, 166.5412658750003629 ) ) ;
#44186 = CARTESIAN_POINT ( 'NONE',  ( -7.778174593052020747, -7.778174593052023411, 109.1875000000000000 ) ) ;
#44188 = CARTESIAN_POINT ( 'NONE',  ( -2.445694354108783219, 206.8125000013656063, 200.4456943541088663 ) ) ;
#44187 = AXIS2_PLACEMENT_3D ( 'NONE', #8732, #60782, #13628 ) ;
#44189 = CARTESIAN_POINT ( 'NONE',  ( 4.000000000000016875, 203.5625000027312126, 199.6568542494924259 ) ) ;
#44190 = CARTESIAN_POINT ( 'NONE',  ( -2.679491924311225848, 111.4583333333333286, -10.00000000000000178 ) ) ;
#44191 = CARTESIAN_POINT ( 'NONE',  ( -4.898587196589412829E-16, 106.6250000000000000, -8.000000000000000000 ) ) ;
#44192 = CARTESIAN_POINT ( 'NONE',  ( -6.676582343750001591, 291.6093750017069510, 0.000000000000000000 ) ) ;
#44193 = PRODUCT_DEFINITION_FORMATION_WITH_SPECIFIED_SOURCE ( 'ANY', '', #68009, .NOT_KNOWN. ) ;
#44194 = CARTESIAN_POINT ( 'NONE',  ( 7.188101187499993827, -2.977408999572645598, 13.01780278187175277 ) ) ;
#44195 = ORIENTED_EDGE ( 'NONE', *, *, #62927, .T. ) ;
#44196 = CARTESIAN_POINT ( 'NONE',  ( 0.000000000000000000, 0.000000000000000000, 36.00000000000000000 ) ) ;
#44197 = CARTESIAN_POINT ( 'NONE',  ( 31.45873412499999944, 206.6875000013656063, 169.9999999999999432 ) ) ;
#44198 = CARTESIAN_POINT ( 'NONE',  ( 7.999999999999998224, 23.71874999590322375, 3.313708498984766493 ) ) ;
#44199 = CARTESIAN_POINT ( 'NONE',  ( -3.458734125000015425, 198.9375000013655779, 142.0000000000000568 ) ) ;
#44200 = CARTESIAN_POINT ( 'NONE',  ( -7.347880794884122694E-16, 5.750000000000000000, 4.000000000000001776 ) ) ;
#44202 = CARTESIAN_POINT ( 'NONE',  ( 3.458734124999960358, 204.6875000013656063, 142.0000000000000568 ) ) ;
#44201 = CARTESIAN_POINT ( 'NONE',  ( -11.00000000000000000, 0.000000000000000000, 0.000000000000000000 ) ) ;
#44203 = CARTESIAN_POINT ( 'NONE',  ( -11.35316468749999785, 259.0104166700807014, -3.042071309553164848 ) ) ;
#44204 = CYLINDRICAL_SURFACE ( 'NONE', #3648, 3.999999999999976019 ) ;
#44205 = CARTESIAN_POINT ( 'NONE',  ( -1.836970198721029983E-15, 95.62499999317203958, 10.00000000000000178 ) ) ;
#44206 = B_SPLINE_CURVE_WITH_KNOTS ( 'NONE', 3,
 ( #66916, #48806, #72190, #14093, #71814, #14467, #71071, #38252 ),
 .UNSPECIFIED., .F., .F.,
 ( 4, 2, 2, 4 ),
 ( 0.005256334970490722167, 0.006570121696661957236, 0.007883908422833192306, 0.01051148187517566418 ),
 .UNSPECIFIED. ) ;
#44207 = CARTESIAN_POINT ( 'NONE',  ( 3.090143665460689970, 225.9995416778970707, -9.510573701245009559 ) ) ;
#44208 = CARTESIAN_POINT ( 'NONE',  ( -2.977408999572647819, 7.188101187499992051, 6.080302781871753659 ) ) ;
#44209 = CARTESIAN_POINT ( 'NONE',  ( -9.832129032723420536, 204.0104166632526983, 5.676582343749997150 ) ) ;
#44210 = CARTESIAN_POINT ( 'NONE',  ( -3.042071309553164404, 2.239583329919349719, -11.35316468749999963 ) ) ;
#44211 = CARTESIAN_POINT ( 'NONE',  ( 3.211159895383560947, 6.187499998634407028, 3.211159895383562723 ) ) ;
#44212 = CARTESIAN_POINT ( 'NONE',  ( -30.82842712474615610, 198.3750000000000284, 172.8284271247465824 ) ) ;
#44214 = CARTESIAN_POINT ( 'NONE',  ( 0.000000000000000000, 300.0000000000000000, 0.000000000000000000 ) ) ;
#44213 = CARTESIAN_POINT ( 'NONE',  ( -2.849036369511732440E-14, 203.3750000027312126, 138.0000000000000568 ) ) ;
#44215 = EDGE_LOOP ( 'NONE', ( #41554, #57112, #43091 ) ) ;
#44216 = CARTESIAN_POINT ( 'NONE',  ( 3.458734124999960358, 203.6250000013656063, 143.4326545832176976 ) ) ;
#44217 = CARTESIAN_POINT ( 'NONE',  ( -9.832129032723420536, 13.69791666325268409, 5.676582343749997150 ) ) ;
#44218 = CARTESIAN_POINT ( 'NONE',  ( -4.556349186104047710, -10.99999999999999822, 100.4687500040967763 ) ) ;
#44219 = CARTESIAN_POINT ( 'NONE',  ( 11.00000000000000000, 1.347111479062088405E-15, 106.9375000040967763 ) ) ;
#44220 = CARTESIAN_POINT ( 'NONE',  ( -24.54126587499999346, 200.1875000013656063, 170.0000000000002842 ) ) ;
#44221 = DIRECTION ( 'NONE',  ( 1.000000000000000000, -0.000000000000000000, -0.000000000000000000 ) ) ;
#44223 = CARTESIAN_POINT ( 'NONE',  ( 11.35316468749999785, 10.57291666325268409, 3.042071309553174174 ) ) ;
#44222 = CARTESIAN_POINT ( 'NONE',  ( 7.188101187500002709, 118.8125000020483810, 2.977408999572649151 ) ) ;
#44224 = CARTESIAN_POINT ( 'NONE',  ( -7.999999999999991118, 0.000000000000000000, 24.83030277982336642 ) ) ;
#44225 =( BOUNDED_CURVE ( )  B_SPLINE_CURVE ( 2, ( #24019, #23280, #15837, #69311, #29689, #63638, #47026, #70062, #18370 ),
 .UNSPECIFIED., .F., .F. ) 
 B_SPLINE_CURVE_WITH_KNOTS ( ( 3, 2, 2, 2, 3 ),
 ( 0.4500000000000002887, 0.4583333333333336479, 0.4666666666666670626, 0.4750000000000004219, 0.4833333333333338366 ),
 .UNSPECIFIED. ) 
 CURVE ( )  GEOMETRIC_REPRESENTATION_ITEM ( )  RATIONAL_B_SPLINE_CURVE ( ( 0.9999999999999974465, 0.9238795325112892920, 1.000000000000000000, 0.9238795325112867385, 1.000000000000000000, 0.9238795325112867385, 1.000000000000000000, 0.9238795325112821866, 1.000000000000004663 ) ) 
 REPRESENTATION_ITEM ( '' )  );
#44226 = CARTESIAN_POINT ( 'NONE',  ( -8.311093377946841443, 123.9062499965860411, 8.311093377946830785 ) ) ;
#44227 = EDGE_CURVE ( 'NONE', #71897, #1378, #47463, .T. ) ;
#44228 = AXIS2_PLACEMENT_3D ( 'NONE', #38524, #3067, #66056 ) ;
#44229 = CARTESIAN_POINT ( 'NONE',  ( -10.00000000000000355, 84.58333332650538239, 2.679491924311223183 ) ) ;
#44230 = CARTESIAN_POINT ( 'NONE',  ( -2.977408999572651815, 123.3125000020483810, 7.188101187500000933 ) ) ;
#44231 = CARTESIAN_POINT ( 'NONE',  ( 2.780723358947928197E-16, 21.68749999863440792, -4.541265875000002339 ) ) ;
#44232 = CARTESIAN_POINT ( 'NONE',  ( 6.123233995736767268E-16, 198.1249999931720538, -10.00000000000000178 ) ) ;
#44233 = CARTESIAN_POINT ( 'NONE',  ( 10.00000000000000711, 145.2083333333333144, -2.679491924311228512 ) ) ;
#44234 = ORIENTED_EDGE ( 'NONE', *, *, #69038, .T. ) ;
#44235 = CARTESIAN_POINT ( 'NONE',  ( 0.7509181236782381808, -65.76106071587273050, 26.27764834702160712 ) ) ;
#44236 = CARTESIAN_POINT ( 'NONE',  ( 4.721056650415999201, 291.2343750017069510, -4.721056650415999201 ) ) ;
#44237 = SURFACE_STYLE_FILL_AREA ( #38584 ) ;
#44238 = CARTESIAN_POINT ( 'NONE',  ( -7.999999999999989342, -3.313708498984762496, 1.111552783920146004 ) ) ;
#44239 = CARTESIAN_POINT ( 'NONE',  ( -2.828427073549516724, 195.0000000000000284, 195.1715728240572219 ) ) ;
#44240 = CARTESIAN_POINT ( 'NONE',  ( -7.320508075688773708, 208.7499999931720254, -7.320508075688774596 ) ) ;
#44241 = CARTESIAN_POINT ( 'NONE',  ( 11.00000000000000355, -4.556349186104044158, 70.84375000409676204 ) ) ;
#44242 = CARTESIAN_POINT ( 'NONE',  ( -7.204075437095965206, -7.204075437095968759, 101.2187500020483668 ) ) ;
#44243 = VERTEX_POINT ( 'NONE', #59903 ) ;
#44244 = EDGE_CURVE ( 'NONE', #11511, #33915, #54141, .T. ) ;
#44245 = CARTESIAN_POINT ( 'NONE',  ( 7.320508075688771044, 156.2499999931720538, 7.320508075688775484 ) ) ;
#44246 = CARTESIAN_POINT ( 'NONE',  ( -11.35316468750000141, 148.8020833299193555, 3.042071309553159963 ) ) ;
#44247 = EDGE_CURVE ( 'NONE', #14457, #5956, #28681, .T. ) ;
#44248 = CARTESIAN_POINT ( 'NONE',  ( 2.445694354108839175, 206.3125000013656063, 195.5543056458912190 ) ) ;
#44249 = CARTESIAN_POINT ( 'NONE',  ( -5.656854249492375253, 5.656854249492375253, 0.8303027839201455595 ) ) ;
#44250 = CARTESIAN_POINT ( 'NONE',  ( 11.35316468749999785, 60.88541666325269119, 3.042071309553174174 ) ) ;
#44251 = ORIENTED_EDGE ( 'NONE', *, *, #11874, .T. ) ;
#44252 = CARTESIAN_POINT ( 'NONE',  ( 10.18810118750000093, -4.220049686691933921, 113.3125000020483668 ) ) ;
#44253 = CARTESIAN_POINT ( 'NONE',  ( -1.881053915767121776, 7.749999998634407916, -4.541265875000002339 ) ) ;
#44254 = ORIENTED_EDGE ( 'NONE', *, *, #71554, .F. ) ;
#44255 = AXIS2_PLACEMENT_3D ( 'NONE', #5431, #69172, #44395 ) ;
#44256 = CARTESIAN_POINT ( 'NONE',  ( 2.977408999572651815, 21.18749999795161187, 7.188101187500000933 ) ) ;
#44257 = CARTESIAN_POINT ( 'NONE',  ( -2.485281374238571761, 287.8750000034139589, -6.000000000000003553 ) ) ;
#44258 = CARTESIAN_POINT ( 'NONE',  ( 1.836970198721029589E-15, 249.3750000068279746, 10.00000000000000000 ) ) ;
#44259 = CARTESIAN_POINT ( 'NONE',  ( 2.977408999572650927, 20.62499999795161543, -7.188101187500001821 ) ) ;
#44260 = CARTESIAN_POINT ( 'NONE',  ( 5.082755093536318824, 5.082755093536319713, 0.9240527818717529929 ) ) ;
#44261 = CARTESIAN_POINT ( 'NONE',  ( -10.18810118749999916, 4.220049686691934809, 111.4375000020483810 ) ) ;
#44262 = DIRECTION ( 'NONE',  ( 1.000000000000000000, -0.000000000000000000, -0.000000000000000000 ) ) ;
#44263 = CARTESIAN_POINT ( 'NONE',  ( -2.828427124746190735, 5.124999997268813168, -2.828427124746191623 ) ) ;
#44264 = CARTESIAN_POINT ( 'NONE',  ( 25.17157287525382259, 207.0000000027312126, 172.8284271247460993 ) ) ;
#44265 = ORIENTED_EDGE ( 'NONE', *, *, #58642, .F. ) ;
#44266 = CARTESIAN_POINT ( 'NONE',  ( 3.458734125000015425, 206.0000000013656347, 196.5673454167823877 ) ) ;
#44267 = CARTESIAN_POINT ( 'NONE',  ( -29.65685424949228732, 195.5625000027311842, 174.0000000000004547 ) ) ;
#44268 = CARTESIAN_POINT ( 'NONE',  ( -10.18810118749999916, 0.000000000000000000, 71.03125000204838102 ) ) ;
#44269 = CARTESIAN_POINT ( 'NONE',  ( 2.780723358947928197E-16, 4.562499998634407028, -4.541265875000002339 ) ) ;
#44270 = DIRECTION ( 'NONE',  ( -0.000000000000000000, -0.000000000000000000, 1.000000000000000000 ) ) ;
#44271 = CARTESIAN_POINT ( 'NONE',  ( 7.188101187499992051, 8.802885111219154394E-16, 23.23655278187175455 ) ) ;
#44272 = ORIENTED_EDGE ( 'NONE', *, *, #8899, .F. ) ;
#44273 = CARTESIAN_POINT ( 'NONE',  ( -6.735557395310442023E-16, 11.00000000000000000, 90.62499999999998579 ) ) ;
#44274 = VERTEX_POINT ( 'NONE', #8217 ) ;
#44275 = CARTESIAN_POINT ( 'NONE',  ( 1.871523826299183495E-15, -10.18810118749999916, 114.5312500020483810 ) ) ;
#44276 = CARTESIAN_POINT ( 'NONE',  ( -7.347880794884122694E-16, 18.75000000000000000, 4.000000000000001776 ) ) ;
#44277 = CARTESIAN_POINT ( 'NONE',  ( 3.458734125000015425, 206.0000000013656347, 196.5673454167823877 ) ) ;
#44278 = CARTESIAN_POINT ( 'NONE',  ( 24.54126587500000412, 200.2500000013656063, 171.4326545832176123 ) ) ;
#44279 = CARTESIAN_POINT ( 'NONE',  ( -5.000000000000005329, 68.33333333333334281, 8.660254037844387298 ) ) ;
#44280 = CARTESIAN_POINT ( 'NONE',  ( -7.188101187500000044, 93.03125000204836681, 0.000000000000000000 ) ) ;
#44281 = CARTESIAN_POINT ( 'NONE',  ( 4.242640687119287435, 291.3750000000000000, 4.242640687119285658 ) ) ;
#44282 = CARTESIAN_POINT ( 'NONE',  ( 23.99999999999998224, 205.8125000027312126, 168.3431457505075741 ) ) ;
#44283 = ORIENTED_EDGE ( 'NONE', *, *, #13983, .T. ) ;
#44284 = CARTESIAN_POINT ( 'NONE',  ( 5.676582343750005144, 220.5729166700806729, 9.832129032723416984 ) ) ;
#44285 = CARTESIAN_POINT ( 'NONE',  ( -4.471435261902951375, -10.26549131683149163, 64.21726486257125543 ) ) ;
#44286 = CARTESIAN_POINT ( 'NONE',  ( -4.000000000000015987, 201.5625000027311842, 140.3431457505076594 ) ) ;
#44287 = LINE ( 'NONE', #54871, #56319 ) ;
#44288 = LINE ( 'NONE', #26543, #58012 ) ;
#44289 = CARTESIAN_POINT ( 'NONE',  ( 9.999999999999998224, 247.7083333333333428, -2.679491924311229401 ) ) ;
#44290 = CARTESIAN_POINT ( 'NONE',  ( -7.320508075688806571, 78.12500000000004263, 7.320508075688797689 ) ) ;
#44291 = CARTESIAN_POINT ( 'NONE',  ( 10.00000000000000000, 184.7916666666666572, 2.679491924311236062 ) ) ;
#44292 = CARTESIAN_POINT ( 'NONE',  ( 29.65685424949229798, 198.1875000027311842, 174.0000000000000284 ) ) ;
#44293 = CARTESIAN_POINT ( 'NONE',  ( 7.188101187499993827, -2.977408999572645598, 22.01780278187175810 ) ) ;
#44294 = CARTESIAN_POINT ( 'NONE',  ( 9.832129032723416984, 155.6770833299193555, 5.676582343750006032 ) ) ;
#44295 = CARTESIAN_POINT ( 'NONE',  ( -2.828427124746153876, 208.0000000027312126, 195.1715728752538439 ) ) ;
#44296 = CARTESIAN_POINT ( 'NONE',  ( -31.28157037813700825, 45.12934964385030412, 65.00000000000000000 ) ) ;
#44297 = CARTESIAN_POINT ( 'NONE',  ( 1.934925017735378189E-11, 153.7500000000015348, 10.00000000000000533 ) ) ;
#44298 = CARTESIAN_POINT ( 'NONE',  ( 8.000000000000001776, 109.3437500040967763, 3.313708498984759387 ) ) ;
#44299 = EDGE_LOOP ( 'NONE', ( #49200, #35604, #73864, #17918 ) ) ;
#44300 = CARTESIAN_POINT ( 'NONE',  ( 8.311093377946834337, 25.46874999658601624, 8.311093377946839666 ) ) ;
#44301 = CARTESIAN_POINT ( 'NONE',  ( 4.556349186104045934, 11.00000000000000000, 77.21875000409679046 ) ) ;
#44302 = VECTOR ( 'NONE', #27714, 1000.000000000000000 ) ;
#44304 = CARTESIAN_POINT ( 'NONE',  ( -4.193070328474943764, 10.26769692241485643, -64.12609983179220308 ) ) ;
#44303 = DIRECTION ( 'NONE',  ( -0.000000000000000000, -0.000000000000000000, 1.000000000000000000 ) ) ;
#44305 = CARTESIAN_POINT ( 'NONE',  ( 4.556349186104052151, -10.99999999999999822, 79.46874999999998579 ) ) ;
#44306 = CARTESIAN_POINT ( 'NONE',  ( 1.432654583217607858, 203.6250000013656063, 138.5412658750000787 ) ) ;
#44307 = CARTESIAN_POINT ( 'NONE',  ( -10.00000000000000000, 49.16666665983869677, -2.679491924311229845 ) ) ;
#44308 = CARTESIAN_POINT ( 'NONE',  ( -5.082755093536324154, 101.8437500020483810, 5.082755093536326818 ) ) ;
#44309 = CARTESIAN_POINT ( 'NONE',  ( -8.342170076843785083E-16, 7.187499998634407028, 4.541265875000002339 ) ) ;
#44310 = CARTESIAN_POINT ( 'NONE',  ( 1.224646799147353454E-15, 300.0000000000000000, -10.00000000000000178 ) ) ;
#44311 = CARTESIAN_POINT ( 'NONE',  ( -4.898587196589407898E-16, 7.999999999999991118, 10.95530277982336642 ) ) ;
#44313 = CARTESIAN_POINT ( 'NONE',  ( 2.679491924311959039, 163.9583333333334565, 9.999999999999579003 ) ) ;
#44312 = DIRECTION ( 'NONE',  ( -0.000000000000000000, 1.000000000000000000, -0.000000000000000000 ) ) ;
#44314 = ORIENTED_EDGE ( 'NONE', *, *, #34722, .T. ) ;
#44315 =( BOUNDED_CURVE ( )  B_SPLINE_CURVE ( 2, ( #42179, #30873, #35076, #41822, #13135, #59190, #6399, #64832, #7500, #13502, #58820, #41461, #58088 ),
 .UNSPECIFIED., .F., .F. ) 
 B_SPLINE_CURVE_WITH_KNOTS ( ( 3, 2, 2, 2, 2, 2, 3 ),
 ( 0.2554347826086956208, 0.2572463768115941241, 0.2590579710144926828, 0.2608695652173912416, 0.2626811594202898559, 0.2644927536231884146, 0.2663043478260869734 ),
 .UNSPECIFIED. ) 
 CURVE ( )  GEOMETRIC_REPRESENTATION_ITEM ( )  RATIONAL_B_SPLINE_CURVE ( ( 1.000000000000001110, 0.9659258262890673130, 1.000000000000000000, 0.9659258262890683122, 1.000000000000000000, 0.9659258262890683122, 1.000000000000000000, 0.9659258262890683122, 1.000000000000000000, 0.9659258262890683122, 1.000000000000000000, 0.9659258262890683122, 1.000000000000000000 ) ) 
 REPRESENTATION_ITEM ( '' )  );
#44316 = VERTEX_POINT ( 'NONE', #42904 ) ;
#44317 = CARTESIAN_POINT ( 'NONE',  ( -5.000000000000000000, -66.10919140997998511, 23.67639547905989161 ) ) ;
#44318 = CARTESIAN_POINT ( 'NONE',  ( 2.445694354108840063, 196.0625000013656063, 200.4456943541088663 ) ) ;
#44319 = CARTESIAN_POINT ( 'NONE',  ( -7.999999999999948486, 3.313708498984799355, 2.236552779823363313 ) ) ;
#44320 = CARTESIAN_POINT ( 'NONE',  ( 7.778174593052021635, 7.778174593052023411, 94.93750000000000000 ) ) ;
#44321 = CARTESIAN_POINT ( 'NONE',  ( 3.042071309553159519, 139.7395833299193555, 11.35316468750000141 ) ) ;
#44322 = ORIENTED_EDGE ( 'NONE', *, *, #30634, .F. ) ;
#44323 = ADVANCED_FACE ( 'NONE', ( #50071, #20648 ), #60263, .F. ) ;
#44324 = CARTESIAN_POINT ( 'NONE',  ( -10.18810118749999916, 4.220049686691934809, 90.06250000204838102 ) ) ;
#44325 = CARTESIAN_POINT ( 'NONE',  ( 1.332431167089188095E-11, 191.2499999999989768, -10.00000000000000533 ) ) ;
#44326 = CARTESIAN_POINT ( 'NONE',  ( 4.000000000000015987, 208.4375000000000853, 199.6568542494924259 ) ) ;
#44328 = CARTESIAN_POINT ( 'NONE',  ( 8.311093377946837890, 131.4062499965860411, -8.311093377946837890 ) ) ;
#44327 = CARTESIAN_POINT ( 'NONE',  ( 2.849036369511732440E-14, 205.2500000000000284, 202.0000000000000000 ) ) ;
#44329 = CARTESIAN_POINT ( 'NONE',  ( 5.000000000000001776, 147.7083333265053682, -8.660254037844389075 ) ) ;
#44330 = EDGE_LOOP ( 'NONE', ( #24994, #60258, #43501, #59686 ) ) ;
#44331 = AXIS2_PLACEMENT_3D ( 'NONE', #12908, #29907, #70994 ) ;
#44332 = CARTESIAN_POINT ( 'NONE',  ( 7.320508075688776373, 256.8750000000000000, 7.320508075688767491 ) ) ;
#44333 = CARTESIAN_POINT ( 'NONE',  ( 44.48374486120344784, 184.9827789239285210, 84.30156509589276936 ) ) ;
#44334 = CARTESIAN_POINT ( 'NONE',  ( 3.042071309553159519, 110.0520833299193413, 11.35316468750000141 ) ) ;
#44335 = CARTESIAN_POINT ( 'NONE',  ( 2.839093476692135984E-14, 200.6875000013656063, 201.4587341250000350 ) ) ;
#44336 = CARTESIAN_POINT ( 'NONE',  ( -5.082755093536325042, 17.90624999795161187, -5.082755093536325930 ) ) ;
#44337 = CARTESIAN_POINT ( 'NONE',  ( -7.204075437095967871, 7.204075437095967871, 85.84375000204836681 ) ) ;
#44338 = CARTESIAN_POINT ( 'NONE',  ( -8.311093377946836114, 22.96874999658601624, -8.311093377946837890 ) ) ;
#44340 = ORIENTED_EDGE ( 'NONE', *, *, #28356, .T. ) ;
#44339 =( BOUNDED_CURVE ( )  B_SPLINE_CURVE ( 2, ( #29557, #18235, #14028, #19330, #60817, #37441, #36332, #49117, #53682, #31027, #8770, #1993, #24985 ),
 .UNSPECIFIED., .F., .F. ) 
 B_SPLINE_CURVE_WITH_KNOTS ( ( 3, 2, 2, 2, 2, 2, 3 ),
 ( 0.2445652173913043514, 0.2463768115942029102, 0.2481884057971014135, 0.2499999999999999722, 0.2518115942028985033, 0.2536231884057970620, 0.2554347826086956208 ),
 .UNSPECIFIED. ) 
 CURVE ( )  GEOMETRIC_REPRESENTATION_ITEM ( )  RATIONAL_B_SPLINE_CURVE ( ( 1.000000000000000000, 0.9659258262890683122, 1.000000000000000000, 0.9659258262890683122, 1.000000000000000000, 0.9659258262890683122, 1.000000000000000000, 0.9659258262890683122, 1.000000000000000000, 0.9659258262890683122, 1.000000000000000000, 0.9659258262890693114, 0.9999999999999990008 ) ) 
 REPRESENTATION_ITEM ( '' )  );
#44341 = CARTESIAN_POINT ( 'NONE',  ( 5.656854249492381470, 89.75000000409677625, 5.656854249492379694 ) ) ;
#44342 = CARTESIAN_POINT ( 'NONE',  ( 3.317071493978883456, -8.008118988124989457, 17.98186528394063188 ) ) ;
#44343 = CARTESIAN_POINT ( 'NONE',  ( -2.754378923186476579E-14, 208.4375000013656063, 145.4587341250000350 ) ) ;
#44344 = CARTESIAN_POINT ( 'NONE',  ( 4.556349186104052151, -10.99999999999999822, 85.65625000409679046 ) ) ;
#44345 = CARTESIAN_POINT ( 'NONE',  ( -7.188101187500002709, 4.312499997951610986, 2.977408999572649151 ) ) ;
#44346 = CARTESIAN_POINT ( 'NONE',  ( -2.765530957081998586, 288.6406250017069510, 6.676582343750001591 ) ) ;
#44347 = ADVANCED_FACE ( 'NONE', ( #48567 ), #67736, .F. ) ;
#44348 = CARTESIAN_POINT ( 'NONE',  ( -2.485281374238187180, 297.1875000000000568, 6.000000000000385469 ) ) ;
#44349 = CARTESIAN_POINT ( 'NONE',  ( 3.499857865026532622, -7.193933550196781823, 0.0006324257780546024528 ) ) ;
#44350 = ORIENTED_EDGE ( 'NONE', *, *, #55945, .F. ) ;
#44351 = CARTESIAN_POINT ( 'NONE',  ( -11.35316468749999785, 148.3854166632526983, -3.042071309553167513 ) ) ;
#44352 = CARTESIAN_POINT ( 'NONE',  ( -6.238412754330611322E-16, 10.18810118749999916, 79.28125000204836681 ) ) ;
#44353 = CARTESIAN_POINT ( 'NONE',  ( -26.56734541678238415, 209.6250000013656063, 166.5412658750003629 ) ) ;
#44354 = CARTESIAN_POINT ( 'NONE',  ( 3.313708498984762496, 26.71875000000000711, 7.999999999999998224 ) ) ;
#44355 = CARTESIAN_POINT ( 'NONE',  ( 1.881053915767121776, 14.62499999863440969, -4.541265875000002339 ) ) ;
#44356 = EDGE_LOOP ( 'NONE', ( #59036, #30228, #23563, #18815 ) ) ;
#44357 = CARTESIAN_POINT ( 'NONE',  ( -2.828427124746152987, 204.2500000027312126, 200.8284271247462129 ) ) ;
#44358 = VECTOR ( 'NONE', #15599, 999.9999999999998863 ) ;
#44359 = CARTESIAN_POINT ( 'NONE',  ( 3.999999999999960032, 210.0000000000000284, 142.0000000000000568 ) ) ;
#44360 = CARTESIAN_POINT ( 'NONE',  ( -29.65685424949246496, 207.1875000027312126, 166.0000000000004263 ) ) ;
#44361 = CARTESIAN_POINT ( 'NONE',  ( -4.898587196589412829E-16, 103.6250000000000000, -8.000000000000000000 ) ) ;
#44362 = VERTEX_POINT ( 'NONE', #43663 ) ;
#44363 = CARTESIAN_POINT ( 'NONE',  ( -5.082755093536326818, 10.40624999795161187, 5.082755093536325042 ) ) ;
#44364 = CARTESIAN_POINT ( 'NONE',  ( 5.000000000000000000, 53.17721328501398403, -43.91924822456213917 ) ) ;
#44365 = CARTESIAN_POINT ( 'NONE',  ( 3.042071309553167069, 186.8229166632527267, -11.35316468749999785 ) ) ;
#44366 = AXIS2_PLACEMENT_3D ( 'NONE', #70140, #35804, #6761 ) ;
#44367 = CARTESIAN_POINT ( 'NONE',  ( 7.188101187500001821, 111.8750000020483668, -2.977408999572651371 ) ) ;
#44368 = CARTESIAN_POINT ( 'NONE',  ( 0.000000000000000000, 22.00000000000000355, 0.000000000000000000 ) ) ;
#44369 = CARTESIAN_POINT ( 'NONE',  ( 3.313708498984762496, -7.999999999999989342, 2.799052779823365977 ) ) ;
#44371 = CARTESIAN_POINT ( 'NONE',  ( 1.469576158976823947E-15, 95.56250000409677625, 8.000000000000000000 ) ) ;
#44370 = CARTESIAN_POINT ( 'NONE',  ( 7.320508075688771044, 131.2499999931720254, 7.320508075688775484 ) ) ;
#44372 = EDGE_LOOP ( 'NONE', ( #14581, #24430, #23748, #9371, #13582, #25892 ) ) ;
#44373 = AXIS2_PLACEMENT_3D ( 'NONE', #27125, #38832, #17294 ) ;
#44374 = CARTESIAN_POINT ( 'NONE',  ( -5.676582343750000703, 263.0729166700806445, -9.832129032723418760 ) ) ;
#44375 = CARTESIAN_POINT ( 'NONE',  ( -2.977408999572647819, 7.188101187499991163, 22.58030278187175099 ) ) ;
#44376 = CARTESIAN_POINT ( 'NONE',  ( 1.469576158976823947E-15, 105.8750000000000000, 8.000000000000000000 ) ) ;
#44377 = CARTESIAN_POINT ( 'NONE',  ( 5.000000000000000000, 10.00000000000000000, 75.19090595827292134 ) ) ;
#44378 = CARTESIAN_POINT ( 'NONE',  ( 0.000000000000000000, 0.000000000000000000, 30.00000000000000000 ) ) ;
#44379 = CARTESIAN_POINT ( 'NONE',  ( -3.458734124999959469, 195.7500000013656063, 199.4326545832176691 ) ) ;
#44380 = ORIENTED_EDGE ( 'NONE', *, *, #69117, .T. ) ;
#44381 = CARTESIAN_POINT ( 'NONE',  ( -8.052558883257647793, 219.3273502760175973, 8.052558883257653122 ) ) ;
#44382 = CARTESIAN_POINT ( 'NONE',  ( 5.656854249492379694, 94.43750000000000000, -5.656854249492380582 ) ) ;
#44383 = CARTESIAN_POINT ( 'NONE',  ( 11.35316468749999785, 120.8854166632526841, 3.042071309553174174 ) ) ;
#44384 = CARTESIAN_POINT ( 'NONE',  ( -5.000000000000000888, -10.53354221205070473, -66.31578581128121641 ) ) ;
#44385 = CARTESIAN_POINT ( 'NONE',  ( 11.00000000000000000, 4.556349186104045934, 72.34374999999998579 ) ) ;
#44388 = CARTESIAN_POINT ( 'NONE',  ( 0.000000000000000000, 28.00000000000000000, 3.999999999999986233 ) ) ;
#44387 = CARTESIAN_POINT ( 'NONE',  ( 24.54126587499998280, 199.1250000013656347, 168.5673454167822740 ) ) ;
#44386 = CARTESIAN_POINT ( 'NONE',  ( 31.45873412499999944, 201.0000000013655779, 168.5673454167822740 ) ) ;
#44389 = VERTEX_POINT ( 'NONE', #4066 ) ;
#44390 = EDGE_CURVE ( 'NONE', #54736, #13039, #3309, .T. ) ;
#44391 = CARTESIAN_POINT ( 'NONE',  ( 9.797174393178825657E-16, 125.0000000000000000, -8.000000000000000000 ) ) ;
#44392 = CARTESIAN_POINT ( 'NONE',  ( -11.00000000000002842, -4.556349186104018401, 113.7812500040967478 ) ) ;
#44393 = CARTESIAN_POINT ( 'NONE',  ( 31.45873412499997812, 198.8750000013656347, 171.4326545832175839 ) ) ;
#44394 = CARTESIAN_POINT ( 'NONE',  ( 3.042071309553159519, 205.0520833299193271, 11.35316468750000141 ) ) ;
#44395 = DIRECTION ( 'NONE',  ( -1.000000000000000000, 0.000000000000000000, 0.000000000000000000 ) ) ;
#44396 = CARTESIAN_POINT ( 'NONE',  ( 10.14468825070462898, 226.0000000000000000, 4.203934788660792954 ) ) ;
#44397 = CARTESIAN_POINT ( 'NONE',  ( -4.541265875000002339, 17.81249999863440792, -5.561446717895856393E-16 ) ) ;
#44398 = CARTESIAN_POINT ( 'NONE',  ( 1.308779242300525114, -49.95118570763320776, 40.70975538998114729 ) ) ;
#44399 = CARTESIAN_POINT ( 'NONE',  ( 7.999999999999991118, 9.797174393178815797E-16, 27.08030277982336642 ) ) ;
#44401 = CARTESIAN_POINT ( 'NONE',  ( -5.656854249492381470, 12.93750000000000355, 5.656854249492379694 ) ) ;
#44400 = CARTESIAN_POINT ( 'NONE',  ( 2.679491924311817375, 186.0416666666666288, -9.999999999999653610 ) ) ;
#44402 = CARTESIAN_POINT ( 'NONE',  ( -2.085542519210945728E-15, 94.53124999658601268, 11.35316468750000141 ) ) ;
#44403 = ORIENTED_EDGE ( 'NONE', *, *, #21981, .T. ) ;
#44404 = CARTESIAN_POINT ( 'NONE',  ( 11.00000000000000000, 4.556349186104045934, 81.34374999999997158 ) ) ;
#44405 = CARTESIAN_POINT ( 'NONE',  ( -1.320432766682874540E-15, 21.09374999795161543, 7.188101187500000044 ) ) ;
#44406 = CARTESIAN_POINT ( 'NONE',  ( 1.836970198721029589E-15, 256.2500000000000568, 10.00000000000000000 ) ) ;
#44407 = CARTESIAN_POINT ( 'NONE',  ( 8.311093377946834337, 257.3437500034139589, -8.311093377946836114 ) ) ;
#44408 = CARTESIAN_POINT ( 'NONE',  ( 5.676582343750001591, 86.61458332991936970, -9.832129032723420536 ) ) ;
#44409 = ORIENTED_EDGE ( 'NONE', *, *, #47622, .F. ) ;
#44410 = CARTESIAN_POINT ( 'NONE',  ( -6.338291171875001240, 299.8046875008535039, 0.000000000000000000 ) ) ;
#44411 = EDGE_CURVE ( 'NONE', #74274, #3133, #61857, .T. ) ;
#44412 = CARTESIAN_POINT ( 'NONE',  ( 7.204075437095968759, -7.204075437095966983, 105.7187500020483810 ) ) ;
#44413 = DIRECTION ( 'NONE',  ( -0.000000000000000000, 1.000000000000000000, -0.000000000000000000 ) ) ;
#44414 = CARTESIAN_POINT ( 'NONE',  ( 2.445694354108840063, 203.0625000013656063, 200.4456943541088663 ) ) ;
#44415 = CARTESIAN_POINT ( 'NONE',  ( -30.82842712474612412, 201.5000000027312126, 172.8284271247466108 ) ) ;
#44417 = CARTESIAN_POINT ( 'NONE',  ( -5.676582343750006032, 89.11458332991935549, 9.832129032723418760 ) ) ;
#44416 = DIRECTION ( 'NONE',  ( -1.000000000000000000, 0.000000000000000000, 0.000000000000000000 ) ) ;
#44418 = CARTESIAN_POINT ( 'NONE',  ( 7.999999999999991118, 9.797174393178815797E-16, 18.26780278392014623 ) ) ;
#44419 = CARTESIAN_POINT ( 'NONE',  ( -28.00000000000002132, 199.6875000013656063, 166.5412658750003629 ) ) ;
#44420 = EDGE_CURVE ( 'NONE', #4004, #21248, #24374, .T. ) ;
#44421 = CARTESIAN_POINT ( 'NONE',  ( -7.320508075688778149, 179.9999999931720254, 7.320508075688769267 ) ) ;
#44422 = FACE_OUTER_BOUND ( 'NONE', #13707, .T. ) ;
#44423 = CARTESIAN_POINT ( 'NONE',  ( 8.311093377946837890, 71.71874999658601268, -8.311093377946837890 ) ) ;
#44424 = CARTESIAN_POINT ( 'NONE',  ( 2.765530957081996366, 293.1406250017069510, -6.676582343750003368 ) ) ;
#44425 = CARTESIAN_POINT ( 'NONE',  ( -10.18810118749999738, -4.220049686691941915, 99.62500000204838102 ) ) ;
#44426 = CARTESIAN_POINT ( 'NONE',  ( 3.042071309553159519, 214.7395833299193271, 11.35316468750000141 ) ) ;
#44427 = ORIENTED_EDGE ( 'NONE', *, *, #49426, .T. ) ;
#44428 = CARTESIAN_POINT ( 'NONE',  ( -2.828427124746192067, 2.625000000000000000, 2.828427124746190735 ) ) ;
#44429 = CARTESIAN_POINT ( 'NONE',  ( 0.000000000000000000, 300.0000000000000000, 0.000000000000000000 ) ) ;
#44430 = CARTESIAN_POINT ( 'NONE',  ( 2.666560895877943341E-14, -16.44602605510714355, 68.55492853905353456 ) ) ;
#44432 = CARTESIAN_POINT ( 'NONE',  ( 3.042071309553159519, 209.7395833299193839, 11.35316468750000141 ) ) ;
#44431 = CARTESIAN_POINT ( 'NONE',  ( -4.000000000000001776, 11.24999999726881406, -4.898587196589415787E-16 ) ) ;
#44433 = VECTOR ( 'NONE', #27942, 1000.000000000000000 ) ;
#44434 = CARTESIAN_POINT ( 'NONE',  ( -2.679491924311228512, 232.0833333401613174, -9.999999999999998224 ) ) ;
#44435 = DIRECTION ( 'NONE',  ( -0.000000000000000000, 1.000000000000000000, -0.000000000000000000 ) ) ;
#44436 = EDGE_CURVE ( 'NONE', #59221, #22353, #42456, .T. ) ;
#44437 = ORIENTED_EDGE ( 'NONE', *, *, #42195, .T. ) ;
#44438 = CARTESIAN_POINT ( 'NONE',  ( -3.042071309553163960, 192.5520833299193271, -11.35316468749999963 ) ) ;
#44439 =( BOUNDED_CURVE ( )  B_SPLINE_CURVE ( 2, ( #3625, #26242, #20588, #38333, #4008, #26621, #67373, #49645, #27742 ),
 .UNSPECIFIED., .F., .F. ) 
 B_SPLINE_CURVE_WITH_KNOTS ( ( 3, 2, 2, 2, 3 ),
 ( 0.5263157894736842923, 0.5328947368421054209, 0.5394736842105263275, 0.5460526315789473450, 0.5526315789473684736 ),
 .UNSPECIFIED. ) 
 CURVE ( )  GEOMETRIC_REPRESENTATION_ITEM ( )  RATIONAL_B_SPLINE_CURVE ( ( 0.9999999999999986677, 0.9238795325112880708, 1.000000000000000000, 0.9238795325112867385, 1.000000000000000000, 0.9238795325112867385, 1.000000000000000000, 0.9238795325112867385, 1.000000000000000000 ) ) 
 REPRESENTATION_ITEM ( '' )  );
#44440 = VECTOR ( 'NONE', #49384, 1000.000000000000000 ) ;
#44441 = CARTESIAN_POINT ( 'NONE',  ( -7.188101187499990274, -2.977408999572651815, 15.08030278187175455 ) ) ;
#44442 = CARTESIAN_POINT ( 'NONE',  ( -26.56734541678238415, 208.3750000013656063, 166.5412658750003629 ) ) ;
#44443 = CARTESIAN_POINT ( 'NONE',  ( -8.000000000000000000, 12.75000000000000178, -9.797174393178825657E-16 ) ) ;
#44444 = ORIENTED_EDGE ( 'NONE', *, *, #13700, .T. ) ;
#44445 = CARTESIAN_POINT ( 'NONE',  ( 5.656854249492381470, 92.75000000409677625, 5.656854249492379694 ) ) ;
#44446 = CARTESIAN_POINT ( 'NONE',  ( 7.320508075688774596, 10.62500000000000000, -7.320508075688774596 ) ) ;
#44447 =( BOUNDED_CURVE ( )  B_SPLINE_CURVE ( 2, ( #46377, #52046, #7503, #57717, #19180, #30141, #7133, #40718, #36173 ),
 .UNSPECIFIED., .F., .F. ) 
 B_SPLINE_CURVE_WITH_KNOTS ( ( 3, 2, 2, 2, 3 ),
 ( 0.9431818181818182323, 0.9488636363636363535, 0.9545454545454545858, 0.9602272727272727071, 0.9659090910434643407 ),
 .UNSPECIFIED. ) 
 CURVE ( )  GEOMETRIC_REPRESENTATION_ITEM ( )  RATIONAL_B_SPLINE_CURVE ( ( 1.000000000000000000, 0.9238795325112867385, 1.000000000000000000, 0.9238795325112867385, 1.000000000000000000, 0.9238795325112867385, 1.000000000000000000, 0.9238795325112867385, 1.000000000000000000 ) ) 
 REPRESENTATION_ITEM ( '' )  );
#44448 = EDGE_CURVE ( 'NONE', #62863, #27541, #61016, .T. ) ;
#44449 = CARTESIAN_POINT ( 'NONE',  ( 4.220049686691934809, 10.18810118749999916, 82.56250000204836681 ) ) ;
#44450 = ORIENTED_EDGE ( 'NONE', *, *, #53779, .F. ) ;
#44451 = CARTESIAN_POINT ( 'NONE',  ( -1.656854249492381248, 20.31250000000000000, -4.000000000000001776 ) ) ;
#44452 = CARTESIAN_POINT ( 'NONE',  ( -8.342170076843785083E-16, 21.06249999863440792, 4.541265875000002339 ) ) ;
#44453 = CARTESIAN_POINT ( 'NONE',  ( 26.34314575050753859, 199.0625000027312126, 173.9999999999997726 ) ) ;
#44454 = ORIENTED_EDGE ( 'NONE', *, *, #58117, .F. ) ;
#44455 = CARTESIAN_POINT ( 'NONE',  ( 2.679491924311228956, 17.91666665983870388, -10.00000000000000000 ) ) ;
#44456 = CARTESIAN_POINT ( 'NONE',  ( -5.082755093536325930, 95.46875000204838102, -5.082755093536325930 ) ) ;
#44459 = CARTESIAN_POINT ( 'NONE',  ( 1.469576158976823947E-15, 91.06250000409676204, 8.000000000000000000 ) ) ;
#44458 = CARTESIAN_POINT ( 'NONE',  ( 3.042071309553163516, 257.4479166700806445, -11.35316468749999785 ) ) ;
#44457 = FACE_OUTER_BOUND ( 'NONE', #29851, .T. ) ;
#44460 = APPLICATION_PROTOCOL_DEFINITION ( 'draft international standard', 'automotive_design', 1998, #50101 ) ;
#44461 = ORIENTED_EDGE ( 'NONE', *, *, #36131, .F. ) ;
#44463 = AXIS2_PLACEMENT_3D ( 'NONE', #41857, #37318, #48991 ) ;
#44462 = CARTESIAN_POINT ( 'NONE',  ( -11.35316468749999963, 259.2187500034140157, 0.000000000000000000 ) ) ;
#44464 = CARTESIAN_POINT ( 'NONE',  ( -5.082755093536319713, 5.082755093536319713, 10.29905278187175455 ) ) ;
#44465 = ORIENTED_EDGE ( 'NONE', *, *, #21867, .F. ) ;
#44466 = EDGE_LOOP ( 'NONE', ( #57997, #21131, #42617, #58371 ) ) ;
#44467 = CARTESIAN_POINT ( 'NONE',  ( 7.204075437095968759, -7.204075437095966983, 72.71875000204838102 ) ) ;
#44468 = CARTESIAN_POINT ( 'NONE',  ( -5.676582343749998039, 77.76041666325268409, -9.832129032723420536 ) ) ;
#44469 = CARTESIAN_POINT ( 'NONE',  ( 7.999999999999971578, -3.313708498984776707, 17.98655277982336997 ) ) ;
#44470 = CARTESIAN_POINT ( 'NONE',  ( 7.778174593052021635, 7.778174593052023411, 90.43749999999998579 ) ) ;
#44473 = CARTESIAN_POINT ( 'NONE',  ( -4.721056650415999201, 291.4843750017070079, -4.721056650415999201 ) ) ;
#44472 = CARTESIAN_POINT ( 'NONE',  ( 31.99999999999997868, 195.4375000027312410, 168.3431457505075173 ) ) ;
#44471 = CYLINDRICAL_SURFACE ( 'NONE', #58848, 7.999999999999991118 ) ;
#44474 = AXIS2_PLACEMENT_3D ( 'NONE', #41639, #52593, #64282 ) ;
#44475 = DIRECTION ( 'NONE',  ( -0.000000000000000000, 1.000000000000000000, -0.000000000000000000 ) ) ;
#44476 = FACE_OUTER_BOUND ( 'NONE', #938, .T. ) ;
#44477 = CARTESIAN_POINT ( 'NONE',  ( 2.839093476692135984E-14, 198.9375000013655779, 201.4587341250000350 ) ) ;
#44478 = CARTESIAN_POINT ( 'NONE',  ( -8.000000000000001776, 9.656249995903221972, 3.313708498984759387 ) ) ;
#44479 = ORIENTED_EDGE ( 'NONE', *, *, #6153, .F. ) ;
#44480 = CARTESIAN_POINT ( 'NONE',  ( 27.99999999999996092, 196.4375000013655779, 173.4587341249998929 ) ) ;
#44481 = CARTESIAN_POINT ( 'NONE',  ( -7.188101187500002709, 19.68749999795161543, 2.977408999572649151 ) ) ;
#44482 = CARTESIAN_POINT ( 'NONE',  ( 9.832129032723416984, 170.6770833299193555, 5.676582343750006032 ) ) ;
#44483 = CARTESIAN_POINT ( 'NONE',  ( 5.656854249492380582, 7.687500000000001776, -5.656854249492380582 ) ) ;
#44484 = CARTESIAN_POINT ( 'NONE',  ( -5.082755093536324154, 106.7187500020483952, 5.082755093536326818 ) ) ;
#44486 = CARTESIAN_POINT ( 'NONE',  ( 2.069125466536428259, -55.78340383128517743, -43.89144373685886791 ) ) ;
#44485 = CARTESIAN_POINT ( 'NONE',  ( 6.123233995736767268E-16, 18.12499999317203248, -10.00000000000000178 ) ) ;
#44487 = CARTESIAN_POINT ( 'NONE',  ( 25.55430564589119768, 206.3125000013656063, 167.5543056458910485 ) ) ;
#44488 = CARTESIAN_POINT ( 'NONE',  ( -2.977408999572648707, -7.188101187499990274, 17.14280278187175455 ) ) ;
#44489 = CARTESIAN_POINT ( 'NONE',  ( 3.999999999999960032, 208.0625000027312410, 143.6568542494924543 ) ) ;
#44490 = CARTESIAN_POINT ( 'NONE',  ( 3.042071309553159519, 59.73958332991934839, 11.35316468750000141 ) ) ;
#44491 = CARTESIAN_POINT ( 'NONE',  ( 7.999973942808394689, -3.313734556176354484, 1.674051741363694168 ) ) ;
#44492 = CARTESIAN_POINT ( 'NONE',  ( -2.679491924311225848, 28.33333332650536818, -10.00000000000000178 ) ) ;
#44493 = CARTESIAN_POINT ( 'NONE',  ( -27.99999999999991118, 200.6250000027312126, 174.0000000000003695 ) ) ;
#44494 = VERTEX_POINT ( 'NONE', #8966 ) ;
#44495 = CARTESIAN_POINT ( 'NONE',  ( 2.828427124746153876, 199.0000000027312126, 144.8284271247462129 ) ) ;
#44496 = CARTESIAN_POINT ( 'NONE',  ( 4.898587196589412829E-16, 19.68749999590322020, -8.000000000000000000 ) ) ;
#44497 = CARTESIAN_POINT ( 'NONE',  ( -3.042071309553164404, 52.23958332991934128, -11.35316468749999963 ) ) ;
#44498 = CARTESIAN_POINT ( 'NONE',  ( 7.778174593052021635, 7.778174593052023411, 74.12500000409677625 ) ) ;
#44499 = CARTESIAN_POINT ( 'NONE',  ( 2.445694354108784108, 198.5625000013656063, 144.4456943541088663 ) ) ;
#44500 = CARTESIAN_POINT ( 'NONE',  ( -5.000000000000000888, 259.1666666666666288, -8.660254037844387298 ) ) ;
#44501 = CARTESIAN_POINT ( 'NONE',  ( -5.000000000000000888, 244.1666666666666572, -8.660254037844387298 ) ) ;
#44504 = EDGE_CURVE ( 'NONE', #58573, #3255, #67430, .T. ) ;
#44503 = CARTESIAN_POINT ( 'NONE',  ( -9.832129032723418760, 42.86458332991934839, -5.676582343750004256 ) ) ;
#44502 = CARTESIAN_POINT ( 'NONE',  ( -2.977408999572650927, 96.87500000204838102, -7.188101187500000933 ) ) ;
#44505 = CARTESIAN_POINT ( 'NONE',  ( 5.656854249492376141, -5.656854249492374365, 8.892802779823364645 ) ) ;
#44506 = CARTESIAN_POINT ( 'NONE',  ( 11.00000000000000000, 1.347111479062088405E-15, 69.24999999999997158 ) ) ;
#44507 = CARTESIAN_POINT ( 'NONE',  ( -11.35316468749999785, 178.0729166632526415, -3.042071309553167513 ) ) ;
#44508 = EDGE_CURVE ( 'NONE', #45738, #44243, #28129, .T. ) ;
#44509 = CARTESIAN_POINT ( 'NONE',  ( -10.00000000000000178, 144.3749999931720538, -1.224646799147353454E-15 ) ) ;
#44510 = CARTESIAN_POINT ( 'NONE',  ( 1.320432766682874540E-15, 103.9062500020483810, 7.188101187500000044 ) ) ;
#44511 = CARTESIAN_POINT ( 'NONE',  ( -1.831236223718799128, -47.38443335155999137, 139.0536985700348680 ) ) ;
#44512 = CARTESIAN_POINT ( 'NONE',  ( -2.085542519210945728E-15, 34.84374999658601268, 11.35316468750000141 ) ) ;
#44513 = VERTEX_POINT ( 'NONE', #60645 ) ;
#44514 = DIRECTION ( 'NONE',  ( 0.000000000000000000, 0.000000000000000000, 1.000000000000000000 ) ) ;
#44515 = CARTESIAN_POINT ( 'NONE',  ( -7.204075437095967871, 7.204075437095967871, 74.96875000204836681 ) ) ;
#44516 = CARTESIAN_POINT ( 'NONE',  ( -1.469576158976823947E-15, 16.12500000000000355, 8.000000000000000000 ) ) ;
#44518 = CARTESIAN_POINT ( 'NONE',  ( 5.676582343749993598, 169.9479166632526983, 9.832129032723422313 ) ) ;
#44517 = DIRECTION ( 'NONE',  ( -1.000000000000000000, 0.000000000000000000, 0.000000000000000000 ) ) ;
#44519 = CARTESIAN_POINT ( 'NONE',  ( 5.656854249492376141, -5.656854249492374365, 13.44905278432982421 ) ) ;
#44520 = CARTESIAN_POINT ( 'NONE',  ( 8.000000000000000000, 9.093750000000001776, -3.313708498984761164 ) ) ;
#44521 = CARTESIAN_POINT ( 'NONE',  ( -5.000000000000000888, 262.2916666734946034, -8.660254037844387298 ) ) ;
#44522 = CARTESIAN_POINT ( 'NONE',  ( -0.8912353796372728398, 51.17464048784120223, -48.53058040617283098 ) ) ;
#44523 = CARTESIAN_POINT ( 'NONE',  ( -7.204075437095967871, 7.204075437095967871, 81.34375000204838102 ) ) ;
#44524 = EDGE_LOOP ( 'NONE', ( #47583, #55434, #27167, #70990, #22723, #10255, #47993, #55975, #69473, #31792, #69858, #48226, #69345, #32150, #56232, #49916, #15463, #66313, #44195, #2292 ) ) ;
#44525 = EDGE_CURVE ( 'NONE', #62352, #2283, #20262, .T. ) ;
#44526 = AXIS2_PLACEMENT_3D ( 'NONE', #51399, #21979, #57076 ) ;
#44527 = DIRECTION ( 'NONE',  ( 1.000000000000000000, -0.000000000000000000, -0.000000000000000000 ) ) ;
#44528 = CARTESIAN_POINT ( 'NONE',  ( -1.656854249492337949, 198.4375000027312410, 138.0000000000000000 ) ) ;
#44529 = CARTESIAN_POINT ( 'NONE',  ( 9.832129032723416984, 110.6770833299193555, 5.676582343750006032 ) ) ;
#44530 = EDGE_CURVE ( 'NONE', #56060, #45292, #74409, .T. ) ;
#44531 = VECTOR ( 'NONE', #19596, 1000.000000000000000 ) ;
#44532 = CARTESIAN_POINT ( 'NONE',  ( -1.881053915767124440, 21.12499999863441147, 4.541265875000001451 ) ) ;
#44533 = ORIENTED_EDGE ( 'NONE', *, *, #8255, .F. ) ;
#44534 = ORIENTED_EDGE ( 'NONE', *, *, #32396, .T. ) ;
#44535 = CARTESIAN_POINT ( 'NONE',  ( -4.541265875000002339, 6.937499998634407916, -5.561446717895856393E-16 ) ) ;
#44536 = CARTESIAN_POINT ( 'NONE',  ( -5.082755093536326818, 8.906249997951610098, 5.082755093536325042 ) ) ;
#44537 = CARTESIAN_POINT ( 'NONE',  ( -5.656854249492380582, 108.5000000040967763, -5.656854249492380582 ) ) ;
#44538 = CARTESIAN_POINT ( 'NONE',  ( -4.220049686691935698, 10.18810118749999916, 91.75000000204836681 ) ) ;
#44539 = CARTESIAN_POINT ( 'NONE',  ( -31.45873412499999944, 203.9375000013656063, 170.0000000000003979 ) ) ;
#44540 = EDGE_CURVE ( 'NONE', #49749, #41682, #70015, .T. ) ;
#44541 = EDGE_CURVE ( 'NONE', #33430, #56422, #28923, .T. ) ;
#44542 =( BOUNDED_CURVE ( )  B_SPLINE_CURVE ( 2, ( #64541, #30205, #6094, #59258, #47177, #7570, #58521, #47912, #24895 ),
 .UNSPECIFIED., .F., .F. ) 
 B_SPLINE_CURVE_WITH_KNOTS ( ( 3, 2, 2, 2, 3 ),
 ( 0.3235294117647058432, 0.3272058823529411242, 0.3308823529411764053, 0.3345588235294116863, 0.3382352941176470229 ),
 .UNSPECIFIED. ) 
 CURVE ( )  GEOMETRIC_REPRESENTATION_ITEM ( )  RATIONAL_B_SPLINE_CURVE ( ( 1.000000000000001110, 0.9238795325112856283, 1.000000000000000000, 0.9238795325112867385, 1.000000000000000000, 0.9238795325112867385, 1.000000000000000000, 0.9238795325112878487, 0.9999999999999988898 ) ) 
 REPRESENTATION_ITEM ( '' )  );
#44543 = CARTESIAN_POINT ( 'NONE',  ( -2.828427124746190735, 7.375000000000000888, -2.828427124746191623 ) ) ;
#44544 = CARTESIAN_POINT ( 'NONE',  ( 2.449293598294707893E-16, 16.99999999726881583, -4.000000000000001776 ) ) ;
#44545 = CARTESIAN_POINT ( 'NONE',  ( -3.211159895383561391, 8.687499998634407916, -3.211159895383561835 ) ) ;
#44546 = CARTESIAN_POINT ( 'NONE',  ( -4.000000000000015099, 199.5625000000000568, 143.6568542494924543 ) ) ;
#44547 = ORIENTED_EDGE ( 'NONE', *, *, #45849, .F. ) ;
#44548 = CARTESIAN_POINT ( 'NONE',  ( 8.000000000000001776, 116.6562500000000000, 3.313708498984759387 ) ) ;
#44550 = CARTESIAN_POINT ( 'NONE',  ( -28.00000000000002842, 200.0000000000000000, 166.0000000000003695 ) ) ;
#44549 = CARTESIAN_POINT ( 'NONE',  ( -30.44569435410886626, 195.5625000013656063, 167.5543056458916169 ) ) ;
#44551 = CARTESIAN_POINT ( 'NONE',  ( -1.881053915767121554, 16.62499999863440436, -4.541265875000002339 ) ) ;
#44552 = CARTESIAN_POINT ( 'NONE',  ( 2.679491924311222739, 70.83333332650538239, 10.00000000000000355 ) ) ;
#44553 = CARTESIAN_POINT ( 'NONE',  ( 2.977408999572650927, -7.188101187499990274, 0.4553027818717525488 ) ) ;
#44554 = ORIENTED_EDGE ( 'NONE', *, *, #60989, .F. ) ;
#44555 = ORIENTED_EDGE ( 'NONE', *, *, #52160, .T. ) ;
#44556 = CARTESIAN_POINT ( 'NONE',  ( -10.18810118749999738, -4.220049686691941915, 91.75000000204836681 ) ) ;
#44557 = CARTESIAN_POINT ( 'NONE',  ( 31.99999999999998579, 204.4375000027312126, 168.3431457505074889 ) ) ;
#44558 = CARTESIAN_POINT ( 'NONE',  ( -31.45873412499997812, 199.0000000013656063, 171.4326545832180386 ) ) ;
#44559 = CARTESIAN_POINT ( 'NONE',  ( 2.020667218593132706E-15, -11.00000000000000000, 109.3750000000000000 ) ) ;
#44560 = CARTESIAN_POINT ( 'NONE',  ( 1.432654583217662481, 208.3750000013656063, 194.5412658750000219 ) ) ;
#44561 = LINE ( 'NONE', #20411, #38658 ) ;
#44562 = EDGE_CURVE ( 'NONE', #59945, #60307, #28581, .T. ) ;
#44563 = CARTESIAN_POINT ( 'NONE',  ( -2.679491924311225848, 126.4583333333333428, -10.00000000000000178 ) ) ;
#44564 = CARTESIAN_POINT ( 'NONE',  ( 5.656854249492379694, 103.4374999999999858, -5.656854249492380582 ) ) ;
#44565 = CARTESIAN_POINT ( 'NONE',  ( -4.088227598258586603E-16, 293.3593750017070079, -6.676582343750001591 ) ) ;
#44566 = CARTESIAN_POINT ( 'NONE',  ( -7.188101187499991163, 2.977408999572646930, 7.767802781871751883 ) ) ;
#44567 = ADVANCED_FACE ( 'NONE', ( #44790 ), #68537, .F. ) ;
#44568 = ORIENTED_EDGE ( 'NONE', *, *, #54463, .T. ) ;
#44569 = CARTESIAN_POINT ( 'NONE',  ( 1.714505518806294638E-15, 0.000000000000000000, -14.00000000000000000 ) ) ;
#44570 = VECTOR ( 'NONE', #60418, 1000.000000000000000 ) ;
#44571 = CARTESIAN_POINT ( 'NONE',  ( 24.54126587499998280, 205.2500000013655779, 171.4326545832175555 ) ) ;
#44572 = CARTESIAN_POINT ( 'NONE',  ( -2.977408999572650039, 1.312499997951610098, -7.188101187500001821 ) ) ;
#44573 = CARTESIAN_POINT ( 'NONE',  ( -2.754378923186476579E-14, 198.1875000013655779, 145.4587341250000350 ) ) ;
#44574 = CARTESIAN_POINT ( 'NONE',  ( 2.977408999572654480, 122.0000000020483810, 7.188101187499999156 ) ) ;
#44576 = CARTESIAN_POINT ( 'NONE',  ( -1.432654583217664701, 203.0000000013655779, 138.5412658750000787 ) ) ;
#44575 = CARTESIAN_POINT ( 'NONE',  ( 10.99999999999999467, 11.00000000000000355, 20.00000000000000000 ) ) ;
#44577 = CARTESIAN_POINT ( 'NONE',  ( -11.35316468749999608, 254.4270833367473585, 3.042071309553173730 ) ) ;
#44578 = CARTESIAN_POINT ( 'NONE',  ( -10.18810118749999916, 0.000000000000000000, 117.5312500020483810 ) ) ;
#44579 = CARTESIAN_POINT ( 'NONE',  ( -10.00000000000000000, 214.1666666598386826, -2.679491924311229845 ) ) ;
#44580 = CARTESIAN_POINT ( 'NONE',  ( 11.35316468749999785, 10.57291666325268409, 3.042071309553174174 ) ) ;
#44581 = EDGE_CURVE ( 'NONE', #69418, #40106, #15117, .T. ) ;
#44582 = CARTESIAN_POINT ( 'NONE',  ( 8.000000000000001776, 100.3437500040967905, 3.313708498984759387 ) ) ;
#44583 = CARTESIAN_POINT ( 'NONE',  ( 3.042071309553167069, 207.1354166632526415, -11.35316468749999785 ) ) ;
#44584 = CARTESIAN_POINT ( 'NONE',  ( 3.211159895383561835, 5.437499998634407028, -3.211159895383561835 ) ) ;
#44585 = CARTESIAN_POINT ( 'NONE',  ( -7.022222184832254577, 9.802124591828755840, 6.291760732204942919E-15 ) ) ;
#44587 = CARTESIAN_POINT ( 'NONE',  ( 8.000000000000001776, 101.8437500040967905, 3.313708498984759387 ) ) ;
#44586 = CARTESIAN_POINT ( 'NONE',  ( 5.000000000000000000, -29.68417822476656553, 4.268394125862919886 ) ) ;
#44588 = ORIENTED_EDGE ( 'NONE', *, *, #72838, .T. ) ;
#44589 = CARTESIAN_POINT ( 'NONE',  ( 1.432654583217607414, 200.5000000013656063, 145.4587341250000634 ) ) ;
#44590 = CARTESIAN_POINT ( 'NONE',  ( 8.311093377946834337, 10.15624999658601801, 8.311093377946839666 ) ) ;
#44591 = CARTESIAN_POINT ( 'NONE',  ( -11.00000000000000000, 0.000000000000000000, 100.1875000040967763 ) ) ;
#44592 = CARTESIAN_POINT ( 'NONE',  ( 2.679491924286489191, 208.9583333333311543, 10.00000000001428369 ) ) ;
#44593 = CARTESIAN_POINT ( 'NONE',  ( -31.45873412499995680, 198.7500000013656063, 171.4326545832181239 ) ) ;
#44594 = CARTESIAN_POINT ( 'NONE',  ( -27.99999999999999645, 210.0000000000000284, 170.0000000000003695 ) ) ;
#44596 = CARTESIAN_POINT ( 'NONE',  ( 11.35316468749999963, 10.98958332991935016, -3.042071309553165293 ) ) ;
#44595 = CARTESIAN_POINT ( 'NONE',  ( 5.082755093536325042, 116.0937500020483810, -5.082755093536325930 ) ) ;
#44597 = CARTESIAN_POINT ( 'NONE',  ( 0.000000000000000000, 22.00000000000000000, 0.000000000000000000 ) ) ;
#44598 = CARTESIAN_POINT ( 'NONE',  ( 3.042071309553167069, 116.8229166632526983, -11.35316468749999785 ) ) ;
#44599 = CARTESIAN_POINT ( 'NONE',  ( 10.00000000000000178, 101.8749999931720396, 0.000000000000000000 ) ) ;
#44600 = CARTESIAN_POINT ( 'NONE',  ( -5.082755093536324154, 118.7187500020483810, 5.082755093536326818 ) ) ;
#44601 = CARTESIAN_POINT ( 'NONE',  ( 4.541265875000002339, 19.49999999863440436, -1.881053915767121554 ) ) ;
#44602 = CARTESIAN_POINT ( 'NONE',  ( -8.660254037844390851, 199.7916666598387110, 4.999999999999998224 ) ) ;
#44603 = CARTESIAN_POINT ( 'NONE',  ( -12.00000000000000178, 5.807951393103176763, -0.7484079198486841555 ) ) ;
#44604 = ORIENTED_EDGE ( 'NONE', *, *, #62565, .T. ) ;
#44605 = DIRECTION ( 'NONE',  ( -0.000000000000000000, 1.000000000000000000, -0.000000000000000000 ) ) ;
#44606 = CARTESIAN_POINT ( 'NONE',  ( -6.676582343750003368, 291.5468750017069510, -2.765530957081996810 ) ) ;
#44607 = CARTESIAN_POINT ( 'NONE',  ( 4.999999999999999112, 52.62579568235167216, 48.70175807018058123 ) ) ;
#44608 = CARTESIAN_POINT ( 'NONE',  ( -4.898587196589407898E-16, 7.999999999999991118, 27.51155278432982598 ) ) ;
#44609 = CARTESIAN_POINT ( 'NONE',  ( 1.656854249492346609, 207.3125000027312126, 138.0000000000000568 ) ) ;
#44610 = CARTESIAN_POINT ( 'NONE',  ( -8.311093377946836114, 258.2812500034140157, -8.311093377946836114 ) ) ;
#44611 = CARTESIAN_POINT ( 'NONE',  ( -10.18810118749999916, 4.220049686691934809, 105.4375000020483668 ) ) ;
#44612 = VERTEX_POINT ( 'NONE', #33862 ) ;
#44613 = VECTOR ( 'NONE', #23679, 1000.000000000000000 ) ;
#44614 = DIRECTION ( 'NONE',  ( 0.000000000000000000, 0.000000000000000000, -1.000000000000000000 ) ) ;
#44615 = CARTESIAN_POINT ( 'NONE',  ( 5.676582343749993598, 160.2604166632526983, 9.832129032723422313 ) ) ;
#44616 = PRESENTATION_STYLE_ASSIGNMENT (( #15555 ) ) ;
#44617 = CARTESIAN_POINT ( 'NONE',  ( -3.458734124999960358, 206.6875000013656063, 198.0000000000000284 ) ) ;
#44618 = DIRECTION ( 'NONE',  ( 0.000000000000000000, 0.000000000000000000, 1.000000000000000000 ) ) ;
#44619 = CARTESIAN_POINT ( 'NONE',  ( -3.042071309553164404, 77.55208332991932707, -11.35316468749999963 ) ) ;
#44620 = ORIENTED_EDGE ( 'NONE', *, *, #72416, .F. ) ;
#44621 = CARTESIAN_POINT ( 'NONE',  ( -7.204075437095967871, 7.204075437095967871, 112.4687500020483810 ) ) ;
#44622 = CARTESIAN_POINT ( 'NONE',  ( 4.541265875000001451, 8.374999998634407916, 1.881053915767124440 ) ) ;
#44623 = EDGE_LOOP ( 'NONE', ( #27653, #69100, #38254 ) ) ;
#44624 = CARTESIAN_POINT ( 'NONE',  ( -8.000000000000001776, 2.343750000000000444, 3.313708498984759387 ) ) ;
#44625 = CYLINDRICAL_SURFACE ( 'NONE', #7113, 3.999999999999976019 ) ;
#44626 = CARTESIAN_POINT ( 'NONE',  ( -23.99999999999995026, 197.8125000027312410, 171.6568542494926817 ) ) ;
#44627 = CARTESIAN_POINT ( 'NONE',  ( -7.188101187500002709, 16.68749999795161543, 2.977408999572649151 ) ) ;
#44628 = FACE_OUTER_BOUND ( 'NONE', #11520, .T. ) ;
#44629 = CARTESIAN_POINT ( 'NONE',  ( 4.220049686691941027, -10.18810118749999738, 110.5000000020483810 ) ) ;
#44630 = AXIS2_PLACEMENT_3D ( 'NONE', #25976, #71635, #49001 ) ;
#44631 = DIRECTION ( 'NONE',  ( -1.000000000000000000, 0.000000000000000000, -0.000000000000000000 ) ) ;
#44632 = CARTESIAN_POINT ( 'NONE',  ( -4.000000000000001776, 7.187499997268813168, -1.656854249492381470 ) ) ;
#44633 = DIRECTION ( 'NONE',  ( -1.000000000000000000, 0.000000000000000000, 0.000000000000000000 ) ) ;
#44634 = AXIS2_PLACEMENT_3D ( 'NONE', #19557, #20296, #61046 ) ;
#44635 = VERTEX_POINT ( 'NONE', #17597 ) ;
#44636 = CARTESIAN_POINT ( 'NONE',  ( -1.432654583217607192, 204.2500000013655779, 194.5412658750000219 ) ) ;
#44637 = CARTESIAN_POINT ( 'NONE',  ( -26.56734541678227757, 209.0000000013655779, 173.4587341250003476 ) ) ;
#44638 = CARTESIAN_POINT ( 'NONE',  ( 2.729893485599593106, 10.18810118750000093, 67.59560438569886287 ) ) ;
#44639 = CARTESIAN_POINT ( 'NONE',  ( 4.541265875000002339, 6.312499998634407028, 0.000000000000000000 ) ) ;
#44640 = CARTESIAN_POINT ( 'NONE',  ( -7.999999999999991118, 0.000000000000000000, 9.830302779823364645 ) ) ;
#44641 = CARTESIAN_POINT ( 'NONE',  ( 7.188101187499992051, 8.802885111219154394E-16, 18.73655278187175455 ) ) ;
#44642 = VERTEX_POINT ( 'NONE', #16094 ) ;
#44643 = CARTESIAN_POINT ( 'NONE',  ( -7.778174593052023411, 7.778174593052023411, 90.81249999999998579 ) ) ;
#44644 = EDGE_LOOP ( 'NONE', ( #58653, #63502, #39192, #51764 ) ) ;
#44645 = CARTESIAN_POINT ( 'NONE',  ( -10.18810118749999916, 0.000000000000000000, 111.1562500020483668 ) ) ;
#44646 = CARTESIAN_POINT ( 'NONE',  ( 26.34314575050764518, 209.0625000027312126, 173.9999999999999147 ) ) ;
#44647 = CARTESIAN_POINT ( 'NONE',  ( 1.432654583217662481, 204.1250000013656063, 194.5412658750000219 ) ) ;
#44648 = CARTESIAN_POINT ( 'NONE',  ( 24.54126587500000412, 199.2500000013656063, 171.4326545832176123 ) ) ;
#44649 = CARTESIAN_POINT ( 'NONE',  ( 4.999999999999993783, 84.16666666666667140, 8.660254037844390851 ) ) ;
#44650 = CARTESIAN_POINT ( 'NONE',  ( -8.000000000000000000, 125.0000000000000000, 0.000000000000000000 ) ) ;
#44651 = CARTESIAN_POINT ( 'NONE',  ( 6.000000000000003553, 293.4374999999998863, 2.485281374238571317 ) ) ;
#44652 = CARTESIAN_POINT ( 'NONE',  ( 26.34314575050764162, 207.0625000027311842, 173.9999999999999147 ) ) ;
#44653 = EDGE_CURVE ( 'NONE', #35739, #64105, #11139, .T. ) ;
#44654 = AXIS2_PLACEMENT_3D ( 'NONE', #65896, #48910, #20237 ) ;
#44655 = ORIENTED_EDGE ( 'NONE', *, *, #48677, .T. ) ;
#44656 =( BOUNDED_CURVE ( )  B_SPLINE_CURVE ( 2, ( #33075, #72283, #27373, #31556, #50393, #73408, #21712, #44741, #54580 ),
 .UNSPECIFIED., .F., .F. ) 
 B_SPLINE_CURVE_WITH_KNOTS ( ( 3, 2, 2, 2, 3 ),
 ( 0.3541666666666646313, 0.3645833333333312609, 0.3749999999999980016, 0.3854166666666646868, 0.3958333333333313164 ),
 .UNSPECIFIED. ) 
 CURVE ( )  GEOMETRIC_REPRESENTATION_ITEM ( )  RATIONAL_B_SPLINE_CURVE ( ( 1.000000000000015099, 0.9238795325112717505, 1.000000000000000000, 0.9238795325112867385, 1.000000000000000000, 0.9238795325112867385, 1.000000000000000000, 0.9238795325113013934, 0.9999999999999853451 ) ) 
 REPRESENTATION_ITEM ( '' )  );
#44657 = CARTESIAN_POINT ( 'NONE',  ( 5.656854249492380582, 8.999999995903221972, -5.656854249492380582 ) ) ;
#44658 = CARTESIAN_POINT ( 'NONE',  ( 5.656854249492380582, 12.18750000000000178, -5.656854249492380582 ) ) ;
#44659 = CARTESIAN_POINT ( 'NONE',  ( 1.656854249492347719, 196.9375000027312410, 146.0000000000000284 ) ) ;
#44660 = CARTESIAN_POINT ( 'NONE',  ( -5.000000000000000888, 67.10993666412713310, 23.06595724273690351 ) ) ;
#44661 = DIRECTION ( 'NONE',  ( -1.000000000000000000, 0.000000000000000000, 0.000000000000000000 ) ) ;
#44662 = CARTESIAN_POINT ( 'NONE',  ( -10.00000000000000000, 254.7916666666666856, -2.679491924311226292 ) ) ;
#44663 = CARTESIAN_POINT ( 'NONE',  ( -10.99999999999991829, 4.556349186104124982, 107.5937500040967336 ) ) ;
#44664 = CARTESIAN_POINT ( 'NONE',  ( -8.660254037844387298, 192.0833333333333428, -5.000000000000004441 ) ) ;
#44665 = EDGE_CURVE ( 'NONE', #26409, #25157, #62133, .T. ) ;
#44666 = CARTESIAN_POINT ( 'NONE',  ( 30.82842712474620939, 198.2500000027312126, 172.8284271247460424 ) ) ;
#44667 = CARTESIAN_POINT ( 'NONE',  ( -5.082755093536319713, 5.082755093536319713, 16.67405278187175810 ) ) ;
#44668 = CARTESIAN_POINT ( 'NONE',  ( -11.35316468750000141, 163.5937499965860127, -1.390361679473963753E-15 ) ) ;
#44669 = CARTESIAN_POINT ( 'NONE',  ( -5.000000000000000888, 53.31073972600139399, 44.28411094576038209 ) ) ;
#44670 = CARTESIAN_POINT ( 'NONE',  ( 7.320508075688907823, 155.6250000000001137, -7.320508075688907823 ) ) ;
#44672 = DIRECTION ( 'NONE',  ( 1.000000000000000000, -0.000000000000000000, -0.000000000000000000 ) ) ;
#44671 = DIRECTION ( 'NONE',  ( 0.000000000000000000, -0.000000000000000000, 1.000000000000000000 ) ) ;
#44673 = ORIENTED_EDGE ( 'NONE', *, *, #65308, .F. ) ;
#44674 = CARTESIAN_POINT ( 'NONE',  ( -11.35316468750000141, 23.80208332991934839, 3.042071309553159963 ) ) ;
#44675 = CARTESIAN_POINT ( 'NONE',  ( -24.54126587499996504, 208.1250000013656063, 171.4326545832179534 ) ) ;
#44677 = CARTESIAN_POINT ( 'NONE',  ( 1.688721909672338040, 10.27943647337372290, -63.64086505882561795 ) ) ;
#44676 = CARTESIAN_POINT ( 'NONE',  ( 1.224646799147353454E-15, 0.000000000000000000, -10.00000000000000178 ) ) ;
#44678 = CARTESIAN_POINT ( 'NONE',  ( -14.71437561237264546, -43.61858406653905007, 197.2871226623139762 ) ) ;
#44679 = CARTESIAN_POINT ( 'NONE',  ( -2.445694354108838731, 204.0625000013656063, 144.4456943541088663 ) ) ;
#44680 = CARTESIAN_POINT ( 'NONE',  ( -8.660254037844387298, 63.95833332650536818, -5.000000000000004441 ) ) ;
#44681 = CARTESIAN_POINT ( 'NONE',  ( -5.082755093536325930, 105.9687500020483952, -5.082755093536325930 ) ) ;
#44682 = CARTESIAN_POINT ( 'NONE',  ( -1.881053915767121554, 6.749999998634407916, -4.541265875000002339 ) ) ;
#44683 = CARTESIAN_POINT ( 'NONE',  ( 38.00000000000000000, -53.00000000000000000, 15.00000000000000178 ) ) ;
#44684 = CARTESIAN_POINT ( 'NONE',  ( 7.999999999999991118, 3.313708498984757611, 6.174052779823364645 ) ) ;
#44685 = CARTESIAN_POINT ( 'NONE',  ( 8.660254037844389075, 165.4166666666666856, -5.000000000000000000 ) ) ;
#44686 = ORIENTED_EDGE ( 'NONE', *, *, #21049, .F. ) ;
#44687 = ORIENTED_EDGE ( 'NONE', *, *, #24659, .T. ) ;
#44688 = CARTESIAN_POINT ( 'NONE',  ( -5.000000000000005329, 223.3333333333333428, 8.660254037844387298 ) ) ;
#44689 = CARTESIAN_POINT ( 'NONE',  ( 1.432654583217664701, 195.0000000013656063, 201.4587341250000065 ) ) ;
#44690 = CARTESIAN_POINT ( 'NONE',  ( -8.311093377946836114, 223.5937500034139589, -8.311093377946836114 ) ) ;
#44691 = B_SPLINE_CURVE_WITH_KNOTS ( 'NONE', 3,
 ( #7811, #65136, #41769, #31185, #25139, #36484, #70446, #53469 ),
 .UNSPECIFIED., .F., .F.,
 ( 4, 2, 2, 4 ),
 ( 0.007010445034807142976, 0.008756443665256694389, 0.01050244229570624493, 0.01399443955660534950 ),
 .UNSPECIFIED. ) ;
#44692 = CARTESIAN_POINT ( 'NONE',  ( -2.085542519210945728E-15, 139.5312499965860411, 11.35316468750000141 ) ) ;
#44693 = ORIENTED_EDGE ( 'NONE', *, *, #41291, .T. ) ;
#44694 = CARTESIAN_POINT ( 'NONE',  ( -4.999999999999992006, 10.25159769123454900, -64.79153472057838314 ) ) ;
#44695 = CARTESIAN_POINT ( 'NONE',  ( 10.18810118749999916, 1.247682550866122264E-15, 89.40625000204838102 ) ) ;
#44696 = CARTESIAN_POINT ( 'NONE',  ( 6.123233995736767268E-16, 46.25000000000000711, -10.00000000000000178 ) ) ;
#44697 = CARTESIAN_POINT ( 'NONE',  ( 4.000000000000015987, 207.5000000000000284, 198.0000000000000284 ) ) ;
#44698 = CARTESIAN_POINT ( 'NONE',  ( 4.000000000000000888, 14.68749999726881406, 1.656854249492384135 ) ) ;
#44699 = CARTESIAN_POINT ( 'NONE',  ( -31.99999999999999289, 197.3750000027312126, 170.0000000000004547 ) ) ;
#44700 = AXIS2_PLACEMENT_3D ( 'NONE', #67508, #15061, #44870 ) ;
#44701 = CARTESIAN_POINT ( 'NONE',  ( -4.556349186104048599, -10.99999999999999822, 95.78124999999998579 ) ) ;
#44702 = VERTEX_POINT ( 'NONE', #11203 ) ;
#44703 = FACE_OUTER_BOUND ( 'NONE', #45417, .T. ) ;
#44704 = CARTESIAN_POINT ( 'NONE',  ( -30.99106816569929634, 173.7267113793454030, 172.4740941932668079 ) ) ;
#44705 = CARTESIAN_POINT ( 'NONE',  ( -11.35316468750000141, 108.8020833299193555, 3.042071309553159963 ) ) ;
#44706 = CARTESIAN_POINT ( 'NONE',  ( 1.432654583217662259, 201.1250000013656347, 194.5412658750000219 ) ) ;
#44707 = CARTESIAN_POINT ( 'NONE',  ( -7.188101187500002709, 19.68749999795161543, 2.977408999572649151 ) ) ;
#44708 = CARTESIAN_POINT ( 'NONE',  ( 7.204075437095968759, -7.204075437095966983, 82.09375000204838102 ) ) ;
#44709 = CARTESIAN_POINT ( 'NONE',  ( 3.042071309553159519, 35.05208332991935549, 11.35316468750000141 ) ) ;
#44710 = VERTEX_POINT ( 'NONE', #34230 ) ;
#44711 = CARTESIAN_POINT ( 'NONE',  ( -3.313708498984816231, 96.96875000409677625, 7.999999999999943157 ) ) ;
#44712 = CARTESIAN_POINT ( 'NONE',  ( -8.008118988124991233, 3.317071493978878127, 17.41936528394063188 ) ) ;
#44713 = FACE_OUTER_BOUND ( 'NONE', #6971, .T. ) ;
#44714 = VECTOR ( 'NONE', #22379, 1000.000000000000000 ) ;
#44715 = CARTESIAN_POINT ( 'NONE',  ( 11.00000000000010836, -4.556349186103939353, 85.84375000409677625 ) ) ;
#44716 = CARTESIAN_POINT ( 'NONE',  ( 7.188101187500000044, 9.468749997951610098, 0.000000000000000000 ) ) ;
#44717 = CARTESIAN_POINT ( 'NONE',  ( -4.721056650415998313, 289.5781250017069510, 4.721056650416000089 ) ) ;
#44718 = DIRECTION ( 'NONE',  ( -0.000000000000000000, -1.000000000000000000, -0.000000000000000000 ) ) ;
#44719 = CARTESIAN_POINT ( 'NONE',  ( 2.977408999572651815, 2.062499997951609654, 7.188101187500000933 ) ) ;
#44720 = ORIENTED_EDGE ( 'NONE', *, *, #69261, .F. ) ;
#44721 = CARTESIAN_POINT ( 'NONE',  ( -2.085542519210945728E-15, 139.8437499965860127, 11.35316468750000141 ) ) ;
#44722 = CARTESIAN_POINT ( 'NONE',  ( -7.204075437095965206, -7.204075437095968759, 76.84375000204838102 ) ) ;
#44723 = CARTESIAN_POINT ( 'NONE',  ( -28.00000000000002487, 208.6875000013656063, 166.5412658750003629 ) ) ;
#44724 = FACE_BOUND ( 'NONE', #50514, .T. ) ;
#44725 = CARTESIAN_POINT ( 'NONE',  ( 1.881053915767122664, 14.24999999863440969, 4.541265875000001451 ) ) ;
#44726 = ORIENTED_EDGE ( 'NONE', *, *, #56751, .T. ) ;
#44727 = CARTESIAN_POINT ( 'NONE',  ( -1.656854249492348607, 200.3125000027312126, 202.0000000000000284 ) ) ;
#44728 = CARTESIAN_POINT ( 'NONE',  ( 1.656854249492347719, 208.8125000000000000, 146.0000000000000284 ) ) ;
#44729 = CARTESIAN_POINT ( 'NONE',  ( -30.82842712474624847, 207.2500000027312126, 167.1715728752542418 ) ) ;
#44730 = ADVANCED_FACE ( 'NONE', ( #57232 ), #74194, .F. ) ;
#44731 = EDGE_CURVE ( 'NONE', #40040, #38312, #54585, .T. ) ;
#44732 = CARTESIAN_POINT ( 'NONE',  ( -8.000000000000000000, 21.65625000000000355, -3.313708498984762496 ) ) ;
#44733 = ORIENTED_EDGE ( 'NONE', *, *, #15375, .T. ) ;
#44734 = CARTESIAN_POINT ( 'NONE',  ( -2.977408999572650039, 8.437499997951611874, -7.188101187500000933 ) ) ;
#44735 = CARTESIAN_POINT ( 'NONE',  ( -25.17157287525373732, 196.7500000027312126, 172.8284271247464972 ) ) ;
#44736 = CARTESIAN_POINT ( 'NONE',  ( -2.603141862248978811, -46.50402002221501618, 151.1788490174893695 ) ) ;
#44737 = CARTESIAN_POINT ( 'NONE',  ( 5.676582343749993598, 189.9479166632526983, 9.832129032723422313 ) ) ;
#44738 = ADVANCED_FACE ( 'NONE', ( #35702 ), #54477, .T. ) ;
#44739 = ADVANCED_FACE ( 'NONE', ( #30036 ), #17152, .F. ) ;
#44740 = CARTESIAN_POINT ( 'NONE',  ( -2.977408999572650927, 107.7500000020483810, -7.188101187500001821 ) ) ;
#44741 = CARTESIAN_POINT ( 'NONE',  ( 2.485281374238939911, 295.3125000000000568, 5.999999999999634959 ) ) ;
#44742 = CARTESIAN_POINT ( 'NONE',  ( -6.676582343750001591, 287.4531250017069510, 0.000000000000000000 ) ) ;
#44744 = CARTESIAN_POINT ( 'NONE',  ( 4.999999999999991118, 94.16666666666667140, 8.660254037844387298 ) ) ;
#44743 = CARTESIAN_POINT ( 'NONE',  ( 9.999999999999998224, 34.99999999999999289, 0.000000000000000000 ) ) ;
#44745 = ORIENTED_EDGE ( 'NONE', *, *, #73889, .T. ) ;
#44746 = CARTESIAN_POINT ( 'NONE',  ( 5.676582343750005144, 255.5729166700806445, 9.832129032723416984 ) ) ;
#44747 = CARTESIAN_POINT ( 'NONE',  ( -5.082755093536319713, 5.082755093536319713, 24.17405278187175455 ) ) ;
#44748 = VECTOR ( 'NONE', #59999, 1000.000000000000000 ) ;
#44749 = CARTESIAN_POINT ( 'NONE',  ( -2.216418498320457786, 51.36626494304663026, 48.60390812669818672 ) ) ;
#44750 = CARTESIAN_POINT ( 'NONE',  ( 29.65685424949231574, 206.0624999999999716, 173.9999999999999147 ) ) ;
#44751 = CARTESIAN_POINT ( 'NONE',  ( -2.997005883566162154, -66.06021892606753454, -26.46015439093728361 ) ) ;
#44752 =( BOUNDED_CURVE ( )  B_SPLINE_CURVE ( 2, ( #50416, #55725, #22474, #15703, #10801, #34204, #22107, #5156, #56465 ),
 .UNSPECIFIED., .F., .F. ) 
 B_SPLINE_CURVE_WITH_KNOTS ( ( 3, 2, 2, 2, 3 ),
 ( 0.7361111111111110494, 0.7430555555555554692, 0.7500000000000000000, 0.7569444444444444198, 0.7638888888888888395 ),
 .UNSPECIFIED. ) 
 CURVE ( )  GEOMETRIC_REPRESENTATION_ITEM ( )  RATIONAL_B_SPLINE_CURVE ( ( 1.000000000000001110, 0.9238795325112855172, 1.000000000000000000, 0.9238795325112867385, 1.000000000000000000, 0.9238795325112867385, 1.000000000000000000, 0.9238795325112867385, 1.000000000000000000 ) ) 
 REPRESENTATION_ITEM ( '' )  );
#44753 = CARTESIAN_POINT ( 'NONE',  ( -1.432654583217608080, 194.8750000013656063, 201.4587341250000350 ) ) ;
#44754 = CARTESIAN_POINT ( 'NONE',  ( -10.00000000000000355, 142.7083333333333712, 2.679491924311223183 ) ) ;
#44755 = CARTESIAN_POINT ( 'NONE',  ( -11.00000000000000000, 0.000000000000000000, 115.1875000040967763 ) ) ;
#44756 = CARTESIAN_POINT ( 'NONE',  ( 0.000000000000000000, 125.0000000000000000, 8.000000000000000000 ) ) ;
#44757 = CARTESIAN_POINT ( 'NONE',  ( 5.656854249492381470, 92.56249999999998579, 5.656854249492379694 ) ) ;
#44758 = CARTESIAN_POINT ( 'NONE',  ( 11.35316468749999963, 126.3020833299193555, -3.042071309553165293 ) ) ;
#44759 = CARTESIAN_POINT ( 'NONE',  ( 5.656854249492379694, 98.93750000000000000, -5.656854249492380582 ) ) ;
#44760 = CARTESIAN_POINT ( 'NONE',  ( 11.00000000000000355, -4.556349186104045046, 72.15624999999997158 ) ) ;
#44763 = CARTESIAN_POINT ( 'NONE',  ( 1.469576158976823947E-15, 118.0625000040967763, 8.000000000000000000 ) ) ;
#44762 = CARTESIAN_POINT ( 'NONE',  ( 28.00000000000001776, 198.4375000013655779, 173.4587341249998929 ) ) ;
#44761 = CARTESIAN_POINT ( 'NONE',  ( 27.99999999999997158, 209.0000000000000284, 173.9999999999999147 ) ) ;
#44764 = ORIENTED_EDGE ( 'NONE', *, *, #39189, .T. ) ;
#44765 = CARTESIAN_POINT ( 'NONE',  ( 8.434195340655811890, 224.5471093110514289, 5.405325235466309053 ) ) ;
#44766 = ADVANCED_FACE ( 'NONE', ( #41359 ), #17972, .F. ) ;
#44767 = CARTESIAN_POINT ( 'NONE',  ( 0.000000000000000000, 300.0000000000000000, 0.000000000000000000 ) ) ;
#44768 = CARTESIAN_POINT ( 'NONE',  ( 29.43265458321766559, 199.1250000013656347, 166.5412658749999650 ) ) ;
#44769 = CARTESIAN_POINT ( 'NONE',  ( 11.35316468749999785, 200.8854166632526699, 3.042071309553174174 ) ) ;
#44770 = CARTESIAN_POINT ( 'NONE',  ( -4.401442555609581635E-16, 119.2812500020483810, -7.188101187500000044 ) ) ;
#44771 = CARTESIAN_POINT ( 'NONE',  ( 2.780723358947928197E-16, 19.56249999863440436, -4.541265875000002339 ) ) ;
#44772 = CARTESIAN_POINT ( 'NONE',  ( 1.506680654948051590, -55.70239491600889892, 43.84725041001744472 ) ) ;
#44773 = CARTESIAN_POINT ( 'NONE',  ( -5.656854249492375253, 5.656854249492375253, 26.14280277982336997 ) ) ;
#44774 = CARTESIAN_POINT ( 'NONE',  ( -48.32285594383906613, 41.53167862176056246, 61.49255443819183142 ) ) ;
#44775 = CARTESIAN_POINT ( 'NONE',  ( -8.311093377946836114, 92.65624999658602690, -8.311093377946837890 ) ) ;
#44776 = ORIENTED_EDGE ( 'NONE', *, *, #58921, .F. ) ;
#44777 =( BOUNDED_CURVE ( )  B_SPLINE_CURVE ( 2, ( #26474, #54800, #43843, #14409, #48744, #2362, #14782, #54429, #37822 ),
 .UNSPECIFIED., .F., .F. ) 
 B_SPLINE_CURVE_WITH_KNOTS ( ( 3, 2, 2, 2, 3 ),
 ( 0.3833333333333335813, 0.3916666666666669405, 0.4000000000000003553, 0.4083333333333337145, 0.4166666666666671293 ),
 .UNSPECIFIED. ) 
 CURVE ( )  GEOMETRIC_REPRESENTATION_ITEM ( )  RATIONAL_B_SPLINE_CURVE ( ( 0.9999999999999980016, 0.9238795325112887369, 1.000000000000000000, 0.9238795325112867385, 1.000000000000000000, 0.9238795325112867385, 1.000000000000000000, 0.9238795325112826307, 1.000000000000003997 ) ) 
 REPRESENTATION_ITEM ( '' )  );
#44778 = DIRECTION ( 'NONE',  ( -0.000000000000000000, -1.000000000000000000, -0.000000000000000000 ) ) ;
#44779 = CARTESIAN_POINT ( 'NONE',  ( -2.977408999572654480, 22.49999999795161543, 7.188101187499999156 ) ) ;
#44780 = CARTESIAN_POINT ( 'NONE',  ( -10.00000000000000000, 222.9166666734946318, -2.679491924311226292 ) ) ;
#44781 = CARTESIAN_POINT ( 'NONE',  ( -9.832129032723415207, 259.6354166700806445, 5.676582343750005144 ) ) ;
#44782 = VECTOR ( 'NONE', #12928, 1000.000000000000000 ) ;
#44783 = CARTESIAN_POINT ( 'NONE',  ( 8.311093377946837890, 106.4062499965859985, -8.311093377946837890 ) ) ;
#44784 = ORIENTED_EDGE ( 'NONE', *, *, #18185, .T. ) ;
#44785 = CARTESIAN_POINT ( 'NONE',  ( 28.00000000000001776, 197.1250000027312126, 173.9999999999999147 ) ) ;
#44786 = CARTESIAN_POINT ( 'NONE',  ( 4.220049686691941027, -10.18810118749999738, 105.6250000020483668 ) ) ;
#44787 = CARTESIAN_POINT ( 'NONE',  ( -2.243032484811285964E-15, 18.31575019322283993, 2.966738217918089671 ) ) ;
#44788 = CARTESIAN_POINT ( 'NONE',  ( -3.458734124999959469, 203.7500000013656063, 199.4326545832176691 ) ) ;
#44789 = CYLINDRICAL_SURFACE ( 'NONE', #16703, 12.00000000000000000 ) ;
#44791 = CARTESIAN_POINT ( 'NONE',  ( -5.676582343749998039, 82.44791666325268409, -9.832129032723420536 ) ) ;
#44790 = FACE_OUTER_BOUND ( 'NONE', #35615, .T. ) ;
#44792 = CARTESIAN_POINT ( 'NONE',  ( -7.999999999999991118, 3.313708498984756723, 14.42405278392014800 ) ) ;
#44793 = CARTESIAN_POINT ( 'NONE',  ( -27.99999999999996447, 202.1875000013656063, 173.4587341250003760 ) ) ;
#44794 = CARTESIAN_POINT ( 'NONE',  ( 6.123233995736767268E-16, 126.2500000000000000, -10.00000000000000178 ) ) ;
#44795 = CARTESIAN_POINT ( 'NONE',  ( 10.00000000000000178, 176.8749999931720538, 0.000000000000000000 ) ) ;
#44796 = CARTESIAN_POINT ( 'NONE',  ( 5.000000000000000000, -53.17721328501367850, 43.91924822456251576 ) ) ;
#44797 = CARTESIAN_POINT ( 'NONE',  ( -5.676582343749998039, 72.76041666325268409, -9.832129032723420536 ) ) ;
#44798 = CARTESIAN_POINT ( 'NONE',  ( 6.676582343750003368, 289.0156250017070079, -2.765530957081997254 ) ) ;
#44799 = CARTESIAN_POINT ( 'NONE',  ( -4.220049686691937474, -10.18810118749999738, 101.3125000020483810 ) ) ;
#44800 = CARTESIAN_POINT ( 'NONE',  ( -9.832129032723418760, 222.8645833299193839, -5.676582343750004256 ) ) ;
#44801 = ORIENTED_EDGE ( 'NONE', *, *, #64767, .T. ) ;
#44802 = CARTESIAN_POINT ( 'NONE',  ( -6.062601303906716588, -5.219661428662635494, 1.000679062340938064 ) ) ;
#44803 = CARTESIAN_POINT ( 'NONE',  ( 4.898587196589412829E-16, 1.687499995903220196, -8.000000000000000000 ) ) ;
#44804 = CARTESIAN_POINT ( 'NONE',  ( -2.160335347077982249, -16.41093803200690715, 68.77481055341485217 ) ) ;
#44805 = CARTESIAN_POINT ( 'NONE',  ( -8.311093377946841443, 208.9062499965860127, 8.311093377946834337 ) ) ;
#44806 = CARTESIAN_POINT ( 'NONE',  ( 4.999999999999997335, 226.4583333401612890, -8.660254037844387298 ) ) ;
#44807 = CARTESIAN_POINT ( 'NONE',  ( 4.721056650415999201, 299.0781250017069510, -4.721056650415999201 ) ) ;
#44808 = EDGE_LOOP ( 'NONE', ( #19266, #40887, #70692, #11806 ) ) ;
#44809 = CARTESIAN_POINT ( 'NONE',  ( -3.042071309553173730, 189.6354166632526983, 11.35316468749999785 ) ) ;
#44810 = B_SPLINE_CURVE_WITH_KNOTS ( 'NONE', 3,
 ( #30800, #19105, #13431, #43884, #48140, #13065, #18377, #59846, #59120, #36103, #53456, #66897, #7429, #55220, #70070, #1416, #24401, #47408, #71148, #7797, #2130, #25122, #35733, #64404, #1775, #3908, #53822, #26515, #70790, #30436 ),
 .UNSPECIFIED., .F., .F.,
 ( 4, 2, 2, 2, 2, 2, 2, 2, 2, 2, 2, 2, 2, 2, 4 ),
 ( 0.05392149607393267874, 0.05640565162188200532, 0.05888980716983133190, 0.06385811826572998506, 0.06634227381367928389, 0.06882642936162858271, 0.07006850713560326682, 0.07131058490957795093, 0.07379474045752736078, 0.07627889600547677063, 0.07876305155342619435, 0.08373136264932509731, 0.08621551819727453492, 0.08869967374522398640, 0.09366798484112280609 ),
 .UNSPECIFIED. ) ;
#44811 = VECTOR ( 'NONE', #28015, 1000.000000000000000 ) ;
#44812 = CARTESIAN_POINT ( 'NONE',  ( -5.082755093536317936, -5.082755093536320601, 16.67405278187175810 ) ) ;
#44813 = CARTESIAN_POINT ( 'NONE',  ( -26.56734541678238415, 206.3750000013656063, 166.5412658750003629 ) ) ;
#44814 = CARTESIAN_POINT ( 'NONE',  ( 8.000000000000000000, 10.50000000000000178, 0.000000000000000000 ) ) ;
#44815 = ORIENTED_EDGE ( 'NONE', *, *, #19750, .F. ) ;
#44816 = ADVANCED_FACE ( 'NONE', ( #40615 ), #7029, .T. ) ;
#44817 = CARTESIAN_POINT ( 'NONE',  ( -3.313708498984762496, 90.96875000409676204, 7.999999999999998224 ) ) ;
#44818 = CARTESIAN_POINT ( 'NONE',  ( -7.320508075688773708, 11.87500000000000000, -7.320508075688774596 ) ) ;
#44819 = CARTESIAN_POINT ( 'NONE',  ( -10.18810118749999916, 0.000000000000000000, 80.03125000204836681 ) ) ;
#44820 = ORIENTED_EDGE ( 'NONE', *, *, #56766, .F. ) ;
#44821 = CARTESIAN_POINT ( 'NONE',  ( 4.000000000000001776, 22.00000000000000000, 0.000000000000000000 ) ) ;
#44822 = CARTESIAN_POINT ( 'NONE',  ( -3.211159895383562723, 17.93749999863440792, 3.211159895383561391 ) ) ;
#44823 = DIRECTION ( 'NONE',  ( 1.000000000000000000, 0.000000000000000000, 0.000000000000000000 ) ) ;
#44824 = VECTOR ( 'NONE', #43556, 1000.000000000000000 ) ;
#44826 = ORIENTED_EDGE ( 'NONE', *, *, #46311, .F. ) ;
#44825 = EDGE_CURVE ( 'NONE', #57937, #61956, #35345, .T. ) ;
#44827 = EDGE_CURVE ( 'NONE', #14172, #4343, #69572, .T. ) ;
#44828 = DIRECTION ( 'NONE',  ( -0.1501682406780869006, 0.1251959390492823898, -0.9807015225527165869 ) ) ;
#44829 = CARTESIAN_POINT ( 'NONE',  ( -7.188101187500001821, 92.56250000204838102, -2.977408999572650483 ) ) ;
#44832 = CARTESIAN_POINT ( 'NONE',  ( 31.99999999999998579, 207.4375000027312410, 168.3431457505074889 ) ) ;
#44831 = CARTESIAN_POINT ( 'NONE',  ( 8.311093377946839666, 245.7812500034139589, 8.311093377946830785 ) ) ;
#44830 = CARTESIAN_POINT ( 'NONE',  ( 31.45873412499999944, 208.6875000013656063, 169.9999999999998863 ) ) ;
#44833 = PRODUCT_CONTEXT ( 'NONE', #16814, 'mechanical' ) ;
#44834 = VECTOR ( 'NONE', #29665, 1000.000000000000000 ) ;
#44835 = EDGE_LOOP ( 'NONE', ( #20257, #74627, #38987, #48795, #69115, #5062, #70956, #23946, #20383, #6859, #1930, #11053, #23452, #9202, #28562, #72456 ) ) ;
#44836 = EDGE_CURVE ( 'NONE', #9385, #17249, #30768, .T. ) ;
#44837 = CARTESIAN_POINT ( 'NONE',  ( 5.676582343750005144, 250.8854166700806729, 9.832129032723416984 ) ) ;
#44838 = CARTESIAN_POINT ( 'NONE',  ( -7.188101187499991163, 2.977408999572646930, 11.89280278187175277 ) ) ;
#44839 = ORIENTED_EDGE ( 'NONE', *, *, #37961, .T. ) ;
#44840 = ORIENTED_EDGE ( 'NONE', *, *, #28735, .T. ) ;
#44841 = CARTESIAN_POINT ( 'NONE',  ( 7.204075437095966983, 7.204075437095967871, 74.59375000204838102 ) ) ;
#44842 = CARTESIAN_POINT ( 'NONE',  ( -11.35316468750000141, 68.59374999658601268, -1.390361679473963753E-15 ) ) ;
#44843 = CARTESIAN_POINT ( 'NONE',  ( 5.656854249492376141, -5.656854249492374365, 17.89280277982336642 ) ) ;
#44844 = CARTESIAN_POINT ( 'NONE',  ( 4.556349186104051263, -10.99999999999999822, 89.96875000000000000 ) ) ;
#44847 = CARTESIAN_POINT ( 'NONE',  ( 1.226468279477575784E-15, 291.8593750017070079, 6.676582343750001591 ) ) ;
#44846 = CARTESIAN_POINT ( 'NONE',  ( 23.99999999999998934, 198.8750000027312126, 169.9999999999999432 ) ) ;
#44845 = CARTESIAN_POINT ( 'NONE',  ( 24.54126587500000412, 209.3750000013656063, 168.5673454167822172 ) ) ;
#44848 = CARTESIAN_POINT ( 'NONE',  ( 2.679491924311228956, 77.91666665983871098, -10.00000000000000000 ) ) ;
#44849 = CARTESIAN_POINT ( 'NONE',  ( 54.00000000000000711, 242.0000000000000284, 20.00000000000001776 ) ) ;
#44850 = EDGE_CURVE ( 'NONE', #25046, #57615, #46073, .T. ) ;
#44851 = CARTESIAN_POINT ( 'NONE',  ( 3.458734125000016757, 198.1250000013656063, 199.4326545832176976 ) ) ;
#44852 = CARTESIAN_POINT ( 'NONE',  ( 5.656854249492380582, 7.499999995903221084, -5.656854249492380582 ) ) ;
#44853 = EDGE_LOOP ( 'NONE', ( #9042, #62503, #70924, #24715 ) ) ;
#44854 = CARTESIAN_POINT ( 'NONE',  ( 29.43265458321766204, 195.8750000013655779, 166.5412658749999650 ) ) ;
#44855 = CARTESIAN_POINT ( 'NONE',  ( -7.188101187500000044, 19.59374999795161543, -8.802885111219163269E-16 ) ) ;
#44856 = AXIS2_PLACEMENT_3D ( 'NONE', #593, #69985, #6609 ) ;
#44857 = CARTESIAN_POINT ( 'NONE',  ( 8.311093377946837890, 171.7187499965860127, -8.311093377946837890 ) ) ;
#44858 = FACE_OUTER_BOUND ( 'NONE', #56798, .T. ) ;
#44859 = CARTESIAN_POINT ( 'NONE',  ( -7.188101187500000044, 106.5312500020483810, 0.000000000000000000 ) ) ;
#44861 = CARTESIAN_POINT ( 'NONE',  ( -0.7581620860327765721, -55.63814191976648971, -43.81219805000106504 ) ) ;
#44860 = CYLINDRICAL_SURFACE ( 'NONE', #10667, 8.000000000000000000 ) ;
#44862 = CARTESIAN_POINT ( 'NONE',  ( 24.54126587499999701, 206.4375000013656063, 169.9999999999998863 ) ) ;
#44863 = CARTESIAN_POINT ( 'NONE',  ( -7.188101187499991163, 2.977408999572646930, 18.26780278187175455 ) ) ;
#44864 = CARTESIAN_POINT ( 'NONE',  ( 1.656854249492347719, 207.9375000027312126, 146.0000000000000284 ) ) ;
#44865 = CARTESIAN_POINT ( 'NONE',  ( 11.35316468750000141, 50.78124999658601979, 0.000000000000000000 ) ) ;
#44866 = CARTESIAN_POINT ( 'NONE',  ( -1.469576158976823947E-15, 20.62500000000000355, 8.000000000000000000 ) ) ;
#44867 = CARTESIAN_POINT ( 'NONE',  ( 10.00000000000000178, 17.08333332650536818, -2.679491924311226736 ) ) ;
#44868 = DIRECTION ( 'NONE',  ( -0.000000000000000000, 1.000000000000000000, 4.689100369878284071E-30 ) ) ;
#44869 = VERTEX_POINT ( 'NONE', #23995 ) ;
#44870 = DIRECTION ( 'NONE',  ( 0.000000000000000000, 0.000000000000000000, 1.000000000000000000 ) ) ;
#44871 = CARTESIAN_POINT ( 'NONE',  ( -1.469576158976823947E-15, 23.43749999590322020, 8.000000000000000000 ) ) ;
#44872 = CARTESIAN_POINT ( 'NONE',  ( -5.676582343749998039, 57.44791666325268409, -9.832129032723420536 ) ) ;
#44873 = CARTESIAN_POINT ( 'NONE',  ( 11.00000000000000355, -4.556349186104045046, 72.34375000409679046 ) ) ;
#44874 = CARTESIAN_POINT ( 'NONE',  ( -2.445694354108839175, 198.3125000013656063, 144.4456943541088663 ) ) ;
#44875 = FACE_OUTER_BOUND ( 'NONE', #44077, .T. ) ;
#44876 = CARTESIAN_POINT ( 'NONE',  ( -2.679491924311287132, 243.9583333333333712, -9.999999999999968026 ) ) ;
#44878 = CARTESIAN_POINT ( 'NONE',  ( -9.832129032723418760, 52.86458332991934839, -5.676582343750004256 ) ) ;
#44877 = CARTESIAN_POINT ( 'NONE',  ( -5.082755093536325930, 95.46875000204838102, -5.082755093536325930 ) ) ;
#44879 = CARTESIAN_POINT ( 'NONE',  ( -5.656854249492375253, 5.656854249492375253, 2.142802779823364645 ) ) ;
#44880 = CARTESIAN_POINT ( 'NONE',  ( 11.00000000000000000, 1.347111479062088405E-15, 97.93750000409677625 ) ) ;
#44881 =( BOUNDED_CURVE ( )  B_SPLINE_CURVE ( 2, ( #61354, #43621, #38730, #2894, #43245, #66632, #21352, #55334, #44376 ),
 .UNSPECIFIED., .F., .F. ) 
 B_SPLINE_CURVE_WITH_KNOTS ( ( 3, 2, 2, 2, 3 ),
 ( 0.5104166666666666297, 0.5156250000000000000, 0.5208333333333333703, 0.5260416666666666297, 0.5312500000000000000 ),
 .UNSPECIFIED. ) 
 CURVE ( )  GEOMETRIC_REPRESENTATION_ITEM ( )  RATIONAL_B_SPLINE_CURVE ( ( 1.000000000000000000, 0.9238795325112867385, 1.000000000000000000, 0.9238795325112867385, 1.000000000000000000, 0.9238795325112867385, 1.000000000000000000, 0.9238795325112867385, 1.000000000000000000 ) ) 
 REPRESENTATION_ITEM ( '' )  );
#44882 = CARTESIAN_POINT ( 'NONE',  ( -2.085542519210945728E-15, 179.5312499965860411, 11.35316468750000141 ) ) ;
#44883 = CARTESIAN_POINT ( 'NONE',  ( -1.836970198721029983E-15, 145.6249999931720538, 10.00000000000000178 ) ) ;
#44884 = VECTOR ( 'NONE', #70830, 1000.000000000000000 ) ;
#44885 = CARTESIAN_POINT ( 'NONE',  ( -5.082755093536324154, 102.2187500020483810, 5.082755093536326818 ) ) ;
#44886 = CARTESIAN_POINT ( 'NONE',  ( -3.000000000000001332, -45.00000000000001421, 139.1455027589170470 ) ) ;
#44887 = CARTESIAN_POINT ( 'NONE',  ( 5.676582343750001591, 31.92708332991935194, -9.832129032723420536 ) ) ;
#44888 = CARTESIAN_POINT ( 'NONE',  ( 7.204075437095968759, -7.204075437095966983, 116.5937500020483810 ) ) ;
#44889 = CARTESIAN_POINT ( 'NONE',  ( -11.35316468750000141, 168.4895833299193839, 3.042071309553159963 ) ) ;
#44890 = ORIENTED_EDGE ( 'NONE', *, *, #31548, .F. ) ;
#44891 = DIRECTION ( 'NONE',  ( -0.000000000000000000, 1.000000000000000000, 4.689100369878284071E-30 ) ) ;
#44892 = CARTESIAN_POINT ( 'NONE',  ( 4.220049686691934809, 10.18810118749999916, 70.18750000204838102 ) ) ;
#44893 = CARTESIAN_POINT ( 'NONE',  ( 30.99999999999998579, 50.00000000000000711, 65.00000000000000000 ) ) ;
#44894 = CARTESIAN_POINT ( 'NONE',  ( -8.311093377946836114, 167.6562499965860411, -8.311093377946837890 ) ) ;
#44895 = CARTESIAN_POINT ( 'NONE',  ( 3.313708498984756279, 7.999999999999991118, 13.91780278432982421 ) ) ;
#44896 = CIRCLE ( 'NONE', #40088, 3.999999999999989786 ) ;
#44897 = CARTESIAN_POINT ( 'NONE',  ( -5.656854249492375253, 5.656854249492375253, 5.142802779823363757 ) ) ;
#44898 = CARTESIAN_POINT ( 'NONE',  ( 9.999999999999998224, 260.8333333401612890, -2.679491924311229401 ) ) ;
#44899 = CARTESIAN_POINT ( 'NONE',  ( 4.104248244544244528, 56.27889056305702553, -44.16174987545804242 ) ) ;
#44900 = CARTESIAN_POINT ( 'NONE',  ( 4.220049686691934809, 10.18810118749999916, 79.56250000204836681 ) ) ;
#44901 = EDGE_LOOP ( 'NONE', ( #40186, #39398, #14642, #29236 ) ) ;
#44902 = CIRCLE ( 'NONE', #70057, 30.99999999999994316 ) ;
#44903 =( BOUNDED_CURVE ( )  B_SPLINE_CURVE ( 2, ( #21869, #10563, #44897, #56600, #4916, #10, #27910, #45632, #22997 ),
 .UNSPECIFIED., .F., .F. ) 
 B_SPLINE_CURVE_WITH_KNOTS ( ( 3, 2, 2, 2, 3 ),
 ( 0.8421052631578948011, 0.8486842105263159297, 0.8552631578947369473, 0.8618421052631578538, 0.8684210526315789824 ),
 .UNSPECIFIED. ) 
 CURVE ( )  GEOMETRIC_REPRESENTATION_ITEM ( )  RATIONAL_B_SPLINE_CURVE ( ( 0.9999999999999986677, 0.9238795325112880708, 1.000000000000000000, 0.9238795325112867385, 1.000000000000000000, 0.9238795325112867385, 1.000000000000000000, 0.9238795325112867385, 1.000000000000000000 ) ) 
 REPRESENTATION_ITEM ( '' )  );
#44904 = CARTESIAN_POINT ( 'NONE',  ( 2.849036369511732440E-14, 204.2500000000000284, 202.0000000000000000 ) ) ;
#44905 = CARTESIAN_POINT ( 'NONE',  ( -8.311093377946836114, 112.9687499965860269, -8.311093377946837890 ) ) ;
#44906 = FACE_OUTER_BOUND ( 'NONE', #24047, .T. ) ;
#44907 = ORIENTED_EDGE ( 'NONE', *, *, #44001, .F. ) ;
#44908 = EDGE_LOOP ( 'NONE', ( #1604, #16260, #36499, #755 ) ) ;
#44909 = EDGE_CURVE ( 'NONE', #72057, #17570, #59234, .T. ) ;
#44910 = CARTESIAN_POINT ( 'NONE',  ( -8.342170076843785083E-16, 6.187499998634407028, 4.541265875000002339 ) ) ;
#44911 = CARTESIAN_POINT ( 'NONE',  ( -2.977408999572654480, 16.49999999795161543, 7.188101187499999156 ) ) ;
#44912 = CARTESIAN_POINT ( 'NONE',  ( 8.000000000000000000, 108.0312500040967620, -3.313708498984762496 ) ) ;
#44913 = CARTESIAN_POINT ( 'NONE',  ( -7.204075437095967871, 7.204075437095967871, 90.34375000204838102 ) ) ;
#44914 = CARTESIAN_POINT ( 'NONE',  ( -30.44569435410883074, 197.8125000013656063, 167.5543056458915885 ) ) ;
#44915 = CARTESIAN_POINT ( 'NONE',  ( -4.000000000000001776, 7.500000000000000000, -4.898587196589415787E-16 ) ) ;
#44916 = CARTESIAN_POINT ( 'NONE',  ( 2.828427124746190291, 20.62499999726881583, 2.828427124746192067 ) ) ;
#44917 = CARTESIAN_POINT ( 'NONE',  ( 4.541265875000001451, 8.249999998634406140, 1.881053915767124440 ) ) ;
#44918 = CARTESIAN_POINT ( 'NONE',  ( -1.656854249492403008, 198.6875000000000284, 146.0000000000000284 ) ) ;
#44919 = EDGE_LOOP ( 'NONE', ( #13082, #11208, #57604, #73058 ) ) ;
#44920 = CARTESIAN_POINT ( 'NONE',  ( 3.313708498984828221, 117.0312499999999858, -7.999999999999932498 ) ) ;
#44921 = CARTESIAN_POINT ( 'NONE',  ( -7.188101187499999156, 109.2500000020483952, 2.977408999572654924 ) ) ;
#44923 = CARTESIAN_POINT ( 'NONE',  ( -2.849036369511732440E-14, 209.2500000000000284, 138.0000000000000568 ) ) ;
#44922 = CARTESIAN_POINT ( 'NONE',  ( -29.43265458321771177, 195.5000000013655779, 166.5412658750003914 ) ) ;
#44924 = SHAPE_REPRESENTATION_RELATIONSHIP ( 'NONE' , 'NONE' ,  #64301, #53434 ) ;
#44925 = EDGE_CURVE ( 'NONE', #3614, #63985, #2587, .T. ) ;
#44926 = CARTESIAN_POINT ( 'NONE',  ( 4.541265875000002339, 22.31249999863440436, 0.000000000000000000 ) ) ;
#44927 = CARTESIAN_POINT ( 'NONE',  ( -2.977408999572647819, 7.188101187499991163, 1.205302781871753215 ) ) ;
#44928 = VERTEX_POINT ( 'NONE', #2099 ) ;
#44929 = EDGE_LOOP ( 'NONE', ( #7232, #25733, #31460, #1440 ) ) ;
#44930 = CARTESIAN_POINT ( 'NONE',  ( -4.220049686691935698, 10.18810118749999916, 91.37500000204838102 ) ) ;
#44931 = CARTESIAN_POINT ( 'NONE',  ( -8.967304722683161700, 219.9183361721456720, 6.468172613360420264 ) ) ;
#44932 = CARTESIAN_POINT ( 'NONE',  ( -25.55430564589119413, 200.5625000013656063, 167.5543056458915316 ) ) ;
#44933 = CARTESIAN_POINT ( 'NONE',  ( -10.99999999999999822, -4.556349186104052151, 107.5937499999999858 ) ) ;
#44934 = CARTESIAN_POINT ( 'NONE',  ( -3.458734124999960358, 207.6250000013656347, 196.5673454167823877 ) ) ;
#44935 = CARTESIAN_POINT ( 'NONE',  ( 13.99999999999999822, 0.000000000000000000, 0.000000000000000000 ) ) ;
#44936 = CARTESIAN_POINT ( 'NONE',  ( -10.00000000000000000, 117.2916666666666430, -2.679491924311229845 ) ) ;
#44937 = AXIS2_PLACEMENT_3D ( 'NONE', #38603, #60476, #32575 ) ;
#44938 = CARTESIAN_POINT ( 'NONE',  ( 1.469576158976823947E-15, 108.8750000000000000, 8.000000000000000000 ) ) ;
#44939 = CARTESIAN_POINT ( 'NONE',  ( 4.721056650415999201, 291.2343750017069510, -4.721056650415999201 ) ) ;
#44940 = CARTESIAN_POINT ( 'NONE',  ( 7.188101187499992051, 8.802885111219154394E-16, 4.111552781871752771 ) ) ;
#44941 = ADVANCED_FACE ( 'NONE', ( #47736 ), #1746, .F. ) ;
#44942 = EDGE_CURVE ( 'NONE', #11938, #33033, #63768, .T. ) ;
#44943 = CARTESIAN_POINT ( 'NONE',  ( 28.00000000000002132, 204.9375000013656063, 166.5412658749999082 ) ) ;
#44944 = CARTESIAN_POINT ( 'NONE',  ( -5.656854249492381470, 26.24999999590322375, 5.656854249492379694 ) ) ;
#44945 = CARTESIAN_POINT ( 'NONE',  ( 2.445694354108782775, 199.5625000013656063, 139.5543056458912190 ) ) ;
#44946 = DIRECTION ( 'NONE',  ( 1.000000000000000000, -1.776356839400250465E-15, 0.000000000000000000 ) ) ;
#44948 = CARTESIAN_POINT ( 'NONE',  ( -3.458734125000016757, 204.1250000013656063, 140.5673454167824161 ) ) ;
#44947 = CARTESIAN_POINT ( 'NONE',  ( -2.249999999999998224, 283.9999999998748308, 5.427273999917394676 ) ) ;
#44949 = CARTESIAN_POINT ( 'NONE',  ( 5.676582343750005144, 245.8854166700806445, 9.832129032723416984 ) ) ;
#44950 = DIRECTION ( 'NONE',  ( -0.000000000000000000, 1.000000000000000000, 0.000000000000000000 ) ) ;
#44951 = CARTESIAN_POINT ( 'NONE',  ( 0.000000000000000000, 51.05255888325788050, 10.99999999999999112 ) ) ;
#44952 = CARTESIAN_POINT ( 'NONE',  ( 26.34314575050763452, 200.5625000000000284, 165.9999999999998863 ) ) ;
#44953 = CARTESIAN_POINT ( 'NONE',  ( -5.676582343750006032, 9.114583329919350163, 9.832129032723418760 ) ) ;
#44954 = CARTESIAN_POINT ( 'NONE',  ( 8.000000000000000000, 100.5312500040967905, -3.313708498984762496 ) ) ;
#44955 = CARTESIAN_POINT ( 'NONE',  ( -8.311093377946841443, 214.2187499965860411, 8.311093377946830785 ) ) ;
#44956 = DIRECTION ( 'NONE',  ( -1.000000000000000000, -0.000000000000000000, -0.000000000000000000 ) ) ;
#44957 = CARTESIAN_POINT ( 'NONE',  ( 27.99999999999999645, 210.0000000000000284, 165.9999999999999147 ) ) ;
#44959 = CARTESIAN_POINT ( 'NONE',  ( -7.999999999999991118, 3.313708498984757167, 29.23655277982336642 ) ) ;
#44958 = CARTESIAN_POINT ( 'NONE',  ( -3.313708498984719864, 25.78124999590322020, -8.000000000000040856 ) ) ;
#44960 = ORIENTED_EDGE ( 'NONE', *, *, #50964, .T. ) ;
#44961 = CARTESIAN_POINT ( 'NONE',  ( -2.445694354108840063, 200.0625000013656063, 139.5543056458912190 ) ) ;
#44962 = CARTESIAN_POINT ( 'NONE',  ( -11.35316468750000141, 8.489583329919348387, 3.042071309553159963 ) ) ;
#44963 = CARTESIAN_POINT ( 'NONE',  ( 7.778174593052023411, -7.778174593052021635, 90.25000000409677625 ) ) ;
#44964 = CARTESIAN_POINT ( 'NONE',  ( 2.485281374238919927, 292.3125000000000568, 5.999999999999654499 ) ) ;
#44965 = CARTESIAN_POINT ( 'NONE',  ( -29.43265458321770822, 197.5000000013656063, 166.5412658750003914 ) ) ;
#44966 = CARTESIAN_POINT ( 'NONE',  ( 3.313708498984752726, 7.031249995903221972, 8.000000000000008882 ) ) ;
#44968 = CARTESIAN_POINT ( 'NONE',  ( -2.085542519210945728E-15, 4.531249996586016238, 11.35316468750000141 ) ) ;
#44967 = CARTESIAN_POINT ( 'NONE',  ( 2.977408999572654480, 117.1250000020483810, 7.188101187499999156 ) ) ;
#44969 = CARTESIAN_POINT ( 'NONE',  ( -7.999999999999991118, 3.313708498984756723, 20.23655277982336642 ) ) ;
#44970 = CARTESIAN_POINT ( 'NONE',  ( -9.832129032723418760, 137.8645833299193555, -5.676582343750004256 ) ) ;
#44971 = CARTESIAN_POINT ( 'NONE',  ( 8.660254037844389075, 102.2916666598386968, -5.000000000000000000 ) ) ;
#44972 = EDGE_CURVE ( 'NONE', #8029, #61067, #51708, .T. ) ;
#44973 = CARTESIAN_POINT ( 'NONE',  ( -4.401442555609581635E-16, 119.6562500020483810, -7.188101187500000044 ) ) ;
#44974 = FACE_OUTER_BOUND ( 'NONE', #22229, .T. ) ;
#44975 = CARTESIAN_POINT ( 'NONE',  ( -24.54126587499999701, 208.4375000013656063, 170.0000000000003411 ) ) ;
#44976 = CARTESIAN_POINT ( 'NONE',  ( 10.00000000000000533, 144.7916666666666856, 2.679491924311237394 ) ) ;
#44977 = ORIENTED_EDGE ( 'NONE', *, *, #31043, .T. ) ;
#44978 = CARTESIAN_POINT ( 'NONE',  ( 0.6474643998350866347, -60.19533971085802904, 22.88219507986015699 ) ) ;
#44979 = CARTESIAN_POINT ( 'NONE',  ( 6.676582343750003368, 289.1718750017070647, -2.765530957081997254 ) ) ;
#44980 = CYLINDRICAL_SURFACE ( 'NONE', #66426, 10.00000000000000178 ) ;
#44981 = CARTESIAN_POINT ( 'NONE',  ( -5.656854249492375253, 5.656854249492375253, 3.830302783920144893 ) ) ;
#44982 = CARTESIAN_POINT ( 'NONE',  ( 3.999999999999960032, 207.0625000027312126, 143.6568542494924259 ) ) ;
#44983 = LINE ( 'NONE', #16657, #33836 ) ;
#44984 = CARTESIAN_POINT ( 'NONE',  ( -4.220049686691935698, 10.18810118749999916, 99.25000000204838102 ) ) ;
#44985 = ORIENTED_EDGE ( 'NONE', *, *, #46321, .T. ) ;
#44986 = DIRECTION ( 'NONE',  ( 1.000000000000000000, 1.776356839400250465E-15, 0.000000000000000000 ) ) ;
#44987 = CARTESIAN_POINT ( 'NONE',  ( 3.042071309553159519, 175.0520833299193555, 11.35316468750000141 ) ) ;
#44988 = CARTESIAN_POINT ( 'NONE',  ( 0.000000000000000000, 207.0000000000000568, 170.0000000000000284 ) ) ;
#44989 = CARTESIAN_POINT ( 'NONE',  ( 2.839093476692135984E-14, 201.9375000013656063, 201.4587341250000350 ) ) ;
#44990 = CARTESIAN_POINT ( 'NONE',  ( -3.313708498984757611, 7.999999999999991118, 0.7365527839201455595 ) ) ;
#44991 = CARTESIAN_POINT ( 'NONE',  ( 11.35316468749999963, 71.30208332991932707, -3.042071309553165293 ) ) ;
#44993 = ORIENTED_EDGE ( 'NONE', *, *, #41588, .F. ) ;
#44992 =( BOUNDED_CURVE ( )  B_SPLINE_CURVE ( 2, ( #48077, #30738, #36040, #59056, #6994, #42415, #54127, #2067, #25056, #19044, #18685, #41691, #1350, #42048, #25431, #35312, #19777, #53391, #71085, #30005, #65433, #1716, #13729, #24334, #52647, #36774, #70003, #71449, #63965, #12277, #58323, #23965, #46973, #66929, #8462, #2811, #32996, #60892, #61269, #43918, #60142, #9214, #21269, #20516, #9965, #61646, #4310, #54505, #49573, #55625, #26930, #48820, #20896, #9598, #71827, #15234, #32617, #37139, #8844, #20144, #72203, #66545, #3941, #26173, #14480, #31482, #43530, #49949, #50316, #25800, #73337, #72964, #14107, #44293, #67307, #42785, #3559, #43160, #66176, #14854, #38265, #15605, #38644, #55996, #31854, #60518, #27300, #65801, #54877, #37519, #3187, #49192, #37894, #32235, #55252, #26549, #72591, #5796, #45773, #45395, #68411, #51431, #51061, #57106, #68049, #34855, #10701, #62741, #11818, #39741, #11081, #51809, #21641, #156, #74443, #28793, #57861, #33735, #34108, #23132, #22014, #73702, #46144, #56737, #15978, #17094, #5419, #39008, #4682, #5056, #44667, #62374, #16711, #28424, #22750, #68785, #67681, #34485, #40116, #69161, #74074, #62011, #63122, #50683, #40491, #11450, #57491, #17470, #63496, #10336, #6167, #22374, #33361, #28052, #45040, #16340, #27677, #29176, #52191, #56362, #39377, #58966, #24239, #47252, #8004, #70279, #31011, #30648, #46517, #36317, #64968, #522, #35948, #6537, #35219, #52929, #1626, #12553, #13277, #1260, #58239, #18222, #24970, #53302, #41237, #29543, #52554, #12182, #41602, #6901, #7274, #18591, #64617, #63870, #47614, #893, #23879, #64243, #23502, #69536, #46888, #30281, #12913, #24606, #69912, #35581, #58595, #13646, #70999, #70637, #59332, #18956, #17847, #41960, #29912, #7643, #53666, #40864, #1978, #47986, #19315, #42327, #65345, #36685, #59696, #19687, #3096, #26080, #61558, #49102, #9879, #9512, #25341, #15146, #43828, #54036, #14767, #60050, #14013, #31765, #55163, #32527, #38178, #44208, #43067, #71735, #3849, #32143, #20051, #37050, #31387, #65709, #20427, #60427, #60801, #72114, #54784, #42696, #26458, #8371, #54413, #61182, #66843, #20810, #49482, #37805, #43443, #66458, #2720, #25708, #48729, #67221, #49860, #9126, #55539, #3469, #48355, #14393, #66083, #2347, #72878, #26845, #72501, #21183, #37427, #15517, #38557, #71361, #8754, #10249, #63038, #51719, #57025, #34027, #39662, #39293, #16254, #21923, #68330, #67, #4224, #62293, #16627, #50598, #34397 ),
 .UNSPECIFIED., .F., .F. ) 
 B_SPLINE_CURVE_WITH_KNOTS ( ( 3, 2, 2, 2, 2, 2, 2, 2, 2, 2, 2, 2, 2, 2, 2, 2, 2, 2, 2, 2, 2, 2, 2, 2, 2, 2, 2, 2, 2, 2, 2, 2, 2, 2, 2, 2, 2, 2, 2, 2, 2, 2, 2, 2, 2, 2, 2, 2, 2, 2, 2, 2, 2, 2, 2, 2, 2, 2, 2, 2, 2, 2, 2, 2, 2, 2, 2, 2, 2, 2, 2, 2, 2, 2, 2, 2, 2, 2, 2, 2, 2, 2, 2, 2, 2, 2, 2, 2, 2, 2, 2, 2, 2, 2, 2, 2, 2, 2, 2, 2, 2, 2, 2, 2, 2, 2, 2, 2, 2, 2, 2, 2, 2, 2, 2, 2, 2, 2, 2, 2, 2, 2, 2, 2, 2, 2, 2, 2, 2, 2, 2, 2, 2, 2, 2, 2, 2, 2, 2, 2, 2, 2, 2, 2, 2, 2, 2, 2, 2, 2, 2, 2, 3 ),
 ( 0.000000000000000000, 0.006578947368421052266, 0.01315789473684210453, 0.01973684210526315680, 0.02631578947368420907, 0.03289473684210526133, 0.03947368421052631360, 0.04605263157894736586, 0.05263157894736841813, 0.05921052631578947040, 0.06578947368421052266, 0.07236842105263158187, 0.07894736842105262720, 0.08552631578947368640, 0.09210526315789473173, 0.09868421052631579093, 0.1052631578947368363, 0.1118421052631578955, 0.1184210526315789408, 0.1250000000000000000, 0.1315789473684210453, 0.1381578947368421184, 0.1447368421052631637, 0.1513157894736842091, 0.1578947368421052544, 0.1644736842105263275, 0.1710526315789473728, 0.1776315789473684181, 0.1842105263157894635, 0.1907894736842105365, 0.1973684210526315819, 0.2039473684210526272, 0.2105263157894736725, 0.2171052631578947456, 0.2236842105263157909, 0.2302631578947368363, 0.2368421052631578816, 0.2434210526315789547, 0.2500000000000000000, 0.2565789473684210731, 0.2631578947368420907, 0.2697368421052631637, 0.2763157894736842368, 0.2828947368421052544, 0.2894736842105263275, 0.2960526315789473450, 0.3026315789473684181, 0.3092105263157894912, 0.3157894736842105088, 0.3223684210526315819, 0.3289473684210526550, 0.3355263157894736725, 0.3421052631578947456, 0.3486842105263157632, 0.3552631578947368363, 0.3618421052631579093, 0.3684210526315789269, 0.3750000000000000000, 0.3815789473684210731, 0.3881578947368420907, 0.3947368421052631637, 0.4013157894736842368, 0.4078947368421052544, 0.4144736842105263275, 0.4210526315789473450, 0.4276315789473684181, 0.4342105263157894912, 0.4407894736842105088, 0.4473684210526315819, 0.4539473684210526550, 0.4605263157894736725, 0.4671052631578947456, 0.4736842105263157632, 0.4802631578947368363, 0.4868421052631579093, 0.4934210526315789269, 0.5000000000000000000, 0.5065789473684210176, 0.5131578947368421462, 0.5197368421052631637, 0.5263157894736841813, 0.5328947368421053099, 0.5394736842105263275, 0.5460526315789473450, 0.5526315789473684736, 0.5592105263157894912, 0.5657894736842105088, 0.5723684210526315264, 0.5789473684210526550, 0.5855263157894736725, 0.5921052631578946901, 0.5986842105263158187, 0.6052631578947368363, 0.6118421052631578538, 0.6184210526315789824, 0.6250000000000000000, 0.6315789473684210176, 0.6381578947368421462, 0.6447368421052631637, 0.6513157894736841813, 0.6578947368421053099, 0.6644736842105263275, 0.6710526315789473450, 0.6776315789473684736, 0.6842105263157894912, 0.6907894736842105088, 0.6973684210526315264, 0.7039473684210526550, 0.7105263157894736725, 0.7171052631578946901, 0.7236842105263158187, 0.7302631578947368363, 0.7368421052631578538, 0.7434210526315789824, 0.7500000000000000000, 0.7565789473684210176, 0.7631578947368421462, 0.7697368421052631637, 0.7763157894736841813, 0.7828947368421053099, 0.7894736842105263275, 0.7960526315789473450, 0.8026315789473684736, 0.8092105263157894912, 0.8157894736842105088, 0.8223684210526315264, 0.8289473684210526550, 0.8355263157894736725, 0.8421052631578946901, 0.8486842105263158187, 0.8552631578947368363, 0.8618421052631578538, 0.8684210526315789824, 0.8750000000000000000, 0.8815789473684210176, 0.8881578947368421462, 0.8947368421052631637, 0.9013157894736841813, 0.9078947368421053099, 0.9144736842105263275, 0.9210526315789473450, 0.9276315789473684736, 0.9342105263157894912, 0.9407894736842105088, 0.9473684210526315264, 0.9539473684210526550, 0.9605263157894736725, 0.9671052631578946901, 0.9736842105263158187, 0.9802631578947368363, 0.9868421052631578538, 0.9934210526315789824, 0.9940576599040155115 ),
 .UNSPECIFIED. ) 
 CURVE ( )  GEOMETRIC_REPRESENTATION_ITEM ( )  RATIONAL_B_SPLINE_CURVE ( ( 1.000000000000000000, 0.9238795325112867385, 1.000000000000000000, 0.9238795325112867385, 1.000000000000000000, 0.9238795325112867385, 1.000000000000000000, 0.9238795325112867385, 1.000000000000000000, 0.9238795325112867385, 1.000000000000000000, 0.9238795325112867385, 1.000000000000000000, 0.9238795325112867385, 1.000000000000000000, 0.9238795325112867385, 1.000000000000000000, 0.9238795325112867385, 1.000000000000000000, 0.9238795325112867385, 1.000000000000000000, 0.9238795325112867385, 1.000000000000000000, 0.9238795325112867385, 1.000000000000000000, 0.9238795325112867385, 1.000000000000000000, 0.9238795325112867385, 1.000000000000000000, 0.9238795325112867385, 1.000000000000000000, 0.9238795325112867385, 1.000000000000000000, 0.9238795325112867385, 1.000000000000000000, 0.9238795325112867385, 1.000000000000000000, 0.9238795325112867385, 1.000000000000000000, 0.9238795325112867385, 1.000000000000000000, 0.9238795325112867385, 1.000000000000000000, 0.9238795325112867385, 1.000000000000000000, 0.9238795325112867385, 1.000000000000000000, 0.9238795325112867385, 1.000000000000000000, 0.9238795325112867385, 1.000000000000000000, 0.9238795325112867385, 1.000000000000000000, 0.9238795325112867385, 1.000000000000000000, 0.9238795325112867385, 1.000000000000000000, 0.9238795325112867385, 1.000000000000000000, 0.9238795325112867385, 1.000000000000000000, 0.9238795325112867385, 1.000000000000000000, 0.9238795325112867385, 1.000000000000000000, 0.9238795325112867385, 1.000000000000000000, 0.9238795325112867385, 1.000000000000000000, 0.9238795325112867385, 1.000000000000000000, 0.9238795325112867385, 1.000000000000000000, 0.9238795325112867385, 1.000000000000000000, 0.9238795325112867385, 1.000000000000000000, 0.9238795325112867385, 1.000000000000000000, 0.9238795325112867385, 1.000000000000000000, 0.9238795325112867385, 1.000000000000000000, 0.9238795325112867385, 1.000000000000000000, 0.9238795325112867385, 1.000000000000000000, 0.9238795325112867385, 1.000000000000000000, 0.9238795325112867385, 1.000000000000000000, 0.9238795325112867385, 1.000000000000000000, 0.9238795325112867385, 1.000000000000000000, 0.9238795325112867385, 1.000000000000000000, 0.9238795325112867385, 1.000000000000000000, 0.9238795325112867385, 1.000000000000000000, 0.9238795325112867385, 1.000000000000000000, 0.9238795325112867385, 1.000000000000000000, 0.9238795325112867385, 1.000000000000000000, 0.9238795325112867385, 1.000000000000000000, 0.9238795325112867385, 1.000000000000000000, 0.9238795325112867385, 1.000000000000000000, 0.9238795325112867385, 1.000000000000000000, 0.9238795325112867385, 1.000000000000000000, 0.9238795325112867385, 1.000000000000000000, 0.9238795325112867385, 1.000000000000000000, 0.9238795325112867385, 1.000000000000000000, 0.9238795325112867385, 1.000000000000000000, 0.9238795325112867385, 1.000000000000000000, 0.9238795325112867385, 1.000000000000000000, 0.9238795325112867385, 1.000000000000000000, 0.9238795325112867385, 1.000000000000000000, 0.9238795325112867385, 1.000000000000000000, 0.9238795325112867385, 1.000000000000000000, 0.9238795325112867385, 1.000000000000000000, 0.9238795325112867385, 1.000000000000000000, 0.9238795325112867385, 1.000000000000000000, 0.9238795325112867385, 1.000000000000000000, 0.9238795325112867385, 1.000000000000000000, 0.9238795325112867385, 1.000000000000000000, 0.9238795325112867385, 1.000000000000000000, 0.9238795325112867385, 1.000000000000000000, 0.9238795325112867385, 1.000000000000000000, 0.9238795325112867385, 1.000000000000000000, 0.9238795325112867385, 1.000000000000000000, 0.9238795325112867385, 1.000000000000000000, 0.9238795325112867385, 1.000000000000000000, 0.9238795325112867385, 1.000000000000000000, 0.9238795325112867385, 1.000000000000000000, 0.9238795325112867385, 1.000000000000000000, 0.9238795325112867385, 1.000000000000000000, 0.9238795325112867385, 1.000000000000000000, 0.9238795325112867385, 1.000000000000000000, 0.9238795325112867385, 1.000000000000000000, 0.9238795325112867385, 1.000000000000000000, 0.9238795325112867385, 1.000000000000000000, 0.9238795325112867385, 1.000000000000000000, 0.9238795325112867385, 1.000000000000000000, 0.9238795325112867385, 1.000000000000000000, 0.9238795325112867385, 1.000000000000000000, 0.9238795325112867385, 1.000000000000000000, 0.9238795325112867385, 1.000000000000000000, 0.9238795325112867385, 1.000000000000000000, 0.9238795325112867385, 1.000000000000000000, 0.9238795325112867385, 1.000000000000000000, 0.9238795325112867385, 1.000000000000000000, 0.9238795325112867385, 1.000000000000000000, 0.9238795325112867385, 1.000000000000000000, 0.9238795325112867385, 1.000000000000000000, 0.9238795325112867385, 1.000000000000000000, 0.9238795325112867385, 1.000000000000000000, 0.9238795325112867385, 1.000000000000000000, 0.9238795325112867385, 1.000000000000000000, 0.9238795325112867385, 1.000000000000000000, 0.9238795325112867385, 1.000000000000000000, 0.9238795325112867385, 1.000000000000000000, 0.9238795325112867385, 1.000000000000000000, 0.9238795325112867385, 1.000000000000000000, 0.9238795325112867385, 1.000000000000000000, 0.9238795325112867385, 1.000000000000000000, 0.9238795325112867385, 1.000000000000000000, 0.9238795325112867385, 1.000000000000000000, 0.9238795325112867385, 1.000000000000000000, 0.9238795325112867385, 1.000000000000000000, 0.9238795325112867385, 1.000000000000000000, 0.9238795325112867385, 1.000000000000000000, 0.9238795325112867385, 1.000000000000000000, 0.9238795325112867385, 1.000000000000000000, 0.9238795325112867385, 1.000000000000000000, 0.9238795325112867385, 1.000000000000000000, 0.9238795325112867385, 1.000000000000000000, 0.9238795325112867385, 1.000000000000000000, 0.9238795325112867385, 1.000000000000000000, 0.9238795325112867385, 1.000000000000000000, 0.9238795325112867385, 1.000000000000000000, 0.9238795325112867385, 1.000000000000000000, 0.9238795325112867385, 1.000000000000000000, 0.9238795325112867385, 1.000000000000000000, 0.9238795325112867385, 1.000000000000000000, 0.9238795325112867385, 1.000000000000000000, 0.9238795325112867385, 1.000000000000000000, 0.9238795325112867385, 1.000000000000000000, 0.9238795325112867385, 1.000000000000000000, 0.9238795325112867385, 1.000000000000000000, 0.9238795325112867385, 1.000000000000000000, 0.9238795325112867385, 1.000000000000000000, 0.9238795325112867385, 1.000000000000000000, 0.9238795325112867385, 1.000000000000000000, 0.9238795325112867385, 1.000000000000000000, 0.9238795325112867385, 1.000000000000000000, 0.9238795325112867385, 1.000000000000000000, 0.9238795325112867385, 1.000000000000000000, 0.9238795325112867385, 1.000000000000000000, 0.9238795325112867385, 1.000000000000000000, 0.9238795325112867385, 1.000000000000000000, 0.9238795325112867385, 1.000000000000000000, 0.9238795325112867385, 1.000000000000000000, 0.9926342558359432244, 0.9866939939076171395 ) ) 
 REPRESENTATION_ITEM ( '' )  );
#44994 = CARTESIAN_POINT ( 'NONE',  ( -4.220049686691937474, -10.18810118749999738, 114.4375000020483668 ) ) ;
#44995 = CARTESIAN_POINT ( 'NONE',  ( -3.211159895383561391, 13.81249999863440614, -3.211159895383561835 ) ) ;
#44996 = ORIENTED_EDGE ( 'NONE', *, *, #57781, .T. ) ;
#44997 = AXIS2_PLACEMENT_3D ( 'NONE', #55960, #3518, #73298 ) ;
#44998 = CARTESIAN_POINT ( 'NONE',  ( -5.656854249492379694, 0.5625000000000000000, -5.656854249492380582 ) ) ;
#44999 = CARTESIAN_POINT ( 'NONE',  ( 2.679491924311222739, 113.9583333333333570, 10.00000000000000355 ) ) ;
#45000 = CARTESIAN_POINT ( 'NONE',  ( 8.660254037844389075, 67.29166665983869677, -5.000000000000000000 ) ) ;
#45001 = CARTESIAN_POINT ( 'NONE',  ( -7.188101187500000044, 18.09374999795161187, -8.802885111219163269E-16 ) ) ;
#45002 = LINE ( 'NONE', #34448, #42365 ) ;
#45003 = EDGE_CURVE ( 'NONE', #38745, #1872, #59432, .T. ) ;
#45004 = CARTESIAN_POINT ( 'NONE',  ( -4.220049686691935698, 10.18810118749999916, 111.2500000020483952 ) ) ;
#45005 = EDGE_CURVE ( 'NONE', #20313, #46612, #48418, .T. ) ;
#45006 = CARTESIAN_POINT ( 'NONE',  ( 4.000000000000016875, 201.5625000027312126, 199.6568542494924259 ) ) ;
#45007 = CARTESIAN_POINT ( 'NONE',  ( 2.449293598294707893E-16, 8.999999997268814056, -4.000000000000001776 ) ) ;
#45008 = CYLINDRICAL_SURFACE ( 'NONE', #36119, 10.00000000000000178 ) ;
#45009 = ORIENTED_EDGE ( 'NONE', *, *, #57637, .T. ) ;
#45010 = CARTESIAN_POINT ( 'NONE',  ( -1.432654583217607858, 203.6250000013656063, 201.4587341250000065 ) ) ;
#45011 = CARTESIAN_POINT ( 'NONE',  ( -31.99999999999995737, 194.4375000027312126, 171.6568542494928522 ) ) ;
#45012 = DIRECTION ( 'NONE',  ( 0.8660254037844408170, 0.4999999999999962808, -0.000000000000000000 ) ) ;
#45013 = EDGE_CURVE ( 'NONE', #25275, #3031, #20554, .T. ) ;
#45014 = CARTESIAN_POINT ( 'NONE',  ( 3.211159895383561835, 10.43749999863440792, -3.211159895383561835 ) ) ;
#45015 = CARTESIAN_POINT ( 'NONE',  ( 10.99999999999999645, -10.99999999999999645, 20.00000000000000000 ) ) ;
#45016 = AXIS2_PLACEMENT_3D ( 'NONE', #61306, #66583, #11387 ) ;
#45017 = CARTESIAN_POINT ( 'NONE',  ( 7.188101187499992051, 8.802885111219154394E-16, 21.73655278187175455 ) ) ;
#45018 = ORIENTED_EDGE ( 'NONE', *, *, #42354, .T. ) ;
#45019 = CARTESIAN_POINT ( 'NONE',  ( -2.726571689596997292E-14, 210.0000000000000284, 138.0000000000000568 ) ) ;
#45020 = EDGE_LOOP ( 'NONE', ( #46033, #58756, #3760, #52970 ) ) ;
#45021 = CARTESIAN_POINT ( 'NONE',  ( -6.238412754330611322E-16, 10.18810118749999916, 107.7812500020483810 ) ) ;
#45022 = DIRECTION ( 'NONE',  ( -0.000000000000000000, 1.000000000000000000, -0.000000000000000000 ) ) ;
#45023 = CARTESIAN_POINT ( 'NONE',  ( -3.458734124999959025, 203.5000000013655779, 199.4326545832176691 ) ) ;
#45024 = CARTESIAN_POINT ( 'NONE',  ( 24.54126587500000412, 201.2500000013656063, 171.4326545832176123 ) ) ;
#45025 = CARTESIAN_POINT ( 'NONE',  ( 2.679491924311222739, 83.95833333333332860, 10.00000000000000355 ) ) ;
#45026 = CARTESIAN_POINT ( 'NONE',  ( -4.898587196589412829E-16, 124.6250000000000000, -8.000000000000000000 ) ) ;
#45027 = CARTESIAN_POINT ( 'NONE',  ( 2.485281374238571317, 290.6875000000000000, -6.000000000000003553 ) ) ;
#45028 = CARTESIAN_POINT ( 'NONE',  ( 25.17157287525377996, 204.7500000027312126, 167.1715728752537586 ) ) ;
#45029 = ORIENTED_EDGE ( 'NONE', *, *, #22346, .F. ) ;
#45030 = CARTESIAN_POINT ( 'NONE',  ( -9.832129032723415207, 219.3229166700806729, 5.676582343750005144 ) ) ;
#45031 = EDGE_CURVE ( 'NONE', #37922, #36060, #67150, .T. ) ;
#45032 = CARTESIAN_POINT ( 'NONE',  ( 3.313708498984756279, 7.999999999999991118, 7.861552779823362869 ) ) ;
#45033 = CARTESIAN_POINT ( 'NONE',  ( -2.849036369511732440E-14, 194.3750000027311842, 138.0000000000000568 ) ) ;
#45034 = DIRECTION ( 'NONE',  ( -0.000000000000000000, 1.000000000000000000, -0.000000000000000000 ) ) ;
#45035 = DIRECTION ( 'NONE',  ( 0.000000000000000000, 0.000000000000000000, 1.000000000000000000 ) ) ;
#45036 = CARTESIAN_POINT ( 'NONE',  ( -6.123233995736766282E-16, 233.7500000000000000, -10.00000000000000000 ) ) ;
#45037 = CARTESIAN_POINT ( 'NONE',  ( 29.65685424949239746, 203.5625000027312126, 165.9999999999999432 ) ) ;
#45038 = CARTESIAN_POINT ( 'NONE',  ( 8.660254037844389075, 195.4166666666666856, -5.000000000000000000 ) ) ;
#45039 = DIRECTION ( 'NONE',  ( 0.000000000000000000, 0.000000000000000000, -1.000000000000000000 ) ) ;
#45040 = CARTESIAN_POINT ( 'NONE',  ( 5.082755093536320601, -5.082755093536318824, 14.42405278187175455 ) ) ;
#45041 = CARTESIAN_POINT ( 'NONE',  ( -8.311093377946836114, 172.9687499965860127, -8.311093377946837890 ) ) ;
#45042 = CARTESIAN_POINT ( 'NONE',  ( -11.00000000000000000, 11.00000000000000000, -6.938893903907228378E-15 ) ) ;
#45043 = CARTESIAN_POINT ( 'NONE',  ( -1.330417324339310703, -42.30397995383646759, 151.0457658719072640 ) ) ;
#45045 = CARTESIAN_POINT ( 'NONE',  ( -4.000000000000001776, 7.249999997268813168, -4.898587196589415787E-16 ) ) ;
#45044 = CARTESIAN_POINT ( 'NONE',  ( 3.458734124999960358, 209.6875000013656063, 142.0000000000000568 ) ) ;
#45046 = EDGE_LOOP ( 'NONE', ( #34891, #54347, #72765, #35898 ) ) ;
#45047 = CARTESIAN_POINT ( 'NONE',  ( 5.676582343749993598, 25.26041666325268764, 9.832129032723422313 ) ) ;
#45048 = CARTESIAN_POINT ( 'NONE',  ( -1.037253499927559108, 194.5743829752848626, 201.4270020984891971 ) ) ;
#45050 = CARTESIAN_POINT ( 'NONE',  ( 1.308779242298710344, -10.28008949575750641, -63.61387346696258049 ) ) ;
#45049 = FACE_OUTER_BOUND ( 'NONE', #28128, .T. ) ;
#45051 = CARTESIAN_POINT ( 'NONE',  ( -28.50353167905964469, -51.84776567077469878, 182.2254167621141505 ) ) ;
#45052 = CARTESIAN_POINT ( 'NONE',  ( -1.432654583217662259, 202.1250000013656063, 145.4587341250000350 ) ) ;
#45053 = CARTESIAN_POINT ( 'NONE',  ( 7.320508075688771044, 61.24999999317203958, 7.320508075688775484 ) ) ;
#45054 = CARTESIAN_POINT ( 'NONE',  ( -2.977408999572650927, 101.3750000020483952, -7.188101187500001821 ) ) ;
#45055 = CARTESIAN_POINT ( 'NONE',  ( 4.541265875000002339, 6.499999998634407028, -1.881053915767121554 ) ) ;
#45056 = CARTESIAN_POINT ( 'NONE',  ( -5.656854249492375253, 5.656854249492375253, 5.142802779823363757 ) ) ;
#45057 = CARTESIAN_POINT ( 'NONE',  ( -2.828427124746190735, 5.124999997268813168, -2.828427124746191623 ) ) ;
#45058 = ORIENTED_EDGE ( 'NONE', *, *, #19001, .F. ) ;
#45059 = ORIENTED_EDGE ( 'NONE', *, *, #47047, .F. ) ;
#45060 = B_SPLINE_CURVE_WITH_KNOTS ( 'NONE', 3,
 ( #27671, #39001, #33730, #74068, #45767, #39371, #68042, #44660, #16333, #62367, #28787, #56732, #27294, #11442, #50310, #17088, #68778, #73331, #39736, #33355 ),
 .UNSPECIFIED., .F., .F.,
 ( 4, 2, 2, 2, 2, 2, 2, 2, 2, 4 ),
 ( 0.000000000000000000, 0.001156441540183992178, 0.001734662310275988158, 0.002312883080367984356, 0.003469324620551976317, 0.004625766160735968711, 0.005782207700919960239, 0.006938649241103952633, 0.008095090781287984927, 0.009251532321472018955 ),
 .UNSPECIFIED. ) ;
#45061 = CARTESIAN_POINT ( 'NONE',  ( -5.656854249492375253, 5.656854249492375253, 11.14280277982336642 ) ) ;
#45062 = CARTESIAN_POINT ( 'NONE',  ( -1.432654583217607414, 195.5000000013656347, 194.5412658750000219 ) ) ;
#45063 = CARTESIAN_POINT ( 'NONE',  ( -8.000000000000000000, 99.49999999999998579, 0.000000000000000000 ) ) ;
#45064 = CARTESIAN_POINT ( 'NONE',  ( -11.35316468749999785, 143.0729166632526983, -3.042071309553167513 ) ) ;
#45065 = VERTEX_POINT ( 'NONE', #37175 ) ;
#45066 = CARTESIAN_POINT ( 'NONE',  ( -5.000000000000001776, 10.82431413986196134, -67.03128830763429846 ) ) ;
#45067 = CARTESIAN_POINT ( 'NONE',  ( -10.18810118749999738, -4.220049686691941915, 88.75000000204836681 ) ) ;
#45068 = DIRECTION ( 'NONE',  ( 0.000000000000000000, 0.000000000000000000, 1.000000000000000000 ) ) ;
#45069 = CARTESIAN_POINT ( 'NONE',  ( 2.828427124746209831, 209.3750000000000284, 200.8284271247462129 ) ) ;
#45070 = CARTESIAN_POINT ( 'NONE',  ( 2.828427124746191623, 14.87499999726881406, -2.828427124746191623 ) ) ;
#45071 = CARTESIAN_POINT ( 'NONE',  ( 11.00000000000000000, 1.347111479062088405E-15, 117.4999999999999716 ) ) ;
#45072 = EDGE_LOOP ( 'NONE', ( #12717, #27566 ) ) ;
#45073 = CARTESIAN_POINT ( 'NONE',  ( 33.78855379685498406, -16.99759590218230088, 154.1484922053565469 ) ) ;
#45074 = CIRCLE ( 'NONE', #8881, 8.999999999999998224 ) ;
#45075 = CARTESIAN_POINT ( 'NONE',  ( -21.92274966597612362, 176.8557779608208875, 147.9630726405050041 ) ) ;
#45076 = CARTESIAN_POINT ( 'NONE',  ( -11.35316468750000141, 108.5937499965860269, -1.390361679473963753E-15 ) ) ;
#45077 = CARTESIAN_POINT ( 'NONE',  ( -1.432654583217607192, 201.2500000013656063, 194.5412658750000219 ) ) ;
#45078 = CARTESIAN_POINT ( 'NONE',  ( -7.188101187500000933, 25.49999999795161187, -2.977408999572651371 ) ) ;
#45079 = CARTESIAN_POINT ( 'NONE',  ( -4.220049686691937474, -10.18810118749999738, 81.81250000204838102 ) ) ;
#45080 = CARTESIAN_POINT ( 'NONE',  ( 9.832129032723420536, 41.51041666325268409, -5.676582343749999815 ) ) ;
#45081 = ORIENTED_EDGE ( 'NONE', *, *, #8471, .T. ) ;
#45082 = CARTESIAN_POINT ( 'NONE',  ( -1.656854249492383468, 4.687500000000000888, 4.000000000000000888 ) ) ;
#45083 = CARTESIAN_POINT ( 'NONE',  ( -8.008118988124991233, 0.000000000000000000, 20.51311528394062833 ) ) ;
#45084 = CARTESIAN_POINT ( 'NONE',  ( 2.445694354108783219, 208.8125000013656063, 139.5543056458912190 ) ) ;
#45085 = CARTESIAN_POINT ( 'NONE',  ( 2.977408999572650927, 11.24999999795161187, -7.188101187500001821 ) ) ;
#45086 = CARTESIAN_POINT ( 'NONE',  ( 1.102182119232618108E-15, 297.3125000034140157, 6.000000000000001776 ) ) ;
#45087 = CARTESIAN_POINT ( 'NONE',  ( 7.347880794884074377E-16, 114.5200769752660932, 47.89721922513225394 ) ) ;
#45088 = CARTESIAN_POINT ( 'NONE',  ( 4.401442555609581635E-16, 2.718749997951610542, -7.188101187500000044 ) ) ;
#45089 = EDGE_CURVE ( 'NONE', #33763, #17458, #19556, .T. ) ;
#45090 = CARTESIAN_POINT ( 'NONE',  ( 5.676582343750001591, 156.9270833299193555, -9.832129032723420536 ) ) ;
#45091 = CARTESIAN_POINT ( 'NONE',  ( -10.18810118749999738, -4.220049686691941915, 79.75000000204838102 ) ) ;
#45092 = CARTESIAN_POINT ( 'NONE',  ( -24.54126587499999701, 195.2500000013656063, 168.5673454167827003 ) ) ;
#45093 = EDGE_CURVE ( 'NONE', #54242, #26409, #7876, .T. ) ;
#45094 = CARTESIAN_POINT ( 'NONE',  ( 0.000000000000000000, 125.0000000000000000, 0.000000000000000000 ) ) ;
#45095 = CARTESIAN_POINT ( 'NONE',  ( -4.541265875000002339, 18.93749999863440436, -5.561446717895856393E-16 ) ) ;
#45096 = EDGE_LOOP ( 'NONE', ( #64037, #24741, #59862, #30399 ) ) ;
#45097 = VECTOR ( 'NONE', #23297, 1000.000000000000000 ) ;
#45098 = CARTESIAN_POINT ( 'NONE',  ( 4.000000000000015987, 198.5625000027312126, 199.6568542494924259 ) ) ;
#45099 = CARTESIAN_POINT ( 'NONE',  ( 3.458734124999960358, 195.6875000013655779, 142.0000000000000568 ) ) ;
#45101 =( BOUNDED_CURVE ( )  B_SPLINE_CURVE ( 2, ( #3324, #4081, #54641, #25939, #37662, #25050, #30731, #2432, #8457 ),
 .UNSPECIFIED., .F., .F. ) 
 B_SPLINE_CURVE_WITH_KNOTS ( ( 3, 2, 2, 2, 3 ),
 ( 0.2000000000000001776, 0.2083333333333335091, 0.2166666666666668406, 0.2250000000000001998, 0.2333333333333335313 ),
 .UNSPECIFIED. ) 
 CURVE ( )  GEOMETRIC_REPRESENTATION_ITEM ( )  RATIONAL_B_SPLINE_CURVE ( ( 0.9999999999999984457, 0.9238795325112882928, 1.000000000000000000, 0.9238795325112867385, 1.000000000000000000, 0.9238795325112867385, 1.000000000000000000, 0.9238795325112849621, 1.000000000000001776 ) ) 
 REPRESENTATION_ITEM ( '' )  );
#45100 = CARTESIAN_POINT ( 'NONE',  ( -29.65685424949246496, 206.1875000027311842, 166.0000000000004263 ) ) ;
#45102 = CARTESIAN_POINT ( 'NONE',  ( -5.656854249492381470, 21.93750000000000355, 5.656854249492379694 ) ) ;
#45103 = ORIENTED_EDGE ( 'NONE', *, *, #58655, .F. ) ;
#45104 = CARTESIAN_POINT ( 'NONE',  ( -7.188101187500000044, 11.71874999795161010, -8.802885111219163269E-16 ) ) ;
#45105 = DIRECTION ( 'NONE',  ( -0.000000000000000000, 0.4789076340208374138, 0.8778652960885079404 ) ) ;
#45106 = CARTESIAN_POINT ( 'NONE',  ( 11.00000000000000000, 1.347111479062088405E-15, 73.93750000409676204 ) ) ;
#45107 = CARTESIAN_POINT ( 'NONE',  ( -8.660254037844390851, 37.91666666666667140, 4.999999999999998224 ) ) ;
#45108 = CARTESIAN_POINT ( 'NONE',  ( 2.977408999572654480, 107.0000000020483810, 7.188101187499999156 ) ) ;
#45109 = CARTESIAN_POINT ( 'NONE',  ( -29.43265458321761230, 207.1250000013656347, 173.4587341250003760 ) ) ;
#45110 = CARTESIAN_POINT ( 'NONE',  ( 7.999999999999950262, -3.313708498984798467, 2.986552779823360204 ) ) ;
#45112 = CARTESIAN_POINT ( 'NONE',  ( -7.778174593052023411, 7.778174593052023411, 74.50000000409676204 ) ) ;
#45111 = CARTESIAN_POINT ( 'NONE',  ( 7.320508075688857197, 80.62500000000005684, -7.320508075688857197 ) ) ;
#45113 = VERTEX_POINT ( 'NONE', #20930 ) ;
#45114 = CARTESIAN_POINT ( 'NONE',  ( 11.35316468749999963, 261.1979166700807014, 3.042071309553159519 ) ) ;
#45115 = PRODUCT_DEFINITION_SHAPE ( 'NONE', 'NONE',  #27458 ) ;
#45116 = CARTESIAN_POINT ( 'NONE',  ( -5.082755093536317936, -5.082755093536320601, 26.04905278187175810 ) ) ;
#45117 = AXIS2_PLACEMENT_3D ( 'NONE', #46397, #47496, #70519 ) ;
#45118 = CARTESIAN_POINT ( 'NONE',  ( 0.8912353796319145705, 51.17464048784069064, 48.53058040617271729 ) ) ;
#45119 = CYLINDRICAL_SURFACE ( 'NONE', #6871, 3.999999999999976019 ) ;
#45120 = CARTESIAN_POINT ( 'NONE',  ( 0.6547826978432315093, -60.19560277018764083, -22.88235556323010300 ) ) ;
#45121 = CARTESIAN_POINT ( 'NONE',  ( -5.000000000000005329, 158.3333333333333428, 8.660254037844387298 ) ) ;
#45122 = CARTESIAN_POINT ( 'NONE',  ( 18.00000000000000000, -10.39230484541328892, -20.69999999999999929 ) ) ;
#45123 = CARTESIAN_POINT ( 'NONE',  ( -30.64284399271075188, 178.3875230420588878, 174.6921329945331536 ) ) ;
#45124 = CYLINDRICAL_SURFACE ( 'NONE', #53202, 8.000000000000000000 ) ;
#45125 = CARTESIAN_POINT ( 'NONE',  ( 9.832129032723420536, 131.5104166632526983, -5.676582343749999815 ) ) ;
#45126 = CARTESIAN_POINT ( 'NONE',  ( 25.17157287525381548, 205.6250000000000284, 167.1715728752537018 ) ) ;
#45127 = CARTESIAN_POINT ( 'NONE',  ( 7.999999999999992895, -7.224685084787812073E-14, 27.26780278391845513 ) ) ;
#45130 = CARTESIAN_POINT ( 'NONE',  ( 5.656854249492379694, 118.6250000040967905, -5.656854249492380582 ) ) ;
#45129 = CARTESIAN_POINT ( 'NONE',  ( 24.54126587499999701, 196.2500000013656631, 171.4326545832175839 ) ) ;
#45128 = CARTESIAN_POINT ( 'NONE',  ( 27.99999999999996092, 194.6875000013655779, 173.4587341249998929 ) ) ;
#45131 = ORIENTED_EDGE ( 'NONE', *, *, #61420, .F. ) ;
#45132 = CARTESIAN_POINT ( 'NONE',  ( 8.681524064790902884, 225.4138481035093662, -4.971750072494869777 ) ) ;
#45133 = CARTESIAN_POINT ( 'NONE',  ( 0.000000000000000000, 125.0000000000000000, 8.000000000000000000 ) ) ;
#45134 = CARTESIAN_POINT ( 'NONE',  ( 11.35316468749999608, 221.9270833367473017, -3.042071309553167069 ) ) ;
#45135 = CARTESIAN_POINT ( 'NONE',  ( 30.44569435410883429, 199.0625000013656063, 167.5543056458911053 ) ) ;
#45136 = CARTESIAN_POINT ( 'NONE',  ( -8.311093377946836114, 202.9687499965860411, -8.311093377946837890 ) ) ;
#45137 = CARTESIAN_POINT ( 'NONE',  ( 5.082755093536325042, 123.5937500020483952, -5.082755093536325930 ) ) ;
#45138 = CARTESIAN_POINT ( 'NONE',  ( -8.342170076843785083E-16, 17.06249999863440792, 4.541265875000002339 ) ) ;
#45139 = CARTESIAN_POINT ( 'NONE',  ( -0.3752463838874934843, -55.62178951997881882, 43.80327721769354810 ) ) ;
#45140 = CARTESIAN_POINT ( 'NONE',  ( 7.999999999999991118, 3.313708498984757611, 21.17405277982336642 ) ) ;
#45142 = CARTESIAN_POINT ( 'NONE',  ( 0.000000000000000000, 125.0000000000000000, 8.000000000000000000 ) ) ;
#45141 = CARTESIAN_POINT ( 'NONE',  ( -49.04048506803781748, 44.15394360280433972, 59.50300479923076580 ) ) ;
#45143 = CARTESIAN_POINT ( 'NONE',  ( -3.042071309553164404, 97.23958332991936970, -11.35316468749999963 ) ) ;
#45144 = ORIENTED_EDGE ( 'NONE', *, *, #20434, .T. ) ;
#45145 = CARTESIAN_POINT ( 'NONE',  ( -1.656854249492444975, 205.8125000027312126, 146.0000000000000000 ) ) ;
#45146 = CARTESIAN_POINT ( 'NONE',  ( -7.188101187500001821, 25.12499999795161187, -2.977408999572651371 ) ) ;
#45147 = CARTESIAN_POINT ( 'NONE',  ( -36.10814071610730736, 146.0000000000000000, 127.0000000000000000 ) ) ;
#45149 = CARTESIAN_POINT ( 'NONE',  ( 8.311093377946834337, 252.3437500034139589, -8.311093377946836114 ) ) ;
#45148 = AXIS2_PLACEMENT_3D ( 'NONE', #71158, #32309, #3629 ) ;
#45150 = CARTESIAN_POINT ( 'NONE',  ( 6.951808397369818766E-16, 102.0312499965860269, -11.35316468750000141 ) ) ;
#45151 = ORIENTED_EDGE ( 'NONE', *, *, #60387, .T. ) ;
#45152 = DIRECTION ( 'NONE',  ( -0.8660254037844389297, -0.4999999999999994449, 0.000000000000000000 ) ) ;
#45153 = CARTESIAN_POINT ( 'NONE',  ( -6.238412754330611322E-16, 10.18810118749999916, 104.7812500020483810 ) ) ;
#45154 = CARTESIAN_POINT ( 'NONE',  ( 10.00000000000000000, 221.6666666598387110, 2.679491924311236062 ) ) ;
#45155 = CARTESIAN_POINT ( 'NONE',  ( -1.432654583217607414, 206.5000000013655779, 194.5412658750000219 ) ) ;
#45156 = CARTESIAN_POINT ( 'NONE',  ( 8.000000000000000000, 118.3437500000000000, -3.313708498984762496 ) ) ;
#45158 = CARTESIAN_POINT ( 'NONE',  ( -9.832129032723420536, 83.69791666325268409, 5.676582343749997150 ) ) ;
#45157 = CARTESIAN_POINT ( 'NONE',  ( 5.656854249492374365, 5.656854249492375253, 22.76780277982336642 ) ) ;
#45159 = CARTESIAN_POINT ( 'NONE',  ( 7.999999999999992895, -3.313708498984756279, 12.17405278392014800 ) ) ;
#45160 = CARTESIAN_POINT ( 'NONE',  ( -30.44569435410883429, 201.8125000013656063, 167.5543056458915885 ) ) ;
#45161 = CARTESIAN_POINT ( 'NONE',  ( 1.656854249492422992, 208.8125000027311842, 194.0000000000000568 ) ) ;
#45162 = ORIENTED_EDGE ( 'NONE', *, *, #74547, .T. ) ;
#45163 = ADVANCED_FACE ( 'NONE', ( #27332 ), #6842, .T. ) ;
#45164 = CARTESIAN_POINT ( 'NONE',  ( 10.00000000000000000, 176.6666666598387110, 2.679491924311236062 ) ) ;
#45165 = EDGE_CURVE ( 'NONE', #27914, #28937, #40267, .T. ) ;
#45166 = CARTESIAN_POINT ( 'NONE',  ( 4.000000000000001776, 6.000000000000000000, 0.000000000000000000 ) ) ;
#45167 = LINE ( 'NONE', #68178, #72618 ) ;
#45168 = CARTESIAN_POINT ( 'NONE',  ( 8.311093377946837890, 81.71874999658601268, -8.311093377946837890 ) ) ;
#45169 = CARTESIAN_POINT ( 'NONE',  ( 6.676582343750004256, 290.8906250017069510, 2.765530957081995478 ) ) ;
#45170 = CARTESIAN_POINT ( 'NONE',  ( 2.977408999572650927, 7.124999997951611874, -7.188101187500000933 ) ) ;
#45171 = CARTESIAN_POINT ( 'NONE',  ( -4.220049686691935698, 10.18810118749999916, 102.2500000020483810 ) ) ;
#45172 = CARTESIAN_POINT ( 'NONE',  ( 3.508320828368888034, 226.7807894534376203, -10.79750125662090632 ) ) ;
#45173 = ORIENTED_EDGE ( 'NONE', *, *, #69841, .F. ) ;
#45174 = CARTESIAN_POINT ( 'NONE',  ( -7.999999999999992895, 4.898587196589407898E-16, 0.000000000000000000 ) ) ;
#45175 = CARTESIAN_POINT ( 'NONE',  ( -3.313708498984720308, 120.2187499999999858, -8.000000000000040856 ) ) ;
#45176 = CARTESIAN_POINT ( 'NONE',  ( 11.35316468749999963, 210.9895833299193839, -3.042071309553165293 ) ) ;
#45177 = CARTESIAN_POINT ( 'NONE',  ( -6.123233995736766282E-16, 231.8750000068279746, -10.00000000000000000 ) ) ;
#45178 = CARTESIAN_POINT ( 'NONE',  ( 0.000000000000000000, 0.000000000000000000, 12.00000000000000000 ) ) ;
#45179 = CARTESIAN_POINT ( 'NONE',  ( -6.676582343750003368, 297.3906250017068942, -2.765530957081996810 ) ) ;
#45180 = ORIENTED_EDGE ( 'NONE', *, *, #71459, .T. ) ;
#45181 = CARTESIAN_POINT ( 'NONE',  ( -5.676582343749998039, 197.7604166632526983, -9.832129032723420536 ) ) ;
#45182 = EDGE_CURVE ( 'NONE', #47672, #41364, #27245, .T. ) ;
#45183 = MECHANICAL_DESIGN_GEOMETRIC_PRESENTATION_REPRESENTATION (  '', ( #54824 ), #62027 ) ;
#45184 = CARTESIAN_POINT ( 'NONE',  ( -31.45873412499998523, 205.7500000013656063, 171.4326545832180386 ) ) ;
#45185 = CARTESIAN_POINT ( 'NONE',  ( -8.000000000000001776, 18.84375000000000355, 3.313708498984759387 ) ) ;
#45186 = VERTEX_POINT ( 'NONE', #5090 ) ;
#45187 = CARTESIAN_POINT ( 'NONE',  ( -5.656854249492378806, 93.87500000409677625, 5.656854249492381470 ) ) ;
#45188 = SURFACE_STYLE_FILL_AREA ( #46298 ) ;
#45189 = CARTESIAN_POINT ( 'NONE',  ( -4.999999999999998224, 11.66666666666666785, -8.660254037844389075 ) ) ;
#45190 = CARTESIAN_POINT ( 'NONE',  ( 10.18810118750000093, -4.220049686691933921, 79.18750000204836681 ) ) ;
#45192 = EDGE_LOOP ( 'NONE', ( #32024, #33332, #40819, #43433 ) ) ;
#45191 =( BOUNDED_CURVE ( )  B_SPLINE_CURVE ( 2, ( #41991, #65001, #13310, #36347, #2010, #59362, #30680, #25373, #20457 ),
 .UNSPECIFIED., .F., .F. ) 
 B_SPLINE_CURVE_WITH_KNOTS ( ( 3, 2, 2, 2, 3 ),
 ( 0.5666666666666670960, 0.5750000000000003997, 0.5833333333333338144, 0.5916666666666671182, 0.6000000000000004219 ),
 .UNSPECIFIED. ) 
 CURVE ( )  GEOMETRIC_REPRESENTATION_ITEM ( )  RATIONAL_B_SPLINE_CURVE ( ( 0.9999999999999958922, 0.9238795325112908463, 1.000000000000000000, 0.9238795325112867385, 1.000000000000000000, 0.9238795325112867385, 1.000000000000000000, 0.9238795325112826307, 1.000000000000003997 ) ) 
 REPRESENTATION_ITEM ( '' )  );
#45193 = CARTESIAN_POINT ( 'NONE',  ( 4.000000000000000888, 20.93750000000000000, 1.656854249492384135 ) ) ;
#45194 = CARTESIAN_POINT ( 'NONE',  ( -3.211159895383562723, 18.93749999863440436, 3.211159895383561391 ) ) ;
#45195 = CARTESIAN_POINT ( 'NONE',  ( 31.34716094839829736, 194.6453746702107992, 168.5383295482856738 ) ) ;
#45196 = CARTESIAN_POINT ( 'NONE',  ( 0.000000000000000000, 0.000000000000000000, 118.0000000000000000 ) ) ;
#45197 = CARTESIAN_POINT ( 'NONE',  ( -5.082755093536325930, 121.3437500020483952, -5.082755093536325930 ) ) ;
#45198 = CARTESIAN_POINT ( 'NONE',  ( 5.000000000000000000, -68.60357193678713372, 20.85024232999320404 ) ) ;
#45201 = DIRECTION ( 'NONE',  ( -1.000000000000000000, 0.000000000000000000, 0.000000000000000000 ) ) ;
#45200 = CARTESIAN_POINT ( 'NONE',  ( -8.311093377946836114, 248.2812500034139589, -8.311093377946836114 ) ) ;
#45199 = CARTESIAN_POINT ( 'NONE',  ( 29.43265458321761585, 207.8750000013656063, 166.5412658749999650 ) ) ;
#45202 = APPLICATION_PROTOCOL_DEFINITION ( 'draft international standard', 'automotive_design', 1998, #60674 ) ;
#45203 = EDGE_LOOP ( 'NONE', ( #65188, #2371, #52996, #43468 ) ) ;
#45204 = CARTESIAN_POINT ( 'NONE',  ( 3.042071309553173286, 255.6770833367473301, 11.35316468749999608 ) ) ;
#45205 = CARTESIAN_POINT ( 'NONE',  ( 2.977408999572646486, 7.188101187499991163, 13.01780278187175277 ) ) ;
#45206 = ORIENTED_EDGE ( 'NONE', *, *, #26624, .T. ) ;
#45207 =( BOUNDED_CURVE ( )  B_SPLINE_CURVE ( 2, ( #61275, #20523, #55259, #50321, #26180, #44298, #67313, #43537, #15611 ),
 .UNSPECIFIED., .F., .F. ) 
 B_SPLINE_CURVE_WITH_KNOTS ( ( 3, 2, 2, 2, 3 ),
 ( 0.3854166666666665741, 0.3906249999999998890, 0.3958333333333332038, 0.4010416666666665741, 0.4062499999999998890 ),
 .UNSPECIFIED. ) 
 CURVE ( )  GEOMETRIC_REPRESENTATION_ITEM ( )  RATIONAL_B_SPLINE_CURVE ( ( 1.000000000000001554, 0.9238795325112850731, 1.000000000000000000, 0.9238795325112867385, 1.000000000000000000, 0.9238795325112867385, 1.000000000000000000, 0.9238795325112884038, 0.9999999999999983347 ) ) 
 REPRESENTATION_ITEM ( '' )  );
#45208 = ORIENTED_EDGE ( 'NONE', *, *, #31884, .T. ) ;
#45209 = CARTESIAN_POINT ( 'NONE',  ( -7.204075437095965206, -7.204075437095968759, 73.84375000204838102 ) ) ;
#45210 = CARTESIAN_POINT ( 'NONE',  ( 3.042071309553167069, 82.13541666325269830, -11.35316468749999785 ) ) ;
#45211 = CARTESIAN_POINT ( 'NONE',  ( 1.469576158976823947E-15, 106.0625000040967763, 8.000000000000000000 ) ) ;
#45212 = CARTESIAN_POINT ( 'NONE',  ( -7.778174593052023411, 7.778174593052023411, 86.31249999999998579 ) ) ;
#45215 = CARTESIAN_POINT ( 'NONE',  ( 4.721056650416000089, 289.9843750017070079, 4.721056650415999201 ) ) ;
#45214 = CARTESIAN_POINT ( 'NONE',  ( 24.54126587499998635, 208.1250000013656063, 168.5673454167822740 ) ) ;
#45213 = CARTESIAN_POINT ( 'NONE',  ( 26.56734541678232731, 208.6250000013655779, 173.4587341249998929 ) ) ;
#45216 = CARTESIAN_POINT ( 'NONE',  ( 8.660254037844389075, 77.29166665983871098, -5.000000000000000000 ) ) ;
#45217 = CARTESIAN_POINT ( 'NONE',  ( 7.000000000000000000, 0.000000000000000000, -14.80000000000000071 ) ) ;
#45218 = AXIS2_PLACEMENT_3D ( 'NONE', #65938, #30871, #48210 ) ;
#45219 = CARTESIAN_POINT ( 'NONE',  ( -8.311093377946841443, 193.9062499965860411, 8.311093377946830785 ) ) ;
#45220 = CARTESIAN_POINT ( 'NONE',  ( -8.000000000000001776, 11.15624999590322020, 3.313708498984759387 ) ) ;
#45221 = ORIENTED_EDGE ( 'NONE', *, *, #3523, .T. ) ;
#45222 = CARTESIAN_POINT ( 'NONE',  ( 26.56734541678232731, 208.6250000013655779, 173.4587341249998929 ) ) ;
#45223 = EDGE_CURVE ( 'NONE', #10294, #1217, #53260, .T. ) ;
#45224 = CARTESIAN_POINT ( 'NONE',  ( 5.082755093536325930, 17.53124999795161543, -5.082755093536325930 ) ) ;
#45225 =( GEOMETRIC_REPRESENTATION_CONTEXT ( 3 ) GLOBAL_UNCERTAINTY_ASSIGNED_CONTEXT ( ( #35281 ) ) GLOBAL_UNIT_ASSIGNED_CONTEXT ( ( #55498, #68199, #29334 ) ) REPRESENTATION_CONTEXT ( 'NONE', 'WORKASPACE' ) );
#45226 = CARTESIAN_POINT ( 'NONE',  ( 11.35316468750000141, 171.0937499965860127, 0.000000000000000000 ) ) ;
#45227 = DIRECTION ( 'NONE',  ( 0.000000000000000000, 1.000000000000000000, 0.000000000000000000 ) ) ;
#45228 = CARTESIAN_POINT ( 'NONE',  ( 7.188101187500000044, 102.7812500020483810, -8.802885111219163269E-16 ) ) ;
#45230 = CARTESIAN_POINT ( 'NONE',  ( -7.320508075688773708, 113.1249999999999858, 7.320508075688764826 ) ) ;
#45229 = CARTESIAN_POINT ( 'NONE',  ( 2.775557561562891351E-14, 210.0000000000000284, 202.0000000000000000 ) ) ;
#45231 = CARTESIAN_POINT ( 'NONE',  ( 30.44569435410879521, 206.8125000013656063, 172.4456943541087526 ) ) ;
#45232 = CARTESIAN_POINT ( 'NONE',  ( -2.977408999572648707, -7.188101187499990274, 18.64280278187175810 ) ) ;
#45233 = CARTESIAN_POINT ( 'NONE',  ( -3.042071309553173730, 54.32291666325269119, 11.35316468749999785 ) ) ;
#45234 = CARTESIAN_POINT ( 'NONE',  ( -1.983802647709429268, -42.74107461072510006, 139.0632304000675390 ) ) ;
#45235 = CARTESIAN_POINT ( 'NONE',  ( 2.849036369511732440E-14, 195.3750000027311842, 202.0000000000000000 ) ) ;
#45236 = ORIENTED_EDGE ( 'NONE', *, *, #69282, .T. ) ;
#45237 = CARTESIAN_POINT ( 'NONE',  ( -7.999999999999991118, 1.505321450683924536E-05, 7.017802358041144828 ) ) ;
#45238 = CARTESIAN_POINT ( 'NONE',  ( -5.656854249492381470, 20.24999999590322375, 5.656854249492379694 ) ) ;
#45239 = CARTESIAN_POINT ( 'NONE',  ( 3.042071309553159519, 59.73958332991933418, 11.35316468750000141 ) ) ;
#45240 = CARTESIAN_POINT ( 'NONE',  ( -4.556349186104045934, 11.00000000000000000, 74.40625000409676204 ) ) ;
#45241 = CARTESIAN_POINT ( 'NONE',  ( 2.445694354108783219, 199.8125000013656063, 139.5543056458912190 ) ) ;
#45242 = CARTESIAN_POINT ( 'NONE',  ( 1.308779242311841839, 10.28008949575769293, 63.61387346695496348 ) ) ;
#45243 = CARTESIAN_POINT ( 'NONE',  ( 4.000000000000015987, 207.5000000000000284, 198.0000000000000284 ) ) ;
#45245 = CARTESIAN_POINT ( 'NONE',  ( -11.35316468750000141, 43.28124999658601268, -1.390361679473963753E-15 ) ) ;
#45244 = CARTESIAN_POINT ( 'NONE',  ( 7.188101187500002709, 96.31250000204838102, 2.977408999572649151 ) ) ;
#45246 = CARTESIAN_POINT ( 'NONE',  ( -4.898587196589407898E-16, 7.999999999999991118, 1.955302779823364645 ) ) ;
#45247 = CARTESIAN_POINT ( 'NONE',  ( 5.656854249492376141, -5.656854249492374365, 4.580302783920145338 ) ) ;
#45248 = CARTESIAN_POINT ( 'NONE',  ( 9.832129032723420536, 176.1979166632526983, -5.676582343749999815 ) ) ;
#45249 = CARTESIAN_POINT ( 'NONE',  ( -8.660254037844387298, 143.9583333265053682, -5.000000000000004441 ) ) ;
#45250 = CARTESIAN_POINT ( 'NONE',  ( 7.188101187500000044, 99.78125000204838102, -8.802885111219163269E-16 ) ) ;
#45251 = CARTESIAN_POINT ( 'NONE',  ( 2.020667218593132706E-15, 219.9523502760175973, 11.00000000000000000 ) ) ;
#45252 = CARTESIAN_POINT ( 'NONE',  ( -5.676582343750006032, 34.42708332991935549, 9.832129032723418760 ) ) ;
#45253 = FACE_OUTER_BOUND ( 'NONE', #32664, .T. ) ;
#45254 = CARTESIAN_POINT ( 'NONE',  ( -3.042071309553164404, 182.2395833299193555, -11.35316468749999963 ) ) ;
#45255 = VERTEX_POINT ( 'NONE', #73735 ) ;
#45256 = CYLINDRICAL_SURFACE ( 'NONE', #52502, 3.999999999999976019 ) ;
#45257 = CARTESIAN_POINT ( 'NONE',  ( 10.18810118749999916, 4.220049686691935698, 68.50000000204838102 ) ) ;
#45258 = CARTESIAN_POINT ( 'NONE',  ( 1.656854249492405451, 196.3125000000000284, 202.0000000000000284 ) ) ;
#45259 = CARTESIAN_POINT ( 'NONE',  ( 31.82098384755875742, 43.37416162849262946, 65.00000000000000000 ) ) ;
#45261 = CARTESIAN_POINT ( 'NONE',  ( 8.311093377946837890, 161.4062499965860695, -8.311093377946837890 ) ) ;
#45260 = CARTESIAN_POINT ( 'NONE',  ( -4.898587196589412829E-16, 103.6250000000000000, -8.000000000000000000 ) ) ;
#45262 = CARTESIAN_POINT ( 'NONE',  ( 5.656854249492374365, 5.656854249492375253, 6.324052784329821542 ) ) ;
#45263 = FACE_OUTER_BOUND ( 'NONE', #37378, .T. ) ;
#45264 = EDGE_CURVE ( 'NONE', #14535, #55545, #6553, .T. ) ;
#45265 = EDGE_CURVE ( 'NONE', #8511, #31876, #47500, .T. ) ;
#45266 = CARTESIAN_POINT ( 'NONE',  ( -3.042071309553166181, 227.8645833367473301, -11.35316468749999608 ) ) ;
#45267 = CARTESIAN_POINT ( 'NONE',  ( -2.069125466540701286, 55.78340383128293212, -43.89144373685724787 ) ) ;
#45268 = CARTESIAN_POINT ( 'NONE',  ( 10.18810118750000093, -4.220049686691933921, 77.68750000204838102 ) ) ;
#45269 = ORIENTED_EDGE ( 'NONE', *, *, #23459, .T. ) ;
#45270 = CARTESIAN_POINT ( 'NONE',  ( -2.828427124746152987, 204.2500000027312126, 200.8284271247462129 ) ) ;
#45271 = CARTESIAN_POINT ( 'NONE',  ( 5.676582343750001591, 111.9270833299193555, -9.832129032723420536 ) ) ;
#45272 = DIRECTION ( 'NONE',  ( 0.000000000000000000, 0.000000000000000000, -1.000000000000000000 ) ) ;
#45273 = EDGE_LOOP ( 'NONE', ( #16439, #69422, #48987, #1303, #21341, #1146, #33817, #35014, #49798, #72739, #35099, #14501, #46290, #48029 ) ) ;
#45274 = ORIENTED_EDGE ( 'NONE', *, *, #69261, .T. ) ;
#45275 = CARTESIAN_POINT ( 'NONE',  ( -4.541265875000002339, 9.874999998634404363, -1.881053915767121998 ) ) ;
#45276 = CARTESIAN_POINT ( 'NONE',  ( -2.977408999572650039, 12.93749999795161365, -7.188101187500001821 ) ) ;
#45277 = EDGE_CURVE ( 'NONE', #69889, #29352, #74109, .T. ) ;
#45278 = CARTESIAN_POINT ( 'NONE',  ( 3.313708498984765161, 109.1562500040967905, 7.999999999999998224 ) ) ;
#45279 = CARTESIAN_POINT ( 'NONE',  ( -26.56734541678238060, 199.6250000013656063, 166.5412658750003629 ) ) ;
#45280 = CARTESIAN_POINT ( 'NONE',  ( 4.000000000000001776, 7.000000000000000000, 0.000000000000000000 ) ) ;
#45281 = CARTESIAN_POINT ( 'NONE',  ( 5.000000000000000000, -50.64189880742087269, -41.08656465431914029 ) ) ;
#45282 = CARTESIAN_POINT ( 'NONE',  ( 1.881053915767122664, 6.124999998634407916, 4.541265875000001451 ) ) ;
#45283 = CARTESIAN_POINT ( 'NONE',  ( 2.828427124746152987, 199.1250000000000284, 139.1715728752538723 ) ) ;
#45284 = ORIENTED_EDGE ( 'NONE', *, *, #20795, .T. ) ;
#45285 = CARTESIAN_POINT ( 'NONE',  ( 5.656854249492374365, 5.656854249492375253, 9.455302783920146226 ) ) ;
#45286 = CARTESIAN_POINT ( 'NONE',  ( 2.977408999572650039, 107.1875000020483810, -7.188101187500001821 ) ) ;
#45288 = DIRECTION ( 'NONE',  ( -1.000000000000000000, 0.000000000000000000, 0.000000000000000000 ) ) ;
#45287 = CARTESIAN_POINT ( 'NONE',  ( 4.556349186104045934, 11.00000000000000000, 78.71875000409676204 ) ) ;
#45289 = CARTESIAN_POINT ( 'NONE',  ( -4.737866951562140549, 16.26762833210766956, -69.68949229523444444 ) ) ;
#45290 = CARTESIAN_POINT ( 'NONE',  ( -2.849036369511732440E-14, 209.2500000000000284, 138.0000000000000568 ) ) ;
#45291 = ORIENTED_EDGE ( 'NONE', *, *, #48501, .T. ) ;
#45292 = VERTEX_POINT ( 'NONE', #33030 ) ;
#45293 = CARTESIAN_POINT ( 'NONE',  ( 1.871523826299183495E-15, -10.18810118749999916, 95.03125000204836681 ) ) ;
#45294 = CARTESIAN_POINT ( 'NONE',  ( -25.55430564589119413, 199.5625000013656063, 167.5543056458915316 ) ) ;
#45295 = CARTESIAN_POINT ( 'NONE',  ( 11.00000000000000000, 4.556349186104045934, 108.3437499999999858 ) ) ;
#45296 = CARTESIAN_POINT ( 'NONE',  ( 3.458734125000016757, 203.1250000013656347, 199.4326545832176691 ) ) ;
#45298 = CARTESIAN_POINT ( 'NONE',  ( 12.00000000000000000, 0.000000000000000000, 0.000000000000000000 ) ) ;
#45297 = DIRECTION ( 'NONE',  ( -1.000000000000000000, 0.000000000000000000, 0.000000000000000000 ) ) ;
#45299 = CARTESIAN_POINT ( 'NONE',  ( 10.00000000000000178, 115.2083333333333144, -2.679491924311226736 ) ) ;
#45300 = CARTESIAN_POINT ( 'NONE',  ( -4.898587196589412829E-16, 105.1250000000000000, -8.000000000000000000 ) ) ;
#45301 = CARTESIAN_POINT ( 'NONE',  ( 2.765530957081996366, 289.2968750017070079, -6.676582343750003368 ) ) ;
#45302 = CARTESIAN_POINT ( 'NONE',  ( -5.082755093536319713, 5.082755093536319713, 4.674052781871752771 ) ) ;
#45303 =( BOUNDED_CURVE ( )  B_SPLINE_CURVE ( 2, ( #67942, #3831, #56258, #62274, #10602, #73232, #21538, #72097, #3450 ),
 .UNSPECIFIED., .F., .F. ) 
 B_SPLINE_CURVE_WITH_KNOTS ( ( 3, 2, 2, 2, 3 ),
 ( 0.3645833333333331483, 0.3697916666666665186, 0.3749999999999998890, 0.3802083333333332038, 0.3854166666666665741 ),
 .UNSPECIFIED. ) 
 CURVE ( )  GEOMETRIC_REPRESENTATION_ITEM ( )  RATIONAL_B_SPLINE_CURVE ( ( 1.000000000000002442, 0.9238795325112842960, 1.000000000000000000, 0.9238795325112867385, 1.000000000000000000, 0.9238795325112867385, 1.000000000000000000, 0.9238795325112884038, 0.9999999999999983347 ) ) 
 REPRESENTATION_ITEM ( '' )  );
#45304 = CARTESIAN_POINT ( 'NONE',  ( -1.469576158976823947E-15, 1.125000000000000222, 8.000000000000000000 ) ) ;
#45305 = CARTESIAN_POINT ( 'NONE',  ( 26.56734541678232731, 207.3750000013656063, 173.4587341249998929 ) ) ;
#45306 = CARTESIAN_POINT ( 'NONE',  ( -2.977408999572654480, 1.874999997951610098, 7.188101187499999156 ) ) ;
#45307 = CARTESIAN_POINT ( 'NONE',  ( 1.432654583217607858, 198.6250000013655779, 138.5412658750000787 ) ) ;
#45308 = CARTESIAN_POINT ( 'NONE',  ( 2.977408999572650039, 124.0625000020483810, -7.188101187500000933 ) ) ;
#45310 = CARTESIAN_POINT ( 'NONE',  ( 3.458734124999959469, 204.7500000013656063, 140.5673454167824161 ) ) ;
#45309 = CARTESIAN_POINT ( 'NONE',  ( 29.65685424949246496, 195.5625000027311842, 166.0000000000000284 ) ) ;
#45311 = CARTESIAN_POINT ( 'NONE',  ( 8.311093377946834337, 242.3437500034139873, -8.311093377946836114 ) ) ;
#45312 = CARTESIAN_POINT ( 'NONE',  ( -8.660254037844390851, 214.7916666598387110, 4.999999999999998224 ) ) ;
#45313 = CARTESIAN_POINT ( 'NONE',  ( 31.99999999999997868, 201.1875000000000284, 171.6568542494923122 ) ) ;
#45314 = CARTESIAN_POINT ( 'NONE',  ( -11.35316468750000141, 18.48958332991934483, 3.042071309553159963 ) ) ;
#45315 = CARTESIAN_POINT ( 'NONE',  ( -4.898587196589412829E-16, 100.8125000040967763, -8.000000000000000000 ) ) ;
#45316 = CARTESIAN_POINT ( 'NONE',  ( 3.042071309553167069, 202.1354166632526983, -11.35316468749999785 ) ) ;
#45317 = CARTESIAN_POINT ( 'NONE',  ( 8.311093377946837890, 1.406249996586016238, -8.311093377946837890 ) ) ;
#45318 = CARTESIAN_POINT ( 'NONE',  ( -8.660254037844387298, 218.9583333265053966, -5.000000000000004441 ) ) ;
#45319 = CARTESIAN_POINT ( 'NONE',  ( 0.000000000000000000, 300.0000000000000000, 0.000000000000000000 ) ) ;
#45320 = ORIENTED_EDGE ( 'NONE', *, *, #71142, .F. ) ;
#45321 = ADVANCED_FACE ( 'NONE', ( #22408 ), #68443, .T. ) ;
#45322 = CARTESIAN_POINT ( 'NONE',  ( 3.458734124999960358, 201.6250000013656063, 143.4326545832176976 ) ) ;
#45323 = CARTESIAN_POINT ( 'NONE',  ( 8.311093377946837890, 26.40624999658601268, -8.311093377946837890 ) ) ;
#45324 = CARTESIAN_POINT ( 'NONE',  ( -7.778174593052023411, 7.778174593052023411, 94.00000000409677625 ) ) ;
#45325 = VECTOR ( 'NONE', #22345, 1000.000000000000000 ) ;
#45326 = CARTESIAN_POINT ( 'NONE',  ( 10.00000000000000178, 210.2083333333333428, -2.679491924311227180 ) ) ;
#45327 = CARTESIAN_POINT ( 'NONE',  ( -26.56734541678228112, 199.0000000013656063, 173.4587341250003476 ) ) ;
#45328 = CARTESIAN_POINT ( 'NONE',  ( -2.751064625579944321E-14, 201.8750000027312126, 146.0000000000000284 ) ) ;
#45330 = CARTESIAN_POINT ( 'NONE',  ( -11.35316468750000141, 3.489583329919349719, 3.042071309553159963 ) ) ;
#45329 = CARTESIAN_POINT ( 'NONE',  ( 7.188101187500000933, 110.0000000020483810, -2.977408999572651371 ) ) ;
#45331 = CARTESIAN_POINT ( 'NONE',  ( -3.313708498984757167, 7.999999999999991118, 18.54905277982336287 ) ) ;
#45332 = CARTESIAN_POINT ( 'NONE',  ( -3.042071309553173730, 129.3229166632526983, 11.35316468749999785 ) ) ;
#45333 = CARTESIAN_POINT ( 'NONE',  ( 5.000000000000001776, 107.7083333265053682, -8.660254037844389075 ) ) ;
#45334 = CARTESIAN_POINT ( 'NONE',  ( -7.188101187499999156, 123.1250000020484094, 2.977408999572654924 ) ) ;
#45335 = FACE_OUTER_BOUND ( 'NONE', #13845, .T. ) ;
#45336 = CARTESIAN_POINT ( 'NONE',  ( -26.56734541678238415, 209.6250000013656063, 166.5412658750003629 ) ) ;
#45337 = CARTESIAN_POINT ( 'NONE',  ( 11.00000000000000000, 1.347111479062088405E-15, 79.74999999999998579 ) ) ;
#45338 = ORIENTED_EDGE ( 'NONE', *, *, #24483, .F. ) ;
#45339 = CARTESIAN_POINT ( 'NONE',  ( 0.4451317748866334134, -67.59323688304569089, 20.03471819849699997 ) ) ;
#45340 = CARTESIAN_POINT ( 'NONE',  ( -1.656854249492383468, 20.43749999726881228, 4.000000000000000888 ) ) ;
#45341 = CARTESIAN_POINT ( 'NONE',  ( 6.676582343750003368, 288.1718750017069510, -2.765530957081997254 ) ) ;
#45342 = CARTESIAN_POINT ( 'NONE',  ( 5.000000000000000000, 50.64189880742059557, 41.08656465431948845 ) ) ;
#45343 = CARTESIAN_POINT ( 'NONE',  ( -7.999999999999991118, 3.313708498984756723, 21.79280278432983309 ) ) ;
#45344 = CARTESIAN_POINT ( 'NONE',  ( 4.999999999999997335, 226.4583333401612890, -8.660254037844387298 ) ) ;
#45345 = EDGE_CURVE ( 'NONE', #22788, #30828, #1705, .T. ) ;
#45346 = FACE_OUTER_BOUND ( 'NONE', #15099, .T. ) ;
#45347 = CARTESIAN_POINT ( 'NONE',  ( -10.18810118749999916, 4.220049686691934809, 97.93750000204836681 ) ) ;
#45348 = ORIENTED_EDGE ( 'NONE', *, *, #61106, .F. ) ;
#45349 = EDGE_CURVE ( 'NONE', #56231, #71873, #36627, .T. ) ;
#45350 = AXIS2_PLACEMENT_3D ( 'NONE', #73368, #37924, #2839 ) ;
#45351 = CARTESIAN_POINT ( 'NONE',  ( 8.660254037844389075, 217.2916666598387110, -5.000000000000000000 ) ) ;
#45352 = CARTESIAN_POINT ( 'NONE',  ( -25.17157282405719343, 195.0000000000000284, 167.1715729264508354 ) ) ;
#45353 = CARTESIAN_POINT ( 'NONE',  ( 1.432654583217664701, 203.0000000013655779, 201.4587341250000065 ) ) ;
#45354 = CARTESIAN_POINT ( 'NONE',  ( -3.042071309553173730, 69.63541666325268409, 11.35316468749999785 ) ) ;
#45355 = ORIENTED_EDGE ( 'NONE', *, *, #757, .F. ) ;
#45356 = CARTESIAN_POINT ( 'NONE',  ( 4.220049686691934809, 10.18810118749999916, 104.6875000020483810 ) ) ;
#45357 = CARTESIAN_POINT ( 'NONE',  ( 4.541265875000001451, 13.37499999863440969, 1.881053915767124440 ) ) ;
#45358 = ORIENTED_EDGE ( 'NONE', *, *, #42649, .F. ) ;
#45359 = CARTESIAN_POINT ( 'NONE',  ( -2.977408999572654480, 25.49999999795161898, 7.188101187499999156 ) ) ;
#45360 = CARTESIAN_POINT ( 'NONE',  ( 2.751064625579944321E-14, 196.8750000027312126, 194.0000000000000568 ) ) ;
#45361 = CARTESIAN_POINT ( 'NONE',  ( 7.188101187500000044, 21.84374999795161543, 0.000000000000000000 ) ) ;
#45362 = EDGE_CURVE ( 'NONE', #18244, #49983, #19658, .T. ) ;
#45363 = FACE_BOUND ( 'NONE', #65953, .T. ) ;
#45364 = CARTESIAN_POINT ( 'NONE',  ( 7.204075437095968759, -7.204075437095966983, 107.5937500020483810 ) ) ;
#45365 = CARTESIAN_POINT ( 'NONE',  ( -4.000000000000001776, 10.18749999726881406, -1.656854249492381470 ) ) ;
#45366 = DIRECTION ( 'NONE',  ( -0.000000000000000000, -0.000000000000000000, 1.000000000000000000 ) ) ;
#45367 = ORIENTED_EDGE ( 'NONE', *, *, #74316, .T. ) ;
#45368 = ADVANCED_FACE ( 'NONE', ( #71676 ), #19997, .F. ) ;
#45369 = CARTESIAN_POINT ( 'NONE',  ( 3.458734125000016313, 203.8750000013656063, 199.4326545832176691 ) ) ;
#45370 = CARTESIAN_POINT ( 'NONE',  ( -31.45873412499999944, 204.6875000013656063, 170.0000000000004547 ) ) ;
#45371 = CARTESIAN_POINT ( 'NONE',  ( 1.656854249492305531, 206.8125000000000284, 146.0000000000000853 ) ) ;
#45372 = CARTESIAN_POINT ( 'NONE',  ( -4.541265875000002339, 10.74999999863440969, -1.881053915767121998 ) ) ;
#45373 = EDGE_CURVE ( 'NONE', #54549, #29688, #19958, .T. ) ;
#45374 = CARTESIAN_POINT ( 'NONE',  ( -1.656854249492401232, 206.4375000027311842, 138.0000000000000284 ) ) ;
#45375 = CARTESIAN_POINT ( 'NONE',  ( -2.977408999572648707, -7.188101187499990274, 16.76780278187175099 ) ) ;
#45376 = ORIENTED_EDGE ( 'NONE', *, *, #44420, .T. ) ;
#45377 = LINE ( 'NONE', #64502, #39776 ) ;
#45378 = ORIENTED_EDGE ( 'NONE', *, *, #36179, .F. ) ;
#45379 = CARTESIAN_POINT ( 'NONE',  ( -4.220049686691937474, -10.18810118749999738, 111.4375000020483810 ) ) ;
#45380 = CARTESIAN_POINT ( 'NONE',  ( 1.836970198721029589E-15, 231.2500000000000000, 10.00000000000000000 ) ) ;
#45381 = CARTESIAN_POINT ( 'NONE',  ( -3.458734124999959025, 202.5000000013656063, 199.4326545832176691 ) ) ;
#45382 = CARTESIAN_POINT ( 'NONE',  ( 30.44569435410879521, 198.8125000013656063, 167.5543056458910485 ) ) ;
#45383 = CARTESIAN_POINT ( 'NONE',  ( -10.00000000000000000, 87.29166666666667140, -2.679491924311229845 ) ) ;
#45384 = CARTESIAN_POINT ( 'NONE',  ( -5.656854249492380582, 121.8125000000000000, -5.656854249492380582 ) ) ;
#45385 = CARTESIAN_POINT ( 'NONE',  ( -6.000000000000001776, 289.0000000000000000, 0.000000000000000000 ) ) ;
#45386 = ORIENTED_EDGE ( 'NONE', *, *, #49430, .F. ) ;
#45387 = AXIS2_PLACEMENT_3D ( 'NONE', #33601, #68283, #56609 ) ;
#45388 = CARTESIAN_POINT ( 'NONE',  ( -4.898587196589407898E-16, 7.999999999999991118, 7.955302779823362869 ) ) ;
#45389 = CARTESIAN_POINT ( 'NONE',  ( 2.828427124746153876, 196.0000000027312126, 144.8284271247462129 ) ) ;
#45390 = CARTESIAN_POINT ( 'NONE',  ( -11.00000000000000000, 0.000000000000000000, 91.00000000000000000 ) ) ;
#45391 = DIRECTION ( 'NONE',  ( 0.000000000000000000, 0.000000000000000000, 1.000000000000000000 ) ) ;
#45392 = CARTESIAN_POINT ( 'NONE',  ( 2.679491924311225848, 238.5416666666666288, -10.00000000000000000 ) ) ;
#45393 = CARTESIAN_POINT ( 'NONE',  ( 28.00000000000001776, 204.5000000000000284, 165.9999999999998863 ) ) ;
#45394 = CARTESIAN_POINT ( 'NONE',  ( -2.679491924311225848, 196.4583333333333428, -10.00000000000000178 ) ) ;
#45395 = CARTESIAN_POINT ( 'NONE',  ( -2.977408999572647819, 7.188101187499992051, 19.58030278187175455 ) ) ;
#45396 = CARTESIAN_POINT ( 'NONE',  ( 3.042071309553159519, 165.0520833299193839, 11.35316468750000141 ) ) ;
#45397 = CARTESIAN_POINT ( 'NONE',  ( -1.173938163346586453E-11, 213.7499999999991189, 10.00000000000000178 ) ) ;
#45398 = CARTESIAN_POINT ( 'NONE',  ( -2.695204135499268183, -43.66808553725495301, 151.1919800546250485 ) ) ;
#45400 = DIRECTION ( 'NONE',  ( -0.000000000000000000, 1.000000000000000000, -1.563033456626094573E-30 ) ) ;
#45399 = DIRECTION ( 'NONE',  ( 0.000000000000000000, 0.000000000000000000, 1.000000000000000000 ) ) ;
#45401 = VERTEX_POINT ( 'NONE', #67529 ) ;
#45402 = CARTESIAN_POINT ( 'NONE',  ( -2.445694354108838731, 197.0625000013656063, 144.4456943541088663 ) ) ;
#45403 = CARTESIAN_POINT ( 'NONE',  ( 6.951808397369818766E-16, 27.34374999658601979, -11.35316468750000141 ) ) ;
#45404 = CARTESIAN_POINT ( 'NONE',  ( 7.778174593052021635, 7.778174593052023411, 110.1250000040967763 ) ) ;
#45405 = CARTESIAN_POINT ( 'NONE',  ( -1.656854249492246467, 198.8125000000000000, 193.9999999999999716 ) ) ;
#45407 = CARTESIAN_POINT ( 'NONE',  ( -1.882291019712477143, -10.12018455450522580, -70.22327770540287872 ) ) ;
#45406 = CARTESIAN_POINT ( 'NONE',  ( -17.99999999999999645, 8.711927089654754042, -1.122611879773020682 ) ) ;
#45408 = CARTESIAN_POINT ( 'NONE',  ( -30.93541659651598152, -51.99989572432781415, 171.9999999999997726 ) ) ;
#45409 = CARTESIAN_POINT ( 'NONE',  ( -3.458734125000015425, 197.0000000013656063, 143.4326545832176976 ) ) ;
#45410 = CARTESIAN_POINT ( 'NONE',  ( -7.320508075688778149, 64.99999999317203958, 7.320508075688769267 ) ) ;
#45411 = CARTESIAN_POINT ( 'NONE',  ( -2.977408999572650927, 105.8750000020483952, -7.188101187500001821 ) ) ;
#45412 = CARTESIAN_POINT ( 'NONE',  ( -3.211159895383561391, 10.81249999863440792, -3.211159895383561835 ) ) ;
#45413 = CARTESIAN_POINT ( 'NONE',  ( -27.99999999999991473, 206.6250000027312126, 174.0000000000003695 ) ) ;
#45414 = CARTESIAN_POINT ( 'NONE',  ( 1.469576158976822172E-15, -7.999999999999991118, 2.705302779823365533 ) ) ;
#45415 = CARTESIAN_POINT ( 'NONE',  ( -27.99999999999999645, 210.0000000000000284, 170.0000000000003695 ) ) ;
#45416 = VERTEX_POINT ( 'NONE', #27528 ) ;
#45417 = EDGE_LOOP ( 'NONE', ( #43231, #26557, #9677, #31472 ) ) ;
#45418 = EDGE_CURVE ( 'NONE', #55503, #18628, #35003, .T. ) ;
#45419 =( BOUNDED_CURVE ( )  B_SPLINE_CURVE ( 2, ( #61534, #50576, #74333, #73593, #16604, #67570, #9857, #44184, #21901 ),
 .UNSPECIFIED., .F., .F. ) 
 B_SPLINE_CURVE_WITH_KNOTS ( ( 3, 2, 2, 2, 3 ),
 ( 0.3157894736842105643, 0.3223684210526316374, 0.3289473684210526550, 0.3355263157894736725, 0.3421052631578947456 ),
 .UNSPECIFIED. ) 
 CURVE ( )  GEOMETRIC_REPRESENTATION_ITEM ( )  RATIONAL_B_SPLINE_CURVE ( ( 0.9999999999999993339, 0.9238795325112874046, 1.000000000000000000, 0.9238795325112867385, 1.000000000000000000, 0.9238795325112867385, 1.000000000000000000, 0.9238795325112867385, 1.000000000000000000 ) ) 
 REPRESENTATION_ITEM ( '' )  );
#45420 = CARTESIAN_POINT ( 'NONE',  ( -8.660254037844481445, 197.9166666666667425, 5.000000000000052403 ) ) ;
#45421 = CARTESIAN_POINT ( 'NONE',  ( 3.458734125000015425, 195.2500000013656063, 196.5673454167823877 ) ) ;
#45422 = AXIS2_PLACEMENT_3D ( 'NONE', #30730, #35664, #977 ) ;
#45423 = CARTESIAN_POINT ( 'NONE',  ( 3.999999999999959144, 198.1875000027312126, 140.3431457505076594 ) ) ;
#45424 = CARTESIAN_POINT ( 'NONE',  ( -5.676582343750006032, 139.1145833299193555, 9.832129032723418760 ) ) ;
#45425 = ORIENTED_EDGE ( 'NONE', *, *, #14826, .F. ) ;
#45426 = CARTESIAN_POINT ( 'NONE',  ( 0.000000000000000000, 0.000000000000000000, -28.00000000000000000 ) ) ;
#45427 = CARTESIAN_POINT ( 'NONE',  ( -7.204075437095967871, 7.204075437095967871, 89.96875000204838102 ) ) ;
#45428 = CARTESIAN_POINT ( 'NONE',  ( -31.34716094839814460, 194.6453746702107992, 171.4616704517149515 ) ) ;
#45429 = CARTESIAN_POINT ( 'NONE',  ( -3.999999999999960032, 208.0000000000000284, 198.0000000000000284 ) ) ;
#45430 = CARTESIAN_POINT ( 'NONE',  ( -2.828427124746153876, 204.8750000000000284, 195.1715728752538439 ) ) ;
#45431 = ORIENTED_EDGE ( 'NONE', *, *, #30340, .T. ) ;
#45432 = CARTESIAN_POINT ( 'NONE',  ( 1.224646799147353454E-15, 300.0000000000000000, -10.00000000000000178 ) ) ;
#45433 = CARTESIAN_POINT ( 'NONE',  ( 10.18810118749999916, 4.220049686691935698, 113.8750000020483668 ) ) ;
#45434 = ORIENTED_EDGE ( 'NONE', *, *, #23941, .F. ) ;
#45435 = ADVANCED_FACE ( 'NONE', ( #61117 ), #15083, .T. ) ;
#45436 = DIRECTION ( 'NONE',  ( -0.000000000000000000, -1.000000000000000000, -0.000000000000000000 ) ) ;
#45437 = CARTESIAN_POINT ( 'NONE',  ( 35.91417783105028150, 173.6629059085598499, 172.9739037162813986 ) ) ;
#45438 = CARTESIAN_POINT ( 'NONE',  ( -5.676582343749998039, 127.7604166632526841, -9.832129032723420536 ) ) ;
#45439 = CARTESIAN_POINT ( 'NONE',  ( 3.458734125000015425, 202.0000000013656063, 196.5673454167823877 ) ) ;
#45440 = CARTESIAN_POINT ( 'NONE',  ( -5.082755093536326818, 25.78124999795161543, 5.082755093536325042 ) ) ;
#45441 = CARTESIAN_POINT ( 'NONE',  ( 10.18810118749999916, 4.220049686691935698, 85.37500000204838102 ) ) ;
#45442 = CARTESIAN_POINT ( 'NONE',  ( -3.042071309553173730, 39.63541666325267698, 11.35316468749999785 ) ) ;
#45443 = ORIENTED_EDGE ( 'NONE', *, *, #18166, .T. ) ;
#45444 = DIRECTION ( 'NONE',  ( -0.000000000000000000, 1.000000000000000000, -4.476705744456276341E-16 ) ) ;
#45445 = CARTESIAN_POINT ( 'NONE',  ( 1.471067592899761672E-15, -8.008118988124991233, 22.38811528394063188 ) ) ;
#45446 = CARTESIAN_POINT ( 'NONE',  ( 3.458734124999960358, 205.6875000013656063, 142.0000000000000568 ) ) ;
#45447 = CARTESIAN_POINT ( 'NONE',  ( 5.082755093536324154, 10.78124999795161187, 5.082755093536326818 ) ) ;
#45448 = CARTESIAN_POINT ( 'NONE',  ( 1.102182119232618108E-15, 296.3125000034140157, 6.000000000000001776 ) ) ;
#45449 = CARTESIAN_POINT ( 'NONE',  ( -47.32259252271279593, 145.2267040872997939, 65.76194439203463560 ) ) ;
#45450 = CARTESIAN_POINT ( 'NONE',  ( 7.188101187500000044, 3.843749997951610542, 0.000000000000000000 ) ) ;
#45451 = CARTESIAN_POINT ( 'NONE',  ( 11.35316468749999963, 156.3020833299192986, -3.042071309553165293 ) ) ;
#45452 = CARTESIAN_POINT ( 'NONE',  ( 7.204075437095966983, 7.204075437095967871, 76.09375000204838102 ) ) ;
#45453 = EDGE_CURVE ( 'NONE', #2593, #69617, #38491, .T. ) ;
#45454 = CARTESIAN_POINT ( 'NONE',  ( -24.54126587499999701, 209.4375000013656063, 170.0000000000003411 ) ) ;
#45455 = EDGE_CURVE ( 'NONE', #48752, #12154, #42661, .T. ) ;
#45456 = CYLINDRICAL_SURFACE ( 'NONE', #65520, 3.000000000000001332 ) ;
#45457 = CARTESIAN_POINT ( 'NONE',  ( 4.541265875000002339, 18.43749999863440792, 0.000000000000000000 ) ) ;
#45458 = ORIENTED_EDGE ( 'NONE', *, *, #38065, .F. ) ;
#45459 = CARTESIAN_POINT ( 'NONE',  ( 1.656854249492405451, 198.4375000027312126, 202.0000000000000284 ) ) ;
#45460 = CARTESIAN_POINT ( 'NONE',  ( 2.828427124746153876, 206.8750000000000284, 144.8284271247462129 ) ) ;
#45461 = CARTESIAN_POINT ( 'NONE',  ( -24.00000000000002842, 206.9375000027312410, 168.3431457505079152 ) ) ;
#45462 = CARTESIAN_POINT ( 'NONE',  ( -2.679491924317145113, 58.54166666666618823, 9.999999999996678213 ) ) ;
#45463 = CARTESIAN_POINT ( 'NONE',  ( -7.999999999999991118, 0.000000000000000000, 8.517802783920146226 ) ) ;
#45464 = VERTEX_POINT ( 'NONE', #60746 ) ;
#45465 = EDGE_CURVE ( 'NONE', #5379, #72263, #21985, .T. ) ;
#45466 = CARTESIAN_POINT ( 'NONE',  ( -5.082755093536326818, 16.40624999795161543, 5.082755093536325042 ) ) ;
#45467 = CARTESIAN_POINT ( 'NONE',  ( -7.999999999999991118, -1.288204405367768053E-10, 8.517802783929960597 ) ) ;
#45468 = CARTESIAN_POINT ( 'NONE',  ( -1.503295408875327865, -47.60365648431734087, 151.0588486906985679 ) ) ;
#45469 = CARTESIAN_POINT ( 'NONE',  ( -5.000000000000005329, 43.33333333333333570, 8.660254037844387298 ) ) ;
#45470 = CARTESIAN_POINT ( 'NONE',  ( 7.188101187500001821, 107.3750000020484094, -2.977408999572651371 ) ) ;
#45471 = DIRECTION ( 'NONE',  ( 0.000000000000000000, 0.000000000000000000, 1.000000000000000000 ) ) ;
#45472 = CARTESIAN_POINT ( 'NONE',  ( -6.000000000000001776, 300.0000000000000000, 0.000000000000000000 ) ) ;
#45474 = CARTESIAN_POINT ( 'NONE',  ( 4.999999999999993783, 196.0416666598387110, 8.660254037844390851 ) ) ;
#45473 = CARTESIAN_POINT ( 'NONE',  ( -27.99999999999995737, 201.5000000000000000, 174.0000000000003695 ) ) ;
#45475 = VERTEX_POINT ( 'NONE', #61494 ) ;
#45476 = CARTESIAN_POINT ( 'NONE',  ( -8.311093377946836114, 243.2812500034139589, -8.311093377946836114 ) ) ;
#45477 = CARTESIAN_POINT ( 'NONE',  ( 7.188101187499991163, 2.977408999572648707, 22.20530278187175810 ) ) ;
#45478 = CARTESIAN_POINT ( 'NONE',  ( -4.330454160167357180, 52.03352386568316490, 48.86100738217030681 ) ) ;
#45479 = CARTESIAN_POINT ( 'NONE',  ( -9.300015335314476772, 220.0000000000000000, 5.337650171418015788 ) ) ;
#45480 = CARTESIAN_POINT ( 'NONE',  ( -8.660254037844387298, 147.0833333333333428, -5.000000000000004441 ) ) ;
#45481 = CARTESIAN_POINT ( 'NONE',  ( -1.432654583217608080, 195.8750000013655779, 201.4587341250000350 ) ) ;
#45482 = CARTESIAN_POINT ( 'NONE',  ( -1.836970198721029983E-15, 163.7500000000000000, 10.00000000000000178 ) ) ;
#45483 = DIRECTION ( 'NONE',  ( 0.000000000000000000, 0.000000000000000000, -1.000000000000000000 ) ) ;
#45484 = SURFACE_STYLE_USAGE ( .BOTH. , #74160 ) ;
#45485 = CARTESIAN_POINT ( 'NONE',  ( 5.000000000000001776, -53.32026166094865971, -44.27875806161964789 ) ) ;
#45486 = CARTESIAN_POINT ( 'NONE',  ( 6.951808397369818766E-16, 127.3437499965860127, -11.35316468750000141 ) ) ;
#45487 = DIRECTION ( 'NONE',  ( 0.000000000000000000, 0.000000000000000000, 1.000000000000000000 ) ) ;
#45488 = CARTESIAN_POINT ( 'NONE',  ( -3.018451720292563716E-14, -16.44602605510714355, -68.55492853905353456 ) ) ;
#45490 = CARTESIAN_POINT ( 'NONE',  ( 30.44569435410879166, 195.8125000013656063, 167.5543056458910485 ) ) ;
#45489 = CARTESIAN_POINT ( 'NONE',  ( 30.44569435410878810, 196.8125000013656063, 172.4456943541087526 ) ) ;
#45491 = ADVANCED_FACE ( 'NONE', ( #32464 ), #9069, .T. ) ;
#45492 = ORIENTED_EDGE ( 'NONE', *, *, #40835, .T. ) ;
#45493 = CARTESIAN_POINT ( 'NONE',  ( 4.545654900257371622, 224.1260959769811905, 8.912008146339848835 ) ) ;
#45494 = ADVANCED_FACE ( 'NONE', ( #55471 ), #32841, .T. ) ;
#45495 = CARTESIAN_POINT ( 'NONE',  ( 0.000000000000000000, 0.000000000000000000, -14.80000000000000071 ) ) ;
#45496 = CARTESIAN_POINT ( 'NONE',  ( 1.432654583217607192, 209.2500000013656063, 145.4587341250000350 ) ) ;
#45497 = VECTOR ( 'NONE', #21645, 1000.000000000000000 ) ;
#45498 = CARTESIAN_POINT ( 'NONE',  ( 37.99999999999999289, 82.00000000000001421, 65.00000000000000000 ) ) ;
#45499 = CARTESIAN_POINT ( 'NONE',  ( 9.832129032723420536, 211.5104166632526699, -5.676582343749999815 ) ) ;
#45500 = CARTESIAN_POINT ( 'NONE',  ( -4.401442555609581635E-16, 120.7812500020483810, -7.188101187500000044 ) ) ;
#45501 = CARTESIAN_POINT ( 'NONE',  ( -8.342170076843785083E-16, 21.06249999863440792, 4.541265875000002339 ) ) ;
#45502 = CARTESIAN_POINT ( 'NONE',  ( -3.734423912264015932, 66.26963445014290244, -26.58791153592997247 ) ) ;
#45503 = CARTESIAN_POINT ( 'NONE',  ( -4.898587196589407898E-16, 7.999999999999991118, 18.45530277982336642 ) ) ;
#45505 = CARTESIAN_POINT ( 'NONE',  ( -32.00000000000003553, 208.3125000027312126, 168.3431457505080857 ) ) ;
#45504 = CARTESIAN_POINT ( 'NONE',  ( -2.828427124746190735, 1.375000000000000222, -2.828427124746191623 ) ) ;
#45506 = CARTESIAN_POINT ( 'NONE',  ( 9.832129032723420536, 91.19791666325269830, -5.676582343749999815 ) ) ;
#45507 = VERTEX_POINT ( 'NONE', #55851 ) ;
#45508 = ADVANCED_FACE ( 'NONE', ( #50540 ), #54729, .T. ) ;
#45509 = DIRECTION ( 'NONE',  ( 0.8660254037844380415, 0.5000000000000009992, 0.000000000000000000 ) ) ;
#45510 = CARTESIAN_POINT ( 'NONE',  ( -1.320432766682874540E-15, 27.09374999795161543, 7.188101187500000044 ) ) ;
#45511 = PLANE ( 'NONE',  #7325 ) ;
#45512 =( BOUNDED_CURVE ( )  B_SPLINE_CURVE ( 2, ( #7843, #20639, #43655, #42536, #59172 ),
 .UNSPECIFIED., .F., .F. ) 
 B_SPLINE_CURVE_WITH_KNOTS ( ( 3, 2, 3 ),
 ( 0.9833333333333340587, 0.9916666666666671404, 1.000000000000000000 ),
 .UNSPECIFIED. ) 
 CURVE ( )  GEOMETRIC_REPRESENTATION_ITEM ( )  RATIONAL_B_SPLINE_CURVE ( ( 0.9999999999999928946, 0.9238795325112938439, 1.000000000000000000, 0.9238795325112867385, 1.000000000000000000 ) ) 
 REPRESENTATION_ITEM ( '' )  );
#45513 = CARTESIAN_POINT ( 'NONE',  ( -9.832129032723418760, 258.8020833367473301, -5.676582343749998927 ) ) ;
#45514 = CARTESIAN_POINT ( 'NONE',  ( 8.311093377946834337, 105.1562499965860269, 8.311093377946839666 ) ) ;
#45515 = ORIENTED_EDGE ( 'NONE', *, *, #25870, .T. ) ;
#45516 = DIRECTION ( 'NONE',  ( -0.000000000000000000, 1.000000000000000000, -0.000000000000000000 ) ) ;
#45517 = CARTESIAN_POINT ( 'NONE',  ( 10.18810118750000093, -4.220049686691933921, 108.8125000020484094 ) ) ;
#45518 = CARTESIAN_POINT ( 'NONE',  ( -5.000000000000005329, 220.2083333265053966, 8.660254037844387298 ) ) ;
#45519 = CARTESIAN_POINT ( 'NONE',  ( 3.458734125000015869, 204.1875000013656063, 198.0000000000000284 ) ) ;
#45520 = CARTESIAN_POINT ( 'NONE',  ( 18.00000000000000355, -3.500879649426325457, -0.1509495798675470069 ) ) ;
#45522 = CARTESIAN_POINT ( 'NONE',  ( 11.35316468749999785, 105.5729166632526983, 3.042071309553174174 ) ) ;
#45521 = CARTESIAN_POINT ( 'NONE',  ( -30.64284399271078740, 271.9999999999999432, 174.6921329945331536 ) ) ;
#45523 = CARTESIAN_POINT ( 'NONE',  ( 5.656854249492374365, 5.656854249492375253, 12.45530278392014623 ) ) ;
#45524 = CARTESIAN_POINT ( 'NONE',  ( -24.54126587500000056, 199.5000000013656063, 168.5673454167827003 ) ) ;
#45525 = CARTESIAN_POINT ( 'NONE',  ( 10.00000000000000178, 170.0000000000000000, 0.000000000000000000 ) ) ;
#45526 = VERTEX_POINT ( 'NONE', #67900 ) ;
#45527 = CARTESIAN_POINT ( 'NONE',  ( -8.660254037844390851, 179.7916666598387110, 4.999999999999998224 ) ) ;
#45528 = CARTESIAN_POINT ( 'NONE',  ( 23.99999999999997868, 200.8125000027312126, 168.3431457505075457 ) ) ;
#45529 = FACE_OUTER_BOUND ( 'NONE', #13113, .T. ) ;
#45530 = CARTESIAN_POINT ( 'NONE',  ( 9.832129032723420536, 86.51041666325268409, -5.676582343749999815 ) ) ;
#45531 = CARTESIAN_POINT ( 'NONE',  ( 6.676582343750001591, 287.9531250017069510, -8.176455196517173205E-16 ) ) ;
#45532 = CARTESIAN_POINT ( 'NONE',  ( 7.188101187500000933, 3.937499997951610986, -2.977408999572650483 ) ) ;
#45533 = EDGE_CURVE ( 'NONE', #25548, #47792, #50383, .T. ) ;
#45534 = CARTESIAN_POINT ( 'NONE',  ( 7.204075437095968759, -7.204075437095966983, 98.59375000204836681 ) ) ;
#45535 = CARTESIAN_POINT ( 'NONE',  ( -3.042071309553164404, 2.552083329919349275, -11.35316468749999963 ) ) ;
#45536 = ORIENTED_EDGE ( 'NONE', *, *, #7959, .F. ) ;
#45537 = CARTESIAN_POINT ( 'NONE',  ( -4.000000000000002665, 1.312499997268813168, 1.656854249492380582 ) ) ;
#45538 = CARTESIAN_POINT ( 'NONE',  ( -3.313708498984765161, 2.343749995903220196, 7.999999999999998224 ) ) ;
#45539 = CARTESIAN_POINT ( 'NONE',  ( 2.828427124746191623, 0.8749999972688131678, -2.828427124746191623 ) ) ;
#45540 = CARTESIAN_POINT ( 'NONE',  ( 9.832129032723416984, 225.3645833299193839, 5.676582343750006032 ) ) ;
#45541 = CARTESIAN_POINT ( 'NONE',  ( -10.00000000000000000, 227.9166666734946034, -2.679491924311226292 ) ) ;
#45542 = CARTESIAN_POINT ( 'NONE',  ( 6.676582343750004256, 296.8906250017068942, 2.765530957081995478 ) ) ;
#45543 = ORIENTED_EDGE ( 'NONE', *, *, #23310, .T. ) ;
#45544 = VECTOR ( 'NONE', #819, 1000.000000000000000 ) ;
#45545 = CARTESIAN_POINT ( 'NONE',  ( 11.35316468749999963, 191.3020833299193839, -3.042071309553165293 ) ) ;
#45546 =( BOUNDED_CURVE ( )  B_SPLINE_CURVE ( 2, ( #30131, #52407, #52772, #1481, #45993, #68634, #23725, #40336, #23352, #1110, #11297, #69009, #17690 ),
 .UNSPECIFIED., .F., .F. ) 
 B_SPLINE_CURVE_WITH_KNOTS ( ( 3, 2, 2, 2, 2, 2, 3 ),
 ( 0.2228260869565217295, 0.2246376811594202882, 0.2264492753623188470, 0.2282608695652174058, 0.2300724637681159646, 0.2318840579710145233, 0.2336956521739130821 ),
 .UNSPECIFIED. ) 
 CURVE ( )  GEOMETRIC_REPRESENTATION_ITEM ( )  RATIONAL_B_SPLINE_CURVE ( ( 1.000000000000000000, 0.9659258262890683122, 1.000000000000000000, 0.9659258262890683122, 1.000000000000000000, 0.9659258262890683122, 1.000000000000000000, 0.9659258262890683122, 1.000000000000000000, 0.9659258262890683122, 1.000000000000000000, 0.9659258262890677571, 1.000000000000000444 ) ) 
 REPRESENTATION_ITEM ( '' )  );
#45547 = CARTESIAN_POINT ( 'NONE',  ( 7.204075437095966983, 7.204075437095967871, 95.59375000204836681 ) ) ;
#45548 = CARTESIAN_POINT ( 'NONE',  ( -27.99999999999996803, 207.9375000013656063, 173.4587341250003760 ) ) ;
#45549 = ADVANCED_FACE ( 'NONE', ( #32081 ), #20366, .T. ) ;
#45550 = CARTESIAN_POINT ( 'NONE',  ( 3.313708498984762052, 18.28125000000000711, -8.000000000000000000 ) ) ;
#45551 = ORIENTED_EDGE ( 'NONE', *, *, #55671, .F. ) ;
#45552 = AXIS2_PLACEMENT_3D ( 'NONE', #9264, #33049, #56048 ) ;
#45553 = PRODUCT_DEFINITION_CONTEXT ( 'detailed design', #61683, 'design' ) ;
#45554 = CARTESIAN_POINT ( 'NONE',  ( 8.000000000000001776, 92.84375000409677625, 3.313708498984759387 ) ) ;
#45555 = SURFACE_STYLE_USAGE ( .BOTH. , #10857 ) ;
#45556 = CARTESIAN_POINT ( 'NONE',  ( 2.679491924311228956, 21.04166666666666075, -10.00000000000000000 ) ) ;
#45557 = AXIS2_PLACEMENT_3D ( 'NONE', #72983, #60538, #8864 ) ;
#45558 =( BOUNDED_CURVE ( )  B_SPLINE_CURVE ( 2, ( #26309, #3321, #20277, #43300, #66314, #14620, #31994, #55015, #49332 ),
 .UNSPECIFIED., .F., .F. ) 
 B_SPLINE_CURVE_WITH_KNOTS ( ( 3, 2, 2, 2, 3 ),
 ( 0.4500000000000002887, 0.4583333333333336479, 0.4666666666666670626, 0.4750000000000004219, 0.4833333333333338366 ),
 .UNSPECIFIED. ) 
 CURVE ( )  GEOMETRIC_REPRESENTATION_ITEM ( )  RATIONAL_B_SPLINE_CURVE ( ( 0.9999999999999974465, 0.9238795325112892920, 1.000000000000000000, 0.9238795325112867385, 1.000000000000000000, 0.9238795325112867385, 1.000000000000000000, 0.9238795325112821866, 1.000000000000004663 ) ) 
 REPRESENTATION_ITEM ( '' )  );
#45559 = CYLINDRICAL_SURFACE ( 'NONE', #7852, 10.00000000000000178 ) ;
#45560 = CARTESIAN_POINT ( 'NONE',  ( 10.18810118750000093, -4.220049686691933921, 83.68750000204836681 ) ) ;
#45561 = ORIENTED_EDGE ( 'NONE', *, *, #52344, .F. ) ;
#45562 = CARTESIAN_POINT ( 'NONE',  ( 1.656854249492381914, 18.81250000000000000, 4.000000000000000888 ) ) ;
#45563 = CARTESIAN_POINT ( 'NONE',  ( 9.000000000000000000, -1.750439824713163617, -0.07547478993377551570 ) ) ;
#45564 = LINE ( 'NONE', #15390, #12560 ) ;
#45565 = CARTESIAN_POINT ( 'NONE',  ( -1.836970198721029983E-15, 15.62499999317203248, 10.00000000000000178 ) ) ;
#45566 = CARTESIAN_POINT ( 'NONE',  ( 2.977408999572654480, 122.0000000020483668, 7.188101187499999156 ) ) ;
#45567 = CARTESIAN_POINT ( 'NONE',  ( 0.8721677472509306028, 51.17354301023034679, 48.53016177276406040 ) ) ;
#45570 = CARTESIAN_POINT ( 'NONE',  ( -8.000000000000000000, 123.6875000040967905, 0.000000000000000000 ) ) ;
#45569 = CARTESIAN_POINT ( 'NONE',  ( -9.832129032723415207, 244.3229166700806445, 5.676582343750005144 ) ) ;
#45568 = CARTESIAN_POINT ( 'NONE',  ( 28.00000000000002132, 208.4375000013656063, 173.4587341249998929 ) ) ;
#45571 = SHAPE_DEFINITION_REPRESENTATION ( #40948, #20419 ) ;
#45572 = ORIENTED_EDGE ( 'NONE', *, *, #45455, .T. ) ;
#45573 = EDGE_CURVE ( 'NONE', #41993, #43604, #14234, .T. ) ;
#45574 = CARTESIAN_POINT ( 'NONE',  ( 5.676582343749997150, 252.5520833367473301, -9.832129032723418760 ) ) ;
#45575 = CARTESIAN_POINT ( 'NONE',  ( 1.320432766682872962E-15, -7.188101187499992051, 10.86155278187175455 ) ) ;
#45576 = VERTEX_POINT ( 'NONE', #45260 ) ;
#45577 = ORIENTED_EDGE ( 'NONE', *, *, #53630, .F. ) ;
#45578 = CARTESIAN_POINT ( 'NONE',  ( 10.18810118749999916, 1.247682550866122264E-15, 75.90625000204836681 ) ) ;
#45579 = CARTESIAN_POINT ( 'NONE',  ( 6.951808397369818766E-16, 87.34374999658602690, -11.35316468750000141 ) ) ;
#45580 = FACE_OUTER_BOUND ( 'NONE', #58193, .T. ) ;
#45581 = CARTESIAN_POINT ( 'NONE',  ( -6.735557395310442023E-16, 11.00000000000000000, 86.12499999999998579 ) ) ;
#45584 = DIRECTION ( 'NONE',  ( 0.000000000000000000, 0.000000000000000000, 1.000000000000000000 ) ) ;
#45583 = CARTESIAN_POINT ( 'NONE',  ( 31.45873412500001010, 207.6250000013656347, 171.4326545832175555 ) ) ;
#45582 = CARTESIAN_POINT ( 'NONE',  ( 24.54126587499998280, 205.5000000013655779, 171.4326545832175555 ) ) ;
#45585 = CYLINDRICAL_SURFACE ( 'NONE', #14252, 6.000000000000001776 ) ;
#45586 = EDGE_CURVE ( 'NONE', #62814, #31018, #9402, .T. ) ;
#45587 = CARTESIAN_POINT ( 'NONE',  ( -3.042071309553164404, 202.2395833299193271, -11.35316468749999963 ) ) ;
#45588 = CARTESIAN_POINT ( 'NONE',  ( -2.445694354108838731, 204.0625000013656063, 144.4456943541088663 ) ) ;
#45589 = ORIENTED_EDGE ( 'NONE', *, *, #41437, .F. ) ;
#45590 = CARTESIAN_POINT ( 'NONE',  ( 25.55430564589115150, 204.5625000013656063, 172.4456943541086957 ) ) ;
#45591 = AXIS2_PLACEMENT_3D ( 'NONE', #16172, #74280, #72800 ) ;
#45592 = CARTESIAN_POINT ( 'NONE',  ( -5.082755093536325042, 17.90624999795161187, -5.082755093536325930 ) ) ;
#45593 = CARTESIAN_POINT ( 'NONE',  ( -5.676582343749998039, 172.7604166632526983, -9.832129032723420536 ) ) ;
#45594 = DIRECTION ( 'NONE',  ( 0.000000000000000000, 0.000000000000000000, 1.000000000000000000 ) ) ;
#45595 = CARTESIAN_POINT ( 'NONE',  ( 7.188101187500000933, 104.3750000020483952, -2.977408999572651371 ) ) ;
#45597 = CARTESIAN_POINT ( 'NONE',  ( -2.679491924311235174, 90.41666665983871098, 10.00000000000000000 ) ) ;
#45596 = DIRECTION ( 'NONE',  ( -0.000000000000000000, 1.000000000000000000, 4.476705744456276341E-16 ) ) ;
#45598 = CARTESIAN_POINT ( 'NONE',  ( 29.43265458321766914, 205.1250000013656347, 166.5412658749999650 ) ) ;
#45599 = CARTESIAN_POINT ( 'NONE',  ( 7.188101187499991163, 2.977408999572648707, 11.70530278187175455 ) ) ;
#45600 = CARTESIAN_POINT ( 'NONE',  ( -8.311093377946836114, 52.65624999658601979, -8.311093377946837890 ) ) ;
#45601 = EDGE_CURVE ( 'NONE', #74324, #48525, #39932, .T. ) ;
#45602 = CARTESIAN_POINT ( 'NONE',  ( -7.999985420792424584, -3.313723078192327698, 1.111553367238835799 ) ) ;
#45603 = CARTESIAN_POINT ( 'NONE',  ( 3.313708498984762496, -7.999999999999989342, 1.355302784329824206 ) ) ;
#45604 = ORIENTED_EDGE ( 'NONE', *, *, #33369, .T. ) ;
#45605 = CARTESIAN_POINT ( 'NONE',  ( 12.00000000000000178, -28.00000000000000000, -3.999999999999989786 ) ) ;
#45606 = CARTESIAN_POINT ( 'NONE',  ( -8.311093377946836114, 67.65624999658599847, -8.311093377946837890 ) ) ;
#45607 = VECTOR ( 'NONE', #7092, 1000.000000000000000 ) ;
#45608 = CARTESIAN_POINT ( 'NONE',  ( 11.00000000000000000, 4.556349186104045934, 75.53125000409676204 ) ) ;
#45609 = CARTESIAN_POINT ( 'NONE',  ( -2.754378923186476579E-14, 199.4375000013655779, 145.4587341250000350 ) ) ;
#45610 = CARTESIAN_POINT ( 'NONE',  ( 3.074111742571302042, 16.37317034319775644, 69.01341173091257986 ) ) ;
#45611 = CARTESIAN_POINT ( 'NONE',  ( -8.660254037844387298, 12.08333333333333570, -5.000000000000004441 ) ) ;
#45613 = CARTESIAN_POINT ( 'NONE',  ( 11.35316468750000141, 55.78124999658601268, 0.000000000000000000 ) ) ;
#45612 = CARTESIAN_POINT ( 'NONE',  ( 2.977408999572650039, 95.18750000204838102, -7.188101187500000933 ) ) ;
#45614 = CARTESIAN_POINT ( 'NONE',  ( -3.313708498984757167, 7.999999999999991118, 3.549052779823362425 ) ) ;
#45615 = CARTESIAN_POINT ( 'NONE',  ( 0.000000000000000000, 45.00000000000000000, 0.000000000000000000 ) ) ;
#45616 = CARTESIAN_POINT ( 'NONE',  ( 8.311093377946837890, 171.4062499965860127, -8.311093377946837890 ) ) ;
#45617 = VECTOR ( 'NONE', #38916, 1000.000000000000000 ) ;
#45618 = CARTESIAN_POINT ( 'NONE',  ( -4.999999999999998224, 143.5416666598386826, -8.660254037844389075 ) ) ;
#45619 = CARTESIAN_POINT ( 'NONE',  ( -7.188101187500001821, 95.93750000204839523, -2.977408999572650483 ) ) ;
#45620 = CARTESIAN_POINT ( 'NONE',  ( -7.999999999999991118, 0.000000000000000000, 17.33030277982336287 ) ) ;
#45621 = CARTESIAN_POINT ( 'NONE',  ( -11.35316468750000141, 48.80208332991934839, 3.042071309553159963 ) ) ;
#45622 = CARTESIAN_POINT ( 'NONE',  ( 1.469576158976823947E-15, 119.5625000040967763, 8.000000000000000000 ) ) ;
#45623 = CARTESIAN_POINT ( 'NONE',  ( -9.832129032723418760, 177.8645833299193555, -5.676582343750004256 ) ) ;
#45624 = ORIENTED_EDGE ( 'NONE', *, *, #16283, .F. ) ;
#45625 = CARTESIAN_POINT ( 'NONE',  ( -7.347880794884122694E-16, 3.750000000000000000, 4.000000000000001776 ) ) ;
#45626 = CARTESIAN_POINT ( 'NONE',  ( 1.871523826299183495E-15, -10.18810118749999916, 74.03125000204836681 ) ) ;
#45627 = CARTESIAN_POINT ( 'NONE',  ( -3.999999999999960032, 197.9375000000000000, 196.3431457505076594 ) ) ;
#45628 = CARTESIAN_POINT ( 'NONE',  ( 31.50643954115454193, 44.24041095553026537, 65.00000000000000000 ) ) ;
#45630 = CARTESIAN_POINT ( 'NONE',  ( -5.676582343749998039, 167.4479166632526983, -9.832129032723420536 ) ) ;
#45629 = CARTESIAN_POINT ( 'NONE',  ( -1.031381239350616097, 194.9470492016643277, 194.1813066841831983 ) ) ;
#45631 = CARTESIAN_POINT ( 'NONE',  ( -3.313708498984757167, 7.999999999999991118, 6.605302784329821542 ) ) ;
#45632 = CARTESIAN_POINT ( 'NONE',  ( 7.999999999999991118, 3.313708498984758055, 4.674052779823363757 ) ) ;
#45633 = CARTESIAN_POINT ( 'NONE',  ( -5.676582343750000703, 223.0729166700806729, -9.832129032723418760 ) ) ;
#45634 = DIRECTION ( 'NONE',  ( -0.000000000000000000, 1.000000000000000000, -0.000000000000000000 ) ) ;
#45635 = VERTEX_POINT ( 'NONE', #10560 ) ;
#45636 = CARTESIAN_POINT ( 'NONE',  ( -5.082755093536317936, -5.082755093536320601, 27.17405278187175455 ) ) ;
#45637 = CARTESIAN_POINT ( 'NONE',  ( 8.311093377946837890, 121.7187499965860411, -8.311093377946837890 ) ) ;
#45638 =( BOUNDED_CURVE ( )  B_SPLINE_CURVE ( 2, ( #61104, #61482, #56951, #9807, #15816, #50160, #10175, #32451, #72426, #49405, #27891 ),
 .UNSPECIFIED., .F., .F. ) 
 B_SPLINE_CURVE_WITH_KNOTS ( ( 3, 2, 2, 2, 2, 3 ),
 ( 0.2117847674899544508, 0.2117848187026179774, 0.2184030942870707759, 0.2250213698715235744, 0.2316396454559763729, 0.2382579061490637251 ),
 .UNSPECIFIED. ) 
 CURVE ( )  GEOMETRIC_REPRESENTATION_ITEM ( )  RATIONAL_B_SPLINE_CURVE ( ( 0.9999988219584774463, 0.9999994109746808135, 1.000000000000000000, 0.9238795325112867385, 1.000000000000000000, 0.9238795325112867385, 1.000000000000000000, 0.9238795325112867385, 1.000000000000000000, 0.9238797037851605998, 0.9999996574530229942 ) ) 
 REPRESENTATION_ITEM ( '' )  );
#45639 = CARTESIAN_POINT ( 'NONE',  ( 32.00000000000000000, 195.3125000000000853, 168.3431457505075457 ) ) ;
#45640 = ORIENTED_EDGE ( 'NONE', *, *, #16441, .T. ) ;
#45641 = CARTESIAN_POINT ( 'NONE',  ( -8.342170076843785083E-16, 7.187499998634407028, 4.541265875000002339 ) ) ;
#45642 = CARTESIAN_POINT ( 'NONE',  ( 4.401442555609581635E-16, 15.84374999795161365, -7.188101187500000044 ) ) ;
#45643 = CARTESIAN_POINT ( 'NONE',  ( 3.313708498984760720, 108.2187500040968047, -8.000000000000000000 ) ) ;
#45644 = CARTESIAN_POINT ( 'NONE',  ( -28.00000000000002132, 199.6875000013656063, 166.5412658750003629 ) ) ;
#45645 = CARTESIAN_POINT ( 'NONE',  ( -4.000000000000001776, 6.437500000000000888, -1.656854249492381470 ) ) ;
#45646 =( BOUNDED_CURVE ( )  B_SPLINE_CURVE ( 2, ( #35332, #51540, #40226, #63229, #6281, #262, #58344, #34589, #57596 ),
 .UNSPECIFIED., .F., .F. ) 
 B_SPLINE_CURVE_WITH_KNOTS ( ( 3, 2, 2, 2, 3 ),
 ( 0.1666666666666668239, 0.1750000000000001554, 0.1833333333333334869, 0.1916666666666668462, 0.2000000000000001776 ),
 .UNSPECIFIED. ) 
 CURVE ( )  GEOMETRIC_REPRESENTATION_ITEM ( )  RATIONAL_B_SPLINE_CURVE ( ( 0.9999999999999984457, 0.9238795325112882928, 1.000000000000000000, 0.9238795325112867385, 1.000000000000000000, 0.9238795325112867385, 1.000000000000000000, 0.9238795325112851842, 1.000000000000001554 ) ) 
 REPRESENTATION_ITEM ( '' )  );
#45647 = CARTESIAN_POINT ( 'NONE',  ( 1.656854249492381914, 21.56249999726881583, 4.000000000000000888 ) ) ;
#45648 = CARTESIAN_POINT ( 'NONE',  ( 2.780723358947928197E-16, 8.562499998634407916, -4.541265875000002339 ) ) ;
#45649 = CARTESIAN_POINT ( 'NONE',  ( -1.656854249492405451, 200.3125000000000284, 138.0000000000000568 ) ) ;
#45650 = VECTOR ( 'NONE', #66321, 1000.000000000000000 ) ;
#45651 = VERTEX_POINT ( 'NONE', #39605 ) ;
#45652 = FILL_AREA_STYLE_COLOUR ( '', #53533 ) ;
#45653 = CARTESIAN_POINT ( 'NONE',  ( 5.082755093536325042, 104.0937500020483810, -5.082755093536325930 ) ) ;
#45654 = CARTESIAN_POINT ( 'NONE',  ( -29.43265458321771177, 194.5000000013656063, 166.5412658750003914 ) ) ;
#45655 = EDGE_CURVE ( 'NONE', #33407, #70596, #74606, .T. ) ;
#45656 = EDGE_CURVE ( 'NONE', #27257, #4330, #46001, .T. ) ;
#45657 = CARTESIAN_POINT ( 'NONE',  ( -1.881053915767121554, 20.62499999863441147, -4.541265875000002339 ) ) ;
#45658 = CARTESIAN_POINT ( 'NONE',  ( -4.401442555609577197E-16, 7.188101187499992051, 1.111552781871753215 ) ) ;
#45659 = ORIENTED_EDGE ( 'NONE', *, *, #25040, .F. ) ;
#45660 = ORIENTED_EDGE ( 'NONE', *, *, #45601, .T. ) ;
#45661 = CARTESIAN_POINT ( 'NONE',  ( 10.18810118749999916, 1.247682550866122264E-15, 95.40625000204836681 ) ) ;
#45662 = CARTESIAN_POINT ( 'NONE',  ( 0.000000000000000000, 0.000000000000000000, -10.77459999999999951 ) ) ;
#45663 = CARTESIAN_POINT ( 'NONE',  ( 5.000000000000000000, -70.11723469343111503, 28.93519894129190817 ) ) ;
#45664 = CARTESIAN_POINT ( 'NONE',  ( -11.00000000000000000, 4.556349186104045934, 99.90624999999998579 ) ) ;
#45665 = CARTESIAN_POINT ( 'NONE',  ( -2.445694354108783219, 203.8125000013656063, 200.4456943541088663 ) ) ;
#45667 = CARTESIAN_POINT ( 'NONE',  ( 11.00000000000000000, 1.347111479062088405E-15, 112.9375000040967763 ) ) ;
#45666 = DIRECTION ( 'NONE',  ( 0.000000000000000000, 0.000000000000000000, 1.000000000000000000 ) ) ;
#45668 = CARTESIAN_POINT ( 'NONE',  ( -4.999999999999998224, 121.6666666666666714, -8.660254037844389075 ) ) ;
#45669 = EDGE_CURVE ( 'NONE', #62597, #58407, #56966, .T. ) ;
#45670 = CARTESIAN_POINT ( 'NONE',  ( -3.313708498984762496, 104.2812499999999858, 7.999999999999998224 ) ) ;
#45671 = CARTESIAN_POINT ( 'NONE',  ( 11.00000000000010836, -4.556349186103939353, 87.34375000409679046 ) ) ;
#45672 = CARTESIAN_POINT ( 'NONE',  ( -7.188101187499991163, 2.977408999572646930, 3.267802781871751439 ) ) ;
#45673 = CARTESIAN_POINT ( 'NONE',  ( 1.656854249492337949, 200.3125000000000000, 202.0000000000000853 ) ) ;
#45674 = CARTESIAN_POINT ( 'NONE',  ( 30.44569435410879521, 207.5625000013656063, 172.4456943541087526 ) ) ;
#45675 = CARTESIAN_POINT ( 'NONE',  ( 8.000000000000000000, 28.31249999590322375, 0.000000000000000000 ) ) ;
#45676 = CARTESIAN_POINT ( 'NONE',  ( 2.445694354108783664, 201.3125000013656063, 144.4456943541088663 ) ) ;
#45677 = CARTESIAN_POINT ( 'NONE',  ( -4.401442555609581635E-16, 121.1562500020483810, -7.188101187500000044 ) ) ;
#45679 = CARTESIAN_POINT ( 'NONE',  ( 0.4888677760596294442, 194.9085675716885078, 194.1142642722682297 ) ) ;
#45678 = CARTESIAN_POINT ( 'NONE',  ( 38.00000000000000000, 37.00000000000000711, 2.785348294322036708E-14 ) ) ;
#45680 = CARTESIAN_POINT ( 'NONE',  ( 3.042071309553173286, 240.6770833367473301, 11.35316468749999608 ) ) ;
#45681 = CARTESIAN_POINT ( 'NONE',  ( -2.977408999572647819, 7.188101187499991163, 25.58030278187175810 ) ) ;
#45682 = CARTESIAN_POINT ( 'NONE',  ( 26.34314575050763452, 199.5625000000000568, 165.9999999999998863 ) ) ;
#45683 = CARTESIAN_POINT ( 'NONE',  ( -2.085542519210945728E-15, 14.53124999658601624, 11.35316468750000141 ) ) ;
#45684 = CYLINDRICAL_SURFACE ( 'NONE', #11047, 10.00000000000000178 ) ;
#45685 = CARTESIAN_POINT ( 'NONE',  ( 9.832129032723416984, 205.6770833299193555, 5.676582343750006032 ) ) ;
#45686 = CARTESIAN_POINT ( 'NONE',  ( -29.65685424949240812, 198.0625000000000284, 166.0000000000004263 ) ) ;
#45687 = CARTESIAN_POINT ( 'NONE',  ( 3.979266480698044450, 124.5000000000001137, -6.940132439340980675 ) ) ;
#45689 = CARTESIAN_POINT ( 'NONE',  ( 2.828427124746191623, 11.87499999726881406, -2.828427124746191623 ) ) ;
#45688 = CARTESIAN_POINT ( 'NONE',  ( -5.656854249492381470, 26.24999999590322375, 5.656854249492379694 ) ) ;
#45690 = ORIENTED_EDGE ( 'NONE', *, *, #36215, .F. ) ;
#45691 = CARTESIAN_POINT ( 'NONE',  ( -2.754378923186476579E-14, 202.4375000013656063, 145.4587341250000350 ) ) ;
#45692 = CARTESIAN_POINT ( 'NONE',  ( 3.042071309553167069, 16.82291666325268054, -11.35316468749999785 ) ) ;
#45693 = CARTESIAN_POINT ( 'NONE',  ( -6.735557395310442023E-16, 11.00000000000000000, 95.31250000409677625 ) ) ;
#45694 = CARTESIAN_POINT ( 'NONE',  ( 10.00000000000000355, 210.0000000000000284, 0.000000000000000000 ) ) ;
#45695 = EDGE_CURVE ( 'NONE', #29121, #2559, #11306, .T. ) ;
#45696 = CARTESIAN_POINT ( 'NONE',  ( -28.00000000000006750, 197.4375000013655779, 166.5412658750003629 ) ) ;
#45697 = CARTESIAN_POINT ( 'NONE',  ( 0.000000000000000000, 19.05255888325788050, 10.99999999999998934 ) ) ;
#45699 = CARTESIAN_POINT ( 'NONE',  ( 6.951808397369818766E-16, 2.031249996586016238, -11.35316468750000141 ) ) ;
#45698 = CARTESIAN_POINT ( 'NONE',  ( -2.977408999572652260, 110.9375000020483810, 7.188101187500000044 ) ) ;
#45700 = CARTESIAN_POINT ( 'NONE',  ( 1.469576158976822172E-15, -7.999999999999991118, 20.70530277982336642 ) ) ;
#45701 = CARTESIAN_POINT ( 'NONE',  ( -11.35316468749999785, 138.0729166632526699, -3.042071309553167513 ) ) ;
#45702 = AXIS2_PLACEMENT_3D ( 'NONE', #46326, #29723, #58410 ) ;
#45703 = CARTESIAN_POINT ( 'NONE',  ( 10.00000000000000178, 102.0833333265053682, -2.679491924311226736 ) ) ;
#45704 = CARTESIAN_POINT ( 'NONE',  ( -5.082755093536324154, 121.7187500020483952, 5.082755093536326818 ) ) ;
#45705 = CARTESIAN_POINT ( 'NONE',  ( 6.123233995736767268E-16, 3.124999993172032919, -10.00000000000000178 ) ) ;
#45706 = CARTESIAN_POINT ( 'NONE',  ( -26.56734541678238415, 207.6250000013656347, 166.5412658750003629 ) ) ;
#45707 = DIRECTION ( 'NONE',  ( -0.000000000000000000, 1.000000000000000000, -0.000000000000000000 ) ) ;
#45708 = VERTEX_POINT ( 'NONE', #17697 ) ;
#45709 = CARTESIAN_POINT ( 'NONE',  ( -1.308779242311917335, -60.23127520339022567, 22.90411807697330104 ) ) ;
#45710 = CARTESIAN_POINT ( 'NONE',  ( 0.000000000000000000, 300.0000000000000000, 0.000000000000000000 ) ) ;
#45711 = CARTESIAN_POINT ( 'NONE',  ( 2.765530957082001251, 295.7656250017069510, 6.676582343750000703 ) ) ;
#45712 = CARTESIAN_POINT ( 'NONE',  ( 5.676582343749993598, 129.9479166632526983, 9.832129032723422313 ) ) ;
#45713 = CARTESIAN_POINT ( 'NONE',  ( -2.828427124746209831, 207.5000000027312126, 139.1715728752538723 ) ) ;
#45714 = CARTESIAN_POINT ( 'NONE',  ( 7.999999999999991118, 9.797174393178815797E-16, 22.63655278432982243 ) ) ;
#45715 = CARTESIAN_POINT ( 'NONE',  ( 2.828427124746152987, 207.2500000027312126, 139.1715728752538723 ) ) ;
#45716 = TOROIDAL_SURFACE ( 'NONE', #7152, 68.99999999999994316, 38.00000000000000000 ) ;
#45717 = CARTESIAN_POINT ( 'NONE',  ( 9.832129032723416984, 256.8229166700806445, -5.676582343750003368 ) ) ;
#45718 = CARTESIAN_POINT ( 'NONE',  ( 7.204075437095968759, -7.204075437095966983, 100.0937500020483668 ) ) ;
#45719 = ORIENTED_EDGE ( 'NONE', *, *, #67296, .T. ) ;
#45720 = CARTESIAN_POINT ( 'NONE',  ( 4.999999999999999112, 10.60557809245594463, 66.49298242784793445 ) ) ;
#45721 = CARTESIAN_POINT ( 'NONE',  ( -30.64284399271078740, -21.00579972956345642, 174.6921329945331536 ) ) ;
#45722 = CARTESIAN_POINT ( 'NONE',  ( 2.445694354108839175, 203.3125000013656063, 195.5543056458912190 ) ) ;
#45723 = CARTESIAN_POINT ( 'NONE',  ( 11.35316468750000141, 71.09374999658601268, 0.000000000000000000 ) ) ;
#45724 = ORIENTED_EDGE ( 'NONE', *, *, #14539, .T. ) ;
#45725 = CARTESIAN_POINT ( 'NONE',  ( -7.204075437095965206, -7.204075437095968759, 109.8437500020483810 ) ) ;
#45726 = CARTESIAN_POINT ( 'NONE',  ( 2.780723358947928197E-16, 11.68749999863440614, -4.541265875000002339 ) ) ;
#45727 = ORIENTED_EDGE ( 'NONE', *, *, #26829, .T. ) ;
#45728 = CARTESIAN_POINT ( 'NONE',  ( 7.999999999999998224, 1.406250000000000000, 3.313708498984766493 ) ) ;
#45729 = CARTESIAN_POINT ( 'NONE',  ( -1.836970198721029983E-15, 20.62499999317203603, 10.00000000000000178 ) ) ;
#45730 = CARTESIAN_POINT ( 'NONE',  ( -4.999999999999998224, -68.02455775458921039, -22.06917953199535276 ) ) ;
#45731 = CARTESIAN_POINT ( 'NONE',  ( 7.188101187499999156, 24.74999999795161543, 2.977408999572654924 ) ) ;
#45732 = DIRECTION ( 'NONE',  ( 0.000000000000000000, -1.000000000000000000, 0.000000000000000000 ) ) ;
#45733 = CARTESIAN_POINT ( 'NONE',  ( 7.204075437095966983, 7.204075437095967871, 106.4687500020483810 ) ) ;
#45734 = PRODUCT_DEFINITION_SHAPE ( 'NONE', 'NONE',  #33048 ) ;
#45735 = CARTESIAN_POINT ( 'NONE',  ( 29.65685424949241522, 208.4375000000000284, 165.9999999999999432 ) ) ;
#45736 = CARTESIAN_POINT ( 'NONE',  ( 2.828427124746191623, 9.874999997268814056, -2.828427124746191623 ) ) ;
#45737 = CARTESIAN_POINT ( 'NONE',  ( 2.449293598294707893E-16, 18.25000000000000000, -4.000000000000001776 ) ) ;
#45738 = VERTEX_POINT ( 'NONE', #22234 ) ;
#45739 = EDGE_CURVE ( 'NONE', #44181, #42810, #51664, .T. ) ;
#45740 = EDGE_CURVE ( 'NONE', #26465, #19551, #7, .T. ) ;
#45741 = FACE_OUTER_BOUND ( 'NONE', #14203, .T. ) ;
#45742 = CARTESIAN_POINT ( 'NONE',  ( 1.432654583217664479, 204.7500000013656063, 201.4587341250000065 ) ) ;
#45744 =( BOUNDED_CURVE ( )  B_SPLINE_CURVE ( 2, ( #54027, #37041, #14002, #47604, #64234, #64608, #18582, #7996, #47977, #60041, #2336, #58585, #24962 ),
 .UNSPECIFIED., .F., .F. ) 
 B_SPLINE_CURVE_WITH_KNOTS ( ( 3, 2, 2, 2, 2, 2, 3 ),
 ( 0.6141304347826087584, 0.6159420289855073172, 0.6177536231884058759, 0.6195652173913044347, 0.6213768115942029935, 0.6231884057971015523, 0.6250000000000001110 ),
 .UNSPECIFIED. ) 
 CURVE ( )  GEOMETRIC_REPRESENTATION_ITEM ( )  RATIONAL_B_SPLINE_CURVE ( ( 0.9999999999999978906, 0.9659258262890704216, 1.000000000000000000, 0.9659258262890683122, 1.000000000000000000, 0.9659258262890683122, 1.000000000000000000, 0.9659258262890683122, 1.000000000000000000, 0.9659258262890683122, 1.000000000000000000, 0.9659258262890662028, 1.000000000000001998 ) ) 
 REPRESENTATION_ITEM ( '' )  );
#45743 = CARTESIAN_POINT ( 'NONE',  ( -29.43265458321756256, 206.8750000013656347, 173.4587341250004044 ) ) ;
#45745 = CARTESIAN_POINT ( 'NONE',  ( 28.00000000000002132, 199.1250000027312126, 173.9999999999999147 ) ) ;
#45746 = CARTESIAN_POINT ( 'NONE',  ( 4.541265875000001451, 10.24999999863440792, 1.881053915767124440 ) ) ;
#45747 = AXIS2_PLACEMENT_3D ( 'NONE', #4312, #15607, #60520 ) ;
#45748 = FACE_OUTER_BOUND ( 'NONE', #41673, .T. ) ;
#45749 = CARTESIAN_POINT ( 'NONE',  ( 2.977408999572646486, 7.188101187499991163, 20.51780278187175455 ) ) ;
#45750 = ORIENTED_EDGE ( 'NONE', *, *, #60386, .T. ) ;
#45751 = CARTESIAN_POINT ( 'NONE',  ( -33.07484552657816579, -21.19745326134420083, 158.8094963175336432 ) ) ;
#45752 = ORIENTED_EDGE ( 'NONE', *, *, #61511, .T. ) ;
#45753 = CARTESIAN_POINT ( 'NONE',  ( 10.18810118750000093, -4.220049686691933033, 110.3125000020483810 ) ) ;
#45754 = FACE_OUTER_BOUND ( 'NONE', #68604, .T. ) ;
#45755 = CARTESIAN_POINT ( 'NONE',  ( -2.445694354108782775, 201.5625000013656063, 200.4456943541088663 ) ) ;
#45756 = CARTESIAN_POINT ( 'NONE',  ( 24.54126587499997569, 197.1250000013656347, 168.5673454167822740 ) ) ;
#45757 = CARTESIAN_POINT ( 'NONE',  ( -10.00000000000000355, 82.70833333333332860, 2.679491924311223183 ) ) ;
#45758 = AXIS2_PLACEMENT_3D ( 'NONE', #67342, #8878, #33397 ) ;
#45759 = EDGE_CURVE ( 'NONE', #15493, #3120, #49341, .T. ) ;
#45760 = CARTESIAN_POINT ( 'NONE',  ( -7.188101187500001821, 89.93750000204840944, -2.977408999572650483 ) ) ;
#45761 = CARTESIAN_POINT ( 'NONE',  ( -3.673940397442060854E-16, 288.7500000000000000, -6.000000000000001776 ) ) ;
#45762 = VERTEX_POINT ( 'NONE', #65192 ) ;
#45763 = EDGE_CURVE ( 'NONE', #37692, #17643, #42558, .T. ) ;
#45764 = FACE_OUTER_BOUND ( 'NONE', #36306, .T. ) ;
#45765 = CARTESIAN_POINT ( 'NONE',  ( -3.074111742570127426, -67.95395293240403589, 20.32712440775640772 ) ) ;
#45766 = CARTESIAN_POINT ( 'NONE',  ( -4.000000000000015987, 197.6250000027312126, 142.0000000000000568 ) ) ;
#45767 = CARTESIAN_POINT ( 'NONE',  ( -5.000000000000000888, 67.91007042436096697, 22.22893179988047763 ) ) ;
#45768 = CARTESIAN_POINT ( 'NONE',  ( 3.313708498984711426, 96.96875000000001421, 8.000000000000053291 ) ) ;
#45769 = CARTESIAN_POINT ( 'NONE',  ( 10.00000000000000000, 242.5000000000000284, -1.224646799147353256E-15 ) ) ;
#45770 = CARTESIAN_POINT ( 'NONE',  ( 11.00000000000000000, 1.347111479062088405E-15, 91.93750000409677625 ) ) ;
#45771 = CARTESIAN_POINT ( 'NONE',  ( -10.18810118749999916, 4.220049686691934809, 69.43750000204838102 ) ) ;
#45772 = CARTESIAN_POINT ( 'NONE',  ( 2.679491924311222739, 203.9583333333333428, 10.00000000000000355 ) ) ;
#45773 = CARTESIAN_POINT ( 'NONE',  ( -5.082755093536319713, 5.082755093536319713, 19.67405278187175455 ) ) ;
#45774 = CARTESIAN_POINT ( 'NONE',  ( -11.35316468749999785, 173.3854166632526983, -3.042071309553167513 ) ) ;
#45775 = FACE_OUTER_BOUND ( 'NONE', #68846, .T. ) ;
#45776 = CARTESIAN_POINT ( 'NONE',  ( 2.020667218593132706E-15, -11.00000000000000000, 97.56250000409677625 ) ) ;
#45778 = CARTESIAN_POINT ( 'NONE',  ( 2.679491924311222739, 85.83333332650538239, 10.00000000000000355 ) ) ;
#45777 = SURFACE_STYLE_USAGE ( .BOTH. , #61651 ) ;
#45779 = ORIENTED_EDGE ( 'NONE', *, *, #2802, .T. ) ;
#45780 = CARTESIAN_POINT ( 'NONE',  ( 2.445694354108783664, 197.3125000013656063, 144.4456943541088663 ) ) ;
#45781 = CARTESIAN_POINT ( 'NONE',  ( 9.832129032723420536, 36.51041666325267698, -5.676582343749999815 ) ) ;
#45782 = CARTESIAN_POINT ( 'NONE',  ( -11.00000000000000000, 4.556349186104045934, 112.0937500040967905 ) ) ;
#45783 = EDGE_CURVE ( 'NONE', #66887, #6411, #47946, .T. ) ;
#45784 = CARTESIAN_POINT ( 'NONE',  ( -29.43265458321771533, 207.5000000013656063, 166.5412658750003914 ) ) ;
#45785 = FACE_OUTER_BOUND ( 'NONE', #57479, .T. ) ;
#45787 = CARTESIAN_POINT ( 'NONE',  ( 23.99999999999997868, 199.8125000000000284, 171.6568542494922553 ) ) ;
#45786 = CARTESIAN_POINT ( 'NONE',  ( -17.99999999999999645, 3.528342445705423991, -0.1857217976155464134 ) ) ;
#45788 = LINE ( 'NONE', #33373, #2464 ) ;
#45789 = CARTESIAN_POINT ( 'NONE',  ( -3.458734125000015425, 200.0000000013656063, 143.4326545832176976 ) ) ;
#45790 = CARTESIAN_POINT ( 'NONE',  ( 10.00000000000000178, 56.87499999317203248, 0.000000000000000000 ) ) ;
#45791 = CARTESIAN_POINT ( 'NONE',  ( -5.082755093536325930, 102.9687500020483810, -5.082755093536325930 ) ) ;
#45792 = CARTESIAN_POINT ( 'NONE',  ( 4.541265875000002339, 10.43749999863440792, 0.000000000000000000 ) ) ;
#45793 = DIRECTION ( 'NONE',  ( 0.000000000000000000, 0.000000000000000000, 1.000000000000000000 ) ) ;
#45794 = CARTESIAN_POINT ( 'NONE',  ( -7.999999999999991118, 0.000000000000000000, 3.830302779823362869 ) ) ;
#45795 = CARTESIAN_POINT ( 'NONE',  ( 2.679491924311149464, 100.8333333265053682, 10.00000000000004619 ) ) ;
#45796 = ORIENTED_EDGE ( 'NONE', *, *, #50082, .F. ) ;
#45797 = ORIENTED_EDGE ( 'NONE', *, *, #1996, .T. ) ;
#45798 = DIRECTION ( 'NONE',  ( -0.000000000000000000, -6.938893903907228378E-16, 1.000000000000000000 ) ) ;
#45799 = DIRECTION ( 'NONE',  ( -0.000000000000000000, 1.000000000000000000, -0.000000000000000000 ) ) ;
#45800 = CARTESIAN_POINT ( 'NONE',  ( -29.74433921902192068, -42.93093941886568388, 161.2115045178713615 ) ) ;
#45801 = CARTESIAN_POINT ( 'NONE',  ( -5.676582343749998039, 142.4479166632526699, -9.832129032723420536 ) ) ;
#45802 = CARTESIAN_POINT ( 'NONE',  ( 4.000000000000001776, 7.000000000000000000, 0.000000000000000000 ) ) ;
#45803 = CARTESIAN_POINT ( 'NONE',  ( -10.18810118749999916, 4.220049686691934809, 85.56250000204838102 ) ) ;
#45804 = CARTESIAN_POINT ( 'NONE',  ( -30.61924198572753397, 194.6825674383569833, 172.5985450115466620 ) ) ;
#45805 = CARTESIAN_POINT ( 'NONE',  ( 2.828427124746208943, 203.6250000000000284, 195.1715728752538439 ) ) ;
#45806 = CARTESIAN_POINT ( 'NONE',  ( -5.656854249492380582, 113.0000000040967763, -5.656854249492380582 ) ) ;
#45807 = CARTESIAN_POINT ( 'NONE',  ( 10.18810118750000093, -4.220049686691933921, 116.6875000020483952 ) ) ;
#45808 = ORIENTED_EDGE ( 'NONE', *, *, #29277, .T. ) ;
#45809 = AXIS2_PLACEMENT_3D ( 'NONE', #16690, #21993, #12802 ) ;
#45810 = CYLINDRICAL_SURFACE ( 'NONE', #10587, 3.999999999999976019 ) ;
#45811 = CARTESIAN_POINT ( 'NONE',  ( 15.12907735394716724, 183.1082765279311673, 142.8489023050493927 ) ) ;
#45812 = CARTESIAN_POINT ( 'NONE',  ( 5.676582343749993598, 125.2604166632526841, 9.832129032723422313 ) ) ;
#45813 = CARTESIAN_POINT ( 'NONE',  ( -2.445694354108782775, 202.5625000013656063, 200.4456943541088663 ) ) ;
#45814 = CARTESIAN_POINT ( 'NONE',  ( -7.188101187500000933, 26.99999999795161898, -2.977408999572651371 ) ) ;
#45815 = CARTESIAN_POINT ( 'NONE',  ( 10.18810118750000093, -4.220049686691933033, 74.68750000204838102 ) ) ;
#45816 = CARTESIAN_POINT ( 'NONE',  ( -11.35316468750000141, 33.59374999658601268, -1.390361679473963753E-15 ) ) ;
#45817 = ORIENTED_EDGE ( 'NONE', *, *, #59303, .F. ) ;
#45818 = CARTESIAN_POINT ( 'NONE',  ( 3.469446951953614189E-15, -11.00000000000000000, 41.99999999999999289 ) ) ;
#45819 = CARTESIAN_POINT ( 'NONE',  ( -4.541265875000003227, 0.9999999986344068059, 1.881053915767121110 ) ) ;
#45820 = CARTESIAN_POINT ( 'NONE',  ( 1.471067592899761672E-15, -8.008118988124991233, 11.88811528394062833 ) ) ;
#45821 = CARTESIAN_POINT ( 'NONE',  ( 1.432654583217607414, 206.5000000013655779, 145.4587341250000634 ) ) ;
#45822 = VECTOR ( 'NONE', #20621, 1000.000000000000000 ) ;
#45823 = AXIS2_PLACEMENT_3D ( 'NONE', #34874, #51080, #17866 ) ;
#45824 = CARTESIAN_POINT ( 'NONE',  ( -1.320432766682874540E-15, 12.09374999795161187, 7.188101187500000044 ) ) ;
#45825 = CARTESIAN_POINT ( 'NONE',  ( -6.000000000000000888, 295.1250000034140157, 2.485281374238575758 ) ) ;
#45826 = LINE ( 'NONE', #68837, #6402 ) ;
#45827 = CARTESIAN_POINT ( 'NONE',  ( -2.977408999572654480, 3.374999997951610098, 7.188101187499999156 ) ) ;
#45828 = CARTESIAN_POINT ( 'NONE',  ( -3.042071309553173730, 154.6354166632526699, 11.35316468749999785 ) ) ;
#45829 = CARTESIAN_POINT ( 'NONE',  ( 1.871523826299183495E-15, -10.18810118749999916, 72.53125000204838102 ) ) ;
#45830 = CARTESIAN_POINT ( 'NONE',  ( -25.55430564589119058, 196.3125000013656063, 167.5543056458915316 ) ) ;
#45831 = CARTESIAN_POINT ( 'NONE',  ( -1.656854249492383468, 15.68750000000000000, 4.000000000000000888 ) ) ;
#45832 = CARTESIAN_POINT ( 'NONE',  ( 2.780723358947928197E-16, 21.68749999863440792, -4.541265875000002339 ) ) ;
#45833 = ORIENTED_EDGE ( 'NONE', *, *, #21416, .T. ) ;
#45834 = EDGE_CURVE ( 'NONE', #55769, #48454, #19177, .T. ) ;
#45835 = CARTESIAN_POINT ( 'NONE',  ( 4.000000000000015099, 199.6875000027312126, 196.3431457505076594 ) ) ;
#45836 = CARTESIAN_POINT ( 'NONE',  ( -2.828427124746208943, 207.6250000000000284, 144.8284271247462129 ) ) ;
#45837 = CARTESIAN_POINT ( 'NONE',  ( -29.65685424949229088, 202.5625000027312126, 174.0000000000004547 ) ) ;
#45838 = CARTESIAN_POINT ( 'NONE',  ( -10.99999999999989164, -4.556349186104158733, 74.78125000409679046 ) ) ;
#45839 = CARTESIAN_POINT ( 'NONE',  ( -5.656854249492373476, -5.656854249492376141, 5.705302783920146226 ) ) ;
#45840 = ORIENTED_EDGE ( 'NONE', *, *, #2931, .T. ) ;
#45841 = CARTESIAN_POINT ( 'NONE',  ( -7.188101187500000044, 19.21874999795161543, -8.802885111219163269E-16 ) ) ;
#45842 = CARTESIAN_POINT ( 'NONE',  ( -3.313708498984759387, -7.999999999999989342, 8.799052783920146226 ) ) ;
#45843 = CARTESIAN_POINT ( 'NONE',  ( -5.000000000000000000, -10.26105934116142215, -64.40045319026754100 ) ) ;
#45844 = CARTESIAN_POINT ( 'NONE',  ( 4.999999999999993783, 39.16666666666667140, 8.660254037844390851 ) ) ;
#45845 = CARTESIAN_POINT ( 'NONE',  ( -4.401442555609581635E-16, 107.6562500020483810, -7.188101187500000044 ) ) ;
#45847 = FACE_OUTER_BOUND ( 'NONE', #48934, .T. ) ;
#45846 = DIRECTION ( 'NONE',  ( -0.000000000000000000, 1.000000000000000000, -0.000000000000000000 ) ) ;
#45848 = VERTEX_POINT ( 'NONE', #64100 ) ;
#45849 = EDGE_CURVE ( 'NONE', #48578, #54437, #36171, .T. ) ;
#45851 = CARTESIAN_POINT ( 'NONE',  ( -9.832129032723418760, 243.4895833367473301, -5.676582343749998927 ) ) ;
#45850 = AXIS2_PLACEMENT_3D ( 'NONE', #52437, #58111, #23387 ) ;
#45852 = CARTESIAN_POINT ( 'NONE',  ( 5.082755093536318824, 5.082755093536319713, 16.29905278187175455 ) ) ;
#45853 = CARTESIAN_POINT ( 'NONE',  ( 1.558072418983279750, 51.25713184919774079, 48.56213741370889636 ) ) ;
#45854 = CARTESIAN_POINT ( 'NONE',  ( -8.892166665161244765, 220.0000000000000284, 6.204661273877360550 ) ) ;
#45855 = CARTESIAN_POINT ( 'NONE',  ( -7.456209740496416494, -61.82228229130281250, -23.87473629694239463 ) ) ;
#45856 = CARTESIAN_POINT ( 'NONE',  ( -8.660254037844387298, 138.9583333265053682, -5.000000000000004441 ) ) ;
#45857 =( BOUNDED_CURVE ( )  B_SPLINE_CURVE ( 2, ( #8486, #43943, #71851, #9990, #15256, #32261, #37919, #31878, #50338 ),
 .UNSPECIFIED., .F., .F. ) 
 B_SPLINE_CURVE_WITH_KNOTS ( ( 3, 2, 2, 2, 3 ),
 ( 0.8833333333333341919, 0.8916666666666676067, 0.9000000000000007994, 0.9083333333333341031, 0.9166666666666674068 ),
 .UNSPECIFIED. ) 
 CURVE ( )  GEOMETRIC_REPRESENTATION_ITEM ( )  RATIONAL_B_SPLINE_CURVE ( ( 0.9999999999999918954, 0.9238795325112948431, 1.000000000000000000, 0.9238795325112867385, 1.000000000000000000, 0.9238795325112867385, 1.000000000000000000, 0.9238795325112796331, 1.000000000000007105 ) ) 
 REPRESENTATION_ITEM ( '' )  );
#45858 = CARTESIAN_POINT ( 'NONE',  ( 2.679491924311222739, 158.9583333333333144, 10.00000000000000355 ) ) ;
#45859 = CYLINDRICAL_SURFACE ( 'NONE', #20074, 3.999999999999976019 ) ;
#45860 = DIRECTION ( 'NONE',  ( -0.8660254037844380415, -0.5000000000000012212, 0.000000000000000000 ) ) ;
#45861 =( BOUNDED_CURVE ( )  B_SPLINE_CURVE ( 2, ( #7173, #12452, #70904, #7905, #19219, #42224, #59954, #65236, #36580 ),
 .UNSPECIFIED., .F., .F. ) 
 B_SPLINE_CURVE_WITH_KNOTS ( ( 3, 2, 2, 2, 3 ),
 ( 0.6000000000000004219, 0.6083333333333338366, 0.6166666666666672514, 0.6250000000000006661, 0.6333333333333339699 ),
 .UNSPECIFIED. ) 
 CURVE ( )  GEOMETRIC_REPRESENTATION_ITEM ( )  RATIONAL_B_SPLINE_CURVE ( ( 0.9999999999999958922, 0.9238795325112908463, 1.000000000000000000, 0.9238795325112867385, 1.000000000000000000, 0.9238795325112867385, 1.000000000000000000, 0.9238795325112806323, 1.000000000000005995 ) ) 
 REPRESENTATION_ITEM ( '' )  );
#45862 = DIRECTION ( 'NONE',  ( 0.000000000000000000, 0.000000000000000000, 1.000000000000000000 ) ) ;
#45863 = CARTESIAN_POINT ( 'NONE',  ( -3.042071309553173730, 134.6354166632526983, 11.35316468749999785 ) ) ;
#45864 = CARTESIAN_POINT ( 'NONE',  ( 0.000000000000000000, 0.000000000000000000, 0.000000000000000000 ) ) ;
#45865 = CARTESIAN_POINT ( 'NONE',  ( -10.99999999999984368, 4.556349186104204030, 107.4062500000000000 ) ) ;
#45868 = DIRECTION ( 'NONE',  ( -0.000000000000000000, -1.000000000000000000, -4.283267841918042741E-17 ) ) ;
#45867 = CARTESIAN_POINT ( 'NONE',  ( 24.54126587499998280, 198.1250000013656063, 168.5673454167822740 ) ) ;
#45866 = CARTESIAN_POINT ( 'NONE',  ( 29.65685424949240101, 209.4375000000000284, 165.9999999999998863 ) ) ;
#45869 = EDGE_LOOP ( 'NONE', ( #16894, #42538, #14619, #52515, #44960, #65144 ) ) ;
#45870 = AXIS2_PLACEMENT_3D ( 'NONE', #11965, #7049, #34996 ) ;
#45871 = CARTESIAN_POINT ( 'NONE',  ( -0.8588954341814998283, -60.21087566322590590, 22.89167302533720871 ) ) ;
#45872 = CONICAL_SURFACE ( 'NONE', #48284, 8.999999999999998224, 1.047197551196595855 ) ;
#45873 = DIRECTION ( 'NONE',  ( 0.000000000000000000, 0.000000000000000000, 1.000000000000000000 ) ) ;
#45874 = CARTESIAN_POINT ( 'NONE',  ( -1.646455035084469998, -7.866828006418148611, 0.000000000000000000 ) ) ;
#45875 = CARTESIAN_POINT ( 'NONE',  ( 5.000000000000000000, -63.84827628760507423, -24.15557308422348015 ) ) ;
#45876 = ADVANCED_FACE ( 'NONE', ( #42180, #41823 ), #30507, .T. ) ;
#45877 = CARTESIAN_POINT ( 'NONE',  ( 8.311093377946834337, 225.4687499965860411, 8.311093377946839666 ) ) ;
#45878 = CARTESIAN_POINT ( 'NONE',  ( 5.082755093536325042, 120.5937500020483952, -5.082755093536325930 ) ) ;
#45879 = CARTESIAN_POINT ( 'NONE',  ( -1.881053915767124440, 2.124999998634406584, 4.541265875000001451 ) ) ;
#45880 = CARTESIAN_POINT ( 'NONE',  ( -2.589639417659010068, -50.10293296561829379, 40.79253907059205631 ) ) ;
#45881 = CARTESIAN_POINT ( 'NONE',  ( -7.999999999999989342, -3.313708498984762496, 21.92405277982336642 ) ) ;
#45882 = CARTESIAN_POINT ( 'NONE',  ( -4.999999999999992895, 225.8333333333333428, 8.660254037844390851 ) ) ;
#45883 = CARTESIAN_POINT ( 'NONE',  ( -5.676582343750006032, 104.1145833299193697, 9.832129032723418760 ) ) ;
#45884 = ORIENTED_EDGE ( 'NONE', *, *, #33802, .T. ) ;
#45885 = EDGE_CURVE ( 'NONE', #50014, #52808, #48582, .T. ) ;
#45886 = DIRECTION ( 'NONE',  ( 1.000000000000000000, -0.000000000000000000, -0.000000000000000000 ) ) ;
#45887 = CARTESIAN_POINT ( 'NONE',  ( 2.977408999572650927, 23.24999999795161187, -7.188101187500001821 ) ) ;
#45888 = DIRECTION ( 'NONE',  ( 0.000000000000000000, 0.000000000000000000, 1.000000000000000000 ) ) ;
#45889 = CARTESIAN_POINT ( 'NONE',  ( -6.951808397369817780E-16, 237.9687500034139873, -11.35316468749999963 ) ) ;
#45890 = CARTESIAN_POINT ( 'NONE',  ( 3.042071309553167069, 96.82291666325269830, -11.35316468749999785 ) ) ;
#45891 = ORIENTED_EDGE ( 'NONE', *, *, #21763, .T. ) ;
#45892 = CARTESIAN_POINT ( 'NONE',  ( -28.00000000000003197, 208.0000000000000284, 166.0000000000003695 ) ) ;
#45893 = CARTESIAN_POINT ( 'NONE',  ( -6.238412754330611322E-16, 10.18810118749999916, 109.2812500020483668 ) ) ;
#45894 = CARTESIAN_POINT ( 'NONE',  ( 7.320508075688771044, 226.2499999931720254, 7.320508075688775484 ) ) ;
#45895 = CARTESIAN_POINT ( 'NONE',  ( -2.445694354108783219, 201.8125000013656063, 200.4456943541088663 ) ) ;
#45896 = CARTESIAN_POINT ( 'NONE',  ( 0.000000000000000000, 0.000000000000000000, 0.000000000000000000 ) ) ;
#45898 = CARTESIAN_POINT ( 'NONE',  ( -8.311093377946841443, 98.90624999658602690, 8.311093377946834337 ) ) ;
#45897 = CARTESIAN_POINT ( 'NONE',  ( 11.00000000000000355, -4.556349186104044158, 97.65624999999998579 ) ) ;
#45899 = CARTESIAN_POINT ( 'NONE',  ( 7.999999999999991118, 3.313708498984757611, 15.36155278392014623 ) ) ;
#45900 = CARTESIAN_POINT ( 'NONE',  ( -31.45873412499999233, 195.9375000013655779, 170.0000000000003979 ) ) ;
#45901 = CARTESIAN_POINT ( 'NONE',  ( 10.00000000000000000, 169.7916666666666856, 2.679491924311235618 ) ) ;
#45902 = ORIENTED_EDGE ( 'NONE', *, *, #70440, .F. ) ;
#45903 = CARTESIAN_POINT ( 'NONE',  ( 10.00000000000000178, 202.0833333265053966, -2.679491924311226736 ) ) ;
#45904 = CARTESIAN_POINT ( 'NONE',  ( 7.999999999999991118, 0.000000000000000000, 30.00000000000000000 ) ) ;
#45905 = EDGE_CURVE ( 'NONE', #64105, #35739, #20640, .T. ) ;
#45906 = CARTESIAN_POINT ( 'NONE',  ( 4.000000000000000888, 9.687499997268814056, 1.656854249492384135 ) ) ;
#45907 = CARTESIAN_POINT ( 'NONE',  ( -5.676582343749998039, 92.76041666325268409, -9.832129032723420536 ) ) ;
#45908 = CARTESIAN_POINT ( 'NONE',  ( -4.721056650415999201, 290.3281250017069510, -4.721056650415999201 ) ) ;
#45909 = CARTESIAN_POINT ( 'NONE',  ( 7.188101187500000044, 5.343749997951610098, 0.000000000000000000 ) ) ;
#45910 = CARTESIAN_POINT ( 'NONE',  ( 10.18810118749999916, 1.247682550866122264E-15, 94.28125000204836681 ) ) ;
#45911 = CARTESIAN_POINT ( 'NONE',  ( -11.35316468750000141, 223.2812499965860127, -1.390361679473963753E-15 ) ) ;
#45912 = VERTEX_POINT ( 'NONE', #59918 ) ;
#45913 = CARTESIAN_POINT ( 'NONE',  ( 0.000000000000000000, 125.0000000000000000, 8.000000000000000000 ) ) ;
#45914 = CARTESIAN_POINT ( 'NONE',  ( -7.999999999998400391, 3.416934844025491914E-06, 16.01767659775488184 ) ) ;
#45915 = CYLINDRICAL_SURFACE ( 'NONE', #27507, 10.00000000000000178 ) ;
#45916 = CARTESIAN_POINT ( 'NONE',  ( 8.311093377946834337, 215.1562499965860127, 8.311093377946839666 ) ) ;
#45917 = DIRECTION ( 'NONE',  ( -0.000000000000000000, -0.000000000000000000, 1.000000000000000000 ) ) ;
#45918 = CARTESIAN_POINT ( 'NONE',  ( -26.34314575050768781, 208.0625000027312126, 166.0000000000003411 ) ) ;
#45919 = CARTESIAN_POINT ( 'NONE',  ( 1.226468279477575784E-15, 295.7031250017069510, 6.676582343750001591 ) ) ;
#45920 = ORIENTED_EDGE ( 'NONE', *, *, #44581, .F. ) ;
#45921 = CARTESIAN_POINT ( 'NONE',  ( -3.673940397442060854E-16, 295.8125000034140157, -6.000000000000001776 ) ) ;
#45922 = CARTESIAN_POINT ( 'NONE',  ( 6.951808397369818766E-16, 202.3437499965860127, -11.35316468750000141 ) ) ;
#45923 = CARTESIAN_POINT ( 'NONE',  ( 10.18810118749999916, 4.220049686691935698, 95.50000000204838102 ) ) ;
#45924 = CARTESIAN_POINT ( 'NONE',  ( -24.54126587499999346, 205.1875000013656063, 170.0000000000003411 ) ) ;
#45925 = CARTESIAN_POINT ( 'NONE',  ( -1.469576158976823947E-15, 20.62500000000000355, 8.000000000000000000 ) ) ;
#45926 = ORIENTED_EDGE ( 'NONE', *, *, #27952, .F. ) ;
#45927 = ADVANCED_FACE ( 'NONE', ( #19914 ), #12410, .F. ) ;
#45928 = CIRCLE ( 'NONE', #64030, 6.000000000000001776 ) ;
#45929 = CARTESIAN_POINT ( 'NONE',  ( -5.082755093536325930, 120.9687500020483952, -5.082755093536325930 ) ) ;
#45930 = CARTESIAN_POINT ( 'NONE',  ( 3.313708498984762496, -7.999999999999989342, 19.29905277982336642 ) ) ;
#45931 = EDGE_CURVE ( 'NONE', #59077, #56693, #39806, .T. ) ;
#45932 = CARTESIAN_POINT ( 'NONE',  ( -10.00000000000000000, 32.29166666666667140, -2.679491924311229845 ) ) ;
#45933 = CARTESIAN_POINT ( 'NONE',  ( 12.00000000000000355, 0.000000000000000000, -25.03750572909317285 ) ) ;
#45934 = CARTESIAN_POINT ( 'NONE',  ( 4.220049686691941027, -10.18810118749999738, 80.50000000204839523 ) ) ;
#45935 = ORIENTED_EDGE ( 'NONE', *, *, #70798, .T. ) ;
#45936 = EDGE_CURVE ( 'NONE', #57226, #68369, #55694, .T. ) ;
#45937 = CARTESIAN_POINT ( 'NONE',  ( -4.000000000000002665, 20.56250000000000355, 1.656854249492380804 ) ) ;
#45938 = CARTESIAN_POINT ( 'NONE',  ( -31.00000000000001066, 82.00000000000001421, 65.00000000000000000 ) ) ;
#45939 = AXIS2_PLACEMENT_3D ( 'NONE', #15152, #61928, #72882 ) ;
#45940 = CARTESIAN_POINT ( 'NONE',  ( 2.170320029193673506, 16.41060967376299473, -68.77687409974411992 ) ) ;
#45941 = DIRECTION ( 'NONE',  ( 1.000000000000000000, -0.000000000000000000, -0.000000000000000000 ) ) ;
#45942 = CARTESIAN_POINT ( 'NONE',  ( 4.999999999999993783, 151.0416666598387110, 8.660254037844390851 ) ) ;
#45943 = CARTESIAN_POINT ( 'NONE',  ( 6.676582343750003368, 294.8906250017069510, 2.765530957081995478 ) ) ;
#45945 = CARTESIAN_POINT ( 'NONE',  ( -11.35316468749999608, 249.1145833367473017, 3.042071309553173730 ) ) ;
#45944 = CARTESIAN_POINT ( 'NONE',  ( 29.43265458321766914, 205.5000000013655779, 173.4587341249998929 ) ) ;
#45946 = PRODUCT_CONTEXT ( 'NONE', #2847, 'mechanical' ) ;
#45947 = ORIENTED_EDGE ( 'NONE', *, *, #58389, .F. ) ;
#45948 = CARTESIAN_POINT ( 'NONE',  ( 3.042071309553173286, 245.6770833367473017, 11.35316468749999608 ) ) ;
#45949 = CARTESIAN_POINT ( 'NONE',  ( 2.977408999572646486, 7.188101187499991163, 5.517802781871753659 ) ) ;
#45950 = ORIENTED_EDGE ( 'NONE', *, *, #29161, .F. ) ;
#45951 = CYLINDRICAL_SURFACE ( 'NONE', #63203, 18.50000000000000000 ) ;
#45952 = CARTESIAN_POINT ( 'NONE',  ( -11.35316468750000141, 83.80208332991934128, 3.042071309553159963 ) ) ;
#45953 = CARTESIAN_POINT ( 'NONE',  ( 2.449293598294707893E-16, 21.25000000000000000, -4.000000000000001776 ) ) ;
#45954 = CARTESIAN_POINT ( 'NONE',  ( -7.778174593052020747, -7.778174593052023411, 80.68750000000000000 ) ) ;
#45957 = CYLINDRICAL_SURFACE ( 'NONE', #31403, 12.00000000000000000 ) ;
#45956 = CARTESIAN_POINT ( 'NONE',  ( 30.44569435410883429, 206.5625000013656063, 172.4456943541086957 ) ) ;
#45955 = CARTESIAN_POINT ( 'NONE',  ( 24.54126587499999701, 207.4375000013656063, 169.9999999999998863 ) ) ;
#45958 = ORIENTED_EDGE ( 'NONE', *, *, #10394, .T. ) ;
#45959 = AXIS2_PLACEMENT_3D ( 'NONE', #58797, #7108, #54617 ) ;
#45960 = CARTESIAN_POINT ( 'NONE',  ( -4.898587196589412829E-16, 114.1250000000000000, -8.000000000000000000 ) ) ;
#45961 = DIRECTION ( 'NONE',  ( -0.000000000000000000, -0.000000000000000000, 1.000000000000000000 ) ) ;
#45962 =( BOUNDED_CURVE ( )  B_SPLINE_CURVE ( 2, ( #51783, #51039, #16315, #131, #23107, #46120, #11057, #39351, #10679 ),
 .UNSPECIFIED., .F., .F. ) 
 B_SPLINE_CURVE_WITH_KNOTS ( ( 3, 2, 2, 2, 3 ),
 ( 0.4204545454545454697, 0.4261363636363636465, 0.4318181818181818232, 0.4375000000000000000, 0.4431818181818181768 ),
 .UNSPECIFIED. ) 
 CURVE ( )  GEOMETRIC_REPRESENTATION_ITEM ( )  RATIONAL_B_SPLINE_CURVE ( ( 1.000000000000000000, 0.9238795325112867385, 1.000000000000000000, 0.9238795325112867385, 1.000000000000000000, 0.9238795325112867385, 1.000000000000000000, 0.9238795325112867385, 1.000000000000000000 ) ) 
 REPRESENTATION_ITEM ( '' )  );
#45963 = CARTESIAN_POINT ( 'NONE',  ( 3.042071309553159519, 199.7395833299193555, 11.35316468750000141 ) ) ;
#45964 = CARTESIAN_POINT ( 'NONE',  ( -1.432654583217664479, 203.7500000013656063, 138.5412658750000787 ) ) ;
#45965 = CARTESIAN_POINT ( 'NONE',  ( 30.44569435410883784, 208.0625000013656063, 167.5543056458911053 ) ) ;
#45966 = EDGE_CURVE ( 'NONE', #29151, #38403, #6982, .T. ) ;
#45967 = CARTESIAN_POINT ( 'NONE',  ( 7.188101187500000044, 15.84374999795161365, 0.000000000000000000 ) ) ;
#45968 = CARTESIAN_POINT ( 'NONE',  ( -11.35316468750000141, 183.8020833299193271, 3.042071309553159963 ) ) ;
#45969 = CARTESIAN_POINT ( 'NONE',  ( 0.000000000000000000, 0.000000000000000000, 118.0000000000000000 ) ) ;
#45970 = CARTESIAN_POINT ( 'NONE',  ( -7.188101187500000933, 98.93750000204836681, -2.977408999572650483 ) ) ;
#45971 = LINE ( 'NONE', #45229, #28757 ) ;
#45972 = CARTESIAN_POINT ( 'NONE',  ( -4.541265875000002339, 9.812499998634406140, -5.561446717895856393E-16 ) ) ;
#45973 = CARTESIAN_POINT ( 'NONE',  ( 31.45873412499998523, 203.8750000013656063, 171.4326545832176123 ) ) ;
#45974 = CARTESIAN_POINT ( 'NONE',  ( -7.188101187499992051, 0.000000000000000000, 7.861552781871751883 ) ) ;
#45975 = CARTESIAN_POINT ( 'NONE',  ( -11.35316468750000141, 58.48958332991934128, 3.042071309553159963 ) ) ;
#45976 = DIRECTION ( 'NONE',  ( 0.000000000000000000, 0.000000000000000000, 1.000000000000000000 ) ) ;
#45977 = CARTESIAN_POINT ( 'NONE',  ( 7.999999999999991118, 3.313708498984757611, 3.230302784329822430 ) ) ;
#45978 = VERTEX_POINT ( 'NONE', #72351 ) ;
#45979 = CARTESIAN_POINT ( 'NONE',  ( 0.000000000000000000, 0.000000000000000000, 0.000000000000000000 ) ) ;
#45980 = LINE ( 'NONE', #70481, #42487 ) ;
#45981 = CARTESIAN_POINT ( 'NONE',  ( 8.311093377946834337, 65.15624999658602690, 8.311093377946839666 ) ) ;
#45982 = CARTESIAN_POINT ( 'NONE',  ( -11.00000000000000000, 4.556349186104045934, 76.09375000409676204 ) ) ;
#45983 = CARTESIAN_POINT ( 'NONE',  ( -2.839093476692135984E-14, 201.9375000013656063, 138.5412658750000503 ) ) ;
#45984 = CARTESIAN_POINT ( 'NONE',  ( -4.465384415997333711, 10.10202268796506431, 70.97396818905025384 ) ) ;
#45986 = CARTESIAN_POINT ( 'NONE',  ( 9.832129032723416984, 60.36458332991934839, 5.676582343750006032 ) ) ;
#45985 = CARTESIAN_POINT ( 'NONE',  ( 7.188101187500000044, 91.90625000204838102, -8.802885111219163269E-16 ) ) ;
#45987 = CARTESIAN_POINT ( 'NONE',  ( 3.313708498984762496, -7.999999999999989342, 5.799052779823364645 ) ) ;
#45988 = CARTESIAN_POINT ( 'NONE',  ( 0.000000000000000000, -28.00000000000000000, 0.000000000000000000 ) ) ;
#45989 = CARTESIAN_POINT ( 'NONE',  ( 11.35316468749999963, 175.9895833299193555, -3.042071309553165293 ) ) ;
#45990 =( BOUNDED_CURVE ( )  B_SPLINE_CURVE ( 2, ( #49854, #37422, #43062, #21549, #20044, #61918, #21176, #72872, #49096 ),
 .UNSPECIFIED., .F., .F. ) 
 B_SPLINE_CURVE_WITH_KNOTS ( ( 3, 2, 2, 2, 3 ),
 ( 0.09375000000000006939, 0.09895833333333339810, 0.1041666666666667407, 0.1093750000000000694, 0.1145833333333333981 ),
 .UNSPECIFIED. ) 
 CURVE ( )  GEOMETRIC_REPRESENTATION_ITEM ( )  RATIONAL_B_SPLINE_CURVE ( ( 0.9999999999999990008, 0.9238795325112877377, 1.000000000000000000, 0.9238795325112867385, 1.000000000000000000, 0.9238795325112867385, 1.000000000000000000, 0.9238795325112857393, 1.000000000000001110 ) ) 
 REPRESENTATION_ITEM ( '' )  );
#45991 = CARTESIAN_POINT ( 'NONE',  ( 8.660254037844389075, 157.2916666598387110, -5.000000000000000000 ) ) ;
#45992 = CARTESIAN_POINT ( 'NONE',  ( -7.188101187500000044, 96.03125000204838102, 0.000000000000000000 ) ) ;
#45993 = CARTESIAN_POINT ( 'NONE',  ( -8.660254037844387298, 53.95833332650536818, -5.000000000000004441 ) ) ;
#45994 = CARTESIAN_POINT ( 'NONE',  ( -9.832129032723420536, 49.01041666325269119, 5.676582343749997150 ) ) ;
#45995 = CARTESIAN_POINT ( 'NONE',  ( -4.220049686691937474, -10.18810118749999738, 116.3125000020483810 ) ) ;
#45996 = CARTESIAN_POINT ( 'NONE',  ( -9.832129032723418760, 187.8645833299193839, -5.676582343750004256 ) ) ;
#45997 = ORIENTED_EDGE ( 'NONE', *, *, #58467, .T. ) ;
#45998 = CARTESIAN_POINT ( 'NONE',  ( 48.05475929102907173, 143.2777182940846785, 62.38327136324791411 ) ) ;
#45999 = CARTESIAN_POINT ( 'NONE',  ( 10.18810118749999916, 4.220049686691935698, 71.50000000204839523 ) ) ;
#46000 = CARTESIAN_POINT ( 'NONE',  ( -1.656854249492348607, 197.1875000000000284, 202.0000000000000284 ) ) ;
#46002 = CARTESIAN_POINT ( 'NONE',  ( -8.311093377946841443, 183.9062499965860411, 8.311093377946834337 ) ) ;
#46001 = LINE ( 'NONE', #62983, #25416 ) ;
#46003 = CARTESIAN_POINT ( 'NONE',  ( -7.999999999999991118, 3.313708498984756723, 8.292802784329824206 ) ) ;
#46004 = DIRECTION ( 'NONE',  ( -0.000000000000000000, 1.000000000000000000, 0.000000000000000000 ) ) ;
#46005 = CARTESIAN_POINT ( 'NONE',  ( -10.00000000000000000, 248.1250000068279746, 0.000000000000000000 ) ) ;
#46006 = DIRECTION ( 'NONE',  ( -0.000000000000000000, -0.000000000000000000, -1.000000000000000000 ) ) ;
#46007 = ORIENTED_EDGE ( 'NONE', *, *, #72395, .T. ) ;
#46008 = SHAPE_REPRESENTATION ( 'MAT-050', ( #24892, #23675, #65835, #816, #42934, #10433, #52606, #29711, #71862, #55028, #39347, #6825, #26067, #3221, #22429, #32087, #74238, #41726, #9183, #864, #18881, #64605 ), #29772 ) ;
#46009 = DIRECTION ( 'NONE',  ( 1.000000000000000000, 0.000000000000000000, -0.000000000000000000 ) ) ;
#46010 = CARTESIAN_POINT ( 'NONE',  ( -5.676582343750006032, 129.4270833299193555, 9.832129032723418760 ) ) ;
#46011 = CARTESIAN_POINT ( 'NONE',  ( 29.65685424949235838, 195.0625000000000000, 173.9999999999999147 ) ) ;
#46012 = ORIENTED_EDGE ( 'NONE', *, *, #70709, .T. ) ;
#46013 = CARTESIAN_POINT ( 'NONE',  ( -4.541265875000003227, 6.999999998634407916, 1.881053915767121110 ) ) ;
#46014 = CARTESIAN_POINT ( 'NONE',  ( 5.082755093536325930, 14.15624999795161187, -5.082755093536325930 ) ) ;
#46015 = CARTESIAN_POINT ( 'NONE',  ( -7.999999999999998224, 101.2812500040967763, 3.313708498984766493 ) ) ;
#46016 = ADVANCED_FACE ( 'NONE', ( #38033 ), #60381, .T. ) ;
#46017 = CARTESIAN_POINT ( 'NONE',  ( -29.43265458321760164, 197.1250000013656347, 173.4587341250003760 ) ) ;
#46018 = EDGE_CURVE ( 'NONE', #33654, #8420, #8982, .T. ) ;
#46019 = CARTESIAN_POINT ( 'NONE',  ( -4.000000000000001776, 8.500000000000000000, -4.898587196589415787E-16 ) ) ;
#46020 = CARTESIAN_POINT ( 'NONE',  ( -4.000000000000001776, 21.18749999726881583, -1.656854249492381470 ) ) ;
#46021 = CARTESIAN_POINT ( 'NONE',  ( 4.541265875000001451, 10.24999999863440792, 1.881053915767124440 ) ) ;
#46022 = CARTESIAN_POINT ( 'NONE',  ( -3.313708498984758943, -7.999999999999989342, 20.79905278392014978 ) ) ;
#46023 = CARTESIAN_POINT ( 'NONE',  ( -2.849036369511732440E-14, 200.2500000000000000, 138.0000000000000568 ) ) ;
#46024 = ORIENTED_EDGE ( 'NONE', *, *, #19272, .F. ) ;
#46025 = CARTESIAN_POINT ( 'NONE',  ( -1.469576158976823947E-15, 23.43749999590322020, 8.000000000000000000 ) ) ;
#46026 = CARTESIAN_POINT ( 'NONE',  ( -4.401442555609581635E-16, 105.7812500020483810, -7.188101187500000044 ) ) ;
#46028 = CARTESIAN_POINT ( 'NONE',  ( -3.313708498984760276, 15.28124999590322197, -8.000000000000000000 ) ) ;
#46027 = DIRECTION ( 'NONE',  ( 0.000000000000000000, 0.000000000000000000, -1.000000000000000000 ) ) ;
#46029 = SHAPE_REPRESENTATION_RELATIONSHIP ( 'NONE' , 'NONE' ,  #61424, #38983 ) ;
#46030 = ORIENTED_EDGE ( 'NONE', *, *, #20580, .F. ) ;
#46031 = CARTESIAN_POINT ( 'NONE',  ( 2.780723358947928197E-16, 21.56249999863440792, -4.541265875000002339 ) ) ;
#46032 = CARTESIAN_POINT ( 'NONE',  ( 2.977408999572646486, 7.188101187499991163, 28.01780278187175455 ) ) ;
#46033 = ORIENTED_EDGE ( 'NONE', *, *, #37588, .T. ) ;
#46034 = ORIENTED_EDGE ( 'NONE', *, *, #70768, .T. ) ;
#46035 = CARTESIAN_POINT ( 'NONE',  ( 1.871523826299183495E-15, -10.18810118749999916, 92.03125000204836681 ) ) ;
#46036 = CARTESIAN_POINT ( 'NONE',  ( -4.000000000000002665, 9.312499997268814056, 1.656854249492380582 ) ) ;
#46037 = CARTESIAN_POINT ( 'NONE',  ( -31.45873412499997812, 198.0000000013656063, 171.4326545832180386 ) ) ;
#46038 = CARTESIAN_POINT ( 'NONE',  ( 11.00000000000000355, -4.556349186104045046, 102.1562499999999858 ) ) ;
#46039 = CARTESIAN_POINT ( 'NONE',  ( -3.458734124999959469, 202.7500000013655779, 199.4326545832176691 ) ) ;
#46041 = CARTESIAN_POINT ( 'NONE',  ( -6.676582343749999815, 297.6718750017070079, 2.765530957082001251 ) ) ;
#46040 = CARTESIAN_POINT ( 'NONE',  ( -2.726571689596997292E-14, 195.0000000000000000, 138.0000000000000568 ) ) ;
#46042 = CARTESIAN_POINT ( 'NONE',  ( 7.320508075688774596, 125.6250000000000142, -7.320508075688774596 ) ) ;
#46043 = CARTESIAN_POINT ( 'NONE',  ( 8.000000000000000000, 100.3437500000000000, -3.313708498984762496 ) ) ;
#46044 = CARTESIAN_POINT ( 'NONE',  ( -4.721056650415998313, 287.7343750017069510, 4.721056650416000089 ) ) ;
#46045 = CARTESIAN_POINT ( 'NONE',  ( -7.188101187499992051, 0.000000000000000000, 6.361552781871754547 ) ) ;
#46046 = CARTESIAN_POINT ( 'NONE',  ( -23.99999999999997868, 208.6875000000000284, 171.6568542494927385 ) ) ;
#46048 = CARTESIAN_POINT ( 'NONE',  ( 26.56734541678238060, 204.0000000013656347, 166.5412658749999650 ) ) ;
#46047 = AXIS2_PLACEMENT_3D ( 'NONE', #3322, #55763, #36908 ) ;
#46049 = CARTESIAN_POINT ( 'NONE',  ( 4.401442555609581635E-16, 1.218749997951610098, -7.188101187500000044 ) ) ;
#46050 = CARTESIAN_POINT ( 'NONE',  ( 12.00000000000000178, -1.170752406943651902, 8.470329472542999693E-17 ) ) ;
#46051 = CARTESIAN_POINT ( 'NONE',  ( -7.188101187499999156, 115.6250000020483810, 2.977408999572654924 ) ) ;
#46053 = CARTESIAN_POINT ( 'NONE',  ( 2.981778917433099974, 194.8314443964915483, 195.5813262573522593 ) ) ;
#46052 = CARTESIAN_POINT ( 'NONE',  ( 30.82842712474616320, 195.5000000027312126, 167.1715728752537018 ) ) ;
#46054 = CARTESIAN_POINT ( 'NONE',  ( -11.35316468749999963, 244.2187500034140157, 0.000000000000000000 ) ) ;
#46055 = CARTESIAN_POINT ( 'NONE',  ( 2.775557561562891351E-14, 210.0000000000000284, 198.0000000000000284 ) ) ;
#46056 = CARTESIAN_POINT ( 'NONE',  ( 10.00000000000000178, 51.87499999317203248, 0.000000000000000000 ) ) ;
#46057 = CARTESIAN_POINT ( 'NONE',  ( 23.99999999999998579, 196.7500000000000000, 169.9999999999998863 ) ) ;
#46058 = CARTESIAN_POINT ( 'NONE',  ( -5.676582343749998039, 12.44791666325268409, -9.832129032723420536 ) ) ;
#46059 = CARTESIAN_POINT ( 'NONE',  ( 5.656854249492379694, 100.6250000040967905, -5.656854249492380582 ) ) ;
#46060 = CARTESIAN_POINT ( 'NONE',  ( 11.35316468749999963, 221.3020833299192986, -3.042071309553165293 ) ) ;
#46061 = CARTESIAN_POINT ( 'NONE',  ( -9.999999999999998224, 240.2083333333333144, 2.679491924311235174 ) ) ;
#46062 = CARTESIAN_POINT ( 'NONE',  ( 0.000000000000000000, -2.500000000000000000, 12.00000000000000000 ) ) ;
#46063 = VERTEX_POINT ( 'NONE', #21037 ) ;
#46064 = CARTESIAN_POINT ( 'NONE',  ( 1.432654583217608080, 198.8750000013656347, 138.5412658750000503 ) ) ;
#46065 = CARTESIAN_POINT ( 'NONE',  ( 9.832129032723420536, 16.19791666325268054, -5.676582343749999815 ) ) ;
#46066 = CARTESIAN_POINT ( 'NONE',  ( 4.556349186104045934, 11.00000000000000000, 92.21875000409677625 ) ) ;
#46067 = CARTESIAN_POINT ( 'NONE',  ( 5.000000000000000000, 10.26105934116143281, 64.40045319026697257 ) ) ;
#46068 = CARTESIAN_POINT ( 'NONE',  ( -30.44569435410875968, 198.8125000013656063, 172.4456943541092642 ) ) ;
#46069 = DIRECTION ( 'NONE',  ( -1.000000000000000000, 0.000000000000000000, 0.000000000000000000 ) ) ;
#46071 = CARTESIAN_POINT ( 'NONE',  ( 3.042071309553167513, 21.82291666325268054, -11.35316468749999785 ) ) ;
#46070 = CARTESIAN_POINT ( 'NONE',  ( -2.977408999572650927, 111.8750000020483810, -7.188101187500000933 ) ) ;
#46072 = CARTESIAN_POINT ( 'NONE',  ( 1.469576158976822172E-15, -7.999999999999991118, 19.20530277982336642 ) ) ;
#46073 = CIRCLE ( 'NONE', #64114, 9.949874371066211864 ) ;
#46074 = CARTESIAN_POINT ( 'NONE',  ( -5.676582343749998039, 132.4479166632526983, -9.832129032723420536 ) ) ;
#46075 = CARTESIAN_POINT ( 'NONE',  ( 7.320508075688771044, 106.2499999931720396, 7.320508075688775484 ) ) ;
#46076 = CARTESIAN_POINT ( 'NONE',  ( 5.082755093536326818, 113.0937500020483810, 5.082755093536325042 ) ) ;
#46077 = CARTESIAN_POINT ( 'NONE',  ( -8.000000000000000000, 120.5937500040967763, -3.313708498984761164 ) ) ;
#46078 = CARTESIAN_POINT ( 'NONE',  ( -28.00000000000002487, 207.6875000013656063, 166.5412658750003629 ) ) ;
#46079 = CARTESIAN_POINT ( 'NONE',  ( -5.000000000000000000, 51.89737250574564342, -42.00009673807059585 ) ) ;
#46080 = ORIENTED_EDGE ( 'NONE', *, *, #19126, .F. ) ;
#46081 = CARTESIAN_POINT ( 'NONE',  ( -3.042071309553163960, 12.55208332991935016, -11.35316468749999963 ) ) ;
#46082 =( BOUNDED_CURVE ( )  B_SPLINE_CURVE ( 2, ( #5548, #22889, #59093, #48111, #59455, #48854, #64373, #64739, #31518 ),
 .UNSPECIFIED., .F., .F. ) 
 B_SPLINE_CURVE_WITH_KNOTS ( ( 3, 2, 2, 2, 3 ),
 ( 0.9062500000000002220, 0.9114583333333335924, 0.9166666666666668517, 0.9218750000000002220, 0.9270833333333335924 ),
 .UNSPECIFIED. ) 
 CURVE ( )  GEOMETRIC_REPRESENTATION_ITEM ( )  RATIONAL_B_SPLINE_CURVE ( ( 0.9999999999999967804, 0.9238795325112899581, 1.000000000000000000, 0.9238795325112867385, 1.000000000000000000, 0.9238795325112867385, 1.000000000000000000, 0.9238795325112835188, 1.000000000000003331 ) ) 
 REPRESENTATION_ITEM ( '' )  );
#46083 = CARTESIAN_POINT ( 'NONE',  ( 2.449293598294707893E-16, 19.99999999726881228, -4.000000000000001776 ) ) ;
#46084 = CARTESIAN_POINT ( 'NONE',  ( -6.676582343750003368, 296.3906250017069510, -2.765530957081996810 ) ) ;
#46085 = CARTESIAN_POINT ( 'NONE',  ( -2.085542519210945728E-15, 134.5312499965860411, 11.35316468750000141 ) ) ;
#46086 = CARTESIAN_POINT ( 'NONE',  ( -5.656854249492373476, -5.656854249492376141, 23.57405278432982598 ) ) ;
#46087 = CARTESIAN_POINT ( 'NONE',  ( 2.584176044310538600, 67.83040087281460728, 20.22720375976279072 ) ) ;
#46088 = CARTESIAN_POINT ( 'NONE',  ( -9.832129032723415207, 254.3229166700806729, 5.676582343750005144 ) ) ;
#46089 = CARTESIAN_POINT ( 'NONE',  ( 10.18810118749999916, 1.247682550866122264E-15, 95.78125000204836681 ) ) ;
#46090 = ORIENTED_EDGE ( 'NONE', *, *, #48755, .T. ) ;
#46091 = EDGE_CURVE ( 'NONE', #20696, #59314, #48956, .T. ) ;
#46092 = EDGE_CURVE ( 'NONE', #55774, #40293, #24818, .T. ) ;
#46093 = CARTESIAN_POINT ( 'NONE',  ( 0.000000000000000000, 0.000000000000000000, 0.000000000000000000 ) ) ;
#46094 = CARTESIAN_POINT ( 'NONE',  ( 5.000000000000001776, 61.58678017309407693, -23.68362420833262405 ) ) ;
#46095 = CARTESIAN_POINT ( 'NONE',  ( 3.458734125000016757, 201.1250000013656347, 199.4326545832176976 ) ) ;
#46096 = CARTESIAN_POINT ( 'NONE',  ( -3.042071309553173730, 94.63541666325269830, 11.35316468749999785 ) ) ;
#46097 = ORIENTED_EDGE ( 'NONE', *, *, #6917, .T. ) ;
#46098 = CARTESIAN_POINT ( 'NONE',  ( 10.18810118749999916, 1.247682550866122264E-15, 108.9062500020483668 ) ) ;
#46099 =( BOUNDED_CURVE ( )  B_SPLINE_CURVE ( 2, ( #51658, #33962, #69012, #67524, #15823, #39226, #17318, #16185, #62226 ),
 .UNSPECIFIED., .F., .F. ) 
 B_SPLINE_CURVE_WITH_KNOTS ( ( 3, 2, 2, 2, 3 ),
 ( 0.5833333333333337034, 0.5916666666666670071, 0.6000000000000004219, 0.6083333333333338366, 0.6166666666666672514 ),
 .UNSPECIFIED. ) 
 CURVE ( )  GEOMETRIC_REPRESENTATION_ITEM ( )  RATIONAL_B_SPLINE_CURVE ( ( 0.9999999999999970024, 0.9238795325112897361, 1.000000000000000000, 0.9238795325112867385, 1.000000000000000000, 0.9238795325112867385, 1.000000000000000000, 0.9238795325112816315, 1.000000000000005107 ) ) 
 REPRESENTATION_ITEM ( '' )  );
#46100 = CARTESIAN_POINT ( 'NONE',  ( -8.342170076843785083E-16, 13.18749999863440792, 4.541265875000002339 ) ) ;
#46101 = ORIENTED_EDGE ( 'NONE', *, *, #16261, .F. ) ;
#46102 = EDGE_LOOP ( 'NONE', ( #56036, #65603, #2584, #42853 ) ) ;
#46103 = CARTESIAN_POINT ( 'NONE',  ( 5.656854249492378806, 1.312500000000000222, 5.656854249492381470 ) ) ;
#46104 = CARTESIAN_POINT ( 'NONE',  ( -1.836970198721029983E-15, 110.6249999931720396, 10.00000000000000178 ) ) ;
#46105 = CARTESIAN_POINT ( 'NONE',  ( -5.000000000000000000, -66.79063484153778063, -23.29724706625406228 ) ) ;
#46106 = CARTESIAN_POINT ( 'NONE',  ( -2.977408999572650039, 22.31249999795161543, -7.188101187500001821 ) ) ;
#46107 = CARTESIAN_POINT ( 'NONE',  ( 11.00000000000000000, 1.347111479062088405E-15, 96.24999999999998579 ) ) ;
#46108 = CARTESIAN_POINT ( 'NONE',  ( 7.204075437095968759, -7.204075437095966983, 103.0937500020483668 ) ) ;
#46109 = VECTOR ( 'NONE', #9442, 1000.000000000000000 ) ;
#46110 = CARTESIAN_POINT ( 'NONE',  ( 1.567784982238203817E-13, 108.7500000000000426, 10.00000000000000533 ) ) ;
#46111 = CARTESIAN_POINT ( 'NONE',  ( -4.000000000000001776, 11.24999999726881406, -4.898587196589415787E-16 ) ) ;
#46112 = CARTESIAN_POINT ( 'NONE',  ( 26.34314575050764162, 209.5625000000000000, 165.9999999999998295 ) ) ;
#46113 = EDGE_LOOP ( 'NONE', ( #53324, #19034, #17804 ) ) ;
#46114 = AXIS2_PLACEMENT_3D ( 'NONE', #43671, #66682, #61023 ) ;
#46115 = CARTESIAN_POINT ( 'NONE',  ( -10.00000000000000000, 263.1250000068279746, 0.000000000000000000 ) ) ;
#46116 = CARTESIAN_POINT ( 'NONE',  ( 1.432654583217662481, 204.1250000013656063, 194.5412658750000219 ) ) ;
#46117 = CARTESIAN_POINT ( 'NONE',  ( -27.99999999999992184, 205.9375000013656063, 173.4587341250003760 ) ) ;
#46118 =( LENGTH_UNIT ( ) NAMED_UNIT ( * ) SI_UNIT ( .MILLI., .METRE. ) );
#46119 = CARTESIAN_POINT ( 'NONE',  ( -3.211159895383562723, 10.93749999863440792, 3.211159895383561391 ) ) ;
#46120 = CARTESIAN_POINT ( 'NONE',  ( -4.000000000000002665, 10.31249999726881406, 1.656854249492380582 ) ) ;
#46121 = CARTESIAN_POINT ( 'NONE',  ( -4.401442555609577197E-16, 7.188101187499992051, 19.11155278187175455 ) ) ;
#46122 = VERTEX_POINT ( 'NONE', #21409 ) ;
#46123 = ORIENTED_EDGE ( 'NONE', *, *, #58161, .T. ) ;
#46124 = CARTESIAN_POINT ( 'NONE',  ( -10.18810118749999916, 0.000000000000000000, 108.1562500020483668 ) ) ;
#46125 = CARTESIAN_POINT ( 'NONE',  ( 2.020667218593132706E-15, -11.00000000000000000, 103.3750000000000000 ) ) ;
#46126 = CARTESIAN_POINT ( 'NONE',  ( -30.82842712474621294, 204.1250000000000284, 167.1715728752542134 ) ) ;
#46127 = CARTESIAN_POINT ( 'NONE',  ( 1.432654583217664479, 201.7500000013655779, 201.4587341250000065 ) ) ;
#46128 = CARTESIAN_POINT ( 'NONE',  ( 27.99999999999996803, 205.6250000027312126, 165.9999999999998863 ) ) ;
#46129 = CARTESIAN_POINT ( 'NONE',  ( 8.660254037844385522, 84.58333333333334281, 5.000000000000005329 ) ) ;
#46130 = CARTESIAN_POINT ( 'NONE',  ( 2.977408999572650039, 91.06250000204838102, -7.188101187500001821 ) ) ;
#46131 = CARTESIAN_POINT ( 'NONE',  ( 3.042071309553159519, 65.05208332991932707, 11.35316468750000141 ) ) ;
#46132 = CARTESIAN_POINT ( 'NONE',  ( 6.000000000000003553, 289.4375000000000000, 2.485281374238571317 ) ) ;
#46133 = ORIENTED_EDGE ( 'NONE', *, *, #42601, .F. ) ;
#46134 = B_SPLINE_CURVE_WITH_KNOTS ( 'NONE', 3,
 ( #42887, #20628, #32722, #60625, #61374, #48549, #55356, #71559, #2916, #54236, #31588, #60246, #44396, #27039, #4047, #38369, #37627, #3661 ),
 .UNSPECIFIED., .F., .F.,
 ( 4, 2, 2, 2, 2, 2, 2, 2, 4 ),
 ( 0.000000000000000000, 0.001314736723651638338, 0.002629473447303276677, 0.003944210170954915232, 0.005258946894606553353, 0.006573683618258192342, 0.007888420341909830463, 0.009203157065561471187, 0.01051789378921311191 ),
 .UNSPECIFIED. ) ;
#46135 = CARTESIAN_POINT ( 'NONE',  ( -27.99999999999991118, 200.6250000027312126, 174.0000000000003695 ) ) ;
#46136 = CARTESIAN_POINT ( 'NONE',  ( 1.558072418987630714, -16.42747873774311884, 68.67104701338894301 ) ) ;
#46137 = CARTESIAN_POINT ( 'NONE',  ( -3.458734125000015425, 207.9375000013656063, 142.0000000000000568 ) ) ;
#46138 = LINE ( 'NONE', #11076, #52712 ) ;
#46139 = DIRECTION ( 'NONE',  ( 1.224646799147353207E-16, 0.000000000000000000, -1.000000000000000000 ) ) ;
#46140 = CARTESIAN_POINT ( 'NONE',  ( -7.320508075688770155, 235.6250000000000000, 7.320508075688774596 ) ) ;
#46141 = CARTESIAN_POINT ( 'NONE',  ( 4.556349186104045934, 11.00000000000000000, 72.71875000409677625 ) ) ;
#46142 = CARTESIAN_POINT ( 'NONE',  ( 10.18810118750000093, -4.220049686691933921, 68.68750000204836681 ) ) ;
#46143 = CARTESIAN_POINT ( 'NONE',  ( 8.660254037844385522, 204.5833333333333428, 5.000000000000005329 ) ) ;
#46144 = CARTESIAN_POINT ( 'NONE',  ( 5.082755093536320601, -5.082755093536318824, 17.42405278187175810 ) ) ;
#46145 = CARTESIAN_POINT ( 'NONE',  ( -9.832129032723418760, 163.1770833299193839, -5.676582343750004256 ) ) ;
#46146 = PLANE ( 'NONE',  #15578 ) ;
#46147 = CARTESIAN_POINT ( 'NONE',  ( 8.660254037844385522, 176.4583333265053682, 5.000000000000005329 ) ) ;
#46149 = CARTESIAN_POINT ( 'NONE',  ( 0.000000000000000000, 0.000000000000000000, 118.0000000000000000 ) ) ;
#46148 = DIRECTION ( 'NONE',  ( 0.000000000000000000, -0.000000000000000000, -1.000000000000000000 ) ) ;
#46150 = EDGE_LOOP ( 'NONE', ( #38651, #48881, #74595, #4101 ) ) ;
#46151 = CARTESIAN_POINT ( 'NONE',  ( 3.458734124999959025, 198.5000000013656347, 140.5673454167824161 ) ) ;
#46152 = CARTESIAN_POINT ( 'NONE',  ( 9.832129032723416984, 40.67708332991935549, 5.676582343750006032 ) ) ;
#46153 = CARTESIAN_POINT ( 'NONE',  ( 11.00000000000000000, 1.347111479062088405E-15, 111.4375000040967763 ) ) ;
#46154 = CARTESIAN_POINT ( 'NONE',  ( -26.56734541678243033, 208.3750000013656063, 166.5412658750003345 ) ) ;
#46155 = CARTESIAN_POINT ( 'NONE',  ( 2.020667218593132706E-15, -11.00000000000000000, 70.37500000000000000 ) ) ;
#46157 = CARTESIAN_POINT ( 'NONE',  ( 28.00000000000001776, 199.5000000000000000, 165.9999999999998863 ) ) ;
#46156 = CARTESIAN_POINT ( 'NONE',  ( 28.00000000000001776, 200.5000000000000000, 165.9999999999998863 ) ) ;
#46158 = CARTESIAN_POINT ( 'NONE',  ( -13.24221748263659748, -41.24981230066703830, 198.0327383062869160 ) ) ;
#46159 = CARTESIAN_POINT ( 'NONE',  ( 2.445694354108783664, 198.3125000013656063, 144.4456943541088663 ) ) ;
#46160 = ADVANCED_FACE ( 'NONE', ( #20663, #55391 ), #2949, .F. ) ;
#46161 = CARTESIAN_POINT ( 'NONE',  ( -8.660254037844387298, 68.95833332650536818, -5.000000000000004441 ) ) ;
#46162 = CARTESIAN_POINT ( 'NONE',  ( 7.188101187500000044, 97.90625000204838102, -8.802885111219163269E-16 ) ) ;
#46163 = CARTESIAN_POINT ( 'NONE',  ( 2.780723358947928197E-16, 12.68749999863440792, -4.541265875000002339 ) ) ;
#46164 = CARTESIAN_POINT ( 'NONE',  ( 3.313708498984762496, -7.999999999999989342, 4.299052779823363757 ) ) ;
#46165 = CARTESIAN_POINT ( 'NONE',  ( 2.828427124746191623, 7.874999997268813168, -2.828427124746191623 ) ) ;
#46166 = ORIENTED_EDGE ( 'NONE', *, *, #10350, .F. ) ;
#46167 = VERTEX_POINT ( 'NONE', #15370 ) ;
#46168 = CARTESIAN_POINT ( 'NONE',  ( -10.00000000000011191, 197.7083333333334281, 2.679491924311252049 ) ) ;
#46169 = CARTESIAN_POINT ( 'NONE',  ( 6.676582343750003368, 299.1718750017069510, -2.765530957081997254 ) ) ;
#46170 = CARTESIAN_POINT ( 'NONE',  ( -10.00000000000001243, 162.2916666666666856, -2.679491924311233841 ) ) ;
#46171 = LINE ( 'NONE', #41263, #61791 ) ;
#46172 = AXIS2_PLACEMENT_3D ( 'NONE', #30330, #52976, #36364 ) ;
#46173 = CARTESIAN_POINT ( 'NONE',  ( -9.832129032723418760, 152.8645833299193555, -5.676582343750004256 ) ) ;
#46174 = DIRECTION ( 'NONE',  ( 0.000000000000000000, 0.000000000000000000, 1.000000000000000000 ) ) ;
#46175 = CARTESIAN_POINT ( 'NONE',  ( -7.204075437095967871, 7.204075437095967871, 82.46875000204836681 ) ) ;
#46176 = CARTESIAN_POINT ( 'NONE',  ( -31.55598681522106475, 194.5891123728962384, 169.4635226781817607 ) ) ;
#46177 = CARTESIAN_POINT ( 'NONE',  ( 1.656854249492403008, 203.6875000000000000, 194.0000000000000853 ) ) ;
#46178 = CARTESIAN_POINT ( 'NONE',  ( -10.99999999999994849, 4.556349186104097448, 113.4062500000000000 ) ) ;
#46179 = CARTESIAN_POINT ( 'NONE',  ( 10.18810118749999916, 1.247682550866122264E-15, 116.7812500020483810 ) ) ;
#46180 = VERTEX_POINT ( 'NONE', #73102 ) ;
#46181 = CARTESIAN_POINT ( 'NONE',  ( 32.24156300664948560, -26.56240014496064461, 164.2514022246716081 ) ) ;
#46182 = CARTESIAN_POINT ( 'NONE',  ( 20.28493003622275026, 177.0489554009944015, 146.4498493592099919 ) ) ;
#46183 = CARTESIAN_POINT ( 'NONE',  ( -3.042071309553173730, 134.6354166632526699, 11.35316468749999785 ) ) ;
#46184 = CARTESIAN_POINT ( 'NONE',  ( -3.458734124999958581, 197.5000000013656063, 199.4326545832176976 ) ) ;
#46185 = CARTESIAN_POINT ( 'NONE',  ( 4.401442555609581635E-16, 26.71874999795161543, -7.188101187500000044 ) ) ;
#46186 = CARTESIAN_POINT ( 'NONE',  ( -4.220049686691935698, 10.18810118749999916, 79.75000000204838102 ) ) ;
#46187 = CARTESIAN_POINT ( 'NONE',  ( -3.042071309553164404, 32.55208332991934128, -11.35316468749999963 ) ) ;
#46188 = ORIENTED_EDGE ( 'NONE', *, *, #62528, .T. ) ;
#46189 = CARTESIAN_POINT ( 'NONE',  ( -7.778174593052020747, -7.778174593052023411, 94.37500000409677625 ) ) ;
#46190 = CARTESIAN_POINT ( 'NONE',  ( -1.881053915767124440, 1.124999998634406584, 4.541265875000001451 ) ) ;
#46191 = CARTESIAN_POINT ( 'NONE',  ( 5.662595241051936235, -5.662595241051934458, 15.07561528394063011 ) ) ;
#46192 = CARTESIAN_POINT ( 'NONE',  ( 3.458734124999959469, 207.7500000013656063, 140.5673454167824161 ) ) ;
#46193 = ADVANCED_FACE ( 'NONE', ( #8605 ), #31997, .F. ) ;
#46194 = EDGE_CURVE ( 'NONE', #31087, #8699, #32757, .T. ) ;
#46195 = CARTESIAN_POINT ( 'NONE',  ( -5.082755093536325042, 7.031249997951611874, -5.082755093536325930 ) ) ;
#46196 = CARTESIAN_POINT ( 'NONE',  ( -6.000000000000003553, 295.0000000034140157, -2.485281374238571317 ) ) ;
#46197 = CARTESIAN_POINT ( 'NONE',  ( -34.69679471024809203, -12.34462646322155699, 148.2170566195945298 ) ) ;
#46198 = CARTESIAN_POINT ( 'NONE',  ( -5.082755093536326818, 7.781249997951610986, 5.082755093536325042 ) ) ;
#46199 = CARTESIAN_POINT ( 'NONE',  ( -5.082755093536319713, 5.082755093536319713, 17.79905278187175455 ) ) ;
#46200 =( BOUNDED_CURVE ( )  B_SPLINE_CURVE ( 2, ( #10703, #56739, #51063, #51811, #40493, #57863, #34110, #6169, #73704, #57108, #22016, #74076, #45397 ),
 .UNSPECIFIED., .F., .F. ) 
 B_SPLINE_CURVE_WITH_KNOTS ( ( 3, 2, 2, 2, 2, 2, 3 ),
 ( 2.653284597091381869, 2.658518511020140807, 2.663752424948899744, 2.668986338877658682, 2.674220252806417619, 2.679454166735176557, 2.684688080663935494 ),
 .UNSPECIFIED. ) 
 CURVE ( )  GEOMETRIC_REPRESENTATION_ITEM ( )  RATIONAL_B_SPLINE_CURVE ( ( 0.9999999999999978906, 0.9659258262890704216, 1.000000000000000000, 0.9659258262890683122, 1.000000000000000000, 0.9659258262890683122, 1.000000000000000000, 0.9659258262890683122, 1.000000000000000000, 0.9659258262890683122, 1.000000000000000000, 0.9659258262891455837, 0.9999999999999227285 ) ) 
 REPRESENTATION_ITEM ( '' )  );
#46201 = EDGE_CURVE ( 'NONE', #64342, #41205, #45101, .T. ) ;
#46202 = CARTESIAN_POINT ( 'NONE',  ( -2.085542519210945728E-15, 149.8437499965860411, 11.35316468750000141 ) ) ;
#46203 = CARTESIAN_POINT ( 'NONE',  ( -10.18810118749999916, 0.000000000000000000, 70.65625000204836681 ) ) ;
#46204 = CIRCLE ( 'NONE', #38981, 71.70204102886728492 ) ;
#46205 = CARTESIAN_POINT ( 'NONE',  ( -30.44569435410879521, 208.0625000013656063, 172.4456943541092357 ) ) ;
#46206 = DIRECTION ( 'NONE',  ( -0.000000000000000000, -1.000000000000000000, -4.283267841918042741E-17 ) ) ;
#46207 = CARTESIAN_POINT ( 'NONE',  ( 3.211159895383560947, 18.31249999863440792, 3.211159895383562723 ) ) ;
#46208 = ORIENTED_EDGE ( 'NONE', *, *, #60460, .F. ) ;
#46209 = CARTESIAN_POINT ( 'NONE',  ( -1.656854249492348607, 198.3125000027312126, 202.0000000000000284 ) ) ;
#46210 = EDGE_CURVE ( 'NONE', #18628, #52951, #17109, .T. ) ;
#46211 = CARTESIAN_POINT ( 'NONE',  ( -2.828427124746209831, 205.3750000000000284, 139.1715728752538723 ) ) ;
#46212 = CARTESIAN_POINT ( 'NONE',  ( -24.00000000000002487, 199.9375000027312126, 168.3431457505079152 ) ) ;
#46213 = CARTESIAN_POINT ( 'NONE',  ( -5.000000000000045297, 58.33333333333338544, 8.660254037844454800 ) ) ;
#46214 = CARTESIAN_POINT ( 'NONE',  ( 7.999999999999991118, 9.797174393178815797E-16, 10.76780278392014800 ) ) ;
#46215 = VERTEX_POINT ( 'NONE', #8089 ) ;
#46216 = CARTESIAN_POINT ( 'NONE',  ( 7.188101187500000044, 16.96874999795161543, 0.000000000000000000 ) ) ;
#46217 = ORIENTED_EDGE ( 'NONE', *, *, #29166, .T. ) ;
#46218 = CARTESIAN_POINT ( 'NONE',  ( -5.999999999999999112, 298.1250000034140157, 2.485281374238575314 ) ) ;
#46219 = CARTESIAN_POINT ( 'NONE',  ( -2.679491924311272477, 45.41666665983869677, 9.999999999999978684 ) ) ;
#46220 = CARTESIAN_POINT ( 'NONE',  ( 4.999999999999993783, 44.16666666666666430, 8.660254037844390851 ) ) ;
#46221 = CARTESIAN_POINT ( 'NONE',  ( 5.082755093536326818, 105.5937500020483810, 5.082755093536325042 ) ) ;
#46222 = CARTESIAN_POINT ( 'NONE',  ( -26.56734541678238415, 206.6250000013656063, 166.5412658750003629 ) ) ;
#46223 = CARTESIAN_POINT ( 'NONE',  ( -23.99999999999999645, 196.8125000000000284, 168.3431457505080289 ) ) ;
#46225 = CARTESIAN_POINT ( 'NONE',  ( -3.313708498984707429, 94.90625000409679046, -8.000000000000055067 ) ) ;
#46224 = FACE_OUTER_BOUND ( 'NONE', #52269, .T. ) ;
#46226 = ORIENTED_EDGE ( 'NONE', *, *, #33057, .T. ) ;
#46227 = CARTESIAN_POINT ( 'NONE',  ( 5.676582343750005144, 250.5729166700807014, 9.832129032723416984 ) ) ;
#46228 = CARTESIAN_POINT ( 'NONE',  ( 1.320432766682872962E-15, -7.188101187499992051, 20.23655278187175455 ) ) ;
#46229 = CARTESIAN_POINT ( 'NONE',  ( -2.591411123064620181, 50.09422832877455534, 40.78779037275248243 ) ) ;
#46230 = DIRECTION ( 'NONE',  ( -0.8191520442889906883, 0.000000000000000000, -0.5735764363510477137 ) ) ;
#46231 = CARTESIAN_POINT ( 'NONE',  ( -9.999999999999998224, 147.2916666666666572, -2.679491924311230289 ) ) ;
#46232 = CARTESIAN_POINT ( 'NONE',  ( 4.999999999999993783, 201.0416666598387110, 8.660254037844390851 ) ) ;
#46233 = CARTESIAN_POINT ( 'NONE',  ( 8.660254037844389075, 155.4166666666666856, -5.000000000000000000 ) ) ;
#46234 = CARTESIAN_POINT ( 'NONE',  ( 0.000000000000000000, 125.0000000000000000, 0.000000000000000000 ) ) ;
#46235 = LINE ( 'NONE', #22848, #38788 ) ;
#46236 = CARTESIAN_POINT ( 'NONE',  ( 3.042071309553167069, 132.1354166632526699, -11.35316468749999785 ) ) ;
#46237 = DIRECTION ( 'NONE',  ( -0.000000000000000000, -1.000000000000000000, -0.000000000000000000 ) ) ;
#46238 = CARTESIAN_POINT ( 'NONE',  ( -4.556349186104045934, 11.00000000000000000, 68.21875000000000000 ) ) ;
#46241 = LINE ( 'NONE', #17947, #4930 ) ;
#46240 = CARTESIAN_POINT ( 'NONE',  ( 24.54126587499997925, 196.1250000013655779, 168.5673454167822740 ) ) ;
#46239 = CARTESIAN_POINT ( 'NONE',  ( 24.54126587499999701, 196.3750000013656063, 168.5673454167822172 ) ) ;
#46242 = VERTEX_POINT ( 'NONE', #60138 ) ;
#46243 = CARTESIAN_POINT ( 'NONE',  ( 8.311093377946837890, 1.718749996586016682, -8.311093377946837890 ) ) ;
#46244 = CARTESIAN_POINT ( 'NONE',  ( -4.794452594515416166, -6.420665270977717221, -0.000000000000000000 ) ) ;
#46245 = CARTESIAN_POINT ( 'NONE',  ( -4.000000000000002665, 11.56250000000000000, 1.656854249492380582 ) ) ;
#46246 = CARTESIAN_POINT ( 'NONE',  ( 8.660254037844385522, 26.45833332650536818, 5.000000000000005329 ) ) ;
#46247 = AXIS2_PLACEMENT_3D ( 'NONE', #63552, #28107, #29233 ) ;
#46248 = CARTESIAN_POINT ( 'NONE',  ( 5.082755093536326818, 118.7187500020483810, 5.082755093536325042 ) ) ;
#46249 = CARTESIAN_POINT ( 'NONE',  ( 2.780723358947928197E-16, 20.56249999863440436, -4.541265875000002339 ) ) ;
#46250 = CARTESIAN_POINT ( 'NONE',  ( -5.126106709314346865, 68.65851429197836353, -20.89429596904543018 ) ) ;
#46251 = CARTESIAN_POINT ( 'NONE',  ( -7.999999999999991118, 3.313708498984756723, 21.73655277982336287 ) ) ;
#46253 = CARTESIAN_POINT ( 'NONE',  ( 9.797174393178825657E-16, 0.5000000000000004441, -8.000000000000000000 ) ) ;
#46252 = CARTESIAN_POINT ( 'NONE',  ( -28.00000000000002842, 202.0000000000000000, 166.0000000000003695 ) ) ;
#46254 = CARTESIAN_POINT ( 'NONE',  ( -9.832129032723418760, 112.8645833299193555, -5.676582343750004256 ) ) ;
#46255 = VERTEX_POINT ( 'NONE', #14100 ) ;
#46256 = CARTESIAN_POINT ( 'NONE',  ( -2.828427124746208943, 205.7500000027312126, 144.8284271247462129 ) ) ;
#46257 = CARTESIAN_POINT ( 'NONE',  ( 2.977408999572650927, 24.74999999795161543, -7.188101187500001821 ) ) ;
#46258 = LINE ( 'NONE', #28913, #61542 ) ;
#46259 = CARTESIAN_POINT ( 'NONE',  ( 9.832129032723416984, 247.1354166700806445, -5.676582343750003368 ) ) ;
#46260 = CARTESIAN_POINT ( 'NONE',  ( 8.311093377946837890, 96.40624999658602690, -8.311093377946837890 ) ) ;
#46261 = VERTEX_POINT ( 'NONE', #66171 ) ;
#46262 = ADVANCED_FACE ( 'NONE', ( #35665 ), #59412, .T. ) ;
#46263 = CARTESIAN_POINT ( 'NONE',  ( 5.000000000000000000, -10.53354221205055907, 66.31578581128081851 ) ) ;
#46264 = CARTESIAN_POINT ( 'NONE',  ( 1.871523826299183495E-15, -10.18810118749999916, 104.0312500020483810 ) ) ;
#46265 = CARTESIAN_POINT ( 'NONE',  ( 6.123233995736767268E-16, 223.1249999931720254, -10.00000000000000178 ) ) ;
#46266 = CARTESIAN_POINT ( 'NONE',  ( -1.432654583217608080, 199.8750000013655779, 201.4587341250000350 ) ) ;
#46267 = LINE ( 'NONE', #35344, #2230 ) ;
#46269 = CARTESIAN_POINT ( 'NONE',  ( 9.832129032723420536, 96.19791666325269830, -5.676582343749999815 ) ) ;
#46268 = CARTESIAN_POINT ( 'NONE',  ( 3.313708498984756279, 7.999999999999991118, 22.86155277982336997 ) ) ;
#46270 = CARTESIAN_POINT ( 'NONE',  ( 1.469576158976822172E-15, -7.999999999999991118, 5.892802783920146226 ) ) ;
#46271 = CARTESIAN_POINT ( 'NONE',  ( -28.00000000000001776, 197.6875000013655779, 166.5412658750003629 ) ) ;
#46272 = CARTESIAN_POINT ( 'NONE',  ( -1.469576158976823947E-15, 27.93749999590322375, 8.000000000000000000 ) ) ;
#46273 = ORIENTED_EDGE ( 'NONE', *, *, #30429, .F. ) ;
#46274 = CARTESIAN_POINT ( 'NONE',  ( 10.00000000000000178, 197.0833333265053398, -2.679491924311226736 ) ) ;
#46275 = CARTESIAN_POINT ( 'NONE',  ( 8.000000000000000000, 115.2499999999999858, -9.797174393178825657E-16 ) ) ;
#46276 = CARTESIAN_POINT ( 'NONE',  ( -47.32259252271279593, 38.77329591270029141, 65.76194439203462139 ) ) ;
#46277 = CARTESIAN_POINT ( 'NONE',  ( 6.951808397369818766E-16, 92.34374999658602690, -11.35316468750000141 ) ) ;
#46278 = CARTESIAN_POINT ( 'NONE',  ( 6.676582343750001591, 289.9531250017069510, -8.176455196517173205E-16 ) ) ;
#46279 = CARTESIAN_POINT ( 'NONE',  ( 2.977408999572652260, 5.062499997951610098, 7.188101187500000044 ) ) ;
#46280 = CARTESIAN_POINT ( 'NONE',  ( -10.18810118749999916, 4.220049686691934809, 96.43750000204836681 ) ) ;
#46281 = CARTESIAN_POINT ( 'NONE',  ( 4.643183940729320724, 226.6963029853575335, -10.42876187888753847 ) ) ;
#46282 = VERTEX_POINT ( 'NONE', #7725 ) ;
#46283 = CARTESIAN_POINT ( 'NONE',  ( 4.000000000000015987, 196.6875000027312126, 196.3431457505076594 ) ) ;
#46284 = CARTESIAN_POINT ( 'NONE',  ( -11.35316468750000141, 218.4895833299193271, 3.042071309553159963 ) ) ;
#46285 = VECTOR ( 'NONE', #64258, 1000.000000000000000 ) ;
#46286 = ADVANCED_FACE ( 'NONE', ( #36399 ), #53384, .F. ) ;
#46287 = DIRECTION ( 'NONE',  ( 0.000000000000000000, 0.000000000000000000, 1.000000000000000000 ) ) ;
#46288 = DIRECTION ( 'NONE',  ( -0.000000000000000000, 1.000000000000000000, -0.000000000000000000 ) ) ;
#46289 = CARTESIAN_POINT ( 'NONE',  ( 2.765530957082001251, 297.7656250017069510, 6.676582343750000703 ) ) ;
#46290 = ORIENTED_EDGE ( 'NONE', *, *, #50467, .F. ) ;
#46291 = CARTESIAN_POINT ( 'NONE',  ( 2.849036369511732440E-14, 199.2500000000000000, 202.0000000000000000 ) ) ;
#46292 = CARTESIAN_POINT ( 'NONE',  ( -3.042071309553173730, 204.6354166632526699, 11.35316468749999785 ) ) ;
#46293 = CARTESIAN_POINT ( 'NONE',  ( 7.204075437095968759, -7.204075437095966983, 87.71875000204836681 ) ) ;
#46294 = CARTESIAN_POINT ( 'NONE',  ( -31.45873412499998523, 204.7500000013656063, 171.4326545832180386 ) ) ;
#46295 = CARTESIAN_POINT ( 'NONE',  ( 3.313708498984762052, 19.78125000000001066, -8.000000000000000000 ) ) ;
#46296 = ORIENTED_EDGE ( 'NONE', *, *, #53720, .T. ) ;
#46297 = CARTESIAN_POINT ( 'NONE',  ( -4.401442555609581635E-16, 123.7812500020483810, -7.188101187500000044 ) ) ;
#46298 = FILL_AREA_STYLE ('',( #48322 ) ) ;
#46299 = EDGE_CURVE ( 'NONE', #39015, #64786, #2806, .T. ) ;
#46300 = CARTESIAN_POINT ( 'NONE',  ( 7.320508075688771044, 34.37500000000000711, 7.320508075688775484 ) ) ;
#46301 = EDGE_CURVE ( 'NONE', #33914, #22922, #63374, .T. ) ;
#46302 = AXIS2_PLACEMENT_3D ( 'NONE', #37684, #72373, #49356 ) ;
#46303 = CARTESIAN_POINT ( 'NONE',  ( -7.999999999961189268, -1.665725685002260109E-05, 4.018425631117963803 ) ) ;
#46304 = CARTESIAN_POINT ( 'NONE',  ( 1.871523826299183495E-15, -10.18810118749999916, 72.90625000204836681 ) ) ;
#46305 = VERTEX_POINT ( 'NONE', #19396 ) ;
#46306 =( BOUNDED_CURVE ( )  B_SPLINE_CURVE ( 2, ( #24102, #47113, #28657, #11680, #35450, #16, #52791, #34717, #39986, #64108, #63730, #11315, #5658, #6029, #45636, #63355, #69400, #17708, #52423, #29776, #22618, #1126, #40723, #17333, #7140, #34349, #70149, #23003, #41469, #18457, #12052, #758, #64483, #68651, #35815, #12780, #57346, #58830, #69029, #40353, #57723, #35085, #30148, #29034, #388, #23370, #58096, #65952, #8991, #36181, #32006, #31629, #47485, #37293, #14257, #1498, #36918, #7509, #42929, #19186, #42189, #54650, #60288, #66325, #65203, #13510, #25946, #54277, #36549, #59200, #53534, #13145, #42566, #7877, #8240, #19550, #2213, #64843, #48592, #30514, #1850, #8614, #2959, #48963, #71600, #59926, #65579, #25207, #24836, #47853, #70874, #14630, #71975, #20289, #59560, #71230, #19921, #30881, #53900, #24479, #43309, #37670, #48222, #60669, #13874, #70508, #25577, #31251, #2589, #18827, #41831, #50094, #33512, #39154, #46199, #44069, #72741, #4831, #33149, #21045, #15004, #27444, #20670, #43689, #15748, #16116, #44812, #67823, #38415, #56143, #66701, #50460, #62156, #10480, #21783, #73475, #38789, #73109, #55772, #32384, #55398, #21417, #49342, #44441, #69215, #26707, #49726, #67452, #67079, #4452, #56515, #28846, #51869, #4088, #210, #9364, #23188, #17526, #27082, #61792, #3708, #9742, #10110, #15378, #40543, #61416, #63548, #11873, #55025, #3332, #26321, #72359, #38041, #61040, #32764, #71047, #46937, #47306, #65019, #35274, #52242, #13330, #69965, #29229, #30332, #1312, #576, #17903, #18273, #57917, #946, #58647, #6954, #18646, #36002, #34909, #47666, #24295, #36366, #12605, #2032, #59019, #63927, #53718, #7328, #70331, #12964, #41654, #6226, #48038, #53351, #65397, #64664, #12237, #58287, #40916, #35632, #29965, #24656, #41288, #6590, #1676, #70688, #23558, #19006, #52978, #42012, #64298, #29597, #46569, #59382, #19367, #23928, #7693, #52610, #30700, #25018, #42380, #69590, #31819, #14443, #43877, #38228, #54840, #8059, #3149, #26894, #60107, #8425, #26135, #31442, #66506, #26509, #61234, #66893, #37478, #72554, #42749, #20859, #37859, #60478, #49535, #43495, #43120, #49154, #54468, #49910, #2775, #72164, #3901, #20475, #14817, #15199, #13694, #9562, #60856, #32577, #72924, #25761, #9176, #55586, #3520, #65765, #21234, #48782, #31060, #32195, #55215, #54088, #71416, #71789, #36736, #20108, #8808, #44260, #59747, #2398, #25396, #48410, #19740, #14068, #37104, #66139, #68378, #21602 ),
 .UNSPECIFIED., .F., .F. ) 
 B_SPLINE_CURVE_WITH_KNOTS ( ( 3, 2, 2, 2, 2, 2, 2, 2, 2, 2, 2, 2, 2, 2, 2, 2, 2, 2, 2, 2, 2, 2, 2, 2, 2, 2, 2, 2, 2, 2, 2, 2, 2, 2, 2, 2, 2, 2, 2, 2, 2, 2, 2, 2, 2, 2, 2, 2, 2, 2, 2, 2, 2, 2, 2, 2, 2, 2, 2, 2, 2, 2, 2, 2, 2, 2, 2, 2, 2, 2, 2, 2, 2, 2, 2, 2, 2, 2, 2, 2, 2, 2, 2, 2, 2, 2, 2, 2, 2, 2, 2, 2, 2, 2, 2, 2, 2, 2, 2, 2, 2, 2, 2, 2, 2, 2, 2, 2, 2, 2, 2, 2, 2, 2, 2, 2, 2, 2, 2, 2, 2, 2, 2, 2, 2, 2, 2, 2, 2, 2, 2, 2, 2, 2, 2, 2, 2, 2, 2, 2, 2, 2, 2, 2, 2, 2, 2, 2, 2, 2, 2, 2, 3 ),
 ( 0.000000000000000000, 0.006578947368421052266, 0.01315789473684210453, 0.01973684210526315680, 0.02631578947368420907, 0.03289473684210526133, 0.03947368421052631360, 0.04605263157894736586, 0.05263157894736841813, 0.05921052631578947040, 0.06578947368421052266, 0.07236842105263158187, 0.07894736842105262720, 0.08552631578947368640, 0.09210526315789473173, 0.09868421052631579093, 0.1052631578947368363, 0.1118421052631578955, 0.1184210526315789408, 0.1250000000000000000, 0.1315789473684210453, 0.1381578947368421184, 0.1447368421052631637, 0.1513157894736842091, 0.1578947368421052544, 0.1644736842105263275, 0.1710526315789473728, 0.1776315789473684181, 0.1842105263157894635, 0.1907894736842105365, 0.1973684210526315819, 0.2039473684210526272, 0.2105263157894736725, 0.2171052631578947456, 0.2236842105263157909, 0.2302631578947368363, 0.2368421052631578816, 0.2434210526315789547, 0.2500000000000000000, 0.2565789473684210731, 0.2631578947368420907, 0.2697368421052631637, 0.2763157894736842368, 0.2828947368421052544, 0.2894736842105263275, 0.2960526315789473450, 0.3026315789473684181, 0.3092105263157894912, 0.3157894736842105088, 0.3223684210526315819, 0.3289473684210526550, 0.3355263157894736725, 0.3421052631578947456, 0.3486842105263157632, 0.3552631578947368363, 0.3618421052631579093, 0.3684210526315789269, 0.3750000000000000000, 0.3815789473684210731, 0.3881578947368420907, 0.3947368421052631637, 0.4013157894736842368, 0.4078947368421052544, 0.4144736842105263275, 0.4210526315789473450, 0.4276315789473684181, 0.4342105263157894912, 0.4407894736842105088, 0.4473684210526315819, 0.4539473684210526550, 0.4605263157894736725, 0.4671052631578947456, 0.4736842105263157632, 0.4802631578947368363, 0.4868421052631579093, 0.4934210526315789269, 0.5000000000000000000, 0.5065789473684210176, 0.5131578947368421462, 0.5197368421052631637, 0.5263157894736841813, 0.5328947368421053099, 0.5394736842105263275, 0.5460526315789473450, 0.5526315789473684736, 0.5592105263157894912, 0.5657894736842105088, 0.5723684210526315264, 0.5789473684210526550, 0.5855263157894736725, 0.5921052631578946901, 0.5986842105263158187, 0.6052631578947368363, 0.6118421052631578538, 0.6184210526315789824, 0.6250000000000001110, 0.6315789473684210176, 0.6381578947368421462, 0.6447368421052631637, 0.6513157894736841813, 0.6578947368421053099, 0.6644736842105263275, 0.6710526315789473450, 0.6776315789473684736, 0.6842105263157894912, 0.6907894736842105088, 0.6973684210526315264, 0.7039473684210526550, 0.7105263157894736725, 0.7171052631578946901, 0.7236842105263158187, 0.7302631578947368363, 0.7368421052631578538, 0.7434210526315789824, 0.7500000000000000000, 0.7565789473684210176, 0.7631578947368421462, 0.7697368421052631637, 0.7763157894736841813, 0.7828947368421053099, 0.7894736842105263275, 0.7960526315789473450, 0.8026315789473684736, 0.8092105263157894912, 0.8157894736842105088, 0.8223684210526315264, 0.8289473684210526550, 0.8355263157894736725, 0.8421052631578946901, 0.8486842105263158187, 0.8552631578947368363, 0.8618421052631578538, 0.8684210526315789824, 0.8749999999999998890, 0.8815789473684210176, 0.8881578947368421462, 0.8947368421052631637, 0.9013157894736841813, 0.9078947368421053099, 0.9144736842105263275, 0.9210526315789473450, 0.9276315789473684736, 0.9342105263157894912, 0.9407894736842105088, 0.9473684210526315264, 0.9539473684210526550, 0.9605263157894736725, 0.9671052631578946901, 0.9736842105263158187, 0.9802631578947368363, 0.9868421052631578538, 0.9934210526315789824, 0.9940576549107595916 ),
 .UNSPECIFIED. ) 
 CURVE ( )  GEOMETRIC_REPRESENTATION_ITEM ( )  RATIONAL_B_SPLINE_CURVE ( ( 1.000000000000000000, 0.9238795325112867385, 1.000000000000000000, 0.9238795325112867385, 1.000000000000000000, 0.9238795325112867385, 1.000000000000000000, 0.9238795325112867385, 1.000000000000000000, 0.9238795325112867385, 1.000000000000000000, 0.9238795325112867385, 1.000000000000000000, 0.9238795325112867385, 1.000000000000000000, 0.9238795325112867385, 1.000000000000000000, 0.9238795325112867385, 1.000000000000000000, 0.9238795325112867385, 1.000000000000000000, 0.9238795325112867385, 1.000000000000000000, 0.9238795325112867385, 1.000000000000000000, 0.9238795325112867385, 1.000000000000000000, 0.9238795325112867385, 1.000000000000000000, 0.9238795325112867385, 1.000000000000000000, 0.9238795325112867385, 1.000000000000000000, 0.9238795325112867385, 1.000000000000000000, 0.9238795325112867385, 1.000000000000000000, 0.9238795325112867385, 1.000000000000000000, 0.9238795325112867385, 1.000000000000000000, 0.9238795325112867385, 1.000000000000000000, 0.9238795325112867385, 1.000000000000000000, 0.9238795325112867385, 1.000000000000000000, 0.9238795325112867385, 1.000000000000000000, 0.9238795325112867385, 1.000000000000000000, 0.9238795325112867385, 1.000000000000000000, 0.9238795325112867385, 1.000000000000000000, 0.9238795325112867385, 1.000000000000000000, 0.9238795325112867385, 1.000000000000000000, 0.9238795325112867385, 1.000000000000000000, 0.9238795325112867385, 1.000000000000000000, 0.9238795325112867385, 1.000000000000000000, 0.9238795325112867385, 1.000000000000000000, 0.9238795325112867385, 1.000000000000000000, 0.9238795325112867385, 1.000000000000000000, 0.9238795325112867385, 1.000000000000000000, 0.9238795325112867385, 1.000000000000000000, 0.9238795325112867385, 1.000000000000000000, 0.9238795325112867385, 1.000000000000000000, 0.9238795325112867385, 1.000000000000000000, 0.9238795325112867385, 1.000000000000000000, 0.9238795325112867385, 1.000000000000000000, 0.9238795325112867385, 1.000000000000000000, 0.9238795325112867385, 1.000000000000000000, 0.9238795325112867385, 1.000000000000000000, 0.9238795325112867385, 1.000000000000000000, 0.9238795325112867385, 1.000000000000000000, 0.9238795325112867385, 1.000000000000000000, 0.9238795325112867385, 1.000000000000000000, 0.9238795325112867385, 1.000000000000000000, 0.9238795325112867385, 1.000000000000000000, 0.9238795325112867385, 1.000000000000000000, 0.9238795325112867385, 1.000000000000000000, 0.9238795325112867385, 1.000000000000000000, 0.9238795325112867385, 1.000000000000000000, 0.9238795325112867385, 1.000000000000000000, 0.9238795325112867385, 1.000000000000000000, 0.9238795325112867385, 1.000000000000000000, 0.9238795325112867385, 1.000000000000000000, 0.9238795325112867385, 1.000000000000000000, 0.9238795325112867385, 1.000000000000000000, 0.9238795325112867385, 1.000000000000000000, 0.9238795325112867385, 1.000000000000000000, 0.9238795325112867385, 1.000000000000000000, 0.9238795325112867385, 1.000000000000000000, 0.9238795325112867385, 1.000000000000000000, 0.9238795325112867385, 1.000000000000000000, 0.9238795325112867385, 1.000000000000000000, 0.9238795325112867385, 1.000000000000000000, 0.9238795325112867385, 1.000000000000000000, 0.9238795325112867385, 1.000000000000000000, 0.9238795325112867385, 1.000000000000000000, 0.9238795325112867385, 1.000000000000000000, 0.9238795325112867385, 1.000000000000000000, 0.9238795325112867385, 1.000000000000000000, 0.9238795325112867385, 1.000000000000000000, 0.9238795325112867385, 1.000000000000000000, 0.9238795325112867385, 1.000000000000000000, 0.9238795325112867385, 1.000000000000000000, 0.9238795325112867385, 1.000000000000000000, 0.9238795325112867385, 1.000000000000000000, 0.9238795325112867385, 1.000000000000000000, 0.9238795325112867385, 1.000000000000000000, 0.9238795325112867385, 1.000000000000000000, 0.9238795325112867385, 1.000000000000000000, 0.9238795325112867385, 1.000000000000000000, 0.9238795325112867385, 1.000000000000000000, 0.9238795325112867385, 1.000000000000000000, 0.9238795325112867385, 1.000000000000000000, 0.9238795325112867385, 1.000000000000000000, 0.9238795325112867385, 1.000000000000000000, 0.9238795325112867385, 1.000000000000000000, 0.9238795325112867385, 1.000000000000000000, 0.9238795325112867385, 1.000000000000000000, 0.9238795325112867385, 1.000000000000000000, 0.9238795325112867385, 1.000000000000000000, 0.9238795325112867385, 1.000000000000000000, 0.9238795325112867385, 1.000000000000000000, 0.9238795325112867385, 1.000000000000000000, 0.9238795325112867385, 1.000000000000000000, 0.9238795325112867385, 1.000000000000000000, 0.9238795325112867385, 1.000000000000000000, 0.9238795325112867385, 1.000000000000000000, 0.9238795325112867385, 1.000000000000000000, 0.9238795325112867385, 1.000000000000000000, 0.9238795325112867385, 1.000000000000000000, 0.9238795325112867385, 1.000000000000000000, 0.9238795325112867385, 1.000000000000000000, 0.9238795325112867385, 1.000000000000000000, 0.9238795325112867385, 1.000000000000000000, 0.9238795325112867385, 1.000000000000000000, 0.9238795325112867385, 1.000000000000000000, 0.9238795325112867385, 1.000000000000000000, 0.9238795325112867385, 1.000000000000000000, 0.9238795325112867385, 1.000000000000000000, 0.9238795325112867385, 1.000000000000000000, 0.9238795325112867385, 1.000000000000000000, 0.9238795325112867385, 1.000000000000000000, 0.9238795325112867385, 1.000000000000000000, 0.9238795325112867385, 1.000000000000000000, 0.9238795325112867385, 1.000000000000000000, 0.9238795325112867385, 1.000000000000000000, 0.9238795325112867385, 1.000000000000000000, 0.9238795325112867385, 1.000000000000000000, 0.9238795325112867385, 1.000000000000000000, 0.9238795325112867385, 1.000000000000000000, 0.9238795325112867385, 1.000000000000000000, 0.9238795325112867385, 1.000000000000000000, 0.9238795325112867385, 1.000000000000000000, 0.9238795325112867385, 1.000000000000000000, 0.9238795325112867385, 1.000000000000000000, 0.9238795325112867385, 1.000000000000000000, 0.9238795325112867385, 1.000000000000000000, 0.9238795325112867385, 1.000000000000000000, 0.9238795325112867385, 1.000000000000000000, 0.9238795325112867385, 1.000000000000000000, 0.9238795325112867385, 1.000000000000000000, 0.9238795325112867385, 1.000000000000000000, 0.9238795325112867385, 1.000000000000000000, 0.9238795325112867385, 1.000000000000000000, 0.9238795325112867385, 1.000000000000000000, 0.9238795325112867385, 1.000000000000000000, 0.9238795325112867385, 1.000000000000000000, 0.9238795325112867385, 1.000000000000000000, 0.9238795325112867385, 1.000000000000000000, 0.9238795325112867385, 1.000000000000000000, 0.9238795325112867385, 1.000000000000000000, 0.9238795325112867385, 1.000000000000000000, 0.9238795325112867385, 1.000000000000000000, 0.9238795325112867385, 1.000000000000000000, 0.9238795325112867385, 1.000000000000000000, 0.9926343136094674113, 0.9866940870930933638 ) ) 
 REPRESENTATION_ITEM ( '' )  );
#46307 = CARTESIAN_POINT ( 'NONE',  ( 9.000000000000001776, -5.196152422706648899, -0.8038475772933779684 ) ) ;
#46308 =( BOUNDED_SURFACE ( )  B_SPLINE_SURFACE ( 3, 2, ( 
 ( #6759, #29763, #58818 ),
 ( #47842, #57711, #63717 ),
 ( #41820, #7128, #6017 ),
 ( #64473, #29021, #63343 ),
 ( #1115, #53152, #12040 ),
 ( #35074, #18445, #747 ),
 ( #41459, #58451, #24827 ),
 ( #35802, #1486, #70498 ),
 ( #18817, #11668, #64830 ),
 ( #13134, #36168, #59188 ),
 ( #7498, #1841, #70863 ),
 ( #19174, #52040, #376 ),
 ( #23357, #71218, #36907 ),
 ( #2947, #2201, #49716 ),
 ( #19538, #36539, #14246 ),
 ( #8603, #13864, #59550 ),
 ( #48579, #37283, #59915 ),
 ( #8231, #38030, #53889 ) ),
 .UNSPECIFIED., .F., .F., .F. ) 
 B_SPLINE_SURFACE_WITH_KNOTS ( ( 4, 2, 2, 2, 2, 2, 2, 2, 4 ),
 ( 3, 3 ),
 ( 0.04202945594032922449, 0.04396162471216792655, 0.04589379348400663555, 0.04782596225584534455, 0.04975813102768404661, 0.05169029979952274867, 0.05265638418544209970, 0.05362246857136145073, 0.05748680611503886179 ),
 ( 0.000000000000000000, 1.000000000000000000 ),
 .UNSPECIFIED. ) 
 GEOMETRIC_REPRESENTATION_ITEM ( )  RATIONAL_B_SPLINE_SURFACE ( (
 ( 1.000000000000000000, 0.6241276099608158434, 1.000000000000000000),
 ( 1.000000000000000000, 0.6218761496800927491, 1.000000000000000000),
 ( 1.000000000000000000, 0.6198047272363291782, 1.000000000000000000),
 ( 1.000000000000000000, 0.6161935119825117102, 1.000000000000000000),
 ( 1.000000000000000000, 0.6146642324080550113, 1.000000000000000000),
 ( 1.000000000000000000, 0.6121850116871446756, 1.000000000000000000),
 ( 1.000000000000000000, 0.6112350889399391640, 1.000000000000000000),
 ( 1.000000000000000000, 0.6099522725973176573, 1.000000000000000000),
 ( 1.000000000000000000, 0.6096208180308001490, 1.000000000000000000),
 ( 1.000000000000000000, 0.6096183796349362582, 1.000000000000000000),
 ( 1.000000000000000000, 0.6099422200102193603, 1.000000000000000000),
 ( 1.000000000000000000, 0.6109087447823151606, 1.000000000000000000),
 ( 1.000000000000000000, 0.6113123981688073361, 1.000000000000000000),
 ( 1.000000000000000000, 0.6122677719809532793, 1.000000000000000000),
 ( 1.000000000000000000, 0.6128199619021084121, 1.000000000000000000),
 ( 1.000000000000000000, 0.6159350830265307719, 1.000000000000000000),
 ( 1.000000000000000000, 0.6195556778515927121, 1.000000000000000000),
 ( 1.000000000000000000, 0.6241278272307889674, 1.000000000000000000) ) ) 
 REPRESENTATION_ITEM ( '' )  SURFACE ( )  );
#46309 = EDGE_CURVE ( 'NONE', #32761, #46261, #32102, .T. ) ;
#46310 = CARTESIAN_POINT ( 'NONE',  ( 0.000000000000000000, 125.0000000000000000, 8.000000000000000000 ) ) ;
#46311 = EDGE_CURVE ( 'NONE', #40533, #24115, #44902, .T. ) ;
#46312 = CARTESIAN_POINT ( 'NONE',  ( -31.66756539373097468, 271.9999999999999432, 167.9999999999998295 ) ) ;
#46313 = CARTESIAN_POINT ( 'NONE',  ( 7.188101187500000044, 123.7812500020483810, -8.802885111219163269E-16 ) ) ;
#46314 = CARTESIAN_POINT ( 'NONE',  ( -2.886287813027996254E-11, 51.14729664189304970, 48.52014062455092613 ) ) ;
#46315 = CARTESIAN_POINT ( 'NONE',  ( -4.721056650415998313, 297.5781250017069510, 4.721056650416000089 ) ) ;
#46317 = CARTESIAN_POINT ( 'NONE',  ( -11.00000000000000000, 0.000000000000000000, 88.18750000409677625 ) ) ;
#46316 = CARTESIAN_POINT ( 'NONE',  ( -9.832129032723415207, 239.3229166700806445, 5.676582343750005144 ) ) ;
#46318 = CONTEXT_DEPENDENT_SHAPE_REPRESENTATION ( #69398, #8055 ) ;
#46319 = ORIENTED_EDGE ( 'NONE', *, *, #60754, .F. ) ;
#46320 = CARTESIAN_POINT ( 'NONE',  ( 11.35316468749999963, 246.5104166700806161, 3.042071309553159519 ) ) ;
#46321 = EDGE_CURVE ( 'NONE', #2485, #56146, #68671, .T. ) ;
#46322 = CARTESIAN_POINT ( 'NONE',  ( -7.188101187499991163, 2.977408999572646930, 4.392802781871752771 ) ) ;
#46323 = VERTEX_POINT ( 'NONE', #50311 ) ;
#46324 = CARTESIAN_POINT ( 'NONE',  ( 10.18810118749999916, 1.247682550866122264E-15, 68.40625000204836681 ) ) ;
#46325 = CARTESIAN_POINT ( 'NONE',  ( -11.35316468750000141, 88.59374999658602690, -1.390361679473963753E-15 ) ) ;
#46326 = CARTESIAN_POINT ( 'NONE',  ( 0.000000000000000000, 125.0000000000000000, 8.000000000000000000 ) ) ;
#46327 = CARTESIAN_POINT ( 'NONE',  ( 4.556349186104051263, -10.99999999999999822, 83.96874999999997158 ) ) ;
#46330 = CARTESIAN_POINT ( 'NONE',  ( 6.676582343750003368, 288.0468750017070079, 2.765530957081995478 ) ) ;
#46329 = CARTESIAN_POINT ( 'NONE',  ( 25.55430564589115860, 207.0625000013656063, 167.5543056458911053 ) ) ;
#46328 = CARTESIAN_POINT ( 'NONE',  ( 25.55430564589115150, 205.5625000013656063, 172.4456943541086957 ) ) ;
#46331 = VERTEX_POINT ( 'NONE', #38639 ) ;
#46332 = LINE ( 'NONE', #17657, #7960 ) ;
#46333 = CARTESIAN_POINT ( 'NONE',  ( 4.000000000000015987, 202.6875000027311842, 196.3431457505076594 ) ) ;
#46334 = CARTESIAN_POINT ( 'NONE',  ( -8.311093377946841443, 203.9062499965859843, 8.311093377946830785 ) ) ;
#46335 = CARTESIAN_POINT ( 'NONE',  ( 2.445694354108783664, 203.3125000013656063, 144.4456943541088663 ) ) ;
#46336 = CARTESIAN_POINT ( 'NONE',  ( 29.43265458321761585, 207.7500000013656063, 173.4587341249998929 ) ) ;
#46337 = CARTESIAN_POINT ( 'NONE',  ( -7.188101187500002709, 22.68749999795161543, 2.977408999572649151 ) ) ;
#46338 = CARTESIAN_POINT ( 'NONE',  ( 9.832129032723420536, 186.5104166632526983, -5.676582343749999815 ) ) ;
#46339 = DIRECTION ( 'NONE',  ( 0.000000000000000000, 0.000000000000000000, 1.000000000000000000 ) ) ;
#46340 = CARTESIAN_POINT ( 'NONE',  ( 2.977408999572654480, 101.0000000020483810, 7.188101187499999156 ) ) ;
#46342 = CARTESIAN_POINT ( 'NONE',  ( -8.660254037844385522, 235.4166666666666572, 5.000000000000004441 ) ) ;
#46341 = CARTESIAN_POINT ( 'NONE',  ( -9.999999999999996447, 207.5000000000000853, -1.224646799147352862E-15 ) ) ;
#46343 = CARTESIAN_POINT ( 'NONE',  ( 1.881053915767121776, 8.499999998634406140, -4.541265875000002339 ) ) ;
#46344 = CARTESIAN_POINT ( 'NONE',  ( 29.43265458321761230, 202.7500000013655779, 173.4587341249998929 ) ) ;
#46345 = CARTESIAN_POINT ( 'NONE',  ( -7.188101187499992051, 0.000000000000000000, 12.36155278187175277 ) ) ;
#46346 = CARTESIAN_POINT ( 'NONE',  ( -5.676582343749998039, 72.44791666325268409, -9.832129032723420536 ) ) ;
#46347 = CARTESIAN_POINT ( 'NONE',  ( 23.99999999999999289, 205.8750000027312126, 169.9999999999999432 ) ) ;
#46348 = CARTESIAN_POINT ( 'NONE',  ( -3.313708498984758943, -7.999999999999989342, 2.667802784329821986 ) ) ;
#46349 = ORIENTED_EDGE ( 'NONE', *, *, #13878, .F. ) ;
#46350 = CARTESIAN_POINT ( 'NONE',  ( 7.999999999999920064, -1.061780717098090627E-06, 7.767802753882760314 ) ) ;
#46351 = DIRECTION ( 'NONE',  ( 0.000000000000000000, 0.000000000000000000, 1.000000000000000000 ) ) ;
#46352 = CARTESIAN_POINT ( 'NONE',  ( 11.35316468749999785, 60.57291666325269119, 3.042071309553174174 ) ) ;
#46353 = CARTESIAN_POINT ( 'NONE',  ( 11.00000000000000355, -4.556349186104045046, 67.84375000409677625 ) ) ;
#46354 = CARTESIAN_POINT ( 'NONE',  ( 3.458734124999960358, 195.6875000013655779, 142.0000000000000568 ) ) ;
#46355 = FACE_OUTER_BOUND ( 'NONE', #29871, .T. ) ;
#46357 = CARTESIAN_POINT ( 'NONE',  ( 5.676582343749993598, 64.94791666325269830, 9.832129032723422313 ) ) ;
#46356 = CARTESIAN_POINT ( 'NONE',  ( 5.082755093536326818, 94.71875000204838102, 5.082755093536325042 ) ) ;
#46358 = VECTOR ( 'NONE', #37431, 1000.000000000000000 ) ;
#46359 = CARTESIAN_POINT ( 'NONE',  ( -5.656854249492373476, -5.656854249492376141, 4.017802779823362869 ) ) ;
#46360 = CARTESIAN_POINT ( 'NONE',  ( 3.313708498984846429, 110.6562500040967763, 7.999999999999918288 ) ) ;
#46362 = CARTESIAN_POINT ( 'NONE',  ( 10.00000000000000178, 152.0833333265053682, -2.679491924311226736 ) ) ;
#46361 = PRODUCT_DEFINITION_SHAPE ( 'NONE', 'NONE',  #74655 ) ;
#46363 = CARTESIAN_POINT ( 'NONE',  ( -7.188101187500001821, 94.43750000204838102, -2.977408999572650483 ) ) ;
#46364 = COLOUR_RGB ( '',0.7921568627450980005, 0.8196078431372548767, 0.9333333333333333481 ) ;
#46365 = CARTESIAN_POINT ( 'NONE',  ( -6.735557395310442023E-16, 11.00000000000000000, 108.6250000000000000 ) ) ;
#46366 = CARTESIAN_POINT ( 'NONE',  ( -11.35316468749999785, 48.38541666325268409, -3.042071309553167957 ) ) ;
#46367 = EDGE_CURVE ( 'NONE', #1593, #8780, #1404, .T. ) ;
#46368 = CARTESIAN_POINT ( 'NONE',  ( 7.204075437095968759, -7.204075437095966983, 115.0937500020483810 ) ) ;
#46369 = CARTESIAN_POINT ( 'NONE',  ( -5.676582343749998039, 182.4479166632526983, -9.832129032723420536 ) ) ;
#46370 = ORIENTED_EDGE ( 'NONE', *, *, #58389, .T. ) ;
#46371 = CARTESIAN_POINT ( 'NONE',  ( 4.000000000000000888, 3.937500000000000000, 1.656854249492384135 ) ) ;
#46372 = CARTESIAN_POINT ( 'NONE',  ( -4.220049686691935698, 10.18810118749999916, 73.37500000204838102 ) ) ;
#46373 = DIRECTION ( 'NONE',  ( -0.000000000000000000, 1.000000000000000000, 4.689100369878284071E-30 ) ) ;
#46375 = CARTESIAN_POINT ( 'NONE',  ( -9.832129032723420536, 173.6979166632526983, 5.676582343749997150 ) ) ;
#46374 = CARTESIAN_POINT ( 'NONE',  ( -2.638998369017515611, 194.9937430236944067, 194.9909928269735246 ) ) ;
#46376 = CARTESIAN_POINT ( 'NONE',  ( 1.469576158976822172E-15, -7.999999999999991118, 7.261552784329822430 ) ) ;
#46377 = CARTESIAN_POINT ( 'NONE',  ( -7.347880794884122694E-16, 21.49999999726881583, 4.000000000000001776 ) ) ;
#46378 = CARTESIAN_POINT ( 'NONE',  ( 8.660254037844389075, 255.2083333401612890, 4.999999999999997335 ) ) ;
#46379 = DIRECTION ( 'NONE',  ( -0.000000000000000000, 1.000000000000000000, -0.000000000000000000 ) ) ;
#46380 = EDGE_LOOP ( 'NONE', ( #32533, #66412, #35225, #7341 ) ) ;
#46381 = CARTESIAN_POINT ( 'NONE',  ( -11.35316468750000141, 168.5937499965860127, -1.390361679473963753E-15 ) ) ;
#46382 = EDGE_CURVE ( 'NONE', #62160, #16346, #61641, .T. ) ;
#46383 = DIRECTION ( 'NONE',  ( -1.000000000000000000, 0.000000000000000000, 0.000000000000000000 ) ) ;
#46384 = CARTESIAN_POINT ( 'NONE',  ( 5.676582343749993598, 130.2604166632526983, 9.832129032723422313 ) ) ;
#46385 = LINE ( 'NONE', #56230, #69484 ) ;
#46386 = VERTEX_POINT ( 'NONE', #21636 ) ;
#46387 = CARTESIAN_POINT ( 'NONE',  ( -8.342170076843785083E-16, 12.18749999863440614, 4.541265875000002339 ) ) ;
#46388 = CARTESIAN_POINT ( 'NONE',  ( 3.313708498984765161, 106.1562500040967763, 7.999999999999998224 ) ) ;
#46389 = EDGE_CURVE ( 'NONE', #42214, #20382, #55619, .T. ) ;
#46390 = ADVANCED_FACE ( 'NONE', ( #9593 ), #33356, .T. ) ;
#46391 = CARTESIAN_POINT ( 'NONE',  ( 4.000000000000000888, 13.93750000000000000, 1.656854249492384135 ) ) ;
#46392 = CARTESIAN_POINT ( 'NONE',  ( -37.29817618843008376, -3.167071582347842362, 131.2282528294346946 ) ) ;
#46393 = CARTESIAN_POINT ( 'NONE',  ( -3.211159895383562723, 10.93749999863440792, 3.211159895383561391 ) ) ;
#46394 = CARTESIAN_POINT ( 'NONE',  ( 7.999999999999991118, 9.797174393178815797E-16, 21.26780278392014623 ) ) ;
#46395 = LINE ( 'NONE', #47494, #67987 ) ;
#46396 = ORIENTED_EDGE ( 'NONE', *, *, #21387, .T. ) ;
#46397 = CARTESIAN_POINT ( 'NONE',  ( 0.000000000000000000, 0.000000000000000000, 118.0000000000000000 ) ) ;
#46398 = CARTESIAN_POINT ( 'NONE',  ( 1.320432766682874540E-15, 102.0312500020483810, 7.188101187500000044 ) ) ;
#46399 = AXIS2_PLACEMENT_3D ( 'NONE', #59972, #53585, #30197 ) ;
#46402 = CARTESIAN_POINT ( 'NONE',  ( -1.469576158976823947E-15, 15.93749999590322197, 8.000000000000000000 ) ) ;
#46401 = CARTESIAN_POINT ( 'NONE',  ( 11.00000000000000000, 1.347111479062088405E-15, 78.43750000409677625 ) ) ;
#46400 =( BOUNDED_CURVE ( )  B_SPLINE_CURVE ( 2, ( #32680, #55311, #3619, #55688, #40924, #5116, #28484, #10760, #17906 ),
 .UNSPECIFIED., .F., .F. ) 
 B_SPLINE_CURVE_WITH_KNOTS ( ( 3, 2, 2, 2, 3 ),
 ( 0.1470588235294118806, 0.1507352941176471617, 0.1544117647058824705, 0.1580882352941177238, 0.1617647058823530326 ),
 .UNSPECIFIED. ) 
 CURVE ( )  GEOMETRIC_REPRESENTATION_ITEM ( )  RATIONAL_B_SPLINE_CURVE ( ( 0.9999999999999976685, 0.9238795325112890700, 1.000000000000000000, 0.9238795325112867385, 1.000000000000000000, 0.9238795325112867385, 1.000000000000000000, 0.9238795325112849621, 1.000000000000001776 ) ) 
 REPRESENTATION_ITEM ( '' )  );
#46403 = ORIENTED_EDGE ( 'NONE', *, *, #25514, .T. ) ;
#46404 = CARTESIAN_POINT ( 'NONE',  ( 2.449293598294707893E-16, 10.25000000000000000, -4.000000000000001776 ) ) ;
#46405 = CARTESIAN_POINT ( 'NONE',  ( -2.977408999572648707, -7.188101187499990274, 27.26780278187175099 ) ) ;
#46406 = ORIENTED_EDGE ( 'NONE', *, *, #50533, .F. ) ;
#46407 = ADVANCED_FACE ( 'NONE', ( #56357 ), #73332, .T. ) ;
#46408 = ORIENTED_EDGE ( 'NONE', *, *, #47285, .F. ) ;
#46409 = CARTESIAN_POINT ( 'NONE',  ( -10.18810118749999916, 4.220049686691934809, 85.56250000204838102 ) ) ;
#46410 = CARTESIAN_POINT ( 'NONE',  ( 1.469576158976823947E-15, 0.000000000000000000, -12.00000000000000000 ) ) ;
#46411 = CARTESIAN_POINT ( 'NONE',  ( -25.55430564589114795, 197.3125000013656063, 172.4456943541091789 ) ) ;
#46412 = CARTESIAN_POINT ( 'NONE',  ( -10.99999999999999822, -4.556349186104052151, 98.59375000000000000 ) ) ;
#46415 = CARTESIAN_POINT ( 'NONE',  ( 6.676582343750001591, 297.1093750017069510, -8.176455196517173205E-16 ) ) ;
#46414 = CARTESIAN_POINT ( 'NONE',  ( 26.34314575050758833, 206.6875000027312126, 165.9999999999998863 ) ) ;
#46413 = LINE ( 'NONE', #46040, #54315 ) ;
#46416 = CARTESIAN_POINT ( 'NONE',  ( -10.00000000000000355, 137.7083333333333428, 2.679491924311223183 ) ) ;
#46417 = CARTESIAN_POINT ( 'NONE',  ( -4.898587196589412829E-16, 99.12499999999998579, -8.000000000000000000 ) ) ;
#46418 = CARTESIAN_POINT ( 'NONE',  ( -1.224646799147353454E-15, 225.9999999999999432, 10.00000000000000178 ) ) ;
#46419 = CARTESIAN_POINT ( 'NONE',  ( 2.977408999572650927, -7.188101187499990274, 2.330302781871754991 ) ) ;
#46421 =( BOUNDED_CURVE ( )  B_SPLINE_CURVE ( 2, ( #26451, #38172, #72495, #67588, #61175, #15884, #43823, #4588, #11356 ),
 .UNSPECIFIED., .F., .F. ) 
 B_SPLINE_CURVE_WITH_KNOTS ( ( 3, 2, 2, 2, 3 ),
 ( 0.1176470588235294934, 0.1213235294117648022, 0.1250000000000001110, 0.1286764705882353921, 0.1323529411764707009 ),
 .UNSPECIFIED. ) 
 CURVE ( )  GEOMETRIC_REPRESENTATION_ITEM ( )  RATIONAL_B_SPLINE_CURVE ( ( 0.9999999999999982236, 0.9238795325112885148, 1.000000000000000000, 0.9238795325112867385, 1.000000000000000000, 0.9238795325112867385, 1.000000000000000000, 0.9238795325112844070, 1.000000000000002220 ) ) 
 REPRESENTATION_ITEM ( '' )  );
#46420 = CARTESIAN_POINT ( 'NONE',  ( 1.656854249492487607, 200.6875000000000284, 194.0000000000001705 ) ) ;
#46422 = CARTESIAN_POINT ( 'NONE',  ( 25.55430564589115150, 203.3125000013656063, 172.4456943541086957 ) ) ;
#46423 = CARTESIAN_POINT ( 'NONE',  ( -7.188101187500002709, 3.187499997951610542, 2.977408999572649151 ) ) ;
#46424 = CARTESIAN_POINT ( 'NONE',  ( -3.317071493978878571, 8.008118988124991233, 3.731865283940628775 ) ) ;
#46425 = CARTESIAN_POINT ( 'NONE',  ( -3.458734125000016313, 196.8750000013656063, 140.5673454167824161 ) ) ;
#46426 = CARTESIAN_POINT ( 'NONE',  ( 7.188101187500002709, 113.1875000020483810, 2.977408999572649151 ) ) ;
#46428 = CARTESIAN_POINT ( 'NONE',  ( 3.649821741245722784, 194.7395660307605283, 198.8504276174034544 ) ) ;
#46427 = PLANE ( 'NONE',  #73302 ) ;
#46429 = CARTESIAN_POINT ( 'NONE',  ( -6.951808397369817780E-16, 247.9687500034140157, -11.35316468749999963 ) ) ;
#46430 = CARTESIAN_POINT ( 'NONE',  ( 54.00000000000000711, 205.0000000000000284, 20.00000000000000000 ) ) ;
#46431 = CARTESIAN_POINT ( 'NONE',  ( 7.188101187499991163, 2.977408999572648707, 25.20530278187175810 ) ) ;
#46432 = CARTESIAN_POINT ( 'NONE',  ( 30.82842712474617031, 200.1250000000000284, 172.8284271247460993 ) ) ;
#46433 = CARTESIAN_POINT ( 'NONE',  ( -11.35316468749999785, 28.07291666325268054, -3.042071309553167513 ) ) ;
#46434 = CARTESIAN_POINT ( 'NONE',  ( 26.34314575050752083, 200.9375000000000284, 173.9999999999998295 ) ) ;
#46435 = CARTESIAN_POINT ( 'NONE',  ( 3.042071309553159519, 220.0520833299193271, 11.35316468750000141 ) ) ;
#46437 = CARTESIAN_POINT ( 'NONE',  ( 0.000000000000000000, 125.0000000000000000, 0.000000000000000000 ) ) ;
#46436 = CYLINDRICAL_SURFACE ( 'NONE', #58828, 20.00000000000001066 ) ;
#46438 = ORIENTED_EDGE ( 'NONE', *, *, #16478, .F. ) ;
#46439 = CARTESIAN_POINT ( 'NONE',  ( 1.432654583217608080, 195.8750000013655779, 138.5412658750000503 ) ) ;
#46440 = CARTESIAN_POINT ( 'NONE',  ( 9.832129032723420536, 26.19791666325268409, -5.676582343749999815 ) ) ;
#46441 = CARTESIAN_POINT ( 'NONE',  ( 7.778174593052021635, 7.778174593052023411, 90.62500000409677625 ) ) ;
#46442 = CARTESIAN_POINT ( 'NONE',  ( 3.458734124999960358, 207.6875000013656063, 142.0000000000000568 ) ) ;
#46443 = CARTESIAN_POINT ( 'NONE',  ( -2.679491924309608919, 151.4583333333332007, -10.00000000000094502 ) ) ;
#46444 = DIRECTION ( 'NONE',  ( -1.000000000000000000, -0.000000000000000000, -0.000000000000000000 ) ) ;
#46446 = CARTESIAN_POINT ( 'NONE',  ( 11.35316468749999785, 15.57291666325268409, 3.042071309553174174 ) ) ;
#46445 = CARTESIAN_POINT ( 'NONE',  ( 7.188101187500000933, 113.0000000020483810, -2.977408999572651371 ) ) ;
#46448 = ADVANCED_FACE ( 'NONE', ( #9958 ), #43913, .F. ) ;
#46447 = CARTESIAN_POINT ( 'NONE',  ( 7.999999999999991118, 3.313708498984757611, 24.17405277982336642 ) ) ;
#46449 = CARTESIAN_POINT ( 'NONE',  ( -3.042071309553164404, 132.2395833299193555, -11.35316468749999963 ) ) ;
#46450 = CARTESIAN_POINT ( 'NONE',  ( 2.679491924311222739, 120.8333333265053540, 10.00000000000000355 ) ) ;
#46451 = CARTESIAN_POINT ( 'NONE',  ( -2.977408999572650927, 115.2500000020484094, -7.188101187500001821 ) ) ;
#46452 = CARTESIAN_POINT ( 'NONE',  ( -31.45873412499999944, 207.9375000013656063, 170.0000000000003979 ) ) ;
#46453 = CYLINDRICAL_SURFACE ( 'NONE', #65499, 11.00000000000000000 ) ;
#46454 = ORIENTED_EDGE ( 'NONE', *, *, #34736, .T. ) ;
#46455 = CARTESIAN_POINT ( 'NONE',  ( -3.042071309553173730, 4.635416663252683200, 11.35316468749999785 ) ) ;
#46456 = EDGE_CURVE ( 'NONE', #55282, #46655, #32612, .T. ) ;
#46457 = CARTESIAN_POINT ( 'NONE',  ( 6.000000000000001776, 289.5000000000000000, -7.347880794884121708E-16 ) ) ;
#46458 = CARTESIAN_POINT ( 'NONE',  ( 2.765530957082001251, 298.7656250017069510, 6.676582343750000703 ) ) ;
#46459 = CARTESIAN_POINT ( 'NONE',  ( 9.832129032723416984, 140.3645833299193555, 5.676582343750006032 ) ) ;
#46460 = CARTESIAN_POINT ( 'NONE',  ( -7.999999999999991118, 3.313708498984756723, 26.29280278432983309 ) ) ;
#46461 = CARTESIAN_POINT ( 'NONE',  ( 58.25034728770824444, 214.6154151734847915, 47.53706141328223111 ) ) ;
#46462 = CARTESIAN_POINT ( 'NONE',  ( 2.085542519210945334E-15, 245.1562500034140157, 11.35316468749999963 ) ) ;
#46463 = CARTESIAN_POINT ( 'NONE',  ( 10.18810118749999916, 1.247682550866122264E-15, 98.78125000204838102 ) ) ;
#46464 = EDGE_LOOP ( 'NONE', ( #18087, #67277, #21821, #64669 ) ) ;
#46465 = VECTOR ( 'NONE', #18008, 999.9999999999998863 ) ;
#46466 = CARTESIAN_POINT ( 'NONE',  ( 10.00000000000000178, 217.0833333265053682, -2.679491924311226736 ) ) ;
#46467 = CYLINDRICAL_SURFACE ( 'NONE', #3822, 10.00000000000000178 ) ;
#46468 = CARTESIAN_POINT ( 'NONE',  ( -9.832129032723420536, 89.01041666325268409, 5.676582343749997150 ) ) ;
#46470 = EDGE_CURVE ( 'NONE', #60307, #39327, #29691, .T. ) ;
#46469 = ORIENTED_EDGE ( 'NONE', *, *, #54201, .T. ) ;
#46471 = CARTESIAN_POINT ( 'NONE',  ( 4.220049686691941027, -10.18810118749999738, 107.1250000020483810 ) ) ;
#46472 = CARTESIAN_POINT ( 'NONE',  ( 4.541265875000001451, 12.37499999863440969, 1.881053915767124440 ) ) ;
#46473 = ORIENTED_EDGE ( 'NONE', *, *, #10257, .F. ) ;
#46474 = ORIENTED_EDGE ( 'NONE', *, *, #8155, .T. ) ;
#46475 = CARTESIAN_POINT ( 'NONE',  ( -5.656854249492381470, 8.437500000000000000, 5.656854249492379694 ) ) ;
#46476 = CARTESIAN_POINT ( 'NONE',  ( 3.211159895383561835, 0.5624999986344069169, -3.211159895383561835 ) ) ;
#46477 = CARTESIAN_POINT ( 'NONE',  ( -2.828427124746152987, 197.2500000027312126, 200.8284271247462129 ) ) ;
#46478 = CARTESIAN_POINT ( 'NONE',  ( -1.320432766682874540E-15, 24.46874999795161543, 7.188101187500000044 ) ) ;
#46479 = CARTESIAN_POINT ( 'NONE',  ( 5.656854249492379694, 121.6250000040967905, -5.656854249492380582 ) ) ;
#46480 = CARTESIAN_POINT ( 'NONE',  ( -4.220049686691937474, -10.18810118749999738, 105.8125000020483952 ) ) ;
#46481 = CARTESIAN_POINT ( 'NONE',  ( -4.000000000000001776, 1.437500000000000444, -1.656854249492381470 ) ) ;
#46482 = CARTESIAN_POINT ( 'NONE',  ( 2.828427124746191623, 8.874999997268814056, -2.828427124746191623 ) ) ;
#46483 = CARTESIAN_POINT ( 'NONE',  ( 2.780723358947928197E-16, 0.5624999986344066949, -4.541265875000002339 ) ) ;
#46484 = VERTEX_POINT ( 'NONE', #49944 ) ;
#46485 = DIRECTION ( 'NONE',  ( -0.000000000000000000, 1.000000000000000000, 4.689100369878284071E-30 ) ) ;
#46486 = CARTESIAN_POINT ( 'NONE',  ( -2.445694354108782775, 198.5625000013656063, 200.4456943541088663 ) ) ;
#46487 = CARTESIAN_POINT ( 'NONE',  ( -26.56734541678242678, 205.3750000013656063, 166.5412658750003345 ) ) ;
#46488 =( NAMED_UNIT ( * ) SI_UNIT ( $, .STERADIAN. ) SOLID_ANGLE_UNIT ( ) );
#46489 = CARTESIAN_POINT ( 'NONE',  ( 3.211159895383560947, 11.18749999863440792, 3.211159895383562723 ) ) ;
#46490 = CARTESIAN_POINT ( 'NONE',  ( -4.000000000000001776, 18.18749999726881583, -1.656854249492381470 ) ) ;
#46491 = CARTESIAN_POINT ( 'NONE',  ( 7.188101187499991163, 2.977408999572648707, 15.83030278187175277 ) ) ;
#46492 = ORIENTED_EDGE ( 'NONE', *, *, #73976, .T. ) ;
#46493 = ORIENTED_EDGE ( 'NONE', *, *, #7139, .F. ) ;
#46494 = CARTESIAN_POINT ( 'NONE',  ( 10.18810118750000093, -4.220049686691933033, 107.3125000020483810 ) ) ;
#46495 = CARTESIAN_POINT ( 'NONE',  ( 5.656854249492379694, 96.12500000409677625, -5.656854249492380582 ) ) ;
#46496 = CARTESIAN_POINT ( 'NONE',  ( -32.00000000000001421, 203.1875000000000284, 168.3431457505080004 ) ) ;
#46497 = CARTESIAN_POINT ( 'NONE',  ( -3.458734124999959025, 200.5000000013655779, 199.4326545832176691 ) ) ;
#46498 = CARTESIAN_POINT ( 'NONE',  ( 30.44569435410879166, 195.8125000013656063, 167.5543056458910485 ) ) ;
#46499 = CARTESIAN_POINT ( 'NONE',  ( 2.679491924311228956, 91.04166666666665719, -10.00000000000000000 ) ) ;
#46500 = CARTESIAN_POINT ( 'NONE',  ( 3.313708498984765161, 119.4687499999999858, 7.999999999999998224 ) ) ;
#46501 = CARTESIAN_POINT ( 'NONE',  ( -9.832129032723420536, 59.01041666325268409, 5.676582343749997150 ) ) ;
#46502 = CARTESIAN_POINT ( 'NONE',  ( 4.242640687119287435, 289.3750000000000000, 4.242640687119285658 ) ) ;
#46503 = CIRCLE ( 'NONE', #26025, 8.000000000000003553 ) ;
#46504 = ORIENTED_EDGE ( 'NONE', *, *, #17795, .F. ) ;
#46505 = EDGE_CURVE ( 'NONE', #33807, #69767, #14600, .T. ) ;
#46506 = CARTESIAN_POINT ( 'NONE',  ( 7.320508075688776373, 251.8750000000000284, 7.320508075688767491 ) ) ;
#46507 = AXIS2_PLACEMENT_3D ( 'NONE', #56000, #9969, #28055 ) ;
#46508 = CARTESIAN_POINT ( 'NONE',  ( 7.999999999999998224, 13.21874999590322375, 3.313708498984766493 ) ) ;
#46509 = CARTESIAN_POINT ( 'NONE',  ( -3.458734125000015425, 205.9375000013656063, 142.0000000000000568 ) ) ;
#46510 = LINE ( 'NONE', #7267, #23771 ) ;
#46511 = FACE_OUTER_BOUND ( 'NONE', #59791, .T. ) ;
#46512 = CARTESIAN_POINT ( 'NONE',  ( 4.999999999999997335, 238.3333333333333428, -8.660254037844387298 ) ) ;
#46513 = DIRECTION ( 'NONE',  ( 0.000000000000000000, 0.000000000000000000, -1.000000000000000000 ) ) ;
#46514 = CARTESIAN_POINT ( 'NONE',  ( -4.556349186104045934, 11.00000000000000000, 117.7187499999999858 ) ) ;
#46515 =( BOUNDED_CURVE ( )  B_SPLINE_CURVE ( 2, ( #66965, #66588, #3596 ),
 .UNSPECIFIED., .F., .T. ) 
 B_SPLINE_CURVE_WITH_KNOTS ( ( 3, 3 ),
 ( 0.9687500000000000000, 0.9722122468226729319 ),
 .UNSPECIFIED. ) 
 CURVE ( )  GEOMETRIC_REPRESENTATION_ITEM ( )  RATIONAL_B_SPLINE_CURVE ( ( 1.000000000000000000, 0.9493988134329905959, 0.9660720450733824016 ) ) 
 REPRESENTATION_ITEM ( '' )  );
#46516 = CARTESIAN_POINT ( 'NONE',  ( 7.320508075688774596, 205.6250000000000000, -7.320508075688774596 ) ) ;
#46517 = CARTESIAN_POINT ( 'NONE',  ( 7.188101187499992051, 8.802885111219154394E-16, 13.11155278187175277 ) ) ;
#46518 = CARTESIAN_POINT ( 'NONE',  ( 3.042071309553159519, 175.0520833299193839, 11.35316468750000141 ) ) ;
#46519 = FACE_OUTER_BOUND ( 'NONE', #18848, .T. ) ;
#46520 = CARTESIAN_POINT ( 'NONE',  ( 0.000000000000000000, 0.000000000000000000, 118.0000000000000000 ) ) ;
#46522 = CARTESIAN_POINT ( 'NONE',  ( 10.00000000000000000, 86.66666665983869677, 2.679491924311235618 ) ) ;
#46521 = CARTESIAN_POINT ( 'NONE',  ( -8.000000000000010658, -3.313708498984740736, 20.42405277982336642 ) ) ;
#46523 = VERTEX_POINT ( 'NONE', #20510 ) ;
#46524 = CARTESIAN_POINT ( 'NONE',  ( 2.445694354108783219, 207.8125000013656063, 139.5543056458912190 ) ) ;
#46525 = CARTESIAN_POINT ( 'NONE',  ( -3.042071309553173730, 39.63541666325267698, 11.35316468749999785 ) ) ;
#46526 = CARTESIAN_POINT ( 'NONE',  ( -10.99999999999999822, -4.556349186104052151, 107.7812500040967763 ) ) ;
#46527 = CARTESIAN_POINT ( 'NONE',  ( -29.43265458321770822, 204.5000000013655779, 166.5412658750003914 ) ) ;
#46528 = DIRECTION ( 'NONE',  ( 0.000000000000000000, -0.000000000000000000, 1.000000000000000000 ) ) ;
#46530 = LINE ( 'NONE', #23892, #71568 ) ;
#46529 = DIRECTION ( 'NONE',  ( 0.000000000000000000, 0.000000000000000000, 1.000000000000000000 ) ) ;
#46532 = EDGE_CURVE ( 'NONE', #73018, #23901, #43525, .T. ) ;
#46531 = CARTESIAN_POINT ( 'NONE',  ( -1.432654583217664479, 198.7500000013656063, 138.5412658750000787 ) ) ;
#46533 = VECTOR ( 'NONE', #53787, 1000.000000000000000 ) ;
#46534 = CARTESIAN_POINT ( 'NONE',  ( -7.320508075688773708, 78.74999999317203958, -7.320508075688774596 ) ) ;
#46535 = CARTESIAN_POINT ( 'NONE',  ( -7.188101187500000044, 97.15625000204839523, 0.000000000000000000 ) ) ;
#46536 = CARTESIAN_POINT ( 'NONE',  ( -4.541265875000002339, 13.93749999863440614, -5.561446717895856393E-16 ) ) ;
#46537 = DIRECTION ( 'NONE',  ( -0.000000000000000000, 1.000000000000000000, -0.000000000000000000 ) ) ;
#46538 = CARTESIAN_POINT ( 'NONE',  ( 3.313708498984762496, -7.999999999999989342, 2.799052779823366421 ) ) ;
#46539 = CARTESIAN_POINT ( 'NONE',  ( -7.347880794884122694E-16, 4.499999997268813168, 4.000000000000001776 ) ) ;
#46540 = ORIENTED_EDGE ( 'NONE', *, *, #63309, .F. ) ;
#46541 = ORIENTED_EDGE ( 'NONE', *, *, #36582, .F. ) ;
#46542 = CARTESIAN_POINT ( 'NONE',  ( -7.320508075688857197, 198.1250000000000853, 7.320508075688848315 ) ) ;
#46543 = CARTESIAN_POINT ( 'NONE',  ( 6.676582343750001591, 297.1093750017069510, -8.176455196517173205E-16 ) ) ;
#46544 = CARTESIAN_POINT ( 'NONE',  ( 2.679491924311228956, 42.91666665983869677, -10.00000000000000000 ) ) ;
#46545 = CARTESIAN_POINT ( 'NONE',  ( 6.951808397369818766E-16, 152.0312499965860411, -11.35316468750000141 ) ) ;
#46546 = CARTESIAN_POINT ( 'NONE',  ( -2.485281374238967000, 297.8125000000000568, -5.999999999999608313 ) ) ;
#46547 = CARTESIAN_POINT ( 'NONE',  ( -6.238412754330611322E-16, 10.18810118749999916, 83.78125000204836681 ) ) ;
#46548 = CARTESIAN_POINT ( 'NONE',  ( -30.14770426596652086, 194.5119512990348198, 167.2119996477674988 ) ) ;
#46549 = CARTESIAN_POINT ( 'NONE',  ( 2.849036369511732440E-14, 205.2500000000000284, 202.0000000000000000 ) ) ;
#46550 = CARTESIAN_POINT ( 'NONE',  ( -8.234290096841624162, 16.03054008682954645, -0.009429105422156794022 ) ) ;
#46551 = CARTESIAN_POINT ( 'NONE',  ( -7.204075437095965206, -7.204075437095968759, 113.2187500020483810 ) ) ;
#46552 = EDGE_LOOP ( 'NONE', ( #59094, #34081, #28023, #5288, #29416 ) ) ;
#46553 = CARTESIAN_POINT ( 'NONE',  ( -2.828427124746152987, 202.2500000027312126, 200.8284271247462129 ) ) ;
#46554 = CARTESIAN_POINT ( 'NONE',  ( 33.12275679046642551, 175.9544041245370920, 155.0238343577928219 ) ) ;
#46555 = CARTESIAN_POINT ( 'NONE',  ( 6.951808397369818766E-16, 127.3437499965860127, -11.35316468750000141 ) ) ;
#46556 = CARTESIAN_POINT ( 'NONE',  ( -2.445694354108783664, 199.3125000013656063, 195.5543056458912190 ) ) ;
#46557 = CARTESIAN_POINT ( 'NONE',  ( 5.082755093536324154, 21.65624999795161543, 5.082755093536326818 ) ) ;
#46558 = CARTESIAN_POINT ( 'NONE',  ( -4.220049686691935698, 10.18810118749999916, 76.75000000204838102 ) ) ;
#46559 = CARTESIAN_POINT ( 'NONE',  ( -9.832129032723418760, 53.17708332991935549, -5.676582343750004256 ) ) ;
#46560 = VERTEX_POINT ( 'NONE', #20891 ) ;
#46561 = CARTESIAN_POINT ( 'NONE',  ( 8.660254037844389075, 37.29166665983869677, -5.000000000000000000 ) ) ;
#46562 = CARTESIAN_POINT ( 'NONE',  ( 0.000000000000000000, 0.000000000000000000, -0.6932054628276118624 ) ) ;
#46563 = CARTESIAN_POINT ( 'NONE',  ( -3.317071493978878571, 8.008118988124991233, 15.73186528394062833 ) ) ;
#46564 = CARTESIAN_POINT ( 'NONE',  ( -2.445694354108840063, 205.0625000013656063, 139.5543056458912190 ) ) ;
#46565 = CARTESIAN_POINT ( 'NONE',  ( -7.188101187500001821, 17.62499999795161187, -2.977408999572651371 ) ) ;
#46566 = CARTESIAN_POINT ( 'NONE',  ( 4.242640687119285658, 295.6875000034139589, -4.242640687119286547 ) ) ;
#46567 = CARTESIAN_POINT ( 'NONE',  ( -12.04178623174921903, -25.57729957216213634, 139.1902360743439147 ) ) ;
#46568 = CARTESIAN_POINT ( 'NONE',  ( -2.977408999572650039, 5.812499997951610098, -7.188101187500001821 ) ) ;
#46569 = CARTESIAN_POINT ( 'NONE',  ( 2.977408999572646486, 7.188101187499992051, 7.017802781871750994 ) ) ;
#46570 = CARTESIAN_POINT ( 'NONE',  ( 10.18810118749999916, 4.220049686691935698, 70.00000000204836681 ) ) ;
#46571 = CARTESIAN_POINT ( 'NONE',  ( -31.45873412499998523, 207.0000000013656063, 171.4326545832180386 ) ) ;
#46572 = CARTESIAN_POINT ( 'NONE',  ( 2.828427124746190291, 2.875000000000000000, 2.828427124746192067 ) ) ;
#46573 = CARTESIAN_POINT ( 'NONE',  ( -1.881053915767121554, 19.74999999863440792, -4.541265875000002339 ) ) ;
#46574 = UNCERTAINTY_MEASURE_WITH_UNIT (LENGTH_MEASURE( 1.000000000000000082E-05 ), #67017, 'distance_accuracy_value', 'NONE');
#46575 = ORIENTED_EDGE ( 'NONE', *, *, #32546, .F. ) ;
#46576 = CARTESIAN_POINT ( 'NONE',  ( 2.849036369511732440E-14, 194.3750000027311842, 202.0000000000000000 ) ) ;
#46577 = CARTESIAN_POINT ( 'NONE',  ( -2.828427124746208943, 206.6250000000000284, 144.8284271247462129 ) ) ;
#46578 = CARTESIAN_POINT ( 'NONE',  ( -26.34314575050753149, 200.6875000027312126, 174.0000000000003411 ) ) ;
#46579 = AXIS2_PLACEMENT_3D ( 'NONE', #1491, #64478, #47106 ) ;
#46580 = CARTESIAN_POINT ( 'NONE',  ( 7.188101187500001821, 114.5000000020483810, -2.977408999572651371 ) ) ;
#46581 = CARTESIAN_POINT ( 'NONE',  ( -3.313708498984757167, 7.999999999999991118, 3.736552783920145338 ) ) ;
#46582 = ORIENTED_EDGE ( 'NONE', *, *, #63461, .T. ) ;
#46583 = CARTESIAN_POINT ( 'NONE',  ( -5.082755093536325042, 16.03124999795161543, -5.082755093536325930 ) ) ;
#46584 = B_SPLINE_CURVE_WITH_KNOTS ( 'NONE', 1,
 ( #49900, #50637 ),
 .UNSPECIFIED., .F., .F.,
 ( 2, 2 ),
 ( 0.000000000000000000, 1.000000000000000000 ),
 .UNSPECIFIED. ) ;
#46585 = VERTEX_POINT ( 'NONE', #60887 ) ;
#46586 = CARTESIAN_POINT ( 'NONE',  ( 29.65685424949224824, 198.0624999999999432, 174.0000000000000284 ) ) ;
#46587 = CARTESIAN_POINT ( 'NONE',  ( -7.071067811865482611, 22.99999999999999645, 1.000000000000000000 ) ) ;
#46588 = CARTESIAN_POINT ( 'NONE',  ( -10.00000000000000178, 47.50000000000000000, -1.224646799147353454E-15 ) ) ;
#46589 = CARTESIAN_POINT ( 'NONE',  ( 7.188101187500000044, 101.2812500020483810, -8.802885111219163269E-16 ) ) ;
#46590 = CARTESIAN_POINT ( 'NONE',  ( -31.45873412499998523, 207.0000000013655779, 171.4326545832180386 ) ) ;
#46591 = CARTESIAN_POINT ( 'NONE',  ( -2.485281374238572649, 299.1874999999999432, 6.000000000000002665 ) ) ;
#46593 = DIRECTION ( 'NONE',  ( 1.000000000000000000, -0.000000000000000000, -0.000000000000000000 ) ) ;
#46592 = CARTESIAN_POINT ( 'NONE',  ( -5.656854249492378806, 89.37500000409679046, 5.656854249492381470 ) ) ;
#46594 = EDGE_LOOP ( 'NONE', ( #61828, #19693, #41213, #50642 ) ) ;
#46595 = CARTESIAN_POINT ( 'NONE',  ( 8.311093377946839666, 240.7812500034140157, 8.311093377946829008 ) ) ;
#46596 = CARTESIAN_POINT ( 'NONE',  ( -2.977408999572648707, -7.188101187499990274, 18.64280278187175810 ) ) ;
#46597 = CARTESIAN_POINT ( 'NONE',  ( 3.999999999999960032, 195.0625000027312126, 143.6568542494924259 ) ) ;
#46598 = DIRECTION ( 'NONE',  ( 0.000000000000000000, 0.000000000000000000, -1.000000000000000000 ) ) ;
#46599 = CARTESIAN_POINT ( 'NONE',  ( -7.320508075688773708, 146.8749999999999716, -7.320508075688774596 ) ) ;
#46600 = CARTESIAN_POINT ( 'NONE',  ( -7.999999999835898379, -3.436314075762838161E-05, 19.01908381112063751 ) ) ;
#46601 = CARTESIAN_POINT ( 'NONE',  ( -2.679491924311235618, 163.5416666666666572, 10.00000000000000000 ) ) ;
#46602 = DIRECTION ( 'NONE',  ( -0.000000000000000000, 1.000000000000000000, 4.689100369878284071E-30 ) ) ;
#46603 = CARTESIAN_POINT ( 'NONE',  ( -1.469576158976823947E-15, 27.93749999590322375, 8.000000000000000000 ) ) ;
#46604 = CARTESIAN_POINT ( 'NONE',  ( 5.656854249492376141, -5.656854249492374365, 4.392802779823363757 ) ) ;
#46605 = CARTESIAN_POINT ( 'NONE',  ( -11.35316468750000141, 143.8020833299193555, 3.042071309553159963 ) ) ;
#46606 = LINE ( 'NONE', #11174, #4740 ) ;
#46607 = CARTESIAN_POINT ( 'NONE',  ( -8.000000000000001776, 5.343750000000000888, 3.313708498984759387 ) ) ;
#46610 = DIRECTION ( 'NONE',  ( 0.000000000000000000, 0.000000000000000000, 1.000000000000000000 ) ) ;
#46609 = CARTESIAN_POINT ( 'NONE',  ( -0.8721677472748865512, -51.17354301023302554, 48.53016177276413146 ) ) ;
#46608 = CARTESIAN_POINT ( 'NONE',  ( 26.34314575050758833, 207.9375000000000000, 173.9999999999999147 ) ) ;
#46611 = VECTOR ( 'NONE', #46230, 1000.000000000000114 ) ;
#46612 = VERTEX_POINT ( 'NONE', #55247 ) ;
#46613 = EDGE_CURVE ( 'NONE', #10820, #34245, #44288, .T. ) ;
#46614 = CARTESIAN_POINT ( 'NONE',  ( 6.951808397369818766E-16, 2.343749996586016682, -11.35316468750000141 ) ) ;
#46615 = CARTESIAN_POINT ( 'NONE',  ( -3.313708498984720308, 118.9062500040967905, -8.000000000000040856 ) ) ;
#46616 = CARTESIAN_POINT ( 'NONE',  ( -11.00000000000000000, 0.000000000000000000, 68.68750000409676204 ) ) ;
#46617 = CARTESIAN_POINT ( 'NONE',  ( -5.778038727434721800, -5.550035267211852030, 0.000000000000000000 ) ) ;
#46618 = CARTESIAN_POINT ( 'NONE',  ( 30.44569435410878810, 195.8125000013656063, 172.4456943541087526 ) ) ;
#46619 = CARTESIAN_POINT ( 'NONE',  ( -8.660254037844390851, 24.79166665983870033, 4.999999999999998224 ) ) ;
#46620 = CARTESIAN_POINT ( 'NONE',  ( 7.188101187500002709, 114.3125000020483952, 2.977408999572649151 ) ) ;
#46621 = CARTESIAN_POINT ( 'NONE',  ( -3.211159895383562723, 20.93749999863440436, 3.211159895383561391 ) ) ;
#46622 = CARTESIAN_POINT ( 'NONE',  ( 0.6474643998348341700, 60.19533971085920854, -22.88219507986035950 ) ) ;
#46623 = CARTESIAN_POINT ( 'NONE',  ( -7.999999999999989342, -3.313708498984762496, 18.92405277982336642 ) ) ;
#46625 = CARTESIAN_POINT ( 'NONE',  ( 0.000000000000000000, 300.0000000000000000, 0.000000000000000000 ) ) ;
#46624 = PLANE ( 'NONE',  #73238 ) ;
#46626 = CARTESIAN_POINT ( 'NONE',  ( -9.832129032723418760, 107.8645833299193555, -5.676582343750004256 ) ) ;
#46627 = ORIENTED_EDGE ( 'NONE', *, *, #42838, .F. ) ;
#46628 = CARTESIAN_POINT ( 'NONE',  ( 2.828427124746190291, 15.62499999726881406, 2.828427124746192067 ) ) ;
#46629 = CARTESIAN_POINT ( 'NONE',  ( -7.188101187500001821, 23.62499999795161543, -2.977408999572651371 ) ) ;
#46630 = CARTESIAN_POINT ( 'NONE',  ( -5.656854249492373476, -5.656854249492376141, 8.517802779823362869 ) ) ;
#46631 = CARTESIAN_POINT ( 'NONE',  ( 5.676582343750005144, 250.8854166700806729, 9.832129032723416984 ) ) ;
#46632 = CARTESIAN_POINT ( 'NONE',  ( -2.085542519210945728E-15, 119.5312499965860269, 11.35316468750000141 ) ) ;
#46633 = VERTEX_POINT ( 'NONE', #66923 ) ;
#46634 = DIRECTION ( 'NONE',  ( -0.000000000000000000, 1.000000000000000000, -0.000000000000000000 ) ) ;
#46635 = CARTESIAN_POINT ( 'NONE',  ( 10.18810118749999916, 4.220049686691935698, 100.0000000020483668 ) ) ;
#46636 = CARTESIAN_POINT ( 'NONE',  ( -1.836970198721029983E-15, 215.6249999931720538, 10.00000000000000178 ) ) ;
#46637 = CARTESIAN_POINT ( 'NONE',  ( -3.458734124999959469, 202.7500000013655779, 199.4326545832176691 ) ) ;
#46638 = CARTESIAN_POINT ( 'NONE',  ( 0.000000000000000000, 125.0000000000000000, 0.000000000000000000 ) ) ;
#46640 = CARTESIAN_POINT ( 'NONE',  ( 8.311093377946834337, 95.15624999658601268, 8.311093377946839666 ) ) ;
#46639 = DIRECTION ( 'NONE',  ( 0.000000000000000000, 0.000000000000000000, -1.000000000000000000 ) ) ;
#46641 = EDGE_CURVE ( 'NONE', #47140, #67997, #21958, .T. ) ;
#46642 = CARTESIAN_POINT ( 'NONE',  ( 1.469576158976822172E-15, -7.999999999999991118, 4.392802783920145338 ) ) ;
#46643 = CARTESIAN_POINT ( 'NONE',  ( -30.44569435410883429, 198.8125000013656063, 167.5543056458915885 ) ) ;
#46644 = CARTESIAN_POINT ( 'NONE',  ( 8.660254037844465458, 175.4166666666667140, -5.000000000000044409 ) ) ;
#46645 = ORIENTED_EDGE ( 'NONE', *, *, #71684, .T. ) ;
#46646 =( BOUNDED_CURVE ( )  B_SPLINE_CURVE ( 2, ( #68102, #33414, #27730, #73387, #56414, #61325, #9651, #50740, #16392, #32289, #43588, #32671, #10755 ),
 .UNSPECIFIED., .F., .F. ) 
 B_SPLINE_CURVE_WITH_KNOTS ( ( 3, 2, 2, 2, 2, 2, 3 ),
 ( 0.4728260869565217850, 0.4746376811594203438, 0.4764492753623189025, 0.4782608695652174058, 0.4800724637681159646, 0.4818840579710144678, 0.4836956521739130266 ),
 .UNSPECIFIED. ) 
 CURVE ( )  GEOMETRIC_REPRESENTATION_ITEM ( )  RATIONAL_B_SPLINE_CURVE ( ( 0.9999999999999990008, 0.9659258262890693114, 1.000000000000000000, 0.9659258262890683122, 1.000000000000000000, 0.9659258262890683122, 1.000000000000000000, 0.9659258262890683122, 1.000000000000000000, 0.9659258262890683122, 1.000000000000000000, 0.9659258262890683122, 1.000000000000000000 ) ) 
 REPRESENTATION_ITEM ( '' )  );
#46647 = CARTESIAN_POINT ( 'NONE',  ( 6.123233995736767268E-16, 193.1249999931720254, -10.00000000000000178 ) ) ;
#46648 = CARTESIAN_POINT ( 'NONE',  ( 26.34314575050765939, 200.6875000027312410, 165.9999999999998579 ) ) ;
#46649 = CYLINDRICAL_SURFACE ( 'NONE', #8738, 3.999999999999976019 ) ;
#46650 = CARTESIAN_POINT ( 'NONE',  ( -2.085542519210945728E-15, 94.84374999658601268, 11.35316468750000141 ) ) ;
#46651 = DIRECTION ( 'NONE',  ( 1.000000000000000000, 0.000000000000000000, 0.000000000000000000 ) ) ;
#46652 = CARTESIAN_POINT ( 'NONE',  ( -2.977408999572650039, 8.812499997951611874, -7.188101187500000933 ) ) ;
#46653 = CARTESIAN_POINT ( 'NONE',  ( 7.204075437095966983, 7.204075437095967871, 94.46875000204838102 ) ) ;
#46654 = CARTESIAN_POINT ( 'NONE',  ( 3.042071309553167069, 7.135416663252682312, -11.35316468749999785 ) ) ;
#46655 = VERTEX_POINT ( 'NONE', #28047 ) ;
#46656 = CARTESIAN_POINT ( 'NONE',  ( 0.000000000000000000, 0.000000000000000000, 30.00000000000000000 ) ) ;
#46657 = CARTESIAN_POINT ( 'NONE',  ( 4.898587196589412829E-16, 19.87500000000000355, -8.000000000000000000 ) ) ;
#46658 = CARTESIAN_POINT ( 'NONE',  ( 11.35316468750000141, 215.7812499965860411, 0.000000000000000000 ) ) ;
#46659 = CARTESIAN_POINT ( 'NONE',  ( 10.18810118750000093, -4.220049686691933921, 79.18750000204836681 ) ) ;
#46660 = CARTESIAN_POINT ( 'NONE',  ( -4.999999999999992895, 218.9583333401613174, 8.660254037844390851 ) ) ;
#46661 = CARTESIAN_POINT ( 'NONE',  ( -8.660254037844387298, 98.95833332650536818, -5.000000000000004441 ) ) ;
#46662 = CARTESIAN_POINT ( 'NONE',  ( -2.765530957081998586, 296.6406250017069510, 6.676582343750001591 ) ) ;
#46663 = ORIENTED_EDGE ( 'NONE', *, *, #8892, .F. ) ;
#46664 = LINE ( 'NONE', #64024, #38905 ) ;
#46665 = CARTESIAN_POINT ( 'NONE',  ( -11.35316468750000141, 213.8020833299193839, 3.042071309553159963 ) ) ;
#46666 = CARTESIAN_POINT ( 'NONE',  ( 7.204075437095966983, 7.204075437095967871, 88.09375000204836681 ) ) ;
#46667 = CARTESIAN_POINT ( 'NONE',  ( -26.56734541678238060, 204.3750000013656063, 166.5412658750003629 ) ) ;
#46668 = CARTESIAN_POINT ( 'NONE',  ( -3.313708498984765161, 19.03125000000000711, 7.999999999999998224 ) ) ;
#46669 = CIRCLE ( 'NONE', #17735, 6.000000000000000000 ) ;
#46670 = ORIENTED_EDGE ( 'NONE', *, *, #7694, .F. ) ;
#46671 = CARTESIAN_POINT ( 'NONE',  ( -2.977408999572650927, 123.8750000020483810, -7.188101187500001821 ) ) ;
#46672 = CARTESIAN_POINT ( 'NONE',  ( -5.000000000000000000, 16.14408868864073554, -27.96238185062347981 ) ) ;
#46673 = CARTESIAN_POINT ( 'NONE',  ( 8.660254037844385522, 34.58333333333333570, 5.000000000000005329 ) ) ;
#46674 = CARTESIAN_POINT ( 'NONE',  ( 0.000000000000000000, 0.000000000000000000, 0.000000000000000000 ) ) ;
#46675 = CARTESIAN_POINT ( 'NONE',  ( -10.18810118749999738, -4.220049686691941915, 74.12500000204836681 ) ) ;
#46676 = ORIENTED_EDGE ( 'NONE', *, *, #29342, .T. ) ;
#46677 = FACE_OUTER_BOUND ( 'NONE', #53916, .T. ) ;
#46678 = CARTESIAN_POINT ( 'NONE',  ( -7.999999999999991118, 0.000000000000000000, 6.830302779823365533 ) ) ;
#46679 = CARTESIAN_POINT ( 'NONE',  ( -2.250000000000000888, -2.250000000000000000, 28.00000000000000000 ) ) ;
#46680 = CARTESIAN_POINT ( 'NONE',  ( 1.320432766682874540E-15, 121.9062500020483810, 7.188101187500000044 ) ) ;
#46681 = LINE ( 'NONE', #12353, #48584 ) ;
#46682 = CARTESIAN_POINT ( 'NONE',  ( 2.765530957082001251, 296.7656250017069510, 6.676582343749999815 ) ) ;
#46684 = CARTESIAN_POINT ( 'NONE',  ( 1.656854249492388576, 206.3124999999999716, 202.0000000000000284 ) ) ;
#46683 = CARTESIAN_POINT ( 'NONE',  ( 9.832129032723416984, 231.8229166700806445, -5.676582343750003368 ) ) ;
#46685 = VERTEX_POINT ( 'NONE', #28788 ) ;
#46686 = PRESENTATION_LAYER_ASSIGNMENT (  '', '', ( #63549 ) ) ;
#46687 = CARTESIAN_POINT ( 'NONE',  ( 2.085542519210945334E-15, 245.4687500034140157, 11.35316468749999963 ) ) ;
#46688 = CARTESIAN_POINT ( 'NONE',  ( 7.188101187499992051, 8.802885111219154394E-16, 3.736552781871751883 ) ) ;
#46689 = ORIENTED_EDGE ( 'NONE', *, *, #31846, .F. ) ;
#46690 = CARTESIAN_POINT ( 'NONE',  ( -7.204075437095965206, -7.204075437095968759, 67.84375000204836681 ) ) ;
#46691 = CARTESIAN_POINT ( 'NONE',  ( 8.311093377946834337, 90.46874999658599847, 8.311093377946839666 ) ) ;
#46692 = CARTESIAN_POINT ( 'NONE',  ( 2.828427124746190291, 20.87500000000000000, 2.828427124746192067 ) ) ;
#46693 = CARTESIAN_POINT ( 'NONE',  ( 11.00000000000000000, 1.347111479062088405E-15, 81.24999999999998579 ) ) ;
#46695 = CARTESIAN_POINT ( 'NONE',  ( 24.54126587500000412, 209.2500000013655779, 171.4326545832175839 ) ) ;
#46694 = CARTESIAN_POINT ( 'NONE',  ( 26.56734541678238415, 206.2500000013656063, 166.5412658749999650 ) ) ;
#46696 = ORIENTED_EDGE ( 'NONE', *, *, #73386, .T. ) ;
#46697 = EDGE_CURVE ( 'NONE', #70312, #36065, #60508, .T. ) ;
#46698 = CARTESIAN_POINT ( 'NONE',  ( -26.34314575050764162, 195.6875000027311842, 174.0000000000004547 ) ) ;
#46699 = CARTESIAN_POINT ( 'NONE',  ( 0.000000000000000000, 0.000000000000000000, 118.0000000000000000 ) ) ;
#46700 = CARTESIAN_POINT ( 'NONE',  ( 11.35316468749999785, 195.5729166632526983, 3.042071309553174174 ) ) ;
#46702 = ADVANCED_FACE ( 'NONE', ( #46511 ), #22369, .T. ) ;
#46701 = CARTESIAN_POINT ( 'NONE',  ( -1.432654583217662481, 204.1250000013656063, 145.4587341250000634 ) ) ;
#46703 = CARTESIAN_POINT ( 'NONE',  ( 25.55430564589119413, 204.3125000013656063, 167.5543056458910485 ) ) ;
#46704 = CARTESIAN_POINT ( 'NONE',  ( -5.082755093536325042, 22.40624999795161543, -5.082755093536325930 ) ) ;
#46705 = CARTESIAN_POINT ( 'NONE',  ( 5.676582343750001591, 186.9270833299193555, -9.832129032723420536 ) ) ;
#46706 = CARTESIAN_POINT ( 'NONE',  ( -5.082755093536324154, 96.21875000204838102, 5.082755093536326818 ) ) ;
#46707 = CARTESIAN_POINT ( 'NONE',  ( 3.999999999999959144, 196.1875000027312126, 140.3431457505076594 ) ) ;
#46708 = CARTESIAN_POINT ( 'NONE',  ( -3.211159895383561391, 11.68749999863440614, -3.211159895383561835 ) ) ;
#46709 = CARTESIAN_POINT ( 'NONE',  ( 25.55430564589119413, 202.3125000013656063, 167.5543056458910485 ) ) ;
#46710 = CARTESIAN_POINT ( 'NONE',  ( 5.082755093536320601, -5.082755093536318824, 12.92405278187175277 ) ) ;
#46711 = CARTESIAN_POINT ( 'NONE',  ( -3.042071309553173730, 74.32291666325268409, 11.35316468749999785 ) ) ;
#46712 = CARTESIAN_POINT ( 'NONE',  ( 27.99999999999996803, 205.6250000027312126, 165.9999999999998863 ) ) ;
#46713 = CARTESIAN_POINT ( 'NONE',  ( -6.062585341144163031, -5.219679969245603957, -0.4430702215468678706 ) ) ;
#46714 = VERTEX_POINT ( 'NONE', #69156 ) ;
#46715 = CARTESIAN_POINT ( 'NONE',  ( -12.00000000000000355, 1.469576158976824342E-15, -14.80000000000000071 ) ) ;
#46716 = CARTESIAN_POINT ( 'NONE',  ( 28.00000000000002487, 206.1250000027312126, 173.9999999999999147 ) ) ;
#46717 = CARTESIAN_POINT ( 'NONE',  ( 5.676582343749993598, 69.94791666325268409, 9.832129032723422313 ) ) ;
#46718 = CARTESIAN_POINT ( 'NONE',  ( -7.204075437095967871, 7.204075437095967871, 116.9687500020483810 ) ) ;
#46719 = CARTESIAN_POINT ( 'NONE',  ( 3.458734124999959469, 194.7500000013656063, 140.5673454167823593 ) ) ;
#46720 = CARTESIAN_POINT ( 'NONE',  ( -2.436599634630690403, 16.39988855009608670, 68.84456747601289806 ) ) ;
#46722 = CARTESIAN_POINT ( 'NONE',  ( -5.676582343750006032, 59.11458332991934839, 9.832129032723418760 ) ) ;
#46721 = CARTESIAN_POINT ( 'NONE',  ( -7.188101187500000933, 89.56250000204838102, -2.977408999572650483 ) ) ;
#46723 = EDGE_CURVE ( 'NONE', #58094, #65387, #56799, .T. ) ;
#46725 = VECTOR ( 'NONE', #34611, 1000.000000000000000 ) ;
#46724 = CARTESIAN_POINT ( 'NONE',  ( -4.898587196589407898E-16, 7.999999999999991118, 27.64280278392014978 ) ) ;
#46726 = CARTESIAN_POINT ( 'NONE',  ( 1.469576158976823947E-15, 110.5625000040967905, 8.000000000000000000 ) ) ;
#46727 = CARTESIAN_POINT ( 'NONE',  ( 2.679491924311222739, 155.8333333265053682, 10.00000000000000355 ) ) ;
#46728 = CARTESIAN_POINT ( 'NONE',  ( -7.188101187499999156, 99.12500000204838102, 2.977408999572654924 ) ) ;
#46729 = CARTESIAN_POINT ( 'NONE',  ( 36.10814071610729314, 133.9999999999999716, 139.0000000000000000 ) ) ;
#46730 = CARTESIAN_POINT ( 'NONE',  ( -11.35316468749999785, 53.38541666325267698, -3.042071309553167957 ) ) ;
#46731 =( BOUNDED_CURVE ( )  B_SPLINE_CURVE ( 2, ( #10936, #73193, #50175, #73558, #74303, #44520, #56222, #16955, #15832 ),
 .UNSPECIFIED., .F., .F. ) 
 B_SPLINE_CURVE_WITH_KNOTS ( ( 3, 2, 2, 2, 3 ),
 ( 0.3194444444444443643, 0.3263888888888888395, 0.3333333333333332593, 0.3402777777777777901, 0.3472222222222222099 ),
 .UNSPECIFIED. ) 
 CURVE ( )  GEOMETRIC_REPRESENTATION_ITEM ( )  RATIONAL_B_SPLINE_CURVE ( ( 1.000000000000000666, 0.9238795325112861834, 1.000000000000000000, 0.9238795325112867385, 1.000000000000000000, 0.9238795325112867385, 1.000000000000000000, 0.9238795325112867385, 1.000000000000000000 ) ) 
 REPRESENTATION_ITEM ( '' )  );
#46732 = CARTESIAN_POINT ( 'NONE',  ( -7.204075437095965206, -7.204075437095968759, 113.2187500020483810 ) ) ;
#46733 = CARTESIAN_POINT ( 'NONE',  ( -2.085542519210945728E-15, 184.5312499965860411, 11.35316468750000141 ) ) ;
#46734 = VERTEX_POINT ( 'NONE', #6162 ) ;
#46735 = CARTESIAN_POINT ( 'NONE',  ( 2.828427124746208943, 205.7500000027312126, 195.1715728752538439 ) ) ;
#46736 = DIRECTION ( 'NONE',  ( 1.000000000000000000, 0.000000000000000000, 0.000000000000000000 ) ) ;
#46737 = CARTESIAN_POINT ( 'NONE',  ( 2.679491924311222739, 160.8333333265053682, 10.00000000000000355 ) ) ;
#46739 = CARTESIAN_POINT ( 'NONE',  ( 3.042071309553159519, 179.7395833299193555, 11.35316468750000141 ) ) ;
#46738 = CARTESIAN_POINT ( 'NONE',  ( 2.828427124746190291, 18.62499999726881583, 2.828427124746192067 ) ) ;
#46740 = CARTESIAN_POINT ( 'NONE',  ( 1.224646799147353454E-15, 300.0000000000000000, -10.00000000000000178 ) ) ;
#46741 = AXIS2_PLACEMENT_3D ( 'NONE', #34248, #39521, #16109 ) ;
#46742 = CARTESIAN_POINT ( 'NONE',  ( -2.679491924311228512, 252.0833333401612606, -9.999999999999998224 ) ) ;
#46743 = CARTESIAN_POINT ( 'NONE',  ( -27.99999999999996092, 206.5000000000000284, 174.0000000000003695 ) ) ;
#46744 = EDGE_LOOP ( 'NONE', ( #12121, #30527 ) ) ;
#46745 = CARTESIAN_POINT ( 'NONE',  ( 11.35316468749999963, 171.3020833299193555, -3.042071309553165293 ) ) ;
#46746 = VECTOR ( 'NONE', #47981, 1000.000000000000114 ) ;
#46747 = EDGE_CURVE ( 'NONE', #43757, #25866, #58114, .T. ) ;
#46748 = DIRECTION ( 'NONE',  ( 0.000000000000000000, -0.000000000000000000, 1.000000000000000000 ) ) ;
#46749 = CARTESIAN_POINT ( 'NONE',  ( -11.35316468749999785, 133.3854166632526699, -3.042071309553167513 ) ) ;
#46750 =( BOUNDED_CURVE ( )  B_SPLINE_CURVE ( 2, ( #56748, #67319, #5067, #45787, #68797, #40129, #49960, #72975, #15616 ),
 .UNSPECIFIED., .F., .F. ) 
 B_SPLINE_CURVE_WITH_KNOTS ( ( 3, 2, 2, 2, 3 ),
 ( 0.6666666666666672958, 0.6750000000000007105, 0.6833333333333340143, 0.6916666666666673180, 0.7000000000000006217 ),
 .UNSPECIFIED. ) 
 CURVE ( )  GEOMETRIC_REPRESENTATION_ITEM ( )  RATIONAL_B_SPLINE_CURVE ( ( 0.9999999999999938938, 0.9238795325112928447, 1.000000000000000000, 0.9238795325112867385, 1.000000000000000000, 0.9238795325112867385, 1.000000000000000000, 0.9238795325112806323, 1.000000000000005995 ) ) 
 REPRESENTATION_ITEM ( '' )  );
#46751 = CARTESIAN_POINT ( 'NONE',  ( 26.34314575050763807, 203.6875000027311842, 165.9999999999998295 ) ) ;
#46752 = EDGE_LOOP ( 'NONE', ( #73343, #69206, #57896 ) ) ;
#46753 = CARTESIAN_POINT ( 'NONE',  ( -7.999999999999998224, 105.7812500040967905, 3.313708498984766493 ) ) ;
#46754 = CARTESIAN_POINT ( 'NONE',  ( 4.000000000000001776, 13.06250000000000000, -1.656854249492381248 ) ) ;
#46755 = DIRECTION ( 'NONE',  ( -1.000000000000000000, -0.000000000000000000, -0.000000000000000000 ) ) ;
#46756 = CARTESIAN_POINT ( 'NONE',  ( -4.541265875000003227, 10.87499999863440969, 1.881053915767121110 ) ) ;
#46757 = CARTESIAN_POINT ( 'NONE',  ( -7.999999999999991118, 0.000000000000000000, 17.51780278392014623 ) ) ;
#46758 = CARTESIAN_POINT ( 'NONE',  ( -2.679491924310637874, 186.4583333333332291, -10.00000000000034284 ) ) ;
#46759 = EDGE_LOOP ( 'NONE', ( #49136, #37864, #53843, #9335, #67119 ) ) ;
#46760 = CARTESIAN_POINT ( 'NONE',  ( -5.656854249492381470, 24.93750000000000355, 5.656854249492379694 ) ) ;
#46761 = CARTESIAN_POINT ( 'NONE',  ( -5.082755093536325930, 107.4687500020483810, -5.082755093536325930 ) ) ;
#46762 = VECTOR ( 'NONE', #57751, 1000.000000000000000 ) ;
#46764 = CARTESIAN_POINT ( 'NONE',  ( 11.00000000000000000, 1.347111479062088405E-15, 99.24999999999998579 ) ) ;
#46763 = LINE ( 'NONE', #16978, #18123 ) ;
#46765 = ORIENTED_EDGE ( 'NONE', *, *, #20580, .T. ) ;
#46766 = CARTESIAN_POINT ( 'NONE',  ( 2.266287154880021859, 10.27715108473168648, -63.73532778936322529 ) ) ;
#46767 = CONICAL_SURFACE ( 'NONE', #14237, 12.00000000000000178, 0.9599310885968795892 ) ;
#46768 = CARTESIAN_POINT ( 'NONE',  ( 1.320432766682872962E-15, -7.188101187499992051, 25.86155278187175810 ) ) ;
#46769 = ORIENTED_EDGE ( 'NONE', *, *, #8357, .T. ) ;
#46770 = ORIENTED_EDGE ( 'NONE', *, *, #14004, .T. ) ;
#46771 = CARTESIAN_POINT ( 'NONE',  ( -10.18810118749999738, -4.220049686691941915, 87.25000000204838102 ) ) ;
#46772 = CARTESIAN_POINT ( 'NONE',  ( 8.000000000000000000, 3.000000000000000444, 0.000000000000000000 ) ) ;
#46773 = CARTESIAN_POINT ( 'NONE',  ( -29.43265458321766914, 195.7500000013656063, 166.5412658750003629 ) ) ;
#46774 = CARTESIAN_POINT ( 'NONE',  ( -4.556349186104047710, -10.99999999999999822, 103.2812499999999858 ) ) ;
#46777 = CARTESIAN_POINT ( 'NONE',  ( -6.676582343750002480, 296.5468750017069510, -2.765530957081996810 ) ) ;
#46776 = CARTESIAN_POINT ( 'NONE',  ( 25.17157287525382259, 206.0000000027312126, 172.8284271247460993 ) ) ;
#46775 = CARTESIAN_POINT ( 'NONE',  ( -10.00000000000000178, 255.9999999999999432, 0.000000000000000000 ) ) ;
#46778 = CARTESIAN_POINT ( 'NONE',  ( 4.999999999999993783, 139.1666666666666856, 8.660254037844390851 ) ) ;
#46779 = CARTESIAN_POINT ( 'NONE',  ( 3.313708498984765161, 102.9687500000000142, 7.999999999999998224 ) ) ;
#46780 = VECTOR ( 'NONE', #5239, 1000.000000000000227 ) ;
#46781 = PLANE ( 'NONE',  #5489 ) ;
#46782 = CARTESIAN_POINT ( 'NONE',  ( -11.00000000000000000, 4.556349186104045934, 78.90624999999998579 ) ) ;
#46783 = VECTOR ( 'NONE', #50591, 1000.000000000000000 ) ;
#46784 = CARTESIAN_POINT ( 'NONE',  ( -10.00000000000000000, 232.9166666734946318, -2.679491924311226292 ) ) ;
#46785 = EDGE_CURVE ( 'NONE', #49614, #48531, #42908, .T. ) ;
#46786 = CARTESIAN_POINT ( 'NONE',  ( 24.54126587499999346, 202.1875000013656063, 169.9999999999998863 ) ) ;
#46787 = CARTESIAN_POINT ( 'NONE',  ( 5.082755093536324154, 6.656249997951610986, 5.082755093536326818 ) ) ;
#46788 = CARTESIAN_POINT ( 'NONE',  ( 1.471067592899761672E-15, -8.008118988124991233, 5.888115283940630995 ) ) ;
#46789 = CARTESIAN_POINT ( 'NONE',  ( -2.754378923186476579E-14, 195.1875000013655779, 145.4587341250000350 ) ) ;
#46790 = CARTESIAN_POINT ( 'NONE',  ( 2.977408999572650039, 113.5625000020483810, -7.188101187500000933 ) ) ;
#46792 = CARTESIAN_POINT ( 'NONE',  ( 0.000000000000000000, 300.0000000000000000, 0.000000000000000000 ) ) ;
#46791 = DIRECTION ( 'NONE',  ( -1.000000000000000000, 0.000000000000000000, -0.000000000000000000 ) ) ;
#46793 = CARTESIAN_POINT ( 'NONE',  ( 8.311093377946834337, 227.3437500034140157, -8.311093377946836114 ) ) ;
#46794 = CARTESIAN_POINT ( 'NONE',  ( 0.000000000000000000, 0.000000000000000000, -10.00000000000000000 ) ) ;
#46795 = CARTESIAN_POINT ( 'NONE',  ( -7.188101187499990274, -2.977408999572651371, 27.45530278187175810 ) ) ;
#46796 = CARTESIAN_POINT ( 'NONE',  ( 23.99999999999997513, 196.8125000000000284, 171.6568542494922553 ) ) ;
#46797 = CARTESIAN_POINT ( 'NONE',  ( 11.35316468749999963, 25.98958332991935194, -3.042071309553165293 ) ) ;
#46798 = CARTESIAN_POINT ( 'NONE',  ( 5.000000000000166089, 25.83333333333352755, -8.660254037844673292 ) ) ;
#46799 = CARTESIAN_POINT ( 'NONE',  ( 11.35316468749999785, 225.8854166632526699, 3.042071309553174174 ) ) ;
#46800 = CYLINDRICAL_SURFACE ( 'NONE', #33181, 3.999999999999976019 ) ;
#46802 = DIRECTION ( 'NONE',  ( 0.000000000000000000, 0.000000000000000000, -1.000000000000000000 ) ) ;
#46801 = CARTESIAN_POINT ( 'NONE',  ( 4.231687259407054036, -16.30907003467246952, 69.42009600258495539 ) ) ;
#46803 = ORIENTED_EDGE ( 'NONE', *, *, #1503, .F. ) ;
#46804 = CARTESIAN_POINT ( 'NONE',  ( 1.432654583217607414, 198.5000000013656347, 145.4587341250000634 ) ) ;
#46805 = CARTESIAN_POINT ( 'NONE',  ( 11.35316468750000141, 20.78124999658601624, 0.000000000000000000 ) ) ;
#46806 = CARTESIAN_POINT ( 'NONE',  ( -11.00000000000000000, 4.556349186104045934, 89.59375000409677625 ) ) ;
#46807 = CARTESIAN_POINT ( 'NONE',  ( 3.458734124999960358, 206.6250000013656063, 143.4326545832176976 ) ) ;
#46808 = CARTESIAN_POINT ( 'NONE',  ( -4.556349186104048599, -10.99999999999999822, 110.9687500040967905 ) ) ;
#46809 = CARTESIAN_POINT ( 'NONE',  ( 11.99999999999999822, 4.673005023400526703, -0.4790896970872614014 ) ) ;
#46811 = CARTESIAN_POINT ( 'NONE',  ( -11.35316468750000141, 18.28124999658601624, -1.390361679473963753E-15 ) ) ;
#46810 = CARTESIAN_POINT ( 'NONE',  ( -7.188101187499999156, 110.7500000020483810, 2.977408999572654924 ) ) ;
#46812 = CARTESIAN_POINT ( 'NONE',  ( 7.999999999999992895, -3.313708498984756279, 14.98655277982336642 ) ) ;
#46813 = CARTESIAN_POINT ( 'NONE',  ( 3.042071309553159519, 144.7395833299193839, 11.35316468750000141 ) ) ;
#46814 = EDGE_CURVE ( 'NONE', #22615, #35470, #32561, .T. ) ;
#46815 = CARTESIAN_POINT ( 'NONE',  ( 2.679491924311222739, 115.8333333265053682, 10.00000000000000355 ) ) ;
#46816 = CARTESIAN_POINT ( 'NONE',  ( -7.188101187500000044, 112.5312500020483952, 0.000000000000000000 ) ) ;
#46817 = CARTESIAN_POINT ( 'NONE',  ( 10.00000000000000178, 172.0833333265053682, -2.679491924311226736 ) ) ;
#46818 = CARTESIAN_POINT ( 'NONE',  ( -24.54126587499999346, 204.4375000013656063, 170.0000000000003411 ) ) ;
#46819 = ORIENTED_EDGE ( 'NONE', *, *, #27549, .T. ) ;
#46820 = CARTESIAN_POINT ( 'NONE',  ( 5.676582343750001591, 6.927083329919350163, -9.832129032723420536 ) ) ;
#46821 = EDGE_CURVE ( 'NONE', #33538, #38802, #30128, .T. ) ;
#46822 = ORIENTED_EDGE ( 'NONE', *, *, #52077, .T. ) ;
#46823 = CARTESIAN_POINT ( 'NONE',  ( -3.407298021520050568, 16.35582233947122432, -69.12343428066031947 ) ) ;
#46824 = CARTESIAN_POINT ( 'NONE',  ( 6.676582343750003368, 299.0156250017069510, -2.765530957081997254 ) ) ;
#46826 = CARTESIAN_POINT ( 'NONE',  ( -5.676582343750006032, 134.1145833299193555, 9.832129032723418760 ) ) ;
#46825 = CARTESIAN_POINT ( 'NONE',  ( 0.000000000000000000, 0.000000000000000000, 0.000000000000000000 ) ) ;
#46827 = CARTESIAN_POINT ( 'NONE',  ( -29.65685424949245075, 207.1875000027312410, 166.0000000000003695 ) ) ;
#46828 = CARTESIAN_POINT ( 'NONE',  ( 7.999999999999992895, -3.313708498984756279, 22.54280278432982954 ) ) ;
#46829 = CARTESIAN_POINT ( 'NONE',  ( 0.000000000000000000, 0.000000000000000000, 118.0000000000000000 ) ) ;
#46830 = CARTESIAN_POINT ( 'NONE',  ( -6.951808397369817780E-16, 242.6562500034140157, -11.35316468749999963 ) ) ;
#46831 = CARTESIAN_POINT ( 'NONE',  ( -10.18810118749999916, 4.220049686691934809, 90.43750000204836681 ) ) ;
#46832 = ORIENTED_EDGE ( 'NONE', *, *, #52675, .F. ) ;
#46833 = AXIS2_PLACEMENT_3D ( 'NONE', #25184, #37646, #20647 ) ;
#46834 = EDGE_CURVE ( 'NONE', #64433, #61509, #56733, .T. ) ;
#46835 = CARTESIAN_POINT ( 'NONE',  ( 10.00000000000000355, 119.7916666666666714, 2.679491924311236506 ) ) ;
#46836 = CARTESIAN_POINT ( 'NONE',  ( -10.49999999999998224, 0.000000000000000000, 118.0000000000000000 ) ) ;
#46837 = EDGE_CURVE ( 'NONE', #29307, #34067, #8583, .T. ) ;
#46838 = CARTESIAN_POINT ( 'NONE',  ( -8.311093377946841443, 89.21874999658602690, 8.311093377946830785 ) ) ;
#46839 = ORIENTED_EDGE ( 'NONE', *, *, #64300, .F. ) ;
#46840 = CARTESIAN_POINT ( 'NONE',  ( 4.220049686691934809, 10.18810118749999916, 107.6875000020483810 ) ) ;
#46841 = CARTESIAN_POINT ( 'NONE',  ( -4.541265875000002339, 17.87499999863441147, -1.881053915767121998 ) ) ;
#46842 = ORIENTED_EDGE ( 'NONE', *, *, #72604, .F. ) ;
#46843 = VERTEX_POINT ( 'NONE', #9683 ) ;
#46844 = CARTESIAN_POINT ( 'NONE',  ( -8.000000000000001776, 5.343750000000000888, 3.313708498984759387 ) ) ;
#46845 = DIRECTION ( 'NONE',  ( -0.8660254037844380415, -0.5000000000000011102, 0.000000000000000000 ) ) ;
#46846 = AXIS2_PLACEMENT_3D ( 'NONE', #39982, #62989, #16959 ) ;
#46847 = CARTESIAN_POINT ( 'NONE',  ( 2.977408999572650927, 22.12499999795161543, -7.188101187500001821 ) ) ;
#46848 = CARTESIAN_POINT ( 'NONE',  ( 1.469576158976823947E-15, 121.0625000040967763, 8.000000000000000000 ) ) ;
#46849 =( BOUNDED_CURVE ( )  B_SPLINE_CURVE ( 2, ( #54663, #2972, #32018, #53546, #65963, #9379, #25592, #71613, #43702 ),
 .UNSPECIFIED., .F., .F. ) 
 B_SPLINE_CURVE_WITH_KNOTS ( ( 3, 2, 2, 2, 3 ),
 ( 0.4374999999999980571, 0.4479166666666647423, 0.4583333333333313719, 0.4687499999999980571, 0.4791666666666647423 ),
 .UNSPECIFIED. ) 
 CURVE ( )  GEOMETRIC_REPRESENTATION_ITEM ( )  RATIONAL_B_SPLINE_CURVE ( ( 1.000000000000014211, 0.9238795325112725276, 1.000000000000000000, 0.9238795325112867385, 1.000000000000000000, 0.9238795325112867385, 1.000000000000000000, 0.9238795325113009493, 0.9999999999999857891 ) ) 
 REPRESENTATION_ITEM ( '' )  );
#46850 = CARTESIAN_POINT ( 'NONE',  ( -10.18810118749999916, 4.220049686691934809, 102.4375000020483810 ) ) ;
#46851 = CARTESIAN_POINT ( 'NONE',  ( 2.828427124746190291, 1.875000000000000222, 2.828427124746192067 ) ) ;
#46852 = CARTESIAN_POINT ( 'NONE',  ( 4.000000000000001776, 13.81249999726881406, -1.656854249492381248 ) ) ;
#46853 = CARTESIAN_POINT ( 'NONE',  ( 27.99999999999997158, 210.0000000000000284, 173.9999999999999147 ) ) ;
#46854 = ORIENTED_EDGE ( 'NONE', *, *, #31273, .T. ) ;
#46855 = ADVANCED_FACE ( 'NONE', ( #20606 ), #27020, .F. ) ;
#46856 = CARTESIAN_POINT ( 'NONE',  ( -7.778174593052020747, -7.778174593052023411, 80.68750000000000000 ) ) ;
#46857 = CARTESIAN_POINT ( 'NONE',  ( 1.432654583217664479, 200.7500000013656347, 201.4587341250000065 ) ) ;
#46858 = ADVANCED_FACE ( 'NONE', ( #4767 ), #71519, .F. ) ;
#46859 = CARTESIAN_POINT ( 'NONE',  ( -24.54126587500002188, 203.2500000013656063, 168.5673454167826435 ) ) ;
#46860 =( BOUNDED_CURVE ( )  B_SPLINE_CURVE ( 3, ( #57743, #6424, #69049, #68670 ),
 .UNSPECIFIED., .F., .F. ) 
 B_SPLINE_CURVE_WITH_KNOTS ( ( 4, 4 ),
 ( 1.209837642689255421, 1.570796326794894338 ),
 .UNSPECIFIED. ) 
 CURVE ( )  GEOMETRIC_REPRESENTATION_ITEM ( )  RATIONAL_B_SPLINE_CURVE ( ( 1.000000000000000000, 0.9891718422399162769, 0.9891718422399162769, 1.000000000000000000 ) ) 
 REPRESENTATION_ITEM ( '' )  );
#46861 = CARTESIAN_POINT ( 'NONE',  ( -4.541265875000002339, 15.74999999863440614, -1.881053915767121998 ) ) ;
#46862 = CARTESIAN_POINT ( 'NONE',  ( 8.660254037844389075, 122.2916666598387110, -5.000000000000000000 ) ) ;
#46863 = CARTESIAN_POINT ( 'NONE',  ( 5.082755093536318824, 5.082755093536319713, 12.92405278187175277 ) ) ;
#46864 = VERTEX_POINT ( 'NONE', #23589 ) ;
#46865 = B_SPLINE_CURVE_WITH_KNOTS ( 'NONE', 3,
 ( #35675, #35317, #46609, #6634, #24699, #29639, #53024, #2072 ),
 .UNSPECIFIED., .F., .F.,
 ( 4, 2, 2, 4 ),
 ( 0.005256334970490777678, 0.006570121696662012747, 0.007883908422833246082, 0.01051148187517571622 ),
 .UNSPECIFIED. ) ;
#46866 = EDGE_CURVE ( 'NONE', #15665, #67456, #63578, .T. ) ;
#46867 = ORIENTED_EDGE ( 'NONE', *, *, #13618, .T. ) ;
#46868 = CARTESIAN_POINT ( 'NONE',  ( -7.204075437095965206, -7.204075437095968759, 106.8437500020483810 ) ) ;
#46869 = CARTESIAN_POINT ( 'NONE',  ( -2.679491924306005579, 98.54166666666711194, 10.00000000000300560 ) ) ;
#46870 = CARTESIAN_POINT ( 'NONE',  ( -29.65685424949234061, 203.4375000000000284, 174.0000000000004547 ) ) ;
#46871 = CARTESIAN_POINT ( 'NONE',  ( 2.754378923186476579E-14, 202.1875000013656063, 194.5412658750000219 ) ) ;
#46872 = CARTESIAN_POINT ( 'NONE',  ( 31.45873412499997812, 194.7500000013656063, 168.5673454167822172 ) ) ;
#46873 = CARTESIAN_POINT ( 'NONE',  ( -8.660254037844390851, 97.91666666666668561, 4.999999999999998224 ) ) ;
#46874 = CARTESIAN_POINT ( 'NONE',  ( 5.656854249492379694, 115.4375000000000000, -5.656854249492380582 ) ) ;
#46875 = CARTESIAN_POINT ( 'NONE',  ( -5.676582343750006032, 59.42708332991934839, 9.832129032723418760 ) ) ;
#46876 = CARTESIAN_POINT ( 'NONE',  ( -2.485281374238572649, 289.1875000000000000, 6.000000000000002665 ) ) ;
#46877 = ORIENTED_EDGE ( 'NONE', *, *, #9343, .T. ) ;
#46878 = DIRECTION ( 'NONE',  ( 0.000000000000000000, 0.000000000000000000, -1.000000000000000000 ) ) ;
#46879 = AXIS2_PLACEMENT_3D ( 'NONE', #6265, #984, #45487 ) ;
#46880 = CARTESIAN_POINT ( 'NONE',  ( -8.000000000000000000, 12.56249999590322197, -9.797174393178825657E-16 ) ) ;
#46881 = CARTESIAN_POINT ( 'NONE',  ( -2.754378923186476579E-14, 208.1875000013656063, 145.4587341250000350 ) ) ;
#46882 = CARTESIAN_POINT ( 'NONE',  ( 2.679491924311224960, 83.95833333333332860, 10.00000000000001243 ) ) ;
#46883 = CARTESIAN_POINT ( 'NONE',  ( 0.000000000000000000, 207.0000000000000568, 207.0000000000000568 ) ) ;
#46884 = CARTESIAN_POINT ( 'NONE',  ( 7.320508075688776373, 221.8750000000000284, 7.320508075688767491 ) ) ;
#46885 = CARTESIAN_POINT ( 'NONE',  ( 0.000000000000000000, 0.000000000000000000, -4.000000000000001776 ) ) ;
#46886 = CARTESIAN_POINT ( 'NONE',  ( -7.204075437095967871, 7.204075437095967871, 70.84375000204836681 ) ) ;
#46887 = CARTESIAN_POINT ( 'NONE',  ( 8.660254037844389075, 220.4166666666666856, -5.000000000000000000 ) ) ;
#46888 = CARTESIAN_POINT ( 'NONE',  ( 7.188101187499992051, 8.802885111219154394E-16, 10.11155278187175455 ) ) ;
#46889 = CARTESIAN_POINT ( 'NONE',  ( 5.676582343750001591, 176.9270833299193555, -9.832129032723420536 ) ) ;
#46890 = CARTESIAN_POINT ( 'NONE',  ( 4.541265875000002339, 0.3749999986344066949, -1.881053915767121554 ) ) ;
#46891 = CARTESIAN_POINT ( 'NONE',  ( 30.82842712474616320, 197.5000000027312126, 167.1715728752537018 ) ) ;
#46893 = DIRECTION ( 'NONE',  ( 1.000000000000000000, -0.000000000000000000, -0.000000000000000000 ) ) ;
#46892 = CARTESIAN_POINT ( 'NONE',  ( 3.313708498984762496, -7.999999999999989342, 20.79905277982336642 ) ) ;
#46894 = ORIENTED_EDGE ( 'NONE', *, *, #9142, .F. ) ;
#46895 = CARTESIAN_POINT ( 'NONE',  ( -2.445694354108840063, 207.0625000013656063, 139.5543056458912190 ) ) ;
#46896 = CARTESIAN_POINT ( 'NONE',  ( 6.951808397369818766E-16, 42.34374999658601979, -11.35316468750000141 ) ) ;
#46897 = CARTESIAN_POINT ( 'NONE',  ( -11.00000000000000000, 0.000000000000000000, 101.6875000040967763 ) ) ;
#46898 = CARTESIAN_POINT ( 'NONE',  ( -26.56734541678243033, 206.3750000013656063, 166.5412658750003345 ) ) ;
#46899 = CARTESIAN_POINT ( 'NONE',  ( 2.679491924311213857, 8.958333333333333925, 10.00000000000000888 ) ) ;
#46901 = CYLINDRICAL_SURFACE ( 'NONE', #4121, 7.999999999999991118 ) ;
#46900 = CYLINDRICAL_SURFACE ( 'NONE', #70155, 11.00000000000000000 ) ;
#46902 = CARTESIAN_POINT ( 'NONE',  ( 3.458734124999959914, 198.4375000013655779, 142.0000000000000568 ) ) ;
#46903 = CARTESIAN_POINT ( 'NONE',  ( -2.679491924311235618, 75.41666665983869677, 10.00000000000000000 ) ) ;
#46904 = CARTESIAN_POINT ( 'NONE',  ( -2.977408999572651815, 95.93750000204839523, 7.188101187500000933 ) ) ;
#46905 = CARTESIAN_POINT ( 'NONE',  ( -8.342170076843785083E-16, 12.18749999863440614, 4.541265875000002339 ) ) ;
#46906 = CARTESIAN_POINT ( 'NONE',  ( -1.836970198721029983E-15, 63.75000000000000000, 10.00000000000000178 ) ) ;
#46907 = CARTESIAN_POINT ( 'NONE',  ( -8.660254037844387298, 48.95833332650536818, -5.000000000000004441 ) ) ;
#46908 = CARTESIAN_POINT ( 'NONE',  ( 2.828427124746190291, 7.624999997268813168, 2.828427124746192067 ) ) ;
#46909 = ORIENTED_EDGE ( 'NONE', *, *, #22155, .T. ) ;
#46910 = ORIENTED_EDGE ( 'NONE', *, *, #19012, .T. ) ;
#46911 = DIRECTION ( 'NONE',  ( -1.000000000000000000, 0.000000000000000000, 0.000000000000000000 ) ) ;
#46912 = CARTESIAN_POINT ( 'NONE',  ( 4.721056650415999201, 296.2343750017069510, -4.721056650415999201 ) ) ;
#46913 = FACE_OUTER_BOUND ( 'NONE', #4568, .T. ) ;
#46914 = CARTESIAN_POINT ( 'NONE',  ( -2.849036369511732440E-14, 198.3750000027312126, 138.0000000000000568 ) ) ;
#46915 = CARTESIAN_POINT ( 'NONE',  ( 6.951808397369818766E-16, 157.0312499965860127, -11.35316468750000141 ) ) ;
#46916 = CARTESIAN_POINT ( 'NONE',  ( 4.220049686691934809, 10.18810118749999916, 85.18750000204838102 ) ) ;
#46917 = CARTESIAN_POINT ( 'NONE',  ( 0.000000000000000000, 300.0000000000000000, 0.000000000000000000 ) ) ;
#46918 = CARTESIAN_POINT ( 'NONE',  ( -2.828427124746152987, 206.1250000000000284, 200.8284271247462129 ) ) ;
#46919 = CARTESIAN_POINT ( 'NONE',  ( 105.0000000000000000, 37.00000000000000000, 20.00000000000000000 ) ) ;
#46920 = CARTESIAN_POINT ( 'NONE',  ( -4.220049686691935698, 10.18810118749999916, 109.7500000020483810 ) ) ;
#46921 = ORIENTED_EDGE ( 'NONE', *, *, #3489, .T. ) ;
#46922 = CARTESIAN_POINT ( 'NONE',  ( -3.999999999999960032, 202.0625000027312410, 196.3431457505076594 ) ) ;
#46923 = CARTESIAN_POINT ( 'NONE',  ( 7.778174593052023411, -7.778174593052021635, 109.7500000040967763 ) ) ;
#46924 = CARTESIAN_POINT ( 'NONE',  ( -5.676582343750006032, 139.4270833299193555, 9.832129032723418760 ) ) ;
#46925 = CARTESIAN_POINT ( 'NONE',  ( 3.458734125000016313, 196.8750000013656347, 199.4326545832176976 ) ) ;
#46926 = CARTESIAN_POINT ( 'NONE',  ( 1.432654583217664701, 208.0000000013656063, 201.4587341250000065 ) ) ;
#46927 = CARTESIAN_POINT ( 'NONE',  ( -6.238412754330611322E-16, 10.18810118749999916, 78.15625000204836681 ) ) ;
#46928 = CARTESIAN_POINT ( 'NONE',  ( 3.042071309553167069, 52.13541666325268409, -11.35316468749999785 ) ) ;
#46929 = ORIENTED_EDGE ( 'NONE', *, *, #37600, .F. ) ;
#46930 = CYLINDRICAL_SURFACE ( 'NONE', #12735, 6.000000000000001776 ) ;
#46931 = CARTESIAN_POINT ( 'NONE',  ( -4.541265875000002339, 5.937499998634407028, -5.561446717895856393E-16 ) ) ;
#46932 = CARTESIAN_POINT ( 'NONE',  ( -8.008118988124991233, 3.317071493978878127, 15.91936528394063011 ) ) ;
#46933 = CARTESIAN_POINT ( 'NONE',  ( -7.188101187500002709, 16.31249999795161543, 2.977408999572649151 ) ) ;
#46934 = CARTESIAN_POINT ( 'NONE',  ( -2.485281374238571761, 291.8750000034140157, -6.000000000000003553 ) ) ;
#46935 = DIRECTION ( 'NONE',  ( 0.000000000000000000, 0.000000000000000000, -1.000000000000000000 ) ) ;
#46936 = CARTESIAN_POINT ( 'NONE',  ( -2.977408999572650039, 8.812499997951611874, -7.188101187500001821 ) ) ;
#46937 = CARTESIAN_POINT ( 'NONE',  ( -7.188101187499992051, 0.000000000000000000, 11.98655278187175277 ) ) ;
#46938 = CARTESIAN_POINT ( 'NONE',  ( 10.18810118749999916, 1.247682550866122264E-15, 74.40625000204836681 ) ) ;
#46939 = CARTESIAN_POINT ( 'NONE',  ( -28.00000000000002132, 205.6875000013656063, 166.5412658750003629 ) ) ;
#46940 = DIRECTION ( 'NONE',  ( -1.000000000000000000, 0.000000000000000000, 0.000000000000000000 ) ) ;
#46941 = CARTESIAN_POINT ( 'NONE',  ( 2.828427124746190291, 3.624999997268813168, 2.828427124746192067 ) ) ;
#46942 = ORIENTED_EDGE ( 'NONE', *, *, #43137, .F. ) ;
#46943 = CIRCLE ( 'NONE', #15652, 3.999999999999976019 ) ;
#46944 = CARTESIAN_POINT ( 'NONE',  ( 4.000000000000015987, 196.5625000027312126, 199.6568542494924259 ) ) ;
#46945 = ADVANCED_FACE ( 'NONE', ( #68872 ), #34939, .F. ) ;
#46946 = CARTESIAN_POINT ( 'NONE',  ( -4.000000000000015987, 206.4375000000000568, 140.3431457505076594 ) ) ;
#46947 = CARTESIAN_POINT ( 'NONE',  ( -29.65685424949229088, 201.5625000027311842, 174.0000000000004547 ) ) ;
#46948 = CARTESIAN_POINT ( 'NONE',  ( 1.320432766682874540E-15, 118.5312500020483810, 7.188101187500000044 ) ) ;
#46949 = CARTESIAN_POINT ( 'NONE',  ( 9.999999999999998224, 250.8333333401613459, -2.679491924311229401 ) ) ;
#46950 = CARTESIAN_POINT ( 'NONE',  ( -5.656854249492375253, 5.656854249492375253, 2.330302783920143561 ) ) ;
#46951 = VERTEX_POINT ( 'NONE', #12272 ) ;
#46952 =( BOUNDED_CURVE ( )  B_SPLINE_CURVE ( 2, ( #10005, #49984, #32276, #42821, #60182, #72244, #14519, #8503, #73001, #21310, #37931, #31520, #66214 ),
 .UNSPECIFIED., .F., .F. ) 
 B_SPLINE_CURVE_WITH_KNOTS ( ( 3, 2, 2, 2, 2, 2, 3 ),
 ( 0.09239130434782608092, 0.09420289855072463969, 0.09601449275362318458, 0.09782608695652174335, 0.09963768115942028825, 0.1014492753623188470, 0.1032608695652173919 ),
 .UNSPECIFIED. ) 
 CURVE ( )  GEOMETRIC_REPRESENTATION_ITEM ( )  RATIONAL_B_SPLINE_CURVE ( ( 1.000000000000000000, 0.9659258262890683122, 1.000000000000000000, 0.9659258262890683122, 1.000000000000000000, 0.9659258262890683122, 1.000000000000000000, 0.9659258262890683122, 1.000000000000000000, 0.9659258262890683122, 1.000000000000000000, 0.9659258262890683122, 1.000000000000000000 ) ) 
 REPRESENTATION_ITEM ( '' )  );
#46953 = ADVANCED_FACE ( 'NONE', ( #57573 ), #29262, .T. ) ;
#46954 = CARTESIAN_POINT ( 'NONE',  ( -5.082755093536325042, 17.53124999795161187, -5.082755093536325930 ) ) ;
#46955 = ORIENTED_EDGE ( 'NONE', *, *, #35899, .T. ) ;
#46956 = CARTESIAN_POINT ( 'NONE',  ( 29.65685424949225180, 200.0625000000000284, 174.0000000000000284 ) ) ;
#46957 = CARTESIAN_POINT ( 'NONE',  ( 6.123233995736767268E-16, 73.12499999317203958, -10.00000000000000178 ) ) ;
#46958 = CARTESIAN_POINT ( 'NONE',  ( 8.660254037844389075, 60.41666666666666430, -5.000000000000000000 ) ) ;
#46959 = CARTESIAN_POINT ( 'NONE',  ( 1.320432766682874540E-15, 100.9062500020483810, 7.188101187500000044 ) ) ;
#46960 = CARTESIAN_POINT ( 'NONE',  ( 3.999999999999960032, 205.1250000027312126, 142.0000000000000568 ) ) ;
#46961 = CARTESIAN_POINT ( 'NONE',  ( -20.11025477313347665, -33.58489503204329907, 193.5920052501028579 ) ) ;
#46962 = EDGE_LOOP ( 'NONE', ( #47651, #68248, #53545, #49640 ) ) ;
#46963 = ORIENTED_EDGE ( 'NONE', *, *, #72663, .T. ) ;
#46964 = CARTESIAN_POINT ( 'NONE',  ( -11.35316468749999608, 249.1145833367473017, 3.042071309553173730 ) ) ;
#46965 = CARTESIAN_POINT ( 'NONE',  ( -2.977408999572647819, 7.188101187499991163, 19.58030278187175455 ) ) ;
#46966 = CARTESIAN_POINT ( 'NONE',  ( -6.362988438888832046E-13, 88.74999999999995737, 9.999999999999998224 ) ) ;
#46967 = CARTESIAN_POINT ( 'NONE',  ( -8.660254037844387298, 73.95833332650536818, -5.000000000000004441 ) ) ;
#46968 = DIRECTION ( 'NONE',  ( 1.000000000000000000, 0.000000000000000000, 0.000000000000000000 ) ) ;
#46969 = CARTESIAN_POINT ( 'NONE',  ( 1.584317714026805320E-12, 163.7500000000001137, 9.999999999999998224 ) ) ;
#46970 = CARTESIAN_POINT ( 'NONE',  ( -10.00000000000000178, 177.5000000000000284, -1.224646799147353454E-15 ) ) ;
#46971 = CARTESIAN_POINT ( 'NONE',  ( -11.00000000000000000, 0.000000000000000000, 76.18750000409677625 ) ) ;
#46972 = CARTESIAN_POINT ( 'NONE',  ( -8.000000000000000000, 118.9062500000000000, -3.313708498984761164 ) ) ;
#46973 = CARTESIAN_POINT ( 'NONE',  ( -7.188101187499992051, 0.000000000000000000, 25.86155278187175810 ) ) ;
#46974 = CARTESIAN_POINT ( 'NONE',  ( 5.676582343749993598, 145.2604166632526699, 9.832129032723422313 ) ) ;
#46975 = CARTESIAN_POINT ( 'NONE',  ( 11.35316468750000141, 0.9374999965860164597, 0.000000000000000000 ) ) ;
#46978 = LINE ( 'NONE', #71455, #7388 ) ;
#46977 = DIRECTION ( 'NONE',  ( 1.000000000000000000, 0.000000000000000000, 0.000000000000000000 ) ) ;
#46976 = CARTESIAN_POINT ( 'NONE',  ( 29.65685424949240101, 205.4375000000000000, 165.9999999999998863 ) ) ;
#46979 = ORIENTED_EDGE ( 'NONE', *, *, #40922, .F. ) ;
#46980 = CARTESIAN_POINT ( 'NONE',  ( -5.000000000000000000, -60.90295814858257017, 23.31388853594792820 ) ) ;
#46981 = CARTESIAN_POINT ( 'NONE',  ( -7.778174593052023411, 7.778174593052023411, 68.50000000409677625 ) ) ;
#46982 = CARTESIAN_POINT ( 'NONE',  ( 0.09215390349082859534, -8.002426153057021097, 0.000000000000000000 ) ) ;
#46983 = CARTESIAN_POINT ( 'NONE',  ( -4.000000000000001776, 11.50000000000000000, -4.898587196589415787E-16 ) ) ;
#46984 = CIRCLE ( 'NONE', #21676, 37.00000000000000711 ) ;
#46985 = CARTESIAN_POINT ( 'NONE',  ( -2.679491924311225848, 33.33333332650536107, -10.00000000000000178 ) ) ;
#46986 = CARTESIAN_POINT ( 'NONE',  ( 7.188101187500000044, 112.9062500020483952, -8.802885111219163269E-16 ) ) ;
#46987 = CARTESIAN_POINT ( 'NONE',  ( -4.541265875000002339, 0.8749999986344069169, -1.881053915767121998 ) ) ;
#46988 = CARTESIAN_POINT ( 'NONE',  ( -0.3794862803194996581, 65.74576272851732028, -26.26831557574448794 ) ) ;
#46989 = CARTESIAN_POINT ( 'NONE',  ( 7.999999999999992895, -3.313708498984756279, 14.98655277982336642 ) ) ;
#46991 = CARTESIAN_POINT ( 'NONE',  ( -50.99999999999994316, -31.99999999999978684, 135.0000000000000000 ) ) ;
#46990 = LINE ( 'NONE', #59439, #27452 ) ;
#46992 = ORIENTED_EDGE ( 'NONE', *, *, #29342, .F. ) ;
#46993 = CARTESIAN_POINT ( 'NONE',  ( 4.999999999999996447, 29.16666666666667140, 8.660254037844394404 ) ) ;
#46994 = CARTESIAN_POINT ( 'NONE',  ( -4.433107781481984588, 226.0000000000000284, -8.987711252925484118 ) ) ;
#46995 = CARTESIAN_POINT ( 'NONE',  ( 11.00000000000000000, 1.347111479062088405E-15, 88.75000000000000000 ) ) ;
#46996 = CARTESIAN_POINT ( 'NONE',  ( 5.676582343749997150, 242.5520833367473301, -9.832129032723418760 ) ) ;
#46997 = CARTESIAN_POINT ( 'NONE',  ( 6.951808397369818766E-16, 122.0312499965860269, -11.35316468750000141 ) ) ;
#46998 = ORIENTED_EDGE ( 'NONE', *, *, #69485, .T. ) ;
#46999 = CARTESIAN_POINT ( 'NONE',  ( -8.259994644541624353, 7.006214462904858387, 117.7099183163968092 ) ) ;
#47000 = VECTOR ( 'NONE', #618, 1000.000000000000000 ) ;
#47001 = CARTESIAN_POINT ( 'NONE',  ( -4.220049686691937474, -10.18810118749999738, 103.9375000020483810 ) ) ;
#47002 = CARTESIAN_POINT ( 'NONE',  ( 47.32259252271278882, 145.2267040872997939, 65.76194439203457875 ) ) ;
#47003 = CARTESIAN_POINT ( 'NONE',  ( -3.458734124999959469, 199.7500000013656063, 199.4326545832176691 ) ) ;
#47004 = DIRECTION ( 'NONE',  ( -0.000000000000000000, 1.000000000000000000, -0.000000000000000000 ) ) ;
#47006 = CARTESIAN_POINT ( 'NONE',  ( 5.676582343750001591, 96.61458332991935549, -9.832129032723420536 ) ) ;
#47005 = DIRECTION ( 'NONE',  ( 0.000000000000000000, 0.000000000000000000, 1.000000000000000000 ) ) ;
#47007 = CARTESIAN_POINT ( 'NONE',  ( 3.313708498984762496, -7.999999999999989342, 7.486552783920144449 ) ) ;
#47008 = CARTESIAN_POINT ( 'NONE',  ( -25.55430564589115150, 198.3125000013656063, 172.4456943541091789 ) ) ;
#47009 = CARTESIAN_POINT ( 'NONE',  ( -2.250000000000000000, 300.0000000000000000, 7.677076266392047543 ) ) ;
#47010 = ORIENTED_EDGE ( 'NONE', *, *, #56330, .T. ) ;
#47011 = CARTESIAN_POINT ( 'NONE',  ( 7.320508075688771044, 196.2499999931719969, 7.320508075688775484 ) ) ;
#47012 = CARTESIAN_POINT ( 'NONE',  ( 3.313708498984721640, 22.21875000000000355, 8.000000000000039080 ) ) ;
#47013 = DIRECTION ( 'NONE',  ( -1.000000000000000000, 0.000000000000000000, 0.000000000000000000 ) ) ;
#47014 = CARTESIAN_POINT ( 'NONE',  ( 11.35316468750000141, 91.09374999658602690, 0.000000000000000000 ) ) ;
#47015 = CARTESIAN_POINT ( 'NONE',  ( 1.102182119232618108E-15, 298.2500000000000000, 6.000000000000001776 ) ) ;
#47016 = CARTESIAN_POINT ( 'NONE',  ( -7.188101187500000933, 14.99999999795161187, -2.977408999572651371 ) ) ;
#47017 = CARTESIAN_POINT ( 'NONE',  ( -4.220049686691937474, -10.18810118749999738, 96.81250000204838102 ) ) ;
#47018 = CARTESIAN_POINT ( 'NONE',  ( -9.832129032723418760, 13.17708332991935194, -5.676582343750004256 ) ) ;
#47019 = ORIENTED_EDGE ( 'NONE', *, *, #69434, .F. ) ;
#47020 = LINE ( 'NONE', #70415, #65720 ) ;
#47021 = CARTESIAN_POINT ( 'NONE',  ( 0.000000000000000000, 0.000000000000000000, 118.0000000000000000 ) ) ;
#47022 = CARTESIAN_POINT ( 'NONE',  ( 6.951808397369818766E-16, 222.0312499965860127, -11.35316468750000141 ) ) ;
#47023 = CARTESIAN_POINT ( 'NONE',  ( 4.220049686691934809, 10.18810118749999916, 78.06250000204838102 ) ) ;
#47024 = CARTESIAN_POINT ( 'NONE',  ( -4.721056650415999201, 294.3281250017069510, -4.721056650415999201 ) ) ;
#47025 = VERTEX_POINT ( 'NONE', #34566 ) ;
#47026 = CARTESIAN_POINT ( 'NONE',  ( 2.828427124746153876, 202.0000000027312126, 144.8284271247462129 ) ) ;
#47027 = CARTESIAN_POINT ( 'NONE',  ( 8.311093377946834337, 205.4687499965859843, 8.311093377946839666 ) ) ;
#47028 = AXIS2_PLACEMENT_3D ( 'NONE', #67841, #43707, #10127 ) ;
#47029 = ADVANCED_FACE ( 'NONE', ( #17182 ), #16799, .T. ) ;
#47030 = EDGE_CURVE ( 'NONE', #1076, #30512, #43103, .T. ) ;
#47031 = CARTESIAN_POINT ( 'NONE',  ( -10.18810118749999738, -4.220049686691941915, 91.75000000204836681 ) ) ;
#47032 = CARTESIAN_POINT ( 'NONE',  ( -31.45873412499998523, 201.7500000013655779, 171.4326545832180386 ) ) ;
#47033 = CARTESIAN_POINT ( 'NONE',  ( -8.000000000000000000, 26.25000000000000711, -9.797174393178825657E-16 ) ) ;
#47034 = VERTEX_POINT ( 'NONE', #6258 ) ;
#47035 = CARTESIAN_POINT ( 'NONE',  ( -26.34314575050753859, 208.6875000027312126, 174.0000000000003411 ) ) ;
#47036 = CARTESIAN_POINT ( 'NONE',  ( 5.082755093536326818, 123.2187500020483952, 5.082755093536325042 ) ) ;
#47037 = FACE_OUTER_BOUND ( 'NONE', #30951, .T. ) ;
#47038 = CARTESIAN_POINT ( 'NONE',  ( -1.836970198721029983E-15, 28.75000000000000000, 10.00000000000000178 ) ) ;
#47039 = VECTOR ( 'NONE', #70907, 1000.000000000000000 ) ;
#47040 = FACE_OUTER_BOUND ( 'NONE', #307, .T. ) ;
#47041 = CARTESIAN_POINT ( 'NONE',  ( -10.18810118749999916, 4.220049686691934809, 76.93750000204839523 ) ) ;
#47042 = ORIENTED_EDGE ( 'NONE', *, *, #72240, .F. ) ;
#47043 = CARTESIAN_POINT ( 'NONE',  ( 2.449293598294707893E-16, 2.999999997268813168, -4.000000000000001776 ) ) ;
#47044 = AXIS2_PLACEMENT_3D ( 'NONE', #53218, #24888, #42618 ) ;
#47045 = DIRECTION ( 'NONE',  ( 0.8660254037844380415, -0.5000000000000013323, 0.000000000000000000 ) ) ;
#47046 = CARTESIAN_POINT ( 'NONE',  ( -2.977408999572650927, 119.7500000020483810, -7.188101187500001821 ) ) ;
#47047 = EDGE_CURVE ( 'NONE', #10894, #65462, #50837, .T. ) ;
#47048 = CARTESIAN_POINT ( 'NONE',  ( -2.295000000000000373, 284.2799999999998590, 5.414444767710663520 ) ) ;
#47049 = CARTESIAN_POINT ( 'NONE',  ( -4.721056650415998313, 295.5781250017069510, 4.721056650416000089 ) ) ;
#47051 = CARTESIAN_POINT ( 'NONE',  ( 2.824543433528785410E-14, 210.0000000000000284, 194.0000000000000568 ) ) ;
#47050 = CARTESIAN_POINT ( 'NONE',  ( 2.085542519210945334E-15, 235.1562500034140157, 11.35316468749999963 ) ) ;
#47052 = ORIENTED_EDGE ( 'NONE', *, *, #15001, .F. ) ;
#47053 = CARTESIAN_POINT ( 'NONE',  ( 3.042071309553173286, 235.6770833367473017, 11.35316468749999608 ) ) ;
#47054 = CARTESIAN_POINT ( 'NONE',  ( 7.188101187499993827, -2.977408999572645598, 6.642802781871754547 ) ) ;
#47055 = EDGE_LOOP ( 'NONE', ( #26163, #29522, #9653, #25777 ) ) ;
#47056 = CARTESIAN_POINT ( 'NONE',  ( 5.656854249492379694, 105.1250000040967763, -5.656854249492380582 ) ) ;
#47057 = CARTESIAN_POINT ( 'NONE',  ( -11.35316468750000141, 98.80208332991932707, 3.042071309553159963 ) ) ;
#47058 = CARTESIAN_POINT ( 'NONE',  ( -4.193030820682219328, 60.66866849074632739, 23.17095654502715973 ) ) ;
#47059 = CARTESIAN_POINT ( 'NONE',  ( 4.556349186104045934, 11.00000000000000000, 86.03124999999998579 ) ) ;
#47062 = CARTESIAN_POINT ( 'NONE',  ( -8.000000000000001776, 2.343750000000000444, 3.313708498984759387 ) ) ;
#47061 = CARTESIAN_POINT ( 'NONE',  ( 24.54126587499998635, 206.1250000013655779, 168.5673454167822740 ) ) ;
#47060 = CARTESIAN_POINT ( 'NONE',  ( 26.56734541678238060, 203.2500000013656063, 166.5412658749999650 ) ) ;
#47063 = ORIENTED_EDGE ( 'NONE', *, *, #20111, .T. ) ;
#47064 = PLANE ( 'NONE',  #50118 ) ;
#47065 = CARTESIAN_POINT ( 'NONE',  ( -36.10814071610732867, 141.0294372515228360, 139.0000000000000000 ) ) ;
#47066 = AXIS2_PLACEMENT_3D ( 'NONE', #13460, #31200, #59511 ) ;
#47067 = CARTESIAN_POINT ( 'NONE',  ( 11.35316468749999785, 210.5729166632526983, 3.042071309553174174 ) ) ;
#47068 =( BOUNDED_CURVE ( )  B_SPLINE_CURVE ( 2, ( #66121, #32562, #3134, #44245, #15553, #38591, #73285, #4258, #9162, #21588, #61590, #50263, #8791 ),
 .UNSPECIFIED., .F., .F. ) 
 B_SPLINE_CURVE_WITH_KNOTS ( ( 3, 2, 2, 2, 2, 2, 3 ),
 ( 0.6684782608695651884, 0.6702898550724637472, 0.6721014492753623060, 0.6739130434782608647, 0.6757246376811594235, 0.6775362318840579823, 0.6793478260869565410 ),
 .UNSPECIFIED. ) 
 CURVE ( )  GEOMETRIC_REPRESENTATION_ITEM ( )  RATIONAL_B_SPLINE_CURVE ( ( 1.000000000000000000, 0.9659258262890683122, 1.000000000000000000, 0.9659258262890683122, 1.000000000000000000, 0.9659258262890683122, 1.000000000000000000, 0.9659258262890683122, 1.000000000000000000, 0.9659258262890683122, 1.000000000000000000, 0.9659258262890683122, 1.000000000000000000 ) ) 
 REPRESENTATION_ITEM ( '' )  );
#47069 = CARTESIAN_POINT ( 'NONE',  ( -2.754378923186476579E-14, 205.1875000013656063, 145.4587341250000350 ) ) ;
#47070 = CARTESIAN_POINT ( 'NONE',  ( 31.45873412499998523, 205.8750000013656063, 171.4326545832175839 ) ) ;
#47071 = CARTESIAN_POINT ( 'NONE',  ( -7.188101187500000044, 21.09374999795161543, -8.802885111219163269E-16 ) ) ;
#47072 = CARTESIAN_POINT ( 'NONE',  ( 11.35316468749999963, 181.3020833299192986, -3.042071309553165293 ) ) ;
#47073 = CARTESIAN_POINT ( 'NONE',  ( 1.320432766682874540E-15, 100.9062500020483810, 7.188101187500000044 ) ) ;
#47074 = CARTESIAN_POINT ( 'NONE',  ( -5.000000000000000000, 64.62379132009284888, -24.09319349500319163 ) ) ;
#47075 = CARTESIAN_POINT ( 'NONE',  ( -26.34314575050764162, 196.9375000000000284, 166.0000000000003695 ) ) ;
#47076 = CARTESIAN_POINT ( 'NONE',  ( -4.541265875000002339, 10.81249999863440792, -5.561446717895856393E-16 ) ) ;
#47077 = CARTESIAN_POINT ( 'NONE',  ( 31.45873412499998523, 202.8750000013656063, 171.4326545832176123 ) ) ;
#47078 = CARTESIAN_POINT ( 'NONE',  ( -5.082755093536319713, 5.082755093536319713, 3.174052781871751439 ) ) ;
#47079 = CARTESIAN_POINT ( 'NONE',  ( -8.311093377946836114, 72.65624999658604111, -8.311093377946837890 ) ) ;
#47080 = CARTESIAN_POINT ( 'NONE',  ( 0.000000000000000000, 0.000000000000000000, 0.000000000000000000 ) ) ;
#47081 = CARTESIAN_POINT ( 'NONE',  ( -4.898587196589407898E-16, 7.999999999999991118, 2.011552784329821542 ) ) ;
#47082 = ORIENTED_EDGE ( 'NONE', *, *, #50467, .T. ) ;
#47083 = DIRECTION ( 'NONE',  ( 1.000000000000000000, 0.000000000000000000, 0.000000000000000000 ) ) ;
#47084 = CARTESIAN_POINT ( 'NONE',  ( 9.832129032723416984, 70.36458332991936970, 5.676582343750006032 ) ) ;
#47085 = CARTESIAN_POINT ( 'NONE',  ( 4.556349186104051263, -10.99999999999999822, 70.65625000409676204 ) ) ;
#47086 = CARTESIAN_POINT ( 'NONE',  ( -1.432654583217664701, 197.0000000013656063, 138.5412658750000787 ) ) ;
#47087 = CARTESIAN_POINT ( 'NONE',  ( -3.728321214232717562, 10.10963409588413953, 70.65936332829922151 ) ) ;
#47089 = CARTESIAN_POINT ( 'NONE',  ( -11.35316468750000141, 63.48958332991935549, 3.042071309553159963 ) ) ;
#47088 = DIRECTION ( 'NONE',  ( 0.000000000000000000, 0.000000000000000000, 1.000000000000000000 ) ) ;
#47090 = CARTESIAN_POINT ( 'NONE',  ( 7.999999999999991118, 3.313708498984757611, 27.36155278392014978 ) ) ;
#47091 = CARTESIAN_POINT ( 'NONE',  ( -10.00000000000000000, 14.16666665983870033, -2.679491924311229845 ) ) ;
#47092 = CARTESIAN_POINT ( 'NONE',  ( -5.000000000000005329, 155.2083333265053682, 8.660254037844387298 ) ) ;
#47093 = CARTESIAN_POINT ( 'NONE',  ( 7.188101187500002709, 98.18750000204838102, 2.977408999572649151 ) ) ;
#47094 = ADVANCED_FACE ( 'NONE', ( #28134 ), #34189, .T. ) ;
#47095 = CARTESIAN_POINT ( 'NONE',  ( 7.320508075688779925, 20.62500000000000000, -7.320508075688779925 ) ) ;
#47096 = CARTESIAN_POINT ( 'NONE',  ( -3.042071309553163960, 47.55208332991934839, -11.35316468749999963 ) ) ;
#47097 = CARTESIAN_POINT ( 'NONE',  ( -4.220049686691937474, -10.18810118749999738, 114.8125000020483668 ) ) ;
#47098 = CARTESIAN_POINT ( 'NONE',  ( 5.676582343750001591, 196.6145833299193839, -9.832129032723420536 ) ) ;
#47099 = ORIENTED_EDGE ( 'NONE', *, *, #43157, .T. ) ;
#47100 = CARTESIAN_POINT ( 'NONE',  ( 4.000000000000001776, 4.000000000000000000, 0.000000000000000000 ) ) ;
#47101 = CARTESIAN_POINT ( 'NONE',  ( -5.656854249492380582, 121.8125000000000000, -5.656854249492380582 ) ) ;
#47102 = CARTESIAN_POINT ( 'NONE',  ( -6.062581705673323107, -5.219684191697756326, -0.2078801478342257869 ) ) ;
#47104 = CARTESIAN_POINT ( 'NONE',  ( -2.085542519210945728E-15, 179.5312499965860411, 11.35316468750000141 ) ) ;
#47103 = CARTESIAN_POINT ( 'NONE',  ( 4.000000000000015987, 195.5625000000000568, 196.3431457505076594 ) ) ;
#47105 = EDGE_CURVE ( 'NONE', #18300, #48454, #30360, .T. ) ;
#47106 = DIRECTION ( 'NONE',  ( -1.000000000000000000, 0.000000000000000000, 0.000000000000000000 ) ) ;
#47107 = CARTESIAN_POINT ( 'NONE',  ( -4.999999999999992895, 253.9583333401613174, 8.660254037844390851 ) ) ;
#47108 = CARTESIAN_POINT ( 'NONE',  ( -32.00000000000001421, 206.1875000000000853, 168.3431457505080289 ) ) ;
#47109 = VECTOR ( 'NONE', #14683, 1000.000000000000000 ) ;
#47110 = ORIENTED_EDGE ( 'NONE', *, *, #55686, .T. ) ;
#47111 = CARTESIAN_POINT ( 'NONE',  ( 8.311093377946834337, 170.4687499965860127, 8.311093377946839666 ) ) ;
#47112 = AXIS2_PLACEMENT_3D ( 'NONE', #69852, #18164, #69478 ) ;
#47113 = CARTESIAN_POINT ( 'NONE',  ( -7.188101187499992051, 2.977408999572646930, 28.39280278187175810 ) ) ;
#47114 = CARTESIAN_POINT ( 'NONE',  ( 9.832129032723420536, 131.5104166632526983, -5.676582343749999815 ) ) ;
#47115 = DIRECTION ( 'NONE',  ( -0.000000000000000000, 1.000000000000000000, -0.000000000000000000 ) ) ;
#47116 = AXIS2_PLACEMENT_3D ( 'NONE', #7737, #7370, #24700 ) ;
#47117 = ORIENTED_EDGE ( 'NONE', *, *, #30702, .T. ) ;
#47118 = ADVANCED_FACE ( 'NONE', ( #36400 ), #42410, .T. ) ;
#47119 = ADVANCED_FACE ( 'NONE', ( #12997 ), #47339, .F. ) ;
#47120 = CARTESIAN_POINT ( 'NONE',  ( 5.656854249492381470, 101.7500000040967905, 5.656854249492379694 ) ) ;
#47121 = ADVANCED_FACE ( 'NONE', ( #54122 ), #71075, .T. ) ;
#47122 = ADVANCED_BREP_SHAPE_REPRESENTATION ( '', ( #66799, #57354 ), #47738 ) ;
#47123 = CARTESIAN_POINT ( 'NONE',  ( 4.000000000000001776, 11.00000000000000000, 0.000000000000000000 ) ) ;
#47124 = CARTESIAN_POINT ( 'NONE',  ( 0.000000000000000000, 2.326828918379971365E-15, -19.00000000000000355 ) ) ;
#47125 = CARTESIAN_POINT ( 'NONE',  ( -4.541265875000002339, 12.74999999863440969, -1.881053915767121998 ) ) ;
#47126 = CARTESIAN_POINT ( 'NONE',  ( -3.313708498984757167, 7.999999999999991118, 21.73655278392014978 ) ) ;
#47127 = LINE ( 'NONE', #70160, #31797 ) ;
#47128 = VERTEX_POINT ( 'NONE', #15053 ) ;
#47129 = CARTESIAN_POINT ( 'NONE',  ( -5.000000000000031974, 178.3333333333333997, 8.660254037844435260 ) ) ;
#47130 = CARTESIAN_POINT ( 'NONE',  ( -2.977408999572651815, 95.93750000204839523, 7.188101187500000933 ) ) ;
#47131 = EDGE_CURVE ( 'NONE', #32492, #40180, #35433, .T. ) ;
#47133 = FACE_OUTER_BOUND ( 'NONE', #64395, .T. ) ;
#47132 = CARTESIAN_POINT ( 'NONE',  ( 1.656854249492280440, 203.9375000027312126, 146.0000000000001421 ) ) ;
#47134 =( NAMED_UNIT ( * ) SI_UNIT ( $, .STERADIAN. ) SOLID_ANGLE_UNIT ( ) );
#47135 = ORIENTED_EDGE ( 'NONE', *, *, #64967, .F. ) ;
#47136 = CARTESIAN_POINT ( 'NONE',  ( -0.6547826978431597889, 10.28110016890869893, -63.57209897671331333 ) ) ;
#47137 = CARTESIAN_POINT ( 'NONE',  ( -31.66756539373085388, -30.58405805906214781, 167.9999999999997726 ) ) ;
#47138 = CARTESIAN_POINT ( 'NONE',  ( 7.188101187499992051, 8.802885111219154394E-16, 26.23655278187175810 ) ) ;
#47139 = ORIENTED_EDGE ( 'NONE', *, *, #47131, .T. ) ;
#47140 = VERTEX_POINT ( 'NONE', #39477 ) ;
#47141 = CARTESIAN_POINT ( 'NONE',  ( -7.204075437095965206, -7.204075437095968759, 85.84375000204836681 ) ) ;
#47142 = UNCERTAINTY_MEASURE_WITH_UNIT (LENGTH_MEASURE( 1.000000000000000082E-05 ), #67191, 'distance_accuracy_value', 'NONE');
#47143 = CARTESIAN_POINT ( 'NONE',  ( -30.44569435410883074, 194.8125000013656063, 167.5543056458915885 ) ) ;
#47144 = CARTESIAN_POINT ( 'NONE',  ( 11.00000000000000355, -4.556349186104045046, 99.15624999999998579 ) ) ;
#47146 = CARTESIAN_POINT ( 'NONE',  ( -14.00000000000000178, 2.249999999994893862, 10.23492587299426404 ) ) ;
#47145 = CARTESIAN_POINT ( 'NONE',  ( 29.65685424949240456, 201.1875000027312694, 173.9999999999999147 ) ) ;
#47147 = CARTESIAN_POINT ( 'NONE',  ( 2.679491924311228956, 131.0416666666666856, -10.00000000000000000 ) ) ;
#47148 = VECTOR ( 'NONE', #16003, 1000.000000000000000 ) ;
#47149 = DIRECTION ( 'NONE',  ( 1.000000000000000000, 0.000000000000000000, -0.000000000000000000 ) ) ;
#47150 = CYLINDRICAL_SURFACE ( 'NONE', #37399, 3.999999999999976019 ) ;
#47151 = CARTESIAN_POINT ( 'NONE',  ( 29.43265458321761230, 201.5000000013655779, 173.4587341249998929 ) ) ;
#47152 = CARTESIAN_POINT ( 'NONE',  ( -5.082755093536325042, 7.406249997951610986, -5.082755093536325930 ) ) ;
#47153 = AXIS2_PLACEMENT_3D ( 'NONE', #27212, #50229, #21555 ) ;
#47154 = CARTESIAN_POINT ( 'NONE',  ( -3.317071493978878571, 8.008118988124991233, 5.231865283940630995 ) ) ;
#47155 = CARTESIAN_POINT ( 'NONE',  ( 1.432654583217607192, 196.2500000013656631, 145.4587341250000634 ) ) ;
#47156 = CARTESIAN_POINT ( 'NONE',  ( -7.188101187500000933, 115.4375000020483810, -2.977408999572650483 ) ) ;
#47158 = FACE_OUTER_BOUND ( 'NONE', #29059, .T. ) ;
#47157 = CARTESIAN_POINT ( 'NONE',  ( 12.00000000000000178, 0.000000000000000000, -31.99999999999998579 ) ) ;
#47159 = CARTESIAN_POINT ( 'NONE',  ( -9.832129032723415207, 229.6354166700806729, 5.676582343750005144 ) ) ;
#47160 = CARTESIAN_POINT ( 'NONE',  ( -26.34314575050764162, 207.9375000000000568, 166.0000000000003695 ) ) ;
#47161 = CARTESIAN_POINT ( 'NONE',  ( 10.00000000000000000, 51.66666665983870388, 2.679491924311235618 ) ) ;
#47163 =( BOUNDED_SURFACE ( )  B_SPLINE_SURFACE ( 1, 2, ( 
 ( #14606, #71205, #9339, #60261, #13848, #55001, #8588, #49702, #66673, #13487, #48937, #30855, #71574, #48196, #55373, #65922, #49315, #43661, #31603, #59536, #3679, #8215, #3308, #7848, #36891, #43284, #65176, #59901, #31227, #42163, #19161, #53876, #26294, #72331, #54251, #19896, #37645, #37268, #66299, #60643, #25551, #14979, #8964, #48565, #31977, #61014, #38015, #10085, #27421, #50811, #16092, #45155, #68165, #4805, #34228, #50437, #61767, #62496, #50069, #28172, #51184, #16839, #33485, #72715, #67052, #55747, #56117, #21019, #9717, #73822, #4426, #44043, #27057, #10825, #57230, #33123, #74192, #73453, #39866, #62868, #5542, #32738, #27798, #33860, #56859, #4064, #22130, #39501, #45519, #56487, #21759, #11201, #5176, #15352, #16464, #44788, #73083, #22497, #15725, #68535, #28544, #38387, #38768, #61391, #21391, #67801, #44414, #67427, #39127, #62131, #10454, #46637, #63241, #40989, #53050, #6294, #7027, #68909, #1013, #17220, #275, #74570, #28921, #5918, #64734, #47373, #45895, #30034, #57990, #23257, #29300, #57608, #18343, #22883, #59087, #7396, #41357, #52310, #58355, #29663, #70399, #17595, #6660, #17970, #51552, #40239, #69657, #24366, #63996, #70034, #646, #23993, #11567, #23630, #64367, #52679, #12311, #46266, #35343, #47003, #69286, #12669, #51937, #34601, #34974, #40613, #13033, #36070, #63615, #18714, #11942, #35700, #58716, #1382, #41722, #31131, #53788, #20552, #60174, #37925, #8496, #47734, #25091, #14886, #70758, #31513, #59450, #49226, #54534, #71482, #2840, #37173, #1744, #43565, #60925, #24725, #48480, #48106, #65466, #30403, #54908, #60550, #31887, #53421, #65831, #43191, #42814, #14138, #7764, #25830, #19074, #8874, #42078, #66207, #54163, #48849, #19437, #2473, #3217, #71858, #13760, #19808, #20173, #8128, #14512, #37550, #65088, #26205, #30766, #66582, #72236, #2097, #13399, #36437, #71116, #42448, #36804, #59814, #25463, #61678, #38297 ),
 ( #56769, #61305, #3976, #16011, #55286, #9630, #21303, #32268, #39771, #3590, #45069, #16371, #32650, #9999, #4714, #4340, #39041, #56031, #20928, #10734, #62043, #43950, #56394, #51095, #73369, #44326, #38676, #10367, #27331, #27708, #50718, #33393, #45429, #33029, #72996, #73734, #55659, #39408, #62408, #28082, #44697, #9246, #26585, #66960, #67339, #49609, #15264, #22042, #15635, #72624, #26963, #68082, #68442, #50347, #33768, #21672, #74108, #22407, #16746, #49979, #5089, #67713, #46918, #68815, #40896, #29576, #35612, #23537, #188, #52959, #69943, #62773, #63902, #17506, #52588, #57893, #46549, #5455, #57139, #925, #18250, #51463, #6200, #41267, #23164, #40153, #11116, #69568, #34140, #28457, #17880, #74477, #12212, #35250, #64276, #12583, #1293, #51842, #28825, #22783, #23908, #46177, #45805, #5830, #58626, #24272, #58268, #69194, #6569, #6934, #40523, #29945, #47283, #17128, #70309, #63528, #29209, #63157, #52222, #18624, #11852, #11484, #34519, #57524, #34887, #554, #64646, #18986, #70669, #54819, #37458, #31799, #13675, #60456, #53330, #19346, #47647, #8405, #12944, #49132, #72145, #31418, #42359, #48389, #19719, #8786, #7673, #71393, #8035, #41635, #35982, #36714, #14424, #54067, #60086, #65375, #65744, #58999, #59726, #54445, #42730, #2376, #13309, #31042, #25372, #65000, #14046, #41990, #7304, #24999, #36346, #3130, #26113, #59361, #30310, #30679, #2753, #37082, #1655, #25741, #48761, #53698, #24636, #71769, #2009, #20085, #48017, #71028, #43099, #66116, #22606, #50538, #40343, #45627, #62600, #74298, #28281, #66488, #34704, #29023, #14798, #39603, #16190, #56594, #6019, #46000, #51663, #22994, #20456, #56964, #34337, #33967, #5279, #73553, #51287, #52042, #6, #37837, #57338, #45258, #68641, #10558, #68270, #69018, #16950, #4910, #10930, #11304, #73927, #4531, #17322, #60834, #9158, #39974, #32175, #62981, #5648, #63345, #28648, #11670, #33589 ) ),
 .UNSPECIFIED., .F., .F., .F. ) 
 B_SPLINE_SURFACE_WITH_KNOTS ( ( 2, 2 ),
 ( 3, 2, 2, 2, 2, 2, 2, 2, 2, 2, 2, 2, 2, 2, 2, 2, 2, 2, 2, 2, 2, 2, 2, 2, 2, 2, 2, 2, 2, 2, 2, 2, 2, 2, 2, 2, 2, 2, 2, 2, 2, 2, 2, 2, 2, 2, 2, 2, 2, 2, 2, 2, 2, 2, 2, 2, 2, 2, 2, 2, 2, 2, 2, 2, 2, 2, 2, 2, 2, 2, 2, 2, 2, 2, 2, 2, 2, 2, 2, 2, 2, 2, 2, 2, 2, 2, 2, 2, 2, 2, 2, 2, 2, 2, 2, 2, 2, 2, 2, 2, 2, 2, 2, 2, 2, 2, 2, 2, 2, 2, 2, 2, 2, 2, 2, 2, 2, 2, 2, 2, 3 ),
 ( 0.000000000000000000, 1.000000000000000000 ),
 ( 0.000000000000000000, 0.008333333333333333218, 0.01666666666666666644, 0.02500000000000000139, 0.03333333333333333287, 0.04166666666666666435, 0.05000000000000000278, 0.05833333333333333426, 0.06666666666666666574, 0.07499999999999999722, 0.08333333333333332871, 0.09166666666666666019, 0.1000000000000000056, 0.1083333333333333370, 0.1166666666666666685, 0.1250000000000000000, 0.1333333333333333315, 0.1416666666666666630, 0.1499999999999999944, 0.1583333333333333259, 0.1666666666666666574, 0.1749999999999999889, 0.1833333333333333204, 0.1916666666666666796, 0.2000000000000000111, 0.2083333333333333426, 0.2166666666666666741, 0.2250000000000000056, 0.2333333333333333370, 0.2416666666666666685, 0.2500000000000000000, 0.2583333333333333592, 0.2666666666666666630, 0.2750000000000000222, 0.2833333333333333259, 0.2916666666666666852, 0.2999999999999999889, 0.3083333333333333481, 0.3166666666666666519, 0.3250000000000000111, 0.3333333333333333148, 0.3416666666666666741, 0.3499999999999999778, 0.3583333333333333370, 0.3666666666666666408, 0.3750000000000000000, 0.3833333333333333592, 0.3916666666666666630, 0.4000000000000000222, 0.4083333333333333259, 0.4166666666666666852, 0.4249999999999999889, 0.4333333333333333481, 0.4416666666666666519, 0.4500000000000000111, 0.4583333333333333148, 0.4666666666666666741, 0.4749999999999999778, 0.4833333333333333370, 0.4916666666666666408, 0.5000000000000000000, 0.5083333333333333037, 0.5166666666666667185, 0.5250000000000000222, 0.5333333333333333259, 0.5416666666666666297, 0.5500000000000000444, 0.5583333333333333481, 0.5666666666666666519, 0.5749999999999999556, 0.5833333333333333703, 0.5916666666666666741, 0.5999999999999999778, 0.6083333333333332815, 0.6166666666666666963, 0.6250000000000000000, 0.6333333333333333037, 0.6416666666666667185, 0.6500000000000000222, 0.6583333333333333259, 0.6666666666666666297, 0.6750000000000000444, 0.6833333333333333481, 0.6916666666666666519, 0.6999999999999999556, 0.7083333333333333703, 0.7166666666666666741, 0.7249999999999999778, 0.7333333333333332815, 0.7416666666666666963, 0.7500000000000000000, 0.7583333333333333037, 0.7666666666666667185, 0.7750000000000000222, 0.7833333333333333259, 0.7916666666666666297, 0.8000000000000000444, 0.8083333333333333481, 0.8166666666666666519, 0.8249999999999999556, 0.8333333333333333703, 0.8416666666666666741, 0.8499999999999999778, 0.8583333333333332815, 0.8666666666666666963, 0.8750000000000000000, 0.8833333333333333037, 0.8916666666666667185, 0.9000000000000000222, 0.9083333333333333259, 0.9166666666666666297, 0.9250000000000000444, 0.9333333333333333481, 0.9416666666666666519, 0.9499999999999999556, 0.9583333333333333703, 0.9666666666666666741, 0.9749999999999999778, 0.9833333333333332815, 0.9916666666666666963, 1.000000000000000000 ),
 .UNSPECIFIED. ) 
 GEOMETRIC_REPRESENTATION_ITEM ( )  RATIONAL_B_SPLINE_SURFACE ( (
 ( 1.000000000000000000, 0.9238795325112867385, 1.000000000000000000, 0.9238795325112867385, 1.000000000000000000, 0.9238795325112867385, 1.000000000000000000, 0.9238795325112867385, 1.000000000000000000, 0.9238795325112867385, 1.000000000000000000, 0.9238795325112867385, 1.000000000000000000, 0.9238795325112867385, 1.000000000000000000, 0.9238795325112867385, 1.000000000000000000, 0.9238795325112867385, 1.000000000000000000, 0.9238795325112867385, 1.000000000000000000, 0.9238795325112867385, 1.000000000000000000, 0.9238795325112867385, 1.000000000000000000, 0.9238795325112867385, 1.000000000000000000, 0.9238795325112867385, 1.000000000000000000, 0.9238795325112867385, 1.000000000000000000, 0.9238795325112867385, 1.000000000000000000, 0.9238795325112867385, 1.000000000000000000, 0.9238795325112867385, 1.000000000000000000, 0.9238795325112867385, 1.000000000000000000, 0.9238795325112867385, 1.000000000000000000, 0.9238795325112867385, 1.000000000000000000, 0.9238795325112867385, 1.000000000000000000, 0.9238795325112867385, 1.000000000000000000, 0.9238795325112867385, 1.000000000000000000, 0.9238795325112867385, 1.000000000000000000, 0.9238795325112867385, 1.000000000000000000, 0.9238795325112867385, 1.000000000000000000, 0.9238795325112867385, 1.000000000000000000, 0.9238795325112867385, 1.000000000000000000, 0.9238795325112867385, 1.000000000000000000, 0.9238795325112867385, 1.000000000000000000, 0.9238795325112867385, 1.000000000000000000, 0.9238795325112867385, 1.000000000000000000, 0.9238795325112867385, 1.000000000000000000, 0.9238795325112867385, 1.000000000000000000, 0.9238795325112867385, 1.000000000000000000, 0.9238795325112867385, 1.000000000000000000, 0.9238795325112867385, 1.000000000000000000, 0.9238795325112867385, 1.000000000000000000, 0.9238795325112867385, 1.000000000000000000, 0.9238795325112867385, 1.000000000000000000, 0.9238795325112867385, 1.000000000000000000, 0.9238795325112867385, 1.000000000000000000, 0.9238795325112867385, 1.000000000000000000, 0.9238795325112867385, 1.000000000000000000, 0.9238795325112867385, 1.000000000000000000, 0.9238795325112867385, 1.000000000000000000, 0.9238795325112867385, 1.000000000000000000, 0.9238795325112867385, 1.000000000000000000, 0.9238795325112867385, 1.000000000000000000, 0.9238795325112867385, 1.000000000000000000, 0.9238795325112867385, 1.000000000000000000, 0.9238795325112867385, 1.000000000000000000, 0.9238795325112867385, 1.000000000000000000, 0.9238795325112867385, 1.000000000000000000, 0.9238795325112867385, 1.000000000000000000, 0.9238795325112867385, 1.000000000000000000, 0.9238795325112867385, 1.000000000000000000, 0.9238795325112867385, 1.000000000000000000, 0.9238795325112867385, 1.000000000000000000, 0.9238795325112867385, 1.000000000000000000, 0.9238795325112867385, 1.000000000000000000, 0.9238795325112867385, 1.000000000000000000, 0.9238795325112867385, 1.000000000000000000, 0.9238795325112867385, 1.000000000000000000, 0.9238795325112867385, 1.000000000000000000, 0.9238795325112867385, 1.000000000000000000, 0.9238795325112867385, 1.000000000000000000, 0.9238795325112867385, 1.000000000000000000, 0.9238795325112867385, 1.000000000000000000, 0.9238795325112867385, 1.000000000000000000, 0.9238795325112867385, 1.000000000000000000, 0.9238795325112867385, 1.000000000000000000, 0.9238795325112867385, 1.000000000000000000, 0.9238795325112867385, 1.000000000000000000, 0.9238795325112867385, 1.000000000000000000, 0.9238795325112867385, 1.000000000000000000, 0.9238795325112867385, 1.000000000000000000, 0.9238795325112867385, 1.000000000000000000, 0.9238795325112867385, 1.000000000000000000, 0.9238795325112867385, 1.000000000000000000, 0.9238795325112867385, 1.000000000000000000, 0.9238795325112867385, 1.000000000000000000, 0.9238795325112867385, 1.000000000000000000, 0.9238795325112867385, 1.000000000000000000, 0.9238795325112867385, 1.000000000000000000, 0.9238795325112867385, 1.000000000000000000, 0.9238795325112867385, 1.000000000000000000, 0.9238795325112867385, 1.000000000000000000, 0.9238795325112867385, 1.000000000000000000, 0.9238795325112867385, 1.000000000000000000, 0.9238795325112867385, 1.000000000000000000, 0.9238795325112867385, 1.000000000000000000, 0.9238795325112867385, 1.000000000000000000, 0.9238795325112867385, 1.000000000000000000, 0.9238795325112867385, 1.000000000000000000, 0.9238795325112867385, 1.000000000000000000, 0.9238795325112867385, 1.000000000000000000, 0.9238795325112867385, 1.000000000000000000, 0.9238795325112867385, 1.000000000000000000, 0.9238795325112867385, 1.000000000000000000, 0.9238795325112867385, 1.000000000000000000, 0.9238795325112867385, 1.000000000000000000, 0.9238795325112867385, 1.000000000000000000, 0.9238795325112867385, 1.000000000000000000, 0.9238795325112867385, 1.000000000000000000, 0.9238795325112867385, 1.000000000000000000, 0.9238795325112867385, 1.000000000000000000, 0.9238795325112867385, 1.000000000000000000, 0.9238795325112867385, 1.000000000000000000, 0.9238795325112867385, 1.000000000000000000, 0.9238795325112867385, 1.000000000000000000, 0.9238795325112867385, 1.000000000000000000, 0.9238795325112867385, 1.000000000000000000, 0.9238795325112867385, 1.000000000000000000, 0.9238795325112867385, 1.000000000000000000, 0.9238795325112867385, 1.000000000000000000, 0.9238795325112867385, 1.000000000000000000, 0.9238795325112867385, 1.000000000000000000, 0.9238795325112867385, 1.000000000000000000),
 ( 1.000000000000000000, 0.9238795325112867385, 1.000000000000000000, 0.9238795325112867385, 1.000000000000000000, 0.9238795325112867385, 1.000000000000000000, 0.9238795325112867385, 1.000000000000000000, 0.9238795325112867385, 1.000000000000000000, 0.9238795325112867385, 1.000000000000000000, 0.9238795325112867385, 1.000000000000000000, 0.9238795325112867385, 1.000000000000000000, 0.9238795325112867385, 1.000000000000000000, 0.9238795325112867385, 1.000000000000000000, 0.9238795325112867385, 1.000000000000000000, 0.9238795325112867385, 1.000000000000000000, 0.9238795325112867385, 1.000000000000000000, 0.9238795325112867385, 1.000000000000000000, 0.9238795325112867385, 1.000000000000000000, 0.9238795325112867385, 1.000000000000000000, 0.9238795325112867385, 1.000000000000000000, 0.9238795325112867385, 1.000000000000000000, 0.9238795325112867385, 1.000000000000000000, 0.9238795325112867385, 1.000000000000000000, 0.9238795325112867385, 1.000000000000000000, 0.9238795325112867385, 1.000000000000000000, 0.9238795325112867385, 1.000000000000000000, 0.9238795325112867385, 1.000000000000000000, 0.9238795325112867385, 1.000000000000000000, 0.9238795325112867385, 1.000000000000000000, 0.9238795325112867385, 1.000000000000000000, 0.9238795325112867385, 1.000000000000000000, 0.9238795325112867385, 1.000000000000000000, 0.9238795325112867385, 1.000000000000000000, 0.9238795325112867385, 1.000000000000000000, 0.9238795325112867385, 1.000000000000000000, 0.9238795325112867385, 1.000000000000000000, 0.9238795325112867385, 1.000000000000000000, 0.9238795325112867385, 1.000000000000000000, 0.9238795325112867385, 1.000000000000000000, 0.9238795325112867385, 1.000000000000000000, 0.9238795325112867385, 1.000000000000000000, 0.9238795325112867385, 1.000000000000000000, 0.9238795325112867385, 1.000000000000000000, 0.9238795325112867385, 1.000000000000000000, 0.9238795325112867385, 1.000000000000000000, 0.9238795325112867385, 1.000000000000000000, 0.9238795325112867385, 1.000000000000000000, 0.9238795325112867385, 1.000000000000000000, 0.9238795325112867385, 1.000000000000000000, 0.9238795325112867385, 1.000000000000000000, 0.9238795325112867385, 1.000000000000000000, 0.9238795325112867385, 1.000000000000000000, 0.9238795325112867385, 1.000000000000000000, 0.9238795325112867385, 1.000000000000000000, 0.9238795325112867385, 1.000000000000000000, 0.9238795325112867385, 1.000000000000000000, 0.9238795325112867385, 1.000000000000000000, 0.9238795325112867385, 1.000000000000000000, 0.9238795325112867385, 1.000000000000000000, 0.9238795325112867385, 1.000000000000000000, 0.9238795325112867385, 1.000000000000000000, 0.9238795325112867385, 1.000000000000000000, 0.9238795325112867385, 1.000000000000000000, 0.9238795325112867385, 1.000000000000000000, 0.9238795325112867385, 1.000000000000000000, 0.9238795325112867385, 1.000000000000000000, 0.9238795325112867385, 1.000000000000000000, 0.9238795325112867385, 1.000000000000000000, 0.9238795325112867385, 1.000000000000000000, 0.9238795325112867385, 1.000000000000000000, 0.9238795325112867385, 1.000000000000000000, 0.9238795325112867385, 1.000000000000000000, 0.9238795325112867385, 1.000000000000000000, 0.9238795325112867385, 1.000000000000000000, 0.9238795325112867385, 1.000000000000000000, 0.9238795325112867385, 1.000000000000000000, 0.9238795325112867385, 1.000000000000000000, 0.9238795325112867385, 1.000000000000000000, 0.9238795325112867385, 1.000000000000000000, 0.9238795325112867385, 1.000000000000000000, 0.9238795325112867385, 1.000000000000000000, 0.9238795325112867385, 1.000000000000000000, 0.9238795325112867385, 1.000000000000000000, 0.9238795325112867385, 1.000000000000000000, 0.9238795325112867385, 1.000000000000000000, 0.9238795325112867385, 1.000000000000000000, 0.9238795325112867385, 1.000000000000000000, 0.9238795325112867385, 1.000000000000000000, 0.9238795325112867385, 1.000000000000000000, 0.9238795325112867385, 1.000000000000000000, 0.9238795325112867385, 1.000000000000000000, 0.9238795325112867385, 1.000000000000000000, 0.9238795325112867385, 1.000000000000000000, 0.9238795325112867385, 1.000000000000000000, 0.9238795325112867385, 1.000000000000000000, 0.9238795325112867385, 1.000000000000000000, 0.9238795325112867385, 1.000000000000000000, 0.9238795325112867385, 1.000000000000000000, 0.9238795325112867385, 1.000000000000000000, 0.9238795325112867385, 1.000000000000000000, 0.9238795325112867385, 1.000000000000000000, 0.9238795325112867385, 1.000000000000000000, 0.9238795325112867385, 1.000000000000000000, 0.9238795325112867385, 1.000000000000000000, 0.9238795325112867385, 1.000000000000000000, 0.9238795325112867385, 1.000000000000000000, 0.9238795325112867385, 1.000000000000000000, 0.9238795325112867385, 1.000000000000000000, 0.9238795325112867385, 1.000000000000000000, 0.9238795325112867385, 1.000000000000000000, 0.9238795325112867385, 1.000000000000000000, 0.9238795325112867385, 1.000000000000000000, 0.9238795325112867385, 1.000000000000000000, 0.9238795325112867385, 1.000000000000000000, 0.9238795325112867385, 1.000000000000000000, 0.9238795325112867385, 1.000000000000000000, 0.9238795325112867385, 1.000000000000000000, 0.9238795325112867385, 1.000000000000000000, 0.9238795325112867385, 1.000000000000000000, 0.9238795325112867385, 1.000000000000000000, 0.9238795325112867385, 1.000000000000000000, 0.9238795325112867385, 1.000000000000000000, 0.9238795325112867385, 1.000000000000000000) ) ) 
 REPRESENTATION_ITEM ( '' )  SURFACE ( )  );
#47162 = CARTESIAN_POINT ( 'NONE',  ( 29.65685424949240101, 197.4375000000000000, 165.9999999999998863 ) ) ;
#47164 = CARTESIAN_POINT ( 'NONE',  ( -5.676582343749998039, 32.44791666325268409, -9.832129032723420536 ) ) ;
#47165 = CARTESIAN_POINT ( 'NONE',  ( 27.99999999999996803, 201.0000000000000000, 173.9999999999999147 ) ) ;
#47166 = CARTESIAN_POINT ( 'NONE',  ( 8.660254037844389075, 2.291666659838699438, -5.000000000000000000 ) ) ;
#47167 = CARTESIAN_POINT ( 'NONE',  ( 27.99999999999996447, 201.6250000027312126, 165.9999999999998863 ) ) ;
#47169 = FACE_OUTER_BOUND ( 'NONE', #9576, .T. ) ;
#47168 = DIRECTION ( 'NONE',  ( -0.000000000000000000, -0.000000000000000000, -1.000000000000000000 ) ) ;
#47170 = VECTOR ( 'NONE', #43648, 1000.000000000000000 ) ;
#47171 = ORIENTED_EDGE ( 'NONE', *, *, #74583, .T. ) ;
#47172 = CARTESIAN_POINT ( 'NONE',  ( 2.445694354108783219, 194.8125000013656063, 139.5543056458912190 ) ) ;
#47173 = CARTESIAN_POINT ( 'NONE',  ( 3.042071309553167069, 31.82291666325268054, -11.35316468749999785 ) ) ;
#47174 = CARTESIAN_POINT ( 'NONE',  ( 7.778174593052023411, -7.778174593052021635, 85.75000000409677625 ) ) ;
#47175 = CARTESIAN_POINT ( 'NONE',  ( -1.432654583217662481, 206.3750000013656063, 145.4587341250000350 ) ) ;
#47176 = CARTESIAN_POINT ( 'NONE',  ( -10.00000000000000711, 152.2916666666667140, -2.679491924311232953 ) ) ;
#47177 = CARTESIAN_POINT ( 'NONE',  ( -6.735557395310442023E-16, 11.00000000000000000, 101.1249999999999858 ) ) ;
#47179 = CARTESIAN_POINT ( 'NONE',  ( -5.676582343750006032, 19.11458332991934839, 9.832129032723418760 ) ) ;
#47178 = CARTESIAN_POINT ( 'NONE',  ( -2.977408999572652260, 106.4375000020483810, 7.188101187500000044 ) ) ;
#47180 = CARTESIAN_POINT ( 'NONE',  ( -5.656854249492375253, 5.656854249492375253, 17.14280277982336287 ) ) ;
#47181 = CARTESIAN_POINT ( 'NONE',  ( -2.085542519210945728E-15, 144.5312499965860411, 11.35316468750000141 ) ) ;
#47182 = CARTESIAN_POINT ( 'NONE',  ( -5.000000000000005329, 120.2083333265053824, 8.660254037844387298 ) ) ;
#47183 = CARTESIAN_POINT ( 'NONE',  ( 1.320432766682874540E-15, 112.9062500020483952, 7.188101187500000044 ) ) ;
#47184 = DIRECTION ( 'NONE',  ( -0.000000000000000000, 1.000000000000000000, -0.000000000000000000 ) ) ;
#47185 = CARTESIAN_POINT ( 'NONE',  ( -30.44569435410879166, 203.0625000013656063, 172.4456943541092357 ) ) ;
#47186 = ORIENTED_EDGE ( 'NONE', *, *, #2034, .T. ) ;
#47187 = CARTESIAN_POINT ( 'NONE',  ( 9.832129032723416984, 5.677083329919350163, 5.676582343750006032 ) ) ;
#47188 =( BOUNDED_CURVE ( )  B_SPLINE_CURVE ( 2, ( #57967, #73431, #1359, #13378, #63975, #6638, #40966, #70379, #52287 ),
 .UNSPECIFIED., .F., .F. ) 
 B_SPLINE_CURVE_WITH_KNOTS ( ( 3, 2, 2, 2, 3 ),
 ( 0.1315789473684210453, 0.1381578947368421184, 0.1447368421052631637, 0.1513157894736842368, 0.1578947368421052821 ),
 .UNSPECIFIED. ) 
 CURVE ( )  GEOMETRIC_REPRESENTATION_ITEM ( )  RATIONAL_B_SPLINE_CURVE ( ( 1.000000000000000000, 0.9238795325112867385, 1.000000000000000000, 0.9238795325112867385, 1.000000000000000000, 0.9238795325112867385, 1.000000000000000000, 0.9238795325112864054, 1.000000000000000222 ) ) 
 REPRESENTATION_ITEM ( '' )  );
#47189 = ORIENTED_EDGE ( 'NONE', *, *, #44909, .F. ) ;
#47190 = CARTESIAN_POINT ( 'NONE',  ( -4.615726161709595488, 16.27701803902710154, -69.62876280158768338 ) ) ;
#47191 = CARTESIAN_POINT ( 'NONE',  ( -4.088227598258586603E-16, 298.2031250017070079, -6.676582343750001591 ) ) ;
#47193 = CARTESIAN_POINT ( 'NONE',  ( -5.676582343749998039, 137.4479166632526983, -9.832129032723420536 ) ) ;
#47192 = CARTESIAN_POINT ( 'NONE',  ( -7.999999999999998224, 108.5937499999999858, 3.313708498984766049 ) ) ;
#47194 = CARTESIAN_POINT ( 'NONE',  ( -2.828427124746190735, 16.12499999726881228, -2.828427124746191623 ) ) ;
#47195 = CARTESIAN_POINT ( 'NONE',  ( 3.313708498984762496, -7.999999999999989342, 16.35530278432982243 ) ) ;
#47196 = VECTOR ( 'NONE', #26364, 1000.000000000000000 ) ;
#47197 = ADVANCED_FACE ( 'NONE', ( #42609 ), #65994, .F. ) ;
#47198 = CARTESIAN_POINT ( 'NONE',  ( 62.11418499370893187, 225.6321991852280462, 45.13563050677449695 ) ) ;
#47199 = CARTESIAN_POINT ( 'NONE',  ( -8.311093377946834337, 249.5312500034139873, 8.311093377946837890 ) ) ;
#47200 = CARTESIAN_POINT ( 'NONE',  ( -7.204075437095965206, -7.204075437095968759, 92.21875000204838102 ) ) ;
#47201 = VERTEX_POINT ( 'NONE', #54695 ) ;
#47202 = CARTESIAN_POINT ( 'NONE',  ( -2.679491924311382611, 205.4166666598386826, 9.999999999999914735 ) ) ;
#47203 = CARTESIAN_POINT ( 'NONE',  ( -4.000000000000002665, 8.562500000000000000, 1.656854249492380582 ) ) ;
#47204 = CARTESIAN_POINT ( 'NONE',  ( 8.311093377946834337, 90.46874999658599847, 8.311093377946839666 ) ) ;
#47205 = CARTESIAN_POINT ( 'NONE',  ( -7.204075437095967871, 7.204075437095967871, 100.4687500020483668 ) ) ;
#47206 = CARTESIAN_POINT ( 'NONE',  ( -1.881053915767124440, 16.12499999863440436, 4.541265875000001451 ) ) ;
#47207 = EDGE_LOOP ( 'NONE', ( #10651, #71588, #48315, #69845, #8074, #69758, #14602, #16667, #57514, #63947, #2756, #73924, #37074, #7332, #8329, #20238, #35812, #15113, #25209, #10163, #63237, #7812, #23847, #61419, #11737, #62534, #59674, #49349, #54904, #1751, #42828, #23026, #38043, #69334, #26010, #51042, #36935, #41157, #25645, #30930, #44907, #67196, #23305, #41346, #44409, #7893, #24105, #52350, #2922, #62875, #27786 ) ) ;
#47208 = VERTEX_POINT ( 'NONE', #71646 ) ;
#47209 = CARTESIAN_POINT ( 'NONE',  ( 5.656854249492380582, 4.687500000000000888, -5.656854249492380582 ) ) ;
#47210 = CARTESIAN_POINT ( 'NONE',  ( -5.082755093536326818, 1.406249997951610320, 5.082755093536325042 ) ) ;
#47211 = CARTESIAN_POINT ( 'NONE',  ( -3.313708498984762496, 119.4687500040967905, 7.999999999999998224 ) ) ;
#47212 = CARTESIAN_POINT ( 'NONE',  ( -6.238412754330611322E-16, 10.18810118749999916, 106.6562500020483810 ) ) ;
#47213 = CIRCLE ( 'NONE', #62897, 3.999999999999986233 ) ;
#47214 = CARTESIAN_POINT ( 'NONE',  ( 1.656854249492381248, 1.187500000000000444, -4.000000000000001776 ) ) ;
#47215 = CARTESIAN_POINT ( 'NONE',  ( -7.347880794884122694E-16, 15.49999999726881406, 4.000000000000001776 ) ) ;
#47216 = CARTESIAN_POINT ( 'NONE',  ( -7.999999999999991118, 3.313708498984757167, 12.92405278392014800 ) ) ;
#47217 = VERTEX_POINT ( 'NONE', #51163 ) ;
#47218 = CARTESIAN_POINT ( 'NONE',  ( -10.99999999999989164, -4.556349186104158733, 80.59374999999998579 ) ) ;
#47219 = CARTESIAN_POINT ( 'NONE',  ( -1.432654583217607192, 198.2500000013656347, 194.5412658750000219 ) ) ;
#47220 = ADVANCED_FACE ( 'NONE', ( #25985 ), #65623, .T. ) ;
#47221 =( REPRESENTATION_RELATIONSHIP ('NONE','NONE', #46008, #66708 ) REPRESENTATION_RELATIONSHIP_WITH_TRANSFORMATION ( #26633 )SHAPE_REPRESENTATION_RELATIONSHIP( ) );
#47223 = DIRECTION ( 'NONE',  ( -0.000000000000000000, 1.000000000000000000, -0.000000000000000000 ) ) ;
#47222 = CARTESIAN_POINT ( 'NONE',  ( -24.54126587500002188, 199.2500000013656063, 168.5673454167826435 ) ) ;
#47224 = EDGE_CURVE ( 'NONE', #48362, #38468, #55242, .T. ) ;
#47225 = CARTESIAN_POINT ( 'NONE',  ( 4.541265875000002339, 14.37499999863440969, -1.881053915767121554 ) ) ;
#47226 = AXIS2_PLACEMENT_3D ( 'NONE', #15189, #32945, #26498 ) ;
#47227 = CARTESIAN_POINT ( 'NONE',  ( 7.778174593052021635, 7.778174593052023411, 84.43749999999998579 ) ) ;
#47228 = CARTESIAN_POINT ( 'NONE',  ( -7.188101187499990274, -2.977408999572651371, 10.58030278187175455 ) ) ;
#47229 = ORIENTED_EDGE ( 'NONE', *, *, #47538, .T. ) ;
#47230 = ORIENTED_EDGE ( 'NONE', *, *, #29495, .T. ) ;
#47231 = CARTESIAN_POINT ( 'NONE',  ( 10.18810118749999916, 1.247682550866122264E-15, 105.9062500020483810 ) ) ;
#47232 = CARTESIAN_POINT ( 'NONE',  ( 8.000000000000000000, 96.03125000409677625, -3.313708498984762496 ) ) ;
#47233 = CARTESIAN_POINT ( 'NONE',  ( -24.00000000000001066, 205.8125000000000000, 168.3431457505080004 ) ) ;
#47234 = CARTESIAN_POINT ( 'NONE',  ( 2.445694354108839619, 198.8125000013656063, 200.4456943541088663 ) ) ;
#47235 = DIRECTION ( 'NONE',  ( -1.000000000000000000, 0.000000000000000000, 0.000000000000000000 ) ) ;
#47236 = CARTESIAN_POINT ( 'NONE',  ( 10.00000000000000178, 100.2083333333333428, -2.679491924311226736 ) ) ;
#47237 = VECTOR ( 'NONE', #52034, 1000.000000000000000 ) ;
#47238 = CARTESIAN_POINT ( 'NONE',  ( 8.000000000000000000, 119.7500000000000000, -9.797174393178825657E-16 ) ) ;
#47239 = CARTESIAN_POINT ( 'NONE',  ( 3.042071309553159519, 55.05208332991934128, 11.35316468750000141 ) ) ;
#47240 = CARTESIAN_POINT ( 'NONE',  ( 4.721056650415999201, 296.2343750017069510, -4.721056650415999201 ) ) ;
#47241 = VERTEX_POINT ( 'NONE', #50789 ) ;
#47242 = CARTESIAN_POINT ( 'NONE',  ( 10.00000000000004086, 189.7916666666667140, 2.679491924311245388 ) ) ;
#47243 = EDGE_CURVE ( 'NONE', #43757, #39207, #72020, .T. ) ;
#47244 = CARTESIAN_POINT ( 'NONE',  ( 5.656854249492380582, 16.49999999590322375, -5.656854249492380582 ) ) ;
#47245 = CARTESIAN_POINT ( 'NONE',  ( 2.445694354108783664, 206.3125000013656063, 144.4456943541088663 ) ) ;
#47246 = CARTESIAN_POINT ( 'NONE',  ( 1.681385197618709730E-11, 51.24999999999869971, -10.00000000000000178 ) ) ;
#47247 = CARTESIAN_POINT ( 'NONE',  ( 1.656854249492381914, 7.812500000000000000, 4.000000000000000888 ) ) ;
#47248 = CARTESIAN_POINT ( 'NONE',  ( -7.320508075688771932, 229.3749999999999716, -7.320508075688771932 ) ) ;
#47249 = CARTESIAN_POINT ( 'NONE',  ( 0.000000000000000000, 300.0000000000000000, 0.000000000000000000 ) ) ;
#47250 = CARTESIAN_POINT ( 'NONE',  ( 7.204075437095968759, -7.204075437095966983, 71.59375000204836681 ) ) ;
#47251 = CARTESIAN_POINT ( 'NONE',  ( -5.000000000000005329, 218.3333333333333428, 8.660254037844387298 ) ) ;
#47252 = CARTESIAN_POINT ( 'NONE',  ( -2.977408999572647819, 7.188101187499992051, 13.58030278187175455 ) ) ;
#47253 = CARTESIAN_POINT ( 'NONE',  ( -2.085542519210945728E-15, 179.8437499965860411, 11.35316468750000141 ) ) ;
#47254 = CARTESIAN_POINT ( 'NONE',  ( 2.780723358947928197E-16, 0.5624999986344066949, -4.541265875000002339 ) ) ;
#47255 = CYLINDRICAL_SURFACE ( 'NONE', #24794, 11.00000000000000000 ) ;
#47257 = DIRECTION ( 'NONE',  ( 1.577021341797097560E-16, -1.000000000000000000, 0.000000000000000000 ) ) ;
#47256 = CARTESIAN_POINT ( 'NONE',  ( -3.999999999999959144, 203.1875000027311842, 199.6568542494924259 ) ) ;
#47258 = VERTEX_POINT ( 'NONE', #66369 ) ;
#47259 = CARTESIAN_POINT ( 'NONE',  ( -3.458734125000015869, 207.1875000013656063, 142.0000000000000568 ) ) ;
#47260 = CARTESIAN_POINT ( 'NONE',  ( 11.35316468750000141, 36.09374999658601979, 0.000000000000000000 ) ) ;
#47261 = CARTESIAN_POINT ( 'NONE',  ( -7.778174593052023411, 7.778174593052023411, 106.0000000040967763 ) ) ;
#47262 = CARTESIAN_POINT ( 'NONE',  ( 11.35316468749999785, 215.8854166632526983, 3.042071309553174174 ) ) ;
#47263 = CARTESIAN_POINT ( 'NONE',  ( -27.99999999999992184, 206.9375000013656063, 173.4587341250003760 ) ) ;
#47264 = CARTESIAN_POINT ( 'NONE',  ( 4.999999999999994671, 9.166666666666666075, 8.660254037844390851 ) ) ;
#47266 = DIRECTION ( 'NONE',  ( -0.000000000000000000, -1.000000000000000000, -0.000000000000000000 ) ) ;
#47265 = CARTESIAN_POINT ( 'NONE',  ( -2.977408999572652260, 121.4375000020483810, 7.188101187500000044 ) ) ;
#47267 = CARTESIAN_POINT ( 'NONE',  ( -1.432654583217662259, 196.1250000013656063, 145.4587341250000350 ) ) ;
#47268 = CARTESIAN_POINT ( 'NONE',  ( -10.00000000000000000, 69.16666665983868256, -2.679491924311229845 ) ) ;
#47269 = CIRCLE ( 'NONE', #66536, 37.00000000000000711 ) ;
#47270 = CARTESIAN_POINT ( 'NONE',  ( -4.401442555609581635E-16, 99.78125000204838102, -7.188101187500000044 ) ) ;
#47271 = CARTESIAN_POINT ( 'NONE',  ( 3.211159895383561835, 15.56249999863440614, -3.211159895383561835 ) ) ;
#47272 = CARTESIAN_POINT ( 'NONE',  ( 0.000000000000000000, 0.000000000000000000, 0.000000000000000000 ) ) ;
#47273 = CARTESIAN_POINT ( 'NONE',  ( 0.5126016559340066392, 0.4114670971541452560, -7.911467097154144312 ) ) ;
#47274 = DIRECTION ( 'NONE',  ( -0.000000000000000000, -1.000000000000000000, -0.000000000000000000 ) ) ;
#47275 = ORIENTED_EDGE ( 'NONE', *, *, #41424, .T. ) ;
#47276 = EDGE_LOOP ( 'NONE', ( #26517, #33528, #61614, #51208 ) ) ;
#47277 = CARTESIAN_POINT ( 'NONE',  ( 2.765530957081996366, 296.2968750017070079, -6.676582343750003368 ) ) ;
#47278 = CARTESIAN_POINT ( 'NONE',  ( -10.00000000000001243, 142.2916666666666856, -2.679491924311233841 ) ) ;
#47279 = CARTESIAN_POINT ( 'NONE',  ( -28.47326357806616315, 194.4587341250000350, 166.5737975347167321 ) ) ;
#47280 = CARTESIAN_POINT ( 'NONE',  ( 5.676582343750001591, 156.6145833299193839, -9.832129032723420536 ) ) ;
#47281 = CARTESIAN_POINT ( 'NONE',  ( -10.18810118749999916, 0.000000000000000000, 81.15625000204838102 ) ) ;
#47282 = CARTESIAN_POINT ( 'NONE',  ( 7.320508075688775484, 5.625000000000000000, -7.320508075688775484 ) ) ;
#47283 = CARTESIAN_POINT ( 'NONE',  ( -3.999999999999960032, 203.0000000000000000, 198.0000000000000284 ) ) ;
#47284 = DIRECTION ( 'NONE',  ( 0.000000000000000000, 0.000000000000000000, 1.000000000000000000 ) ) ;
#47285 = EDGE_CURVE ( 'NONE', #62397, #56611, #55068, .T. ) ;
#47286 = CARTESIAN_POINT ( 'NONE',  ( 1.871523826299183495E-15, -10.18810118749999916, 108.9062500020483668 ) ) ;
#47287 = ORIENTED_EDGE ( 'NONE', *, *, #31636, .T. ) ;
#47288 =( BOUNDED_CURVE ( )  B_SPLINE_CURVE ( 2, ( #30491, #42903, #8589, #31228, #2934, #48938, #2563, #25552, #13488, #48566, #65923, #70849, #53508 ),
 .UNSPECIFIED., .F., .F. ) 
 B_SPLINE_CURVE_WITH_KNOTS ( ( 3, 2, 2, 2, 2, 2, 3 ),
 ( 0.9262938265175630903, 0.9315262799636203628, 0.9367587334096776353, 0.9419911868557350187, 0.9472236403017922912, 0.9524560937478495637, 0.9576885471939067251 ),
 .UNSPECIFIED. ) 
 CURVE ( )  GEOMETRIC_REPRESENTATION_ITEM ( )  RATIONAL_B_SPLINE_CURVE ( ( 0.9999999999999990008, 0.9659258262890693114, 1.000000000000000000, 0.9659258262890683122, 1.000000000000000000, 0.9659258262890683122, 1.000000000000000000, 0.9659258262890683122, 1.000000000000000000, 0.9659258262890683122, 1.000000000000000000, 0.9659258262891518010, 0.9999999999999165112 ) ) 
 REPRESENTATION_ITEM ( '' )  );
#47289 = DIRECTION ( 'NONE',  ( -7.885106708985487801E-17, 1.000000000000000000, -0.000000000000000000 ) ) ;
#47290 = VECTOR ( 'NONE', #15742, 1000.000000000000000 ) ;
#47291 = CARTESIAN_POINT ( 'NONE',  ( -2.085542519210945728E-15, 144.8437499965860411, 11.35316468750000141 ) ) ;
#47292 = CARTESIAN_POINT ( 'NONE',  ( 2.445694354108839619, 197.8125000013656063, 200.4456943541088663 ) ) ;
#47293 = CARTESIAN_POINT ( 'NONE',  ( 3.458734124999959914, 194.4587341250000065, 142.0000000000000568 ) ) ;
#47295 = EDGE_CURVE ( 'NONE', #43701, #16032, #38087, .T. ) ;
#47294 = CARTESIAN_POINT ( 'NONE',  ( 10.18810118749999916, 1.247682550866122264E-15, 74.78125000204836681 ) ) ;
#47296 = B_SPLINE_CURVE_WITH_KNOTS ( 'NONE', 3,
 ( #42397, #49173, #48427, #71430, #43141, #66524, #2792, #55233, #66156, #42767, #66910, #37498, #48799, #65783, #26914, #72183, #37875, #8825 ),
 .UNSPECIFIED., .F., .F.,
 ( 4, 2, 2, 2, 2, 2, 2, 2, 4 ),
 ( 0.000000000000000000, 0.06250000000000000000, 0.1250000000000000000, 0.1875000000000000000, 0.2500000000000000000, 0.3125000000000000000, 0.3750000000000000000, 0.4375000000000000000, 0.5000000000000000000 ),
 .UNSPECIFIED. ) ;
#47297 = CARTESIAN_POINT ( 'NONE',  ( -3.042071309553173730, 49.63541666325267698, 11.35316468749999785 ) ) ;
#47298 = ORIENTED_EDGE ( 'NONE', *, *, #49305, .F. ) ;
#47299 = CARTESIAN_POINT ( 'NONE',  ( -7.320508075688782590, 28.12500000000000355, 7.320508075688774596 ) ) ;
#47300 = CARTESIAN_POINT ( 'NONE',  ( 3.211159895383561835, 4.562499998634407028, -3.211159895383561835 ) ) ;
#47301 = CARTESIAN_POINT ( 'NONE',  ( 8.008118988124991233, 9.807117285998411148E-16, 12.26311528394063011 ) ) ;
#47302 = CARTESIAN_POINT ( 'NONE',  ( -5.082755093536326818, 13.40624999795161187, 5.082755093536325042 ) ) ;
#47303 = CARTESIAN_POINT ( 'NONE',  ( -4.242640687119285658, 294.1875000034139589, 4.242640687119287435 ) ) ;
#47304 = CARTESIAN_POINT ( 'NONE',  ( 3.360070523759410399, 124.5134190293533010, -7.253681227061663073 ) ) ;
#47305 = CARTESIAN_POINT ( 'NONE',  ( -7.188101187500001821, 11.99999999795161187, -2.977408999572651371 ) ) ;
#47306 = CARTESIAN_POINT ( 'NONE',  ( -7.188101187499992051, 2.977408999572646930, 11.89280278187175277 ) ) ;
#47307 =( BOUNDED_CURVE ( )  B_SPLINE_CURVE ( 2, ( #22087, #33815, #74524, #68490, #21714, #73410, #4383, #68864, #50395, #45111, #11158, #33077, #67759 ),
 .UNSPECIFIED., .F., .F. ) 
 B_SPLINE_CURVE_WITH_KNOTS ( ( 3, 2, 2, 2, 2, 2, 3 ),
 ( 0.9890912047459377021, 0.9943250801786815973, 0.9995589556114257146, 1.004792831044169832, 1.010026706476913949, 1.015260581909658066, 1.020494457342402184 ),
 .UNSPECIFIED. ) 
 CURVE ( )  GEOMETRIC_REPRESENTATION_ITEM ( )  RATIONAL_B_SPLINE_CURVE ( ( 1.000000000000001110, 0.9659258262890673130, 1.000000000000000000, 0.9659258262890683122, 1.000000000000000000, 0.9659258262890683122, 1.000000000000000000, 0.9659258262890683122, 1.000000000000000000, 0.9659258262890683122, 1.000000000000000000, 0.9659258262891643465, 0.9999999999999039657 ) ) 
 REPRESENTATION_ITEM ( '' )  );
#47308 = CARTESIAN_POINT ( 'NONE',  ( -10.18810118749999916, 0.000000000000000000, 69.15625000204836681 ) ) ;
#47309 = EDGE_CURVE ( 'NONE', #60564, #21067, #13244, .T. ) ;
#47310 = CARTESIAN_POINT ( 'NONE',  ( -31.45873412500001010, 206.8750000013656347, 168.5673454167827572 ) ) ;
#47311 = EDGE_CURVE ( 'NONE', #62350, #22045, #63592, .T. ) ;
#47312 = CARTESIAN_POINT ( 'NONE',  ( 1.881053915767122664, 22.24999999863440792, 4.541265875000001451 ) ) ;
#47313 = ORIENTED_EDGE ( 'NONE', *, *, #71387, .T. ) ;
#47314 = CARTESIAN_POINT ( 'NONE',  ( 3.458734125000015425, 208.9375000013656063, 198.0000000000000284 ) ) ;
#47315 = CARTESIAN_POINT ( 'NONE',  ( 3.999999999999960032, 200.9375000000000284, 143.6568542494924543 ) ) ;
#47316 = CARTESIAN_POINT ( 'NONE',  ( -25.17157287525373732, 195.7500000027312126, 172.8284271247464972 ) ) ;
#47317 = ADVANCED_FACE ( 'NONE', ( #41337 ), #5897, .T. ) ;
#47318 = CARTESIAN_POINT ( 'NONE',  ( -4.541265875000002339, 1.812499998634406584, -5.561446717895856393E-16 ) ) ;
#47319 = CARTESIAN_POINT ( 'NONE',  ( -5.082755093536324154, 116.8437500020483810, 5.082755093536326818 ) ) ;
#47320 = CARTESIAN_POINT ( 'NONE',  ( 36.10814071610729314, 133.9999999999999716, 139.0000000000000000 ) ) ;
#47321 = CARTESIAN_POINT ( 'NONE',  ( -5.656854249492373476, -5.656854249492376141, -0.2946972160798554397 ) ) ;
#47322 = ORIENTED_EDGE ( 'NONE', *, *, #17707, .F. ) ;
#47323 = CARTESIAN_POINT ( 'NONE',  ( -5.082755093536325042, 22.03124999795161543, -5.082755093536325930 ) ) ;
#47324 = ORIENTED_EDGE ( 'NONE', *, *, #5284, .T. ) ;
#47325 = CARTESIAN_POINT ( 'NONE',  ( 4.999999999999997335, 256.4583333401613459, -8.660254037844387298 ) ) ;
#47326 = CARTESIAN_POINT ( 'NONE',  ( 5.656854249492380582, 13.68750000000000178, -5.656854249492380582 ) ) ;
#47327 = CARTESIAN_POINT ( 'NONE',  ( 29.43265458321766914, 207.5000000013656063, 173.4587341249998929 ) ) ;
#47328 = CARTESIAN_POINT ( 'NONE',  ( 7.320508075688774596, 50.62500000000000711, -7.320508075688774596 ) ) ;
#47329 = CARTESIAN_POINT ( 'NONE',  ( 1.320432766682874540E-15, 102.4062500020483810, 7.188101187500000044 ) ) ;
#47330 = CARTESIAN_POINT ( 'NONE',  ( 4.242640687119285658, 294.6249999999999432, -4.242640687119286547 ) ) ;
#47332 = CARTESIAN_POINT ( 'NONE',  ( 38.00000000000000000, 53.00000000000000000, 15.00000000000000178 ) ) ;
#47331 = CARTESIAN_POINT ( 'NONE',  ( -38.00000000000002132, 50.00000000000000711, 69.99999999999998579 ) ) ;
#47333 = ORIENTED_EDGE ( 'NONE', *, *, #52070, .F. ) ;
#47334 = CARTESIAN_POINT ( 'NONE',  ( 8.311093377946834337, 237.0312500034140157, -8.311093377946836114 ) ) ;
#47335 = CARTESIAN_POINT ( 'NONE',  ( 7.188101187499991163, 2.977408999572648707, 14.70530278187175455 ) ) ;
#47336 = CARTESIAN_POINT ( 'NONE',  ( -1.836970198721029983E-15, 65.62499999317203958, 10.00000000000000178 ) ) ;
#47337 = CARTESIAN_POINT ( 'NONE',  ( -4.999999999999998224, 73.54166665983869677, -8.660254037844389075 ) ) ;
#47338 = CARTESIAN_POINT ( 'NONE',  ( 7.999999999752645863, -6.290875383172500320E-05, 1.767801038436179750 ) ) ;
#47339 = CYLINDRICAL_SURFACE ( 'NONE', #58049, 3.999999999999976019 ) ;
#47340 = LINE ( 'NONE', #63206, #7784 ) ;
#47341 = CARTESIAN_POINT ( 'NONE',  ( -10.00000000000000000, 177.2916666666666856, -2.679491924311229845 ) ) ;
#47342 = CARTESIAN_POINT ( 'NONE',  ( -3.673940397442060854E-16, 297.8125000034140157, -6.000000000000001776 ) ) ;
#47343 = CARTESIAN_POINT ( 'NONE',  ( -4.898587196589412829E-16, 118.6250000000000000, -8.000000000000000000 ) ) ;
#47344 = CARTESIAN_POINT ( 'NONE',  ( -0.8761883848953855303, -67.61551161115575326, 20.05282165013548834 ) ) ;
#47345 = CARTESIAN_POINT ( 'NONE',  ( 11.35316468749999963, 146.3020833299193555, -3.042071309553165293 ) ) ;
#47346 = CARTESIAN_POINT ( 'NONE',  ( 23.99999999999999645, 201.6875000000000284, 168.3431457505074889 ) ) ;
#47347 = CARTESIAN_POINT ( 'NONE',  ( 8.000000000000001776, 97.34375000409679046, 3.313708498984759387 ) ) ;
#47350 = CARTESIAN_POINT ( 'NONE',  ( -2.485281374238217822, 294.1875000000000568, 6.000000000000357048 ) ) ;
#47349 = CARTESIAN_POINT ( 'NONE',  ( 7.320508075688774596, 107.4999999931720254, -7.320508075688774596 ) ) ;
#47348 = CARTESIAN_POINT ( 'NONE',  ( 32.00000000000000000, 208.2500000000000284, 169.9999999999999432 ) ) ;
#47351 = EDGE_LOOP ( 'NONE', ( #58705, #26057, #20308, #61109 ) ) ;
#47352 = CIRCLE ( 'NONE', #14813, 15.99999999999998579 ) ;
#47353 = CARTESIAN_POINT ( 'NONE',  ( 3.313708498984762496, 10.21875000000000178, 7.999999999999998224 ) ) ;
#47354 = CARTESIAN_POINT ( 'NONE',  ( -8.999999999999998224, 0.000000000000000000, 0.000000000000000000 ) ) ;
#47355 = CARTESIAN_POINT ( 'NONE',  ( -1.432654583217664479, 207.7500000013656063, 138.5412658750000787 ) ) ;
#47356 = CARTESIAN_POINT ( 'NONE',  ( -4.000000000000015987, 202.5625000000000000, 143.6568542494924259 ) ) ;
#47357 = CARTESIAN_POINT ( 'NONE',  ( 10.00000000000000000, 41.66666665983870388, 2.679491924311236062 ) ) ;
#47358 = CARTESIAN_POINT ( 'NONE',  ( -2.977408999572650927, 116.3750000020483810, -7.188101187500001821 ) ) ;
#47359 = CARTESIAN_POINT ( 'NONE',  ( -1.881053915767124440, 6.124999998634407916, 4.541265875000001451 ) ) ;
#47360 = CARTESIAN_POINT ( 'NONE',  ( 30.64284399271082293, -37.99999999999981526, 174.6921329945330683 ) ) ;
#47361 = CARTESIAN_POINT ( 'NONE',  ( 3.313708498984762496, -7.999999999999989342, 17.79905277982336642 ) ) ;
#47363 = DIRECTION ( 'NONE',  ( 1.000000000000000000, -0.000000000000000000, -0.000000000000000000 ) ) ;
#47362 = CARTESIAN_POINT ( 'NONE',  ( -32.00000000000000000, 203.2500000000000000, 170.0000000000003979 ) ) ;
#47364 = ORIENTED_EDGE ( 'NONE', *, *, #50562, .F. ) ;
#47365 = CARTESIAN_POINT ( 'NONE',  ( 5.656854249492379694, 93.12500000409677625, -5.656854249492380582 ) ) ;
#47366 = FACE_OUTER_BOUND ( 'NONE', #10724, .T. ) ;
#47367 = CARTESIAN_POINT ( 'NONE',  ( -11.35316468749999963, 244.2187500034140157, 0.000000000000000000 ) ) ;
#47368 = CARTESIAN_POINT ( 'NONE',  ( -8.311093377946836114, 112.6562499965860127, -8.311093377946837890 ) ) ;
#47369 = ORIENTED_EDGE ( 'NONE', *, *, #41757, .F. ) ;
#47370 = CARTESIAN_POINT ( 'NONE',  ( -27.99999999999990763, 196.6250000027312126, 174.0000000000003695 ) ) ;
#47371 = CARTESIAN_POINT ( 'NONE',  ( 10.18810118750000093, -4.220049686691933921, 101.3125000020483810 ) ) ;
#47372 = CARTESIAN_POINT ( 'NONE',  ( 7.778174593052021635, 7.778174593052023411, 86.12500000409677625 ) ) ;
#47373 = CARTESIAN_POINT ( 'NONE',  ( -1.432654583217608080, 201.8750000013656063, 201.4587341250000350 ) ) ;
#47374 = LINE ( 'NONE', #22884, #21520 ) ;
#47376 = CARTESIAN_POINT ( 'NONE',  ( 9.832129032723416984, 110.3645833299193555, 5.676582343750006032 ) ) ;
#47375 = DIRECTION ( 'NONE',  ( 0.000000000000000000, 0.000000000000000000, 1.000000000000000000 ) ) ;
#47377 = CARTESIAN_POINT ( 'NONE',  ( -7.999999999999991118, 3.313708498984756723, 9.924052783920146226 ) ) ;
#47378 = CARTESIAN_POINT ( 'NONE',  ( -29.43265458321760164, 196.1250000013655779, 173.4587341250003760 ) ) ;
#47379 = EDGE_CURVE ( 'NONE', #25157, #35750, #52807, .T. ) ;
#47380 = CARTESIAN_POINT ( 'NONE',  ( 2.679491924311149464, 80.83333332650533976, 10.00000000000004619 ) ) ;
#47381 = ORIENTED_EDGE ( 'NONE', *, *, #32937, .F. ) ;
#47382 = CARTESIAN_POINT ( 'NONE',  ( -5.000000000000005329, 200.2083333265053682, 8.660254037844387298 ) ) ;
#47383 = CARTESIAN_POINT ( 'NONE',  ( -11.00000000000010303, -4.556349186103947346, 73.09375000000000000 ) ) ;
#47384 = AXIS2_PLACEMENT_3D ( 'NONE', #56679, #34055, #57050 ) ;
#47385 = FACE_OUTER_BOUND ( 'NONE', #36085, .T. ) ;
#47386 = CARTESIAN_POINT ( 'NONE',  ( 5.676582343749993598, 105.2604166632526841, 9.832129032723422313 ) ) ;
#47387 = CARTESIAN_POINT ( 'NONE',  ( 0.000000000000000000, 0.000000000000000000, -8.000000000000000000 ) ) ;
#47388 = CARTESIAN_POINT ( 'NONE',  ( 5.082755093536325930, 11.53124999795161187, -5.082755093536325930 ) ) ;
#47390 = EDGE_CURVE ( 'NONE', #70797, #57404, #27689, .T. ) ;
#47389 = CARTESIAN_POINT ( 'NONE',  ( -6.238412754330611322E-16, 10.18810118749999916, 93.15625000204836681 ) ) ;
#47391 = CARTESIAN_POINT ( 'NONE',  ( -3.042071309553164404, 12.55208332991935194, -11.35316468749999963 ) ) ;
#47392 = ORIENTED_EDGE ( 'NONE', *, *, #22567, .F. ) ;
#47393 = CARTESIAN_POINT ( 'NONE',  ( -10.00000000000001421, 137.7083333333333428, 2.679491924311226292 ) ) ;
#47394 = FACE_OUTER_BOUND ( 'NONE', #63381, .T. ) ;
#47395 = CARTESIAN_POINT ( 'NONE',  ( 11.00000000000000000, 1.347111479062088405E-15, 102.2500000000000000 ) ) ;
#47396 = CARTESIAN_POINT ( 'NONE',  ( -10.18810118749999916, 4.220049686691934809, 75.43750000204836681 ) ) ;
#47397 = DIRECTION ( 'NONE',  ( 0.000000000000000000, 1.000000000000000000, 0.000000000000000000 ) ) ;
#47398 = CARTESIAN_POINT ( 'NONE',  ( -10.00000000000000355, 149.5833333265053682, 2.679491924311223183 ) ) ;
#47399 = CARTESIAN_POINT ( 'NONE',  ( -4.088227598258586603E-16, 293.2031250017069510, -6.676582343750001591 ) ) ;
#47400 = CARTESIAN_POINT ( 'NONE',  ( -4.556349186104045934, 11.00000000000000000, 89.40625000409677625 ) ) ;
#47401 = CARTESIAN_POINT ( 'NONE',  ( 11.35316468749999963, 206.3020833299193271, -3.042071309553165293 ) ) ;
#47402 = CARTESIAN_POINT ( 'NONE',  ( 7.204075437095966983, 7.204075437095967871, 86.59375000204836681 ) ) ;
#47403 =( BOUNDED_SURFACE ( )  B_SPLINE_SURFACE ( 1, 2, ( 
 ( #35911, #64208, #30241, #58197, #23467, #57825, #12512, #7601, #12146, #35544, #13243, #53631, #30609, #47577, #70600, #36277, #35182, #63830, #18917, #24200, #52519, #6130, #46479, #29136, #58558, #856, #52890, #6863, #46848, #52151, #41561, #487, #69499, #23841, #1941, #69126, #40824, #40455, #69870, #18183, #11779, #64934, #17431, #29875, #1221, #47211, #70245, #64577, #12874, #58930, #7237, #3056, #37766, #49441, #3425, #48689, #9088, #53993, #32101, #49060, #71695, #20013, #2304, #55121, #43785, #72069, #26039, #31725, #31342, #8332, #13970, #60384, #66800, #70962, #55492, #54373, #8710, #42660, #26414, #72460, #30974, #37013, #14726, #25301, #65303, #59655, #15103, #43024, #43402, #20388, #42289, #20767, #66047, #19647, #9466, #13608, #66417, #48320, #38135, #60765, #14354, #61136, #54747, #19279, #32484, #25670, #36646, #60014, #71326, #65672, #7972, #2683, #37382, #24930, #47944, #50188, #44165, #33237, #68288, #11322, #38513, #34355, #33987, #49818, #39621, #16585, #3807, #39250, #9837, #61514, #56235, #4929, #15846, #62621, #4550, #32864, #28298, #73573, #10207, #55868, #62998, #73210, #50935, #67179, #15475, #62249, #10951, #56982, #5296, #61885, #27926, #4185, #73947, #51305, #74317, #45278, #22249, #10576, #21883, #27545, #27171, #21515, #44537, #16968, #22624, #45643, #67549, #44912, #68658, #38880, #50559, #26804, #39994, #72835, #67918, #21141, #16211, #33606, #56615, #58466, #29041, #70154, #12421, #12057, #18091, #52059, #70511, #46388, #23749, #47488, #763, #46753, #12784, #57355, #35819, #35454, #64486, #18830, #69406, #69774, #58833, #57730, #23, #40729, #63361, #6036, #394, #41834, #64113, #11687, #18461, #6777, #17713, #51677, #52795, #41106, #23009, #40361, #63737, #5665, #23376, #6412, #29417, #29782, #1130, #28663, #41472, #24108, #7144, #35091, #24484, #1504, #64847, #69036, #47120, #30151, #53168, #34725, #13148, #46015, #58101, #17339, #52428, #30519, #2216, #65209, #65583, #65955, #48598, #1853, #48968, #19925, #37296, #60292, #66705, #25949, #31254, #20295, #48228, #13514, #47856, #54282, #49346, #25210, #2594, #3336, #43693, #20674, #14634, #43312, #26326, #71234, #53903, #60673, #14260, #19555, #70876, #36553, #19191, #25583, #42570, #42935, #71603, #36922, #24839, #8620, #59565, #42193, #13880, #36188, #59204, #7881, #53538, #59929, #8243, #30886, #66329, #8994, #31634, #54653, #2963, #72364, #71980, #37675, #32010, #55029, #7513, #27833, #39533, #68198, #38794, #73856, #44074, #22160, #39158, #61797, #10114, #67085, #45187, #33891, #62161, #16120, #21787, #21421, #73115, #4092, #50464, #56893, #61045, #45554, #44445, #73479, #32768, #16496, #62529, #21050, #27086, #4835, #15382, #10856, #27449, #5207, #38419, #32389, #67457, #61421, #9750, #55776, #74227, #44817, #50099, #50842, #10486, #55403, #49730, #28205, #33153, #33518, #56520, #3713, #51218, #56147, #15754, #22533, #26711, #15010, #4461, #38044, #9368, #67829, #72746, #35009, #16872, #24026, #51971 ),
 ( #6330, #29333, #18378, #46671, #46297, #18007, #11600, #74603, #34262, #23288, #47036, #40273, #69318, #52714, #70072, #68570, #58387, #64031, #39897, #57642, #34636, #1047, #52342, #5952, #22916, #68941, #51586, #63650, #309, #679, #40646, #17627, #28578, #23665, #45929, #17251, #28951, #62902, #11234, #11977, #63273, #58024, #69693, #41023, #57265, #5580, #12343, #29698, #35377, #6693, #58658, #40557, #29608, #40931, #69228, #13340, #36377, #41300, #11886, #42024, #46948, #59392, #70345, #63941, #7338, #24307, #23940, #29975, #12249, #7705, #58298, #35645, #30711, #12615, #6966, #24667, #17537, #47678, #47319, #1689, #53731, #6603, #588, #69601, #35286, #2043, #1324, #23569, #30344, #18657, #34920, #29242, #25030, #52992, #12976, #41666, #57931, #53363, #64310, #52622, #63559, #6238, #64677, #46580, #52254, #36013, #59031, #70699, #19018, #17915, #958, #69977, #18286, #65031, #71424, #19752, #31071, #25771, #71799, #37869, #31455, #42759, #13704, #2785, #60864, #56624, #8070, #4939, #4560, #19377, #9186, #32207, #48050, #8817, #54100, #2412, #48792, #49166, #60117, #55226, #20119, #25407, #73584, #43133, #54480, #48421, #33618, #65776, #20487, #36748, #59760, #31829, #27557, #50567, #21891, #66149, #72175, #14079, #43505, #44921, #67929, #14828, #66516, #54848, #14454, #37490, #37114, #8435, #60491, #62259, #16222, #3158, #39261, #26147, #42391, #10586, #71059, #65407, #46761, #69786, #32, #45286, #773, #5675, #18101, #29050, #74326, #40738, #57741, #57366, #63371, #22632, #41117, #16977, #69047, #64122, #46026, #17351, #58110, #27936, #6421, #6045, #35101, #12429, #40003, #40372, #29427, #28306, #68296, #11331, #52436, #12065, #35463, #63007, #45653, #23759, #52069, #68667, #62631, #5305, #39632, #11697, #34364, #34735, #406, #28673, #16593, #23386, #56990, #10962, #51687, #58476, #50944, #51315, #22257, #23019, #46398, #33997, #73956, #69415, #17722, #63747, #35828, #48237, #36197, #36930, #24848, #1514, #59576, #19565, #31264, #59937, #30529, #65594, #58843, #13891, #30895, #53547, #1862, #7155, #8250, #25593, #53912, #7889, #13524, #13160, #64855, #70520, #42203, #48609, #52804, #37305, #59213, #65219, #24494, #54292, #2604, #12796, #18838, #71245, #30159, #71614, #41846, #1139, #2225, #47866, #24117, #64496, #7524, #29794, #47497, #70886, #19201, #36562, #25223, #6784, #42580, #19935, #42943, #65964, #14269, #47130, #70163, #18470, #41481, #53177, #44456, #66338, #38430, #27095, #14644, #61433, #50111, #54664, #26335, #37685, #15022, #15393, #72757, #25958, #73127, #44085, #9759, #32780, #16129, #21433, #55413, #67470, #72374, #60685, #71990, #3722, #73491, #49357, #26721, #27462, #67837, #44829, #20303, #49741, #21798, #20685, #21061, #50476, #60301, #8631, #38804, #15767, #31644, #43703, #3345, #10124, #55787, #66718, #43323, #9005, #32019, #67096, #38056, #4103, #61806, #61056, #48977, #33161, #55039, #9380, #32399, #2973, #56156, #4472, #33530, #68579, #56904, #4848, #69327 ) ),
 .UNSPECIFIED., .F., .F., .F. ) 
 B_SPLINE_SURFACE_WITH_KNOTS ( ( 2, 2 ),
 ( 3, 2, 2, 2, 2, 2, 2, 2, 2, 2, 2, 2, 2, 2, 2, 2, 2, 2, 2, 2, 2, 2, 2, 2, 2, 2, 2, 2, 2, 2, 2, 2, 2, 2, 2, 2, 2, 2, 2, 2, 2, 2, 2, 2, 2, 2, 2, 2, 2, 2, 2, 2, 2, 2, 2, 2, 2, 2, 2, 2, 2, 2, 2, 2, 2, 2, 2, 2, 2, 2, 2, 2, 2, 2, 2, 2, 2, 2, 2, 2, 2, 2, 2, 2, 2, 2, 2, 2, 2, 2, 2, 2, 2, 2, 2, 2, 2, 2, 2, 2, 2, 2, 2, 2, 2, 2, 2, 2, 2, 2, 2, 2, 2, 2, 2, 2, 2, 2, 2, 2, 2, 2, 2, 2, 2, 2, 2, 2, 2, 2, 2, 2, 2, 2, 2, 2, 2, 2, 2, 2, 2, 2, 2, 2, 2, 2, 2, 2, 2, 2, 2, 2, 2, 2, 2, 2, 2, 2, 2, 2, 2, 2, 2, 2, 2, 2, 2, 2, 2, 2, 2, 2, 2, 2, 2, 2, 2, 2, 2, 2, 2, 2, 2, 2, 2, 2, 2, 3 ),
 ( 0.000000000000000000, 1.000000000000000000 ),
 ( 0.000000000000000000, 0.005208333333333333044, 0.01041666666666666609, 0.01562500000000000000, 0.02083333333333333218, 0.02604166666666666782, 0.03125000000000000000, 0.03645833333333333565, 0.04166666666666666435, 0.04687500000000000000, 0.05208333333333333565, 0.05729166666666666435, 0.06250000000000000000, 0.06770833333333332871, 0.07291666666666667129, 0.07812500000000000000, 0.08333333333333332871, 0.08854166666666667129, 0.09375000000000000000, 0.09895833333333332871, 0.1041666666666666713, 0.1093750000000000000, 0.1145833333333333287, 0.1197916666666666713, 0.1250000000000000000, 0.1302083333333333426, 0.1354166666666666574, 0.1406250000000000000, 0.1458333333333333426, 0.1510416666666666574, 0.1562500000000000000, 0.1614583333333333426, 0.1666666666666666574, 0.1718750000000000000, 0.1770833333333333426, 0.1822916666666666574, 0.1875000000000000000, 0.1927083333333333426, 0.1979166666666666574, 0.2031250000000000000, 0.2083333333333333426, 0.2135416666666666574, 0.2187500000000000000, 0.2239583333333333426, 0.2291666666666666574, 0.2343750000000000000, 0.2395833333333333426, 0.2447916666666666574, 0.2500000000000000000, 0.2552083333333333148, 0.2604166666666666852, 0.2656250000000000000, 0.2708333333333333148, 0.2760416666666666852, 0.2812500000000000000, 0.2864583333333333148, 0.2916666666666666852, 0.2968750000000000000, 0.3020833333333333148, 0.3072916666666666852, 0.3125000000000000000, 0.3177083333333333148, 0.3229166666666666852, 0.3281250000000000000, 0.3333333333333333148, 0.3385416666666666852, 0.3437500000000000000, 0.3489583333333333148, 0.3541666666666666852, 0.3593750000000000000, 0.3645833333333333148, 0.3697916666666666852, 0.3750000000000000000, 0.3802083333333333148, 0.3854166666666666852, 0.3906250000000000000, 0.3958333333333333148, 0.4010416666666666852, 0.4062500000000000000, 0.4114583333333333148, 0.4166666666666666852, 0.4218750000000000000, 0.4270833333333333148, 0.4322916666666666852, 0.4375000000000000000, 0.4427083333333333148, 0.4479166666666666852, 0.4531250000000000000, 0.4583333333333333148, 0.4635416666666666852, 0.4687500000000000000, 0.4739583333333333148, 0.4791666666666666852, 0.4843750000000000000, 0.4895833333333333148, 0.4947916666666666852, 0.5000000000000000000, 0.5052083333333333703, 0.5104166666666666297, 0.5156250000000000000, 0.5208333333333333703, 0.5260416666666666297, 0.5312500000000000000, 0.5364583333333333703, 0.5416666666666666297, 0.5468750000000000000, 0.5520833333333333703, 0.5572916666666666297, 0.5625000000000000000, 0.5677083333333333703, 0.5729166666666666297, 0.5781250000000000000, 0.5833333333333333703, 0.5885416666666666297, 0.5937500000000000000, 0.5989583333333333703, 0.6041666666666666297, 0.6093750000000000000, 0.6145833333333333703, 0.6197916666666666297, 0.6250000000000000000, 0.6302083333333333703, 0.6354166666666666297, 0.6406250000000000000, 0.6458333333333333703, 0.6510416666666666297, 0.6562500000000000000, 0.6614583333333333703, 0.6666666666666666297, 0.6718750000000000000, 0.6770833333333333703, 0.6822916666666666297, 0.6875000000000000000, 0.6927083333333333703, 0.6979166666666666297, 0.7031250000000000000, 0.7083333333333333703, 0.7135416666666666297, 0.7187500000000000000, 0.7239583333333333703, 0.7291666666666666297, 0.7343750000000000000, 0.7395833333333333703, 0.7447916666666666297, 0.7500000000000000000, 0.7552083333333333703, 0.7604166666666666297, 0.7656250000000000000, 0.7708333333333333703, 0.7760416666666666297, 0.7812500000000000000, 0.7864583333333333703, 0.7916666666666666297, 0.7968750000000000000, 0.8020833333333333703, 0.8072916666666666297, 0.8125000000000000000, 0.8177083333333333703, 0.8229166666666666297, 0.8281250000000000000, 0.8333333333333333703, 0.8385416666666666297, 0.8437500000000000000, 0.8489583333333333703, 0.8541666666666666297, 0.8593750000000000000, 0.8645833333333333703, 0.8697916666666666297, 0.8750000000000000000, 0.8802083333333333703, 0.8854166666666666297, 0.8906250000000000000, 0.8958333333333333703, 0.9010416666666666297, 0.9062500000000000000, 0.9114583333333333703, 0.9166666666666666297, 0.9218750000000000000, 0.9270833333333333703, 0.9322916666666666297, 0.9375000000000000000, 0.9427083333333333703, 0.9479166666666666297, 0.9531250000000000000, 0.9583333333333333703, 0.9635416666666666297, 0.9687500000000000000, 0.9722122500602408124 ),
 .UNSPECIFIED. ) 
 GEOMETRIC_REPRESENTATION_ITEM ( )  RATIONAL_B_SPLINE_SURFACE ( (
 ( 1.000000000000000000, 0.9238795325112867385, 1.000000000000000000, 0.9238795325112867385, 1.000000000000000000, 0.9238795325112867385, 1.000000000000000000, 0.9238795325112867385, 1.000000000000000000, 0.9238795325112867385, 1.000000000000000000, 0.9238795325112867385, 1.000000000000000000, 0.9238795325112867385, 1.000000000000000000, 0.9238795325112867385, 1.000000000000000000, 0.9238795325112867385, 1.000000000000000000, 0.9238795325112867385, 1.000000000000000000, 0.9238795325112867385, 1.000000000000000000, 0.9238795325112867385, 1.000000000000000000, 0.9238795325112867385, 1.000000000000000000, 0.9238795325112867385, 1.000000000000000000, 0.9238795325112867385, 1.000000000000000000, 0.9238795325112867385, 1.000000000000000000, 0.9238795325112867385, 1.000000000000000000, 0.9238795325112867385, 1.000000000000000000, 0.9238795325112867385, 1.000000000000000000, 0.9238795325112867385, 1.000000000000000000, 0.9238795325112867385, 1.000000000000000000, 0.9238795325112867385, 1.000000000000000000, 0.9238795325112867385, 1.000000000000000000, 0.9238795325112867385, 1.000000000000000000, 0.9238795325112867385, 1.000000000000000000, 0.9238795325112867385, 1.000000000000000000, 0.9238795325112867385, 1.000000000000000000, 0.9238795325112867385, 1.000000000000000000, 0.9238795325112867385, 1.000000000000000000, 0.9238795325112867385, 1.000000000000000000, 0.9238795325112867385, 1.000000000000000000, 0.9238795325112867385, 1.000000000000000000, 0.9238795325112867385, 1.000000000000000000, 0.9238795325112867385, 1.000000000000000000, 0.9238795325112867385, 1.000000000000000000, 0.9238795325112867385, 1.000000000000000000, 0.9238795325112867385, 1.000000000000000000, 0.9238795325112867385, 1.000000000000000000, 0.9238795325112867385, 1.000000000000000000, 0.9238795325112867385, 1.000000000000000000, 0.9238795325112867385, 1.000000000000000000, 0.9238795325112867385, 1.000000000000000000, 0.9238795325112867385, 1.000000000000000000, 0.9238795325112867385, 1.000000000000000000, 0.9238795325112867385, 1.000000000000000000, 0.9238795325112867385, 1.000000000000000000, 0.9238795325112867385, 1.000000000000000000, 0.9238795325112867385, 1.000000000000000000, 0.9238795325112867385, 1.000000000000000000, 0.9238795325112867385, 1.000000000000000000, 0.9238795325112867385, 1.000000000000000000, 0.9238795325112867385, 1.000000000000000000, 0.9238795325112867385, 1.000000000000000000, 0.9238795325112867385, 1.000000000000000000, 0.9238795325112867385, 1.000000000000000000, 0.9238795325112867385, 1.000000000000000000, 0.9238795325112867385, 1.000000000000000000, 0.9238795325112867385, 1.000000000000000000, 0.9238795325112867385, 1.000000000000000000, 0.9238795325112867385, 1.000000000000000000, 0.9238795325112867385, 1.000000000000000000, 0.9238795325112867385, 1.000000000000000000, 0.9238795325112867385, 1.000000000000000000, 0.9238795325112867385, 1.000000000000000000, 0.9238795325112867385, 1.000000000000000000, 0.9238795325112867385, 1.000000000000000000, 0.9238795325112867385, 1.000000000000000000, 0.9238795325112867385, 1.000000000000000000, 0.9238795325112867385, 1.000000000000000000, 0.9238795325112867385, 1.000000000000000000, 0.9238795325112867385, 1.000000000000000000, 0.9238795325112867385, 1.000000000000000000, 0.9238795325112867385, 1.000000000000000000, 0.9238795325112867385, 1.000000000000000000, 0.9238795325112867385, 1.000000000000000000, 0.9238795325112867385, 1.000000000000000000, 0.9238795325112867385, 1.000000000000000000, 0.9238795325112867385, 1.000000000000000000, 0.9238795325112867385, 1.000000000000000000, 0.9238795325112867385, 1.000000000000000000, 0.9238795325112867385, 1.000000000000000000, 0.9238795325112867385, 1.000000000000000000, 0.9238795325112867385, 1.000000000000000000, 0.9238795325112867385, 1.000000000000000000, 0.9238795325112867385, 1.000000000000000000, 0.9238795325112867385, 1.000000000000000000, 0.9238795325112867385, 1.000000000000000000, 0.9238795325112867385, 1.000000000000000000, 0.9238795325112867385, 1.000000000000000000, 0.9238795325112867385, 1.000000000000000000, 0.9238795325112867385, 1.000000000000000000, 0.9238795325112867385, 1.000000000000000000, 0.9238795325112867385, 1.000000000000000000, 0.9238795325112867385, 1.000000000000000000, 0.9238795325112867385, 1.000000000000000000, 0.9238795325112867385, 1.000000000000000000, 0.9238795325112867385, 1.000000000000000000, 0.9238795325112867385, 1.000000000000000000, 0.9238795325112867385, 1.000000000000000000, 0.9238795325112867385, 1.000000000000000000, 0.9238795325112867385, 1.000000000000000000, 0.9238795325112867385, 1.000000000000000000, 0.9238795325112867385, 1.000000000000000000, 0.9238795325112867385, 1.000000000000000000, 0.9238795325112867385, 1.000000000000000000, 0.9238795325112867385, 1.000000000000000000, 0.9238795325112867385, 1.000000000000000000, 0.9238795325112867385, 1.000000000000000000, 0.9238795325112867385, 1.000000000000000000, 0.9238795325112867385, 1.000000000000000000, 0.9238795325112867385, 1.000000000000000000, 0.9238795325112867385, 1.000000000000000000, 0.9238795325112867385, 1.000000000000000000, 0.9238795325112867385, 1.000000000000000000, 0.9238795325112867385, 1.000000000000000000, 0.9238795325112867385, 1.000000000000000000, 0.9238795325112867385, 1.000000000000000000, 0.9238795325112867385, 1.000000000000000000, 0.9238795325112867385, 1.000000000000000000, 0.9238795325112867385, 1.000000000000000000, 0.9238795325112867385, 1.000000000000000000, 0.9238795325112867385, 1.000000000000000000, 0.9238795325112867385, 1.000000000000000000, 0.9238795325112867385, 1.000000000000000000, 0.9238795325112867385, 1.000000000000000000, 0.9238795325112867385, 1.000000000000000000, 0.9238795325112867385, 1.000000000000000000, 0.9238795325112867385, 1.000000000000000000, 0.9238795325112867385, 1.000000000000000000, 0.9238795325112867385, 1.000000000000000000, 0.9238795325112867385, 1.000000000000000000, 0.9238795325112867385, 1.000000000000000000, 0.9238795325112867385, 1.000000000000000000, 0.9238795325112867385, 1.000000000000000000, 0.9238795325112867385, 1.000000000000000000, 0.9238795325112867385, 1.000000000000000000, 0.9238795325112867385, 1.000000000000000000, 0.9238795325112867385, 1.000000000000000000, 0.9238795325112867385, 1.000000000000000000, 0.9238795325112867385, 1.000000000000000000, 0.9238795325112867385, 1.000000000000000000, 0.9238795325112867385, 1.000000000000000000, 0.9238795325112867385, 1.000000000000000000, 0.9238795325112867385, 1.000000000000000000, 0.9238795325112867385, 1.000000000000000000, 0.9238795325112867385, 1.000000000000000000, 0.9238795325112867385, 1.000000000000000000, 0.9238795325112867385, 1.000000000000000000, 0.9238795325112867385, 1.000000000000000000, 0.9238795325112867385, 1.000000000000000000, 0.9238795325112867385, 1.000000000000000000, 0.9238795325112867385, 1.000000000000000000, 0.9238795325112867385, 1.000000000000000000, 0.9238795325112867385, 1.000000000000000000, 0.9238795325112867385, 1.000000000000000000, 0.9238795325112867385, 1.000000000000000000, 0.9238795325112867385, 1.000000000000000000, 0.9238795325112867385, 1.000000000000000000, 0.9238795325112867385, 1.000000000000000000, 0.9238795325112867385, 1.000000000000000000, 0.9238795325112867385, 1.000000000000000000, 0.9238795325112867385, 1.000000000000000000, 0.9238795325112867385, 1.000000000000000000, 0.9238795325112867385, 1.000000000000000000, 0.9238795325112867385, 1.000000000000000000, 0.9238795325112867385, 1.000000000000000000, 0.9238795325112867385, 1.000000000000000000, 0.9238795325112867385, 1.000000000000000000, 0.9238795325112867385, 1.000000000000000000, 0.9238795325112867385, 1.000000000000000000, 0.9238795325112867385, 1.000000000000000000, 0.9238795325112867385, 1.000000000000000000, 0.9238795325112867385, 1.000000000000000000, 0.9238795325112867385, 1.000000000000000000, 0.9238795325112867385, 1.000000000000000000, 0.9238795325112867385, 1.000000000000000000, 0.9238795325112867385, 1.000000000000000000, 0.9238795325112867385, 1.000000000000000000, 0.9238795325112867385, 1.000000000000000000, 0.9238795325112867385, 1.000000000000000000, 0.9238795325112867385, 1.000000000000000000, 0.9238795325112867385, 1.000000000000000000, 0.9238795325112867385, 1.000000000000000000, 0.9238795325112867385, 1.000000000000000000, 0.9238795325112867385, 1.000000000000000000, 0.9238795325112867385, 1.000000000000000000, 0.9493987661155159907, 0.9660720762559202868),
 ( 1.000000000000000000, 0.9238795325112867385, 1.000000000000000000, 0.9238795325112867385, 1.000000000000000000, 0.9238795325112867385, 1.000000000000000000, 0.9238795325112867385, 1.000000000000000000, 0.9238795325112867385, 1.000000000000000000, 0.9238795325112867385, 1.000000000000000000, 0.9238795325112867385, 1.000000000000000000, 0.9238795325112867385, 1.000000000000000000, 0.9238795325112867385, 1.000000000000000000, 0.9238795325112867385, 1.000000000000000000, 0.9238795325112867385, 1.000000000000000000, 0.9238795325112867385, 1.000000000000000000, 0.9238795325112867385, 1.000000000000000000, 0.9238795325112867385, 1.000000000000000000, 0.9238795325112867385, 1.000000000000000000, 0.9238795325112867385, 1.000000000000000000, 0.9238795325112867385, 1.000000000000000000, 0.9238795325112867385, 1.000000000000000000, 0.9238795325112867385, 1.000000000000000000, 0.9238795325112867385, 1.000000000000000000, 0.9238795325112867385, 1.000000000000000000, 0.9238795325112867385, 1.000000000000000000, 0.9238795325112867385, 1.000000000000000000, 0.9238795325112867385, 1.000000000000000000, 0.9238795325112867385, 1.000000000000000000, 0.9238795325112867385, 1.000000000000000000, 0.9238795325112867385, 1.000000000000000000, 0.9238795325112867385, 1.000000000000000000, 0.9238795325112867385, 1.000000000000000000, 0.9238795325112867385, 1.000000000000000000, 0.9238795325112867385, 1.000000000000000000, 0.9238795325112867385, 1.000000000000000000, 0.9238795325112867385, 1.000000000000000000, 0.9238795325112867385, 1.000000000000000000, 0.9238795325112867385, 1.000000000000000000, 0.9238795325112867385, 1.000000000000000000, 0.9238795325112867385, 1.000000000000000000, 0.9238795325112867385, 1.000000000000000000, 0.9238795325112867385, 1.000000000000000000, 0.9238795325112867385, 1.000000000000000000, 0.9238795325112867385, 1.000000000000000000, 0.9238795325112867385, 1.000000000000000000, 0.9238795325112867385, 1.000000000000000000, 0.9238795325112867385, 1.000000000000000000, 0.9238795325112867385, 1.000000000000000000, 0.9238795325112867385, 1.000000000000000000, 0.9238795325112867385, 1.000000000000000000, 0.9238795325112867385, 1.000000000000000000, 0.9238795325112867385, 1.000000000000000000, 0.9238795325112867385, 1.000000000000000000, 0.9238795325112867385, 1.000000000000000000, 0.9238795325112867385, 1.000000000000000000, 0.9238795325112867385, 1.000000000000000000, 0.9238795325112867385, 1.000000000000000000, 0.9238795325112867385, 1.000000000000000000, 0.9238795325112867385, 1.000000000000000000, 0.9238795325112867385, 1.000000000000000000, 0.9238795325112867385, 1.000000000000000000, 0.9238795325112867385, 1.000000000000000000, 0.9238795325112867385, 1.000000000000000000, 0.9238795325112867385, 1.000000000000000000, 0.9238795325112867385, 1.000000000000000000, 0.9238795325112867385, 1.000000000000000000, 0.9238795325112867385, 1.000000000000000000, 0.9238795325112867385, 1.000000000000000000, 0.9238795325112867385, 1.000000000000000000, 0.9238795325112867385, 1.000000000000000000, 0.9238795325112867385, 1.000000000000000000, 0.9238795325112867385, 1.000000000000000000, 0.9238795325112867385, 1.000000000000000000, 0.9238795325112867385, 1.000000000000000000, 0.9238795325112867385, 1.000000000000000000, 0.9238795325112867385, 1.000000000000000000, 0.9238795325112867385, 1.000000000000000000, 0.9238795325112867385, 1.000000000000000000, 0.9238795325112867385, 1.000000000000000000, 0.9238795325112867385, 1.000000000000000000, 0.9238795325112867385, 1.000000000000000000, 0.9238795325112867385, 1.000000000000000000, 0.9238795325112867385, 1.000000000000000000, 0.9238795325112867385, 1.000000000000000000, 0.9238795325112867385, 1.000000000000000000, 0.9238795325112867385, 1.000000000000000000, 0.9238795325112867385, 1.000000000000000000, 0.9238795325112867385, 1.000000000000000000, 0.9238795325112867385, 1.000000000000000000, 0.9238795325112867385, 1.000000000000000000, 0.9238795325112867385, 1.000000000000000000, 0.9238795325112867385, 1.000000000000000000, 0.9238795325112867385, 1.000000000000000000, 0.9238795325112867385, 1.000000000000000000, 0.9238795325112867385, 1.000000000000000000, 0.9238795325112867385, 1.000000000000000000, 0.9238795325112867385, 1.000000000000000000, 0.9238795325112867385, 1.000000000000000000, 0.9238795325112867385, 1.000000000000000000, 0.9238795325112867385, 1.000000000000000000, 0.9238795325112867385, 1.000000000000000000, 0.9238795325112867385, 1.000000000000000000, 0.9238795325112867385, 1.000000000000000000, 0.9238795325112867385, 1.000000000000000000, 0.9238795325112867385, 1.000000000000000000, 0.9238795325112867385, 1.000000000000000000, 0.9238795325112867385, 1.000000000000000000, 0.9238795325112867385, 1.000000000000000000, 0.9238795325112867385, 1.000000000000000000, 0.9238795325112867385, 1.000000000000000000, 0.9238795325112867385, 1.000000000000000000, 0.9238795325112867385, 1.000000000000000000, 0.9238795325112867385, 1.000000000000000000, 0.9238795325112867385, 1.000000000000000000, 0.9238795325112867385, 1.000000000000000000, 0.9238795325112867385, 1.000000000000000000, 0.9238795325112867385, 1.000000000000000000, 0.9238795325112867385, 1.000000000000000000, 0.9238795325112867385, 1.000000000000000000, 0.9238795325112867385, 1.000000000000000000, 0.9238795325112867385, 1.000000000000000000, 0.9238795325112867385, 1.000000000000000000, 0.9238795325112867385, 1.000000000000000000, 0.9238795325112867385, 1.000000000000000000, 0.9238795325112867385, 1.000000000000000000, 0.9238795325112867385, 1.000000000000000000, 0.9238795325112867385, 1.000000000000000000, 0.9238795325112867385, 1.000000000000000000, 0.9238795325112867385, 1.000000000000000000, 0.9238795325112867385, 1.000000000000000000, 0.9238795325112867385, 1.000000000000000000, 0.9238795325112867385, 1.000000000000000000, 0.9238795325112867385, 1.000000000000000000, 0.9238795325112867385, 1.000000000000000000, 0.9238795325112867385, 1.000000000000000000, 0.9238795325112867385, 1.000000000000000000, 0.9238795325112867385, 1.000000000000000000, 0.9238795325112867385, 1.000000000000000000, 0.9238795325112867385, 1.000000000000000000, 0.9238795325112867385, 1.000000000000000000, 0.9238795325112867385, 1.000000000000000000, 0.9238795325112867385, 1.000000000000000000, 0.9238795325112867385, 1.000000000000000000, 0.9238795325112867385, 1.000000000000000000, 0.9238795325112867385, 1.000000000000000000, 0.9238795325112867385, 1.000000000000000000, 0.9238795325112867385, 1.000000000000000000, 0.9238795325112867385, 1.000000000000000000, 0.9238795325112867385, 1.000000000000000000, 0.9238795325112867385, 1.000000000000000000, 0.9238795325112867385, 1.000000000000000000, 0.9238795325112867385, 1.000000000000000000, 0.9238795325112867385, 1.000000000000000000, 0.9238795325112867385, 1.000000000000000000, 0.9238795325112867385, 1.000000000000000000, 0.9238795325112867385, 1.000000000000000000, 0.9238795325112867385, 1.000000000000000000, 0.9238795325112867385, 1.000000000000000000, 0.9238795325112867385, 1.000000000000000000, 0.9238795325112867385, 1.000000000000000000, 0.9238795325112867385, 1.000000000000000000, 0.9238795325112867385, 1.000000000000000000, 0.9238795325112867385, 1.000000000000000000, 0.9238795325112867385, 1.000000000000000000, 0.9238795325112867385, 1.000000000000000000, 0.9238795325112867385, 1.000000000000000000, 0.9238795325112867385, 1.000000000000000000, 0.9238795325112867385, 1.000000000000000000, 0.9238795325112867385, 1.000000000000000000, 0.9238795325112867385, 1.000000000000000000, 0.9238795325112867385, 1.000000000000000000, 0.9238795325112867385, 1.000000000000000000, 0.9238795325112867385, 1.000000000000000000, 0.9238795325112867385, 1.000000000000000000, 0.9238795325112867385, 1.000000000000000000, 0.9238795325112867385, 1.000000000000000000, 0.9238795325112867385, 1.000000000000000000, 0.9238795325112867385, 1.000000000000000000, 0.9238795325112867385, 1.000000000000000000, 0.9238795325112867385, 1.000000000000000000, 0.9238795325112867385, 1.000000000000000000, 0.9238795325112867385, 1.000000000000000000, 0.9238795325112867385, 1.000000000000000000, 0.9238795325112867385, 1.000000000000000000, 0.9238795325112867385, 1.000000000000000000, 0.9238795325112867385, 1.000000000000000000, 0.9238795325112867385, 1.000000000000000000, 0.9238795325112867385, 1.000000000000000000, 0.9238795325112867385, 1.000000000000000000, 0.9493987661155159907, 0.9660720762559202868) ) ) 
 REPRESENTATION_ITEM ( '' )  SURFACE ( )  );
#47404 = CARTESIAN_POINT ( 'NONE',  ( -26.56734541678232375, 203.0000000013655779, 173.4587341250003760 ) ) ;
#47405 = CARTESIAN_POINT ( 'NONE',  ( -8.000000000000001776, 21.84375000000000355, 3.313708498984759387 ) ) ;
#47406 = VERTEX_POINT ( 'NONE', #53028 ) ;
#47407 = AXIS2_PLACEMENT_3D ( 'NONE', #32550, #3493, #50251 ) ;
#47408 = CARTESIAN_POINT ( 'NONE',  ( -24.09428029662548454, -50.77845604291201198, 150.4777531985531027 ) ) ;
#47409 = CARTESIAN_POINT ( 'NONE',  ( -1.656854249492348607, 208.3125000027312126, 202.0000000000000284 ) ) ;
#47410 = CARTESIAN_POINT ( 'NONE',  ( 6.123233995736767268E-16, 26.25000000000000355, -10.00000000000000178 ) ) ;
#47411 = CARTESIAN_POINT ( 'NONE',  ( 7.999999999932789763, 3.279097096261179525E-05, 13.76780373625499010 ) ) ;
#47412 = CARTESIAN_POINT ( 'NONE',  ( 10.18810118749999916, 1.247682550866122264E-15, 73.28125000204838102 ) ) ;
#47413 = VERTEX_POINT ( 'NONE', #12289 ) ;
#47414 = CARTESIAN_POINT ( 'NONE',  ( -7.188101187500002709, 5.812499997951611874, 2.977408999572649151 ) ) ;
#47415 = LINE ( 'NONE', #70439, #2926 ) ;
#47416 = CARTESIAN_POINT ( 'NONE',  ( 11.00000000000000000, 1.347111479062088405E-15, 93.43750000409677625 ) ) ;
#47417 = CARTESIAN_POINT ( 'NONE',  ( -4.401442555609581635E-16, 116.6562500020483810, -7.188101187500000044 ) ) ;
#47418 = CARTESIAN_POINT ( 'NONE',  ( 2.295000000000000373, 284.2799999999998590, 5.414445227811098604 ) ) ;
#47419 = CARTESIAN_POINT ( 'NONE',  ( 6.676582343750002480, 295.0156250017069510, -2.765530957081997254 ) ) ;
#47421 = CARTESIAN_POINT ( 'NONE',  ( -3.999999999999960032, 209.1250000027312126, 198.0000000000000284 ) ) ;
#47420 = CARTESIAN_POINT ( 'NONE',  ( -3.042071309553166625, 227.8645833367473301, -11.35316468749999608 ) ) ;
#47422 = ITEM_DEFINED_TRANSFORMATION ( 'NONE', 'NONE', #10433,  #57354 ) ;
#47423 = ORIENTED_EDGE ( 'NONE', *, *, #66288, .T. ) ;
#47424 = CARTESIAN_POINT ( 'NONE',  ( 5.676582343750005144, 235.8854166700806729, 9.832129032723416984 ) ) ;
#47425 = CARTESIAN_POINT ( 'NONE',  ( 5.082755093536318824, 5.082755093536319713, 3.924052781871752327 ) ) ;
#47426 = VECTOR ( 'NONE', #44262, 1000.000000000000000 ) ;
#47427 = CARTESIAN_POINT ( 'NONE',  ( 1.432654583217662481, 204.3750000013656063, 194.5412658750000219 ) ) ;
#47428 = ORIENTED_EDGE ( 'NONE', *, *, #4710, .T. ) ;
#47429 = CARTESIAN_POINT ( 'NONE',  ( -6.238412754330611322E-16, 10.18810118749999916, 70.28125000204838102 ) ) ;
#47430 = CARTESIAN_POINT ( 'NONE',  ( 8.311093377946834337, 100.4687499965860269, 8.311093377946839666 ) ) ;
#47431 = CARTESIAN_POINT ( 'NONE',  ( 0.000000000000000000, 0.000000000000000000, 0.000000000000000000 ) ) ;
#47432 = CARTESIAN_POINT ( 'NONE',  ( 11.00000000000000000, 1.347111479062088405E-15, 78.24999999999998579 ) ) ;
#47435 = CARTESIAN_POINT ( 'NONE',  ( -1.656854249492263564, 201.8124999999999716, 194.0000000000000000 ) ) ;
#47434 = CARTESIAN_POINT ( 'NONE',  ( 29.43265458321761230, 202.8750000013656347, 166.5412658749999650 ) ) ;
#47433 = CARTESIAN_POINT ( 'NONE',  ( 28.00000000000002132, 202.1875000013656063, 166.5412658749999082 ) ) ;
#47436 = EDGE_LOOP ( 'NONE', ( #57084, #59288, #65172, #37295 ) ) ;
#47437 = LINE ( 'NONE', #70462, #63363 ) ;
#47438 = CARTESIAN_POINT ( 'NONE',  ( 2.326828918379975309E-15, 265.0000000000000000, 19.00000000000003553 ) ) ;
#47439 = CARTESIAN_POINT ( 'NONE',  ( -9.832129032723418760, 207.8645833299193555, -5.676582343750004256 ) ) ;
#47440 = CARTESIAN_POINT ( 'NONE',  ( -2.445694354108839619, 202.8125000013656063, 139.5543056458912190 ) ) ;
#47441 = EDGE_CURVE ( 'NONE', #4761, #13563, #58560, .T. ) ;
#47442 = CARTESIAN_POINT ( 'NONE',  ( 25.55430564589119413, 200.3125000013656063, 167.5543056458910485 ) ) ;
#47443 = EDGE_CURVE ( 'NONE', #64267, #42385, #71016, .T. ) ;
#47444 = CARTESIAN_POINT ( 'NONE',  ( 7.188101187500001821, 21.93749999795161543, -2.977408999572650483 ) ) ;
#47445 = CARTESIAN_POINT ( 'NONE',  ( -5.676582343750006032, 179.4270833299193555, 9.832129032723418760 ) ) ;
#47446 = CARTESIAN_POINT ( 'NONE',  ( 7.188101187500000044, 99.78125000204838102, -8.802885111219163269E-16 ) ) ;
#47447 = CARTESIAN_POINT ( 'NONE',  ( -2.775557561562891351E-14, 210.0000000000000284, 142.0000000000000568 ) ) ;
#47448 = CARTESIAN_POINT ( 'NONE',  ( -30.82842712474615610, 196.3750000000000284, 172.8284271247465824 ) ) ;
#47449 = CARTESIAN_POINT ( 'NONE',  ( 1.881053915767121776, 13.49999999863440969, -4.541265875000002339 ) ) ;
#47450 = CARTESIAN_POINT ( 'NONE',  ( 25.55430564589115150, 200.5625000013656063, 172.4456943541086957 ) ) ;
#47451 = CARTESIAN_POINT ( 'NONE',  ( 1.320432766682872962E-15, -7.188101187499992051, 6.736552781871754547 ) ) ;
#47452 = CARTESIAN_POINT ( 'NONE',  ( -5.676582343750006032, 69.11458332991936970, 9.832129032723418760 ) ) ;
#47453 = CARTESIAN_POINT ( 'NONE',  ( 0.000000000000000000, -3.149999999999999911, 11.00000000000000000 ) ) ;
#47454 = DIRECTION ( 'NONE',  ( -0.000000000000000000, 1.000000000000000000, -1.563033456626094573E-30 ) ) ;
#47455 = ORIENTED_EDGE ( 'NONE', *, *, #5667, .T. ) ;
#47456 = CARTESIAN_POINT ( 'NONE',  ( 1.836970198721029589E-15, 224.3750000068279746, 10.00000000000000000 ) ) ;
#47458 = CARTESIAN_POINT ( 'NONE',  ( 2.020667218593132706E-15, -11.00000000000000000, 116.8749999999999858 ) ) ;
#47457 = VECTOR ( 'NONE', #24744, 1000.000000000000000 ) ;
#47459 = CARTESIAN_POINT ( 'NONE',  ( 8.311093377946834337, 75.15624999658602690, 8.311093377946839666 ) ) ;
#47460 = CARTESIAN_POINT ( 'NONE',  ( -10.18810118749999916, 0.000000000000000000, 117.1562500020483810 ) ) ;
#47461 = CARTESIAN_POINT ( 'NONE',  ( -2.839093476692135984E-14, 195.9375000013655779, 138.5412658750000503 ) ) ;
#47462 = CARTESIAN_POINT ( 'NONE',  ( -0.8912353796322802779, 16.44139524822730891, 68.58382889509240954 ) ) ;
#47464 = CARTESIAN_POINT ( 'NONE',  ( -3.042071309553163960, 67.23958332991934128, -11.35316468749999963 ) ) ;
#47463 = LINE ( 'NONE', #36893, #1505 ) ;
#47465 = CARTESIAN_POINT ( 'NONE',  ( -3.313708498984758943, -7.999999999999989342, 26.79905278392014623 ) ) ;
#47466 = EDGE_CURVE ( 'NONE', #5172, #54540, #70102, .T. ) ;
#47467 = CARTESIAN_POINT ( 'NONE',  ( -2.496229509220055931, 194.6789702782472773, 139.2862435838018769 ) ) ;
#47468 = CARTESIAN_POINT ( 'NONE',  ( -7.320508075688778149, 149.9999999931720538, 7.320508075688769267 ) ) ;
#47469 = CARTESIAN_POINT ( 'NONE',  ( 7.188101187500002709, 93.68750000204838102, 2.977408999572649151 ) ) ;
#47470 = CARTESIAN_POINT ( 'NONE',  ( -24.42570115618304882, 194.9664015783983473, 168.2699142173232474 ) ) ;
#47471 = CARTESIAN_POINT ( 'NONE',  ( 8.311093377946837890, 61.71874999658601979, -8.311093377946837890 ) ) ;
#47472 = CARTESIAN_POINT ( 'NONE',  ( -10.18810118749999916, 4.220049686691934809, 112.9375000020483810 ) ) ;
#47473 = CARTESIAN_POINT ( 'NONE',  ( -9.832129032723420536, 193.6979166632526983, 5.676582343749997150 ) ) ;
#47474 = EDGE_LOOP ( 'NONE', ( #19236, #50573, #31881, #22640 ) ) ;
#47475 = CARTESIAN_POINT ( 'NONE',  ( 2.751064625579944321E-14, 205.8750000027312126, 194.0000000000000568 ) ) ;
#47476 = CARTESIAN_POINT ( 'NONE',  ( -8.000000000000000000, 121.9062500000000000, -3.313708498984761164 ) ) ;
#47477 = DIRECTION ( 'NONE',  ( 0.000000000000000000, 0.000000000000000000, 1.000000000000000000 ) ) ;
#47478 = CARTESIAN_POINT ( 'NONE',  ( 9.832129032723420536, 181.1979166632526983, -5.676582343749999815 ) ) ;
#47479 = DIRECTION ( 'NONE',  ( -0.000000000000000000, 1.000000000000000000, -0.000000000000000000 ) ) ;
#47480 = CARTESIAN_POINT ( 'NONE',  ( 9.999999999999998224, 245.8333333401613174, -2.679491924311229401 ) ) ;
#47481 = CARTESIAN_POINT ( 'NONE',  ( -37.99999999999999289, 37.00000000000000000, 20.00000000000000000 ) ) ;
#47482 = ORIENTED_EDGE ( 'NONE', *, *, #81, .T. ) ;
#47483 = CARTESIAN_POINT ( 'NONE',  ( -9.832129032723420536, 169.0104166632526983, 5.676582343749997150 ) ) ;
#47484 = VECTOR ( 'NONE', #44828, 1000.000000000000114 ) ;
#47485 = CARTESIAN_POINT ( 'NONE',  ( -4.401442555609577197E-16, 7.188101187499992051, 23.61155278187175455 ) ) ;
#47486 = CARTESIAN_POINT ( 'NONE',  ( 10.92737078412413609, 225.9999999999999147, -3.080083792328916825 ) ) ;
#47487 = ORIENTED_EDGE ( 'NONE', *, *, #58332, .F. ) ;
#47488 = CARTESIAN_POINT ( 'NONE',  ( -3.313708498984762496, 105.9687500040967620, 7.999999999999998224 ) ) ;
#47489 = CARTESIAN_POINT ( 'NONE',  ( -7.347880794884122694E-16, 11.75000000000000000, 4.000000000000001776 ) ) ;
#47490 = LINE ( 'NONE', #36191, #27554 ) ;
#47491 = CARTESIAN_POINT ( 'NONE',  ( 3.211159895383560947, 11.18749999863440792, 3.211159895383562723 ) ) ;
#47492 = CARTESIAN_POINT ( 'NONE',  ( -7.999999999999991118, 0.000000000000000000, 19.01780278392014623 ) ) ;
#47494 = CARTESIAN_POINT ( 'NONE',  ( -10.99999999999999645, -11.00000000000000000, -6.938893903907228378E-15 ) ) ;
#47493 = AXIS2_PLACEMENT_3D ( 'NONE', #27674, #51058, #32993 ) ;
#47495 = ORIENTED_EDGE ( 'NONE', *, *, #52425, .F. ) ;
#47496 = DIRECTION ( 'NONE',  ( -0.000000000000000000, -0.000000000000000000, -1.000000000000000000 ) ) ;
#47497 = CARTESIAN_POINT ( 'NONE',  ( -5.082755093536325930, 96.96875000204838102, -5.082755093536325930 ) ) ;
#47499 = CARTESIAN_POINT ( 'NONE',  ( -25.17157287525385811, 205.0000000027312126, 167.1715728752541281 ) ) ;
#47498 = CARTESIAN_POINT ( 'NONE',  ( 1.656854249492538234, 196.6875000000000284, 194.0000000000001990 ) ) ;
#47500 =( BOUNDED_CURVE ( )  B_SPLINE_CURVE ( 2, ( #56395, #18162, #10000, #44698, #62044, #41178, #45070, #10735, #64188 ),
 .UNSPECIFIED., .F., .F. ) 
 B_SPLINE_CURVE_WITH_KNOTS ( ( 3, 2, 2, 2, 3 ),
 ( 0.6250000000000000000, 0.6306818181818182323, 0.6363636363636363535, 0.6420454545454545858, 0.6477272727272727071 ),
 .UNSPECIFIED. ) 
 CURVE ( )  GEOMETRIC_REPRESENTATION_ITEM ( )  RATIONAL_B_SPLINE_CURVE ( ( 1.000000000000000000, 0.9238795325112867385, 1.000000000000000000, 0.9238795325112867385, 1.000000000000000000, 0.9238795325112867385, 1.000000000000000000, 0.9238795325112867385, 1.000000000000000000 ) ) 
 REPRESENTATION_ITEM ( '' )  );
#47501 = ORIENTED_EDGE ( 'NONE', *, *, #51306, .F. ) ;
#47502 = CARTESIAN_POINT ( 'NONE',  ( 2.436599634630545630, 16.39988855009607605, -68.84456747601286963 ) ) ;
#47503 = CARTESIAN_POINT ( 'NONE',  ( -8.000000000000000000, 104.0937500040967905, -3.313708498984761164 ) ) ;
#47504 = ADVANCED_FACE ( 'NONE', ( #42344 ), #65361, .T. ) ;
#47505 = CARTESIAN_POINT ( 'NONE',  ( 7.188101187499992051, 8.802885111219154394E-16, 24.73655278187175810 ) ) ;
#47506 = ORIENTED_EDGE ( 'NONE', *, *, #28652, .T. ) ;
#47507 = ORIENTED_EDGE ( 'NONE', *, *, #58117, .T. ) ;
#47508 = CARTESIAN_POINT ( 'NONE',  ( 10.18810118749999916, 4.220049686691935698, 85.00000000204838102 ) ) ;
#47509 = CARTESIAN_POINT ( 'NONE',  ( -7.320508075688773708, 113.7499999931720254, -7.320508075688774596 ) ) ;
#47510 = CARTESIAN_POINT ( 'NONE',  ( -11.00000000000000000, 0.000000000000000000, 96.99999999999998579 ) ) ;
#47513 = CARTESIAN_POINT ( 'NONE',  ( -2.765530957081996810, 299.4218750017069510, -6.676582343750002480 ) ) ;
#47512 = CARTESIAN_POINT ( 'NONE',  ( 28.00000000000002132, 200.1250000027312126, 173.9999999999999147 ) ) ;
#47511 = CYLINDRICAL_SURFACE ( 'NONE', #11995, 10.00000000000000178 ) ;
#47514 = CARTESIAN_POINT ( 'NONE',  ( -7.320508075688773708, 131.8749999999999716, -7.320508075688774596 ) ) ;
#47515 = CARTESIAN_POINT ( 'NONE',  ( -4.000000000000001776, 0.4375000000000002220, -1.656854249492381470 ) ) ;
#47516 = CARTESIAN_POINT ( 'NONE',  ( 18.00000000000000000, 10.39230484541329247, -1.607695154586745501 ) ) ;
#47517 = DIRECTION ( 'NONE',  ( -0.000000000000000000, -0.000000000000000000, 1.000000000000000000 ) ) ;
#47518 = CARTESIAN_POINT ( 'NONE',  ( 31.45873412499999944, 201.6875000013656063, 169.9999999999999432 ) ) ;
#47519 = CARTESIAN_POINT ( 'NONE',  ( 5.082755093536324154, 8.156249997951611874, 5.082755093536326818 ) ) ;
#47520 = MECHANICAL_DESIGN_GEOMETRIC_PRESENTATION_REPRESENTATION (  '', ( #28273 ), #12698 ) ;
#47521 = CARTESIAN_POINT ( 'NONE',  ( 3.317071493978877683, 8.008118988124991233, 3.544365283940628775 ) ) ;
#47522 = CARTESIAN_POINT ( 'NONE',  ( -2.839093476692135984E-14, 195.6875000013655779, 138.5412658750000503 ) ) ;
#47523 = CARTESIAN_POINT ( 'NONE',  ( -5.082755093536325930, 115.3437500020483810, -5.082755093536325930 ) ) ;
#47525 = CARTESIAN_POINT ( 'NONE',  ( -6.891449706541976639, -51.31760009879133833, -41.45518442798706360 ) ) ;
#47524 = CARTESIAN_POINT ( 'NONE',  ( -7.320508075688771932, 249.3750000000000000, -7.320508075688771932 ) ) ;
#47526 = CARTESIAN_POINT ( 'NONE',  ( 11.35316468749999608, 231.9270833367473585, -3.042071309553167069 ) ) ;
#47527 = CARTESIAN_POINT ( 'NONE',  ( 0.000000000000000000, 0.000000000000000000, -21.50000000000000000 ) ) ;
#47528 = CARTESIAN_POINT ( 'NONE',  ( -4.401442555609577197E-16, 7.188101187499992051, 19.48655278187175455 ) ) ;
#47529 = CARTESIAN_POINT ( 'NONE',  ( 31.99999999999999289, 196.2500000000000000, 169.9999999999999432 ) ) ;
#47530 = CARTESIAN_POINT ( 'NONE',  ( 6.951808397369818766E-16, 22.03124999658601624, -11.35316468750000141 ) ) ;
#47531 = CARTESIAN_POINT ( 'NONE',  ( 10.00000000000033040, 25.20833333333352755, -2.679491924311314666 ) ) ;
#47532 = CARTESIAN_POINT ( 'NONE',  ( -11.35316468750000141, 223.8020833299192986, 3.042071309553159963 ) ) ;
#47533 = FACE_BOUND ( 'NONE', #63821, .T. ) ;
#47534 = CARTESIAN_POINT ( 'NONE',  ( -11.00000000000005151, 4.556349186103993532, 99.90624999999997158 ) ) ;
#47535 = ORIENTED_EDGE ( 'NONE', *, *, #49440, .F. ) ;
#47536 = CARTESIAN_POINT ( 'NONE',  ( -7.778174593052023411, 7.778174593052023411, 104.5000000040967763 ) ) ;
#47538 = EDGE_CURVE ( 'NONE', #13039, #30692, #4126, .T. ) ;
#47537 = CARTESIAN_POINT ( 'NONE',  ( -3.458734125000015425, 195.2500000013656063, 143.4326545832176976 ) ) ;
#47539 = EDGE_CURVE ( 'NONE', #36985, #52335, #52945, .T. ) ;
#47540 = CARTESIAN_POINT ( 'NONE',  ( -3.042071309553173730, 39.32291666325267698, 11.35316468749999785 ) ) ;
#47541 = CARTESIAN_POINT ( 'NONE',  ( 2.020667218593132706E-15, -11.00000000000000000, 87.06250000409676204 ) ) ;
#47542 = CARTESIAN_POINT ( 'NONE',  ( -3.458734125000015425, 206.2500000013655779, 143.4326545832176976 ) ) ;
#47543 = CARTESIAN_POINT ( 'NONE',  ( 0.000000000000000000, 117.6259055164962462, 36.30610930966346217 ) ) ;
#47544 = LINE ( 'NONE', #58163, #15410 ) ;
#47546 = CARTESIAN_POINT ( 'NONE',  ( 5.676582343750001591, 36.61458332991934839, -9.832129032723420536 ) ) ;
#47545 = CARTESIAN_POINT ( 'NONE',  ( 7.188101187500000044, 103.9062500020483810, -8.802885111219163269E-16 ) ) ;
#47547 = CARTESIAN_POINT ( 'NONE',  ( 5.656854249492376141, -5.656854249492374365, 17.89280277982336642 ) ) ;
#47548 = CARTESIAN_POINT ( 'NONE',  ( -5.676582343750006032, 144.1145833299193555, 9.832129032723418760 ) ) ;
#47549 = CARTESIAN_POINT ( 'NONE',  ( 8.660254037844389075, 117.2916666598386968, -5.000000000000000000 ) ) ;
#47550 = CARTESIAN_POINT ( 'NONE',  ( -7.188101187500001821, 115.4375000020483810, -2.977408999572650483 ) ) ;
#47551 = FACE_OUTER_BOUND ( 'NONE', #70147, .T. ) ;
#47552 = CARTESIAN_POINT ( 'NONE',  ( -30.44569435410883784, 206.8125000013656063, 167.5543056458915885 ) ) ;
#47553 = ORIENTED_EDGE ( 'NONE', *, *, #57729, .F. ) ;
#47554 = CARTESIAN_POINT ( 'NONE',  ( -9.832129032723420536, 4.010416663252683200, 5.676582343749997150 ) ) ;
#47555 = ORIENTED_EDGE ( 'NONE', *, *, #25211, .F. ) ;
#47556 = CARTESIAN_POINT ( 'NONE',  ( 6.000000000000003553, 289.5625000000001137, -2.485281374238571761 ) ) ;
#47558 = CARTESIAN_POINT ( 'NONE',  ( -5.676582343749998039, 142.4479166632526699, -9.832129032723420536 ) ) ;
#47557 = CARTESIAN_POINT ( 'NONE',  ( -6.735557395310442023E-16, 11.00000000000000000, 92.31250000409677625 ) ) ;
#47559 = CARTESIAN_POINT ( 'NONE',  ( -4.000000000000001776, 3.500000000000000000, -4.898587196589415787E-16 ) ) ;
#47560 = CARTESIAN_POINT ( 'NONE',  ( -5.656854249492375253, 5.656854249492375253, 15.69905278432982776 ) ) ;
#47561 = CIRCLE ( 'NONE', #15018, 71.70204102886728492 ) ;
#47562 = CARTESIAN_POINT ( 'NONE',  ( 10.00000000000000000, 225.6250000068279746, -1.224646799147353256E-15 ) ) ;
#47563 = CARTESIAN_POINT ( 'NONE',  ( 11.35316468749999963, 246.1979166700806445, 3.042071309553159519 ) ) ;
#47564 = EDGE_CURVE ( 'NONE', #65881, #47792, #62861, .T. ) ;
#47565 = CARTESIAN_POINT ( 'NONE',  ( 10.18810118750000093, -4.220049686691933921, 91.18750000204836681 ) ) ;
#47566 = ORIENTED_EDGE ( 'NONE', *, *, #73059, .F. ) ;
#47567 = CARTESIAN_POINT ( 'NONE',  ( -2.679491924311226292, 203.3333333265053966, -10.00000000000000178 ) ) ;
#47568 = CARTESIAN_POINT ( 'NONE',  ( 11.00000000000000000, 1.347111479062088405E-15, 100.9375000040967763 ) ) ;
#47569 = CARTESIAN_POINT ( 'NONE',  ( -8.311093377946836114, 92.96874999658602690, -8.311093377946837890 ) ) ;
#47570 = CARTESIAN_POINT ( 'NONE',  ( 10.18810118750000093, -4.220049686691933921, 101.3125000020483810 ) ) ;
#47571 = CARTESIAN_POINT ( 'NONE',  ( 1.881053915767122664, 16.24999999863440436, 4.541265875000001451 ) ) ;
#47572 = VERTEX_POINT ( 'NONE', #61939 ) ;
#47573 = VERTEX_POINT ( 'NONE', #73634 ) ;
#47574 = CARTESIAN_POINT ( 'NONE',  ( 3.313708498984762496, 7.218750000000000888, 7.999999999999998224 ) ) ;
#47575 = CARTESIAN_POINT ( 'NONE',  ( 1.334622868157815783E-15, 10.39230484541327293, -10.80000000000000071 ) ) ;
#47576 = CARTESIAN_POINT ( 'NONE',  ( 7.188101187500001821, 0.5624999979516098758, -2.977408999572650483 ) ) ;
#47577 = CARTESIAN_POINT ( 'NONE',  ( -3.313708498984762496, 122.4687500040967763, 7.999999999999998224 ) ) ;
#47578 = CARTESIAN_POINT ( 'NONE',  ( 7.204075437095966983, 7.204075437095967871, 97.46875000204838102 ) ) ;
#47579 = CONICAL_SURFACE ( 'NONE', #31986, 3.999999999999976019, 0.7853981633974496113 ) ;
#47580 = CARTESIAN_POINT ( 'NONE',  ( -7.347880794884122694E-16, 0.7500000000000002220, 4.000000000000001776 ) ) ;
#47581 = CARTESIAN_POINT ( 'NONE',  ( -1.656854249492381248, 15.06249999726881406, -4.000000000000001776 ) ) ;
#47582 = CARTESIAN_POINT ( 'NONE',  ( 1.881053915767121998, 0.4999999986344067504, -4.541265875000002339 ) ) ;
#47583 = ORIENTED_EDGE ( 'NONE', *, *, #53325, .F. ) ;
#47584 = CARTESIAN_POINT ( 'NONE',  ( -2.839093476692135984E-14, 207.6875000013656063, 138.5412658750000503 ) ) ;
#47585 = CARTESIAN_POINT ( 'NONE',  ( 2.445694354108839619, 199.8125000013656063, 200.4456943541088663 ) ) ;
#47587 = CARTESIAN_POINT ( 'NONE',  ( 0.000000000000000000, 300.0000000000000000, 0.000000000000000000 ) ) ;
#47586 = CARTESIAN_POINT ( 'NONE',  ( -31.45873412500002431, 202.6250000013656063, 168.5673454167828140 ) ) ;
#47588 = CARTESIAN_POINT ( 'NONE',  ( -8.342170076843785083E-16, 16.06249999863440436, 4.541265875000002339 ) ) ;
#47589 = CARTESIAN_POINT ( 'NONE',  ( 5.499987861550171608, 9.526286449755788865, 67.99927393035380874 ) ) ;
#47590 = CARTESIAN_POINT ( 'NONE',  ( 1.320432766682872962E-15, -7.188101187499992051, 12.36155278187175277 ) ) ;
#47591 = ORIENTED_EDGE ( 'NONE', *, *, #11097, .T. ) ;
#47592 =( BOUNDED_CURVE ( )  B_SPLINE_CURVE ( 2, ( #29838, #6467, #30572, #29097, #64539, #41888, #41523, #12836, #29470, #58890, #36607, #59256, #449, #13202, #52850, #35873, #18146, #1182, #53594, #7199, #12475, #7568, #36240, #19241, #41161, #69831, #23428, #1905, #35506, #63790, #70565, #24893, #46442, #24534, #52480, #42251, #18516, #817, #47910, #30202, #52117, #70929, #58519, #65264, #69460, #53223, #17768, #23804, #40784, #46807, #24163, #13569, #12108, #47175, #1555, #47542, #18882, #60345, #13933, #49399, #53957, #30937, #38473, #2270, #43747, #15065, #36975, #8673, #3391, #3016, #14687, #54708, #19609, #9427, #60726, #42622, #55083, #49785, #72031, #19979, #37347, #37728, #20347, #54335, #25998, #43364, #31307, #66380, #8296, #25264, #66007, #59980, #21108, #44131, #25635, #72799, #2646, #20729, #32062, #48283, #26375, #14312, #7932, #48650, #66761, #67141, #71658, #61098, #31688, #15436, #26767, #71289, #65637, #9048, #38100, #32445, #42988, #72419, #55454, #3765, #49023, #4888, #56201, #21842, #45983, #11287, #16932, #51269, #39214, #68253, #39586, #5632, #27509, #16548, #27884, #17306, #32823, #56575, #34317, #73910, #5261, #28632, #50895, #73534, #16171, #62581, #22214, #33946, #56945, #10913, #22977, #62214, #50519, #74279, #38846, #39956, #62961, #51646, #45241, #61476, #55833, #22589, #28262, #27139, #45609, #10540, #10169, #30936, #68623, #68999, #57321, #4149, #4514, #9800, #50154, #73171, #15810, #21478, #44499, #67512, #61849, #33205, #44874, #67880, #33572, #58436, #35060, #733, #24812, #64817, #70484, #41807, #40325, #1101, #53138, #52763, #24077, #17681, #70124, #47827, #18803, #40698, #63329, #47086, #11655, #57697, #18430, #52024, #41445, #64457, #13119, #24452, #30490, #29390, #6384, #34689, #1471, #52397, #362, #7115, #47461, #58073, #30121, #36155, #46354, #12757, #23715, #35429, #23344, #29749, #59175, #69745, #7485, #6005, #35789, #29006, #63702, #69371, #12027, #46719, #53507 ),
 .UNSPECIFIED., .F., .F. ) 
 B_SPLINE_CURVE_WITH_KNOTS ( ( 3, 2, 2, 2, 2, 2, 2, 2, 2, 2, 2, 2, 2, 2, 2, 2, 2, 2, 2, 2, 2, 2, 2, 2, 2, 2, 2, 2, 2, 2, 2, 2, 2, 2, 2, 2, 2, 2, 2, 2, 2, 2, 2, 2, 2, 2, 2, 2, 2, 2, 2, 2, 2, 2, 2, 2, 2, 2, 2, 2, 2, 2, 2, 2, 2, 2, 2, 2, 2, 2, 2, 2, 2, 2, 2, 2, 2, 2, 2, 2, 2, 2, 2, 2, 2, 2, 2, 2, 2, 2, 2, 2, 2, 2, 2, 2, 2, 2, 2, 2, 2, 2, 2, 2, 2, 2, 2, 2, 2, 2, 2, 2, 2, 2, 2, 2, 2, 2, 2, 2, 3 ),
 ( 0.000000000000000000, 0.008333333333333333218, 0.01666666666666666644, 0.02500000000000000139, 0.03333333333333333287, 0.04166666666666666435, 0.05000000000000000278, 0.05833333333333333426, 0.06666666666666666574, 0.07499999999999999722, 0.08333333333333332871, 0.09166666666666666019, 0.1000000000000000056, 0.1083333333333333370, 0.1166666666666666685, 0.1250000000000000000, 0.1333333333333333315, 0.1416666666666666630, 0.1499999999999999944, 0.1583333333333333259, 0.1666666666666666574, 0.1749999999999999889, 0.1833333333333333204, 0.1916666666666666796, 0.2000000000000000111, 0.2083333333333333426, 0.2166666666666666741, 0.2250000000000000056, 0.2333333333333333370, 0.2416666666666666685, 0.2500000000000000000, 0.2583333333333333592, 0.2666666666666666630, 0.2750000000000000222, 0.2833333333333333259, 0.2916666666666666852, 0.2999999999999999889, 0.3083333333333333481, 0.3166666666666666519, 0.3250000000000000111, 0.3333333333333333148, 0.3416666666666666741, 0.3499999999999999778, 0.3583333333333333370, 0.3666666666666666408, 0.3750000000000000000, 0.3833333333333333592, 0.3916666666666666630, 0.4000000000000000222, 0.4083333333333333259, 0.4166666666666666852, 0.4249999999999999889, 0.4333333333333333481, 0.4416666666666666519, 0.4500000000000000111, 0.4583333333333333148, 0.4666666666666666741, 0.4749999999999999778, 0.4833333333333333370, 0.4916666666666666408, 0.5000000000000000000, 0.5083333333333333037, 0.5166666666666667185, 0.5250000000000000222, 0.5333333333333333259, 0.5416666666666666297, 0.5500000000000000444, 0.5583333333333333481, 0.5666666666666666519, 0.5749999999999999556, 0.5833333333333333703, 0.5916666666666666741, 0.5999999999999999778, 0.6083333333333332815, 0.6166666666666666963, 0.6250000000000000000, 0.6333333333333333037, 0.6416666666666667185, 0.6500000000000000222, 0.6583333333333333259, 0.6666666666666666297, 0.6750000000000000444, 0.6833333333333333481, 0.6916666666666666519, 0.6999999999999999556, 0.7083333333333333703, 0.7166666666666666741, 0.7249999999999999778, 0.7333333333333332815, 0.7416666666666666963, 0.7500000000000000000, 0.7583333333333333037, 0.7666666666666667185, 0.7750000000000000222, 0.7833333333333333259, 0.7916666666666666297, 0.8000000000000000444, 0.8083333333333333481, 0.8166666666666666519, 0.8249999999999999556, 0.8333333333333333703, 0.8416666666666666741, 0.8499999999999999778, 0.8583333333333332815, 0.8666666666666666963, 0.8750000000000000000, 0.8833333333333333037, 0.8916666666666667185, 0.9000000000000000222, 0.9083333333333333259, 0.9166666666666666297, 0.9250000000000000444, 0.9333333333333333481, 0.9416666666666666519, 0.9499999999999999556, 0.9583333333333333703, 0.9666666666666666741, 0.9749999999999999778, 0.9833333333333332815, 0.9916666666666666963, 1.000000000000000000 ),
 .UNSPECIFIED. ) 
 CURVE ( )  GEOMETRIC_REPRESENTATION_ITEM ( )  RATIONAL_B_SPLINE_CURVE ( ( 1.000000000000000000, 0.9238795325112867385, 1.000000000000000000, 0.9238795325112867385, 1.000000000000000000, 0.9238795325112867385, 1.000000000000000000, 0.9238795325112867385, 1.000000000000000000, 0.9238795325112867385, 1.000000000000000000, 0.9238795325112867385, 1.000000000000000000, 0.9238795325112867385, 1.000000000000000000, 0.9238795325112867385, 1.000000000000000000, 0.9238795325112867385, 1.000000000000000000, 0.9238795325112867385, 1.000000000000000000, 0.9238795325112867385, 1.000000000000000000, 0.9238795325112867385, 1.000000000000000000, 0.9238795325112867385, 1.000000000000000000, 0.9238795325112867385, 1.000000000000000000, 0.9238795325112867385, 1.000000000000000000, 0.9238795325112867385, 1.000000000000000000, 0.9238795325112867385, 1.000000000000000000, 0.9238795325112867385, 1.000000000000000000, 0.9238795325112867385, 1.000000000000000000, 0.9238795325112867385, 1.000000000000000000, 0.9238795325112867385, 1.000000000000000000, 0.9238795325112867385, 1.000000000000000000, 0.9238795325112867385, 1.000000000000000000, 0.9238795325112867385, 1.000000000000000000, 0.9238795325112867385, 1.000000000000000000, 0.9238795325112867385, 1.000000000000000000, 0.9238795325112867385, 1.000000000000000000, 0.9238795325112867385, 1.000000000000000000, 0.9238795325112867385, 1.000000000000000000, 0.9238795325112867385, 1.000000000000000000, 0.9238795325112867385, 1.000000000000000000, 0.9238795325112867385, 1.000000000000000000, 0.9238795325112867385, 1.000000000000000000, 0.9238795325112867385, 1.000000000000000000, 0.9238795325112867385, 1.000000000000000000, 0.9238795325112867385, 1.000000000000000000, 0.9238795325112867385, 1.000000000000000000, 0.9238795325112867385, 1.000000000000000000, 0.9238795325112867385, 1.000000000000000000, 0.9238795325112867385, 1.000000000000000000, 0.9238795325112867385, 1.000000000000000000, 0.9238795325112867385, 1.000000000000000000, 0.9238795325112867385, 1.000000000000000000, 0.9238795325112867385, 1.000000000000000000, 0.9238795325112867385, 1.000000000000000000, 0.9238795325112867385, 1.000000000000000000, 0.9238795325112867385, 1.000000000000000000, 0.9238795325112867385, 1.000000000000000000, 0.9238795325112867385, 1.000000000000000000, 0.9238795325112867385, 1.000000000000000000, 0.9238795325112867385, 1.000000000000000000, 0.9238795325112867385, 1.000000000000000000, 0.9238795325112867385, 1.000000000000000000, 0.9238795325112867385, 1.000000000000000000, 0.9238795325112867385, 1.000000000000000000, 0.9238795325112867385, 1.000000000000000000, 0.9238795325112867385, 1.000000000000000000, 0.9238795325112867385, 1.000000000000000000, 0.9238795325112867385, 1.000000000000000000, 0.9238795325112867385, 1.000000000000000000, 0.9238795325112867385, 1.000000000000000000, 0.9238795325112867385, 1.000000000000000000, 0.9238795325112867385, 1.000000000000000000, 0.9238795325112867385, 1.000000000000000000, 0.9238795325112867385, 1.000000000000000000, 0.9238795325112867385, 1.000000000000000000, 0.9238795325112867385, 1.000000000000000000, 0.9238795325112867385, 1.000000000000000000, 0.9238795325112867385, 1.000000000000000000, 0.9238795325112867385, 1.000000000000000000, 0.9238795325112867385, 1.000000000000000000, 0.9238795325112867385, 1.000000000000000000, 0.9238795325112867385, 1.000000000000000000, 0.9238795325112867385, 1.000000000000000000, 0.9238795325112867385, 1.000000000000000000, 0.9238795325112867385, 1.000000000000000000, 0.9238795325112867385, 1.000000000000000000, 0.9238795325112867385, 1.000000000000000000, 0.9238795325112867385, 1.000000000000000000, 0.9238795325112867385, 1.000000000000000000, 0.9238795325112867385, 1.000000000000000000, 0.9238795325112867385, 1.000000000000000000, 0.9238795325112867385, 1.000000000000000000, 0.9238795325112867385, 1.000000000000000000, 0.9238795325112867385, 1.000000000000000000, 0.9238795325112867385, 1.000000000000000000, 0.9238795325112867385, 1.000000000000000000, 0.9238795325112867385, 1.000000000000000000, 0.9238795325112867385, 1.000000000000000000, 0.9238795325112867385, 1.000000000000000000, 0.9238795325112867385, 1.000000000000000000, 0.9238795325112867385, 1.000000000000000000, 0.9238795325112867385, 1.000000000000000000, 0.9238795325112867385, 1.000000000000000000, 0.9238795325112867385, 1.000000000000000000, 0.9238795325112867385, 1.000000000000000000, 0.9238795325112867385, 1.000000000000000000, 0.9238795325112867385, 1.000000000000000000, 0.9238795325112867385, 1.000000000000000000, 0.9238795325112867385, 1.000000000000000000, 0.9238795325112867385, 1.000000000000000000, 0.9238795325112867385, 1.000000000000000000, 0.9238795325112867385, 1.000000000000000000, 0.9238795325112867385, 1.000000000000000000, 0.9238795325112867385, 1.000000000000000000, 0.9238795325112867385, 1.000000000000000000, 0.9238795325112867385, 1.000000000000000000, 0.9238795325112867385, 1.000000000000000000, 0.9238795325112867385, 1.000000000000000000, 0.9238795325112867385, 1.000000000000000000, 0.9238795325112867385, 1.000000000000000000, 0.9238795325112867385, 1.000000000000000000, 0.9238795325112867385, 1.000000000000000000, 0.9238795325112867385, 1.000000000000000000, 0.9238795325112867385, 1.000000000000000000, 0.9238795325112867385, 1.000000000000000000, 0.9238795325112867385, 1.000000000000000000, 0.9238795325112867385, 1.000000000000000000, 0.9238795325112867385, 1.000000000000000000, 0.9238795325112867385, 1.000000000000000000 ) ) 
 REPRESENTATION_ITEM ( '' )  );
#47593 = ORIENTED_EDGE ( 'NONE', *, *, #49514, .F. ) ;
#47594 = CARTESIAN_POINT ( 'NONE',  ( 7.204075437095966983, 7.204075437095967871, 101.5937500020483668 ) ) ;
#47595 = CARTESIAN_POINT ( 'NONE',  ( -10.52975931929888453, -14.70525031332738664, -0.04683108270950248064 ) ) ;
#47596 = CARTESIAN_POINT ( 'NONE',  ( -28.00000000000002842, 204.0000000000000284, 166.0000000000003695 ) ) ;
#47597 = CARTESIAN_POINT ( 'NONE',  ( 2.754378923186476579E-14, 197.1875000013655779, 194.5412658750000219 ) ) ;
#47598 = CARTESIAN_POINT ( 'NONE',  ( -8.000000000000000000, 12.46874999590322197, -3.313708498984762496 ) ) ;
#47599 = CARTESIAN_POINT ( 'NONE',  ( -5.000000000000005329, 88.33333333333332860, 8.660254037844387298 ) ) ;
#47600 = ADVANCED_FACE ( 'NONE', ( #3485 ), #48393, .F. ) ;
#47601 = CARTESIAN_POINT ( 'NONE',  ( 5.656854249492381470, 119.5625000000000000, 5.656854249492379694 ) ) ;
#47602 = CARTESIAN_POINT ( 'NONE',  ( -6.676582343750001591, 297.6093750017069510, 0.000000000000000000 ) ) ;
#47603 = ORIENTED_EDGE ( 'NONE', *, *, #32233, .F. ) ;
#47604 = CARTESIAN_POINT ( 'NONE',  ( -7.320508075688773708, 143.7499999931719969, -7.320508075688774596 ) ) ;
#47605 = CARTESIAN_POINT ( 'NONE',  ( -8.000000000000001776, 17.15624999590322020, 3.313708498984759387 ) ) ;
#47606 = CARTESIAN_POINT ( 'NONE',  ( 2.445694354108782775, 208.5625000013656063, 139.5543056458912190 ) ) ;
#47607 = CARTESIAN_POINT ( 'NONE',  ( 8.000000000000000000, 11.90624999590322375, -3.313708498984761164 ) ) ;
#47608 = CARTESIAN_POINT ( 'NONE',  ( 8.000000000000005329, 9.797174393178833546E-16, -14.77459999999999951 ) ) ;
#47609 = CARTESIAN_POINT ( 'NONE',  ( 1.836970198721029589E-15, 221.2500000000000000, 10.00000000000000000 ) ) ;
#47610 = FACE_OUTER_BOUND ( 'NONE', #20919, .T. ) ;
#47611 = CARTESIAN_POINT ( 'NONE',  ( 2.020667218593132706E-15, -11.00000000000000000, 110.8749999999999858 ) ) ;
#47612 = CARTESIAN_POINT ( 'NONE',  ( -7.320508075688773708, 216.8750000000000000, -7.320508075688774596 ) ) ;
#47613 =( BOUNDED_CURVE ( )  B_SPLINE_CURVE ( 2, ( #21377, #68153, #10812, #27409, #55360, #50425, #44401, #73439, #21747 ),
 .UNSPECIFIED., .F., .F. ) 
 B_SPLINE_CURVE_WITH_KNOTS ( ( 3, 2, 2, 2, 3 ),
 ( 0.4583333333333333148, 0.4652777777777777901, 0.4722222222222222099, 0.4791666666666666852, 0.4861111111111111049 ),
 .UNSPECIFIED. ) 
 CURVE ( )  GEOMETRIC_REPRESENTATION_ITEM ( )  RATIONAL_B_SPLINE_CURVE ( ( 1.000000000000000000, 0.9238795325112867385, 1.000000000000000000, 0.9238795325112867385, 1.000000000000000000, 0.9238795325112867385, 1.000000000000000000, 0.9238795325112867385, 1.000000000000000000 ) ) 
 REPRESENTATION_ITEM ( '' )  );
#47614 = CARTESIAN_POINT ( 'NONE',  ( -5.082755093536319713, 5.082755093536319713, 10.67405278187175455 ) ) ;
#47615 = CARTESIAN_POINT ( 'NONE',  ( -9.832129032723418760, 178.1770833299193555, -5.676582343750004256 ) ) ;
#47616 = CARTESIAN_POINT ( 'NONE',  ( -3.211159895383562723, 0.9374999986344068059, 3.211159895383561391 ) ) ;
#47617 = PLANE ( 'NONE',  #65613 ) ;
#47619 = CARTESIAN_POINT ( 'NONE',  ( 1.656854249492381248, 5.187500000000000888, -4.000000000000001776 ) ) ;
#47618 = CARTESIAN_POINT ( 'NONE',  ( -3.313708498984759387, -7.999999999999989342, 20.61155277982336997 ) ) ;
#47620 = ORIENTED_EDGE ( 'NONE', *, *, #50287, .F. ) ;
#47622 = EDGE_CURVE ( 'NONE', #2559, #64356, #68230, .T. ) ;
#47621 = CARTESIAN_POINT ( 'NONE',  ( -3.458734125000016313, 194.8750000013656063, 140.5673454167824161 ) ) ;
#47623 = CARTESIAN_POINT ( 'NONE',  ( 5.676582343750001591, 51.92708332991935549, -9.832129032723420536 ) ) ;
#47624 = CARTESIAN_POINT ( 'NONE',  ( 11.00000000000000000, 4.556349186104045934, 104.0312500040967763 ) ) ;
#47625 = AXIS2_PLACEMENT_3D ( 'NONE', #10471, #73839, #22145 ) ;
#47626 = CARTESIAN_POINT ( 'NONE',  ( -5.676582343750006032, 219.4270833299193555, 9.832129032723418760 ) ) ;
#47627 = CARTESIAN_POINT ( 'NONE',  ( -26.56734541678243033, 205.3750000013656063, 166.5412658750003345 ) ) ;
#47628 = CARTESIAN_POINT ( 'NONE',  ( 11.00000000000000000, 1.347111479062088405E-15, 79.93750000409677625 ) ) ;
#47630 = CARTESIAN_POINT ( 'NONE',  ( -8.660254037844373087, 102.9166666666666572, 4.999999999999987566 ) ) ;
#47629 = CARTESIAN_POINT ( 'NONE',  ( -5.082755093536324154, 122.8437500020483952, 5.082755093536326818 ) ) ;
#47631 = CARTESIAN_POINT ( 'NONE',  ( -11.00000000000010658, 4.556349186103942017, 87.90625000000000000 ) ) ;
#47632 = EDGE_CURVE ( 'NONE', #44389, #1774, #40704, .T. ) ;
#47633 = CARTESIAN_POINT ( 'NONE',  ( -7.320508075688778149, 74.99999999317202537, 7.320508075688769267 ) ) ;
#47634 = AXIS2_PLACEMENT_3D ( 'NONE', #59393, #7339, #19019 ) ;
#47635 = CARTESIAN_POINT ( 'NONE',  ( 7.188101187500001821, 96.50000000204838102, -2.977408999572651371 ) ) ;
#47636 = CARTESIAN_POINT ( 'NONE',  ( -3.211159895383562723, 17.06249999863440792, 3.211159895383561391 ) ) ;
#47637 = CARTESIAN_POINT ( 'NONE',  ( -29.65685424949244009, 206.1875000027311842, 166.0000000000003979 ) ) ;
#47638 = CARTESIAN_POINT ( 'NONE',  ( 4.000000000000000888, 10.68749999726881406, 1.656854249492384135 ) ) ;
#47639 = CARTESIAN_POINT ( 'NONE',  ( 7.778174593052023411, -7.778174593052021635, 67.75000000409677625 ) ) ;
#47640 = VERTEX_POINT ( 'NONE', #13112 ) ;
#47641 = VERTEX_POINT ( 'NONE', #8581 ) ;
#47642 = CARTESIAN_POINT ( 'NONE',  ( -4.721056650415998313, 297.7343750017069510, 4.721056650416000089 ) ) ;
#47643 = CARTESIAN_POINT ( 'NONE',  ( -5.000000000000011546, 143.3333333333333428, 8.660254037844397956 ) ) ;
#47644 = CARTESIAN_POINT ( 'NONE',  ( 0.000000000000000000, 51.05255888325788050, 0.000000000000000000 ) ) ;
#47645 = CARTESIAN_POINT ( 'NONE',  ( -3.042071309553164404, 162.2395833299193271, -11.35316468749999963 ) ) ;
#47646 = CARTESIAN_POINT ( 'NONE',  ( 5.094045771088254959, 8.823157229062946527, 67.15552375567561683 ) ) ;
#47647 = CARTESIAN_POINT ( 'NONE',  ( 4.000000000000015987, 201.5000000000000000, 198.0000000000000284 ) ) ;
#47648 = CARTESIAN_POINT ( 'NONE',  ( -9.000000000000023093, 15.58845726811988541, 0.000000000000000000 ) ) ;
#47649 = EDGE_CURVE ( 'NONE', #23384, #29935, #48930, .T. ) ;
#47650 = CARTESIAN_POINT ( 'NONE',  ( 10.18810118749999916, 1.247682550866122264E-15, 107.7812500020483810 ) ) ;
#47651 = ORIENTED_EDGE ( 'NONE', *, *, #71387, .F. ) ;
#47652 = CARTESIAN_POINT ( 'NONE',  ( 2.849036369511732440E-14, 202.3750000027312126, 202.0000000000000000 ) ) ;
#47653 = CARTESIAN_POINT ( 'NONE',  ( 10.99999999999992006, -4.556349186104122317, 109.8437500040967620 ) ) ;
#47654 = CARTESIAN_POINT ( 'NONE',  ( 6.951808397369818766E-16, 147.3437499965860411, -11.35316468750000141 ) ) ;
#47655 = CARTESIAN_POINT ( 'NONE',  ( -2.445694354108783664, 200.3125000013656063, 195.5543056458912190 ) ) ;
#47656 = CARTESIAN_POINT ( 'NONE',  ( 6.000000000000003553, 298.6250000034140157, -2.485281374238571761 ) ) ;
#47657 = CARTESIAN_POINT ( 'NONE',  ( -4.220049686691935698, 10.18810118749999916, 73.75000000204836681 ) ) ;
#47658 = CARTESIAN_POINT ( 'NONE',  ( -8.311093377946841443, 49.21874999658600558, 8.311093377946830785 ) ) ;
#47659 = ORIENTED_EDGE ( 'NONE', *, *, #8136, .T. ) ;
#47660 = CARTESIAN_POINT ( 'NONE',  ( 1.881053915767121998, 5.624999998634407028, -4.541265875000002339 ) ) ;
#47661 = CARTESIAN_POINT ( 'NONE',  ( -5.662595241051933570, -5.662595241051936235, 10.20061528394063188 ) ) ;
#47662 = CARTESIAN_POINT ( 'NONE',  ( 2.977408999572651815, 15.18749999795161365, 7.188101187500000933 ) ) ;
#47663 = CARTESIAN_POINT ( 'NONE',  ( -4.242640687119285658, 292.1875000034139589, 4.242640687119287435 ) ) ;
#47664 = DIRECTION ( 'NONE',  ( 6.308085367188390241E-16, 0.000000000000000000, -1.000000000000000000 ) ) ;
#47665 = CARTESIAN_POINT ( 'NONE',  ( 7.188101187499999156, 11.24999999795161187, 2.977408999572654924 ) ) ;
#47666 = CARTESIAN_POINT ( 'NONE',  ( -4.401442555609577197E-16, 7.188101187499992051, 10.11155278187175455 ) ) ;
#47667 =( REPRESENTATION_RELATIONSHIP ('NONE','NONE', #46008, #2150 ) REPRESENTATION_RELATIONSHIP_WITH_TRANSFORMATION ( #6347 )SHAPE_REPRESENTATION_RELATIONSHIP( ) );
#47668 = CARTESIAN_POINT ( 'NONE',  ( -10.18810118749999916, 0.000000000000000000, 117.5312500020483810 ) ) ;
#47669 = EDGE_CURVE ( 'NONE', #66522, #66166, #62941, .T. ) ;
#47670 = DIRECTION ( 'NONE',  ( 0.000000000000000000, 0.000000000000000000, -1.000000000000000000 ) ) ;
#47671 = CARTESIAN_POINT ( 'NONE',  ( 1.656854249492381914, 3.562499997268812724, 4.000000000000000888 ) ) ;
#47672 = VERTEX_POINT ( 'NONE', #36148 ) ;
#47673 = CARTESIAN_POINT ( 'NONE',  ( -3.999999999999960032, 196.1250000027311842, 198.0000000000000284 ) ) ;
#47674 = AXIS2_PLACEMENT_3D ( 'NONE', #40166, #22798, #28471 ) ;
#47675 = CARTESIAN_POINT ( 'NONE',  ( 3.999999999999959144, 201.0625000000000000, 140.3431457505076594 ) ) ;
#47676 = CARTESIAN_POINT ( 'NONE',  ( -30.82842712474624136, 196.2500000027312126, 167.1715728752542418 ) ) ;
#47677 = CARTESIAN_POINT ( 'NONE',  ( 1.881053915767122664, 1.124999998634406584, 4.541265875000001451 ) ) ;
#47678 = CARTESIAN_POINT ( 'NONE',  ( -2.977408999572651815, 116.9375000020483952, 7.188101187500000933 ) ) ;
#47679 = VECTOR ( 'NONE', #31739, 1000.000000000000000 ) ;
#47680 = DIRECTION ( 'NONE',  ( -0.000000000000000000, 1.000000000000000000, -0.000000000000000000 ) ) ;
#47681 = CARTESIAN_POINT ( 'NONE',  ( 7.999999999999991118, 3.313708498984757611, 1.861552783920143117 ) ) ;
#47682 = VERTEX_POINT ( 'NONE', #70478 ) ;
#47683 = CARTESIAN_POINT ( 'NONE',  ( -1.320432766682874540E-15, 22.59374999795161187, 7.188101187500000044 ) ) ;
#47684 = ORIENTED_EDGE ( 'NONE', *, *, #45003, .F. ) ;
#47685 = CARTESIAN_POINT ( 'NONE',  ( -1.432654583217607192, 208.2500000013656063, 194.5412658750000219 ) ) ;
#47686 = CARTESIAN_POINT ( 'NONE',  ( 28.00000000000001776, 203.4375000013656063, 173.4587341249998929 ) ) ;
#47687 = CARTESIAN_POINT ( 'NONE',  ( -2.679491924311235618, 53.54166666666667140, 10.00000000000000000 ) ) ;
#47688 = CARTESIAN_POINT ( 'NONE',  ( 5.082755093536325042, 99.96875000204838102, -5.082755093536325930 ) ) ;
#47689 = CARTESIAN_POINT ( 'NONE',  ( -4.242640687119285658, 297.1250000000000000, 4.242640687119287435 ) ) ;
#47691 = CARTESIAN_POINT ( 'NONE',  ( -29.15421671454355135, -42.85086343433406597, 180.6117556560664639 ) ) ;
#47690 = CARTESIAN_POINT ( 'NONE',  ( 32.88366962843983998, 175.6453849665569464, 160.0580059460211828 ) ) ;
#47692 = EDGE_LOOP ( 'NONE', ( #55290, #36570, #60540, #41 ) ) ;
#47693 = VECTOR ( 'NONE', #24998, 1000.000000000000000 ) ;
#47694 = CARTESIAN_POINT ( 'NONE',  ( 11.35316468749999963, 231.1979166700806161, 3.042071309553159519 ) ) ;
#47695 = CARTESIAN_POINT ( 'NONE',  ( -5.082755093536319713, 5.082755093536319713, 13.67405278187175455 ) ) ;
#47696 = CARTESIAN_POINT ( 'NONE',  ( 5.126144196591297941, 52.42426806216620605, 49.01287729762282197 ) ) ;
#47697 = CARTESIAN_POINT ( 'NONE',  ( -7.999999999999991118, 0.000000000000000000, 3.830302779823362869 ) ) ;
#47698 = CARTESIAN_POINT ( 'NONE',  ( 18.00000000000000000, 10.39230484541325161, -20.69999999999999929 ) ) ;
#47699 = CARTESIAN_POINT ( 'NONE',  ( -7.320508075688771932, 259.3750000000000568, -7.320508075688771932 ) ) ;
#47701 = ADVANCED_FACE ( 'NONE', ( #48190 ), #53132, .F. ) ;
#47700 = CARTESIAN_POINT ( 'NONE',  ( -7.778174593052023411, 7.778174593052023411, 116.5000000040967905 ) ) ;
#47702 = CARTESIAN_POINT ( 'NONE',  ( 2.679491924311228956, 181.0416666666666856, -10.00000000000000000 ) ) ;
#47703 = CARTESIAN_POINT ( 'NONE',  ( 24.54126587499998635, 209.2500000013655779, 171.4326545832175555 ) ) ;
#47704 = CARTESIAN_POINT ( 'NONE',  ( 27.99999999999996447, 198.6250000027312126, 165.9999999999998863 ) ) ;
#47705 = CARTESIAN_POINT ( 'NONE',  ( 11.00000000000010836, -4.556349186103939353, 69.34375000409676204 ) ) ;
#47706 = CARTESIAN_POINT ( 'NONE',  ( -5.676582343750006032, 139.4270833299193555, 9.832129032723418760 ) ) ;
#47707 = DIRECTION ( 'NONE',  ( -0.000000000000000000, -0.000000000000000000, 1.000000000000000000 ) ) ;
#47708 = CARTESIAN_POINT ( 'NONE',  ( 8.000000000000000000, 97.53125000409676204, -3.313708498984762496 ) ) ;
#47711 = DIRECTION ( 'NONE',  ( -0.000000000000000000, -0.000000000000000000, 1.000000000000000000 ) ) ;
#47710 = PLANE ( 'NONE',  #27355 ) ;
#47709 = CARTESIAN_POINT ( 'NONE',  ( 25.17157287525378351, 204.8750000000000284, 172.8284271247460424 ) ) ;
#47712 = VERTEX_POINT ( 'NONE', #25544 ) ;
#47713 = CARTESIAN_POINT ( 'NONE',  ( 11.35316468749999963, 6.302083329919350163, -3.042071309553165293 ) ) ;
#47714 = CARTESIAN_POINT ( 'NONE',  ( -4.898587196589412829E-16, 88.81250000409677625, -8.000000000000000000 ) ) ;
#47715 = CARTESIAN_POINT ( 'NONE',  ( -9.000000000000000000, -1.750439824713162729, -0.07547478993377626511 ) ) ;
#47716 = CARTESIAN_POINT ( 'NONE',  ( -3.458734125000015425, 205.0000000013655779, 143.4326545832176976 ) ) ;
#47717 =( BOUNDED_CURVE ( )  B_SPLINE_CURVE ( 2, ( #8657, #59961, #9032, #55064, #24873, #7549, #49382, #20713, #14295, #47892, #72401, #43729, #70912 ),
 .UNSPECIFIED., .F., .F. ) 
 B_SPLINE_CURVE_WITH_KNOTS ( ( 3, 2, 2, 2, 2, 2, 3 ),
 ( 0.4166666666666664076, 0.4259259259259256525, 0.4351851851851848973, 0.4444444444444441422, 0.4537037037037034981, 0.4629629629629627430, 0.4722222222222219878 ),
 .UNSPECIFIED. ) 
 CURVE ( )  GEOMETRIC_REPRESENTATION_ITEM ( )  RATIONAL_B_SPLINE_CURVE ( ( 1.000000000000001110, 0.9659258262890673130, 1.000000000000000000, 0.9659258262890683122, 1.000000000000000000, 0.9659258262890683122, 1.000000000000000000, 0.9659258262890683122, 1.000000000000000000, 0.9659258262890683122, 1.000000000000000000, 0.9659258262890690894, 0.9999999999999992228 ) ) 
 REPRESENTATION_ITEM ( '' )  );
#47718 = CARTESIAN_POINT ( 'NONE',  ( 2.849036369511732440E-14, 204.2500000000000284, 202.0000000000000000 ) ) ;
#47719 = ADVANCED_FACE ( 'NONE', ( #65167 ), #19516, .F. ) ;
#47720 = CARTESIAN_POINT ( 'NONE',  ( 7.320508075688774596, 32.49999999317203248, -7.320508075688774596 ) ) ;
#47721 = CARTESIAN_POINT ( 'NONE',  ( -4.401442555609581635E-16, 117.7812500020483810, -7.188101187500000044 ) ) ;
#47722 = CARTESIAN_POINT ( 'NONE',  ( -3.211159895383562723, 6.062499998634407028, 3.211159895383561391 ) ) ;
#47723 = CARTESIAN_POINT ( 'NONE',  ( 7.778174593052023411, -7.778174593052021635, 85.56249999999998579 ) ) ;
#47724 = CARTESIAN_POINT ( 'NONE',  ( -3.313708498984758943, -7.999999999999989342, 13.11155277982336465 ) ) ;
#47725 = CARTESIAN_POINT ( 'NONE',  ( -4.556349186104045934, 11.00000000000000000, 101.4062500040967763 ) ) ;
#47726 = ORIENTED_EDGE ( 'NONE', *, *, #74600, .F. ) ;
#47727 = CARTESIAN_POINT ( 'NONE',  ( -7.347880794884122694E-16, 19.49999999726881228, 4.000000000000001776 ) ) ;
#47728 = CARTESIAN_POINT ( 'NONE',  ( 11.35316468749999963, 226.5104166700806445, 3.042071309553159519 ) ) ;
#47729 = CARTESIAN_POINT ( 'NONE',  ( 3.042071309553159519, 109.7395833299193697, 11.35316468750000141 ) ) ;
#47730 = EDGE_LOOP ( 'NONE', ( #49739, #65045, #37540 ) ) ;
#47731 = CARTESIAN_POINT ( 'NONE',  ( 5.471491410962281421, 9.542682104092435225, 117.5000000000000568 ) ) ;
#47732 = CARTESIAN_POINT ( 'NONE',  ( 7.204075437095966983, 7.204075437095967871, 101.5937500020483668 ) ) ;
#47733 = DIRECTION ( 'NONE',  ( -0.000000000000000000, 1.000000000000000000, -0.000000000000000000 ) ) ;
#47734 = CARTESIAN_POINT ( 'NONE',  ( 1.432654583217662481, 198.3750000013655779, 194.5412658750000219 ) ) ;
#47735 = CARTESIAN_POINT ( 'NONE',  ( -4.898587196589407898E-16, 7.999999999999991118, 27.45530277982336642 ) ) ;
#47737 = CARTESIAN_POINT ( 'NONE',  ( -3.042071309553173730, 114.3229166632526841, 11.35316468749999785 ) ) ;
#47736 = FACE_OUTER_BOUND ( 'NONE', #50270, .T. ) ;
#47738 =( GEOMETRIC_REPRESENTATION_CONTEXT ( 3 ) GLOBAL_UNCERTAINTY_ASSIGNED_CONTEXT ( ( #6595 ) ) GLOBAL_UNIT_ASSIGNED_CONTEXT ( ( #32875, #43800, #44177 ) ) REPRESENTATION_CONTEXT ( 'NONE', 'WORKASPACE' ) );
#47739 = CARTESIAN_POINT ( 'NONE',  ( -29.65685424949234772, 207.4375000000000284, 174.0000000000004547 ) ) ;
#47740 = CARTESIAN_POINT ( 'NONE',  ( -4.898587196589407898E-16, 7.999999999999991118, 6.642802783920143561 ) ) ;
#47741 = ORIENTED_EDGE ( 'NONE', *, *, #8431, .T. ) ;
#47742 = CARTESIAN_POINT ( 'NONE',  ( 5.000000000000001776, 202.7083333265053682, -8.660254037844389075 ) ) ;
#47743 = EDGE_CURVE ( 'NONE', #40340, #11129, #65216, .T. ) ;
#47744 = CARTESIAN_POINT ( 'NONE',  ( -4.898587196589412829E-16, 112.8125000040967905, -8.000000000000000000 ) ) ;
#47745 = CARTESIAN_POINT ( 'NONE',  ( -2.828427124746190735, 9.375000000000000000, -2.828427124746191623 ) ) ;
#47746 = CARTESIAN_POINT ( 'NONE',  ( 3.042071309553167513, 102.1354166632526841, -11.35316468749999785 ) ) ;
#47747 = CARTESIAN_POINT ( 'NONE',  ( -3.458734124999958581, 208.5000000013656063, 199.4326545832176976 ) ) ;
#47748 = CARTESIAN_POINT ( 'NONE',  ( -7.188101187500002709, 12.18749999795161365, 2.977408999572649151 ) ) ;
#47749 = CARTESIAN_POINT ( 'NONE',  ( -10.18810118749999916, 0.000000000000000000, 89.03125000204836681 ) ) ;
#47750 = ADVANCED_FACE ( 'NONE', ( #24446 ), #36518, .F. ) ;
#47751 = CARTESIAN_POINT ( 'NONE',  ( -5.676582343750006032, 9.427083329919350163, 9.832129032723418760 ) ) ;
#47752 = VERTEX_POINT ( 'NONE', #20254 ) ;
#47753 = DIRECTION ( 'NONE',  ( 0.000000000000000000, 0.000000000000000000, 1.000000000000000000 ) ) ;
#47754 = CARTESIAN_POINT ( 'NONE',  ( 2.828427124746209831, 196.5000000027312126, 200.8284271247462129 ) ) ;
#47755 = CARTESIAN_POINT ( 'NONE',  ( 11.27292232226671054, 225.9999999999999432, 1.347431162485829281 ) ) ;
#47756 = CARTESIAN_POINT ( 'NONE',  ( 10.18810118750000093, -4.220049686691933921, 71.68750000204836681 ) ) ;
#47757 = CARTESIAN_POINT ( 'NONE',  ( 3.260352326811678303, 22.00000000000002842, 2.654260131296421132 ) ) ;
#47758 = CARTESIAN_POINT ( 'NONE',  ( 2.679491924326688590, 201.0416666666652930, -9.999999999991077360 ) ) ;
#47759 = CARTESIAN_POINT ( 'NONE',  ( 4.721056650415999201, 291.0781250017069510, -4.721056650415999201 ) ) ;
#47760 = CARTESIAN_POINT ( 'NONE',  ( 4.000000000000015987, 204.6875000027312126, 196.3431457505076594 ) ) ;
#47761 = CARTESIAN_POINT ( 'NONE',  ( -3.042071309553163960, 217.5520833299193555, -11.35316468749999963 ) ) ;
#47762 = AXIS2_PLACEMENT_3D ( 'NONE', #46562, #11866, #5104 ) ;
#47763 = CARTESIAN_POINT ( 'NONE',  ( -10.18810118749999916, 0.000000000000000000, 90.15625000204838102 ) ) ;
#47764 = EDGE_CURVE ( 'NONE', #21170, #57934, #59894, .T. ) ;
#47765 = CARTESIAN_POINT ( 'NONE',  ( -31.45873412499999944, 201.6875000013656063, 170.0000000000003979 ) ) ;
#47766 = CARTESIAN_POINT ( 'NONE',  ( 4.898587196589412829E-16, 21.37500000000000355, -8.000000000000000000 ) ) ;
#47767 = CARTESIAN_POINT ( 'NONE',  ( 1.881053915767122664, 13.24999999863441147, 4.541265875000001451 ) ) ;
#47768 = ORIENTED_EDGE ( 'NONE', *, *, #30229, .T. ) ;
#47769 = CARTESIAN_POINT ( 'NONE',  ( -28.00000000000008171, 209.1250000027312126, 166.0000000000003695 ) ) ;
#47770 = CARTESIAN_POINT ( 'NONE',  ( 1.656854249492405451, 207.4375000027311842, 202.0000000000000284 ) ) ;
#47771 = CARTESIAN_POINT ( 'NONE',  ( -1.432654583217662481, 197.3750000013656063, 145.4587341250000634 ) ) ;
#47772 = CARTESIAN_POINT ( 'NONE',  ( 2.828427124746152987, 205.2500000027312126, 139.1715728752538723 ) ) ;
#47773 = CARTESIAN_POINT ( 'NONE',  ( 5.000000000000002665, 14.32120916179452230, -69.86289779849464310 ) ) ;
#47774 = CARTESIAN_POINT ( 'NONE',  ( 4.220049686691941027, -10.18810118749999738, 68.50000000204838102 ) ) ;
#47775 = ORIENTED_EDGE ( 'NONE', *, *, #19546, .T. ) ;
#47776 = CARTESIAN_POINT ( 'NONE',  ( 2.977408999572652260, 7.687499997951611874, 7.188101187500000044 ) ) ;
#47777 = ADVANCED_FACE ( 'NONE', ( #59169 ), #54246, .F. ) ;
#47778 = DIRECTION ( 'NONE',  ( 0.000000000000000000, 0.000000000000000000, 1.000000000000000000 ) ) ;
#47779 = CARTESIAN_POINT ( 'NONE',  ( 2.977408999572650039, 121.0625000020483668, -7.188101187500001821 ) ) ;
#47780 = CARTESIAN_POINT ( 'NONE',  ( 1.469576158976823947E-15, 116.5625000040967763, 8.000000000000000000 ) ) ;
#47781 = CARTESIAN_POINT ( 'NONE',  ( -2.295000000000000373, 261.4319999999996753, 5.413230550752030190 ) ) ;
#47782 = CARTESIAN_POINT ( 'NONE',  ( -6.676582343749999815, 290.5156250017069510, 2.765530957082001251 ) ) ;
#47783 = ADVANCED_FACE ( 'NONE', ( #71566 ), #1818, .T. ) ;
#47785 = CYLINDRICAL_SURFACE ( 'NONE', #8451, 8.000000000000000000 ) ;
#47784 = CARTESIAN_POINT ( 'NONE',  ( 8.311093377946834337, 237.0312500034139873, -8.311093377946836114 ) ) ;
#47786 = CONTEXT_DEPENDENT_SHAPE_REPRESENTATION ( #53963, #34326 ) ;
#47787 = EDGE_LOOP ( 'NONE', ( #480, #48911, #16984, #28577 ) ) ;
#47788 = CARTESIAN_POINT ( 'NONE',  ( -9.832129032723415207, 224.6354166700806729, 5.676582343750005144 ) ) ;
#47789 = CARTESIAN_POINT ( 'NONE',  ( 1.320432766682872962E-15, -7.188101187499992051, 0.3615527818717524378 ) ) ;
#47791 = EDGE_CURVE ( 'NONE', #57840, #50950, #70840, .T. ) ;
#47790 = CARTESIAN_POINT ( 'NONE',  ( 3.458734125000015425, 202.2500000013656063, 196.5673454167823877 ) ) ;
#47792 = VERTEX_POINT ( 'NONE', #7478 ) ;
#47793 = CARTESIAN_POINT ( 'NONE',  ( 2.751064625579944321E-14, 209.7500000000000284, 194.0000000000000568 ) ) ;
#47794 = CARTESIAN_POINT ( 'NONE',  ( 6.951808397369818766E-16, 102.3437499965860127, -11.35316468750000141 ) ) ;
#47795 = CARTESIAN_POINT ( 'NONE',  ( -8.660254037844383745, 122.0833333333333428, -5.000000000000003553 ) ) ;
#47796 = CARTESIAN_POINT ( 'NONE',  ( 7.778174593052023411, -7.778174593052021635, 79.56249999999998579 ) ) ;
#47799 = CARTESIAN_POINT ( 'NONE',  ( -30.82842712474615965, 205.3750000000000284, 172.8284271247465824 ) ) ;
#47798 = CARTESIAN_POINT ( 'NONE',  ( 29.43265458321766559, 206.5000000013655779, 173.4587341249998929 ) ) ;
#47797 = CARTESIAN_POINT ( 'NONE',  ( 25.55430564589119413, 202.3125000013656063, 167.5543056458910485 ) ) ;
#47800 = ORIENTED_EDGE ( 'NONE', *, *, #70313, .F. ) ;
#47801 = CARTESIAN_POINT ( 'NONE',  ( 1.656854249492381248, 19.18749999999999645, -4.000000000000001776 ) ) ;
#47802 = CARTESIAN_POINT ( 'NONE',  ( -5.000000000000005329, 180.2083333265053682, 8.660254037844387298 ) ) ;
#47803 = CARTESIAN_POINT ( 'NONE',  ( -3.042071309553173730, 219.3229166632526699, 11.35316468749999785 ) ) ;
#47804 = CARTESIAN_POINT ( 'NONE',  ( -2.839093476692135984E-14, 201.6875000013656063, 138.5412658750000503 ) ) ;
#47805 = VECTOR ( 'NONE', #29272, 1000.000000000000000 ) ;
#47806 = CARTESIAN_POINT ( 'NONE',  ( 30.44569435410883429, 201.0625000013656063, 167.5543056458911053 ) ) ;
#47807 = DIRECTION ( 'NONE',  ( -0.000000000000000000, -0.000000000000000000, 1.000000000000000000 ) ) ;
#47808 = CARTESIAN_POINT ( 'NONE',  ( 5.676582343749993598, 195.2604166632526983, 9.832129032723422313 ) ) ;
#47809 = CARTESIAN_POINT ( 'NONE',  ( 11.00000000000000000, 1.347111479062088405E-15, 70.74999999999998579 ) ) ;
#47810 = CARTESIAN_POINT ( 'NONE',  ( 3.729367062499960195, 194.8437500006828031, 142.0000000000000568 ) ) ;
#47811 = CARTESIAN_POINT ( 'NONE',  ( -25.17157287525377640, 198.6250000000000284, 172.8284271247465256 ) ) ;
#47812 = CARTESIAN_POINT ( 'NONE',  ( 1.881053915767122664, 16.12499999863440792, 4.541265875000001451 ) ) ;
#47813 = CARTESIAN_POINT ( 'NONE',  ( 30.44569435410878810, 197.8125000013656063, 172.4456943541087526 ) ) ;
#47814 = CARTESIAN_POINT ( 'NONE',  ( 1.320432766682872962E-15, -7.188101187499992051, 3.736552781871751883 ) ) ;
#47815 = CARTESIAN_POINT ( 'NONE',  ( -11.35316468749999785, 73.07291666325268409, -3.042071309553167513 ) ) ;
#47816 = EDGE_CURVE ( 'NONE', #72356, #19023, #21880, .T. ) ;
#47817 = EDGE_CURVE ( 'NONE', #10908, #65516, #14665, .T. ) ;
#47818 = CARTESIAN_POINT ( 'NONE',  ( -5.000000000000000888, -53.18690467503099484, 43.91652490638204398 ) ) ;
#47819 = CARTESIAN_POINT ( 'NONE',  ( 0.000000000000000000, 237.9999999999999716, 0.000000000000000000 ) ) ;
#47820 = ORIENTED_EDGE ( 'NONE', *, *, #38882, .F. ) ;
#47821 = FACE_OUTER_BOUND ( 'NONE', #34352, .T. ) ;
#47822 = DIRECTION ( 'NONE',  ( -0.8660254037844380415, -0.5000000000000011102, 0.000000000000000000 ) ) ;
#47823 = CARTESIAN_POINT ( 'NONE',  ( 11.35316468749999785, 80.57291666325268409, 3.042071309553174174 ) ) ;
#47824 = ORIENTED_EDGE ( 'NONE', *, *, #19552, .T. ) ;
#47825 = CARTESIAN_POINT ( 'NONE',  ( -4.220049686691935698, 10.18810118749999916, 84.25000000204838102 ) ) ;
#47826 = CARTESIAN_POINT ( 'NONE',  ( -10.99999999999999822, -4.556349186104052151, 67.28125000409676204 ) ) ;
#47827 = CARTESIAN_POINT ( 'NONE',  ( -3.458734125000015425, 197.2500000013656063, 143.4326545832176976 ) ) ;
#47828 = DIRECTION ( 'NONE',  ( 0.000000000000000000, 0.000000000000000000, 1.000000000000000000 ) ) ;
#47830 = CARTESIAN_POINT ( 'NONE',  ( -8.311093377946836114, 72.65624999658601268, -8.311093377946837890 ) ) ;
#47829 = CARTESIAN_POINT ( 'NONE',  ( -7.347880794884122694E-16, 13.49999999726881406, 4.000000000000001776 ) ) ;
#47831 = CARTESIAN_POINT ( 'NONE',  ( 5.656854249492374365, 5.656854249492375253, 25.95530278392014623 ) ) ;
#47832 = CARTESIAN_POINT ( 'NONE',  ( 2.449293598294707893E-16, 13.25000000000000000, -4.000000000000001776 ) ) ;
#47833 = CARTESIAN_POINT ( 'NONE',  ( -7.320508075688778149, 164.9999999931720822, 7.320508075688769267 ) ) ;
#47834 = CARTESIAN_POINT ( 'NONE',  ( 5.082755093536326818, 93.59375000204838102, 5.082755093536325042 ) ) ;
#47835 = CARTESIAN_POINT ( 'NONE',  ( -24.68676758239197255, 194.9812539062533574, 167.7597446909301198 ) ) ;
#47836 = CARTESIAN_POINT ( 'NONE',  ( -2.085542519210945728E-15, 64.84374999658601268, 11.35316468750000141 ) ) ;
#47837 =( BOUNDED_CURVE ( )  B_SPLINE_CURVE ( 2, ( #43898, #49554, #38245, #14087, #49928, #31462, #72943, #65413, #59768, #8077, #31078, #54106, #60124 ),
 .UNSPECIFIED., .F., .F. ) 
 B_SPLINE_CURVE_WITH_KNOTS ( ( 3, 2, 2, 2, 2, 2, 3 ),
 ( 2.527683269455331949, 2.532917274740161151, 2.538151280024989909, 2.543385285309819110, 2.548619290594648312, 2.553853295879477070, 2.559087301164306272 ),
 .UNSPECIFIED. ) 
 CURVE ( )  GEOMETRIC_REPRESENTATION_ITEM ( )  RATIONAL_B_SPLINE_CURVE ( ( 1.000000000000219158, 0.9659258262888491542, 1.000000000000000000, 0.9659258262890684232, 1.000000000000000000, 0.9659258262890684232, 1.000000000000000000, 0.9659258262890684232, 1.000000000000000000, 0.9659258262890684232, 1.000000000000000000, 0.9659258262890705327, 0.9999999999999978906 ) ) 
 REPRESENTATION_ITEM ( '' )  );
#47838 = CARTESIAN_POINT ( 'NONE',  ( -10.18810118749999916, 0.000000000000000000, 114.5312500020483810 ) ) ;
#47839 = CARTESIAN_POINT ( 'NONE',  ( 3.042071309553167069, 201.8229166632526415, -11.35316468749999785 ) ) ;
#47840 = ORIENTED_EDGE ( 'NONE', *, *, #41051, .T. ) ;
#47841 = EDGE_CURVE ( 'NONE', #51478, #38312, #15342, .T. ) ;
#47842 = CARTESIAN_POINT ( 'NONE',  ( 4.737866951562526907, 68.48668487056681897, 20.75656675268901097 ) ) ;
#47843 = CARTESIAN_POINT ( 'NONE',  ( -5.656854249492378806, 122.1875000000000000, 5.656854249492381470 ) ) ;
#47844 = CARTESIAN_POINT ( 'NONE',  ( 2.751064625579944321E-14, 195.7500000000000000, 194.0000000000000568 ) ) ;
#47846 = CARTESIAN_POINT ( 'NONE',  ( -11.35316468749999785, 188.0729166632526983, -3.042071309553167957 ) ) ;
#47845 = CARTESIAN_POINT ( 'NONE',  ( 7.320508075688771044, 263.1249999999999432, -7.320508075688771932 ) ) ;
#47847 = AXIS2_PLACEMENT_3D ( 'NONE', #20043, #20421, #71356 ) ;
#47848 = LINE ( 'NONE', #23736, #73091 ) ;
#47849 = CARTESIAN_POINT ( 'NONE',  ( -8.660254037844385522, 238.5416666734946318, 5.000000000000004441 ) ) ;
#47850 = CARTESIAN_POINT ( 'NONE',  ( -4.999999999999998224, 188.5416666598387110, -8.660254037844389075 ) ) ;
#47851 = ORIENTED_EDGE ( 'NONE', *, *, #11808, .T. ) ;
#47852 = CARTESIAN_POINT ( 'NONE',  ( 11.35316468749999785, 180.8854166632526699, 3.042071309553174174 ) ) ;
#47853 = CARTESIAN_POINT ( 'NONE',  ( 7.188101187499993827, -2.977408999572645598, 20.14280278187176165 ) ) ;
#47854 = CARTESIAN_POINT ( 'NONE',  ( 25.17157287525377996, 203.7500000027312126, 167.1715728752537586 ) ) ;
#47855 = EDGE_LOOP ( 'NONE', ( #32004, #67367, #46188, #66498 ) ) ;
#47856 = CARTESIAN_POINT ( 'NONE',  ( -4.898587196589412829E-16, 99.31250000409677625, -8.000000000000000000 ) ) ;
#47857 = CARTESIAN_POINT ( 'NONE',  ( -5.000000000000005329, 3.333333333333333481, 8.660254037844387298 ) ) ;
#47858 = VECTOR ( 'NONE', #18297, 1000.000000000000000 ) ;
#47859 = CARTESIAN_POINT ( 'NONE',  ( 1.656854249492381248, 12.18750000000000000, -4.000000000000001776 ) ) ;
#47860 = CARTESIAN_POINT ( 'NONE',  ( 9.797174393178825657E-16, 125.0000000000000000, -8.000000000000000000 ) ) ;
#47861 = CARTESIAN_POINT ( 'NONE',  ( 1.881053915767121998, 17.49999999863440436, -4.541265875000002339 ) ) ;
#47862 = CARTESIAN_POINT ( 'NONE',  ( 7.999999999999992895, -3.313708498984756279, 15.17405278392014623 ) ) ;
#47863 = CARTESIAN_POINT ( 'NONE',  ( -7.320508075688779925, 188.1250000000000000, 7.320508075688771932 ) ) ;
#47864 = VERTEX_POINT ( 'NONE', #38006 ) ;
#47865 = CARTESIAN_POINT ( 'NONE',  ( 4.999999999999999112, -15.47455834364811267, -69.96446835377027185 ) ) ;
#47866 = CARTESIAN_POINT ( 'NONE',  ( -2.977408999572651815, 97.43750000204839523, 7.188101187500000933 ) ) ;
#47867 = ADVANCED_FACE ( 'NONE', ( #26668 ), #10076, .T. ) ;
#47869 = CARTESIAN_POINT ( 'NONE',  ( 2.828427124746191623, 13.87499999726881406, -2.828427124746191623 ) ) ;
#47868 = CARTESIAN_POINT ( 'NONE',  ( 6.326249034914468552E-13, 178.7500000000000853, 10.00000000000000533 ) ) ;
#47870 = DIRECTION ( 'NONE',  ( 1.000000000000000000, 0.000000000000000000, 0.000000000000000000 ) ) ;
#47871 = ORIENTED_EDGE ( 'NONE', *, *, #26397, .F. ) ;
#47872 = CARTESIAN_POINT ( 'NONE',  ( -7.320508075688907823, 156.8750000000001137, -7.320508075688907823 ) ) ;
#47873 = CARTESIAN_POINT ( 'NONE',  ( 2.085542519210945334E-15, 260.4687500034140157, 11.35316468749999963 ) ) ;
#47874 = CARTESIAN_POINT ( 'NONE',  ( 7.188101187499993827, -2.977408999572645598, 20.14280278187176165 ) ) ;
#47875 = ORIENTED_EDGE ( 'NONE', *, *, #49514, .T. ) ;
#47876 = EDGE_CURVE ( 'NONE', #26401, #65370, #38378, .T. ) ;
#47877 = ORIENTED_EDGE ( 'NONE', *, *, #2363, .T. ) ;
#47878 = CARTESIAN_POINT ( 'NONE',  ( -6.238412754330611322E-16, 10.18810118749999916, 88.28125000204836681 ) ) ;
#47879 = CARTESIAN_POINT ( 'NONE',  ( -8.660254037844390851, 114.7916666598387110, 4.999999999999998224 ) ) ;
#47880 = CARTESIAN_POINT ( 'NONE',  ( -4.556349186104045934, 11.00000000000000000, 95.21874999999998579 ) ) ;
#47883 = CARTESIAN_POINT ( 'NONE',  ( 2.765530957082001251, 292.9218750017069510, 6.676582343749999815 ) ) ;
#47882 = CARTESIAN_POINT ( 'NONE',  ( 25.17157287525381903, 202.0000000027312126, 172.8284271247460993 ) ) ;
#47881 = FACE_OUTER_BOUND ( 'NONE', #62576, .T. ) ;
#47884 = CARTESIAN_POINT ( 'NONE',  ( -2.679491924311235618, 128.5416666666666288, 10.00000000000000000 ) ) ;
#47885 = CARTESIAN_POINT ( 'NONE',  ( -11.00000000000000000, 0.000000000000000000, 84.99999999999998579 ) ) ;
#47886 = DIRECTION ( 'NONE',  ( -0.000000000000000000, 1.000000000000000000, -0.000000000000000000 ) ) ;
#47887 = CARTESIAN_POINT ( 'NONE',  ( 4.242640687119287435, 290.4375000034140157, 4.242640687119285658 ) ) ;
#47888 = CARTESIAN_POINT ( 'NONE',  ( 5.656854249492380582, 4.499999995903220196, -5.656854249492380582 ) ) ;
#47889 = CARTESIAN_POINT ( 'NONE',  ( 26.56734541678232375, 200.3750000013656063, 173.4587341249998929 ) ) ;
#47890 = CARTESIAN_POINT ( 'NONE',  ( -7.188101187500001821, 7.499999997951610986, -2.977408999572651371 ) ) ;
#47891 = CARTESIAN_POINT ( 'NONE',  ( -4.898587196589407898E-16, 7.999999999999991118, 23.14280278392014978 ) ) ;
#47892 = CARTESIAN_POINT ( 'NONE',  ( -7.320508075688771932, 242.5000000068279746, -7.320508075688771932 ) ) ;
#47893 = CARTESIAN_POINT ( 'NONE',  ( 5.082755093536326818, 107.0937500020483810, 5.082755093536325042 ) ) ;
#47895 = CARTESIAN_POINT ( 'NONE',  ( -5.000000000000005329, 133.3333333333333712, 8.660254037844387298 ) ) ;
#47894 = CARTESIAN_POINT ( 'NONE',  ( -10.00000000000000000, 250.0000000000000000, 0.000000000000000000 ) ) ;
#47896 = CARTESIAN_POINT ( 'NONE',  ( 5.676582343749997150, 222.5520833367473017, -9.832129032723418760 ) ) ;
#47897 = CARTESIAN_POINT ( 'NONE',  ( 2.449293598294707893E-16, 12.25000000000000000, -4.000000000000001776 ) ) ;
#47898 = CARTESIAN_POINT ( 'NONE',  ( -5.082755093536319713, 5.082755093536319713, 19.67405278187175455 ) ) ;
#47899 = CARTESIAN_POINT ( 'NONE',  ( 31.99999999999999289, 195.2500000000000000, 169.9999999999999432 ) ) ;
#47900 = CARTESIAN_POINT ( 'NONE',  ( 3.042071309553159519, 34.73958332991934839, 11.35316468750000141 ) ) ;
#47901 = CARTESIAN_POINT ( 'NONE',  ( 4.898587196589412829E-16, 9.375000000000001776, -8.000000000000000000 ) ) ;
#47902 = CARTESIAN_POINT ( 'NONE',  ( -7.320508075688773708, 3.749999993172032475, -7.320508075688774596 ) ) ;
#47903 = CARTESIAN_POINT ( 'NONE',  ( 27.99999999999999645, 210.0000000000000284, 165.9999999999999147 ) ) ;
#47904 = SURFACE_STYLE_USAGE ( .BOTH. , #27408 ) ;
#47905 = ORIENTED_EDGE ( 'NONE', *, *, #6856, .F. ) ;
#47906 = DIRECTION ( 'NONE',  ( 0.000000000000000000, 0.000000000000000000, 1.000000000000000000 ) ) ;
#47907 = CARTESIAN_POINT ( 'NONE',  ( -1.656854249492358155, 14.68750000000000000, 4.000000000000024869 ) ) ;
#47908 = CARTESIAN_POINT ( 'NONE',  ( -5.676582343749998039, 37.44791666325267698, -9.832129032723420536 ) ) ;
#47909 = CARTESIAN_POINT ( 'NONE',  ( -7.778174593052023411, 7.778174593052023411, 85.00000000409677625 ) ) ;
#47910 = CARTESIAN_POINT ( 'NONE',  ( -2.445694354108839175, 207.3125000013656063, 144.4456943541088663 ) ) ;
#47911 = CARTESIAN_POINT ( 'NONE',  ( -10.00000000000000888, 152.5000000000000284, -1.224646799147354440E-15 ) ) ;
#47912 = CARTESIAN_POINT ( 'NONE',  ( 10.99999999999994849, 4.556349186104097448, 100.8437500000000142 ) ) ;
#47914 = CARTESIAN_POINT ( 'NONE',  ( -9.832129032723420536, 33.69791666325268409, 5.676582343749997150 ) ) ;
#47913 = CARTESIAN_POINT ( 'NONE',  ( 5.082755093536326818, 106.7187500020483952, 5.082755093536325042 ) ) ;
#47915 = CARTESIAN_POINT ( 'NONE',  ( 5.656854249492374365, 5.656854249492375253, 13.76780277982336465 ) ) ;
#47916 = CARTESIAN_POINT ( 'NONE',  ( -11.35316468750000141, 148.4895833299193555, 3.042071309553159963 ) ) ;
#47917 = CARTESIAN_POINT ( 'NONE',  ( -5.000000000000005329, 115.2083333265053682, 8.660254037844387298 ) ) ;
#47918 = CARTESIAN_POINT ( 'NONE',  ( -2.977408999572650927, 107.7500000020483810, -7.188101187500001821 ) ) ;
#47919 = DIRECTION ( 'NONE',  ( -1.577021341797097560E-16, 1.000000000000000000, 0.000000000000000000 ) ) ;
#47920 = CARTESIAN_POINT ( 'NONE',  ( -29.43265458321761230, 206.1250000013655779, 173.4587341250003760 ) ) ;
#47921 = ORIENTED_EDGE ( 'NONE', *, *, #37693, .T. ) ;
#47922 = CARTESIAN_POINT ( 'NONE',  ( 8.311093377946834337, 20.46874999658601624, 8.311093377946839666 ) ) ;
#47923 = ORIENTED_EDGE ( 'NONE', *, *, #19434, .T. ) ;
#47924 = CARTESIAN_POINT ( 'NONE',  ( 2.449293598294707893E-16, 7.250000000000000000, -4.000000000000001776 ) ) ;
#47925 = LINE ( 'NONE', #59632, #37756 ) ;
#47927 = CARTESIAN_POINT ( 'NONE',  ( 5.676582343750001591, 151.6145833299193555, -9.832129032723420536 ) ) ;
#47926 = CARTESIAN_POINT ( 'NONE',  ( -21.58999975740480792, -26.27687770201866613, 145.2393037872558637 ) ) ;
#47928 = CARTESIAN_POINT ( 'NONE',  ( 2.449293598294707893E-16, 3.250000000000000444, -4.000000000000001776 ) ) ;
#47929 = CARTESIAN_POINT ( 'NONE',  ( -3.313708498984757167, 7.999999999999991118, 15.60530278432982421 ) ) ;
#47930 = CARTESIAN_POINT ( 'NONE',  ( -1.469576158976823947E-15, 14.62500000000000178, 8.000000000000000000 ) ) ;
#47931 = CARTESIAN_POINT ( 'NONE',  ( -5.676582343749992710, 234.7395833367473301, 9.832129032723422313 ) ) ;
#47932 = CARTESIAN_POINT ( 'NONE',  ( -4.220049686691937474, -10.18810118749999738, 92.31250000204838102 ) ) ;
#47933 = ORIENTED_EDGE ( 'NONE', *, *, #52505, .F. ) ;
#47934 = CARTESIAN_POINT ( 'NONE',  ( 4.898587196589415787E-16, 0.000000000000000000, 4.000000000000001776 ) ) ;
#47935 = CARTESIAN_POINT ( 'NONE',  ( -3.673940397442060854E-16, 291.8125000034140157, -6.000000000000001776 ) ) ;
#47936 = CARTESIAN_POINT ( 'NONE',  ( -3.042071309553173730, 99.63541666325268409, 11.35316468749999785 ) ) ;
#47937 = CARTESIAN_POINT ( 'NONE',  ( 7.204075437095968759, -7.204075437095966983, 102.7187500020483668 ) ) ;
#47938 = CARTESIAN_POINT ( 'NONE',  ( 1.881053915767122664, 18.24999999863440792, 4.541265875000001451 ) ) ;
#47939 = VERTEX_POINT ( 'NONE', #72322 ) ;
#47940 = VERTEX_POINT ( 'NONE', #43652 ) ;
#47941 = CARTESIAN_POINT ( 'NONE',  ( 5.656854249492380582, 3.187500000000000444, -5.656854249492380582 ) ) ;
#47942 = CARTESIAN_POINT ( 'NONE',  ( -4.541265875000002339, 0.8749999986344069169, -1.881053915767121998 ) ) ;
#47943 = CARTESIAN_POINT ( 'NONE',  ( 7.188101187500000044, 4.968749997951610986, 0.000000000000000000 ) ) ;
#47944 = CARTESIAN_POINT ( 'NONE',  ( -5.656854249492380582, 113.0000000040967763, -5.656854249492380582 ) ) ;
#47945 = VECTOR ( 'NONE', #73831, 1000.000000000000227 ) ;
#47946 =( BOUNDED_CURVE ( )  B_SPLINE_CURVE ( 2, ( #53892, #25200, #1118, #47845, #71592, #1489, #70866, #48213, #12773, #36910, #70501, #1843, #13136 ),
 .UNSPECIFIED., .F., .F. ) 
 B_SPLINE_CURVE_WITH_KNOTS ( ( 3, 2, 2, 2, 2, 2, 3 ),
 ( 0.02777777777777718296, 0.03703703703703645211, 0.04629629629629572474, 0.05555555555555498348, 0.06481481481481425611, 0.07407407407407351485, 0.08333333333333278747 ),
 .UNSPECIFIED. ) 
 CURVE ( )  GEOMETRIC_REPRESENTATION_ITEM ( )  RATIONAL_B_SPLINE_CURVE ( ( 1.000000000000002220, 0.9659258262890662028, 1.000000000000000000, 0.9659258262890683122, 1.000000000000000000, 0.9659258262890683122, 1.000000000000000000, 0.9659258262890683122, 1.000000000000000000, 0.9659258262890683122, 1.000000000000000000, 0.9659258262890703106, 0.9999999999999980016 ) ) 
 REPRESENTATION_ITEM ( '' )  );
#47948 = EDGE_CURVE ( 'NONE', #57466, #20924, #48364, .T. ) ;
#47947 = CARTESIAN_POINT ( 'NONE',  ( 10.18810118750000093, -4.220049686691933921, 100.1875000020483668 ) ) ;
#47949 = ADVANCED_FACE ( 'NONE', ( #15716 ), #21009, .T. ) ;
#47950 = CARTESIAN_POINT ( 'NONE',  ( -8.660254037844390851, 159.7916666598387110, 4.999999999999998224 ) ) ;
#47951 = CARTESIAN_POINT ( 'NONE',  ( 1.656854249492381914, 0.8125000000000004441, 4.000000000000000888 ) ) ;
#47952 = CARTESIAN_POINT ( 'NONE',  ( -2.828427124746192067, 13.37499999726881406, 2.828427124746190735 ) ) ;
#47953 = CARTESIAN_POINT ( 'NONE',  ( -1.881053915767121776, 3.624999998634406584, -4.541265875000002339 ) ) ;
#47954 = VERTEX_POINT ( 'NONE', #62122 ) ;
#47955 = EDGE_CURVE ( 'NONE', #20642, #45762, #27788, .T. ) ;
#47956 = VECTOR ( 'NONE', #4980, 1000.000000000000000 ) ;
#47957 = LINE ( 'NONE', #7979, #16338 ) ;
#47958 = CARTESIAN_POINT ( 'NONE',  ( -1.432654583217607192, 197.2500000013656063, 194.5412658750000219 ) ) ;
#47960 = CARTESIAN_POINT ( 'NONE',  ( -10.00000000000000355, 224.5833333265053398, 2.679491924311223183 ) ) ;
#47959 = CARTESIAN_POINT ( 'NONE',  ( -29.43265458321771177, 201.5000000013655779, 166.5412658750003914 ) ) ;
#47961 = CARTESIAN_POINT ( 'NONE',  ( 4.541265875000001451, 13.24999999863441147, 1.881053915767124440 ) ) ;
#47962 = CARTESIAN_POINT ( 'NONE',  ( -7.778174593052023411, 7.778174593052023411, 84.81249999999998579 ) ) ;
#47963 = CARTESIAN_POINT ( 'NONE',  ( 5.082755093536318824, 5.082755093536319713, 11.42405278187175455 ) ) ;
#47964 = ORIENTED_EDGE ( 'NONE', *, *, #38622, .F. ) ;
#47965 = ORIENTED_EDGE ( 'NONE', *, *, #20881, .T. ) ;
#47966 = CARTESIAN_POINT ( 'NONE',  ( 4.220049686691934809, 10.18810118749999916, 106.1875000020483810 ) ) ;
#47967 = CARTESIAN_POINT ( 'NONE',  ( 8.000000000000000000, 26.90624999590322730, -3.313708498984761164 ) ) ;
#47968 = CARTESIAN_POINT ( 'NONE',  ( -24.54126587499999346, 205.4375000013656063, 170.0000000000003411 ) ) ;
#47969 = CARTESIAN_POINT ( 'NONE',  ( -26.34314575050758123, 199.5625000000000568, 174.0000000000003411 ) ) ;
#47970 = CARTESIAN_POINT ( 'NONE',  ( 2.445694354108838731, 197.0625000013656063, 195.5543056458912190 ) ) ;
#47971 = DIRECTION ( 'NONE',  ( -0.000000000000000000, -1.000000000000000000, -0.000000000000000000 ) ) ;
#47972 = CARTESIAN_POINT ( 'NONE',  ( -7.320508075688778149, 98.12499999999998579, 7.320508075688769267 ) ) ;
#47973 = CARTESIAN_POINT ( 'NONE',  ( 8.000000000000000000, 116.7499999999999858, -9.797174393178825657E-16 ) ) ;
#47974 = CARTESIAN_POINT ( 'NONE',  ( -2.765530957081998586, 296.7968750017070079, 6.676582343750001591 ) ) ;
#47975 = EDGE_CURVE ( 'NONE', #44702, #11605, #37841, .T. ) ;
#47976 = ORIENTED_EDGE ( 'NONE', *, *, #10373, .T. ) ;
#47977 = CARTESIAN_POINT ( 'NONE',  ( -8.660254037844390851, 144.7916666598387110, 4.999999999999998224 ) ) ;
#47978 = CARTESIAN_POINT ( 'NONE',  ( -3.313708498984765161, 15.84374999590322197, 7.999999999999998224 ) ) ;
#47979 = CARTESIAN_POINT ( 'NONE',  ( 2.445694354108782775, 202.5625000013656063, 139.5543056458912190 ) ) ;
#47980 = CARTESIAN_POINT ( 'NONE',  ( -10.00000000000000178, 104.3749999931720396, -1.224646799147353454E-15 ) ) ;
#47981 = DIRECTION ( 'NONE',  ( 0.8191520442889907994, 1.003171929053523514E-16, -0.5735764363510476027 ) ) ;
#47982 = CARTESIAN_POINT ( 'NONE',  ( 2.679491924311225848, 228.5416666666666572, -10.00000000000000000 ) ) ;
#47983 = CARTESIAN_POINT ( 'NONE',  ( 2.020667218593132706E-15, -11.00000000000000000, 91.56250000409677625 ) ) ;
#47984 = CARTESIAN_POINT ( 'NONE',  ( -7.778174593052020747, -7.778174593052023411, 112.1875000000000000 ) ) ;
#47985 = CARTESIAN_POINT ( 'NONE',  ( 8.660254037844385522, 214.5833333333333428, 5.000000000000005329 ) ) ;
#47986 = CARTESIAN_POINT ( 'NONE',  ( 2.977408999572650927, -7.188101187499990274, 8.330302781871752771 ) ) ;
#47987 = CARTESIAN_POINT ( 'NONE',  ( -11.35316468750000141, 183.8020833299193271, 3.042071309553159963 ) ) ;
#47988 = DIRECTION ( 'NONE',  ( -0.000000000000000000, 1.000000000000000000, -0.000000000000000000 ) ) ;
#47989 = CARTESIAN_POINT ( 'NONE',  ( 1.881053915767121776, 1.499999998634406806, -4.541265875000002339 ) ) ;
#47990 = LINE ( 'NONE', #14397, #46358 ) ;
#47992 = DIRECTION ( 'NONE',  ( 1.000000000000000000, -0.000000000000000000, 0.000000000000000000 ) ) ;
#47991 = CYLINDRICAL_SURFACE ( 'NONE', #14146, 3.999999999999976019 ) ;
#47993 = ORIENTED_EDGE ( 'NONE', *, *, #66801, .T. ) ;
#47994 = CARTESIAN_POINT ( 'NONE',  ( -2.445694354108840063, 208.0625000013656063, 139.5543056458912190 ) ) ;
#47995 = CARTESIAN_POINT ( 'NONE',  ( 9.832129032723420536, 51.51041666325269119, -5.676582343749999815 ) ) ;
#47996 = CARTESIAN_POINT ( 'NONE',  ( -6.735557395310442023E-16, 11.00000000000000000, 105.8125000040967763 ) ) ;
#47997 = CARTESIAN_POINT ( 'NONE',  ( 6.951808397369818766E-16, 217.3437499965860411, -11.35316468750000141 ) ) ;
#47998 = CARTESIAN_POINT ( 'NONE',  ( -24.54126587499996504, 206.1250000013656063, 171.4326545832179534 ) ) ;
#47999 = CARTESIAN_POINT ( 'NONE',  ( 0.000000000000000000, 0.000000000000000000, 0.000000000000000000 ) ) ;
#48001 = CARTESIAN_POINT ( 'NONE',  ( 8.000000000000000000, 119.7500000000000000, -9.797174393178825657E-16 ) ) ;
#48000 = CARTESIAN_POINT ( 'NONE',  ( -11.00000000000000000, 0.000000000000000000, 107.4999999999999858 ) ) ;
#48002 = CARTESIAN_POINT ( 'NONE',  ( 3.458734124999959914, 195.3750000013656063, 143.4326545832176976 ) ) ;
#48003 = CARTESIAN_POINT ( 'NONE',  ( -11.35316468750000141, 108.2812499965860269, -1.390361679473963753E-15 ) ) ;
#48004 = AXIS2_PLACEMENT_3D ( 'NONE', #31492, #43540, #54514 ) ;
#48005 = CARTESIAN_POINT ( 'NONE',  ( 2.679491924311222739, 80.83333332650535397, 10.00000000000000355 ) ) ;
#48006 = CARTESIAN_POINT ( 'NONE',  ( 2.977408999572650039, 90.68750000204838102, -7.188101187500001821 ) ) ;
#48007 = CARTESIAN_POINT ( 'NONE',  ( -4.541265875000003227, 16.99999999863440792, 1.881053915767121110 ) ) ;
#48008 = CARTESIAN_POINT ( 'NONE',  ( 4.000000000000000888, 10.93750000000000178, 1.656854249492384135 ) ) ;
#48009 = CARTESIAN_POINT ( 'NONE',  ( 11.00000000000000000, 1.347111479062088405E-15, 67.93750000409676204 ) ) ;
#48010 = ORIENTED_EDGE ( 'NONE', *, *, #60568, .T. ) ;
#48011 = EDGE_LOOP ( 'NONE', ( #21276, #51765, #12722, #50663 ) ) ;
#48012 = CARTESIAN_POINT ( 'NONE',  ( 6.676582343750001591, 295.1093750017069510, -8.176455196517173205E-16 ) ) ;
#48013 = FACE_OUTER_BOUND ( 'NONE', #41243, .T. ) ;
#48014 = CARTESIAN_POINT ( 'NONE',  ( 11.35316468750000141, 165.7812499965860411, 0.000000000000000000 ) ) ;
#48015 = CARTESIAN_POINT ( 'NONE',  ( 10.00000000000000178, 1.874999993172032697, 0.000000000000000000 ) ) ;
#48016 = AXIS2_PLACEMENT_3D ( 'NONE', #26270, #9314, #8191 ) ;
#48017 = CARTESIAN_POINT ( 'NONE',  ( 2.828427124746209831, 198.3750000000000284, 200.8284271247462129 ) ) ;
#48018 = DIRECTION ( 'NONE',  ( 0.000000000000000000, 0.000000000000000000, 1.000000000000000000 ) ) ;
#48019 = CARTESIAN_POINT ( 'NONE',  ( -7.204075437095967871, 7.204075437095967871, 111.3437500020483810 ) ) ;
#48020 = ORIENTED_EDGE ( 'NONE', *, *, #18919, .T. ) ;
#48021 = AXIS2_PLACEMENT_3D ( 'NONE', #25620, #49769, #60331 ) ;
#48022 = CARTESIAN_POINT ( 'NONE',  ( 39.97324732667616587, 0.000000000000000000, 113.7582050592233429 ) ) ;
#48023 = DIRECTION ( 'NONE',  ( -0.000000000000000000, -0.000000000000000000, -1.000000000000000000 ) ) ;
#48024 = CARTESIAN_POINT ( 'NONE',  ( -11.35316468749999785, 148.3854166632526983, -3.042071309553167957 ) ) ;
#48025 = CARTESIAN_POINT ( 'NONE',  ( 1.432654583217662259, 195.1250000013656063, 194.5412658750000219 ) ) ;
#48026 = CARTESIAN_POINT ( 'NONE',  ( -2.485281374238268004, 291.1875000000000568, 6.000000000000304645 ) ) ;
#48027 = CARTESIAN_POINT ( 'NONE',  ( 1.871523826299183495E-15, -10.18810118749999916, 69.90625000204836681 ) ) ;
#48028 = CARTESIAN_POINT ( 'NONE',  ( -8.311093377946836114, 42.96874999658601268, -8.311093377946837890 ) ) ;
#48029 = ORIENTED_EDGE ( 'NONE', *, *, #62383, .F. ) ;
#48030 = DIRECTION ( 'NONE',  ( -1.000000000000000000, 0.000000000000000000, 0.000000000000000000 ) ) ;
#48031 = CARTESIAN_POINT ( 'NONE',  ( 2.780723358947928197E-16, 3.687499998634407472, -4.541265875000002339 ) ) ;
#48032 = CARTESIAN_POINT ( 'NONE',  ( 1.471067592899761672E-15, -8.008118988124991233, 8.888115283940630107 ) ) ;
#48033 = EDGE_CURVE ( 'NONE', #4336, #46261, #20636, .T. ) ;
#48034 = CARTESIAN_POINT ( 'NONE',  ( -1.320432766682874540E-15, 16.59374999795161543, 7.188101187500000044 ) ) ;
#48035 = CARTESIAN_POINT ( 'NONE',  ( -4.242640687119285658, 293.1875000034139589, 4.242640687119287435 ) ) ;
#48036 = CARTESIAN_POINT ( 'NONE',  ( 2.020667218593132706E-15, 219.9523502760175973, 11.00000000000000000 ) ) ;
#48037 = CARTESIAN_POINT ( 'NONE',  ( -5.082755093536325042, 13.40624999795161187, -5.082755093536325930 ) ) ;
#48038 = CARTESIAN_POINT ( 'NONE',  ( -7.188101187499992051, 2.977408999572646930, 8.892802781871754547 ) ) ;
#48039 = CARTESIAN_POINT ( 'NONE',  ( 4.220049686691941027, -10.18810118749999738, 116.5000000020483810 ) ) ;
#48040 =( BOUNDED_CURVE ( )  B_SPLINE_CURVE ( 2, ( #62220, #33578, #26773, #27515, #16177, #49791, #50526, #39220, #43753, #4155, #73541, #67886, #21114 ),
 .UNSPECIFIED., .F., .F. ) 
 B_SPLINE_CURVE_WITH_KNOTS ( ( 3, 2, 2, 2, 2, 2, 3 ),
 ( 2.559087301164306272, 2.564320718348052530, 2.569554135531799233, 2.574787552715545935, 2.580020969899292194, 2.585254387083038896, 2.590487804266785599 ),
 .UNSPECIFIED. ) 
 CURVE ( )  GEOMETRIC_REPRESENTATION_ITEM ( )  RATIONAL_B_SPLINE_CURVE ( ( 1.000000000000001998, 0.9659258262890662028, 1.000000000000000000, 0.9659258262890683122, 1.000000000000000000, 0.9659258262890683122, 1.000000000000000000, 0.9659258262890683122, 1.000000000000000000, 0.9659258262890683122, 1.000000000000000000, 0.9659258262890704216, 0.9999999999999978906 ) ) 
 REPRESENTATION_ITEM ( '' )  );
#48041 = CYLINDRICAL_SURFACE ( 'NONE', #28154, 3.999999999999976019 ) ;
#48042 = CARTESIAN_POINT ( 'NONE',  ( -4.000000000000001776, 1.249999997268813168, -4.898587196589415787E-16 ) ) ;
#48043 = EDGE_LOOP ( 'NONE', ( #4477, #1958, #65199, #24216 ) ) ;
#48044 = EDGE_CURVE ( 'NONE', #55449, #72546, #11834, .T. ) ;
#48045 = CARTESIAN_POINT ( 'NONE',  ( -1.656854249492348607, 197.3125000027312126, 202.0000000000000284 ) ) ;
#48046 = CARTESIAN_POINT ( 'NONE',  ( 3.999999999999960032, 202.0000000000000000, 142.0000000000000568 ) ) ;
#48047 = CARTESIAN_POINT ( 'NONE',  ( -25.17157287525374088, 197.7500000027312126, 172.8284271247464972 ) ) ;
#48048 = ADVANCED_FACE ( 'NONE', ( #43274 ), #66290, .F. ) ;
#48049 = CARTESIAN_POINT ( 'NONE',  ( -8.342170076843785083E-16, 4.062499998634407028, 4.541265875000002339 ) ) ;
#48050 = CARTESIAN_POINT ( 'NONE',  ( -4.401442555609581635E-16, 111.7812500020483810, -7.188101187500000044 ) ) ;
#48051 = DIRECTION ( 'NONE',  ( -1.000000000000000000, 0.000000000000000000, 0.000000000000000000 ) ) ;
#48052 = CARTESIAN_POINT ( 'NONE',  ( 7.999999999999992895, -3.313708498984756279, 0.1740527839201450044 ) ) ;
#48053 = VERTEX_POINT ( 'NONE', #31967 ) ;
#48055 =( BOUNDED_CURVE ( )  B_SPLINE_CURVE ( 2, ( #11473, #34507, #46908, #69932, #5818, #28813, #46165, #34876, #57882 ),
 .UNSPECIFIED., .F., .F. ) 
 B_SPLINE_CURVE_WITH_KNOTS ( ( 3, 2, 2, 2, 3 ),
 ( 0.3068181818181818232, 0.3125000000000000000, 0.3181818181818181768, 0.3238636363636363535, 0.3295454545454545303 ),
 .UNSPECIFIED. ) 
 CURVE ( )  GEOMETRIC_REPRESENTATION_ITEM ( )  RATIONAL_B_SPLINE_CURVE ( ( 1.000000000000000000, 0.9238795325112867385, 1.000000000000000000, 0.9238795325112867385, 1.000000000000000000, 0.9238795325112867385, 1.000000000000000000, 0.9238795325112867385, 1.000000000000000000 ) ) 
 REPRESENTATION_ITEM ( '' )  );
#48054 = CARTESIAN_POINT ( 'NONE',  ( -2.977408999572654480, 22.49999999795161187, 7.188101187499999156 ) ) ;
#48056 = ORIENTED_EDGE ( 'NONE', *, *, #19444, .F. ) ;
#48057 = DIRECTION ( 'NONE',  ( -0.000000000000000000, 1.000000000000000000, -0.000000000000000000 ) ) ;
#48058 = DIRECTION ( 'NONE',  ( -0.000000000000000000, -1.000000000000000000, -0.000000000000000000 ) ) ;
#48059 = CARTESIAN_POINT ( 'NONE',  ( 24.54126587499998280, 205.1250000013656347, 168.5673454167822740 ) ) ;
#48060 = CARTESIAN_POINT ( 'NONE',  ( -2.679491924311225848, 56.45833333333333570, -10.00000000000000178 ) ) ;
#48061 = AXIS2_PLACEMENT_3D ( 'NONE', #65762, #14064, #60104 ) ;
#48062 = CARTESIAN_POINT ( 'NONE',  ( -7.188101187500000044, 99.03125000204838102, 0.000000000000000000 ) ) ;
#48063 = CARTESIAN_POINT ( 'NONE',  ( -6.000000000000000888, 298.0625000000000568, 2.485281374238575758 ) ) ;
#48064 = EDGE_CURVE ( 'NONE', #64507, #62698, #61004, .T. ) ;
#48066 = CARTESIAN_POINT ( 'NONE',  ( -25.07381373783670142, -41.26957671354230683, 188.2315966371032516 ) ) ;
#48065 = CARTESIAN_POINT ( 'NONE',  ( 29.65685424949240812, 207.1875000027312126, 173.9999999999999147 ) ) ;
#48067 = ORIENTED_EDGE ( 'NONE', *, *, #74133, .T. ) ;
#48068 = CARTESIAN_POINT ( 'NONE',  ( 9.832129032723420536, 235.9895833367473301, 5.676582343749996262 ) ) ;
#48069 = CARTESIAN_POINT ( 'NONE',  ( 7.320508075688759497, 89.37500000000001421, 7.320508075688763050 ) ) ;
#48070 = FACE_OUTER_BOUND ( 'NONE', #41729, .T. ) ;
#48071 = CARTESIAN_POINT ( 'NONE',  ( -5.656854249492375253, 5.656854249492375253, 2.330302783920143561 ) ) ;
#48072 = CARTESIAN_POINT ( 'NONE',  ( 24.23812689673033205, 194.8931109331406333, 168.9283172946348657 ) ) ;
#48073 = FACE_OUTER_BOUND ( 'NONE', #52073, .T. ) ;
#48074 = CARTESIAN_POINT ( 'NONE',  ( 2.679491924311228956, 176.0416666666666572, -10.00000000000000000 ) ) ;
#48075 = CARTESIAN_POINT ( 'NONE',  ( 7.999999999999991118, 9.797174393178815797E-16, 6.080302779823364645 ) ) ;
#48076 = DIRECTION ( 'NONE',  ( -0.000000000000000000, 1.000000000000000000, -0.000000000000000000 ) ) ;
#48077 = CARTESIAN_POINT ( 'NONE',  ( -7.188101187499992051, 0.000000000000000000, 28.86155278187175810 ) ) ;
#48078 = CARTESIAN_POINT ( 'NONE',  ( -3.042071309553164404, 147.5520833299193271, -11.35316468749999963 ) ) ;
#48079 = DIRECTION ( 'NONE',  ( 0.000000000000000000, 0.000000000000000000, -1.000000000000000000 ) ) ;
#48080 = CARTESIAN_POINT ( 'NONE',  ( -7.999999999999998224, 117.5937500000000000, 3.313708498984766049 ) ) ;
#48082 = CARTESIAN_POINT ( 'NONE',  ( -11.00000000000000000, 0.000000000000000000, 96.99999999999998579 ) ) ;
#48081 = CARTESIAN_POINT ( 'NONE',  ( 29.65685424949235482, 207.0625000000000568, 173.9999999999999147 ) ) ;
#48083 = VERTEX_POINT ( 'NONE', #63232 ) ;
#48084 = CARTESIAN_POINT ( 'NONE',  ( -3.042071309553173730, 14.63541666325268231, 11.35316468749999785 ) ) ;
#48085 = LINE ( 'NONE', #19054, #27488 ) ;
#48086 = CARTESIAN_POINT ( 'NONE',  ( 1.567784982238203817E-13, 113.7500000000000284, 10.00000000000000533 ) ) ;
#48087 = DIRECTION ( 'NONE',  ( -1.000000000000000000, 0.000000000000000000, 0.000000000000000000 ) ) ;
#48088 = CARTESIAN_POINT ( 'NONE',  ( -3.458734125000015425, 207.9375000013656063, 142.0000000000000568 ) ) ;
#48089 = LINE ( 'NONE', #41703, #59470 ) ;
#48090 = CARTESIAN_POINT ( 'NONE',  ( -8.660254037844387298, 38.95833332650536818, -5.000000000000004441 ) ) ;
#48091 = CARTESIAN_POINT ( 'NONE',  ( 2.977408999572650039, 113.1875000020483810, -7.188101187500001821 ) ) ;
#48092 = CARTESIAN_POINT ( 'NONE',  ( 1.881053915767121776, 5.624999998634407028, -4.541265875000002339 ) ) ;
#48093 = CARTESIAN_POINT ( 'NONE',  ( 1.317228840344749186, 65.80815776305091447, -26.30638062134158872 ) ) ;
#48094 = CARTESIAN_POINT ( 'NONE',  ( -4.898587196589407898E-16, 7.999999999999991118, 12.45530277982336642 ) ) ;
#48096 = PLANE ( 'NONE',  #23340 ) ;
#48095 = CARTESIAN_POINT ( 'NONE',  ( 1.836970198721029589E-15, 239.3750000068279746, 10.00000000000000000 ) ) ;
#48097 = VERTEX_POINT ( 'NONE', #34219 ) ;
#48098 = CARTESIAN_POINT ( 'NONE',  ( 2.824543433528785410E-14, 210.0000000000000284, 194.0000000000000568 ) ) ;
#48099 = DIRECTION ( 'NONE',  ( 0.8660254037844312691, 0.5000000000000128786, 0.000000000000000000 ) ) ;
#48100 = CARTESIAN_POINT ( 'NONE',  ( 5.676582343750005144, 230.8854166700806729, 9.832129032723416984 ) ) ;
#48101 = CARTESIAN_POINT ( 'NONE',  ( 8.311093377946837890, 121.4062499965860127, -8.311093377946837890 ) ) ;
#48102 = ORIENTED_EDGE ( 'NONE', *, *, #53263, .T. ) ;
#48103 = CARTESIAN_POINT ( 'NONE',  ( 2.828427124746208943, 198.6250000000000284, 195.1715728752538439 ) ) ;
#48104 = CARTESIAN_POINT ( 'NONE',  ( -10.18810118749999916, 0.000000000000000000, 93.15625000204836681 ) ) ;
#48105 = LINE ( 'NONE', #59449, #7974 ) ;
#48106 = CARTESIAN_POINT ( 'NONE',  ( 1.432654583217662481, 197.3750000013656063, 194.5412658750000219 ) ) ;
#48107 = CARTESIAN_POINT ( 'NONE',  ( 2.824543433528785410E-14, 210.0000000000000284, 194.0000000000000568 ) ) ;
#48109 = CARTESIAN_POINT ( 'NONE',  ( -9.832129032723418760, 107.8645833299193555, -5.676582343750004256 ) ) ;
#48108 = CARTESIAN_POINT ( 'NONE',  ( 6.682541319018295845, 220.0000000000001137, 7.585481667126755312 ) ) ;
#48110 = CARTESIAN_POINT ( 'NONE',  ( -25.17157287525377996, 209.6250000000000284, 172.8284271247465256 ) ) ;
#48111 = CARTESIAN_POINT ( 'NONE',  ( -7.999999999999998224, 92.09375000000000000, 3.313708498984766049 ) ) ;
#48112 = ORIENTED_EDGE ( 'NONE', *, *, #8272, .F. ) ;
#48113 = APPLICATION_CONTEXT ( 'automotive_design' ) ;
#48114 = B_SPLINE_CURVE_WITH_KNOTS ( 'NONE', 3,
 ( #51757, #22324, #35171, #50633, #104, #22703, #45720, #68365, #39329, #10653, #11031, #68734, #23082, #69111, #17418, #19636, #35532, #53249, #58917, #59283, #6851, #64924 ),
 .UNSPECIFIED., .F., .F.,
 ( 4, 2, 2, 2, 2, 2, 2, 2, 2, 2, 4 ),
 ( 0.000000000000000000, 0.001156727053362482157, 0.001735090580043723235, 0.002313454106724964314, 0.003470181160087444303, 0.004048544686768682996, 0.004626908213449921689, 0.005783635266812366983, 0.006940362320174811410, 0.008097089373537256704, 0.009253816426899701131 ),
 .UNSPECIFIED. ) ;
#48115 = CARTESIAN_POINT ( 'NONE',  ( -7.320508075688773708, 203.7499999931720538, -7.320508075688774596 ) ) ;
#48116 = AXIS2_PLACEMENT_3D ( 'NONE', #59626, #24543, #53233 ) ;
#48117 = CARTESIAN_POINT ( 'NONE',  ( 11.00000000000000000, 1.347111479062088405E-15, 73.74999999999998579 ) ) ;
#48118 = CARTESIAN_POINT ( 'NONE',  ( 10.99999999999978861, 4.556349186104256432, 83.03125000409679046 ) ) ;
#48119 = CARTESIAN_POINT ( 'NONE',  ( 11.35316468749999785, 105.8854166632526983, 3.042071309553174174 ) ) ;
#48120 = CARTESIAN_POINT ( 'NONE',  ( 2.445694354108838731, 209.0625000013656063, 195.5543056458912190 ) ) ;
#48121 = CARTESIAN_POINT ( 'NONE',  ( -5.082755093536325042, 13.40624999795161187, -5.082755093536325930 ) ) ;
#48122 = CARTESIAN_POINT ( 'NONE',  ( 7.204075437095966983, 7.204075437095967871, 91.46875000204838102 ) ) ;
#48123 = CARTESIAN_POINT ( 'NONE',  ( -3.042071309553173730, 4.635416663252684089, 11.35316468749999785 ) ) ;
#48124 = ORIENTED_EDGE ( 'NONE', *, *, #28849, .T. ) ;
#48125 = CARTESIAN_POINT ( 'NONE',  ( 7.320508075688771044, 181.2499999931720254, 7.320508075688775484 ) ) ;
#48126 = CARTESIAN_POINT ( 'NONE',  ( -8.008118988124989457, -3.317071493978883900, 26.60686528394063188 ) ) ;
#48127 = DIRECTION ( 'NONE',  ( 0.000000000000000000, 0.000000000000000000, -1.000000000000000000 ) ) ;
#48128 = CARTESIAN_POINT ( 'NONE',  ( -4.220049686691935698, 10.18810118749999916, 75.25000000204836681 ) ) ;
#48129 = EDGE_CURVE ( 'NONE', #48555, #3208, #39991, .T. ) ;
#48130 = CARTESIAN_POINT ( 'NONE',  ( -3.313708498984816231, 98.46875000409676204, 7.999999999999943157 ) ) ;
#48131 = CYLINDRICAL_SURFACE ( 'NONE', #31869, 4.000000000000001776 ) ;
#48132 = CARTESIAN_POINT ( 'NONE',  ( -4.721056650415998313, 294.5781250017069510, 4.721056650416000089 ) ) ;
#48133 = CARTESIAN_POINT ( 'NONE',  ( 3.407298021520018594, 51.68473891414078025, -48.72627478609679486 ) ) ;
#48134 = CARTESIAN_POINT ( 'NONE',  ( 38.00000000000000000, -63.00000000000000000, 10.00000000000006217 ) ) ;
#48135 = CARTESIAN_POINT ( 'NONE',  ( 10.18810118749999916, 4.220049686691935698, 80.50000000204839523 ) ) ;
#48136 = CARTESIAN_POINT ( 'NONE',  ( -24.54126587499997925, 197.1250000013656347, 171.4326545832179818 ) ) ;
#48137 = CARTESIAN_POINT ( 'NONE',  ( 4.898587196589412829E-16, 22.87500000000000355, -8.000000000000000000 ) ) ;
#48138 = CARTESIAN_POINT ( 'NONE',  ( -1.881053915767121554, 10.74999999863440969, -4.541265875000002339 ) ) ;
#48139 = ORIENTED_EDGE ( 'NONE', *, *, #6602, .T. ) ;
#48140 = CARTESIAN_POINT ( 'NONE',  ( -13.52903678635354723, -41.76888711651481856, 142.1038761753728181 ) ) ;
#48141 = DIRECTION ( 'NONE',  ( -0.000000000000000000, -0.000000000000000000, -1.000000000000000000 ) ) ;
#48142 = CARTESIAN_POINT ( 'NONE',  ( -3.458734125000016757, 198.1250000013656063, 140.5673454167824161 ) ) ;
#48143 = CARTESIAN_POINT ( 'NONE',  ( 1.656854249492347719, 205.9375000027311842, 146.0000000000000284 ) ) ;
#48144 = ADVANCED_FACE ( 'NONE', ( #637 ), #11559, .T. ) ;
#48145 = CARTESIAN_POINT ( 'NONE',  ( 5.000000000000000000, 15.48016642534403253, -69.96422921944753170 ) ) ;
#48146 = CARTESIAN_POINT ( 'NONE',  ( 7.204075437095966983, 7.204075437095967871, 70.46875000204836681 ) ) ;
#48147 = ORIENTED_EDGE ( 'NONE', *, *, #52790, .T. ) ;
#48148 = CARTESIAN_POINT ( 'NONE',  ( -5.082755093536326818, 4.406249997951610986, 5.082755093536325042 ) ) ;
#48149 = DIRECTION ( 'NONE',  ( 0.000000000000000000, 0.000000000000000000, 1.000000000000000000 ) ) ;
#48150 = CARTESIAN_POINT ( 'NONE',  ( -4.401442555609581635E-16, 121.1562500020483810, -7.188101187500000044 ) ) ;
#48151 = CARTESIAN_POINT ( 'NONE',  ( -4.437079077512471770, 22.00000000000000355, 0.01162584019489742125 ) ) ;
#48152 = CARTESIAN_POINT ( 'NONE',  ( 4.721056650416000089, 292.8281250017069510, 4.721056650415999201 ) ) ;
#48153 = EDGE_CURVE ( 'NONE', #12049, #11773, #68900, .T. ) ;
#48155 = CARTESIAN_POINT ( 'NONE',  ( 10.00000000000000000, 136.6666666598387110, 2.679491924311235618 ) ) ;
#48154 = CARTESIAN_POINT ( 'NONE',  ( -9.832129032723418760, 238.4895833367473301, -5.676582343749998927 ) ) ;
#48156 =( BOUNDED_CURVE ( )  B_SPLINE_CURVE ( 2, ( #64123, #64498, #13525, #25224, #65220, #7525, #2605, #54293, #18471 ),
 .UNSPECIFIED., .F., .F. ) 
 B_SPLINE_CURVE_WITH_KNOTS ( ( 3, 2, 2, 2, 3 ),
 ( 0.5416666666666666297, 0.5486111111111111605, 0.5555555555555555802, 0.5625000000000000000, 0.5694444444444444198 ),
 .UNSPECIFIED. ) 
 CURVE ( )  GEOMETRIC_REPRESENTATION_ITEM ( )  RATIONAL_B_SPLINE_CURVE ( ( 1.000000000000000000, 0.9238795325112867385, 1.000000000000000000, 0.9238795325112867385, 1.000000000000000000, 0.9238795325112867385, 1.000000000000000000, 0.9238795325112867385, 1.000000000000000000 ) ) 
 REPRESENTATION_ITEM ( '' )  );
#48157 = ORIENTED_EDGE ( 'NONE', *, *, #11739, .T. ) ;
#48158 = EDGE_CURVE ( 'NONE', #30597, #72156, #65287, .T. ) ;
#48160 = CIRCLE ( 'NONE', #32515, 70.50000000000000000 ) ;
#48159 = CARTESIAN_POINT ( 'NONE',  ( 9.832129032723420536, 221.3020833367473301, 5.676582343749996262 ) ) ;
#48161 = CARTESIAN_POINT ( 'NONE',  ( 7.188101187499993827, -2.977408999572645598, 3.642802781871751883 ) ) ;
#48162 = CARTESIAN_POINT ( 'NONE',  ( 2.824543433528785410E-14, 210.0000000000000284, 194.0000000000000568 ) ) ;
#48163 = CARTESIAN_POINT ( 'NONE',  ( 3.458734125000015869, 201.1875000013656063, 198.0000000000000284 ) ) ;
#48164 = ORIENTED_EDGE ( 'NONE', *, *, #37814, .F. ) ;
#48165 = CARTESIAN_POINT ( 'NONE',  ( 0.000000000000000000, 1.806524977843537691E-16, 0.000000000000000000 ) ) ;
#48166 = CARTESIAN_POINT ( 'NONE',  ( -3.313708498984762052, 97.71874999999998579, -8.000000000000000000 ) ) ;
#48167 = CARTESIAN_POINT ( 'NONE',  ( 8.311093377946837890, 106.7187499965860269, -8.311093377946837890 ) ) ;
#48168 = CARTESIAN_POINT ( 'NONE',  ( -3.171697045051319909E-12, 121.2500000000002558, -10.00000000000000178 ) ) ;
#48169 = CARTESIAN_POINT ( 'NONE',  ( 7.778174593052023411, -7.778174593052021635, 75.06249999999997158 ) ) ;
#48172 = DIRECTION ( 'NONE',  ( 1.000000000000000000, 0.000000000000000000, 0.000000000000000000 ) ) ;
#48171 = CARTESIAN_POINT ( 'NONE',  ( 31.45873412499999944, 202.6875000013656063, 169.9999999999998863 ) ) ;
#48170 = CARTESIAN_POINT ( 'NONE',  ( 24.54126587499999346, 201.4375000013656063, 169.9999999999998863 ) ) ;
#48173 = ORIENTED_EDGE ( 'NONE', *, *, #5242, .T. ) ;
#48174 = CIRCLE ( 'NONE', #39728, 71.70204102886728492 ) ;
#48175 = DIRECTION ( 'NONE',  ( -0.000000000000000000, 1.000000000000000000, -4.476705744456276341E-16 ) ) ;
#48176 = CARTESIAN_POINT ( 'NONE',  ( 3.042071309553159519, 214.7395833299193271, 11.35316468750000141 ) ) ;
#48177 = CARTESIAN_POINT ( 'NONE',  ( 3.458734124999959914, 199.3750000013656063, 143.4326545832176976 ) ) ;
#48178 = CARTESIAN_POINT ( 'NONE',  ( 31.45873412499999944, 201.0000000013655779, 168.5673454167822740 ) ) ;
#48179 = CARTESIAN_POINT ( 'NONE',  ( -10.99999999999999822, -4.556349186104052151, 115.2812500040967763 ) ) ;
#48180 = EDGE_CURVE ( 'NONE', #54025, #43761, #33010, .T. ) ;
#48181 = CARTESIAN_POINT ( 'NONE',  ( -8.311093377946836114, 187.9687499965860411, -8.311093377946837890 ) ) ;
#48182 = CARTESIAN_POINT ( 'NONE',  ( -7.188101187500000044, 91.53125000204836681, 0.000000000000000000 ) ) ;
#48183 = CARTESIAN_POINT ( 'NONE',  ( -31.99999999999999289, 197.2500000000000000, 170.0000000000003979 ) ) ;
#48184 = CARTESIAN_POINT ( 'NONE',  ( 3.211159895383561835, 14.43749999863440792, -3.211159895383561835 ) ) ;
#48185 = CARTESIAN_POINT ( 'NONE',  ( 24.54126587499998990, 197.4375000013655779, 169.9999999999998863 ) ) ;
#48186 = CARTESIAN_POINT ( 'NONE',  ( 1.320432766682872962E-15, -7.188101187499992051, 5.236552781871753659 ) ) ;
#48187 = CARTESIAN_POINT ( 'NONE',  ( -3.042071309553164404, 87.23958332991934128, -11.35316468749999963 ) ) ;
#48188 = VERTEX_POINT ( 'NONE', #5534 ) ;
#48189 = CARTESIAN_POINT ( 'NONE',  ( -28.00000000000002487, 195.0000000000000000, 166.0000000000003695 ) ) ;
#48190 = FACE_OUTER_BOUND ( 'NONE', #69713, .T. ) ;
#48191 = ORIENTED_EDGE ( 'NONE', *, *, #23779, .F. ) ;
#48192 = DIRECTION ( 'NONE',  ( 0.000000000000000000, -0.000000000000000000, -1.000000000000000000 ) ) ;
#48193 = CARTESIAN_POINT ( 'NONE',  ( 3.042071309553159519, 79.73958332991934128, 11.35316468750000141 ) ) ;
#48194 = CARTESIAN_POINT ( 'NONE',  ( 1.871523826299183495E-15, -10.18810118749999916, 86.40625000204838102 ) ) ;
#48195 = CARTESIAN_POINT ( 'NONE',  ( -7.204075437095965206, -7.204075437095968759, 112.8437500020483810 ) ) ;
#48196 = CARTESIAN_POINT ( 'NONE',  ( -1.432654583217608080, 208.8750000013656347, 201.4587341250000350 ) ) ;
#48197 = DIRECTION ( 'NONE',  ( 0.000000000000000000, 0.000000000000000000, 1.000000000000000000 ) ) ;
#48199 = CARTESIAN_POINT ( 'NONE',  ( 3.042071309553167513, 76.82291666325269830, -11.35316468749999785 ) ) ;
#48198 = CARTESIAN_POINT ( 'NONE',  ( 3.313708498984765161, 103.1562500040967905, 7.999999999999998224 ) ) ;
#48200 = CARTESIAN_POINT ( 'NONE',  ( 5.656854249492376141, -5.656854249492374365, 22.58030278392014623 ) ) ;
#48201 = CARTESIAN_POINT ( 'NONE',  ( 4.000000000000001776, 13.00000000000000178, 0.000000000000000000 ) ) ;
#48202 = AXIS2_PLACEMENT_3D ( 'NONE', #3173, #73970, #20885 ) ;
#48203 = CARTESIAN_POINT ( 'NONE',  ( 6.123233995736767268E-16, 173.1249999931720538, -10.00000000000000178 ) ) ;
#48204 = CARTESIAN_POINT ( 'NONE',  ( 7.188101187500001821, 90.87500000204838102, -2.977408999572651371 ) ) ;
#48205 = CARTESIAN_POINT ( 'NONE',  ( 5.000000000000000000, -50.64189880742116401, 41.08656465431877791 ) ) ;
#48206 = CARTESIAN_POINT ( 'NONE',  ( 5.676582343750001591, 56.92708332991935549, -9.832129032723420536 ) ) ;
#48207 = CARTESIAN_POINT ( 'NONE',  ( 7.204075437095968759, -7.204075437095966983, 106.0937500020483810 ) ) ;
#48208 = CARTESIAN_POINT ( 'NONE',  ( -11.35316468750000141, 193.4895833299193271, 3.042071309553159963 ) ) ;
#48209 = ORIENTED_EDGE ( 'NONE', *, *, #54476, .F. ) ;
#48210 = DIRECTION ( 'NONE',  ( 0.000000000000000000, 0.000000000000000000, 1.000000000000000000 ) ) ;
#48211 = CARTESIAN_POINT ( 'NONE',  ( -25.17157287525385811, 199.0000000027312126, 167.1715728752541281 ) ) ;
#48212 = CARTESIAN_POINT ( 'NONE',  ( -0.8588954341814981630, 49.93020820668157000, 40.69831139579171264 ) ) ;
#48214 = CARTESIAN_POINT ( 'NONE',  ( -5.676582343749998039, 187.4479166632526983, -9.832129032723420536 ) ) ;
#48213 = CARTESIAN_POINT ( 'NONE',  ( 10.00000000000000178, 262.2916666666666288, 2.679491924311222739 ) ) ;
#48215 = FACE_OUTER_BOUND ( 'NONE', #11618, .T. ) ;
#48216 = CARTESIAN_POINT ( 'NONE',  ( 5.000000000000004441, 234.7916666734946602, 8.660254037844385522 ) ) ;
#48217 = CARTESIAN_POINT ( 'NONE',  ( -31.99999999999997868, 200.3125000000000284, 171.6568542494928238 ) ) ;
#48218 = ORIENTED_EDGE ( 'NONE', *, *, #1278, .T. ) ;
#48219 = ADVANCED_FACE ( 'NONE', ( #33850 ), #16829, .F. ) ;
#48220 = CARTESIAN_POINT ( 'NONE',  ( 11.35316468749999963, 181.3020833299193271, -3.042071309553165293 ) ) ;
#48221 = VECTOR ( 'NONE', #33258, 1000.000000000000000 ) ;
#48222 = CARTESIAN_POINT ( 'NONE',  ( 5.082755093536318824, 5.082755093536319713, 18.92405278187175455 ) ) ;
#48223 = EDGE_CURVE ( 'NONE', #6191, #54592, #29291, .T. ) ;
#48224 = FACE_OUTER_BOUND ( 'NONE', #4368, .T. ) ;
#48225 = AXIS2_PLACEMENT_3D ( 'NONE', #28896, #10802, #62111 ) ;
#48226 = ORIENTED_EDGE ( 'NONE', *, *, #40363, .F. ) ;
#48227 = CIRCLE ( 'NONE', #42192, 19.00000000000003553 ) ;
#48228 = CARTESIAN_POINT ( 'NONE',  ( -5.656854249492380582, 99.50000000409679046, -5.656854249492380582 ) ) ;
#48229 = LINE ( 'NONE', #71604, #16884 ) ;
#48230 = EDGE_CURVE ( 'NONE', #63519, #70220, #6651, .T. ) ;
#48231 = CARTESIAN_POINT ( 'NONE',  ( 2.828427124746191623, 16.12500000000000000, -2.828427124746191623 ) ) ;
#48232 = CARTESIAN_POINT ( 'NONE',  ( -8.342170076843785083E-16, 15.06249999863440792, 4.541265875000002339 ) ) ;
#48233 = CARTESIAN_POINT ( 'NONE',  ( -3.313708498984758943, -7.999999999999989342, 14.79905278392014978 ) ) ;
#48234 = DIRECTION ( 'NONE',  ( 1.000000000000000000, -0.000000000000000000, -0.000000000000000000 ) ) ;
#48235 = VERTEX_POINT ( 'NONE', #40604 ) ;
#48236 = CARTESIAN_POINT ( 'NONE',  ( -6.735557395310442023E-16, 11.00000000000000000, 72.62500000000000000 ) ) ;
#48237 = CARTESIAN_POINT ( 'NONE',  ( -2.977408999572650927, 101.3750000020483952, -7.188101187500001821 ) ) ;
#48240 = CIRCLE ( 'NONE', #56727, 10.00000000000000000 ) ;
#48239 = CARTESIAN_POINT ( 'NONE',  ( -11.00000000000000000, 0.000000000000000000, 101.6875000040967763 ) ) ;
#48238 = CARTESIAN_POINT ( 'NONE',  ( -8.000000000000000000, 92.09375000409679046, -3.313708498984761164 ) ) ;
#48241 = DIRECTION ( 'NONE',  ( 2.444036937190193349E-14, -1.000000000000000000, 4.876176775795935793E-29 ) ) ;
#48242 = EDGE_LOOP ( 'NONE', ( #9252, #45206, #16947, #22630 ) ) ;
#48243 = EDGE_CURVE ( 'NONE', #26308, #37641, #1277, .T. ) ;
#48244 = CARTESIAN_POINT ( 'NONE',  ( -5.676582343750000703, 263.3854166700806445, -9.832129032723418760 ) ) ;
#48245 = CARTESIAN_POINT ( 'NONE',  ( 2.977408999572650927, -7.188101187499990274, 16.95530278187175455 ) ) ;
#48246 = ORIENTED_EDGE ( 'NONE', *, *, #916, .T. ) ;
#48247 = ORIENTED_EDGE ( 'NONE', *, *, #72278, .T. ) ;
#48248 = CARTESIAN_POINT ( 'NONE',  ( 10.18810118749999916, 1.247682550866122264E-15, 78.90625000204836681 ) ) ;
#48249 = CARTESIAN_POINT ( 'NONE',  ( -2.804140485925949776E-11, 67.59332269700094287, -20.03478791450258001 ) ) ;
#48250 = CARTESIAN_POINT ( 'NONE',  ( 11.00000000000000355, -4.556349186104045046, 93.15625000000000000 ) ) ;
#48253 = CARTESIAN_POINT ( 'NONE',  ( 6.676582343750001591, 296.1093750017069510, -8.176455196517173205E-16 ) ) ;
#48252 = CARTESIAN_POINT ( 'NONE',  ( 24.00000000000000355, 199.9375000027312126, 171.6568542494923122 ) ) ;
#48251 = CARTESIAN_POINT ( 'NONE',  ( 0.000000000000000000, 300.0000000000000000, 6.000000000000001776 ) ) ;
#48254 = CARTESIAN_POINT ( 'NONE',  ( -8.660254037844387298, 152.0833333333333428, -5.000000000000004441 ) ) ;
#48255 = CARTESIAN_POINT ( 'NONE',  ( -26.34314575050764873, 204.0625000027312410, 166.0000000000004263 ) ) ;
#48256 = CARTESIAN_POINT ( 'NONE',  ( 1.656854249492327735, 208.9375000027311842, 146.0000000000000853 ) ) ;
#48257 = FACE_OUTER_BOUND ( 'NONE', #21413, .T. ) ;
#48258 = CARTESIAN_POINT ( 'NONE',  ( 8.000000000000000000, 5.812499995903220196, 0.000000000000000000 ) ) ;
#48259 = AXIS2_PLACEMENT_3D ( 'NONE', #40017, #51701, #18115 ) ;
#48260 = CARTESIAN_POINT ( 'NONE',  ( 25.55430564589119058, 197.0625000013656063, 167.5543056458910485 ) ) ;
#48261 = CARTESIAN_POINT ( 'NONE',  ( -7.188101187500001821, 10.49999999795161010, -2.977408999572651371 ) ) ;
#48262 = CARTESIAN_POINT ( 'NONE',  ( -3.313708498984757167, 7.999999999999991118, 26.23655278392014623 ) ) ;
#48263 = CYLINDRICAL_SURFACE ( 'NONE', #5812, 4.000000000000001776 ) ;
#48264 = CARTESIAN_POINT ( 'NONE',  ( -7.188101187500000933, 109.4375000020483810, -2.977408999572650483 ) ) ;
#48266 = CARTESIAN_POINT ( 'NONE',  ( 2.030339228148215693E-11, 166.2499999999984368, -10.00000000000000178 ) ) ;
#48265 = FACE_OUTER_BOUND ( 'NONE', #8259, .T. ) ;
#48267 = CARTESIAN_POINT ( 'NONE',  ( 2.085542519210945334E-15, 235.4687500034139873, 11.35316468749999963 ) ) ;
#48268 = CARTESIAN_POINT ( 'NONE',  ( 24.54126587500000767, 209.3750000013656063, 168.5673454167822172 ) ) ;
#48269 = CARTESIAN_POINT ( 'NONE',  ( 7.188101187499992051, 8.802885111219154394E-16, 19.11155278187175455 ) ) ;
#48270 = CARTESIAN_POINT ( 'NONE',  ( 27.99999999999996447, 196.0000000000000000, 173.9999999999999147 ) ) ;
#48271 = CARTESIAN_POINT ( 'NONE',  ( -11.35316468750000141, 48.48958332991934839, 3.042071309553159963 ) ) ;
#48272 =( BOUNDED_CURVE ( )  B_SPLINE_CURVE ( 2, ( #54453, #2761, #8793, #49521, #66494, #72541, #54827, #3136, #20847, #43865, #66880, #15185, #2017 ),
 .UNSPECIFIED., .F., .F. ) 
 B_SPLINE_CURVE_WITH_KNOTS ( ( 3, 2, 2, 2, 2, 2, 3 ),
 ( 2.716084159200326198, 2.721317171148036618, 2.726550183095747037, 2.731783195043457457, 2.737016206991167877, 2.742249218938878297, 2.747482230802302361 ),
 .UNSPECIFIED. ) 
 CURVE ( )  GEOMETRIC_REPRESENTATION_ITEM ( )  RATIONAL_B_SPLINE_CURVE ( ( 1.000000000000004219, 0.9659258262890640934, 1.000000000000000000, 0.9659258262890683122, 1.000000000000000000, 0.9659258262890683122, 1.000000000000000000, 0.9659258262890683122, 1.000000000000000000, 0.9659258262890683122, 1.000000000000000000, 0.9659258262890683122, 1.000000000000000000 ) ) 
 REPRESENTATION_ITEM ( '' )  );
#48273 = CARTESIAN_POINT ( 'NONE',  ( 8.660254037844390851, 150.4166666666666572, -5.000000000000001776 ) ) ;
#48275 = CARTESIAN_POINT ( 'NONE',  ( 2.679491924311222739, 5.833333326505364624, 10.00000000000000355 ) ) ;
#48274 =( BOUNDED_CURVE ( )  B_SPLINE_CURVE ( 2, ( #21388, #26675, #62128, #67423, #15722, #38765, #16461, #73819, #61010, #33482, #61764, #56484, #4801 ),
 .UNSPECIFIED., .F., .F. ) 
 B_SPLINE_CURVE_WITH_KNOTS ( ( 3, 2, 2, 2, 2, 2, 3 ),
 ( 0.8858695652173912416, 0.8876811594202896893, 0.8894927536231882481, 0.8913043478260869179, 0.8931159420289854767, 0.8949275362318840354, 0.8967391304347825942 ),
 .UNSPECIFIED. ) 
 CURVE ( )  GEOMETRIC_REPRESENTATION_ITEM ( )  RATIONAL_B_SPLINE_CURVE ( ( 1.000000000000001998, 0.9659258262890662028, 1.000000000000000000, 0.9659258262890683122, 1.000000000000000000, 0.9659258262890683122, 1.000000000000000000, 0.9659258262890683122, 1.000000000000000000, 0.9659258262890683122, 1.000000000000000000, 0.9659258262890683122, 1.000000000000000000 ) ) 
 REPRESENTATION_ITEM ( '' )  );
#48276 = CARTESIAN_POINT ( 'NONE',  ( -6.123233995736766282E-16, 238.7500000000000284, -10.00000000000000000 ) ) ;
#48277 = FACE_OUTER_BOUND ( 'NONE', #42245, .T. ) ;
#48278 = ORIENTED_EDGE ( 'NONE', *, *, #29495, .F. ) ;
#48279 = CARTESIAN_POINT ( 'NONE',  ( -1.836970198721029983E-15, 130.6249999931720254, 10.00000000000000178 ) ) ;
#48280 = DIRECTION ( 'NONE',  ( -0.000000000000000000, -1.000000000000000000, -0.000000000000000000 ) ) ;
#48281 = CARTESIAN_POINT ( 'NONE',  ( 5.676582343750001591, 31.61458332991935194, -9.832129032723420536 ) ) ;
#48282 = CARTESIAN_POINT ( 'NONE',  ( 4.556349186104051263, -10.99999999999999822, 88.65625000409679046 ) ) ;
#48283 = CARTESIAN_POINT ( 'NONE',  ( 1.432654583217607414, 203.5000000013655779, 145.4587341250000350 ) ) ;
#48284 = AXIS2_PLACEMENT_3D ( 'NONE', #40606, #69650, #63608 ) ;
#48285 = CARTESIAN_POINT ( 'NONE',  ( 1.347111479062088405E-15, -3.149999999999999911, -11.00000000000000000 ) ) ;
#48287 = CARTESIAN_POINT ( 'NONE',  ( 9.832129032723416984, 30.36458332991935194, 5.676582343750006032 ) ) ;
#48286 = CARTESIAN_POINT ( 'NONE',  ( 7.188101187500000044, 106.9062500020483810, -8.802885111219163269E-16 ) ) ;
#48288 = CARTESIAN_POINT ( 'NONE',  ( -3.313708498984757167, 7.999999999999991118, 15.54905277982336465 ) ) ;
#48289 = CARTESIAN_POINT ( 'NONE',  ( -9.832129032723418760, 147.8645833299193555, -5.676582343750004256 ) ) ;
#48290 = CARTESIAN_POINT ( 'NONE',  ( 10.00000000000000178, 131.8749999931720254, 0.000000000000000000 ) ) ;
#48291 = CARTESIAN_POINT ( 'NONE',  ( -5.082755093536324154, 111.2187500020483810, 5.082755093536326818 ) ) ;
#48292 = CARTESIAN_POINT ( 'NONE',  ( -24.54126587500000056, 203.5000000013655779, 168.5673454167827003 ) ) ;
#48293 = ORIENTED_EDGE ( 'NONE', *, *, #42545, .T. ) ;
#48294 = CARTESIAN_POINT ( 'NONE',  ( 2.679491924311222739, 20.83333332650536462, 10.00000000000000355 ) ) ;
#48295 = CARTESIAN_POINT ( 'NONE',  ( -3.042071309553163960, 27.55208332991935194, -11.35316468749999963 ) ) ;
#48296 = ORIENTED_EDGE ( 'NONE', *, *, #67619, .F. ) ;
#48297 = DIRECTION ( 'NONE',  ( -0.000000000000000000, -0.000000000000000000, -1.000000000000000000 ) ) ;
#48298 = CARTESIAN_POINT ( 'NONE',  ( -5.099999999999999645, 6.245698675651499853E-16, -0.6301867843887376530 ) ) ;
#48300 = CARTESIAN_POINT ( 'NONE',  ( -5.676582343749998039, 152.4479166632526983, -9.832129032723420536 ) ) ;
#48299 = CARTESIAN_POINT ( 'NONE',  ( 11.00000000000005151, 4.556349186103993532, 92.03125000409677625 ) ) ;
#48301 = CARTESIAN_POINT ( 'NONE',  ( -27.99999999999999645, 210.0000000000000284, 170.0000000000003695 ) ) ;
#48302 = CARTESIAN_POINT ( 'NONE',  ( 3.313708498984756279, 7.999999999999991118, 19.91780278432982954 ) ) ;
#48303 = CARTESIAN_POINT ( 'NONE',  ( -5.447323953993864265, -4.689931814214729044, 0.5319290643893268555 ) ) ;
#48304 = CARTESIAN_POINT ( 'NONE',  ( -3.042071309553159075, 239.9479166700806729, 11.35316468749999963 ) ) ;
#48305 = CARTESIAN_POINT ( 'NONE',  ( -4.220049686691935698, 10.18810118749999916, 88.75000000204836681 ) ) ;
#48306 = ORIENTED_EDGE ( 'NONE', *, *, #60667, .F. ) ;
#48307 = ADVANCED_FACE ( 'NONE', ( #62487 ), #69275, .T. ) ;
#48308 = CARTESIAN_POINT ( 'NONE',  ( 5.656854249492378806, 20.62499999590322375, 5.656854249492381470 ) ) ;
#48309 = CARTESIAN_POINT ( 'NONE',  ( -14.00000000000000178, -2.250000000005106138, 7.677076266390546522 ) ) ;
#48310 = CARTESIAN_POINT ( 'NONE',  ( -3.042071309553164404, 107.5520833299193555, -11.35316468749999963 ) ) ;
#48311 = CARTESIAN_POINT ( 'NONE',  ( 7.204075437095968759, -7.204075437095966983, 99.71875000204838102 ) ) ;
#48312 = EDGE_CURVE ( 'NONE', #31018, #28928, #37384, .T. ) ;
#48313 = CARTESIAN_POINT ( 'NONE',  ( 1.881053915767122664, 15.24999999863440969, 4.541265875000001451 ) ) ;
#48314 = EDGE_LOOP ( 'NONE', ( #49331, #42703, #12506, #26069 ) ) ;
#48315 = ORIENTED_EDGE ( 'NONE', *, *, #31376, .T. ) ;
#48316 = VECTOR ( 'NONE', #67674, 1000.000000000000000 ) ;
#48317 = CARTESIAN_POINT ( 'NONE',  ( 7.999999999999998224, 8.906250000000001776, 3.313708498984766493 ) ) ;
#48318 = CARTESIAN_POINT ( 'NONE',  ( 3.211159895383560947, 5.312499998634407028, 3.211159895383562723 ) ) ;
#48319 = CARTESIAN_POINT ( 'NONE',  ( -5.082755093536326818, 4.406249997951610986, 5.082755093536325042 ) ) ;
#48320 = CARTESIAN_POINT ( 'NONE',  ( -8.000000000000000000, 114.5937500040967763, -3.313708498984761608 ) ) ;
#48321 = CARTESIAN_POINT ( 'NONE',  ( -4.220049686691935698, 10.18810118749999916, 100.7500000020483526 ) ) ;
#48322 = FILL_AREA_STYLE_COLOUR ( '', #64503 ) ;
#48323 = CARTESIAN_POINT ( 'NONE',  ( -4.000000000000001776, 3.500000000000000000, -4.898587196589415787E-16 ) ) ;
#48324 = CARTESIAN_POINT ( 'NONE',  ( -1.656854249492381248, 14.06249999726881406, -4.000000000000001776 ) ) ;
#48325 = CARTESIAN_POINT ( 'NONE',  ( -4.541265875000002339, 5.812499998634406140, -5.561446717895856393E-16 ) ) ;
#48326 = CARTESIAN_POINT ( 'NONE',  ( 3.458734124999959914, 209.4375000013656063, 142.0000000000000568 ) ) ;
#48327 = CARTESIAN_POINT ( 'NONE',  ( -3.458734124999959914, 195.3750000013656063, 196.5673454167823877 ) ) ;
#48329 = CARTESIAN_POINT ( 'NONE',  ( -5.000000000000170530, 23.33333333333352400, 8.660254037844671515 ) ) ;
#48328 = CARTESIAN_POINT ( 'NONE',  ( -28.00000000000007105, 200.4375000013656063, 166.5412658750003629 ) ) ;
#48330 = CARTESIAN_POINT ( 'NONE',  ( -3.211159895383561391, 15.68749999863440436, -3.211159895383561835 ) ) ;
#48331 = CARTESIAN_POINT ( 'NONE',  ( 4.556349186104045934, 11.00000000000000000, 84.53125000000000000 ) ) ;
#48332 = CARTESIAN_POINT ( 'NONE',  ( -5.082755093536319713, 5.082755093536319713, 4.299052781871752771 ) ) ;
#48333 = VERTEX_POINT ( 'NONE', #12660 ) ;
#48334 = ORIENTED_EDGE ( 'NONE', *, *, #40214, .T. ) ;
#48335 = CARTESIAN_POINT ( 'NONE',  ( -10.18810118749999916, 4.220049686691934809, 97.56250000204836681 ) ) ;
#48336 = CARTESIAN_POINT ( 'NONE',  ( 11.00000000000002132, 4.556349186104026394, 114.5312500040967620 ) ) ;
#48337 = CONICAL_SURFACE ( 'NONE', #54395, 8.999999999999998224, 1.047197551196595855 ) ;
#48338 = CARTESIAN_POINT ( 'NONE',  ( -27.99999999999996447, 204.1875000013656063, 173.4587341250003760 ) ) ;
#48339 = CARTESIAN_POINT ( 'NONE',  ( -24.00000000000001066, 200.8125000000000284, 168.3431457505080004 ) ) ;
#48340 = CARTESIAN_POINT ( 'NONE',  ( 3.458734125000015425, 196.0000000013656347, 196.5673454167823877 ) ) ;
#48341 = CARTESIAN_POINT ( 'NONE',  ( -7.347880794884122694E-16, 1.750000000000000222, 4.000000000000001776 ) ) ;
#48342 = CARTESIAN_POINT ( 'NONE',  ( -10.00000000000000355, 107.7083333333333428, 2.679491924311223183 ) ) ;
#48343 = CARTESIAN_POINT ( 'NONE',  ( 1.469576158976823947E-15, 114.8750000000000000, 8.000000000000000000 ) ) ;
#48344 = CARTESIAN_POINT ( 'NONE',  ( -6.676582343750001591, 295.6093750017069510, 0.000000000000000000 ) ) ;
#48345 = ORIENTED_EDGE ( 'NONE', *, *, #19932, .F. ) ;
#48346 = DIRECTION ( 'NONE',  ( -0.000000000000000000, 0.000000000000000000, 1.000000000000000000 ) ) ;
#48347 = CARTESIAN_POINT ( 'NONE',  ( 7.999999999999998224, 20.71874999590322375, 3.313708498984766493 ) ) ;
#48348 = CARTESIAN_POINT ( 'NONE',  ( 1.432654583217607858, 204.6250000013655779, 138.5412658750000787 ) ) ;
#48349 = DIRECTION ( 'NONE',  ( -0.000000000000000000, 1.000000000000000000, -0.000000000000000000 ) ) ;
#48350 = CARTESIAN_POINT ( 'NONE',  ( 2.828427124746190291, 7.875000000000000000, 2.828427124746192067 ) ) ;
#48351 = CARTESIAN_POINT ( 'NONE',  ( 7.320508075688771044, 223.1250000000000284, -7.320508075688771932 ) ) ;
#48352 = CARTESIAN_POINT ( 'NONE',  ( -4.000000000000001776, 3.187499997268814056, -1.656854249492381470 ) ) ;
#48353 = CARTESIAN_POINT ( 'NONE',  ( 11.00000000000000000, 4.556349186104045934, 115.8437500000000000 ) ) ;
#48354 = CARTESIAN_POINT ( 'NONE',  ( 7.320508075688771044, 219.3750000000000000, 7.320508075688775484 ) ) ;
#48355 = CARTESIAN_POINT ( 'NONE',  ( -4.401442555609577197E-16, 7.188101187499992051, 2.986552781871751439 ) ) ;
#48356 = CARTESIAN_POINT ( 'NONE',  ( 8.311093377946837890, 191.7187499965860127, -8.311093377946837890 ) ) ;
#48357 = LINE ( 'NONE', #42329, #63649 ) ;
#48358 = CARTESIAN_POINT ( 'NONE',  ( 3.211159895383560947, 3.187499998634407028, 3.211159895383562723 ) ) ;
#48359 = CARTESIAN_POINT ( 'NONE',  ( 0.000000000000000000, 300.0000000000000000, 0.000000000000000000 ) ) ;
#48361 = DIRECTION ( 'NONE',  ( 0.000000000000000000, 0.000000000000000000, -1.000000000000000000 ) ) ;
#48360 = CARTESIAN_POINT ( 'NONE',  ( 2.751064625579944321E-14, 202.8750000027312126, 194.0000000000000568 ) ) ;
#48362 = VERTEX_POINT ( 'NONE', #36796 ) ;
#48363 =( BOUNDED_CURVE ( )  B_SPLINE_CURVE ( 2, ( #65190, #24092, #47843, #70864, #36169, #47476, #47101, #53890, #59189 ),
 .UNSPECIFIED., .F., .F. ) 
 B_SPLINE_CURVE_WITH_KNOTS ( ( 3, 2, 2, 2, 3 ),
 ( 0.07291666666666671293, 0.07812500000000005551, 0.08333333333333338422, 0.08854166666666674068, 0.09375000000000006939 ),
 .UNSPECIFIED. ) 
 CURVE ( )  GEOMETRIC_REPRESENTATION_ITEM ( )  RATIONAL_B_SPLINE_CURVE ( ( 0.9999999999999994449, 0.9238795325112872936, 1.000000000000000000, 0.9238795325112867385, 1.000000000000000000, 0.9238795325112867385, 1.000000000000000000, 0.9238795325112857393, 1.000000000000001110 ) ) 
 REPRESENTATION_ITEM ( '' )  );
#48364 = CIRCLE ( 'NONE', #72508, 71.70204102886728492 ) ;
#48365 = CARTESIAN_POINT ( 'NONE',  ( 1.432654583217608080, 205.8750000013656063, 138.5412658750000503 ) ) ;
#48366 = CARTESIAN_POINT ( 'NONE',  ( -2.085542519210945728E-15, 44.84374999658602690, 11.35316468750000141 ) ) ;
#48367 = CARTESIAN_POINT ( 'NONE',  ( 4.556349186104045934, 11.00000000000000000, 105.7187500040967763 ) ) ;
#48368 = CARTESIAN_POINT ( 'NONE',  ( 5.676582343750001591, 221.9270833299193555, -9.832129032723420536 ) ) ;
#48369 = CARTESIAN_POINT ( 'NONE',  ( -31.45873412499996391, 202.7500000013655779, 171.4326545832181239 ) ) ;
#48370 = CARTESIAN_POINT ( 'NONE',  ( 38.00000000000000000, 272.0000000000000000, 3.791916237172776494E-14 ) ) ;
#48372 = CARTESIAN_POINT ( 'NONE',  ( -2.679491924311222295, 231.0416666666666856, 10.00000000000000178 ) ) ;
#48371 = CARTESIAN_POINT ( 'NONE',  ( -2.977408999572650927, 122.3750000020483952, -7.188101187500000933 ) ) ;
#48373 = CARTESIAN_POINT ( 'NONE',  ( -1.432654583217664479, 196.7500000013656063, 138.5412658750000787 ) ) ;
#48374 = CARTESIAN_POINT ( 'NONE',  ( 3.042071309553159519, 104.7395833299193555, 11.35316468750000141 ) ) ;
#48375 = EDGE_CURVE ( 'NONE', #71473, #3567, #56142, .T. ) ;
#48376 = EDGE_CURVE ( 'NONE', #56463, #11938, #4564, .T. ) ;
#48377 = CARTESIAN_POINT ( 'NONE',  ( 10.00000000000000178, 87.08333332650535397, -2.679491924311226736 ) ) ;
#48378 = CARTESIAN_POINT ( 'NONE',  ( -7.188101187500001821, 89.56250000204838102, -2.977408999572650483 ) ) ;
#48379 = CARTESIAN_POINT ( 'NONE',  ( -4.541265875000002339, 14.87499999863441147, -1.881053915767121998 ) ) ;
#48380 = DIRECTION ( 'NONE',  ( -0.000000000000000000, -1.000000000000000000, -0.000000000000000000 ) ) ;
#48381 = CARTESIAN_POINT ( 'NONE',  ( -3.313708498984759387, -7.999999999999989342, 1.111552779823364201 ) ) ;
#48382 = ORIENTED_EDGE ( 'NONE', *, *, #68834, .F. ) ;
#48383 = CARTESIAN_POINT ( 'NONE',  ( -6.101298592596269721, 226.0000000000000000, 7.950093002584347701 ) ) ;
#48384 = ORIENTED_EDGE ( 'NONE', *, *, #53301, .T. ) ;
#48385 = CARTESIAN_POINT ( 'NONE',  ( 2.765530957082001251, 294.9218750017070647, 6.676582343750000703 ) ) ;
#48386 = CARTESIAN_POINT ( 'NONE',  ( 10.00000000000000178, 187.0833333265053398, -2.679491924311226736 ) ) ;
#48387 = CARTESIAN_POINT ( 'NONE',  ( -11.35316468749999785, 163.0729166632526415, -3.042071309553167513 ) ) ;
#48388 = CARTESIAN_POINT ( 'NONE',  ( 0.000000000000000000, 1.224646799147352862E-15, -9.999999999999996447 ) ) ;
#48389 = CARTESIAN_POINT ( 'NONE',  ( -3.999999999999959144, 201.0625000000000000, 199.6568542494924259 ) ) ;
#48390 = CARTESIAN_POINT ( 'NONE',  ( -10.00000000000004441, 192.2916666666666856, -2.679491924311241835 ) ) ;
#48391 = CARTESIAN_POINT ( 'NONE',  ( -6.238412754330611322E-16, 10.18810118749999916, 108.1562500020483668 ) ) ;
#48392 = EDGE_LOOP ( 'NONE', ( #45458, #10555, #63111, #43128 ) ) ;
#48393 =( BOUNDED_SURFACE ( )  B_SPLINE_SURFACE ( 1, 2, ( 
 ( #61198, #67609, #15906, #4241, #49118, #9528, #10266, #27228, #8771, #56290, #15533, #33293, #43460, #72892, #21199, #14783, #60441, #60818, #9894, #21570, #61574, #4608, #37442, #37823, #20444, #27603, #15163, #43844, #50614, #54801, #3113, #26097, #21939, #66100, #32543, #3867, #14410, #55554, #31781, #26862, #67237, #72130, #49877, #66475, #50244, #9141, #38574, #73266, #32159, #55180, #44224, #32924, #26475, #72518, #20827, #66857, #23433, #46447, #57789, #27986, #17025, #69465, #6097, #62309, #35151, #69092, #63794, #22306, #51736, #86, #68346, #39311, #39676, #63420, #454, #40422, #57415, #52485, #29475, #16643, #63053, #52122, #11748, #29103, #56669, #28721, #822, #57040, #23063, #17773, #62675, #40788, #28352, #5721, #45700, #11378, #74371, #11010, #40049, #44969, #34412, #34043, #12113, #6472, #17398, #68714, #33663, #5351, #4985, #34786, #46072, #67975, #58166, #16270, #10636, #50991, #74003, #45331, #51361, #22682, #8301, #54340, #59261, #30942, #47547, #59985, #59622, #24898, #29843, #65642, #64544, #58895, #47180, #42628, #18521, #53962, #23809, #7573, #19246, #2275, #53228, #24539, #70571, #52855, #31312, #35511, #1187, #64903, #7204, #48288, #70934, #42257, #41893, #41166, #53599, #46812, #35878, #65269, #18151, #1910, #69836, #18887, #1560, #41529, #30208, #13207, #71293, #36246, #47915, #7937, #64176, #13574, #30577, #36612, #12841, #58524, #12480, #36980, #19614, #70212, #13938, #6831, #24168, #25269, #38479, #3396, #3771, #26004, #15815, #71664, #43752, #66011, #19984, #38103, #8678, #66766, #72425, #44136, #50159, #55838, #60731, #73176, #67146, #27143, #60351, #4154, #42993, #21483, #38850, #15070, #31693, #9053, #54713, #32067, #61854, #20734, #61103, #21113, #37352, #49404, #44505, #43369, #48655, #15441, #14692, #10174, #61481, #55089, #49790, #9806, #25640, #3020, #49028, #72036, #67517, #32828, #20352, #72804, #9433, #33210, #26380, #2651, #32450, #55459, #14317, #66386, #37733, #26772, #5636, #29010, #68258, #6009, #51274, #45987, #12031, #62219, #34693, #74284, #50901, #62586, #22981, #40702, #4893, #28267, #10545, #56950, #33577, #56580, #62966, #16553, #63334, #17686, #46359, #5267, #39590, #63706, #27890, #45614, #56206, #68628, #57325, #67885, #22594, #52029, #69003, #57701, #28636, #17310, #73915, #22219, #16937, #39962, #44879, #27514, #45246, #11291, #366, #23348, #40329, #39219, #34322, #69375, #11659, #73540, #4519, #51650, #50524, #10918, #20105 ),
 ( #21848, #33952, #16176, #42167, #1829, #70852, #46724, #18807, #42546, #47090, #41811, #19165, #58441, #7853, #18434, #47465, #35793, #1475, #64462, #6750, #7119, #65558, #24456, #52767, #47831, #71209, #59180, #58807, #23719, #1105, #69749, #53511, #70489, #35064, #2190, #58077, #30859, #59540, #64821, #7489, #18063, #24816, #19527, #6388, #13123, #65180, #30126, #29394, #13492, #36159, #41078, #25187, #24081, #70128, #29753, #53880, #41449, #36530, #52401, #30494, #48200, #737, #12761, #53142, #64088, #12398, #35431, #25555, #19901, #55006, #71951, #67057, #59905, #60265, #42906, #32742, #37649, #66303, #15356, #2566, #48569, #71579, #9721, #50074, #31981, #26298, #55751, #31231, #4068, #73087, #3311, #65926, #20264, #14230, #43288, #21395, #8968, #49319, #32363, #37272, #60647, #27061, #54628, #8219, #26682, #25925, #44418, #49706, #14610, #61018, #21023, #36895, #8592, #31606, #2937, #13853, #72719, #48941, #9344, #72335, #38392, #20650, #54255, #43665, #66677, #14982, #38019, #55377, #3683, #44048, #61395, #4808, #17223, #62500, #57234, #23261, #73456, #45899, #10829, #62136, #73826, #34233, #51941, #16096, #39505, #21764, #68170, #44792, #67805, #74196, #27802, #74574, #28925, #57612, #16468, #50816, #279, #39131, #40243, #39870, #62872, #33864, #10089, #22501, #67433, #22133, #5546, #61771, #45523, #15729, #56863, #45159, #10458, #5180, #28176, #63246, #51188, #68539, #28548, #38770, #16843, #11205, #51555, #56491, #4430, #33127, #5922, #11572, #33489, #34605, #27425, #56122, #22887, #68913, #50440, #47377, #69661, #60453, #40617, #12672, #34978, #63619, #7031, #52314, #35705, #41361, #14043, #20082, #25737, #29667, #43096, #37079, #71766, #29304, #48758, #30039, #31415, #17974, #66113, #52683, #58720, #47007, #53054, #1018, #40993, #18347, #54816, #1386, #64000, #60082, #8783, #71390, #70038, #57994, #12315, #6298, #65741, #24370, #46270, #14421, #69289, #37455, #31795, #19715, #42727, #650, #8402, #3127, #17600, #54442, #2750, #64371, #11946, #23635, #46642, #35347, #58359, #6664, #23997, #49511, #44981, #20838, #33305, #56682, #61585, #21582, #4619, #55565, #26874, #49888, #32172, #62321, #37833, #55192, #67251, #9541, #27617, #72142, #72530, #3498, #67986, #72903, #3878, #50627, #14795, #60831, #9155, #21953, #10647, #44238, #38585, #16281, #15545, #26110, #9904, #27240, #26486, #21211, #73645, #15918, #39323, #50256, #38949, #43855, #66868, #32935, #55941, #15176, #20454 ),
 ( #43472, #33678, #73278, #49130, #38207, #4252, #44608, #61211, #66485, #32555, #67622, #56303, #61950, #10278, #12496, #64191, #28366, #23076, #12126, #46460, #40803, #16655, #63435, #35526, #17039, #58180, #17790, #62686, #51750, #29489, #63810, #22317, #69853, #29116, #23823, #57053, #11762, #34799, #51375, #74016, #74385, #23446, #35164, #467, #17412, #4999, #27998, #22696, #46086, #6485, #69479, #52499, #39686, #57804, #51007, #40064, #6111, #837, #45714, #46828, #63069, #40435, #5735, #69106, #34427, #68726, #98, #45343, #52135, #11391, #18165, #41180, #68360, #28733, #11024, #57429, #34058, #5366, #70946, #58538, #25656, #6845, #31327, #8317, #65286, #7952, #70226, #48302, #43008, #14336, #19261, #65656, #7586, #20000, #19630, #59636, #64559, #48672, #24554, #18901, #7221, #2664, #53242, #13952, #29859, #42274, #53978, #36993, #13224, #59276, #30592, #12855, #66028, #18536, #35894, #24913, #41908, #60000, #52871, #30224, #58911, #71679, #53611, #36261, #54355, #47195, #41543, #1573, #1202, #24184, #1925, #13592, #47560, #47929, #70584, #36630, #30957, #64916, #2288, #25284, #71310, #42644, #61497, #50174, #73192, #37368, #9819, #9450, #61120, #26396, #49045, #44895, #14711, #37749, #44148, #49422, #44519, #73557, #27530, #32467, #20752, #21866, #9072, #61869, #32843, #55853, #55475, #54732, #67163, #67902, #72444, #4170, #31709, #15458, #60369, #3787, #15086, #32084, #43768, #27157, #8694, #21500, #60749, #67531, #3039, #15831, #26787, #49804, #66782, #72052, #26022, #50542, #10192, #55104, #33223, #20369, #56221, #3412, #38865, #38121, #38493, #72820, #43386, #66403, #21127, #4535, #33593, #11308, #73931, #39978, #68645, #46003, #6022, #34707, #56968, #29026, #69021, #52045, #27909, #57716, #10562, #381, #46376, #62985, #50917, #5283, #22236, #28285, #69391, #45631, #16954, #22996, #45262, #22610, #23361, #62604, #62235, #17325, #33972, #17699, #40346, #51291, #9, #63348, #39235, #68274, #16570, #39607, #40717, #11673, #10934, #16194, #5650, #56598, #34341, #4915, #74302, #57341, #28651, #51666, #22971, #33940, #5255, #52758, #51639, #45977, #34310, #29743, #5626, #18053, #41439, #46348, #6378, #64078, #40319, #11649, #34684, #16926, #47081, #22582, #6740, #356, #10907, #23337, #12021, #45603, #5999, #58431, #727, #41068, #40692, #69365, #39950, #62955, #29000, #17676, #74273, #56939, #11280, #52018, #12388, #35422, #23709, #68617, #57690, #1094, #46713, #28256, #24071 ) ),
 .UNSPECIFIED., .F., .F., .F. ) 
 B_SPLINE_SURFACE_WITH_KNOTS ( ( 2, 1, 2 ),
 ( 3, 2, 2, 2, 2, 2, 2, 2, 2, 2, 2, 2, 2, 2, 2, 2, 2, 2, 2, 2, 2, 2, 2, 2, 2, 2, 2, 2, 2, 2, 2, 2, 2, 2, 2, 2, 2, 2, 2, 2, 2, 2, 2, 2, 2, 2, 2, 2, 2, 2, 2, 2, 2, 2, 2, 2, 2, 2, 2, 2, 2, 2, 2, 2, 2, 2, 2, 2, 2, 2, 2, 2, 2, 2, 2, 2, 2, 2, 2, 2, 2, 2, 2, 2, 2, 2, 2, 2, 2, 2, 2, 2, 2, 2, 2, 2, 2, 2, 2, 2, 2, 2, 2, 2, 2, 2, 2, 2, 2, 2, 2, 2, 2, 2, 2, 2, 2, 2, 2, 2, 2, 2, 2, 2, 2, 2, 2, 2, 2, 2, 2, 2, 2, 2, 2, 2, 2, 2, 2, 2, 2, 2, 2, 2, 2, 2, 2, 2, 2, 2, 2, 2, 2, 2, 3 ),
 ( 0.000000000000000000, 1.000000000000000000, 1.100000000000000089 ),
 ( -0.01003998210305807881, 0.000000000000000000, 0.006578947368421052266, 0.01315789473684210453, 0.01973684210526315680, 0.02631578947368420907, 0.03289473684210526133, 0.03947368421052631360, 0.04605263157894736586, 0.05263157894736841813, 0.05921052631578947040, 0.06578947368421052266, 0.07236842105263158187, 0.07894736842105262720, 0.08552631578947368640, 0.09210526315789473173, 0.09868421052631579093, 0.1052631578947368363, 0.1118421052631578955, 0.1184210526315789408, 0.1250000000000000000, 0.1315789473684210453, 0.1381578947368421184, 0.1447368421052631637, 0.1513157894736842091, 0.1578947368421052544, 0.1644736842105263275, 0.1710526315789473728, 0.1776315789473684181, 0.1842105263157894635, 0.1907894736842105365, 0.1973684210526315819, 0.2039473684210526272, 0.2105263157894736725, 0.2171052631578947456, 0.2236842105263157909, 0.2302631578947368363, 0.2368421052631578816, 0.2434210526315789547, 0.2500000000000000000, 0.2565789473684210731, 0.2631578947368420907, 0.2697368421052631637, 0.2763157894736842368, 0.2828947368421052544, 0.2894736842105263275, 0.2960526315789473450, 0.3026315789473684181, 0.3092105263157894912, 0.3157894736842105088, 0.3223684210526315819, 0.3289473684210526550, 0.3355263157894736725, 0.3421052631578947456, 0.3486842105263157632, 0.3552631578947368363, 0.3618421052631579093, 0.3684210526315789269, 0.3750000000000000000, 0.3815789473684210731, 0.3881578947368420907, 0.3947368421052631637, 0.4013157894736842368, 0.4078947368421052544, 0.4144736842105263275, 0.4210526315789473450, 0.4276315789473684181, 0.4342105263157894912, 0.4407894736842105088, 0.4473684210526315819, 0.4539473684210526550, 0.4605263157894736725, 0.4671052631578947456, 0.4736842105263157632, 0.4802631578947368363, 0.4868421052631579093, 0.4934210526315789269, 0.5000000000000000000, 0.5065789473684210176, 0.5131578947368421462, 0.5197368421052631637, 0.5263157894736841813, 0.5328947368421053099, 0.5394736842105263275, 0.5460526315789473450, 0.5526315789473684736, 0.5592105263157894912, 0.5657894736842105088, 0.5723684210526315264, 0.5789473684210526550, 0.5855263157894736725, 0.5921052631578946901, 0.5986842105263158187, 0.6052631578947368363, 0.6118421052631578538, 0.6184210526315789824, 0.6250000000000000000, 0.6315789473684210176, 0.6381578947368421462, 0.6447368421052631637, 0.6513157894736841813, 0.6578947368421053099, 0.6644736842105263275, 0.6710526315789473450, 0.6776315789473684736, 0.6842105263157894912, 0.6907894736842105088, 0.6973684210526315264, 0.7039473684210526550, 0.7105263157894736725, 0.7171052631578946901, 0.7236842105263158187, 0.7302631578947368363, 0.7368421052631578538, 0.7434210526315789824, 0.7500000000000000000, 0.7565789473684210176, 0.7631578947368421462, 0.7697368421052631637, 0.7763157894736841813, 0.7828947368421053099, 0.7894736842105263275, 0.7960526315789473450, 0.8026315789473684736, 0.8092105263157894912, 0.8157894736842105088, 0.8223684210526315264, 0.8289473684210526550, 0.8355263157894736725, 0.8421052631578946901, 0.8486842105263158187, 0.8552631578947368363, 0.8618421052631578538, 0.8684210526315789824, 0.8750000000000000000, 0.8815789473684210176, 0.8881578947368421462, 0.8947368421052631637, 0.9013157894736841813, 0.9078947368421053099, 0.9144736842105263275, 0.9210526315789473450, 0.9276315789473684736, 0.9342105263157894912, 0.9407894736842105088, 0.9473684210526315264, 0.9539473684210526550, 0.9605263157894736725, 0.9671052631578946901, 0.9736842105263158187, 0.9802631578947368363, 0.9868421052631578538, 0.9934210526315789824, 0.9940576339661463257, 1.003998210305807826 ),
 .UNSPECIFIED. ) 
 GEOMETRIC_REPRESENTATION_ITEM ( )  RATIONAL_B_SPLINE_SURFACE ( (
 ( 1.000000000000000000, 1.000000000000000000, 1.000000000000000000, 0.9238795325112867385, 1.000000000000000000, 0.9238795325112867385, 1.000000000000000000, 0.9238795325112867385, 1.000000000000000000, 0.9238795325112867385, 1.000000000000000000, 0.9238795325112867385, 1.000000000000000000, 0.9238795325112867385, 1.000000000000000000, 0.9238795325112867385, 1.000000000000000000, 0.9238795325112867385, 1.000000000000000000, 0.9238795325112867385, 1.000000000000000000, 0.9238795325112867385, 1.000000000000000000, 0.9238795325112867385, 1.000000000000000000, 0.9238795325112867385, 1.000000000000000000, 0.9238795325112867385, 1.000000000000000000, 0.9238795325112867385, 1.000000000000000000, 0.9238795325112867385, 1.000000000000000000, 0.9238795325112867385, 1.000000000000000000, 0.9238795325112867385, 1.000000000000000000, 0.9238795325112867385, 1.000000000000000000, 0.9238795325112867385, 1.000000000000000000, 0.9238795325112867385, 1.000000000000000000, 0.9238795325112867385, 1.000000000000000000, 0.9238795325112867385, 1.000000000000000000, 0.9238795325112867385, 1.000000000000000000, 0.9238795325112867385, 1.000000000000000000, 0.9238795325112867385, 1.000000000000000000, 0.9238795325112867385, 1.000000000000000000, 0.9238795325112867385, 1.000000000000000000, 0.9238795325112867385, 1.000000000000000000, 0.9238795325112867385, 1.000000000000000000, 0.9238795325112867385, 1.000000000000000000, 0.9238795325112867385, 1.000000000000000000, 0.9238795325112867385, 1.000000000000000000, 0.9238795325112867385, 1.000000000000000000, 0.9238795325112867385, 1.000000000000000000, 0.9238795325112867385, 1.000000000000000000, 0.9238795325112867385, 1.000000000000000000, 0.9238795325112867385, 1.000000000000000000, 0.9238795325112867385, 1.000000000000000000, 0.9238795325112867385, 1.000000000000000000, 0.9238795325112867385, 1.000000000000000000, 0.9238795325112867385, 1.000000000000000000, 0.9238795325112867385, 1.000000000000000000, 0.9238795325112867385, 1.000000000000000000, 0.9238795325112867385, 1.000000000000000000, 0.9238795325112867385, 1.000000000000000000, 0.9238795325112867385, 1.000000000000000000, 0.9238795325112867385, 1.000000000000000000, 0.9238795325112867385, 1.000000000000000000, 0.9238795325112867385, 1.000000000000000000, 0.9238795325112867385, 1.000000000000000000, 0.9238795325112867385, 1.000000000000000000, 0.9238795325112867385, 1.000000000000000000, 0.9238795325112867385, 1.000000000000000000, 0.9238795325112867385, 1.000000000000000000, 0.9238795325112867385, 1.000000000000000000, 0.9238795325112867385, 1.000000000000000000, 0.9238795325112867385, 1.000000000000000000, 0.9238795325112867385, 1.000000000000000000, 0.9238795325112867385, 1.000000000000000000, 0.9238795325112867385, 1.000000000000000000, 0.9238795325112867385, 1.000000000000000000, 0.9238795325112867385, 1.000000000000000000, 0.9238795325112867385, 1.000000000000000000, 0.9238795325112867385, 1.000000000000000000, 0.9238795325112867385, 1.000000000000000000, 0.9238795325112867385, 1.000000000000000000, 0.9238795325112867385, 1.000000000000000000, 0.9238795325112867385, 1.000000000000000000, 0.9238795325112867385, 1.000000000000000000, 0.9238795325112867385, 1.000000000000000000, 0.9238795325112867385, 1.000000000000000000, 0.9238795325112867385, 1.000000000000000000, 0.9238795325112867385, 1.000000000000000000, 0.9238795325112867385, 1.000000000000000000, 0.9238795325112867385, 1.000000000000000000, 0.9238795325112867385, 1.000000000000000000, 0.9238795325112867385, 1.000000000000000000, 0.9238795325112867385, 1.000000000000000000, 0.9238795325112867385, 1.000000000000000000, 0.9238795325112867385, 1.000000000000000000, 0.9238795325112867385, 1.000000000000000000, 0.9238795325112867385, 1.000000000000000000, 0.9238795325112867385, 1.000000000000000000, 0.9238795325112867385, 1.000000000000000000, 0.9238795325112867385, 1.000000000000000000, 0.9238795325112867385, 1.000000000000000000, 0.9238795325112867385, 1.000000000000000000, 0.9238795325112867385, 1.000000000000000000, 0.9238795325112867385, 1.000000000000000000, 0.9238795325112867385, 1.000000000000000000, 0.9238795325112867385, 1.000000000000000000, 0.9238795325112867385, 1.000000000000000000, 0.9238795325112867385, 1.000000000000000000, 0.9238795325112867385, 1.000000000000000000, 0.9238795325112867385, 1.000000000000000000, 0.9238795325112867385, 1.000000000000000000, 0.9238795325112867385, 1.000000000000000000, 0.9238795325112867385, 1.000000000000000000, 0.9238795325112867385, 1.000000000000000000, 0.9238795325112867385, 1.000000000000000000, 0.9238795325112867385, 1.000000000000000000, 0.9238795325112867385, 1.000000000000000000, 0.9238795325112867385, 1.000000000000000000, 0.9238795325112867385, 1.000000000000000000, 0.9238795325112867385, 1.000000000000000000, 0.9238795325112867385, 1.000000000000000000, 0.9238795325112867385, 1.000000000000000000, 0.9238795325112867385, 1.000000000000000000, 0.9238795325112867385, 1.000000000000000000, 0.9238795325112867385, 1.000000000000000000, 0.9238795325112867385, 1.000000000000000000, 0.9238795325112867385, 1.000000000000000000, 0.9238795325112867385, 1.000000000000000000, 0.9238795325112867385, 1.000000000000000000, 0.9238795325112867385, 1.000000000000000000, 0.9238795325112867385, 1.000000000000000000, 0.9238795325112867385, 1.000000000000000000, 0.9238795325112867385, 1.000000000000000000, 0.9238795325112867385, 1.000000000000000000, 0.9238795325112867385, 1.000000000000000000, 0.9238795325112867385, 1.000000000000000000, 0.9238795325112867385, 1.000000000000000000, 0.9238795325112867385, 1.000000000000000000, 0.9238795325112867385, 1.000000000000000000, 0.9238795325112867385, 1.000000000000000000, 0.9238795325112867385, 1.000000000000000000, 0.9238795325112867385, 1.000000000000000000, 0.9238795325112867385, 1.000000000000000000, 0.9238795325112867385, 1.000000000000000000, 0.9238795325112867385, 1.000000000000000000, 0.9238795325112867385, 1.000000000000000000, 0.9238795325112867385, 1.000000000000000000, 0.9238795325112867385, 1.000000000000000000, 0.9238795325112867385, 1.000000000000000000, 0.9238795325112867385, 1.000000000000000000, 0.9238795325112867385, 1.000000000000000000, 0.9238795325112867385, 1.000000000000000000, 0.9238795325112867385, 1.000000000000000000, 0.9238795325112867385, 1.000000000000000000, 0.9238795325112867385, 1.000000000000000000, 0.9238795325112867385, 1.000000000000000000, 0.9238795325112867385, 1.000000000000000000, 0.9238795325112867385, 1.000000000000000000, 0.9238795325112867385, 1.000000000000000000, 0.9238795325112867385, 1.000000000000000000, 0.9238795325112867385, 1.000000000000000000, 0.9238795325112867385, 1.000000000000000000, 0.9238795325112867385, 1.000000000000000000, 0.9238795325112867385, 1.000000000000000000, 0.9238795325112867385, 1.000000000000000000, 0.9238795325112867385, 1.000000000000000000, 0.9926345559451579259, 0.9866944779689741374, 0.9866944779689741374, 0.9866944779689741374),
 ( 1.000000000000000000, 1.000000000000000000, 1.000000000000000000, 0.9238795325112867385, 1.000000000000000000, 0.9238795325112867385, 1.000000000000000000, 0.9238795325112867385, 1.000000000000000000, 0.9238795325112867385, 1.000000000000000000, 0.9238795325112867385, 1.000000000000000000, 0.9238795325112867385, 1.000000000000000000, 0.9238795325112867385, 1.000000000000000000, 0.9238795325112867385, 1.000000000000000000, 0.9238795325112867385, 1.000000000000000000, 0.9238795325112867385, 1.000000000000000000, 0.9238795325112867385, 1.000000000000000000, 0.9238795325112867385, 1.000000000000000000, 0.9238795325112867385, 1.000000000000000000, 0.9238795325112867385, 1.000000000000000000, 0.9238795325112867385, 1.000000000000000000, 0.9238795325112867385, 1.000000000000000000, 0.9238795325112867385, 1.000000000000000000, 0.9238795325112867385, 1.000000000000000000, 0.9238795325112867385, 1.000000000000000000, 0.9238795325112867385, 1.000000000000000000, 0.9238795325112867385, 1.000000000000000000, 0.9238795325112867385, 1.000000000000000000, 0.9238795325112867385, 1.000000000000000000, 0.9238795325112867385, 1.000000000000000000, 0.9238795325112867385, 1.000000000000000000, 0.9238795325112867385, 1.000000000000000000, 0.9238795325112867385, 1.000000000000000000, 0.9238795325112867385, 1.000000000000000000, 0.9238795325112867385, 1.000000000000000000, 0.9238795325112867385, 1.000000000000000000, 0.9238795325112867385, 1.000000000000000000, 0.9238795325112867385, 1.000000000000000000, 0.9238795325112867385, 1.000000000000000000, 0.9238795325112867385, 1.000000000000000000, 0.9238795325112867385, 1.000000000000000000, 0.9238795325112867385, 1.000000000000000000, 0.9238795325112867385, 1.000000000000000000, 0.9238795325112867385, 1.000000000000000000, 0.9238795325112867385, 1.000000000000000000, 0.9238795325112867385, 1.000000000000000000, 0.9238795325112867385, 1.000000000000000000, 0.9238795325112867385, 1.000000000000000000, 0.9238795325112867385, 1.000000000000000000, 0.9238795325112867385, 1.000000000000000000, 0.9238795325112867385, 1.000000000000000000, 0.9238795325112867385, 1.000000000000000000, 0.9238795325112867385, 1.000000000000000000, 0.9238795325112867385, 1.000000000000000000, 0.9238795325112867385, 1.000000000000000000, 0.9238795325112867385, 1.000000000000000000, 0.9238795325112867385, 1.000000000000000000, 0.9238795325112867385, 1.000000000000000000, 0.9238795325112867385, 1.000000000000000000, 0.9238795325112867385, 1.000000000000000000, 0.9238795325112867385, 1.000000000000000000, 0.9238795325112867385, 1.000000000000000000, 0.9238795325112867385, 1.000000000000000000, 0.9238795325112867385, 1.000000000000000000, 0.9238795325112867385, 1.000000000000000000, 0.9238795325112867385, 1.000000000000000000, 0.9238795325112867385, 1.000000000000000000, 0.9238795325112867385, 1.000000000000000000, 0.9238795325112867385, 1.000000000000000000, 0.9238795325112867385, 1.000000000000000000, 0.9238795325112867385, 1.000000000000000000, 0.9238795325112867385, 1.000000000000000000, 0.9238795325112867385, 1.000000000000000000, 0.9238795325112867385, 1.000000000000000000, 0.9238795325112867385, 1.000000000000000000, 0.9238795325112867385, 1.000000000000000000, 0.9238795325112867385, 1.000000000000000000, 0.9238795325112867385, 1.000000000000000000, 0.9238795325112867385, 1.000000000000000000, 0.9238795325112867385, 1.000000000000000000, 0.9238795325112867385, 1.000000000000000000, 0.9238795325112867385, 1.000000000000000000, 0.9238795325112867385, 1.000000000000000000, 0.9238795325112867385, 1.000000000000000000, 0.9238795325112867385, 1.000000000000000000, 0.9238795325112867385, 1.000000000000000000, 0.9238795325112867385, 1.000000000000000000, 0.9238795325112867385, 1.000000000000000000, 0.9238795325112867385, 1.000000000000000000, 0.9238795325112867385, 1.000000000000000000, 0.9238795325112867385, 1.000000000000000000, 0.9238795325112867385, 1.000000000000000000, 0.9238795325112867385, 1.000000000000000000, 0.9238795325112867385, 1.000000000000000000, 0.9238795325112867385, 1.000000000000000000, 0.9238795325112867385, 1.000000000000000000, 0.9238795325112867385, 1.000000000000000000, 0.9238795325112867385, 1.000000000000000000, 0.9238795325112867385, 1.000000000000000000, 0.9238795325112867385, 1.000000000000000000, 0.9238795325112867385, 1.000000000000000000, 0.9238795325112867385, 1.000000000000000000, 0.9238795325112867385, 1.000000000000000000, 0.9238795325112867385, 1.000000000000000000, 0.9238795325112867385, 1.000000000000000000, 0.9238795325112867385, 1.000000000000000000, 0.9238795325112867385, 1.000000000000000000, 0.9238795325112867385, 1.000000000000000000, 0.9238795325112867385, 1.000000000000000000, 0.9238795325112867385, 1.000000000000000000, 0.9238795325112867385, 1.000000000000000000, 0.9238795325112867385, 1.000000000000000000, 0.9238795325112867385, 1.000000000000000000, 0.9238795325112867385, 1.000000000000000000, 0.9238795325112867385, 1.000000000000000000, 0.9238795325112867385, 1.000000000000000000, 0.9238795325112867385, 1.000000000000000000, 0.9238795325112867385, 1.000000000000000000, 0.9238795325112867385, 1.000000000000000000, 0.9238795325112867385, 1.000000000000000000, 0.9238795325112867385, 1.000000000000000000, 0.9238795325112867385, 1.000000000000000000, 0.9238795325112867385, 1.000000000000000000, 0.9238795325112867385, 1.000000000000000000, 0.9238795325112867385, 1.000000000000000000, 0.9238795325112867385, 1.000000000000000000, 0.9238795325112867385, 1.000000000000000000, 0.9238795325112867385, 1.000000000000000000, 0.9238795325112867385, 1.000000000000000000, 0.9238795325112867385, 1.000000000000000000, 0.9238795325112867385, 1.000000000000000000, 0.9238795325112867385, 1.000000000000000000, 0.9238795325112867385, 1.000000000000000000, 0.9238795325112867385, 1.000000000000000000, 0.9238795325112867385, 1.000000000000000000, 0.9238795325112867385, 1.000000000000000000, 0.9238795325112867385, 1.000000000000000000, 0.9238795325112867385, 1.000000000000000000, 0.9238795325112867385, 1.000000000000000000, 0.9238795325112867385, 1.000000000000000000, 0.9238795325112867385, 1.000000000000000000, 0.9238795325112867385, 1.000000000000000000, 0.9238795325112867385, 1.000000000000000000, 0.9238795325112867385, 1.000000000000000000, 0.9238795325112867385, 1.000000000000000000, 0.9238795325112867385, 1.000000000000000000, 0.9238795325112867385, 1.000000000000000000, 0.9238795325112867385, 1.000000000000000000, 0.9238795325112867385, 1.000000000000000000, 0.9238795325112867385, 1.000000000000000000, 0.9238795325112867385, 1.000000000000000000, 0.9238795325112867385, 1.000000000000000000, 0.9238795325112867385, 1.000000000000000000, 0.9238795325112867385, 1.000000000000000000, 0.9238795325112867385, 1.000000000000000000, 0.9238795325112867385, 1.000000000000000000, 0.9238795325112867385, 1.000000000000000000, 0.9926345559451579259, 0.9866944779689741374, 0.9866944779689741374, 0.9866944779689741374),
 ( 1.000000000000000000, 1.000000000000000000, 1.000000000000000000, 0.9238795325112867385, 1.000000000000000000, 0.9238795325112867385, 1.000000000000000000, 0.9238795325112867385, 1.000000000000000000, 0.9238795325112867385, 1.000000000000000000, 0.9238795325112867385, 1.000000000000000000, 0.9238795325112867385, 1.000000000000000000, 0.9238795325112867385, 1.000000000000000000, 0.9238795325112867385, 1.000000000000000000, 0.9238795325112867385, 1.000000000000000000, 0.9238795325112867385, 1.000000000000000000, 0.9238795325112867385, 1.000000000000000000, 0.9238795325112867385, 1.000000000000000000, 0.9238795325112867385, 1.000000000000000000, 0.9238795325112867385, 1.000000000000000000, 0.9238795325112867385, 1.000000000000000000, 0.9238795325112867385, 1.000000000000000000, 0.9238795325112867385, 1.000000000000000000, 0.9238795325112867385, 1.000000000000000000, 0.9238795325112867385, 1.000000000000000000, 0.9238795325112867385, 1.000000000000000000, 0.9238795325112867385, 1.000000000000000000, 0.9238795325112867385, 1.000000000000000000, 0.9238795325112867385, 1.000000000000000000, 0.9238795325112867385, 1.000000000000000000, 0.9238795325112867385, 1.000000000000000000, 0.9238795325112867385, 1.000000000000000000, 0.9238795325112867385, 1.000000000000000000, 0.9238795325112867385, 1.000000000000000000, 0.9238795325112867385, 1.000000000000000000, 0.9238795325112867385, 1.000000000000000000, 0.9238795325112867385, 1.000000000000000000, 0.9238795325112867385, 1.000000000000000000, 0.9238795325112867385, 1.000000000000000000, 0.9238795325112867385, 1.000000000000000000, 0.9238795325112867385, 1.000000000000000000, 0.9238795325112867385, 1.000000000000000000, 0.9238795325112867385, 1.000000000000000000, 0.9238795325112867385, 1.000000000000000000, 0.9238795325112867385, 1.000000000000000000, 0.9238795325112867385, 1.000000000000000000, 0.9238795325112867385, 1.000000000000000000, 0.9238795325112867385, 1.000000000000000000, 0.9238795325112867385, 1.000000000000000000, 0.9238795325112867385, 1.000000000000000000, 0.9238795325112867385, 1.000000000000000000, 0.9238795325112867385, 1.000000000000000000, 0.9238795325112867385, 1.000000000000000000, 0.9238795325112867385, 1.000000000000000000, 0.9238795325112867385, 1.000000000000000000, 0.9238795325112867385, 1.000000000000000000, 0.9238795325112867385, 1.000000000000000000, 0.9238795325112867385, 1.000000000000000000, 0.9238795325112867385, 1.000000000000000000, 0.9238795325112867385, 1.000000000000000000, 0.9238795325112867385, 1.000000000000000000, 0.9238795325112867385, 1.000000000000000000, 0.9238795325112867385, 1.000000000000000000, 0.9238795325112867385, 1.000000000000000000, 0.9238795325112867385, 1.000000000000000000, 0.9238795325112867385, 1.000000000000000000, 0.9238795325112867385, 1.000000000000000000, 0.9238795325112867385, 1.000000000000000000, 0.9238795325112867385, 1.000000000000000000, 0.9238795325112867385, 1.000000000000000000, 0.9238795325112867385, 1.000000000000000000, 0.9238795325112867385, 1.000000000000000000, 0.9238795325112867385, 1.000000000000000000, 0.9238795325112867385, 1.000000000000000000, 0.9238795325112867385, 1.000000000000000000, 0.9238795325112867385, 1.000000000000000000, 0.9238795325112867385, 1.000000000000000000, 0.9238795325112867385, 1.000000000000000000, 0.9238795325112867385, 1.000000000000000000, 0.9238795325112867385, 1.000000000000000000, 0.9238795325112867385, 1.000000000000000000, 0.9238795325112867385, 1.000000000000000000, 0.9238795325112867385, 1.000000000000000000, 0.9238795325112867385, 1.000000000000000000, 0.9238795325112867385, 1.000000000000000000, 0.9238795325112867385, 1.000000000000000000, 0.9238795325112867385, 1.000000000000000000, 0.9238795325112867385, 1.000000000000000000, 0.9238795325112867385, 1.000000000000000000, 0.9238795325112867385, 1.000000000000000000, 0.9238795325112867385, 1.000000000000000000, 0.9238795325112867385, 1.000000000000000000, 0.9238795325112867385, 1.000000000000000000, 0.9238795325112867385, 1.000000000000000000, 0.9238795325112867385, 1.000000000000000000, 0.9238795325112867385, 1.000000000000000000, 0.9238795325112867385, 1.000000000000000000, 0.9238795325112867385, 1.000000000000000000, 0.9238795325112867385, 1.000000000000000000, 0.9238795325112867385, 1.000000000000000000, 0.9238795325112867385, 1.000000000000000000, 0.9238795325112867385, 1.000000000000000000, 0.9238795325112867385, 1.000000000000000000, 0.9238795325112867385, 1.000000000000000000, 0.9238795325112867385, 1.000000000000000000, 0.9238795325112867385, 1.000000000000000000, 0.9238795325112867385, 1.000000000000000000, 0.9238795325112867385, 1.000000000000000000, 0.9238795325112867385, 1.000000000000000000, 0.9238795325112867385, 1.000000000000000000, 0.9238795325112867385, 1.000000000000000000, 0.9238795325112867385, 1.000000000000000000, 0.9238795325112867385, 1.000000000000000000, 0.9238795325112867385, 1.000000000000000000, 0.9238795325112867385, 1.000000000000000000, 0.9238795325112867385, 1.000000000000000000, 0.9238795325112867385, 1.000000000000000000, 0.9238795325112867385, 1.000000000000000000, 0.9238795325112867385, 1.000000000000000000, 0.9238795325112867385, 1.000000000000000000, 0.9238795325112867385, 1.000000000000000000, 0.9238795325112867385, 1.000000000000000000, 0.9238795325112867385, 1.000000000000000000, 0.9238795325112867385, 1.000000000000000000, 0.9238795325112867385, 1.000000000000000000, 0.9238795325112867385, 1.000000000000000000, 0.9238795325112867385, 1.000000000000000000, 0.9238795325112867385, 1.000000000000000000, 0.9238795325112867385, 1.000000000000000000, 0.9238795325112867385, 1.000000000000000000, 0.9238795325112867385, 1.000000000000000000, 0.9238795325112867385, 1.000000000000000000, 0.9238795325112867385, 1.000000000000000000, 0.9238795325112867385, 1.000000000000000000, 0.9238795325112867385, 1.000000000000000000, 0.9238795325112867385, 1.000000000000000000, 0.9238795325112867385, 1.000000000000000000, 0.9238795325112867385, 1.000000000000000000, 0.9238795325112867385, 1.000000000000000000, 0.9238795325112867385, 1.000000000000000000, 0.9238795325112867385, 1.000000000000000000, 0.9238795325112867385, 1.000000000000000000, 0.9238795325112867385, 1.000000000000000000, 0.9238795325112867385, 1.000000000000000000, 0.9238795325112867385, 1.000000000000000000, 0.9238795325112867385, 1.000000000000000000, 0.9238795325112867385, 1.000000000000000000, 0.9238795325112867385, 1.000000000000000000, 0.9238795325112867385, 1.000000000000000000, 0.9238795325112867385, 1.000000000000000000, 0.9238795325112867385, 1.000000000000000000, 0.9238795325112867385, 1.000000000000000000, 0.9238795325112867385, 1.000000000000000000, 0.9238795325112867385, 1.000000000000000000, 0.9238795325112867385, 1.000000000000000000, 0.9238795325112867385, 1.000000000000000000, 0.9238795325112867385, 1.000000000000000000, 0.9926345559451579259, 0.9866944779689741374, 0.9866944779689741374, 0.9866944779689741374) ) ) 
 REPRESENTATION_ITEM ( '' )  SURFACE ( )  );
#48394 = CARTESIAN_POINT ( 'NONE',  ( 1.308779242300813994, 49.95118570763349908, -40.70975538998080623 ) ) ;
#48395 = DIRECTION ( 'NONE',  ( -0.000000000000000000, -0.000000000000000000, -1.000000000000000000 ) ) ;
#48396 = CARTESIAN_POINT ( 'NONE',  ( -11.35316468750000141, 138.8020833299193271, 3.042071309553159963 ) ) ;
#48397 = CARTESIAN_POINT ( 'NONE',  ( 2.445694354108838731, 196.0625000013656063, 195.5543056458912190 ) ) ;
#48398 = CARTESIAN_POINT ( 'NONE',  ( -4.242640687119285658, 291.1249999999999432, 4.242640687119287435 ) ) ;
#48399 = CARTESIAN_POINT ( 'NONE',  ( 7.204075437095966983, 7.204075437095967871, 73.46875000204838102 ) ) ;
#48400 = CARTESIAN_POINT ( 'NONE',  ( -11.35316468749999785, 68.38541666325268409, -3.042071309553167513 ) ) ;
#48401 = ORIENTED_EDGE ( 'NONE', *, *, #28849, .F. ) ;
#48402 = CARTESIAN_POINT ( 'NONE',  ( 0.000000000000000000, 0.000000000000000000, -14.80000000000000071 ) ) ;
#48403 = CARTESIAN_POINT ( 'NONE',  ( 1.881053915767121998, 3.624999998634407028, -4.541265875000002339 ) ) ;
#48404 = CARTESIAN_POINT ( 'NONE',  ( 8.008118988124993010, -3.317071493978877239, 10.66936528394063011 ) ) ;
#48405 = ORIENTED_EDGE ( 'NONE', *, *, #21321, .F. ) ;
#48406 = CARTESIAN_POINT ( 'NONE',  ( -5.082755093536326818, 22.40624999795161187, 5.082755093536325042 ) ) ;
#48407 = CARTESIAN_POINT ( 'NONE',  ( 6.000000000000003553, 293.5000000034140157, 2.485281374238571317 ) ) ;
#48408 = CARTESIAN_POINT ( 'NONE',  ( 3.979266480698044450, 124.5000000000001137, -6.940132439340980675 ) ) ;
#48409 = CARTESIAN_POINT ( 'NONE',  ( -7.188101187500002709, 13.68749999795161365, 2.977408999572649151 ) ) ;
#48410 = CARTESIAN_POINT ( 'NONE',  ( 5.082755093536320601, -5.082755093536318824, 0.5490527818717526598 ) ) ;
#48411 = CARTESIAN_POINT ( 'NONE',  ( -7.204075437095967871, 7.204075437095967871, 67.46875000204836681 ) ) ;
#48412 =( BOUNDED_CURVE ( )  B_SPLINE_CURVE ( 2, ( #19823, #14528, #30785, #48125, #53805, #31149, #42829, #54181, #26219, #65847, #31528, #59467, #14157 ),
 .UNSPECIFIED., .F., .F. ) 
 B_SPLINE_CURVE_WITH_KNOTS ( ( 3, 2, 2, 2, 2, 2, 3 ),
 ( 0.7771739130434782705, 0.7789855072463768293, 0.7807971014492754991, 0.7826086956521740579, 0.7844202898550726166, 0.7862318840579712864, 0.7880434782608697342 ),
 .UNSPECIFIED. ) 
 CURVE ( )  GEOMETRIC_REPRESENTATION_ITEM ( )  RATIONAL_B_SPLINE_CURVE ( ( 1.000000000000000000, 0.9659258262890683122, 1.000000000000000000, 0.9659258262890683122, 1.000000000000000000, 0.9659258262890683122, 1.000000000000000000, 0.9659258262890683122, 1.000000000000000000, 0.9659258262890683122, 1.000000000000000000, 0.9659258262890640934, 1.000000000000004219 ) ) 
 REPRESENTATION_ITEM ( '' )  );
#48413 = DIRECTION ( 'NONE',  ( 1.000000000000000000, 0.000000000000000000, 0.000000000000000000 ) ) ;
#48414 = CARTESIAN_POINT ( 'NONE',  ( -4.000000000000001776, 4.187499997268813168, -1.656854249492381470 ) ) ;
#48415 = EDGE_LOOP ( 'NONE', ( #25910, #65094 ) ) ;
#48416 = CIRCLE ( 'NONE', #71311, 37.00000000000000711 ) ;
#48417 = CARTESIAN_POINT ( 'NONE',  ( -1.432654583217607192, 206.2500000013656063, 194.5412658750000219 ) ) ;
#48418 = CIRCLE ( 'NONE', #60487, 10.50000000000000000 ) ;
#48419 = CARTESIAN_POINT ( 'NONE',  ( -24.00000000000002132, 196.9375000027312410, 168.3431457505079152 ) ) ;
#48420 = CARTESIAN_POINT ( 'NONE',  ( 1.881053915767121776, 0.4999999986344067504, -4.541265875000002339 ) ) ;
#48421 = CARTESIAN_POINT ( 'NONE',  ( -7.188101187500001821, 110.5625000020483810, -2.977408999572650483 ) ) ;
#48422 = CARTESIAN_POINT ( 'NONE',  ( -3.673940397442060854E-16, 294.7500000000000000, -6.000000000000001776 ) ) ;
#48423 = CARTESIAN_POINT ( 'NONE',  ( -4.401442555609577197E-16, 7.188101187499992051, 23.61155278187175455 ) ) ;
#48424 = ORIENTED_EDGE ( 'NONE', *, *, #29706, .F. ) ;
#48425 = CARTESIAN_POINT ( 'NONE',  ( 5.082755093536325930, 23.15624999795161543, -5.082755093536325930 ) ) ;
#48426 = VERTEX_POINT ( 'NONE', #18333 ) ;
#48427 = CARTESIAN_POINT ( 'NONE',  ( 7.796785530332603464, 2.081694232947989054, -0.000000000000000000 ) ) ;
#48428 = CARTESIAN_POINT ( 'NONE',  ( 1.432654583217664479, 207.7500000013656063, 201.4587341250000065 ) ) ;
#48429 = CARTESIAN_POINT ( 'NONE',  ( 29.43265458321761230, 204.8750000013656063, 166.5412658749999650 ) ) ;
#48430 = CARTESIAN_POINT ( 'NONE',  ( 8.660254037844385522, 64.58333333333334281, 5.000000000000005329 ) ) ;
#48431 = CARTESIAN_POINT ( 'NONE',  ( 7.188101187500001821, 92.37500000204839523, -2.977408999572651371 ) ) ;
#48432 = CARTESIAN_POINT ( 'NONE',  ( -2.485281374238571761, 295.8125000000000000, -6.000000000000003553 ) ) ;
#48434 = CARTESIAN_POINT ( 'NONE',  ( 2.849036369511732440E-14, 197.3750000027312126, 202.0000000000000000 ) ) ;
#48433 = DIRECTION ( 'NONE',  ( 0.000000000000000000, 0.7071067811865465735, 0.7071067811865484609 ) ) ;
#48435 = VERTEX_POINT ( 'NONE', #70750 ) ;
#48436 = CARTESIAN_POINT ( 'NONE',  ( -3.042071309553159075, 229.9479166700806161, 11.35316468749999963 ) ) ;
#48437 = EDGE_CURVE ( 'NONE', #26901, #44928, #24395, .T. ) ;
#48438 = CIRCLE ( 'NONE', #53262, 27.99999999999998224 ) ;
#48439 = CARTESIAN_POINT ( 'NONE',  ( 3.999999999999960032, 199.0625000027312126, 143.6568542494924543 ) ) ;
#48440 = DIRECTION ( 'NONE',  ( -0.000000000000000000, -0.000000000000000000, 1.000000000000000000 ) ) ;
#48441 = CARTESIAN_POINT ( 'NONE',  ( -2.775557561562891351E-14, 210.0000000000000284, 142.0000000000000568 ) ) ;
#48442 = CARTESIAN_POINT ( 'NONE',  ( -10.00000000000000000, 264.7916666666666856, -2.679491924311226292 ) ) ;
#48443 = CARTESIAN_POINT ( 'NONE',  ( 11.00000000000000888, 4.556349186104037940, 116.0312500040967905 ) ) ;
#48444 = CARTESIAN_POINT ( 'NONE',  ( -8.660254037844390851, 177.9166666666666572, 4.999999999999998224 ) ) ;
#48445 = PLANE ( 'NONE',  #59574 ) ;
#48446 = CARTESIAN_POINT ( 'NONE',  ( 5.000000000000004441, 239.7916666734946318, 8.660254037844385522 ) ) ;
#48447 = CARTESIAN_POINT ( 'NONE',  ( 3.313708498984762496, -7.999999999999989342, 4.299052779823362869 ) ) ;
#48448 = CARTESIAN_POINT ( 'NONE',  ( 8.311093377946834337, 155.4687499965859843, 8.311093377946839666 ) ) ;
#48449 = DIRECTION ( 'NONE',  ( 0.000000000000000000, 0.000000000000000000, 1.000000000000000000 ) ) ;
#48450 = CARTESIAN_POINT ( 'NONE',  ( 10.00000000000000178, 27.08333332650536462, -2.679491924311226736 ) ) ;
#48453 = CARTESIAN_POINT ( 'NONE',  ( -6.000000000000003553, 293.9374999999998863, -2.485281374238571317 ) ) ;
#48452 = CARTESIAN_POINT ( 'NONE',  ( -2.679491924311226292, 83.33333332650536818, -10.00000000000000178 ) ) ;
#48451 = CARTESIAN_POINT ( 'NONE',  ( 32.00000000000000711, 203.3125000000000284, 168.3431457505075741 ) ) ;
#48454 = VERTEX_POINT ( 'NONE', #1004 ) ;
#48455 = CARTESIAN_POINT ( 'NONE',  ( 5.676582343749993598, 10.26041666325268409, 9.832129032723422313 ) ) ;
#48456 = CARTESIAN_POINT ( 'NONE',  ( 2.449293598294707893E-16, 18.25000000000000000, -4.000000000000001776 ) ) ;
#48457 = DIRECTION ( 'NONE',  ( 0.1513591288559071046, -8.467839242509013420E-17, 0.9884788384745426537 ) ) ;
#48458 = CARTESIAN_POINT ( 'NONE',  ( -2.445694354108839619, 205.8125000013656063, 139.5543056458912190 ) ) ;
#48459 = CARTESIAN_POINT ( 'NONE',  ( -3.893442805679455887, 124.6581723871223488, -6.826363913033100417 ) ) ;
#48460 = VECTOR ( 'NONE', #40212, 1000.000000000000000 ) ;
#48461 = CARTESIAN_POINT ( 'NONE',  ( -2.679491924311235618, 35.41666665983870388, 10.00000000000000000 ) ) ;
#48462 = CARTESIAN_POINT ( 'NONE',  ( 5.082755093536325042, 108.5937500020483810, -5.082755093536325930 ) ) ;
#48463 = CARTESIAN_POINT ( 'NONE',  ( -3.211159895383562723, 5.062499998634407028, 3.211159895383561391 ) ) ;
#48464 = CARTESIAN_POINT ( 'NONE',  ( 3.728321214196736566, 66.24762070555856042, -26.57448171418095484 ) ) ;
#48465 = CARTESIAN_POINT ( 'NONE',  ( -3.313708498984758943, -7.999999999999989342, 14.61155277982336465 ) ) ;
#48467 = DIRECTION ( 'NONE',  ( 0.000000000000000000, 0.000000000000000000, 1.000000000000000000 ) ) ;
#48466 = CARTESIAN_POINT ( 'NONE',  ( 4.242640687119287435, 291.4375000034140157, 4.242640687119285658 ) ) ;
#48468 = ORIENTED_EDGE ( 'NONE', *, *, #36830, .F. ) ;
#48469 = CARTESIAN_POINT ( 'NONE',  ( 3.313708498984869077, 93.21875000409677625, -7.999999999999892530 ) ) ;
#48470 = CARTESIAN_POINT ( 'NONE',  ( -7.778174593052023411, 7.778174593052023411, 82.00000000409676204 ) ) ;
#48471 = CARTESIAN_POINT ( 'NONE',  ( -9.832129032723415207, 229.6354166700806729, 5.676582343750005144 ) ) ;
#48472 = VECTOR ( 'NONE', #4628, 1000.000000000000000 ) ;
#48473 = CARTESIAN_POINT ( 'NONE',  ( -11.35316468750000141, 133.2812499965860127, -1.390361679473963753E-15 ) ) ;
#48474 = ORIENTED_EDGE ( 'NONE', *, *, #28295, .T. ) ;
#48475 = DIRECTION ( 'NONE',  ( -1.000000000000000000, 0.000000000000000000, 0.000000000000000000 ) ) ;
#48476 = EDGE_CURVE ( 'NONE', #9708, #18825, #30397, .T. ) ;
#48477 = EDGE_CURVE ( 'NONE', #3, #37917, #73751, .T. ) ;
#48478 = CARTESIAN_POINT ( 'NONE',  ( -6.238412754330611322E-16, 10.18810118749999916, 94.28125000204836681 ) ) ;
#48479 = CARTESIAN_POINT ( 'NONE',  ( 38.00000000000000000, 242.0000000000000284, 20.00000000000002132 ) ) ;
#48480 = CARTESIAN_POINT ( 'NONE',  ( 2.754378923186476579E-14, 197.4375000013655779, 194.5412658750000219 ) ) ;
#48481 = LINE ( 'NONE', #31132, #60624 ) ;
#48483 = CARTESIAN_POINT ( 'NONE',  ( 8.311093377946837890, 106.4062499965860127, -8.311093377946837890 ) ) ;
#48482 = CARTESIAN_POINT ( 'NONE',  ( 5.539869284409778771, 219.9999999999998863, 8.691086950455378712 ) ) ;
#48484 = CARTESIAN_POINT ( 'NONE',  ( -23.99999999999999289, 208.7500000000000284, 170.0000000000003411 ) ) ;
#48485 = CARTESIAN_POINT ( 'NONE',  ( 10.00000000000000000, 146.6666666598386826, 2.679491924311235618 ) ) ;
#48486 = ORIENTED_EDGE ( 'NONE', *, *, #32847, .T. ) ;
#48487 = CARTESIAN_POINT ( 'NONE',  ( 5.656854249492381470, 112.2500000040967763, 5.656854249492379694 ) ) ;
#48488 = CARTESIAN_POINT ( 'NONE',  ( -1.656854249492381248, 9.312500000000000000, -4.000000000000001776 ) ) ;
#48489 = CARTESIAN_POINT ( 'NONE',  ( -5.676582343749998039, 107.7604166632526841, -9.832129032723420536 ) ) ;
#48490 = CARTESIAN_POINT ( 'NONE',  ( -2.445694354108783664, 208.3125000013656063, 195.5543056458912190 ) ) ;
#48491 = CARTESIAN_POINT ( 'NONE',  ( -2.977408999572654480, 9.374999997951610098, 7.188101187499999156 ) ) ;
#48492 =( BOUNDED_CURVE ( )  B_SPLINE_CURVE ( 2, ( #44232, #49124, #10272, #61203, #20449, #9899, #9534, #56297, #44602, #37448, #3872, #66480, #43849 ),
 .UNSPECIFIED., .F., .F. ) 
 B_SPLINE_CURVE_WITH_KNOTS ( ( 3, 2, 2, 2, 2, 2, 3 ),
 ( 0.8532608695652174058, 0.8550724637681159646, 0.8568840579710145233, 0.8586956521739130821, 0.8605072463768116409, 0.8623188405797101996, 0.8641304347826086474 ),
 .UNSPECIFIED. ) 
 CURVE ( )  GEOMETRIC_REPRESENTATION_ITEM ( )  RATIONAL_B_SPLINE_CURVE ( ( 1.000000000000000000, 0.9659258262890683122, 1.000000000000000000, 0.9659258262890683122, 1.000000000000000000, 0.9659258262890683122, 1.000000000000000000, 0.9659258262890683122, 1.000000000000000000, 0.9659258262890683122, 1.000000000000000000, 0.9659258262890683122, 1.000000000000000000 ) ) 
 REPRESENTATION_ITEM ( '' )  );
#48493 = CARTESIAN_POINT ( 'NONE',  ( -10.18810118749999916, 0.000000000000000000, 87.53125000204836681 ) ) ;
#48494 = CARTESIAN_POINT ( 'NONE',  ( -9.832129032723420536, 19.01041666325268409, 5.676582343749997150 ) ) ;
#48495 = VERTEX_POINT ( 'NONE', #59442 ) ;
#48496 = CARTESIAN_POINT ( 'NONE',  ( -3.317071493978878571, 8.008118988124991233, 24.73186528394063544 ) ) ;
#48497 = CARTESIAN_POINT ( 'NONE',  ( 10.00000000000000000, 116.6666666598387110, 2.679491924311235618 ) ) ;
#48498 = CARTESIAN_POINT ( 'NONE',  ( -4.220049686691937474, -10.18810118749999738, 74.31250000204836681 ) ) ;
#48499 = CARTESIAN_POINT ( 'NONE',  ( 49.70177871865296026, 50.00000000000000711, 57.99999999999999289 ) ) ;
#48500 = CARTESIAN_POINT ( 'NONE',  ( 4.721056650416000089, 293.8281250017069510, 4.721056650415999201 ) ) ;
#48501 = EDGE_CURVE ( 'NONE', #29980, #1076, #30759, .T. ) ;
#48502 = CARTESIAN_POINT ( 'NONE',  ( 4.000000000000016875, 204.5625000027312126, 199.6568542494924259 ) ) ;
#48503 = CARTESIAN_POINT ( 'NONE',  ( 5.676582343750001591, 216.9270833299193555, -9.832129032723420536 ) ) ;
#48504 = CARTESIAN_POINT ( 'NONE',  ( 8.311093377946834337, 135.4687499965860411, 8.311093377946839666 ) ) ;
#48505 = CARTESIAN_POINT ( 'NONE',  ( 7.204075437095968759, -7.204075437095966983, 83.21875000204836681 ) ) ;
#48506 = CARTESIAN_POINT ( 'NONE',  ( -26.56734541678238060, 200.3750000013656063, 166.5412658750003629 ) ) ;
#48507 =( BOUNDED_CURVE ( )  B_SPLINE_CURVE ( 2, ( #37344, #70926, #9045, #60723, #8670, #59976, #49020, #61095, #66377 ),
 .UNSPECIFIED., .F., .F. ) 
 B_SPLINE_CURVE_WITH_KNOTS ( ( 3, 2, 2, 2, 3 ),
 ( 0.9117647058823529216, 0.9154411764705882026, 0.9191176470588233727, 0.9227941176470587648, 0.9264705882352940458 ),
 .UNSPECIFIED. ) 
 CURVE ( )  GEOMETRIC_REPRESENTATION_ITEM ( )  RATIONAL_B_SPLINE_CURVE ( ( 1.000000000000000000, 0.9238795325112867385, 1.000000000000000000, 0.9238795325112867385, 1.000000000000000000, 0.9238795325112867385, 1.000000000000000000, 0.9238795325112890700, 0.9999999999999976685 ) ) 
 REPRESENTATION_ITEM ( '' )  );
#48508 = CARTESIAN_POINT ( 'NONE',  ( -1.469576158976823947E-15, 25.12500000000000355, 8.000000000000000000 ) ) ;
#48509 = CARTESIAN_POINT ( 'NONE',  ( -4.541265875000002339, 12.87499999863440969, -1.881053915767121998 ) ) ;
#48510 = VERTEX_POINT ( 'NONE', #36061 ) ;
#48511 = CARTESIAN_POINT ( 'NONE',  ( -1.656854249492347719, 207.9375000027312126, 194.0000000000000853 ) ) ;
#48512 = CARTESIAN_POINT ( 'NONE',  ( -1.432654583217664701, 197.0000000013656347, 138.5412658750000787 ) ) ;
#48513 = CARTESIAN_POINT ( 'NONE',  ( 3.999999999999960032, 204.1250000027312126, 142.0000000000000568 ) ) ;
#48514 = CARTESIAN_POINT ( 'NONE',  ( -5.000000000000047073, 171.6666666666667425, -8.660254037844470787 ) ) ;
#48515 = CARTESIAN_POINT ( 'NONE',  ( 5.094050593753887135, 8.823154444699161658, 67.53052362291680311 ) ) ;
#48516 = ORIENTED_EDGE ( 'NONE', *, *, #66343, .T. ) ;
#48517 = CARTESIAN_POINT ( 'NONE',  ( 5.082755093536325930, 3.656249997951610542, -5.082755093536325930 ) ) ;
#48518 = CARTESIAN_POINT ( 'NONE',  ( -11.97472659780681603, -25.76607261614005395, 198.5950153741617612 ) ) ;
#48519 = FACE_OUTER_BOUND ( 'NONE', #8038, .T. ) ;
#48520 = CARTESIAN_POINT ( 'NONE',  ( 1.320432766682874540E-15, 115.9062500020483810, 7.188101187500000044 ) ) ;
#48521 = CARTESIAN_POINT ( 'NONE',  ( 1.468605411411143757, -19.93670996121502625, -1.118160017449617349 ) ) ;
#48522 = CARTESIAN_POINT ( 'NONE',  ( -4.721056650415998313, 293.5781250017069510, 4.721056650416000089 ) ) ;
#48524 = DIRECTION ( 'NONE',  ( -1.621639297089430499E-05, 1.883468370551372626E-05, 0.9999999996911416167 ) ) ;
#48523 = CARTESIAN_POINT ( 'NONE',  ( -8.311093377946836114, 223.2812500034140157, -8.311093377946836114 ) ) ;
#48525 = VERTEX_POINT ( 'NONE', #59078 ) ;
#48526 = CARTESIAN_POINT ( 'NONE',  ( 3.042071309553173286, 225.6770833367473017, 11.35316468749999608 ) ) ;
#48527 = CARTESIAN_POINT ( 'NONE',  ( 7.188101187499992051, 8.802885111219154394E-16, 2.236552781871750550 ) ) ;
#48528 = CARTESIAN_POINT ( 'NONE',  ( 6.123233995736767268E-16, 168.1249999931720538, -10.00000000000000178 ) ) ;
#48529 = DIRECTION ( 'NONE',  ( -0.000000000000000000, -0.000000000000000000, -1.000000000000000000 ) ) ;
#48530 = CARTESIAN_POINT ( 'NONE',  ( 1.432654583217664701, 198.0000000013656063, 201.4587341250000065 ) ) ;
#48531 = VERTEX_POINT ( 'NONE', #71107 ) ;
#48532 = CARTESIAN_POINT ( 'NONE',  ( -10.99999999999996092, 4.556349186104085902, 114.9062499999999716 ) ) ;
#48533 = CARTESIAN_POINT ( 'NONE',  ( 8.000000000000000000, 98.84374999999998579, -3.313708498984762496 ) ) ;
#48534 = CARTESIAN_POINT ( 'NONE',  ( -11.35316468750000141, 118.8020833299193413, 3.042071309553159963 ) ) ;
#48535 = CARTESIAN_POINT ( 'NONE',  ( 2.751064625579944321E-14, 208.7500000000000284, 194.0000000000000568 ) ) ;
#48536 = CARTESIAN_POINT ( 'NONE',  ( 4.556349186104051263, -10.99999999999999822, 74.96874999999998579 ) ) ;
#48539 = FACE_OUTER_BOUND ( 'NONE', #32859, .T. ) ;
#48538 = CARTESIAN_POINT ( 'NONE',  ( 25.55430564589119058, 201.3125000013656063, 172.4456943541087526 ) ) ;
#48537 = CARTESIAN_POINT ( 'NONE',  ( 24.54126587500000056, 204.3750000013656063, 168.5673454167822172 ) ) ;
#48540 = ORIENTED_EDGE ( 'NONE', *, *, #13084, .F. ) ;
#48541 = EDGE_CURVE ( 'NONE', #46612, #64105, #30394, .T. ) ;
#48542 = LINE ( 'NONE', #19137, #63377 ) ;
#48543 = CARTESIAN_POINT ( 'NONE',  ( 8.311093377946837890, 216.4062499965860127, -8.311093377946837890 ) ) ;
#48544 = CARTESIAN_POINT ( 'NONE',  ( -3.458734125000015425, 200.0000000013656347, 143.4326545832176976 ) ) ;
#48545 = CARTESIAN_POINT ( 'NONE',  ( 24.54126587499998280, 201.5000000013655779, 171.4326545832175555 ) ) ;
#48546 = CARTESIAN_POINT ( 'NONE',  ( -2.977408999572654480, 27.37499999795161187, 7.188101187499999156 ) ) ;
#48547 = CARTESIAN_POINT ( 'NONE',  ( 11.35316468750000141, 191.0937499965860127, 0.000000000000000000 ) ) ;
#48548 = CARTESIAN_POINT ( 'NONE',  ( -7.188101187500000933, 89.93750000204839523, -2.977408999572650483 ) ) ;
#48549 = CARTESIAN_POINT ( 'NONE',  ( 7.247622103906887325, 225.9999999999999147, 7.486376043179081563 ) ) ;
#48550 = CARTESIAN_POINT ( 'NONE',  ( 1.881053915767121776, 14.49999999863440969, -4.541265875000002339 ) ) ;
#48551 = CARTESIAN_POINT ( 'NONE',  ( 24.54126587499998280, 199.5000000013656063, 171.4326545832175555 ) ) ;
#48552 = CARTESIAN_POINT ( 'NONE',  ( 5.082755093536318824, 5.082755093536319713, 1.299052781871753215 ) ) ;
#48553 = FACE_OUTER_BOUND ( 'NONE', #35520, .T. ) ;
#48554 = CARTESIAN_POINT ( 'NONE',  ( -11.35316468750000141, 78.48958332991935549, 3.042071309553159963 ) ) ;
#48555 = VERTEX_POINT ( 'NONE', #8485 ) ;
#48556 = CARTESIAN_POINT ( 'NONE',  ( 10.00000000000001066, 140.0000000000000284, 0.000000000000000000 ) ) ;
#48557 = CARTESIAN_POINT ( 'NONE',  ( 27.99999999999999645, 210.0000000000000284, 169.9999999999999147 ) ) ;
#48558 = CARTESIAN_POINT ( 'NONE',  ( -8.000000000000000000, 9.468749995903223748, -3.313708498984762496 ) ) ;
#48559 = LINE ( 'NONE', #66667, #26818 ) ;
#48560 = CARTESIAN_POINT ( 'NONE',  ( -11.35316468750000141, 88.48958332991934128, 3.042071309553159963 ) ) ;
#48561 = ORIENTED_EDGE ( 'NONE', *, *, #69523, .T. ) ;
#48562 = CARTESIAN_POINT ( 'NONE',  ( 10.18810118749999916, 4.220049686691935698, 89.87500000204836681 ) ) ;
#48563 = EDGE_CURVE ( 'NONE', #18004, #27943, #8970, .T. ) ;
#48564 = CARTESIAN_POINT ( 'NONE',  ( -6.238412754330611322E-16, 10.18810118749999916, 110.7812500020483668 ) ) ;
#48565 = CARTESIAN_POINT ( 'NONE',  ( 1.432654583217664701, 207.0000000013656063, 201.4587341250000065 ) ) ;
#48566 = CARTESIAN_POINT ( 'NONE',  ( 7.320508075688796801, 75.62500000000002842, -7.320508075688796801 ) ) ;
#48568 = CARTESIAN_POINT ( 'NONE',  ( -8.311093377946841443, 73.90624999658601268, 8.311093377946834337 ) ) ;
#48567 = FACE_OUTER_BOUND ( 'NONE', #56263, .T. ) ;
#48569 = CARTESIAN_POINT ( 'NONE',  ( -5.656854249492373476, -5.656854249492376141, 20.70530278392014623 ) ) ;
#48570 = FACE_OUTER_BOUND ( 'NONE', #7841, .T. ) ;
#48571 = CARTESIAN_POINT ( 'NONE',  ( -10.00000000000000355, 174.5833333265053682, 2.679491924311223183 ) ) ;
#48572 = CARTESIAN_POINT ( 'NONE',  ( -4.401442555609581635E-16, 91.15625000204838102, -7.188101187500000044 ) ) ;
#48573 = CARTESIAN_POINT ( 'NONE',  ( -24.07989181644099475, 194.9176386608073699, 170.1288133823554745 ) ) ;
#48574 = CARTESIAN_POINT ( 'NONE',  ( -11.35316468749999785, 63.38541666325269119, -3.042071309553167957 ) ) ;
#48575 = CARTESIAN_POINT ( 'NONE',  ( 4.721056650415999201, 295.0781250017069510, -4.721056650415999201 ) ) ;
#48576 = CARTESIAN_POINT ( 'NONE',  ( 10.18810118749999916, 4.220049686691935698, 109.3750000020483810 ) ) ;
#48577 = CARTESIAN_POINT ( 'NONE',  ( 11.35316468749999963, 200.9895833299193839, -3.042071309553165293 ) ) ;
#48578 = VERTEX_POINT ( 'NONE', #39031 ) ;
#48579 = CARTESIAN_POINT ( 'NONE',  ( -4.336811714529519968, 68.30918023749056545, 20.61428864874217481 ) ) ;
#48580 = CARTESIAN_POINT ( 'NONE',  ( 0.000000000000000000, 0.000000000000000000, 0.000000000000000000 ) ) ;
#48581 = CARTESIAN_POINT ( 'NONE',  ( 5.656854249492378806, 14.62499999590322020, 5.656854249492381470 ) ) ;
#48583 = CARTESIAN_POINT ( 'NONE',  ( 9.832129032723416984, 190.3645833299193839, 5.676582343750006032 ) ) ;
#48582 = LINE ( 'NONE', #30139, #50925 ) ;
#48584 = VECTOR ( 'NONE', #34274, 999.9999999999998863 ) ;
#48585 = CARTESIAN_POINT ( 'NONE',  ( 27.99999999999996447, 199.6250000027312126, 165.9999999999998863 ) ) ;
#48586 = CARTESIAN_POINT ( 'NONE',  ( 5.000000000000004441, 239.7916666734946318, 8.660254037844385522 ) ) ;
#48587 = FACE_OUTER_BOUND ( 'NONE', #72656, .T. ) ;
#48588 = EDGE_CURVE ( 'NONE', #56250, #3815, #60962, .T. ) ;
#48589 = ORIENTED_EDGE ( 'NONE', *, *, #62177, .T. ) ;
#48590 = CARTESIAN_POINT ( 'NONE',  ( 9.832129032723420536, 181.5104166632526699, -5.676582343749999815 ) ) ;
#48591 = EDGE_CURVE ( 'NONE', #66964, #16528, #16660, .T. ) ;
#48592 = CARTESIAN_POINT ( 'NONE',  ( -5.082755093536317936, -5.082755093536320601, 21.17405278187175455 ) ) ;
#48593 = B_SPLINE_CURVE_WITH_KNOTS ( 'NONE', 3,
 ( #38373, #61754, #33107, #4413, #73438, #21746, #44774, #6280, #74556, #69271, #45141, #34960, #57216, #5530, #40225, #73809, #4790, #57975, #10442, #23614 ),
 .UNSPECIFIED., .F., .F.,
 ( 4, 2, 2, 2, 2, 2, 2, 2, 2, 4 ),
 ( 2.081668171172168513E-17, 0.003663249189234797469, 0.004579061486543501390, 0.005494873783852205311, 0.007326498378469627898, 0.009158122973087049618, 0.01098974756770447307, 0.01190555986501318567, 0.01282137216232190000, 0.01465299675693934600 ),
 .UNSPECIFIED. ) ;
#48594 = CARTESIAN_POINT ( 'NONE',  ( -9.999999999999996447, 92.70833333333332860, 2.679491924311221407 ) ) ;
#48595 = VERTEX_POINT ( 'NONE', #15255 ) ;
#48596 = EDGE_CURVE ( 'NONE', #33763, #53267, #62035, .T. ) ;
#48597 = EDGE_CURVE ( 'NONE', #3455, #20924, #68037, .T. ) ;
#48598 = CARTESIAN_POINT ( 'NONE',  ( 8.000000000000000000, 100.4375000040967763, -9.797174393178825657E-16 ) ) ;
#48599 =( BOUNDED_CURVE ( )  B_SPLINE_CURVE ( 2, ( #72205, #67683, #72966, #21271, #3943, #43162, #15980, #33363, #37896 ),
 .UNSPECIFIED., .F., .F. ) 
 B_SPLINE_CURVE_WITH_KNOTS ( ( 3, 2, 2, 2, 3 ),
 ( 0.2833333333333336590, 0.2916666666666669627, 0.3000000000000002665, 0.3083333333333335702, 0.3166666666666668184 ),
 .UNSPECIFIED. ) 
 CURVE ( )  GEOMETRIC_REPRESENTATION_ITEM ( )  RATIONAL_B_SPLINE_CURVE ( ( 0.9999999999999970024, 0.9238795325112897361, 1.000000000000000000, 0.9238795325112867385, 1.000000000000000000, 0.9238795325112867385, 1.000000000000000000, 0.9238795325112851842, 1.000000000000001554 ) ) 
 REPRESENTATION_ITEM ( '' )  );
#48600 = CARTESIAN_POINT ( 'NONE',  ( 25.17157287525381903, 208.6250000000000284, 167.1715728752537018 ) ) ;
#48601 = EDGE_CURVE ( 'NONE', #8103, #62523, #20165, .T. ) ;
#48602 = AXIS2_PLACEMENT_3D ( 'NONE', #50029, #65884, #26638 ) ;
#48603 = CARTESIAN_POINT ( 'NONE',  ( -4.000000000000001776, 14.43750000000000000, -1.656854249492381470 ) ) ;
#48604 = CARTESIAN_POINT ( 'NONE',  ( -4.541265875000003227, 15.87499999863440436, 1.881053915767121110 ) ) ;
#48605 = CARTESIAN_POINT ( 'NONE',  ( 1.469576158976822172E-15, -7.999999999999991118, 13.39280278392014623 ) ) ;
#48606 = DIRECTION ( 'NONE',  ( -1.000000000000000000, 0.000000000000000000, 0.000000000000000000 ) ) ;
#48607 = ORIENTED_EDGE ( 'NONE', *, *, #21322, .T. ) ;
#48608 = LINE ( 'NONE', #53911, #19792 ) ;
#48609 = CARTESIAN_POINT ( 'NONE',  ( -2.977408999572651815, 98.93750000204838102, 7.188101187500000933 ) ) ;
#48610 = CARTESIAN_POINT ( 'NONE',  ( -11.35316468749999785, 258.6979166700807014, -3.042071309553164848 ) ) ;
#48611 = SHAPE_DEFINITION_REPRESENTATION ( #19743, #69137 ) ;
#48612 = VERTEX_POINT ( 'NONE', #14502 ) ;
#48613 = CARTESIAN_POINT ( 'NONE',  ( -11.00000000000000000, 0.000000000000000000, 83.49999999999998579 ) ) ;
#48614 = CARTESIAN_POINT ( 'NONE',  ( -2.977408999572647819, 7.188101187499991163, 20.70530278187175455 ) ) ;
#48615 = EDGE_LOOP ( 'NONE', ( #49745, #54672, #62412, #42927 ) ) ;
#48616 = VERTEX_POINT ( 'NONE', #3209 ) ;
#48617 = CARTESIAN_POINT ( 'NONE',  ( -6.238412754330611322E-16, 10.18810118749999916, 77.78125000204836681 ) ) ;
#48618 = CARTESIAN_POINT ( 'NONE',  ( -2.085542519210945728E-15, 64.84374999658601268, 11.35316468750000141 ) ) ;
#48619 = CARTESIAN_POINT ( 'NONE',  ( 10.00000000000000178, 92.08333332650536818, -2.679491924311226736 ) ) ;
#48620 = CARTESIAN_POINT ( 'NONE',  ( -10.99999999999999822, -4.556349186104052151, 92.59374999999998579 ) ) ;
#48623 = CARTESIAN_POINT ( 'NONE',  ( -4.088227598258586603E-16, 292.3593750017070079, -6.676582343750001591 ) ) ;
#48622 = CARTESIAN_POINT ( 'NONE',  ( 31.99999999999999289, 199.3750000027312126, 169.9999999999998863 ) ) ;
#48621 = CARTESIAN_POINT ( 'NONE',  ( 11.00000000000010836, -4.556349186103939353, 105.1562499999999858 ) ) ;
#48624 = CARTESIAN_POINT ( 'NONE',  ( 10.00000000000000178, 145.2083333333333144, -2.679491924311226736 ) ) ;
#48625 = CARTESIAN_POINT ( 'NONE',  ( 11.00000000000000000, 1.347111479062088405E-15, 75.43750000409676204 ) ) ;
#48626 = CARTESIAN_POINT ( 'NONE',  ( -3.313708498984870410, 90.96875000409676204, 7.999999999999890754 ) ) ;
#48627 = CARTESIAN_POINT ( 'NONE',  ( 2.449293598294707893E-16, 13.25000000000000000, -4.000000000000001776 ) ) ;
#48628 = CARTESIAN_POINT ( 'NONE',  ( 8.000000000000000000, 5.906249995903220196, -3.313708498984761608 ) ) ;
#48629 = CARTESIAN_POINT ( 'NONE',  ( 26.56734541678238060, 200.0000000013656347, 166.5412658749999650 ) ) ;
#48630 = CARTESIAN_POINT ( 'NONE',  ( -7.188101187500000044, 10.59374999795161187, -8.802885111219163269E-16 ) ) ;
#48631 = CARTESIAN_POINT ( 'NONE',  ( -5.656854249492373476, -5.656854249492376141, 23.70530278392014978 ) ) ;
#48632 = CARTESIAN_POINT ( 'NONE',  ( 2.828427124746191623, 5.874999997268813168, -2.828427124746191623 ) ) ;
#48633 = CARTESIAN_POINT ( 'NONE',  ( -7.188101187500000933, 110.9375000020483810, -2.977408999572650483 ) ) ;
#48635 = CARTESIAN_POINT ( 'NONE',  ( -4.000000000000002665, 16.56250000000000000, 1.656854249492380582 ) ) ;
#48634 = CARTESIAN_POINT ( 'NONE',  ( -2.679491924311235174, 20.41666665983869677, 10.00000000000000000 ) ) ;
#48636 = CARTESIAN_POINT ( 'NONE',  ( -11.35316468749999963, 219.2187500034139873, 0.000000000000000000 ) ) ;
#48637 = CARTESIAN_POINT ( 'NONE',  ( 4.898587196589412829E-16, 21.37500000000000355, -8.000000000000000000 ) ) ;
#48638 = CARTESIAN_POINT ( 'NONE',  ( 2.977408999572646486, 7.188101187499991163, 19.39280278187176165 ) ) ;
#48639 = CARTESIAN_POINT ( 'NONE',  ( 0.000000000000000000, 0.000000000000000000, 10.00000000000000178 ) ) ;
#48640 = CARTESIAN_POINT ( 'NONE',  ( -9.832129032723418760, 37.86458332991934839, -5.676582343750004256 ) ) ;
#48641 = EDGE_CURVE ( 'NONE', #23857, #29800, #26197, .T. ) ;
#48642 = CARTESIAN_POINT ( 'NONE',  ( 7.320508075688776373, 150.6250000000000000, -7.320508075688776373 ) ) ;
#48643 = CARTESIAN_POINT ( 'NONE',  ( -7.320508075688778149, 14.99999999317203425, 7.320508075688769267 ) ) ;
#48644 = ORIENTED_EDGE ( 'NONE', *, *, #50697, .F. ) ;
#48645 = CARTESIAN_POINT ( 'NONE',  ( -10.00000000000000178, 129.3749999931720254, -1.224646799147353454E-15 ) ) ;
#48646 = B_SPLINE_CURVE_WITH_KNOTS ( 'NONE', 3,
 ( #47486, #29779, #41832, #36550, #7141, #35817, #1499, #70509, #24481, #64845, #13146, #36183, #25208, #59201, #30515, #53535 ),
 .UNSPECIFIED., .F., .F.,
 ( 4, 2, 2, 2, 2, 2, 2, 4 ),
 ( 0.000000000000000000, 0.002635095253036493727, 0.003952642879554739072, 0.005270190506072984851, 0.006587738132591231498, 0.007905285759109476409, 0.009222833385627722189, 0.01054038101214596797 ),
 .UNSPECIFIED. ) ;
#48647 = DIRECTION ( 'NONE',  ( 0.000000000000000000, -1.000000000000000000, -0.000000000000000000 ) ) ;
#48648 = CARTESIAN_POINT ( 'NONE',  ( 11.35316468749999963, 30.98958332991935194, -3.042071309553165293 ) ) ;
#48649 = CARTESIAN_POINT ( 'NONE',  ( -11.00000000000000000, 0.000000000000000000, 82.18750000409677625 ) ) ;
#48650 = CARTESIAN_POINT ( 'NONE',  ( -3.458734125000015425, 203.2500000013655495, 143.4326545832176976 ) ) ;
#48651 = CARTESIAN_POINT ( 'NONE',  ( -4.999999999999992895, 260.8333333333333712, 8.660254037844390851 ) ) ;
#48652 = DIRECTION ( 'NONE',  ( -0.000000000000000000, -0.000000000000000000, 1.000000000000000000 ) ) ;
#48654 = CARTESIAN_POINT ( 'NONE',  ( 5.676582343750001591, 31.61458332991935194, -9.832129032723420536 ) ) ;
#48653 = CARTESIAN_POINT ( 'NONE',  ( 2.977408999572650039, 105.6875000020483952, -7.188101187500000933 ) ) ;
#48655 = CARTESIAN_POINT ( 'NONE',  ( 1.469576158976822172E-15, -7.999999999999991118, 8.705302779823362869 ) ) ;
#48656 = CARTESIAN_POINT ( 'NONE',  ( 5.676582343750001591, 156.6145833299193839, -9.832129032723420536 ) ) ;
#48657 = ADVANCED_FACE ( 'NONE', ( #14879 ), #37918, .F. ) ;
#48658 = CARTESIAN_POINT ( 'NONE',  ( 10.00000000000000178, 132.0833333265053398, -2.679491924311226736 ) ) ;
#48659 = CARTESIAN_POINT ( 'NONE',  ( -7.188101187500001821, 109.4375000020483810, -2.977408999572650483 ) ) ;
#48660 = VECTOR ( 'NONE', #1708, 1000.000000000000000 ) ;
#48661 = ORIENTED_EDGE ( 'NONE', *, *, #38040, .T. ) ;
#48662 = LINE ( 'NONE', #25276, #3857 ) ;
#48663 = CARTESIAN_POINT ( 'NONE',  ( -9.832129032723418760, 28.17708332991935194, -5.676582343750004256 ) ) ;
#48664 = ORIENTED_EDGE ( 'NONE', *, *, #42517, .T. ) ;
#48665 = CARTESIAN_POINT ( 'NONE',  ( 4.898587196589412829E-16, 18.37500000000000355, -8.000000000000000000 ) ) ;
#48666 = CARTESIAN_POINT ( 'NONE',  ( 1.871523826299183495E-15, -10.18810118749999916, 80.03125000204836681 ) ) ;
#48667 = CARTESIAN_POINT ( 'NONE',  ( -28.00000000000002487, 197.0000000000000000, 166.0000000000003695 ) ) ;
#48668 = PRODUCT_RELATED_PRODUCT_CATEGORY ( 'part', '', ( #42631 ) ) ;
#48670 = CARTESIAN_POINT ( 'NONE',  ( -2.085542519210945728E-15, 154.5312499965860127, 11.35316468750000141 ) ) ;
#48669 = CARTESIAN_POINT ( 'NONE',  ( -20.56108207772482643, -28.52085825003521080, 145.2189059375704687 ) ) ;
#48671 = CARTESIAN_POINT ( 'NONE',  ( -7.188101187500000044, 1.593749997951610320, -8.802885111219163269E-16 ) ) ;
#48672 = CARTESIAN_POINT ( 'NONE',  ( -7.999999999999989342, -3.313708498984762496, 18.98030278432982954 ) ) ;
#48673 = CARTESIAN_POINT ( 'NONE',  ( -25.40387798348978166, -22.52342783027560813, 187.7747974912569759 ) ) ;
#48674 = CARTESIAN_POINT ( 'NONE',  ( -3.042071309553159075, 229.9479166700806161, 11.35316468749999963 ) ) ;
#48675 = CARTESIAN_POINT ( 'NONE',  ( 4.220049686691941027, -10.18810118749999738, 86.50000000204838102 ) ) ;
#48676 = EDGE_LOOP ( 'NONE', ( #2817, #30539 ) ) ;
#48677 = EDGE_CURVE ( 'NONE', #57404, #21228, #19529, .T. ) ;
#48678 = CARTESIAN_POINT ( 'NONE',  ( 5.656854249492380582, 1.499999995903219974, -5.656854249492380582 ) ) ;
#48679 = CARTESIAN_POINT ( 'NONE',  ( -4.242640687119285658, 292.1875000034139589, 4.242640687119287435 ) ) ;
#48680 = CARTESIAN_POINT ( 'NONE',  ( -5.676582343749998039, 107.7604166632526841, -9.832129032723420536 ) ) ;
#48681 = CARTESIAN_POINT ( 'NONE',  ( -6.238412754330611322E-16, 10.18810118749999916, 101.7812500020483810 ) ) ;
#48682 = EDGE_CURVE ( 'NONE', #31332, #33217, #56760, .T. ) ;
#48683 = CARTESIAN_POINT ( 'NONE',  ( 1.881053915767121998, 19.62499999863441147, -4.541265875000002339 ) ) ;
#48684 = EDGE_LOOP ( 'NONE', ( #5601, #58189, #52494, #33566 ) ) ;
#48685 = EDGE_LOOP ( 'NONE', ( #26501, #56167, #72549, #61815 ) ) ;
#48686 = VECTOR ( 'NONE', #49738, 1000.000000000000000 ) ;
#48687 = CARTESIAN_POINT ( 'NONE',  ( 2.780723358947928197E-16, 3.687499998634407472, -4.541265875000002339 ) ) ;
#48688 = CARTESIAN_POINT ( 'NONE',  ( -7.188101187500002709, 27.18749999795162609, 2.977408999572649151 ) ) ;
#48689 = CARTESIAN_POINT ( 'NONE',  ( 8.000000000000000000, 118.5312500040968047, -3.313708498984762496 ) ) ;
#48690 = CARTESIAN_POINT ( 'NONE',  ( 4.220049686691941027, -10.18810118749999738, 100.0000000020483668 ) ) ;
#48691 = CARTESIAN_POINT ( 'NONE',  ( -24.54126587499998280, 204.3750000013656063, 171.4326545832179818 ) ) ;
#48692 = FACE_OUTER_BOUND ( 'NONE', #38287, .T. ) ;
#48693 = EDGE_CURVE ( 'NONE', #27168, #7738, #36505, .T. ) ;
#48694 = CARTESIAN_POINT ( 'NONE',  ( 1.656854249492381914, 3.812500000000000000, 4.000000000000000888 ) ) ;
#48695 = CARTESIAN_POINT ( 'NONE',  ( 2.449293598294707893E-16, 18.99999999726881228, -4.000000000000001776 ) ) ;
#48696 = CARTESIAN_POINT ( 'NONE',  ( 4.541265875000002339, 3.374999998634407028, -1.881053915767121776 ) ) ;
#48697 = CARTESIAN_POINT ( 'NONE',  ( -3.458734125000015425, 208.0000000013656347, 143.4326545832176976 ) ) ;
#48698 = CARTESIAN_POINT ( 'NONE',  ( 24.00000000000000711, 207.6875000000000284, 168.3431457505074889 ) ) ;
#48700 = CARTESIAN_POINT ( 'NONE',  ( -7.320508075688773708, 223.7499999931720538, -7.320508075688774596 ) ) ;
#48699 = CARTESIAN_POINT ( 'NONE',  ( -28.00000000000007105, 201.4375000013656063, 166.5412658750003629 ) ) ;
#48701 = CARTESIAN_POINT ( 'NONE',  ( -3.211159895383561391, 17.68749999863440792, -3.211159895383561835 ) ) ;
#48702 = DIRECTION ( 'NONE',  ( -0.000000000000000000, 1.000000000000000000, -0.000000000000000000 ) ) ;
#48703 = CARTESIAN_POINT ( 'NONE',  ( -2.977408999572647819, 7.188101187499991163, 5.705302781871753659 ) ) ;
#48704 = ORIENTED_EDGE ( 'NONE', *, *, #73472, .F. ) ;
#48705 =( BOUNDED_CURVE ( )  B_SPLINE_CURVE ( 2, ( #31494, #42796, #72216, #54139, #14490, #66558, #37907, #65812, #49587 ),
 .UNSPECIFIED., .F., .F. ) 
 B_SPLINE_CURVE_WITH_KNOTS ( ( 3, 2, 2, 2, 3 ),
 ( 0.2395833333333330928, 0.2447916666666664076, 0.2499999999999997780, 0.2552083333333330928, 0.2604166666666664631 ),
 .UNSPECIFIED. ) 
 CURVE ( )  GEOMETRIC_REPRESENTATION_ITEM ( )  RATIONAL_B_SPLINE_CURVE ( ( 1.000000000000003553, 0.9238795325112830747, 1.000000000000000000, 0.9238795325112867385, 1.000000000000000000, 0.9238795325112867385, 1.000000000000000000, 0.9238795325112899581, 0.9999999999999967804 ) ) 
 REPRESENTATION_ITEM ( '' )  );
#48706 =( BOUNDED_CURVE ( )  B_SPLINE_CURVE ( 2, ( #55328, #45110, #68123, #44369, #67380, #39083, #16417, #39450, #62450 ),
 .UNSPECIFIED., .F., .F. ) 
 B_SPLINE_CURVE_WITH_KNOTS ( ( 3, 2, 2, 2, 3 ),
 ( 0.9210526315789474561, 0.9276315789473685847, 0.9342105263157896022, 0.9407894736842106198, 0.9473684210526316374 ),
 .UNSPECIFIED. ) 
 CURVE ( )  GEOMETRIC_REPRESENTATION_ITEM ( )  RATIONAL_B_SPLINE_CURVE ( ( 0.9999999999999986677, 0.9238795325112880708, 1.000000000000000000, 0.9238795325112867385, 1.000000000000000000, 0.9238795325112867385, 1.000000000000000000, 0.9238795325112854062, 1.000000000000001332 ) ) 
 REPRESENTATION_ITEM ( '' )  );
#48707 = ORIENTED_EDGE ( 'NONE', *, *, #49121, .T. ) ;
#48708 = CARTESIAN_POINT ( 'NONE',  ( -10.18810118749999916, 4.220049686691934809, 96.06250000204836681 ) ) ;
#48709 = CARTESIAN_POINT ( 'NONE',  ( -10.00000000000000000, 220.0000000000000000, 0.000000000000000000 ) ) ;
#48710 = CARTESIAN_POINT ( 'NONE',  ( -24.54126587499999346, 204.4375000013656063, 170.0000000000003411 ) ) ;
#48711 = CARTESIAN_POINT ( 'NONE',  ( -23.99999999999998934, 199.7500000000000000, 170.0000000000003411 ) ) ;
#48712 = CARTESIAN_POINT ( 'NONE',  ( -3.458734124999959914, 196.4375000013655779, 198.0000000000000284 ) ) ;
#48713 = CARTESIAN_POINT ( 'NONE',  ( 12.00000000000000000, 0.000000000000000000, 0.000000000000000000 ) ) ;
#48714 = CARTESIAN_POINT ( 'NONE',  ( 4.999999999999993783, 109.1666666666666714, 8.660254037844390851 ) ) ;
#48715 = CARTESIAN_POINT ( 'NONE',  ( -3.313708498984762052, 114.2187500000000000, -8.000000000000000000 ) ) ;
#48716 = CARTESIAN_POINT ( 'NONE',  ( 6.676582343750003368, 294.1718750017070079, -2.765530957081997254 ) ) ;
#48717 = EDGE_CURVE ( 'NONE', #31137, #8706, #65792, .T. ) ;
#48718 = ORIENTED_EDGE ( 'NONE', *, *, #51396, .F. ) ;
#48719 = CARTESIAN_POINT ( 'NONE',  ( 10.00000000000004263, 190.0000000000000284, 0.000000000000000000 ) ) ;
#48720 = CARTESIAN_POINT ( 'NONE',  ( -3.313708498984765161, 20.34374999590322020, 7.999999999999998224 ) ) ;
#48721 = CARTESIAN_POINT ( 'NONE',  ( 3.458734124999959025, 201.5000000013655779, 140.5673454167824161 ) ) ;
#48722 = CARTESIAN_POINT ( 'NONE',  ( -4.000000000000002665, 5.562500000000000000, 1.656854249492380582 ) ) ;
#48723 = DIRECTION ( 'NONE',  ( 0.000000000000000000, 0.000000000000000000, 1.000000000000000000 ) ) ;
#48724 = CARTESIAN_POINT ( 'NONE',  ( -5.676582343749992710, 250.0520833367473301, 9.832129032723422313 ) ) ;
#48725 = CARTESIAN_POINT ( 'NONE',  ( -10.99999999999999822, -4.556349186104053040, 91.28125000409677625 ) ) ;
#48726 = CARTESIAN_POINT ( 'NONE',  ( -11.00000000000000000, 0.000000000000000000, 111.9999999999999858 ) ) ;
#48727 = CARTESIAN_POINT ( 'NONE',  ( -9.832129032723420536, 3.697916663252683200, 5.676582343749997150 ) ) ;
#48728 = EDGE_CURVE ( 'NONE', #31087, #21048, #73512, .T. ) ;
#48729 = CARTESIAN_POINT ( 'NONE',  ( -5.082755093536317936, -5.082755093536320601, 3.549052781871751883 ) ) ;
#48730 = CARTESIAN_POINT ( 'NONE',  ( -3.042071309553164404, 197.5520833299193555, -11.35316468749999963 ) ) ;
#48731 = LINE ( 'NONE', #14015, #64836 ) ;
#48732 = CARTESIAN_POINT ( 'NONE',  ( 3.211159895383560947, 8.187499998634406140, 3.211159895383562723 ) ) ;
#48733 = CARTESIAN_POINT ( 'NONE',  ( -5.656854249492378806, 99.87500000409679046, 5.656854249492381470 ) ) ;
#48735 = LINE ( 'NONE', #9518, #57982 ) ;
#48734 = DIRECTION ( 'NONE',  ( -0.000000000000000000, -0.000000000000000000, -1.000000000000000000 ) ) ;
#48736 = ORIENTED_EDGE ( 'NONE', *, *, #71578, .F. ) ;
#48737 = CARTESIAN_POINT ( 'NONE',  ( -2.445694354108839175, 203.3125000013656063, 144.4456943541088663 ) ) ;
#48738 = CARTESIAN_POINT ( 'NONE',  ( 8.311093377946834337, 50.46874999658601979, 8.311093377946839666 ) ) ;
#48739 = CARTESIAN_POINT ( 'NONE',  ( 2.020667218593132706E-15, -11.00000000000000000, 97.56250000409677625 ) ) ;
#48740 = CARTESIAN_POINT ( 'NONE',  ( 10.99999999999989697, -4.556349186104149851, 106.8437500040967620 ) ) ;
#48741 = CARTESIAN_POINT ( 'NONE',  ( -29.43265458321755546, 199.8750000013656063, 173.4587341250004044 ) ) ;
#48742 = CYLINDRICAL_SURFACE ( 'NONE', #70731, 7.000000000000000000 ) ;
#48744 = CARTESIAN_POINT ( 'NONE',  ( 3.999999999999960032, 204.0000000000000284, 142.0000000000000568 ) ) ;
#48743 = CARTESIAN_POINT ( 'NONE',  ( -4.556349186104048599, -10.99999999999999822, 107.7812500000000000 ) ) ;
#48745 = CARTESIAN_POINT ( 'NONE',  ( -3.458734125000015425, 194.9375000013655779, 142.0000000000000568 ) ) ;
#48746 = CARTESIAN_POINT ( 'NONE',  ( -9.832129032723420536, 123.6979166632526983, 5.676582343749997150 ) ) ;
#48747 = CARTESIAN_POINT ( 'NONE',  ( 2.679491924311222739, 85.83333332650538239, 10.00000000000000355 ) ) ;
#48748 = CARTESIAN_POINT ( 'NONE',  ( -2.977408999572650927, 93.87500000204836681, -7.188101187500001821 ) ) ;
#48749 = CARTESIAN_POINT ( 'NONE',  ( 3.211159895383560947, 22.31249999863440792, 3.211159895383562723 ) ) ;
#48750 = CARTESIAN_POINT ( 'NONE',  ( -26.34314575050763096, 204.5624999999999716, 174.0000000000003979 ) ) ;
#48751 = CYLINDRICAL_SURFACE ( 'NONE', #12449, 10.00000000000000178 ) ;
#48752 = VERTEX_POINT ( 'NONE', #17871 ) ;
#48753 = CARTESIAN_POINT ( 'NONE',  ( -4.433077647033921487, 225.9999999999999147, 8.987638501916837441 ) ) ;
#48754 = ORIENTED_EDGE ( 'NONE', *, *, #34044, .F. ) ;
#48755 = EDGE_CURVE ( 'NONE', #33138, #68174, #25241, .T. ) ;
#48756 = CARTESIAN_POINT ( 'NONE',  ( -4.721056650415998313, 292.7343750017069510, 4.721056650416000089 ) ) ;
#48757 = DIRECTION ( 'NONE',  ( -0.000000000000000000, -0.000000000000000000, 1.000000000000000000 ) ) ;
#48758 = CARTESIAN_POINT ( 'NONE',  ( -4.898587196589407898E-16, 7.999999999999991118, 8.142802783920144449 ) ) ;
#48759 = CARTESIAN_POINT ( 'NONE',  ( 8.311093377946834337, 175.1562499965860127, 8.311093377946839666 ) ) ;
#48760 = CARTESIAN_POINT ( 'NONE',  ( 9.000000000000000000, 4.355963544827403666, -0.5613059398865194449 ) ) ;
#48761 = CARTESIAN_POINT ( 'NONE',  ( 2.751064625579944321E-14, 198.7500000000000000, 194.0000000000000568 ) ) ;
#48762 = CIRCLE ( 'NONE', #10217, 12.00000000000000178 ) ;
#48763 = CARTESIAN_POINT ( 'NONE',  ( -10.18810118749999916, 0.000000000000000000, 104.0312500020483810 ) ) ;
#48764 = VERTEX_POINT ( 'NONE', #63520 ) ;
#48765 = CARTESIAN_POINT ( 'NONE',  ( -1.317228840347983265, 55.68607278123570126, -43.83834608838444069 ) ) ;
#48766 = CIRCLE ( 'NONE', #17433, 4.000000000000000000 ) ;
#48767 = CARTESIAN_POINT ( 'NONE',  ( -5.000000000000000000, 70.11723469343073134, 28.93519894129288517 ) ) ;
#48768 = CARTESIAN_POINT ( 'NONE',  ( -8.311093377946836114, 152.9687499965859843, -8.311093377946837890 ) ) ;
#48769 = CARTESIAN_POINT ( 'NONE',  ( -2.445694354108783664, 196.3125000013656063, 195.5543056458912190 ) ) ;
#48770 = CARTESIAN_POINT ( 'NONE',  ( -1.432654583217608080, 206.8750000013656347, 201.4587341250000350 ) ) ;
#48771 = CARTESIAN_POINT ( 'NONE',  ( -10.18810118749999916, 4.220049686691934809, 70.93750000204838102 ) ) ;
#48772 = CARTESIAN_POINT ( 'NONE',  ( -11.35316468749999785, 58.38541666325268409, -3.042071309553167513 ) ) ;
#48773 = ORIENTED_EDGE ( 'NONE', *, *, #54802, .F. ) ;
#48774 = DIRECTION ( 'NONE',  ( 0.000000000000000000, 0.000000000000000000, -1.000000000000000000 ) ) ;
#48775 = CARTESIAN_POINT ( 'NONE',  ( -3.211159895383562723, 9.062499998634407916, 3.211159895383561391 ) ) ;
#48776 = CARTESIAN_POINT ( 'NONE',  ( -8.008118988124989457, -3.317071493978883900, 10.10686528394063188 ) ) ;
#48777 = ORIENTED_EDGE ( 'NONE', *, *, #23627, .F. ) ;
#48778 = CARTESIAN_POINT ( 'NONE',  ( 2.977408999572650927, 18.74999999795161898, -7.188101187500001821 ) ) ;
#48779 = CARTESIAN_POINT ( 'NONE',  ( -3.673940397442060854E-16, 289.8125000034140157, -6.000000000000001776 ) ) ;
#48780 = DIRECTION ( 'NONE',  ( 1.000000000000000000, 0.000000000000000000, 0.000000000000000000 ) ) ;
#48781 = CARTESIAN_POINT ( 'NONE',  ( -5.082755093536325042, 14.90624999795161187, -5.082755093536325930 ) ) ;
#48782 = CARTESIAN_POINT ( 'NONE',  ( 1.320432766682872962E-15, -7.188101187499992051, 1.861552781871753881 ) ) ;
#48783 = CARTESIAN_POINT ( 'NONE',  ( -10.18810118749999916, 4.220049686691934809, 115.9375000020483668 ) ) ;
#48784 = CYLINDRICAL_SURFACE ( 'NONE', #53474, 8.000000000000000000 ) ;
#48785 = CARTESIAN_POINT ( 'NONE',  ( -4.000000000000001776, 8.249999997268814056, -4.898587196589415787E-16 ) ) ;
#48786 = EDGE_LOOP ( 'NONE', ( #22524, #66128, #57883, #9065 ) ) ;
#48787 = B_SPLINE_CURVE_WITH_KNOTS ( 'NONE', 3,
 ( #11483, #52221, #74107, #17878, #22406, #16370, #34518, #28456, #6199, #45804, #51841, #57138, #57523, #45428, #56392, #62406, #39407, #40895, #51094, #46176, #63901, #68441, #5088, #553, #29208, #23163, #33767, #46548, #74475, #56768, #69193, #22782, #33392, #73733 ),
 .UNSPECIFIED., .F., .F.,
 ( 4, 2, 2, 2, 2, 2, 2, 2, 2, 2, 2, 2, 2, 2, 2, 2, 4 ),
 ( 0.009106795846385649928, 0.009781323166192857840, 0.01045585048600006749, 0.01113037780580727540, 0.01180490512561448505, 0.01247943244542169296, 0.01315395976522890087, 0.01382848708503611398, 0.01450301440484332710, 0.01517754172465054022, 0.01585206904445775333, 0.01652659636426496992, 0.01720112368407217956, 0.01787565100387939615, 0.01855017832368660927, 0.01922470564349382238, 0.01989923296330103550 ),
 .UNSPECIFIED. ) ;
#48788 = CARTESIAN_POINT ( 'NONE',  ( -2.445694354108782775, 206.5625000013656063, 200.4456943541088663 ) ) ;
#48789 = CARTESIAN_POINT ( 'NONE',  ( -28.00000000000007816, 198.1250000027312126, 166.0000000000003695 ) ) ;
#48790 = EDGE_CURVE ( 'NONE', #12947, #62352, #73725, .T. ) ;
#48791 = CARTESIAN_POINT ( 'NONE',  ( -4.541265875000002339, 4.749999998634407028, -1.881053915767121998 ) ) ;
#48792 = CARTESIAN_POINT ( 'NONE',  ( 7.188101187500000044, 111.4062500020483810, -8.802885111219163269E-16 ) ) ;
#48793 = DIRECTION ( 'NONE',  ( -0.000000000000000000, -0.000000000000000000, -1.000000000000000000 ) ) ;
#48794 = CARTESIAN_POINT ( 'NONE',  ( -2.977408999572647819, 7.188101187499991163, 23.70530278187175810 ) ) ;
#48795 = ORIENTED_EDGE ( 'NONE', *, *, #33981, .T. ) ;
#48796 = CARTESIAN_POINT ( 'NONE',  ( 7.188101187500000044, 22.96874999795161543, 0.000000000000000000 ) ) ;
#48797 = ORIENTED_EDGE ( 'NONE', *, *, #10002, .T. ) ;
#48798 = CARTESIAN_POINT ( 'NONE',  ( 7.204075437095968759, -7.204075437095966983, 116.2187500020483810 ) ) ;
#48799 = CARTESIAN_POINT ( 'NONE',  ( -4.906935342930776045, 6.406660676655467235, 0.000000000000000000 ) ) ;
#48800 = CARTESIAN_POINT ( 'NONE',  ( -2.445694354108782775, 207.5625000013656063, 200.4456943541088663 ) ) ;
#48801 = CARTESIAN_POINT ( 'NONE',  ( 25.55430564589115505, 202.0625000013656063, 167.5543056458911053 ) ) ;
#48802 = CARTESIAN_POINT ( 'NONE',  ( -2.679491924311235618, 63.54166666666667851, 10.00000000000000000 ) ) ;
#48803 = CARTESIAN_POINT ( 'NONE',  ( -7.188101187499999156, 91.62500000204838102, 2.977408999572654924 ) ) ;
#48804 = CARTESIAN_POINT ( 'NONE',  ( -6.000000000000000888, 295.0625000000000000, 2.485281374238575758 ) ) ;
#48805 = AXIS2_PLACEMENT_3D ( 'NONE', #63154, #16743, #11481 ) ;
#48807 = FACE_OUTER_BOUND ( 'NONE', #72382, .T. ) ;
#48806 = CARTESIAN_POINT ( 'NONE',  ( 0.4368895104719984768, -51.14729664189336944, -48.52014062455057086 ) ) ;
#48808 = EDGE_CURVE ( 'NONE', #70885, #13802, #20307, .T. ) ;
#48809 =( BOUNDED_CURVE ( )  B_SPLINE_CURVE ( 2, ( #33245, #44920, #5304, #61524, #28305, #44548, #67558, #33617, #67928 ),
 .UNSPECIFIED., .F., .F. ) 
 B_SPLINE_CURVE_WITH_KNOTS ( ( 3, 2, 2, 2, 3 ),
 ( 0.2187500000000001388, 0.2239583333333333703, 0.2291666666666666019, 0.2343749999999998335, 0.2395833333333330928 ),
 .UNSPECIFIED. ) 
 CURVE ( )  GEOMETRIC_REPRESENTATION_ITEM ( )  RATIONAL_B_SPLINE_CURVE ( ( 0.9999999999999980016, 0.9238795325112887369, 1.000000000000000000, 0.9238795325112867385, 1.000000000000000000, 0.9238795325112867385, 1.000000000000000000, 0.9238795325112904022, 0.9999999999999963363 ) ) 
 REPRESENTATION_ITEM ( '' )  );
#48810 = ORIENTED_EDGE ( 'NONE', *, *, #32915, .T. ) ;
#48811 = CARTESIAN_POINT ( 'NONE',  ( -5.676582343749992710, 229.7395833367473301, 9.832129032723422313 ) ) ;
#48812 = CARTESIAN_POINT ( 'NONE',  ( 8.000000000000000000, 12.09375000000000178, -3.313708498984761164 ) ) ;
#48813 = CARTESIAN_POINT ( 'NONE',  ( 2.828427124746152987, 201.2500000027312126, 139.1715728752538723 ) ) ;
#48814 = CARTESIAN_POINT ( 'NONE',  ( 3.999999999999959144, 197.1875000027312410, 140.3431457505076594 ) ) ;
#48815 = CARTESIAN_POINT ( 'NONE',  ( 24.07989181644096277, 194.9176386608072562, 169.8711866176451508 ) ) ;
#48816 = LINE ( 'NONE', #20141, #24613 ) ;
#48817 = CARTESIAN_POINT ( 'NONE',  ( -4.999999999999998224, 181.6666666666666572, -8.660254037844389075 ) ) ;
#48818 = ADVANCED_FACE ( 'NONE', ( #29569 ), #19254, .T. ) ;
#48819 = CARTESIAN_POINT ( 'NONE',  ( 7.320508075688771044, 241.2500000068279462, -7.320508075688771932 ) ) ;
#48820 = CARTESIAN_POINT ( 'NONE',  ( -2.977408999572647819, 7.188101187499992051, 24.08030278187175099 ) ) ;
#48821 = CARTESIAN_POINT ( 'NONE',  ( 3.042071309553167069, 152.1354166632526983, -11.35316468749999785 ) ) ;
#48822 = CARTESIAN_POINT ( 'NONE',  ( 7.999999999999991118, 9.797174393178815797E-16, 22.76780278392014623 ) ) ;
#48823 = CARTESIAN_POINT ( 'NONE',  ( -6.123233995736766282E-16, 261.8750000068280315, -10.00000000000000000 ) ) ;
#48826 = CARTESIAN_POINT ( 'NONE',  ( -3.673940397442060854E-16, 293.7500000000000000, -6.000000000000001776 ) ) ;
#48825 = CARTESIAN_POINT ( 'NONE',  ( 1.656854249492337949, 199.4375000027312410, 202.0000000000000853 ) ) ;
#48824 = CARTESIAN_POINT ( 'NONE',  ( 25.17157287525378351, 200.8750000000000284, 172.8284271247460424 ) ) ;
#48827 = ORIENTED_EDGE ( 'NONE', *, *, #17263, .T. ) ;
#48828 = CARTESIAN_POINT ( 'NONE',  ( -5.676582343749998039, 7.760416663252684089, -9.832129032723420536 ) ) ;
#48829 = DIRECTION ( 'NONE',  ( 0.000000000000000000, 0.000000000000000000, -1.000000000000000000 ) ) ;
#48830 = CARTESIAN_POINT ( 'NONE',  ( -1.656854249492309972, 207.8124999999999716, 194.0000000000000284 ) ) ;
#48831 = CARTESIAN_POINT ( 'NONE',  ( -2.828427124746152987, 196.2500000027312126, 200.8284271247462129 ) ) ;
#48832 = CARTESIAN_POINT ( 'NONE',  ( 3.458734124999959914, 208.3750000013656063, 143.4326545832176976 ) ) ;
#48833 =( BOUNDED_CURVE ( )  B_SPLINE_CURVE ( 2, ( #10253, #33280, #56279, #4597, #27592, #72, #6461, #23051, #28709 ),
 .UNSPECIFIED., .F., .F. ) 
 B_SPLINE_CURVE_WITH_KNOTS ( ( 3, 2, 2, 2, 3 ),
 ( 0.08333333333333352300, 0.09166666666666679897, 0.1000000000000000888, 0.1083333333333333787, 0.1166666666666666546 ),
 .UNSPECIFIED. ) 
 CURVE ( )  GEOMETRIC_REPRESENTATION_ITEM ( )  RATIONAL_B_SPLINE_CURVE ( ( 0.9999999999999982236, 0.9238795325112885148, 1.000000000000000000, 0.9238795325112867385, 1.000000000000000000, 0.9238795325112867385, 1.000000000000000000, 0.9238795325112868495, 0.9999999999999998890 ) ) 
 REPRESENTATION_ITEM ( '' )  );
#48834 = CARTESIAN_POINT ( 'NONE',  ( 2.679491924311228956, 42.91666665983869677, -10.00000000000000000 ) ) ;
#48835 = CARTESIAN_POINT ( 'NONE',  ( 1.320432766682874540E-15, 106.5312500020483810, 7.188101187500000044 ) ) ;
#48836 = CARTESIAN_POINT ( 'NONE',  ( 3.211159895383561835, 5.562499998634407028, -3.211159895383561835 ) ) ;
#48837 = CARTESIAN_POINT ( 'NONE',  ( 1.882291019709091628, 65.87523470713929896, -26.34730193751198968 ) ) ;
#48838 = CARTESIAN_POINT ( 'NONE',  ( 5.656854249492376141, -5.656854249492374365, 8.892802779823364645 ) ) ;
#48840 = CARTESIAN_POINT ( 'NONE',  ( -11.00000000000000000, 0.000000000000000000, 104.6875000040967763 ) ) ;
#48839 = CARTESIAN_POINT ( 'NONE',  ( 11.00000000000000000, 1.347111479062088405E-15, 118.0000000000000000 ) ) ;
#48841 = EDGE_LOOP ( 'NONE', ( #74151, #24702, #13008, #54300 ) ) ;
#48842 = CARTESIAN_POINT ( 'NONE',  ( -5.000000000000000000, -67.91996363552676996, 22.23680535815869774 ) ) ;
#48843 = CARTESIAN_POINT ( 'NONE',  ( 11.35316468749999963, 236.7187500034139873, -1.390361679473963556E-15 ) ) ;
#48844 = CARTESIAN_POINT ( 'NONE',  ( 5.676582343749993598, 134.9479166632526983, 9.832129032723422313 ) ) ;
#48845 = ORIENTED_EDGE ( 'NONE', *, *, #39491, .F. ) ;
#48846 = CARTESIAN_POINT ( 'NONE',  ( -2.849036369511732440E-14, 200.2500000000000000, 138.0000000000000568 ) ) ;
#48847 = CARTESIAN_POINT ( 'NONE',  ( 7.204075437095968759, -7.204075437095966983, 96.71875000204838102 ) ) ;
#48848 = DIRECTION ( 'NONE',  ( -1.000000000000000000, -0.000000000000000000, -0.000000000000000000 ) ) ;
#48849 = CARTESIAN_POINT ( 'NONE',  ( 3.458734125000015425, 196.2500000013656631, 196.5673454167823877 ) ) ;
#48850 = DIRECTION ( 'NONE',  ( 1.000000000000000000, 0.000000000000000000, 0.000000000000000000 ) ) ;
#48852 = CARTESIAN_POINT ( 'NONE',  ( -9.832129032723418760, 132.8645833299193555, -5.676582343750004256 ) ) ;
#48851 = CARTESIAN_POINT ( 'NONE',  ( -4.898587196589412829E-16, 94.62499999999998579, -8.000000000000000000 ) ) ;
#48853 = CARTESIAN_POINT ( 'NONE',  ( -25.17157287525377996, 207.6250000000000284, 172.8284271247465256 ) ) ;
#48854 = CARTESIAN_POINT ( 'NONE',  ( -8.000000000000000000, 91.90625000000000000, -3.313708498984761164 ) ) ;
#48855 = ORIENTED_EDGE ( 'NONE', *, *, #25648, .F. ) ;
#48856 = CARTESIAN_POINT ( 'NONE',  ( -8.000000000000000000, 110.0000000000000000, 0.000000000000000000 ) ) ;
#48857 = SHAPE_REPRESENTATION ( 'clamping lever', ( #57354 ), #18781 ) ;
#48858 = CARTESIAN_POINT ( 'NONE',  ( 12.00000000000000178, 28.00000000000000000, 0.000000000000000000 ) ) ;
#48859 = CARTESIAN_POINT ( 'NONE',  ( 9.832129032723420536, 101.5104166632526841, -5.676582343749999815 ) ) ;
#48860 = CARTESIAN_POINT ( 'NONE',  ( -1.432654583217607858, 207.6250000013656063, 201.4587341250000065 ) ) ;
#48861 = CARTESIAN_POINT ( 'NONE',  ( -2.977408999572650039, 20.81249999795161543, -7.188101187500000933 ) ) ;
#48862 = CARTESIAN_POINT ( 'NONE',  ( 4.220049686691941027, -10.18810118749999738, 89.50000000204836681 ) ) ;
#48863 = CARTESIAN_POINT ( 'NONE',  ( -11.35316468750000141, 28.59374999658601624, -1.390361679473963753E-15 ) ) ;
#48864 = ORIENTED_EDGE ( 'NONE', *, *, #42627, .F. ) ;
#48865 = CARTESIAN_POINT ( 'NONE',  ( -1.736494649863607131, 67.70200331863343024, -20.12302832235386418 ) ) ;
#48866 = CARTESIAN_POINT ( 'NONE',  ( -5.662595241051933570, -5.662595241051936235, 25.20061528394063544 ) ) ;
#48867 = CARTESIAN_POINT ( 'NONE',  ( 11.00000000000010836, -4.556349186103939353, 102.3437500040967905 ) ) ;
#48868 = EDGE_CURVE ( 'NONE', #3122, #16691, #48662, .T. ) ;
#48869 = DIRECTION ( 'NONE',  ( -1.000000000000000000, -0.000000000000000000, -0.000000000000000000 ) ) ;
#48870 = CARTESIAN_POINT ( 'NONE',  ( 7.188101187499999156, 3.374999997951610098, 2.977408999572654924 ) ) ;
#48871 = CARTESIAN_POINT ( 'NONE',  ( -6.676582343750001591, 290.4531250017069510, 0.000000000000000000 ) ) ;
#48872 = VECTOR ( 'NONE', #39424, 999.9999999999998863 ) ;
#48873 = CARTESIAN_POINT ( 'NONE',  ( -2.828427124746208943, 199.6250000000000284, 144.8284271247462129 ) ) ;
#48874 = CARTESIAN_POINT ( 'NONE',  ( -2.085542519210945728E-15, 219.8437499965860411, 11.35316468750000141 ) ) ;
#48875 = CARTESIAN_POINT ( 'NONE',  ( -11.35316468750000141, 143.5937499965860411, -1.390361679473963753E-15 ) ) ;
#48876 = CARTESIAN_POINT ( 'NONE',  ( -4.220049686691935698, 10.18810118749999916, 85.37500000204839523 ) ) ;
#48877 = AXIS2_PLACEMENT_3D ( 'NONE', #54388, #43416, #43802 ) ;
#48878 = CARTESIAN_POINT ( 'NONE',  ( -26.56734541678232375, 201.0000000013655779, 173.4587341250003760 ) ) ;
#48879 = CARTESIAN_POINT ( 'NONE',  ( -2.751064625579944321E-14, 198.7500000000000000, 146.0000000000000284 ) ) ;
#48880 = CARTESIAN_POINT ( 'NONE',  ( 2.780723358947928197E-16, 11.68749999863440614, -4.541265875000002339 ) ) ;
#48881 = ORIENTED_EDGE ( 'NONE', *, *, #43131, .T. ) ;
#48882 = CARTESIAN_POINT ( 'NONE',  ( 1.656854249492403008, 201.8125000027312126, 194.0000000000000853 ) ) ;
#48883 = CARTESIAN_POINT ( 'NONE',  ( -3.458734125000015425, 199.2500000013656063, 143.4326545832176976 ) ) ;
#48884 = CARTESIAN_POINT ( 'NONE',  ( -4.000000000000015987, 204.6250000027312126, 142.0000000000000568 ) ) ;
#48885 = CARTESIAN_POINT ( 'NONE',  ( 5.000000000000000000, 10.26105934116143459, -64.40045319026695836 ) ) ;
#48886 = ORIENTED_EDGE ( 'NONE', *, *, #4001, .F. ) ;
#48887 = CARTESIAN_POINT ( 'NONE',  ( -2.977408999572654480, 5.999999997951610986, 7.188101187499999156 ) ) ;
#48888 = CARTESIAN_POINT ( 'NONE',  ( -14.05609634983435541, -21.36520000172663813, 197.6313249932136102 ) ) ;
#48889 = FACE_OUTER_BOUND ( 'NONE', #69490, .T. ) ;
#48890 = CARTESIAN_POINT ( 'NONE',  ( 3.042071309553159519, 189.7395833299193271, 11.35316468750000141 ) ) ;
#48891 = EDGE_CURVE ( 'NONE', #8905, #16375, #53617, .T. ) ;
#48892 = CARTESIAN_POINT ( 'NONE',  ( -2.977408999572650927, 113.7500000020483668, -7.188101187500001821 ) ) ;
#48893 = CARTESIAN_POINT ( 'NONE',  ( 1.226468279477575784E-15, 293.7031250017069510, 6.676582343750001591 ) ) ;
#48895 = CARTESIAN_POINT ( 'NONE',  ( -1.656854249492358155, 15.43749999726881406, 4.000000000000024869 ) ) ;
#48894 = CARTESIAN_POINT ( 'NONE',  ( 5.000000000000001776, 132.7083333265053682, -8.660254037844389075 ) ) ;
#48896 = ORIENTED_EDGE ( 'NONE', *, *, #5924, .F. ) ;
#48897 = CARTESIAN_POINT ( 'NONE',  ( -11.35316468749999963, 229.2187500034139873, 0.000000000000000000 ) ) ;
#48898 = CARTESIAN_POINT ( 'NONE',  ( 2.977408999572650927, -7.188101187499990274, 27.83030278187176165 ) ) ;
#48899 = LINE ( 'NONE', #3269, #72698 ) ;
#48900 = CARTESIAN_POINT ( 'NONE',  ( 0.000000000000000000, 300.0000000000000000, 0.000000000000000000 ) ) ;
#48901 = CARTESIAN_POINT ( 'NONE',  ( 1.432654583217664701, 200.0000000013656347, 201.4587341250000065 ) ) ;
#48902 = ORIENTED_EDGE ( 'NONE', *, *, #39463, .T. ) ;
#48903 = DIRECTION ( 'NONE',  ( -0.000000000000000000, 1.000000000000000000, -0.000000000000000000 ) ) ;
#48904 = CARTESIAN_POINT ( 'NONE',  ( -5.656854249492378806, 95.18750000000000000, 5.656854249492381470 ) ) ;
#48905 = CARTESIAN_POINT ( 'NONE',  ( 3.042071309553159519, 110.0520833299193271, 11.35316468750000141 ) ) ;
#48906 = CARTESIAN_POINT ( 'NONE',  ( 0.000000000000000000, 0.000000000000000000, 0.000000000000000000 ) ) ;
#48907 = CARTESIAN_POINT ( 'NONE',  ( -11.00000000000000000, 0.000000000000000000, 78.99999999999998579 ) ) ;
#48910 = DIRECTION ( 'NONE',  ( -0.000000000000000000, -0.000000000000000000, 1.000000000000000000 ) ) ;
#48909 = CARTESIAN_POINT ( 'NONE',  ( 29.43265458321761230, 200.8750000013656063, 166.5412658749999650 ) ) ;
#48908 = CARTESIAN_POINT ( 'NONE',  ( 31.45873412499999233, 200.9375000013656063, 169.9999999999999432 ) ) ;
#48911 = ORIENTED_EDGE ( 'NONE', *, *, #34321, .F. ) ;
#48912 = CARTESIAN_POINT ( 'NONE',  ( 8.000000000000000000, 100.2499999999999858, -9.797174393178825657E-16 ) ) ;
#48913 = VECTOR ( 'NONE', #21987, 1000.000000000000000 ) ;
#48914 = EDGE_CURVE ( 'NONE', #35319, #6969, #20741, .T. ) ;
#48915 = CARTESIAN_POINT ( 'NONE',  ( 8.311093377946837890, 226.4062499965860411, -8.311093377946837890 ) ) ;
#48916 = CARTESIAN_POINT ( 'NONE',  ( 2.445694354108782775, 201.5625000013656063, 139.5543056458912190 ) ) ;
#48917 = CARTESIAN_POINT ( 'NONE',  ( 28.00000000000002132, 202.1875000013656063, 166.5412658749999082 ) ) ;
#48918 = CARTESIAN_POINT ( 'NONE',  ( -4.556349186104047710, -10.99999999999999822, 113.9687500040967905 ) ) ;
#48919 = CARTESIAN_POINT ( 'NONE',  ( -11.35316468750000141, 198.5937499965860127, -1.390361679473963753E-15 ) ) ;
#48920 = CARTESIAN_POINT ( 'NONE',  ( 2.977408999572654480, 92.00000000204838102, 7.188101187499999156 ) ) ;
#48921 = DIRECTION ( 'NONE',  ( -0.000000000000000000, 1.000000000000000000, -0.000000000000000000 ) ) ;
#48922 = CARTESIAN_POINT ( 'NONE',  ( -3.211159895383561391, 15.68749999863440436, -3.211159895383561835 ) ) ;
#48923 = CARTESIAN_POINT ( 'NONE',  ( 27.99999999999996447, 198.6875000013655779, 173.4587341249998929 ) ) ;
#48924 = CARTESIAN_POINT ( 'NONE',  ( -7.999999999999989342, -3.313708498984762496, 24.92405277982336997 ) ) ;
#48925 = DIRECTION ( 'NONE',  ( -0.000000000000000000, 1.000000000000000000, -0.000000000000000000 ) ) ;
#48926 = CARTESIAN_POINT ( 'NONE',  ( -3.042071309553164404, 77.23958332991935549, -11.35316468749999963 ) ) ;
#48927 = ORIENTED_EDGE ( 'NONE', *, *, #42187, .T. ) ;
#48928 =( BOUNDED_CURVE ( )  B_SPLINE_CURVE ( 2, ( #42287, #19277, #36644, #12143, #7235, #36275, #59291, #6500, #1585 ),
 .UNSPECIFIED., .F., .F. ) 
 B_SPLINE_CURVE_WITH_KNOTS ( ( 3, 2, 2, 2, 3 ),
 ( 0.4027777777777776791, 0.4097222222222220989, 0.4166666666666666297, 0.4236111111111110494, 0.4305555555555555247 ),
 .UNSPECIFIED. ) 
 CURVE ( )  GEOMETRIC_REPRESENTATION_ITEM ( )  RATIONAL_B_SPLINE_CURVE ( ( 1.000000000000001110, 0.9238795325112855172, 1.000000000000000000, 0.9238795325112867385, 1.000000000000000000, 0.9238795325112867385, 1.000000000000000000, 0.9238795325112872936, 0.9999999999999994449 ) ) 
 REPRESENTATION_ITEM ( '' )  );
#48929 = CARTESIAN_POINT ( 'NONE',  ( 2.679491924292086047, 138.9583333333316375, 10.00000000001106670 ) ) ;
#48930 = LINE ( 'NONE', #42895, #25482 ) ;
#48931 = CARTESIAN_POINT ( 'NONE',  ( 0.000000000000000000, 0.000000000000000000, -4.000000000000001776 ) ) ;
#48932 = DIRECTION ( 'NONE',  ( -0.000000000000000000, 1.000000000000000000, -0.000000000000000000 ) ) ;
#48933 = CARTESIAN_POINT ( 'NONE',  ( 6.951808397369818766E-16, 92.03124999658602690, -11.35316468750000141 ) ) ;
#48934 = EDGE_LOOP ( 'NONE', ( #56027, #7307, #33757, #781 ) ) ;
#48935 = CARTESIAN_POINT ( 'NONE',  ( 7.204075437095966983, 7.204075437095967871, 85.46875000204836681 ) ) ;
#48936 = CARTESIAN_POINT ( 'NONE',  ( -10.18810118749999916, 4.220049686691934809, 114.0625000020483668 ) ) ;
#48937 = CARTESIAN_POINT ( 'NONE',  ( 2.445694354108840063, 209.0625000013656063, 200.4456943541088663 ) ) ;
#48938 = CARTESIAN_POINT ( 'NONE',  ( 10.00000000000003375, 74.79166666666668561, 2.679491924311244500 ) ) ;
#48940 = CARTESIAN_POINT ( 'NONE',  ( -2.085542519210945728E-15, 74.53124999658602690, 11.35316468750000141 ) ) ;
#48939 = CARTESIAN_POINT ( 'NONE',  ( -5.000000000000000000, 68.60357193678683529, 20.85024232999420946 ) ) ;
#48941 = CARTESIAN_POINT ( 'NONE',  ( -3.313708498984757167, 7.999999999999991118, 17.23655278392014978 ) ) ;
#48942 = DIRECTION ( 'NONE',  ( -0.000000000000000000, -0.000000000000000000, 1.000000000000000000 ) ) ;
#48943 = VECTOR ( 'NONE', #40522, 1000.000000000000000 ) ;
#48944 = CARTESIAN_POINT ( 'NONE',  ( -5.000000000000005329, 170.2083333265053682, 8.660254037844387298 ) ) ;
#48945 = CARTESIAN_POINT ( 'NONE',  ( 3.999999999999960032, 200.1250000027312126, 142.0000000000000568 ) ) ;
#48946 = CARTESIAN_POINT ( 'NONE',  ( -24.54718095033810243, 194.8728775736659600, 171.7645726005719382 ) ) ;
#48947 = CARTESIAN_POINT ( 'NONE',  ( 9.832129032723416984, 60.67708332991934839, 5.676582343750006032 ) ) ;
#48948 = CARTESIAN_POINT ( 'NONE',  ( -6.676582343750003368, 295.3906250017068942, -2.765530957081996810 ) ) ;
#48949 = CARTESIAN_POINT ( 'NONE',  ( 7.204075437095968759, -7.204075437095966983, 107.5937500020483810 ) ) ;
#48950 = CARTESIAN_POINT ( 'NONE',  ( -11.35316468750000141, 213.2812499965860411, -1.390361679473963753E-15 ) ) ;
#48952 = ORIENTED_EDGE ( 'NONE', *, *, #3794, .F. ) ;
#48951 =( BOUNDED_CURVE ( )  B_SPLINE_CURVE ( 2, ( #5596, #29715, #17269, #51604, #57658, #74619, #6707, #63665, #5964 ),
 .UNSPECIFIED., .F., .F. ) 
 B_SPLINE_CURVE_WITH_KNOTS ( ( 3, 2, 2, 2, 3 ),
 ( 0.8124999999999983347, 0.8229166666666649643, 0.8333333333333317050, 0.8437499999999983347, 0.8541666666666649643 ),
 .UNSPECIFIED. ) 
 CURVE ( )  GEOMETRIC_REPRESENTATION_ITEM ( )  RATIONAL_B_SPLINE_CURVE ( ( 1.000000000000012212, 0.9238795325112745260, 1.000000000000000000, 0.9238795325112867385, 1.000000000000000000, 0.9238795325112867385, 1.000000000000000000, 0.9238795325112989509, 0.9999999999999877875 ) ) 
 REPRESENTATION_ITEM ( '' )  );
#48953 = LINE ( 'NONE', #42177, #70521 ) ;
#48954 = CARTESIAN_POINT ( 'NONE',  ( 0.8588954341814944993, -60.21087566322576379, -22.89167302533761728 ) ) ;
#48955 = CARTESIAN_POINT ( 'NONE',  ( 2.449293598294707893E-16, 16.99999999726881583, -4.000000000000001776 ) ) ;
#48957 = CARTESIAN_POINT ( 'NONE',  ( -3.042071309553163960, 192.2395833299193555, -11.35316468749999963 ) ) ;
#48956 = LINE ( 'NONE', #14249, #18228 ) ;
#48958 = CARTESIAN_POINT ( 'NONE',  ( 4.898587196589412829E-16, 3.187499995903220640, -8.000000000000000000 ) ) ;
#48959 = CARTESIAN_POINT ( 'NONE',  ( 7.320508075688776373, 240.0000000068279178, 7.320508075688767491 ) ) ;
#48960 = CARTESIAN_POINT ( 'NONE',  ( -8.660254037844387298, 188.9583333265053966, -5.000000000000004441 ) ) ;
#48961 = EDGE_LOOP ( 'NONE', ( #46894, #43093, #73149, #69934, #60851 ) ) ;
#48962 = CARTESIAN_POINT ( 'NONE',  ( -8.311093377946836114, 187.9687499965860127, -8.311093377946837890 ) ) ;
#48963 = CARTESIAN_POINT ( 'NONE',  ( -2.977408999572647819, 7.188101187499992051, 20.70530278187175810 ) ) ;
#48964 = CARTESIAN_POINT ( 'NONE',  ( -2.679491924316975471, 93.54166666666615981, 9.999999999996678213 ) ) ;
#48965 = EDGE_LOOP ( 'NONE', ( #50784, #27838, #17705, #73217 ) ) ;
#48966 = EDGE_CURVE ( 'NONE', #13169, #19469, #63831, .T. ) ;
#48967 = AXIS2_PLACEMENT_3D ( 'NONE', #18473, #64125, #58479 ) ;
#48968 = CARTESIAN_POINT ( 'NONE',  ( 5.656854249492381470, 100.2500000040967905, 5.656854249492379694 ) ) ;
#48969 = CARTESIAN_POINT ( 'NONE',  ( 3.426202465283471721, 194.4587341250000350, 141.5267364219330943 ) ) ;
#48970 = CARTESIAN_POINT ( 'NONE',  ( 1.656854249492381248, 14.18750000000000000, -4.000000000000001776 ) ) ;
#48971 = CARTESIAN_POINT ( 'NONE',  ( 4.541265875000002339, 16.37499999863440436, -1.881053915767121776 ) ) ;
#48972 = CARTESIAN_POINT ( 'NONE',  ( -5.656854249492373476, -5.656854249492376141, 16.20530278392014978 ) ) ;
#48973 = CARTESIAN_POINT ( 'NONE',  ( 28.89281933948924319, 194.7383503587969642, 166.3628827488052195 ) ) ;
#48975 = EDGE_CURVE ( 'NONE', #52445, #24629, #13583, .T. ) ;
#48974 = ORIENTED_EDGE ( 'NONE', *, *, #6431, .F. ) ;
#48976 = FACE_OUTER_BOUND ( 'NONE', #73186, .T. ) ;
#48977 = CARTESIAN_POINT ( 'NONE',  ( 5.082755093536326818, 90.21875000204838102, 5.082755093536325042 ) ) ;
#48979 = CARTESIAN_POINT ( 'NONE',  ( -8.311093377946836114, 263.2812500034139589, -8.311093377946836114 ) ) ;
#48978 = DIRECTION ( 'NONE',  ( -0.000000000000000000, -1.000000000000000000, -0.000000000000000000 ) ) ;
#48980 =( NAMED_UNIT ( * ) PLANE_ANGLE_UNIT ( ) SI_UNIT ( $, .RADIAN. ) );
#48981 = ORIENTED_EDGE ( 'NONE', *, *, #30709, .T. ) ;
#48982 = EDGE_CURVE ( 'NONE', #64048, #3350, #54474, .T. ) ;
#48983 = AXIS2_PLACEMENT_3D ( 'NONE', #71223, #3702, #31246 ) ;
#48984 = CARTESIAN_POINT ( 'NONE',  ( -4.193030820682226434, 50.40097124335192547, -40.95512985424939245 ) ) ;
#48985 = CARTESIAN_POINT ( 'NONE',  ( -5.082755093536317936, -5.082755093536320601, 21.17405278187175455 ) ) ;
#48986 = VECTOR ( 'NONE', #22846, 1000.000000000000000 ) ;
#48987 = ORIENTED_EDGE ( 'NONE', *, *, #44448, .F. ) ;
#48988 = ORIENTED_EDGE ( 'NONE', *, *, #51211, .T. ) ;
#48989 = CARTESIAN_POINT ( 'NONE',  ( 10.18810118749999916, 4.220049686691935698, 80.50000000204839523 ) ) ;
#48990 = CARTESIAN_POINT ( 'NONE',  ( -8.311093377946841443, 79.21874999658601268, 8.311093377946830785 ) ) ;
#48991 = DIRECTION ( 'NONE',  ( 0.000000000000000000, 0.000000000000000000, -1.000000000000000000 ) ) ;
#48992 = CARTESIAN_POINT ( 'NONE',  ( -4.556349186104045934, 11.00000000000000000, 93.71874999999998579 ) ) ;
#48995 = CARTESIAN_POINT ( 'NONE',  ( 1.226468279477575784E-15, 294.8593750017070079, 6.676582343750001591 ) ) ;
#48994 = CARTESIAN_POINT ( 'NONE',  ( 27.99999999999996092, 196.6250000027312126, 165.9999999999998863 ) ) ;
#48993 = CARTESIAN_POINT ( 'NONE',  ( 26.56734541678238415, 209.2500000013655779, 166.5412658749999650 ) ) ;
#48996 = CARTESIAN_POINT ( 'NONE',  ( 4.999999999999993783, 144.1666666666666572, 8.660254037844390851 ) ) ;
#48997 = DIRECTION ( 'NONE',  ( -0.000000000000000000, -0.000000000000000000, 1.000000000000000000 ) ) ;
#48998 = CARTESIAN_POINT ( 'NONE',  ( 6.123233995736767268E-16, 163.1249999931720254, -10.00000000000000178 ) ) ;
#48999 = EDGE_CURVE ( 'NONE', #21239, #18569, #52056, .T. ) ;
#49000 = CARTESIAN_POINT ( 'NONE',  ( -2.445694354108783219, 199.8125000013656063, 200.4456943541088663 ) ) ;
#49001 = DIRECTION ( 'NONE',  ( 0.000000000000000000, -1.000000000000000000, 0.000000000000000000 ) ) ;
#49002 = CARTESIAN_POINT ( 'NONE',  ( 7.999999999999998224, 2.718749995903220196, 3.313708498984766493 ) ) ;
#49003 = CARTESIAN_POINT ( 'NONE',  ( 31.45873412499997812, 200.6250000013655779, 171.4326545832175839 ) ) ;
#49004 = CARTESIAN_POINT ( 'NONE',  ( -7.188101187500000044, 13.59374999795161187, -8.802885111219163269E-16 ) ) ;
#49005 = CARTESIAN_POINT ( 'NONE',  ( -3.313708498984757167, 7.999999999999991118, 23.23655278392014623 ) ) ;
#49006 = CARTESIAN_POINT ( 'NONE',  ( 2.775557558920088989E-14, -48.00000000000001421, 151.0000000000000284 ) ) ;
#49007 = CARTESIAN_POINT ( 'NONE',  ( 2.977408999572650039, 109.0625000020483810, -7.188101187500000933 ) ) ;
#49009 = CARTESIAN_POINT ( 'NONE',  ( -4.000000000000001776, 16.50000000000000000, -4.898587196589415787E-16 ) ) ;
#49008 = CARTESIAN_POINT ( 'NONE',  ( -5.999999999999999112, 293.1250000034141294, 2.485281374238575314 ) ) ;
#49010 = CARTESIAN_POINT ( 'NONE',  ( 8.660254037844387298, 134.5833333333333428, 5.000000000000007105 ) ) ;
#49011 = CARTESIAN_POINT ( 'NONE',  ( 37.94562015984924130, 146.0000000000000000, 126.9999999999999716 ) ) ;
#49012 = CARTESIAN_POINT ( 'NONE',  ( 7.188101187499991163, 2.977408999572648707, 23.70530278187175810 ) ) ;
#49013 = CARTESIAN_POINT ( 'NONE',  ( 31.99999999999999289, 200.3750000027312126, 169.9999999999998863 ) ) ;
#49014 = CARTESIAN_POINT ( 'NONE',  ( -11.35316468750000141, 38.48958332991935549, 3.042071309553159963 ) ) ;
#49015 = CARTESIAN_POINT ( 'NONE',  ( -2.926785083138225622E-14, 16.44602605510714355, 68.55492853905353456 ) ) ;
#49016 = CARTESIAN_POINT ( 'NONE',  ( -4.999999999999998224, 8.541666659838698550, -8.660254037844389075 ) ) ;
#49017 = ORIENTED_EDGE ( 'NONE', *, *, #45695, .T. ) ;
#49018 = VECTOR ( 'NONE', #35303, 1000.000000000000000 ) ;
#49019 = CARTESIAN_POINT ( 'NONE',  ( -8.660254037844387298, 128.9583333265053966, -5.000000000000004441 ) ) ;
#49020 = CARTESIAN_POINT ( 'NONE',  ( 7.778174593052021635, 7.778174593052023411, 69.62500000409677625 ) ) ;
#49021 = CARTESIAN_POINT ( 'NONE',  ( -3.042071309553164404, 47.23958332991935549, -11.35316468749999963 ) ) ;
#49022 = CARTESIAN_POINT ( 'NONE',  ( -4.556349186104045934, 11.00000000000000000, 78.90625000409677625 ) ) ;
#49023 = CARTESIAN_POINT ( 'NONE',  ( -3.458734125000015869, 202.1875000013656063, 142.0000000000000568 ) ) ;
#49024 = CARTESIAN_POINT ( 'NONE',  ( -4.231687259407060253, -68.27410168872928864, -20.58597903916688665 ) ) ;
#49025 = CARTESIAN_POINT ( 'NONE',  ( -28.00000000000002842, 203.0000000000000000, 166.0000000000003695 ) ) ;
#49027 = CARTESIAN_POINT ( 'NONE',  ( -9.832129032723418760, 32.86458332991934839, -5.676582343750004256 ) ) ;
#49026 = CARTESIAN_POINT ( 'NONE',  ( 5.082755093536326818, 100.7187500020483810, 5.082755093536325042 ) ) ;
#49028 = CARTESIAN_POINT ( 'NONE',  ( 5.656854249492374365, 5.656854249492375253, 7.767802779823362869 ) ) ;
#49029 = CARTESIAN_POINT ( 'NONE',  ( 1.017526493066789772, 0.4019176081028156267, -7.852628965127530059 ) ) ;
#49030 = CARTESIAN_POINT ( 'NONE',  ( 9.832129032723420536, 156.1979166632526983, -5.676582343749999815 ) ) ;
#49031 = CARTESIAN_POINT ( 'NONE',  ( 7.320508075688774596, 122.4999999931720254, -7.320508075688774596 ) ) ;
#49032 = EDGE_CURVE ( 'NONE', #26852, #46122, #12266, .T. ) ;
#49033 = CARTESIAN_POINT ( 'NONE',  ( -7.188101187500001821, 107.9375000020483810, -2.977408999572650483 ) ) ;
#49034 = ORIENTED_EDGE ( 'NONE', *, *, #28863, .F. ) ;
#49035 = DIRECTION ( 'NONE',  ( -0.000000000000000000, 1.000000000000000000, -0.000000000000000000 ) ) ;
#49036 = CARTESIAN_POINT ( 'NONE',  ( 5.676582343749993598, 15.26041666325268409, 9.832129032723422313 ) ) ;
#49037 = LINE ( 'NONE', #66395, #1497 ) ;
#49038 = ORIENTED_EDGE ( 'NONE', *, *, #61439, .F. ) ;
#49039 = CARTESIAN_POINT ( 'NONE',  ( -30.82842712474615965, 204.3750000000000284, 172.8284271247465824 ) ) ;
#49040 = CARTESIAN_POINT ( 'NONE',  ( 10.18810118749999916, 1.247682550866122264E-15, 74.40625000204836681 ) ) ;
#49041 = CARTESIAN_POINT ( 'NONE',  ( 0.000000000000000000, 300.0000000000000000, 10.00000000000000178 ) ) ;
#49043 = CARTESIAN_POINT ( 'NONE',  ( -9.832129032723420536, 158.6979166632526983, 5.676582343749997150 ) ) ;
#49042 = CARTESIAN_POINT ( 'NONE',  ( 4.000000000000000888, 21.93750000000000355, 1.656854249492384135 ) ) ;
#49044 = CARTESIAN_POINT ( 'NONE',  ( 4.401442555609581635E-16, 1.218749997951610098, -7.188101187500000044 ) ) ;
#49045 = CARTESIAN_POINT ( 'NONE',  ( -4.898587196589407898E-16, 7.999999999999991118, 14.01155278432982421 ) ) ;
#49046 = CARTESIAN_POINT ( 'NONE',  ( -11.00000000000000000, 0.000000000000000000, 108.9999999999999858 ) ) ;
#49047 = CARTESIAN_POINT ( 'NONE',  ( 3.042071309553163960, 232.4479166700806161, -11.35316468749999785 ) ) ;
#49048 = CARTESIAN_POINT ( 'NONE',  ( -10.18810118749999738, -4.220049686691941915, 86.12500000204836681 ) ) ;
#49049 = ORIENTED_EDGE ( 'NONE', *, *, #31353, .T. ) ;
#49050 =( BOUNDED_CURVE ( )  B_SPLINE_CURVE ( 2, ( #8632, #55040, #31645, #72375, #61434, #10125, #9761, #55788, #27097 ),
 .UNSPECIFIED., .F., .F. ) 
 B_SPLINE_CURVE_WITH_KNOTS ( ( 3, 2, 2, 2, 3 ),
 ( 0.5789473684210527660, 0.5855263157894737835, 0.5921052631578946901, 0.5986842105263158187, 0.6052631578947368363 ),
 .UNSPECIFIED. ) 
 CURVE ( )  GEOMETRIC_REPRESENTATION_ITEM ( )  RATIONAL_B_SPLINE_CURVE ( ( 0.9999999999999986677, 0.9238795325112880708, 1.000000000000000000, 0.9238795325112867385, 1.000000000000000000, 0.9238795325112867385, 1.000000000000000000, 0.9238795325112867385, 1.000000000000000000 ) ) 
 REPRESENTATION_ITEM ( '' )  );
#49051 = LINE ( 'NONE', #3045, #2770 ) ;
#49052 = CARTESIAN_POINT ( 'NONE',  ( -2.485281374238895502, 291.8750000034140157, -5.999999999999677591 ) ) ;
#49053 = CARTESIAN_POINT ( 'NONE',  ( 5.676582343749993598, 105.2604166632526841, 9.832129032723422313 ) ) ;
#49054 = CARTESIAN_POINT ( 'NONE',  ( -10.18810118749999916, 4.220049686691934809, 94.56250000204838102 ) ) ;
#49055 = CARTESIAN_POINT ( 'NONE',  ( -3.211159895383562723, 20.06249999863440436, 3.211159895383561391 ) ) ;
#49056 = ORIENTED_EDGE ( 'NONE', *, *, #52249, .T. ) ;
#49057 = VERTEX_POINT ( 'NONE', #55096 ) ;
#49058 = CARTESIAN_POINT ( 'NONE',  ( 1.881053915767121776, 4.624999998634407028, -4.541265875000002339 ) ) ;
#49059 = CARTESIAN_POINT ( 'NONE',  ( -5.082755093536326818, 10.40624999795161187, 5.082755093536325042 ) ) ;
#49060 = CARTESIAN_POINT ( 'NONE',  ( 3.313708498984765161, 118.1562500040967763, 7.999999999999998224 ) ) ;
#49061 = CARTESIAN_POINT ( 'NONE',  ( -7.204075437095967871, 7.204075437095967871, 97.84375000204836681 ) ) ;
#49062 = CARTESIAN_POINT ( 'NONE',  ( -25.55430564589119413, 201.5625000013656063, 167.5543056458915316 ) ) ;
#49063 =( NAMED_UNIT ( * ) PLANE_ANGLE_UNIT ( ) SI_UNIT ( $, .RADIAN. ) );
#49064 = CARTESIAN_POINT ( 'NONE',  ( 4.000000000000001776, 3.000000000000000000, 0.000000000000000000 ) ) ;
#49065 = CARTESIAN_POINT ( 'NONE',  ( -4.000000000000001776, 20.18749999726881228, -1.656854249492381470 ) ) ;
#49066 = CARTESIAN_POINT ( 'NONE',  ( 1.881053915767122664, 3.124999998634406584, 4.541265875000001451 ) ) ;
#49067 = AXIS2_PLACEMENT_3D ( 'NONE', #42691, #26838, #9504 ) ;
#49068 = CARTESIAN_POINT ( 'NONE',  ( -2.445694354108839619, 207.8125000013656063, 139.5543056458912190 ) ) ;
#49069 = CARTESIAN_POINT ( 'NONE',  ( 2.445694354108839619, 195.8125000013656063, 200.4456943541088663 ) ) ;
#49071 = CARTESIAN_POINT ( 'NONE',  ( -7.778174593052020747, -7.778174593052023411, 95.87500000409676204 ) ) ;
#49070 = CARTESIAN_POINT ( 'NONE',  ( -24.54126587499998990, 195.1875000013655779, 170.0000000000002842 ) ) ;
#49072 =( NAMED_UNIT ( * ) SI_UNIT ( $, .STERADIAN. ) SOLID_ANGLE_UNIT ( ) );
#49073 = ADVANCED_FACE ( 'NONE', ( #3402 ), #26386, .F. ) ;
#49074 = CARTESIAN_POINT ( 'NONE',  ( -3.211159895383562723, 17.93749999863440792, 3.211159895383561391 ) ) ;
#49075 = CARTESIAN_POINT ( 'NONE',  ( 2.696298182373501717, -46.32987163626484062, 151.1921358781021922 ) ) ;
#49076 = CARTESIAN_POINT ( 'NONE',  ( -5.082755093536319713, 5.082755093536319713, 7.299052781871751883 ) ) ;
#49077 = VERTEX_POINT ( 'NONE', #61487 ) ;
#49078 = ORIENTED_EDGE ( 'NONE', *, *, #13130, .F. ) ;
#49079 = CARTESIAN_POINT ( 'NONE',  ( 10.18810118749999916, 4.220049686691935698, 100.0000000020483952 ) ) ;
#49080 = CARTESIAN_POINT ( 'NONE',  ( 12.00000000000000000, 0.000000000000000000, -28.00000000000000000 ) ) ;
#49081 = CARTESIAN_POINT ( 'NONE',  ( -31.45873412499999944, 202.9375000013656063, 170.0000000000003979 ) ) ;
#49082 = CARTESIAN_POINT ( 'NONE',  ( -31.99999999999997868, 199.3125000000000853, 171.6568542494928238 ) ) ;
#49083 = CARTESIAN_POINT ( 'NONE',  ( 3.458734125000015869, 209.1875000013656063, 198.0000000000000284 ) ) ;
#49084 = DIRECTION ( 'NONE',  ( 0.000000000000000000, 0.000000000000000000, 1.000000000000000000 ) ) ;
#49085 = CARTESIAN_POINT ( 'NONE',  ( -7.320508075688778149, 108.1250000000000284, 7.320508075688769267 ) ) ;
#49086 = CARTESIAN_POINT ( 'NONE',  ( 3.313708498984760720, 109.5312500000000142, -8.000000000000000000 ) ) ;
#49087 = CARTESIAN_POINT ( 'NONE',  ( -4.088227598258586603E-16, 292.3593750017070079, -6.676582343750001591 ) ) ;
#49088 = CARTESIAN_POINT ( 'NONE',  ( -2.977408999572648707, -7.188101187499990274, 12.64280278187175277 ) ) ;
#49089 = VERTEX_POINT ( 'NONE', #45251 ) ;
#49090 = MECHANICAL_DESIGN_GEOMETRIC_PRESENTATION_REPRESENTATION (  '', ( #63549 ), #17776 ) ;
#49091 = CARTESIAN_POINT ( 'NONE',  ( -1.469576158976823947E-15, 19.12500000000000355, 8.000000000000000000 ) ) ;
#49092 = EDGE_CURVE ( 'NONE', #59754, #25774, #50165, .T. ) ;
#49093 = CARTESIAN_POINT ( 'NONE',  ( 5.656854249492378806, 20.62499999590322375, 5.656854249492381470 ) ) ;
#49094 = CARTESIAN_POINT ( 'NONE',  ( -3.458734125000015425, 204.9375000013656063, 142.0000000000000568 ) ) ;
#49095 = CARTESIAN_POINT ( 'NONE',  ( -1.656854249492381248, 5.312500000000000888, -4.000000000000001776 ) ) ;
#49096 = CARTESIAN_POINT ( 'NONE',  ( 1.469576158976823947E-15, 120.8750000000000000, 8.000000000000000000 ) ) ;
#49097 = CARTESIAN_POINT ( 'NONE',  ( -3.042071309553166181, 253.1770833367473017, -11.35316468749999608 ) ) ;
#49098 = CARTESIAN_POINT ( 'NONE',  ( -2.828427124746153876, 207.0000000027312126, 195.1715728752538439 ) ) ;
#49099 = CARTESIAN_POINT ( 'NONE',  ( -7.778174593052023411, 7.778174593052023411, 114.8125000000000000 ) ) ;
#49100 = CARTESIAN_POINT ( 'NONE',  ( -8.311093377946836114, 7.656249996586014461, -8.311093377946837890 ) ) ;
#49101 = EDGE_CURVE ( 'NONE', #17509, #41950, #55494, .T. ) ;
#49102 = CARTESIAN_POINT ( 'NONE',  ( 2.977408999572646486, 7.188101187499992051, 7.392802781871750994 ) ) ;
#49103 = CARTESIAN_POINT ( 'NONE',  ( -2.085542519210945728E-15, 189.8437499965860127, 11.35316468750000141 ) ) ;
#49104 = CARTESIAN_POINT ( 'NONE',  ( 4.556349186104052151, -10.99999999999999822, 101.9687500000000000 ) ) ;
#49105 = CARTESIAN_POINT ( 'NONE',  ( -8.342170076843785083E-16, 7.062499998634407028, 4.541265875000002339 ) ) ;
#49106 = DIRECTION ( 'NONE',  ( 0.000000000000000000, 0.000000000000000000, -1.000000000000000000 ) ) ;
#49108 = CARTESIAN_POINT ( 'NONE',  ( -4.000000000000015987, 206.5000000000000284, 142.0000000000000568 ) ) ;
#49107 = DIRECTION ( 'NONE',  ( -1.000000000000000000, 0.000000000000000000, 0.000000000000000000 ) ) ;
#49109 = ORIENTED_EDGE ( 'NONE', *, *, #18252, .F. ) ;
#49110 = CARTESIAN_POINT ( 'NONE',  ( -2.445694354108839175, 204.3125000013656063, 144.4456943541088663 ) ) ;
#49111 = CARTESIAN_POINT ( 'NONE',  ( 9.832129032723416984, 10.36458332991935016, 5.676582343750006032 ) ) ;
#49112 = CARTESIAN_POINT ( 'NONE',  ( 11.00000000000000000, 1.347111479062088405E-15, 97.93750000409677625 ) ) ;
#49113 = CARTESIAN_POINT ( 'NONE',  ( 0.000000000000000000, -7.499999999999890754, 0.000000000000000000 ) ) ;
#49114 = CARTESIAN_POINT ( 'NONE',  ( -30.44569435410886982, 202.5625000013656063, 167.5543056458916169 ) ) ;
#49115 = CARTESIAN_POINT ( 'NONE',  ( 0.000000000000000000, -20.78460969082658494, -20.69999999999999929 ) ) ;
#49117 = CARTESIAN_POINT ( 'NONE',  ( -10.00000000000000355, 59.58333332650536107, 2.679491924311223183 ) ) ;
#49116 = CARTESIAN_POINT ( 'NONE',  ( 2.977408999572650039, 119.1875000020483952, -7.188101187500000933 ) ) ;
#49118 = CARTESIAN_POINT ( 'NONE',  ( -5.656854249492375253, 5.656854249492375253, 29.14280277982336642 ) ) ;
#49119 = CARTESIAN_POINT ( 'NONE',  ( -9.832129032723418760, 117.8645833299193697, -5.676582343750004256 ) ) ;
#49120 = CARTESIAN_POINT ( 'NONE',  ( -7.320508075688778149, 94.99999999317202537, 7.320508075688769267 ) ) ;
#49121 = EDGE_CURVE ( 'NONE', #55604, #3980, #31158, .T. ) ;
#49122 = CARTESIAN_POINT ( 'NONE',  ( 2.977408999572650039, 92.18750000204838102, -7.188101187500001821 ) ) ;
#49123 = CARTESIAN_POINT ( 'NONE',  ( 4.541265875000001451, 21.37499999863441147, 1.881053915767124440 ) ) ;
#49124 = CARTESIAN_POINT ( 'NONE',  ( -2.679491924311226292, 198.3333333265053398, -10.00000000000000178 ) ) ;
#49125 = CARTESIAN_POINT ( 'NONE',  ( -1.836970198721029983E-15, 143.7500000000000284, 10.00000000000000178 ) ) ;
#49126 = ORIENTED_EDGE ( 'NONE', *, *, #1611, .T. ) ;
#49127 = CARTESIAN_POINT ( 'NONE',  ( -9.935911514116300580, 225.9999999999999432, -1.307310426733117481 ) ) ;
#49128 = EDGE_CURVE ( 'NONE', #61049, #44090, #16559, .T. ) ;
#49129 = CARTESIAN_POINT ( 'NONE',  ( -6.676582343750003368, 293.5468750017070079, -2.765530957081996810 ) ) ;
#49130 = CARTESIAN_POINT ( 'NONE',  ( -7.999999999999991118, 3.313708498984756723, 27.79280278432983309 ) ) ;
#49131 = CARTESIAN_POINT ( 'NONE',  ( 3.042071309553167069, 171.8229166632526983, -11.35316468749999785 ) ) ;
#49132 = CARTESIAN_POINT ( 'NONE',  ( 1.656854249492405451, 201.3125000000000568, 202.0000000000000284 ) ) ;
#49133 = DIRECTION ( 'NONE',  ( -0.000000000000000000, 1.000000000000000000, 4.476705744456276341E-16 ) ) ;
#49134 = AXIS2_PLACEMENT_3D ( 'NONE', #2648, #26769, #36977 ) ;
#49135 = CARTESIAN_POINT ( 'NONE',  ( -6.238412754330611322E-16, 10.18810118749999916, 102.1562500020483810 ) ) ;
#49136 = ORIENTED_EDGE ( 'NONE', *, *, #23183, .F. ) ;
#49137 = DIRECTION ( 'NONE',  ( 0.000000000000000000, 0.000000000000000000, -1.000000000000000000 ) ) ;
#49138 = CARTESIAN_POINT ( 'NONE',  ( 11.35316468750000141, 161.0937499965860127, 0.000000000000000000 ) ) ;
#49139 = CARTESIAN_POINT ( 'NONE',  ( -2.445694354108782775, 195.5625000013656063, 200.4456943541088663 ) ) ;
#49140 = CARTESIAN_POINT ( 'NONE',  ( 1.432654583217662481, 205.3750000013656063, 194.5412658750000219 ) ) ;
#49141 =( BOUNDED_CURVE ( )  B_SPLINE_CURVE ( 2, ( #73940, #21877, #52054, #45639, #29036, #57349, #390, #46011, #16964 ),
 .UNSPECIFIED., .F., .F. ) 
 B_SPLINE_CURVE_WITH_KNOTS ( ( 3, 2, 2, 2, 3 ),
 ( 0.9666666666666674512, 0.9750000000000005329, 0.9833333333333336146, 0.9916666666666669183, 1.000000000000000000 ),
 .UNSPECIFIED. ) 
 CURVE ( )  GEOMETRIC_REPRESENTATION_ITEM ( )  RATIONAL_B_SPLINE_CURVE ( ( 0.9999999999999928946, 0.9238795325112938439, 1.000000000000000000, 0.9238795325112867385, 1.000000000000000000, 0.9238795325112867385, 1.000000000000000000, 0.9238795325112867385, 1.000000000000000000 ) ) 
 REPRESENTATION_ITEM ( '' )  );
#49142 = CARTESIAN_POINT ( 'NONE',  ( 7.204075437095968759, -7.204075437095966983, 73.09375000204838102 ) ) ;
#49143 = CARTESIAN_POINT ( 'NONE',  ( -3.042071309553173730, 59.63541666325267698, 11.35316468749999785 ) ) ;
#49144 = ORIENTED_EDGE ( 'NONE', *, *, #20488, .F. ) ;
#49145 = CARTESIAN_POINT ( 'NONE',  ( 0.000000000000000000, 0.000000000000000000, -14.00000000000000178 ) ) ;
#49146 = CARTESIAN_POINT ( 'NONE',  ( -8.342170076843785083E-16, 10.18749999863440614, 4.541265875000002339 ) ) ;
#49147 = ORIENTED_EDGE ( 'NONE', *, *, #32678, .F. ) ;
#49148 = EDGE_CURVE ( 'NONE', #26525, #32606, #66244, .T. ) ;
#49149 = CARTESIAN_POINT ( 'NONE',  ( 5.082755093536325930, 18.65624999795161187, -5.082755093536325930 ) ) ;
#49150 = CARTESIAN_POINT ( 'NONE',  ( -4.242640687119285658, 287.1875000034139589, 4.242640687119287435 ) ) ;
#49151 = CIRCLE ( 'NONE', #52783, 15.99999999999998579 ) ;
#49152 = CARTESIAN_POINT ( 'NONE',  ( -26.34314575050763452, 197.6875000027312126, 174.0000000000004547 ) ) ;
#49153 = CARTESIAN_POINT ( 'NONE',  ( -2.977408999572650039, 16.31249999795161543, -7.188101187500001821 ) ) ;
#49154 = CARTESIAN_POINT ( 'NONE',  ( 7.188101187499992051, 8.802885111219154394E-16, 3.736552781871751883 ) ) ;
#49155 = ADVANCED_FACE ( 'NONE', ( #74289 ), #38484, .T. ) ;
#49156 = VECTOR ( 'NONE', #18218, 1000.000000000000000 ) ;
#49157 = CARTESIAN_POINT ( 'NONE',  ( 4.220049686691934809, 10.18810118749999916, 114.0625000020483668 ) ) ;
#49158 = ADVANCED_FACE ( 'NONE', ( #56211 ), #15076, .T. ) ;
#49159 =( BOUNDED_CURVE ( )  B_SPLINE_CURVE ( 2, ( #14010, #37046, #67217, #15143, #38175, #66840, #16250, #21919, #55536 ),
 .UNSPECIFIED., .F., .F. ) 
 B_SPLINE_CURVE_WITH_KNOTS ( ( 3, 2, 2, 2, 3 ),
 ( 0.2395833333333330928, 0.2447916666666664076, 0.2499999999999997780, 0.2552083333333330928, 0.2604166666666664631 ),
 .UNSPECIFIED. ) 
 CURVE ( )  GEOMETRIC_REPRESENTATION_ITEM ( )  RATIONAL_B_SPLINE_CURVE ( ( 1.000000000000003553, 0.9238795325112830747, 1.000000000000000000, 0.9238795325112867385, 1.000000000000000000, 0.9238795325112867385, 1.000000000000000000, 0.9238795325112899581, 0.9999999999999967804 ) ) 
 REPRESENTATION_ITEM ( '' )  );
#49160 = LINE ( 'NONE', #72167, #47426 ) ;
#49161 = CARTESIAN_POINT ( 'NONE',  ( -1.656854249492381248, 7.062499997268812280, -4.000000000000001776 ) ) ;
#49162 = ORIENTED_EDGE ( 'NONE', *, *, #39433, .T. ) ;
#49163 = CARTESIAN_POINT ( 'NONE',  ( 3.458734125000015425, 208.0000000013656347, 196.5673454167823877 ) ) ;
#49164 = CARTESIAN_POINT ( 'NONE',  ( -24.54126587499996504, 207.1250000013656347, 171.4326545832179534 ) ) ;
#49165 = CARTESIAN_POINT ( 'NONE',  ( -4.541265875000002339, 5.749999998634407028, -1.881053915767121998 ) ) ;
#49166 = CARTESIAN_POINT ( 'NONE',  ( 7.188101187500002709, 111.3125000020483810, 2.977408999572649151 ) ) ;
#49167 = CARTESIAN_POINT ( 'NONE',  ( 1.469576158976823947E-15, 93.87499999999998579, 8.000000000000000000 ) ) ;
#49168 = CARTESIAN_POINT ( 'NONE',  ( -7.188101187499991163, 2.977408999572646930, 26.89280278187175455 ) ) ;
#49169 = ORIENTED_EDGE ( 'NONE', *, *, #8136, .F. ) ;
#49170 = DIRECTION ( 'NONE',  ( 1.000000000000000000, -0.000000000000000000, -0.000000000000000000 ) ) ;
#49171 = ORIENTED_EDGE ( 'NONE', *, *, #1837, .F. ) ;
#49172 = CARTESIAN_POINT ( 'NONE',  ( -7.320508075688775484, 3.124999999999998224, 7.320508075688766603 ) ) ;
#49173 = CARTESIAN_POINT ( 'NONE',  ( 7.999999999999994671, 1.060658008479643977, 0.000000000000000000 ) ) ;
#49174 = CARTESIAN_POINT ( 'NONE',  ( 0.000000000000000000, 0.000000000000000000, 0.000000000000000000 ) ) ;
#49175 = CARTESIAN_POINT ( 'NONE',  ( 24.54126587499999346, 205.1875000013656063, 169.9999999999999432 ) ) ;
#49176 = CARTESIAN_POINT ( 'NONE',  ( 7.320508075688774596, 65.62500000000000000, -7.320508075688774596 ) ) ;
#49177 = CARTESIAN_POINT ( 'NONE',  ( 2.977408999572654480, 95.00000000204836681, 7.188101187499999156 ) ) ;
#49178 = CARTESIAN_POINT ( 'NONE',  ( 4.242640687119287435, 292.3750000000000000, 4.242640687119285658 ) ) ;
#49180 = DIRECTION ( 'NONE',  ( 0.000000000000000000, -0.000000000000000000, 1.000000000000000000 ) ) ;
#49179 = CARTESIAN_POINT ( 'NONE',  ( -3.166186134455097228E-13, 141.2500000000000284, -9.999999999999998224 ) ) ;
#49181 = ORIENTED_EDGE ( 'NONE', *, *, #51015, .F. ) ;
#49182 = CARTESIAN_POINT ( 'NONE',  ( -11.35316468749999963, 223.9062500034139873, 0.000000000000000000 ) ) ;
#49183 = ADVANCED_FACE ( 'NONE', ( #9440 ), #32457, .F. ) ;
#49184 = FACE_OUTER_BOUND ( 'NONE', #56764, .T. ) ;
#49185 = CARTESIAN_POINT ( 'NONE',  ( -2.828427124746209831, 201.5000000027312126, 139.1715728752538723 ) ) ;
#49186 = CYLINDRICAL_SURFACE ( 'NONE', #30981, 11.00000000000000000 ) ;
#49187 = CARTESIAN_POINT ( 'NONE',  ( 8.000000000000014211, -3.313708498984734518, 22.48655277982336997 ) ) ;
#49188 = CARTESIAN_POINT ( 'NONE',  ( 10.00000000000000000, 257.5000000000000000, -1.224646799147353256E-15 ) ) ;
#49189 = PLANE ( 'NONE',  #36692 ) ;
#49190 = CARTESIAN_POINT ( 'NONE',  ( 8.660254037844385522, 184.5833333333333428, 5.000000000000005329 ) ) ;
#49191 = FACE_OUTER_BOUND ( 'NONE', #24285, .T. ) ;
#49192 = CARTESIAN_POINT ( 'NONE',  ( 2.977408999572650927, -7.188101187499990274, 20.33030278187175810 ) ) ;
#49193 = CARTESIAN_POINT ( 'NONE',  ( -8.311093377946841443, 149.2187499965860411, 8.311093377946830785 ) ) ;
#49194 = FACE_OUTER_BOUND ( 'NONE', #48011, .T. ) ;
#49195 = CARTESIAN_POINT ( 'NONE',  ( 27.99999999999999645, 210.0000000000000284, 169.9999999999999147 ) ) ;
#49196 = LINE ( 'NONE', #72207, #19840 ) ;
#49199 = CARTESIAN_POINT ( 'NONE',  ( -3.313708498984765161, 17.53125000000000711, 7.999999999999998224 ) ) ;
#49198 = CARTESIAN_POINT ( 'NONE',  ( 7.999999999999991118, 9.797174393178815797E-16, 25.58030277982336997 ) ) ;
#49197 = CARTESIAN_POINT ( 'NONE',  ( 31.99999999999998579, 204.1875000000000568, 171.6568542494923122 ) ) ;
#49200 = ORIENTED_EDGE ( 'NONE', *, *, #25172, .F. ) ;
#49201 = AXIS2_PLACEMENT_3D ( 'NONE', #62560, #68977, #33925 ) ;
#49202 = CARTESIAN_POINT ( 'NONE',  ( -3.042071309553164404, 12.55208332991935194, -11.35316468749999963 ) ) ;
#49203 = CARTESIAN_POINT ( 'NONE',  ( -2.828427124746153876, 198.8750000000000284, 195.1715728752538439 ) ) ;
#49205 = DIRECTION ( 'NONE',  ( -0.000000000000000000, 1.000000000000000000, -1.563033456626094573E-30 ) ) ;
#49204 = CARTESIAN_POINT ( 'NONE',  ( -5.656854249492373476, -5.656854249492376141, -0.2946972160798554397 ) ) ;
#49206 = DIRECTION ( 'NONE',  ( 0.000000000000000000, 0.000000000000000000, -1.000000000000000000 ) ) ;
#49207 = CARTESIAN_POINT ( 'NONE',  ( -2.839093476692135984E-14, 204.6875000013656063, 138.5412658750000503 ) ) ;
#49208 = AXIS2_PLACEMENT_3D ( 'NONE', #14388, #10243, #49476 ) ;
#49209 = CARTESIAN_POINT ( 'NONE',  ( 6.123233995736767268E-16, 48.12499999317203958, -10.00000000000000178 ) ) ;
#49210 = CARTESIAN_POINT ( 'NONE',  ( 7.188101187500002709, 111.3125000020483810, 2.977408999572649151 ) ) ;
#49211 = CARTESIAN_POINT ( 'NONE',  ( -4.541265875000002339, 6.937499998634407916, -5.561446717895856393E-16 ) ) ;
#49212 = CARTESIAN_POINT ( 'NONE',  ( 6.123233995736767268E-16, 221.2500000000000000, -10.00000000000000178 ) ) ;
#49213 = CARTESIAN_POINT ( 'NONE',  ( -5.656854249492375253, 5.656854249492375253, 8.142802779823362869 ) ) ;
#49215 = CARTESIAN_POINT ( 'NONE',  ( 7.320508075688771044, 164.3750000000000568, 7.320508075688775484 ) ) ;
#49214 = CARTESIAN_POINT ( 'NONE',  ( 0.000000000000000000, 300.0000000000000000, 10.00000000000000178 ) ) ;
#49216 = ORIENTED_EDGE ( 'NONE', *, *, #6730, .F. ) ;
#49217 = CARTESIAN_POINT ( 'NONE',  ( -4.999999999999998224, 221.6666666666666856, -8.660254037844389075 ) ) ;
#49218 = CARTESIAN_POINT ( 'NONE',  ( -7.999988082670040690, 3.313720416314709816, 14.42405230710402186 ) ) ;
#49219 = CARTESIAN_POINT ( 'NONE',  ( -11.00000000000000000, 0.000000000000000000, 95.49999999999998579 ) ) ;
#49220 = CARTESIAN_POINT ( 'NONE',  ( -8.311093377946836114, 127.6562499965860411, -8.311093377946837890 ) ) ;
#49221 = VERTEX_POINT ( 'NONE', #27148 ) ;
#49222 = LINE ( 'NONE', #70755, #23511 ) ;
#49223 = ADVANCED_FACE ( 'NONE', ( #50907 ), #73547, .F. ) ;
#49224 = CARTESIAN_POINT ( 'NONE',  ( -7.204075437095967871, 7.204075437095967871, 95.96875000204838102 ) ) ;
#49225 = DIRECTION ( 'NONE',  ( -1.000000000000000000, 0.000000000000000000, 0.000000000000000000 ) ) ;
#49226 = CARTESIAN_POINT ( 'NONE',  ( 1.432654583217664701, 198.0000000013656063, 201.4587341250000065 ) ) ;
#49227 = CARTESIAN_POINT ( 'NONE',  ( 31.99999999999999289, 197.2500000000000000, 169.9999999999999432 ) ) ;
#49228 = CARTESIAN_POINT ( 'NONE',  ( 5.676582343749993598, 124.9479166632526983, 9.832129032723422313 ) ) ;
#49229 = CARTESIAN_POINT ( 'NONE',  ( 10.00000000000000178, 146.8749999931720538, 0.000000000000000000 ) ) ;
#49230 = VERTEX_POINT ( 'NONE', #12402 ) ;
#49231 = CARTESIAN_POINT ( 'NONE',  ( -3.313708498984789141, 109.7187499999999858, -7.999999999999974243 ) ) ;
#49232 = CARTESIAN_POINT ( 'NONE',  ( -30.64415807102234268, 173.4395964365057523, 174.7231612473717348 ) ) ;
#49233 = CARTESIAN_POINT ( 'NONE',  ( 11.35316468749999963, 121.3020833299193555, -3.042071309553165293 ) ) ;
#49234 = CARTESIAN_POINT ( 'NONE',  ( -3.458734124999959914, 208.4375000013656063, 198.0000000000000284 ) ) ;
#49235 = CARTESIAN_POINT ( 'NONE',  ( 7.188101187500000044, 20.34374999795161543, 0.000000000000000000 ) ) ;
#49236 = CARTESIAN_POINT ( 'NONE',  ( 7.204075437095966983, 7.204075437095967871, 88.46875000204838102 ) ) ;
#49237 = CARTESIAN_POINT ( 'NONE',  ( 8.311093377946837890, 16.71874999658601268, -8.311093377946837890 ) ) ;
#49238 = ORIENTED_EDGE ( 'NONE', *, *, #70602, .T. ) ;
#49239 = CARTESIAN_POINT ( 'NONE',  ( -6.123233995736766282E-16, 258.7500000000000568, -10.00000000000000000 ) ) ;
#49240 = CARTESIAN_POINT ( 'NONE',  ( 8.008118988124993010, -3.317071493978877239, 27.16936528394063544 ) ) ;
#49241 = CARTESIAN_POINT ( 'NONE',  ( -6.123233995736766282E-16, 238.7500000000000284, -10.00000000000000000 ) ) ;
#49242 = CARTESIAN_POINT ( 'NONE',  ( -2.751064625579944321E-14, 200.7500000000000000, 146.0000000000000284 ) ) ;
#49243 = CARTESIAN_POINT ( 'NONE',  ( 2.977408999572651815, 4.687499997951610986, 7.188101187500000933 ) ) ;
#49244 = CARTESIAN_POINT ( 'NONE',  ( -6.676582343750000703, 287.5156250017069510, 2.765530957082001251 ) ) ;
#49245 = CARTESIAN_POINT ( 'NONE',  ( 0.000000000000000000, 237.9999999999999716, 0.000000000000000000 ) ) ;
#49246 = FACE_OUTER_BOUND ( 'NONE', #11650, .T. ) ;
#49247 = EDGE_CURVE ( 'NONE', #7225, #6516, #68952, .T. ) ;
#49248 = ORIENTED_EDGE ( 'NONE', *, *, #35143, .T. ) ;
#49249 = CARTESIAN_POINT ( 'NONE',  ( 5.676582343749993598, 145.2604166632526699, 9.832129032723422313 ) ) ;
#49250 = CARTESIAN_POINT ( 'NONE',  ( 1.871523826299183495E-15, -10.18810118749999916, 83.03125000204838102 ) ) ;
#49251 = CARTESIAN_POINT ( 'NONE',  ( -25.55430564589119413, 200.3125000013656063, 167.5543056458915316 ) ) ;
#49252 = EDGE_CURVE ( 'NONE', #59062, #69825, #48416, .T. ) ;
#49253 = CARTESIAN_POINT ( 'NONE',  ( -74.99999999999998579, 242.0000000000000284, 42.00000000000003553 ) ) ;
#49254 = CARTESIAN_POINT ( 'NONE',  ( 4.541265875000002339, 15.43749999863440614, 0.000000000000000000 ) ) ;
#49255 = ORIENTED_EDGE ( 'NONE', *, *, #14309, .F. ) ;
#49256 = AXIS2_PLACEMENT_3D ( 'NONE', #27636, #51023, #68002 ) ;
#49257 = CARTESIAN_POINT ( 'NONE',  ( 4.000000000000015987, 202.5625000027312126, 199.6568542494924259 ) ) ;
#49258 =( BOUNDED_CURVE ( )  B_SPLINE_CURVE ( 2, ( #5198, #45918, #41011, #74217, #34252, #68191, #10476, #68930, #11966 ),
 .UNSPECIFIED., .F., .F. ) 
 B_SPLINE_CURVE_WITH_KNOTS ( ( 3, 2, 2, 2, 3 ),
 ( 0.06666666666666672125, 0.07500000000000006661, 0.08333333333333339810, 0.09166666666666672958, 0.1000000000000000888 ),
 .UNSPECIFIED. ) 
 CURVE ( )  GEOMETRIC_REPRESENTATION_ITEM ( )  RATIONAL_B_SPLINE_CURVE ( ( 0.9999999999999994449, 0.9238795325112872936, 1.000000000000000000, 0.9238795325112867385, 1.000000000000000000, 0.9238795325112867385, 1.000000000000000000, 0.9238795325112859613, 1.000000000000000666 ) ) 
 REPRESENTATION_ITEM ( '' )  );
#49259 = CARTESIAN_POINT ( 'NONE',  ( -2.445694354108840063, 198.0625000013656063, 139.5543056458912190 ) ) ;
#49260 = CARTESIAN_POINT ( 'NONE',  ( -1.656854249492405451, 205.4375000027312126, 138.0000000000000568 ) ) ;
#49261 = CARTESIAN_POINT ( 'NONE',  ( 7.999999999999998224, 5.906250000000000888, 3.313708498984766049 ) ) ;
#49262 = EDGE_LOOP ( 'NONE', ( #30815, #72762, #58723, #36566, #72854 ) ) ;
#49263 = CARTESIAN_POINT ( 'NONE',  ( -2.977408999572654480, 13.49999999795161187, 7.188101187499999156 ) ) ;
#49264 = CARTESIAN_POINT ( 'NONE',  ( -20.03439145747709205, -15.25864258333471746, 193.6707515143633884 ) ) ;
#49265 = CYLINDRICAL_SURFACE ( 'NONE', #37879, 10.00000000000000178 ) ;
#49266 = CARTESIAN_POINT ( 'NONE',  ( -3.042071309553164404, 192.2395833299193555, -11.35316468749999963 ) ) ;
#49267 = CARTESIAN_POINT ( 'NONE',  ( 1.320432766682874540E-15, 111.4062500020483810, 7.188101187500000044 ) ) ;
#49268 = CARTESIAN_POINT ( 'NONE',  ( -2.250000000000000888, -2.250000000000000000, 0.000000000000000000 ) ) ;
#49269 = CARTESIAN_POINT ( 'NONE',  ( 4.721056650416000089, 290.8281250017069510, 4.721056650415999201 ) ) ;
#49271 = CARTESIAN_POINT ( 'NONE',  ( 4.999999999999999112, 95.83333333333334281, -8.660254037844383745 ) ) ;
#49270 = CARTESIAN_POINT ( 'NONE',  ( 6.123233995736767268E-16, 133.1249999931720254, -10.00000000000000178 ) ) ;
#49272 = VERTEX_POINT ( 'NONE', #40707 ) ;
#49273 =( BOUNDED_CURVE ( )  B_SPLINE_CURVE ( 2, ( #9220, #55258, #26555, #20901, #15610, #43923, #20149, #66933, #37144 ),
 .UNSPECIFIED., .F., .F. ) 
 B_SPLINE_CURVE_WITH_KNOTS ( ( 3, 2, 2, 2, 3 ),
 ( 0.4166666666666671293, 0.4250000000000003775, 0.4333333333333336812, 0.4416666666666669849, 0.4500000000000002887 ),
 .UNSPECIFIED. ) 
 CURVE ( )  GEOMETRIC_REPRESENTATION_ITEM ( )  RATIONAL_B_SPLINE_CURVE ( ( 0.9999999999999958922, 0.9238795325112908463, 1.000000000000000000, 0.9238795325112867385, 1.000000000000000000, 0.9238795325112867385, 1.000000000000000000, 0.9238795325112841850, 1.000000000000002442 ) ) 
 REPRESENTATION_ITEM ( '' )  );
#49274 = CARTESIAN_POINT ( 'NONE',  ( 5.676582343749997150, 232.5520833367473301, -9.832129032723418760 ) ) ;
#49275 = CARTESIAN_POINT ( 'NONE',  ( -4.401442555609577197E-16, 7.188101187499992051, 2.611552781871750994 ) ) ;
#49276 = CARTESIAN_POINT ( 'NONE',  ( -7.347880794884122694E-16, 2.499999997268813168, 4.000000000000001776 ) ) ;
#49277 = CARTESIAN_POINT ( 'NONE',  ( 4.898587196589412829E-16, 19.68749999590322020, -8.000000000000000000 ) ) ;
#49278 = CARTESIAN_POINT ( 'NONE',  ( -3.228176881614594596, -60.48309044411862345, -23.05774181791981547 ) ) ;
#49279 = CARTESIAN_POINT ( 'NONE',  ( 1.432654583217662481, 198.3750000013655779, 194.5412658750000219 ) ) ;
#49280 = EDGE_LOOP ( 'NONE', ( #56244, #6313, #63621, #17359 ) ) ;
#49281 = CARTESIAN_POINT ( 'NONE',  ( 3.313708498984762496, 23.71875000000000355, 7.999999999999998224 ) ) ;
#49282 = CARTESIAN_POINT ( 'NONE',  ( -7.999999999999998224, 96.59375000000000000, 3.313708498984766493 ) ) ;
#49283 = CARTESIAN_POINT ( 'NONE',  ( -8.311093377946836114, 112.9687499965860269, -8.311093377946837890 ) ) ;
#49284 = CARTESIAN_POINT ( 'NONE',  ( 10.00000000000000178, 212.0833333265053682, -2.679491924311226736 ) ) ;
#49285 = CARTESIAN_POINT ( 'NONE',  ( 11.00000000000000355, -4.556349186104045046, 70.65625000000000000 ) ) ;
#49288 = CARTESIAN_POINT ( 'NONE',  ( 7.778174593052021635, 7.778174593052023411, 110.1250000040967763 ) ) ;
#49287 = CARTESIAN_POINT ( 'NONE',  ( 30.44569435410879521, 200.8125000013656063, 167.5543056458910485 ) ) ;
#49286 = CARTESIAN_POINT ( 'NONE',  ( 29.43265458321766559, 199.1250000013656347, 166.5412658749999650 ) ) ;
#49289 = ORIENTED_EDGE ( 'NONE', *, *, #54673, .T. ) ;
#49290 = CARTESIAN_POINT ( 'NONE',  ( 32.00000000000000000, 205.3750000027312126, 169.9999999999998863 ) ) ;
#49291 = CARTESIAN_POINT ( 'NONE',  ( -3.042071309553173730, 224.3229166632527267, 11.35316468749999785 ) ) ;
#49292 = CARTESIAN_POINT ( 'NONE',  ( 1.432654583217607858, 195.6250000013656063, 138.5412658750000787 ) ) ;
#49293 = CARTESIAN_POINT ( 'NONE',  ( 31.45873412499999233, 196.9375000013655779, 169.9999999999999432 ) ) ;
#49294 = AXIS2_PLACEMENT_3D ( 'NONE', #52265, #51137, #45471 ) ;
#49295 = CARTESIAN_POINT ( 'NONE',  ( 11.00000000000000000, 1.347111479062088405E-15, 109.9375000040967763 ) ) ;
#49296 = CARTESIAN_POINT ( 'NONE',  ( -5.676582343749998039, 187.7604166632526983, -9.832129032723420536 ) ) ;
#49297 = CARTESIAN_POINT ( 'NONE',  ( -2.977408999572650927, 92.75000000204839523, -7.188101187500000933 ) ) ;
#49298 = DIRECTION ( 'NONE',  ( 1.000000000000000000, 1.577021341797097560E-16, 0.000000000000000000 ) ) ;
#49299 = CARTESIAN_POINT ( 'NONE',  ( 4.541265875000001451, 17.24999999863440792, 1.881053915767124440 ) ) ;
#49300 = CARTESIAN_POINT ( 'NONE',  ( 3.496982156811260900, -51.71401992552191018, 48.73755072030270696 ) ) ;
#49301 = CARTESIAN_POINT ( 'NONE',  ( 3.313708498984756279, 7.999999999999991118, 27.36155277982336642 ) ) ;
#49302 = CYLINDRICAL_SURFACE ( 'NONE', #12232, 11.00000000000000000 ) ;
#49303 = CARTESIAN_POINT ( 'NONE',  ( -3.042071309553173730, 84.32291666325268409, 11.35316468749999785 ) ) ;
#49304 = VERTEX_POINT ( 'NONE', #63711 ) ;
#49305 = EDGE_CURVE ( 'NONE', #56251, #42029, #73959, .T. ) ;
#49306 = CARTESIAN_POINT ( 'NONE',  ( 5.656854249492381470, 92.56249999999998579, 5.656854249492379694 ) ) ;
#49307 = CARTESIAN_POINT ( 'NONE',  ( -7.188101187500001821, 19.12499999795161187, -2.977408999572651371 ) ) ;
#49308 = CARTESIAN_POINT ( 'NONE',  ( 4.999999999999997335, 233.3333333333333428, -8.660254037844387298 ) ) ;
#49309 = CARTESIAN_POINT ( 'NONE',  ( 5.676582343749993598, 94.94791666325269830, 9.832129032723422313 ) ) ;
#49310 = VERTEX_POINT ( 'NONE', #45620 ) ;
#49311 = CARTESIAN_POINT ( 'NONE',  ( -10.18810118749999916, 4.220049686691934809, 84.43750000204838102 ) ) ;
#49312 = AXIS2_PLACEMENT_3D ( 'NONE', #9877, #26843, #20808 ) ;
#49313 = CARTESIAN_POINT ( 'NONE',  ( 4.220049686691934809, 10.18810118749999916, 112.1875000020483810 ) ) ;
#49314 = CARTESIAN_POINT ( 'NONE',  ( -30.99999999999992895, -31.99999999999978684, 205.0000000000000284 ) ) ;
#49315 = CARTESIAN_POINT ( 'NONE',  ( -3.458734124999960358, 208.6875000013656063, 198.0000000000000284 ) ) ;
#49316 = DIRECTION ( 'NONE',  ( -1.000000000000000000, -0.000000000000000000, -0.000000000000000000 ) ) ;
#49318 = CARTESIAN_POINT ( 'NONE',  ( 8.311093377946837890, 91.40624999658602690, -8.311093377946837890 ) ) ;
#49317 = CARTESIAN_POINT ( 'NONE',  ( -2.775557561562891351E-14, 210.0000000000000284, 142.0000000000000568 ) ) ;
#49319 = CARTESIAN_POINT ( 'NONE',  ( -7.999999999999989342, -3.313708498984762496, 19.11155278392014623 ) ) ;
#49320 = CARTESIAN_POINT ( 'NONE',  ( -7.347880794884122694E-16, 14.75000000000000178, 4.000000000000001776 ) ) ;
#49321 = EDGE_CURVE ( 'NONE', #37225, #8408, #22389, .T. ) ;
#49322 = AXIS2_PLACEMENT_3D ( 'NONE', #60429, #66460, #2722 ) ;
#49323 = EDGE_CURVE ( 'NONE', #27541, #11598, #58081, .T. ) ;
#49324 = CARTESIAN_POINT ( 'NONE',  ( -7.320508075688778149, 174.9999999931720538, 7.320508075688769267 ) ) ;
#49325 = CARTESIAN_POINT ( 'NONE',  ( -4.556349186104045934, 11.00000000000000000, 113.2187500000000000 ) ) ;
#49326 = CARTESIAN_POINT ( 'NONE',  ( 5.000000000000000000, -52.85372778481357869, 48.38359481482874713 ) ) ;
#49327 = CARTESIAN_POINT ( 'NONE',  ( 11.35316468749999785, 70.88541666325266988, 3.042071309553174174 ) ) ;
#49328 = CARTESIAN_POINT ( 'NONE',  ( -2.765530957081996810, 293.2656250017068942, -6.676582343750003368 ) ) ;
#49329 = CARTESIAN_POINT ( 'NONE',  ( -10.18810118749999916, 4.220049686691934809, 109.9375000020483810 ) ) ;
#49330 = CARTESIAN_POINT ( 'NONE',  ( 11.35316468749999963, 205.9895833299193271, -3.042071309553165293 ) ) ;
#49331 = ORIENTED_EDGE ( 'NONE', *, *, #56617, .T. ) ;
#49332 = CARTESIAN_POINT ( 'NONE',  ( -2.751064625579944321E-14, 202.7500000000000000, 146.0000000000000284 ) ) ;
#49333 = CARTESIAN_POINT ( 'NONE',  ( -2.751064625579944321E-14, 205.8750000027312126, 146.0000000000000284 ) ) ;
#49334 = CARTESIAN_POINT ( 'NONE',  ( -1.704527592502766309, 49.99193291617112322, 40.73198448289741691 ) ) ;
#49336 = CARTESIAN_POINT ( 'NONE',  ( -8.311093377946841443, 198.9062499965860411, 8.311093377946834337 ) ) ;
#49335 = DIRECTION ( 'NONE',  ( 0.000000000000000000, 0.000000000000000000, -1.000000000000000000 ) ) ;
#49337 = CARTESIAN_POINT ( 'NONE',  ( 0.000000000000000000, 0.000000000000000000, 0.000000000000000000 ) ) ;
#49338 = CARTESIAN_POINT ( 'NONE',  ( -7.320508075688771932, 242.5000000068279178, -7.320508075688771932 ) ) ;
#49339 = ORIENTED_EDGE ( 'NONE', *, *, #43157, .F. ) ;
#49340 = CARTESIAN_POINT ( 'NONE',  ( -11.35316468749999785, 178.3854166632526699, -3.042071309553167957 ) ) ;
#49341 = B_SPLINE_CURVE_WITH_KNOTS ( 'NONE', 3,
 ( #12043, #4912, #6020, #35077, #58089, #6400, #27906, #50915 ),
 .UNSPECIFIED., .F., .F.,
 ( 4, 2, 2, 4 ),
 ( 0.005256334970460276035, 0.006570121696639122204, 0.007883908422817968373, 0.01051148187517565204 ),
 .UNSPECIFIED. ) ;
#49342 = CARTESIAN_POINT ( 'NONE',  ( -5.082755093536317936, -5.082755093536320601, 15.17405278187175455 ) ) ;
#49343 = CARTESIAN_POINT ( 'NONE',  ( -7.320508075688767491, 91.87500000000001421, -7.320508075688768379 ) ) ;
#49344 = ORIENTED_EDGE ( 'NONE', *, *, #71666, .F. ) ;
#49345 = EDGE_CURVE ( 'NONE', #34824, #47258, #741, .T. ) ;
#49346 = CARTESIAN_POINT ( 'NONE',  ( 5.656854249492379694, 99.12500000409677625, -5.656854249492380582 ) ) ;
#49347 = CARTESIAN_POINT ( 'NONE',  ( 10.00000000000000178, 5.208333333333333037, -2.679491924311226736 ) ) ;
#49348 = CIRCLE ( 'NONE', #10805, 19.00000000000000355 ) ;
#49349 = ORIENTED_EDGE ( 'NONE', *, *, #25789, .F. ) ;
#49350 = CARTESIAN_POINT ( 'NONE',  ( -2.828427124746192067, 15.62500000000000000, 2.828427124746190735 ) ) ;
#49351 = CARTESIAN_POINT ( 'NONE',  ( -4.541265875000002339, 20.74999999863440436, -1.881053915767121998 ) ) ;
#49352 = CARTESIAN_POINT ( 'NONE',  ( -3.313708498984757167, 7.999999999999991118, 15.73655278392014267 ) ) ;
#49353 = CARTESIAN_POINT ( 'NONE',  ( -7.999999999999991118, 3.313708498984757167, 18.92405278392014978 ) ) ;
#49354 = VECTOR ( 'NONE', #62030, 1000.000000000000000 ) ;
#49355 = ORIENTED_EDGE ( 'NONE', *, *, #64835, .F. ) ;
#49356 = DIRECTION ( 'NONE',  ( 0.000000000000000000, 0.000000000000000000, 1.000000000000000000 ) ) ;
#49357 = CARTESIAN_POINT ( 'NONE',  ( -2.977408999572651815, 92.93750000204839523, 7.188101187500000933 ) ) ;
#49360 = CARTESIAN_POINT ( 'NONE',  ( -6.676582343750001591, 299.5312500017070079, 0.000000000000000000 ) ) ;
#49359 = CARTESIAN_POINT ( 'NONE',  ( -3.042071309553166625, 252.8645833367473301, -11.35316468749999608 ) ) ;
#49358 = DIRECTION ( 'NONE',  ( 1.000000000000000000, 0.000000000000000000, 0.000000000000000000 ) ) ;
#49361 = EDGE_LOOP ( 'NONE', ( #71300, #35561, #21577, #60869 ) ) ;
#49362 = CARTESIAN_POINT ( 'NONE',  ( 11.35316468749999963, 261.5104166700807014, 3.042071309553159519 ) ) ;
#49363 = CARTESIAN_POINT ( 'NONE',  ( -4.401442555609577197E-16, 7.188101187499992051, 17.61155278187175810 ) ) ;
#49364 = ORIENTED_EDGE ( 'NONE', *, *, #2154, .F. ) ;
#49365 =( BOUNDED_CURVE ( )  B_SPLINE_CURVE ( 2, ( #34145, #57144, #17132, #5836, #56400, #22790, #5094, #51469, #16016 ),
 .UNSPECIFIED., .F., .F. ) 
 B_SPLINE_CURVE_WITH_KNOTS ( ( 3, 2, 2, 2, 3 ),
 ( 0.1470588235294118529, 0.1507352941176471339, 0.1544117647058824427, 0.1580882352941177238, 0.1617647058823530326 ),
 .UNSPECIFIED. ) 
 CURVE ( )  GEOMETRIC_REPRESENTATION_ITEM ( )  RATIONAL_B_SPLINE_CURVE ( ( 0.9999999999999982236, 0.9238795325112885148, 1.000000000000000000, 0.9238795325112867385, 1.000000000000000000, 0.9238795325112867385, 1.000000000000000000, 0.9238795325112849621, 1.000000000000001776 ) ) 
 REPRESENTATION_ITEM ( '' )  );
#49366 = ORIENTED_EDGE ( 'NONE', *, *, #67611, .T. ) ;
#49367 = CARTESIAN_POINT ( 'NONE',  ( 4.220049686691934809, 10.18810118749999916, 80.68750000204836681 ) ) ;
#49368 = CARTESIAN_POINT ( 'NONE',  ( -11.35316468750000141, 78.80208332991935549, 3.042071309553159963 ) ) ;
#49369 = CARTESIAN_POINT ( 'NONE',  ( -8.000000000000000000, 105.6875000040967763, 0.000000000000000000 ) ) ;
#49370 = CARTESIAN_POINT ( 'NONE',  ( -7.778174593052023411, 7.778174593052023411, 90.81249999999998579 ) ) ;
#49373 = CARTESIAN_POINT ( 'NONE',  ( -6.676582343749999815, 294.6718750017070079, 2.765530957082001251 ) ) ;
#49372 = CARTESIAN_POINT ( 'NONE',  ( 28.00000000000002132, 198.1250000027312126, 173.9999999999999147 ) ) ;
#49371 = CARTESIAN_POINT ( 'NONE',  ( 0.000000000000000000, 0.000000000000000000, 30.00000000000000000 ) ) ;
#49374 = CARTESIAN_POINT ( 'NONE',  ( -27.99999999999991118, 203.6250000027312126, 174.0000000000003695 ) ) ;
#49375 = DIRECTION ( 'NONE',  ( -0.000000000000000000, 1.000000000000000000, -0.000000000000000000 ) ) ;
#49376 = CARTESIAN_POINT ( 'NONE',  ( 2.754378923186476579E-14, 197.4375000013655779, 194.5412658750000219 ) ) ;
#49377 = CARTESIAN_POINT ( 'NONE',  ( 3.313708498984762052, 4.593749995903220196, -8.000000000000000000 ) ) ;
#49378 = CARTESIAN_POINT ( 'NONE',  ( 29.43265458321761230, 200.5000000013655779, 173.4587341249998929 ) ) ;
#49379 = EDGE_CURVE ( 'NONE', #27119, #19863, #45546, .T. ) ;
#49380 = CARTESIAN_POINT ( 'NONE',  ( 2.977408999572651815, 14.06249999795161365, 7.188101187500000933 ) ) ;
#49381 = CARTESIAN_POINT ( 'NONE',  ( -4.898587196589407898E-16, 7.999999999999991118, 26.14280278392014623 ) ) ;
#49382 = CARTESIAN_POINT ( 'NONE',  ( -10.00000000000000000, 243.1250000068280031, 0.000000000000000000 ) ) ;
#49383 = CARTESIAN_POINT ( 'NONE',  ( -2.977408999572650927, 110.7500000020483810, -7.188101187500000933 ) ) ;
#49385 = FACE_OUTER_BOUND ( 'NONE', #15472, .T. ) ;
#49384 = DIRECTION ( 'NONE',  ( -0.000000000000000000, -0.000000000000000000, -1.000000000000000000 ) ) ;
#49386 = CARTESIAN_POINT ( 'NONE',  ( -9.832129032723415207, 219.6354166700806445, 5.676582343750005144 ) ) ;
#49387 = CARTESIAN_POINT ( 'NONE',  ( -23.99999999999999289, 207.7500000000000284, 170.0000000000003411 ) ) ;
#49388 = CARTESIAN_POINT ( 'NONE',  ( -4.401442555609577197E-16, 7.188101187499992051, 13.48655278187175455 ) ) ;
#49389 = CARTESIAN_POINT ( 'NONE',  ( -4.000000000000015987, 208.5625000027312410, 140.3431457505076594 ) ) ;
#49390 = CARTESIAN_POINT ( 'NONE',  ( -8.311093377946841443, 43.90624999658601268, 8.311093377946830785 ) ) ;
#49391 = CARTESIAN_POINT ( 'NONE',  ( 1.736494649845416349, 16.42394793108440254, 68.69316892220884085 ) ) ;
#49392 = CARTESIAN_POINT ( 'NONE',  ( 2.679491924311228956, 2.916666659838698994, -10.00000000000000000 ) ) ;
#49393 = CARTESIAN_POINT ( 'NONE',  ( 2.828427124746191623, 17.12500000000000000, -2.828427124746191623 ) ) ;
#49394 = ORIENTED_EDGE ( 'NONE', *, *, #64472, .F. ) ;
#49395 = CARTESIAN_POINT ( 'NONE',  ( 10.00000000000000178, 141.8749999931720538, 0.000000000000000000 ) ) ;
#49396 = CARTESIAN_POINT ( 'NONE',  ( -2.828427124746190735, 8.124999997268814056, -2.828427124746191623 ) ) ;
#49397 = CARTESIAN_POINT ( 'NONE',  ( 6.951808397369818766E-16, 52.03124999658601979, -11.35316468750000141 ) ) ;
#49398 = CARTESIAN_POINT ( 'NONE',  ( 7.778174593052023411, -7.778174593052021635, 81.25000000409676204 ) ) ;
#49399 = CARTESIAN_POINT ( 'NONE',  ( -1.432654583217664701, 206.0000000013656063, 138.5412658750000787 ) ) ;
#49400 = CARTESIAN_POINT ( 'NONE',  ( -2.978189300774432354E-14, -67.59332269700065865, -20.03478791450352858 ) ) ;
#49401 = CARTESIAN_POINT ( 'NONE',  ( 8.000000000000000000, 25.40624999590322730, -3.313708498984761164 ) ) ;
#49403 = CARTESIAN_POINT ( 'NONE',  ( 9.832129032723420536, 41.19791666325268409, -5.676582343749999815 ) ) ;
#49402 = CARTESIAN_POINT ( 'NONE',  ( 7.188101187500000933, 101.0000000020483810, -2.977408999572651371 ) ) ;
#49404 = CARTESIAN_POINT ( 'NONE',  ( 7.999999999999992895, -3.313708498984756279, 8.986552779823366421 ) ) ;
#49405 = CARTESIAN_POINT ( 'NONE',  ( 7.999994293450985339, 3.313714205533765611, 21.36155301224097158 ) ) ;
#49406 = CARTESIAN_POINT ( 'NONE',  ( -8.311093377946841443, 163.9062499965859843, 8.311093377946830785 ) ) ;
#49407 = AXIS2_PLACEMENT_3D ( 'NONE', #54775, #73604, #26070 ) ;
#49408 = CARTESIAN_POINT ( 'NONE',  ( 6.123233995736767268E-16, 133.1249999931720254, -10.00000000000000178 ) ) ;
#49409 = CARTESIAN_POINT ( 'NONE',  ( 5.082755093536326818, 111.5937500020483810, 5.082755093536325042 ) ) ;
#49410 = ORIENTED_EDGE ( 'NONE', *, *, #61871, .T. ) ;
#49411 = DIRECTION ( 'NONE',  ( 0.000000000000000000, 0.000000000000000000, -1.000000000000000000 ) ) ;
#49412 = CARTESIAN_POINT ( 'NONE',  ( 9.832129032723416984, 20.67708332991935194, 5.676582343750006032 ) ) ;
#49413 = CARTESIAN_POINT ( 'NONE',  ( -3.999999999999960032, 196.9375000000000284, 196.3431457505076594 ) ) ;
#49414 = ORIENTED_EDGE ( 'NONE', *, *, #20996, .F. ) ;
#49415 = CARTESIAN_POINT ( 'NONE',  ( -29.65685424949232285, 205.5625000027311842, 174.0000000000003411 ) ) ;
#49416 = CARTESIAN_POINT ( 'NONE',  ( 10.18810118749999916, 4.220049686691935698, 77.50000000204839523 ) ) ;
#49417 = DIRECTION ( 'NONE',  ( -0.000000000000000000, -0.000000000000000000, -1.000000000000000000 ) ) ;
#49419 = CARTESIAN_POINT ( 'NONE',  ( 5.676582343750001591, 156.6145833299193839, -9.832129032723420536 ) ) ;
#49418 = CARTESIAN_POINT ( 'NONE',  ( -7.188101187499992051, 0.000000000000000000, 28.67405278187175810 ) ) ;
#49420 = CARTESIAN_POINT ( 'NONE',  ( -2.977408999572650039, 1.312499997951610098, -7.188101187500000933 ) ) ;
#49421 = VECTOR ( 'NONE', #59430, 1000.000000000000000 ) ;
#49422 = CARTESIAN_POINT ( 'NONE',  ( 7.999999999999992895, -3.313708498984756279, 13.54280278432982598 ) ) ;
#49423 = CARTESIAN_POINT ( 'NONE',  ( -20.91786611113093031, -27.59247207081794784, 192.8793035041884991 ) ) ;
#49424 = AXIS2_PLACEMENT_3D ( 'NONE', #14588, #48921, #71934 ) ;
#49425 = EDGE_CURVE ( 'NONE', #48083, #25046, #37617, .T. ) ;
#49426 = EDGE_CURVE ( 'NONE', #45416, #1129, #58100, .T. ) ;
#49427 = CARTESIAN_POINT ( 'NONE',  ( 5.676582343749997150, 237.2395833367473301, -9.832129032723418760 ) ) ;
#49428 = CARTESIAN_POINT ( 'NONE',  ( 7.204075437095966983, 7.204075437095967871, 85.46875000204836681 ) ) ;
#49429 = ORIENTED_EDGE ( 'NONE', *, *, #38714, .F. ) ;
#49430 = EDGE_CURVE ( 'NONE', #47413, #29990, #54803, .T. ) ;
#49431 = CARTESIAN_POINT ( 'NONE',  ( 4.556349186104052151, -10.99999999999999822, 90.15625000409677625 ) ) ;
#49432 = CARTESIAN_POINT ( 'NONE',  ( -2.485281374238227592, 292.2500000034139589, 6.000000000000345501 ) ) ;
#49433 = CARTESIAN_POINT ( 'NONE',  ( 9.832129032723416984, 105.6770833299193413, 5.676582343750006032 ) ) ;
#49434 = CARTESIAN_POINT ( 'NONE',  ( 4.220049686691934809, 10.18810118749999916, 92.68750000204838102 ) ) ;
#49435 = CARTESIAN_POINT ( 'NONE',  ( 4.541265875000002339, 21.43749999863440792, 0.000000000000000000 ) ) ;
#49436 = EDGE_LOOP ( 'NONE', ( #72613, #21837, #11694, #62900 ) ) ;
#49437 = ORIENTED_EDGE ( 'NONE', *, *, #25193, .F. ) ;
#49438 = CARTESIAN_POINT ( 'NONE',  ( -3.211159895383562723, 4.062499998634407028, 3.211159895383561391 ) ) ;
#49439 = CARTESIAN_POINT ( 'NONE',  ( -7.188101187500001821, 5.624999997951611874, -2.977408999572651371 ) ) ;
#49440 = EDGE_CURVE ( 'NONE', #27289, #19989, #34034, .T. ) ;
#49441 = CARTESIAN_POINT ( 'NONE',  ( 3.313708498984760720, 118.7187500040967905, -8.000000000000000000 ) ) ;
#49442 = VECTOR ( 'NONE', #55240, 1000.000000000000000 ) ;
#49443 = CARTESIAN_POINT ( 'NONE',  ( -10.18810118749999916, 4.220049686691934809, 94.93750000204838102 ) ) ;
#49444 = CARTESIAN_POINT ( 'NONE',  ( -31.45873412499999944, 201.8750000013656063, 168.5673454167827572 ) ) ;
#49445 = PRESENTATION_STYLE_ASSIGNMENT (( #19649 ) ) ;
#49446 = CARTESIAN_POINT ( 'NONE',  ( 4.000000000000000888, 4.937500000000001776, 1.656854249492384135 ) ) ;
#49447 = CARTESIAN_POINT ( 'NONE',  ( -4.000000000000001776, 17.24999999726881583, -4.898587196589415787E-16 ) ) ;
#49448 = CARTESIAN_POINT ( 'NONE',  ( -1.881053915767124440, 3.999999998634406584, 4.541265875000001451 ) ) ;
#49449 = CARTESIAN_POINT ( 'NONE',  ( -1.656854249492405451, 203.3125000000000284, 138.0000000000000568 ) ) ;
#49450 = VERTEX_POINT ( 'NONE', #14614 ) ;
#49451 = CARTESIAN_POINT ( 'NONE',  ( 25.17157287525378706, 207.8750000000000284, 172.8284271247460424 ) ) ;
#49453 = CARTESIAN_POINT ( 'NONE',  ( -10.99999999999994671, -4.556349186104105442, 95.78125000409679046 ) ) ;
#49452 = CARTESIAN_POINT ( 'NONE',  ( -25.55430564589111953, 198.0625000013656063, 172.4456943541091505 ) ) ;
#49454 = CARTESIAN_POINT ( 'NONE',  ( -4.541265875000002339, 17.74999999863440792, -1.881053915767121998 ) ) ;
#49455 = AXIS2_PLACEMENT_3D ( 'NONE', #6423, #73957, #33 ) ;
#49456 = DIRECTION ( 'NONE',  ( -0.000000000000000000, 1.000000000000000000, -0.000000000000000000 ) ) ;
#49457 = CARTESIAN_POINT ( 'NONE',  ( 7.188101187499992051, 8.802885111219154394E-16, 6.736552781871754547 ) ) ;
#49458 = ORIENTED_EDGE ( 'NONE', *, *, #7633, .T. ) ;
#49459 = ORIENTED_EDGE ( 'NONE', *, *, #39948, .T. ) ;
#49460 = CARTESIAN_POINT ( 'NONE',  ( 7.204075437095968759, -7.204075437095966983, 98.21875000204838102 ) ) ;
#49461 = CARTESIAN_POINT ( 'NONE',  ( -27.99999999999996447, 203.1875000013656063, 173.4587341250003760 ) ) ;
#49462 = CARTESIAN_POINT ( 'NONE',  ( -23.99999999999998934, 201.7500000000000000, 170.0000000000003411 ) ) ;
#49463 = CARTESIAN_POINT ( 'NONE',  ( -2.445694354108783219, 207.8125000013656063, 200.4456943541088663 ) ) ;
#49464 = CARTESIAN_POINT ( 'NONE',  ( 5.000000000000040856, 60.83333333333337833, -8.660254037844454800 ) ) ;
#49465 = CARTESIAN_POINT ( 'NONE',  ( 6.123233995736767268E-16, 106.2500000000000142, -10.00000000000000178 ) ) ;
#49466 = CIRCLE ( 'NONE', #26582, 5.000000000000000000 ) ;
#49467 = CARTESIAN_POINT ( 'NONE',  ( 5.656854249492379694, 113.9375000000000000, -5.656854249492380582 ) ) ;
#49468 = CARTESIAN_POINT ( 'NONE',  ( 6.676582343750004256, 291.0468750017070079, 2.765530957081995478 ) ) ;
#49469 = AXIS2_PLACEMENT_3D ( 'NONE', #69277, #34594, #73815 ) ;
#49470 = CARTESIAN_POINT ( 'NONE',  ( 2.977408999572650927, -7.188101187499990274, 9.830302781871752771 ) ) ;
#49471 = VERTEX_POINT ( 'NONE', #59545 ) ;
#49472 = CARTESIAN_POINT ( 'NONE',  ( -8.660254037844390851, 174.7916666598387110, 4.999999999999998224 ) ) ;
#49473 = CARTESIAN_POINT ( 'NONE',  ( 3.313708498984762052, 18.09374999590322375, -8.000000000000000000 ) ) ;
#49474 = CARTESIAN_POINT ( 'NONE',  ( 3.458734124999959025, 203.5000000013655779, 140.5673454167824161 ) ) ;
#49475 = CARTESIAN_POINT ( 'NONE',  ( -1.836970198721029983E-15, 185.6249999931720538, 10.00000000000000178 ) ) ;
#49477 = CARTESIAN_POINT ( 'NONE',  ( -1.432654583217662481, 203.3750000013656063, 145.4587341250000634 ) ) ;
#49476 = DIRECTION ( 'NONE',  ( 0.000000000000000000, 0.000000000000000000, -1.000000000000000000 ) ) ;
#49478 = CARTESIAN_POINT ( 'NONE',  ( -9.832129032723415207, 259.6354166700806445, 5.676582343750005144 ) ) ;
#49479 = DIRECTION ( 'NONE',  ( -0.000000000000000000, -0.000000000000000000, 1.000000000000000000 ) ) ;
#49480 = DIRECTION ( 'NONE',  ( 0.000000000000000000, 0.000000000000000000, 1.000000000000000000 ) ) ;
#49481 = CARTESIAN_POINT ( 'NONE',  ( 10.00000000000000178, 225.2083333333333144, -2.679491924311226736 ) ) ;
#49482 = CARTESIAN_POINT ( 'NONE',  ( 7.188101187499992051, 8.802885111219154394E-16, 4.111552781871752771 ) ) ;
#49483 = CARTESIAN_POINT ( 'NONE',  ( 8.311093377946837890, 196.7187499965860127, -8.311093377946837890 ) ) ;
#49484 = DIRECTION ( 'NONE',  ( -0.000000000000000000, 1.000000000000000000, -0.000000000000000000 ) ) ;
#49485 = CARTESIAN_POINT ( 'NONE',  ( -8.342170076843785083E-16, 5.062499998634407028, 4.541265875000002339 ) ) ;
#49486 = FACE_OUTER_BOUND ( 'NONE', #2641, .T. ) ;
#49488 = DIRECTION ( 'NONE',  ( 0.000000000000000000, 0.000000000000000000, 1.000000000000000000 ) ) ;
#49487 = DIRECTION ( 'NONE',  ( -0.000000000000000000, 1.000000000000000000, -0.000000000000000000 ) ) ;
#49489 = ORIENTED_EDGE ( 'NONE', *, *, #1104, .T. ) ;
#49490 = EDGE_CURVE ( 'NONE', #58474, #44494, #24822, .T. ) ;
#49491 = CARTESIAN_POINT ( 'NONE',  ( 3.458734124999960358, 204.6875000013656063, 142.0000000000000568 ) ) ;
#49492 = CARTESIAN_POINT ( 'NONE',  ( 9.832129032723416984, 5.364583329919349275, 5.676582343750006032 ) ) ;
#49493 = CARTESIAN_POINT ( 'NONE',  ( 11.00000000000000000, 4.556349186104045934, 101.0312500040967620 ) ) ;
#49494 = CYLINDRICAL_SURFACE ( 'NONE', #23848, 3.999999999999976019 ) ;
#49495 = CARTESIAN_POINT ( 'NONE',  ( -24.54126587499996148, 201.1250000013656347, 171.4326545832179534 ) ) ;
#49496 = CYLINDRICAL_SURFACE ( 'NONE', #32190, 11.99999999999999645 ) ;
#49498 = CARTESIAN_POINT ( 'NONE',  ( 5.656854249492381470, 119.5625000000000000, 5.656854249492379694 ) ) ;
#49497 = CARTESIAN_POINT ( 'NONE',  ( 7.188101187500002709, 115.8125000020483952, 2.977408999572649151 ) ) ;
#49499 = DIRECTION ( 'NONE',  ( -0.000000000000000000, -1.000000000000000000, -0.000000000000000000 ) ) ;
#49500 =( BOUNDED_CURVE ( )  B_SPLINE_CURVE ( 2, ( #73528, #50889, #33565, #38467, #73903, #67873, #22208, #38094, #45235 ),
 .UNSPECIFIED., .F., .F. ) 
 B_SPLINE_CURVE_WITH_KNOTS ( ( 3, 2, 2, 2, 3 ),
 ( 0.8833333333333341919, 0.8916666666666676067, 0.9000000000000007994, 0.9083333333333341031, 0.9166666666666674068 ),
 .UNSPECIFIED. ) 
 CURVE ( )  GEOMETRIC_REPRESENTATION_ITEM ( )  RATIONAL_B_SPLINE_CURVE ( ( 0.9999999999999918954, 0.9238795325112948431, 1.000000000000000000, 0.9238795325112867385, 1.000000000000000000, 0.9238795325112867385, 1.000000000000000000, 0.9238795325112796331, 1.000000000000007105 ) ) 
 REPRESENTATION_ITEM ( '' )  );
#49501 = CARTESIAN_POINT ( 'NONE',  ( 11.35316468749999785, 120.5729166632526699, 3.042071309553174174 ) ) ;
#49502 = CARTESIAN_POINT ( 'NONE',  ( -1.836970198721029983E-15, 95.62499999317203958, 10.00000000000000178 ) ) ;
#49503 = CARTESIAN_POINT ( 'NONE',  ( -7.188101187500001821, 92.56250000204838102, -2.977408999572650483 ) ) ;
#49504 = CARTESIAN_POINT ( 'NONE',  ( 4.541265875000002339, 18.49999999863440436, -1.881053915767121554 ) ) ;
#49505 = CARTESIAN_POINT ( 'NONE',  ( 7.999999999999992895, -3.313708498984756279, 25.67405278392014978 ) ) ;
#49506 = DIRECTION ( 'NONE',  ( 0.000000000000000000, 0.000000000000000000, 1.000000000000000000 ) ) ;
#49507 = EDGE_LOOP ( 'NONE', ( #66645, #73591, #66949, #72091, #67168, #19569, #45572, #17966, #31754, #53865, #47877, #54923, #61405, #47775, #45367, #68925, #18894, #22583, #70414, #15347, #49458, #58048, #3043, #48124, #2322, #13406, #68214, #69887, #33523, #19939, #60030, #70101, #57345, #58037, #62228, #73024, #40480, #178, #70704, #29500, #6839, #12991, #16659, #15031, #59024, #34144, #41458, #31489, #73878, #52705, #50851, #41556, #26344, #57551, #15914, #42394, #67468, #33381, #898, #10508, #24777, #37471, #8778, #4374, #43555, #20683, #5228, #9222, #8821, #17497, #37850, #1860, #67638, #44840, #60958, #43166, #961, #19358, #65864, #13354, #47287, #20362, #44655, #63972, #16360, #59729, #1068, #11035, #63189, #43941, #32189, #5200, #19730, #54061 ) ) ;
#49508 = CARTESIAN_POINT ( 'NONE',  ( -4.000000000000015987, 200.6875000027312126, 143.6568542494924259 ) ) ;
#49509 = CARTESIAN_POINT ( 'NONE',  ( -2.765530957081998586, 292.7968750017070079, 6.676582343750001591 ) ) ;
#49510 = CARTESIAN_POINT ( 'NONE',  ( 5.000000000000001776, 187.7083333265053966, -8.660254037844389075 ) ) ;
#49511 = CARTESIAN_POINT ( 'NONE',  ( -7.999999999999991118, 3.313708498984756723, 3.924052783920144893 ) ) ;
#49512 = CARTESIAN_POINT ( 'NONE',  ( 5.676582343750001591, 171.6145833299193555, -9.832129032723420536 ) ) ;
#49513 = CARTESIAN_POINT ( 'NONE',  ( 3.999999999999960032, 198.0000000000000000, 142.0000000000000568 ) ) ;
#49514 = EDGE_CURVE ( 'NONE', #31332, #2280, #60483, .T. ) ;
#49515 = CARTESIAN_POINT ( 'NONE',  ( -4.999999999999998224, 203.5416666598387110, -8.660254037844389075 ) ) ;
#49516 = CARTESIAN_POINT ( 'NONE',  ( -5.000000000000000000, -29.68417822476656553, 4.268394125862918997 ) ) ;
#49517 = CARTESIAN_POINT ( 'NONE',  ( 10.18810118749999916, 1.247682550866122264E-15, 106.2812500020483810 ) ) ;
#49518 = ORIENTED_EDGE ( 'NONE', *, *, #23102, .F. ) ;
#49519 = CARTESIAN_POINT ( 'NONE',  ( -30.82842712474624491, 199.2500000027312126, 167.1715728752542418 ) ) ;
#49520 = CARTESIAN_POINT ( 'NONE',  ( -9.832129032723418760, 153.1770833299193555, -5.676582343750004256 ) ) ;
#49521 = CARTESIAN_POINT ( 'NONE',  ( -7.320508075688777261, 216.8750000000000000, -7.320508075688778149 ) ) ;
#49522 = CARTESIAN_POINT ( 'NONE',  ( 3.458734125000015425, 207.2500000013655779, 196.5673454167823877 ) ) ;
#49523 = DIRECTION ( 'NONE',  ( 0.000000000000000000, 0.000000000000000000, 1.000000000000000000 ) ) ;
#49524 = CARTESIAN_POINT ( 'NONE',  ( 9.832129032723420536, 61.51041666325268409, -5.676582343749999815 ) ) ;
#49525 = ORIENTED_EDGE ( 'NONE', *, *, #58545, .T. ) ;
#49526 = CARTESIAN_POINT ( 'NONE',  ( -10.18810118749999738, -4.220049686691941915, 112.7500000020483810 ) ) ;
#49527 = CARTESIAN_POINT ( 'NONE',  ( 3.211159895383561835, 9.562499998634406140, -3.211159895383561835 ) ) ;
#49528 = ORIENTED_EDGE ( 'NONE', *, *, #39212, .F. ) ;
#49529 = CARTESIAN_POINT ( 'NONE',  ( -1.320432766682874540E-15, 24.09374999795161543, 7.188101187500000044 ) ) ;
#49530 = CARTESIAN_POINT ( 'NONE',  ( -6.000000000000003553, 290.0000000034140157, -2.485281374238571317 ) ) ;
#49531 = AXIS2_PLACEMENT_3D ( 'NONE', #13392, #54153, #71108 ) ;
#49532 = CARTESIAN_POINT ( 'NONE',  ( -2.222453528114265639E-12, 168.7499999999998295, 10.00000000000000178 ) ) ;
#49533 = CARTESIAN_POINT ( 'NONE',  ( 5.082755093536324154, 20.15624999795161543, 5.082755093536326818 ) ) ;
#49534 = ADVANCED_FACE ( 'NONE', ( #54632 ), #60651, .T. ) ;
#49535 = CARTESIAN_POINT ( 'NONE',  ( 2.977408999572646486, 7.188101187499992051, 4.017802781871751883 ) ) ;
#49536 = CARTESIAN_POINT ( 'NONE',  ( -4.220049686691935698, 10.18810118749999916, 112.7500000020483810 ) ) ;
#49537 = EDGE_CURVE ( 'NONE', #13268, #66327, #54260, .T. ) ;
#49538 = AXIS2_PLACEMENT_3D ( 'NONE', #41735, #52322, #46651 ) ;
#49539 = CARTESIAN_POINT ( 'NONE',  ( -37.94562015984924841, 38.00000000000001421, 126.9999999999999716 ) ) ;
#49540 = CARTESIAN_POINT ( 'NONE',  ( 4.000000000000001776, 7.812499997268813168, -1.656854249492381248 ) ) ;
#49541 = CARTESIAN_POINT ( 'NONE',  ( -23.99999999999996447, 208.8125000027312126, 171.6568542494926817 ) ) ;
#49542 = VECTOR ( 'NONE', #12918, 1000.000000000000000 ) ;
#49543 = ORIENTED_EDGE ( 'NONE', *, *, #31043, .F. ) ;
#49544 = ADVANCED_FACE ( 'NONE', ( #24462 ), #59183, .T. ) ;
#49545 = CARTESIAN_POINT ( 'NONE',  ( 1.432654583217664479, 205.7500000013656063, 201.4587341250000065 ) ) ;
#49546 = CARTESIAN_POINT ( 'NONE',  ( -29.65685424949245430, 194.1875000027312126, 166.0000000000004263 ) ) ;
#49547 = CARTESIAN_POINT ( 'NONE',  ( 4.541265875000002339, 7.374999998634408804, -1.881053915767121554 ) ) ;
#49548 = ADVANCED_FACE ( 'NONE', ( #13128 ), #19906, .F. ) ;
#49549 = CARTESIAN_POINT ( 'NONE',  ( -2.828427124746192067, 13.62500000000000000, 2.828427124746190735 ) ) ;
#49550 = CARTESIAN_POINT ( 'NONE',  ( -7.188101187499992051, 0.000000000000000000, 25.48655278187175810 ) ) ;
#49551 = ORIENTED_EDGE ( 'NONE', *, *, #67147, .T. ) ;
#49552 = ORIENTED_EDGE ( 'NONE', *, *, #6764, .F. ) ;
#49553 = CARTESIAN_POINT ( 'NONE',  ( 4.220049686691934809, 10.18810118749999916, 116.6875000020483952 ) ) ;
#49554 = CARTESIAN_POINT ( 'NONE',  ( -2.679491924295767102, 201.4583333333319501, -10.00000000000892442 ) ) ;
#49555 = CARTESIAN_POINT ( 'NONE',  ( 1.432654583217664479, 204.7500000013656063, 201.4587341250000065 ) ) ;
#49556 = CARTESIAN_POINT ( 'NONE',  ( 24.54126587499998280, 198.1250000013656063, 168.5673454167822740 ) ) ;
#49557 = CARTESIAN_POINT ( 'NONE',  ( -10.00000000000000000, 67.29166666666667140, -2.679491924311229845 ) ) ;
#49558 = AXIS2_PLACEMENT_3D ( 'NONE', #13360, #37136, #24327 ) ;
#49559 = CARTESIAN_POINT ( 'NONE',  ( -5.082755093536325930, 91.34375000204838102, -5.082755093536325930 ) ) ;
#49560 = CARTESIAN_POINT ( 'NONE',  ( -6.000000000000003553, 291.9374999999999432, -2.485281374238571317 ) ) ;
#49562 = PLANE ( 'NONE',  #48202 ) ;
#49561 = CARTESIAN_POINT ( 'NONE',  ( 29.65685424949235482, 207.5625000027312126, 165.9999999999998863 ) ) ;
#49563 = VERTEX_POINT ( 'NONE', #59910 ) ;
#49564 = CARTESIAN_POINT ( 'NONE',  ( 5.656854249492378806, 8.624999995903221972, 5.656854249492381470 ) ) ;
#49565 = CARTESIAN_POINT ( 'NONE',  ( -2.216418498312179075, -16.40908668940157611, 68.78644440154799611 ) ) ;
#49566 = CARTESIAN_POINT ( 'NONE',  ( 2.828427124746152987, 199.2500000027312126, 139.1715728752538723 ) ) ;
#49567 = CARTESIAN_POINT ( 'NONE',  ( 7.999999999843520726, -5.003525229023116430E-05, 24.26780136833107093 ) ) ;
#49568 = DIRECTION ( 'NONE',  ( -0.000000000000000000, -0.000000000000000000, -1.000000000000000000 ) ) ;
#49569 = CARTESIAN_POINT ( 'NONE',  ( 2.679491924311235174, 251.4583333333333428, 9.999999999999998224 ) ) ;
#49570 = CARTESIAN_POINT ( 'NONE',  ( -38.00000000000000000, 272.0000000000000000, 20.00000000000003553 ) ) ;
#49571 = CARTESIAN_POINT ( 'NONE',  ( -10.00000000000000178, 192.5000000000000000, -1.224646799147353454E-15 ) ) ;
#49572 = CARTESIAN_POINT ( 'NONE',  ( 11.35316468750000141, 1.093749996586016682, 0.000000000000000000 ) ) ;
#49573 = CARTESIAN_POINT ( 'NONE',  ( -7.188101187499992051, 0.000000000000000000, 24.36155278187175810 ) ) ;
#49574 = CARTESIAN_POINT ( 'NONE',  ( -11.35316468750000141, 158.5937499965860127, -1.390361679473963753E-15 ) ) ;
#49575 = FACE_OUTER_BOUND ( 'NONE', #28520, .T. ) ;
#49576 = CARTESIAN_POINT ( 'NONE',  ( 5.094044972490348933, 8.823157690132404696, 67.53052377765949643 ) ) ;
#49577 = CARTESIAN_POINT ( 'NONE',  ( -4.556349186104048599, -10.99999999999999822, 82.46875000409677625 ) ) ;
#49579 = LINE ( 'NONE', #38271, #33902 ) ;
#49578 = CARTESIAN_POINT ( 'NONE',  ( -11.00000000000000000, 0.000000000000000000, 118.0000000000000000 ) ) ;
#49580 = EDGE_LOOP ( 'NONE', ( #53088, #47591, #69653, #2889 ) ) ;
#49581 = CARTESIAN_POINT ( 'NONE',  ( -5.676582343749998039, 22.76041666325268409, -9.832129032723420536 ) ) ;
#49582 = VECTOR ( 'NONE', #54284, 1000.000000000000114 ) ;
#49583 = CARTESIAN_POINT ( 'NONE',  ( 11.00000000000000000, 1.347111479062088405E-15, 76.93750000409677625 ) ) ;
#49584 = EDGE_CURVE ( 'NONE', #39015, #34530, #7493, .T. ) ;
#49586 = CARTESIAN_POINT ( 'NONE',  ( 6.123233995736767268E-16, 33.12499999317203248, -10.00000000000000178 ) ) ;
#49585 = CYLINDRICAL_SURFACE ( 'NONE', #27560, 10.99999999999999645 ) ;
#49587 = CARTESIAN_POINT ( 'NONE',  ( -4.898587196589412829E-16, 115.6250000000000000, -8.000000000000000000 ) ) ;
#49588 = CARTESIAN_POINT ( 'NONE',  ( 1.432654583217607858, 204.6250000013656063, 138.5412658750000787 ) ) ;
#49589 = CARTESIAN_POINT ( 'NONE',  ( -10.00000000000000355, 44.58333332650536818, 2.679491924311223183 ) ) ;
#49590 = VECTOR ( 'NONE', #38922, 1000.000000000000000 ) ;
#49591 = CARTESIAN_POINT ( 'NONE',  ( -7.188101187500001821, 110.5625000020483810, -2.977408999572650483 ) ) ;
#49592 = CARTESIAN_POINT ( 'NONE',  ( -1.881053915767124440, 7.124999998634407916, 4.541265875000001451 ) ) ;
#49593 = CARTESIAN_POINT ( 'NONE',  ( 2.679491924311226292, 218.9583333333333428, 10.00000000000001421 ) ) ;
#49594 = CARTESIAN_POINT ( 'NONE',  ( -7.999999999999989342, -3.313708498984762496, 6.924052779823366421 ) ) ;
#49596 = CARTESIAN_POINT ( 'NONE',  ( 2.828427124746190291, 0.8750000000000002220, 2.828427124746192067 ) ) ;
#49595 = CARTESIAN_POINT ( 'NONE',  ( 1.037253499927448308, 194.5743829752848626, 138.5729979015108881 ) ) ;
#49597 = ORIENTED_EDGE ( 'NONE', *, *, #29605, .F. ) ;
#49598 =( BOUNDED_CURVE ( )  B_SPLINE_CURVE ( 2, ( #66316, #74214, #45539, #27074, #16484 ),
 .UNSPECIFIED., .F., .F. ) 
 B_SPLINE_CURVE_WITH_KNOTS ( ( 3, 2, 3 ),
 ( 0.000000000000000000, 0.005681818181818181976, 0.01136363636363636395 ),
 .UNSPECIFIED. ) 
 CURVE ( )  GEOMETRIC_REPRESENTATION_ITEM ( )  RATIONAL_B_SPLINE_CURVE ( ( 1.000000000000000000, 0.9238795325112867385, 1.000000000000000000, 0.9238795325112867385, 1.000000000000000000 ) ) 
 REPRESENTATION_ITEM ( '' )  );
#49599 = ORIENTED_EDGE ( 'NONE', *, *, #52654, .T. ) ;
#49600 = EDGE_CURVE ( 'NONE', #17893, #53923, #68840, .T. ) ;
#49601 = CARTESIAN_POINT ( 'NONE',  ( 5.000000000000004441, 30.83333333333333925, -8.660254037844390851 ) ) ;
#49602 = CARTESIAN_POINT ( 'NONE',  ( 7.999999999999991118, 3.313708498984758055, 1.674052779823364423 ) ) ;
#49603 = CARTESIAN_POINT ( 'NONE',  ( -11.35316468749999963, 224.2187500034139873, 0.000000000000000000 ) ) ;
#49604 = CARTESIAN_POINT ( 'NONE',  ( -5.676582343750006032, 134.1145833299193555, 9.832129032723418760 ) ) ;
#49605 = ORIENTED_EDGE ( 'NONE', *, *, #41016, .T. ) ;
#49606 = CARTESIAN_POINT ( 'NONE',  ( -6.000000000000001776, 298.0000000000000000, 0.000000000000000000 ) ) ;
#49607 = CARTESIAN_POINT ( 'NONE',  ( 7.204075437095966983, 7.204075437095967871, 95.59375000204836681 ) ) ;
#49608 = CARTESIAN_POINT ( 'NONE',  ( 27.99999999999999645, 210.0000000000000284, 173.9999999999998863 ) ) ;
#49609 = CARTESIAN_POINT ( 'NONE',  ( -1.656854249492348607, 207.1875000000000284, 202.0000000000000284 ) ) ;
#49610 = CARTESIAN_POINT ( 'NONE',  ( -7.320508075688778149, 154.9999999931720538, 7.320508075688769267 ) ) ;
#49612 = CARTESIAN_POINT ( 'NONE',  ( 9.832129032723420536, 121.1979166632526983, -5.676582343749999815 ) ) ;
#49611 = CARTESIAN_POINT ( 'NONE',  ( 30.82842712474616675, 196.1250000000000284, 172.8284271247460993 ) ) ;
#49613 = CYLINDRICAL_SURFACE ( 'NONE', #16836, 10.00000000000000000 ) ;
#49614 = VERTEX_POINT ( 'NONE', #2196 ) ;
#49615 = EDGE_CURVE ( 'NONE', #17647, #58637, #61618, .T. ) ;
#49616 = CYLINDRICAL_SURFACE ( 'NONE', #52113, 8.000000000000000000 ) ;
#49617 = CARTESIAN_POINT ( 'NONE',  ( 3.042071309553159519, 115.0520833299193555, 11.35316468750000141 ) ) ;
#49618 = CARTESIAN_POINT ( 'NONE',  ( 3.458734125000015425, 205.9375000013656063, 198.0000000000000284 ) ) ;
#49619 = CARTESIAN_POINT ( 'NONE',  ( 7.188101187500000933, 15.93749999795161365, -2.977408999572650483 ) ) ;
#49620 = CARTESIAN_POINT ( 'NONE',  ( 10.18810118749999916, 1.247682550866122264E-15, 85.28125000204836681 ) ) ;
#49621 = CARTESIAN_POINT ( 'NONE',  ( -5.676582343749998039, 22.76041666325268409, -9.832129032723420536 ) ) ;
#49623 = ORIENTED_EDGE ( 'NONE', *, *, #25899, .F. ) ;
#49622 =( BOUNDED_CURVE ( )  B_SPLINE_CURVE ( 2, ( #59935, #71242, #31260, #7886, #66715, #3719, #30891, #65961, #54289 ),
 .UNSPECIFIED., .F., .F. ) 
 B_SPLINE_CURVE_WITH_KNOTS ( ( 3, 2, 2, 2, 3 ),
 ( 0.9333333333333341253, 0.9416666666666674290, 0.9500000000000007327, 0.9583333333333341475, 0.9666666666666674512 ),
 .UNSPECIFIED. ) 
 CURVE ( )  GEOMETRIC_REPRESENTATION_ITEM ( )  RATIONAL_B_SPLINE_CURVE ( ( 0.9999999999999928946, 0.9238795325112938439, 1.000000000000000000, 0.9238795325112867385, 1.000000000000000000, 0.9238795325112867385, 1.000000000000000000, 0.9238795325112796331, 1.000000000000007105 ) ) 
 REPRESENTATION_ITEM ( '' )  );
#49624 = CARTESIAN_POINT ( 'NONE',  ( -4.898587196589412829E-16, 96.31250000409677625, -8.000000000000000000 ) ) ;
#49625 = CARTESIAN_POINT ( 'NONE',  ( -3.317071493978880348, -8.008118988124989457, 26.79436528394063188 ) ) ;
#49626 = CARTESIAN_POINT ( 'NONE',  ( 1.432654583217608080, 208.8750000013656347, 138.5412658750000503 ) ) ;
#49627 = PRODUCT_DEFINITION ( 'UNKNOWN', '', #74308, #40272 ) ;
#49628 = CARTESIAN_POINT ( 'NONE',  ( 3.999999999999960032, 201.0000000000000000, 142.0000000000000568 ) ) ;
#49629 = CARTESIAN_POINT ( 'NONE',  ( -7.188101187500000044, 1.218749997951610098, -8.802885111219163269E-16 ) ) ;
#49630 = CARTESIAN_POINT ( 'NONE',  ( -2.765530957081998586, 290.6406250017069510, 6.676582343750001591 ) ) ;
#49631 = CARTESIAN_POINT ( 'NONE',  ( 0.000000000000000000, 125.0000000000000000, 8.000000000000000000 ) ) ;
#49632 = CARTESIAN_POINT ( 'NONE',  ( -8.000000000000000000, 16.96874999590322730, -3.313708498984762496 ) ) ;
#49633 = ORIENTED_EDGE ( 'NONE', *, *, #31063, .F. ) ;
#49634 = CARTESIAN_POINT ( 'NONE',  ( -5.676582343750006032, 144.4270833299193555, 9.832129032723418760 ) ) ;
#49635 = CARTESIAN_POINT ( 'NONE',  ( -4.220049686691935698, 10.18810118749999916, 80.87500000204836681 ) ) ;
#49636 = ADVANCED_FACE ( 'NONE', ( #44422 ), #67437, .T. ) ;
#49637 = CARTESIAN_POINT ( 'NONE',  ( -25.55430564589119058, 197.3125000013656063, 167.5543056458915316 ) ) ;
#49638 = CARTESIAN_POINT ( 'NONE',  ( 8.000000000000000000, 27.00000000000000355, 0.000000000000000000 ) ) ;
#49639 = CARTESIAN_POINT ( 'NONE',  ( -4.541265875000002339, 14.93749999863440792, -5.561446717895856393E-16 ) ) ;
#49640 = ORIENTED_EDGE ( 'NONE', *, *, #8071, .F. ) ;
#49641 = CARTESIAN_POINT ( 'NONE',  ( -3.999999999999960032, 203.1250000027312126, 198.0000000000000284 ) ) ;
#49642 = CARTESIAN_POINT ( 'NONE',  ( -2.828427124746209831, 208.3750000000000284, 139.1715728752538723 ) ) ;
#49643 = CARTESIAN_POINT ( 'NONE',  ( -23.99999999999995737, 203.8125000027312410, 171.6568542494926817 ) ) ;
#49644 = AXIS2_PLACEMENT_3D ( 'NONE', #60498, #37122, #20496 ) ;
#49645 = CARTESIAN_POINT ( 'NONE',  ( 7.999999999999991118, 3.313708498984758055, 13.67405277982336465 ) ) ;
#49646 = VERTEX_POINT ( 'NONE', #62141 ) ;
#49647 = CARTESIAN_POINT ( 'NONE',  ( -7.188101187500000044, 13.21874999795161187, -8.802885111219163269E-16 ) ) ;
#49648 = CARTESIAN_POINT ( 'NONE',  ( 7.999999999999992895, -3.313708498984756279, 9.174052783920146226 ) ) ;
#49649 = CARTESIAN_POINT ( 'NONE',  ( 7.071067811865482611, 22.99999999999999645, 1.000000000000000000 ) ) ;
#49650 = CARTESIAN_POINT ( 'NONE',  ( -11.35316468749999785, 193.0729166632526415, -3.042071309553167513 ) ) ;
#49651 = CARTESIAN_POINT ( 'NONE',  ( -7.188101187500000044, 114.0312500020483952, 0.000000000000000000 ) ) ;
#49652 = CARTESIAN_POINT ( 'NONE',  ( -3.673940397442060854E-16, 290.8125000034140157, -6.000000000000001776 ) ) ;
#49653 = CARTESIAN_POINT ( 'NONE',  ( 6.676582343750003368, 287.8906250017069510, 2.765530957081995478 ) ) ;
#49655 = CARTESIAN_POINT ( 'NONE',  ( -18.00000000000000355, -3.500879649426325457, -0.1509495798675467015 ) ) ;
#49654 = CARTESIAN_POINT ( 'NONE',  ( -1.836970198721029983E-15, 130.6249999931720254, 10.00000000000000178 ) ) ;
#49656 = VERTEX_POINT ( 'NONE', #32748 ) ;
#49657 = CARTESIAN_POINT ( 'NONE',  ( 9.832129032723416984, 256.8229166700806445, -5.676582343750003368 ) ) ;
#49658 = AXIS2_PLACEMENT_3D ( 'NONE', #67633, #60845, #49523 ) ;
#49659 = CARTESIAN_POINT ( 'NONE',  ( 2.977408999572646486, 7.188101187499991163, 25.39280278187176165 ) ) ;
#49660 = LINE ( 'NONE', #60602, #26907 ) ;
#49661 = CARTESIAN_POINT ( 'NONE',  ( -5.656854249492375253, 5.656854249492375253, 15.83030278392014800 ) ) ;
#49662 = CARTESIAN_POINT ( 'NONE',  ( 1.308779242313053537, -60.23127520338580609, -22.90411807697111257 ) ) ;
#49663 = CARTESIAN_POINT ( 'NONE',  ( -1.432654583217607414, 198.5000000013656347, 194.5412658750000219 ) ) ;
#49664 = CYLINDRICAL_SURFACE ( 'NONE', #26897, 8.000000000000000000 ) ;
#49665 = DIRECTION ( 'NONE',  ( 1.000000000000000000, 0.000000000000000000, -0.000000000000000000 ) ) ;
#49666 = CARTESIAN_POINT ( 'NONE',  ( -3.313708498984762052, 94.71874999999998579, -8.000000000000000000 ) ) ;
#49667 = CARTESIAN_POINT ( 'NONE',  ( 11.35316468749999785, 115.8854166632526841, 3.042071309553174174 ) ) ;
#49668 = CARTESIAN_POINT ( 'NONE',  ( 8.000000000000000000, 98.84375000000000000, -3.313708498984762496 ) ) ;
#49669 = CARTESIAN_POINT ( 'NONE',  ( -11.00000000000000000, 4.556349186104045934, 69.90624999999998579 ) ) ;
#49672 = CARTESIAN_POINT ( 'NONE',  ( 0.000000000000000000, 0.000000000000000000, 0.000000000000000000 ) ) ;
#49671 = CARTESIAN_POINT ( 'NONE',  ( 24.54126587500000056, 201.2500000013656063, 171.4326545832175839 ) ) ;
#49670 = CARTESIAN_POINT ( 'NONE',  ( 27.99999999999996447, 198.6875000013655779, 173.4587341249998929 ) ) ;
#49673 = EDGE_LOOP ( 'NONE', ( #72780, #42396, #9831, #61582 ) ) ;
#49674 = AXIS2_PLACEMENT_3D ( 'NONE', #42550, #71957, #37276 ) ;
#49675 = CARTESIAN_POINT ( 'NONE',  ( 31.99999999999998579, 205.4375000027312126, 168.3431457505074889 ) ) ;
#49676 = EDGE_CURVE ( 'NONE', #31901, #50470, #42209, .T. ) ;
#49677 = CARTESIAN_POINT ( 'NONE',  ( 11.35316468749999963, 220.9895833299193555, -3.042071309553165293 ) ) ;
#49678 = VECTOR ( 'NONE', #51186, 1000.000000000000000 ) ;
#49679 = CARTESIAN_POINT ( 'NONE',  ( 3.458734124999959914, 197.3750000013656063, 143.4326545832176976 ) ) ;
#49680 = CARTESIAN_POINT ( 'NONE',  ( 26.56734541678237704, 197.2500000013656063, 166.5412658749999650 ) ) ;
#49681 = CARTESIAN_POINT ( 'NONE',  ( 11.00000000000000000, 1.347111479062088405E-15, 112.9375000040967763 ) ) ;
#49682 = CARTESIAN_POINT ( 'NONE',  ( 5.676582343749993598, 210.2604166632526699, 9.832129032723422313 ) ) ;
#49683 = DIRECTION ( 'NONE',  ( -1.000000000000000000, 0.000000000000000000, 0.000000000000000000 ) ) ;
#49684 = CYLINDRICAL_SURFACE ( 'NONE', #26518, 10.00000000000000178 ) ;
#49685 = CARTESIAN_POINT ( 'NONE',  ( 4.541265875000001451, 19.24999999863440436, 1.881053915767124440 ) ) ;
#49686 = CARTESIAN_POINT ( 'NONE',  ( 29.43265458321766204, 196.1250000013656063, 166.5412658749999650 ) ) ;
#49687 = CARTESIAN_POINT ( 'NONE',  ( 3.313708498984762496, -7.999999999999989342, 25.29905277982336642 ) ) ;
#49689 = DIRECTION ( 'NONE',  ( 0.000000000000000000, 0.000000000000000000, -1.000000000000000000 ) ) ;
#49688 = CARTESIAN_POINT ( 'NONE',  ( 4.999999999999991118, 184.1666666666666856, 8.660254037844387298 ) ) ;
#49690 = CARTESIAN_POINT ( 'NONE',  ( 11.35316468749999785, 85.57291666325268409, 3.042071309553174174 ) ) ;
#49691 = VERTEX_POINT ( 'NONE', #4437 ) ;
#49692 = EDGE_CURVE ( 'NONE', #44612, #50104, #38774, .T. ) ;
#49693 = DIRECTION ( 'NONE',  ( 0.000000000000000000, 0.000000000000000000, -1.000000000000000000 ) ) ;
#49694 = CARTESIAN_POINT ( 'NONE',  ( -5.082755093536325042, 17.53124999795161187, -5.082755093536325930 ) ) ;
#49695 = CARTESIAN_POINT ( 'NONE',  ( -8.660254037844387298, 222.7083333401613174, -4.999999999999999112 ) ) ;
#49696 = CARTESIAN_POINT ( 'NONE',  ( 9.832129032723420536, 261.3020833367473301, 5.676582343749996262 ) ) ;
#49697 = CARTESIAN_POINT ( 'NONE',  ( -3.042071309553164404, 92.23958332991935549, -11.35316468749999963 ) ) ;
#49698 = VERTEX_POINT ( 'NONE', #44052 ) ;
#49699 = CARTESIAN_POINT ( 'NONE',  ( 29.65685424949240456, 208.1875000027312126, 173.9999999999999716 ) ) ;
#49700 = CARTESIAN_POINT ( 'NONE',  ( -4.220049686691935698, 10.18810118749999916, 112.3750000020483810 ) ) ;
#49701 = LINE ( 'NONE', #55746, #71929 ) ;
#49702 = CARTESIAN_POINT ( 'NONE',  ( 3.458734125000015425, 209.2500000013655779, 196.5673454167823877 ) ) ;
#49703 = CARTESIAN_POINT ( 'NONE',  ( 3.313708498984697215, 117.9687499999999858, 8.000000000000063949 ) ) ;
#49705 = CARTESIAN_POINT ( 'NONE',  ( 8.311093377946837890, 81.40624999658601268, -8.311093377946837890 ) ) ;
#49704 = CARTESIAN_POINT ( 'NONE',  ( 1.469576158976823947E-15, 121.0625000040967763, 8.000000000000000000 ) ) ;
#49706 = CARTESIAN_POINT ( 'NONE',  ( 7.999999999999992895, -3.313708498984756279, 18.17405278392014623 ) ) ;
#49707 = CARTESIAN_POINT ( 'NONE',  ( -31.45873412499999944, 201.9375000013656063, 170.0000000000003979 ) ) ;
#49708 = DIRECTION ( 'NONE',  ( 0.000000000000000000, 0.000000000000000000, -1.000000000000000000 ) ) ;
#49709 = CARTESIAN_POINT ( 'NONE',  ( 8.660254037844389075, 182.2916666598387110, -5.000000000000000000 ) ) ;
#49710 = CARTESIAN_POINT ( 'NONE',  ( 2.980397541819803653, -45.39460101182298501, 139.1435789998069765 ) ) ;
#49711 = CARTESIAN_POINT ( 'NONE',  ( 8.311093377946837890, 76.71874999658601268, -8.311093377946837890 ) ) ;
#49712 = CARTESIAN_POINT ( 'NONE',  ( -6.676582343750000703, 294.5156250017069510, 2.765530957082001251 ) ) ;
#49713 = CARTESIAN_POINT ( 'NONE',  ( 4.220049686691941027, -10.18810118749999738, 106.0000000020483668 ) ) ;
#49714 = CARTESIAN_POINT ( 'NONE',  ( 9.832129032723416984, 205.3645833299193555, 5.676582343750006032 ) ) ;
#49715 = ORIENTED_EDGE ( 'NONE', *, *, #2490, .T. ) ;
#49716 = CARTESIAN_POINT ( 'NONE',  ( -3.228176881614092331, 60.48309044411788449, 23.05774181791989008 ) ) ;
#49717 = CARTESIAN_POINT ( 'NONE',  ( 2.828427124746190291, 3.624999997268813168, 2.828427124746192067 ) ) ;
#49719 = CARTESIAN_POINT ( 'NONE',  ( -3.042071309553163960, 202.2395833299193555, -11.35316468749999963 ) ) ;
#49718 = CARTESIAN_POINT ( 'NONE',  ( -1.656854249492383468, 11.43749999726881406, 4.000000000000000888 ) ) ;
#49720 = FACE_OUTER_BOUND ( 'NONE', #29031, .T. ) ;
#49721 = CARTESIAN_POINT ( 'NONE',  ( 8.660254037844389075, 220.2083333401613174, 4.999999999999997335 ) ) ;
#49722 = CARTESIAN_POINT ( 'NONE',  ( -4.721056650415999201, 299.3281250017069510, -4.721056650415999201 ) ) ;
#49723 = ORIENTED_EDGE ( 'NONE', *, *, #50675, .T. ) ;
#49724 = CARTESIAN_POINT ( 'NONE',  ( -11.35316468750000141, 193.8020833299193271, 3.042071309553159963 ) ) ;
#49725 =( BOUNDED_SURFACE ( )  B_SPLINE_SURFACE ( 1, 2, ( 
 ( #72790, #43736, #32434, #73159, #21831, #20719, #67129, #26367, #73524, #49389, #27129, #15424, #21467, #38463, #37717, #66750, #3755, #44489, #61466, #44864, #72408, #15056, #9791, #4504, #32813, #27497, #67869, #38090, #61839, #43354, #14678, #61087, #60717, #9416, #9038, #55445, #55821, #56192, #32051, #4139, #55071, #3380, #26756, #49774, #50144, #67502, #15801, #38836, #33195, #59488, #30439, #48143, #26241, #59850, #24762, #42114, #36843, #37211, #7800, #49260, #53459, #2504, #47772, #1777, #71518, #65125, #25499, #31172, #2876, #8910, #14546, #19474, #48884, #54197, #31922, #30803, #19842, #66243, #54570, #70794, #48513, #19108, #42486, #13435, #8164, #72274, #36471, #42850, #65867, #14176, #54943, #60208, #2134, #7433, #71895, #71152, #25126, #65503, #3251, #13798, #53825, #60584, #8532, #31547, #20587, #25862, #20209, #43229, #43600, #37584, #66614, #36106, #59123, #26541, #66921, #13721, #72195, #38258, #36766, #20508, #60136, #44286, #49185, #20890, #37512, #25792, #48813, #59778, #8087, #55617, #54499, #71818, #37134, #15226, #54870, #61261, #31090, #43523, #9207, #9591, #43153, #14473, #60511, #19770, #49942, #54119, #20137, #8836, #3179, #66169, #31847, #72956, #71442, #26166, #42778, #2430, #37887, #66538, #49566, #32610, #25423, #48439, #43911, #21262, #14847, #65795, #3934, #26924, #14098, #8455, #60885, #32227, #55245, #3551, #72584, #31475, #2804, #73330, #10696, #28045, #55990, #38637, #21634, #62366, #45766, #68777, #57484, #56731, #27293, #61639, #67300, #33354, #33729, #16705, #11441, #44659, #74067, #22367, #15971, #9956, #62004, #11075, #22745, #62735, #5050, #149, #51801, #39000, #51055, #22006, #45389, #32989, #4303, #10329, #17087, #63115, #40109, #51425, #56355, #34477, #50676, #74437, #5789, #28786, #68405, #39735, #23125, #50309, #15598, #4674, #5413, #67672, #34103, #27670, #73695, #39370, #45033, #68041, #16332, #57098, #28418 ),
 ( #1972, #6894, #53294, #69904, #58231, #6530, #69154, #40483, #13270, #12176, #29536, #69528, #24600, #12546, #47606, #17462, #29906, #41596, #70630, #886, #46881, #18216, #52184, #7635, #46137, #52547, #41229, #35574, #23871, #64236, #30641, #29169, #58588, #515, #34849, #70272, #52920, #7266, #64961, #11810, #63488, #1619, #53660, #1253, #57854, #41953, #36309, #6160, #23495, #24231, #47245, #18584, #64610, #12906, #35940, #58959, #46509, #30275, #18949, #17840, #40856, #63863, #59326, #35214, #26449, #15138, #14386, #59690, #70992, #24964, #65702, #43060, #49094, #43821, #2339, #31757, #54777, #48348, #19309, #19679, #43436, #55154, #20420, #37420, #32518, #9503, #71355, #66076, #54406, #20042, #42319, #65337, #42690, #3460, #20802, #49474, #9119, #14006, #72493, #8364, #32136, #66835, #38170, #3088, #60420, #61173, #7998, #55531, #37043, #37799, #47979, #72107, #54029, #13639, #71728, #8747, #26073, #66452, #14759, #36678, #60043, #2713, #60794, #31004, #25333, #31380, #25701, #48721, #22657, #33639, #45676, #63029, #32899, #57016, #40027, #11354, #38549, #5329, #61550, #68691, #73242, #50589, #62652, #39654, #73607, #10986, #3841, #27962, #21914, #27580, #67586, #15509, #34389, #9872, #27204, #72870, #15882, #17001, #44945, #67212, #55904, #4586, #4961, #50221, #26837, #21174, #67953, #4215, #44199, #39283, #21547, #16245, #62285, #45307, #51339, #28331, #61916, #16619, #10613, #74347, #44573, #56646, #34019, #22284, #38914, #50967, #10241, #33268, #56267, #73981, #49852, #68321, #41143, #29452, #23785, #53204, #58500, #23410, #28697, #70187, #69439, #46425, #63772, #1537, #17750, #34763, #7180, #11723, #40399, #18496, #64148, #47155, #430, #64882, #63397, #24143, #41505, #13184, #52461, #799, #47522, #64521, #69811, #23039, #12819, #30186, #40765, #24517, #46789, #35854, #18863, #58869, #18127, #12458, #52098, #12089, #70547, #41869, #6071, #35488, #57765 ) ),
 .UNSPECIFIED., .F., .F., .F. ) 
 B_SPLINE_SURFACE_WITH_KNOTS ( ( 2, 2 ),
 ( 3, 2, 2, 2, 2, 2, 2, 2, 2, 2, 2, 2, 2, 2, 2, 2, 2, 2, 2, 2, 2, 2, 2, 2, 2, 2, 2, 2, 2, 2, 2, 2, 2, 2, 2, 2, 2, 2, 2, 2, 2, 2, 2, 2, 2, 2, 2, 2, 2, 2, 2, 2, 2, 2, 2, 2, 2, 2, 2, 2, 2, 2, 2, 2, 2, 2, 2, 2, 2, 2, 2, 2, 2, 2, 2, 2, 2, 2, 2, 2, 2, 2, 2, 2, 2, 2, 2, 2, 2, 2, 2, 2, 2, 2, 2, 2, 2, 2, 2, 2, 2, 2, 2, 2, 2, 2, 2, 2, 2, 2, 2, 2, 2, 2, 2, 2, 2, 2, 2, 2, 3 ),
 ( 0.000000000000000000, 1.000000000000000000 ),
 ( 0.000000000000000000, 0.008333333333333333218, 0.01666666666666666644, 0.02500000000000000139, 0.03333333333333333287, 0.04166666666666666435, 0.05000000000000000278, 0.05833333333333333426, 0.06666666666666666574, 0.07499999999999999722, 0.08333333333333332871, 0.09166666666666666019, 0.1000000000000000056, 0.1083333333333333370, 0.1166666666666666685, 0.1250000000000000000, 0.1333333333333333315, 0.1416666666666666630, 0.1499999999999999944, 0.1583333333333333259, 0.1666666666666666574, 0.1749999999999999889, 0.1833333333333333204, 0.1916666666666666796, 0.2000000000000000111, 0.2083333333333333426, 0.2166666666666666741, 0.2250000000000000056, 0.2333333333333333370, 0.2416666666666666685, 0.2500000000000000000, 0.2583333333333333592, 0.2666666666666666630, 0.2750000000000000222, 0.2833333333333333259, 0.2916666666666666852, 0.2999999999999999889, 0.3083333333333333481, 0.3166666666666666519, 0.3250000000000000111, 0.3333333333333333148, 0.3416666666666666741, 0.3499999999999999778, 0.3583333333333333370, 0.3666666666666666408, 0.3750000000000000000, 0.3833333333333333592, 0.3916666666666666630, 0.4000000000000000222, 0.4083333333333333259, 0.4166666666666666852, 0.4249999999999999889, 0.4333333333333333481, 0.4416666666666666519, 0.4500000000000000111, 0.4583333333333333148, 0.4666666666666666741, 0.4749999999999999778, 0.4833333333333333370, 0.4916666666666666408, 0.5000000000000000000, 0.5083333333333333037, 0.5166666666666667185, 0.5250000000000000222, 0.5333333333333333259, 0.5416666666666666297, 0.5500000000000000444, 0.5583333333333333481, 0.5666666666666666519, 0.5749999999999999556, 0.5833333333333333703, 0.5916666666666666741, 0.5999999999999999778, 0.6083333333333332815, 0.6166666666666666963, 0.6250000000000000000, 0.6333333333333333037, 0.6416666666666667185, 0.6500000000000000222, 0.6583333333333333259, 0.6666666666666666297, 0.6750000000000000444, 0.6833333333333333481, 0.6916666666666666519, 0.6999999999999999556, 0.7083333333333333703, 0.7166666666666666741, 0.7249999999999999778, 0.7333333333333332815, 0.7416666666666666963, 0.7500000000000000000, 0.7583333333333333037, 0.7666666666666667185, 0.7750000000000000222, 0.7833333333333333259, 0.7916666666666666297, 0.8000000000000000444, 0.8083333333333333481, 0.8166666666666666519, 0.8249999999999999556, 0.8333333333333333703, 0.8416666666666666741, 0.8499999999999999778, 0.8583333333333332815, 0.8666666666666666963, 0.8750000000000000000, 0.8833333333333333037, 0.8916666666666667185, 0.9000000000000000222, 0.9083333333333333259, 0.9166666666666666297, 0.9250000000000000444, 0.9333333333333333481, 0.9416666666666666519, 0.9499999999999999556, 0.9583333333333333703, 0.9666666666666666741, 0.9749999999999999778, 0.9833333333333332815, 0.9916666666666666963, 1.000000000000000000 ),
 .UNSPECIFIED. ) 
 GEOMETRIC_REPRESENTATION_ITEM ( )  RATIONAL_B_SPLINE_SURFACE ( (
 ( 1.000000000000000000, 0.9238795325112867385, 1.000000000000000000, 0.9238795325112867385, 1.000000000000000000, 0.9238795325112867385, 1.000000000000000000, 0.9238795325112867385, 1.000000000000000000, 0.9238795325112867385, 1.000000000000000000, 0.9238795325112867385, 1.000000000000000000, 0.9238795325112867385, 1.000000000000000000, 0.9238795325112867385, 1.000000000000000000, 0.9238795325112867385, 1.000000000000000000, 0.9238795325112867385, 1.000000000000000000, 0.9238795325112867385, 1.000000000000000000, 0.9238795325112867385, 1.000000000000000000, 0.9238795325112867385, 1.000000000000000000, 0.9238795325112867385, 1.000000000000000000, 0.9238795325112867385, 1.000000000000000000, 0.9238795325112867385, 1.000000000000000000, 0.9238795325112867385, 1.000000000000000000, 0.9238795325112867385, 1.000000000000000000, 0.9238795325112867385, 1.000000000000000000, 0.9238795325112867385, 1.000000000000000000, 0.9238795325112867385, 1.000000000000000000, 0.9238795325112867385, 1.000000000000000000, 0.9238795325112867385, 1.000000000000000000, 0.9238795325112867385, 1.000000000000000000, 0.9238795325112867385, 1.000000000000000000, 0.9238795325112867385, 1.000000000000000000, 0.9238795325112867385, 1.000000000000000000, 0.9238795325112867385, 1.000000000000000000, 0.9238795325112867385, 1.000000000000000000, 0.9238795325112867385, 1.000000000000000000, 0.9238795325112867385, 1.000000000000000000, 0.9238795325112867385, 1.000000000000000000, 0.9238795325112867385, 1.000000000000000000, 0.9238795325112867385, 1.000000000000000000, 0.9238795325112867385, 1.000000000000000000, 0.9238795325112867385, 1.000000000000000000, 0.9238795325112867385, 1.000000000000000000, 0.9238795325112867385, 1.000000000000000000, 0.9238795325112867385, 1.000000000000000000, 0.9238795325112867385, 1.000000000000000000, 0.9238795325112867385, 1.000000000000000000, 0.9238795325112867385, 1.000000000000000000, 0.9238795325112867385, 1.000000000000000000, 0.9238795325112867385, 1.000000000000000000, 0.9238795325112867385, 1.000000000000000000, 0.9238795325112867385, 1.000000000000000000, 0.9238795325112867385, 1.000000000000000000, 0.9238795325112867385, 1.000000000000000000, 0.9238795325112867385, 1.000000000000000000, 0.9238795325112867385, 1.000000000000000000, 0.9238795325112867385, 1.000000000000000000, 0.9238795325112867385, 1.000000000000000000, 0.9238795325112867385, 1.000000000000000000, 0.9238795325112867385, 1.000000000000000000, 0.9238795325112867385, 1.000000000000000000, 0.9238795325112867385, 1.000000000000000000, 0.9238795325112867385, 1.000000000000000000, 0.9238795325112867385, 1.000000000000000000, 0.9238795325112867385, 1.000000000000000000, 0.9238795325112867385, 1.000000000000000000, 0.9238795325112867385, 1.000000000000000000, 0.9238795325112867385, 1.000000000000000000, 0.9238795325112867385, 1.000000000000000000, 0.9238795325112867385, 1.000000000000000000, 0.9238795325112867385, 1.000000000000000000, 0.9238795325112867385, 1.000000000000000000, 0.9238795325112867385, 1.000000000000000000, 0.9238795325112867385, 1.000000000000000000, 0.9238795325112867385, 1.000000000000000000, 0.9238795325112867385, 1.000000000000000000, 0.9238795325112867385, 1.000000000000000000, 0.9238795325112867385, 1.000000000000000000, 0.9238795325112867385, 1.000000000000000000, 0.9238795325112867385, 1.000000000000000000, 0.9238795325112867385, 1.000000000000000000, 0.9238795325112867385, 1.000000000000000000, 0.9238795325112867385, 1.000000000000000000, 0.9238795325112867385, 1.000000000000000000, 0.9238795325112867385, 1.000000000000000000, 0.9238795325112867385, 1.000000000000000000, 0.9238795325112867385, 1.000000000000000000, 0.9238795325112867385, 1.000000000000000000, 0.9238795325112867385, 1.000000000000000000, 0.9238795325112867385, 1.000000000000000000, 0.9238795325112867385, 1.000000000000000000, 0.9238795325112867385, 1.000000000000000000, 0.9238795325112867385, 1.000000000000000000, 0.9238795325112867385, 1.000000000000000000, 0.9238795325112867385, 1.000000000000000000, 0.9238795325112867385, 1.000000000000000000, 0.9238795325112867385, 1.000000000000000000, 0.9238795325112867385, 1.000000000000000000, 0.9238795325112867385, 1.000000000000000000, 0.9238795325112867385, 1.000000000000000000, 0.9238795325112867385, 1.000000000000000000, 0.9238795325112867385, 1.000000000000000000, 0.9238795325112867385, 1.000000000000000000, 0.9238795325112867385, 1.000000000000000000, 0.9238795325112867385, 1.000000000000000000, 0.9238795325112867385, 1.000000000000000000, 0.9238795325112867385, 1.000000000000000000, 0.9238795325112867385, 1.000000000000000000, 0.9238795325112867385, 1.000000000000000000, 0.9238795325112867385, 1.000000000000000000, 0.9238795325112867385, 1.000000000000000000, 0.9238795325112867385, 1.000000000000000000, 0.9238795325112867385, 1.000000000000000000, 0.9238795325112867385, 1.000000000000000000, 0.9238795325112867385, 1.000000000000000000, 0.9238795325112867385, 1.000000000000000000, 0.9238795325112867385, 1.000000000000000000, 0.9238795325112867385, 1.000000000000000000, 0.9238795325112867385, 1.000000000000000000, 0.9238795325112867385, 1.000000000000000000, 0.9238795325112867385, 1.000000000000000000, 0.9238795325112867385, 1.000000000000000000, 0.9238795325112867385, 1.000000000000000000, 0.9238795325112867385, 1.000000000000000000, 0.9238795325112867385, 1.000000000000000000, 0.9238795325112867385, 1.000000000000000000),
 ( 1.000000000000000000, 0.9238795325112867385, 1.000000000000000000, 0.9238795325112867385, 1.000000000000000000, 0.9238795325112867385, 1.000000000000000000, 0.9238795325112867385, 1.000000000000000000, 0.9238795325112867385, 1.000000000000000000, 0.9238795325112867385, 1.000000000000000000, 0.9238795325112867385, 1.000000000000000000, 0.9238795325112867385, 1.000000000000000000, 0.9238795325112867385, 1.000000000000000000, 0.9238795325112867385, 1.000000000000000000, 0.9238795325112867385, 1.000000000000000000, 0.9238795325112867385, 1.000000000000000000, 0.9238795325112867385, 1.000000000000000000, 0.9238795325112867385, 1.000000000000000000, 0.9238795325112867385, 1.000000000000000000, 0.9238795325112867385, 1.000000000000000000, 0.9238795325112867385, 1.000000000000000000, 0.9238795325112867385, 1.000000000000000000, 0.9238795325112867385, 1.000000000000000000, 0.9238795325112867385, 1.000000000000000000, 0.9238795325112867385, 1.000000000000000000, 0.9238795325112867385, 1.000000000000000000, 0.9238795325112867385, 1.000000000000000000, 0.9238795325112867385, 1.000000000000000000, 0.9238795325112867385, 1.000000000000000000, 0.9238795325112867385, 1.000000000000000000, 0.9238795325112867385, 1.000000000000000000, 0.9238795325112867385, 1.000000000000000000, 0.9238795325112867385, 1.000000000000000000, 0.9238795325112867385, 1.000000000000000000, 0.9238795325112867385, 1.000000000000000000, 0.9238795325112867385, 1.000000000000000000, 0.9238795325112867385, 1.000000000000000000, 0.9238795325112867385, 1.000000000000000000, 0.9238795325112867385, 1.000000000000000000, 0.9238795325112867385, 1.000000000000000000, 0.9238795325112867385, 1.000000000000000000, 0.9238795325112867385, 1.000000000000000000, 0.9238795325112867385, 1.000000000000000000, 0.9238795325112867385, 1.000000000000000000, 0.9238795325112867385, 1.000000000000000000, 0.9238795325112867385, 1.000000000000000000, 0.9238795325112867385, 1.000000000000000000, 0.9238795325112867385, 1.000000000000000000, 0.9238795325112867385, 1.000000000000000000, 0.9238795325112867385, 1.000000000000000000, 0.9238795325112867385, 1.000000000000000000, 0.9238795325112867385, 1.000000000000000000, 0.9238795325112867385, 1.000000000000000000, 0.9238795325112867385, 1.000000000000000000, 0.9238795325112867385, 1.000000000000000000, 0.9238795325112867385, 1.000000000000000000, 0.9238795325112867385, 1.000000000000000000, 0.9238795325112867385, 1.000000000000000000, 0.9238795325112867385, 1.000000000000000000, 0.9238795325112867385, 1.000000000000000000, 0.9238795325112867385, 1.000000000000000000, 0.9238795325112867385, 1.000000000000000000, 0.9238795325112867385, 1.000000000000000000, 0.9238795325112867385, 1.000000000000000000, 0.9238795325112867385, 1.000000000000000000, 0.9238795325112867385, 1.000000000000000000, 0.9238795325112867385, 1.000000000000000000, 0.9238795325112867385, 1.000000000000000000, 0.9238795325112867385, 1.000000000000000000, 0.9238795325112867385, 1.000000000000000000, 0.9238795325112867385, 1.000000000000000000, 0.9238795325112867385, 1.000000000000000000, 0.9238795325112867385, 1.000000000000000000, 0.9238795325112867385, 1.000000000000000000, 0.9238795325112867385, 1.000000000000000000, 0.9238795325112867385, 1.000000000000000000, 0.9238795325112867385, 1.000000000000000000, 0.9238795325112867385, 1.000000000000000000, 0.9238795325112867385, 1.000000000000000000, 0.9238795325112867385, 1.000000000000000000, 0.9238795325112867385, 1.000000000000000000, 0.9238795325112867385, 1.000000000000000000, 0.9238795325112867385, 1.000000000000000000, 0.9238795325112867385, 1.000000000000000000, 0.9238795325112867385, 1.000000000000000000, 0.9238795325112867385, 1.000000000000000000, 0.9238795325112867385, 1.000000000000000000, 0.9238795325112867385, 1.000000000000000000, 0.9238795325112867385, 1.000000000000000000, 0.9238795325112867385, 1.000000000000000000, 0.9238795325112867385, 1.000000000000000000, 0.9238795325112867385, 1.000000000000000000, 0.9238795325112867385, 1.000000000000000000, 0.9238795325112867385, 1.000000000000000000, 0.9238795325112867385, 1.000000000000000000, 0.9238795325112867385, 1.000000000000000000, 0.9238795325112867385, 1.000000000000000000, 0.9238795325112867385, 1.000000000000000000, 0.9238795325112867385, 1.000000000000000000, 0.9238795325112867385, 1.000000000000000000, 0.9238795325112867385, 1.000000000000000000, 0.9238795325112867385, 1.000000000000000000, 0.9238795325112867385, 1.000000000000000000, 0.9238795325112867385, 1.000000000000000000, 0.9238795325112867385, 1.000000000000000000, 0.9238795325112867385, 1.000000000000000000, 0.9238795325112867385, 1.000000000000000000, 0.9238795325112867385, 1.000000000000000000, 0.9238795325112867385, 1.000000000000000000, 0.9238795325112867385, 1.000000000000000000, 0.9238795325112867385, 1.000000000000000000, 0.9238795325112867385, 1.000000000000000000, 0.9238795325112867385, 1.000000000000000000, 0.9238795325112867385, 1.000000000000000000, 0.9238795325112867385, 1.000000000000000000, 0.9238795325112867385, 1.000000000000000000, 0.9238795325112867385, 1.000000000000000000, 0.9238795325112867385, 1.000000000000000000, 0.9238795325112867385, 1.000000000000000000, 0.9238795325112867385, 1.000000000000000000, 0.9238795325112867385, 1.000000000000000000, 0.9238795325112867385, 1.000000000000000000, 0.9238795325112867385, 1.000000000000000000, 0.9238795325112867385, 1.000000000000000000) ) ) 
 REPRESENTATION_ITEM ( '' )  SURFACE ( )  );
#49726 = CARTESIAN_POINT ( 'NONE',  ( -5.082755093536319713, 5.082755093536319713, 14.79905278187175455 ) ) ;
#49727 = CARTESIAN_POINT ( 'NONE',  ( 6.123233995736767268E-16, 91.25000000000001421, -10.00000000000000178 ) ) ;
#49728 = CARTESIAN_POINT ( 'NONE',  ( -8.000000000000000000, 14.15625000000000355, -3.313708498984762496 ) ) ;
#49729 = ORIENTED_EDGE ( 'NONE', *, *, #4466, .T. ) ;
#49730 = CARTESIAN_POINT ( 'NONE',  ( -5.656854249492380582, 90.50000000409677625, -5.656854249492380582 ) ) ;
#49731 = CIRCLE ( 'NONE', #17197, 3.999999999999976019 ) ;
#49732 = CARTESIAN_POINT ( 'NONE',  ( -8.660254037844390851, 17.91666666666666785, 4.999999999999998224 ) ) ;
#49733 =( BOUNDED_CURVE ( )  B_SPLINE_CURVE ( 2, ( #23213, #57566, #5875, #28871, #51891, #15682, #69989, #34932, #12263 ),
 .UNSPECIFIED., .F., .F. ) 
 B_SPLINE_CURVE_WITH_KNOTS ( ( 3, 2, 2, 2, 3 ),
 ( 0.3229166666666665186, 0.3281249999999998335, 0.3333333333333331483, 0.3385416666666665186, 0.3437499999999998335 ),
 .UNSPECIFIED. ) 
 CURVE ( )  GEOMETRIC_REPRESENTATION_ITEM ( )  RATIONAL_B_SPLINE_CURVE ( ( 1.000000000000002442, 0.9238795325112842960, 1.000000000000000000, 0.9238795325112867385, 1.000000000000000000, 0.9238795325112867385, 1.000000000000000000, 0.9238795325112891810, 0.9999999999999975575 ) ) 
 REPRESENTATION_ITEM ( '' )  );
#49734 = VERTEX_POINT ( 'NONE', #10094 ) ;
#49735 = CARTESIAN_POINT ( 'NONE',  ( -4.000000000000002665, 17.56250000000000355, 1.656854249492380804 ) ) ;
#49736 = CARTESIAN_POINT ( 'NONE',  ( 4.541265875000001451, 20.24999999863440436, 1.881053915767124440 ) ) ;
#49737 = CARTESIAN_POINT ( 'NONE',  ( -3.313708498984757167, 7.999999999999991118, 6.736552783920144449 ) ) ;
#49738 = DIRECTION ( 'NONE',  ( -0.000000000000000000, 1.000000000000000000, 4.476705744456276341E-16 ) ) ;
#49739 = ORIENTED_EDGE ( 'NONE', *, *, #68754, .F. ) ;
#49740 = FILL_AREA_STYLE_COLOUR ( '', #46364 ) ;
#49741 = CARTESIAN_POINT ( 'NONE',  ( -2.977408999572650927, 92.37500000204839523, -7.188101187500001821 ) ) ;
#49743 = CARTESIAN_POINT ( 'NONE',  ( 1.469576158976823947E-15, 109.0625000040967905, 8.000000000000000000 ) ) ;
#49742 = CARTESIAN_POINT ( 'NONE',  ( -5.000000000000000888, 257.2916666734946034, -8.660254037844387298 ) ) ;
#49744 = DIRECTION ( 'NONE',  ( 1.000000000000000000, 0.000000000000000000, 0.000000000000000000 ) ) ;
#49745 = ORIENTED_EDGE ( 'NONE', *, *, #32107, .T. ) ;
#49746 = ADVANCED_FACE ( 'NONE', ( #4814 ), #38024, .T. ) ;
#49747 = CARTESIAN_POINT ( 'NONE',  ( 2.085542519210945334E-15, 250.4687500034140157, 11.35316468749999963 ) ) ;
#49748 = CARTESIAN_POINT ( 'NONE',  ( 1.320432766682872962E-15, -7.188101187499992051, 13.86155278187175455 ) ) ;
#49749 = VERTEX_POINT ( 'NONE', #22139 ) ;
#49750 = ORIENTED_EDGE ( 'NONE', *, *, #68085, .F. ) ;
#49751 = CARTESIAN_POINT ( 'NONE',  ( 1.871523826299183495E-15, -10.18810118749999916, 83.03125000204838102 ) ) ;
#49752 = CARTESIAN_POINT ( 'NONE',  ( 9.832129032723420536, 71.51041666325268409, -5.676582343749999815 ) ) ;
#49753 = CARTESIAN_POINT ( 'NONE',  ( -4.898587196589412829E-16, 105.3125000040967763, -8.000000000000000000 ) ) ;
#49754 = CARTESIAN_POINT ( 'NONE',  ( 7.778174593052021635, 7.778174593052023411, 87.43749999999998579 ) ) ;
#49757 = CARTESIAN_POINT ( 'NONE',  ( -4.088227598258586603E-16, 289.3593750017070079, -6.676582343750001591 ) ) ;
#49756 = CARTESIAN_POINT ( 'NONE',  ( 31.99999999999997868, 197.4375000027312126, 168.3431457505075173 ) ) ;
#49755 = CARTESIAN_POINT ( 'NONE',  ( 27.99999999999999645, 210.0000000000000284, 173.9999999999998863 ) ) ;
#49758 = CARTESIAN_POINT ( 'NONE',  ( 11.00000000000010836, -4.556349186103939353, 84.15624999999998579 ) ) ;
#49759 = CARTESIAN_POINT ( 'NONE',  ( 29.65685424949235482, 209.0625000000000284, 173.9999999999999716 ) ) ;
#49760 = EDGE_CURVE ( 'NONE', #3175, #25916, #45167, .T. ) ;
#49761 = CARTESIAN_POINT ( 'NONE',  ( 1.432654583217664701, 197.0000000013656063, 201.4587341250000065 ) ) ;
#49762 = CARTESIAN_POINT ( 'NONE',  ( -3.313708498984760720, 10.78124999590322197, -8.000000000000000000 ) ) ;
#49763 = ORIENTED_EDGE ( 'NONE', *, *, #7352, .F. ) ;
#49764 = CARTESIAN_POINT ( 'NONE',  ( 31.45873412499999233, 195.6875000013655779, 169.9999999999999432 ) ) ;
#49765 = CARTESIAN_POINT ( 'NONE',  ( 7.188101187500001821, 14.43749999795161365, -2.977408999572650483 ) ) ;
#49766 = CARTESIAN_POINT ( 'NONE',  ( -3.042071309553173730, 169.6354166632526699, 11.35316468749999785 ) ) ;
#49767 = FACE_OUTER_BOUND ( 'NONE', #73762, .T. ) ;
#49768 = CARTESIAN_POINT ( 'NONE',  ( -5.082755093536325930, 106.3437500020483810, -5.082755093536325930 ) ) ;
#49770 = CYLINDRICAL_SURFACE ( 'NONE', #11283, 8.000000000000000000 ) ;
#49769 = DIRECTION ( 'NONE',  ( -0.000000000000000000, 1.000000000000000000, 4.689100369878284071E-30 ) ) ;
#49771 = CARTESIAN_POINT ( 'NONE',  ( 25.55430564589119413, 205.3125000013656063, 167.5543056458910485 ) ) ;
#49772 = ADVANCED_FACE ( 'NONE', ( #67062 ), #4072, .T. ) ;
#49773 = CARTESIAN_POINT ( 'NONE',  ( -7.188101187499992051, 0.000000000000000000, 13.86155278187175455 ) ) ;
#49774 = CARTESIAN_POINT ( 'NONE',  ( -1.656854249492405451, 206.4375000027311842, 138.0000000000000568 ) ) ;
#49775 = CARTESIAN_POINT ( 'NONE',  ( -8.311093377946841443, 38.90624999658599847, 8.311093377946830785 ) ) ;
#49776 = DIRECTION ( 'NONE',  ( 1.000000000000000000, -0.000000000000000000, -0.000000000000000000 ) ) ;
#49777 = CARTESIAN_POINT ( 'NONE',  ( -7.320508075688773708, 23.74999999317202892, -7.320508075688774596 ) ) ;
#49778 = CARTESIAN_POINT ( 'NONE',  ( -27.99999999999999645, 210.0000000000000284, 170.0000000000003695 ) ) ;
#49779 = ORIENTED_EDGE ( 'NONE', *, *, #37693, .F. ) ;
#49780 = LINE ( 'NONE', #55827, #19364 ) ;
#49781 = AXIS2_PLACEMENT_3D ( 'NONE', #18740, #71507, #19831 ) ;
#49782 = DIRECTION ( 'NONE',  ( -0.8660254037844312691, 0.5000000000000128786, 0.000000000000000000 ) ) ;
#49783 = CARTESIAN_POINT ( 'NONE',  ( -3.042071309553173730, 49.32291666325266988, 11.35316468749999785 ) ) ;
#49784 = CARTESIAN_POINT ( 'NONE',  ( -4.556349186104047710, -10.99999999999999822, 77.96875000409679046 ) ) ;
#49785 = CARTESIAN_POINT ( 'NONE',  ( 1.432654583217608080, 204.8750000013656063, 138.5412658750000503 ) ) ;
#49786 = CARTESIAN_POINT ( 'NONE',  ( 1.506680654954607457, 10.12163528317106120, 70.16331425390788468 ) ) ;
#49787 = CARTESIAN_POINT ( 'NONE',  ( -11.00000000000000000, 0.000000000000000000, 79.18750000409677625 ) ) ;
#49789 = CARTESIAN_POINT ( 'NONE',  ( 6.951808397369818766E-16, 47.03124999658601979, -11.35316468750000141 ) ) ;
#49788 = CARTESIAN_POINT ( 'NONE',  ( 7.188101187500000044, 99.40625000204838102, -8.802885111219163269E-16 ) ) ;
#49790 = CARTESIAN_POINT ( 'NONE',  ( -5.656854249492375253, 5.656854249492375253, 8.142802779823362869 ) ) ;
#49791 = CARTESIAN_POINT ( 'NONE',  ( 9.999999999999996447, 204.7916666666667140, 2.679491924311235174 ) ) ;
#49792 = CARTESIAN_POINT ( 'NONE',  ( 9.832129032723420536, 161.1979166632526983, -5.676582343749999815 ) ) ;
#49793 = CARTESIAN_POINT ( 'NONE',  ( 2.679491924311228956, 127.9166666598386968, -10.00000000000000000 ) ) ;
#49794 = CARTESIAN_POINT ( 'NONE',  ( 5.082755093536325042, 104.4687500020483952, -5.082755093536325930 ) ) ;
#49795 = DIRECTION ( 'NONE',  ( -0.000000000000000000, -1.000000000000000000, -0.000000000000000000 ) ) ;
#49796 = CARTESIAN_POINT ( 'NONE',  ( -3.042071309553173730, 39.63541666325267698, 11.35316468749999785 ) ) ;
#49797 = CARTESIAN_POINT ( 'NONE',  ( -4.000000000000015987, 195.6875000027312126, 143.6568542494924259 ) ) ;
#49798 = ORIENTED_EDGE ( 'NONE', *, *, #59349, .F. ) ;
#49799 = DIRECTION ( 'NONE',  ( -0.000000000000000000, 1.000000000000000000, -0.000000000000000000 ) ) ;
#49800 = CARTESIAN_POINT ( 'NONE',  ( -6.238412754330611322E-16, 10.18810118749999916, 77.78125000204836681 ) ) ;
#49801 = CARTESIAN_POINT ( 'NONE',  ( -11.00000000000000000, 0.000000000000000000, 99.99999999999998579 ) ) ;
#49803 = CARTESIAN_POINT ( 'NONE',  ( 8.311093377946834337, 170.1562499965860127, 8.311093377946839666 ) ) ;
#49802 = DIRECTION ( 'NONE',  ( 0.000000000000000000, 0.000000000000000000, 1.000000000000000000 ) ) ;
#49804 = CARTESIAN_POINT ( 'NONE',  ( 7.999999999999992895, -3.313708498984756279, 10.54280278432982598 ) ) ;
#49805 = CARTESIAN_POINT ( 'NONE',  ( -30.46864743399846986, -21.01145865389314338, 175.8297559005563642 ) ) ;
#49806 = CARTESIAN_POINT ( 'NONE',  ( 8.311093377946834337, 227.0312500034140157, -8.311093377946836114 ) ) ;
#49807 = CARTESIAN_POINT ( 'NONE',  ( 1.871523826299183495E-15, -10.18810118749999916, 84.90625000204838102 ) ) ;
#49808 = ORIENTED_EDGE ( 'NONE', *, *, #22673, .T. ) ;
#49809 = DIRECTION ( 'NONE',  ( 0.000000000000000000, -1.000000000000000000, 0.000000000000000000 ) ) ;
#49810 = CARTESIAN_POINT ( 'NONE',  ( -4.556349186104045934, 11.00000000000000000, 105.7187499999999858 ) ) ;
#49811 = CARTESIAN_POINT ( 'NONE',  ( 11.35316468749999785, 110.8854166632526699, 3.042071309553174174 ) ) ;
#49812 = CARTESIAN_POINT ( 'NONE',  ( -4.220049686691935698, 10.18810118749999916, 94.37500000204839523 ) ) ;
#49813 = CARTESIAN_POINT ( 'NONE',  ( -3.211159895383562723, 21.06249999863440792, 3.211159895383561391 ) ) ;
#49814 = ORIENTED_EDGE ( 'NONE', *, *, #23291, .T. ) ;
#49815 = VERTEX_POINT ( 'NONE', #55382 ) ;
#49816 = CARTESIAN_POINT ( 'NONE',  ( 2.780723358947928197E-16, 5.687499998634407028, -4.541265875000002339 ) ) ;
#49817 = CARTESIAN_POINT ( 'NONE',  ( -1.320432766682874540E-15, 7.593749997951611874, 7.188101187500000044 ) ) ;
#49818 = CARTESIAN_POINT ( 'NONE',  ( 3.313708498984765161, 112.1562500040967763, 7.999999999999998224 ) ) ;
#49819 = CARTESIAN_POINT ( 'NONE',  ( -6.238412754330611322E-16, 10.18810118749999916, 91.65625000204836681 ) ) ;
#49820 = CARTESIAN_POINT ( 'NONE',  ( -28.00000000000002132, 202.6875000013656063, 166.5412658750003629 ) ) ;
#49821 = CARTESIAN_POINT ( 'NONE',  ( -5.656854249492373476, -5.656854249492376141, 19.01780277982336642 ) ) ;
#49822 =( BOUNDED_CURVE ( )  B_SPLINE_CURVE ( 2, ( #51414, #33342, #15586, #39725, #62354, #38626, #4289, #27657, #44276 ),
 .UNSPECIFIED., .F., .F. ) 
 B_SPLINE_CURVE_WITH_KNOTS ( ( 3, 2, 2, 2, 3 ),
 ( 0.8295454545454545858, 0.8352272727272727071, 0.8409090909090909394, 0.8465909090909090606, 0.8522727272727272929 ),
 .UNSPECIFIED. ) 
 CURVE ( )  GEOMETRIC_REPRESENTATION_ITEM ( )  RATIONAL_B_SPLINE_CURVE ( ( 1.000000000000000000, 0.9238795325112867385, 1.000000000000000000, 0.9238795325112867385, 1.000000000000000000, 0.9238795325112867385, 1.000000000000000000, 0.9238795325112867385, 1.000000000000000000 ) ) 
 REPRESENTATION_ITEM ( '' )  );
#49823 = CARTESIAN_POINT ( 'NONE',  ( 2.449293598294707893E-16, 4.250000000000000000, -4.000000000000001776 ) ) ;
#49824 = CARTESIAN_POINT ( 'NONE',  ( -4.000000000000002665, 17.31249999726881938, 1.656854249492380804 ) ) ;
#49825 = CARTESIAN_POINT ( 'NONE',  ( -3.211159895383561391, 7.687499998634407028, -3.211159895383561835 ) ) ;
#49826 = CARTESIAN_POINT ( 'NONE',  ( -2.828427124746208943, 202.6250000000000284, 144.8284271247462129 ) ) ;
#49827 = ORIENTED_EDGE ( 'NONE', *, *, #17341, .F. ) ;
#49828 = LINE ( 'NONE', #2316, #5328 ) ;
#49830 = CARTESIAN_POINT ( 'NONE',  ( 2.679491924311168560, 236.6666666734946602, -10.00000000000003375 ) ) ;
#49829 = CARTESIAN_POINT ( 'NONE',  ( -29.43265458321755546, 196.8750000013656063, 173.4587341250004044 ) ) ;
#49831 = CARTESIAN_POINT ( 'NONE',  ( 1.881053915767122664, 17.12499999863440436, 4.541265875000001451 ) ) ;
#49832 = CARTESIAN_POINT ( 'NONE',  ( 6.676582343750002480, 299.0156250017069510, -2.765530957081997254 ) ) ;
#49833 = CARTESIAN_POINT ( 'NONE',  ( 5.082755093536320601, -5.082755093536318824, 9.549052781871754547 ) ) ;
#49834 = ORIENTED_EDGE ( 'NONE', *, *, #74065, .T. ) ;
#49835 = ORIENTED_EDGE ( 'NONE', *, *, #56867, .F. ) ;
#49836 = CARTESIAN_POINT ( 'NONE',  ( -4.220049686691935698, 10.18810118749999916, 98.87500000204838102 ) ) ;
#49837 = CARTESIAN_POINT ( 'NONE',  ( 5.000000000000000000, 10.26105934116143281, 64.40045319026697257 ) ) ;
#49838 = CARTESIAN_POINT ( 'NONE',  ( -26.56734541678238060, 199.6250000013656063, 166.5412658750003629 ) ) ;
#49839 = CARTESIAN_POINT ( 'NONE',  ( 2.020667218593132706E-15, -11.00000000000000000, 106.3750000000000000 ) ) ;
#49840 = CARTESIAN_POINT ( 'NONE',  ( 3.458734125000015869, 208.1875000013656063, 198.0000000000000284 ) ) ;
#49841 = CARTESIAN_POINT ( 'NONE',  ( -4.000000000000001776, 21.18749999726881583, -1.656854249492381470 ) ) ;
#49842 = CARTESIAN_POINT ( 'NONE',  ( -10.00000000000000178, 107.5000000000000142, -1.224646799147353454E-15 ) ) ;
#49843 = EDGE_CURVE ( 'NONE', #4458, #17509, #41836, .T. ) ;
#49844 = CARTESIAN_POINT ( 'NONE',  ( -8.000000000000000000, 114.4999999999999858, 0.000000000000000000 ) ) ;
#49845 = CARTESIAN_POINT ( 'NONE',  ( -4.721056650415999201, 293.4843750017070079, -4.721056650415999201 ) ) ;
#49846 = CARTESIAN_POINT ( 'NONE',  ( -5.082755093536319713, 5.082755093536319713, 10.67405278187175455 ) ) ;
#49847 = VERTEX_POINT ( 'NONE', #5930 ) ;
#49848 = DIRECTION ( 'NONE',  ( 0.000000000000000000, 0.000000000000000000, -1.000000000000000000 ) ) ;
#49849 = CARTESIAN_POINT ( 'NONE',  ( 26.56734541678232731, 208.3750000013656063, 173.4587341249998929 ) ) ;
#49850 = CARTESIAN_POINT ( 'NONE',  ( -3.313708498984765161, 21.84374999590322375, 7.999999999999998224 ) ) ;
#49851 = AXIS2_PLACEMENT_3D ( 'NONE', #52155, #23470, #28019 ) ;
#49852 = CARTESIAN_POINT ( 'NONE',  ( 2.445694354108782775, 197.5625000013656063, 139.5543056458912190 ) ) ;
#49853 = CARTESIAN_POINT ( 'NONE',  ( -19.99999999999992895, -32.55154106607723463, 145.8082228544479051 ) ) ;
#49855 = CARTESIAN_POINT ( 'NONE',  ( 3.458734124999960358, 203.6250000013656063, 143.4326545832176976 ) ) ;
#49854 = CARTESIAN_POINT ( 'NONE',  ( -4.898587196589412829E-16, 121.6250000000000000, -8.000000000000000000 ) ) ;
#49856 = CARTESIAN_POINT ( 'NONE',  ( 5.676582343749997150, 252.5520833367473301, -9.832129032723418760 ) ) ;
#49857 = LINE ( 'NONE', #32904, #60809 ) ;
#49858 = DIRECTION ( 'NONE',  ( -0.000000000000000000, 1.000000000000000000, -1.563033456626094573E-30 ) ) ;
#49859 = CARTESIAN_POINT ( 'NONE',  ( 4.089758525567003034, 225.9150540747923515, -9.185782198135839849 ) ) ;
#49860 = CARTESIAN_POINT ( 'NONE',  ( -7.188101187499992051, 0.000000000000000000, 3.361552781871751883 ) ) ;
#49861 = CARTESIAN_POINT ( 'NONE',  ( 9.832129032723420536, 211.5104166632526699, -5.676582343749999815 ) ) ;
#49862 = CARTESIAN_POINT ( 'NONE',  ( 3.042071309553167069, 1.822916663252682756, -11.35316468749999785 ) ) ;
#49863 = CARTESIAN_POINT ( 'NONE',  ( -4.541265875000003227, 5.874999998634406140, 1.881053915767121110 ) ) ;
#49864 = CARTESIAN_POINT ( 'NONE',  ( -9.000000000000035527, -15.58845726811991739, -20.69999999999999929 ) ) ;
#49866 = CARTESIAN_POINT ( 'NONE',  ( 4.242640687119287435, 297.3750000000000000, 4.242640687119285658 ) ) ;
#49865 = DIRECTION ( 'NONE',  ( -0.000000000000000000, 1.000000000000000000, 4.689100369878284071E-30 ) ) ;
#49867 = ORIENTED_EDGE ( 'NONE', *, *, #14652, .F. ) ;
#49868 = CARTESIAN_POINT ( 'NONE',  ( 2.445694354108784108, 204.5625000013656063, 144.4456943541088663 ) ) ;
#49869 = CARTESIAN_POINT ( 'NONE',  ( 11.35316468750000141, 5.781249996586016238, 0.000000000000000000 ) ) ;
#49870 = CARTESIAN_POINT ( 'NONE',  ( 11.00000000000000355, -4.556349186104045046, 96.34375000409677625 ) ) ;
#49871 = DIRECTION ( 'NONE',  ( -1.000000000000000000, -0.000000000000000000, -0.000000000000000000 ) ) ;
#49872 = ADVANCED_FACE ( 'NONE', ( #68547 ), #16850, .T. ) ;
#49873 = CARTESIAN_POINT ( 'NONE',  ( -26.56734541678243033, 200.3750000013656063, 166.5412658750003345 ) ) ;
#49874 = LINE ( 'NONE', #72889, #38223 ) ;
#49876 = CARTESIAN_POINT ( 'NONE',  ( -2.085542519210945728E-15, 9.531249996586018014, 11.35316468750000141 ) ) ;
#49875 = CARTESIAN_POINT ( 'NONE',  ( -2.977408999572650927, 117.8750000020483810, -7.188101187500000933 ) ) ;
#49877 = CARTESIAN_POINT ( 'NONE',  ( 7.999999999999991118, 9.797174393178815797E-16, 25.58030277982336997 ) ) ;
#49878 = CARTESIAN_POINT ( 'NONE',  ( -3.042071309553164404, 122.2395833299193271, -11.35316468749999963 ) ) ;
#49879 = CARTESIAN_POINT ( 'NONE',  ( -10.00000000000000178, 89.37499999317203958, -1.224646799147353454E-15 ) ) ;
#49880 = CARTESIAN_POINT ( 'NONE',  ( 7.188101187500000044, 119.2812500020483810, -8.802885111219163269E-16 ) ) ;
#49881 = CARTESIAN_POINT ( 'NONE',  ( 3.211159895383561835, 18.56249999863440436, -3.211159895383561835 ) ) ;
#49882 = LINE ( 'NONE', #66862, #25327 ) ;
#49883 = CARTESIAN_POINT ( 'NONE',  ( 1.491046635511791134E-11, 146.2499999999988631, -9.999999999999998224 ) ) ;
#49884 = VERTEX_POINT ( 'NONE', #46276 ) ;
#49885 = LINE ( 'NONE', #72900, #59307 ) ;
#49886 = CARTESIAN_POINT ( 'NONE',  ( -6.676582343750001591, 289.6093750017069510, 0.000000000000000000 ) ) ;
#49887 = CARTESIAN_POINT ( 'NONE',  ( -7.347880794884122694E-16, 12.49999999726881406, 4.000000000000001776 ) ) ;
#49888 = CARTESIAN_POINT ( 'NONE',  ( 3.313708498984762496, -7.999999999999989342, 2.986552783920144449 ) ) ;
#49889 = VECTOR ( 'NONE', #9263, 1000.000000000000000 ) ;
#49890 = DIRECTION ( 'NONE',  ( 0.000000000000000000, -0.000000000000000000, -1.000000000000000000 ) ) ;
#49891 = CARTESIAN_POINT ( 'NONE',  ( 7.320508075688774596, 202.4999999931720538, -7.320508075688774596 ) ) ;
#49892 = FACE_OUTER_BOUND ( 'NONE', #28944, .T. ) ;
#49893 = CARTESIAN_POINT ( 'NONE',  ( 10.18810118750000093, -4.220049686691933921, 101.6875000020483810 ) ) ;
#49894 = ORIENTED_EDGE ( 'NONE', *, *, #47443, .F. ) ;
#49895 = B_SPLINE_CURVE_WITH_KNOTS ( 'NONE', 3,
 ( #63741, #58837, #29421, #7517, #7148, #70157, #35822, #12790 ),
 .UNSPECIFIED., .F., .F.,
 ( 4, 2, 2, 4 ),
 ( 0.005257893453559909711, 0.006567392922673239916, 0.007876892391786568387, 0.01049589133001322880 ),
 .UNSPECIFIED. ) ;
#49896 = CARTESIAN_POINT ( 'NONE',  ( 2.849036369511732440E-14, 198.3750000027312126, 202.0000000000000000 ) ) ;
#49897 = CARTESIAN_POINT ( 'NONE',  ( 8.311093377946834337, 160.4687499965860411, 8.311093377946839666 ) ) ;
#49898 = CARTESIAN_POINT ( 'NONE',  ( -11.00000000000000000, 0.000000000000000000, 98.49999999999998579 ) ) ;
#49899 = CARTESIAN_POINT ( 'NONE',  ( 3.458734125000015869, 207.1875000013656063, 198.0000000000000284 ) ) ;
#49900 = CARTESIAN_POINT ( 'NONE',  ( -7.188101187499992051, 0.000000000000000000, 28.86155278187175810 ) ) ;
#49901 = CARTESIAN_POINT ( 'NONE',  ( -3.042071309553164404, 62.55208332991934839, -11.35316468749999963 ) ) ;
#49902 = EDGE_LOOP ( 'NONE', ( #58415, #41353, #65632 ) ) ;
#49903 = CARTESIAN_POINT ( 'NONE',  ( -10.18810118749999916, 0.000000000000000000, 114.1562500020483810 ) ) ;
#49904 = CARTESIAN_POINT ( 'NONE',  ( -3.211159895383561391, 8.812499998634407916, -3.211159895383561835 ) ) ;
#49905 = ORIENTED_EDGE ( 'NONE', *, *, #20887, .F. ) ;
#49906 = CARTESIAN_POINT ( 'NONE',  ( 2.977408999572651815, 24.18749999795161543, 7.188101187500000933 ) ) ;
#49907 = CARTESIAN_POINT ( 'NONE',  ( 6.000000000000001776, 288.5625000034140157, -7.347880794884121708E-16 ) ) ;
#49908 = CARTESIAN_POINT ( 'NONE',  ( -25.17157287525385811, 198.0000000027312126, 167.1715728752541281 ) ) ;
#49909 = CARTESIAN_POINT ( 'NONE',  ( 7.188101187500001821, 20.43749999795161187, -2.977408999572650483 ) ) ;
#49910 = CARTESIAN_POINT ( 'NONE',  ( 5.082755093536320601, -5.082755093536318824, 3.549052781871751883 ) ) ;
#49911 = CARTESIAN_POINT ( 'NONE',  ( -10.18810118749999916, 0.000000000000000000, 108.5312500020483810 ) ) ;
#49912 = PRODUCT ( 'square bolt', 'square bolt', '', ( #22178 ) ) ;
#49913 = CARTESIAN_POINT ( 'NONE',  ( 1.504109706850426109, -42.39693258347419658, 151.0589245267576644 ) ) ;
#49914 = CARTESIAN_POINT ( 'NONE',  ( -4.000000000000002665, 5.312499997268813168, 1.656854249492380804 ) ) ;
#49915 = CARTESIAN_POINT ( 'NONE',  ( 1.656854249492381248, 18.18750000000000000, -4.000000000000001776 ) ) ;
#49916 = ORIENTED_EDGE ( 'NONE', *, *, #14168, .F. ) ;
#49917 = EDGE_CURVE ( 'NONE', #10305, #13303, #16212, .T. ) ;
#49918 = CARTESIAN_POINT ( 'NONE',  ( -2.445694354108783664, 205.3125000013656063, 195.5543056458912190 ) ) ;
#49919 = CARTESIAN_POINT ( 'NONE',  ( -31.45873412500002431, 208.6250000013655779, 168.5673454167828140 ) ) ;
#49920 = CARTESIAN_POINT ( 'NONE',  ( 10.18810118749999916, 4.220049686691935698, 71.87500000204836681 ) ) ;
#49921 = CARTESIAN_POINT ( 'NONE',  ( -1.881053915767121554, 4.624999998634407028, -4.541265875000002339 ) ) ;
#49922 = DIRECTION ( 'NONE',  ( 1.000000000000000000, 0.000000000000000000, 0.000000000000000000 ) ) ;
#49923 = CARTESIAN_POINT ( 'NONE',  ( 1.320432766682872962E-15, -7.188101187499992051, 25.86155278187175810 ) ) ;
#49924 = VERTEX_POINT ( 'NONE', #23642 ) ;
#49925 = CARTESIAN_POINT ( 'NONE',  ( -4.556349186104045934, 11.00000000000000000, 90.71874999999998579 ) ) ;
#49926 = VERTEX_POINT ( 'NONE', #62878 ) ;
#49927 = CARTESIAN_POINT ( 'NONE',  ( -10.18810118749999916, 0.000000000000000000, 117.1562500020483810 ) ) ;
#49928 = CARTESIAN_POINT ( 'NONE',  ( -8.660254037844387298, 202.0833333333333428, -5.000000000000004441 ) ) ;
#49929 = CARTESIAN_POINT ( 'NONE',  ( 3.458734125000015425, 202.9375000013656063, 198.0000000000000284 ) ) ;
#49930 = CARTESIAN_POINT ( 'NONE',  ( 25.55430564589115505, 199.0625000013656063, 167.5543056458911053 ) ) ;
#49931 = CARTESIAN_POINT ( 'NONE',  ( 4.999999999999993783, 64.16666666666667140, 8.660254037844390851 ) ) ;
#49932 = AXIS2_PLACEMENT_3D ( 'NONE', #37968, #66249, #55324 ) ;
#49933 = ADVANCED_FACE ( 'NONE', ( #35354 ), #58365, .T. ) ;
#49934 = CARTESIAN_POINT ( 'NONE',  ( -2.977408999572650927, 94.25000000204838102, -7.188101187500001821 ) ) ;
#49935 = CARTESIAN_POINT ( 'NONE',  ( -3.673940397442060854E-16, 291.7500000000000000, -6.000000000000001776 ) ) ;
#49936 = CARTESIAN_POINT ( 'NONE',  ( 32.00000000000000000, 206.3750000027312126, 169.9999999999998863 ) ) ;
#49937 = ORIENTED_EDGE ( 'NONE', *, *, #21654, .F. ) ;
#49938 =( BOUNDED_SURFACE ( )  B_SPLINE_SURFACE ( 3, 2, ( 
 ( #61685, #49232, #55666 ),
 ( #4347, #44704, #10006 ),
 ( #37932, #20560, #3983 ),
 ( #3225, #60558, #60932 ),
 ( #67719, #39047, #27337 ),
 ( #61312, #4720, #33038 ),
 ( #31895, #50354, #56401 ),
 ( #73373, #62050, #9254 ),
 ( #32277, #10375, #50726 ),
 ( #26972, #45075, #73741 ),
 ( #14520, #54916, #72245 ),
 ( #72632, #66966, #38306 ),
 ( #52227, #16752, #40901 ),
 ( #34893, #29214, #5096 ),
 ( #931, #5462, #51850 ),
 ( #39778, #63909, #51471 ),
 ( #68822, #34524, #22791 ),
 ( #40158, #23914, #57529 ),
 ( #6207, #29581, #17511 ),
 ( #62416, #63164, #11489 ),
 ( #5837, #68089, #35257 ),
 ( #28831, #23170, #45811 ),
 ( #194, #17134, #16378 ),
 ( #559, #46182, #28463 ),
 ( #39417, #10741, #58273 ),
 ( #74484, #62781, #12221 ),
 ( #23542, #33775, #69200 ),
 ( #46554, #40527, #63533 ),
 ( #74114, #52594, #28087 ),
 ( #11858, #57900, #69575 ),
 ( #17886, #6575, #56775 ),
 ( #11123, #51102, #22415 ),
 ( #45437, #68452, #34146 ),
 ( #57146, #13679, #41273 ) ),
 .UNSPECIFIED., .F., .F., .F. ) 
 B_SPLINE_SURFACE_WITH_KNOTS ( ( 4, 2, 2, 2, 2, 2, 2, 2, 2, 2, 2, 2, 2, 2, 2, 2, 4 ),
 ( 3, 3 ),
 ( 1.398180355084344573, 1.616106892397525918, 1.834033429710707042, 2.051959967023888165, 2.269886504337069510, 2.487813041650250856, 2.705739578963432201, 2.923666116276613547, 3.141592653589794892, 3.359519190902976238, 3.577445728216157583, 3.795372265529338929, 4.013298802842520274, 4.231225340155701176, 4.449151877468882077, 4.667078414782062978, 4.885004952095244768 ),
 ( 0.000000000000000000, 1.000000000000000000 ),
 .UNSPECIFIED. ) 
 GEOMETRIC_REPRESENTATION_ITEM ( )  RATIONAL_B_SPLINE_SURFACE ( (
 ( 1.000000000000000000, 0.7147553065756221402, 1.000000000000000000),
 ( 1.000000000000000000, 0.7115858121534747172, 1.000000000000000000),
 ( 1.000000000000000000, 0.7083342461907259358, 1.000000000000000000),
 ( 1.000000000000000000, 0.7018176610181855457, 1.000000000000000000),
 ( 1.000000000000000000, 0.6985527070788675186, 1.000000000000000000),
 ( 1.000000000000000000, 0.6921661235331102446, 1.000000000000000000),
 ( 1.000000000000000000, 0.6890447671308475019, 1.000000000000000000),
 ( 1.000000000000000000, 0.6831019955317740866, 1.000000000000000000),
 ( 1.000000000000000000, 0.6802808894116101346, 1.000000000000000000),
 ( 1.000000000000000000, 0.6750859627294230059, 1.000000000000000000),
 ( 1.000000000000000000, 0.6727124631768420793, 1.000000000000000000),
 ( 1.000000000000000000, 0.6685412636674606945, 1.000000000000000000),
 ( 1.000000000000000000, 0.6667438609243098169, 1.000000000000000000),
 ( 1.000000000000000000, 0.6638251156788782525, 1.000000000000000000),
 ( 1.000000000000000000, 0.6627040045098303578, 1.000000000000000000),
 ( 1.000000000000000000, 0.6612017554393337937, 1.000000000000000000),
 ( 1.000000000000000000, 0.6608207446963441090, 1.000000000000000000),
 ( 1.000000000000000000, 0.6608207446963441090, 1.000000000000000000),
 ( 1.000000000000000000, 0.6612017554394790109, 1.000000000000000000),
 ( 1.000000000000000000, 0.6627040045096851406, 1.000000000000000000),
 ( 1.000000000000000000, 0.6638251156787329244, 1.000000000000000000),
 ( 1.000000000000000000, 0.6667438609244551451, 1.000000000000000000),
 ( 1.000000000000000000, 0.6685412636674631370, 1.000000000000000000),
 ( 1.000000000000000000, 0.6727124631768445218, 1.000000000000000000),
 ( 1.000000000000000000, 0.6750859627290272114, 1.000000000000000000),
 ( 1.000000000000000000, 0.6802808894120059291, 1.000000000000000000),
 ( 1.000000000000000000, 0.6831019955315804637, 1.000000000000000000),
 ( 1.000000000000000000, 0.6890447671310415689, 1.000000000000000000),
 ( 1.000000000000000000, 0.6921661235304776838, 1.000000000000000000),
 ( 1.000000000000000000, 0.6985527070815005235, 1.000000000000000000),
 ( 1.000000000000000000, 0.7018176610177988550, 1.000000000000000000),
 ( 1.000000000000000000, 0.7083342461911121823, 1.000000000000000000),
 ( 1.000000000000000000, 0.7115858121531838387, 1.000000000000000000),
 ( 1.000000000000000000, 0.7147553065756238055, 1.000000000000000000) ) ) 
 REPRESENTATION_ITEM ( '' )  SURFACE ( )  );
#49939 = ADVANCED_FACE ( 'NONE', ( #23267 ), #46649, .F. ) ;
#49940 = CARTESIAN_POINT ( 'NONE',  ( 5.676582343749997150, 222.2395833367473017, -9.832129032723418760 ) ) ;
#49941 = CARTESIAN_POINT ( 'NONE',  ( 0.000000000000000000, 20.39230484541327471, -10.20000000000000284 ) ) ;
#49942 = CARTESIAN_POINT ( 'NONE',  ( 3.999999999999960032, 200.1250000027312126, 142.0000000000000568 ) ) ;
#49943 = DIRECTION ( 'NONE',  ( -1.000000000000000000, 0.000000000000000000, 0.000000000000000000 ) ) ;
#49944 = CARTESIAN_POINT ( 'NONE',  ( -28.00000000000000000, 191.0000000000000284, 170.0000000000003695 ) ) ;
#49945 = CARTESIAN_POINT ( 'NONE',  ( 2.679491924311225848, 248.5416666666666856, -10.00000000000000000 ) ) ;
#49946 = CARTESIAN_POINT ( 'NONE',  ( -10.00000000000004263, 77.70833333333338544, 2.679491924311233397 ) ) ;
#49947 = CARTESIAN_POINT ( 'NONE',  ( 5.000000000000001776, 185.8333333333333428, -8.660254037844389075 ) ) ;
#49948 = FILL_AREA_STYLE_COLOUR ( '', #10285 ) ;
#49949 = CARTESIAN_POINT ( 'NONE',  ( -2.977408999572647819, 7.188101187499992051, 22.58030278187175455 ) ) ;
#49950 = CARTESIAN_POINT ( 'NONE',  ( -11.35316468749999785, 148.3854166632526983, -3.042071309553167513 ) ) ;
#49951 = CARTESIAN_POINT ( 'NONE',  ( -11.00000000000000000, 0.000000000000000000, 88.18750000409677625 ) ) ;
#49952 = CARTESIAN_POINT ( 'NONE',  ( 10.00000000000000000, 260.6250000068279746, -1.224646799147353256E-15 ) ) ;
#49953 = DIRECTION ( 'NONE',  ( 0.000000000000000000, 1.000000000000000000, 0.000000000000000000 ) ) ;
#49955 = CYLINDRICAL_SURFACE ( 'NONE', #14577, 11.00000000000000000 ) ;
#49954 = CARTESIAN_POINT ( 'NONE',  ( -8.660254037844390851, 84.79166665983869677, 4.999999999999998224 ) ) ;
#49956 = ORIENTED_EDGE ( 'NONE', *, *, #25598, .T. ) ;
#49957 = CARTESIAN_POINT ( 'NONE',  ( -2.085542519210945728E-15, 24.84374999658601624, 11.35316468750000141 ) ) ;
#49958 = ADVANCED_FACE ( 'NONE', ( #45529 ), #41283, .F. ) ;
#49960 = CARTESIAN_POINT ( 'NONE',  ( 25.17157287525381548, 199.6250000000000284, 167.1715728752537018 ) ) ;
#49959 = CARTESIAN_POINT ( 'NONE',  ( -4.898587196589412829E-16, 97.62499999999998579, -8.000000000000000000 ) ) ;
#49961 = CARTESIAN_POINT ( 'NONE',  ( 7.778174593052023411, -7.778174593052021635, 79.56249999999998579 ) ) ;
#49962 = CARTESIAN_POINT ( 'NONE',  ( 1.432654583217607192, 203.2500000013655495, 145.4587341250000350 ) ) ;
#49963 = CARTESIAN_POINT ( 'NONE',  ( -10.00000000000000178, 49.37499999317203248, -1.224646799147353454E-15 ) ) ;
#49964 = PRESENTATION_LAYER_ASSIGNMENT (  '', '', ( #54824 ) ) ;
#49965 = CARTESIAN_POINT ( 'NONE',  ( 5.082755093536325042, 107.0937500020483810, -5.082755093536325930 ) ) ;
#49966 = CARTESIAN_POINT ( 'NONE',  ( 4.541265875000002339, 6.437499998634407028, 0.000000000000000000 ) ) ;
#49967 = CARTESIAN_POINT ( 'NONE',  ( -7.999999999999991118, 0.000000000000000000, 6.830302779823365533 ) ) ;
#49969 = CARTESIAN_POINT ( 'NONE',  ( 6.123233995736767268E-16, 161.2500000000000000, -10.00000000000000178 ) ) ;
#49968 = CARTESIAN_POINT ( 'NONE',  ( 2.485281374238919927, 291.3750000034139589, 5.999999999999654499 ) ) ;
#49970 = ORIENTED_EDGE ( 'NONE', *, *, #35639, .T. ) ;
#49971 = ORIENTED_EDGE ( 'NONE', *, *, #13614, .F. ) ;
#49972 = CARTESIAN_POINT ( 'NONE',  ( -7.320508075688773708, 221.8750000000000284, -7.320508075688774596 ) ) ;
#49973 = CARTESIAN_POINT ( 'NONE',  ( -26.08087491822010406, -41.84332358895906623, 153.2365425615005847 ) ) ;
#49974 = CARTESIAN_POINT ( 'NONE',  ( 8.311093377946834337, 125.1562499965860411, 8.311093377946839666 ) ) ;
#49975 = ORIENTED_EDGE ( 'NONE', *, *, #41335, .T. ) ;
#49976 = CARTESIAN_POINT ( 'NONE',  ( 32.00000000000000000, 201.3125000000000284, 168.3431457505075457 ) ) ;
#49977 = CARTESIAN_POINT ( 'NONE',  ( -4.220049686691935698, 10.18810118749999916, 86.87500000204836681 ) ) ;
#49978 = CARTESIAN_POINT ( 'NONE',  ( 0.000000000000000000, 0.000000000000000000, 118.0000000000000000 ) ) ;
#49979 = CARTESIAN_POINT ( 'NONE',  ( 1.656854249492405451, 206.3125000000000284, 202.0000000000000284 ) ) ;
#49981 = CARTESIAN_POINT ( 'NONE',  ( -3.042071309553163960, 122.2395833299193271, -11.35316468749999963 ) ) ;
#49980 = DIRECTION ( 'NONE',  ( 0.000000000000000000, 0.000000000000000000, 1.000000000000000000 ) ) ;
#49982 = DIRECTION ( 'NONE',  ( 0.000000000000000000, 0.000000000000000000, -1.000000000000000000 ) ) ;
#49983 = VERTEX_POINT ( 'NONE', #57241 ) ;
#49984 = CARTESIAN_POINT ( 'NONE',  ( -2.679491924311226292, 23.33333332650536818, -10.00000000000000178 ) ) ;
#49985 = EDGE_CURVE ( 'NONE', #66203, #29969, #23492, .T. ) ;
#49986 = CARTESIAN_POINT ( 'NONE',  ( 45.49866705521328214, 185.8289241312458273, 77.67342763857470800 ) ) ;
#49987 = CARTESIAN_POINT ( 'NONE',  ( -9.832129032723420536, 119.0104166632526841, 5.676582343749997150 ) ) ;
#49988 = CARTESIAN_POINT ( 'NONE',  ( 1.432654583217662259, 205.1250000013656347, 194.5412658750000219 ) ) ;
#49989 = CARTESIAN_POINT ( 'NONE',  ( 4.401442555609581635E-16, 17.71874999795161187, -7.188101187500000044 ) ) ;
#49990 = CARTESIAN_POINT ( 'NONE',  ( 10.18810118750000093, -4.220049686691933033, 82.18750000204836681 ) ) ;
#49991 = CARTESIAN_POINT ( 'NONE',  ( 11.35316468750000141, 26.09374999658601624, 0.000000000000000000 ) ) ;
#49992 = ORIENTED_EDGE ( 'NONE', *, *, #51405, .F. ) ;
#49993 = CARTESIAN_POINT ( 'NONE',  ( 0.000000000000000000, 300.0000000000000000, 0.000000000000000000 ) ) ;
#49994 = CARTESIAN_POINT ( 'NONE',  ( 5.662595241051936235, -5.662595241051934458, 18.07561528394063188 ) ) ;
#49995 = CARTESIAN_POINT ( 'NONE',  ( 1.836970198721029589E-15, 236.2500000000000284, 10.00000000000000178 ) ) ;
#49996 = CARTESIAN_POINT ( 'NONE',  ( 1.102182119232618108E-15, 298.3125000034140157, 6.000000000000001776 ) ) ;
#49997 = CARTESIAN_POINT ( 'NONE',  ( 7.188101187500001821, 2.062499997951610098, -2.977408999572650483 ) ) ;
#49998 = CARTESIAN_POINT ( 'NONE',  ( -4.721056650415998313, 290.5781250017069510, 4.721056650416000089 ) ) ;
#49999 = CARTESIAN_POINT ( 'NONE',  ( -18.00000000000000000, 10.39230484541324628, -20.69999999999999929 ) ) ;
#50000 = CARTESIAN_POINT ( 'NONE',  ( 7.188101187500001821, 0.9374999979516100979, -2.977408999572650483 ) ) ;
#50001 = ORIENTED_EDGE ( 'NONE', *, *, #8254, .T. ) ;
#50002 = CARTESIAN_POINT ( 'NONE',  ( -9.832129032723420536, 144.0104166632526699, 5.676582343749997150 ) ) ;
#50003 = CARTESIAN_POINT ( 'NONE',  ( -6.238412754330611322E-16, 10.18810118749999916, 74.78125000204836681 ) ) ;
#50004 = CARTESIAN_POINT ( 'NONE',  ( -29.43265458321766559, 194.5000000013656063, 166.5412658750003629 ) ) ;
#50005 = CARTESIAN_POINT ( 'NONE',  ( -1.656854249492321074, 198.3125000000000853, 137.9999999999999716 ) ) ;
#50006 = CARTESIAN_POINT ( 'NONE',  ( -4.541265875000002339, 17.87499999863441147, -1.881053915767121998 ) ) ;
#50007 = ORIENTED_EDGE ( 'NONE', *, *, #44653, .F. ) ;
#50008 = CARTESIAN_POINT ( 'NONE',  ( 2.849036369511732440E-14, 205.3750000027312126, 202.0000000000000000 ) ) ;
#50009 = VECTOR ( 'NONE', #58754, 1000.000000000000000 ) ;
#50010 = CARTESIAN_POINT ( 'NONE',  ( -1.432654583217662481, 196.3750000013656063, 145.4587341250000634 ) ) ;
#50011 = CARTESIAN_POINT ( 'NONE',  ( -27.99999999999991118, 204.6250000027312126, 174.0000000000003695 ) ) ;
#50012 = AXIS2_PLACEMENT_3D ( 'NONE', #66928, #45039, #26929 ) ;
#50013 = CARTESIAN_POINT ( 'NONE',  ( 4.898587196589412829E-16, 6.375000000000000888, -8.000000000000000000 ) ) ;
#50014 = VERTEX_POINT ( 'NONE', #63252 ) ;
#50015 = CARTESIAN_POINT ( 'NONE',  ( 5.082755093536325930, 11.15624999795161187, -5.082755093536325930 ) ) ;
#50016 = CARTESIAN_POINT ( 'NONE',  ( -25.28061399944827059, -12.82819220331784926, 187.9640033798334002 ) ) ;
#50017 = CARTESIAN_POINT ( 'NONE',  ( 0.000000000000000000, 101.0525588832578734, -7.949999999999993960 ) ) ;
#50018 = B_SPLINE_CURVE_WITH_KNOTS ( 'NONE', 3,
 ( #68125, #16419, #39453, #62452, #5134, #28127, #22454, #65790, #7351 ),
 .UNSPECIFIED., .F., .F.,
 ( 4, 2, 2, 1, 4 ),
 ( 0.5000000000000000000, 0.5566067453737802984, 0.5707584317172254007, 0.5849101180606703920, 0.6132134907475605967 ),
 .UNSPECIFIED. ) ;
#50019 = CARTESIAN_POINT ( 'NONE',  ( -2.085542519210945728E-15, 184.5312499965860411, 11.35316468750000141 ) ) ;
#50020 = CARTESIAN_POINT ( 'NONE',  ( 5.082755093536326818, 114.5937500020483810, 5.082755093536325042 ) ) ;
#50021 = CARTESIAN_POINT ( 'NONE',  ( 1.656854249492432318, 207.8125000027312410, 194.0000000000000568 ) ) ;
#50022 = CARTESIAN_POINT ( 'NONE',  ( -6.676582343749999815, 288.5156250017069510, 2.765530957082001251 ) ) ;
#50024 = DIRECTION ( 'NONE',  ( -0.000000000000000000, 1.000000000000000000, 4.476705744456276341E-16 ) ) ;
#50023 = CARTESIAN_POINT ( 'NONE',  ( -5.676582343749992710, 224.7395833367473301, 9.832129032723422313 ) ) ;
#50025 = ORIENTED_EDGE ( 'NONE', *, *, #34457, .F. ) ;
#50026 = EDGE_CURVE ( 'NONE', #34824, #9367, #842, .T. ) ;
#50027 = CARTESIAN_POINT ( 'NONE',  ( -11.35316468749999608, 219.4270833367473301, 3.042071309553173730 ) ) ;
#50028 = CARTESIAN_POINT ( 'NONE',  ( 1.320432766682872962E-15, -7.188101187499992051, 24.73655278187175810 ) ) ;
#50029 = CARTESIAN_POINT ( 'NONE',  ( -27.99999999999999645, 210.0000000000000284, 170.0000000000003695 ) ) ;
#50030 = LINE ( 'NONE', #21353, #21453 ) ;
#50031 = CARTESIAN_POINT ( 'NONE',  ( -0.4451317748866462920, -67.59323688304517930, -20.03471819849869817 ) ) ;
#50032 =( BOUNDED_CURVE ( )  B_SPLINE_CURVE ( 2, ( #65238, #46782, #70905, #794, #41864, #1532, #12084, #24512, #1159 ),
 .UNSPECIFIED., .F., .F. ) 
 B_SPLINE_CURVE_WITH_KNOTS ( ( 3, 2, 2, 2, 3 ),
 ( 0.7647058823529411242, 0.7683823529411765163, 0.7720588235294117974, 0.7757352941176470784, 0.7794117647058823595 ),
 .UNSPECIFIED. ) 
 CURVE ( )  GEOMETRIC_REPRESENTATION_ITEM ( )  RATIONAL_B_SPLINE_CURVE ( ( 1.000000000000000000, 0.9238795325112867385, 1.000000000000000000, 0.9238795325112867385, 1.000000000000000000, 0.9238795325112867385, 1.000000000000000000, 0.9238795325112867385, 1.000000000000000000 ) ) 
 REPRESENTATION_ITEM ( '' )  );
#50033 = CARTESIAN_POINT ( 'NONE',  ( 2.445694354108840063, 196.0625000013656063, 200.4456943541088663 ) ) ;
#50034 = ORIENTED_EDGE ( 'NONE', *, *, #41835, .F. ) ;
#50035 = CARTESIAN_POINT ( 'NONE',  ( -4.118099735505520442, 8.014718854569423456, 4.446287698374634477E-15 ) ) ;
#50036 = CARTESIAN_POINT ( 'NONE',  ( 8.000000000000000000, 91.34375000000000000, -3.313708498984762496 ) ) ;
#50037 = CARTESIAN_POINT ( 'NONE',  ( -8.311093377946841443, 114.2187499965860269, 8.311093377946830785 ) ) ;
#50038 = CARTESIAN_POINT ( 'NONE',  ( -5.000000000000000000, -16.24494643555759410, -69.83755725260751035 ) ) ;
#50039 = CARTESIAN_POINT ( 'NONE',  ( 11.00000000000000000, 4.556349186104045934, 73.84374999999998579 ) ) ;
#50042 = CARTESIAN_POINT ( 'NONE',  ( 0.000000000000000000, 300.0000000000000000, 6.000000000000001776 ) ) ;
#50041 = CARTESIAN_POINT ( 'NONE',  ( 24.54126587499998280, 201.1250000013656347, 168.5673454167822740 ) ) ;
#50040 = CARTESIAN_POINT ( 'NONE',  ( 29.43265458321761230, 198.7500000013656063, 173.4587341249998929 ) ) ;
#50043 = ORIENTED_EDGE ( 'NONE', *, *, #7136, .T. ) ;
#50044 = CARTESIAN_POINT ( 'NONE',  ( -7.347880794884122694E-16, 1.750000000000000222, 4.000000000000001776 ) ) ;
#50045 = CARTESIAN_POINT ( 'NONE',  ( 6.000000000000003553, 287.5000000034140157, 2.485281374238571317 ) ) ;
#50046 = CARTESIAN_POINT ( 'NONE',  ( 26.56734541678237704, 196.2500000013656631, 166.5412658749999650 ) ) ;
#50047 = ADVANCED_FACE ( 'NONE', ( #47385 ), #55724, .F. ) ;
#50048 = CARTESIAN_POINT ( 'NONE',  ( 11.35316468749999785, 205.8854166632526415, 3.042071309553174174 ) ) ;
#50049 = FACE_BOUND ( 'NONE', #41802, .T. ) ;
#50050 = CARTESIAN_POINT ( 'NONE',  ( 0.000000000000000000, 125.0000000000000000, 0.000000000000000000 ) ) ;
#50051 = CARTESIAN_POINT ( 'NONE',  ( 3.211159895383561835, 19.43749999863440436, -3.211159895383561835 ) ) ;
#50052 = CARTESIAN_POINT ( 'NONE',  ( 0.8997857290928857887, -51.17549659653120386, 48.53090770943006049 ) ) ;
#50053 = CARTESIAN_POINT ( 'NONE',  ( -3.313708498984757167, 7.999999999999991118, 27.54905277982337353 ) ) ;
#50055 = CARTESIAN_POINT ( 'NONE',  ( -7.999999999999991118, 0.000000000000000000, 9.830302779823364645 ) ) ;
#50054 = CARTESIAN_POINT ( 'NONE',  ( -11.00000000000000000, 0.000000000000000000, 86.50000000000000000 ) ) ;
#50056 = CARTESIAN_POINT ( 'NONE',  ( -8.311093377946841443, 88.90624999658602690, 8.311093377946830785 ) ) ;
#50057 = EDGE_LOOP ( 'NONE', ( #64894, #56106 ) ) ;
#50058 = ADVANCED_FACE ( 'NONE', ( #2479 ), #2107, .F. ) ;
#50059 =( BOUNDED_CURVE ( )  B_SPLINE_CURVE ( 2, ( #28994, #57684, #22963, #58060, #11273, #69732, #34305, #350, #63688, #5620, #12015, #18047, #41062 ),
 .UNSPECIFIED., .F., .F. ) 
 B_SPLINE_CURVE_WITH_KNOTS ( ( 3, 2, 2, 2, 2, 2, 3 ),
 ( 1.334491602770097263, 1.339725126200808969, 1.344958649631520675, 1.350192173062232381, 1.355425696492944088, 1.360659219923655794, 1.365892743354367500 ),
 .UNSPECIFIED. ) 
 CURVE ( )  GEOMETRIC_REPRESENTATION_ITEM ( )  RATIONAL_B_SPLINE_CURVE ( ( 1.000000000000001998, 0.9659258262890663138, 1.000000000000000000, 0.9659258262890684232, 1.000000000000000000, 0.9659258262890684232, 1.000000000000000000, 0.9659258262890684232, 1.000000000000000000, 0.9659258262890684232, 1.000000000000000000, 0.9659258262890684232, 1.000000000000000000 ) ) 
 REPRESENTATION_ITEM ( '' )  );
#50060 = CARTESIAN_POINT ( 'NONE',  ( -2.775557561562891351E-14, 210.0000000000000284, 146.0000000000000284 ) ) ;
#50061 = CARTESIAN_POINT ( 'NONE',  ( -2.977408999572654480, 20.99999999795161898, 7.188101187499999156 ) ) ;
#50062 = CARTESIAN_POINT ( 'NONE',  ( -5.000000000000000888, 222.2916666734946602, -8.660254037844387298 ) ) ;
#50063 = CARTESIAN_POINT ( 'NONE',  ( 11.35316468749999963, 256.5104166700807014, 3.042071309553159519 ) ) ;
#50064 = CARTESIAN_POINT ( 'NONE',  ( 8.311093377946834337, 85.15624999658602690, 8.311093377946839666 ) ) ;
#50065 = ORIENTED_EDGE ( 'NONE', *, *, #3806, .F. ) ;
#50066 = PLANE ( 'NONE',  #22258 ) ;
#50067 = CARTESIAN_POINT ( 'NONE',  ( 10.18810118749999916, 1.247682550866122264E-15, 105.9062500020483810 ) ) ;
#50068 = CARTESIAN_POINT ( 'NONE',  ( 5.009999999999998899, 0.000000000000000000, -0.6932054628276118624 ) ) ;
#50069 = CARTESIAN_POINT ( 'NONE',  ( 2.445694354108840063, 206.0625000013656063, 200.4456943541088663 ) ) ;
#50070 = CARTESIAN_POINT ( 'NONE',  ( 18.00000000000000355, 0.000000000000000000, 0.000000000000000000 ) ) ;
#50072 = CARTESIAN_POINT ( 'NONE',  ( 3.042071309553167513, 86.82291666325266988, -11.35316468749999785 ) ) ;
#50071 = FACE_BOUND ( 'NONE', #61880, .T. ) ;
#50073 = AXIS2_PLACEMENT_3D ( 'NONE', #21495, #57336, #21860 ) ;
#50074 = CARTESIAN_POINT ( 'NONE',  ( -7.999999999999991118, 3.313708498984756723, 20.42405278392014978 ) ) ;
#50075 = CARTESIAN_POINT ( 'NONE',  ( -31.45873412499999233, 200.9375000013656063, 170.0000000000003979 ) ) ;
#50076 = CARTESIAN_POINT ( 'NONE',  ( 4.000000000000016875, 208.5625000027311842, 199.6568542494924259 ) ) ;
#50077 = CARTESIAN_POINT ( 'NONE',  ( 4.999999999999993783, 181.0416666598387110, 8.660254037844390851 ) ) ;
#50078 = VECTOR ( 'NONE', #73029, 1000.000000000000000 ) ;
#50079 = CARTESIAN_POINT ( 'NONE',  ( 5.000000000000000000, -53.55895565990308427, 45.41404144516045704 ) ) ;
#50080 = CARTESIAN_POINT ( 'NONE',  ( -3.042071309553173730, 69.63541666325268409, 11.35316468749999785 ) ) ;
#50081 = CARTESIAN_POINT ( 'NONE',  ( 4.721056650415999201, 293.0781250017069510, -4.721056650415999201 ) ) ;
#50082 = EDGE_CURVE ( 'NONE', #46255, #66256, #70232, .T. ) ;
#50083 = CARTESIAN_POINT ( 'NONE',  ( -7.204075437095965206, -7.204075437095968759, 99.71875000204838102 ) ) ;
#50084 = CARTESIAN_POINT ( 'NONE',  ( -3.042071309553173730, 214.3229166632526983, 11.35316468749999785 ) ) ;
#50085 = EDGE_LOOP ( 'NONE', ( #31642, #54940, #25063 ) ) ;
#50086 = CARTESIAN_POINT ( 'NONE',  ( -2.828427124746192067, 1.374999997268813168, 2.828427124746190735 ) ) ;
#50087 = CYLINDRICAL_SURFACE ( 'NONE', #46047, 3.999999999999976019 ) ;
#50088 = LINE ( 'NONE', #10473, #7003 ) ;
#50089 = CARTESIAN_POINT ( 'NONE',  ( -8.311093377946836114, 207.6562499965860127, -8.311093377946837890 ) ) ;
#50090 = CARTESIAN_POINT ( 'NONE',  ( -2.679491924311222295, 219.1666666734946602, 10.00000000000000178 ) ) ;
#50091 = CARTESIAN_POINT ( 'NONE',  ( 11.00000000000000000, 1.347111479062088405E-15, 72.43750000409676204 ) ) ;
#50092 = ORIENTED_EDGE ( 'NONE', *, *, #30218, .F. ) ;
#50093 = CARTESIAN_POINT ( 'NONE',  ( 11.35316468749999785, 195.8854166632526415, 3.042071309553174174 ) ) ;
#50094 = CARTESIAN_POINT ( 'NONE',  ( -7.188101187499990274, -2.977408999572651815, 18.08030278187175455 ) ) ;
#50095 = CARTESIAN_POINT ( 'NONE',  ( -27.99999999999996803, 205.9375000013656063, 173.4587341250003760 ) ) ;
#50096 = CARTESIAN_POINT ( 'NONE',  ( 3.313708498984762496, 11.71875000000000000, 7.999999999999998224 ) ) ;
#50097 = ORIENTED_EDGE ( 'NONE', *, *, #29056, .F. ) ;
#50098 = EDGE_CURVE ( 'NONE', #41307, #16897, #64165, .T. ) ;
#50099 = CARTESIAN_POINT ( 'NONE',  ( -5.656854249492378806, 90.87500000409677625, 5.656854249492381470 ) ) ;
#50100 = EDGE_CURVE ( 'NONE', #42039, #7034, #3970, .T. ) ;
#50101 = APPLICATION_CONTEXT ( 'automotive_design' ) ;
#50102 = CARTESIAN_POINT ( 'NONE',  ( 10.00000000000000178, 10.00000000000000000, 0.000000000000000000 ) ) ;
#50103 = CARTESIAN_POINT ( 'NONE',  ( 10.18810118750000093, -4.220049686691933921, 82.18750000204836681 ) ) ;
#50104 = VERTEX_POINT ( 'NONE', #25471 ) ;
#50105 = EDGE_CURVE ( 'NONE', #46282, #6126, #62504, .T. ) ;
#50106 = CARTESIAN_POINT ( 'NONE',  ( 1.656854249492381248, 21.18750000000000000, -4.000000000000001776 ) ) ;
#50107 = CARTESIAN_POINT ( 'NONE',  ( -1.881053915767124440, 20.99999999863440792, 4.541265875000001451 ) ) ;
#50108 = CARTESIAN_POINT ( 'NONE',  ( -7.999999999999991118, 0.000000000000000000, 7.017802783920144449 ) ) ;
#50109 = CARTESIAN_POINT ( 'NONE',  ( 25.17157287525377996, 198.7500000027312126, 167.1715728752537586 ) ) ;
#50110 = ORIENTED_EDGE ( 'NONE', *, *, #36316, .T. ) ;
#50111 = CARTESIAN_POINT ( 'NONE',  ( 7.188101187500000044, 94.90625000204838102, -8.802885111219163269E-16 ) ) ;
#50114 = FACE_OUTER_BOUND ( 'NONE', #60867, .T. ) ;
#50113 = CARTESIAN_POINT ( 'NONE',  ( 11.35316468749999963, 261.4062500034140157, -1.390361679473963556E-15 ) ) ;
#50112 = DIRECTION ( 'NONE',  ( 0.000000000000000000, 0.000000000000000000, 1.000000000000000000 ) ) ;
#50115 = APPLICATION_PROTOCOL_DEFINITION ( 'draft international standard', 'automotive_design', 1998, #54403 ) ;
#50116 = ORIENTED_EDGE ( 'NONE', *, *, #44448, .T. ) ;
#50117 = CARTESIAN_POINT ( 'NONE',  ( 3.042071309553163960, 257.7604166700806445, -11.35316468749999785 ) ) ;
#50118 = AXIS2_PLACEMENT_3D ( 'NONE', #41422, #18407, #7462 ) ;
#50119 = CARTESIAN_POINT ( 'NONE',  ( -7.188101187499991163, 2.977408999572646930, 13.39280278187175455 ) ) ;
#50120 = VERTEX_POINT ( 'NONE', #64743 ) ;
#50121 = EDGE_LOOP ( 'NONE', ( #50487, #1494, #18989, #50341 ) ) ;
#50122 = CARTESIAN_POINT ( 'NONE',  ( 10.18810118750000093, -4.220049686691933033, 74.31250000204836681 ) ) ;
#50123 = CARTESIAN_POINT ( 'NONE',  ( -5.676582343749998039, 72.76041666325268409, -9.832129032723420536 ) ) ;
#50124 = DIRECTION ( 'NONE',  ( 0.000000000000000000, -1.000000000000000000, 0.000000000000000000 ) ) ;
#50125 = CARTESIAN_POINT ( 'NONE',  ( 11.00000000000000000, 4.556349186104045934, 91.84374999999998579 ) ) ;
#50128 = CARTESIAN_POINT ( 'NONE',  ( 6.676582343750001591, 292.1093750017069510, -8.176455196517173205E-16 ) ) ;
#50127 = CARTESIAN_POINT ( 'NONE',  ( 26.34314575050758833, 198.6875000027312126, 165.9999999999998863 ) ) ;
#50126 = CARTESIAN_POINT ( 'NONE',  ( -26.34314575050756346, 205.6875000027312126, 174.0000000000003979 ) ) ;
#50129 = CARTESIAN_POINT ( 'NONE',  ( -7.778174593052020747, -7.778174593052023411, 83.68750000000000000 ) ) ;
#50130 = DIRECTION ( 'NONE',  ( 1.000000000000000000, 0.000000000000000000, 0.000000000000000000 ) ) ;
#50131 = CARTESIAN_POINT ( 'NONE',  ( 1.432654583217664701, 200.0000000013656063, 201.4587341250000065 ) ) ;
#50132 = CARTESIAN_POINT ( 'NONE',  ( 3.313708498984762052, 10.59374999590322020, -8.000000000000000000 ) ) ;
#50133 = AXIS2_PLACEMENT_3D ( 'NONE', #71857, #25829, #20551 ) ;
#50134 = VERTEX_POINT ( 'NONE', #25838 ) ;
#50135 = CARTESIAN_POINT ( 'NONE',  ( 25.55430564589119768, 209.3125000013656063, 167.5543056458910485 ) ) ;
#50136 = CARTESIAN_POINT ( 'NONE',  ( -7.188101187500001821, 14.99999999795161187, -2.977408999572651371 ) ) ;
#50137 = CARTESIAN_POINT ( 'NONE',  ( -5.676582343750006032, 164.4270833299193555, 9.832129032723418760 ) ) ;
#50138 = CARTESIAN_POINT ( 'NONE',  ( 7.778174593052023411, -7.778174593052021635, 99.25000000409679046 ) ) ;
#50139 = CARTESIAN_POINT ( 'NONE',  ( -2.977408999572650927, 106.2500000020484094, -7.188101187500000933 ) ) ;
#50141 = CARTESIAN_POINT ( 'NONE',  ( 1.780377099649257167, -51.29164421682789765, -48.57534666485256025 ) ) ;
#50140 = DIRECTION ( 'NONE',  ( 0.000000000000000000, -1.000000000000000000, 0.000000000000000000 ) ) ;
#50142 = CARTESIAN_POINT ( 'NONE',  ( 28.00000000000002487, 207.1875000013656063, 166.5412658749999082 ) ) ;
#50143 = CARTESIAN_POINT ( 'NONE',  ( 2.977408999572650927, -7.188101187499990274, 18.83030278187175099 ) ) ;
#50144 = CARTESIAN_POINT ( 'NONE',  ( -2.849036369511732440E-14, 206.3750000027312126, 138.0000000000000568 ) ) ;
#50145 = CARTESIAN_POINT ( 'NONE',  ( 5.676582343750001591, 51.61458332991934839, -9.832129032723420536 ) ) ;
#50146 = CARTESIAN_POINT ( 'NONE',  ( 4.898587196589412829E-16, 21.37500000000000355, -8.000000000000000000 ) ) ;
#50147 = CARTESIAN_POINT ( 'NONE',  ( 8.660254037844389075, 17.29166665983869677, -5.000000000000000000 ) ) ;
#50148 = CARTESIAN_POINT ( 'NONE',  ( -31.99999999999999289, 200.3750000027312126, 170.0000000000004547 ) ) ;
#50149 = VERTEX_POINT ( 'NONE', #7773 ) ;
#50150 = CARTESIAN_POINT ( 'NONE',  ( 6.123233995736767268E-16, 143.1249999931720538, -10.00000000000000178 ) ) ;
#50151 = CARTESIAN_POINT ( 'NONE',  ( -3.313708498984800688, 22.78124999590322020, -7.999999999999958256 ) ) ;
#50152 = CARTESIAN_POINT ( 'NONE',  ( -2.085542519210945728E-15, 44.53124999658601979, 11.35316468750000141 ) ) ;
#50153 = CARTESIAN_POINT ( 'NONE',  ( -7.778174593052020747, -7.778174593052023411, 74.87500000409677625 ) ) ;
#50154 = CARTESIAN_POINT ( 'NONE',  ( 2.445694354108783219, 198.8125000013656063, 139.5543056458912190 ) ) ;
#50155 = FACE_OUTER_BOUND ( 'NONE', #35105, .T. ) ;
#50156 = CARTESIAN_POINT ( 'NONE',  ( -2.679491924324485019, 13.54166666666547769, 9.999999999992347455 ) ) ;
#50158 = CARTESIAN_POINT ( 'NONE',  ( 5.676582343749993598, 44.94791666325267698, 9.832129032723422313 ) ) ;
#50157 = CARTESIAN_POINT ( 'NONE',  ( -7.188101187500000044, 97.15625000204839523, 0.000000000000000000 ) ) ;
#50159 = CARTESIAN_POINT ( 'NONE',  ( -4.898587196589407898E-16, 7.999999999999991118, 10.95530277982336642 ) ) ;
#50160 = CARTESIAN_POINT ( 'NONE',  ( -3.313708498984757611, 7.999999999999991118, 21.73655278392014623 ) ) ;
#50161 =( BOUNDED_CURVE ( )  B_SPLINE_CURVE ( 2, ( #41129, #40387, #10975, #12444, #418, #62642, #74338, #23398, #69799 ),
 .UNSPECIFIED., .F., .F. ) 
 B_SPLINE_CURVE_WITH_KNOTS ( ( 3, 2, 2, 2, 3 ),
 ( 0.7291666666666649643, 0.7395833333333317050, 0.7499999999999983347, 0.7604166666666649643, 0.7708333333333317050 ),
 .UNSPECIFIED. ) 
 CURVE ( )  GEOMETRIC_REPRESENTATION_ITEM ( )  RATIONAL_B_SPLINE_CURVE ( ( 1.000000000000012212, 0.9238795325112745260, 1.000000000000000000, 0.9238795325112867385, 1.000000000000000000, 0.9238795325112867385, 1.000000000000000000, 0.9238795325112989509, 0.9999999999999877875 ) ) 
 REPRESENTATION_ITEM ( '' )  );
#50162 = CARTESIAN_POINT ( 'NONE',  ( -11.35316468749999785, 168.0729166632526699, -3.042071309553167513 ) ) ;
#50163 = CARTESIAN_POINT ( 'NONE',  ( -7.320508075688778149, 144.9999999931719969, 7.320508075688769267 ) ) ;
#50164 = CARTESIAN_POINT ( 'NONE',  ( -2.977408999572650927, 104.7500000020483810, -7.188101187500001821 ) ) ;
#50165 = LINE ( 'NONE', #39596, #12305 ) ;
#50166 = CARTESIAN_POINT ( 'NONE',  ( 6.951808397369818766E-16, 32.34374999658601268, -11.35316468750000141 ) ) ;
#50167 = DIRECTION ( 'NONE',  ( 0.000000000000000000, 0.000000000000000000, -1.000000000000000000 ) ) ;
#50168 = ORIENTED_EDGE ( 'NONE', *, *, #56608, .F. ) ;
#50169 = DIRECTION ( 'NONE',  ( 0.000000000000000000, 0.000000000000000000, 1.000000000000000000 ) ) ;
#50170 = CARTESIAN_POINT ( 'NONE',  ( -10.18810118749999916, 0.000000000000000000, 75.15625000204836681 ) ) ;
#50171 = CARTESIAN_POINT ( 'NONE',  ( 35.89412776602885913, 39.44128785059449172, 65.00000000000000000 ) ) ;
#50173 = CARTESIAN_POINT ( 'NONE',  ( 6.951808397369818766E-16, 172.0312499965860411, -11.35316468750000141 ) ) ;
#50172 = CARTESIAN_POINT ( 'NONE',  ( 1.881637226502129035E-11, 6.249999999998538058, -10.00000000000000178 ) ) ;
#50174 = CARTESIAN_POINT ( 'NONE',  ( -3.313708498984758943, -7.999999999999989342, 14.66780278432982598 ) ) ;
#50175 = CARTESIAN_POINT ( 'NONE',  ( 5.656854249492378806, 8.812500000000000000, 5.656854249492381470 ) ) ;
#50176 = CARTESIAN_POINT ( 'NONE',  ( 5.000000000000004441, 259.7916666734946034, 8.660254037844385522 ) ) ;
#50177 = CARTESIAN_POINT ( 'NONE',  ( -2.219371606100929206, 51.37365828841677740, -48.60677221569366679 ) ) ;
#50178 = CARTESIAN_POINT ( 'NONE',  ( 4.220049686691941027, -10.18810118749999738, 83.50000000204840944 ) ) ;
#50179 = ORIENTED_EDGE ( 'NONE', *, *, #3343, .T. ) ;
#50180 = CYLINDRICAL_SURFACE ( 'NONE', #32891, 11.00000000000000000 ) ;
#50181 = CARTESIAN_POINT ( 'NONE',  ( 4.556349186104045934, 11.00000000000000000, 105.5312500000000142 ) ) ;
#50182 = CARTESIAN_POINT ( 'NONE',  ( -8.311093377946836114, 117.9687499965860127, -8.311093377946837890 ) ) ;
#50183 = CARTESIAN_POINT ( 'NONE',  ( -4.541265875000003227, 20.99999999863440792, 1.881053915767121110 ) ) ;
#50184 = VERTEX_POINT ( 'NONE', #65476 ) ;
#50185 = ORIENTED_EDGE ( 'NONE', *, *, #70525, .T. ) ;
#50186 = CARTESIAN_POINT ( 'NONE',  ( 4.541265875000002339, 8.499999998634406140, -1.881053915767121554 ) ) ;
#50187 = CARTESIAN_POINT ( 'NONE',  ( 7.188101187500000044, 6.468749997951610986, 0.000000000000000000 ) ) ;
#50188 = CARTESIAN_POINT ( 'NONE',  ( -3.313708498984762052, 112.9062500040967763, -8.000000000000000000 ) ) ;
#50189 = ADVANCED_FACE ( 'NONE', ( #53797 ), #71492, .F. ) ;
#50190 = CARTESIAN_POINT ( 'NONE',  ( -7.204075437095967871, 7.204075437095967871, 91.84375000204838102 ) ) ;
#50191 = AXIS2_PLACEMENT_3D ( 'NONE', #29027, #24096, #35446 ) ;
#50192 = CARTESIAN_POINT ( 'NONE',  ( -31.45873412499999233, 200.9375000013656063, 170.0000000000003979 ) ) ;
#50193 = EDGE_CURVE ( 'NONE', #300, #39682, #25582, .T. ) ;
#50194 = CARTESIAN_POINT ( 'NONE',  ( 2.449293598294707893E-16, 6.250000000000000000, -4.000000000000001776 ) ) ;
#50195 = CARTESIAN_POINT ( 'NONE',  ( 1.656854249492381248, 18.93749999726881228, -4.000000000000001776 ) ) ;
#50196 = CARTESIAN_POINT ( 'NONE',  ( -4.541265875000002339, 6.749999998634407916, -1.881053915767121998 ) ) ;
#50197 = CARTESIAN_POINT ( 'NONE',  ( -4.000000000000015987, 196.4375000000000568, 140.3431457505076594 ) ) ;
#50198 = ORIENTED_EDGE ( 'NONE', *, *, #35471, .F. ) ;
#50199 =( NAMED_UNIT ( * ) SI_UNIT ( $, .STERADIAN. ) SOLID_ANGLE_UNIT ( ) );
#50201 = CARTESIAN_POINT ( 'NONE',  ( 2.020667218593132706E-15, -11.00000000000000000, 96.06250000409677625 ) ) ;
#50200 = CARTESIAN_POINT ( 'NONE',  ( -24.54126587499996148, 198.1250000013656063, 171.4326545832179534 ) ) ;
#50202 = CARTESIAN_POINT ( 'NONE',  ( 1.881053915767121776, 17.49999999863440436, -4.541265875000002339 ) ) ;
#50203 = CARTESIAN_POINT ( 'NONE',  ( 8.660254037844389075, 72.29166665983869677, -5.000000000000000000 ) ) ;
#50204 = CARTESIAN_POINT ( 'NONE',  ( 7.188101187499991163, 2.977408999572648707, 27.83030278187176165 ) ) ;
#50205 = ORIENTED_EDGE ( 'NONE', *, *, #72251, .F. ) ;
#50206 = ORIENTED_EDGE ( 'NONE', *, *, #45182, .T. ) ;
#50207 = CARTESIAN_POINT ( 'NONE',  ( -7.204075437095967871, 7.204075437095967871, 94.46875000204838102 ) ) ;
#50208 = CARTESIAN_POINT ( 'NONE',  ( -27.99999999999996447, 200.1875000013656063, 173.4587341250003760 ) ) ;
#50209 = CARTESIAN_POINT ( 'NONE',  ( -6.735557395310442023E-16, 11.00000000000000000, 108.6250000000000000 ) ) ;
#50211 = CARTESIAN_POINT ( 'NONE',  ( -1.432654583217607414, 208.5000000013656063, 194.5412658750000219 ) ) ;
#50210 = VECTOR ( 'NONE', #68130, 1000.000000000000000 ) ;
#50212 = CARTESIAN_POINT ( 'NONE',  ( 8.660254037844385522, 124.5833333333333428, 5.000000000000005329 ) ) ;
#50213 = CARTESIAN_POINT ( 'NONE',  ( 3.313708498984760720, 108.0312499999999858, -8.000000000000000000 ) ) ;
#50214 = CARTESIAN_POINT ( 'NONE',  ( -6.676582343750001591, 293.6093750017069510, 0.000000000000000000 ) ) ;
#50215 = PRODUCT_DEFINITION_FORMATION_WITH_SPECIFIED_SOURCE ( 'ANY', '', #4763, .NOT_KNOWN. ) ;
#50216 = CARTESIAN_POINT ( 'NONE',  ( -7.188101187499992051, 0.000000000000000000, 7.861552781871751883 ) ) ;
#50217 = EDGE_LOOP ( 'NONE', ( #8729, #21420, #25205, #16023 ) ) ;
#50218 = CARTESIAN_POINT ( 'NONE',  ( -2.679491924311235174, 175.4166666598387110, 10.00000000000000000 ) ) ;
#50219 = CARTESIAN_POINT ( 'NONE',  ( 31.45873412499998523, 208.6250000013655779, 171.4326545832175839 ) ) ;
#50220 = CARTESIAN_POINT ( 'NONE',  ( 4.898587196589412829E-16, 24.18749999590322375, -8.000000000000000000 ) ) ;
#50221 = CARTESIAN_POINT ( 'NONE',  ( 1.432654583217607192, 199.2500000013656063, 145.4587341250000634 ) ) ;
#50222 = CARTESIAN_POINT ( 'NONE',  ( -5.082755093536324154, 123.2187500020483952, 5.082755093536326818 ) ) ;
#50224 = CARTESIAN_POINT ( 'NONE',  ( 1.432654583217607414, 201.5000000013655779, 145.4587341250000634 ) ) ;
#50223 = DIRECTION ( 'NONE',  ( -7.885106708985487801E-17, 1.000000000000000000, -0.000000000000000000 ) ) ;
#50225 = CARTESIAN_POINT ( 'NONE',  ( -9.832129032723418760, 253.8020833367473017, -5.676582343749998927 ) ) ;
#50226 = DIRECTION ( 'NONE',  ( 0.000000000000000000, 0.000000000000000000, -1.000000000000000000 ) ) ;
#50227 = CARTESIAN_POINT ( 'NONE',  ( 6.123233995736767268E-16, 213.1249999931720538, -10.00000000000000178 ) ) ;
#50228 = CARTESIAN_POINT ( 'NONE',  ( -8.660254037844387298, 222.0833333333333428, -5.000000000000004441 ) ) ;
#50229 = DIRECTION ( 'NONE',  ( 0.000000000000000000, 0.000000000000000000, -1.000000000000000000 ) ) ;
#50230 = CARTESIAN_POINT ( 'NONE',  ( -8.311093377946836114, 202.9687499965860411, -8.311093377946837890 ) ) ;
#50231 = CARTESIAN_POINT ( 'NONE',  ( -4.000000000000015987, 197.6250000027312126, 142.0000000000000568 ) ) ;
#50232 = CARTESIAN_POINT ( 'NONE',  ( 4.541265875000001451, 6.249999998634407916, 1.881053915767124440 ) ) ;
#50233 = DIRECTION ( 'NONE',  ( -1.000000000000000000, 0.000000000000000000, 0.000000000000000000 ) ) ;
#50235 = CARTESIAN_POINT ( 'NONE',  ( 8.000000000000000000, 102.0312500040967763, -3.313708498984762496 ) ) ;
#50234 = CARTESIAN_POINT ( 'NONE',  ( -23.99999999999998934, 205.7500000000000284, 170.0000000000003411 ) ) ;
#50236 = ORIENTED_EDGE ( 'NONE', *, *, #35471, .T. ) ;
#50237 = CARTESIAN_POINT ( 'NONE',  ( 2.445694354108784108, 199.5625000013656063, 144.4456943541088663 ) ) ;
#50238 = CARTESIAN_POINT ( 'NONE',  ( -11.35316468750000141, 3.489583329919349719, 3.042071309553159963 ) ) ;
#50239 = CARTESIAN_POINT ( 'NONE',  ( -11.00000000000000000, 0.000000000000000000, 98.68750000409677625 ) ) ;
#50240 = CARTESIAN_POINT ( 'NONE',  ( -26.56734541678242678, 196.3750000013656063, 166.5412658750003345 ) ) ;
#50241 = FACE_OUTER_BOUND ( 'NONE', #1793, .T. ) ;
#50243 = CARTESIAN_POINT ( 'NONE',  ( 6.951808397369818766E-16, 7.031249996586016238, -11.35316468750000141 ) ) ;
#50242 = CARTESIAN_POINT ( 'NONE',  ( -7.188101187500000933, 116.5625000020483810, -2.977408999572650483 ) ) ;
#50244 = CARTESIAN_POINT ( 'NONE',  ( 5.656854249492376141, -5.656854249492374365, 25.39280277982336642 ) ) ;
#50245 = CARTESIAN_POINT ( 'NONE',  ( -5.676582343750006032, 124.1145833299193555, 9.832129032723418760 ) ) ;
#50246 = AXIS2_PLACEMENT_3D ( 'NONE', #49314, #8963, #9716 ) ;
#50247 = CARTESIAN_POINT ( 'NONE',  ( -8.660254037844390851, 99.79166665983871098, 4.999999999999998224 ) ) ;
#50248 = CARTESIAN_POINT ( 'NONE',  ( 2.977408999572650039, 121.0625000020483668, -7.188101187500001821 ) ) ;
#50249 = CARTESIAN_POINT ( 'NONE',  ( -1.881053915767121554, 19.74999999863440792, -4.541265875000002339 ) ) ;
#50250 = DIRECTION ( 'NONE',  ( -1.000000000000000000, 0.000000000000000000, 0.000000000000000000 ) ) ;
#50251 = DIRECTION ( 'NONE',  ( 0.000000000000000000, 0.000000000000000000, -1.000000000000000000 ) ) ;
#50252 = ORIENTED_EDGE ( 'NONE', *, *, #43625, .F. ) ;
#50253 = CARTESIAN_POINT ( 'NONE',  ( -2.679491924307398687, 116.4583333333330302, -10.00000000000221512 ) ) ;
#50254 = CARTESIAN_POINT ( 'NONE',  ( 4.721056650415999201, 290.2343750017069510, -4.721056650415999201 ) ) ;
#50255 = FILL_AREA_STYLE ('',( #33677 ) ) ;
#50256 = CARTESIAN_POINT ( 'NONE',  ( 3.313708498984762496, -7.999999999999989342, -0.01344721607985516210 ) ) ;
#50257 = CARTESIAN_POINT ( 'NONE',  ( 0.000000000000000000, 15.08051212944140218, 15.04081104653146994 ) ) ;
#50258 = CARTESIAN_POINT ( 'NONE',  ( -11.35316468749999785, 263.6979166700807014, -3.042071309553164848 ) ) ;
#50259 = CARTESIAN_POINT ( 'NONE',  ( 1.871523826299183495E-15, -10.18810118749999916, 104.4062500020483810 ) ) ;
#50260 = ORIENTED_EDGE ( 'NONE', *, *, #21519, .T. ) ;
#50261 = EDGE_CURVE ( 'NONE', #49221, #68433, #3911, .T. ) ;
#50262 = ADVANCED_FACE ( 'NONE', ( #66215 ), #36813, .F. ) ;
#50263 = CARTESIAN_POINT ( 'NONE',  ( 2.679491924311228956, 157.9166666598386826, -10.00000000000000000 ) ) ;
#50264 = CARTESIAN_POINT ( 'NONE',  ( 3.042071309553159519, 160.0520833299193555, 11.35316468750000141 ) ) ;
#50265 = CARTESIAN_POINT ( 'NONE',  ( -7.999999999999981348, 3.313708498984767381, 24.73655277982336287 ) ) ;
#50266 = CARTESIAN_POINT ( 'NONE',  ( 3.458734125000015425, 204.2500000013655779, 196.5673454167823877 ) ) ;
#50267 = CARTESIAN_POINT ( 'NONE',  ( 2.679491924311226292, 231.6666666734946034, -10.00000000000000000 ) ) ;
#50268 = CARTESIAN_POINT ( 'NONE',  ( -11.35316468750000141, 78.80208332991935549, 3.042071309553159963 ) ) ;
#50270 = EDGE_LOOP ( 'NONE', ( #50097, #43805, #2536, #36855 ) ) ;
#50269 =( BOUNDED_CURVE ( )  B_SPLINE_CURVE ( 2, ( #10772, #51885, #28865, #46218, #21708, #16785, #40188, #63191, #39078 ),
 .UNSPECIFIED., .F., .F. ) 
 B_SPLINE_CURVE_WITH_KNOTS ( ( 3, 2, 2, 2, 3 ),
 ( 0.06249999999999773792, 0.07291666666666440921, 0.08333333333333108051, 0.09374999999999775180, 0.1041666666666644370 ),
 .UNSPECIFIED. ) 
 CURVE ( )  GEOMETRIC_REPRESENTATION_ITEM ( )  RATIONAL_B_SPLINE_CURVE ( ( 1.000000000000016431, 0.9238795325112701962, 1.000000000000000000, 0.9238795325112867385, 1.000000000000000000, 0.9238795325112867385, 1.000000000000000000, 0.9238795325113030588, 0.9999999999999836797 ) ) 
 REPRESENTATION_ITEM ( '' )  );
#50271 = CARTESIAN_POINT ( 'NONE',  ( -7.204075437095965206, -7.204075437095968759, 114.3437500020483810 ) ) ;
#50272 = CARTESIAN_POINT ( 'NONE',  ( -1.881053915767124440, 10.12499999863440792, 4.541265875000001451 ) ) ;
#50273 = ORIENTED_EDGE ( 'NONE', *, *, #10577, .T. ) ;
#50274 = AXIS2_PLACEMENT_3D ( 'NONE', #74454, #34496, #17104 ) ;
#50275 = EDGE_CURVE ( 'NONE', #70764, #55422, #23938, .T. ) ;
#50276 = CARTESIAN_POINT ( 'NONE',  ( -8.000000000000001776, 0.8437500000000000000, 3.313708498984759387 ) ) ;
#50277 = CARTESIAN_POINT ( 'NONE',  ( 2.485281374238571317, 287.7500000034140157, -6.000000000000003553 ) ) ;
#50278 = FACE_OUTER_BOUND ( 'NONE', #61707, .T. ) ;
#50279 = CARTESIAN_POINT ( 'NONE',  ( -7.188101187500001821, 19.49999999795161898, -2.977408999572651371 ) ) ;
#50280 = CARTESIAN_POINT ( 'NONE',  ( 4.556349186104052151, -10.99999999999999822, 103.6562500040967905 ) ) ;
#50281 = CARTESIAN_POINT ( 'NONE',  ( 7.204075437095966983, 7.204075437095967871, 110.9687500020483810 ) ) ;
#50282 = DIRECTION ( 'NONE',  ( -0.8660271417563482066, 1.588872886645881945E-06, -0.4999969897297438237 ) ) ;
#50283 = CARTESIAN_POINT ( 'NONE',  ( 4.000000000000001776, 5.749999997268813168, 0.000000000000000000 ) ) ;
#50284 = CARTESIAN_POINT ( 'NONE',  ( -4.000000000000015987, 208.6250000027312126, 142.0000000000000568 ) ) ;
#50285 = ORIENTED_EDGE ( 'NONE', *, *, #32915, .F. ) ;
#50286 = CARTESIAN_POINT ( 'NONE',  ( 2.445694354108838731, 202.0625000013656063, 195.5543056458912190 ) ) ;
#50287 = EDGE_CURVE ( 'NONE', #22437, #26371, #7631, .T. ) ;
#50288 = CARTESIAN_POINT ( 'NONE',  ( -26.34314575050752794, 194.6875000027312126, 174.0000000000003411 ) ) ;
#50289 = CARTESIAN_POINT ( 'NONE',  ( 4.000000000000000888, 12.68749999726881406, 1.656854249492384135 ) ) ;
#50290 = AXIS2_PLACEMENT_3D ( 'NONE', #10705, #62744, #46148 ) ;
#50291 = CARTESIAN_POINT ( 'NONE',  ( 4.541265875000002339, 5.312499998634407028, 0.000000000000000000 ) ) ;
#50292 = CARTESIAN_POINT ( 'NONE',  ( -8.000000000000003553, 9.797174393178831574E-16, -14.80000000000000071 ) ) ;
#50293 = CARTESIAN_POINT ( 'NONE',  ( -7.188101187499991163, 2.977408999572646930, 17.89280278187175455 ) ) ;
#50294 = ORIENTED_EDGE ( 'NONE', *, *, #39004, .F. ) ;
#50295 = CARTESIAN_POINT ( 'NONE',  ( 0.000000000000000000, 0.000000000000000000, -10.00000000000000000 ) ) ;
#50296 = ORIENTED_EDGE ( 'NONE', *, *, #40727, .T. ) ;
#50297 = CARTESIAN_POINT ( 'NONE',  ( 7.204075437095966983, 7.204075437095967871, 113.5937500020483810 ) ) ;
#50298 = CARTESIAN_POINT ( 'NONE',  ( -10.67658234375000070, 264.6093750017070079, 0.000000000000000000 ) ) ;
#50299 = CARTESIAN_POINT ( 'NONE',  ( -1.432654583217607192, 203.2500000013656063, 194.5412658750000219 ) ) ;
#50300 = CARTESIAN_POINT ( 'NONE',  ( 25.55430564589115505, 200.0625000013656063, 167.5543056458911053 ) ) ;
#50301 = CARTESIAN_POINT ( 'NONE',  ( 7.320508075688774596, 75.62500000000000000, -7.320508075688774596 ) ) ;
#50302 = CARTESIAN_POINT ( 'NONE',  ( 1.926036052266958176, 89.59560469603701449, -7.188101187500001821 ) ) ;
#50303 = CARTESIAN_POINT ( 'NONE',  ( -2.485281374238571761, 291.8125000000000000, -6.000000000000003553 ) ) ;
#50304 = CARTESIAN_POINT ( 'NONE',  ( 23.99999999999997868, 204.8125000027312126, 168.3431457505075741 ) ) ;
#50305 = ADVANCED_FACE ( 'NONE', ( #21311 ), #49616, .T. ) ;
#50306 = EDGE_LOOP ( 'NONE', ( #20903, #19173, #71062, #69185 ) ) ;
#50307 = CARTESIAN_POINT ( 'NONE',  ( 7.999999999999998224, 8.718749995903221972, 3.313708498984766049 ) ) ;
#50308 = CARTESIAN_POINT ( 'NONE',  ( 0.000000000000000000, 54.99999999999999289, 8.000000000000000000 ) ) ;
#50309 = CARTESIAN_POINT ( 'NONE',  ( 1.656854249492347719, 194.9375000027312126, 146.0000000000000284 ) ) ;
#50310 = CARTESIAN_POINT ( 'NONE',  ( -5.000000000000000000, 63.46149047932892984, 24.14127879314137815 ) ) ;
#50311 = CARTESIAN_POINT ( 'NONE',  ( 2.751064625579944321E-14, 197.8750000027312126, 194.0000000000000568 ) ) ;
#50312 = CARTESIAN_POINT ( 'NONE',  ( -4.999999999999992895, 245.8333333333333428, 8.660254037844390851 ) ) ;
#50313 = CIRCLE ( 'NONE', #52655, 30.99999999999997158 ) ;
#50314 = CARTESIAN_POINT ( 'NONE',  ( -1.836970198721029983E-15, 193.7500000000000000, 10.00000000000000178 ) ) ;
#50315 = FILL_AREA_STYLE ('',( #49948 ) ) ;
#50316 = CARTESIAN_POINT ( 'NONE',  ( -4.401442555609577197E-16, 7.188101187499992051, 22.48655278187175455 ) ) ;
#50317 = CARTESIAN_POINT ( 'NONE',  ( -9.832129032723418760, 173.1770833299193555, -5.676582343750004256 ) ) ;
#50318 = CARTESIAN_POINT ( 'NONE',  ( 0.000000000000000000, 300.0000000000000000, 10.00000000000000178 ) ) ;
#50319 = CARTESIAN_POINT ( 'NONE',  ( -5.000000000000000000, 52.63864145287860197, 42.88977517748130452 ) ) ;
#50320 = CYLINDRICAL_SURFACE ( 'NONE', #33145, 4.000000000000001776 ) ;
#50321 = CARTESIAN_POINT ( 'NONE',  ( 8.000000000000000000, 109.5312500040968047, -3.313708498984762496 ) ) ;
#50322 = VERTEX_POINT ( 'NONE', #38683 ) ;
#50323 = CARTESIAN_POINT ( 'NONE',  ( -3.042071309553173730, 29.63541666325268054, 11.35316468749999785 ) ) ;
#50324 = CARTESIAN_POINT ( 'NONE',  ( -31.45873412500002786, 208.6250000013656063, 168.5673454167828140 ) ) ;
#50326 = CARTESIAN_POINT ( 'NONE',  ( -0.6474643998436649950, -10.28110762191874805, -63.57179091896463063 ) ) ;
#50325 = CARTESIAN_POINT ( 'NONE',  ( 3.459103461385761413, -7.213501455148458419, -0.0001169852011744028255 ) ) ;
#50327 = DIRECTION ( 'NONE',  ( 0.000000000000000000, 2.238352872228138170E-16, -1.000000000000000000 ) ) ;
#50328 = CARTESIAN_POINT ( 'NONE',  ( 3.458734124999959914, 204.4375000013656063, 142.0000000000000568 ) ) ;
#50329 = CARTESIAN_POINT ( 'NONE',  ( 7.320508075688771044, 51.24999999317203958, 7.320508075688775484 ) ) ;
#50330 = CARTESIAN_POINT ( 'NONE',  ( -5.082755093536324154, 103.3437500020483668, 5.082755093536326818 ) ) ;
#50331 = CARTESIAN_POINT ( 'NONE',  ( -3.211159895383562723, 8.062499998634406140, 3.211159895383561391 ) ) ;
#50332 = CARTESIAN_POINT ( 'NONE',  ( 8.660254037844394404, 219.5833333333333428, 5.000000000000011546 ) ) ;
#50333 = CARTESIAN_POINT ( 'NONE',  ( -4.898587196589407898E-16, 7.999999999999991118, 6.455302779823365533 ) ) ;
#50334 = VERTEX_POINT ( 'NONE', #8882 ) ;
#50335 = ORIENTED_EDGE ( 'NONE', *, *, #20794, .T. ) ;
#50336 = DIRECTION ( 'NONE',  ( -0.000000000000000000, 1.000000000000000000, -0.000000000000000000 ) ) ;
#50337 = CARTESIAN_POINT ( 'NONE',  ( 3.458734125000016757, 195.1250000013656063, 199.4326545832176976 ) ) ;
#50338 = CARTESIAN_POINT ( 'NONE',  ( -2.849036369511732440E-14, 196.2500000000000000, 138.0000000000000568 ) ) ;
#50339 = CARTESIAN_POINT ( 'NONE',  ( -11.35316468749999608, 219.4270833367473585, 3.042071309553173730 ) ) ;
#50340 = CARTESIAN_POINT ( 'NONE',  ( 8.311093377946834337, 140.1562499965860127, 8.311093377946839666 ) ) ;
#50341 = ORIENTED_EDGE ( 'NONE', *, *, #38594, .F. ) ;
#50342 = ADVANCED_FACE ( 'NONE', ( #9637 ), #49938, .F. ) ;
#50343 = ADVANCED_FACE ( 'NONE', ( #58631 ), #1661, .F. ) ;
#50344 = CARTESIAN_POINT ( 'NONE',  ( -5.000000000000000888, 11.44657803507906024, -68.01244171956641082 ) ) ;
#50345 = CARTESIAN_POINT ( 'NONE',  ( -7.204075437095965206, -7.204075437095968759, 90.34375000204838102 ) ) ;
#50346 = CARTESIAN_POINT ( 'NONE',  ( 7.778174593052021635, 7.778174593052023411, 93.43749999999998579 ) ) ;
#50347 = CARTESIAN_POINT ( 'NONE',  ( 1.656854249492403008, 206.6875000000000284, 194.0000000000000853 ) ) ;
#50348 = CARTESIAN_POINT ( 'NONE',  ( 9.999999999999998224, 247.7083333333333428, -2.679491924311229401 ) ) ;
#50349 = CARTESIAN_POINT ( 'NONE',  ( -7.999999999835898379, -3.436314075762838161E-05, 19.01908381112063751 ) ) ;
#50350 = ORIENTED_EDGE ( 'NONE', *, *, #58559, .F. ) ;
#50351 = PRESENTATION_LAYER_ASSIGNMENT (  '', '', ( #74482 ) ) ;
#50352 = ADVANCED_FACE ( 'NONE', ( #59367 ), #53335, .T. ) ;
#50353 = CARTESIAN_POINT ( 'NONE',  ( 37.42586205935411670, -2.873244719482776155, 130.3943765886380106 ) ) ;
#50354 = CARTESIAN_POINT ( 'NONE',  ( -28.27213368402390969, 175.6923493050193770, 157.0765971110028261 ) ) ;
#50355 = CARTESIAN_POINT ( 'NONE',  ( -3.042071309553173730, 109.6354166632526699, 11.35316468749999785 ) ) ;
#50356 = CARTESIAN_POINT ( 'NONE',  ( 2.445694354108838731, 201.0625000013656063, 195.5543056458912190 ) ) ;
#50357 = CARTESIAN_POINT ( 'NONE',  ( -5.082755093536325042, 19.40624999795161543, -5.082755093536325930 ) ) ;
#50358 = CARTESIAN_POINT ( 'NONE',  ( 1.871523826299183495E-15, -10.18810118749999916, 80.40625000204838102 ) ) ;
#50359 = CARTESIAN_POINT ( 'NONE',  ( -5.676582343750006032, 34.42708332991935549, 9.832129032723418760 ) ) ;
#50360 = ORIENTED_EDGE ( 'NONE', *, *, #67402, .F. ) ;
#50361 = CARTESIAN_POINT ( 'NONE',  ( -8.000000000000000000, 96.59375000409679046, -3.313708498984761164 ) ) ;
#50362 = CARTESIAN_POINT ( 'NONE',  ( 8.008118988124991233, 9.807117285998411148E-16, 18.26311528394063188 ) ) ;
#50363 = LINE ( 'NONE', #21687, #49889 ) ;
#50364 = EDGE_CURVE ( 'NONE', #41364, #68174, #59005, .T. ) ;
#50365 = EDGE_CURVE ( 'NONE', #18351, #37225, #2759, .T. ) ;
#50366 = DIRECTION ( 'NONE',  ( -0.000000000000000000, -0.000000000000000000, -1.000000000000000000 ) ) ;
#50367 = CARTESIAN_POINT ( 'NONE',  ( -5.082755093536325042, 5.531249997951610986, -5.082755093536325930 ) ) ;
#50368 = CARTESIAN_POINT ( 'NONE',  ( 6.676582343750001591, 289.9531250017069510, -8.176455196517173205E-16 ) ) ;
#50369 = CARTESIAN_POINT ( 'NONE',  ( -8.000000000000000000, 17.06249999590322375, -9.797174393178825657E-16 ) ) ;
#50370 = ORIENTED_EDGE ( 'NONE', *, *, #34293, .T. ) ;
#50371 = EDGE_CURVE ( 'NONE', #2929, #18351, #6118, .T. ) ;
#50372 = CARTESIAN_POINT ( 'NONE',  ( -5.676582343749998039, 137.7604166632526983, -9.832129032723420536 ) ) ;
#50373 = CARTESIAN_POINT ( 'NONE',  ( 4.220049686691941027, -10.18810118749999738, 77.12500000204838102 ) ) ;
#50374 = CARTESIAN_POINT ( 'NONE',  ( -29.43265458321766559, 208.7500000013656063, 166.5412658750003629 ) ) ;
#50375 = CARTESIAN_POINT ( 'NONE',  ( 5.000000000000000000, 0.000000000000000000, 0.000000000000000000 ) ) ;
#50376 = CARTESIAN_POINT ( 'NONE',  ( 3.211159895383560947, 14.31249999863440792, 3.211159895383562723 ) ) ;
#50377 = ORIENTED_EDGE ( 'NONE', *, *, #7143, .T. ) ;
#50378 = CARTESIAN_POINT ( 'NONE',  ( 1.656854249492405451, 203.4375000027312126, 202.0000000000000284 ) ) ;
#50379 = EDGE_CURVE ( 'NONE', #23110, #29212, #7310, .T. ) ;
#50380 = CONICAL_SURFACE ( 'NONE', #58749, 6.900000000000001243, 0.9599310885968755924 ) ;
#50381 = CARTESIAN_POINT ( 'NONE',  ( -1.432654583217662481, 195.3750000013656063, 145.4587341250000634 ) ) ;
#50383 =( BOUNDED_CURVE ( )  B_SPLINE_CURVE ( 2, ( #3036, #26019, #14708, #49042, #72049 ),
 .UNSPECIFIED., .F., .F. ) 
 B_SPLINE_CURVE_WITH_KNOTS ( ( 3, 2, 3 ),
 ( 0.9886363636363636465, 0.9943181818181817677, 1.000000000000000000 ),
 .UNSPECIFIED. ) 
 CURVE ( )  GEOMETRIC_REPRESENTATION_ITEM ( )  RATIONAL_B_SPLINE_CURVE ( ( 1.000000000000000000, 0.9238795325112867385, 1.000000000000000000, 0.9238795325112867385, 1.000000000000000000 ) ) 
 REPRESENTATION_ITEM ( '' )  );
#50382 = CARTESIAN_POINT ( 'NONE',  ( -32.00000000000003553, 207.3125000027312126, 168.3431457505080573 ) ) ;
#50384 = AXIS2_PLACEMENT_3D ( 'NONE', #56560, #27491, #3748 ) ;
#50385 = CARTESIAN_POINT ( 'NONE',  ( -5.656854249492379694, 21.56250000000000355, -5.656854249492380582 ) ) ;
#50386 = ORIENTED_EDGE ( 'NONE', *, *, #56567, .F. ) ;
#50387 = CARTESIAN_POINT ( 'NONE',  ( 5.082755093536325930, 12.65624999795161187, -5.082755093536325930 ) ) ;
#50388 = CARTESIAN_POINT ( 'NONE',  ( -4.999999999999998224, 208.5416666598387394, -8.660254037844389075 ) ) ;
#50389 = CARTESIAN_POINT ( 'NONE',  ( 5.000000000000000000, 53.21762015693931147, -47.70201125340150838 ) ) ;
#50390 = CARTESIAN_POINT ( 'NONE',  ( 6.951808397369818766E-16, 182.0312499965860411, -11.35316468750000141 ) ) ;
#50391 = VECTOR ( 'NONE', #24135, 1000.000000000000000 ) ;
#50392 = CARTESIAN_POINT ( 'NONE',  ( 7.188101187500002709, 104.1875000020483668, 2.977408999572649151 ) ) ;
#50393 = CARTESIAN_POINT ( 'NONE',  ( 6.000000000000001776, 295.5000000000000000, -7.347880794884121708E-16 ) ) ;
#50394 = CARTESIAN_POINT ( 'NONE',  ( -4.088227598258586603E-16, 288.2031250017069510, -6.676582343750001591 ) ) ;
#50396 = CARTESIAN_POINT ( 'NONE',  ( -7.320508075688780814, 68.12500000000000000, 7.320508075688771932 ) ) ;
#50395 = CARTESIAN_POINT ( 'NONE',  ( 8.660254037844484998, 80.41666666666672825, -5.000000000000056843 ) ) ;
#50397 = VERTEX_POINT ( 'NONE', #69948 ) ;
#50398 = AXIS2_PLACEMENT_3D ( 'NONE', #28333, #39285, #33641 ) ;
#50399 = CARTESIAN_POINT ( 'NONE',  ( 9.832129032723420536, 255.9895833367473301, 5.676582343749996262 ) ) ;
#50400 = CARTESIAN_POINT ( 'NONE',  ( 7.188101187499993827, -2.977408999572645598, 22.01780278187175810 ) ) ;
#50401 = CARTESIAN_POINT ( 'NONE',  ( -1.836970198721029983E-15, 10.62499999317203425, 10.00000000000000178 ) ) ;
#50402 = FACE_OUTER_BOUND ( 'NONE', #70405, .T. ) ;
#50403 = CARTESIAN_POINT ( 'NONE',  ( -2.436599634630704614, -67.82108862182700193, -20.21956363439016258 ) ) ;
#50404 = CARTESIAN_POINT ( 'NONE',  ( -3.614602657737266966, 22.00000000000000000, 2.764888201658305178 ) ) ;
#50405 = CARTESIAN_POINT ( 'NONE',  ( -10.00000000000000178, 147.5000000000000284, -1.224646799147353454E-15 ) ) ;
#50406 = CARTESIAN_POINT ( 'NONE',  ( -11.00000000000001421, -4.556349186104037052, 115.2812500040967763 ) ) ;
#50407 = FACE_OUTER_BOUND ( 'NONE', #46380, .T. ) ;
#50408 = CARTESIAN_POINT ( 'NONE',  ( 5.656854249492381470, 97.06250000000000000, 5.656854249492379694 ) ) ;
#50409 = CARTESIAN_POINT ( 'NONE',  ( -9.832129032723418760, 128.1770833299193555, -5.676582343750004256 ) ) ;
#50410 = DIRECTION ( 'NONE',  ( 0.000000000000000000, 0.000000000000000000, -1.000000000000000000 ) ) ;
#50411 = CARTESIAN_POINT ( 'NONE',  ( -7.778174593052023411, 7.778174593052023411, 68.31249999999998579 ) ) ;
#50414 = DIRECTION ( 'NONE',  ( -0.000000000000000000, 1.000000000000000000, -0.000000000000000000 ) ) ;
#50413 = CARTESIAN_POINT ( 'NONE',  ( 27.99999999999996447, 194.9375000013655779, 166.5412658749999082 ) ) ;
#50412 = CARTESIAN_POINT ( 'NONE',  ( 25.55430564589119413, 200.3125000013656063, 167.5543056458910485 ) ) ;
#50415 = ORIENTED_EDGE ( 'NONE', *, *, #46367, .T. ) ;
#50416 = CARTESIAN_POINT ( 'NONE',  ( 4.898587196589412829E-16, 19.87500000000000355, -8.000000000000000000 ) ) ;
#50417 = DIRECTION ( 'NONE',  ( 0.000000000000000000, 0.000000000000000000, 1.000000000000000000 ) ) ;
#50418 = CARTESIAN_POINT ( 'NONE',  ( 26.56734541678238060, 199.2500000013656063, 166.5412658749999650 ) ) ;
#50419 = CARTESIAN_POINT ( 'NONE',  ( 8.311093377946837890, 211.7187499965860127, -8.311093377946837890 ) ) ;
#50420 = CARTESIAN_POINT ( 'NONE',  ( -7.188101187499999156, 122.7500000020483952, 2.977408999572654924 ) ) ;
#50421 = CARTESIAN_POINT ( 'NONE',  ( 1.881053915767121776, 17.49999999863440436, -4.541265875000002339 ) ) ;
#50422 = CARTESIAN_POINT ( 'NONE',  ( 27.99999999999996092, 196.6875000013655779, 173.4587341249998929 ) ) ;
#50423 = CARTESIAN_POINT ( 'NONE',  ( 2.977408999572650927, -7.188101187499990274, 0.8303027818717529929 ) ) ;
#50425 = CARTESIAN_POINT ( 'NONE',  ( -8.000000000000001776, 12.84375000000000355, 3.313708498984759387 ) ) ;
#50424 = LINE ( 'NONE', #38754, #55216 ) ;
#50426 = CARTESIAN_POINT ( 'NONE',  ( 9.832129032723416984, 90.36458332991935549, 5.676582343750006032 ) ) ;
#50427 = ORIENTED_EDGE ( 'NONE', *, *, #10955, .T. ) ;
#50428 = CARTESIAN_POINT ( 'NONE',  ( 26.34314575050762031, 204.6875000027312126, 165.9999999999998295 ) ) ;
#50429 = CARTESIAN_POINT ( 'NONE',  ( -7.188101187500002709, 20.81249999795161543, 2.977408999572649151 ) ) ;
#50430 = CARTESIAN_POINT ( 'NONE',  ( 0.000000000000000000, 125.0000000000000000, 8.000000000000000000 ) ) ;
#50431 = CARTESIAN_POINT ( 'NONE',  ( -8.311093377946836114, 263.5937500034140157, -8.311093377946836114 ) ) ;
#50432 = CARTESIAN_POINT ( 'NONE',  ( 6.951808397369818766E-16, 97.03124999658602690, -11.35316468750000141 ) ) ;
#50433 = EDGE_LOOP ( 'NONE', ( #12806, #60211, #45431, #45817 ) ) ;
#50434 = ADVANCED_FACE ( 'NONE', ( #70674 ), #6939, .T. ) ;
#50435 = CARTESIAN_POINT ( 'NONE',  ( 27.99999999999996092, 196.6250000027312126, 165.9999999999998863 ) ) ;
#50436 = CARTESIAN_POINT ( 'NONE',  ( -7.204075437095967871, 7.204075437095967871, 104.9687500020483810 ) ) ;
#50437 = CARTESIAN_POINT ( 'NONE',  ( 3.458734125000015425, 206.2500000013656063, 196.5673454167823877 ) ) ;
#50438 = CARTESIAN_POINT ( 'NONE',  ( -29.65685424949235838, 201.5625000027311557, 174.0000000000003126 ) ) ;
#50439 = CARTESIAN_POINT ( 'NONE',  ( -3.042071309553163960, 87.23958332991935549, -11.35316468749999963 ) ) ;
#50440 = CARTESIAN_POINT ( 'NONE',  ( -7.999999999999991118, 0.000000000000000000, 10.01780278392014623 ) ) ;
#50441 = CARTESIAN_POINT ( 'NONE',  ( -31.45873412499997812, 200.0000000013656347, 171.4326545832180386 ) ) ;
#50442 = CARTESIAN_POINT ( 'NONE',  ( -3.313708498984765161, 21.84374999590322375, 7.999999999999998224 ) ) ;
#50443 = CARTESIAN_POINT ( 'NONE',  ( 10.00000000000000178, 186.8749999931720538, 0.000000000000000000 ) ) ;
#50444 = CARTESIAN_POINT ( 'NONE',  ( 5.000000000000000888, -51.74377041917559694, 41.86884046506250456 ) ) ;
#50445 = CARTESIAN_POINT ( 'NONE',  ( -11.35316468750000141, 68.80208332991935549, 3.042071309553159963 ) ) ;
#50446 = CARTESIAN_POINT ( 'NONE',  ( -4.088227598258586603E-16, 290.2031250017069510, -6.676582343750001591 ) ) ;
#50447 = CARTESIAN_POINT ( 'NONE',  ( 4.220049686691934809, 10.18810118749999916, 100.5625000020483668 ) ) ;
#50448 = CARTESIAN_POINT ( 'NONE',  ( 5.676582343750001591, 206.6145833299193555, -9.832129032723420536 ) ) ;
#50449 = ORIENTED_EDGE ( 'NONE', *, *, #26613, .T. ) ;
#50450 = DIRECTION ( 'NONE',  ( 0.000000000000000000, 0.000000000000000000, -1.000000000000000000 ) ) ;
#50451 = CARTESIAN_POINT ( 'NONE',  ( -29.65685424949241167, 203.1875000027311842, 166.0000000000003695 ) ) ;
#50452 = DIRECTION ( 'NONE',  ( 1.000000000000000000, 0.000000000000000000, 0.000000000000000000 ) ) ;
#50453 = CARTESIAN_POINT ( 'NONE',  ( 3.042071309553159519, 199.7395833299193555, 11.35316468750000141 ) ) ;
#50454 = AXIS2_PLACEMENT_3D ( 'NONE', #3654, #54228, #31579 ) ;
#50455 = CARTESIAN_POINT ( 'NONE',  ( -7.320508075688771932, 222.5000000068280031, -7.320508075688771932 ) ) ;
#50456 = CARTESIAN_POINT ( 'NONE',  ( -10.00000000000000000, 252.9166666734946602, -2.679491924311226292 ) ) ;
#50457 = ORIENTED_EDGE ( 'NONE', *, *, #12372, .T. ) ;
#50458 = CARTESIAN_POINT ( 'NONE',  ( 11.35316468749999963, 196.3020833299193271, -3.042071309553165293 ) ) ;
#50459 = EDGE_CURVE ( 'NONE', #61992, #22328, #54360, .T. ) ;
#50460 = CARTESIAN_POINT ( 'NONE',  ( -2.977408999572647819, 7.188101187499992051, 16.20530278187175099 ) ) ;
#50461 = CARTESIAN_POINT ( 'NONE',  ( -24.54126587499998635, 207.1250000013656347, 171.4326545832179818 ) ) ;
#50462 = CARTESIAN_POINT ( 'NONE',  ( -3.313708498984760720, 10.96875000000000178, -8.000000000000000000 ) ) ;
#50463 = ORIENTED_EDGE ( 'NONE', *, *, #42716, .F. ) ;
#50464 = CARTESIAN_POINT ( 'NONE',  ( 5.656854249492379694, 93.12500000409677625, -5.656854249492380582 ) ) ;
#50465 = ADVANCED_FACE ( 'NONE', ( #53705 ), #42442, .T. ) ;
#50466 = CARTESIAN_POINT ( 'NONE',  ( 8.660254037844389075, 10.41666666666666785, -5.000000000000000000 ) ) ;
#50467 = EDGE_CURVE ( 'NONE', #70980, #34808, #60092, .T. ) ;
#50468 = CARTESIAN_POINT ( 'NONE',  ( -7.204075437095965206, -7.204075437095968759, 80.21875000204836681 ) ) ;
#50470 = VERTEX_POINT ( 'NONE', #64651 ) ;
#50469 =( BOUNDED_CURVE ( )  B_SPLINE_CURVE ( 2, ( #1891, #31677, #36960, #7917, #72406, #37715, #60715, #42974, #24878 ),
 .UNSPECIFIED., .F., .F. ) 
 B_SPLINE_CURVE_WITH_KNOTS ( ( 3, 2, 2, 2, 3 ),
 ( 0.8541666666666649643, 0.8645833333333317050, 0.8749999999999984457, 0.8854166666666650753, 0.8958333333333318160 ),
 .UNSPECIFIED. ) 
 CURVE ( )  GEOMETRIC_REPRESENTATION_ITEM ( )  RATIONAL_B_SPLINE_CURVE ( ( 1.000000000000012212, 0.9238795325112745260, 1.000000000000000000, 0.9238795325112867385, 1.000000000000000000, 0.9238795325112867385, 1.000000000000000000, 0.9238795325112980628, 0.9999999999999886757 ) ) 
 REPRESENTATION_ITEM ( '' )  );
#50471 = CARTESIAN_POINT ( 'NONE',  ( 4.000000000000000888, 21.93750000000000355, 1.656854249492384135 ) ) ;
#50472 = CARTESIAN_POINT ( 'NONE',  ( 3.211159895383561835, 19.43749999863440436, -3.211159895383561835 ) ) ;
#50473 = CARTESIAN_POINT ( 'NONE',  ( 31.42478664712817960, 194.6389826057386472, 168.7494685811212491 ) ) ;
#50474 = ORIENTED_EDGE ( 'NONE', *, *, #18214, .F. ) ;
#50475 = CARTESIAN_POINT ( 'NONE',  ( -11.00000000000000000, 0.000000000000000000, 118.0000000000000000 ) ) ;
#50476 = CARTESIAN_POINT ( 'NONE',  ( 7.188101187500001821, 92.00000000204838102, -2.977408999572651371 ) ) ;
#50479 = CARTESIAN_POINT ( 'NONE',  ( 4.000000000000015987, 197.5000000000000000, 198.0000000000000284 ) ) ;
#50478 = CARTESIAN_POINT ( 'NONE',  ( 9.832129032723416984, 246.8229166700806729, -5.676582343750003368 ) ) ;
#50477 = CARTESIAN_POINT ( 'NONE',  ( 25.55430564589115860, 206.0625000013656063, 167.5543056458911053 ) ) ;
#50480 = APPLICATION_PROTOCOL_DEFINITION ( 'draft international standard', 'automotive_design', 1998, #70807 ) ;
#50481 = VERTEX_POINT ( 'NONE', #24642 ) ;
#50482 = CARTESIAN_POINT ( 'NONE',  ( -9.832129032723415207, 254.6354166700806729, 5.676582343750005144 ) ) ;
#50483 = ADVANCED_FACE ( 'NONE', ( #25378 ), #35988, .T. ) ;
#50484 = CARTESIAN_POINT ( 'NONE',  ( 5.082755093536318824, 5.082755093536319713, 11.42405278187175455 ) ) ;
#50485 = ORIENTED_EDGE ( 'NONE', *, *, #73863, .T. ) ;
#50486 =( BOUNDED_CURVE ( )  B_SPLINE_CURVE ( 2, ( #65044, #53379, #24681, #19033, #8450, #18298, #1703, #24321, #48434 ),
 .UNSPECIFIED., .F., .F. ) 
 B_SPLINE_CURVE_WITH_KNOTS ( ( 3, 2, 2, 2, 3 ),
 ( 0.7500000000000006661, 0.7583333333333339699, 0.7666666666666672736, 0.7750000000000005773, 0.7833333333333338810 ),
 .UNSPECIFIED. ) 
 CURVE ( )  GEOMETRIC_REPRESENTATION_ITEM ( )  RATIONAL_B_SPLINE_CURVE ( ( 0.9999999999999938938, 0.9238795325112928447, 1.000000000000000000, 0.9238795325112867385, 1.000000000000000000, 0.9238795325112867385, 1.000000000000000000, 0.9238795325112816315, 1.000000000000005107 ) ) 
 REPRESENTATION_ITEM ( '' )  );
#50487 = ORIENTED_EDGE ( 'NONE', *, *, #38096, .T. ) ;
#50488 = CARTESIAN_POINT ( 'NONE',  ( -4.220049686691935698, 10.18810118749999916, 74.87500000204836681 ) ) ;
#50489 = CARTESIAN_POINT ( 'NONE',  ( 5.676582343749993598, 75.26041666325268409, 9.832129032723422313 ) ) ;
#50490 = CYLINDRICAL_SURFACE ( 'NONE', #40854, 10.00000000000000178 ) ;
#50491 = CARTESIAN_POINT ( 'NONE',  ( 7.778174593052021635, 7.778174593052023411, 91.93749999999998579 ) ) ;
#50494 = CARTESIAN_POINT ( 'NONE',  ( 1.226468279477575784E-15, 288.8593750017070079, 6.676582343750001591 ) ) ;
#50493 = CARTESIAN_POINT ( 'NONE',  ( 28.00000000000002132, 199.1250000027312126, 173.9999999999999147 ) ) ;
#50492 = CARTESIAN_POINT ( 'NONE',  ( 25.55430564589115505, 209.5625000013656063, 172.4456943541086957 ) ) ;
#50495 = AXIS2_PLACEMENT_3D ( 'NONE', #30684, #36350, #23541 ) ;
#50496 = DIRECTION ( 'NONE',  ( 0.000000000000000000, 0.000000000000000000, 1.000000000000000000 ) ) ;
#50497 = CARTESIAN_POINT ( 'NONE',  ( 0.000000000000000000, 300.0000000000000000, 0.000000000000000000 ) ) ;
#50498 = CARTESIAN_POINT ( 'NONE',  ( 1.432654583217662481, 199.3750000013656063, 194.5412658750000219 ) ) ;
#50499 = CARTESIAN_POINT ( 'NONE',  ( -3.313708498984760720, 6.281249995903221084, -8.000000000000000000 ) ) ;
#50500 = VERTEX_POINT ( 'NONE', #19724 ) ;
#50501 = CARTESIAN_POINT ( 'NONE',  ( 27.99999999999996803, 208.6875000013656063, 173.4587341249998929 ) ) ;
#50502 = CARTESIAN_POINT ( 'NONE',  ( 4.401442555609581635E-16, 14.71874999795161187, -7.188101187500000044 ) ) ;
#50503 = CARTESIAN_POINT ( 'NONE',  ( -11.35316468750000141, 173.5937499965860411, -1.390361679473963753E-15 ) ) ;
#50504 = CARTESIAN_POINT ( 'NONE',  ( 1.469576158976823947E-15, 105.8750000000000000, 8.000000000000000000 ) ) ;
#50505 = CARTESIAN_POINT ( 'NONE',  ( 2.977408999572650039, 101.5625000020483952, -7.188101187500000933 ) ) ;
#50507 = DIRECTION ( 'NONE',  ( 0.000000000000000000, 0.000000000000000000, 1.000000000000000000 ) ) ;
#50506 = CARTESIAN_POINT ( 'NONE',  ( 2.775557561562891351E-14, 210.0000000000000284, 170.0000000000000284 ) ) ;
#50508 = CARTESIAN_POINT ( 'NONE',  ( 24.54126587499998635, 208.5000000013656063, 171.4326545832175555 ) ) ;
#50509 = CARTESIAN_POINT ( 'NONE',  ( 1.320432766682872962E-15, -7.188101187499992051, 18.73655278187175455 ) ) ;
#50510 = DIRECTION ( 'NONE',  ( 1.000000000000000000, 0.000000000000000000, 0.000000000000000000 ) ) ;
#50511 = CARTESIAN_POINT ( 'NONE',  ( 3.042071309553159519, 54.73958332991934839, 11.35316468750000141 ) ) ;
#50512 = DIRECTION ( 'NONE',  ( -0.000000000000000000, -0.000000000000000000, -1.000000000000000000 ) ) ;
#50513 = CARTESIAN_POINT ( 'NONE',  ( 5.000000000000001776, 17.70833332650536818, -8.660254037844389075 ) ) ;
#50514 = EDGE_LOOP ( 'NONE', ( #14179, #14882, #53186, #4944, #27367 ) ) ;
#50515 = DIRECTION ( 'NONE',  ( 0.000000000000000000, 0.02418647091589873691, -0.9997074645238147594 ) ) ;
#50516 = CARTESIAN_POINT ( 'NONE',  ( -8.000000000000000000, 23.06249999590322020, -9.797174393178825657E-16 ) ) ;
#50517 = CARTESIAN_POINT ( 'NONE',  ( -11.35316468750000141, 53.28124999658601979, -1.390361679473963753E-15 ) ) ;
#50518 = CARTESIAN_POINT ( 'NONE',  ( 7.778174593052021635, 7.778174593052023411, 72.62500000409677625 ) ) ;
#50519 = CARTESIAN_POINT ( 'NONE',  ( -3.458734125000015869, 200.1875000013656063, 142.0000000000000568 ) ) ;
#50520 = DIRECTION ( 'NONE',  ( -0.000000000000000000, 1.000000000000000000, 4.689100369878284071E-30 ) ) ;
#50521 = CARTESIAN_POINT ( 'NONE',  ( -7.320508075688770155, 245.6250000000000000, 7.320508075688774596 ) ) ;
#50523 = CARTESIAN_POINT ( 'NONE',  ( -11.35316468749999785, 43.07291666325267698, -3.042071309553167957 ) ) ;
#50522 = CARTESIAN_POINT ( 'NONE',  ( -7.188101187500000933, 94.06250000204838102, -2.977408999572650483 ) ) ;
#50525 = EDGE_CURVE ( 'NONE', #10770, #15213, #44896, .T. ) ;
#50524 = CARTESIAN_POINT ( 'NONE',  ( -6.062585341144163031, -5.219679969245603957, 1.000679773946673290 ) ) ;
#50526 = CARTESIAN_POINT ( 'NONE',  ( 10.00000000000000000, 205.0000000000000284, 0.000000000000000000 ) ) ;
#50527 = CARTESIAN_POINT ( 'NONE',  ( -5.676582343750006032, 179.1145833299193555, 9.832129032723418760 ) ) ;
#50529 = CARTESIAN_POINT ( 'NONE',  ( 8.660254037844385522, 136.4583333265053682, 5.000000000000005329 ) ) ;
#50528 = PRODUCT_DEFINITION_SHAPE ( 'NONE', 'NONE',  #51928 ) ;
#50530 = CARTESIAN_POINT ( 'NONE',  ( -2.977408999572651815, 103.8125000020483952, 7.188101187500000933 ) ) ;
#50531 = CARTESIAN_POINT ( 'NONE',  ( -3.360070523760016581, 0.4865809706466538986, -7.253681227061384185 ) ) ;
#50532 = CARTESIAN_POINT ( 'NONE',  ( 11.35316468749999785, 40.88541666325268409, 3.042071309553174174 ) ) ;
#50533 = EDGE_CURVE ( 'NONE', #27023, #44612, #26880, .T. ) ;
#50534 = CARTESIAN_POINT ( 'NONE',  ( 10.18810118750000093, -4.220049686691933033, 116.6875000020483952 ) ) ;
#50535 = ORIENTED_EDGE ( 'NONE', *, *, #40654, .F. ) ;
#50536 = CARTESIAN_POINT ( 'NONE',  ( 27.99999999999999645, 210.0000000000000284, 169.9999999999999147 ) ) ;
#50537 = CARTESIAN_POINT ( 'NONE',  ( -7.204075437095965206, -7.204075437095968759, 70.84375000204836681 ) ) ;
#50538 = CARTESIAN_POINT ( 'NONE',  ( -3.999999999999959144, 198.0625000000000284, 199.6568542494924259 ) ) ;
#50539 = CYLINDRICAL_SURFACE ( 'NONE', #460, 5.000000000000000888 ) ;
#50541 = CARTESIAN_POINT ( 'NONE',  ( -5.676582343749998039, 172.4479166632526983, -9.832129032723420536 ) ) ;
#50540 = FACE_OUTER_BOUND ( 'NONE', #43311, .T. ) ;
#50542 = CARTESIAN_POINT ( 'NONE',  ( -3.313708498984758943, -7.999999999999989342, 10.16780278432982598 ) ) ;
#50543 = CARTESIAN_POINT ( 'NONE',  ( -11.00000000000000000, 0.000000000000000000, 79.18750000409677625 ) ) ;
#50544 = CARTESIAN_POINT ( 'NONE',  ( -9.832129032723415207, 224.3229166700806729, 5.676582343750005144 ) ) ;
#50545 = CARTESIAN_POINT ( 'NONE',  ( 5.126106709302933773, 52.42424824936820471, -49.01286957842418701 ) ) ;
#50546 = CARTESIAN_POINT ( 'NONE',  ( -10.18810118749999738, -4.220049686691941915, 81.62500000204836681 ) ) ;
#50547 = VERTEX_POINT ( 'NONE', #15924 ) ;
#50548 = APPLICATION_CONTEXT ( 'automotive_design' ) ;
#50549 = EDGE_CURVE ( 'NONE', #46167, #38779, #3242, .T. ) ;
#50550 = AXIS2_PLACEMENT_3D ( 'NONE', #17096, #524, #39379 ) ;
#50551 = LINE ( 'NONE', #15466, #41201 ) ;
#50552 = CARTESIAN_POINT ( 'NONE',  ( 8.311093377946834337, 115.4687499965860269, 8.311093377946839666 ) ) ;
#50553 = DIRECTION ( 'NONE',  ( -0.000000000000000000, 1.000000000000000000, -4.476705744456276341E-16 ) ) ;
#50554 = ORIENTED_EDGE ( 'NONE', *, *, #35277, .F. ) ;
#50555 = ORIENTED_EDGE ( 'NONE', *, *, #5266, .F. ) ;
#50556 = CARTESIAN_POINT ( 'NONE',  ( 4.541265875000002339, 9.499999998634406140, -1.881053915767121554 ) ) ;
#50557 = CIRCLE ( 'NONE', #38511, 70.50000000000000000 ) ;
#50558 = CARTESIAN_POINT ( 'NONE',  ( -5.082755093536325042, 14.53124999795161187, -5.082755093536325930 ) ) ;
#50559 = CARTESIAN_POINT ( 'NONE',  ( 5.656854249492381470, 107.7500000040967763, 5.656854249492379694 ) ) ;
#50560 = CARTESIAN_POINT ( 'NONE',  ( -4.220049686691935698, 10.18810118749999916, 93.25000000204838102 ) ) ;
#50561 = CARTESIAN_POINT ( 'NONE',  ( -31.45873412499999944, 197.8750000013656063, 168.5673454167827572 ) ) ;
#50562 = EDGE_CURVE ( 'NONE', #30512, #46323, #10953, .T. ) ;
#50563 = CARTESIAN_POINT ( 'NONE',  ( 1.656854249492381248, 9.187500000000000000, -4.000000000000001776 ) ) ;
#50564 = CARTESIAN_POINT ( 'NONE',  ( 4.541265875000002339, 8.374999998634407916, -1.881053915767121776 ) ) ;
#50565 = CARTESIAN_POINT ( 'NONE',  ( -4.000000000000015987, 197.5000000000000000, 142.0000000000000568 ) ) ;
#50566 = ORIENTED_EDGE ( 'NONE', *, *, #18926, .T. ) ;
#50567 = CARTESIAN_POINT ( 'NONE',  ( 7.188101187500002709, 109.8125000020483952, 2.977408999572649151 ) ) ;
#50569 = CARTESIAN_POINT ( 'NONE',  ( 3.313708498984756279, 7.999999999999991118, 16.86155277982336642 ) ) ;
#50568 = CARTESIAN_POINT ( 'NONE',  ( -30.44569435410875613, 196.8125000013656063, 172.4456943541092642 ) ) ;
#50570 =( LENGTH_UNIT ( ) NAMED_UNIT ( * ) SI_UNIT ( .MILLI., .METRE. ) );
#50571 = CARTESIAN_POINT ( 'NONE',  ( 3.211159895383561835, 21.43749999863440792, -3.211159895383561835 ) ) ;
#50572 = CARTESIAN_POINT ( 'NONE',  ( -5.082755093536317936, -5.082755093536320601, 1.674052781871753659 ) ) ;
#50573 = ORIENTED_EDGE ( 'NONE', *, *, #70067, .T. ) ;
#50574 = ORIENTED_EDGE ( 'NONE', *, *, #25734, .F. ) ;
#50575 = CARTESIAN_POINT ( 'NONE',  ( 7.204075437095968759, -7.204075437095966983, 90.71875000204838102 ) ) ;
#50576 = CARTESIAN_POINT ( 'NONE',  ( -7.999999999999968914, 3.313708498984778039, 20.23655277982336287 ) ) ;
#50577 = CARTESIAN_POINT ( 'NONE',  ( -26.56734541678232731, 201.2500000013656063, 173.4587341250003760 ) ) ;
#50578 = CARTESIAN_POINT ( 'NONE',  ( -7.778174593052020747, -7.778174593052023411, 107.6874999999999858 ) ) ;
#50579 = CARTESIAN_POINT ( 'NONE',  ( -3.458734124999959469, 205.7500000013656063, 199.4326545832176691 ) ) ;
#50580 = DIRECTION ( 'NONE',  ( -0.000000000000000000, 1.000000000000000000, -0.000000000000000000 ) ) ;
#50581 = CARTESIAN_POINT ( 'NONE',  ( -10.00000000000000000, 127.2916666666666714, -2.679491924311229845 ) ) ;
#50582 = CARTESIAN_POINT ( 'NONE',  ( 8.000000000000000000, 106.2500000000000000, -9.797174393178825657E-16 ) ) ;
#50583 = CARTESIAN_POINT ( 'NONE',  ( -4.721056650415998313, 290.7343750017069510, 4.721056650416000089 ) ) ;
#50584 = CARTESIAN_POINT ( 'NONE',  ( -7.188101187499990274, -2.977408999572651371, 6.455302781871754547 ) ) ;
#50585 =( BOUNDED_CURVE ( )  B_SPLINE_CURVE ( 2, ( #14749, #73597, #37790, #49841, #60786, #26439, #72484, #43811, #66826 ),
 .UNSPECIFIED., .F., .F. ) 
 B_SPLINE_CURVE_WITH_KNOTS ( ( 3, 2, 2, 2, 3 ),
 ( 0.9204545454545455252, 0.9261363636363637575, 0.9318181818181817677, 0.9375000000000000000, 0.9431818181818182323 ),
 .UNSPECIFIED. ) 
 CURVE ( )  GEOMETRIC_REPRESENTATION_ITEM ( )  RATIONAL_B_SPLINE_CURVE ( ( 0.9999999999999985567, 0.9238795325112881818, 1.000000000000000000, 0.9238795325112867385, 1.000000000000000000, 0.9238795325112867385, 1.000000000000000000, 0.9238795325112867385, 1.000000000000000000 ) ) 
 REPRESENTATION_ITEM ( '' )  );
#50586 = CYLINDRICAL_SURFACE ( 'NONE', #16877, 10.00000000000000178 ) ;
#50587 = CARTESIAN_POINT ( 'NONE',  ( 29.43265458321761585, 207.5000000013655779, 173.4587341249998929 ) ) ;
#50588 = CARTESIAN_POINT ( 'NONE',  ( 4.898587196589412829E-16, 27.18749999590322375, -8.000000000000000000 ) ) ;
#50589 = CARTESIAN_POINT ( 'NONE',  ( 1.432654583217607858, 200.6250000013655779, 138.5412658750000787 ) ) ;
#50590 = CARTESIAN_POINT ( 'NONE',  ( -5.082755093536325930, 122.8437500020483952, -5.082755093536325930 ) ) ;
#50592 = CARTESIAN_POINT ( 'NONE',  ( 1.432654583217607414, 203.5000000013655779, 145.4587341250000634 ) ) ;
#50591 = DIRECTION ( 'NONE',  ( 1.000000000000000000, 0.000000000000000000, 1.836970198721037823E-16 ) ) ;
#50593 = CARTESIAN_POINT ( 'NONE',  ( 8.311093377946839666, 236.0937500034139589, 8.311093377946829008 ) ) ;
#50594 = CARTESIAN_POINT ( 'NONE',  ( 8.000000000000000000, 0.000000000000000000, 0.000000000000000000 ) ) ;
#50595 = CARTESIAN_POINT ( 'NONE',  ( -1.836970198721029983E-15, 215.6249999931720538, 10.00000000000000178 ) ) ;
#50596 = CARTESIAN_POINT ( 'NONE',  ( 23.99999999999998934, 200.7500000000000000, 169.9999999999998863 ) ) ;
#50597 = CARTESIAN_POINT ( 'NONE',  ( 8.311093377946834337, 15.15624999658601624, 8.311093377946839666 ) ) ;
#50598 = CARTESIAN_POINT ( 'NONE',  ( -5.272366635369878374, -4.893143551702761052, 0.5406094755204297053 ) ) ;
#50599 = CARTESIAN_POINT ( 'NONE',  ( -5.676582343750006032, 209.4270833299193555, 9.832129032723418760 ) ) ;
#50600 = CARTESIAN_POINT ( 'NONE',  ( -4.000000000000016875, 197.5625000027312126, 140.3431457505076594 ) ) ;
#50601 = DIRECTION ( 'NONE',  ( -1.000000000000000000, 0.000000000000000000, 0.000000000000000000 ) ) ;
#50603 = CARTESIAN_POINT ( 'NONE',  ( -7.347880794884122694E-16, 11.49999999726881406, 4.000000000000001776 ) ) ;
#50602 = DIRECTION ( 'NONE',  ( -0.000000000000000000, 1.000000000000000000, -4.476705744456276341E-16 ) ) ;
#50604 = ORIENTED_EDGE ( 'NONE', *, *, #3904, .F. ) ;
#50605 = VECTOR ( 'NONE', #60145, 1000.000000000000000 ) ;
#50606 = CARTESIAN_POINT ( 'NONE',  ( -2.754378923186476579E-14, 199.4375000013655779, 145.4587341250000350 ) ) ;
#50607 = CARTESIAN_POINT ( 'NONE',  ( 3.042071309553167069, 11.82291666325268231, -11.35316468749999785 ) ) ;
#50608 = CARTESIAN_POINT ( 'NONE',  ( -7.778174593052023411, 7.778174593052023411, 92.50000000409677625 ) ) ;
#50609 = CARTESIAN_POINT ( 'NONE',  ( -4.193030820683908644, 10.26769724739506984, 64.12608639927678666 ) ) ;
#50610 = CARTESIAN_POINT ( 'NONE',  ( -25.55430564589111953, 198.0625000013656063, 172.4456943541091505 ) ) ;
#50611 = DIRECTION ( 'NONE',  ( 0.000000000000000000, 0.000000000000000000, 1.000000000000000000 ) ) ;
#50613 = CARTESIAN_POINT ( 'NONE',  ( -11.35316468750000141, 3.281249996586016238, -1.390361679473963753E-15 ) ) ;
#50612 = CARTESIAN_POINT ( 'NONE',  ( 2.977408999572650039, 114.6875000020484094, -7.188101187500000933 ) ) ;
#50615 = EDGE_CURVE ( 'NONE', #53701, #35109, #70203, .T. ) ;
#50614 = CARTESIAN_POINT ( 'NONE',  ( 5.656854249492376141, -5.656854249492374365, 26.89280277982336642 ) ) ;
#50616 = CARTESIAN_POINT ( 'NONE',  ( 11.35316468749999785, 135.5729166632526983, 3.042071309553174174 ) ) ;
#50617 = CARTESIAN_POINT ( 'NONE',  ( 10.00000000000000000, 101.6666666598386826, 2.679491924311236062 ) ) ;
#50618 = CARTESIAN_POINT ( 'NONE',  ( -5.082755093536325930, 119.8437500020483810, -5.082755093536325930 ) ) ;
#50619 = DIRECTION ( 'NONE',  ( -0.000000000000000000, 1.000000000000000000, -0.000000000000000000 ) ) ;
#50620 = CARTESIAN_POINT ( 'NONE',  ( -27.99999999999996803, 208.1875000013656063, 173.4587341250003760 ) ) ;
#50621 = DIRECTION ( 'NONE',  ( 1.000000000000000000, 0.000000000000000000, -0.000000000000000000 ) ) ;
#50622 = VERTEX_POINT ( 'NONE', #72911 ) ;
#50623 = CARTESIAN_POINT ( 'NONE',  ( 9.832129032723420536, 1.510416663252683422, -5.676582343749999815 ) ) ;
#50624 = EDGE_CURVE ( 'NONE', #18394, #33017, #47068, .T. ) ;
#50625 = CARTESIAN_POINT ( 'NONE',  ( 6.676582343750004256, 288.0468750017070079, 2.765530957081995478 ) ) ;
#50626 = CARTESIAN_POINT ( 'NONE',  ( 5.000000000000000000, 52.16438407847101644, 42.28020805311251706 ) ) ;
#50627 = CARTESIAN_POINT ( 'NONE',  ( 7.999999999999992895, -3.313708498984756279, 1.674052783920142895 ) ) ;
#50628 = CARTESIAN_POINT ( 'NONE',  ( -23.99999999999998934, 198.7500000000000000, 170.0000000000003411 ) ) ;
#50629 = CARTESIAN_POINT ( 'NONE',  ( 8.311093377946839666, 260.7812500034140157, 8.311093377946829008 ) ) ;
#50630 = CARTESIAN_POINT ( 'NONE',  ( -10.18810118749999916, 4.220049686691934809, 96.43750000204836681 ) ) ;
#50631 = VERTEX_POINT ( 'NONE', #9910 ) ;
#50632 = AXIS2_PLACEMENT_3D ( 'NONE', #66255, #50024, #38343 ) ;
#50633 = CARTESIAN_POINT ( 'NONE',  ( 5.000000000000000000, 10.38759426015435139, 65.74583990312709147 ) ) ;
#50634 = CARTESIAN_POINT ( 'NONE',  ( -11.35316468749999785, 163.3854166632526699, -3.042071309553167957 ) ) ;
#50635 = PLANE ( 'NONE',  #27836 ) ;
#50636 = CARTESIAN_POINT ( 'NONE',  ( 1.432654583217662481, 203.3750000013656063, 194.5412658750000219 ) ) ;
#50637 = CARTESIAN_POINT ( 'NONE',  ( -7.999999999999991118, 0.000000000000000000, 29.33030277982336642 ) ) ;
#50638 = CARTESIAN_POINT ( 'NONE',  ( -11.35316468750000141, 78.59374999658601268, -1.390361679473963753E-15 ) ) ;
#50639 = ORIENTED_EDGE ( 'NONE', *, *, #10268, .T. ) ;
#50640 = CARTESIAN_POINT ( 'NONE',  ( 1.871523826299183495E-15, -10.18810118749999916, 116.0312500020483810 ) ) ;
#50641 = CARTESIAN_POINT ( 'NONE',  ( -3.211159895383561391, 11.81249999863440614, -3.211159895383561835 ) ) ;
#50642 = ORIENTED_EDGE ( 'NONE', *, *, #8548, .T. ) ;
#50643 = CARTESIAN_POINT ( 'NONE',  ( -1.469576158976823947E-15, 2.625000000000000444, 8.000000000000000000 ) ) ;
#50644 = CARTESIAN_POINT ( 'NONE',  ( 8.660254037844385522, 66.45833332650536818, 5.000000000000005329 ) ) ;
#50645 = CARTESIAN_POINT ( 'NONE',  ( -2.977408999572654480, 16.87499999795161543, 7.188101187499999156 ) ) ;
#50646 = CARTESIAN_POINT ( 'NONE',  ( -2.751064625579944321E-14, 199.7500000000000000, 146.0000000000000284 ) ) ;
#50647 = CARTESIAN_POINT ( 'NONE',  ( -7.204075437095967871, 7.204075437095967871, 108.3437500020483810 ) ) ;
#50648 = AXIS2_PLACEMENT_3D ( 'NONE', #17453, #63479, #47235 ) ;
#50649 = CARTESIAN_POINT ( 'NONE',  ( 4.000000000000015987, 201.6875000027311842, 196.3431457505076594 ) ) ;
#50650 = CARTESIAN_POINT ( 'NONE',  ( -7.347880794884122694E-16, 9.499999997268814056, 4.000000000000001776 ) ) ;
#50651 = FACE_OUTER_BOUND ( 'NONE', #44623, .T. ) ;
#50652 = AXIS2_PLACEMENT_3D ( 'NONE', #54331, #25994, #58886 ) ;
#50653 = EDGE_LOOP ( 'NONE', ( #14507, #8144, #28313, #29652 ) ) ;
#50654 = AXIS2_PLACEMENT_3D ( 'NONE', #50050, #15708, #9701 ) ;
#50655 = CARTESIAN_POINT ( 'NONE',  ( -3.458734124999959914, 203.3750000013656063, 196.5673454167823877 ) ) ;
#50656 = CARTESIAN_POINT ( 'NONE',  ( -31.45873412500002431, 207.6250000013656347, 168.5673454167828140 ) ) ;
#50657 = CARTESIAN_POINT ( 'NONE',  ( 30.82842712474620939, 199.2500000027312126, 172.8284271247460424 ) ) ;
#50658 = CARTESIAN_POINT ( 'NONE',  ( -4.541265875000002339, 8.812499998634407916, -5.561446717895856393E-16 ) ) ;
#50659 = CARTESIAN_POINT ( 'NONE',  ( 8.000000000000000000, 94.43750000409679046, -9.797174393178825657E-16 ) ) ;
#50660 = CARTESIAN_POINT ( 'NONE',  ( 7.188101187499992051, 8.802885111219154394E-16, 20.23655278187175099 ) ) ;
#50661 = ORIENTED_EDGE ( 'NONE', *, *, #643, .T. ) ;
#50662 = DIRECTION ( 'NONE',  ( -0.000000000000000000, -1.000000000000000000, -0.000000000000000000 ) ) ;
#50663 = ORIENTED_EDGE ( 'NONE', *, *, #10876, .F. ) ;
#50664 = CARTESIAN_POINT ( 'NONE',  ( -7.204075437095965206, -7.204075437095968759, 111.3437500020483810 ) ) ;
#50665 = CARTESIAN_POINT ( 'NONE',  ( 0.000000000000000000, 300.0000000000000000, 10.00000000000000178 ) ) ;
#50666 = CARTESIAN_POINT ( 'NONE',  ( -3.458734124999959914, 204.3750000013656063, 196.5673454167823877 ) ) ;
#50667 = CARTESIAN_POINT ( 'NONE',  ( 29.43265458321761230, 197.8750000013656063, 166.5412658749999650 ) ) ;
#50668 = CARTESIAN_POINT ( 'NONE',  ( 6.123233995736767268E-16, 86.25000000000001421, -10.00000000000000178 ) ) ;
#50669 = CARTESIAN_POINT ( 'NONE',  ( 8.000000000000001776, 122.6562500000000000, 3.313708498984759387 ) ) ;
#50670 = CARTESIAN_POINT ( 'NONE',  ( -6.000000000000001776, 292.0000000000000000, 0.000000000000000000 ) ) ;
#50671 = CARTESIAN_POINT ( 'NONE',  ( 29.65685424949240456, 203.1875000027312126, 173.9999999999999147 ) ) ;
#50672 = ORIENTED_EDGE ( 'NONE', *, *, #68450, .T. ) ;
#50673 = ADVANCED_FACE ( 'NONE', ( #32941 ), #37674, .T. ) ;
#50674 = DIRECTION ( 'NONE',  ( -0.000000000000000000, 1.000000000000000000, -0.000000000000000000 ) ) ;
#50675 = EDGE_CURVE ( 'NONE', #17960, #2769, #67628, .T. ) ;
#50676 = CARTESIAN_POINT ( 'NONE',  ( -2.849036369511732440E-14, 195.3750000027311842, 138.0000000000000568 ) ) ;
#50677 = DIRECTION ( 'NONE',  ( -0.000000000000000000, 1.000000000000000000, -0.000000000000000000 ) ) ;
#50678 = DIRECTION ( 'NONE',  ( 0.000000000000000000, -1.000000000000000000, 0.000000000000000000 ) ) ;
#50679 = CARTESIAN_POINT ( 'NONE',  ( -7.320508075688771932, 249.3750000000000284, -7.320508075688771932 ) ) ;
#50680 = CARTESIAN_POINT ( 'NONE',  ( 7.999999999999991118, 9.797174393178815797E-16, 7.580302779823366421 ) ) ;
#50681 = CARTESIAN_POINT ( 'NONE',  ( 10.00000000000000178, 200.0000000000000000, 0.000000000000000000 ) ) ;
#50682 = CARTESIAN_POINT ( 'NONE',  ( 0.000000000000000000, 45.00000000000000000, -8.749999999999998224 ) ) ;
#50683 = CARTESIAN_POINT ( 'NONE',  ( -7.188101187499990274, -2.977408999572651815, 15.45530278187175632 ) ) ;
#50684 = CARTESIAN_POINT ( 'NONE',  ( 11.35316468749999963, 171.3020833299193555, -3.042071309553165293 ) ) ;
#50685 = CARTESIAN_POINT ( 'NONE',  ( -7.999999999929542582, -2.214810345207895024E-05, 22.01864141485938831 ) ) ;
#50686 = CARTESIAN_POINT ( 'NONE',  ( -32.73498202863738982, 41.77901764534865237, 65.00000000000000000 ) ) ;
#50687 = CARTESIAN_POINT ( 'NONE',  ( -11.00000000000000000, 0.000000000000000000, 82.18750000409677625 ) ) ;
#50689 = CARTESIAN_POINT ( 'NONE',  ( -8.000000000000000000, 9.797174393178827630E-16, 3.577867169202164632E-15 ) ) ;
#50688 = DIRECTION ( 'NONE',  ( 0.000000000000000000, 0.000000000000000000, 1.000000000000000000 ) ) ;
#50690 = ORIENTED_EDGE ( 'NONE', *, *, #989, .F. ) ;
#50691 = CARTESIAN_POINT ( 'NONE',  ( -8.311093377946836114, 17.96874999658601979, -8.311093377946837890 ) ) ;
#50692 = CARTESIAN_POINT ( 'NONE',  ( -25.17157287525377640, 200.6250000000000284, 172.8284271247465256 ) ) ;
#50694 = CARTESIAN_POINT ( 'NONE',  ( -0.8588954341814977189, 10.28066745654381720, -63.58998442112849858 ) ) ;
#50693 = FACE_OUTER_BOUND ( 'NONE', #68730, .T. ) ;
#50695 = CARTESIAN_POINT ( 'NONE',  ( 0.000000000000000000, 125.0000000000000000, 0.000000000000000000 ) ) ;
#50697 = EDGE_CURVE ( 'NONE', #29352, #59314, #8522, .T. ) ;
#50696 = CARTESIAN_POINT ( 'NONE',  ( -1.432654583217662259, 204.1250000013656063, 145.4587341250000350 ) ) ;
#50698 = CIRCLE ( 'NONE', #25376, 9.000000000000001776 ) ;
#50699 = CARTESIAN_POINT ( 'NONE',  ( -10.00000000000000355, 59.58333332650535397, 2.679491924311223183 ) ) ;
#50700 = CARTESIAN_POINT ( 'NONE',  ( 1.320432766682874540E-15, 102.0312500020483810, 7.188101187500000044 ) ) ;
#50701 = CARTESIAN_POINT ( 'NONE',  ( -1.881053915767121554, 9.749999998634406140, -4.541265875000002339 ) ) ;
#50702 = DIRECTION ( 'NONE',  ( 0.000000000000000000, 1.000000000000000000, 0.000000000000000000 ) ) ;
#50703 = CARTESIAN_POINT ( 'NONE',  ( 5.656854249492376141, -5.656854249492374365, 1.392802779823364201 ) ) ;
#50704 = CARTESIAN_POINT ( 'NONE',  ( 2.030339228148215693E-11, 166.2499999999984368, -10.00000000000000178 ) ) ;
#50705 = ORIENTED_EDGE ( 'NONE', *, *, #27957, .T. ) ;
#50706 = EDGE_LOOP ( 'NONE', ( #35677, #404, #7059, #70360 ) ) ;
#50707 =( BOUNDED_CURVE ( )  B_SPLINE_CURVE ( 2, ( #47901, #23419, #18505, #24525, #70556, #17759, #64530, #53212, #40773 ),
 .UNSPECIFIED., .F., .F. ) 
 B_SPLINE_CURVE_WITH_KNOTS ( ( 3, 2, 2, 2, 3 ),
 ( 0.3472222222222222099, 0.3541666666666666852, 0.3611111111111111049, 0.3680555555555555802, 0.3750000000000000000 ),
 .UNSPECIFIED. ) 
 CURVE ( )  GEOMETRIC_REPRESENTATION_ITEM ( )  RATIONAL_B_SPLINE_CURVE ( ( 1.000000000000000000, 0.9238795325112867385, 1.000000000000000000, 0.9238795325112867385, 1.000000000000000000, 0.9238795325112867385, 1.000000000000000000, 0.9238795325112867385, 1.000000000000000000 ) ) 
 REPRESENTATION_ITEM ( '' )  );
#50708 =( BOUNDED_CURVE ( )  B_SPLINE_CURVE ( 2, ( #13587, #62770, #59631, #7947, #51092, #39768, #11113, #21122, #54726 ),
 .UNSPECIFIED., .F., .F. ) 
 B_SPLINE_CURVE_WITH_KNOTS ( ( 3, 2, 2, 2, 3 ),
 ( 0.01847903363950017044, 0.02083333333333333218, 0.02777777777777777624, 0.03472222222222222376, 0.04166666666666666435 ),
 .UNSPECIFIED. ) 
 CURVE ( )  GEOMETRIC_REPRESENTATION_ITEM ( )  RATIONAL_B_SPLINE_CURVE ( ( 0.9658850645339662755, 0.9741937033643515154, 1.000000000000000000, 0.9238795325112867385, 1.000000000000000000, 0.9238795325112867385, 1.000000000000000000, 0.9238795325112867385, 1.000000000000000000 ) ) 
 REPRESENTATION_ITEM ( '' )  );
#50709 = CARTESIAN_POINT ( 'NONE',  ( -0.4320110153365220862, -49.91454558245964535, -40.68976686129133213 ) ) ;
#50710 = CARTESIAN_POINT ( 'NONE',  ( -7.999999999999989342, -3.313708498984762496, 14.61155278392014800 ) ) ;
#50711 = DIRECTION ( 'NONE',  ( 0.8660254037844379305, 0.5000000000000011102, 0.000000000000000000 ) ) ;
#50712 = CARTESIAN_POINT ( 'NONE',  ( -11.35316468749999963, 219.2187500034139873, 0.000000000000000000 ) ) ;
#50713 = CARTESIAN_POINT ( 'NONE',  ( -11.35316468750000141, 138.4895833299193271, 3.042071309553159963 ) ) ;
#50714 = ORIENTED_EDGE ( 'NONE', *, *, #32846, .F. ) ;
#50715 = CARTESIAN_POINT ( 'NONE',  ( -7.999999999999989342, -3.313708498984762496, 10.11155278392014623 ) ) ;
#50716 = CARTESIAN_POINT ( 'NONE',  ( 4.220049686691934809, 10.18810118749999916, 86.68750000204836681 ) ) ;
#50717 = CARTESIAN_POINT ( 'NONE',  ( -7.347880794884122694E-16, 7.499999997268813168, 4.000000000000001776 ) ) ;
#50718 = CARTESIAN_POINT ( 'NONE',  ( -2.828427124746152987, 208.1250000000000284, 200.8284271247462129 ) ) ;
#50719 = CARTESIAN_POINT ( 'NONE',  ( -1.469576158976823947E-15, 18.93749999590322020, 8.000000000000000000 ) ) ;
#50720 = CARTESIAN_POINT ( 'NONE',  ( -11.00000000000000000, 0.000000000000000000, 113.4999999999999858 ) ) ;
#50721 = AXIS2_PLACEMENT_3D ( 'NONE', #35424, #69367, #39410 ) ;
#50722 = CARTESIAN_POINT ( 'NONE',  ( -4.898587196589412829E-16, 100.6249999999999858, -8.000000000000000000 ) ) ;
#50723 = ORIENTED_EDGE ( 'NONE', *, *, #24311, .F. ) ;
#50724 = CARTESIAN_POINT ( 'NONE',  ( 32.91008470507601658, -22.18307313467122555, 159.8854973932241705 ) ) ;
#50725 = AXIS2_PLACEMENT_3D ( 'NONE', #1394, #24006, #71126 ) ;
#50726 = CARTESIAN_POINT ( 'NONE',  ( -25.17741886378425775, 181.7850574557801338, 151.7745050278459757 ) ) ;
#50727 = CARTESIAN_POINT ( 'NONE',  ( -8.311093377946841443, 109.2187499965860127, 8.311093377946834337 ) ) ;
#50728 = CARTESIAN_POINT ( 'NONE',  ( 3.458734125000015425, 204.0000000013656063, 196.5673454167823877 ) ) ;
#50729 = CARTESIAN_POINT ( 'NONE',  ( -2.977408999572654480, 21.37499999795161543, 7.188101187499999156 ) ) ;
#50730 = CARTESIAN_POINT ( 'NONE',  ( 7.204075437095966983, 7.204075437095967871, 82.46875000204836681 ) ) ;
#50731 = CARTESIAN_POINT ( 'NONE',  ( -5.676582343750006032, 39.42708332991935549, 9.832129032723418760 ) ) ;
#50732 = ORIENTED_EDGE ( 'NONE', *, *, #44227, .F. ) ;
#50733 = DIRECTION ( 'NONE',  ( -0.000000000000000000, 1.000000000000000000, -0.000000000000000000 ) ) ;
#50734 = CARTESIAN_POINT ( 'NONE',  ( -5.662595241051933570, -5.662595241051936235, 22.20061528394063188 ) ) ;
#50735 = CARTESIAN_POINT ( 'NONE',  ( 9.797174393178825657E-16, 125.0000000000000000, -8.000000000000000000 ) ) ;
#50736 = AXIS2_PLACEMENT_3D ( 'NONE', #69165, #45400, #23137 ) ;
#50737 = CARTESIAN_POINT ( 'NONE',  ( -1.656854249492381248, 7.312500000000000000, -4.000000000000001776 ) ) ;
#50738 = CARTESIAN_POINT ( 'NONE',  ( -2.977408999572654480, 7.499999997951610986, 7.188101187499999156 ) ) ;
#50739 = CARTESIAN_POINT ( 'NONE',  ( 4.242640687119287435, 297.4375000034140157, 4.242640687119285658 ) ) ;
#50740 = CARTESIAN_POINT ( 'NONE',  ( 10.00000000000000178, 112.0833333265053682, -2.679491924311226736 ) ) ;
#50741 = CARTESIAN_POINT ( 'NONE',  ( 5.082755093536325930, 2.531249997951610542, -5.082755093536325930 ) ) ;
#50742 = CARTESIAN_POINT ( 'NONE',  ( 9.832129032723416984, 155.6770833299193555, 5.676582343750006032 ) ) ;
#50743 = CARTESIAN_POINT ( 'NONE',  ( -10.18810118749999738, -4.220049686691941915, 78.25000000204836681 ) ) ;
#50744 = ADVANCED_BREP_SHAPE_REPRESENTATION ( '', ( #67548, #57354 ), #51355 ) ;
#50745 = CARTESIAN_POINT ( 'NONE',  ( -30.44569435410878810, 195.8125000013656063, 172.4456943541092357 ) ) ;
#50746 = CARTESIAN_POINT ( 'NONE',  ( 4.000000000000001776, 3.000000000000000000, 0.000000000000000000 ) ) ;
#50747 = CARTESIAN_POINT ( 'NONE',  ( 3.211159895383561835, 17.56249999863440792, -3.211159895383561835 ) ) ;
#50748 = ORIENTED_EDGE ( 'NONE', *, *, #15763, .T. ) ;
#50749 = CARTESIAN_POINT ( 'NONE',  ( 2.828427124746208943, 200.7500000027312126, 195.1715728752538439 ) ) ;
#50750 = CARTESIAN_POINT ( 'NONE',  ( -3.458734125000016757, 196.1250000013655779, 140.5673454167824161 ) ) ;
#50751 = CARTESIAN_POINT ( 'NONE',  ( -30.82842712474612767, 206.5000000027312126, 172.8284271247466108 ) ) ;
#50752 = EDGE_CURVE ( 'NONE', #53500, #16650, #60841, .T. ) ;
#50753 = CARTESIAN_POINT ( 'NONE',  ( -27.99999999999999645, 210.0000000000000284, 174.0000000000003411 ) ) ;
#50754 = ORIENTED_EDGE ( 'NONE', *, *, #74046, .F. ) ;
#50755 = CARTESIAN_POINT ( 'NONE',  ( -1.320432766682874540E-15, 9.093749997951610098, 7.188101187500000044 ) ) ;
#50756 = CARTESIAN_POINT ( 'NONE',  ( -7.320508075688773708, 208.7499999931719969, -7.320508075688774596 ) ) ;
#50757 = CARTESIAN_POINT ( 'NONE',  ( -10.99999999999999822, -4.556349186104053040, 73.28125000409677625 ) ) ;
#50758 = CARTESIAN_POINT ( 'NONE',  ( 2.679491924311222739, 38.95833333333333570, 10.00000000000000355 ) ) ;
#50759 = CARTESIAN_POINT ( 'NONE',  ( -5.082755093536324154, 105.2187500020483952, 5.082755093536326818 ) ) ;
#50760 = MECHANICAL_DESIGN_GEOMETRIC_PRESENTATION_REPRESENTATION (  '', ( #11042 ), #53196 ) ;
#50761 = CARTESIAN_POINT ( 'NONE',  ( -24.54126587500000767, 208.5000000013656063, 168.5673454167827003 ) ) ;
#50762 = CARTESIAN_POINT ( 'NONE',  ( -2.765530957081998142, 287.6406250017069510, 6.676582343750000703 ) ) ;
#50764 = CARTESIAN_POINT ( 'NONE',  ( 2.828427124746152987, 201.2500000027312126, 139.1715728752538723 ) ) ;
#50763 = CARTESIAN_POINT ( 'NONE',  ( 0.000000000000000000, 51.05255888325788050, -10.19999999999999396 ) ) ;
#50765 = ORIENTED_EDGE ( 'NONE', *, *, #585, .T. ) ;
#50766 = CARTESIAN_POINT ( 'NONE',  ( -5.676582343750000703, 258.0729166700806445, -9.832129032723418760 ) ) ;
#50767 = CARTESIAN_POINT ( 'NONE',  ( 5.082755093536318824, 5.082755093536319713, 23.79905278187175455 ) ) ;
#50768 = VECTOR ( 'NONE', #67961, 1000.000000000000000 ) ;
#50769 = CARTESIAN_POINT ( 'NONE',  ( -0.7581620860329574274, 55.63814191977067480, 43.81219805000592515 ) ) ;
#50770 = DIRECTION ( 'NONE',  ( -0.000000000000000000, 1.000000000000000000, -0.000000000000000000 ) ) ;
#50771 = CARTESIAN_POINT ( 'NONE',  ( 5.086519500889780332, -60.91611154180146315, -23.32191296475813758 ) ) ;
#50772 = CARTESIAN_POINT ( 'NONE',  ( -2.445694354108783219, 196.8125000013656063, 200.4456943541088663 ) ) ;
#50773 = CARTESIAN_POINT ( 'NONE',  ( 2.679491924311228956, 166.0416666666666572, -10.00000000000000000 ) ) ;
#50774 = LINE ( 'NONE', #8930, #42567 ) ;
#50775 = CARTESIAN_POINT ( 'NONE',  ( 18.00000000000000000, 10.39230484541329247, -1.607695154586745501 ) ) ;
#50776 = CARTESIAN_POINT ( 'NONE',  ( 5.000000000000000000, -53.18690467503068220, -43.91652490638241346 ) ) ;
#50777 = CARTESIAN_POINT ( 'NONE',  ( -3.042071309553173730, 129.6354166632526415, 11.35316468749999785 ) ) ;
#50778 = CARTESIAN_POINT ( 'NONE',  ( -4.999999999999999112, -15.48016642534408405, -69.96422921944751749 ) ) ;
#50779 = CARTESIAN_POINT ( 'NONE',  ( -6.735557395310442023E-16, 11.00000000000000000, 71.12500000000000000 ) ) ;
#50780 = CIRCLE ( 'NONE', #60406, 10.00000000000000000 ) ;
#50783 = DIRECTION ( 'NONE',  ( 0.000000000000000000, 0.000000000000000000, -1.000000000000000000 ) ) ;
#50782 = CARTESIAN_POINT ( 'NONE',  ( 24.54126587499998990, 197.1875000013655779, 169.9999999999999432 ) ) ;
#50781 = CARTESIAN_POINT ( 'NONE',  ( 25.55430564589119058, 195.3125000013656063, 167.5543056458910485 ) ) ;
#50784 = ORIENTED_EDGE ( 'NONE', *, *, #13029, .F. ) ;
#50785 = EDGE_CURVE ( 'NONE', #24567, #40096, #17796, .T. ) ;
#50786 = EDGE_CURVE ( 'NONE', #52055, #51031, #63441, .T. ) ;
#50787 = CARTESIAN_POINT ( 'NONE',  ( 1.656854249492381248, 2.187500000000000444, -4.000000000000001776 ) ) ;
#50788 = DIRECTION ( 'NONE',  ( 1.000000000000000000, 0.000000000000000000, 0.000000000000000000 ) ) ;
#50789 = CARTESIAN_POINT ( 'NONE',  ( 18.00000000000000000, 0.000000000000000000, 19.00000000000000355 ) ) ;
#50790 = CARTESIAN_POINT ( 'NONE',  ( 24.54126587500000056, 199.3750000013656063, 168.5673454167822172 ) ) ;
#50791 = CARTESIAN_POINT ( 'NONE',  ( 5.676582343750001591, 206.9270833299193555, -9.832129032723420536 ) ) ;
#50792 = CARTESIAN_POINT ( 'NONE',  ( 1.320432766682874540E-15, 118.5312500020483810, 7.188101187500000044 ) ) ;
#50793 = CARTESIAN_POINT ( 'NONE',  ( 2.780723358947928197E-16, 18.56249999863440436, -4.541265875000002339 ) ) ;
#50794 = CARTESIAN_POINT ( 'NONE',  ( 31.45873412499999233, 195.9375000013655779, 169.9999999999999432 ) ) ;
#50795 = CARTESIAN_POINT ( 'NONE',  ( 3.313708498984762496, -7.999999999999989342, 23.79905277982336642 ) ) ;
#50797 = FACE_OUTER_BOUND ( 'NONE', #24355, .T. ) ;
#50796 = CARTESIAN_POINT ( 'NONE',  ( -1.656854249492382580, 1.312500000000000444, -4.000000000000000000 ) ) ;
#50798 = CARTESIAN_POINT ( 'NONE',  ( 5.676582343750001591, 96.61458332991935549, -9.832129032723420536 ) ) ;
#50799 = ORIENTED_EDGE ( 'NONE', *, *, #72510, .T. ) ;
#50800 = DIRECTION ( 'NONE',  ( -0.000000000000000000, 1.000000000000000000, -4.476705744456276341E-16 ) ) ;
#50801 = CARTESIAN_POINT ( 'NONE',  ( 2.977408999572651815, 19.68749999795161543, 7.188101187500000933 ) ) ;
#50802 = FACE_OUTER_BOUND ( 'NONE', #12859, .T. ) ;
#50803 =( BOUNDED_CURVE ( )  B_SPLINE_CURVE ( 2, ( #19606, #19238, #49396, #15062, #42248, #43360, #13566, #36604, #31304 ),
 .UNSPECIFIED., .F., .F. ) 
 B_SPLINE_CURVE_WITH_KNOTS ( ( 3, 2, 2, 2, 3 ),
 ( 0.3295454545454545303, 0.3352272727272727071, 0.3409090909090909394, 0.3465909090909091717, 0.3522727272727273484 ),
 .UNSPECIFIED. ) 
 CURVE ( )  GEOMETRIC_REPRESENTATION_ITEM ( )  RATIONAL_B_SPLINE_CURVE ( ( 1.000000000000000000, 0.9238795325112867385, 1.000000000000000000, 0.9238795325112867385, 1.000000000000000000, 0.9238795325112867385, 1.000000000000000000, 0.9238795325112859613, 1.000000000000000666 ) ) 
 REPRESENTATION_ITEM ( '' )  );
#50804 = CARTESIAN_POINT ( 'NONE',  ( -3.042071309553159075, 255.2604166700806445, 11.35316468749999963 ) ) ;
#50805 = AXIS2_PLACEMENT_3D ( 'NONE', #19889, #30483, #65915 ) ;
#50806 = CARTESIAN_POINT ( 'NONE',  ( -8.311093377946841443, 108.9062499965860127, 8.311093377946830785 ) ) ;
#50807 = EDGE_LOOP ( 'NONE', ( #3884, #62065, #48345 ) ) ;
#50808 = CARTESIAN_POINT ( 'NONE',  ( 38.00000000000000000, 52.99999999999992895, -6.791607979884335933E-15 ) ) ;
#50809 = CARTESIAN_POINT ( 'NONE',  ( -10.18810118749999738, -4.220049686691941915, 105.2500000020483952 ) ) ;
#50810 = CARTESIAN_POINT ( 'NONE',  ( -29.43265458321766559, 195.7500000013656063, 166.5412658750003629 ) ) ;
#50811 = CARTESIAN_POINT ( 'NONE',  ( -3.458734124999960358, 206.6250000013656063, 196.5673454167823877 ) ) ;
#50812 = CARTESIAN_POINT ( 'NONE',  ( 5.656854249492379694, 118.4375000000000000, -5.656854249492380582 ) ) ;
#50814 = CARTESIAN_POINT ( 'NONE',  ( 5.676582343750001591, 81.61458332991935549, -9.832129032723420536 ) ) ;
#50813 = CARTESIAN_POINT ( 'NONE',  ( -7.778174593052020747, -7.778174593052023411, 97.18749999999998579 ) ) ;
#50815 = ADVANCED_FACE ( 'NONE', ( #33686 ), #5741, .T. ) ;
#50816 = CARTESIAN_POINT ( 'NONE',  ( 7.999999999999992895, -3.313708498984756279, 13.67405278392014978 ) ) ;
#50817 = CARTESIAN_POINT ( 'NONE',  ( -31.45873412499997812, 199.0000000013656063, 171.4326545832180386 ) ) ;
#50818 = EDGE_LOOP ( 'NONE', ( #51389, #39732, #31832, #40515 ) ) ;
#50819 = CARTESIAN_POINT ( 'NONE',  ( -8.660254037844387298, 188.9583333265053966, -5.000000000000004441 ) ) ;
#50820 = CARTESIAN_POINT ( 'NONE',  ( -5.000000000000000000, -16.24494643555759410, 69.83755725260752456 ) ) ;
#50821 = DIRECTION ( 'NONE',  ( 0.000000000000000000, 0.000000000000000000, 1.000000000000000000 ) ) ;
#50822 = CARTESIAN_POINT ( 'NONE',  ( 11.35316468749999963, 71.30208332991932707, -3.042071309553165293 ) ) ;
#50823 = CARTESIAN_POINT ( 'NONE',  ( -4.721056650415998313, 288.5781250017069510, 4.721056650416000089 ) ) ;
#50824 = CARTESIAN_POINT ( 'NONE',  ( -3.166186134455097228E-13, 211.2500000000000568, -9.999999999999998224 ) ) ;
#50825 = CARTESIAN_POINT ( 'NONE',  ( -6.238412754330611322E-16, 10.18810118749999916, 100.6562500020483810 ) ) ;
#50826 = CARTESIAN_POINT ( 'NONE',  ( 11.35316468749999963, 220.9895833299193555, -3.042071309553165293 ) ) ;
#50827 = EDGE_LOOP ( 'NONE', ( #30948, #59104 ) ) ;
#50828 = CARTESIAN_POINT ( 'NONE',  ( 7.999999999999991118, 9.797174393178815797E-16, 28.58030277982336642 ) ) ;
#50829 = CARTESIAN_POINT ( 'NONE',  ( -6.338291171875001240, 299.2578125025604550, 0.000000000000000000 ) ) ;
#50830 = CARTESIAN_POINT ( 'NONE',  ( -7.000000000000000000, 8.572527594031473190E-16, -0.7002075382097148193 ) ) ;
#50831 = CARTESIAN_POINT ( 'NONE',  ( -2.085542519210945728E-15, 209.5312499965860411, 11.35316468750000141 ) ) ;
#50832 = CARTESIAN_POINT ( 'NONE',  ( -8.660254037844387298, 222.7083333401613174, -4.999999999999999112 ) ) ;
#50833 = CARTESIAN_POINT ( 'NONE',  ( -5.000000000000005329, 100.2083333265053682, 8.660254037844387298 ) ) ;
#50834 = CARTESIAN_POINT ( 'NONE',  ( 6.676582343750004256, 298.8906250017069510, 2.765530957081995478 ) ) ;
#50835 = ORIENTED_EDGE ( 'NONE', *, *, #27022, .T. ) ;
#50836 = CARTESIAN_POINT ( 'NONE',  ( 5.676582343750001591, 191.9270833299193555, -9.832129032723420536 ) ) ;
#50837 =( BOUNDED_CURVE ( )  B_SPLINE_CURVE ( 2, ( #23221, #63961, #58318, #46599, #45480, #46231, #52642, #978, #5141, #23961, #10787, #33823, #39827 ),
 .UNSPECIFIED., .F., .F. ) 
 B_SPLINE_CURVE_WITH_KNOTS ( ( 3, 2, 2, 2, 2, 2, 3 ),
 ( 1.836885797912684914, 1.842119258028978912, 1.847352718145273132, 1.852586178261567573, 1.857819638377861793, 1.863053098494156234, 1.868286558610450454 ),
 .UNSPECIFIED. ) 
 CURVE ( )  GEOMETRIC_REPRESENTATION_ITEM ( )  RATIONAL_B_SPLINE_CURVE ( ( 1.000000000000097922, 0.9659258262889700575, 0.9999999999999998890, 0.9659258262890682012, 0.9999999999999998890, 0.9659258262890682012, 0.9999999999999998890, 0.9659258262890682012, 0.9999999999999998890, 0.9659258262890682012, 0.9999999999999998890, 0.9659258262892623792, 0.9999999999998057110 ) ) 
 REPRESENTATION_ITEM ( '' )  );
#50838 = VECTOR ( 'NONE', #28385, 1000.000000000000000 ) ;
#50839 = CARTESIAN_POINT ( 'NONE',  ( -25.55430564589119768, 206.3125000013656063, 167.5543056458915316 ) ) ;
#50840 = CARTESIAN_POINT ( 'NONE',  ( -5.656854249492379694, 11.06250000000000178, -5.656854249492380582 ) ) ;
#50841 = VERTEX_POINT ( 'NONE', #73651 ) ;
#50842 = CARTESIAN_POINT ( 'NONE',  ( -7.999999999999998224, 90.78125000409681888, 3.313708498984766493 ) ) ;
#50843 = CARTESIAN_POINT ( 'NONE',  ( 10.00000000000000000, 14.79166666666666607, 2.679491924311236062 ) ) ;
#50844 = CARTESIAN_POINT ( 'NONE',  ( 10.18810118749999916, 1.247682550866122264E-15, 82.28125000204838102 ) ) ;
#50845 = ORIENTED_EDGE ( 'NONE', *, *, #74221, .F. ) ;
#50846 = CARTESIAN_POINT ( 'NONE',  ( -4.000000000000001776, 19.43750000000000000, -1.656854249492381470 ) ) ;
#50847 = CARTESIAN_POINT ( 'NONE',  ( 3.211159895383561835, 20.43749999863440436, -3.211159895383561835 ) ) ;
#50848 = DIRECTION ( 'NONE',  ( 0.000000000000000000, -1.000000000000000000, 0.000000000000000000 ) ) ;
#50849 = AXIS2_PLACEMENT_3D ( 'NONE', #69380, #71583, #31611 ) ;
#50850 = EDGE_CURVE ( 'NONE', #27032, #63005, #73090, .T. ) ;
#50851 = ORIENTED_EDGE ( 'NONE', *, *, #3789, .T. ) ;
#50852 = CARTESIAN_POINT ( 'NONE',  ( 2.679491924311222739, 15.83333332650536640, 10.00000000000000355 ) ) ;
#50853 = CARTESIAN_POINT ( 'NONE',  ( -7.188101187500001821, 122.9375000020483810, -2.977408999572650483 ) ) ;
#50856 = CARTESIAN_POINT ( 'NONE',  ( 1.656854249492321074, 197.3125000000000568, 202.0000000000001137 ) ) ;
#50855 = CARTESIAN_POINT ( 'NONE',  ( -11.35316468749999963, 248.9062500034139873, 0.000000000000000000 ) ) ;
#50854 = CARTESIAN_POINT ( 'NONE',  ( 26.56734541678233441, 209.0000000013656063, 166.5412658749999650 ) ) ;
#50857 = APPLICATION_PROTOCOL_DEFINITION ( 'draft international standard', 'automotive_design', 1998, #58827 ) ;
#50858 = VECTOR ( 'NONE', #24368, 1000.000000000000000 ) ;
#50859 = EDGE_LOOP ( 'NONE', ( #47381, #22937, #44126 ) ) ;
#50860 = CARTESIAN_POINT ( 'NONE',  ( 3.042071309553163960, 252.7604166700806445, -11.35316468749999785 ) ) ;
#50861 = CARTESIAN_POINT ( 'NONE',  ( -4.401442555609577197E-16, 7.188101187499992051, 11.61155278187175632 ) ) ;
#50862 = ORIENTED_EDGE ( 'NONE', *, *, #23566, .T. ) ;
#50863 = ORIENTED_EDGE ( 'NONE', *, *, #21425, .F. ) ;
#50864 = CARTESIAN_POINT ( 'NONE',  ( 4.220049686691934809, 10.18810118749999916, 74.68750000204838102 ) ) ;
#50865 = CARTESIAN_POINT ( 'NONE',  ( 11.35316468749999785, 85.88541666325268409, 3.042071309553174174 ) ) ;
#50866 = FACE_OUTER_BOUND ( 'NONE', #9567, .T. ) ;
#50867 = CARTESIAN_POINT ( 'NONE',  ( -11.00000000000000000, 0.000000000000000000, 86.50000000000000000 ) ) ;
#50870 = CARTESIAN_POINT ( 'NONE',  ( 4.721056650415999201, 288.2343750017069510, -4.721056650415999201 ) ) ;
#50869 = CARTESIAN_POINT ( 'NONE',  ( 23.99999999999997513, 194.8125000027312126, 168.3431457505075741 ) ) ;
#50868 = CARTESIAN_POINT ( 'NONE',  ( 31.45873412499998523, 207.8750000013656063, 171.4326545832175839 ) ) ;
#50871 = EDGE_CURVE ( 'NONE', #38797, #70301, #5006, .T. ) ;
#50872 = CARTESIAN_POINT ( 'NONE',  ( 1.469576158976823947E-15, 114.8750000000000000, 8.000000000000000000 ) ) ;
#50873 = CARTESIAN_POINT ( 'NONE',  ( 9.491012693392001592E-16, 125.0000000000000000, 7.500000000000020428 ) ) ;
#50874 = CARTESIAN_POINT ( 'NONE',  ( 6.951808397369818766E-16, 197.0312499965860411, -11.35316468750000141 ) ) ;
#50875 = CARTESIAN_POINT ( 'NONE',  ( 3.313708498984762496, 8.531249995903221972, 7.999999999999998224 ) ) ;
#50876 = ORIENTED_EDGE ( 'NONE', *, *, #26969, .F. ) ;
#50877 = CARTESIAN_POINT ( 'NONE',  ( 29.43265458321760519, 195.5000000013655779, 173.4587341249998929 ) ) ;
#50878 = CARTESIAN_POINT ( 'NONE',  ( -7.188101187500001821, 17.99999999795161898, -2.977408999572651371 ) ) ;
#50879 = AXIS2_PLACEMENT_3D ( 'NONE', #14461, #26155, #43511 ) ;
#50880 = CARTESIAN_POINT ( 'NONE',  ( 5.676582343750001591, 171.9270833299193555, -9.832129032723420536 ) ) ;
#50881 = CARTESIAN_POINT ( 'NONE',  ( 0.000000000000000000, 125.0000000000000000, 0.000000000000000000 ) ) ;
#50882 = CARTESIAN_POINT ( 'NONE',  ( -5.082755093536325930, 103.3437500020483668, -5.082755093536325930 ) ) ;
#50884 = CARTESIAN_POINT ( 'NONE',  ( 0.6474643998346684137, -49.91423208894351404, -40.68959583910973521 ) ) ;
#50883 = CARTESIAN_POINT ( 'NONE',  ( 1.656854249492381914, 17.56249999726881938, 4.000000000000000888 ) ) ;
#50885 = CARTESIAN_POINT ( 'NONE',  ( 26.56734541678238060, 205.2500000013655779, 166.5412658749999650 ) ) ;
#50886 = CARTESIAN_POINT ( 'NONE',  ( 5.082755093536318824, 5.082755093536319713, 16.29905278187175455 ) ) ;
#50887 = CARTESIAN_POINT ( 'NONE',  ( 9.832129032723416984, 60.36458332991935549, 5.676582343750006032 ) ) ;
#50888 = DIRECTION ( 'NONE',  ( -0.000000000000000000, 1.000000000000000000, 4.476705744456276341E-16 ) ) ;
#50889 = CARTESIAN_POINT ( 'NONE',  ( 1.656854249492538234, 195.8125000027312126, 194.0000000000001990 ) ) ;
#50890 = ORIENTED_EDGE ( 'NONE', *, *, #12287, .F. ) ;
#50891 = CARTESIAN_POINT ( 'NONE',  ( 0.000000000000000000, 19.05255888325788050, 0.000000000000000000 ) ) ;
#50892 = CARTESIAN_POINT ( 'NONE',  ( -4.556349186104045934, 11.00000000000000000, 80.40625000409676204 ) ) ;
#50893 = CARTESIAN_POINT ( 'NONE',  ( -5.676582343750006032, 59.11458332991934839, 9.832129032723418760 ) ) ;
#50894 = CARTESIAN_POINT ( 'NONE',  ( -10.99999999999999822, -4.556349186104052151, 76.28125000409676204 ) ) ;
#50895 = CARTESIAN_POINT ( 'NONE',  ( 2.445694354108783219, 200.8125000013656063, 139.5543056458912190 ) ) ;
#50896 = CARTESIAN_POINT ( 'NONE',  ( 3.223881452105103573, 10.27322224982961529, 63.89771963198208482 ) ) ;
#50897 = CARTESIAN_POINT ( 'NONE',  ( -8.660254037844385522, 245.4166666666666856, 5.000000000000004441 ) ) ;
#50899 = CARTESIAN_POINT ( 'NONE',  ( 9.832129032723416984, 45.36458332991934839, 5.676582343750006032 ) ) ;
#50898 = CARTESIAN_POINT ( 'NONE',  ( -7.188101187499999156, 91.25000000204838102, 2.977408999572654924 ) ) ;
#50900 = EDGE_CURVE ( 'NONE', #16735, #41123, #29123, .T. ) ;
#50901 = CARTESIAN_POINT ( 'NONE',  ( -7.999999999999991118, 0.000000000000000000, 5.330302779823363757 ) ) ;
#50902 = CARTESIAN_POINT ( 'NONE',  ( -4.898587196589412829E-16, 115.6250000000000000, -8.000000000000000000 ) ) ;
#50903 = CARTESIAN_POINT ( 'NONE',  ( -11.35316468750000141, 173.2812499965860411, -1.390361679473963753E-15 ) ) ;
#50904 = CARTESIAN_POINT ( 'NONE',  ( 6.123233995736767268E-16, 148.1249999931720538, -10.00000000000000178 ) ) ;
#50905 = AXIS2_PLACEMENT_3D ( 'NONE', #74213, #27819, #39145 ) ;
#50906 = CARTESIAN_POINT ( 'NONE',  ( -5.082755093536325930, 104.8437500020483810, -5.082755093536325930 ) ) ;
#50907 = FACE_OUTER_BOUND ( 'NONE', #20776, .T. ) ;
#50908 = CARTESIAN_POINT ( 'NONE',  ( 8.311093377946837890, 31.71874999658601979, -8.311093377946837890 ) ) ;
#50909 = CARTESIAN_POINT ( 'NONE',  ( 6.951808397369818766E-16, 187.0312499965860127, -11.35316468750000141 ) ) ;
#50910 = ORIENTED_EDGE ( 'NONE', *, *, #14826, .T. ) ;
#50911 = CARTESIAN_POINT ( 'NONE',  ( 1.469576158976823947E-15, 100.0625000040967763, 8.000000000000000000 ) ) ;
#50912 = CARTESIAN_POINT ( 'NONE',  ( -4.220049686691937474, -10.18810118749999738, 69.43750000204838102 ) ) ;
#50913 = CARTESIAN_POINT ( 'NONE',  ( -3.999999999999960032, 196.0000000000000000, 198.0000000000000284 ) ) ;
#50914 = CARTESIAN_POINT ( 'NONE',  ( 4.898587196589412829E-16, 16.87500000000000000, -8.000000000000000000 ) ) ;
#50916 = CARTESIAN_POINT ( 'NONE',  ( 11.35316468750000141, 160.7812499965860127, 0.000000000000000000 ) ) ;
#50915 = CARTESIAN_POINT ( 'NONE',  ( 5.000000000000000000, -68.60357193678713372, 20.85024232999320404 ) ) ;
#50917 = CARTESIAN_POINT ( 'NONE',  ( -5.656854249492373476, -5.656854249492376141, 7.074052784329822430 ) ) ;
#50918 = AXIS2_PLACEMENT_3D ( 'NONE', #70769, #19083, #8138 ) ;
#50919 = EDGE_CURVE ( 'NONE', #41754, #43896, #58156, .T. ) ;
#50920 = CARTESIAN_POINT ( 'NONE',  ( 0.000000000000000000, 0.000000000000000000, 30.00000000000000000 ) ) ;
#50921 = CARTESIAN_POINT ( 'NONE',  ( -8.311093377946836114, 223.2812500034140157, -8.311093377946836114 ) ) ;
#50922 = CARTESIAN_POINT ( 'NONE',  ( -6.308070865140195771, 51.03903544636535372, -41.30321721933843548 ) ) ;
#50923 = CARTESIAN_POINT ( 'NONE',  ( 10.18810118749999916, 4.220049686691935698, 77.87500000204838102 ) ) ;
#50924 = EDGE_LOOP ( 'NONE', ( #43272, #45236, #47506, #15746 ) ) ;
#50925 = VECTOR ( 'NONE', #13503, 1000.000000000000000 ) ;
#50926 = EDGE_CURVE ( 'NONE', #68433, #55117, #51381, .T. ) ;
#50927 = DIRECTION ( 'NONE',  ( 0.000000000000000000, 0.000000000000000000, -1.000000000000000000 ) ) ;
#50928 = CARTESIAN_POINT ( 'NONE',  ( 11.35316468749999785, 120.8854166632526841, 3.042071309553174174 ) ) ;
#50929 =( BOUNDED_CURVE ( )  B_SPLINE_CURVE ( 2, ( #17507, #67715, #62775, #68816, #40154, #10369, #34142, #22785, #33396 ),
 .UNSPECIFIED., .F., .F. ) 
 B_SPLINE_CURVE_WITH_KNOTS ( ( 3, 2, 2, 2, 3 ),
 ( 0.1770833333333334259, 0.1822916666666667407, 0.1875000000000001110, 0.1927083333333334814, 0.1979166666666667962 ),
 .UNSPECIFIED. ) 
 CURVE ( )  GEOMETRIC_REPRESENTATION_ITEM ( )  RATIONAL_B_SPLINE_CURVE ( ( 0.9999999999999987788, 0.9238795325112879597, 1.000000000000000000, 0.9238795325112867385, 1.000000000000000000, 0.9238795325112867385, 1.000000000000000000, 0.9238795325112847401, 1.000000000000001998 ) ) 
 REPRESENTATION_ITEM ( '' )  );
#50930 = CARTESIAN_POINT ( 'NONE',  ( -1.349999999999999867, 255.9999999999997726, 5.686520093750665694 ) ) ;
#50931 = ORIENTED_EDGE ( 'NONE', *, *, #48808, .T. ) ;
#50932 = ORIENTED_EDGE ( 'NONE', *, *, #44247, .T. ) ;
#50933 = CARTESIAN_POINT ( 'NONE',  ( -1.881053915767121554, 8.749999998634406140, -4.541265875000002339 ) ) ;
#50934 = CARTESIAN_POINT ( 'NONE',  ( -1.320432766682874540E-15, 13.59374999795161187, 7.188101187500000044 ) ) ;
#50935 = CARTESIAN_POINT ( 'NONE',  ( -5.656854249492378806, 110.3750000040967763, 5.656854249492381470 ) ) ;
#50936 = CARTESIAN_POINT ( 'NONE',  ( -26.56734541678232375, 200.2500000013656631, 173.4587341250003760 ) ) ;
#50937 = CARTESIAN_POINT ( 'NONE',  ( 2.828427124746190291, 7.875000000000000000, 2.828427124746192067 ) ) ;
#50938 =( BOUNDED_CURVE ( )  B_SPLINE_CURVE ( 2, ( #67599, #67227, #43834, #50235, #21561, #44587, #21928, #34032, #27976 ),
 .UNSPECIFIED., .F., .F. ) 
 B_SPLINE_CURVE_WITH_KNOTS ( ( 3, 2, 2, 2, 3 ),
 ( 0.5937500000000000000, 0.5989583333333333703, 0.6041666666666666297, 0.6093750000000000000, 0.6145833333333333703 ),
 .UNSPECIFIED. ) 
 CURVE ( )  GEOMETRIC_REPRESENTATION_ITEM ( )  RATIONAL_B_SPLINE_CURVE ( ( 1.000000000000000000, 0.9238795325112867385, 1.000000000000000000, 0.9238795325112867385, 1.000000000000000000, 0.9238795325112867385, 1.000000000000000000, 0.9238795325112867385, 1.000000000000000000 ) ) 
 REPRESENTATION_ITEM ( '' )  );
#50939 = CARTESIAN_POINT ( 'NONE',  ( 2.828427124746191623, 21.87499999726881583, -2.828427124746191623 ) ) ;
#50940 = CARTESIAN_POINT ( 'NONE',  ( -3.211159895383561391, 6.687499998634407028, -3.211159895383561835 ) ) ;
#50941 = CARTESIAN_POINT ( 'NONE',  ( 2.828427124746153876, 199.8750000000000284, 144.8284271247462129 ) ) ;
#50942 = ORIENTED_EDGE ( 'NONE', *, *, #9011, .T. ) ;
#50943 = CARTESIAN_POINT ( 'NONE',  ( -7.999984110674186688, 3.313724388310563373, 9.924052148183214683 ) ) ;
#50944 = CARTESIAN_POINT ( 'NONE',  ( 7.188101187500000044, 102.4062500020483810, -8.802885111219163269E-16 ) ) ;
#50946 = CARTESIAN_POINT ( 'NONE',  ( -9.000000000000023093, 15.58845726811988541, 0.000000000000000000 ) ) ;
#50945 = DIRECTION ( 'NONE',  ( -0.000000000000000000, -1.000000000000000000, -4.283267841918042741E-17 ) ) ;
#50947 =( NAMED_UNIT ( * ) SI_UNIT ( $, .STERADIAN. ) SOLID_ANGLE_UNIT ( ) );
#50948 = FACE_OUTER_BOUND ( 'NONE', #18109, .T. ) ;
#50949 = DIRECTION ( 'NONE',  ( -0.000000000000000000, 1.000000000000000000, -0.000000000000000000 ) ) ;
#50950 = VERTEX_POINT ( 'NONE', #11399 ) ;
#50951 = ADVANCED_FACE ( 'NONE', ( #28741 ), #16289, .T. ) ;
#50952 = VERTEX_POINT ( 'NONE', #57435 ) ;
#50953 = CARTESIAN_POINT ( 'NONE',  ( 7.204075437095968759, -7.204075437095966983, 92.21875000204838102 ) ) ;
#50954 = CARTESIAN_POINT ( 'NONE',  ( -28.00000000000002132, 201.6875000013656063, 166.5412658750003629 ) ) ;
#50955 = CARTESIAN_POINT ( 'NONE',  ( -4.556349186104045934, 11.00000000000000000, 108.7187499999999858 ) ) ;
#50956 = CARTESIAN_POINT ( 'NONE',  ( 2.839093476692135984E-14, 201.9375000013656063, 201.4587341250000350 ) ) ;
#50957 = CARTESIAN_POINT ( 'NONE',  ( 105.0000000000000000, -70.00000000000001421, 201.0000000000000000 ) ) ;
#50958 = CARTESIAN_POINT ( 'NONE',  ( -8.660254037844390851, 127.9166666666666856, 4.999999999999998224 ) ) ;
#50959 = VECTOR ( 'NONE', #56790, 1000.000000000000000 ) ;
#50960 = CARTESIAN_POINT ( 'NONE',  ( -8.000000000000000000, 105.4062500000000000, -3.313708498984761608 ) ) ;
#50961 = CARTESIAN_POINT ( 'NONE',  ( 1.560533225284023162, 225.9999999999998863, 9.885282897026870685 ) ) ;
#50962 = CARTESIAN_POINT ( 'NONE',  ( 2.977408999572650927, -7.188101187499990274, 3.830302781871751883 ) ) ;
#50963 = DIRECTION ( 'NONE',  ( 0.000000000000000000, 0.000000000000000000, -1.000000000000000000 ) ) ;
#50964 = EDGE_CURVE ( 'NONE', #9987, #59197, #72665, .T. ) ;
#50965 = CARTESIAN_POINT ( 'NONE',  ( 31.45873412499999944, 208.6875000013656063, 169.9999999999999432 ) ) ;
#50966 = CARTESIAN_POINT ( 'NONE',  ( -7.188101187500002709, 1.687499997951610098, 2.977408999572649151 ) ) ;
#50967 = CARTESIAN_POINT ( 'NONE',  ( -3.458734125000016313, 197.8750000013656063, 140.5673454167824161 ) ) ;
#50968 = CARTESIAN_POINT ( 'NONE',  ( -7.347880794884122694E-16, 4.750000000000000000, 4.000000000000001776 ) ) ;
#50970 = CARTESIAN_POINT ( 'NONE',  ( -2.445694354108839175, 202.3125000013656063, 144.4456943541088663 ) ) ;
#50969 = FACE_OUTER_BOUND ( 'NONE', #5730, .T. ) ;
#50971 = CARTESIAN_POINT ( 'NONE',  ( -3.042071309553159075, 245.2604166700806729, 11.35316468749999963 ) ) ;
#50972 = CARTESIAN_POINT ( 'NONE',  ( 1.224646799147353454E-15, 300.0000000000000000, -10.00000000000000178 ) ) ;
#50973 = CARTESIAN_POINT ( 'NONE',  ( 23.99999999999998934, 201.7500000000000000, 169.9999999999998863 ) ) ;
#50974 = CARTESIAN_POINT ( 'NONE',  ( -11.35316468749999785, 13.07291666325268409, -3.042071309553167513 ) ) ;
#50975 = CARTESIAN_POINT ( 'NONE',  ( 8.000000000000000000, 122.7500000000000000, -9.797174393178825657E-16 ) ) ;
#50976 = CARTESIAN_POINT ( 'NONE',  ( 6.951808397369818766E-16, 212.3437499965860411, -11.35316468750000141 ) ) ;
#50977 = CARTESIAN_POINT ( 'NONE',  ( -2.679491924311226292, 133.3333333265053398, -10.00000000000000178 ) ) ;
#50978 = CARTESIAN_POINT ( 'NONE',  ( 27.99999999999999645, 210.0000000000000284, 169.9999999999999147 ) ) ;
#50979 = PRODUCT_DEFINITION ( 'UNKNOWN', '', #53833, #74226 ) ;
#50981 = CARTESIAN_POINT ( 'NONE',  ( 4.000000000000001776, 11.74999999726881406, 0.000000000000000000 ) ) ;
#50980 = CARTESIAN_POINT ( 'NONE',  ( 2.828427124746153876, 203.0000000027312126, 144.8284271247462129 ) ) ;
#50982 = ORIENTED_EDGE ( 'NONE', *, *, #22400, .F. ) ;
#50983 = CARTESIAN_POINT ( 'NONE',  ( -3.458734125000015869, 201.1875000013656063, 142.0000000000000568 ) ) ;
#50984 = CARTESIAN_POINT ( 'NONE',  ( 9.832129032723416984, 20.36458332991935194, 5.676582343750006032 ) ) ;
#50985 = CARTESIAN_POINT ( 'NONE',  ( 2.020667218593132706E-15, -11.00000000000000000, 91.56250000409677625 ) ) ;
#50986 = CARTESIAN_POINT ( 'NONE',  ( 10.00000000000000000, 227.5000000000000000, -1.224646799147353256E-15 ) ) ;
#50987 = CARTESIAN_POINT ( 'NONE',  ( -24.54126587500001833, 198.2500000013656347, 168.5673454167826435 ) ) ;
#50988 = CARTESIAN_POINT ( 'NONE',  ( -1.469576158976823947E-15, 6.937499995903221084, 8.000000000000000000 ) ) ;
#50990 = CARTESIAN_POINT ( 'NONE',  ( 3.042071309553159519, 4.739583329919349275, 11.35316468750000141 ) ) ;
#50989 = CARTESIAN_POINT ( 'NONE',  ( 7.188101187500000044, 112.9062500020483952, -8.802885111219163269E-16 ) ) ;
#50991 = CARTESIAN_POINT ( 'NONE',  ( -7.999999999999991118, 3.313708498984756723, 18.73655277982336642 ) ) ;
#50992 = CARTESIAN_POINT ( 'NONE',  ( 11.35316468749999963, 135.9895833299193271, -3.042071309553165293 ) ) ;
#50993 = EDGE_CURVE ( 'NONE', #21755, #60656, #48114, .T. ) ;
#50994 = CARTESIAN_POINT ( 'NONE',  ( -8.660254037844387298, 103.9583333265053824, -5.000000000000004441 ) ) ;
#50995 = CARTESIAN_POINT ( 'NONE',  ( -4.401442555609581635E-16, 118.1562500020483810, -7.188101187500000044 ) ) ;
#50996 = CARTESIAN_POINT ( 'NONE',  ( -2.679491924311226292, 3.333333326505365513, -10.00000000000000178 ) ) ;
#50997 = CARTESIAN_POINT ( 'NONE',  ( -26.56734541678232731, 208.2500000013656063, 173.4587341250003760 ) ) ;
#50998 = AXIS2_PLACEMENT_3D ( 'NONE', #13400, #8497, #48850 ) ;
#50999 = CARTESIAN_POINT ( 'NONE',  ( -4.999999999999998224, 52.84634075987170831, -43.22150062466479170 ) ) ;
#51000 = ORIENTED_EDGE ( 'NONE', *, *, #33764, .T. ) ;
#51001 = CARTESIAN_POINT ( 'NONE',  ( 1.317228840344650820, -65.80815776305074394, 26.30638062134261190 ) ) ;
#51002 = B_SPLINE_CURVE_WITH_KNOTS ( 'NONE', 3,
 ( #31641, #2970, #25954, #48973, #71987, #43319, #66335, #21794, #39165, #33527, #22926, #32776, #55784, #45195, #50473, #15762, #22542, #56901, #4100, #61803, #39908, #68205, #62168, #39542, #57273, #10121, #5213, #4469, #10866, #5588, #33903, #16885, #73862, #68577 ),
 .UNSPECIFIED., .F., .F.,
 ( 4, 2, 2, 2, 2, 2, 2, 2, 2, 2, 2, 2, 2, 2, 2, 2, 4 ),
 ( 0.009106795846385969118, 0.009781323166193241214, 0.01045585048600051505, 0.01113037780580778888, 0.01180490512561506097, 0.01247943244542233307, 0.01315395976522960690, 0.01382848708503687900, 0.01450301440484415283, 0.01517754172465142493, 0.01585206904445869702, 0.01652659636426597259, 0.01720112368407324469, 0.01787565100388052372, 0.01855017832368780623, 0.01922470564349508526, 0.01989923296330236430 ),
 .UNSPECIFIED. ) ;
#51003 = ADVANCED_FACE ( 'NONE', ( #7227 ), #30230, .T. ) ;
#51004 = CARTESIAN_POINT ( 'NONE',  ( 5.656854249492379694, 107.9374999999999858, -5.656854249492380582 ) ) ;
#51005 = CARTESIAN_POINT ( 'NONE',  ( -6.676582343750001591, 288.6093750017069510, 0.000000000000000000 ) ) ;
#51006 =( LENGTH_UNIT ( ) NAMED_UNIT ( * ) SI_UNIT ( .MILLI., .METRE. ) );
#51007 = CARTESIAN_POINT ( 'NONE',  ( -4.898587196589407898E-16, 7.999999999999991118, 23.01155278432982598 ) ) ;
#51008 = CARTESIAN_POINT ( 'NONE',  ( 2.679491924311226292, 226.6666666734946034, -10.00000000000000000 ) ) ;
#51009 = CARTESIAN_POINT ( 'NONE',  ( 11.35316468749999608, 256.6145833367473301, -3.042071309553167069 ) ) ;
#51010 = CARTESIAN_POINT ( 'NONE',  ( 4.220049686691941027, -10.18810118749999738, 100.0000000020483668 ) ) ;
#51011 = ORIENTED_EDGE ( 'NONE', *, *, #58134, .F. ) ;
#51012 = CARTESIAN_POINT ( 'NONE',  ( 5.000000000000001776, 217.7083333265053682, -8.660254037844389075 ) ) ;
#51013 = DIRECTION ( 'NONE',  ( -0.000000000000000000, -1.000000000000000000, -0.000000000000000000 ) ) ;
#51014 = CARTESIAN_POINT ( 'NONE',  ( 2.754378923186476579E-14, 201.4375000013656063, 194.5412658750000219 ) ) ;
#51015 = EDGE_CURVE ( 'NONE', #51123, #22089, #13338, .T. ) ;
#51016 = CARTESIAN_POINT ( 'NONE',  ( 9.832129032723416984, 75.67708332991934128, 5.676582343750006032 ) ) ;
#51017 = ORIENTED_EDGE ( 'NONE', *, *, #42187, .F. ) ;
#51018 = CARTESIAN_POINT ( 'NONE',  ( 7.204075437095966983, 7.204075437095967871, 115.0937500020483810 ) ) ;
#51019 = CARTESIAN_POINT ( 'NONE',  ( -1.881053915767124440, 13.12499999863440969, 4.541265875000001451 ) ) ;
#51020 = ORIENTED_EDGE ( 'NONE', *, *, #46201, .T. ) ;
#51021 = AXIS2_PLACEMENT_3D ( 'NONE', #53575, #54694, #3003 ) ;
#51022 = CARTESIAN_POINT ( 'NONE',  ( 2.977408999572650927, 26.24999999795161898, -7.188101187500001821 ) ) ;
#51023 = DIRECTION ( 'NONE',  ( -0.000000000000000000, 1.000000000000000000, -0.000000000000000000 ) ) ;
#51024 = CARTESIAN_POINT ( 'NONE',  ( -5.000000000000000000, -60.90295814858238543, -23.31388853594834032 ) ) ;
#51025 = CARTESIAN_POINT ( 'NONE',  ( -2.977408999572654480, 24.37499999795161543, 7.188101187499999156 ) ) ;
#51026 = DIRECTION ( 'NONE',  ( 0.000000000000000000, 0.000000000000000000, 1.000000000000000000 ) ) ;
#51027 = CARTESIAN_POINT ( 'NONE',  ( 10.18810118749999916, 1.247682550866122264E-15, 112.2812500020483810 ) ) ;
#51028 = FACE_OUTER_BOUND ( 'NONE', #8134, .T. ) ;
#51029 = CARTESIAN_POINT ( 'NONE',  ( 2.449293598294707893E-16, 9.999999997268814056, -4.000000000000001776 ) ) ;
#51030 = CARTESIAN_POINT ( 'NONE',  ( 12.00000000000000000, 6.928203230275491009, -14.00000000000000178 ) ) ;
#51031 = VERTEX_POINT ( 'NONE', #70591 ) ;
#51032 = EDGE_CURVE ( 'NONE', #10283, #14049, #67360, .T. ) ;
#51033 = CARTESIAN_POINT ( 'NONE',  ( 1.432654583217662481, 203.1250000013656347, 194.5412658750000219 ) ) ;
#51034 = EDGE_CURVE ( 'NONE', #51512, #22380, #70654, .T. ) ;
#51036 =( BOUNDED_CURVE ( )  B_SPLINE_CURVE ( 2, ( #32607, #3932, #20888, #39368, #43909, #73693, #67670, #62364, #38997 ),
 .UNSPECIFIED., .F., .F. ) 
 B_SPLINE_CURVE_WITH_KNOTS ( ( 3, 2, 2, 2, 3 ),
 ( 0.8437500000000002220, 0.8489583333333335924, 0.8541666666666668517, 0.8593750000000002220, 0.8645833333333335924 ),
 .UNSPECIFIED. ) 
 CURVE ( )  GEOMETRIC_REPRESENTATION_ITEM ( )  RATIONAL_B_SPLINE_CURVE ( ( 0.9999999999999967804, 0.9238795325112899581, 1.000000000000000000, 0.9238795325112867385, 1.000000000000000000, 0.9238795325112867385, 1.000000000000000000, 0.9238795325112835188, 1.000000000000003331 ) ) 
 REPRESENTATION_ITEM ( '' )  );
#51035 = CARTESIAN_POINT ( 'NONE',  ( -24.54126587499996148, 204.1250000013656063, 171.4326545832179534 ) ) ;
#51037 = CARTESIAN_POINT ( 'NONE',  ( 3.999999999999960032, 206.9375000000000284, 143.6568542494924259 ) ) ;
#51038 = CARTESIAN_POINT ( 'NONE',  ( 1.881053915767122664, 9.124999998634407916, 4.541265875000001451 ) ) ;
#51039 = CARTESIAN_POINT ( 'NONE',  ( -1.656854249492381248, 10.06249999726881406, -4.000000000000001776 ) ) ;
#51040 = CIRCLE ( 'NONE', #18527, 7.000000000000000000 ) ;
#51041 = CARTESIAN_POINT ( 'NONE',  ( 5.082755093536320601, -5.082755093536318824, 18.54905278187175455 ) ) ;
#51042 = ORIENTED_EDGE ( 'NONE', *, *, #25483, .F. ) ;
#51043 = EDGE_CURVE ( 'NONE', #5243, #49926, #1931, .T. ) ;
#51044 = ORIENTED_EDGE ( 'NONE', *, *, #60187, .T. ) ;
#51045 = CARTESIAN_POINT ( 'NONE',  ( 7.204075437095968759, -7.204075437095966983, 111.7187500020483810 ) ) ;
#51046 = CARTESIAN_POINT ( 'NONE',  ( -11.00000000000000000, 0.000000000000000000, 97.18750000409677625 ) ) ;
#51047 = CARTESIAN_POINT ( 'NONE',  ( 3.458734125000015425, 205.0000000013655779, 196.5673454167823877 ) ) ;
#51048 = CARTESIAN_POINT ( 'NONE',  ( 31.45873412499999233, 200.6875000013656063, 169.9999999999998863 ) ) ;
#51049 = CARTESIAN_POINT ( 'NONE',  ( -4.999999999999998224, 86.66666666666667140, -8.660254037844389075 ) ) ;
#51050 = CARTESIAN_POINT ( 'NONE',  ( -7.999999999999998224, 122.0937500000000000, 3.313708498984766493 ) ) ;
#51051 = CARTESIAN_POINT ( 'NONE',  ( 6.000000000000003553, 288.4375000000000000, 2.485281374238571317 ) ) ;
#51052 = ORIENTED_EDGE ( 'NONE', *, *, #25162, .T. ) ;
#51053 = CYLINDRICAL_SURFACE ( 'NONE', #51782, 11.00000000000000000 ) ;
#51054 = CARTESIAN_POINT ( 'NONE',  ( -6.298842414732763295, -61.32333038069151598, 23.57034304878679976 ) ) ;
#51055 = CARTESIAN_POINT ( 'NONE',  ( 3.999999999999960032, 196.1250000027311842, 142.0000000000000568 ) ) ;
#51056 = PLANE ( 'NONE',  #18925 ) ;
#51057 = CARTESIAN_POINT ( 'NONE',  ( 4.999999999999997335, 243.3333333333333428, -8.660254037844387298 ) ) ;
#51058 = DIRECTION ( 'NONE',  ( -0.000000000000000000, 1.000000000000000000, 4.689100369878284071E-30 ) ) ;
#51059 = EDGE_CURVE ( 'NONE', #46167, #493, #42279, .T. ) ;
#51060 = CARTESIAN_POINT ( 'NONE',  ( -7.320508075688778149, 198.1250000000000000, 7.320508075688769267 ) ) ;
#51061 = CARTESIAN_POINT ( 'NONE',  ( 5.082755093536318824, 5.082755093536319713, 19.29905278187175455 ) ) ;
#51062 = CARTESIAN_POINT ( 'NONE',  ( 3.042071309553167069, 167.1354166632526415, -11.35316468749999785 ) ) ;
#51063 = CARTESIAN_POINT ( 'NONE',  ( -5.000000000000109246, 211.6666666666667993, -8.660254037844580921 ) ) ;
#51064 = CARTESIAN_POINT ( 'NONE',  ( 7.778174593052023411, -7.778174593052021635, 82.75000000409676204 ) ) ;
#51066 = CARTESIAN_POINT ( 'NONE',  ( 2.849036369511732440E-14, 208.3750000027312126, 202.0000000000000000 ) ) ;
#51065 = SURFACE_STYLE_FILL_AREA ( #40120 ) ;
#51067 = ORIENTED_EDGE ( 'NONE', *, *, #44942, .T. ) ;
#51068 = AXIS2_PLACEMENT_3D ( 'NONE', #59711, #59346, #19701 ) ;
#51069 = CARTESIAN_POINT ( 'NONE',  ( -2.445694354108838731, 199.0625000013656063, 144.4456943541088663 ) ) ;
#51070 = CARTESIAN_POINT ( 'NONE',  ( 11.35316468750000141, 26.09374999658601624, 0.000000000000000000 ) ) ;
#51071 = CARTESIAN_POINT ( 'NONE',  ( -7.778174593052020747, -7.778174593052023411, 110.8750000040967763 ) ) ;
#51072 = CARTESIAN_POINT ( 'NONE',  ( -26.34314575050757767, 200.9375000000000284, 166.0000000000004263 ) ) ;
#51074 = CARTESIAN_POINT ( 'NONE',  ( 4.471435261903841329, -10.26549131683148985, -64.21726486257124122 ) ) ;
#51073 = CARTESIAN_POINT ( 'NONE',  ( -1.836970198721029983E-15, 220.6249999931720538, 10.00000000000000178 ) ) ;
#51075 = CARTESIAN_POINT ( 'NONE',  ( 18.00000000000000000, -10.39230484541328892, -21.50000000000000000 ) ) ;
#51076 = CARTESIAN_POINT ( 'NONE',  ( 3.458734124999959914, 199.3750000013656063, 143.4326545832176976 ) ) ;
#51077 = CARTESIAN_POINT ( 'NONE',  ( 5.000000000000001776, 62.70833332650536818, -8.660254037844389075 ) ) ;
#51078 = CARTESIAN_POINT ( 'NONE',  ( 2.977408999572654480, 103.6250000020483810, 7.188101187499999156 ) ) ;
#51079 = CARTESIAN_POINT ( 'NONE',  ( 3.211159895383561835, 11.56249999863440614, -3.211159895383561835 ) ) ;
#51080 = DIRECTION ( 'NONE',  ( -0.000000000000000000, -0.000000000000000000, 1.000000000000000000 ) ) ;
#51081 = CARTESIAN_POINT ( 'NONE',  ( 7.999999999999992895, -3.313708498984756279, 4.486552779823363757 ) ) ;
#51082 = CARTESIAN_POINT ( 'NONE',  ( 1.704527592502775635, -49.99193291617169876, 40.73198448289673479 ) ) ;
#51083 = ORIENTED_EDGE ( 'NONE', *, *, #56168, .T. ) ;
#51084 = ORIENTED_EDGE ( 'NONE', *, *, #48693, .T. ) ;
#51085 = EDGE_CURVE ( 'NONE', #64471, #26128, #2783, .T. ) ;
#51086 = CARTESIAN_POINT ( 'NONE',  ( -3.313708498984757611, 7.999999999999991118, 11.04905277982336642 ) ) ;
#51087 = CARTESIAN_POINT ( 'NONE',  ( -3.458734124999960358, 195.6875000013655779, 198.0000000000000284 ) ) ;
#51088 = CARTESIAN_POINT ( 'NONE',  ( 1.584317714026805320E-12, 163.7500000000001137, 9.999999999999998224 ) ) ;
#51089 = CARTESIAN_POINT ( 'NONE',  ( 6.123233995736767268E-16, 43.12499999317203248, -10.00000000000000178 ) ) ;
#51090 = CARTESIAN_POINT ( 'NONE',  ( 6.951808397369818766E-16, 142.0312499965860411, -11.35316468750000141 ) ) ;
#51091 = ORIENTED_EDGE ( 'NONE', *, *, #21631, .F. ) ;
#51092 = CARTESIAN_POINT ( 'NONE',  ( -8.000000000000000000, 0.7500000000000000000, -9.797174393178825657E-16 ) ) ;
#51093 = CARTESIAN_POINT ( 'NONE',  ( 4.220049686691941027, -10.18810118749999738, 89.12500000204836681 ) ) ;
#51094 = CARTESIAN_POINT ( 'NONE',  ( -31.60757109211649762, 194.6015308780792168, 169.9129482759651069 ) ) ;
#51095 = CARTESIAN_POINT ( 'NONE',  ( 4.000000000000015099, 208.5625000000000000, 196.3431457505076594 ) ) ;
#51096 = CARTESIAN_POINT ( 'NONE',  ( -1.656854249492280440, 204.8125000000000284, 194.0000000000000284 ) ) ;
#51097 = CARTESIAN_POINT ( 'NONE',  ( 3.594044162775203777, 89.15552387383502264, -6.225081946264263699 ) ) ;
#51098 = CARTESIAN_POINT ( 'NONE',  ( 4.220049686691934809, 10.18810118749999916, 114.0625000020483668 ) ) ;
#51099 = ORIENTED_EDGE ( 'NONE', *, *, #23828, .F. ) ;
#51100 = APPLICATION_CONTEXT ( 'automotive_design' ) ;
#51101 = CYLINDRICAL_SURFACE ( 'NONE', #2191, 10.00000000000000000 ) ;
#51102 = CARTESIAN_POINT ( 'NONE',  ( 31.08702224744855869, 174.0168584738492541, 170.2012752884360225 ) ) ;
#51103 = CARTESIAN_POINT ( 'NONE',  ( -9.832129032723420536, 129.0104166632526983, 5.676582343749997150 ) ) ;
#51104 = CARTESIAN_POINT ( 'NONE',  ( 3.458734125000015425, 202.9375000013656063, 198.0000000000000284 ) ) ;
#51105 = CARTESIAN_POINT ( 'NONE',  ( 7.188101187499999156, 26.24999999795161543, 2.977408999572654924 ) ) ;
#51106 = CARTESIAN_POINT ( 'NONE',  ( -7.204075437095967871, 7.204075437095967871, 81.34375000204838102 ) ) ;
#51107 = CARTESIAN_POINT ( 'NONE',  ( -11.35316468750000141, 33.80208332991934839, 3.042071309553159963 ) ) ;
#51108 = ORIENTED_EDGE ( 'NONE', *, *, #71440, .T. ) ;
#51109 = LINE ( 'NONE', #35265, #15157 ) ;
#51110 = FACE_OUTER_BOUND ( 'NONE', #30067, .T. ) ;
#51111 = CARTESIAN_POINT ( 'NONE',  ( -5.662595241051935346, 5.662595241051935346, 18.82561528394063188 ) ) ;
#51112 = CARTESIAN_POINT ( 'NONE',  ( -2.839093476692135984E-14, 205.9375000013656063, 138.5412658750000503 ) ) ;
#51113 = CARTESIAN_POINT ( 'NONE',  ( -7.188101187500002709, 11.81249999795161187, 2.977408999572649151 ) ) ;
#51114 = CARTESIAN_POINT ( 'NONE',  ( 6.000000000000003553, 295.6250000034140157, -2.485281374238571761 ) ) ;
#51115 = CARTESIAN_POINT ( 'NONE',  ( -11.40310758942533731, -27.92336628524488873, 139.7248639375075072 ) ) ;
#51116 = CARTESIAN_POINT ( 'NONE',  ( 2.977408999572650927, 4.124999997951610986, -7.188101187500001821 ) ) ;
#51117 = EDGE_CURVE ( 'NONE', #67846, #70240, #49051, .T. ) ;
#51118 = CARTESIAN_POINT ( 'NONE',  ( -11.35316468750000141, 158.5937499965860127, -1.390361679473963753E-15 ) ) ;
#51119 = CARTESIAN_POINT ( 'NONE',  ( 1.871523826299183495E-15, -10.18810118749999916, 80.03125000204836681 ) ) ;
#51120 = CARTESIAN_POINT ( 'NONE',  ( -31.45873412499997812, 194.7500000013656063, 171.4326545832180386 ) ) ;
#51121 = CARTESIAN_POINT ( 'NONE',  ( -75.00000000000001421, 242.0000000000000284, 20.00000000000002132 ) ) ;
#51122 = CARTESIAN_POINT ( 'NONE',  ( 3.211159895383560947, 20.31249999863440436, 3.211159895383562723 ) ) ;
#51123 = VERTEX_POINT ( 'NONE', #37373 ) ;
#51124 = CIRCLE ( 'NONE', #21012, 18.00000000000000000 ) ;
#51125 = CARTESIAN_POINT ( 'NONE',  ( 2.828427124746209831, 197.5000000027312126, 200.8284271247462129 ) ) ;
#51126 = EDGE_CURVE ( 'NONE', #33772, #38706, #32473, .T. ) ;
#51127 = CARTESIAN_POINT ( 'NONE',  ( 2.828427124746152987, 209.1250000000000284, 139.1715728752538723 ) ) ;
#51128 = CARTESIAN_POINT ( 'NONE',  ( -28.00000000000008171, 206.1250000027312126, 166.0000000000003695 ) ) ;
#51129 = CARTESIAN_POINT ( 'NONE',  ( 12.00000000000000178, 1.469576158976824144E-15, -21.47459999999999525 ) ) ;
#51130 = ORIENTED_EDGE ( 'NONE', *, *, #51862, .F. ) ;
#51131 = EDGE_CURVE ( 'NONE', #38757, #33088, #57238, .T. ) ;
#51132 = CARTESIAN_POINT ( 'NONE',  ( 7.188101187499999156, 15.37499999795161187, 2.977408999572654924 ) ) ;
#51133 = LINE ( 'NONE', #51503, #36395 ) ;
#51134 = LINE ( 'NONE', #20967, #65589 ) ;
#51135 = CARTESIAN_POINT ( 'NONE',  ( 10.00000000000000000, 34.79166666666666430, 2.679491924311236062 ) ) ;
#51136 = CARTESIAN_POINT ( 'NONE',  ( -2.977408999572651815, 105.3125000020483668, 7.188101187500000933 ) ) ;
#51137 = DIRECTION ( 'NONE',  ( -0.000000000000000000, 1.000000000000000000, -0.000000000000000000 ) ) ;
#51138 = CARTESIAN_POINT ( 'NONE',  ( -6.676582343750001591, 290.4531250017069510, 0.000000000000000000 ) ) ;
#51140 = CARTESIAN_POINT ( 'NONE',  ( -7.999999999999998224, 95.28125000409677625, 3.313708498984766049 ) ) ;
#51139 = CARTESIAN_POINT ( 'NONE',  ( -23.99999999999998934, 201.7500000000000000, 170.0000000000003411 ) ) ;
#51141 = ORIENTED_EDGE ( 'NONE', *, *, #16399, .F. ) ;
#51142 = CARTESIAN_POINT ( 'NONE',  ( 3.042071309553163960, 252.4479166700806729, -11.35316468749999785 ) ) ;
#51143 = PRODUCT ( 'stud', 'stud', '', ( #44833 ) ) ;
#51144 = CARTESIAN_POINT ( 'NONE',  ( -2.977408999572647819, 7.188101187499991163, 21.08030278187175810 ) ) ;
#51145 = VECTOR ( 'NONE', #73866, 1000.000000000000000 ) ;
#51146 = CARTESIAN_POINT ( 'NONE',  ( -8.577559645643342279, 220.0000000000000284, 6.763852041043552532 ) ) ;
#51147 = CARTESIAN_POINT ( 'NONE',  ( 0.000000000000000000, 125.0000000000000000, 0.000000000000000000 ) ) ;
#51148 = CARTESIAN_POINT ( 'NONE',  ( 2.839093476692135984E-14, 196.9375000013655779, 201.4587341250000350 ) ) ;
#51149 =( BOUNDED_CURVE ( )  B_SPLINE_CURVE ( 2, ( #46616, #35322, #46981, #19055, #18694, #42058, #18321, #17950, #2078 ),
 .UNSPECIFIED., .F., .F. ) 
 B_SPLINE_CURVE_WITH_KNOTS ( ( 3, 2, 2, 2, 3 ),
 ( 0.9411764705882353921, 0.9448529411764706731, 0.9485294117647058432, 0.9522058823529411242, 0.9558823529411765163 ),
 .UNSPECIFIED. ) 
 CURVE ( )  GEOMETRIC_REPRESENTATION_ITEM ( )  RATIONAL_B_SPLINE_CURVE ( ( 0.9999999999999976685, 0.9238795325112890700, 1.000000000000000000, 0.9238795325112867385, 1.000000000000000000, 0.9238795325112867385, 1.000000000000000000, 0.9238795325112867385, 1.000000000000000000 ) ) 
 REPRESENTATION_ITEM ( '' )  );
#51150 = CARTESIAN_POINT ( 'NONE',  ( -4.999999999999998224, 166.6666666666666856, -8.660254037844389075 ) ) ;
#51151 = LINE ( 'NONE', #39830, #23295 ) ;
#51152 = CARTESIAN_POINT ( 'NONE',  ( 12.04876049975178631, 13.82825457289349558, -0.1850551574587529224 ) ) ;
#51153 =( BOUNDED_CURVE ( )  B_SPLINE_CURVE ( 2, ( #17386, #5709, #34400, #442, #45318, #27974, #23421, #34774, #68333, #57401, #28708, #11734, #28340 ),
 .UNSPECIFIED., .F., .F. ) 
 B_SPLINE_CURVE_WITH_KNOTS ( ( 3, 2, 2, 2, 2, 2, 3 ),
 ( 0.9402173913043480047, 0.9420289855072465635, 0.9438405797101451222, 0.9456521739130436810, 0.9474637681159421287, 0.9492753623188406875, 0.9510869565217392463 ),
 .UNSPECIFIED. ) 
 CURVE ( )  GEOMETRIC_REPRESENTATION_ITEM ( )  RATIONAL_B_SPLINE_CURVE ( ( 0.9999999999999957812, 0.9659258262890725311, 1.000000000000000000, 0.9659258262890683122, 1.000000000000000000, 0.9659258262890683122, 1.000000000000000000, 0.9659258262890683122, 1.000000000000000000, 0.9659258262890683122, 1.000000000000000000, 0.9659258262890662028, 1.000000000000001998 ) ) 
 REPRESENTATION_ITEM ( '' )  );
#51154 = CARTESIAN_POINT ( 'NONE',  ( -7.999999999999998224, 90.59375000000000000, 3.313708498984766493 ) ) ;
#51155 = CARTESIAN_POINT ( 'NONE',  ( -11.35316468750000141, 133.8020833299193555, 3.042071309553159963 ) ) ;
#51156 = CARTESIAN_POINT ( 'NONE',  ( 26.34314575050773755, 198.5625000000000000, 165.9999999999998010 ) ) ;
#51159 = CARTESIAN_POINT ( 'NONE',  ( 1.656854249492433206, 197.1875000000000284, 138.0000000000001705 ) ) ;
#51158 = CARTESIAN_POINT ( 'NONE',  ( 29.43265458321766204, 195.5000000013655779, 173.4587341249998929 ) ) ;
#51157 = CARTESIAN_POINT ( 'NONE',  ( 25.17157287525381903, 209.6250000000000284, 167.1715728752537018 ) ) ;
#51160 = ORIENTED_EDGE ( 'NONE', *, *, #53428, .T. ) ;
#51161 = CARTESIAN_POINT ( 'NONE',  ( 7.080414546044030644, 225.6242882639226082, -7.067909898757898546 ) ) ;
#51162 = DIRECTION ( 'NONE',  ( 0.000000000000000000, 0.000000000000000000, 1.000000000000000000 ) ) ;
#51163 = CARTESIAN_POINT ( 'NONE',  ( 11.00000000000000000, 1.347111479062088405E-15, 76.74999999999998579 ) ) ;
#51164 = CARTESIAN_POINT ( 'NONE',  ( 26.56734541678237704, 195.2500000013656063, 166.5412658749999650 ) ) ;
#51165 = CARTESIAN_POINT ( 'NONE',  ( 5.676582343750001591, 211.9270833299193555, -9.832129032723420536 ) ) ;
#51166 = CARTESIAN_POINT ( 'NONE',  ( -5.082755093536324154, 118.3437500020483810, 5.082755093536326818 ) ) ;
#51167 = CARTESIAN_POINT ( 'NONE',  ( -1.881053915767121554, 1.749999998634407250, -4.541265875000002339 ) ) ;
#51168 = CARTESIAN_POINT ( 'NONE',  ( -0.7509181236817221716, -55.63764137817485533, 43.81192498625236453 ) ) ;
#51169 = CARTESIAN_POINT ( 'NONE',  ( 3.313708498984762496, -7.999999999999989342, 19.29905277982336642 ) ) ;
#51170 = CARTESIAN_POINT ( 'NONE',  ( -30.82842712474624847, 208.2500000027312126, 167.1715728752542418 ) ) ;
#51171 = CARTESIAN_POINT ( 'NONE',  ( 11.35316468749999963, 90.98958332991935549, -3.042071309553165293 ) ) ;
#51172 = VERTEX_POINT ( 'NONE', #67541 ) ;
#51173 = DIRECTION ( 'NONE',  ( 0.000000000000000000, 0.000000000000000000, 1.000000000000000000 ) ) ;
#51174 = CARTESIAN_POINT ( 'NONE',  ( -5.082755093536326818, 26.90624999795161543, 5.082755093536325042 ) ) ;
#51175 = CARTESIAN_POINT ( 'NONE',  ( 12.00000000000000000, -6.928203230275538971, -14.80000000000000071 ) ) ;
#51176 = EDGE_CURVE ( 'NONE', #45762, #42810, #66621, .T. ) ;
#51178 = CARTESIAN_POINT ( 'NONE',  ( 5.676582343749997150, 262.5520833367473301, -9.832129032723418760 ) ) ;
#51177 = VECTOR ( 'NONE', #11445, 1000.000000000000000 ) ;
#51179 = CARTESIAN_POINT ( 'NONE',  ( 11.35316468749999963, 95.98958332991935549, -3.042071309553165293 ) ) ;
#51180 = ORIENTED_EDGE ( 'NONE', *, *, #10691, .T. ) ;
#51181 = CARTESIAN_POINT ( 'NONE',  ( 0.000000000000000000, 0.000000000000000000, -20.69999999999999929 ) ) ;
#51182 = CARTESIAN_POINT ( 'NONE',  ( 10.18810118749999916, 1.247682550866122264E-15, 104.4062500020483810 ) ) ;
#51183 = CARTESIAN_POINT ( 'NONE',  ( -4.999999999999998224, 218.5416666598387110, -8.660254037844389075 ) ) ;
#51184 = CARTESIAN_POINT ( 'NONE',  ( 2.839093476692135984E-14, 205.9375000013656063, 201.4587341250000350 ) ) ;
#51185 = DIRECTION ( 'NONE',  ( 1.000000000000000000, 2.701921919735176973E-32, -6.308085367188386297E-16 ) ) ;
#51187 = CARTESIAN_POINT ( 'NONE',  ( 11.35316468750000141, 105.7812499965860269, 0.000000000000000000 ) ) ;
#51186 = DIRECTION ( 'NONE',  ( -0.000000000000000000, 1.000000000000000000, -1.563033456626094573E-30 ) ) ;
#51188 = CARTESIAN_POINT ( 'NONE',  ( -5.656854249492373476, -5.656854249492376141, 11.70530278392014445 ) ) ;
#51189 = CARTESIAN_POINT ( 'NONE',  ( -31.45873412499997812, 201.0000000013655779, 171.4326545832180386 ) ) ;
#51190 = FACE_OUTER_BOUND ( 'NONE', #45273, .T. ) ;
#51191 = ORIENTED_EDGE ( 'NONE', *, *, #42128, .F. ) ;
#51192 = CARTESIAN_POINT ( 'NONE',  ( -8.660254037844390851, 184.7916666598387110, 4.999999999999998224 ) ) ;
#51193 = CARTESIAN_POINT ( 'NONE',  ( 4.000000000000000888, 5.937500000000000000, 1.656854249492384135 ) ) ;
#51194 = CARTESIAN_POINT ( 'NONE',  ( 2.385302041791413252, -46.82989226316983888, 139.0917130241418818 ) ) ;
#51195 = CARTESIAN_POINT ( 'NONE',  ( -2.085542519210945728E-15, 84.84374999658601268, 11.35316468750000141 ) ) ;
#51196 = CARTESIAN_POINT ( 'NONE',  ( -4.088227598258586603E-16, 291.2031250017069510, -6.676582343750001591 ) ) ;
#51197 = CARTESIAN_POINT ( 'NONE',  ( 2.977408999572650927, 4.124999997951610986, -7.188101187500000933 ) ) ;
#51198 = CARTESIAN_POINT ( 'NONE',  ( 4.220049686691934809, 10.18810118749999916, 102.0625000020483810 ) ) ;
#51199 = CARTESIAN_POINT ( 'NONE',  ( 11.35316468749999963, 225.9895833299193839, -3.042071309553165293 ) ) ;
#51200 = ORIENTED_EDGE ( 'NONE', *, *, #59781, .F. ) ;
#51201 = CARTESIAN_POINT ( 'NONE',  ( -2.828427124746190735, 2.375000000000000000, -2.828427124746191623 ) ) ;
#51202 = DIRECTION ( 'NONE',  ( -0.000000000000000000, 1.000000000000000000, -0.000000000000000000 ) ) ;
#51203 = CARTESIAN_POINT ( 'NONE',  ( 2.128287106641264010E-14, -42.00000000000000711, 139.0000000000000568 ) ) ;
#51204 = CARTESIAN_POINT ( 'NONE',  ( 5.676582343749993598, 219.9479166632526983, 9.832129032723422313 ) ) ;
#51205 = CARTESIAN_POINT ( 'NONE',  ( 10.00000000000000178, 225.4166666734946602, 2.679491924311222739 ) ) ;
#51206 = CARTESIAN_POINT ( 'NONE',  ( -5.000000000000097700, 158.3333333333334565, 8.660254037844545394 ) ) ;
#51207 = CARTESIAN_POINT ( 'NONE',  ( 6.676582343750003368, 298.0156250017070079, -2.765530957081997254 ) ) ;
#51208 = ORIENTED_EDGE ( 'NONE', *, *, #9530, .F. ) ;
#51209 = CARTESIAN_POINT ( 'NONE',  ( 6.951808397369818766E-16, 192.3437499965860127, -11.35316468750000141 ) ) ;
#51210 = ADVANCED_FACE ( 'NONE', ( #43393, #55482 ), #31715, .T. ) ;
#51211 = EDGE_CURVE ( 'NONE', #51876, #61876, #3417, .T. ) ;
#51212 = CARTESIAN_POINT ( 'NONE',  ( -4.220049686691937474, -10.18810118749999738, 97.93750000204836681 ) ) ;
#51213 = COLOUR_RGB ( '',0.7921568627450980005, 0.8196078431372548767, 0.9333333333333333481 ) ;
#51214 = CARTESIAN_POINT ( 'NONE',  ( -30.44569435410879521, 205.8125000013656063, 172.4456943541092357 ) ) ;
#51215 = CARTESIAN_POINT ( 'NONE',  ( -8.000000000000000000, 20.25000000000000355, -9.797174393178825657E-16 ) ) ;
#51216 = ORIENTED_EDGE ( 'NONE', *, *, #5578, .T. ) ;
#51217 = ADVANCED_FACE ( 'NONE', ( #25661 ), #50180, .T. ) ;
#51218 = CARTESIAN_POINT ( 'NONE',  ( 8.000000000000000000, 89.93750000409677625, -9.797174393178825657E-16 ) ) ;
#51219 = CARTESIAN_POINT ( 'NONE',  ( -5.952395412842847122, -17.34799259689866702, -0.1532218116813779951 ) ) ;
#51220 = CARTESIAN_POINT ( 'NONE',  ( 7.320508075688774596, 20.62499999999999289, -7.320508075688774596 ) ) ;
#51221 = CARTESIAN_POINT ( 'NONE',  ( -4.220049686691935698, 10.18810118749999916, 82.75000000204838102 ) ) ;
#51222 = ORIENTED_EDGE ( 'NONE', *, *, #10232, .F. ) ;
#51223 = CARTESIAN_POINT ( 'NONE',  ( 2.828427124746191623, 19.12500000000000000, -2.828427124746191623 ) ) ;
#51224 = CARTESIAN_POINT ( 'NONE',  ( 23.99999999999997868, 198.8125000027312126, 168.3431457505075457 ) ) ;
#51225 = CARTESIAN_POINT ( 'NONE',  ( 1.656854249492381248, 4.937499997268813168, -4.000000000000001776 ) ) ;
#51226 = CARTESIAN_POINT ( 'NONE',  ( 5.082755093536325042, 122.4687500020483952, -5.082755093536325930 ) ) ;
#51227 = EDGE_CURVE ( 'NONE', #69151, #31186, #10501, .T. ) ;
#51228 = CARTESIAN_POINT ( 'NONE',  ( 4.999999999999999112, -66.11467145570902915, 23.67355326543016858 ) ) ;
#51231 = CARTESIAN_POINT ( 'NONE',  ( -2.751064625579944321E-14, 199.8750000027312126, 146.0000000000000284 ) ) ;
#51230 = CARTESIAN_POINT ( 'NONE',  ( -3.042071309553159075, 249.9479166700806729, 11.35316468749999963 ) ) ;
#51229 = CARTESIAN_POINT ( 'NONE',  ( 27.99999999999997158, 205.9375000013656063, 166.5412658749999082 ) ) ;
#51232 = APPLICATION_PROTOCOL_DEFINITION ( 'draft international standard', 'automotive_design', 1998, #61683 ) ;
#51233 = VERTEX_POINT ( 'NONE', #37755 ) ;
#51234 = CARTESIAN_POINT ( 'NONE',  ( 11.35316468749999608, 246.9270833367472733, -3.042071309553167069 ) ) ;
#51235 = CARTESIAN_POINT ( 'NONE',  ( -7.188101187499992051, 0.000000000000000000, 14.98655278187175455 ) ) ;
#51236 = ORIENTED_EDGE ( 'NONE', *, *, #16314, .T. ) ;
#51237 = ORIENTED_EDGE ( 'NONE', *, *, #21654, .T. ) ;
#51238 = CARTESIAN_POINT ( 'NONE',  ( 4.220049686691941027, -10.18810118749999738, 74.12500000204836681 ) ) ;
#51239 = CARTESIAN_POINT ( 'NONE',  ( -8.311093377946836114, 87.96874999658602690, -8.311093377946837890 ) ) ;
#51240 = DIRECTION ( 'NONE',  ( -0.000000000000000000, -1.000000000000000000, -4.283267841918042741E-17 ) ) ;
#51241 = CARTESIAN_POINT ( 'NONE',  ( -4.556349186104047710, -10.99999999999999822, 83.78125000000000000 ) ) ;
#51244 = CARTESIAN_POINT ( 'NONE',  ( -6.676582343750002480, 291.5468750017069510, -2.765530957081996810 ) ) ;
#51243 = CARTESIAN_POINT ( 'NONE',  ( 24.54126587499998635, 209.1250000013656631, 168.5673454167822740 ) ) ;
#51242 = CARTESIAN_POINT ( 'NONE',  ( 31.45873412499999944, 205.9375000013656063, 169.9999999999999432 ) ) ;
#51245 = CARTESIAN_POINT ( 'NONE',  ( -60.51222946527267510, 219.8985979011596044, 46.02364178679460593 ) ) ;
#51246 = DIRECTION ( 'NONE',  ( 0.000000000000000000, 0.000000000000000000, 1.000000000000000000 ) ) ;
#51247 = AXIS2_PLACEMENT_3D ( 'NONE', #69015, #73551, #4907 ) ;
#51248 =( BOUNDED_CURVE ( )  B_SPLINE_CURVE ( 2, ( #20870, #15579, #72937, #20489, #50659, #38619, #43506, #37491, #67654 ),
 .UNSPECIFIED., .F., .F. ) 
 B_SPLINE_CURVE_WITH_KNOTS ( ( 3, 2, 2, 2, 3 ),
 ( 0.8020833333333334814, 0.8072916666666667407, 0.8125000000000001110, 0.8177083333333334814, 0.8229166666666667407 ),
 .UNSPECIFIED. ) 
 CURVE ( )  GEOMETRIC_REPRESENTATION_ITEM ( )  RATIONAL_B_SPLINE_CURVE ( ( 0.9999999999999983347, 0.9238795325112884038, 1.000000000000000000, 0.9238795325112867385, 1.000000000000000000, 0.9238795325112867385, 1.000000000000000000, 0.9238795325112850731, 1.000000000000001554 ) ) 
 REPRESENTATION_ITEM ( '' )  );
#51249 = CARTESIAN_POINT ( 'NONE',  ( -3.042071309553173730, 194.3229166632526699, 11.35316468749999785 ) ) ;
#51250 = CARTESIAN_POINT ( 'NONE',  ( 8.000000000000000000, 8.812499995903221972, 0.000000000000000000 ) ) ;
#51251 = ORIENTED_EDGE ( 'NONE', *, *, #4638, .T. ) ;
#51252 = CARTESIAN_POINT ( 'NONE',  ( 30.44569435410883074, 195.8125000013656063, 167.5543056458911053 ) ) ;
#51253 = CARTESIAN_POINT ( 'NONE',  ( -2.977408999572654480, 19.87499999795161543, 7.188101187499999156 ) ) ;
#51254 = CARTESIAN_POINT ( 'NONE',  ( 3.042071309553167069, 167.1354166632526415, -11.35316468749999785 ) ) ;
#51255 = CARTESIAN_POINT ( 'NONE',  ( 3.313708498984762496, 7.218750000000000888, 7.999999999999998224 ) ) ;
#51256 = CARTESIAN_POINT ( 'NONE',  ( 5.082755093536326818, 101.0937500020483810, 5.082755093536325042 ) ) ;
#51258 = CARTESIAN_POINT ( 'NONE',  ( -7.320508075688773708, 88.74999999317202537, -7.320508075688774596 ) ) ;
#51257 = CARTESIAN_POINT ( 'NONE',  ( 0.000000000000000000, 300.0000000000000000, 10.00000000000000178 ) ) ;
#51259 = CARTESIAN_POINT ( 'NONE',  ( 24.54126587499998280, 205.5000000013655779, 171.4326545832175555 ) ) ;
#51260 = CARTESIAN_POINT ( 'NONE',  ( -2.977408999572648707, -7.188101187499990274, 11.14280278187175810 ) ) ;
#51261 = CARTESIAN_POINT ( 'NONE',  ( 8.311093377946837890, 51.40624999658602690, -8.311093377946837890 ) ) ;
#51262 = CARTESIAN_POINT ( 'NONE',  ( 5.656854249492376141, -5.656854249492374365, 1.580302783920146226 ) ) ;
#51263 = CARTESIAN_POINT ( 'NONE',  ( -5.656854249492378806, 119.3750000040967905, 5.656854249492381470 ) ) ;
#51264 = ORIENTED_EDGE ( 'NONE', *, *, #66753, .T. ) ;
#51265 = CARTESIAN_POINT ( 'NONE',  ( -7.999999999971585396, 1.424435121157765920E-05, 7.017269882810325932 ) ) ;
#51266 = CARTESIAN_POINT ( 'NONE',  ( -3.313708498984805573, 23.34374999590321664, 7.999999999999956479 ) ) ;
#51267 = CARTESIAN_POINT ( 'NONE',  ( 8.311093377946837890, 61.40624999658602690, -8.311093377946837890 ) ) ;
#51268 = CARTESIAN_POINT ( 'NONE',  ( -10.99999999999999822, -4.556349186104052151, 73.28125000409677625 ) ) ;
#51269 = CARTESIAN_POINT ( 'NONE',  ( 3.458734124999959469, 201.7500000013655779, 140.5673454167823593 ) ) ;
#51270 = PLANE ( 'NONE',  #45591 ) ;
#51271 = CARTESIAN_POINT ( 'NONE',  ( 2.828427124746209831, 207.3750000000000284, 200.8284271247462129 ) ) ;
#51273 = CARTESIAN_POINT ( 'NONE',  ( -3.042071309553163960, 62.23958332991934128, -11.35316468749999963 ) ) ;
#51272 = CARTESIAN_POINT ( 'NONE',  ( -4.401442555609581635E-16, 95.28125000204836681, -7.188101187500000044 ) ) ;
#51274 = CARTESIAN_POINT ( 'NONE',  ( 5.656854249492376141, -5.656854249492374365, 5.892802779823364645 ) ) ;
#51275 = CARTESIAN_POINT ( 'NONE',  ( -10.00000000000000355, 14.58333332650536462, 2.679491924311223183 ) ) ;
#51276 = CARTESIAN_POINT ( 'NONE',  ( -3.042071309553173730, 169.3229166632526699, 11.35316468749999785 ) ) ;
#51277 =( BOUNDED_CURVE ( )  B_SPLINE_CURVE ( 2, ( #53037, #2458, #24353, #19424, #47362, #41710, #13020, #7384, #70746 ),
 .UNSPECIFIED., .F., .F. ) 
 B_SPLINE_CURVE_WITH_KNOTS ( ( 3, 2, 2, 2, 3 ),
 ( 0.4333333333333336812, 0.4416666666666669849, 0.4500000000000003997, 0.4583333333333337034, 0.4666666666666670626 ),
 .UNSPECIFIED. ) 
 CURVE ( )  GEOMETRIC_REPRESENTATION_ITEM ( )  RATIONAL_B_SPLINE_CURVE ( ( 0.9999999999999970024, 0.9238795325112897361, 1.000000000000000000, 0.9238795325112867385, 1.000000000000000000, 0.9238795325112867385, 1.000000000000000000, 0.9238795325112831858, 1.000000000000003553 ) ) 
 REPRESENTATION_ITEM ( '' )  );
#51278 = CARTESIAN_POINT ( 'NONE',  ( -7.320508075688773708, 138.7499999931720254, -7.320508075688774596 ) ) ;
#51279 = CARTESIAN_POINT ( 'NONE',  ( 7.188101187500002709, 104.1875000020483668, 2.977408999572649151 ) ) ;
#51280 = CARTESIAN_POINT ( 'NONE',  ( -2.603585389454555976, -46.50326054477230286, 139.1093334085009303 ) ) ;
#51281 = CARTESIAN_POINT ( 'NONE',  ( -11.35316468750000141, 33.80208332991935549, 3.042071309553159963 ) ) ;
#51282 = CARTESIAN_POINT ( 'NONE',  ( -3.673940397442060854E-16, 295.8125000034140157, -6.000000000000001776 ) ) ;
#51283 = CARTESIAN_POINT ( 'NONE',  ( -9.832129032723420536, 188.6979166632526983, 5.676582343749997150 ) ) ;
#51284 = ORIENTED_EDGE ( 'NONE', *, *, #37058, .T. ) ;
#51285 = CARTESIAN_POINT ( 'NONE',  ( 49.58482923361744099, 136.4532658507989140, 58.24946605281415657 ) ) ;
#51286 = CARTESIAN_POINT ( 'NONE',  ( 7.204075437095968759, -7.204075437095966983, 74.21875000204836681 ) ) ;
#51287 = CARTESIAN_POINT ( 'NONE',  ( 2.828427124746208943, 196.6250000000000284, 195.1715728752538439 ) ) ;
#51288 = CARTESIAN_POINT ( 'NONE',  ( 34.77943304252697487, 39.95293522172878653, 65.00000000000001421 ) ) ;
#51290 = CARTESIAN_POINT ( 'NONE',  ( 3.042071309553159519, 159.7395833299193555, 11.35316468750000141 ) ) ;
#51289 = CARTESIAN_POINT ( 'NONE',  ( 2.828427124746191623, 18.87499999726881228, -2.828427124746191623 ) ) ;
#51291 = CARTESIAN_POINT ( 'NONE',  ( -7.999999999999989342, -3.313708498984762496, 5.480302784329825094 ) ) ;
#51292 = CARTESIAN_POINT ( 'NONE',  ( 11.00000000000000000, 1.347111479062088405E-15, 79.93750000409677625 ) ) ;
#51293 = CARTESIAN_POINT ( 'NONE',  ( 2.679491924311225848, 261.6666666734946602, -10.00000000000000000 ) ) ;
#51294 = DIRECTION ( 'NONE',  ( -0.000000000000000000, -0.000000000000000000, 1.000000000000000000 ) ) ;
#51295 = ORIENTED_EDGE ( 'NONE', *, *, #62415, .F. ) ;
#51296 =( BOUNDED_CURVE ( )  B_SPLINE_CURVE ( 2, ( #61783, #27435, #39883, #10101, #73099, #45537, #50086, #4078, #68186 ),
 .UNSPECIFIED., .F., .F. ) 
 B_SPLINE_CURVE_WITH_KNOTS ( ( 3, 2, 2, 2, 3 ),
 ( 0.01136363636363636395, 0.01704545454545454419, 0.02272727272727272790, 0.02840909090909090814, 0.03409090909090908839 ),
 .UNSPECIFIED. ) 
 CURVE ( )  GEOMETRIC_REPRESENTATION_ITEM ( )  RATIONAL_B_SPLINE_CURVE ( ( 1.000000000000000000, 0.9238795325112867385, 1.000000000000000000, 0.9238795325112867385, 1.000000000000000000, 0.9238795325112867385, 1.000000000000000000, 0.9238795325112867385, 1.000000000000000000 ) ) 
 REPRESENTATION_ITEM ( '' )  );
#51297 = DIRECTION ( 'NONE',  ( 0.000000000000000000, 0.000000000000000000, 1.000000000000000000 ) ) ;
#51298 = CARTESIAN_POINT ( 'NONE',  ( -9.832129032723420536, 114.0104166632526983, 5.676582343749997150 ) ) ;
#51299 = CARTESIAN_POINT ( 'NONE',  ( 7.320508075688774596, 12.49999999317203425, -7.320508075688774596 ) ) ;
#51300 = ORIENTED_EDGE ( 'NONE', *, *, #25602, .T. ) ;
#51301 = CARTESIAN_POINT ( 'NONE',  ( 4.541265875000001451, 8.374999998634406140, 1.881053915767124440 ) ) ;
#51302 = EDGE_CURVE ( 'NONE', #20100, #63756, #8323, .T. ) ;
#51303 = CARTESIAN_POINT ( 'NONE',  ( 5.082755093536325930, 15.65624999795161365, -5.082755093536325930 ) ) ;
#51304 =( GEOMETRIC_REPRESENTATION_CONTEXT ( 3 ) GLOBAL_UNCERTAINTY_ASSIGNED_CONTEXT ( ( #40549 ) ) GLOBAL_UNIT_ASSIGNED_CONTEXT ( ( #52528, #35922, #64944 ) ) REPRESENTATION_CONTEXT ( 'NONE', 'WORKASPACE' ) );
#51305 = CARTESIAN_POINT ( 'NONE',  ( 8.000000000000001776, 109.3437500040967905, 3.313708498984759387 ) ) ;
#51306 = EDGE_CURVE ( 'NONE', #25296, #4993, #43014, .T. ) ;
#51307 = CARTESIAN_POINT ( 'NONE',  ( -25.55430564589115150, 198.3125000013656063, 172.4456943541091789 ) ) ;
#51308 = VECTOR ( 'NONE', #58570, 1000.000000000000000 ) ;
#51309 = CARTESIAN_POINT ( 'NONE',  ( -2.828427124746192067, 6.625000000000000000, 2.828427124746190735 ) ) ;
#51310 = CARTESIAN_POINT ( 'NONE',  ( -4.000000000000001776, 22.18749999726881583, -1.656854249492381470 ) ) ;
#51311 = CARTESIAN_POINT ( 'NONE',  ( 4.541265875000002339, 7.374999998634407916, -1.881053915767121776 ) ) ;
#51312 = CARTESIAN_POINT ( 'NONE',  ( -2.828427124746208943, 197.6250000000000284, 144.8284271247462129 ) ) ;
#51313 = ORIENTED_EDGE ( 'NONE', *, *, #70879, .F. ) ;
#51314 = CARTESIAN_POINT ( 'NONE',  ( 10.92737078412413609, 225.9999999999999147, -3.080083792328916825 ) ) ;
#51315 = CARTESIAN_POINT ( 'NONE',  ( 7.188101187500002709, 102.3125000020483810, 2.977408999572649151 ) ) ;
#51316 = ADVANCED_FACE ( 'NONE', ( #14343 ), #26030, .T. ) ;
#51318 = LINE ( 'NONE', #74328, #68349 ) ;
#51317 = CARTESIAN_POINT ( 'NONE',  ( -31.45873412499999233, 194.6875000013655779, 170.0000000000004547 ) ) ;
#51319 =( LENGTH_UNIT ( ) NAMED_UNIT ( * ) SI_UNIT ( .MILLI., .METRE. ) );
#51320 = CARTESIAN_POINT ( 'NONE',  ( -4.541265875000003227, 20.87499999863441147, 1.881053915767121110 ) ) ;
#51321 = CARTESIAN_POINT ( 'NONE',  ( 5.082755093536320601, -5.082755093536318824, 2.049052781871754103 ) ) ;
#51322 = EDGE_LOOP ( 'NONE', ( #65129, #2830, #50714, #4021 ) ) ;
#51323 = ORIENTED_EDGE ( 'NONE', *, *, #48597, .T. ) ;
#51324 = CARTESIAN_POINT ( 'NONE',  ( 1.871523826299183495E-15, -10.18810118749999916, 93.53125000204836681 ) ) ;
#51325 = FACE_OUTER_BOUND ( 'NONE', #13604, .T. ) ;
#51326 = CARTESIAN_POINT ( 'NONE',  ( -31.45873412499999944, 201.9375000013656063, 170.0000000000003979 ) ) ;
#51327 = CARTESIAN_POINT ( 'NONE',  ( -7.778174593052023411, 7.778174593052023411, 105.8124999999999858 ) ) ;
#51328 = CARTESIAN_POINT ( 'NONE',  ( 3.458734125000016757, 204.1250000013656063, 199.4326545832176691 ) ) ;
#51330 = CARTESIAN_POINT ( 'NONE',  ( 1.734723475976807489E-15, -16.00000000000000355, 38.34805510287551300 ) ) ;
#51329 = CARTESIAN_POINT ( 'NONE',  ( 23.99999999999997868, 202.8125000027312126, 168.3431457505075457 ) ) ;
#51331 = CARTESIAN_POINT ( 'NONE',  ( 7.320508075688771044, 119.3750000000000142, 7.320508075688775484 ) ) ;
#51332 = B_SPLINE_CURVE_WITH_KNOTS ( 'NONE', 3,
 ( #59927, #8241, #31631, #4089, #32765, #54651, #67080, #60671, #55399, #31252, #44071, #43310 ),
 .UNSPECIFIED., .F., .F.,
 ( 4, 2, 2, 2, 2, 4 ),
 ( 0.000000000000000000, 0.002547658444427994794, 0.005095316888855989587, 0.006369146111069987418, 0.007642975333283985248, 0.01019063377771197744 ),
 .UNSPECIFIED. ) ;
#51333 = CARTESIAN_POINT ( 'NONE',  ( 8.000000000000000000, 106.3437500000000000, -3.313708498984762496 ) ) ;
#51334 = CARTESIAN_POINT ( 'NONE',  ( 4.721056650415999201, 288.2343750017069510, -4.721056650415999201 ) ) ;
#51335 = CARTESIAN_POINT ( 'NONE',  ( -4.401442555609577197E-16, 7.188101187499992051, 5.986552781871753659 ) ) ;
#51336 = CARTESIAN_POINT ( 'NONE',  ( -5.656854249492380582, 102.5000000040967905, -5.656854249492380582 ) ) ;
#51337 = CARTESIAN_POINT ( 'NONE',  ( 25.55430564589119768, 206.0625000013656063, 167.5543056458910485 ) ) ;
#51338 = CARTESIAN_POINT ( 'NONE',  ( -3.313708498984765161, 27.84374999590322375, 7.999999999999998224 ) ) ;
#51339 = CARTESIAN_POINT ( 'NONE',  ( 2.445694354108782775, 198.5625000013656063, 139.5543056458912190 ) ) ;
#51340 = CARTESIAN_POINT ( 'NONE',  ( 7.188101187500002709, 122.1875000020483810, 2.977408999572649151 ) ) ;
#51341 = CARTESIAN_POINT ( 'NONE',  ( 3.742616585878813851, 194.7527601235051691, 198.3689192493877158 ) ) ;
#51342 = CARTESIAN_POINT ( 'NONE',  ( 9.832129032723420536, 246.3020833367473301, 5.676582343749996262 ) ) ;
#51343 = CARTESIAN_POINT ( 'NONE',  ( 30.82842712474616675, 198.1250000000000284, 172.8284271247460993 ) ) ;
#51344 = CARTESIAN_POINT ( 'NONE',  ( -5.676582343749998039, 17.44791666325268409, -9.832129032723420536 ) ) ;
#51345 = CARTESIAN_POINT ( 'NONE',  ( 2.679491924305073436, 1.041666666667218299, -10.00000000000355094 ) ) ;
#51346 = CARTESIAN_POINT ( 'NONE',  ( 9.832129032723416984, 210.6770833299193555, 5.676582343750006032 ) ) ;
#51347 = CARTESIAN_POINT ( 'NONE',  ( -24.00000000000000355, 196.8125000000000284, 168.3431457505080004 ) ) ;
#51348 = CARTESIAN_POINT ( 'NONE',  ( -11.00000000000000000, 0.000000000000000000, 103.1875000040967763 ) ) ;
#51350 = CARTESIAN_POINT ( 'NONE',  ( 5.656854249492374365, 5.656854249492375253, 28.76780277982336642 ) ) ;
#51349 = CARTESIAN_POINT ( 'NONE',  ( 3.999999999999960032, 203.0625000027311842, 143.6568542494924259 ) ) ;
#51351 = ORIENTED_EDGE ( 'NONE', *, *, #70144, .F. ) ;
#51352 = CARTESIAN_POINT ( 'NONE',  ( 3.458734124999959469, 201.7500000013655779, 140.5673454167824161 ) ) ;
#51353 = CARTESIAN_POINT ( 'NONE',  ( 11.35316468749999963, 25.98958332991935194, -3.042071309553165293 ) ) ;
#51354 = CARTESIAN_POINT ( 'NONE',  ( 4.556349186104045934, 11.00000000000000000, 93.71875000409676204 ) ) ;
#51355 =( GEOMETRIC_REPRESENTATION_CONTEXT ( 3 ) GLOBAL_UNCERTAINTY_ASSIGNED_CONTEXT ( ( #581 ) ) GLOBAL_UNIT_ASSIGNED_CONTEXT ( ( #26051, #31737, #49072 ) ) REPRESENTATION_CONTEXT ( 'NONE', 'WORKASPACE' ) );
#51356 = CARTESIAN_POINT ( 'NONE',  ( 2.679491924311082407, 211.0416666666666572, -10.00000000000008349 ) ) ;
#51357 = CARTESIAN_POINT ( 'NONE',  ( -31.45873412500002075, 198.6250000013656063, 168.5673454167828140 ) ) ;
#51358 = LINE ( 'NONE', #63417, #5749 ) ;
#51360 = CARTESIAN_POINT ( 'NONE',  ( -11.35316468750000141, 8.489583329919348387, 3.042071309553159963 ) ) ;
#51359 = CARTESIAN_POINT ( 'NONE',  ( 2.977408999572654480, 114.1250000020483952, 7.188101187499999156 ) ) ;
#51361 = CARTESIAN_POINT ( 'NONE',  ( -4.898587196589407898E-16, 7.999999999999991118, 18.45530277982336642 ) ) ;
#51362 = CARTESIAN_POINT ( 'NONE',  ( 8.311093377946834337, 130.1562499965860411, 8.311093377946839666 ) ) ;
#51363 = CARTESIAN_POINT ( 'NONE',  ( 10.00000000000000000, 96.66666665983871098, 2.679491924311236062 ) ) ;
#51364 = CARTESIAN_POINT ( 'NONE',  ( 2.977408999572654480, 123.5000000020483952, 7.188101187499999156 ) ) ;
#51365 = CARTESIAN_POINT ( 'NONE',  ( 2.170320029194602984, 67.76782500014425636, -20.17643218080212719 ) ) ;
#51366 = CARTESIAN_POINT ( 'NONE',  ( -25.55430564589115505, 209.3125000013656063, 172.4456943541091789 ) ) ;
#51367 = LINE ( 'NONE', #16649, #41391 ) ;
#51368 = EDGE_LOOP ( 'NONE', ( #36519, #32655 ) ) ;
#51369 = CARTESIAN_POINT ( 'NONE',  ( -10.00000000000000533, 117.2916666666666714, -2.679491924311231177 ) ) ;
#51370 =( BOUNDED_SURFACE ( )  B_SPLINE_SURFACE ( 1, 2, ( 
 ( #23416, #52837, #34769, #70194, #18502, #41511, #68696, #63778, #69817, #64154, #63034, #29458, #23791, #11359, #52467, #46795, #74352, #11729, #804, #18133, #5703, #69445, #22662, #12463, #40770, #69075, #40405, #57771, #64527, #52104, #57021, #63403, #6076, #5334, #12095, #45681, #40032, #29084, #436, #46431, #17756, #14301, #19969, #25987, #24879, #53578, #60335, #13922, #1892, #66371, #70553, #43353, #19231, #31294, #13189, #49012, #2258, #24523, #8285, #64888, #18869, #72022, #65996, #71276, #53209, #8663, #30192, #19595, #53945, #36594, #36227, #59244, #7555, #20336, #31678, #54697, #42975, #42238, #54325, #70918, #37337, #65251, #7186, #36961, #3006, #13556, #71648, #35860, #30562, #59605, #2636, #30923, #42611, #7918, #59967, #25624, #65625, #25252, #47898, #1543, #47528, #48638, #41875, #58875, #48269, #73158, #4138, #50143, #50509, #45232, #3754, #4503, #66749, #44863, #67868, #33561, #21466, #14677, #9037, #72407, #72789, #37716, #55444, #38462, #61465, #44488, #15800, #60716, #27496, #55820, #16161, #67128, #56565, #4880, #50886, #26366, #67501, #73523, #21830, #20718, #38835, #56191, #43735, #61838, #39202, #32050, #44119, #10157, #33194, #15055, #27128, #55070, #62204, #10529, #26755, #38089, #15423, #27875, #9790, #73900, #49773, #61086, #3379, #22205, #49388, #9415, #32433, #21096, #32812, #35418, #46710, #52387, #58428, #57312, #11276, #18050, #46345, #34308, #24068, #28252, #1091, #51636, #63691, #45599, #6736, #34681, #56936, #40689, #22579, #51260, #29740, #23706, #52015, #11646, #68989, #68614, #16923, #39946, #52755, #64075, #41065, #723, #65876, #12018, #68244, #69735, #5252, #57687, #69362, #62951, #12383, #16536, #353, #17672, #39577, #5623, #23333, #5995, #62572, #10903, #28623, #33937, #22967, #28997, #45974, #35051, #74270, #17298, #40316, #63320, #58063, #6374, #29380, #36145, #7475, #2919, #47451, #64447, #30480, #53129, #60249, #8575, #64807, #14215, #1462, #59889, #71193, #12748, #7104, #37254, #65165, #65544, #48186, #35779, #31214, #19149, #41798, #31591, #58794, #19512, #24443, #65909, #42530, #13476, #25169, #53863, #18421, #54612, #47814, #41435, #53497, #70475, #13836, #30112, #47078, #70115, #36881, #1814, #18793, #13109, #59166, #24800, #19884, #70837, #42152, #2548, #36515, #8202, #59524, #30842, #7837, #2175, #54239, #25539, #48552, #71562, #42890, #3664, #8950, #50423, #21003, #32346, #31962, #10441, #9704 ),
 ( #66284, #21375, #60628, #43269, #73437, #20249, #14965, #61000, #56473, #26280, #14591, #9326, #54987, #39113, #62117, #43647, #67787, #3294, #38753, #50053, #37630, #49301, #16079, #44029, #44399, #27042, #72318, #10071, #72702, #20631, #33471, #66658, #73069, #38002, #44773, #67413, #67038, #4050, #32725, #71937, #25907, #26664, #55359, #49687, #15337, #15711, #38372, #48924, #61377, #61753, #55733, #33106, #56103, #4412, #27407, #21745, #16823, #12295, #34959, #50795, #40599, #28530, #63227, #68521, #51538, #16449, #17957, #74555, #40975, #69270, #57215, #62481, #29286, #22867, #11188, #10811, #63982, #11554, #260, #45881, #68895, #46251, #11927, #33845, #51922, #62852, #5904, #45140, #23243, #39485, #22116, #52296, #73808, #34588, #17205, #5529, #56843, #5164, #28158, #35330, #632, #23613, #57974, #34213, #17581, #69643, #6279, #51169, #40224, #57594, #74178, #46623, #4789, #28904, #63600, #27782, #45503, #68152, #22482, #39851, #29649, #30022, #71470, #47361, #24712, #70387, #19063, #41343, #6646, #58342, #13749, #13386, #65452, #19796, #13019, #7750, #2085, #12656, #70745, #23981, #71103, #42065, #18702, #64353, #59074, #25450, #53409, #42436, #41709, #35687, #52664, #65073, #1000, #46989, #58702, #7013, #30755, #48465, #36792, #59802, #42802, #64723, #1367, #8115, #36424, #24352, #14126, #18328, #65819, #36057, #53776, #53036, #70022, #47724, #7383, #25077, #30390, #1732, #59438, #31120, #48094, #19423, #54148, #2457, #54894, #2827, #67326, #61665, #3578, #31501, #31873, #60537, #3960, #3205, #8863, #20537, #44311, #43551, #8481, #38284, #21288, #72222, #72982, #15623, #66194, #14874, #32636, #32255, #43937, #9233, #61289, #9616, #66946, #66565, #26193, #54522, #25819, #20916, #48838, #67700, #37913, #15250, #26570, #72610, #38663, #37160, #49213, #26949, #14498, #9984, #33015, #56016, #55645, #60162, #71844, #20161, #60910, #43178, #55273, #49594, #49967, #4328, #27317, #37537, #50333, #73355, #21659, #44684, #57881, #34875, #52209, #27694, #22771, #28812, #176, #22031, #68804, #57511, #45056, #17116, #5817, #10355, #62031, #40138, #23152, #51081, #51830, #46164, #68068, #68430, #11472, #11104, #45794, #62761, #63144, #34506, #69182, #22393, #39395, #33379, #56380, #74463, #4701, #46538, #45414, #17493, #5442, #51450, #40512, #15997, #5076, #63516, #16357, #11839, #6188, #29197, #542, #39026, #50703, #73721, #74095, #62394, #56756, #39759, #34127 ) ),
 .UNSPECIFIED., .F., .F., .F. ) 
 B_SPLINE_SURFACE_WITH_KNOTS ( ( 2, 2 ),
 ( 3, 2, 2, 2, 2, 2, 2, 2, 2, 2, 2, 2, 2, 2, 2, 2, 2, 2, 2, 2, 2, 2, 2, 2, 2, 2, 2, 2, 2, 2, 2, 2, 2, 2, 2, 2, 2, 2, 2, 2, 2, 2, 2, 2, 2, 2, 2, 2, 2, 2, 2, 2, 2, 2, 2, 2, 2, 2, 2, 2, 2, 2, 2, 2, 2, 2, 2, 2, 2, 2, 2, 2, 2, 2, 2, 2, 2, 2, 2, 2, 2, 2, 2, 2, 2, 2, 2, 2, 2, 2, 2, 2, 2, 2, 2, 2, 2, 2, 2, 2, 2, 2, 2, 2, 2, 2, 2, 2, 2, 2, 2, 2, 2, 2, 2, 2, 2, 2, 2, 2, 2, 2, 2, 2, 2, 2, 2, 2, 2, 2, 2, 2, 2, 2, 2, 2, 2, 2, 2, 2, 2, 2, 2, 2, 2, 2, 2, 2, 2, 2, 2, 2, 3 ),
 ( 0.000000000000000000, 1.000000000000000000 ),
 ( 0.000000000000000000, 0.006578947368421052266, 0.01315789473684210453, 0.01973684210526315680, 0.02631578947368420907, 0.03289473684210526133, 0.03947368421052631360, 0.04605263157894736586, 0.05263157894736841813, 0.05921052631578947040, 0.06578947368421052266, 0.07236842105263158187, 0.07894736842105262720, 0.08552631578947368640, 0.09210526315789473173, 0.09868421052631579093, 0.1052631578947368363, 0.1118421052631578955, 0.1184210526315789408, 0.1250000000000000000, 0.1315789473684210453, 0.1381578947368421184, 0.1447368421052631637, 0.1513157894736842091, 0.1578947368421052544, 0.1644736842105263275, 0.1710526315789473728, 0.1776315789473684181, 0.1842105263157894635, 0.1907894736842105365, 0.1973684210526315819, 0.2039473684210526272, 0.2105263157894736725, 0.2171052631578947456, 0.2236842105263157909, 0.2302631578947368363, 0.2368421052631578816, 0.2434210526315789547, 0.2500000000000000000, 0.2565789473684210731, 0.2631578947368420907, 0.2697368421052631637, 0.2763157894736842368, 0.2828947368421052544, 0.2894736842105263275, 0.2960526315789473450, 0.3026315789473684181, 0.3092105263157894912, 0.3157894736842105088, 0.3223684210526315819, 0.3289473684210526550, 0.3355263157894736725, 0.3421052631578947456, 0.3486842105263157632, 0.3552631578947368363, 0.3618421052631579093, 0.3684210526315789269, 0.3750000000000000000, 0.3815789473684210731, 0.3881578947368420907, 0.3947368421052631637, 0.4013157894736842368, 0.4078947368421052544, 0.4144736842105263275, 0.4210526315789473450, 0.4276315789473684181, 0.4342105263157894912, 0.4407894736842105088, 0.4473684210526315819, 0.4539473684210526550, 0.4605263157894736725, 0.4671052631578947456, 0.4736842105263157632, 0.4802631578947368363, 0.4868421052631579093, 0.4934210526315789269, 0.5000000000000000000, 0.5065789473684210176, 0.5131578947368421462, 0.5197368421052631637, 0.5263157894736841813, 0.5328947368421053099, 0.5394736842105263275, 0.5460526315789473450, 0.5526315789473684736, 0.5592105263157894912, 0.5657894736842105088, 0.5723684210526315264, 0.5789473684210526550, 0.5855263157894736725, 0.5921052631578946901, 0.5986842105263158187, 0.6052631578947368363, 0.6118421052631578538, 0.6184210526315789824, 0.6250000000000000000, 0.6315789473684210176, 0.6381578947368421462, 0.6447368421052631637, 0.6513157894736841813, 0.6578947368421053099, 0.6644736842105263275, 0.6710526315789473450, 0.6776315789473684736, 0.6842105263157894912, 0.6907894736842105088, 0.6973684210526315264, 0.7039473684210526550, 0.7105263157894736725, 0.7171052631578946901, 0.7236842105263158187, 0.7302631578947368363, 0.7368421052631578538, 0.7434210526315789824, 0.7500000000000000000, 0.7565789473684210176, 0.7631578947368421462, 0.7697368421052631637, 0.7763157894736841813, 0.7828947368421053099, 0.7894736842105263275, 0.7960526315789473450, 0.8026315789473684736, 0.8092105263157894912, 0.8157894736842105088, 0.8223684210526315264, 0.8289473684210526550, 0.8355263157894736725, 0.8421052631578946901, 0.8486842105263158187, 0.8552631578947368363, 0.8618421052631578538, 0.8684210526315789824, 0.8750000000000000000, 0.8815789473684210176, 0.8881578947368421462, 0.8947368421052631637, 0.9013157894736841813, 0.9078947368421053099, 0.9144736842105263275, 0.9210526315789473450, 0.9276315789473684736, 0.9342105263157894912, 0.9407894736842105088, 0.9473684210526315264, 0.9539473684210526550, 0.9605263157894736725, 0.9671052631578946901, 0.9736842105263158187, 0.9802631578947368363, 0.9868421052631578538, 0.9934210526315789824, 0.9940576599040155115 ),
 .UNSPECIFIED. ) 
 GEOMETRIC_REPRESENTATION_ITEM ( )  RATIONAL_B_SPLINE_SURFACE ( (
 ( 1.000000000000000000, 0.9238795325112867385, 1.000000000000000000, 0.9238795325112867385, 1.000000000000000000, 0.9238795325112867385, 1.000000000000000000, 0.9238795325112867385, 1.000000000000000000, 0.9238795325112867385, 1.000000000000000000, 0.9238795325112867385, 1.000000000000000000, 0.9238795325112867385, 1.000000000000000000, 0.9238795325112867385, 1.000000000000000000, 0.9238795325112867385, 1.000000000000000000, 0.9238795325112867385, 1.000000000000000000, 0.9238795325112867385, 1.000000000000000000, 0.9238795325112867385, 1.000000000000000000, 0.9238795325112867385, 1.000000000000000000, 0.9238795325112867385, 1.000000000000000000, 0.9238795325112867385, 1.000000000000000000, 0.9238795325112867385, 1.000000000000000000, 0.9238795325112867385, 1.000000000000000000, 0.9238795325112867385, 1.000000000000000000, 0.9238795325112867385, 1.000000000000000000, 0.9238795325112867385, 1.000000000000000000, 0.9238795325112867385, 1.000000000000000000, 0.9238795325112867385, 1.000000000000000000, 0.9238795325112867385, 1.000000000000000000, 0.9238795325112867385, 1.000000000000000000, 0.9238795325112867385, 1.000000000000000000, 0.9238795325112867385, 1.000000000000000000, 0.9238795325112867385, 1.000000000000000000, 0.9238795325112867385, 1.000000000000000000, 0.9238795325112867385, 1.000000000000000000, 0.9238795325112867385, 1.000000000000000000, 0.9238795325112867385, 1.000000000000000000, 0.9238795325112867385, 1.000000000000000000, 0.9238795325112867385, 1.000000000000000000, 0.9238795325112867385, 1.000000000000000000, 0.9238795325112867385, 1.000000000000000000, 0.9238795325112867385, 1.000000000000000000, 0.9238795325112867385, 1.000000000000000000, 0.9238795325112867385, 1.000000000000000000, 0.9238795325112867385, 1.000000000000000000, 0.9238795325112867385, 1.000000000000000000, 0.9238795325112867385, 1.000000000000000000, 0.9238795325112867385, 1.000000000000000000, 0.9238795325112867385, 1.000000000000000000, 0.9238795325112867385, 1.000000000000000000, 0.9238795325112867385, 1.000000000000000000, 0.9238795325112867385, 1.000000000000000000, 0.9238795325112867385, 1.000000000000000000, 0.9238795325112867385, 1.000000000000000000, 0.9238795325112867385, 1.000000000000000000, 0.9238795325112867385, 1.000000000000000000, 0.9238795325112867385, 1.000000000000000000, 0.9238795325112867385, 1.000000000000000000, 0.9238795325112867385, 1.000000000000000000, 0.9238795325112867385, 1.000000000000000000, 0.9238795325112867385, 1.000000000000000000, 0.9238795325112867385, 1.000000000000000000, 0.9238795325112867385, 1.000000000000000000, 0.9238795325112867385, 1.000000000000000000, 0.9238795325112867385, 1.000000000000000000, 0.9238795325112867385, 1.000000000000000000, 0.9238795325112867385, 1.000000000000000000, 0.9238795325112867385, 1.000000000000000000, 0.9238795325112867385, 1.000000000000000000, 0.9238795325112867385, 1.000000000000000000, 0.9238795325112867385, 1.000000000000000000, 0.9238795325112867385, 1.000000000000000000, 0.9238795325112867385, 1.000000000000000000, 0.9238795325112867385, 1.000000000000000000, 0.9238795325112867385, 1.000000000000000000, 0.9238795325112867385, 1.000000000000000000, 0.9238795325112867385, 1.000000000000000000, 0.9238795325112867385, 1.000000000000000000, 0.9238795325112867385, 1.000000000000000000, 0.9238795325112867385, 1.000000000000000000, 0.9238795325112867385, 1.000000000000000000, 0.9238795325112867385, 1.000000000000000000, 0.9238795325112867385, 1.000000000000000000, 0.9238795325112867385, 1.000000000000000000, 0.9238795325112867385, 1.000000000000000000, 0.9238795325112867385, 1.000000000000000000, 0.9238795325112867385, 1.000000000000000000, 0.9238795325112867385, 1.000000000000000000, 0.9238795325112867385, 1.000000000000000000, 0.9238795325112867385, 1.000000000000000000, 0.9238795325112867385, 1.000000000000000000, 0.9238795325112867385, 1.000000000000000000, 0.9238795325112867385, 1.000000000000000000, 0.9238795325112867385, 1.000000000000000000, 0.9238795325112867385, 1.000000000000000000, 0.9238795325112867385, 1.000000000000000000, 0.9238795325112867385, 1.000000000000000000, 0.9238795325112867385, 1.000000000000000000, 0.9238795325112867385, 1.000000000000000000, 0.9238795325112867385, 1.000000000000000000, 0.9238795325112867385, 1.000000000000000000, 0.9238795325112867385, 1.000000000000000000, 0.9238795325112867385, 1.000000000000000000, 0.9238795325112867385, 1.000000000000000000, 0.9238795325112867385, 1.000000000000000000, 0.9238795325112867385, 1.000000000000000000, 0.9238795325112867385, 1.000000000000000000, 0.9238795325112867385, 1.000000000000000000, 0.9238795325112867385, 1.000000000000000000, 0.9238795325112867385, 1.000000000000000000, 0.9238795325112867385, 1.000000000000000000, 0.9238795325112867385, 1.000000000000000000, 0.9238795325112867385, 1.000000000000000000, 0.9238795325112867385, 1.000000000000000000, 0.9238795325112867385, 1.000000000000000000, 0.9238795325112867385, 1.000000000000000000, 0.9238795325112867385, 1.000000000000000000, 0.9238795325112867385, 1.000000000000000000, 0.9238795325112867385, 1.000000000000000000, 0.9238795325112867385, 1.000000000000000000, 0.9238795325112867385, 1.000000000000000000, 0.9238795325112867385, 1.000000000000000000, 0.9238795325112867385, 1.000000000000000000, 0.9238795325112867385, 1.000000000000000000, 0.9238795325112867385, 1.000000000000000000, 0.9238795325112867385, 1.000000000000000000, 0.9238795325112867385, 1.000000000000000000, 0.9238795325112867385, 1.000000000000000000, 0.9238795325112867385, 1.000000000000000000, 0.9238795325112867385, 1.000000000000000000, 0.9238795325112867385, 1.000000000000000000, 0.9238795325112867385, 1.000000000000000000, 0.9238795325112867385, 1.000000000000000000, 0.9238795325112867385, 1.000000000000000000, 0.9238795325112867385, 1.000000000000000000, 0.9238795325112867385, 1.000000000000000000, 0.9238795325112867385, 1.000000000000000000, 0.9238795325112867385, 1.000000000000000000, 0.9238795325112867385, 1.000000000000000000, 0.9238795325112867385, 1.000000000000000000, 0.9238795325112867385, 1.000000000000000000, 0.9238795325112867385, 1.000000000000000000, 0.9238795325112867385, 1.000000000000000000, 0.9238795325112867385, 1.000000000000000000, 0.9238795325112867385, 1.000000000000000000, 0.9238795325112867385, 1.000000000000000000, 0.9238795325112867385, 1.000000000000000000, 0.9238795325112867385, 1.000000000000000000, 0.9238795325112867385, 1.000000000000000000, 0.9238795325112867385, 1.000000000000000000, 0.9238795325112867385, 1.000000000000000000, 0.9238795325112867385, 1.000000000000000000, 0.9238795325112867385, 1.000000000000000000, 0.9238795325112867385, 1.000000000000000000, 0.9238795325112867385, 1.000000000000000000, 0.9238795325112867385, 1.000000000000000000, 0.9238795325112867385, 1.000000000000000000, 0.9926342558359432244, 0.9866939939076171395),
 ( 1.000000000000000000, 0.9238795325112867385, 1.000000000000000000, 0.9238795325112867385, 1.000000000000000000, 0.9238795325112867385, 1.000000000000000000, 0.9238795325112867385, 1.000000000000000000, 0.9238795325112867385, 1.000000000000000000, 0.9238795325112867385, 1.000000000000000000, 0.9238795325112867385, 1.000000000000000000, 0.9238795325112867385, 1.000000000000000000, 0.9238795325112867385, 1.000000000000000000, 0.9238795325112867385, 1.000000000000000000, 0.9238795325112867385, 1.000000000000000000, 0.9238795325112867385, 1.000000000000000000, 0.9238795325112867385, 1.000000000000000000, 0.9238795325112867385, 1.000000000000000000, 0.9238795325112867385, 1.000000000000000000, 0.9238795325112867385, 1.000000000000000000, 0.9238795325112867385, 1.000000000000000000, 0.9238795325112867385, 1.000000000000000000, 0.9238795325112867385, 1.000000000000000000, 0.9238795325112867385, 1.000000000000000000, 0.9238795325112867385, 1.000000000000000000, 0.9238795325112867385, 1.000000000000000000, 0.9238795325112867385, 1.000000000000000000, 0.9238795325112867385, 1.000000000000000000, 0.9238795325112867385, 1.000000000000000000, 0.9238795325112867385, 1.000000000000000000, 0.9238795325112867385, 1.000000000000000000, 0.9238795325112867385, 1.000000000000000000, 0.9238795325112867385, 1.000000000000000000, 0.9238795325112867385, 1.000000000000000000, 0.9238795325112867385, 1.000000000000000000, 0.9238795325112867385, 1.000000000000000000, 0.9238795325112867385, 1.000000000000000000, 0.9238795325112867385, 1.000000000000000000, 0.9238795325112867385, 1.000000000000000000, 0.9238795325112867385, 1.000000000000000000, 0.9238795325112867385, 1.000000000000000000, 0.9238795325112867385, 1.000000000000000000, 0.9238795325112867385, 1.000000000000000000, 0.9238795325112867385, 1.000000000000000000, 0.9238795325112867385, 1.000000000000000000, 0.9238795325112867385, 1.000000000000000000, 0.9238795325112867385, 1.000000000000000000, 0.9238795325112867385, 1.000000000000000000, 0.9238795325112867385, 1.000000000000000000, 0.9238795325112867385, 1.000000000000000000, 0.9238795325112867385, 1.000000000000000000, 0.9238795325112867385, 1.000000000000000000, 0.9238795325112867385, 1.000000000000000000, 0.9238795325112867385, 1.000000000000000000, 0.9238795325112867385, 1.000000000000000000, 0.9238795325112867385, 1.000000000000000000, 0.9238795325112867385, 1.000000000000000000, 0.9238795325112867385, 1.000000000000000000, 0.9238795325112867385, 1.000000000000000000, 0.9238795325112867385, 1.000000000000000000, 0.9238795325112867385, 1.000000000000000000, 0.9238795325112867385, 1.000000000000000000, 0.9238795325112867385, 1.000000000000000000, 0.9238795325112867385, 1.000000000000000000, 0.9238795325112867385, 1.000000000000000000, 0.9238795325112867385, 1.000000000000000000, 0.9238795325112867385, 1.000000000000000000, 0.9238795325112867385, 1.000000000000000000, 0.9238795325112867385, 1.000000000000000000, 0.9238795325112867385, 1.000000000000000000, 0.9238795325112867385, 1.000000000000000000, 0.9238795325112867385, 1.000000000000000000, 0.9238795325112867385, 1.000000000000000000, 0.9238795325112867385, 1.000000000000000000, 0.9238795325112867385, 1.000000000000000000, 0.9238795325112867385, 1.000000000000000000, 0.9238795325112867385, 1.000000000000000000, 0.9238795325112867385, 1.000000000000000000, 0.9238795325112867385, 1.000000000000000000, 0.9238795325112867385, 1.000000000000000000, 0.9238795325112867385, 1.000000000000000000, 0.9238795325112867385, 1.000000000000000000, 0.9238795325112867385, 1.000000000000000000, 0.9238795325112867385, 1.000000000000000000, 0.9238795325112867385, 1.000000000000000000, 0.9238795325112867385, 1.000000000000000000, 0.9238795325112867385, 1.000000000000000000, 0.9238795325112867385, 1.000000000000000000, 0.9238795325112867385, 1.000000000000000000, 0.9238795325112867385, 1.000000000000000000, 0.9238795325112867385, 1.000000000000000000, 0.9238795325112867385, 1.000000000000000000, 0.9238795325112867385, 1.000000000000000000, 0.9238795325112867385, 1.000000000000000000, 0.9238795325112867385, 1.000000000000000000, 0.9238795325112867385, 1.000000000000000000, 0.9238795325112867385, 1.000000000000000000, 0.9238795325112867385, 1.000000000000000000, 0.9238795325112867385, 1.000000000000000000, 0.9238795325112867385, 1.000000000000000000, 0.9238795325112867385, 1.000000000000000000, 0.9238795325112867385, 1.000000000000000000, 0.9238795325112867385, 1.000000000000000000, 0.9238795325112867385, 1.000000000000000000, 0.9238795325112867385, 1.000000000000000000, 0.9238795325112867385, 1.000000000000000000, 0.9238795325112867385, 1.000000000000000000, 0.9238795325112867385, 1.000000000000000000, 0.9238795325112867385, 1.000000000000000000, 0.9238795325112867385, 1.000000000000000000, 0.9238795325112867385, 1.000000000000000000, 0.9238795325112867385, 1.000000000000000000, 0.9238795325112867385, 1.000000000000000000, 0.9238795325112867385, 1.000000000000000000, 0.9238795325112867385, 1.000000000000000000, 0.9238795325112867385, 1.000000000000000000, 0.9238795325112867385, 1.000000000000000000, 0.9238795325112867385, 1.000000000000000000, 0.9238795325112867385, 1.000000000000000000, 0.9238795325112867385, 1.000000000000000000, 0.9238795325112867385, 1.000000000000000000, 0.9238795325112867385, 1.000000000000000000, 0.9238795325112867385, 1.000000000000000000, 0.9238795325112867385, 1.000000000000000000, 0.9238795325112867385, 1.000000000000000000, 0.9238795325112867385, 1.000000000000000000, 0.9238795325112867385, 1.000000000000000000, 0.9238795325112867385, 1.000000000000000000, 0.9238795325112867385, 1.000000000000000000, 0.9238795325112867385, 1.000000000000000000, 0.9238795325112867385, 1.000000000000000000, 0.9238795325112867385, 1.000000000000000000, 0.9238795325112867385, 1.000000000000000000, 0.9238795325112867385, 1.000000000000000000, 0.9238795325112867385, 1.000000000000000000, 0.9238795325112867385, 1.000000000000000000, 0.9238795325112867385, 1.000000000000000000, 0.9238795325112867385, 1.000000000000000000, 0.9238795325112867385, 1.000000000000000000, 0.9238795325112867385, 1.000000000000000000, 0.9238795325112867385, 1.000000000000000000, 0.9238795325112867385, 1.000000000000000000, 0.9238795325112867385, 1.000000000000000000, 0.9238795325112867385, 1.000000000000000000, 0.9238795325112867385, 1.000000000000000000, 0.9238795325112867385, 1.000000000000000000, 0.9238795325112867385, 1.000000000000000000, 0.9238795325112867385, 1.000000000000000000, 0.9238795325112867385, 1.000000000000000000, 0.9238795325112867385, 1.000000000000000000, 0.9238795325112867385, 1.000000000000000000, 0.9238795325112867385, 1.000000000000000000, 0.9238795325112867385, 1.000000000000000000, 0.9238795325112867385, 1.000000000000000000, 0.9238795325112867385, 1.000000000000000000, 0.9926342558359432244, 0.9866939939076171395) ) ) 
 REPRESENTATION_ITEM ( '' )  SURFACE ( )  );
#51371 = DIRECTION ( 'NONE',  ( -0.000000000000000000, 1.000000000000000000, -0.000000000000000000 ) ) ;
#51372 = CARTESIAN_POINT ( 'NONE',  ( -6.676582343750000703, 298.5156250017070079, 2.765530957082001251 ) ) ;
#51373 = CARTESIAN_POINT ( 'NONE',  ( 6.951808397369818766E-16, 132.0312499965860127, -11.35316468750000141 ) ) ;
#51374 = CARTESIAN_POINT ( 'NONE',  ( 4.999999999999999112, 53.39837237779229184, 47.14918772354995724 ) ) ;
#51375 = CARTESIAN_POINT ( 'NONE',  ( -4.898587196589407898E-16, 7.999999999999991118, 24.51155278432982598 ) ) ;
#51376 = CARTESIAN_POINT ( 'NONE',  ( 8.660254037844385522, 226.0416666734946602, -5.000000000000003553 ) ) ;
#51377 = CARTESIAN_POINT ( 'NONE',  ( 5.676582343749997150, 257.2395833367473301, -9.832129032723418760 ) ) ;
#51378 = CARTESIAN_POINT ( 'NONE',  ( 1.871523826299183495E-15, -10.18810118749999916, 98.40625000204838102 ) ) ;
#51379 = EDGE_LOOP ( 'NONE', ( #33062, #43872, #56804, #56154 ) ) ;
#51380 = AXIS2_PLACEMENT_3D ( 'NONE', #49978, #62042, #49225 ) ;
#51381 = LINE ( 'NONE', #57059, #55828 ) ;
#51382 = FILL_AREA_STYLE ('',( #33687 ) ) ;
#51383 = CARTESIAN_POINT ( 'NONE',  ( 1.432654583217664701, 202.0000000013656063, 201.4587341250000065 ) ) ;
#51384 = CARTESIAN_POINT ( 'NONE',  ( -5.676582343749998039, 72.76041666325268409, -9.832129032723420536 ) ) ;
#51385 = EDGE_LOOP ( 'NONE', ( #52444, #58403 ) ) ;
#51386 = CARTESIAN_POINT ( 'NONE',  ( 10.18810118750000093, -4.220049686691933921, 110.3125000020483810 ) ) ;
#51387 =( BOUNDED_SURFACE ( )  B_SPLINE_SURFACE ( 3, 2, ( 
 ( #34476, #57853, #33728 ),
 ( #56730, #28044, #17461 ),
 ( #40482, #39734, #51054 ),
 ( #62734, #34102, #51424 ),
 ( #45765, #5788, #51800 ),
 ( #11809, #34848, #9902 ),
 ( #38946, #16278, #22313 ),
 ( #68356, #27994, #45709 ),
 ( #4616, #34053, #67983 ),
 ( #45339, #62318, #44978 ),
 ( #74012, #44235, #16651 ),
 ( #32932, #51001, #61946 ),
 ( #39683, #10275, #55938 ),
 ( #61583, #39320, #3875 ),
 ( #5360, #10644, #40059 ),
 ( #21578, #17033, #22691 ),
 ( #33673, #56677, #73642 ),
 ( #4249, #62683, #4994 ) ),
 .UNSPECIFIED., .F., .F., .F. ) 
 B_SPLINE_SURFACE_WITH_KNOTS ( ( 4, 2, 2, 2, 2, 2, 2, 2, 4 ),
 ( 3, 3 ),
 ( 0.04202945594032910653, 0.04396162471216781553, 0.04589379348400653147, 0.04782596225584524741, 0.04975813102768396334, 0.05169029979952267928, 0.05265638418544203725, 0.05362246857136138828, 0.05748680611503881321 ),
 ( 0.000000000000000000, 1.000000000000000000 ),
 .UNSPECIFIED. ) 
 GEOMETRIC_REPRESENTATION_ITEM ( )  RATIONAL_B_SPLINE_SURFACE ( (
 ( 1.000000000000000000, 0.6241276099608162875, 1.000000000000000000),
 ( 1.000000000000000000, 0.6218761496800390143, 1.000000000000000000),
 ( 1.000000000000000000, 0.6198047272364022309, 1.000000000000000000),
 ( 1.000000000000000000, 0.6161935119824402118, 1.000000000000000000),
 ( 1.000000000000000000, 0.6146642324079480968, 1.000000000000000000),
 ( 1.000000000000000000, 0.6121850116872522563, 1.000000000000000000),
 ( 1.000000000000000000, 0.6112350889399755793, 1.000000000000000000),
 ( 1.000000000000000000, 0.6099522725972823523, 1.000000000000000000),
 ( 1.000000000000000000, 0.6096208180307279845, 1.000000000000000000),
 ( 1.000000000000000000, 0.6096183796350086448, 1.000000000000000000),
 ( 1.000000000000000000, 0.6099422200101831670, 1.000000000000000000),
 ( 1.000000000000000000, 0.6109087447823332573, 1.000000000000000000),
 ( 1.000000000000000000, 0.6113123981688617370, 1.000000000000000000),
 ( 1.000000000000000000, 0.6122677719808993224, 1.000000000000000000),
 ( 1.000000000000000000, 0.6128199619020365807, 1.000000000000000000),
 ( 1.000000000000000000, 0.6159350830268174315, 1.000000000000000000),
 ( 1.000000000000000000, 0.6195556778513785501, 1.000000000000000000),
 ( 1.000000000000000000, 0.6241278272307889674, 1.000000000000000000) ) ) 
 REPRESENTATION_ITEM ( '' )  SURFACE ( )  );
#51388 = CARTESIAN_POINT ( 'NONE',  ( -1.881053915767124440, 11.12499999863440969, 4.541265875000001451 ) ) ;
#51389 = ORIENTED_EDGE ( 'NONE', *, *, #43779, .F. ) ;
#51390 = CARTESIAN_POINT ( 'NONE',  ( -7.188101187500002709, 25.31249999795161543, 2.977408999572649151 ) ) ;
#51391 = CARTESIAN_POINT ( 'NONE',  ( -10.00000000000000000, 109.1666666598386968, -2.679491924311229845 ) ) ;
#51392 = DIRECTION ( 'NONE',  ( 0.8660254037844377084, -0.5000000000000017764, 0.000000000000000000 ) ) ;
#51393 = CARTESIAN_POINT ( 'NONE',  ( -2.977408999572654480, 21.37499999795161543, 7.188101187499999156 ) ) ;
#51394 = CARTESIAN_POINT ( 'NONE',  ( 1.502314598737163567E-15, -20.78460969082658494, -21.50000000000000000 ) ) ;
#51395 = CARTESIAN_POINT ( 'NONE',  ( -10.18810118749999738, -4.220049686691941915, 104.1250000020483810 ) ) ;
#51396 = EDGE_CURVE ( 'NONE', #21207, #33772, #36504, .T. ) ;
#51397 = CARTESIAN_POINT ( 'NONE',  ( 8.660254037844383745, 110.4166666666666714, -4.999999999999997335 ) ) ;
#51398 = CARTESIAN_POINT ( 'NONE',  ( -1.656854249492381248, 11.06249999726881406, -4.000000000000001776 ) ) ;
#51399 = CARTESIAN_POINT ( 'NONE',  ( 0.000000000000000000, 125.0000000000000000, 0.000000000000000000 ) ) ;
#51400 = ORIENTED_EDGE ( 'NONE', *, *, #70798, .F. ) ;
#51401 = CARTESIAN_POINT ( 'NONE',  ( -5.000000000000000000, -18.53862685874495853, -23.57305537018139674 ) ) ;
#51402 = CARTESIAN_POINT ( 'NONE',  ( -3.458734124999959914, 204.4375000013656063, 198.0000000000000284 ) ) ;
#51403 = CARTESIAN_POINT ( 'NONE',  ( -26.56734541678227757, 205.0000000013655779, 173.4587341250003476 ) ) ;
#51404 = CARTESIAN_POINT ( 'NONE',  ( 2.828427124746152987, 207.1250000000000284, 139.1715728752538723 ) ) ;
#51405 = EDGE_CURVE ( 'NONE', #41903, #72372, #73854, .T. ) ;
#51406 = CARTESIAN_POINT ( 'NONE',  ( -1.881053915767121554, 8.624999998634406140, -4.541265875000002339 ) ) ;
#51407 = CARTESIAN_POINT ( 'NONE',  ( 4.000000000000001776, 16.00000000000000000, 0.000000000000000000 ) ) ;
#51408 = CARTESIAN_POINT ( 'NONE',  ( 7.188101187499991163, 2.977408999572648707, 18.83030278187175099 ) ) ;
#51409 = EDGE_LOOP ( 'NONE', ( #28392, #54439 ) ) ;
#51410 = EDGE_CURVE ( 'NONE', #69045, #53254, #40265, .T. ) ;
#51411 = CARTESIAN_POINT ( 'NONE',  ( -4.242640687119286547, 291.8750000000000000, -4.242640687119286547 ) ) ;
#51412 = ORIENTED_EDGE ( 'NONE', *, *, #23939, .T. ) ;
#51413 = CARTESIAN_POINT ( 'NONE',  ( 7.204075437095968759, -7.204075437095966983, 110.2187500020483810 ) ) ;
#51414 = CARTESIAN_POINT ( 'NONE',  ( 2.449293598294707893E-16, 18.25000000000000000, -4.000000000000001776 ) ) ;
#51415 = CARTESIAN_POINT ( 'NONE',  ( -1.432654583217607858, 198.6250000013655779, 201.4587341250000065 ) ) ;
#51416 = CARTESIAN_POINT ( 'NONE',  ( 24.54126587499997569, 196.1250000013656063, 168.5673454167822740 ) ) ;
#51417 = CARTESIAN_POINT ( 'NONE',  ( 7.320508075688774596, 80.62500000000000000, -7.320508075688774596 ) ) ;
#51418 = CARTESIAN_POINT ( 'NONE',  ( -3.313708498984762052, 124.7187500000000000, -8.000000000000000000 ) ) ;
#51419 = CARTESIAN_POINT ( 'NONE',  ( 1.102182119232618108E-15, 290.2500000000000000, 6.000000000000001776 ) ) ;
#51420 = ORIENTED_EDGE ( 'NONE', *, *, #38391, .T. ) ;
#51421 = VECTOR ( 'NONE', #52426, 1000.000000000000000 ) ;
#51422 = CARTESIAN_POINT ( 'NONE',  ( 4.242640687119287435, 294.3750000000000000, 4.242640687119285658 ) ) ;
#51423 = EDGE_CURVE ( 'NONE', #1735, #55418, #26340, .T. ) ;
#51424 = CARTESIAN_POINT ( 'NONE',  ( -5.086519500887583867, -60.91611154180644405, 23.32191296476066356 ) ) ;
#51425 = CARTESIAN_POINT ( 'NONE',  ( -4.000000000000015987, 195.5625000027311842, 140.3431457505076594 ) ) ;
#51426 = CARTESIAN_POINT ( 'NONE',  ( 8.660254037844385522, 56.45833332650536818, 5.000000000000005329 ) ) ;
#51427 = CARTESIAN_POINT ( 'NONE',  ( -5.656854249492379694, 23.06250000000000355, -5.656854249492380582 ) ) ;
#51428 = CARTESIAN_POINT ( 'NONE',  ( 10.00000000000000178, 237.2916666666666288, 2.679491924311222739 ) ) ;
#51429 = CARTESIAN_POINT ( 'NONE',  ( -11.00000000000000000, 0.000000000000000000, 88.00000000000000000 ) ) ;
#51430 = CARTESIAN_POINT ( 'NONE',  ( 7.320508075688771044, 199.3750000000000000, 7.320508075688775484 ) ) ;
#51431 = CARTESIAN_POINT ( 'NONE',  ( 2.977408999572646486, 7.188101187499992051, 19.39280278187176165 ) ) ;
#51432 = CARTESIAN_POINT ( 'NONE',  ( -11.35316468749999785, 168.3854166632526699, -3.042071309553167513 ) ) ;
#51433 = DIRECTION ( 'NONE',  ( 1.000000000000000000, 0.000000000000000000, 0.000000000000000000 ) ) ;
#51434 = DIRECTION ( 'NONE',  ( 0.000000000000000000, 0.000000000000000000, -1.000000000000000000 ) ) ;
#51436 = CARTESIAN_POINT ( 'NONE',  ( 8.000000000000000000, 10.40624999590321842, -3.313708498984761164 ) ) ;
#51435 = DIRECTION ( 'NONE',  ( -2.771571441169508074E-17, -1.000000000000000000, -2.238352872228138663E-16 ) ) ;
#51437 = VERTEX_POINT ( 'NONE', #45921 ) ;
#51438 = CARTESIAN_POINT ( 'NONE',  ( -2.445694354108839619, 198.8125000013656063, 139.5543056458912190 ) ) ;
#51439 = CARTESIAN_POINT ( 'NONE',  ( 8.311093377946834337, 40.46874999658601979, 8.311093377946839666 ) ) ;
#51440 = CARTESIAN_POINT ( 'NONE',  ( -11.00000000000000000, 0.000000000000000000, 112.1875000040967763 ) ) ;
#51441 = CARTESIAN_POINT ( 'NONE',  ( -31.45873412499999944, 207.6875000013656063, 170.0000000000004547 ) ) ;
#51442 = DIRECTION ( 'NONE',  ( 0.000000000000000000, 0.000000000000000000, 1.000000000000000000 ) ) ;
#51443 = CARTESIAN_POINT ( 'NONE',  ( -2.124081043562908722, 10.27770035960974759, -63.71262442773669932 ) ) ;
#51444 = CARTESIAN_POINT ( 'NONE',  ( -11.55698479651917410, -36.78417955641780424, 198.7667097343568230 ) ) ;
#51445 = CARTESIAN_POINT ( 'NONE',  ( 3.458734124999959914, 199.4375000013655779, 142.0000000000000568 ) ) ;
#51446 = CARTESIAN_POINT ( 'NONE',  ( 5.000000000000001776, 67.70833332650536818, -8.660254037844389075 ) ) ;
#51447 = CARTESIAN_POINT ( 'NONE',  ( -7.188101187500001821, 103.0625000020483810, -2.977408999572650483 ) ) ;
#51448 = CARTESIAN_POINT ( 'NONE',  ( 3.211159895383560947, 14.31249999863440792, 3.211159895383562723 ) ) ;
#51449 = DIRECTION ( 'NONE',  ( 0.8660254037844379305, 0.5000000000000011102, 0.000000000000000000 ) ) ;
#51450 = CARTESIAN_POINT ( 'NONE',  ( -7.999999999999989342, -3.313708498984762496, 2.424052779823365533 ) ) ;
#51451 = DIRECTION ( 'NONE',  ( 0.000000000000000000, 0.000000000000000000, 1.000000000000000000 ) ) ;
#51452 = ORIENTED_EDGE ( 'NONE', *, *, #31376, .F. ) ;
#51453 = ORIENTED_EDGE ( 'NONE', *, *, #32970, .F. ) ;
#51454 = CARTESIAN_POINT ( 'NONE',  ( 3.369429374625377172, -50.21921270641806956, -40.85597392306833342 ) ) ;
#51455 = CARTESIAN_POINT ( 'NONE',  ( 3.458734125000015869, 195.1875000013655779, 198.0000000000000284 ) ) ;
#51456 = LINE ( 'NONE', #39401, #47148 ) ;
#51457 = AXIS2_PLACEMENT_3D ( 'NONE', #15333, #32721, #4045 ) ;
#51458 = EDGE_CURVE ( 'NONE', #12103, #52340, #60590, .T. ) ;
#51459 = CARTESIAN_POINT ( 'NONE',  ( -9.832129032723420536, 138.6979166632526983, 5.676582343749997150 ) ) ;
#51460 = CARTESIAN_POINT ( 'NONE',  ( 7.320508075688763050, 105.6250000000000142, -7.320508075688763050 ) ) ;
#51461 = CARTESIAN_POINT ( 'NONE',  ( 4.220049686691941027, -10.18810118749999738, 86.12500000204836681 ) ) ;
#51462 = CARTESIAN_POINT ( 'NONE',  ( 8.000000000000000000, 4.593750000000000888, -3.313708498984761164 ) ) ;
#51463 = CARTESIAN_POINT ( 'NONE',  ( -3.999999999999960032, 204.9375000000000284, 196.3431457505076594 ) ) ;
#51464 = CARTESIAN_POINT ( 'NONE',  ( -8.000000000000001776, 18.65624999590322375, 3.313708498984759387 ) ) ;
#51465 = CARTESIAN_POINT ( 'NONE',  ( 7.897089018260699866, -1.490448377887923836, -0.000000000000000000 ) ) ;
#51466 = EDGE_CURVE ( 'NONE', #33088, #13669, #11397, .T. ) ;
#51467 = CARTESIAN_POINT ( 'NONE',  ( 7.204075437095966983, 7.204075437095967871, 113.9687500020483810 ) ) ;
#51468 = ORIENTED_EDGE ( 'NONE', *, *, #66046, .F. ) ;
#51469 = CARTESIAN_POINT ( 'NONE',  ( 11.00000000000007994, 4.556349186103967774, 108.5312500040967905 ) ) ;
#51470 = AXIS2_PLACEMENT_3D ( 'NONE', #61733, #67016, #67768 ) ;
#51471 = CARTESIAN_POINT ( 'NONE',  ( -4.503730643522685817, 183.6423555172976876, 139.2463417149593568 ) ) ;
#51472 = CARTESIAN_POINT ( 'NONE',  ( -9.832129032723418760, 123.1770833299193555, -5.676582343750004256 ) ) ;
#51473 = CARTESIAN_POINT ( 'NONE',  ( -2.445694354108782775, 201.5625000013656063, 200.4456943541088663 ) ) ;
#51474 = CARTESIAN_POINT ( 'NONE',  ( 7.188101187500000933, 26.43749999795162253, -2.977408999572650483 ) ) ;
#51476 = EDGE_CURVE ( 'NONE', #64638, #24567, #46664, .T. ) ;
#51475 = CARTESIAN_POINT ( 'NONE',  ( -4.220049686691935698, 10.18810118749999916, 78.25000000204838102 ) ) ;
#51477 = CARTESIAN_POINT ( 'NONE',  ( -3.042071309553164404, 42.55208332991933418, -11.35316468749999963 ) ) ;
#51478 = VERTEX_POINT ( 'NONE', #23658 ) ;
#51479 = DIRECTION ( 'NONE',  ( -0.000000000000000000, 1.000000000000000000, -0.000000000000000000 ) ) ;
#51480 = CARTESIAN_POINT ( 'NONE',  ( -3.211159895383561391, 0.8124999986344069169, -3.211159895383561835 ) ) ;
#51481 = CARTESIAN_POINT ( 'NONE',  ( -5.662595241051935346, 5.662595241051935346, 23.32561528394063188 ) ) ;
#51482 = CARTESIAN_POINT ( 'NONE',  ( -3.458734125000015425, 207.2500000013655779, 143.4326545832176976 ) ) ;
#51483 = CARTESIAN_POINT ( 'NONE',  ( -5.082755093536326818, 8.906249997951610098, 5.082755093536325042 ) ) ;
#51484 = CARTESIAN_POINT ( 'NONE',  ( -4.242640687119286547, 297.9375000034140157, -4.242640687119286547 ) ) ;
#51485 = CARTESIAN_POINT ( 'NONE',  ( -11.00000000000052935, -31.17830422493387843, 140.3677189386882276 ) ) ;
#51486 = CARTESIAN_POINT ( 'NONE',  ( 2.977408999572650927, 5.624999997951610986, -7.188101187500001821 ) ) ;
#51487 =( BOUNDED_CURVE ( )  B_SPLINE_CURVE ( 2, ( #46853, #36282, #18188, #64212, #13249, #18558, #35549, #46112, #41569 ),
 .UNSPECIFIED., .F., .F. ) 
 B_SPLINE_CURVE_WITH_KNOTS ( ( 3, 2, 2, 2, 3 ),
 ( 0.000000000000000000, 0.008333333333333340157, 0.01666666666666668031, 0.02500000000000002220, 0.03333333333333336063 ),
 .UNSPECIFIED. ) 
 CURVE ( )  GEOMETRIC_REPRESENTATION_ITEM ( )  RATIONAL_B_SPLINE_CURVE ( ( 1.000000000000000000, 0.9238795325112867385, 1.000000000000000000, 0.9238795325112867385, 1.000000000000000000, 0.9238795325112867385, 1.000000000000000000, 0.9238795325112865164, 1.000000000000000222 ) ) 
 REPRESENTATION_ITEM ( '' )  );
#51488 = CARTESIAN_POINT ( 'NONE',  ( -11.35316468750000141, 153.5937499965860127, -1.390361679473963753E-15 ) ) ;
#51489 = VECTOR ( 'NONE', #43036, 1000.000000000000114 ) ;
#51490 = CARTESIAN_POINT ( 'NONE',  ( 7.204075437095966983, 7.204075437095967871, 74.59375000204838102 ) ) ;
#51491 = CARTESIAN_POINT ( 'NONE',  ( -27.99999999999996092, 195.9375000013655779, 173.4587341250003760 ) ) ;
#51492 = CARTESIAN_POINT ( 'NONE',  ( -4.000000000000001776, 15.43749999999999822, -1.656854249492381470 ) ) ;
#51493 = CARTESIAN_POINT ( 'NONE',  ( -1.881053915767124440, 18.12499999863440792, 4.541265875000001451 ) ) ;
#51494 = ORIENTED_EDGE ( 'NONE', *, *, #40075, .T. ) ;
#51495 = CARTESIAN_POINT ( 'NONE',  ( 2.849036369511732440E-14, 198.3750000027312126, 202.0000000000000000 ) ) ;
#51496 = CARTESIAN_POINT ( 'NONE',  ( 2.828427124746152987, 206.1250000000000284, 139.1715728752538723 ) ) ;
#51497 = CARTESIAN_POINT ( 'NONE',  ( -32.00000000000002842, 201.3125000027312126, 168.3431457505080573 ) ) ;
#51498 = EDGE_CURVE ( 'NONE', #13141, #10343, #42587, .T. ) ;
#51499 = CARTESIAN_POINT ( 'NONE',  ( 11.00000000000000000, 1.347111479062088405E-15, 75.43750000409676204 ) ) ;
#51500 = CARTESIAN_POINT ( 'NONE',  ( -5.656854249492375253, 5.656854249492375253, 5.330302783920146226 ) ) ;
#51501 = ORIENTED_EDGE ( 'NONE', *, *, #25586, .F. ) ;
#51502 = CARTESIAN_POINT ( 'NONE',  ( 7.188101187499999156, 19.87499999795161543, 2.977408999572654924 ) ) ;
#51503 = CARTESIAN_POINT ( 'NONE',  ( 9.797174393178825657E-16, 125.0000000000000000, -8.000000000000000000 ) ) ;
#51504 = VECTOR ( 'NONE', #34783, 1000.000000000000000 ) ;
#51505 = LINE ( 'NONE', #40939, #64434 ) ;
#51506 = CARTESIAN_POINT ( 'NONE',  ( 10.00000000000000178, 45.20833333333332860, -2.679491924311226736 ) ) ;
#51507 = CARTESIAN_POINT ( 'NONE',  ( -4.401442555609581635E-16, 106.1562500020483810, -7.188101187500000044 ) ) ;
#51508 = CARTESIAN_POINT ( 'NONE',  ( -26.56734541678238415, 208.6250000013656063, 166.5412658750003629 ) ) ;
#51509 = CARTESIAN_POINT ( 'NONE',  ( -23.99999999999997158, 196.6875000000000284, 171.6568542494927385 ) ) ;
#51511 = CARTESIAN_POINT ( 'NONE',  ( 4.556349186104045934, 11.00000000000000000, 74.21875000409676204 ) ) ;
#51510 = CARTESIAN_POINT ( 'NONE',  ( 9.797174393178825657E-16, 125.0000000000000000, -8.000000000000000000 ) ) ;
#51512 = VERTEX_POINT ( 'NONE', #35369 ) ;
#51513 = CARTESIAN_POINT ( 'NONE',  ( 5.676582343750005144, 245.5729166700806729, 9.832129032723416984 ) ) ;
#51514 = CARTESIAN_POINT ( 'NONE',  ( 5.082755093536318824, 5.082755093536319713, 17.79905278187175810 ) ) ;
#51515 = CARTESIAN_POINT ( 'NONE',  ( 0.4451317748862709811, 51.14719335908506537, 48.52010116548684238 ) ) ;
#51516 = LINE ( 'NONE', #28133, #50210 ) ;
#51517 = CARTESIAN_POINT ( 'NONE',  ( 24.17985302810937398, 194.9464753018649787, 171.0086001198536962 ) ) ;
#51518 = CARTESIAN_POINT ( 'NONE',  ( -4.999999999999998224, 138.5416666598387110, -8.660254037844389075 ) ) ;
#51519 = CARTESIAN_POINT ( 'NONE',  ( -7.320508075688778149, 163.1250000000000284, 7.320508075688769267 ) ) ;
#51520 = DIRECTION ( 'NONE',  ( -1.000000000000000000, 2.701921919735179162E-32, -6.308085367188390241E-16 ) ) ;
#51521 = CARTESIAN_POINT ( 'NONE',  ( 8.000000000000000000, 91.25000000000000000, -9.797174393178825657E-16 ) ) ;
#51522 = CARTESIAN_POINT ( 'NONE',  ( 5.656854249492381470, 91.06249999999998579, 5.656854249492379694 ) ) ;
#51523 = CARTESIAN_POINT ( 'NONE',  ( 5.676582343749993598, 125.2604166632526841, 9.832129032723422313 ) ) ;
#51524 = CARTESIAN_POINT ( 'NONE',  ( -5.656854249492375253, 5.656854249492375253, 27.83030278392014978 ) ) ;
#51527 = CARTESIAN_POINT ( 'NONE',  ( -2.751064625579944321E-14, 201.7500000000000000, 146.0000000000000284 ) ) ;
#51526 = CARTESIAN_POINT ( 'NONE',  ( 29.43265458321760519, 195.8750000013655779, 166.5412658749999650 ) ) ;
#51525 = CARTESIAN_POINT ( 'NONE',  ( 29.43265458321766204, 195.1250000013656063, 166.5412658749999650 ) ) ;
#51528 = ORIENTED_EDGE ( 'NONE', *, *, #63833, .F. ) ;
#51529 = CARTESIAN_POINT ( 'NONE',  ( -0.4320110153365229189, -60.19564456717424150, 22.88238106212085654 ) ) ;
#51530 = FACE_OUTER_BOUND ( 'NONE', #2353, .T. ) ;
#51531 = APPLICATION_CONTEXT ( 'automotive_design' ) ;
#51532 = AXIS2_PLACEMENT_3D ( 'NONE', #64162, #12469, #52844 ) ;
#51533 = CARTESIAN_POINT ( 'NONE',  ( 24.54126587499997925, 195.5000000013655779, 171.4326545832175555 ) ) ;
#51534 = CARTESIAN_POINT ( 'NONE',  ( 11.35316468749999963, 221.3020833299192986, -3.042071309553165293 ) ) ;
#51535 = CARTESIAN_POINT ( 'NONE',  ( -5.082755093536325930, 123.9687500020483952, -5.082755093536325930 ) ) ;
#51536 = CARTESIAN_POINT ( 'NONE',  ( -4.541265875000002339, 1.937499998634406806, -5.561446717895856393E-16 ) ) ;
#51537 = CARTESIAN_POINT ( 'NONE',  ( -1.308779242310801116, 60.23127520339139807, -22.90411807697349289 ) ) ;
#51538 = CARTESIAN_POINT ( 'NONE',  ( -7.999999999999991118, 0.000000000000000000, 23.33030277982336642 ) ) ;
#51540 = CARTESIAN_POINT ( 'NONE',  ( -29.65685424949237259, 207.4375000000000284, 174.0000000000003695 ) ) ;
#51539 = DIRECTION ( 'NONE',  ( 0.000000000000000000, 0.000000000000000000, 1.000000000000000000 ) ) ;
#51541 = CARTESIAN_POINT ( 'NONE',  ( 9.832129032723416984, 100.3645833299193697, 5.676582343750006032 ) ) ;
#51542 = ORIENTED_EDGE ( 'NONE', *, *, #27632, .T. ) ;
#51543 = CARTESIAN_POINT ( 'NONE',  ( -4.000000000000001776, 19.18749999726881228, -1.656854249492381470 ) ) ;
#51544 = CARTESIAN_POINT ( 'NONE',  ( 5.082755093536324154, 22.78124999795161187, 5.082755093536326818 ) ) ;
#51545 = CARTESIAN_POINT ( 'NONE',  ( 3.313708498984762496, -7.999999999999989342, 8.799052779823364645 ) ) ;
#51546 = CARTESIAN_POINT ( 'NONE',  ( 2.085542519210945334E-15, 245.4687500034140157, 11.35316468749999963 ) ) ;
#51547 = CARTESIAN_POINT ( 'NONE',  ( -9.832129032723418760, 102.8645833299193697, -5.676582343750004256 ) ) ;
#51548 = ORIENTED_EDGE ( 'NONE', *, *, #26397, .T. ) ;
#51549 = CARTESIAN_POINT ( 'NONE',  ( 5.000000000000000888, -14.70421557449305361, 69.92631206022691970 ) ) ;
#51550 = CARTESIAN_POINT ( 'NONE',  ( -6.238412754330611322E-16, 10.18810118749999916, 107.7812500020483810 ) ) ;
#51551 = CARTESIAN_POINT ( 'NONE',  ( -7.320508075688778149, 224.9999999931720254, 7.320508075688769267 ) ) ;
#51552 = CARTESIAN_POINT ( 'NONE',  ( -3.458734124999960358, 200.6875000013656063, 198.0000000000000284 ) ) ;
#51553 = DIRECTION ( 'NONE',  ( -0.000000000000000000, 1.000000000000000000, 4.476705744456276341E-16 ) ) ;
#51554 = CARTESIAN_POINT ( 'NONE',  ( 5.676582343749993598, 99.94791666325268409, 9.832129032723422313 ) ) ;
#51555 = CARTESIAN_POINT ( 'NONE',  ( -4.898587196589407898E-16, 7.999999999999991118, 11.14280278392014800 ) ) ;
#51556 = CARTESIAN_POINT ( 'NONE',  ( -30.44569435410878810, 197.0625000013656063, 172.4456943541092357 ) ) ;
#51557 = EDGE_CURVE ( 'NONE', #61509, #62325, #44225, .T. ) ;
#51558 = CARTESIAN_POINT ( 'NONE',  ( -3.313708498984805573, 27.84374999590322020, 7.999999999999956479 ) ) ;
#51559 = ORIENTED_EDGE ( 'NONE', *, *, #48966, .T. ) ;
#51560 = CARTESIAN_POINT ( 'NONE',  ( 2.679491924311222739, 200.8333333265053398, 10.00000000000000355 ) ) ;
#51561 = DIRECTION ( 'NONE',  ( 0.000000000000000000, 0.000000000000000000, 1.000000000000000000 ) ) ;
#51562 = CARTESIAN_POINT ( 'NONE',  ( 0.9662696845636871146, -47.84692511509527435, 139.0145297348084057 ) ) ;
#51563 = CARTESIAN_POINT ( 'NONE',  ( 3.042071309553167513, 82.13541666325269830, -11.35316468749999785 ) ) ;
#51564 = CARTESIAN_POINT ( 'NONE',  ( 4.721056650416000089, 288.8281250017069510, 4.721056650415999201 ) ) ;
#51565 = CARTESIAN_POINT ( 'NONE',  ( -7.188101187500002709, 6.187499997951610986, 2.977408999572649151 ) ) ;
#51567 = EDGE_CURVE ( 'NONE', #17054, #34668, #28186, .T. ) ;
#51566 = CARTESIAN_POINT ( 'NONE',  ( -4.220049686691935698, 10.18810118749999916, 97.75000000204838102 ) ) ;
#51568 = CARTESIAN_POINT ( 'NONE',  ( -2.085542519210945728E-15, 224.5312499965860127, 11.35316468750000141 ) ) ;
#51569 = EDGE_LOOP ( 'NONE', ( #24417, #54359, #56897, #24099 ) ) ;
#51570 = CARTESIAN_POINT ( 'NONE',  ( 7.999999999999988454, -3.313708498984764272, 28.48655277982336997 ) ) ;
#51571 = DIRECTION ( 'NONE',  ( 0.000000000000000000, -1.000000000000000000, 0.000000000000000000 ) ) ;
#51572 = CARTESIAN_POINT ( 'NONE',  ( -7.999999999999998224, 120.5937500000000000, 3.313708498984766049 ) ) ;
#51573 = CARTESIAN_POINT ( 'NONE',  ( -9.832129032723420536, 213.6979166632526983, 5.676582343749997150 ) ) ;
#51574 = CARTESIAN_POINT ( 'NONE',  ( -47.32259252271279593, 191.7059220763548240, 65.76194439203463560 ) ) ;
#51575 = CARTESIAN_POINT ( 'NONE',  ( 1.226468279477575784E-15, 296.7031250017070079, 6.676582343750001591 ) ) ;
#51576 = ORIENTED_EDGE ( 'NONE', *, *, #39210, .F. ) ;
#51577 = DIRECTION ( 'NONE',  ( 0.000000000000000000, -0.000000000000000000, 1.000000000000000000 ) ) ;
#51578 = CARTESIAN_POINT ( 'NONE',  ( 8.311093377946837890, 211.7187499965860127, -8.311093377946837890 ) ) ;
#51579 = CARTESIAN_POINT ( 'NONE',  ( -4.220049686691935698, 10.18810118749999916, 92.87500000204838102 ) ) ;
#51580 = VECTOR ( 'NONE', #7556, 1000.000000000000000 ) ;
#51581 = CARTESIAN_POINT ( 'NONE',  ( -26.56734541678238060, 205.3750000013656063, 166.5412658750003629 ) ) ;
#51582 = CARTESIAN_POINT ( 'NONE',  ( 8.000000000000000000, 16.59375000000000711, -3.313708498984761608 ) ) ;
#51583 = VERTEX_POINT ( 'NONE', #1768 ) ;
#51584 = AXIS2_PLACEMENT_3D ( 'NONE', #10996, #61560, #32909 ) ;
#51585 = PRODUCT_DEFINITION_CONTEXT ( 'detailed design', #60674, 'design' ) ;
#51586 = CARTESIAN_POINT ( 'NONE',  ( 5.082755093536326818, 121.7187500020483952, 5.082755093536325042 ) ) ;
#51587 = CARTESIAN_POINT ( 'NONE',  ( -8.000000000000010658, -3.313708498984740736, 18.92405277982336642 ) ) ;
#51588 = CARTESIAN_POINT ( 'NONE',  ( -7.320508075688773708, 26.87500000000000355, -7.320508075688774596 ) ) ;
#51589 = AXIS2_PLACEMENT_3D ( 'NONE', #61290, #44312, #14499 ) ;
#51590 = LINE ( 'NONE', #40649, #60836 ) ;
#51591 = CARTESIAN_POINT ( 'NONE',  ( -10.18810118749999916, 4.220049686691934809, 79.93750000204839523 ) ) ;
#51592 = ORIENTED_EDGE ( 'NONE', *, *, #70693, .F. ) ;
#51593 = CARTESIAN_POINT ( 'NONE',  ( 2.828427124746191623, 20.12500000000000000, -2.828427124746191623 ) ) ;
#51594 =( BOUNDED_CURVE ( )  B_SPLINE_CURVE ( 2, ( #8669, #1550, #47536, #7563, #70561, #18877, #59613, #25260, #71285 ),
 .UNSPECIFIED., .F., .F. ) 
 B_SPLINE_CURVE_WITH_KNOTS ( ( 3, 2, 2, 2, 3 ),
 ( 0.2352941176470586815, 0.2389705882352939903, 0.2426470588235292714, 0.2463235294117645802, 0.2499999999999998612 ),
 .UNSPECIFIED. ) 
 CURVE ( )  GEOMETRIC_REPRESENTATION_ITEM ( )  RATIONAL_B_SPLINE_CURVE ( ( 1.000000000000002887, 0.9238795325112838519, 1.000000000000000000, 0.9238795325112867385, 1.000000000000000000, 0.9238795325112867385, 1.000000000000000000, 0.9238795325112896251, 0.9999999999999971134 ) ) 
 REPRESENTATION_ITEM ( '' )  );
#51595 = CARTESIAN_POINT ( 'NONE',  ( -2.572420464602065859, 21.96751355773091774, 3.849899326165059144 ) ) ;
#51596 =( BOUNDED_CURVE ( )  B_SPLINE_CURVE ( 2, ( #56278, #4596, #44212, #55543, #3853, #20814, #4228, #67225, #26849 ),
 .UNSPECIFIED., .F., .F. ) 
 B_SPLINE_CURVE_WITH_KNOTS ( ( 3, 2, 2, 2, 3 ),
 ( 0.7666666666666673846, 0.7750000000000006883, 0.7833333333333339921, 0.7916666666666672958, 0.8000000000000007105 ),
 .UNSPECIFIED. ) 
 CURVE ( )  GEOMETRIC_REPRESENTATION_ITEM ( )  RATIONAL_B_SPLINE_CURVE ( ( 0.9999999999999938938, 0.9238795325112928447, 1.000000000000000000, 0.9238795325112867385, 1.000000000000000000, 0.9238795325112867385, 1.000000000000000000, 0.9238795325112806323, 1.000000000000005995 ) ) 
 REPRESENTATION_ITEM ( '' )  );
#51597 = CARTESIAN_POINT ( 'NONE',  ( 0.4368895104448404787, 16.44602605510734605, -68.55492853905226980 ) ) ;
#51598 = CARTESIAN_POINT ( 'NONE',  ( -13.99999999999999822, 0.000000000000000000, 0.000000000000000000 ) ) ;
#51599 = CARTESIAN_POINT ( 'NONE',  ( -7.188101187500000044, 124.5312500020483810, 0.000000000000000000 ) ) ;
#51600 = CARTESIAN_POINT ( 'NONE',  ( 5.000000000000000000, 52.35862550122891435, 48.98731492261470777 ) ) ;
#51601 = CARTESIAN_POINT ( 'NONE',  ( 2.765530957081996366, 295.1406250017069510, -6.676582343750002480 ) ) ;
#51604 = CARTESIAN_POINT ( 'NONE',  ( -5.999999999999999112, 289.1250000034141294, 2.485281374238575314 ) ) ;
#51603 = CARTESIAN_POINT ( 'NONE',  ( -6.951808397369817780E-16, 242.6562500034140157, -11.35316468749999963 ) ) ;
#51602 = CARTESIAN_POINT ( 'NONE',  ( 31.45873412499999944, 205.6875000013656063, 169.9999999999998863 ) ) ;
#51605 = PRODUCT_CONTEXT ( 'NONE', #18274, 'mechanical' ) ;
#51606 = EDGE_LOOP ( 'NONE', ( #48147, #42846, #36726, #38814 ) ) ;
#51607 = CARTESIAN_POINT ( 'NONE',  ( 3.042071309553163960, 237.7604166700806161, -11.35316468749999785 ) ) ;
#51608 = CARTESIAN_POINT ( 'NONE',  ( -2.977408999572647819, 7.188101187499991163, 7.205302781871750994 ) ) ;
#51609 = VERTEX_POINT ( 'NONE', #19096 ) ;
#51610 = EDGE_CURVE ( 'NONE', #26967, #38945, #53447, .T. ) ;
#51611 = ORIENTED_EDGE ( 'NONE', *, *, #46092, .T. ) ;
#51612 = CARTESIAN_POINT ( 'NONE',  ( -10.18810118749999916, 4.220049686691934809, 75.06250000204836681 ) ) ;
#51613 = CARTESIAN_POINT ( 'NONE',  ( -8.311093377946841443, 89.21874999658602690, 8.311093377946830785 ) ) ;
#51614 = CARTESIAN_POINT ( 'NONE',  ( 5.000000000000000000, 60.90295814858223622, 23.31388853594876664 ) ) ;
#51615 = CARTESIAN_POINT ( 'NONE',  ( -11.00000000000000000, 4.556349186104045934, 81.90625000000000000 ) ) ;
#51618 = CYLINDRICAL_SURFACE ( 'NONE', #15732, 11.00000000000000000 ) ;
#51617 = CARTESIAN_POINT ( 'NONE',  ( 31.45873412499999944, 206.6875000013656063, 169.9999999999998863 ) ) ;
#51616 = CARTESIAN_POINT ( 'NONE',  ( 31.45873412500001010, 208.0000000013656347, 168.5673454167822740 ) ) ;
#51619 = VERTEX_POINT ( 'NONE', #65491 ) ;
#51620 = CYLINDRICAL_SURFACE ( 'NONE', #3159, 17.50000000000000000 ) ;
#51621 = CYLINDRICAL_SURFACE ( 'NONE', #49201, 4.000000000000001776 ) ;
#51622 = CARTESIAN_POINT ( 'NONE',  ( -9.832129032723420536, 203.6979166632526983, 5.676582343749997150 ) ) ;
#51623 = EDGE_CURVE ( 'NONE', #68174, #66108, #3687, .T. ) ;
#51624 = CARTESIAN_POINT ( 'NONE',  ( 2.445694354108782775, 204.5625000013656063, 139.5543056458912190 ) ) ;
#51625 = EDGE_CURVE ( 'NONE', #29110, #28748, #51945, .T. ) ;
#51626 = CARTESIAN_POINT ( 'NONE',  ( 31.45873412499999944, 207.9375000013656063, 169.9999999999999432 ) ) ;
#51627 = AXIS2_PLACEMENT_3D ( 'NONE', #52025, #36156, #23345 ) ;
#51628 = CARTESIAN_POINT ( 'NONE',  ( -2.977408999572650039, 14.81249999795161543, -7.188101187500001821 ) ) ;
#51629 = CARTESIAN_POINT ( 'NONE',  ( -8.311093377946836114, 177.9687499965860127, -8.311093377946837890 ) ) ;
#51630 = DIRECTION ( 'NONE',  ( 1.836970198721037823E-16, -4.283267841918042125E-17, 1.000000000000000000 ) ) ;
#51631 = CARTESIAN_POINT ( 'NONE',  ( -2.977408999572650927, 100.2500000020483810, -7.188101187500000933 ) ) ;
#51633 = CARTESIAN_POINT ( 'NONE',  ( -8.660254037844390851, 89.79166665983869677, 4.999999999999998224 ) ) ;
#51632 = DIRECTION ( 'NONE',  ( 0.000000000000000000, 0.000000000000000000, 1.000000000000000000 ) ) ;
#51634 = CARTESIAN_POINT ( 'NONE',  ( 1.881053915767122664, 11.12499999863440792, 4.541265875000001451 ) ) ;
#51635 = CARTESIAN_POINT ( 'NONE',  ( 30.44569435410879166, 200.8125000013656063, 172.4456943541087526 ) ) ;
#51636 = CARTESIAN_POINT ( 'NONE',  ( 2.977408999572646486, 7.188101187499991163, 11.89280278187175810 ) ) ;
#51637 = CARTESIAN_POINT ( 'NONE',  ( -11.35316468750000141, 58.28124999658601268, -1.390361679473963753E-15 ) ) ;
#51638 = DIRECTION ( 'NONE',  ( 0.000000000000000000, 0.000000000000000000, 1.000000000000000000 ) ) ;
#51639 = CARTESIAN_POINT ( 'NONE',  ( 5.656854249492374365, 5.656854249492375253, 3.324052784329822430 ) ) ;
#51640 = ORIENTED_EDGE ( 'NONE', *, *, #41790, .T. ) ;
#51641 = CARTESIAN_POINT ( 'NONE',  ( 11.02092980224260543, 7.493469672506262391, -0.7454400371385366819 ) ) ;
#51642 = CARTESIAN_POINT ( 'NONE',  ( 2.775557561562891351E-14, 210.0000000000000284, 198.0000000000000284 ) ) ;
#51643 = CARTESIAN_POINT ( 'NONE',  ( -11.35316468750000141, 58.28124999658601268, -1.390361679473963753E-15 ) ) ;
#51644 = AXIS2_PLACEMENT_3D ( 'NONE', #24787, #18039, #70825 ) ;
#51645 = CARTESIAN_POINT ( 'NONE',  ( -7.778174593052020747, -7.778174593052023411, 73.37500000409677625 ) ) ;
#51646 = CARTESIAN_POINT ( 'NONE',  ( 1.432654583217608080, 199.8750000013656063, 138.5412658750000503 ) ) ;
#51647 = CARTESIAN_POINT ( 'NONE',  ( -1.506524674528488372, 10.12152537343924941, 70.16785718945649819 ) ) ;
#51649 = CARTESIAN_POINT ( 'NONE',  ( -11.35316468749999785, 58.07291666325268409, -3.042071309553167957 ) ) ;
#51648 = CARTESIAN_POINT ( 'NONE',  ( -2.977408999572652260, 92.93750000204839523, 7.188101187500000044 ) ) ;
#51650 = CARTESIAN_POINT ( 'NONE',  ( -5.867873826482948196, -5.445834672501801421, 1.009359820037964095 ) ) ;
#51651 = DIRECTION ( 'NONE',  ( 0.000000000000000000, 0.000000000000000000, -1.000000000000000000 ) ) ;
#51652 = CARTESIAN_POINT ( 'NONE',  ( -8.311093377946841443, 173.9062499965860411, 8.311093377946830785 ) ) ;
#51653 = CIRCLE ( 'NONE', #27517, 10.00000000000000178 ) ;
#51654 = CARTESIAN_POINT ( 'NONE',  ( 7.320508075688771044, 146.2499999931719969, 7.320508075688775484 ) ) ;
#51655 = CARTESIAN_POINT ( 'NONE',  ( -2.977408999572651815, 99.31250000204839523, 7.188101187500000933 ) ) ;
#51656 = DIRECTION ( 'NONE',  ( -0.000000000000000000, -0.000000000000000000, 1.000000000000000000 ) ) ;
#51657 = CARTESIAN_POINT ( 'NONE',  ( -3.042071309553163960, 42.55208332991934128, -11.35316468749999963 ) ) ;
#51658 = CARTESIAN_POINT ( 'NONE',  ( 2.849036369511732440E-14, 201.2500000000000000, 202.0000000000000000 ) ) ;
#51659 = CARTESIAN_POINT ( 'NONE',  ( -11.35316468750000141, 178.4895833299193555, 3.042071309553159963 ) ) ;
#51660 = ORIENTED_EDGE ( 'NONE', *, *, #14403, .F. ) ;
#51661 = LINE ( 'NONE', #5277, #34430 ) ;
#51662 = CARTESIAN_POINT ( 'NONE',  ( -7.204075437095967871, 7.204075437095967871, 68.96875000204836681 ) ) ;
#51663 = CARTESIAN_POINT ( 'NONE',  ( -2.828427124746152987, 197.1250000000000284, 200.8284271247462129 ) ) ;
#51665 = CARTESIAN_POINT ( 'NONE',  ( -8.311093377946836114, 182.6562499965860411, -8.311093377946837890 ) ) ;
#51664 = LINE ( 'NONE', #56596, #2557 ) ;
#51666 = CARTESIAN_POINT ( 'NONE',  ( -7.999999999999991118, 3.313708498984756723, 3.792802784329823318 ) ) ;
#51667 = FACE_OUTER_BOUND ( 'NONE', #44901, .T. ) ;
#51668 = CARTESIAN_POINT ( 'NONE',  ( 5.000000000000004441, 249.7916666734946318, 8.660254037844385522 ) ) ;
#51669 = CARTESIAN_POINT ( 'NONE',  ( -30.82842712474616320, 206.3750000000000284, 172.8284271247465824 ) ) ;
#51670 = VERTEX_POINT ( 'NONE', #2494 ) ;
#51671 = DIRECTION ( 'NONE',  ( 0.000000000000000000, 0.000000000000000000, 1.000000000000000000 ) ) ;
#51672 = CARTESIAN_POINT ( 'NONE',  ( 11.35316468749999785, 125.8854166632526983, 3.042071309553174174 ) ) ;
#51673 = CARTESIAN_POINT ( 'NONE',  ( 2.679491924311222739, 10.83333332650536640, 10.00000000000000355 ) ) ;
#51674 = ORIENTED_EDGE ( 'NONE', *, *, #53996, .F. ) ;
#51675 = CARTESIAN_POINT ( 'NONE',  ( -1.881053915767124440, 9.124999998634407916, 4.541265875000001451 ) ) ;
#51676 = CARTESIAN_POINT ( 'NONE',  ( -7.188101187500000044, 14.71874999795161187, -8.802885111219163269E-16 ) ) ;
#51677 = CARTESIAN_POINT ( 'NONE',  ( 3.313708498984760720, 103.7187500040967763, -8.000000000000000000 ) ) ;
#51678 = CARTESIAN_POINT ( 'NONE',  ( -31.45873412499999233, 198.9375000013655779, 170.0000000000003979 ) ) ;
#51679 = VECTOR ( 'NONE', #68879, 1000.000000000000000 ) ;
#51680 = CARTESIAN_POINT ( 'NONE',  ( 2.449293598294707893E-16, 8.250000000000000000, -4.000000000000001776 ) ) ;
#51681 = CARTESIAN_POINT ( 'NONE',  ( -7.347880794884122694E-16, 20.49999999726881583, 4.000000000000001776 ) ) ;
#51682 = CARTESIAN_POINT ( 'NONE',  ( -4.541265875000002339, 13.81249999863440614, -5.561446717895856393E-16 ) ) ;
#51683 = CARTESIAN_POINT ( 'NONE',  ( -7.999999999999991118, 3.313708498984756723, 21.92405278392015333 ) ) ;
#51684 = CARTESIAN_POINT ( 'NONE',  ( -2.828427124746208943, 196.6250000000000284, 144.8284271247462129 ) ) ;
#51685 = ORIENTED_EDGE ( 'NONE', *, *, #71486, .T. ) ;
#51686 = CARTESIAN_POINT ( 'NONE',  ( -4.898587196589412829E-16, 99.31250000409677625, -8.000000000000000000 ) ) ;
#51687 = CARTESIAN_POINT ( 'NONE',  ( 5.082755093536325042, 102.5937500020483668, -5.082755093536325930 ) ) ;
#51690 = DIRECTION ( 'NONE',  ( 1.000000000000000000, -0.000000000000000000, -0.000000000000000000 ) ) ;
#51689 = CARTESIAN_POINT ( 'NONE',  ( -7.347880794884122694E-16, 10.49999999726881406, 4.000000000000001776 ) ) ;
#51688 =( BOUNDED_CURVE ( )  B_SPLINE_CURVE ( 2, ( #26808, #51972, #61139, #45930, #63651, #310, #49821, #51587, #62530 ),
 .UNSPECIFIED., .F., .F. ) 
 B_SPLINE_CURVE_WITH_KNOTS ( ( 3, 2, 2, 2, 3 ),
 ( 0.3421052631578947456, 0.3486842105263157632, 0.3552631578947368363, 0.3618421052631579649, 0.3684210526315789824 ),
 .UNSPECIFIED. ) 
 CURVE ( )  GEOMETRIC_REPRESENTATION_ITEM ( )  RATIONAL_B_SPLINE_CURVE ( ( 1.000000000000000000, 0.9238795325112867385, 1.000000000000000000, 0.9238795325112867385, 1.000000000000000000, 0.9238795325112867385, 1.000000000000000000, 0.9238795325112860723, 1.000000000000000666 ) ) 
 REPRESENTATION_ITEM ( '' )  );
#51691 = CARTESIAN_POINT ( 'NONE',  ( -8.342170076843785083E-16, 22.06249999863440792, 4.541265875000002339 ) ) ;
#51692 = EDGE_CURVE ( 'NONE', #53176, #51725, #34549, .T. ) ;
#51693 = CARTESIAN_POINT ( 'NONE',  ( -4.401442555609577197E-16, 7.188101187499992051, 2.611552781871750994 ) ) ;
#51694 = ORIENTED_EDGE ( 'NONE', *, *, #64252, .T. ) ;
#51695 = ORIENTED_EDGE ( 'NONE', *, *, #15669, .F. ) ;
#51696 = CARTESIAN_POINT ( 'NONE',  ( -10.18810118749999916, 4.220049686691934809, 90.06250000204838102 ) ) ;
#51697 = CARTESIAN_POINT ( 'NONE',  ( -31.99999999999995737, 195.4375000027312126, 171.6568542494928522 ) ) ;
#51698 = CARTESIAN_POINT ( 'NONE',  ( -31.45873412499999944, 197.8750000013656063, 168.5673454167827572 ) ) ;
#51699 = CARTESIAN_POINT ( 'NONE',  ( -7.778174593052020747, -7.778174593052023411, 103.1874999999999858 ) ) ;
#51700 = CARTESIAN_POINT ( 'NONE',  ( 2.839093476692135984E-14, 202.9375000013656063, 201.4587341250000350 ) ) ;
#51702 = CARTESIAN_POINT ( 'NONE',  ( -4.721056650415998313, 298.7343750017069510, 4.721056650416000089 ) ) ;
#51701 = DIRECTION ( 'NONE',  ( -0.000000000000000000, -0.000000000000000000, -1.000000000000000000 ) ) ;
#51703 = CARTESIAN_POINT ( 'NONE',  ( -7.320508075688773708, 116.8750000000000000, -7.320508075688774596 ) ) ;
#51704 = CARTESIAN_POINT ( 'NONE',  ( 3.313708498984760720, 100.5312500000000000, -8.000000000000000000 ) ) ;
#51705 = CARTESIAN_POINT ( 'NONE',  ( -2.765530957081996810, 288.4218750017070079, -6.676582343750003368 ) ) ;
#51706 = CARTESIAN_POINT ( 'NONE',  ( 5.082755093536318824, 5.082755093536319713, 4.299052781871752771 ) ) ;
#51708 =( BOUNDED_CURVE ( )  B_SPLINE_CURVE ( 2, ( #31889, #26587, #25465, #66961, #14514, #37552, #72238, #31133, #36806 ),
 .UNSPECIFIED., .F., .F. ) 
 B_SPLINE_CURVE_WITH_KNOTS ( ( 3, 2, 2, 2, 3 ),
 ( 0.8000000000000007105, 0.8083333333333340143, 0.8166666666666673180, 0.8250000000000006217, 0.8333333333333340365 ),
 .UNSPECIFIED. ) 
 CURVE ( )  GEOMETRIC_REPRESENTATION_ITEM ( )  RATIONAL_B_SPLINE_CURVE ( ( 0.9999999999999938938, 0.9238795325112928447, 1.000000000000000000, 0.9238795325112867385, 1.000000000000000000, 0.9238795325112867385, 1.000000000000000000, 0.9238795325112806323, 1.000000000000005995 ) ) 
 REPRESENTATION_ITEM ( '' )  );
#51707 = CARTESIAN_POINT ( 'NONE',  ( -8.000000000000000000, 102.5937500040967763, -3.313708498984761164 ) ) ;
#51709 = CARTESIAN_POINT ( 'NONE',  ( 26.56734541678232375, 201.3750000013656347, 173.4587341249998929 ) ) ;
#51710 = CARTESIAN_POINT ( 'NONE',  ( 7.999999999999998224, 28.21874999590322375, 3.313708498984766493 ) ) ;
#51711 = CARTESIAN_POINT ( 'NONE',  ( 11.99999999999999822, -5.801387104618779489, -0.7465129729868814623 ) ) ;
#51712 = CARTESIAN_POINT ( 'NONE',  ( -2.977408999572650927, 121.2500000020483952, -7.188101187500000933 ) ) ;
#51714 = CARTESIAN_POINT ( 'NONE',  ( 2.250000000000000000, 284.0000000000000000, 5.562148865321749014 ) ) ;
#51713 = CARTESIAN_POINT ( 'NONE',  ( 38.00000000000000000, 52.99999999999999289, 25.00000000000000000 ) ) ;
#51715 = CARTESIAN_POINT ( 'NONE',  ( -5.676582343750000703, 243.3854166700806445, -9.832129032723418760 ) ) ;
#51716 = CARTESIAN_POINT ( 'NONE',  ( 7.778174593052021635, 7.778174593052023411, 85.93749999999998579 ) ) ;
#51717 = CARTESIAN_POINT ( 'NONE',  ( 23.99999999999999645, 197.6875000000000000, 168.3431457505075173 ) ) ;
#51718 = CARTESIAN_POINT ( 'NONE',  ( 11.35316468749999963, 15.98958332991934839, -3.042071309553165293 ) ) ;
#51719 = CARTESIAN_POINT ( 'NONE',  ( -2.977408999572647819, 7.188101187499992051, 1.580302781871753659 ) ) ;
#51720 = CARTESIAN_POINT ( 'NONE',  ( -2.085542519210945728E-15, 224.8437499965860127, 11.35316468750000141 ) ) ;
#51721 = CARTESIAN_POINT ( 'NONE',  ( -23.99999999999997513, 198.6875000000000284, 171.6568542494927385 ) ) ;
#51722 = CARTESIAN_POINT ( 'NONE',  ( -4.999999999999992895, 240.8333333333333428, 8.660254037844390851 ) ) ;
#51724 = CARTESIAN_POINT ( 'NONE',  ( 13.99999999999999822, 0.000000000000000000, 0.000000000000000000 ) ) ;
#51723 = CARTESIAN_POINT ( 'NONE',  ( -0.4369882809986812555, 51.14729664189420077, 48.52014062455138088 ) ) ;
#51725 = VERTEX_POINT ( 'NONE', #37573 ) ;
#51727 = ADVANCED_FACE ( 'NONE', ( #8519 ), #70423, .T. ) ;
#51726 = CARTESIAN_POINT ( 'NONE',  ( 3.458734124999960358, 200.6250000013655779, 143.4326545832176976 ) ) ;
#51728 = ADVANCED_FACE ( 'NONE', ( #42836 ), #13056, .T. ) ;
#51729 = CARTESIAN_POINT ( 'NONE',  ( -9.832129032723420536, 28.69791666325268409, 5.676582343749997150 ) ) ;
#51730 = CARTESIAN_POINT ( 'NONE',  ( -10.99999999999999822, -4.556349186104052151, 94.28125000409676204 ) ) ;
#51731 = DIRECTION ( 'NONE',  ( 0.000000000000000000, -1.000000000000000000, 0.000000000000000000 ) ) ;
#51732 = CARTESIAN_POINT ( 'NONE',  ( -31.45873412500002075, 196.6250000013656063, 168.5673454167828140 ) ) ;
#51733 = DIRECTION ( 'NONE',  ( 0.000000000000000000, 0.000000000000000000, 1.000000000000000000 ) ) ;
#51735 = CARTESIAN_POINT ( 'NONE',  ( -11.35316468749999785, 23.07291666325268054, -3.042071309553167957 ) ) ;
#51734 = CARTESIAN_POINT ( 'NONE',  ( 7.188101187500000044, 109.9062500020483810, -8.802885111219163269E-16 ) ) ;
#51736 = CARTESIAN_POINT ( 'NONE',  ( -5.656854249492375253, 5.656854249492375253, 23.14280277982336642 ) ) ;
#51737 = CARTESIAN_POINT ( 'NONE',  ( -11.35316468750000141, 133.2812499965860127, -1.390361679473963753E-15 ) ) ;
#51738 = ADVANCED_FACE ( 'NONE', ( #14164 ), #31536, .T. ) ;
#51739 = CARTESIAN_POINT ( 'NONE',  ( 2.679491924311228956, 102.9166666598386826, -10.00000000000000000 ) ) ;
#51740 = CARTESIAN_POINT ( 'NONE',  ( 5.082755093536326818, 114.5937500020483810, 5.082755093536325042 ) ) ;
#51741 = CARTESIAN_POINT ( 'NONE',  ( 37.99999999999999289, 50.00000000000000711, 57.99999999999999289 ) ) ;
#51742 = CARTESIAN_POINT ( 'NONE',  ( -24.54126587499999701, 209.4375000013656063, 170.0000000000003411 ) ) ;
#51743 = CARTESIAN_POINT ( 'NONE',  ( -5.000000000000000000, 53.50771145605737189, -45.03482491321273073 ) ) ;
#51744 = ORIENTED_EDGE ( 'NONE', *, *, #28892, .F. ) ;
#51745 = CARTESIAN_POINT ( 'NONE',  ( 11.35316468749999963, 11.30208332991934839, -3.042071309553165293 ) ) ;
#51746 = CARTESIAN_POINT ( 'NONE',  ( -2.828427124746192067, 20.37499999726881228, 2.828427124746190735 ) ) ;
#51747 = CARTESIAN_POINT ( 'NONE',  ( 6.676582343750001591, 298.9531250017069510, -8.176455196517173205E-16 ) ) ;
#51748 = CARTESIAN_POINT ( 'NONE',  ( -2.085542519210945728E-15, 139.5312499965860411, 11.35316468750000141 ) ) ;
#51749 = CARTESIAN_POINT ( 'NONE',  ( 5.000000000000000888, 53.20585484986760605, 47.69738026034786316 ) ) ;
#51750 = CARTESIAN_POINT ( 'NONE',  ( 5.656854249492376141, -5.656854249492374365, 25.44905278432982954 ) ) ;
#51751 = CARTESIAN_POINT ( 'NONE',  ( -2.849036369511732440E-14, 207.3750000027312126, 138.0000000000000568 ) ) ;
#51752 = AXIS2_PLACEMENT_3D ( 'NONE', #22595, #57702, #738 ) ;
#51753 = CARTESIAN_POINT ( 'NONE',  ( -3.042071309553166181, 257.8645833367473301, -11.35316468749999608 ) ) ;
#51754 = EDGE_CURVE ( 'NONE', #33835, #5549, #24563, .T. ) ;
#51755 = CARTESIAN_POINT ( 'NONE',  ( -10.18810118749999916, 4.220049686691934809, 99.43750000204836681 ) ) ;
#51756 = ORIENTED_EDGE ( 'NONE', *, *, #21337, .T. ) ;
#51757 = CARTESIAN_POINT ( 'NONE',  ( 5.000000000000000000, 10.26105934116143281, 64.40045319026697257 ) ) ;
#51758 = DIRECTION ( 'NONE',  ( 0.000000000000000000, -0.000000000000000000, 1.000000000000000000 ) ) ;
#51759 = CARTESIAN_POINT ( 'NONE',  ( -1.432654583217607414, 201.5000000013655779, 194.5412658750000219 ) ) ;
#51760 = CARTESIAN_POINT ( 'NONE',  ( 9.832129032723416984, 70.67708332991935549, 5.676582343750006032 ) ) ;
#51761 = VERTEX_POINT ( 'NONE', #67733 ) ;
#51762 = CARTESIAN_POINT ( 'NONE',  ( 4.220049686691934809, 10.18810118749999916, 106.1875000020483810 ) ) ;
#51763 = CARTESIAN_POINT ( 'NONE',  ( -8.342170076843785083E-16, 14.18749999863440792, 4.541265875000002339 ) ) ;
#51764 = ORIENTED_EDGE ( 'NONE', *, *, #36932, .F. ) ;
#51765 = ORIENTED_EDGE ( 'NONE', *, *, #23518, .T. ) ;
#51766 = CARTESIAN_POINT ( 'NONE',  ( 2.977408999572651815, 27.18749999795161898, 7.188101187500000933 ) ) ;
#51767 = CARTESIAN_POINT ( 'NONE',  ( -8.660254037844387298, 108.9583333265053682, -5.000000000000004441 ) ) ;
#51768 = CARTESIAN_POINT ( 'NONE',  ( 2.849036369511732440E-14, 197.3750000027312126, 202.0000000000000000 ) ) ;
#51769 = CARTESIAN_POINT ( 'NONE',  ( -2.977408999572654480, 25.87499999795161543, 7.188101187499999156 ) ) ;
#51770 = LINE ( 'NONE', #117, #44811 ) ;
#51771 = CARTESIAN_POINT ( 'NONE',  ( -7.204075437095967871, 7.204075437095967871, 106.8437500020483810 ) ) ;
#51772 = PRODUCT ( 'spindle', 'spindle', '', ( #28594 ) ) ;
#51773 = CARTESIAN_POINT ( 'NONE',  ( -28.00000000000008171, 209.5625000013656063, 166.0000000000003695 ) ) ;
#51774 = CARTESIAN_POINT ( 'NONE',  ( 4.000000000000001776, 8.749999997268814056, 0.000000000000000000 ) ) ;
#51775 = DIRECTION ( 'NONE',  ( -0.000000000000000000, 1.000000000000000000, -0.000000000000000000 ) ) ;
#51776 = ORIENTED_EDGE ( 'NONE', *, *, #46091, .T. ) ;
#51777 = CARTESIAN_POINT ( 'NONE',  ( -2.726571689596997292E-14, 210.0000000000000284, 138.0000000000000568 ) ) ;
#51778 = CARTESIAN_POINT ( 'NONE',  ( -3.458734124999959914, 203.4375000013656063, 198.0000000000000284 ) ) ;
#51779 = CARTESIAN_POINT ( 'NONE',  ( -31.45873412500002431, 206.6250000013656063, 168.5673454167828140 ) ) ;
#51780 = CARTESIAN_POINT ( 'NONE',  ( 29.65685424949245075, 199.5625000027312126, 165.9999999999999716 ) ) ;
#51781 = CARTESIAN_POINT ( 'NONE',  ( -4.541265875000003227, 11.87499999863440969, 1.881053915767121110 ) ) ;
#51782 = AXIS2_PLACEMENT_3D ( 'NONE', #68403, #22363, #74064 ) ;
#51783 = CARTESIAN_POINT ( 'NONE',  ( 2.449293598294707893E-16, 9.999999997268814056, -4.000000000000001776 ) ) ;
#51784 = CARTESIAN_POINT ( 'NONE',  ( -5.082755093536317936, -5.082755093536320601, 21.17405278187175455 ) ) ;
#51785 = ORIENTED_EDGE ( 'NONE', *, *, #67567, .F. ) ;
#51786 = VERTEX_POINT ( 'NONE', #38697 ) ;
#51787 = CARTESIAN_POINT ( 'NONE',  ( -10.18810118749999738, -4.220049686691941915, 108.2500000020483810 ) ) ;
#51788 = CARTESIAN_POINT ( 'NONE',  ( 10.99999999999994849, 4.556349186104097448, 96.53125000409677625 ) ) ;
#51789 = CARTESIAN_POINT ( 'NONE',  ( -25.17157287525382259, 205.8750000000000284, 167.1715728752541565 ) ) ;
#51790 = CARTESIAN_POINT ( 'NONE',  ( -3.458734124999959025, 201.5000000013655779, 199.4326545832176691 ) ) ;
#51791 = CARTESIAN_POINT ( 'NONE',  ( 30.44569435410879166, 196.8125000013656063, 167.5543056458910485 ) ) ;
#51792 = CARTESIAN_POINT ( 'NONE',  ( 10.00000000000000000, 79.79166666666668561, 2.679491924311236062 ) ) ;
#51793 = EDGE_CURVE ( 'NONE', #53587, #14276, #18655, .T. ) ;
#51794 = AXIS2_PLACEMENT_3D ( 'NONE', #36593, #59604, #8662 ) ;
#51795 = CARTESIAN_POINT ( 'NONE',  ( 1.320432766682874540E-15, 90.40625000204838102, 7.188101187500000044 ) ) ;
#51796 = CARTESIAN_POINT ( 'NONE',  ( -3.042071309553173730, 59.63541666325267698, 11.35316468749999785 ) ) ;
#51797 = CARTESIAN_POINT ( 'NONE',  ( 2.485281374238575314, 290.3124999999999432, 6.000000000000000888 ) ) ;
#51798 = ORIENTED_EDGE ( 'NONE', *, *, #33167, .F. ) ;
#51799 = CARTESIAN_POINT ( 'NONE',  ( 10.00000000000000178, 252.2916666666666856, 2.679491924311222739 ) ) ;
#51800 = CARTESIAN_POINT ( 'NONE',  ( -4.471435261917410919, -60.74652839096143708, 23.21845616858397676 ) ) ;
#51801 = CARTESIAN_POINT ( 'NONE',  ( 2.828427124746152987, 196.2500000027312126, 139.1715728752538723 ) ) ;
#51802 = CARTESIAN_POINT ( 'NONE',  ( 5.000000000000001776, 57.70833332650537528, -8.660254037844389075 ) ) ;
#51803 = CARTESIAN_POINT ( 'NONE',  ( 5.656854249492378806, 5.624999995903220196, 5.656854249492381470 ) ) ;
#51804 = CARTESIAN_POINT ( 'NONE',  ( -2.679491924311228512, 238.9583333333333144, -9.999999999999998224 ) ) ;
#51805 = CARTESIAN_POINT ( 'NONE',  ( 11.00000000000000000, 1.347111479062088405E-15, 72.43750000409676204 ) ) ;
#51806 = CARTESIAN_POINT ( 'NONE',  ( 1.871523826299183495E-15, -10.18810118749999916, 68.40625000204836681 ) ) ;
#51807 =( BOUNDED_CURVE ( )  B_SPLINE_CURVE ( 2, ( #3517, #32192, #72551, #21599, #51767, #51391, #28751, #28382, #114, #34072, #74030, #4641, #46104 ),
 .UNSPECIFIED., .F., .F. ) 
 B_SPLINE_CURVE_WITH_KNOTS ( ( 3, 2, 2, 2, 2, 2, 3 ),
 ( 0.4619565217391304879, 0.4637681159420290466, 0.4655797101449276054, 0.4673913043478261642, 0.4692028985507246674, 0.4710144927536232262, 0.4728260869565217850 ),
 .UNSPECIFIED. ) 
 CURVE ( )  GEOMETRIC_REPRESENTATION_ITEM ( )  RATIONAL_B_SPLINE_CURVE ( ( 0.9999999999999990008, 0.9659258262890693114, 1.000000000000000000, 0.9659258262890683122, 1.000000000000000000, 0.9659258262890683122, 1.000000000000000000, 0.9659258262890683122, 1.000000000000000000, 0.9659258262890683122, 1.000000000000000000, 0.9659258262890673130, 1.000000000000001110 ) ) 
 REPRESENTATION_ITEM ( '' )  );
#51808 = CARTESIAN_POINT ( 'NONE',  ( 4.999999999999993783, 199.1666666666666856, 8.660254037844390851 ) ) ;
#51809 = CARTESIAN_POINT ( 'NONE',  ( -7.188101187499990274, -2.977408999572651815, 18.45530278187175455 ) ) ;
#51810 = CARTESIAN_POINT ( 'NONE',  ( 3.042071309553167069, 162.1354166632526983, -11.35316468749999785 ) ) ;
#51811 = CARTESIAN_POINT ( 'NONE',  ( -7.320508075688936245, 211.8750000000000853, -7.320508075688936245 ) ) ;
#51812 = CARTESIAN_POINT ( 'NONE',  ( 2.679491924311222739, 175.8333333265053966, 10.00000000000000355 ) ) ;
#51814 = CARTESIAN_POINT ( 'NONE',  ( -2.485281374238967000, 296.8750000034140726, -5.999999999999608313 ) ) ;
#51813 = CARTESIAN_POINT ( 'NONE',  ( 30.64284399271082293, 271.9999999999999432, 174.6921329945330683 ) ) ;
#51815 = VERTEX_POINT ( 'NONE', #45087 ) ;
#51817 = EDGE_CURVE ( 'NONE', #64471, #69918, #38319, .T. ) ;
#51816 = CARTESIAN_POINT ( 'NONE',  ( -2.445694354108839619, 195.8125000013656063, 139.5543056458912190 ) ) ;
#51818 = CARTESIAN_POINT ( 'NONE',  ( 11.35316468749999963, 36.30208332991935549, -3.042071309553165293 ) ) ;
#51819 = CARTESIAN_POINT ( 'NONE',  ( 4.556349186104051263, -10.99999999999999822, 109.6562500040967905 ) ) ;
#51820 = CARTESIAN_POINT ( 'NONE',  ( -25.55430564589123321, 209.3125000013656063, 167.5543056458915032 ) ) ;
#51821 = DIRECTION ( 'NONE',  ( 1.000000000000000000, -0.000000000000000000, -0.000000000000000000 ) ) ;
#51823 = FACE_OUTER_BOUND ( 'NONE', #6233, .T. ) ;
#51822 = CARTESIAN_POINT ( 'NONE',  ( 4.999999999999993783, 221.0416666598387110, 8.660254037844390851 ) ) ;
#51824 = CARTESIAN_POINT ( 'NONE',  ( 26.34314575050765939, 201.6875000027312410, 165.9999999999998579 ) ) ;
#51825 = CARTESIAN_POINT ( 'NONE',  ( -3.458734125000015425, 198.0000000013656063, 143.4326545832176976 ) ) ;
#51826 = CARTESIAN_POINT ( 'NONE',  ( 2.679491924311228956, 62.91666665983868967, -10.00000000000000000 ) ) ;
#51827 = CARTESIAN_POINT ( 'NONE',  ( -2.977408999572651815, 104.9375000020483810, 7.188101187500000933 ) ) ;
#51828 = CARTESIAN_POINT ( 'NONE',  ( -4.541265875000002339, 11.87499999863440969, -1.881053915767121998 ) ) ;
#51829 = CARTESIAN_POINT ( 'NONE',  ( 1.502314598737163567E-15, -20.78460969082658494, -20.69999999999999929 ) ) ;
#51830 = CARTESIAN_POINT ( 'NONE',  ( 5.656854249492376141, -5.656854249492374365, 4.392802779823363757 ) ) ;
#51831 = CARTESIAN_POINT ( 'NONE',  ( -4.193030820682222881, -50.40097124335162704, 40.95512985424973351 ) ) ;
#51832 = VERTEX_POINT ( 'NONE', #56051 ) ;
#51833 = ORIENTED_EDGE ( 'NONE', *, *, #30709, .F. ) ;
#51834 = CARTESIAN_POINT ( 'NONE',  ( -2.679491924304188810, 196.4583333333328596, -10.00000000000419043 ) ) ;
#51835 = CARTESIAN_POINT ( 'NONE',  ( -4.721056650415999201, 297.4843750017070079, -4.721056650415999201 ) ) ;
#51836 = SURFACE_STYLE_FILL_AREA ( #23158 ) ;
#51837 = DIRECTION ( 'NONE',  ( -0.000000000000000000, 1.000000000000000000, -0.000000000000000000 ) ) ;
#51838 = CARTESIAN_POINT ( 'NONE',  ( -3.042071309553164404, 142.2395833299193839, -11.35316468749999963 ) ) ;
#51839 = CARTESIAN_POINT ( 'NONE',  ( -7.347880794884122694E-16, 6.750000000000000000, 4.000000000000001776 ) ) ;
#51840 = CARTESIAN_POINT ( 'NONE',  ( 10.18810118749999916, 4.220049686691935698, 82.00000000204836681 ) ) ;
#51841 = CARTESIAN_POINT ( 'NONE',  ( -30.76847783166666872, 194.6767860410252240, 172.4299946856685040 ) ) ;
#51842 = CARTESIAN_POINT ( 'NONE',  ( -3.999999999999960032, 203.9375000000000000, 196.3431457505076594 ) ) ;
#51843 = CYLINDRICAL_SURFACE ( 'NONE', #20483, 8.000000000000000000 ) ;
#51844 = ADVANCED_FACE ( 'NONE', ( #16029 ), #72261, .T. ) ;
#51845 = CARTESIAN_POINT ( 'NONE',  ( -10.18810118749999916, 4.220049686691934809, 117.4375000020483810 ) ) ;
#51846 = EDGE_LOOP ( 'NONE', ( #28314, #45284, #70606, #10969 ) ) ;
#51847 = EDGE_CURVE ( 'NONE', #63005, #56250, #67357, .T. ) ;
#51848 = AXIS2_PLACEMENT_3D ( 'NONE', #59233, #41500, #7176 ) ;
#51849 = CARTESIAN_POINT ( 'NONE',  ( 1.469576158976823947E-15, 96.87499999999998579, 8.000000000000000000 ) ) ;
#51850 = CARTESIAN_POINT ( 'NONE',  ( -8.901020801742189903, 183.4979971941717167, 140.2200920701657196 ) ) ;
#51851 = CARTESIAN_POINT ( 'NONE',  ( -8.311093377946836114, 122.9687499965860127, -8.311093377946837890 ) ) ;
#51852 = CARTESIAN_POINT ( 'NONE',  ( 2.445694354108839619, 200.8125000013656063, 200.4456943541088663 ) ) ;
#51853 = CARTESIAN_POINT ( 'NONE',  ( 7.188101187500000933, 24.93749999795161543, -2.977408999572650483 ) ) ;
#51854 = CARTESIAN_POINT ( 'NONE',  ( 10.18810118750000093, -4.220049686691933033, 77.68750000204838102 ) ) ;
#51855 = CARTESIAN_POINT ( 'NONE',  ( -5.676582343749998039, 37.76041666325267698, -9.832129032723420536 ) ) ;
#51856 = ORIENTED_EDGE ( 'NONE', *, *, #13168, .F. ) ;
#51857 = CARTESIAN_POINT ( 'NONE',  ( 27.99999999999999645, 195.0000000000000000, 169.9999999999999147 ) ) ;
#51858 = CARTESIAN_POINT ( 'NONE',  ( -1.881053915767124440, 2.124999998634406584, 4.541265875000001451 ) ) ;
#51859 = CARTESIAN_POINT ( 'NONE',  ( -4.903558642999205574E-16, 8.008118988124991233, 14.13811528394063188 ) ) ;
#51860 = CARTESIAN_POINT ( 'NONE',  ( 1.432654583217608080, 206.8750000013656347, 138.5412658750000503 ) ) ;
#51861 = CIRCLE ( 'NONE', #19298, 71.70204102886728492 ) ;
#51862 = EDGE_CURVE ( 'NONE', #23203, #62806, #47352, .T. ) ;
#51863 = EDGE_CURVE ( 'NONE', #8159, #71834, #62063, .T. ) ;
#51864 = VECTOR ( 'NONE', #1294, 1000.000000000000000 ) ;
#51865 = CARTESIAN_POINT ( 'NONE',  ( -7.188101187500000044, 7.218749997951610986, -8.802885111219163269E-16 ) ) ;
#51866 = CARTESIAN_POINT ( 'NONE',  ( -3.673940397442060854E-16, 297.8125000034140157, -6.000000000000001776 ) ) ;
#51867 = CARTESIAN_POINT ( 'NONE',  ( -19.25037841756599732, -15.80982980707932839, 137.0612338252263100 ) ) ;
#51868 = CARTESIAN_POINT ( 'NONE',  ( 7.188101187499999156, 3.749999997951610542, 2.977408999572654924 ) ) ;
#51869 = CARTESIAN_POINT ( 'NONE',  ( 7.188101187499992051, 8.802885111219154394E-16, 14.23655278187175455 ) ) ;
#51870 = CARTESIAN_POINT ( 'NONE',  ( -9.832129032723420536, 154.0104166632526983, 5.676582343749997150 ) ) ;
#51871 = CARTESIAN_POINT ( 'NONE',  ( 10.18810118749999916, 4.220049686691935698, 68.50000000204838102 ) ) ;
#51872 = EDGE_CURVE ( 'NONE', #20252, #41754, #18450, .T. ) ;
#51873 = CARTESIAN_POINT ( 'NONE',  ( -26.56734541678238415, 207.6250000013656347, 166.5412658750003629 ) ) ;
#51874 = CARTESIAN_POINT ( 'NONE',  ( -8.000000000000003553, 9.797174393178831574E-16, -25.03750572909317285 ) ) ;
#51875 = CARTESIAN_POINT ( 'NONE',  ( 4.541265875000002339, 19.43749999863440436, 0.000000000000000000 ) ) ;
#51876 = VERTEX_POINT ( 'NONE', #49999 ) ;
#51877 = CARTESIAN_POINT ( 'NONE',  ( -2.828427124746152987, 199.2500000027312126, 200.8284271247462129 ) ) ;
#51878 = AXIS2_PLACEMENT_3D ( 'NONE', #3495, #72526, #20835 ) ;
#51879 = CARTESIAN_POINT ( 'NONE',  ( -1.656854249492405451, 208.3125000000000000, 138.0000000000000568 ) ) ;
#51880 = CARTESIAN_POINT ( 'NONE',  ( -30.82842712474612412, 201.5000000027312126, 172.8284271247466108 ) ) ;
#51881 = CARTESIAN_POINT ( 'NONE',  ( -10.00000000000007816, 57.29166666666671404, -2.679491924311251605 ) ) ;
#51882 = CARTESIAN_POINT ( 'NONE',  ( 7.999999999999992895, -3.313708498984756279, 10.67405278392014623 ) ) ;
#51883 = ORIENTED_EDGE ( 'NONE', *, *, #34911, .T. ) ;
#51884 = CARTESIAN_POINT ( 'NONE',  ( -7.188101187500000933, 14.62499999795161187, -2.977408999572651371 ) ) ;
#51885 = CARTESIAN_POINT ( 'NONE',  ( -2.485281374238159646, 298.2500000034140157, 6.000000000000414779 ) ) ;
#51886 = CARTESIAN_POINT ( 'NONE',  ( 0.4320110153364595806, -10.28109898471437589, -63.57214792341208920 ) ) ;
#51887 = CARTESIAN_POINT ( 'NONE',  ( -1.836970198721029983E-15, 38.75000000000000000, 10.00000000000000178 ) ) ;
#51888 = CARTESIAN_POINT ( 'NONE',  ( 2.977408999572654480, 108.5000000020483810, 7.188101187499999156 ) ) ;
#51889 = CARTESIAN_POINT ( 'NONE',  ( -25.55430564589115505, 208.3125000013656063, 172.4456943541091789 ) ) ;
#51890 = CARTESIAN_POINT ( 'NONE',  ( -2.849036369511732440E-14, 205.3750000027312126, 138.0000000000000568 ) ) ;
#51892 = CARTESIAN_POINT ( 'NONE',  ( 2.679491924311228956, 197.9166666598386826, -10.00000000000000000 ) ) ;
#51891 = CARTESIAN_POINT ( 'NONE',  ( -8.000000000000000000, 111.6875000040967905, 0.000000000000000000 ) ) ;
#51893 = EDGE_LOOP ( 'NONE', ( #36235, #13259, #39157, #37616, #23648 ) ) ;
#51895 = CARTESIAN_POINT ( 'NONE',  ( 8.311093377946834337, 242.0312500034140157, -8.311093377946836114 ) ) ;
#51894 = AXIS2_PLACEMENT_3D ( 'NONE', #31279, #13173, #42592 ) ;
#51896 = CARTESIAN_POINT ( 'NONE',  ( 7.188101187499992051, 8.802885111219154394E-16, 17.61155278187175810 ) ) ;
#51897 = CARTESIAN_POINT ( 'NONE',  ( -7.320508075688778149, 9.999999993172032475, 7.320508075688769267 ) ) ;
#51898 = CARTESIAN_POINT ( 'NONE',  ( -9.418986816871308676, 219.9999999999999716, 5.041166117107052536 ) ) ;
#51900 = ADVANCED_FACE ( 'NONE', ( #62429 ), #73754, .F. ) ;
#51899 = CYLINDRICAL_SURFACE ( 'NONE', #2969, 8.000000000000000000 ) ;
#51901 = CARTESIAN_POINT ( 'NONE',  ( 7.320508075688774596, 155.6250000000000284, -7.320508075688774596 ) ) ;
#51902 = CYLINDRICAL_SURFACE ( 'NONE', #14036, 4.000000000000001776 ) ;
#51903 = LINE ( 'NONE', #34570, #43986 ) ;
#51904 = LINE ( 'NONE', #17563, #12269 ) ;
#51905 = CARTESIAN_POINT ( 'NONE',  ( 3.042071309553159519, 130.0520833299193555, 11.35316468750000141 ) ) ;
#51906 = FACE_OUTER_BOUND ( 'NONE', #8047, .T. ) ;
#51907 = CARTESIAN_POINT ( 'NONE',  ( -7.999999999999991118, 3.313708498984757167, 27.92405278392015333 ) ) ;
#51910 = CARTESIAN_POINT ( 'NONE',  ( -7.778174593052023411, 7.778174593052023411, 85.00000000409677625 ) ) ;
#51909 = CARTESIAN_POINT ( 'NONE',  ( 24.54126587499999701, 195.2500000013656063, 171.4326545832175839 ) ) ;
#51908 = CARTESIAN_POINT ( 'NONE',  ( 31.45873412499999944, 196.0000000013656347, 168.5673454167822740 ) ) ;
#51911 = EDGE_LOOP ( 'NONE', ( #22855, #19993, #40996, #38038 ) ) ;
#51912 = CARTESIAN_POINT ( 'NONE',  ( 5.000000000000000000, -60.90295814858255596, 23.31388853594792110 ) ) ;
#51913 = AXIS2_PLACEMENT_3D ( 'NONE', #56109, #37638, #15344 ) ;
#51914 = CARTESIAN_POINT ( 'NONE',  ( 0.000000000000000000, 0.000000000000000000, 29.33030277982336642 ) ) ;
#51915 = CARTESIAN_POINT ( 'NONE',  ( -8.000000000000005329, 0.000000000000000000, -14.77459999999999951 ) ) ;
#51916 = CARTESIAN_POINT ( 'NONE',  ( 5.000000000000000000, -68.60357193678697740, -20.85024232999374050 ) ) ;
#51917 = EDGE_CURVE ( 'NONE', #73747, #64725, #46646, .T. ) ;
#51918 = CARTESIAN_POINT ( 'NONE',  ( -4.999999999999998224, 18.54166665983870033, -8.660254037844389075 ) ) ;
#51919 = CARTESIAN_POINT ( 'NONE',  ( -2.977408999572651815, 121.4375000020483668, 7.188101187500000933 ) ) ;
#51920 = CARTESIAN_POINT ( 'NONE',  ( -4.541265875000002339, 20.74999999863440436, -1.881053915767121998 ) ) ;
#51921 = CARTESIAN_POINT ( 'NONE',  ( 0.4451317748864607737, 67.59323688304490929, -20.03471819849965030 ) ) ;
#51922 = CARTESIAN_POINT ( 'NONE',  ( -4.898587196589407898E-16, 7.999999999999991118, 21.45530277982336642 ) ) ;
#51924 = CARTESIAN_POINT ( 'NONE',  ( 23.99999999999999645, 196.6875000000000284, 168.3431457505074889 ) ) ;
#51923 = CARTESIAN_POINT ( 'NONE',  ( 3.472923220124667587, -7.207533209433660382, -2.138143543582478310E-15 ) ) ;
#51925 = CARTESIAN_POINT ( 'NONE',  ( -11.35316468750000141, 103.2812499965860269, -1.390361679473963753E-15 ) ) ;
#51926 = EDGE_LOOP ( 'NONE', ( #39526, #40514, #57288, #72767 ) ) ;
#51927 = CARTESIAN_POINT ( 'NONE',  ( -4.000000000000016875, 205.5625000027312126, 140.3431457505076594 ) ) ;
#51929 = CARTESIAN_POINT ( 'NONE',  ( 7.188101187500000044, 22.96874999795161543, 0.000000000000000000 ) ) ;
#51928 = PRODUCT_DEFINITION ( 'UNKNOWN', '', #44193, #56892 ) ;
#51930 = CARTESIAN_POINT ( 'NONE',  ( 8.660254037844525854, 40.41666666666676377, -5.000000000000079936 ) ) ;
#51931 = CARTESIAN_POINT ( 'NONE',  ( 8.311093377946839666, 246.0937500034139873, 8.311093377946830785 ) ) ;
#51932 = CARTESIAN_POINT ( 'NONE',  ( 5.676582343750001591, 101.6145833299193697, -9.832129032723420536 ) ) ;
#51933 = EDGE_LOOP ( 'NONE', ( #19157, #70875 ) ) ;
#51934 = CARTESIAN_POINT ( 'NONE',  ( 5.000000000000000000, -14.13320814749868326, 69.81894086168452418 ) ) ;
#51935 = CARTESIAN_POINT ( 'NONE',  ( -10.18810118749999738, -4.220049686691941915, 103.7500000020483668 ) ) ;
#51936 = CARTESIAN_POINT ( 'NONE',  ( 2.679491924311228956, 217.9166666598387110, -10.00000000000000000 ) ) ;
#51937 = CARTESIAN_POINT ( 'NONE',  ( -2.445694354108784108, 199.5625000013656063, 195.5543056458912190 ) ) ;
#51938 = CARTESIAN_POINT ( 'NONE',  ( -4.076600168545496672E-14, -10.39230484541327471, -0.8038475772933779684 ) ) ;
#51940 = CARTESIAN_POINT ( 'NONE',  ( 5.676582343749993598, 94.94791666325269830, 9.832129032723422313 ) ) ;
#51939 = CARTESIAN_POINT ( 'NONE',  ( -3.999999999999960032, 206.0625000027312410, 196.3431457505076594 ) ) ;
#51941 = CARTESIAN_POINT ( 'NONE',  ( 1.469576158976822172E-15, -7.999999999999991118, 14.89280278392014623 ) ) ;
#51942 = CARTESIAN_POINT ( 'NONE',  ( -31.45873412499999233, 194.9375000013655779, 170.0000000000003979 ) ) ;
#51943 = CARTESIAN_POINT ( 'NONE',  ( 4.898587196589412829E-16, 27.18749999590322375, -8.000000000000000000 ) ) ;
#51944 = ORIENTED_EDGE ( 'NONE', *, *, #34293, .F. ) ;
#51945 =( BOUNDED_CURVE ( )  B_SPLINE_CURVE ( 2, ( #2865, #42101, #43213, #53812, #8151, #71139, #36828, #19463, #65113, #42474, #3239, #59837, #13424 ),
 .UNSPECIFIED., .F., .F. ) 
 B_SPLINE_CURVE_WITH_KNOTS ( ( 3, 2, 2, 2, 2, 2, 3 ),
 ( 0.5380434782608695121, 0.5398550724637680709, 0.5416666666666666297, 0.5434782608695651884, 0.5452898550724637472, 0.5471014492753623060, 0.5489130434782608647 ),
 .UNSPECIFIED. ) 
 CURVE ( )  GEOMETRIC_REPRESENTATION_ITEM ( )  RATIONAL_B_SPLINE_CURVE ( ( 1.000000000000000000, 0.9659258262890683122, 1.000000000000000000, 0.9659258262890683122, 1.000000000000000000, 0.9659258262890683122, 1.000000000000000000, 0.9659258262890683122, 1.000000000000000000, 0.9659258262890683122, 1.000000000000000000, 0.9659258262890683122, 1.000000000000000000 ) ) 
 REPRESENTATION_ITEM ( '' )  );
#51946 = CARTESIAN_POINT ( 'NONE',  ( -7.320508075688778149, 189.9999999931720538, 7.320508075688769267 ) ) ;
#51947 = EDGE_CURVE ( 'NONE', #49077, #4470, #62372, .T. ) ;
#51948 = CARTESIAN_POINT ( 'NONE',  ( 1.656854249492381914, 5.812500000000000000, 4.000000000000000888 ) ) ;
#51949 = CARTESIAN_POINT ( 'NONE',  ( 2.828427124746190291, 9.624999997268814056, 2.828427124746192067 ) ) ;
#51950 = CARTESIAN_POINT ( 'NONE',  ( -2.085542519210945728E-15, 89.84374999658602690, 11.35316468750000141 ) ) ;
#51951 = CARTESIAN_POINT ( 'NONE',  ( -4.088227598258586603E-16, 288.2031250017069510, -6.676582343750001591 ) ) ;
#51952 = CARTESIAN_POINT ( 'NONE',  ( -2.977408999572654480, 4.874999997951610986, 7.188101187499999156 ) ) ;
#51953 = CARTESIAN_POINT ( 'NONE',  ( 10.18810118749999916, 4.220049686691935698, 97.37500000204839523 ) ) ;
#51954 = CARTESIAN_POINT ( 'NONE',  ( 11.35316468750000141, 220.7812499965860127, 0.000000000000000000 ) ) ;
#51955 = ORIENTED_EDGE ( 'NONE', *, *, #15942, .F. ) ;
#51956 = B_SPLINE_CURVE_WITH_KNOTS ( 'NONE', 3,
 ( #3969, #3584, #15257, #55280, #4334, #38291, #61299, #55654, #27325, #49973, #72990, #38670, #73362, #21666, #16004, #39035, #22401, #57519, #45800, #68436, #63152, #58623, #11111, #69939 ),
 .UNSPECIFIED., .F., .F.,
 ( 4, 2, 2, 2, 2, 2, 2, 2, 2, 2, 2, 4 ),
 ( 0.03856548449537325340, 0.04003590933863943740, 0.04150633418190562141, 0.04444718386843798941, 0.04591760871170417341, 0.04738803355497035741, 0.05032888324150265602, 0.05179930808476884696, 0.05326973292803503790, 0.05621058261456741978, 0.05915143230109981554, 0.06209228198763219742 ),
 .UNSPECIFIED. ) ;
#51957 = DIRECTION ( 'NONE',  ( -0.000000000000000000, -0.000000000000000000, -1.000000000000000000 ) ) ;
#51958 = DIRECTION ( 'NONE',  ( 1.000000000000000000, 0.000000000000000000, 0.000000000000000000 ) ) ;
#51959 = CARTESIAN_POINT ( 'NONE',  ( 11.35316468749999785, 220.5729166632526415, 3.042071309553174174 ) ) ;
#51960 = CARTESIAN_POINT ( 'NONE',  ( 3.313708498984756279, 7.999999999999991118, 11.04905278392014978 ) ) ;
#51961 = CARTESIAN_POINT ( 'NONE',  ( -7.320508075688912264, 158.1250000000000853, 7.320508075688904270 ) ) ;
#51962 = CARTESIAN_POINT ( 'NONE',  ( -6.676582343750001591, 298.4531250017069510, 0.000000000000000000 ) ) ;
#51963 = EDGE_LOOP ( 'NONE', ( #46769, #43597, #24492, #35382 ) ) ;
#51964 = CARTESIAN_POINT ( 'NONE',  ( -2.995737153982818146, -51.55860531535488178, -48.67776149471355041 ) ) ;
#51965 = CARTESIAN_POINT ( 'NONE',  ( -3.042071309553163960, 202.5520833299193555, -11.35316468749999963 ) ) ;
#51966 = CARTESIAN_POINT ( 'NONE',  ( -7.204075437095967871, 7.204075437095967871, 88.46875000204838102 ) ) ;
#51967 = ADVANCED_FACE ( 'NONE', ( #52240 ), #382, .T. ) ;
#51968 = CARTESIAN_POINT ( 'NONE',  ( -26.56734541678232375, 205.0000000013655779, 173.4587341250003760 ) ) ;
#51969 = CARTESIAN_POINT ( 'NONE',  ( 8.000000000000000000, 18.09375000000000355, -3.313708498984761608 ) ) ;
#51970 = ORIENTED_EDGE ( 'NONE', *, *, #6422, .F. ) ;
#51971 = CARTESIAN_POINT ( 'NONE',  ( 3.999985685286083115, 88.68677412680156635, -6.928211494859724873 ) ) ;
#51972 = CARTESIAN_POINT ( 'NONE',  ( 7.999999999999992895, -3.313708498984756279, 19.48655277982336642 ) ) ;
#51973 = CARTESIAN_POINT ( 'NONE',  ( 8.660254037844389075, 30.41666666666666785, -5.000000000000000000 ) ) ;
#51974 = PRESENTATION_LAYER_ASSIGNMENT (  '', '', ( #72431 ) ) ;
#51975 = CARTESIAN_POINT ( 'NONE',  ( 4.898587196589412829E-16, 7.875000000000001776, -8.000000000000000000 ) ) ;
#51976 = CARTESIAN_POINT ( 'NONE',  ( -6.238412754330611322E-16, 10.18810118749999916, 75.15625000204836681 ) ) ;
#51977 = ORIENTED_EDGE ( 'NONE', *, *, #29718, .F. ) ;
#51978 = CARTESIAN_POINT ( 'NONE',  ( 8.000000000000001776, 113.6562500000000000, 3.313708498984759387 ) ) ;
#51979 = CIRCLE ( 'NONE', #53165, 92.50000000000000000 ) ;
#51980 = CARTESIAN_POINT ( 'NONE',  ( -7.999999999999991118, 3.313708498984757167, 6.736552779823365533 ) ) ;
#51981 = DIRECTION ( 'NONE',  ( -0.000000000000000000, 1.000000000000000000, -4.476705744456276341E-16 ) ) ;
#51982 = CARTESIAN_POINT ( 'NONE',  ( -5.000000000000000000, -10.38759426015435139, 65.74583990312709147 ) ) ;
#51983 = CARTESIAN_POINT ( 'NONE',  ( 6.123233995736767268E-16, 153.1249999931720538, -10.00000000000000178 ) ) ;
#51984 = CARTESIAN_POINT ( 'NONE',  ( -6.676582343749999815, 294.5156250017069510, 2.765530957082001251 ) ) ;
#51985 = EDGE_CURVE ( 'NONE', #74626, #7590, #1213, .T. ) ;
#51987 = CARTESIAN_POINT ( 'NONE',  ( 1.656854249492444975, 206.6875000000000284, 194.0000000000000853 ) ) ;
#51986 = CARTESIAN_POINT ( 'NONE',  ( 3.042071309553173286, 240.3645833367473301, 11.35316468749999608 ) ) ;
#51988 = CONTEXT_DEPENDENT_SHAPE_REPRESENTATION ( #43370, #12032 ) ;
#51989 = EDGE_LOOP ( 'NONE', ( #12055, #31148, #72749, #11678 ) ) ;
#51990 = CARTESIAN_POINT ( 'NONE',  ( -8.311093377946836114, 243.5937500034140157, -8.311093377946836114 ) ) ;
#51991 = CARTESIAN_POINT ( 'NONE',  ( -2.977408999572648707, -7.188101187499990274, 6.267802781871754547 ) ) ;
#51992 = EDGE_CURVE ( 'NONE', #1123, #40106, #45826, .T. ) ;
#51993 = ORIENTED_EDGE ( 'NONE', *, *, #16701, .F. ) ;
#51994 = CARTESIAN_POINT ( 'NONE',  ( 0.000000000000000000, 0.000000000000000000, 0.000000000000000000 ) ) ;
#51995 = CARTESIAN_POINT ( 'NONE',  ( 9.832129032723416984, 85.67708332991935549, 5.676582343750006032 ) ) ;
#51996 = PLANE ( 'NONE',  #45702 ) ;
#51997 = CARTESIAN_POINT ( 'NONE',  ( 11.00000000000000355, -4.556349186104045046, 84.15624999999998579 ) ) ;
#52000 = CARTESIAN_POINT ( 'NONE',  ( 4.898587196589412829E-16, 1.875000000000000444, -8.000000000000000000 ) ) ;
#51999 = CARTESIAN_POINT ( 'NONE',  ( 28.00000000000002132, 207.4375000013656063, 173.4587341249998929 ) ) ;
#51998 = CARTESIAN_POINT ( 'NONE',  ( 24.54126587500000412, 208.3750000013656063, 168.5673454167822172 ) ) ;
#52001 = VERTEX_POINT ( 'NONE', #22430 ) ;
#52002 = AXIS2_PLACEMENT_3D ( 'NONE', #47819, #41801, #42155 ) ;
#52003 = CARTESIAN_POINT ( 'NONE',  ( -54.04090307507133417, 206.4287802646885268, 51.39467995780781706 ) ) ;
#52004 = CARTESIAN_POINT ( 'NONE',  ( -5.676582343750006032, 199.1145833299193555, 9.832129032723418760 ) ) ;
#52005 = CARTESIAN_POINT ( 'NONE',  ( 2.445694354108783664, 206.3125000013656063, 144.4456943541088663 ) ) ;
#52006 = CARTESIAN_POINT ( 'NONE',  ( 26.56734541678232375, 204.6250000013655779, 173.4587341249998929 ) ) ;
#52007 = CARTESIAN_POINT ( 'NONE',  ( 4.401442555609581635E-16, 23.71874999795161543, -7.188101187500000044 ) ) ;
#52008 = CARTESIAN_POINT ( 'NONE',  ( 9.832129032723416984, 185.6770833299193555, 5.676582343750006032 ) ) ;
#52009 = FACE_OUTER_BOUND ( 'NONE', #57247, .T. ) ;
#52010 = CARTESIAN_POINT ( 'NONE',  ( -7.188101187499999156, 99.12500000204838102, 2.977408999572654924 ) ) ;
#52012 = CARTESIAN_POINT ( 'NONE',  ( 4.000000000000000888, 9.937499999999998224, 1.656854249492384135 ) ) ;
#52011 = LINE ( 'NONE', #34304, #1051 ) ;
#52013 = CARTESIAN_POINT ( 'NONE',  ( -1.881053915767121554, 8.624999998634406140, -4.541265875000002339 ) ) ;
#52014 = CARTESIAN_POINT ( 'NONE',  ( 31.45873412500001010, 203.0000000013655779, 168.5673454167822740 ) ) ;
#52015 = CARTESIAN_POINT ( 'NONE',  ( -7.188101187499992051, 0.000000000000000000, 10.86155278187175455 ) ) ;
#52016 = CARTESIAN_POINT ( 'NONE',  ( 3.042071309553159519, 64.73958332991935549, 11.35316468750000141 ) ) ;
#52017 = CARTESIAN_POINT ( 'NONE',  ( 0.000000000000000000, 0.000000000000000000, 11.00000000000000000 ) ) ;
#52018 = CARTESIAN_POINT ( 'NONE',  ( 7.999999999999992895, -3.313708498984756279, 0.04280278432982297099 ) ) ;
#52019 = ORIENTED_EDGE ( 'NONE', *, *, #50365, .F. ) ;
#52020 = CARTESIAN_POINT ( 'NONE',  ( 0.000000000000000000, 0.000000000000000000, 118.0000000000000000 ) ) ;
#52021 = CARTESIAN_POINT ( 'NONE',  ( 29.65685424949237969, 206.5625000027312410, 165.9999999999999147 ) ) ;
#52022 = CARTESIAN_POINT ( 'NONE',  ( 8.311093377946837890, 56.40624999658600558, -8.311093377946837890 ) ) ;
#52023 = CARTESIAN_POINT ( 'NONE',  ( 4.556349186104051263, -10.99999999999999822, 69.15625000409676204 ) ) ;
#52024 = CARTESIAN_POINT ( 'NONE',  ( 3.458734124999959469, 196.7500000013656063, 140.5673454167823593 ) ) ;
#52026 = AXIS2_PLACEMENT_3D ( 'NONE', #33644, #49479, #72498 ) ;
#52025 = CARTESIAN_POINT ( 'NONE',  ( 0.000000000000000000, 0.000000000000000000, -10.20000000000000462 ) ) ;
#52028 = CARTESIAN_POINT ( 'NONE',  ( -2.085542519210945728E-15, 54.53124999658601979, 11.35316468750000141 ) ) ;
#52027 = CARTESIAN_POINT ( 'NONE',  ( -4.401442555609581635E-16, 90.78125000204836681, -7.188101187500000044 ) ) ;
#52029 = CARTESIAN_POINT ( 'NONE',  ( 7.999999999999992895, -3.313708498984756279, 2.986552779823361981 ) ) ;
#52030 = CARTESIAN_POINT ( 'NONE',  ( -0.2454044849291622254, 194.9147657458008780, 145.9147657458008496 ) ) ;
#52031 = CARTESIAN_POINT ( 'NONE',  ( 6.123233995736767268E-16, 158.1249999931720254, -10.00000000000000178 ) ) ;
#52032 = CARTESIAN_POINT ( 'NONE',  ( 2.977408999572654480, 96.50000000204838102, 7.188101187499999156 ) ) ;
#52033 = VECTOR ( 'NONE', #65294, 1000.000000000000000 ) ;
#52034 = DIRECTION ( 'NONE',  ( 1.000000000000000000, 0.000000000000000000, -1.826024711554534406E-16 ) ) ;
#52035 = CARTESIAN_POINT ( 'NONE',  ( 6.951808397369818766E-16, 47.34374999658602690, -11.35316468750000141 ) ) ;
#52036 =( BOUNDED_CURVE ( )  B_SPLINE_CURVE ( 2, ( #53116, #1451, #34670, #35766, #17658, #30469, #6723, #40677, #24432, #29730, #47802, #13097, #57673 ),
 .UNSPECIFIED., .F., .F. ) 
 B_SPLINE_CURVE_WITH_KNOTS ( ( 3, 2, 2, 2, 2, 2, 3 ),
 ( 0.7663043478260869179, 0.7681159420289854767, 0.7699275362318840354, 0.7717391304347825942, 0.7735507246376811530, 0.7753623188405797118, 0.7771739130434782705 ),
 .UNSPECIFIED. ) 
 CURVE ( )  GEOMETRIC_REPRESENTATION_ITEM ( )  RATIONAL_B_SPLINE_CURVE ( ( 1.000000000000000000, 0.9659258262890683122, 1.000000000000000000, 0.9659258262890683122, 1.000000000000000000, 0.9659258262890683122, 1.000000000000000000, 0.9659258262890683122, 1.000000000000000000, 0.9659258262890683122, 1.000000000000000000, 0.9659258262890683122, 1.000000000000000000 ) ) 
 REPRESENTATION_ITEM ( '' )  );
#52037 = CARTESIAN_POINT ( 'NONE',  ( 10.18810118749999916, 1.247682550866122264E-15, 110.7812500020483668 ) ) ;
#52038 = CARTESIAN_POINT ( 'NONE',  ( -8.311093377946841443, 178.9062499965859843, 8.311093377946830785 ) ) ;
#52039 = ORIENTED_EDGE ( 'NONE', *, *, #65332, .F. ) ;
#52040 = CARTESIAN_POINT ( 'NONE',  ( -1.317228840344501606, 65.80815776305036024, 26.30638062134577382 ) ) ;
#52041 = CARTESIAN_POINT ( 'NONE',  ( -10.18810118749999916, 0.000000000000000000, 70.65625000204836681 ) ) ;
#52042 = CARTESIAN_POINT ( 'NONE',  ( 4.000000000000015099, 196.5625000000000284, 196.3431457505076594 ) ) ;
#52044 = CARTESIAN_POINT ( 'NONE',  ( -11.35316468749999785, 183.0729166632526983, -3.042071309553167957 ) ) ;
#52043 = DIRECTION ( 'NONE',  ( -1.000000000000000000, 0.000000000000000000, -0.000000000000000000 ) ) ;
#52045 = CARTESIAN_POINT ( 'NONE',  ( 7.999999999999991118, 3.313708498984757611, 7.730302784329822430 ) ) ;
#52046 = CARTESIAN_POINT ( 'NONE',  ( 1.656854249492381914, 21.56249999726881583, 4.000000000000000888 ) ) ;
#52047 = CARTESIAN_POINT ( 'NONE',  ( -5.000000000000000888, 252.2916666734946602, -8.660254037844387298 ) ) ;
#52048 = DIRECTION ( 'NONE',  ( -0.000000000000000000, -1.000000000000000000, -0.000000000000000000 ) ) ;
#52049 = EDGE_LOOP ( 'NONE', ( #43650, #40651, #55137, #35110 ) ) ;
#52050 = CARTESIAN_POINT ( 'NONE',  ( 9.832129032723416984, 165.6770833299193555, 5.676582343750006032 ) ) ;
#52051 = FACE_OUTER_BOUND ( 'NONE', #44644, .T. ) ;
#52052 = CARTESIAN_POINT ( 'NONE',  ( -9.832129032723418760, 123.1770833299193555, -5.676582343750004256 ) ) ;
#52053 =( BOUNDED_CURVE ( )  B_SPLINE_CURVE ( 2, ( #71645, #42235, #42608, #7183, #49009, #48635, #53942, #60332, #8660 ),
 .UNSPECIFIED., .F., .F. ) 
 B_SPLINE_CURVE_WITH_KNOTS ( ( 3, 2, 2, 2, 3 ),
 ( 0.7386363636363636465, 0.7443181818181817677, 0.7500000000000000000, 0.7556818181818182323, 0.7613636363636363535 ),
 .UNSPECIFIED. ) 
 CURVE ( )  GEOMETRIC_REPRESENTATION_ITEM ( )  RATIONAL_B_SPLINE_CURVE ( ( 1.000000000000000000, 0.9238795325112867385, 1.000000000000000000, 0.9238795325112867385, 1.000000000000000000, 0.9238795325112867385, 1.000000000000000000, 0.9238795325112867385, 1.000000000000000000 ) ) 
 REPRESENTATION_ITEM ( '' )  );
#52054 = CARTESIAN_POINT ( 'NONE',  ( 30.82842712474619873, 195.3750000000000284, 167.1715728752537586 ) ) ;
#52055 = VERTEX_POINT ( 'NONE', #17150 ) ;
#52056 = CIRCLE ( 'NONE', #2665, 70.50000000000000000 ) ;
#52057 = CARTESIAN_POINT ( 'NONE',  ( -1.881053915767124440, 12.12499999863440969, 4.541265875000001451 ) ) ;
#52058 = CARTESIAN_POINT ( 'NONE',  ( -1.320432766682874540E-15, 15.09374999795161187, 7.188101187500000044 ) ) ;
#52059 = CARTESIAN_POINT ( 'NONE',  ( 8.000000000000001776, 106.3437500040967763, 3.313708498984759387 ) ) ;
#52060 = EDGE_CURVE ( 'NONE', #57640, #73379, #13785, .T. ) ;
#52061 = CARTESIAN_POINT ( 'NONE',  ( -30.44569435410879166, 199.0625000013656063, 172.4456943541092357 ) ) ;
#52062 = CARTESIAN_POINT ( 'NONE',  ( 1.656854249492381248, 10.18750000000000000, -4.000000000000001776 ) ) ;
#52063 = CARTESIAN_POINT ( 'NONE',  ( -2.828427124746190735, 22.12499999726881583, -2.828427124746191623 ) ) ;
#52064 = CARTESIAN_POINT ( 'NONE',  ( -4.541265875000002339, 11.81249999863440614, -5.561446717895856393E-16 ) ) ;
#52065 = CARTESIAN_POINT ( 'NONE',  ( 7.999999999999992895, -3.313708498984756279, 18.17405278392014623 ) ) ;
#52066 = CARTESIAN_POINT ( 'NONE',  ( 1.491046635511791134E-11, 146.2499999999988631, -9.999999999999998224 ) ) ;
#52067 = ORIENTED_EDGE ( 'NONE', *, *, #44942, .F. ) ;
#52068 = DIRECTION ( 'NONE',  ( 0.7071067811865525687, 0.7071067811865425767, -0.000000000000000000 ) ) ;
#52069 = CARTESIAN_POINT ( 'NONE',  ( 7.188101187500000044, 103.9062500020483810, -8.802885111219163269E-16 ) ) ;
#52070 = EDGE_CURVE ( 'NONE', #25226, #7497, #2030, .T. ) ;
#52072 = CARTESIAN_POINT ( 'NONE',  ( 11.00000000000000000, 1.347111479062088405E-15, 96.43750000409677625 ) ) ;
#52071 = CARTESIAN_POINT ( 'NONE',  ( 38.00000000000000000, 63.00000000000000000, 10.00000000000006217 ) ) ;
#52073 = EDGE_LOOP ( 'NONE', ( #62635, #13028, #58345, #72432 ) ) ;
#52074 = CARTESIAN_POINT ( 'NONE',  ( -4.000000000000002665, 10.56250000000000000, 1.656854249492380582 ) ) ;
#52075 = TOROIDAL_SURFACE ( 'NONE', #50879, 68.99999999999994316, 38.00000000000000000 ) ;
#52076 = CARTESIAN_POINT ( 'NONE',  ( -2.977408999572648707, -7.188101187499990274, 25.76780278187175810 ) ) ;
#52077 = EDGE_CURVE ( 'NONE', #38888, #47939, #29963, .T. ) ;
#52078 = ORIENTED_EDGE ( 'NONE', *, *, #51458, .T. ) ;
#52079 = B_SPLINE_CURVE_WITH_KNOTS ( 'NONE', 3,
 ( #28804, #57873, #17105, #45786, #40503, #28062, #45406, #35594 ),
 .UNSPECIFIED., .F., .F.,
 ( 4, 2, 2, 4 ),
 ( 0.02905455086391281472, 0.03168444077422613581, 0.03431433068453945689, 0.03957411050516609907 ),
 .UNSPECIFIED. ) ;
#52080 = B_SPLINE_CURVE_WITH_KNOTS ( 'NONE', 3,
 ( #70738, #13743, #64718, #14120, #37155, #42430, #36052, #59797, #36787, #30750, #7007, #53030, #65447, #70381, #8110, #48459, #65067, #24346, #54142, #25071, #2451, #60156 ),
 .UNSPECIFIED., .F., .F.,
 ( 4, 2, 2, 2, 2, 2, 2, 2, 2, 2, 4 ),
 ( 0.000000000000000000, 0.001531360831348023465, 0.002297041247022034872, 0.003062721662696046062, 0.004594082494044070611, 0.006125443325392096461, 0.006891123741066107651, 0.007656804156740118841, 0.009188164988088146426, 0.01071952581943617401, 0.01225088665078420333 ),
 .UNSPECIFIED. ) ;
#52081 = ORIENTED_EDGE ( 'NONE', *, *, #46834, .T. ) ;
#52082 = CARTESIAN_POINT ( 'NONE',  ( -7.204075437095965206, -7.204075437095968759, 84.34375000204836681 ) ) ;
#52083 = CARTESIAN_POINT ( 'NONE',  ( 2.449293598294707893E-16, 8.999999997268814056, -4.000000000000001776 ) ) ;
#52084 = CARTESIAN_POINT ( 'NONE',  ( -27.99999999999996092, 196.1875000013655779, 173.4587341250003760 ) ) ;
#52085 = CARTESIAN_POINT ( 'NONE',  ( -7.778174593052020747, -7.778174593052023411, 98.68749999999998579 ) ) ;
#52088 = CARTESIAN_POINT ( 'NONE',  ( -6.676582343750002480, 298.5468750017069510, -2.765530957081996810 ) ) ;
#52087 = CARTESIAN_POINT ( 'NONE',  ( 24.00000000000001066, 205.9375000027311842, 171.6568542494923122 ) ) ;
#52086 = FACE_BOUND ( 'NONE', #27612, .T. ) ;
#52089 = CARTESIAN_POINT ( 'NONE',  ( 7.320508075688774596, 135.6249999999999432, -7.320508075688774596 ) ) ;
#52090 = CARTESIAN_POINT ( 'NONE',  ( -7.999999999999998224, 99.59374999999998579, 3.313708498984766493 ) ) ;
#52091 = CARTESIAN_POINT ( 'NONE',  ( 6.676582343750004256, 288.0468750017070079, 2.765530957081995478 ) ) ;
#52092 = CARTESIAN_POINT ( 'NONE',  ( -7.188101187499990274, -2.977408999572651371, 1.955302781871753881 ) ) ;
#52093 = CARTESIAN_POINT ( 'NONE',  ( 8.000000000000000000, 1.500000000000000000, 0.000000000000000000 ) ) ;
#52095 = CARTESIAN_POINT ( 'NONE',  ( 31.45873412499998523, 203.6250000013656063, 171.4326545832175839 ) ) ;
#52094 = AXIS2_PLACEMENT_3D ( 'NONE', #30553, #42600, #30914 ) ;
#52096 = CARTESIAN_POINT ( 'NONE',  ( 5.082755093536325930, 5.531249997951610098, -5.082755093536325930 ) ) ;
#52097 = CARTESIAN_POINT ( 'NONE',  ( 5.662595241051936235, -5.662595241051934458, 3.075615283940628331 ) ) ;
#52098 = CARTESIAN_POINT ( 'NONE',  ( -2.445694354108839619, 194.8125000013656063, 139.5543056458912190 ) ) ;
#52099 = CARTESIAN_POINT ( 'NONE',  ( -2.977408999572650927, 113.7500000020483810, -7.188101187500000933 ) ) ;
#52101 = DIRECTION ( 'NONE',  ( 0.000000000000000000, 0.000000000000000000, 1.000000000000000000 ) ) ;
#52100 = FILL_AREA_STYLE ('',( #63031 ) ) ;
#52102 = CARTESIAN_POINT ( 'NONE',  ( 9.832129032723416984, 237.1354166700806445, -5.676582343750003368 ) ) ;
#52103 = CARTESIAN_POINT ( 'NONE',  ( -31.58827465454502814, 43.93882196680915087, 65.00000000000001421 ) ) ;
#52104 = CARTESIAN_POINT ( 'NONE',  ( -2.977408999572648707, -7.188101187499990274, 26.14280278187176165 ) ) ;
#52105 = CARTESIAN_POINT ( 'NONE',  ( 31.99999999999997868, 200.1875000000000568, 171.6568542494923122 ) ) ;
#52106 = CARTESIAN_POINT ( 'NONE',  ( 11.35316468749999785, 25.57291666325268409, 3.042071309553174174 ) ) ;
#52107 = CARTESIAN_POINT ( 'NONE',  ( -1.237384350715592869E-11, 93.74999999999903366, 9.999999999999998224 ) ) ;
#52108 = CARTESIAN_POINT ( 'NONE',  ( -3.042071309553173730, 224.6354166632526983, 11.35316468749999785 ) ) ;
#52109 = CARTESIAN_POINT ( 'NONE',  ( 8.000000000000000000, 124.2500000000000000, -9.797174393178825657E-16 ) ) ;
#52111 = CARTESIAN_POINT ( 'NONE',  ( -3.458734124999911508, 194.4587341250001202, 198.1584999238177431 ) ) ;
#52110 = CARTESIAN_POINT ( 'NONE',  ( 0.000000000000000000, 220.0000000000000284, -11.00000000000000000 ) ) ;
#52112 = ORIENTED_EDGE ( 'NONE', *, *, #29418, .F. ) ;
#52113 = AXIS2_PLACEMENT_3D ( 'NONE', #26212, #22047, #27715 ) ;
#52114 = CARTESIAN_POINT ( 'NONE',  ( -1.432654583217664701, 197.0000000013656347, 138.5412658750000787 ) ) ;
#52115 = CARTESIAN_POINT ( 'NONE',  ( 11.35316468750000141, 25.78124999658601624, 0.000000000000000000 ) ) ;
#52116 = CARTESIAN_POINT ( 'NONE',  ( -11.00000000000000000, 4.556349186104045934, 94.09375000409679046 ) ) ;
#52117 = CARTESIAN_POINT ( 'NONE',  ( -3.458734125000015869, 207.1875000013656063, 142.0000000000000568 ) ) ;
#52118 = CARTESIAN_POINT ( 'NONE',  ( 1.934925017735378189E-11, 153.7500000000015348, 10.00000000000000533 ) ) ;
#52119 = CARTESIAN_POINT ( 'NONE',  ( -4.000000000000015987, 201.6875000027311842, 143.6568542494924259 ) ) ;
#52121 = CARTESIAN_POINT ( 'NONE',  ( -5.676582343749998039, 17.44791666325268409, -9.832129032723420536 ) ) ;
#52120 = CARTESIAN_POINT ( 'NONE',  ( 7.188101187500000933, 114.5000000020483810, -2.977408999572651371 ) ) ;
#52122 = CARTESIAN_POINT ( 'NONE',  ( -7.999999999999989342, -3.313708498984762496, 21.92405277982336642 ) ) ;
#52123 = CARTESIAN_POINT ( 'NONE',  ( 5.676582343749993598, 139.9479166632526983, 9.832129032723422313 ) ) ;
#52124 = CARTESIAN_POINT ( 'NONE',  ( -1.836970198721029983E-15, 120.6249999931720396, 10.00000000000000178 ) ) ;
#52125 = CARTESIAN_POINT ( 'NONE',  ( -7.188101187500000044, 117.0312500020483810, 0.000000000000000000 ) ) ;
#52126 = CARTESIAN_POINT ( 'NONE',  ( 0.000000000000000000, 0.000000000000000000, 0.000000000000000000 ) ) ;
#52127 = CARTESIAN_POINT ( 'NONE',  ( 11.00000000000000000, 1.347111479062088405E-15, 102.4375000040967763 ) ) ;
#52128 = CARTESIAN_POINT ( 'NONE',  ( -4.999999999999953815, -52.35862550122923409, -48.98731492261434539 ) ) ;
#52129 = ORIENTED_EDGE ( 'NONE', *, *, #27395, .F. ) ;
#52130 = CARTESIAN_POINT ( 'NONE',  ( 8.311093377946834337, 10.46874999658601624, 8.311093377946839666 ) ) ;
#52131 = CARTESIAN_POINT ( 'NONE',  ( 0.000000000000000000, 125.0000000000000000, 8.000000000000000000 ) ) ;
#52132 = CARTESIAN_POINT ( 'NONE',  ( -4.721056650415999201, 298.3281250017069510, -4.721056650415999201 ) ) ;
#52133 = CARTESIAN_POINT ( 'NONE',  ( 11.35316468749999785, 145.5729166632526983, 3.042071309553174174 ) ) ;
#52134 = LINE ( 'NONE', #52870, #70018 ) ;
#52135 = CARTESIAN_POINT ( 'NONE',  ( -5.656854249492375253, 5.656854249492375253, 21.69905278432982243 ) ) ;
#52136 = CARTESIAN_POINT ( 'NONE',  ( -28.00000000000002842, 199.0000000000000000, 166.0000000000003695 ) ) ;
#52137 = CARTESIAN_POINT ( 'NONE',  ( -5.676582343749992710, 249.7395833367473301, 9.832129032723422313 ) ) ;
#52138 = CARTESIAN_POINT ( 'NONE',  ( 10.18810118750000093, -4.220049686691933921, 95.68750000204838102 ) ) ;
#52139 = EDGE_LOOP ( 'NONE', ( #50799, #26408, #34475, #11787 ) ) ;
#52140 = DIRECTION ( 'NONE',  ( -0.000000000000000000, -1.000000000000000000, -0.000000000000000000 ) ) ;
#52141 = FACE_OUTER_BOUND ( 'NONE', #65747, .T. ) ;
#52142 = CARTESIAN_POINT ( 'NONE',  ( 8.311093377946834337, 95.46874999658601268, 8.311093377946839666 ) ) ;
#52143 = ORIENTED_EDGE ( 'NONE', *, *, #1657, .T. ) ;
#52144 = CARTESIAN_POINT ( 'NONE',  ( -6.238412754330611322E-16, 10.18810118749999916, 106.2812500020483810 ) ) ;
#52145 = CARTESIAN_POINT ( 'NONE',  ( 1.881053915767121998, 14.62499999863440969, -4.541265875000002339 ) ) ;
#52146 = ORIENTED_EDGE ( 'NONE', *, *, #55602, .F. ) ;
#52147 = ORIENTED_EDGE ( 'NONE', *, *, #59129, .T. ) ;
#52148 = CARTESIAN_POINT ( 'NONE',  ( 8.000000000000000000, 6.093750000000000888, -3.313708498984761608 ) ) ;
#52149 = CARTESIAN_POINT ( 'NONE',  ( -5.656854249492380582, 110.0000000040967763, -5.656854249492380582 ) ) ;
#52150 = CARTESIAN_POINT ( 'NONE',  ( -7.188101187500000044, 24.09374999795161543, -8.802885111219163269E-16 ) ) ;
#52151 = CARTESIAN_POINT ( 'NONE',  ( -3.313708498984762496, 120.9687500040967905, 7.999999999999998224 ) ) ;
#52152 =( BOUNDED_CURVE ( )  B_SPLINE_CURVE ( 2, ( #74411, #33701, #57452, #22339, #63089, #490, #38971, #61977, #10302 ),
 .UNSPECIFIED., .F., .F. ) 
 B_SPLINE_CURVE_WITH_KNOTS ( ( 3, 2, 2, 2, 3 ),
 ( 0.3500000000000004219, 0.3583333333333337256, 0.3666666666666669738, 0.3750000000000002776, 0.3833333333333335813 ),
 .UNSPECIFIED. ) 
 CURVE ( )  GEOMETRIC_REPRESENTATION_ITEM ( )  RATIONAL_B_SPLINE_CURVE ( ( 0.9999999999999958922, 0.9238795325112908463, 1.000000000000000000, 0.9238795325112867385, 1.000000000000000000, 0.9238795325112867385, 1.000000000000000000, 0.9238795325112847401, 1.000000000000001998 ) ) 
 REPRESENTATION_ITEM ( '' )  );
#52153 = CARTESIAN_POINT ( 'NONE',  ( -7.204075437095965206, -7.204075437095968759, 102.7187500020483668 ) ) ;
#52154 = AXIS2_PLACEMENT_3D ( 'NONE', #2556, #48932, #36886 ) ;
#52155 = CARTESIAN_POINT ( 'NONE',  ( -27.99999999999999645, 210.0000000000000284, 170.0000000000003695 ) ) ;
#52156 = CARTESIAN_POINT ( 'NONE',  ( 1.656854249492381248, 11.93749999726881406, -4.000000000000001776 ) ) ;
#52157 = CARTESIAN_POINT ( 'NONE',  ( -3.211159895383561391, 0.6874999986344068059, -3.211159895383561835 ) ) ;
#52158 = ORIENTED_EDGE ( 'NONE', *, *, #72082, .F. ) ;
#52159 = VECTOR ( 'NONE', #19268, 1000.000000000000000 ) ;
#52160 = EDGE_CURVE ( 'NONE', #3031, #30042, #59642, .T. ) ;
#52161 = DIRECTION ( 'NONE',  ( 0.000000000000000000, 0.000000000000000000, -1.000000000000000000 ) ) ;
#52162 = CARTESIAN_POINT ( 'NONE',  ( 2.445694354108838731, 198.0625000013656063, 195.5543056458912190 ) ) ;
#52163 = CARTESIAN_POINT ( 'NONE',  ( -29.43265458321771177, 203.5000000013655779, 166.5412658750003914 ) ) ;
#52164 =( NAMED_UNIT ( * ) PLANE_ANGLE_UNIT ( ) SI_UNIT ( $, .RADIAN. ) );
#52165 =( BOUNDED_CURVE ( )  B_SPLINE_CURVE ( 2, ( #58998, #42358, #36713, #53329, #6568, #1292, #12582, #7672, #25371 ),
 .UNSPECIFIED., .F., .F. ) 
 B_SPLINE_CURVE_WITH_KNOTS ( ( 3, 2, 2, 2, 3 ),
 ( 0.6842105263157894912, 0.6907894736842105088, 0.6973684210526316374, 0.7039473684210527660, 0.7105263157894737835 ),
 .UNSPECIFIED. ) 
 CURVE ( )  GEOMETRIC_REPRESENTATION_ITEM ( )  RATIONAL_B_SPLINE_CURVE ( ( 1.000000000000000000, 0.9238795325112867385, 1.000000000000000000, 0.9238795325112867385, 1.000000000000000000, 0.9238795325112867385, 1.000000000000000000, 0.9238795325112854062, 1.000000000000001332 ) ) 
 REPRESENTATION_ITEM ( '' )  );
#52166 = CARTESIAN_POINT ( 'NONE',  ( 2.780723358947928197E-16, 9.562499998634406140, -4.541265875000002339 ) ) ;
#52167 = CARTESIAN_POINT ( 'NONE',  ( 2.828427124746191623, 16.12500000000000000, -2.828427124746191623 ) ) ;
#52168 = CARTESIAN_POINT ( 'NONE',  ( -5.082755093536319713, 5.082755093536319713, 13.29905278187175277 ) ) ;
#52169 = ORIENTED_EDGE ( 'NONE', *, *, #40214, .F. ) ;
#52170 = ORIENTED_EDGE ( 'NONE', *, *, #24398, .T. ) ;
#52171 = CARTESIAN_POINT ( 'NONE',  ( 10.18810118749999916, 1.247682550866122264E-15, 113.4062500020483810 ) ) ;
#52172 = CARTESIAN_POINT ( 'NONE',  ( -16.53139458858884581, -11.24020457502486892, -1.118160017449591814 ) ) ;
#52173 = CARTESIAN_POINT ( 'NONE',  ( -30.82842712474615965, 204.3750000000000284, 172.8284271247465824 ) ) ;
#52174 = CARTESIAN_POINT ( 'NONE',  ( -2.445694354108782775, 199.5625000013656063, 200.4456943541088663 ) ) ;
#52175 = CARTESIAN_POINT ( 'NONE',  ( 29.43265458321760519, 195.8750000013655779, 166.5412658749999650 ) ) ;
#52176 = CARTESIAN_POINT ( 'NONE',  ( -10.00000000000000355, 92.70833333333332860, 2.679491924311223183 ) ) ;
#52177 = CARTESIAN_POINT ( 'NONE',  ( 8.000000000000000000, 119.8437500000000142, -3.313708498984762496 ) ) ;
#52178 = CARTESIAN_POINT ( 'NONE',  ( 8.311093377946837890, 66.71874999658602690, -8.311093377946837890 ) ) ;
#52179 = CARTESIAN_POINT ( 'NONE',  ( 2.485281374238571317, 289.6874999999999432, -6.000000000000003553 ) ) ;
#52180 = EDGE_CURVE ( 'NONE', #49089, #33033, #60068, .T. ) ;
#52181 = ORIENTED_EDGE ( 'NONE', *, *, #48999, .T. ) ;
#52182 = CARTESIAN_POINT ( 'NONE',  ( 4.000000000000015987, 203.5000000000000000, 198.0000000000000284 ) ) ;
#52183 = CARTESIAN_POINT ( 'NONE',  ( 3.511653767259352410, -16.35475815726353233, 69.12977678000895310 ) ) ;
#52184 = CARTESIAN_POINT ( 'NONE',  ( -2.445694354108838731, 208.0625000013656063, 144.4456943541088663 ) ) ;
#52185 = CARTESIAN_POINT ( 'NONE',  ( 10.00000000000000888, 84.79166666666668561, 2.679491924311237838 ) ) ;
#52186 = CARTESIAN_POINT ( 'NONE',  ( 28.31625444984002371, 194.4587341250000350, 173.4478902384277603 ) ) ;
#52187 = CARTESIAN_POINT ( 'NONE',  ( -2.679491924311222295, 236.0416666666666856, 10.00000000000000178 ) ) ;
#52188 = CARTESIAN_POINT ( 'NONE',  ( 0.000000000000000000, 9.032624889217688457E-17, 4.000000000000000000 ) ) ;
#52189 = CARTESIAN_POINT ( 'NONE',  ( 4.220049686691941027, -10.18810118749999738, 68.50000000204838102 ) ) ;
#52190 = CARTESIAN_POINT ( 'NONE',  ( -8.660254037844390851, 207.9166666666666572, 4.999999999999998224 ) ) ;
#52191 = CARTESIAN_POINT ( 'NONE',  ( -5.082755093536317936, -5.082755093536320601, 14.04905278187175455 ) ) ;
#52192 = CARTESIAN_POINT ( 'NONE',  ( 8.311093377946834337, 175.4687499965860127, 8.311093377946839666 ) ) ;
#52193 = CARTESIAN_POINT ( 'NONE',  ( 16.00000000000000711, 16.00000000000000355, 20.00000000000000000 ) ) ;
#52194 = CARTESIAN_POINT ( 'NONE',  ( -2.903053168685532981, -44.21814323542975700, 151.2230508638683943 ) ) ;
#52196 = CARTESIAN_POINT ( 'NONE',  ( 4.999999999999993783, 86.04166665983869677, 8.660254037844390851 ) ) ;
#52195 = CARTESIAN_POINT ( 'NONE',  ( 0.000000000000000000, 300.0000000000000000, 0.000000000000000000 ) ) ;
#52197 = ORIENTED_EDGE ( 'NONE', *, *, #56237, .F. ) ;
#52198 = CARTESIAN_POINT ( 'NONE',  ( -3.458734125000015869, 208.1875000013656063, 142.0000000000000568 ) ) ;
#52199 = CARTESIAN_POINT ( 'NONE',  ( -8.311093377946836114, 42.96874999658601268, -8.311093377946837890 ) ) ;
#52200 = CARTESIAN_POINT ( 'NONE',  ( 4.556349186104045934, 11.00000000000000000, 110.2187500040968047 ) ) ;
#52201 = CARTESIAN_POINT ( 'NONE',  ( -27.99999999999991829, 204.9375000013656063, 173.4587341250003760 ) ) ;
#52203 = CARTESIAN_POINT ( 'NONE',  ( -4.556349186104048599, -10.99999999999999822, 107.9687500040967905 ) ) ;
#52202 = CARTESIAN_POINT ( 'NONE',  ( 10.00000000000000178, 222.0833333265053682, -2.679491924311226736 ) ) ;
#52204 = CARTESIAN_POINT ( 'NONE',  ( 3.458734124999959914, 197.3750000013656063, 143.4326545832176976 ) ) ;
#52205 = CARTESIAN_POINT ( 'NONE',  ( -2.679491924311235618, 70.41666665983869677, 10.00000000000000000 ) ) ;
#52206 = CARTESIAN_POINT ( 'NONE',  ( 2.977408999572654480, 99.12500000204838102, 7.188101187499999156 ) ) ;
#52207 = CARTESIAN_POINT ( 'NONE',  ( 3.211159895383560947, 13.31249999863440792, 3.211159895383562723 ) ) ;
#52208 = CARTESIAN_POINT ( 'NONE',  ( 2.849036369511732440E-14, 198.3750000027312126, 202.0000000000000000 ) ) ;
#52209 = CARTESIAN_POINT ( 'NONE',  ( 5.656854249492376141, -5.656854249492374365, 5.892802779823364645 ) ) ;
#52210 = FACE_OUTER_BOUND ( 'NONE', #64289, .T. ) ;
#52211 = ORIENTED_EDGE ( 'NONE', *, *, #74129, .T. ) ;
#52212 = ORIENTED_EDGE ( 'NONE', *, *, #65599, .F. ) ;
#52213 = CARTESIAN_POINT ( 'NONE',  ( 11.00000000000002487, 4.556349186104019289, 115.8437500000000000 ) ) ;
#52214 = CARTESIAN_POINT ( 'NONE',  ( -6.676582343750003368, 298.5468750017069510, -2.765530957081996810 ) ) ;
#52215 = DIRECTION ( 'NONE',  ( -0.000000000000000000, 1.000000000000000000, -0.000000000000000000 ) ) ;
#52216 = CARTESIAN_POINT ( 'NONE',  ( 7.320508075688771044, 41.24999999317203248, 7.320508075688775484 ) ) ;
#52217 = AXIS2_PLACEMENT_3D ( 'NONE', #49778, #44868, #68247 ) ;
#52218 = CARTESIAN_POINT ( 'NONE',  ( 11.35316468749999785, 150.5729166632526699, 3.042071309553174174 ) ) ;
#52219 = CARTESIAN_POINT ( 'NONE',  ( -1.522892193876115035E-11, 103.7499999999988205, 10.00000000000000178 ) ) ;
#52220 = CARTESIAN_POINT ( 'NONE',  ( -10.18810118749999916, 0.000000000000000000, 84.15625000204838102 ) ) ;
#52221 = CARTESIAN_POINT ( 'NONE',  ( -28.22735846810414273, 194.7564787015573700, 173.7564787015576542 ) ) ;
#52222 = CARTESIAN_POINT ( 'NONE',  ( 2.828427124746208943, 202.6250000000000284, 195.1715728752538439 ) ) ;
#52223 = CYLINDRICAL_SURFACE ( 'NONE', #57912, 11.00000000000000000 ) ;
#52224 = CARTESIAN_POINT ( 'NONE',  ( -10.18810118749999916, 0.000000000000000000, 114.5312500020483810 ) ) ;
#52225 = ORIENTED_EDGE ( 'NONE', *, *, #68733, .F. ) ;
#52226 = CARTESIAN_POINT ( 'NONE',  ( 3.313708498984762496, 17.53124999590322375, 7.999999999999998224 ) ) ;
#52227 = CARTESIAN_POINT ( 'NONE',  ( -17.56925112072165263, 178.1485276299164582, 137.8365335656544346 ) ) ;
#52228 = CARTESIAN_POINT ( 'NONE',  ( 6.951808397369818766E-16, 122.3437499965860269, -11.35316468750000141 ) ) ;
#52229 = CARTESIAN_POINT ( 'NONE',  ( 2.445694354108838731, 199.0625000013656063, 195.5543056458912190 ) ) ;
#52230 = CARTESIAN_POINT ( 'NONE',  ( -1.320432766682874540E-15, 25.96874999795161543, 7.188101187500000044 ) ) ;
#52231 = CARTESIAN_POINT ( 'NONE',  ( -10.18810118749999916, 0.000000000000000000, 78.53125000204836681 ) ) ;
#52232 = CARTESIAN_POINT ( 'NONE',  ( 6.951808397369818766E-16, 47.34374999658602690, -11.35316468750000141 ) ) ;
#52233 = ORIENTED_EDGE ( 'NONE', *, *, #61637, .F. ) ;
#52234 = CARTESIAN_POINT ( 'NONE',  ( -8.000000000000000000, 125.0000000000000000, -1.469576158976823947E-15 ) ) ;
#52235 = CARTESIAN_POINT ( 'NONE',  ( -4.541265875000002339, 0.9374999986344068059, -5.561446717895856393E-16 ) ) ;
#52236 = CARTESIAN_POINT ( 'NONE',  ( -8.008118988124991233, 0.000000000000000000, 11.51311528394062833 ) ) ;
#52237 = CARTESIAN_POINT ( 'NONE',  ( -3.458734125000015425, 205.2500000013655779, 143.4326545832176976 ) ) ;
#52238 = CARTESIAN_POINT ( 'NONE',  ( -1.320432766682874540E-15, 9.093749997951610098, 7.188101187500000044 ) ) ;
#52239 = CARTESIAN_POINT ( 'NONE',  ( -6.000000000000000888, 296.1250000034139589, 2.485281374238575758 ) ) ;
#52240 = FACE_OUTER_BOUND ( 'NONE', #9083, .T. ) ;
#52241 = CARTESIAN_POINT ( 'NONE',  ( -7.188101187500000044, 3.093749997951610098, -8.802885111219163269E-16 ) ) ;
#52242 = CARTESIAN_POINT ( 'NONE',  ( -4.401442555609577197E-16, 7.188101187499992051, 11.61155278187175632 ) ) ;
#52243 = CARTESIAN_POINT ( 'NONE',  ( -10.18810118749999738, -4.220049686691941915, 72.25000000204836681 ) ) ;
#52244 = CIRCLE ( 'NONE', #6478, 3.999999999999986233 ) ;
#52245 = CARTESIAN_POINT ( 'NONE',  ( -30.44569435410879521, 207.0625000013656063, 172.4456943541092357 ) ) ;
#52246 = DIRECTION ( 'NONE',  ( 0.000000000000000000, 0.000000000000000000, -1.000000000000000000 ) ) ;
#52247 = CARTESIAN_POINT ( 'NONE',  ( -8.342170076843785083E-16, 21.18749999863440792, 4.541265875000002339 ) ) ;
#52248 = ORIENTED_EDGE ( 'NONE', *, *, #3049, .T. ) ;
#52249 = EDGE_CURVE ( 'NONE', #22437, #13532, #37476, .T. ) ;
#52250 = CARTESIAN_POINT ( 'NONE',  ( -1.656854249492347719, 195.9375000027312126, 194.0000000000000853 ) ) ;
#52251 = CARTESIAN_POINT ( 'NONE',  ( -2.828427124746208943, 204.6250000000000284, 144.8284271247462129 ) ) ;
#52252 = CARTESIAN_POINT ( 'NONE',  ( -25.17157287525374088, 201.7500000027312126, 172.8284271247464972 ) ) ;
#52253 = ADVANCED_FACE ( 'NONE', ( #7326 ), #59745, .T. ) ;
#52254 = CARTESIAN_POINT ( 'NONE',  ( 7.188101187500000044, 114.4062500020483810, -8.802885111219163269E-16 ) ) ;
#52255 = CARTESIAN_POINT ( 'NONE',  ( 10.00000000000000178, 250.4166666734946602, 2.679491924311222739 ) ) ;
#52256 = CARTESIAN_POINT ( 'NONE',  ( 3.313708498984762496, -7.999999999999989342, 7.486552783920144449 ) ) ;
#52257 = ORIENTED_EDGE ( 'NONE', *, *, #10588, .T. ) ;
#52258 =( BOUNDED_CURVE ( )  B_SPLINE_CURVE ( 2, ( #33574, #22216, #38475, #5263, #45243, #4151, #51271, #67882, #16173 ),
 .UNSPECIFIED., .F., .F. ) 
 B_SPLINE_CURVE_WITH_KNOTS ( ( 3, 2, 2, 2, 3 ),
 ( 0.1500000000000002442, 0.1583333333333335202, 0.1666666666666667962, 0.1750000000000000722, 0.1833333333333333481 ),
 .UNSPECIFIED. ) 
 CURVE ( )  GEOMETRIC_REPRESENTATION_ITEM ( )  RATIONAL_B_SPLINE_CURVE ( ( 0.9999999999999976685, 0.9238795325112890700, 1.000000000000000000, 0.9238795325112867385, 1.000000000000000000, 0.9238795325112867385, 1.000000000000000000, 0.9238795325112865164, 1.000000000000000222 ) ) 
 REPRESENTATION_ITEM ( '' )  );
#52259 = CARTESIAN_POINT ( 'NONE',  ( 4.401442555609581635E-16, 18.84374999795161187, -7.188101187500000044 ) ) ;
#52260 = EDGE_LOOP ( 'NONE', ( #18510, #47905 ) ) ;
#52261 = CARTESIAN_POINT ( 'NONE',  ( -7.320508075688778149, 44.99999999317203958, 7.320508075688769267 ) ) ;
#52262 = CARTESIAN_POINT ( 'NONE',  ( 2.679491924311228956, 46.04166666666666430, -10.00000000000000000 ) ) ;
#52263 = VECTOR ( 'NONE', #20539, 1000.000000000000000 ) ;
#52264 = CARTESIAN_POINT ( 'NONE',  ( 5.082755093536325042, 98.46875000204838102, -5.082755093536325930 ) ) ;
#52265 = CARTESIAN_POINT ( 'NONE',  ( 0.000000000000000000, -3.149999999999999911, 0.000000000000000000 ) ) ;
#52266 = CARTESIAN_POINT ( 'NONE',  ( -2.751064625579944321E-14, 204.8750000027312126, 146.0000000000000284 ) ) ;
#52267 = EDGE_CURVE ( 'NONE', #17730, #24196, #65392, .T. ) ;
#52268 = PLANE ( 'NONE',  #24120 ) ;
#52269 = EDGE_LOOP ( 'NONE', ( #23602, #33623, #3636, #49750 ) ) ;
#52270 = CARTESIAN_POINT ( 'NONE',  ( -3.042071309553159075, 244.9479166700806445, 11.35316468749999963 ) ) ;
#52271 = CARTESIAN_POINT ( 'NONE',  ( -7.188101187499992051, 0.000000000000000000, 18.36155278187175455 ) ) ;
#52272 = CARTESIAN_POINT ( 'NONE',  ( 4.999999999999985789, 89.16666666666665719, 8.660254037844378416 ) ) ;
#52273 = CARTESIAN_POINT ( 'NONE',  ( 32.00000000000000000, 206.2500000000000284, 169.9999999999999432 ) ) ;
#52274 = DIRECTION ( 'NONE',  ( -0.000000000000000000, -0.000000000000000000, 1.000000000000000000 ) ) ;
#52275 = CARTESIAN_POINT ( 'NONE',  ( -6.000000000000001776, 300.0000000000000000, 0.000000000000000000 ) ) ;
#52276 = CARTESIAN_POINT ( 'NONE',  ( 7.320508075688774596, 160.6249999999999716, -7.320508075688774596 ) ) ;
#52277 = DIRECTION ( 'NONE',  ( -0.000000000000000000, 1.000000000000000000, -0.000000000000000000 ) ) ;
#52278 = CARTESIAN_POINT ( 'NONE',  ( -32.88367528069134949, 175.6453838037559194, 160.0579690329453229 ) ) ;
#52279 = CARTESIAN_POINT ( 'NONE',  ( 4.999999999999999112, -53.50771145605675372, -45.03482491321348391 ) ) ;
#52280 = CARTESIAN_POINT ( 'NONE',  ( 9.832129032723416984, 140.6770833299193555, 5.676582343750006032 ) ) ;
#52281 = CARTESIAN_POINT ( 'NONE',  ( -3.673940397442060854E-16, 293.8125000034140157, -6.000000000000001776 ) ) ;
#52282 = CARTESIAN_POINT ( 'NONE',  ( 5.000000000000000000, -52.35862550122924830, -48.98731492261435250 ) ) ;
#52285 = CARTESIAN_POINT ( 'NONE',  ( -14.00000000000000178, 2.249999999994893862, 10.23492587299426404 ) ) ;
#52284 = CARTESIAN_POINT ( 'NONE',  ( 10.00000000000000178, 107.0833333265053398, -2.679491924311226736 ) ) ;
#52283 = CARTESIAN_POINT ( 'NONE',  ( 28.00000000000001776, 204.5000000000000284, 165.9999999999998863 ) ) ;
#52286 = ORIENTED_EDGE ( 'NONE', *, *, #49490, .F. ) ;
#52287 = CARTESIAN_POINT ( 'NONE',  ( -7.999999999999991118, 0.000000000000000000, 24.83030277982336642 ) ) ;
#52288 = CARTESIAN_POINT ( 'NONE',  ( 8.660254037844481445, 195.4166666666667425, -5.000000000000054179 ) ) ;
#52289 = CARTESIAN_POINT ( 'NONE',  ( 25.55430564589114795, 195.5625000013656063, 172.4456943541086957 ) ) ;
#52290 = EDGE_CURVE ( 'NONE', #21207, #22380, #71045, .T. ) ;
#52291 = CARTESIAN_POINT ( 'NONE',  ( -2.679491924311235618, 25.41666665983869677, 10.00000000000000000 ) ) ;
#52292 = AXIS2_PLACEMENT_3D ( 'NONE', #11415, #11049, #69129 ) ;
#52293 = CARTESIAN_POINT ( 'NONE',  ( 7.188101187500001821, 116.0000000020483810, -2.977408999572651371 ) ) ;
#52294 = CARTESIAN_POINT ( 'NONE',  ( 3.211159895383561835, 1.562499998634406806, -3.211159895383561835 ) ) ;
#52295 = CARTESIAN_POINT ( 'NONE',  ( -2.990854866097343745, 66.07503719301357137, -26.46919450145105301 ) ) ;
#52296 = CARTESIAN_POINT ( 'NONE',  ( 3.313708498984762496, -7.999999999999989342, 20.79905277982336642 ) ) ;
#52298 = CYLINDRICAL_SURFACE ( 'NONE', #43795, 10.00000000000000178 ) ;
#52297 = LINE ( 'NONE', #39486, #31061 ) ;
#52299 = CARTESIAN_POINT ( 'NONE',  ( 5.676582343750001591, 106.6145833299193555, -9.832129032723420536 ) ) ;
#52300 = ORIENTED_EDGE ( 'NONE', *, *, #17571, .T. ) ;
#52301 = CARTESIAN_POINT ( 'NONE',  ( 0.000000000000000000, 125.0000000000000000, 0.000000000000000000 ) ) ;
#52302 = CARTESIAN_POINT ( 'NONE',  ( -5.082755093536325042, 23.53124999795161543, -5.082755093536325930 ) ) ;
#52303 = CARTESIAN_POINT ( 'NONE',  ( 0.000000000000000000, 0.000000000000000000, 28.00000000000000000 ) ) ;
#52304 = CARTESIAN_POINT ( 'NONE',  ( -3.042071309553166625, 248.1770833367473017, -11.35316468749999608 ) ) ;
#52305 = CARTESIAN_POINT ( 'NONE',  ( -9.832129032723420536, 113.6979166632526983, 5.676582343749997150 ) ) ;
#52306 = ORIENTED_EDGE ( 'NONE', *, *, #52704, .F. ) ;
#52307 = CARTESIAN_POINT ( 'NONE',  ( 4.898587196589412829E-16, 25.87500000000000711, -8.000000000000000000 ) ) ;
#52308 = CARTESIAN_POINT ( 'NONE',  ( -10.18810118749999916, 0.000000000000000000, 103.6562500020483810 ) ) ;
#52309 = CARTESIAN_POINT ( 'NONE',  ( -10.00000000000000000, 219.1666666598387110, -2.679491924311229845 ) ) ;
#52310 = CARTESIAN_POINT ( 'NONE',  ( 3.458734125000016757, 201.1250000013656347, 199.4326545832176691 ) ) ;
#52311 = DIRECTION ( 'NONE',  ( -0.000000000000000000, 1.000000000000000000, -0.000000000000000000 ) ) ;
#52313 = CARTESIAN_POINT ( 'NONE',  ( 8.311093377946837890, 96.40624999658602690, -8.311093377946837890 ) ) ;
#52312 = DIRECTION ( 'NONE',  ( -1.000000000000000000, 0.000000000000000000, 0.000000000000000000 ) ) ;
#52314 = CARTESIAN_POINT ( 'NONE',  ( 7.999999999999992895, -3.313708498984756279, 9.174052783920144449 ) ) ;
#52315 = CARTESIAN_POINT ( 'NONE',  ( -29.43265458321766559, 195.7500000013656063, 166.5412658750003629 ) ) ;
#52316 = CARTESIAN_POINT ( 'NONE',  ( 7.320508075688774596, 170.6250000000000000, -7.320508075688774596 ) ) ;
#52317 = VERTEX_POINT ( 'NONE', #65395 ) ;
#52318 = CARTESIAN_POINT ( 'NONE',  ( 5.000000000000001776, 197.7083333265053966, -8.660254037844389075 ) ) ;
#52319 = CARTESIAN_POINT ( 'NONE',  ( 5.094044972490348933, 8.823157690132404696, 67.53052377765949643 ) ) ;
#52320 = CARTESIAN_POINT ( 'NONE',  ( 2.775557559380704872E-14, -48.00000000000001421, 139.0000000000000568 ) ) ;
#52321 = CARTESIAN_POINT ( 'NONE',  ( -9.832129032723420536, 94.01041666325268409, 5.676582343749997150 ) ) ;
#52322 = DIRECTION ( 'NONE',  ( -0.000000000000000000, -0.000000000000000000, 1.000000000000000000 ) ) ;
#52323 = CARTESIAN_POINT ( 'NONE',  ( 7.188101187499999156, 6.749999997951610986, 2.977408999572654924 ) ) ;
#52324 = CARTESIAN_POINT ( 'NONE',  ( 10.18810118749999916, 4.220049686691935698, 94.37500000204839523 ) ) ;
#52325 = CARTESIAN_POINT ( 'NONE',  ( 8.311093377946834337, 220.1562499965860127, 8.311093377946839666 ) ) ;
#52326 = VERTEX_POINT ( 'NONE', #59380 ) ;
#52327 = CARTESIAN_POINT ( 'NONE',  ( 2.828427124746190291, 20.62499999726881583, 2.828427124746192067 ) ) ;
#52328 = CARTESIAN_POINT ( 'NONE',  ( 4.000000000000016875, 196.5625000027312126, 199.6568542494924259 ) ) ;
#52329 = CARTESIAN_POINT ( 'NONE',  ( 8.311093377946837890, 216.4062499965860127, -8.311093377946837890 ) ) ;
#52330 = CARTESIAN_POINT ( 'NONE',  ( -7.204075437095965206, -7.204075437095968759, 80.21875000204836681 ) ) ;
#52331 = AXIS2_PLACEMENT_3D ( 'NONE', #59572, #48234, #19931 ) ;
#52332 = CARTESIAN_POINT ( 'NONE',  ( 4.000754058696052162, 22.00000000000000000, 0.7008730298822498650 ) ) ;
#52333 = CARTESIAN_POINT ( 'NONE',  ( 3.979266480698044450, 124.5000000000001137, -6.940132439340980675 ) ) ;
#52334 = CARTESIAN_POINT ( 'NONE',  ( 4.721056650415999201, 297.0781250017069510, -4.721056650415999201 ) ) ;
#52335 = VERTEX_POINT ( 'NONE', #20106 ) ;
#52336 = CARTESIAN_POINT ( 'NONE',  ( -3.042071309553173730, 214.6354166632526983, 11.35316468749999785 ) ) ;
#52337 = CARTESIAN_POINT ( 'NONE',  ( 10.18810118749999916, 1.247682550866122264E-15, 90.90625000204836681 ) ) ;
#52338 = CARTESIAN_POINT ( 'NONE',  ( -31.45873412500001010, 203.6250000013656063, 168.5673454167827572 ) ) ;
#52339 = CARTESIAN_POINT ( 'NONE',  ( 4.898587196589412829E-16, 19.87500000000000355, -8.000000000000000000 ) ) ;
#52340 = VERTEX_POINT ( 'NONE', #24654 ) ;
#52341 = B_SPLINE_CURVE_WITH_KNOTS ( 'NONE', 3,
 ( #21559, #27591, #26462, #15150, #44585, #32911 ),
 .UNSPECIFIED., .F., .F.,
 ( 4, 2, 4 ),
 ( 2.380729645499322951E-07, 0.003505341553885846402, 0.007010445034807142976 ),
 .UNSPECIFIED. ) ;
#52342 = CARTESIAN_POINT ( 'NONE',  ( 5.082755093536325042, 122.0937500020483952, -5.082755093536325930 ) ) ;
#52343 = LINE ( 'NONE', #11235, #12741 ) ;
#52344 = EDGE_CURVE ( 'NONE', #61133, #64958, #65972, .T. ) ;
#52345 = CARTESIAN_POINT ( 'NONE',  ( -8.660254037844390851, 32.91666666666667140, 4.999999999999998224 ) ) ;
#52346 = EDGE_CURVE ( 'NONE', #50950, #19551, #71414, .T. ) ;
#52347 = VECTOR ( 'NONE', #19829, 1000.000000000000000 ) ;
#52348 = CARTESIAN_POINT ( 'NONE',  ( 0.000000000000000000, 300.0000000000000000, 0.000000000000000000 ) ) ;
#52349 = CARTESIAN_POINT ( 'NONE',  ( 10.18810118750000093, -4.220049686691933921, 77.68750000204838102 ) ) ;
#52350 = ORIENTED_EDGE ( 'NONE', *, *, #44508, .F. ) ;
#52351 = CARTESIAN_POINT ( 'NONE',  ( -5.082755093536326818, 1.406249997951610320, 5.082755093536325042 ) ) ;
#52352 = DIRECTION ( 'NONE',  ( 0.000000000000000000, 0.000000000000000000, -1.000000000000000000 ) ) ;
#52353 = CARTESIAN_POINT ( 'NONE',  ( -5.000000000000000000, -11.82742353449332917, 68.45184936927694253 ) ) ;
#52354 = CARTESIAN_POINT ( 'NONE',  ( 1.739508062058411131, 51.27839935804142613, 48.57027215863440262 ) ) ;
#52355 = CARTESIAN_POINT ( 'NONE',  ( -6.676582343749999815, 297.5156250017070079, 2.765530957082001251 ) ) ;
#52357 = CARTESIAN_POINT ( 'NONE',  ( -10.99999999999978684, -4.556349186104264426, 88.28125000409679046 ) ) ;
#52356 = CARTESIAN_POINT ( 'NONE',  ( -9.832129032723418760, 233.4895833367473301, -5.676582343749998927 ) ) ;
#52358 = CONTEXT_DEPENDENT_SHAPE_REPRESENTATION ( #63095, #46361 ) ;
#52359 = ORIENTED_EDGE ( 'NONE', *, *, #43260, .F. ) ;
#52360 = ADVANCED_FACE ( 'NONE', ( #37101 ), #54466, .F. ) ;
#52361 = CARTESIAN_POINT ( 'NONE',  ( -8.311093377946834337, 239.8437500034139873, 8.311093377946837890 ) ) ;
#52362 = CARTESIAN_POINT ( 'NONE',  ( -2.977408999572647819, 7.188101187499991163, 4.205302781871751883 ) ) ;
#52363 = ADVANCED_FACE ( 'NONE', ( #50278 ), #54838, .T. ) ;
#52364 = ORIENTED_EDGE ( 'NONE', *, *, #61982, .F. ) ;
#52365 = CARTESIAN_POINT ( 'NONE',  ( 10.18810118749999916, 4.220049686691935698, 70.00000000204836681 ) ) ;
#52366 = CARTESIAN_POINT ( 'NONE',  ( 5.676582343750001591, 86.92708332991935549, -9.832129032723420536 ) ) ;
#52367 = CARTESIAN_POINT ( 'NONE',  ( -10.53333261448112346, 14.70318727039197881, 2.005774019098183203E-15 ) ) ;
#52368 = CARTESIAN_POINT ( 'NONE',  ( 4.556349186104051263, -10.99999999999999822, 82.46874999999998579 ) ) ;
#52371 = CARTESIAN_POINT ( 'NONE',  ( -1.469576158976823947E-15, 2.625000000000000444, 8.000000000000000000 ) ) ;
#52370 = CARTESIAN_POINT ( 'NONE',  ( 28.00000000000001776, 195.1250000027311842, 173.9999999999999147 ) ) ;
#52369 = CARTESIAN_POINT ( 'NONE',  ( 24.54126587499998635, 207.5000000013655779, 171.4326545832175555 ) ) ;
#52372 = EDGE_LOOP ( 'NONE', ( #65771, #25348, #24121, #27244 ) ) ;
#52373 = CARTESIAN_POINT ( 'NONE',  ( -26.34314575050759188, 196.0625000027312126, 166.0000000000004263 ) ) ;
#52374 = DIRECTION ( 'NONE',  ( -1.000000000000000000, 0.000000000000000000, 0.000000000000000000 ) ) ;
#52375 = CARTESIAN_POINT ( 'NONE',  ( 11.35316468750000141, 195.7812499965860127, 0.000000000000000000 ) ) ;
#52376 =( BOUNDED_CURVE ( )  B_SPLINE_CURVE ( 3, ( #34748, #13171, #18850, #25606 ),
 .UNSPECIFIED., .F., .F. ) 
 B_SPLINE_CURVE_WITH_KNOTS ( ( 4, 4 ),
 ( 4.745773451018401090, 4.898297765737375187 ),
 .UNSPECIFIED. ) 
 CURVE ( )  GEOMETRIC_REPRESENTATION_ITEM ( )  RATIONAL_B_SPLINE_CURVE ( ( 1.000000000000000000, 0.9980623005163389294, 0.9980623005163389294, 1.000000000000000000 ) ) 
 REPRESENTATION_ITEM ( '' )  );
#52377 = CARTESIAN_POINT ( 'NONE',  ( -3.458734125000015425, 205.9375000013656063, 142.0000000000000568 ) ) ;
#52378 = CARTESIAN_POINT ( 'NONE',  ( 28.00000000000002487, 206.1875000013656063, 166.5412658749999082 ) ) ;
#52379 = CARTESIAN_POINT ( 'NONE',  ( 2.977408999572650927, 20.62499999795161543, -7.188101187500001821 ) ) ;
#52380 = EDGE_CURVE ( 'NONE', #16071, #6572, #5666, .T. ) ;
#52381 = CARTESIAN_POINT ( 'NONE',  ( 8.311093377946837890, 186.7187499965860127, -8.311093377946837890 ) ) ;
#52382 = CARTESIAN_POINT ( 'NONE',  ( 5.082755093536326818, 96.59375000204838102, 5.082755093536325042 ) ) ;
#52384 = CARTESIAN_POINT ( 'NONE',  ( -7.347880794884122694E-16, 9.750000000000000000, 4.000000000000001776 ) ) ;
#52383 = DIRECTION ( 'NONE',  ( -0.000000000000000000, 0.000000000000000000, 1.000000000000000000 ) ) ;
#52385 = CARTESIAN_POINT ( 'NONE',  ( 2.780723358947928197E-16, 10.56249999863440792, -4.541265875000002339 ) ) ;
#52386 = CARTESIAN_POINT ( 'NONE',  ( 31.45873412499997812, 200.8750000013656063, 171.4326545832176123 ) ) ;
#52387 = CARTESIAN_POINT ( 'NONE',  ( 2.977408999572650927, -7.188101187499990274, 12.83030278187175277 ) ) ;
#52388 = CARTESIAN_POINT ( 'NONE',  ( 8.311093377946837890, 71.40624999658602690, -8.311093377946837890 ) ) ;
#52389 = EDGE_CURVE ( 'NONE', #26323, #46305, #38938, .T. ) ;
#52390 = DIRECTION ( 'NONE',  ( -0.000000000000000000, 1.000000000000000000, -0.000000000000000000 ) ) ;
#52391 = CARTESIAN_POINT ( 'NONE',  ( -2.828427124746208943, 201.6250000000000284, 144.8284271247462129 ) ) ;
#52392 = ORIENTED_EDGE ( 'NONE', *, *, #59046, .T. ) ;
#52393 = CARTESIAN_POINT ( 'NONE',  ( 3.313708498984762496, -7.999999999999989342, 7.486552783920144449 ) ) ;
#52394 = CARTESIAN_POINT ( 'NONE',  ( -10.99999999999989164, -4.556349186104158733, 80.78125000409679046 ) ) ;
#52395 = CARTESIAN_POINT ( 'NONE',  ( 5.676582343750001591, 71.61458332991935549, -9.832129032723420536 ) ) ;
#52396 = CARTESIAN_POINT ( 'NONE',  ( -10.18810118749999916, 4.220049686691934809, 117.0625000020483668 ) ) ;
#52397 = CARTESIAN_POINT ( 'NONE',  ( -3.458734125000016757, 196.1250000013656063, 140.5673454167823593 ) ) ;
#52398 = CARTESIAN_POINT ( 'NONE',  ( -2.219371606097579441, 16.40787039054625396, 68.79427927095593986 ) ) ;
#52400 = CARTESIAN_POINT ( 'NONE',  ( 9.832129032723420536, 56.19791666325268409, -5.676582343749999815 ) ) ;
#52399 = CARTESIAN_POINT ( 'NONE',  ( -2.977408999572652260, 89.93750000204839523, 7.188101187500000044 ) ) ;
#52401 = CARTESIAN_POINT ( 'NONE',  ( 7.999999999999991118, 9.797174393178815797E-16, 22.76780278392014623 ) ) ;
#52402 = CARTESIAN_POINT ( 'NONE',  ( 8.000000000000000000, 111.0312500040967763, -3.313708498984762496 ) ) ;
#52404 = CARTESIAN_POINT ( 'NONE',  ( 10.00000000000000178, 161.8749999931720254, 0.000000000000000000 ) ) ;
#52403 = PRODUCT_DEFINITION_SHAPE ( 'NONE', 'NONE',  #74654 ) ;
#52405 = CARTESIAN_POINT ( 'NONE',  ( -5.082755093536325930, 94.34375000204838102, -5.082755093536325930 ) ) ;
#52406 = VECTOR ( 'NONE', #47045, 999.9999999999997726 ) ;
#52407 = CARTESIAN_POINT ( 'NONE',  ( -2.679491924311226292, 53.33333332650536107, -10.00000000000000178 ) ) ;
#52408 = CARTESIAN_POINT ( 'NONE',  ( -8.311093377946841443, 54.21874999658601979, 8.311093377946834337 ) ) ;
#52409 = CARTESIAN_POINT ( 'NONE',  ( -4.220049686691937474, -10.18810118749999738, 113.3125000020483668 ) ) ;
#52410 = CARTESIAN_POINT ( 'NONE',  ( 11.35316468750000141, 180.7812499965860411, 0.000000000000000000 ) ) ;
#52411 = ORIENTED_EDGE ( 'NONE', *, *, #32090, .F. ) ;
#52412 = FACE_OUTER_BOUND ( 'NONE', #51322, .T. ) ;
#52413 = CARTESIAN_POINT ( 'NONE',  ( -1.469576158976823947E-15, 12.93749999590322197, 8.000000000000000000 ) ) ;
#52415 = CARTESIAN_POINT ( 'NONE',  ( -5.676582343750006032, 184.1145833299193555, 9.832129032723418760 ) ) ;
#52414 = CARTESIAN_POINT ( 'NONE',  ( -1.764475369138369887, 194.9673491673439401, 194.4371566899129959 ) ) ;
#52416 = EDGE_CURVE ( 'NONE', #35360, #64164, #35320, .T. ) ;
#52417 = CARTESIAN_POINT ( 'NONE',  ( -1.836970198721029983E-15, 83.75000000000000000, 10.00000000000000178 ) ) ;
#52418 = CARTESIAN_POINT ( 'NONE',  ( 1.836970198721029589E-15, 254.3750000068280031, 10.00000000000000000 ) ) ;
#52419 = CARTESIAN_POINT ( 'NONE',  ( 13.99999999999999822, -2.250000000005106138, 7.677076266390546522 ) ) ;
#52420 = ORIENTED_EDGE ( 'NONE', *, *, #62304, .F. ) ;
#52421 = ADVANCED_FACE ( 'NONE', ( #26133 ), #15564, .F. ) ;
#52422 = CARTESIAN_POINT ( 'NONE',  ( -8.311093377946841443, 164.2187499965860411, 8.311093377946834337 ) ) ;
#52423 = CARTESIAN_POINT ( 'NONE',  ( -5.082755093536319713, 5.082755093536319713, 26.79905278187175455 ) ) ;
#52424 = CARTESIAN_POINT ( 'NONE',  ( 3.042071309553159519, 135.0520833299193555, 11.35316468750000141 ) ) ;
#52425 = EDGE_CURVE ( 'NONE', #21248, #74465, #22081, .T. ) ;
#52426 = DIRECTION ( 'NONE',  ( -0.000000000000000000, -0.000000000000000000, -1.000000000000000000 ) ) ;
#52427 = ORIENTED_EDGE ( 'NONE', *, *, #71804, .T. ) ;
#52428 = CARTESIAN_POINT ( 'NONE',  ( -5.656854249492380582, 101.0000000040967905, -5.656854249492380582 ) ) ;
#52429 = CARTESIAN_POINT ( 'NONE',  ( 2.828427124746191623, 13.12500000000000000, -2.828427124746191623 ) ) ;
#52430 = CARTESIAN_POINT ( 'NONE',  ( -38.32546752959855496, -1.189519027697512055, 124.5193363645423545 ) ) ;
#52431 = CARTESIAN_POINT ( 'NONE',  ( -4.541265875000002339, 10.81249999863440792, -5.561446717895856393E-16 ) ) ;
#52432 = CARTESIAN_POINT ( 'NONE',  ( 5.656854249492374365, 5.656854249492375253, 21.45530278392014623 ) ) ;
#52433 = CARTESIAN_POINT ( 'NONE',  ( -1.656854249492403008, 195.6875000000000284, 146.0000000000000284 ) ) ;
#52434 = ORIENTED_EDGE ( 'NONE', *, *, #46821, .F. ) ;
#52435 = CARTESIAN_POINT ( 'NONE',  ( 3.999999999999960032, 204.9375000000000284, 143.6568542494924259 ) ) ;
#52436 = CARTESIAN_POINT ( 'NONE',  ( -5.082755093536325930, 104.4687500020483952, -5.082755093536325930 ) ) ;
#52438 = CARTESIAN_POINT ( 'NONE',  ( 1.102182119232618108E-15, 293.2500000000000000, 6.000000000000001776 ) ) ;
#52437 = CARTESIAN_POINT ( 'NONE',  ( 16.00000000000000711, 0.000000000000000000, 38.34805510287551300 ) ) ;
#52439 = DIRECTION ( 'NONE',  ( -3.491481338843133355E-15, 1.000000000000000000, 0.000000000000000000 ) ) ;
#52440 = EDGE_LOOP ( 'NONE', ( #40693, #50457, #36916, #5343 ) ) ;
#52441 = CARTESIAN_POINT ( 'NONE',  ( -3.496982156820191978, 16.35094707925454216, -69.15443034747076467 ) ) ;
#52442 = PRESENTATION_LAYER_ASSIGNMENT (  '', '', ( #66877 ) ) ;
#52443 = CARTESIAN_POINT ( 'NONE',  ( 7.188101187499993827, -2.977408999572645598, 26.14280278187175455 ) ) ;
#52444 = ORIENTED_EDGE ( 'NONE', *, *, #63145, .T. ) ;
#52445 = VERTEX_POINT ( 'NONE', #72162 ) ;
#52446 = CARTESIAN_POINT ( 'NONE',  ( -10.18810118749999916, 4.220049686691934809, 88.56250000204838102 ) ) ;
#52447 = CARTESIAN_POINT ( 'NONE',  ( -28.00000000000007461, 195.1250000027311842, 166.0000000000003695 ) ) ;
#52448 = CARTESIAN_POINT ( 'NONE',  ( -31.45873412499999233, 195.9375000013655779, 170.0000000000003979 ) ) ;
#52449 = CARTESIAN_POINT ( 'NONE',  ( -6.735557395310442023E-16, 11.00000000000000000, 99.62499999999998579 ) ) ;
#52452 = CARTESIAN_POINT ( 'NONE',  ( -2.765530957081998142, 296.7968750017070079, 6.676582343750000703 ) ) ;
#52451 = CARTESIAN_POINT ( 'NONE',  ( 31.99999999999998579, 205.4375000027312126, 168.3431457505075173 ) ) ;
#52450 = CARTESIAN_POINT ( 'NONE',  ( 26.34314575050763807, 202.6875000027312126, 165.9999999999998295 ) ) ;
#52453 = CARTESIAN_POINT ( 'NONE',  ( -1.836970198721029983E-15, 128.7500000000000000, 10.00000000000000178 ) ) ;
#52454 = CARTESIAN_POINT ( 'NONE',  ( -5.656854249492378806, 101.1875000000000000, 5.656854249492381470 ) ) ;
#52455 = CARTESIAN_POINT ( 'NONE',  ( -6.676582343750001591, 289.6093750017069510, 0.000000000000000000 ) ) ;
#52456 = CARTESIAN_POINT ( 'NONE',  ( -5.082755093536317936, -5.082755093536320601, 2.049052781871754103 ) ) ;
#52457 = CARTESIAN_POINT ( 'NONE',  ( -27.99999999999996092, 208.5000000000000284, 174.0000000000003695 ) ) ;
#52458 = CARTESIAN_POINT ( 'NONE',  ( 24.54126587500000056, 202.1250000013656063, 168.5673454167822172 ) ) ;
#52459 = CARTESIAN_POINT ( 'NONE',  ( 7.188101187500000044, 3.843749997951610542, 0.000000000000000000 ) ) ;
#52460 = CARTESIAN_POINT ( 'NONE',  ( 3.317071493978883456, -8.008118988124989457, 2.981865283940628331 ) ) ;
#52461 = CARTESIAN_POINT ( 'NONE',  ( -2.445694354108839619, 195.8125000013656063, 139.5543056458912190 ) ) ;
#52462 = CARTESIAN_POINT ( 'NONE',  ( 7.188101187500002709, 114.6875000020484094, 2.977408999572649151 ) ) ;
#52464 = CARTESIAN_POINT ( 'NONE',  ( 3.003894787873386818, 194.6986583611032984, 200.1718283400802534 ) ) ;
#52463 = CARTESIAN_POINT ( 'NONE',  ( -9.999999999999998224, 250.2083333333333144, 2.679491924311235174 ) ) ;
#52465 = CARTESIAN_POINT ( 'NONE',  ( 3.042071309553163960, 227.7604166700806445, -11.35316468749999785 ) ) ;
#52466 = DIRECTION ( 'NONE',  ( -0.000000000000000000, 1.000000000000000000, 4.476705744456276341E-16 ) ) ;
#52467 = CARTESIAN_POINT ( 'NONE',  ( -5.082755093536317936, -5.082755093536320601, 27.54905278187175455 ) ) ;
#52469 =( BOUNDED_CURVE ( )  B_SPLINE_CURVE ( 2, ( #50044, #27033, #11180, #68512, #21737, #57206, #73060, #50787, #16072 ),
 .UNSPECIFIED., .F., .F. ) 
 B_SPLINE_CURVE_WITH_KNOTS ( ( 3, 2, 2, 2, 3 ),
 ( 0.07954545454545454419, 0.08522727272727272096, 0.09090909090909091161, 0.09659090909090908839, 0.1022727272727272790 ),
 .UNSPECIFIED. ) 
 CURVE ( )  GEOMETRIC_REPRESENTATION_ITEM ( )  RATIONAL_B_SPLINE_CURVE ( ( 1.000000000000000000, 0.9238795325112867385, 1.000000000000000000, 0.9238795325112867385, 1.000000000000000000, 0.9238795325112867385, 1.000000000000000000, 0.9238795325112867385, 1.000000000000000000 ) ) 
 REPRESENTATION_ITEM ( '' )  );
#52468 = CARTESIAN_POINT ( 'NONE',  ( 32.00000000000000000, 197.3125000000000568, 168.3431457505075741 ) ) ;
#52470 = CARTESIAN_POINT ( 'NONE',  ( -8.311093377946841443, 28.90624999658601979, 8.311093377946830785 ) ) ;
#52471 = CARTESIAN_POINT ( 'NONE',  ( 2.679491924289742144, 23.95833333333158777, 10.00000000001278444 ) ) ;
#52472 = CARTESIAN_POINT ( 'NONE',  ( -3.042071309553164404, 217.5520833299193555, -11.35316468749999963 ) ) ;
#52473 = CARTESIAN_POINT ( 'NONE',  ( -30.93541659651598152, -51.99989572432781415, 171.9999999999997726 ) ) ;
#52475 = CARTESIAN_POINT ( 'NONE',  ( -38.00000000000000000, -52.99999999999999289, 25.00000000000000000 ) ) ;
#52474 = CARTESIAN_POINT ( 'NONE',  ( -2.995737153994215252, 51.55860531535790869, 48.67776149471519886 ) ) ;
#52476 = VERTEX_POINT ( 'NONE', #56322 ) ;
#52477 = CARTESIAN_POINT ( 'NONE',  ( 1.432654583217608080, 194.8750000013656063, 138.5412658750000503 ) ) ;
#52478 = CARTESIAN_POINT ( 'NONE',  ( -2.085542519210945728E-15, 19.53124999658601979, 11.35316468750000141 ) ) ;
#52479 = CARTESIAN_POINT ( 'NONE',  ( 7.778174593052023411, -7.778174593052021635, 88.75000000409677625 ) ) ;
#52480 = CARTESIAN_POINT ( 'NONE',  ( 2.445694354108784108, 207.5625000013656063, 144.4456943541088663 ) ) ;
#52481 = CARTESIAN_POINT ( 'NONE',  ( -6.000000000000001776, 295.0625000034140157, 0.000000000000000000 ) ) ;
#52482 = CARTESIAN_POINT ( 'NONE',  ( 0.000000000000000000, 300.0000000000000000, 10.00000000000000178 ) ) ;
#52484 = CARTESIAN_POINT ( 'NONE',  ( -3.042071309553163960, 17.23958332991935194, -11.35316468749999963 ) ) ;
#52483 = CARTESIAN_POINT ( 'NONE',  ( 1.320432766682874540E-15, 109.5312500020483810, 7.188101187500000044 ) ) ;
#52485 = CARTESIAN_POINT ( 'NONE',  ( 3.313708498984762496, -7.999999999999989342, 22.29905277982336287 ) ) ;
#52486 = CARTESIAN_POINT ( 'NONE',  ( -9.832129032723420536, 143.6979166632526699, 5.676582343749997150 ) ) ;
#52487 = CARTESIAN_POINT ( 'NONE',  ( -2.679491924311235618, 115.4166666598386968, 10.00000000000000000 ) ) ;
#52488 = CARTESIAN_POINT ( 'NONE',  ( -5.082755093536325930, 116.8437500020483810, -5.082755093536325930 ) ) ;
#52489 = CARTESIAN_POINT ( 'NONE',  ( 2.679491924311228956, 172.9166666598386826, -10.00000000000000000 ) ) ;
#52490 = CARTESIAN_POINT ( 'NONE',  ( -28.00000000000002487, 206.6875000013656063, 166.5412658750003629 ) ) ;
#52491 = VERTEX_POINT ( 'NONE', #55213 ) ;
#52492 = CARTESIAN_POINT ( 'NONE',  ( -3.042071309553173730, 14.63541666325268231, 11.35316468749999785 ) ) ;
#52493 =( BOUNDED_CURVE ( )  B_SPLINE_CURVE ( 2, ( #64072, #36415, #68986, #12380, #40313, #59429, #30747, #63317, #2077, #45230, #10901, #33935, #48086 ),
 .UNSPECIFIED., .F., .F. ) 
 B_SPLINE_CURVE_WITH_KNOTS ( ( 3, 2, 2, 2, 2, 2, 3 ),
 ( 1.397287049208421728, 1.402520683848244909, 1.407754318488068090, 1.412987953127891272, 1.418221587767714453, 1.423455222407537857, 1.428688857047360816 ),
 .UNSPECIFIED. ) 
 CURVE ( )  GEOMETRIC_REPRESENTATION_ITEM ( )  RATIONAL_B_SPLINE_CURVE ( ( 1.000000000000238032, 0.9659258262888302804, 1.000000000000000000, 0.9659258262890683122, 1.000000000000000000, 0.9659258262890683122, 1.000000000000000000, 0.9659258262890683122, 1.000000000000000000, 0.9659258262890683122, 1.000000000000000000, 0.9659258262890683122, 1.000000000000000000 ) ) 
 REPRESENTATION_ITEM ( '' )  );
#52494 = ORIENTED_EDGE ( 'NONE', *, *, #1211, .F. ) ;
#52495 = DIRECTION ( 'NONE',  ( 1.000000000000000000, 0.000000000000000000, 0.000000000000000000 ) ) ;
#52496 = CARTESIAN_POINT ( 'NONE',  ( 4.721056650415999201, 297.0781250017069510, -4.721056650415999201 ) ) ;
#52497 = CARTESIAN_POINT ( 'NONE',  ( 3.042071309553159519, 139.7395833299193839, 11.35316468750000141 ) ) ;
#52498 = CARTESIAN_POINT ( 'NONE',  ( -1.656854249492377029, 3.687500000000000888, 4.000000000000007994 ) ) ;
#52499 = CARTESIAN_POINT ( 'NONE',  ( -7.999999999999991118, 3.313708498984756723, 23.29280278432983309 ) ) ;
#52500 = CARTESIAN_POINT ( 'NONE',  ( 56.59224446838397427, 211.2645079806148374, 48.87444646355286437 ) ) ;
#52501 = CARTESIAN_POINT ( 'NONE',  ( -3.042071309553166181, 252.8645833367473301, -11.35316468749999608 ) ) ;
#52502 = AXIS2_PLACEMENT_3D ( 'NONE', #50536, #5646, #44514 ) ;
#52503 = CARTESIAN_POINT ( 'NONE',  ( -10.18810118749999738, -4.220049686691941915, 92.12500000204836681 ) ) ;
#52504 = ORIENTED_EDGE ( 'NONE', *, *, #66706, .F. ) ;
#52505 = EDGE_CURVE ( 'NONE', #63519, #14543, #34099, .T. ) ;
#52506 = AXIS2_PLACEMENT_3D ( 'NONE', #73678, #44270, #49922 ) ;
#52507 = CARTESIAN_POINT ( 'NONE',  ( -1.656854249492521136, 197.6874999999999432, 145.9999999999999147 ) ) ;
#52508 = CARTESIAN_POINT ( 'NONE',  ( -4.000000000000001776, 8.437500000000000000, -1.656854249492381470 ) ) ;
#52509 = CARTESIAN_POINT ( 'NONE',  ( 11.35316468749999785, 90.88541666325266988, 3.042071309553174174 ) ) ;
#52510 = EDGE_LOOP ( 'NONE', ( #55221, #1985, #18178, #10681 ) ) ;
#52511 = CARTESIAN_POINT ( 'NONE',  ( -4.220049686691937474, -10.18810118749999738, 108.4375000020483668 ) ) ;
#52512 = EDGE_CURVE ( 'NONE', #36620, #69862, #71457, .T. ) ;
#52513 = CARTESIAN_POINT ( 'NONE',  ( -1.881053915767121776, 16.74999999863440436, -4.541265875000002339 ) ) ;
#52514 = ORIENTED_EDGE ( 'NONE', *, *, #68773, .F. ) ;
#52515 = ORIENTED_EDGE ( 'NONE', *, *, #71378, .T. ) ;
#52516 = CARTESIAN_POINT ( 'NONE',  ( 5.656854249492380582, 7.687500000000001776, -5.656854249492380582 ) ) ;
#52517 = CARTESIAN_POINT ( 'NONE',  ( 4.541265875000002339, 1.499999998634407028, -1.881053915767121554 ) ) ;
#52518 = CARTESIAN_POINT ( 'NONE',  ( -5.082755093536325042, 26.90624999795161898, -5.082755093536325930 ) ) ;
#52519 = CARTESIAN_POINT ( 'NONE',  ( -4.898587196589412829E-16, 121.8125000040967763, -8.000000000000000000 ) ) ;
#52520 = CARTESIAN_POINT ( 'NONE',  ( 10.18810118749999916, 4.220049686691935698, 101.8750000020483810 ) ) ;
#52521 = CARTESIAN_POINT ( 'NONE',  ( 0.000000000000000000, 300.0000000000000000, 15.99999999999998579 ) ) ;
#52522 = CARTESIAN_POINT ( 'NONE',  ( 2.828427124746190291, 14.62499999726881406, 2.828427124746192067 ) ) ;
#52523 = CARTESIAN_POINT ( 'NONE',  ( 0.000000000000000000, 300.0000000000000000, 10.00000000000000178 ) ) ;
#52524 = ORIENTED_EDGE ( 'NONE', *, *, #13442, .F. ) ;
#52525 = FACE_OUTER_BOUND ( 'NONE', #8960, .T. ) ;
#52526 = CARTESIAN_POINT ( 'NONE',  ( 3.458734125000015425, 197.0000000013656347, 196.5673454167823877 ) ) ;
#52527 = CARTESIAN_POINT ( 'NONE',  ( -25.55430564589122966, 204.3125000013656063, 167.5543056458915032 ) ) ;
#52528 =( LENGTH_UNIT ( ) NAMED_UNIT ( * ) SI_UNIT ( .MILLI., .METRE. ) );
#52529 = CARTESIAN_POINT ( 'NONE',  ( 4.541265875000001451, 15.24999999863440969, 1.881053915767124440 ) ) ;
#52530 = CARTESIAN_POINT ( 'NONE',  ( 0.000000000000000000, 0.000000000000000000, 0.000000000000000000 ) ) ;
#52531 = CARTESIAN_POINT ( 'NONE',  ( -4.401442555609577197E-16, 7.188101187499992051, 10.11155278187175455 ) ) ;
#52532 = VERTEX_POINT ( 'NONE', #49532 ) ;
#52533 = ORIENTED_EDGE ( 'NONE', *, *, #2596, .F. ) ;
#52534 = CARTESIAN_POINT ( 'NONE',  ( 10.18810118750000093, -4.220049686691933033, 105.8125000020483952 ) ) ;
#52535 = CARTESIAN_POINT ( 'NONE',  ( 6.123233995736767268E-16, 96.25000000000000000, -10.00000000000000178 ) ) ;
#52536 = CARTESIAN_POINT ( 'NONE',  ( -32.00000000000000000, 204.2500000000000284, 170.0000000000003979 ) ) ;
#52537 = CARTESIAN_POINT ( 'NONE',  ( 1.432654583217664479, 199.7500000013656063, 201.4587341250000065 ) ) ;
#52538 = FACE_BOUND ( 'NONE', #62298, .T. ) ;
#52539 = CARTESIAN_POINT ( 'NONE',  ( 6.123233995736767268E-16, 91.25000000000001421, -10.00000000000000178 ) ) ;
#52540 = CARTESIAN_POINT ( 'NONE',  ( -8.000000000000000000, 117.5000000000000000, 0.000000000000000000 ) ) ;
#52541 = CARTESIAN_POINT ( 'NONE',  ( -11.35316468750000141, 63.80208332991934839, 3.042071309553159963 ) ) ;
#52542 = CARTESIAN_POINT ( 'NONE',  ( -4.088227598258586603E-16, 298.3593750017070079, -6.676582343750001591 ) ) ;
#52543 = EDGE_LOOP ( 'NONE', ( #37094, #63805, #28072, #60838 ) ) ;
#52544 = CARTESIAN_POINT ( 'NONE',  ( 4.000000000000016875, 203.4375000000000284, 199.6568542494924259 ) ) ;
#52545 = AXIS2_PLACEMENT_3D ( 'NONE', #1078, #13096, #59153 ) ;
#52546 = CARTESIAN_POINT ( 'NONE',  ( -3.313708498984765161, 14.34374999590322375, 7.999999999999998224 ) ) ;
#52547 = CARTESIAN_POINT ( 'NONE',  ( -3.458734125000016313, 207.8750000013656063, 140.5673454167824161 ) ) ;
#52548 = CARTESIAN_POINT ( 'NONE',  ( 3.313708498984762496, 11.53124999590322375, 7.999999999999998224 ) ) ;
#52549 = CARTESIAN_POINT ( 'NONE',  ( 7.999999999999991118, 1.469576158976822369E-15, 25.76780278392172008 ) ) ;
#52550 = CARTESIAN_POINT ( 'NONE',  ( -2.679491924311228512, 223.9583333333333428, -9.999999999999998224 ) ) ;
#52551 = CARTESIAN_POINT ( 'NONE',  ( -2.485281374238895502, 292.8124999999999432, -5.999999999999677591 ) ) ;
#52552 = CARTESIAN_POINT ( 'NONE',  ( -10.18810118749999916, 4.220049686691934809, 70.93750000204838102 ) ) ;
#52553 = CARTESIAN_POINT ( 'NONE',  ( 4.999999999999993783, 219.1666666666666856, 8.660254037844390851 ) ) ;
#52554 = CARTESIAN_POINT ( 'NONE',  ( 5.082755093536320601, -5.082755093536318824, 11.42405278187175455 ) ) ;
#52555 = CARTESIAN_POINT ( 'NONE',  ( -3.042071309553164404, 177.5520833299193839, -11.35316468749999963 ) ) ;
#52556 = CARTESIAN_POINT ( 'NONE',  ( 1.881053915767122664, 3.124999998634407028, 4.541265875000001451 ) ) ;
#52558 = CARTESIAN_POINT ( 'NONE',  ( -14.00000000000000178, 2.249999999994893862, 10.23492587299426404 ) ) ;
#52557 = CARTESIAN_POINT ( 'NONE',  ( 5.656854249492376141, -5.656854249492374365, 20.89280277982336642 ) ) ;
#52559 = VERTEX_POINT ( 'NONE', #72552 ) ;
#52560 = CARTESIAN_POINT ( 'NONE',  ( 2.445694354108782775, 194.5625000013656063, 139.5543056458912190 ) ) ;
#52561 = CARTESIAN_POINT ( 'NONE',  ( -2.085542519210945728E-15, 34.84374999658601268, 11.35316468750000141 ) ) ;
#52562 = CARTESIAN_POINT ( 'NONE',  ( -4.556349186104047710, -10.99999999999999822, 104.9687500040967763 ) ) ;
#52563 = CARTESIAN_POINT ( 'NONE',  ( -30.44569435410875968, 203.8125000013656063, 172.4456943541092642 ) ) ;
#52564 = CARTESIAN_POINT ( 'NONE',  ( 3.313708498984757167, 4.031249995903219308, 8.000000000000001776 ) ) ;
#52566 = CARTESIAN_POINT ( 'NONE',  ( 5.841566664369303132E-15, 13.85640646055103531, -14.80000000000000071 ) ) ;
#52565 = CARTESIAN_POINT ( 'NONE',  ( -3.313708498984693218, 115.9062500040967620, -8.000000000000065725 ) ) ;
#52567 = CARTESIAN_POINT ( 'NONE',  ( -3.458734125000015425, 200.9375000013656063, 142.0000000000000568 ) ) ;
#52568 = EDGE_CURVE ( 'NONE', #20975, #44642, #20857, .T. ) ;
#52569 = EDGE_CURVE ( 'NONE', #32440, #64909, #22334, .T. ) ;
#52570 = AXIS2_PLACEMENT_3D ( 'NONE', #8127, #7395, #1743 ) ;
#52571 = CARTESIAN_POINT ( 'NONE',  ( 7.320508075688774596, 72.49999999317203958, -7.320508075688774596 ) ) ;
#52572 = CARTESIAN_POINT ( 'NONE',  ( -7.188101187499999156, 97.25000000204839523, 2.977408999572654924 ) ) ;
#52573 = CARTESIAN_POINT ( 'NONE',  ( 2.780723358947928197E-16, 10.68749999863440792, -4.541265875000002339 ) ) ;
#52574 = CARTESIAN_POINT ( 'NONE',  ( 8.660254037844385522, 55.41666666666666430, -4.999999999999997335 ) ) ;
#52575 = CARTESIAN_POINT ( 'NONE',  ( 6.716570278246744685, 0.2636345205237095035, -3.927716332986086911 ) ) ;
#52576 = CARTESIAN_POINT ( 'NONE',  ( 4.193070328474941100, -50.40098303874172103, 40.95513628906654446 ) ) ;
#52577 = ORIENTED_EDGE ( 'NONE', *, *, #64012, .F. ) ;
#52578 = VERTEX_POINT ( 'NONE', #22713 ) ;
#52579 = CARTESIAN_POINT ( 'NONE',  ( 7.320508075688774596, 22.49999999317202892, -7.320508075688774596 ) ) ;
#52580 = CARTESIAN_POINT ( 'NONE',  ( -2.765530957081996810, 297.4218750017069510, -6.676582343750003368 ) ) ;
#52581 = PLANE ( 'NONE',  #25439 ) ;
#52582 = CARTESIAN_POINT ( 'NONE',  ( -5.000000000000000000, -32.28817737728140003, -1.075528555105620399E-13 ) ) ;
#52583 = CARTESIAN_POINT ( 'NONE',  ( -3.042071309553164404, 152.2395833299193271, -11.35316468749999963 ) ) ;
#52584 = EDGE_CURVE ( 'NONE', #2013, #30714, #29241, .T. ) ;
#52585 = EDGE_CURVE ( 'NONE', #37723, #53254, #72267, .T. ) ;
#52586 = CARTESIAN_POINT ( 'NONE',  ( 7.204075437095968759, -7.204075437095966983, 84.71875000204836681 ) ) ;
#52587 = CARTESIAN_POINT ( 'NONE',  ( 2.824543433528785410E-14, 210.0000000000000284, 194.0000000000000568 ) ) ;
#52588 = CARTESIAN_POINT ( 'NONE',  ( 2.828427124746209831, 205.3750000000000284, 200.8284271247462129 ) ) ;
#52589 = DIRECTION ( 'NONE',  ( 1.000000000000000000, 0.000000000000000000, 0.000000000000000000 ) ) ;
#52590 = CARTESIAN_POINT ( 'NONE',  ( 10.18810118750000093, -4.220049686691933921, 107.6875000020483810 ) ) ;
#52591 = ORIENTED_EDGE ( 'NONE', *, *, #3124, .T. ) ;
#52592 =( BOUNDED_CURVE ( )  B_SPLINE_CURVE ( 2, ( #16236, #32889, #38537, #10230, #38160, #44189, #61538, #55519, #27950 ),
 .UNSPECIFIED., .F., .F. ) 
 B_SPLINE_CURVE_WITH_KNOTS ( ( 3, 2, 2, 2, 3 ),
 ( 0.3500000000000004219, 0.3583333333333337256, 0.3666666666666669738, 0.3750000000000002776, 0.3833333333333335813 ),
 .UNSPECIFIED. ) 
 CURVE ( )  GEOMETRIC_REPRESENTATION_ITEM ( )  RATIONAL_B_SPLINE_CURVE ( ( 0.9999999999999958922, 0.9238795325112908463, 1.000000000000000000, 0.9238795325112867385, 1.000000000000000000, 0.9238795325112867385, 1.000000000000000000, 0.9238795325112847401, 1.000000000000001998 ) ) 
 REPRESENTATION_ITEM ( '' )  );
#52593 = DIRECTION ( 'NONE',  ( 0.000000000000000000, 0.000000000000000000, -1.000000000000000000 ) ) ;
#52594 = CARTESIAN_POINT ( 'NONE',  ( 29.13614168215335454, 175.4267435998110898, 159.1571751346110659 ) ) ;
#52595 = CARTESIAN_POINT ( 'NONE',  ( 3.042071309553159519, 125.0520833299193555, 11.35316468750000141 ) ) ;
#52596 = CARTESIAN_POINT ( 'NONE',  ( 3.458734125000015425, 198.9375000013655779, 198.0000000000000284 ) ) ;
#52597 = CARTESIAN_POINT ( 'NONE',  ( 4.242640687119287435, 298.4375000034140157, 4.242640687119285658 ) ) ;
#52598 = CARTESIAN_POINT ( 'NONE',  ( -7.204075437095965206, -7.204075437095968759, 78.71875000204836681 ) ) ;
#52599 = CARTESIAN_POINT ( 'NONE',  ( -2.085542519210945728E-15, 49.84374999658601268, 11.35316468750000141 ) ) ;
#52600 = ORIENTED_EDGE ( 'NONE', *, *, #42494, .T. ) ;
#52601 = DIRECTION ( 'NONE',  ( -0.000000000000000000, 1.000000000000000000, 0.000000000000000000 ) ) ;
#52602 = CARTESIAN_POINT ( 'NONE',  ( -3.211159895383561391, 1.812499998634406584, -3.211159895383561835 ) ) ;
#52603 = CARTESIAN_POINT ( 'NONE',  ( 3.317071493978877683, 8.008118988124991233, 15.54436528394063188 ) ) ;
#52604 = CARTESIAN_POINT ( 'NONE',  ( -7.188101187500000044, 14.71874999795161187, -8.802885111219163269E-16 ) ) ;
#52605 = CARTESIAN_POINT ( 'NONE',  ( -2.485281374238572649, 293.2500000034140157, 6.000000000000002665 ) ) ;
#52606 = AXIS2_PLACEMENT_3D ( 'NONE', #12068, #12432, #70889 ) ;
#52607 = ADVANCED_FACE ( 'NONE', ( #57070 ), #29134, .T. ) ;
#52608 = CARTESIAN_POINT ( 'NONE',  ( -47.73904998337091143, 144.1604321045476809, 63.58670016157662275 ) ) ;
#52609 = CARTESIAN_POINT ( 'NONE',  ( 5.082755093536324154, 3.656249997951610542, 5.082755093536326818 ) ) ;
#52610 = CARTESIAN_POINT ( 'NONE',  ( 5.082755093536320601, -5.082755093536318824, 6.549052781871754547 ) ) ;
#52611 =( BOUNDED_CURVE ( )  B_SPLINE_CURVE ( 2, ( #9365, #60289, #42568, #61041, #8616, #61417, #32385, #25947, #66702, #26322, #13876 ),
 .UNSPECIFIED., .F., .F. ) 
 B_SPLINE_CURVE_WITH_KNOTS ( ( 3, 2, 2, 2, 2, 3 ),
 ( 0.3970965164372073364, 0.3970965350674087180, 0.4037148106518655410, 0.4103330862363223086, 0.4169513618207791872, 0.4235696451107979765 ),
 .UNSPECIFIED. ) 
 CURVE ( )  GEOMETRIC_REPRESENTATION_ITEM ( )  RATIONAL_B_SPLINE_CURVE ( ( 0.9999995714485965248, 0.9999997857236950782, 1.000000000000000000, 0.9238795325112867385, 1.000000000000000000, 0.9238795325112867385, 1.000000000000000000, 0.9238795325112867385, 1.000000000000000000, 0.9238795325112867385, 1.000000000000000000 ) ) 
 REPRESENTATION_ITEM ( '' )  );
#52612 = CARTESIAN_POINT ( 'NONE',  ( 10.18810118749999916, 1.247682550866122264E-15, 69.90625000204836681 ) ) ;
#52613 = CARTESIAN_POINT ( 'NONE',  ( -25.55430564589115505, 207.3125000013656063, 172.4456943541091789 ) ) ;
#52614 = CARTESIAN_POINT ( 'NONE',  ( -1.836970198721029983E-15, 65.62499999317203958, 10.00000000000000178 ) ) ;
#52615 = CARTESIAN_POINT ( 'NONE',  ( -4.541265875000002339, 21.87499999863441147, -1.881053915767121998 ) ) ;
#52616 = UNCERTAINTY_MEASURE_WITH_UNIT (LENGTH_MEASURE( 1.000000000000000082E-05 ), #19402, 'distance_accuracy_value', 'NONE');
#52617 = ORIENTED_EDGE ( 'NONE', *, *, #42630, .F. ) ;
#52618 = CARTESIAN_POINT ( 'NONE',  ( 4.000000000000015987, 195.6250000027311842, 198.0000000000000284 ) ) ;
#52619 = CARTESIAN_POINT ( 'NONE',  ( -4.000000000000015099, 207.5625000000000284, 143.6568542494924543 ) ) ;
#52620 = CARTESIAN_POINT ( 'NONE',  ( -27.99999999999991118, 203.6250000027312126, 174.0000000000003695 ) ) ;
#52621 = VECTOR ( 'NONE', #40357, 1000.000000000000000 ) ;
#52622 = CARTESIAN_POINT ( 'NONE',  ( -2.977408999572650927, 114.8750000020483810, -7.188101187500001821 ) ) ;
#52623 = CARTESIAN_POINT ( 'NONE',  ( -11.00000000000000000, 4.556349186104045934, 94.09375000409679046 ) ) ;
#52624 = CARTESIAN_POINT ( 'NONE',  ( 7.999999999999992895, -3.313708498984756279, 1.674052783920142895 ) ) ;
#52625 = ADVANCED_BREP_SHAPE_REPRESENTATION ( '', ( #18038, #57354 ), #69405 ) ;
#52626 = VERTEX_POINT ( 'NONE', #74405 ) ;
#52627 = CARTESIAN_POINT ( 'NONE',  ( -1.320432766682874540E-15, 18.09374999795161187, 7.188101187500000044 ) ) ;
#52628 = ORIENTED_EDGE ( 'NONE', *, *, #21704, .F. ) ;
#52629 = DIRECTION ( 'NONE',  ( 1.000000000000000000, -0.000000000000000000, 0.000000000000000000 ) ) ;
#52630 = CARTESIAN_POINT ( 'NONE',  ( 4.193070328474939323, -10.26769692241485998, -64.12609983179218887 ) ) ;
#52631 = CARTESIAN_POINT ( 'NONE',  ( 4.999999999999993783, 59.16666666666667140, 8.660254037844390851 ) ) ;
#52632 = CARTESIAN_POINT ( 'NONE',  ( 2.977408999572654480, 101.0000000020483810, 7.188101187499999156 ) ) ;
#52633 = CARTESIAN_POINT ( 'NONE',  ( -31.45873412500001010, 205.8750000013656063, 168.5673454167827572 ) ) ;
#52634 = CARTESIAN_POINT ( 'NONE',  ( 0.8419854211626194296, -10.28111362163632769, 63.57154293063803152 ) ) ;
#52636 = DIRECTION ( 'NONE',  ( 0.000000000000000000, -0.000000000000000000, 1.000000000000000000 ) ) ;
#52635 = CARTESIAN_POINT ( 'NONE',  ( -2.485281374238855090, 287.8750000034139589, -5.999999999999718447 ) ) ;
#52637 = ORIENTED_EDGE ( 'NONE', *, *, #6709, .T. ) ;
#52638 = CARTESIAN_POINT ( 'NONE',  ( -3.042071309553166181, 247.8645833367472733, -11.35316468749999608 ) ) ;
#52639 = CARTESIAN_POINT ( 'NONE',  ( 7.188101187499991163, 2.977408999572648707, 17.70530278187175455 ) ) ;
#52640 = CARTESIAN_POINT ( 'NONE',  ( 5.000000000000000000, 11.14555136602165142, 27.84144949604463193 ) ) ;
#52641 = CARTESIAN_POINT ( 'NONE',  ( -10.00000000000000000, 74.16666665983869677, -2.679491924311229845 ) ) ;
#52642 = CARTESIAN_POINT ( 'NONE',  ( -10.00000000000000178, 147.5000000000000284, -1.224646799147353454E-15 ) ) ;
#52643 = FACE_OUTER_BOUND ( 'NONE', #47692, .T. ) ;
#52644 = CARTESIAN_POINT ( 'NONE',  ( 2.679491924311222739, 168.9583333333333428, 10.00000000000000355 ) ) ;
#52645 = CARTESIAN_POINT ( 'NONE',  ( -1.469576158976823947E-15, 22.12500000000000355, 8.000000000000000000 ) ) ;
#52646 = DIRECTION ( 'NONE',  ( 1.000000000000000000, 0.000000000000000000, 0.000000000000000000 ) ) ;
#52647 = CARTESIAN_POINT ( 'NONE',  ( 7.188101187499992051, 8.802885111219154394E-16, 26.61155278187175810 ) ) ;
#52648 = CARTESIAN_POINT ( 'NONE',  ( -5.676582343750006032, 144.4270833299193555, 9.832129032723418760 ) ) ;
#52649 = FACE_OUTER_BOUND ( 'NONE', #700, .T. ) ;
#52650 = CARTESIAN_POINT ( 'NONE',  ( -8.000000000000000000, 5.250000000000000888, -9.797174393178825657E-16 ) ) ;
#52651 = CARTESIAN_POINT ( 'NONE',  ( 32.00000000000000711, 206.3125000000000284, 168.3431457505075741 ) ) ;
#52652 = AXIS2_PLACEMENT_3D ( 'NONE', #60978, #38347, #2895 ) ;
#52653 = ORIENTED_EDGE ( 'NONE', *, *, #24022, .F. ) ;
#52654 = EDGE_CURVE ( 'NONE', #37917, #69045, #11409, .T. ) ;
#52655 = AXIS2_PLACEMENT_3D ( 'NONE', #65634, #48647, #19976 ) ;
#52656 = CARTESIAN_POINT ( 'NONE',  ( 6.424498079411709028, 225.6958308926248833, -7.668941570935106533 ) ) ;
#52657 = CARTESIAN_POINT ( 'NONE',  ( -25.17157287525382614, 209.8750000000000284, 167.1715728752541565 ) ) ;
#52658 = CARTESIAN_POINT ( 'NONE',  ( 3.458734124999959914, 209.4375000013656063, 142.0000000000000568 ) ) ;
#52659 = CARTESIAN_POINT ( 'NONE',  ( 5.000000000000000000, -67.91996363552661364, -22.23680535815918446 ) ) ;
#52660 = CARTESIAN_POINT ( 'NONE',  ( 10.00000000000000178, 42.08333332650537528, -2.679491924311226736 ) ) ;
#52661 = CARTESIAN_POINT ( 'NONE',  ( 7.188101187500001821, 114.5000000020483810, -2.977408999572651371 ) ) ;
#52662 = CARTESIAN_POINT ( 'NONE',  ( 3.211159895383560947, 21.18749999863440792, 3.211159895383562723 ) ) ;
#52663 = CARTESIAN_POINT ( 'NONE',  ( -2.266287154886550415, -50.05783744175262484, 40.76793781259078031 ) ) ;
#52664 = CARTESIAN_POINT ( 'NONE',  ( 5.656854249492374365, 5.656854249492375253, 15.26780277982336642 ) ) ;
#52666 = CARTESIAN_POINT ( 'NONE',  ( -7.320508075688770155, 225.6250000000000000, 7.320508075688774596 ) ) ;
#52665 = CARTESIAN_POINT ( 'NONE',  ( 10.99999999999989342, 4.556349186104152515, 101.0312500040967763 ) ) ;
#52667 = ORIENTED_EDGE ( 'NONE', *, *, #2314, .F. ) ;
#52668 = DIRECTION ( 'NONE',  ( 0.000000000000000000, 0.000000000000000000, -1.000000000000000000 ) ) ;
#52669 = CARTESIAN_POINT ( 'NONE',  ( -2.977408999572650039, 23.43749999795161898, -7.188101187500001821 ) ) ;
#52670 = CARTESIAN_POINT ( 'NONE',  ( -28.00000000000007816, 198.1250000027312126, 166.0000000000003695 ) ) ;
#52671 = CARTESIAN_POINT ( 'NONE',  ( 2.085542519210945334E-15, 240.4687500034139873, 11.35316468749999963 ) ) ;
#52672 = CARTESIAN_POINT ( 'NONE',  ( -9.832129032723420536, 118.6979166632526841, 5.676582343749997150 ) ) ;
#52673 = ORIENTED_EDGE ( 'NONE', *, *, #58852, .F. ) ;
#52674 = CARTESIAN_POINT ( 'NONE',  ( -10.11200329296622868, 3.728704622900627985, 117.7636805921466703 ) ) ;
#52675 = EDGE_CURVE ( 'NONE', #67207, #545, #57675, .T. ) ;
#52676 = ADVANCED_FACE ( 'NONE', ( #10162 ), #73164, .F. ) ;
#52677 = CARTESIAN_POINT ( 'NONE',  ( -10.18810118749999916, 4.220049686691934809, 99.06250000204836681 ) ) ;
#52678 = CARTESIAN_POINT ( 'NONE',  ( 8.660254037844389075, 222.2916666598387110, -5.000000000000000000 ) ) ;
#52679 = CARTESIAN_POINT ( 'NONE',  ( 1.432654583217664701, 200.0000000013656347, 201.4587341250000065 ) ) ;
#52680 = DIRECTION ( 'NONE',  ( 0.000000000000000000, 0.000000000000000000, 1.000000000000000000 ) ) ;
#52682 = CARTESIAN_POINT ( 'NONE',  ( 6.951808397369818766E-16, 102.0312499965860269, -11.35316468750000141 ) ) ;
#52681 = CARTESIAN_POINT ( 'NONE',  ( 0.000000000000000000, 15.99999999999998579, -1.000000000000000000 ) ) ;
#52683 = CARTESIAN_POINT ( 'NONE',  ( 7.999999999999992895, -3.313708498984756279, 7.674052783920145338 ) ) ;
#52684 = CARTESIAN_POINT ( 'NONE',  ( -24.54126587499999701, 196.5000000013656063, 168.5673454167827003 ) ) ;
#52685 = CARTESIAN_POINT ( 'NONE',  ( -8.000000000000000000, 27.56249999590322375, -9.797174393178825657E-16 ) ) ;
#52686 = ORIENTED_EDGE ( 'NONE', *, *, #51302, .F. ) ;
#52687 = EDGE_CURVE ( 'NONE', #68592, #46063, #19098, .T. ) ;
#52688 = CARTESIAN_POINT ( 'NONE',  ( 5.000000000000001776, 192.7083333265053966, -8.660254037844389075 ) ) ;
#52689 = DIRECTION ( 'NONE',  ( 0.000000000000000000, 0.000000000000000000, 1.000000000000000000 ) ) ;
#52690 = CARTESIAN_POINT ( 'NONE',  ( -11.00000000000010658, 4.556349186103942017, 100.0937500040967763 ) ) ;
#52691 = CARTESIAN_POINT ( 'NONE',  ( 5.676582343749993598, 90.26041666325268409, 9.832129032723422313 ) ) ;
#52692 = CARTESIAN_POINT ( 'NONE',  ( -6.676582343750001591, 287.4531250017069510, 0.000000000000000000 ) ) ;
#52693 = CARTESIAN_POINT ( 'NONE',  ( -7.188101187500000044, 9.093749997951611874, -8.802885111219163269E-16 ) ) ;
#52694 = CARTESIAN_POINT ( 'NONE',  ( 7.204075437095966983, 7.204075437095967871, 95.96875000204838102 ) ) ;
#52695 = CARTESIAN_POINT ( 'NONE',  ( -11.35316468750000141, 3.802083329919349275, 3.042071309553159963 ) ) ;
#52696 = ORIENTED_EDGE ( 'NONE', *, *, #57962, .T. ) ;
#52697 = CARTESIAN_POINT ( 'NONE',  ( 7.999999999999991118, 9.797174393178815797E-16, 27.08030277982336642 ) ) ;
#52698 = CARTESIAN_POINT ( 'NONE',  ( 1.829534547818520540, -42.61436550504831899, 139.0536033650462002 ) ) ;
#52699 = CARTESIAN_POINT ( 'NONE',  ( 3.042071309553167513, 216.8229166632526699, -11.35316468749999785 ) ) ;
#52700 = CARTESIAN_POINT ( 'NONE',  ( 10.18810118749999916, 1.247682550866122264E-15, 80.78125000204838102 ) ) ;
#52701 = DIRECTION ( 'NONE',  ( -1.000000000000000000, 0.000000000000000000, 0.000000000000000000 ) ) ;
#52702 = CARTESIAN_POINT ( 'NONE',  ( -2.679491924311087736, 150.4166666598387110, 10.00000000000008349 ) ) ;
#52703 = CARTESIAN_POINT ( 'NONE',  ( -6.676582343750003368, 293.3906250017069510, -2.765530957081996810 ) ) ;
#52704 = EDGE_CURVE ( 'NONE', #23461, #61992, #41786, .T. ) ;
#52705 = ORIENTED_EDGE ( 'NONE', *, *, #26791, .T. ) ;
#52706 = CARTESIAN_POINT ( 'NONE',  ( -0.8761883848702536337, -51.17400877215151667, -48.53033992007411968 ) ) ;
#52707 = CARTESIAN_POINT ( 'NONE',  ( 3.042071309553159519, 205.0520833299192986, 11.35316468750000141 ) ) ;
#52708 = CARTESIAN_POINT ( 'NONE',  ( -10.18810118749999916, 4.220049686691934809, 91.56250000204836681 ) ) ;
#52709 =( BOUNDED_CURVE ( )  B_SPLINE_CURVE ( 2, ( #38717, #20213, #43606, #61715, #66619, #26625, #4013, #54203, #27002 ),
 .UNSPECIFIED., .F., .F. ) 
 B_SPLINE_CURVE_WITH_KNOTS ( ( 3, 2, 2, 2, 3 ),
 ( 0.08333333333333352300, 0.09166666666666679897, 0.1000000000000000888, 0.1083333333333333787, 0.1166666666666666546 ),
 .UNSPECIFIED. ) 
 CURVE ( )  GEOMETRIC_REPRESENTATION_ITEM ( )  RATIONAL_B_SPLINE_CURVE ( ( 0.9999999999999982236, 0.9238795325112885148, 1.000000000000000000, 0.9238795325112867385, 1.000000000000000000, 0.9238795325112867385, 1.000000000000000000, 0.9238795325112868495, 0.9999999999999998890 ) ) 
 REPRESENTATION_ITEM ( '' )  );
#52710 = CARTESIAN_POINT ( 'NONE',  ( -30.44569435410879166, 201.8125000013656063, 172.4456943541092357 ) ) ;
#52711 = CARTESIAN_POINT ( 'NONE',  ( -8.000000000000000000, 17.15625000000000000, -3.313708498984762496 ) ) ;
#52712 = VECTOR ( 'NONE', #22368, 1000.000000000000000 ) ;
#52713 = ORIENTED_EDGE ( 'NONE', *, *, #32803, .F. ) ;
#52714 = CARTESIAN_POINT ( 'NONE',  ( -2.977408999572651815, 122.9375000020483810, 7.188101187500000933 ) ) ;
#52715 = CARTESIAN_POINT ( 'NONE',  ( -3.999999999999959144, 207.1875000027312126, 199.6568542494924259 ) ) ;
#52716 = CARTESIAN_POINT ( 'NONE',  ( -10.00000000000000000, 27.29166666666666430, -2.679491924311229845 ) ) ;
#52717 = AXIS2_PLACEMENT_3D ( 'NONE', #67391, #43248, #55714 ) ;
#52718 = CARTESIAN_POINT ( 'NONE',  ( -26.34314575050767715, 197.5625000000000568, 174.0000000000004547 ) ) ;
#52719 = CARTESIAN_POINT ( 'NONE',  ( -10.18810118749999916, 4.220049686691934809, 75.43750000204836681 ) ) ;
#52720 = ORIENTED_EDGE ( 'NONE', *, *, #59637, .T. ) ;
#52721 = CARTESIAN_POINT ( 'NONE',  ( 8.000000000000000000, 113.7500000000000000, -9.797174393178825657E-16 ) ) ;
#52722 = DIRECTION ( 'NONE',  ( 0.000000000000000000, 0.000000000000000000, 1.000000000000000000 ) ) ;
#52723 = CARTESIAN_POINT ( 'NONE',  ( -7.999999999999991118, 9.797174393178815797E-16, 30.00000000000000000 ) ) ;
#52724 = CARTESIAN_POINT ( 'NONE',  ( -7.188101187499999156, 115.6250000020483810, 2.977408999572654924 ) ) ;
#52725 = CARTESIAN_POINT ( 'NONE',  ( -0.4590000000000000746, 284.2799999999998590, 5.818592113970287194 ) ) ;
#52726 = CARTESIAN_POINT ( 'NONE',  ( 6.676582343750001591, 295.9531250017069510, -8.176455196517173205E-16 ) ) ;
#52728 = CARTESIAN_POINT ( 'NONE',  ( 11.00000000000000000, 1.347111479062088405E-15, 88.93750000409677625 ) ) ;
#52727 = CARTESIAN_POINT ( 'NONE',  ( 5.676582343749997150, 237.2395833367473301, -9.832129032723418760 ) ) ;
#52729 = ITEM_DEFINED_TRANSFORMATION ( 'NONE', 'NONE', #42934,  #57354 ) ;
#52730 = VERTEX_POINT ( 'NONE', #55825 ) ;
#52731 = VECTOR ( 'NONE', #18961, 1000.000000000000000 ) ;
#52732 = CARTESIAN_POINT ( 'NONE',  ( -11.35316468749999608, 239.4270833367473301, 3.042071309553173730 ) ) ;
#52733 = CARTESIAN_POINT ( 'NONE',  ( 7.188101187499992051, 8.802885111219154394E-16, 6.736552781871754547 ) ) ;
#52734 = ORIENTED_EDGE ( 'NONE', *, *, #28214, .F. ) ;
#52735 = CARTESIAN_POINT ( 'NONE',  ( 2.729887517050593182, 10.18810118749999916, 67.22060451829244698 ) ) ;
#52736 = CARTESIAN_POINT ( 'NONE',  ( -11.35316468749999785, 103.3854166632526699, -3.042071309553167513 ) ) ;
#52737 = CARTESIAN_POINT ( 'NONE',  ( -0.8419854211626145446, 60.19512794652348475, 22.88206588978842504 ) ) ;
#52738 = CARTESIAN_POINT ( 'NONE',  ( 11.00000000000000000, 1.347111479062088405E-15, 82.74999999999998579 ) ) ;
#52741 = CARTESIAN_POINT ( 'NONE',  ( -8.000000000000000000, 2.156250000000000444, -3.313708498984762496 ) ) ;
#52740 = CARTESIAN_POINT ( 'NONE',  ( 31.45873412499999944, 204.6875000013656063, 169.9999999999998863 ) ) ;
#52739 = CARTESIAN_POINT ( 'NONE',  ( 24.54126587499999346, 204.4375000013656063, 169.9999999999998863 ) ) ;
#52742 = ORIENTED_EDGE ( 'NONE', *, *, #55602, .T. ) ;
#52743 = EDGE_CURVE ( 'NONE', #870, #20600, #49500, .T. ) ;
#52744 = DIRECTION ( 'NONE',  ( -0.000000000000000000, 1.000000000000000000, -0.000000000000000000 ) ) ;
#52745 = DIRECTION ( 'NONE',  ( 0.000000000000000000, 0.000000000000000000, 1.000000000000000000 ) ) ;
#52746 = CARTESIAN_POINT ( 'NONE',  ( 3.042071309553159519, 219.7395833299193271, 11.35316468750000141 ) ) ;
#52747 = CARTESIAN_POINT ( 'NONE',  ( -3.458734125000015425, 207.0000000013656063, 143.4326545832176976 ) ) ;
#52748 = CARTESIAN_POINT ( 'NONE',  ( 26.56734541678238415, 207.2500000013655779, 166.5412658749999650 ) ) ;
#52749 = CARTESIAN_POINT ( 'NONE',  ( -7.188101187500002709, 25.68749999795162253, 2.977408999572649151 ) ) ;
#52750 = CARTESIAN_POINT ( 'NONE',  ( -8.311093377946841443, 174.2187499965860127, 8.311093377946830785 ) ) ;
#52751 = CARTESIAN_POINT ( 'NONE',  ( 2.977408999572650039, 98.56250000204838102, -7.188101187500000933 ) ) ;
#52752 = CARTESIAN_POINT ( 'NONE',  ( -5.999999999999999112, 296.1250000034140726, 2.485281374238575314 ) ) ;
#52753 = CARTESIAN_POINT ( 'NONE',  ( -4.541265875000002339, 8.749999998634406140, -1.881053915767121998 ) ) ;
#52754 = CARTESIAN_POINT ( 'NONE',  ( 30.44569435410883429, 203.0625000013656063, 167.5543056458911053 ) ) ;
#52755 = CARTESIAN_POINT ( 'NONE',  ( 5.082755093536318824, 5.082755093536319713, 10.29905278187175455 ) ) ;
#52756 = CARTESIAN_POINT ( 'NONE',  ( -3.042071309553173730, 69.32291666325268409, 11.35316468749999785 ) ) ;
#52757 = CARTESIAN_POINT ( 'NONE',  ( 0.000000000000000000, 300.0000000000000000, 0.000000000000000000 ) ) ;
#52758 = CARTESIAN_POINT ( 'NONE',  ( 3.313708498984756279, 7.999999999999991118, 3.417802784329822430 ) ) ;
#52759 = ORIENTED_EDGE ( 'NONE', *, *, #6951, .F. ) ;
#52760 = LINE ( 'NONE', #25176, #57965 ) ;
#52761 = CARTESIAN_POINT ( 'NONE',  ( 11.35316468750000141, 80.78124999658602690, 0.000000000000000000 ) ) ;
#52762 = CARTESIAN_POINT ( 'NONE',  ( 11.00000000000000000, 1.347111479062088405E-15, 69.43750000409676204 ) ) ;
#52763 = CARTESIAN_POINT ( 'NONE',  ( 1.432654583217607414, 197.5000000013656063, 145.4587341250000350 ) ) ;
#52764 = CARTESIAN_POINT ( 'NONE',  ( 4.000000000000001776, 8.749999997268814056, 0.000000000000000000 ) ) ;
#52766 = CARTESIAN_POINT ( 'NONE',  ( -8.311093377946836114, 62.65624999658601979, -8.311093377946837890 ) ) ;
#52765 = CARTESIAN_POINT ( 'NONE',  ( 1.926037949307475072, 89.22060463630471361, -7.188101187500000933 ) ) ;
#52768 = AXIS2_PLACEMENT_3D ( 'NONE', #8137, #19446, #2106 ) ;
#52767 = CARTESIAN_POINT ( 'NONE',  ( 3.313708498984756279, 7.999999999999991118, 26.04905278392014623 ) ) ;
#52769 = CARTESIAN_POINT ( 'NONE',  ( 2.751064625579944321E-14, 203.8750000027312126, 194.0000000000000568 ) ) ;
#52770 = CARTESIAN_POINT ( 'NONE',  ( 8.660254037844385522, 156.4583333265053966, 5.000000000000005329 ) ) ;
#52771 = CARTESIAN_POINT ( 'NONE',  ( 1.320432766682874540E-15, 96.40625000204838102, 7.188101187500000044 ) ) ;
#52772 = CARTESIAN_POINT ( 'NONE',  ( -4.999999999999998224, 53.54166665983870388, -8.660254037844389075 ) ) ;
#52773 = CARTESIAN_POINT ( 'NONE',  ( -5.676582343750006032, 44.42708332991934839, 9.832129032723418760 ) ) ;
#52774 = CARTESIAN_POINT ( 'NONE',  ( -7.204075437095965206, -7.204075437095968759, 110.2187500020483810 ) ) ;
#52775 = CARTESIAN_POINT ( 'NONE',  ( 9.832129032723420536, 196.1979166632526983, -5.676582343749999815 ) ) ;
#52776 = ORIENTED_EDGE ( 'NONE', *, *, #5651, .F. ) ;
#52777 = CARTESIAN_POINT ( 'NONE',  ( 2.828427124746209831, 205.5000000027312126, 200.8284271247462129 ) ) ;
#52778 = DIRECTION ( 'NONE',  ( -0.000000000000000000, 1.000000000000000000, -0.000000000000000000 ) ) ;
#52779 = DIRECTION ( 'NONE',  ( -0.000000000000000000, 1.000000000000000000, -1.563033456626094573E-30 ) ) ;
#52781 = CARTESIAN_POINT ( 'NONE',  ( 9.832129032723420536, 186.1979166632526983, -5.676582343749999815 ) ) ;
#52780 = CARTESIAN_POINT ( 'NONE',  ( 0.000000000000000000, 0.000000000000000000, -4.000000000000001776 ) ) ;
#52782 = CARTESIAN_POINT ( 'NONE',  ( -12.00000000000000355, 1.469576158976824342E-15, -21.50000000000000000 ) ) ;
#52783 = AXIS2_PLACEMENT_3D ( 'NONE', #73999, #16637, #39671 ) ;
#52784 = CARTESIAN_POINT ( 'NONE',  ( -6.123233995736766282E-16, 246.8750000068280031, -10.00000000000000000 ) ) ;
#52785 = DIRECTION ( 'NONE',  ( 0.000000000000000000, 0.000000000000000000, -1.000000000000000000 ) ) ;
#52786 = EDGE_CURVE ( 'NONE', #56693, #19432, #26805, .T. ) ;
#52787 = ORIENTED_EDGE ( 'NONE', *, *, #20488, .T. ) ;
#52788 = CARTESIAN_POINT ( 'NONE',  ( 3.042071309553167513, 162.1354166632526699, -11.35316468749999785 ) ) ;
#52789 = MECHANICAL_DESIGN_GEOMETRIC_PRESENTATION_REPRESENTATION (  '', ( #56399 ), #39537 ) ;
#52790 = EDGE_CURVE ( 'NONE', #40180, #40560, #65362, .T. ) ;
#52791 = CARTESIAN_POINT ( 'NONE',  ( 5.082755093536318824, 5.082755093536319713, 27.92405278187175455 ) ) ;
#52792 = CARTESIAN_POINT ( 'NONE',  ( -8.311093377946836114, 132.9687499965860411, -8.311093377946837890 ) ) ;
#52793 = DIRECTION ( 'NONE',  ( 1.000000000000000000, 0.000000000000000000, 0.000000000000000000 ) ) ;
#52794 = ORIENTED_EDGE ( 'NONE', *, *, #18005, .F. ) ;
#52795 = CARTESIAN_POINT ( 'NONE',  ( 5.656854249492379694, 103.6250000040967763, -5.656854249492380582 ) ) ;
#52796 = EDGE_CURVE ( 'NONE', #10215, #38154, #21516, .T. ) ;
#52797 = CARTESIAN_POINT ( 'NONE',  ( -1.656854249492381248, 10.31250000000000000, -4.000000000000001776 ) ) ;
#52798 = DIRECTION ( 'NONE',  ( 0.000000000000000000, 0.000000000000000000, 1.000000000000000000 ) ) ;
#52799 = CARTESIAN_POINT ( 'NONE',  ( 3.211159895383561835, 13.43749999863440614, -3.211159895383561835 ) ) ;
#52800 = CARTESIAN_POINT ( 'NONE',  ( -4.898587196589407898E-16, 7.999999999999991118, 17.14280278392014978 ) ) ;
#52801 = CARTESIAN_POINT ( 'NONE',  ( -10.00000000000000355, 187.2916666666666572, -2.679491924311231177 ) ) ;
#52802 = ORIENTED_EDGE ( 'NONE', *, *, #61267, .T. ) ;
#52803 = FACE_OUTER_BOUND ( 'NONE', #17655, .T. ) ;
#52804 = CARTESIAN_POINT ( 'NONE',  ( -5.082755093536324154, 98.84375000204838102, 5.082755093536326818 ) ) ;
#52806 = CARTESIAN_POINT ( 'NONE',  ( 3.313708498984794915, 120.2187500040967905, -7.999999999999967137 ) ) ;
#52805 = CARTESIAN_POINT ( 'NONE',  ( 0.000000000000000000, 300.0000000000000000, 0.000000000000000000 ) ) ;
#52807 =( BOUNDED_CURVE ( )  B_SPLINE_CURVE ( 2, ( #28524, #11921, #28897, #23975, #39844, #63221, #74549, #64345, #17574 ),
 .UNSPECIFIED., .F., .F. ) 
 B_SPLINE_CURVE_WITH_KNOTS ( ( 3, 2, 2, 2, 3 ),
 ( 0.8666666666666673624, 0.8750000000000006661, 0.8833333333333339699, 0.8916666666666674956, 0.9000000000000007994 ),
 .UNSPECIFIED. ) 
 CURVE ( )  GEOMETRIC_REPRESENTATION_ITEM ( )  RATIONAL_B_SPLINE_CURVE ( ( 0.9999999999999938938, 0.9238795325112928447, 1.000000000000000000, 0.9238795325112867385, 1.000000000000000000, 0.9238795325112867385, 1.000000000000000000, 0.9238795325112796331, 1.000000000000007105 ) ) 
 REPRESENTATION_ITEM ( '' )  );
#52808 = VERTEX_POINT ( 'NONE', #692 ) ;
#52809 = CARTESIAN_POINT ( 'NONE',  ( 0.7509181236784587821, 10.12341933770226277, -70.08957333326497974 ) ) ;
#52811 = CYLINDRICAL_SURFACE ( 'NONE', #45809, 10.00000000000000178 ) ;
#52810 = VECTOR ( 'NONE', #43334, 1000.000000000000000 ) ;
#52812 = CARTESIAN_POINT ( 'NONE',  ( 1.320432766682872962E-15, -7.188101187499992051, 27.36155278187175455 ) ) ;
#52813 = ORIENTED_EDGE ( 'NONE', *, *, #73567, .T. ) ;
#52814 = ORIENTED_EDGE ( 'NONE', *, *, #14412, .T. ) ;
#52815 = CARTESIAN_POINT ( 'NONE',  ( 7.204075437095966983, 7.204075437095967871, 88.09375000204836681 ) ) ;
#52816 = CARTESIAN_POINT ( 'NONE',  ( -31.45873412499999233, 194.9375000013655779, 170.0000000000003979 ) ) ;
#52817 = CARTESIAN_POINT ( 'NONE',  ( 11.00000000000000000, 4.556349186104045934, 100.8437499999999858 ) ) ;
#52820 = CARTESIAN_POINT ( 'NONE',  ( 6.676582343750003368, 297.0468750017069510, 2.765530957081995478 ) ) ;
#52819 = CARTESIAN_POINT ( 'NONE',  ( 29.65685424949235127, 201.5625000027311842, 165.9999999999998863 ) ) ;
#52818 = CARTESIAN_POINT ( 'NONE',  ( -29.65685424949236193, 198.1875000027311842, 166.0000000000003411 ) ) ;
#52821 = CARTESIAN_POINT ( 'NONE',  ( 10.00000000000000178, 130.2083333333333712, -2.679491924311226736 ) ) ;
#52822 = CARTESIAN_POINT ( 'NONE',  ( 3.313708498984760720, 99.03124999999998579, -8.000000000000000000 ) ) ;
#52823 = CIRCLE ( 'NONE', #60021, 10.99999999999999645 ) ;
#52824 = CARTESIAN_POINT ( 'NONE',  ( 11.00000000000000000, 1.347111479062088405E-15, 97.74999999999998579 ) ) ;
#52825 = CARTESIAN_POINT ( 'NONE',  ( -4.401442555609577197E-16, 7.188101187499992051, 1.486552781871753437 ) ) ;
#52826 = EDGE_CURVE ( 'NONE', #27743, #2057, #62066, .T. ) ;
#52827 = VECTOR ( 'NONE', #32901, 1000.000000000000000 ) ;
#52828 = CARTESIAN_POINT ( 'NONE',  ( -3.673940397442060854E-16, 290.8125000034140157, -6.000000000000001776 ) ) ;
#52829 = CARTESIAN_POINT ( 'NONE',  ( 31.45873412499997812, 201.6250000013656063, 171.4326545832175839 ) ) ;
#52830 = CARTESIAN_POINT ( 'NONE',  ( -7.188101187500000044, 6.093749997951610986, -8.802885111219163269E-16 ) ) ;
#52831 = CARTESIAN_POINT ( 'NONE',  ( -5.662595241051935346, 5.662595241051935346, 0.8256152839406295518 ) ) ;
#52832 = CARTESIAN_POINT ( 'NONE',  ( -4.401442555609581635E-16, 115.1562500020483810, -7.188101187500000044 ) ) ;
#52834 = CARTESIAN_POINT ( 'NONE',  ( 0.9804963856519454124, 194.6309867350711613, 201.5048895931090840 ) ) ;
#52833 = DIRECTION ( 'NONE',  ( 0.000000000000000000, 0.000000000000000000, 1.000000000000000000 ) ) ;
#52835 = CARTESIAN_POINT ( 'NONE',  ( 9.832129032723420536, 226.3020833367473301, 5.676582343749996262 ) ) ;
#52836 = CARTESIAN_POINT ( 'NONE',  ( -3.313708498984708317, 90.78125000000002842, 8.000000000000053291 ) ) ;
#52837 = CARTESIAN_POINT ( 'NONE',  ( -7.188101187499991163, 2.977408999572646930, 28.76780278187175455 ) ) ;
#52838 = CARTESIAN_POINT ( 'NONE',  ( 25.17157287525381193, 197.6250000000000284, 167.1715728752537018 ) ) ;
#52839 = CARTESIAN_POINT ( 'NONE',  ( -5.676582343750006032, 29.11458332991935194, 9.832129032723418760 ) ) ;
#52840 = EDGE_CURVE ( 'NONE', #64164, #66501, #10870, .T. ) ;
#52841 = CARTESIAN_POINT ( 'NONE',  ( 7.320508075689014404, 25.62500000000018829, -7.320508075689014404 ) ) ;
#52842 = CARTESIAN_POINT ( 'NONE',  ( 9.832129032723416984, 220.6770833299193555, 5.676582343750006032 ) ) ;
#52843 = FACE_OUTER_BOUND ( 'NONE', #15121, .T. ) ;
#52845 = DIRECTION ( 'NONE',  ( -0.000000000000000000, -0.000000000000000000, 1.000000000000000000 ) ) ;
#52844 = DIRECTION ( 'NONE',  ( 1.224646799147353207E-16, -1.000000000000000000, 0.000000000000000000 ) ) ;
#52846 = ORIENTED_EDGE ( 'NONE', *, *, #33893, .T. ) ;
#52847 = CARTESIAN_POINT ( 'NONE',  ( -3.458734125000015425, 196.2500000013656631, 143.4326545832176976 ) ) ;
#52848 = CARTESIAN_POINT ( 'NONE',  ( -8.311093377946836114, 32.65624999658600558, -8.311093377946837890 ) ) ;
#52849 = CARTESIAN_POINT ( 'NONE',  ( -7.778174593052020747, -7.778174593052023411, 83.87500000409677625 ) ) ;
#52850 = CARTESIAN_POINT ( 'NONE',  ( 2.445694354108783219, 208.8125000013656063, 139.5543056458912190 ) ) ;
#52851 = CARTESIAN_POINT ( 'NONE',  ( -30.44569435410875613, 194.8125000013656063, 172.4456943541092642 ) ) ;
#52852 = DIRECTION ( 'NONE',  ( 1.000000000000000000, 1.084202172485504434E-16, 0.000000000000000000 ) ) ;
#52854 = CARTESIAN_POINT ( 'NONE',  ( 5.676582343750001591, 16.61458332991935194, -9.832129032723420536 ) ) ;
#52853 = CARTESIAN_POINT ( 'NONE',  ( -7.188101187500000933, 107.5625000020483810, -2.977408999572650483 ) ) ;
#52855 = CARTESIAN_POINT ( 'NONE',  ( -3.313708498984758943, -7.999999999999989342, 16.11155277982336642 ) ) ;
#52856 = CARTESIAN_POINT ( 'NONE',  ( -11.35316468750000141, 148.2812499965860411, -1.390361679473963753E-15 ) ) ;
#52857 = EDGE_CURVE ( 'NONE', #3120, #4298, #17342, .T. ) ;
#52858 = CARTESIAN_POINT ( 'NONE',  ( 2.679491924311228956, 112.9166666598387252, -10.00000000000000000 ) ) ;
#52859 = CARTESIAN_POINT ( 'NONE',  ( -2.977408999572651815, 115.8125000020484094, 7.188101187500000933 ) ) ;
#52860 = DIRECTION ( 'NONE',  ( 1.000000000000000000, 1.577021341797097560E-16, 0.000000000000000000 ) ) ;
#52861 = CARTESIAN_POINT ( 'NONE',  ( -26.56734541678238415, 206.6250000013656063, 166.5412658750003629 ) ) ;
#52862 = ORIENTED_EDGE ( 'NONE', *, *, #42516, .F. ) ;
#52863 = CARTESIAN_POINT ( 'NONE',  ( -9.832129032723418760, 8.177083329919350163, -5.676582343750004256 ) ) ;
#52864 = ORIENTED_EDGE ( 'NONE', *, *, #15774, .F. ) ;
#52865 = ADVANCED_FACE ( 'NONE', ( #22930 ), #68580, .F. ) ;
#52866 = CARTESIAN_POINT ( 'NONE',  ( -10.99999999999994671, -4.556349186104105442, 100.0937500000000000 ) ) ;
#52867 = CARTESIAN_POINT ( 'NONE',  ( -4.721056650415998313, 297.5781250017069510, 4.721056650416000089 ) ) ;
#52869 = CARTESIAN_POINT ( 'NONE',  ( -9.832129032723420536, 138.6979166632526983, 5.676582343749997150 ) ) ;
#52868 = CARTESIAN_POINT ( 'NONE',  ( -24.83888924784116270, -22.87511254730129906, 146.5755188694719493 ) ) ;
#52870 = CARTESIAN_POINT ( 'NONE',  ( 4.898587196589415787E-16, 0.000000000000000000, 4.000000000000001776 ) ) ;
#52871 = CARTESIAN_POINT ( 'NONE',  ( -4.898587196589407898E-16, 7.999999999999991118, 17.01155278432982954 ) ) ;
#52872 = CARTESIAN_POINT ( 'NONE',  ( 3.313708498984761608, 15.28125000000000355, -8.000000000000000000 ) ) ;
#52873 = CARTESIAN_POINT ( 'NONE',  ( 3.042071309553173286, 250.3645833367473301, 11.35316468749999608 ) ) ;
#52874 = CARTESIAN_POINT ( 'NONE',  ( -4.220049686691935698, 10.18810118749999916, 90.25000000204838102 ) ) ;
#52875 = ORIENTED_EDGE ( 'NONE', *, *, #4838, .F. ) ;
#52876 = EDGE_CURVE ( 'NONE', #21239, #45651, #30845, .T. ) ;
#52877 = AXIS2_PLACEMENT_3D ( 'NONE', #40990, #11568, #57231 ) ;
#52878 = CARTESIAN_POINT ( 'NONE',  ( -2.828427124746209831, 197.3750000000000284, 139.1715728752538723 ) ) ;
#52879 = CARTESIAN_POINT ( 'NONE',  ( -1.656854249492371034, 8.687500000000000000, 4.000000000000013323 ) ) ;
#52880 = UNCERTAINTY_MEASURE_WITH_UNIT (LENGTH_MEASURE( 1.000000000000000082E-05 ), #11761, 'distance_accuracy_value', 'NONE');
#52881 = CARTESIAN_POINT ( 'NONE',  ( 3.042071309553167069, 87.13541666325268409, -11.35316468749999785 ) ) ;
#52882 = CARTESIAN_POINT ( 'NONE',  ( -10.18810118749999738, -4.220049686691941915, 105.2500000020483952 ) ) ;
#52883 = CARTESIAN_POINT ( 'NONE',  ( 4.541265875000001451, 17.37499999863440436, 1.881053915767124440 ) ) ;
#52884 = ORIENTED_EDGE ( 'NONE', *, *, #48891, .F. ) ;
#52885 = ORIENTED_EDGE ( 'NONE', *, *, #15788, .T. ) ;
#52886 = CARTESIAN_POINT ( 'NONE',  ( 3.313708498984762496, 2.718750000000000888, 7.999999999999998224 ) ) ;
#52887 = DIRECTION ( 'NONE',  ( 0.8660254037844380415, -0.5000000000000013323, 0.000000000000000000 ) ) ;
#52888 = VECTOR ( 'NONE', #40079, 999.9999999999998863 ) ;
#52889 = CARTESIAN_POINT ( 'NONE',  ( 4.401442555609581635E-16, 2.343749997951610098, -7.188101187500000044 ) ) ;
#52890 = CARTESIAN_POINT ( 'NONE',  ( 5.656854249492381470, 121.2500000040967905, 5.656854249492379694 ) ) ;
#52891 = CARTESIAN_POINT ( 'NONE',  ( -4.220049686691937474, -10.18810118749999738, 101.3125000020483810 ) ) ;
#52892 = CARTESIAN_POINT ( 'NONE',  ( -4.000000000000001776, 0.5000000000000002220, -4.898587196589415787E-16 ) ) ;
#52893 = CARTESIAN_POINT ( 'NONE',  ( 4.000000000000001776, 14.81249999726881406, -1.656854249492381248 ) ) ;
#52894 = CARTESIAN_POINT ( 'NONE',  ( 2.449293598294707893E-16, 10.99999999726881406, -4.000000000000001776 ) ) ;
#52895 = ORIENTED_EDGE ( 'NONE', *, *, #22789, .T. ) ;
#52896 = CARTESIAN_POINT ( 'NONE',  ( -1.469576158976823947E-15, 5.437499995903221084, 8.000000000000000000 ) ) ;
#52897 = CARTESIAN_POINT ( 'NONE',  ( -3.458734124999959025, 199.5000000013656063, 199.4326545832176691 ) ) ;
#52899 = CARTESIAN_POINT ( 'NONE',  ( -5.000000000000005329, 225.2083333265053966, 8.660254037844387298 ) ) ;
#52898 = CARTESIAN_POINT ( 'NONE',  ( -28.00000000000007105, 199.4375000013655779, 166.5412658750003629 ) ) ;
#52900 = CARTESIAN_POINT ( 'NONE',  ( -4.541265875000002339, 14.81249999863440792, -5.561446717895856393E-16 ) ) ;
#52901 = CARTESIAN_POINT ( 'NONE',  ( 1.656854249492381914, 11.81250000000000000, 4.000000000000000888 ) ) ;
#52902 = CARTESIAN_POINT ( 'NONE',  ( -2.977408999572648707, -7.188101187499990274, 10.76780278187175632 ) ) ;
#52903 = ORIENTED_EDGE ( 'NONE', *, *, #43390, .T. ) ;
#52904 =( BOUNDED_CURVE ( )  B_SPLINE_CURVE ( 2, ( #3471, #65711, #1980, #49104, #72116, #24972, #43445, #31013, #20429 ),
 .UNSPECIFIED., .F., .F. ) 
 B_SPLINE_CURVE_WITH_KNOTS ( ( 3, 2, 2, 2, 3 ),
 ( 0.3088235294117646634, 0.3124999999999999445, 0.3161764705882352255, 0.3198529411764705066, 0.3235294117647058432 ),
 .UNSPECIFIED. ) 
 CURVE ( )  GEOMETRIC_REPRESENTATION_ITEM ( )  RATIONAL_B_SPLINE_CURVE ( ( 1.000000000000001110, 0.9238795325112856283, 1.000000000000000000, 0.9238795325112867385, 1.000000000000000000, 0.9238795325112867385, 1.000000000000000000, 0.9238795325112878487, 0.9999999999999988898 ) ) 
 REPRESENTATION_ITEM ( '' )  );
#52905 = ORIENTED_EDGE ( 'NONE', *, *, #6849, .F. ) ;
#52906 = CARTESIAN_POINT ( 'NONE',  ( 7.204075437095966983, 7.204075437095967871, 106.0937500020483810 ) ) ;
#52907 = CARTESIAN_POINT ( 'NONE',  ( 7.778174593052023411, -7.778174593052021635, 103.5624999999999858 ) ) ;
#52908 = CARTESIAN_POINT ( 'NONE',  ( -27.99999999999996092, 206.5000000000000284, 174.0000000000003695 ) ) ;
#52909 = CARTESIAN_POINT ( 'NONE',  ( -3.458734124999959914, 200.4375000013656063, 198.0000000000000284 ) ) ;
#52910 = CARTESIAN_POINT ( 'NONE',  ( 25.55430564589118703, 196.3125000013656063, 172.4456943541087526 ) ) ;
#52911 = CARTESIAN_POINT ( 'NONE',  ( -2.679491924311235618, 98.54166666666667140, 10.00000000000000000 ) ) ;
#52912 = CARTESIAN_POINT ( 'NONE',  ( 5.656854249492379694, 118.4375000000000000, -5.656854249492380582 ) ) ;
#52913 = CARTESIAN_POINT ( 'NONE',  ( 5.676582343749993598, 65.26041666325268409, 9.832129032723422313 ) ) ;
#52914 = CARTESIAN_POINT ( 'NONE',  ( 6.676582343750004256, 296.0468750017069510, 2.765530957081995478 ) ) ;
#52915 = EDGE_CURVE ( 'NONE', #7738, #1129, #46681, .T. ) ;
#52916 = ORIENTED_EDGE ( 'NONE', *, *, #3044, .T. ) ;
#52917 = CARTESIAN_POINT ( 'NONE',  ( 4.556349186104045934, 11.00000000000000000, 74.03125000000000000 ) ) ;
#52918 = AXIS2_PLACEMENT_3D ( 'NONE', #18314, #70727, #19046 ) ;
#52919 = CARTESIAN_POINT ( 'NONE',  ( 5.656854249492378806, 14.62499999590322020, 5.656854249492381470 ) ) ;
#52920 = CARTESIAN_POINT ( 'NONE',  ( -2.754378923186476579E-14, 207.1875000013656063, 145.4587341250000350 ) ) ;
#52921 = CARTESIAN_POINT ( 'NONE',  ( 8.000000000000000000, 11.81249999590322197, 0.000000000000000000 ) ) ;
#52922 = CARTESIAN_POINT ( 'NONE',  ( 1.224646799147353454E-15, 300.0000000000000000, -10.00000000000000178 ) ) ;
#52923 = CARTESIAN_POINT ( 'NONE',  ( -7.320508075688770155, 225.6249999999999716, 7.320508075688774596 ) ) ;
#52924 = CARTESIAN_POINT ( 'NONE',  ( -3.673940397442060854E-16, 292.7500000000000000, -6.000000000000001776 ) ) ;
#52925 = CARTESIAN_POINT ( 'NONE',  ( -6.238412754330611322E-16, 10.18810118749999916, 69.15625000204836681 ) ) ;
#52926 = CARTESIAN_POINT ( 'NONE',  ( -2.679491924311225848, 211.4583333333333144, -10.00000000000000178 ) ) ;
#52927 = EDGE_CURVE ( 'NONE', #67635, #71847, #16047, .T. ) ;
#52928 =( BOUNDED_CURVE ( )  B_SPLINE_CURVE ( 2, ( #64622, #6906, #18596, #71366, #70642, #29917, #24244, #47619, #70284 ),
 .UNSPECIFIED., .F., .F. ) 
 B_SPLINE_CURVE_WITH_KNOTS ( ( 3, 2, 2, 2, 3 ),
 ( 0.2159090909090909116, 0.2215909090909090884, 0.2272727272727272652, 0.2329545454545454419, 0.2386363636363636465 ),
 .UNSPECIFIED. ) 
 CURVE ( )  GEOMETRIC_REPRESENTATION_ITEM ( )  RATIONAL_B_SPLINE_CURVE ( ( 1.000000000000000000, 0.9238795325112867385, 1.000000000000000000, 0.9238795325112867385, 1.000000000000000000, 0.9238795325112867385, 1.000000000000000000, 0.9238795325112867385, 1.000000000000000000 ) ) 
 REPRESENTATION_ITEM ( '' )  );
#52929 = CARTESIAN_POINT ( 'NONE',  ( -7.188101187499990274, -2.977408999572651815, 12.45530278187175277 ) ) ;
#52930 = CARTESIAN_POINT ( 'NONE',  ( -11.35316468750000141, 178.8020833299193271, 3.042071309553159963 ) ) ;
#52931 = CARTESIAN_POINT ( 'NONE',  ( 3.211159895383561835, 1.437499998634406806, -3.211159895383561835 ) ) ;
#52932 = CARTESIAN_POINT ( 'NONE',  ( -4.556349186104048599, -10.99999999999999822, 97.46875000409677625 ) ) ;
#52934 = DIRECTION ( 'NONE',  ( -1.000000000000000000, -1.577021341797097560E-16, 0.000000000000000000 ) ) ;
#52933 = FACE_OUTER_BOUND ( 'NONE', #1692, .T. ) ;
#52935 = ORIENTED_EDGE ( 'NONE', *, *, #57385, .T. ) ;
#52936 = AXIS2_PLACEMENT_3D ( 'NONE', #3466, #10247, #49480 ) ;
#52937 = CARTESIAN_POINT ( 'NONE',  ( 3.458734124999959469, 207.7500000013656063, 140.5673454167824161 ) ) ;
#52938 = CARTESIAN_POINT ( 'NONE',  ( -8.311093377946836114, 32.96874999658600558, -8.311093377946837890 ) ) ;
#52939 = CARTESIAN_POINT ( 'NONE',  ( 2.020667218593132706E-15, -11.00000000000000000, 102.0625000040967763 ) ) ;
#52940 = CARTESIAN_POINT ( 'NONE',  ( -9.832129032723418760, 218.1770833299193555, -5.676582343750004256 ) ) ;
#52941 = CARTESIAN_POINT ( 'NONE',  ( -26.56734541678228112, 207.0000000013655779, 173.4587341250003476 ) ) ;
#52942 = LINE ( 'NONE', #29555, #22584 ) ;
#52944 = CARTESIAN_POINT ( 'NONE',  ( 0.000000000000000000, 0.000000000000000000, 0.000000000000000000 ) ) ;
#52943 = CARTESIAN_POINT ( 'NONE',  ( 2.977408999572654480, 121.6250000020483810, 7.188101187499999156 ) ) ;
#52945 = LINE ( 'NONE', #1275, #60433 ) ;
#52946 = CARTESIAN_POINT ( 'NONE',  ( -7.320508075688778149, 69.99999999317203958, 7.320508075688769267 ) ) ;
#52947 = CARTESIAN_POINT ( 'NONE',  ( -5.082755093536325930, 99.96875000204838102, -5.082755093536325930 ) ) ;
#52948 = CARTESIAN_POINT ( 'NONE',  ( 3.211159895383560947, 18.31249999863440792, 3.211159895383562723 ) ) ;
#52949 = FACE_BOUND ( 'NONE', #36906, .T. ) ;
#52950 = CARTESIAN_POINT ( 'NONE',  ( 6.155571212629570077, 0.2837926415812287440, -4.791828655132197134 ) ) ;
#52951 = VERTEX_POINT ( 'NONE', #58399 ) ;
#52952 = ORIENTED_EDGE ( 'NONE', *, *, #56034, .F. ) ;
#52953 = CARTESIAN_POINT ( 'NONE',  ( 6.676582343750004256, 299.0468750017069510, 2.765530957081995478 ) ) ;
#52954 = CARTESIAN_POINT ( 'NONE',  ( -8.660254037844397956, 142.0833333333333712, -5.000000000000010658 ) ) ;
#52955 = CARTESIAN_POINT ( 'NONE',  ( 2.849036369511732440E-14, 197.2500000000000000, 202.0000000000000000 ) ) ;
#52956 = CARTESIAN_POINT ( 'NONE',  ( -5.676582343750006032, 154.1145833299193555, 9.832129032723418760 ) ) ;
#52957 = CARTESIAN_POINT ( 'NONE',  ( -7.204075437095965206, -7.204075437095968759, 81.34375000204838102 ) ) ;
#52958 = CARTESIAN_POINT ( 'NONE',  ( 11.00000000000000000, 1.347111479062088405E-15, 118.0000000000000000 ) ) ;
#52959 = CARTESIAN_POINT ( 'NONE',  ( 1.656854249492403008, 205.6875000000000284, 194.0000000000000853 ) ) ;
#52960 = CARTESIAN_POINT ( 'NONE',  ( 38.00000000000000000, -52.99999999999999289, 25.00000000000000000 ) ) ;
#52961 = CARTESIAN_POINT ( 'NONE',  ( -10.18810118749999738, -4.220049686691941915, 110.1250000020483810 ) ) ;
#52962 = ORIENTED_EDGE ( 'NONE', *, *, #4551, .F. ) ;
#52963 = CARTESIAN_POINT ( 'NONE',  ( -5.656854249492378806, 113.1875000000000000, 5.656854249492381470 ) ) ;
#52964 = DIRECTION ( 'NONE',  ( -0.000000000000000000, 1.000000000000000000, -0.000000000000000000 ) ) ;
#52965 = CARTESIAN_POINT ( 'NONE',  ( -8.311093377946836114, 142.9687499965859843, -8.311093377946837890 ) ) ;
#52966 = CARTESIAN_POINT ( 'NONE',  ( 3.458734125000016313, 199.8750000013656063, 199.4326545832176976 ) ) ;
#52967 = CARTESIAN_POINT ( 'NONE',  ( 3.458734125000016757, 209.1250000013656347, 199.4326545832176976 ) ) ;
#52968 = CARTESIAN_POINT ( 'NONE',  ( 10.18810118749999916, 1.247682550866122264E-15, 79.28125000204836681 ) ) ;
#52969 = CARTESIAN_POINT ( 'NONE',  ( -11.35316468750000141, 53.59374999658601979, -1.390361679473963753E-15 ) ) ;
#52970 = ORIENTED_EDGE ( 'NONE', *, *, #57207, .F. ) ;
#52971 = CARTESIAN_POINT ( 'NONE',  ( -5.000000000000008882, 28.33333333333333925, 8.660254037844390851 ) ) ;
#52972 = CARTESIAN_POINT ( 'NONE',  ( -1.881053915767121776, 4.749999998634407028, -4.541265875000002339 ) ) ;
#52973 = CARTESIAN_POINT ( 'NONE',  ( -5.662595241051935346, 5.662595241051935346, 12.82561528394063011 ) ) ;
#52974 = CARTESIAN_POINT ( 'NONE',  ( -1.320432766682874540E-15, 18.09374999795161187, 7.188101187500000044 ) ) ;
#52975 = CARTESIAN_POINT ( 'NONE',  ( 6.000000000000003553, 291.6250000034139589, -2.485281374238571761 ) ) ;
#52976 = DIRECTION ( 'NONE',  ( -0.000000000000000000, 1.000000000000000000, -0.000000000000000000 ) ) ;
#52977 = CARTESIAN_POINT ( 'NONE',  ( 7.188101187500000044, 11.34374999795161187, 0.000000000000000000 ) ) ;
#52978 = CARTESIAN_POINT ( 'NONE',  ( -7.188101187499992051, 2.977408999572646930, 7.392802781871750994 ) ) ;
#52979 = APPLICATION_CONTEXT ( 'automotive_design' ) ;
#52980 = CARTESIAN_POINT ( 'NONE',  ( 10.18810118750000093, -4.220049686691933921, 74.31250000204836681 ) ) ;
#52981 = VECTOR ( 'NONE', #73339, 1000.000000000000000 ) ;
#52982 = CARTESIAN_POINT ( 'NONE',  ( -29.43265458321760519, 205.1250000013656347, 173.4587341250003760 ) ) ;
#52983 = CARTESIAN_POINT ( 'NONE',  ( -47.32259252271279593, 145.2267040872997939, 65.76194439203463560 ) ) ;
#52984 = CARTESIAN_POINT ( 'NONE',  ( -2.828427124746190735, 1.124999997268813390, -2.828427124746191623 ) ) ;
#52985 = ORIENTED_EDGE ( 'NONE', *, *, #5179, .T. ) ;
#52986 = VECTOR ( 'NONE', #30741, 1000.000000000000000 ) ;
#52987 = CARTESIAN_POINT ( 'NONE',  ( -2.828427124746152987, 196.2500000027312126, 200.8284271247462129 ) ) ;
#52988 = CARTESIAN_POINT ( 'NONE',  ( 2.828427124746152987, 208.1250000000000284, 139.1715728752538723 ) ) ;
#52989 = CARTESIAN_POINT ( 'NONE',  ( -23.99999999999995737, 199.8125000027312410, 171.6568542494926817 ) ) ;
#52990 = ADVANCED_FACE ( 'NONE', ( #56905 ), #14321, .F. ) ;
#52991 = CARTESIAN_POINT ( 'NONE',  ( 4.541265875000002339, 1.312499998634406584, 0.000000000000000000 ) ) ;
#52992 = CARTESIAN_POINT ( 'NONE',  ( -2.977408999572651815, 115.4375000020483810, 7.188101187500000933 ) ) ;
#52993 = EDGE_CURVE ( 'NONE', #20252, #8242, #66926, .T. ) ;
#52994 = CARTESIAN_POINT ( 'NONE',  ( -30.93541659651597797, -37.99999999999981526, 171.9999999999998295 ) ) ;
#52995 = CARTESIAN_POINT ( 'NONE',  ( 5.656854249492376141, -5.656854249492374365, 3.080302783920144005 ) ) ;
#52996 = ORIENTED_EDGE ( 'NONE', *, *, #71458, .T. ) ;
#52997 = CARTESIAN_POINT ( 'NONE',  ( 7.188101187500000044, 25.96874999795161543, 0.000000000000000000 ) ) ;
#52998 = ORIENTED_EDGE ( 'NONE', *, *, #65095, .T. ) ;
#52999 = CARTESIAN_POINT ( 'NONE',  ( 32.00000000000000000, 200.3125000000000284, 168.3431457505075457 ) ) ;
#53000 = CARTESIAN_POINT ( 'NONE',  ( -6.000000000000012434, 10.39230484541325694, 0.000000000000000000 ) ) ;
#53001 = CARTESIAN_POINT ( 'NONE',  ( 26.56734541678238060, 206.3750000013656063, 173.4587341249998929 ) ) ;
#53002 = CARTESIAN_POINT ( 'NONE',  ( 2.679491924311228956, 56.04166666666667140, -10.00000000000000000 ) ) ;
#53003 = CARTESIAN_POINT ( 'NONE',  ( -5.082755093536324154, 97.71875000204838102, 5.082755093536326818 ) ) ;
#53004 = CARTESIAN_POINT ( 'NONE',  ( 2.828427124746152987, 205.2500000027312126, 139.1715728752538723 ) ) ;
#53006 = CARTESIAN_POINT ( 'NONE',  ( -7.347880794884122694E-16, 6.750000000000000000, 4.000000000000001776 ) ) ;
#53005 = CARTESIAN_POINT ( 'NONE',  ( 0.000000000000000000, 300.0000000000000000, 0.000000000000000000 ) ) ;
#53007 = EDGE_CURVE ( 'NONE', #35916, #65881, #5745, .T. ) ;
#53008 = ORIENTED_EDGE ( 'NONE', *, *, #20906, .T. ) ;
#53009 = CARTESIAN_POINT ( 'NONE',  ( 3.042071309553163960, 232.4479166700806161, -11.35316468749999785 ) ) ;
#53010 = CARTESIAN_POINT ( 'NONE',  ( 2.977408999572650927, -7.188101187499990274, 15.83030278187175277 ) ) ;
#53011 = CARTESIAN_POINT ( 'NONE',  ( -2.849036369511732440E-14, 195.3750000027311842, 138.0000000000000568 ) ) ;
#53012 = CARTESIAN_POINT ( 'NONE',  ( 7.999999999999991118, 0.000000000000000000, 30.00000000000000000 ) ) ;
#53013 = DIRECTION ( 'NONE',  ( -0.000000000000000000, 1.000000000000000000, 2.238352872228138170E-16 ) ) ;
#53014 = CARTESIAN_POINT ( 'NONE',  ( 8.660254037844385522, 257.9166666666666856, -5.000000000000003553 ) ) ;
#53015 = CARTESIAN_POINT ( 'NONE',  ( 8.660254037844385522, 179.5833333333333428, 5.000000000000005329 ) ) ;
#53017 = DIRECTION ( 'NONE',  ( 0.000000000000000000, -1.000000000000000000, 0.000000000000000000 ) ) ;
#53016 = B_SPLINE_CURVE_WITH_KNOTS ( 'NONE', 3,
 ( #22394, #51831, #16734, #74464, #40513, #23525, #68431, #51082, #39760, #69183, #52576, #12202 ),
 .UNSPECIFIED., .F., .F.,
 ( 4, 2, 2, 2, 2, 4 ),
 ( 0.000000000000000000, 0.002547658444427995227, 0.005095316888855990455, 0.006369146111069988285, 0.007642975333283986983, 0.01019063377771197917 ),
 .UNSPECIFIED. ) ;
#53018 = CARTESIAN_POINT ( 'NONE',  ( 8.000000000000001776, 91.15625000000000000, 3.313708498984759387 ) ) ;
#53019 = CARTESIAN_POINT ( 'NONE',  ( -0.4369882810000410012, -67.59332269700179552, 20.03478791450388030 ) ) ;
#53020 = CARTESIAN_POINT ( 'NONE',  ( 3.042071309553159519, 140.0520833299193271, 11.35316468750000141 ) ) ;
#53021 = CYLINDRICAL_SURFACE ( 'NONE', #52918, 4.000000000000001776 ) ;
#53022 = DIRECTION ( 'NONE',  ( 0.000000000000000000, 0.000000000000000000, 1.000000000000000000 ) ) ;
#53025 = DIRECTION ( 'NONE',  ( 1.652117596168387509E-16, 4.283267841918042741E-17, -1.000000000000000000 ) ) ;
#53024 = CARTESIAN_POINT ( 'NONE',  ( -4.231687259407056700, -51.96503165405702873, 48.83411696341828190 ) ) ;
#53023 = CARTESIAN_POINT ( 'NONE',  ( 31.99999999999998579, 208.1875000000000853, 171.6568542494923122 ) ) ;
#53026 = ORIENTED_EDGE ( 'NONE', *, *, #54802, .T. ) ;
#53027 = CARTESIAN_POINT ( 'NONE',  ( 5.730382604041190930, 225.7665013914169947, -8.216451592654051339 ) ) ;
#53028 = CARTESIAN_POINT ( 'NONE',  ( -11.00000000000000000, 0.000000000000000000, 91.18750000409677625 ) ) ;
#53029 =( BOUNDED_CURVE ( )  B_SPLINE_CURVE ( 2, ( #71117, #54535, #25464, #54909, #47735, #59451, #71483, #60551, #42815 ),
 .UNSPECIFIED., .F., .F. ) 
 B_SPLINE_CURVE_WITH_KNOTS ( ( 3, 2, 2, 2, 3 ),
 ( 0.05263157894736845976, 0.05921052631578951897, 0.06578947368421057817, 0.07236842105263163738, 0.07894736842105269659 ),
 .UNSPECIFIED. ) 
 CURVE ( )  GEOMETRIC_REPRESENTATION_ITEM ( )  RATIONAL_B_SPLINE_CURVE ( ( 0.9999999999999995559, 0.9238795325112871826, 1.000000000000000000, 0.9238795325112867385, 1.000000000000000000, 0.9238795325112867385, 1.000000000000000000, 0.9238795325112859613, 1.000000000000000888 ) ) 
 REPRESENTATION_ITEM ( '' )  );
#53030 = CARTESIAN_POINT ( 'NONE',  ( -5.309927858096890496, 124.6926540804226988, -5.729198325116819035 ) ) ;
#53031 = CIRCLE ( 'NONE', #42126, 92.50000000000000000 ) ;
#53032 = CARTESIAN_POINT ( 'NONE',  ( 2.679491924311222739, 40.83333332650536818, 10.00000000000000355 ) ) ;
#53033 = CARTESIAN_POINT ( 'NONE',  ( 5.082755093536325042, 113.0937500020483810, -5.082755093536325930 ) ) ;
#53034 = CARTESIAN_POINT ( 'NONE',  ( -4.541265875000003227, 2.999999998634407028, 1.881053915767121110 ) ) ;
#53035 = CARTESIAN_POINT ( 'NONE',  ( 1.780377099649100181, 67.71330631781181353, -20.13219356122023385 ) ) ;
#53036 = CARTESIAN_POINT ( 'NONE',  ( 3.313708498984762496, -7.999999999999989342, 13.29905277982336465 ) ) ;
#53038 = CARTESIAN_POINT ( 'NONE',  ( -8.660254037844387298, 224.5833333333333712, -4.999999999999999112 ) ) ;
#53037 = CARTESIAN_POINT ( 'NONE',  ( -27.99999999999995737, 203.5000000000000000, 174.0000000000003695 ) ) ;
#53039 = ORIENTED_EDGE ( 'NONE', *, *, #55869, .T. ) ;
#53040 = CARTESIAN_POINT ( 'NONE',  ( 6.000000000000001776, 292.5625000034140157, -7.347880794884121708E-16 ) ) ;
#53041 = CARTESIAN_POINT ( 'NONE',  ( -9.679794093948311584, 225.9999999999999716, -2.594496013589457917 ) ) ;
#53042 = CARTESIAN_POINT ( 'NONE',  ( -7.778174593052020747, -7.778174593052023411, 115.1875000000000000 ) ) ;
#53043 = CARTESIAN_POINT ( 'NONE',  ( 5.676582343750005144, 245.8854166700806445, 9.832129032723416984 ) ) ;
#53044 = CARTESIAN_POINT ( 'NONE',  ( -8.311093377946841443, 118.9062499965860269, 8.311093377946830785 ) ) ;
#53045 = ORIENTED_EDGE ( 'NONE', *, *, #41094, .T. ) ;
#53046 = CARTESIAN_POINT ( 'NONE',  ( -4.527972964883675289, 9.877574257516585021, 117.6444479903747151 ) ) ;
#53047 = VECTOR ( 'NONE', #56396, 1000.000000000000000 ) ;
#53048 = CARTESIAN_POINT ( 'NONE',  ( 10.18810118749999916, 1.247682550866122264E-15, 98.40625000204838102 ) ) ;
#53049 = CARTESIAN_POINT ( 'NONE',  ( 7.320508075688774596, 227.4999999931720254, -7.320508075688774596 ) ) ;
#53050 = CARTESIAN_POINT ( 'NONE',  ( -2.445694354108784108, 202.5625000013656063, 195.5543056458912190 ) ) ;
#53051 = CARTESIAN_POINT ( 'NONE',  ( 62.39047978708148889, 229.6205190061017447, 45.00000000000000000 ) ) ;
#53053 = CARTESIAN_POINT ( 'NONE',  ( 5.676582343749993598, 114.9479166632526983, 9.832129032723422313 ) ) ;
#53052 = CARTESIAN_POINT ( 'NONE',  ( 2.751064625579944321E-14, 205.8750000027312126, 194.0000000000000568 ) ) ;
#53054 = CARTESIAN_POINT ( 'NONE',  ( 1.469576158976822172E-15, -7.999999999999991118, 7.392802783920144449 ) ) ;
#53055 = CARTESIAN_POINT ( 'NONE',  ( -31.45873412499997812, 197.0000000013656347, 171.4326545832180386 ) ) ;
#53056 = CYLINDRICAL_SURFACE ( 'NONE', #8379, 18.50000000000000000 ) ;
#53057 = VERTEX_POINT ( 'NONE', #20970 ) ;
#53058 = CARTESIAN_POINT ( 'NONE',  ( 8.660254037844385522, 196.4583333265053966, 5.000000000000005329 ) ) ;
#53059 = CARTESIAN_POINT ( 'NONE',  ( -6.735557395310442023E-16, 11.00000000000000000, 83.31250000409676204 ) ) ;
#53060 = CARTESIAN_POINT ( 'NONE',  ( 3.042071309553167513, 107.1354166632526841, -11.35316468749999785 ) ) ;
#53061 = CYLINDRICAL_SURFACE ( 'NONE', #50725, 10.00000000000000000 ) ;
#53062 = CARTESIAN_POINT ( 'NONE',  ( 2.977408999572650927, 11.62499999795161187, -7.188101187500000933 ) ) ;
#53063 = CARTESIAN_POINT ( 'NONE',  ( 10.18810118750000093, -4.220049686691933033, 94.18750000204836681 ) ) ;
#53064 = CARTESIAN_POINT ( 'NONE',  ( 11.35316468750000141, 11.09374999658601624, 0.000000000000000000 ) ) ;
#53065 = VERTEX_POINT ( 'NONE', #60970 ) ;
#53066 = CARTESIAN_POINT ( 'NONE',  ( 0.000000000000000000, 0.000000000000000000, 0.000000000000000000 ) ) ;
#53067 = CARTESIAN_POINT ( 'NONE',  ( 5.656854249492379694, 99.12500000409677625, -5.656854249492380582 ) ) ;
#53068 = CARTESIAN_POINT ( 'NONE',  ( 11.33169192104559997, 226.0000000000000000, -1.645653018074211493 ) ) ;
#53069 = CARTESIAN_POINT ( 'NONE',  ( 4.220049686691941027, -10.18810118749999738, 74.50000000204838102 ) ) ;
#53070 = CARTESIAN_POINT ( 'NONE',  ( 3.680852415662204891, 22.00000000000001066, 1.883217705396645014 ) ) ;
#53071 = CARTESIAN_POINT ( 'NONE',  ( 0.000000000000000000, 0.000000000000000000, 41.99999999999999289 ) ) ;
#53072 = CARTESIAN_POINT ( 'NONE',  ( 6.676582343750003368, 294.0156250017070079, -2.765530957081997254 ) ) ;
#53073 = VERTEX_POINT ( 'NONE', #20218 ) ;
#53074 = CARTESIAN_POINT ( 'NONE',  ( -6.735557395310442023E-16, 11.00000000000000000, 89.31250000409676204 ) ) ;
#53075 = CARTESIAN_POINT ( 'NONE',  ( 9.832129032723416984, 205.6770833299193555, 5.676582343750006032 ) ) ;
#53076 = AXIS2_PLACEMENT_3D ( 'NONE', #29623, #63954, #52636 ) ;
#53077 = CARTESIAN_POINT ( 'NONE',  ( -10.18810118749999916, 4.220049686691934809, 87.06250000204838102 ) ) ;
#53078 = EDGE_CURVE ( 'NONE', #71712, #46560, #18212, .T. ) ;
#53079 = CARTESIAN_POINT ( 'NONE',  ( -27.99999999999996447, 203.9375000013656063, 173.4587341250003760 ) ) ;
#53080 = CARTESIAN_POINT ( 'NONE',  ( 8.000000000000000000, 22.50000000000000355, 0.000000000000000000 ) ) ;
#53081 = ORIENTED_EDGE ( 'NONE', *, *, #64579, .T. ) ;
#53082 = CARTESIAN_POINT ( 'NONE',  ( 1.224646799147353454E-15, 255.9999999999999432, -10.00000000000000178 ) ) ;
#53083 = CARTESIAN_POINT ( 'NONE',  ( 2.751064625579944321E-14, 208.8750000027312126, 194.0000000000000568 ) ) ;
#53084 = CARTESIAN_POINT ( 'NONE',  ( 6.123233995736767268E-16, 31.25000000000000000, -10.00000000000000178 ) ) ;
#53085 = VECTOR ( 'NONE', #13264, 1000.000000000000000 ) ;
#53086 = CARTESIAN_POINT ( 'NONE',  ( -5.000000000000000888, 12.55543720214795478, 69.09376167622116327 ) ) ;
#53087 = CARTESIAN_POINT ( 'NONE',  ( -7.204075437095965206, -7.204075437095968759, 77.21875000204836681 ) ) ;
#53088 = ORIENTED_EDGE ( 'NONE', *, *, #66976, .F. ) ;
#53089 = CARTESIAN_POINT ( 'NONE',  ( 5.082755093536324154, 4.781249997951610986, 5.082755093536326818 ) ) ;
#53090 = LINE ( 'NONE', #18015, #8906 ) ;
#53091 = EDGE_CURVE ( 'NONE', #6837, #67176, #36934, .T. ) ;
#53092 = EDGE_CURVE ( 'NONE', #31972, #28551, #67757, .T. ) ;
#53093 = CARTESIAN_POINT ( 'NONE',  ( -9.000000000000000000, -5.196152422706644458, -10.20000000000000284 ) ) ;
#53094 = CARTESIAN_POINT ( 'NONE',  ( -7.188101187500000044, 115.5312500020483952, 0.000000000000000000 ) ) ;
#53095 = AXIS2_PLACEMENT_3D ( 'NONE', #42535, #41803, #48192 ) ;
#53096 = CARTESIAN_POINT ( 'NONE',  ( -1.377000000000000002, 272.8559999999997672, 5.668134320366531753 ) ) ;
#53097 = CARTESIAN_POINT ( 'NONE',  ( -4.088227598258586603E-16, 295.2031250017069510, -6.676582343750001591 ) ) ;
#53099 = CARTESIAN_POINT ( 'NONE',  ( 7.320508075688771044, 136.2499999931720538, 7.320508075688775484 ) ) ;
#53098 = CARTESIAN_POINT ( 'NONE',  ( 3.042071309553163516, 232.4479166700806445, -11.35316468749999785 ) ) ;
#53100 = ITEM_DEFINED_TRANSFORMATION ( 'NONE', 'NONE', #6825,  #57354 ) ;
#53101 = EDGE_LOOP ( 'NONE', ( #28361, #61980, #35282, #49171, #10660, #915, #51011, #17159, #53308, #9150, #74020, #29503, #43861, #56003, #66233, #71410, #32291, #52776, #36523, #20873, #64500, #37450, #17051, #37434, #53255, #72192, #6016, #65888, #696, #2323, #54010, #34346, #57745, #19070 ) ) ;
#53102 = B_SPLINE_CURVE_WITH_KNOTS ( 'NONE', 3,
 ( #17029, #10640, #11016, #4990, #51365, #63799, #22687, #40055 ),
 .UNSPECIFIED., .F., .F.,
 ( 4, 2, 2, 4 ),
 ( 0.005256334970462575411, 0.006570121696640842182, 0.007883908422819108086, 0.01051148187517563469 ),
 .UNSPECIFIED. ) ;
#53103 = CARTESIAN_POINT ( 'NONE',  ( 5.676582343750005144, 245.8854166700806445, 9.832129032723416984 ) ) ;
#53104 = CARTESIAN_POINT ( 'NONE',  ( -4.401442555609577197E-16, 7.188101187499992051, 4.111552781871752771 ) ) ;
#53105 = CARTESIAN_POINT ( 'NONE',  ( -3.458734124999960358, 204.6875000013656063, 198.0000000000000284 ) ) ;
#53106 = ORIENTED_EDGE ( 'NONE', *, *, #46389, .T. ) ;
#53107 = CARTESIAN_POINT ( 'NONE',  ( 5.094045771088254959, 8.823157229062946527, 67.15552375567561683 ) ) ;
#53108 = CARTESIAN_POINT ( 'NONE',  ( -3.042071309553164404, 107.5520833299193555, -11.35316468749999963 ) ) ;
#53109 = FACE_OUTER_BOUND ( 'NONE', #67374, .T. ) ;
#53110 = CARTESIAN_POINT ( 'NONE',  ( 11.00000000000000000, 4.556349186104045934, 78.34374999999998579 ) ) ;
#53113 = CARTESIAN_POINT ( 'NONE',  ( -5.656854249492379694, 2.062500000000000444, -5.656854249492380582 ) ) ;
#53112 = CARTESIAN_POINT ( 'NONE',  ( 25.55430564589115505, 204.0625000013656063, 167.5543056458911053 ) ) ;
#53111 = CARTESIAN_POINT ( 'NONE',  ( 29.43265458321766559, 204.1250000013656063, 166.5412658749999650 ) ) ;
#53114 = ORIENTED_EDGE ( 'NONE', *, *, #21868, .F. ) ;
#53115 = DIRECTION ( 'NONE',  ( 1.000000000000000000, 0.000000000000000000, 0.000000000000000000 ) ) ;
#53116 = CARTESIAN_POINT ( 'NONE',  ( 6.123233995736767268E-16, 178.1249999931720538, -10.00000000000000178 ) ) ;
#53117 = EDGE_CURVE ( 'NONE', #46122, #60284, #32313, .T. ) ;
#53118 = VECTOR ( 'NONE', #50414, 1000.000000000000000 ) ;
#53119 = CARTESIAN_POINT ( 'NONE',  ( 5.676582343749993598, 214.9479166632526983, 9.832129032723422313 ) ) ;
#53120 = CARTESIAN_POINT ( 'NONE',  ( 1.432654583217607192, 204.2500000013655779, 145.4587341250000634 ) ) ;
#53121 = CARTESIAN_POINT ( 'NONE',  ( 24.54126587499998635, 207.5000000013655779, 171.4326545832175555 ) ) ;
#53122 = CARTESIAN_POINT ( 'NONE',  ( -1.320432766682874540E-15, 24.46874999795161543, 7.188101187500000044 ) ) ;
#53123 = CARTESIAN_POINT ( 'NONE',  ( 9.832129032723420536, 181.5104166632526699, -5.676582343749999815 ) ) ;
#53124 = CARTESIAN_POINT ( 'NONE',  ( 5.082755093536325042, 95.46875000204838102, -5.082755093536325930 ) ) ;
#53125 = DIRECTION ( 'NONE',  ( 0.000000000000000000, 0.000000000000000000, 1.000000000000000000 ) ) ;
#53126 = CARTESIAN_POINT ( 'NONE',  ( -30.82842712474615610, 197.3750000000000284, 172.8284271247465824 ) ) ;
#53127 = CARTESIAN_POINT ( 'NONE',  ( 1.881053915767122664, 10.12499999863440792, 4.541265875000001451 ) ) ;
#53128 = CARTESIAN_POINT ( 'NONE',  ( 28.00000000000002132, 201.1875000013656063, 166.5412658749999082 ) ) ;
#53129 = CARTESIAN_POINT ( 'NONE',  ( -7.188101187499990274, -2.977408999572651371, 6.455302781871754547 ) ) ;
#53130 = CARTESIAN_POINT ( 'NONE',  ( -11.35316468750000141, 68.48958332991935549, 3.042071309553159963 ) ) ;
#53131 = FACE_OUTER_BOUND ( 'NONE', #16827, .T. ) ;
#53132 = CYLINDRICAL_SURFACE ( 'NONE', #54421, 3.999999999999976019 ) ;
#53133 = ORIENTED_EDGE ( 'NONE', *, *, #62967, .F. ) ;
#53134 = CARTESIAN_POINT ( 'NONE',  ( 105.0000000000000000, 210.0000000000000568, 139.0000000000000284 ) ) ;
#53135 = LINE ( 'NONE', #35426, #71398 ) ;
#53136 = CARTESIAN_POINT ( 'NONE',  ( 5.676582343750001591, 81.61458332991935549, -9.832129032723420536 ) ) ;
#53137 = CARTESIAN_POINT ( 'NONE',  ( 11.00000000000000000, 4.556349186104045934, 71.03125000409677625 ) ) ;
#53138 = CARTESIAN_POINT ( 'NONE',  ( 2.445694354108784108, 197.5625000013656063, 144.4456943541088663 ) ) ;
#53139 = CARTESIAN_POINT ( 'NONE',  ( -31.24282280673623902, -33.02374444324331648, 167.9999999999997726 ) ) ;
#53141 = CARTESIAN_POINT ( 'NONE',  ( 11.35316468749999785, 70.57291666325268409, 3.042071309553174174 ) ) ;
#53140 = CARTESIAN_POINT ( 'NONE',  ( -1.656854249492405895, 13.06249999726881761, -3.999999999999976463 ) ) ;
#53142 = CARTESIAN_POINT ( 'NONE',  ( -3.313708498984758943, -7.999999999999989342, 22.29905278392014623 ) ) ;
#53143 = DIRECTION ( 'NONE',  ( -0.000000000000000000, 1.000000000000000000, 4.476705744456276341E-16 ) ) ;
#53144 = CARTESIAN_POINT ( 'NONE',  ( -2.679491924311235618, 160.4166666598386541, 10.00000000000000000 ) ) ;
#53145 = CARTESIAN_POINT ( 'NONE',  ( -4.401442555609581635E-16, 95.65625000204838102, -7.188101187500000044 ) ) ;
#53146 = DIRECTION ( 'NONE',  ( -0.000000000000000000, 1.000000000000000000, -0.000000000000000000 ) ) ;
#53147 = CARTESIAN_POINT ( 'NONE',  ( 9.832129032723416984, 45.67708332991934839, 5.676582343750006032 ) ) ;
#53148 =( BOUNDED_SURFACE ( )  B_SPLINE_SURFACE ( 1, 2, ( 
 ( #51599, #62917, #62540, #33905, #5216, #691, #58033, #74614, #46313, #68954, #56530, #22544, #28217, #62171, #6341, #29346, #11243, #50853, #11986, #16888, #23674, #40283, #51226, #40657, #17264, #34273, #63284, #45566, #46680, #57653, #28963, #69704, #73867, #22172, #45197, #18016, #48150, #47779, #25135, #54205, #30077, #30449, #71159, #18389, #35385, #1428, #24037, #41401, #35744, #2513, #24768, #47046, #30809, #59132, #12352, #1058, #24412, #41035, #58761, #41765, #64773, #1783, #19115, #64042, #53832, #7441, #19480, #70442, #59856, #36850, #25507, #29710, #70801, #2141, #42495, #70082, #42120, #59494, #64414, #65131, #7807, #58398, #7071, #12712, #47417, #13443, #53465, #6703, #65510, #36480, #13805, #8170, #48520, #31180, #13076, #52724, #53094, #18757, #36111, #66623, #10039, #37593, #14928, #38720, #4379, #56070, #50020, #55701, #61718, #60592, #14556, #21346, #49651, #8917, #31555, #48892, #8541, #37970, #3261, #3631, #60969, #72282, #60217, #43993, #25872, #54579, #31929, #27372, #71526, #20217, #65875, #26249, #54951, #37219, #27007, #44367, #9289, #14182, #71903, #38339, #49267, #73035, #32312, #66251, #72667, #9672, #67379, #15679, #20594, #4017, #43236, #33074, #20969, #43610, #55326, #26628, #19853, #42857, #67003, #15302, #61346, #32692, #2884, #39448, #11155, #69238, #21711, #6247, #56809, #34179, #68121, #51888, #228, #56436, #62448, #40192, #27748, #5872, #10775, #44740, #45845, #33436, #23209, #45470, #5130, #4756, #34929, #45108, #22829, #16049, #39081, #57181, #11524, #63194, #34558, #33812, #51507, #62086, #68860, #57563, #28868, #17171, #46221, #5498, #68486, #51136, #50759, #73775, #22084, #63569, #17547, #16788, #40566, #39815, #67756, #28123, #16415, #50392, #11895, #57941, #22450, #10408, #73407, #74146, #62820, #74521, #28498, #42035, #59041, #58669, #64687, #967, #42400, #18295, #70356, #19387, #47329, #18667, #59403, #29251, #7718, #7348, #36388, #65417, #41311, #41678, #30721, #29619, #46589, #12623, #35294, #52632, #46959, #13715, #36024, #58308, #65041, #53376, #69610, #63950, #36759, #12986, #47688, #30355, #17926, #13350, #1336, #23950, #59772, #40941, #1700, #6612, #48062, #24678, #70710, #19028, #53742, #596, #52264, #29986, #23579, #64319, #69987, #35654, #12260, #6975, #53003, #2053, #24318, #25041, #71069, #37504, #72577, #15591, #42771, #38630, #38250, #54112, #43903, #20882, #8081, #43515, #14091, #65787, #60502, #9198, #20130, #66914, #8829, #31840, #60129, #8447, #37126, #21255, #3928, #49177, #15219, #72188, #2422, #43145, #54491, #31082, #26919, #49934, #54859, #25417, #55611, #3170, #72947, #32219, #2796, #61253, #37880, #26159, #66529, #25784, #44280, #71812, #20500, #67291, #14839, #60875, #9585, #48431, #32602, #55237, #71434, #19764, #66161, #3543, #31467, #48803, #14465, #26534, #49559, #61998, #4667, #46130, #68400, #15964, #74432, #11070, #27285, #21626, #51795, #5043, #5408, #62730, #4294, #45760, #33723, #56348, #69148, #50302, #34096, #38993, #5782 ),
 ( #44650, #39362, #10689, #51418, #45026, #33347, #73323, #16326, #22739, #17455, #67666, #61632, #17082, #32983, #68771, #40104, #9950, #22360, #10321, #27664, #62359, #57092, #73688, #63109, #56725, #50669, #11435, #28039, #68033, #22000, #55984, #51050, #28410, #74061, #45384, #16698, #34472, #57476, #28778, #39729, #142, #23118, #35935, #1612, #53287, #7260, #12899, #24224, #58580, #6888, #18942, #18208, #7626, #59321, #1966, #52177, #47238, #24595, #47601, #46500, #18578, #30270, #69520, #41589, #70624, #34841, #6523, #17834, #69897, #70265, #52912, #6154, #41948, #64602, #58952, #64956, #70988, #13266, #35567, #36303, #52540, #40848, #509, #29899, #53655, #29530, #1247, #30635, #47973, #24958, #40476, #63481, #11803, #878, #58224, #57848, #29162, #23864, #23488, #63856, #12171, #35207, #46874, #41222, #64230, #12539, #7993, #66445, #48343, #54023, #60038, #26830, #49844, #42684, #13634, #48715, #37037, #59684, #49467, #43813, #60413, #36672, #71350, #60788, #71721, #72487, #37414, #13998, #72100, #32128, #66828, #20796, #43053, #3452, #19672, #26442, #43430, #66070, #14378, #65696, #15130, #38162, #14752, #20413, #26065, #25695, #2707, #8358, #54771, #61164, #65330, #19304, #20037, #3081, #31374, #9495, #32509, #25328, #54400, #9112, #8739, #55522, #31751, #30999, #37792, #49086, #2331, #55147, #3834, #42314, #38906, #21907, #44938, #56639, #73973, #72862, #10978, #74341, #4208, #61908, #62645, #50213, #28323, #10233, #67204, #68315, #39277, #15502, #55894, #56260, #21167, #33261, #67945, #16239, #4954, #22278, #44191, #34013, #62278, #51333, #50582, #40020, #16993, #34382, #9863, #27954, #57008, #5321, #27197, #50960, #39648, #73234, #45300, #22650, #38539, #4576, #21540, #27574, #16612, #10605, #61540, #45670, #68684, #63023, #11347, #28690, #57382, #33633, #5692, #73600, #44564, #32892, #67576, #15873, #17740, #46779, #19865, #60231, #37233, #31194, #36862, #42871, #40755, #69431, #2529, #29812, #63764, #11713, #29070, #63389, #18119, #58133, #58494, #69803, #52454, #40391, #25149, #6063, #34753, #12082, #8556, #51704, #423, #46043, #6442, #35118, #17367, #8183, #25521, #41133, #69063, #52090, #19492, #29443, #54218, #64140, #46417, #52822, #65525, #48533, #71541, #792, #59870, #23402, #65890, #1157, #23776, #12450, #35480, #14196, #51, #48166, #71174, #6800, #42508, #13818, #23034, #57758, #50408, #2900, #62101, #37984, #15316, #49282, #33090, #60608, #66266, #72298, #39098, #31570, #54966, #25885, #60983, #20610, #71918, #61736, #56087, #72683, #48904, #8932, #73050, #9304, #10053, #49666, #26262, #9687, #44382, #4396, #27389, #55341, #15695, #31943, #38737, #55716, #3644, #26644, #3275, #73422, #21727, #4031, #32707, #38352, #32328, #14945, #43628, #67019, #44757, #20231, #54594, #20985, #61360, #66638, #67770, #16064, #37608, #44009, #21358, #27025, #43250, #50036, #14573, #67393, #51522, #4772, #68136, #68504, #33454, #51154, #34194, #57198, #68877, #11539, #10424, #23225, #74537, #63583, #62836 ) ),
 .UNSPECIFIED., .F., .F., .F. ) 
 B_SPLINE_SURFACE_WITH_KNOTS ( ( 2, 2 ),
 ( 3, 2, 2, 2, 2, 2, 2, 2, 2, 2, 2, 2, 2, 2, 2, 2, 2, 2, 2, 2, 2, 2, 2, 2, 2, 2, 2, 2, 2, 2, 2, 2, 2, 2, 2, 2, 2, 2, 2, 2, 2, 2, 2, 2, 2, 2, 2, 2, 2, 2, 2, 2, 2, 2, 2, 2, 2, 2, 2, 2, 2, 2, 2, 2, 2, 2, 2, 2, 2, 2, 2, 2, 2, 2, 2, 2, 2, 2, 2, 2, 2, 2, 2, 2, 2, 2, 2, 2, 2, 2, 2, 2, 2, 2, 2, 2, 2, 2, 2, 2, 2, 2, 2, 2, 2, 2, 2, 2, 2, 2, 2, 2, 2, 2, 2, 2, 2, 2, 2, 2, 2, 2, 2, 2, 2, 2, 2, 2, 2, 2, 2, 2, 2, 2, 2, 2, 2, 2, 2, 2, 2, 2, 2, 2, 2, 2, 2, 2, 2, 2, 2, 2, 2, 2, 2, 2, 2, 2, 2, 2, 2, 2, 2, 2, 2, 2, 2, 2, 2, 2, 2, 2, 2, 2, 2, 2, 2, 2, 2, 2, 2, 2, 2, 2, 2, 2, 2, 2, 3 ),
 ( 0.000000000000000000, 1.000000000000000000 ),
 ( 0.000000000000000000, 0.005208333333333333044, 0.01041666666666666609, 0.01562500000000000000, 0.02083333333333333218, 0.02604166666666666782, 0.03125000000000000000, 0.03645833333333333565, 0.04166666666666666435, 0.04687500000000000000, 0.05208333333333333565, 0.05729166666666666435, 0.06250000000000000000, 0.06770833333333332871, 0.07291666666666667129, 0.07812500000000000000, 0.08333333333333332871, 0.08854166666666667129, 0.09375000000000000000, 0.09895833333333332871, 0.1041666666666666713, 0.1093750000000000000, 0.1145833333333333287, 0.1197916666666666713, 0.1250000000000000000, 0.1302083333333333426, 0.1354166666666666574, 0.1406250000000000000, 0.1458333333333333426, 0.1510416666666666574, 0.1562500000000000000, 0.1614583333333333426, 0.1666666666666666574, 0.1718750000000000000, 0.1770833333333333426, 0.1822916666666666574, 0.1875000000000000000, 0.1927083333333333426, 0.1979166666666666574, 0.2031250000000000000, 0.2083333333333333426, 0.2135416666666666574, 0.2187500000000000000, 0.2239583333333333426, 0.2291666666666666574, 0.2343750000000000000, 0.2395833333333333426, 0.2447916666666666574, 0.2500000000000000000, 0.2552083333333333148, 0.2604166666666666852, 0.2656250000000000000, 0.2708333333333333148, 0.2760416666666666852, 0.2812500000000000000, 0.2864583333333333148, 0.2916666666666666852, 0.2968750000000000000, 0.3020833333333333148, 0.3072916666666666852, 0.3125000000000000000, 0.3177083333333333148, 0.3229166666666666852, 0.3281250000000000000, 0.3333333333333333148, 0.3385416666666666852, 0.3437500000000000000, 0.3489583333333333148, 0.3541666666666666852, 0.3593750000000000000, 0.3645833333333333148, 0.3697916666666666852, 0.3750000000000000000, 0.3802083333333333148, 0.3854166666666666852, 0.3906250000000000000, 0.3958333333333333148, 0.4010416666666666852, 0.4062500000000000000, 0.4114583333333333148, 0.4166666666666666852, 0.4218750000000000000, 0.4270833333333333148, 0.4322916666666666852, 0.4375000000000000000, 0.4427083333333333148, 0.4479166666666666852, 0.4531250000000000000, 0.4583333333333333148, 0.4635416666666666852, 0.4687500000000000000, 0.4739583333333333148, 0.4791666666666666852, 0.4843750000000000000, 0.4895833333333333148, 0.4947916666666666852, 0.5000000000000000000, 0.5052083333333333703, 0.5104166666666666297, 0.5156250000000000000, 0.5208333333333333703, 0.5260416666666666297, 0.5312500000000000000, 0.5364583333333333703, 0.5416666666666666297, 0.5468750000000000000, 0.5520833333333333703, 0.5572916666666666297, 0.5625000000000000000, 0.5677083333333333703, 0.5729166666666666297, 0.5781250000000000000, 0.5833333333333333703, 0.5885416666666666297, 0.5937500000000000000, 0.5989583333333333703, 0.6041666666666666297, 0.6093750000000000000, 0.6145833333333333703, 0.6197916666666666297, 0.6250000000000000000, 0.6302083333333333703, 0.6354166666666666297, 0.6406250000000000000, 0.6458333333333333703, 0.6510416666666666297, 0.6562500000000000000, 0.6614583333333333703, 0.6666666666666666297, 0.6718750000000000000, 0.6770833333333333703, 0.6822916666666666297, 0.6875000000000000000, 0.6927083333333333703, 0.6979166666666666297, 0.7031250000000000000, 0.7083333333333333703, 0.7135416666666666297, 0.7187500000000000000, 0.7239583333333333703, 0.7291666666666666297, 0.7343750000000000000, 0.7395833333333333703, 0.7447916666666666297, 0.7500000000000000000, 0.7552083333333333703, 0.7604166666666666297, 0.7656250000000000000, 0.7708333333333333703, 0.7760416666666666297, 0.7812500000000000000, 0.7864583333333333703, 0.7916666666666666297, 0.7968750000000000000, 0.8020833333333333703, 0.8072916666666666297, 0.8125000000000000000, 0.8177083333333333703, 0.8229166666666666297, 0.8281250000000000000, 0.8333333333333333703, 0.8385416666666666297, 0.8437500000000000000, 0.8489583333333333703, 0.8541666666666666297, 0.8593750000000000000, 0.8645833333333333703, 0.8697916666666666297, 0.8750000000000000000, 0.8802083333333333703, 0.8854166666666666297, 0.8906250000000000000, 0.8958333333333333703, 0.9010416666666666297, 0.9062500000000000000, 0.9114583333333333703, 0.9166666666666666297, 0.9218750000000000000, 0.9270833333333333703, 0.9322916666666666297, 0.9375000000000000000, 0.9427083333333333703, 0.9479166666666666297, 0.9531250000000000000, 0.9583333333333333703, 0.9635416666666666297, 0.9687500000000000000, 0.9722122468226729319, 0.9819343692908996113 ),
 .UNSPECIFIED. ) 
 GEOMETRIC_REPRESENTATION_ITEM ( )  RATIONAL_B_SPLINE_SURFACE ( (
 ( 1.000000000000000000, 0.9238795325112867385, 1.000000000000000000, 0.9238795325112867385, 1.000000000000000000, 0.9238795325112867385, 1.000000000000000000, 0.9238795325112867385, 1.000000000000000000, 0.9238795325112867385, 1.000000000000000000, 0.9238795325112867385, 1.000000000000000000, 0.9238795325112867385, 1.000000000000000000, 0.9238795325112867385, 1.000000000000000000, 0.9238795325112867385, 1.000000000000000000, 0.9238795325112867385, 1.000000000000000000, 0.9238795325112867385, 1.000000000000000000, 0.9238795325112867385, 1.000000000000000000, 0.9238795325112867385, 1.000000000000000000, 0.9238795325112867385, 1.000000000000000000, 0.9238795325112867385, 1.000000000000000000, 0.9238795325112867385, 1.000000000000000000, 0.9238795325112867385, 1.000000000000000000, 0.9238795325112867385, 1.000000000000000000, 0.9238795325112867385, 1.000000000000000000, 0.9238795325112867385, 1.000000000000000000, 0.9238795325112867385, 1.000000000000000000, 0.9238795325112867385, 1.000000000000000000, 0.9238795325112867385, 1.000000000000000000, 0.9238795325112867385, 1.000000000000000000, 0.9238795325112867385, 1.000000000000000000, 0.9238795325112867385, 1.000000000000000000, 0.9238795325112867385, 1.000000000000000000, 0.9238795325112867385, 1.000000000000000000, 0.9238795325112867385, 1.000000000000000000, 0.9238795325112867385, 1.000000000000000000, 0.9238795325112867385, 1.000000000000000000, 0.9238795325112867385, 1.000000000000000000, 0.9238795325112867385, 1.000000000000000000, 0.9238795325112867385, 1.000000000000000000, 0.9238795325112867385, 1.000000000000000000, 0.9238795325112867385, 1.000000000000000000, 0.9238795325112867385, 1.000000000000000000, 0.9238795325112867385, 1.000000000000000000, 0.9238795325112867385, 1.000000000000000000, 0.9238795325112867385, 1.000000000000000000, 0.9238795325112867385, 1.000000000000000000, 0.9238795325112867385, 1.000000000000000000, 0.9238795325112867385, 1.000000000000000000, 0.9238795325112867385, 1.000000000000000000, 0.9238795325112867385, 1.000000000000000000, 0.9238795325112867385, 1.000000000000000000, 0.9238795325112867385, 1.000000000000000000, 0.9238795325112867385, 1.000000000000000000, 0.9238795325112867385, 1.000000000000000000, 0.9238795325112867385, 1.000000000000000000, 0.9238795325112867385, 1.000000000000000000, 0.9238795325112867385, 1.000000000000000000, 0.9238795325112867385, 1.000000000000000000, 0.9238795325112867385, 1.000000000000000000, 0.9238795325112867385, 1.000000000000000000, 0.9238795325112867385, 1.000000000000000000, 0.9238795325112867385, 1.000000000000000000, 0.9238795325112867385, 1.000000000000000000, 0.9238795325112867385, 1.000000000000000000, 0.9238795325112867385, 1.000000000000000000, 0.9238795325112867385, 1.000000000000000000, 0.9238795325112867385, 1.000000000000000000, 0.9238795325112867385, 1.000000000000000000, 0.9238795325112867385, 1.000000000000000000, 0.9238795325112867385, 1.000000000000000000, 0.9238795325112867385, 1.000000000000000000, 0.9238795325112867385, 1.000000000000000000, 0.9238795325112867385, 1.000000000000000000, 0.9238795325112867385, 1.000000000000000000, 0.9238795325112867385, 1.000000000000000000, 0.9238795325112867385, 1.000000000000000000, 0.9238795325112867385, 1.000000000000000000, 0.9238795325112867385, 1.000000000000000000, 0.9238795325112867385, 1.000000000000000000, 0.9238795325112867385, 1.000000000000000000, 0.9238795325112867385, 1.000000000000000000, 0.9238795325112867385, 1.000000000000000000, 0.9238795325112867385, 1.000000000000000000, 0.9238795325112867385, 1.000000000000000000, 0.9238795325112867385, 1.000000000000000000, 0.9238795325112867385, 1.000000000000000000, 0.9238795325112867385, 1.000000000000000000, 0.9238795325112867385, 1.000000000000000000, 0.9238795325112867385, 1.000000000000000000, 0.9238795325112867385, 1.000000000000000000, 0.9238795325112867385, 1.000000000000000000, 0.9238795325112867385, 1.000000000000000000, 0.9238795325112867385, 1.000000000000000000, 0.9238795325112867385, 1.000000000000000000, 0.9238795325112867385, 1.000000000000000000, 0.9238795325112867385, 1.000000000000000000, 0.9238795325112867385, 1.000000000000000000, 0.9238795325112867385, 1.000000000000000000, 0.9238795325112867385, 1.000000000000000000, 0.9238795325112867385, 1.000000000000000000, 0.9238795325112867385, 1.000000000000000000, 0.9238795325112867385, 1.000000000000000000, 0.9238795325112867385, 1.000000000000000000, 0.9238795325112867385, 1.000000000000000000, 0.9238795325112867385, 1.000000000000000000, 0.9238795325112867385, 1.000000000000000000, 0.9238795325112867385, 1.000000000000000000, 0.9238795325112867385, 1.000000000000000000, 0.9238795325112867385, 1.000000000000000000, 0.9238795325112867385, 1.000000000000000000, 0.9238795325112867385, 1.000000000000000000, 0.9238795325112867385, 1.000000000000000000, 0.9238795325112867385, 1.000000000000000000, 0.9238795325112867385, 1.000000000000000000, 0.9238795325112867385, 1.000000000000000000, 0.9238795325112867385, 1.000000000000000000, 0.9238795325112867385, 1.000000000000000000, 0.9238795325112867385, 1.000000000000000000, 0.9238795325112867385, 1.000000000000000000, 0.9238795325112867385, 1.000000000000000000, 0.9238795325112867385, 1.000000000000000000, 0.9238795325112867385, 1.000000000000000000, 0.9238795325112867385, 1.000000000000000000, 0.9238795325112867385, 1.000000000000000000, 0.9238795325112867385, 1.000000000000000000, 0.9238795325112867385, 1.000000000000000000, 0.9238795325112867385, 1.000000000000000000, 0.9238795325112867385, 1.000000000000000000, 0.9238795325112867385, 1.000000000000000000, 0.9238795325112867385, 1.000000000000000000, 0.9238795325112867385, 1.000000000000000000, 0.9238795325112867385, 1.000000000000000000, 0.9238795325112867385, 1.000000000000000000, 0.9238795325112867385, 1.000000000000000000, 0.9238795325112867385, 1.000000000000000000, 0.9238795325112867385, 1.000000000000000000, 0.9238795325112867385, 1.000000000000000000, 0.9238795325112867385, 1.000000000000000000, 0.9238795325112867385, 1.000000000000000000, 0.9238795325112867385, 1.000000000000000000, 0.9238795325112867385, 1.000000000000000000, 0.9238795325112867385, 1.000000000000000000, 0.9238795325112867385, 1.000000000000000000, 0.9238795325112867385, 1.000000000000000000, 0.9238795325112867385, 1.000000000000000000, 0.9238795325112867385, 1.000000000000000000, 0.9238795325112867385, 1.000000000000000000, 0.9238795325112867385, 1.000000000000000000, 0.9238795325112867385, 1.000000000000000000, 0.9238795325112867385, 1.000000000000000000, 0.9238795325112867385, 1.000000000000000000, 0.9238795325112867385, 1.000000000000000000, 0.9238795325112867385, 1.000000000000000000, 0.9238795325112867385, 1.000000000000000000, 0.9238795325112867385, 1.000000000000000000, 0.9238795325112867385, 1.000000000000000000, 0.9238795325112867385, 1.000000000000000000, 0.9238795325112867385, 1.000000000000000000, 0.9238795325112867385, 1.000000000000000000, 0.9238795325112867385, 1.000000000000000000, 0.9238795325112867385, 1.000000000000000000, 0.9238795325112867385, 1.000000000000000000, 0.9238795325112867385, 1.000000000000000000, 0.9238795325112867385, 1.000000000000000000, 0.9238795325112867385, 1.000000000000000000, 0.9238795325112867385, 1.000000000000000000, 0.9238795325112867385, 1.000000000000000000, 0.9238795325112867385, 1.000000000000000000, 0.9238795325112867385, 1.000000000000000000, 0.9238795325112867385, 1.000000000000000000, 0.9238795325112867385, 1.000000000000000000, 0.9238795325112867385, 1.000000000000000000, 0.9238795325112867385, 1.000000000000000000, 0.9238795325112867385, 1.000000000000000000, 0.9238795325112867385, 1.000000000000000000, 0.9238795325112867385, 1.000000000000000000, 0.9238795325112867385, 1.000000000000000000, 0.9238795325112867385, 1.000000000000000000, 0.9238795325112867385, 1.000000000000000000, 0.9238795325112867385, 1.000000000000000000, 0.9238795325112867385, 1.000000000000000000, 0.9238795325112867385, 1.000000000000000000, 0.9238795325112867385, 1.000000000000000000, 0.9238795325112867385, 1.000000000000000000, 0.9238795325112867385, 1.000000000000000000, 0.9238795325112867385, 1.000000000000000000, 0.9238795325112867385, 1.000000000000000000, 0.9238795325112867385, 1.000000000000000000, 0.9238795325112867385, 1.000000000000000000, 0.9238795325112867385, 1.000000000000000000, 0.9238795325112867385, 1.000000000000000000, 0.9493988134329905959, 0.9660720450733824016, 0.9660720450733824016, 0.9660720450733824016),
 ( 1.000000000000000000, 0.9238795325112867385, 1.000000000000000000, 0.9238795325112867385, 1.000000000000000000, 0.9238795325112867385, 1.000000000000000000, 0.9238795325112867385, 1.000000000000000000, 0.9238795325112867385, 1.000000000000000000, 0.9238795325112867385, 1.000000000000000000, 0.9238795325112867385, 1.000000000000000000, 0.9238795325112867385, 1.000000000000000000, 0.9238795325112867385, 1.000000000000000000, 0.9238795325112867385, 1.000000000000000000, 0.9238795325112867385, 1.000000000000000000, 0.9238795325112867385, 1.000000000000000000, 0.9238795325112867385, 1.000000000000000000, 0.9238795325112867385, 1.000000000000000000, 0.9238795325112867385, 1.000000000000000000, 0.9238795325112867385, 1.000000000000000000, 0.9238795325112867385, 1.000000000000000000, 0.9238795325112867385, 1.000000000000000000, 0.9238795325112867385, 1.000000000000000000, 0.9238795325112867385, 1.000000000000000000, 0.9238795325112867385, 1.000000000000000000, 0.9238795325112867385, 1.000000000000000000, 0.9238795325112867385, 1.000000000000000000, 0.9238795325112867385, 1.000000000000000000, 0.9238795325112867385, 1.000000000000000000, 0.9238795325112867385, 1.000000000000000000, 0.9238795325112867385, 1.000000000000000000, 0.9238795325112867385, 1.000000000000000000, 0.9238795325112867385, 1.000000000000000000, 0.9238795325112867385, 1.000000000000000000, 0.9238795325112867385, 1.000000000000000000, 0.9238795325112867385, 1.000000000000000000, 0.9238795325112867385, 1.000000000000000000, 0.9238795325112867385, 1.000000000000000000, 0.9238795325112867385, 1.000000000000000000, 0.9238795325112867385, 1.000000000000000000, 0.9238795325112867385, 1.000000000000000000, 0.9238795325112867385, 1.000000000000000000, 0.9238795325112867385, 1.000000000000000000, 0.9238795325112867385, 1.000000000000000000, 0.9238795325112867385, 1.000000000000000000, 0.9238795325112867385, 1.000000000000000000, 0.9238795325112867385, 1.000000000000000000, 0.9238795325112867385, 1.000000000000000000, 0.9238795325112867385, 1.000000000000000000, 0.9238795325112867385, 1.000000000000000000, 0.9238795325112867385, 1.000000000000000000, 0.9238795325112867385, 1.000000000000000000, 0.9238795325112867385, 1.000000000000000000, 0.9238795325112867385, 1.000000000000000000, 0.9238795325112867385, 1.000000000000000000, 0.9238795325112867385, 1.000000000000000000, 0.9238795325112867385, 1.000000000000000000, 0.9238795325112867385, 1.000000000000000000, 0.9238795325112867385, 1.000000000000000000, 0.9238795325112867385, 1.000000000000000000, 0.9238795325112867385, 1.000000000000000000, 0.9238795325112867385, 1.000000000000000000, 0.9238795325112867385, 1.000000000000000000, 0.9238795325112867385, 1.000000000000000000, 0.9238795325112867385, 1.000000000000000000, 0.9238795325112867385, 1.000000000000000000, 0.9238795325112867385, 1.000000000000000000, 0.9238795325112867385, 1.000000000000000000, 0.9238795325112867385, 1.000000000000000000, 0.9238795325112867385, 1.000000000000000000, 0.9238795325112867385, 1.000000000000000000, 0.9238795325112867385, 1.000000000000000000, 0.9238795325112867385, 1.000000000000000000, 0.9238795325112867385, 1.000000000000000000, 0.9238795325112867385, 1.000000000000000000, 0.9238795325112867385, 1.000000000000000000, 0.9238795325112867385, 1.000000000000000000, 0.9238795325112867385, 1.000000000000000000, 0.9238795325112867385, 1.000000000000000000, 0.9238795325112867385, 1.000000000000000000, 0.9238795325112867385, 1.000000000000000000, 0.9238795325112867385, 1.000000000000000000, 0.9238795325112867385, 1.000000000000000000, 0.9238795325112867385, 1.000000000000000000, 0.9238795325112867385, 1.000000000000000000, 0.9238795325112867385, 1.000000000000000000, 0.9238795325112867385, 1.000000000000000000, 0.9238795325112867385, 1.000000000000000000, 0.9238795325112867385, 1.000000000000000000, 0.9238795325112867385, 1.000000000000000000, 0.9238795325112867385, 1.000000000000000000, 0.9238795325112867385, 1.000000000000000000, 0.9238795325112867385, 1.000000000000000000, 0.9238795325112867385, 1.000000000000000000, 0.9238795325112867385, 1.000000000000000000, 0.9238795325112867385, 1.000000000000000000, 0.9238795325112867385, 1.000000000000000000, 0.9238795325112867385, 1.000000000000000000, 0.9238795325112867385, 1.000000000000000000, 0.9238795325112867385, 1.000000000000000000, 0.9238795325112867385, 1.000000000000000000, 0.9238795325112867385, 1.000000000000000000, 0.9238795325112867385, 1.000000000000000000, 0.9238795325112867385, 1.000000000000000000, 0.9238795325112867385, 1.000000000000000000, 0.9238795325112867385, 1.000000000000000000, 0.9238795325112867385, 1.000000000000000000, 0.9238795325112867385, 1.000000000000000000, 0.9238795325112867385, 1.000000000000000000, 0.9238795325112867385, 1.000000000000000000, 0.9238795325112867385, 1.000000000000000000, 0.9238795325112867385, 1.000000000000000000, 0.9238795325112867385, 1.000000000000000000, 0.9238795325112867385, 1.000000000000000000, 0.9238795325112867385, 1.000000000000000000, 0.9238795325112867385, 1.000000000000000000, 0.9238795325112867385, 1.000000000000000000, 0.9238795325112867385, 1.000000000000000000, 0.9238795325112867385, 1.000000000000000000, 0.9238795325112867385, 1.000000000000000000, 0.9238795325112867385, 1.000000000000000000, 0.9238795325112867385, 1.000000000000000000, 0.9238795325112867385, 1.000000000000000000, 0.9238795325112867385, 1.000000000000000000, 0.9238795325112867385, 1.000000000000000000, 0.9238795325112867385, 1.000000000000000000, 0.9238795325112867385, 1.000000000000000000, 0.9238795325112867385, 1.000000000000000000, 0.9238795325112867385, 1.000000000000000000, 0.9238795325112867385, 1.000000000000000000, 0.9238795325112867385, 1.000000000000000000, 0.9238795325112867385, 1.000000000000000000, 0.9238795325112867385, 1.000000000000000000, 0.9238795325112867385, 1.000000000000000000, 0.9238795325112867385, 1.000000000000000000, 0.9238795325112867385, 1.000000000000000000, 0.9238795325112867385, 1.000000000000000000, 0.9238795325112867385, 1.000000000000000000, 0.9238795325112867385, 1.000000000000000000, 0.9238795325112867385, 1.000000000000000000, 0.9238795325112867385, 1.000000000000000000, 0.9238795325112867385, 1.000000000000000000, 0.9238795325112867385, 1.000000000000000000, 0.9238795325112867385, 1.000000000000000000, 0.9238795325112867385, 1.000000000000000000, 0.9238795325112867385, 1.000000000000000000, 0.9238795325112867385, 1.000000000000000000, 0.9238795325112867385, 1.000000000000000000, 0.9238795325112867385, 1.000000000000000000, 0.9238795325112867385, 1.000000000000000000, 0.9238795325112867385, 1.000000000000000000, 0.9238795325112867385, 1.000000000000000000, 0.9238795325112867385, 1.000000000000000000, 0.9238795325112867385, 1.000000000000000000, 0.9238795325112867385, 1.000000000000000000, 0.9238795325112867385, 1.000000000000000000, 0.9238795325112867385, 1.000000000000000000, 0.9238795325112867385, 1.000000000000000000, 0.9238795325112867385, 1.000000000000000000, 0.9238795325112867385, 1.000000000000000000, 0.9238795325112867385, 1.000000000000000000, 0.9238795325112867385, 1.000000000000000000, 0.9238795325112867385, 1.000000000000000000, 0.9238795325112867385, 1.000000000000000000, 0.9238795325112867385, 1.000000000000000000, 0.9238795325112867385, 1.000000000000000000, 0.9238795325112867385, 1.000000000000000000, 0.9238795325112867385, 1.000000000000000000, 0.9238795325112867385, 1.000000000000000000, 0.9238795325112867385, 1.000000000000000000, 0.9238795325112867385, 1.000000000000000000, 0.9238795325112867385, 1.000000000000000000, 0.9238795325112867385, 1.000000000000000000, 0.9238795325112867385, 1.000000000000000000, 0.9238795325112867385, 1.000000000000000000, 0.9238795325112867385, 1.000000000000000000, 0.9238795325112867385, 1.000000000000000000, 0.9238795325112867385, 1.000000000000000000, 0.9238795325112867385, 1.000000000000000000, 0.9238795325112867385, 1.000000000000000000, 0.9238795325112867385, 1.000000000000000000, 0.9238795325112867385, 1.000000000000000000, 0.9238795325112867385, 1.000000000000000000, 0.9238795325112867385, 1.000000000000000000, 0.9238795325112867385, 1.000000000000000000, 0.9238795325112867385, 1.000000000000000000, 0.9238795325112867385, 1.000000000000000000, 0.9238795325112867385, 1.000000000000000000, 0.9238795325112867385, 1.000000000000000000, 0.9238795325112867385, 1.000000000000000000, 0.9493988134329905959, 0.9660720450733824016, 0.9660720450733824016, 0.9660720450733824016) ) ) 
 REPRESENTATION_ITEM ( '' )  SURFACE ( )  );
#53149 = CARTESIAN_POINT ( 'NONE',  ( 7.204075437095966983, 7.204075437095967871, 112.4687500020483810 ) ) ;
#53150 = CARTESIAN_POINT ( 'NONE',  ( -11.35316468749999785, 193.0729166632526415, -3.042071309553167513 ) ) ;
#53151 = EDGE_LOOP ( 'NONE', ( #70429, #1523, #5585, #25421 ) ) ;
#53152 = CARTESIAN_POINT ( 'NONE',  ( 2.620431783929131786, 65.99617417813951192, 26.42108291244571561 ) ) ;
#53153 = CARTESIAN_POINT ( 'NONE',  ( -6.238412754330611322E-16, 10.18810118749999916, 67.28125000204838102 ) ) ;
#53154 = CARTESIAN_POINT ( 'NONE',  ( 10.00000000000000000, 161.6666666598386826, 2.679491924311235618 ) ) ;
#53156 = CARTESIAN_POINT ( 'NONE',  ( 3.042071309553159519, 174.7395833299193555, 11.35316468750000141 ) ) ;
#53155 = DIRECTION ( 'NONE',  ( -0.000000000000000000, -1.000000000000000000, -0.000000000000000000 ) ) ;
#53157 = FACE_OUTER_BOUND ( 'NONE', #32772, .T. ) ;
#53158 = CARTESIAN_POINT ( 'NONE',  ( -2.679491924311228512, 247.0833333401613174, -9.999999999999998224 ) ) ;
#53159 = CARTESIAN_POINT ( 'NONE',  ( -2.679491924311078410, 188.3333333265053682, -10.00000000000008527 ) ) ;
#53160 = ORIENTED_EDGE ( 'NONE', *, *, #50364, .F. ) ;
#53161 = CARTESIAN_POINT ( 'NONE',  ( -5.676582343750006032, 174.4270833299193555, 9.832129032723418760 ) ) ;
#53162=STYLED_ITEM('',(#74692),#18038);
#53163 = PLANE ( 'NONE',  #25500 ) ;
#53164 = CARTESIAN_POINT ( 'NONE',  ( 3.594042629939374400, 89.53052393364181683, -6.225082831242716885 ) ) ;
#53165 = AXIS2_PLACEMENT_3D ( 'NONE', #19321, #46893, #69917 ) ;
#53166 = ORIENTED_EDGE ( 'NONE', *, *, #12611, .T. ) ;
#53167 = ADVANCED_FACE ( 'NONE', ( #9673 ), #4380, .F. ) ;
#53168 = CARTESIAN_POINT ( 'NONE',  ( 1.469576158976823947E-15, 101.5625000040967763, 8.000000000000000000 ) ) ;
#53169 = CARTESIAN_POINT ( 'NONE',  ( -2.828427124746192067, 12.62500000000000000, 2.828427124746190735 ) ) ;
#53170 = CARTESIAN_POINT ( 'NONE',  ( 0.000000000000000000, -7.999999999999991118, 29.33030277982336642 ) ) ;
#53171 = CARTESIAN_POINT ( 'NONE',  ( 1.881053915767122664, 10.12499999863440792, 4.541265875000001451 ) ) ;
#53172 = CARTESIAN_POINT ( 'NONE',  ( -5.656854249492373476, -5.656854249492376141, 17.70530278392014623 ) ) ;
#53173 = CARTESIAN_POINT ( 'NONE',  ( -4.000000000000015987, 195.5000000000000000, 142.0000000000000568 ) ) ;
#53174 = AXIS2_PLACEMENT_3D ( 'NONE', #4168, #4533, #21864 ) ;
#53176 = VERTEX_POINT ( 'NONE', #66624 ) ;
#53175 = EDGE_CURVE ( 'NONE', #39873, #9385, #15303, .T. ) ;
#53177 = CARTESIAN_POINT ( 'NONE',  ( -7.188101187500001821, 95.56250000204838102, -2.977408999572650483 ) ) ;
#53179 = CARTESIAN_POINT ( 'NONE',  ( 1.656854249492381914, 13.56249999726881406, 4.000000000000000888 ) ) ;
#53178 = CARTESIAN_POINT ( 'NONE',  ( 2.828427124746152987, 204.2500000027312126, 139.1715728752538723 ) ) ;
#53180 = ORIENTED_EDGE ( 'NONE', *, *, #39622, .F. ) ;
#53181 = EDGE_CURVE ( 'NONE', #7770, #59197, #23287, .T. ) ;
#53182 = CARTESIAN_POINT ( 'NONE',  ( 2.069125466538726865, 10.11940336925073503, -70.25556669587955128 ) ) ;
#53183 = DIRECTION ( 'NONE',  ( -1.000000000000000000, -0.000000000000000000, 0.000000000000000000 ) ) ;
#53184 = CARTESIAN_POINT ( 'NONE',  ( -7.188101187499992051, 0.000000000000000000, 25.48655278187175810 ) ) ;
#53185 = ORIENTED_EDGE ( 'NONE', *, *, #37814, .T. ) ;
#53186 = ORIENTED_EDGE ( 'NONE', *, *, #17273, .F. ) ;
#53187 = CARTESIAN_POINT ( 'NONE',  ( 7.204075437095968759, -7.204075437095966983, 89.21875000204838102 ) ) ;
#53188 = UNCERTAINTY_MEASURE_WITH_UNIT (LENGTH_MEASURE( 1.000000000000000082E-05 ), #50570, 'distance_accuracy_value', 'NONE');
#53189 = CARTESIAN_POINT ( 'NONE',  ( -27.99999999999996092, 195.1875000013655779, 173.4587341250003760 ) ) ;
#53190 = CARTESIAN_POINT ( 'NONE',  ( 7.778174593052021635, 7.778174593052023411, 100.9374999999999858 ) ) ;
#53193 = CARTESIAN_POINT ( 'NONE',  ( 2.765530957081996366, 297.2968750017070079, -6.676582343750002480 ) ) ;
#53192 = CARTESIAN_POINT ( 'NONE',  ( 30.82842712474620939, 201.2500000027312126, 172.8284271247460424 ) ) ;
#53191 = CARTESIAN_POINT ( 'NONE',  ( 2.775557561562891351E-14, -70.00000000000000000, 151.0000000000000284 ) ) ;
#53194 = CARTESIAN_POINT ( 'NONE',  ( -4.999999999999998224, 131.6666666666666856, -8.660254037844389075 ) ) ;
#53195 = CARTESIAN_POINT ( 'NONE',  ( 10.99999999999986855, 4.556349186104178273, 105.5312500040967763 ) ) ;
#53196 =( GEOMETRIC_REPRESENTATION_CONTEXT ( 3 ) GLOBAL_UNCERTAINTY_ASSIGNED_CONTEXT ( ( #845 ) ) GLOBAL_UNIT_ASSIGNED_CONTEXT ( ( #3126, #9154, #25369 ) ) REPRESENTATION_CONTEXT ( 'NONE', 'WORKASPACE' ) );
#53197 = CARTESIAN_POINT ( 'NONE',  ( 1.320432766682872962E-15, -7.188101187499992051, 2.236552781871754103 ) ) ;
#53198 = EDGE_CURVE ( 'NONE', #15239, #52491, #15680, .T. ) ;
#53199 = CARTESIAN_POINT ( 'NONE',  ( 3.313708498984756279, 7.999999999999991118, 15.36155277982336642 ) ) ;
#53200 = CARTESIAN_POINT ( 'NONE',  ( 30.44569435410883429, 201.8125000013656063, 167.5543056458911053 ) ) ;
#53201 = CARTESIAN_POINT ( 'NONE',  ( 5.082755093536324154, 3.656249997951610542, 5.082755093536326818 ) ) ;
#53202 = AXIS2_PLACEMENT_3D ( 'NONE', #62464, #22099, #45862 ) ;
#53203 = CARTESIAN_POINT ( 'NONE',  ( -3.317071493978880348, -8.008118988124989457, 1.294365283940630107 ) ) ;
#53204 = CARTESIAN_POINT ( 'NONE',  ( 1.432654583217607192, 197.2500000013656063, 145.4587341250000634 ) ) ;
#53205 = CARTESIAN_POINT ( 'NONE',  ( -7.188101187500000044, 117.0312500020483810, 0.000000000000000000 ) ) ;
#53206 = CARTESIAN_POINT ( 'NONE',  ( 4.898587196589412829E-16, 3.187499995903220640, -8.000000000000000000 ) ) ;
#53207 = CARTESIAN_POINT ( 'NONE',  ( 8.311093377946839666, 226.0937500034140157, 8.311093377946829008 ) ) ;
#53208 = CARTESIAN_POINT ( 'NONE',  ( -25.17157287525382614, 207.8750000000000284, 167.1715728752541565 ) ) ;
#53209 = CARTESIAN_POINT ( 'NONE',  ( -7.188101187499992051, 0.000000000000000000, 22.86155278187175455 ) ) ;
#53210 = DIRECTION ( 'NONE',  ( 0.000000000000000000, 0.000000000000000000, 1.000000000000000000 ) ) ;
#53211 = CARTESIAN_POINT ( 'NONE',  ( 6.951808397369818766E-16, 27.03124999658601979, -11.35316468750000141 ) ) ;
#53212 = CARTESIAN_POINT ( 'NONE',  ( -3.313708498984765161, 10.03125000000000178, 7.999999999999998224 ) ) ;
#53213 = CARTESIAN_POINT ( 'NONE',  ( -2.085542519210945728E-15, 219.8437499965860411, 11.35316468750000141 ) ) ;
#53214 = CARTESIAN_POINT ( 'NONE',  ( 8.000000000000000000, 112.3437499999999858, -3.313708498984762496 ) ) ;
#53215 = CARTESIAN_POINT ( 'NONE',  ( -1.469576158976823947E-15, 24.93749999590322375, 8.000000000000000000 ) ) ;
#53216 = AXIS2_PLACEMENT_3D ( 'NONE', #21005, #38755, #15339 ) ;
#53217 = ORIENTED_EDGE ( 'NONE', *, *, #17399, .T. ) ;
#53218 = CARTESIAN_POINT ( 'NONE',  ( 0.000000000000000000, 0.000000000000000000, 0.000000000000000000 ) ) ;
#53219 = EDGE_CURVE ( 'NONE', #23868, #71352, #44656, .T. ) ;
#53220 = CARTESIAN_POINT ( 'NONE',  ( 2.445694354108784108, 197.5625000013656063, 144.4456943541088663 ) ) ;
#53221 = CARTESIAN_POINT ( 'NONE',  ( -3.042071309553164404, 37.23958332991934839, -11.35316468749999963 ) ) ;
#53222 = CARTESIAN_POINT ( 'NONE',  ( -4.556349186104047710, -10.99999999999999822, 88.46875000409677625 ) ) ;
#53223 = CARTESIAN_POINT ( 'NONE',  ( 1.432654583217608080, 206.8750000013656347, 138.5412658750000503 ) ) ;
#53224 = DIRECTION ( 'NONE',  ( 0.8660254037844379305, -0.5000000000000012212, 0.000000000000000000 ) ) ;
#53225 = CARTESIAN_POINT ( 'NONE',  ( -1.469576158976823947E-15, 2.625000000000000444, 8.000000000000000000 ) ) ;
#53227 = CARTESIAN_POINT ( 'NONE',  ( -11.35316468749999785, 13.07291666325268409, -3.042071309553167957 ) ) ;
#53226 = CARTESIAN_POINT ( 'NONE',  ( -5.082755093536324154, 103.3437500020483668, 5.082755093536326818 ) ) ;
#53228 = CARTESIAN_POINT ( 'NONE',  ( 5.656854249492376141, -5.656854249492374365, 16.39280277982336287 ) ) ;
#53229 = CARTESIAN_POINT ( 'NONE',  ( -3.042071309553164404, 152.2395833299193271, -11.35316468749999963 ) ) ;
#53230 = CARTESIAN_POINT ( 'NONE',  ( -10.00000000000000000, 114.1666666598386968, -2.679491924311229845 ) ) ;
#53231 = ADVANCED_FACE ( 'NONE', ( #2885 ), #25873, .F. ) ;
#53232 = CARTESIAN_POINT ( 'NONE',  ( 1.320432766682874540E-15, 114.4062500020483810, 7.188101187500000044 ) ) ;
#53233 = DIRECTION ( 'NONE',  ( 1.000000000000000000, 0.000000000000000000, 0.000000000000000000 ) ) ;
#53234 = CARTESIAN_POINT ( 'NONE',  ( -31.45873412499998523, 204.0000000013656347, 171.4326545832180386 ) ) ;
#53235 = VERTEX_POINT ( 'NONE', #14558 ) ;
#53236 = CARTESIAN_POINT ( 'NONE',  ( 3.042071309553167513, 12.13541666325268231, -11.35316468749999785 ) ) ;
#53237 = ORIENTED_EDGE ( 'NONE', *, *, #67089, .T. ) ;
#53238 = LINE ( 'NONE', #52131, #43775 ) ;
#53240 = CARTESIAN_POINT ( 'NONE',  ( 3.042071309553167513, 136.8229166632526699, -11.35316468749999785 ) ) ;
#53239 = CARTESIAN_POINT ( 'NONE',  ( -4.898587196589412829E-16, 108.1250000000000000, -8.000000000000000000 ) ) ;
#53241 = CARTESIAN_POINT ( 'NONE',  ( 0.000000000000000000, 300.0000000000000000, 0.000000000000000000 ) ) ;
#53242 = CARTESIAN_POINT ( 'NONE',  ( -4.898587196589407898E-16, 7.999999999999991118, 18.51155278432982243 ) ) ;
#53243 =( BOUNDED_CURVE ( )  B_SPLINE_CURVE ( 2, ( #12408, #25198, #48211, #30137, #63719, #19539, #19175, #1487, #70499 ),
 .UNSPECIFIED., .F., .F. ) 
 B_SPLINE_CURVE_WITH_KNOTS ( ( 3, 2, 2, 2, 3 ),
 ( 0.6666666666666672958, 0.6750000000000007105, 0.6833333333333340143, 0.6916666666666673180, 0.7000000000000006217 ),
 .UNSPECIFIED. ) 
 CURVE ( )  GEOMETRIC_REPRESENTATION_ITEM ( )  RATIONAL_B_SPLINE_CURVE ( ( 0.9999999999999938938, 0.9238795325112928447, 1.000000000000000000, 0.9238795325112867385, 1.000000000000000000, 0.9238795325112867385, 1.000000000000000000, 0.9238795325112806323, 1.000000000000005995 ) ) 
 REPRESENTATION_ITEM ( '' )  );
#53244 = AXIS2_PLACEMENT_3D ( 'NONE', #48557, #47454, #2553 ) ;
#53245 = CARTESIAN_POINT ( 'NONE',  ( 49.59292767147987746, 197.7804099379733032, 58.14609736359237502 ) ) ;
#53246 = CARTESIAN_POINT ( 'NONE',  ( -8.311093377946836114, 248.2812500034139873, -8.311093377946836114 ) ) ;
#53247 = CARTESIAN_POINT ( 'NONE',  ( 10.18810118749999916, 4.220049686691935698, 89.87500000204836681 ) ) ;
#53248 = ORIENTED_EDGE ( 'NONE', *, *, #46367, .F. ) ;
#53249 = CARTESIAN_POINT ( 'NONE',  ( 4.999999999999999112, 14.31098243164692008, 69.87317657433686691 ) ) ;
#53250 = DIRECTION ( 'NONE',  ( -0.000000000000000000, 1.000000000000000000, -0.000000000000000000 ) ) ;
#53251 = CARTESIAN_POINT ( 'NONE',  ( -11.35316468750000141, 88.59374999658602690, -1.390361679473963753E-15 ) ) ;
#53252 = CARTESIAN_POINT ( 'NONE',  ( -4.220049686691937474, -10.18810118749999738, 100.9375000020483810 ) ) ;
#53253 = CARTESIAN_POINT ( 'NONE',  ( -1.881053915767124440, 18.12499999863441147, 4.541265875000001451 ) ) ;
#53254 = VERTEX_POINT ( 'NONE', #20596 ) ;
#53255 = ORIENTED_EDGE ( 'NONE', *, *, #17743, .F. ) ;
#53256 = CARTESIAN_POINT ( 'NONE',  ( 4.898587196589412829E-16, 3.375000000000000444, -8.000000000000000000 ) ) ;
#53257 = CARTESIAN_POINT ( 'NONE',  ( -9.000000000000000000, -5.196152422706644458, -10.20000000000000284 ) ) ;
#53258 = CARTESIAN_POINT ( 'NONE',  ( -2.977408999572650039, 0.9374999979516102089, -7.188101187500001821 ) ) ;
#53259 = CARTESIAN_POINT ( 'NONE',  ( -7.778174593052023411, 7.778174593052023411, 96.81250000000000000 ) ) ;
#53260 =( BOUNDED_CURVE ( )  B_SPLINE_CURVE ( 2, ( #35523, #62774, #16372, #4341, #68083, #51464, #16012, #21304, #50719 ),
 .UNSPECIFIED., .F., .F. ) 
 B_SPLINE_CURVE_WITH_KNOTS ( ( 3, 2, 2, 2, 3 ),
 ( 0.6249999999999998890, 0.6319444444444443088, 0.6388888888888888395, 0.6458333333333333703, 0.6527777777777777901 ),
 .UNSPECIFIED. ) 
 CURVE ( )  GEOMETRIC_REPRESENTATION_ITEM ( )  RATIONAL_B_SPLINE_CURVE ( ( 1.000000000000001110, 0.9238795325112855172, 1.000000000000000000, 0.9238795325112867385, 1.000000000000000000, 0.9238795325112867385, 1.000000000000000000, 0.9238795325112867385, 1.000000000000000000 ) ) 
 REPRESENTATION_ITEM ( '' )  );
#53261 = CARTESIAN_POINT ( 'NONE',  ( 4.220049686691934809, 10.18810118749999916, 100.5625000020483668 ) ) ;
#53262 = AXIS2_PLACEMENT_3D ( 'NONE', #70118, #6739, #41067 ) ;
#53263 = EDGE_CURVE ( 'NONE', #31201, #20088, #68588, .T. ) ;
#53264 = CARTESIAN_POINT ( 'NONE',  ( -8.000000000000001776, 6.843750000000000888, 3.313708498984759387 ) ) ;
#53265 = CARTESIAN_POINT ( 'NONE',  ( -1.656854249492383691, 15.43749999726881583, 4.000000000000000888 ) ) ;
#53266 = CARTESIAN_POINT ( 'NONE',  ( -4.541265875000003227, 0.8749999986344068059, 1.881053915767121110 ) ) ;
#53267 = VERTEX_POINT ( 'NONE', #39449 ) ;
#53268 = CARTESIAN_POINT ( 'NONE',  ( 2.445694354108783664, 208.3125000013656063, 144.4456943541088663 ) ) ;
#53269 = CARTESIAN_POINT ( 'NONE',  ( -3.458734124999959914, 200.3750000013656063, 196.5673454167823877 ) ) ;
#53271 = CARTESIAN_POINT ( 'NONE',  ( -10.00000000000033040, 22.29166666666685970, -2.679491924311318662 ) ) ;
#53270 = CARTESIAN_POINT ( 'NONE',  ( -30.44569435410886982, 200.5625000013656063, 167.5543056458916169 ) ) ;
#53272 = EDGE_CURVE ( 'NONE', #24907, #20010, #64923, .T. ) ;
#53273 = CARTESIAN_POINT ( 'NONE',  ( 3.211159895383561835, 15.43749999863440614, -3.211159895383561835 ) ) ;
#53274 = AXIS2_PLACEMENT_3D ( 'NONE', #3178, #43910, #20136 ) ;
#53276 = CARTESIAN_POINT ( 'NONE',  ( 2.449293598294707893E-16, 12.25000000000000000, -4.000000000000001776 ) ) ;
#53275 =( BOUNDED_CURVE ( )  B_SPLINE_CURVE ( 2, ( #52697, #18362, #23274, #70052, #41740, #57625, #5938, #64387, #35361 ),
 .UNSPECIFIED., .F., .F. ) 
 B_SPLINE_CURVE_WITH_KNOTS ( ( 3, 2, 2, 2, 3 ),
 ( 0.07894736842105269659, 0.08552631578947372804, 0.09210526315789474561, 0.09868421052631579093, 0.1052631578947368085 ),
 .UNSPECIFIED. ) 
 CURVE ( )  GEOMETRIC_REPRESENTATION_ITEM ( )  RATIONAL_B_SPLINE_CURVE ( ( 0.9999999999999992228, 0.9238795325112875156, 1.000000000000000000, 0.9238795325112867385, 1.000000000000000000, 0.9238795325112867385, 1.000000000000000000, 0.9238795325112870716, 0.9999999999999996669 ) ) 
 REPRESENTATION_ITEM ( '' )  );
#53277 = CARTESIAN_POINT ( 'NONE',  ( -2.977408999572647819, 7.188101187499991163, 11.70530278187175099 ) ) ;
#53278 = ORIENTED_EDGE ( 'NONE', *, *, #12056, .F. ) ;
#53279 = ORIENTED_EDGE ( 'NONE', *, *, #58983, .T. ) ;
#53280 = CARTESIAN_POINT ( 'NONE',  ( 7.204075437095968759, -7.204075437095966983, 104.2187500020483810 ) ) ;
#53281 = CARTESIAN_POINT ( 'NONE',  ( -2.726571689596997292E-14, 210.0000000000000284, 138.0000000000000568 ) ) ;
#53282 = CARTESIAN_POINT ( 'NONE',  ( -25.17157287525377640, 204.6250000000000284, 172.8284271247465256 ) ) ;
#53283 = CARTESIAN_POINT ( 'NONE',  ( -2.445694354108782775, 194.5625000013656063, 200.4456943541088663 ) ) ;
#53284 = CARTESIAN_POINT ( 'NONE',  ( 0.000000000000000000, 220.0000000000000284, 0.000000000000000000 ) ) ;
#53285 = CARTESIAN_POINT ( 'NONE',  ( -4.999999999999998224, 96.66666666666668561, -8.660254037844389075 ) ) ;
#53286 = VECTOR ( 'NONE', #60739, 1000.000000000000000 ) ;
#53287 = CARTESIAN_POINT ( 'NONE',  ( 1.469576158976823947E-15, 120.8750000000000000, 8.000000000000000000 ) ) ;
#53288 = CARTESIAN_POINT ( 'NONE',  ( 2.765530957082001251, 296.9218750017069510, 6.676582343750000703 ) ) ;
#53289 = ORIENTED_EDGE ( 'NONE', *, *, #3124, .F. ) ;
#53290 = AXIS2_PLACEMENT_3D ( 'NONE', #36439, #13035, #47005 ) ;
#53291 = CARTESIAN_POINT ( 'NONE',  ( 11.00000000000000000, 1.347111479062088405E-15, 73.74999999999998579 ) ) ;
#53292 = EDGE_CURVE ( 'NONE', #42724, #66327, #64922, .T. ) ;
#53293 = CARTESIAN_POINT ( 'NONE',  ( -3.313708498984760720, 15.28124999590322197, -8.000000000000000000 ) ) ;
#53294 = CARTESIAN_POINT ( 'NONE',  ( 2.445694354108783664, 209.3125000013656063, 144.4456943541088663 ) ) ;
#53295 = CARTESIAN_POINT ( 'NONE',  ( -5.000000000000000000, -60.11723469343116477, 46.25570701698070764 ) ) ;
#53296 = DIRECTION ( 'NONE',  ( 1.000000000000000000, 0.000000000000000000, 0.000000000000000000 ) ) ;
#53297 = CARTESIAN_POINT ( 'NONE',  ( 8.660254037844385522, 227.9166666666666856, -5.000000000000003553 ) ) ;
#53298 = CARTESIAN_POINT ( 'NONE',  ( 10.99999999999995026, -4.556349186104096560, 91.84375000409677625 ) ) ;
#53299 = CARTESIAN_POINT ( 'NONE',  ( -7.204075437095965206, -7.204075437095968759, 68.21875000204836681 ) ) ;
#53300 = CARTESIAN_POINT ( 'NONE',  ( 6.123233995736767268E-16, 216.2500000000000284, -10.00000000000000178 ) ) ;
#53301 = EDGE_CURVE ( 'NONE', #4298, #3, #35840, .T. ) ;
#53302 = CARTESIAN_POINT ( 'NONE',  ( 7.188101187499992051, 2.977408999572647819, 11.70530278187175632 ) ) ;
#53303 = CARTESIAN_POINT ( 'NONE',  ( 5.676582343749993598, 175.2604166632526699, 9.832129032723422313 ) ) ;
#53304 = CARTESIAN_POINT ( 'NONE',  ( 4.541265875000001451, 2.249999998634407028, 1.881053915767124440 ) ) ;
#53305 = DIRECTION ( 'NONE',  ( -0.000000000000000000, 1.000000000000000000, 4.476705744456276341E-16 ) ) ;
#53307 = DIRECTION ( 'NONE',  ( 7.885106708985487801E-17, -1.000000000000000000, 0.000000000000000000 ) ) ;
#53306 = CARTESIAN_POINT ( 'NONE',  ( -28.00000000000001776, 194.5625000013656063, 166.5412658750003629 ) ) ;
#53308 = ORIENTED_EDGE ( 'NONE', *, *, #4299, .F. ) ;
#53309 = CARTESIAN_POINT ( 'NONE',  ( 1.432654583217607858, 194.6250000013655779, 138.5412658750000787 ) ) ;
#53310 = CARTESIAN_POINT ( 'NONE',  ( 8.311093377946837890, 51.71874999658601979, -8.311093377946837890 ) ) ;
#53311 = CARTESIAN_POINT ( 'NONE',  ( -7.778174593052023411, 7.778174593052023411, 107.5000000040967763 ) ) ;
#53312 = CARTESIAN_POINT ( 'NONE',  ( -3.042071309553173730, 214.6354166632526983, 11.35316468749999785 ) ) ;
#53313 = CARTESIAN_POINT ( 'NONE',  ( -31.45873412499996391, 204.7500000013655779, 171.4326545832181239 ) ) ;
#53314 = CARTESIAN_POINT ( 'NONE',  ( -10.00000000000000355, 124.5833333265053682, 2.679491924311223183 ) ) ;
#53316 = LINE ( 'NONE', #1640, #46285 ) ;
#53315 = CARTESIAN_POINT ( 'NONE',  ( -4.401442555609581635E-16, 123.7812500020483810, -7.188101187500000044 ) ) ;
#53317 = CARTESIAN_POINT ( 'NONE',  ( 2.445694354108782775, 195.5625000013656063, 139.5543056458912190 ) ) ;
#53318 = CARTESIAN_POINT ( 'NONE',  ( 7.320508075688771044, 76.24999999317203958, 7.320508075688775484 ) ) ;
#53319 = CARTESIAN_POINT ( 'NONE',  ( -2.977408999572651815, 98.93750000204838102, 7.188101187500000933 ) ) ;
#53320 = CARTESIAN_POINT ( 'NONE',  ( -3.211159895383562723, 16.06249999863440436, 3.211159895383561391 ) ) ;
#53321 = CARTESIAN_POINT ( 'NONE',  ( -5.000000000000007994, 73.33333333333332860, 8.660254037844390851 ) ) ;
#53322 = CARTESIAN_POINT ( 'NONE',  ( 4.519822870821364802, 0.3270240920704938770, -6.395220799012816038 ) ) ;
#53323 = VERTEX_POINT ( 'NONE', #40014 ) ;
#53325 = EDGE_CURVE ( 'NONE', #5560, #74626, #52376, .T. ) ;
#53324 = ORIENTED_EDGE ( 'NONE', *, *, #56083, .T. ) ;
#53326 = CARTESIAN_POINT ( 'NONE',  ( -2.765530957081998586, 298.7968750017069510, 6.676582343750001591 ) ) ;
#53327 = CARTESIAN_POINT ( 'NONE',  ( -1.656854249492287101, 195.4375000027312126, 137.9999999999998863 ) ) ;
#53328 = CARTESIAN_POINT ( 'NONE',  ( 5.676582343750001591, 151.6145833299193555, -9.832129032723420536 ) ) ;
#53329 = CARTESIAN_POINT ( 'NONE',  ( -3.313708498984757611, 7.999999999999991118, 9.549052779823364645 ) ) ;
#53330 = CARTESIAN_POINT ( 'NONE',  ( 2.828427124746208943, 201.6250000000000284, 195.1715728752538439 ) ) ;
#53331 = CARTESIAN_POINT ( 'NONE',  ( -7.470240680701166980, 16.47166422291241616, -0.04683108270947877738 ) ) ;
#53332 = CARTESIAN_POINT ( 'NONE',  ( -10.18810118749999738, -4.220049686691941915, 107.1250000020483810 ) ) ;
#53333 = ORIENTED_EDGE ( 'NONE', *, *, #46210, .F. ) ;
#53334 = CARTESIAN_POINT ( 'NONE',  ( 2.751064625579944321E-14, 201.8750000027312126, 194.0000000000000568 ) ) ;
#53335 = PLANE ( 'NONE',  #30448 ) ;
#53336 = CARTESIAN_POINT ( 'NONE',  ( 9.832129032723420536, 136.5104166632526983, -5.676582343749999815 ) ) ;
#53337 = CARTESIAN_POINT ( 'NONE',  ( 3.458734125000015425, 199.0000000013656063, 196.5673454167823877 ) ) ;
#53338 = CARTESIAN_POINT ( 'NONE',  ( 0.000000000000000000, 0.000000000000000000, 118.0000000000000000 ) ) ;
#53339 = CARTESIAN_POINT ( 'NONE',  ( -6.238412754330611322E-16, 10.18810118749999916, 69.15625000204836681 ) ) ;
#53340 = CARTESIAN_POINT ( 'NONE',  ( -8.311093377946841443, 54.21874999658601979, 8.311093377946830785 ) ) ;
#53341 = VERTEX_POINT ( 'NONE', #63016 ) ;
#53342 = CARTESIAN_POINT ( 'NONE',  ( -7.999999999999991118, 0.000000000000000000, 12.83030277982336465 ) ) ;
#53343 = CARTESIAN_POINT ( 'NONE',  ( -3.211159895383561391, 5.812499998634407028, -3.211159895383561835 ) ) ;
#53344 = CARTESIAN_POINT ( 'NONE',  ( 3.317071493978883456, -8.008118988124989457, 11.98186528394062655 ) ) ;
#53345 = ADVANCED_FACE ( 'NONE', ( #30905 ), #13904, .F. ) ;
#53346 = VECTOR ( 'NONE', #28004, 1000.000000000000000 ) ;
#53347 = CARTESIAN_POINT ( 'NONE',  ( -7.188101187500002709, 14.81249999795161543, 2.977408999572649151 ) ) ;
#53348 = CARTESIAN_POINT ( 'NONE',  ( -3.673940397442060854E-16, 290.8125000034140157, -6.000000000000001776 ) ) ;
#53349 = CARTESIAN_POINT ( 'NONE',  ( 1.224646799147353454E-15, 300.0000000000000000, -10.00000000000000178 ) ) ;
#53350 = CARTESIAN_POINT ( 'NONE',  ( 2.977408999572650927, 14.62499999795161010, -7.188101187500001821 ) ) ;
#53351 = CARTESIAN_POINT ( 'NONE',  ( -5.082755093536319713, 5.082755093536319713, 8.799052781871752771 ) ) ;
#53352 = ADVANCED_FACE ( 'NONE', ( #71256 ), #7536, .F. ) ;
#53353 = CARTESIAN_POINT ( 'NONE',  ( -10.18810118749999738, -4.220049686691941915, 70.75000000204836681 ) ) ;
#53354 =( BOUNDED_CURVE ( )  B_SPLINE_CURVE ( 2, ( #70490, #65181, #13124, #20265, #43290, #24817, #66304, #36160, #42907, #54256, #18808, #64823, #14611 ),
 .UNSPECIFIED., .F., .F. ) 
 B_SPLINE_CURVE_WITH_KNOTS ( ( 3, 2, 2, 2, 2, 2, 3 ),
 ( 1.617086391009537660, 1.622319942449755636, 1.627553493889973169, 1.632787045330191145, 1.638020596770409121, 1.643254148210627097, 1.648487699650845073 ),
 .UNSPECIFIED. ) 
 CURVE ( )  GEOMETRIC_REPRESENTATION_ITEM ( )  RATIONAL_B_SPLINE_CURVE ( ( 0.9999999999999791278, 0.9659258262890892954, 1.000000000000000000, 0.9659258262890684232, 1.000000000000000000, 0.9659258262890684232, 1.000000000000000000, 0.9659258262890684232, 1.000000000000000000, 0.9659258262890684232, 1.000000000000000000, 0.9659258262890684232, 1.000000000000000000 ) ) 
 REPRESENTATION_ITEM ( '' )  );
#53355 = EDGE_CURVE ( 'NONE', #62930, #19023, #66791, .T. ) ;
#53356 = CARTESIAN_POINT ( 'NONE',  ( 0.000000000000000000, 0.000000000000000000, -0.7002075382097148193 ) ) ;
#53357 = CARTESIAN_POINT ( 'NONE',  ( -4.000000000000001776, 3.187499997268814056, -1.656854249492381470 ) ) ;
#53358 = VERTEX_POINT ( 'NONE', #48249 ) ;
#53359 = CARTESIAN_POINT ( 'NONE',  ( 2.828427124746209831, 196.5000000027312126, 200.8284271247462129 ) ) ;
#53360 = CARTESIAN_POINT ( 'NONE',  ( -1.656854249492403008, 201.6875000000000000, 146.0000000000000284 ) ) ;
#53361 = CARTESIAN_POINT ( 'NONE',  ( -31.99999999999999289, 199.3750000027312126, 170.0000000000004547 ) ) ;
#53362 = CARTESIAN_POINT ( 'NONE',  ( 2.780723358947928197E-16, 2.562499998634407028, -4.541265875000002339 ) ) ;
#53363 = CARTESIAN_POINT ( 'NONE',  ( -7.188101187500001821, 115.0625000020483952, -2.977408999572650483 ) ) ;
#53364 = DIRECTION ( 'NONE',  ( -1.000000000000000000, 0.000000000000000000, 1.281975129857798973E-14 ) ) ;
#53365 = CARTESIAN_POINT ( 'NONE',  ( 7.999999999999992895, -3.313708498984756279, 4.674052783920145338 ) ) ;
#53366 = ORIENTED_EDGE ( 'NONE', *, *, #52585, .F. ) ;
#53367 = EDGE_CURVE ( 'NONE', #54369, #29990, #36943, .T. ) ;
#53368 = EDGE_CURVE ( 'NONE', #4422, #39299, #72649, .T. ) ;
#53370 =( BOUNDED_CURVE ( )  B_SPLINE_CURVE ( 2, ( #41697, #13735, #71833, #20150, #64710, #36046, #13007, #53762, #59790 ),
 .UNSPECIFIED., .F., .F. ) 
 B_SPLINE_CURVE_WITH_KNOTS ( ( 3, 2, 2, 2, 3 ),
 ( 0.4000000000000003553, 0.4083333333333336590, 0.4166666666666670182, 0.4250000000000003220, 0.4333333333333336812 ),
 .UNSPECIFIED. ) 
 CURVE ( )  GEOMETRIC_REPRESENTATION_ITEM ( )  RATIONAL_B_SPLINE_CURVE ( ( 0.9999999999999970024, 0.9238795325112897361, 1.000000000000000000, 0.9238795325112867385, 1.000000000000000000, 0.9238795325112867385, 1.000000000000000000, 0.9238795325112837409, 1.000000000000003109 ) ) 
 REPRESENTATION_ITEM ( '' )  );
#53369 = CARTESIAN_POINT ( 'NONE',  ( 4.401442555609581635E-16, 23.34374999795161543, -7.188101187500000044 ) ) ;
#53371 = ORIENTED_EDGE ( 'NONE', *, *, #39818, .T. ) ;
#53372 = CARTESIAN_POINT ( 'NONE',  ( 7.320508075688776373, 255.0000000068279746, 7.320508075688767491 ) ) ;
#53373 = CARTESIAN_POINT ( 'NONE',  ( 3.458734125000016313, 207.8750000013656063, 199.4326545832176691 ) ) ;
#53374 = CARTESIAN_POINT ( 'NONE',  ( 31.45873412499998523, 204.7500000013655779, 168.5673454167822172 ) ) ;
#53375 = CARTESIAN_POINT ( 'NONE',  ( -7.320508075688778149, 58.12499999999999289, 7.320508075688769267 ) ) ;
#53376 = CARTESIAN_POINT ( 'NONE',  ( -7.188101187500001821, 100.4375000020483668, -2.977408999572650483 ) ) ;
#53377 = CARTESIAN_POINT ( 'NONE',  ( 2.485281374238571317, 295.6875000000000000, -6.000000000000003553 ) ) ;
#53379 = CARTESIAN_POINT ( 'NONE',  ( 1.656854249492504705, 197.8125000027312694, 194.0000000000001990 ) ) ;
#53378 = CARTESIAN_POINT ( 'NONE',  ( 2.249999999999999112, 2.250000000000000000, 28.00000000000000000 ) ) ;
#53380 = EDGE_LOOP ( 'NONE', ( #30323, #48067, #2428, #72581 ) ) ;
#53381 = CARTESIAN_POINT ( 'NONE',  ( -9.832129032723418760, 228.4895833367473585, -5.676582343749998927 ) ) ;
#53382 = CARTESIAN_POINT ( 'NONE',  ( -7.188101187499992051, 0.000000000000000000, 10.86155278187175455 ) ) ;
#53383 = CARTESIAN_POINT ( 'NONE',  ( 3.999999999999959144, 195.1875000027312410, 140.3431457505076594 ) ) ;
#53384 = CYLINDRICAL_SURFACE ( 'NONE', #67781, 3.999999999999976019 ) ;
#53385 = CARTESIAN_POINT ( 'NONE',  ( 24.14031152995217511, 194.9033115224686412, 169.3054215075829916 ) ) ;
#53386 = DIRECTION ( 'NONE',  ( -0.000000000000000000, 1.000000000000000000, 0.000000000000000000 ) ) ;
#53387 = CARTESIAN_POINT ( 'NONE',  ( 5.000000000000001776, 180.8333333333333428, -8.660254037844389075 ) ) ;
#53388 = CARTESIAN_POINT ( 'NONE',  ( -3.673940397442060854E-16, 299.7500000000000000, -6.000000000000001776 ) ) ;
#53389 = EDGE_CURVE ( 'NONE', #45507, #60229, #69775, .T. ) ;
#53390 = CARTESIAN_POINT ( 'NONE',  ( 10.00000000000000178, 240.4166666734946318, 2.679491924311222739 ) ) ;
#53391 = CARTESIAN_POINT ( 'NONE',  ( -7.188101187499992051, 2.977408999572646930, 27.26780278187175455 ) ) ;
#53392 = CARTESIAN_POINT ( 'NONE',  ( 11.35316468749999785, 140.8854166632526415, 3.042071309553174174 ) ) ;
#53393 = CARTESIAN_POINT ( 'NONE',  ( 25.17157287525381548, 201.6250000000000284, 167.1715728752537018 ) ) ;
#53394 = CARTESIAN_POINT ( 'NONE',  ( -3.673940397442060854E-16, 291.7500000000000000, -6.000000000000001776 ) ) ;
#53397 = CARTESIAN_POINT ( 'NONE',  ( 18.00000000000000355, 0.000000000000000000, 0.000000000000000000 ) ) ;
#53396 = CARTESIAN_POINT ( 'NONE',  ( 11.00000000000000000, 1.347111479062088405E-15, 118.0000000000000000 ) ) ;
#53395 = CARTESIAN_POINT ( 'NONE',  ( 30.82842712474617386, 208.1250000000000284, 172.8284271247460993 ) ) ;
#53398 = ORIENTED_EDGE ( 'NONE', *, *, #1759, .T. ) ;
#53399 = AXIS2_PLACEMENT_3D ( 'NONE', #15656, #10389, #9267 ) ;
#53400 = CARTESIAN_POINT ( 'NONE',  ( 11.35316468749999785, 5.885416663252683200, 3.042071309553174174 ) ) ;
#53401 = CARTESIAN_POINT ( 'NONE',  ( 25.17157287525377996, 197.7500000027312126, 167.1715728752537586 ) ) ;
#53402 = PLANE ( 'NONE',  #65078 ) ;
#53403 = CARTESIAN_POINT ( 'NONE',  ( -2.839093476692135984E-14, 205.6875000013656063, 138.5412658750000503 ) ) ;
#53404 = CARTESIAN_POINT ( 'NONE',  ( 2.751064625579944321E-14, 195.8750000027311842, 194.0000000000000568 ) ) ;
#53405 = CARTESIAN_POINT ( 'NONE',  ( -8.660254037844390851, 29.79166665983870388, 4.999999999999998224 ) ) ;
#53406 = CARTESIAN_POINT ( 'NONE',  ( 5.082755093536326818, 117.2187500020483810, 5.082755093536325042 ) ) ;
#53407 = CARTESIAN_POINT ( 'NONE',  ( -3.211159895383562723, 3.062499998634407028, 3.211159895383561391 ) ) ;
#53408 = CARTESIAN_POINT ( 'NONE',  ( 5.126144196591289059, 68.65853088339399335, -20.89430926782988962 ) ) ;
#53409 = CARTESIAN_POINT ( 'NONE',  ( -5.656854249492375253, 5.656854249492375253, 15.64280277982336642 ) ) ;
#53411 = CARTESIAN_POINT ( 'NONE',  ( 2.020667218593132706E-15, -11.00000000000000000, 105.0625000040967763 ) ) ;
#53410 = CARTESIAN_POINT ( 'NONE',  ( -9.000000000000017764, -15.58845726811988719, 0.000000000000000000 ) ) ;
#53412 = ORIENTED_EDGE ( 'NONE', *, *, #50365, .T. ) ;
#53413 = CARTESIAN_POINT ( 'NONE',  ( 7.320508075688771044, 221.2500000068279746, -7.320508075688771932 ) ) ;
#53414 = CARTESIAN_POINT ( 'NONE',  ( 7.999999999988127719, 1.377684776014802281E-05, 21.26780317368888618 ) ) ;
#53415 = CARTESIAN_POINT ( 'NONE',  ( 11.35316468749999963, 226.7187500034139873, -1.390361679473963556E-15 ) ) ;
#53416 = CARTESIAN_POINT ( 'NONE',  ( -3.042071309553164404, 112.2395833299193697, -11.35316468749999963 ) ) ;
#53417 = VERTEX_POINT ( 'NONE', #71626 ) ;
#53418 = CARTESIAN_POINT ( 'NONE',  ( -7.999999999999991118, -1.759549274430992710E-05, 5.517803281724177111 ) ) ;
#53419 = CARTESIAN_POINT ( 'NONE',  ( 10.18810118750000093, -4.220049686691933921, 98.31250000204836681 ) ) ;
#53420 = CARTESIAN_POINT ( 'NONE',  ( -4.556349186104045934, 11.00000000000000000, 86.40625000409677625 ) ) ;
#53421 = CARTESIAN_POINT ( 'NONE',  ( 1.432654583217664701, 197.0000000013656347, 201.4587341250000065 ) ) ;
#53422 = CARTESIAN_POINT ( 'NONE',  ( 4.000000000000001776, 0.7499999972688131678, 0.000000000000000000 ) ) ;
#53424 = CARTESIAN_POINT ( 'NONE',  ( 5.676582343750001591, 106.6145833299193555, -9.832129032723420536 ) ) ;
#53423 = CARTESIAN_POINT ( 'NONE',  ( -9.999999999999998224, 182.7083333333333428, 2.679491924311222295 ) ) ;
#53425 = CARTESIAN_POINT ( 'NONE',  ( -25.17157287525382614, 207.8750000000000284, 167.1715728752541565 ) ) ;
#53426 = CARTESIAN_POINT ( 'NONE',  ( 8.660254037844389075, 49.58333333333333570, 5.000000000000007994 ) ) ;
#53427 = ORIENTED_EDGE ( 'NONE', *, *, #62904, .T. ) ;
#53428 = EDGE_CURVE ( 'NONE', #64725, #5834, #67807, .T. ) ;
#53429 = CARTESIAN_POINT ( 'NONE',  ( 8.660254037844385522, 206.4583333265053682, 5.000000000000005329 ) ) ;
#53430 = CARTESIAN_POINT ( 'NONE',  ( -4.556349186104048599, -10.99999999999999822, 73.28124999999997158 ) ) ;
#53431 = AXIS2_PLACEMENT_3D ( 'NONE', #32080, #26392, #67528 ) ;
#53432 = DIRECTION ( 'NONE',  ( -0.000000000000000000, -0.000000000000000000, -1.000000000000000000 ) ) ;
#53433 = CARTESIAN_POINT ( 'NONE',  ( 8.311093377946837890, 96.71874999658599847, -8.311093377946837890 ) ) ;
#53434 = ADVANCED_BREP_SHAPE_REPRESENTATION ( '', ( #66045, #57354 ), #44151 ) ;
#53435 = CARTESIAN_POINT ( 'NONE',  ( -2.445694354108782775, 208.5625000013656063, 200.4456943541088663 ) ) ;
#53436 = CARTESIAN_POINT ( 'NONE',  ( -1.320432766682874540E-15, 13.96874999795161187, 7.188101187500000044 ) ) ;
#53437 = CARTESIAN_POINT ( 'NONE',  ( 10.18810118749999916, 1.247682550866122264E-15, 86.78125000204836681 ) ) ;
#53438 = CARTESIAN_POINT ( 'NONE',  ( -9.832129032723418760, 3.177083329919349719, -5.676582343750004256 ) ) ;
#53439 = VERTEX_POINT ( 'NONE', #53925 ) ;
#53440 = PLANE ( 'NONE',  #15102 ) ;
#53441 = DIRECTION ( 'NONE',  ( 0.000000000000000000, 0.000000000000000000, -1.000000000000000000 ) ) ;
#53442 = CARTESIAN_POINT ( 'NONE',  ( -11.00000000000000000, 0.000000000000000000, 103.0000000000000000 ) ) ;
#53443 = CARTESIAN_POINT ( 'NONE',  ( 4.220049686691934809, 10.18810118749999916, 73.56250000204835260 ) ) ;
#53444 = CYLINDRICAL_SURFACE ( 'NONE', #20549, 6.000000000000001776 ) ;
#53445 = CARTESIAN_POINT ( 'NONE',  ( 10.00000000000000000, 199.7916666666666572, 2.679491924311235618 ) ) ;
#53446 = CARTESIAN_POINT ( 'NONE',  ( 2.765530957081996366, 294.1406250017069510, -6.676582343750003368 ) ) ;
#53447 = LINE ( 'NONE', #64757, #16005 ) ;
#53448 = CARTESIAN_POINT ( 'NONE',  ( 10.99653194014283564, 225.8365693605616116, 3.659777347618654808 ) ) ;
#53449 = ADVANCED_FACE ( 'NONE', ( #2238 ), #50490, .T. ) ;
#53450 = CARTESIAN_POINT ( 'NONE',  ( -7.204075437095965206, -7.204075437095968759, 90.34375000204838102 ) ) ;
#53451 = CARTESIAN_POINT ( 'NONE',  ( -25.55430564589115150, 203.0625000013656063, 172.4456943541091789 ) ) ;
#53452 = EDGE_CURVE ( 'NONE', #45113, #73073, #15781, .T. ) ;
#53453 = CARTESIAN_POINT ( 'NONE',  ( -3.313708498984765161, 26.53125000000000355, 7.999999999999998224 ) ) ;
#53454 = CARTESIAN_POINT ( 'NONE',  ( -1.881053915767124440, 10.12499999863440792, 4.541265875000001451 ) ) ;
#53455 = VERTEX_POINT ( 'NONE', #73140 ) ;
#53456 = CARTESIAN_POINT ( 'NONE',  ( -19.67382924195849725, -48.49768232664703049, 146.0311653248315622 ) ) ;
#53457 = CARTESIAN_POINT ( 'NONE',  ( -3.999999999999960032, 209.1250000027312126, 198.0000000000000284 ) ) ;
#53458 = CARTESIAN_POINT ( 'NONE',  ( 3.458734124999960358, 197.6250000013656063, 143.4326545832176976 ) ) ;
#53459 = CARTESIAN_POINT ( 'NONE',  ( -2.849036369511732440E-14, 205.3750000027312126, 138.0000000000000568 ) ) ;
#53460 = CARTESIAN_POINT ( 'NONE',  ( 30.82842712474621294, 208.2500000027312126, 172.8284271247460424 ) ) ;
#53461 = CARTESIAN_POINT ( 'NONE',  ( -4.220049686691937474, -10.18810118749999738, 72.81250000204836681 ) ) ;
#53462 = ORIENTED_EDGE ( 'NONE', *, *, #53219, .T. ) ;
#53463 = CARTESIAN_POINT ( 'NONE',  ( -5.082755093536326818, 7.406249997951610986, 5.082755093536325042 ) ) ;
#53464 = CARTESIAN_POINT ( 'NONE',  ( 2.020667218593132706E-15, -11.00000000000000000, 112.3749999999999858 ) ) ;
#53465 = CARTESIAN_POINT ( 'NONE',  ( 5.082755093536325042, 116.4687500020483810, -5.082755093536325930 ) ) ;
#53466 = CARTESIAN_POINT ( 'NONE',  ( -4.310155712710913356, 22.00000000000000000, 1.403903855516097421 ) ) ;
#53467 = CARTESIAN_POINT ( 'NONE',  ( -4.088227598258586603E-16, 291.2031250017069510, -6.676582343750001591 ) ) ;
#53469 = CARTESIAN_POINT ( 'NONE',  ( 7.806255641895631925E-15, 13.85640646055103709, -1.071796769724504550 ) ) ;
#53468 = CARTESIAN_POINT ( 'NONE',  ( -6.951808397369817780E-16, 227.6562500034139873, -11.35316468749999963 ) ) ;
#53470 =( BOUNDED_CURVE ( )  B_SPLINE_CURVE ( 2, ( #5695, #46420, #16997, #63026, #39280, #22654, #40760, #45673, #74344 ),
 .UNSPECIFIED., .F., .F. ) 
 B_SPLINE_CURVE_WITH_KNOTS ( ( 3, 2, 2, 2, 3 ),
 ( 0.6166666666666672514, 0.6250000000000005551, 0.6333333333333337478, 0.6416666666666671626, 0.6500000000000004663 ),
 .UNSPECIFIED. ) 
 CURVE ( )  GEOMETRIC_REPRESENTATION_ITEM ( )  RATIONAL_B_SPLINE_CURVE ( ( 0.9999999999999948930, 0.9238795325112918455, 1.000000000000000000, 0.9238795325112867385, 1.000000000000000000, 0.9238795325112867385, 1.000000000000000000, 0.9238795325112826307, 1.000000000000003997 ) ) 
 REPRESENTATION_ITEM ( '' )  );
#53471 = ORIENTED_EDGE ( 'NONE', *, *, #19767, .F. ) ;
#53472 = CARTESIAN_POINT ( 'NONE',  ( -5.676582343750000703, 223.3854166700806729, -9.832129032723418760 ) ) ;
#53473 = CARTESIAN_POINT ( 'NONE',  ( -7.188101187499991163, 2.977408999572646930, 2.892802781871751439 ) ) ;
#53474 = AXIS2_PLACEMENT_3D ( 'NONE', #66142, #9179, #15201 ) ;
#53475 = CARTESIAN_POINT ( 'NONE',  ( 1.432654583217662481, 202.3750000013655779, 194.5412658750000219 ) ) ;
#53476 = VERTEX_POINT ( 'NONE', #27109 ) ;
#53477 = CARTESIAN_POINT ( 'NONE',  ( 3.313708498984760276, 105.2187500040967905, -8.000000000000000000 ) ) ;
#53478 = CARTESIAN_POINT ( 'NONE',  ( -2.085542519210945728E-15, 94.84374999658601268, 11.35316468750000141 ) ) ;
#53479 = CARTESIAN_POINT ( 'NONE',  ( -8.660254037844387298, 122.9166666666666998, 4.999999999999997335 ) ) ;
#53480 = CARTESIAN_POINT ( 'NONE',  ( 7.778174593052021635, 7.778174593052023411, 75.43749999999998579 ) ) ;
#53483 = CARTESIAN_POINT ( 'NONE',  ( -11.00000000000000000, 0.000000000000000000, 113.4999999999999858 ) ) ;
#53482 = CARTESIAN_POINT ( 'NONE',  ( 25.55430564589119413, 206.3125000013656063, 172.4456943541087526 ) ) ;
#53481 = CARTESIAN_POINT ( 'NONE',  ( 29.43265458321761230, 202.7500000013655779, 173.4587341249998929 ) ) ;
#53484 = VERTEX_POINT ( 'NONE', #62184 ) ;
#53485 = CARTESIAN_POINT ( 'NONE',  ( 4.000000000000001776, 19.06250000000000000, -1.656854249492381248 ) ) ;
#53486 = DIRECTION ( 'NONE',  ( 0.000000000000000000, 0.000000000000000000, -1.000000000000000000 ) ) ;
#53487 = CARTESIAN_POINT ( 'NONE',  ( -11.35316468750000141, 218.2812499965860411, -1.390361679473963753E-15 ) ) ;
#53488 = CARTESIAN_POINT ( 'NONE',  ( 2.445694354108783664, 202.3125000013656063, 144.4456943541088663 ) ) ;
#53489 = CARTESIAN_POINT ( 'NONE',  ( 29.43265458321761230, 201.7500000013655779, 173.4587341249998929 ) ) ;
#53490 = CARTESIAN_POINT ( 'NONE',  ( 2.977408999572651815, 21.56249999795161898, 7.188101187500000933 ) ) ;
#53491 = CARTESIAN_POINT ( 'NONE',  ( 8.311093377946837890, 191.7187499965860127, -8.311093377946837890 ) ) ;
#53492 = CARTESIAN_POINT ( 'NONE',  ( 5.082755093536326818, 93.59375000204838102, 5.082755093536325042 ) ) ;
#53493 = CARTESIAN_POINT ( 'NONE',  ( -4.999999999999944045, 68.60357193678724741, -20.85024232999276350 ) ) ;
#53494 = CARTESIAN_POINT ( 'NONE',  ( 2.449293598294707893E-16, 18.99999999726881228, -4.000000000000001776 ) ) ;
#53495 = CARTESIAN_POINT ( 'NONE',  ( -1.881053915767124440, 14.99999999863440969, 4.541265875000001451 ) ) ;
#53496 = CARTESIAN_POINT ( 'NONE',  ( 27.99999999999996447, 199.6875000013656063, 173.4587341249998929 ) ) ;
#53497 = CARTESIAN_POINT ( 'NONE',  ( -5.082755093536317936, -5.082755093536320601, 3.549052781871751883 ) ) ;
#53498 = CARTESIAN_POINT ( 'NONE',  ( 3.042071309553159519, 69.73958332991935549, 11.35316468750000141 ) ) ;
#53499 = CARTESIAN_POINT ( 'NONE',  ( -5.000000000000000000, -53.12474899268202222, 47.87640533067842341 ) ) ;
#53500 = VERTEX_POINT ( 'NONE', #21810 ) ;
#53501 = FACE_BOUND ( 'NONE', #58173, .T. ) ;
#53503 = DIRECTION ( 'NONE',  ( -1.000000000000000000, 0.000000000000000000, -0.000000000000000000 ) ) ;
#53502 = AXIS2_PLACEMENT_3D ( 'NONE', #12195, #28805, #58981 ) ;
#53504 = CARTESIAN_POINT ( 'NONE',  ( -2.085542519210945728E-15, 79.53124999658602690, 11.35316468750000141 ) ) ;
#53505 = CARTESIAN_POINT ( 'NONE',  ( 10.18810118749999916, 4.220049686691935698, 85.37500000204839523 ) ) ;
#53506 = CARTESIAN_POINT ( 'NONE',  ( 4.556349186104045934, 11.00000000000000000, 69.71875000409677625 ) ) ;
#53507 = CARTESIAN_POINT ( 'NONE',  ( 3.458734124999960358, 194.6875000013655779, 142.0000000000000568 ) ) ;
#53508 = CARTESIAN_POINT ( 'NONE',  ( 1.268984979720182487E-11, 76.24999999999903366, -10.00000000000000178 ) ) ;
#53510 = CARTESIAN_POINT ( 'NONE',  ( -5.676582343749998039, 67.44791666325268409, -9.832129032723420536 ) ) ;
#53509 = CARTESIAN_POINT ( 'NONE',  ( -5.656854249492380582, 123.5000000040967905, -5.656854249492380582 ) ) ;
#53511 = CARTESIAN_POINT ( 'NONE',  ( -3.313708498984758943, -7.999999999999989342, 25.29905278392014623 ) ) ;
#53512 = CARTESIAN_POINT ( 'NONE',  ( 4.000000000000000888, 12.93750000000000355, 1.656854249492384135 ) ) ;
#53513 = EDGE_CURVE ( 'NONE', #22871, #25965, #21066, .T. ) ;
#53514 = ADVANCED_FACE ( 'NONE', ( #38443 ), #22743, .T. ) ;
#53515 = CARTESIAN_POINT ( 'NONE',  ( 7.320508075688771044, 171.2499999931719969, 7.320508075688775484 ) ) ;
#53516 = CARTESIAN_POINT ( 'NONE',  ( 3.594050593751920264, 89.53052362291684574, -6.225078233346985179 ) ) ;
#53517 = CARTESIAN_POINT ( 'NONE',  ( -24.17985302810928516, 194.9464753018651209, 168.9913998801469859 ) ) ;
#53518 = CARTESIAN_POINT ( 'NONE',  ( -11.35316468750000141, 58.59374999658601979, -1.390361679473963753E-15 ) ) ;
#53519 = CARTESIAN_POINT ( 'NONE',  ( -6.238412754330611322E-16, 10.18810118749999916, 111.1562500020483668 ) ) ;
#53520 = CARTESIAN_POINT ( 'NONE',  ( 9.832129032723420536, 201.1979166632526983, -5.676582343749999815 ) ) ;
#53521 = ORIENTED_EDGE ( 'NONE', *, *, #26447, .T. ) ;
#53522 = CARTESIAN_POINT ( 'NONE',  ( 2.828427124746190291, 3.875000000000000000, 2.828427124746192067 ) ) ;
#53523 = CARTESIAN_POINT ( 'NONE',  ( -36.10814071610730736, 50.00000000000000000, 139.0000000000000000 ) ) ;
#53524 = CARTESIAN_POINT ( 'NONE',  ( 27.99999999999999645, 210.0000000000000284, 165.9999999999999147 ) ) ;
#53526 = CARTESIAN_POINT ( 'NONE',  ( 11.35316468750000141, 195.7812499965860127, 0.000000000000000000 ) ) ;
#53525 = DIRECTION ( 'NONE',  ( -0.000000000000000000, 1.000000000000000000, -4.476705744456276341E-16 ) ) ;
#53527 = FACE_OUTER_BOUND ( 'NONE', #31741, .T. ) ;
#53528 = EDGE_CURVE ( 'NONE', #33233, #49310, #31648, .T. ) ;
#53529 = CARTESIAN_POINT ( 'NONE',  ( 7.320508075688776373, 245.0000000068279462, 7.320508075688767491 ) ) ;
#53530 = DIRECTION ( 'NONE',  ( -1.000000000000000000, -0.000000000000000000, -0.000000000000000000 ) ) ;
#53531 = VERTEX_POINT ( 'NONE', #27476 ) ;
#53532 = CARTESIAN_POINT ( 'NONE',  ( -3.042071309553163960, 182.5520833299193271, -11.35316468749999963 ) ) ;
#53533 = COLOUR_RGB ( '',0.7921568627450980005, 0.8196078431372548767, 0.9333333333333333481 ) ;
#53534 = CARTESIAN_POINT ( 'NONE',  ( 5.082755093536318824, 5.082755093536319713, 21.92405278187175455 ) ) ;
#53535 = CARTESIAN_POINT ( 'NONE',  ( 3.090148520752590944, 225.9998984954551418, -9.510618362637927703 ) ) ;
#53536 = ORIENTED_EDGE ( 'NONE', *, *, #32608, .T. ) ;
#53537 = EDGE_CURVE ( 'NONE', #27684, #30150, #42023, .T. ) ;
#53538 = CARTESIAN_POINT ( 'NONE',  ( -4.898587196589412829E-16, 96.31250000409677625, -8.000000000000000000 ) ) ;
#53539 = CARTESIAN_POINT ( 'NONE',  ( -4.000000000000001776, 13.50000000000000000, -4.898587196589415787E-16 ) ) ;
#53540 = CARTESIAN_POINT ( 'NONE',  ( 27.99999999999999645, 210.0000000000000284, 169.9999999999999147 ) ) ;
#53541 = CARTESIAN_POINT ( 'NONE',  ( 4.541265875000001451, 17.24999999863440792, 1.881053915767124440 ) ) ;
#53542 = CARTESIAN_POINT ( 'NONE',  ( -5.656854249492373476, -5.656854249492376141, 13.20530278392014623 ) ) ;
#53544 = CARTESIAN_POINT ( 'NONE',  ( -7.320508075688776373, 186.8749999999999432, -7.320508075688777261 ) ) ;
#53543 = AXIS2_PLACEMENT_3D ( 'NONE', #56433, #5128, #10773 ) ;
#53545 = ORIENTED_EDGE ( 'NONE', *, *, #25483, .T. ) ;
#53546 = CARTESIAN_POINT ( 'NONE',  ( 6.000000000000003553, 293.6250000034140157, -2.485281374238571761 ) ) ;
#53547 = CARTESIAN_POINT ( 'NONE',  ( -7.188101187500001821, 100.0625000020483952, -2.977408999572650483 ) ) ;
#53549 = CARTESIAN_POINT ( 'NONE',  ( 4.000000000000000888, 6.687499997268813168, 1.656854249492384135 ) ) ;
#53548 = CARTESIAN_POINT ( 'NONE',  ( 4.000000000000015987, 196.5625000000000284, 196.3431457505076594 ) ) ;
#53550 = DIRECTION ( 'NONE',  ( 0.000000000000000000, 0.000000000000000000, 1.000000000000000000 ) ) ;
#53551 = VERTEX_POINT ( 'NONE', #16141 ) ;
#53552 = CARTESIAN_POINT ( 'NONE',  ( 7.188101187500000044, 27.46874999795161543, 0.000000000000000000 ) ) ;
#53553 = CARTESIAN_POINT ( 'NONE',  ( 3.042071309553173286, 260.6770833367473301, 11.35316468749999608 ) ) ;
#53554 = CARTESIAN_POINT ( 'NONE',  ( 2.977408999572646486, 7.188101187499991163, 22.01780278187175455 ) ) ;
#53555 = ORIENTED_EDGE ( 'NONE', *, *, #40331, .T. ) ;
#53556 = ORIENTED_EDGE ( 'NONE', *, *, #43052, .T. ) ;
#53557 = CARTESIAN_POINT ( 'NONE',  ( 10.18810118749999916, 1.247682550866122264E-15, 87.90625000204838102 ) ) ;
#53558 = CARTESIAN_POINT ( 'NONE',  ( 7.999999999732929190, -6.536825277765295045E-05, 6.267800880277100362 ) ) ;
#53559 = CARTESIAN_POINT ( 'NONE',  ( -4.556349186104047710, -10.99999999999999822, 97.28124999999997158 ) ) ;
#53562 = CARTESIAN_POINT ( 'NONE',  ( -6.676582343750001591, 293.6093750017069510, 0.000000000000000000 ) ) ;
#53561 = CARTESIAN_POINT ( 'NONE',  ( 25.17157287525381903, 203.0000000027312126, 172.8284271247460993 ) ) ;
#53560 = DIRECTION ( 'NONE',  ( 0.000000000000000000, 0.000000000000000000, 1.000000000000000000 ) ) ;
#53563 = CARTESIAN_POINT ( 'NONE',  ( 4.999999999999993783, 129.1666666666666856, 8.660254037844390851 ) ) ;
#53564 = CARTESIAN_POINT ( 'NONE',  ( -5.000000000000000000, 70.11723469343132820, -28.93519894129142145 ) ) ;
#53565 = PLANE ( 'NONE',  #62447 ) ;
#53566 = CARTESIAN_POINT ( 'NONE',  ( 1.836970198721029589E-15, 234.3750000068279746, 10.00000000000000000 ) ) ;
#53567 = CARTESIAN_POINT ( 'NONE',  ( -5.656854249492381470, 2.249999995903220196, 5.656854249492379694 ) ) ;
#53568 = CARTESIAN_POINT ( 'NONE',  ( 31.45873412499999944, 197.7500000013656063, 168.5673454167822740 ) ) ;
#53569 = CARTESIAN_POINT ( 'NONE',  ( -7.188101187500001821, 5.999999997951610098, -2.977408999572651371 ) ) ;
#53570 = VECTOR ( 'NONE', #41400, 1000.000000000000000 ) ;
#53571 = CARTESIAN_POINT ( 'NONE',  ( -3.317071493978878571, 8.008118988124991233, 2.231865283940627886 ) ) ;
#53572 = CARTESIAN_POINT ( 'NONE',  ( -11.00000000000000533, -11.00000000000000355, 20.00000000000000000 ) ) ;
#53573 = CARTESIAN_POINT ( 'NONE',  ( -4.401442555609581635E-16, 113.6562500020483952, -7.188101187500000044 ) ) ;
#53575 = CARTESIAN_POINT ( 'NONE',  ( 0.000000000000000000, 45.00000000000000000, 0.000000000000000000 ) ) ;
#53574 = CARTESIAN_POINT ( 'NONE',  ( -8.660254037844385522, 250.4166666666666856, 5.000000000000004441 ) ) ;
#53576 = CARTESIAN_POINT ( 'NONE',  ( -9.832129032723415207, 224.6354166700806729, 5.676582343750005144 ) ) ;
#53577 = CYLINDRICAL_SURFACE ( 'NONE', #51794, 3.999999999999976019 ) ;
#53578 = CARTESIAN_POINT ( 'NONE',  ( -2.977408999572648707, -7.188101187499990274, 24.64280278187176165 ) ) ;
#53579 = DIRECTION ( 'NONE',  ( 0.000000000000000000, -1.000000000000000000, 0.000000000000000000 ) ) ;
#53580 = CARTESIAN_POINT ( 'NONE',  ( 6.951808397369818766E-16, 32.03124999658601979, -11.35316468750000141 ) ) ;
#53581 =( BOUNDED_CURVE ( )  B_SPLINE_CURVE ( 2, ( #65260, #37343, #24530, #31303, #49019, #2642, #48645, #7195, #2266, #30931, #71654, #13564, #48279 ),
 .UNSPECIFIED., .F., .F. ) 
 B_SPLINE_CURVE_WITH_KNOTS ( ( 3, 2, 2, 2, 2, 2, 3 ),
 ( 0.5489130434782608647, 0.5507246376811594235, 0.5525362318840579823, 0.5543478260869565410, 0.5561594202898549888, 0.5579710144927535476, 0.5597826086956521063 ),
 .UNSPECIFIED. ) 
 CURVE ( )  GEOMETRIC_REPRESENTATION_ITEM ( )  RATIONAL_B_SPLINE_CURVE ( ( 1.000000000000000000, 0.9659258262890683122, 1.000000000000000000, 0.9659258262890683122, 1.000000000000000000, 0.9659258262890683122, 1.000000000000000000, 0.9659258262890683122, 1.000000000000000000, 0.9659258262890683122, 1.000000000000000000, 0.9659258262890704216, 0.9999999999999978906 ) ) 
 REPRESENTATION_ITEM ( '' )  );
#53582 = CARTESIAN_POINT ( 'NONE',  ( -2.828427124746152987, 203.1250000000000284, 200.8284271247462129 ) ) ;
#53584 = CARTESIAN_POINT ( 'NONE',  ( -1.836970198721029983E-15, 5.624999993172032475, 10.00000000000000178 ) ) ;
#53583 =( BOUNDED_CURVE ( )  B_SPLINE_CURVE ( 2, ( #39744, #51812, #23135, #35584, #46147, #69164, #41240, #17473, #40867, #63873, #64246, #12556, #58598 ),
 .UNSPECIFIED., .F., .F. ) 
 B_SPLINE_CURVE_WITH_KNOTS ( ( 3, 2, 2, 2, 2, 2, 3 ),
 ( 0.7554347826086956763, 0.7572463768115942351, 0.7590579710144927938, 0.7608695652173913526, 0.7626811594202898004, 0.7644927536231883591, 0.7663043478260869179 ),
 .UNSPECIFIED. ) 
 CURVE ( )  GEOMETRIC_REPRESENTATION_ITEM ( )  RATIONAL_B_SPLINE_CURVE ( ( 1.000000000000000000, 0.9659258262890683122, 1.000000000000000000, 0.9659258262890683122, 1.000000000000000000, 0.9659258262890683122, 1.000000000000000000, 0.9659258262890683122, 1.000000000000000000, 0.9659258262890683122, 1.000000000000000000, 0.9659258262890683122, 1.000000000000000000 ) ) 
 REPRESENTATION_ITEM ( '' )  );
#53585 = DIRECTION ( 'NONE',  ( 0.000000000000000000, -1.000000000000000000, 0.000000000000000000 ) ) ;
#53586 = DIRECTION ( 'NONE',  ( -0.000000000000000000, 1.000000000000000000, 4.476705744456276341E-16 ) ) ;
#53587 = VERTEX_POINT ( 'NONE', #16519 ) ;
#53588 = CYLINDRICAL_SURFACE ( 'NONE', #31439, 19.00000000000000355 ) ;
#53589 = ADVANCED_FACE ( 'NONE', ( #39180 ), #56544, .T. ) ;
#53590 = ADVANCED_FACE ( 'NONE', ( #50866 ), #32412, .F. ) ;
#53591 = CARTESIAN_POINT ( 'NONE',  ( 1.432654583217608080, 197.8750000013656063, 138.5412658750000503 ) ) ;
#53592 = CARTESIAN_POINT ( 'NONE',  ( -9.832129032723418760, 32.86458332991934839, -5.676582343750004256 ) ) ;
#53593 = CARTESIAN_POINT ( 'NONE',  ( 11.00000000000000000, 4.556349186104045934, 86.03125000409676204 ) ) ;
#53594 = CARTESIAN_POINT ( 'NONE',  ( 2.445694354108784108, 208.5625000013656063, 144.4456943541088663 ) ) ;
#53595 = CARTESIAN_POINT ( 'NONE',  ( -28.47326357806616315, 194.4587341250000350, 166.5737975347167321 ) ) ;
#53596 = DIRECTION ( 'NONE',  ( 0.000000000000000000, -1.000000000000000000, -0.000000000000000000 ) ) ;
#53598 = CARTESIAN_POINT ( 'NONE',  ( -5.676582343750006032, 34.11458332991934839, 9.832129032723418760 ) ) ;
#53597 = CARTESIAN_POINT ( 'NONE',  ( -7.188101187500000044, 103.1562500020483810, 0.000000000000000000 ) ) ;
#53599 = CARTESIAN_POINT ( 'NONE',  ( 7.999999999999991118, 9.797174393178815797E-16, 15.08030277982336642 ) ) ;
#53600 = CARTESIAN_POINT ( 'NONE',  ( -2.085542519210945728E-15, 149.5312499965860411, 11.35316468750000141 ) ) ;
#53601 = CARTESIAN_POINT ( 'NONE',  ( 10.00000000000000178, 116.8749999931720396, 0.000000000000000000 ) ) ;
#53602 = CARTESIAN_POINT ( 'NONE',  ( -7.188101187500000044, 109.5312500020483810, 0.000000000000000000 ) ) ;
#53603 = CARTESIAN_POINT ( 'NONE',  ( 0.000000000000000000, 0.000000000000000000, 0.000000000000000000 ) ) ;
#53604 = CARTESIAN_POINT ( 'NONE',  ( -27.99999999999996447, 205.1875000013656063, 173.4587341250003760 ) ) ;
#53605 = EDGE_LOOP ( 'NONE', ( #73473, #62074, #68932, #16976, #45808, #25097, #59573, #46349, #11976, #53746, #11120, #57373, #17632, #19349, #69682, #59491 ) ) ;
#53606 = CARTESIAN_POINT ( 'NONE',  ( 5.676582343750001591, 26.92708332991935194, -9.832129032723420536 ) ) ;
#53607 = ORIENTED_EDGE ( 'NONE', *, *, #45966, .F. ) ;
#53608 = CARTESIAN_POINT ( 'NONE',  ( 4.000000000000001776, 7.062500000000000000, -1.656854249492381248 ) ) ;
#53610 = CARTESIAN_POINT ( 'NONE',  ( -8.311093377946836114, 157.6562499965860411, -8.311093377946837890 ) ) ;
#53609 = CARTESIAN_POINT ( 'NONE',  ( -3.313708498984708317, 108.7812500000000142, 8.000000000000053291 ) ) ;
#53611 = CARTESIAN_POINT ( 'NONE',  ( 7.999999999999991118, 9.797174393178815797E-16, 16.63655278432982954 ) ) ;
#53612 = CARTESIAN_POINT ( 'NONE',  ( 1.836970198721029589E-15, 224.3750000068279746, 10.00000000000000000 ) ) ;
#53613 = EDGE_CURVE ( 'NONE', #9713, #54330, #28782, .T. ) ;
#53614 = CARTESIAN_POINT ( 'NONE',  ( -5.676582343750000703, 243.0729166700806445, -9.832129032723418760 ) ) ;
#53615 = CARTESIAN_POINT ( 'NONE',  ( 1.871523826299183495E-15, -10.18810118749999916, 89.40625000204838102 ) ) ;
#53616 = EDGE_LOOP ( 'NONE', ( #36117, #1370, #40645, #41397, #58853, #26580, #57739, #61093, #4937, #25528, #53462, #68087, #36074, #70614, #44764, #16384, #27046, #47010, #66062, #31965, #46034, #14633, #1064, #51559, #29658, #45884, #27104, #35242 ) ) ;
#53617 = B_SPLINE_CURVE_WITH_KNOTS ( 'NONE', 3,
 ( #13944, #36986, #31318, #42265, #72433, #23902, #65277, #54345, #19621 ),
 .UNSPECIFIED., .F., .F.,
 ( 4, 2, 1, 2, 4 ),
 ( 0.000000000000000000, 0.001314083742622694853, 0.002628167485245389706, 0.003942251227868084559, 0.005256334970490779412 ),
 .UNSPECIFIED. ) ;
#53618 = ADVANCED_FACE ( 'NONE', ( #72770 ), #44100, .T. ) ;
#53619 = CARTESIAN_POINT ( 'NONE',  ( 8.660254037844390851, 120.4166666666666714, -5.000000000000001776 ) ) ;
#53620 = CARTESIAN_POINT ( 'NONE',  ( 1.224646799147353454E-15, 300.0000000000000000, -10.00000000000000178 ) ) ;
#53621 = CARTESIAN_POINT ( 'NONE',  ( -11.35316468749999785, 83.38541666325265567, -3.042071309553167513 ) ) ;
#53622 = CARTESIAN_POINT ( 'NONE',  ( 7.204075437095966983, 7.204075437095967871, 100.0937500020483668 ) ) ;
#53623 = CARTESIAN_POINT ( 'NONE',  ( -1.881053915767124440, 17.12499999863440436, 4.541265875000001451 ) ) ;
#53624 = VERTEX_POINT ( 'NONE', #35400 ) ;
#53625 = ORIENTED_EDGE ( 'NONE', *, *, #68944, .F. ) ;
#53626 = CARTESIAN_POINT ( 'NONE',  ( 8.000000000000000000, 7.593750000000001776, -3.313708498984761608 ) ) ;
#53627 = CARTESIAN_POINT ( 'NONE',  ( -3.211159895383561391, 0.8124999986344069169, -3.211159895383561835 ) ) ;
#53628 = CARTESIAN_POINT ( 'NONE',  ( 5.082755093536324154, 4.781249997951610986, 5.082755093536326818 ) ) ;
#53629 = CIRCLE ( 'NONE', #42773, 18.00000000000000355 ) ;
#53630 = EDGE_CURVE ( 'NONE', #61876, #39105, #28972, .T. ) ;
#53631 = CARTESIAN_POINT ( 'NONE',  ( 3.313708498984765161, 122.6562500040968047, 7.999999999999998224 ) ) ;
#53632 = CARTESIAN_POINT ( 'NONE',  ( 10.18810118749999916, 1.247682550866122264E-15, 98.78125000204838102 ) ) ;
#53633 = CARTESIAN_POINT ( 'NONE',  ( 38.00000000000000000, 53.00000000000000000, 15.00000000000000178 ) ) ;
#53634 = VECTOR ( 'NONE', #4309, 1000.000000000000000 ) ;
#53635 = CARTESIAN_POINT ( 'NONE',  ( -3.313708498984760276, 6.468750000000001776, -8.000000000000000000 ) ) ;
#53636 = CARTESIAN_POINT ( 'NONE',  ( -4.000000000000001776, 16.24999999726881228, -4.898587196589415787E-16 ) ) ;
#53637 = CARTESIAN_POINT ( 'NONE',  ( -3.211159895383561391, 3.687499998634407028, -3.211159895383561835 ) ) ;
#53638 = VERTEX_POINT ( 'NONE', #17279 ) ;
#53639 = CARTESIAN_POINT ( 'NONE',  ( 3.458734124999959914, 207.3750000013656063, 143.4326545832176976 ) ) ;
#53640 = CARTESIAN_POINT ( 'NONE',  ( 2.839093476692135984E-14, 197.6875000013655779, 201.4587341250000350 ) ) ;
#53642 = DIRECTION ( 'NONE',  ( 0.000000000000000000, 0.000000000000000000, 1.000000000000000000 ) ) ;
#53641 = CARTESIAN_POINT ( 'NONE',  ( -27.99999999999991829, 200.9375000013656063, 173.4587341250003760 ) ) ;
#53643 =( LENGTH_UNIT ( ) NAMED_UNIT ( * ) SI_UNIT ( .MILLI., .METRE. ) );
#53644 = CARTESIAN_POINT ( 'NONE',  ( 1.881053915767122664, 14.12499999863440969, 4.541265875000001451 ) ) ;
#53645 = CARTESIAN_POINT ( 'NONE',  ( -7.778174593052023411, 7.778174593052023411, 68.31249999999998579 ) ) ;
#53646 = CARTESIAN_POINT ( 'NONE',  ( 7.188101187499992051, 8.802885111219154394E-16, 12.73655278187175277 ) ) ;
#53647 = ORIENTED_EDGE ( 'NONE', *, *, #52380, .T. ) ;
#53648 = ORIENTED_EDGE ( 'NONE', *, *, #67089, .F. ) ;
#53649 = CARTESIAN_POINT ( 'NONE',  ( -4.220049686691937474, -10.18810118749999738, 102.4375000020483810 ) ) ;
#53650 = DIRECTION ( 'NONE',  ( -0.000000000000000000, -1.000000000000000000, -4.283267841918042741E-17 ) ) ;
#53651 = CARTESIAN_POINT ( 'NONE',  ( -25.17157287525382259, 201.8750000000000284, 167.1715728752541565 ) ) ;
#53652 = CARTESIAN_POINT ( 'NONE',  ( 2.445694354108839619, 197.8125000013656063, 200.4456943541088663 ) ) ;
#53653 = CARTESIAN_POINT ( 'NONE',  ( -11.35316468749999963, 264.2187500034140157, 0.000000000000000000 ) ) ;
#53654 = CARTESIAN_POINT ( 'NONE',  ( -2.679491924311235618, 88.54166666666668561, 10.00000000000000000 ) ) ;
#53655 = CARTESIAN_POINT ( 'NONE',  ( -4.898587196589412829E-16, 117.1250000000000000, -8.000000000000000000 ) ) ;
#53656 = CARTESIAN_POINT ( 'NONE',  ( -4.721056650415998313, 295.7343750017069510, 4.721056650416000089 ) ) ;
#53657 = VERTEX_POINT ( 'NONE', #35031 ) ;
#53658 = CARTESIAN_POINT ( 'NONE',  ( 4.556349186104052151, -10.99999999999999822, 109.4687499999999858 ) ) ;
#53659 = CARTESIAN_POINT ( 'NONE',  ( 8.000000000000000000, 17.81249999590322375, 0.000000000000000000 ) ) ;
#53660 = CARTESIAN_POINT ( 'NONE',  ( -2.445694354108839619, 206.8125000013656063, 139.5543056458912190 ) ) ;
#53661 = CARTESIAN_POINT ( 'NONE',  ( 1.656854249492381248, 8.187500000000000000, -4.000000000000001776 ) ) ;
#53662 = CARTESIAN_POINT ( 'NONE',  ( -4.999999999999992895, 230.8333333333333428, 8.660254037844390851 ) ) ;
#53663 = CARTESIAN_POINT ( 'NONE',  ( 2.751064625579944321E-14, 206.8750000027312126, 194.0000000000000568 ) ) ;
#53664 = CARTESIAN_POINT ( 'NONE',  ( -4.556349186104047710, -10.99999999999999822, 113.7812500000000142 ) ) ;
#53665 = CARTESIAN_POINT ( 'NONE',  ( -8.660254037844387298, 212.0833333333333428, -5.000000000000004441 ) ) ;
#53666 = CARTESIAN_POINT ( 'NONE',  ( 7.188101187499992051, 8.802885111219154394E-16, 8.611552781871752771 ) ) ;
#53667 = CARTESIAN_POINT ( 'NONE',  ( 3.042071309553167069, 182.1354166632526699, -11.35316468749999785 ) ) ;
#53668 = CARTESIAN_POINT ( 'NONE',  ( -3.211159895383562723, 1.937499998634406806, 3.211159895383561391 ) ) ;
#53669 = CARTESIAN_POINT ( 'NONE',  ( 10.00000000000000000, 242.5000000000000284, -1.224646799147353256E-15 ) ) ;
#53670 = LINE ( 'NONE', #31017, #17015 ) ;
#53671 = ORIENTED_EDGE ( 'NONE', *, *, #395, .F. ) ;
#53672 =( BOUNDED_CURVE ( )  B_SPLINE_CURVE ( 2, ( #57457, #23474, #12882, #35918, #24207, #63838, #46856, #47218, #58937 ),
 .UNSPECIFIED., .F., .F. ) 
 B_SPLINE_CURVE_WITH_KNOTS ( ( 3, 2, 2, 2, 3 ),
 ( 0.7205882352941176405, 0.7242647058823529216, 0.7279411764705880916, 0.7316176470588233727, 0.7352941176470587648 ),
 .UNSPECIFIED. ) 
 CURVE ( )  GEOMETRIC_REPRESENTATION_ITEM ( )  RATIONAL_B_SPLINE_CURVE ( ( 1.000000000000000000, 0.9238795325112867385, 1.000000000000000000, 0.9238795325112867385, 1.000000000000000000, 0.9238795325112867385, 1.000000000000000000, 0.9238795325112890700, 0.9999999999999976685 ) ) 
 REPRESENTATION_ITEM ( '' )  );
#53673 = ADVANCED_FACE ( 'NONE', ( #70095 ), #51996, .T. ) ;
#53674 = CARTESIAN_POINT ( 'NONE',  ( 3.458734124999959469, 208.7500000013656063, 140.5673454167824161 ) ) ;
#53675 = CARTESIAN_POINT ( 'NONE',  ( -9.832129032723418760, 53.17708332991935549, -5.676582343750004256 ) ) ;
#53676 = CARTESIAN_POINT ( 'NONE',  ( 11.00000000000000000, 4.556349186104045934, 105.5312500040967905 ) ) ;
#53677 = VECTOR ( 'NONE', #73187, 1000.000000000000000 ) ;
#53678 = CARTESIAN_POINT ( 'NONE',  ( 9.832129032723420536, 221.5104166632526983, -5.676582343749999815 ) ) ;
#53679 = CARTESIAN_POINT ( 'NONE',  ( -31.45873412499999944, 203.6875000013656063, 170.0000000000004547 ) ) ;
#53680 = CARTESIAN_POINT ( 'NONE',  ( -6.735557395310442023E-16, 11.00000000000000000, 95.31250000409677625 ) ) ;
#53682 = CARTESIAN_POINT ( 'NONE',  ( -8.660254037844390851, 59.79166665983870388, 4.999999999999998224 ) ) ;
#53681 = CARTESIAN_POINT ( 'NONE',  ( 2.977408999572650039, 120.6875000020483952, -7.188101187500000933 ) ) ;
#53683 = CARTESIAN_POINT ( 'NONE',  ( -2.445694354108838731, 195.0625000013656063, 144.4456943541088663 ) ) ;
#53684 =( BOUNDED_CURVE ( )  B_SPLINE_CURVE ( 2, ( #74422, #28029, #23478, #46490, #22728, #69511, #17823, #40837, #35195 ),
 .UNSPECIFIED., .F., .F. ) 
 B_SPLINE_CURVE_WITH_KNOTS ( ( 3, 2, 2, 2, 3 ),
 ( 0.7840909090909090606, 0.7897727272727272929, 0.7954545454545454142, 0.8011363636363637575, 0.8068181818181818787 ),
 .UNSPECIFIED. ) 
 CURVE ( )  GEOMETRIC_REPRESENTATION_ITEM ( )  RATIONAL_B_SPLINE_CURVE ( ( 1.000000000000000000, 0.9238795325112867385, 1.000000000000000000, 0.9238795325112867385, 1.000000000000000000, 0.9238795325112867385, 1.000000000000000000, 0.9238795325112852952, 1.000000000000001554 ) ) 
 REPRESENTATION_ITEM ( '' )  );
#53685 = CARTESIAN_POINT ( 'NONE',  ( -2.085542519210945728E-15, 104.5312499965860269, 11.35316468750000141 ) ) ;
#53686 = CARTESIAN_POINT ( 'NONE',  ( 6.123233995736767268E-16, 78.12499999317202537, -10.00000000000000178 ) ) ;
#53687 = AXIS2_PLACEMENT_3D ( 'NONE', #56429, #60963, #32686 ) ;
#53688 = CARTESIAN_POINT ( 'NONE',  ( -4.401442555609581635E-16, 90.78125000204836681, -7.188101187500000044 ) ) ;
#53689 = CARTESIAN_POINT ( 'NONE',  ( -3.211159895383561391, 16.81249999863440436, -3.211159895383561835 ) ) ;
#53690 = CARTESIAN_POINT ( 'NONE',  ( -30.82842712474624491, 204.2500000027312126, 167.1715728752542418 ) ) ;
#53691 = CARTESIAN_POINT ( 'NONE',  ( -8.000000000000021316, -3.313708498984730522, 23.42405277982336642 ) ) ;
#53692 = ORIENTED_EDGE ( 'NONE', *, *, #63473, .F. ) ;
#53693 = ORIENTED_EDGE ( 'NONE', *, *, #16099, .T. ) ;
#53694 = CARTESIAN_POINT ( 'NONE',  ( -6.676582343750001591, 292.6093750017069510, 0.000000000000000000 ) ) ;
#53695 = DIRECTION ( 'NONE',  ( 0.000000000000000000, 0.000000000000000000, 1.000000000000000000 ) ) ;
#53696 = CARTESIAN_POINT ( 'NONE',  ( 5.676582343750001591, 166.6145833299193555, -9.832129032723420536 ) ) ;
#53697 = CARTESIAN_POINT ( 'NONE',  ( 2.679491924311228956, 2.916666659838698994, -10.00000000000000000 ) ) ;
#53698 = CARTESIAN_POINT ( 'NONE',  ( 1.656854249492403008, 198.6875000000000284, 194.0000000000000853 ) ) ;
#53699 = DIRECTION ( 'NONE',  ( -0.000000000000000000, 1.000000000000000000, 0.000000000000000000 ) ) ;
#53700 = CARTESIAN_POINT ( 'NONE',  ( -10.18810118749999916, 4.220049686691934809, 111.4375000020483810 ) ) ;
#53701 = VERTEX_POINT ( 'NONE', #22946 ) ;
#53702 =( BOUNDED_CURVE ( )  B_SPLINE_CURVE ( 2, ( #58790, #63687, #7833, #52752, #41061, #41431, #2171, #35775, #12379 ),
 .UNSPECIFIED., .F., .F. ) 
 B_SPLINE_CURVE_WITH_KNOTS ( ( 3, 2, 2, 2, 3 ),
 ( 0.2291666666666645480, 0.2395833333333312609, 0.2499999999999979183, 0.2604166666666646313, 0.2708333333333312609 ),
 .UNSPECIFIED. ) 
 CURVE ( )  GEOMETRIC_REPRESENTATION_ITEM ( )  RATIONAL_B_SPLINE_CURVE ( ( 1.000000000000015321, 0.9238795325112713064, 1.000000000000000000, 0.9238795325112867385, 1.000000000000000000, 0.9238795325112867385, 1.000000000000000000, 0.9238795325113017265, 0.9999999999999850120 ) ) 
 REPRESENTATION_ITEM ( '' )  );
#53703 = ADVANCED_FACE ( 'NONE', ( #45580 ), #18401, .T. ) ;
#53704 = CARTESIAN_POINT ( 'NONE',  ( -3.313708498984842432, 112.7187499999999858, -7.999999999999920064 ) ) ;
#53705 = FACE_OUTER_BOUND ( 'NONE', #44835, .T. ) ;
#53706 = CARTESIAN_POINT ( 'NONE',  ( -5.676582343749998039, 142.7604166632526699, -9.832129032723420536 ) ) ;
#53707 = CARTESIAN_POINT ( 'NONE',  ( 1.656854249492440978, 206.8125000027312126, 194.0000000000001137 ) ) ;
#53708 = CARTESIAN_POINT ( 'NONE',  ( 10.18810118750000093, -4.220049686691933033, 68.68750000204838102 ) ) ;
#53709 = CARTESIAN_POINT ( 'NONE',  ( 11.35316468749999963, 46.30208332991934128, -3.042071309553165293 ) ) ;
#53710 = VERTEX_POINT ( 'NONE', #39927 ) ;
#53711 = CARTESIAN_POINT ( 'NONE',  ( -5.656854249492373476, -5.656854249492376141, 13.01780277982336465 ) ) ;
#53712 = CARTESIAN_POINT ( 'NONE',  ( -4.541265875000002339, 4.874999998634406140, -1.881053915767121998 ) ) ;
#53713 = CARTESIAN_POINT ( 'NONE',  ( 8.008118988124991233, 3.317071493978879015, 6.356865283940630995 ) ) ;
#53714 = CARTESIAN_POINT ( 'NONE',  ( 7.188101187499999156, 13.87499999795161187, 2.977408999572654924 ) ) ;
#53715 = CARTESIAN_POINT ( 'NONE',  ( -3.673940397442060854E-16, 291.8125000034140157, -6.000000000000001776 ) ) ;
#53716 = CARTESIAN_POINT ( 'NONE',  ( 4.000000000000015987, 202.5000000000000000, 198.0000000000000284 ) ) ;
#53717 = CARTESIAN_POINT ( 'NONE',  ( 2.977408999572651815, 9.562499997951608322, 7.188101187500000933 ) ) ;
#53718 = CARTESIAN_POINT ( 'NONE',  ( 2.977408999572650927, -7.188101187499990274, 9.455302781871752771 ) ) ;
#53719 = CARTESIAN_POINT ( 'NONE',  ( 7.204075437095968759, -7.204075437095966983, 116.5937500020483810 ) ) ;
#53720 = EDGE_CURVE ( 'NONE', #2769, #44073, #42463, .T. ) ;
#53721 =( BOUNDED_CURVE ( )  B_SPLINE_CURVE ( 2, ( #36086, #59105, #6678, #30420, #1031, #29681, #64750, #47393, #41376, #58008, #24011, #12685, #69302 ),
 .UNSPECIFIED., .F., .F. ) 
 B_SPLINE_CURVE_WITH_KNOTS ( ( 3, 2, 2, 2, 2, 2, 3 ),
 ( 1.711289316333768351, 1.716522046495266629, 1.721754776656765129, 1.726987506818263407, 1.732220236979761685, 1.737452967141260185, 1.742685697302758463 ),
 .UNSPECIFIED. ) 
 CURVE ( )  GEOMETRIC_REPRESENTATION_ITEM ( )  RATIONAL_B_SPLINE_CURVE ( ( 1.000000000000001998, 0.9659258262890662028, 1.000000000000000000, 0.9659258262890683122, 1.000000000000000000, 0.9659258262890683122, 1.000000000000000000, 0.9659258262890683122, 1.000000000000000000, 0.9659258262890683122, 1.000000000000000000, 0.9659258262893397617, 0.9999999999997285505 ) ) 
 REPRESENTATION_ITEM ( '' )  );
#53722 = EDGE_CURVE ( 'NONE', #61381, #33430, #25897, .T. ) ;
#53723 = CYLINDRICAL_SURFACE ( 'NONE', #22164, 11.00000000000000000 ) ;
#53724 = CARTESIAN_POINT ( 'NONE',  ( -1.656854249492383691, 2.437499997268814056, 4.000000000000000888 ) ) ;
#53725 = ORIENTED_EDGE ( 'NONE', *, *, #25585, .T. ) ;
#53726 = CARTESIAN_POINT ( 'NONE',  ( 4.000000000000015099, 196.6875000027312126, 196.3431457505076594 ) ) ;
#53727 = CIRCLE ( 'NONE', #70587, 12.00000000000000178 ) ;
#53728 = CARTESIAN_POINT ( 'NONE',  ( 1.656854249492348607, 203.1875000000000284, 138.0000000000000568 ) ) ;
#53729 = CARTESIAN_POINT ( 'NONE',  ( -29.65685424949228732, 196.5625000027312126, 174.0000000000004547 ) ) ;
#53730 = CARTESIAN_POINT ( 'NONE',  ( 4.541265875000001451, 3.249999998634406584, 1.881053915767124440 ) ) ;
#53731 = CARTESIAN_POINT ( 'NONE',  ( -7.188101187500000044, 116.6562500020483810, 0.000000000000000000 ) ) ;
#53732 = ADVANCED_FACE ( 'NONE', ( #18030, #62933 ), #1071, .T. ) ;
#53733 = CARTESIAN_POINT ( 'NONE',  ( -28.00000000000002842, 209.8437500006828031, 166.2706329375003804 ) ) ;
#53734 = CARTESIAN_POINT ( 'NONE',  ( -7.999999999999991118, 0.000000000000000000, 1.017802783920145782 ) ) ;
#53735 = ORIENTED_EDGE ( 'NONE', *, *, #36094, .T. ) ;
#53736 = CARTESIAN_POINT ( 'NONE',  ( -7.188101187500002709, 20.81249999795161543, 2.977408999572649151 ) ) ;
#53737 = ORIENTED_EDGE ( 'NONE', *, *, #32745, .F. ) ;
#53738 = LINE ( 'NONE', #9194, #32805 ) ;
#53739 = CARTESIAN_POINT ( 'NONE',  ( 6.000000000000001776, 296.5000000000000000, -7.347880794884121708E-16 ) ) ;
#53740 = CARTESIAN_POINT ( 'NONE',  ( 28.00000000000001776, 201.4375000013656063, 173.4587341249998929 ) ) ;
#53741 = CARTESIAN_POINT ( 'NONE',  ( 7.320508075688771044, 54.37500000000000000, 7.320508075688775484 ) ) ;
#53742 = CARTESIAN_POINT ( 'NONE',  ( -4.401442555609581635E-16, 98.65625000204838102, -7.188101187500000044 ) ) ;
#53743 = CARTESIAN_POINT ( 'NONE',  ( 6.000000000000003553, 296.5625000000000000, -2.485281374238571761 ) ) ;
#53745 = CARTESIAN_POINT ( 'NONE',  ( -27.64040105425268479, -42.47909655985780120, 184.0500010904650310 ) ) ;
#53744 = CARTESIAN_POINT ( 'NONE',  ( -3.673940397442060854E-16, 287.8125000034140157, -6.000000000000001776 ) ) ;
#53746 = ORIENTED_EDGE ( 'NONE', *, *, #55931, .F. ) ;
#53747 = CARTESIAN_POINT ( 'NONE',  ( 8.311093377946839666, 235.7812500034139589, 8.311093377946829008 ) ) ;
#53748 = CARTESIAN_POINT ( 'NONE',  ( 5.107860025164002948, 50.62490018645832635, 41.07729128472288949 ) ) ;
#53749 = CARTESIAN_POINT ( 'NONE',  ( -5.000000000000000000, 60.90295814858271939, -23.31388853594749833 ) ) ;
#53750 = CARTESIAN_POINT ( 'NONE',  ( 5.656854249492374365, 5.656854249492375253, 1.955302783920143117 ) ) ;
#53751 = CARTESIAN_POINT ( 'NONE',  ( 25.10295958197927746, 194.8478348442015999, 167.4604882576522584 ) ) ;
#53752 = PLANE ( 'NONE',  #74017 ) ;
#53753 = CARTESIAN_POINT ( 'NONE',  ( 2.679491924311222739, 173.9583333333333144, 10.00000000000000355 ) ) ;
#53754 = CARTESIAN_POINT ( 'NONE',  ( 0.000000000000000000, 0.000000000000000000, 30.00000000000000000 ) ) ;
#53755 =( NAMED_UNIT ( * ) SI_UNIT ( $, .STERADIAN. ) SOLID_ANGLE_UNIT ( ) );
#53756 = FACE_OUTER_BOUND ( 'NONE', #25140, .T. ) ;
#53757 = CARTESIAN_POINT ( 'NONE',  ( 9.832129032723416984, 145.6770833299193555, 5.676582343750006032 ) ) ;
#53758 = CARTESIAN_POINT ( 'NONE',  ( 1.469576158976823947E-15, 108.8750000000000000, 8.000000000000000000 ) ) ;
#53759 = FACE_OUTER_BOUND ( 'NONE', #39336, .T. ) ;
#53762 = CARTESIAN_POINT ( 'NONE',  ( 26.34314575050768426, 203.5625000000000284, 165.9999999999998295 ) ) ;
#53761 = DIRECTION ( 'NONE',  ( -0.000000000000000000, -0.000000000000000000, -1.000000000000000000 ) ) ;
#53760 = CARTESIAN_POINT ( 'NONE',  ( 25.17157287525381548, 204.6250000000000284, 167.1715728752537018 ) ) ;
#53763 = ADVANCED_FACE ( 'NONE', ( #69340 ), #5231, .T. ) ;
#53764 = EDGE_LOOP ( 'NONE', ( #26227, #35177 ) ) ;
#53765 = CARTESIAN_POINT ( 'NONE',  ( 5.676582343750001591, 11.92708332991935016, -9.832129032723420536 ) ) ;
#53766 = CARTESIAN_POINT ( 'NONE',  ( 2.143584681480918963, 88.75185463835309463, -8.000000000000000000 ) ) ;
#53767 = ADVANCED_FACE ( 'NONE', ( #68970 ), #11999, .T. ) ;
#53768 = CARTESIAN_POINT ( 'NONE',  ( -5.000000000000005329, 90.20833332650536818, 8.660254037844387298 ) ) ;
#53769 = FACE_OUTER_BOUND ( 'NONE', #6870, .T. ) ;
#53770 = CARTESIAN_POINT ( 'NONE',  ( 3.458734124999959914, 207.3750000013656063, 143.4326545832176976 ) ) ;
#53771 = CARTESIAN_POINT ( 'NONE',  ( -5.656854249492381470, 5.249999995903221084, 5.656854249492379694 ) ) ;
#53772 = CARTESIAN_POINT ( 'NONE',  ( 2.679491924311222739, 35.83333332650536818, 10.00000000000000355 ) ) ;
#53773 = CARTESIAN_POINT ( 'NONE',  ( 5.082755093536325042, 114.5937500020483810, -5.082755093536325930 ) ) ;
#53774 = CARTESIAN_POINT ( 'NONE',  ( 3.211159895383560947, 5.312499998634407028, 3.211159895383562723 ) ) ;
#53775 = CARTESIAN_POINT ( 'NONE',  ( -7.778174593052020747, -7.778174593052023411, 85.18749999999998579 ) ) ;
#53776 = CARTESIAN_POINT ( 'NONE',  ( 5.656854249492376141, -5.656854249492374365, 13.39280277982336465 ) ) ;
#53777 = CARTESIAN_POINT ( 'NONE',  ( -3.673940397442060854E-16, 291.8125000034140157, -6.000000000000001776 ) ) ;
#53778 = VERTEX_POINT ( 'NONE', #34287 ) ;
#53779 = EDGE_CURVE ( 'NONE', #61205, #11312, #69716, .T. ) ;
#53780 = CARTESIAN_POINT ( 'NONE',  ( 7.320508075688775484, 29.37500000000000355, 7.320508075688779037 ) ) ;
#53781 = CARTESIAN_POINT ( 'NONE',  ( 5.656854249492381470, 109.0624999999999858, 5.656854249492379694 ) ) ;
#53782 = CARTESIAN_POINT ( 'NONE',  ( -9.832129032723415207, 224.6354166700806729, 5.676582343750005144 ) ) ;
#53783 = CARTESIAN_POINT ( 'NONE',  ( 9.832129032723420536, 111.1979166632526983, -5.676582343749999815 ) ) ;
#53784 = ORIENTED_EDGE ( 'NONE', *, *, #57898, .F. ) ;
#53785 = CARTESIAN_POINT ( 'NONE',  ( 1.656854249492504705, 198.6875000000000284, 194.0000000000001990 ) ) ;
#53786 = CARTESIAN_POINT ( 'NONE',  ( 4.220049686691941027, -10.18810118749999738, 93.62500000204838102 ) ) ;
#53787 = DIRECTION ( 'NONE',  ( 0.8660254037844381525, 0.5000000000000008882, 0.000000000000000000 ) ) ;
#53788 = CARTESIAN_POINT ( 'NONE',  ( -3.458734124999960358, 198.6875000013655779, 198.0000000000000284 ) ) ;
#53789 = CARTESIAN_POINT ( 'NONE',  ( 0.000000000000000000, 75.00000000000000000, 11.00000000000000000 ) ) ;
#53791 = CARTESIAN_POINT ( 'NONE',  ( -8.311093377946841443, 113.9062499965860127, 8.311093377946834337 ) ) ;
#53790 = CARTESIAN_POINT ( 'NONE',  ( -19.30232404099007582, 180.3952738753220331, 120.2370213099772371 ) ) ;
#53792 = CARTESIAN_POINT ( 'NONE',  ( -23.99999999999999289, 209.7500000000000284, 170.0000000000003411 ) ) ;
#53793 = CARTESIAN_POINT ( 'NONE',  ( 7.999999999999989342, -3.268493847551538582E-05, 6.267801859212078774 ) ) ;
#53794 = VERTEX_POINT ( 'NONE', #53845 ) ;
#53795 = CARTESIAN_POINT ( 'NONE',  ( 10.00000000000000178, 211.8749999931720538, 0.000000000000000000 ) ) ;
#53796 = CARTESIAN_POINT ( 'NONE',  ( -2.751064625579944321E-14, 205.7500000000000284, 146.0000000000000284 ) ) ;
#53797 = FACE_OUTER_BOUND ( 'NONE', #179, .T. ) ;
#53798 = CARTESIAN_POINT ( 'NONE',  ( -8.311093377946836114, 102.9687499965859985, -8.311093377946837890 ) ) ;
#53799 = DIRECTION ( 'NONE',  ( 0.000000000000000000, 0.000000000000000000, -1.000000000000000000 ) ) ;
#53800 = CARTESIAN_POINT ( 'NONE',  ( -5.082755093536325042, 14.90624999795161187, -5.082755093536325930 ) ) ;
#53801 =( BOUNDED_CURVE ( )  B_SPLINE_CURVE ( 2, ( #1282, #42720, #12572, #48008, #12933, #65733, #14035, #2001, #42350 ),
 .UNSPECIFIED., .F., .F. ) 
 B_SPLINE_CURVE_WITH_KNOTS ( ( 3, 2, 2, 2, 3 ),
 ( 0.4886363636363636465, 0.4943181818181818232, 0.5000000000000000000, 0.5056818181818182323, 0.5113636363636363535 ),
 .UNSPECIFIED. ) 
 CURVE ( )  GEOMETRIC_REPRESENTATION_ITEM ( )  RATIONAL_B_SPLINE_CURVE ( ( 1.000000000000000000, 0.9238795325112867385, 1.000000000000000000, 0.9238795325112867385, 1.000000000000000000, 0.9238795325112867385, 1.000000000000000000, 0.9238795325112867385, 1.000000000000000000 ) ) 
 REPRESENTATION_ITEM ( '' )  );
#53802 = CARTESIAN_POINT ( 'NONE',  ( 7.204075437095968759, -7.204075437095966983, 89.59375000204838102 ) ) ;
#53803 = CARTESIAN_POINT ( 'NONE',  ( -5.676582343750006032, 4.427083329919350163, 9.832129032723418760 ) ) ;
#53804 = VERTEX_POINT ( 'NONE', #30823 ) ;
#53805 = CARTESIAN_POINT ( 'NONE',  ( 8.660254037844385522, 181.4583333265053682, 5.000000000000005329 ) ) ;
#53806 = CARTESIAN_POINT ( 'NONE',  ( 5.662595241051934458, 5.662595241051935346, 24.45061528394063188 ) ) ;
#53807 = CARTESIAN_POINT ( 'NONE',  ( 38.00000000000000000, 205.0000000000000284, 20.00000000000002132 ) ) ;
#53808 = CARTESIAN_POINT ( 'NONE',  ( -10.18810118749999916, 4.220049686691934809, 72.43750000204838102 ) ) ;
#53809 = DIRECTION ( 'NONE',  ( 5.551115147383500873E-15, 0.5000000000000113243, 0.8660254037844320463 ) ) ;
#53810 = CARTESIAN_POINT ( 'NONE',  ( -3.313708498984816231, 93.96875000409676204, 7.999999999999943157 ) ) ;
#53811 = CARTESIAN_POINT ( 'NONE',  ( 1.226468279477575784E-15, 294.7031250017069510, 6.676582343750001591 ) ) ;
#53812 = CARTESIAN_POINT ( 'NONE',  ( 7.320508075688771044, 126.2499999931720396, 7.320508075688775484 ) ) ;
#53813 = CARTESIAN_POINT ( 'NONE',  ( -5.676582343749998039, 222.7604166632526983, -9.832129032723420536 ) ) ;
#53814 = AXIS2_PLACEMENT_3D ( 'NONE', #32085, #9821, #55106 ) ;
#53815 = CARTESIAN_POINT ( 'NONE',  ( 7.204075437095966983, 7.204075437095967871, 80.59375000204838102 ) ) ;
#53816 = ADVANCED_FACE ( 'NONE', ( #54220 ), #24424, .T. ) ;
#53817 = CARTESIAN_POINT ( 'NONE',  ( -27.99999999999996447, 198.9375000013655779, 173.4587341250003760 ) ) ;
#53818 =( BOUNDED_CURVE ( )  B_SPLINE_CURVE ( 2, ( #14221, #71569, #49308, #30850, #14599, #19891, #53871, #3302, #1821, #43277, #42158, #30486, #37639 ),
 .UNSPECIFIED., .F., .F. ) 
 B_SPLINE_CURVE_WITH_KNOTS ( ( 3, 2, 2, 2, 2, 2, 3 ),
 ( 0.6944444444444444198, 0.7037037037037037202, 0.7129629629629629095, 0.7222222222222222099, 0.7314814814814815103, 0.7407407407407406996, 0.7500000000000000000 ),
 .UNSPECIFIED. ) 
 CURVE ( )  GEOMETRIC_REPRESENTATION_ITEM ( )  RATIONAL_B_SPLINE_CURVE ( ( 1.000000000000000000, 0.9659258262890683122, 1.000000000000000000, 0.9659258262890683122, 1.000000000000000000, 0.9659258262890683122, 1.000000000000000000, 0.9659258262890683122, 1.000000000000000000, 0.9659258262890683122, 1.000000000000000000, 0.9659258262890683122, 1.000000000000000000 ) ) 
 REPRESENTATION_ITEM ( '' )  );
#53819 = CARTESIAN_POINT ( 'NONE',  ( 7.999999999999998224, 23.90625000000000000, 3.313708498984766493 ) ) ;
#53820 = CARTESIAN_POINT ( 'NONE',  ( 1.881053915767122664, 10.24999999863440792, 4.541265875000001451 ) ) ;
#53821 = ORIENTED_EDGE ( 'NONE', *, *, #58116, .T. ) ;
#53822 = CARTESIAN_POINT ( 'NONE',  ( -30.02843915197690805, -51.97725902804302933, 162.2548226003614218 ) ) ;
#53823 = CARTESIAN_POINT ( 'NONE',  ( -3.999999999999959144, 206.1875000027311842, 199.6568542494924259 ) ) ;
#53824 = CARTESIAN_POINT ( 'NONE',  ( -3.458734125000015869, 197.1875000013655779, 142.0000000000000568 ) ) ;
#53825 = CARTESIAN_POINT ( 'NONE',  ( -2.751064625579944321E-14, 202.8750000027312126, 146.0000000000000284 ) ) ;
#53826 = CARTESIAN_POINT ( 'NONE',  ( 5.000000000000000000, 16.24494643555759410, -69.83755725260752456 ) ) ;
#53827 = CARTESIAN_POINT ( 'NONE',  ( -4.220049686691935698, 10.18810118749999916, 70.75000000204836681 ) ) ;
#53828 = VERTEX_POINT ( 'NONE', #7084 ) ;
#53829 = CARTESIAN_POINT ( 'NONE',  ( 2.977408999572650927, 2.249999997951610098, -7.188101187500000933 ) ) ;
#53830 = VECTOR ( 'NONE', #54215, 1000.000000000000000 ) ;
#53831 = CARTESIAN_POINT ( 'NONE',  ( -7.320508075688778149, 29.99999999317203248, 7.320508075688769267 ) ) ;
#53832 = CARTESIAN_POINT ( 'NONE',  ( -7.188101187500000044, 118.5312500020483810, 0.000000000000000000 ) ) ;
#53833 = PRODUCT_DEFINITION_FORMATION_WITH_SPECIFIED_SOURCE ( 'ANY', '', #49912, .NOT_KNOWN. ) ;
#53834 = CARTESIAN_POINT ( 'NONE',  ( -4.195582579073398932, 22.00000000000000355, 1.737867247408543925 ) ) ;
#53835 = CARTESIAN_POINT ( 'NONE',  ( -2.765530957081998142, 292.6406250017069510, 6.676582343750000703 ) ) ;
#53837 = CARTESIAN_POINT ( 'NONE',  ( 4.999999999999993783, 136.0416666598387110, 8.660254037844390851 ) ) ;
#53836 = CARTESIAN_POINT ( 'NONE',  ( 5.676582343750005144, 235.5729166700806729, 9.832129032723416984 ) ) ;
#53838 = ORIENTED_EDGE ( 'NONE', *, *, #22351, .T. ) ;
#53839 = CARTESIAN_POINT ( 'NONE',  ( 5.676582343749997150, 222.5520833367473017, -9.832129032723418760 ) ) ;
#53840 = CARTESIAN_POINT ( 'NONE',  ( 5.082755093536320601, -5.082755093536318824, 0.5490527818717526598 ) ) ;
#53841 = CARTESIAN_POINT ( 'NONE',  ( -1.469576158976823947E-15, 15.93749999590322197, 8.000000000000000000 ) ) ;
#53842 = CARTESIAN_POINT ( 'NONE',  ( -2.445694354108784108, 197.5625000013656063, 195.5543056458912190 ) ) ;
#53843 = ORIENTED_EDGE ( 'NONE', *, *, #36921, .F. ) ;
#53844 = CARTESIAN_POINT ( 'NONE',  ( 11.35316468749999963, 106.3020833299193413, -3.042071309553165293 ) ) ;
#53845 = CARTESIAN_POINT ( 'NONE',  ( 6.123233995736767268E-16, 43.12499999317203248, -10.00000000000000178 ) ) ;
#53846 = CARTESIAN_POINT ( 'NONE',  ( 11.00000000000000000, 4.556349186104045934, 76.84374999999998579 ) ) ;
#53848 = CARTESIAN_POINT ( 'NONE',  ( 27.99999999999996803, 202.9375000013656063, 166.5412658749999082 ) ) ;
#53847 = CARTESIAN_POINT ( 'NONE',  ( 30.44569435410879166, 202.8125000013656063, 172.4456943541087526 ) ) ;
#53849 = VERTEX_POINT ( 'NONE', #8558 ) ;
#53850 = CARTESIAN_POINT ( 'NONE',  ( 4.531193156845207581E-15, 210.0000000000000284, 133.0000000000000284 ) ) ;
#53851 = EDGE_CURVE ( 'NONE', #22380, #38706, #396, .T. ) ;
#53852 = CARTESIAN_POINT ( 'NONE',  ( 6.951808397369818766E-16, 207.0312499965860411, -11.35316468750000141 ) ) ;
#53853 = CARTESIAN_POINT ( 'NONE',  ( -3.458734125000016313, 201.8750000013656063, 140.5673454167824161 ) ) ;
#53854 = VECTOR ( 'NONE', #4425, 1000.000000000000000 ) ;
#53855 = CARTESIAN_POINT ( 'NONE',  ( 24.54126587499999346, 200.4375000013656063, 169.9999999999998863 ) ) ;
#53856 = CARTESIAN_POINT ( 'NONE',  ( -5.082755093536325042, 26.90624999795161898, -5.082755093536325930 ) ) ;
#53857 = CARTESIAN_POINT ( 'NONE',  ( -2.085542519210945728E-15, 194.8437499965860127, 11.35316468750000141 ) ) ;
#53858 = CARTESIAN_POINT ( 'NONE',  ( 1.320432766682874540E-15, 94.90625000204838102, 7.188101187500000044 ) ) ;
#53859 = FACE_OUTER_BOUND ( 'NONE', #37257, .T. ) ;
#53860 = CARTESIAN_POINT ( 'NONE',  ( -32.00000000000000711, 196.1875000000000568, 168.3431457505080004 ) ) ;
#53861 = CARTESIAN_POINT ( 'NONE',  ( 1.881053915767122664, 13.12499999863440969, 4.541265875000001451 ) ) ;
#53862 = CARTESIAN_POINT ( 'NONE',  ( 26.56734541678232731, 200.6250000013656063, 173.4587341249998929 ) ) ;
#53863 = CARTESIAN_POINT ( 'NONE',  ( 7.188101187499993827, -2.977408999572645598, 4.017802781871751883 ) ) ;
#53864 = CARTESIAN_POINT ( 'NONE',  ( 11.35316468749999963, 85.98958332991936970, -3.042071309553165293 ) ) ;
#53865 = ORIENTED_EDGE ( 'NONE', *, *, #37951, .T. ) ;
#53866 = ADVANCED_FACE ( 'NONE', ( #31572 ), #36864, .T. ) ;
#53867 = CARTESIAN_POINT ( 'NONE',  ( 7.320508075688781702, 140.6250000000000284, -7.320508075688781702 ) ) ;
#53868 = CARTESIAN_POINT ( 'NONE',  ( -2.849036369511732440E-14, 201.2500000000000000, 138.0000000000000568 ) ) ;
#53869 = ORIENTED_EDGE ( 'NONE', *, *, #66876, .F. ) ;
#53870 = CARTESIAN_POINT ( 'NONE',  ( -2.679491924311159234, 46.45833333333334281, -10.00000000000007105 ) ) ;
#53871 = CARTESIAN_POINT ( 'NONE',  ( 10.00000000000000000, 232.5000000000000000, -1.224646799147353256E-15 ) ) ;
#53872 = CARTESIAN_POINT ( 'NONE',  ( 8.311093377946837890, 71.40624999658602690, -8.311093377946837890 ) ) ;
#53873 = ORIENTED_EDGE ( 'NONE', *, *, #69784, .T. ) ;
#53874 = CARTESIAN_POINT ( 'NONE',  ( -4.220049686691937474, -10.18810118749999738, 87.81250000204838102 ) ) ;
#53875 = CARTESIAN_POINT ( 'NONE',  ( 4.220049686691941027, -10.18810118749999738, 114.6250000020483810 ) ) ;
#53876 = CARTESIAN_POINT ( 'NONE',  ( -3.458734124999959469, 207.7500000013656063, 199.4326545832176691 ) ) ;
#53877 = CARTESIAN_POINT ( 'NONE',  ( -4.231687259407056700, 16.30907003467247307, 69.42009600258496960 ) ) ;
#53879 = CARTESIAN_POINT ( 'NONE',  ( 8.311093377946837890, 76.40624999658602690, -8.311093377946837890 ) ) ;
#53878 = CARTESIAN_POINT ( 'NONE',  ( -8.000000000000000000, 123.6875000040967905, 0.000000000000000000 ) ) ;
#53880 = CARTESIAN_POINT ( 'NONE',  ( 3.313708498984756279, 7.999999999999991118, 23.04905278392014623 ) ) ;
#53881 = CARTESIAN_POINT ( 'NONE',  ( -2.841757666793576517E-14, 194.6037658790967271, 138.3962341209032445 ) ) ;
#53882 = CARTESIAN_POINT ( 'NONE',  ( 7.320508075688774596, 172.4999999931719969, -7.320508075688774596 ) ) ;
#53883 = CARTESIAN_POINT ( 'NONE',  ( -5.082755093536324154, 90.21875000204838102, 5.082755093536326818 ) ) ;
#53884 = CARTESIAN_POINT ( 'NONE',  ( -27.99999999999999289, 194.7622595281507358, 173.7622595281509916 ) ) ;
#53885 = CARTESIAN_POINT ( 'NONE',  ( 8.311093377946834337, 55.46874999658601268, 8.311093377946839666 ) ) ;
#53886 = CARTESIAN_POINT ( 'NONE',  ( -4.220049686691937474, -10.18810118749999738, 107.3125000020483810 ) ) ;
#53887 = CARTESIAN_POINT ( 'NONE',  ( -3.042071309553173730, 194.3229166632526699, 11.35316468749999785 ) ) ;
#53888 = VERTEX_POINT ( 'NONE', #1443 ) ;
#53889 = CARTESIAN_POINT ( 'NONE',  ( -7.456209740496419158, 61.82228229130262775, 23.87473629694281030 ) ) ;
#53890 = CARTESIAN_POINT ( 'NONE',  ( -3.313708498984727413, 121.7187499999999858, -8.000000000000033751 ) ) ;
#53891 = CARTESIAN_POINT ( 'NONE',  ( 5.000000000000000000, 60.90295814858223622, 23.31388853594876664 ) ) ;
#53893 = CARTESIAN_POINT ( 'NONE',  ( -11.35316468750000141, 188.2812499965860127, -1.390361679473963753E-15 ) ) ;
#53892 = CARTESIAN_POINT ( 'NONE',  ( -6.123233995736766282E-16, 263.7500000000000568, -10.00000000000000000 ) ) ;
#53894 = VECTOR ( 'NONE', #50677, 1000.000000000000000 ) ;
#53895 = CARTESIAN_POINT ( 'NONE',  ( -2.679491924311226292, 193.3333333265053682, -10.00000000000000178 ) ) ;
#53896 = CARTESIAN_POINT ( 'NONE',  ( 2.679491924311225848, 241.6666666734946318, -10.00000000000000000 ) ) ;
#53897 = ORIENTED_EDGE ( 'NONE', *, *, #71055, .F. ) ;
#53898 = CARTESIAN_POINT ( 'NONE',  ( -5.676582343749998039, 182.7604166632526699, -9.832129032723420536 ) ) ;
#53899 = CLOSED_SHELL ( 'NONE', ( #66345, #55306, #44941, #53732, #28816, #62794 ) ) ;
#53900 = CARTESIAN_POINT ( 'NONE',  ( -5.082755093536319713, 5.082755093536319713, 19.29905278187175455 ) ) ;
#53901 = CARTESIAN_POINT ( 'NONE',  ( 23.99999999999998934, 203.8750000027312126, 169.9999999999999432 ) ) ;
#53902 = ORIENTED_EDGE ( 'NONE', *, *, #72950, .F. ) ;
#53903 = CARTESIAN_POINT ( 'NONE',  ( -8.000000000000000000, 98.18750000409677625, 0.000000000000000000 ) ) ;
#53904 =( BOUNDED_CURVE ( )  B_SPLINE_CURVE ( 2, ( #34644, #18014, #28212, #74611, #23296, #28586, #35015, #22924, #47043 ),
 .UNSPECIFIED., .F., .F. ) 
 B_SPLINE_CURVE_WITH_KNOTS ( ( 3, 2, 2, 2, 3 ),
 ( 0.07954545454545454419, 0.08522727272727272096, 0.09090909090909091161, 0.09659090909090908839, 0.1022727272727272790 ),
 .UNSPECIFIED. ) 
 CURVE ( )  GEOMETRIC_REPRESENTATION_ITEM ( )  RATIONAL_B_SPLINE_CURVE ( ( 1.000000000000000000, 0.9238795325112867385, 1.000000000000000000, 0.9238795325112867385, 1.000000000000000000, 0.9238795325112867385, 1.000000000000000000, 0.9238795325112867385, 1.000000000000000000 ) ) 
 REPRESENTATION_ITEM ( '' )  );
#53905 = CARTESIAN_POINT ( 'NONE',  ( 6.123233995736767268E-16, 6.250000000000000000, -10.00000000000000178 ) ) ;
#53906 = CARTESIAN_POINT ( 'NONE',  ( -7.347880794884122694E-16, 15.75000000000000000, 4.000000000000001776 ) ) ;
#53907 = CARTESIAN_POINT ( 'NONE',  ( -4.541265875000002339, 15.81249999863440436, -5.561446717895856393E-16 ) ) ;
#53908 = CARTESIAN_POINT ( 'NONE',  ( -3.313708498984757167, 7.999999999999991118, 11.23655278392014445 ) ) ;
#53909 = CARTESIAN_POINT ( 'NONE',  ( 0.000000000000000000, 0.000000000000000000, 0.000000000000000000 ) ) ;
#53910 = VERTEX_POINT ( 'NONE', #25151 ) ;
#53911 = CARTESIAN_POINT ( 'NONE',  ( 5.000000000000000000, 70.11723469343132820, -28.93519894129142145 ) ) ;
#53912 = CARTESIAN_POINT ( 'NONE',  ( 5.082755093536325042, 99.59375000204838102, -5.082755093536325930 ) ) ;
#53914 = CARTESIAN_POINT ( 'NONE',  ( 5.656854249492381470, 119.7500000040967905, 5.656854249492379694 ) ) ;
#53913 = FACE_OUTER_BOUND ( 'NONE', #44330, .T. ) ;
#53915 =( LENGTH_UNIT ( ) NAMED_UNIT ( * ) SI_UNIT ( .MILLI., .METRE. ) );
#53917 = ADVANCED_FACE ( 'NONE', ( #53109 ), #71176, .T. ) ;
#53916 = EDGE_LOOP ( 'NONE', ( #41535, #10422, #60450, #38624, #24809, #45376 ) ) ;
#53918 = EDGE_CURVE ( 'NONE', #38960, #57815, #10758, .T. ) ;
#53919 = DIRECTION ( 'NONE',  ( 0.000000000000000000, 0.000000000000000000, -1.000000000000000000 ) ) ;
#53920 = CARTESIAN_POINT ( 'NONE',  ( -4.401442555609577197E-16, 7.188101187499992051, 20.61155278187175455 ) ) ;
#53921 = EDGE_LOOP ( 'NONE', ( #73466, #67797, #20634, #48896 ) ) ;
#53922 = AXIS2_PLACEMENT_3D ( 'NONE', #58206, #11788, #125 ) ;
#53923 = VERTEX_POINT ( 'NONE', #12726 ) ;
#53924 = CARTESIAN_POINT ( 'NONE',  ( -10.18810118749999738, -4.220049686691941915, 78.25000000204838102 ) ) ;
#53925 = CARTESIAN_POINT ( 'NONE',  ( 27.99999999999997158, 210.0000000000000284, 173.9999999999999147 ) ) ;
#53926 = CARTESIAN_POINT ( 'NONE',  ( 7.778174593052021635, 7.778174593052023411, 93.43749999999998579 ) ) ;
#53929 = CARTESIAN_POINT ( 'NONE',  ( 6.676582343750003368, 293.0468750017069510, 2.765530957081995478 ) ) ;
#53928 = CARTESIAN_POINT ( 'NONE',  ( 27.99999999999996447, 200.6250000027312126, 165.9999999999998863 ) ) ;
#53927 = CARTESIAN_POINT ( 'NONE',  ( -32.00000000000002842, 198.3125000027312126, 168.3431457505080857 ) ) ;
#53930 = CARTESIAN_POINT ( 'NONE',  ( 10.00000000000000178, 150.0000000000000284, 0.000000000000000000 ) ) ;
#53931 = CARTESIAN_POINT ( 'NONE',  ( -2.828427124746190735, 0.3750000000000001665, -2.828427124746191623 ) ) ;
#53932 = DIRECTION ( 'NONE',  ( -1.000000000000000000, 0.000000000000000000, 0.000000000000000000 ) ) ;
#53933 = VECTOR ( 'NONE', #20349, 1000.000000000000000 ) ;
#53934 = CARTESIAN_POINT ( 'NONE',  ( 5.000000000000000000, -10.26105934116143459, 64.40045319026695836 ) ) ;
#53935 = CARTESIAN_POINT ( 'NONE',  ( -3.313708498984765161, 2.343749995903220196, 7.999999999999998224 ) ) ;
#53936 = CARTESIAN_POINT ( 'NONE',  ( 25.55430564589115150, 198.3125000013656063, 172.4456943541086957 ) ) ;
#53937 = CARTESIAN_POINT ( 'NONE',  ( -7.188101187500000044, 12.09374999795161187, -8.802885111219163269E-16 ) ) ;
#53938 = CARTESIAN_POINT ( 'NONE',  ( 5.656854249492376141, -5.656854249492374365, 25.58030278392014978 ) ) ;
#53939 = CARTESIAN_POINT ( 'NONE',  ( 5.099999999999999645, 0.000000000000000000, -10.14441321561125520 ) ) ;
#53940 = CARTESIAN_POINT ( 'NONE',  ( 5.082755093536325042, 110.4687500020483810, -5.082755093536325930 ) ) ;
#53942 = CARTESIAN_POINT ( 'NONE',  ( -2.828427124746192067, 16.62500000000000000, 2.828427124746190735 ) ) ;
#53941 = CARTESIAN_POINT ( 'NONE',  ( -28.00000000000002487, 209.6875000013656063, 166.5412658750003629 ) ) ;
#53943 = CARTESIAN_POINT ( 'NONE',  ( -8.311093377946836114, 228.5937500034139873, -8.311093377946836114 ) ) ;
#53944 = CARTESIAN_POINT ( 'NONE',  ( -4.000000000000002665, 12.56250000000000000, 1.656854249492380582 ) ) ;
#53945 = CARTESIAN_POINT ( 'NONE',  ( -4.401442555609577197E-16, 7.188101187499992051, 22.48655278187175455 ) ) ;
#53946 = LINE ( 'NONE', #19970, #9406 ) ;
#53947 = CARTESIAN_POINT ( 'NONE',  ( 5.676582343750001591, 41.61458332991935549, -9.832129032723420536 ) ) ;
#53948 = CARTESIAN_POINT ( 'NONE',  ( 0.4369882809721246097, 16.44602605510714355, 68.55492853905350614 ) ) ;
#53949 = CARTESIAN_POINT ( 'NONE',  ( -8.660254037844387298, 8.958333326505366401, -5.000000000000004441 ) ) ;
#53950 = SPHERICAL_SURFACE ( 'NONE', #13852, 38.34805510287551300 ) ;
#53951 = PRESENTATION_STYLE_ASSIGNMENT (( #47904 ) ) ;
#53952 = ORIENTED_EDGE ( 'NONE', *, *, #48868, .T. ) ;
#53953 = CARTESIAN_POINT ( 'NONE',  ( 0.000000000000000000, 0.000000000000000000, 0.000000000000000000 ) ) ;
#53954 = CARTESIAN_POINT ( 'NONE',  ( -4.000000000000002665, 14.56250000000000000, 1.656854249492380582 ) ) ;
#53955 = CARTESIAN_POINT ( 'NONE',  ( 5.676582343749993598, 29.94791666325268409, 9.832129032723422313 ) ) ;
#53956 = CARTESIAN_POINT ( 'NONE',  ( 11.00000000000000000, 1.347111479062088405E-15, 84.43750000409677625 ) ) ;
#53957 = CARTESIAN_POINT ( 'NONE',  ( -2.839093476692135984E-14, 205.9375000013656063, 138.5412658750000503 ) ) ;
#53958 = LINE ( 'NONE', #66762, #37202 ) ;
#53959 = DIRECTION ( 'NONE',  ( 1.000000000000000000, -0.000000000000000000, 0.000000000000000000 ) ) ;
#53961 = CARTESIAN_POINT ( 'NONE',  ( 11.35316468749999963, 35.98958332991934128, -3.042071309553165293 ) ) ;
#53960 = CARTESIAN_POINT ( 'NONE',  ( -5.082755093536325930, 104.4687500020483952, -5.082755093536325930 ) ) ;
#53962 = CARTESIAN_POINT ( 'NONE',  ( 3.313708498984756279, 7.999999999999991118, 16.86155277982336642 ) ) ;
#53963 =( REPRESENTATION_RELATIONSHIP ('NONE','NONE', #46008, #22414 ) REPRESENTATION_RELATIONSHIP_WITH_TRANSFORMATION ( #36485 )SHAPE_REPRESENTATION_RELATIONSHIP( ) );
#53964 = CARTESIAN_POINT ( 'NONE',  ( -3.042071309553173730, 154.3229166632527267, 11.35316468749999785 ) ) ;
#53965 = VECTOR ( 'NONE', #13928, 1000.000000000000000 ) ;
#53966 = CARTESIAN_POINT ( 'NONE',  ( -7.320508075688773708, 128.7499999931720538, -7.320508075688774596 ) ) ;
#53967 = CARTESIAN_POINT ( 'NONE',  ( 2.977408999572654480, 108.5000000020483810, 7.188101187499999156 ) ) ;
#53968 = CARTESIAN_POINT ( 'NONE',  ( -29.43265458321766559, 203.7500000013656063, 166.5412658750003629 ) ) ;
#53969 = EDGE_LOOP ( 'NONE', ( #67702, #41490, #59805 ) ) ;
#53970 = CARTESIAN_POINT ( 'NONE',  ( -1.836970198721029983E-15, 20.62499999317203603, 10.00000000000000178 ) ) ;
#53971 = CARTESIAN_POINT ( 'NONE',  ( -2.085542519210945728E-15, 19.84374999658601979, 11.35316468750000141 ) ) ;
#53972 = ORIENTED_EDGE ( 'NONE', *, *, #44154, .T. ) ;
#53973 = CARTESIAN_POINT ( 'NONE',  ( -3.018451720292563716E-14, -16.44602605510714355, -68.55492853905353456 ) ) ;
#53974 = LINE ( 'NONE', #15455, #67908 ) ;
#53976 = CARTESIAN_POINT ( 'NONE',  ( 9.832129032723416984, 155.3645833299193839, 5.676582343750006032 ) ) ;
#53975 = DIRECTION ( 'NONE',  ( 0.000000000000000000, 0.000000000000000000, 1.000000000000000000 ) ) ;
#53977 = CARTESIAN_POINT ( 'NONE',  ( -7.188101187500000933, 1.499999997951610098, -2.977408999572651371 ) ) ;
#53978 = CARTESIAN_POINT ( 'NONE',  ( 7.999999999999991118, 9.797174393178815797E-16, 18.13655278432982243 ) ) ;
#53979 = CARTESIAN_POINT ( 'NONE',  ( 54.47603529178351778, 207.2498654739821689, 50.94393749907032998 ) ) ;
#53980 = CARTESIAN_POINT ( 'NONE',  ( -5.676582343750000703, 238.0729166700806445, -9.832129032723418760 ) ) ;
#53981 = CARTESIAN_POINT ( 'NONE',  ( 4.220049686691941027, -10.18810118749999738, 94.00000000204838102 ) ) ;
#53982 = ORIENTED_EDGE ( 'NONE', *, *, #27022, .F. ) ;
#53983 = CARTESIAN_POINT ( 'NONE',  ( 3.313708498984721640, 20.53124999590322020, 8.000000000000039080 ) ) ;
#53984 = CARTESIAN_POINT ( 'NONE',  ( -5.000000000000000000, -10.26105934116142215, -64.40045319026754100 ) ) ;
#53985 = CARTESIAN_POINT ( 'NONE',  ( 9.832129032723416984, 100.6770833299193555, 5.676582343750006032 ) ) ;
#53986 = CARTESIAN_POINT ( 'NONE',  ( -7.204075437095967871, 7.204075437095967871, 101.9687500020483668 ) ) ;
#53987 = CARTESIAN_POINT ( 'NONE',  ( 4.541265875000002339, 15.43749999863440614, 0.000000000000000000 ) ) ;
#53988 = ORIENTED_EDGE ( 'NONE', *, *, #5862, .F. ) ;
#53989 = ORIENTED_EDGE ( 'NONE', *, *, #10880, .T. ) ;
#53990 = CARTESIAN_POINT ( 'NONE',  ( 8.000000000000000000, 13.50000000000000178, 0.000000000000000000 ) ) ;
#53991 = CARTESIAN_POINT ( 'NONE',  ( -1.881053915767121554, 4.749999998634407028, -4.541265875000002339 ) ) ;
#53992 = CARTESIAN_POINT ( 'NONE',  ( 4.401442555609581635E-16, 5.343749997951610986, -7.188101187500000044 ) ) ;
#53993 = CARTESIAN_POINT ( 'NONE',  ( 8.000000000000001776, 118.3437500040967763, 3.313708498984759387 ) ) ;
#53994 = CARTESIAN_POINT ( 'NONE',  ( -4.220049686691935698, 10.18810118749999916, 97.75000000204838102 ) ) ;
#53995 = CONICAL_SURFACE ( 'NONE', #63804, 3.999999999999976019, 0.7853981633974491672 ) ;
#53996 = EDGE_CURVE ( 'NONE', #43418, #69933, #55309, .T. ) ;
#53997 = CARTESIAN_POINT ( 'NONE',  ( -3.469446951953614189E-15, 16.00000000000000000, 38.34805510287551300 ) ) ;
#53998 = CARTESIAN_POINT ( 'NONE',  ( 4.000000000000001776, 1.062500000000000222, -1.656854249492381248 ) ) ;
#53999 = CARTESIAN_POINT ( 'NONE',  ( 1.656854249492381914, 12.56249999726881406, 4.000000000000000888 ) ) ;
#54000 = CARTESIAN_POINT ( 'NONE',  ( 1.881053915767121998, 4.499999998634407028, -4.541265875000002339 ) ) ;
#54001 = ORIENTED_EDGE ( 'NONE', *, *, #21484, .T. ) ;
#54002 = DIRECTION ( 'NONE',  ( 1.000000000000000000, 0.000000000000000000, 1.652117596168387509E-16 ) ) ;
#54003 = CARTESIAN_POINT ( 'NONE',  ( -2.445694354108782775, 195.5625000013656063, 200.4456943541088663 ) ) ;
#54005 = CARTESIAN_POINT ( 'NONE',  ( -3.313708498984765161, 16.03125000000000355, 7.999999999999998224 ) ) ;
#54004 = CARTESIAN_POINT ( 'NONE',  ( -27.99999999999991829, 199.9375000013656063, 173.4587341250003760 ) ) ;
#54006 = VECTOR ( 'NONE', #74267, 1000.000000000000000 ) ;
#54007 = CARTESIAN_POINT ( 'NONE',  ( 4.541265875000002339, 15.31249999863440614, 0.000000000000000000 ) ) ;
#54008 = CARTESIAN_POINT ( 'NONE',  ( 2.679491924311228956, 122.9166666598386968, -10.00000000000000000 ) ) ;
#54009 = CARTESIAN_POINT ( 'NONE',  ( -7.188101187499991163, 2.977408999572646930, 5.892802781871754547 ) ) ;
#54010 = ORIENTED_EDGE ( 'NONE', *, *, #41182, .F. ) ;
#54011 =( BOUNDED_CURVE ( )  B_SPLINE_CURVE ( 2, ( #2465, #25456, #48470, #71475, #19800, #63989, #61671, #66952, #9239 ),
 .UNSPECIFIED., .F., .F. ) 
 B_SPLINE_CURVE_WITH_KNOTS ( ( 3, 2, 2, 2, 3 ),
 ( 0.6764705882352939348, 0.6801470588235292158, 0.6838235294117644969, 0.6874999999999998890, 0.6911764705882351700 ),
 .UNSPECIFIED. ) 
 CURVE ( )  GEOMETRIC_REPRESENTATION_ITEM ( )  RATIONAL_B_SPLINE_CURVE ( ( 1.000000000000004663, 0.9238795325112821866, 1.000000000000000000, 0.9238795325112867385, 1.000000000000000000, 0.9238795325112867385, 1.000000000000000000, 0.9238795325112890700, 0.9999999999999976685 ) ) 
 REPRESENTATION_ITEM ( '' )  );
#54012 =( BOUNDED_CURVE ( )  B_SPLINE_CURVE ( 2, ( #35407, #52373, #30099, #1450, #24431, #29729, #709, #46698, #64435 ),
 .UNSPECIFIED., .F., .F. ) 
 B_SPLINE_CURVE_WITH_KNOTS ( ( 3, 2, 2, 2, 3 ),
 ( 0.8666666666666673624, 0.8750000000000006661, 0.8833333333333339699, 0.8916666666666674956, 0.9000000000000007994 ),
 .UNSPECIFIED. ) 
 CURVE ( )  GEOMETRIC_REPRESENTATION_ITEM ( )  RATIONAL_B_SPLINE_CURVE ( ( 0.9999999999999938938, 0.9238795325112928447, 1.000000000000000000, 0.9238795325112867385, 1.000000000000000000, 0.9238795325112867385, 1.000000000000000000, 0.9238795325112796331, 1.000000000000007105 ) ) 
 REPRESENTATION_ITEM ( '' )  );
#54013 = ORIENTED_EDGE ( 'NONE', *, *, #30867, .F. ) ;
#54014 = CARTESIAN_POINT ( 'NONE',  ( 4.220049686691934809, 10.18810118749999916, 101.6875000020483810 ) ) ;
#54015 = CARTESIAN_POINT ( 'NONE',  ( -38.00000000000000000, 52.99999999999999289, 25.00000000000000000 ) ) ;
#54016 = CARTESIAN_POINT ( 'NONE',  ( -24.54126587499998280, 203.3750000013656063, 171.4326545832179818 ) ) ;
#54017 = CARTESIAN_POINT ( 'NONE',  ( -23.99999999999997513, 199.6875000000000000, 171.6568542494927385 ) ) ;
#54018 = CARTESIAN_POINT ( 'NONE',  ( 2.754378923186476579E-14, 198.1875000013655779, 194.5412658750000219 ) ) ;
#54019 = CARTESIAN_POINT ( 'NONE',  ( -3.313708498984765161, 12.84374999590322197, 7.999999999999998224 ) ) ;
#54020 = CARTESIAN_POINT ( 'NONE',  ( -10.00000000000000000, 102.2916666666666572, -2.679491924311229845 ) ) ;
#54021 = ADVANCED_FACE ( 'NONE', ( #13820 ), #59872, .F. ) ;
#54022 = EDGE_CURVE ( 'NONE', #66166, #16792, #39366, .T. ) ;
#54023 = CARTESIAN_POINT ( 'NONE',  ( -3.313708498984762496, 114.7812500000000000, 7.999999999999998224 ) ) ;
#54024 = CARTESIAN_POINT ( 'NONE',  ( -6.676582343750000703, 296.6718750017069510, 2.765530957082001251 ) ) ;
#54025 = VERTEX_POINT ( 'NONE', #71543 ) ;
#54026 = EDGE_CURVE ( 'NONE', #45113, #28745, #8068, .T. ) ;
#54027 = CARTESIAN_POINT ( 'NONE',  ( 6.123233995736767268E-16, 143.1249999931720538, -10.00000000000000178 ) ) ;
#54028 = CARTESIAN_POINT ( 'NONE',  ( 3.313708498984762052, 12.09374999590322020, -8.000000000000000000 ) ) ;
#54029 = CARTESIAN_POINT ( 'NONE',  ( 3.458734124999959914, 202.4375000013656063, 142.0000000000000568 ) ) ;
#54030 = CARTESIAN_POINT ( 'NONE',  ( -2.828427124746190735, 5.375000000000000000, -2.828427124746191623 ) ) ;
#54031 = CARTESIAN_POINT ( 'NONE',  ( 2.828427124746191623, 8.125000000000000000, -2.828427124746191623 ) ) ;
#54032 = CARTESIAN_POINT ( 'NONE',  ( 1.836970198721029589E-15, 226.2500000000000000, 10.00000000000000000 ) ) ;
#54033 = CARTESIAN_POINT ( 'NONE',  ( -4.556349186104048599, -10.99999999999999822, 91.46875000409676204 ) ) ;
#54034 = CARTESIAN_POINT ( 'NONE',  ( -4.556349186104047710, -10.99999999999999822, 110.7812500000000000 ) ) ;
#54035 = CARTESIAN_POINT ( 'NONE',  ( 7.320508075688771044, 214.3749999999999716, 7.320508075688775484 ) ) ;
#54036 = CARTESIAN_POINT ( 'NONE',  ( 2.977408999572650927, -7.188101187499990274, 6.830302781871754547 ) ) ;
#54037 = CARTESIAN_POINT ( 'NONE',  ( -9.832129032723420536, 189.0104166632526983, 5.676582343749997150 ) ) ;
#54038 = LINE ( 'NONE', #54786, #13009 ) ;
#54039 = CARTESIAN_POINT ( 'NONE',  ( -3.211159895383562723, 3.937499998634406584, 3.211159895383561391 ) ) ;
#54040 = LINE ( 'NONE', #42700, #66987 ) ;
#54042 = CARTESIAN_POINT ( 'NONE',  ( 8.000000000000003553, 0.000000000000000000, -25.03750572909317285 ) ) ;
#54041 = DIRECTION ( 'NONE',  ( -0.000000000000000000, 1.000000000000000000, -0.000000000000000000 ) ) ;
#54043 = ORIENTED_EDGE ( 'NONE', *, *, #26302, .T. ) ;
#54044 = CARTESIAN_POINT ( 'NONE',  ( -1.432654583217662481, 203.3750000013656063, 145.4587341250000634 ) ) ;
#54045 = CARTESIAN_POINT ( 'NONE',  ( 11.35316468750000141, 46.09374999658602690, 0.000000000000000000 ) ) ;
#54046 = CARTESIAN_POINT ( 'NONE',  ( -11.00000000000000000, 4.556349186104045934, 107.5937500040967763 ) ) ;
#54047 = CARTESIAN_POINT ( 'NONE',  ( -9.832129032723418760, 223.1770833299193555, -5.676582343750004256 ) ) ;
#54048 = EDGE_CURVE ( 'NONE', #15213, #10770, #17979, .T. ) ;
#54049 = CARTESIAN_POINT ( 'NONE',  ( -26.56734541678243033, 202.3750000013656063, 166.5412658750003345 ) ) ;
#54050 = CARTESIAN_POINT ( 'NONE',  ( -10.99999999999989342, 4.556349186104152515, 71.40624999999995737 ) ) ;
#54052 = CARTESIAN_POINT ( 'NONE',  ( 8.000000000000001776, 119.6562499999999858, 3.313708498984759387 ) ) ;
#54051 = CARTESIAN_POINT ( 'NONE',  ( -7.188101187500000044, 124.1562500020483810, 0.000000000000000000 ) ) ;
#54053 = CARTESIAN_POINT ( 'NONE',  ( -30.99999999999992895, -31.99999999999978684, 167.9999999999997726 ) ) ;
#54054 = CARTESIAN_POINT ( 'NONE',  ( -9.832129032723420536, 103.6979166632526841, 5.676582343749997150 ) ) ;
#54055 = AXIS2_PLACEMENT_3D ( 'NONE', #5543, #51553, #52680 ) ;
#54056 = CARTESIAN_POINT ( 'NONE',  ( -1.836970198721029983E-15, 90.62499999317203958, 10.00000000000000178 ) ) ;
#54057 = CARTESIAN_POINT ( 'NONE',  ( 7.188101187500001821, 92.00000000204838102, -2.977408999572651371 ) ) ;
#54058 = CARTESIAN_POINT ( 'NONE',  ( -1.881053915767121554, 16.74999999863440792, -4.541265875000002339 ) ) ;
#54059 = CARTESIAN_POINT ( 'NONE',  ( -8.660254037844390851, 72.08333333333334281, -5.000000000000007105 ) ) ;
#54060 = CYLINDRICAL_SURFACE ( 'NONE', #8853, 10.00000000000000178 ) ;
#54061 = ORIENTED_EDGE ( 'NONE', *, *, #35551, .T. ) ;
#54062 = ORIENTED_EDGE ( 'NONE', *, *, #46389, .F. ) ;
#54063 = CARTESIAN_POINT ( 'NONE',  ( -4.088227598258586603E-16, 292.3593750017070079, -6.676582343750001591 ) ) ;
#54064 = CARTESIAN_POINT ( 'NONE',  ( -8.311093377946841443, 168.9062499965860411, 8.311093377946830785 ) ) ;
#54065 = CARTESIAN_POINT ( 'NONE',  ( 11.00000000000000000, 1.347111479062088405E-15, 94.93750000409677625 ) ) ;
#54066 = CONICAL_SURFACE ( 'NONE', #64874, 7.949999999999993960, 0.04496966185232758456 ) ;
#54067 = CARTESIAN_POINT ( 'NONE',  ( 4.000000000000015987, 200.4375000000000568, 199.6568542494924259 ) ) ;
#54068 = CARTESIAN_POINT ( 'NONE',  ( 7.778174593052023411, -7.778174593052021635, 70.75000000409677625 ) ) ;
#54069 = CARTESIAN_POINT ( 'NONE',  ( -4.220049686691937474, -10.18810118749999738, 108.8125000020484094 ) ) ;
#54070 = ORIENTED_EDGE ( 'NONE', *, *, #67401, .F. ) ;
#54071 = VECTOR ( 'NONE', #70111, 1000.000000000000000 ) ;
#54072 = CARTESIAN_POINT ( 'NONE',  ( 6.891449706525156316, 51.31760009878723139, -41.45518442798378800 ) ) ;
#54073 = CARTESIAN_POINT ( 'NONE',  ( -7.347880794884122694E-16, 17.75000000000000355, 4.000000000000001776 ) ) ;
#54074 = CARTESIAN_POINT ( 'NONE',  ( 6.951808397369818766E-16, 142.3437499965860411, -11.35316468750000141 ) ) ;
#54075 = CARTESIAN_POINT ( 'NONE',  ( 4.000000000000015987, 206.6250000027312126, 198.0000000000000284 ) ) ;
#54076 = CARTESIAN_POINT ( 'NONE',  ( 2.977408999572652260, 27.56249999795161187, 7.188101187500000044 ) ) ;
#54077 = CARTESIAN_POINT ( 'NONE',  ( -10.18810118749999916, 4.220049686691934809, 72.43750000204838102 ) ) ;
#54078 = CARTESIAN_POINT ( 'NONE',  ( 8.311093377946834337, 65.46874999658601268, 8.311093377946839666 ) ) ;
#54079 = VERTEX_POINT ( 'NONE', #67021 ) ;
#54080 = FACE_OUTER_BOUND ( 'NONE', #4053, .T. ) ;
#54081 = CARTESIAN_POINT ( 'NONE',  ( 4.541265875000002339, 6.499999998634407916, -1.881053915767121776 ) ) ;
#54082 = CARTESIAN_POINT ( 'NONE',  ( 8.008118988124993010, -3.317071493978877239, 7.669365283940628331 ) ) ;
#54083 = UNCERTAINTY_MEASURE_WITH_UNIT (LENGTH_MEASURE( 1.000000000000000082E-05 ), #32779, 'distance_accuracy_value', 'NONE');
#54084 = CARTESIAN_POINT ( 'NONE',  ( -7.188101187500000044, 20.71874999795161543, -8.802885111219163269E-16 ) ) ;
#54085 = CARTESIAN_POINT ( 'NONE',  ( -2.485281374238571761, 293.8750000034139589, -6.000000000000003553 ) ) ;
#54086 = CARTESIAN_POINT ( 'NONE',  ( 1.714702201362999334, 124.5469634165301898, -7.773580895186444906 ) ) ;
#54087 = CARTESIAN_POINT ( 'NONE',  ( 2.977408999572650927, 11.62499999795161365, -7.188101187500001821 ) ) ;
#54088 = CARTESIAN_POINT ( 'NONE',  ( -7.188101187499992051, 0.000000000000000000, 1.486552781871753437 ) ) ;
#54089 = CARTESIAN_POINT ( 'NONE',  ( 1.871523826299183495E-15, -10.18810118749999916, 68.03125000204838102 ) ) ;
#54090 = PRODUCT ( 'MAT-050', 'MAT-050', '', ( #37308 ) ) ;
#54091 = CARTESIAN_POINT ( 'NONE',  ( 4.898587196589412829E-16, 12.37500000000000178, -8.000000000000000000 ) ) ;
#54092 = CARTESIAN_POINT ( 'NONE',  ( 4.000000000000000888, 3.687499997268813168, 1.656854249492384135 ) ) ;
#54093 = ORIENTED_EDGE ( 'NONE', *, *, #35358, .F. ) ;
#54094 = EDGE_CURVE ( 'NONE', #25519, #51832, #15772, .T. ) ;
#54095 = CARTESIAN_POINT ( 'NONE',  ( 3.458734125000015425, 205.0000000013655779, 196.5673454167823877 ) ) ;
#54096 = CARTESIAN_POINT ( 'NONE',  ( 3.999999999999959144, 204.0625000000000000, 140.3431457505076594 ) ) ;
#54097 = CARTESIAN_POINT ( 'NONE',  ( -31.99999999999999289, 197.3750000027312126, 170.0000000000004547 ) ) ;
#54098 = CARTESIAN_POINT ( 'NONE',  ( -1.881053915767124440, 2.999999998634407028, 4.541265875000001451 ) ) ;
#54100 = CARTESIAN_POINT ( 'NONE',  ( 5.082755093536325042, 111.5937500020483810, -5.082755093536325930 ) ) ;
#54099 = AXIS2_PLACEMENT_3D ( 'NONE', #58776, #65527, #18773 ) ;
#54101 = CARTESIAN_POINT ( 'NONE',  ( -4.242640687119285658, 295.1249999999999432, 4.242640687119287435 ) ) ;
#54102 = CARTESIAN_POINT ( 'NONE',  ( 3.313708498984756279, 7.999999999999991118, 2.049052783920143117 ) ) ;
#54103 = ORIENTED_EDGE ( 'NONE', *, *, #43009, .F. ) ;
#54104 = CARTESIAN_POINT ( 'NONE',  ( -1.320432766682874540E-15, 25.59374999795161543, 7.188101187500000044 ) ) ;
#54105 = VERTEX_POINT ( 'NONE', #55718 ) ;
#54106 = CARTESIAN_POINT ( 'NONE',  ( -2.679491924311382611, 203.5416666666666572, 9.999999999999912959 ) ) ;
#54107 = CARTESIAN_POINT ( 'NONE',  ( 3.458734125000016313, 208.8750000013656347, 199.4326545832176691 ) ) ;
#54108 = CARTESIAN_POINT ( 'NONE',  ( 31.45873412499999944, 203.6875000013656063, 169.9999999999998863 ) ) ;
#54109 = CARTESIAN_POINT ( 'NONE',  ( -8.660254037844387298, 57.08333333333334281, -5.000000000000004441 ) ) ;
#54110 = CIRCLE ( 'NONE', #62519, 5.099999999999999645 ) ;
#54111 = EDGE_CURVE ( 'NONE', #55396, #23868, #31204, .T. ) ;
#54112 = CARTESIAN_POINT ( 'NONE',  ( 7.188101187500002709, 96.68750000204836681, 2.977408999572649151 ) ) ;
#54113 = CARTESIAN_POINT ( 'NONE',  ( 2.485281374238571317, 296.6875000000000568, -6.000000000000003553 ) ) ;
#54115 = CARTESIAN_POINT ( 'NONE',  ( -24.00875902089660840, -40.50424123436440027, 189.6191649576120994 ) ) ;
#54114 = FACE_OUTER_BOUND ( 'NONE', #42588, .T. ) ;
#54116 =( BOUNDED_CURVE ( )  B_SPLINE_CURVE ( 2, ( #48879, #3246, #72654, #4366, #21333, #20202, #73022, #50005, #43222 ),
 .UNSPECIFIED., .F., .F. ) 
 B_SPLINE_CURVE_WITH_KNOTS ( ( 3, 2, 2, 2, 3 ),
 ( 0.7500000000000006661, 0.7583333333333339699, 0.7666666666666672736, 0.7750000000000005773, 0.7833333333333338810 ),
 .UNSPECIFIED. ) 
 CURVE ( )  GEOMETRIC_REPRESENTATION_ITEM ( )  RATIONAL_B_SPLINE_CURVE ( ( 0.9999999999999938938, 0.9238795325112928447, 1.000000000000000000, 0.9238795325112867385, 1.000000000000000000, 0.9238795325112867385, 1.000000000000000000, 0.9238795325112816315, 1.000000000000005107 ) ) 
 REPRESENTATION_ITEM ( '' )  );
#54117 = ORIENTED_EDGE ( 'NONE', *, *, #5325, .T. ) ;
#54118 = CARTESIAN_POINT ( 'NONE',  ( 5.676582343750005144, 235.5729166700806729, 9.832129032723416984 ) ) ;
#54119 = CARTESIAN_POINT ( 'NONE',  ( 3.999999999999960032, 200.0625000027312410, 143.6568542494924543 ) ) ;
#54120 = CARTESIAN_POINT ( 'NONE',  ( -10.00000000000000178, 74.37499999317203958, -1.224646799147353454E-15 ) ) ;
#54121 = CARTESIAN_POINT ( 'NONE',  ( -7.999999999999991118, -1.759625989565808730E-05, 2.517803281745877975 ) ) ;
#54122 = FACE_OUTER_BOUND ( 'NONE', #70390, .T. ) ;
#54123 = FACE_OUTER_BOUND ( 'NONE', #38062, .T. ) ;
#54124 = CARTESIAN_POINT ( 'NONE',  ( -7.320508075688778149, 173.1249999999999716, 7.320508075688769267 ) ) ;
#54125 = CARTESIAN_POINT ( 'NONE',  ( 74.99999999999998579, 0.000000000000000000, 69.99999999999997158 ) ) ;
#54126 = FILL_AREA_STYLE ('',( #31097 ) ) ;
#54127 = CARTESIAN_POINT ( 'NONE',  ( 5.082755093536318824, 5.082755093536319713, 28.29905278187175810 ) ) ;
#54128 = CARTESIAN_POINT ( 'NONE',  ( -2.085542519210945728E-15, 149.8437499965860411, 11.35316468750000141 ) ) ;
#54129 = DIRECTION ( 'NONE',  ( 1.000000000000000000, 0.000000000000000000, -0.000000000000000000 ) ) ;
#54130 = CARTESIAN_POINT ( 'NONE',  ( 3.313708498984815343, 97.71875000409676204, -7.999999999999944933 ) ) ;
#54133 = LINE ( 'NONE', #65807, #29037 ) ;
#54132 = DIRECTION ( 'NONE',  ( -0.000000000000000000, -0.000000000000000000, -1.000000000000000000 ) ) ;
#54131 = CARTESIAN_POINT ( 'NONE',  ( 30.82842712474620228, 203.3750000000000284, 167.1715728752537586 ) ) ;
#54134 = ORIENTED_EDGE ( 'NONE', *, *, #64585, .F. ) ;
#54135 = CARTESIAN_POINT ( 'NONE',  ( -5.676582343750006032, 14.42708332991935016, 9.832129032723418760 ) ) ;
#54136 = EDGE_CURVE ( 'NONE', #67442, #18291, #12787, .T. ) ;
#54137 = DIRECTION ( 'NONE',  ( -0.000000000000000000, -0.000000000000000000, -1.000000000000000000 ) ) ;
#54138 = CARTESIAN_POINT ( 'NONE',  ( 2.849036369511732440E-14, 208.2500000000000284, 202.0000000000000000 ) ) ;
#54139 = CARTESIAN_POINT ( 'NONE',  ( -7.999999999999998224, 116.0937500000000000, 3.313708498984766049 ) ) ;
#54140 = CARTESIAN_POINT ( 'NONE',  ( -2.839093476692135984E-14, 206.6875000013656063, 138.5412658750000503 ) ) ;
#54141 =( BOUNDED_CURVE ( )  B_SPLINE_CURVE ( 2, ( #13121, #53140, #70486, #30857, #18805, #1827, #24814, #13489, #47829 ),
 .UNSPECIFIED., .F., .F. ) 
 B_SPLINE_CURVE_WITH_KNOTS ( ( 3, 2, 2, 2, 3 ),
 ( 0.5568181818181818787, 0.5625000000000001110, 0.5681818181818183433, 0.5738636363636363535, 0.5795454545454545858 ),
 .UNSPECIFIED. ) 
 CURVE ( )  GEOMETRIC_REPRESENTATION_ITEM ( )  RATIONAL_B_SPLINE_CURVE ( ( 0.9999999999999985567, 0.9238795325112881818, 1.000000000000000000, 0.9238795325112867385, 1.000000000000000000, 0.9238795325112867385, 1.000000000000000000, 0.9238795325112867385, 1.000000000000000000 ) ) 
 REPRESENTATION_ITEM ( '' )  );
#54142 = CARTESIAN_POINT ( 'NONE',  ( -2.009711600462664727, 124.6176558922824569, -7.638752868991079303 ) ) ;
#54143 = EDGE_CURVE ( 'NONE', #61723, #48752, #37986, .T. ) ;
#54144 = CARTESIAN_POINT ( 'NONE',  ( -4.999999999999998224, 33.54166665983870388, -8.660254037844389075 ) ) ;
#54145 = CARTESIAN_POINT ( 'NONE',  ( -5.082755093536325930, 108.9687500020483810, -5.082755093536325930 ) ) ;
#54146 = CARTESIAN_POINT ( 'NONE',  ( 1.881053915767122664, 3.249999998634406584, 4.541265875000001451 ) ) ;
#54147 = CARTESIAN_POINT ( 'NONE',  ( -7.999999999999989342, -3.313708498984762496, 13.11155278392014623 ) ) ;
#54148 = CARTESIAN_POINT ( 'NONE',  ( 5.656854249492374365, 5.656854249492375253, 12.26780277982336642 ) ) ;
#54150 = DIRECTION ( 'NONE',  ( 0.7578158005275104081, 0.6524685528597132800, 0.000000000000000000 ) ) ;
#54149 = FACE_OUTER_BOUND ( 'NONE', #7353, .T. ) ;
#54151 = ORIENTED_EDGE ( 'NONE', *, *, #9203, .T. ) ;
#54152 = CARTESIAN_POINT ( 'NONE',  ( 6.000000000000003553, 292.5000000034140157, 2.485281374238571317 ) ) ;
#54153 = DIRECTION ( 'NONE',  ( -0.000000000000000000, 1.000000000000000000, -1.563033456626094573E-30 ) ) ;
#54154 = EDGE_CURVE ( 'NONE', #55362, #62597, #33664, .T. ) ;
#54155 = CARTESIAN_POINT ( 'NONE',  ( -11.35316468749999608, 224.4270833367473017, 3.042071309553173730 ) ) ;
#54156 = CARTESIAN_POINT ( 'NONE',  ( 8.311093377946834337, 130.1562499965860411, 8.311093377946839666 ) ) ;
#54157 = ORIENTED_EDGE ( 'NONE', *, *, #65700, .F. ) ;
#54158 = ADVANCED_FACE ( 'NONE', ( #57200 ), #28515, .F. ) ;
#54159 = B_SPLINE_CURVE_WITH_KNOTS ( 'NONE', 5,
 ( #39608, #56970, #5285, #40347, #55854, #58457 ),
 .UNSPECIFIED., .F., .F.,
 ( 6, 6 ),
 ( 0.000000000000000000, 1.000000000000000000 ),
 .UNSPECIFIED. ) ;
#54160 = CARTESIAN_POINT ( 'NONE',  ( 1.656854249492321074, 198.3125000000000853, 202.0000000000001137 ) ) ;
#54161 = CARTESIAN_POINT ( 'NONE',  ( 10.18810118750000093, -4.220049686691933921, 92.31250000204838102 ) ) ;
#54162 = CARTESIAN_POINT ( 'NONE',  ( 10.99999999999989342, 4.556349186104152515, 86.03125000409676204 ) ) ;
#54163 = CARTESIAN_POINT ( 'NONE',  ( 2.445694354108839175, 196.3125000013656063, 195.5543056458912190 ) ) ;
#54164 = CARTESIAN_POINT ( 'NONE',  ( 0.000000000000000000, 125.0000000000000000, 0.000000000000000000 ) ) ;
#54166 = CARTESIAN_POINT ( 'NONE',  ( 8.311093377946837890, 111.4062499965860269, -8.311093377946837890 ) ) ;
#54165 = DIRECTION ( 'NONE',  ( -0.000000000000000000, -0.000000000000000000, 1.000000000000000000 ) ) ;
#54167 = CARTESIAN_POINT ( 'NONE',  ( -29.65685424949234772, 209.4375000000000284, 174.0000000000004547 ) ) ;
#54168 = CARTESIAN_POINT ( 'NONE',  ( 8.660254037844385522, 146.4583333265053682, 5.000000000000005329 ) ) ;
#54169 = ORIENTED_EDGE ( 'NONE', *, *, #5832, .T. ) ;
#54170 = VECTOR ( 'NONE', #11051, 1000.000000000000000 ) ;
#54171 = CARTESIAN_POINT ( 'NONE',  ( 3.999999999999959144, 206.0625000000000000, 140.3431457505076594 ) ) ;
#54172 = EDGE_CURVE ( 'NONE', #67283, #49304, #17565, .T. ) ;
#54173 = DIRECTION ( 'NONE',  ( 1.000000000000000000, 0.000000000000000000, -0.000000000000000000 ) ) ;
#54174 = CARTESIAN_POINT ( 'NONE',  ( 9.832129032723416984, 105.6770833299193413, 5.676582343750006032 ) ) ;
#54175 = CARTESIAN_POINT ( 'NONE',  ( 3.458734125000015425, 205.0000000013655779, 196.5673454167823877 ) ) ;
#54176 = CARTESIAN_POINT ( 'NONE',  ( 7.188101187500000044, 12.84374999795161187, 0.000000000000000000 ) ) ;
#54177 = CARTESIAN_POINT ( 'NONE',  ( -10.18810118749999916, 4.220049686691934809, 88.93750000204839523 ) ) ;
#54178 = CARTESIAN_POINT ( 'NONE',  ( 6.951808397369818766E-16, 7.343749996586017126, -11.35316468750000141 ) ) ;
#54180 = ORIENTED_EDGE ( 'NONE', *, *, #21981, .F. ) ;
#54179 = AXIS2_PLACEMENT_3D ( 'NONE', #42612, #53579, #7187 ) ;
#54181 = CARTESIAN_POINT ( 'NONE',  ( 10.00000000000000178, 182.0833333265053682, -2.679491924311226736 ) ) ;
#54182 = CARTESIAN_POINT ( 'NONE',  ( -8.008118988124991233, 3.317071493978878127, 24.91936528394063899 ) ) ;
#54183 = CARTESIAN_POINT ( 'NONE',  ( 11.00000000000000000, 1.347111479062088405E-15, 102.4375000040967763 ) ) ;
#54184 = CARTESIAN_POINT ( 'NONE',  ( -6.238412754330611322E-16, 10.18810118749999916, 76.65625000204836681 ) ) ;
#54185 = DIRECTION ( 'NONE',  ( 0.000000000000000000, 0.000000000000000000, 1.000000000000000000 ) ) ;
#54186 = CARTESIAN_POINT ( 'NONE',  ( -7.999999999999998224, 93.78125000409679046, 3.313708498984766049 ) ) ;
#54187 = CARTESIAN_POINT ( 'NONE',  ( 4.721056650416000089, 291.8281250017069510, 4.721056650415999201 ) ) ;
#54188 = CARTESIAN_POINT ( 'NONE',  ( 2.751064625579944321E-14, 204.8750000027312126, 194.0000000000000568 ) ) ;
#54189 = CARTESIAN_POINT ( 'NONE',  ( 3.042071309553167069, 132.1354166632526699, -11.35316468749999785 ) ) ;
#54190 = CARTESIAN_POINT ( 'NONE',  ( 10.18810118749999916, 1.247682550866122264E-15, 84.90625000204838102 ) ) ;
#54191 = CARTESIAN_POINT ( 'NONE',  ( -24.54126587499999346, 199.1875000013655779, 170.0000000000003411 ) ) ;
#54192 = CARTESIAN_POINT ( 'NONE',  ( 8.000000000000000000, 21.00000000000000355, 0.000000000000000000 ) ) ;
#54193 = CARTESIAN_POINT ( 'NONE',  ( 4.541265875000002339, 12.43749999863440792, 0.000000000000000000 ) ) ;
#54194 = ORIENTED_EDGE ( 'NONE', *, *, #2393, .F. ) ;
#54195 = CARTESIAN_POINT ( 'NONE',  ( -2.828427124746153876, 206.0000000027312126, 195.1715728752538439 ) ) ;
#54196 = CARTESIAN_POINT ( 'NONE',  ( -3.458734125000015425, 197.2500000013656063, 143.4326545832176976 ) ) ;
#54197 = CARTESIAN_POINT ( 'NONE',  ( -4.000000000000015987, 204.5625000027312126, 140.3431457505076594 ) ) ;
#54198 = CARTESIAN_POINT ( 'NONE',  ( 5.000000000000000888, 12.55543720214775583, -69.09376167622102116 ) ) ;
#54199 = CARTESIAN_POINT ( 'NONE',  ( 10.18810118750000093, -4.220049686691933921, 70.18750000204838102 ) ) ;
#54200 = ORIENTED_EDGE ( 'NONE', *, *, #41293, .F. ) ;
#54201 = EDGE_CURVE ( 'NONE', #38154, #50134, #23064, .T. ) ;
#54202 = CARTESIAN_POINT ( 'NONE',  ( -7.188101187500000933, 5.624999997951610986, -2.977408999572651371 ) ) ;
#54203 = CARTESIAN_POINT ( 'NONE',  ( -1.656854249492407449, 208.3125000000000000, 138.0000000000000284 ) ) ;
#54204 = CARTESIAN_POINT ( 'NONE',  ( -2.679491924311226292, 28.33333332650536818, -10.00000000000000178 ) ) ;
#54205 = CARTESIAN_POINT ( 'NONE',  ( 7.188101187500001821, 120.8750000020483810, -2.977408999572651371 ) ) ;
#54206 = CARTESIAN_POINT ( 'NONE',  ( -3.422326672995520180, 21.99999999999999645, -2.553026752608630101 ) ) ;
#54207 = CARTESIAN_POINT ( 'NONE',  ( 2.765530957082001251, 291.7656250017069510, 6.676582343749999815 ) ) ;
#54209 = DIRECTION ( 'NONE',  ( 0.000000000000000000, 0.000000000000000000, 1.000000000000000000 ) ) ;
#54208 = CARTESIAN_POINT ( 'NONE',  ( 2.679491924311075302, 130.8333333265053682, 10.00000000000008704 ) ) ;
#54210 = ORIENTED_EDGE ( 'NONE', *, *, #56126, .F. ) ;
#54211 = EDGE_CURVE ( 'NONE', #62209, #55468, #7205, .T. ) ;
#54213 = AXIS2_PLACEMENT_3D ( 'NONE', #71250, #36937, #53919 ) ;
#54212 = CARTESIAN_POINT ( 'NONE',  ( 3.042071309553163960, 232.7604166700806445, -11.35316468749999785 ) ) ;
#54214 = CARTESIAN_POINT ( 'NONE',  ( 7.188101187499991163, 2.977408999572648707, 26.70530278187175455 ) ) ;
#54215 = DIRECTION ( 'NONE',  ( -0.000000000000000000, -1.000000000000000000, -0.000000000000000000 ) ) ;
#54216 = CARTESIAN_POINT ( 'NONE',  ( -3.458734124999960358, 197.6875000013655779, 198.0000000000000284 ) ) ;
#54217 = ORIENTED_EDGE ( 'NONE', *, *, #16793, .F. ) ;
#54218 = CARTESIAN_POINT ( 'NONE',  ( -5.656854249492380582, 99.31250000000000000, -5.656854249492380582 ) ) ;
#54219 = CARTESIAN_POINT ( 'NONE',  ( -8.311093377946836114, 102.9687499965859985, -8.311093377946837890 ) ) ;
#54220 = FACE_OUTER_BOUND ( 'NONE', #67656, .T. ) ;
#54221 = PRODUCT_DEFINITION ( 'UNKNOWN', '', #42987, #41126 ) ;
#54222 = CARTESIAN_POINT ( 'NONE',  ( 11.00000000000000000, 1.347111479062088405E-15, 75.24999999999998579 ) ) ;
#54225 = CARTESIAN_POINT ( 'NONE',  ( 54.00000000000000000, 37.00000000000000000, 0.000000000000000000 ) ) ;
#54224 = CARTESIAN_POINT ( 'NONE',  ( 29.43265458321761585, 205.8750000013656063, 166.5412658749999650 ) ) ;
#54223 = CARTESIAN_POINT ( 'NONE',  ( 26.56734541678232375, 203.6250000013656063, 173.4587341249998929 ) ) ;
#54226 = VERTEX_POINT ( 'NONE', #22467 ) ;
#54227 = AXIS2_PLACEMENT_3D ( 'NONE', #23228, #63968, #11175 ) ;
#54228 = DIRECTION ( 'NONE',  ( -0.5000000000000009992, -0.8660254037844380415, 0.000000000000000000 ) ) ;
#54229 = CARTESIAN_POINT ( 'NONE',  ( 3.042071309553167069, 211.8229166632527267, -11.35316468749999785 ) ) ;
#54230 = CARTESIAN_POINT ( 'NONE',  ( -2.754378923186476579E-14, 201.1875000013656063, 145.4587341250000350 ) ) ;
#54231 = CARTESIAN_POINT ( 'NONE',  ( 24.54126587499998280, 202.5000000013656063, 171.4326545832175555 ) ) ;
#54232 = EDGE_CURVE ( 'NONE', #74324, #41307, #68506, .T. ) ;
#54233 = CARTESIAN_POINT ( 'NONE',  ( -1.320432766682874540E-15, 27.46874999795161543, 7.188101187500000044 ) ) ;
#54234 = CARTESIAN_POINT ( 'NONE',  ( -3.042071309553164404, 197.5520833299193555, -11.35316468749999963 ) ) ;
#54235 = CARTESIAN_POINT ( 'NONE',  ( -5.082755093536324154, 93.21875000204838102, 5.082755093536326818 ) ) ;
#54236 = CARTESIAN_POINT ( 'NONE',  ( 9.150885453380622536, 225.9999999999998863, 5.663720741180870100 ) ) ;
#54237 = CARTESIAN_POINT ( 'NONE',  ( -8.342170076843785083E-16, 15.06249999863440792, 4.541265875000002339 ) ) ;
#54238 = CARTESIAN_POINT ( 'NONE',  ( 31.45873412499997812, 199.8750000013656063, 171.4326545832176123 ) ) ;
#54239 = CARTESIAN_POINT ( 'NONE',  ( -4.401442555609577197E-16, 7.188101187499992051, 1.486552781871753437 ) ) ;
#54240 = DIRECTION ( 'NONE',  ( 0.000000000000000000, 0.000000000000000000, 1.000000000000000000 ) ) ;
#54241 = CARTESIAN_POINT ( 'NONE',  ( -11.35316468749999785, 88.07291666325266988, -3.042071309553167513 ) ) ;
#54242 = VERTEX_POINT ( 'NONE', #22850 ) ;
#54243 =( BOUNDED_CURVE ( )  B_SPLINE_CURVE ( 2, ( #2848, #32656, #25837, #38682, #3982, #60931, #61684, #19815, #71866 ),
 .UNSPECIFIED., .F., .F. ) 
 B_SPLINE_CURVE_WITH_KNOTS ( ( 3, 2, 2, 2, 3 ),
 ( 0.7941176470588234837, 0.7977941176470588758, 0.8014705882352941568, 0.8051470588235294379, 0.8088235294117647189 ),
 .UNSPECIFIED. ) 
 CURVE ( )  GEOMETRIC_REPRESENTATION_ITEM ( )  RATIONAL_B_SPLINE_CURVE ( ( 1.000000000000000000, 0.9238795325112867385, 1.000000000000000000, 0.9238795325112867385, 1.000000000000000000, 0.9238795325112867385, 1.000000000000000000, 0.9238795325112867385, 1.000000000000000000 ) ) 
 REPRESENTATION_ITEM ( '' )  );
#54244 = ADVANCED_FACE ( 'NONE', ( #51906 ), #23227, .T. ) ;
#54245 = CARTESIAN_POINT ( 'NONE',  ( -32.00000000000000711, 195.1875000000000000, 168.3431457505080289 ) ) ;
#54246 = CYLINDRICAL_SURFACE ( 'NONE', #53244, 3.999999999999976019 ) ;
#54247 = FACE_BOUND ( 'NONE', #4580, .T. ) ;
#54248 = CARTESIAN_POINT ( 'NONE',  ( -8.311093377946836114, 87.65624999658601268, -8.311093377946837890 ) ) ;
#54249 = CARTESIAN_POINT ( 'NONE',  ( 1.871523826299183495E-15, -10.18810118749999916, 89.40625000204838102 ) ) ;
#54250 = CARTESIAN_POINT ( 'NONE',  ( -10.18810118749999916, 0.000000000000000000, 111.1562500020483668 ) ) ;
#54251 = CARTESIAN_POINT ( 'NONE',  ( -2.445694354108784108, 207.5625000013656063, 195.5543056458912190 ) ) ;
#54252 = CARTESIAN_POINT ( 'NONE',  ( 7.999999999999998224, 23.71874999590322020, 3.313708498984766049 ) ) ;
#54254 = CARTESIAN_POINT ( 'NONE',  ( 6.951808397369818766E-16, 77.03124999658601268, -11.35316468750000141 ) ) ;
#54253 = CARTESIAN_POINT ( 'NONE',  ( -25.17157287525374443, 206.7500000027312126, 172.8284271247464972 ) ) ;
#54255 = CARTESIAN_POINT ( 'NONE',  ( 7.999999999999991118, 9.797174393178815797E-16, 16.76780278392014978 ) ) ;
#54256 = CARTESIAN_POINT ( 'NONE',  ( 7.320508075688774596, 130.6250000000000284, -7.320508075688774596 ) ) ;
#54257 = VECTOR ( 'NONE', #40980, 1000.000000000000000 ) ;
#54258 = CARTESIAN_POINT ( 'NONE',  ( -2.679491924311235618, 170.4166666598386541, 10.00000000000000000 ) ) ;
#54259 = CARTESIAN_POINT ( 'NONE',  ( -2.977408999572650927, 89.75000000204839523, -7.188101187500001821 ) ) ;
#54260 = LINE ( 'NONE', #8596, #56902 ) ;
#54261 = CARTESIAN_POINT ( 'NONE',  ( 6.951808397369818766E-16, 67.34374999658601268, -11.35316468750000141 ) ) ;
#54262 = CARTESIAN_POINT ( 'NONE',  ( 4.721056650415999201, 292.0781250017069510, -4.721056650415999201 ) ) ;
#54263 = ADVANCED_FACE ( 'NONE', ( #39469 ), #23597, .T. ) ;
#54264 = CARTESIAN_POINT ( 'NONE',  ( 4.220049686691941027, -10.18810118749999738, 104.5000000020483668 ) ) ;
#54265 = CARTESIAN_POINT ( 'NONE',  ( 6.951808397369818766E-16, 192.0312499965860127, -11.35316468750000141 ) ) ;
#54266 = ORIENTED_EDGE ( 'NONE', *, *, #47309, .T. ) ;
#54267 = DIRECTION ( 'NONE',  ( 0.000000000000000000, 0.000000000000000000, 1.000000000000000000 ) ) ;
#54268 = CARTESIAN_POINT ( 'NONE',  ( 2.828427124746191623, 3.874999997268813168, -2.828427124746191623 ) ) ;
#54269 = CARTESIAN_POINT ( 'NONE',  ( -5.000000000000000000, 50.64189880742059557, 41.08656465431948845 ) ) ;
#54271 = CARTESIAN_POINT ( 'NONE',  ( 8.311093377946834337, 195.1562499965860411, 8.311093377946839666 ) ) ;
#54270 = DIRECTION ( 'NONE',  ( 0.000000000000000000, 0.000000000000000000, 1.000000000000000000 ) ) ;
#54272 = CARTESIAN_POINT ( 'NONE',  ( 2.775557561562891351E-14, -70.00000000000000000, 170.0000000000000000 ) ) ;
#54273 = CARTESIAN_POINT ( 'NONE',  ( -6.123233995736766282E-16, 241.8750000068280031, -10.00000000000000000 ) ) ;
#54274 = CARTESIAN_POINT ( 'NONE',  ( -7.320508075688778149, 189.9999999931720538, 7.320508075688769267 ) ) ;
#54275 = ORIENTED_EDGE ( 'NONE', *, *, #53368, .F. ) ;
#54276 = CARTESIAN_POINT ( 'NONE',  ( 8.311093377946834337, 185.4687499965860127, 8.311093377946839666 ) ) ;
#54277 = CARTESIAN_POINT ( 'NONE',  ( -2.977408999572647819, 7.188101187499992051, 22.20530278187175455 ) ) ;
#54278 = CARTESIAN_POINT ( 'NONE',  ( 1.469576158976823947E-15, 110.5625000040967905, 8.000000000000000000 ) ) ;
#54279 = AXIS2_PLACEMENT_3D ( 'NONE', #44767, #67780, #51162 ) ;
#54280 = ORIENTED_EDGE ( 'NONE', *, *, #23608, .T. ) ;
#54281 = VECTOR ( 'NONE', #43644, 1000.000000000000000 ) ;
#54282 = CARTESIAN_POINT ( 'NONE',  ( 3.313708498984760720, 99.21875000409680467, -8.000000000000000000 ) ) ;
#54283 = ADVANCED_FACE ( 'NONE', ( #52649 ), #63967, .T. ) ;
#54284 = DIRECTION ( 'NONE',  ( -0.8660254037844397068, -0.4999999999999981126, 0.000000000000000000 ) ) ;
#54285 = EDGE_CURVE ( 'NONE', #14563, #37485, #46606, .T. ) ;
#54286 = CARTESIAN_POINT ( 'NONE',  ( 1.656854249492381914, 15.81250000000000178, 4.000000000000000888 ) ) ;
#54287 = CARTESIAN_POINT ( 'NONE',  ( 3.211159895383560947, 15.18749999863440792, 3.211159895383562723 ) ) ;
#54288 = CARTESIAN_POINT ( 'NONE',  ( 3.313708498984756279, 7.999999999999991118, 11.04905278392014800 ) ) ;
#54289 = CARTESIAN_POINT ( 'NONE',  ( -27.99999999999995381, 195.5000000000000000, 174.0000000000003695 ) ) ;
#54290 = VERTEX_POINT ( 'NONE', #16433 ) ;
#54291 = CARTESIAN_POINT ( 'NONE',  ( 4.999999999999999112, -14.31098243164691652, -69.87317657433686691 ) ) ;
#54292 = CARTESIAN_POINT ( 'NONE',  ( -2.977408999572650927, 98.37500000204840944, -7.188101187500001821 ) ) ;
#54295 = CIRCLE ( 'NONE', #47066, 9.000000000000001776 ) ;
#54294 = CARTESIAN_POINT ( 'NONE',  ( 8.000000000000000000, 119.9375000040967763, -9.797174393178825657E-16 ) ) ;
#54293 = CARTESIAN_POINT ( 'NONE',  ( 3.313708498984761608, 16.59374999590322375, -8.000000000000000000 ) ) ;
#54296 = DIRECTION ( 'NONE',  ( 1.000000000000000000, 0.000000000000000000, 0.000000000000000000 ) ) ;
#54297 = ORIENTED_EDGE ( 'NONE', *, *, #19940, .T. ) ;
#54298 = CARTESIAN_POINT ( 'NONE',  ( 1.704527592502767863, 49.99193291617198298, -40.73198448289638662 ) ) ;
#54299 = CARTESIAN_POINT ( 'NONE',  ( 5.082755093536320601, -5.082755093536318824, 17.04905278187175810 ) ) ;
#54300 = ORIENTED_EDGE ( 'NONE', *, *, #46837, .F. ) ;
#54301 = EDGE_CURVE ( 'NONE', #28093, #32715, #58325, .T. ) ;
#54302 = EDGE_LOOP ( 'NONE', ( #29430, #72525, #50554, #32785 ) ) ;
#54303 = CARTESIAN_POINT ( 'NONE',  ( 10.18810118749999916, 1.247682550866122264E-15, 80.40625000204838102 ) ) ;
#54304 = CARTESIAN_POINT ( 'NONE',  ( 5.676582343750001591, 61.92708332991934839, -9.832129032723420536 ) ) ;
#54305 = CARTESIAN_POINT ( 'NONE',  ( 8.660254037844385522, 91.45833332650536818, 5.000000000000005329 ) ) ;
#54306 = CARTESIAN_POINT ( 'NONE',  ( 2.020667218593132706E-15, -11.00000000000000000, 95.87499999999998579 ) ) ;
#54309 = CARTESIAN_POINT ( 'NONE',  ( -6.676582343750001591, 294.6093750017069510, 0.000000000000000000 ) ) ;
#54308 = CARTESIAN_POINT ( 'NONE',  ( 23.99999999999998934, 199.8750000027312126, 169.9999999999999432 ) ) ;
#54307 = CARTESIAN_POINT ( 'NONE',  ( 0.000000000000000000, 22.00000000000000355, 8.000000000000003553 ) ) ;
#54310 = CARTESIAN_POINT ( 'NONE',  ( 10.00000000000000178, 150.2083333333333428, -2.679491924311226736 ) ) ;
#54311 = CARTESIAN_POINT ( 'NONE',  ( -2.849036369511732440E-14, 204.2500000000000284, 138.0000000000000568 ) ) ;
#54312 = CARTESIAN_POINT ( 'NONE',  ( 30.82842712474620583, 209.3750000000000284, 167.1715728752537586 ) ) ;
#54313 = DIRECTION ( 'NONE',  ( -0.000000000000000000, 1.000000000000000000, -0.000000000000000000 ) ) ;
#54314 = CARTESIAN_POINT ( 'NONE',  ( -5.656854249492381470, 5.249999995903221084, 5.656854249492379694 ) ) ;
#54315 = VECTOR ( 'NONE', #58490, 1000.000000000000000 ) ;
#54316 = CARTESIAN_POINT ( 'NONE',  ( 26.56734541678232375, 198.3750000013655779, 173.4587341249998929 ) ) ;
#54317 = CARTESIAN_POINT ( 'NONE',  ( 2.977408999572650927, 10.12499999795161187, -7.188101187500001821 ) ) ;
#54318 = CARTESIAN_POINT ( 'NONE',  ( 3.313708498984762496, -7.999999999999989342, 23.98655278392014978 ) ) ;
#54319 = CARTESIAN_POINT ( 'NONE',  ( 2.828427124746190291, 5.624999997268813168, 2.828427124746192067 ) ) ;
#54320 = CARTESIAN_POINT ( 'NONE',  ( -7.188101187500000044, 109.5312500020483810, 0.000000000000000000 ) ) ;
#54322 = DIRECTION ( 'NONE',  ( 0.000000000000000000, -0.000000000000000000, -1.000000000000000000 ) ) ;
#54321 = DIRECTION ( 'NONE',  ( -0.000000000000000000, 1.000000000000000000, -0.000000000000000000 ) ) ;
#54323 = CARTESIAN_POINT ( 'NONE',  ( 7.320508075688777261, 135.6249999999999716, -7.320508075688777261 ) ) ;
#54324 = CARTESIAN_POINT ( 'NONE',  ( 31.45873412500001010, 209.0000000013656063, 168.5673454167822740 ) ) ;
#54325 = CARTESIAN_POINT ( 'NONE',  ( -5.082755093536317936, -5.082755093536320601, 21.54905278187175455 ) ) ;
#54326 = CARTESIAN_POINT ( 'NONE',  ( 30.82842712474619873, 196.3750000000000284, 167.1715728752537586 ) ) ;
#54327 = CARTESIAN_POINT ( 'NONE',  ( -11.35316468750000141, 43.48958332991935549, 3.042071309553159963 ) ) ;
#54328 = CARTESIAN_POINT ( 'NONE',  ( -1.656854249492381248, 6.312500000000000000, -4.000000000000001776 ) ) ;
#54329 = CARTESIAN_POINT ( 'NONE',  ( -10.00000000000000000, 14.16666665983870210, -2.679491924311229845 ) ) ;
#54330 = VERTEX_POINT ( 'NONE', #33830 ) ;
#54331 = CARTESIAN_POINT ( 'NONE',  ( 0.000000000000000000, 0.000000000000000000, 0.000000000000000000 ) ) ;
#54332 = CARTESIAN_POINT ( 'NONE',  ( 2.449293598294707893E-16, 14.25000000000000000, -4.000000000000001776 ) ) ;
#54333 = CARTESIAN_POINT ( 'NONE',  ( 6.951808397369818766E-16, 42.03124999658601268, -11.35316468750000141 ) ) ;
#54334 = CARTESIAN_POINT ( 'NONE',  ( 7.778174593052021635, 7.778174593052023411, 83.12500000409676204 ) ) ;
#54335 = CARTESIAN_POINT ( 'NONE',  ( 1.432654583217607414, 204.5000000013655779, 145.4587341250000350 ) ) ;
#54336 = CARTESIAN_POINT ( 'NONE',  ( -4.242640687119286547, 298.8750000000000000, -4.242640687119286547 ) ) ;
#54337 = CARTESIAN_POINT ( 'NONE',  ( -11.00000000000000000, 0.000000000000000000, 118.0000000000000000 ) ) ;
#54339 = CARTESIAN_POINT ( 'NONE',  ( -3.042071309553173730, 39.32291666325267698, 11.35316468749999785 ) ) ;
#54338 = CARTESIAN_POINT ( 'NONE',  ( -5.082755093536324154, 107.8437500020483810, 5.082755093536326818 ) ) ;
#54340 = CARTESIAN_POINT ( 'NONE',  ( 7.999999999999991118, 3.313708498984757611, 18.17405277982336642 ) ) ;
#54341 = CARTESIAN_POINT ( 'NONE',  ( -3.042071309553173730, 164.3229166632526415, 11.35316468749999785 ) ) ;
#54342 = CARTESIAN_POINT ( 'NONE',  ( -2.679491924311235618, 125.4166666598386968, 10.00000000000000000 ) ) ;
#54343 = CARTESIAN_POINT ( 'NONE',  ( 5.082755093536326818, 107.0937500020483810, 5.082755093536325042 ) ) ;
#54344 = ORIENTED_EDGE ( 'NONE', *, *, #13597, .F. ) ;
#54345 = CARTESIAN_POINT ( 'NONE',  ( 0.4369882809721256645, -67.59332269700064444, -20.03478791450352503 ) ) ;
#54346 = CARTESIAN_POINT ( 'NONE',  ( 5.676582343749993598, 25.26041666325268764, 9.832129032723422313 ) ) ;
#54347 = ORIENTED_EDGE ( 'NONE', *, *, #4416, .T. ) ;
#54348 = CARTESIAN_POINT ( 'NONE',  ( -32.00000000000003553, 205.3125000027312126, 168.3431457505080857 ) ) ;
#54349 = CARTESIAN_POINT ( 'NONE',  ( -7.204075437095965206, -7.204075437095968759, 79.84375000204838102 ) ) ;
#54350 = CARTESIAN_POINT ( 'NONE',  ( -30.64284399271078740, 271.9999999999999432, 174.6921329945331536 ) ) ;
#54352 = CARTESIAN_POINT ( 'NONE',  ( -5.676582343750006032, 149.1145833299193555, 9.832129032723418760 ) ) ;
#54351 = CARTESIAN_POINT ( 'NONE',  ( -20.04020123427919486, -30.91468120080561377, 145.4868234293612090 ) ) ;
#54353 = CARTESIAN_POINT ( 'NONE',  ( 9.797174393178825657E-16, 125.0000000000000000, -8.000000000000000000 ) ) ;
#54354 = AXIS2_PLACEMENT_3D ( 'NONE', #44214, #32149, #73256 ) ;
#54355 = CARTESIAN_POINT ( 'NONE',  ( 5.656854249492376141, -5.656854249492374365, 16.44905278432982954 ) ) ;
#54356 = CARTESIAN_POINT ( 'NONE',  ( -29.63216573525020436, -21.08125295631979768, 179.1787732309172441 ) ) ;
#54357 = CARTESIAN_POINT ( 'NONE',  ( -8.311093377946836114, 228.2812500034140157, -8.311093377946836114 ) ) ;
#54358 = CARTESIAN_POINT ( 'NONE',  ( 4.220049686691934809, 10.18810118749999916, 84.06250000204838102 ) ) ;
#54359 = ORIENTED_EDGE ( 'NONE', *, *, #31532, .T. ) ;
#54360 =( BOUNDED_CURVE ( )  B_SPLINE_CURVE ( 2, ( #65381, #2381, #42366, #30685, #18257, #24278, #41640, #36352, #54073 ),
 .UNSPECIFIED., .F., .F. ) 
 B_SPLINE_CURVE_WITH_KNOTS ( ( 3, 2, 2, 2, 3 ),
 ( 0.7840909090909090606, 0.7897727272727272929, 0.7954545454545454142, 0.8011363636363637575, 0.8068181818181818787 ),
 .UNSPECIFIED. ) 
 CURVE ( )  GEOMETRIC_REPRESENTATION_ITEM ( )  RATIONAL_B_SPLINE_CURVE ( ( 1.000000000000000000, 0.9238795325112867385, 1.000000000000000000, 0.9238795325112867385, 1.000000000000000000, 0.9238795325112867385, 1.000000000000000000, 0.9238795325112852952, 1.000000000000001554 ) ) 
 REPRESENTATION_ITEM ( '' )  );
#54361 = EDGE_CURVE ( 'NONE', #64315, #53073, #56827, .T. ) ;
#54362 = DIRECTION ( 'NONE',  ( -0.000000000000000000, 1.000000000000000000, -0.000000000000000000 ) ) ;
#54363 = CARTESIAN_POINT ( 'NONE',  ( -3.999999999999959144, 199.1875000027312410, 199.6568542494924259 ) ) ;
#54364 = ADVANCED_BREP_SHAPE_REPRESENTATION ( '', ( #17160, #57354 ), #64563 ) ;
#54365 = CARTESIAN_POINT ( 'NONE',  ( 8.311093377946834337, 105.4687499965860127, 8.311093377946839666 ) ) ;
#54366 = CARTESIAN_POINT ( 'NONE',  ( -7.204075437095967871, 7.204075437095967871, 103.4687500020483668 ) ) ;
#54367 = CARTESIAN_POINT ( 'NONE',  ( 1.881053915767122664, 19.24999999863440436, 4.541265875000001451 ) ) ;
#54368 = ORIENTED_EDGE ( 'NONE', *, *, #23212, .F. ) ;
#54369 = VERTEX_POINT ( 'NONE', #74163 ) ;
#54370 = AXIS2_PLACEMENT_3D ( 'NONE', #29171, #5052, #46139 ) ;
#54371 = CARTESIAN_POINT ( 'NONE',  ( 4.541265875000002339, 2.437499998634407028, 0.000000000000000000 ) ) ;
#54372 = CARTESIAN_POINT ( 'NONE',  ( 5.082755093536325930, 0.6562499979516100979, -5.082755093536325930 ) ) ;
#54373 = CARTESIAN_POINT ( 'NONE',  ( 3.313708498984765161, 116.6562500040968047, 7.999999999999998224 ) ) ;
#54374 = ADVANCED_FACE ( 'NONE', ( #34196 ), #53021, .T. ) ;
#54375 = CARTESIAN_POINT ( 'NONE',  ( -7.204075437095965206, -7.204075437095968759, 96.71875000204838102 ) ) ;
#54376 = CARTESIAN_POINT ( 'NONE',  ( -24.54126587500000056, 204.5000000013656063, 168.5673454167827003 ) ) ;
#54377 = CARTESIAN_POINT ( 'NONE',  ( 0.000000000000000000, 125.0000000000000000, 0.000000000000000000 ) ) ;
#54378 = EDGE_CURVE ( 'NONE', #545, #69783, #14892, .T. ) ;
#54379 = CARTESIAN_POINT ( 'NONE',  ( 4.000000000000001776, 5.062500000000001776, -1.656854249492381248 ) ) ;
#54380 = CARTESIAN_POINT ( 'NONE',  ( 1.656854249492381248, 17.93749999726881583, -4.000000000000001776 ) ) ;
#54381 = CARTESIAN_POINT ( 'NONE',  ( -1.881053915767124440, 2.999999998634407028, 4.541265875000001451 ) ) ;
#54382 = PLANE ( 'NONE',  #23449 ) ;
#54383 = FACE_OUTER_BOUND ( 'NONE', #51926, .T. ) ;
#54384 = COLOUR_RGB ( '',0.7921568627450980005, 0.8196078431372548767, 0.9333333333333333481 ) ;
#54386 = DIRECTION ( 'NONE',  ( 0.000000000000000000, 0.000000000000000000, 1.000000000000000000 ) ) ;
#54385 = CARTESIAN_POINT ( 'NONE',  ( -26.56734541678227757, 203.0000000013655779, 173.4587341250003476 ) ) ;
#54387 = CARTESIAN_POINT ( 'NONE',  ( 4.541265875000001451, 18.24999999863440792, 1.881053915767124440 ) ) ;
#54388 = CARTESIAN_POINT ( 'NONE',  ( 5.000000000000000000, -16.14408868864072844, 27.96238185062368586 ) ) ;
#54389 = AXIS2_PLACEMENT_3D ( 'NONE', #73360, #22776, #21664 ) ;
#54390 = CARTESIAN_POINT ( 'NONE',  ( -7.188101187499992051, 0.000000000000000000, 5.986552781871753659 ) ) ;
#54391 = ORIENTED_EDGE ( 'NONE', *, *, #8487, .F. ) ;
#54392 = ORIENTED_EDGE ( 'NONE', *, *, #70346, .F. ) ;
#54393 = CARTESIAN_POINT ( 'NONE',  ( 1.871523826299183495E-15, -10.18810118749999916, 96.53125000204838102 ) ) ;
#54394 = CARTESIAN_POINT ( 'NONE',  ( -7.778174593052023411, 7.778174593052023411, 115.0000000040967905 ) ) ;
#54395 = AXIS2_PLACEMENT_3D ( 'NONE', #31215, #46802, #29832 ) ;
#54396 = CARTESIAN_POINT ( 'NONE',  ( -28.00000000000002132, 205.6875000013656063, 166.5412658750003629 ) ) ;
#54397 = CARTESIAN_POINT ( 'NONE',  ( -29.65685424949241167, 199.0625000000000284, 166.0000000000004263 ) ) ;
#54398 = CARTESIAN_POINT ( 'NONE',  ( 3.458734125000016313, 196.8750000013656063, 199.4326545832176691 ) ) ;
#54399 = CARTESIAN_POINT ( 'NONE',  ( -7.320508075688778149, 113.1250000000000142, 7.320508075688769267 ) ) ;
#54400 = CARTESIAN_POINT ( 'NONE',  ( -5.656854249492378806, 110.1875000000000000, 5.656854249492381470 ) ) ;
#54401 = CARTESIAN_POINT ( 'NONE',  ( -2.765530957081996810, 296.4218750017070079, -6.676582343750003368 ) ) ;
#54402 = ORIENTED_EDGE ( 'NONE', *, *, #71713, .T. ) ;
#54403 = APPLICATION_CONTEXT ( 'automotive_design' ) ;
#54404 = CARTESIAN_POINT ( 'NONE',  ( 7.778174593052023411, -7.778174593052021635, 109.5625000000000000 ) ) ;
#54405 = CARTESIAN_POINT ( 'NONE',  ( -5.656854249492381470, 18.74999999590322020, 5.656854249492379694 ) ) ;
#54406 = CARTESIAN_POINT ( 'NONE',  ( -3.458734125000015425, 203.9375000013656063, 142.0000000000000568 ) ) ;
#54407 = CARTESIAN_POINT ( 'NONE',  ( -20.04126766827750572, -33.09544091703538982, 145.9388831141634171 ) ) ;
#54408 = CARTESIAN_POINT ( 'NONE',  ( 5.656854249492379694, 114.1250000040967763, -5.656854249492380582 ) ) ;
#54409 = CARTESIAN_POINT ( 'NONE',  ( 5.676582343750005144, 255.8854166700806445, 9.832129032723416984 ) ) ;
#54410 = CARTESIAN_POINT ( 'NONE',  ( 1.102182119232618108E-15, 289.2500000000000000, 6.000000000000001776 ) ) ;
#54411 = CARTESIAN_POINT ( 'NONE',  ( 11.00000000000000000, 4.556349186104045934, 112.8437500000000000 ) ) ;
#54412 = CARTESIAN_POINT ( 'NONE',  ( 3.042071309553159519, 4.739583329919349275, 11.35316468750000141 ) ) ;
#54413 = CARTESIAN_POINT ( 'NONE',  ( -4.401442555609577197E-16, 7.188101187499992051, 4.486552781871752771 ) ) ;
#54414 = CARTESIAN_POINT ( 'NONE',  ( -8.311093377946841443, 189.2187499965860411, 8.311093377946830785 ) ) ;
#54415 = FACE_OUTER_BOUND ( 'NONE', #52372, .T. ) ;
#54416 = CARTESIAN_POINT ( 'NONE',  ( -4.541265875000002339, 5.812499998634406140, -5.561446717895856393E-16 ) ) ;
#54417 = CARTESIAN_POINT ( 'NONE',  ( 7.320508075688776373, 241.8749999999999716, 7.320508075688767491 ) ) ;
#54419 = CYLINDRICAL_SURFACE ( 'NONE', #43500, 7.999999999999991118 ) ;
#54418 = CARTESIAN_POINT ( 'NONE',  ( -5.656854249492378806, 107.3750000040967763, 5.656854249492381470 ) ) ;
#54420 = VERTEX_POINT ( 'NONE', #60144 ) ;
#54421 = AXIS2_PLACEMENT_3D ( 'NONE', #35783, #18797, #59528 ) ;
#54422 = CARTESIAN_POINT ( 'NONE',  ( 3.458734124999959469, 202.7500000013655779, 140.5673454167824161 ) ) ;
#54423 = CARTESIAN_POINT ( 'NONE',  ( -11.35316468750000141, 48.59374999658601268, -1.390361679473963753E-15 ) ) ;
#54424 = CARTESIAN_POINT ( 'NONE',  ( -10.99999999999999822, -4.556349186104052151, 97.28125000409677625 ) ) ;
#54425 = CYLINDRICAL_SURFACE ( 'NONE', #26416, 3.999999999999976019 ) ;
#54426 = CARTESIAN_POINT ( 'NONE',  ( -24.54126587500001833, 203.2500000013655495, 168.5673454167826435 ) ) ;
#54427 = CARTESIAN_POINT ( 'NONE',  ( 6.742326029964707423, 8.814023156139338511, 117.4676415472669788 ) ) ;
#54429 = CARTESIAN_POINT ( 'NONE',  ( 1.656854249492280440, 203.8125000000000568, 146.0000000000001421 ) ) ;
#54428 = CARTESIAN_POINT ( 'NONE',  ( 5.000000000000000000, 60.90295814858223622, 23.31388853594876664 ) ) ;
#54430 = CARTESIAN_POINT ( 'NONE',  ( 1.432654583217607858, 195.6250000013656063, 138.5412658750000787 ) ) ;
#54431 = CARTESIAN_POINT ( 'NONE',  ( -11.35316468750000141, 128.2812499965860127, -1.390361679473963753E-15 ) ) ;
#54432 = CARTESIAN_POINT ( 'NONE',  ( -4.999999999999998224, 93.54166665983871098, -8.660254037844389075 ) ) ;
#54433 = CARTESIAN_POINT ( 'NONE',  ( -2.977408999572651815, 91.43750000204838102, 7.188101187500000933 ) ) ;
#54434 = CARTESIAN_POINT ( 'NONE',  ( 1.881053915767122664, 15.24999999863440969, 4.541265875000001451 ) ) ;
#54435 = CARTESIAN_POINT ( 'NONE',  ( 0.000000000000000000, 0.000000000000000000, -0.6932054628276118624 ) ) ;
#54436 = CARTESIAN_POINT ( 'NONE',  ( 5.000000000000000000, -68.60357193678697740, -20.85024232999374050 ) ) ;
#54437 = VERTEX_POINT ( 'NONE', #65057 ) ;
#54438 = CARTESIAN_POINT ( 'NONE',  ( -7.950158476760519122, 225.9999999999998863, 6.101342341042199635 ) ) ;
#54439 = ORIENTED_EDGE ( 'NONE', *, *, #39052, .F. ) ;
#54440 = CARTESIAN_POINT ( 'NONE',  ( 6.676582343750001591, 294.1093750017069510, -8.176455196517173205E-16 ) ) ;
#54441 = CARTESIAN_POINT ( 'NONE',  ( -4.000000000000001776, 12.24999999726881406, -4.898587196589415787E-16 ) ) ;
#54442 = CARTESIAN_POINT ( 'NONE',  ( 7.999999999999991118, 3.313708498984757611, 4.861552783920145338 ) ) ;
#54443 = CARTESIAN_POINT ( 'NONE',  ( -3.042071309553173730, 174.3229166632526983, 11.35316468749999785 ) ) ;
#54444 = CARTESIAN_POINT ( 'NONE',  ( -3.999999999999960032, 201.1250000027312126, 198.0000000000000284 ) ) ;
#54445 = CARTESIAN_POINT ( 'NONE',  ( -3.999999999999959144, 200.0625000000000568, 199.6568542494924259 ) ) ;
#54446 = CARTESIAN_POINT ( 'NONE',  ( 6.123233995736767268E-16, 83.12499999317203958, -10.00000000000000178 ) ) ;
#54447 = CARTESIAN_POINT ( 'NONE',  ( -6.238412754330611322E-16, 10.18810118749999916, 106.6562500020483810 ) ) ;
#54448 = ORIENTED_EDGE ( 'NONE', *, *, #74038, .F. ) ;
#54449 = CARTESIAN_POINT ( 'NONE',  ( -3.728321214210839063, 56.13798660966043741, -44.08488161416902784 ) ) ;
#54450 = AXIS2_PLACEMENT_3D ( 'NONE', #17797, #53250, #28742 ) ;
#54451 = DIRECTION ( 'NONE',  ( 0.000000000000000000, 0.000000000000000000, 1.000000000000000000 ) ) ;
#54452 = CARTESIAN_POINT ( 'NONE',  ( 3.042071309553167513, 137.1354166632526983, -11.35316468749999785 ) ) ;
#54453 = CARTESIAN_POINT ( 'NONE',  ( 6.350741970897364085E-13, 216.2499999999999432, -9.999999999999998224 ) ) ;
#54454 = CARTESIAN_POINT ( 'NONE',  ( 1.432654583217662481, 207.3750000013656063, 194.5412658750000219 ) ) ;
#54455 =( BOUNDED_CURVE ( )  B_SPLINE_CURVE ( 2, ( #13505, #71594, #20665, #66694, #14997, #55393, #61034, #25202, #30876 ),
 .UNSPECIFIED., .F., .F. ) 
 B_SPLINE_CURVE_WITH_KNOTS ( ( 3, 2, 2, 2, 3 ),
 ( 0.4166666666666671293, 0.4250000000000003775, 0.4333333333333336812, 0.4416666666666669849, 0.4500000000000002887 ),
 .UNSPECIFIED. ) 
 CURVE ( )  GEOMETRIC_REPRESENTATION_ITEM ( )  RATIONAL_B_SPLINE_CURVE ( ( 0.9999999999999958922, 0.9238795325112908463, 1.000000000000000000, 0.9238795325112867385, 1.000000000000000000, 0.9238795325112867385, 1.000000000000000000, 0.9238795325112841850, 1.000000000000002442 ) ) 
 REPRESENTATION_ITEM ( '' )  );
#54456 = CARTESIAN_POINT ( 'NONE',  ( 10.18810118750000093, -4.220049686691933033, 70.18750000204838102 ) ) ;
#54457 = CARTESIAN_POINT ( 'NONE',  ( 3.042071309553159519, 65.05208332991932707, 11.35316468750000141 ) ) ;
#54458 = ORIENTED_EDGE ( 'NONE', *, *, #32107, .F. ) ;
#54459 = CARTESIAN_POINT ( 'NONE',  ( -27.99999999999991473, 208.6250000027312126, 174.0000000000003695 ) ) ;
#54460 = CARTESIAN_POINT ( 'NONE',  ( -3.211159895383562723, 5.062499998634407028, 3.211159895383561391 ) ) ;
#54461 = CARTESIAN_POINT ( 'NONE',  ( -5.662595241051935346, 5.662595241051935346, 8.325615283940630107 ) ) ;
#54462 = ORIENTED_EDGE ( 'NONE', *, *, #25789, .T. ) ;
#54463 = EDGE_CURVE ( 'NONE', #9367, #26719, #74621, .T. ) ;
#54464 = CARTESIAN_POINT ( 'NONE',  ( -5.082755093536325042, 20.53124999795161543, -5.082755093536325930 ) ) ;
#54465 = CARTESIAN_POINT ( 'NONE',  ( -6.000000000000001776, 290.0625000034140157, 0.000000000000000000 ) ) ;
#54466 = CYLINDRICAL_SURFACE ( 'NONE', #67827, 3.999999999999976019 ) ;
#54467 = CARTESIAN_POINT ( 'NONE',  ( -2.977408999572650039, 13.31249999795161187, -7.188101187500001821 ) ) ;
#54468 = CARTESIAN_POINT ( 'NONE',  ( 7.188101187499993827, -2.977408999572645598, 3.642802781871751883 ) ) ;
#54469 = CARTESIAN_POINT ( 'NONE',  ( -7.204075437095965206, -7.204075437095968759, 116.2187500020483810 ) ) ;
#54470 =( BOUNDED_CURVE ( )  B_SPLINE_CURVE ( 2, ( #63509, #5809, #58609, #17484, #70293, #52203, #535, #24254, #23515 ),
 .UNSPECIFIED., .F., .F. ) 
 B_SPLINE_CURVE_WITH_KNOTS ( ( 3, 2, 2, 2, 3 ),
 ( 0.1617647058823530326, 0.1654411764705883137, 0.1691176470588236225, 0.1727941176470589035, 0.1764705882352942123 ),
 .UNSPECIFIED. ) 
 CURVE ( )  GEOMETRIC_REPRESENTATION_ITEM ( )  RATIONAL_B_SPLINE_CURVE ( ( 0.9999999999999982236, 0.9238795325112885148, 1.000000000000000000, 0.9238795325112867385, 1.000000000000000000, 0.9238795325112867385, 1.000000000000000000, 0.9238795325112849621, 1.000000000000001776 ) ) 
 REPRESENTATION_ITEM ( '' )  );
#54471 = CARTESIAN_POINT ( 'NONE',  ( 1.829567600301109653, -42.61442074515464640, 151.0875869205108017 ) ) ;
#54472 = CARTESIAN_POINT ( 'NONE',  ( 2.449293598294707893E-16, 2.999999997268813168, -4.000000000000001776 ) ) ;
#54473 = ORIENTED_EDGE ( 'NONE', *, *, #70336, .T. ) ;
#54474 = CIRCLE ( 'NONE', #23117, 12.00000000000000000 ) ;
#54475 = CARTESIAN_POINT ( 'NONE',  ( 2.445694354108839619, 206.8125000013656063, 200.4456943541088663 ) ) ;
#54476 = EDGE_CURVE ( 'NONE', #46843, #56876, #43262, .T. ) ;
#54477 = CONICAL_SURFACE ( 'NONE', #53290, 10.99999999999998934, 0.5235987755982931535 ) ;
#54478 = CARTESIAN_POINT ( 'NONE',  ( -23.99999999999998934, 198.8750000027312126, 170.0000000000002842 ) ) ;
#54479 = CARTESIAN_POINT ( 'NONE',  ( 4.541265875000001451, 1.249999998634407028, 1.881053915767124440 ) ) ;
#54480 = CARTESIAN_POINT ( 'NONE',  ( -7.188101187500000044, 110.6562500020483810, 0.000000000000000000 ) ) ;
#54481 = CARTESIAN_POINT ( 'NONE',  ( 11.00000000000000000, 1.347111479062088405E-15, 103.7500000000000000 ) ) ;
#54482 = CARTESIAN_POINT ( 'NONE',  ( 5.082755093536318824, 5.082755093536319713, 23.42405278187175455 ) ) ;
#54483 = ORIENTED_EDGE ( 'NONE', *, *, #73564, .T. ) ;
#54484 = CARTESIAN_POINT ( 'NONE',  ( -7.188101187500000044, 23.71874999795161543, -8.802885111219163269E-16 ) ) ;
#54485 = ORIENTED_EDGE ( 'NONE', *, *, #48477, .T. ) ;
#54486 = CARTESIAN_POINT ( 'NONE',  ( 7.204075437095968759, -7.204075437095966983, 114.7187500020483810 ) ) ;
#54487 = DIRECTION ( 'NONE',  ( -0.000000000000000000, -0.000000000000000000, 1.000000000000000000 ) ) ;
#54488 = CARTESIAN_POINT ( 'NONE',  ( -2.445694354108782775, 208.5625000013656063, 200.4456943541088663 ) ) ;
#54489 = CARTESIAN_POINT ( 'NONE',  ( 24.54126587499999346, 202.1875000013656063, 169.9999999999999432 ) ) ;
#54490 = CARTESIAN_POINT ( 'NONE',  ( -1.836970198721029983E-15, 73.75000000000001421, 10.00000000000000178 ) ) ;
#54491 = CARTESIAN_POINT ( 'NONE',  ( -7.188101187500000044, 94.53125000204836681, 0.000000000000000000 ) ) ;
#54492 = CARTESIAN_POINT ( 'NONE',  ( -3.673940397442060854E-16, 296.7500000000000000, -6.000000000000001776 ) ) ;
#54494 = CARTESIAN_POINT ( 'NONE',  ( -5.000000000000000888, 254.1666666666666572, -8.660254037844387298 ) ) ;
#54493 = CARTESIAN_POINT ( 'NONE',  ( 25.17157287525382259, 209.0000000027312126, 172.8284271247460993 ) ) ;
#54495 = ORIENTED_EDGE ( 'NONE', *, *, #8548, .F. ) ;
#54496 = CARTESIAN_POINT ( 'NONE',  ( 9.832129032723420536, 230.9895833367473301, 5.676582343749996262 ) ) ;
#54497 = AXIS2_PLACEMENT_3D ( 'NONE', #19599, #49776, #61090 ) ;
#54498 = CARTESIAN_POINT ( 'NONE',  ( 11.00000000000000000, 1.347111479062088405E-15, 87.43750000409677625 ) ) ;
#54499 = CARTESIAN_POINT ( 'NONE',  ( 2.828427124746153876, 201.0000000027312126, 144.8284271247462129 ) ) ;
#54500 = DIRECTION ( 'NONE',  ( -0.000000000000000000, -0.000000000000000000, -1.000000000000000000 ) ) ;
#54501 = CARTESIAN_POINT ( 'NONE',  ( -7.320508075688770155, 260.6249999999999432, 7.320508075688774596 ) ) ;
#54502 = DIRECTION ( 'NONE',  ( -1.000000000000000000, 0.000000000000000000, 0.000000000000000000 ) ) ;
#54503 = CARTESIAN_POINT ( 'NONE',  ( 5.000000000000001776, 190.8333333333333428, -8.660254037844389075 ) ) ;
#54504 = CARTESIAN_POINT ( 'NONE',  ( 2.020667218593132706E-15, -11.00000000000000000, 89.87499999999998579 ) ) ;
#54505 = CARTESIAN_POINT ( 'NONE',  ( -7.188101187499990274, -2.977408999572651815, 24.45530278187175810 ) ) ;
#54506 = CARTESIAN_POINT ( 'NONE',  ( -8.311093377946836114, 152.9687499965859558, -8.311093377946837890 ) ) ;
#54507 = CARTESIAN_POINT ( 'NONE',  ( 4.242640687119287435, 294.4375000034140157, 4.242640687119285658 ) ) ;
#54508 = DIRECTION ( 'NONE',  ( -0.000000000000000000, -1.000000000000000000, -4.283267841918042741E-17 ) ) ;
#54511 = CARTESIAN_POINT ( 'NONE',  ( -4.242640687119286547, 293.8750000000000000, -4.242640687119286547 ) ) ;
#54510 = CARTESIAN_POINT ( 'NONE',  ( -2.679491924311235174, 85.41666665983869677, 10.00000000000000000 ) ) ;
#54509 = CARTESIAN_POINT ( 'NONE',  ( 29.65685424949235482, 203.0625000000000284, 173.9999999999999147 ) ) ;
#54512 = ORIENTED_EDGE ( 'NONE', *, *, #7273, .T. ) ;
#54513 = CARTESIAN_POINT ( 'NONE',  ( -8.311093377946841443, 14.21874999658601979, 8.311093377946830785 ) ) ;
#54514 = DIRECTION ( 'NONE',  ( 0.000000000000000000, 0.000000000000000000, -1.000000000000000000 ) ) ;
#54515 = CARTESIAN_POINT ( 'NONE',  ( 0.000000000000000000, 300.0000000000000000, 0.000000000000000000 ) ) ;
#54516 = CARTESIAN_POINT ( 'NONE',  ( 1.432654583217607858, 205.6250000013656063, 138.5412658750000787 ) ) ;
#54517 = CIRCLE ( 'NONE', #11122, 8.000000000000000000 ) ;
#54518 = CARTESIAN_POINT ( 'NONE',  ( 10.00000000000000000, 46.66666665983868967, 2.679491924311236062 ) ) ;
#54519 = CARTESIAN_POINT ( 'NONE',  ( 1.320432766682874540E-15, 111.0312500020483810, 7.188101187500000044 ) ) ;
#54520 = CARTESIAN_POINT ( 'NONE',  ( 2.780723358947928197E-16, 4.687499998634407028, -4.541265875000002339 ) ) ;
#54521 = CARTESIAN_POINT ( 'NONE',  ( 3.544144923083450749, 60.54353712382587105, -23.09461823984437956 ) ) ;
#54522 = CARTESIAN_POINT ( 'NONE',  ( 7.999999999999991118, 3.313708498984757611, 9.174052779823364645 ) ) ;
#54523 = DIRECTION ( 'NONE',  ( -0.000000000000000000, -0.000000000000000000, -1.000000000000000000 ) ) ;
#54524 = ORIENTED_EDGE ( 'NONE', *, *, #38594, .T. ) ;
#54525 = CARTESIAN_POINT ( 'NONE',  ( 5.656854249492374365, 5.656854249492375253, 1.767802779823364423 ) ) ;
#54526 = CARTESIAN_POINT ( 'NONE',  ( 11.35316468749999608, 231.9270833367473301, -3.042071309553167513 ) ) ;
#54527 = AXIS2_PLACEMENT_3D ( 'NONE', #18724, #53432, #13769 ) ;
#54528 = CARTESIAN_POINT ( 'NONE',  ( -8.311093377946841443, 133.9062499965860411, 8.311093377946830785 ) ) ;
#54529 = ORIENTED_EDGE ( 'NONE', *, *, #24114, .F. ) ;
#54530 = EDGE_CURVE ( 'NONE', #53638, #62209, #64047, .T. ) ;
#54531 = CARTESIAN_POINT ( 'NONE',  ( 2.828427124746209831, 198.3750000000000284, 200.8284271247462129 ) ) ;
#54532 = CARTESIAN_POINT ( 'NONE',  ( -10.18810118749999738, -4.220049686691941915, 96.25000000204838102 ) ) ;
#54533 = CARTESIAN_POINT ( 'NONE',  ( -5.656854249492375253, 5.656854249492375253, 20.33030278392014623 ) ) ;
#54534 = CARTESIAN_POINT ( 'NONE',  ( 2.839093476692135984E-14, 197.9375000013655779, 201.4587341250000350 ) ) ;
#54535 = CARTESIAN_POINT ( 'NONE',  ( -7.999999999999974243, 3.313708498984772710, 27.73655277982335932 ) ) ;
#54537 = CARTESIAN_POINT ( 'NONE',  ( -2.085542519210945728E-15, 119.5312499965860269, 11.35316468750000141 ) ) ;
#54536 = CARTESIAN_POINT ( 'NONE',  ( 32.00000000000000000, 196.3125000000000284, 168.3431457505075457 ) ) ;
#54538 = CARTESIAN_POINT ( 'NONE',  ( -30.82842712474621649, 208.1250000000000284, 167.1715728752542134 ) ) ;
#54539 = CARTESIAN_POINT ( 'NONE',  ( 4.999999999999993783, 81.04166665983871098, 8.660254037844390851 ) ) ;
#54540 = VERTEX_POINT ( 'NONE', #37141 ) ;
#54541 = VECTOR ( 'NONE', #66540, 1000.000000000000000 ) ;
#54542 = DIRECTION ( 'NONE',  ( -0.000000000000000000, -0.000000000000000000, -1.000000000000000000 ) ) ;
#54543 = CARTESIAN_POINT ( 'NONE',  ( 12.00000000000000000, 28.00000000000000000, 0.000000000000000000 ) ) ;
#54544 = CARTESIAN_POINT ( 'NONE',  ( 8.311093377946837890, 106.7187499965860269, -8.311093377946837890 ) ) ;
#54545 = CARTESIAN_POINT ( 'NONE',  ( 2.445694354108838731, 208.0625000013656063, 195.5543056458912190 ) ) ;
#54546 = CARTESIAN_POINT ( 'NONE',  ( -7.188101187500000933, 11.99999999795161187, -2.977408999572651371 ) ) ;
#54547 = CARTESIAN_POINT ( 'NONE',  ( -7.204075437095967871, 7.204075437095967871, 90.34375000204838102 ) ) ;
#54548 = CARTESIAN_POINT ( 'NONE',  ( -8.311093377946841443, 19.21874999658601979, 8.311093377946830785 ) ) ;
#54549 = VERTEX_POINT ( 'NONE', #53758 ) ;
#54550 = CARTESIAN_POINT ( 'NONE',  ( -4.217983994794429314, 68.29231466825656582, -20.60018752343895088 ) ) ;
#54551 = CARTESIAN_POINT ( 'NONE',  ( 2.679491924311306672, 244.5833333401612606, 9.999999999999957367 ) ) ;
#54552 = CARTESIAN_POINT ( 'NONE',  ( 10.92737078412413609, 225.9999999999999147, -3.080083792328916825 ) ) ;
#54553 = CARTESIAN_POINT ( 'NONE',  ( 10.18810118749999916, 1.247682550866122264E-15, 71.78125000204838102 ) ) ;
#54554 = ADVANCED_FACE ( 'NONE', ( #8097 ), #2069, .F. ) ;
#54555 = CARTESIAN_POINT ( 'NONE',  ( -10.00000000000000000, 264.0625000034140157, 0.000000000000000000 ) ) ;
#54556 = CARTESIAN_POINT ( 'NONE',  ( -6.000000000000003553, 299.0000000034139589, -2.485281374238571317 ) ) ;
#54557 = CARTESIAN_POINT ( 'NONE',  ( 4.000000000000015987, 204.6250000027312126, 198.0000000000000284 ) ) ;
#54558 = CARTESIAN_POINT ( 'NONE',  ( 8.311093377946837890, 221.7187499965860127, -8.311093377946837890 ) ) ;
#54559 = ADVANCED_FACE ( 'NONE', ( #23967 ), #25058, .T. ) ;
#54560 = CARTESIAN_POINT ( 'NONE',  ( 11.35316468749999963, 136.3020833299193555, -3.042071309553165293 ) ) ;
#54561 = CARTESIAN_POINT ( 'NONE',  ( 4.220049686691941027, -10.18810118749999738, 83.12500000204835260 ) ) ;
#54562 = CARTESIAN_POINT ( 'NONE',  ( -29.43265458321766559, 199.5000000013656063, 166.5412658750003629 ) ) ;
#54563 = CARTESIAN_POINT ( 'NONE',  ( 4.898587196589412829E-16, 24.37500000000000355, -8.000000000000000000 ) ) ;
#54564 = CARTESIAN_POINT ( 'NONE',  ( 4.541265875000001451, 11.37499999863440969, 1.881053915767124440 ) ) ;
#54565 = VERTEX_POINT ( 'NONE', #42417 ) ;
#54566 = CARTESIAN_POINT ( 'NONE',  ( 4.000000000000015099, 201.6875000027312126, 196.3431457505076594 ) ) ;
#54567 = ADVANCED_FACE ( 'NONE', ( #65435 ), #64337, .T. ) ;
#54568 =( BOUNDED_CURVE ( )  B_SPLINE_CURVE ( 2, ( #1861, #25957, #60300, #20684, #48236, #71244, #14268, #30894, #20302 ),
 .UNSPECIFIED., .F., .F. ) 
 B_SPLINE_CURVE_WITH_KNOTS ( ( 3, 2, 2, 2, 3 ),
 ( 0.8823529411764706731, 0.8860294117647059542, 0.8897058823529412352, 0.8933823529411766273, 0.8970588235294119084 ),
 .UNSPECIFIED. ) 
 CURVE ( )  GEOMETRIC_REPRESENTATION_ITEM ( )  RATIONAL_B_SPLINE_CURVE ( ( 0.9999999999999976685, 0.9238795325112890700, 1.000000000000000000, 0.9238795325112867385, 1.000000000000000000, 0.9238795325112867385, 1.000000000000000000, 0.9238795325112844070, 1.000000000000002220 ) ) 
 REPRESENTATION_ITEM ( '' )  );
#54569 = CARTESIAN_POINT ( 'NONE',  ( -2.754378923186476579E-14, 200.4375000013656063, 145.4587341250000350 ) ) ;
#54570 = CARTESIAN_POINT ( 'NONE',  ( 2.828427124746152987, 204.2500000027312126, 139.1715728752538723 ) ) ;
#54571 = CARTESIAN_POINT ( 'NONE',  ( 27.99999999999996803, 208.6250000027312126, 165.9999999999998863 ) ) ;
#54572 = AXIS2_PLACEMENT_3D ( 'NONE', #9501, #32516, #23964 ) ;
#54573 = ORIENTED_EDGE ( 'NONE', *, *, #45739, .F. ) ;
#54574 = CARTESIAN_POINT ( 'NONE',  ( -5.082755093536325042, 4.031249997951610986, -5.082755093536325930 ) ) ;
#54575 = CARTESIAN_POINT ( 'NONE',  ( -13.37704301675528207, -22.50206576122104707, 197.9698155523694254 ) ) ;
#54576 = DIRECTION ( 'NONE',  ( -0.000000000000000000, 1.000000000000000000, -0.000000000000000000 ) ) ;
#54577 = AXIS2_PLACEMENT_3D ( 'NONE', #67270, #66891, #21600 ) ;
#54578 = CARTESIAN_POINT ( 'NONE',  ( -5.676582343750006032, 184.1145833299193555, 9.832129032723418760 ) ) ;
#54579 = CARTESIAN_POINT ( 'NONE',  ( -2.977408999572651815, 112.8125000020483952, 7.188101187500000933 ) ) ;
#54580 = CARTESIAN_POINT ( 'NONE',  ( 1.102182119232618108E-15, 295.2500000000000000, 6.000000000000001776 ) ) ;
#54581 = CARTESIAN_POINT ( 'NONE',  ( 4.721056650415999201, 291.0781250017069510, -4.721056650415999201 ) ) ;
#54583 = CARTESIAN_POINT ( 'NONE',  ( 5.000000000000000000, 60.11723469343052528, 46.25570701698154608 ) ) ;
#54582 = CARTESIAN_POINT ( 'NONE',  ( -32.00000000000001421, 209.1875000000000284, 168.3431457505080289 ) ) ;
#54584 = ORIENTED_EDGE ( 'NONE', *, *, #43297, .T. ) ;
#54585 =( BOUNDED_CURVE ( )  B_SPLINE_CURVE ( 2, ( #68911, #11569, #34603, #57610, #5920, #51939, #277, #13401, #53052 ),
 .UNSPECIFIED., .F., .F. ) 
 B_SPLINE_CURVE_WITH_KNOTS ( ( 3, 2, 2, 2, 3 ),
 ( 0.1833333333333333481, 0.1916666666666667629, 0.2000000000000001776, 0.2083333333333335646, 0.2166666666666669516 ),
 .UNSPECIFIED. ) 
 CURVE ( )  GEOMETRIC_REPRESENTATION_ITEM ( )  RATIONAL_B_SPLINE_CURVE ( ( 0.9999999999999997780, 0.9238795325112869605, 1.000000000000000000, 0.9238795325112867385, 1.000000000000000000, 0.9238795325112867385, 1.000000000000000000, 0.9238795325112841850, 1.000000000000002442 ) ) 
 REPRESENTATION_ITEM ( '' )  );
#54586 = CARTESIAN_POINT ( 'NONE',  ( 8.311093377946834337, 227.3437500034140157, -8.311093377946836114 ) ) ;
#54587 = ADVANCED_FACE ( 'NONE', ( #71087 ), #7208, .F. ) ;
#54588 = CARTESIAN_POINT ( 'NONE',  ( -5.082755093536319713, 5.082755093536319713, 2.799052781871750994 ) ) ;
#54589 = DIRECTION ( 'NONE',  ( -0.000000000000000000, 1.000000000000000000, -0.000000000000000000 ) ) ;
#54590 = CARTESIAN_POINT ( 'NONE',  ( -5.000000000000000000, 10.26105934116142215, 64.40045319026754100 ) ) ;
#54591 = CARTESIAN_POINT ( 'NONE',  ( -2.445694354108784108, 198.5625000013656063, 195.5543056458912190 ) ) ;
#54592 = VERTEX_POINT ( 'NONE', #13004 ) ;
#54593 = CARTESIAN_POINT ( 'NONE',  ( -4.242640687119286547, 298.9375000034140157, -4.242640687119286547 ) ) ;
#54594 = CARTESIAN_POINT ( 'NONE',  ( 1.469576158976823947E-15, 92.37499999999998579, 8.000000000000000000 ) ) ;
#54595 = CARTESIAN_POINT ( 'NONE',  ( -3.042071309553173730, 119.6354166632526841, 11.35316468749999785 ) ) ;
#54596 = DIRECTION ( 'NONE',  ( -0.000000000000000000, 1.000000000000000000, -0.000000000000000000 ) ) ;
#54597 = CARTESIAN_POINT ( 'NONE',  ( -4.556349186104045934, 11.00000000000000000, 78.71874999999998579 ) ) ;
#54600 = DIRECTION ( 'NONE',  ( -0.000000000000000000, 1.000000000000000000, -0.000000000000000000 ) ) ;
#54599 = CARTESIAN_POINT ( 'NONE',  ( 28.00000000000001776, 199.4375000013655779, 173.4587341249998929 ) ) ;
#54598 = CARTESIAN_POINT ( 'NONE',  ( 24.54126587499997925, 197.5000000013656063, 171.4326545832175555 ) ) ;
#54601 = ORIENTED_EDGE ( 'NONE', *, *, #1411, .T. ) ;
#54602 = LINE ( 'NONE', #36501, #4642 ) ;
#54603 = CARTESIAN_POINT ( 'NONE',  ( 8.311093377946837890, 221.4062499965860411, -8.311093377946837890 ) ) ;
#54604 = CARTESIAN_POINT ( 'NONE',  ( -3.458734125000016313, 200.8750000013656063, 140.5673454167824161 ) ) ;
#54605 = CARTESIAN_POINT ( 'NONE',  ( 26.56734541678232375, 203.6250000013656063, 173.4587341249998929 ) ) ;
#54606 = CARTESIAN_POINT ( 'NONE',  ( 4.556349186104051263, -10.99999999999999822, 114.1562500040967763 ) ) ;
#54607 = CARTESIAN_POINT ( 'NONE',  ( -2.085542519210945728E-15, 189.8437499965860127, 11.35316468750000141 ) ) ;
#54608 = CARTESIAN_POINT ( 'NONE',  ( 5.082755093536325042, 90.96875000204838102, -5.082755093536325930 ) ) ;
#54609 = DIRECTION ( 'NONE',  ( -0.000000000000000000, -0.000000000000000000, 1.000000000000000000 ) ) ;
#54610 = CARTESIAN_POINT ( 'NONE',  ( 4.541265875000001451, 13.24999999863441147, 1.881053915767124440 ) ) ;
#54611 = CARTESIAN_POINT ( 'NONE',  ( 25.55430564589119413, 199.3125000013656063, 167.5543056458910485 ) ) ;
#54612 = CARTESIAN_POINT ( 'NONE',  ( 2.977408999572650927, -7.188101187499990274, 3.830302781871751883 ) ) ;
#54613 = CARTESIAN_POINT ( 'NONE',  ( -5.000000000000000000, 29.68417822476651580, 4.268394125863326671 ) ) ;
#54614 = CARTESIAN_POINT ( 'NONE',  ( -11.35316468750000141, 88.48958332991934128, 3.042071309553159963 ) ) ;
#54615 = ORIENTED_EDGE ( 'NONE', *, *, #49600, .F. ) ;
#54616 = CARTESIAN_POINT ( 'NONE',  ( 7.320508075688779037, 139.3750000000000000, 7.320508075688782590 ) ) ;
#54617 = DIRECTION ( 'NONE',  ( 0.000000000000000000, 0.000000000000000000, 1.000000000000000000 ) ) ;
#54618 = CYLINDRICAL_SURFACE ( 'NONE', #10940, 3.999999999999976019 ) ;
#54619 = CARTESIAN_POINT ( 'NONE',  ( -1.656854249492305531, 206.8125000000000284, 194.0000000000000284 ) ) ;
#54620 = CARTESIAN_POINT ( 'NONE',  ( -5.676582343750006032, 89.11458332991935549, 9.832129032723418760 ) ) ;
#54621 = ORIENTED_EDGE ( 'NONE', *, *, #69408, .F. ) ;
#54622 = CARTESIAN_POINT ( 'NONE',  ( 10.18810118749999916, 1.247682550866122264E-15, 86.78125000204836681 ) ) ;
#54623 = CARTESIAN_POINT ( 'NONE',  ( 1.871523826299183495E-15, -10.18810118749999916, 116.0312500020483810 ) ) ;
#54624 = CARTESIAN_POINT ( 'NONE',  ( -5.656854249492378806, 102.6875000000000000, 5.656854249492381470 ) ) ;
#54625 = CARTESIAN_POINT ( 'NONE',  ( 30.82842712474617386, 207.1250000000000284, 172.8284271247460993 ) ) ;
#54627 = CARTESIAN_POINT ( 'NONE',  ( 6.951808397369818766E-16, 72.03124999658602690, -11.35316468750000141 ) ) ;
#54626 = CARTESIAN_POINT ( 'NONE',  ( 5.656854249492379694, 121.6250000040967905, -5.656854249492380582 ) ) ;
#54628 = CARTESIAN_POINT ( 'NONE',  ( -4.898587196589407898E-16, 7.999999999999991118, 18.64280278392014623 ) ) ;
#54629 = CARTESIAN_POINT ( 'NONE',  ( 2.828427124746190291, 12.87500000000000178, 2.828427124746192067 ) ) ;
#54630 = CARTESIAN_POINT ( 'NONE',  ( 8.660254037844385522, 171.4583333265053682, 5.000000000000005329 ) ) ;
#54631 = CARTESIAN_POINT ( 'NONE',  ( -2.977408999572651815, 90.31250000204838102, 7.188101187500000933 ) ) ;
#54632 = FACE_OUTER_BOUND ( 'NONE', #17448, .T. ) ;
#54633 = CARTESIAN_POINT ( 'NONE',  ( -5.676582343750006032, 59.42708332991934839, 9.832129032723418760 ) ) ;
#54634 = CARTESIAN_POINT ( 'NONE',  ( -4.721056650415998313, 295.5781250017069510, 4.721056650416000089 ) ) ;
#54635 = CARTESIAN_POINT ( 'NONE',  ( 7.204075437095968759, -7.204075437095966983, 104.5937500020483810 ) ) ;
#54636 = CARTESIAN_POINT ( 'NONE',  ( -2.085542519210945728E-15, 209.5312499965860411, 11.35316468750000141 ) ) ;
#54637 = ORIENTED_EDGE ( 'NONE', *, *, #72510, .F. ) ;
#54638 = CARTESIAN_POINT ( 'NONE',  ( -3.313708498984759387, -7.999999999999989342, 26.79905278392014623 ) ) ;
#54639 = CARTESIAN_POINT ( 'NONE',  ( -11.00000000000000533, 0.000000000000000000, 41.99999999999999289 ) ) ;
#54640 = CARTESIAN_POINT ( 'NONE',  ( 5.000000000000000000, 67.66743717231469191, 22.54291394825019168 ) ) ;
#54642 = CARTESIAN_POINT ( 'NONE',  ( -11.35316468750000141, 198.4895833299193555, 3.042071309553159963 ) ) ;
#54641 = CARTESIAN_POINT ( 'NONE',  ( 25.17157287525378706, 206.8750000000000284, 172.8284271247460424 ) ) ;
#54643 = AXIS2_PLACEMENT_3D ( 'NONE', #57277, #5960, #29347 ) ;
#54644 = CYLINDRICAL_SURFACE ( 'NONE', #17662, 12.00000000000000355 ) ;
#54645 = CARTESIAN_POINT ( 'NONE',  ( -10.00000000000000000, 237.9166666734946602, -2.679491924311226292 ) ) ;
#54646 = CARTESIAN_POINT ( 'NONE',  ( 7.999999999999991118, 1.076704741343554046E-05, 12.26780308853677148 ) ) ;
#54647 = ORIENTED_EDGE ( 'NONE', *, *, #11313, .F. ) ;
#54648 = CARTESIAN_POINT ( 'NONE',  ( 5.676582343749993598, 175.2604166632526699, 9.832129032723422313 ) ) ;
#54649 = EDGE_CURVE ( 'NONE', #7001, #6837, #22616, .T. ) ;
#54650 = CARTESIAN_POINT ( 'NONE',  ( -2.977408999572647819, -7.188101187499990274, 22.76780278187175455 ) ) ;
#54651 = CARTESIAN_POINT ( 'NONE',  ( -0.4320110153365262495, 60.19564456717440493, -22.88238106212044087 ) ) ;
#54652 = EDGE_LOOP ( 'NONE', ( #65312, #22179, #38529 ) ) ;
#54653 = CARTESIAN_POINT ( 'NONE',  ( 3.313708498984765161, 95.65625000409679046, 7.999999999999998224 ) ) ;
#54654 = CARTESIAN_POINT ( 'NONE',  ( -8.660254037844390851, 7.916666666666666963, 4.999999999999998224 ) ) ;
#54655 = ADVANCED_FACE ( 'NONE', ( #49575 ), #32237, .T. ) ;
#54656 = AXIS2_PLACEMENT_3D ( 'NONE', #35889, #24179, #18531 ) ;
#54657 = ADVANCED_FACE ( 'NONE', ( #20146 ), #55998, .T. ) ;
#54658 = CARTESIAN_POINT ( 'NONE',  ( 2.828427124746190291, 14.87500000000000178, 2.828427124746192067 ) ) ;
#54659 = CARTESIAN_POINT ( 'NONE',  ( -4.541265875000003227, 13.87499999863440792, 1.881053915767121110 ) ) ;
#54660 = CARTESIAN_POINT ( 'NONE',  ( -7.999999999999991118, 3.313708498984756723, 14.42405278392014800 ) ) ;
#54661 = CARTESIAN_POINT ( 'NONE',  ( -4.898587196589412829E-16, 93.12499999999998579, -8.000000000000000000 ) ) ;
#54662 = EDGE_LOOP ( 'NONE', ( #41040, #64111, #54615, #66342, #60379 ) ) ;
#54663 = CARTESIAN_POINT ( 'NONE',  ( -3.673940397442060854E-16, 293.8125000034140157, -6.000000000000001776 ) ) ;
#54664 = CARTESIAN_POINT ( 'NONE',  ( 7.188101187500002709, 94.81250000204838102, 2.977408999572649151 ) ) ;
#54666 = CARTESIAN_POINT ( 'NONE',  ( 8.311093377946834337, 257.0312500034139020, -8.311093377946836114 ) ) ;
#54665 = CARTESIAN_POINT ( 'NONE',  ( -2.679491924311265816, 83.54166666666672825, 10.00000000000011546 ) ) ;
#54667 = CARTESIAN_POINT ( 'NONE',  ( 1424.688200795887269, 710.9677537767815920, 917.4921604560587411 ) ) ;
#54668 = ORIENTED_EDGE ( 'NONE', *, *, #30593, .F. ) ;
#54669 = CARTESIAN_POINT ( 'NONE',  ( -8.311093377946836114, 263.5937500034140157, -8.311093377946836114 ) ) ;
#54670 = ADVANCED_FACE ( 'NONE', ( #49194 ), #39010, .T. ) ;
#54671 = CARTESIAN_POINT ( 'NONE',  ( 1.320432766682872962E-15, -7.188101187499992051, 18.36155278187175455 ) ) ;
#54672 = ORIENTED_EDGE ( 'NONE', *, *, #41186, .T. ) ;
#54673 = EDGE_CURVE ( 'NONE', #13626, #43538, #72593, .T. ) ;
#54674 =( BOUNDED_CURVE ( )  B_SPLINE_CURVE ( 2, ( #63050, #44966, #83, #23060, #11375, #69089, #17395, #67972, #40419 ),
 .UNSPECIFIED., .F., .F. ) 
 B_SPLINE_CURVE_WITH_KNOTS ( ( 3, 2, 2, 2, 3 ),
 ( 0.2083333333333333148, 0.2152777777777777624, 0.2222222222222221821, 0.2291666666666666574, 0.2361111111111111049 ),
 .UNSPECIFIED. ) 
 CURVE ( )  GEOMETRIC_REPRESENTATION_ITEM ( )  RATIONAL_B_SPLINE_CURVE ( ( 1.000000000000000222, 0.9238795325112864054, 1.000000000000000000, 0.9238795325112867385, 1.000000000000000000, 0.9238795325112867385, 1.000000000000000000, 0.9238795325112867385, 1.000000000000000000 ) ) 
 REPRESENTATION_ITEM ( '' )  );
#54675 = ORIENTED_EDGE ( 'NONE', *, *, #24398, .F. ) ;
#54676 = CARTESIAN_POINT ( 'NONE',  ( -10.18810118749999916, 4.220049686691934809, 81.06250000204836681 ) ) ;
#54677 = CARTESIAN_POINT ( 'NONE',  ( -3.042071309553173730, 74.63541666325268409, 11.35316468749999785 ) ) ;
#54678 = CARTESIAN_POINT ( 'NONE',  ( 5.000000000000001776, 92.70833332650536818, -8.660254037844389075 ) ) ;
#54679 = CARTESIAN_POINT ( 'NONE',  ( 7.778174593052021635, 7.778174593052023411, 96.43749999999998579 ) ) ;
#54682 = CARTESIAN_POINT ( 'NONE',  ( 4.721056650415999201, 292.2343750017069510, -4.721056650415999201 ) ) ;
#54681 = CARTESIAN_POINT ( 'NONE',  ( 30.82842712474616320, 197.5000000027312126, 167.1715728752537018 ) ) ;
#54680 = CARTESIAN_POINT ( 'NONE',  ( -23.99999999999996092, 205.8125000027312126, 171.6568542494926817 ) ) ;
#54683 = CARTESIAN_POINT ( 'NONE',  ( -2.679491924311225848, 151.4583333333333428, -10.00000000000000178 ) ) ;
#54684 = VECTOR ( 'NONE', #14417, 1000.000000000000114 ) ;
#54685 = CARTESIAN_POINT ( 'NONE',  ( -1.836970198721029983E-15, 165.6249999931720254, 10.00000000000000178 ) ) ;
#54686 = CARTESIAN_POINT ( 'NONE',  ( -2.445694354108783219, 198.8125000013656063, 200.4456943541088663 ) ) ;
#54687 = CARTESIAN_POINT ( 'NONE',  ( 1.102182119232618108E-15, 293.2500000000000000, 6.000000000000001776 ) ) ;
#54688 = CARTESIAN_POINT ( 'NONE',  ( 28.00000000000002132, 198.9375000013655779, 166.5412658749999082 ) ) ;
#54689 = CARTESIAN_POINT ( 'NONE',  ( -1.320432766682874540E-15, 12.46874999795161187, 7.188101187500000044 ) ) ;
#54690 = CARTESIAN_POINT ( 'NONE',  ( 7.999999999999991118, 9.797174393178815797E-16, 24.26780278392014978 ) ) ;
#54691 = DIRECTION ( 'NONE',  ( -0.000000000000000000, 1.000000000000000000, -0.000000000000000000 ) ) ;
#54692 = CARTESIAN_POINT ( 'NONE',  ( 2.977408999572654480, 113.0000000020483810, 7.188101187499999156 ) ) ;
#54694 = DIRECTION ( 'NONE',  ( -0.000000000000000000, -1.000000000000000000, -0.000000000000000000 ) ) ;
#54693 = CARTESIAN_POINT ( 'NONE',  ( -2.485281374238217822, 293.2500000034140157, 6.000000000000357048 ) ) ;
#54695 = CARTESIAN_POINT ( 'NONE',  ( 28.00000000000001421, 195.5000000000000000, 165.9999999999998863 ) ) ;
#54696 = CARTESIAN_POINT ( 'NONE',  ( 27.99999999999996803, 209.6875000013656063, 173.4587341249998929 ) ) ;
#54697 = CARTESIAN_POINT ( 'NONE',  ( 2.977408999572650927, -7.188101187499990274, 21.83030278187175810 ) ) ;
#54698 = CYLINDRICAL_SURFACE ( 'NONE', #35965, 5.099999999999999645 ) ;
#54699 = CARTESIAN_POINT ( 'NONE',  ( 8.311093377946834337, 45.15624999658601268, 8.311093377946839666 ) ) ;
#54700 = CARTESIAN_POINT ( 'NONE',  ( -4.000000000000002665, 6.562500000000000000, 1.656854249492380582 ) ) ;
#54701 = CARTESIAN_POINT ( 'NONE',  ( 6.123233995736767268E-16, 8.124999993172032475, -10.00000000000000178 ) ) ;
#54702 = VERTEX_POINT ( 'NONE', #66931 ) ;
#54703 = ADVANCED_FACE ( 'NONE', ( #32998 ), #15236, .T. ) ;
#54704 = CARTESIAN_POINT ( 'NONE',  ( -36.10814071610730736, 49.99999999999998579, 139.0000000000000000 ) ) ;
#54705 = CARTESIAN_POINT ( 'NONE',  ( -2.828427124746192067, 14.62500000000000000, 2.828427124746190735 ) ) ;
#54706 = CARTESIAN_POINT ( 'NONE',  ( -5.676582343750006032, 49.11458332991935549, 9.832129032723418760 ) ) ;
#54707 = CARTESIAN_POINT ( 'NONE',  ( 7.778174593052023411, -7.778174593052021635, 78.25000000409676204 ) ) ;
#54708 = CARTESIAN_POINT ( 'NONE',  ( -3.458734125000015425, 205.2500000013655779, 143.4326545832176976 ) ) ;
#54709 = CARTESIAN_POINT ( 'NONE',  ( -4.242640687119285658, 299.1250000000000000, 4.242640687119287435 ) ) ;
#54710 = DIRECTION ( 'NONE',  ( 0.000000000000000000, 0.8536788251726021848, 0.5207998305029730712 ) ) ;
#54712 = CARTESIAN_POINT ( 'NONE',  ( 6.951808397369818766E-16, 27.03124999658601979, -11.35316468750000141 ) ) ;
#54711 = CARTESIAN_POINT ( 'NONE',  ( 7.188101187500000044, 100.9062500020483810, -8.802885111219163269E-16 ) ) ;
#54714 = EDGE_CURVE ( 'NONE', #45978, #1178, #49348, .T. ) ;
#54713 = CARTESIAN_POINT ( 'NONE',  ( -5.656854249492375253, 5.656854249492375253, 9.642802779823364645 ) ) ;
#54715 = CARTESIAN_POINT ( 'NONE',  ( -5.000000000000005329, 50.20833332650537528, 8.660254037844387298 ) ) ;
#54716 = CARTESIAN_POINT ( 'NONE',  ( 9.832129032723416984, 155.3645833299193839, 5.676582343750006032 ) ) ;
#54718 = CARTESIAN_POINT ( 'NONE',  ( -5.000000000000005329, 130.2083333265053966, 8.660254037844387298 ) ) ;
#54717 = PRODUCT ( 'plain washer (type a)_is_IS 2016 A- 14', 'plain washer (type a)_is_IS 2016 A- 14', '', ( #57659 ) ) ;
#54719 = CARTESIAN_POINT ( 'NONE',  ( -2.977408999572651815, 111.3125000020483810, 7.188101187500000933 ) ) ;
#54720 = ORIENTED_EDGE ( 'NONE', *, *, #41588, .T. ) ;
#54721 = CARTESIAN_POINT ( 'NONE',  ( 7.320508075688771044, 21.24999999317203248, 7.320508075688775484 ) ) ;
#54722 = CARTESIAN_POINT ( 'NONE',  ( 9.832129032723420536, 16.51041666325268054, -5.676582343749999815 ) ) ;
#54723 = EDGE_CURVE ( 'NONE', #14049, #30219, #60894, .T. ) ;
#54724 = CARTESIAN_POINT ( 'NONE',  ( -1.656854249492538234, 195.8125000027312126, 145.9999999999998863 ) ) ;
#54725 = VERTEX_POINT ( 'NONE', #21643 ) ;
#54726 = CARTESIAN_POINT ( 'NONE',  ( -1.469576158976823947E-15, 1.125000000000000222, 8.000000000000000000 ) ) ;
#54727 = CARTESIAN_POINT ( 'NONE',  ( -7.204075437095965206, -7.204075437095968759, 78.34375000204838102 ) ) ;
#54728 = FACE_OUTER_BOUND ( 'NONE', #4264, .T. ) ;
#54730 = CARTESIAN_POINT ( 'NONE',  ( 8.311093377946837890, 151.4062499965860127, -8.311093377946837890 ) ) ;
#54729 = CYLINDRICAL_SURFACE ( 'NONE', #53174, 11.00000000000000000 ) ;
#54731 = CARTESIAN_POINT ( 'NONE',  ( 5.082755093536324154, 2.156249997951610542, 5.082755093536326818 ) ) ;
#54732 = CARTESIAN_POINT ( 'NONE',  ( 3.313708498984756279, 7.999999999999991118, 12.41780278432982421 ) ) ;
#54733 = CARTESIAN_POINT ( 'NONE',  ( -27.96674631054437299, -21.41150722326580791, 183.4226951199153746 ) ) ;
#54734 = CARTESIAN_POINT ( 'NONE',  ( -11.35316468749999785, 238.6979166700806729, -3.042071309553164848 ) ) ;
#54735 = CARTESIAN_POINT ( 'NONE',  ( -4.220049686691937474, -10.18810118749999738, 84.81250000204838102 ) ) ;
#54736 = VERTEX_POINT ( 'NONE', #49951 ) ;
#54737 = CARTESIAN_POINT ( 'NONE',  ( -2.679491924311226292, 118.3333333265053966, -10.00000000000000178 ) ) ;
#54738 = CARTESIAN_POINT ( 'NONE',  ( -11.00000000000000000, 0.000000000000000000, 109.1875000040967763 ) ) ;
#54739 = CARTESIAN_POINT ( 'NONE',  ( -5.676582343749998039, 102.7604166632526841, -9.832129032723420536 ) ) ;
#54740 = CARTESIAN_POINT ( 'NONE',  ( 1.871523826299183495E-15, -10.18810118749999916, 96.53125000204838102 ) ) ;
#54741 = CARTESIAN_POINT ( 'NONE',  ( 10.00000000000001066, 15.00000000000000533, 0.000000000000000000 ) ) ;
#54742 = VERTEX_POINT ( 'NONE', #9600 ) ;
#54743 = VERTEX_POINT ( 'NONE', #54879 ) ;
#54744 = VECTOR ( 'NONE', #30296, 1000.000000000000000 ) ;
#54745 = CARTESIAN_POINT ( 'NONE',  ( 4.541265875000002339, 5.437499998634407028, 0.000000000000000000 ) ) ;
#54746 = CARTESIAN_POINT ( 'NONE',  ( -2.977408999572654480, 10.49999999795161010, 7.188101187499999156 ) ) ;
#54747 = CARTESIAN_POINT ( 'NONE',  ( 5.656854249492379694, 114.1250000040967763, -5.656854249492380582 ) ) ;
#54748 = CARTESIAN_POINT ( 'NONE',  ( 4.220049686691941027, -10.18810118749999738, 95.50000000204838102 ) ) ;
#54749 = CARTESIAN_POINT ( 'NONE',  ( -29.43265458321760519, 204.1250000013656063, 173.4587341250003760 ) ) ;
#54750 = CARTESIAN_POINT ( 'NONE',  ( -8.660254037844387298, 158.9583333265053966, -5.000000000000004441 ) ) ;
#54751 = CARTESIAN_POINT ( 'NONE',  ( -7.347880794884122694E-16, 3.750000000000000000, 4.000000000000001776 ) ) ;
#54752 = CARTESIAN_POINT ( 'NONE',  ( -4.000000000000001776, 18.18749999726881228, -1.656854249492381470 ) ) ;
#54753 = CARTESIAN_POINT ( 'NONE',  ( 3.211159895383560947, 3.187499998634407028, 3.211159895383562723 ) ) ;
#54754 = CARTESIAN_POINT ( 'NONE',  ( 8.000000000000000000, 95.75000000000000000, -9.797174393178825657E-16 ) ) ;
#54755 = CARTESIAN_POINT ( 'NONE',  ( 2.445694354108838731, 196.0625000013656063, 195.5543056458912190 ) ) ;
#54757 = CYLINDRICAL_SURFACE ( 'NONE', #38237, 20.00000000000001066 ) ;
#54756 = CARTESIAN_POINT ( 'NONE',  ( -25.55430564589122611, 195.3125000013656063, 167.5543056458915032 ) ) ;
#54758 = CARTESIAN_POINT ( 'NONE',  ( 3.211159895383561835, 16.43749999863440436, -3.211159895383561835 ) ) ;
#54759 = CARTESIAN_POINT ( 'NONE',  ( -11.00000000000000000, 0.000000000000000000, 99.99999999999998579 ) ) ;
#54760 = CIRCLE ( 'NONE', #33082, 3.999999999999976019 ) ;
#54761 = CARTESIAN_POINT ( 'NONE',  ( 7.188101187499991163, 2.977408999572648707, 6.830302781871755435 ) ) ;
#54762 = ORIENTED_EDGE ( 'NONE', *, *, #43692, .T. ) ;
#54763 = ORIENTED_EDGE ( 'NONE', *, *, #36305, .F. ) ;
#54764 = CARTESIAN_POINT ( 'NONE',  ( -6.238412754330611322E-16, 10.18810118749999916, 95.78125000204836681 ) ) ;
#54765 = CARTESIAN_POINT ( 'NONE',  ( 7.999999999999998224, 26.71874999590322375, 3.313708498984766049 ) ) ;
#54766 = CARTESIAN_POINT ( 'NONE',  ( -24.54126587499998280, 204.3750000013656063, 171.4326545832179818 ) ) ;
#54767 = CARTESIAN_POINT ( 'NONE',  ( -26.34314575050758123, 200.5625000000000284, 174.0000000000003411 ) ) ;
#54768 = CARTESIAN_POINT ( 'NONE',  ( -1.432654583217607192, 195.2500000013656063, 194.5412658750000219 ) ) ;
#54769 = CARTESIAN_POINT ( 'NONE',  ( -26.34314575050763807, 202.0625000027312126, 166.0000000000003979 ) ) ;
#54770 = CARTESIAN_POINT ( 'NONE',  ( -8.660254037844387298, 107.0833333333333428, -5.000000000000004441 ) ) ;
#54771 = CARTESIAN_POINT ( 'NONE',  ( -4.898587196589412829E-16, 111.1250000000000000, -8.000000000000000000 ) ) ;
#54772 = CARTESIAN_POINT ( 'NONE',  ( -6.676582343750000703, 290.6718750017070079, 2.765530957082001251 ) ) ;
#54773 = CARTESIAN_POINT ( 'NONE',  ( -2.977408999572648707, -7.188101187499990274, 11.14280278187175810 ) ) ;
#54774 = VERTEX_POINT ( 'NONE', #32619 ) ;
#54775 = CARTESIAN_POINT ( 'NONE',  ( 0.000000000000000000, 0.000000000000000000, 0.000000000000000000 ) ) ;
#54776 = CARTESIAN_POINT ( 'NONE',  ( 3.313708498984762496, 19.03124999590322375, 7.999999999999998224 ) ) ;
#54777 = CARTESIAN_POINT ( 'NONE',  ( -2.839093476692135984E-14, 204.6875000013656063, 138.5412658750000503 ) ) ;
#54778 = CARTESIAN_POINT ( 'NONE',  ( -7.347880794884122694E-16, 16.75000000000000000, 4.000000000000001776 ) ) ;
#54779 = CARTESIAN_POINT ( 'NONE',  ( 4.898587196589412829E-16, 1.875000000000000444, -8.000000000000000000 ) ) ;
#54780 = CARTESIAN_POINT ( 'NONE',  ( -11.35316468749999785, 254.0104166700806729, -3.042071309553164848 ) ) ;
#54781 = CARTESIAN_POINT ( 'NONE',  ( -3.999999999999959144, 207.1875000027312126, 199.6568542494924259 ) ) ;
#54782 = CARTESIAN_POINT ( 'NONE',  ( -6.735557395310442023E-16, 11.00000000000000000, 116.1249999999999858 ) ) ;
#54783 = CARTESIAN_POINT ( 'NONE',  ( -8.660254037844390851, 222.9166666666666856, 4.999999999999998224 ) ) ;
#54784 = CARTESIAN_POINT ( 'NONE',  ( -7.188101187499992051, 0.000000000000000000, 4.861552781871752771 ) ) ;
#54785 = CARTESIAN_POINT ( 'NONE',  ( 11.35316468749999785, 195.8854166632526415, 3.042071309553174174 ) ) ;
#54786 = CARTESIAN_POINT ( 'NONE',  ( 7.999999999999991118, 0.000000000000000000, 30.00000000000000000 ) ) ;
#54787 = CARTESIAN_POINT ( 'NONE',  ( 3.211159895383561835, 4.437499998634407028, -3.211159895383561835 ) ) ;
#54788 = DIRECTION ( 'NONE',  ( 1.000000000000000000, -0.000000000000000000, -0.000000000000000000 ) ) ;
#54790 = CARTESIAN_POINT ( 'NONE',  ( 6.000000000000001776, 297.5000000000000000, -7.347880794884121708E-16 ) ) ;
#54789 = CARTESIAN_POINT ( 'NONE',  ( -2.828427124746190735, 14.12499999726881406, -2.828427124746191623 ) ) ;
#54791 = ORIENTED_EDGE ( 'NONE', *, *, #45763, .F. ) ;
#54792 = AXIS2_PLACEMENT_3D ( 'NONE', #52188, #70276, #69908 ) ;
#54793 = CARTESIAN_POINT ( 'NONE',  ( -3.458734125000015425, 205.2500000013655779, 143.4326545832176976 ) ) ;
#54794 = CARTESIAN_POINT ( 'NONE',  ( -9.832129032723420536, 3.697916663252683200, 5.676582343749997150 ) ) ;
#54795 = CARTESIAN_POINT ( 'NONE',  ( 4.556349186104045934, 11.00000000000000000, 99.71875000409676204 ) ) ;
#54796 = CARTESIAN_POINT ( 'NONE',  ( -7.778174593052020747, -7.778174593052023411, 106.3750000040967763 ) ) ;
#54797 = CARTESIAN_POINT ( 'NONE',  ( -25.55430564589111953, 203.0625000013656063, 172.4456943541091505 ) ) ;
#54798 = LINE ( 'NONE', #3482, #71968 ) ;
#54800 = CARTESIAN_POINT ( 'NONE',  ( 1.656854249492382358, 204.1875000000000284, 138.0000000000001137 ) ) ;
#54799 = CARTESIAN_POINT ( 'NONE',  ( -7.188101187500000044, 119.6562500020483810, 0.000000000000000000 ) ) ;
#54802 = EDGE_CURVE ( 'NONE', #53828, #53624, #48599, .T. ) ;
#54801 = CARTESIAN_POINT ( 'NONE',  ( 3.313708498984762496, -7.999999999999989342, 26.79905277982337353 ) ) ;
#54803 =( BOUNDED_CURVE ( )  B_SPLINE_CURVE ( 3, ( #46729, #14238, #55009, #30498 ),
 .UNSPECIFIED., .F., .F. ) 
 B_SPLINE_CURVE_WITH_KNOTS ( ( 4, 4 ),
 ( 3.141592653589793116, 4.712388980384691450 ),
 .UNSPECIFIED. ) 
 CURVE ( )  GEOMETRIC_REPRESENTATION_ITEM ( )  RATIONAL_B_SPLINE_CURVE ( ( 1.000000000000000000, 0.8047378541243646044, 0.8047378541243646044, 1.000000000000000000 ) ) 
 REPRESENTATION_ITEM ( '' )  );
#54804 = CARTESIAN_POINT ( 'NONE',  ( 9.832129032723420536, 121.1979166632526983, -5.676582343749999815 ) ) ;
#54805 = CARTESIAN_POINT ( 'NONE',  ( -2.679491924311225848, 83.33333332650536818, -10.00000000000000178 ) ) ;
#54806 = CARTESIAN_POINT ( 'NONE',  ( -7.188101187499999156, 89.75000000204839523, 2.977408999572654924 ) ) ;
#54807 = CARTESIAN_POINT ( 'NONE',  ( -3.211159895383562723, 19.06249999863440436, 3.211159895383561391 ) ) ;
#54808 = CARTESIAN_POINT ( 'NONE',  ( 1.474731560294312738, -9.540868182094932592, -0.3570196857253685185 ) ) ;
#54809 = CARTESIAN_POINT ( 'NONE',  ( 6.123233995736767268E-16, 103.1249999931720396, -10.00000000000000178 ) ) ;
#54810 = EDGE_LOOP ( 'NONE', ( #51351, #23617, #72232, #68155 ) ) ;
#54811 = CARTESIAN_POINT ( 'NONE',  ( -2.828427124746209831, 200.5000000027312126, 139.1715728752538723 ) ) ;
#54812 = ORIENTED_EDGE ( 'NONE', *, *, #61609, .T. ) ;
#54813 = EDGE_CURVE ( 'NONE', #38243, #19453, #33228, .T. ) ;
#54814 = CARTESIAN_POINT ( 'NONE',  ( 6.676582343750004256, 294.0468750017070079, 2.765530957081995478 ) ) ;
#54815 = CARTESIAN_POINT ( 'NONE',  ( 2.679491924311376394, 187.9166666598386541, -9.999999999999914735 ) ) ;
#54816 = CARTESIAN_POINT ( 'NONE',  ( -7.999999999999991118, 0.000000000000000000, 7.017802783920144449 ) ) ;
#54817 = CARTESIAN_POINT ( 'NONE',  ( -9.832129032723420536, 163.6979166632526983, 5.676582343749997150 ) ) ;
#54818 = CARTESIAN_POINT ( 'NONE',  ( -3.999999999999960032, 201.0625000027312126, 196.3431457505076594 ) ) ;
#54819 = CARTESIAN_POINT ( 'NONE',  ( -3.999999999999960032, 201.9375000000000284, 196.3431457505076594 ) ) ;
#54820 = CARTESIAN_POINT ( 'NONE',  ( -10.99999999999999822, -4.556349186104053040, 70.28125000409676204 ) ) ;
#54821 = VECTOR ( 'NONE', #67158, 1000.000000000000000 ) ;
#54822 = CARTESIAN_POINT ( 'NONE',  ( 4.220049686691934809, 10.18810118749999916, 106.5625000020483668 ) ) ;
#54823 = EDGE_LOOP ( 'NONE', ( #47507, #1148, #71165, #2103 ) ) ;
#54824=STYLED_ITEM('',(#74713),#66162);
#54825 = DIRECTION ( 'NONE',  ( -0.000000000000000000, -1.000000000000000000, -0.000000000000000000 ) ) ;
#54826 = CARTESIAN_POINT ( 'NONE',  ( 6.951808397369818766E-16, 157.3437499965860127, -11.35316468750000141 ) ) ;
#54827 = CARTESIAN_POINT ( 'NONE',  ( -10.00000000000000533, 217.5000000000000284, -1.224646799147354045E-15 ) ) ;
#54828 = CARTESIAN_POINT ( 'NONE',  ( -2.445694354108783219, 206.8125000013656063, 200.4456943541088663 ) ) ;
#54829 = CARTESIAN_POINT ( 'NONE',  ( 7.204075437095968759, -7.204075437095966983, 71.59375000204836681 ) ) ;
#54830 = CARTESIAN_POINT ( 'NONE',  ( 9.832129032723420536, 56.51041666325268409, -5.676582343749999815 ) ) ;
#54831 = ORIENTED_EDGE ( 'NONE', *, *, #11595, .T. ) ;
#54832 = CARTESIAN_POINT ( 'NONE',  ( -2.775557561562891351E-14, 210.0000000000000284, 142.0000000000000568 ) ) ;
#54833 = CARTESIAN_POINT ( 'NONE',  ( 3.211159895383561835, 8.562499998634407916, -3.211159895383561835 ) ) ;
#54834 = CARTESIAN_POINT ( 'NONE',  ( 1.471067592899761672E-15, -8.008118988124991233, 7.388115283940628331 ) ) ;
#54835 = VERTEX_POINT ( 'NONE', #22752 ) ;
#54836 = CARTESIAN_POINT ( 'NONE',  ( 2.977408999572650927, 23.24999999795161187, -7.188101187500001821 ) ) ;
#54837 = CARTESIAN_POINT ( 'NONE',  ( -2.485281374238571761, 288.8750000034140157, -6.000000000000003553 ) ) ;
#54838 = CYLINDRICAL_SURFACE ( 'NONE', #44937, 11.00000000000000000 ) ;
#54839 = CARTESIAN_POINT ( 'NONE',  ( 7.188101187500001821, 15.93749999795161543, -2.977408999572650483 ) ) ;
#54840 = CARTESIAN_POINT ( 'NONE',  ( -2.977408999572647819, 7.188101187499992051, 5.705302781871753659 ) ) ;
#54841 = CARTESIAN_POINT ( 'NONE',  ( -6.238412754330611322E-16, 10.18810118749999916, 117.1562500020483810 ) ) ;
#54842 = CARTESIAN_POINT ( 'NONE',  ( 0.1982902916130831472, -42.00000000000000711, 151.0000000000000568 ) ) ;
#54843 = CARTESIAN_POINT ( 'NONE',  ( -1.656854249492381248, 6.062499997268813168, -4.000000000000001776 ) ) ;
#54844 = EDGE_LOOP ( 'NONE', ( #29881, #67703, #18141, #14418, #11770, #74025 ) ) ;
#54845 = CARTESIAN_POINT ( 'NONE',  ( 2.445694354108838731, 206.0625000013656063, 195.5543056458912190 ) ) ;
#54846 = CARTESIAN_POINT ( 'NONE',  ( -23.99999999999995026, 195.8125000027312126, 171.6568542494926817 ) ) ;
#54847 = CARTESIAN_POINT ( 'NONE',  ( 1.881053915767122664, 8.124999998634407916, 4.541265875000001451 ) ) ;
#54848 = CARTESIAN_POINT ( 'NONE',  ( -2.977408999572650927, 108.8750000020483810, -7.188101187500001821 ) ) ;
#54849 = CARTESIAN_POINT ( 'NONE',  ( 23.99999999999998934, 204.7500000000000284, 169.9999999999998863 ) ) ;
#54850 = CARTESIAN_POINT ( 'NONE',  ( -5.082755093536317936, -5.082755093536320601, 24.17405278187175455 ) ) ;
#54851 = VERTEX_POINT ( 'NONE', #52193 ) ;
#54852 = LINE ( 'NONE', #50295, #31314 ) ;
#54853 = ORIENTED_EDGE ( 'NONE', *, *, #45655, .T. ) ;
#54854 = CARTESIAN_POINT ( 'NONE',  ( -10.18810118749999916, 0.000000000000000000, 114.1562500020483810 ) ) ;
#54855 = CARTESIAN_POINT ( 'NONE',  ( 7.778174593052023411, -7.778174593052021635, 84.25000000409677625 ) ) ;
#54856 = CARTESIAN_POINT ( 'NONE',  ( 2.839093476692135984E-14, 206.6875000013656063, 201.4587341250000350 ) ) ;
#54857 = CARTESIAN_POINT ( 'NONE',  ( 25.55430564589115505, 204.0625000013656063, 167.5543056458911053 ) ) ;
#54858 = CARTESIAN_POINT ( 'NONE',  ( -1.836970198721029983E-15, 63.75000000000000000, 10.00000000000000178 ) ) ;
#54859 = CARTESIAN_POINT ( 'NONE',  ( -4.401442555609581635E-16, 94.15625000204838102, -7.188101187500000044 ) ) ;
#54860 = CARTESIAN_POINT ( 'NONE',  ( 6.000000000000003553, 295.4374999999999432, 2.485281374238571317 ) ) ;
#54861 = CIRCLE ( 'NONE', #28369, 11.00000000000000000 ) ;
#54863 = CARTESIAN_POINT ( 'NONE',  ( -9.999999999999998224, 255.2083333333333712, 2.679491924311235174 ) ) ;
#54862 = CARTESIAN_POINT ( 'NONE',  ( 32.16793986848087172, 176.1252570847143772, 164.7322117711578642 ) ) ;
#54864 = ORIENTED_EDGE ( 'NONE', *, *, #40263, .F. ) ;
#54865 = EDGE_CURVE ( 'NONE', #44090, #54774, #64487, .T. ) ;
#54866 = ADVANCED_FACE ( 'NONE', ( #56364 ), #46146, .T. ) ;
#54867 = CARTESIAN_POINT ( 'NONE',  ( -11.35316468749999608, 224.1145833367473301, 3.042071309553173730 ) ) ;
#54868 = VECTOR ( 'NONE', #32234, 1000.000000000000000 ) ;
#54869 = FACE_OUTER_BOUND ( 'NONE', #65808, .T. ) ;
#54870 = CARTESIAN_POINT ( 'NONE',  ( -2.828427124746208943, 200.7500000027312126, 144.8284271247462129 ) ) ;
#54871 = CARTESIAN_POINT ( 'NONE',  ( 11.00000000000000000, 1.347111479062088405E-15, 118.0000000000000000 ) ) ;
#54872 = DIRECTION ( 'NONE',  ( -0.000000000000000000, 1.000000000000000000, -0.000000000000000000 ) ) ;
#54873 = CARTESIAN_POINT ( 'NONE',  ( -4.999999999999992895, 250.8333333333333428, 8.660254037844390851 ) ) ;
#54874 = DIRECTION ( 'NONE',  ( -0.000000000000000000, -1.000000000000000000, -0.000000000000000000 ) ) ;
#54875 = CARTESIAN_POINT ( 'NONE',  ( -7.320508075688773708, 186.8750000000000000, -7.320508075688774596 ) ) ;
#54876 = CARTESIAN_POINT ( 'NONE',  ( -11.00000000000000000, 0.000000000000000000, 89.50000000000000000 ) ) ;
#54877 = CARTESIAN_POINT ( 'NONE',  ( 7.188101187499992051, 8.802885111219154394E-16, 20.61155278187175455 ) ) ;
#54878 = CARTESIAN_POINT ( 'NONE',  ( 5.676582343749993598, 160.2604166632526983, 9.832129032723422313 ) ) ;
#54879 = CARTESIAN_POINT ( 'NONE',  ( -50.99999999999994316, -31.99999999999978684, 171.9999999999997726 ) ) ;
#54880 = CARTESIAN_POINT ( 'NONE',  ( -31.00000000000001776, 49.38896263239215045, 65.00000000000001421 ) ) ;
#54881 = CYLINDRICAL_SURFACE ( 'NONE', #57357, 3.999999999999976019 ) ;
#54884 = CARTESIAN_POINT ( 'NONE',  ( -2.485281374238172081, 297.2500000034139589, 6.000000000000400568 ) ) ;
#54883 = CARTESIAN_POINT ( 'NONE',  ( 2.849036369511732440E-14, 199.3750000027312126, 202.0000000000000000 ) ) ;
#54882 = CARTESIAN_POINT ( 'NONE',  ( 26.34314575050763452, 203.5625000000000000, 165.9999999999998863 ) ) ;
#54885 = ORIENTED_EDGE ( 'NONE', *, *, #2490, .F. ) ;
#54886 = CARTESIAN_POINT ( 'NONE',  ( 3.042071309553159519, 15.05208332991935194, 11.35316468750000141 ) ) ;
#54887 = CARTESIAN_POINT ( 'NONE',  ( 4.000000000000015987, 200.6875000027312126, 196.3431457505076594 ) ) ;
#54888 = CARTESIAN_POINT ( 'NONE',  ( 10.00000000000000178, 32.08333332650535397, -2.679491924311226736 ) ) ;
#54889 = CARTESIAN_POINT ( 'NONE',  ( -1.432654583217664479, 201.7500000013655779, 138.5412658750000787 ) ) ;
#54890 = CARTESIAN_POINT ( 'NONE',  ( -7.320508075688773708, 48.74999999317203248, -7.320508075688774596 ) ) ;
#54891 = CARTESIAN_POINT ( 'NONE',  ( -7.188101187500001821, 107.5625000020483810, -2.977408999572650483 ) ) ;
#54892 = CARTESIAN_POINT ( 'NONE',  ( 1.881053915767121776, 9.624999998634404363, -4.541265875000002339 ) ) ;
#54893 = CARTESIAN_POINT ( 'NONE',  ( 7.320508075688779925, 219.3750000000000000, 7.320508075688784366 ) ) ;
#54894 = CARTESIAN_POINT ( 'NONE',  ( 7.999999999999991118, 9.797174393178815797E-16, 12.08030277982336642 ) ) ;
#54896 = CARTESIAN_POINT ( 'NONE',  ( -7.999987203421805582, -3.313721295562947144, 17.61155329591527519 ) ) ;
#54895 = FACE_OUTER_BOUND ( 'NONE', #12936, .T. ) ;
#54897 = ORIENTED_EDGE ( 'NONE', *, *, #34553, .T. ) ;
#54898 =( BOUNDED_CURVE ( )  B_SPLINE_CURVE ( 2, ( #48998, #8271, #38077, #72008, #15409, #3740, #25239, #37703, #19582, #60322, #36949, #72777, #54685 ),
 .UNSPECIFIED., .F., .F. ) 
 B_SPLINE_CURVE_WITH_KNOTS ( ( 3, 2, 2, 2, 2, 2, 3 ),
 ( 0.7010869565217391353, 0.7028985507246376940, 0.7047101449275362528, 0.7065217391304348116, 0.7083333333333332593, 0.7101449275362318181, 0.7119565217391303769 ),
 .UNSPECIFIED. ) 
 CURVE ( )  GEOMETRIC_REPRESENTATION_ITEM ( )  RATIONAL_B_SPLINE_CURVE ( ( 1.000000000000000000, 0.9659258262890683122, 1.000000000000000000, 0.9659258262890683122, 1.000000000000000000, 0.9659258262890683122, 1.000000000000000000, 0.9659258262890683122, 1.000000000000000000, 0.9659258262890683122, 1.000000000000000000, 0.9659258262890704216, 0.9999999999999978906 ) ) 
 REPRESENTATION_ITEM ( '' )  );
#54899 = B_SPLINE_CURVE_WITH_KNOTS ( 'NONE', 3,
 ( #729, #5257, #57692, #11282, #28629, #63697, #51641, #56941 ),
 .UNSPECIFIED., .F., .F.,
 ( 4, 2, 2, 4 ),
 ( 0.007010445034807182875, 0.008756443665256715206, 0.01050244229570624840, 0.01399443955660531827 ),
 .UNSPECIFIED. ) ;
#54900 = CARTESIAN_POINT ( 'NONE',  ( -4.999999999999998224, -64.42874436516127901, 24.11656705754152341 ) ) ;
#54901 = CARTESIAN_POINT ( 'NONE',  ( 3.313708498984721640, 26.71875000000000000, 8.000000000000039080 ) ) ;
#54902 = CARTESIAN_POINT ( 'NONE',  ( -8.311093377946836114, 228.5937500034139873, -8.311093377946836114 ) ) ;
#54903 = CARTESIAN_POINT ( 'NONE',  ( 11.35316468750000141, 130.7812499965860127, 0.000000000000000000 ) ) ;
#54904 = ORIENTED_EDGE ( 'NONE', *, *, #40791, .F. ) ;
#54905 = CARTESIAN_POINT ( 'NONE',  ( 7.999999999999991118, 9.797174393178815797E-16, 4.767802783920145338 ) ) ;
#54906 = CARTESIAN_POINT ( 'NONE',  ( 4.220049686691934809, 10.18810118749999916, 92.68750000204838102 ) ) ;
#54907 = CARTESIAN_POINT ( 'NONE',  ( 7.999999999999991118, 3.313708498984758055, 19.86155278392014978 ) ) ;
#54908 = CARTESIAN_POINT ( 'NONE',  ( 3.458734125000015869, 197.1875000013655779, 198.0000000000000284 ) ) ;
#54909 = CARTESIAN_POINT ( 'NONE',  ( -3.313708498984757611, 7.999999999999991118, 27.54905277982337353 ) ) ;
#54911 = CARTESIAN_POINT ( 'NONE',  ( 6.951808397369818766E-16, 127.0312499965860269, -11.35316468750000141 ) ) ;
#54910 = CARTESIAN_POINT ( 'NONE',  ( 0.000000000000000000, 0.000000000000000000, -20.42428869268542968 ) ) ;
#54912 = EDGE_CURVE ( 'NONE', #63044, #17271, #65021, .T. ) ;
#54913 = CARTESIAN_POINT ( 'NONE',  ( -7.347880794884122694E-16, 19.49999999726881228, 4.000000000000001776 ) ) ;
#54914 = ORIENTED_EDGE ( 'NONE', *, *, #43815, .T. ) ;
#54915 = CARTESIAN_POINT ( 'NONE',  ( 8.660254037844385522, 257.9166666666666856, -5.000000000000003553 ) ) ;
#54916 = CARTESIAN_POINT ( 'NONE',  ( -20.28493003623160007, 177.0489554009581639, 146.4498493591373460 ) ) ;
#54917 = CARTESIAN_POINT ( 'NONE',  ( -5.676582343749998039, 117.7604166632526841, -9.832129032723420536 ) ) ;
#54918 = CARTESIAN_POINT ( 'NONE',  ( 3.458734125000015425, 207.0000000013655779, 196.5673454167823877 ) ) ;
#54919 = CARTESIAN_POINT ( 'NONE',  ( -1.320432766682874540E-15, 16.96874999795161543, 7.188101187500000044 ) ) ;
#54920 = CARTESIAN_POINT ( 'NONE',  ( -10.18810118749999738, -4.220049686691941915, 90.62500000204836681 ) ) ;
#54921 = CARTESIAN_POINT ( 'NONE',  ( 11.35316468749999785, 20.88541666325268764, 3.042071309553174174 ) ) ;
#54923 = ORIENTED_EDGE ( 'NONE', *, *, #49305, .T. ) ;
#54922 =( BOUNDED_CURVE ( )  B_SPLINE_CURVE ( 2, ( #54138, #72215, #66557, #14867, #66939, #14489, #31493, #48830, #43170 ),
 .UNSPECIFIED., .F., .F. ) 
 B_SPLINE_CURVE_WITH_KNOTS ( ( 3, 2, 2, 2, 3 ),
 ( 0.1166666666666666546, 0.1250000000000000555, 0.1333333333333334425, 0.1416666666666668573, 0.1500000000000002442 ),
 .UNSPECIFIED. ) 
 CURVE ( )  GEOMETRIC_REPRESENTATION_ITEM ( )  RATIONAL_B_SPLINE_CURVE ( ( 1.000000000000000222, 0.9238795325112867385, 1.000000000000000000, 0.9238795325112867385, 1.000000000000000000, 0.9238795325112867385, 1.000000000000000000, 0.9238795325112844070, 1.000000000000002220 ) ) 
 REPRESENTATION_ITEM ( '' )  );
#54924 = CARTESIAN_POINT ( 'NONE',  ( 0.000000000000000000, 300.0000000000000000, 0.000000000000000000 ) ) ;
#54925 = CARTESIAN_POINT ( 'NONE',  ( -4.903558642999205574E-16, 8.008118988124991233, 26.13811528394063188 ) ) ;
#54926 = CARTESIAN_POINT ( 'NONE',  ( -1.432654583217662481, 208.3750000013656063, 145.4587341250000634 ) ) ;
#54927 = DIRECTION ( 'NONE',  ( 0.000000000000000000, 0.000000000000000000, 1.000000000000000000 ) ) ;
#54928 = CARTESIAN_POINT ( 'NONE',  ( 7.188101187499999156, 4.874999997951610098, 2.977408999572654924 ) ) ;
#54929 = CARTESIAN_POINT ( 'NONE',  ( -4.721056650415999201, 289.3281250017069510, -4.721056650415999201 ) ) ;
#54930 = AXIS2_PLACEMENT_3D ( 'NONE', #48402, #64657, #48030 ) ;
#54931 = CARTESIAN_POINT ( 'NONE',  ( -1.656854249492337949, 199.3125000000001137, 138.0000000000000000 ) ) ;
#54932 = CARTESIAN_POINT ( 'NONE',  ( -8.311093377946841443, 219.2187499965860127, 8.311093377946834337 ) ) ;
#54933 = EDGE_LOOP ( 'NONE', ( #61168, #2163, #9855, #40778 ) ) ;
#54934 = CARTESIAN_POINT ( 'NONE',  ( -3.042071309553173730, 144.6354166632526983, 11.35316468749999785 ) ) ;
#54935 = CARTESIAN_POINT ( 'NONE',  ( 1.871523826299183495E-15, -10.18810118749999916, 86.03125000204836681 ) ) ;
#54936 = AXIS2_PLACEMENT_3D ( 'NONE', #22075, #9281, #61712 ) ;
#54937 = CARTESIAN_POINT ( 'NONE',  ( -31.45873412499999944, 200.6250000013655779, 168.5673454167827572 ) ) ;
#54938 = DIRECTION ( 'NONE',  ( 0.000000000000000000, -1.000000000000000000, 0.000000000000000000 ) ) ;
#54939 = CARTESIAN_POINT ( 'NONE',  ( 1.881053915767122664, 15.24999999863440969, 4.541265875000001451 ) ) ;
#54940 = ORIENTED_EDGE ( 'NONE', *, *, #31783, .F. ) ;
#54941 = CARTESIAN_POINT ( 'NONE',  ( 2.751064625579944321E-14, 202.8750000027312126, 194.0000000000000568 ) ) ;
#54942 = CARTESIAN_POINT ( 'NONE',  ( -1.432654583217662481, 199.3750000013656063, 145.4587341250000634 ) ) ;
#54943 = CARTESIAN_POINT ( 'NONE',  ( -2.828427124746209831, 203.5000000027312126, 139.1715728752538723 ) ) ;
#54944 = ADVANCED_FACE ( 'NONE', ( #69538 ), #11083, .T. ) ;
#54945 = CARTESIAN_POINT ( 'NONE',  ( -3.313708498984762496, 104.2812499999999858, 7.999999999999998224 ) ) ;
#54946 = ORIENTED_EDGE ( 'NONE', *, *, #7668, .F. ) ;
#54947 = CARTESIAN_POINT ( 'NONE',  ( 5.082755093536325930, 9.656249997951610098, -5.082755093536325930 ) ) ;
#54948 = CARTESIAN_POINT ( 'NONE',  ( 2.020667218593132706E-15, -11.00000000000000000, 76.37499999999998579 ) ) ;
#54949 = CARTESIAN_POINT ( 'NONE',  ( 2.828427124746190291, 19.87500000000000000, 2.828427124746192067 ) ) ;
#54950 = CARTESIAN_POINT ( 'NONE',  ( 6.951808397369818766E-16, 192.0312499965860127, -11.35316468750000141 ) ) ;
#54951 = CARTESIAN_POINT ( 'NONE',  ( -4.401442555609581635E-16, 112.1562500020483952, -7.188101187500000044 ) ) ;
#54952 = CARTESIAN_POINT ( 'NONE',  ( 4.000000000000016875, 207.5625000027312126, 199.6568542494924259 ) ) ;
#54953 = CARTESIAN_POINT ( 'NONE',  ( -6.676582343749999815, 291.5156250017069510, 2.765530957082001251 ) ) ;
#54955 = CARTESIAN_POINT ( 'NONE',  ( 9.999999999999994671, 94.79166666666667140, 2.679491924311234730 ) ) ;
#54954 = CARTESIAN_POINT ( 'NONE',  ( 0.000000000000000000, 18.31575019322283637, 2.966738217918095000 ) ) ;
#54956 =( REPRESENTATION_RELATIONSHIP ('NONE','NONE', #46008, #22863 ) REPRESENTATION_RELATIONSHIP_WITH_TRANSFORMATION ( #20974 )SHAPE_REPRESENTATION_RELATIONSHIP( ) );
#54957 = ORIENTED_EDGE ( 'NONE', *, *, #22410, .T. ) ;
#54958 = CARTESIAN_POINT ( 'NONE',  ( -3.042071309553166181, 228.1770833367473301, -11.35316468749999608 ) ) ;
#54959 = CARTESIAN_POINT ( 'NONE',  ( -2.977408999572647819, 7.188101187499991163, 27.08030278187175810 ) ) ;
#54960 = CARTESIAN_POINT ( 'NONE',  ( 4.556349186104052151, -10.99999999999999822, 92.96875000000000000 ) ) ;
#54961 = CARTESIAN_POINT ( 'NONE',  ( 7.999999999999991118, 3.313708498984758055, 15.36155278392014623 ) ) ;
#54962 = DIRECTION ( 'NONE',  ( 1.000000000000000000, 0.000000000000000000, 0.000000000000000000 ) ) ;
#54963 = CARTESIAN_POINT ( 'NONE',  ( -1.432654583217608080, 198.8750000013656347, 201.4587341250000350 ) ) ;
#54964 = CARTESIAN_POINT ( 'NONE',  ( 2.020667218593132706E-15, -11.00000000000000000, 115.5625000040967763 ) ) ;
#54965 = CARTESIAN_POINT ( 'NONE',  ( 7.778174593052021635, 7.778174593052023411, 114.4375000000000000 ) ) ;
#54966 = CARTESIAN_POINT ( 'NONE',  ( 5.656854249492379694, 95.93750000000000000, -5.656854249492380582 ) ) ;
#54967 = CARTESIAN_POINT ( 'NONE',  ( -5.676582343750006032, 119.4270833299193555, 9.832129032723418760 ) ) ;
#54968 = CARTESIAN_POINT ( 'NONE',  ( 26.34314575050754925, 205.9375000000000000, 173.9999999999998863 ) ) ;
#54969 = CARTESIAN_POINT ( 'NONE',  ( -6.735557395310442023E-16, 11.00000000000000000, 69.62499999999998579 ) ) ;
#54972 = DIRECTION ( 'NONE',  ( -0.000000000000000000, -1.000000000000000000, -4.283267841918042741E-17 ) ) ;
#54971 = CARTESIAN_POINT ( 'NONE',  ( 26.56734541678237704, 200.3750000013656063, 173.4587341249998929 ) ) ;
#54970 = CARTESIAN_POINT ( 'NONE',  ( 31.45873412499999944, 200.0000000013656347, 168.5673454167822740 ) ) ;
#54973 = EDGE_LOOP ( 'NONE', ( #24566, #35928, #68185, #53625 ) ) ;
#54974 = ADVANCED_FACE ( 'NONE', ( #45775 ), #11452, .F. ) ;
#54975 = ADVANCED_FACE ( 'NONE', ( #46519 ), #69163, .T. ) ;
#54976 = CARTESIAN_POINT ( 'NONE',  ( 30.82842712474617031, 205.5000000027312126, 167.1715728752537018 ) ) ;
#54977 = CARTESIAN_POINT ( 'NONE',  ( -27.31189167431821119, 229.0752414545900990, -20.81150119242884600 ) ) ;
#54979 = ADVANCED_FACE ( 'NONE', ( #22376 ), #5798, .F. ) ;
#54978 = CARTESIAN_POINT ( 'NONE',  ( -2.445694354108838731, 200.0625000013656063, 144.4456943541088663 ) ) ;
#54980 = CARTESIAN_POINT ( 'NONE',  ( 31.45873412499999944, 202.9375000013656063, 169.9999999999999432 ) ) ;
#54981 = CARTESIAN_POINT ( 'NONE',  ( -10.99999999999999822, -4.556349186104052151, 113.7812500040967763 ) ) ;
#54982 = CARTESIAN_POINT ( 'NONE',  ( -9.832129032723420536, 199.0104166632526983, 5.676582343749997150 ) ) ;
#54983 = CARTESIAN_POINT ( 'NONE',  ( -5.082755093536325930, 91.34375000204838102, -5.082755093536325930 ) ) ;
#54984 = CYLINDRICAL_SURFACE ( 'NONE', #27774, 10.00000000000000178 ) ;
#54985 = CARTESIAN_POINT ( 'NONE',  ( -4.541265875000003227, 13.87499999863440969, 1.881053915767121110 ) ) ;
#54986 = CARTESIAN_POINT ( 'NONE',  ( 30.44569435410883429, 198.0625000013656063, 167.5543056458911053 ) ) ;
#54987 = CARTESIAN_POINT ( 'NONE',  ( 1.469576158976822172E-15, -7.999999999999991118, 28.20530277982336642 ) ) ;
#54988 = LINE ( 'NONE', #3295, #47170 ) ;
#54989 = CARTESIAN_POINT ( 'NONE',  ( 6.951808397369818766E-16, 82.03124999658602690, -11.35316468750000141 ) ) ;
#54990 = VERTEX_POINT ( 'NONE', #33737 ) ;
#54991 = CARTESIAN_POINT ( 'NONE',  ( -31.99999999999999289, 195.2500000000000000, 170.0000000000003979 ) ) ;
#54992 = CARTESIAN_POINT ( 'NONE',  ( 1.469576158976823947E-15, 92.37499999999998579, 8.000000000000000000 ) ) ;
#54993 = CARTESIAN_POINT ( 'NONE',  ( -5.082755093536326818, 19.40624999795161543, 5.082755093536325042 ) ) ;
#54994 = CARTESIAN_POINT ( 'NONE',  ( 5.000000000000073719, 39.16666666666676377, 8.660254037844529407 ) ) ;
#54995 = CARTESIAN_POINT ( 'NONE',  ( 0.000000000000000000, 0.000000000000000000, 0.000000000000000000 ) ) ;
#54996 = CARTESIAN_POINT ( 'NONE',  ( -3.042071309553164404, 87.23958332991934128, -11.35316468749999963 ) ) ;
#54997 = ORIENTED_EDGE ( 'NONE', *, *, #12435, .F. ) ;
#54998 = CARTESIAN_POINT ( 'NONE',  ( 10.18810118749999916, 1.247682550866122264E-15, 89.78125000204836681 ) ) ;
#54999 = CARTESIAN_POINT ( 'NONE',  ( -10.18810118749999916, 0.000000000000000000, 112.6562500020483810 ) ) ;
#55000 = CARTESIAN_POINT ( 'NONE',  ( 6.123233995736767268E-16, 21.25000000000000000, -10.00000000000000178 ) ) ;
#55001 = CARTESIAN_POINT ( 'NONE',  ( 1.432654583217662481, 209.3750000013656063, 194.5412658750000219 ) ) ;
#55002 = FACE_OUTER_BOUND ( 'NONE', #63439, .T. ) ;
#55004 = CARTESIAN_POINT ( 'NONE',  ( 11.35316468749999785, 80.57291666325268409, 3.042071309553174174 ) ) ;
#55003 = DIRECTION ( 'NONE',  ( 0.000000000000000000, -1.000000000000000000, -2.238352872228138170E-16 ) ) ;
#55005 = EDGE_CURVE ( 'NONE', #17320, #73073, #46200, .T. ) ;
#55006 = CARTESIAN_POINT ( 'NONE',  ( -3.313708498984757167, 7.999999999999991118, 21.73655278392014978 ) ) ;
#55007 = CARTESIAN_POINT ( 'NONE',  ( -31.99999999999999289, 196.3750000027311842, 170.0000000000004547 ) ) ;
#55008 = CARTESIAN_POINT ( 'NONE',  ( -2.679491924311225848, 173.3333333265053398, -10.00000000000000178 ) ) ;
#55009 = CARTESIAN_POINT ( 'NONE',  ( 36.86924962228697922, 146.0000000000000000, 134.0294372515228360 ) ) ;
#55010 = CARTESIAN_POINT ( 'NONE',  ( 8.311093377946834337, 65.46874999658601268, 8.311093377946839666 ) ) ;
#55011 = CARTESIAN_POINT ( 'NONE',  ( -2.765530957081998586, 294.6406250017069510, 6.676582343750001591 ) ) ;
#55012 = CARTESIAN_POINT ( 'NONE',  ( 4.220049686691934809, 10.18810118749999916, 108.0625000020483810 ) ) ;
#55013 = CARTESIAN_POINT ( 'NONE',  ( -8.311093377946836114, 202.6562499965860127, -8.311093377946837890 ) ) ;
#55014 = EDGE_LOOP ( 'NONE', ( #56781, #21733, #68994, #10372 ) ) ;
#55015 = CARTESIAN_POINT ( 'NONE',  ( 1.656854249492271780, 202.8125000000000284, 146.0000000000001137 ) ) ;
#55016 = CARTESIAN_POINT ( 'NONE',  ( 3.373128826976384165, -60.49298623944814324, -23.06377889928852554 ) ) ;
#55017 = CARTESIAN_POINT ( 'NONE',  ( 2.265596578422603396E-15, -3.149999999999999911, -18.50000000000000000 ) ) ;
#55018 = CARTESIAN_POINT ( 'NONE',  ( -8.311093377946841443, 193.9062499965860411, 8.311093377946834337 ) ) ;
#55019 = CARTESIAN_POINT ( 'NONE',  ( 7.999999999999998224, 2.718749995903220640, 3.313708498984766049 ) ) ;
#55020 = CARTESIAN_POINT ( 'NONE',  ( -7.320508075688770155, 243.7500000068279462, 7.320508075688774596 ) ) ;
#55021 = CARTESIAN_POINT ( 'NONE',  ( 2.449293598294707893E-16, 20.25000000000000000, -4.000000000000001776 ) ) ;
#55022 = ORIENTED_EDGE ( 'NONE', *, *, #58052, .T. ) ;
#55023 = CARTESIAN_POINT ( 'NONE',  ( 8.311093377946837890, 176.7187499965860127, -8.311093377946837890 ) ) ;
#55024 =( BOUNDED_CURVE ( )  B_SPLINE_CURVE ( 2, ( #20526, #66555, #43169, #54887, #15241, #33005, #71836, #37904, #2820 ),
 .UNSPECIFIED., .F., .F. ) 
 B_SPLINE_CURVE_WITH_KNOTS ( ( 3, 2, 2, 2, 3 ),
 ( 0.5500000000000005995, 0.5583333333333337922, 0.5666666666666670960, 0.5750000000000003997, 0.5833333333333337034 ),
 .UNSPECIFIED. ) 
 CURVE ( )  GEOMETRIC_REPRESENTATION_ITEM ( )  RATIONAL_B_SPLINE_CURVE ( ( 0.9999999999999948930, 0.9238795325112918455, 1.000000000000000000, 0.9238795325112867385, 1.000000000000000000, 0.9238795325112867385, 1.000000000000000000, 0.9238795325112837409, 1.000000000000003109 ) ) 
 REPRESENTATION_ITEM ( '' )  );
#55025 = CARTESIAN_POINT ( 'NONE',  ( 7.188101187499992051, 8.802885111219154394E-16, 12.73655278187175277 ) ) ;
#55026 = CARTESIAN_POINT ( 'NONE',  ( -24.54126587499999701, 209.1875000013656063, 170.0000000000003411 ) ) ;
#55027 = VERTEX_POINT ( 'NONE', #16713 ) ;
#55028 = AXIS2_PLACEMENT_3D ( 'NONE', #58113, #6425, #52439 ) ;
#55029 = CARTESIAN_POINT ( 'NONE',  ( -8.000000000000000000, 95.09375000409679046, -3.313708498984761608 ) ) ;
#55030 = CARTESIAN_POINT ( 'NONE',  ( 2.679491924311222739, 3.958333333333333925, 10.00000000000000355 ) ) ;
#55031 =( BOUNDED_CURVE ( )  B_SPLINE_CURVE ( 2, ( #40195, #56074, #5501, #16052, #61721, #28126, #44743, #33439, #10779, #27751, #68124, #56813, #22833 ),
 .UNSPECIFIED., .F., .F. ) 
 B_SPLINE_CURVE_WITH_KNOTS ( ( 3, 2, 2, 2, 2, 2, 3 ),
 ( 0.4238920256284931520, 0.4291260266837255144, 0.4343600277389579878, 0.4395940287941904057, 0.4448280298494227680, 0.4500620309046552414, 0.4552960319598876593 ),
 .UNSPECIFIED. ) 
 CURVE ( )  GEOMETRIC_REPRESENTATION_ITEM ( )  RATIONAL_B_SPLINE_CURVE ( ( 0.9999999999999984457, 0.9659258262890697555, 1.000000000000000000, 0.9659258262890682012, 1.000000000000000000, 0.9659258262890682012, 1.000000000000000000, 0.9659258262890682012, 1.000000000000000000, 0.9659258262890682012, 1.000000000000000000, 0.9659258262890900726, 0.9999999999999781286 ) ) 
 REPRESENTATION_ITEM ( '' )  );
#55032 = CARTESIAN_POINT ( 'NONE',  ( 2.828427124746191623, 17.12500000000000000, -2.828427124746191623 ) ) ;
#55033 = CARTESIAN_POINT ( 'NONE',  ( -3.211159895383562723, 16.93749999863440436, 3.211159895383561391 ) ) ;
#55034 = CARTESIAN_POINT ( 'NONE',  ( 3.313708498984762496, -7.999999999999989342, 14.98655278392014623 ) ) ;
#55035 = CARTESIAN_POINT ( 'NONE',  ( -7.999999999835898379, -3.436314075762838161E-05, 19.01908381112063751 ) ) ;
#55036 = ADVANCED_FACE ( 'NONE', ( #39743 ), #17774, .F. ) ;
#55037 = ORIENTED_EDGE ( 'NONE', *, *, #7857, .T. ) ;
#55038 = CARTESIAN_POINT ( 'NONE',  ( 5.000000000000000000, -10.25159769123455256, -64.79153472057839735 ) ) ;
#55039 = CARTESIAN_POINT ( 'NONE',  ( 1.320432766682874540E-15, 90.03125000204838102, 7.188101187500000044 ) ) ;
#55042 = CARTESIAN_POINT ( 'NONE',  ( 0.8761883848702568534, -51.17400877215189325, 48.53033992007376440 ) ) ;
#55041 = CARTESIAN_POINT ( 'NONE',  ( -8.311093377946836114, 253.2812500034140442, -8.311093377946836114 ) ) ;
#55040 = CARTESIAN_POINT ( 'NONE',  ( -7.999999999999948486, 3.313708498984799355, 12.73655277982336465 ) ) ;
#55043 = DIRECTION ( 'NONE',  ( 0.000000000000000000, 1.000000000000000000, 0.000000000000000000 ) ) ;
#55044 = ORIENTED_EDGE ( 'NONE', *, *, #34628, .F. ) ;
#55045 = CARTESIAN_POINT ( 'NONE',  ( -3.313708498984707429, 100.9062500040967905, -8.000000000000055067 ) ) ;
#55046 = CARTESIAN_POINT ( 'NONE',  ( 2.977408999572650927, -7.188101187499990274, 19.95530278187175810 ) ) ;
#55047 = VERTEX_POINT ( 'NONE', #28358 ) ;
#55048 = ORIENTED_EDGE ( 'NONE', *, *, #9451, .T. ) ;
#55049 = CARTESIAN_POINT ( 'NONE',  ( -7.204075437095965206, -7.204075437095968759, 82.84375000204838102 ) ) ;
#55050 = CARTESIAN_POINT ( 'NONE',  ( 9.832129032723416984, 75.67708332991934128, 5.676582343750006032 ) ) ;
#55051 = CARTESIAN_POINT ( 'NONE',  ( -8.000000000000053291, -3.313708498984698547, 17.42405277982336287 ) ) ;
#55052 = CARTESIAN_POINT ( 'NONE',  ( 11.00000000000000355, -4.556349186104045046, 90.15625000000000000 ) ) ;
#55055 = CARTESIAN_POINT ( 'NONE',  ( 6.676582343750001591, 293.1093750017069510, -8.176455196517173205E-16 ) ) ;
#55054 = CARTESIAN_POINT ( 'NONE',  ( 25.17157287525377996, 198.7500000027312126, 167.1715728752537586 ) ) ;
#55053 = CARTESIAN_POINT ( 'NONE',  ( -1.001543065824775909E-15, -10.39230484541329247, -10.80000000000000071 ) ) ;
#55056 = CYLINDRICAL_SURFACE ( 'NONE', #29673, 8.000000000000000000 ) ;
#55057 = CARTESIAN_POINT ( 'NONE',  ( -5.656854249492378806, 90.87500000409677625, 5.656854249492381470 ) ) ;
#55058 = CARTESIAN_POINT ( 'NONE',  ( -3.458734124999959469, 197.7500000013656063, 199.4326545832176976 ) ) ;
#55059 = CARTESIAN_POINT ( 'NONE',  ( 7.347880794884121708E-16, 300.0000000000000000, -6.000000000000001776 ) ) ;
#55060 = CARTESIAN_POINT ( 'NONE',  ( 5.656854249492378806, 2.624999995903220196, 5.656854249492381470 ) ) ;
#55061 = CARTESIAN_POINT ( 'NONE',  ( 24.54126587499998280, 198.2500000013656347, 171.4326545832175555 ) ) ;
#55062 = CARTESIAN_POINT ( 'NONE',  ( 5.082755093536325930, 8.531249997951611874, -5.082755093536325930 ) ) ;
#55063 = CARTESIAN_POINT ( 'NONE',  ( -5.873835977744188419, -5.451354504359680497, -0.3078279556938505190 ) ) ;
#55064 = CARTESIAN_POINT ( 'NONE',  ( -7.320508075688770155, 243.7500000068279462, 7.320508075688774596 ) ) ;
#55065 = CARTESIAN_POINT ( 'NONE',  ( -4.401442555609581635E-16, 109.1562500020483810, -7.188101187500000044 ) ) ;
#55067 = CARTESIAN_POINT ( 'NONE',  ( 4.336811714529654083, -52.00708776950327916, -48.85034107298358208 ) ) ;
#55066 = FACE_BOUND ( 'NONE', #65698, .T. ) ;
#55068 = LINE ( 'NONE', #3377, #47196 ) ;
#55069 = CYLINDRICAL_SURFACE ( 'NONE', #71053, 3.999999999999976019 ) ;
#55070 = CARTESIAN_POINT ( 'NONE',  ( 7.188101187499991163, 2.977408999572648707, 14.70530278187175455 ) ) ;
#55071 = CARTESIAN_POINT ( 'NONE',  ( -4.000000000000015987, 206.6250000027312126, 142.0000000000000568 ) ) ;
#55072 = CARTESIAN_POINT ( 'NONE',  ( -9.832129032723420536, 38.69791666325269119, 5.676582343749997150 ) ) ;
#55073 = CARTESIAN_POINT ( 'NONE',  ( -1.967015505459129087E-11, 148.7499999999984936, 10.00000000000000533 ) ) ;
#55074 = CARTESIAN_POINT ( 'NONE',  ( 10.00000000000000178, 11.87499999317203248, 0.000000000000000000 ) ) ;
#55075 = CARTESIAN_POINT ( 'NONE',  ( 10.99999999999989697, -4.556349186104149851, 72.15624999999998579 ) ) ;
#55076 = ORIENTED_EDGE ( 'NONE', *, *, #2954, .F. ) ;
#55077 = VECTOR ( 'NONE', #2733, 1000.000000000000000 ) ;
#55078 = CARTESIAN_POINT ( 'NONE',  ( 2.679491924311081963, 142.9166666598387110, -10.00000000000008349 ) ) ;
#55079 = CARTESIAN_POINT ( 'NONE',  ( 0.000000000000000000, 101.0525588832578734, 0.000000000000000000 ) ) ;
#55080 = CARTESIAN_POINT ( 'NONE',  ( 11.35316468749999963, 50.98958332991934839, -3.042071309553165293 ) ) ;
#55081 = CARTESIAN_POINT ( 'NONE',  ( -4.556349186104047710, -10.99999999999999822, 82.46875000409677625 ) ) ;
#55082 = PRODUCT_DEFINITION_FORMATION_WITH_SPECIFIED_SOURCE ( 'ANY', '', #8304, .NOT_KNOWN. ) ;
#55083 = CARTESIAN_POINT ( 'NONE',  ( -2.839093476692135984E-14, 204.9375000013656063, 138.5412658750000503 ) ) ;
#55084 = CARTESIAN_POINT ( 'NONE',  ( -4.898587196589412829E-16, 114.3125000040967905, -8.000000000000000000 ) ) ;
#55085 = FACE_OUTER_BOUND ( 'NONE', #10657, .T. ) ;
#55087 = CARTESIAN_POINT ( 'NONE',  ( -11.35316468750000141, 28.28124999658601624, -1.390361679473963753E-15 ) ) ;
#55086 = CARTESIAN_POINT ( 'NONE',  ( 2.977408999572650039, 98.18750000204835260, -7.188101187500000933 ) ) ;
#55088 = ADVANCED_FACE ( 'NONE', ( #45335 ), #68718, .T. ) ;
#55089 = CARTESIAN_POINT ( 'NONE',  ( -7.999999999999991118, 3.313708498984756723, 8.236552779823362869 ) ) ;
#55090 = CARTESIAN_POINT ( 'NONE',  ( -7.320508075688773708, 48.74999999317203248, -7.320508075688774596 ) ) ;
#55091 = CARTESIAN_POINT ( 'NONE',  ( 8.311093377946837890, 166.4062499965860127, -8.311093377946837890 ) ) ;
#55092 = EDGE_CURVE ( 'NONE', #38802, #7386, #30774, .T. ) ;
#55093 = CARTESIAN_POINT ( 'NONE',  ( -5.000000000000005329, 125.2083333265053540, 8.660254037844387298 ) ) ;
#55094 = CARTESIAN_POINT ( 'NONE',  ( 2.977408999572650039, 106.0625000020483668, -7.188101187500001821 ) ) ;
#55095 = ORIENTED_EDGE ( 'NONE', *, *, #52927, .T. ) ;
#55096 = CARTESIAN_POINT ( 'NONE',  ( 11.00000000000000000, 1.347111479062088405E-15, 100.7499999999999858 ) ) ;
#55097 = CARTESIAN_POINT ( 'NONE',  ( 5.676582343750001591, 16.92708332991935194, -9.832129032723420536 ) ) ;
#55098 = ORIENTED_EDGE ( 'NONE', *, *, #59311, .T. ) ;
#55099 = LINE ( 'NONE', #25650, #36761 ) ;
#55100 = CARTESIAN_POINT ( 'NONE',  ( 7.204075437095968759, -7.204075437095966983, 80.21875000204836681 ) ) ;
#55101 = CARTESIAN_POINT ( 'NONE',  ( -2.751064625579944321E-14, 203.7500000000000284, 146.0000000000000284 ) ) ;
#55102 = CARTESIAN_POINT ( 'NONE',  ( 8.311093377946837890, 156.4062499965860411, -8.311093377946837890 ) ) ;
#55103 = DIRECTION ( 'NONE',  ( 0.000000000000000000, 0.000000000000000000, 1.000000000000000000 ) ) ;
#55104 = CARTESIAN_POINT ( 'NONE',  ( -7.999999999999989342, -3.313708498984762496, 9.980302784329824206 ) ) ;
#55105 = EDGE_CURVE ( 'NONE', #53358, #24578, #53102, .T. ) ;
#55106 = DIRECTION ( 'NONE',  ( 0.000000000000000000, 0.000000000000000000, 1.000000000000000000 ) ) ;
#55107 = CARTESIAN_POINT ( 'NONE',  ( 3.042071309553163960, 237.4479166700806729, -11.35316468749999785 ) ) ;
#55108 = CARTESIAN_POINT ( 'NONE',  ( -10.18810118749999916, 0.000000000000000000, 83.03125000204838102 ) ) ;
#55109 = ORIENTED_EDGE ( 'NONE', *, *, #72447, .T. ) ;
#55110 = CIRCLE ( 'NONE', #57480, 7.000000000000000000 ) ;
#55111 = EDGE_CURVE ( 'NONE', #61723, #9076, #40918, .T. ) ;
#55112 = CARTESIAN_POINT ( 'NONE',  ( 11.00000000000000000, 1.347111479062088405E-15, 90.43750000409676204 ) ) ;
#55113 = CARTESIAN_POINT ( 'NONE',  ( -6.000000000000001776, 292.0625000034140157, 0.000000000000000000 ) ) ;
#55114 = CARTESIAN_POINT ( 'NONE',  ( -8.311093377946836114, 97.96874999658599847, -8.311093377946837890 ) ) ;
#55115 = CARTESIAN_POINT ( 'NONE',  ( 1.871523826299183495E-15, -10.18810118749999916, 95.03125000204836681 ) ) ;
#55116 = CARTESIAN_POINT ( 'NONE',  ( -1.881053915767124440, 19.12499999863441147, 4.541265875000001451 ) ) ;
#55117 = VERTEX_POINT ( 'NONE', #51741 ) ;
#55118 = ORIENTED_EDGE ( 'NONE', *, *, #20866, .F. ) ;
#55119 = CARTESIAN_POINT ( 'NONE',  ( 4.541265875000002339, 3.437499998634407028, 0.000000000000000000 ) ) ;
#55120 = CARTESIAN_POINT ( 'NONE',  ( 7.188101187500001821, 11.06249999795161187, -2.977408999572650483 ) ) ;
#55121 = CARTESIAN_POINT ( 'NONE',  ( -7.999999999999998224, 117.7812500040967905, 3.313708498984766493 ) ) ;
#55122 = CARTESIAN_POINT ( 'NONE',  ( -10.18810118749999738, -4.220049686691941915, 93.62500000204838102 ) ) ;
#55123 = CARTESIAN_POINT ( 'NONE',  ( -31.45873412500001010, 202.8750000013656347, 168.5673454167827572 ) ) ;
#55124 = FACE_OUTER_BOUND ( 'NONE', #60581, .T. ) ;
#55125 =( BOUNDED_CURVE ( )  B_SPLINE_CURVE ( 2, ( #8456, #3180, #67301, #72196, #9592, #37513, #25793, #14099, #20509, #31476, #49567 ),
 .UNSPECIFIED., .F., .F. ) 
 B_SPLINE_CURVE_WITH_KNOTS ( ( 3, 2, 2, 2, 2, 3 ),
 ( 0.1058924239672156403, 0.1125106849357718625, 0.1191289605202222601, 0.1257472361046726717, 0.1323655116891230554, 0.1323655657721681533 ),
 .UNSPECIFIED. ) 
 CURVE ( )  GEOMETRIC_REPRESENTATION_ITEM ( )  RATIONAL_B_SPLINE_CURVE ( ( 0.9999996637896906293, 0.9238797006168126824, 1.000000000000000000, 0.9238795325112867385, 1.000000000000000000, 0.9238795325112867385, 1.000000000000000000, 0.9238795325112867385, 1.000000000000000000, 0.9999993779608262745, 0.9999987559318189723 ) ) 
 REPRESENTATION_ITEM ( '' )  );
#55126 = CARTESIAN_POINT ( 'NONE',  ( -7.347880794884122694E-16, 4.750000000000000000, 4.000000000000001776 ) ) ;
#55127 = CARTESIAN_POINT ( 'NONE',  ( 2.828427124746190291, 18.62499999726881583, 2.828427124746192067 ) ) ;
#55128 = CARTESIAN_POINT ( 'NONE',  ( 3.211159895383560947, 5.187499998634407028, 3.211159895383562723 ) ) ;
#55129 = AXIS2_PLACEMENT_3D ( 'NONE', #4587, #57017, #44946 ) ;
#55130 = ORIENTED_EDGE ( 'NONE', *, *, #20693, .F. ) ;
#55131 = ADVANCED_FACE ( 'NONE', ( #44974 ), #12117, .T. ) ;
#55133 = DIRECTION ( 'NONE',  ( 0.000000000000000000, 0.000000000000000000, 1.000000000000000000 ) ) ;
#55132 = CARTESIAN_POINT ( 'NONE',  ( -31.45873412499999233, 195.6875000013655779, 170.0000000000004547 ) ) ;
#55134 = CARTESIAN_POINT ( 'NONE',  ( 4.541265875000002339, 16.37499999863440436, -1.881053915767121554 ) ) ;
#55135 = CARTESIAN_POINT ( 'NONE',  ( 4.721056650415999201, 299.0781250017069510, -4.721056650415999201 ) ) ;
#55136 = CARTESIAN_POINT ( 'NONE',  ( -2.977408999572647819, 7.188101187499991163, 7.205302781871750994 ) ) ;
#55137 = ORIENTED_EDGE ( 'NONE', *, *, #47649, .T. ) ;
#55138 = EDGE_CURVE ( 'NONE', #44243, #53657, #4782, .T. ) ;
#55139 = VERTEX_POINT ( 'NONE', #40426 ) ;
#55140 = CARTESIAN_POINT ( 'NONE',  ( 7.204075437095968759, -7.204075437095966983, 101.2187500020483668 ) ) ;
#55141 = CYLINDRICAL_SURFACE ( 'NONE', #44187, 3.999999999999976019 ) ;
#55142 = CARTESIAN_POINT ( 'NONE',  ( -25.55430564589115150, 205.3125000013656063, 172.4456943541091789 ) ) ;
#55143 = CARTESIAN_POINT ( 'NONE',  ( -30.82842712474621294, 202.1250000000000284, 167.1715728752542134 ) ) ;
#55144 = CARTESIAN_POINT ( 'NONE',  ( 2.445694354108839175, 208.3125000013656063, 195.5543056458912190 ) ) ;
#55145 = DIRECTION ( 'NONE',  ( -0.000000000000000000, 1.000000000000000000, -0.000000000000000000 ) ) ;
#55146 = CARTESIAN_POINT ( 'NONE',  ( 10.00000000000000000, 104.7916666666666572, 2.679491924311236062 ) ) ;
#55147 = CARTESIAN_POINT ( 'NONE',  ( 8.000000000000000000, 109.3437499999999858, -3.313708498984762496 ) ) ;
#55148 = CARTESIAN_POINT ( 'NONE',  ( -6.676582343750003368, 291.5468750017069510, -2.765530957081996810 ) ) ;
#55149 = CARTESIAN_POINT ( 'NONE',  ( 7.188101187499991163, 2.977408999572648707, 8.705302781871752771 ) ) ;
#55150 = ORIENTED_EDGE ( 'NONE', *, *, #17599, .T. ) ;
#55151 = CARTESIAN_POINT ( 'NONE',  ( -38.00000000000000000, 272.0000000000000000, 3.791916237172779019E-14 ) ) ;
#55152 = ADVANCED_FACE ( 'NONE', ( #63425 ), #9573, .T. ) ;
#55153 = CARTESIAN_POINT ( 'NONE',  ( -1.469576158976823947E-15, 21.93749999590322375, 8.000000000000000000 ) ) ;
#55154 = CARTESIAN_POINT ( 'NONE',  ( 3.458734124999959914, 204.3750000013656063, 143.4326545832176976 ) ) ;
#55155 = CARTESIAN_POINT ( 'NONE',  ( -10.00000000000000355, 184.5833333265053113, 2.679491924311223183 ) ) ;
#55157 = CARTESIAN_POINT ( 'NONE',  ( -3.458734125000015425, 201.2500000013656063, 143.4326545832176976 ) ) ;
#55156 = LINE ( 'NONE', #44201, #52827 ) ;
#55158 = ADVANCED_BREP_SHAPE_REPRESENTATION ( '', ( #16907, #57354 ), #21241 ) ;
#55159 = CARTESIAN_POINT ( 'NONE',  ( 8.311093377946839666, 261.0937500034140157, 8.311093377946829008 ) ) ;
#55160 = CARTESIAN_POINT ( 'NONE',  ( -28.00000000000002842, 209.8437500006828031, 166.2706329375003804 ) ) ;
#55161 = CARTESIAN_POINT ( 'NONE',  ( 7.778174593052023411, -7.778174593052021635, 111.0625000000000000 ) ) ;
#55162 = CARTESIAN_POINT ( 'NONE',  ( 7.320508075688771044, 224.3749999999999716, 7.320508075688775484 ) ) ;
#55163 = CARTESIAN_POINT ( 'NONE',  ( -7.188101187499992051, 0.000000000000000000, 6.361552781871754547 ) ) ;
#55164 = CARTESIAN_POINT ( 'NONE',  ( -8.311093377946836114, 192.9687499965859843, -8.311093377946837890 ) ) ;
#55165 = CARTESIAN_POINT ( 'NONE',  ( 7.320508075688774596, 192.4999999931720538, -7.320508075688774596 ) ) ;
#55166 = CARTESIAN_POINT ( 'NONE',  ( 2.780723358947928197E-16, 5.562499998634407028, -4.541265875000002339 ) ) ;
#55167 = CARTESIAN_POINT ( 'NONE',  ( 0.000000000000000000, 0.000000000000000000, 118.0000000000000000 ) ) ;
#55168 = PRODUCT_RELATED_PRODUCT_CATEGORY ( 'part', '', ( #20355 ) ) ;
#55170 = LINE ( 'NONE', #27218, #12166 ) ;
#55169 = DIRECTION ( 'NONE',  ( -0.8660254037844380415, -0.5000000000000012212, 0.000000000000000000 ) ) ;
#55171 = EDGE_LOOP ( 'NONE', ( #68884, #25495, #18480, #39784, #1285, #50863, #63562, #68438, #65506, #45131, #69014, #27319, #26922, #34311, #19838, #32264, #17194, #59775, #73106, #44454, #51576, #57130, #70171, #52434, #65870, #35008, #46929, #62180, #21349, #11161, #67263, #41479, #26333, #71772, #11704, #41069, #59558, #57648, #37525, #32057 ) ) ;
#55172 = CARTESIAN_POINT ( 'NONE',  ( -2.445694354108839175, 205.3125000013656063, 144.4456943541088663 ) ) ;
#55173 = CARTESIAN_POINT ( 'NONE',  ( -9.832129032723418760, 2.864583329919349719, -5.676582343750004256 ) ) ;
#55174 = CARTESIAN_POINT ( 'NONE',  ( -11.00000000000000000, 4.556349186104045934, 97.09375000409679046 ) ) ;
#55175 = CARTESIAN_POINT ( 'NONE',  ( 2.849036369511732440E-14, 205.3750000027312126, 202.0000000000000000 ) ) ;
#55176 = CARTESIAN_POINT ( 'NONE',  ( -25.55430564589122966, 202.3125000013656063, 167.5543056458915032 ) ) ;
#55177 = CARTESIAN_POINT ( 'NONE',  ( 11.00000000000001066, 4.556349186104036164, 117.3437500000000142 ) ) ;
#55179 = CARTESIAN_POINT ( 'NONE',  ( 3.313708498984800688, 120.0312499999999716, -7.999999999999958256 ) ) ;
#55178 = CARTESIAN_POINT ( 'NONE',  ( 2.977408999572654480, 118.6250000020483810, 7.188101187499999156 ) ) ;
#55180 = CARTESIAN_POINT ( 'NONE',  ( -7.999999999999989342, -3.313708498984762496, 24.92405277982336997 ) ) ;
#55181 = CARTESIAN_POINT ( 'NONE',  ( 9.832129032723420536, 126.1979166632526983, -5.676582343749999815 ) ) ;
#55182 = EDGE_CURVE ( 'NONE', #9475, #32512, #56334, .T. ) ;
#55183 = CARTESIAN_POINT ( 'NONE',  ( 8.660254037844385522, 86.45833332650538239, 5.000000000000005329 ) ) ;
#55184 = CARTESIAN_POINT ( 'NONE',  ( 5.082755093536325042, 93.59375000204838102, -5.082755093536325930 ) ) ;
#55185 = CARTESIAN_POINT ( 'NONE',  ( -1.881053915767124440, 20.12499999863441147, 4.541265875000001451 ) ) ;
#55186 = CARTESIAN_POINT ( 'NONE',  ( 3.734486434573635272, -8.236198097127193307, -0.01899995639454811480 ) ) ;
#55187 = CARTESIAN_POINT ( 'NONE',  ( -4.999999999999998224, 38.54166665983869677, -8.660254037844389075 ) ) ;
#55188 = ORIENTED_EDGE ( 'NONE', *, *, #48641, .F. ) ;
#55189 = CYLINDRICAL_SURFACE ( 'NONE', #51878, 3.999999999999976019 ) ;
#55190 = CARTESIAN_POINT ( 'NONE',  ( 6.676582343750001591, 292.1093750017069510, -8.176455196517173205E-16 ) ) ;
#55191 = CYLINDRICAL_SURFACE ( 'NONE', #3767, 11.00000000000000000 ) ;
#55192 = CARTESIAN_POINT ( 'NONE',  ( -7.999999999999989342, -3.313708498984762496, 2.611552783920144005 ) ) ;
#55193 = CARTESIAN_POINT ( 'NONE',  ( -3.042071309553164404, 167.2395833299193839, -11.35316468749999963 ) ) ;
#55194 = CARTESIAN_POINT ( 'NONE',  ( 4.898587196589412829E-16, 24.37500000000000355, -8.000000000000000000 ) ) ;
#55195 = CARTESIAN_POINT ( 'NONE',  ( -8.660254037844390851, 204.7916666598387110, 4.999999999999998224 ) ) ;
#55196 = CARTESIAN_POINT ( 'NONE',  ( 4.556349186104045934, 11.00000000000000000, 69.53124999999998579 ) ) ;
#55197 = CIRCLE ( 'NONE', #3366, 6.000000000000001776 ) ;
#55198 = CARTESIAN_POINT ( 'NONE',  ( 10.18810118749999916, 1.247682550866122264E-15, 103.2812500020483810 ) ) ;
#55199 = ORIENTED_EDGE ( 'NONE', *, *, #29256, .F. ) ;
#55200 = CARTESIAN_POINT ( 'NONE',  ( -1.656854249492416109, 198.3125000027312126, 201.9999999999999432 ) ) ;
#55201 = CARTESIAN_POINT ( 'NONE',  ( -3.042071309553173730, 149.6354166632526983, 11.35316468749999785 ) ) ;
#55202 = CARTESIAN_POINT ( 'NONE',  ( -1.432654583217607858, 194.6250000013656063, 201.4587341250000065 ) ) ;
#55203 = CARTESIAN_POINT ( 'NONE',  ( 3.458734125000015869, 206.1875000013656063, 198.0000000000000284 ) ) ;
#55204 = CARTESIAN_POINT ( 'NONE',  ( -10.18810118749999916, 4.220049686691934809, 67.93750000204838102 ) ) ;
#55205 = CARTESIAN_POINT ( 'NONE',  ( 11.35316468749999785, 65.88541666325268409, 3.042071309553174174 ) ) ;
#55206 = ORIENTED_EDGE ( 'NONE', *, *, #34271, .T. ) ;
#55207 = CARTESIAN_POINT ( 'NONE',  ( -10.18810118749999916, 0.000000000000000000, 112.6562500020483810 ) ) ;
#55208 = CARTESIAN_POINT ( 'NONE',  ( 2.780723358947928197E-16, 7.687499998634407028, -4.541265875000002339 ) ) ;
#55209 = ORIENTED_EDGE ( 'NONE', *, *, #7927, .T. ) ;
#55210 = CARTESIAN_POINT ( 'NONE',  ( 4.401442555609581635E-16, 23.34374999795161543, -7.188101187500000044 ) ) ;
#55211 = CARTESIAN_POINT ( 'NONE',  ( -6.000000000000000888, 289.1250000034140726, 2.485281374238575758 ) ) ;
#55212 = VECTOR ( 'NONE', #44956, 1000.000000000000000 ) ;
#55213 = CARTESIAN_POINT ( 'NONE',  ( -2.250000000000000888, -2.250000000000000000, 0.000000000000000000 ) ) ;
#55214 = CARTESIAN_POINT ( 'NONE',  ( 5.082755093536324154, 17.15624999795161543, 5.082755093536326818 ) ) ;
#55215 = CARTESIAN_POINT ( 'NONE',  ( -7.188101187499990274, -2.977408999572651815, 1.580302781871753659 ) ) ;
#55216 = VECTOR ( 'NONE', #9705, 1000.000000000000000 ) ;
#55217 = CARTESIAN_POINT ( 'NONE',  ( 5.094050593753887135, 8.823154444699161658, 67.15552362291680311 ) ) ;
#55218 = DIRECTION ( 'NONE',  ( 0.000000000000000000, 0.000000000000000000, 1.000000000000000000 ) ) ;
#55219 = CARTESIAN_POINT ( 'NONE',  ( -1.656854249492383691, 4.437499997268813168, 4.000000000000000888 ) ) ;
#55220 = CARTESIAN_POINT ( 'NONE',  ( -21.37908376636208985, -49.53694815986835920, 147.5481716400113328 ) ) ;
#55221 = ORIENTED_EDGE ( 'NONE', *, *, #32514, .F. ) ;
#55222 = CARTESIAN_POINT ( 'NONE',  ( -3.458734124999959914, 208.3750000013656063, 196.5673454167823877 ) ) ;
#55223 = ADVANCED_FACE ( 'NONE', ( #35883 ), #70938, .T. ) ;
#55224 = CARTESIAN_POINT ( 'NONE',  ( -29.65685424949245430, 195.1875000027312410, 166.0000000000004263 ) ) ;
#55225 = CARTESIAN_POINT ( 'NONE',  ( -3.211159895383562723, 7.937499998634407028, 3.211159895383561391 ) ) ;
#55226 = CARTESIAN_POINT ( 'NONE',  ( 2.977408999572654480, 111.1250000020483810, 7.188101187499999156 ) ) ;
#55227 = CARTESIAN_POINT ( 'NONE',  ( -5.999999999999999112, 290.0625000000000000, 2.485281374238575314 ) ) ;
#55228 = CARTESIAN_POINT ( 'NONE',  ( 1.320432766682872962E-15, -7.188101187499992051, 27.36155278187175455 ) ) ;
#55229 = ORIENTED_EDGE ( 'NONE', *, *, #10905, .T. ) ;
#55230 = EDGE_CURVE ( 'NONE', #61413, #60403, #24044, .T. ) ;
#55231 = DIRECTION ( 'NONE',  ( 1.000000000000000000, 0.000000000000000000, -1.281975129857798973E-14 ) ) ;
#55232 = ORIENTED_EDGE ( 'NONE', *, *, #17317, .F. ) ;
#55233 = CARTESIAN_POINT ( 'NONE',  ( 2.081755106360743568, 7.796932491752575523, -0.000000000000000000 ) ) ;
#55234 = CARTESIAN_POINT ( 'NONE',  ( -3.458734124999959914, 202.4375000013656063, 198.0000000000000284 ) ) ;
#55235 = CARTESIAN_POINT ( 'NONE',  ( 28.00000000000001776, 200.4375000013656063, 173.4587341249998929 ) ) ;
#55236 = CARTESIAN_POINT ( 'NONE',  ( -10.00000000000000355, 62.70833333333333570, 2.679491924311223183 ) ) ;
#55237 = CARTESIAN_POINT ( 'NONE',  ( 7.188101187500002709, 92.18750000204838102, 2.977408999572649151 ) ) ;
#55238 = CARTESIAN_POINT ( 'NONE',  ( -6.000000000000003553, 292.9374999999999432, -2.485281374238571317 ) ) ;
#55240 = DIRECTION ( 'NONE',  ( -0.000000000000000000, 1.000000000000000000, -0.000000000000000000 ) ) ;
#55239 = CARTESIAN_POINT ( 'NONE',  ( 26.34314575050764162, 208.0625000027312410, 173.9999999999999147 ) ) ;
#55241 = ORIENTED_EDGE ( 'NONE', *, *, #26029, .T. ) ;
#55242 =( BOUNDED_CURVE ( )  B_SPLINE_CURVE ( 2, ( #9035, #9413, #13920, #36959, #49010, #8283, #32431, #31292, #37335, #54323, #8661, #31676, #3004 ),
 .UNSPECIFIED., .F., .F. ) 
 B_SPLINE_CURVE_WITH_KNOTS ( ( 3, 2, 2, 2, 2, 2, 3 ),
 ( 1.679891585307146773, 1.685124540478250443, 1.690357495649354114, 1.695590450820457784, 1.700823405991561010, 1.706056361162664681, 1.711289316333768351 ),
 .UNSPECIFIED. ) 
 CURVE ( )  GEOMETRIC_REPRESENTATION_ITEM ( )  RATIONAL_B_SPLINE_CURVE ( ( 1.000000000000037526, 0.9659258262890306757, 1.000000000000000000, 0.9659258262890683122, 1.000000000000000000, 0.9659258262890683122, 1.000000000000000000, 0.9659258262890683122, 1.000000000000000000, 0.9659258262890683122, 1.000000000000000000, 0.9659258262890704216, 0.9999999999999978906 ) ) 
 REPRESENTATION_ITEM ( '' )  );
#55243 = DIRECTION ( 'NONE',  ( 0.000000000000000000, 0.000000000000000000, 1.000000000000000000 ) ) ;
#55244 = CARTESIAN_POINT ( 'NONE',  ( -2.990854866088966002, -10.11452374054218240, 70.45725801587769865 ) ) ;
#55245 = CARTESIAN_POINT ( 'NONE',  ( -2.849036369511732440E-14, 198.3750000027312126, 138.0000000000000568 ) ) ;
#55246 = CARTESIAN_POINT ( 'NONE',  ( 2.775557561562891351E-14, 210.0000000000000284, 202.0000000000000000 ) ) ;
#55247 = CARTESIAN_POINT ( 'NONE',  ( -10.50000000000000000, 1.285879139104720831E-15, -20.42428869268542968 ) ) ;
#55248 = CARTESIAN_POINT ( 'NONE',  ( -10.00000000000000000, 245.0000000000000284, 0.000000000000000000 ) ) ;
#55249 = LINE ( 'NONE', #25796, #31905 ) ;
#55250 = CARTESIAN_POINT ( 'NONE',  ( -4.999999999999998224, 186.6666666666666856, -8.660254037844389075 ) ) ;
#55251 = CARTESIAN_POINT ( 'NONE',  ( -11.00000000000010303, -4.556349186103947346, 110.5937499999999716 ) ) ;
#55252 = CARTESIAN_POINT ( 'NONE',  ( -5.082755093536317936, -5.082755093536320601, 20.04905278187175455 ) ) ;
#55253 = CARTESIAN_POINT ( 'NONE',  ( -3.042071309553164404, 152.5520833299193271, -11.35316468749999963 ) ) ;
#55254 = CARTESIAN_POINT ( 'NONE',  ( 11.99999999999999822, 0.000000000000000000, 0.000000000000000000 ) ) ;
#55255 = CARTESIAN_POINT ( 'NONE',  ( -5.000000000000000000, 53.17721328501306033, 43.91924822456324762 ) ) ;
#55256 = FACE_OUTER_BOUND ( 'NONE', #12596, .T. ) ;
#55259 = CARTESIAN_POINT ( 'NONE',  ( 5.656854249492379694, 109.6250000040967763, -5.656854249492380582 ) ) ;
#55258 = CARTESIAN_POINT ( 'NONE',  ( -1.656854249492470732, 202.8125000027312126, 145.9999999999999716 ) ) ;
#55257 = CARTESIAN_POINT ( 'NONE',  ( 30.82842712474620228, 201.3750000000000284, 167.1715728752537586 ) ) ;
#55260 = VERTEX_POINT ( 'NONE', #6835 ) ;
#55261 = AXIS2_PLACEMENT_3D ( 'NONE', #30100, #70104, #52745 ) ;
#55262 = CARTESIAN_POINT ( 'NONE',  ( 6.951808397369818766E-16, 22.34374999658601979, -11.35316468750000141 ) ) ;
#55263 = CARTESIAN_POINT ( 'NONE',  ( 7.320508075688771044, 96.24999999317202537, 7.320508075688775484 ) ) ;
#55265 = DIRECTION ( 'NONE',  ( 0.000000000000000000, 0.000000000000000000, -1.000000000000000000 ) ) ;
#55264 = DIRECTION ( 'NONE',  ( -0.000000000000000000, 1.000000000000000000, -0.000000000000000000 ) ) ;
#55266 = CARTESIAN_POINT ( 'NONE',  ( -30.64284399271078740, 38.00000000000000711, 174.6921329945331252 ) ) ;
#55267 = CARTESIAN_POINT ( 'NONE',  ( 2.445694354108783664, 202.3125000013656063, 144.4456943541088663 ) ) ;
#55268 = VECTOR ( 'NONE', #24875, 1000.000000000000000 ) ;
#55269 = CARTESIAN_POINT ( 'NONE',  ( -7.320508075688778149, 49.99999999317202537, 7.320508075688769267 ) ) ;
#55270 = CARTESIAN_POINT ( 'NONE',  ( -4.401442555609581635E-16, 108.7812500020483810, -7.188101187500000044 ) ) ;
#55271 = CARTESIAN_POINT ( 'NONE',  ( -4.541265875000003227, 7.999999998634407028, 1.881053915767121110 ) ) ;
#55272 = CARTESIAN_POINT ( 'NONE',  ( 7.320508075688761274, 100.6249999999999716, -7.320508075688761274 ) ) ;
#55273 = CARTESIAN_POINT ( 'NONE',  ( -5.656854249492373476, -5.656854249492376141, 7.017802779823365533 ) ) ;
#55275 = CARTESIAN_POINT ( 'NONE',  ( 1.656854249492381914, 0.8125000000000004441, 4.000000000000000888 ) ) ;
#55274 = CARTESIAN_POINT ( 'NONE',  ( 12.00000000000000178, 28.00000000000000000, 3.999999999999986233 ) ) ;
#55276 = ORIENTED_EDGE ( 'NONE', *, *, #36030, .T. ) ;
#55277 = ORIENTED_EDGE ( 'NONE', *, *, #38998, .T. ) ;
#55278 = CARTESIAN_POINT ( 'NONE',  ( -10.00000000000000178, 222.5000000000000000, -1.224646799147353256E-15 ) ) ;
#55279 = CARTESIAN_POINT ( 'NONE',  ( 3.313708498984756279, 7.999999999999991118, 14.04905278392014800 ) ) ;
#55280 = CARTESIAN_POINT ( 'NONE',  ( -22.80014585274940941, -39.34393049308034307, 148.9928290591344080 ) ) ;
#55281 = CARTESIAN_POINT ( 'NONE',  ( -11.35316468750000141, 123.4895833299193555, 3.042071309553159963 ) ) ;
#55282 = VERTEX_POINT ( 'NONE', #59266 ) ;
#55283 = CARTESIAN_POINT ( 'NONE',  ( -4.999999999999999112, 13.22058908515350062, -69.49198671174478648 ) ) ;
#55284 = CARTESIAN_POINT ( 'NONE',  ( -10.18810118749999916, 0.000000000000000000, 96.15625000204838102 ) ) ;
#55285 = CARTESIAN_POINT ( 'NONE',  ( -5.656854249492378806, 93.68750000000000000, 5.656854249492381470 ) ) ;
#55286 = CARTESIAN_POINT ( 'NONE',  ( 2.751064625579944321E-14, 209.7500000000000284, 194.0000000000000568 ) ) ;
#55288 = CARTESIAN_POINT ( 'NONE',  ( -11.35316468750000141, 123.2812499965860269, -1.390361679473963753E-15 ) ) ;
#55287 = DIRECTION ( 'NONE',  ( -0.000000000000000000, 1.000000000000000000, -0.000000000000000000 ) ) ;
#55289 = FACE_OUTER_BOUND ( 'NONE', #15933, .T. ) ;
#55290 = ORIENTED_EDGE ( 'NONE', *, *, #22173, .T. ) ;
#55291 = CARTESIAN_POINT ( 'NONE',  ( 49.61047886775523352, 47.55761547386373422, 58.18749371922437064 ) ) ;
#55292 = CARTESIAN_POINT ( 'NONE',  ( -9.832129032723418760, 118.1770833299193555, -5.676582343750004256 ) ) ;
#55293 = CARTESIAN_POINT ( 'NONE',  ( 1.432654583217662259, 207.1250000013656347, 194.5412658750000219 ) ) ;
#55294 = CARTESIAN_POINT ( 'NONE',  ( 7.188101187499999156, 15.74999999795161365, 2.977408999572654924 ) ) ;
#55295 = CARTESIAN_POINT ( 'NONE',  ( -6.238412754330611322E-16, 10.18810118749999916, 82.65625000204838102 ) ) ;
#55296 = CARTESIAN_POINT ( 'NONE',  ( 6.951808397369818766E-16, 22.34374999658601979, -11.35316468750000141 ) ) ;
#55297 = ORIENTED_EDGE ( 'NONE', *, *, #58116, .F. ) ;
#55298 = CARTESIAN_POINT ( 'NONE',  ( -6.000000000000021316, -10.39230484541325161, 0.000000000000000000 ) ) ;
#55299 = CARTESIAN_POINT ( 'NONE',  ( 10.00000000000000178, 245.4166666734946318, 2.679491924311222739 ) ) ;
#55300 = CARTESIAN_POINT ( 'NONE',  ( 11.00000000000000000, 1.347111479062088405E-15, 112.9375000040967763 ) ) ;
#55301 = CARTESIAN_POINT ( 'NONE',  ( 7.188101187500000044, 1.968749997951610320, 0.000000000000000000 ) ) ;
#55302 = CARTESIAN_POINT ( 'NONE',  ( -6.676582343750001591, 287.4531250017069510, 0.000000000000000000 ) ) ;
#55303 = CARTESIAN_POINT ( 'NONE',  ( -6.062591786044946751, -5.219672483564715471, -0.3118205092643556720 ) ) ;
#55304 = CYLINDRICAL_SURFACE ( 'NONE', #26776, 10.00000000000000178 ) ;
#55305 = ORIENTED_EDGE ( 'NONE', *, *, #743, .F. ) ;
#55306 = ADVANCED_FACE ( 'NONE', ( #18155 ), #23815, .F. ) ;
#55307 = CARTESIAN_POINT ( 'NONE',  ( 6.951808397369818766E-16, 147.3437499965860411, -11.35316468750000141 ) ) ;
#55308 = CARTESIAN_POINT ( 'NONE',  ( -10.18810118749999738, -4.220049686691941915, 85.75000000204838102 ) ) ;
#55309 = CIRCLE ( 'NONE', #54099, 11.00000000000000000 ) ;
#55310 = CARTESIAN_POINT ( 'NONE',  ( -30.44569435410879166, 197.8125000013656063, 172.4456943541092357 ) ) ;
#55311 = CARTESIAN_POINT ( 'NONE',  ( -10.99999999999989342, 4.556349186104152515, 110.4062500000000142 ) ) ;
#55312 = CARTESIAN_POINT ( 'NONE',  ( 4.541265875000002339, 14.43749999863440792, 0.000000000000000000 ) ) ;
#55313 = ORIENTED_EDGE ( 'NONE', *, *, #66578, .F. ) ;
#55314 = VECTOR ( 'NONE', #1508, 1000.000000000000000 ) ;
#55315 = CARTESIAN_POINT ( 'NONE',  ( 2.828427124746209831, 203.5000000027312126, 200.8284271247462129 ) ) ;
#55316 = ADVANCED_FACE ( 'NONE', ( #30946 ), #29480, .T. ) ;
#55317 = CARTESIAN_POINT ( 'NONE',  ( -4.000000000000015987, 208.4375000000000853, 140.3431457505076594 ) ) ;
#55318 = CARTESIAN_POINT ( 'NONE',  ( -29.65685424949229443, 206.5625000027312126, 174.0000000000004547 ) ) ;
#55319 = CARTESIAN_POINT ( 'NONE',  ( -2.249999999999998224, 283.9999999998748308, 5.427273999917394676 ) ) ;
#55320 = ADVANCED_FACE ( 'NONE', ( #47551 ), #827, .F. ) ;
#55321 = ORIENTED_EDGE ( 'NONE', *, *, #38204, .T. ) ;
#55322 = CARTESIAN_POINT ( 'NONE',  ( 7.188101187500000044, 12.46874999795161187, 0.000000000000000000 ) ) ;
#55323 = CARTESIAN_POINT ( 'NONE',  ( -16.39879824506198247, -18.30767282889565806, 196.3167295749472885 ) ) ;
#55324 = DIRECTION ( 'NONE',  ( 0.000000000000000000, 0.000000000000000000, 1.000000000000000000 ) ) ;
#55325 = CARTESIAN_POINT ( 'NONE',  ( -5.676582343749998039, 192.4479166632526983, -9.832129032723420536 ) ) ;
#55326 = CARTESIAN_POINT ( 'NONE',  ( 5.082755093536326818, 110.0937500020483810, 5.082755093536325042 ) ) ;
#55327 = CARTESIAN_POINT ( 'NONE',  ( -2.485281374238227592, 291.2500000034139589, 6.000000000000345501 ) ) ;
#55328 = CARTESIAN_POINT ( 'NONE',  ( 7.999999999999991118, 9.797174393178815797E-16, 3.080302779823361981 ) ) ;
#55330 = CARTESIAN_POINT ( 'NONE',  ( -8.660254037844389075, 67.08333333333335702, -5.000000000000006217 ) ) ;
#55329 = CARTESIAN_POINT ( 'NONE',  ( 2.085542519210945334E-15, 220.1562500034139873, 11.35316468749999963 ) ) ;
#55331 = ORIENTED_EDGE ( 'NONE', *, *, #26545, .F. ) ;
#55332 = CARTESIAN_POINT ( 'NONE',  ( 11.35316468749999608, 251.6145833367473585, -3.042071309553167069 ) ) ;
#55333 = CARTESIAN_POINT ( 'NONE',  ( -7.188101187499991163, 2.977408999572646930, 25.76780278187175810 ) ) ;
#55334 = CARTESIAN_POINT ( 'NONE',  ( 3.313708498984765161, 105.9687500000000000, 7.999999999999998224 ) ) ;
#55335 = CYLINDRICAL_SURFACE ( 'NONE', #65873, 10.00000000000000000 ) ;
#55336 = CARTESIAN_POINT ( 'NONE',  ( 6.298842414730434491, -61.32333038069613451, -23.57034304879013575 ) ) ;
#55337 =( BOUNDED_SURFACE ( )  B_SPLINE_SURFACE ( 1, 2, ( 
 ( #67989, #50258, #17042, #10280, #5369, #28736, #39689, #61954, #56684, #100, #27620, #34059, #74389, #73280, #62688, #50629, #10649, #4254, #5002, #68728, #21955, #22698, #9906, #11027, #32938, #15920, #15549, #44610, #67625, #51753, #73648, #16284, #51377, #33681, #45717, #51009, #40066, #63071, #67254, #39324, #11394, #38951, #34429, #55944, #27242, #6846, #46088, #40437, #29119, #29492, #69107, #57808, #24186, #52501, #17415, #469, #58913, #30595, #35167, #24556, #23825, #13227, #64918, #7588, #6113, #52873, #7223, #30226, #52137, #47199, #12857, #18903, #29861, #58182, #36263, #53246, #63437, #70229, #839, #35896, #41183, #1205, #11764, #34802, #1576, #47563, #23450, #64193, #70586, #6487, #46462, #69481, #18538, #17792, #40805, #63815, #12129, #41546, #59279, #41910, #53614, #1927, #46830, #69856, #18168, #12498, #35529, #58541, #64562, #66405, #25287, #20372, #2290, #15088, #66032, #48304, #60751, #14338, #32469, #72446, #19264, #54734, #36632, #2667, #53980, #38123, #71681, #55107, #49427, #37370, #42276, #19632, #71313, #14713, #42646, #65658, #31711, #70948, #13955, #36997, #47931, #55479, #65289, #9074, #32086, #60002, #25658, #43389, #20001, #3041, #43011, #49047, #26024, #72055, #31330, #37751, #66784, #60371, #24915, #20755, #13594, #3414, #59639, #48674, #8319, #61122, #8697, #26399, #43770, #9453, #7956, #54357, #30959, #45266, #73194, #21502, #10564, #49806, #32848, #15833, #26790, #34344, #72822, #39609, #10938, #55855, #56223, #73933, #73560, #33595, #50544, #27911, #4917, #56601, #10194, #50921, #45633, #67904, #38867, #33224, #22237, #21870, #68276, #16198, #39237, #62607, #3791, #67536, #16572, #4172, #33974, #56971, #22612, #62237, #21129, #44149, #61499 ),
 ( #5286, #11310, #28287, #67165, #44521, #62988, #15460, #51293, #27159, #68647, #74306, #44898, #16958, #39981, #38497, #9822, #50176, #61873, #4537, #27532, #17702, #41826, #7134, #12776, #58823, #57343, #18079, #70145, #69765, #41095, #34711, #12413, #64837, #35810, #28653, #18452, #6404, #64103, #46378, #29409, #69025, #70504, #52418, #18823, #47107, #35080, #40348, #30142, #384, #41465, #13139, #6766, #52047, #46742, #5654, #23364, #24097, #64479, #63350, #29770, #40719, #753, #17327, #29028, #51668, #69393, #63725, #11, #57719, #22999, #12047, #11675, #46005, #6024, #58092, #24475, #23737, #53158, #52784, #35447, #1121, #58458, #1492, #47480, #65947, #43684, #14253, #53529, #30877, #20666, #1846, #37289, #65195, #55020, #60282, #2583, #8608, #42925, #7504, #49338, #66696, #30510, #54273, #53896, #71224, #36174, #60664, #66320, #37665, #59194, #71595, #48959, #48586, #19917, #13506, #31623, #24832, #14625, #47849, #71970, #59922, #54645, #25203, #8236, #70869, #72354, #31247, #19181, #25942, #13870, #42183, #8985, #2208, #20284, #36545, #2952, #48216, #25572, #59556, #19544, #43305, #32001, #7872, #3328, #42562, #26316, #65573, #36914, #16486, #44434, #45177, #32379, #39148, #55394, #38410, #38036, #67074, #44064, #28194, #10847, #62520, #22150, #21411, #62152, #67448, #21040, #56509, #61035, #22521, #45541, #4825, #15745, #21779, #67819, #33881, #55767, #44806, #56138, #14998, #9360, #61411, #51205, #4084, #4448, #38784, #10475, #3703, #61787, #27823, #16111, #27439, #10106, #33506, #33143, #50832, #50455, #73470, #73843, #26701, #27077, #68190, #15373, #39523, #56881, #5197, #74216, #49721, #72737, #9737, #73104, #32759, #50090, #46660, #297, #68559, #22905, #6682 ) ),
 .UNSPECIFIED., .F., .F., .T. ) 
 B_SPLINE_SURFACE_WITH_KNOTS ( ( 2, 2 ),
 ( 3, 2, 2, 2, 2, 2, 2, 2, 2, 2, 2, 2, 2, 2, 2, 2, 2, 2, 2, 2, 2, 2, 2, 2, 2, 2, 2, 2, 2, 2, 2, 2, 2, 2, 2, 2, 2, 2, 2, 2, 2, 2, 2, 2, 2, 2, 2, 2, 2, 2, 2, 2, 2, 2, 2, 2, 2, 2, 2, 2, 2, 2, 2, 2, 2, 2, 2, 2, 2, 2, 2, 2, 2, 2, 2, 2, 2, 2, 2, 2, 2, 2, 2, 2, 2, 2, 2, 2, 2, 2, 2, 2, 2, 2, 2, 2, 2, 2, 2, 2, 2, 2, 2, 2, 2, 2, 2, 2, 3 ),
 ( 0.000000000000000000, 1.000000000000000000 ),
 ( 0.000000000000000000, 0.009259259259259258745, 0.01851851851851851749, 0.02777777777777777624, 0.03703703703703703498, 0.04629629629629629373, 0.05555555555555555247, 0.06481481481481481122, 0.07407407407407406996, 0.08333333333333332871, 0.09259259259259258745, 0.1018518518518518462, 0.1111111111111111049, 0.1203703703703703637, 0.1296296296296296224, 0.1388888888888888951, 0.1481481481481481399, 0.1574074074074074125, 0.1666666666666666574, 0.1759259259259259300, 0.1851851851851851749, 0.1944444444444444475, 0.2037037037037036924, 0.2129629629629629650, 0.2222222222222222099, 0.2314814814814814825, 0.2407407407407407274, 0.2500000000000000000, 0.2592592592592592449, 0.2685185185185185452, 0.2777777777777777901, 0.2870370370370370350, 0.2962962962962962798, 0.3055555555555555802, 0.3148148148148148251, 0.3240740740740740700, 0.3333333333333333148, 0.3425925925925926152, 0.3518518518518518601, 0.3611111111111111049, 0.3703703703703703498, 0.3796296296296296502, 0.3888888888888888951, 0.3981481481481481399, 0.4074074074074073848, 0.4166666666666666852, 0.4259259259259259300, 0.4351851851851851749, 0.4444444444444444198, 0.4537037037037037202, 0.4629629629629629650, 0.4722222222222222099, 0.4814814814814814548, 0.4907407407407407551, 0.5000000000000000000, 0.5092592592592593004, 0.5185185185185184897, 0.5277777777777777901, 0.5370370370370370905, 0.5462962962962962798, 0.5555555555555555802, 0.5648148148148147696, 0.5740740740740740700, 0.5833333333333333703, 0.5925925925925925597, 0.6018518518518518601, 0.6111111111111111605, 0.6203703703703703498, 0.6296296296296296502, 0.6388888888888888395, 0.6481481481481481399, 0.6574074074074074403, 0.6666666666666666297, 0.6759259259259259300, 0.6851851851851852304, 0.6944444444444444198, 0.7037037037037037202, 0.7129629629629629095, 0.7222222222222222099, 0.7314814814814815103, 0.7407407407407406996, 0.7500000000000000000, 0.7592592592592593004, 0.7685185185185184897, 0.7777777777777777901, 0.7870370370370370905, 0.7962962962962962798, 0.8055555555555555802, 0.8148148148148147696, 0.8240740740740740700, 0.8333333333333333703, 0.8425925925925925597, 0.8518518518518518601, 0.8611111111111111605, 0.8703703703703703498, 0.8796296296296296502, 0.8888888888888888395, 0.8981481481481481399, 0.9074074074074074403, 0.9166666666666666297, 0.9259259259259259300, 0.9351851851851852304, 0.9444444444444444198, 0.9537037037037037202, 0.9629629629629629095, 0.9722222222222222099, 0.9814814814814815103, 0.9907407407407406996, 1.000000000000000000 ),
 .UNSPECIFIED. ) 
 GEOMETRIC_REPRESENTATION_ITEM ( )  RATIONAL_B_SPLINE_SURFACE ( (
 ( 1.000000000000000000, 0.9659258262890683122, 1.000000000000000000, 0.9659258262890683122, 1.000000000000000000, 0.9659258262890683122, 1.000000000000000000, 0.9659258262890683122, 1.000000000000000000, 0.9659258262890683122, 1.000000000000000000, 0.9659258262890683122, 1.000000000000000000, 0.9659258262890683122, 1.000000000000000000, 0.9659258262890683122, 1.000000000000000000, 0.9659258262890683122, 1.000000000000000000, 0.9659258262890683122, 1.000000000000000000, 0.9659258262890683122, 1.000000000000000000, 0.9659258262890683122, 1.000000000000000000, 0.9659258262890683122, 1.000000000000000000, 0.9659258262890683122, 1.000000000000000000, 0.9659258262890683122, 1.000000000000000000, 0.9659258262890683122, 1.000000000000000000, 0.9659258262890683122, 1.000000000000000000, 0.9659258262890683122, 1.000000000000000000, 0.9659258262890683122, 1.000000000000000000, 0.9659258262890683122, 1.000000000000000000, 0.9659258262890683122, 1.000000000000000000, 0.9659258262890683122, 1.000000000000000000, 0.9659258262890683122, 1.000000000000000000, 0.9659258262890683122, 1.000000000000000000, 0.9659258262890683122, 1.000000000000000000, 0.9659258262890683122, 1.000000000000000000, 0.9659258262890683122, 1.000000000000000000, 0.9659258262890683122, 1.000000000000000000, 0.9659258262890683122, 1.000000000000000000, 0.9659258262890683122, 1.000000000000000000, 0.9659258262890683122, 1.000000000000000000, 0.9659258262890683122, 1.000000000000000000, 0.9659258262890683122, 1.000000000000000000, 0.9659258262890683122, 1.000000000000000000, 0.9659258262890683122, 1.000000000000000000, 0.9659258262890683122, 1.000000000000000000, 0.9659258262890683122, 1.000000000000000000, 0.9659258262890683122, 1.000000000000000000, 0.9659258262890683122, 1.000000000000000000, 0.9659258262890683122, 1.000000000000000000, 0.9659258262890683122, 1.000000000000000000, 0.9659258262890683122, 1.000000000000000000, 0.9659258262890683122, 1.000000000000000000, 0.9659258262890683122, 1.000000000000000000, 0.9659258262890683122, 1.000000000000000000, 0.9659258262890683122, 1.000000000000000000, 0.9659258262890683122, 1.000000000000000000, 0.9659258262890683122, 1.000000000000000000, 0.9659258262890683122, 1.000000000000000000, 0.9659258262890683122, 1.000000000000000000, 0.9659258262890683122, 1.000000000000000000, 0.9659258262890683122, 1.000000000000000000, 0.9659258262890683122, 1.000000000000000000, 0.9659258262890683122, 1.000000000000000000, 0.9659258262890683122, 1.000000000000000000, 0.9659258262890683122, 1.000000000000000000, 0.9659258262890683122, 1.000000000000000000, 0.9659258262890683122, 1.000000000000000000, 0.9659258262890683122, 1.000000000000000000, 0.9659258262890683122, 1.000000000000000000, 0.9659258262890683122, 1.000000000000000000, 0.9659258262890683122, 1.000000000000000000, 0.9659258262890683122, 1.000000000000000000, 0.9659258262890683122, 1.000000000000000000, 0.9659258262890683122, 1.000000000000000000, 0.9659258262890683122, 1.000000000000000000, 0.9659258262890683122, 1.000000000000000000, 0.9659258262890683122, 1.000000000000000000, 0.9659258262890683122, 1.000000000000000000, 0.9659258262890683122, 1.000000000000000000, 0.9659258262890683122, 1.000000000000000000, 0.9659258262890683122, 1.000000000000000000, 0.9659258262890683122, 1.000000000000000000, 0.9659258262890683122, 1.000000000000000000, 0.9659258262890683122, 1.000000000000000000, 0.9659258262890683122, 1.000000000000000000, 0.9659258262890683122, 1.000000000000000000, 0.9659258262890683122, 1.000000000000000000, 0.9659258262890683122, 1.000000000000000000, 0.9659258262890683122, 1.000000000000000000, 0.9659258262890683122, 1.000000000000000000, 0.9659258262890683122, 1.000000000000000000, 0.9659258262890683122, 1.000000000000000000, 0.9659258262890683122, 1.000000000000000000, 0.9659258262890683122, 1.000000000000000000, 0.9659258262890683122, 1.000000000000000000, 0.9659258262890683122, 1.000000000000000000, 0.9659258262890683122, 1.000000000000000000, 0.9659258262890683122, 1.000000000000000000, 0.9659258262890683122, 1.000000000000000000, 0.9659258262890683122, 1.000000000000000000, 0.9659258262890683122, 1.000000000000000000, 0.9659258262890683122, 1.000000000000000000, 0.9659258262890683122, 1.000000000000000000, 0.9659258262890683122, 1.000000000000000000, 0.9659258262890683122, 1.000000000000000000, 0.9659258262890683122, 1.000000000000000000, 0.9659258262890683122, 1.000000000000000000, 0.9659258262890683122, 1.000000000000000000, 0.9659258262890683122, 1.000000000000000000, 0.9659258262890683122, 1.000000000000000000, 0.9659258262890683122, 1.000000000000000000, 0.9659258262890683122, 1.000000000000000000, 0.9659258262890683122, 1.000000000000000000, 0.9659258262890683122, 1.000000000000000000, 0.9659258262890683122, 1.000000000000000000, 0.9659258262890683122, 1.000000000000000000, 0.9659258262890683122, 1.000000000000000000),
 ( 1.000000000000000000, 0.9659258262890683122, 1.000000000000000000, 0.9659258262890683122, 1.000000000000000000, 0.9659258262890683122, 1.000000000000000000, 0.9659258262890683122, 1.000000000000000000, 0.9659258262890683122, 1.000000000000000000, 0.9659258262890683122, 1.000000000000000000, 0.9659258262890683122, 1.000000000000000000, 0.9659258262890683122, 1.000000000000000000, 0.9659258262890683122, 1.000000000000000000, 0.9659258262890683122, 1.000000000000000000, 0.9659258262890683122, 1.000000000000000000, 0.9659258262890683122, 1.000000000000000000, 0.9659258262890683122, 1.000000000000000000, 0.9659258262890683122, 1.000000000000000000, 0.9659258262890683122, 1.000000000000000000, 0.9659258262890683122, 1.000000000000000000, 0.9659258262890683122, 1.000000000000000000, 0.9659258262890683122, 1.000000000000000000, 0.9659258262890683122, 1.000000000000000000, 0.9659258262890683122, 1.000000000000000000, 0.9659258262890683122, 1.000000000000000000, 0.9659258262890683122, 1.000000000000000000, 0.9659258262890683122, 1.000000000000000000, 0.9659258262890683122, 1.000000000000000000, 0.9659258262890683122, 1.000000000000000000, 0.9659258262890683122, 1.000000000000000000, 0.9659258262890683122, 1.000000000000000000, 0.9659258262890683122, 1.000000000000000000, 0.9659258262890683122, 1.000000000000000000, 0.9659258262890683122, 1.000000000000000000, 0.9659258262890683122, 1.000000000000000000, 0.9659258262890683122, 1.000000000000000000, 0.9659258262890683122, 1.000000000000000000, 0.9659258262890683122, 1.000000000000000000, 0.9659258262890683122, 1.000000000000000000, 0.9659258262890683122, 1.000000000000000000, 0.9659258262890683122, 1.000000000000000000, 0.9659258262890683122, 1.000000000000000000, 0.9659258262890683122, 1.000000000000000000, 0.9659258262890683122, 1.000000000000000000, 0.9659258262890683122, 1.000000000000000000, 0.9659258262890683122, 1.000000000000000000, 0.9659258262890683122, 1.000000000000000000, 0.9659258262890683122, 1.000000000000000000, 0.9659258262890683122, 1.000000000000000000, 0.9659258262890683122, 1.000000000000000000, 0.9659258262890683122, 1.000000000000000000, 0.9659258262890683122, 1.000000000000000000, 0.9659258262890683122, 1.000000000000000000, 0.9659258262890683122, 1.000000000000000000, 0.9659258262890683122, 1.000000000000000000, 0.9659258262890683122, 1.000000000000000000, 0.9659258262890683122, 1.000000000000000000, 0.9659258262890683122, 1.000000000000000000, 0.9659258262890683122, 1.000000000000000000, 0.9659258262890683122, 1.000000000000000000, 0.9659258262890683122, 1.000000000000000000, 0.9659258262890683122, 1.000000000000000000, 0.9659258262890683122, 1.000000000000000000, 0.9659258262890683122, 1.000000000000000000, 0.9659258262890683122, 1.000000000000000000, 0.9659258262890683122, 1.000000000000000000, 0.9659258262890683122, 1.000000000000000000, 0.9659258262890683122, 1.000000000000000000, 0.9659258262890683122, 1.000000000000000000, 0.9659258262890683122, 1.000000000000000000, 0.9659258262890683122, 1.000000000000000000, 0.9659258262890683122, 1.000000000000000000, 0.9659258262890683122, 1.000000000000000000, 0.9659258262890683122, 1.000000000000000000, 0.9659258262890683122, 1.000000000000000000, 0.9659258262890683122, 1.000000000000000000, 0.9659258262890683122, 1.000000000000000000, 0.9659258262890683122, 1.000000000000000000, 0.9659258262890683122, 1.000000000000000000, 0.9659258262890683122, 1.000000000000000000, 0.9659258262890683122, 1.000000000000000000, 0.9659258262890683122, 1.000000000000000000, 0.9659258262890683122, 1.000000000000000000, 0.9659258262890683122, 1.000000000000000000, 0.9659258262890683122, 1.000000000000000000, 0.9659258262890683122, 1.000000000000000000, 0.9659258262890683122, 1.000000000000000000, 0.9659258262890683122, 1.000000000000000000, 0.9659258262890683122, 1.000000000000000000, 0.9659258262890683122, 1.000000000000000000, 0.9659258262890683122, 1.000000000000000000, 0.9659258262890683122, 1.000000000000000000, 0.9659258262890683122, 1.000000000000000000, 0.9659258262890683122, 1.000000000000000000, 0.9659258262890683122, 1.000000000000000000, 0.9659258262890683122, 1.000000000000000000, 0.9659258262890683122, 1.000000000000000000, 0.9659258262890683122, 1.000000000000000000, 0.9659258262890683122, 1.000000000000000000, 0.9659258262890683122, 1.000000000000000000, 0.9659258262890683122, 1.000000000000000000, 0.9659258262890683122, 1.000000000000000000, 0.9659258262890683122, 1.000000000000000000, 0.9659258262890683122, 1.000000000000000000, 0.9659258262890683122, 1.000000000000000000, 0.9659258262890683122, 1.000000000000000000, 0.9659258262890683122, 1.000000000000000000, 0.9659258262890683122, 1.000000000000000000, 0.9659258262890683122, 1.000000000000000000, 0.9659258262890683122, 1.000000000000000000, 0.9659258262890683122, 1.000000000000000000, 0.9659258262890683122, 1.000000000000000000) ) ) 
 REPRESENTATION_ITEM ( '' )  SURFACE ( )  );
#55338 = CARTESIAN_POINT ( 'NONE',  ( -3.458734124999959469, 200.7500000013656347, 199.4326545832176691 ) ) ;
#55339 = DIRECTION ( 'NONE',  ( 1.000000000000000000, -0.000000000000000000, 0.000000000000000000 ) ) ;
#55340 = CARTESIAN_POINT ( 'NONE',  ( -1.469576158976823947E-15, 23.62500000000000355, 8.000000000000000000 ) ) ;
#55341 = CARTESIAN_POINT ( 'NONE',  ( 8.000000000000001776, 94.15624999999998579, 3.313708498984759387 ) ) ;
#55342 = CARTESIAN_POINT ( 'NONE',  ( 11.35316468749999785, 110.8854166632526699, 3.042071309553174174 ) ) ;
#55343 = CARTESIAN_POINT ( 'NONE',  ( 23.99999999999997868, 205.8125000000000000, 171.6568542494922553 ) ) ;
#55344 = CARTESIAN_POINT ( 'NONE',  ( 4.556349186104045934, 11.00000000000000000, 71.03124999999998579 ) ) ;
#55347 = CARTESIAN_POINT ( 'NONE',  ( 16.52771754582130015, -11.24232751665652508, -1.116934336526976379 ) ) ;
#55346 = CARTESIAN_POINT ( 'NONE',  ( 25.55430564589115505, 202.0625000013656063, 167.5543056458911053 ) ) ;
#55345 = CARTESIAN_POINT ( 'NONE',  ( 26.56734541678238060, 200.2500000013656631, 166.5412658749999650 ) ) ;
#55348 = ORIENTED_EDGE ( 'NONE', *, *, #9152, .T. ) ;
#55349 = CARTESIAN_POINT ( 'NONE',  ( 8.000000000000000000, 100.3437500000000000, -3.313708498984762496 ) ) ;
#55350 = CARTESIAN_POINT ( 'NONE',  ( -11.35316468750000141, 223.4895833299193555, 3.042071309553159963 ) ) ;
#55351 = CARTESIAN_POINT ( 'NONE',  ( 3.458734124999959025, 196.5000000013656063, 140.5673454167824161 ) ) ;
#55352 = CARTESIAN_POINT ( 'NONE',  ( 24.54126587499998990, 197.4375000013655779, 169.9999999999998863 ) ) ;
#55353 = CARTESIAN_POINT ( 'NONE',  ( -2.977408999572650039, 26.81249999795161543, -7.188101187500001821 ) ) ;
#55354 = CARTESIAN_POINT ( 'NONE',  ( 11.35316468749999785, 210.8854166632526983, 3.042071309553174174 ) ) ;
#55355 = CARTESIAN_POINT ( 'NONE',  ( 4.556349186104052151, -10.99999999999999822, 70.46874999999998579 ) ) ;
#55356 = CARTESIAN_POINT ( 'NONE',  ( 7.600546564020412177, 225.9999999999997726, 7.213721669030190853 ) ) ;
#55357 = CARTESIAN_POINT ( 'NONE',  ( 4.541265875000002339, 17.31249999863440792, 0.000000000000000000 ) ) ;
#55358 = CARTESIAN_POINT ( 'NONE',  ( 3.223881452091941213, -50.20043732027839667, 40.84573126306743518 ) ) ;
#55359 = CARTESIAN_POINT ( 'NONE',  ( 5.656854249492376141, -5.656854249492374365, 25.39280277982336642 ) ) ;
#55360 = CARTESIAN_POINT ( 'NONE',  ( -8.000000000000000000, 12.75000000000000178, -9.797174393178825657E-16 ) ) ;
#55361 = CARTESIAN_POINT ( 'NONE',  ( -5.676582343750006032, 79.11458332991935549, 9.832129032723418760 ) ) ;
#55362 = VERTEX_POINT ( 'NONE', #7578 ) ;
#55363 =( BOUNDED_CURVE ( )  B_SPLINE_CURVE ( 2, ( #18330, #41345, #64355, #12658, #35689, #58704, #30023, #2459, #65454 ),
 .UNSPECIFIED., .F., .F. ) 
 B_SPLINE_CURVE_WITH_KNOTS ( ( 3, 2, 2, 2, 3 ),
 ( 0.8472222222222222099, 0.8541666666666666297, 0.8611111111111111605, 0.8680555555555555802, 0.8750000000000000000 ),
 .UNSPECIFIED. ) 
 CURVE ( )  GEOMETRIC_REPRESENTATION_ITEM ( )  RATIONAL_B_SPLINE_CURVE ( ( 1.000000000000000000, 0.9238795325112867385, 1.000000000000000000, 0.9238795325112867385, 1.000000000000000000, 0.9238795325112867385, 1.000000000000000000, 0.9238795325112867385, 1.000000000000000000 ) ) 
 REPRESENTATION_ITEM ( '' )  );
#55364 = CARTESIAN_POINT ( 'NONE',  ( 12.00000000000000000, 4.898587196589398038E-16, -24.00000000000001421 ) ) ;
#55365 = CARTESIAN_POINT ( 'NONE',  ( 7.188101187500000044, 16.96874999795161543, 0.000000000000000000 ) ) ;
#55366 = CARTESIAN_POINT ( 'NONE',  ( -37.99999999999999289, 205.0000000000000284, 0.000000000000000000 ) ) ;
#55367 = CARTESIAN_POINT ( 'NONE',  ( 8.311093377946839666, 251.0937500034139873, 8.311093377946830785 ) ) ;
#55368 = CARTESIAN_POINT ( 'NONE',  ( -5.676582343749998039, 87.44791666325268409, -9.832129032723420536 ) ) ;
#55369 = EDGE_LOOP ( 'NONE', ( #14428, #54093, #47495 ) ) ;
#55370 = CARTESIAN_POINT ( 'NONE',  ( 23.99999999999997513, 196.8125000027312410, 168.3431457505075457 ) ) ;
#55371 = CARTESIAN_POINT ( 'NONE',  ( 10.18810118750000093, -4.220049686691933921, 113.3125000020483668 ) ) ;
#55372 = CARTESIAN_POINT ( 'NONE',  ( -31.45873412499997812, 196.0000000013656347, 171.4326545832180386 ) ) ;
#55373 = CARTESIAN_POINT ( 'NONE',  ( -2.445694354108783219, 208.8125000013656063, 200.4456943541088663 ) ) ;
#55374 = CARTESIAN_POINT ( 'NONE',  ( 3.313708498984800688, 118.5312499999999858, -7.999999999999958256 ) ) ;
#55376 = CARTESIAN_POINT ( 'NONE',  ( -8.311093377946836114, 87.65624999658601268, -8.311093377946837890 ) ) ;
#55375 = CARTESIAN_POINT ( 'NONE',  ( 2.775557561562891351E-14, -70.00000000000000000, 170.0000000000000000 ) ) ;
#55377 = CARTESIAN_POINT ( 'NONE',  ( -3.313708498984758943, -7.999999999999989342, 16.29905278392014623 ) ) ;
#55378 = CARTESIAN_POINT ( 'NONE',  ( -28.00000000000002132, 202.6875000013656063, 166.5412658750003629 ) ) ;
#55379 = CARTESIAN_POINT ( 'NONE',  ( -8.000000000000001776, 21.65624999590322375, 3.313708498984759387 ) ) ;
#55380 = CARTESIAN_POINT ( 'NONE',  ( 2.679491924311222739, 185.8333333265053398, 10.00000000000000355 ) ) ;
#55381 = EDGE_CURVE ( 'NONE', #51876, #38945, #7211, .T. ) ;
#55382 = CARTESIAN_POINT ( 'NONE',  ( -1.836970198721029983E-15, 95.62499999317203958, 10.00000000000000178 ) ) ;
#55383 = CARTESIAN_POINT ( 'NONE',  ( -11.35316468750000141, 73.59374999658602690, -1.390361679473963753E-15 ) ) ;
#55384 = CARTESIAN_POINT ( 'NONE',  ( -4.721056650415999201, 292.3281250017069510, -4.721056650415999201 ) ) ;
#55385 = CARTESIAN_POINT ( 'NONE',  ( -10.18810118749999738, -4.220049686691941915, 107.1250000020483810 ) ) ;
#55386 = CARTESIAN_POINT ( 'NONE',  ( 9.832129032723420536, 211.1979166632526983, -5.676582343749999815 ) ) ;
#55387 = ORIENTED_EDGE ( 'NONE', *, *, #8639, .F. ) ;
#55388 = LINE ( 'NONE', #65189, #56121 ) ;
#55389 = CARTESIAN_POINT ( 'NONE',  ( -1.688721909672324495, -60.25432409644719201, -22.91817940688312660 ) ) ;
#55390 = CARTESIAN_POINT ( 'NONE',  ( 5.000000000000000888, 66.79212039439808279, 23.29662735513495164 ) ) ;
#55392 = CARTESIAN_POINT ( 'NONE',  ( 8.311093377946834337, 210.1562499965860127, 8.311093377946839666 ) ) ;
#55391 = FACE_OUTER_BOUND ( 'NONE', #34254, .T. ) ;
#55393 = CARTESIAN_POINT ( 'NONE',  ( -4.000000000000016875, 203.4375000000000284, 140.3431457505076594 ) ) ;
#55394 = CARTESIAN_POINT ( 'NONE',  ( 7.320508075688771044, 231.2500000068279462, -7.320508075688771932 ) ) ;
#55395 = CARTESIAN_POINT ( 'NONE',  ( -6.676582343750001591, 299.4531250017069510, 0.000000000000000000 ) ) ;
#55396 = VERTEX_POINT ( 'NONE', #30581 ) ;
#55397 = CARTESIAN_POINT ( 'NONE',  ( 11.35316468749999963, 201.3020833299193555, -3.042071309553165293 ) ) ;
#55398 = CARTESIAN_POINT ( 'NONE',  ( 1.320432766682872962E-15, -7.188101187499992051, 15.36155278187175277 ) ) ;
#55399 = CARTESIAN_POINT ( 'NONE',  ( -2.124081043562903837, 60.31560147600205113, -22.95556260996129794 ) ) ;
#55400 = CARTESIAN_POINT ( 'NONE',  ( -8.000000000000000000, 12.65625000000000178, -3.313708498984762496 ) ) ;
#55401 = EDGE_LOOP ( 'NONE', ( #27279, #16912, #527, #72929 ) ) ;
#55402 = EDGE_CURVE ( 'NONE', #13802, #63081, #72243, .T. ) ;
#55403 = CARTESIAN_POINT ( 'NONE',  ( -8.000000000000000000, 90.59375000409677625, -3.313708498984761608 ) ) ;
#55404 = CARTESIAN_POINT ( 'NONE',  ( -8.660254037844390851, 12.91666666666666785, 4.999999999999998224 ) ) ;
#55405 = AXIS2_PLACEMENT_3D ( 'NONE', #3561, #26551, #8846 ) ;
#55406 = ORIENTED_EDGE ( 'NONE', *, *, #18760, .F. ) ;
#55407 = CARTESIAN_POINT ( 'NONE',  ( -1.656854249492381248, 17.31250000000000355, -4.000000000000001776 ) ) ;
#55408 = CARTESIAN_POINT ( 'NONE',  ( 4.541265875000002339, 20.37499999863441147, -1.881053915767121776 ) ) ;
#55409 = CARTESIAN_POINT ( 'NONE',  ( -5.656854249492373476, -5.656854249492376141, 7.205302783920144449 ) ) ;
#55410 = VECTOR ( 'NONE', #54508, 1000.000000000000000 ) ;
#55411 = ORIENTED_EDGE ( 'NONE', *, *, #3142, .T. ) ;
#55412 = DIRECTION ( 'NONE',  ( -0.000000000000000000, 1.000000000000000000, -1.563033456626094573E-30 ) ) ;
#55413 = CARTESIAN_POINT ( 'NONE',  ( 5.082755093536325042, 93.59375000204838102, -5.082755093536325930 ) ) ;
#55414 = ADVANCED_FACE ( 'NONE', ( #41170 ), #18525, .F. ) ;
#55417 = DIRECTION ( 'NONE',  ( 1.000000000000000000, 0.000000000000000000, -0.000000000000000000 ) ) ;
#55416 = CARTESIAN_POINT ( 'NONE',  ( -24.00000000000002487, 204.9375000027312126, 168.3431457505079152 ) ) ;
#55415 = CARTESIAN_POINT ( 'NONE',  ( -4.999999999999992895, 258.9583333401613459, 8.660254037844390851 ) ) ;
#55418 = VERTEX_POINT ( 'NONE', #19251 ) ;
#55419 = CARTESIAN_POINT ( 'NONE',  ( -11.35316468749999608, 259.4270833367472164, 3.042071309553173730 ) ) ;
#55420 = CARTESIAN_POINT ( 'NONE',  ( 5.082755093536318824, 5.082755093536319713, 15.92405278187175632 ) ) ;
#55421 = ORIENTED_EDGE ( 'NONE', *, *, #43289, .T. ) ;
#55422 = VERTEX_POINT ( 'NONE', #42262 ) ;
#55423 = CARTESIAN_POINT ( 'NONE',  ( -10.18810118749999916, 4.220049686691934809, 79.56250000204836681 ) ) ;
#55424 = CARTESIAN_POINT ( 'NONE',  ( -11.35316468750000141, 73.59374999658602690, -1.390361679473963753E-15 ) ) ;
#55425 = CARTESIAN_POINT ( 'NONE',  ( -27.99999999999999645, 210.0000000000000284, 170.0000000000003695 ) ) ;
#55426 = CARTESIAN_POINT ( 'NONE',  ( 11.00000000000000000, 4.556349186104045934, 87.34374999999998579 ) ) ;
#55429 = CARTESIAN_POINT ( 'NONE',  ( 6.676582343750003368, 291.0468750017070079, 2.765530957081995478 ) ) ;
#55428 = CARTESIAN_POINT ( 'NONE',  ( 25.17157287525381548, 196.0000000027312126, 172.8284271247460993 ) ) ;
#55427 = FACE_OUTER_BOUND ( 'NONE', #14187, .T. ) ;
#55430 = CARTESIAN_POINT ( 'NONE',  ( 11.00000000000000000, 1.347111479062088405E-15, 84.24999999999998579 ) ) ;
#55431 = CARTESIAN_POINT ( 'NONE',  ( 0.000000000000000000, 300.0000000000000000, 6.000000000000001776 ) ) ;
#55432 = CARTESIAN_POINT ( 'NONE',  ( 3.458734125000015869, 197.1875000013655779, 198.0000000000000284 ) ) ;
#55433 = CARTESIAN_POINT ( 'NONE',  ( 5.656854249492380582, 11.99999999590322197, -5.656854249492380582 ) ) ;
#55434 = ORIENTED_EDGE ( 'NONE', *, *, #21795, .T. ) ;
#55435 = CARTESIAN_POINT ( 'NONE',  ( 26.56734541678238415, 208.2500000013656063, 166.5412658749999650 ) ) ;
#55436 = CARTESIAN_POINT ( 'NONE',  ( 7.188101187499999156, 14.24999999795161010, 2.977408999572654924 ) ) ;
#55437 = CARTESIAN_POINT ( 'NONE',  ( 5.656854249492374365, 5.656854249492375253, 25.95530278392014623 ) ) ;
#55438 = DIRECTION ( 'NONE',  ( 0.000000000000000000, 0.000000000000000000, 1.000000000000000000 ) ) ;
#55439 = CARTESIAN_POINT ( 'NONE',  ( 7.188101187500002709, 107.1875000020483810, 2.977408999572649151 ) ) ;
#55441 = CARTESIAN_POINT ( 'NONE',  ( -1.781595147096349363, -51.28498669165043111, -48.57279346520105179 ) ) ;
#55440 = CARTESIAN_POINT ( 'NONE',  ( -2.679491924311226292, 18.33333332650536818, -10.00000000000000178 ) ) ;
#55442 = CARTESIAN_POINT ( 'NONE',  ( 11.35316468749999963, 221.7187500034139873, -1.390361679473963556E-15 ) ) ;
#55443 = CARTESIAN_POINT ( 'NONE',  ( 26.56734541678233086, 208.6250000013656063, 173.4587341249998929 ) ) ;
#55444 = CARTESIAN_POINT ( 'NONE',  ( 5.082755093536320601, -5.082755093536318824, 17.42405278187175810 ) ) ;
#55445 = CARTESIAN_POINT ( 'NONE',  ( 1.656854249492347719, 206.9375000027312410, 146.0000000000000284 ) ) ;
#55446 = CARTESIAN_POINT ( 'NONE',  ( 11.35316468749999963, 40.98958332991935549, -3.042071309553165293 ) ) ;
#55447 = FACE_OUTER_BOUND ( 'NONE', #23584, .T. ) ;
#55448 = CARTESIAN_POINT ( 'NONE',  ( 2.679491924311228956, 17.91666665983870033, -10.00000000000000000 ) ) ;
#55449 = VERTEX_POINT ( 'NONE', #64181 ) ;
#55450 = CARTESIAN_POINT ( 'NONE',  ( 7.999999999999991118, 9.797174393178815797E-16, 9.080302779823364645 ) ) ;
#55451 = CARTESIAN_POINT ( 'NONE',  ( -18.00000000000000000, -10.39230484541329247, -1.607695154586745501 ) ) ;
#55452 = CARTESIAN_POINT ( 'NONE',  ( 8.311093377946834337, 45.15624999658601268, 8.311093377946839666 ) ) ;
#55453 = CARTESIAN_POINT ( 'NONE',  ( -11.00000000000000000, 0.000000000000000000, 79.18750000409677625 ) ) ;
#55454 = CARTESIAN_POINT ( 'NONE',  ( -2.445694354108839175, 202.3125000013656063, 144.4456943541088663 ) ) ;
#55455 = CARTESIAN_POINT ( 'NONE',  ( -2.679491924311081963, 261.0416666666666856, 10.00000000000008171 ) ) ;
#55456 = CARTESIAN_POINT ( 'NONE',  ( 3.313708498984762496, 25.03124999590322375, 7.999999999999998224 ) ) ;
#55458 = CARTESIAN_POINT ( 'NONE',  ( 11.35316468750000141, 50.78124999658601268, 0.000000000000000000 ) ) ;
#55457 = CARTESIAN_POINT ( 'NONE',  ( 1.320432766682874540E-15, 97.53125000204838102, 7.188101187500000044 ) ) ;
#55459 = CARTESIAN_POINT ( 'NONE',  ( -7.999999999999991118, 3.313708498984756723, 6.736552779823365533 ) ) ;
#55460 = CARTESIAN_POINT ( 'NONE',  ( -75.00000000000000000, 0.000000000000000000, 42.00000000000002132 ) ) ;
#55461 =( BOUNDED_CURVE ( )  B_SPLINE_CURVE ( 2, ( #464, #41176, #13588, #63806, #12491, #35521, #29855, #52866, #49801 ),
 .UNSPECIFIED., .F., .F. ) 
 B_SPLINE_CURVE_WITH_KNOTS ( ( 3, 2, 2, 2, 3 ),
 ( 0.3382352941176470229, 0.3419117647058823040, 0.3455882352941175850, 0.3492647058823528661, 0.3529411764705882026 ),
 .UNSPECIFIED. ) 
 CURVE ( )  GEOMETRIC_REPRESENTATION_ITEM ( )  RATIONAL_B_SPLINE_CURVE ( ( 1.000000000000001110, 0.9238795325112856283, 1.000000000000000000, 0.9238795325112867385, 1.000000000000000000, 0.9238795325112867385, 1.000000000000000000, 0.9238795325112878487, 0.9999999999999988898 ) ) 
 REPRESENTATION_ITEM ( '' )  );
#55462 = CARTESIAN_POINT ( 'NONE',  ( -2.085542519210945728E-15, 164.5312499965860127, 11.35316468750000141 ) ) ;
#55463 = CIRCLE ( 'NONE', #54213, 10.00000000000000000 ) ;
#55464 = CARTESIAN_POINT ( 'NONE',  ( 10.00000000000000178, 126.8749999931720396, 0.000000000000000000 ) ) ;
#55465 = CARTESIAN_POINT ( 'NONE',  ( 5.082755093536325042, 101.4687500020483810, -5.082755093536325930 ) ) ;
#55466 = CARTESIAN_POINT ( 'NONE',  ( 11.35316468749999785, 35.88541666325268409, 3.042071309553174174 ) ) ;
#55467 = CARTESIAN_POINT ( 'NONE',  ( -2.751064625579944321E-14, 195.8750000027311842, 146.0000000000000284 ) ) ;
#55468 = VERTEX_POINT ( 'NONE', #41533 ) ;
#55469 = CARTESIAN_POINT ( 'NONE',  ( 7.204075437095966983, 7.204075437095967871, 79.09375000204838102 ) ) ;
#55470 = FACE_BOUND ( 'NONE', #56716, .T. ) ;
#55472 = CARTESIAN_POINT ( 'NONE',  ( 6.951808397369818766E-16, 162.0312499965860127, -11.35316468750000141 ) ) ;
#55471 = FACE_OUTER_BOUND ( 'NONE', #21053, .T. ) ;
#55473 = CARTESIAN_POINT ( 'NONE',  ( -27.99999999999999645, 210.0000000000000284, 170.0000000000003695 ) ) ;
#55474 = VECTOR ( 'NONE', #5157, 1000.000000000000000 ) ;
#55475 = CARTESIAN_POINT ( 'NONE',  ( -4.898587196589407898E-16, 7.999999999999991118, 12.51155278432982421 ) ) ;
#55476 = EDGE_CURVE ( 'NONE', #61626, #12433, #13580, .T. ) ;
#55477 = CARTESIAN_POINT ( 'NONE',  ( -21.38761108821279322, -26.62525806848194421, 192.4427279250102458 ) ) ;
#55478 = AXIS2_PLACEMENT_3D ( 'NONE', #27234, #38580, #32549 ) ;
#55479 = CARTESIAN_POINT ( 'NONE',  ( -8.311093377946834337, 234.5312500034139589, 8.311093377946837890 ) ) ;
#55480 = CARTESIAN_POINT ( 'NONE',  ( 7.204075437095966983, 7.204075437095967871, 86.96875000204836681 ) ) ;
#55481 = ORIENTED_EDGE ( 'NONE', *, *, #19554, .F. ) ;
#55482 = FACE_OUTER_BOUND ( 'NONE', #38764, .T. ) ;
#55483 = CYLINDRICAL_SURFACE ( 'NONE', #21895, 3.999999999999976019 ) ;
#55484 = CARTESIAN_POINT ( 'NONE',  ( 5.676582343750001591, 106.9270833299193413, -9.832129032723420536 ) ) ;
#55485 = CARTESIAN_POINT ( 'NONE',  ( -10.18810118749999916, 0.000000000000000000, 97.65625000204838102 ) ) ;
#55486 = CARTESIAN_POINT ( 'NONE',  ( -4.541265875000002339, 19.87499999863441147, -1.881053915767121998 ) ) ;
#55487 = VERTEX_POINT ( 'NONE', #5025 ) ;
#55488 = ORIENTED_EDGE ( 'NONE', *, *, #57616, .T. ) ;
#55489 = CARTESIAN_POINT ( 'NONE',  ( -3.211159895383562723, 5.062499998634407028, 3.211159895383561391 ) ) ;
#55490 = EDGE_CURVE ( 'NONE', #445, #20745, #30333, .T. ) ;
#55491 = CARTESIAN_POINT ( 'NONE',  ( 2.977408999572650927, 11.24999999795161187, -7.188101187500001821 ) ) ;
#55492 = CARTESIAN_POINT ( 'NONE',  ( 5.656854249492381470, 116.7500000040967905, 5.656854249492379694 ) ) ;
#55493 = AXIS2_PLACEMENT_3D ( 'NONE', #695, #30453, #35748 ) ;
#55494 = B_SPLINE_CURVE_WITH_KNOTS ( 'NONE', 3,
 ( #10923, #9811, #73920, #22599, #27520, #62224, #68263, #44511, #67522, #15821, #72811, #51280, #3776, #21118, #33214, #73182, #27897, #44886 ),
 .UNSPECIFIED., .F., .F.,
 ( 4, 2, 2, 2, 2, 2, 2, 2, 4 ),
 ( 0.009384855993314511480, 0.009971557501196359405, 0.01055825900907820733, 0.01114496051696005526, 0.01173166202484190318, 0.01231836353272375284, 0.01290506504060560077, 0.01349176654848744869, 0.01407846805636929662 ),
 .UNSPECIFIED. ) ;
#55495 = CARTESIAN_POINT ( 'NONE',  ( 7.204075437095966983, 7.204075437095967871, 94.46875000204838102 ) ) ;
#55496 = ADVANCED_FACE ( 'NONE', ( #5390 ), #61979, .T. ) ;
#55497 = CARTESIAN_POINT ( 'NONE',  ( -27.99999999999996447, 203.1875000013656063, 173.4587341250003760 ) ) ;
#55498 =( LENGTH_UNIT ( ) NAMED_UNIT ( * ) SI_UNIT ( .MILLI., .METRE. ) );
#55499 = CARTESIAN_POINT ( 'NONE',  ( -7.347880794884122694E-16, 5.750000000000000000, 4.000000000000001776 ) ) ;
#55500 = CARTESIAN_POINT ( 'NONE',  ( -1.656854249492381248, 19.06249999726881228, -4.000000000000001776 ) ) ;
#55501 = CARTESIAN_POINT ( 'NONE',  ( -4.541265875000002339, 7.749999998634407916, -1.881053915767121998 ) ) ;
#55502 = CARTESIAN_POINT ( 'NONE',  ( -2.828427124746208943, 200.6250000000000284, 144.8284271247462129 ) ) ;
#55503 = VERTEX_POINT ( 'NONE', #27644 ) ;
#55504 = CARTESIAN_POINT ( 'NONE',  ( 23.99999999999998224, 207.8125000000000000, 171.6568542494922553 ) ) ;
#55505 = ADVANCED_FACE ( 'NONE', ( #50651 ), #45008, .T. ) ;
#55507 = CARTESIAN_POINT ( 'NONE',  ( -7.999999999999991118, 0.000000000000000000, 17.33030277982336287 ) ) ;
#55506 = CARTESIAN_POINT ( 'NONE',  ( -24.54126587499995793, 197.1250000013656347, 171.4326545832179534 ) ) ;
#55508 = CARTESIAN_POINT ( 'NONE',  ( -1.881053915767124440, 16.99999999863440792, 4.541265875000001451 ) ) ;
#55509 = CIRCLE ( 'NONE', #65126, 9.999999999999998224 ) ;
#55510 = CARTESIAN_POINT ( 'NONE',  ( 3.000000000000000888, -45.19590738606609648, 151.2383369607063344 ) ) ;
#55511 = CARTESIAN_POINT ( 'NONE',  ( 5.082755093536320601, -5.082755093536318824, 8.049052781871752771 ) ) ;
#55512 = ORIENTED_EDGE ( 'NONE', *, *, #72199, .F. ) ;
#55513 = ORIENTED_EDGE ( 'NONE', *, *, #55111, .F. ) ;
#55514 = CARTESIAN_POINT ( 'NONE',  ( -10.18810118749999916, 0.000000000000000000, 99.15625000204838102 ) ) ;
#55515 = CARTESIAN_POINT ( 'NONE',  ( 6.000000000000003553, 288.5625000000000000, -2.485281374238571761 ) ) ;
#55516 = CARTESIAN_POINT ( 'NONE',  ( -24.54126587500000412, 201.5000000013655779, 168.5673454167827003 ) ) ;
#55517 = CARTESIAN_POINT ( 'NONE',  ( -6.735557395310442023E-16, 11.00000000000000000, 110.1249999999999858 ) ) ;
#55518 = CARTESIAN_POINT ( 'NONE',  ( -3.458734124999960358, 208.6875000013656063, 198.0000000000000284 ) ) ;
#55519 = CARTESIAN_POINT ( 'NONE',  ( 1.656854249492371256, 203.4375000027311557, 202.0000000000000000 ) ) ;
#55520 = CARTESIAN_POINT ( 'NONE',  ( 10.00000000000000000, 109.7916666666666572, 2.679491924311236062 ) ) ;
#55521 = VECTOR ( 'NONE', #50366, 1000.000000000000000 ) ;
#55522 = CARTESIAN_POINT ( 'NONE',  ( -8.000000000000000000, 109.9062499999999858, -3.313708498984761608 ) ) ;
#55523 = CARTESIAN_POINT ( 'NONE',  ( 4.721056650416000089, 291.9843750017070079, 4.721056650415999201 ) ) ;
#55524 = AXIS2_PLACEMENT_3D ( 'NONE', #41714, #24358, #25082 ) ;
#55525 = CARTESIAN_POINT ( 'NONE',  ( 5.082755093536318824, 5.082755093536319713, 13.29905278187175277 ) ) ;
#55526 = EDGE_LOOP ( 'NONE', ( #4465, #51776, #48644, #73963 ) ) ;
#55527 = DIRECTION ( 'NONE',  ( 0.000000000000000000, 0.000000000000000000, 1.000000000000000000 ) ) ;
#55529 = EDGE_CURVE ( 'NONE', #2280, #37130, #22341, .T. ) ;
#55528 = CARTESIAN_POINT ( 'NONE',  ( 31.45873412499998523, 205.6250000013656063, 171.4326545832175839 ) ) ;
#55530 = CARTESIAN_POINT ( 'NONE',  ( -5.656854249492379694, 22.87499999590322375, -5.656854249492380582 ) ) ;
#55531 = CARTESIAN_POINT ( 'NONE',  ( -1.432654583217664479, 202.7500000013655779, 138.5412658750000787 ) ) ;
#55532 = CARTESIAN_POINT ( 'NONE',  ( -20.32317157256123608, -34.69963365420603196, 146.4047638185813014 ) ) ;
#55534 = CARTESIAN_POINT ( 'NONE',  ( 1.432654583217607414, 202.5000000013656063, 145.4587341250000634 ) ) ;
#55533 = CARTESIAN_POINT ( 'NONE',  ( -2.775557561562891351E-14, 210.0000000000000284, 142.0000000000000568 ) ) ;
#55535 = CARTESIAN_POINT ( 'NONE',  ( 3.042071309553173286, 255.6770833367473301, 11.35316468749999608 ) ) ;
#55536 = CARTESIAN_POINT ( 'NONE',  ( -4.898587196589412829E-16, 114.3125000040967905, -8.000000000000000000 ) ) ;
#55537 = CARTESIAN_POINT ( 'NONE',  ( -4.999999999999998224, 93.54166665983871098, -8.660254037844389075 ) ) ;
#55538 = CARTESIAN_POINT ( 'NONE',  ( 5.000000000000001776, 225.8333333333333712, -8.660254037844389075 ) ) ;
#55539 = CARTESIAN_POINT ( 'NONE',  ( -5.082755093536319713, 5.082755093536319713, 3.174052781871751439 ) ) ;
#55540 = CARTESIAN_POINT ( 'NONE',  ( 11.35316468749999785, 190.8854166632526983, 3.042071309553174174 ) ) ;
#55541 = CARTESIAN_POINT ( 'NONE',  ( -10.00000000000000178, 134.3749999931720254, -1.224646799147353454E-15 ) ) ;
#55542 = CARTESIAN_POINT ( 'NONE',  ( -3.211159895383561391, 5.687499998634407028, -3.211159895383561835 ) ) ;
#55543 = CARTESIAN_POINT ( 'NONE',  ( -31.99999999999997868, 198.3125000000000284, 171.6568542494928238 ) ) ;
#55544 = CARTESIAN_POINT ( 'NONE',  ( -8.000000000000000000, 107.1875000040967905, 0.000000000000000000 ) ) ;
#55545 = VERTEX_POINT ( 'NONE', #34080 ) ;
#55546 = CARTESIAN_POINT ( 'NONE',  ( -1.432654583217664701, 204.0000000013656347, 138.5412658750000787 ) ) ;
#55547 = CARTESIAN_POINT ( 'NONE',  ( -9.832129032723418760, 7.864583329919350163, -5.676582343750004256 ) ) ;
#55548 = CARTESIAN_POINT ( 'NONE',  ( -11.00000000000000000, 0.000000000000000000, 97.18750000409677625 ) ) ;
#55549 = CARTESIAN_POINT ( 'NONE',  ( 4.000000000000001776, 19.81249999726881228, -1.656854249492381248 ) ) ;
#55550 = CARTESIAN_POINT ( 'NONE',  ( -29.43265458321755546, 200.8750000013656063, 173.4587341250004044 ) ) ;
#55551 = CARTESIAN_POINT ( 'NONE',  ( 0.000000000000000000, 300.0000000000000000, 0.000000000000000000 ) ) ;
#55553 = CARTESIAN_POINT ( 'NONE',  ( -9.832129032723418760, 2.864583329919349719, -5.676582343750004256 ) ) ;
#55552 = CARTESIAN_POINT ( 'NONE',  ( 2.977408999572654480, 120.1250000020484094, 7.188101187499999156 ) ) ;
#55554 = CARTESIAN_POINT ( 'NONE',  ( -3.313708498984757167, 7.999999999999991118, 26.04905277982336997 ) ) ;
#55555 = CARTESIAN_POINT ( 'NONE',  ( -5.676582343750006032, 119.1145833299193697, 9.832129032723418760 ) ) ;
#55556 = CARTESIAN_POINT ( 'NONE',  ( -1.836970198721029983E-15, 85.62499999317203958, 10.00000000000000178 ) ) ;
#55557 = CARTESIAN_POINT ( 'NONE',  ( 1.320432766682874540E-15, 118.9062500020483810, 7.188101187500000044 ) ) ;
#55558 = CARTESIAN_POINT ( 'NONE',  ( 4.541265875000002339, 20.43749999863440436, 0.000000000000000000 ) ) ;
#55559 = CARTESIAN_POINT ( 'NONE',  ( 0.000000000000000000, 75.00000000000000000, 11.00000000000000000 ) ) ;
#55560 = CYLINDRICAL_SURFACE ( 'NONE', #73906, 5.000000000000000888 ) ;
#55561 = VERTEX_POINT ( 'NONE', #9930 ) ;
#55562 = CARTESIAN_POINT ( 'NONE',  ( 3.153939666463620179E-13, 118.7500000000000426, 9.999999999999998224 ) ) ;
#55563 = CARTESIAN_POINT ( 'NONE',  ( -4.088227598258586603E-16, 290.3593750017070079, -6.676582343750001591 ) ) ;
#55564 = CARTESIAN_POINT ( 'NONE',  ( -4.000000000000002665, 12.31249999726881406, 1.656854249492380582 ) ) ;
#55565 = CARTESIAN_POINT ( 'NONE',  ( 7.999999999999992895, -3.313708498984756279, 3.174052783920144893 ) ) ;
#55566 = CARTESIAN_POINT ( 'NONE',  ( 0.000000000000000000, 1.806524977843537691E-16, 0.000000000000000000 ) ) ;
#55567 = CARTESIAN_POINT ( 'NONE',  ( -8.660254037844387298, 208.9583333265053682, -5.000000000000004441 ) ) ;
#55568 = CARTESIAN_POINT ( 'NONE',  ( -4.898587196589412829E-16, 103.6250000000000000, -8.000000000000000000 ) ) ;
#55569 = CARTESIAN_POINT ( 'NONE',  ( 1.871523826299183495E-15, -10.18810118749999916, 102.9062500020483810 ) ) ;
#55570 = ORIENTED_EDGE ( 'NONE', *, *, #45533, .F. ) ;
#55571 = CARTESIAN_POINT ( 'NONE',  ( 5.656854249492378806, 22.12499999590322375, 5.656854249492381470 ) ) ;
#55572 = CARTESIAN_POINT ( 'NONE',  ( -5.676582343750006032, 149.4270833299193555, 9.832129032723418760 ) ) ;
#55573 = CARTESIAN_POINT ( 'NONE',  ( -3.458734124999960358, 205.6875000013656063, 198.0000000000000284 ) ) ;
#55574 = EDGE_CURVE ( 'NONE', #49471, #74050, #11417, .T. ) ;
#55575 = CARTESIAN_POINT ( 'NONE',  ( -3.042071309553164404, 67.55208332991935549, -11.35316468749999963 ) ) ;
#55577 = VERTEX_POINT ( 'NONE', #28022 ) ;
#55576 =( BOUNDED_CURVE ( )  B_SPLINE_CURVE ( 2, ( #61902, #44931, #67938, #16232, #32885 ),
 .UNSPECIFIED., .F., .F. ) 
 B_SPLINE_CURVE_WITH_KNOTS ( ( 3, 2, 3 ),
 ( 0.9871528671839122637, 0.9907407407407406996, 1.000000000000000000 ),
 .UNSPECIFIED. ) 
 CURVE ( )  GEOMETRIC_REPRESENTATION_ITEM ( )  RATIONAL_B_SPLINE_CURVE ( ( 0.9838255637299375689, 0.9867965867025509930, 1.000000000000000000, 0.9659258262890683122, 1.000000000000000000 ) ) 
 REPRESENTATION_ITEM ( '' )  );
#55578 = CARTESIAN_POINT ( 'NONE',  ( -4.220049686691935698, 10.18810118749999916, 115.3750000020483810 ) ) ;
#55579 = CARTESIAN_POINT ( 'NONE',  ( 4.541265875000002339, 9.437499998634407916, 0.000000000000000000 ) ) ;
#55580 = VERTEX_POINT ( 'NONE', #51030 ) ;
#55581 = CARTESIAN_POINT ( 'NONE',  ( -7.188101187500001821, 20.62499999795161543, -2.977408999572651371 ) ) ;
#55582 = CARTESIAN_POINT ( 'NONE',  ( -4.242640687119286547, 289.9375000034140157, -4.242640687119286547 ) ) ;
#55583 = AXIS2_PLACEMENT_3D ( 'NONE', #18246, #41262, #41630 ) ;
#55584 = CARTESIAN_POINT ( 'NONE',  ( -5.000000000000000888, 247.2916666734946318, -8.660254037844387298 ) ) ;
#55585 = CARTESIAN_POINT ( 'NONE',  ( 7.188101187500001821, 17.43749999795161543, -2.977408999572650483 ) ) ;
#55586 = CARTESIAN_POINT ( 'NONE',  ( 7.188101187499992051, 8.802885111219154394E-16, 2.236552781871750550 ) ) ;
#55587 = CARTESIAN_POINT ( 'NONE',  ( 10.18810118750000093, -4.220049686691933921, 110.6875000020483952 ) ) ;
#55588 = EDGE_CURVE ( 'NONE', #19469, #271, #68751, .T. ) ;
#55589 = DIRECTION ( 'NONE',  ( -0.000000000000000000, -1.000000000000000000, -0.000000000000000000 ) ) ;
#55590 = CARTESIAN_POINT ( 'NONE',  ( -2.828427124746190735, 6.124999997268813168, -2.828427124746191623 ) ) ;
#55591 = CARTESIAN_POINT ( 'NONE',  ( -25.17157287525374443, 207.7500000027312126, 172.8284271247464972 ) ) ;
#55592 = CIRCLE ( 'NONE', #11000, 18.00000000000000355 ) ;
#55593 = EDGE_LOOP ( 'NONE', ( #66347, #31262, #39028, #35028 ) ) ;
#55594 = CARTESIAN_POINT ( 'NONE',  ( -3.458734124999959025, 207.5000000013655779, 199.4326545832176691 ) ) ;
#55595 = CARTESIAN_POINT ( 'NONE',  ( -31.45873412499996746, 207.7500000013656063, 171.4326545832181239 ) ) ;
#55596 = CARTESIAN_POINT ( 'NONE',  ( 10.18810118749999916, 1.247682550866122264E-15, 71.78125000204838102 ) ) ;
#55597 = EDGE_CURVE ( 'NONE', #57226, #870, #16681, .T. ) ;
#55598 = CARTESIAN_POINT ( 'NONE',  ( 1.881053915767122664, 5.124999998634406140, 4.541265875000001451 ) ) ;
#55599 = CARTESIAN_POINT ( 'NONE',  ( -3.673940397442060854E-16, 289.7500000000000000, -6.000000000000001776 ) ) ;
#55600 = CARTESIAN_POINT ( 'NONE',  ( -5.082755093536317936, -5.082755093536320601, 27.17405278187175455 ) ) ;
#55601 = ORIENTED_EDGE ( 'NONE', *, *, #6228, .F. ) ;
#55602 = EDGE_CURVE ( 'NONE', #69992, #44702, #56708, .T. ) ;
#55603 = PLANE ( 'NONE',  #61423 ) ;
#55604 = VERTEX_POINT ( 'NONE', #74041 ) ;
#55605 = CARTESIAN_POINT ( 'NONE',  ( -4.220049686691935698, 10.18810118749999916, 116.8750000020483952 ) ) ;
#55606 = CARTESIAN_POINT ( 'NONE',  ( -7.778174593052020747, -7.778174593052023411, 83.87500000409677625 ) ) ;
#55607 = CARTESIAN_POINT ( 'NONE',  ( 2.445694354108838731, 203.0625000013656063, 195.5543056458912190 ) ) ;
#55608 = CARTESIAN_POINT ( 'NONE',  ( 29.43265458321766204, 197.5000000013656063, 173.4587341249998929 ) ) ;
#55609 = CARTESIAN_POINT ( 'NONE',  ( 4.999999999999993783, 69.16666666666667140, 8.660254037844390851 ) ) ;
#55610 = AXIS2_PLACEMENT_3D ( 'NONE', #54053, #19331, #29927 ) ;
#55611 = CARTESIAN_POINT ( 'NONE',  ( 5.082755093536325042, 93.96875000204838102, -5.082755093536325930 ) ) ;
#55612 = CARTESIAN_POINT ( 'NONE',  ( -3.673940397442060854E-16, 292.7500000000000000, -6.000000000000001776 ) ) ;
#55613 = CARTESIAN_POINT ( 'NONE',  ( 0.000000000000000000, 300.0000000000000000, 10.00000000000000178 ) ) ;
#55614 = ORIENTED_EDGE ( 'NONE', *, *, #49615, .F. ) ;
#55615 = CARTESIAN_POINT ( 'NONE',  ( -7.347880794884122694E-16, 3.499999997268812724, 4.000000000000001776 ) ) ;
#55616 = CARTESIAN_POINT ( 'NONE',  ( -4.737866951552680561, -16.26762833211037318, 69.68949229522927169 ) ) ;
#55617 = CARTESIAN_POINT ( 'NONE',  ( 3.999999999999960032, 201.0625000027312126, 143.6568542494924543 ) ) ;
#55618 = DIRECTION ( 'NONE',  ( -0.000000000000000000, -0.000000000000000000, -1.000000000000000000 ) ) ;
#55619 = LINE ( 'NONE', #21264, #48316 ) ;
#55620 = CARTESIAN_POINT ( 'NONE',  ( -8.660254037844387298, 249.5833333333333428, -4.999999999999999112 ) ) ;
#55621 = EDGE_CURVE ( 'NONE', #46612, #20313, #19193, .T. ) ;
#55622 = CARTESIAN_POINT ( 'NONE',  ( -11.00000000000000000, 0.000000000000000000, 107.6875000040967763 ) ) ;
#55623 = CARTESIAN_POINT ( 'NONE',  ( -5.000000000000005329, 193.3333333333333712, 8.660254037844387298 ) ) ;
#55624 = CARTESIAN_POINT ( 'NONE',  ( -3.458734124999959914, 194.5625000013656063, 198.0000000000000284 ) ) ;
#55625 = CARTESIAN_POINT ( 'NONE',  ( -7.188101187499992051, 2.977408999572646930, 24.26780278187175810 ) ) ;
#55626 = CARTESIAN_POINT ( 'NONE',  ( 3.042071309553159519, 160.0520833299193555, 11.35316468750000141 ) ) ;
#55627 = DIRECTION ( 'NONE',  ( 0.000000000000000000, 0.000000000000000000, -1.000000000000000000 ) ) ;
#55628 = CARTESIAN_POINT ( 'NONE',  ( -4.999999999999999112, 51.30314553820166168, 41.49361401976570107 ) ) ;
#55629 = CARTESIAN_POINT ( 'NONE',  ( 2.679491924336306674, 156.0416666666645540, -9.999999999985730526 ) ) ;
#55631 = CARTESIAN_POINT ( 'NONE',  ( -8.000000000000000000, 17.15625000000000000, -3.313708498984762496 ) ) ;
#55630 = CARTESIAN_POINT ( 'NONE',  ( -10.00000000000000178, 84.37499999317203958, -1.224646799147353454E-15 ) ) ;
#55632 = ORIENTED_EDGE ( 'NONE', *, *, #54361, .F. ) ;
#55633 = CARTESIAN_POINT ( 'NONE',  ( -11.35316468750000141, 18.80208332991934839, 3.042071309553159963 ) ) ;
#55634 = VECTOR ( 'NONE', #48457, 1000.000000000000114 ) ;
#55635 = DIRECTION ( 'NONE',  ( 1.000000000000000000, 0.000000000000000000, 0.000000000000000000 ) ) ;
#55637 = CARTESIAN_POINT ( 'NONE',  ( 4.737866951551791495, -16.26762833211076043, -69.68949229522870326 ) ) ;
#55636 = CARTESIAN_POINT ( 'NONE',  ( -3.313708498984759387, -7.999999999999989342, -0.2009472160798553286 ) ) ;
#55638 = CARTESIAN_POINT ( 'NONE',  ( 2.751064625579944321E-14, 195.8750000027311842, 194.0000000000000568 ) ) ;
#55639 = CARTESIAN_POINT ( 'NONE',  ( 3.458734124999959914, 201.3750000013656347, 143.4326545832176976 ) ) ;
#55640 = CARTESIAN_POINT ( 'NONE',  ( 8.660254037844385522, 46.45833332650536818, 5.000000000000005329 ) ) ;
#55641 = AXIS2_PLACEMENT_3D ( 'NONE', #32474, #4542, #50927 ) ;
#55642 = CARTESIAN_POINT ( 'NONE',  ( -2.977408999572650927, 107.3750000020484094, -7.188101187500001821 ) ) ;
#55643 = CARTESIAN_POINT ( 'NONE',  ( 2.780723358947928197E-16, 6.687499998634407028, -4.541265875000002339 ) ) ;
#55644 = CARTESIAN_POINT ( 'NONE',  ( 10.00000000000001421, 220.0000000000000000, 0.000000000000000000 ) ) ;
#55645 = CARTESIAN_POINT ( 'NONE',  ( 7.999999999999991118, 9.797174393178815797E-16, 7.580302779823366421 ) ) ;
#55647 = CARTESIAN_POINT ( 'NONE',  ( -7.999994982332486515, -3.313713516652264435, 20.61155298467860320 ) ) ;
#55646 = CARTESIAN_POINT ( 'NONE',  ( 2.968631558800352455, 194.5024059583199971, 140.1296420989537239 ) ) ;
#55648 = VERTEX_POINT ( 'NONE', #4276 ) ;
#55649 = ORIENTED_EDGE ( 'NONE', *, *, #28766, .T. ) ;
#55650 = CARTESIAN_POINT ( 'NONE',  ( -5.000000000000000000, -68.48952624890536356, 21.22548696402875734 ) ) ;
#55651 = DIRECTION ( 'NONE',  ( 0.000000000000000000, 0.000000000000000000, -1.000000000000000000 ) ) ;
#55652 = CARTESIAN_POINT ( 'NONE',  ( 7.999999999999991118, 9.797174393178815797E-16, 1.580302779823364201 ) ) ;
#55653 = EDGE_CURVE ( 'NONE', #22328, #9782, #12481, .T. ) ;
#55654 = CARTESIAN_POINT ( 'NONE',  ( -25.28356999513048109, -41.40371770032956533, 152.0568237941338907 ) ) ;
#55655 = CARTESIAN_POINT ( 'NONE',  ( -5.676582343749998039, 122.4479166632526983, -9.832129032723420536 ) ) ;
#55656 = ORIENTED_EDGE ( 'NONE', *, *, #45265, .F. ) ;
#55657 = CARTESIAN_POINT ( 'NONE',  ( -5.000000000000000000, 11.32881245867859121, -67.85521288293392672 ) ) ;
#55658 = CARTESIAN_POINT ( 'NONE',  ( 10.18810118750000093, -4.220049686691933921, 89.31250000204838102 ) ) ;
#55659 = CARTESIAN_POINT ( 'NONE',  ( 2.751064625579944321E-14, 207.7500000000000284, 194.0000000000000568 ) ) ;
#55661 = CARTESIAN_POINT ( 'NONE',  ( 11.35316468750000141, 130.7812499965860127, 0.000000000000000000 ) ) ;
#55660 = CARTESIAN_POINT ( 'NONE',  ( -7.999999999999998224, 95.09375000000000000, 3.313708498984766049 ) ) ;
#55662 = EDGE_CURVE ( 'NONE', #16471, #68939, #15327, .T. ) ;
#55663 = CARTESIAN_POINT ( 'NONE',  ( 7.999999999999991118, 9.797174393178815797E-16, 19.58030277982336642 ) ) ;
#55664 = ORIENTED_EDGE ( 'NONE', *, *, #49247, .T. ) ;
#55665 = LINE ( 'NONE', #20934, #58808 ) ;
#55666 = CARTESIAN_POINT ( 'NONE',  ( -30.53930338426081548, 178.2937657132232516, 175.3245609024662315 ) ) ;
#55667 = CARTESIAN_POINT ( 'NONE',  ( 8.311093377946834337, 120.4687499965860269, 8.311093377946839666 ) ) ;
#55668 = CARTESIAN_POINT ( 'NONE',  ( 2.754378923186476579E-14, 207.1875000013656063, 194.5412658750000219 ) ) ;
#55669 = CARTESIAN_POINT ( 'NONE',  ( -7.188101187500002709, 16.68749999795161543, 2.977408999572649151 ) ) ;
#55671 = EDGE_CURVE ( 'NONE', #7527, #1761, #41204, .T. ) ;
#55670 = CARTESIAN_POINT ( 'NONE',  ( 10.18810118749999916, 1.247682550866122264E-15, 83.78125000204838102 ) ) ;
#55672 = CARTESIAN_POINT ( 'NONE',  ( 8.311093377946834337, 25.46874999658601624, 8.311093377946839666 ) ) ;
#55673 = VERTEX_POINT ( 'NONE', #12517 ) ;
#55674 = CARTESIAN_POINT ( 'NONE',  ( -2.828427124746190735, 4.375000000000000000, -2.828427124746191623 ) ) ;
#55675 = CARTESIAN_POINT ( 'NONE',  ( -3.317071493978878571, 8.008118988124991233, 20.23186528394063544 ) ) ;
#55676 = CYLINDRICAL_SURFACE ( 'NONE', #57113, 9.999999999999998224 ) ;
#55677 = VECTOR ( 'NONE', #56498, 1000.000000000000000 ) ;
#55678 = CARTESIAN_POINT ( 'NONE',  ( -2.849036369511732440E-14, 201.2500000000000000, 138.0000000000000568 ) ) ;
#55679 = CARTESIAN_POINT ( 'NONE',  ( -7.188101187500000044, 4.218749997951610986, -8.802885111219163269E-16 ) ) ;
#55680 = CARTESIAN_POINT ( 'NONE',  ( 4.721056650415999201, 290.0781250017069510, -4.721056650415999201 ) ) ;
#55681 = CARTESIAN_POINT ( 'NONE',  ( -49.61047886775524063, 136.4423845261362374, 58.18749371922434932 ) ) ;
#55682 = CARTESIAN_POINT ( 'NONE',  ( -25.17157287525377996, 206.6250000000000284, 172.8284271247465256 ) ) ;
#55683 = ORIENTED_EDGE ( 'NONE', *, *, #46532, .T. ) ;
#55684 = CARTESIAN_POINT ( 'NONE',  ( -8.311093377946836114, 147.9687499965860411, -8.311093377946837890 ) ) ;
#55685 = CARTESIAN_POINT ( 'NONE',  ( 4.220049686691941027, -10.18810118749999738, 78.62500000204838102 ) ) ;
#55686 = EDGE_CURVE ( 'NONE', #70510, #59338, #25470, .T. ) ;
#55687 = CARTESIAN_POINT ( 'NONE',  ( -28.00000000000001776, 195.4375000013655779, 166.5412658750003629 ) ) ;
#55688 = CARTESIAN_POINT ( 'NONE',  ( -4.556349186104045934, 11.00000000000000000, 110.2187499999999858 ) ) ;
#55689 = CARTESIAN_POINT ( 'NONE',  ( -1.881053915767124440, 16.12499999863440792, 4.541265875000001451 ) ) ;
#55690 = VERTEX_POINT ( 'NONE', #64938 ) ;
#55691 = CARTESIAN_POINT ( 'NONE',  ( 4.000000000000015987, 201.6250000027312126, 198.0000000000000284 ) ) ;
#55692 = CARTESIAN_POINT ( 'NONE',  ( -1.432654583217664701, 195.0000000013656063, 138.5412658750000787 ) ) ;
#55694 =( BOUNDED_CURVE ( )  B_SPLINE_CURVE ( 2, ( #2580, #29766, #24094, #47103, #70141, #18448, #41462, #64476, #35805 ),
 .UNSPECIFIED., .F., .F. ) 
 B_SPLINE_CURVE_WITH_KNOTS ( ( 3, 2, 2, 2, 3 ),
 ( 0.9500000000000009548, 0.9583333333333343695, 0.9666666666666675622, 0.9750000000000007550, 0.9833333333333340587 ),
 .UNSPECIFIED. ) 
 CURVE ( )  GEOMETRIC_REPRESENTATION_ITEM ( )  RATIONAL_B_SPLINE_CURVE ( ( 0.9999999999999908962, 0.9238795325112958423, 1.000000000000000000, 0.9238795325112867385, 1.000000000000000000, 0.9238795325112867385, 1.000000000000000000, 0.9238795325112796331, 1.000000000000007105 ) ) 
 REPRESENTATION_ITEM ( '' )  );
#55693 = CARTESIAN_POINT ( 'NONE',  ( -26.34314575050769491, 205.0625000027312126, 166.0000000000003695 ) ) ;
#55695 = CARTESIAN_POINT ( 'NONE',  ( 8.000000000000000000, 6.000000000000000888, 0.000000000000000000 ) ) ;
#55696 = EDGE_LOOP ( 'NONE', ( #6636, #38428, #41491, #36427 ) ) ;
#55697 = CARTESIAN_POINT ( 'NONE',  ( 4.401442555609581635E-16, 9.843749997951610098, -7.188101187500000044 ) ) ;
#55698 = CARTESIAN_POINT ( 'NONE',  ( -6.362988438888832046E-13, 88.74999999999995737, 9.999999999999998224 ) ) ;
#55699 = CARTESIAN_POINT ( 'NONE',  ( -4.556349186104048599, -10.99999999999999822, 73.46875000409677625 ) ) ;
#55700 = CARTESIAN_POINT ( 'NONE',  ( -11.35316468749999785, 183.0729166632526983, -3.042071309553167513 ) ) ;
#55701 = CARTESIAN_POINT ( 'NONE',  ( 2.977408999572654480, 114.5000000020483810, 7.188101187499999156 ) ) ;
#55702 = DIRECTION ( 'NONE',  ( -0.000000000000000000, -1.000000000000000000, -0.000000000000000000 ) ) ;
#55703 = CARTESIAN_POINT ( 'NONE',  ( 2.765530957081996366, 288.1406250017070647, -6.676582343750002480 ) ) ;
#55705 = CARTESIAN_POINT ( 'NONE',  ( 7.320508075688769267, 95.62499999999998579, -7.320508075688769267 ) ) ;
#55704 = CARTESIAN_POINT ( 'NONE',  ( 2.679491924311228956, 132.9166666598386826, -10.00000000000000000 ) ) ;
#55706 = ORIENTED_EDGE ( 'NONE', *, *, #37107, .T. ) ;
#55707 = CARTESIAN_POINT ( 'NONE',  ( 8.311093377946834337, 262.0312500034139589, -8.311093377946836114 ) ) ;
#55708 = VECTOR ( 'NONE', #73100, 1000.000000000000000 ) ;
#55709 = CARTESIAN_POINT ( 'NONE',  ( -5.082755093536317936, -5.082755093536320601, 21.54905278187175455 ) ) ;
#55710 = CARTESIAN_POINT ( 'NONE',  ( 2.449293598294707893E-16, 1.999999997268813168, -4.000000000000001776 ) ) ;
#55711 = CARTESIAN_POINT ( 'NONE',  ( 7.999999999999998224, 19.21874999590322020, 3.313708498984766049 ) ) ;
#55712 = CARTESIAN_POINT ( 'NONE',  ( 2.591411123064221389, -60.37037679142930102, -22.98897912932425314 ) ) ;
#55713 = CARTESIAN_POINT ( 'NONE',  ( 3.458734125000016757, 195.1250000013656063, 199.4326545832176691 ) ) ;
#55714 = DIRECTION ( 'NONE',  ( 0.000000000000000000, 0.000000000000000000, 1.000000000000000000 ) ) ;
#55715 = CARTESIAN_POINT ( 'NONE',  ( -5.499999999999992006, 219.5356836093509685, 9.526279441628830114 ) ) ;
#55716 = CARTESIAN_POINT ( 'NONE',  ( -3.313708498984762496, 93.78125000000000000, 7.999999999999998224 ) ) ;
#55717 = CARTESIAN_POINT ( 'NONE',  ( -3.042071309553164404, 112.5520833299193413, -11.35316468749999963 ) ) ;
#55718 = CARTESIAN_POINT ( 'NONE',  ( 1.469576158976823947E-15, 104.3750000000000000, 8.000000000000000000 ) ) ;
#55719 = CARTESIAN_POINT ( 'NONE',  ( -11.00000000000000000, 0.000000000000000000, 71.49999999999998579 ) ) ;
#55722 = CARTESIAN_POINT ( 'NONE',  ( -7.778174593052023411, 7.778174593052023411, 110.5000000040967763 ) ) ;
#55721 = CARTESIAN_POINT ( 'NONE',  ( 29.43265458321766559, 199.5000000013656063, 173.4587341249998929 ) ) ;
#55720 = CARTESIAN_POINT ( 'NONE',  ( 30.44569435410883074, 197.0625000013656063, 167.5543056458911053 ) ) ;
#55723 = ORIENTED_EDGE ( 'NONE', *, *, #49379, .F. ) ;
#55724 = TOROIDAL_SURFACE ( 'NONE', #65329, 5.000000000000000000, 7.000000000000000000 ) ;
#55725 = CARTESIAN_POINT ( 'NONE',  ( -3.313708498984719864, 19.96874999999999645, -8.000000000000040856 ) ) ;
#55726 = CARTESIAN_POINT ( 'NONE',  ( -3.458734125000015425, 199.0000000013656063, 143.4326545832176976 ) ) ;
#55727 = CARTESIAN_POINT ( 'NONE',  ( 31.45873412499997812, 197.8750000013656063, 171.4326545832175839 ) ) ;
#55728 = CARTESIAN_POINT ( 'NONE',  ( -11.35316468750000141, 213.8020833299193839, 3.042071309553159963 ) ) ;
#55729 = DIRECTION ( 'NONE',  ( 0.000000000000000000, 0.000000000000000000, -1.000000000000000000 ) ) ;
#55730 = CARTESIAN_POINT ( 'NONE',  ( 4.898587196589412829E-16, 3.375000000000000444, -8.000000000000000000 ) ) ;
#55731 = CARTESIAN_POINT ( 'NONE',  ( -3.211159895383561391, 17.68749999863440792, -3.211159895383561835 ) ) ;
#55732 = CARTESIAN_POINT ( 'NONE',  ( 1.781595147087996267, -51.28498669164731183, 48.57279346520238761 ) ) ;
#55733 = CARTESIAN_POINT ( 'NONE',  ( -5.656854249492375253, 5.656854249492375253, 24.64280277982336642 ) ) ;
#55735 = CARTESIAN_POINT ( 'NONE',  ( -31.99999999999996447, 208.4375000027312126, 171.6568542494928522 ) ) ;
#55734 = FILL_AREA_STYLE_COLOUR ( '', #10609 ) ;
#55736 = CARTESIAN_POINT ( 'NONE',  ( -5.676582343750006032, 89.11458332991935549, 9.832129032723418760 ) ) ;
#55737 = VERTEX_POINT ( 'NONE', #70249 ) ;
#55738 = CARTESIAN_POINT ( 'NONE',  ( 26.34314575050760254, 205.0625000027312126, 173.9999999999998863 ) ) ;
#55739 = CARTESIAN_POINT ( 'NONE',  ( 7.188101187499999156, 18.37499999795161187, 2.977408999572654924 ) ) ;
#55740 = CARTESIAN_POINT ( 'NONE',  ( -5.656854249492378806, 108.8750000040967763, 5.656854249492381470 ) ) ;
#55741 = CARTESIAN_POINT ( 'NONE',  ( 11.35316468749999608, 261.9270833367472733, -3.042071309553167513 ) ) ;
#55742 = CARTESIAN_POINT ( 'NONE',  ( -3.042071309553173730, 94.32291666325266988, 11.35316468749999785 ) ) ;
#55743 = ORIENTED_EDGE ( 'NONE', *, *, #72447, .F. ) ;
#55744 = FACE_OUTER_BOUND ( 'NONE', #829, .T. ) ;
#55745 = CARTESIAN_POINT ( 'NONE',  ( 4.220049686691941027, -10.18810118749999738, 108.6250000020483668 ) ) ;
#55746 = CARTESIAN_POINT ( 'NONE',  ( 0.000000000000000000, 300.0000000000000000, 10.00000000000000178 ) ) ;
#55747 = CARTESIAN_POINT ( 'NONE',  ( -3.458734124999960358, 205.6250000013656063, 196.5673454167823877 ) ) ;
#55748 = CARTESIAN_POINT ( 'NONE',  ( 8.000000000000001776, 118.1562500000000000, 3.313708498984759387 ) ) ;
#55750 = CARTESIAN_POINT ( 'NONE',  ( 5.676582343749993598, 89.94791666325269830, 9.832129032723422313 ) ) ;
#55749 = CARTESIAN_POINT ( 'NONE',  ( 0.000000000000000000, 0.000000000000000000, -14.77459999999999951 ) ) ;
#55751 = CARTESIAN_POINT ( 'NONE',  ( -4.898587196589407898E-16, 7.999999999999991118, 20.14280278392014623 ) ) ;
#55752 = CARTESIAN_POINT ( 'NONE',  ( -25.55430564589115150, 200.3125000013656063, 172.4456943541091789 ) ) ;
#55753 = EDGE_CURVE ( 'NONE', #38779, #47140, #69876, .T. ) ;
#55754 = CARTESIAN_POINT ( 'NONE',  ( 4.000000000000015987, 208.6875000027312410, 196.3431457505076594 ) ) ;
#55755 = CARTESIAN_POINT ( 'NONE',  ( -1.836970198721029983E-15, 185.6249999931720538, 10.00000000000000178 ) ) ;
#55756 = CARTESIAN_POINT ( 'NONE',  ( 5.000000000000000000, -53.57153130924498896, 46.19535935661046011 ) ) ;
#55757 = CARTESIAN_POINT ( 'NONE',  ( -9.832129032723418760, 78.17708332991935549, -5.676582343750004256 ) ) ;
#55758 = CARTESIAN_POINT ( 'NONE',  ( -4.088227598258586603E-16, 295.2031250017069510, -6.676582343750001591 ) ) ;
#55760 = EDGE_CURVE ( 'NONE', #53439, #2215, #51487, .T. ) ;
#55759 = CARTESIAN_POINT ( 'NONE',  ( 1.871523826299183495E-15, -10.18810118749999916, 98.40625000204838102 ) ) ;
#55761 = CARTESIAN_POINT ( 'NONE',  ( 11.35316468749999963, 210.9895833299193839, -3.042071309553165293 ) ) ;
#55762 = ORIENTED_EDGE ( 'NONE', *, *, #74133, .F. ) ;
#55763 = DIRECTION ( 'NONE',  ( -0.000000000000000000, 1.000000000000000000, 4.689100369878284071E-30 ) ) ;
#55764 = CARTESIAN_POINT ( 'NONE',  ( 0.1983877408473751491, -42.00000000000002842, 139.0000000000000568 ) ) ;
#55766 = CARTESIAN_POINT ( 'NONE',  ( -5.676582343749998039, 202.4479166632526983, -9.832129032723420536 ) ) ;
#55765 = CARTESIAN_POINT ( 'NONE',  ( -1.656854249492381248, 19.31250000000000000, -4.000000000000001776 ) ) ;
#55767 = CARTESIAN_POINT ( 'NONE',  ( 2.679491924311225848, 226.6666666734946034, -10.00000000000000000 ) ) ;
#55768 = CARTESIAN_POINT ( 'NONE',  ( -5.000000000000000888, 252.2916666734946602, -8.660254037844387298 ) ) ;
#55769 = VERTEX_POINT ( 'NONE', #30245 ) ;
#55770 = CARTESIAN_POINT ( 'NONE',  ( -11.35316468749999785, 198.3854166632526699, -3.042071309553167957 ) ) ;
#55771 = CIRCLE ( 'NONE', #24404, 10.19999999999999396 ) ;
#55772 = CARTESIAN_POINT ( 'NONE',  ( 5.082755093536320601, -5.082755093536318824, 15.54905278187175455 ) ) ;
#55773 = CARTESIAN_POINT ( 'NONE',  ( 5.656854249492380582, 10.68750000000000178, -5.656854249492380582 ) ) ;
#55774 = VERTEX_POINT ( 'NONE', #52894 ) ;
#55775 = AXIS2_PLACEMENT_3D ( 'NONE', #17996, #51577, #58017 ) ;
#55776 = CARTESIAN_POINT ( 'NONE',  ( 3.313708498984765161, 91.15625000409676204, 7.999999999999998224 ) ) ;
#55777 = CARTESIAN_POINT ( 'NONE',  ( -10.00000000000000178, 17.50000000000000000, -1.224646799147353454E-15 ) ) ;
#55778 = CARTESIAN_POINT ( 'NONE',  ( -10.18810118749999916, 4.220049686691934809, 78.43750000204838102 ) ) ;
#55780 = VERTEX_POINT ( 'NONE', #40459 ) ;
#55779 =( BOUNDED_CURVE ( )  B_SPLINE_CURVE ( 2, ( #70006, #54130, #58688, #47708, #70728, #47347, #42418, #42051, #70371 ),
 .UNSPECIFIED., .F., .F. ) 
 B_SPLINE_CURVE_WITH_KNOTS ( ( 3, 2, 2, 2, 3 ),
 ( 0.7187500000000001110, 0.7239583333333334814, 0.7291666666666667407, 0.7343750000000001110, 0.7395833333333334814 ),
 .UNSPECIFIED. ) 
 CURVE ( )  GEOMETRIC_REPRESENTATION_ITEM ( )  RATIONAL_B_SPLINE_CURVE ( ( 0.9999999999999983347, 0.9238795325112884038, 1.000000000000000000, 0.9238795325112867385, 1.000000000000000000, 0.9238795325112867385, 1.000000000000000000, 0.9238795325112850731, 1.000000000000001554 ) ) 
 REPRESENTATION_ITEM ( '' )  );
#55781 = CARTESIAN_POINT ( 'NONE',  ( 1.656854249492381914, 21.81250000000000355, 4.000000000000000888 ) ) ;
#55782 = CARTESIAN_POINT ( 'NONE',  ( -4.541265875000002339, 19.81249999863440436, -5.561446717895856393E-16 ) ) ;
#55783 = CARTESIAN_POINT ( 'NONE',  ( 3.313708498984762496, -7.999999999999989342, 10.48655278392014800 ) ) ;
#55784 = CARTESIAN_POINT ( 'NONE',  ( 31.15206608112011466, 194.6581652650363594, 168.1297425406502271 ) ) ;
#55785 = ORIENTED_EDGE ( 'NONE', *, *, #28999, .T. ) ;
#55786 = CARTESIAN_POINT ( 'NONE',  ( 4.000000000000000888, 4.687499997268813168, 1.656854249492384135 ) ) ;
#55787 = CARTESIAN_POINT ( 'NONE',  ( -7.188101187500000044, 91.15625000204838102, 0.000000000000000000 ) ) ;
#55790 = DIRECTION ( 'NONE',  ( -0.8660254037844381525, 0.5000000000000008882, 0.000000000000000000 ) ) ;
#55789 = CARTESIAN_POINT ( 'NONE',  ( -6.951808397369817780E-16, 262.6562500034140157, -11.35316468749999963 ) ) ;
#55788 = CARTESIAN_POINT ( 'NONE',  ( 7.999999999999991118, 3.313708498984758055, 12.17405277982336642 ) ) ;
#55791 = APPLICATION_PROTOCOL_DEFINITION ( 'draft international standard', 'automotive_design', 1998, #32274 ) ;
#55792 = ORIENTED_EDGE ( 'NONE', *, *, #15942, .T. ) ;
#55793 = CARTESIAN_POINT ( 'NONE',  ( -9.832129032723415207, 259.6354166700806445, 5.676582343750005144 ) ) ;
#55794 = CARTESIAN_POINT ( 'NONE',  ( 1.320432766682872962E-15, -7.188101187499992051, 15.36155278187175277 ) ) ;
#55795 = ORIENTED_EDGE ( 'NONE', *, *, #44504, .T. ) ;
#55796 =( BOUNDED_CURVE ( )  B_SPLINE_CURVE ( 2, ( #65075, #42804, #31875, #37162, #53411, #30757, #71472, #1734, #48840 ),
 .UNSPECIFIED., .F., .F. ) 
 B_SPLINE_CURVE_WITH_KNOTS ( ( 3, 2, 2, 2, 3 ),
 ( 0.2205882352941175018, 0.2242647058823528106, 0.2279411764705880916, 0.2316176470588234004, 0.2352941176470586815 ),
 .UNSPECIFIED. ) 
 CURVE ( )  GEOMETRIC_REPRESENTATION_ITEM ( )  RATIONAL_B_SPLINE_CURVE ( ( 1.000000000000002887, 0.9238795325112838519, 1.000000000000000000, 0.9238795325112867385, 1.000000000000000000, 0.9238795325112867385, 1.000000000000000000, 0.9238795325112896251, 0.9999999999999971134 ) ) 
 REPRESENTATION_ITEM ( '' )  );
#55797 = ORIENTED_EDGE ( 'NONE', *, *, #4109, .F. ) ;
#55798 = CARTESIAN_POINT ( 'NONE',  ( 7.204075437095966983, 7.204075437095967871, 71.59375000204836681 ) ) ;
#55799 = CARTESIAN_POINT ( 'NONE',  ( 8.311093377946837890, 71.71874999658601268, -8.311093377946837890 ) ) ;
#55800 = CARTESIAN_POINT ( 'NONE',  ( 0.000000000000000000, 0.000000000000000000, 41.99999999999999289 ) ) ;
#55801 = CARTESIAN_POINT ( 'NONE',  ( 2.020667218593132706E-15, -11.00000000000000000, 88.37499999999998579 ) ) ;
#55804 = CARTESIAN_POINT ( 'NONE',  ( -6.676582343749999815, 288.6718750017069510, 2.765530957082001251 ) ) ;
#55803 = CARTESIAN_POINT ( 'NONE',  ( 29.65685424949240101, 197.1875000027312694, 173.9999999999999147 ) ) ;
#55802 = CARTESIAN_POINT ( 'NONE',  ( -24.00000000000002842, 205.9375000027312126, 168.3431457505079152 ) ) ;
#55805 = CARTESIAN_POINT ( 'NONE',  ( -11.00000000000000000, 0.000000000000000000, 83.49999999999998579 ) ) ;
#55806 = DIRECTION ( 'NONE',  ( -0.000000000000000000, -0.000000000000000000, 1.000000000000000000 ) ) ;
#55807 = CARTESIAN_POINT ( 'NONE',  ( 2.754378923186476579E-14, 200.4375000013656063, 194.5412658750000219 ) ) ;
#55808 = EDGE_CURVE ( 'NONE', #36810, #73904, #1226, .T. ) ;
#55809 = CARTESIAN_POINT ( 'NONE',  ( 7.999999999999998224, 10.21874999590321842, 3.313708498984766493 ) ) ;
#55810 = EDGE_CURVE ( 'NONE', #46633, #56773, #71724, .T. ) ;
#55811 = VERTEX_POINT ( 'NONE', #57272 ) ;
#55812 = CARTESIAN_POINT ( 'NONE',  ( 25.55430564589115505, 209.5625000013656063, 172.4456943541086957 ) ) ;
#55813 = CARTESIAN_POINT ( 'NONE',  ( -1.320432766682874540E-15, 18.46874999795161187, 7.188101187500000044 ) ) ;
#55814 = CARTESIAN_POINT ( 'NONE',  ( 11.35316468749999963, 166.3020833299193271, -3.042071309553165293 ) ) ;
#55815 = FACE_OUTER_BOUND ( 'NONE', #58665, .T. ) ;
#55816 = CARTESIAN_POINT ( 'NONE',  ( -4.401442555609581635E-16, 104.6562500020483810, -7.188101187500000044 ) ) ;
#55818 = CARTESIAN_POINT ( 'NONE',  ( 0.8912353796322691757, -51.17464048783892139, -48.53058040617464286 ) ) ;
#55817 = FACE_OUTER_BOUND ( 'NONE', #19893, .T. ) ;
#55819 = CARTESIAN_POINT ( 'NONE',  ( 24.54126587500000767, 207.3750000013656063, 168.5673454167822172 ) ) ;
#55820 = CARTESIAN_POINT ( 'NONE',  ( -7.188101187499991163, 2.977408999572646930, 16.76780278187175099 ) ) ;
#55821 = CARTESIAN_POINT ( 'NONE',  ( -2.751064625579944321E-14, 206.8750000027312126, 146.0000000000000284 ) ) ;
#55822 = CARTESIAN_POINT ( 'NONE',  ( -11.35316468750000141, 53.28124999658602690, -1.390361679473963753E-15 ) ) ;
#55823 = DIRECTION ( 'NONE',  ( 0.000000000000000000, 0.000000000000000000, 1.000000000000000000 ) ) ;
#55824 = CARTESIAN_POINT ( 'NONE',  ( 10.00000000000000178, 26.87499999317203603, 0.000000000000000000 ) ) ;
#55825 = CARTESIAN_POINT ( 'NONE',  ( 6.123233995736767268E-16, 91.25000000000001421, -10.00000000000000178 ) ) ;
#55826 = ORIENTED_EDGE ( 'NONE', *, *, #31345, .F. ) ;
#55827 = CARTESIAN_POINT ( 'NONE',  ( 0.000000000000000000, 300.0000000000000000, 10.00000000000000178 ) ) ;
#55828 = VECTOR ( 'NONE', #74394, 1000.000000000000000 ) ;
#55829 = CARTESIAN_POINT ( 'NONE',  ( -1.469576158976823947E-15, 20.43749999590322375, 8.000000000000000000 ) ) ;
#55830 = ADVANCED_FACE ( 'NONE', ( #46677 ), #28958, .F. ) ;
#55831 = CARTESIAN_POINT ( 'NONE',  ( -2.085542519210945728E-15, 49.53124999658601268, 11.35316468750000141 ) ) ;
#55832 = CARTESIAN_POINT ( 'NONE',  ( 4.556349186104051263, -10.99999999999999822, 79.65625000409677625 ) ) ;
#55833 = CARTESIAN_POINT ( 'NONE',  ( 3.458734124999960358, 199.6875000013656063, 142.0000000000000568 ) ) ;
#55834 = CYLINDRICAL_SURFACE ( 'NONE', #13060, 10.00000000000000178 ) ;
#55835 = CARTESIAN_POINT ( 'NONE',  ( -10.00000000000000000, 245.0000000000000284, 0.000000000000000000 ) ) ;
#55837 = CARTESIAN_POINT ( 'NONE',  ( -11.35316468750000141, 43.48958332991934839, 3.042071309553159963 ) ) ;
#55836 = CARTESIAN_POINT ( 'NONE',  ( -4.401442555609581635E-16, 99.78125000204838102, -7.188101187500000044 ) ) ;
#55838 = CARTESIAN_POINT ( 'NONE',  ( 3.313708498984756279, 7.999999999999991118, 10.86155277982336820 ) ) ;
#55839 = CYLINDRICAL_SURFACE ( 'NONE', #74636, 7.999999999999991118 ) ;
#55840 = CARTESIAN_POINT ( 'NONE',  ( 8.311093377946837890, 161.4062499965860411, -8.311093377946837890 ) ) ;
#55841 = CARTESIAN_POINT ( 'NONE',  ( 5.000000000000001776, 142.7083333265053682, -8.660254037844389075 ) ) ;
#55842 = CARTESIAN_POINT ( 'NONE',  ( -5.082755093536325930, 101.8437500020483810, -5.082755093536325930 ) ) ;
#55843 = CARTESIAN_POINT ( 'NONE',  ( 0.000000000000000000, 300.0000000000000000, 0.000000000000000000 ) ) ;
#55844 = CARTESIAN_POINT ( 'NONE',  ( 3.042071309553159519, 40.05208332991935549, 11.35316468750000141 ) ) ;
#55845 = VECTOR ( 'NONE', #57954, 1000.000000000000000 ) ;
#55846 = CARTESIAN_POINT ( 'NONE',  ( -2.679491924311308448, 80.41666665983868256, 9.999999999999957367 ) ) ;
#55847 = EDGE_LOOP ( 'NONE', ( #73892, #67256, #33340, #45589 ) ) ;
#55848 = CARTESIAN_POINT ( 'NONE',  ( 49.36078510129537733, 138.2065558490915009, 58.74518531386929965 ) ) ;
#55849 = CARTESIAN_POINT ( 'NONE',  ( -7.204075437095965206, -7.204075437095968759, 75.34375000204838102 ) ) ;
#55850 = FACE_OUTER_BOUND ( 'NONE', #73962, .T. ) ;
#55852 = CARTESIAN_POINT ( 'NONE',  ( 6.951808397369818766E-16, 167.0312499965860411, -11.35316468750000141 ) ) ;
#55851 = CARTESIAN_POINT ( 'NONE',  ( -1.836970198721029983E-15, 90.62499999317203958, 10.00000000000000178 ) ) ;
#55853 = CARTESIAN_POINT ( 'NONE',  ( -3.313708498984757167, 7.999999999999991118, 12.60530278432982421 ) ) ;
#55854 = CARTESIAN_POINT ( 'NONE',  ( 2.250000000000000444, 278.3999999999996930, 5.425975448606632945 ) ) ;
#55855 = CARTESIAN_POINT ( 'NONE',  ( 3.042071309553173286, 225.3645833367473301, 11.35316468749999608 ) ) ;
#55856 = CARTESIAN_POINT ( 'NONE',  ( 2.620431783921520541, 55.87941608673474292, -43.94382193462354991 ) ) ;
#55857 = EDGE_CURVE ( 'NONE', #10942, #12530, #35741, .T. ) ;
#55858 = CARTESIAN_POINT ( 'NONE',  ( -4.220049686691935698, 10.18810118749999916, 87.25000000204838102 ) ) ;
#55859 = VERTEX_POINT ( 'NONE', #74234 ) ;
#55860 = CARTESIAN_POINT ( 'NONE',  ( -11.00000000000000000, 0.000000000000000000, 89.68750000409677625 ) ) ;
#55861 = CARTESIAN_POINT ( 'NONE',  ( 2.751064625579944321E-14, 203.8750000027312126, 194.0000000000000568 ) ) ;
#55862 = CARTESIAN_POINT ( 'NONE',  ( -3.042071309553164404, 112.5520833299193413, -11.35316468749999963 ) ) ;
#55863 = CARTESIAN_POINT ( 'NONE',  ( 8.660254037844390851, 14.58333333333333925, 5.000000000000009770 ) ) ;
#55864 = ORIENTED_EDGE ( 'NONE', *, *, #473, .F. ) ;
#55865 = ORIENTED_EDGE ( 'NONE', *, *, #70130, .T. ) ;
#55866 = CARTESIAN_POINT ( 'NONE',  ( 3.211159895383561835, 9.562499998634406140, -3.211159895383561835 ) ) ;
#55867 = CARTESIAN_POINT ( 'NONE',  ( -2.977408999572650039, 9.937499997951610098, -7.188101187500001821 ) ) ;
#55868 = CARTESIAN_POINT ( 'NONE',  ( 3.313708498984765161, 110.6562500040967905, 7.999999999999998224 ) ) ;
#55869 = EDGE_CURVE ( 'NONE', #57513, #59211, #53904, .T. ) ;
#55870 = CARTESIAN_POINT ( 'NONE',  ( 4.220049686691934809, 10.18810118749999916, 94.56250000204838102 ) ) ;
#55871 = CARTESIAN_POINT ( 'NONE',  ( -31.45873412499997812, 201.0000000013655779, 171.4326545832180386 ) ) ;
#55872 = CARTESIAN_POINT ( 'NONE',  ( 2.828427124746190291, 2.875000000000000000, 2.828427124746192067 ) ) ;
#55873 = CARTESIAN_POINT ( 'NONE',  ( 4.000000000000001776, 18.81249999726881228, -1.656854249492381248 ) ) ;
#55874 = CARTESIAN_POINT ( 'NONE',  ( -4.541265875000002339, 8.812499998634407916, -5.561446717895856393E-16 ) ) ;
#55875 = CARTESIAN_POINT ( 'NONE',  ( 3.999999999999960032, 203.9375000000000000, 143.6568542494924543 ) ) ;
#55876 = ORIENTED_EDGE ( 'NONE', *, *, #3880, .F. ) ;
#55877 = CARTESIAN_POINT ( 'NONE',  ( -3.313708498984757611, 7.999999999999991118, 9.736552783920146226 ) ) ;
#55878 = PRODUCT_DEFINITION_CONTEXT ( 'detailed design', #64107, 'design' ) ;
#55880 = CARTESIAN_POINT ( 'NONE',  ( 10.00000000000000000, 235.6250000068279746, -1.224646799147353256E-15 ) ) ;
#55879 = CARTESIAN_POINT ( 'NONE',  ( -29.43265458321755546, 195.8750000013655779, 173.4587341250004044 ) ) ;
#55881 = CARTESIAN_POINT ( 'NONE',  ( 1.881053915767122664, 20.12499999863441147, 4.541265875000001451 ) ) ;
#55882 = DIRECTION ( 'NONE',  ( 0.000000000000000000, 0.000000000000000000, 1.000000000000000000 ) ) ;
#55883 = CARTESIAN_POINT ( 'NONE',  ( 7.188101187499991163, 2.977408999572648707, 0.8303027818717529929 ) ) ;
#55884 = ORIENTED_EDGE ( 'NONE', *, *, #38998, .F. ) ;
#55885 = VERTEX_POINT ( 'NONE', #45938 ) ;
#55886 = CARTESIAN_POINT ( 'NONE',  ( 10.18810118749999916, 4.220049686691935698, 89.50000000204836681 ) ) ;
#55887 = CARTESIAN_POINT ( 'NONE',  ( 5.656854249492379694, 91.62500000409677625, -5.656854249492380582 ) ) ;
#55888 = CARTESIAN_POINT ( 'NONE',  ( -25.55430564589115150, 201.3125000013656063, 172.4456943541091789 ) ) ;
#55889 = CARTESIAN_POINT ( 'NONE',  ( 7.778174593052023411, -7.778174593052021635, 106.5624999999999858 ) ) ;
#55890 = CARTESIAN_POINT ( 'NONE',  ( 2.839093476692135984E-14, 205.9375000013656063, 201.4587341250000350 ) ) ;
#55891 = LINE ( 'NONE', #4205, #38606 ) ;
#55892 = CARTESIAN_POINT ( 'NONE',  ( 2.679491924311222739, 118.9583333333333428, 10.00000000000000355 ) ) ;
#55893 = EDGE_CURVE ( 'NONE', #52001, #17336, #38501, .T. ) ;
#55894 = CARTESIAN_POINT ( 'NONE',  ( 1.469576158976823947E-15, 107.3750000000000000, 8.000000000000000000 ) ) ;
#55895 = CARTESIAN_POINT ( 'NONE',  ( -6.676582343750003368, 290.5468750017071216, -2.765530957081996810 ) ) ;
#55896 = CARTESIAN_POINT ( 'NONE',  ( 5.082755093536318824, 5.082755093536319713, 10.29905278187175455 ) ) ;
#55897 = ORIENTED_EDGE ( 'NONE', *, *, #35227, .T. ) ;
#55898 =( BOUNDED_CURVE ( )  B_SPLINE_CURVE ( 2, ( #24849, #12797, #12430, #35830, #36563, #48238, #59578, #30532, #25594 ),
 .UNSPECIFIED., .F., .F. ) 
 B_SPLINE_CURVE_WITH_KNOTS ( ( 3, 2, 2, 2, 3 ),
 ( 0.8645833333333335924, 0.8697916666666668517, 0.8750000000000002220, 0.8802083333333337034, 0.8854166666666669627 ),
 .UNSPECIFIED. ) 
 CURVE ( )  GEOMETRIC_REPRESENTATION_ITEM ( )  RATIONAL_B_SPLINE_CURVE ( ( 0.9999999999999967804, 0.9238795325112899581, 1.000000000000000000, 0.9238795325112867385, 1.000000000000000000, 0.9238795325112867385, 1.000000000000000000, 0.9238795325112818535, 1.000000000000004885 ) ) 
 REPRESENTATION_ITEM ( '' )  );
#55899 = CARTESIAN_POINT ( 'NONE',  ( -5.656854249492378806, 102.8750000040967763, 5.656854249492381470 ) ) ;
#55900 = EDGE_CURVE ( 'NONE', #327, #8398, #866, .T. ) ;
#55901 = CARTESIAN_POINT ( 'NONE',  ( 29.43265458321766559, 208.8750000013656347, 166.5412658749999650 ) ) ;
#55902 = CARTESIAN_POINT ( 'NONE',  ( -1.469576158976823947E-15, 18.93749999590322020, 8.000000000000000000 ) ) ;
#55903 = VECTOR ( 'NONE', #40547, 1000.000000000000000 ) ;
#55904 = CARTESIAN_POINT ( 'NONE',  ( 3.458734124999959914, 199.4375000013655779, 142.0000000000000568 ) ) ;
#55905 = CARTESIAN_POINT ( 'NONE',  ( 5.082755093536325042, 119.4687500020483810, -5.082755093536325930 ) ) ;
#55907 = CARTESIAN_POINT ( 'NONE',  ( 2.445694354108783219, 202.8125000013656063, 139.5543056458912190 ) ) ;
#55906 = CARTESIAN_POINT ( 'NONE',  ( 2.828427073549516724, 195.0000000000000284, 144.8284271759428634 ) ) ;
#55908 = CARTESIAN_POINT ( 'NONE',  ( -3.042071309553159075, 260.2604166700805877, 11.35316468749999963 ) ) ;
#55909 = DIRECTION ( 'NONE',  ( -0.000000000000000000, 1.000000000000000000, -1.563033456626094573E-30 ) ) ;
#55910 = CARTESIAN_POINT ( 'NONE',  ( -10.00000000000000355, 214.5833333265053682, 2.679491924311223183 ) ) ;
#55911 = CARTESIAN_POINT ( 'NONE',  ( -5.000000000000005329, 223.3333333333333428, 8.660254037844387298 ) ) ;
#55912 = CARTESIAN_POINT ( 'NONE',  ( 10.00000000000000000, 0.2083333333333323989, -2.679491924311226736 ) ) ;
#55913 = CARTESIAN_POINT ( 'NONE',  ( -9.832129032723418760, 213.1770833299193555, -5.676582343750004256 ) ) ;
#55914 = CARTESIAN_POINT ( 'NONE',  ( -10.00000000000000355, 134.5833333265053682, 2.679491924311223183 ) ) ;
#55915 = CARTESIAN_POINT ( 'NONE',  ( -3.211159895383561391, 7.687499998634407028, -3.211159895383561835 ) ) ;
#55916 = CARTESIAN_POINT ( 'NONE',  ( 4.242640687119287435, 290.3750000000000000, 4.242640687119285658 ) ) ;
#55918 = CARTESIAN_POINT ( 'NONE',  ( -4.000000000000015987, 206.5625000000000000, 143.6568542494924259 ) ) ;
#55917 = CARTESIAN_POINT ( 'NONE',  ( 3.999999999999960032, 203.1250000027312126, 142.0000000000000568 ) ) ;
#55919 = EDGE_LOOP ( 'NONE', ( #38412, #56519, #51099, #3213 ) ) ;
#55921 = EDGE_CURVE ( 'NONE', #15853, #44362, #73481, .T. ) ;
#55920 = CARTESIAN_POINT ( 'NONE',  ( -1.432654583217664701, 202.0000000013656063, 138.5412658750000787 ) ) ;
#55922 = EDGE_CURVE ( 'NONE', #31066, #64829, #61617, .T. ) ;
#55923 = CARTESIAN_POINT ( 'NONE',  ( 5.676582343750001591, 11.61458332991935016, -9.832129032723420536 ) ) ;
#55924 = CARTESIAN_POINT ( 'NONE',  ( -7.778174593052020747, -7.778174593052023411, 95.87500000409676204 ) ) ;
#55925 = CARTESIAN_POINT ( 'NONE',  ( -2.828427124746209831, 205.3750000000000284, 139.1715728752538723 ) ) ;
#55926 = CARTESIAN_POINT ( 'NONE',  ( -30.44569435410886626, 196.5625000013656063, 167.5543056458916169 ) ) ;
#55927 = CARTESIAN_POINT ( 'NONE',  ( 7.778174593052021635, 7.778174593052023411, 117.4375000000000000 ) ) ;
#55929 = CARTESIAN_POINT ( 'NONE',  ( 5.676582343750001591, 1.614583329919349497, -9.832129032723420536 ) ) ;
#55928 = CARTESIAN_POINT ( 'NONE',  ( 1.320432766682874540E-15, 117.0312500020483810, 7.188101187500000044 ) ) ;
#55930 = CARTESIAN_POINT ( 'NONE',  ( -5.676582343749998039, 117.4479166632526841, -9.832129032723420536 ) ) ;
#55931 = EDGE_CURVE ( 'NONE', #15493, #16375, #48160, .T. ) ;
#55932 = CARTESIAN_POINT ( 'NONE',  ( -10.00000000000000355, 99.58333332650538239, 2.679491924311223183 ) ) ;
#55933 = CARTESIAN_POINT ( 'NONE',  ( 2.977408999572654480, 119.0000000020483810, 7.188101187499999156 ) ) ;
#55934 = CARTESIAN_POINT ( 'NONE',  ( 1.881053915767122664, 21.24999999863440436, 4.541265875000001451 ) ) ;
#55935 = CARTESIAN_POINT ( 'NONE',  ( 0.000000000000000000, 125.0000000000000000, 0.000000000000000000 ) ) ;
#55936 = CARTESIAN_POINT ( 'NONE',  ( -10.00000000000000000, 39.16666665983869677, -2.679491924311229845 ) ) ;
#55937 = ORIENTED_EDGE ( 'NONE', *, *, #65254, .T. ) ;
#55938 = CARTESIAN_POINT ( 'NONE',  ( 2.589639417652957132, -60.37884160280833612, 22.99414321703618924 ) ) ;
#55939 = CARTESIAN_POINT ( 'NONE',  ( -6.676582343750003368, 289.5468750017069510, -2.765530957081996810 ) ) ;
#55940 = CARTESIAN_POINT ( 'NONE',  ( 4.999999999999998224, 53.32026166094831154, 44.27875806162001027 ) ) ;
#55941 = CARTESIAN_POINT ( 'NONE',  ( -6.062585341144163031, -5.219679969245603957, -0.3118202219565458511 ) ) ;
#55942 = CIRCLE ( 'NONE', #13714, 17.50000000000000000 ) ;
#55943 = DIRECTION ( 'NONE',  ( -1.000000000000000000, 0.000000000000000000, -1.652117596168387509E-16 ) ) ;
#55944 = CARTESIAN_POINT ( 'NONE',  ( -3.042071309553159075, 254.9479166700806729, 11.35316468749999963 ) ) ;
#55945 = EDGE_CURVE ( 'NONE', #33430, #25548, #20178, .T. ) ;
#55946 = CARTESIAN_POINT ( 'NONE',  ( -7.204075437095967871, 7.204075437095967871, 100.8437500020483668 ) ) ;
#55947 = VERTEX_POINT ( 'NONE', #9190 ) ;
#55948 = CARTESIAN_POINT ( 'NONE',  ( 0.000000000000000000, 0.000000000000000000, 0.000000000000000000 ) ) ;
#55949 = CARTESIAN_POINT ( 'NONE',  ( -3.042071309553163960, 152.5520833299193555, -11.35316468749999963 ) ) ;
#55950 = DIRECTION ( 'NONE',  ( 0.000000000000000000, 0.000000000000000000, -1.000000000000000000 ) ) ;
#55951 = CARTESIAN_POINT ( 'NONE',  ( 2.445694354108840063, 204.0625000013656063, 200.4456943541088663 ) ) ;
#55952 = CARTESIAN_POINT ( 'NONE',  ( 7.320508075688771044, 231.2500000068279746, -7.320508075688771932 ) ) ;
#55953 = CARTESIAN_POINT ( 'NONE',  ( 8.311093377946837890, 76.71874999658599847, -8.311093377946837890 ) ) ;
#55954 = ORIENTED_EDGE ( 'NONE', *, *, #67737, .F. ) ;
#55955 = CARTESIAN_POINT ( 'NONE',  ( -4.220049686691937474, -10.18810118749999738, 115.9375000020483668 ) ) ;
#55956 = CARTESIAN_POINT ( 'NONE',  ( -4.541265875000002339, 9.874999998634404363, -1.881053915767121998 ) ) ;
#55957 = ORIENTED_EDGE ( 'NONE', *, *, #49537, .T. ) ;
#55958 = CARTESIAN_POINT ( 'NONE',  ( -8.000000000000000000, 0.7500000000000000000, -9.797174393178825657E-16 ) ) ;
#55959 = CARTESIAN_POINT ( 'NONE',  ( -2.485281374238572649, 288.2500000034140726, 6.000000000000002665 ) ) ;
#55960 = CARTESIAN_POINT ( 'NONE',  ( -2.775557561562891351E-14, 210.0000000000000284, 142.0000000000000568 ) ) ;
#55961 = CARTESIAN_POINT ( 'NONE',  ( 2.977408999572651815, 18.56249999795161187, 7.188101187500000933 ) ) ;
#55962 = DIRECTION ( 'NONE',  ( 0.000000000000000000, 0.000000000000000000, 1.000000000000000000 ) ) ;
#55963 = CARTESIAN_POINT ( 'NONE',  ( 10.18810118750000093, -4.220049686691933921, 109.1875000020483810 ) ) ;
#55964 = AXIS2_PLACEMENT_3D ( 'NONE', #31355, #32112, #2692 ) ;
#55965 = CARTESIAN_POINT ( 'NONE',  ( 2.846263374404472746, -44.03201140620412701, 151.2142471918900810 ) ) ;
#55966 = CARTESIAN_POINT ( 'NONE',  ( 2.828427124746191623, 6.874999997268813168, -2.828427124746191623 ) ) ;
#55967 = CARTESIAN_POINT ( 'NONE',  ( 7.347880794884121708E-16, 300.0000000000000000, -6.000000000000001776 ) ) ;
#55968 = ORIENTED_EDGE ( 'NONE', *, *, #35527, .F. ) ;
#55969 = CARTESIAN_POINT ( 'NONE',  ( 3.458734125000015425, 203.0000000013655779, 196.5673454167823877 ) ) ;
#55970 = CARTESIAN_POINT ( 'NONE',  ( -30.82842712474624136, 194.2500000027312126, 167.1715728752542418 ) ) ;
#55971 = CARTESIAN_POINT ( 'NONE',  ( 10.18810118749999916, 4.220049686691935698, 70.37500000204838102 ) ) ;
#55972 = CARTESIAN_POINT ( 'NONE',  ( -3.211159895383561391, 5.687499998634407028, -3.211159895383561835 ) ) ;
#55973 = CARTESIAN_POINT ( 'NONE',  ( 3.313708498984762496, -7.999999999999989342, 10.29905277982336465 ) ) ;
#55974 = CARTESIAN_POINT ( 'NONE',  ( 1.320432766682872962E-15, -7.188101187499992051, 22.86155278187175455 ) ) ;
#55975 = ORIENTED_EDGE ( 'NONE', *, *, #65954, .T. ) ;
#55976 = CARTESIAN_POINT ( 'NONE',  ( -11.00000000000000000, 0.000000000000000000, 91.00000000000000000 ) ) ;
#55977 = ORIENTED_EDGE ( 'NONE', *, *, #3790, .F. ) ;
#55978 = DIRECTION ( 'NONE',  ( 0.000000000000000000, 0.000000000000000000, -1.000000000000000000 ) ) ;
#55979 = LINE ( 'NONE', #16693, #28003 ) ;
#55980 = CARTESIAN_POINT ( 'NONE',  ( -2.445694354108783664, 205.3125000013656063, 195.5543056458912190 ) ) ;
#55981 = CARTESIAN_POINT ( 'NONE',  ( 30.44569435410883074, 199.5625000013656063, 172.4456943541086957 ) ) ;
#55982 = CARTESIAN_POINT ( 'NONE',  ( -2.679491924311225848, 71.45833333333332860, -10.00000000000000178 ) ) ;
#55983 = EDGE_CURVE ( 'NONE', #16346, #46633, #61246, .T. ) ;
#55984 = CARTESIAN_POINT ( 'NONE',  ( -5.656854249492378806, 122.1875000000000000, 5.656854249492381470 ) ) ;
#55985 = CARTESIAN_POINT ( 'NONE',  ( -4.242640687119286547, 292.8750000000000000, -4.242640687119286547 ) ) ;
#55986 = CARTESIAN_POINT ( 'NONE',  ( 25.17157287525381903, 204.0000000027312126, 172.8284271247460993 ) ) ;
#55987 = ORIENTED_EDGE ( 'NONE', *, *, #2757, .F. ) ;
#55988 = CARTESIAN_POINT ( 'NONE',  ( -11.35316468749999608, 219.1145833367473017, 3.042071309553173730 ) ) ;
#55989 = FACE_OUTER_BOUND ( 'NONE', #73429, .T. ) ;
#55990 = CARTESIAN_POINT ( 'NONE',  ( -2.751064625579944321E-14, 197.8750000027312126, 146.0000000000000284 ) ) ;
#55991 = CARTESIAN_POINT ( 'NONE',  ( -3.313708498984760276, 22.96875000000000355, -8.000000000000000000 ) ) ;
#55992 = CARTESIAN_POINT ( 'NONE',  ( 10.00000000000000000, 247.5000000000000000, -1.224646799147353256E-15 ) ) ;
#55993 = CARTESIAN_POINT ( 'NONE',  ( 30.82842712474616675, 203.5000000027312126, 167.1715728752537018 ) ) ;
#55994 = CARTESIAN_POINT ( 'NONE',  ( -10.00000000000000355, 192.7083333333333428, 2.679491924311223183 ) ) ;
#55995 = LINE ( 'NONE', #32616, #22323 ) ;
#55996 = CARTESIAN_POINT ( 'NONE',  ( -2.977408999572647819, 7.188101187499992051, 21.08030278187175810 ) ) ;
#55997 = CARTESIAN_POINT ( 'NONE',  ( 5.676582343749993598, 170.2604166632526983, 9.832129032723422313 ) ) ;
#55998 = CYLINDRICAL_SURFACE ( 'NONE', #45747, 4.000000000000001776 ) ;
#55999 = CARTESIAN_POINT ( 'NONE',  ( -5.000000000000000888, 53.09993190648213357, 43.73864582539290780 ) ) ;
#56000 = CARTESIAN_POINT ( 'NONE',  ( 0.000000000000000000, 75.00000000000000000, 0.000000000000000000 ) ) ;
#56002 = CARTESIAN_POINT ( 'NONE',  ( -3.313708498984719864, 16.96874999999999289, -8.000000000000040856 ) ) ;
#56001 = CARTESIAN_POINT ( 'NONE',  ( 0.000000000000000000, 300.0000000000000000, 0.000000000000000000 ) ) ;
#56003 = ORIENTED_EDGE ( 'NONE', *, *, #34726, .F. ) ;
#56004 = CARTESIAN_POINT ( 'NONE',  ( -5.676582343750006032, 29.42708332991935194, 9.832129032723418760 ) ) ;
#56005 = AXIS2_PLACEMENT_3D ( 'NONE', #31769, #54788, #24609 ) ;
#56006 = FACE_BOUND ( 'NONE', #1266, .T. ) ;
#56008 = CARTESIAN_POINT ( 'NONE',  ( -6.308070865131614191, -10.25011764679139503, -64.85270989089528371 ) ) ;
#56007 = CARTESIAN_POINT ( 'NONE',  ( 2.751064625579944321E-14, 200.8750000027312126, 194.0000000000000568 ) ) ;
#56009 = CARTESIAN_POINT ( 'NONE',  ( -17.05177509603550590, -46.35863725427757487, 195.9004682482653266 ) ) ;
#56010 = CARTESIAN_POINT ( 'NONE',  ( 2.445694354108783664, 201.3125000013656063, 144.4456943541088663 ) ) ;
#56011 = EDGE_CURVE ( 'NONE', #55859, #55811, #27915, .T. ) ;
#56012 = CARTESIAN_POINT ( 'NONE',  ( -2.679491924311225848, 53.33333332650536107, -10.00000000000000178 ) ) ;
#56013 = CARTESIAN_POINT ( 'NONE',  ( -7.188101187500000044, 101.6562500020483810, 0.000000000000000000 ) ) ;
#56014 = CARTESIAN_POINT ( 'NONE',  ( 4.541265875000002339, 8.499999998634406140, -1.881053915767121554 ) ) ;
#56015 = CARTESIAN_POINT ( 'NONE',  ( 5.000000000000007994, 220.8333333333333428, -8.660254037844397956 ) ) ;
#56016 = CARTESIAN_POINT ( 'NONE',  ( 7.999999999999991118, 3.313708498984757611, 7.674052779823366421 ) ) ;
#56017 = CARTESIAN_POINT ( 'NONE',  ( -4.000000000000002665, 5.312499997268812280, 1.656854249492380582 ) ) ;
#56018 = ORIENTED_EDGE ( 'NONE', *, *, #64580, .F. ) ;
#56019 = EDGE_LOOP ( 'NONE', ( #46992, #60190, #8547, #49344 ) ) ;
#56020 =( BOUNDED_CURVE ( )  B_SPLINE_CURVE ( 2, ( #33313, #50265, #56311, #68366, #22325, #62695, #5372, #11032, #67994 ),
 .UNSPECIFIED., .F., .F. ) 
 B_SPLINE_CURVE_WITH_KNOTS ( ( 3, 2, 2, 2, 3 ),
 ( 0.1578947368421052821, 0.1644736842105263552, 0.1710526315789474006, 0.1776315789473684459, 0.1842105263157894912 ),
 .UNSPECIFIED. ) 
 CURVE ( )  GEOMETRIC_REPRESENTATION_ITEM ( )  RATIONAL_B_SPLINE_CURVE ( ( 0.9999999999999996669, 0.9238795325112870716, 1.000000000000000000, 0.9238795325112867385, 1.000000000000000000, 0.9238795325112867385, 1.000000000000000000, 0.9238795325112864054, 1.000000000000000222 ) ) 
 REPRESENTATION_ITEM ( '' )  );
#56021 =( BOUNDED_CURVE ( )  B_SPLINE_CURVE ( 2, ( #1158, #59592, #53931, #47515, #24511, #24866, #70180, #65611, #35847 ),
 .UNSPECIFIED., .F., .F. ) 
 B_SPLINE_CURVE_WITH_KNOTS ( ( 3, 2, 2, 2, 3 ),
 ( 0.01136363636363636395, 0.01704545454545454419, 0.02272727272727272790, 0.02840909090909090814, 0.03409090909090908839 ),
 .UNSPECIFIED. ) 
 CURVE ( )  GEOMETRIC_REPRESENTATION_ITEM ( )  RATIONAL_B_SPLINE_CURVE ( ( 1.000000000000000000, 0.9238795325112867385, 1.000000000000000000, 0.9238795325112867385, 1.000000000000000000, 0.9238795325112867385, 1.000000000000000000, 0.9238795325112867385, 1.000000000000000000 ) ) 
 REPRESENTATION_ITEM ( '' )  );
#56022 = CARTESIAN_POINT ( 'NONE',  ( -5.000000000000000000, -67.10422270468713180, 23.07049055144742766 ) ) ;
#56023 = DIRECTION ( 'NONE',  ( 1.000000000000000000, 0.000000000000000000, -0.000000000000000000 ) ) ;
#56024 = CARTESIAN_POINT ( 'NONE',  ( -4.898587196589407898E-16, 7.999999999999991118, 1.955302779823364645 ) ) ;
#56025 = CARTESIAN_POINT ( 'NONE',  ( -6.735557395310442023E-16, 11.00000000000000000, 95.12499999999998579 ) ) ;
#56026 = CARTESIAN_POINT ( 'NONE',  ( -8.311093377946841443, 143.9062499965860127, 8.311093377946830785 ) ) ;
#56027 = ORIENTED_EDGE ( 'NONE', *, *, #46091, .F. ) ;
#56028 = PLANE ( 'NONE',  #15042 ) ;
#56029 = CARTESIAN_POINT ( 'NONE',  ( -10.18810118749999916, 4.220049686691934809, 88.56250000204836681 ) ) ;
#56030 = CARTESIAN_POINT ( 'NONE',  ( -7.999999999999991118, 3.313708498984757167, 20.42405278392015333 ) ) ;
#56031 = CARTESIAN_POINT ( 'NONE',  ( -3.999999999999960032, 208.9375000000000284, 196.3431457505076594 ) ) ;
#56033 = CARTESIAN_POINT ( 'NONE',  ( 8.311093377946834337, 125.1562499965860269, 8.311093377946839666 ) ) ;
#56032 = CARTESIAN_POINT ( 'NONE',  ( -2.849036369511732440E-14, 195.2500000000000000, 138.0000000000000568 ) ) ;
#56034 = EDGE_CURVE ( 'NONE', #73747, #9554, #37494, .T. ) ;
#56035 = DIRECTION ( 'NONE',  ( -0.000000000000000000, 1.000000000000000000, -0.000000000000000000 ) ) ;
#56036 = ORIENTED_EDGE ( 'NONE', *, *, #16314, .F. ) ;
#56037 = ADVANCED_FACE ( 'NONE', ( #60495 ), #55603, .T. ) ;
#56038 = CARTESIAN_POINT ( 'NONE',  ( 4.999999999999997335, 258.3333333333333712, -8.660254037844387298 ) ) ;
#56039 = CARTESIAN_POINT ( 'NONE',  ( 11.35316468750000141, 111.0937499965860127, 0.000000000000000000 ) ) ;
#56040 = CARTESIAN_POINT ( 'NONE',  ( -3.458734124999959914, 202.3750000013656063, 196.5673454167823877 ) ) ;
#56041 = CARTESIAN_POINT ( 'NONE',  ( 2.977408999572650927, 16.12499999795161543, -7.188101187500000933 ) ) ;
#56042 = CARTESIAN_POINT ( 'NONE',  ( -7.204075437095965206, -7.204075437095968759, 83.21875000204836681 ) ) ;
#56043 = CARTESIAN_POINT ( 'NONE',  ( -8.311093377946836114, 32.96874999658600558, -8.311093377946837890 ) ) ;
#56044 = ORIENTED_EDGE ( 'NONE', *, *, #1830, .F. ) ;
#56045 = CARTESIAN_POINT ( 'NONE',  ( 5.656854249492379694, 90.12500000409677625, -5.656854249492380582 ) ) ;
#56046 = CARTESIAN_POINT ( 'NONE',  ( 3.317071493978877683, 8.008118988124991233, 18.54436528394063188 ) ) ;
#56047 = CARTESIAN_POINT ( 'NONE',  ( 10.00000000000000178, 237.2916666666666288, 2.679491924311222739 ) ) ;
#56048 = DIRECTION ( 'NONE',  ( -1.000000000000000000, 0.000000000000000000, 0.000000000000000000 ) ) ;
#56049 = CARTESIAN_POINT ( 'NONE',  ( 7.188101187500001821, 5.062499997951610098, -2.977408999572650483 ) ) ;
#56050 = CARTESIAN_POINT ( 'NONE',  ( 1.226468279477575784E-15, 287.7031250017069510, 6.676582343750001591 ) ) ;
#56051 = CARTESIAN_POINT ( 'NONE',  ( 1.469576158976823947E-15, 98.37499999999998579, 8.000000000000000000 ) ) ;
#56052 = CARTESIAN_POINT ( 'NONE',  ( -1.469576158976823947E-15, 17.43749999590322375, 8.000000000000000000 ) ) ;
#56053 = VERTEX_POINT ( 'NONE', #38986 ) ;
#56054 = CARTESIAN_POINT ( 'NONE',  ( 11.35316468750000141, 141.0937499965860127, 0.000000000000000000 ) ) ;
#56055 = CARTESIAN_POINT ( 'NONE',  ( 4.220049686691934809, 10.18810118749999916, 77.68750000204838102 ) ) ;
#56056 = EDGE_CURVE ( 'NONE', #44513, #14535, #54852, .T. ) ;
#56057 = CARTESIAN_POINT ( 'NONE',  ( -26.56734541678232731, 209.2500000013655779, 173.4587341250003760 ) ) ;
#56058 = CARTESIAN_POINT ( 'NONE',  ( 7.999999999999991118, 9.797174393178815797E-16, 21.08030277982336642 ) ) ;
#56059 = CARTESIAN_POINT ( 'NONE',  ( 1.881053915767122664, 17.24999999863440792, 4.541265875000001451 ) ) ;
#56060 = VERTEX_POINT ( 'NONE', #67658 ) ;
#56061 = CARTESIAN_POINT ( 'NONE',  ( 2.828427124746208943, 204.7500000027312126, 195.1715728752538439 ) ) ;
#56062 = VECTOR ( 'NONE', #45152, 1000.000000000000227 ) ;
#56063 = CARTESIAN_POINT ( 'NONE',  ( 3.999999999999960032, 209.0000000000000284, 142.0000000000000568 ) ) ;
#56064 = CARTESIAN_POINT ( 'NONE',  ( -23.99999999999996447, 206.8125000027312126, 171.6568542494926817 ) ) ;
#56065 = ORIENTED_EDGE ( 'NONE', *, *, #10507, .T. ) ;
#56066 = CARTESIAN_POINT ( 'NONE',  ( 7.188101187499999156, 12.37499999795161187, 2.977408999572654924 ) ) ;
#56067 = CARTESIAN_POINT ( 'NONE',  ( -28.00000000000007461, 197.1250000027312126, 166.0000000000003695 ) ) ;
#56068 = CARTESIAN_POINT ( 'NONE',  ( 5.000000000000000000, 53.35645474066845395, -47.33026262608697010 ) ) ;
#56069 = CARTESIAN_POINT ( 'NONE',  ( -8.311093377946841443, 188.9062499965859843, 8.311093377946830785 ) ) ;
#56070 = CARTESIAN_POINT ( 'NONE',  ( 7.188101187500002709, 114.6875000020484094, 2.977408999572649151 ) ) ;
#56071 = CARTESIAN_POINT ( 'NONE',  ( -6.000000000000003553, 291.0000000034139589, -2.485281374238571317 ) ) ;
#56072 = CARTESIAN_POINT ( 'NONE',  ( 4.721056650416000089, 289.8281250017069510, 4.721056650415999201 ) ) ;
#56073 = EDGE_CURVE ( 'NONE', #34562, #50500, #68888, .T. ) ;
#56075 = CARTESIAN_POINT ( 'NONE',  ( 1.656854249492263564, 200.9375000027312694, 146.0000000000001421 ) ) ;
#56074 = CARTESIAN_POINT ( 'NONE',  ( 2.679491924311332873, 33.95833333333334991, 9.999999999999936051 ) ) ;
#56076 = ORIENTED_EDGE ( 'NONE', *, *, #14446, .T. ) ;
#56077 = CARTESIAN_POINT ( 'NONE',  ( 8.311093377946834337, 257.0312500034139020, -8.311093377946836114 ) ) ;
#56078 = CARTESIAN_POINT ( 'NONE',  ( -7.188101187499990274, -2.977408999572651371, 24.45530278187175455 ) ) ;
#56079 = CYLINDRICAL_SURFACE ( 'NONE', #64302, 7.999999999999991118 ) ;
#56080 = FACE_OUTER_BOUND ( 'NONE', #47855, .T. ) ;
#56081 = CARTESIAN_POINT ( 'NONE',  ( 4.465349678524231258, -66.51625814178485996, -26.73836809291886496 ) ) ;
#56083 = EDGE_CURVE ( 'NONE', #18244, #2602, #14320, .T. ) ;
#56082 = CARTESIAN_POINT ( 'NONE',  ( 1.432654583217662481, 195.3750000013656063, 194.5412658750000219 ) ) ;
#56084 = CARTESIAN_POINT ( 'NONE',  ( 10.00000000000000178, 145.0000000000000284, 0.000000000000000000 ) ) ;
#56085 = CARTESIAN_POINT ( 'NONE',  ( -7.778174593052020747, -7.778174593052023411, 115.3750000040967905 ) ) ;
#56086 = CARTESIAN_POINT ( 'NONE',  ( 15.05053643744962777, 12.09517842721670355, -0.7140392532422370486 ) ) ;
#56087 = CARTESIAN_POINT ( 'NONE',  ( 1.469576158976823947E-15, 95.37499999999998579, 8.000000000000000000 ) ) ;
#56088 = CARTESIAN_POINT ( 'NONE',  ( 11.35316468750000141, 121.0937499965860269, 0.000000000000000000 ) ) ;
#56089 = CARTESIAN_POINT ( 'NONE',  ( 8.000000000000001776, 98.65625000000001421, 3.313708498984759387 ) ) ;
#56090 = CARTESIAN_POINT ( 'NONE',  ( -11.00000000000000000, 0.000000000000000000, 68.49999999999997158 ) ) ;
#56093 = CARTESIAN_POINT ( 'NONE',  ( -10.99999999999993427, 4.556349186104110771, 110.5937500040967620 ) ) ;
#56092 = CARTESIAN_POINT ( 'NONE',  ( 30.44569435410883074, 200.5625000013656063, 172.4456943541086957 ) ) ;
#56091 = CARTESIAN_POINT ( 'NONE',  ( 31.45873412499997812, 198.8750000013656347, 171.4326545832175839 ) ) ;
#56094 = ORIENTED_EDGE ( 'NONE', *, *, #50919, .F. ) ;
#56095 = CARTESIAN_POINT ( 'NONE',  ( 9.527714560998933990, 225.2503231660761003, -3.092998227472968598 ) ) ;
#56096 = CARTESIAN_POINT ( 'NONE',  ( 7.778174593052023411, -7.778174593052021635, 114.2500000040967763 ) ) ;
#56097 = CARTESIAN_POINT ( 'NONE',  ( 29.43265458321766559, 200.1250000013656063, 166.5412658749999650 ) ) ;
#56098 = EDGE_CURVE ( 'NONE', #26323, #55545, #30166, .T. ) ;
#56099 = CARTESIAN_POINT ( 'NONE',  ( 9.832129032723420536, 206.5104166632526983, -5.676582343749999815 ) ) ;
#56100 = CARTESIAN_POINT ( 'NONE',  ( -2.977408999572650927, 119.3750000020483810, -7.188101187500001821 ) ) ;
#56101 = CARTESIAN_POINT ( 'NONE',  ( -1.881053915767121554, 17.62499999863440436, -4.541265875000002339 ) ) ;
#56102 = CARTESIAN_POINT ( 'NONE',  ( 30.44569435410883074, 195.0625000013656063, 167.5543056458911053 ) ) ;
#56103 = CARTESIAN_POINT ( 'NONE',  ( -4.898587196589407898E-16, 7.999999999999991118, 24.45530277982336642 ) ) ;
#56104 = FACE_OUTER_BOUND ( 'NONE', #8378, .T. ) ;
#56105 = CARTESIAN_POINT ( 'NONE',  ( -9.832129032723418760, 97.86458332991935549, -5.676582343750004256 ) ) ;
#56106 = ORIENTED_EDGE ( 'NONE', *, *, #66900, .T. ) ;
#56107 = DIRECTION ( 'NONE',  ( -0.000000000000000000, 1.000000000000000000, 4.476705744456276341E-16 ) ) ;
#56108 = CARTESIAN_POINT ( 'NONE',  ( -7.188101187500001821, 17.62499999795161187, -2.977408999572651371 ) ) ;
#56109 = CARTESIAN_POINT ( 'NONE',  ( 0.000000000000000000, 210.0000000000000284, 170.0000000000000284 ) ) ;
#56110 =( BOUNDED_CURVE ( )  B_SPLINE_CURVE ( 2, ( #44803, #33140, #16483, #27436, #39520, #67816, #22518, #45538, #34247 ),
 .UNSPECIFIED., .F., .F. ) 
 B_SPLINE_CURVE_WITH_KNOTS ( ( 3, 2, 2, 2, 3 ),
 ( 0.01388888888888889159, 0.02083333333333333565, 0.02777777777777777624, 0.03472222222222222376, 0.04166666666666666435 ),
 .UNSPECIFIED. ) 
 CURVE ( )  GEOMETRIC_REPRESENTATION_ITEM ( )  RATIONAL_B_SPLINE_CURVE ( ( 1.000000000000000000, 0.9238795325112867385, 1.000000000000000000, 0.9238795325112867385, 1.000000000000000000, 0.9238795325112867385, 1.000000000000000000, 0.9238795325112867385, 1.000000000000000000 ) ) 
 REPRESENTATION_ITEM ( '' )  );
#56111 = CARTESIAN_POINT ( 'NONE',  ( -3.042071309553166625, 263.1770833367473301, -11.35316468749999608 ) ) ;
#56112 = CARTESIAN_POINT ( 'NONE',  ( -8.311093377946836114, 97.65624999658602690, -8.311093377946837890 ) ) ;
#56113 = ORIENTED_EDGE ( 'NONE', *, *, #66528, .T. ) ;
#56114 = CARTESIAN_POINT ( 'NONE',  ( 26.34314575050768426, 196.6875000027311842, 165.9999999999998010 ) ) ;
#56115 = CARTESIAN_POINT ( 'NONE',  ( -4.220049686691937474, -10.18810118749999738, 109.9375000020483952 ) ) ;
#56116 = CARTESIAN_POINT ( 'NONE',  ( -26.56734541678237704, 195.6250000013656063, 166.5412658750003629 ) ) ;
#56117 = CARTESIAN_POINT ( 'NONE',  ( -2.445694354108784108, 205.5625000013656063, 195.5543056458912190 ) ) ;
#56118 = FACE_OUTER_BOUND ( 'NONE', #8730, .T. ) ;
#56120 = CARTESIAN_POINT ( 'NONE',  ( -11.35316468749999785, 88.07291666325266988, -3.042071309553167957 ) ) ;
#56119 = CARTESIAN_POINT ( 'NONE',  ( 4.556349186104052151, -10.99999999999999822, 97.46874999999998579 ) ) ;
#56121 = VECTOR ( 'NONE', #26695, 1000.000000000000000 ) ;
#56122 = CARTESIAN_POINT ( 'NONE',  ( -3.313708498984758943, -7.999999999999989342, 10.29905278392014623 ) ) ;
#56123 = CARTESIAN_POINT ( 'NONE',  ( -31.45873412499999944, 201.8750000013656063, 168.5673454167827572 ) ) ;
#56124 = DIRECTION ( 'NONE',  ( -0.000000000000000000, -0.000000000000000000, 1.000000000000000000 ) ) ;
#56125 = CARTESIAN_POINT ( 'NONE',  ( -4.999999999999998224, 178.5416666598387110, -8.660254037844389075 ) ) ;
#56126 = EDGE_CURVE ( 'NONE', #50952, #61963, #45377, .T. ) ;
#56127 = CIRCLE ( 'NONE', #59715, 7.500000000000020428 ) ;
#56128 = CARTESIAN_POINT ( 'NONE',  ( 5.000000000000000888, -53.36732872257306326, 44.46877392682749530 ) ) ;
#56129 = CARTESIAN_POINT ( 'NONE',  ( 3.042071309553159519, 70.05208332991934128, 11.35316468750000141 ) ) ;
#56130 = CARTESIAN_POINT ( 'NONE',  ( 2.765530957081996366, 290.1406250017069510, -6.676582343750003368 ) ) ;
#56131 = CARTESIAN_POINT ( 'NONE',  ( -10.18810118749999916, 4.220049686691934809, 102.4375000020483810 ) ) ;
#56132 = CARTESIAN_POINT ( 'NONE',  ( -9.832129032723420536, 208.6979166632526983, 5.676582343749997150 ) ) ;
#56133 = VERTEX_POINT ( 'NONE', #68764 ) ;
#56134 = DIRECTION ( 'NONE',  ( -1.000000000000000000, 0.000000000000000000, 0.000000000000000000 ) ) ;
#56135 = LINE ( 'NONE', #61784, #313 ) ;
#56136 = CARTESIAN_POINT ( 'NONE',  ( 0.000000000000000000, 0.000000000000000000, -10.00000000000000000 ) ) ;
#56137 = CARTESIAN_POINT ( 'NONE',  ( 3.042071309553167513, 211.8229166632526699, -11.35316468749999785 ) ) ;
#56138 = CARTESIAN_POINT ( 'NONE',  ( 7.320508075688771044, 226.2500000068279746, -7.320508075688771932 ) ) ;
#56139 = CARTESIAN_POINT ( 'NONE',  ( 7.778174593052023411, -7.778174593052021635, 72.25000000409677625 ) ) ;
#56140 = ORIENTED_EDGE ( 'NONE', *, *, #34546, .F. ) ;
#56141 = CARTESIAN_POINT ( 'NONE',  ( -8.311093377946836114, 192.9687499965860127, -8.311093377946837890 ) ) ;
#56142 =( BOUNDED_CURVE ( )  B_SPLINE_CURVE ( 2, ( #14130, #48469, #47365, #71474, #35691, #25454, #18706, #59806, #1736 ),
 .UNSPECIFIED., .F., .F. ) 
 B_SPLINE_CURVE_WITH_KNOTS ( ( 3, 2, 2, 2, 3 ),
 ( 0.8437500000000002220, 0.8489583333333335924, 0.8541666666666668517, 0.8593750000000002220, 0.8645833333333335924 ),
 .UNSPECIFIED. ) 
 CURVE ( )  GEOMETRIC_REPRESENTATION_ITEM ( )  RATIONAL_B_SPLINE_CURVE ( ( 0.9999999999999967804, 0.9238795325112899581, 1.000000000000000000, 0.9238795325112867385, 1.000000000000000000, 0.9238795325112867385, 1.000000000000000000, 0.9238795325112835188, 1.000000000000003331 ) ) 
 REPRESENTATION_ITEM ( '' )  );
#56143 = CARTESIAN_POINT ( 'NONE',  ( -7.188101187499992051, 2.977408999572646930, 16.39280278187175455 ) ) ;
#56144 = CARTESIAN_POINT ( 'NONE',  ( -24.54126587500000412, 208.2500000013656063, 168.5673454167827003 ) ) ;
#56145 = CARTESIAN_POINT ( 'NONE',  ( 8.000000000000000000, 9.093750000000001776, -3.313708498984761608 ) ) ;
#56146 = VERTEX_POINT ( 'NONE', #62723 ) ;
#56147 = CARTESIAN_POINT ( 'NONE',  ( 8.000000000000001776, 89.84375000409677625, 3.313708498984759387 ) ) ;
#56148 = CARTESIAN_POINT ( 'NONE',  ( -10.00000000000000000, 17.29166666666666430, -2.679491924311229845 ) ) ;
#56149 = CARTESIAN_POINT ( 'NONE',  ( 7.204075437095966983, 7.204075437095967871, 80.96875000204836681 ) ) ;
#56150 = ORIENTED_EDGE ( 'NONE', *, *, #47948, .F. ) ;
#56151 = CARTESIAN_POINT ( 'NONE',  ( -2.828427124746190735, 21.37500000000000000, -2.828427124746191623 ) ) ;
#56152 = CARTESIAN_POINT ( 'NONE',  ( 2.780723358947928197E-16, 18.56249999863440436, -4.541265875000002339 ) ) ;
#56153 = CARTESIAN_POINT ( 'NONE',  ( 23.99999999999998934, 198.8750000027312126, 169.9999999999999432 ) ) ;
#56154 = ORIENTED_EDGE ( 'NONE', *, *, #36230, .F. ) ;
#56155 = PRESENTATION_STYLE_ASSIGNMENT (( #38429 ) ) ;
#56156 = CARTESIAN_POINT ( 'NONE',  ( -7.188101187500000044, 89.65625000204838102, 0.000000000000000000 ) ) ;
#56157 = AXIS2_PLACEMENT_3D ( 'NONE', #25011, #72157, #3141 ) ;
#56158 = ADVANCED_FACE ( 'NONE', ( #22352 ), #52811, .T. ) ;
#56161 = CARTESIAN_POINT ( 'NONE',  ( 0.000000000000000000, 0.000000000000000000, 0.000000000000000000 ) ) ;
#56160 = CARTESIAN_POINT ( 'NONE',  ( 9.832129032723420536, 250.9895833367473017, 5.676582343749996262 ) ) ;
#56159 = CARTESIAN_POINT ( 'NONE',  ( -2.679491924311358186, 257.0833333401612890, -9.999999999999923617 ) ) ;
#56162 = SHAPE_DEFINITION_REPRESENTATION ( #16795, #5031 ) ;
#56163 = ORIENTED_EDGE ( 'NONE', *, *, #1329, .F. ) ;
#56164 = CARTESIAN_POINT ( 'NONE',  ( 11.35316468749999608, 256.9270833367473301, -3.042071309553167069 ) ) ;
#56165 = AXIS2_PLACEMENT_3D ( 'NONE', #63125, #6170, #69915 ) ;
#56166 = CARTESIAN_POINT ( 'NONE',  ( -7.188101187499990274, -2.977408999572651371, 12.08030278187175099 ) ) ;
#56167 = ORIENTED_EDGE ( 'NONE', *, *, #21071, .T. ) ;
#56168 = EDGE_CURVE ( 'NONE', #69421, #53624, #35834, .T. ) ;
#56169 = VERTEX_POINT ( 'NONE', #70528 ) ;
#56170 = CARTESIAN_POINT ( 'NONE',  ( 10.18810118750000093, -4.220049686691933033, 72.81250000204838102 ) ) ;
#56171 = CARTESIAN_POINT ( 'NONE',  ( -2.085542519210945728E-15, 69.84374999658601268, 11.35316468750000141 ) ) ;
#56172 = CARTESIAN_POINT ( 'NONE',  ( 1.469576158976822172E-15, -7.999999999999991118, 17.70530277982336642 ) ) ;
#56173 = CARTESIAN_POINT ( 'NONE',  ( 4.556349186104051263, -10.99999999999999822, 91.46874999999998579 ) ) ;
#56176 = CARTESIAN_POINT ( 'NONE',  ( -4.721056650415999201, 289.4843750017070079, -4.721056650415999201 ) ) ;
#56175 = CARTESIAN_POINT ( 'NONE',  ( 30.82842712474620939, 198.2500000027312126, 172.8284271247460424 ) ) ;
#56174 = CARTESIAN_POINT ( 'NONE',  ( 26.56734541678232731, 209.6250000013656063, 173.4587341249998929 ) ) ;
#56177 = CARTESIAN_POINT ( 'NONE',  ( 7.778174593052021635, 7.778174593052023411, 88.93749999999998579 ) ) ;
#56178 = CARTESIAN_POINT ( 'NONE',  ( -3.999999999999960032, 199.9375000000000000, 196.3431457505076594 ) ) ;
#56179 = CARTESIAN_POINT ( 'NONE',  ( -3.458734124999960358, 199.6250000013656063, 196.5673454167823877 ) ) ;
#56180 = CARTESIAN_POINT ( 'NONE',  ( -8.000000000000000000, 7.968749995903221972, -3.313708498984762496 ) ) ;
#56181 = VECTOR ( 'NONE', #1012, 1000.000000000000000 ) ;
#56182 = ORIENTED_EDGE ( 'NONE', *, *, #39043, .F. ) ;
#56183 = CARTESIAN_POINT ( 'NONE',  ( 26.56734541678232731, 209.6250000013656063, 173.4587341249998929 ) ) ;
#56184 = CARTESIAN_POINT ( 'NONE',  ( 2.977408999572650927, 14.62499999795161010, -7.188101187500001821 ) ) ;
#56185 = CARTESIAN_POINT ( 'NONE',  ( -11.35316468749999785, 173.3854166632526983, -3.042071309553167513 ) ) ;
#56186 = CARTESIAN_POINT ( 'NONE',  ( 8.000000000000000000, 7.593750000000001776, -3.313708498984761164 ) ) ;
#56187 = CARTESIAN_POINT ( 'NONE',  ( 7.188101187500000933, 102.8750000020483810, -2.977408999572651371 ) ) ;
#56189 = CARTESIAN_POINT ( 'NONE',  ( -0.3794862803193519429, -55.62190996747714422, -43.80334292620955949 ) ) ;
#56188 = DIRECTION ( 'NONE',  ( 0.000000000000000000, -1.000000000000000000, -4.476705744456276341E-16 ) ) ;
#56190 = CARTESIAN_POINT ( 'NONE',  ( 31.45873412500001010, 207.0000000013655779, 168.5673454167822740 ) ) ;
#56191 = CARTESIAN_POINT ( 'NONE',  ( -2.977408999572648707, -7.188101187499990274, 15.64280278187175632 ) ) ;
#56192 = CARTESIAN_POINT ( 'NONE',  ( -1.656854249492403008, 206.8125000027312126, 146.0000000000000284 ) ) ;
#56193 = CARTESIAN_POINT ( 'NONE',  ( 3.042071309553167069, 51.82291666325266988, -11.35316468749999785 ) ) ;
#56194 = CARTESIAN_POINT ( 'NONE',  ( 10.00000000000000178, 22.08333332650536818, -2.679491924311226736 ) ) ;
#56195 = CARTESIAN_POINT ( 'NONE',  ( -11.00000000000010303, -4.556349186103947346, 71.59374999999998579 ) ) ;
#56196 = ORIENTED_EDGE ( 'NONE', *, *, #60921, .T. ) ;
#56197 = CARTESIAN_POINT ( 'NONE',  ( 5.000000000000001776, 142.7083333265053682, -8.660254037844389075 ) ) ;
#56198 = CYLINDRICAL_SURFACE ( 'NONE', #65380, 6.000000000000000000 ) ;
#56199 = CARTESIAN_POINT ( 'NONE',  ( -11.35316468750000141, 43.48958332991934839, 3.042071309553159963 ) ) ;
#56200 = CARTESIAN_POINT ( 'NONE',  ( 7.778174593052023411, -7.778174593052021635, 76.75000000409676204 ) ) ;
#56201 = CARTESIAN_POINT ( 'NONE',  ( -2.445694354108840063, 202.0625000013656063, 139.5543056458912190 ) ) ;
#56202 = CARTESIAN_POINT ( 'NONE',  ( 7.000000000000000000, -2.500000000000000000, 0.000000000000000000 ) ) ;
#56203 = CARTESIAN_POINT ( 'NONE',  ( -4.000000000000016875, 196.5625000027312126, 140.3431457505076594 ) ) ;
#56205 = CARTESIAN_POINT ( 'NONE',  ( 3.042071309553159519, 49.73958332991934839, 11.35316468750000141 ) ) ;
#56204 = CARTESIAN_POINT ( 'NONE',  ( 1.320432766682874540E-15, 99.03125000204838102, 7.188101187500000044 ) ) ;
#56206 = CARTESIAN_POINT ( 'NONE',  ( -4.898587196589407898E-16, 7.999999999999991118, 3.455302779823362425 ) ) ;
#56207 = CARTESIAN_POINT ( 'NONE',  ( 0.000000000000000000, 9.980871413050930352E-15, 81.50000000000000000 ) ) ;
#56208 = CARTESIAN_POINT ( 'NONE',  ( 6.951808397369818766E-16, 177.0312499965860411, -11.35316468750000141 ) ) ;
#56209 = CARTESIAN_POINT ( 'NONE',  ( 8.660254037844389075, 142.2916666598386826, -5.000000000000000000 ) ) ;
#56210 = CARTESIAN_POINT ( 'NONE',  ( -7.188101187499999156, 102.1250000020483810, 2.977408999572654924 ) ) ;
#56211 = FACE_OUTER_BOUND ( 'NONE', #44466, .T. ) ;
#56212 = CARTESIAN_POINT ( 'NONE',  ( 11.35316468750000141, 36.09374999658601979, 0.000000000000000000 ) ) ;
#56213 = CARTESIAN_POINT ( 'NONE',  ( 2.485281374238196062, 295.7500000034141863, -6.000000000000377476 ) ) ;
#56214 = VERTEX_POINT ( 'NONE', #1144 ) ;
#56215 = CYLINDRICAL_SURFACE ( 'NONE', #51247, 4.000000000000001776 ) ;
#56216 = CARTESIAN_POINT ( 'NONE',  ( 10.18810118749999916, 4.220049686691935698, 73.00000000204836681 ) ) ;
#56217 = DIRECTION ( 'NONE',  ( -0.000000000000000000, -1.000000000000000000, -0.000000000000000000 ) ) ;
#56218 = CARTESIAN_POINT ( 'NONE',  ( 33.33057127554769039, 41.08277773008951783, 64.99999999999998579 ) ) ;
#56220 = CARTESIAN_POINT ( 'NONE',  ( 9.832129032723416984, 170.3645833299193555, 5.676582343750006032 ) ) ;
#56219 = DIRECTION ( 'NONE',  ( -0.000000000000000000, -0.000000000000000000, -1.000000000000000000 ) ) ;
#56221 = CARTESIAN_POINT ( 'NONE',  ( -5.656854249492375253, 5.656854249492375253, 9.699052784329824206 ) ) ;
#56222 = CARTESIAN_POINT ( 'NONE',  ( 5.656854249492380582, 9.187500000000001776, -5.656854249492380582 ) ) ;
#56223 = CARTESIAN_POINT ( 'NONE',  ( 2.085542519210945334E-15, 225.1562500034139873, 11.35316468749999963 ) ) ;
#56224 = CARTESIAN_POINT ( 'NONE',  ( -1.780377099653301709, 51.29164421682977348, -48.57534666485153707 ) ) ;
#56225 = CARTESIAN_POINT ( 'NONE',  ( 4.220049686691941027, -10.18810118749999738, 79.00000000204838102 ) ) ;
#56226 = ORIENTED_EDGE ( 'NONE', *, *, #39302, .T. ) ;
#56227 = FACE_OUTER_BOUND ( 'NONE', #68355, .T. ) ;
#56228 = CARTESIAN_POINT ( 'NONE',  ( -2.085542519210945728E-15, 114.8437499965860127, 11.35316468750000141 ) ) ;
#56229 =( BOUNDED_CURVE ( )  B_SPLINE_CURVE ( 2, ( #21946, #57421, #62315, #5357, #56674, #17781, #74377, #57795, #52127 ),
 .UNSPECIFIED., .F., .F. ) 
 B_SPLINE_CURVE_WITH_KNOTS ( ( 3, 2, 2, 2, 3 ),
 ( 0.2647058823529410132, 0.2683823529411762943, 0.2720588235294115753, 0.2757352941176469674, 0.2794117647058822484 ),
 .UNSPECIFIED. ) 
 CURVE ( )  GEOMETRIC_REPRESENTATION_ITEM ( )  RATIONAL_B_SPLINE_CURVE ( ( 1.000000000000003553, 0.9238795325112832968, 1.000000000000000000, 0.9238795325112867385, 1.000000000000000000, 0.9238795325112867385, 1.000000000000000000, 0.9238795325112890700, 0.9999999999999976685 ) ) 
 REPRESENTATION_ITEM ( '' )  );
#56230 = CARTESIAN_POINT ( 'NONE',  ( -5.000000000000000000, 60.11723469343148452, -46.25570701698029552 ) ) ;
#56231 = VERTEX_POINT ( 'NONE', #68025 ) ;
#56232 = ORIENTED_EDGE ( 'NONE', *, *, #71509, .T. ) ;
#56233 = CARTESIAN_POINT ( 'NONE',  ( -4.541265875000002339, 8.937499998634407916, -5.561446717895856393E-16 ) ) ;
#56234 = CARTESIAN_POINT ( 'NONE',  ( 4.401442555609581635E-16, 6.843749997951611874, -7.188101187500000044 ) ) ;
#56235 = CARTESIAN_POINT ( 'NONE',  ( -5.656854249492380582, 111.5000000040967763, -5.656854249492380582 ) ) ;
#56236 = CARTESIAN_POINT ( 'NONE',  ( 7.204075437095968759, -7.204075437095966983, 92.59375000204838102 ) ) ;
#56237 = EDGE_CURVE ( 'NONE', #8879, #50547, #70168, .T. ) ;
#56238 = AXIS2_PLACEMENT_3D ( 'NONE', #35895, #72445, #15459 ) ;
#56239 = CARTESIAN_POINT ( 'NONE',  ( -26.56734541678232375, 204.2500000013655779, 173.4587341250003760 ) ) ;
#56240 = CARTESIAN_POINT ( 'NONE',  ( -7.347880794884122694E-16, 7.750000000000000000, 4.000000000000001776 ) ) ;
#56241 =( BOUNDED_SURFACE ( )  B_SPLINE_SURFACE ( 1, 2, ( 
 ( #9268, #50000, #14910, #20950, #66982, #15657, #38320, #38698, #32290, #61699, #10021, #33053, #4361, #44719, #16030, #39063, #56415, #4736, #50741, #73755, #45088, #68103, #16393, #62430, #52241, #22431, #57543, #45827, #68467, #74497, #52609, #51868, #45450, #16767, #28845, #51116, #5852, #40174, #41287, #57160, #63177, #12236, #35273, #575, #11872, #11504, #18272, #23557, #35631, #945, #209, #51486, #63926, #46568, #12604, #23187, #29596, #68838, #40915, #58646, #39794, #64297, #69589, #62798, #6589, #17525, #17151, #22806, #28101, #74128, #17902, #11138, #34160, #58286, #46198, #34908, #6225, #5476, #28478, #34537, #69214, #40542, #23927, #63547, #57916, #46936, #29228, #69964, #14442, #37477, #1675, #13693, #19739, #53717, #36365, #19005, #36735, #42379, #6953, #30699, #71788, #29964, #37102, #31441, #43119, #59746, #8057, #20107, #31059, #59018, #42011, #47665, #52977, #14067, #25017, #54087, #1311, #24294, #7692, #47305, #59381, #65018, #66137, #36001, #13329, #65764, #60106, #2397, #65396, #2031, #70330, #25395, #18645, #54467, #48037, #30331, #42748, #48409, #41653, #71046, #8424, #70687, #2774, #64663, #12963, #7327, #71415, #53350, #25760, #19366, #48781, #24655, #21973, #73665, #32955, #60477, #8807, #67641, #32576, #67271, #38604, #54839, #43494, #43876, #31818, #49153, #33324, #3519, #26893, #44627, #61604, #50645, #68004, #16300, #55214, #15565, #73299, #55585, #15198, #72553, #9923, #21233, #3148, #9561, #45001, #26134, #15937, #10298, #72163, #55961, #4271, #20473, #27261, #37858, #20858, #26508, #66505, #38966, #3899, #50279, #66892, #61233, #14816, #60855, #9175, #38227, #49533, #32194, #21601, #49909, #72923, #44259, #61970, #56323, #4644, #27638, #16675, #74406, #11044, #51393, #855, #68745, #68377, #34074, #45361, #17430, #23840, #46847, #39705, #46106, #69869, #40823, #74032, #63829, #39340, #23466, #63453, #33697, #17059, #57071, #5018, #5383, #12144, #63086, #62705, #40081, #28384, #22714, #52150, #11778, #28014, #51025, #46478, #34817, #35181, #45731, #22335, #62337, #69125, #6129, #11410, #34447, #58196, #57446, #5754, #10665, #28754, #51769, #116, #23095, #40454, #57823, #29507, #29135, #486, #69498, #17807, #6501, #52518, #56702, #1587, #48688, #25669, #59653, #60013, #30973, #65302, #8331, #24571 ),
 ( #6862, #47576, #54372, #24199, #70243, #53258, #64576, #30240, #2682, #70599, #47210, #12873, #18553, #70961, #18182, #41197, #41559, #24929, #64207, #19646, #52889, #42659, #12511, #2303, #42288, #35542, #18916, #35910, #58557, #58929, #65670, #41922, #29874, #1220, #64933, #7236, #13242, #36276, #31341, #59292, #7600, #25300, #48319, #13607, #1940, #30608, #53628, #36645, #47943, #13969, #19278, #7970, #53992, #71325, #37011, #49439, #73209, #37765, #9836, #27544, #8709, #33235, #44164, #31724, #50187, #61135, #60764, #20386, #56234, #10206, #67178, #71693, #20012, #4184, #43784, #26803, #49817, #26038, #72834, #38512, #61513, #38879, #9465, #3424, #20766, #15101, #4549, #14353, #26413, #43401, #44536, #32862, #43023, #27170, #61883, #72459, #21514, #66044, #14725, #67547, #66798, #55867, #37381, #72068, #15845, #60383, #49059, #54746, #38134, #3054, #66416, #9086, #32100, #55120, #32483, #55491, #3805, #21140, #15474, #67917, #39248, #23008, #11321, #17338, #4928, #62248, #393, #16967, #5664, #10575, #33605, #40360, #56614, #45276, #6035, #62620, #73946, #39620, #27925, #10950, #50934, #34724, #56981, #68657, #57353, #22, #46014, #39993, #33986, #16584, #50558, #73572, #51676, #29040, #69035, #28661, #52058, #5295, #28297, #63360, #62997, #22248, #51303, #74315, #45642, #11686, #57728, #68287, #21882, #22623, #34354, #44911, #16209, #4795, #43653, #62123, #55365, #37637, #67043, #31968, #16084, #21382, #49694, #56108, #15717, #26286, #72323, #9331, #27789, #10447, #73444, #55739, #27048, #61383, #44035, #20637, #10077, #4056, #15343, #49307, #32351, #4418, #54993, #73814, #3300, #50801, #38759, #66664, #21751, #32731, #3671, #14970, #43275, #56479, #61759, #66291, #14597, #50429, #38379, #50061, #44405, #60635, #38007, #26669, #8956, #61005, #39119, #72707, #9709, #27413, #67418, #33477, #21010, #73075, #33114, #44779, #67793, #68901, #51544, #34220, #51929, #57600, #29654, #45887, #12302, #52669, #52302, #46629, #58347, #28912, #266, #35335, #23249, #74184, #57221, #62858, #22121, #29292, #40230, #46257, #28536, #22874, #6652, #45146, #68157, #74562, #11192, #16456, #40605, #33851, #39493, #17211, #10816, #63233, #62488, #28164, #22489, #5535, #68527, #11560, #56849, #34593, #51174, #16830, #45510, #69276, #5168, #39857, #5910 ) ),
 .UNSPECIFIED., .F., .F., .F. ) 
 B_SPLINE_SURFACE_WITH_KNOTS ( ( 2, 2 ),
 ( 3, 2, 2, 2, 2, 2, 2, 2, 2, 2, 2, 2, 2, 2, 2, 2, 2, 2, 2, 2, 2, 2, 2, 2, 2, 2, 2, 2, 2, 2, 2, 2, 2, 2, 2, 2, 2, 2, 2, 2, 2, 2, 2, 2, 2, 2, 2, 2, 2, 2, 2, 2, 2, 2, 2, 2, 2, 2, 2, 2, 2, 2, 2, 2, 2, 2, 2, 2, 2, 2, 2, 2, 2, 2, 2, 2, 2, 2, 2, 2, 2, 2, 2, 2, 2, 2, 2, 2, 2, 2, 2, 2, 2, 2, 2, 2, 2, 2, 2, 2, 2, 2, 2, 2, 2, 2, 2, 2, 2, 2, 2, 2, 2, 2, 2, 2, 2, 2, 2, 2, 2, 2, 2, 2, 2, 2, 2, 2, 2, 2, 2, 2, 2, 2, 2, 2, 2, 2, 2, 2, 2, 2, 2, 2, 3 ),
 ( 0.000000000000000000, 1.000000000000000000 ),
 ( 0.000000000000000000, 0.006944444444444444059, 0.01388888888888888812, 0.02083333333333333218, 0.02777777777777777624, 0.03472222222222222376, 0.04166666666666666435, 0.04861111111111111188, 0.05555555555555555247, 0.06250000000000000000, 0.06944444444444444753, 0.07638888888888889506, 0.08333333333333332871, 0.09027777777777777624, 0.09722222222222222376, 0.1041666666666666713, 0.1111111111111111049, 0.1180555555555555525, 0.1250000000000000000, 0.1319444444444444475, 0.1388888888888888951, 0.1458333333333333426, 0.1527777777777777901, 0.1597222222222222099, 0.1666666666666666574, 0.1736111111111111049, 0.1805555555555555525, 0.1875000000000000000, 0.1944444444444444475, 0.2013888888888888951, 0.2083333333333333426, 0.2152777777777777901, 0.2222222222222222099, 0.2291666666666666574, 0.2361111111111111049, 0.2430555555555555525, 0.2500000000000000000, 0.2569444444444444198, 0.2638888888888888951, 0.2708333333333333148, 0.2777777777777777901, 0.2847222222222222099, 0.2916666666666666852, 0.2986111111111111049, 0.3055555555555555802, 0.3125000000000000000, 0.3194444444444444198, 0.3263888888888888951, 0.3333333333333333148, 0.3402777777777777901, 0.3472222222222222099, 0.3541666666666666852, 0.3611111111111111049, 0.3680555555555555802, 0.3750000000000000000, 0.3819444444444444198, 0.3888888888888888951, 0.3958333333333333148, 0.4027777777777777901, 0.4097222222222222099, 0.4166666666666666852, 0.4236111111111111049, 0.4305555555555555802, 0.4375000000000000000, 0.4444444444444444198, 0.4513888888888888951, 0.4583333333333333148, 0.4652777777777777901, 0.4722222222222222099, 0.4791666666666666852, 0.4861111111111111049, 0.4930555555555555802, 0.5000000000000000000, 0.5069444444444444198, 0.5138888888888888395, 0.5208333333333333703, 0.5277777777777777901, 0.5347222222222222099, 0.5416666666666666297, 0.5486111111111111605, 0.5555555555555555802, 0.5625000000000000000, 0.5694444444444444198, 0.5763888888888888395, 0.5833333333333333703, 0.5902777777777777901, 0.5972222222222222099, 0.6041666666666666297, 0.6111111111111111605, 0.6180555555555555802, 0.6250000000000000000, 0.6319444444444444198, 0.6388888888888888395, 0.6458333333333333703, 0.6527777777777777901, 0.6597222222222222099, 0.6666666666666666297, 0.6736111111111111605, 0.6805555555555555802, 0.6875000000000000000, 0.6944444444444444198, 0.7013888888888888395, 0.7083333333333333703, 0.7152777777777777901, 0.7222222222222222099, 0.7291666666666666297, 0.7361111111111111605, 0.7430555555555555802, 0.7500000000000000000, 0.7569444444444444198, 0.7638888888888888395, 0.7708333333333333703, 0.7777777777777777901, 0.7847222222222222099, 0.7916666666666666297, 0.7986111111111111605, 0.8055555555555555802, 0.8125000000000000000, 0.8194444444444444198, 0.8263888888888888395, 0.8333333333333333703, 0.8402777777777777901, 0.8472222222222222099, 0.8541666666666666297, 0.8611111111111111605, 0.8680555555555555802, 0.8750000000000000000, 0.8819444444444444198, 0.8888888888888888395, 0.8958333333333333703, 0.9027777777777777901, 0.9097222222222222099, 0.9166666666666666297, 0.9236111111111111605, 0.9305555555555555802, 0.9375000000000000000, 0.9444444444444444198, 0.9513888888888888395, 0.9583333333333333703, 0.9652777777777777901, 0.9722222222222222099, 0.9791666666666666297, 0.9861111111111111605, 0.9930555555555555802, 1.000000000000000000 ),
 .UNSPECIFIED. ) 
 GEOMETRIC_REPRESENTATION_ITEM ( )  RATIONAL_B_SPLINE_SURFACE ( (
 ( 1.000000000000000000, 0.9238795325112867385, 1.000000000000000000, 0.9238795325112867385, 1.000000000000000000, 0.9238795325112867385, 1.000000000000000000, 0.9238795325112867385, 1.000000000000000000, 0.9238795325112867385, 1.000000000000000000, 0.9238795325112867385, 1.000000000000000000, 0.9238795325112867385, 1.000000000000000000, 0.9238795325112867385, 1.000000000000000000, 0.9238795325112867385, 1.000000000000000000, 0.9238795325112867385, 1.000000000000000000, 0.9238795325112867385, 1.000000000000000000, 0.9238795325112867385, 1.000000000000000000, 0.9238795325112867385, 1.000000000000000000, 0.9238795325112867385, 1.000000000000000000, 0.9238795325112867385, 1.000000000000000000, 0.9238795325112867385, 1.000000000000000000, 0.9238795325112867385, 1.000000000000000000, 0.9238795325112867385, 1.000000000000000000, 0.9238795325112867385, 1.000000000000000000, 0.9238795325112867385, 1.000000000000000000, 0.9238795325112867385, 1.000000000000000000, 0.9238795325112867385, 1.000000000000000000, 0.9238795325112867385, 1.000000000000000000, 0.9238795325112867385, 1.000000000000000000, 0.9238795325112867385, 1.000000000000000000, 0.9238795325112867385, 1.000000000000000000, 0.9238795325112867385, 1.000000000000000000, 0.9238795325112867385, 1.000000000000000000, 0.9238795325112867385, 1.000000000000000000, 0.9238795325112867385, 1.000000000000000000, 0.9238795325112867385, 1.000000000000000000, 0.9238795325112867385, 1.000000000000000000, 0.9238795325112867385, 1.000000000000000000, 0.9238795325112867385, 1.000000000000000000, 0.9238795325112867385, 1.000000000000000000, 0.9238795325112867385, 1.000000000000000000, 0.9238795325112867385, 1.000000000000000000, 0.9238795325112867385, 1.000000000000000000, 0.9238795325112867385, 1.000000000000000000, 0.9238795325112867385, 1.000000000000000000, 0.9238795325112867385, 1.000000000000000000, 0.9238795325112867385, 1.000000000000000000, 0.9238795325112867385, 1.000000000000000000, 0.9238795325112867385, 1.000000000000000000, 0.9238795325112867385, 1.000000000000000000, 0.9238795325112867385, 1.000000000000000000, 0.9238795325112867385, 1.000000000000000000, 0.9238795325112867385, 1.000000000000000000, 0.9238795325112867385, 1.000000000000000000, 0.9238795325112867385, 1.000000000000000000, 0.9238795325112867385, 1.000000000000000000, 0.9238795325112867385, 1.000000000000000000, 0.9238795325112867385, 1.000000000000000000, 0.9238795325112867385, 1.000000000000000000, 0.9238795325112867385, 1.000000000000000000, 0.9238795325112867385, 1.000000000000000000, 0.9238795325112867385, 1.000000000000000000, 0.9238795325112867385, 1.000000000000000000, 0.9238795325112867385, 1.000000000000000000, 0.9238795325112867385, 1.000000000000000000, 0.9238795325112867385, 1.000000000000000000, 0.9238795325112867385, 1.000000000000000000, 0.9238795325112867385, 1.000000000000000000, 0.9238795325112867385, 1.000000000000000000, 0.9238795325112867385, 1.000000000000000000, 0.9238795325112867385, 1.000000000000000000, 0.9238795325112867385, 1.000000000000000000, 0.9238795325112867385, 1.000000000000000000, 0.9238795325112867385, 1.000000000000000000, 0.9238795325112867385, 1.000000000000000000, 0.9238795325112867385, 1.000000000000000000, 0.9238795325112867385, 1.000000000000000000, 0.9238795325112867385, 1.000000000000000000, 0.9238795325112867385, 1.000000000000000000, 0.9238795325112867385, 1.000000000000000000, 0.9238795325112867385, 1.000000000000000000, 0.9238795325112867385, 1.000000000000000000, 0.9238795325112867385, 1.000000000000000000, 0.9238795325112867385, 1.000000000000000000, 0.9238795325112867385, 1.000000000000000000, 0.9238795325112867385, 1.000000000000000000, 0.9238795325112867385, 1.000000000000000000, 0.9238795325112867385, 1.000000000000000000, 0.9238795325112867385, 1.000000000000000000, 0.9238795325112867385, 1.000000000000000000, 0.9238795325112867385, 1.000000000000000000, 0.9238795325112867385, 1.000000000000000000, 0.9238795325112867385, 1.000000000000000000, 0.9238795325112867385, 1.000000000000000000, 0.9238795325112867385, 1.000000000000000000, 0.9238795325112867385, 1.000000000000000000, 0.9238795325112867385, 1.000000000000000000, 0.9238795325112867385, 1.000000000000000000, 0.9238795325112867385, 1.000000000000000000, 0.9238795325112867385, 1.000000000000000000, 0.9238795325112867385, 1.000000000000000000, 0.9238795325112867385, 1.000000000000000000, 0.9238795325112867385, 1.000000000000000000, 0.9238795325112867385, 1.000000000000000000, 0.9238795325112867385, 1.000000000000000000, 0.9238795325112867385, 1.000000000000000000, 0.9238795325112867385, 1.000000000000000000, 0.9238795325112867385, 1.000000000000000000, 0.9238795325112867385, 1.000000000000000000, 0.9238795325112867385, 1.000000000000000000, 0.9238795325112867385, 1.000000000000000000, 0.9238795325112867385, 1.000000000000000000, 0.9238795325112867385, 1.000000000000000000, 0.9238795325112867385, 1.000000000000000000, 0.9238795325112867385, 1.000000000000000000, 0.9238795325112867385, 1.000000000000000000, 0.9238795325112867385, 1.000000000000000000, 0.9238795325112867385, 1.000000000000000000, 0.9238795325112867385, 1.000000000000000000, 0.9238795325112867385, 1.000000000000000000, 0.9238795325112867385, 1.000000000000000000, 0.9238795325112867385, 1.000000000000000000, 0.9238795325112867385, 1.000000000000000000, 0.9238795325112867385, 1.000000000000000000, 0.9238795325112867385, 1.000000000000000000, 0.9238795325112867385, 1.000000000000000000, 0.9238795325112867385, 1.000000000000000000, 0.9238795325112867385, 1.000000000000000000, 0.9238795325112867385, 1.000000000000000000, 0.9238795325112867385, 1.000000000000000000, 0.9238795325112867385, 1.000000000000000000, 0.9238795325112867385, 1.000000000000000000, 0.9238795325112867385, 1.000000000000000000, 0.9238795325112867385, 1.000000000000000000, 0.9238795325112867385, 1.000000000000000000, 0.9238795325112867385, 1.000000000000000000, 0.9238795325112867385, 1.000000000000000000, 0.9238795325112867385, 1.000000000000000000, 0.9238795325112867385, 1.000000000000000000, 0.9238795325112867385, 1.000000000000000000, 0.9238795325112867385, 1.000000000000000000, 0.9238795325112867385, 1.000000000000000000, 0.9238795325112867385, 1.000000000000000000, 0.9238795325112867385, 1.000000000000000000, 0.9238795325112867385, 1.000000000000000000, 0.9238795325112867385, 1.000000000000000000, 0.9238795325112867385, 1.000000000000000000, 0.9238795325112867385, 1.000000000000000000, 0.9238795325112867385, 1.000000000000000000),
 ( 1.000000000000000000, 0.9238795325112867385, 1.000000000000000000, 0.9238795325112867385, 1.000000000000000000, 0.9238795325112867385, 1.000000000000000000, 0.9238795325112867385, 1.000000000000000000, 0.9238795325112867385, 1.000000000000000000, 0.9238795325112867385, 1.000000000000000000, 0.9238795325112867385, 1.000000000000000000, 0.9238795325112867385, 1.000000000000000000, 0.9238795325112867385, 1.000000000000000000, 0.9238795325112867385, 1.000000000000000000, 0.9238795325112867385, 1.000000000000000000, 0.9238795325112867385, 1.000000000000000000, 0.9238795325112867385, 1.000000000000000000, 0.9238795325112867385, 1.000000000000000000, 0.9238795325112867385, 1.000000000000000000, 0.9238795325112867385, 1.000000000000000000, 0.9238795325112867385, 1.000000000000000000, 0.9238795325112867385, 1.000000000000000000, 0.9238795325112867385, 1.000000000000000000, 0.9238795325112867385, 1.000000000000000000, 0.9238795325112867385, 1.000000000000000000, 0.9238795325112867385, 1.000000000000000000, 0.9238795325112867385, 1.000000000000000000, 0.9238795325112867385, 1.000000000000000000, 0.9238795325112867385, 1.000000000000000000, 0.9238795325112867385, 1.000000000000000000, 0.9238795325112867385, 1.000000000000000000, 0.9238795325112867385, 1.000000000000000000, 0.9238795325112867385, 1.000000000000000000, 0.9238795325112867385, 1.000000000000000000, 0.9238795325112867385, 1.000000000000000000, 0.9238795325112867385, 1.000000000000000000, 0.9238795325112867385, 1.000000000000000000, 0.9238795325112867385, 1.000000000000000000, 0.9238795325112867385, 1.000000000000000000, 0.9238795325112867385, 1.000000000000000000, 0.9238795325112867385, 1.000000000000000000, 0.9238795325112867385, 1.000000000000000000, 0.9238795325112867385, 1.000000000000000000, 0.9238795325112867385, 1.000000000000000000, 0.9238795325112867385, 1.000000000000000000, 0.9238795325112867385, 1.000000000000000000, 0.9238795325112867385, 1.000000000000000000, 0.9238795325112867385, 1.000000000000000000, 0.9238795325112867385, 1.000000000000000000, 0.9238795325112867385, 1.000000000000000000, 0.9238795325112867385, 1.000000000000000000, 0.9238795325112867385, 1.000000000000000000, 0.9238795325112867385, 1.000000000000000000, 0.9238795325112867385, 1.000000000000000000, 0.9238795325112867385, 1.000000000000000000, 0.9238795325112867385, 1.000000000000000000, 0.9238795325112867385, 1.000000000000000000, 0.9238795325112867385, 1.000000000000000000, 0.9238795325112867385, 1.000000000000000000, 0.9238795325112867385, 1.000000000000000000, 0.9238795325112867385, 1.000000000000000000, 0.9238795325112867385, 1.000000000000000000, 0.9238795325112867385, 1.000000000000000000, 0.9238795325112867385, 1.000000000000000000, 0.9238795325112867385, 1.000000000000000000, 0.9238795325112867385, 1.000000000000000000, 0.9238795325112867385, 1.000000000000000000, 0.9238795325112867385, 1.000000000000000000, 0.9238795325112867385, 1.000000000000000000, 0.9238795325112867385, 1.000000000000000000, 0.9238795325112867385, 1.000000000000000000, 0.9238795325112867385, 1.000000000000000000, 0.9238795325112867385, 1.000000000000000000, 0.9238795325112867385, 1.000000000000000000, 0.9238795325112867385, 1.000000000000000000, 0.9238795325112867385, 1.000000000000000000, 0.9238795325112867385, 1.000000000000000000, 0.9238795325112867385, 1.000000000000000000, 0.9238795325112867385, 1.000000000000000000, 0.9238795325112867385, 1.000000000000000000, 0.9238795325112867385, 1.000000000000000000, 0.9238795325112867385, 1.000000000000000000, 0.9238795325112867385, 1.000000000000000000, 0.9238795325112867385, 1.000000000000000000, 0.9238795325112867385, 1.000000000000000000, 0.9238795325112867385, 1.000000000000000000, 0.9238795325112867385, 1.000000000000000000, 0.9238795325112867385, 1.000000000000000000, 0.9238795325112867385, 1.000000000000000000, 0.9238795325112867385, 1.000000000000000000, 0.9238795325112867385, 1.000000000000000000, 0.9238795325112867385, 1.000000000000000000, 0.9238795325112867385, 1.000000000000000000, 0.9238795325112867385, 1.000000000000000000, 0.9238795325112867385, 1.000000000000000000, 0.9238795325112867385, 1.000000000000000000, 0.9238795325112867385, 1.000000000000000000, 0.9238795325112867385, 1.000000000000000000, 0.9238795325112867385, 1.000000000000000000, 0.9238795325112867385, 1.000000000000000000, 0.9238795325112867385, 1.000000000000000000, 0.9238795325112867385, 1.000000000000000000, 0.9238795325112867385, 1.000000000000000000, 0.9238795325112867385, 1.000000000000000000, 0.9238795325112867385, 1.000000000000000000, 0.9238795325112867385, 1.000000000000000000, 0.9238795325112867385, 1.000000000000000000, 0.9238795325112867385, 1.000000000000000000, 0.9238795325112867385, 1.000000000000000000, 0.9238795325112867385, 1.000000000000000000, 0.9238795325112867385, 1.000000000000000000, 0.9238795325112867385, 1.000000000000000000, 0.9238795325112867385, 1.000000000000000000, 0.9238795325112867385, 1.000000000000000000, 0.9238795325112867385, 1.000000000000000000, 0.9238795325112867385, 1.000000000000000000, 0.9238795325112867385, 1.000000000000000000, 0.9238795325112867385, 1.000000000000000000, 0.9238795325112867385, 1.000000000000000000, 0.9238795325112867385, 1.000000000000000000, 0.9238795325112867385, 1.000000000000000000, 0.9238795325112867385, 1.000000000000000000, 0.9238795325112867385, 1.000000000000000000, 0.9238795325112867385, 1.000000000000000000, 0.9238795325112867385, 1.000000000000000000, 0.9238795325112867385, 1.000000000000000000, 0.9238795325112867385, 1.000000000000000000, 0.9238795325112867385, 1.000000000000000000, 0.9238795325112867385, 1.000000000000000000, 0.9238795325112867385, 1.000000000000000000, 0.9238795325112867385, 1.000000000000000000, 0.9238795325112867385, 1.000000000000000000, 0.9238795325112867385, 1.000000000000000000, 0.9238795325112867385, 1.000000000000000000, 0.9238795325112867385, 1.000000000000000000, 0.9238795325112867385, 1.000000000000000000, 0.9238795325112867385, 1.000000000000000000, 0.9238795325112867385, 1.000000000000000000, 0.9238795325112867385, 1.000000000000000000, 0.9238795325112867385, 1.000000000000000000, 0.9238795325112867385, 1.000000000000000000, 0.9238795325112867385, 1.000000000000000000, 0.9238795325112867385, 1.000000000000000000, 0.9238795325112867385, 1.000000000000000000, 0.9238795325112867385, 1.000000000000000000, 0.9238795325112867385, 1.000000000000000000, 0.9238795325112867385, 1.000000000000000000, 0.9238795325112867385, 1.000000000000000000) ) ) 
 REPRESENTATION_ITEM ( '' )  SURFACE ( )  );
#56242 = CARTESIAN_POINT ( 'NONE',  ( -4.541265875000003227, 6.874999998634407916, 1.881053915767121110 ) ) ;
#56243 = CARTESIAN_POINT ( 'NONE',  ( 3.999999999999960032, 199.0000000000000000, 142.0000000000000568 ) ) ;
#56244 = ORIENTED_EDGE ( 'NONE', *, *, #12860, .T. ) ;
#56245 = EDGE_CURVE ( 'NONE', #7053, #28042, #56717, .T. ) ;
#56247 = CARTESIAN_POINT ( 'NONE',  ( -27.99999999999995737, 199.5000000000000000, 174.0000000000003695 ) ) ;
#56246 = CARTESIAN_POINT ( 'NONE',  ( -29.43265458321755901, 197.8750000013656063, 173.4587341250004044 ) ) ;
#56248 = CARTESIAN_POINT ( 'NONE',  ( 4.541265875000001451, 22.24999999863440792, 1.881053915767124440 ) ) ;
#56249 = CARTESIAN_POINT ( 'NONE',  ( 5.082755093536318824, 5.082755093536319713, 2.424052781871750994 ) ) ;
#56250 = VERTEX_POINT ( 'NONE', #73681 ) ;
#56251 = VERTEX_POINT ( 'NONE', #68392 ) ;
#56252 = CARTESIAN_POINT ( 'NONE',  ( -4.220049686691937474, -10.18810118749999738, 91.93750000204836681 ) ) ;
#56253 = CARTESIAN_POINT ( 'NONE',  ( 6.000000000000003553, 288.4375000000000000, 2.485281374238571317 ) ) ;
#56254 = CARTESIAN_POINT ( 'NONE',  ( -31.45873412499998523, 202.0000000013656063, 171.4326545832180386 ) ) ;
#56255 = CARTESIAN_POINT ( 'NONE',  ( -4.556349186104045934, 11.00000000000000000, 107.2187500000000000 ) ) ;
#56257 = CARTESIAN_POINT ( 'NONE',  ( 2.445694354108839175, 206.3125000013656063, 195.5543056458912190 ) ) ;
#56256 = AXIS2_PLACEMENT_3D ( 'NONE', #31091, #8088, #2060 ) ;
#56258 = CARTESIAN_POINT ( 'NONE',  ( -5.656854249492378806, 111.6875000000000000, 5.656854249492381470 ) ) ;
#56259 = CARTESIAN_POINT ( 'NONE',  ( -7.320508075688773708, 126.8750000000000142, -7.320508075688774596 ) ) ;
#56260 = CARTESIAN_POINT ( 'NONE',  ( -3.313708498984762496, 107.2812499999999858, 7.999999999999998224 ) ) ;
#56261 = CARTESIAN_POINT ( 'NONE',  ( -2.765530957081998586, 292.7968750017070079, 6.676582343750001591 ) ) ;
#56262 = CARTESIAN_POINT ( 'NONE',  ( 5.082755093536318824, 5.082755093536319713, 5.799052781871753659 ) ) ;
#56263 = EDGE_LOOP ( 'NONE', ( #51191, #12307, #73590, #20293 ) ) ;
#56264 = LINE ( 'NONE', #44196, #36180 ) ;
#56265 = CARTESIAN_POINT ( 'NONE',  ( 29.43265458321761585, 206.5000000013655779, 173.4587341249998929 ) ) ;
#56266 = CARTESIAN_POINT ( 'NONE',  ( -7.188101187500001821, 1.499999997951610542, -2.977408999572651371 ) ) ;
#56267 = CARTESIAN_POINT ( 'NONE',  ( -2.839093476692135984E-14, 197.6875000013655779, 138.5412658750000503 ) ) ;
#56268 = CARTESIAN_POINT ( 'NONE',  ( 7.188101187500000933, 120.8750000020483810, -2.977408999572651371 ) ) ;
#56270 = CARTESIAN_POINT ( 'NONE',  ( 3.458734124999960358, 204.6250000013655779, 143.4326545832176976 ) ) ;
#56269 = CYLINDRICAL_SURFACE ( 'NONE', #49208, 10.00000000000000000 ) ;
#56271 = CARTESIAN_POINT ( 'NONE',  ( -5.676582343749992710, 245.0520833367473301, 9.832129032723422313 ) ) ;
#56272 = FACE_OUTER_BOUND ( 'NONE', #17825, .T. ) ;
#56273 = PLANE ( 'NONE',  #49312 ) ;
#56274 = CARTESIAN_POINT ( 'NONE',  ( -8.311093377946836114, 12.65624999658601801, -8.311093377946837890 ) ) ;
#56275 = DIRECTION ( 'NONE',  ( -0.000000000000000000, 1.000000000000000000, 4.689100369878284071E-30 ) ) ;
#56276 = CARTESIAN_POINT ( 'NONE',  ( -11.35316468750000141, 213.8020833299193839, 3.042071309553159963 ) ) ;
#56277 = CARTESIAN_POINT ( 'NONE',  ( -25.17157287525374088, 202.7500000027312126, 172.8284271247464972 ) ) ;
#56278 = CARTESIAN_POINT ( 'NONE',  ( -27.99999999999995737, 198.5000000000000000, 174.0000000000003695 ) ) ;
#56280 = CARTESIAN_POINT ( 'NONE',  ( -2.828427124746209831, 206.3750000000000284, 139.1715728752538723 ) ) ;
#56279 = CARTESIAN_POINT ( 'NONE',  ( 2.828427124746208943, 208.6250000000000284, 195.1715728752538439 ) ) ;
#56281 = ORIENTED_EDGE ( 'NONE', *, *, #23200, .F. ) ;
#56282 = CARTESIAN_POINT ( 'NONE',  ( 2.445694354108783219, 201.8125000013656063, 139.5543056458912190 ) ) ;
#56283 = CARTESIAN_POINT ( 'NONE',  ( 8.311093377946834337, 15.15624999658601624, 8.311093377946839666 ) ) ;
#56284 = CARTESIAN_POINT ( 'NONE',  ( -6.735557395310442023E-16, 11.00000000000000000, 92.31250000409677625 ) ) ;
#56285 = CARTESIAN_POINT ( 'NONE',  ( -0.8419854211627070262, 10.28111362163633125, 63.57154293063805994 ) ) ;
#56286 = CARTESIAN_POINT ( 'NONE',  ( -29.43265458321755546, 198.8750000013656063, 173.4587341250004044 ) ) ;
#56287 = CARTESIAN_POINT ( 'NONE',  ( -75.00000000000001421, 272.0000000000000000, 20.00000000000003553 ) ) ;
#56289 = CARTESIAN_POINT ( 'NONE',  ( -3.042071309553163960, 12.23958332991935016, -11.35316468749999963 ) ) ;
#56288 = CARTESIAN_POINT ( 'NONE',  ( -2.977408999572650927, 116.3750000020483810, -7.188101187500000933 ) ) ;
#56290 = CARTESIAN_POINT ( 'NONE',  ( 7.999999999999991118, 3.313708498984757611, 28.67405277982336642 ) ) ;
#56291 = B_SPLINE_CURVE_WITH_KNOTS ( 'NONE', 3,
 ( #10345, #63133, #34117, #17103, #45048, #34866, #56370, #68794, #40126, #57871, #74085, #68421, #17481, #11461, #39749, #67690, #34495, #165 ),
 .UNSPECIFIED., .F., .F.,
 ( 4, 2, 2, 2, 2, 2, 2, 2, 4 ),
 ( 0.01486571574505584671, 0.01549490539733654020, 0.01612409504961723195, 0.01675328470189792543, 0.01738247435417861891, 0.01801166400645931240, 0.01864085365874000588, 0.01927004331102069937, 0.01989923296330139285 ),
 .UNSPECIFIED. ) ;
#56292 = CARTESIAN_POINT ( 'NONE',  ( -3.042071309553173730, 134.3229166632526983, 11.35316468749999785 ) ) ;
#56293 = VECTOR ( 'NONE', #7369, 1000.000000000000000 ) ;
#56294 = CARTESIAN_POINT ( 'NONE',  ( 5.000000000000001776, 102.7083333265053824, -8.660254037844389075 ) ) ;
#56295 = CARTESIAN_POINT ( 'NONE',  ( 7.188101187500002709, 122.1875000020483668, 2.977408999572649151 ) ) ;
#56296 = CARTESIAN_POINT ( 'NONE',  ( -4.541265875000003227, 21.99999999863440792, 1.881053915767121110 ) ) ;
#56297 = CARTESIAN_POINT ( 'NONE',  ( -10.00000000000000355, 199.5833333265053398, 2.679491924311223183 ) ) ;
#56298 = FACE_OUTER_BOUND ( 'NONE', #60011, .T. ) ;
#56299 = ORIENTED_EDGE ( 'NONE', *, *, #54649, .T. ) ;
#56300 = CARTESIAN_POINT ( 'NONE',  ( 18.00000000000000000, 0.000000000000000000, 0.000000000000000000 ) ) ;
#56301 = CARTESIAN_POINT ( 'NONE',  ( -6.676582343750001591, 291.6093750017069510, 0.000000000000000000 ) ) ;
#56302 = CARTESIAN_POINT ( 'NONE',  ( 4.999999999999999112, 53.18690467503036956, 43.91652490638277584 ) ) ;
#56303 = CARTESIAN_POINT ( 'NONE',  ( 7.999999999999992895, -3.313708498984756279, 27.04280278432983309 ) ) ;
#56304 = CARTESIAN_POINT ( 'NONE',  ( 3.407298021510790864, 68.04056125360874319, 20.39715949456173050 ) ) ;
#56305 = CARTESIAN_POINT ( 'NONE',  ( 3.313708498984765161, 102.9687499999999858, 7.999999999999998224 ) ) ;
#56306 = CARTESIAN_POINT ( 'NONE',  ( 10.18810118749999916, 1.247682550866122264E-15, 97.28125000204838102 ) ) ;
#56307 = EDGE_LOOP ( 'NONE', ( #19572, #10781, #11336, #52067, #46670, #50463 ) ) ;
#56308 = EDGE_CURVE ( 'NONE', #70823, #24126, #39722, .T. ) ;
#56309 = CARTESIAN_POINT ( 'NONE',  ( -3.999999999999960032, 198.0625000027312410, 196.3431457505076594 ) ) ;
#56310 = CARTESIAN_POINT ( 'NONE',  ( 3.042071309553159519, 150.0520833299193555, 11.35316468750000141 ) ) ;
#56311 = CARTESIAN_POINT ( 'NONE',  ( -5.656854249492375253, 5.656854249492375253, 24.64280277982336642 ) ) ;
#56312 = CARTESIAN_POINT ( 'NONE',  ( 3.458734125000016757, 203.1250000013656347, 199.4326545832176976 ) ) ;
#56313 = DIRECTION ( 'NONE',  ( -0.000000000000000000, 1.000000000000000000, -0.000000000000000000 ) ) ;
#56314 = CARTESIAN_POINT ( 'NONE',  ( 11.35316468749999785, 70.88541666325265567, 3.042071309553174174 ) ) ;
#56315 = EDGE_LOOP ( 'NONE', ( #18778, #23366, #6349, #39162 ) ) ;
#56316 = CARTESIAN_POINT ( 'NONE',  ( 4.220049686691934809, 10.18810118749999916, 115.1875000020483668 ) ) ;
#56317 = CARTESIAN_POINT ( 'NONE',  ( -8.342170076843785083E-16, 8.187499998634406140, 4.541265875000002339 ) ) ;
#56318 = ORIENTED_EDGE ( 'NONE', *, *, #56411, .T. ) ;
#56319 = VECTOR ( 'NONE', #61640, 1000.000000000000000 ) ;
#56320 = CARTESIAN_POINT ( 'NONE',  ( 3.313708498984762496, 1.218750000000000222, 7.999999999999998224 ) ) ;
#56321 = CARTESIAN_POINT ( 'NONE',  ( -3.313708498984815343, 109.9062500040967905, -7.999999999999944933 ) ) ;
#56322 = CARTESIAN_POINT ( 'NONE',  ( -7.347880794884122694E-16, 4.499999997268813168, 4.000000000000001776 ) ) ;
#56323 = CARTESIAN_POINT ( 'NONE',  ( -2.977408999572650039, 20.81249999795161543, -7.188101187500001821 ) ) ;
#56324 = CARTESIAN_POINT ( 'NONE',  ( -2.751064625579944321E-14, 200.8750000027312126, 146.0000000000000284 ) ) ;
#56325 = CARTESIAN_POINT ( 'NONE',  ( -7.204075437095965206, -7.204075437095968759, 111.7187500020483810 ) ) ;
#56326 = CARTESIAN_POINT ( 'NONE',  ( 7.320508075688769267, 110.6249999999999858, -7.320508075688769267 ) ) ;
#56327 = CARTESIAN_POINT ( 'NONE',  ( 4.000000000000001776, 11.81249999726881228, -1.656854249492381248 ) ) ;
#56328 = CARTESIAN_POINT ( 'NONE',  ( 2.824543433528785410E-14, 210.0000000000000284, 194.0000000000000568 ) ) ;
#56329 = EDGE_LOOP ( 'NONE', ( #30655, #43013 ) ) ;
#56330 = EDGE_CURVE ( 'NONE', #6481, #29411, #69333, .T. ) ;
#56331 = ADVANCED_FACE ( 'NONE', ( #64863 ), #63102, .T. ) ;
#56332 = CARTESIAN_POINT ( 'NONE',  ( -3.458734124999959914, 201.3750000013656347, 196.5673454167823877 ) ) ;
#56334 =( BOUNDED_CURVE ( )  B_SPLINE_CURVE ( 2, ( #69470, #17780, #40793, #18892, #12845, #64549, #1192, #46817, #7941, #69843, #35515, #52489, #24174 ),
 .UNSPECIFIED., .F., .F. ) 
 B_SPLINE_CURVE_WITH_KNOTS ( ( 3, 2, 2, 2, 2, 2, 3 ),
 ( 0.7336956521739129711, 0.7355072463768115298, 0.7373188405797100886, 0.7391304347826086474, 0.7409420289855072062, 0.7427536231884057649, 0.7445652173913043237 ),
 .UNSPECIFIED. ) 
 CURVE ( )  GEOMETRIC_REPRESENTATION_ITEM ( )  RATIONAL_B_SPLINE_CURVE ( ( 1.000000000000001998, 0.9659258262890662028, 1.000000000000000000, 0.9659258262890683122, 1.000000000000000000, 0.9659258262890683122, 1.000000000000000000, 0.9659258262890683122, 1.000000000000000000, 0.9659258262890683122, 1.000000000000000000, 0.9659258262890683122, 1.000000000000000000 ) ) 
 REPRESENTATION_ITEM ( '' )  );
#56333 = CARTESIAN_POINT ( 'NONE',  ( -25.55430564589111953, 209.0625000013656063, 172.4456943541091505 ) ) ;
#56335 = CARTESIAN_POINT ( 'NONE',  ( 2.828427124746191623, 12.87499999726881406, -2.828427124746191623 ) ) ;
#56336=STYLED_ITEM('',(#74706),#40499);
#56337 = CARTESIAN_POINT ( 'NONE',  ( -4.541265875000002339, 6.812499998634407028, -5.561446717895856393E-16 ) ) ;
#56338 = DIRECTION ( 'NONE',  ( -0.000000000000000000, -1.000000000000000000, -4.283267841918042741E-17 ) ) ;
#56339 = CARTESIAN_POINT ( 'NONE',  ( 2.977408999572646486, 7.188101187499991163, 17.51780278187175455 ) ) ;
#56340 = ORIENTED_EDGE ( 'NONE', *, *, #38449, .T. ) ;
#56341 = CARTESIAN_POINT ( 'NONE',  ( -5.082755093536325042, 26.53124999795161543, -5.082755093536325930 ) ) ;
#56342 = ORIENTED_EDGE ( 'NONE', *, *, #51131, .F. ) ;
#56343 = CARTESIAN_POINT ( 'NONE',  ( -7.204075437095967871, 7.204075437095967871, 107.9687500020483810 ) ) ;
#56344 = CARTESIAN_POINT ( 'NONE',  ( -2.886287813027996254E-11, 51.14729664189304970, 48.52014062455092613 ) ) ;
#56345 = CARTESIAN_POINT ( 'NONE',  ( 2.839093476692135984E-14, 203.6875000013656063, 201.4587341250000350 ) ) ;
#56346 = CARTESIAN_POINT ( 'NONE',  ( 30.44569435410879521, 199.8125000013656063, 167.5543056458910485 ) ) ;
#56347 = CARTESIAN_POINT ( 'NONE',  ( -2.679491924311235618, 83.54166666666664298, 10.00000000000000000 ) ) ;
#56348 = CARTESIAN_POINT ( 'NONE',  ( -2.977408999572650927, 89.75000000204839523, -7.188101187500001821 ) ) ;
#56349 = CARTESIAN_POINT ( 'NONE',  ( -4.242640687119286547, 290.8750000000000000, -4.242640687119286547 ) ) ;
#56350 = EDGE_CURVE ( 'NONE', #45186, #35289, #35633, .T. ) ;
#56351 = CARTESIAN_POINT ( 'NONE',  ( 32.00000000000000000, 203.3750000027312126, 169.9999999999998863 ) ) ;
#56352 = ORIENTED_EDGE ( 'NONE', *, *, #33476, .F. ) ;
#56353 = LINE ( 'NONE', #27668, #24101 ) ;
#56354 = CARTESIAN_POINT ( 'NONE',  ( 2.219371606101167238, -16.40787039054615093, 68.79427927095674988 ) ) ;
#56355 = CARTESIAN_POINT ( 'NONE',  ( -2.828427124746209831, 195.5000000027312126, 139.1715728752538723 ) ) ;
#56356 = CARTESIAN_POINT ( 'NONE',  ( -1.836970198721029983E-15, 55.62499999317203958, 10.00000000000000178 ) ) ;
#56357 = FACE_OUTER_BOUND ( 'NONE', #5425, .T. ) ;
#56358 = CARTESIAN_POINT ( 'NONE',  ( -2.679491924311222295, 256.0416666666666856, 10.00000000000000178 ) ) ;
#56359 = CARTESIAN_POINT ( 'NONE',  ( -8.660254037844417496, 77.08333333333337123, -5.000000000000023093 ) ) ;
#56360 = CARTESIAN_POINT ( 'NONE',  ( 8.660254037844389075, 205.4166666666666856, -5.000000000000000000 ) ) ;
#56361 = CARTESIAN_POINT ( 'NONE',  ( 0.000000000000000000, 125.0000000000000000, 8.000000000000000000 ) ) ;
#56362 = CARTESIAN_POINT ( 'NONE',  ( -7.188101187499990274, -2.977408999572651815, 13.95530278187175455 ) ) ;
#56363 = CARTESIAN_POINT ( 'NONE',  ( 9.832129032723416984, 170.6770833299193555, 5.676582343750006032 ) ) ;
#56364 = FACE_OUTER_BOUND ( 'NONE', #68905, .T. ) ;
#56365 = CARTESIAN_POINT ( 'NONE',  ( -7.778174593052020747, -7.778174593052023411, 82.37500000409677625 ) ) ;
#56367 = CARTESIAN_POINT ( 'NONE',  ( -2.828427124746192067, 7.374999997268813168, 2.828427124746190735 ) ) ;
#56366 = PLANE ( 'NONE',  #50290 ) ;
#56368 = ORIENTED_EDGE ( 'NONE', *, *, #25585, .F. ) ;
#56369 = CARTESIAN_POINT ( 'NONE',  ( -11.35316468750000141, 23.59374999658601979, -1.390361679473963753E-15 ) ) ;
#56370 = CARTESIAN_POINT ( 'NONE',  ( -1.616960574868709921, 194.5560245358154532, 201.1741968415167889 ) ) ;
#56371 = VECTOR ( 'NONE', #31309, 1000.000000000000000 ) ;
#56373 = CARTESIAN_POINT ( 'NONE',  ( -5.107860025166345075, -10.26152767799330690, -64.38109526788291248 ) ) ;
#56372 = DIRECTION ( 'NONE',  ( -0.000000000000000000, 1.000000000000000000, -0.000000000000000000 ) ) ;
#56374 = CYLINDRICAL_SURFACE ( 'NONE', #63921, 8.000000000000000000 ) ;
#56375 = CARTESIAN_POINT ( 'NONE',  ( -3.458734125000016313, 203.8750000013656063, 140.5673454167823593 ) ) ;
#56376 = CARTESIAN_POINT ( 'NONE',  ( -4.999999999999998224, 63.54166665983869677, -8.660254037844389075 ) ) ;
#56377 = CARTESIAN_POINT ( 'NONE',  ( 5.082755093536325042, 102.5937500020483668, -5.082755093536325930 ) ) ;
#56378 = CARTESIAN_POINT ( 'NONE',  ( -1.881053915767124440, 10.12499999863440792, 4.541265875000001451 ) ) ;
#56379 = CARTESIAN_POINT ( 'NONE',  ( 9.999999999999994671, 54.79166666666666430, 2.679491924311234285 ) ) ;
#56380 = CARTESIAN_POINT ( 'NONE',  ( 7.999999999999991118, 9.797174393178815797E-16, 3.080302779823361981 ) ) ;
#56381 = CARTESIAN_POINT ( 'NONE',  ( 9.999999999999998224, 164.7916666666666856, 2.679491924311235618 ) ) ;
#56382 = ORIENTED_EDGE ( 'NONE', *, *, #42258, .T. ) ;
#56383 = ORIENTED_EDGE ( 'NONE', *, *, #74544, .T. ) ;
#56384 = CARTESIAN_POINT ( 'NONE',  ( -3.999999999999959144, 205.1875000027312126, 199.6568542494924259 ) ) ;
#56385 = CARTESIAN_POINT ( 'NONE',  ( 2.754378923186476579E-14, 196.4375000013655779, 194.5412658750000219 ) ) ;
#56386 = LINE ( 'NONE', #27700, #26629 ) ;
#56387 = CARTESIAN_POINT ( 'NONE',  ( 3.042071309553173286, 220.6770833367472733, 11.35316468749999608 ) ) ;
#56388 = CARTESIAN_POINT ( 'NONE',  ( -5.676582343749998039, 137.4479166632526983, -9.832129032723420536 ) ) ;
#56389 = ORIENTED_EDGE ( 'NONE', *, *, #4731, .F. ) ;
#56390 = CARTESIAN_POINT ( 'NONE',  ( -5.656854249492373476, -5.656854249492376141, 10.20530278392014623 ) ) ;
#56391 = CARTESIAN_POINT ( 'NONE',  ( -10.18810118749999916, 0.000000000000000000, 88.65625000204838102 ) ) ;
#56392 = CARTESIAN_POINT ( 'NONE',  ( -31.42478664712804104, 194.6389826057388461, 171.2505314188794330 ) ) ;
#56393 = AXIS2_PLACEMENT_3D ( 'NONE', #38924, #15148, #67223 ) ;
#56394 = CARTESIAN_POINT ( 'NONE',  ( 2.828427124746208943, 208.6250000000000284, 195.1715728752538439 ) ) ;
#56395 = CARTESIAN_POINT ( 'NONE',  ( -7.347880794884122694E-16, 14.49999999726881406, 4.000000000000001776 ) ) ;
#56396 = DIRECTION ( 'NONE',  ( -0.000000000000000000, 1.000000000000000000, -0.000000000000000000 ) ) ;
#56397 = CARTESIAN_POINT ( 'NONE',  ( 1.347111479062088405E-15, 0.000000000000000000, -11.00000000000000000 ) ) ;
#56398 = ORIENTED_EDGE ( 'NONE', *, *, #782, .T. ) ;
#56399=STYLED_ITEM('',(#74678),#42204);
#56400 = CARTESIAN_POINT ( 'NONE',  ( -6.735557395310442023E-16, 11.00000000000000000, 108.8125000040967763 ) ) ;
#56401 = CARTESIAN_POINT ( 'NONE',  ( -28.52237390288164676, 180.9141530225708721, 157.6490779871871268 ) ) ;
#56402 = CARTESIAN_POINT ( 'NONE',  ( 11.35316468749999963, 111.3020833299193413, -3.042071309553165293 ) ) ;
#56403 = CARTESIAN_POINT ( 'NONE',  ( -3.458734124999959914, 202.4375000013656063, 198.0000000000000284 ) ) ;
#56404 = CARTESIAN_POINT ( 'NONE',  ( 2.977408999572652260, 26.06249999795161543, 7.188101187500000044 ) ) ;
#56405 = CARTESIAN_POINT ( 'NONE',  ( -6.238412754330611322E-16, 10.18810118749999916, 85.65625000204838102 ) ) ;
#56406 = CARTESIAN_POINT ( 'NONE',  ( 5.676582343750001591, 36.92708332991935549, -9.832129032723420536 ) ) ;
#56407 = ORIENTED_EDGE ( 'NONE', *, *, #62793, .F. ) ;
#56408 = CARTESIAN_POINT ( 'NONE',  ( -3.458734124999960358, 209.6875000013656063, 198.0000000000000284 ) ) ;
#56409 = CARTESIAN_POINT ( 'NONE',  ( -3.317071493978880348, -8.008118988124989457, 20.79436528394063188 ) ) ;
#56410 = CARTESIAN_POINT ( 'NONE',  ( -5.656854249492375253, 5.656854249492375253, 23.33030278392014978 ) ) ;
#56411 = EDGE_CURVE ( 'NONE', #19065, #73307, #4839, .T. ) ;
#56412 = CARTESIAN_POINT ( 'NONE',  ( 7.188101187500001821, 9.562499997951608322, -2.977408999572650483 ) ) ;
#56413 = CARTESIAN_POINT ( 'NONE',  ( 2.485281374238575314, 295.3750000034139589, 6.000000000000000888 ) ) ;
#56414 = CARTESIAN_POINT ( 'NONE',  ( 8.660254037844385522, 111.4583333265053682, 5.000000000000005329 ) ) ;
#56415 = CARTESIAN_POINT ( 'NONE',  ( 7.188101187500000044, 2.343749997951610098, 0.000000000000000000 ) ) ;
#56416 = EDGE_LOOP ( 'NONE', ( #18963, #61510, #29902, #59914 ) ) ;
#56417 = CARTESIAN_POINT ( 'NONE',  ( -11.35316468749999785, 153.3854166632526699, -3.042071309553167513 ) ) ;
#56418 = CARTESIAN_POINT ( 'NONE',  ( 10.18810118749999916, 1.247682550866122264E-15, 75.90625000204836681 ) ) ;
#56419 = CARTESIAN_POINT ( 'NONE',  ( -31.45873412499999233, 194.6875000013655779, 170.0000000000003979 ) ) ;
#56420 = CARTESIAN_POINT ( 'NONE',  ( -30.93541659651597797, 271.9999999999999432, 171.9999999999998295 ) ) ;
#56421 = CARTESIAN_POINT ( 'NONE',  ( 4.541265875000001451, 14.37499999863440969, 1.881053915767124440 ) ) ;
#56422 = VERTEX_POINT ( 'NONE', #28032 ) ;
#56423 = EDGE_CURVE ( 'NONE', #52808, #40745, #43313, .T. ) ;
#56424 = CARTESIAN_POINT ( 'NONE',  ( -2.828427124746152987, 201.2500000027312126, 200.8284271247462129 ) ) ;
#56425 = CARTESIAN_POINT ( 'NONE',  ( 1.656854249492347719, 209.8125000000000000, 146.0000000000000284 ) ) ;
#56426 = B_SPLINE_CURVE_WITH_KNOTS ( 'NONE', 3,
 ( #5698, #51711, #58, #17375, #46050, #29819 ),
 .UNSPECIFIED., .F., .F.,
 ( 4, 2, 4 ),
 ( 0.01236082503524029742, 0.01586526280559109534, 0.01936970057594189498 ),
 .UNSPECIFIED. ) ;
#56427 = CARTESIAN_POINT ( 'NONE',  ( -26.34314575050753859, 206.6875000027312126, 174.0000000000003411 ) ) ;
#56428 = AXIS2_PLACEMENT_3D ( 'NONE', #20701, #43719, #31659 ) ;
#56429 = CARTESIAN_POINT ( 'NONE',  ( 5.000000000000000000, -10.00000000000000000, 75.19090595827292134 ) ) ;
#56430 = ORIENTED_EDGE ( 'NONE', *, *, #73136, .F. ) ;
#56431 = CARTESIAN_POINT ( 'NONE',  ( -7.188101187500000933, 8.624999997951611874, -2.977408999572651371 ) ) ;
#56432 = DIRECTION ( 'NONE',  ( -0.000000000000000000, -1.000000000000000000, -0.000000000000000000 ) ) ;
#56433 = CARTESIAN_POINT ( 'NONE',  ( 0.000000000000000000, 0.000000000000000000, -10.80000000000000071 ) ) ;
#56434 = CARTESIAN_POINT ( 'NONE',  ( 7.320508075688774596, 35.62500000000000711, -7.320508075688774596 ) ) ;
#56435 = AXIS2_PLACEMENT_3D ( 'NONE', #24386, #58735, #51958 ) ;
#56436 = CARTESIAN_POINT ( 'NONE',  ( -2.977408999572651815, 108.3125000020483810, 7.188101187500000933 ) ) ;
#56437 = CARTESIAN_POINT ( 'NONE',  ( -25.55430564589119768, 209.5625000013656063, 167.5543056458915316 ) ) ;
#56438 = CARTESIAN_POINT ( 'NONE',  ( 4.721056650415999201, 289.0781250017069510, -4.721056650415999201 ) ) ;
#56439 = EDGE_CURVE ( 'NONE', #5598, #60666, #59205, .T. ) ;
#56441 = CARTESIAN_POINT ( 'NONE',  ( -10.00000000000000355, 67.29166666666667140, -2.679491924311231177 ) ) ;
#56440 = FACE_OUTER_BOUND ( 'NONE', #32305, .T. ) ;
#56442 = ORIENTED_EDGE ( 'NONE', *, *, #36684, .T. ) ;
#56443 = AXIS2_PLACEMENT_3D ( 'NONE', #36590, #41507, #64523 ) ;
#56444 = CARTESIAN_POINT ( 'NONE',  ( -8.311093377946834337, 254.5312500034139873, 8.311093377946837890 ) ) ;
#56445 = CARTESIAN_POINT ( 'NONE',  ( 7.188101187499993827, -2.977408999572645598, 25.01780278187175455 ) ) ;
#56446 = CARTESIAN_POINT ( 'NONE',  ( -1.506680654954638987, 55.70239491600216297, 43.84725041001183143 ) ) ;
#56447 = CARTESIAN_POINT ( 'NONE',  ( 49.70177871865296026, 50.00000000000007105, 57.99999999999998579 ) ) ;
#56448 = CARTESIAN_POINT ( 'NONE',  ( -2.726571689596997292E-14, 210.0000000000000284, 138.0000000000000568 ) ) ;
#56449 = CARTESIAN_POINT ( 'NONE',  ( -3.941655914118860071, 22.00000000000000355, 2.274490667310467451 ) ) ;
#56450 =( BOUNDED_CURVE ( )  B_SPLINE_CURVE ( 2, ( #21281, #26942, #49961, #44305, #67320, #15617, #38656, #8108, #25442 ),
 .UNSPECIFIED., .F., .F. ) 
 B_SPLINE_CURVE_WITH_KNOTS ( ( 3, 2, 2, 2, 3 ),
 ( 0.7500000000000000000, 0.7536764705882352811, 0.7573529411764705621, 0.7610294117647058432, 0.7647058823529411242 ),
 .UNSPECIFIED. ) 
 CURVE ( )  GEOMETRIC_REPRESENTATION_ITEM ( )  RATIONAL_B_SPLINE_CURVE ( ( 1.000000000000000000, 0.9238795325112867385, 1.000000000000000000, 0.9238795325112867385, 1.000000000000000000, 0.9238795325112867385, 1.000000000000000000, 0.9238795325112867385, 1.000000000000000000 ) ) 
 REPRESENTATION_ITEM ( '' )  );
#56451 = CARTESIAN_POINT ( 'NONE',  ( -10.00000000000000000, 152.2916666666666856, -2.679491924311229845 ) ) ;
#56452 = CYLINDRICAL_SURFACE ( 'NONE', #51470, 3.999999999999976019 ) ;
#56453 = CARTESIAN_POINT ( 'NONE',  ( 10.52975931929885789, 14.70525031332736177, -0.04683108270947845125 ) ) ;
#56454 =( BOUNDED_CURVE ( )  B_SPLINE_CURVE ( 2, ( #40943, #23951, #230, #46223, #11897, #51509, #6976, #1337, #5874 ),
 .UNSPECIFIED., .F., .F. ) 
 B_SPLINE_CURVE_WITH_KNOTS ( ( 3, 2, 2, 2, 3 ),
 ( 0.8666666666666673624, 0.8750000000000006661, 0.8833333333333339699, 0.8916666666666674956, 0.9000000000000007994 ),
 .UNSPECIFIED. ) 
 CURVE ( )  GEOMETRIC_REPRESENTATION_ITEM ( )  RATIONAL_B_SPLINE_CURVE ( ( 0.9999999999999938938, 0.9238795325112928447, 1.000000000000000000, 0.9238795325112867385, 1.000000000000000000, 0.9238795325112867385, 1.000000000000000000, 0.9238795325112796331, 1.000000000000007105 ) ) 
 REPRESENTATION_ITEM ( '' )  );
#56455 = DIRECTION ( 'NONE',  ( 0.000000000000000000, 0.000000000000000000, 1.000000000000000000 ) ) ;
#56456 = CARTESIAN_POINT ( 'NONE',  ( -9.832129032723420536, 124.0104166632526841, 5.676582343749997150 ) ) ;
#56457 = CARTESIAN_POINT ( 'NONE',  ( -6.000000000000003553, 295.9374999999999432, -2.485281374238571317 ) ) ;
#56458 = CARTESIAN_POINT ( 'NONE',  ( -4.556349186104045934, 11.00000000000000000, 72.71874999999997158 ) ) ;
#56461 = CARTESIAN_POINT ( 'NONE',  ( 0.000000000000000000, 0.5000000000000004441, 0.000000000000000000 ) ) ;
#56460 = CARTESIAN_POINT ( 'NONE',  ( 30.44569435410879166, 196.8125000013656063, 167.5543056458910485 ) ) ;
#56459 = CARTESIAN_POINT ( 'NONE',  ( 26.34314575050763807, 208.5625000000000000, 165.9999999999998863 ) ) ;
#56462 = EDGE_CURVE ( 'NONE', #19443, #4330, #70975, .T. ) ;
#56463 = VERTEX_POINT ( 'NONE', #7894 ) ;
#56464 = EDGE_CURVE ( 'NONE', #34088, #5951, #55463, .T. ) ;
#56465 = CARTESIAN_POINT ( 'NONE',  ( -1.469576158976823947E-15, 20.62500000000000355, 8.000000000000000000 ) ) ;
#56466 = DIRECTION ( 'NONE',  ( 0.000000000000000000, 0.000000000000000000, -1.000000000000000000 ) ) ;
#56467 = CARTESIAN_POINT ( 'NONE',  ( 30.44569435410878810, 197.8125000013656063, 172.4456943541087526 ) ) ;
#56468 = EDGE_CURVE ( 'NONE', #74609, #19989, #15, .T. ) ;
#56469 = CARTESIAN_POINT ( 'NONE',  ( 11.35316468749999963, 206.3020833299193271, -3.042071309553165293 ) ) ;
#56470 = CARTESIAN_POINT ( 'NONE',  ( 7.188101187500000044, 118.9062500020483810, -8.802885111219163269E-16 ) ) ;
#56471 = CARTESIAN_POINT ( 'NONE',  ( -3.211159895383561391, 18.68749999863440436, -3.211159895383561835 ) ) ;
#56472 = CARTESIAN_POINT ( 'NONE',  ( 4.737866951550043559, -52.21905653846192052, 48.93292554253444138 ) ) ;
#56473 = CARTESIAN_POINT ( 'NONE',  ( 7.999999999999991118, 9.797174393178815797E-16, 28.58030277982336642 ) ) ;
#56475 = CARTESIAN_POINT ( 'NONE',  ( -27.99999999999991473, 208.6250000027312126, 174.0000000000003695 ) ) ;
#56474 = CARTESIAN_POINT ( 'NONE',  ( 2.449293598294707893E-16, 1.250000000000000222, -4.000000000000001776 ) ) ;
#56476 = CARTESIAN_POINT ( 'NONE',  ( -8.311093377946836114, 97.65624999658602690, -8.311093377946837890 ) ) ;
#56477 = ORIENTED_EDGE ( 'NONE', *, *, #59300, .F. ) ;
#56478 = CARTESIAN_POINT ( 'NONE',  ( -7.778174593052023411, 7.778174593052023411, 81.81249999999998579 ) ) ;
#56479 = CARTESIAN_POINT ( 'NONE',  ( -2.977408999572650039, 20.43749999795161187, -7.188101187500001821 ) ) ;
#56480 = CARTESIAN_POINT ( 'NONE',  ( -2.775557561562891351E-14, 210.0000000000000284, 142.0000000000000568 ) ) ;
#56481 = CARTESIAN_POINT ( 'NONE',  ( 11.35316468749999608, 256.9270833367473301, -3.042071309553167513 ) ) ;
#56482 = CARTESIAN_POINT ( 'NONE',  ( -11.35316468750000141, 108.4895833299193413, 3.042071309553159963 ) ) ;
#56483 = ORIENTED_EDGE ( 'NONE', *, *, #64252, .F. ) ;
#56484 = CARTESIAN_POINT ( 'NONE',  ( 2.679491924311228956, 207.9166666598387110, -10.00000000000000000 ) ) ;
#56485 = CARTESIAN_POINT ( 'NONE',  ( 10.18810118750000093, -4.220049686691933921, 105.8125000020483952 ) ) ;
#56486 = CARTESIAN_POINT ( 'NONE',  ( -30.44569435410878810, 196.0625000013656063, 172.4456943541092357 ) ) ;
#56487 = CARTESIAN_POINT ( 'NONE',  ( 3.458734125000016757, 204.1250000013656063, 199.4326545832176691 ) ) ;
#56488 = DIRECTION ( 'NONE',  ( 0.000000000000000000, 0.000000000000000000, 1.000000000000000000 ) ) ;
#56490 = CARTESIAN_POINT ( 'NONE',  ( -9.832129032723420536, 88.69791666325268409, 5.676582343749997150 ) ) ;
#56489 = CARTESIAN_POINT ( 'NONE',  ( -3.313708498984757611, 7.999999999999991118, 23.04905277982336287 ) ) ;
#56491 = CARTESIAN_POINT ( 'NONE',  ( 3.313708498984756279, 7.999999999999991118, 11.04905278392014800 ) ) ;
#56492 = CARTESIAN_POINT ( 'NONE',  ( -24.54126587499998280, 200.3750000013656063, 171.4326545832179818 ) ) ;
#56493 = DIRECTION ( 'NONE',  ( -0.000000000000000000, -1.000000000000000000, -0.000000000000000000 ) ) ;
#56494 = ORIENTED_EDGE ( 'NONE', *, *, #59880, .F. ) ;
#56495 = CARTESIAN_POINT ( 'NONE',  ( 10.00000000000000000, 181.6666666598387394, 2.679491924311236062 ) ) ;
#56496 = VECTOR ( 'NONE', #28991, 1000.000000000000000 ) ;
#56497 = CARTESIAN_POINT ( 'NONE',  ( 28.00000000000001776, 196.1250000027311842, 173.9999999999999147 ) ) ;
#56498 = DIRECTION ( 'NONE',  ( -1.000000000000000000, -0.000000000000000000, -0.000000000000000000 ) ) ;
#56499 = CARTESIAN_POINT ( 'NONE',  ( -2.085542519210945728E-15, 79.84374999658601268, 11.35316468750000141 ) ) ;
#56500 = CARTESIAN_POINT ( 'NONE',  ( -6.676582343750003368, 290.3906250017070647, -2.765530957081996810 ) ) ;
#56501 = CARTESIAN_POINT ( 'NONE',  ( 10.18810118750000093, -4.220049686691933033, 100.1875000020483952 ) ) ;
#56502 = CARTESIAN_POINT ( 'NONE',  ( -3.042071309553164404, 217.2395833299192986, -11.35316468749999963 ) ) ;
#56503 = ORIENTED_EDGE ( 'NONE', *, *, #69873, .T. ) ;
#56504 = CARTESIAN_POINT ( 'NONE',  ( -7.347880794884122694E-16, 2.750000000000000000, 4.000000000000001776 ) ) ;
#56505 = CARTESIAN_POINT ( 'NONE',  ( -28.00000000000007816, 203.1250000027312126, 166.0000000000003695 ) ) ;
#56506 = CYLINDRICAL_SURFACE ( 'NONE', #46741, 3.999999999999976019 ) ;
#56507 = CARTESIAN_POINT ( 'NONE',  ( -11.35316468750000141, 203.2812499965860411, -1.390361679473963753E-15 ) ) ;
#56508 = AXIS2_PLACEMENT_3D ( 'NONE', #3704, #44435, #8986 ) ;
#56509 = CARTESIAN_POINT ( 'NONE',  ( -8.660254037844385522, 228.5416666734946602, 5.000000000000004441 ) ) ;
#56510 = CARTESIAN_POINT ( 'NONE',  ( -3.428378827827392783, -16.35907404636618523, -69.10239319626211341 ) ) ;
#56511 = CARTESIAN_POINT ( 'NONE',  ( 11.00000000000000000, 1.347111479062088405E-15, 67.93750000409676204 ) ) ;
#56512 = ORIENTED_EDGE ( 'NONE', *, *, #4730, .F. ) ;
#56513 = CARTESIAN_POINT ( 'NONE',  ( -2.085542519210945728E-15, 189.8437499965860127, 11.35316468750000141 ) ) ;
#56514 = AXIS2_PLACEMENT_3D ( 'NONE', #47447, #30108, #64071 ) ;
#56515 = CARTESIAN_POINT ( 'NONE',  ( 5.082755093536318824, 5.082755093536319713, 14.42405278187175455 ) ) ;
#56516 = EDGE_CURVE ( 'NONE', #12488, #23710, #46984, .T. ) ;
#56517 = CARTESIAN_POINT ( 'NONE',  ( -25.55430564589119768, 208.3125000013656063, 167.5543056458915316 ) ) ;
#56518 = CARTESIAN_POINT ( 'NONE',  ( -3.313708498984760720, 9.468750000000000000, -8.000000000000000000 ) ) ;
#56519 = ORIENTED_EDGE ( 'NONE', *, *, #13144, .T. ) ;
#56520 = CARTESIAN_POINT ( 'NONE',  ( 5.656854249492379694, 90.12500000409677625, -5.656854249492380582 ) ) ;
#56521 = CARTESIAN_POINT ( 'NONE',  ( -5.000000000000005329, 8.333333333333333925, 8.660254037844387298 ) ) ;
#56522 = ADVANCED_FACE ( 'NONE', ( #60308 ), #66449, .T. ) ;
#56523 = CARTESIAN_POINT ( 'NONE',  ( -10.18810118749999916, 0.000000000000000000, 81.53125000204838102 ) ) ;
#56524 = ORIENTED_EDGE ( 'NONE', *, *, #72397, .T. ) ;
#56525 = CARTESIAN_POINT ( 'NONE',  ( 2.828427124746190291, 20.87500000000000000, 2.828427124746192067 ) ) ;
#56526 = CARTESIAN_POINT ( 'NONE',  ( -8.342170076843785083E-16, 19.06249999863440436, 4.541265875000002339 ) ) ;
#56527 = PRODUCT_RELATED_PRODUCT_CATEGORY ( 'part', '', ( #54090 ) ) ;
#56528 = CARTESIAN_POINT ( 'NONE',  ( 0.8721677472502531447, 16.44158143986616949, -68.58266913489720196 ) ) ;
#56529 = ORIENTED_EDGE ( 'NONE', *, *, #51176, .T. ) ;
#56530 = CARTESIAN_POINT ( 'NONE',  ( 5.082755093536326818, 123.5937500020483952, 5.082755093536325042 ) ) ;
#56533 = CARTESIAN_POINT ( 'NONE',  ( -1.469576158976823947E-15, 3.937499995903220640, 8.000000000000000000 ) ) ;
#56532 = CARTESIAN_POINT ( 'NONE',  ( -5.676582343750000703, 243.0729166700806445, -9.832129032723418760 ) ) ;
#56531 = CARTESIAN_POINT ( 'NONE',  ( 25.55430564589119413, 206.3125000013656063, 172.4456943541087526 ) ) ;
#56534 = SHAPE_DEFINITION_REPRESENTATION ( #10783, #63845 ) ;
#56535 = ORIENTED_EDGE ( 'NONE', *, *, #73450, .F. ) ;
#56536 = EDGE_CURVE ( 'NONE', #63061, #62856, #15968, .T. ) ;
#56537 = CARTESIAN_POINT ( 'NONE',  ( 11.35316468749999963, 251.7187500034139873, -1.390361679473963556E-15 ) ) ;
#56538 = CARTESIAN_POINT ( 'NONE',  ( 7.188101187499993827, -2.977408999572645598, 15.64280278187175277 ) ) ;
#56539 = VERTEX_POINT ( 'NONE', #38635 ) ;
#56540 = EDGE_CURVE ( 'NONE', #111, #17357, #43773, .T. ) ;
#56541 = ORIENTED_EDGE ( 'NONE', *, *, #6696, .F. ) ;
#56542 = CARTESIAN_POINT ( 'NONE',  ( 4.220049686691941027, -10.18810118749999738, 77.12500000204838102 ) ) ;
#56543 = CARTESIAN_POINT ( 'NONE',  ( -5.676582343749998039, 82.76041666325268409, -9.832129032723420536 ) ) ;
#56544 = CYLINDRICAL_SURFACE ( 'NONE', #57732, 12.00000000000000355 ) ;
#56545 = CARTESIAN_POINT ( 'NONE',  ( -4.556349186104047710, -10.99999999999999822, 86.78124999999998579 ) ) ;
#56548 = CARTESIAN_POINT ( 'NONE',  ( 2.765530957081996366, 288.2968750017070079, -6.676582343750002480 ) ) ;
#56547 = CARTESIAN_POINT ( 'NONE',  ( 28.00000000000002132, 209.4375000013656063, 173.4587341249998929 ) ) ;
#56546 = CARTESIAN_POINT ( 'NONE',  ( 27.99999999999996803, 206.6875000013656063, 173.4587341249998929 ) ) ;
#56549 =( BOUNDED_SURFACE ( )  B_SPLINE_SURFACE ( 1, 2, ( 
 ( #18310, #6992, #13000, #47703, #59054, #19043, #42047, #7729, #30736, #55901, #40025, #63027, #50965, #50219, #39652, #16617, #39281, #49849, #21172, #73978, #38547, #27960, #28329, #27578, #67210, #10983, #33637, #22282, #62650, #32897, #45674, #50587, #62283, #45305, #73605, #33266, #11352, #34017, #72868, #21545, #38911, #26835, #21912, #10611, #44197, #68689, #68319, #56265, #5326, #67949, #15507, #57014, #56644, #16998, #51337, #9868, #61548, #74345, #73240, #4958, #22655, #55528, #61913, #4213, #3839, #27202, #10239, #44571, #4583, #67584, #15880, #16243, #44943, #41501, #64518, #6446, #7177, #17746, #12816, #57388, #69436, #11719, #29075, #63769, #70544, #40396, #34760, #46048, #58497, #41139, #12086, #35123, #63394, #52095, #57762, #64145, #34387, #69067, #46422, #12455, #18860, #35851, #17371, #58866, #5696, #18493, #6803, #427, #23406, #58139, #29448, #40762, #24514, #29816, #6068, #41866, #46786, #52458, #30183, #796, #28695, #35484, #53200, #1534, #47518, #52829, #18124, #47151, #64879, #51709, #56, #23781, #69808, #1162, #23037, #24140, #70184, #19586, #9028, #30915, #2626, #49003, #66362, #49378, #60326, #47889, #14667, #42966, #3370, #25615, #36219, #48629, #7546, #32041, #19960, #20327, #59958, #65987, #14292, #13913, #65617, #37329, #37707, #8654, #31669, #60708, #71638, #7909, #54688, #43726, #59237, #2997, #25978, #71266, #59596, #13547, #43344, #54316, #53936, #55061, #30554, #72013, #70909, #13181, #26357, #72398, #20709, #53568, #1884, #24870, #19223, #42229, #65241, #8276, #36585, #42602, #2250, #25243, #48260, #36952, #31286, #21457, #28244, #72781, #44111, #3744, #16152, #73515, #44480, #67494, #21087, #61457, #67120, #21822, #66740, #26745, #4129, #44854, #51252, #68236, #49764, #16529, #15045, #50877, #39193, #9783, #32802, #15792, #38827, #27120, #56928, #62196, #15414, #74262, #4495, #61829, #39568, #38455, #38081, #67860, #73893 ),
 ( #56557, #56183, #55812, #10521, #5244, #33553, #50135, #73150, #10149, #33186, #4872, #27867, #10895, #27487, #22197, #61078, #50501, #45222, #62564, #33929, #22571, #9405, #32424, #55435, #12738, #28613, #45965, #23324, #51626, #6727, #17289, #46336, #35411, #68980, #30104, #53121, #41057, #40308, #29733, #52748, #29371, #39937, #11267, #64066, #74642, #18042, #18412, #17663, #57302, #1083, #23698, #12375, #24060, #22957, #35770, #40681, #52378, #58420, #63683, #69352, #1454, #47070, #62943, #11637, #28988, #16913, #12010, #714, #34299, #58786, #70107, #35043, #7095, #63310, #34673, #58055, #57677, #41427, #5986, #6366, #64439, #52006, #45590, #68605, #5614, #343, #46703, #69727, #8195, #18784, #64798, #19877, #7467, #71555, #71930, #71186, #36137, #54605, #2540, #42882, #60242, #1806, #14585, #19505, #31206, #65902, #42523, #2167, #54980, #2912, #41789, #65157, #7829, #70467, #65537, #54231, #13100, #37622, #14208, #25161, #48917, #36873, #59158, #37245, #25532, #60619, #20242, #53489, #30472, #8567, #19140, #48545, #43261, #25900, #30833, #24792, #66277, #36507, #47806, #48178, #70828, #31583, #13828, #42144, #8943, #31955, #13468, #59516, #53855, #24435, #47442, #59882, #15706, #56097, #10435, #10804, #21369, #16444, #43640, #66649, #20995, #22111, #9698, #73432, #27402, #50790, #14957, #50418, #4406, #44768, #45135, #67406, #32719, #44393, #26273, #39108, #67782, #38748, #72694, #21740, #68147, #16074, #32340, #3657, #15330, #73062, #62112, #33465, #39479, #55727, #56467, #3287, #26657, #4783, #10065, #27777, #55352, #61748, #33101, #49680, #73803, #62475, #33840, #4043, #49293, #72311, #44021, #20624, #37995, #60993, #67031, #9319, #38366, #61372, #27036, #50046, #57210, #34583, #62847, #17952, #28525, #57589, #46618, #5524, #41338, #64346, #52289, #51533, #40969, #63977, #40594, #51164, #22477, #627, #39845, #29280, #29644, #28898, #68515, #12290, #34954 ) ),
 .UNSPECIFIED., .F., .F., .F. ) 
 B_SPLINE_SURFACE_WITH_KNOTS ( ( 2, 2 ),
 ( 3, 2, 2, 2, 2, 2, 2, 2, 2, 2, 2, 2, 2, 2, 2, 2, 2, 2, 2, 2, 2, 2, 2, 2, 2, 2, 2, 2, 2, 2, 2, 2, 2, 2, 2, 2, 2, 2, 2, 2, 2, 2, 2, 2, 2, 2, 2, 2, 2, 2, 2, 2, 2, 2, 2, 2, 2, 2, 2, 2, 2, 2, 2, 2, 2, 2, 2, 2, 2, 2, 2, 2, 2, 2, 2, 2, 2, 2, 2, 2, 2, 2, 2, 2, 2, 2, 2, 2, 2, 2, 2, 2, 2, 2, 2, 2, 2, 2, 2, 2, 2, 2, 2, 2, 2, 2, 2, 2, 2, 2, 2, 2, 2, 2, 2, 2, 2, 2, 2, 2, 3 ),
 ( 0.000000000000000000, 1.000000000000000000 ),
 ( 0.000000000000000000, 0.008333333333333333218, 0.01666666666666666644, 0.02500000000000000139, 0.03333333333333333287, 0.04166666666666666435, 0.05000000000000000278, 0.05833333333333333426, 0.06666666666666666574, 0.07499999999999999722, 0.08333333333333332871, 0.09166666666666666019, 0.1000000000000000056, 0.1083333333333333370, 0.1166666666666666685, 0.1250000000000000000, 0.1333333333333333315, 0.1416666666666666630, 0.1499999999999999944, 0.1583333333333333259, 0.1666666666666666574, 0.1749999999999999889, 0.1833333333333333204, 0.1916666666666666796, 0.2000000000000000111, 0.2083333333333333426, 0.2166666666666666741, 0.2250000000000000056, 0.2333333333333333370, 0.2416666666666666685, 0.2500000000000000000, 0.2583333333333333592, 0.2666666666666666630, 0.2750000000000000222, 0.2833333333333333259, 0.2916666666666666852, 0.2999999999999999889, 0.3083333333333333481, 0.3166666666666666519, 0.3250000000000000111, 0.3333333333333333148, 0.3416666666666666741, 0.3499999999999999778, 0.3583333333333333370, 0.3666666666666666408, 0.3750000000000000000, 0.3833333333333333592, 0.3916666666666666630, 0.4000000000000000222, 0.4083333333333333259, 0.4166666666666666852, 0.4249999999999999889, 0.4333333333333333481, 0.4416666666666666519, 0.4500000000000000111, 0.4583333333333333148, 0.4666666666666666741, 0.4749999999999999778, 0.4833333333333333370, 0.4916666666666666408, 0.5000000000000000000, 0.5083333333333333037, 0.5166666666666667185, 0.5250000000000000222, 0.5333333333333333259, 0.5416666666666666297, 0.5500000000000000444, 0.5583333333333333481, 0.5666666666666666519, 0.5749999999999999556, 0.5833333333333333703, 0.5916666666666666741, 0.5999999999999999778, 0.6083333333333332815, 0.6166666666666666963, 0.6250000000000000000, 0.6333333333333333037, 0.6416666666666667185, 0.6500000000000000222, 0.6583333333333333259, 0.6666666666666666297, 0.6750000000000000444, 0.6833333333333333481, 0.6916666666666666519, 0.6999999999999999556, 0.7083333333333333703, 0.7166666666666666741, 0.7249999999999999778, 0.7333333333333332815, 0.7416666666666666963, 0.7500000000000000000, 0.7583333333333333037, 0.7666666666666667185, 0.7750000000000000222, 0.7833333333333333259, 0.7916666666666666297, 0.8000000000000000444, 0.8083333333333333481, 0.8166666666666666519, 0.8249999999999999556, 0.8333333333333333703, 0.8416666666666666741, 0.8499999999999999778, 0.8583333333333332815, 0.8666666666666666963, 0.8750000000000000000, 0.8833333333333333037, 0.8916666666666667185, 0.9000000000000000222, 0.9083333333333333259, 0.9166666666666666297, 0.9250000000000000444, 0.9333333333333333481, 0.9416666666666666519, 0.9499999999999999556, 0.9583333333333333703, 0.9666666666666666741, 0.9749999999999999778, 0.9833333333333332815, 0.9916666666666666963, 1.000000000000000000 ),
 .UNSPECIFIED. ) 
 GEOMETRIC_REPRESENTATION_ITEM ( )  RATIONAL_B_SPLINE_SURFACE ( (
 ( 1.000000000000000000, 0.9238795325112867385, 1.000000000000000000, 0.9238795325112867385, 1.000000000000000000, 0.9238795325112867385, 1.000000000000000000, 0.9238795325112867385, 1.000000000000000000, 0.9238795325112867385, 1.000000000000000000, 0.9238795325112867385, 1.000000000000000000, 0.9238795325112867385, 1.000000000000000000, 0.9238795325112867385, 1.000000000000000000, 0.9238795325112867385, 1.000000000000000000, 0.9238795325112867385, 1.000000000000000000, 0.9238795325112867385, 1.000000000000000000, 0.9238795325112867385, 1.000000000000000000, 0.9238795325112867385, 1.000000000000000000, 0.9238795325112867385, 1.000000000000000000, 0.9238795325112867385, 1.000000000000000000, 0.9238795325112867385, 1.000000000000000000, 0.9238795325112867385, 1.000000000000000000, 0.9238795325112867385, 1.000000000000000000, 0.9238795325112867385, 1.000000000000000000, 0.9238795325112867385, 1.000000000000000000, 0.9238795325112867385, 1.000000000000000000, 0.9238795325112867385, 1.000000000000000000, 0.9238795325112867385, 1.000000000000000000, 0.9238795325112867385, 1.000000000000000000, 0.9238795325112867385, 1.000000000000000000, 0.9238795325112867385, 1.000000000000000000, 0.9238795325112867385, 1.000000000000000000, 0.9238795325112867385, 1.000000000000000000, 0.9238795325112867385, 1.000000000000000000, 0.9238795325112867385, 1.000000000000000000, 0.9238795325112867385, 1.000000000000000000, 0.9238795325112867385, 1.000000000000000000, 0.9238795325112867385, 1.000000000000000000, 0.9238795325112867385, 1.000000000000000000, 0.9238795325112867385, 1.000000000000000000, 0.9238795325112867385, 1.000000000000000000, 0.9238795325112867385, 1.000000000000000000, 0.9238795325112867385, 1.000000000000000000, 0.9238795325112867385, 1.000000000000000000, 0.9238795325112867385, 1.000000000000000000, 0.9238795325112867385, 1.000000000000000000, 0.9238795325112867385, 1.000000000000000000, 0.9238795325112867385, 1.000000000000000000, 0.9238795325112867385, 1.000000000000000000, 0.9238795325112867385, 1.000000000000000000, 0.9238795325112867385, 1.000000000000000000, 0.9238795325112867385, 1.000000000000000000, 0.9238795325112867385, 1.000000000000000000, 0.9238795325112867385, 1.000000000000000000, 0.9238795325112867385, 1.000000000000000000, 0.9238795325112867385, 1.000000000000000000, 0.9238795325112867385, 1.000000000000000000, 0.9238795325112867385, 1.000000000000000000, 0.9238795325112867385, 1.000000000000000000, 0.9238795325112867385, 1.000000000000000000, 0.9238795325112867385, 1.000000000000000000, 0.9238795325112867385, 1.000000000000000000, 0.9238795325112867385, 1.000000000000000000, 0.9238795325112867385, 1.000000000000000000, 0.9238795325112867385, 1.000000000000000000, 0.9238795325112867385, 1.000000000000000000, 0.9238795325112867385, 1.000000000000000000, 0.9238795325112867385, 1.000000000000000000, 0.9238795325112867385, 1.000000000000000000, 0.9238795325112867385, 1.000000000000000000, 0.9238795325112867385, 1.000000000000000000, 0.9238795325112867385, 1.000000000000000000, 0.9238795325112867385, 1.000000000000000000, 0.9238795325112867385, 1.000000000000000000, 0.9238795325112867385, 1.000000000000000000, 0.9238795325112867385, 1.000000000000000000, 0.9238795325112867385, 1.000000000000000000, 0.9238795325112867385, 1.000000000000000000, 0.9238795325112867385, 1.000000000000000000, 0.9238795325112867385, 1.000000000000000000, 0.9238795325112867385, 1.000000000000000000, 0.9238795325112867385, 1.000000000000000000, 0.9238795325112867385, 1.000000000000000000, 0.9238795325112867385, 1.000000000000000000, 0.9238795325112867385, 1.000000000000000000, 0.9238795325112867385, 1.000000000000000000, 0.9238795325112867385, 1.000000000000000000, 0.9238795325112867385, 1.000000000000000000, 0.9238795325112867385, 1.000000000000000000, 0.9238795325112867385, 1.000000000000000000, 0.9238795325112867385, 1.000000000000000000, 0.9238795325112867385, 1.000000000000000000, 0.9238795325112867385, 1.000000000000000000, 0.9238795325112867385, 1.000000000000000000, 0.9238795325112867385, 1.000000000000000000, 0.9238795325112867385, 1.000000000000000000, 0.9238795325112867385, 1.000000000000000000, 0.9238795325112867385, 1.000000000000000000, 0.9238795325112867385, 1.000000000000000000, 0.9238795325112867385, 1.000000000000000000, 0.9238795325112867385, 1.000000000000000000, 0.9238795325112867385, 1.000000000000000000, 0.9238795325112867385, 1.000000000000000000, 0.9238795325112867385, 1.000000000000000000, 0.9238795325112867385, 1.000000000000000000, 0.9238795325112867385, 1.000000000000000000, 0.9238795325112867385, 1.000000000000000000, 0.9238795325112867385, 1.000000000000000000, 0.9238795325112867385, 1.000000000000000000, 0.9238795325112867385, 1.000000000000000000, 0.9238795325112867385, 1.000000000000000000, 0.9238795325112867385, 1.000000000000000000, 0.9238795325112867385, 1.000000000000000000, 0.9238795325112867385, 1.000000000000000000, 0.9238795325112867385, 1.000000000000000000, 0.9238795325112867385, 1.000000000000000000, 0.9238795325112867385, 1.000000000000000000, 0.9238795325112867385, 1.000000000000000000, 0.9238795325112867385, 1.000000000000000000, 0.9238795325112867385, 1.000000000000000000, 0.9238795325112867385, 1.000000000000000000, 0.9238795325112867385, 1.000000000000000000, 0.9238795325112867385, 1.000000000000000000, 0.9238795325112867385, 1.000000000000000000, 0.9238795325112867385, 1.000000000000000000),
 ( 1.000000000000000000, 0.9238795325112867385, 1.000000000000000000, 0.9238795325112867385, 1.000000000000000000, 0.9238795325112867385, 1.000000000000000000, 0.9238795325112867385, 1.000000000000000000, 0.9238795325112867385, 1.000000000000000000, 0.9238795325112867385, 1.000000000000000000, 0.9238795325112867385, 1.000000000000000000, 0.9238795325112867385, 1.000000000000000000, 0.9238795325112867385, 1.000000000000000000, 0.9238795325112867385, 1.000000000000000000, 0.9238795325112867385, 1.000000000000000000, 0.9238795325112867385, 1.000000000000000000, 0.9238795325112867385, 1.000000000000000000, 0.9238795325112867385, 1.000000000000000000, 0.9238795325112867385, 1.000000000000000000, 0.9238795325112867385, 1.000000000000000000, 0.9238795325112867385, 1.000000000000000000, 0.9238795325112867385, 1.000000000000000000, 0.9238795325112867385, 1.000000000000000000, 0.9238795325112867385, 1.000000000000000000, 0.9238795325112867385, 1.000000000000000000, 0.9238795325112867385, 1.000000000000000000, 0.9238795325112867385, 1.000000000000000000, 0.9238795325112867385, 1.000000000000000000, 0.9238795325112867385, 1.000000000000000000, 0.9238795325112867385, 1.000000000000000000, 0.9238795325112867385, 1.000000000000000000, 0.9238795325112867385, 1.000000000000000000, 0.9238795325112867385, 1.000000000000000000, 0.9238795325112867385, 1.000000000000000000, 0.9238795325112867385, 1.000000000000000000, 0.9238795325112867385, 1.000000000000000000, 0.9238795325112867385, 1.000000000000000000, 0.9238795325112867385, 1.000000000000000000, 0.9238795325112867385, 1.000000000000000000, 0.9238795325112867385, 1.000000000000000000, 0.9238795325112867385, 1.000000000000000000, 0.9238795325112867385, 1.000000000000000000, 0.9238795325112867385, 1.000000000000000000, 0.9238795325112867385, 1.000000000000000000, 0.9238795325112867385, 1.000000000000000000, 0.9238795325112867385, 1.000000000000000000, 0.9238795325112867385, 1.000000000000000000, 0.9238795325112867385, 1.000000000000000000, 0.9238795325112867385, 1.000000000000000000, 0.9238795325112867385, 1.000000000000000000, 0.9238795325112867385, 1.000000000000000000, 0.9238795325112867385, 1.000000000000000000, 0.9238795325112867385, 1.000000000000000000, 0.9238795325112867385, 1.000000000000000000, 0.9238795325112867385, 1.000000000000000000, 0.9238795325112867385, 1.000000000000000000, 0.9238795325112867385, 1.000000000000000000, 0.9238795325112867385, 1.000000000000000000, 0.9238795325112867385, 1.000000000000000000, 0.9238795325112867385, 1.000000000000000000, 0.9238795325112867385, 1.000000000000000000, 0.9238795325112867385, 1.000000000000000000, 0.9238795325112867385, 1.000000000000000000, 0.9238795325112867385, 1.000000000000000000, 0.9238795325112867385, 1.000000000000000000, 0.9238795325112867385, 1.000000000000000000, 0.9238795325112867385, 1.000000000000000000, 0.9238795325112867385, 1.000000000000000000, 0.9238795325112867385, 1.000000000000000000, 0.9238795325112867385, 1.000000000000000000, 0.9238795325112867385, 1.000000000000000000, 0.9238795325112867385, 1.000000000000000000, 0.9238795325112867385, 1.000000000000000000, 0.9238795325112867385, 1.000000000000000000, 0.9238795325112867385, 1.000000000000000000, 0.9238795325112867385, 1.000000000000000000, 0.9238795325112867385, 1.000000000000000000, 0.9238795325112867385, 1.000000000000000000, 0.9238795325112867385, 1.000000000000000000, 0.9238795325112867385, 1.000000000000000000, 0.9238795325112867385, 1.000000000000000000, 0.9238795325112867385, 1.000000000000000000, 0.9238795325112867385, 1.000000000000000000, 0.9238795325112867385, 1.000000000000000000, 0.9238795325112867385, 1.000000000000000000, 0.9238795325112867385, 1.000000000000000000, 0.9238795325112867385, 1.000000000000000000, 0.9238795325112867385, 1.000000000000000000, 0.9238795325112867385, 1.000000000000000000, 0.9238795325112867385, 1.000000000000000000, 0.9238795325112867385, 1.000000000000000000, 0.9238795325112867385, 1.000000000000000000, 0.9238795325112867385, 1.000000000000000000, 0.9238795325112867385, 1.000000000000000000, 0.9238795325112867385, 1.000000000000000000, 0.9238795325112867385, 1.000000000000000000, 0.9238795325112867385, 1.000000000000000000, 0.9238795325112867385, 1.000000000000000000, 0.9238795325112867385, 1.000000000000000000, 0.9238795325112867385, 1.000000000000000000, 0.9238795325112867385, 1.000000000000000000, 0.9238795325112867385, 1.000000000000000000, 0.9238795325112867385, 1.000000000000000000, 0.9238795325112867385, 1.000000000000000000, 0.9238795325112867385, 1.000000000000000000, 0.9238795325112867385, 1.000000000000000000, 0.9238795325112867385, 1.000000000000000000, 0.9238795325112867385, 1.000000000000000000, 0.9238795325112867385, 1.000000000000000000, 0.9238795325112867385, 1.000000000000000000, 0.9238795325112867385, 1.000000000000000000, 0.9238795325112867385, 1.000000000000000000, 0.9238795325112867385, 1.000000000000000000, 0.9238795325112867385, 1.000000000000000000, 0.9238795325112867385, 1.000000000000000000, 0.9238795325112867385, 1.000000000000000000, 0.9238795325112867385, 1.000000000000000000, 0.9238795325112867385, 1.000000000000000000, 0.9238795325112867385, 1.000000000000000000, 0.9238795325112867385, 1.000000000000000000, 0.9238795325112867385, 1.000000000000000000, 0.9238795325112867385, 1.000000000000000000, 0.9238795325112867385, 1.000000000000000000, 0.9238795325112867385, 1.000000000000000000) ) ) 
 REPRESENTATION_ITEM ( '' )  SURFACE ( )  );
#56550 = AXIS2_PLACEMENT_3D ( 'NONE', #59181, #53143, #13854 ) ;
#56551 = CARTESIAN_POINT ( 'NONE',  ( 6.123233995736767268E-16, 78.12499999317202537, -10.00000000000000178 ) ) ;
#56552 = CARTESIAN_POINT ( 'NONE',  ( 3.313708498984765161, 101.4687500000000000, 7.999999999999998224 ) ) ;
#56553 =( BOUNDED_CURVE ( )  B_SPLINE_CURVE ( 2, ( #28216, #10868, #16503, #55786, #5215, #15766, #39543, #51225, #74236 ),
 .UNSPECIFIED., .F., .F. ) 
 B_SPLINE_CURVE_WITH_KNOTS ( ( 3, 2, 2, 2, 3 ),
 ( 0.1704545454545454697, 0.1761363636363636742, 0.1818181818181818232, 0.1875000000000000000, 0.1931818181818181768 ),
 .UNSPECIFIED. ) 
 CURVE ( )  GEOMETRIC_REPRESENTATION_ITEM ( )  RATIONAL_B_SPLINE_CURVE ( ( 0.9999999999999996669, 0.9238795325112870716, 1.000000000000000000, 0.9238795325112867385, 1.000000000000000000, 0.9238795325112867385, 1.000000000000000000, 0.9238795325112867385, 1.000000000000000000 ) ) 
 REPRESENTATION_ITEM ( '' )  );
#56554 = CARTESIAN_POINT ( 'NONE',  ( 3.042071309553159519, 204.7395833299193271, 11.35316468750000141 ) ) ;
#56555 = CARTESIAN_POINT ( 'NONE',  ( -3.313708498984760720, 7.781249995903221972, -8.000000000000000000 ) ) ;
#56556 = ORIENTED_EDGE ( 'NONE', *, *, #16396, .F. ) ;
#56557 = CARTESIAN_POINT ( 'NONE',  ( 27.99999999999996803, 209.6875000013656063, 173.4587341249998929 ) ) ;
#56558 = CARTESIAN_POINT ( 'NONE',  ( 5.082755093536325930, 14.53124999795161187, -5.082755093536325930 ) ) ;
#56559 = CARTESIAN_POINT ( 'NONE',  ( 9.832129032723416984, 165.6770833299193555, 5.676582343750006032 ) ) ;
#56560 = CARTESIAN_POINT ( 'NONE',  ( 0.000000000000000000, 300.0000000000000000, 0.000000000000000000 ) ) ;
#56561 = CARTESIAN_POINT ( 'NONE',  ( 1.320432766682874540E-15, 106.9062500020483810, 7.188101187500000044 ) ) ;
#56563 = CARTESIAN_POINT ( 'NONE',  ( 5.126144196591278401, -52.42426806216655422, -49.01287729762245959 ) ) ;
#56562 = LINE ( 'NONE', #51257, #66057 ) ;
#56564 = CARTESIAN_POINT ( 'NONE',  ( 31.45873412499998523, 206.8750000013656347, 171.4326545832176123 ) ) ;
#56565 = CARTESIAN_POINT ( 'NONE',  ( -4.401442555609577197E-16, 7.188101187499992051, 16.48655278187175810 ) ) ;
#56566 = CARTESIAN_POINT ( 'NONE',  ( -8.311093377946836114, 57.65624999658601979, -8.311093377946837890 ) ) ;
#56567 = EDGE_CURVE ( 'NONE', #18299, #8118, #56353, .T. ) ;
#56568 = CARTESIAN_POINT ( 'NONE',  ( 1.469576158976822172E-15, -7.999999999999991118, 1.392802783920146004 ) ) ;
#56569 = CARTESIAN_POINT ( 'NONE',  ( 4.000000000000000888, 16.93750000000000000, 1.656854249492384135 ) ) ;
#56570 = ORIENTED_EDGE ( 'NONE', *, *, #62415, .T. ) ;
#56571 = CARTESIAN_POINT ( 'NONE',  ( 9.797174393178825657E-16, 125.0000000000000000, -8.000000000000000000 ) ) ;
#56572 = CARTESIAN_POINT ( 'NONE',  ( 28.00000000000002132, 204.1250000027312126, 173.9999999999999147 ) ) ;
#56573 = CARTESIAN_POINT ( 'NONE',  ( -5.676582343749998039, 67.44791666325268409, -9.832129032723420536 ) ) ;
#56574 = CARTESIAN_POINT ( 'NONE',  ( -11.00000000000000000, 0.000000000000000000, 76.18750000409677625 ) ) ;
#56575 = CARTESIAN_POINT ( 'NONE',  ( -3.458734125000016757, 201.1250000013656347, 140.5673454167823593 ) ) ;
#56576 = CARTESIAN_POINT ( 'NONE',  ( 5.126106709314341536, 16.23426604260439632, 69.90716554747308464 ) ) ;
#56577 = CARTESIAN_POINT ( 'NONE',  ( -8.660254037844387298, 244.5833333333333428, -4.999999999999999112 ) ) ;
#56579 = CARTESIAN_POINT ( 'NONE',  ( 11.35316468749999785, 50.57291666325268409, 3.042071309553174174 ) ) ;
#56578 = CARTESIAN_POINT ( 'NONE',  ( 1.320432766682874540E-15, 93.03125000204836681, 7.188101187500000044 ) ) ;
#56580 = CARTESIAN_POINT ( 'NONE',  ( 7.999999999999992895, -3.313708498984756279, 4.486552779823363757 ) ) ;
#56581 = CARTESIAN_POINT ( 'NONE',  ( -30.93541659651597442, -36.99696054459029426, 171.9999999999997726 ) ) ;
#56582 = CARTESIAN_POINT ( 'NONE',  ( 11.35316468749999785, 170.5729166632526983, 3.042071309553174174 ) ) ;
#56583 =( BOUNDED_CURVE ( )  B_SPLINE_CURVE ( 2, ( #48095, #42066, #70023, #41344, #1001, #65453, #64354, #18703, #7751, #12657, #35688, #58703, #7014 ),
 .UNSPECIFIED., .F., .F. ) 
 B_SPLINE_CURVE_WITH_KNOTS ( ( 3, 2, 2, 2, 2, 2, 3 ),
 ( 0.5277777777777775681, 0.5370370370370368684, 0.5462962962962960578, 0.5555555555555553582, 0.5648148148148145475, 0.5740740740740738479, 0.5833333333333331483 ),
 .UNSPECIFIED. ) 
 CURVE ( )  GEOMETRIC_REPRESENTATION_ITEM ( )  RATIONAL_B_SPLINE_CURVE ( ( 1.000000000000000888, 0.9659258262890675351, 1.000000000000000000, 0.9659258262890683122, 1.000000000000000000, 0.9659258262890683122, 1.000000000000000000, 0.9659258262890683122, 1.000000000000000000, 0.9659258262890683122, 1.000000000000000000, 0.9659258262890690894, 0.9999999999999992228 ) ) 
 REPRESENTATION_ITEM ( '' )  );
#56585 = CARTESIAN_POINT ( 'NONE',  ( -10.00000000000000178, 139.3749999931720538, -1.224646799147353454E-15 ) ) ;
#56584 = PRODUCT_DEFINITION_SHAPE ( 'NONE', 'NONE',  #25152 ) ;
#56586 = CARTESIAN_POINT ( 'NONE',  ( -2.977408999572651815, 102.3125000020483810, 7.188101187500000933 ) ) ;
#56587 = CARTESIAN_POINT ( 'NONE',  ( -1.714702201363321965, 0.4530365834698286132, -7.773580895186361417 ) ) ;
#56588 = CARTESIAN_POINT ( 'NONE',  ( -8.311093377946836114, 32.96874999658600558, -8.311093377946837890 ) ) ;
#56589 = CARTESIAN_POINT ( 'NONE',  ( -10.00000000000000355, 79.58333332650536818, 2.679491924311223183 ) ) ;
#56590 = CARTESIAN_POINT ( 'NONE',  ( 6.951808397369818766E-16, 182.0312499965860411, -11.35316468750000141 ) ) ;
#56591 = VERTEX_POINT ( 'NONE', #55615 ) ;
#56592 = FACE_OUTER_BOUND ( 'NONE', #71478, .T. ) ;
#56593 = CARTESIAN_POINT ( 'NONE',  ( 4.220049686691934809, 10.18810118749999916, 68.68750000204836681 ) ) ;
#56594 = CARTESIAN_POINT ( 'NONE',  ( 1.656854249492405451, 197.3125000000000568, 202.0000000000000284 ) ) ;
#56595 = CARTESIAN_POINT ( 'NONE',  ( 36.77746154251568811, 39.17984125877857338, 64.99999999999998579 ) ) ;
#56597 = CARTESIAN_POINT ( 'NONE',  ( -3.042071309553163960, 167.2395833299193555, -11.35316468749999963 ) ) ;
#56596 = CARTESIAN_POINT ( 'NONE',  ( 12.00000000000000000, 0.000000000000000000, -31.99999999999998579 ) ) ;
#56598 = CARTESIAN_POINT ( 'NONE',  ( 3.313708498984762496, -7.999999999999989342, 4.355302784329824206 ) ) ;
#56599 = EDGE_CURVE ( 'NONE', #21899, #30502, #28899, .T. ) ;
#56600 = CARTESIAN_POINT ( 'NONE',  ( -3.313708498984757611, 7.999999999999991118, 5.049052779823363757 ) ) ;
#56601 = CARTESIAN_POINT ( 'NONE',  ( -11.35316468749999785, 223.6979166700806445, -3.042071309553164848 ) ) ;
#56602 = CARTESIAN_POINT ( 'NONE',  ( -2.997005883569377804, 55.94527535363560844, -43.97975057404802612 ) ) ;
#56603 = CARTESIAN_POINT ( 'NONE',  ( -4.220049686691935698, 10.18810118749999916, 79.75000000204838102 ) ) ;
#56604 = ORIENTED_EDGE ( 'NONE', *, *, #19674, .T. ) ;
#56605 = EDGE_CURVE ( 'NONE', #1872, #68569, #51036, .T. ) ;
#56606 = CARTESIAN_POINT ( 'NONE',  ( -3.999999999999960032, 204.0000000000000284, 198.0000000000000284 ) ) ;
#56607 = CARTESIAN_POINT ( 'NONE',  ( 8.311093377946837890, 111.7187499965859985, -8.311093377946837890 ) ) ;
#56608 = EDGE_CURVE ( 'NONE', #69323, #39904, #72193, .T. ) ;
#56609 = DIRECTION ( 'NONE',  ( 1.000000000000000000, 0.000000000000000000, 0.000000000000000000 ) ) ;
#56610 = VERTEX_POINT ( 'NONE', #9589 ) ;
#56611 = VERTEX_POINT ( 'NONE', #16702 ) ;
#56612 = CARTESIAN_POINT ( 'NONE',  ( -3.211159895383562723, 7.062499998634407028, 3.211159895383561391 ) ) ;
#56613 = AXIS2_PLACEMENT_3D ( 'NONE', #26176, #37897, #62014 ) ;
#56614 = CARTESIAN_POINT ( 'NONE',  ( 4.401442555609581635E-16, 12.84374999795161187, -7.188101187500000044 ) ) ;
#56615 = CARTESIAN_POINT ( 'NONE',  ( -5.656854249492380582, 107.0000000040967763, -5.656854249492380582 ) ) ;
#56616 = CARTESIAN_POINT ( 'NONE',  ( -31.45873412499999944, 199.8750000013655779, 168.5673454167827572 ) ) ;
#56617 = EDGE_CURVE ( 'NONE', #18980, #34052, #68688, .T. ) ;
#56618 = CARTESIAN_POINT ( 'NONE',  ( 4.000000000000001776, 10.00000000000000000, 0.000000000000000000 ) ) ;
#56619 = CARTESIAN_POINT ( 'NONE',  ( -2.828427124746192067, 21.37499999726881583, 2.828427124746190735 ) ) ;
#56620 = CARTESIAN_POINT ( 'NONE',  ( -3.211159895383561391, 9.687499998634406140, -3.211159895383561835 ) ) ;
#56621 = CARTESIAN_POINT ( 'NONE',  ( 3.999999999999960032, 198.0000000000000000, 142.0000000000000568 ) ) ;
#56622 = ORIENTED_EDGE ( 'NONE', *, *, #61982, .T. ) ;
#56623 = CARTESIAN_POINT ( 'NONE',  ( 0.000000000000000000, 45.00000000000000000, 0.000000000000000000 ) ) ;
#56624 = CARTESIAN_POINT ( 'NONE',  ( -2.977408999572651815, 112.4375000020483810, 7.188101187500000933 ) ) ;
#56626 = CARTESIAN_POINT ( 'NONE',  ( 1.836970198721029589E-15, 239.3750000068279746, 10.00000000000000000 ) ) ;
#56625 = CARTESIAN_POINT ( 'NONE',  ( 4.531193156845207581E-15, 195.0000000000000284, 133.0000000000000284 ) ) ;
#56627 = CARTESIAN_POINT ( 'NONE',  ( -4.541265875000002339, 20.81249999863440436, -5.561446717895856393E-16 ) ) ;
#56628 = CARTESIAN_POINT ( 'NONE',  ( -5.082755093536317936, -5.082755093536320601, 0.1740527818717522990 ) ) ;
#56629 = EDGE_LOOP ( 'NONE', ( #68638, #43510, #32551, #28278, #35756 ) ) ;
#56630 = B_SPLINE_CURVE_WITH_KNOTS ( 'NONE', 3,
 ( #28905, #51923, #23244, #16450 ),
 .UNSPECIFIED., .F., .F.,
 ( 4, 4 ),
 ( 0.000000000000000000, 4.515620356819685806E-05 ),
 .UNSPECIFIED. ) ;
#56631 = ORIENTED_EDGE ( 'NONE', *, *, #38361, .T. ) ;
#56632 = CARTESIAN_POINT ( 'NONE',  ( -10.18810118749999738, -4.220049686691941915, 93.25000000204838102 ) ) ;
#56633 = CARTESIAN_POINT ( 'NONE',  ( -2.726571689596997292E-14, 210.0000000000000284, 138.0000000000000568 ) ) ;
#56634 = CARTESIAN_POINT ( 'NONE',  ( -24.54126587499998280, 200.3750000013656063, 171.4326545832179818 ) ) ;
#56635 = CARTESIAN_POINT ( 'NONE',  ( -10.99999999999999822, -4.556349186104052151, 104.5937499999999716 ) ) ;
#56636 = CARTESIAN_POINT ( 'NONE',  ( 2.445694354108839175, 209.3125000013656063, 195.5543056458912190 ) ) ;
#56637 = LINE ( 'NONE', #68312, #49442 ) ;
#56638 = CARTESIAN_POINT ( 'NONE',  ( -10.00000000000000178, 127.5000000000000000, -1.224646799147353454E-15 ) ) ;
#56639 = CARTESIAN_POINT ( 'NONE',  ( -3.313708498984762496, 108.7812500000000000, 7.999999999999998224 ) ) ;
#56640 = CARTESIAN_POINT ( 'NONE',  ( -6.676582343750003368, 288.5468750017070079, -2.765530957081996810 ) ) ;
#56641 = CARTESIAN_POINT ( 'NONE',  ( 7.188101187499991163, 2.977408999572648707, 7.205302781871754547 ) ) ;
#56642 = CARTESIAN_POINT ( 'NONE',  ( -5.656854249492380582, 97.81250000000000000, -5.656854249492380582 ) ) ;
#56643 = VECTOR ( 'NONE', #39354, 1000.000000000000000 ) ;
#56644 = CARTESIAN_POINT ( 'NONE',  ( 24.54126587499999701, 206.1875000013656063, 169.9999999999998863 ) ) ;
#56645 = CARTESIAN_POINT ( 'NONE',  ( 8.000000000000000000, 25.31249999590322375, 0.000000000000000000 ) ) ;
#56646 = CARTESIAN_POINT ( 'NONE',  ( -1.432654583217662481, 198.1250000013656063, 145.4587341250000634 ) ) ;
#56647 = CARTESIAN_POINT ( 'NONE',  ( 7.188101187500000044, 122.2812500020483810, -8.802885111219163269E-16 ) ) ;
#56649 = CARTESIAN_POINT ( 'NONE',  ( -3.458734125000016757, 203.1250000013656347, 140.5673454167824161 ) ) ;
#56648 = DIRECTION ( 'NONE',  ( -0.000000000000000000, 1.000000000000000000, -1.563033456626094573E-30 ) ) ;
#56650 = CARTESIAN_POINT ( 'NONE',  ( -3.042071309553159075, 240.2604166700806729, 11.35316468749999963 ) ) ;
#56651 = CARTESIAN_POINT ( 'NONE',  ( -10.00000000000000178, 214.3749999931720538, -1.224646799147353454E-15 ) ) ;
#56652 = CARTESIAN_POINT ( 'NONE',  ( 27.99999999999996803, 204.0000000000000284, 173.9999999999999147 ) ) ;
#56653 = CARTESIAN_POINT ( 'NONE',  ( -3.042071309553164404, 12.23958332991935194, -11.35316468749999963 ) ) ;
#56654 = CARTESIAN_POINT ( 'NONE',  ( 7.320508075688773708, 0.6249999999999988898, -7.320508075688773708 ) ) ;
#56655 = CARTESIAN_POINT ( 'NONE',  ( 6.951808397369818766E-16, 207.3437499965860411, -11.35316468750000141 ) ) ;
#56656 = CARTESIAN_POINT ( 'NONE',  ( -6.000000000000037303, -10.39230484541327826, -14.00000000000000178 ) ) ;
#56658 = FACE_OUTER_BOUND ( 'NONE', #145, .T. ) ;
#56657 = CARTESIAN_POINT ( 'NONE',  ( -4.556349186104048599, -10.99999999999999822, 88.28124999999998579 ) ) ;
#56659 = ORIENTED_EDGE ( 'NONE', *, *, #15516, .T. ) ;
#56660 = AXIS2_PLACEMENT_3D ( 'NONE', #3291, #14962, #49298 ) ;
#56661 = CARTESIAN_POINT ( 'NONE',  ( -2.445694354108840063, 201.0625000013656063, 139.5543056458912190 ) ) ;
#56662 = CARTESIAN_POINT ( 'NONE',  ( -11.35316468750000141, 23.28124999658601979, -1.390361679473963753E-15 ) ) ;
#56663 = CARTESIAN_POINT ( 'NONE',  ( -4.556349186104047710, -10.99999999999999822, 91.46875000409676204 ) ) ;
#56664 = CARTESIAN_POINT ( 'NONE',  ( -2.250000000000000888, -2.250000000000000000, 28.00000000000000000 ) ) ;
#56665 = CARTESIAN_POINT ( 'NONE',  ( -28.00000000000007105, 198.4375000013655779, 166.5412658750003629 ) ) ;
#56666 = FACE_OUTER_BOUND ( 'NONE', #66775, .T. ) ;
#56668 = CARTESIAN_POINT ( 'NONE',  ( -7.320508075688771932, 229.3749999999999716, -7.320508075688771932 ) ) ;
#56667 = CARTESIAN_POINT ( 'NONE',  ( 7.188101187500000044, 111.4062500020483810, -8.802885111219163269E-16 ) ) ;
#56669 = CARTESIAN_POINT ( 'NONE',  ( -5.656854249492375253, 5.656854249492375253, 21.64280277982336997 ) ) ;
#56670 = CARTESIAN_POINT ( 'NONE',  ( -9.832129032723420536, 128.6979166632526983, 5.676582343749997150 ) ) ;
#56671 = ADVANCED_FACE ( 'NONE', ( #45764 ), #62733, .F. ) ;
#56672 = CARTESIAN_POINT ( 'NONE',  ( 8.660254037844385522, 106.4583333265053682, 5.000000000000005329 ) ) ;
#56673 = CARTESIAN_POINT ( 'NONE',  ( 7.188101187500000044, 120.7812500020483810, -8.802885111219163269E-16 ) ) ;
#56674 = CARTESIAN_POINT ( 'NONE',  ( -6.735557395310442023E-16, 11.00000000000000000, 102.8125000040967763 ) ) ;
#56675 = CARTESIAN_POINT ( 'NONE',  ( -5.000000000000000000, 53.39837237779330081, -47.14918772354884879 ) ) ;
#56676 = VERTEX_POINT ( 'NONE', #40852 ) ;
#56677 = CARTESIAN_POINT ( 'NONE',  ( 3.728321214240235548, -66.24762070548278814, 26.57448171413092197 ) ) ;
#56678 =( BOUNDED_SURFACE ( )  B_SPLINE_SURFACE ( 1, 2, ( 
 ( #1219, #69868, #46476, #13606, #18915, #41196, #53627, #47942, #41921, #64932, #40821, #12510, #30606, #64575, #63827, #58195, #24198, #52517, #70242, #58927, #18552, #1939, #854, #23839, #24928, #70959, #9085, #61134, #60763, #32481, #66415, #21139, #54371, #71324, #37380, #60012, #67177, #15473, #71692, #44163, #8330, #66797, #3423, #19645, #13967, #38510, #72066, #72458, #55119, #42658, #38133, #26037, #48687, #61512, #65669, #26410, #31340, #72833, #49438, #20384, #32099, #20765, #25299, #9834, #43783, #37010, #9464, #49058, #20011, #53991, #2681, #15100, #25668, #2301, #55489, #43400, #3804, #26802, #48318, #43021, #54745, #66043, #14351, #60382, #49816, #8708, #31723, #3053, #14724, #37764, #4548, #73208, #44910, #21881, #5662, #67915, #40359, #62996, #4183, #68656, #22622, #32861, #68286, #38877, #44535, #46013, #56612, #69034, #45641, #10574, #15844, #57352, #27924, #39247, #61882, #17337, #16583, #28296, #73945, #22246, #74314, #39992, #10205, #5294, #16208, #33985, #21513, #51301, #67546, #50186, #28660, #27169, #39619, #50933, #33604, #33234, #56233, #27543, #63359, #51675, #20, #11320, #62247, #16966, #4927, #50556, #55866, #23007, #10949, #73571, #34353, #45275, #62618, #56980, #31543, #53454, #42481, #53820, #43223, #57727, #59118, #25858, #1773, #2128, #24757, #48138, #69404, #34721, #11685, #42845, #65497, #19837, #19468, #65863, #25120, #54564, #13063, #29039, #70788, #17712, #48880, #71890, #30434, #2871, #40728, #25494, #36838, #52057, #46387, #20203, #30798, #31166, #54193, #63734, #13792, #2500, #6033, #42108, #59844, #48509, #36101, #71146, #392, #71514, #8158, #47767, #7427, #13429, #23375, #7795, #14171, #19103, #65119, #36466, #37205, #59482, #60204, #8528, #66610, #15664, #33422, #44725, #50376, #56421, #55312, #9275, #16038, #44355, #32296, #22069, #26235, #73761, #49639, #61706, #43596, #4743, #32681, #54939, #38705, #20583, #49254, #27736, #21699, #26993, #37580, #60580, #20957, #3620, #31917, #67742, #39069, #55689, #8904, #60957, #14916, #33061, #26616, #9659, #72655, #67366, #4367, #3247, #10027, #73394, #43978, #27360, #62073, #37957, #66990, #56059, #61331, #73023, #38326, #10397, #50747, #21334, #15290, #4003, #72270, #50006, #66239, #14542, #952, #51493, #28854, #10761, #46207, #57550, #45457, #34166, #34914, #22436, #580, #23562, #63933, #5857, #45095, #39436, #28108, #28485, #68107, #11143, #68845, #17158, #51875, #69221, #16401, #57924, #11510, #46573, #22815, #12243, #35280, #6594, #56797, #215, #6232, #29234, #51122, #23194, #33799, #69595, #17907, #34542, #62435, #39799, #68473, #11879, #62805, #63182, #57166, #17531, #52247, #5117, #40548, #40925, #5482, #58292, #29601, #74135, #45832, #63553, #40179, #52615, #16774, #74505, #25023, #30704, #30336, #47312, #41295, #69971, #7699 ),
 ( #7331, #29968, #37109, #60111, #41658, #65770, #52984, #36742, #48042, #64305, #58652, #14072, #42016, #42384, #71051, #12609, #8063, #70691, #18650, #8429, #35637, #19370, #1316, #42753, #65400, #65024, #2036, #53724, #18279, #31446, #24661, #6959, #59023, #70339, #13697, #24301, #54472, #23932, #59752, #53357, #64668, #12969, #36006, #1681, #71419, #47671, #46941, #54092, #19010, #31065, #2403, #13333, #59385, #36369, #25399, #48414, #19746, #38972, #67276, #55219, #60481, #27265, #72559, #9180, #8811, #61978, #61237, #72927, #43882, #66896, #44263, #9929, #31824, #49914, #60859, #3907, #43126, #21237, #37483, #20113, #50283, #71792, #9565, #20863, #3525, #54843, #55590, #15571, #3152, #26899, #38609, #66143, #32199, #61611, #32962, #26140, #15202, #14448, #55966, #32583, #14820, #49161, #26514, #44632, #38232, #4275, #37863, #72168, #20480, #73305, #15944, #43499, #66509, #49540, #21607, #67646, #10303, #33329, #2779, #25766, #48785, #6134, #34451, #74040, #12151, #16305, #63835, #39710, #51774, #33702, #46482, #22720, #45007, #28760, #10670, #39343, #69502, #11785, #17064, #27643, #50650, #11050, #22340, #21978, #34822, #29140, #45736, #73670, #51029, #5024, #23099, #45365, #74412, #68381, #57453, #69130, #68012, #5760, #40458, #16680, #17436, #63457, #56707, #34079, #120, #51398, #63090, #28390, #46111, #57828, #11416, #62711, #28020, #62340, #57075, #40086, #5389, #56327, #68750, #52156, #491, #23471, #17812, #4649, #40829, #24935, #12516, #65310, #13611, #53999, #70604, #35186, #29512, #18187, #18557, #58200, #1225, #58934, #7240, #18922, #36281, #6505, #47952, #1591, #36650, #12878, #2310, #25307, #71331, #46852, #41928, #70968, #19282, #48324, #24576, #23845, #7606, #64211, #69875, #19652, #59660, #64937, #52522, #859, #64582, #52893, #41203, #7976, #30978, #47581, #35548, #29879, #58563, #1946, #24204, #53265, #47215, #13248, #42293, #6867, #59297, #42665, #70248, #65676, #41568, #35914, #30244, #30613, #53636, #20773, #60769, #38142, #15110, #43792, #20394, #37391, #31350, #60019, #72465, #8338, #44544, #43408, #66808, #3430, #49447, #49824, #13975, #3062, #3812, #66051, #44170, #67184, #32868, #61142, #37017, #54380, #71701, #72077, #2689, #54752, #37773, #9095, #9472, #32489, #25675, #26810, #55127, #15481, #66422, #55873, #4189, #50195, #48695, #55500, #72841, #21148, #20019, #38517, #61520, #43029, #9842, #27178, #14359, #14734, #73214, #21522, #60392, #26421, #8718, #31730, #26045, #49065, #32109, #68291, #34729, #62626, #51681, #4934, #44916, #4556, #10957, #6039, #33612, #67923, #16216, #16973, #57734, #46020, #26, #29044, #56619, #10581, #17344, #45647, #27931, #23379, #27551, #400, #50939, #63002, #39256, #73579, #52063, #51310, #11326, #33992, #56986, #34358, #23013, #21887, #39999, #73950, #68662 ) ),
 .UNSPECIFIED., .F., .F., .F. ) 
 B_SPLINE_SURFACE_WITH_KNOTS ( ( 2, 2 ),
 ( 3, 2, 2, 2, 2, 2, 2, 2, 2, 2, 2, 2, 2, 2, 2, 2, 2, 2, 2, 2, 2, 2, 2, 2, 2, 2, 2, 2, 2, 2, 2, 2, 2, 2, 2, 2, 2, 2, 2, 2, 2, 2, 2, 2, 2, 2, 2, 2, 2, 2, 2, 2, 2, 2, 2, 2, 2, 2, 2, 2, 2, 2, 2, 2, 2, 2, 2, 2, 2, 2, 2, 2, 2, 2, 2, 2, 2, 2, 2, 2, 2, 2, 2, 2, 2, 2, 2, 2, 2, 2, 2, 2, 2, 2, 2, 2, 2, 2, 2, 2, 2, 2, 2, 2, 2, 2, 2, 2, 2, 2, 2, 2, 2, 2, 2, 2, 2, 2, 2, 2, 2, 2, 2, 2, 2, 2, 2, 2, 2, 2, 2, 2, 2, 2, 2, 2, 2, 2, 2, 2, 2, 2, 2, 2, 2, 2, 2, 2, 2, 2, 2, 2, 2, 2, 2, 2, 2, 2, 2, 2, 2, 2, 2, 2, 2, 2, 2, 2, 2, 2, 2, 2, 2, 2, 2, 2, 3 ),
 ( 0.000000000000000000, 1.000000000000000000 ),
 ( 0.000000000000000000, 0.005681818181818181976, 0.01136363636363636395, 0.01704545454545454419, 0.02272727272727272790, 0.02840909090909090814, 0.03409090909090908839, 0.03977272727272727210, 0.04545454545454545581, 0.05113636363636363952, 0.05681818181818181629, 0.06250000000000000000, 0.06818181818181817677, 0.07386363636363636742, 0.07954545454545454419, 0.08522727272727272096, 0.09090909090909091161, 0.09659090909090908839, 0.1022727272727272790, 0.1079545454545454558, 0.1136363636363636326, 0.1193181818181818232, 0.1250000000000000000, 0.1306818181818181768, 0.1363636363636363535, 0.1420454545454545581, 0.1477272727272727348, 0.1534090909090909116, 0.1590909090909090884, 0.1647727272727272652, 0.1704545454545454419, 0.1761363636363636465, 0.1818181818181818232, 0.1875000000000000000, 0.1931818181818181768, 0.1988636363636363535, 0.2045454545454545581, 0.2102272727272727348, 0.2159090909090909116, 0.2215909090909090884, 0.2272727272727272652, 0.2329545454545454419, 0.2386363636363636465, 0.2443181818181818232, 0.2500000000000000000, 0.2556818181818181768, 0.2613636363636363535, 0.2670454545454545303, 0.2727272727272727071, 0.2784090909090908839, 0.2840909090909091161, 0.2897727272727272929, 0.2954545454545454697, 0.3011363636363636465, 0.3068181818181818232, 0.3125000000000000000, 0.3181818181818181768, 0.3238636363636363535, 0.3295454545454545303, 0.3352272727272727071, 0.3409090909090908839, 0.3465909090909091161, 0.3522727272727272929, 0.3579545454545454697, 0.3636363636363636465, 0.3693181818181818232, 0.3750000000000000000, 0.3806818181818181768, 0.3863636363636363535, 0.3920454545454545303, 0.3977272727272727071, 0.4034090909090908839, 0.4090909090909091161, 0.4147727272727272929, 0.4204545454545454697, 0.4261363636363636465, 0.4318181818181818232, 0.4375000000000000000, 0.4431818181818181768, 0.4488636363636363535, 0.4545454545454545303, 0.4602272727272727071, 0.4659090909090908839, 0.4715909090909091161, 0.4772727272727272929, 0.4829545454545454697, 0.4886363636363636465, 0.4943181818181818232, 0.5000000000000000000, 0.5056818181818182323, 0.5113636363636363535, 0.5170454545454545858, 0.5227272727272727071, 0.5284090909090909394, 0.5340909090909090606, 0.5397727272727272929, 0.5454545454545454142, 0.5511363636363636465, 0.5568181818181817677, 0.5625000000000000000, 0.5681818181818182323, 0.5738636363636363535, 0.5795454545454545858, 0.5852272727272727071, 0.5909090909090909394, 0.5965909090909090606, 0.6022727272727272929, 0.6079545454545454142, 0.6136363636363636465, 0.6193181818181817677, 0.6250000000000000000, 0.6306818181818182323, 0.6363636363636363535, 0.6420454545454545858, 0.6477272727272727071, 0.6534090909090909394, 0.6590909090909090606, 0.6647727272727272929, 0.6704545454545454142, 0.6761363636363636465, 0.6818181818181817677, 0.6875000000000000000, 0.6931818181818182323, 0.6988636363636363535, 0.7045454545454545858, 0.7102272727272727071, 0.7159090909090909394, 0.7215909090909090606, 0.7272727272727272929, 0.7329545454545454142, 0.7386363636363636465, 0.7443181818181817677, 0.7500000000000000000, 0.7556818181818182323, 0.7613636363636363535, 0.7670454545454545858, 0.7727272727272727071, 0.7784090909090909394, 0.7840909090909090606, 0.7897727272727272929, 0.7954545454545454142, 0.8011363636363636465, 0.8068181818181817677, 0.8125000000000000000, 0.8181818181818182323, 0.8238636363636363535, 0.8295454545454545858, 0.8352272727272727071, 0.8409090909090909394, 0.8465909090909090606, 0.8522727272727272929, 0.8579545454545454142, 0.8636363636363636465, 0.8693181818181817677, 0.8750000000000000000, 0.8806818181818182323, 0.8863636363636363535, 0.8920454545454545858, 0.8977272727272727071, 0.9034090909090909394, 0.9090909090909090606, 0.9147727272727272929, 0.9204545454545454142, 0.9261363636363636465, 0.9318181818181817677, 0.9375000000000000000, 0.9431818181818182323, 0.9488636363636363535, 0.9545454545454545858, 0.9602272727272727071, 0.9659090909090909394, 0.9715909090909090606, 0.9772727272727272929, 0.9829545454545454142, 0.9886363636363636465, 0.9943181818181817677, 1.000000000000000000 ),
 .UNSPECIFIED. ) 
 GEOMETRIC_REPRESENTATION_ITEM ( )  RATIONAL_B_SPLINE_SURFACE ( (
 ( 1.000000000000000000, 0.9238795325112867385, 1.000000000000000000, 0.9238795325112867385, 1.000000000000000000, 0.9238795325112867385, 1.000000000000000000, 0.9238795325112867385, 1.000000000000000000, 0.9238795325112867385, 1.000000000000000000, 0.9238795325112867385, 1.000000000000000000, 0.9238795325112867385, 1.000000000000000000, 0.9238795325112867385, 1.000000000000000000, 0.9238795325112867385, 1.000000000000000000, 0.9238795325112867385, 1.000000000000000000, 0.9238795325112867385, 1.000000000000000000, 0.9238795325112867385, 1.000000000000000000, 0.9238795325112867385, 1.000000000000000000, 0.9238795325112867385, 1.000000000000000000, 0.9238795325112867385, 1.000000000000000000, 0.9238795325112867385, 1.000000000000000000, 0.9238795325112867385, 1.000000000000000000, 0.9238795325112867385, 1.000000000000000000, 0.9238795325112867385, 1.000000000000000000, 0.9238795325112867385, 1.000000000000000000, 0.9238795325112867385, 1.000000000000000000, 0.9238795325112867385, 1.000000000000000000, 0.9238795325112867385, 1.000000000000000000, 0.9238795325112867385, 1.000000000000000000, 0.9238795325112867385, 1.000000000000000000, 0.9238795325112867385, 1.000000000000000000, 0.9238795325112867385, 1.000000000000000000, 0.9238795325112867385, 1.000000000000000000, 0.9238795325112867385, 1.000000000000000000, 0.9238795325112867385, 1.000000000000000000, 0.9238795325112867385, 1.000000000000000000, 0.9238795325112867385, 1.000000000000000000, 0.9238795325112867385, 1.000000000000000000, 0.9238795325112867385, 1.000000000000000000, 0.9238795325112867385, 1.000000000000000000, 0.9238795325112867385, 1.000000000000000000, 0.9238795325112867385, 1.000000000000000000, 0.9238795325112867385, 1.000000000000000000, 0.9238795325112867385, 1.000000000000000000, 0.9238795325112867385, 1.000000000000000000, 0.9238795325112867385, 1.000000000000000000, 0.9238795325112867385, 1.000000000000000000, 0.9238795325112867385, 1.000000000000000000, 0.9238795325112867385, 1.000000000000000000, 0.9238795325112867385, 1.000000000000000000, 0.9238795325112867385, 1.000000000000000000, 0.9238795325112867385, 1.000000000000000000, 0.9238795325112867385, 1.000000000000000000, 0.9238795325112867385, 1.000000000000000000, 0.9238795325112867385, 1.000000000000000000, 0.9238795325112867385, 1.000000000000000000, 0.9238795325112867385, 1.000000000000000000, 0.9238795325112867385, 1.000000000000000000, 0.9238795325112867385, 1.000000000000000000, 0.9238795325112867385, 1.000000000000000000, 0.9238795325112867385, 1.000000000000000000, 0.9238795325112867385, 1.000000000000000000, 0.9238795325112867385, 1.000000000000000000, 0.9238795325112867385, 1.000000000000000000, 0.9238795325112867385, 1.000000000000000000, 0.9238795325112867385, 1.000000000000000000, 0.9238795325112867385, 1.000000000000000000, 0.9238795325112867385, 1.000000000000000000, 0.9238795325112867385, 1.000000000000000000, 0.9238795325112867385, 1.000000000000000000, 0.9238795325112867385, 1.000000000000000000, 0.9238795325112867385, 1.000000000000000000, 0.9238795325112867385, 1.000000000000000000, 0.9238795325112867385, 1.000000000000000000, 0.9238795325112867385, 1.000000000000000000, 0.9238795325112867385, 1.000000000000000000, 0.9238795325112867385, 1.000000000000000000, 0.9238795325112867385, 1.000000000000000000, 0.9238795325112867385, 1.000000000000000000, 0.9238795325112867385, 1.000000000000000000, 0.9238795325112867385, 1.000000000000000000, 0.9238795325112867385, 1.000000000000000000, 0.9238795325112867385, 1.000000000000000000, 0.9238795325112867385, 1.000000000000000000, 0.9238795325112867385, 1.000000000000000000, 0.9238795325112867385, 1.000000000000000000, 0.9238795325112867385, 1.000000000000000000, 0.9238795325112867385, 1.000000000000000000, 0.9238795325112867385, 1.000000000000000000, 0.9238795325112867385, 1.000000000000000000, 0.9238795325112867385, 1.000000000000000000, 0.9238795325112867385, 1.000000000000000000, 0.9238795325112867385, 1.000000000000000000, 0.9238795325112867385, 1.000000000000000000, 0.9238795325112867385, 1.000000000000000000, 0.9238795325112867385, 1.000000000000000000, 0.9238795325112867385, 1.000000000000000000, 0.9238795325112867385, 1.000000000000000000, 0.9238795325112867385, 1.000000000000000000, 0.9238795325112867385, 1.000000000000000000, 0.9238795325112867385, 1.000000000000000000, 0.9238795325112867385, 1.000000000000000000, 0.9238795325112867385, 1.000000000000000000, 0.9238795325112867385, 1.000000000000000000, 0.9238795325112867385, 1.000000000000000000, 0.9238795325112867385, 1.000000000000000000, 0.9238795325112867385, 1.000000000000000000, 0.9238795325112867385, 1.000000000000000000, 0.9238795325112867385, 1.000000000000000000, 0.9238795325112867385, 1.000000000000000000, 0.9238795325112867385, 1.000000000000000000, 0.9238795325112867385, 1.000000000000000000, 0.9238795325112867385, 1.000000000000000000, 0.9238795325112867385, 1.000000000000000000, 0.9238795325112867385, 1.000000000000000000, 0.9238795325112867385, 1.000000000000000000, 0.9238795325112867385, 1.000000000000000000, 0.9238795325112867385, 1.000000000000000000, 0.9238795325112867385, 1.000000000000000000, 0.9238795325112867385, 1.000000000000000000, 0.9238795325112867385, 1.000000000000000000, 0.9238795325112867385, 1.000000000000000000, 0.9238795325112867385, 1.000000000000000000, 0.9238795325112867385, 1.000000000000000000, 0.9238795325112867385, 1.000000000000000000, 0.9238795325112867385, 1.000000000000000000, 0.9238795325112867385, 1.000000000000000000, 0.9238795325112867385, 1.000000000000000000, 0.9238795325112867385, 1.000000000000000000, 0.9238795325112867385, 1.000000000000000000, 0.9238795325112867385, 1.000000000000000000, 0.9238795325112867385, 1.000000000000000000, 0.9238795325112867385, 1.000000000000000000, 0.9238795325112867385, 1.000000000000000000, 0.9238795325112867385, 1.000000000000000000, 0.9238795325112867385, 1.000000000000000000, 0.9238795325112867385, 1.000000000000000000, 0.9238795325112867385, 1.000000000000000000, 0.9238795325112867385, 1.000000000000000000, 0.9238795325112867385, 1.000000000000000000, 0.9238795325112867385, 1.000000000000000000, 0.9238795325112867385, 1.000000000000000000, 0.9238795325112867385, 1.000000000000000000, 0.9238795325112867385, 1.000000000000000000, 0.9238795325112867385, 1.000000000000000000, 0.9238795325112867385, 1.000000000000000000, 0.9238795325112867385, 1.000000000000000000, 0.9238795325112867385, 1.000000000000000000, 0.9238795325112867385, 1.000000000000000000, 0.9238795325112867385, 1.000000000000000000, 0.9238795325112867385, 1.000000000000000000, 0.9238795325112867385, 1.000000000000000000, 0.9238795325112867385, 1.000000000000000000, 0.9238795325112867385, 1.000000000000000000, 0.9238795325112867385, 1.000000000000000000, 0.9238795325112867385, 1.000000000000000000, 0.9238795325112867385, 1.000000000000000000, 0.9238795325112867385, 1.000000000000000000, 0.9238795325112867385, 1.000000000000000000, 0.9238795325112867385, 1.000000000000000000, 0.9238795325112867385, 1.000000000000000000, 0.9238795325112867385, 1.000000000000000000, 0.9238795325112867385, 1.000000000000000000, 0.9238795325112867385, 1.000000000000000000, 0.9238795325112867385, 1.000000000000000000, 0.9238795325112867385, 1.000000000000000000, 0.9238795325112867385, 1.000000000000000000, 0.9238795325112867385, 1.000000000000000000, 0.9238795325112867385, 1.000000000000000000, 0.9238795325112867385, 1.000000000000000000, 0.9238795325112867385, 1.000000000000000000, 0.9238795325112867385, 1.000000000000000000, 0.9238795325112867385, 1.000000000000000000, 0.9238795325112867385, 1.000000000000000000, 0.9238795325112867385, 1.000000000000000000, 0.9238795325112867385, 1.000000000000000000, 0.9238795325112867385, 1.000000000000000000, 0.9238795325112867385, 1.000000000000000000, 0.9238795325112867385, 1.000000000000000000, 0.9238795325112867385, 1.000000000000000000, 0.9238795325112867385, 1.000000000000000000),
 ( 1.000000000000000000, 0.9238795325112867385, 1.000000000000000000, 0.9238795325112867385, 1.000000000000000000, 0.9238795325112867385, 1.000000000000000000, 0.9238795325112867385, 1.000000000000000000, 0.9238795325112867385, 1.000000000000000000, 0.9238795325112867385, 1.000000000000000000, 0.9238795325112867385, 1.000000000000000000, 0.9238795325112867385, 1.000000000000000000, 0.9238795325112867385, 1.000000000000000000, 0.9238795325112867385, 1.000000000000000000, 0.9238795325112867385, 1.000000000000000000, 0.9238795325112867385, 1.000000000000000000, 0.9238795325112867385, 1.000000000000000000, 0.9238795325112867385, 1.000000000000000000, 0.9238795325112867385, 1.000000000000000000, 0.9238795325112867385, 1.000000000000000000, 0.9238795325112867385, 1.000000000000000000, 0.9238795325112867385, 1.000000000000000000, 0.9238795325112867385, 1.000000000000000000, 0.9238795325112867385, 1.000000000000000000, 0.9238795325112867385, 1.000000000000000000, 0.9238795325112867385, 1.000000000000000000, 0.9238795325112867385, 1.000000000000000000, 0.9238795325112867385, 1.000000000000000000, 0.9238795325112867385, 1.000000000000000000, 0.9238795325112867385, 1.000000000000000000, 0.9238795325112867385, 1.000000000000000000, 0.9238795325112867385, 1.000000000000000000, 0.9238795325112867385, 1.000000000000000000, 0.9238795325112867385, 1.000000000000000000, 0.9238795325112867385, 1.000000000000000000, 0.9238795325112867385, 1.000000000000000000, 0.9238795325112867385, 1.000000000000000000, 0.9238795325112867385, 1.000000000000000000, 0.9238795325112867385, 1.000000000000000000, 0.9238795325112867385, 1.000000000000000000, 0.9238795325112867385, 1.000000000000000000, 0.9238795325112867385, 1.000000000000000000, 0.9238795325112867385, 1.000000000000000000, 0.9238795325112867385, 1.000000000000000000, 0.9238795325112867385, 1.000000000000000000, 0.9238795325112867385, 1.000000000000000000, 0.9238795325112867385, 1.000000000000000000, 0.9238795325112867385, 1.000000000000000000, 0.9238795325112867385, 1.000000000000000000, 0.9238795325112867385, 1.000000000000000000, 0.9238795325112867385, 1.000000000000000000, 0.9238795325112867385, 1.000000000000000000, 0.9238795325112867385, 1.000000000000000000, 0.9238795325112867385, 1.000000000000000000, 0.9238795325112867385, 1.000000000000000000, 0.9238795325112867385, 1.000000000000000000, 0.9238795325112867385, 1.000000000000000000, 0.9238795325112867385, 1.000000000000000000, 0.9238795325112867385, 1.000000000000000000, 0.9238795325112867385, 1.000000000000000000, 0.9238795325112867385, 1.000000000000000000, 0.9238795325112867385, 1.000000000000000000, 0.9238795325112867385, 1.000000000000000000, 0.9238795325112867385, 1.000000000000000000, 0.9238795325112867385, 1.000000000000000000, 0.9238795325112867385, 1.000000000000000000, 0.9238795325112867385, 1.000000000000000000, 0.9238795325112867385, 1.000000000000000000, 0.9238795325112867385, 1.000000000000000000, 0.9238795325112867385, 1.000000000000000000, 0.9238795325112867385, 1.000000000000000000, 0.9238795325112867385, 1.000000000000000000, 0.9238795325112867385, 1.000000000000000000, 0.9238795325112867385, 1.000000000000000000, 0.9238795325112867385, 1.000000000000000000, 0.9238795325112867385, 1.000000000000000000, 0.9238795325112867385, 1.000000000000000000, 0.9238795325112867385, 1.000000000000000000, 0.9238795325112867385, 1.000000000000000000, 0.9238795325112867385, 1.000000000000000000, 0.9238795325112867385, 1.000000000000000000, 0.9238795325112867385, 1.000000000000000000, 0.9238795325112867385, 1.000000000000000000, 0.9238795325112867385, 1.000000000000000000, 0.9238795325112867385, 1.000000000000000000, 0.9238795325112867385, 1.000000000000000000, 0.9238795325112867385, 1.000000000000000000, 0.9238795325112867385, 1.000000000000000000, 0.9238795325112867385, 1.000000000000000000, 0.9238795325112867385, 1.000000000000000000, 0.9238795325112867385, 1.000000000000000000, 0.9238795325112867385, 1.000000000000000000, 0.9238795325112867385, 1.000000000000000000, 0.9238795325112867385, 1.000000000000000000, 0.9238795325112867385, 1.000000000000000000, 0.9238795325112867385, 1.000000000000000000, 0.9238795325112867385, 1.000000000000000000, 0.9238795325112867385, 1.000000000000000000, 0.9238795325112867385, 1.000000000000000000, 0.9238795325112867385, 1.000000000000000000, 0.9238795325112867385, 1.000000000000000000, 0.9238795325112867385, 1.000000000000000000, 0.9238795325112867385, 1.000000000000000000, 0.9238795325112867385, 1.000000000000000000, 0.9238795325112867385, 1.000000000000000000, 0.9238795325112867385, 1.000000000000000000, 0.9238795325112867385, 1.000000000000000000, 0.9238795325112867385, 1.000000000000000000, 0.9238795325112867385, 1.000000000000000000, 0.9238795325112867385, 1.000000000000000000, 0.9238795325112867385, 1.000000000000000000, 0.9238795325112867385, 1.000000000000000000, 0.9238795325112867385, 1.000000000000000000, 0.9238795325112867385, 1.000000000000000000, 0.9238795325112867385, 1.000000000000000000, 0.9238795325112867385, 1.000000000000000000, 0.9238795325112867385, 1.000000000000000000, 0.9238795325112867385, 1.000000000000000000, 0.9238795325112867385, 1.000000000000000000, 0.9238795325112867385, 1.000000000000000000, 0.9238795325112867385, 1.000000000000000000, 0.9238795325112867385, 1.000000000000000000, 0.9238795325112867385, 1.000000000000000000, 0.9238795325112867385, 1.000000000000000000, 0.9238795325112867385, 1.000000000000000000, 0.9238795325112867385, 1.000000000000000000, 0.9238795325112867385, 1.000000000000000000, 0.9238795325112867385, 1.000000000000000000, 0.9238795325112867385, 1.000000000000000000, 0.9238795325112867385, 1.000000000000000000, 0.9238795325112867385, 1.000000000000000000, 0.9238795325112867385, 1.000000000000000000, 0.9238795325112867385, 1.000000000000000000, 0.9238795325112867385, 1.000000000000000000, 0.9238795325112867385, 1.000000000000000000, 0.9238795325112867385, 1.000000000000000000, 0.9238795325112867385, 1.000000000000000000, 0.9238795325112867385, 1.000000000000000000, 0.9238795325112867385, 1.000000000000000000, 0.9238795325112867385, 1.000000000000000000, 0.9238795325112867385, 1.000000000000000000, 0.9238795325112867385, 1.000000000000000000, 0.9238795325112867385, 1.000000000000000000, 0.9238795325112867385, 1.000000000000000000, 0.9238795325112867385, 1.000000000000000000, 0.9238795325112867385, 1.000000000000000000, 0.9238795325112867385, 1.000000000000000000, 0.9238795325112867385, 1.000000000000000000, 0.9238795325112867385, 1.000000000000000000, 0.9238795325112867385, 1.000000000000000000, 0.9238795325112867385, 1.000000000000000000, 0.9238795325112867385, 1.000000000000000000, 0.9238795325112867385, 1.000000000000000000, 0.9238795325112867385, 1.000000000000000000, 0.9238795325112867385, 1.000000000000000000, 0.9238795325112867385, 1.000000000000000000, 0.9238795325112867385, 1.000000000000000000, 0.9238795325112867385, 1.000000000000000000, 0.9238795325112867385, 1.000000000000000000, 0.9238795325112867385, 1.000000000000000000, 0.9238795325112867385, 1.000000000000000000, 0.9238795325112867385, 1.000000000000000000, 0.9238795325112867385, 1.000000000000000000, 0.9238795325112867385, 1.000000000000000000, 0.9238795325112867385, 1.000000000000000000, 0.9238795325112867385, 1.000000000000000000, 0.9238795325112867385, 1.000000000000000000, 0.9238795325112867385, 1.000000000000000000, 0.9238795325112867385, 1.000000000000000000, 0.9238795325112867385, 1.000000000000000000, 0.9238795325112867385, 1.000000000000000000, 0.9238795325112867385, 1.000000000000000000, 0.9238795325112867385, 1.000000000000000000, 0.9238795325112867385, 1.000000000000000000, 0.9238795325112867385, 1.000000000000000000, 0.9238795325112867385, 1.000000000000000000, 0.9238795325112867385, 1.000000000000000000, 0.9238795325112867385, 1.000000000000000000, 0.9238795325112867385, 1.000000000000000000, 0.9238795325112867385, 1.000000000000000000) ) ) 
 REPRESENTATION_ITEM ( '' )  SURFACE ( )  );
#56679 = CARTESIAN_POINT ( 'NONE',  ( 0.000000000000000000, 300.0000000000000000, 0.000000000000000000 ) ) ;
#56680 = CARTESIAN_POINT ( 'NONE',  ( -6.676582343750000703, 290.6718750017070079, 2.765530957082001251 ) ) ;
#56681 = CARTESIAN_POINT ( 'NONE',  ( 5.000000000000000888, 53.12474899268135431, 47.87640533067916948 ) ) ;
#56682 = CARTESIAN_POINT ( 'NONE',  ( 3.313708498984756279, 7.999999999999991118, 3.549052783920144893 ) ) ;
#56683 = CARTESIAN_POINT ( 'NONE',  ( 0.000000000000000000, 125.0000000000000000, 8.000000000000000000 ) ) ;
#56684 = CARTESIAN_POINT ( 'NONE',  ( 5.676582343749997150, 262.2395833367473301, -9.832129032723418760 ) ) ;
#56685 = CARTESIAN_POINT ( 'NONE',  ( -4.220049686691935698, 10.18810118749999916, 96.25000000204838102 ) ) ;
#56686 = ORIENTED_EDGE ( 'NONE', *, *, #47379, .F. ) ;
#56687 = EDGE_CURVE ( 'NONE', #64324, #29716, #58767, .T. ) ;
#56688 = VECTOR ( 'NONE', #37223, 1000.000000000000000 ) ;
#56689 = CARTESIAN_POINT ( 'NONE',  ( 5.000000000000000000, 10.00000000000000000, -75.19090595827292134 ) ) ;
#56690 = SURFACE_SIDE_STYLE ('',( #74395 ) ) ;
#56691 = CARTESIAN_POINT ( 'NONE',  ( 2.445694354108839175, 202.3125000013656063, 195.5543056458912190 ) ) ;
#56692 = CARTESIAN_POINT ( 'NONE',  ( 6.951808397369818766E-16, 82.34374999658601268, -11.35316468750000141 ) ) ;
#56693 = VERTEX_POINT ( 'NONE', #46135 ) ;
#56694 = CARTESIAN_POINT ( 'NONE',  ( 4.220049686691934809, 10.18810118749999916, 113.6875000020483952 ) ) ;
#56695 = EDGE_CURVE ( 'NONE', #18027, #50547, #72172, .T. ) ;
#56696 =( BOUNDED_CURVE ( )  B_SPLINE_CURVE ( 2, ( #1787, #25876, #19119, #18762, #59137, #64777, #42499, #48895, #71908 ),
 .UNSPECIFIED., .F., .F. ) 
 B_SPLINE_CURVE_WITH_KNOTS ( ( 3, 2, 2, 2, 3 ),
 ( 0.6477272727272727071, 0.6534090909090909394, 0.6590909090909091717, 0.6647727272727274039, 0.6704545454545455252 ),
 .UNSPECIFIED. ) 
 CURVE ( )  GEOMETRIC_REPRESENTATION_ITEM ( )  RATIONAL_B_SPLINE_CURVE ( ( 1.000000000000000000, 0.9238795325112867385, 1.000000000000000000, 0.9238795325112867385, 1.000000000000000000, 0.9238795325112867385, 1.000000000000000000, 0.9238795325112852952, 1.000000000000001554 ) ) 
 REPRESENTATION_ITEM ( '' )  );
#56697 = CARTESIAN_POINT ( 'NONE',  ( 1.881053915767122664, 11.24999999863441147, 4.541265875000001451 ) ) ;
#56698 = ORIENTED_EDGE ( 'NONE', *, *, #61345, .F. ) ;
#56699 = CARTESIAN_POINT ( 'NONE',  ( 7.188101187499999156, 25.87499999795161543, 2.977408999572654924 ) ) ;
#56700 = CARTESIAN_POINT ( 'NONE',  ( 2.679491924315057449, 116.0416666666663303, -9.999999999997791988 ) ) ;
#56701 = CARTESIAN_POINT ( 'NONE',  ( -2.828427124746153876, 197.0000000027312126, 195.1715728752538439 ) ) ;
#56702 = CARTESIAN_POINT ( 'NONE',  ( -7.188101187500001821, 26.99999999795161543, -2.977408999572651371 ) ) ;
#56703 = CARTESIAN_POINT ( 'NONE',  ( -2.775557561562891351E-14, 210.0000000000000284, 146.0000000000000284 ) ) ;
#56704 = CARTESIAN_POINT ( 'NONE',  ( 10.18810118749999916, 1.247682550866122264E-15, 107.7812500020483810 ) ) ;
#56705 = VECTOR ( 'NONE', #25959, 1000.000000000000000 ) ;
#56706 = CARTESIAN_POINT ( 'NONE',  ( 47.32259252271281014, 0.000000000000000000, 65.76194439203456454 ) ) ;
#56707 = CARTESIAN_POINT ( 'NONE',  ( 2.828427124746191623, 10.87499999726881406, -2.828427124746191623 ) ) ;
#56708 = LINE ( 'NONE', #21608, #74624 ) ;
#56709 = ORIENTED_EDGE ( 'NONE', *, *, #39463, .F. ) ;
#56710 = CARTESIAN_POINT ( 'NONE',  ( 2.839093476692135984E-14, 204.6875000013656063, 201.4587341250000350 ) ) ;
#56711 = CARTESIAN_POINT ( 'NONE',  ( -24.54126587499999701, 207.1875000013656063, 170.0000000000002842 ) ) ;
#56712 = CARTESIAN_POINT ( 'NONE',  ( 31.99999999999997868, 199.4375000027312126, 168.3431457505074889 ) ) ;
#56713 = CARTESIAN_POINT ( 'NONE',  ( 4.541265875000002339, 10.37499999863440792, -1.881053915767121554 ) ) ;
#56714 = CARTESIAN_POINT ( 'NONE',  ( 1.656854249492381248, 0.1875000000000001943, -4.000000000000001776 ) ) ;
#56715 = CARTESIAN_POINT ( 'NONE',  ( -4.401442555609577197E-16, 7.188101187499992051, 16.11155278187175455 ) ) ;
#56716 = EDGE_LOOP ( 'NONE', ( #46696, #66577 ) ) ;
#56717 = LINE ( 'NONE', #5773, #40970 ) ;
#56718 = ORIENTED_EDGE ( 'NONE', *, *, #58983, .F. ) ;
#56719 = CARTESIAN_POINT ( 'NONE',  ( -10.18810118749999916, 4.220049686691934809, 112.5625000020483810 ) ) ;
#56720 = LINE ( 'NONE', #61994, #56930 ) ;
#56721 = CARTESIAN_POINT ( 'NONE',  ( 3.458734125000015425, 205.9375000013656063, 198.0000000000000284 ) ) ;
#56722 = CARTESIAN_POINT ( 'NONE',  ( 26.56734541678237704, 198.3750000013656063, 173.4587341249998929 ) ) ;
#56723 = CARTESIAN_POINT ( 'NONE',  ( 10.00000000000000178, 85.00000000000000000, 0.000000000000000000 ) ) ;
#56724 = EDGE_CURVE ( 'NONE', #10198, #55282, #74172, .T. ) ;
#56725 = CARTESIAN_POINT ( 'NONE',  ( 8.000000000000000000, 122.7500000000000000, -9.797174393178825657E-16 ) ) ;
#56726 = CARTESIAN_POINT ( 'NONE',  ( 4.721056650416000089, 298.9843750017070079, 4.721056650415999201 ) ) ;
#56727 = AXIS2_PLACEMENT_3D ( 'NONE', #35763, #29727, #337 ) ;
#56728 = ORIENTED_EDGE ( 'NONE', *, *, #41486, .F. ) ;
#56729 = CARTESIAN_POINT ( 'NONE',  ( 2.849036369511732440E-14, 203.2500000000000000, 202.0000000000000000 ) ) ;
#56730 = CARTESIAN_POINT ( 'NONE',  ( -4.737866951563228568, -68.48668487056878007, 20.75656675268391638 ) ) ;
#56731 = CARTESIAN_POINT ( 'NONE',  ( -1.656854249492405451, 197.4375000027312126, 138.0000000000000568 ) ) ;
#56732 = CARTESIAN_POINT ( 'NONE',  ( -5.000000000000000000, 65.00666015986153923, 24.03732210400620062 ) ) ;
#56733 = LINE ( 'NONE', #56448, #41114 ) ;
#56734 = CARTESIAN_POINT ( 'NONE',  ( 9.999999999999998224, 242.7083333333333428, -2.679491924311229401 ) ) ;
#56735 = CARTESIAN_POINT ( 'NONE',  ( 30.82842712474620228, 204.3750000000000284, 167.1715728752537586 ) ) ;
#56736 = CARTESIAN_POINT ( 'NONE',  ( -10.00000000000000178, 197.5000000000000000, -1.224646799147353454E-15 ) ) ;
#56737 = CARTESIAN_POINT ( 'NONE',  ( 2.977408999572650927, -7.188101187499990274, 17.33030278187175455 ) ) ;
#56738 = CARTESIAN_POINT ( 'NONE',  ( -9.832129032723418760, 168.1770833299193555, -5.676582343750004256 ) ) ;
#56739 = CARTESIAN_POINT ( 'NONE',  ( -2.679491924311433237, 211.4583333333334849, -10.00000000000014033 ) ) ;
#56740 = CARTESIAN_POINT ( 'NONE',  ( 2.775557561822899905E-14, -42.00000000000000711, 151.0000000000000284 ) ) ;
#56742 = CARTESIAN_POINT ( 'NONE',  ( -5.999999999999999112, 297.1250000034141294, 2.485281374238575314 ) ) ;
#56741 = FACE_OUTER_BOUND ( 'NONE', #73514, .T. ) ;
#56743 = ORIENTED_EDGE ( 'NONE', *, *, #43462, .T. ) ;
#56744 = CARTESIAN_POINT ( 'NONE',  ( 11.35316468749999963, 26.30208332991934839, -3.042071309553165293 ) ) ;
#56745 = CARTESIAN_POINT ( 'NONE',  ( 7.778174593052023411, -7.778174593052021635, 112.7500000040967763 ) ) ;
#56746 = CARTESIAN_POINT ( 'NONE',  ( -26.56734541678228112, 208.0000000013656063, 173.4587341250003476 ) ) ;
#56748 = CARTESIAN_POINT ( 'NONE',  ( 27.99999999999996803, 200.0000000000000000, 173.9999999999999147 ) ) ;
#56747 = CARTESIAN_POINT ( 'NONE',  ( 0.000000000000000000, 0.000000000000000000, -28.00000000000000000 ) ) ;
#56749 = CARTESIAN_POINT ( 'NONE',  ( -12.10377610768008161, -38.62207949530581885, 198.5409546172315061 ) ) ;
#56750 = CARTESIAN_POINT ( 'NONE',  ( 3.458734124999959914, 197.4375000013655779, 142.0000000000000568 ) ) ;
#56751 = EDGE_CURVE ( 'NONE', #28343, #18004, #41227, .T. ) ;
#56752 = CARTESIAN_POINT ( 'NONE',  ( 10.00000000000000000, 61.66666665983871098, 2.679491924311236062 ) ) ;
#56753 = CARTESIAN_POINT ( 'NONE',  ( 7.188101187500000044, 100.9062500020483810, -8.802885111219163269E-16 ) ) ;
#56754 = CARTESIAN_POINT ( 'NONE',  ( 2.780723358947928197E-16, 13.68749999863440614, -4.541265875000002339 ) ) ;
#56755 = LINE ( 'NONE', #28069, #25286 ) ;
#56756 = CARTESIAN_POINT ( 'NONE',  ( -5.656854249492373476, -5.656854249492376141, 1.017802779823363757 ) ) ;
#56757 = CARTESIAN_POINT ( 'NONE',  ( 7.999999999999992895, -3.313708498984756279, 21.17405278392015333 ) ) ;
#56758 = ORIENTED_EDGE ( 'NONE', *, *, #58993, .F. ) ;
#56759 = ORIENTED_EDGE ( 'NONE', *, *, #47030, .F. ) ;
#56760 = LINE ( 'NONE', #34131, #42386 ) ;
#56761 = CARTESIAN_POINT ( 'NONE',  ( 1.432654583217662481, 196.3750000013656063, 194.5412658750000219 ) ) ;
#56762 = CARTESIAN_POINT ( 'NONE',  ( -9.832129032723418760, 223.8020833367473301, -5.676582343749998927 ) ) ;
#56763 = CARTESIAN_POINT ( 'NONE',  ( 5.676582343750001591, 141.6145833299193555, -9.832129032723420536 ) ) ;
#56764 = EDGE_LOOP ( 'NONE', ( #64859, #70302, #33726, #32594, #44720 ) ) ;
#56765 = CARTESIAN_POINT ( 'NONE',  ( 30.82842712474620228, 201.3750000000000284, 167.1715728752537586 ) ) ;
#56766 = EDGE_CURVE ( 'NONE', #10672, #62018, #57852, .T. ) ;
#56767 = CARTESIAN_POINT ( 'NONE',  ( 4.220049686691941027, -10.18810118749999738, 90.62500000204836681 ) ) ;
#56768 = CARTESIAN_POINT ( 'NONE',  ( -29.56585189577901573, 194.4922901696101576, 166.8703325185142319 ) ) ;
#56769 = CARTESIAN_POINT ( 'NONE',  ( -3.999999999999960032, 210.0000000000000284, 198.0000000000000284 ) ) ;
#56770 = CARTESIAN_POINT ( 'NONE',  ( 6.366783985983791361, -4.860392236259310828, -0.000000000000000000 ) ) ;
#56771 = AXIS2_PLACEMENT_3D ( 'NONE', #32352, #67419, #73076 ) ;
#56772 = CARTESIAN_POINT ( 'NONE',  ( -6.238412754330611322E-16, 10.18810118749999916, 114.1562500020483810 ) ) ;
#56773 = VERTEX_POINT ( 'NONE', #6158 ) ;
#56774 = CARTESIAN_POINT ( 'NONE',  ( 8.000000000000001776, 106.3437500040967763, 3.313708498984759387 ) ) ;
#56775 = CARTESIAN_POINT ( 'NONE',  ( 30.86618291540373349, 179.6247977656714454, 166.3462567337799101 ) ) ;
#56776 = CARTESIAN_POINT ( 'NONE',  ( 8.311093377946834337, 130.4687499965860411, 8.311093377946839666 ) ) ;
#56777 = CARTESIAN_POINT ( 'NONE',  ( 2.754378923186476579E-14, 202.1875000013656063, 194.5412658750000219 ) ) ;
#56778 = CARTESIAN_POINT ( 'NONE',  ( -2.977408999572654480, 22.87499999795161543, 7.188101187499999156 ) ) ;
#56779 = CARTESIAN_POINT ( 'NONE',  ( 10.18810118749999916, 4.220049686691935698, 82.37500000204838102 ) ) ;
#56780 = CARTESIAN_POINT ( 'NONE',  ( -8.311093377946836114, 37.96874999658601979, -8.311093377946837890 ) ) ;
#56781 = ORIENTED_EDGE ( 'NONE', *, *, #39276, .F. ) ;
#56782 = DIRECTION ( 'NONE',  ( -0.000000000000000000, 1.000000000000000000, -0.000000000000000000 ) ) ;
#56783 = CARTESIAN_POINT ( 'NONE',  ( -8.342170076843785083E-16, 1.187499998634406806, 4.541265875000002339 ) ) ;
#56784 = CARTESIAN_POINT ( 'NONE',  ( 1.471067592899761672E-15, -8.008118988124991233, 20.88811528394063188 ) ) ;
#56785 = CARTESIAN_POINT ( 'NONE',  ( -1.432654583217662481, 206.3750000013656063, 145.4587341250000634 ) ) ;
#56786 = AXIS2_PLACEMENT_3D ( 'NONE', #30743, #53025, #2816 ) ;
#56787 = CARTESIAN_POINT ( 'NONE',  ( -2.977408999572650039, 11.43749999795161010, -7.188101187500001821 ) ) ;
#56788 = CARTESIAN_POINT ( 'NONE',  ( -2.485281374238572649, 296.2500000034140726, 6.000000000000002665 ) ) ;
#56789 = EDGE_CURVE ( 'NONE', #35502, #9105, #53031, .T. ) ;
#56790 = DIRECTION ( 'NONE',  ( -0.000000000000000000, 1.000000000000000000, -0.000000000000000000 ) ) ;
#56791 = DIRECTION ( 'NONE',  ( 0.000000000000000000, 0.000000000000000000, 1.000000000000000000 ) ) ;
#56792 =( BOUNDED_CURVE ( )  B_SPLINE_CURVE ( 2, ( #19936, #68957, #64685, #4849, #22546, #28219, #28591, #50854, #41676, #21799, #68582, #16130, #44830, #62920, #33531, #16890, #45568, #17267, #1334, #5962, #10871, #56906, #39913, #67839, #73492, #45199, #57656, #24316, #29983, #11614, #73869, #47327, #33907, #34651, #70354, #18665, #5594, #11246, #12984, #10497, #36021, #39169, #40286, #39547, #68210, #5218, #59039, #16506, #27846, #53001, #56531, #22175, #27463, #62172, #50477, #62542, #51229, #74240, #34276, #57279, #51602, #74617, #22933, #45944, #63287, #19385, #30353, #1697, #49175, #48059, #42398, #30719, #60500, #48429, #8827, #53374, #42769, #2794, #31838, #36756, #8079, #13348, #43513, #59401, #37500, #65785, #54857, #2420, #71432, #24676, #31080, #26157, #54108, #59770, #3168, #19761, #47686, #25414, #65415, #14089, #72185, #20128, #71067, #20498, #25038, #7346, #37124, #60126, #2051, #13712, #8444, #66158, #43143, #31464, #14463, #70707, #54489, #25781, #48801, #71810, #19026, #66526, #14837, #37877, #42032, #7715, #65039, #36386, #53740, #74058, #32217, #45024, #66912, #15588, #62356, #4291, #61629, #16695, #32980, #27283, #51048, #72945, #21253, #9196, #55235, #28037, #26916, #44278, #9582, #39359, #50300, #10687, #3540, #21624, #56346, #33720, #38628, #9948, #55981, #15217, #22357, #38247, #5040, #44648, #73321, #27659, #49930, #67663, #15962, #67289, #45382, #32600, #26532, #38991, #61996, #68397, #10318, #56722, #33344, #73685, #4665, #49556, #72575, #43900, #20879, #50667, #60873, #21998, #68030, #16324, #61251, #55608, #3926, #57846, #507, #28408, #11066, #45756, #34839, #18206, #41219, #34094, #51791, #6521, #1244, #17080, #6151, #40474, #40846, #63107, #52910, #57090, #29157, #51416, #5406, #23486, #68769, #52175, #46498, #29528, #12535, #11433, #69518, #69146, #17832, #74430, #22736, #57474, #69894, #35565, #64227, #23862, #34470, #58578, #23115, #46872, #6886, #29897, #63854, #12169, #24222 ),
 .UNSPECIFIED., .F., .F. ) 
 B_SPLINE_CURVE_WITH_KNOTS ( ( 3, 2, 2, 2, 2, 2, 2, 2, 2, 2, 2, 2, 2, 2, 2, 2, 2, 2, 2, 2, 2, 2, 2, 2, 2, 2, 2, 2, 2, 2, 2, 2, 2, 2, 2, 2, 2, 2, 2, 2, 2, 2, 2, 2, 2, 2, 2, 2, 2, 2, 2, 2, 2, 2, 2, 2, 2, 2, 2, 2, 2, 2, 2, 2, 2, 2, 2, 2, 2, 2, 2, 2, 2, 2, 2, 2, 2, 2, 2, 2, 2, 2, 2, 2, 2, 2, 2, 2, 2, 2, 2, 2, 2, 2, 2, 2, 2, 2, 2, 2, 2, 2, 2, 2, 2, 2, 2, 2, 2, 2, 2, 2, 2, 2, 2, 2, 2, 2, 2, 2, 3 ),
 ( 0.000000000000000000, 0.008333333333333333218, 0.01666666666666666644, 0.02500000000000000139, 0.03333333333333333287, 0.04166666666666666435, 0.05000000000000000278, 0.05833333333333333426, 0.06666666666666666574, 0.07499999999999999722, 0.08333333333333332871, 0.09166666666666666019, 0.1000000000000000056, 0.1083333333333333370, 0.1166666666666666685, 0.1250000000000000000, 0.1333333333333333315, 0.1416666666666666630, 0.1499999999999999944, 0.1583333333333333259, 0.1666666666666666574, 0.1749999999999999889, 0.1833333333333333204, 0.1916666666666666796, 0.2000000000000000111, 0.2083333333333333426, 0.2166666666666666741, 0.2250000000000000056, 0.2333333333333333370, 0.2416666666666666685, 0.2500000000000000000, 0.2583333333333333592, 0.2666666666666666630, 0.2750000000000000222, 0.2833333333333333259, 0.2916666666666666852, 0.2999999999999999889, 0.3083333333333333481, 0.3166666666666666519, 0.3250000000000000111, 0.3333333333333333148, 0.3416666666666666741, 0.3499999999999999778, 0.3583333333333333370, 0.3666666666666666408, 0.3750000000000000000, 0.3833333333333333592, 0.3916666666666666630, 0.4000000000000000222, 0.4083333333333333259, 0.4166666666666666852, 0.4249999999999999889, 0.4333333333333333481, 0.4416666666666666519, 0.4500000000000000111, 0.4583333333333333148, 0.4666666666666666741, 0.4749999999999999778, 0.4833333333333333370, 0.4916666666666666408, 0.5000000000000000000, 0.5083333333333333037, 0.5166666666666667185, 0.5250000000000000222, 0.5333333333333333259, 0.5416666666666666297, 0.5500000000000000444, 0.5583333333333333481, 0.5666666666666666519, 0.5749999999999999556, 0.5833333333333333703, 0.5916666666666666741, 0.5999999999999999778, 0.6083333333333332815, 0.6166666666666666963, 0.6250000000000000000, 0.6333333333333333037, 0.6416666666666667185, 0.6500000000000000222, 0.6583333333333333259, 0.6666666666666666297, 0.6750000000000000444, 0.6833333333333333481, 0.6916666666666666519, 0.6999999999999999556, 0.7083333333333333703, 0.7166666666666666741, 0.7249999999999999778, 0.7333333333333332815, 0.7416666666666666963, 0.7500000000000000000, 0.7583333333333333037, 0.7666666666666667185, 0.7750000000000000222, 0.7833333333333333259, 0.7916666666666666297, 0.8000000000000000444, 0.8083333333333333481, 0.8166666666666666519, 0.8249999999999999556, 0.8333333333333333703, 0.8416666666666666741, 0.8499999999999999778, 0.8583333333333332815, 0.8666666666666666963, 0.8750000000000000000, 0.8833333333333333037, 0.8916666666666667185, 0.9000000000000000222, 0.9083333333333333259, 0.9166666666666666297, 0.9250000000000000444, 0.9333333333333333481, 0.9416666666666666519, 0.9499999999999999556, 0.9583333333333333703, 0.9666666666666666741, 0.9749999999999999778, 0.9833333333333332815, 0.9916666666666666963, 0.9985233269883845297 ),
 .UNSPECIFIED. ) 
 CURVE ( )  GEOMETRIC_REPRESENTATION_ITEM ( )  RATIONAL_B_SPLINE_CURVE ( ( 1.000000000000000000, 0.9238795325112867385, 1.000000000000000000, 0.9238795325112867385, 1.000000000000000000, 0.9238795325112867385, 1.000000000000000000, 0.9238795325112867385, 1.000000000000000000, 0.9238795325112867385, 1.000000000000000000, 0.9238795325112867385, 1.000000000000000000, 0.9238795325112867385, 1.000000000000000000, 0.9238795325112867385, 1.000000000000000000, 0.9238795325112867385, 1.000000000000000000, 0.9238795325112867385, 1.000000000000000000, 0.9238795325112867385, 1.000000000000000000, 0.9238795325112867385, 1.000000000000000000, 0.9238795325112867385, 1.000000000000000000, 0.9238795325112867385, 1.000000000000000000, 0.9238795325112867385, 1.000000000000000000, 0.9238795325112867385, 1.000000000000000000, 0.9238795325112867385, 1.000000000000000000, 0.9238795325112867385, 1.000000000000000000, 0.9238795325112867385, 1.000000000000000000, 0.9238795325112867385, 1.000000000000000000, 0.9238795325112867385, 1.000000000000000000, 0.9238795325112867385, 1.000000000000000000, 0.9238795325112867385, 1.000000000000000000, 0.9238795325112867385, 1.000000000000000000, 0.9238795325112867385, 1.000000000000000000, 0.9238795325112867385, 1.000000000000000000, 0.9238795325112867385, 1.000000000000000000, 0.9238795325112867385, 1.000000000000000000, 0.9238795325112867385, 1.000000000000000000, 0.9238795325112867385, 1.000000000000000000, 0.9238795325112867385, 1.000000000000000000, 0.9238795325112867385, 1.000000000000000000, 0.9238795325112867385, 1.000000000000000000, 0.9238795325112867385, 1.000000000000000000, 0.9238795325112867385, 1.000000000000000000, 0.9238795325112867385, 1.000000000000000000, 0.9238795325112867385, 1.000000000000000000, 0.9238795325112867385, 1.000000000000000000, 0.9238795325112867385, 1.000000000000000000, 0.9238795325112867385, 1.000000000000000000, 0.9238795325112867385, 1.000000000000000000, 0.9238795325112867385, 1.000000000000000000, 0.9238795325112867385, 1.000000000000000000, 0.9238795325112867385, 1.000000000000000000, 0.9238795325112867385, 1.000000000000000000, 0.9238795325112867385, 1.000000000000000000, 0.9238795325112867385, 1.000000000000000000, 0.9238795325112867385, 1.000000000000000000, 0.9238795325112867385, 1.000000000000000000, 0.9238795325112867385, 1.000000000000000000, 0.9238795325112867385, 1.000000000000000000, 0.9238795325112867385, 1.000000000000000000, 0.9238795325112867385, 1.000000000000000000, 0.9238795325112867385, 1.000000000000000000, 0.9238795325112867385, 1.000000000000000000, 0.9238795325112867385, 1.000000000000000000, 0.9238795325112867385, 1.000000000000000000, 0.9238795325112867385, 1.000000000000000000, 0.9238795325112867385, 1.000000000000000000, 0.9238795325112867385, 1.000000000000000000, 0.9238795325112867385, 1.000000000000000000, 0.9238795325112867385, 1.000000000000000000, 0.9238795325112867385, 1.000000000000000000, 0.9238795325112867385, 1.000000000000000000, 0.9238795325112867385, 1.000000000000000000, 0.9238795325112867385, 1.000000000000000000, 0.9238795325112867385, 1.000000000000000000, 0.9238795325112867385, 1.000000000000000000, 0.9238795325112867385, 1.000000000000000000, 0.9238795325112867385, 1.000000000000000000, 0.9238795325112867385, 1.000000000000000000, 0.9238795325112867385, 1.000000000000000000, 0.9238795325112867385, 1.000000000000000000, 0.9238795325112867385, 1.000000000000000000, 0.9238795325112867385, 1.000000000000000000, 0.9238795325112867385, 1.000000000000000000, 0.9238795325112867385, 1.000000000000000000, 0.9238795325112867385, 1.000000000000000000, 0.9238795325112867385, 1.000000000000000000, 0.9238795325112867385, 1.000000000000000000, 0.9238795325112867385, 1.000000000000000000, 0.9238795325112867385, 1.000000000000000000, 0.9238795325112867385, 1.000000000000000000, 0.9238795325112867385, 1.000000000000000000, 0.9238795325112867385, 1.000000000000000000, 0.9238795325112867385, 1.000000000000000000, 0.9238795325112867385, 1.000000000000000000, 0.9238795325112867385, 1.000000000000000000, 0.9238795325112867385, 1.000000000000000000, 0.9238795325112867385, 1.000000000000000000, 0.9238795325112867385, 1.000000000000000000, 0.9238795325112867385, 1.000000000000000000, 0.9238795325112867385, 1.000000000000000000, 0.9238795325112867385, 1.000000000000000000, 0.9238795325112867385, 1.000000000000000000, 0.9238795325112867385, 1.000000000000000000, 0.9238795325112867385, 1.000000000000000000, 0.9238795325112867385, 1.000000000000000000, 0.9238795325112867385, 1.000000000000000000, 0.9238795325112867385, 1.000000000000000000, 0.9238795325112867385, 1.000000000000000000, 0.9238795325112867385, 1.000000000000000000, 0.9238795325112867385, 1.000000000000000000, 0.9238795325112867385, 1.000000000000000000, 0.9238795325112867385, 1.000000000000000000, 0.9238795325112867385, 1.000000000000000000, 0.9238795325112867385, 1.000000000000000000, 0.9238795325112867385, 1.000000000000000000, 0.9238795325112867385, 1.000000000000000000, 0.9238795325112867385, 1.000000000000000000, 0.9238795325112867385, 1.000000000000000000, 0.9238795325112867385, 1.000000000000000000, 0.9238795325112867385, 1.000000000000000000, 0.9238795325112867385, 1.000000000000000000, 0.9238795325112867385, 1.000000000000000000, 0.9238795325112867385, 1.000000000000000000, 0.9238795325112867385, 1.000000000000000000, 0.9238795325112867385, 1.000000000000000000, 0.9238795325112867385, 1.000000000000000000, 0.9373681373079431056, 0.9778031724869039598 ) ) 
 REPRESENTATION_ITEM ( '' )  );
#56793 = CARTESIAN_POINT ( 'NONE',  ( -8.311093377946836114, 157.9687499965860127, -8.311093377946837890 ) ) ;
#56794 = CARTESIAN_POINT ( 'NONE',  ( -10.18810118749999916, 0.000000000000000000, 75.15625000204836681 ) ) ;
#56795 = CARTESIAN_POINT ( 'NONE',  ( -30.44569435410883074, 195.5625000013656063, 167.5543056458915885 ) ) ;
#56796 = CARTESIAN_POINT ( 'NONE',  ( 0.000000000000000000, 0.000000000000000000, 30.00000000000000000 ) ) ;
#56797 = CARTESIAN_POINT ( 'NONE',  ( -3.211159895383562723, 20.06249999863440436, 3.211159895383561391 ) ) ;
#56798 = EDGE_LOOP ( 'NONE', ( #8085, #32788, #12804, #4702 ) ) ;
#56799 = CIRCLE ( 'NONE', #54370, 6.000000000000005329 ) ;
#56800 = CARTESIAN_POINT ( 'NONE',  ( -2.828427124746153876, 200.0000000027312126, 195.1715728752538439 ) ) ;
#56801 = CARTESIAN_POINT ( 'NONE',  ( -2.839093476692135984E-14, 195.9375000013655779, 138.5412658750000503 ) ) ;
#56802 = CARTESIAN_POINT ( 'NONE',  ( -32.00000000000000000, 204.3750000027312126, 170.0000000000004547 ) ) ;
#56803 = LINE ( 'NONE', #51129, #68177 ) ;
#56804 = ORIENTED_EDGE ( 'NONE', *, *, #2406, .F. ) ;
#56805 = CARTESIAN_POINT ( 'NONE',  ( 4.401442555609581635E-16, 14.34374999795161187, -7.188101187500000044 ) ) ;
#56806 = DIRECTION ( 'NONE',  ( 0.000000000000000000, -0.8778652960885079404, 0.4789076340208374138 ) ) ;
#56807 = CARTESIAN_POINT ( 'NONE',  ( -2.846155565392938236, -45.96854017595656927, 151.2142286236573625 ) ) ;
#56808 = CARTESIAN_POINT ( 'NONE',  ( -2.679491924311235618, 38.54166666666665719, 10.00000000000000000 ) ) ;
#56809 = CARTESIAN_POINT ( 'NONE',  ( 7.188101187500000044, 108.7812500020483810, -8.802885111219163269E-16 ) ) ;
#56810 = AXIS2_PLACEMENT_3D ( 'NONE', #24267, #6564, #2006 ) ;
#56811 = CARTESIAN_POINT ( 'NONE',  ( -27.99999999999996803, 208.1875000013656063, 173.4587341250003760 ) ) ;
#56812 = CARTESIAN_POINT ( 'NONE',  ( -4.721056650415998313, 289.5781250017069510, 4.721056650416000089 ) ) ;
#56814 = CARTESIAN_POINT ( 'NONE',  ( -11.00000000000010658, 4.556349186103942017, 74.59375000409676204 ) ) ;
#56813 = CARTESIAN_POINT ( 'NONE',  ( 2.679491924312774831, 36.04166666666652930, -9.999999999999104716 ) ) ;
#56815 = VERTEX_POINT ( 'NONE', #22742 ) ;
#56816 = CARTESIAN_POINT ( 'NONE',  ( -6.951808397369817780E-16, 252.6562500034140157, -11.35316468749999963 ) ) ;
#56817 = CARTESIAN_POINT ( 'NONE',  ( 5.082755093536320601, -5.082755093536318824, 23.42405278187175455 ) ) ;
#56818 = CARTESIAN_POINT ( 'NONE',  ( 2.589639417653039288, 50.10293296561670218, 40.79253907059217710 ) ) ;
#56819 = CARTESIAN_POINT ( 'NONE',  ( 5.000000000000000000, -60.90295814858238543, -23.31388853594834032 ) ) ;
#56820 = CARTESIAN_POINT ( 'NONE',  ( 0.000000000000000000, 125.0000000000000000, 0.000000000000000000 ) ) ;
#56821 = CARTESIAN_POINT ( 'NONE',  ( -2.445694354108783219, 194.8125000013656063, 200.4456943541088663 ) ) ;
#56822 = CARTESIAN_POINT ( 'NONE',  ( -8.660254037844387298, 167.0833333333333428, -5.000000000000004441 ) ) ;
#56823 = CARTESIAN_POINT ( 'NONE',  ( -6.000000000000003553, 299.9374999999999432, -2.485281374238571317 ) ) ;
#56824 = SURFACE_STYLE_FILL_AREA ( #33827 ) ;
#56825 = CARTESIAN_POINT ( 'NONE',  ( 4.999999999999999112, -50.98458432551128539, -41.27351214092455933 ) ) ;
#56826 = CARTESIAN_POINT ( 'NONE',  ( 8.311093377946834337, 125.4687499965860127, 8.311093377946839666 ) ) ;
#56827 = LINE ( 'NONE', #5148, #33666 ) ;
#56828 = CARTESIAN_POINT ( 'NONE',  ( 3.313708498984756279, 7.999999999999991118, 27.54905278392014623 ) ) ;
#56829 = VECTOR ( 'NONE', #74180, 1000.000000000000000 ) ;
#56832 = CARTESIAN_POINT ( 'NONE',  ( 10.99999999999989342, 4.556349186104152515, 84.53125000409679046 ) ) ;
#56831 = CARTESIAN_POINT ( 'NONE',  ( 26.56734541678237704, 198.3750000013655779, 173.4587341249998929 ) ) ;
#56830 = CARTESIAN_POINT ( 'NONE',  ( 30.44569435410878810, 194.8125000013656063, 172.4456943541087526 ) ) ;
#56833 = ORIENTED_EDGE ( 'NONE', *, *, #15384, .F. ) ;
#56834 = ADVANCED_FACE ( 'NONE', ( #513 ), #51053, .T. ) ;
#56835 = CARTESIAN_POINT ( 'NONE',  ( 2.905213938366133508, 223.9844880932393210, 9.586977549355461647 ) ) ;
#56836 = DIRECTION ( 'NONE',  ( -0.000000000000000000, 1.000000000000000000, -0.000000000000000000 ) ) ;
#56837 = CARTESIAN_POINT ( 'NONE',  ( -4.556349186104048599, -10.99999999999999822, 112.4687500040967905 ) ) ;
#56838 = CARTESIAN_POINT ( 'NONE',  ( 5.000000000000000000, -67.10422270468698969, -23.07049055144788952 ) ) ;
#56839 = CARTESIAN_POINT ( 'NONE',  ( -11.35316468750000141, 208.8020833299193555, 3.042071309553159963 ) ) ;
#56840 = CARTESIAN_POINT ( 'NONE',  ( -2.977408999572651815, 118.4375000020483810, 7.188101187500000933 ) ) ;
#56841 = CARTESIAN_POINT ( 'NONE',  ( -3.211159895383562723, 17.93749999863440792, 3.211159895383561391 ) ) ;
#56842 = CARTESIAN_POINT ( 'NONE',  ( 2.620431783923081959, -55.87941608673214233, 43.94382193462615049 ) ) ;
#56843 = CARTESIAN_POINT ( 'NONE',  ( -7.999999999999991118, 0.000000000000000000, 20.33030277982336642 ) ) ;
#56845 = LINE ( 'NONE', #22484, #62840 ) ;
#56844 = CARTESIAN_POINT ( 'NONE',  ( 2.449293598294707893E-16, 11.99999999726881406, -4.000000000000001776 ) ) ;
#56846 = CARTESIAN_POINT ( 'NONE',  ( -11.35316468750000141, 93.28124999658602690, -1.390361679473963753E-15 ) ) ;
#56847 = ORIENTED_EDGE ( 'NONE', *, *, #33610, .F. ) ;
#56848 = DIRECTION ( 'NONE',  ( 0.000000000000000000, 1.000000000000000000, 0.000000000000000000 ) ) ;
#56849 = CARTESIAN_POINT ( 'NONE',  ( -7.188101187500000044, 26.71874999795161543, -8.802885111219163269E-16 ) ) ;
#56850 = CARTESIAN_POINT ( 'NONE',  ( 5.000000000000081712, 40.83333333333342097, -8.660254037844525854 ) ) ;
#56851 = CARTESIAN_POINT ( 'NONE',  ( 11.35316468749999963, 251.5104166700806729, 3.042071309553159519 ) ) ;
#56852 = VECTOR ( 'NONE', #20334, 1000.000000000000000 ) ;
#56853 = CARTESIAN_POINT ( 'NONE',  ( 9.832129032723416984, 100.3645833299193697, 5.676582343750006032 ) ) ;
#56854 = ORIENTED_EDGE ( 'NONE', *, *, #42577, .T. ) ;
#56855 = DIRECTION ( 'NONE',  ( 1.000000000000000000, -0.000000000000000000, 0.000000000000000000 ) ) ;
#56856 = EDGE_CURVE ( 'NONE', #22034, #37225, #66902, .T. ) ;
#56857 = CARTESIAN_POINT ( 'NONE',  ( 4.220049686691934809, 10.18810118749999916, 104.6875000020483810 ) ) ;
#56858 = CARTESIAN_POINT ( 'NONE',  ( -2.679491924311235618, 225.4166666598386826, 10.00000000000000000 ) ) ;
#56859 = CARTESIAN_POINT ( 'NONE',  ( 2.754378923186476579E-14, 204.4375000013656063, 194.5412658750000219 ) ) ;
#56860 = CARTESIAN_POINT ( 'NONE',  ( -32.00000000000002842, 201.3125000027312126, 168.3431457505080857 ) ) ;
#56862 = CARTESIAN_POINT ( 'NONE',  ( -2.085542519210945728E-15, 94.53124999658601268, 11.35316468750000141 ) ) ;
#56861 = CARTESIAN_POINT ( 'NONE',  ( 0.000000000000000000, 0.000000000000000000, -1.050311307314560239 ) ) ;
#56863 = CARTESIAN_POINT ( 'NONE',  ( 7.999999999999991118, 9.797174393178815797E-16, 12.26780278392014623 ) ) ;
#56864 = CARTESIAN_POINT ( 'NONE',  ( -31.45873412499999944, 199.8750000013655779, 168.5673454167827572 ) ) ;
#56865 = CARTESIAN_POINT ( 'NONE',  ( 2.449293598294707893E-16, 16.25000000000000000, -4.000000000000001776 ) ) ;
#56866 = ORIENTED_EDGE ( 'NONE', *, *, #61830, .F. ) ;
#56867 = EDGE_CURVE ( 'NONE', #12530, #36130, #38045, .T. ) ;
#56868 = CARTESIAN_POINT ( 'NONE',  ( 2.679491924311222739, 180.8333333265053966, 10.00000000000000355 ) ) ;
#56869 = DIRECTION ( 'NONE',  ( -0.000000000000000000, -0.000000000000000000, 1.000000000000000000 ) ) ;
#56870 = DIRECTION ( 'NONE',  ( 0.000000000000000000, 0.000000000000000000, -1.000000000000000000 ) ) ;
#56871 = CARTESIAN_POINT ( 'NONE',  ( -5.676582343750006032, 84.42708332991935549, 9.832129032723418760 ) ) ;
#56872 = CARTESIAN_POINT ( 'NONE',  ( 1.226468279477575784E-15, 290.7031250017069510, 6.676582343750001591 ) ) ;
#56873 = CARTESIAN_POINT ( 'NONE',  ( 4.401442555609581635E-16, 5.718749997951610986, -7.188101187500000044 ) ) ;
#56874 = CARTESIAN_POINT ( 'NONE',  ( 10.18810118749999916, 4.220049686691935698, 103.3750000020483952 ) ) ;
#56875 = CARTESIAN_POINT ( 'NONE',  ( -8.311093377946836114, 222.6562499965860411, -8.311093377946837890 ) ) ;
#56876 = VERTEX_POINT ( 'NONE', #31002 ) ;
#56877 = CARTESIAN_POINT ( 'NONE',  ( 0.000000000000000000, 0.000000000000000000, -14.00000000000000178 ) ) ;
#56878 = CARTESIAN_POINT ( 'NONE',  ( 5.656854249492379694, 115.6250000040967905, -5.656854249492380582 ) ) ;
#56879 = CARTESIAN_POINT ( 'NONE',  ( 0.000000000000000000, 0.000000000000000000, 41.99999999999999289 ) ) ;
#56880 = CARTESIAN_POINT ( 'NONE',  ( 9.832129032723416984, 210.3645833299193555, 5.676582343750006032 ) ) ;
#56881 = CARTESIAN_POINT ( 'NONE',  ( 9.999999999999998224, 220.8333333401613174, -2.679491924311229401 ) ) ;
#56882 = CARTESIAN_POINT ( 'NONE',  ( -1.836970198721029983E-15, 100.6249999931720396, 10.00000000000000178 ) ) ;
#56883 = CARTESIAN_POINT ( 'NONE',  ( -2.765530957081998586, 297.6406250017070079, 6.676582343750001591 ) ) ;
#56884 = EDGE_CURVE ( 'NONE', #44635, #48188, #45744, .T. ) ;
#56885 = ORIENTED_EDGE ( 'NONE', *, *, #65928, .F. ) ;
#56886 = CARTESIAN_POINT ( 'NONE',  ( 11.35316468749999785, 200.8854166632526983, 3.042071309553174174 ) ) ;
#56887 = CARTESIAN_POINT ( 'NONE',  ( -4.220049686691937474, -10.18810118749999738, 96.43750000204836681 ) ) ;
#56888 = CIRCLE ( 'NONE', #26747, 3.999999999999988010 ) ;
#56889 = CARTESIAN_POINT ( 'NONE',  ( -25.55430564589119413, 205.3125000013656063, 167.5543056458915316 ) ) ;
#56890 = CARTESIAN_POINT ( 'NONE',  ( 8.000000000000000000, 15.00000000000000355, 0.000000000000000000 ) ) ;
#56891 = ORIENTED_EDGE ( 'NONE', *, *, #15182, .F. ) ;
#56892 = PRODUCT_DEFINITION_CONTEXT ( 'detailed design', #51100, 'design' ) ;
#56893 = CARTESIAN_POINT ( 'NONE',  ( 8.000000000000000000, 93.03125000409677625, -3.313708498984762496 ) ) ;
#56894 = CARTESIAN_POINT ( 'NONE',  ( 1.224646799147353256E-15, 265.0000000000000000, 10.00000000000000000 ) ) ;
#56895 = CARTESIAN_POINT ( 'NONE',  ( 2.679491924311228956, 16.04166666666666785, -10.00000000000000000 ) ) ;
#56896 = CARTESIAN_POINT ( 'NONE',  ( -6.238412754330611322E-16, 10.18810118749999916, 78.15625000204836681 ) ) ;
#56897 = ORIENTED_EDGE ( 'NONE', *, *, #52786, .F. ) ;
#56898 = CARTESIAN_POINT ( 'NONE',  ( 4.000000000000001776, 21.00000000000000000, 0.000000000000000000 ) ) ;
#56899 =( BOUNDED_CURVE ( )  B_SPLINE_CURVE ( 2, ( #64700, #36036, #47700, #6259, #13362, #19774, #42045, #48443, #31094 ),
 .UNSPECIFIED., .F., .F. ) 
 B_SPLINE_CURVE_WITH_KNOTS ( ( 3, 2, 2, 2, 3 ),
 ( 0.000000000000000000, 0.003676470588235296235, 0.007352941176470592470, 0.01102941176470589001, 0.01470588235294118494 ),
 .UNSPECIFIED. ) 
 CURVE ( )  GEOMETRIC_REPRESENTATION_ITEM ( )  RATIONAL_B_SPLINE_CURVE ( ( 1.000000000000000000, 0.9238795325112867385, 1.000000000000000000, 0.9238795325112867385, 1.000000000000000000, 0.9238795325112867385, 1.000000000000000000, 0.9238795325112865164, 1.000000000000000222 ) ) 
 REPRESENTATION_ITEM ( '' )  );
#56900 = CARTESIAN_POINT ( 'NONE',  ( -8.342170076843785083E-16, 18.06249999863440792, 4.541265875000002339 ) ) ;
#56901 = CARTESIAN_POINT ( 'NONE',  ( 31.61180006176080681, 194.6073834165950132, 169.8621511762734997 ) ) ;
#56902 = VECTOR ( 'NONE', #25930, 1000.000000000000227 ) ;
#56903 = CARTESIAN_POINT ( 'NONE',  ( 8.660254037844389075, 17.29166665983869677, -5.000000000000000000 ) ) ;
#56904 = CARTESIAN_POINT ( 'NONE',  ( -4.401442555609581635E-16, 89.28125000204838102, -7.188101187500000044 ) ) ;
#56905 = FACE_OUTER_BOUND ( 'NONE', #33704, .T. ) ;
#56908 = LINE ( 'NONE', #10873, #13295 ) ;
#56907 = CARTESIAN_POINT ( 'NONE',  ( -9.832129032723415207, 249.3229166700806729, 5.676582343750005144 ) ) ;
#56906 = CARTESIAN_POINT ( 'NONE',  ( 24.54126587499998635, 208.1250000013656063, 168.5673454167822740 ) ) ;
#56909 = SHAPE_DEFINITION_REPRESENTATION ( #68631, #4585 ) ;
#56910 = CIRCLE ( 'NONE', #29230, 5.000000000000000000 ) ;
#56911 = ORIENTED_EDGE ( 'NONE', *, *, #55857, .F. ) ;
#56912 = CARTESIAN_POINT ( 'NONE',  ( -11.35316468749999963, 249.2187500034139873, 0.000000000000000000 ) ) ;
#56913 = CARTESIAN_POINT ( 'NONE',  ( -7.188101187499990274, -2.977408999572651371, 15.08030278187175455 ) ) ;
#56914 = EDGE_LOOP ( 'NONE', ( #46474, #30347, #21879, #7865 ) ) ;
#56915 = ORIENTED_EDGE ( 'NONE', *, *, #49321, .T. ) ;
#56916 = CARTESIAN_POINT ( 'NONE',  ( -7.204075437095965206, -7.204075437095968759, 72.34375000204836681 ) ) ;
#56917 = CARTESIAN_POINT ( 'NONE',  ( -2.085542519210945728E-15, 84.84374999658601268, 11.35316468750000141 ) ) ;
#56918 = DIRECTION ( 'NONE',  ( 0.000000000000000000, 0.000000000000000000, 1.000000000000000000 ) ) ;
#56919 = CARTESIAN_POINT ( 'NONE',  ( -4.556349186104047710, -10.99999999999999822, 80.78124999999998579 ) ) ;
#56922 = CARTESIAN_POINT ( 'NONE',  ( 2.765530957082001251, 289.9218750017069510, 6.676582343749999815 ) ) ;
#56921 = CARTESIAN_POINT ( 'NONE',  ( 23.99999999999998579, 194.8750000027311842, 169.9999999999999432 ) ) ;
#56920 = CARTESIAN_POINT ( 'NONE',  ( 31.45873412499999944, 208.9375000013656063, 169.9999999999999432 ) ) ;
#56923 = DIRECTION ( 'NONE',  ( -0.000000000000000000, 1.000000000000000000, -1.563033456626094573E-30 ) ) ;
#56924 = CARTESIAN_POINT ( 'NONE',  ( -3.999999999999959144, 200.0625000000000284, 199.6568542494924259 ) ) ;
#56925 = CARTESIAN_POINT ( 'NONE',  ( -2.085542519210945728E-15, 199.5312499965860411, 11.35316468750000141 ) ) ;
#56926 = CARTESIAN_POINT ( 'NONE',  ( 8.000000000000000000, 10.31249999590322020, 0.000000000000000000 ) ) ;
#56927 = ORIENTED_EDGE ( 'NONE', *, *, #44562, .T. ) ;
#56928 = CARTESIAN_POINT ( 'NONE',  ( 25.55430564589119058, 195.0625000013656063, 167.5543056458910485 ) ) ;
#56929 = CARTESIAN_POINT ( 'NONE',  ( 7.188101187500001821, 18.93749999795161187, -2.977408999572650483 ) ) ;
#56930 = VECTOR ( 'NONE', #27281, 1000.000000000000000 ) ;
#56931 = CARTESIAN_POINT ( 'NONE',  ( 5.676582343750001591, 166.9270833299193555, -9.832129032723420536 ) ) ;
#56932 = CARTESIAN_POINT ( 'NONE',  ( 5.082755093536325042, 104.4687500020483952, -5.082755093536325930 ) ) ;
#56934 = CARTESIAN_POINT ( 'NONE',  ( -10.00000000000000000, 234.7916666666666856, -2.679491924311226292 ) ) ;
#56933 = CARTESIAN_POINT ( 'NONE',  ( 4.000000000000000888, 16.68749999726881583, 1.656854249492384135 ) ) ;
#56935 = CARTESIAN_POINT ( 'NONE',  ( 27.99999999999996803, 207.6875000013656063, 173.4587341249998929 ) ) ;
#56936 = CARTESIAN_POINT ( 'NONE',  ( 5.082755093536320601, -5.082755093536318824, 11.42405278187175455 ) ) ;
#56937 = CARTESIAN_POINT ( 'NONE',  ( -5.676582343750006032, 54.11458332991934839, 9.832129032723418760 ) ) ;
#56938 = CARTESIAN_POINT ( 'NONE',  ( -1.505592673977224738, -42.39769117051795888, 139.0361489862156930 ) ) ;
#56939 = CARTESIAN_POINT ( 'NONE',  ( 7.999999999999991118, 3.313708498984757611, 0.2303027843298232069 ) ) ;
#56940 = ORIENTED_EDGE ( 'NONE', *, *, #1429, .T. ) ;
#56941 = CARTESIAN_POINT ( 'NONE',  ( 12.00000000000000000, 6.928203230275542523, -1.071796769724504550 ) ) ;
#56942 = FACE_OUTER_BOUND ( 'NONE', #63916, .T. ) ;
#56943 = CARTESIAN_POINT ( 'NONE',  ( -11.35316468750000141, 63.48958332991935549, 3.042071309553159963 ) ) ;
#56944 = CARTESIAN_POINT ( 'NONE',  ( -6.735557395310442023E-16, 11.00000000000000000, 74.31250000409676204 ) ) ;
#56945 = CARTESIAN_POINT ( 'NONE',  ( -2.754378923186476579E-14, 200.4375000013656063, 145.4587341250000350 ) ) ;
#56946 = CARTESIAN_POINT ( 'NONE',  ( 4.737866951562321738, 16.26762833210778680, 69.68949229523451550 ) ) ;
#56947 = CARTESIAN_POINT ( 'NONE',  ( -4.999999999999998224, 11.66666666666666785, -8.660254037844389075 ) ) ;
#56949 = CARTESIAN_POINT ( 'NONE',  ( -5.676582343750006032, 49.11458332991935549, 9.832129032723418760 ) ) ;
#56948 = CARTESIAN_POINT ( 'NONE',  ( -2.977408999572652260, 91.43750000204838102, 7.188101187500000044 ) ) ;
#56950 = CARTESIAN_POINT ( 'NONE',  ( 7.999999999999991118, 3.313708498984757611, 4.674052779823363757 ) ) ;
#56951 = CARTESIAN_POINT ( 'NONE',  ( -7.999999999999991118, 0.000000000000000000, 22.01780278392014623 ) ) ;
#56952 = CARTESIAN_POINT ( 'NONE',  ( 9.832129032723420536, 171.1979166632526983, -5.676582343749999815 ) ) ;
#56953 = ADVANCED_FACE ( 'NONE', ( #42317 ), #31378, .T. ) ;
#56954 = CARTESIAN_POINT ( 'NONE',  ( 5.000000000000001776, 147.7083333265053682, -8.660254037844389075 ) ) ;
#56955 = VECTOR ( 'NONE', #7111, 1000.000000000000000 ) ;
#56956 = CARTESIAN_POINT ( 'NONE',  ( -7.188101187499999156, 105.1250000020483668, 2.977408999572654924 ) ) ;
#56957 = DIRECTION ( 'NONE',  ( -0.000000000000000000, 1.000000000000000000, -0.000000000000000000 ) ) ;
#56958 = CARTESIAN_POINT ( 'NONE',  ( -9.832129032723420536, 29.01041666325268764, 5.676582343749997150 ) ) ;
#56959 = CARTESIAN_POINT ( 'NONE',  ( 10.18810118749999916, 1.247682550866122264E-15, 116.7812500020483810 ) ) ;
#56960 = CARTESIAN_POINT ( 'NONE',  ( -11.35316468749999785, 188.0729166632526983, -3.042071309553167513 ) ) ;
#56961 = EDGE_LOOP ( 'NONE', ( #4670, #58192, #72537, #3743 ) ) ;
#56962 = CARTESIAN_POINT ( 'NONE',  ( 1.469576158976823947E-15, 107.3750000000000000, 8.000000000000000000 ) ) ;
#56963 = CARTESIAN_POINT ( 'NONE',  ( -10.18810118749999916, 0.000000000000000000, 72.15625000204836681 ) ) ;
#56964 = CARTESIAN_POINT ( 'NONE',  ( -3.999999999999960032, 196.9375000000000284, 196.3431457505076594 ) ) ;
#56965 = CARTESIAN_POINT ( 'NONE',  ( 31.01747540368007350, 47.55161448135750391, 65.00000000000000000 ) ) ;
#56967 = CARTESIAN_POINT ( 'NONE',  ( -11.35316468749999785, 163.0729166632526699, -3.042071309553167957 ) ) ;
#56966 = LINE ( 'NONE', #18075, #35098 ) ;
#56968 = CARTESIAN_POINT ( 'NONE',  ( -4.898587196589407898E-16, 7.999999999999991118, 8.011552784329822430 ) ) ;
#56969 = AXIS2_PLACEMENT_3D ( 'NONE', #73093, #67809, #50821 ) ;
#56970 = CARTESIAN_POINT ( 'NONE',  ( 2.250000000000001332, 261.5999999999996248, 5.425975922785162275 ) ) ;
#56971 = CARTESIAN_POINT ( 'NONE',  ( -3.042071309553159075, 219.9479166700806445, 11.35316468749999963 ) ) ;
#56972 = CYLINDRICAL_SURFACE ( 'NONE', #20322, 10.00000000000000178 ) ;
#56973 = ORIENTED_EDGE ( 'NONE', *, *, #43058, .F. ) ;
#56974 = ADVANCED_FACE ( 'NONE', ( #35938 ), #70628, .T. ) ;
#56975 = CARTESIAN_POINT ( 'NONE',  ( 0.000000000000000000, 300.0000000000000000, 0.000000000000000000 ) ) ;
#56976 = CARTESIAN_POINT ( 'NONE',  ( -2.085542519210945728E-15, 109.8437499965860269, 11.35316468750000141 ) ) ;
#56977 = EDGE_CURVE ( 'NONE', #17226, #32089, #2335, .T. ) ;
#56978 = FACE_OUTER_BOUND ( 'NONE', #32283, .T. ) ;
#56979 = ORIENTED_EDGE ( 'NONE', *, *, #28240, .F. ) ;
#56980 = CARTESIAN_POINT ( 'NONE',  ( -4.541265875000003227, 9.999999998634407916, 1.881053915767121110 ) ) ;
#56981 = CARTESIAN_POINT ( 'NONE',  ( 5.082755093536324154, 13.78124999795161010, 5.082755093536326818 ) ) ;
#56982 = CARTESIAN_POINT ( 'NONE',  ( -3.313708498984762052, 109.9062500040967905, -8.000000000000000000 ) ) ;
#56983 = CARTESIAN_POINT ( 'NONE',  ( -25.55430564589119413, 199.5625000013656063, 167.5543056458915316 ) ) ;
#56984 = EDGE_CURVE ( 'NONE', #32512, #24671, #10064, .T. ) ;
#56985 = CARTESIAN_POINT ( 'NONE',  ( 4.000000000000000888, 7.937500000000000888, 1.656854249492384135 ) ) ;
#56986 = CARTESIAN_POINT ( 'NONE',  ( -2.828427124746192067, 22.37499999726881583, 2.828427124746190735 ) ) ;
#56987 = CARTESIAN_POINT ( 'NONE',  ( 3.211159895383560947, 6.187499998634407028, 3.211159895383562723 ) ) ;
#56988 = CARTESIAN_POINT ( 'NONE',  ( -4.000000000000015987, 198.4375000000000568, 140.3431457505076594 ) ) ;
#56989 = ORIENTED_EDGE ( 'NONE', *, *, #35268, .T. ) ;
#56990 = CARTESIAN_POINT ( 'NONE',  ( -4.401442555609581635E-16, 102.7812500020483810, -7.188101187500000044 ) ) ;
#56993 = CARTESIAN_POINT ( 'NONE',  ( -8.000000000000000000, 123.5000000000000000, 0.000000000000000000 ) ) ;
#56992 = PLANE ( 'NONE',  #25314 ) ;
#56991 =( BOUNDED_CURVE ( )  B_SPLINE_CURVE ( 2, ( #70002, #74536, #22847, #13365, #54504, #59417, #31481, #3186, #54876 ),
 .UNSPECIFIED., .F., .F. ) 
 B_SPLINE_CURVE_WITH_KNOTS ( ( 3, 2, 2, 2, 3 ),
 ( 0.5441176470588233727, 0.5477941176470587648, 0.5514705882352940458, 0.5551470588235293269, 0.5588235294117646079 ),
 .UNSPECIFIED. ) 
 CURVE ( )  GEOMETRIC_REPRESENTATION_ITEM ( )  RATIONAL_B_SPLINE_CURVE ( ( 1.000000000000002220, 0.9238795325112844070, 1.000000000000000000, 0.9238795325112867385, 1.000000000000000000, 0.9238795325112867385, 1.000000000000000000, 0.9238795325112890700, 0.9999999999999976685 ) ) 
 REPRESENTATION_ITEM ( '' )  );
#56994 =( NAMED_UNIT ( * ) PLANE_ANGLE_UNIT ( ) SI_UNIT ( $, .RADIAN. ) );
#56995 = CARTESIAN_POINT ( 'NONE',  ( -3.211159895383562723, 21.93749999863440792, 3.211159895383561391 ) ) ;
#56996 = CARTESIAN_POINT ( 'NONE',  ( 7.188101187499992051, 8.802885111219154394E-16, 2.236552781871750550 ) ) ;
#56997 = VERTEX_POINT ( 'NONE', #21544 ) ;
#56998 = VERTEX_POINT ( 'NONE', #61170 ) ;
#56999 = CARTESIAN_POINT ( 'NONE',  ( -10.18810118749999916, 4.220049686691934809, 91.56250000204838102 ) ) ;
#57000 = CARTESIAN_POINT ( 'NONE',  ( 29.65685424949235838, 204.1875000027311842, 173.9999999999999432 ) ) ;
#57001 = CARTESIAN_POINT ( 'NONE',  ( -24.54126587500000412, 198.5000000013656063, 168.5673454167827003 ) ) ;
#57002 = CARTESIAN_POINT ( 'NONE',  ( -11.00000000000000000, 0.000000000000000000, 108.9999999999999858 ) ) ;
#57003 = CARTESIAN_POINT ( 'NONE',  ( -2.445694354108783219, 204.8125000013656063, 200.4456943541088663 ) ) ;
#57005 = CARTESIAN_POINT ( 'NONE',  ( -7.320508075688771932, 254.3750000000000284, -7.320508075688771932 ) ) ;
#57004 = CYLINDRICAL_SURFACE ( 'NONE', #57947, 11.00000000000000000 ) ;
#57006 = EDGE_CURVE ( 'NONE', #70764, #70088, #26446, .T. ) ;
#57007 = CARTESIAN_POINT ( 'NONE',  ( -8.660254037844390851, 117.9166666666666714, 4.999999999999998224 ) ) ;
#57008 = CARTESIAN_POINT ( 'NONE',  ( -5.656854249492378806, 105.6874999999999858, 5.656854249492381470 ) ) ;
#57009 = CARTESIAN_POINT ( 'NONE',  ( 2.765530957081996366, 288.2968750017070647, -6.676582343750003368 ) ) ;
#57010 = CARTESIAN_POINT ( 'NONE',  ( -7.188101187499991163, 2.977408999572646930, 6.267802781871754547 ) ) ;
#57011 = ADVANCED_FACE ( 'NONE', ( #14383 ), #10860, .T. ) ;
#57013 =( BOUNDED_CURVE ( )  B_SPLINE_CURVE ( 2, ( #42971, #71644, #61462, #65992, #14673, #3750, #14297, #8659, #31674 ),
 .UNSPECIFIED., .F., .F. ) 
 B_SPLINE_CURVE_WITH_KNOTS ( ( 3, 2, 2, 2, 3 ),
 ( 0.5500000000000005995, 0.5583333333333337922, 0.5666666666666670960, 0.5750000000000003997, 0.5833333333333337034 ),
 .UNSPECIFIED. ) 
 CURVE ( )  GEOMETRIC_REPRESENTATION_ITEM ( )  RATIONAL_B_SPLINE_CURVE ( ( 0.9999999999999948930, 0.9238795325112918455, 1.000000000000000000, 0.9238795325112867385, 1.000000000000000000, 0.9238795325112867385, 1.000000000000000000, 0.9238795325112837409, 1.000000000000003109 ) ) 
 REPRESENTATION_ITEM ( '' )  );
#57012 = CARTESIAN_POINT ( 'NONE',  ( 4.898587196589415787E-16, 0.000000000000000000, 4.000000000000001776 ) ) ;
#57014 = CARTESIAN_POINT ( 'NONE',  ( 24.54126587499998635, 206.2500000013656063, 171.4326545832175555 ) ) ;
#57015 = CARTESIAN_POINT ( 'NONE',  ( -3.313708498984765161, 24.84374999590322020, 7.999999999999998224 ) ) ;
#57016 = CARTESIAN_POINT ( 'NONE',  ( -1.432654583217662481, 201.1250000013656347, 145.4587341250000634 ) ) ;
#57017 = DIRECTION ( 'NONE',  ( -0.000000000000000000, -0.000000000000000000, -1.000000000000000000 ) ) ;
#57019 = CARTESIAN_POINT ( 'NONE',  ( -2.775557561562891351E-14, 210.0000000000000284, 146.0000000000000284 ) ) ;
#57018 = LINE ( 'NONE', #5331, #37154 ) ;
#57020 = CARTESIAN_POINT ( 'NONE',  ( 3.042071309553173286, 245.6770833367473017, 11.35316468749999608 ) ) ;
#57021 = CARTESIAN_POINT ( 'NONE',  ( -5.082755093536317936, -5.082755093536320601, 26.04905278187175810 ) ) ;
#57022 = CARTESIAN_POINT ( 'NONE',  ( 27.99999999999996803, 200.0000000000000000, 173.9999999999999147 ) ) ;
#57023 = CARTESIAN_POINT ( 'NONE',  ( 11.35316468749999963, 20.98958332991935549, -3.042071309553165293 ) ) ;
#57024 = EDGE_CURVE ( 'NONE', #17458, #68962, #43434, .T. ) ;
#57025 = CARTESIAN_POINT ( 'NONE',  ( -4.401442555609577197E-16, 7.188101187499992051, 1.486552781871753437 ) ) ;
#57026 = CARTESIAN_POINT ( 'NONE',  ( -9.832129032723420536, 209.0104166632526699, 5.676582343749997150 ) ) ;
#57027 = CARTESIAN_POINT ( 'NONE',  ( 11.35316468749999963, 0.9895833299193491639, -3.042071309553165293 ) ) ;
#57028 = DIRECTION ( 'NONE',  ( 0.000000000000000000, -1.000000000000000000, 0.000000000000000000 ) ) ;
#57030 = CARTESIAN_POINT ( 'NONE',  ( 0.000000000000000000, 195.0000000000000284, 207.0000000000000568 ) ) ;
#57029 = LINE ( 'NONE', #44586, #41895 ) ;
#57031 = ORIENTED_EDGE ( 'NONE', *, *, #69703, .T. ) ;
#57032 = CARTESIAN_POINT ( 'NONE',  ( -2.445694354108839175, 201.3125000013656063, 144.4456943541088663 ) ) ;
#57033 = CARTESIAN_POINT ( 'NONE',  ( 11.35316468749999785, 20.57291666325268409, 3.042071309553174174 ) ) ;
#57034 = CARTESIAN_POINT ( 'NONE',  ( -4.556349186104047710, -10.99999999999999822, 89.96875000409677625 ) ) ;
#57035 = CARTESIAN_POINT ( 'NONE',  ( 8.660254037844389075, 210.4166666666666572, -5.000000000000000888 ) ) ;
#57036 = CARTESIAN_POINT ( 'NONE',  ( -26.56734541678228112, 196.0000000013656063, 173.4587341250003476 ) ) ;
#57037 = DIRECTION ( 'NONE',  ( -0.000000000000000000, 1.000000000000000000, -0.000000000000000000 ) ) ;
#57039 = CARTESIAN_POINT ( 'NONE',  ( 3.042071309553167513, 6.822916663252683200, -11.35316468749999785 ) ) ;
#57038 = CARTESIAN_POINT ( 'NONE',  ( -7.188101187500000044, 113.6562500020483810, 0.000000000000000000 ) ) ;
#57040 = CARTESIAN_POINT ( 'NONE',  ( 3.313708498984756279, 7.999999999999991118, 21.36155277982336997 ) ) ;
#57041 = CARTESIAN_POINT ( 'NONE',  ( 9.832129032723420536, 141.1979166632526699, -5.676582343749999815 ) ) ;
#57042 = CARTESIAN_POINT ( 'NONE',  ( -7.320508075688773708, 108.7499999931720254, -7.320508075688774596 ) ) ;
#57043 = CARTESIAN_POINT ( 'NONE',  ( -4.401442555609581635E-16, 121.1562500020483810, -7.188101187500000044 ) ) ;
#57044 = CARTESIAN_POINT ( 'NONE',  ( -8.000000000000001776, 14.15624999590322730, 3.313708498984759387 ) ) ;
#57045 = CARTESIAN_POINT ( 'NONE',  ( -25.55430564589119768, 208.5625000013656063, 167.5543056458915316 ) ) ;
#57046 = AXIS2_PLACEMENT_3D ( 'NONE', #42270, #69848, #65281 ) ;
#57047 = CARTESIAN_POINT ( 'NONE',  ( -5.000000000000000000, 53.55923425356163392, -45.42020841079019533 ) ) ;
#57048 = ORIENTED_EDGE ( 'NONE', *, *, #12218, .F. ) ;
#57049 = CARTESIAN_POINT ( 'NONE',  ( -10.00000000000000888, 117.7083333333333428, 2.679491924311224071 ) ) ;
#57050 = DIRECTION ( 'NONE',  ( 0.000000000000000000, 0.000000000000000000, 1.000000000000000000 ) ) ;
#57051 = CARTESIAN_POINT ( 'NONE',  ( 2.765530957081996366, 289.2968750017070079, -6.676582343750003368 ) ) ;
#57052 = CARTESIAN_POINT ( 'NONE',  ( 0.000000000000000000, 300.0000000000000000, 0.000000000000000000 ) ) ;
#57053 = CARTESIAN_POINT ( 'NONE',  ( -7.999999999999991118, 3.313708498984756723, 24.79280278432983664 ) ) ;
#57054 = CARTESIAN_POINT ( 'NONE',  ( 2.828427124746153876, 197.8750000000000284, 144.8284271247462129 ) ) ;
#57055 = CARTESIAN_POINT ( 'NONE',  ( 1.469576158976823947E-15, 102.8750000000000000, 8.000000000000000000 ) ) ;
#57056 = CARTESIAN_POINT ( 'NONE',  ( -10.18810118749999738, -4.220049686691941915, 99.62500000204838102 ) ) ;
#57057 = ORIENTED_EDGE ( 'NONE', *, *, #31636, .F. ) ;
#57058 = ADVANCED_FACE ( 'NONE', ( #66450 ), #50586, .T. ) ;
#57059 = CARTESIAN_POINT ( 'NONE',  ( 37.99999999999999289, 50.00000000000000711, 57.99999999999999289 ) ) ;
#57060 = CARTESIAN_POINT ( 'NONE',  ( 11.00000000000000000, 1.347111479062088405E-15, 97.74999999999998579 ) ) ;
#57061 = CARTESIAN_POINT ( 'NONE',  ( 2.754378923186476579E-14, 203.4375000013656063, 194.5412658750000219 ) ) ;
#57062 = CARTESIAN_POINT ( 'NONE',  ( 5.676582343749993598, 75.26041666325268409, 9.832129032723422313 ) ) ;
#57063 = ORIENTED_EDGE ( 'NONE', *, *, #40663, .T. ) ;
#57064 = CARTESIAN_POINT ( 'NONE',  ( -4.220049686691937474, -10.18810118749999738, 106.9375000020483810 ) ) ;
#57065 = CARTESIAN_POINT ( 'NONE',  ( 2.780723358947928197E-16, 13.68749999863440614, -4.541265875000002339 ) ) ;
#57066 = ORIENTED_EDGE ( 'NONE', *, *, #58421, .T. ) ;
#57067 = AXIS2_PLACEMENT_3D ( 'NONE', #2633, #2256, #25249 ) ;
#57068 = CARTESIAN_POINT ( 'NONE',  ( -5.082755093536325042, 26.53124999795161543, -5.082755093536325930 ) ) ;
#57069 = CARTESIAN_POINT ( 'NONE',  ( -19.99999999999993250, -31.99999999999978684, 205.0000000000000284 ) ) ;
#57070 = FACE_OUTER_BOUND ( 'NONE', #1582, .T. ) ;
#57071 = CARTESIAN_POINT ( 'NONE',  ( 7.188101187499999156, 23.24999999795161187, 2.977408999572654924 ) ) ;
#57072 = CARTESIAN_POINT ( 'NONE',  ( 0.000000000000000000, 0.000000000000000000, -10.00000000000000000 ) ) ;
#57073 = CARTESIAN_POINT ( 'NONE',  ( 4.220049686691941027, -10.18810118749999738, 106.0000000020483668 ) ) ;
#57074 = DIRECTION ( 'NONE',  ( 0.000000000000000000, -1.000000000000000000, 0.000000000000000000 ) ) ;
#57075 = CARTESIAN_POINT ( 'NONE',  ( 2.828427124746190291, 11.62499999726881406, 2.828427124746192067 ) ) ;
#57076 = DIRECTION ( 'NONE',  ( 0.000000000000000000, 0.000000000000000000, 1.000000000000000000 ) ) ;
#57077 = ORIENTED_EDGE ( 'NONE', *, *, #6917, .F. ) ;
#57078 = ADVANCED_FACE ( 'NONE', ( #38167 ), #73239, .T. ) ;
#57079 = CARTESIAN_POINT ( 'NONE',  ( 3.458734125000015425, 200.9375000013656063, 198.0000000000000284 ) ) ;
#57080 = CARTESIAN_POINT ( 'NONE',  ( -24.54126587500002188, 205.2500000013655779, 168.5673454167826435 ) ) ;
#57081 = CARTESIAN_POINT ( 'NONE',  ( -1.881053915767121554, 9.624999998634404363, -4.541265875000002339 ) ) ;
#57082 = CIRCLE ( 'NONE', #72748, 7.499999999999992895 ) ;
#57083 = CARTESIAN_POINT ( 'NONE',  ( 5.082755093536318824, 5.082755093536319713, 21.92405278187175455 ) ) ;
#57084 = ORIENTED_EDGE ( 'NONE', *, *, #51466, .T. ) ;
#57085 = CARTESIAN_POINT ( 'NONE',  ( -4.242640687119285658, 292.1249999999999432, 4.242640687119287435 ) ) ;
#57086 = EDGE_LOOP ( 'NONE', ( #48864, #2147, #54529, #15751 ) ) ;
#57087 = CARTESIAN_POINT ( 'NONE',  ( -4.220049686691937474, -10.18810118749999738, 112.9375000020483810 ) ) ;
#57088 = DIRECTION ( 'NONE',  ( -1.000000000000000000, -0.000000000000000000, 0.000000000000000000 ) ) ;
#57089 = CARTESIAN_POINT ( 'NONE',  ( -3.458734124999959914, 200.3750000013656063, 196.5673454167823877 ) ) ;
#57090 = CARTESIAN_POINT ( 'NONE',  ( 24.54126587500000056, 196.2500000013656347, 171.4326545832176123 ) ) ;
#57091 = CARTESIAN_POINT ( 'NONE',  ( -7.320508075688773708, 76.87499999999998579, -7.320508075688774596 ) ) ;
#57092 = CARTESIAN_POINT ( 'NONE',  ( 3.313708498984760720, 123.0312499999999858, -8.000000000000000000 ) ) ;
#57093 = CARTESIAN_POINT ( 'NONE',  ( -4.242640687119285658, 289.1249999999999432, 4.242640687119287435 ) ) ;
#57094 = EDGE_CURVE ( 'NONE', #51619, #34267, #7630, .T. ) ;
#57095 = ORIENTED_EDGE ( 'NONE', *, *, #62531, .T. ) ;
#57096 = CARTESIAN_POINT ( 'NONE',  ( 10.99999999999992006, -4.556349186104122317, 109.6562499999999858 ) ) ;
#57097 = CARTESIAN_POINT ( 'NONE',  ( 1.506524674532313535, -10.12152537343867031, 70.16785718946155725 ) ) ;
#57098 = CARTESIAN_POINT ( 'NONE',  ( 3.999999999999959144, 194.1875000027312126, 140.3431457505076594 ) ) ;
#57099 = CARTESIAN_POINT ( 'NONE',  ( 2.020667218593132706E-15, -11.00000000000000000, 91.37499999999998579 ) ) ;
#57100 = CARTESIAN_POINT ( 'NONE',  ( 7.999999999999991118, 3.313708498984758055, 25.86155278392014267 ) ) ;
#57101 = CARTESIAN_POINT ( 'NONE',  ( 7.320508075688771044, 238.1249999999999716, -7.320508075688771932 ) ) ;
#57102 = CARTESIAN_POINT ( 'NONE',  ( 31.99999999999998579, 204.1875000000000853, 171.6568542494923122 ) ) ;
#57103 =( BOUNDED_CURVE ( )  B_SPLINE_CURVE ( 2, ( #20999, #16724, #57872, #11092, #166, #27038, #67034, #26660, #34118 ),
 .UNSPECIFIED., .F., .F. ) 
 B_SPLINE_CURVE_WITH_KNOTS ( ( 3, 2, 2, 2, 3 ),
 ( 0.06666666666666672125, 0.07500000000000006661, 0.08333333333333339810, 0.09166666666666672958, 0.1000000000000000888 ),
 .UNSPECIFIED. ) 
 CURVE ( )  GEOMETRIC_REPRESENTATION_ITEM ( )  RATIONAL_B_SPLINE_CURVE ( ( 0.9999999999999994449, 0.9238795325112872936, 1.000000000000000000, 0.9238795325112867385, 1.000000000000000000, 0.9238795325112867385, 1.000000000000000000, 0.9238795325112859613, 1.000000000000000666 ) ) 
 REPRESENTATION_ITEM ( '' )  );
#57104 = CARTESIAN_POINT ( 'NONE',  ( -8.660254037844390851, 197.9166666666666856, 4.999999999999998224 ) ) ;
#57105 = ADVANCED_FACE ( 'NONE', ( #32896 ), #27201, .F. ) ;
#57106 = CARTESIAN_POINT ( 'NONE',  ( 7.188101187499992051, 2.977408999572647819, 19.20530278187175455 ) ) ;
#57107 = CARTESIAN_POINT ( 'NONE',  ( 6.951808397369818766E-16, 167.3437499965860127, -11.35316468750000141 ) ) ;
#57108 = CARTESIAN_POINT ( 'NONE',  ( -7.320508075688939797, 213.1250000000000853, 7.320508075688932692 ) ) ;
#57109 = CARTESIAN_POINT ( 'NONE',  ( 31.99999999999997868, 197.4375000027312126, 168.3431457505074889 ) ) ;
#57111 = CARTESIAN_POINT ( 'NONE',  ( 8.000000000000000000, 10.31249999590322020, 0.000000000000000000 ) ) ;
#57110 = CYLINDRICAL_SURFACE ( 'NONE', #67169, 10.00000000000000178 ) ;
#57112 = ORIENTED_EDGE ( 'NONE', *, *, #20079, .T. ) ;
#57113 = AXIS2_PLACEMENT_3D ( 'NONE', #10016, #33047, #3234 ) ;
#57114 = CARTESIAN_POINT ( 'NONE',  ( 2.445694354108783664, 198.3125000013656063, 144.4456943541088663 ) ) ;
#57115 = CARTESIAN_POINT ( 'NONE',  ( -9.832129032723418760, 38.17708332991935549, -5.676582343750004256 ) ) ;
#57116 = CARTESIAN_POINT ( 'NONE',  ( -10.99999999999999822, -4.556349186104052151, 112.2812500040967763 ) ) ;
#57117 = CARTESIAN_POINT ( 'NONE',  ( -25.55430564589111953, 209.0625000013656063, 172.4456943541091505 ) ) ;
#57118 = CARTESIAN_POINT ( 'NONE',  ( -7.778174593052020747, -7.778174593052023411, 70.18749999999998579 ) ) ;
#57120 = CARTESIAN_POINT ( 'NONE',  ( 1.506680654948938658, -10.12163528317107719, -70.16331425389822130 ) ) ;
#57119 = CARTESIAN_POINT ( 'NONE',  ( 7.320508075688771044, 221.2499999931720538, 7.320508075688775484 ) ) ;
#57121 = CARTESIAN_POINT ( 'NONE',  ( -29.52074869199887885, -51.94789886732490913, 179.5111983649387071 ) ) ;
#57122 = CARTESIAN_POINT ( 'NONE',  ( 3.458734124999959914, 200.4375000013656063, 142.0000000000000568 ) ) ;
#57123 = CARTESIAN_POINT ( 'NONE',  ( 8.660254037844389075, 67.29166665983869677, -5.000000000000000000 ) ) ;
#57124 = CARTESIAN_POINT ( 'NONE',  ( 5.082755093536325042, 104.0937500020483810, -5.082755093536325930 ) ) ;
#57125 = CARTESIAN_POINT ( 'NONE',  ( -1.881053915767124440, 14.12499999863440969, 4.541265875000001451 ) ) ;
#57126 = CARTESIAN_POINT ( 'NONE',  ( -32.00000000000003553, 206.3125000027312126, 168.3431457505080857 ) ) ;
#57127 = CARTESIAN_POINT ( 'NONE',  ( 7.313652169806020176, 0.2330964041442518675, -2.525252314552933086 ) ) ;
#57128 = FACE_OUTER_BOUND ( 'NONE', #38565, .T. ) ;
#57129 = ORIENTED_EDGE ( 'NONE', *, *, #51211, .F. ) ;
#57130 = ORIENTED_EDGE ( 'NONE', *, *, #33912, .F. ) ;
#57131 = CARTESIAN_POINT ( 'NONE',  ( -2.828427124746152987, 205.2500000027312126, 200.8284271247462129 ) ) ;
#57132 = CARTESIAN_POINT ( 'NONE',  ( 1.469576158976822172E-15, -7.999999999999991118, 14.89280278392014623 ) ) ;
#57133 = LINE ( 'NONE', #34882, #7373 ) ;
#57134 = DIRECTION ( 'NONE',  ( 1.000000000000000000, 0.000000000000000000, 0.000000000000000000 ) ) ;
#57135 = CARTESIAN_POINT ( 'NONE',  ( -9.832129032723418760, 142.8645833299193555, -5.676582343750004256 ) ) ;
#57136 = DIRECTION ( 'NONE',  ( -1.000000000000000000, -0.000000000000000000, -0.000000000000000000 ) ) ;
#57137 = CARTESIAN_POINT ( 'NONE',  ( 7.204075437095966983, 7.204075437095967871, 91.09375000204838102 ) ) ;
#57138 = CARTESIAN_POINT ( 'NONE',  ( -31.03434905890962270, 194.6645454233662633, 172.0669317922800303 ) ) ;
#57139 = CARTESIAN_POINT ( 'NONE',  ( -2.828427124746152987, 205.1250000000000284, 200.8284271247462129 ) ) ;
#57140 = CARTESIAN_POINT ( 'NONE',  ( 2.679491924311139250, 248.5416666666666856, -10.00000000000004796 ) ) ;
#57141 = LINE ( 'NONE', #45432, #53047 ) ;
#57142 = CARTESIAN_POINT ( 'NONE',  ( -10.18810118749999738, -4.220049686691941915, 116.1250000020483810 ) ) ;
#57143 = ORIENTED_EDGE ( 'NONE', *, *, #47743, .T. ) ;
#57144 = CARTESIAN_POINT ( 'NONE',  ( -10.99999999999991829, 4.556349186104124982, 109.0937500040967763 ) ) ;
#57145 = VECTOR ( 'NONE', #59473, 1000.000000000000000 ) ;
#57146 = CARTESIAN_POINT ( 'NONE',  ( 35.46499747849647122, 173.3340168152039666, 175.5502016142357320 ) ) ;
#57147 = CARTESIAN_POINT ( 'NONE',  ( 6.951808397369818766E-16, 132.3437499965860127, -11.35316468750000141 ) ) ;
#57148 = CARTESIAN_POINT ( 'NONE',  ( -1.432654583217607858, 201.6250000013656063, 201.4587341250000065 ) ) ;
#57149 = CARTESIAN_POINT ( 'NONE',  ( -5.082755093536326818, 24.28124999795161543, 5.082755093536325042 ) ) ;
#57150 = CARTESIAN_POINT ( 'NONE',  ( -10.18810118749999916, 4.220049686691934809, 79.93750000204838102 ) ) ;
#57151 = CARTESIAN_POINT ( 'NONE',  ( -9.832129032723418760, 33.17708332991934839, -5.676582343750004256 ) ) ;
#57152 = ORIENTED_EDGE ( 'NONE', *, *, #25641, .T. ) ;
#57153 = CARTESIAN_POINT ( 'NONE',  ( -1.836970198721029983E-15, 35.62499999317203248, 10.00000000000000178 ) ) ;
#57154 = CARTESIAN_POINT ( 'NONE',  ( 4.541265875000002339, 0.4374999986344068059, 0.000000000000000000 ) ) ;
#57155 = CARTESIAN_POINT ( 'NONE',  ( -8.008118988124991233, 0.000000000000000000, 22.01311528394063188 ) ) ;
#57156 = CARTESIAN_POINT ( 'NONE',  ( -2.839093476692135984E-14, 206.9375000013656063, 138.5412658750000503 ) ) ;
#57157 = CARTESIAN_POINT ( 'NONE',  ( 7.188101187499999156, 7.874999997951610986, 2.977408999572654924 ) ) ;
#57158 = CARTESIAN_POINT ( 'NONE',  ( 6.000000000000003553, 294.5000000034139589, 2.485281374238571317 ) ) ;
#57159 = CARTESIAN_POINT ( 'NONE',  ( -18.25964289199068347, -16.57744543794718339, 137.1161668676152772 ) ) ;
#57160 = CARTESIAN_POINT ( 'NONE',  ( -7.188101187500001821, 4.499999997951610098, -2.977408999572651371 ) ) ;
#57161 = CARTESIAN_POINT ( 'NONE',  ( 3.042071309553167069, 152.1354166632526983, -11.35316468749999785 ) ) ;
#57162 = CARTESIAN_POINT ( 'NONE',  ( 10.18810118749999916, 1.247682550866122264E-15, 80.40625000204838102 ) ) ;
#57163 = CARTESIAN_POINT ( 'NONE',  ( -31.45873412499999944, 196.6250000013656063, 168.5673454167827572 ) ) ;
#57164 = ADVANCED_FACE ( 'NONE', ( #3456 ), #15134, .T. ) ;
#57165 = DIRECTION ( 'NONE',  ( 0.000000000000000000, 0.000000000000000000, 1.000000000000000000 ) ) ;
#57166 = CARTESIAN_POINT ( 'NONE',  ( -3.211159895383562723, 21.06249999863440792, 3.211159895383561391 ) ) ;
#57167 = ORIENTED_EDGE ( 'NONE', *, *, #21049, .T. ) ;
#57168 = VECTOR ( 'NONE', #11907, 1000.000000000000000 ) ;
#57169 = CARTESIAN_POINT ( 'NONE',  ( -2.828427124746153876, 198.0000000027312126, 195.1715728752538439 ) ) ;
#57170 = CARTESIAN_POINT ( 'NONE',  ( 1.656854249492347719, 207.8125000000000284, 146.0000000000000284 ) ) ;
#57171 = CARTESIAN_POINT ( 'NONE',  ( -26.34314575050769491, 202.0625000027312410, 166.0000000000003695 ) ) ;
#57172 = EDGE_CURVE ( 'NONE', #64725, #40886, #3838, .T. ) ;
#57173 = EDGE_CURVE ( 'NONE', #52340, #64048, #7247, .T. ) ;
#57174 = CARTESIAN_POINT ( 'NONE',  ( -10.00000000000008171, 57.50000000000004974, -1.224646799147362920E-15 ) ) ;
#57175 = CARTESIAN_POINT ( 'NONE',  ( 5.656854249492376141, -5.656854249492374365, 9.080302783920146226 ) ) ;
#57176 = EDGE_LOOP ( 'NONE', ( #35888, #69739, #37581, #988 ) ) ;
#57177 = CARTESIAN_POINT ( 'NONE',  ( 2.977408999572652260, 19.68749999795161543, 7.188101187500000044 ) ) ;
#57178 = FACE_OUTER_BOUND ( 'NONE', #61668, .T. ) ;
#57179 = CARTESIAN_POINT ( 'NONE',  ( 4.999999999999998224, 52.63864145287949725, -42.88977517748021029 ) ) ;
#57180 = CARTESIAN_POINT ( 'NONE',  ( 6.123233995736767268E-16, 41.25000000000000000, -10.00000000000000178 ) ) ;
#57181 = CARTESIAN_POINT ( 'NONE',  ( -7.188101187499999156, 106.6250000020483952, 2.977408999572654924 ) ) ;
#57182 = CARTESIAN_POINT ( 'NONE',  ( -29.43265458321761230, 208.1250000013656063, 173.4587341250003760 ) ) ;
#57183 = CARTESIAN_POINT ( 'NONE',  ( 1.656854249492365705, 205.3125000027312126, 138.0000000000000853 ) ) ;
#57185 = CARTESIAN_POINT ( 'NONE',  ( -8.000000000000000000, 95.18750000409679046, 0.000000000000000000 ) ) ;
#57184 = CYLINDRICAL_SURFACE ( 'NONE', #67100, 8.000000000000000000 ) ;
#57186 = ORIENTED_EDGE ( 'NONE', *, *, #31714, .F. ) ;
#57187 = CARTESIAN_POINT ( 'NONE',  ( -11.35316468749999785, 238.6979166700806729, -3.042071309553164848 ) ) ;
#57188 = PRODUCT_DEFINITION_SHAPE ( 'NONE', 'NONE',  #74664 ) ;
#57189 = CARTESIAN_POINT ( 'NONE',  ( 1.320432766682872962E-15, -7.188101187499992051, 18.73655278187175455 ) ) ;
#57190 = VECTOR ( 'NONE', #22098, 1000.000000000000000 ) ;
#57191 = CARTESIAN_POINT ( 'NONE',  ( -0.4501631047668632757, 51.14740050675958116, 48.52018030598983955 ) ) ;
#57192 = CARTESIAN_POINT ( 'NONE',  ( -6.000000000000001776, 287.0625000034140157, 0.000000000000000000 ) ) ;
#57193 = DIRECTION ( 'NONE',  ( -0.000000000000000000, 1.000000000000000000, -0.000000000000000000 ) ) ;
#57194 = CARTESIAN_POINT ( 'NONE',  ( -1.432654583217607414, 197.5000000013656063, 194.5412658750000219 ) ) ;
#57195 = CARTESIAN_POINT ( 'NONE',  ( -5.000000000000005329, 163.3333333333333428, 8.660254037844387298 ) ) ;
#57196 = LINE ( 'NONE', #17939, #19663 ) ;
#57197 = CARTESIAN_POINT ( 'NONE',  ( 4.531193156845207581E-15, 210.0000000000000284, 133.0000000000000284 ) ) ;
#57198 = CARTESIAN_POINT ( 'NONE',  ( -8.000000000000000000, 90.40624999999998579, -3.313708498984761608 ) ) ;
#57199 = CARTESIAN_POINT ( 'NONE',  ( -11.35316468749999785, 128.3854166632526699, -3.042071309553167513 ) ) ;
#57200 = FACE_OUTER_BOUND ( 'NONE', #20358, .T. ) ;
#57201 = PLANE ( 'NONE',  #6034 ) ;
#57204 = CARTESIAN_POINT ( 'NONE',  ( 1.656854249492263564, 201.8124999999999716, 146.0000000000001421 ) ) ;
#57203 = CARTESIAN_POINT ( 'NONE',  ( 30.44569435410882718, 194.5625000013656063, 172.4456943541086957 ) ) ;
#57202 = CARTESIAN_POINT ( 'NONE',  ( 24.54126587499997925, 195.5000000013655779, 171.4326545832175555 ) ) ;
#57205 = ORIENTED_EDGE ( 'NONE', *, *, #73800, .F. ) ;
#57206 = CARTESIAN_POINT ( 'NONE',  ( 4.000000000000001776, 2.062500000000000000, -1.656854249492381248 ) ) ;
#57207 = EDGE_CURVE ( 'NONE', #17422, #8416, #56264, .T. ) ;
#57208 = FACE_OUTER_BOUND ( 'NONE', #122, .T. ) ;
#57209 = CARTESIAN_POINT ( 'NONE',  ( -0.1292575518527070144, -8.001915877911162767, -0.000000000000000000 ) ) ;
#57210 = CARTESIAN_POINT ( 'NONE',  ( 28.00000000000001776, 196.1875000013655779, 166.5412658749999082 ) ) ;
#57211 = CARTESIAN_POINT ( 'NONE',  ( -8.311093377946841443, 219.2187499965859843, 8.311093377946830785 ) ) ;
#57212 = CARTESIAN_POINT ( 'NONE',  ( 2.977408999572650039, 123.6875000020484094, -7.188101187500001821 ) ) ;
#57213 = CARTESIAN_POINT ( 'NONE',  ( 4.541265875000001451, 22.24999999863440792, 1.881053915767124440 ) ) ;
#57214 = CARTESIAN_POINT ( 'NONE',  ( -3.728321214209889156, -56.13798660964528864, 44.08488161418000573 ) ) ;
#57215 = CARTESIAN_POINT ( 'NONE',  ( 5.656854249492374365, 5.656854249492375253, 22.76780277982336642 ) ) ;
#57217 = CARTESIAN_POINT ( 'NONE',  ( -9.999999999999998224, 225.2083333333333144, 2.679491924311235174 ) ) ;
#57216 = CARTESIAN_POINT ( 'NONE',  ( -49.36078510129538444, 45.79344415090853460, 58.74518531386928544 ) ) ;
#57218 = CARTESIAN_POINT ( 'NONE',  ( -8.311093377946841443, 98.90624999658604111, 8.311093377946830785 ) ) ;
#57219 = EDGE_LOOP ( 'NONE', ( #61532, #66771, #69033, #65688 ) ) ;
#57220 = DIRECTION ( 'NONE',  ( -0.000000000000000000, 1.000000000000000000, -0.000000000000000000 ) ) ;
#57221 = CARTESIAN_POINT ( 'NONE',  ( 5.082755093536324154, 24.28124999795161543, 5.082755093536326818 ) ) ;
#57222 = DIRECTION ( 'NONE',  ( 0.000000000000000000, -1.000000000000000000, 0.000000000000000000 ) ) ;
#57224 = CARTESIAN_POINT ( 'NONE',  ( -8.311093377946834337, 239.8437500034139873, 8.311093377946837890 ) ) ;
#57223 = AXIS2_PLACEMENT_3D ( 'NONE', #8751, #13643, #1975 ) ;
#57225 = CARTESIAN_POINT ( 'NONE',  ( 8.311093377946837890, 101.4062499965859985, -8.311093377946837890 ) ) ;
#57226 = VERTEX_POINT ( 'NONE', #67209 ) ;
#57227 = CARTESIAN_POINT ( 'NONE',  ( -2.299997487996822354, 10.65384601377883023, 117.6108347966737426 ) ) ;
#57228 = CARTESIAN_POINT ( 'NONE',  ( 7.204075437095968759, -7.204075437095966983, 107.2187500020483810 ) ) ;
#57229 = CARTESIAN_POINT ( 'NONE',  ( 8.660254037844385522, 221.4583333265053966, 5.000000000000005329 ) ) ;
#57230 = CARTESIAN_POINT ( 'NONE',  ( 2.445694354108840063, 205.0625000013656063, 200.4456943541088663 ) ) ;
#57231 = DIRECTION ( 'NONE',  ( 0.000000000000000000, 0.000000000000000000, 1.000000000000000000 ) ) ;
#57233 = CARTESIAN_POINT ( 'NONE',  ( -8.311093377946836114, 97.65624999658602690, -8.311093377946837890 ) ) ;
#57232 = FACE_OUTER_BOUND ( 'NONE', #4828, .T. ) ;
#57234 = CARTESIAN_POINT ( 'NONE',  ( -4.898587196589407898E-16, 7.999999999999991118, 15.64280278392014800 ) ) ;
#57235 = CARTESIAN_POINT ( 'NONE',  ( -24.54126587499998990, 197.4375000013655779, 170.0000000000003411 ) ) ;
#57236 = CARTESIAN_POINT ( 'NONE',  ( 6.123233995736767268E-16, 128.1249999931720254, -10.00000000000000178 ) ) ;
#57237 = ORIENTED_EDGE ( 'NONE', *, *, #67516, .T. ) ;
#57238 =( BOUNDED_CURVE ( )  B_SPLINE_CURVE ( 2, ( #55112, #27163, #3795, #49431, #2672, #72825, #32854, #72058, #55860 ),
 .UNSPECIFIED., .F., .F. ) 
 B_SPLINE_CURVE_WITH_KNOTS ( ( 3, 2, 2, 2, 3 ),
 ( 0.5147058823529412352, 0.5183823529411765163, 0.5220588235294116863, 0.5257352941176468564, 0.5294117647058820264 ),
 .UNSPECIFIED. ) 
 CURVE ( )  GEOMETRIC_REPRESENTATION_ITEM ( )  RATIONAL_B_SPLINE_CURVE ( ( 0.9999999999999976685, 0.9238795325112890700, 1.000000000000000000, 0.9238795325112867385, 1.000000000000000000, 0.9238795325112867385, 1.000000000000000000, 0.9238795325112936219, 0.9999999999999931166 ) ) 
 REPRESENTATION_ITEM ( '' )  );
#57239 = CARTESIAN_POINT ( 'NONE',  ( -7.320508075688778149, 194.9999999931720538, 7.320508075688769267 ) ) ;
#57240 = CARTESIAN_POINT ( 'NONE',  ( 23.99999999999998934, 200.8750000027312126, 169.9999999999999432 ) ) ;
#57241 = CARTESIAN_POINT ( 'NONE',  ( -19.99999999999993250, -31.99999999999978684, 145.6940130594346670 ) ) ;
#57242 = CARTESIAN_POINT ( 'NONE',  ( -5.676582343749998039, 87.76041666325268409, -9.832129032723420536 ) ) ;
#57243 = CARTESIAN_POINT ( 'NONE',  ( 2.765530957081996366, 289.1406250017069510, -6.676582343750003368 ) ) ;
#57244 = CARTESIAN_POINT ( 'NONE',  ( -2.977408999572654480, 7.874999997951610986, 7.188101187499999156 ) ) ;
#57245 = CARTESIAN_POINT ( 'NONE',  ( 7.204075437095968759, -7.204075437095966983, 103.0937500020483668 ) ) ;
#57246 = CARTESIAN_POINT ( 'NONE',  ( 8.311093377946837890, 1.718749996586016682, -8.311093377946837890 ) ) ;
#57247 = EDGE_LOOP ( 'NONE', ( #66786, #17987, #50007, #6321 ) ) ;
#57248 = CARTESIAN_POINT ( 'NONE',  ( -7.320508075688778149, 69.99999999317203958, 7.320508075688769267 ) ) ;
#57249 = CARTESIAN_POINT ( 'NONE',  ( 6.123233995736767268E-16, 101.2500000000000000, -10.00000000000000178 ) ) ;
#57250 = FACE_OUTER_BOUND ( 'NONE', #2138, .T. ) ;
#57251 = CARTESIAN_POINT ( 'NONE',  ( -5.676582343750006032, 214.1145833299193555, 9.832129032723418760 ) ) ;
#57252 = CARTESIAN_POINT ( 'NONE',  ( 10.00000000000000178, 46.87499999317203958, 0.000000000000000000 ) ) ;
#57253 = CARTESIAN_POINT ( 'NONE',  ( -8.999999999999998224, 0.000000000000000000, 0.000000000000000000 ) ) ;
#57254 = CARTESIAN_POINT ( 'NONE',  ( 2.765530957081996366, 298.1406250017069510, -6.676582343750003368 ) ) ;
#57255 = AXIS2_PLACEMENT_3D ( 'NONE', #66204, #2094, #25827 ) ;
#57256 = EDGE_LOOP ( 'NONE', ( #67350, #11239, #45162, #71714 ) ) ;
#57257 = CARTESIAN_POINT ( 'NONE',  ( 4.217983994794715308, 51.98644305215067618, -48.84278562423046566 ) ) ;
#57258 = CARTESIAN_POINT ( 'NONE',  ( -11.35316468750000141, 208.8020833299193555, 3.042071309553159963 ) ) ;
#57259 = CARTESIAN_POINT ( 'NONE',  ( -4.220049686691937474, -10.18810118749999738, 93.43750000204836681 ) ) ;
#57260 = EDGE_CURVE ( 'NONE', #14040, #44316, #12902, .T. ) ;
#57261 = VECTOR ( 'NONE', #70965, 1000.000000000000000 ) ;
#57262 = CARTESIAN_POINT ( 'NONE',  ( -30.44569435410883784, 206.5625000013656063, 167.5543056458915885 ) ) ;
#57263 = CARTESIAN_POINT ( 'NONE',  ( -8.000000000000000000, 15.75000000000000355, -9.797174393178825657E-16 ) ) ;
#57264 = ORIENTED_EDGE ( 'NONE', *, *, #62486, .F. ) ;
#57265 = CARTESIAN_POINT ( 'NONE',  ( 1.320432766682874540E-15, 120.0312500020483810, 7.188101187500000044 ) ) ;
#57266 = CARTESIAN_POINT ( 'NONE',  ( -2.955318825516840775, -19.07835557137326532, -0.7126204852947463086 ) ) ;
#57267 = CARTESIAN_POINT ( 'NONE',  ( -4.999999999999998224, 21.66666666666666785, -8.660254037844389075 ) ) ;
#57268 = CARTESIAN_POINT ( 'NONE',  ( -8.000000000000000000, 8.156250000000001776, -3.313708498984762496 ) ) ;
#57269 = CARTESIAN_POINT ( 'NONE',  ( -4.220049686691937474, -10.18810118749999738, 81.81250000204838102 ) ) ;
#57270 = ORIENTED_EDGE ( 'NONE', *, *, #40331, .F. ) ;
#57271 = CARTESIAN_POINT ( 'NONE',  ( 4.000000000000001776, 20.00000000000000000, 0.000000000000000000 ) ) ;
#57272 = CARTESIAN_POINT ( 'NONE',  ( 1.102182119232618108E-15, 299.2500000000000000, 6.000000000000001776 ) ) ;
#57273 = CARTESIAN_POINT ( 'NONE',  ( 30.94238183655217256, 194.5434106550123374, 171.9871435362137504 ) ) ;
#57274 = EDGE_CURVE ( 'NONE', #23017, #52578, #53470, .T. ) ;
#57275 = EDGE_CURVE ( 'NONE', #66991, #42278, #61169, .T. ) ;
#57276 = CARTESIAN_POINT ( 'NONE',  ( -5.000000000000001776, -10.82431413986196134, 67.03128830763429846 ) ) ;
#57277 = CARTESIAN_POINT ( 'NONE',  ( 105.0000000000000000, 37.00000000000000000, 0.000000000000000000 ) ) ;
#57278 = CARTESIAN_POINT ( 'NONE',  ( -4.088227598258586603E-16, 297.2031250017070079, -6.676582343750001591 ) ) ;
#57281 = CARTESIAN_POINT ( 'NONE',  ( -1.656854249492337949, 199.4375000027312410, 138.0000000000000000 ) ) ;
#57280 = CARTESIAN_POINT ( 'NONE',  ( 5.676582343749997150, 247.2395833367473301, -9.832129032723418760 ) ) ;
#57279 = CARTESIAN_POINT ( 'NONE',  ( 31.45873412499998523, 205.7500000013656063, 168.5673454167822172 ) ) ;
#57282 = APPLICATION_PROTOCOL_DEFINITION ( 'draft international standard', 'automotive_design', 1998, #2847 ) ;
#57283 = ORIENTED_EDGE ( 'NONE', *, *, #36676, .F. ) ;
#57284 = ADVANCED_FACE ( 'NONE', ( #62648 ), #6445, .T. ) ;
#57285 = CARTESIAN_POINT ( 'NONE',  ( 5.676582343749997150, 237.5520833367473301, -9.832129032723418760 ) ) ;
#57286 = CARTESIAN_POINT ( 'NONE',  ( -2.977408999572648707, -7.188101187499990274, 13.76780278187175455 ) ) ;
#57287 = ORIENTED_EDGE ( 'NONE', *, *, #36921, .T. ) ;
#57288 = ORIENTED_EDGE ( 'NONE', *, *, #4747, .T. ) ;
#57289 = CARTESIAN_POINT ( 'NONE',  ( -10.18810118749999916, 4.220049686691934809, 72.06250000204836681 ) ) ;
#57290 = CARTESIAN_POINT ( 'NONE',  ( -3.042071309553173730, 94.63541666325269830, 11.35316468749999785 ) ) ;
#57291 = CARTESIAN_POINT ( 'NONE',  ( -16.52771754582129660, 11.24232751665648422, -1.116934336526962390 ) ) ;
#57292 = CARTESIAN_POINT ( 'NONE',  ( -6.735557395310442023E-16, 11.00000000000000000, 83.12499999999998579 ) ) ;
#57295 = FACE_OUTER_BOUND ( 'NONE', #55919, .T. ) ;
#57294 = CARTESIAN_POINT ( 'NONE',  ( 29.43265458321766559, 207.5000000013655779, 173.4587341249998929 ) ) ;
#57293 = CARTESIAN_POINT ( 'NONE',  ( 24.54126587499998635, 208.5000000013656063, 171.4326545832175555 ) ) ;
#57296 = CARTESIAN_POINT ( 'NONE',  ( -56.56060386279985153, 211.2026708385327254, 48.90167542805480139 ) ) ;
#57297 = FACE_BOUND ( 'NONE', #40264, .T. ) ;
#57298 = VECTOR ( 'NONE', #31902, 1000.000000000000000 ) ;
#57299 = EDGE_CURVE ( 'NONE', #6481, #44928, #11351, .T. ) ;
#57300 = CARTESIAN_POINT ( 'NONE',  ( 5.676582343749993598, 199.9479166632526983, 9.832129032723422313 ) ) ;
#57301 = CARTESIAN_POINT ( 'NONE',  ( 1.432654583217607192, 205.2500000013655779, 145.4587341250000634 ) ) ;
#57302 = CARTESIAN_POINT ( 'NONE',  ( 27.99999999999996803, 206.6875000013656063, 173.4587341249998929 ) ) ;
#57303 = CARTESIAN_POINT ( 'NONE',  ( -7.188101187500001821, 19.49999999795161898, -2.977408999572651371 ) ) ;
#57304 = CIRCLE ( 'NONE', #64566, 8.000000000000005329 ) ;
#57305 = CARTESIAN_POINT ( 'NONE',  ( -5.676582343749998039, 162.7604166632526983, -9.832129032723420536 ) ) ;
#57306 = DIRECTION ( 'NONE',  ( 0.000000000000000000, 0.000000000000000000, -1.000000000000000000 ) ) ;
#57307 = CARTESIAN_POINT ( 'NONE',  ( -5.082755093536325930, 100.3437500020483810, -5.082755093536325930 ) ) ;
#57309 = CARTESIAN_POINT ( 'NONE',  ( -8.660254037844387298, 88.95833332650536818, -5.000000000000004441 ) ) ;
#57308 = DIRECTION ( 'NONE',  ( -0.000000000000000000, -1.000000000000000000, -0.000000000000000000 ) ) ;
#57310 = CARTESIAN_POINT ( 'NONE',  ( 4.541265875000002339, 10.31249999863440792, 0.000000000000000000 ) ) ;
#57311 = CARTESIAN_POINT ( 'NONE',  ( 31.45873412499999944, 201.9375000013656063, 169.9999999999999432 ) ) ;
#57312 = CARTESIAN_POINT ( 'NONE',  ( -2.977408999572648707, -7.188101187499990274, 12.64280278187175277 ) ) ;
#57313 = CARTESIAN_POINT ( 'NONE',  ( 8.311093377946837890, 56.40624999658600558, -8.311093377946837890 ) ) ;
#57314 = CARTESIAN_POINT ( 'NONE',  ( -7.999999999961167951, -1.666173683171983354E-05, 1.018425797410095646 ) ) ;
#57315 = CARTESIAN_POINT ( 'NONE',  ( -7.999999999999998224, 119.2812500040967905, 3.313708498984766049 ) ) ;
#57316 = VERTEX_POINT ( 'NONE', #10982 ) ;
#57317 = FACE_OUTER_BOUND ( 'NONE', #27712, .T. ) ;
#57318 = CARTESIAN_POINT ( 'NONE',  ( 7.778174593052021635, 7.778174593052023411, 80.12500000409677625 ) ) ;
#57319 = CARTESIAN_POINT ( 'NONE',  ( -9.832129032723418760, 62.86458332991935549, -5.676582343750004256 ) ) ;
#57320 = CARTESIAN_POINT ( 'NONE',  ( -4.556349186104045934, 11.00000000000000000, 77.40625000409676204 ) ) ;
#57321 = CARTESIAN_POINT ( 'NONE',  ( -2.445694354108840063, 199.0625000013656063, 139.5543056458912190 ) ) ;
#57322 = CARTESIAN_POINT ( 'NONE',  ( 2.216418498319753017, 16.40908668940204151, 68.78644440154937456 ) ) ;
#57324 = CARTESIAN_POINT ( 'NONE',  ( 3.042071309553159519, 59.73958332991933418, 11.35316468750000141 ) ) ;
#57323 = CARTESIAN_POINT ( 'NONE',  ( -4.401442555609581635E-16, 93.78125000204836681, -7.188101187500000044 ) ) ;
#57325 = CARTESIAN_POINT ( 'NONE',  ( 5.656854249492374365, 5.656854249492375253, 3.267802779823362425 ) ) ;
#57326 = CARTESIAN_POINT ( 'NONE',  ( 3.313708498984679895, 111.2187500040967905, -8.000000000000081712 ) ) ;
#57327 = CARTESIAN_POINT ( 'NONE',  ( -2.085542519210945728E-15, 174.5312499965860411, 11.35316468750000141 ) ) ;
#57328 = CARTESIAN_POINT ( 'NONE',  ( 5.000000000000001776, 137.7083333265053682, -8.660254037844389075 ) ) ;
#57329 = CARTESIAN_POINT ( 'NONE',  ( -2.977408999572651815, 94.81250000204838102, 7.188101187500000933 ) ) ;
#57330 = CARTESIAN_POINT ( 'NONE',  ( 0.000000000000000000, 0.000000000000000000, -20.69999999999999929 ) ) ;
#57331 = CARTESIAN_POINT ( 'NONE',  ( 3.042071309553167513, 52.13541666325268409, -11.35316468749999785 ) ) ;
#57332 =( BOUNDED_CURVE ( )  B_SPLINE_CURVE ( 2, ( #69676, #42094, #53067, #69303, #1401, #12329, #17989, #11585, #17614 ),
 .UNSPECIFIED., .F., .F. ) 
 B_SPLINE_CURVE_WITH_KNOTS ( ( 3, 2, 2, 2, 3 ),
 ( 0.6770833333333334814, 0.6822916666666667407, 0.6875000000000001110, 0.6927083333333334814, 0.6979166666666667407 ),
 .UNSPECIFIED. ) 
 CURVE ( )  GEOMETRIC_REPRESENTATION_ITEM ( )  RATIONAL_B_SPLINE_CURVE ( ( 0.9999999999999983347, 0.9238795325112884038, 1.000000000000000000, 0.9238795325112867385, 1.000000000000000000, 0.9238795325112867385, 1.000000000000000000, 0.9238795325112850731, 1.000000000000001554 ) ) 
 REPRESENTATION_ITEM ( '' )  );
#57333 = CARTESIAN_POINT ( 'NONE',  ( 0.000000000000000000, 300.0000000000000000, 10.00000000000000178 ) ) ;
#57334 = CARTESIAN_POINT ( 'NONE',  ( -5.676582343750006032, 184.1145833299193555, 9.832129032723418760 ) ) ;
#57335 = VERTEX_POINT ( 'NONE', #12085 ) ;
#57336 = DIRECTION ( 'NONE',  ( -0.000000000000000000, 1.000000000000000000, -0.000000000000000000 ) ) ;
#57337 = CARTESIAN_POINT ( 'NONE',  ( 7.204075437095966983, 7.204075437095967871, 70.09375000204836681 ) ) ;
#57338 = CARTESIAN_POINT ( 'NONE',  ( 2.828427124746209831, 196.3750000000000284, 200.8284271247462129 ) ) ;
#57340 = CARTESIAN_POINT ( 'NONE',  ( 8.311093377946834337, 185.1562499965860411, 8.311093377946839666 ) ) ;
#57339 = CARTESIAN_POINT ( 'NONE',  ( 31.99999999999998579, 203.1875000000000284, 171.6568542494923122 ) ) ;
#57341 = CARTESIAN_POINT ( 'NONE',  ( -7.999999999999989342, -3.313708498984762496, 3.980302784329822874 ) ) ;
#57342 = CARTESIAN_POINT ( 'NONE',  ( -7.778174593052020747, -7.778174593052023411, 79.37500000409677625 ) ) ;
#57343 = CARTESIAN_POINT ( 'NONE',  ( -10.00000000000000000, 257.9166666734946602, -2.679491924311226292 ) ) ;
#57344 = FACE_BOUND ( 'NONE', #61124, .T. ) ;
#57345 = ORIENTED_EDGE ( 'NONE', *, *, #30633, .T. ) ;
#57346 = CARTESIAN_POINT ( 'NONE',  ( -4.401442555609577197E-16, 7.188101187499992051, 25.11155278187175810 ) ) ;
#57347 = CARTESIAN_POINT ( 'NONE',  ( -3.042071309553164404, 127.5520833299193555, -11.35316468749999963 ) ) ;
#57348 =( BOUNDED_CURVE ( )  B_SPLINE_CURVE ( 2, ( #19966, #42972, #59602, #19592, #59964, #30189, #70550, #70915, #58872, #65248, #47895, #14298, #30559 ),
 .UNSPECIFIED., .F., .F. ) 
 B_SPLINE_CURVE_WITH_KNOTS ( ( 3, 2, 2, 2, 2, 2, 3 ),
 ( 1.648487699650845073, 1.653721680593561949, 1.658955661536279047, 1.664189642478995923, 1.669423623421712799, 1.674657604364429897, 1.679891585307146773 ),
 .UNSPECIFIED. ) 
 CURVE ( )  GEOMETRIC_REPRESENTATION_ITEM ( )  RATIONAL_B_SPLINE_CURVE ( ( 0.9999999999999998890, 0.9659258262890682012, 0.9999999999999998890, 0.9659258262890682012, 0.9999999999999998890, 0.9659258262890682012, 0.9999999999999998890, 0.9659258262890682012, 0.9999999999999998890, 0.9659258262890682012, 0.9999999999999998890, 0.9659258262891058378, 0.9999999999999622524 ) ) 
 REPRESENTATION_ITEM ( '' )  );
#57349 = CARTESIAN_POINT ( 'NONE',  ( 31.99999999999997868, 195.1875000000000000, 171.6568542494923122 ) ) ;
#57350 = ORIENTED_EDGE ( 'NONE', *, *, #14492, .T. ) ;
#57351 = ADVANCED_FACE ( 'NONE', ( #54 ), #63767, .T. ) ;
#57352 = CARTESIAN_POINT ( 'NONE',  ( 4.541265875000001451, 7.374999998634408804, 1.881053915767124440 ) ) ;
#57353 = CARTESIAN_POINT ( 'NONE',  ( 7.188101187500000044, 13.96874999795161187, 0.000000000000000000 ) ) ;
#57354 = AXIS2_PLACEMENT_3D ( 'NONE', #63097, #11422, #34459 ) ;
#57355 = CARTESIAN_POINT ( 'NONE',  ( -8.000000000000000000, 105.5937500040967763, -3.313708498984761608 ) ) ;
#57356 = CARTESIAN_POINT ( 'NONE',  ( -27.99999999999996092, 197.1875000013655779, 173.4587341250003760 ) ) ;
#57357 = AXIS2_PLACEMENT_3D ( 'NONE', #41053, #14858, #58050 ) ;
#57358 = CARTESIAN_POINT ( 'NONE',  ( 4.000000000000001776, 7.062500000000000000, -1.656854249492381248 ) ) ;
#57359 = CARTESIAN_POINT ( 'NONE',  ( 6.123233995736767268E-16, 53.12499999317203958, -10.00000000000000178 ) ) ;
#57360 = CARTESIAN_POINT ( 'NONE',  ( 2.780723358947928197E-16, 11.56249999863440614, -4.541265875000002339 ) ) ;
#57361 = CARTESIAN_POINT ( 'NONE',  ( 3.313708498984762496, -7.999999999999989342, 22.48655278392014623 ) ) ;
#57362 = CARTESIAN_POINT ( 'NONE',  ( 2.828427124746152987, 197.1250000000000284, 139.1715728752538723 ) ) ;
#57364 = ORIENTED_EDGE ( 'NONE', *, *, #12875, .T. ) ;
#57363 = EDGE_CURVE ( 'NONE', #65259, #46523, #1911, .T. ) ;
#57365 = DIRECTION ( 'NONE',  ( -0.000000000000000000, 1.000000000000000000, -0.000000000000000000 ) ) ;
#57366 = CARTESIAN_POINT ( 'NONE',  ( -2.977408999572651815, 106.4375000020483810, 7.188101187500000933 ) ) ;
#57367 = CYLINDRICAL_SURFACE ( 'NONE', #68748, 10.00000000000000178 ) ;
#57368 =( NAMED_UNIT ( * ) SI_UNIT ( $, .STERADIAN. ) SOLID_ANGLE_UNIT ( ) );
#57370 = VECTOR ( 'NONE', #66487, 1000.000000000000000 ) ;
#57369 = CARTESIAN_POINT ( 'NONE',  ( -1.881053915767124440, 20.99999999863440792, 4.541265875000001451 ) ) ;
#57371 = CARTESIAN_POINT ( 'NONE',  ( -2.977408999572647819, 7.188101187499991163, 28.20530278187175455 ) ) ;
#57372 = ORIENTED_EDGE ( 'NONE', *, *, #61207, .T. ) ;
#57373 = ORIENTED_EDGE ( 'NONE', *, *, #59765, .F. ) ;
#57374 = CARTESIAN_POINT ( 'NONE',  ( 10.18810118750000093, -4.220049686691933033, 93.81250000204838102 ) ) ;
#57375 = DIRECTION ( 'NONE',  ( -0.000000000000000000, -0.000000000000000000, -1.000000000000000000 ) ) ;
#57376 = CARTESIAN_POINT ( 'NONE',  ( -31.45873412499999233, 196.9375000013655779, 170.0000000000003979 ) ) ;
#57377 = CARTESIAN_POINT ( 'NONE',  ( 11.00000000000000000, 1.347111479062088405E-15, 100.7499999999999858 ) ) ;
#57378 = CARTESIAN_POINT ( 'NONE',  ( 2.754378923186476579E-14, 203.4375000013656063, 194.5412658750000219 ) ) ;
#57380 = CARTESIAN_POINT ( 'NONE',  ( 2.765530957081996366, 299.2968750017070079, -6.676582343750002480 ) ) ;
#57379 = CARTESIAN_POINT ( 'NONE',  ( 2.020667218593132706E-15, -11.00000000000000000, 86.87499999999998579 ) ) ;
#57381 = CARTESIAN_POINT ( 'NONE',  ( 2.679491924311222739, 123.9583333333333286, 10.00000000000000355 ) ) ;
#57382 = CARTESIAN_POINT ( 'NONE',  ( -5.656854249492380582, 103.8125000000000000, -5.656854249492380582 ) ) ;
#57383 = CARTESIAN_POINT ( 'NONE',  ( 4.721056650416000089, 288.9843750017070079, 4.721056650415999201 ) ) ;
#57384 = CARTESIAN_POINT ( 'NONE',  ( -2.977408999572648707, -7.188101187499990274, 5.142802781871752771 ) ) ;
#57385 = EDGE_CURVE ( 'NONE', #51832, #43757, #9635, .T. ) ;
#57386 = DIRECTION ( 'NONE',  ( 0.000000000000000000, 0.000000000000000000, 1.000000000000000000 ) ) ;
#57387 = EDGE_CURVE ( 'NONE', #45255, #57513, #29074, .T. ) ;
#57388 = CARTESIAN_POINT ( 'NONE',  ( 29.43265458321761230, 204.5000000013656063, 173.4587341249998929 ) ) ;
#57389 = CARTESIAN_POINT ( 'NONE',  ( -8.000000000000001776, 24.65624999590322730, 3.313708498984759387 ) ) ;
#57390 = DIRECTION ( 'NONE',  ( 1.000000000000000000, -0.000000000000000000, 0.000000000000000000 ) ) ;
#57391 = CARTESIAN_POINT ( 'NONE',  ( -7.188101187500000933, 121.4375000020483810, -2.977408999572650483 ) ) ;
#57393 = CARTESIAN_POINT ( 'NONE',  ( 0.2454044849291649733, 194.9147657458009917, 194.0852342541993494 ) ) ;
#57392 = SURFACE_STYLE_USAGE ( .BOTH. , #34391 ) ;
#57394 = CARTESIAN_POINT ( 'NONE',  ( -9.832129032723418760, 243.8020833367473301, -5.676582343749998927 ) ) ;
#57395 = CARTESIAN_POINT ( 'NONE',  ( -1.836970198721029983E-15, 50.62499999317203248, 10.00000000000000178 ) ) ;
#57396 = CARTESIAN_POINT ( 'NONE',  ( 30.82842712474619873, 198.3750000000000284, 167.1715728752537586 ) ) ;
#57397 = CARTESIAN_POINT ( 'NONE',  ( -9.832129032723420536, 13.69791666325268409, 5.676582343749997150 ) ) ;
#57398 = CARTESIAN_POINT ( 'NONE',  ( 3.313708498984744732, 122.4687499999999858, 8.000000000000019540 ) ) ;
#57399 = CARTESIAN_POINT ( 'NONE',  ( -11.35316468750000141, 203.5937499965860127, -1.390361679473963753E-15 ) ) ;
#57400 = CARTESIAN_POINT ( 'NONE',  ( -26.34314575050757412, 196.5625000000000284, 174.0000000000003411 ) ) ;
#57401 = CARTESIAN_POINT ( 'NONE',  ( -7.320508075688778149, 219.9999999931720538, 7.320508075688769267 ) ) ;
#57403 = CARTESIAN_POINT ( 'NONE',  ( 0.000000000000000000, 0.000000000000000000, 0.000000000000000000 ) ) ;
#57402 = CARTESIAN_POINT ( 'NONE',  ( -23.99999999999997513, 205.6875000000000284, 171.6568542494927385 ) ) ;
#57404 = VERTEX_POINT ( 'NONE', #11717 ) ;
#57405 = ADVANCED_FACE ( 'NONE', ( #34759 ), #42226, .F. ) ;
#57406 = CARTESIAN_POINT ( 'NONE',  ( 1.432654583217607414, 202.5000000013656063, 145.4587341250000634 ) ) ;
#57407 = CARTESIAN_POINT ( 'NONE',  ( -11.35316468750000141, 28.48958332991934839, 3.042071309553159963 ) ) ;
#57408 = CARTESIAN_POINT ( 'NONE',  ( 4.556349186104051263, -10.99999999999999822, 93.15625000409676204 ) ) ;
#57409 =( GEOMETRIC_REPRESENTATION_CONTEXT ( 3 ) GLOBAL_UNCERTAINTY_ASSIGNED_CONTEXT ( ( #53188 ) ) GLOBAL_UNIT_ASSIGNED_CONTEXT ( ( #50570, #56994, #34740 ) ) REPRESENTATION_CONTEXT ( 'NONE', 'WORKASPACE' ) );
#57410 = CARTESIAN_POINT ( 'NONE',  ( 7.320508075688771044, 209.3750000000000000, 7.320508075688775484 ) ) ;
#57411 = CARTESIAN_POINT ( 'NONE',  ( -27.99999999999991473, 195.9375000013655779, 173.4587341250003760 ) ) ;
#57412 = CARTESIAN_POINT ( 'NONE',  ( 2.250000000000000444, 283.9999999999998863, 5.427273995025124975 ) ) ;
#57414 = CARTESIAN_POINT ( 'NONE',  ( -11.35316468749999785, 18.07291666325267698, -3.042071309553167957 ) ) ;
#57413 = CARTESIAN_POINT ( 'NONE',  ( -4.401442555609581635E-16, 111.7812500020483810, -7.188101187500000044 ) ) ;
#57415 = CARTESIAN_POINT ( 'NONE',  ( 5.656854249492376141, -5.656854249492374365, 22.39280277982336997 ) ) ;
#57416 = CARTESIAN_POINT ( 'NONE',  ( -5.676582343750006032, 134.1145833299193555, 9.832129032723418760 ) ) ;
#57417 = CARTESIAN_POINT ( 'NONE',  ( -10.00000000000000178, 104.3749999931720396, -1.224646799147353454E-15 ) ) ;
#57418 = EDGE_CURVE ( 'NONE', #34061, #9236, #7544, .T. ) ;
#57419 = CARTESIAN_POINT ( 'NONE',  ( -4.401442555609581635E-16, 116.6562500020483810, -7.188101187500000044 ) ) ;
#57420 = CARTESIAN_POINT ( 'NONE',  ( -5.000000000000005329, 5.208333326505366401, 8.660254037844387298 ) ) ;
#57421 = CARTESIAN_POINT ( 'NONE',  ( -11.00000000000015810, 4.556349186103888727, 103.0937500040967905 ) ) ;
#57422 = CARTESIAN_POINT ( 'NONE',  ( 5.656854249492376141, -5.656854249492374365, 0.08030278392014492117 ) ) ;
#57423 = ORIENTED_EDGE ( 'NONE', *, *, #73865, .T. ) ;
#57424 = CARTESIAN_POINT ( 'NONE',  ( -2.085542519210945728E-15, 9.843749996586018014, 11.35316468750000141 ) ) ;
#57425 = CARTESIAN_POINT ( 'NONE',  ( -10.99999999999999645, -11.00000000000000000, -6.938893903907228378E-15 ) ) ;
#57426 = CARTESIAN_POINT ( 'NONE',  ( 2.765530957081996366, 298.1406250017069510, -6.676582343750003368 ) ) ;
#57427 = CARTESIAN_POINT ( 'NONE',  ( -8.311093377946841443, 123.9062499965860269, 8.311093377946834337 ) ) ;
#57428 = CARTESIAN_POINT ( 'NONE',  ( 4.999999999999999112, 50.98458432551099406, 41.27351214092492881 ) ) ;
#57429 = CARTESIAN_POINT ( 'NONE',  ( 7.999999999999992895, -3.313708498984756279, 21.04280278432983309 ) ) ;
#57430 = DIRECTION ( 'NONE',  ( -0.000000000000000000, 1.000000000000000000, -0.000000000000000000 ) ) ;
#57431 = PLANE ( 'NONE',  #63922 ) ;
#57432 = CARTESIAN_POINT ( 'NONE',  ( 7.204075437095968759, -7.204075437095966983, 98.59375000204836681 ) ) ;
#57433 = ORIENTED_EDGE ( 'NONE', *, *, #38714, .T. ) ;
#57434 = AXIS2_PLACEMENT_3D ( 'NONE', #58098, #6410, #52793 ) ;
#57435 = CARTESIAN_POINT ( 'NONE',  ( 37.99999999999999289, 39.09128788536428800, 65.00000000000000000 ) ) ;
#57436 = CARTESIAN_POINT ( 'NONE',  ( 5.000000000000001776, 62.32183698944635353, -23.94439461060335361 ) ) ;
#57437 = CARTESIAN_POINT ( 'NONE',  ( -3.458734124999959469, 202.7500000013655779, 199.4326545832176976 ) ) ;
#57438 = CARTESIAN_POINT ( 'NONE',  ( -8.311093377946841443, 74.21874999658601268, 8.311093377946830785 ) ) ;
#57439 = EDGE_LOOP ( 'NONE', ( #21806, #21796, #33002, #48405 ) ) ;
#57440 = CARTESIAN_POINT ( 'NONE',  ( -10.18810118749999916, 0.000000000000000000, 106.6562500020483668 ) ) ;
#57441 = CARTESIAN_POINT ( 'NONE',  ( -3.211159895383561391, 12.81249999863440792, -3.211159895383561835 ) ) ;
#57442 = ORIENTED_EDGE ( 'NONE', *, *, #50926, .T. ) ;
#57443 = CARTESIAN_POINT ( 'NONE',  ( 7.188101187500000044, 27.46874999795161543, 0.000000000000000000 ) ) ;
#57444 = CARTESIAN_POINT ( 'NONE',  ( 8.248616681371277227E-12, 116.2499999999993747, -10.00000000000000178 ) ) ;
#57445 = CARTESIAN_POINT ( 'NONE',  ( -1.656854249492229592, 196.9375000027311842, 193.9999999999999147 ) ) ;
#57446 = CARTESIAN_POINT ( 'NONE',  ( -7.188101187500001821, 25.49999999795161898, -2.977408999572651371 ) ) ;
#57447 = PLANE ( 'NONE',  #237 ) ;
#57448 = ADVANCED_FACE ( 'NONE', ( #48257 ), #41137, .T. ) ;
#57449 =( BOUNDED_CURVE ( )  B_SPLINE_CURVE ( 2, ( #5388, #33328, #28759, #40457, #5023, #63456, #62710, #23098, #29139 ),
 .UNSPECIFIED., .F., .F. ) 
 B_SPLINE_CURVE_WITH_KNOTS ( ( 3, 2, 2, 2, 3 ),
 ( 0.8235294117647058432, 0.8272058823529411242, 0.8308823529411766273, 0.8345588235294119084, 0.8382352941176471894 ),
 .UNSPECIFIED. ) 
 CURVE ( )  GEOMETRIC_REPRESENTATION_ITEM ( )  RATIONAL_B_SPLINE_CURVE ( ( 1.000000000000000000, 0.9238795325112867385, 1.000000000000000000, 0.9238795325112867385, 1.000000000000000000, 0.9238795325112867385, 1.000000000000000000, 0.9238795325112844070, 1.000000000000002220 ) ) 
 REPRESENTATION_ITEM ( '' )  );
#57450 = CARTESIAN_POINT ( 'NONE',  ( -6.238412754330611322E-16, 10.18810118749999916, 103.6562500020483810 ) ) ;
#57451 = ADVANCED_FACE ( 'NONE', ( #70182 ), #18492, .F. ) ;
#57452 = CARTESIAN_POINT ( 'NONE',  ( 2.828427124746208943, 204.6250000000000284, 195.1715728752538439 ) ) ;
#57453 = CARTESIAN_POINT ( 'NONE',  ( -2.828427124746192067, 10.37499999726881406, 2.828427124746190735 ) ) ;
#57454 = DIRECTION ( 'NONE',  ( 0.000000000000000000, 0.000000000000000000, -1.000000000000000000 ) ) ;
#57455 = VERTEX_POINT ( 'NONE', #53934 ) ;
#57456 = AXIS2_PLACEMENT_3D ( 'NONE', #64597, #12532, #1241 ) ;
#57457 = CARTESIAN_POINT ( 'NONE',  ( 11.00000000000000000, 1.347111479062088405E-15, 81.24999999999998579 ) ) ;
#57458 = CARTESIAN_POINT ( 'NONE',  ( 3.458734125000016313, 200.8750000013656063, 199.4326545832176691 ) ) ;
#57459 = CARTESIAN_POINT ( 'NONE',  ( -30.44569435410887337, 206.5625000013656063, 167.5543056458916169 ) ) ;
#57460 = SHAPE_REPRESENTATION_RELATIONSHIP ( 'NONE' , 'NONE' ,  #22268, #25601 ) ;
#57461 =( BOUNDED_CURVE ( )  B_SPLINE_CURVE ( 2, ( #63572, #971, #29253, #11898, #23582, #64690, #6250, #41313, #42037, #35297, #17550, #59043, #6617 ),
 .UNSPECIFIED., .F., .F. ) 
 B_SPLINE_CURVE_WITH_KNOTS ( ( 3, 2, 2, 2, 2, 2, 3 ),
 ( 0.1358695652173912971, 0.1376811594202898559, 0.1394927536231884146, 0.1413043478260869179, 0.1431159420289854767, 0.1449275362318840354, 0.1467391304347825942 ),
 .UNSPECIFIED. ) 
 CURVE ( )  GEOMETRIC_REPRESENTATION_ITEM ( )  RATIONAL_B_SPLINE_CURVE ( ( 1.000000000000000000, 0.9659258262890683122, 1.000000000000000000, 0.9659258262890683122, 1.000000000000000000, 0.9659258262890683122, 1.000000000000000000, 0.9659258262890683122, 1.000000000000000000, 0.9659258262890683122, 1.000000000000000000, 0.9659258262890688673, 0.9999999999999994449 ) ) 
 REPRESENTATION_ITEM ( '' )  );
#57462 = ADVANCED_FACE ( 'NONE', ( #2248 ), #47150, .F. ) ;
#57463 = CARTESIAN_POINT ( 'NONE',  ( -1.881053915767121554, 11.62499999863440969, -4.541265875000002339 ) ) ;
#57464 = CARTESIAN_POINT ( 'NONE',  ( 25.17157287525381548, 204.6250000000000284, 167.1715728752537018 ) ) ;
#57465 = CARTESIAN_POINT ( 'NONE',  ( 5.082755093536320601, -5.082755093536318824, 17.04905278187175810 ) ) ;
#57466 = VERTEX_POINT ( 'NONE', #65615 ) ;
#57467 = CARTESIAN_POINT ( 'NONE',  ( -5.656854249492378806, 104.3750000040967763, 5.656854249492381470 ) ) ;
#57468 = ORIENTED_EDGE ( 'NONE', *, *, #67583, .T. ) ;
#57469 = CARTESIAN_POINT ( 'NONE',  ( 1.871523826299183495E-15, -10.18810118749999916, 108.5312500020483810 ) ) ;
#57470 = PRODUCT_RELATED_PRODUCT_CATEGORY ( 'part', '', ( #68009 ) ) ;
#57471 = CARTESIAN_POINT ( 'NONE',  ( -56.00000000000004974, -70.00000000000001421, 167.9999999999997442 ) ) ;
#57472 = CARTESIAN_POINT ( 'NONE',  ( -25.17157287525382259, 204.8750000000000284, 167.1715728752541565 ) ) ;
#57473 = CARTESIAN_POINT ( 'NONE',  ( -1.432654583217607192, 198.2500000013656347, 194.5412658750000219 ) ) ;
#57474 = CARTESIAN_POINT ( 'NONE',  ( 24.54126587500000056, 195.2500000013656063, 171.4326545832176123 ) ) ;
#57475 = CARTESIAN_POINT ( 'NONE',  ( -10.00000000000000355, 77.70833333333332860, 2.679491924311223183 ) ) ;
#57476 = CARTESIAN_POINT ( 'NONE',  ( 3.313708498984760720, 121.5312500000000142, -8.000000000000000000 ) ) ;
#57477 = CARTESIAN_POINT ( 'NONE',  ( 11.35316468749999963, 56.30208332991934839, -3.042071309553165293 ) ) ;
#57478 = CARTESIAN_POINT ( 'NONE',  ( -6.676582343750003368, 298.5468750017069510, -2.765530957081996810 ) ) ;
#57479 = EDGE_LOOP ( 'NONE', ( #41384, #49525, #38984, #58465 ) ) ;
#57480 = AXIS2_PLACEMENT_3D ( 'NONE', #70165, #70523, #18472 ) ;
#57481 = CARTESIAN_POINT ( 'NONE',  ( 7.320508075688771044, 253.1250000000000000, -7.320508075688771932 ) ) ;
#57482 = EDGE_CURVE ( 'NONE', #23575, #52476, #19221, .T. ) ;
#57483 = CARTESIAN_POINT ( 'NONE',  ( 1.882291019712136082, -10.12018455450522580, 70.22327770540285030 ) ) ;
#57484 = CARTESIAN_POINT ( 'NONE',  ( -2.828427124746209831, 197.5000000027312126, 139.1715728752538723 ) ) ;
#57485 = CARTESIAN_POINT ( 'NONE',  ( 7.320508075688774596, 57.49999999317203248, -7.320508075688774596 ) ) ;
#57486 = CARTESIAN_POINT ( 'NONE',  ( 5.656854249492380582, 5.999999995903221084, -5.656854249492380582 ) ) ;
#57487 = CARTESIAN_POINT ( 'NONE',  ( -8.660254037844387298, 239.5833333333333428, -4.999999999999999112 ) ) ;
#57488 = CARTESIAN_POINT ( 'NONE',  ( -29.65685424949234417, 202.5625000027312410, 174.0000000000003979 ) ) ;
#57489 = CARTESIAN_POINT ( 'NONE',  ( 4.220049686691941027, -10.18810118749999738, 71.50000000204839523 ) ) ;
#57490 = CARTESIAN_POINT ( 'NONE',  ( 10.00000000000000178, 195.2083333333333428, -2.679491924311226736 ) ) ;
#57491 = CARTESIAN_POINT ( 'NONE',  ( -5.082755093536319713, 5.082755093536319713, 15.17405278187175455 ) ) ;
#57492 = CARTESIAN_POINT ( 'NONE',  ( 8.311093377946834337, 165.4687499965859843, 8.311093377946839666 ) ) ;
#57493 = DIRECTION ( 'NONE',  ( -1.000000000000000000, 0.000000000000000000, 0.000000000000000000 ) ) ;
#57494 = CYLINDRICAL_SURFACE ( 'NONE', #56165, 8.000000000000000000 ) ;
#57496 = CARTESIAN_POINT ( 'NONE',  ( -28.00000000000001776, 194.4587341250000350, 166.5412658750003629 ) ) ;
#57495 = FILL_AREA_STYLE_COLOUR ( '', #6955 ) ;
#57497 = ORIENTED_EDGE ( 'NONE', *, *, #55810, .T. ) ;
#57498 = B_SPLINE_CURVE_WITH_KNOTS ( 'NONE', 3,
 ( #22903, #21777, #73468, #4080, #68556, #44804, #67445, #22519, #16859, #44430 ),
 .UNSPECIFIED., .F., .F.,
 ( 4, 2, 2, 2, 4 ),
 ( 0.000000000000000000, 0.001314083742622693986, 0.002628167485245387971, 0.003942251227868081957, 0.005256334970490775943 ),
 .UNSPECIFIED. ) ;
#57499 = CARTESIAN_POINT ( 'NONE',  ( -3.458734125000016313, 198.8750000013656347, 140.5673454167824161 ) ) ;
#57500 = CARTESIAN_POINT ( 'NONE',  ( -2.085542519210945728E-15, 39.84374999658601979, 11.35316468750000141 ) ) ;
#57501 = CARTESIAN_POINT ( 'NONE',  ( 11.00000000000000000, 4.556349186104045934, 113.0312500040967763 ) ) ;
#57502 = CARTESIAN_POINT ( 'NONE',  ( -24.54126587499996504, 209.1250000013656347, 171.4326545832179534 ) ) ;
#57503 = CYLINDRICAL_SURFACE ( 'NONE', #59920, 3.999999999999986233 ) ;
#57505 = LINE ( 'NONE', #52566, #54744 ) ;
#57504 = DIRECTION ( 'NONE',  ( 0.000000000000000000, 0.000000000000000000, 1.000000000000000000 ) ) ;
#57506 = CARTESIAN_POINT ( 'NONE',  ( -1.432654583217664479, 199.7500000013656063, 138.5412658750000787 ) ) ;
#57507 = CARTESIAN_POINT ( 'NONE',  ( -7.320508075688773708, 68.74999999317201116, -7.320508075688774596 ) ) ;
#57508 = CARTESIAN_POINT ( 'NONE',  ( -7.188101187499999156, 103.2500000020483810, 2.977408999572654924 ) ) ;
#57509 = CARTESIAN_POINT ( 'NONE',  ( -4.541265875000002339, 10.87499999863440792, -1.881053915767121998 ) ) ;
#57510 = CARTESIAN_POINT ( 'NONE',  ( 10.00000000000005151, 64.79166666666668561, 2.679491924311249385 ) ) ;
#57511 = CARTESIAN_POINT ( 'NONE',  ( -7.999999999999991118, 3.313708498984756723, 5.236552779823363757 ) ) ;
#57512 = DIRECTION ( 'NONE',  ( -0.000000000000000000, 1.000000000000000000, 4.689100369878284071E-30 ) ) ;
#57513 = VERTEX_POINT ( 'NONE', #36216 ) ;
#57514 = ORIENTED_EDGE ( 'NONE', *, *, #58132, .F. ) ;
#57515 = DIRECTION ( 'NONE',  ( -0.000000000000000000, 1.000000000000000000, -0.000000000000000000 ) ) ;
#57516 = CARTESIAN_POINT ( 'NONE',  ( -6.676582343750000703, 297.6718750017070079, 2.765530957082001251 ) ) ;
#57517 = CARTESIAN_POINT ( 'NONE',  ( -8.660254037844399733, 162.9166666666666856, 5.000000000000003553 ) ) ;
#57518 = AXIS2_PLACEMENT_3D ( 'NONE', #63507, #23143, #21371 ) ;
#57519 = CARTESIAN_POINT ( 'NONE',  ( -29.45134917122205209, -42.89584244968524729, 160.2744645009697138 ) ) ;
#57520 = CARTESIAN_POINT ( 'NONE',  ( -5.676582343750006032, 144.1145833299193555, 9.832129032723418760 ) ) ;
#57521 = CARTESIAN_POINT ( 'NONE',  ( 1.592277918221149080E-13, 106.2500000000000142, -10.00000000000000178 ) ) ;
#57522 = CARTESIAN_POINT ( 'NONE',  ( -7.204075437095965206, -7.204075437095968759, 82.84375000204838102 ) ) ;
#57523 = CARTESIAN_POINT ( 'NONE',  ( -31.15206608111996189, 194.6581652650363878, 171.8702574593503414 ) ) ;
#57524 = CARTESIAN_POINT ( 'NONE',  ( 1.656854249492405451, 202.3125000000000000, 202.0000000000000284 ) ) ;
#57525 = CARTESIAN_POINT ( 'NONE',  ( -6.735557395310442023E-16, 11.00000000000000000, 113.1249999999999858 ) ) ;
#57526 = CARTESIAN_POINT ( 'NONE',  ( 7.204075437095968759, -7.204075437095966983, 116.5937500020483810 ) ) ;
#57527 = ORIENTED_EDGE ( 'NONE', *, *, #2738, .F. ) ;
#57528 = CARTESIAN_POINT ( 'NONE',  ( 1.347111479062088405E-15, 0.000000000000000000, -11.00000000000000000 ) ) ;
#57529 = CARTESIAN_POINT ( 'NONE',  ( 2.251907551946699559, 183.6788756342477029, 139.0000000000000853 ) ) ;
#57530 = CARTESIAN_POINT ( 'NONE',  ( 11.35316468750000141, 131.0937499965860127, 0.000000000000000000 ) ) ;
#57531 = CARTESIAN_POINT ( 'NONE',  ( 3.458734125000015425, 201.0000000013655779, 196.5673454167823877 ) ) ;
#57532 = CARTESIAN_POINT ( 'NONE',  ( -7.188101187500000933, 23.99999999795161543, -2.977408999572651371 ) ) ;
#57533 = CARTESIAN_POINT ( 'NONE',  ( -4.220049686691937474, -10.18810118749999738, 74.31250000204836681 ) ) ;
#57534 = CARTESIAN_POINT ( 'NONE',  ( 6.951808397369818766E-16, 37.34374999658601979, -11.35316468750000141 ) ) ;
#57535 = ORIENTED_EDGE ( 'NONE', *, *, #73366, .F. ) ;
#57536 = CARTESIAN_POINT ( 'NONE',  ( -2.679491924311227624, 26.45833333333333925, -10.00000000000000888 ) ) ;
#57537 = CARTESIAN_POINT ( 'NONE',  ( -4.541265875000002339, 1.937499998634406806, -5.561446717895856393E-16 ) ) ;
#57538 = CARTESIAN_POINT ( 'NONE',  ( 5.662595241051934458, 5.662595241051935346, 12.45061528394063011 ) ) ;
#57539 = CARTESIAN_POINT ( 'NONE',  ( -1.432654583217662481, 205.3750000013656063, 145.4587341250000634 ) ) ;
#57540 = CARTESIAN_POINT ( 'NONE',  ( 2.977408999572650927, 6.749999997951611874, -7.188101187500001821 ) ) ;
#57541 = CARTESIAN_POINT ( 'NONE',  ( 6.000000000000003553, 297.6250000034140726, -2.485281374238571761 ) ) ;
#57542 = CARTESIAN_POINT ( 'NONE',  ( -19.59549724906859325, -15.56487351423710308, 137.0580289693109535 ) ) ;
#57543 = CARTESIAN_POINT ( 'NONE',  ( -5.082755093536326818, 3.281249997951610098, 5.082755093536325042 ) ) ;
#57544 = ADVANCED_FACE ( 'NONE', ( #64878 ), #13179, .T. ) ;
#57545 = CARTESIAN_POINT ( 'NONE',  ( 8.311093377946834337, 160.4687499965860127, 8.311093377946839666 ) ) ;
#57546 = CARTESIAN_POINT ( 'NONE',  ( -6.238412754330611322E-16, 10.18810118749999916, 73.28125000204838102 ) ) ;
#57547 = CARTESIAN_POINT ( 'NONE',  ( -25.55430564589115150, 205.3125000013656063, 172.4456943541091789 ) ) ;
#57548 = EDGE_CURVE ( 'NONE', #46560, #16691, #17331, .T. ) ;
#57549 = CARTESIAN_POINT ( 'NONE',  ( 4.000000000000000888, 2.937500000000000000, 1.656854249492384135 ) ) ;
#57550 = CARTESIAN_POINT ( 'NONE',  ( 4.541265875000001451, 18.37499999863441147, 1.881053915767124440 ) ) ;
#57551 = ORIENTED_EDGE ( 'NONE', *, *, #21440, .T. ) ;
#57552 = CARTESIAN_POINT ( 'NONE',  ( 2.828427124746209831, 199.5000000027312126, 200.8284271247462129 ) ) ;
#57553 = CARTESIAN_POINT ( 'NONE',  ( -4.000000000000015099, 205.5625000000000284, 143.6568542494924543 ) ) ;
#57554 = CARTESIAN_POINT ( 'NONE',  ( -28.00000000000007816, 203.1250000027312126, 166.0000000000003695 ) ) ;
#57555 = CARTESIAN_POINT ( 'NONE',  ( 5.000000000000004441, 249.7916666734946318, 8.660254037844385522 ) ) ;
#57556 = CARTESIAN_POINT ( 'NONE',  ( 5.656854249492376141, -5.656854249492374365, 6.080302783920147114 ) ) ;
#57557 = ORIENTED_EDGE ( 'NONE', *, *, #13029, .T. ) ;
#57558 =( BOUNDED_CURVE ( )  B_SPLINE_CURVE ( 2, ( #44866, #67131, #15427, #73526, #38465, #32815, #4141, #27132, #50146 ),
 .UNSPECIFIED., .F., .F. ) 
 B_SPLINE_CURVE_WITH_KNOTS ( ( 3, 2, 2, 2, 3 ),
 ( 0.7638888888888888395, 0.7708333333333333703, 0.7777777777777779011, 0.7847222222222223209, 0.7916666666666667407 ),
 .UNSPECIFIED. ) 
 CURVE ( )  GEOMETRIC_REPRESENTATION_ITEM ( )  RATIONAL_B_SPLINE_CURVE ( ( 1.000000000000000000, 0.9238795325112867385, 1.000000000000000000, 0.9238795325112867385, 1.000000000000000000, 0.9238795325112867385, 1.000000000000000000, 0.9238795325112855172, 1.000000000000001110 ) ) 
 REPRESENTATION_ITEM ( '' )  );
#57559 = CARTESIAN_POINT ( 'NONE',  ( -2.977408999572650039, 15.93749999795161365, -7.188101187500000933 ) ) ;
#57560 = CARTESIAN_POINT ( 'NONE',  ( -8.660254037844387298, 208.9583333265053682, -5.000000000000004441 ) ) ;
#57561 = CARTESIAN_POINT ( 'NONE',  ( -0.1960660428291157720, -48.00000000000003553, 151.0000000000000568 ) ) ;
#57562 = CARTESIAN_POINT ( 'NONE',  ( 10.00000000000000000, 39.79166666666667140, 2.679491924311236062 ) ) ;
#57563 = CARTESIAN_POINT ( 'NONE',  ( 7.188101187500001821, 105.8750000020483952, -2.977408999572651371 ) ) ;
#57564 = CARTESIAN_POINT ( 'NONE',  ( -27.99999999999996803, 207.1875000013656063, 173.4587341250003760 ) ) ;
#57565 = CARTESIAN_POINT ( 'NONE',  ( 3.369429374625374951, -10.27270496052241278, 63.91910092334654792 ) ) ;
#57567 = CARTESIAN_POINT ( 'NONE',  ( 11.00000000000000000, 4.556349186104045934, 74.03125000409677625 ) ) ;
#57566 = CARTESIAN_POINT ( 'NONE',  ( -3.313708498984681672, 111.9687500040968047, 8.000000000000078160 ) ) ;
#57568 = ORIENTED_EDGE ( 'NONE', *, *, #65292, .T. ) ;
#57569 = CARTESIAN_POINT ( 'NONE',  ( -11.35316468749999963, 243.9062500034140157, 0.000000000000000000 ) ) ;
#57570 = CARTESIAN_POINT ( 'NONE',  ( 2.977408999572646486, 7.188101187499991163, 17.89280278187175455 ) ) ;
#57571 = CARTESIAN_POINT ( 'NONE',  ( 1.296342370383217313, 49.95006747299250804, 40.70914535207719354 ) ) ;
#57572 = DIRECTION ( 'NONE',  ( -0.000000000000000000, 1.000000000000000000, -0.000000000000000000 ) ) ;
#57573 = FACE_OUTER_BOUND ( 'NONE', #27151, .T. ) ;
#57574 = DIRECTION ( 'NONE',  ( -0.000000000000000000, 1.000000000000000000, 4.689100369878284071E-30 ) ) ;
#57575 = CARTESIAN_POINT ( 'NONE',  ( -7.320508075688773708, 161.8750000000000000, -7.320508075688774596 ) ) ;
#57576 = CARTESIAN_POINT ( 'NONE',  ( 0.000000000000000000, 0.000000000000000000, -4.000000000000001776 ) ) ;
#57577 = DIRECTION ( 'NONE',  ( 0.000000000000000000, 0.000000000000000000, 1.000000000000000000 ) ) ;
#57578 = CARTESIAN_POINT ( 'NONE',  ( 5.676582343750001591, 126.9270833299193697, -9.832129032723420536 ) ) ;
#57579 = CARTESIAN_POINT ( 'NONE',  ( 25.17157287525378351, 198.8750000000000284, 172.8284271247460424 ) ) ;
#57580 = CARTESIAN_POINT ( 'NONE',  ( 4.898587196589412829E-16, 4.875000000000000888, -8.000000000000000000 ) ) ;
#57583 = CARTESIAN_POINT ( 'NONE',  ( -11.00000000000000000, 0.000000000000000000, 85.18750000409677625 ) ) ;
#57582 = CARTESIAN_POINT ( 'NONE',  ( 26.56734541678237349, 195.3750000013656063, 173.4587341249998929 ) ) ;
#57581 = CARTESIAN_POINT ( 'NONE',  ( 30.44569435410883074, 195.0625000013656063, 167.5543056458911053 ) ) ;
#57584 = EDGE_LOOP ( 'NONE', ( #1917, #22878, #37027, #15715, #63249 ) ) ;
#57585 = CARTESIAN_POINT ( 'NONE',  ( 3.313708498984802020, 10.78125000000000000, -7.999999999999958256 ) ) ;
#57586 = CARTESIAN_POINT ( 'NONE',  ( 27.99999999999996447, 201.6250000027312126, 165.9999999999998863 ) ) ;
#57587 = CARTESIAN_POINT ( 'NONE',  ( 5.000000000000055955, 195.8333333333334281, -8.660254037844481445 ) ) ;
#57588 = VECTOR ( 'NONE', #40776, 1000.000000000000000 ) ;
#57589 = CARTESIAN_POINT ( 'NONE',  ( 31.45873412499997812, 195.8750000013655779, 171.4326545832175839 ) ) ;
#57590 = CARTESIAN_POINT ( 'NONE',  ( -4.999999999999998224, 23.54166665983870033, -8.660254037844389075 ) ) ;
#57591 = CARTESIAN_POINT ( 'NONE',  ( 5.082755093536325042, 122.0937500020483952, -5.082755093536325930 ) ) ;
#57592 = CARTESIAN_POINT ( 'NONE',  ( 4.541265875000001451, 2.374999998634407028, 1.881053915767124440 ) ) ;
#57593 = CARTESIAN_POINT ( 'NONE',  ( -0.7581620860321414135, 65.76154746682149721, -26.27794529688514658 ) ) ;
#57594 = CARTESIAN_POINT ( 'NONE',  ( -3.313708498984758943, -7.999999999999989342, 19.11155277982336997 ) ) ;
#57596 = CARTESIAN_POINT ( 'NONE',  ( -28.00000000000003197, 207.0000000000000284, 166.0000000000003695 ) ) ;
#57595 = FACE_BOUND ( 'NONE', #71227, .T. ) ;
#57597 = CARTESIAN_POINT ( 'NONE',  ( -9.832129032723420536, 108.6979166632526983, 5.676582343749997150 ) ) ;
#57598 = ORIENTED_EDGE ( 'NONE', *, *, #67048, .F. ) ;
#57599 = CARTESIAN_POINT ( 'NONE',  ( 2.828427124746191623, 15.87499999726881406, -2.828427124746191623 ) ) ;
#57600 = CARTESIAN_POINT ( 'NONE',  ( 7.188101187500001821, 23.06249999795161187, -2.977408999572650483 ) ) ;
#57601 = DIRECTION ( 'NONE',  ( 0.000000000000000000, 0.000000000000000000, 1.000000000000000000 ) ) ;
#57602 = CARTESIAN_POINT ( 'NONE',  ( 2.085542519210945334E-15, 250.4687500034140157, 11.35316468749999963 ) ) ;
#57603 = CARTESIAN_POINT ( 'NONE',  ( 5.676582343750001591, 106.6145833299193555, -9.832129032723420536 ) ) ;
#57604 = ORIENTED_EDGE ( 'NONE', *, *, #36709, .F. ) ;
#57605 = CARTESIAN_POINT ( 'NONE',  ( 4.999999999999999112, -10.82378452496227261, 67.02990231369372509 ) ) ;
#57606 = CARTESIAN_POINT ( 'NONE',  ( -10.18810118749999916, 0.000000000000000000, 102.1562500020483810 ) ) ;
#57607 = CARTESIAN_POINT ( 'NONE',  ( -1.836970198721029983E-15, 225.6249999931720254, 10.00000000000000178 ) ) ;
#57608 = CARTESIAN_POINT ( 'NONE',  ( -1.432654583217607414, 201.5000000013655779, 194.5412658750000219 ) ) ;
#57609 = FACE_OUTER_BOUND ( 'NONE', #18662, .T. ) ;
#57611 = CARTESIAN_POINT ( 'NONE',  ( 3.042071309553159519, 104.7395833299193555, 11.35316468750000141 ) ) ;
#57610 = CARTESIAN_POINT ( 'NONE',  ( -3.999999999999959144, 206.1875000027312126, 199.6568542494924259 ) ) ;
#57612 = CARTESIAN_POINT ( 'NONE',  ( 7.999999999999991118, 3.313708498984757611, 13.86155278392014623 ) ) ;
#57613 = CARTESIAN_POINT ( 'NONE',  ( -25.55430564589119058, 196.5625000013656063, 167.5543056458915316 ) ) ;
#57614 = CARTESIAN_POINT ( 'NONE',  ( -1.300830538084598961E-11, 173.7499999999989768, 10.00000000000000178 ) ) ;
#57615 = VERTEX_POINT ( 'NONE', #35849 ) ;
#57616 = EDGE_CURVE ( 'NONE', #60098, #14756, #63593, .T. ) ;
#57617 = CARTESIAN_POINT ( 'NONE',  ( -2.679491924311225848, 193.3333333265053966, -10.00000000000000178 ) ) ;
#57618 = DIRECTION ( 'NONE',  ( -0.000000000000000000, -1.000000000000000000, -4.283267841918042741E-17 ) ) ;
#57619 = CARTESIAN_POINT ( 'NONE',  ( 8.311093377946837890, 86.71874999658601268, -8.311093377946837890 ) ) ;
#57620 = CARTESIAN_POINT ( 'NONE',  ( 4.721056650416000089, 287.8281250017069510, 4.721056650415999201 ) ) ;
#57621 = CARTESIAN_POINT ( 'NONE',  ( 7.188101187499999156, 8.249999997951611874, 2.977408999572654924 ) ) ;
#57622 = CARTESIAN_POINT ( 'NONE',  ( 10.18810118750000093, -4.220049686691933033, 97.18750000204836681 ) ) ;
#57623 = CARTESIAN_POINT ( 'NONE',  ( -5.676582343750006032, 219.1145833299193839, 9.832129032723418760 ) ) ;
#57624 = ORIENTED_EDGE ( 'NONE', *, *, #44825, .F. ) ;
#57625 = CARTESIAN_POINT ( 'NONE',  ( -3.313708498984759387, -7.999999999999989342, 26.61155277982336997 ) ) ;
#57626 = CARTESIAN_POINT ( 'NONE',  ( 2.981007339808865453, -44.60935554269958914, 139.1436377913152569 ) ) ;
#57627 = CARTESIAN_POINT ( 'NONE',  ( -9.832129032723420536, 218.6979166632526983, 5.676582343749997150 ) ) ;
#57628 = DIRECTION ( 'NONE',  ( 0.000000000000000000, 0.000000000000000000, -1.000000000000000000 ) ) ;
#57629 = CARTESIAN_POINT ( 'NONE',  ( -0.4368895104720005862, -16.44602605510715421, -68.55492853905352035 ) ) ;
#57630 = CARTESIAN_POINT ( 'NONE',  ( 2.765530957081996366, 296.1406250017070647, -6.676582343750003368 ) ) ;
#57631 = ORIENTED_EDGE ( 'NONE', *, *, #38065, .T. ) ;
#57633 = AXIS2_PLACEMENT_3D ( 'NONE', #31690, #72422, #20731 ) ;
#57632 = DIRECTION ( 'NONE',  ( -0.000000000000000000, -0.000000000000000000, 1.000000000000000000 ) ) ;
#57634 = CARTESIAN_POINT ( 'NONE',  ( -3.042071309553163960, 212.5520833299193839, -11.35316468749999963 ) ) ;
#57635 = EDGE_CURVE ( 'NONE', #41296, #52445, #25019, .T. ) ;
#57636 = CARTESIAN_POINT ( 'NONE',  ( -7.204075437095967871, 7.204075437095967871, 86.96875000204836681 ) ) ;
#57637 = EDGE_CURVE ( 'NONE', #53417, #54743, #61484, .T. ) ;
#57638 = CARTESIAN_POINT ( 'NONE',  ( -24.54126587500000412, 206.2500000013656063, 168.5673454167827003 ) ) ;
#57639 = CARTESIAN_POINT ( 'NONE',  ( 4.898587196589412829E-16, 15.37500000000000355, -8.000000000000000000 ) ) ;
#57640 = VERTEX_POINT ( 'NONE', #8652 ) ;
#57641 = B_SPLINE_CURVE_WITH_KNOTS ( 'NONE', 3,
 ( #45843, #6610, #63192, #58667, #11893, #51886, #12983, #29617, #28496, #226, #52630, #594 ),
 .UNSPECIFIED., .F., .F.,
 ( 4, 2, 2, 2, 2, 4 ),
 ( 1.618164387277533384E-15, 0.002547658444429638010, 0.005095316888857658391, 0.006369146111071668365, 0.007642975333285679206, 0.01019063377771369655 ),
 .UNSPECIFIED. ) ;
#57642 = CARTESIAN_POINT ( 'NONE',  ( -2.977408999572650927, 122.3750000020483952, -7.188101187500001821 ) ) ;
#57643 = DIRECTION ( 'NONE',  ( -0.000000000000000000, 1.000000000000000000, -0.000000000000000000 ) ) ;
#57644 = CARTESIAN_POINT ( 'NONE',  ( 7.320508075688774596, 30.62500000000000000, -7.320508075688774596 ) ) ;
#57645 =( GEOMETRIC_REPRESENTATION_CONTEXT ( 3 ) GLOBAL_UNCERTAINTY_ASSIGNED_CONTEXT ( ( #29498 ) ) GLOBAL_UNIT_ASSIGNED_CONTEXT ( ( #16824, #33846, #40600 ) ) REPRESENTATION_CONTEXT ( 'NONE', 'WORKASPACE' ) );
#57646 = CARTESIAN_POINT ( 'NONE',  ( -36.10814071610730736, 49.99999999999998579, 139.0000000000000000 ) ) ;
#57647 = CARTESIAN_POINT ( 'NONE',  ( 10.18810118749999916, 1.247682550866122264E-15, 76.28125000204836681 ) ) ;
#57648 = ORIENTED_EDGE ( 'NONE', *, *, #37676, .F. ) ;
#57649 = CARTESIAN_POINT ( 'NONE',  ( -1.881053915767121554, 3.624999998634406584, -4.541265875000002339 ) ) ;
#57650 = CARTESIAN_POINT ( 'NONE',  ( 8.000000000000000000, 113.8437500000000000, -3.313708498984762496 ) ) ;
#57651 = CARTESIAN_POINT ( 'NONE',  ( 5.656854249492374365, 5.656854249492375253, 6.267802779823364645 ) ) ;
#57652 = PLANE ( 'NONE',  #23469 ) ;
#57653 = CARTESIAN_POINT ( 'NONE',  ( -2.977408999572651815, 121.8125000020483810, 7.188101187500000933 ) ) ;
#57654 = CARTESIAN_POINT ( 'NONE',  ( 5.000000000000000000, -61.58678017309387798, 23.68362420833305038 ) ) ;
#57655 = CARTESIAN_POINT ( 'NONE',  ( -4.088227598258586603E-16, 296.2031250017070079, -6.676582343750001591 ) ) ;
#57658 = CARTESIAN_POINT ( 'NONE',  ( -6.000000000000001776, 289.0625000034140157, 0.000000000000000000 ) ) ;
#57657 = CARTESIAN_POINT ( 'NONE',  ( 3.042071309553173286, 250.3645833367473301, 11.35316468749999608 ) ) ;
#57656 = CARTESIAN_POINT ( 'NONE',  ( 30.44569435410879876, 207.8125000013656063, 167.5543056458910485 ) ) ;
#57659 = PRODUCT_CONTEXT ( 'NONE', #41407, 'mechanical' ) ;
#57660 = ORIENTED_EDGE ( 'NONE', *, *, #26521, .T. ) ;
#57661 = CARTESIAN_POINT ( 'NONE',  ( -9.832129032723415207, 234.6354166700806445, 5.676582343750005144 ) ) ;
#57662 = CARTESIAN_POINT ( 'NONE',  ( -2.977408999572648707, -7.188101187499990274, 9.267802781871756324 ) ) ;
#57663 = EDGE_LOOP ( 'NONE', ( #72065, #28728, #45750, #777 ) ) ;
#57664 = CARTESIAN_POINT ( 'NONE',  ( -6.238412754330611322E-16, 10.18810118749999916, 67.28125000204838102 ) ) ;
#57665 = CARTESIAN_POINT ( 'NONE',  ( 9.832129032723420536, 91.51041666325268409, -5.676582343749999815 ) ) ;
#57666 = CARTESIAN_POINT ( 'NONE',  ( 4.000000000000001776, 21.06250000000000000, -1.656854249492381248 ) ) ;
#57667 = CARTESIAN_POINT ( 'NONE',  ( -4.556349186104045934, 11.00000000000000000, 86.21874999999998579 ) ) ;
#57670 = CARTESIAN_POINT ( 'NONE',  ( 5.000000000000003553, 70.83333333333334281, -8.660254037844390851 ) ) ;
#57669 = CARTESIAN_POINT ( 'NONE',  ( 30.82842712474620583, 194.2500000027312126, 172.8284271247460424 ) ) ;
#57668 = CARTESIAN_POINT ( 'NONE',  ( 25.55430564589119768, 208.3125000013656063, 167.5543056458910485 ) ) ;
#57671 = VERTEX_POINT ( 'NONE', #54687 ) ;
#57672 = CARTESIAN_POINT ( 'NONE',  ( 2.679491924311296014, 75.83333332650536818, 9.999999999999959144 ) ) ;
#57673 = CARTESIAN_POINT ( 'NONE',  ( -1.836970198721029983E-15, 180.6249999931720538, 10.00000000000000178 ) ) ;
#57674 = CARTESIAN_POINT ( 'NONE',  ( -9.832129032723420536, 198.6979166632526983, 5.676582343749997150 ) ) ;
#57675 =( BOUNDED_CURVE ( )  B_SPLINE_CURVE ( 2, ( #63828, #485, #23465, #69497, #40822, #39339, #62336, #10664, #61843 ),
 .UNSPECIFIED., .F., .F. ) 
 B_SPLINE_CURVE_WITH_KNOTS ( ( 3, 2, 2, 2, 3 ),
 ( 0.7794117647058822484, 0.7830882352941175295, 0.7867647058823528106, 0.7904411764705880916, 0.7941176470588233727 ),
 .UNSPECIFIED. ) 
 CURVE ( )  GEOMETRIC_REPRESENTATION_ITEM ( )  RATIONAL_B_SPLINE_CURVE ( ( 1.000000000000002220, 0.9238795325112844070, 1.000000000000000000, 0.9238795325112867385, 1.000000000000000000, 0.9238795325112867385, 1.000000000000000000, 0.9238795325112890700, 0.9999999999999976685 ) ) 
 REPRESENTATION_ITEM ( '' )  );
#57676 = CARTESIAN_POINT ( 'NONE',  ( -1.432654583217662481, 205.1250000013656347, 145.4587341250000634 ) ) ;
#57677 = CARTESIAN_POINT ( 'NONE',  ( 31.45873412499999944, 204.9375000013656063, 169.9999999999999432 ) ) ;
#57678 = VECTOR ( 'NONE', #28545, 1000.000000000000000 ) ;
#57679 = CARTESIAN_POINT ( 'NONE',  ( -2.977408999572650039, 22.31249999795161543, -7.188101187500001821 ) ) ;
#57680 = CARTESIAN_POINT ( 'NONE',  ( 9.832129032723416984, 175.6770833299193555, 5.676582343750006032 ) ) ;
#57681 = CARTESIAN_POINT ( 'NONE',  ( -2.250000000000000888, -2.250000000000000000, 28.00000000000000000 ) ) ;
#57682 = CARTESIAN_POINT ( 'NONE',  ( 5.082755093536326818, 98.09375000204838102, 5.082755093536325042 ) ) ;
#57684 = CARTESIAN_POINT ( 'NONE',  ( -2.679491924311077966, 106.4583333333333144, -10.00000000000008171 ) ) ;
#57683 = CARTESIAN_POINT ( 'NONE',  ( -7.347880794884122694E-16, 15.75000000000000000, 4.000000000000001776 ) ) ;
#57685 = CARTESIAN_POINT ( 'NONE',  ( 4.541265875000001451, 9.249999998634406140, 1.881053915767124440 ) ) ;
#57686 = CARTESIAN_POINT ( 'NONE',  ( 26.56734541678232731, 201.6250000013656063, 173.4587341249998929 ) ) ;
#57687 = CARTESIAN_POINT ( 'NONE',  ( -7.188101187499990274, -2.977408999572651371, 9.455302781871754547 ) ) ;
#57688 = CARTESIAN_POINT ( 'NONE',  ( -11.35316468749999785, 63.07291666325268409, -3.042071309553167513 ) ) ;
#57689 = DIRECTION ( 'NONE',  ( 0.000000000000000000, 0.000000000000000000, -1.000000000000000000 ) ) ;
#57690 = CARTESIAN_POINT ( 'NONE',  ( -5.656854249492373476, -5.656854249492376141, -0.4259472156701774592 ) ) ;
#57691 = VERTEX_POINT ( 'NONE', #72011 ) ;
#57692 = CARTESIAN_POINT ( 'NONE',  ( 7.020684431968935435, 9.803012413858334995, -0.02533325329315222127 ) ) ;
#57693 = CARTESIAN_POINT ( 'NONE',  ( 4.556349186104052151, -10.99999999999999822, 116.9687500000000142 ) ) ;
#57694 = CARTESIAN_POINT ( 'NONE',  ( 5.676582343750001591, 56.61458332991934839, -9.832129032723420536 ) ) ;
#57695 = AXIS2_PLACEMENT_3D ( 'NONE', #60704, #14662, #53932 ) ;
#57696 = CARTESIAN_POINT ( 'NONE',  ( 11.00000000000000355, -4.556349186104045046, 76.84375000409676204 ) ) ;
#57697 = CARTESIAN_POINT ( 'NONE',  ( 1.432654583217608080, 196.8750000013656347, 138.5412658750000503 ) ) ;
#57698 = CARTESIAN_POINT ( 'NONE',  ( -5.107860025160073647, 10.26152767799289123, 64.38109526790010761 ) ) ;
#57700 = CARTESIAN_POINT ( 'NONE',  ( 6.951808397369818766E-16, 62.03124999658601979, -11.35316468750000141 ) ) ;
#57699 = CARTESIAN_POINT ( 'NONE',  ( 7.188101187500000044, 94.90625000204838102, -8.802885111219163269E-16 ) ) ;
#57701 = CARTESIAN_POINT ( 'NONE',  ( 3.313708498984762496, -7.999999999999989342, 2.799052779823366421 ) ) ;
#57702 = DIRECTION ( 'NONE',  ( -0.000000000000000000, -0.9659258262890700886, -0.2588190451025146888 ) ) ;
#57703 = CIRCLE ( 'NONE', #37210, 6.000000000000001776 ) ;
#57704 = CARTESIAN_POINT ( 'NONE',  ( -10.00000000000000178, 149.3749999931720538, -1.224646799147353454E-15 ) ) ;
#57705 = CARTESIAN_POINT ( 'NONE',  ( 7.188101187500001821, 98.37500000204840944, -2.977408999572651371 ) ) ;
#57706 = DIRECTION ( 'NONE',  ( 0.000000000000000000, 0.000000000000000000, 1.000000000000000000 ) ) ;
#57707 = CARTESIAN_POINT ( 'NONE',  ( -11.35316468749999785, 43.38541666325267698, -3.042071309553167957 ) ) ;
#57708 = CARTESIAN_POINT ( 'NONE',  ( -7.204075437095967871, 7.204075437095967871, 111.3437500020483810 ) ) ;
#57709 = CARTESIAN_POINT ( 'NONE',  ( 8.311093377946837890, 176.4062499965859843, -8.311093377946837890 ) ) ;
#57710 = EDGE_LOOP ( 'NONE', ( #59268, #50065, #35392, #264 ) ) ;
#57711 = CARTESIAN_POINT ( 'NONE',  ( 4.104248244562368697, 66.38464254922966745, 26.65807398667948291 ) ) ;
#57712 = CARTESIAN_POINT ( 'NONE',  ( 1.871523826299183495E-15, -10.18810118749999916, 72.53125000204838102 ) ) ;
#57713 = CYLINDRICAL_SURFACE ( 'NONE', #40756, 4.000000000000001776 ) ;
#57715 = CARTESIAN_POINT ( 'NONE',  ( -3.042071309553173730, 174.3229166632526983, 11.35316468749999785 ) ) ;
#57714 = DIRECTION ( 'NONE',  ( 1.000000000000000000, -0.000000000000000000, -0.000000000000000000 ) ) ;
#57716 = CARTESIAN_POINT ( 'NONE',  ( 7.999999999999992895, -3.313708498984756279, 7.542802784329822430 ) ) ;
#57717 = CARTESIAN_POINT ( 'NONE',  ( 4.000000000000000888, 21.68749999726881583, 1.656854249492384135 ) ) ;
#57718 = EDGE_CURVE ( 'NONE', #51725, #746, #32769, .T. ) ;
#57719 = CARTESIAN_POINT ( 'NONE',  ( -4.999999999999992895, 248.9583333401613174, 8.660254037844390851 ) ) ;
#57720 = CARTESIAN_POINT ( 'NONE',  ( 11.00000000000000000, 1.347111479062088405E-15, 75.24999999999998579 ) ) ;
#57721 = ORIENTED_EDGE ( 'NONE', *, *, #50697, .T. ) ;
#57722 = CARTESIAN_POINT ( 'NONE',  ( 5.676582343749993598, 165.2604166632526983, 9.832129032723422313 ) ) ;
#57723 = CARTESIAN_POINT ( 'NONE',  ( 7.188101187499992051, 8.802885111219154394E-16, 24.73655278187175810 ) ) ;
#57724 = CARTESIAN_POINT ( 'NONE',  ( -5.676582343750006032, 134.4270833299193555, 9.832129032723418760 ) ) ;
#57725 = CARTESIAN_POINT ( 'NONE',  ( 2.249999999999997335, 255.9999999999998295, 5.427273999917215264 ) ) ;
#57726 = ORIENTED_EDGE ( 'NONE', *, *, #30960, .F. ) ;
#57727 = CARTESIAN_POINT ( 'NONE',  ( 4.541265875000001451, 10.37499999863440792, 1.881053915767124440 ) ) ;
#57728 = CARTESIAN_POINT ( 'NONE',  ( -5.082755093536325042, 16.03124999795161543, -5.082755093536325930 ) ) ;
#57729 = EDGE_CURVE ( 'NONE', #14276, #31901, #9026, .T. ) ;
#57730 = CARTESIAN_POINT ( 'NONE',  ( 8.000000000000001776, 104.8437500040967763, 3.313708498984759387 ) ) ;
#57731 = CARTESIAN_POINT ( 'NONE',  ( -31.45873412499999233, 197.9375000013655779, 170.0000000000003979 ) ) ;
#57732 = AXIS2_PLACEMENT_3D ( 'NONE', #4861, #27857, #15035 ) ;
#57733 = CARTESIAN_POINT ( 'NONE',  ( -4.000000000000002665, 11.56249999999999822, 1.656854249492380804 ) ) ;
#57734 = CARTESIAN_POINT ( 'NONE',  ( -2.828427124746190735, 21.12499999726881583, -2.828427124746191623 ) ) ;
#57735 = CARTESIAN_POINT ( 'NONE',  ( 4.541265875000002339, 10.37499999863440969, -1.881053915767121776 ) ) ;
#57736 = CARTESIAN_POINT ( 'NONE',  ( -5.656854249492375253, 5.656854249492375253, 18.83030278392014623 ) ) ;
#57737 = DIRECTION ( 'NONE',  ( -0.000000000000000000, 1.000000000000000000, -0.000000000000000000 ) ) ;
#57738 = AXIS2_PLACEMENT_3D ( 'NONE', #23753, #40731, #17716 ) ;
#57739 = ORIENTED_EDGE ( 'NONE', *, *, #7189, .T. ) ;
#57740 = CARTESIAN_POINT ( 'NONE',  ( -8.660254037844435260, 177.0833333333333712, -5.000000000000031086 ) ) ;
#57741 = CARTESIAN_POINT ( 'NONE',  ( 1.320432766682874540E-15, 106.5312500020483810, 7.188101187500000044 ) ) ;
#57743 = CARTESIAN_POINT ( 'NONE',  ( 47.32259252271278882, 38.77329591270031983, 65.76194439203456454 ) ) ;
#57742 = DIRECTION ( 'NONE',  ( -1.000000000000000000, 0.000000000000000000, 0.000000000000000000 ) ) ;
#57744 =( NAMED_UNIT ( * ) PLANE_ANGLE_UNIT ( ) SI_UNIT ( $, .RADIAN. ) );
#57745 = ORIENTED_EDGE ( 'NONE', *, *, #47669, .F. ) ;
#57746 = CARTESIAN_POINT ( 'NONE',  ( 4.541265875000001451, 21.24999999863440436, 1.881053915767124440 ) ) ;
#57747 = CARTESIAN_POINT ( 'NONE',  ( -4.401442555609577197E-16, 7.188101187499992051, 22.11155278187175455 ) ) ;
#57748 = EDGE_LOOP ( 'NONE', ( #31912, #14245, #15551, #73317, #8554, #15946, #19380, #41966 ) ) ;
#57749 = VERTEX_POINT ( 'NONE', #48627 ) ;
#57750 = CARTESIAN_POINT ( 'NONE',  ( 7.204075437095968759, -7.204075437095966983, 84.71875000204836681 ) ) ;
#57751 = DIRECTION ( 'NONE',  ( -0.000000000000000000, 1.000000000000000000, -0.000000000000000000 ) ) ;
#57752 = CARTESIAN_POINT ( 'NONE',  ( -24.54126587499998990, 196.4375000013655779, 170.0000000000003411 ) ) ;
#57753 = CARTESIAN_POINT ( 'NONE',  ( 11.00000000000000000, 1.347111479062088405E-15, 102.2500000000000000 ) ) ;
#57756 = CARTESIAN_POINT ( 'NONE',  ( -6.676582343750002480, 299.5468750017069510, -2.765530957081996810 ) ) ;
#57755 = CARTESIAN_POINT ( 'NONE',  ( 24.00000000000000355, 204.9375000027312410, 171.6568542494923122 ) ) ;
#57754 = CARTESIAN_POINT ( 'NONE',  ( 0.000000000000000000, 125.0000000000000000, 0.000000000000000000 ) ) ;
#57757 = CARTESIAN_POINT ( 'NONE',  ( 2.679491924311222739, 138.9583333333333712, 10.00000000000000355 ) ) ;
#57758 = CARTESIAN_POINT ( 'NONE',  ( 8.000000000000001776, 97.15625000000000000, 3.313708498984759387 ) ) ;
#57759 = CARTESIAN_POINT ( 'NONE',  ( 2.765530957082001251, 288.9218750017069510, 6.676582343750000703 ) ) ;
#57760 = CARTESIAN_POINT ( 'NONE',  ( -5.082755093536319713, 5.082755093536319713, 6.174052781871754547 ) ) ;
#57761 = CARTESIAN_POINT ( 'NONE',  ( -26.34314575050763807, 208.9375000000000284, 166.0000000000003411 ) ) ;
#57762 = CARTESIAN_POINT ( 'NONE',  ( 30.44569435410879166, 203.5625000013656063, 172.4456943541087526 ) ) ;
#57763 = CARTESIAN_POINT ( 'NONE',  ( -7.188101187500001821, 4.499999997951610098, -2.977408999572651371 ) ) ;
#57764 = CARTESIAN_POINT ( 'NONE',  ( 5.662595241051936235, -5.662595241051934458, 1.575615283940630107 ) ) ;
#57765 = CARTESIAN_POINT ( 'NONE',  ( 3.458734124999959914, 194.4375000013656063, 142.0000000000000568 ) ) ;
#57766 = CARTESIAN_POINT ( 'NONE',  ( 5.082755093536325042, 114.9687500020483810, -5.082755093536325930 ) ) ;
#57768 = CARTESIAN_POINT ( 'NONE',  ( 3.637049425642478351, 194.7916240854007697, 196.9005725204635553 ) ) ;
#57767 =( LENGTH_UNIT ( ) NAMED_UNIT ( * ) SI_UNIT ( .MILLI., .METRE. ) );
#57769 = CARTESIAN_POINT ( 'NONE',  ( 11.35316468749999963, 241.5104166700806729, 3.042071309553159519 ) ) ;
#57770 = CARTESIAN_POINT ( 'NONE',  ( -3.313708498984765161, 4.031250000000000888, 7.999999999999998224 ) ) ;
#57771 = CARTESIAN_POINT ( 'NONE',  ( 2.977408999572650927, -7.188101187499990274, 26.33030278187175810 ) ) ;
#57773 =( BOUNDED_CURVE ( )  B_SPLINE_CURVE ( 2, ( #73383, #50737, #43968, #67730, #32668, #33411, #10385, #4732, #14906 ),
 .UNSPECIFIED., .F., .F. ) 
 B_SPLINE_CURVE_WITH_KNOTS ( ( 3, 2, 2, 2, 3 ),
 ( 0.3295454545454545303, 0.3352272727272727071, 0.3409090909090908839, 0.3465909090909091161, 0.3522727272727272929 ),
 .UNSPECIFIED. ) 
 CURVE ( )  GEOMETRIC_REPRESENTATION_ITEM ( )  RATIONAL_B_SPLINE_CURVE ( ( 1.000000000000000000, 0.9238795325112867385, 1.000000000000000000, 0.9238795325112867385, 1.000000000000000000, 0.9238795325112867385, 1.000000000000000000, 0.9238795325112867385, 1.000000000000000000 ) ) 
 REPRESENTATION_ITEM ( '' )  );
#57772 = CARTESIAN_POINT ( 'NONE',  ( 23.99999999999999645, 196.6875000000000000, 168.3431457505075173 ) ) ;
#57774 = CARTESIAN_POINT ( 'NONE',  ( 3.042071309553167069, 21.82291666325268054, -11.35316468749999785 ) ) ;
#57775 = CARTESIAN_POINT ( 'NONE',  ( -1.656854249492271780, 202.8125000000000284, 193.9999999999999716 ) ) ;
#57776 = CARTESIAN_POINT ( 'NONE',  ( 5.676582343749993598, 225.2604166632526983, 9.832129032723422313 ) ) ;
#57777 = CARTESIAN_POINT ( 'NONE',  ( 8.000000000000000000, 124.3437500000000000, -3.313708498984762496 ) ) ;
#57779 = CARTESIAN_POINT ( 'NONE',  ( -8.660254037844532959, 42.91666666666677088, 5.000000000000080824 ) ) ;
#57778 = CARTESIAN_POINT ( 'NONE',  ( -1.736494649864163131, 51.27805538754891757, 48.57014059985818477 ) ) ;
#57780 = ORIENTED_EDGE ( 'NONE', *, *, #28344, .T. ) ;
#57781 = EDGE_CURVE ( 'NONE', #51123, #37372, #19957, .T. ) ;
#57782 = CARTESIAN_POINT ( 'NONE',  ( 3.458734124999959469, 194.7500000013656063, 140.5673454167824161 ) ) ;
#57783 = CARTESIAN_POINT ( 'NONE',  ( -8.311093377946841443, 18.90624999658601624, 8.311093377946830785 ) ) ;
#57784 = CARTESIAN_POINT ( 'NONE',  ( 4.556349186104045934, 11.00000000000000000, 90.71875000409676204 ) ) ;
#57785 = CARTESIAN_POINT ( 'NONE',  ( -11.00000000000000533, 11.00000000000000000, 41.99999999999999289 ) ) ;
#57786 = FACE_OUTER_BOUND ( 'NONE', #50924, .T. ) ;
#57788 = CARTESIAN_POINT ( 'NONE',  ( 5.676582343750001591, 21.61458332991935194, -9.832129032723420536 ) ) ;
#57787 = CARTESIAN_POINT ( 'NONE',  ( -2.977408999572650927, 108.8750000020483952, -7.188101187500000933 ) ) ;
#57789 = CARTESIAN_POINT ( 'NONE',  ( 7.999999999999991118, 9.797174393178815797E-16, 24.08030277982336642 ) ) ;
#57790 = CARTESIAN_POINT ( 'NONE',  ( -11.35316468750000141, 138.4895833299193271, 3.042071309553159963 ) ) ;
#57791 = AXIS2_PLACEMENT_3D ( 'NONE', #1915, #52860, #47919 ) ;
#57792 = CARTESIAN_POINT ( 'NONE',  ( 2.679491924311222739, 110.8333333265053824, 10.00000000000000355 ) ) ;
#57793 = CARTESIAN_POINT ( 'NONE',  ( 2.977408999572650039, 116.5625000020483810, -7.188101187500001821 ) ) ;
#57794 = CARTESIAN_POINT ( 'NONE',  ( -4.999999999999998224, 3.541666659838699438, -8.660254037844389075 ) ) ;
#57795 = CARTESIAN_POINT ( 'NONE',  ( 10.99999999999989342, 4.556349186104152515, 102.5312500040967763 ) ) ;
#57796 = CARTESIAN_POINT ( 'NONE',  ( -5.000000000000000000, -53.21762015693864356, -47.70201125340226156 ) ) ;
#57797 = ORIENTED_EDGE ( 'NONE', *, *, #11398, .F. ) ;
#57798 = CARTESIAN_POINT ( 'NONE',  ( -8.311093377946836114, 12.96874999658601446, -8.311093377946837890 ) ) ;
#57799 =( BOUNDED_CURVE ( )  B_SPLINE_CURVE ( 2, ( #40487, #6898, #40860, #29909, #63492, #63119, #24235, #52551, #52924 ),
 .UNSPECIFIED., .F., .F. ) 
 B_SPLINE_CURVE_WITH_KNOTS ( ( 3, 2, 2, 2, 3 ),
 ( 0.5624999999999981126, 0.5729166666666647423, 0.5833333333333314830, 0.5937499999999982236, 0.6041666666666648533 ),
 .UNSPECIFIED. ) 
 CURVE ( )  GEOMETRIC_REPRESENTATION_ITEM ( )  RATIONAL_B_SPLINE_CURVE ( ( 1.000000000000013767, 0.9238795325112729717, 1.000000000000000000, 0.9238795325112867385, 1.000000000000000000, 0.9238795325112867385, 1.000000000000000000, 0.9238795325112997281, 0.9999999999999870104 ) ) 
 REPRESENTATION_ITEM ( '' )  );
#57800 = CARTESIAN_POINT ( 'NONE',  ( -2.751064625579944321E-14, 201.8750000027312126, 146.0000000000000284 ) ) ;
#57801 = CARTESIAN_POINT ( 'NONE',  ( -2.765530957081996810, 296.2656250017069510, -6.676582343750003368 ) ) ;
#57802 = CARTESIAN_POINT ( 'NONE',  ( 6.951808397369818766E-16, 137.0312499965860411, -11.35316468750000141 ) ) ;
#57803 = CARTESIAN_POINT ( 'NONE',  ( -2.828427124746192067, 3.625000000000000000, 2.828427124746190735 ) ) ;
#57804 = CARTESIAN_POINT ( 'NONE',  ( -3.313708498984757167, 7.999999999999991118, 23.10530278432982954 ) ) ;
#57805 = CYLINDRICAL_SURFACE ( 'NONE', #15223, 10.00000000000000178 ) ;
#57806 = CIRCLE ( 'NONE', #51752, 6.000000000000015099 ) ;
#57807 = ADVANCED_FACE ( 'NONE', ( #65985 ), #3526, .F. ) ;
#57808 = CARTESIAN_POINT ( 'NONE',  ( -8.311093377946836114, 253.2812500034139873, -8.311093377946836114 ) ) ;
#57809 = CARTESIAN_POINT ( 'NONE',  ( 1.871523826299183495E-15, -10.18810118749999916, 95.40625000204836681 ) ) ;
#57810 = ORIENTED_EDGE ( 'NONE', *, *, #47564, .F. ) ;
#57811 = EDGE_CURVE ( 'NONE', #38509, #5172, #44810, .T. ) ;
#57812 = CARTESIAN_POINT ( 'NONE',  ( -38.00000000000000000, 53.00000000000000000, 15.00000000000000178 ) ) ;
#57813 = CARTESIAN_POINT ( 'NONE',  ( 4.999999999999999112, 65.75515815785567497, -23.82162496270573016 ) ) ;
#57814 = CARTESIAN_POINT ( 'NONE',  ( -8.311093377946841443, 84.21874999658599847, 8.311093377946830785 ) ) ;
#57815 = VERTEX_POINT ( 'NONE', #53082 ) ;
#57816 = CARTESIAN_POINT ( 'NONE',  ( 4.220049686691941027, -10.18810118749999738, 108.6250000020483668 ) ) ;
#57817 = CARTESIAN_POINT ( 'NONE',  ( -4.541265875000002339, 13.93749999863440614, -5.561446717895856393E-16 ) ) ;
#57818 = VERTEX_POINT ( 'NONE', #19470 ) ;
#57819 = ORIENTED_EDGE ( 'NONE', *, *, #70879, .T. ) ;
#57820 = CARTESIAN_POINT ( 'NONE',  ( -8.000000000000000000, 8.156250000000001776, -3.313708498984762496 ) ) ;
#57821 = DIRECTION ( 'NONE',  ( -6.558680509637771650E-18, -1.000000000000000000, 0.000000000000000000 ) ) ;
#57822 = DIRECTION ( 'NONE',  ( -0.5000000000000017764, -0.8660254037844377084, 0.000000000000000000 ) ) ;
#57823 = CARTESIAN_POINT ( 'NONE',  ( 7.188101187499999156, 26.24999999795161898, 2.977408999572654924 ) ) ;
#57824 = EDGE_CURVE ( 'NONE', #5951, #34088, #35011, .T. ) ;
#57825 = CARTESIAN_POINT ( 'NONE',  ( 3.313708498984760720, 123.2187500040967763, -8.000000000000000000 ) ) ;
#57826 = CARTESIAN_POINT ( 'NONE',  ( 10.18810118750000093, -4.220049686691933921, 103.1875000020483810 ) ) ;
#57827 = CARTESIAN_POINT ( 'NONE',  ( 9.999999999999996447, 110.0000000000000000, 0.000000000000000000 ) ) ;
#57828 = CARTESIAN_POINT ( 'NONE',  ( -4.000000000000002665, 11.31249999726881583, 1.656854249492380804 ) ) ;
#57829 = CARTESIAN_POINT ( 'NONE',  ( -3.313708498984757611, 7.999999999999991118, 12.73655278392014623 ) ) ;
#57830 = ORIENTED_EDGE ( 'NONE', *, *, #17216, .F. ) ;
#57831 = LINE ( 'NONE', #41206, #2125 ) ;
#57832 = CARTESIAN_POINT ( 'NONE',  ( 3.458734125000016313, 199.8750000013655779, 199.4326545832176691 ) ) ;
#57833 = APPLICATION_CONTEXT ( 'automotive_design' ) ;
#57834 = CARTESIAN_POINT ( 'NONE',  ( -31.45873412500002431, 203.6250000013656063, 168.5673454167828140 ) ) ;
#57835 =( LENGTH_UNIT ( ) NAMED_UNIT ( * ) SI_UNIT ( .MILLI., .METRE. ) );
#57836 = CARTESIAN_POINT ( 'NONE',  ( 1.881053915767121776, 11.49999999863440792, -4.541265875000002339 ) ) ;
#57837 = AXIS2_PLACEMENT_3D ( 'NONE', #5786, #11439, #11807 ) ;
#57838 = ADVANCED_FACE ( 'NONE', ( #70430 ), #40464, .F. ) ;
#57839 = CARTESIAN_POINT ( 'NONE',  ( 7.188101187499993827, -2.977408999572645598, 14.14280278187175455 ) ) ;
#57840 = VERTEX_POINT ( 'NONE', #10963 ) ;
#57841 = VERTEX_POINT ( 'NONE', #22260 ) ;
#57842 = CARTESIAN_POINT ( 'NONE',  ( 10.18810118749999916, 4.220049686691935698, 107.5000000020483668 ) ) ;
#57843 = CARTESIAN_POINT ( 'NONE',  ( 2.775557561562891351E-14, 210.0000000000000284, 202.0000000000000000 ) ) ;
#57844 = CARTESIAN_POINT ( 'NONE',  ( -29.65685424949241167, 204.0625000000000000, 166.0000000000004263 ) ) ;
#57845 = CARTESIAN_POINT ( 'NONE',  ( 2.445694354108838731, 202.0625000013656063, 195.5543056458912190 ) ) ;
#57846 = CARTESIAN_POINT ( 'NONE',  ( 26.56734541678237349, 197.3750000013656063, 173.4587341249998929 ) ) ;
#57847 = CARTESIAN_POINT ( 'NONE',  ( -8.660254037844390851, 87.91666666666667140, 4.999999999999998224 ) ) ;
#57848 = CARTESIAN_POINT ( 'NONE',  ( -7.999999999999998224, 116.0937500000000000, 3.313708498984766493 ) ) ;
#57849 = CARTESIAN_POINT ( 'NONE',  ( 11.35316468750000141, 66.09374999658601268, 0.000000000000000000 ) ) ;
#57850 = CARTESIAN_POINT ( 'NONE',  ( -4.242640687119285658, 288.1249999999999432, 4.242640687119287435 ) ) ;
#57851 = ORIENTED_EDGE ( 'NONE', *, *, #53537, .T. ) ;
#57852 = LINE ( 'NONE', #18213, #67459 ) ;
#57853 = CARTESIAN_POINT ( 'NONE',  ( -4.465349678524266785, -66.51625814178508733, 26.73836809291843153 ) ) ;
#57854 = CARTESIAN_POINT ( 'NONE',  ( -2.839093476692135984E-14, 206.6875000013656063, 138.5412658750000503 ) ) ;
#57855 = CARTESIAN_POINT ( 'NONE',  ( 8.660254037844396180, 85.41666666666668561, -5.000000000000005329 ) ) ;
#57856 = CARTESIAN_POINT ( 'NONE',  ( 8.000000000000000000, 97.25000000000000000, -9.797174393178825657E-16 ) ) ;
#57857 = CARTESIAN_POINT ( 'NONE',  ( -6.123233995736766282E-16, 238.7500000000000284, -10.00000000000000000 ) ) ;
#57858 = PLANE ( 'NONE',  #54792 ) ;
#57859 = CARTESIAN_POINT ( 'NONE',  ( -4.220049686691937474, -10.18810118749999738, 69.81250000204835260 ) ) ;
#57860 = CARTESIAN_POINT ( 'NONE',  ( -10.00000000000000178, 207.5000000000000284, -1.224646799147353454E-15 ) ) ;
#57861 = CARTESIAN_POINT ( 'NONE',  ( -4.401442555609577197E-16, 7.188101187499992051, 17.98655278187175810 ) ) ;
#57862 = CARTESIAN_POINT ( 'NONE',  ( 8.311093377946834337, 180.4687499965859843, 8.311093377946839666 ) ) ;
#57863 = CARTESIAN_POINT ( 'NONE',  ( -10.00000000000022204, 212.2916666666667993, -2.679491924311289797 ) ) ;
#57864 = CARTESIAN_POINT ( 'NONE',  ( -11.00000000000000000, 0.000000000000000000, 97.18750000409677625 ) ) ;
#57866 = FACE_OUTER_BOUND ( 'NONE', #69027, .T. ) ;
#57865 = CARTESIAN_POINT ( 'NONE',  ( -4.999999999999992895, 228.9583333401612890, 8.660254037844390851 ) ) ;
#57867 = ORIENTED_EDGE ( 'NONE', *, *, #35040, .F. ) ;
#57868 = CARTESIAN_POINT ( 'NONE',  ( 1.432654583217608080, 208.8750000013656347, 138.5412658750000503 ) ) ;
#57869 = CARTESIAN_POINT ( 'NONE',  ( 5.676582343750001591, 36.92708332991935549, -9.832129032723420536 ) ) ;
#57870 = CARTESIAN_POINT ( 'NONE',  ( -11.00000000000000000, 4.556349186104045934, 109.0937500040967905 ) ) ;
#57871 = CARTESIAN_POINT ( 'NONE',  ( -2.454488697237479755, 194.5261102419721908, 200.5402859678918617 ) ) ;
#57872 = CARTESIAN_POINT ( 'NONE',  ( 25.17157287525382259, 208.0000000027312126, 172.8284271247460993 ) ) ;
#57874 = LINE ( 'NONE', #40504, #20959 ) ;
#57873 = CARTESIAN_POINT ( 'NONE',  ( -18.00000000000000355, 0.8785859941773035420, 1.985868744837707145E-15 ) ) ;
#57875 = CARTESIAN_POINT ( 'NONE',  ( -3.458734125000016313, 197.8750000013656063, 140.5673454167823593 ) ) ;
#57876 = CIRCLE ( 'NONE', #67490, 14.00000000000000000 ) ;
#57877 = CARTESIAN_POINT ( 'NONE',  ( -5.000000000000005329, 65.20833332650536818, 8.660254037844387298 ) ) ;
#57878 = CARTESIAN_POINT ( 'NONE',  ( -5.082755093536325930, 98.46875000204838102, -5.082755093536325930 ) ) ;
#57879 = CARTESIAN_POINT ( 'NONE',  ( -1.881053915767124440, 12.12499999863440969, 4.541265875000001451 ) ) ;
#57880 = CARTESIAN_POINT ( 'NONE',  ( 5.000000000000027534, 65.83333333333337123, -8.660254037844433483 ) ) ;
#57881 = CARTESIAN_POINT ( 'NONE',  ( 7.999999999999991118, 9.797174393178815797E-16, 6.080302779823364645 ) ) ;
#57882 = CARTESIAN_POINT ( 'NONE',  ( 2.449293598294707893E-16, 7.999999997268813168, -4.000000000000001776 ) ) ;
#57883 = ORIENTED_EDGE ( 'NONE', *, *, #73598, .T. ) ;
#57884 = ORIENTED_EDGE ( 'NONE', *, *, #41051, .F. ) ;
#57885 = CARTESIAN_POINT ( 'NONE',  ( -7.778174593052023411, 7.778174593052023411, 116.3125000000000000 ) ) ;
#57886 = CARTESIAN_POINT ( 'NONE',  ( -6.676582343750003368, 297.5468750017069510, -2.765530957081996810 ) ) ;
#57887 = CARTESIAN_POINT ( 'NONE',  ( 9.797174393178825657E-16, 125.0000000000000000, -8.000000000000000000 ) ) ;
#57888 = CARTESIAN_POINT ( 'NONE',  ( -7.320508075688771932, 86.87500000000001421, -7.320508075688773708 ) ) ;
#57889 = CARTESIAN_POINT ( 'NONE',  ( 5.676582343749993598, 159.9479166632526983, 9.832129032723422313 ) ) ;
#57890 = CARTESIAN_POINT ( 'NONE',  ( -3.313708498984775375, 6.843749995903221084, 7.999999999999988454 ) ) ;
#57891 = CARTESIAN_POINT ( 'NONE',  ( -4.220049686691935698, 10.18810118749999916, 85.37500000204839523 ) ) ;
#57892 = CARTESIAN_POINT ( 'NONE',  ( 105.0000000000000000, 205.0000000000000284, 20.00000000000000000 ) ) ;
#57893 = CARTESIAN_POINT ( 'NONE',  ( 1.656854249492405451, 205.3125000000000568, 202.0000000000000284 ) ) ;
#57894 = CYLINDRICAL_SURFACE ( 'NONE', #31373, 8.000000000000000000 ) ;
#57895 = CARTESIAN_POINT ( 'NONE',  ( 4.220049686691934809, 10.18810118749999916, 117.0625000020483668 ) ) ;
#57896 = ORIENTED_EDGE ( 'NONE', *, *, #4830, .F. ) ;
#57897 =( BOUNDED_CURVE ( )  B_SPLINE_CURVE ( 2, ( #4996, #27995, #51004, #40060, #34423, #69102, #5732, #35160, #13220 ),
 .UNSPECIFIED., .F., .F. ) 
 B_SPLINE_CURVE_WITH_KNOTS ( ( 3, 2, 2, 2, 3 ),
 ( 0.4687499999999998890, 0.4739583333333332593, 0.4791666666666666297, 0.4843750000000000000, 0.4895833333333333148 ),
 .UNSPECIFIED. ) 
 CURVE ( )  GEOMETRIC_REPRESENTATION_ITEM ( )  RATIONAL_B_SPLINE_CURVE ( ( 1.000000000000001554, 0.9238795325112850731, 1.000000000000000000, 0.9238795325112867385, 1.000000000000000000, 0.9238795325112867385, 1.000000000000000000, 0.9238795325112867385, 1.000000000000000000 ) ) 
 REPRESENTATION_ITEM ( '' )  );
#57898 = EDGE_CURVE ( 'NONE', #52559, #8159, #46763, .T. ) ;
#57899 = CARTESIAN_POINT ( 'NONE',  ( 36.32979099710041737, -5.792970758617062899, 137.5524717672482780 ) ) ;
#57900 = CARTESIAN_POINT ( 'NONE',  ( 30.39335777030632002, 174.8762529804578207, 163.4693516532806541 ) ) ;
#57901 = CARTESIAN_POINT ( 'NONE',  ( 3.042071309553159519, 135.0520833299193555, 11.35316468750000141 ) ) ;
#57902 = CARTESIAN_POINT ( 'NONE',  ( 2.754378923186476579E-14, 197.1875000013655779, 194.5412658750000219 ) ) ;
#57903 = CARTESIAN_POINT ( 'NONE',  ( -2.977408999572650039, 25.31249999795161543, -7.188101187500000933 ) ) ;
#57904 = CARTESIAN_POINT ( 'NONE',  ( 4.220049686691934809, 10.18810118749999916, 76.56250000204836681 ) ) ;
#57905 = CARTESIAN_POINT ( 'NONE',  ( -11.35316468750000141, 48.80208332991934128, 3.042071309553159963 ) ) ;
#57906 = ORIENTED_EDGE ( 'NONE', *, *, #63812, .F. ) ;
#57907 = CARTESIAN_POINT ( 'NONE',  ( 4.556349186104052151, -10.99999999999999822, 94.65625000409680467 ) ) ;
#57908 = CARTESIAN_POINT ( 'NONE',  ( -4.541265875000003227, 1.999999998634407028, 1.881053915767121110 ) ) ;
#57909 = CARTESIAN_POINT ( 'NONE',  ( -3.317071493978880348, -8.008118988124989457, 11.79436528394062833 ) ) ;
#57910 = CARTESIAN_POINT ( 'NONE',  ( -3.458734125000015425, 206.2500000013656063, 143.4326545832176976 ) ) ;
#57911 = VECTOR ( 'NONE', #61921, 1000.000000000000000 ) ;
#57912 = AXIS2_PLACEMENT_3D ( 'NONE', #70670, #18987, #17881 ) ;
#57913 = CARTESIAN_POINT ( 'NONE',  ( -7.188101187500002709, 7.312499997951610986, 2.977408999572649151 ) ) ;
#57914 = CARTESIAN_POINT ( 'NONE',  ( -4.242640687119285658, 297.1875000034139589, 4.242640687119287435 ) ) ;
#57915 = CARTESIAN_POINT ( 'NONE',  ( -15.10145118338216719, -19.83835122548060426, 137.7459079296164077 ) ) ;
#57916 = CARTESIAN_POINT ( 'NONE',  ( 4.401442555609581635E-16, 8.718749997951611874, -7.188101187500000044 ) ) ;
#57917 = CARTESIAN_POINT ( 'NONE',  ( -2.977408999572647819, -7.188101187499990274, 10.76780278187175632 ) ) ;
#57918 =( BOUNDED_CURVE ( )  B_SPLINE_CURVE ( 2, ( #42946, #15395, #25960, #48979, #38807, #14647, #55789, #37307, #60304, #71993, #65966, #38432, #50113, #44087, #14271, #26338, #33163, #3724, #8633, #31646, #60687, #9382, #72760, #25595, #4105, #48610, #71616, #37687, #61435, #32400, #20687, #44458, #67098, #54666, #2975, #61808, #43324, #20305, #26723, #72376, #73129, #66339, #21435, #67472, #9762, #15769, #32021, #32782, #43706, #27098, #9007, #55041, #3347, #49359, #66720, #15024, #38059, #11615, #5219, #16131, #10498, #4474, #56160, #34277, #28220, #57657, #39914, #51230, #62921, #33532, #56907, #45945, #50855, #40660, #63664, #45200, #74241, #5963, #11247, #22547, #57280, #27464, #50478, #33908, #73493, #21800, #28966, #44831, #68958, #4850, #67840, #16891, #39170, #73870, #45569, #16507, #10872, #68583, #63288, #5595, #56532, #28592, #51603, #62173, #11988, #74618, #27847, #22934, #17268, #22176, #40287, #68211, #34652, #51986, #62543, #39548, #324, #23302, #46316, #69330, #17641, #6345, #48154, #24040, #6706, #7074, #42498, #1432, #52727, #47784, #71163, #59136, #58764, #23678, #1061, #69707, #53836, #29714, #47050, #30080, #7444, #70085, #13446, #18020, #41038, #58401, #52356, #70804, #7810, #1786, #694, #53098, #65513, #36114, #46683, #64045, #18392, #35023, #19483, #41404, #2145, #58036, #29349, #64418, #19118, #41768, #24415, #25138, #30452, #12355, #35389, #12715, #35747, #47420, #53468, #70445, #30812, #18761, #24771, #64776, #13079, #42123, #65135, #36483, #59497, #60972, #9292, #20598, #50023, #66254, #2887, #3634, #65879, #43997, #37596, #48523, #42860, #26252, #36853, #13808, #66626, #8920, #31932, #14932, #25510, #31184, #61349, #59860, #73039, #32315, #55329, #71529, #15305, #37973, #19856, #9675, #32696 ),
 .UNSPECIFIED., .F., .F. ) 
 B_SPLINE_CURVE_WITH_KNOTS ( ( 3, 2, 2, 2, 2, 2, 2, 2, 2, 2, 2, 2, 2, 2, 2, 2, 2, 2, 2, 2, 2, 2, 2, 2, 2, 2, 2, 2, 2, 2, 2, 2, 2, 2, 2, 2, 2, 2, 2, 2, 2, 2, 2, 2, 2, 2, 2, 2, 2, 2, 2, 2, 2, 2, 2, 2, 2, 2, 2, 2, 2, 2, 2, 2, 2, 2, 2, 2, 2, 2, 2, 2, 2, 2, 2, 2, 2, 2, 2, 2, 2, 2, 2, 2, 2, 2, 2, 2, 2, 2, 2, 2, 2, 2, 2, 2, 2, 2, 2, 2, 2, 2, 2, 2, 2, 2, 2, 2, 3 ),
 ( 0.000000000000000000, 0.009259259259259258745, 0.01851851851851851749, 0.02777777777777777624, 0.03703703703703703498, 0.04629629629629629373, 0.05555555555555555247, 0.06481481481481481122, 0.07407407407407406996, 0.08333333333333332871, 0.09259259259259258745, 0.1018518518518518462, 0.1111111111111111049, 0.1203703703703703637, 0.1296296296296296224, 0.1388888888888888951, 0.1481481481481481399, 0.1574074074074074125, 0.1666666666666666574, 0.1759259259259259300, 0.1851851851851851749, 0.1944444444444444475, 0.2037037037037036924, 0.2129629629629629650, 0.2222222222222222099, 0.2314814814814814825, 0.2407407407407407274, 0.2500000000000000000, 0.2592592592592592449, 0.2685185185185185452, 0.2777777777777777901, 0.2870370370370370350, 0.2962962962962962798, 0.3055555555555555802, 0.3148148148148148251, 0.3240740740740740700, 0.3333333333333333148, 0.3425925925925926152, 0.3518518518518518601, 0.3611111111111111049, 0.3703703703703703498, 0.3796296296296296502, 0.3888888888888888951, 0.3981481481481481399, 0.4074074074074073848, 0.4166666666666666852, 0.4259259259259259300, 0.4351851851851851749, 0.4444444444444444198, 0.4537037037037037202, 0.4629629629629629650, 0.4722222222222222099, 0.4814814814814814548, 0.4907407407407407551, 0.5000000000000000000, 0.5092592592592593004, 0.5185185185185184897, 0.5277777777777777901, 0.5370370370370370905, 0.5462962962962962798, 0.5555555555555555802, 0.5648148148148147696, 0.5740740740740740700, 0.5833333333333333703, 0.5925925925925925597, 0.6018518518518518601, 0.6111111111111111605, 0.6203703703703703498, 0.6296296296296296502, 0.6388888888888888395, 0.6481481481481481399, 0.6574074074074074403, 0.6666666666666666297, 0.6759259259259259300, 0.6851851851851852304, 0.6944444444444444198, 0.7037037037037037202, 0.7129629629629629095, 0.7222222222222222099, 0.7314814814814815103, 0.7407407407407406996, 0.7500000000000000000, 0.7592592592592593004, 0.7685185185185184897, 0.7777777777777777901, 0.7870370370370370905, 0.7962962962962962798, 0.8055555555555555802, 0.8148148148148147696, 0.8240740740740740700, 0.8333333333333333703, 0.8425925925925925597, 0.8518518518518518601, 0.8611111111111111605, 0.8703703703703703498, 0.8796296296296296502, 0.8888888888888888395, 0.8981481481481481399, 0.9074074074074074403, 0.9166666666666666297, 0.9259259259259259300, 0.9351851851851852304, 0.9444444444444444198, 0.9537037037037037202, 0.9629629629629629095, 0.9722222222222222099, 0.9814814814814815103, 0.9907407407407406996, 1.000000000000000000 ),
 .UNSPECIFIED. ) 
 CURVE ( )  GEOMETRIC_REPRESENTATION_ITEM ( )  RATIONAL_B_SPLINE_CURVE ( ( 1.000000000000000000, 0.9659258262890683122, 1.000000000000000000, 0.9659258262890683122, 1.000000000000000000, 0.9659258262890683122, 1.000000000000000000, 0.9659258262890683122, 1.000000000000000000, 0.9659258262890683122, 1.000000000000000000, 0.9659258262890683122, 1.000000000000000000, 0.9659258262890683122, 1.000000000000000000, 0.9659258262890683122, 1.000000000000000000, 0.9659258262890683122, 1.000000000000000000, 0.9659258262890683122, 1.000000000000000000, 0.9659258262890683122, 1.000000000000000000, 0.9659258262890683122, 1.000000000000000000, 0.9659258262890683122, 1.000000000000000000, 0.9659258262890683122, 1.000000000000000000, 0.9659258262890683122, 1.000000000000000000, 0.9659258262890683122, 1.000000000000000000, 0.9659258262890683122, 1.000000000000000000, 0.9659258262890683122, 1.000000000000000000, 0.9659258262890683122, 1.000000000000000000, 0.9659258262890683122, 1.000000000000000000, 0.9659258262890683122, 1.000000000000000000, 0.9659258262890683122, 1.000000000000000000, 0.9659258262890683122, 1.000000000000000000, 0.9659258262890683122, 1.000000000000000000, 0.9659258262890683122, 1.000000000000000000, 0.9659258262890683122, 1.000000000000000000, 0.9659258262890683122, 1.000000000000000000, 0.9659258262890683122, 1.000000000000000000, 0.9659258262890683122, 1.000000000000000000, 0.9659258262890683122, 1.000000000000000000, 0.9659258262890683122, 1.000000000000000000, 0.9659258262890683122, 1.000000000000000000, 0.9659258262890683122, 1.000000000000000000, 0.9659258262890683122, 1.000000000000000000, 0.9659258262890683122, 1.000000000000000000, 0.9659258262890683122, 1.000000000000000000, 0.9659258262890683122, 1.000000000000000000, 0.9659258262890683122, 1.000000000000000000, 0.9659258262890683122, 1.000000000000000000, 0.9659258262890683122, 1.000000000000000000, 0.9659258262890683122, 1.000000000000000000, 0.9659258262890683122, 1.000000000000000000, 0.9659258262890683122, 1.000000000000000000, 0.9659258262890683122, 1.000000000000000000, 0.9659258262890683122, 1.000000000000000000, 0.9659258262890683122, 1.000000000000000000, 0.9659258262890683122, 1.000000000000000000, 0.9659258262890683122, 1.000000000000000000, 0.9659258262890683122, 1.000000000000000000, 0.9659258262890683122, 1.000000000000000000, 0.9659258262890683122, 1.000000000000000000, 0.9659258262890683122, 1.000000000000000000, 0.9659258262890683122, 1.000000000000000000, 0.9659258262890683122, 1.000000000000000000, 0.9659258262890683122, 1.000000000000000000, 0.9659258262890683122, 1.000000000000000000, 0.9659258262890683122, 1.000000000000000000, 0.9659258262890683122, 1.000000000000000000, 0.9659258262890683122, 1.000000000000000000, 0.9659258262890683122, 1.000000000000000000, 0.9659258262890683122, 1.000000000000000000, 0.9659258262890683122, 1.000000000000000000, 0.9659258262890683122, 1.000000000000000000, 0.9659258262890683122, 1.000000000000000000, 0.9659258262890683122, 1.000000000000000000, 0.9659258262890683122, 1.000000000000000000, 0.9659258262890683122, 1.000000000000000000, 0.9659258262890683122, 1.000000000000000000, 0.9659258262890683122, 1.000000000000000000, 0.9659258262890683122, 1.000000000000000000, 0.9659258262890683122, 1.000000000000000000, 0.9659258262890683122, 1.000000000000000000, 0.9659258262890683122, 1.000000000000000000, 0.9659258262890683122, 1.000000000000000000, 0.9659258262890683122, 1.000000000000000000, 0.9659258262890683122, 1.000000000000000000, 0.9659258262890683122, 1.000000000000000000, 0.9659258262890683122, 1.000000000000000000, 0.9659258262890683122, 1.000000000000000000, 0.9659258262890683122, 1.000000000000000000, 0.9659258262890683122, 1.000000000000000000, 0.9659258262890683122, 1.000000000000000000, 0.9659258262890683122, 1.000000000000000000, 0.9659258262890683122, 1.000000000000000000, 0.9659258262890683122, 1.000000000000000000, 0.9659258262890683122, 1.000000000000000000, 0.9659258262890683122, 1.000000000000000000, 0.9659258262890683122, 1.000000000000000000, 0.9659258262890683122, 1.000000000000000000, 0.9659258262890683122, 1.000000000000000000, 0.9659258262890683122, 1.000000000000000000, 0.9659258262890683122, 1.000000000000000000, 0.9659258262890683122, 1.000000000000000000, 0.9659258262890683122, 1.000000000000000000, 0.9659258262890683122, 1.000000000000000000, 0.9659258262890683122, 1.000000000000000000, 0.9659258262890683122, 1.000000000000000000, 0.9659258262890683122, 1.000000000000000000, 0.9659258262890683122, 1.000000000000000000, 0.9659258262890683122, 1.000000000000000000, 0.9659258262890683122, 1.000000000000000000, 0.9659258262890683122, 1.000000000000000000, 0.9659258262890683122, 1.000000000000000000, 0.9659258262890683122, 1.000000000000000000, 0.9659258262890683122, 1.000000000000000000, 0.9659258262890683122, 1.000000000000000000, 0.9659258262890683122, 1.000000000000000000, 0.9659258262890683122, 1.000000000000000000 ) ) 
 REPRESENTATION_ITEM ( '' )  );
#57919 = CARTESIAN_POINT ( 'NONE',  ( 7.204075437095966983, 7.204075437095967871, 73.09375000204838102 ) ) ;
#57920 = ADVANCED_FACE ( 'NONE', ( #28675 ), #35102, .F. ) ;
#57921 = CARTESIAN_POINT ( 'NONE',  ( -27.99999999999996803, 206.1875000013656063, 173.4587341250003760 ) ) ;
#57922 = EDGE_CURVE ( 'NONE', #47939, #63554, #60287, .T. ) ;
#57923 = CARTESIAN_POINT ( 'NONE',  ( 2.775557561562891351E-14, 210.0000000000000284, 170.0000000000000284 ) ) ;
#57924 = CARTESIAN_POINT ( 'NONE',  ( 1.881053915767121776, 19.62499999863441147, -4.541265875000002339 ) ) ;
#57925 = UNCERTAINTY_MEASURE_WITH_UNIT (LENGTH_MEASURE( 1.000000000000000082E-05 ), #46118, 'distance_accuracy_value', 'NONE');
#57926 = ORIENTED_EDGE ( 'NONE', *, *, #7880, .T. ) ;
#57927 = CARTESIAN_POINT ( 'NONE',  ( -1.656854249492348607, 201.3125000027312126, 202.0000000000000284 ) ) ;
#57928 = VECTOR ( 'NONE', #13094, 1000.000000000000000 ) ;
#57929 = CARTESIAN_POINT ( 'NONE',  ( -4.000000000000015099, 204.5625000000000000, 143.6568542494924543 ) ) ;
#57930 = CARTESIAN_POINT ( 'NONE',  ( -28.00000000000007816, 202.1250000027312126, 166.0000000000003695 ) ) ;
#57931 = CARTESIAN_POINT ( 'NONE',  ( -7.188101187500000044, 115.1562500020483810, 0.000000000000000000 ) ) ;
#57932 = CARTESIAN_POINT ( 'NONE',  ( -4.556349186104048599, -10.99999999999999822, 74.96875000409677625 ) ) ;
#57933 = CARTESIAN_POINT ( 'NONE',  ( 5.656854249492376141, -5.656854249492374365, 10.58030278392014800 ) ) ;
#57934 = VERTEX_POINT ( 'NONE', #51689 ) ;
#57935 = ADVANCED_FACE ( 'NONE', ( #33998 ), #57367, .T. ) ;
#57936 = CARTESIAN_POINT ( 'NONE',  ( 2.977408999572650927, 18.74999999795161543, -7.188101187500000933 ) ) ;
#57937 = VERTEX_POINT ( 'NONE', #40375 ) ;
#57938 = CARTESIAN_POINT ( 'NONE',  ( 32.00000000000000000, 198.3125000000000284, 168.3431457505075457 ) ) ;
#57939 = CARTESIAN_POINT ( 'NONE',  ( 2.775557561562891351E-14, 271.9999999999999432, 151.0000000000000568 ) ) ;
#57940 = CARTESIAN_POINT ( 'NONE',  ( -8.660254037844387298, 47.08333333333333570, -5.000000000000004441 ) ) ;
#57941 = CARTESIAN_POINT ( 'NONE',  ( 2.977408999572654480, 104.0000000020483810, 7.188101187499999156 ) ) ;
#57942 = CARTESIAN_POINT ( 'NONE',  ( -24.54126587499998635, 206.3750000013656063, 171.4326545832179818 ) ) ;
#57943 = CARTESIAN_POINT ( 'NONE',  ( -3.373128826976394379, -10.27267468567300135, 63.92035228378879452 ) ) ;
#57945 = CARTESIAN_POINT ( 'NONE',  ( 10.00000000000000178, 196.8749999931720254, 0.000000000000000000 ) ) ;
#57944 = CARTESIAN_POINT ( 'NONE',  ( -6.000000000000003553, 288.0000000034140157, -2.485281374238571317 ) ) ;
#57946 = ORIENTED_EDGE ( 'NONE', *, *, #22259, .F. ) ;
#57948 = CARTESIAN_POINT ( 'NONE',  ( 11.35316468749999963, 246.1979166700806445, 3.042071309553159519 ) ) ;
#57947 = AXIS2_PLACEMENT_3D ( 'NONE', #29065, #39645, #45297 ) ;
#57949 = CARTESIAN_POINT ( 'NONE',  ( -7.188101187499992051, 0.000000000000000000, 16.86155278187175810 ) ) ;
#57950 = CARTESIAN_POINT ( 'NONE',  ( 2.679491924310923867, 88.95833333333327175, 10.00000000000015454 ) ) ;
#57951 = CARTESIAN_POINT ( 'NONE',  ( 1.656854249492504705, 198.8125000027312126, 194.0000000000001990 ) ) ;
#57952 = CARTESIAN_POINT ( 'NONE',  ( 5.656854249492376141, -5.656854249492374365, 19.58030278392014978 ) ) ;
#57953 = CARTESIAN_POINT ( 'NONE',  ( 10.00000000000000178, 160.0000000000000000, 0.000000000000000000 ) ) ;
#57954 = DIRECTION ( 'NONE',  ( -0.000000000000000000, -1.000000000000000000, -0.000000000000000000 ) ) ;
#57955 = DIRECTION ( 'NONE',  ( -0.000000000000000000, 1.000000000000000000, -0.000000000000000000 ) ) ;
#57956 = CARTESIAN_POINT ( 'NONE',  ( 5.000000000000000888, -53.20585484986793290, -47.69738026034749367 ) ) ;
#57957 = CARTESIAN_POINT ( 'NONE',  ( -11.35316468750000141, 133.5937499965860127, -1.390361679473963753E-15 ) ) ;
#57958 = DIRECTION ( 'NONE',  ( 0.5000000000000014433, 0.8660254037844379305, -0.000000000000000000 ) ) ;
#57961 = CARTESIAN_POINT ( 'NONE',  ( 4.556349186104045934, 11.00000000000000000, 84.71875000409677625 ) ) ;
#57960 = CARTESIAN_POINT ( 'NONE',  ( 30.44569435410882718, 196.5625000013656063, 172.4456943541086957 ) ) ;
#57959 = CARTESIAN_POINT ( 'NONE',  ( 26.56734541678232375, 195.6250000013656063, 173.4587341249998929 ) ) ;
#57962 = EDGE_CURVE ( 'NONE', #24773, #68143, #20622, .T. ) ;
#57963 = EDGE_LOOP ( 'NONE', ( #20964, #18425, #29384, #13158 ) ) ;
#57964 = CARTESIAN_POINT ( 'NONE',  ( -1.656854249492365705, 206.1875000000000853, 202.0000000000000000 ) ) ;
#57965 = VECTOR ( 'NONE', #18426, 1000.000000000000000 ) ;
#57966 = ADVANCED_FACE ( 'NONE', ( #39634 ), #56992, .T. ) ;
#57967 = CARTESIAN_POINT ( 'NONE',  ( 7.999999999999991118, 9.797174393178815797E-16, 25.58030277982336997 ) ) ;
#57968 = CARTESIAN_POINT ( 'NONE',  ( 10.00000000000010658, 194.7916666666667425, 2.679491924311264039 ) ) ;
#57969 = CARTESIAN_POINT ( 'NONE',  ( 5.000000000000000000, -68.48952624890522145, -21.22548696402925117 ) ) ;
#57970 = CARTESIAN_POINT ( 'NONE',  ( -7.320508075688778149, 24.99999999317203603, 7.320508075688769267 ) ) ;
#57971 = CARTESIAN_POINT ( 'NONE',  ( 2.977408999572654480, 117.1250000020483952, 7.188101187499999156 ) ) ;
#57972 = CARTESIAN_POINT ( 'NONE',  ( -1.881053915767121554, 0.7499999986344069169, -4.541265875000002339 ) ) ;
#57973 = CARTESIAN_POINT ( 'NONE',  ( -1.780377099653247974, -51.29164421682995822, 48.57534666485132391 ) ) ;
#57974 = CARTESIAN_POINT ( 'NONE',  ( 5.656854249492374365, 5.656854249492375253, 19.76780277982336642 ) ) ;
#57976 = DIRECTION ( 'NONE',  ( -0.000000000000000000, 1.000000000000000000, -0.000000000000000000 ) ) ;
#57975 = CARTESIAN_POINT ( 'NONE',  ( -49.67894393727055302, 48.76488615825680739, 58.04780024834198571 ) ) ;
#57977 = CARTESIAN_POINT ( 'NONE',  ( -8.311093377946841443, 103.9062499965860269, 8.311093377946830785 ) ) ;
#57978 = EDGE_LOOP ( 'NONE', ( #41627, #66716, #27737, #20151 ) ) ;
#57979 = ADVANCED_FACE ( 'NONE', ( #12066 ), #5306, .T. ) ;
#57980 = DIRECTION ( 'NONE',  ( -0.000000000000000000, -1.000000000000000000, -0.000000000000000000 ) ) ;
#57981 = DIRECTION ( 'NONE',  ( -0.000000000000000000, 1.000000000000000000, -0.000000000000000000 ) ) ;
#57982 = VECTOR ( 'NONE', #20816, 1000.000000000000000 ) ;
#57983 = CARTESIAN_POINT ( 'NONE',  ( 3.155198069298572835E-14, 192.0000000000000284, 201.0000000000000000 ) ) ;
#57984 = CARTESIAN_POINT ( 'NONE',  ( 11.35316468749999963, 246.5104166700806445, 3.042071309553159519 ) ) ;
#57985 = CARTESIAN_POINT ( 'NONE',  ( -11.35316468749999785, 113.0729166632526841, -3.042071309553167513 ) ) ;
#57986 = ORIENTED_EDGE ( 'NONE', *, *, #66956, .F. ) ;
#57987 = CARTESIAN_POINT ( 'NONE',  ( 5.000000000000000000, -11.00774715070946108, 67.37702390743022818 ) ) ;
#57988 = CARTESIAN_POINT ( 'NONE',  ( 4.220049686691941027, -10.18810118749999738, 102.6250000020483810 ) ) ;
#57989 = CARTESIAN_POINT ( 'NONE',  ( -8.660254037844387298, 213.9583333265053682, -5.000000000000004441 ) ) ;
#57990 = CARTESIAN_POINT ( 'NONE',  ( -3.458734124999960358, 201.6875000013656063, 198.0000000000000284 ) ) ;
#57991 = DIRECTION ( 'NONE',  ( 0.000000000000000000, 0.000000000000000000, -1.000000000000000000 ) ) ;
#57993 = CARTESIAN_POINT ( 'NONE',  ( -9.832129032723420536, 103.6979166632526841, 5.676582343749997150 ) ) ;
#57992 = CARTESIAN_POINT ( 'NONE',  ( -8.660254037844385522, 182.0833333333333712, -5.000000000000003553 ) ) ;
#57994 = CARTESIAN_POINT ( 'NONE',  ( 7.999999999999991118, 3.313708498984757611, 6.361552783920146226 ) ) ;
#57995 = CARTESIAN_POINT ( 'NONE',  ( -29.43265458321760164, 197.1250000013656347, 173.4587341250003760 ) ) ;
#57996 = CARTESIAN_POINT ( 'NONE',  ( -7.188101187499992051, 0.000000000000000000, 28.48655278187175810 ) ) ;
#57997 = ORIENTED_EDGE ( 'NONE', *, *, #70464, .T. ) ;
#57998 = CARTESIAN_POINT ( 'NONE',  ( 2.679491924311222739, 195.8333333265053682, 10.00000000000000355 ) ) ;
#57999 = CARTESIAN_POINT ( 'NONE',  ( 3.999999999999960032, 207.9375000000000000, 143.6568542494924259 ) ) ;
#58000 = CARTESIAN_POINT ( 'NONE',  ( 4.556349186104045934, 11.00000000000000000, 99.71875000409677625 ) ) ;
#58001 = CARTESIAN_POINT ( 'NONE',  ( -8.311093377946841443, 94.21874999658601268, 8.311093377946834337 ) ) ;
#58002 = ADVANCED_BREP_SHAPE_REPRESENTATION ( '', ( #41383, #57354 ), #51304 ) ;
#58003 = LINE ( 'NONE', #47387, #36292 ) ;
#58004 = CARTESIAN_POINT ( 'NONE',  ( -2.977408999572654480, 3.374999997951610986, 7.188101187499999156 ) ) ;
#58005 = CARTESIAN_POINT ( 'NONE',  ( 1.871523826299183495E-15, -10.18810118749999916, 93.90625000204836681 ) ) ;
#58006 = CARTESIAN_POINT ( 'NONE',  ( -5.676582343749998039, 217.4479166632526983, -9.832129032723420536 ) ) ;
#58007 = ORIENTED_EDGE ( 'NONE', *, *, #26545, .T. ) ;
#58008 = CARTESIAN_POINT ( 'NONE',  ( -7.320508075688786143, 138.1250000000000000, 7.320508075688777261 ) ) ;
#58009 = CARTESIAN_POINT ( 'NONE',  ( -39.97324732667617297, 0.000000000000000000, 113.7582050592233998 ) ) ;
#58010 = CARTESIAN_POINT ( 'NONE',  ( -11.35316468750000141, 218.2812499965860411, -1.390361679473963753E-15 ) ) ;
#58011 = CARTESIAN_POINT ( 'NONE',  ( 10.18810118749999916, 4.220049686691935698, 82.37500000204838102 ) ) ;
#58012 = VECTOR ( 'NONE', #49568, 1000.000000000000000 ) ;
#58013 = CARTESIAN_POINT ( 'NONE',  ( -46.46053351546693477, 188.1068786666309336, 71.39178048200130888 ) ) ;
#58014 = CARTESIAN_POINT ( 'NONE',  ( -5.000000000000000000, 0.000000000000000000, 0.000000000000000000 ) ) ;
#58015 = CARTESIAN_POINT ( 'NONE',  ( 2.765530957082001251, 298.7656250017069510, 6.676582343750000703 ) ) ;
#58016 = ORIENTED_EDGE ( 'NONE', *, *, #66554, .T. ) ;
#58017 = DIRECTION ( 'NONE',  ( -1.000000000000000000, 0.000000000000000000, 0.000000000000000000 ) ) ;
#58018 = CARTESIAN_POINT ( 'NONE',  ( -11.35316468750000141, 208.5937499965860411, -1.390361679473963753E-15 ) ) ;
#58019 = CARTESIAN_POINT ( 'NONE',  ( 7.204075437095968759, -7.204075437095966983, 92.21875000204838102 ) ) ;
#58020 =( BOUNDED_CURVE ( )  B_SPLINE_CURVE ( 2, ( #28254, #44491, #51262, #16540, #56568, #4882, #67504, #45602, #57314 ),
 .UNSPECIFIED., .F., .F. ) 
 B_SPLINE_CURVE_WITH_KNOTS ( ( 3, 2, 2, 2, 3 ),
 ( 0.9265586498208127075, 0.9331768574084092771, 0.9397951329928664332, 0.9464134085773237004, 0.9530316461170064146 ),
 .UNSPECIFIED. ) 
 CURVE ( )  GEOMETRIC_REPRESENTATION_ITEM ( )  RATIONAL_B_SPLINE_CURVE ( ( 0.9999984358766603743, 0.9238803145809916240, 1.000000000000000000, 0.9238795325112867385, 1.000000000000000000, 0.9238795325112867385, 1.000000000000000000, 0.9238799700853922436, 0.9999991248568196323 ) ) 
 REPRESENTATION_ITEM ( '' )  );
#58021 = CARTESIAN_POINT ( 'NONE',  ( -31.45873412499999944, 204.6875000013656063, 170.0000000000003979 ) ) ;
#58022 = CARTESIAN_POINT ( 'NONE',  ( -3.313708498984765161, 17.53125000000000711, 7.999999999999998224 ) ) ;
#58023 = VERTEX_POINT ( 'NONE', #6046 ) ;
#58024 = CARTESIAN_POINT ( 'NONE',  ( 7.188101187500002709, 120.3125000020483668, 2.977408999572649151 ) ) ;
#58025 = CARTESIAN_POINT ( 'NONE',  ( -4.999999999999998224, 26.66666666666666785, -8.660254037844389075 ) ) ;
#58026 = CARTESIAN_POINT ( 'NONE',  ( -8.000000000000001776, 8.343750000000001776, 3.313708498984759387 ) ) ;
#58027 = CARTESIAN_POINT ( 'NONE',  ( 10.18810118749999916, 4.220049686691935698, 74.87500000204836681 ) ) ;
#58028 = ORIENTED_EDGE ( 'NONE', *, *, #70566, .T. ) ;
#58029 = CARTESIAN_POINT ( 'NONE',  ( 8.999999999999998224, 0.000000000000000000, 0.000000000000000000 ) ) ;
#58030 = AXIS2_PLACEMENT_3D ( 'NONE', #18140, #52845, #25908 ) ;
#58031 = FACE_OUTER_BOUND ( 'NONE', #42532, .T. ) ;
#58032 = DIRECTION ( 'NONE',  ( -0.000000000000000000, -0.000000000000000000, 1.000000000000000000 ) ) ;
#58033 = CARTESIAN_POINT ( 'NONE',  ( 5.082755093536325042, 123.9687500020483952, -5.082755093536325930 ) ) ;
#58034 = CARTESIAN_POINT ( 'NONE',  ( 2.679491924311228956, 152.9166666598387394, -10.00000000000000000 ) ) ;
#58035 = CARTESIAN_POINT ( 'NONE',  ( 4.721056650416000089, 297.8281250017069510, 4.721056650415999201 ) ) ;
#58036 = CARTESIAN_POINT ( 'NONE',  ( 3.042071309553173286, 230.3645833367473017, 11.35316468749999608 ) ) ;
#58037 = ORIENTED_EDGE ( 'NONE', *, *, #61369, .T. ) ;
#58038 = CARTESIAN_POINT ( 'NONE',  ( -5.676582343749992710, 240.0520833367473301, 9.832129032723422313 ) ) ;
#58039 = CARTESIAN_POINT ( 'NONE',  ( -7.188101187499991163, 2.977408999572646930, 5.892802781871754547 ) ) ;
#58040 = VERTEX_POINT ( 'NONE', #34366 ) ;
#58041 = CARTESIAN_POINT ( 'NONE',  ( 7.204075437095968759, -7.204075437095966983, 71.21875000204836681 ) ) ;
#58042 = CARTESIAN_POINT ( 'NONE',  ( 5.676582343750001591, 81.92708332991935549, -9.832129032723420536 ) ) ;
#58043 = CARTESIAN_POINT ( 'NONE',  ( 4.193070328474943764, 60.66867996115621509, 23.17096354272623415 ) ) ;
#58044 = CARTESIAN_POINT ( 'NONE',  ( 4.556349186104045934, 11.00000000000000000, 81.53125000000000000 ) ) ;
#58047 = FACE_OUTER_BOUND ( 'NONE', #34465, .T. ) ;
#58046 = CARTESIAN_POINT ( 'NONE',  ( 28.00000000000001776, 194.1250000027311842, 173.9999999999999147 ) ) ;
#58045 = CARTESIAN_POINT ( 'NONE',  ( 27.99999999999996447, 205.6875000013656063, 173.4587341249998929 ) ) ;
#58048 = ORIENTED_EDGE ( 'NONE', *, *, #45031, .T. ) ;
#58049 = AXIS2_PLACEMENT_3D ( 'NONE', #19040, #2807, #59413 ) ;
#58050 = DIRECTION ( 'NONE',  ( 0.000000000000000000, 0.000000000000000000, 1.000000000000000000 ) ) ;
#58051 = CYLINDRICAL_SURFACE ( 'NONE', #61277, 11.00000000000000000 ) ;
#58052 = EDGE_CURVE ( 'NONE', #38816, #64638, #29051, .T. ) ;
#58053 = CARTESIAN_POINT ( 'NONE',  ( 8.311093377946834337, 205.1562499965859843, 8.311093377946839666 ) ) ;
#58054 = CARTESIAN_POINT ( 'NONE',  ( -1.432654583217662481, 206.1250000013655779, 145.4587341250000634 ) ) ;
#58055 = CARTESIAN_POINT ( 'NONE',  ( 31.45873412500001010, 205.0000000013655779, 168.5673454167822740 ) ) ;
#58056 = CARTESIAN_POINT ( 'NONE',  ( -5.082755093536325042, 25.40624999795161543, -5.082755093536325930 ) ) ;
#58057 = CARTESIAN_POINT ( 'NONE',  ( 3.042071309553159519, 175.0520833299193839, 11.35316468750000141 ) ) ;
#58058 = CARTESIAN_POINT ( 'NONE',  ( 7.188101187500000044, 96.78125000204838102, -8.802885111219163269E-16 ) ) ;
#58060 = CARTESIAN_POINT ( 'NONE',  ( -7.320508075688769267, 106.8750000000000284, -7.320508075688770155 ) ) ;
#58059 = CARTESIAN_POINT ( 'NONE',  ( -5.000000000000000888, 65.00653492603765926, -24.02639942437745191 ) ) ;
#58061 = CARTESIAN_POINT ( 'NONE',  ( -4.541265875000003227, 9.874999998634404363, 1.881053915767121110 ) ) ;
#58062 = CARTESIAN_POINT ( 'NONE',  ( 24.54126587499999346, 204.4375000013656063, 169.9999999999998863 ) ) ;
#58063 = CARTESIAN_POINT ( 'NONE',  ( 5.082755093536318824, 5.082755093536319713, 7.299052781871751883 ) ) ;
#58064 = CARTESIAN_POINT ( 'NONE',  ( -3.042071309553164404, 62.23958332991934839, -11.35316468749999963 ) ) ;
#58065 = EDGE_CURVE ( 'NONE', #72690, #6581, #36218, .T. ) ;
#58066 = CARTESIAN_POINT ( 'NONE',  ( 24.00000000000000711, 205.9375000027312126, 171.6568542494923122 ) ) ;
#58067 = CARTESIAN_POINT ( 'NONE',  ( -8.000000000000000000, 119.0937500040967905, -3.313708498984761164 ) ) ;
#58068 = VERTEX_POINT ( 'NONE', #33619 ) ;
#58069 = CARTESIAN_POINT ( 'NONE',  ( 7.778174593052023411, -7.778174593052021635, 75.06249999999997158 ) ) ;
#58070 = CARTESIAN_POINT ( 'NONE',  ( -2.726571689596997292E-14, 210.0000000000000284, 138.0000000000000568 ) ) ;
#58071 = CARTESIAN_POINT ( 'NONE',  ( -5.676582343750006032, 64.11458332991935549, 9.832129032723418760 ) ) ;
#58072 = CARTESIAN_POINT ( 'NONE',  ( -4.556349186104045934, 11.00000000000000000, 68.40625000409677625 ) ) ;
#58073 = CARTESIAN_POINT ( 'NONE',  ( 1.432654583217608080, 195.8750000013655779, 138.5412658750000503 ) ) ;
#58074 = LINE ( 'NONE', #6385, #22702 ) ;
#58076 = CARTESIAN_POINT ( 'NONE',  ( 5.676582343749993598, 54.94791666325268409, 9.832129032723422313 ) ) ;
#58075 = CARTESIAN_POINT ( 'NONE',  ( 1.320432766682874540E-15, 96.03125000204838102, 7.188101187500000044 ) ) ;
#58077 = CARTESIAN_POINT ( 'NONE',  ( -7.999999999999991118, 3.313708498984756723, 24.92405278392015333 ) ) ;
#58078 = CARTESIAN_POINT ( 'NONE',  ( -10.00000000000000178, 14.37499999317203425, -1.224646799147353454E-15 ) ) ;
#58079 = CARTESIAN_POINT ( 'NONE',  ( -4.999999999999998224, 153.5416666598387110, -8.660254037844389075 ) ) ;
#58080 = CARTESIAN_POINT ( 'NONE',  ( 7.188101187500001821, 93.87500000204836681, -2.977408999572651371 ) ) ;
#58081 = LINE ( 'NONE', #29398, #47237 ) ;
#58082 = CARTESIAN_POINT ( 'NONE',  ( -9.832129032723420536, 54.01041666325268409, 5.676582343749997150 ) ) ;
#58083 = CARTESIAN_POINT ( 'NONE',  ( 7.204075437095968759, -7.204075437095966983, 113.5937500020483810 ) ) ;
#58084 = CARTESIAN_POINT ( 'NONE',  ( 11.35316468749999785, 185.5729166632526983, 3.042071309553174174 ) ) ;
#58085 = EDGE_LOOP ( 'NONE', ( #15897, #5004, #4128, #59720 ) ) ;
#58086 = CARTESIAN_POINT ( 'NONE',  ( -32.60989089554323783, -21.10814940924306526, 161.8459686935492812 ) ) ;
#58087 = CARTESIAN_POINT ( 'NONE',  ( 0.000000000000000000, 0.000000000000000000, 118.0000000000000000 ) ) ;
#58088 = CARTESIAN_POINT ( 'NONE',  ( 6.123233995736767268E-16, 63.12499999317203248, -10.00000000000000178 ) ) ;
#58090 = CARTESIAN_POINT ( 'NONE',  ( 5.676582343749993598, 174.9479166632526699, 9.832129032723422313 ) ) ;
#58089 = CARTESIAN_POINT ( 'NONE',  ( 2.170320029193293809, -67.76782500014387267, 20.17643218080241496 ) ) ;
#58091 = CARTESIAN_POINT ( 'NONE',  ( -3.313708498984765161, 11.34374999590322197, 7.999999999999998224 ) ) ;
#58092 = CARTESIAN_POINT ( 'NONE',  ( -8.660254037844387298, 247.7083333401613174, -4.999999999999999112 ) ) ;
#58093 = CARTESIAN_POINT ( 'NONE',  ( 7.999999999714877852, 6.754118554053788561E-05, 0.2678047518895779744 ) ) ;
#58094 = VERTEX_POINT ( 'NONE', #56625 ) ;
#58095 = CARTESIAN_POINT ( 'NONE',  ( 11.35316468749999963, 166.3020833299193271, -3.042071309553165293 ) ) ;
#58096 = CARTESIAN_POINT ( 'NONE',  ( -5.082755093536317936, -5.082755093536320601, 24.17405278187175455 ) ) ;
#58097 = CARTESIAN_POINT ( 'NONE',  ( 11.35316468750000141, 136.0937499965860127, 0.000000000000000000 ) ) ;
#58098 = CARTESIAN_POINT ( 'NONE',  ( 0.000000000000000000, 0.000000000000000000, 41.99999999999999289 ) ) ;
#58099 = EDGE_LOOP ( 'NONE', ( #34432, #30615, #67982, #44008 ) ) ;
#58100 = CIRCLE ( 'NONE', #8695, 5.000000000000000888 ) ;
#58101 = CARTESIAN_POINT ( 'NONE',  ( -8.000000000000000000, 101.1875000040967763, 0.000000000000000000 ) ) ;
#58102 = AXIS2_PLACEMENT_3D ( 'NONE', #58608, #22385, #12566 ) ;
#58103 = CARTESIAN_POINT ( 'NONE',  ( 2.449293598294707893E-16, 12.25000000000000000, -4.000000000000001776 ) ) ;
#58104 = CARTESIAN_POINT ( 'NONE',  ( -35.08316577992787444, -10.52114692595101353, 145.6937887528720807 ) ) ;
#58105 = CARTESIAN_POINT ( 'NONE',  ( 4.541265875000002339, 11.31249999863440614, 0.000000000000000000 ) ) ;
#58106 = CARTESIAN_POINT ( 'NONE',  ( 7.999999999999991118, 3.313708498984757611, 22.86155278392014623 ) ) ;
#58107 = CARTESIAN_POINT ( 'NONE',  ( 2.828427124746152987, 196.1250000000000284, 139.1715728752538723 ) ) ;
#58108 = ORIENTED_EDGE ( 'NONE', *, *, #68659, .T. ) ;
#58109 = CARTESIAN_POINT ( 'NONE',  ( -2.220555325575947149E-11, 176.2500000000017621, -10.00000000000000533 ) ) ;
#58110 = CARTESIAN_POINT ( 'NONE',  ( 5.082755093536325042, 105.5937500020483810, -5.082755093536325930 ) ) ;
#58112 = CARTESIAN_POINT ( 'NONE',  ( -2.828427124746209831, 209.3750000000000284, 139.1715728752538723 ) ) ;
#58111 = DIRECTION ( 'NONE',  ( -1.000000000000000000, 0.000000000000000000, 0.000000000000000000 ) ) ;
#58113 = CARTESIAN_POINT ( 'NONE',  ( 1424.688200795879766, 864.9677537767864806, 997.8421604560428477 ) ) ;
#58114 =( BOUNDED_CURVE ( )  B_SPLINE_CURVE ( 2, ( #17464, #68407, #40485, #63490, #57856, #40858, #17842, #45768, #63865 ),
 .UNSPECIFIED., .F., .F. ) 
 B_SPLINE_CURVE_WITH_KNOTS ( ( 3, 2, 2, 2, 3 ),
 ( 0.7604166666666667407, 0.7656250000000001110, 0.7708333333333334814, 0.7760416666666667407, 0.7812500000000001110 ),
 .UNSPECIFIED. ) 
 CURVE ( )  GEOMETRIC_REPRESENTATION_ITEM ( )  RATIONAL_B_SPLINE_CURVE ( ( 0.9999999999999983347, 0.9238795325112884038, 1.000000000000000000, 0.9238795325112867385, 1.000000000000000000, 0.9238795325112867385, 1.000000000000000000, 0.9238795325112850731, 1.000000000000001554 ) ) 
 REPRESENTATION_ITEM ( '' )  );
#58116 = EDGE_CURVE ( 'NONE', #34808, #29797, #4940, .T. ) ;
#58115 = ORIENTED_EDGE ( 'NONE', *, *, #38255, .F. ) ;
#58117 = EDGE_CURVE ( 'NONE', #21929, #38634, #48156, .T. ) ;
#58118 = CARTESIAN_POINT ( 'NONE',  ( 2.997005883564160644, 10.11494357242049524, -70.43990496500994425 ) ) ;
#58119 = AXIS2_PLACEMENT_3D ( 'NONE', #15803, #9793, #33563 ) ;
#58120 = CARTESIAN_POINT ( 'NONE',  ( 2.977408999572646486, 7.188101187499991163, 26.51780278187175455 ) ) ;
#58121 = VERTEX_POINT ( 'NONE', #7891 ) ;
#58122 = B_SPLINE_CURVE_WITH_KNOTS ( 'NONE', 3,
 ( #62908, #12346, #6697, #18382, #35737, #7065, #30071, #16878, #39901, #53086, #42115, #65127, #24405, #13436, #14177, #13800, #36473, #20210, #19110, #59489 ),
 .UNSPECIFIED., .F., .F.,
 ( 4, 2, 2, 2, 2, 2, 2, 2, 2, 4 ),
 ( 0.000000000000000000, 0.001156441540183927559, 0.001734662310275893616, 0.002312883080367859456, 0.003469324620551791135, 0.004625766160735723248, 0.005782207700919654060, 0.006938649241103586607, 0.008095090781287518286, 0.009251532321471449966 ),
 .UNSPECIFIED. ) ;
#58123 = ORIENTED_EDGE ( 'NONE', *, *, #64067, .F. ) ;
#58124 = CARTESIAN_POINT ( 'NONE',  ( 7.204075437095968759, -7.204075437095966983, 86.21875000204836681 ) ) ;
#58125 = CARTESIAN_POINT ( 'NONE',  ( -27.99999999999990763, 195.6250000027311842, 174.0000000000003695 ) ) ;
#58126 = CARTESIAN_POINT ( 'NONE',  ( -24.54126587499997569, 196.3750000013656063, 171.4326545832179818 ) ) ;
#58127 = CARTESIAN_POINT ( 'NONE',  ( -7.778174593052023411, 7.778174593052023411, 98.31250000000000000 ) ) ;
#58130 = CARTESIAN_POINT ( 'NONE',  ( 1.226468279477575784E-15, 296.8593750017070079, 6.676582343750001591 ) ) ;
#58129 = CARTESIAN_POINT ( 'NONE',  ( 23.99999999999997868, 203.8125000027312410, 168.3431457505075741 ) ) ;
#58128 = CARTESIAN_POINT ( 'NONE',  ( 23.99999999999998934, 202.8750000027312126, 169.9999999999999432 ) ) ;
#58131 = CARTESIAN_POINT ( 'NONE',  ( 7.320508075688774596, 130.6250000000000284, -7.320508075688774596 ) ) ;
#58132 = EDGE_CURVE ( 'NONE', #3567, #31249, #55898, .T. ) ;
#58134 = EDGE_CURVE ( 'NONE', #61189, #4164, #28353, .T. ) ;
#58133 = CARTESIAN_POINT ( 'NONE',  ( 3.313708498984765161, 101.4687499999999858, 7.999999999999998224 ) ) ;
#58135 = CARTESIAN_POINT ( 'NONE',  ( -4.721056650415998313, 288.7343750017069510, 4.721056650416000089 ) ) ;
#58136 = CARTESIAN_POINT ( 'NONE',  ( -7.188101187499991163, 2.977408999572646930, 1.767802781871753881 ) ) ;
#58137 = CARTESIAN_POINT ( 'NONE',  ( -25.17157287525377996, 208.6250000000000284, 172.8284271247465256 ) ) ;
#58139 = CARTESIAN_POINT ( 'NONE',  ( 31.45873412499998523, 202.6250000013656063, 171.4326545832175839 ) ) ;
#58138 = VECTOR ( 'NONE', #3698, 1000.000000000000000 ) ;
#58140 = CARTESIAN_POINT ( 'NONE',  ( -2.977408999572650039, 4.312499997951610098, -7.188101187500001821 ) ) ;
#58141 = CARTESIAN_POINT ( 'NONE',  ( -8.008118988124991233, 3.317071493978878127, 3.919365283940628775 ) ) ;
#58142 = DIRECTION ( 'NONE',  ( 0.000000000000000000, 0.000000000000000000, 1.000000000000000000 ) ) ;
#58143 = CARTESIAN_POINT ( 'NONE',  ( -5.082755093536325930, 116.8437500020483810, -5.082755093536325930 ) ) ;
#58145 = CARTESIAN_POINT ( 'NONE',  ( 3.391401283215903728, 194.7190068104547720, 199.5463616947160119 ) ) ;
#58144 = CARTESIAN_POINT ( 'NONE',  ( -7.320508075688770155, 250.6249999999999432, 7.320508075688774596 ) ) ;
#58146 = CARTESIAN_POINT ( 'NONE',  ( 5.676582343750005144, 225.8854166700806729, 9.832129032723416984 ) ) ;
#58147 = FACE_OUTER_BOUND ( 'NONE', #54652, .T. ) ;
#58148 = CARTESIAN_POINT ( 'NONE',  ( 7.320508075688774596, 52.49999999317203958, -7.320508075688774596 ) ) ;
#58149 = CARTESIAN_POINT ( 'NONE',  ( 31.99999999999999289, 199.2500000000000000, 169.9999999999999432 ) ) ;
#58150 = CARTESIAN_POINT ( 'NONE',  ( -11.35316468750000141, 23.48958332991934483, 3.042071309553159963 ) ) ;
#58151 = CARTESIAN_POINT ( 'NONE',  ( -11.35316468750000141, 223.5937499965860127, -1.390361679473963753E-15 ) ) ;
#58152 = CARTESIAN_POINT ( 'NONE',  ( -2.775557561562891351E-14, 210.0000000000000284, 142.0000000000000568 ) ) ;
#58154 = CARTESIAN_POINT ( 'NONE',  ( -3.313708498984816231, 96.78125000000002842, 7.999999999999943157 ) ) ;
#58153 = CARTESIAN_POINT ( 'NONE',  ( 2.170320029210516921, -16.41060967376241564, 68.77687409974784316 ) ) ;
#58155 = ORIENTED_EDGE ( 'NONE', *, *, #11877, .F. ) ;
#58156 = CIRCLE ( 'NONE', #17195, 18.00000000000000000 ) ;
#58157 = CARTESIAN_POINT ( 'NONE',  ( -2.754378923186476579E-14, 195.4375000013655779, 145.4587341250000350 ) ) ;
#58158 = CARTESIAN_POINT ( 'NONE',  ( -8.311093377946841443, 28.90624999658601979, 8.311093377946830785 ) ) ;
#58159 = CARTESIAN_POINT ( 'NONE',  ( -6.735557395310442023E-16, 11.00000000000000000, 89.31250000409676204 ) ) ;
#58160 = CARTESIAN_POINT ( 'NONE',  ( -2.828427073549516724, 195.0000000000000284, 195.1715728240572219 ) ) ;
#58161 = EDGE_CURVE ( 'NONE', #41296, #21159, #35465, .T. ) ;
#58162 = CARTESIAN_POINT ( 'NONE',  ( -5.000000000000001776, 151.6666666666666856, -8.660254037844394404 ) ) ;
#58163 = CARTESIAN_POINT ( 'NONE',  ( 0.000000000000000000, 300.0000000000000000, 10.00000000000000178 ) ) ;
#58165 = CARTESIAN_POINT ( 'NONE',  ( -8.311093377946841443, 18.90624999658601979, 8.311093377946834337 ) ) ;
#58164 = CARTESIAN_POINT ( 'NONE',  ( 2.977408999572654480, 111.1250000020483810, 7.188101187499999156 ) ) ;
#58166 = CARTESIAN_POINT ( 'NONE',  ( -5.656854249492373476, -5.656854249492376141, 19.01780277982336642 ) ) ;
#58167 = VECTOR ( 'NONE', #53155, 1000.000000000000000 ) ;
#58168 = CARTESIAN_POINT ( 'NONE',  ( -2.085542519210945728E-15, 154.5312499965860127, 11.35316468750000141 ) ) ;
#58169 = CARTESIAN_POINT ( 'NONE',  ( 7.320508075688771044, 121.2499999931720254, 7.320508075688775484 ) ) ;
#58170 = CARTESIAN_POINT ( 'NONE',  ( -5.082755093536325930, 113.8437500020483810, -5.082755093536325930 ) ) ;
#58171 = CARTESIAN_POINT ( 'NONE',  ( -5.656854249492381470, 14.24999999590322375, 5.656854249492379694 ) ) ;
#58172 = DIRECTION ( 'NONE',  ( -0.000000000000000000, -1.000000000000000000, -0.000000000000000000 ) ) ;
#58173 = EDGE_LOOP ( 'NONE', ( #12769, #22774 ) ) ;
#58174 = CARTESIAN_POINT ( 'NONE',  ( 3.042071309553167513, 2.135416663252682756, -11.35316468749999785 ) ) ;
#58175 = ORIENTED_EDGE ( 'NONE', *, *, #71726, .T. ) ;
#58176 = CYLINDRICAL_SURFACE ( 'NONE', #54656, 6.000000000000001776 ) ;
#58177 = CARTESIAN_POINT ( 'NONE',  ( 2.765530957081996366, 299.1406250017068942, -6.676582343750003368 ) ) ;
#58178 = CARTESIAN_POINT ( 'NONE',  ( -9.832129032723420536, 143.6979166632526699, 5.676582343749997150 ) ) ;
#58179 = PRESENTATION_STYLE_ASSIGNMENT (( #35163 ) ) ;
#58180 = CARTESIAN_POINT ( 'NONE',  ( 7.999999999999991118, 3.313708498984757611, 25.73030278432982598 ) ) ;
#58181 = CARTESIAN_POINT ( 'NONE',  ( -7.778174593052023411, 7.778174593052023411, 91.00000000409677625 ) ) ;
#58182 = CARTESIAN_POINT ( 'NONE',  ( -11.35316468749999785, 248.6979166700806445, -3.042071309553164848 ) ) ;
#58183 = CARTESIAN_POINT ( 'NONE',  ( 7.204075437095966983, 7.204075437095967871, 92.96875000204838102 ) ) ;
#58184 = ORIENTED_EDGE ( 'NONE', *, *, #42763, .T. ) ;
#58185 = CARTESIAN_POINT ( 'NONE',  ( -4.000000000000015987, 197.5625000000000568, 143.6568542494924259 ) ) ;
#58186 = DIRECTION ( 'NONE',  ( -0.000000000000000000, 1.000000000000000000, -0.000000000000000000 ) ) ;
#58187 = UNCERTAINTY_MEASURE_WITH_UNIT (LENGTH_MEASURE( 1.000000000000000082E-05 ), #51006, 'distance_accuracy_value', 'NONE');
#58188 = CARTESIAN_POINT ( 'NONE',  ( -5.676582343749998039, 87.76041666325268409, -9.832129032723420536 ) ) ;
#58189 = ORIENTED_EDGE ( 'NONE', *, *, #50900, .F. ) ;
#58190 = CARTESIAN_POINT ( 'NONE',  ( 10.18810118750000093, -4.220049686691933921, 108.8125000020484094 ) ) ;
#58191 = CARTESIAN_POINT ( 'NONE',  ( -4.541265875000002339, 16.93749999863440436, -5.561446717895856393E-16 ) ) ;
#58192 = ORIENTED_EDGE ( 'NONE', *, *, #45669, .T. ) ;
#58193 = EDGE_LOOP ( 'NONE', ( #26909, #39567, #34033, #20222 ) ) ;
#58194 = CARTESIAN_POINT ( 'NONE',  ( -5.656854249492379694, 8.062500000000001776, -5.656854249492380582 ) ) ;
#58195 = CARTESIAN_POINT ( 'NONE',  ( 4.541265875000001451, 1.374999998634407250, 1.881053915767124440 ) ) ;
#58196 = CARTESIAN_POINT ( 'NONE',  ( -5.082755093536325042, 25.40624999795161543, -5.082755093536325930 ) ) ;
#58197 = CARTESIAN_POINT ( 'NONE',  ( -3.313708498984762052, 123.4062500040967905, -8.000000000000000000 ) ) ;
#58198 = CARTESIAN_POINT ( 'NONE',  ( 1.871523826299183495E-15, -10.18810118749999916, 102.9062500020483810 ) ) ;
#58199 = DIRECTION ( 'NONE',  ( 0.000000000000000000, 1.000000000000000000, 0.000000000000000000 ) ) ;
#58200 = CARTESIAN_POINT ( 'NONE',  ( 1.656854249492381248, 12.93749999726881583, -4.000000000000001776 ) ) ;
#58201 = CARTESIAN_POINT ( 'NONE',  ( 3.211159895383560947, 1.187499998634406806, 3.211159895383562723 ) ) ;
#58202 = ORIENTED_EDGE ( 'NONE', *, *, #43815, .F. ) ;
#58203 = B_SPLINE_CURVE_WITH_KNOTS ( 'NONE', 1,
 ( #45570, #6346 ),
 .UNSPECIFIED., .F., .F.,
 ( 2, 2 ),
 ( 0.000000000000000000, 1.000000000000000000 ),
 .UNSPECIFIED. ) ;
#58204 = EDGE_CURVE ( 'NONE', #39497, #14172, #71295, .T. ) ;
#58205 = ADVANCED_FACE ( 'NONE', ( #53913 ), #19566, .T. ) ;
#58206 = CARTESIAN_POINT ( 'NONE',  ( 0.000000000000000000, 0.000000000000000000, 0.000000000000000000 ) ) ;
#58207 = CARTESIAN_POINT ( 'NONE',  ( 3.458734125000015425, 198.9375000013655779, 198.0000000000000284 ) ) ;
#58208 = CARTESIAN_POINT ( 'NONE',  ( -30.44569435410876324, 206.8125000013656063, 172.4456943541092642 ) ) ;
#58209 = CARTESIAN_POINT ( 'NONE',  ( 2.828427124746153876, 206.8750000000000284, 144.8284271247462129 ) ) ;
#58210 = CARTESIAN_POINT ( 'NONE',  ( 3.211159895383561835, 8.437499998634407916, -3.211159895383561835 ) ) ;
#58211 = CARTESIAN_POINT ( 'NONE',  ( -1.966770576099810657E-11, 61.25000000000153477, -9.999999999999998224 ) ) ;
#58212 = CARTESIAN_POINT ( 'NONE',  ( -7.188101187499992051, 0.000000000000000000, 10.48655278187175455 ) ) ;
#58213 = ORIENTED_EDGE ( 'NONE', *, *, #49148, .F. ) ;
#58214 =( BOUNDED_CURVE ( )  B_SPLINE_CURVE ( 2, ( #47897, #19594, #13555, #7554, #30561, #53944, #70917, #30922, #72021 ),
 .UNSPECIFIED., .F., .F. ) 
 B_SPLINE_CURVE_WITH_KNOTS ( ( 3, 2, 2, 2, 3 ),
 ( 0.5568181818181818787, 0.5625000000000001110, 0.5681818181818183433, 0.5738636363636363535, 0.5795454545454545858 ),
 .UNSPECIFIED. ) 
 CURVE ( )  GEOMETRIC_REPRESENTATION_ITEM ( )  RATIONAL_B_SPLINE_CURVE ( ( 0.9999999999999985567, 0.9238795325112881818, 1.000000000000000000, 0.9238795325112867385, 1.000000000000000000, 0.9238795325112867385, 1.000000000000000000, 0.9238795325112867385, 1.000000000000000000 ) ) 
 REPRESENTATION_ITEM ( '' )  );
#58215 = ORIENTED_EDGE ( 'NONE', *, *, #33059, .F. ) ;
#58216 = CARTESIAN_POINT ( 'NONE',  ( -10.18810118749999916, 0.000000000000000000, 103.6562500020483810 ) ) ;
#58217 = CARTESIAN_POINT ( 'NONE',  ( -9.999999999999991118, 97.70833333333332860, 2.679491924311220075 ) ) ;
#58218 = CARTESIAN_POINT ( 'NONE',  ( -28.00000000000002842, 203.0000000000000000, 166.0000000000003695 ) ) ;
#58219 = CARTESIAN_POINT ( 'NONE',  ( 1.432654583217664479, 200.7500000013656347, 201.4587341250000065 ) ) ;
#58220 = CARTESIAN_POINT ( 'NONE',  ( 38.00000000000000000, 53.00000000000000711, 9.999999999999991118 ) ) ;
#58221 = CARTESIAN_POINT ( 'NONE',  ( -10.00000000000000000, 97.29166666666667140, -2.679491924311229845 ) ) ;
#58222 = EDGE_CURVE ( 'NONE', #53624, #61757, #4344, .T. ) ;
#58223 = EDGE_CURVE ( 'NONE', #24322, #60275, #59214, .T. ) ;
#58224 = CARTESIAN_POINT ( 'NONE',  ( -5.656854249492378806, 116.1875000000000000, 5.656854249492381470 ) ) ;
#58225 = CARTESIAN_POINT ( 'NONE',  ( -3.042071309553164404, 67.55208332991935549, -11.35316468749999963 ) ) ;
#58226 = CARTESIAN_POINT ( 'NONE',  ( 1.226468279477575784E-15, 298.8593750017070079, 6.676582343750001591 ) ) ;
#58227 = ORIENTED_EDGE ( 'NONE', *, *, #58559, .T. ) ;
#58228 = EDGE_CURVE ( 'NONE', #49691, #37587, #41365, .T. ) ;
#58229 = CARTESIAN_POINT ( 'NONE',  ( -6.123233995736766282E-16, 253.7500000000000284, -10.00000000000000000 ) ) ;
#58230 = CARTESIAN_POINT ( 'NONE',  ( -3.313708498984760720, 13.78124999590322552, -8.000000000000000000 ) ) ;
#58231 = CARTESIAN_POINT ( 'NONE',  ( -2.754378923186476579E-14, 209.1875000013656063, 145.4587341250000350 ) ) ;
#58232 = CARTESIAN_POINT ( 'NONE',  ( -5.000000000000005329, 105.2083333265053824, 8.660254037844387298 ) ) ;
#58233 = CARTESIAN_POINT ( 'NONE',  ( -3.313708498984757611, 7.999999999999991118, 26.23655278392014623 ) ) ;
#58234 = CARTESIAN_POINT ( 'NONE',  ( -2.679491924311222295, 241.0416666666666288, 10.00000000000000178 ) ) ;
#58235 = CARTESIAN_POINT ( 'NONE',  ( -28.00000000000007816, 202.1250000027312126, 166.0000000000003695 ) ) ;
#58236 = CARTESIAN_POINT ( 'NONE',  ( 2.020667218593132706E-15, -11.00000000000000000, 116.8749999999999858 ) ) ;
#58237 = CARTESIAN_POINT ( 'NONE',  ( -5.000000000000005329, 213.3333333333333428, 8.660254037844387298 ) ) ;
#58238 =( BOUNDED_CURVE ( )  B_SPLINE_CURVE ( 2, ( #50603, #34402, #22670, #5342, #50981, #40039, #45689, #33653, #73 ),
 .UNSPECIFIED., .F., .F. ) 
 B_SPLINE_CURVE_WITH_KNOTS ( ( 3, 2, 2, 2, 3 ),
 ( 0.4886363636363636465, 0.4943181818181818232, 0.5000000000000000000, 0.5056818181818182323, 0.5113636363636363535 ),
 .UNSPECIFIED. ) 
 CURVE ( )  GEOMETRIC_REPRESENTATION_ITEM ( )  RATIONAL_B_SPLINE_CURVE ( ( 1.000000000000000000, 0.9238795325112867385, 1.000000000000000000, 0.9238795325112867385, 1.000000000000000000, 0.9238795325112867385, 1.000000000000000000, 0.9238795325112867385, 1.000000000000000000 ) ) 
 REPRESENTATION_ITEM ( '' )  );
#58239 = CARTESIAN_POINT ( 'NONE',  ( -4.401442555609577197E-16, 7.188101187499992051, 11.98655278187175632 ) ) ;
#58240 = CARTESIAN_POINT ( 'NONE',  ( -3.042071309553164404, 187.5520833299193555, -11.35316468749999963 ) ) ;
#58241 = CARTESIAN_POINT ( 'NONE',  ( -8.342170076843785083E-16, 3.062499998634406584, 4.541265875000002339 ) ) ;
#58242 = CARTESIAN_POINT ( 'NONE',  ( 11.00000000000000000, 1.347111479062088405E-15, 97.93750000409677625 ) ) ;
#58243 = DIRECTION ( 'NONE',  ( 1.000000000000000000, -0.000000000000000000, -0.000000000000000000 ) ) ;
#58244 = ORIENTED_EDGE ( 'NONE', *, *, #58770, .T. ) ;
#58245 = CARTESIAN_POINT ( 'NONE',  ( -2.445694354108839619, 194.8125000013656063, 139.5543056458912190 ) ) ;
#58246 = CARTESIAN_POINT ( 'NONE',  ( 3.042071309553159519, 40.05208332991935549, 11.35316468750000141 ) ) ;
#58247 = CARTESIAN_POINT ( 'NONE',  ( 4.556349186104045934, 11.00000000000000000, 108.7187500040967763 ) ) ;
#58248 = EDGE_CURVE ( 'NONE', #71793, #68916, #67471, .T. ) ;
#58249 = CARTESIAN_POINT ( 'NONE',  ( -26.56734541678228112, 206.0000000013656063, 173.4587341250003476 ) ) ;
#58250 = DIRECTION ( 'NONE',  ( -0.000000000000000000, -1.000000000000000000, -0.000000000000000000 ) ) ;
#58251 = CARTESIAN_POINT ( 'NONE',  ( 6.123233995736767268E-16, 223.1249999931720254, -10.00000000000000178 ) ) ;
#58252 = CARTESIAN_POINT ( 'NONE',  ( -2.839093476692135984E-14, 198.6875000013655779, 138.5412658750000503 ) ) ;
#58253 = CARTESIAN_POINT ( 'NONE',  ( 6.123233995736767268E-16, 73.12499999317203958, -10.00000000000000178 ) ) ;
#58254 = CARTESIAN_POINT ( 'NONE',  ( -2.977408999572650927, 98.37500000204840944, -7.188101187500001821 ) ) ;
#58255 = CARTESIAN_POINT ( 'NONE',  ( -4.541265875000002339, 11.93749999863440614, -5.561446717895856393E-16 ) ) ;
#58256 = CARTESIAN_POINT ( 'NONE',  ( 7.320508075688936245, 215.6250000000001421, -7.320508075688936245 ) ) ;
#58257 = CARTESIAN_POINT ( 'NONE',  ( -2.828427124746192067, 4.374999997268814056, 2.828427124746190735 ) ) ;
#58258 = EDGE_LOOP ( 'NONE', ( #38212, #32028, #45221, #69606 ) ) ;
#58259 = ORIENTED_EDGE ( 'NONE', *, *, #52568, .F. ) ;
#58260 = CARTESIAN_POINT ( 'NONE',  ( 0.000000000000000000, 0.000000000000000000, -10.00000000000000000 ) ) ;
#58261 = CARTESIAN_POINT ( 'NONE',  ( -4.721056650415998313, 298.7343750017069510, 4.721056650416000089 ) ) ;
#58262 = DIRECTION ( 'NONE',  ( 0.000000000000000000, -0.5207998305029790664, 0.8536788251725986321 ) ) ;
#58263 = CARTESIAN_POINT ( 'NONE',  ( 0.000000000000000000, 0.000000000000000000, -10.20000000000000462 ) ) ;
#58264 = VECTOR ( 'NONE', #37594, 1000.000000000000000 ) ;
#58265 = CARTESIAN_POINT ( 'NONE',  ( -3.042071309553173730, 159.3229166632526699, 11.35316468749999785 ) ) ;
#58266 = CARTESIAN_POINT ( 'NONE',  ( -10.18810118749999738, -4.220049686691941915, 85.75000000204838102 ) ) ;
#58267 = CYLINDRICAL_SURFACE ( 'NONE', #15183, 10.00000000000000178 ) ;
#58268 = CARTESIAN_POINT ( 'NONE',  ( 2.828427124746209831, 203.3750000000000284, 200.8284271247462129 ) ) ;
#58269 = FACE_OUTER_BOUND ( 'NONE', #68026, .T. ) ;
#58270 = CARTESIAN_POINT ( 'NONE',  ( -4.220049686691935698, 10.18810118749999916, 112.7500000020483810 ) ) ;
#58271 = ORIENTED_EDGE ( 'NONE', *, *, #47955, .T. ) ;
#58272 = DIRECTION ( 'NONE',  ( 0.7071067811865401342, 8.659560562354842879E-17, -0.7071067811865549002 ) ) ;
#58273 = CARTESIAN_POINT ( 'NONE',  ( 22.27911678678798069, 182.2961259327863388, 148.3271588659208646 ) ) ;
#58274 = CARTESIAN_POINT ( 'NONE',  ( -11.35316468749999785, 123.3854166632526699, -3.042071309553167957 ) ) ;
#58275 = CARTESIAN_POINT ( 'NONE',  ( -3.458734124999959914, 198.3750000013656063, 196.5673454167823877 ) ) ;
#58276 = CARTESIAN_POINT ( 'NONE',  ( -1.432654583217607414, 209.5000000013656063, 194.5412658750000219 ) ) ;
#58277 = CARTESIAN_POINT ( 'NONE',  ( -10.18810118749999916, 4.220049686691934809, 75.43750000204836681 ) ) ;
#58278 = CARTESIAN_POINT ( 'NONE',  ( 8.311093377946834337, 50.46874999658601979, 8.311093377946839666 ) ) ;
#58279 = ORIENTED_EDGE ( 'NONE', *, *, #11448, .T. ) ;
#58280 = CARTESIAN_POINT ( 'NONE',  ( 11.00000000000000355, -4.556349186104044158, 94.84375000409677625 ) ) ;
#58281 = CARTESIAN_POINT ( 'NONE',  ( -3.211159895383561391, 2.812499998634407028, -3.211159895383561835 ) ) ;
#58282 = CARTESIAN_POINT ( 'NONE',  ( 5.662595241051934458, 5.662595241051935346, 15.45061528394063011 ) ) ;
#58283 = CARTESIAN_POINT ( 'NONE',  ( 2.977408999572650927, 14.24999999795161010, -7.188101187500001821 ) ) ;
#58284 = CARTESIAN_POINT ( 'NONE',  ( -6.000000000000000888, 292.1250000034140157, 2.485281374238575758 ) ) ;
#58285 = CARTESIAN_POINT ( 'NONE',  ( -11.79731652672780662, -26.35074500299052147, 139.3730105126419403 ) ) ;
#58286 = CARTESIAN_POINT ( 'NONE',  ( -7.188101187500002709, 7.687499997951611874, 2.977408999572649151 ) ) ;
#58287 = CARTESIAN_POINT ( 'NONE',  ( 5.082755093536318824, 5.082755093536319713, 8.424052781871752771 ) ) ;
#58288 = APPLICATION_CONTEXT ( 'automotive_design' ) ;
#58289 = CARTESIAN_POINT ( 'NONE',  ( -4.220049686691937474, -10.18810118749999738, 70.93750000204838102 ) ) ;
#58290 = CARTESIAN_POINT ( 'NONE',  ( -25.55430564589115505, 208.3125000013656063, 172.4456943541091789 ) ) ;
#58291 = CARTESIAN_POINT ( 'NONE',  ( -8.660254037844387298, 63.95833332650536818, -5.000000000000004441 ) ) ;
#58292 = CARTESIAN_POINT ( 'NONE',  ( 4.541265875000002339, 21.49999999863440792, -1.881053915767121554 ) ) ;
#58293 = ORIENTED_EDGE ( 'NONE', *, *, #56884, .T. ) ;
#58294 = EDGE_CURVE ( 'NONE', #13320, #2612, #38525, .T. ) ;
#58295 = CARTESIAN_POINT ( 'NONE',  ( -3.999999999999960032, 195.1250000027311842, 198.0000000000000284 ) ) ;
#58296 = CARTESIAN_POINT ( 'NONE',  ( -2.849036369511732440E-14, 207.2500000000000284, 138.0000000000000568 ) ) ;
#58297 = CARTESIAN_POINT ( 'NONE',  ( -26.34314575050753149, 201.6875000027312126, 174.0000000000003411 ) ) ;
#58298 = CARTESIAN_POINT ( 'NONE',  ( 5.082755093536325042, 117.5937500020483810, -5.082755093536325930 ) ) ;
#58299 = CARTESIAN_POINT ( 'NONE',  ( 4.556349186104045934, 11.00000000000000000, 93.71875000409676204 ) ) ;
#58300 = CARTESIAN_POINT ( 'NONE',  ( 7.999999999999991118, 9.797174393178815797E-16, 3.267802783920144449 ) ) ;
#58301 = ORIENTED_EDGE ( 'NONE', *, *, #51567, .T. ) ;
#58302 = CARTESIAN_POINT ( 'NONE',  ( -7.188101187500000044, 14.71874999795161187, -8.802885111219163269E-16 ) ) ;
#58303 = ORIENTED_EDGE ( 'NONE', *, *, #12241, .T. ) ;
#58304 = CARTESIAN_POINT ( 'NONE',  ( 27.99999999999996803, 200.0000000000000000, 173.9999999999999147 ) ) ;
#58305 = DIRECTION ( 'NONE',  ( -0.000000000000000000, 1.000000000000000000, -4.476705744456276341E-16 ) ) ;
#58306 = CARTESIAN_POINT ( 'NONE',  ( 10.00000000000000178, 50.00000000000000000, 0.000000000000000000 ) ) ;
#58307 = CIRCLE ( 'NONE', #482, 6.999999999999999112 ) ;
#58308 = CARTESIAN_POINT ( 'NONE',  ( -7.188101187499999156, 100.6250000020483810, 2.977408999572654924 ) ) ;
#58309 = CARTESIAN_POINT ( 'NONE',  ( -28.00000000000002132, 204.6875000013656063, 166.5412658750003629 ) ) ;
#58310 = CARTESIAN_POINT ( 'NONE',  ( -6.000000000000003553, 298.9375000000000000, -2.485281374238571317 ) ) ;
#58311 = CARTESIAN_POINT ( 'NONE',  ( 1.224646799147353454E-15, 300.0000000000000000, -10.00000000000000178 ) ) ;
#58312 = ORIENTED_EDGE ( 'NONE', *, *, #65700, .T. ) ;
#58313 = ADVANCED_FACE ( 'NONE', ( #14646 ), #9381, .F. ) ;
#58314 = CARTESIAN_POINT ( 'NONE',  ( 9.832129032723416984, 241.8229166700806445, -5.676582343750003368 ) ) ;
#58315 = CARTESIAN_POINT ( 'NONE',  ( -2.977408999572648707, -7.188101187499990274, 20.14280278187176165 ) ) ;
#58316 = CARTESIAN_POINT ( 'NONE',  ( 9.999999999999985789, 90.00000000000001421, 0.000000000000000000 ) ) ;
#58317 = LINE ( 'NONE', #53012, #14231 ) ;
#58318 = CARTESIAN_POINT ( 'NONE',  ( -4.999999999999998224, 146.6666666666666572, -8.660254037844389075 ) ) ;
#58319 = CARTESIAN_POINT ( 'NONE',  ( -3.313708498984759387, -7.999999999999989342, 19.29905278392014978 ) ) ;
#58320 = CARTESIAN_POINT ( 'NONE',  ( 7.320508075688774596, 165.6250000000000284, -7.320508075688774596 ) ) ;
#58321 = CYLINDRICAL_SURFACE ( 'NONE', #32960, 8.000000000000000000 ) ;
#58322 = CARTESIAN_POINT ( 'NONE',  ( -31.57689670703662443, 176.8634628171951135, 168.5921286597449011 ) ) ;
#58323 = CARTESIAN_POINT ( 'NONE',  ( -5.082755093536317936, -5.082755093536320601, 26.04905278187175810 ) ) ;
#58324 = CARTESIAN_POINT ( 'NONE',  ( -3.042071309553164404, 137.5520833299193555, -11.35316468749999963 ) ) ;
#58325 = LINE ( 'NONE', #62838, #66148 ) ;
#58326 = CARTESIAN_POINT ( 'NONE',  ( -11.00000000000000000, 0.000000000000000000, 107.4999999999999858 ) ) ;
#58329 = LINE ( 'NONE', #6635, #65205 ) ;
#58328 = CARTESIAN_POINT ( 'NONE',  ( 28.00000000000001421, 194.4375000013656063, 173.4587341249998929 ) ) ;
#58327 = CARTESIAN_POINT ( 'NONE',  ( 25.17157287525381903, 207.6250000000000284, 167.1715728752537018 ) ) ;
#58330 = ORIENTED_EDGE ( 'NONE', *, *, #42112, .T. ) ;
#58331 = CARTESIAN_POINT ( 'NONE',  ( -7.522341449313134198, 6.049278984716041307, -0.3563104543936375102 ) ) ;
#58332 = EDGE_CURVE ( 'NONE', #5036, #9311, #5222, .T. ) ;
#58333 = CARTESIAN_POINT ( 'NONE',  ( -9.000000000000001776, -4.351040328464083728, -0.5598847297401622347 ) ) ;
#58334 = CARTESIAN_POINT ( 'NONE',  ( 1.181073143174618423, -7.934766031977416922, 0.000000000000000000 ) ) ;
#58335 =( BOUNDED_CURVE ( )  B_SPLINE_CURVE ( 2, ( #30544, #60317, #65232, #13536, #42959, #71258, #36575, #70176, #13906 ),
 .UNSPECIFIED., .F., .F. ) 
 B_SPLINE_CURVE_WITH_KNOTS ( ( 3, 2, 2, 2, 3 ),
 ( 0.8333333333333340365, 0.8416666666666673402, 0.8500000000000006439, 0.8583333333333339477, 0.8666666666666673624 ),
 .UNSPECIFIED. ) 
 CURVE ( )  GEOMETRIC_REPRESENTATION_ITEM ( )  RATIONAL_B_SPLINE_CURVE ( ( 0.9999999999999938938, 0.9238795325112928447, 1.000000000000000000, 0.9238795325112867385, 1.000000000000000000, 0.9238795325112867385, 1.000000000000000000, 0.9238795325112806323, 1.000000000000005995 ) ) 
 REPRESENTATION_ITEM ( '' )  );
#58336 = CARTESIAN_POINT ( 'NONE',  ( 5.000000000000000000, -66.10919140997980037, -23.67639547906034991 ) ) ;
#58337 = EDGE_CURVE ( 'NONE', #24245, #35502, #28954, .T. ) ;
#58338 = CARTESIAN_POINT ( 'NONE',  ( 2.679491924311228956, 32.91666665983868967, -10.00000000000000000 ) ) ;
#58339 = CARTESIAN_POINT ( 'NONE',  ( -7.188101187500001821, 113.5625000020483668, -2.977408999572650483 ) ) ;
#58340 = CARTESIAN_POINT ( 'NONE',  ( 2.780723358947928197E-16, 21.56249999863440792, -4.541265875000002339 ) ) ;
#58341 = CARTESIAN_POINT ( 'NONE',  ( -1.317228840348880325, -55.68607278122971849, 43.83834608838142088 ) ) ;
#58342 = CARTESIAN_POINT ( 'NONE',  ( -7.999999999999991118, 3.313708498984756723, 17.23655277982336642 ) ) ;
#58344 = CARTESIAN_POINT ( 'NONE',  ( -30.82842712474621649, 207.1250000000000284, 167.1715728752542134 ) ) ;
#58343 = CARTESIAN_POINT ( 'NONE',  ( -4.000000000000001776, 1.500000000000000222, -4.898587196589415787E-16 ) ) ;
#58345 = ORIENTED_EDGE ( 'NONE', *, *, #61609, .F. ) ;
#58346 = DIRECTION ( 'NONE',  ( 0.000000000000000000, -0.000000000000000000, 1.000000000000000000 ) ) ;
#58347 = CARTESIAN_POINT ( 'NONE',  ( -7.188101187500000044, 23.71874999795161543, -8.802885111219163269E-16 ) ) ;
#58348 = CARTESIAN_POINT ( 'NONE',  ( -10.00000000000005329, 62.29166666666670693, -2.679491924311244944 ) ) ;
#58349 = CARTESIAN_POINT ( 'NONE',  ( -8.311093377946834337, 249.8437500034139589, 8.311093377946837890 ) ) ;
#58350 = CARTESIAN_POINT ( 'NONE',  ( 11.35316468749999785, 120.5729166632526699, 3.042071309553174174 ) ) ;
#58351 = ORIENTED_EDGE ( 'NONE', *, *, #37634, .F. ) ;
#58352 = CARTESIAN_POINT ( 'NONE',  ( -10.46351411367761486, 2.360032084838133759, 117.7839813612980038 ) ) ;
#58353 = CARTESIAN_POINT ( 'NONE',  ( 7.204075437095966983, 7.204075437095967871, 100.0937500020483668 ) ) ;
#58354 = CARTESIAN_POINT ( 'NONE',  ( -1.836970198721029983E-15, 220.6249999931720538, 10.00000000000000178 ) ) ;
#58355 = CARTESIAN_POINT ( 'NONE',  ( 2.445694354108840063, 201.0625000013656063, 200.4456943541088663 ) ) ;
#58356 = CARTESIAN_POINT ( 'NONE',  ( -1.656854249492381248, 6.062499997268813168, -4.000000000000001776 ) ) ;
#58358 = CARTESIAN_POINT ( 'NONE',  ( 9.832129032723420536, 101.1979166632526841, -5.676582343749999815 ) ) ;
#58357 = CARTESIAN_POINT ( 'NONE',  ( -8.660254037844389075, 182.9166666666666856, 4.999999999999997335 ) ) ;
#58359 = CARTESIAN_POINT ( 'NONE',  ( -5.656854249492373476, -5.656854249492376141, 4.205302783920145338 ) ) ;
#58360 = CARTESIAN_POINT ( 'NONE',  ( -26.56734541678237704, 197.6250000013656063, 166.5412658750003629 ) ) ;
#58361 = ORIENTED_EDGE ( 'NONE', *, *, #48180, .F. ) ;
#58362 = CARTESIAN_POINT ( 'NONE',  ( -10.00000000000000000, 194.1666666598387110, -2.679491924311229845 ) ) ;
#58363 = CARTESIAN_POINT ( 'NONE',  ( 37.99999999999999289, 50.00000000000000711, 65.00000000000000000 ) ) ;
#58364 = EDGE_CURVE ( 'NONE', #62698, #53065, #43415, .T. ) ;
#58365 = CYLINDRICAL_SURFACE ( 'NONE', #32844, 30.99999999999997158 ) ;
#58366 = CARTESIAN_POINT ( 'NONE',  ( -11.35316468750000141, 83.80208332991934128, 3.042071309553159963 ) ) ;
#58367 = CARTESIAN_POINT ( 'NONE',  ( -2.445694354108783664, 209.3125000013656063, 195.5543056458912190 ) ) ;
#58368 = CARTESIAN_POINT ( 'NONE',  ( -1.320432766682874540E-15, 3.468749997951610986, 7.188101187500000044 ) ) ;
#58369 = CARTESIAN_POINT ( 'NONE',  ( 1.871523826299183495E-15, -10.18810118749999916, 96.90625000204838102 ) ) ;
#58370 = CARTESIAN_POINT ( 'NONE',  ( -5.676582343750006032, 14.42708332991935016, 9.832129032723418760 ) ) ;
#58371 = ORIENTED_EDGE ( 'NONE', *, *, #38360, .F. ) ;
#58372 = CARTESIAN_POINT ( 'NONE',  ( 0.000000000000000000, 0.000000000000000000, 41.99999999999999289 ) ) ;
#58373 = CARTESIAN_POINT ( 'NONE',  ( 0.9677818261170547665, -42.15358416805125330, 139.0145768240332700 ) ) ;
#58374 = CARTESIAN_POINT ( 'NONE',  ( -11.35316468750000141, 213.2812499965860411, -1.390361679473963753E-15 ) ) ;
#58375 = CARTESIAN_POINT ( 'NONE',  ( -4.220049686691937474, -10.18810118749999738, 81.81250000204838102 ) ) ;
#58376 = AXIS2_PLACEMENT_3D ( 'NONE', #53909, #14640, #8628 ) ;
#58377 = DIRECTION ( 'NONE',  ( -0.000000000000000000, 1.000000000000000000, 4.476705744456276341E-16 ) ) ;
#58378 = CARTESIAN_POINT ( 'NONE',  ( -8.000000000000000000, 93.59375000409677625, -3.313708498984761164 ) ) ;
#58379 = CARTESIAN_POINT ( 'NONE',  ( 6.676582343750001591, 295.9531250017069510, -8.176455196517173205E-16 ) ) ;
#58380 = ORIENTED_EDGE ( 'NONE', *, *, #13294, .F. ) ;
#58381 = CARTESIAN_POINT ( 'NONE',  ( 11.00000000000000000, 1.347111479062088405E-15, 88.93750000409677625 ) ) ;
#58382 = CARTESIAN_POINT ( 'NONE',  ( 11.35316468749999963, 211.3020833299193839, -3.042071309553165293 ) ) ;
#58383 = CARTESIAN_POINT ( 'NONE',  ( -6.238412754330611322E-16, 10.18810118749999916, 91.28125000204836681 ) ) ;
#58384 = CARTESIAN_POINT ( 'NONE',  ( -26.56734541678232375, 204.0000000013656347, 173.4587341250003760 ) ) ;
#58385 = CARTESIAN_POINT ( 'NONE',  ( 8.000000000000000000, 19.59375000000000711, -3.313708498984761608 ) ) ;
#58386 = ORIENTED_EDGE ( 'NONE', *, *, #11012, .F. ) ;
#58387 = CARTESIAN_POINT ( 'NONE',  ( -7.188101187500000044, 122.6562500020483810, 0.000000000000000000 ) ) ;
#58388 = CARTESIAN_POINT ( 'NONE',  ( 4.000000000000015987, 207.5625000027312126, 199.6568542494924259 ) ) ;
#58389 = EDGE_CURVE ( 'NONE', #13756, #26953, #49050, .T. ) ;
#58390 = CARTESIAN_POINT ( 'NONE',  ( 2.679491924311222739, 28.95833333333333215, 10.00000000000000355 ) ) ;
#58391 = CARTESIAN_POINT ( 'NONE',  ( -5.000000000000000000, 11.14555136602165142, 27.84144949604463193 ) ) ;
#58392 = CARTESIAN_POINT ( 'NONE',  ( 10.18810118750000093, -4.220049686691933921, 73.18750000204838102 ) ) ;
#58393 = VERTEX_POINT ( 'NONE', #73128 ) ;
#58394 = ADVANCED_FACE ( 'NONE', ( #44457 ), #15768, .T. ) ;
#58395 = DIRECTION ( 'NONE',  ( 0.000000000000000000, 0.000000000000000000, 1.000000000000000000 ) ) ;
#58396 = CARTESIAN_POINT ( 'NONE',  ( -7.778174593052020747, -7.778174593052023411, 112.1875000000000000 ) ) ;
#58397 = DIRECTION ( 'NONE',  ( -9.637352644315595243E-17, 1.000000000000000000, 0.000000000000000000 ) ) ;
#58398 = CARTESIAN_POINT ( 'NONE',  ( -7.188101187500001821, 116.9375000020483952, -2.977408999572650483 ) ) ;
#58399 = CARTESIAN_POINT ( 'NONE',  ( 7.999999999752645863, -6.290875383172500320E-05, 1.767801038436179750 ) ) ;
#58400 = CARTESIAN_POINT ( 'NONE',  ( 6.676582343750002480, 296.0156250017069510, -2.765530957081997254 ) ) ;
#58402 = CARTESIAN_POINT ( 'NONE',  ( 2.828427124746209831, 206.3750000000000284, 200.8284271247462129 ) ) ;
#58401 = CARTESIAN_POINT ( 'NONE',  ( -11.35316468749999785, 233.6979166700806445, -3.042071309553164848 ) ) ;
#58403 = ORIENTED_EDGE ( 'NONE', *, *, #12160, .T. ) ;
#58404 = EDGE_CURVE ( 'NONE', #48235, #49614, #56792, .T. ) ;
#58405 = CARTESIAN_POINT ( 'NONE',  ( -11.35316468749999963, 239.2187500034139873, 0.000000000000000000 ) ) ;
#58406 = CARTESIAN_POINT ( 'NONE',  ( 7.188101187499991163, 2.977408999572648707, 8.330302781871752771 ) ) ;
#58407 = VERTEX_POINT ( 'NONE', #46128 ) ;
#58408 = CARTESIAN_POINT ( 'NONE',  ( 10.18810118750000093, -4.220049686691933033, 71.31250000204836681 ) ) ;
#58409 = CARTESIAN_POINT ( 'NONE',  ( 9.832129032723420536, 101.5104166632526841, -5.676582343749999815 ) ) ;
#58410 = DIRECTION ( 'NONE',  ( 0.000000000000000000, 0.000000000000000000, 1.000000000000000000 ) ) ;
#58411 = CARTESIAN_POINT ( 'NONE',  ( 4.556349186104051263, -10.99999999999999822, 85.46874999999998579 ) ) ;
#58414 = DIRECTION ( 'NONE',  ( -0.000000000000000000, -0.000000000000000000, -1.000000000000000000 ) ) ;
#58413 = CARTESIAN_POINT ( 'NONE',  ( 24.54126587499999346, 204.1875000013656063, 169.9999999999999432 ) ) ;
#58412 = CARTESIAN_POINT ( 'NONE',  ( 25.55430564589115150, 203.5625000013656063, 172.4456943541086957 ) ) ;
#58415 = ORIENTED_EDGE ( 'NONE', *, *, #21506, .F. ) ;
#58416 = DIRECTION ( 'NONE',  ( -0.000000000000000000, 1.000000000000000000, 4.689100369878284071E-30 ) ) ;
#58417 = DIRECTION ( 'NONE',  ( 0.000000000000000000, 0.000000000000000000, -1.000000000000000000 ) ) ;
#58418 = CARTESIAN_POINT ( 'NONE',  ( 9.832129032723420536, 211.1979166632526983, -5.676582343749999815 ) ) ;
#58419 = CARTESIAN_POINT ( 'NONE',  ( 3.458734124999959025, 206.5000000013655779, 140.5673454167824161 ) ) ;
#58420 = CARTESIAN_POINT ( 'NONE',  ( 29.43265458321766559, 206.1250000013655779, 166.5412658749999650 ) ) ;
#58421 = EDGE_CURVE ( 'NONE', #57455, #30587, #11801, .T. ) ;
#58422 = CARTESIAN_POINT ( 'NONE',  ( 7.188101187499999156, 24.74999999795161543, 2.977408999572654924 ) ) ;
#58423 = CARTESIAN_POINT ( 'NONE',  ( -3.042071309553164404, 177.5520833299193839, -11.35316468749999963 ) ) ;
#58424 = CARTESIAN_POINT ( 'NONE',  ( 2.977408999572654480, 99.50000000204838102, 7.188101187499999156 ) ) ;
#58425 = DIRECTION ( 'NONE',  ( -0.000000000000000000, 1.000000000000000000, -0.000000000000000000 ) ) ;
#58426 = CARTESIAN_POINT ( 'NONE',  ( -3.211159895383561391, 10.68749999863440792, -3.211159895383561835 ) ) ;
#58427 = CARTESIAN_POINT ( 'NONE',  ( 28.00000000000002132, 202.1875000013656063, 166.5412658749999082 ) ) ;
#58428 = CARTESIAN_POINT ( 'NONE',  ( 1.320432766682872962E-15, -7.188101187499992051, 12.73655278187175277 ) ) ;
#58429 = CARTESIAN_POINT ( 'NONE',  ( -8.311093377946836114, 67.65624999658599847, -8.311093377946837890 ) ) ;
#58430 = DIRECTION ( 'NONE',  ( 0.000000000000000000, 0.000000000000000000, 1.000000000000000000 ) ) ;
#58431 = CARTESIAN_POINT ( 'NONE',  ( -3.313708498984758943, -7.999999999999989342, 1.167802784329823984 ) ) ;
#58432 = ORIENTED_EDGE ( 'NONE', *, *, #11362, .F. ) ;
#58433 = CARTESIAN_POINT ( 'NONE',  ( -2.828427124746209831, 203.5000000027312126, 139.1715728752538723 ) ) ;
#58434 = CARTESIAN_POINT ( 'NONE',  ( -11.35316468750000141, 78.48958332991935549, 3.042071309553159963 ) ) ;
#58435 = CARTESIAN_POINT ( 'NONE',  ( 11.00000000000000355, -4.556349186104045046, 70.84375000409676204 ) ) ;
#58436 = CARTESIAN_POINT ( 'NONE',  ( -3.458734125000016757, 198.1250000013656063, 140.5673454167823593 ) ) ;
#58437 = CARTESIAN_POINT ( 'NONE',  ( -0.7509181236784702174, 10.12341933770169256, 70.08957333326500816 ) ) ;
#58439 = CARTESIAN_POINT ( 'NONE',  ( -8.311093377946841443, 53.90624999658601979, 8.311093377946834337 ) ) ;
#58438 = CARTESIAN_POINT ( 'NONE',  ( 2.977408999572654480, 90.12500000204836681, 7.188101187499999156 ) ) ;
#58440 = VECTOR ( 'NONE', #37809, 1000.000000000000000 ) ;
#58441 = CARTESIAN_POINT ( 'NONE',  ( 5.656854249492376141, -5.656854249492374365, 27.08030278392014978 ) ) ;
#58442 = DIRECTION ( 'NONE',  ( -0.000000000000000000, 1.000000000000000000, -0.000000000000000000 ) ) ;
#58443 = CARTESIAN_POINT ( 'NONE',  ( 7.320508075688774596, 152.4999999931720538, -7.320508075688774596 ) ) ;
#58444 = CARTESIAN_POINT ( 'NONE',  ( 1.320432766682874540E-15, 94.90625000204838102, 7.188101187500000044 ) ) ;
#58445 = CARTESIAN_POINT ( 'NONE',  ( 10.00000000000001066, 20.00000000000000355, 0.000000000000000000 ) ) ;
#58446 = CARTESIAN_POINT ( 'NONE',  ( -8.311093377946841443, 49.21874999658600558, 8.311093377946834337 ) ) ;
#58447 =( BOUNDED_CURVE ( )  B_SPLINE_CURVE ( 2, ( #60137, #3935, #43912, #66922, #15227, #38259, #72957, #21263, #150 ),
 .UNSPECIFIED., .F., .F. ) 
 B_SPLINE_CURVE_WITH_KNOTS ( ( 3, 2, 2, 2, 3 ),
 ( 0.7794117647058823595, 0.7830882352941176405, 0.7867647058823529216, 0.7904411764705882026, 0.7941176470588234837 ),
 .UNSPECIFIED. ) 
 CURVE ( )  GEOMETRIC_REPRESENTATION_ITEM ( )  RATIONAL_B_SPLINE_CURVE ( ( 1.000000000000000000, 0.9238795325112867385, 1.000000000000000000, 0.9238795325112867385, 1.000000000000000000, 0.9238795325112867385, 1.000000000000000000, 0.9238795325112867385, 1.000000000000000000 ) ) 
 REPRESENTATION_ITEM ( '' )  );
#58448 = CARTESIAN_POINT ( 'NONE',  ( -4.220049686691937474, -10.18810118749999738, 110.3125000020483810 ) ) ;
#58449 = CARTESIAN_POINT ( 'NONE',  ( 11.35316468749999963, 190.9895833299193271, -3.042071309553165293 ) ) ;
#58450 = ORIENTED_EDGE ( 'NONE', *, *, #64606, .F. ) ;
#58452 =( BOUNDED_CURVE ( )  B_SPLINE_CURVE ( 2, ( #3781, #49415, #14330, #9066, #72437, #54348, #26390, #72815, #36989 ),
 .UNSPECIFIED., .F., .F. ) 
 B_SPLINE_CURVE_WITH_KNOTS ( ( 3, 2, 2, 2, 3 ),
 ( 0.2333333333333335313, 0.2416666666666668628, 0.2500000000000002220, 0.2583333333333335813, 0.2666666666666668850 ),
 .UNSPECIFIED. ) 
 CURVE ( )  GEOMETRIC_REPRESENTATION_ITEM ( )  RATIONAL_B_SPLINE_CURVE ( ( 0.9999999999999982236, 0.9238795325112885148, 1.000000000000000000, 0.9238795325112867385, 1.000000000000000000, 0.9238795325112867385, 1.000000000000000000, 0.9238795325112847401, 1.000000000000001998 ) ) 
 REPRESENTATION_ITEM ( '' )  );
#58451 = CARTESIAN_POINT ( 'NONE',  ( 1.506680654955621534, 65.82403019916786491, 26.31606384388625131 ) ) ;
#58453 = CARTESIAN_POINT ( 'NONE',  ( 0.000000000000000000, 125.0000000000000000, 0.000000000000000000 ) ) ;
#58454 = PLANE ( 'NONE',  #44366 ) ;
#58456 = CARTESIAN_POINT ( 'NONE',  ( -2.085542519210945728E-15, 174.5312499965860411, 11.35316468750000141 ) ) ;
#58455 = CARTESIAN_POINT ( 'NONE',  ( -27.99999999999991118, 200.6250000027312126, 174.0000000000003695 ) ) ;
#58457 = CARTESIAN_POINT ( 'NONE',  ( 2.250000000000000444, 283.9999999999998863, 5.427273995025124975 ) ) ;
#58458 = CARTESIAN_POINT ( 'NONE',  ( 7.320508075688771044, 246.2500000068279746, -7.320508075688771932 ) ) ;
#58459 = DIRECTION ( 'NONE',  ( -0.000000000000000000, -1.000000000000000000, -0.000000000000000000 ) ) ;
#58460 = ORIENTED_EDGE ( 'NONE', *, *, #61439, .T. ) ;
#58461 = CARTESIAN_POINT ( 'NONE',  ( 3.042071309553167513, 167.1354166632526699, -11.35316468749999785 ) ) ;
#58462 = DIRECTION ( 'NONE',  ( 0.000000000000000000, 0.000000000000000000, 1.000000000000000000 ) ) ;
#58463 = CARTESIAN_POINT ( 'NONE',  ( -11.35316468750000141, 123.8020833299193271, 3.042071309553159963 ) ) ;
#58464 = CARTESIAN_POINT ( 'NONE',  ( -8.000000000000000000, 3.468749995903220196, -3.313708498984762496 ) ) ;
#58465 = ORIENTED_EDGE ( 'NONE', *, *, #8106, .F. ) ;
#58466 = CARTESIAN_POINT ( 'NONE',  ( -3.313708498984762052, 106.9062500040967763, -8.000000000000000000 ) ) ;
#58467 = EDGE_CURVE ( 'NONE', #24188, #38816, #55509, .T. ) ;
#58468 = ADVANCED_FACE ( 'NONE', ( #52538, #139 ), #876, .T. ) ;
#58469 = CARTESIAN_POINT ( 'NONE',  ( -1.656854249492381248, 13.31250000000000000, -4.000000000000001776 ) ) ;
#58470 = PLANE ( 'NONE',  #57738 ) ;
#58471 = CARTESIAN_POINT ( 'NONE',  ( 3.211159895383561835, 11.43749999863440614, -3.211159895383561835 ) ) ;
#58472 = CARTESIAN_POINT ( 'NONE',  ( 7.999999999999991118, 9.797174393178815797E-16, 18.26780278392014623 ) ) ;
#58473 = CARTESIAN_POINT ( 'NONE',  ( -1.469576158976823947E-15, 10.12500000000000178, 8.000000000000000000 ) ) ;
#58474 = VERTEX_POINT ( 'NONE', #70263 ) ;
#58475 = CARTESIAN_POINT ( 'NONE',  ( -10.00000000000005329, 177.2916666666667140, -2.679491924311244944 ) ) ;
#58476 = CARTESIAN_POINT ( 'NONE',  ( 7.188101187500001821, 102.5000000020483810, -2.977408999572651371 ) ) ;
#58477 = CIRCLE ( 'NONE', #12625, 8.749999999999998224 ) ;
#58478 = CARTESIAN_POINT ( 'NONE',  ( -11.00000000000000000, 0.000000000000000000, 98.49999999999998579 ) ) ;
#58479 = DIRECTION ( 'NONE',  ( 1.000000000000000000, 0.000000000000000000, 0.000000000000000000 ) ) ;
#58480 = ORIENTED_EDGE ( 'NONE', *, *, #8790, .F. ) ;
#58481 = CARTESIAN_POINT ( 'NONE',  ( -4.471435261917971360, 10.26549131683129623, -64.21726486257941247 ) ) ;
#58482 = CIRCLE ( 'NONE', #4257, 34.85072926314708752 ) ;
#58483 = CARTESIAN_POINT ( 'NONE',  ( -5.082755093536317936, -5.082755093536320601, 24.17405278187175455 ) ) ;
#58484 = ORIENTED_EDGE ( 'NONE', *, *, #27952, .T. ) ;
#58485 = ORIENTED_EDGE ( 'NONE', *, *, #55893, .F. ) ;
#58486 = CARTESIAN_POINT ( 'NONE',  ( -7.204075437095965206, -7.204075437095968759, 88.84375000204838102 ) ) ;
#58487 = UNCERTAINTY_MEASURE_WITH_UNIT (LENGTH_MEASURE( 1.000000000000000082E-05 ), #51319, 'distance_accuracy_value', 'NONE');
#58488 = CARTESIAN_POINT ( 'NONE',  ( -31.45873412499997812, 196.0000000013656063, 171.4326545832180386 ) ) ;
#58489 = CARTESIAN_POINT ( 'NONE',  ( 4.556349186104045934, 11.00000000000000000, 99.53125000000001421 ) ) ;
#58492 = CARTESIAN_POINT ( 'NONE',  ( -6.676582343750001591, 296.6093750017069510, 0.000000000000000000 ) ) ;
#58491 = CARTESIAN_POINT ( 'NONE',  ( 30.82842712474616675, 201.5000000027312126, 167.1715728752537018 ) ) ;
#58490 = DIRECTION ( 'NONE',  ( 8.659560562354940254E-17, 0.7071067811865465735, -0.7071067811865484609 ) ) ;
#58493 = CARTESIAN_POINT ( 'NONE',  ( 6.123233995736767268E-16, 136.2500000000000000, -10.00000000000000178 ) ) ;
#58494 = CARTESIAN_POINT ( 'NONE',  ( 1.469576158976823947E-15, 101.3750000000000000, 8.000000000000000000 ) ) ;
#58495 = CARTESIAN_POINT ( 'NONE',  ( -27.99999999999995737, 203.5000000000000000, 174.0000000000003695 ) ) ;
#58496 = CARTESIAN_POINT ( 'NONE',  ( 0.000000000000000000, 0.000000000000000000, 0.000000000000000000 ) ) ;
#58497 = CARTESIAN_POINT ( 'NONE',  ( 28.00000000000002132, 203.9375000013656063, 166.5412658749999082 ) ) ;
#58498 = CARTESIAN_POINT ( 'NONE',  ( 2.977408999572650927, 5.624999997951610986, -7.188101187500001821 ) ) ;
#58499 = CARTESIAN_POINT ( 'NONE',  ( 8.008118988124991233, 3.317071493978879015, 4.856865283940630107 ) ) ;
#58500 = CARTESIAN_POINT ( 'NONE',  ( -2.754378923186476579E-14, 197.1875000013655779, 145.4587341250000350 ) ) ;
#58501 = CARTESIAN_POINT ( 'NONE',  ( 5.082755093536326818, 116.0937500020483810, 5.082755093536325042 ) ) ;
#58503 = CARTESIAN_POINT ( 'NONE',  ( 1.895132620089674313, 194.6589491196967288, 201.1395742274239353 ) ) ;
#58502 = CARTESIAN_POINT ( 'NONE',  ( 0.000000000000000000, 125.0000000000000000, 0.000000000000000000 ) ) ;
#58504 = CARTESIAN_POINT ( 'NONE',  ( 5.676582343749997150, 232.5520833367473301, -9.832129032723418760 ) ) ;
#58505 = CARTESIAN_POINT ( 'NONE',  ( -32.92256969242384912, 41.53940249566237952, 64.99999999999998579 ) ) ;
#58506 = CARTESIAN_POINT ( 'NONE',  ( 7.320508075688771044, 51.24999999317203248, 7.320508075688775484 ) ) ;
#58507 = CARTESIAN_POINT ( 'NONE',  ( 23.99999999999997513, 197.8125000000000284, 171.6568542494922553 ) ) ;
#58508 = B_SPLINE_CURVE_WITH_KNOTS ( 'NONE', 3,
 ( #3579, #31874, #66195, #26571, #49595, #19797, #60163, #65820, #20917, #72611, #43938, #37161, #55646, #25820, #14127, #66947, #15251, #38285 ),
 .UNSPECIFIED., .F., .F.,
 ( 4, 2, 2, 2, 2, 2, 2, 2, 4 ),
 ( 0.01486571574505567324, 0.01549490539733627999, 0.01612409504961688847, 0.01675328470189749522, 0.01738247435417810197, 0.01801166400645870871, 0.01864085365873931546, 0.01927004331101992221, 0.01989923296330052896 ),
 .UNSPECIFIED. ) ;
#58509 = CARTESIAN_POINT ( 'NONE',  ( -11.35316468749999785, 23.07291666325268054, -3.042071309553167513 ) ) ;
#58510 = CARTESIAN_POINT ( 'NONE',  ( -32.00000000000000711, 199.1875000000000284, 168.3431457505080289 ) ) ;
#58511 = CARTESIAN_POINT ( 'NONE',  ( 9.832129032723420536, 216.5104166632526983, -5.676582343749999815 ) ) ;
#58512 = FACE_OUTER_BOUND ( 'NONE', #9547, .T. ) ;
#58514 = CARTESIAN_POINT ( 'NONE',  ( 38.00000000000000000, 53.00000000000000000, 15.00000000000000178 ) ) ;
#58513 = CARTESIAN_POINT ( 'NONE',  ( -6.735557395310442023E-16, 11.00000000000000000, 99.62499999999998579 ) ) ;
#58515 = ORIENTED_EDGE ( 'NONE', *, *, #42545, .F. ) ;
#58516 = CARTESIAN_POINT ( 'NONE',  ( 3.458734124999960358, 195.6250000013656063, 143.4326545832176976 ) ) ;
#58517 = CARTESIAN_POINT ( 'NONE',  ( -9.832129032723420536, 33.69791666325268409, 5.676582343749997150 ) ) ;
#58518 = CARTESIAN_POINT ( 'NONE',  ( -4.556349186104045934, 11.00000000000000000, 86.40625000409677625 ) ) ;
#58519 = CARTESIAN_POINT ( 'NONE',  ( -2.445694354108840063, 207.0625000013656063, 139.5543056458912190 ) ) ;
#58520 = PLANE ( 'NONE',  #40809 ) ;
#58521 = CARTESIAN_POINT ( 'NONE',  ( 7.778174593052021635, 7.778174593052023411, 100.9374999999999858 ) ) ;
#58523 = CARTESIAN_POINT ( 'NONE',  ( -11.35316468750000141, 18.48958332991934483, 3.042071309553159963 ) ) ;
#58522 = CARTESIAN_POINT ( 'NONE',  ( -5.082755093536325930, 105.9687500020483952, -5.082755093536325930 ) ) ;
#58524 = CARTESIAN_POINT ( 'NONE',  ( -3.313708498984758943, -7.999999999999989342, 13.11155277982336465 ) ) ;
#58525 = CARTESIAN_POINT ( 'NONE',  ( -9.832129032723420536, 148.6979166632526983, 5.676582343749997150 ) ) ;
#58526 = CARTESIAN_POINT ( 'NONE',  ( -7.320508075688778149, 119.9999999931720396, 7.320508075688769267 ) ) ;
#58527 = CARTESIAN_POINT ( 'NONE',  ( -7.188101187499999156, 114.1250000020483952, 2.977408999572654924 ) ) ;
#58528 = DIRECTION ( 'NONE',  ( 0.000000000000000000, 0.000000000000000000, 1.000000000000000000 ) ) ;
#58529 = CARTESIAN_POINT ( 'NONE',  ( -29.43265458321766559, 204.7500000013656063, 166.5412658750003629 ) ) ;
#58530 = ORIENTED_EDGE ( 'NONE', *, *, #65207, .F. ) ;
#58531 = CARTESIAN_POINT ( 'NONE',  ( -8.311093377946841443, 4.218749996586016238, 8.311093377946834337 ) ) ;
#58532 = ORIENTED_EDGE ( 'NONE', *, *, #68019, .T. ) ;
#58533 = FACE_OUTER_BOUND ( 'NONE', #47474, .T. ) ;
#58534 = CARTESIAN_POINT ( 'NONE',  ( 1.226468279477575784E-15, 297.7031250017070079, 6.676582343750001591 ) ) ;
#58536 = CARTESIAN_POINT ( 'NONE',  ( 8.311093377946837890, 141.4062499965860127, -8.311093377946837890 ) ) ;
#58535 = CARTESIAN_POINT ( 'NONE',  ( 2.679491924311306672, 246.4583333333333144, 9.999999999999957367 ) ) ;
#58537 = CARTESIAN_POINT ( 'NONE',  ( 5.000000000000000000, 52.35862550122993042, -48.98731492261362064 ) ) ;
#58538 = CARTESIAN_POINT ( 'NONE',  ( -3.313708498984758943, -7.999999999999989342, 20.66780278432982598 ) ) ;
#58539 =( BOUNDED_CURVE ( )  B_SPLINE_CURVE ( 2, ( #20889, #8454, #15597, #43152, #38636, #31474, #72955, #61260, #54498 ),
 .UNSPECIFIED., .F., .F. ) 
 B_SPLINE_CURVE_WITH_KNOTS ( ( 3, 2, 2, 2, 3 ),
 ( 0.5588235294117644969, 0.5624999999999997780, 0.5661764705882350590, 0.5698529411764704511, 0.5735294117647057321 ),
 .UNSPECIFIED. ) 
 CURVE ( )  GEOMETRIC_REPRESENTATION_ITEM ( )  RATIONAL_B_SPLINE_CURVE ( ( 1.000000000000004663, 0.9238795325112821866, 1.000000000000000000, 0.9238795325112867385, 1.000000000000000000, 0.9238795325112867385, 1.000000000000000000, 0.9238795325112890700, 0.9999999999999976685 ) ) 
 REPRESENTATION_ITEM ( '' )  );
#58540 = CARTESIAN_POINT ( 'NONE',  ( 59.05816676805604004, 216.3380951397245155, 46.96481239528198870 ) ) ;
#58541 = CARTESIAN_POINT ( 'NONE',  ( 11.35316468749999608, 241.6145833367473585, -3.042071309553167069 ) ) ;
#58542 = CIRCLE ( 'NONE', #68169, 7.141428428542858420 ) ;
#58543 = CARTESIAN_POINT ( 'NONE',  ( -10.18810118749999916, 4.220049686691934809, 93.43750000204836681 ) ) ;
#58544 = EDGE_LOOP ( 'NONE', ( #18896, #60555, #58532, #29325 ) ) ;
#58545 = EDGE_CURVE ( 'NONE', #16961, #33538, #36075, .T. ) ;
#58546 = EDGE_CURVE ( 'NONE', #41315, #33033, #33818, .T. ) ;
#58547 = AXIS2_PLACEMENT_3D ( 'NONE', #3821, #48702, #44179 ) ;
#58548 = CARTESIAN_POINT ( 'NONE',  ( 10.00000000000000533, 120.2083333333333428, -2.679491924311227624 ) ) ;
#58549 = CARTESIAN_POINT ( 'NONE',  ( -7.347880794884122694E-16, 8.750000000000000000, 4.000000000000001776 ) ) ;
#58550 = CARTESIAN_POINT ( 'NONE',  ( 9.832129032723420536, 91.51041666325268409, -5.676582343749999815 ) ) ;
#58551 = CARTESIAN_POINT ( 'NONE',  ( -6.238412754330611322E-16, 10.18810118749999916, 104.7812500020483810 ) ) ;
#58552 = CARTESIAN_POINT ( 'NONE',  ( -1.881053915767121776, 15.74999999863440436, -4.541265875000002339 ) ) ;
#58553 = ORIENTED_EDGE ( 'NONE', *, *, #49490, .T. ) ;
#58554 = ORIENTED_EDGE ( 'NONE', *, *, #51625, .T. ) ;
#58555 = CARTESIAN_POINT ( 'NONE',  ( -5.656854249492381470, 5.437500000000000888, 5.656854249492379694 ) ) ;
#58556 = CARTESIAN_POINT ( 'NONE',  ( -4.898587196589412829E-16, 106.6250000000000000, -8.000000000000000000 ) ) ;
#58557 = CARTESIAN_POINT ( 'NONE',  ( -1.320432766682874540E-15, 3.093749997951610542, 7.188101187500000044 ) ) ;
#58558 = CARTESIAN_POINT ( 'NONE',  ( 8.000000000000000000, 121.4375000040967763, -9.797174393178825657E-16 ) ) ;
#58559 = EDGE_CURVE ( 'NONE', #4846, #54105, #42862, .T. ) ;
#58560 =( BOUNDED_CURVE ( )  B_SPLINE_CURVE ( 2, ( #52658, #17951, #625, #45496, #69636, #63976, #6639, #29643, #42797, #37152, #13013, #59796, #8858, #13379, #8109, #60155, #24706, #48832, #59431, #13741, #2079, #42428, #19789, #36051, #48088, #71839, #42059, #47355, #14119, #36417, #14491, #20155, #25070, #53770, #2823, #64716, #59067, #7376, #43172, #70737, #71096, #30383, #65813, #70380, #54140, #1360, #19416, #65446, #19056, #7743, #30749, #25813, #36786, #2450, #8475, #24345, #25443, #31112, #48458, #65066, #53403, #54516, #66189, #31495, #1726, #71464, #37531, #60531, #18695, #31866, #41702, #47716, #32250, #61660, #9978, #3573, #49207, #49588, #73349, #10349, #50328, #21653, #27688, #33374, #38278, #50696, #44679, #4695, #37908, #56375, #72217, #73715, #16352, #44306, #60905, #61283, #9228, #9611, #39390, #49962, #21282, #14869, #26943, #22026, #20911, #26188, #67694, #66941, #68062, #15991, #32630, #27312, #62025, #3200, #55267, #26563, #72603, #45052, #39022, #43931, #62389, #66559, #10714, #54889, #20531, #15618, #43543, #3954, #15245, #55639, #56010, #72977, #67321, #38657, #33009, #4323, #52567, #28438, #40879, #64259, #69175, #40131, #536, #18236, #57122, #5811, #62755, #34500, #11096, #34121, #40506, #45789, #63884, #69926, #23893, #57506, #906, #5435, #63511, #11833, #51445, #51076, #17486, #39754, #23147, #28807, #23516, #6552, #12196, #17108, #29558, #46531, #58252, #16728, #35233, #74089, #46902, #41251, #46159, #74458, #63138, #11466, #34870, #51825, #170, #57875, #22766, #6183, #33747, #29191, #68799, #69550, #56750, #52204, #17861, #22388, #5069, #68425, #28065, #45409, #12568, #70294, #31402, #48373, #7289, #8020, #1994, #65726, #13293, #43084, #59347, #30665, #2736, #47267, #30297, #58982, #36701, #60067, #24622, #37067, #7659, #54430, #53317, #19702, #35596, #48002, #31028, #14029, #41974, #36333, #53683, #18608, #48745, #24255, #41619, #24986, #70653, #8389, #58610, #1641, #64631 ),
 .UNSPECIFIED., .F., .F. ) 
 B_SPLINE_CURVE_WITH_KNOTS ( ( 3, 2, 2, 2, 2, 2, 2, 2, 2, 2, 2, 2, 2, 2, 2, 2, 2, 2, 2, 2, 2, 2, 2, 2, 2, 2, 2, 2, 2, 2, 2, 2, 2, 2, 2, 2, 2, 2, 2, 2, 2, 2, 2, 2, 2, 2, 2, 2, 2, 2, 2, 2, 2, 2, 2, 2, 2, 2, 2, 2, 2, 2, 2, 2, 2, 2, 2, 2, 2, 2, 2, 2, 2, 2, 2, 2, 2, 2, 2, 2, 2, 2, 2, 2, 2, 2, 2, 2, 2, 2, 2, 2, 2, 2, 2, 2, 2, 2, 2, 2, 2, 2, 2, 2, 2, 2, 2, 2, 2, 2, 2, 2, 2, 2, 2, 2, 2, 2, 2, 2, 3 ),
 ( 0.000000000000000000, 0.008333333333333333218, 0.01666666666666666644, 0.02500000000000000139, 0.03333333333333333287, 0.04166666666666666435, 0.05000000000000000278, 0.05833333333333333426, 0.06666666666666666574, 0.07499999999999999722, 0.08333333333333332871, 0.09166666666666666019, 0.1000000000000000056, 0.1083333333333333370, 0.1166666666666666685, 0.1250000000000000000, 0.1333333333333333315, 0.1416666666666666630, 0.1499999999999999944, 0.1583333333333333259, 0.1666666666666666574, 0.1749999999999999889, 0.1833333333333333204, 0.1916666666666666796, 0.2000000000000000111, 0.2083333333333333426, 0.2166666666666666741, 0.2250000000000000056, 0.2333333333333333370, 0.2416666666666666685, 0.2500000000000000000, 0.2583333333333333592, 0.2666666666666666630, 0.2750000000000000222, 0.2833333333333333259, 0.2916666666666666852, 0.2999999999999999889, 0.3083333333333333481, 0.3166666666666666519, 0.3250000000000000111, 0.3333333333333333148, 0.3416666666666666741, 0.3499999999999999778, 0.3583333333333333370, 0.3666666666666666408, 0.3750000000000000000, 0.3833333333333333592, 0.3916666666666666630, 0.4000000000000000222, 0.4083333333333333259, 0.4166666666666666852, 0.4249999999999999889, 0.4333333333333333481, 0.4416666666666666519, 0.4500000000000000111, 0.4583333333333333148, 0.4666666666666666741, 0.4749999999999999778, 0.4833333333333333370, 0.4916666666666666408, 0.5000000000000000000, 0.5083333333333333037, 0.5166666666666667185, 0.5250000000000000222, 0.5333333333333333259, 0.5416666666666666297, 0.5500000000000000444, 0.5583333333333333481, 0.5666666666666666519, 0.5749999999999999556, 0.5833333333333333703, 0.5916666666666666741, 0.5999999999999999778, 0.6083333333333332815, 0.6166666666666666963, 0.6250000000000000000, 0.6333333333333333037, 0.6416666666666667185, 0.6500000000000000222, 0.6583333333333333259, 0.6666666666666666297, 0.6750000000000000444, 0.6833333333333333481, 0.6916666666666666519, 0.6999999999999999556, 0.7083333333333333703, 0.7166666666666666741, 0.7249999999999999778, 0.7333333333333332815, 0.7416666666666666963, 0.7500000000000000000, 0.7583333333333333037, 0.7666666666666667185, 0.7750000000000000222, 0.7833333333333333259, 0.7916666666666666297, 0.8000000000000000444, 0.8083333333333333481, 0.8166666666666666519, 0.8249999999999999556, 0.8333333333333333703, 0.8416666666666666741, 0.8499999999999999778, 0.8583333333333332815, 0.8666666666666666963, 0.8750000000000000000, 0.8833333333333333037, 0.8916666666666667185, 0.9000000000000000222, 0.9083333333333333259, 0.9166666666666666297, 0.9250000000000000444, 0.9333333333333333481, 0.9416666666666666519, 0.9499999999999999556, 0.9583333333333333703, 0.9666666666666666741, 0.9749999999999999778, 0.9833333333333332815, 0.9916666666666666963, 0.9985233269883790896 ),
 .UNSPECIFIED. ) 
 CURVE ( )  GEOMETRIC_REPRESENTATION_ITEM ( )  RATIONAL_B_SPLINE_CURVE ( ( 1.000000000000000000, 0.9238795325112867385, 1.000000000000000000, 0.9238795325112867385, 1.000000000000000000, 0.9238795325112867385, 1.000000000000000000, 0.9238795325112867385, 1.000000000000000000, 0.9238795325112867385, 1.000000000000000000, 0.9238795325112867385, 1.000000000000000000, 0.9238795325112867385, 1.000000000000000000, 0.9238795325112867385, 1.000000000000000000, 0.9238795325112867385, 1.000000000000000000, 0.9238795325112867385, 1.000000000000000000, 0.9238795325112867385, 1.000000000000000000, 0.9238795325112867385, 1.000000000000000000, 0.9238795325112867385, 1.000000000000000000, 0.9238795325112867385, 1.000000000000000000, 0.9238795325112867385, 1.000000000000000000, 0.9238795325112867385, 1.000000000000000000, 0.9238795325112867385, 1.000000000000000000, 0.9238795325112867385, 1.000000000000000000, 0.9238795325112867385, 1.000000000000000000, 0.9238795325112867385, 1.000000000000000000, 0.9238795325112867385, 1.000000000000000000, 0.9238795325112867385, 1.000000000000000000, 0.9238795325112867385, 1.000000000000000000, 0.9238795325112867385, 1.000000000000000000, 0.9238795325112867385, 1.000000000000000000, 0.9238795325112867385, 1.000000000000000000, 0.9238795325112867385, 1.000000000000000000, 0.9238795325112867385, 1.000000000000000000, 0.9238795325112867385, 1.000000000000000000, 0.9238795325112867385, 1.000000000000000000, 0.9238795325112867385, 1.000000000000000000, 0.9238795325112867385, 1.000000000000000000, 0.9238795325112867385, 1.000000000000000000, 0.9238795325112867385, 1.000000000000000000, 0.9238795325112867385, 1.000000000000000000, 0.9238795325112867385, 1.000000000000000000, 0.9238795325112867385, 1.000000000000000000, 0.9238795325112867385, 1.000000000000000000, 0.9238795325112867385, 1.000000000000000000, 0.9238795325112867385, 1.000000000000000000, 0.9238795325112867385, 1.000000000000000000, 0.9238795325112867385, 1.000000000000000000, 0.9238795325112867385, 1.000000000000000000, 0.9238795325112867385, 1.000000000000000000, 0.9238795325112867385, 1.000000000000000000, 0.9238795325112867385, 1.000000000000000000, 0.9238795325112867385, 1.000000000000000000, 0.9238795325112867385, 1.000000000000000000, 0.9238795325112867385, 1.000000000000000000, 0.9238795325112867385, 1.000000000000000000, 0.9238795325112867385, 1.000000000000000000, 0.9238795325112867385, 1.000000000000000000, 0.9238795325112867385, 1.000000000000000000, 0.9238795325112867385, 1.000000000000000000, 0.9238795325112867385, 1.000000000000000000, 0.9238795325112867385, 1.000000000000000000, 0.9238795325112867385, 1.000000000000000000, 0.9238795325112867385, 1.000000000000000000, 0.9238795325112867385, 1.000000000000000000, 0.9238795325112867385, 1.000000000000000000, 0.9238795325112867385, 1.000000000000000000, 0.9238795325112867385, 1.000000000000000000, 0.9238795325112867385, 1.000000000000000000, 0.9238795325112867385, 1.000000000000000000, 0.9238795325112867385, 1.000000000000000000, 0.9238795325112867385, 1.000000000000000000, 0.9238795325112867385, 1.000000000000000000, 0.9238795325112867385, 1.000000000000000000, 0.9238795325112867385, 1.000000000000000000, 0.9238795325112867385, 1.000000000000000000, 0.9238795325112867385, 1.000000000000000000, 0.9238795325112867385, 1.000000000000000000, 0.9238795325112867385, 1.000000000000000000, 0.9238795325112867385, 1.000000000000000000, 0.9238795325112867385, 1.000000000000000000, 0.9238795325112867385, 1.000000000000000000, 0.9238795325112867385, 1.000000000000000000, 0.9238795325112867385, 1.000000000000000000, 0.9238795325112867385, 1.000000000000000000, 0.9238795325112867385, 1.000000000000000000, 0.9238795325112867385, 1.000000000000000000, 0.9238795325112867385, 1.000000000000000000, 0.9238795325112867385, 1.000000000000000000, 0.9238795325112867385, 1.000000000000000000, 0.9238795325112867385, 1.000000000000000000, 0.9238795325112867385, 1.000000000000000000, 0.9238795325112867385, 1.000000000000000000, 0.9238795325112867385, 1.000000000000000000, 0.9238795325112867385, 1.000000000000000000, 0.9238795325112867385, 1.000000000000000000, 0.9238795325112867385, 1.000000000000000000, 0.9238795325112867385, 1.000000000000000000, 0.9238795325112867385, 1.000000000000000000, 0.9238795325112867385, 1.000000000000000000, 0.9238795325112867385, 1.000000000000000000, 0.9238795325112867385, 1.000000000000000000, 0.9238795325112867385, 1.000000000000000000, 0.9238795325112867385, 1.000000000000000000, 0.9238795325112867385, 1.000000000000000000, 0.9238795325112867385, 1.000000000000000000, 0.9238795325112867385, 1.000000000000000000, 0.9238795325112867385, 1.000000000000000000, 0.9238795325112867385, 1.000000000000000000, 0.9238795325112867385, 1.000000000000000000, 0.9238795325112867385, 1.000000000000000000, 0.9238795325112867385, 1.000000000000000000, 0.9238795325112867385, 1.000000000000000000, 0.9238795325112867385, 1.000000000000000000, 0.9238795325112867385, 1.000000000000000000, 0.9238795325112867385, 1.000000000000000000, 0.9238795325112867385, 1.000000000000000000, 0.9238795325112867385, 1.000000000000000000, 0.9238795325112867385, 1.000000000000000000, 0.9238795325112867385, 1.000000000000000000, 0.9238795325112867385, 1.000000000000000000, 0.9238795325112867385, 1.000000000000000000, 0.9238795325112867385, 1.000000000000000000, 0.9238795325112867385, 1.000000000000000000, 0.9238795325112867385, 1.000000000000000000, 0.9373681373079927326, 0.9778031724868398999 ) ) 
 REPRESENTATION_ITEM ( '' )  );
#58561 = CARTESIAN_POINT ( 'NONE',  ( 1.871523826299183495E-15, -10.18810118749999916, 101.4062500020483810 ) ) ;
#58562 = CARTESIAN_POINT ( 'NONE',  ( 1.656854249492381248, 0.1875000000000001943, -4.000000000000001776 ) ) ;
#58563 = CARTESIAN_POINT ( 'NONE',  ( -4.000000000000001776, 15.24999999726881406, -4.898587196589415787E-16 ) ) ;
#58564 = VERTEX_POINT ( 'NONE', #48341 ) ;
#58565 = CARTESIAN_POINT ( 'NONE',  ( -3.313708498984765161, 5.343749995903221084, 7.999999999999998224 ) ) ;
#58566 = CARTESIAN_POINT ( 'NONE',  ( -2.445694354108782775, 200.5625000013656063, 200.4456943541088663 ) ) ;
#58568 = CARTESIAN_POINT ( 'NONE',  ( -10.00000000000033218, 22.50000000000019185, -1.224646799147393686E-15 ) ) ;
#58567 = CARTESIAN_POINT ( 'NONE',  ( -31.45873412500001720, 199.6250000013656063, 168.5673454167828140 ) ) ;
#58569 = CARTESIAN_POINT ( 'NONE',  ( -4.541265875000002339, 13.74999999863440969, -1.881053915767121998 ) ) ;
#58570 = DIRECTION ( 'NONE',  ( -0.000000000000000000, -0.000000000000000000, -1.000000000000000000 ) ) ;
#58571 = CARTESIAN_POINT ( 'NONE',  ( -7.188101187499991163, 2.977408999572646930, 10.39280278187175810 ) ) ;
#58572 = ORIENTED_EDGE ( 'NONE', *, *, #70648, .F. ) ;
#58573 = VERTEX_POINT ( 'NONE', #58950 ) ;
#58574 = CARTESIAN_POINT ( 'NONE',  ( -4.220049686691937474, -10.18810118749999738, 106.9375000020483810 ) ) ;
#58575 = CARTESIAN_POINT ( 'NONE',  ( -12.04876049975181296, -13.82825457289352755, -0.1850551574587747938 ) ) ;
#58576 = CARTESIAN_POINT ( 'NONE',  ( -30.82842712474621294, 205.1250000000000284, 167.1715728752542134 ) ) ;
#58577 = CARTESIAN_POINT ( 'NONE',  ( 1.432654583217662481, 200.1250000013656063, 194.5412658750000219 ) ) ;
#58578 = CARTESIAN_POINT ( 'NONE',  ( 29.43265458321760519, 194.8750000013656347, 166.5412658749999650 ) ) ;
#58579 = CARTESIAN_POINT ( 'NONE',  ( 7.320508075688771044, 94.37500000000000000, 7.320508075688775484 ) ) ;
#58580 = CARTESIAN_POINT ( 'NONE',  ( -8.000000000000000000, 120.5000000000000000, 0.000000000000000000 ) ) ;
#58581 = CARTESIAN_POINT ( 'NONE',  ( -8.311093377946841443, 64.21874999658601268, 8.311093377946830785 ) ) ;
#58582 = CARTESIAN_POINT ( 'NONE',  ( 4.721056650415999201, 297.2343750017069510, -4.721056650415999201 ) ) ;
#58583 =( GEOMETRIC_REPRESENTATION_CONTEXT ( 3 ) GLOBAL_UNCERTAINTY_ASSIGNED_CONTEXT ( ( #29235 ) ) GLOBAL_UNIT_ASSIGNED_CONTEXT ( ( #30986, #36288, #1953 ) ) REPRESENTATION_CONTEXT ( 'NONE', 'WORKASPACE' ) );
#58584 = ORIENTED_EDGE ( 'NONE', *, *, #29591, .T. ) ;
#58585 = CARTESIAN_POINT ( 'NONE',  ( -2.679491924311087736, 145.4166666598386826, 10.00000000000008349 ) ) ;
#58586 = AXIS2_PLACEMENT_3D ( 'NONE', #48359, #1629, #2350 ) ;
#58587 = CARTESIAN_POINT ( 'NONE',  ( -8.000000000000000000, 15.56249999590322197, -9.797174393178825657E-16 ) ) ;
#58588 = CARTESIAN_POINT ( 'NONE',  ( 3.458734124999959914, 207.4375000013656063, 142.0000000000000568 ) ) ;
#58589 = CARTESIAN_POINT ( 'NONE',  ( 5.000000000000007105, 85.83333333333335702, -8.660254037844396180 ) ) ;
#58590 = FILL_AREA_STYLE_COLOUR ( '', #68449 ) ;
#58591 = CARTESIAN_POINT ( 'NONE',  ( -7.320508075688770155, 230.6250000000000284, 7.320508075688774596 ) ) ;
#58592 = DIRECTION ( 'NONE',  ( 0.000000000000000000, 0.000000000000000000, -1.000000000000000000 ) ) ;
#58593 = CARTESIAN_POINT ( 'NONE',  ( -7.204075437095967871, 7.204075437095967871, 67.84375000204836681 ) ) ;
#58594 = CARTESIAN_POINT ( 'NONE',  ( 4.999999999999993783, 209.1666666666666572, 8.660254037844390851 ) ) ;
#58595 = CARTESIAN_POINT ( 'NONE',  ( -5.082755093536317936, -5.082755093536320601, 9.549052781871754547 ) ) ;
#58596 = CARTESIAN_POINT ( 'NONE',  ( -8.311093377946836114, 187.9687499965860411, -8.311093377946837890 ) ) ;
#58597 = CARTESIAN_POINT ( 'NONE',  ( -4.541265875000002339, 0.7499999986344069169, -1.881053915767121998 ) ) ;
#58598 = CARTESIAN_POINT ( 'NONE',  ( 6.123233995736767268E-16, 178.1249999931720538, -10.00000000000000178 ) ) ;
#58600 = DIRECTION ( 'NONE',  ( 0.000000000000000000, -0.000000000000000000, 1.000000000000000000 ) ) ;
#58599 = CARTESIAN_POINT ( 'NONE',  ( 8.000000000000014211, -3.313708498984734518, 20.98655277982335932 ) ) ;
#58601 = VERTEX_POINT ( 'NONE', #53653 ) ;
#58602 = CARTESIAN_POINT ( 'NONE',  ( -3.458734125000015425, 194.9375000013655779, 142.0000000000000568 ) ) ;
#58603 = CARTESIAN_POINT ( 'NONE',  ( -3.042071309553164404, 32.55208332991934128, -11.35316468749999963 ) ) ;
#58604 = CARTESIAN_POINT ( 'NONE',  ( 11.00000000000000000, 1.347111479062088405E-15, 106.9375000040967763 ) ) ;
#58605 = CARTESIAN_POINT ( 'NONE',  ( 11.35316468750000141, 221.0937499965860127, 0.000000000000000000 ) ) ;
#58606 = CARTESIAN_POINT ( 'NONE',  ( -31.45873412499999944, 206.6875000013656063, 170.0000000000004547 ) ) ;
#58607 = CARTESIAN_POINT ( 'NONE',  ( -1.836970198721029983E-15, 125.6249999931720254, 10.00000000000000178 ) ) ;
#58609 = CARTESIAN_POINT ( 'NONE',  ( 7.778174593052023411, -7.778174593052021635, 108.2500000040967763 ) ) ;
#58608 = CARTESIAN_POINT ( 'NONE',  ( 2.775557561562891351E-14, 271.9999999999999432, 170.0000000000000284 ) ) ;
#58610 = CARTESIAN_POINT ( 'NONE',  ( 2.445694354108782775, 194.5625000013656063, 139.5543056458912190 ) ) ;
#58611 = VECTOR ( 'NONE', #37081, 1000.000000000000000 ) ;
#58612 = EDGE_CURVE ( 'NONE', #39173, #14438, #18940, .T. ) ;
#58613 = CARTESIAN_POINT ( 'NONE',  ( 10.00000000000000000, 81.66666665983869677, 2.679491924311236062 ) ) ;
#58614 = CARTESIAN_POINT ( 'NONE',  ( -7.188101187499999156, 98.75000000204838102, 2.977408999572654924 ) ) ;
#58615 = CARTESIAN_POINT ( 'NONE',  ( -8.342170076843785083E-16, 18.18749999863440792, 4.541265875000002339 ) ) ;
#58616 = CYLINDRICAL_SURFACE ( 'NONE', #32587, 11.00000000000000000 ) ;
#58617 = DIRECTION ( 'NONE',  ( -0.000000000000000000, 1.000000000000000000, -1.563033456626094573E-30 ) ) ;
#58618 = DIRECTION ( 'NONE',  ( 0.000000000000000000, 2.238352872228138170E-16, -1.000000000000000000 ) ) ;
#58619 = ORIENTED_EDGE ( 'NONE', *, *, #64089, .F. ) ;
#58620 = ORIENTED_EDGE ( 'NONE', *, *, #71991, .T. ) ;
#58621 = CARTESIAN_POINT ( 'NONE',  ( -6.676582343750003368, 299.5468750017069510, -2.765530957081996810 ) ) ;
#58622 = CARTESIAN_POINT ( 'NONE',  ( -2.679491924311376838, 141.4583333333333428, -9.999999999999928946 ) ) ;
#58623 = CARTESIAN_POINT ( 'NONE',  ( -30.75960933714538825, -42.99850569349359120, 166.0223858372369250 ) ) ;
#58624 = CARTESIAN_POINT ( 'NONE',  ( -9.832129032723420536, 158.6979166632526983, 5.676582343749997150 ) ) ;
#58625 = CARTESIAN_POINT ( 'NONE',  ( -4.220049686691937474, -10.18810118749999738, 85.93750000204839523 ) ) ;
#58626 = CARTESIAN_POINT ( 'NONE',  ( 4.000000000000015987, 203.5000000000000000, 198.0000000000000284 ) ) ;
#58627 = FACE_BOUND ( 'NONE', #62732, .T. ) ;
#58628 = CARTESIAN_POINT ( 'NONE',  ( 1.871523826299183495E-15, -10.18810118749999916, 111.9062500020483810 ) ) ;
#58629 = ORIENTED_EDGE ( 'NONE', *, *, #58223, .T. ) ;
#58630 = FACE_OUTER_BOUND ( 'NONE', #20459, .T. ) ;
#58631 = FACE_OUTER_BOUND ( 'NONE', #71156, .T. ) ;
#58632 = CARTESIAN_POINT ( 'NONE',  ( -3.042071309553173730, 139.6354166632526699, 11.35316468749999785 ) ) ;
#58633 = CARTESIAN_POINT ( 'NONE',  ( 1.432654583217664479, 196.7500000013656063, 201.4587341250000065 ) ) ;
#58634 = CARTESIAN_POINT ( 'NONE',  ( -3.458734124999960358, 209.6875000013656063, 198.0000000000000284 ) ) ;
#58635 = CARTESIAN_POINT ( 'NONE',  ( -10.18810118749999738, -4.220049686691941915, 75.62500000204838102 ) ) ;
#58636 = CARTESIAN_POINT ( 'NONE',  ( -11.35316468749999785, 48.38541666325268409, -3.042071309553167513 ) ) ;
#58637 = VERTEX_POINT ( 'NONE', #30268 ) ;
#58638 = CARTESIAN_POINT ( 'NONE',  ( -8.660254037844390851, 27.08333333333333925, -5.000000000000007994 ) ) ;
#58639 = CARTESIAN_POINT ( 'NONE',  ( -1.881053915767124440, 3.124999998634407028, 4.541265875000001451 ) ) ;
#58640 = CARTESIAN_POINT ( 'NONE',  ( 8.008118988124991233, 9.807117285998411148E-16, 13.76311528394063011 ) ) ;
#58641 = EDGE_CURVE ( 'NONE', #4004, #71916, #65694, .T. ) ;
#58642 = EDGE_CURVE ( 'NONE', #30848, #36205, #36301, .T. ) ;
#58643 = CARTESIAN_POINT ( 'NONE',  ( 4.401442555609581635E-16, 14.34374999795161187, -7.188101187500000044 ) ) ;
#58644 = CARTESIAN_POINT ( 'NONE',  ( -6.000000000000001776, 293.0625000034140157, 0.000000000000000000 ) ) ;
#58645 = CARTESIAN_POINT ( 'NONE',  ( -33.89651676036610439, -12.20582025699173201, 146.7502335348651741 ) ) ;
#58646 = CARTESIAN_POINT ( 'NONE',  ( -2.977408999572654480, 6.374999997951610098, 7.188101187499999156 ) ) ;
#58647 = CARTESIAN_POINT ( 'NONE',  ( -7.188101187499990274, -2.977408999572651815, 10.58030278187175455 ) ) ;
#58648 = CARTESIAN_POINT ( 'NONE',  ( 7.204075437095968759, -7.204075437095966983, 69.71875000204836681 ) ) ;
#58649 =( BOUNDED_CURVE ( )  B_SPLINE_CURVE ( 2, ( #11485, #17129, #62410, #27710, #44699, #68444, #39773, #4716, #11118 ),
 .UNSPECIFIED., .F., .F. ) 
 B_SPLINE_CURVE_WITH_KNOTS ( ( 3, 2, 2, 2, 3 ),
 ( 0.7666666666666673846, 0.7750000000000006883, 0.7833333333333339921, 0.7916666666666672958, 0.8000000000000007105 ),
 .UNSPECIFIED. ) 
 CURVE ( )  GEOMETRIC_REPRESENTATION_ITEM ( )  RATIONAL_B_SPLINE_CURVE ( ( 0.9999999999999938938, 0.9238795325112928447, 1.000000000000000000, 0.9238795325112867385, 1.000000000000000000, 0.9238795325112867385, 1.000000000000000000, 0.9238795325112806323, 1.000000000000005995 ) ) 
 REPRESENTATION_ITEM ( '' )  );
#58650 = CARTESIAN_POINT ( 'NONE',  ( -24.54126587500000056, 205.5000000013655779, 168.5673454167827003 ) ) ;
#58651 = CARTESIAN_POINT ( 'NONE',  ( 6.123233995736767268E-16, 63.12499999317203248, -10.00000000000000178 ) ) ;
#58652 = CARTESIAN_POINT ( 'NONE',  ( -2.828427124746192067, 1.374999997268813168, 2.828427124746190735 ) ) ;
#58653 = ORIENTED_EDGE ( 'NONE', *, *, #10778, .F. ) ;
#58654 = CARTESIAN_POINT ( 'NONE',  ( 1.432654583217662481, 209.1250000013656631, 194.5412658750000219 ) ) ;
#58655 = EDGE_CURVE ( 'NONE', #44173, #8420, #1496, .T. ) ;
#58656 = CARTESIAN_POINT ( 'NONE',  ( -2.751064625579944321E-14, 204.7500000000000284, 146.0000000000000284 ) ) ;
#58657 = CARTESIAN_POINT ( 'NONE',  ( -27.99999999999991118, 200.6250000027312126, 174.0000000000003695 ) ) ;
#58658 = CARTESIAN_POINT ( 'NONE',  ( -5.082755093536325930, 119.4687500020483810, -5.082755093536325930 ) ) ;
#58659 = DIRECTION ( 'NONE',  ( 0.000000000000000000, 1.000000000000000000, 0.000000000000000000 ) ) ;
#58660 = VECTOR ( 'NONE', #13727, 1000.000000000000000 ) ;
#58661 = CARTESIAN_POINT ( 'NONE',  ( -7.999999999999989342, -3.313708498984762496, 2.611552783920144005 ) ) ;
#58662 = ORIENTED_EDGE ( 'NONE', *, *, #52060, .T. ) ;
#58664 =( BOUNDED_CURVE ( )  B_SPLINE_CURVE ( 2, ( #38286, #61291, #9618, #34128, #543, #23153, #58257, #40885, #46539 ),
 .UNSPECIFIED., .F., .F. ) 
 B_SPLINE_CURVE_WITH_KNOTS ( ( 3, 2, 2, 2, 3 ),
 ( 0.1477272727272727348, 0.1534090909090909116, 0.1590909090909091161, 0.1647727272727272929, 0.1704545454545454697 ),
 .UNSPECIFIED. ) 
 CURVE ( )  GEOMETRIC_REPRESENTATION_ITEM ( )  RATIONAL_B_SPLINE_CURVE ( ( 1.000000000000000000, 0.9238795325112867385, 1.000000000000000000, 0.9238795325112867385, 1.000000000000000000, 0.9238795325112867385, 1.000000000000000000, 0.9238795325112864054, 1.000000000000000444 ) ) 
 REPRESENTATION_ITEM ( '' )  );
#58663 = CARTESIAN_POINT ( 'NONE',  ( 7.188101187499999156, 24.37499999795161543, 2.977408999572654924 ) ) ;
#58665 = EDGE_LOOP ( 'NONE', ( #25948, #7447, #71342, #12880 ) ) ;
#58666 = LINE ( 'NONE', #13346, #19532 ) ;
#58667 = CARTESIAN_POINT ( 'NONE',  ( -1.688721909672437294, -10.27943647337372290, -63.64086505882561795 ) ) ;
#58668 = CARTESIAN_POINT ( 'NONE',  ( -4.999999999999998224, 56.66666666666667140, -8.660254037844389075 ) ) ;
#58669 = CARTESIAN_POINT ( 'NONE',  ( 2.977408999572650039, 103.0625000020483810, -7.188101187500001821 ) ) ;
#58670 = CARTESIAN_POINT ( 'NONE',  ( 1.656854249492297093, 204.9375000027312126, 146.0000000000000853 ) ) ;
#58672 = CARTESIAN_POINT ( 'NONE',  ( -19.99999999999993250, -31.99999999999978684, 193.6854385646540209 ) ) ;
#58671 = PLANE ( 'NONE',  #4478 ) ;
#58673 = ORIENTED_EDGE ( 'NONE', *, *, #69902, .T. ) ;
#58674 = ORIENTED_EDGE ( 'NONE', *, *, #56308, .T. ) ;
#58675 = CARTESIAN_POINT ( 'NONE',  ( 11.35316468749999608, 246.6145833367472733, -3.042071309553167069 ) ) ;
#58676 = CARTESIAN_POINT ( 'NONE',  ( -5.082755093536317936, -5.082755093536320601, 15.54905278187175632 ) ) ;
#58677 = LINE ( 'NONE', #6986, #48660 ) ;
#58678 = CARTESIAN_POINT ( 'NONE',  ( 7.999999999999991118, 9.797174393178815797E-16, 3.080302779823361981 ) ) ;
#58679 = CARTESIAN_POINT ( 'NONE',  ( -4.000000000000001776, 17.18749999726881583, -1.656854249492381470 ) ) ;
#58680 = CARTESIAN_POINT ( 'NONE',  ( 2.679491924311225848, 258.5416666666666856, -10.00000000000000000 ) ) ;
#58681 = CARTESIAN_POINT ( 'NONE',  ( 7.999999999999992895, -3.313708498984756279, 19.67405278392015333 ) ) ;
#58682 = CARTESIAN_POINT ( 'NONE',  ( -7.320508075688773708, 176.8750000000000000, -7.320508075688774596 ) ) ;
#58683 = CARTESIAN_POINT ( 'NONE',  ( 7.999999999999950262, -3.313708498984798467, 5.986552779823362869 ) ) ;
#58684 = LINE ( 'NONE', #68876, #21089 ) ;
#58685 = CARTESIAN_POINT ( 'NONE',  ( -7.778174593052020747, -7.778174593052023411, 68.87500000409677625 ) ) ;
#58686 = CARTESIAN_POINT ( 'NONE',  ( -11.35316468749999785, 143.3854166632526983, -3.042071309553167513 ) ) ;
#58687 = CARTESIAN_POINT ( 'NONE',  ( 0.000000000000000000, 0.000000000000000000, -10.77459999999999951 ) ) ;
#58688 = CARTESIAN_POINT ( 'NONE',  ( 5.656854249492379694, 97.62500000409677625, -5.656854249492380582 ) ) ;
#58691 = CARTESIAN_POINT ( 'NONE',  ( -8.660254037844390851, 167.9166666666666856, 5.000000000000000000 ) ) ;
#58690 = CARTESIAN_POINT ( 'NONE',  ( -5.656854249492375253, 5.656854249492375253, 26.14280277982336997 ) ) ;
#58689 = CARTESIAN_POINT ( 'NONE',  ( 26.34314575050763807, 206.5625000000000000, 165.9999999999998863 ) ) ;
#58692 = AXIS2_PLACEMENT_3D ( 'NONE', #43622, #61355, #3270 ) ;
#58693 = EDGE_LOOP ( 'NONE', ( #38613, #60432, #5034, #20433, #2177 ) ) ;
#58694 = CARTESIAN_POINT ( 'NONE',  ( -11.35316468749999785, 3.385416663252682756, -3.042071309553167513 ) ) ;
#58695 = CARTESIAN_POINT ( 'NONE',  ( 1.469576158976823947E-15, 103.0625000040967763, 8.000000000000000000 ) ) ;
#58696 = CARTESIAN_POINT ( 'NONE',  ( 3.262048642599709058, -7.308067487734634327, -0.000000000000000000 ) ) ;
#58697 = CARTESIAN_POINT ( 'NONE',  ( -5.656854249492379694, 4.874999995903221084, -5.656854249492380582 ) ) ;
#58698 = CARTESIAN_POINT ( 'NONE',  ( -8.660254037844387298, 33.95833332650536818, -5.000000000000004441 ) ) ;
#58699 = CARTESIAN_POINT ( 'NONE',  ( 7.188101187500000044, 115.9062500020483810, -8.802885111219163269E-16 ) ) ;
#58700 = CARTESIAN_POINT ( 'NONE',  ( 4.541265875000002339, 5.499999998634407028, -1.881053915767121554 ) ) ;
#58701 = CARTESIAN_POINT ( 'NONE',  ( 11.00000000000000000, 1.347111479062088405E-15, 85.75000000000000000 ) ) ;
#58702 = CARTESIAN_POINT ( 'NONE',  ( 5.656854249492376141, -5.656854249492374365, 14.89280277982336642 ) ) ;
#58704 = CARTESIAN_POINT ( 'NONE',  ( -8.000000000000001776, 24.65624999590322730, 3.313708498984759387 ) ) ;
#58703 = CARTESIAN_POINT ( 'NONE',  ( -2.679491924311287132, 237.0833333401613743, -9.999999999999968026 ) ) ;
#58705 = ORIENTED_EDGE ( 'NONE', *, *, #33607, .T. ) ;
#58706 = CARTESIAN_POINT ( 'NONE',  ( 10.00000000000000000, 220.6250000068279746, -1.224646799147353256E-15 ) ) ;
#58707 = CARTESIAN_POINT ( 'NONE',  ( -9.999960627438866823, 226.0000000000000284, -0.6562093533521858868 ) ) ;
#58708 = CARTESIAN_POINT ( 'NONE',  ( 2.020667218593132706E-15, -11.00000000000000000, 115.3749999999999858 ) ) ;
#58709 = CARTESIAN_POINT ( 'NONE',  ( -9.832129032723415207, 249.6354166700806445, 5.676582343750005144 ) ) ;
#58710 = CARTESIAN_POINT ( 'NONE',  ( -5.676582343749998039, 112.4479166632526983, -9.832129032723420536 ) ) ;
#58711 = ORIENTED_EDGE ( 'NONE', *, *, #24212, .T. ) ;
#58712 = EDGE_CURVE ( 'NONE', #27943, #1761, #60286, .T. ) ;
#58713 = CARTESIAN_POINT ( 'NONE',  ( -31.99999999999998579, 208.3125000000000000, 171.6568542494928238 ) ) ;
#58714 = CARTESIAN_POINT ( 'NONE',  ( 10.18810118750000093, -4.220049686691933921, 99.81250000204838102 ) ) ;
#58715 = CARTESIAN_POINT ( 'NONE',  ( 46.89594099591772647, 145.9999999999999716, 68.54827124808608119 ) ) ;
#58716 = CARTESIAN_POINT ( 'NONE',  ( 2.839093476692135984E-14, 198.9375000013655779, 201.4587341250000350 ) ) ;
#58717 = CARTESIAN_POINT ( 'NONE',  ( 75.00000000000001421, 242.0000000000000284, 20.00000000000002132 ) ) ;
#58719 = CARTESIAN_POINT ( 'NONE',  ( 11.35316468750000141, 115.7812499965860269, 0.000000000000000000 ) ) ;
#58718 = CARTESIAN_POINT ( 'NONE',  ( 27.99999999999999645, 210.0000000000000284, 169.9999999999999147 ) ) ;
#58720 = CARTESIAN_POINT ( 'NONE',  ( 5.656854249492376141, -5.656854249492374365, 7.580302783920144449 ) ) ;
#58721 = CARTESIAN_POINT ( 'NONE',  ( -31.45873412499999944, 195.8750000013655779, 168.5673454167827572 ) ) ;
#58722 = CARTESIAN_POINT ( 'NONE',  ( 2.679491924311370177, 145.8333333265053966, 9.999999999999918288 ) ) ;
#58723 = ORIENTED_EDGE ( 'NONE', *, *, #12647, .T. ) ;
#58724 = AXIS2_PLACEMENT_3D ( 'NONE', #47331, #12626, #19032 ) ;
#58725 = CARTESIAN_POINT ( 'NONE',  ( 7.320508075688771044, 191.2499999931720538, 7.320508075688775484 ) ) ;
#58726 = CARTESIAN_POINT ( 'NONE',  ( 8.000000000000000000, 112.5312500040967905, -3.313708498984762496 ) ) ;
#58727 = CARTESIAN_POINT ( 'NONE',  ( -7.347880794884122694E-16, 9.750000000000000000, 4.000000000000001776 ) ) ;
#58728 = CARTESIAN_POINT ( 'NONE',  ( 11.35316468750000141, 96.09374999658601268, 0.000000000000000000 ) ) ;
#58729 = CARTESIAN_POINT ( 'NONE',  ( 4.000000000000016875, 205.4375000000000284, 199.6568542494924259 ) ) ;
#58730 = CARTESIAN_POINT ( 'NONE',  ( 5.082755093536324154, 9.656249997951610098, 5.082755093536326818 ) ) ;
#58731 = CARTESIAN_POINT ( 'NONE',  ( 1.871523826299183495E-15, -10.18810118749999916, 92.40625000204836681 ) ) ;
#58732 = CARTESIAN_POINT ( 'NONE',  ( 11.35316468749999785, 10.88541666325268586, 3.042071309553174174 ) ) ;
#58733 = EDGE_LOOP ( 'NONE', ( #58817, #65779, #17543, #26036 ) ) ;
#58734 = CARTESIAN_POINT ( 'NONE',  ( -3.255014963930524218E-15, -13.85640646055106728, -14.80000000000000071 ) ) ;
#58735 = DIRECTION ( 'NONE',  ( -0.000000000000000000, -0.000000000000000000, 1.000000000000000000 ) ) ;
#58736 = CARTESIAN_POINT ( 'NONE',  ( -5.676582343749998039, 217.4479166632526983, -9.832129032723420536 ) ) ;
#58737 = CARTESIAN_POINT ( 'NONE',  ( 1.871523826299183495E-15, -10.18810118749999916, 78.90625000204836681 ) ) ;
#58738 = EDGE_CURVE ( 'NONE', #20975, #17422, #32631, .T. ) ;
#58739 = LINE ( 'NONE', #74592, #59131 ) ;
#58740 = LINE ( 'NONE', #36459, #52347 ) ;
#58741 = CARTESIAN_POINT ( 'NONE',  ( -4.721056650415999201, 291.3281250017069510, -4.721056650415999201 ) ) ;
#58742 = ORIENTED_EDGE ( 'NONE', *, *, #38256, .F. ) ;
#58743 = CARTESIAN_POINT ( 'NONE',  ( 2.751064625579944321E-14, 199.7500000000000000, 194.0000000000000568 ) ) ;
#58744 = CARTESIAN_POINT ( 'NONE',  ( 11.35316468750000141, 211.0937499965860411, 0.000000000000000000 ) ) ;
#58745 = EDGE_CURVE ( 'NONE', #3455, #31632, #18575, .T. ) ;
#58746 = CARTESIAN_POINT ( 'NONE',  ( 10.18810118749999916, 4.220049686691935698, 89.50000000204836681 ) ) ;
#58747 = CARTESIAN_POINT ( 'NONE',  ( -29.43265458321760519, 203.8750000013656063, 173.4587341250003760 ) ) ;
#58748 = CARTESIAN_POINT ( 'NONE',  ( 3.313708498984762496, 22.21875000000000355, 7.999999999999998224 ) ) ;
#58749 = AXIS2_PLACEMENT_3D ( 'NONE', #61262, #48440, #26925 ) ;
#58750 = ORIENTED_EDGE ( 'NONE', *, *, #50525, .T. ) ;
#58751 = CARTESIAN_POINT ( 'NONE',  ( 2.828427124746209831, 207.5000000027312126, 200.8284271247462129 ) ) ;
#58752 = EDGE_CURVE ( 'NONE', #55139, #49656, #9741, .T. ) ;
#58753 = CARTESIAN_POINT ( 'NONE',  ( 10.00000000000000178, 30.00000000000000355, 0.000000000000000000 ) ) ;
#58754 = DIRECTION ( 'NONE',  ( -0.000000000000000000, -0.000000000000000000, 1.000000000000000000 ) ) ;
#58755 = CARTESIAN_POINT ( 'NONE',  ( -10.18810118749999916, 4.220049686691934809, 72.43750000204838102 ) ) ;
#58756 = ORIENTED_EDGE ( 'NONE', *, *, #52568, .T. ) ;
#58757 = DIRECTION ( 'NONE',  ( -0.000000000000000000, 1.000000000000000000, -0.000000000000000000 ) ) ;
#58758 = CARTESIAN_POINT ( 'NONE',  ( 0.000000000000000000, 0.000000000000000000, 0.000000000000000000 ) ) ;
#58759 = EDGE_CURVE ( 'NONE', #51786, #68916, #8722, .T. ) ;
#58760 = LINE ( 'NONE', #46312, #53570 ) ;
#58761 = CARTESIAN_POINT ( 'NONE',  ( 5.082755093536326818, 119.0937500020483810, 5.082755093536325042 ) ) ;
#58762 = CARTESIAN_POINT ( 'NONE',  ( 0.4589999999999999636, 261.4319999999996753, 5.805285082142985331 ) ) ;
#58763 = CARTESIAN_POINT ( 'NONE',  ( 4.721056650416000089, 295.8281250017069510, 4.721056650415999201 ) ) ;
#58765 = DIRECTION ( 'NONE',  ( 0.000000000000000000, -0.8778652960884978373, -0.4789076340208558435 ) ) ;
#58764 = CARTESIAN_POINT ( 'NONE',  ( 11.35316468749999963, 236.4062500034140157, -1.390361679473963556E-15 ) ) ;
#58766 = ITEM_DEFINED_TRANSFORMATION ( 'NONE', 'NONE', #22429,  #57354 ) ;
#58767 =( BOUNDED_CURVE ( )  B_SPLINE_CURVE ( 2, ( #34845, #69901, #40107, #35212, #63113, #23493, #51422, #63860, #28414 ),
 .UNSPECIFIED., .F., .F. ) 
 B_SPLINE_CURVE_WITH_KNOTS ( ( 3, 2, 2, 2, 3 ),
 ( 0.4374999999999980571, 0.4479166666666647423, 0.4583333333333313719, 0.4687499999999980571, 0.4791666666666647423 ),
 .UNSPECIFIED. ) 
 CURVE ( )  GEOMETRIC_REPRESENTATION_ITEM ( )  RATIONAL_B_SPLINE_CURVE ( ( 1.000000000000014211, 0.9238795325112725276, 1.000000000000000000, 0.9238795325112867385, 1.000000000000000000, 0.9238795325112867385, 1.000000000000000000, 0.9238795325113009493, 0.9999999999999857891 ) ) 
 REPRESENTATION_ITEM ( '' )  );
#58768 = ORIENTED_EDGE ( 'NONE', *, *, #42173, .F. ) ;
#58769 = CARTESIAN_POINT ( 'NONE',  ( -8.311093377946834337, 244.8437500034140157, 8.311093377946837890 ) ) ;
#58770 = EDGE_CURVE ( 'NONE', #28197, #46655, #52592, .T. ) ;
#58771 = CARTESIAN_POINT ( 'NONE',  ( 7.188101187499992051, 8.802885111219154394E-16, 5.236552781871753659 ) ) ;
#58772 = CARTESIAN_POINT ( 'NONE',  ( -2.445694354108783219, 201.8125000013656063, 200.4456943541088663 ) ) ;
#58773 = VERTEX_POINT ( 'NONE', #9861 ) ;
#58774 = CARTESIAN_POINT ( 'NONE',  ( -10.18810118749999738, -4.220049686691941915, 67.75000000204836681 ) ) ;
#58775 = CARTESIAN_POINT ( 'NONE',  ( -9.832129032723418760, 103.1770833299193555, -5.676582343750004256 ) ) ;
#58776 = CARTESIAN_POINT ( 'NONE',  ( 0.000000000000000000, 54.99999999999999289, 0.000000000000000000 ) ) ;
#58777 = CARTESIAN_POINT ( 'NONE',  ( 2.020667218593132706E-15, -11.00000000000000000, 76.37499999999998579 ) ) ;
#58780 = CARTESIAN_POINT ( 'NONE',  ( 2.679491924305930084, 71.04166666666714036, -10.00000000000306244 ) ) ;
#58779 = CARTESIAN_POINT ( 'NONE',  ( 31.45873412499998523, 205.7500000013656063, 168.5673454167822172 ) ) ;
#58778 = CARTESIAN_POINT ( 'NONE',  ( 29.43265458321766559, 202.1250000013656063, 166.5412658749999650 ) ) ;
#58781 = ORIENTED_EDGE ( 'NONE', *, *, #29122, .T. ) ;
#58782 = FACE_OUTER_BOUND ( 'NONE', #43869, .T. ) ;
#58783 = LINE ( 'NONE', #12734, #63700 ) ;
#58784 = CARTESIAN_POINT ( 'NONE',  ( -5.676582343750006032, 214.1145833299193555, 9.832129032723418760 ) ) ;
#58785 = CARTESIAN_POINT ( 'NONE',  ( 1.432654583217607858, 204.6250000013655779, 138.5412658750000787 ) ) ;
#58786 = CARTESIAN_POINT ( 'NONE',  ( 24.54126587500000056, 205.3750000013656063, 168.5673454167822172 ) ) ;
#58787 = CARTESIAN_POINT ( 'NONE',  ( 7.188101187500000044, 26.34374999795161543, 0.000000000000000000 ) ) ;
#58788 = CARTESIAN_POINT ( 'NONE',  ( -9.832129032723420536, 179.0104166632526699, 5.676582343749997150 ) ) ;
#58789 = CARTESIAN_POINT ( 'NONE',  ( 2.977408999572654480, 96.50000000204838102, 7.188101187499999156 ) ) ;
#58790 = CARTESIAN_POINT ( 'NONE',  ( 1.102182119232618108E-15, 296.3125000034140157, 6.000000000000001776 ) ) ;
#58791 = CARTESIAN_POINT ( 'NONE',  ( -31.99999999999997868, 195.3125000000000853, 171.6568542494928238 ) ) ;
#58792 = CARTESIAN_POINT ( 'NONE',  ( 4.541265875000002339, 11.31249999863440614, 0.000000000000000000 ) ) ;
#58793 = CARTESIAN_POINT ( 'NONE',  ( 31.45873412499999944, 201.0000000013655779, 168.5673454167822740 ) ) ;
#58794 = CARTESIAN_POINT ( 'NONE',  ( -5.082755093536319713, 5.082755093536319713, 4.674052781871752771 ) ) ;
#58795 = CARTESIAN_POINT ( 'NONE',  ( 6.951808397369818766E-16, 67.03124999658602690, -11.35316468750000141 ) ) ;
#58796 = FACE_OUTER_BOUND ( 'NONE', #71612, .T. ) ;
#58797 = CARTESIAN_POINT ( 'NONE',  ( 0.000000000000000000, 125.0000000000000000, 0.000000000000000000 ) ) ;
#58798 = EDGE_LOOP ( 'NONE', ( #39404, #10960 ) ) ;
#58799 = CARTESIAN_POINT ( 'NONE',  ( 6.123233995736767268E-16, 11.25000000000000178, -10.00000000000000178 ) ) ;
#58800 = CARTESIAN_POINT ( 'NONE',  ( 4.898587196589415787E-16, 0.000000000000000000, 4.000000000000001776 ) ) ;
#58801 = CARTESIAN_POINT ( 'NONE',  ( 8.311093377946837890, 81.40624999658601268, -8.311093377946837890 ) ) ;
#58802 = CARTESIAN_POINT ( 'NONE',  ( -4.220049686691935698, 10.18810118749999916, 116.8750000020483668 ) ) ;
#58803 = LINE ( 'NONE', #70848, #62407 ) ;
#58804 = CARTESIAN_POINT ( 'NONE',  ( -31.01286907374194257, -35.49843713210861296, 167.9999999999997726 ) ) ;
#58806 = CARTESIAN_POINT ( 'NONE',  ( 6.951808397369818766E-16, 67.03124999658602690, -11.35316468750000141 ) ) ;
#58805 = CARTESIAN_POINT ( 'NONE',  ( 6.000000000000000000, 7.347880794884119736E-16, -10.77459999999999951 ) ) ;
#58808 = VECTOR ( 'NONE', #43956, 1000.000000000000000 ) ;
#58807 = CARTESIAN_POINT ( 'NONE',  ( 7.999999999999992895, -3.313708498984756279, 25.67405278392015333 ) ) ;
#58809 = CARTESIAN_POINT ( 'NONE',  ( -1.885018014105924955, 194.8695402653108317, 145.4147183048736451 ) ) ;
#58810 = CARTESIAN_POINT ( 'NONE',  ( -2.679491924311225848, 158.3333333265053113, -10.00000000000000178 ) ) ;
#58811 = CARTESIAN_POINT ( 'NONE',  ( 1.320432766682874540E-15, 97.90625000204839523, 7.188101187500000044 ) ) ;
#58812 = DIRECTION ( 'NONE',  ( 0.000000000000000000, 0.000000000000000000, 1.000000000000000000 ) ) ;
#58813 = CARTESIAN_POINT ( 'NONE',  ( -11.35316468750000141, 43.59374999658601979, -1.390361679473963753E-15 ) ) ;
#58814 = EDGE_CURVE ( 'NONE', #3720, #38699, #55891, .T. ) ;
#58815 = CARTESIAN_POINT ( 'NONE',  ( 10.18810118750000093, -4.220049686691933033, 112.1875000020483810 ) ) ;
#58816 = CARTESIAN_POINT ( 'NONE',  ( -2.085542519210945728E-15, 194.5312499965860127, 11.35316468750000141 ) ) ;
#58817 = ORIENTED_EDGE ( 'NONE', *, *, #52840, .F. ) ;
#58818 = CARTESIAN_POINT ( 'NONE',  ( 7.456155213548061766, 61.82225697226374450, 23.87472085067569694 ) ) ;
#58819 = CARTESIAN_POINT ( 'NONE',  ( -7.347880794884122694E-16, 16.49999999726881228, 4.000000000000001776 ) ) ;
#58820 = CARTESIAN_POINT ( 'NONE',  ( 5.000000000000001776, 62.70833332650536818, -8.660254037844389075 ) ) ;
#58821 = CARTESIAN_POINT ( 'NONE',  ( 9.832129032723416984, 175.3645833299193555, 5.676582343750006032 ) ) ;
#58822 = FACE_OUTER_BOUND ( 'NONE', #72971, .T. ) ;
#58823 = CARTESIAN_POINT ( 'NONE',  ( -10.00000000000000000, 258.1250000068279746, 0.000000000000000000 ) ) ;
#58824 = CARTESIAN_POINT ( 'NONE',  ( 7.999999999971009856, 2.153409470846384379E-05, 12.26780339315719814 ) ) ;
#58825 = ORIENTED_EDGE ( 'NONE', *, *, #60201, .T. ) ;
#58826 = CARTESIAN_POINT ( 'NONE',  ( -8.311093377946836114, 162.9687499965860411, -8.311093377946837890 ) ) ;
#58827 = APPLICATION_CONTEXT ( 'automotive_design' ) ;
#58828 = AXIS2_PLACEMENT_3D ( 'NONE', #12101, #8290, #31301 ) ;
#58829 = EDGE_CURVE ( 'NONE', #35953, #53341, #32507, .T. ) ;
#58830 = CARTESIAN_POINT ( 'NONE',  ( 2.977408999572646486, 7.188101187499992051, 25.01780278187175810 ) ) ;
#58831 = LINE ( 'NONE', #17710, #18906 ) ;
#58832 = ORIENTED_EDGE ( 'NONE', *, *, #1749, .F. ) ;
#58833 = CARTESIAN_POINT ( 'NONE',  ( 8.000000000000000000, 104.9375000040967763, -9.797174393178825657E-16 ) ) ;
#58834 = EDGE_CURVE ( 'NONE', #20010, #26283, #21905, .T. ) ;
#58835 = EDGE_CURVE ( 'NONE', #5359, #50397, #45303, .T. ) ;
#58836 = CARTESIAN_POINT ( 'NONE',  ( 1.656854249492381248, 11.18749999999999822, -4.000000000000001776 ) ) ;
#58837 = CARTESIAN_POINT ( 'NONE',  ( 4.881900264494500874, 7.573738413550456627, 4.181378144120852046E-15 ) ) ;
#58838 = CARTESIAN_POINT ( 'NONE',  ( -3.211159895383562723, 9.937499998634406140, 3.211159895383561391 ) ) ;
#58839 = CARTESIAN_POINT ( 'NONE',  ( 1.469576158976822172E-15, -7.999999999999991118, 19.39280278392014978 ) ) ;
#58840 = CARTESIAN_POINT ( 'NONE',  ( -1.656854249492405451, 195.3125000000000853, 138.0000000000000568 ) ) ;
#58841 = ORIENTED_EDGE ( 'NONE', *, *, #43343, .F. ) ;
#58842 = CARTESIAN_POINT ( 'NONE',  ( -2.679491924327887187, 178.5416666666652361, 9.999999999990450306 ) ) ;
#58843 = CARTESIAN_POINT ( 'NONE',  ( -5.082755093536324154, 100.3437500020483810, 5.082755093536326818 ) ) ;
#58845 = CARTESIAN_POINT ( 'NONE',  ( 7.778174593052023411, -7.778174593052021635, 99.06250000000000000 ) ) ;
#58844 = DIRECTION ( 'NONE',  ( -0.000000000000000000, -1.000000000000000000, -0.000000000000000000 ) ) ;
#58846 = ORIENTED_EDGE ( 'NONE', *, *, #60187, .F. ) ;
#58847 = CARTESIAN_POINT ( 'NONE',  ( 0.6474643998349955964, 10.28110762191874805, -63.57179091896464485 ) ) ;
#58849 = CARTESIAN_POINT ( 'NONE',  ( 1.102182119232618108E-15, 292.2500000000000000, 6.000000000000001776 ) ) ;
#58848 = AXIS2_PLACEMENT_3D ( 'NONE', #49371, #10138, #26350 ) ;
#58850 = CARTESIAN_POINT ( 'NONE',  ( 2.977408999572650927, -7.188101187499990274, 25.95530278187175455 ) ) ;
#58851 = EDGE_LOOP ( 'NONE', ( #4599, #27417, #32098, #32210 ) ) ;
#58852 = EDGE_CURVE ( 'NONE', #71456, #22076, #44561, .T. ) ;
#58853 = ORIENTED_EDGE ( 'NONE', *, *, #6099, .T. ) ;
#58854 = CARTESIAN_POINT ( 'NONE',  ( -6.238412754330611322E-16, 10.18810118749999916, 83.78125000204836681 ) ) ;
#58855 = CARTESIAN_POINT ( 'NONE',  ( -30.44569435410883074, 196.8125000013656063, 167.5543056458915885 ) ) ;
#58856 = CARTESIAN_POINT ( 'NONE',  ( 2.020667218593132706E-15, -11.00000000000000000, 101.8750000000000000 ) ) ;
#58859 = CARTESIAN_POINT ( 'NONE',  ( 1.226468279477575784E-15, 297.8593750017070079, 6.676582343750001591 ) ) ;
#58858 = CARTESIAN_POINT ( 'NONE',  ( 25.17157287525377996, 202.7500000027312126, 167.1715728752537586 ) ) ;
#58857 = DIRECTION ( 'NONE',  ( -0.000000000000000000, -0.000000000000000000, -1.000000000000000000 ) ) ;
#58860 = CARTESIAN_POINT ( 'NONE',  ( -8.660254037844387298, 137.0833333333333428, -5.000000000000004441 ) ) ;
#58861 = VECTOR ( 'NONE', #66737, 1000.000000000000000 ) ;
#58862 = CARTESIAN_POINT ( 'NONE',  ( -30.64284399271078740, -21.00579972956345642, 174.6921329945331536 ) ) ;
#58863 = CARTESIAN_POINT ( 'NONE',  ( -30.99999999999992895, -31.99999999999978684, 135.0000000000000000 ) ) ;
#58864 = COLOUR_RGB ( '',0.7921568627450980005, 0.8196078431372548767, 0.9333333333333333481 ) ;
#58865 = CARTESIAN_POINT ( 'NONE',  ( 0.000000000000000000, 0.000000000000000000, 30.00000000000000000 ) ) ;
#58866 = CARTESIAN_POINT ( 'NONE',  ( 26.56734541678238060, 203.0000000013655779, 166.5412658749999650 ) ) ;
#58867 = CARTESIAN_POINT ( 'NONE',  ( -1.320432766682874540E-15, 7.968749997951610986, 7.188101187500000044 ) ) ;
#58868 = CARTESIAN_POINT ( 'NONE',  ( -5.662595241051935346, 5.662595241051935346, 3.825615283940628775 ) ) ;
#58869 = CARTESIAN_POINT ( 'NONE',  ( -3.458734125000015425, 195.0000000013656063, 143.4326545832176976 ) ) ;
#58870 = CARTESIAN_POINT ( 'NONE',  ( 5.082755093536326818, 117.5937500020483810, 5.082755093536325042 ) ) ;
#58872 = CARTESIAN_POINT ( 'NONE',  ( -8.660254037844390851, 132.9166666666667140, 4.999999999999998224 ) ) ;
#58871 = CARTESIAN_POINT ( 'NONE',  ( -2.679491924311121043, 251.0416666666666572, 10.00000000000005862 ) ) ;
#58873 = CARTESIAN_POINT ( 'NONE',  ( -5.676582343750000703, 228.3854166700806729, -9.832129032723418760 ) ) ;
#58874 = CARTESIAN_POINT ( 'NONE',  ( -4.898587196589412829E-16, 90.12500000000000000, -8.000000000000000000 ) ) ;
#58875 = CARTESIAN_POINT ( 'NONE',  ( 7.188101187499991163, 2.977408999572648707, 19.20530278187175810 ) ) ;
#58876 = CARTESIAN_POINT ( 'NONE',  ( 29.65685424949240101, 195.4375000000000000, 165.9999999999998863 ) ) ;
#58877 = CARTESIAN_POINT ( 'NONE',  ( -3.042071309553173730, 34.32291666325268409, 11.35316468749999785 ) ) ;
#58878 =( BOUNDED_CURVE ( )  B_SPLINE_CURVE ( 2, ( #40981, #28537, #10817, #51545, #39494, #10448, #46630, #5911, #11193 ),
 .UNSPECIFIED., .F., .F. ) 
 B_SPLINE_CURVE_WITH_KNOTS ( ( 3, 2, 2, 2, 3 ),
 ( 0.7105263157894737835, 0.7171052631578948011, 0.7236842105263159297, 0.7302631578947369473, 0.7368421052631579649 ),
 .UNSPECIFIED. ) 
 CURVE ( )  GEOMETRIC_REPRESENTATION_ITEM ( )  RATIONAL_B_SPLINE_CURVE ( ( 0.9999999999999986677, 0.9238795325112880708, 1.000000000000000000, 0.9238795325112867385, 1.000000000000000000, 0.9238795325112867385, 1.000000000000000000, 0.9238795325112854062, 1.000000000000001332 ) ) 
 REPRESENTATION_ITEM ( '' )  );
#58879 = CARTESIAN_POINT ( 'NONE',  ( 2.751064625579944321E-14, 202.7500000000000000, 194.0000000000000568 ) ) ;
#58881 = CARTESIAN_POINT ( 'NONE',  ( -2.085542519210945728E-15, 214.8437499965860411, 11.35316468750000141 ) ) ;
#58880 =( BOUNDED_CURVE ( )  B_SPLINE_CURVE ( 2, ( #47167, #31300, #6818, #25257, #59610, #36966, #29830, #59249, #18507 ),
 .UNSPECIFIED., .F., .F. ) 
 B_SPLINE_CURVE_WITH_KNOTS ( ( 3, 2, 2, 2, 3 ),
 ( 0.5000000000000004441, 0.5083333333333337478, 0.5166666666666671626, 0.5250000000000004663, 0.5333333333333337700 ),
 .UNSPECIFIED. ) 
 CURVE ( )  GEOMETRIC_REPRESENTATION_ITEM ( )  RATIONAL_B_SPLINE_CURVE ( ( 0.9999999999999958922, 0.9238795325112908463, 1.000000000000000000, 0.9238795325112867385, 1.000000000000000000, 0.9238795325112867385, 1.000000000000000000, 0.9238795325112826307, 1.000000000000003997 ) ) 
 REPRESENTATION_ITEM ( '' )  );
#58882 = CARTESIAN_POINT ( 'NONE',  ( -1.040834085586084257E-14, 82.00000000000001421, 65.00000000000000000 ) ) ;
#58883 = CARTESIAN_POINT ( 'NONE',  ( -3.407298021519794773, 51.68473891413969312, 48.72627478609783225 ) ) ;
#58884 = ORIENTED_EDGE ( 'NONE', *, *, #43297, .F. ) ;
#58885 = EDGE_CURVE ( 'NONE', #61426, #15999, #50698, .T. ) ;
#58886 = DIRECTION ( 'NONE',  ( -1.000000000000000000, 1.776356839400250465E-15, 0.000000000000000000 ) ) ;
#58887 = CARTESIAN_POINT ( 'NONE',  ( -7.999999999999991118, 0.000000000000000000, 18.83030277982336642 ) ) ;
#58888 = CARTESIAN_POINT ( 'NONE',  ( 3.042071309553159519, 29.73958332991934839, 11.35316468750000141 ) ) ;
#58889 = CARTESIAN_POINT ( 'NONE',  ( -10.99999999999999822, -4.556349186104052151, 83.78125000409679046 ) ) ;
#58890 = CARTESIAN_POINT ( 'NONE',  ( -3.458734125000016757, 209.1250000013656347, 140.5673454167823593 ) ) ;
#58891 = CARTESIAN_POINT ( 'NONE',  ( -6.000000000000003553, 295.0000000034139589, -2.485281374238571317 ) ) ;
#58892 = CARTESIAN_POINT ( 'NONE',  ( -1.656854249492478948, 201.8125000027312410, 146.0000000000000000 ) ) ;
#58894 = CARTESIAN_POINT ( 'NONE',  ( 11.35316468749999785, 25.57291666325268409, 3.042071309553174174 ) ) ;
#58893 = CARTESIAN_POINT ( 'NONE',  ( 5.082755093536326818, 103.7187500020483810, 5.082755093536325042 ) ) ;
#58896 = EDGE_CURVE ( 'NONE', #56422, #45848, #50585, .T. ) ;
#58895 = CARTESIAN_POINT ( 'NONE',  ( -7.999999999999991118, 3.313708498984756723, 17.23655277982336642 ) ) ;
#58897 = CARTESIAN_POINT ( 'NONE',  ( 9.832129032723416984, 150.3645833299193555, 5.676582343750006032 ) ) ;
#58898 = CARTESIAN_POINT ( 'NONE',  ( 7.320508075688771044, 111.2499999931720396, 7.320508075688775484 ) ) ;
#58899 = CARTESIAN_POINT ( 'NONE',  ( 7.188101187500001821, 111.8750000020483668, -2.977408999572651371 ) ) ;
#58900 = CARTESIAN_POINT ( 'NONE',  ( 17.99999999999998934, 0.000000000000000000, 0.000000000000000000 ) ) ;
#58901 = CARTESIAN_POINT ( 'NONE',  ( -26.56734541678232375, 204.2500000013655779, 173.4587341250003760 ) ) ;
#58902 = ORIENTED_EDGE ( 'NONE', *, *, #13708, .F. ) ;
#58903 = CARTESIAN_POINT ( 'NONE',  ( -8.311093377946836114, 2.968749996586016238, -8.311093377946837890 ) ) ;
#58904 = EDGE_CURVE ( 'NONE', #60808, #52491, #15128, .T. ) ;
#58905 = EDGE_LOOP ( 'NONE', ( #14682, #54831, #23920, #26345 ) ) ;
#58906 = CARTESIAN_POINT ( 'NONE',  ( 4.242640687119287435, 289.3750000000000000, 4.242640687119285658 ) ) ;
#58907 = CARTESIAN_POINT ( 'NONE',  ( 1.226468279477575784E-15, 296.7031250017070079, 6.676582343750001591 ) ) ;
#58909 = CARTESIAN_POINT ( 'NONE',  ( 9.832129032723416984, 135.3645833299193555, 5.676582343750006032 ) ) ;
#58908 = CARTESIAN_POINT ( 'NONE',  ( -5.656854249492380582, 108.3124999999999858, -5.656854249492380582 ) ) ;
#58910 = CARTESIAN_POINT ( 'NONE',  ( -1.656854249492383468, 16.43749999726881228, 4.000000000000000888 ) ) ;
#58911 = CARTESIAN_POINT ( 'NONE',  ( 5.656854249492374365, 5.656854249492375253, 16.82405278432982954 ) ) ;
#58912 = CYLINDRICAL_SURFACE ( 'NONE', #28553, 11.00000000000000000 ) ;
#58913 = CARTESIAN_POINT ( 'NONE',  ( 5.676582343749997150, 252.2395833367473301, -9.832129032723418760 ) ) ;
#58914 = CARTESIAN_POINT ( 'NONE',  ( 4.220049686691941027, -10.18810118749999738, 89.50000000204836681 ) ) ;
#58915 = ORIENTED_EDGE ( 'NONE', *, *, #28909, .T. ) ;
#58916 = AXIS2_PLACEMENT_3D ( 'NONE', #10086, #73084, #21392 ) ;
#58917 = CARTESIAN_POINT ( 'NONE',  ( 4.999999999999999112, 14.70234347858786528, 69.93881661156081009 ) ) ;
#58918 = CARTESIAN_POINT ( 'NONE',  ( 5.000000000000000000, 64.62627855237467145, -24.10294814404638686 ) ) ;
#58919 = B_SPLINE_CURVE_WITH_KNOTS ( 'NONE', 3,
 ( #37190, #8512, #54550, #2857, #25845, #48865, #65105, #60940, #14902 ),
 .UNSPECIFIED., .F., .F.,
 ( 4, 2, 1, 2, 4 ),
 ( 0.000000000000000000, 0.001314083742615642985, 0.002628167485231287272, 0.003942251227846931341, 0.005256334970462575411 ),
 .UNSPECIFIED. ) ;
#58920 = CARTESIAN_POINT ( 'NONE',  ( -5.676582343749998039, 92.76041666325268409, -9.832129032723420536 ) ) ;
#58921 = EDGE_CURVE ( 'NONE', #55648, #42638, #46413, .T. ) ;
#58922 = CARTESIAN_POINT ( 'NONE',  ( 1.871523826299183495E-15, -10.18810118749999916, 101.0312500020483810 ) ) ;
#58923 = CARTESIAN_POINT ( 'NONE',  ( -4.541265875000003227, 17.99999999863440792, 1.881053915767121110 ) ) ;
#58924 = ORIENTED_EDGE ( 'NONE', *, *, #66753, .F. ) ;
#58925 = VERTEX_POINT ( 'NONE', #68681 ) ;
#58926 = CARTESIAN_POINT ( 'NONE',  ( -5.656854249492379694, 6.562500000000001776, -5.656854249492380582 ) ) ;
#58927 = CARTESIAN_POINT ( 'NONE',  ( 1.881053915767121776, 1.624999998634407028, -4.541265875000002339 ) ) ;
#58928 = VECTOR ( 'NONE', #70598, 1000.000000000000000 ) ;
#58929 = CARTESIAN_POINT ( 'NONE',  ( 2.977408999572651815, 3.187499997951610098, 7.188101187500000933 ) ) ;
#58930 = CARTESIAN_POINT ( 'NONE',  ( -8.000000000000000000, 119.0937500040967905, -3.313708498984761608 ) ) ;
#58931 = CARTESIAN_POINT ( 'NONE',  ( 10.18810118749999916, 4.220049686691935698, 97.37500000204839523 ) ) ;
#58932 = CARTESIAN_POINT ( 'NONE',  ( 30.82842712474617386, 208.1250000000000284, 172.8284271247460993 ) ) ;
#58933 = EDGE_CURVE ( 'NONE', #53849, #59630, #63760, .T. ) ;
#58934 = CARTESIAN_POINT ( 'NONE',  ( -1.656854249492381248, 13.06249999726881406, -4.000000000000001776 ) ) ;
#58935 = CARTESIAN_POINT ( 'NONE',  ( -4.541265875000002339, 0.7499999986344069169, -1.881053915767121998 ) ) ;
#58936 = ORIENTED_EDGE ( 'NONE', *, *, #33802, .F. ) ;
#58937 = CARTESIAN_POINT ( 'NONE',  ( -11.00000000000000000, 0.000000000000000000, 80.49999999999998579 ) ) ;
#58938 = CARTESIAN_POINT ( 'NONE',  ( 2.839093476692135984E-14, 200.6875000013656063, 201.4587341250000350 ) ) ;
#58940 = CARTESIAN_POINT ( 'NONE',  ( 4.898587196589412829E-16, 15.37500000000000355, -8.000000000000000000 ) ) ;
#58939 = CARTESIAN_POINT ( 'NONE',  ( -24.54126587499996148, 202.1250000013656063, 171.4326545832179534 ) ) ;
#58941 = CARTESIAN_POINT ( 'NONE',  ( 3.211159895383561835, 14.43749999863440792, -3.211159895383561835 ) ) ;
#58942 = CARTESIAN_POINT ( 'NONE',  ( -6.735557395310442023E-16, 11.00000000000000000, 68.12499999999998579 ) ) ;
#58943 = CARTESIAN_POINT ( 'NONE',  ( -7.188101187499990274, -2.977408999572651371, 13.58030278187175277 ) ) ;
#58944 = ORIENTED_EDGE ( 'NONE', *, *, #45013, .T. ) ;
#58945 = ORIENTED_EDGE ( 'NONE', *, *, #33706, .T. ) ;
#58946 = CARTESIAN_POINT ( 'NONE',  ( -4.220049686691935698, 10.18810118749999916, 106.3750000020483668 ) ) ;
#58947 = CARTESIAN_POINT ( 'NONE',  ( -2.679491924311223183, 96.45833333333331439, -9.999999999999989342 ) ) ;
#58948 = CARTESIAN_POINT ( 'NONE',  ( -31.99999999999998579, 205.3125000000000568, 171.6568542494928238 ) ) ;
#58949 = CARTESIAN_POINT ( 'NONE',  ( 1.432654583217664479, 194.7500000013656063, 201.4587341250000065 ) ) ;
#58950 = CARTESIAN_POINT ( 'NONE',  ( -11.00000000000000000, 0.000000000000000000, 67.18750000409676204 ) ) ;
#58951 = CARTESIAN_POINT ( 'NONE',  ( 8.660254037844385522, 99.58333333333334281, 5.000000000000005329 ) ) ;
#58952 = CARTESIAN_POINT ( 'NONE',  ( 5.656854249492381470, 118.0625000000000000, 5.656854249492379694 ) ) ;
#58953 = CARTESIAN_POINT ( 'NONE',  ( -6.676582343750001591, 296.6093750017069510, 0.000000000000000000 ) ) ;
#58954 = ORIENTED_EDGE ( 'NONE', *, *, #68399, .F. ) ;
#58955 = ADVANCED_FACE ( 'NONE', ( #68311 ), #57004, .T. ) ;
#58956 = CARTESIAN_POINT ( 'NONE',  ( -7.778174593052023411, 7.778174593052023411, 74.31249999999998579 ) ) ;
#58957 = VECTOR ( 'NONE', #54596, 1000.000000000000000 ) ;
#58958 = CARTESIAN_POINT ( 'NONE',  ( -5.656854249492379694, 12.37499999590322197, -5.656854249492380582 ) ) ;
#58959 = CARTESIAN_POINT ( 'NONE',  ( -3.458734125000015425, 206.0000000013656347, 143.4326545832176976 ) ) ;
#58960 = CARTESIAN_POINT ( 'NONE',  ( -2.679491924311226292, 103.3333333265053824, -10.00000000000000178 ) ) ;
#58961 = CARTESIAN_POINT ( 'NONE',  ( 5.656854249492381470, 113.7500000040967763, 5.656854249492379694 ) ) ;
#58962 = CARTESIAN_POINT ( 'NONE',  ( -11.35316468749999785, 264.0104166700807014, -3.042071309553164848 ) ) ;
#58963 = CYLINDRICAL_SURFACE ( 'NONE', #66796, 10.00000000000000178 ) ;
#58964 = CARTESIAN_POINT ( 'NONE',  ( 7.204075437095968759, -7.204075437095966983, 70.09375000204836681 ) ) ;
#58965 = CARTESIAN_POINT ( 'NONE',  ( -10.00000000000000000, 212.2916666666666572, -2.679491924311229845 ) ) ;
#58966 = CARTESIAN_POINT ( 'NONE',  ( -7.188101187499992051, 2.977408999572646930, 13.76780278187175455 ) ) ;
#58967 = CARTESIAN_POINT ( 'NONE',  ( 3.042071309553159519, 185.0520833299193555, 11.35316468750000141 ) ) ;
#58968 = CARTESIAN_POINT ( 'NONE',  ( -4.541265875000003227, 2.874999998634407028, 1.881053915767121110 ) ) ;
#58969 = CARTESIAN_POINT ( 'NONE',  ( 2.679491924311168560, 243.5416666666666856, -10.00000000000003375 ) ) ;
#58971 = CARTESIAN_POINT ( 'NONE',  ( 0.000000000000000000, 0.000000000000000000, -10.80000000000000071 ) ) ;
#58970 = CARTESIAN_POINT ( 'NONE',  ( 2.775557561562891351E-14, 210.0000000000000284, 198.0000000000000284 ) ) ;
#58972 = EDGE_LOOP ( 'NONE', ( #63906, #43554 ) ) ;
#58973 = AXIS2_PLACEMENT_3D ( 'NONE', #45615, #28637, #51651 ) ;
#58974 = CARTESIAN_POINT ( 'NONE',  ( -3.458734125000016757, 209.1250000013656631, 140.5673454167824161 ) ) ;
#58975 = CARTESIAN_POINT ( 'NONE',  ( 5.676582343749993598, 50.26041666325269119, 9.832129032723422313 ) ) ;
#58976 = CARTESIAN_POINT ( 'NONE',  ( -7.778174593052020747, -7.778174593052023411, 106.3750000040967763 ) ) ;
#58977 = CARTESIAN_POINT ( 'NONE',  ( -11.35316468749999785, 223.3854166632526699, -3.042071309553167513 ) ) ;
#58978 = CARTESIAN_POINT ( 'NONE',  ( -24.54126587499996148, 205.1250000013656347, 171.4326545832179534 ) ) ;
#58979 = CARTESIAN_POINT ( 'NONE',  ( 4.556349186104045934, 11.00000000000000000, 71.03124999999998579 ) ) ;
#58981 = DIRECTION ( 'NONE',  ( 0.000000000000000000, 0.000000000000000000, 1.000000000000000000 ) ) ;
#58980 = CARTESIAN_POINT ( 'NONE',  ( 11.00000000000000000, 4.556349186104045934, 71.03125000409676204 ) ) ;
#58983 = EDGE_CURVE ( 'NONE', #47208, #47258, #16875, .T. ) ;
#58982 = CARTESIAN_POINT ( 'NONE',  ( -3.458734125000015425, 196.0000000013656063, 143.4326545832176976 ) ) ;
#58984 =( BOUNDED_CURVE ( )  B_SPLINE_CURVE ( 2, ( #21989, #62720, #63099, #56714, #34831 ),
 .UNSPECIFIED., .F., .F. ) 
 B_SPLINE_CURVE_WITH_KNOTS ( ( 3, 2, 3 ),
 ( 0.000000000000000000, 0.005681818181818181976, 0.01136363636363636395 ),
 .UNSPECIFIED. ) 
 CURVE ( )  GEOMETRIC_REPRESENTATION_ITEM ( )  RATIONAL_B_SPLINE_CURVE ( ( 1.000000000000000000, 0.9238795325112867385, 1.000000000000000000, 0.9238795325112867385, 1.000000000000000000 ) ) 
 REPRESENTATION_ITEM ( '' )  );
#58985 = VECTOR ( 'NONE', #62662, 1000.000000000000000 ) ;
#58986 = CARTESIAN_POINT ( 'NONE',  ( 8.660254037844389075, 72.29166665983869677, -5.000000000000000000 ) ) ;
#58987 = CARTESIAN_POINT ( 'NONE',  ( 7.188101187500002709, 96.31250000204838102, 2.977408999572649151 ) ) ;
#58988 = CARTESIAN_POINT ( 'NONE',  ( -1.881053915767124440, 17.12499999863440436, 4.541265875000001451 ) ) ;
#58989 = CARTESIAN_POINT ( 'NONE',  ( 1.656854249492369036, 10.93749999726881583, -4.000000000000014211 ) ) ;
#58990 = CARTESIAN_POINT ( 'NONE',  ( 0.000000000000000000, 0.000000000000000000, 0.000000000000000000 ) ) ;
#58991 = ORIENTED_EDGE ( 'NONE', *, *, #8579, .F. ) ;
#58992 = VERTEX_POINT ( 'NONE', #34750 ) ;
#58993 = EDGE_CURVE ( 'NONE', #16691, #1871, #50161, .T. ) ;
#58994 = CARTESIAN_POINT ( 'NONE',  ( -6.676582343750001591, 299.6093750017069510, 0.000000000000000000 ) ) ;
#58995 = DIRECTION ( 'NONE',  ( -0.000000000000000000, -0.000000000000000000, -1.000000000000000000 ) ) ;
#58996 = CARTESIAN_POINT ( 'NONE',  ( -5.000000000000009770, 18.33333333333333570, 8.660254037844392627 ) ) ;
#58997 = CARTESIAN_POINT ( 'NONE',  ( 9.832129032723420536, 161.1979166632526983, -5.676582343749999815 ) ) ;
#58998 = CARTESIAN_POINT ( 'NONE',  ( -7.999999999999991118, 0.000000000000000000, 9.830302779823364645 ) ) ;
#58999 = CARTESIAN_POINT ( 'NONE',  ( -1.656854249492348607, 200.1875000000000568, 202.0000000000000284 ) ) ;
#59000 = CARTESIAN_POINT ( 'NONE',  ( -8.618100331995474761, 15.80894714424573344, 2.003974074085267026E-15 ) ) ;
#59001 = CARTESIAN_POINT ( 'NONE',  ( -10.18810118749999916, 0.000000000000000000, 111.5312500020483668 ) ) ;
#59002 = EDGE_LOOP ( 'NONE', ( #6049, #67617, #42284, #24917 ) ) ;
#59003 =( BOUNDED_CURVE ( )  B_SPLINE_CURVE ( 2, ( #23952, #30357, #46592, #69614, #17929, #40944, #13352, #18670, #63953 ),
 .UNSPECIFIED., .F., .F. ) 
 B_SPLINE_CURVE_WITH_KNOTS ( ( 3, 2, 2, 2, 3 ),
 ( 0.9479166666666665186, 0.9531249999999998890, 0.9583333333333332593, 0.9635416666666666297, 0.9687500000000000000 ),
 .UNSPECIFIED. ) 
 CURVE ( )  GEOMETRIC_REPRESENTATION_ITEM ( )  RATIONAL_B_SPLINE_CURVE ( ( 1.000000000000001554, 0.9238795325112850731, 1.000000000000000000, 0.9238795325112867385, 1.000000000000000000, 0.9238795325112867385, 1.000000000000000000, 0.9238795325112867385, 1.000000000000000000 ) ) 
 REPRESENTATION_ITEM ( '' )  );
#59004 = CARTESIAN_POINT ( 'NONE',  ( 7.999999999999998224, 17.71874999590322730, 3.313708498984766049 ) ) ;
#59005 = LINE ( 'NONE', #42735, #18387 ) ;
#59006 = CARTESIAN_POINT ( 'NONE',  ( 11.35316468750000141, 146.0937499965860411, 0.000000000000000000 ) ) ;
#59007 = CARTESIAN_POINT ( 'NONE',  ( -3.458734124999959914, 199.3750000013656063, 196.5673454167823877 ) ) ;
#59008 = CARTESIAN_POINT ( 'NONE',  ( -3.673940397442060854E-16, 298.8125000034140157, -6.000000000000001776 ) ) ;
#59009 = CARTESIAN_POINT ( 'NONE',  ( -10.18810118749999916, 0.000000000000000000, 69.53125000204838102 ) ) ;
#59010 = CARTESIAN_POINT ( 'NONE',  ( -11.35316468750000141, 48.59374999658601268, -1.390361679473963753E-15 ) ) ;
#59011 = EDGE_LOOP ( 'NONE', ( #15877, #26055, #32767, #19089 ) ) ;
#59012 = CARTESIAN_POINT ( 'NONE',  ( 5.000000000000000000, 29.68417822476661527, -4.268394125862720934 ) ) ;
#59013 = CARTESIAN_POINT ( 'NONE',  ( -4.541265875000003227, 3.999999998634406584, 1.881053915767121110 ) ) ;
#59014 = CARTESIAN_POINT ( 'NONE',  ( -8.008118988124991233, 3.317071493978878127, 14.41936528394063188 ) ) ;
#59015 = CARTESIAN_POINT ( 'NONE',  ( 2.977408999572651815, 13.68749999795161365, 7.188101187500000933 ) ) ;
#59016 = CARTESIAN_POINT ( 'NONE',  ( -3.673940397442060854E-16, 292.8125000034140157, -6.000000000000001776 ) ) ;
#59017 = CARTESIAN_POINT ( 'NONE',  ( 49.70177871865296026, 272.0000000000000000, 57.99999999999999289 ) ) ;
#59018 = CARTESIAN_POINT ( 'NONE',  ( 2.977408999572651815, 11.06249999795161187, 7.188101187500000933 ) ) ;
#59019 = CARTESIAN_POINT ( 'NONE',  ( 7.188101187499993827, -2.977408999572645598, 9.642802781871756324 ) ) ;
#59020 = CARTESIAN_POINT ( 'NONE',  ( -10.18810118749999738, -4.220049686691941915, 73.75000000204836681 ) ) ;
#59021 = CARTESIAN_POINT ( 'NONE',  ( -29.43265458321766559, 205.7500000013656063, 166.5412658750003629 ) ) ;
#59022 = CARTESIAN_POINT ( 'NONE',  ( -5.000000000000005329, 65.20833332650536818, 8.660254037844387298 ) ) ;
#59023 = CARTESIAN_POINT ( 'NONE',  ( 4.000000000000001776, 2.749999997268813168, 0.000000000000000000 ) ) ;
#59024 = ORIENTED_EDGE ( 'NONE', *, *, #10091, .T. ) ;
#59025 = EDGE_CURVE ( 'NONE', #23374, #43617, #6132, .T. ) ;
#59026 = AXIS2_PLACEMENT_3D ( 'NONE', #6454, #29457, #24148 ) ;
#59027 = CARTESIAN_POINT ( 'NONE',  ( -1.656854249492348607, 196.3125000027312126, 202.0000000000000284 ) ) ;
#59028 = CARTESIAN_POINT ( 'NONE',  ( 2.828427124746152987, 202.1250000000000284, 139.1715728752538723 ) ) ;
#59029 = CARTESIAN_POINT ( 'NONE',  ( -29.65685424949245785, 199.1875000027312694, 166.0000000000004263 ) ) ;
#59030 = CARTESIAN_POINT ( 'NONE',  ( 3.211159895383560947, 4.187499998634407028, 3.211159895383562723 ) ) ;
#59031 = CARTESIAN_POINT ( 'NONE',  ( 5.082755093536326818, 114.2187500020483810, 5.082755093536325042 ) ) ;
#59032 = DIRECTION ( 'NONE',  ( 1.281975129857798973E-14, 0.000000000000000000, 1.000000000000000000 ) ) ;
#59033 = CARTESIAN_POINT ( 'NONE',  ( 2.977408999572646486, 7.188101187499991163, 28.01780278187175455 ) ) ;
#59034 = VERTEX_POINT ( 'NONE', #16990 ) ;
#59035 = CARTESIAN_POINT ( 'NONE',  ( 7.188101187500000044, 21.46874999795161543, 0.000000000000000000 ) ) ;
#59036 = ORIENTED_EDGE ( 'NONE', *, *, #68936, .T. ) ;
#59037 = CARTESIAN_POINT ( 'NONE',  ( 10.00000000000000178, 255.4166666734946602, 2.679491924311222739 ) ) ;
#59038 = CARTESIAN_POINT ( 'NONE',  ( 3.458734125000015425, 208.0000000013656347, 196.5673454167823877 ) ) ;
#59039 = CARTESIAN_POINT ( 'NONE',  ( 30.44569435410883429, 206.5625000013656063, 172.4456943541086957 ) ) ;
#59040 = CARTESIAN_POINT ( 'NONE',  ( 7.320508075688774596, 55.62499999999999289, -7.320508075688774596 ) ) ;
#59041 = CARTESIAN_POINT ( 'NONE',  ( -4.401442555609581635E-16, 103.1562500020483810, -7.188101187500000044 ) ) ;
#59042 = CARTESIAN_POINT ( 'NONE',  ( 1.102182119232618108E-15, 296.2500000000000000, 6.000000000000001776 ) ) ;
#59044 = CARTESIAN_POINT ( 'NONE',  ( -20.27232155875134012, -34.51210842437127013, 193.4532132907935988 ) ) ;
#59043 = CARTESIAN_POINT ( 'NONE',  ( -2.679491924311272477, 35.41666665983871098, 9.999999999999978684 ) ) ;
#59045 = ORIENTED_EDGE ( 'NONE', *, *, #24375, .T. ) ;
#59046 = EDGE_CURVE ( 'NONE', #26967, #728, #35066, .T. ) ;
#59047 = EDGE_CURVE ( 'NONE', #73379, #3727, #6437, .T. ) ;
#59048 = CARTESIAN_POINT ( 'NONE',  ( -11.35316468749999963, 233.9062500034139873, 0.000000000000000000 ) ) ;
#59049 = CARTESIAN_POINT ( 'NONE',  ( 2.977408999572650927, -7.188101187499990274, 11.33030278187175632 ) ) ;
#59050 = DIRECTION ( 'NONE',  ( 0.000000000000000000, 0.000000000000000000, 1.000000000000000000 ) ) ;
#59051 = CARTESIAN_POINT ( 'NONE',  ( 1.836970198721029589E-15, 261.2500000000000568, 10.00000000000000000 ) ) ;
#59052 = CARTESIAN_POINT ( 'NONE',  ( -7.999970022586251339, -3.313738476398500943, 19.11155398332591915 ) ) ;
#59053 = CARTESIAN_POINT ( 'NONE',  ( -5.000000000000005329, 178.3333333333333428, 8.660254037844387298 ) ) ;
#59054 = CARTESIAN_POINT ( 'NONE',  ( 24.54126587499999701, 209.1875000013656063, 169.9999999999998863 ) ) ;
#59055 =( NAMED_UNIT ( * ) PLANE_ANGLE_UNIT ( ) SI_UNIT ( $, .RADIAN. ) );
#59056 = CARTESIAN_POINT ( 'NONE',  ( -2.977408999572647819, 7.188101187499992051, 28.58030278187176521 ) ) ;
#59057 = CARTESIAN_POINT ( 'NONE',  ( 9.832129032723416984, 135.6770833299193555, 5.676582343750006032 ) ) ;
#59058 = DIRECTION ( 'NONE',  ( 0.000000000000000000, 0.000000000000000000, 1.000000000000000000 ) ) ;
#59061 = CARTESIAN_POINT ( 'NONE',  ( -2.679491924292381810, 166.4583333333316943, -10.00000000001088374 ) ) ;
#59060 = CARTESIAN_POINT ( 'NONE',  ( 10.00000000000000178, 106.8749999931720396, 0.000000000000000000 ) ) ;
#59059 = CARTESIAN_POINT ( 'NONE',  ( 24.00000000000001066, 206.6875000000000284, 168.3431457505075173 ) ) ;
#59062 = VERTEX_POINT ( 'NONE', #47 ) ;
#59063 = ADVANCED_FACE ( 'NONE', ( #52086, #6059 ), #63386, .T. ) ;
#59064 = CARTESIAN_POINT ( 'NONE',  ( 8.000000000000000000, 10.59375000000000178, -3.313708498984761164 ) ) ;
#59065 = CARTESIAN_POINT ( 'NONE',  ( 6.123233995736767268E-16, 26.25000000000000355, -10.00000000000000178 ) ) ;
#59066 = CARTESIAN_POINT ( 'NONE',  ( -1.836970198721029983E-15, 205.6249999931720538, 10.00000000000000178 ) ) ;
#59067 = CARTESIAN_POINT ( 'NONE',  ( -2.754378923186476579E-14, 207.1875000013656063, 145.4587341250000350 ) ) ;
#59068 = DIRECTION ( 'NONE',  ( -0.000000000000000000, 1.000000000000000000, -0.000000000000000000 ) ) ;
#59069 = VECTOR ( 'NONE', #55243, 1000.000000000000000 ) ;
#59070 = CARTESIAN_POINT ( 'NONE',  ( 10.00000000000000178, 31.87499999317203248, 0.000000000000000000 ) ) ;
#59071 = CARTESIAN_POINT ( 'NONE',  ( -2.977408999572651815, 113.9375000020483952, 7.188101187500000933 ) ) ;
#59072 = CARTESIAN_POINT ( 'NONE',  ( -4.541265875000002339, 5.874999998634407028, -1.881053915767121998 ) ) ;
#59073 = CARTESIAN_POINT ( 'NONE',  ( 4.336811714529170025, 68.30918023748891699, -20.61428864874696032 ) ) ;
#59074 = CARTESIAN_POINT ( 'NONE',  ( -7.999999999999991118, 0.000000000000000000, 15.83030277982336642 ) ) ;
#59076 = CARTESIAN_POINT ( 'NONE',  ( 7.320508075688774596, 7.499999993172032475, -7.320508075688774596 ) ) ;
#59075 = CARTESIAN_POINT ( 'NONE',  ( -6.735557395310442023E-16, 11.00000000000000000, 101.3125000040967763 ) ) ;
#59077 = VERTEX_POINT ( 'NONE', #11710 ) ;
#59078 = CARTESIAN_POINT ( 'NONE',  ( -14.00000000000000178, 0.000000000000000000, -17.50000000000000000 ) ) ;
#59079 = CARTESIAN_POINT ( 'NONE',  ( -4.500000000000012434, 7.794228634059945371, -10.20000000000000462 ) ) ;
#59080 = CARTESIAN_POINT ( 'NONE',  ( 9.832129032723416984, 232.1354166700806445, -5.676582343750003368 ) ) ;
#59081 = CARTESIAN_POINT ( 'NONE',  ( -3.042071309553173730, 119.3229166632526699, 11.35316468749999785 ) ) ;
#59082 = ORIENTED_EDGE ( 'NONE', *, *, #67632, .F. ) ;
#59083 = FACE_OUTER_BOUND ( 'NONE', #27467, .T. ) ;
#59084 = VECTOR ( 'NONE', #926, 1000.000000000000000 ) ;
#59085 = CARTESIAN_POINT ( 'NONE',  ( 10.18810118749999916, 1.247682550866122264E-15, 99.90625000204838102 ) ) ;
#59086 = CARTESIAN_POINT ( 'NONE',  ( 47.11462393093395207, 145.7394130188241377, 67.12012181809809874 ) ) ;
#59087 = CARTESIAN_POINT ( 'NONE',  ( 2.445694354108839175, 201.3125000013656063, 195.5543056458912190 ) ) ;
#59088 = CYLINDRICAL_SURFACE ( 'NONE', #70271, 8.000000000000000000 ) ;
#59090 = CARTESIAN_POINT ( 'NONE',  ( 9.832129032723420536, 116.1979166632526841, -5.676582343749999815 ) ) ;
#59089 = CARTESIAN_POINT ( 'NONE',  ( -33.48318503342263597, 175.8115626168855101, 156.1427595010634377 ) ) ;
#59091 = ADVANCED_FACE ( 'NONE', ( #12078 ), #29439, .T. ) ;
#59092 = CARTESIAN_POINT ( 'NONE',  ( -32.00000000000001421, 207.1875000000000284, 168.3431457505080004 ) ) ;
#59093 = CARTESIAN_POINT ( 'NONE',  ( -5.656854249492378806, 92.18749999999998579, 5.656854249492381470 ) ) ;
#59094 = ORIENTED_EDGE ( 'NONE', *, *, #65254, .F. ) ;
#59095 = CARTESIAN_POINT ( 'NONE',  ( -7.320508075688778149, 204.9999999931720254, 7.320508075688769267 ) ) ;
#59096 = CARTESIAN_POINT ( 'NONE',  ( 8.000000000000001776, 112.3437500040967905, 3.313708498984759387 ) ) ;
#59097 = DIRECTION ( 'NONE',  ( 0.000000000000000000, 0.000000000000000000, -1.000000000000000000 ) ) ;
#59098 = CARTESIAN_POINT ( 'NONE',  ( 3.042071309553159519, 100.0520833299193555, 11.35316468750000141 ) ) ;
#59099 = CARTESIAN_POINT ( 'NONE',  ( -5.000000000000000000, 18.53862685874493010, -23.57305537018094554 ) ) ;
#59100 = CARTESIAN_POINT ( 'NONE',  ( -7.188101187500002709, 15.18749999795161365, 2.977408999572649151 ) ) ;
#59101 =( BOUNDED_CURVE ( )  B_SPLINE_CURVE ( 2, ( #28181, #28930, #16473, #17605, #40623, #57999, #74578, #39136, #27809 ),
 .UNSPECIFIED., .F., .F. ) 
 B_SPLINE_CURVE_WITH_KNOTS ( ( 3, 2, 2, 2, 3 ),
 ( 0.1166666666666666546, 0.1250000000000000555, 0.1333333333333334425, 0.1416666666666668573, 0.1500000000000002442 ),
 .UNSPECIFIED. ) 
 CURVE ( )  GEOMETRIC_REPRESENTATION_ITEM ( )  RATIONAL_B_SPLINE_CURVE ( ( 1.000000000000000222, 0.9238795325112867385, 1.000000000000000000, 0.9238795325112867385, 1.000000000000000000, 0.9238795325112867385, 1.000000000000000000, 0.9238795325112844070, 1.000000000000002220 ) ) 
 REPRESENTATION_ITEM ( '' )  );
#59102 = CARTESIAN_POINT ( 'NONE',  ( 10.18810118749999916, 4.220049686691935698, 92.87500000204838102 ) ) ;
#59103 = CARTESIAN_POINT ( 'NONE',  ( -9.832129032723420536, 14.01041666325268409, 5.676582343749997150 ) ) ;
#59104 = ORIENTED_EDGE ( 'NONE', *, *, #7688, .T. ) ;
#59105 = CARTESIAN_POINT ( 'NONE',  ( -2.679491924311081519, 136.4583333333333144, -10.00000000000009770 ) ) ;
#59106 = CARTESIAN_POINT ( 'NONE',  ( 2.603828935537542577, -43.49700039518273798, 139.1093513339536401 ) ) ;
#59107 = CARTESIAN_POINT ( 'NONE',  ( -7.778174593052023411, 7.778174593052023411, 102.8124999999999858 ) ) ;
#59108 = CARTESIAN_POINT ( 'NONE',  ( -6.238412754330611322E-16, 10.18810118749999916, 72.15625000204836681 ) ) ;
#59109 = CARTESIAN_POINT ( 'NONE',  ( 1.469576158976823947E-15, 115.0625000040967905, 8.000000000000000000 ) ) ;
#59110 = CARTESIAN_POINT ( 'NONE',  ( -7.320508075688773708, 148.7499999931720254, -7.320508075688774596 ) ) ;
#59111 = CARTESIAN_POINT ( 'NONE',  ( -2.765530957081998586, 293.6406250017069510, 6.676582343750001591 ) ) ;
#59112 = CARTESIAN_POINT ( 'NONE',  ( 2.160335347094620939, 51.35526406371981523, -48.59969451235843962 ) ) ;
#59113 = CARTESIAN_POINT ( 'NONE',  ( 9.832129032723420536, 221.5104166632526983, -5.676582343749999815 ) ) ;
#59114 = CARTESIAN_POINT ( 'NONE',  ( -10.18810118749999916, 4.220049686691934809, 90.06250000204838102 ) ) ;
#59115 = CARTESIAN_POINT ( 'NONE',  ( -31.45873412500001010, 204.6250000013655779, 168.5673454167827572 ) ) ;
#59116 =( BOUNDED_CURVE ( )  B_SPLINE_CURVE ( 2, ( #43240, #26253, #44744, #14933, #73040, #54955, #37974, #3265, #60973, #55705, #49271, #10412, #33078 ),
 .UNSPECIFIED., .F., .F. ) 
 B_SPLINE_CURVE_WITH_KNOTS ( ( 3, 2, 2, 2, 2, 2, 3 ),
 ( 1.177487769121809080, 1.182721478772594148, 1.187955188423379438, 1.193188898074164506, 1.198422607724949573, 1.203656317375734863, 1.208890027026519931 ),
 .UNSPECIFIED. ) 
 CURVE ( )  GEOMETRIC_REPRESENTATION_ITEM ( )  RATIONAL_B_SPLINE_CURVE ( ( 1.000000000000081490, 0.9659258262889869329, 1.000000000000000000, 0.9659258262890684232, 1.000000000000000000, 0.9659258262890684232, 1.000000000000000000, 0.9659258262890684232, 1.000000000000000000, 0.9659258262890684232, 1.000000000000000000, 0.9659258262890684232, 1.000000000000000000 ) ) 
 REPRESENTATION_ITEM ( '' )  );
#59117 = CARTESIAN_POINT ( 'NONE',  ( -5.656854249492379694, 23.06250000000000355, -5.656854249492380582 ) ) ;
#59118 = CARTESIAN_POINT ( 'NONE',  ( 4.541265875000002339, 10.43749999863440792, 0.000000000000000000 ) ) ;
#59119 = ORIENTED_EDGE ( 'NONE', *, *, #62927, .F. ) ;
#59120 = CARTESIAN_POINT ( 'NONE',  ( -17.97431660307913148, -47.19385343660658094, 144.7330103597662401 ) ) ;
#59121 = CARTESIAN_POINT ( 'NONE',  ( 1.656854249492405451, 208.4375000027311842, 202.0000000000000284 ) ) ;
#59122 = CARTESIAN_POINT ( 'NONE',  ( 1.432654583217608080, 197.8750000013656063, 138.5412658750000503 ) ) ;
#59123 = CARTESIAN_POINT ( 'NONE',  ( 3.999999999999960032, 202.1250000027312126, 142.0000000000000568 ) ) ;
#59124 = CARTESIAN_POINT ( 'NONE',  ( 5.000000000000000888, 13.57926339724853371, -69.65188861886713312 ) ) ;
#59125 = CARTESIAN_POINT ( 'NONE',  ( 7.204075437095968759, -7.204075437095966983, 77.59375000204838102 ) ) ;
#59126 = ORIENTED_EDGE ( 'NONE', *, *, #4054, .T. ) ;
#59127 = CARTESIAN_POINT ( 'NONE',  ( -1.320432766682874540E-15, 6.093749997951610986, 7.188101187500000044 ) ) ;
#59128 = PLANE ( 'NONE',  #22149 ) ;
#59129 = EDGE_CURVE ( 'NONE', #30692, #41579, #24581, .T. ) ;
#59130 = ADVANCED_FACE ( 'NONE', ( #41495 ), #8265, .F. ) ;
#59131 = VECTOR ( 'NONE', #45917, 1000.000000000000000 ) ;
#59132 = CARTESIAN_POINT ( 'NONE',  ( 2.977408999572650039, 119.5625000020483810, -7.188101187500001821 ) ) ;
#59133 = CIRCLE ( 'NONE', #49469, 70.50000000000000000 ) ;
#59134 = CARTESIAN_POINT ( 'NONE',  ( -2.295000000000000373, 267.1439999999997212, 5.415579320905394844 ) ) ;
#59135 = CARTESIAN_POINT ( 'NONE',  ( 1.226468279477575784E-15, 290.7031250017069510, 6.676582343750001591 ) ) ;
#59137 = CARTESIAN_POINT ( 'NONE',  ( -4.000000000000001776, 15.24999999726881406, -4.898587196589415787E-16 ) ) ;
#59136 = CARTESIAN_POINT ( 'NONE',  ( 11.35316468749999608, 236.6145833367473301, -3.042071309553167513 ) ) ;
#59138 = CONTEXT_DEPENDENT_SHAPE_REPRESENTATION ( #7695, #63201 ) ;
#59139 = ORIENTED_EDGE ( 'NONE', *, *, #45265, .T. ) ;
#59140 = CARTESIAN_POINT ( 'NONE',  ( 9.832129032723420536, 231.3020833367473301, 5.676582343749996262 ) ) ;
#59141 = CARTESIAN_POINT ( 'NONE',  ( 2.977408999572646486, 7.188101187499991163, 26.89280278187175455 ) ) ;
#59142 = CARTESIAN_POINT ( 'NONE',  ( -3.458734124999960358, 202.6250000013656063, 196.5673454167823877 ) ) ;
#59143 = ORIENTED_EDGE ( 'NONE', *, *, #20102, .T. ) ;
#59144 = CARTESIAN_POINT ( 'NONE',  ( -10.18810118749999916, 0.000000000000000000, 67.65625000204836681 ) ) ;
#59145 = CARTESIAN_POINT ( 'NONE',  ( 5.676582343750001591, 96.92708332991935549, -9.832129032723420536 ) ) ;
#59146 = CARTESIAN_POINT ( 'NONE',  ( -1.656854249492336173, 209.1875000000000568, 202.0000000000000284 ) ) ;
#59147 = CARTESIAN_POINT ( 'NONE',  ( 4.556349186104045934, 11.00000000000000000, 75.53124999999998579 ) ) ;
#59150 = FACE_OUTER_BOUND ( 'NONE', #64607, .T. ) ;
#59149 = CARTESIAN_POINT ( 'NONE',  ( 31.45873412499998523, 204.7500000013656063, 168.5673454167822172 ) ) ;
#59148 = CARTESIAN_POINT ( 'NONE',  ( 29.43265458321766559, 203.1250000013656347, 166.5412658749999650 ) ) ;
#59151 = VERTEX_POINT ( 'NONE', #19950 ) ;
#59152 = EDGE_CURVE ( 'NONE', #13169, #73371, #1876, .T. ) ;
#59153 = DIRECTION ( 'NONE',  ( 0.000000000000000000, 0.000000000000000000, 1.000000000000000000 ) ) ;
#59154 = CARTESIAN_POINT ( 'NONE',  ( 27.99999999999996803, 208.6250000027312126, 165.9999999999998863 ) ) ;
#59155 = CARTESIAN_POINT ( 'NONE',  ( 6.951808397369818766E-16, 217.0312499965860411, -11.35316468750000141 ) ) ;
#59157 = EDGE_CURVE ( 'NONE', #27850, #64213, #8533, .T. ) ;
#59156 = CARTESIAN_POINT ( 'NONE',  ( -2.839093476692135984E-14, 199.6875000013656063, 138.5412658750000503 ) ) ;
#59158 = CARTESIAN_POINT ( 'NONE',  ( 30.44569435410883429, 202.0625000013656063, 167.5543056458911053 ) ) ;
#59159 = CARTESIAN_POINT ( 'NONE',  ( 5.082755093536324154, 26.15624999795161543, 5.082755093536326818 ) ) ;
#59160 = CARTESIAN_POINT ( 'NONE',  ( 11.35316468750000141, 196.0937499965860127, 0.000000000000000000 ) ) ;
#59161 = CARTESIAN_POINT ( 'NONE',  ( 7.778174593052023411, -7.778174593052021635, 70.56249999999998579 ) ) ;
#59162 = CARTESIAN_POINT ( 'NONE',  ( 2.828427124746152987, 196.2500000027312126, 139.1715728752538723 ) ) ;
#59163 = CARTESIAN_POINT ( 'NONE',  ( -28.00000000000002487, 195.0000000000000000, 166.0000000000003695 ) ) ;
#59164 = CARTESIAN_POINT ( 'NONE',  ( -4.541265875000002339, 13.81249999863440614, -5.561446717895856393E-16 ) ) ;
#59165 = CARTESIAN_POINT ( 'NONE',  ( 31.45873412499999233, 199.9375000013656063, 169.9999999999999432 ) ) ;
#59166 = CARTESIAN_POINT ( 'NONE',  ( 7.188101187499992051, 8.802885111219154394E-16, 2.611552781871750994 ) ) ;
#59167 = CARTESIAN_POINT ( 'NONE',  ( 5.676582343750001591, 71.61458332991935549, -9.832129032723420536 ) ) ;
#59168 = CARTESIAN_POINT ( 'NONE',  ( 28.00000000000002487, 206.1250000027312126, 173.9999999999999147 ) ) ;
#59169 = FACE_OUTER_BOUND ( 'NONE', #16542, .T. ) ;
#59170 = VERTEX_POINT ( 'NONE', #24862 ) ;
#59171 = FACE_OUTER_BOUND ( 'NONE', #67359, .T. ) ;
#59172 = CARTESIAN_POINT ( 'NONE',  ( -3.999999999999960032, 195.0000000000000000, 198.0000000000000284 ) ) ;
#59173 = CARTESIAN_POINT ( 'NONE',  ( -5.676582343750006032, 69.11458332991936970, 9.832129032723418760 ) ) ;
#59174 = CARTESIAN_POINT ( 'NONE',  ( -4.556349186104045934, 11.00000000000000000, 71.40625000409677625 ) ) ;
#59175 = CARTESIAN_POINT ( 'NONE',  ( -2.445694354108839175, 195.3125000013656063, 144.4456943541088663 ) ) ;
#59176 = CARTESIAN_POINT ( 'NONE',  ( -30.95103850725454109, -36.74533461631524744, 167.9999999999997726 ) ) ;
#59178 = CARTESIAN_POINT ( 'NONE',  ( 9.832129032723416984, 70.36458332991936970, 5.676582343750006032 ) ) ;
#59177 = CARTESIAN_POINT ( 'NONE',  ( -3.313708498984758055, 123.4062500040967905, -8.000000000000001776 ) ) ;
#59179 = EDGE_CURVE ( 'NONE', #29602, #72546, #30174, .T. ) ;
#59180 = CARTESIAN_POINT ( 'NONE',  ( 7.999999999999991118, 9.797174393178815797E-16, 25.76780278392014978 ) ) ;
#59181 = CARTESIAN_POINT ( 'NONE',  ( 2.775557561562891351E-14, 210.0000000000000284, 198.0000000000000284 ) ) ;
#59182 = CARTESIAN_POINT ( 'NONE',  ( -10.00000000000000355, 159.5833333265053398, 2.679491924311223183 ) ) ;
#59183 = CYLINDRICAL_SURFACE ( 'NONE', #49674, 10.00000000000000178 ) ;
#59184 = CARTESIAN_POINT ( 'NONE',  ( 11.35316468749999963, 61.30208332991934839, -3.042071309553165293 ) ) ;
#59185 = CARTESIAN_POINT ( 'NONE',  ( -10.18810118749999916, 4.220049686691934809, 111.4375000020483810 ) ) ;
#59186 = CARTESIAN_POINT ( 'NONE',  ( 9.832129032723416984, 200.3645833299193555, 5.676582343750006032 ) ) ;
#59187 = ORIENTED_EDGE ( 'NONE', *, *, #19650, .F. ) ;
#59188 = CARTESIAN_POINT ( 'NONE',  ( -0.6474643998350495533, 60.19533971085391499, 22.88219507985867196 ) ) ;
#59189 = CARTESIAN_POINT ( 'NONE',  ( -4.898587196589412829E-16, 121.6250000000000000, -8.000000000000000000 ) ) ;
#59190 = CARTESIAN_POINT ( 'NONE',  ( 10.00000000000000000, 61.66666665983870388, 2.679491924311235618 ) ) ;
#59192 = CARTESIAN_POINT ( 'NONE',  ( 5.676582343749993598, 189.9479166632526983, 9.832129032723422313 ) ) ;
#59191 = DIRECTION ( 'NONE',  ( 1.000000000000000000, 0.000000000000000000, 0.000000000000000000 ) ) ;
#59193 = CARTESIAN_POINT ( 'NONE',  ( 3.313708498984762496, 2.531249995903220196, 7.999999999999998224 ) ) ;
#59194 = CARTESIAN_POINT ( 'NONE',  ( 10.00000000000000178, 240.4166666734946318, 2.679491924311222739 ) ) ;
#59195 = CARTESIAN_POINT ( 'NONE',  ( -10.00000000000000178, 189.3749999931720254, -1.224646799147353454E-15 ) ) ;
#59196 = AXIS2_PLACEMENT_3D ( 'NONE', #10646, #63068, #16654 ) ;
#59197 = VERTEX_POINT ( 'NONE', #54307 ) ;
#59198 = CARTESIAN_POINT ( 'NONE',  ( 6.951808397369818766E-16, 177.3437499965860411, -11.35316468750000141 ) ) ;
#59199 = VECTOR ( 'NONE', #25283, 1000.000000000000000 ) ;
#59200 = CARTESIAN_POINT ( 'NONE',  ( 2.977408999572646486, 7.188101187499992051, 22.01780278187175455 ) ) ;
#59201 = CARTESIAN_POINT ( 'NONE',  ( 3.959805771731846225, 226.0000000000000568, -9.326041370300968580 ) ) ;
#59202 = CIRCLE ( 'NONE', #56786, 11.49999999999999112 ) ;
#59203 = ORIENTED_EDGE ( 'NONE', *, *, #43692, .F. ) ;
#59204 = CARTESIAN_POINT ( 'NONE',  ( -5.656854249492380582, 96.50000000409677625, -5.656854249492380582 ) ) ;
#59205 =( BOUNDED_CURVE ( )  B_SPLINE_CURVE ( 2, ( #48613, #31270, #61063, #2610, #71619, #20692, #71995, #42950, #70893 ),
 .UNSPECIFIED., .F., .F. ) 
 B_SPLINE_CURVE_WITH_KNOTS ( ( 3, 2, 2, 2, 3 ),
 ( 0.6764705882352940458, 0.6801470588235293269, 0.6838235294117647189, 0.6875000000000000000, 0.6911764705882352811 ),
 .UNSPECIFIED. ) 
 CURVE ( )  GEOMETRIC_REPRESENTATION_ITEM ( )  RATIONAL_B_SPLINE_CURVE ( ( 1.000000000000002220, 0.9238795325112844070, 1.000000000000000000, 0.9238795325112867385, 1.000000000000000000, 0.9238795325112867385, 1.000000000000000000, 0.9238795325112867385, 1.000000000000000000 ) ) 
 REPRESENTATION_ITEM ( '' )  );
#59206 = CARTESIAN_POINT ( 'NONE',  ( -7.347880794884122694E-16, 10.75000000000000000, 4.000000000000001776 ) ) ;
#59207 = DIRECTION ( 'NONE',  ( -0.000000000000000000, 1.000000000000000000, -4.476705744456276341E-16 ) ) ;
#59208 = CARTESIAN_POINT ( 'NONE',  ( 4.541265875000002339, 17.31249999863440792, 0.000000000000000000 ) ) ;
#59209 = CARTESIAN_POINT ( 'NONE',  ( 7.999999999999991118, 9.797174393178815797E-16, 16.76780278392014978 ) ) ;
#59210 = CARTESIAN_POINT ( 'NONE',  ( 1.656854249492348607, 195.1875000000000000, 138.0000000000000568 ) ) ;
#59211 = VERTEX_POINT ( 'NONE', #2618 ) ;
#59212 = LINE ( 'NONE', #7523, #18630 ) ;
#59213 = CARTESIAN_POINT ( 'NONE',  ( -7.188101187500000044, 98.65625000204838102, 0.000000000000000000 ) ) ;
#59215 = CARTESIAN_POINT ( 'NONE',  ( 4.000000000000000888, 13.68749999726881583, 1.656854249492384135 ) ) ;
#59214 = LINE ( 'NONE', #38806, #14493 ) ;
#59216 = CARTESIAN_POINT ( 'NONE',  ( 1424.688200795866351, 850.9677537768168349, 997.8421604560583091 ) ) ;
#59217 = ORIENTED_EDGE ( 'NONE', *, *, #882, .T. ) ;
#59218 = CARTESIAN_POINT ( 'NONE',  ( 2.696524195522682164E-11, 156.2499999999978968, -10.00000000000000178 ) ) ;
#59219 = DIRECTION ( 'NONE',  ( -0.000000000000000000, 1.000000000000000000, -0.000000000000000000 ) ) ;
#59220 = CARTESIAN_POINT ( 'NONE',  ( 1.320432766682872962E-15, -7.188101187499992051, 22.86155278187175455 ) ) ;
#59221 = VERTEX_POINT ( 'NONE', #53191 ) ;
#59222 = ORIENTED_EDGE ( 'NONE', *, *, #26143, .F. ) ;
#59223 = CARTESIAN_POINT ( 'NONE',  ( 1.871523826299183495E-15, -10.18810118749999916, 87.53125000204836681 ) ) ;
#59224 = CARTESIAN_POINT ( 'NONE',  ( -5.204170427930421283E-15, 20.78460969082654231, -1.607695154586745501 ) ) ;
#59225 = CARTESIAN_POINT ( 'NONE',  ( 4.556349186104045934, 11.00000000000000000, 93.53125000000000000 ) ) ;
#59228 = CARTESIAN_POINT ( 'NONE',  ( -4.721056650415999201, 294.4843750017070079, -4.721056650415999201 ) ) ;
#59227 = CARTESIAN_POINT ( 'NONE',  ( 30.82842712474620939, 200.2500000027312126, 172.8284271247460424 ) ) ;
#59226 = CARTESIAN_POINT ( 'NONE',  ( -31.99999999999995737, 198.4375000027312126, 171.6568542494928522 ) ) ;
#59229 = CARTESIAN_POINT ( 'NONE',  ( -1.836970198721029983E-15, 138.7500000000000000, 10.00000000000000178 ) ) ;
#59230 = CARTESIAN_POINT ( 'NONE',  ( -24.00000000000000711, 203.8125000000000000, 168.3431457505080289 ) ) ;
#59231 = AXIS2_PLACEMENT_3D ( 'NONE', #45495, #45873, #39843 ) ;
#59232 = CARTESIAN_POINT ( 'NONE',  ( 5.082755093536320601, -5.082755093536318824, 2.424052781871754103 ) ) ;
#59233 = CARTESIAN_POINT ( 'NONE',  ( 0.000000000000000000, 20.39230484541327471, -10.20000000000000284 ) ) ;
#59234 = B_SPLINE_CURVE_WITH_KNOTS ( 'NONE', 3,
 ( #42080, #70036, #18716, #41724, #24727, #64736 ),
 .UNSPECIFIED., .F., .F.,
 ( 4, 2, 4 ),
 ( 0.4500003403313557193, 0.4750001701656778597, 0.5000000000000000000 ),
 .UNSPECIFIED. ) ;
#59235 = CARTESIAN_POINT ( 'NONE',  ( -5.656854249492379694, 3.374999995903220640, -5.656854249492380582 ) ) ;
#59236 = EDGE_CURVE ( 'NONE', #38154, #27000, #1153, .T. ) ;
#59237 = CARTESIAN_POINT ( 'NONE',  ( 30.44569435410883429, 198.8125000013656063, 167.5543056458911053 ) ) ;
#59238 = CARTESIAN_POINT ( 'NONE',  ( -1.320432766682874540E-15, 4.968749997951610986, 7.188101187500000044 ) ) ;
#59239 = CARTESIAN_POINT ( 'NONE',  ( 8.008118988124993010, -3.317071493978877239, 6.169365283940631883 ) ) ;
#59240 = CARTESIAN_POINT ( 'NONE',  ( 0.000000000000000000, 0.000000000000000000, 0.000000000000000000 ) ) ;
#59241 = CARTESIAN_POINT ( 'NONE',  ( 7.188101187500000044, 116.2812500020483810, -8.802885111219163269E-16 ) ) ;
#59242 = FACE_OUTER_BOUND ( 'NONE', #73943, .T. ) ;
#59243 = CARTESIAN_POINT ( 'NONE',  ( 11.35316468749999963, 231.7187500034139873, -1.390361679473963556E-15 ) ) ;
#59244 = CARTESIAN_POINT ( 'NONE',  ( 7.188101187499991163, 2.977408999572648707, 22.20530278187175810 ) ) ;
#59245 = LINE ( 'NONE', #65252, #51580 ) ;
#59246 = CARTESIAN_POINT ( 'NONE',  ( 5.676582343750001591, 31.61458332991935194, -9.832129032723420536 ) ) ;
#59247 = CARTESIAN_POINT ( 'NONE',  ( -6.331740687315345895E-14, -13.85640646055103531, -1.071796769724504550 ) ) ;
#59248 = CARTESIAN_POINT ( 'NONE',  ( 9.832129032723420536, 221.5104166632526983, -5.676582343749999815 ) ) ;
#59249 = CARTESIAN_POINT ( 'NONE',  ( 29.65685424949234061, 201.1875000027312694, 174.0000000000000284 ) ) ;
#59250 = CARTESIAN_POINT ( 'NONE',  ( 11.00000000000000000, 1.347111479062088405E-15, 118.0000000000000000 ) ) ;
#59251 = ORIENTED_EDGE ( 'NONE', *, *, #27773, .T. ) ;
#59252 = DIRECTION ( 'NONE',  ( 1.000000000000000000, 0.000000000000000000, 0.000000000000000000 ) ) ;
#59253 = CARTESIAN_POINT ( 'NONE',  ( -3.458734125000016757, 197.1250000013656347, 140.5673454167824161 ) ) ;
#59254 = CARTESIAN_POINT ( 'NONE',  ( 5.676582343749993598, 39.94791666325268409, 9.832129032723422313 ) ) ;
#59255 = CARTESIAN_POINT ( 'NONE',  ( 4.556349186104045934, 11.00000000000000000, 86.21875000409680467 ) ) ;
#59256 = CARTESIAN_POINT ( 'NONE',  ( -1.432654583217664701, 209.0000000013656063, 138.5412658750000787 ) ) ;
#59257 = CARTESIAN_POINT ( 'NONE',  ( -27.99999999999991473, 194.9375000013655779, 173.4587341250003760 ) ) ;
#59258 = CARTESIAN_POINT ( 'NONE',  ( -4.556349186104045934, 11.00000000000000000, 101.2187500000000000 ) ) ;
#59260 = CARTESIAN_POINT ( 'NONE',  ( -5.676582343750006032, 39.11458332991934839, 9.832129032723418760 ) ) ;
#59259 = CARTESIAN_POINT ( 'NONE',  ( -5.082755093536324154, 104.8437500020483810, 5.082755093536326818 ) ) ;
#59261 = CARTESIAN_POINT ( 'NONE',  ( 7.999999999999991118, 9.797174393178815797E-16, 18.08030277982336642 ) ) ;
#59262 = CARTESIAN_POINT ( 'NONE',  ( -11.35316468750000141, 143.4895833299193839, 3.042071309553159963 ) ) ;
#59263 = ADVANCED_FACE ( 'NONE', ( #47881 ), #53995, .F. ) ;
#59264 = CARTESIAN_POINT ( 'NONE',  ( 7.320508075688771044, 116.2499999931720254, 7.320508075688775484 ) ) ;
#59265 = CARTESIAN_POINT ( 'NONE',  ( 7.188101187500001821, 108.8750000020483810, -2.977408999572651371 ) ) ;
#59266 = CARTESIAN_POINT ( 'NONE',  ( 2.849036369511732440E-14, 203.2500000000000000, 202.0000000000000000 ) ) ;
#59267 = CARTESIAN_POINT ( 'NONE',  ( -30.44569435410879521, 206.0625000013656063, 172.4456943541092357 ) ) ;
#59268 = ORIENTED_EDGE ( 'NONE', *, *, #10577, .F. ) ;
#59269 = CARTESIAN_POINT ( 'NONE',  ( -5.676582343750006032, 24.42708332991935194, 9.832129032723418760 ) ) ;
#59270 = EDGE_CURVE ( 'NONE', #13196, #25157, #58335, .T. ) ;
#59271 = ORIENTED_EDGE ( 'NONE', *, *, #18252, .T. ) ;
#59272 = CARTESIAN_POINT ( 'NONE',  ( 4.999999999999994671, 105.8333333333333286, -8.660254037844376640 ) ) ;
#59273 = DIRECTION ( 'NONE',  ( -0.000000000000000000, 1.000000000000000000, -0.000000000000000000 ) ) ;
#59275 = CARTESIAN_POINT ( 'NONE',  ( -11.35316468749999785, 143.0729166632526983, -3.042071309553167957 ) ) ;
#59274 = CARTESIAN_POINT ( 'NONE',  ( -19.99999999999993250, -31.46213522578591437, 145.5826352683941707 ) ) ;
#59276 = CARTESIAN_POINT ( 'NONE',  ( 3.313708498984762496, -7.999999999999989342, 17.85530278432982598 ) ) ;
#59277 = AXIS2_PLACEMENT_3D ( 'NONE', #13660, #59712, #64985 ) ;
#59278 = CARTESIAN_POINT ( 'NONE',  ( 62.39047978708148889, 227.5926696121481712, 44.99999999999999289 ) ) ;
#59279 = CARTESIAN_POINT ( 'NONE',  ( -9.832129032723418760, 243.4895833367473301, -5.676582343749998927 ) ) ;
#59280 = CARTESIAN_POINT ( 'NONE',  ( 1.871523826299183495E-15, -10.18810118749999916, 90.90625000204838102 ) ) ;
#59281 = ORIENTED_EDGE ( 'NONE', *, *, #70153, .F. ) ;
#59282 = ADVANCED_FACE ( 'NONE', ( #24131 ), #47511, .T. ) ;
#59283 = CARTESIAN_POINT ( 'NONE',  ( 4.999999999999999112, 15.47455834364811622, 69.96446835377025764 ) ) ;
#59284 = CARTESIAN_POINT ( 'NONE',  ( 29.65685424949243654, 205.4375000000000284, 165.9999999999999147 ) ) ;
#59285 = CARTESIAN_POINT ( 'NONE',  ( -5.676582343750006032, 94.42708332991935549, 9.832129032723418760 ) ) ;
#59286 = CARTESIAN_POINT ( 'NONE',  ( 7.204075437095966983, 7.204075437095967871, 101.5937500020483668 ) ) ;
#59287 = CARTESIAN_POINT ( 'NONE',  ( -3.211159895383561391, 18.81249999863440436, -3.211159895383561835 ) ) ;
#59288 = ORIENTED_EDGE ( 'NONE', *, *, #123, .T. ) ;
#59289 = ORIENTED_EDGE ( 'NONE', *, *, #39892, .F. ) ;
#59290 = CARTESIAN_POINT ( 'NONE',  ( 7.999999999999998224, 7.406250000000000888, 3.313708498984766493 ) ) ;
#59291 = CARTESIAN_POINT ( 'NONE',  ( -5.656854249492381470, 11.43750000000000178, 5.656854249492379694 ) ) ;
#59292 = CARTESIAN_POINT ( 'NONE',  ( -7.188101187500001821, 4.124999997951610986, -2.977408999572651371 ) ) ;
#59293 = CARTESIAN_POINT ( 'NONE',  ( -11.00000000000000000, 0.000000000000000000, 96.99999999999998579 ) ) ;
#59294 = CARTESIAN_POINT ( 'NONE',  ( -7.204075437095965206, -7.204075437095968759, 99.71875000204838102 ) ) ;
#59295 = AXIS2_PLACEMENT_3D ( 'NONE', #47080, #40691, #57689 ) ;
#59296 = CARTESIAN_POINT ( 'NONE',  ( -4.000000000000002665, 1.562500000000000666, 1.656854249492380804 ) ) ;
#59297 = CARTESIAN_POINT ( 'NONE',  ( 4.000000000000001776, 15.74999999726881406, 0.000000000000000000 ) ) ;
#59298 = CARTESIAN_POINT ( 'NONE',  ( 3.211159895383561835, 5.437499998634407028, -3.211159895383561835 ) ) ;
#59299 = EDGE_LOOP ( 'NONE', ( #68197, #67557, #48540, #71130 ) ) ;
#59300 = EDGE_CURVE ( 'NONE', #9758, #16071, #70432, .T. ) ;
#59301 = CARTESIAN_POINT ( 'NONE',  ( 2.445694354108782775, 207.5625000013656063, 139.5543056458912190 ) ) ;
#59302 = CARTESIAN_POINT ( 'NONE',  ( 2.754378923186476579E-14, 198.1875000013655779, 194.5412658750000219 ) ) ;
#59303 = EDGE_CURVE ( 'NONE', #49304, #12752, #41994, .T. ) ;
#59305 = CARTESIAN_POINT ( 'NONE',  ( -5.656854249492379694, 15.56250000000000355, -5.656854249492380582 ) ) ;
#59304 = CARTESIAN_POINT ( 'NONE',  ( -31.45873412499999944, 201.6875000013656063, 170.0000000000004547 ) ) ;
#59306 = CARTESIAN_POINT ( 'NONE',  ( -4.541265875000002339, 13.81249999863440614, -5.561446717895856393E-16 ) ) ;
#59307 = VECTOR ( 'NONE', #44605, 1000.000000000000000 ) ;
#59308 = CARTESIAN_POINT ( 'NONE',  ( -11.00000000000000000, 0.000000000000000000, 68.49999999999997158 ) ) ;
#59309 = CARTESIAN_POINT ( 'NONE',  ( 2.977408999572650927, -7.188101187499990274, 15.45530278187175455 ) ) ;
#59310 = ORIENTED_EDGE ( 'NONE', *, *, #6221, .T. ) ;
#59311 = EDGE_CURVE ( 'NONE', #111, #66661, #61820, .T. ) ;
#59312 =( BOUNDED_CURVE ( )  B_SPLINE_CURVE ( 2, ( #33942, #23711, #58069, #6001, #39952, #62577, #29002, #23339, #10909 ),
 .UNSPECIFIED., .F., .F. ) 
 B_SPLINE_CURVE_WITH_KNOTS ( ( 3, 2, 2, 2, 3 ),
 ( 0.8382352941176471894, 0.8419117647058824705, 0.8455882352941177516, 0.8492647058823530326, 0.8529411764705883137 ),
 .UNSPECIFIED. ) 
 CURVE ( )  GEOMETRIC_REPRESENTATION_ITEM ( )  RATIONAL_B_SPLINE_CURVE ( ( 0.9999999999999976685, 0.9238795325112890700, 1.000000000000000000, 0.9238795325112867385, 1.000000000000000000, 0.9238795325112867385, 1.000000000000000000, 0.9238795325112844070, 1.000000000000002220 ) ) 
 REPRESENTATION_ITEM ( '' )  );
#59313 =( BOUNDED_CURVE ( )  B_SPLINE_CURVE ( 2, ( #51839, #22780, #185, #65280, #45802, #53608, #1920, #24908, #47924 ),
 .UNSPECIFIED., .F., .F. ) 
 B_SPLINE_CURVE_WITH_KNOTS ( ( 3, 2, 2, 2, 3 ),
 ( 0.3068181818181818232, 0.3125000000000000000, 0.3181818181818181768, 0.3238636363636363535, 0.3295454545454545303 ),
 .UNSPECIFIED. ) 
 CURVE ( )  GEOMETRIC_REPRESENTATION_ITEM ( )  RATIONAL_B_SPLINE_CURVE ( ( 1.000000000000000000, 0.9238795325112867385, 1.000000000000000000, 0.9238795325112867385, 1.000000000000000000, 0.9238795325112867385, 1.000000000000000000, 0.9238795325112867385, 1.000000000000000000 ) ) 
 REPRESENTATION_ITEM ( '' )  );
#59314 = VERTEX_POINT ( 'NONE', #9775 ) ;
#59315 = CARTESIAN_POINT ( 'NONE',  ( 4.220049686691941027, -10.18810118749999738, 102.6250000020483810 ) ) ;
#59316 = CARTESIAN_POINT ( 'NONE',  ( -28.00000000000002842, 201.0000000000000000, 166.0000000000003695 ) ) ;
#59317 = CARTESIAN_POINT ( 'NONE',  ( -3.458734124999959914, 195.3750000013656063, 196.5673454167823877 ) ) ;
#59318 = CARTESIAN_POINT ( 'NONE',  ( -28.00000000000007816, 202.1250000027312126, 166.0000000000003695 ) ) ;
#59319 = CARTESIAN_POINT ( 'NONE',  ( 5.000000000000001776, 95.83333333333334281, -8.660254037844389075 ) ) ;
#59320 = AXIS2_PLACEMENT_3D ( 'NONE', #16183, #49795, #4161 ) ;
#59321 = CARTESIAN_POINT ( 'NONE',  ( 3.313708498984760720, 120.0312500000000142, -8.000000000000000000 ) ) ;
#59322 = CARTESIAN_POINT ( 'NONE',  ( 1.226468279477575784E-15, 297.8593750017070079, 6.676582343750001591 ) ) ;
#59323 = ORIENTED_EDGE ( 'NONE', *, *, #21984, .F. ) ;
#59324 = CARTESIAN_POINT ( 'NONE',  ( 3.153939666463620179E-13, 188.7500000000000284, 9.999999999999998224 ) ) ;
#59325 = CARTESIAN_POINT ( 'NONE',  ( 5.656854249492378806, 17.62499999590322375, 5.656854249492381470 ) ) ;
#59326 = CARTESIAN_POINT ( 'NONE',  ( 2.445694354108782775, 205.5625000013656063, 139.5543056458912190 ) ) ;
#59327 = CARTESIAN_POINT ( 'NONE',  ( -8.660254037844392627, 52.91666666666666430, 4.999999999999999112 ) ) ;
#59328 = CARTESIAN_POINT ( 'NONE',  ( 8.660254037844385522, 222.9166666666666856, -5.000000000000003553 ) ) ;
#59329 = DIRECTION ( 'NONE',  ( -0.1513591288559072157, 0.000000000000000000, 0.9884788384745425427 ) ) ;
#59330 = CARTESIAN_POINT ( 'NONE',  ( -4.556349186104045934, 11.00000000000000000, 113.2187499999999858 ) ) ;
#59331 = CARTESIAN_POINT ( 'NONE',  ( 10.00000000000000000, 209.7916666666667140, 2.679491924311236062 ) ) ;
#59332 = CARTESIAN_POINT ( 'NONE',  ( -5.082755093536319713, 5.082755093536319713, 9.174052781871752771 ) ) ;
#59333 = CARTESIAN_POINT ( 'NONE',  ( -8.311093377946841443, 184.2187499965860127, 8.311093377946830785 ) ) ;
#59334 = CARTESIAN_POINT ( 'NONE',  ( 38.00000000000000000, 52.99999999999999289, 25.00000000000000000 ) ) ;
#59335 = CARTESIAN_POINT ( 'NONE',  ( -1.881053915767121554, 1.624999998634407028, -4.541265875000002339 ) ) ;
#59336 = CARTESIAN_POINT ( 'NONE',  ( 9.999999999999998224, 242.7083333333333428, -2.679491924311229401 ) ) ;
#59337 = DIRECTION ( 'NONE',  ( -0.000000000000000000, 1.000000000000000000, -0.000000000000000000 ) ) ;
#59338 = VERTEX_POINT ( 'NONE', #32794 ) ;
#59339 = CARTESIAN_POINT ( 'NONE',  ( -2.445694354108840063, 209.0625000013656063, 139.5543056458912190 ) ) ;
#59340 = CARTESIAN_POINT ( 'NONE',  ( -8.311093377946836114, 52.96874999658601268, -8.311093377946837890 ) ) ;
#59341 = CARTESIAN_POINT ( 'NONE',  ( 4.556349186104045934, 11.00000000000000000, 102.7187500040967620 ) ) ;
#59342 = CARTESIAN_POINT ( 'NONE',  ( -8.311093377946841443, 214.2187499965860411, 8.311093377946830785 ) ) ;
#59343 = CARTESIAN_POINT ( 'NONE',  ( -27.99999999999992184, 205.9375000013656063, 173.4587341250003760 ) ) ;
#59344 = FACE_OUTER_BOUND ( 'NONE', #35461, .T. ) ;
#59346 = DIRECTION ( 'NONE',  ( -0.000000000000000000, 1.000000000000000000, -0.000000000000000000 ) ) ;
#59345 = CARTESIAN_POINT ( 'NONE',  ( 7.188101187500000933, 122.0000000020483810, -2.977408999572651371 ) ) ;
#59347 = CARTESIAN_POINT ( 'NONE',  ( 2.445694354108783664, 196.3125000013656063, 144.4456943541088663 ) ) ;
#59348 = CARTESIAN_POINT ( 'NONE',  ( -8.311093377946836114, 102.6562499965860269, -8.311093377946837890 ) ) ;
#59349 = EDGE_CURVE ( 'NONE', #25822, #2846, #14658, .T. ) ;
#59350 = CARTESIAN_POINT ( 'NONE',  ( -4.999999999999998224, 78.54166665983871098, -8.660254037844389075 ) ) ;
#59351 = CARTESIAN_POINT ( 'NONE',  ( 2.977408999572654480, 97.62500000204836681, 7.188101187499999156 ) ) ;
#59352 = CARTESIAN_POINT ( 'NONE',  ( -1.881053915767121554, 15.74999999863440614, -4.541265875000002339 ) ) ;
#59353 = CARTESIAN_POINT ( 'NONE',  ( 4.500000000000006217, -7.794228634059941818, 0.000000000000000000 ) ) ;
#59354 = CARTESIAN_POINT ( 'NONE',  ( -6.062601303906716588, -5.219661428662635494, 1.000679062340938064 ) ) ;
#59355 = ORIENTED_EDGE ( 'NONE', *, *, #22567, .T. ) ;
#59356 = ORIENTED_EDGE ( 'NONE', *, *, #38365, .T. ) ;
#59357 = CARTESIAN_POINT ( 'NONE',  ( 4.721056650415999201, 294.2343750017069510, -4.721056650415999201 ) ) ;
#59358 = FACE_OUTER_BOUND ( 'NONE', #16717, .T. ) ;
#59359 = CARTESIAN_POINT ( 'NONE',  ( 3.042071309553159519, 159.7395833299193839, 11.35316468750000141 ) ) ;
#59360 = CARTESIAN_POINT ( 'NONE',  ( 10.00000000000000355, 5.208333333333333037, -2.679491924311226736 ) ) ;
#59361 = CARTESIAN_POINT ( 'NONE',  ( -1.656854249492348607, 199.1875000000000000, 202.0000000000000284 ) ) ;
#59362 = CARTESIAN_POINT ( 'NONE',  ( -32.00000000000000711, 201.1875000000000284, 168.3431457505080289 ) ) ;
#59363 = CARTESIAN_POINT ( 'NONE',  ( -10.18810118749999916, 4.220049686691934809, 109.9375000020483952 ) ) ;
#59364 = ORIENTED_EDGE ( 'NONE', *, *, #36305, .T. ) ;
#59365 = DIRECTION ( 'NONE',  ( -0.000000000000000000, 1.000000000000000000, -0.000000000000000000 ) ) ;
#59366 = VECTOR ( 'NONE', #21474, 1000.000000000000000 ) ;
#59367 = FACE_OUTER_BOUND ( 'NONE', #2946, .T. ) ;
#59368 = CARTESIAN_POINT ( 'NONE',  ( 9.832129032723416984, 140.6770833299193555, 5.676582343750006032 ) ) ;
#59369 = CARTESIAN_POINT ( 'NONE',  ( 3.458734125000015425, 198.0000000013656063, 196.5673454167823877 ) ) ;
#59370 = CARTESIAN_POINT ( 'NONE',  ( 5.082755093536324154, 27.65624999795161543, 5.082755093536326818 ) ) ;
#59371 = CARTESIAN_POINT ( 'NONE',  ( 7.204075437095966983, 7.204075437095967871, 71.96875000204836681 ) ) ;
#59372 = CARTESIAN_POINT ( 'NONE',  ( 11.35316468749999785, 55.88541666325266988, 3.042071309553174174 ) ) ;
#59373 = EDGE_LOOP ( 'NONE', ( #21250, #19274, #44801 ) ) ;
#59374 = FACE_OUTER_BOUND ( 'NONE', #17909, .T. ) ;
#59375 = CARTESIAN_POINT ( 'NONE',  ( 3.211159895383560947, 5.312499998634407028, 3.211159895383562723 ) ) ;
#59376 = CARTESIAN_POINT ( 'NONE',  ( 5.662595241051936235, -5.662595241051934458, 9.075615283940630107 ) ) ;
#59377 = AXIS2_PLACEMENT_3D ( 'NONE', #20181, #36079, #19447 ) ;
#59378 = CARTESIAN_POINT ( 'NONE',  ( -5.082755093536325042, 13.03124999795161187, -5.082755093536325930 ) ) ;
#59379 = CARTESIAN_POINT ( 'NONE',  ( -2.485281374238571761, 292.8750000034139589, -6.000000000000003553 ) ) ;
#59380 = CARTESIAN_POINT ( 'NONE',  ( 1.836970198721029589E-15, 226.2500000000000000, 10.00000000000000000 ) ) ;
#59381 = CARTESIAN_POINT ( 'NONE',  ( -7.188101187500000044, 12.09374999795161187, -8.802885111219163269E-16 ) ) ;
#59382 = CARTESIAN_POINT ( 'NONE',  ( 5.082755093536318824, 5.082755093536319713, 6.924052781871750994 ) ) ;
#59383 = CARTESIAN_POINT ( 'NONE',  ( -7.204075437095965206, -7.204075437095968759, 114.7187500020483810 ) ) ;
#59384 = CARTESIAN_POINT ( 'NONE',  ( 27.99999999999997158, 209.0000000000000284, 173.9999999999999147 ) ) ;
#59385 = CARTESIAN_POINT ( 'NONE',  ( 2.449293598294707893E-16, 3.999999997268813168, -4.000000000000001776 ) ) ;
#59386 = EDGE_LOOP ( 'NONE', ( #3892, #31654, #6608, #39437 ) ) ;
#59387 = CARTESIAN_POINT ( 'NONE',  ( -1.656854249492347719, 196.9375000027312410, 194.0000000000000853 ) ) ;
#59388 = ADVANCED_FACE ( 'NONE', ( #55427 ), #44471, .F. ) ;
#59389 = CARTESIAN_POINT ( 'NONE',  ( 1.656854249492347719, 200.8125000000000284, 146.0000000000000284 ) ) ;
#59390 = CARTESIAN_POINT ( 'NONE',  ( -25.17157287525374088, 198.7500000027312126, 172.8284271247464972 ) ) ;
#59391 = CARTESIAN_POINT ( 'NONE',  ( -4.541265875000002339, 2.812499998634407028, -5.561446717895856393E-16 ) ) ;
#59392 = CARTESIAN_POINT ( 'NONE',  ( -2.977408999572651815, 118.4375000020483810, 7.188101187500000933 ) ) ;
#59393 = CARTESIAN_POINT ( 'NONE',  ( 0.000000000000000000, 0.000000000000000000, 30.00000000000000000 ) ) ;
#59394 = CARTESIAN_POINT ( 'NONE',  ( -3.313708498984758943, -7.999999999999989342, 2.799052783920144005 ) ) ;
#59395 = ORIENTED_EDGE ( 'NONE', *, *, #33260, .F. ) ;
#59396 = EDGE_CURVE ( 'NONE', #15999, #39667, #37132, .T. ) ;
#59397 = CARTESIAN_POINT ( 'NONE',  ( 2.977408999572652260, 24.18749999795161543, 7.188101187500000044 ) ) ;
#59398 = ORIENTED_EDGE ( 'NONE', *, *, #16196, .T. ) ;
#59399 = CARTESIAN_POINT ( 'NONE',  ( 30.82842712474620228, 200.3750000000000284, 167.1715728752537586 ) ) ;
#59400 = CARTESIAN_POINT ( 'NONE',  ( -3.458734124999959914, 206.4375000013656063, 198.0000000000000284 ) ) ;
#59401 = CARTESIAN_POINT ( 'NONE',  ( 24.54126587500000412, 204.2500000013655779, 171.4326545832176123 ) ) ;
#59402 = CARTESIAN_POINT ( 'NONE',  ( -1.836970198721029983E-15, 53.75000000000000711, 10.00000000000000178 ) ) ;
#59403 = CARTESIAN_POINT ( 'NONE',  ( -5.082755093536324154, 102.2187500020483810, 5.082755093536326818 ) ) ;
#59404 = CARTESIAN_POINT ( 'NONE',  ( 2.485281374238575314, 298.3124999999999432, 6.000000000000000888 ) ) ;
#59406 = CARTESIAN_POINT ( 'NONE',  ( -20.84899715379480867, -36.24810969123834781, 192.9422563093208680 ) ) ;
#59405 = DIRECTION ( 'NONE',  ( -0.000000000000000000, 1.000000000000000000, -0.000000000000000000 ) ) ;
#59407 =( BOUNDED_SURFACE ( )  B_SPLINE_SURFACE ( 1, 2, ( 
 ( #43969, #14162, #42833, #8894, #60945, #66978, #61696, #20192, #49629, #72644, #66229, #37195, #37571, #61323, #73014, #38317, #55301, #49997, #43211, #3994, #32287, #72259, #26983, #3609, #26605, #21324, #9649, #60195, #20947, #25850, #26223, #48870, #66601, #33050, #71878, #15280, #14907, #9265, #38695, #32669, #55679, #44345, #67355, #15654, #31907, #49243, #10018, #54928, #14531, #56049, #60570, #3237, #4358, #27350, #50367, #20572, #73384, #37946, #65852, #8517, #31534, #2862, #39791, #11869, #63175, #34157, #62061, #57540, #69210, #33790, #46195, #16764, #51865, #57913, #6222, #50738, #17148, #62795, #11501, #57157, #39060, #39428, #74125, #5849, #11134, #29225, #73752, #62427, #5473, #40538, #51483, #63544, #52238, #22058, #206, #21690, #44716, #56412, #23184, #4733, #34905, #16389, #68464, #28842, #17522, #28475, #67731, #33412, #40170, #34534, #45447, #10753, #27727, #16027, #10386, #45085, #68100, #56787, #5108, #74494, #28098, #51113, #22427, #22803, #45824, #68835, #69586, #41650, #63923, #17899, #35998, #6586, #64660, #70327, #59378, #1672, #12960, #35628, #47302, #7689, #30696, #59015, #7323, #53714, #19002, #40912, #30327, #58283, #58643, #29593, #24291, #65393, #52604, #53347, #18642, #24652, #71043, #47662, #70684, #2028, #42008, #65016, #41284, #6949, #19362, #64294, #942, #25014, #23924, #46933, #36362, #13325, #48034, #18269, #8053, #69961, #42376, #13690, #31056, #36732, #59743, #572, #23553, #46565, #12233, #35270, #12601, #29961, #52974, #1307, #9558, #15562, #32573, #26130, #49149, #48778, #60474, #20855, #38601, #2771, #72160, #8421, #71785, #31815, #15195, #20470, #61600, #31437, #20103, #43490, #72920, #9172, #21230, #9920, #54464, #55581, #54084, #2394, #14063, #3896, #37099, #44256, #43115, #66502, #38224, #61229, #14814, #25391, #65761, #72550, #43873, #3146, #66134, #60103, #48406, #71412, #26890, #66889, #67267, #19736, #37855, #42745, #25757, #54836, #55210, #14439, #37473, #8804, #60852, #32191, #3516, #26505, #49529, #49906, #28012, #17055, #34071, #22332, #68001, #5014, #40078, #63083, #68374, #16671, #11407, #51390, #27258, #45359, #15934, #16297, #38964, #56699, #23091, #61967, #39702, #51022, #74029, #28750, #57068, #5380, #34444, #62702, #74403, #73661, #39337, #51766, #21970, #10295, #57443 ),
 ( #11040, #4639, #63450, #28381, #5751, #22711, #44998, #62334, #55958, #50276, #113, #10661, #33694, #56320, #46103, #45728, #69122, #4268, #68742, #17427, #40451, #32952, #73296, #21598, #33321, #44624, #67639, #27635, #50643, #52886, #41195, #6860, #70958, #19276, #47941, #41920, #53256, #1938, #24927, #35540, #483, #17805, #12509, #12871, #35179, #42286, #6127, #1218, #23463, #29132, #47209, #40820, #24197, #29872, #70597, #35908, #70241, #46844, #58555, #18914, #64931, #18551, #41557, #13240, #30238, #52148, #64574, #69495, #69867, #63826, #58926, #11775, #12142, #7234, #1584, #24569, #7598, #47574, #36274, #59290, #30605, #53626, #52516, #18180, #34813, #853, #58194, #57820, #6499, #29505, #46475, #23838, #64205, #9366, #73852, #48317, #33151, #56145, #22157, #38417, #9746, #56518, #4456, #4090, #30971, #27447, #39156, #3710, #16118, #61418, #21785, #27830, #44814, #32766, #55773, #61042, #72744, #50462, #50840, #13966, #27084, #19644, #65300, #42657, #61794, #50096, #73477, #73112, #7968, #32386, #44072, #67825, #21419, #13605, #65668, #55400, #44443, #10482, #67455, #33514, #36643, #37009, #62159, #59650, #53990, #25298, #4833, #71323, #2300, #26709, #15750, #49728, #21047, #38791, #67081, #15380, #10112, #63646, #68938, #34259, #56890, #63271, #35374, #11975, #57639, #10854, #6328, #18003, #57263, #69690, #40270, #677, #6691, #23663, #17248, #11597, #39894, #51582, #35007, #29696, #68568, #34632, #74224, #52711, #22528, #40643, #5950, #58022, #28949, #62526, #62899, #22913, #29330, #51969, #1044, #45550, #11231, #306, #64028, #23285, #12341, #45185, #16868, #46668, #68196, #16492, #5204, #41021, #28202, #58385, #5576, #46295, #52339, #39530, #69316, #33888, #51215, #28576, #74601, #17625, #45925, #35731, #31542, #60203, #54192, #65496, #14170, #37204, #47766, #12700, #30066, #24756, #25119, #47405, #8527, #18375, #65118, #58748, #41389, #59481, #53080, #13428, #19102, #8157, #48137, #36465, #59117, #70787, #31165, #2499, #7794, #30797, #25493, #42480, #64402, #53819, #7058, #7426, #1414, #42107, #54563, #24399, #2127, #71145, #19467, #19836, #13791, #36837, #48508, #59843, #71513, #64761, #30433, #42844, #13062, #70428, #65862, #18745, #41753, #24024, #47033, #70068, #36100, #53453, #1772, #44354, #67365, #33421, #49638 ) ),
 .UNSPECIFIED., .F., .F., .F. ) 
 B_SPLINE_SURFACE_WITH_KNOTS ( ( 2, 2 ),
 ( 3, 2, 2, 2, 2, 2, 2, 2, 2, 2, 2, 2, 2, 2, 2, 2, 2, 2, 2, 2, 2, 2, 2, 2, 2, 2, 2, 2, 2, 2, 2, 2, 2, 2, 2, 2, 2, 2, 2, 2, 2, 2, 2, 2, 2, 2, 2, 2, 2, 2, 2, 2, 2, 2, 2, 2, 2, 2, 2, 2, 2, 2, 2, 2, 2, 2, 2, 2, 2, 2, 2, 2, 2, 2, 2, 2, 2, 2, 2, 2, 2, 2, 2, 2, 2, 2, 2, 2, 2, 2, 2, 2, 2, 2, 2, 2, 2, 2, 2, 2, 2, 2, 2, 2, 2, 2, 2, 2, 2, 2, 2, 2, 2, 2, 2, 2, 2, 2, 2, 2, 2, 2, 2, 2, 2, 2, 2, 2, 2, 2, 2, 2, 2, 2, 2, 2, 2, 2, 2, 2, 2, 2, 2, 2, 3 ),
 ( 0.000000000000000000, 1.000000000000000000 ),
 ( 0.000000000000000000, 0.006944444444444444059, 0.01388888888888888812, 0.02083333333333333218, 0.02777777777777777624, 0.03472222222222222376, 0.04166666666666666435, 0.04861111111111111188, 0.05555555555555555247, 0.06250000000000000000, 0.06944444444444444753, 0.07638888888888889506, 0.08333333333333332871, 0.09027777777777777624, 0.09722222222222222376, 0.1041666666666666713, 0.1111111111111111049, 0.1180555555555555525, 0.1250000000000000000, 0.1319444444444444475, 0.1388888888888888951, 0.1458333333333333426, 0.1527777777777777901, 0.1597222222222222099, 0.1666666666666666574, 0.1736111111111111049, 0.1805555555555555525, 0.1875000000000000000, 0.1944444444444444475, 0.2013888888888888951, 0.2083333333333333426, 0.2152777777777777901, 0.2222222222222222099, 0.2291666666666666574, 0.2361111111111111049, 0.2430555555555555525, 0.2500000000000000000, 0.2569444444444444198, 0.2638888888888888951, 0.2708333333333333148, 0.2777777777777777901, 0.2847222222222222099, 0.2916666666666666852, 0.2986111111111111049, 0.3055555555555555802, 0.3125000000000000000, 0.3194444444444444198, 0.3263888888888888951, 0.3333333333333333148, 0.3402777777777777901, 0.3472222222222222099, 0.3541666666666666852, 0.3611111111111111049, 0.3680555555555555802, 0.3750000000000000000, 0.3819444444444444198, 0.3888888888888888951, 0.3958333333333333148, 0.4027777777777777901, 0.4097222222222222099, 0.4166666666666666852, 0.4236111111111111049, 0.4305555555555555802, 0.4375000000000000000, 0.4444444444444444198, 0.4513888888888888951, 0.4583333333333333148, 0.4652777777777777901, 0.4722222222222222099, 0.4791666666666666852, 0.4861111111111111049, 0.4930555555555555802, 0.5000000000000000000, 0.5069444444444444198, 0.5138888888888888395, 0.5208333333333333703, 0.5277777777777777901, 0.5347222222222222099, 0.5416666666666666297, 0.5486111111111111605, 0.5555555555555555802, 0.5625000000000000000, 0.5694444444444444198, 0.5763888888888888395, 0.5833333333333333703, 0.5902777777777777901, 0.5972222222222222099, 0.6041666666666666297, 0.6111111111111111605, 0.6180555555555555802, 0.6250000000000000000, 0.6319444444444444198, 0.6388888888888888395, 0.6458333333333333703, 0.6527777777777777901, 0.6597222222222222099, 0.6666666666666666297, 0.6736111111111111605, 0.6805555555555555802, 0.6875000000000000000, 0.6944444444444444198, 0.7013888888888888395, 0.7083333333333333703, 0.7152777777777777901, 0.7222222222222222099, 0.7291666666666666297, 0.7361111111111111605, 0.7430555555555555802, 0.7500000000000000000, 0.7569444444444444198, 0.7638888888888888395, 0.7708333333333333703, 0.7777777777777777901, 0.7847222222222222099, 0.7916666666666666297, 0.7986111111111111605, 0.8055555555555555802, 0.8125000000000000000, 0.8194444444444444198, 0.8263888888888888395, 0.8333333333333333703, 0.8402777777777777901, 0.8472222222222222099, 0.8541666666666666297, 0.8611111111111111605, 0.8680555555555555802, 0.8750000000000000000, 0.8819444444444444198, 0.8888888888888888395, 0.8958333333333333703, 0.9027777777777777901, 0.9097222222222222099, 0.9166666666666666297, 0.9236111111111111605, 0.9305555555555555802, 0.9375000000000000000, 0.9444444444444444198, 0.9513888888888888395, 0.9583333333333333703, 0.9652777777777777901, 0.9722222222222222099, 0.9791666666666666297, 0.9861111111111111605, 0.9930555555555555802, 1.000000000000000000 ),
 .UNSPECIFIED. ) 
 GEOMETRIC_REPRESENTATION_ITEM ( )  RATIONAL_B_SPLINE_SURFACE ( (
 ( 1.000000000000000000, 0.9238795325112867385, 1.000000000000000000, 0.9238795325112867385, 1.000000000000000000, 0.9238795325112867385, 1.000000000000000000, 0.9238795325112867385, 1.000000000000000000, 0.9238795325112867385, 1.000000000000000000, 0.9238795325112867385, 1.000000000000000000, 0.9238795325112867385, 1.000000000000000000, 0.9238795325112867385, 1.000000000000000000, 0.9238795325112867385, 1.000000000000000000, 0.9238795325112867385, 1.000000000000000000, 0.9238795325112867385, 1.000000000000000000, 0.9238795325112867385, 1.000000000000000000, 0.9238795325112867385, 1.000000000000000000, 0.9238795325112867385, 1.000000000000000000, 0.9238795325112867385, 1.000000000000000000, 0.9238795325112867385, 1.000000000000000000, 0.9238795325112867385, 1.000000000000000000, 0.9238795325112867385, 1.000000000000000000, 0.9238795325112867385, 1.000000000000000000, 0.9238795325112867385, 1.000000000000000000, 0.9238795325112867385, 1.000000000000000000, 0.9238795325112867385, 1.000000000000000000, 0.9238795325112867385, 1.000000000000000000, 0.9238795325112867385, 1.000000000000000000, 0.9238795325112867385, 1.000000000000000000, 0.9238795325112867385, 1.000000000000000000, 0.9238795325112867385, 1.000000000000000000, 0.9238795325112867385, 1.000000000000000000, 0.9238795325112867385, 1.000000000000000000, 0.9238795325112867385, 1.000000000000000000, 0.9238795325112867385, 1.000000000000000000, 0.9238795325112867385, 1.000000000000000000, 0.9238795325112867385, 1.000000000000000000, 0.9238795325112867385, 1.000000000000000000, 0.9238795325112867385, 1.000000000000000000, 0.9238795325112867385, 1.000000000000000000, 0.9238795325112867385, 1.000000000000000000, 0.9238795325112867385, 1.000000000000000000, 0.9238795325112867385, 1.000000000000000000, 0.9238795325112867385, 1.000000000000000000, 0.9238795325112867385, 1.000000000000000000, 0.9238795325112867385, 1.000000000000000000, 0.9238795325112867385, 1.000000000000000000, 0.9238795325112867385, 1.000000000000000000, 0.9238795325112867385, 1.000000000000000000, 0.9238795325112867385, 1.000000000000000000, 0.9238795325112867385, 1.000000000000000000, 0.9238795325112867385, 1.000000000000000000, 0.9238795325112867385, 1.000000000000000000, 0.9238795325112867385, 1.000000000000000000, 0.9238795325112867385, 1.000000000000000000, 0.9238795325112867385, 1.000000000000000000, 0.9238795325112867385, 1.000000000000000000, 0.9238795325112867385, 1.000000000000000000, 0.9238795325112867385, 1.000000000000000000, 0.9238795325112867385, 1.000000000000000000, 0.9238795325112867385, 1.000000000000000000, 0.9238795325112867385, 1.000000000000000000, 0.9238795325112867385, 1.000000000000000000, 0.9238795325112867385, 1.000000000000000000, 0.9238795325112867385, 1.000000000000000000, 0.9238795325112867385, 1.000000000000000000, 0.9238795325112867385, 1.000000000000000000, 0.9238795325112867385, 1.000000000000000000, 0.9238795325112867385, 1.000000000000000000, 0.9238795325112867385, 1.000000000000000000, 0.9238795325112867385, 1.000000000000000000, 0.9238795325112867385, 1.000000000000000000, 0.9238795325112867385, 1.000000000000000000, 0.9238795325112867385, 1.000000000000000000, 0.9238795325112867385, 1.000000000000000000, 0.9238795325112867385, 1.000000000000000000, 0.9238795325112867385, 1.000000000000000000, 0.9238795325112867385, 1.000000000000000000, 0.9238795325112867385, 1.000000000000000000, 0.9238795325112867385, 1.000000000000000000, 0.9238795325112867385, 1.000000000000000000, 0.9238795325112867385, 1.000000000000000000, 0.9238795325112867385, 1.000000000000000000, 0.9238795325112867385, 1.000000000000000000, 0.9238795325112867385, 1.000000000000000000, 0.9238795325112867385, 1.000000000000000000, 0.9238795325112867385, 1.000000000000000000, 0.9238795325112867385, 1.000000000000000000, 0.9238795325112867385, 1.000000000000000000, 0.9238795325112867385, 1.000000000000000000, 0.9238795325112867385, 1.000000000000000000, 0.9238795325112867385, 1.000000000000000000, 0.9238795325112867385, 1.000000000000000000, 0.9238795325112867385, 1.000000000000000000, 0.9238795325112867385, 1.000000000000000000, 0.9238795325112867385, 1.000000000000000000, 0.9238795325112867385, 1.000000000000000000, 0.9238795325112867385, 1.000000000000000000, 0.9238795325112867385, 1.000000000000000000, 0.9238795325112867385, 1.000000000000000000, 0.9238795325112867385, 1.000000000000000000, 0.9238795325112867385, 1.000000000000000000, 0.9238795325112867385, 1.000000000000000000, 0.9238795325112867385, 1.000000000000000000, 0.9238795325112867385, 1.000000000000000000, 0.9238795325112867385, 1.000000000000000000, 0.9238795325112867385, 1.000000000000000000, 0.9238795325112867385, 1.000000000000000000, 0.9238795325112867385, 1.000000000000000000, 0.9238795325112867385, 1.000000000000000000, 0.9238795325112867385, 1.000000000000000000, 0.9238795325112867385, 1.000000000000000000, 0.9238795325112867385, 1.000000000000000000, 0.9238795325112867385, 1.000000000000000000, 0.9238795325112867385, 1.000000000000000000, 0.9238795325112867385, 1.000000000000000000, 0.9238795325112867385, 1.000000000000000000, 0.9238795325112867385, 1.000000000000000000, 0.9238795325112867385, 1.000000000000000000, 0.9238795325112867385, 1.000000000000000000, 0.9238795325112867385, 1.000000000000000000, 0.9238795325112867385, 1.000000000000000000, 0.9238795325112867385, 1.000000000000000000, 0.9238795325112867385, 1.000000000000000000, 0.9238795325112867385, 1.000000000000000000, 0.9238795325112867385, 1.000000000000000000, 0.9238795325112867385, 1.000000000000000000, 0.9238795325112867385, 1.000000000000000000, 0.9238795325112867385, 1.000000000000000000, 0.9238795325112867385, 1.000000000000000000, 0.9238795325112867385, 1.000000000000000000, 0.9238795325112867385, 1.000000000000000000, 0.9238795325112867385, 1.000000000000000000, 0.9238795325112867385, 1.000000000000000000, 0.9238795325112867385, 1.000000000000000000, 0.9238795325112867385, 1.000000000000000000, 0.9238795325112867385, 1.000000000000000000, 0.9238795325112867385, 1.000000000000000000, 0.9238795325112867385, 1.000000000000000000, 0.9238795325112867385, 1.000000000000000000, 0.9238795325112867385, 1.000000000000000000, 0.9238795325112867385, 1.000000000000000000, 0.9238795325112867385, 1.000000000000000000, 0.9238795325112867385, 1.000000000000000000, 0.9238795325112867385, 1.000000000000000000, 0.9238795325112867385, 1.000000000000000000, 0.9238795325112867385, 1.000000000000000000, 0.9238795325112867385, 1.000000000000000000),
 ( 1.000000000000000000, 0.9238795325112867385, 1.000000000000000000, 0.9238795325112867385, 1.000000000000000000, 0.9238795325112867385, 1.000000000000000000, 0.9238795325112867385, 1.000000000000000000, 0.9238795325112867385, 1.000000000000000000, 0.9238795325112867385, 1.000000000000000000, 0.9238795325112867385, 1.000000000000000000, 0.9238795325112867385, 1.000000000000000000, 0.9238795325112867385, 1.000000000000000000, 0.9238795325112867385, 1.000000000000000000, 0.9238795325112867385, 1.000000000000000000, 0.9238795325112867385, 1.000000000000000000, 0.9238795325112867385, 1.000000000000000000, 0.9238795325112867385, 1.000000000000000000, 0.9238795325112867385, 1.000000000000000000, 0.9238795325112867385, 1.000000000000000000, 0.9238795325112867385, 1.000000000000000000, 0.9238795325112867385, 1.000000000000000000, 0.9238795325112867385, 1.000000000000000000, 0.9238795325112867385, 1.000000000000000000, 0.9238795325112867385, 1.000000000000000000, 0.9238795325112867385, 1.000000000000000000, 0.9238795325112867385, 1.000000000000000000, 0.9238795325112867385, 1.000000000000000000, 0.9238795325112867385, 1.000000000000000000, 0.9238795325112867385, 1.000000000000000000, 0.9238795325112867385, 1.000000000000000000, 0.9238795325112867385, 1.000000000000000000, 0.9238795325112867385, 1.000000000000000000, 0.9238795325112867385, 1.000000000000000000, 0.9238795325112867385, 1.000000000000000000, 0.9238795325112867385, 1.000000000000000000, 0.9238795325112867385, 1.000000000000000000, 0.9238795325112867385, 1.000000000000000000, 0.9238795325112867385, 1.000000000000000000, 0.9238795325112867385, 1.000000000000000000, 0.9238795325112867385, 1.000000000000000000, 0.9238795325112867385, 1.000000000000000000, 0.9238795325112867385, 1.000000000000000000, 0.9238795325112867385, 1.000000000000000000, 0.9238795325112867385, 1.000000000000000000, 0.9238795325112867385, 1.000000000000000000, 0.9238795325112867385, 1.000000000000000000, 0.9238795325112867385, 1.000000000000000000, 0.9238795325112867385, 1.000000000000000000, 0.9238795325112867385, 1.000000000000000000, 0.9238795325112867385, 1.000000000000000000, 0.9238795325112867385, 1.000000000000000000, 0.9238795325112867385, 1.000000000000000000, 0.9238795325112867385, 1.000000000000000000, 0.9238795325112867385, 1.000000000000000000, 0.9238795325112867385, 1.000000000000000000, 0.9238795325112867385, 1.000000000000000000, 0.9238795325112867385, 1.000000000000000000, 0.9238795325112867385, 1.000000000000000000, 0.9238795325112867385, 1.000000000000000000, 0.9238795325112867385, 1.000000000000000000, 0.9238795325112867385, 1.000000000000000000, 0.9238795325112867385, 1.000000000000000000, 0.9238795325112867385, 1.000000000000000000, 0.9238795325112867385, 1.000000000000000000, 0.9238795325112867385, 1.000000000000000000, 0.9238795325112867385, 1.000000000000000000, 0.9238795325112867385, 1.000000000000000000, 0.9238795325112867385, 1.000000000000000000, 0.9238795325112867385, 1.000000000000000000, 0.9238795325112867385, 1.000000000000000000, 0.9238795325112867385, 1.000000000000000000, 0.9238795325112867385, 1.000000000000000000, 0.9238795325112867385, 1.000000000000000000, 0.9238795325112867385, 1.000000000000000000, 0.9238795325112867385, 1.000000000000000000, 0.9238795325112867385, 1.000000000000000000, 0.9238795325112867385, 1.000000000000000000, 0.9238795325112867385, 1.000000000000000000, 0.9238795325112867385, 1.000000000000000000, 0.9238795325112867385, 1.000000000000000000, 0.9238795325112867385, 1.000000000000000000, 0.9238795325112867385, 1.000000000000000000, 0.9238795325112867385, 1.000000000000000000, 0.9238795325112867385, 1.000000000000000000, 0.9238795325112867385, 1.000000000000000000, 0.9238795325112867385, 1.000000000000000000, 0.9238795325112867385, 1.000000000000000000, 0.9238795325112867385, 1.000000000000000000, 0.9238795325112867385, 1.000000000000000000, 0.9238795325112867385, 1.000000000000000000, 0.9238795325112867385, 1.000000000000000000, 0.9238795325112867385, 1.000000000000000000, 0.9238795325112867385, 1.000000000000000000, 0.9238795325112867385, 1.000000000000000000, 0.9238795325112867385, 1.000000000000000000, 0.9238795325112867385, 1.000000000000000000, 0.9238795325112867385, 1.000000000000000000, 0.9238795325112867385, 1.000000000000000000, 0.9238795325112867385, 1.000000000000000000, 0.9238795325112867385, 1.000000000000000000, 0.9238795325112867385, 1.000000000000000000, 0.9238795325112867385, 1.000000000000000000, 0.9238795325112867385, 1.000000000000000000, 0.9238795325112867385, 1.000000000000000000, 0.9238795325112867385, 1.000000000000000000, 0.9238795325112867385, 1.000000000000000000, 0.9238795325112867385, 1.000000000000000000, 0.9238795325112867385, 1.000000000000000000, 0.9238795325112867385, 1.000000000000000000, 0.9238795325112867385, 1.000000000000000000, 0.9238795325112867385, 1.000000000000000000, 0.9238795325112867385, 1.000000000000000000, 0.9238795325112867385, 1.000000000000000000, 0.9238795325112867385, 1.000000000000000000, 0.9238795325112867385, 1.000000000000000000, 0.9238795325112867385, 1.000000000000000000, 0.9238795325112867385, 1.000000000000000000, 0.9238795325112867385, 1.000000000000000000, 0.9238795325112867385, 1.000000000000000000, 0.9238795325112867385, 1.000000000000000000, 0.9238795325112867385, 1.000000000000000000, 0.9238795325112867385, 1.000000000000000000, 0.9238795325112867385, 1.000000000000000000, 0.9238795325112867385, 1.000000000000000000, 0.9238795325112867385, 1.000000000000000000, 0.9238795325112867385, 1.000000000000000000, 0.9238795325112867385, 1.000000000000000000, 0.9238795325112867385, 1.000000000000000000, 0.9238795325112867385, 1.000000000000000000, 0.9238795325112867385, 1.000000000000000000, 0.9238795325112867385, 1.000000000000000000, 0.9238795325112867385, 1.000000000000000000, 0.9238795325112867385, 1.000000000000000000, 0.9238795325112867385, 1.000000000000000000, 0.9238795325112867385, 1.000000000000000000, 0.9238795325112867385, 1.000000000000000000, 0.9238795325112867385, 1.000000000000000000, 0.9238795325112867385, 1.000000000000000000, 0.9238795325112867385, 1.000000000000000000, 0.9238795325112867385, 1.000000000000000000, 0.9238795325112867385, 1.000000000000000000, 0.9238795325112867385, 1.000000000000000000, 0.9238795325112867385, 1.000000000000000000, 0.9238795325112867385, 1.000000000000000000, 0.9238795325112867385, 1.000000000000000000, 0.9238795325112867385, 1.000000000000000000, 0.9238795325112867385, 1.000000000000000000) ) ) 
 REPRESENTATION_ITEM ( '' )  SURFACE ( )  );
#59408 = ORIENTED_EDGE ( 'NONE', *, *, #45005, .T. ) ;
#59409 = CARTESIAN_POINT ( 'NONE',  ( 8.311093377946839666, 225.7812500034140157, 8.311093377946829008 ) ) ;
#59410 = CARTESIAN_POINT ( 'NONE',  ( 7.320508075688762162, 90.62500000000001421, -7.320508075688762162 ) ) ;
#59411 = DIRECTION ( 'NONE',  ( 0.000000000000000000, -1.000000000000000000, 0.000000000000000000 ) ) ;
#59412 = CYLINDRICAL_SURFACE ( 'NONE', #49558, 4.000000000000001776 ) ;
#59413 = DIRECTION ( 'NONE',  ( 0.000000000000000000, 0.000000000000000000, 1.000000000000000000 ) ) ;
#59414 = CARTESIAN_POINT ( 'NONE',  ( 0.000000000000000000, 0.000000000000000000, 118.0000000000000000 ) ) ;
#59415 = CARTESIAN_POINT ( 'NONE',  ( 10.00000000000000178, 170.2083333333333428, -2.679491924311226736 ) ) ;
#59416 = FACE_OUTER_BOUND ( 'NONE', #15842, .T. ) ;
#59417 = CARTESIAN_POINT ( 'NONE',  ( -4.556349186104048599, -10.99999999999999822, 89.78125000000000000 ) ) ;
#59418 = CARTESIAN_POINT ( 'NONE',  ( -3.407298021520221543, -68.04056125361168483, 20.39715949456294908 ) ) ;
#59419 = CARTESIAN_POINT ( 'NONE',  ( -3.042071309553164404, 142.5520833299193271, -11.35316468749999963 ) ) ;
#59420 = CARTESIAN_POINT ( 'NONE',  ( -11.00000000000000000, 0.000000000000000000, 76.18750000409677625 ) ) ;
#59421 = CARTESIAN_POINT ( 'NONE',  ( 11.00000000000000000, 1.347111479062088405E-15, 81.43750000409677625 ) ) ;
#59424 = CARTESIAN_POINT ( 'NONE',  ( 17.99999999999999645, 3.528342445705438202, -0.1857217976155470518 ) ) ;
#59423 = FACE_OUTER_BOUND ( 'NONE', #13258, .T. ) ;
#59422 = CARTESIAN_POINT ( 'NONE',  ( 23.99999999999998934, 204.7500000000000284, 169.9999999999998863 ) ) ;
#59425 = ORIENTED_EDGE ( 'NONE', *, *, #4137, .T. ) ;
#59426 = AXIS2_PLACEMENT_3D ( 'NONE', #41549, #42650, #29864 ) ;
#59427 = CARTESIAN_POINT ( 'NONE',  ( 8.311093377946834337, 5.468749996586017126, 8.311093377946839666 ) ) ;
#59428 = CARTESIAN_POINT ( 'NONE',  ( 4.898587196589412829E-16, 7.687499995903221084, -8.000000000000000000 ) ) ;
#59429 = CARTESIAN_POINT ( 'NONE',  ( -9.999999999999992895, 112.2916666666666714, -2.679491924311228068 ) ) ;
#59430 = DIRECTION ( 'NONE',  ( -0.000000000000000000, 1.000000000000000000, 4.689100369878284071E-30 ) ) ;
#59431 = CARTESIAN_POINT ( 'NONE',  ( 2.445694354108783664, 208.3125000013656063, 144.4456943541088663 ) ) ;
#59432 =( BOUNDED_CURVE ( )  B_SPLINE_CURVE ( 2, ( #59816, #9631, #42450, #55660, #14888, #37927, #65468, #43952, #48851 ),
 .UNSPECIFIED., .F., .F. ) 
 B_SPLINE_CURVE_WITH_KNOTS ( ( 3, 2, 2, 2, 3 ),
 ( 0.8229166666666667407, 0.8281250000000001110, 0.8333333333333334814, 0.8385416666666668517, 0.8437500000000002220 ),
 .UNSPECIFIED. ) 
 CURVE ( )  GEOMETRIC_REPRESENTATION_ITEM ( )  RATIONAL_B_SPLINE_CURVE ( ( 0.9999999999999983347, 0.9238795325112884038, 1.000000000000000000, 0.9238795325112867385, 1.000000000000000000, 0.9238795325112867385, 1.000000000000000000, 0.9238795325112835188, 1.000000000000003331 ) ) 
 REPRESENTATION_ITEM ( '' )  );
#59433 = CARTESIAN_POINT ( 'NONE',  ( 4.898587196589412829E-16, 4.687499995903220196, -8.000000000000000000 ) ) ;
#59434 = CARTESIAN_POINT ( 'NONE',  ( -7.320508075688778149, 29.99999999317203603, 7.320508075688769267 ) ) ;
#59435 = CARTESIAN_POINT ( 'NONE',  ( 5.082755093536326818, 114.2187500020483810, 5.082755093536325042 ) ) ;
#59436 = CARTESIAN_POINT ( 'NONE',  ( 4.541265875000002339, 4.437499998634407028, 0.000000000000000000 ) ) ;
#59437 = CARTESIAN_POINT ( 'NONE',  ( -7.999999999999861444, -9.580972845112835701E-07, 13.01783880491507261 ) ) ;
#59438 = CARTESIAN_POINT ( 'NONE',  ( -5.656854249492375253, 5.656854249492375253, 12.64280277982336287 ) ) ;
#59440 = CARTESIAN_POINT ( 'NONE',  ( 8.999999999999998224, 0.000000000000000000, 0.000000000000000000 ) ) ;
#59439 = CARTESIAN_POINT ( 'NONE',  ( 9.797174393178825657E-16, 125.0000000000000000, -8.000000000000000000 ) ) ;
#59441 = ORIENTED_EDGE ( 'NONE', *, *, #35627, .T. ) ;
#59442 = CARTESIAN_POINT ( 'NONE',  ( -2.751064625579944321E-14, 209.7500000000000284, 146.0000000000000284 ) ) ;
#59443 = CARTESIAN_POINT ( 'NONE',  ( -5.000000000000023981, 61.66666666666669272, -8.660254037844433483 ) ) ;
#59444 = CARTESIAN_POINT ( 'NONE',  ( -3.042071309553159075, 225.2604166700806161, 11.35316468749999963 ) ) ;
#59445 = CARTESIAN_POINT ( 'NONE',  ( 5.676582343749993598, 119.9479166632526841, 9.832129032723422313 ) ) ;
#59446 = ORIENTED_EDGE ( 'NONE', *, *, #43886, .T. ) ;
#59447 = CARTESIAN_POINT ( 'NONE',  ( 3.748303087376534393, 10.32408853373171809, 117.5267128448309677 ) ) ;
#59448 = CARTESIAN_POINT ( 'NONE',  ( -10.18810118749999916, 0.000000000000000000, 94.65625000204836681 ) ) ;
#59449 = CARTESIAN_POINT ( 'NONE',  ( 6.000000000000000000, 7.347880794884119736E-16, -10.77459999999999951 ) ) ;
#59450 = CARTESIAN_POINT ( 'NONE',  ( 2.445694354108840063, 198.0625000013656063, 200.4456943541088663 ) ) ;
#59451 = CARTESIAN_POINT ( 'NONE',  ( 3.313708498984756279, 7.999999999999991118, 27.36155277982336642 ) ) ;
#59453 = CARTESIAN_POINT ( 'NONE',  ( -11.35316468749999785, 118.0729166632526841, -3.042071309553167957 ) ) ;
#59452 = CARTESIAN_POINT ( 'NONE',  ( -1.001543065824775909E-15, -10.39230484541329247, -10.80000000000000071 ) ) ;
#59454 = CARTESIAN_POINT ( 'NONE',  ( -28.00000000000003197, 209.0000000000000284, 166.0000000000003695 ) ) ;
#59455 = CARTESIAN_POINT ( 'NONE',  ( -8.000000000000000000, 92.00000000000000000, 0.000000000000000000 ) ) ;
#59456 = ORIENTED_EDGE ( 'NONE', *, *, #71167, .T. ) ;
#59457 = CARTESIAN_POINT ( 'NONE',  ( 10.00000000000000000, 211.6666666598386541, 2.679491924311236062 ) ) ;
#59458 = CARTESIAN_POINT ( 'NONE',  ( -4.898587196589412829E-16, 99.12499999999998579, -8.000000000000000000 ) ) ;
#59459 = AXIS2_PLACEMENT_3D ( 'NONE', #54350, #9446, #72048 ) ;
#59460 = DIRECTION ( 'NONE',  ( 1.000000000000000000, -0.000000000000000000, -0.000000000000000000 ) ) ;
#59461 = CARTESIAN_POINT ( 'NONE',  ( -11.35316468750000141, 103.5937499965860269, -1.390361679473963753E-15 ) ) ;
#59462 = CARTESIAN_POINT ( 'NONE',  ( -12.00000000000000000, 1.469576158976823947E-15, 6.938893903907228378E-15 ) ) ;
#59463 = CARTESIAN_POINT ( 'NONE',  ( 7.188101187500000933, 12.93749999795161187, -2.977408999572650483 ) ) ;
#59464 = CARTESIAN_POINT ( 'NONE',  ( 4.220049686691934809, 10.18810118749999916, 91.56250000204838102 ) ) ;
#59465 = CARTESIAN_POINT ( 'NONE',  ( 9.832129032723416984, 5.677083329919350163, 5.676582343750006032 ) ) ;
#59466 = ORIENTED_EDGE ( 'NONE', *, *, #3880, .T. ) ;
#59467 = CARTESIAN_POINT ( 'NONE',  ( 2.679491924310934969, 182.9166666598387394, -10.00000000000017053 ) ) ;
#59468 = CARTESIAN_POINT ( 'NONE',  ( 8.660254037844385522, 246.0416666734946318, -5.000000000000003553 ) ) ;
#59469 = CARTESIAN_POINT ( 'NONE',  ( -10.99999999999989164, -4.556349186104158733, 101.7812500040967763 ) ) ;
#59470 = VECTOR ( 'NONE', #71465, 1000.000000000000000 ) ;
#59471 = CARTESIAN_POINT ( 'NONE',  ( 7.204075437095966983, 7.204075437095967871, 73.46875000204838102 ) ) ;
#59472 = CARTESIAN_POINT ( 'NONE',  ( -1.062900648031719353, 21.99999999999998934, 4.384117386624189372 ) ) ;
#59473 = DIRECTION ( 'NONE',  ( 1.000000000000000000, -0.000000000000000000, -0.000000000000000000 ) ) ;
#59474 = CARTESIAN_POINT ( 'NONE',  ( 6.676582343750003368, 293.0156250017070079, -2.765530957081997254 ) ) ;
#59475 = CARTESIAN_POINT ( 'NONE',  ( -4.000000000000015987, 199.5000000000000000, 142.0000000000000568 ) ) ;
#59476 = DIRECTION ( 'NONE',  ( 1.000000000000000000, -0.000000000000000000, -0.000000000000000000 ) ) ;
#59477 = EDGE_CURVE ( 'NONE', #53267, #68962, #11835, .T. ) ;
#59478 = ADVANCED_FACE ( 'NONE', ( #3736 ), #26735, .T. ) ;
#59479 = CARTESIAN_POINT ( 'NONE',  ( 7.204075437095966983, 7.204075437095967871, 85.09375000204836681 ) ) ;
#59480 = CARTESIAN_POINT ( 'NONE',  ( -30.44569435410879166, 199.8125000013656063, 172.4456943541092357 ) ) ;
#59481 = CARTESIAN_POINT ( 'NONE',  ( 7.999999999999998224, 22.40625000000000355, 3.313708498984766493 ) ) ;
#59482 = CARTESIAN_POINT ( 'NONE',  ( -4.541265875000002339, 13.87499999863440969, -1.881053915767121998 ) ) ;
#59483 = ORIENTED_EDGE ( 'NONE', *, *, #67930, .T. ) ;
#59484 = AXIS2_PLACEMENT_3D ( 'NONE', #37334, #25621, #54322 ) ;
#59485 = CARTESIAN_POINT ( 'NONE',  ( -27.99999999999991473, 208.6250000027312126, 174.0000000000003695 ) ) ;
#59486 = CARTESIAN_POINT ( 'NONE',  ( -2.828427124746152987, 206.2500000027312126, 200.8284271247462129 ) ) ;
#59487 = CARTESIAN_POINT ( 'NONE',  ( -2.445694354108839175, 199.3125000013656063, 144.4456943541088663 ) ) ;
#59488 = CARTESIAN_POINT ( 'NONE',  ( 3.999999999999960032, 206.0625000027312694, 143.6568542494924543 ) ) ;
#59489 = CARTESIAN_POINT ( 'NONE',  ( -5.000000000000000000, 10.26105934116142215, 64.40045319026754100 ) ) ;
#59490 = CARTESIAN_POINT ( 'NONE',  ( 10.18810118750000093, -4.220049686691933921, 68.68750000204836681 ) ) ;
#59491 = ORIENTED_EDGE ( 'NONE', *, *, #27807, .F. ) ;
#59492 = CARTESIAN_POINT ( 'NONE',  ( -5.082755093536325042, 2.531249997951610542, -5.082755093536325930 ) ) ;
#59493 = CARTESIAN_POINT ( 'NONE',  ( -10.00000000000000178, 29.37499999317203248, -1.224646799147353454E-15 ) ) ;
#59494 = CARTESIAN_POINT ( 'NONE',  ( -2.977408999572651815, 117.3125000020483810, 7.188101187500000933 ) ) ;
#59495 = CARTESIAN_POINT ( 'NONE',  ( -0.4590000000000000746, 272.8559999999997672, 5.793779103868386571 ) ) ;
#59496 = CARTESIAN_POINT ( 'NONE',  ( -4.088227598258586603E-16, 293.2031250017069510, -6.676582343750001591 ) ) ;
#59498 = CARTESIAN_POINT ( 'NONE',  ( 0.000000000000000000, 0.000000000000000000, 0.000000000000000000 ) ) ;
#59497 = CARTESIAN_POINT ( 'NONE',  ( 5.676582343750005144, 225.5729166700806729, 9.832129032723416984 ) ) ;
#59499 = VERTEX_POINT ( 'NONE', #66732 ) ;
#59500 = CARTESIAN_POINT ( 'NONE',  ( 5.676582343750005144, 230.8854166700806729, 9.832129032723416984 ) ) ;
#59501 = CARTESIAN_POINT ( 'NONE',  ( 5.082755093536318824, 5.082755093536319713, 2.424052781871750994 ) ) ;
#59502 = CIRCLE ( 'NONE', #16122, 12.00000000000000000 ) ;
#59503 = CARTESIAN_POINT ( 'NONE',  ( 8.000000000000000000, 3.093750000000000888, -3.313708498984761164 ) ) ;
#59504 = CARTESIAN_POINT ( 'NONE',  ( 2.445694354108839175, 202.3125000013656063, 195.5543056458912190 ) ) ;
#59505 = ORIENTED_EDGE ( 'NONE', *, *, #49615, .T. ) ;
#59506 = CARTESIAN_POINT ( 'NONE',  ( 11.35316468749999785, 100.8854166632526841, 3.042071309553174174 ) ) ;
#59507 = DIRECTION ( 'NONE',  ( -0.000000000000000000, 1.000000000000000000, -0.000000000000000000 ) ) ;
#59508 = CARTESIAN_POINT ( 'NONE',  ( -10.99999999999999822, -4.556349186104052151, 77.59374999999998579 ) ) ;
#59511 = DIRECTION ( 'NONE',  ( -1.000000000000000000, 0.000000000000000000, 0.000000000000000000 ) ) ;
#59510 = CARTESIAN_POINT ( 'NONE',  ( 26.56734541678233086, 206.0000000013656347, 166.5412658749999650 ) ) ;
#59509 = CARTESIAN_POINT ( 'NONE',  ( 24.54126587499999346, 202.4375000013656063, 169.9999999999998863 ) ) ;
#59512 = ORIENTED_EDGE ( 'NONE', *, *, #71284, .F. ) ;
#59513 = CARTESIAN_POINT ( 'NONE',  ( 3.313708498984711426, 99.96875000000000000, 8.000000000000053291 ) ) ;
#59514 = CARTESIAN_POINT ( 'NONE',  ( -8.311093377946836114, 212.6562499965860411, -8.311093377946837890 ) ) ;
#59515 = CARTESIAN_POINT ( 'NONE',  ( 1.432654583217607858, 200.6250000013655779, 138.5412658750000787 ) ) ;
#59516 = CARTESIAN_POINT ( 'NONE',  ( 24.54126587499998280, 200.5000000013656063, 171.4326545832175555 ) ) ;
#59517 = DIRECTION ( 'NONE',  ( -0.000000000000000000, 1.000000000000000000, -0.000000000000000000 ) ) ;
#59518 = CARTESIAN_POINT ( 'NONE',  ( -3.042071309553173730, 189.6354166632526983, 11.35316468749999785 ) ) ;
#59519 = CARTESIAN_POINT ( 'NONE',  ( 2.977408999572650039, 92.56250000204838102, -7.188101187500000933 ) ) ;
#59520 = FACE_OUTER_BOUND ( 'NONE', #330, .T. ) ;
#59521 = CARTESIAN_POINT ( 'NONE',  ( -25.17157287525377285, 196.6250000000000284, 172.8284271247465256 ) ) ;
#59522 = CARTESIAN_POINT ( 'NONE',  ( 4.541265875000002339, 12.37499999863440969, -1.881053915767121554 ) ) ;
#59523 = CARTESIAN_POINT ( 'NONE',  ( 24.54126587499999346, 198.4375000013655779, 169.9999999999998863 ) ) ;
#59524 = CARTESIAN_POINT ( 'NONE',  ( -7.188101187499992051, 0.000000000000000000, 1.861552781871753881 ) ) ;
#59525 = CARTESIAN_POINT ( 'NONE',  ( 11.35316468749999785, 80.57291666325268409, 3.042071309553174174 ) ) ;
#59526 =( BOUNDED_CURVE ( )  B_SPLINE_CURVE ( 2, ( #11776, #10662, #33695, #69123, #68743, #5015, #52149, #56321, #29133 ),
 .UNSPECIFIED., .F., .F. ) 
 B_SPLINE_CURVE_WITH_KNOTS ( ( 3, 2, 2, 2, 3 ),
 ( 0.3645833333333331483, 0.3697916666666665186, 0.3749999999999998890, 0.3802083333333332038, 0.3854166666666665741 ),
 .UNSPECIFIED. ) 
 CURVE ( )  GEOMETRIC_REPRESENTATION_ITEM ( )  RATIONAL_B_SPLINE_CURVE ( ( 1.000000000000002442, 0.9238795325112842960, 1.000000000000000000, 0.9238795325112867385, 1.000000000000000000, 0.9238795325112867385, 1.000000000000000000, 0.9238795325112884038, 0.9999999999999983347 ) ) 
 REPRESENTATION_ITEM ( '' )  );
#59527 = LINE ( 'NONE', #43273, #73768 ) ;
#59528 = DIRECTION ( 'NONE',  ( 0.000000000000000000, 0.000000000000000000, 1.000000000000000000 ) ) ;
#59529 = ORIENTED_EDGE ( 'NONE', *, *, #68362, .T. ) ;
#59530 = FACE_BOUND ( 'NONE', #46752, .T. ) ;
#59531 = CARTESIAN_POINT ( 'NONE',  ( 1.469576158976823947E-15, 97.06250000409677625, 8.000000000000000000 ) ) ;
#59532 = CARTESIAN_POINT ( 'NONE',  ( -11.35316468750000141, 78.28124999658601268, -1.390361679473963753E-15 ) ) ;
#59533 = VERTEX_POINT ( 'NONE', #3360 ) ;
#59534 = CARTESIAN_POINT ( 'NONE',  ( 7.204075437095966983, 7.204075437095967871, 83.96875000204836681 ) ) ;
#59535 = CARTESIAN_POINT ( 'NONE',  ( 11.00000000000000000, 4.556349186104045934, 69.53125000409677625 ) ) ;
#59536 = CARTESIAN_POINT ( 'NONE',  ( -1.432654583217607414, 208.5000000013656063, 194.5412658750000219 ) ) ;
#59537 = CARTESIAN_POINT ( 'NONE',  ( 8.000000000000000000, 23.90624999590322375, -3.313708498984761164 ) ) ;
#59539 = CARTESIAN_POINT ( 'NONE',  ( 9.832129032723420536, 76.19791666325269830, -5.676582343749999815 ) ) ;
#59538 = CARTESIAN_POINT ( 'NONE',  ( -1.739508062077478989, 67.70228923712431879, 20.12326043015404764 ) ) ;
#59540 = CARTESIAN_POINT ( 'NONE',  ( -3.313708498984757167, 7.999999999999991118, 24.73655278392014978 ) ) ;
#59541 = DIRECTION ( 'NONE',  ( 0.000000000000000000, -0.000000000000000000, -1.000000000000000000 ) ) ;
#59542 = CARTESIAN_POINT ( 'NONE',  ( -2.679491924311225848, 168.3333333265053966, -10.00000000000000178 ) ) ;
#59543 = CARTESIAN_POINT ( 'NONE',  ( 1.320432766682874540E-15, 91.90625000204838102, 7.188101187500000044 ) ) ;
#59544 = EDGE_CURVE ( 'NONE', #24721, #25147, #20318, .T. ) ;
#59545 = CARTESIAN_POINT ( 'NONE',  ( -3.458734124999959914, 209.4375000013656063, 198.0000000000000284 ) ) ;
#59546 = CARTESIAN_POINT ( 'NONE',  ( 9.832129032723420536, 56.51041666325268409, -5.676582343749999815 ) ) ;
#59547 = CARTESIAN_POINT ( 'NONE',  ( 1.871523826299183495E-15, -10.18810118749999916, 107.4062500020483668 ) ) ;
#59548 = CARTESIAN_POINT ( 'NONE',  ( 8.311093377946837890, 196.4062499965860411, -8.311093377946837890 ) ) ;
#59549 = ORIENTED_EDGE ( 'NONE', *, *, #69293, .F. ) ;
#59550 = CARTESIAN_POINT ( 'NONE',  ( -5.107860025165151363, 60.88642786445262090, 23.30380398316496482 ) ) ;
#59551 = FACE_OUTER_BOUND ( 'NONE', #60010, .T. ) ;
#59552 = CARTESIAN_POINT ( 'NONE',  ( 8.660254037844389075, 162.2916666598387110, -5.000000000000000000 ) ) ;
#59554 = CARTESIAN_POINT ( 'NONE',  ( -3.042071309553173730, 199.3229166632526983, 11.35316468749999785 ) ) ;
#59553 = CARTESIAN_POINT ( 'NONE',  ( -23.99999999999995026, 200.8125000027312126, 171.6568542494926817 ) ) ;
#59555 = CARTESIAN_POINT ( 'NONE',  ( 0.000000000000000000, 300.0000000000000000, 0.000000000000000000 ) ) ;
#59556 = CARTESIAN_POINT ( 'NONE',  ( 1.836970198721029589E-15, 234.3750000068279746, 10.00000000000000000 ) ) ;
#59557 = CARTESIAN_POINT ( 'NONE',  ( 9.797174393178825657E-16, 125.0000000000000000, -8.000000000000000000 ) ) ;
#59558 = ORIENTED_EDGE ( 'NONE', *, *, #38204, .F. ) ;
#59559 = CARTESIAN_POINT ( 'NONE',  ( -3.042071309553163960, 177.5520833299193555, -11.35316468749999963 ) ) ;
#59560 = CARTESIAN_POINT ( 'NONE',  ( -5.082755093536317936, -5.082755093536320601, 19.67405278187175455 ) ) ;
#59561 = CARTESIAN_POINT ( 'NONE',  ( 0.000000000000000000, 0.000000000000000000, -4.000000000000001776 ) ) ;
#59562 = VERTEX_POINT ( 'NONE', #15037 ) ;
#59563 = ADVANCED_FACE ( 'NONE', ( #67484 ), #72772, .T. ) ;
#59564 = ADVANCED_FACE ( 'NONE', ( #9394 ), #32414, .T. ) ;
#59565 = CARTESIAN_POINT ( 'NONE',  ( -5.656854249492378806, 96.87500000409677625, 5.656854249492381470 ) ) ;
#59567 = EDGE_CURVE ( 'NONE', #59034, #34777, #66012, .T. ) ;
#59566 = CYLINDRICAL_SURFACE ( 'NONE', #44634, 6.000000000000001776 ) ;
#59568 = CARTESIAN_POINT ( 'NONE',  ( 1.656854249492381914, 17.81250000000000355, 4.000000000000000888 ) ) ;
#59569 = CARTESIAN_POINT ( 'NONE',  ( -4.541265875000002339, 17.74999999863440792, -1.881053915767121998 ) ) ;
#59570 = CARTESIAN_POINT ( 'NONE',  ( 5.656854249492374365, 5.656854249492375253, 12.45530278392014623 ) ) ;
#59572 = CARTESIAN_POINT ( 'NONE',  ( 12.00000000000000000, 0.000000000000000000, -28.00000000000000000 ) ) ;
#59571 = AXIS2_PLACEMENT_3D ( 'NONE', #14477, #9211, #37516 ) ;
#59573 = ORIENTED_EDGE ( 'NONE', *, *, #39918, .T. ) ;
#59574 = AXIS2_PLACEMENT_3D ( 'NONE', #24692, #64333, #19776 ) ;
#59575 = CARTESIAN_POINT ( 'NONE',  ( 38.00000000000000000, -52.99999999999999289, 25.00000000000000000 ) ) ;
#59576 = CARTESIAN_POINT ( 'NONE',  ( 7.188101187500000044, 100.9062500020483810, -8.802885111219163269E-16 ) ) ;
#59577 = ADVANCED_FACE ( 'NONE', ( #73142 ), #24137, .F. ) ;
#59579 = CARTESIAN_POINT ( 'NONE',  ( 5.656854249492379694, 120.1250000040967905, -5.656854249492380582 ) ) ;
#59578 = CARTESIAN_POINT ( 'NONE',  ( -5.656854249492380582, 92.00000000409677625, -5.656854249492380582 ) ) ;
#59580 = ORIENTED_EDGE ( 'NONE', *, *, #10673, .T. ) ;
#59581 = CARTESIAN_POINT ( 'NONE',  ( 3.373128826976389938, 50.22031155377564460, -40.85657338450008069 ) ) ;
#59582 = CARTESIAN_POINT ( 'NONE',  ( -5.082755093536317936, -5.082755093536320601, 18.17405278187175455 ) ) ;
#59583 = EDGE_LOOP ( 'NONE', ( #7879, #50179, #51955, #45561, #49034 ) ) ;
#59584 = ORIENTED_EDGE ( 'NONE', *, *, #62454, .F. ) ;
#59585 = CARTESIAN_POINT ( 'NONE',  ( 10.18810118750000093, -4.220049686691933033, 78.81250000204838102 ) ) ;
#59586 = CARTESIAN_POINT ( 'NONE',  ( 2.679491924311155682, 92.91666665983871098, -10.00000000000004441 ) ) ;
#59587 = CARTESIAN_POINT ( 'NONE',  ( -11.00000000000000000, 4.556349186104045934, 95.40624999999998579 ) ) ;
#59590 = CARTESIAN_POINT ( 'NONE',  ( 2.765530957081996366, 293.2968750017070079, -6.676582343750002480 ) ) ;
#59589 = CARTESIAN_POINT ( 'NONE',  ( 28.00000000000002132, 201.1250000027312126, 173.9999999999999147 ) ) ;
#59588 = DIRECTION ( 'NONE',  ( -0.000000000000000000, 1.000000000000000000, -0.000000000000000000 ) ) ;
#59591 = CARTESIAN_POINT ( 'NONE',  ( -8.660254037844390851, 152.9166666666666856, 4.999999999999998224 ) ) ;
#59592 = CARTESIAN_POINT ( 'NONE',  ( -1.656854249492381248, 0.3125000000000002220, -4.000000000000001776 ) ) ;
#59593 = CARTESIAN_POINT ( 'NONE',  ( 1.320432766682872962E-15, -7.188101187499992051, 0.7365527818717527708 ) ) ;
#59594 = DIRECTION ( 'NONE',  ( 1.000000000000000000, 0.000000000000000000, 0.000000000000000000 ) ) ;
#59595 = CARTESIAN_POINT ( 'NONE',  ( 5.656854249492378806, 5.624999995903220196, 5.656854249492381470 ) ) ;
#59596 = CARTESIAN_POINT ( 'NONE',  ( 30.44569435410879166, 198.5625000013656063, 172.4456943541087526 ) ) ;
#59597 = CARTESIAN_POINT ( 'NONE',  ( 5.082755093536324154, 11.15624999795161187, 5.082755093536326818 ) ) ;
#59598 = CARTESIAN_POINT ( 'NONE',  ( -7.999999999999991118, 0.000000000000000000, 28.01780278392014978 ) ) ;
#59599 = DIRECTION ( 'NONE',  ( 0.000000000000000000, 0.000000000000000000, 1.000000000000000000 ) ) ;
#59600 = CARTESIAN_POINT ( 'NONE',  ( -5.082755093536325930, 109.3437500020483810, -5.082755093536325930 ) ) ;
#59602 = CARTESIAN_POINT ( 'NONE',  ( -4.999999999999998224, 131.6666666666667140, -8.660254037844389075 ) ) ;
#59601 =( NAMED_UNIT ( * ) PLANE_ANGLE_UNIT ( ) SI_UNIT ( $, .RADIAN. ) );
#59603 = CARTESIAN_POINT ( 'NONE',  ( 9.832129032723416984, 227.1354166700806729, -5.676582343750003368 ) ) ;
#59604 = DIRECTION ( 'NONE',  ( -0.000000000000000000, 1.000000000000000000, -1.563033456626094573E-30 ) ) ;
#59605 = CARTESIAN_POINT ( 'NONE',  ( 7.188101187499993827, -2.977408999572645598, 20.51780278187175455 ) ) ;
#59606 = CARTESIAN_POINT ( 'NONE',  ( -18.89444362769112118, 5.999999999999950262, 167.9999999999997726 ) ) ;
#59607 = CARTESIAN_POINT ( 'NONE',  ( 8.311093377946834337, 25.15624999658601268, 8.311093377946839666 ) ) ;
#59608 = CARTESIAN_POINT ( 'NONE',  ( 8.660254037844389075, 149.5833333333333144, 5.000000000000007105 ) ) ;
#59609 = CARTESIAN_POINT ( 'NONE',  ( 8.660254037844385522, 6.458333326505366401, 5.000000000000005329 ) ) ;
#59610 = CARTESIAN_POINT ( 'NONE',  ( 32.00000000000000000, 201.3750000027312126, 169.9999999999998863 ) ) ;
#59611 = DIRECTION ( 'NONE',  ( -0.000000000000000000, 1.000000000000000000, -0.000000000000000000 ) ) ;
#59612 = ORIENTED_EDGE ( 'NONE', *, *, #1319, .T. ) ;
#59613 = CARTESIAN_POINT ( 'NONE',  ( 7.778174593052021635, 7.778174593052023411, 104.1250000040967763 ) ) ;
#59614 = CARTESIAN_POINT ( 'NONE',  ( -7.347880794884122694E-16, 14.75000000000000178, 4.000000000000001776 ) ) ;
#59615 = CARTESIAN_POINT ( 'NONE',  ( 3.042071309553159519, 39.73958332991934128, 11.35316468750000141 ) ) ;
#59616 = CARTESIAN_POINT ( 'NONE',  ( 7.778174593052021635, 7.778174593052023411, 86.12500000409677625 ) ) ;
#59617 = CARTESIAN_POINT ( 'NONE',  ( 75.00000000000001421, 242.0000000000000284, 20.00000000000002132 ) ) ;
#59618 = CARTESIAN_POINT ( 'NONE',  ( 23.99999999999999645, 202.6875000000000284, 168.3431457505074889 ) ) ;
#59619 = CARTESIAN_POINT ( 'NONE',  ( 27.99999999999996803, 200.0000000000000000, 173.9999999999999147 ) ) ;
#59621 = CARTESIAN_POINT ( 'NONE',  ( -11.35316468750000141, 28.48958332991934839, 3.042071309553159963 ) ) ;
#59620 = CARTESIAN_POINT ( 'NONE',  ( 7.188101187500002709, 106.8125000020483952, 2.977408999572649151 ) ) ;
#59622 = CARTESIAN_POINT ( 'NONE',  ( 1.469576158976822172E-15, -7.999999999999991118, 17.70530277982336642 ) ) ;
#59623 = CARTESIAN_POINT ( 'NONE',  ( -11.35316468750000141, 153.2812499965860127, -1.390361679473963753E-15 ) ) ;
#59624 = CARTESIAN_POINT ( 'NONE',  ( 2.679491924311228956, 122.9166666598386968, -10.00000000000000000 ) ) ;
#59625 = CARTESIAN_POINT ( 'NONE',  ( -7.188101187499999156, 109.6250000020483952, 2.977408999572654924 ) ) ;
#59626 = CARTESIAN_POINT ( 'NONE',  ( 0.000000000000000000, 0.000000000000000000, 0.000000000000000000 ) ) ;
#59627 = CARTESIAN_POINT ( 'NONE',  ( -26.56734541678238060, 204.6250000013655779, 166.5412658750003629 ) ) ;
#59628 = EDGE_LOOP ( 'NONE', ( #52814, #68219, #64763, #62091, #40964, #20096 ) ) ;
#59629 = CARTESIAN_POINT ( 'NONE',  ( 5.676582343750001591, 21.92708332991935194, -9.832129032723420536 ) ) ;
#59630 = VERTEX_POINT ( 'NONE', #59606 ) ;
#59631 = CARTESIAN_POINT ( 'NONE',  ( -5.656854249492379694, 0.5625000000000000000, -5.656854249492380582 ) ) ;
#59632 = CARTESIAN_POINT ( 'NONE',  ( 54.00000000000000000, 37.00000000000000711, 4.085831468968142743E-14 ) ) ;
#59634 = CARTESIAN_POINT ( 'NONE',  ( -11.35316468750000141, 148.2812499965860411, -1.390361679473963753E-15 ) ) ;
#59633 = CARTESIAN_POINT ( 'NONE',  ( -25.44220607266933598, -22.50438833763057289, 146.9907766063561212 ) ) ;
#59635 = CARTESIAN_POINT ( 'NONE',  ( -5.082755093536325042, 1.406249997951610320, -5.082755093536325930 ) ) ;
#59636 = CARTESIAN_POINT ( 'NONE',  ( -3.313708498984758943, -7.999999999999989342, 19.16780278432982954 ) ) ;
#59637 = EDGE_CURVE ( 'NONE', #2971, #69151, #41876, .T. ) ;
#59638 = CARTESIAN_POINT ( 'NONE',  ( 52.83422997672269616, 204.1666909556982432, 52.87948297946047660 ) ) ;
#59639 = CARTESIAN_POINT ( 'NONE',  ( 2.085542519210945334E-15, 230.1562500034139873, 11.35316468749999963 ) ) ;
#59640 = CARTESIAN_POINT ( 'NONE',  ( -7.204075437095965206, -7.204075437095968759, 89.21875000204838102 ) ) ;
#59641 = ORIENTED_EDGE ( 'NONE', *, *, #40490, .F. ) ;
#59642 =( BOUNDED_CURVE ( )  B_SPLINE_CURVE ( 2, ( #31440, #70329, #41652, #12962, #2773, #43118, #25016, #19365, #25759 ),
 .UNSPECIFIED., .F., .F. ) 
 B_SPLINE_CURVE_WITH_KNOTS ( ( 3, 2, 2, 2, 3 ),
 ( 0.1562500000000001110, 0.1614583333333334536, 0.1666666666666667407, 0.1718750000000000833, 0.1770833333333334259 ),
 .UNSPECIFIED. ) 
 CURVE ( )  GEOMETRIC_REPRESENTATION_ITEM ( )  RATIONAL_B_SPLINE_CURVE ( ( 0.9999999999999983347, 0.9238795325112884038, 1.000000000000000000, 0.9238795325112867385, 1.000000000000000000, 0.9238795325112867385, 1.000000000000000000, 0.9238795325112855172, 1.000000000000001110 ) ) 
 REPRESENTATION_ITEM ( '' )  );
#59643 = CARTESIAN_POINT ( 'NONE',  ( 5.000000000000003553, 120.8333333333333286, -8.660254037844390851 ) ) ;
#59644 = CARTESIAN_POINT ( 'NONE',  ( -2.751064625579944321E-14, 198.8750000027312126, 146.0000000000000284 ) ) ;
#59645 = CARTESIAN_POINT ( 'NONE',  ( -3.042071309553164404, 102.5520833299193555, -11.35316468749999963 ) ) ;
#59646 = CARTESIAN_POINT ( 'NONE',  ( -10.18810118749999738, -4.220049686691941915, 100.7500000020483526 ) ) ;
#59647 = CARTESIAN_POINT ( 'NONE',  ( -1.881053915767121776, 18.74999999863440436, -4.541265875000002339 ) ) ;
#59648 = ORIENTED_EDGE ( 'NONE', *, *, #38912, .T. ) ;
#59649 = VERTEX_POINT ( 'NONE', #48639 ) ;
#59650 = CARTESIAN_POINT ( 'NONE',  ( 7.999999999999998224, 13.40625000000000178, 3.313708498984766493 ) ) ;
#59651 = LINE ( 'NONE', #12872, #16718 ) ;
#59652 = EDGE_CURVE ( 'NONE', #33983, #45292, #18870, .T. ) ;
#59653 = CARTESIAN_POINT ( 'NONE',  ( -2.977408999572654480, 27.37499999795161187, 7.188101187499999156 ) ) ;
#59654 = VECTOR ( 'NONE', #46634, 1000.000000000000000 ) ;
#59655 = CARTESIAN_POINT ( 'NONE',  ( 3.313708498984760720, 115.7187500040967763, -8.000000000000000000 ) ) ;
#59656 = CARTESIAN_POINT ( 'NONE',  ( -10.18810118749999916, 4.220049686691934809, 99.43750000204836681 ) ) ;
#59657 = CARTESIAN_POINT ( 'NONE',  ( -7.020684431968946093, -9.803012413858361640, -0.02533325329316988769 ) ) ;
#59658 = AXIS2_PLACEMENT_3D ( 'NONE', #37015, #60017, #2686 ) ;
#59659 = FACE_OUTER_BOUND ( 'NONE', #61113, .T. ) ;
#59660 = CARTESIAN_POINT ( 'NONE',  ( -7.347880794884122694E-16, 14.49999999726881406, 4.000000000000001776 ) ) ;
#59661 = CARTESIAN_POINT ( 'NONE',  ( -3.211159895383562723, 4.937499998634407028, 3.211159895383561391 ) ) ;
#59662 = ORIENTED_EDGE ( 'NONE', *, *, #11517, .F. ) ;
#59663 = DIRECTION ( 'NONE',  ( -1.000000000000000000, -0.000000000000000000, -0.000000000000000000 ) ) ;
#59664 = CARTESIAN_POINT ( 'NONE',  ( 25.17157287525381903, 207.6250000000000284, 167.1715728752537018 ) ) ;
#59665 = EDGE_CURVE ( 'NONE', #31861, #56591, #53946, .T. ) ;
#59667 = CARTESIAN_POINT ( 'NONE',  ( -2.319934922699201535E-11, 23.74999999999819522, 10.00000000000000178 ) ) ;
#59666 = CARTESIAN_POINT ( 'NONE',  ( -27.99999999999991829, 202.9375000013656063, 173.4587341250003760 ) ) ;
#59668 =( NAMED_UNIT ( * ) SI_UNIT ( $, .STERADIAN. ) SOLID_ANGLE_UNIT ( ) );
#59669 = EDGE_CURVE ( 'NONE', #54242, #13196, #59245, .T. ) ;
#59670 = CARTESIAN_POINT ( 'NONE',  ( 1.881053915767122664, 15.12499999863441147, 4.541265875000001451 ) ) ;
#59671 = CARTESIAN_POINT ( 'NONE',  ( -11.00000000000000000, 0.000000000000000000, 118.0000000000000000 ) ) ;
#59672 = CARTESIAN_POINT ( 'NONE',  ( 7.188101187499991163, 2.977408999572648707, 9.830302781871752771 ) ) ;
#59673 = ORIENTED_EDGE ( 'NONE', *, *, #41593, .F. ) ;
#59674 = ORIENTED_EDGE ( 'NONE', *, *, #53613, .F. ) ;
#59675 = CARTESIAN_POINT ( 'NONE',  ( 7.204075437095968759, -7.204075437095966983, 105.7187500020483810 ) ) ;
#59676 = LINE ( 'NONE', #13990, #12881 ) ;
#59677 = CARTESIAN_POINT ( 'NONE',  ( -26.56734541678238060, 203.6250000013656063, 166.5412658750003629 ) ) ;
#59678 = CARTESIAN_POINT ( 'NONE',  ( -24.00000000000001066, 201.8125000000000000, 168.3431457505080004 ) ) ;
#59679 = CARTESIAN_POINT ( 'NONE',  ( 3.458734125000015425, 194.9375000013655779, 198.0000000000000284 ) ) ;
#59680 = CARTESIAN_POINT ( 'NONE',  ( 3.313708498984765161, 104.4687500000000000, 7.999999999999998224 ) ) ;
#59681 = CARTESIAN_POINT ( 'NONE',  ( -5.000000000000005329, 113.3333333333333428, 8.660254037844387298 ) ) ;
#59682 = ADVANCED_FACE ( 'NONE', ( #25988, #35861 ), #71277, .T. ) ;
#59683 = ADVANCED_FACE ( 'NONE', ( #19232 ), #2259, .T. ) ;
#59684 = CARTESIAN_POINT ( 'NONE',  ( 3.313708498984760720, 114.0312500000000000, -8.000000000000000000 ) ) ;
#59685 = CARTESIAN_POINT ( 'NONE',  ( 4.721056650416000089, 294.9843750017070079, 4.721056650415999201 ) ) ;
#59686 = ORIENTED_EDGE ( 'NONE', *, *, #34629, .F. ) ;
#59687 = CARTESIAN_POINT ( 'NONE',  ( 5.000000000000022204, 190.8333333333333712, -8.660254037844422825 ) ) ;
#59688 = EDGE_CURVE ( 'NONE', #4761, #40449, #65626, .T. ) ;
#59689 = CARTESIAN_POINT ( 'NONE',  ( 5.656854249492380582, 17.99999999590322375, -5.656854249492380582 ) ) ;
#59690 = CARTESIAN_POINT ( 'NONE',  ( 1.432654583217607192, 205.2500000013655779, 145.4587341250000634 ) ) ;
#59691 = CARTESIAN_POINT ( 'NONE',  ( 0.000000000000000000, 125.0000000000000000, 8.000000000000000000 ) ) ;
#59692 = CARTESIAN_POINT ( 'NONE',  ( -5.000000000000000888, 229.1666666666666856, -8.660254037844387298 ) ) ;
#59693 = CARTESIAN_POINT ( 'NONE',  ( 7.778174593052023411, -7.778174593052021635, 91.75000000409677625 ) ) ;
#59694 = CARTESIAN_POINT ( 'NONE',  ( -10.99999999999999822, -4.556349186104052151, 110.5937499999999858 ) ) ;
#59695 = CARTESIAN_POINT ( 'NONE',  ( -7.320508075688778149, 218.1250000000000000, 7.320508075688769267 ) ) ;
#59696 = CARTESIAN_POINT ( 'NONE',  ( -7.188101187499992051, 0.000000000000000000, 7.861552781871751883 ) ) ;
#59697 = CARTESIAN_POINT ( 'NONE',  ( 11.35316468749999963, 196.3020833299193271, -3.042071309553165293 ) ) ;
#59698 = CARTESIAN_POINT ( 'NONE',  ( -2.726571689596997292E-14, 210.0000000000000284, 138.0000000000000568 ) ) ;
#59699 = CARTESIAN_POINT ( 'NONE',  ( -4.541265875000002339, 3.812499998634407028, -5.561446717895856393E-16 ) ) ;
#59700 = CARTESIAN_POINT ( 'NONE',  ( 7.320508075688771044, 243.1249999999999716, -7.320508075688771932 ) ) ;
#59702 = CARTESIAN_POINT ( 'NONE',  ( 5.656854249492380582, 10.49999999590322020, -5.656854249492380582 ) ) ;
#59701 = LINE ( 'NONE', #66463, #4541 ) ;
#59703 = ORIENTED_EDGE ( 'NONE', *, *, #71135, .T. ) ;
#59704 = CARTESIAN_POINT ( 'NONE',  ( 2.445694354108784108, 203.5625000013656063, 144.4456943541088663 ) ) ;
#59705 = CARTESIAN_POINT ( 'NONE',  ( 11.35316468750000141, 51.09374999658601268, 0.000000000000000000 ) ) ;
#59706 = CARTESIAN_POINT ( 'NONE',  ( -11.00000000000000000, 0.000000000000000000, 106.1875000040967620 ) ) ;
#59707 = AXIS2_PLACEMENT_3D ( 'NONE', #32754, #68554, #39144 ) ;
#59708 = CARTESIAN_POINT ( 'NONE',  ( 11.35316468750000141, 226.0937499965860127, 0.000000000000000000 ) ) ;
#59709 = CARTESIAN_POINT ( 'NONE',  ( -24.54126587499996148, 202.1250000013656063, 171.4326545832179534 ) ) ;
#59711 = CARTESIAN_POINT ( 'NONE',  ( 0.000000000000000000, 125.0000000000000000, 0.000000000000000000 ) ) ;
#59710 = CARTESIAN_POINT ( 'NONE',  ( 11.00000000000000000, 1.347111479062088405E-15, 108.2499999999999858 ) ) ;
#59712 = DIRECTION ( 'NONE',  ( -0.000000000000000000, -0.000000000000000000, -1.000000000000000000 ) ) ;
#59713 = CARTESIAN_POINT ( 'NONE',  ( 3.042071309553159519, 109.7395833299193697, 11.35316468750000141 ) ) ;
#59714 = CARTESIAN_POINT ( 'NONE',  ( 4.999999999999993783, 76.04166665983871098, 8.660254037844390851 ) ) ;
#59715 = AXIS2_PLACEMENT_3D ( 'NONE', #4197, #49456, #55882 ) ;
#59716 = CARTESIAN_POINT ( 'NONE',  ( -7.188101187500000044, 94.15625000204838102, 0.000000000000000000 ) ) ;
#59717 = CARTESIAN_POINT ( 'NONE',  ( -3.211159895383561391, 15.81249999863440436, -3.211159895383561835 ) ) ;
#59718 = CYLINDRICAL_SURFACE ( 'NONE', #1246, 11.00000000000000000 ) ;
#59719 = DIRECTION ( 'NONE',  ( 0.000000000000000000, 0.000000000000000000, -1.000000000000000000 ) ) ;
#59720 = ORIENTED_EDGE ( 'NONE', *, *, #56350, .T. ) ;
#59721 = ORIENTED_EDGE ( 'NONE', *, *, #58835, .T. ) ;
#59722 = CARTESIAN_POINT ( 'NONE',  ( 6.676582343750004256, 293.0468750017069510, 2.765530957081995478 ) ) ;
#59723 = CARTESIAN_POINT ( 'NONE',  ( 8.000000000000000000, 28.31249999590322375, 0.000000000000000000 ) ) ;
#59724 = CARTESIAN_POINT ( 'NONE',  ( -3.042071309553164404, 172.2395833299193839, -11.35316468749999963 ) ) ;
#59725 = CARTESIAN_POINT ( 'NONE',  ( 2.679491924311222739, 3.958333333333333481, 10.00000000000000533 ) ) ;
#59726 = CARTESIAN_POINT ( 'NONE',  ( -2.828427124746152987, 200.1250000000000284, 200.8284271247462129 ) ) ;
#59727 = CARTESIAN_POINT ( 'NONE',  ( -8.660254037844428154, 192.9166666666666856, 5.000000000000020428 ) ) ;
#59728 = CARTESIAN_POINT ( 'NONE',  ( 10.18810118750000093, -4.220049686691933921, 109.1875000020483810 ) ) ;
#59729 = ORIENTED_EDGE ( 'NONE', *, *, #27893, .T. ) ;
#59730 = CARTESIAN_POINT ( 'NONE',  ( -7.999999999999998224, 113.0937500000000000, 3.313708498984766049 ) ) ;
#59731 = CARTESIAN_POINT ( 'NONE',  ( -7.778174593052020747, -7.778174593052023411, 109.3750000040967763 ) ) ;
#59732 = CARTESIAN_POINT ( 'NONE',  ( -9.832129032723418760, 138.1770833299193555, -5.676582343750004256 ) ) ;
#59733 = CARTESIAN_POINT ( 'NONE',  ( 2.754378923186476579E-14, 196.1875000013655779, 194.5412658750000219 ) ) ;
#59734 = CARTESIAN_POINT ( 'NONE',  ( -2.445694354108784108, 208.5625000013656063, 195.5543056458912190 ) ) ;
#59735 =( BOUNDED_CURVE ( )  B_SPLINE_CURVE ( 2, ( #32919, #20821, #37818, #43839, #3480, #14024, #55925, #27223, #37062 ),
 .UNSPECIFIED., .F., .F. ) 
 B_SPLINE_CURVE_WITH_KNOTS ( ( 3, 2, 2, 2, 3 ),
 ( 0.2833333333333336590, 0.2916666666666669627, 0.3000000000000002665, 0.3083333333333335702, 0.3166666666666668184 ),
 .UNSPECIFIED. ) 
 CURVE ( )  GEOMETRIC_REPRESENTATION_ITEM ( )  RATIONAL_B_SPLINE_CURVE ( ( 0.9999999999999970024, 0.9238795325112897361, 1.000000000000000000, 0.9238795325112867385, 1.000000000000000000, 0.9238795325112867385, 1.000000000000000000, 0.9238795325112851842, 1.000000000000001554 ) ) 
 REPRESENTATION_ITEM ( '' )  );
#59737 = EDGE_CURVE ( 'NONE', #53804, #25147, #73739, .T. ) ;
#59736 = CARTESIAN_POINT ( 'NONE',  ( -7.204075437095965206, -7.204075437095968759, 68.21875000204836681 ) ) ;
#59738 = CARTESIAN_POINT ( 'NONE',  ( 3.042071309553167069, 57.13541666325268409, -11.35316468749999785 ) ) ;
#59739 = ORIENTED_EDGE ( 'NONE', *, *, #43713, .T. ) ;
#59740 = CARTESIAN_POINT ( 'NONE',  ( 3.313708498984762496, -7.999999999999989342, 13.29905277982336465 ) ) ;
#59741 = CARTESIAN_POINT ( 'NONE',  ( -1.881053915767124440, 6.124999998634407916, 4.541265875000001451 ) ) ;
#59742 = CARTESIAN_POINT ( 'NONE',  ( 8.008118988124993010, -3.317071493978877239, 9.169365283940628331 ) ) ;
#59743 = CARTESIAN_POINT ( 'NONE',  ( 4.401442555609581635E-16, 17.34374999795161187, -7.188101187500000044 ) ) ;
#59744 = CARTESIAN_POINT ( 'NONE',  ( 6.000000000000001776, 290.5625000034140157, -7.347880794884121708E-16 ) ) ;
#59745 = CYLINDRICAL_SURFACE ( 'NONE', #46172, 10.00000000000000178 ) ;
#59746 = CARTESIAN_POINT ( 'NONE',  ( -7.188101187500002709, 10.68749999795161187, 2.977408999572649151 ) ) ;
#59747 = CARTESIAN_POINT ( 'NONE',  ( 7.188101187499992051, 2.977408999572647819, 0.8303027818717529929 ) ) ;
#59748 = CARTESIAN_POINT ( 'NONE',  ( -7.204075437095965206, -7.204075437095968759, 67.84375000204836681 ) ) ;
#59749 = ADVANCED_FACE ( 'NONE', ( #8664 ), #54698, .F. ) ;
#59750 =( BOUNDED_CURVE ( )  B_SPLINE_CURVE ( 2, ( #68132, #62832, #51518, #22843, #45856, #32704, #29263, #28881, #12998, #69999, #1346, #70721, #35305 ),
 .UNSPECIFIED., .F., .F. ) 
 B_SPLINE_CURVE_WITH_KNOTS ( ( 3, 2, 2, 2, 2, 2, 3 ),
 ( 0.5923913043478260532, 0.5942028985507246119, 0.5960144927536231707, 0.5978260869565217295, 0.5996376811594202882, 0.6014492753623188470, 0.6032608695652174058 ),
 .UNSPECIFIED. ) 
 CURVE ( )  GEOMETRIC_REPRESENTATION_ITEM ( )  RATIONAL_B_SPLINE_CURVE ( ( 1.000000000000000000, 0.9659258262890683122, 1.000000000000000000, 0.9659258262890683122, 1.000000000000000000, 0.9659258262890683122, 1.000000000000000000, 0.9659258262890683122, 1.000000000000000000, 0.9659258262890683122, 1.000000000000000000, 0.9659258262890683122, 1.000000000000000000 ) ) 
 REPRESENTATION_ITEM ( '' )  );
#59751 = CARTESIAN_POINT ( 'NONE',  ( -2.679491924311226292, 63.33333332650536818, -10.00000000000000178 ) ) ;
#59752 = CARTESIAN_POINT ( 'NONE',  ( -2.828427124746190735, 3.124999997268813168, -2.828427124746191623 ) ) ;
#59753 = PRODUCT_RELATED_PRODUCT_CATEGORY ( 'part', '', ( #61975 ) ) ;
#59754 = VERTEX_POINT ( 'NONE', #44120 ) ;
#59755 = CARTESIAN_POINT ( 'NONE',  ( 4.000000000000015099, 194.6875000027312126, 196.3431457505076594 ) ) ;
#59756 = CARTESIAN_POINT ( 'NONE',  ( 1.656854249492348607, 201.1875000000000284, 138.0000000000000568 ) ) ;
#59757 = CARTESIAN_POINT ( 'NONE',  ( -29.65685424949245430, 197.1875000027312694, 166.0000000000004263 ) ) ;
#59758 = ADVANCED_FACE ( 'NONE', ( #10158 ), #49725, .F. ) ;
#59759 = CARTESIAN_POINT ( 'NONE',  ( -1.881053915767121554, 2.624999998634406584, -4.541265875000002339 ) ) ;
#59760 = CARTESIAN_POINT ( 'NONE',  ( 5.082755093536325042, 110.0937500020483810, -5.082755093536325930 ) ) ;
#59761 = CIRCLE ( 'NONE', #69407, 5.099999999999999645 ) ;
#59762 = DIRECTION ( 'NONE',  ( 0.8191520442889907994, 1.003171929053523514E-16, -0.5735764363510474917 ) ) ;
#59763 = CARTESIAN_POINT ( 'NONE',  ( -2.977408999572647819, 7.188101187499991163, 28.20530278187175455 ) ) ;
#59764 = ORIENTED_EDGE ( 'NONE', *, *, #59477, .T. ) ;
#59765 = EDGE_CURVE ( 'NONE', #58637, #3120, #61217, .T. ) ;
#59766 = CARTESIAN_POINT ( 'NONE',  ( -5.082755093536326818, 25.40624999795161543, 5.082755093536325042 ) ) ;
#59767 = ORIENTED_EDGE ( 'NONE', *, *, #45003, .T. ) ;
#59768 = CARTESIAN_POINT ( 'NONE',  ( -8.660254037844390851, 202.9166666666666856, 4.999999999999998224 ) ) ;
#59769 = CARTESIAN_POINT ( 'NONE',  ( 3.458734125000015425, 207.0000000013656063, 196.5673454167823877 ) ) ;
#59770 = CARTESIAN_POINT ( 'NONE',  ( 31.45873412500001010, 203.6250000013656063, 171.4326545832175555 ) ) ;
#59771 = CARTESIAN_POINT ( 'NONE',  ( -10.00000000000000355, 52.70833333333334281, 2.679491924311223183 ) ) ;
#59772 = CARTESIAN_POINT ( 'NONE',  ( 1.320432766682874540E-15, 99.40625000204838102, 7.188101187500000044 ) ) ;
#59773 = CARTESIAN_POINT ( 'NONE',  ( 4.242640687119285658, 297.6250000000000000, -4.242640687119286547 ) ) ;
#59774 = CARTESIAN_POINT ( 'NONE',  ( 23.99999999999999289, 208.8750000027312126, 169.9999999999999432 ) ) ;
#59775 = ORIENTED_EDGE ( 'NONE', *, *, #26049, .F. ) ;
#59776 = CONICAL_SURFACE ( 'NONE', #45350, 8.999999999999998224, 1.047197551196595855 ) ;
#59777 = CARTESIAN_POINT ( 'NONE',  ( -5.676582343750000703, 228.0729166700806729, -9.832129032723418760 ) ) ;
#59778 = CARTESIAN_POINT ( 'NONE',  ( 3.999999999999959144, 201.1875000027312694, 140.3431457505076594 ) ) ;
#59779 = DIRECTION ( 'NONE',  ( 0.000000000000000000, 0.000000000000000000, 1.000000000000000000 ) ) ;
#59780 = CARTESIAN_POINT ( 'NONE',  ( -4.999999999999992895, 260.8333333333333712, 8.660254037844390851 ) ) ;
#59781 = EDGE_CURVE ( 'NONE', #19, #5379, #56426, .T. ) ;
#59782 = DIRECTION ( 'NONE',  ( -1.000000000000000000, 0.000000000000000000, 0.000000000000000000 ) ) ;
#59783 = CARTESIAN_POINT ( 'NONE',  ( 2.679491924311228956, 171.0416666666666572, -10.00000000000000000 ) ) ;
#59784 = CARTESIAN_POINT ( 'NONE',  ( 105.0000000000000000, 38.00000000000000000, 139.0000000000000000 ) ) ;
#59785 = CARTESIAN_POINT ( 'NONE',  ( -11.00000000000000000, 0.000000000000000000, 68.68750000409676204 ) ) ;
#59786 = CARTESIAN_POINT ( 'NONE',  ( -8.311093377946841443, 159.2187499965860127, 8.311093377946830785 ) ) ;
#59787 = DIRECTION ( 'NONE',  ( -1.000000000000000000, -0.000000000000000000, -0.000000000000000000 ) ) ;
#59790 = CARTESIAN_POINT ( 'NONE',  ( 28.00000000000001776, 203.5000000000000000, 165.9999999999998863 ) ) ;
#59789 = LINE ( 'NONE', #3193, #39478 ) ;
#59788 = CARTESIAN_POINT ( 'NONE',  ( 26.34314575050758833, 204.9375000000000284, 173.9999999999999147 ) ) ;
#59791 = EDGE_LOOP ( 'NONE', ( #74330, #24032, #15806, #20784 ) ) ;
#59792 = CARTESIAN_POINT ( 'NONE',  ( -2.085542519210945728E-15, 9.843749996586018014, 11.35316468750000141 ) ) ;
#59793 = LINE ( 'NONE', #30381, #17862 ) ;
#59794 = CARTESIAN_POINT ( 'NONE',  ( 4.330454160157055199, -16.29811171461376063, -69.49285720718685866 ) ) ;
#59795 = CARTESIAN_POINT ( 'NONE',  ( -31.99999999999997868, 196.3125000000000284, 171.6568542494928238 ) ) ;
#59796 = CARTESIAN_POINT ( 'NONE',  ( -1.432654583217664479, 208.7500000013656063, 138.5412658750000787 ) ) ;
#59797 = CARTESIAN_POINT ( 'NONE',  ( -6.951749144819291182, 124.7465970749896229, -3.470743364672778331 ) ) ;
#59798 = CARTESIAN_POINT ( 'NONE',  ( 10.00000000000000000, 36.66666665983869677, 2.679491924311236062 ) ) ;
#59799 = CARTESIAN_POINT ( 'NONE',  ( -7.188101187499999156, 110.7500000020483668, 2.977408999572654924 ) ) ;
#59800 = CARTESIAN_POINT ( 'NONE',  ( 1.881053915767121776, 4.624999998634407028, -4.541265875000002339 ) ) ;
#59801 = LINE ( 'NONE', #15622, #67467 ) ;
#59802 = CARTESIAN_POINT ( 'NONE',  ( -7.999999999999989342, -3.313708498984762496, 14.42405277982336465 ) ) ;
#59804 = CARTESIAN_POINT ( 'NONE',  ( -8.000000000000001776, 26.34375000000000711, 3.313708498984759387 ) ) ;
#59803 = CARTESIAN_POINT ( 'NONE',  ( 6.000000000000001776, 291.5625000034140157, -7.347880794884121708E-16 ) ) ;
#59805 = ORIENTED_EDGE ( 'NONE', *, *, #11609, .T. ) ;
#59806 = CARTESIAN_POINT ( 'NONE',  ( 3.313708498984657247, 92.65625000409677625, 8.000000000000106581 ) ) ;
#59807 = CARTESIAN_POINT ( 'NONE',  ( 10.99999999999997691, -4.556349186104070803, 115.6562500000000000 ) ) ;
#59808 = CARTESIAN_POINT ( 'NONE',  ( 3.042071309553163516, 232.7604166700806161, -11.35316468749999785 ) ) ;
#59809 = CARTESIAN_POINT ( 'NONE',  ( 11.35316468749999785, 125.5729166632526983, 3.042071309553174174 ) ) ;
#59810 = ORIENTED_EDGE ( 'NONE', *, *, #56536, .F. ) ;
#59811 = DIRECTION ( 'NONE',  ( 0.000000000000000000, 0.000000000000000000, -1.000000000000000000 ) ) ;
#59812 = CARTESIAN_POINT ( 'NONE',  ( 7.204075437095966983, 7.204075437095967871, 92.59375000204838102 ) ) ;
#59813 = CARTESIAN_POINT ( 'NONE',  ( 0.000000000000000000, 300.0000000000000000, 0.000000000000000000 ) ) ;
#59814 = CARTESIAN_POINT ( 'NONE',  ( -1.432654583217608080, 194.8750000013656063, 201.4587341250000350 ) ) ;
#59815 = LINE ( 'NONE', #14513, #24485 ) ;
#59817 = CARTESIAN_POINT ( 'NONE',  ( -2.085542519210945728E-15, 114.5312499965860269, 11.35316468750000141 ) ) ;
#59816 = CARTESIAN_POINT ( 'NONE',  ( 1.469576158976823947E-15, 95.37499999999998579, 8.000000000000000000 ) ) ;
#59818 = CARTESIAN_POINT ( 'NONE',  ( -31.99999999999998579, 209.3125000000000568, 171.6568542494928238 ) ) ;
#59819 = EDGE_CURVE ( 'NONE', #19306, #66501, #31257, .T. ) ;
#59820 = ORIENTED_EDGE ( 'NONE', *, *, #55922, .F. ) ;
#59821 = CARTESIAN_POINT ( 'NONE',  ( -2.679491924311225848, 213.3333333265053682, -10.00000000000000178 ) ) ;
#59822 = CARTESIAN_POINT ( 'NONE',  ( 2.828427124746153876, 205.8750000000000284, 144.8284271247462129 ) ) ;
#59823 = CARTESIAN_POINT ( 'NONE',  ( 8.311093377946837890, 101.7187499965860127, -8.311093377946837890 ) ) ;
#59824 = CARTESIAN_POINT ( 'NONE',  ( 2.839093476692135984E-14, 204.6875000013656063, 201.4587341250000350 ) ) ;
#59825 = CARTESIAN_POINT ( 'NONE',  ( -5.082755093536326818, 10.78124999795161187, 5.082755093536325042 ) ) ;
#59827 = ADVANCED_FACE ( 'NONE', ( #6449 ), #66365, .T. ) ;
#59826 = CARTESIAN_POINT ( 'NONE',  ( -6.238412754330611322E-16, 10.18810118749999916, 91.65625000204836681 ) ) ;
#59828 = CARTESIAN_POINT ( 'NONE',  ( 5.676582343749993598, 5.260416663252683200, 9.832129032723422313 ) ) ;
#59829 = ORIENTED_EDGE ( 'NONE', *, *, #45586, .F. ) ;
#59830 = LINE ( 'NONE', #7780, #22320 ) ;
#59831 = CARTESIAN_POINT ( 'NONE',  ( -8.008118988124991233, 3.317071493978878127, 27.91936528394063544 ) ) ;
#59832 = CARTESIAN_POINT ( 'NONE',  ( 11.44979897117363699, 225.9999999999999432, -0.1323599981037845985 ) ) ;
#59833 = CARTESIAN_POINT ( 'NONE',  ( 10.18810118749999916, 1.247682550866122264E-15, 76.28125000204836681 ) ) ;
#59834 = DIRECTION ( 'NONE',  ( 0.000000000000000000, 0.000000000000000000, 1.000000000000000000 ) ) ;
#59835 = DIRECTION ( 'NONE',  ( -0.000000000000000000, -1.000000000000000000, -0.000000000000000000 ) ) ;
#59836 = CARTESIAN_POINT ( 'NONE',  ( 1.226468279477575784E-15, 293.7031250017069510, 6.676582343750001591 ) ) ;
#59837 = CARTESIAN_POINT ( 'NONE',  ( 2.679491924311228956, 127.9166666598386968, -10.00000000000000000 ) ) ;
#59838 = CARTESIAN_POINT ( 'NONE',  ( 11.35316468749999785, 220.8854166632526699, 3.042071309553174174 ) ) ;
#59839 = CARTESIAN_POINT ( 'NONE',  ( 6.951808397369818766E-16, 127.3437499965860127, -11.35316468750000141 ) ) ;
#59840 = CARTESIAN_POINT ( 'NONE',  ( -7.204075437095965206, -7.204075437095968759, 82.84375000204838102 ) ) ;
#59841 = EDGE_CURVE ( 'NONE', #27667, #8238, #1049, .T. ) ;
#59842 = CARTESIAN_POINT ( 'NONE',  ( -26.56734541678238060, 199.3750000013656063, 166.5412658750003629 ) ) ;
#59843 = CARTESIAN_POINT ( 'NONE',  ( 3.313708498984762496, 25.21875000000000711, 7.999999999999998224 ) ) ;
#59844 = CARTESIAN_POINT ( 'NONE',  ( -3.211159895383561391, 12.81249999863440792, -3.211159895383561835 ) ) ;
#59845 = ORIENTED_EDGE ( 'NONE', *, *, #69177, .T. ) ;
#59846 = CARTESIAN_POINT ( 'NONE',  ( -17.41027957807906290, -46.69348151157597471, 144.3427545490948489 ) ) ;
#59847 = CARTESIAN_POINT ( 'NONE',  ( -3.999999999999960032, 206.1250000027312126, 198.0000000000000284 ) ) ;
#59848 =( BOUNDED_CURVE ( )  B_SPLINE_CURVE ( 2, ( #22719, #45735, #68380, #5759, #70603, #30612, #58932, #13246, #12515 ),
 .UNSPECIFIED., .F., .F. ) 
 B_SPLINE_CURVE_WITH_KNOTS ( ( 3, 2, 2, 2, 3 ),
 ( 0.1000000000000000888, 0.1083333333333334203, 0.1166666666666667657, 0.1250000000000001110, 0.1333333333333334425 ),
 .UNSPECIFIED. ) 
 CURVE ( )  GEOMETRIC_REPRESENTATION_ITEM ( )  RATIONAL_B_SPLINE_CURVE ( ( 0.9999999999999992228, 0.9238795325112875156, 1.000000000000000000, 0.9238795325112867385, 1.000000000000000000, 0.9238795325112867385, 1.000000000000000000, 0.9238795325112857393, 1.000000000000001110 ) ) 
 REPRESENTATION_ITEM ( '' )  );
#59849 = CARTESIAN_POINT ( 'NONE',  ( 1.432654583217607414, 199.5000000013656063, 145.4587341250000634 ) ) ;
#59850 = CARTESIAN_POINT ( 'NONE',  ( -1.656854249492403008, 205.8125000027312126, 146.0000000000000284 ) ) ;
#59851 = DIRECTION ( 'NONE',  ( 0.000000000000000000, 0.2588190451025143557, -0.9659258262890699775 ) ) ;
#59852 = CARTESIAN_POINT ( 'NONE',  ( -6.238412754330611322E-16, 10.18810118749999916, 69.15625000204836681 ) ) ;
#59853 = ORIENTED_EDGE ( 'NONE', *, *, #3904, .T. ) ;
#59854 = CARTESIAN_POINT ( 'NONE',  ( 2.977408999572650927, 6.749999997951611874, -7.188101187500000933 ) ) ;
#59855 = CARTESIAN_POINT ( 'NONE',  ( 0.000000000000000000, 15.99999999999998579, 0.000000000000000000 ) ) ;
#59856 = CARTESIAN_POINT ( 'NONE',  ( -4.401442555609581635E-16, 118.1562500020483810, -7.188101187500000044 ) ) ;
#59857 = EDGE_CURVE ( 'NONE', #68369, #20600, #63467, .T. ) ;
#59858 = CARTESIAN_POINT ( 'NONE',  ( -4.352425261977313831, 21.99999999999996803, -0.6811922050314749288 ) ) ;
#59859 = CARTESIAN_POINT ( 'NONE',  ( 6.676582343750003368, 293.8906250017069510, 2.765530957081995478 ) ) ;
#59861 = CARTESIAN_POINT ( 'NONE',  ( 6.123233995736767268E-16, 138.1249999931720538, -10.00000000000000178 ) ) ;
#59860 = CARTESIAN_POINT ( 'NONE',  ( 8.311093377946839666, 220.7812500034139873, 8.311093377946830785 ) ) ;
#59862 = ORIENTED_EDGE ( 'NONE', *, *, #18600, .F. ) ;
#59863 =( BOUNDED_CURVE ( )  B_SPLINE_CURVE ( 2, ( #37836, #15546, #38586, #32174, #54444, #54818, #14423, #9542, #4253 ),
 .UNSPECIFIED., .F., .F. ) 
 B_SPLINE_CURVE_WITH_KNOTS ( ( 3, 2, 2, 2, 3 ),
 ( 0.5166666666666670515, 0.5250000000000003553, 0.5333333333333337700, 0.5416666666666671848, 0.5500000000000005995 ),
 .UNSPECIFIED. ) 
 CURVE ( )  GEOMETRIC_REPRESENTATION_ITEM ( )  RATIONAL_B_SPLINE_CURVE ( ( 0.9999999999999970024, 0.9238795325112897361, 1.000000000000000000, 0.9238795325112867385, 1.000000000000000000, 0.9238795325112867385, 1.000000000000000000, 0.9238795325112816315, 1.000000000000005107 ) ) 
 REPRESENTATION_ITEM ( '' )  );
#59864 = CARTESIAN_POINT ( 'NONE',  ( 11.35316468749999608, 231.9270833367473585, -3.042071309553167069 ) ) ;
#59865 = CARTESIAN_POINT ( 'NONE',  ( -7.188101187499990274, -2.977408999572651371, 27.45530278187175810 ) ) ;
#59866 = CARTESIAN_POINT ( 'NONE',  ( 0.000000000000000000, 0.000000000000000000, -10.00000000000000000 ) ) ;
#59867 = CARTESIAN_POINT ( 'NONE',  ( 2.445694354108839175, 198.3125000013656063, 195.5543056458912190 ) ) ;
#59868 = ORIENTED_EDGE ( 'NONE', *, *, #46747, .T. ) ;
#59869 = CARTESIAN_POINT ( 'NONE',  ( 8.000000000000000000, 24.00000000000000355, 0.000000000000000000 ) ) ;
#59870 = CARTESIAN_POINT ( 'NONE',  ( 5.656854249492381470, 98.56250000000000000, 5.656854249492379694 ) ) ;
#59871 = CARTESIAN_POINT ( 'NONE',  ( -2.085542519210945728E-15, 99.84374999658601268, 11.35316468750000141 ) ) ;
#59872 = CYLINDRICAL_SURFACE ( 'NONE', #37246, 3.999999999999976019 ) ;
#59873 = CARTESIAN_POINT ( 'NONE',  ( -4.556349186104045934, 11.00000000000000000, 77.21875000000001421 ) ) ;
#59875 = CARTESIAN_POINT ( 'NONE',  ( 31.45873412500001010, 202.6250000013656063, 171.4326545832175555 ) ) ;
#59874 = CARTESIAN_POINT ( 'NONE',  ( 27.99999999999996447, 202.6875000013656063, 173.4587341249998929 ) ) ;
#59876 = ORIENTED_EDGE ( 'NONE', *, *, #35644, .T. ) ;
#59877 = CARTESIAN_POINT ( 'NONE',  ( -4.898587196589412829E-16, 103.8125000040967763, -8.000000000000000000 ) ) ;
#59878 = CARTESIAN_POINT ( 'NONE',  ( -5.676582343750006032, 219.1145833299193839, 9.832129032723418760 ) ) ;
#59879 = CARTESIAN_POINT ( 'NONE',  ( -1.432654583217662481, 200.1250000013656063, 145.4587341250000634 ) ) ;
#59880 = EDGE_CURVE ( 'NONE', #12693, #54725, #42232, .T. ) ;
#59881 = VECTOR ( 'NONE', #20132, 1000.000000000000000 ) ;
#59882 = CARTESIAN_POINT ( 'NONE',  ( 26.56734541678238060, 200.2500000013656631, 166.5412658749999650 ) ) ;
#59883 = CARTESIAN_POINT ( 'NONE',  ( 2.020667218593132706E-15, -11.00000000000000000, 115.5625000040967763 ) ) ;
#59884 = CARTESIAN_POINT ( 'NONE',  ( 3.042071309553167069, 197.1354166632526415, -11.35316468749999785 ) ) ;
#59885 = CARTESIAN_POINT ( 'NONE',  ( -2.977408999572652260, 91.81250000204838102, 7.188101187500000044 ) ) ;
#59886 = CARTESIAN_POINT ( 'NONE',  ( -32.00000000000000711, 198.1875000000000853, 168.3431457505080004 ) ) ;
#59887 = CARTESIAN_POINT ( 'NONE',  ( 4.541265875000002339, 14.37499999863440969, -1.881053915767121554 ) ) ;
#59888 = CARTESIAN_POINT ( 'NONE',  ( 30.44569435410883429, 199.0625000013656063, 167.5543056458911053 ) ) ;
#59889 = CARTESIAN_POINT ( 'NONE',  ( 2.977408999572646486, 7.188101187499991163, 5.892802781871754547 ) ) ;
#59890 = CARTESIAN_POINT ( 'NONE',  ( -3.673940397442060854E-16, 293.7500000000000000, -6.000000000000001776 ) ) ;
#59891 = CARTESIAN_POINT ( 'NONE',  ( -9.832129032723420536, 83.69791666325268409, 5.676582343749997150 ) ) ;
#59892 = ORIENTED_EDGE ( 'NONE', *, *, #21146, .F. ) ;
#59893 = DIRECTION ( 'NONE',  ( -0.000000000000000000, -0.000000000000000000, 1.000000000000000000 ) ) ;
#59894 = LINE ( 'NONE', #8208, #37569 ) ;
#59895 = CARTESIAN_POINT ( 'NONE',  ( -8.660254037844408614, 47.08333333333334991, -5.000000000000017764 ) ) ;
#59896 = DIRECTION ( 'NONE',  ( -1.000000000000000000, 0.000000000000000000, 0.000000000000000000 ) ) ;
#59897 = CARTESIAN_POINT ( 'NONE',  ( 3.042071309553159519, 69.73958332991935549, 11.35316468750000141 ) ) ;
#59898 = ORIENTED_EDGE ( 'NONE', *, *, #29148, .F. ) ;
#59899 = CARTESIAN_POINT ( 'NONE',  ( -6.238412754330611322E-16, 10.18810118749999916, 87.15625000204838102 ) ) ;
#59900 = CARTESIAN_POINT ( 'NONE',  ( -7.204075437095965206, -7.204075437095968759, 111.3437500020483810 ) ) ;
#59901 = CARTESIAN_POINT ( 'NONE',  ( 1.432654583217664701, 208.0000000013656347, 201.4587341250000065 ) ) ;
#59902 = CARTESIAN_POINT ( 'NONE',  ( -1.739508062077478767, 16.42388987907938258, 68.69353258878824420 ) ) ;
#59904 = CARTESIAN_POINT ( 'NONE',  ( -11.35316468750000141, 73.48958332991934128, 3.042071309553159963 ) ) ;
#59903 = CARTESIAN_POINT ( 'NONE',  ( 1.469576158976823947E-15, 121.0625000040967763, 8.000000000000000000 ) ) ;
#59905 = CARTESIAN_POINT ( 'NONE',  ( 5.656854249492374365, 5.656854249492375253, 21.45530278392014623 ) ) ;
#59906 = EDGE_CURVE ( 'NONE', #1423, #68675, #32044, .T. ) ;
#59907 = CARTESIAN_POINT ( 'NONE',  ( 4.000000000000001776, 13.06250000000000000, -1.656854249492381248 ) ) ;
#59908 = CARTESIAN_POINT ( 'NONE',  ( -8.660254037844387298, 173.9583333265053682, -5.000000000000004441 ) ) ;
#59909 = CARTESIAN_POINT ( 'NONE',  ( -5.656854249492378806, 113.3750000040967763, 5.656854249492381470 ) ) ;
#59910 = CARTESIAN_POINT ( 'NONE',  ( -2.751064625579944321E-14, 202.7500000000000000, 146.0000000000000284 ) ) ;
#59911 = CARTESIAN_POINT ( 'NONE',  ( 11.35316468750000141, 66.09374999658601268, 0.000000000000000000 ) ) ;
#59912 = CARTESIAN_POINT ( 'NONE',  ( 10.18810118749999916, 4.220049686691935698, 104.8750000020483668 ) ) ;
#59913 = CARTESIAN_POINT ( 'NONE',  ( -11.35316468750000141, 198.2812499965860411, -1.390361679473963753E-15 ) ) ;
#59914 = ORIENTED_EDGE ( 'NONE', *, *, #38709, .F. ) ;
#59915 = CARTESIAN_POINT ( 'NONE',  ( -6.308070865121395698, 61.28915309318116300, 23.54949267155276971 ) ) ;
#59916 = CARTESIAN_POINT ( 'NONE',  ( 2.828427124746152987, 206.2500000027312126, 139.1715728752538723 ) ) ;
#59917 = CARTESIAN_POINT ( 'NONE',  ( 5.000000000000001776, 68.60357193678683529, 20.85024232999420946 ) ) ;
#59919 = CARTESIAN_POINT ( 'NONE',  ( 8.311093377946837890, 186.4062499965860411, -8.311093377946837890 ) ) ;
#59918 = CARTESIAN_POINT ( 'NONE',  ( -31.05507224581700143, 5.999999999999963585, 171.9999999999997726 ) ) ;
#59920 = AXIS2_PLACEMENT_3D ( 'NONE', #28803, #51821, #17482 ) ;
#59921 = CARTESIAN_POINT ( 'NONE',  ( 5.656854249492380582, 2.999999995903220196, -5.656854249492380582 ) ) ;
#59922 = CARTESIAN_POINT ( 'NONE',  ( -10.00000000000000000, 238.1250000068279746, 0.000000000000000000 ) ) ;
#59923 = LINE ( 'NONE', #8237, #33615 ) ;
#59924 = ORIENTED_EDGE ( 'NONE', *, *, #30634, .T. ) ;
#59925 = CARTESIAN_POINT ( 'NONE',  ( -2.085542519210945728E-15, 179.8437499965860411, 11.35316468750000141 ) ) ;
#59926 = CARTESIAN_POINT ( 'NONE',  ( 2.977408999572646486, 7.188101187499992051, 20.51780278187175810 ) ) ;
#59927 = CARTESIAN_POINT ( 'NONE',  ( 5.000000000000000000, 60.90295814858271939, -23.31388853594749833 ) ) ;
#59928 = ORIENTED_EDGE ( 'NONE', *, *, #65680, .F. ) ;
#59929 = CARTESIAN_POINT ( 'NONE',  ( 3.313708498984760720, 96.21875000409680467, -8.000000000000000000 ) ) ;
#59930 = CARTESIAN_POINT ( 'NONE',  ( 24.00000000000000711, 208.6875000000000284, 168.3431457505074889 ) ) ;
#59931 = PRESENTATION_LAYER_ASSIGNMENT (  '', '', ( #56336 ) ) ;
#59932 = CARTESIAN_POINT ( 'NONE',  ( 1.656854249492381248, 15.18750000000000000, -4.000000000000001776 ) ) ;
#59933 = CARTESIAN_POINT ( 'NONE',  ( 2.780723358947928197E-16, 14.56249999863440792, -4.541265875000002339 ) ) ;
#59934 = CARTESIAN_POINT ( 'NONE',  ( 3.313708498984762496, -7.999999999999989342, 11.98655278392014445 ) ) ;
#59935 = CARTESIAN_POINT ( 'NONE',  ( -28.00000000000002487, 196.0000000000000000, 166.0000000000003695 ) ) ;
#59936 = VERTEX_POINT ( 'NONE', #49006 ) ;
#59937 = CARTESIAN_POINT ( 'NONE',  ( 2.977408999572654480, 100.6250000020483810, 7.188101187499999156 ) ) ;
#59938 = CARTESIAN_POINT ( 'NONE',  ( 7.320508075688812788, 180.6250000000000284, -7.320508075688812788 ) ) ;
#59939 = DIRECTION ( 'NONE',  ( 1.000000000000000000, 0.000000000000000000, 0.000000000000000000 ) ) ;
#59940 = EDGE_LOOP ( 'NONE', ( #38715, #13678, #37958, #43988 ) ) ;
#59941 = CARTESIAN_POINT ( 'NONE',  ( -5.656854249492380582, 101.0000000040967905, -5.656854249492380582 ) ) ;
#59942 = CARTESIAN_POINT ( 'NONE',  ( 7.188101187499993827, -2.977408999572645598, 18.64280278187175810 ) ) ;
#59943 = ORIENTED_EDGE ( 'NONE', *, *, #46641, .T. ) ;
#59944 =( BOUNDED_CURVE ( )  B_SPLINE_CURVE ( 2, ( #7656, #64256, #30294, #35593, #53680, #71013, #6549, #19328, #42341 ),
 .UNSPECIFIED., .F., .F. ) 
 B_SPLINE_CURVE_WITH_KNOTS ( ( 3, 2, 2, 2, 3 ),
 ( 0.4117647058823528661, 0.4154411764705882026, 0.4191176470588234837, 0.4227941176470588203, 0.4264705882352941013 ),
 .UNSPECIFIED. ) 
 CURVE ( )  GEOMETRIC_REPRESENTATION_ITEM ( )  RATIONAL_B_SPLINE_CURVE ( ( 1.000000000000001110, 0.9238795325112856283, 1.000000000000000000, 0.9238795325112867385, 1.000000000000000000, 0.9238795325112867385, 1.000000000000000000, 0.9238795325112867385, 1.000000000000000000 ) ) 
 REPRESENTATION_ITEM ( '' )  );
#59945 = VERTEX_POINT ( 'NONE', #60329 ) ;
#59946 = CARTESIAN_POINT ( 'NONE',  ( -10.18810118749999916, 0.000000000000000000, 78.15625000204836681 ) ) ;
#59947 = CARTESIAN_POINT ( 'NONE',  ( 11.35316468750000141, 56.09374999658601979, 0.000000000000000000 ) ) ;
#59948 = CARTESIAN_POINT ( 'NONE',  ( 1.472282454178701849, 19.93458701958330082, -1.116934336526971272 ) ) ;
#59949 = CARTESIAN_POINT ( 'NONE',  ( 4.556349186104045934, 11.00000000000000000, 98.03124999999997158 ) ) ;
#59952 = CARTESIAN_POINT ( 'NONE',  ( -4.088227598258586603E-16, 294.3593750017070079, -6.676582343750001591 ) ) ;
#59951 = CARTESIAN_POINT ( 'NONE',  ( 31.99999999999999289, 200.3750000027312126, 169.9999999999998863 ) ) ;
#59950 = CARTESIAN_POINT ( 'NONE',  ( -11.00000000000000000, 0.000000000000000000, 86.50000000000000000 ) ) ;
#59953 = CARTESIAN_POINT ( 'NONE',  ( -10.00000000000000000, 147.2916666666666288, -2.679491924311229845 ) ) ;
#59954 = CARTESIAN_POINT ( 'NONE',  ( 25.17157287525377996, 199.7500000027312126, 167.1715728752537586 ) ) ;
#59955 = CARTESIAN_POINT ( 'NONE',  ( -11.00000000000000000, 0.000000000000000000, 91.00000000000000000 ) ) ;
#59956 = CARTESIAN_POINT ( 'NONE',  ( 7.999999999999991118, 9.797174393178815797E-16, 15.08030277982336642 ) ) ;
#59957 = CARTESIAN_POINT ( 'NONE',  ( 3.313708498984762052, 1.593749995903220196, -8.000000000000000000 ) ) ;
#59958 = CARTESIAN_POINT ( 'NONE',  ( 31.45873412499999233, 199.6875000013656063, 169.9999999999999432 ) ) ;
#59959 = CARTESIAN_POINT ( 'NONE',  ( 2.977408999572651815, 12.56249999795161365, 7.188101187500000933 ) ) ;
#59960 = CARTESIAN_POINT ( 'NONE',  ( 5.656854249492376141, -5.656854249492374365, 27.08030278392014978 ) ) ;
#59961 = CARTESIAN_POINT ( 'NONE',  ( -2.679491924311150353, 244.1666666734946887, 10.00000000000004441 ) ) ;
#59962 = CARTESIAN_POINT ( 'NONE',  ( 5.082755093536325042, 111.9687500020483810, -5.082755093536325930 ) ) ;
#59964 = CARTESIAN_POINT ( 'NONE',  ( -8.660254037844387298, 132.0833333333333712, -5.000000000000004441 ) ) ;
#59963 = CARTESIAN_POINT ( 'NONE',  ( -8.660254037844387298, 18.95833332650536818, -5.000000000000004441 ) ) ;
#59965 = CARTESIAN_POINT ( 'NONE',  ( 3.042071309553173286, 220.6770833367472733, 11.35316468749999608 ) ) ;
#59966 = CARTESIAN_POINT ( 'NONE',  ( 25.55430564589119768, 209.3125000013656063, 167.5543056458910485 ) ) ;
#59967 = CARTESIAN_POINT ( 'NONE',  ( -5.082755093536317936, -5.082755093536320601, 20.04905278187175455 ) ) ;
#59968 = CARTESIAN_POINT ( 'NONE',  ( 30.82842712474616675, 200.5000000027312126, 167.1715728752537018 ) ) ;
#59969 = CARTESIAN_POINT ( 'NONE',  ( 11.35316468750000141, 40.78124999658601268, 0.000000000000000000 ) ) ;
#59970 = CARTESIAN_POINT ( 'NONE',  ( -4.000000000000001776, 6.437500000000000888, -1.656854249492381470 ) ) ;
#59971 = CARTESIAN_POINT ( 'NONE',  ( -4.999999999999998224, 13.54166665983870033, -8.660254037844389075 ) ) ;
#59972 = CARTESIAN_POINT ( 'NONE',  ( -10.00000000000000178, 225.9999999999999432, 0.000000000000000000 ) ) ;
#59973 = CARTESIAN_POINT ( 'NONE',  ( 1.267086777181619559E-12, 183.7500000000001137, 10.00000000000000178 ) ) ;
#59974 = EDGE_LOOP ( 'NONE', ( #50765, #37179, #54275, #20566 ) ) ;
#59975 = DIRECTION ( 'NONE',  ( 1.000000000000000000, 0.000000000000000000, 0.000000000000000000 ) ) ;
#59976 = CARTESIAN_POINT ( 'NONE',  ( 4.556349186104045934, 11.00000000000000000, 69.71875000409677625 ) ) ;
#59977 = ADVANCED_FACE ( 'NONE', ( #25618 ), #42969, .T. ) ;
#59978 = CARTESIAN_POINT ( 'NONE',  ( 8.311093377946837890, 41.40624999658601268, -8.311093377946837890 ) ) ;
#59979 = CARTESIAN_POINT ( 'NONE',  ( -4.556349186104045934, 11.00000000000000000, 83.40625000409676204 ) ) ;
#59980 = CARTESIAN_POINT ( 'NONE',  ( -1.432654583217664701, 204.0000000013656063, 138.5412658750000787 ) ) ;
#59981 = LINE ( 'NONE', #25636, #60071 ) ;
#59982 = CARTESIAN_POINT ( 'NONE',  ( 5.656854249492380582, 25.49999999590322375, -5.656854249492380582 ) ) ;
#59984 = CARTESIAN_POINT ( 'NONE',  ( 8.311093377946837890, 31.40624999658601979, -8.311093377946837890 ) ) ;
#59983 = CARTESIAN_POINT ( 'NONE',  ( 7.188101187500002709, 103.8125000020483952, 2.977408999572649151 ) ) ;
#59985 = CARTESIAN_POINT ( 'NONE',  ( 3.313708498984762496, -7.999999999999989342, 17.79905277982336642 ) ) ;
#59986 = CARTESIAN_POINT ( 'NONE',  ( 11.35316468749999963, 155.9895833299193555, -3.042071309553165293 ) ) ;
#59987 = VECTOR ( 'NONE', #29464, 1000.000000000000000 ) ;
#59988 = CARTESIAN_POINT ( 'NONE',  ( -1.836970198721029983E-15, 125.6249999931720254, 10.00000000000000178 ) ) ;
#59989 = CARTESIAN_POINT ( 'NONE',  ( -7.188101187499999156, 108.1250000020483810, 2.977408999572654924 ) ) ;
#59990 = ORIENTED_EDGE ( 'NONE', *, *, #57962, .F. ) ;
#59991 = CARTESIAN_POINT ( 'NONE',  ( 0.7361406979141439377, 9.967293815311101923, -0.5584673446549246467 ) ) ;
#59992 = CARTESIAN_POINT ( 'NONE',  ( -9.832129032723418760, 23.17708332991934839, -5.676582343750004256 ) ) ;
#59993 = VERTEX_POINT ( 'NONE', #53939 ) ;
#59994 = CARTESIAN_POINT ( 'NONE',  ( 0.000000000000000000, 300.0000000000000000, 0.000000000000000000 ) ) ;
#59995 = CARTESIAN_POINT ( 'NONE',  ( 1.871523826299183495E-15, -10.18810118749999916, 84.53125000204836681 ) ) ;
#59996 = CARTESIAN_POINT ( 'NONE',  ( -27.99999999999995381, 197.5000000000000000, 174.0000000000003695 ) ) ;
#59998 = CARTESIAN_POINT ( 'NONE',  ( 11.35316468749999963, 155.9895833299193555, -3.042071309553165293 ) ) ;
#59997 = CARTESIAN_POINT ( 'NONE',  ( -27.23239143871326817, -21.62909802479688537, 148.4619828294406148 ) ) ;
#59999 = DIRECTION ( 'NONE',  ( -0.000000000000000000, -1.000000000000000000, -0.000000000000000000 ) ) ;
#60000 = CARTESIAN_POINT ( 'NONE',  ( -3.313708498984757167, 7.999999999999991118, 17.10530278432982598 ) ) ;
#60001 = FACE_OUTER_BOUND ( 'NONE', #25278, .T. ) ;
#60002 = CARTESIAN_POINT ( 'NONE',  ( -11.35316468749999785, 233.6979166700806161, -3.042071309553164848 ) ) ;
#60003 = ADVANCED_FACE ( 'NONE', ( #20331 ), #37710, .F. ) ;
#60004 = CARTESIAN_POINT ( 'NONE',  ( -6.238412754330611322E-16, 10.18810118749999916, 85.65625000204838102 ) ) ;
#60005 = EDGE_LOOP ( 'NONE', ( #18997, #2981, #6270 ) ) ;
#60006 = CARTESIAN_POINT ( 'NONE',  ( -2.726571689596997292E-14, 210.0000000000000284, 138.0000000000000568 ) ) ;
#60007 = CARTESIAN_POINT ( 'NONE',  ( -5.676582343750006032, 104.4270833299193555, 9.832129032723418760 ) ) ;
#60008 = CARTESIAN_POINT ( 'NONE',  ( -7.204075437095965206, -7.204075437095968759, 99.34375000204836681 ) ) ;
#60009 = CARTESIAN_POINT ( 'NONE',  ( 4.541265875000001451, 19.37499999863440792, 1.881053915767124440 ) ) ;
#60010 = EDGE_LOOP ( 'NONE', ( #12163, #52112, #58944, #44555 ) ) ;
#60011 = EDGE_LOOP ( 'NONE', ( #34362, #52392 ) ) ;
#60012 = CARTESIAN_POINT ( 'NONE',  ( 1.881053915767121776, 2.624999998634407028, -4.541265875000002339 ) ) ;
#60013 = CARTESIAN_POINT ( 'NONE',  ( -1.320432766682874540E-15, 27.46874999795161543, 7.188101187500000044 ) ) ;
#60014 = CARTESIAN_POINT ( 'NONE',  ( 3.313708498984765161, 113.6562500040967905, 7.999999999999998224 ) ) ;
#60015 = VECTOR ( 'NONE', #36666, 1000.000000000000000 ) ;
#60016 = CARTESIAN_POINT ( 'NONE',  ( 1.871523826299183495E-15, -10.18810118749999916, 96.90625000204838102 ) ) ;
#60017 = DIRECTION ( 'NONE',  ( -0.000000000000000000, 1.000000000000000000, -0.000000000000000000 ) ) ;
#60018 = CARTESIAN_POINT ( 'NONE',  ( 4.000000000000000888, 5.937500000000000000, 1.656854249492384135 ) ) ;
#60019 = CARTESIAN_POINT ( 'NONE',  ( 4.000000000000001776, 16.81249999726881228, -1.656854249492381248 ) ) ;
#60020 = CARTESIAN_POINT ( 'NONE',  ( 4.541265875000002339, 4.374999998634407028, -1.881053915767121776 ) ) ;
#60021 = AXIS2_PLACEMENT_3D ( 'NONE', #70181, #64516, #12814 ) ;
#60022 = CARTESIAN_POINT ( 'NONE',  ( 3.458734124999959914, 208.3750000013656063, 143.4326545832176976 ) ) ;
#60023 = CARTESIAN_POINT ( 'NONE',  ( 1.432654583217664479, 194.7500000013656063, 201.4587341250000065 ) ) ;
#60025 = CARTESIAN_POINT ( 'NONE',  ( 5.841566664369303132E-15, 13.85640646055103531, -14.00000000000000178 ) ) ;
#60024 = CARTESIAN_POINT ( 'NONE',  ( -30.44569435410875968, 201.8125000013656063, 172.4456943541092642 ) ) ;
#60026 = CARTESIAN_POINT ( 'NONE',  ( 4.541265875000002339, 19.37499999863440792, -1.881053915767121554 ) ) ;
#60027 = CARTESIAN_POINT ( 'NONE',  ( 10.00000000000000178, 122.0833333265053682, -2.679491924311226736 ) ) ;
#60028 = CARTESIAN_POINT ( 'NONE',  ( 5.082755093536318824, 5.082755093536319713, 9.924052781871754547 ) ) ;
#60029 = EDGE_LOOP ( 'NONE', ( #31568, #55632, #17694, #37120 ) ) ;
#60030 = ORIENTED_EDGE ( 'NONE', *, *, #4836, .T. ) ;
#60031 = CARTESIAN_POINT ( 'NONE',  ( 1.871523826299183495E-15, -10.18810118749999916, 98.03125000204838102 ) ) ;
#60032 = LINE ( 'NONE', #25320, #26129 ) ;
#60033 = CARTESIAN_POINT ( 'NONE',  ( -29.43265458321761230, 206.1250000013656063, 173.4587341250003760 ) ) ;
#60034 = CARTESIAN_POINT ( 'NONE',  ( -25.17157287525377640, 199.6250000000000284, 172.8284271247465256 ) ) ;
#60035 = CARTESIAN_POINT ( 'NONE',  ( 2.445694354108839619, 196.8125000013656063, 200.4456943541088663 ) ) ;
#60036 = CARTESIAN_POINT ( 'NONE',  ( -8.660254037844387298, 32.91666666666667140, 4.999999999999996447 ) ) ;
#60037 = CARTESIAN_POINT ( 'NONE',  ( 4.999999999999993783, 114.1666666666666856, 8.660254037844390851 ) ) ;
#60038 = CARTESIAN_POINT ( 'NONE',  ( -5.656854249492378806, 114.6875000000000000, 5.656854249492381470 ) ) ;
#60039 = CARTESIAN_POINT ( 'NONE',  ( -6.676582343750003368, 294.5468750017069510, -2.765530957081996810 ) ) ;
#60040 = ORIENTED_EDGE ( 'NONE', *, *, #16611, .F. ) ;
#60041 = CARTESIAN_POINT ( 'NONE',  ( -7.320508075688778149, 144.9999999931719969, 7.320508075688769267 ) ) ;
#60042 = CARTESIAN_POINT ( 'NONE',  ( -8.000000000000000000, 19.96874999590322375, -3.313708498984762496 ) ) ;
#60043 = CARTESIAN_POINT ( 'NONE',  ( -3.458734125000015425, 201.9375000013656063, 142.0000000000000568 ) ) ;
#60044 = CARTESIAN_POINT ( 'NONE',  ( -10.00000000000000178, 184.3749999931720538, -1.224646799147353454E-15 ) ) ;
#60045 = CARTESIAN_POINT ( 'NONE',  ( 8.000000000000000000, 113.9375000040967763, -9.797174393178825657E-16 ) ) ;
#60046 = CARTESIAN_POINT ( 'NONE',  ( -2.679491924311222295, 221.0416666666667140, 10.00000000000000178 ) ) ;
#60047 = CARTESIAN_POINT ( 'NONE',  ( -2.828427124746192067, 3.374999997268813612, 2.828427124746190735 ) ) ;
#60048 = CARTESIAN_POINT ( 'NONE',  ( -11.00000000000000000, 4.556349186104045934, 110.4062500000000000 ) ) ;
#60049 = CARTESIAN_POINT ( 'NONE',  ( 8.311093377946837890, 1.406249996586016682, -8.311093377946837890 ) ) ;
#60050 = CARTESIAN_POINT ( 'NONE',  ( -2.977408999572647819, -7.188101187499990274, 6.642802781871754547 ) ) ;
#60051 = CARTESIAN_POINT ( 'NONE',  ( 11.35316468750000141, 191.0937499965860127, 0.000000000000000000 ) ) ;
#60052 = CARTESIAN_POINT ( 'NONE',  ( -1.836970198721029983E-15, 190.6249999931720254, 10.00000000000000178 ) ) ;
#60053 = CARTESIAN_POINT ( 'NONE',  ( -4.541265875000003227, 7.874999998634407028, 1.881053915767121110 ) ) ;
#60054 = CARTESIAN_POINT ( 'NONE',  ( 11.00000000000000000, 1.347111479062088405E-15, 91.74999999999998579 ) ) ;
#60056 = PLANE ( 'NONE',  #27841 ) ;
#60055 = FACE_OUTER_BOUND ( 'NONE', #11496, .T. ) ;
#60057 = VERTEX_POINT ( 'NONE', #13916 ) ;
#60059 = ADVANCED_FACE ( 'NONE', ( #43347 ), #73442, .F. ) ;
#60058 = CARTESIAN_POINT ( 'NONE',  ( 1.432654583217608080, 202.8750000013656347, 138.5412658750000503 ) ) ;
#60060 = CARTESIAN_POINT ( 'NONE',  ( -8.311093377946841443, 49.21874999658600558, 8.311093377946830785 ) ) ;
#60061 = CARTESIAN_POINT ( 'NONE',  ( 4.556349186104051263, -10.99999999999999822, 99.15625000409677625 ) ) ;
#60062 = FACE_OUTER_BOUND ( 'NONE', #48685, .T. ) ;
#60063 = CARTESIAN_POINT ( 'NONE',  ( -27.99999999999991829, 199.9375000013656063, 173.4587341250003760 ) ) ;
#60064 = DIRECTION ( 'NONE',  ( -0.000000000000000000, 1.000000000000000000, -0.000000000000000000 ) ) ;
#60066 = CARTESIAN_POINT ( 'NONE',  ( -9.999999999999998224, 230.2083333333333428, 2.679491924311235174 ) ) ;
#60065 = CARTESIAN_POINT ( 'NONE',  ( 2.977408999572654480, 123.1250000020484094, 7.188101187499999156 ) ) ;
#60067 = CARTESIAN_POINT ( 'NONE',  ( -3.458734125000016313, 195.8750000013655779, 140.5673454167823593 ) ) ;
#60068 =( BOUNDED_CURVE ( )  B_SPLINE_CURVE ( 2, ( #48036, #25394, #42378 ),
 .UNSPECIFIED., .F., .T. ) 
 B_SPLINE_CURVE_WITH_KNOTS ( ( 3, 3 ),
 ( 0.02777777777777780052, 0.02886181444060835141 ),
 .UNSPECIFIED. ) 
 CURVE ( )  GEOMETRIC_REPRESENTATION_ITEM ( )  RATIONAL_B_SPLINE_CURVE ( ( 1.000000000000000000, 0.9960107334157028980, 0.9929555612582052770 ) ) 
 REPRESENTATION_ITEM ( '' )  );
#60069 = CARTESIAN_POINT ( 'NONE',  ( -9.832129032723420536, 113.6979166632526983, 5.676582343749997150 ) ) ;
#60070 = EDGE_CURVE ( 'NONE', #32440, #5866, #47717, .T. ) ;
#60071 = VECTOR ( 'NONE', #66381, 1000.000000000000000 ) ;
#60072 = CARTESIAN_POINT ( 'NONE',  ( 10.00000000000000000, 91.66666665983869677, 2.679491924311236062 ) ) ;
#60073 = CARTESIAN_POINT ( 'NONE',  ( -4.401442555609581635E-16, 92.28125000204836681, -7.188101187500000044 ) ) ;
#60074 = CARTESIAN_POINT ( 'NONE',  ( -1.881053915767121554, 17.74999999863440792, -4.541265875000002339 ) ) ;
#60075 = CARTESIAN_POINT ( 'NONE',  ( -10.00000000000000533, 72.29166666666667140, -2.679491924311231621 ) ) ;
#60076 = CARTESIAN_POINT ( 'NONE',  ( 3.313708498984762496, -7.999999999999989342, 1.299052779823363979 ) ) ;
#60077 = VERTEX_POINT ( 'NONE', #37332 ) ;
#60078 = CARTESIAN_POINT ( 'NONE',  ( -1.656854249492354825, 200.4375000027311842, 138.0000000000000284 ) ) ;
#60079 = EDGE_LOOP ( 'NONE', ( #3730, #56318 ) ) ;
#60080 = CARTESIAN_POINT ( 'NONE',  ( 4.721056650415999201, 295.2343750017069510, -4.721056650415999201 ) ) ;
#60081 = CARTESIAN_POINT ( 'NONE',  ( 3.008240453400888764E-14, 271.9999999999999432, 189.0000000000000284 ) ) ;
#60082 = CARTESIAN_POINT ( 'NONE',  ( -3.313708498984757167, 7.999999999999991118, 6.736552783920144449 ) ) ;
#60083 = CARTESIAN_POINT ( 'NONE',  ( -8.311093377946841443, 173.9062499965860411, 8.311093377946830785 ) ) ;
#60084 = LINE ( 'NONE', #26112, #36899 ) ;
#60085 = VECTOR ( 'NONE', #30153, 1000.000000000000000 ) ;
#60086 = CARTESIAN_POINT ( 'NONE',  ( 2.828427124746209831, 200.3750000000000284, 200.8284271247462129 ) ) ;
#60087 = CARTESIAN_POINT ( 'NONE',  ( -2.751064625579944321E-14, 195.8750000027311842, 146.0000000000000284 ) ) ;
#60088 = ADVANCED_FACE ( 'NONE', ( #19226 ), #65245, .T. ) ;
#60089 = CARTESIAN_POINT ( 'NONE',  ( 7.204075437095966983, 7.204075437095967871, 107.9687500020483810 ) ) ;
#60090 = ORIENTED_EDGE ( 'NONE', *, *, #59857, .T. ) ;
#60091 = CARTESIAN_POINT ( 'NONE',  ( -0.4451317748924059625, 51.14719335908522169, -48.52010116548709817 ) ) ;
#60092 = LINE ( 'NONE', #2015, #67778 ) ;
#60093 = CARTESIAN_POINT ( 'NONE',  ( 9.832129032723420536, 141.5104166632526699, -5.676582343749999815 ) ) ;
#60094 = CARTESIAN_POINT ( 'NONE',  ( -1.432654583217607192, 196.2500000013656347, 194.5412658750000219 ) ) ;
#60095 = CARTESIAN_POINT ( 'NONE',  ( 2.839093476692135984E-14, 203.9375000013656063, 201.4587341250000350 ) ) ;
#60096 = CARTESIAN_POINT ( 'NONE',  ( 7.204075437095968759, -7.204075437095966983, 70.09375000204836681 ) ) ;
#60097 = CARTESIAN_POINT ( 'NONE',  ( -9.832129032723420536, 69.01041666325268409, 5.676582343749997150 ) ) ;
#60098 = VERTEX_POINT ( 'NONE', #7912 ) ;
#60099 = CARTESIAN_POINT ( 'NONE',  ( -26.34314575050770202, 209.0625000027312126, 166.0000000000003126 ) ) ;
#60100 = CARTESIAN_POINT ( 'NONE',  ( -4.541265875000002339, 4.937499998634407916, -5.561446717895856393E-16 ) ) ;
#60101 = CARTESIAN_POINT ( 'NONE',  ( -8.008118988124991233, 3.317071493978878127, 8.419365283940628331 ) ) ;
#60102 = ORIENTED_EDGE ( 'NONE', *, *, #39301, .T. ) ;
#60103 = CARTESIAN_POINT ( 'NONE',  ( -7.188101187500002709, 22.31249999795161187, 2.977408999572649151 ) ) ;
#60104 = DIRECTION ( 'NONE',  ( 0.000000000000000000, 0.000000000000000000, -1.000000000000000000 ) ) ;
#60105 = CARTESIAN_POINT ( 'NONE',  ( 2.751064625579944321E-14, 202.7500000000000000, 194.0000000000000568 ) ) ;
#60106 = CARTESIAN_POINT ( 'NONE',  ( 5.082755093536324154, 12.65624999795161187, 5.082755093536326818 ) ) ;
#60107 = CARTESIAN_POINT ( 'NONE',  ( 7.188101187499992051, 2.977408999572647819, 5.330302781871753659 ) ) ;
#60108 = CARTESIAN_POINT ( 'NONE',  ( 4.220049686691934809, 10.18810118749999916, 115.5625000020483810 ) ) ;
#60109 = ADVANCED_FACE ( 'NONE', ( #25246 ), #48263, .T. ) ;
#60110 = DIRECTION ( 'NONE',  ( -0.000000000000000000, 1.000000000000000000, -0.000000000000000000 ) ) ;
#60111 = CARTESIAN_POINT ( 'NONE',  ( 1.656854249492381248, 0.9374999972688131678, -4.000000000000001776 ) ) ;
#60112 = ORIENTED_EDGE ( 'NONE', *, *, #48728, .T. ) ;
#60113 = CARTESIAN_POINT ( 'NONE',  ( 1.432654583217664479, 208.7500000013656063, 201.4587341250000065 ) ) ;
#60114 = CARTESIAN_POINT ( 'NONE',  ( -25.17157287525385456, 196.0000000027312126, 167.1715728752541281 ) ) ;
#60115 = CARTESIAN_POINT ( 'NONE',  ( -8.342170076843785083E-16, 2.062499998634406584, 4.541265875000002339 ) ) ;
#60117 = CARTESIAN_POINT ( 'NONE',  ( 5.082755093536326818, 111.2187500020483810, 5.082755093536325042 ) ) ;
#60116 = AXIS2_PLACEMENT_3D ( 'NONE', #45864, #46237, #40959 ) ;
#60118 = FACE_OUTER_BOUND ( 'NONE', #4799, .T. ) ;
#60119 = CARTESIAN_POINT ( 'NONE',  ( -5.082755093536319713, 5.082755093536319713, 22.29905278187175455 ) ) ;
#60120 = ORIENTED_EDGE ( 'NONE', *, *, #26526, .T. ) ;
#60121 = CARTESIAN_POINT ( 'NONE',  ( -5.082755093536326818, 20.90624999795161543, 5.082755093536325042 ) ) ;
#60122 = VERTEX_POINT ( 'NONE', #36955 ) ;
#60123 = CARTESIAN_POINT ( 'NONE',  ( -8.660254037844387298, 2.916666666666664742, 4.999999999999995559 ) ) ;
#60124 = CARTESIAN_POINT ( 'NONE',  ( -3.190679070438223991E-13, 203.7500000000000000, 10.00000000000000533 ) ) ;
#60125 = CARTESIAN_POINT ( 'NONE',  ( 2.485281374238950125, 296.3125000000001705, 5.999999999999625189 ) ) ;
#60126 = CARTESIAN_POINT ( 'NONE',  ( 31.45873412499998523, 202.7500000013655779, 168.5673454167822172 ) ) ;
#60127 = CARTESIAN_POINT ( 'NONE',  ( -8.660254037844387298, 72.08333333333332860, -5.000000000000004441 ) ) ;
#60128 = VECTOR ( 'NONE', #69496, 1000.000000000000000 ) ;
#60129 = CARTESIAN_POINT ( 'NONE',  ( 5.082755093536325042, 95.46875000204838102, -5.082755093536325930 ) ) ;
#60130 = CARTESIAN_POINT ( 'NONE',  ( -2.485281374238572649, 297.1875000000000000, 6.000000000000002665 ) ) ;
#60132 = CARTESIAN_POINT ( 'NONE',  ( -25.76220260446628885, -41.68111043767994062, 187.2530570791431614 ) ) ;
#60131 = CARTESIAN_POINT ( 'NONE',  ( 24.00000000000001066, 207.9375000027312126, 171.6568542494923122 ) ) ;
#60133 = ORIENTED_EDGE ( 'NONE', *, *, #18609, .T. ) ;
#60134 = CARTESIAN_POINT ( 'NONE',  ( -3.042071309553159075, 224.9479166700806445, 11.35316468749999963 ) ) ;
#60135 = CYLINDRICAL_SURFACE ( 'NONE', #53274, 11.00000000000000000 ) ;
#60136 = CARTESIAN_POINT ( 'NONE',  ( -4.000000000000015987, 201.6250000027312126, 142.0000000000000568 ) ) ;
#60137 = CARTESIAN_POINT ( 'NONE',  ( 11.00000000000000000, 1.347111479062088405E-15, 78.24999999999998579 ) ) ;
#60138 = CARTESIAN_POINT ( 'NONE',  ( 2.966170491840901068E-11, 66.24999999999768363, -9.999999999999998224 ) ) ;
#60139 = CARTESIAN_POINT ( 'NONE',  ( 8.000000000000001776, 107.8437500040967905, 3.313708498984759387 ) ) ;
#60140 = CARTESIAN_POINT ( 'NONE',  ( 8.660254037844389075, 180.4166666666666572, -5.000000000000000000 ) ) ;
#60141 = DIRECTION ( 'NONE',  ( -1.000000000000000000, 0.000000000000000000, 0.000000000000000000 ) ) ;
#60142 = CARTESIAN_POINT ( 'NONE',  ( 7.188101187499992051, 8.802885111219154394E-16, 25.11155278187175810 ) ) ;
#60143 = CARTESIAN_POINT ( 'NONE',  ( -11.35316468750000141, 148.8020833299193555, 3.042071309553159963 ) ) ;
#60144 = CARTESIAN_POINT ( 'NONE',  ( 6.000000000000024869, 10.39230484541325339, -14.00000000000000178 ) ) ;
#60145 = DIRECTION ( 'NONE',  ( 0.000000000000000000, 0.000000000000000000, 1.000000000000000000 ) ) ;
#60148 = LINE ( 'NONE', #70374, #71178 ) ;
#60147 = CARTESIAN_POINT ( 'NONE',  ( 105.0000000000000000, 229.6205190061017447, 90.00000000000000000 ) ) ;
#60146 = CARTESIAN_POINT ( 'NONE',  ( 30.82842712474620228, 202.3750000000000284, 167.1715728752537586 ) ) ;
#60149 = EDGE_LOOP ( 'NONE', ( #55570, #5750, #70815, #22741 ) ) ;
#60150 = CARTESIAN_POINT ( 'NONE',  ( 11.35316468749999785, 10.88541666325268586, 3.042071309553174174 ) ) ;
#60151 = ADVANCED_FACE ( 'NONE', ( #55815 ), #38830, .T. ) ;
#60152 = CARTESIAN_POINT ( 'NONE',  ( -11.00000000000000000, 0.000000000000000000, 77.68750000409677625 ) ) ;
#60153 = DIRECTION ( 'NONE',  ( -0.000000000000000000, 1.000000000000000000, 4.689100369878284071E-30 ) ) ;
#60154 = CARTESIAN_POINT ( 'NONE',  ( 0.000000000000000000, 0.000000000000000000, 0.000000000000000000 ) ) ;
#60155 = CARTESIAN_POINT ( 'NONE',  ( 3.458734124999958581, 208.5000000013656063, 140.5673454167823593 ) ) ;
#60156 = CARTESIAN_POINT ( 'NONE',  ( -4.850062511589670794E-16, 124.5792468245269475, -7.920753175473082663 ) ) ;
#60157 = ADVANCED_FACE ( 'NONE', ( #49767, #9786 ), #32807, .F. ) ;
#60158 = CARTESIAN_POINT ( 'NONE',  ( -4.999999999999998224, 43.54166665983870388, -8.660254037844389075 ) ) ;
#60159 = CARTESIAN_POINT ( 'NONE',  ( 7.188101187500001821, 111.5000000020483810, -2.977408999572651371 ) ) ;
#60160 = CARTESIAN_POINT ( 'NONE',  ( 4.541265875000002339, 5.437499998634407028, 0.000000000000000000 ) ) ;
#60161 = DIRECTION ( 'NONE',  ( -1.000000000000000000, 0.000000000000000000, 0.000000000000000000 ) ) ;
#60162 = CARTESIAN_POINT ( 'NONE',  ( 7.999999999999992895, -3.313708498984756279, 7.486552779823366421 ) ) ;
#60164 = CARTESIAN_POINT ( 'NONE',  ( -27.99999999999991118, 201.6250000027312126, 174.0000000000003695 ) ) ;
#60163 = CARTESIAN_POINT ( 'NONE',  ( 1.616960574868474554, 194.5560245358154816, 138.8258031584831542 ) ) ;
#60165 = VERTEX_POINT ( 'NONE', #38458 ) ;
#60166 =( BOUNDED_CURVE ( )  B_SPLINE_CURVE ( 2, ( #21689, #44715, #62060, #44344, #26222, #20571, #60944, #15279, #72258 ),
 .UNSPECIFIED., .F., .F. ) 
 B_SPLINE_CURVE_WITH_KNOTS ( ( 3, 2, 2, 2, 3 ),
 ( 0.6029411764705880916, 0.6066176470588233727, 0.6102941176470586537, 0.6139705882352939348, 0.6176470588235292158 ),
 .UNSPECIFIED. ) 
 CURVE ( )  GEOMETRIC_REPRESENTATION_ITEM ( )  RATIONAL_B_SPLINE_CURVE ( ( 1.000000000000002220, 0.9238795325112844070, 1.000000000000000000, 0.9238795325112867385, 1.000000000000000000, 0.9238795325112867385, 1.000000000000000000, 0.9238795325112912904, 0.9999999999999954481 ) ) 
 REPRESENTATION_ITEM ( '' )  );
#60167 = CARTESIAN_POINT ( 'NONE',  ( -10.50000000000000000, 1.285879139104720831E-15, -21.50000000000000000 ) ) ;
#60168 = CARTESIAN_POINT ( 'NONE',  ( 4.000000000000001776, 1.806524977843537691E-16, 0.000000000000000000 ) ) ;
#60169 = CARTESIAN_POINT ( 'NONE',  ( -3.042071309553166625, 233.1770833367472733, -11.35316468749999608 ) ) ;
#60170 = CARTESIAN_POINT ( 'NONE',  ( -9.832129032723418760, 122.8645833299193555, -5.676582343750004256 ) ) ;
#60171 = ORIENTED_EDGE ( 'NONE', *, *, #68500, .F. ) ;
#60172 = CARTESIAN_POINT ( 'NONE',  ( -0.4325856884189893115, 10.91672922346751839, 117.5849391215780457 ) ) ;
#60173 = CARTESIAN_POINT ( 'NONE',  ( -4.220049686691935698, 10.18810118749999916, 95.87500000204838102 ) ) ;
#60174 = CARTESIAN_POINT ( 'NONE',  ( -2.445694354108784108, 198.5625000013656063, 195.5543056458912190 ) ) ;
#60175 = FACE_OUTER_BOUND ( 'NONE', #46102, .T. ) ;
#60177 = CARTESIAN_POINT ( 'NONE',  ( 6.951808397369818766E-16, 112.0312499965860269, -11.35316468750000141 ) ) ;
#60176 = CARTESIAN_POINT ( 'NONE',  ( 7.320508075688792360, 45.62500000000002132, -7.320508075688792360 ) ) ;
#60178 = CARTESIAN_POINT ( 'NONE',  ( -32.00000000000001421, 208.1875000000000853, 168.3431457505080004 ) ) ;
#60179 = CARTESIAN_POINT ( 'NONE',  ( -5.656854249492375253, 5.656854249492375253, 6.830302783920143561 ) ) ;
#60180 = ORIENTED_EDGE ( 'NONE', *, *, #49692, .F. ) ;
#60181 = ADVANCED_FACE ( 'NONE', ( #73153 ), #5247, .T. ) ;
#60182 = CARTESIAN_POINT ( 'NONE',  ( -8.660254037844387298, 23.95833332650536462, -5.000000000000004441 ) ) ;
#60183 = CARTESIAN_POINT ( 'NONE',  ( -11.35316468750000141, 98.59374999658601268, -1.390361679473963753E-15 ) ) ;
#60184 = CARTESIAN_POINT ( 'NONE',  ( -1.432654583217607858, 204.6250000013656063, 201.4587341250000065 ) ) ;
#60185 = CARTESIAN_POINT ( 'NONE',  ( 5.082755093536324154, 14.15624999795161187, 5.082755093536326818 ) ) ;
#60186 = CARTESIAN_POINT ( 'NONE',  ( 4.220049686691941027, -10.18810118749999738, 91.00000000204836681 ) ) ;
#60187 = EDGE_CURVE ( 'NONE', #56169, #4846, #60733, .T. ) ;
#60188 = CARTESIAN_POINT ( 'NONE',  ( 3.042071309553167069, 27.13541666325268409, -11.35316468749999785 ) ) ;
#60190 = ORIENTED_EDGE ( 'NONE', *, *, #64580, .T. ) ;
#60189 =( BOUNDED_SURFACE ( )  B_SPLINE_SURFACE ( 1, 2, ( 
 ( #16025, #39058, #62059, #10384, #33410, #66599, #32286, #73011, #37942, #3606, #73750, #22057, #26604, #49626, #45084, #68099, #39427, #72642, #20945, #31904, #44343, #54926, #28474, #62791, #63920, #204, #10751, #40537, #23182, #5106, #11133, #46192, #40911, #69209, #74124, #5472, #17521, #22426, #6218, #51482, #34156, #12231, #63543, #33786, #57156, #51860, #62426, #74493, #11868, #22801, #34904, #45821, #39788, #56785, #28097, #57910, #11500, #68832, #40169, #17144, #51112, #23552, #69585, #569, #45446, #68462, #16763, #63174, #34533, #57539, #29223, #52237, #5848, #28841, #46564, #17898, #10244, #33642, #39286, #45310, #44202, #56270, #38552, #27207, #62287, #15141, #32521, #66838, #21550, #44948, #22287, #72873, #21917, #43824, #27583, #9506, #38173, #49855, #26452, #50592, #10616, #49477, #9874, #21177, #20805, #56649, #4964, #44576, #72496, #61176, #55907, #3463, #32902, #67215, #68324, #55534, #15512, #27965, #50970, #4589, #38917, #61553, #16622, #73610, #62655, #4218, #33271, #67955, #16248, #73245, #73984, #50224, #39657, #10989, #3844, #55157, #67589, #26840, #15885, #61919, #20586, #19473, #8531, #2133, #14175, #31546, #66242, #14545, #54569, #70793, #13434, #65502, #19107, #42113, #2875, #25861, #31170, #71894, #42485, #42849, #3250, #7432, #65866, #59849, #37209, #54942, #59487, #48883, #25125, #20208, #26240, #43227, #37583, #71517, #60583, #8909, #31921, #8163, #19841, #60207, #30438, #65124, #71151, #36105, #13797, #48142, #49259, #7799, #72273, #59122, #43599, #36470, #13069, #53458, #36842, #1776, #24761, #47771, #30802, #54196, #53824, #2503, #25498, #48512, #26997, #62077, #38329, #20961, #66613, #28112, #10400, #67370, #43984, #50010, #73027, #14920, #4748, #50750, #33427, #62438, #56801, #27740, #22073, #68111, #45099, #61335, #66994, #27364, #73764, #50381, #38711, #21702, #16405, #39439, #5120, #55692, #67746, #21338, #61709, #10766, #26619 ),
 ( #44359, #16041, #32300, #56425, #72658, #33804, #15667, #9663, #73398, #10030, #33065, #15293, #32684, #4006, #51127, #74138, #56063, #22439, #3623, #44728, #39073, #4370, #37962, #60960, #9278, #55317, #49642, #51879, #69226, #63557, #52988, #62810, #11146, #1321, #34169, #57170, #586, #5860, #45836, #52619, #12247, #5487, #17163, #69975, #58296, #40182, #6600, #12613, #68850, #35642, #45460, #219, #40929, #34547, #46577, #63938, #23936, #46946, #35284, #28488, #63185, #23198, #51496, #74508, #29606, #69598, #22820, #11514, #17912, #6963, #956, #57553, #28858, #18283, #46211, #41298, #17535, #40552, #68476, #64308, #16778, #11883, #23567, #39804, #58656, #34917, #52251, #57929, #29972, #6236, #29239, #38144, #13336, #12973, #72843, #54096, #61145, #55875, #19373, #9844, #30707, #13701, #20775, #42020, #43794, #38519, #42388, #49449, #44172, #53728, #3814, #30341, #8066, #36373, #2039, #15112, #25027, #7334, #49826, #32870, #61522, #24304, #36009, #19014, #72467, #64672, #59028, #18653, #48046, #71056, #67186, #7702, #25404, #53360, #66810, #1685, #9474, #65403, #65028, #31068, #36745, #59756, #24664, #47675, #70695, #47315, #21150, #59389, #32491, #2408, #55502, #26812, #15483, #70342, #41663, #45649, #46023, #68293, #10583, #27933, #22255, #73216, #50941, #33614, #23016, #62256, #5301, #44546, #74323, #10214, #68664, #4936, #73581, #62628, #45283, #73953, #56243, #4558, #33243, #17347, #29, #44918, #40001, #15852, #33994, #56988, #27553, #28303, #16975, #63004, #69044, #16590, #56621, #39629, #10959, #11693, #21524, #67556, #51312, #39258, #50565, #11328, #34361, #38887, #21889, #28670, #57362, #67925, #5673, #40369, #16219, #63368, #34732, #22629, #51684, #4191, #27180, #50197, #61891, #36194, #1511, #40734, #58107, #35460, #63744, #12062, #70517, #7151, #23382, #52433, #30156, #19198, #53173, #35097, #69781, #58840, #6418, #59210, #41113, #29424, #65215 ) ),
 .UNSPECIFIED., .F., .F., .F. ) 
 B_SPLINE_SURFACE_WITH_KNOTS ( ( 2, 2 ),
 ( 3, 2, 2, 2, 2, 2, 2, 2, 2, 2, 2, 2, 2, 2, 2, 2, 2, 2, 2, 2, 2, 2, 2, 2, 2, 2, 2, 2, 2, 2, 2, 2, 2, 2, 2, 2, 2, 2, 2, 2, 2, 2, 2, 2, 2, 2, 2, 2, 2, 2, 2, 2, 2, 2, 2, 2, 2, 2, 2, 2, 2, 2, 2, 2, 2, 2, 2, 2, 2, 2, 2, 2, 2, 2, 2, 2, 2, 2, 2, 2, 2, 2, 2, 2, 2, 2, 2, 2, 2, 2, 2, 2, 2, 2, 2, 2, 2, 2, 2, 2, 2, 2, 2, 2, 2, 2, 2, 2, 2, 2, 2, 2, 2, 2, 2, 2, 2, 2, 2, 2, 3 ),
 ( 0.000000000000000000, 1.000000000000000000 ),
 ( 0.000000000000000000, 0.008333333333333333218, 0.01666666666666666644, 0.02500000000000000139, 0.03333333333333333287, 0.04166666666666666435, 0.05000000000000000278, 0.05833333333333333426, 0.06666666666666666574, 0.07499999999999999722, 0.08333333333333332871, 0.09166666666666666019, 0.1000000000000000056, 0.1083333333333333370, 0.1166666666666666685, 0.1250000000000000000, 0.1333333333333333315, 0.1416666666666666630, 0.1499999999999999944, 0.1583333333333333259, 0.1666666666666666574, 0.1749999999999999889, 0.1833333333333333204, 0.1916666666666666796, 0.2000000000000000111, 0.2083333333333333426, 0.2166666666666666741, 0.2250000000000000056, 0.2333333333333333370, 0.2416666666666666685, 0.2500000000000000000, 0.2583333333333333592, 0.2666666666666666630, 0.2750000000000000222, 0.2833333333333333259, 0.2916666666666666852, 0.2999999999999999889, 0.3083333333333333481, 0.3166666666666666519, 0.3250000000000000111, 0.3333333333333333148, 0.3416666666666666741, 0.3499999999999999778, 0.3583333333333333370, 0.3666666666666666408, 0.3750000000000000000, 0.3833333333333333592, 0.3916666666666666630, 0.4000000000000000222, 0.4083333333333333259, 0.4166666666666666852, 0.4249999999999999889, 0.4333333333333333481, 0.4416666666666666519, 0.4500000000000000111, 0.4583333333333333148, 0.4666666666666666741, 0.4749999999999999778, 0.4833333333333333370, 0.4916666666666666408, 0.5000000000000000000, 0.5083333333333333037, 0.5166666666666667185, 0.5250000000000000222, 0.5333333333333333259, 0.5416666666666666297, 0.5500000000000000444, 0.5583333333333333481, 0.5666666666666666519, 0.5749999999999999556, 0.5833333333333333703, 0.5916666666666666741, 0.5999999999999999778, 0.6083333333333332815, 0.6166666666666666963, 0.6250000000000000000, 0.6333333333333333037, 0.6416666666666667185, 0.6500000000000000222, 0.6583333333333333259, 0.6666666666666666297, 0.6750000000000000444, 0.6833333333333333481, 0.6916666666666666519, 0.6999999999999999556, 0.7083333333333333703, 0.7166666666666666741, 0.7249999999999999778, 0.7333333333333332815, 0.7416666666666666963, 0.7500000000000000000, 0.7583333333333333037, 0.7666666666666667185, 0.7750000000000000222, 0.7833333333333333259, 0.7916666666666666297, 0.8000000000000000444, 0.8083333333333333481, 0.8166666666666666519, 0.8249999999999999556, 0.8333333333333333703, 0.8416666666666666741, 0.8499999999999999778, 0.8583333333333332815, 0.8666666666666666963, 0.8750000000000000000, 0.8833333333333333037, 0.8916666666666667185, 0.9000000000000000222, 0.9083333333333333259, 0.9166666666666666297, 0.9250000000000000444, 0.9333333333333333481, 0.9416666666666666519, 0.9499999999999999556, 0.9583333333333333703, 0.9666666666666666741, 0.9749999999999999778, 0.9833333333333332815, 0.9916666666666666963, 1.000000000000000000 ),
 .UNSPECIFIED. ) 
 GEOMETRIC_REPRESENTATION_ITEM ( )  RATIONAL_B_SPLINE_SURFACE ( (
 ( 1.000000000000000000, 0.9238795325112867385, 1.000000000000000000, 0.9238795325112867385, 1.000000000000000000, 0.9238795325112867385, 1.000000000000000000, 0.9238795325112867385, 1.000000000000000000, 0.9238795325112867385, 1.000000000000000000, 0.9238795325112867385, 1.000000000000000000, 0.9238795325112867385, 1.000000000000000000, 0.9238795325112867385, 1.000000000000000000, 0.9238795325112867385, 1.000000000000000000, 0.9238795325112867385, 1.000000000000000000, 0.9238795325112867385, 1.000000000000000000, 0.9238795325112867385, 1.000000000000000000, 0.9238795325112867385, 1.000000000000000000, 0.9238795325112867385, 1.000000000000000000, 0.9238795325112867385, 1.000000000000000000, 0.9238795325112867385, 1.000000000000000000, 0.9238795325112867385, 1.000000000000000000, 0.9238795325112867385, 1.000000000000000000, 0.9238795325112867385, 1.000000000000000000, 0.9238795325112867385, 1.000000000000000000, 0.9238795325112867385, 1.000000000000000000, 0.9238795325112867385, 1.000000000000000000, 0.9238795325112867385, 1.000000000000000000, 0.9238795325112867385, 1.000000000000000000, 0.9238795325112867385, 1.000000000000000000, 0.9238795325112867385, 1.000000000000000000, 0.9238795325112867385, 1.000000000000000000, 0.9238795325112867385, 1.000000000000000000, 0.9238795325112867385, 1.000000000000000000, 0.9238795325112867385, 1.000000000000000000, 0.9238795325112867385, 1.000000000000000000, 0.9238795325112867385, 1.000000000000000000, 0.9238795325112867385, 1.000000000000000000, 0.9238795325112867385, 1.000000000000000000, 0.9238795325112867385, 1.000000000000000000, 0.9238795325112867385, 1.000000000000000000, 0.9238795325112867385, 1.000000000000000000, 0.9238795325112867385, 1.000000000000000000, 0.9238795325112867385, 1.000000000000000000, 0.9238795325112867385, 1.000000000000000000, 0.9238795325112867385, 1.000000000000000000, 0.9238795325112867385, 1.000000000000000000, 0.9238795325112867385, 1.000000000000000000, 0.9238795325112867385, 1.000000000000000000, 0.9238795325112867385, 1.000000000000000000, 0.9238795325112867385, 1.000000000000000000, 0.9238795325112867385, 1.000000000000000000, 0.9238795325112867385, 1.000000000000000000, 0.9238795325112867385, 1.000000000000000000, 0.9238795325112867385, 1.000000000000000000, 0.9238795325112867385, 1.000000000000000000, 0.9238795325112867385, 1.000000000000000000, 0.9238795325112867385, 1.000000000000000000, 0.9238795325112867385, 1.000000000000000000, 0.9238795325112867385, 1.000000000000000000, 0.9238795325112867385, 1.000000000000000000, 0.9238795325112867385, 1.000000000000000000, 0.9238795325112867385, 1.000000000000000000, 0.9238795325112867385, 1.000000000000000000, 0.9238795325112867385, 1.000000000000000000, 0.9238795325112867385, 1.000000000000000000, 0.9238795325112867385, 1.000000000000000000, 0.9238795325112867385, 1.000000000000000000, 0.9238795325112867385, 1.000000000000000000, 0.9238795325112867385, 1.000000000000000000, 0.9238795325112867385, 1.000000000000000000, 0.9238795325112867385, 1.000000000000000000, 0.9238795325112867385, 1.000000000000000000, 0.9238795325112867385, 1.000000000000000000, 0.9238795325112867385, 1.000000000000000000, 0.9238795325112867385, 1.000000000000000000, 0.9238795325112867385, 1.000000000000000000, 0.9238795325112867385, 1.000000000000000000, 0.9238795325112867385, 1.000000000000000000, 0.9238795325112867385, 1.000000000000000000, 0.9238795325112867385, 1.000000000000000000, 0.9238795325112867385, 1.000000000000000000, 0.9238795325112867385, 1.000000000000000000, 0.9238795325112867385, 1.000000000000000000, 0.9238795325112867385, 1.000000000000000000, 0.9238795325112867385, 1.000000000000000000, 0.9238795325112867385, 1.000000000000000000, 0.9238795325112867385, 1.000000000000000000, 0.9238795325112867385, 1.000000000000000000, 0.9238795325112867385, 1.000000000000000000, 0.9238795325112867385, 1.000000000000000000, 0.9238795325112867385, 1.000000000000000000, 0.9238795325112867385, 1.000000000000000000, 0.9238795325112867385, 1.000000000000000000, 0.9238795325112867385, 1.000000000000000000, 0.9238795325112867385, 1.000000000000000000, 0.9238795325112867385, 1.000000000000000000, 0.9238795325112867385, 1.000000000000000000, 0.9238795325112867385, 1.000000000000000000, 0.9238795325112867385, 1.000000000000000000, 0.9238795325112867385, 1.000000000000000000, 0.9238795325112867385, 1.000000000000000000, 0.9238795325112867385, 1.000000000000000000, 0.9238795325112867385, 1.000000000000000000, 0.9238795325112867385, 1.000000000000000000, 0.9238795325112867385, 1.000000000000000000, 0.9238795325112867385, 1.000000000000000000, 0.9238795325112867385, 1.000000000000000000, 0.9238795325112867385, 1.000000000000000000, 0.9238795325112867385, 1.000000000000000000, 0.9238795325112867385, 1.000000000000000000, 0.9238795325112867385, 1.000000000000000000, 0.9238795325112867385, 1.000000000000000000, 0.9238795325112867385, 1.000000000000000000, 0.9238795325112867385, 1.000000000000000000, 0.9238795325112867385, 1.000000000000000000, 0.9238795325112867385, 1.000000000000000000, 0.9238795325112867385, 1.000000000000000000, 0.9238795325112867385, 1.000000000000000000, 0.9238795325112867385, 1.000000000000000000, 0.9238795325112867385, 1.000000000000000000, 0.9238795325112867385, 1.000000000000000000, 0.9238795325112867385, 1.000000000000000000, 0.9238795325112867385, 1.000000000000000000, 0.9238795325112867385, 1.000000000000000000),
 ( 1.000000000000000000, 0.9238795325112867385, 1.000000000000000000, 0.9238795325112867385, 1.000000000000000000, 0.9238795325112867385, 1.000000000000000000, 0.9238795325112867385, 1.000000000000000000, 0.9238795325112867385, 1.000000000000000000, 0.9238795325112867385, 1.000000000000000000, 0.9238795325112867385, 1.000000000000000000, 0.9238795325112867385, 1.000000000000000000, 0.9238795325112867385, 1.000000000000000000, 0.9238795325112867385, 1.000000000000000000, 0.9238795325112867385, 1.000000000000000000, 0.9238795325112867385, 1.000000000000000000, 0.9238795325112867385, 1.000000000000000000, 0.9238795325112867385, 1.000000000000000000, 0.9238795325112867385, 1.000000000000000000, 0.9238795325112867385, 1.000000000000000000, 0.9238795325112867385, 1.000000000000000000, 0.9238795325112867385, 1.000000000000000000, 0.9238795325112867385, 1.000000000000000000, 0.9238795325112867385, 1.000000000000000000, 0.9238795325112867385, 1.000000000000000000, 0.9238795325112867385, 1.000000000000000000, 0.9238795325112867385, 1.000000000000000000, 0.9238795325112867385, 1.000000000000000000, 0.9238795325112867385, 1.000000000000000000, 0.9238795325112867385, 1.000000000000000000, 0.9238795325112867385, 1.000000000000000000, 0.9238795325112867385, 1.000000000000000000, 0.9238795325112867385, 1.000000000000000000, 0.9238795325112867385, 1.000000000000000000, 0.9238795325112867385, 1.000000000000000000, 0.9238795325112867385, 1.000000000000000000, 0.9238795325112867385, 1.000000000000000000, 0.9238795325112867385, 1.000000000000000000, 0.9238795325112867385, 1.000000000000000000, 0.9238795325112867385, 1.000000000000000000, 0.9238795325112867385, 1.000000000000000000, 0.9238795325112867385, 1.000000000000000000, 0.9238795325112867385, 1.000000000000000000, 0.9238795325112867385, 1.000000000000000000, 0.9238795325112867385, 1.000000000000000000, 0.9238795325112867385, 1.000000000000000000, 0.9238795325112867385, 1.000000000000000000, 0.9238795325112867385, 1.000000000000000000, 0.9238795325112867385, 1.000000000000000000, 0.9238795325112867385, 1.000000000000000000, 0.9238795325112867385, 1.000000000000000000, 0.9238795325112867385, 1.000000000000000000, 0.9238795325112867385, 1.000000000000000000, 0.9238795325112867385, 1.000000000000000000, 0.9238795325112867385, 1.000000000000000000, 0.9238795325112867385, 1.000000000000000000, 0.9238795325112867385, 1.000000000000000000, 0.9238795325112867385, 1.000000000000000000, 0.9238795325112867385, 1.000000000000000000, 0.9238795325112867385, 1.000000000000000000, 0.9238795325112867385, 1.000000000000000000, 0.9238795325112867385, 1.000000000000000000, 0.9238795325112867385, 1.000000000000000000, 0.9238795325112867385, 1.000000000000000000, 0.9238795325112867385, 1.000000000000000000, 0.9238795325112867385, 1.000000000000000000, 0.9238795325112867385, 1.000000000000000000, 0.9238795325112867385, 1.000000000000000000, 0.9238795325112867385, 1.000000000000000000, 0.9238795325112867385, 1.000000000000000000, 0.9238795325112867385, 1.000000000000000000, 0.9238795325112867385, 1.000000000000000000, 0.9238795325112867385, 1.000000000000000000, 0.9238795325112867385, 1.000000000000000000, 0.9238795325112867385, 1.000000000000000000, 0.9238795325112867385, 1.000000000000000000, 0.9238795325112867385, 1.000000000000000000, 0.9238795325112867385, 1.000000000000000000, 0.9238795325112867385, 1.000000000000000000, 0.9238795325112867385, 1.000000000000000000, 0.9238795325112867385, 1.000000000000000000, 0.9238795325112867385, 1.000000000000000000, 0.9238795325112867385, 1.000000000000000000, 0.9238795325112867385, 1.000000000000000000, 0.9238795325112867385, 1.000000000000000000, 0.9238795325112867385, 1.000000000000000000, 0.9238795325112867385, 1.000000000000000000, 0.9238795325112867385, 1.000000000000000000, 0.9238795325112867385, 1.000000000000000000, 0.9238795325112867385, 1.000000000000000000, 0.9238795325112867385, 1.000000000000000000, 0.9238795325112867385, 1.000000000000000000, 0.9238795325112867385, 1.000000000000000000, 0.9238795325112867385, 1.000000000000000000, 0.9238795325112867385, 1.000000000000000000, 0.9238795325112867385, 1.000000000000000000, 0.9238795325112867385, 1.000000000000000000, 0.9238795325112867385, 1.000000000000000000, 0.9238795325112867385, 1.000000000000000000, 0.9238795325112867385, 1.000000000000000000, 0.9238795325112867385, 1.000000000000000000, 0.9238795325112867385, 1.000000000000000000, 0.9238795325112867385, 1.000000000000000000, 0.9238795325112867385, 1.000000000000000000, 0.9238795325112867385, 1.000000000000000000, 0.9238795325112867385, 1.000000000000000000, 0.9238795325112867385, 1.000000000000000000, 0.9238795325112867385, 1.000000000000000000, 0.9238795325112867385, 1.000000000000000000, 0.9238795325112867385, 1.000000000000000000, 0.9238795325112867385, 1.000000000000000000, 0.9238795325112867385, 1.000000000000000000, 0.9238795325112867385, 1.000000000000000000, 0.9238795325112867385, 1.000000000000000000, 0.9238795325112867385, 1.000000000000000000, 0.9238795325112867385, 1.000000000000000000, 0.9238795325112867385, 1.000000000000000000, 0.9238795325112867385, 1.000000000000000000, 0.9238795325112867385, 1.000000000000000000, 0.9238795325112867385, 1.000000000000000000, 0.9238795325112867385, 1.000000000000000000, 0.9238795325112867385, 1.000000000000000000, 0.9238795325112867385, 1.000000000000000000, 0.9238795325112867385, 1.000000000000000000) ) ) 
 REPRESENTATION_ITEM ( '' )  SURFACE ( )  );
#60191 = CARTESIAN_POINT ( 'NONE',  ( 1.656854249492356157, 20.93749999726881228, -4.000000000000026645 ) ) ;
#60192 = CARTESIAN_POINT ( 'NONE',  ( -8.008118988124991233, 3.317071493978878127, 26.41936528394063188 ) ) ;
#60193 = CARTESIAN_POINT ( 'NONE',  ( -10.18810118749999738, -4.220049686691941915, 72.62500000204836681 ) ) ;
#60194 = CARTESIAN_POINT ( 'NONE',  ( -0.3671489098107383886, 21.99999999999999645, 4.453226760635411452 ) ) ;
#60195 = CARTESIAN_POINT ( 'NONE',  ( -2.977408999572654480, 2.999999997951610542, 7.188101187499999156 ) ) ;
#60196 = CARTESIAN_POINT ( 'NONE',  ( -4.721056650415998313, 291.5781250017069510, 4.721056650416000089 ) ) ;
#60197 = CARTESIAN_POINT ( 'NONE',  ( 8.311093377946834337, 220.4687499965860127, 8.311093377946839666 ) ) ;
#60198 = CARTESIAN_POINT ( 'NONE',  ( 3.042071309553167069, 137.1354166632526983, -11.35316468749999785 ) ) ;
#60199 = CARTESIAN_POINT ( 'NONE',  ( -10.18810118749999916, 4.220049686691934809, 84.06250000204838102 ) ) ;
#60200 = ADVANCED_FACE ( 'NONE', ( #4132 ), #15049, .F. ) ;
#60201 = EDGE_CURVE ( 'NONE', #32974, #11019, #12051, .T. ) ;
#60202 = CARTESIAN_POINT ( 'NONE',  ( -25.55430564589119413, 199.3125000013656063, 167.5543056458915316 ) ) ;
#60203 = CARTESIAN_POINT ( 'NONE',  ( 7.999999999999998224, 20.90625000000000355, 3.313708498984766493 ) ) ;
#60204 = CARTESIAN_POINT ( 'NONE',  ( -4.541265875000002339, 13.93749999863440614, -5.561446717895856393E-16 ) ) ;
#60205 = ORIENTED_EDGE ( 'NONE', *, *, #62693, .F. ) ;
#60206 = CARTESIAN_POINT ( 'NONE',  ( 2.828427124746208943, 202.7500000027312126, 195.1715728752538439 ) ) ;
#60207 = CARTESIAN_POINT ( 'NONE',  ( 1.432654583217607414, 198.5000000013656347, 145.4587341250000634 ) ) ;
#60208 = CARTESIAN_POINT ( 'NONE',  ( -1.656854249492405451, 203.4375000027312126, 138.0000000000000568 ) ) ;
#60209 = CARTESIAN_POINT ( 'NONE',  ( -3.166186134455097228E-13, 171.2500000000000284, -9.999999999999998224 ) ) ;
#60210 = DIRECTION ( 'NONE',  ( 0.8660254037844380415, -0.5000000000000009992, 0.000000000000000000 ) ) ;
#60211 = ORIENTED_EDGE ( 'NONE', *, *, #8384, .T. ) ;
#60212 = CARTESIAN_POINT ( 'NONE',  ( 7.188101187500000933, 5.062499997951610098, -2.977408999572650483 ) ) ;
#60213 = CARTESIAN_POINT ( 'NONE',  ( -15.04621553396602707, -19.93110780747396404, 197.1054176773724578 ) ) ;
#60214 = EDGE_CURVE ( 'NONE', #29969, #8618, #34324, .T. ) ;
#60215 = CARTESIAN_POINT ( 'NONE',  ( -5.000000000000005329, 30.20833332650536818, 8.660254037844387298 ) ) ;
#60216 = CARTESIAN_POINT ( 'NONE',  ( -8.311093377946836114, 182.6562499965860411, -8.311093377946837890 ) ) ;
#60217 = CARTESIAN_POINT ( 'NONE',  ( 5.082755093536326818, 113.0937500020483810, 5.082755093536325042 ) ) ;
#60218 = CARTESIAN_POINT ( 'NONE',  ( -0.4590000000000000746, 278.5679999999998699, 5.805285082143462283 ) ) ;
#60219 = CARTESIAN_POINT ( 'NONE',  ( -4.721056650415998313, 291.5781250017069510, 4.721056650416000089 ) ) ;
#60220 = ADVANCED_FACE ( 'NONE', ( #44858 ), #21461, .T. ) ;
#60221 = CARTESIAN_POINT ( 'NONE',  ( -27.99999999999996092, 209.5000000000000284, 174.0000000000003695 ) ) ;
#60222 = ORIENTED_EDGE ( 'NONE', *, *, #5591, .F. ) ;
#60223 = CARTESIAN_POINT ( 'NONE',  ( 5.676582343750005144, 225.8854166700806729, 9.832129032723416984 ) ) ;
#60224 = CARTESIAN_POINT ( 'NONE',  ( 7.188101187499993827, -2.977408999572645598, 28.01780278187175455 ) ) ;
#60225 = CARTESIAN_POINT ( 'NONE',  ( -4.000000000000002665, 2.312499997268813168, 1.656854249492380582 ) ) ;
#60226 = CARTESIAN_POINT ( 'NONE',  ( -7.999999999999991118, 3.313708498984757167, 15.92405278392014445 ) ) ;
#60228 = EDGE_CURVE ( 'NONE', #22020, #70268, #35191, .T. ) ;
#60227 = CARTESIAN_POINT ( 'NONE',  ( -1.432654583217607414, 199.5000000013656063, 194.5412658750000219 ) ) ;
#60229 = VERTEX_POINT ( 'NONE', #31109 ) ;
#60230 = CARTESIAN_POINT ( 'NONE',  ( -6.735557395310442023E-16, 11.00000000000000000, 114.6249999999999858 ) ) ;
#60231 = CARTESIAN_POINT ( 'NONE',  ( -3.313708498984762496, 102.7812499999999858, 7.999999999999998224 ) ) ;
#60232 = CARTESIAN_POINT ( 'NONE',  ( -9.832129032723420536, 114.0104166632526983, 5.676582343749997150 ) ) ;
#60233 = DIRECTION ( 'NONE',  ( 0.000000000000000000, 0.000000000000000000, 1.000000000000000000 ) ) ;
#60234 = CARTESIAN_POINT ( 'NONE',  ( -11.00000000000000000, 4.556349186104045934, 74.40624999999998579 ) ) ;
#60237 = CYLINDRICAL_SURFACE ( 'NONE', #66340, 7.999999999999991118 ) ;
#60236 = CARTESIAN_POINT ( 'NONE',  ( 31.45873412499999944, 198.6250000013655779, 171.4326545832175555 ) ) ;
#60235 = CARTESIAN_POINT ( 'NONE',  ( 24.54126587499999346, 198.4375000013655779, 169.9999999999998863 ) ) ;
#60238 = ORIENTED_EDGE ( 'NONE', *, *, #48601, .T. ) ;
#60239 = LINE ( 'NONE', #53850, #24819 ) ;
#60240 = CARTESIAN_POINT ( 'NONE',  ( 11.35316468749999785, 225.5729166632526983, 3.042071309553174174 ) ) ;
#60241 = CARTESIAN_POINT ( 'NONE',  ( -1.432654583217664479, 202.7500000013655779, 138.5412658750000787 ) ) ;
#60242 = CARTESIAN_POINT ( 'NONE',  ( 24.54126587499999346, 203.4375000013656063, 169.9999999999998863 ) ) ;
#60243 = CARTESIAN_POINT ( 'NONE',  ( 11.00000000000000000, 4.556349186104045934, 114.5312500040968047 ) ) ;
#60244 = CARTESIAN_POINT ( 'NONE',  ( -5.676582343749998039, 197.7604166632526983, -9.832129032723420536 ) ) ;
#60245 = CARTESIAN_POINT ( 'NONE',  ( 5.082755093536326818, 92.09375000204838102, 5.082755093536325042 ) ) ;
#60246 = CARTESIAN_POINT ( 'NONE',  ( 9.919492326333610777, 226.0000000000000000, 4.581766860447704204 ) ) ;
#60247 = CARTESIAN_POINT ( 'NONE',  ( 1.881053915767121776, 15.49999999863440792, -4.541265875000002339 ) ) ;
#60248 = CARTESIAN_POINT ( 'NONE',  ( 30.44569435410879166, 199.8125000013656063, 172.4456943541087526 ) ) ;
#60249 = CARTESIAN_POINT ( 'NONE',  ( -7.188101187499992051, 0.000000000000000000, 6.361552781871754547 ) ) ;
#60250 = CARTESIAN_POINT ( 'NONE',  ( 2.775557561562891351E-14, 195.0000000000000000, 202.0000000000000000 ) ) ;
#60251 = CARTESIAN_POINT ( 'NONE',  ( -9.832129032723418760, 87.86458332991935549, -5.676582343750004256 ) ) ;
#60252 = ORIENTED_EDGE ( 'NONE', *, *, #24852, .F. ) ;
#60253 = CARTESIAN_POINT ( 'NONE',  ( 8.660254037844392627, 139.5833333333333712, 5.000000000000009770 ) ) ;
#60254 = CARTESIAN_POINT ( 'NONE',  ( -1.656854249492354825, 201.3125000000000284, 138.0000000000000284 ) ) ;
#60255 = CARTESIAN_POINT ( 'NONE',  ( -1.469576158976823947E-15, 9.937499995903220196, 8.000000000000000000 ) ) ;
#60256 = CARTESIAN_POINT ( 'NONE',  ( -2.828427124746152987, 207.1250000000000284, 200.8284271247462129 ) ) ;
#60257 = CARTESIAN_POINT ( 'NONE',  ( -2.085542519210945728E-15, 94.53124999658601268, 11.35316468750000141 ) ) ;
#60258 = ORIENTED_EDGE ( 'NONE', *, *, #24035, .T. ) ;
#60259 = CARTESIAN_POINT ( 'NONE',  ( 4.220049686691941027, -10.18810118749999738, 86.50000000204838102 ) ) ;
#60260 = CARTESIAN_POINT ( 'NONE',  ( -4.220049686691937474, -10.18810118749999738, 111.4375000020483810 ) ) ;
#60261 = CARTESIAN_POINT ( 'NONE',  ( -1.432654583217607414, 209.5000000013656063, 194.5412658750000219 ) ) ;
#60262 = CYLINDRICAL_SURFACE ( 'NONE', #15478, 3.999999999999976019 ) ;
#60264 = CARTESIAN_POINT ( 'NONE',  ( 11.35316468749999785, 75.57291666325269830, 3.042071309553174174 ) ) ;
#60263 = PLANE ( 'NONE',  #18352 ) ;
#60265 = CARTESIAN_POINT ( 'NONE',  ( 7.999999999999991118, 3.313708498984757611, 21.36155278392014978 ) ) ;
#60266 = CARTESIAN_POINT ( 'NONE',  ( -3.742616585878841384, 194.7527601235050838, 141.6310807506124263 ) ) ;
#60267 = VECTOR ( 'NONE', #33440, 1000.000000000000000 ) ;
#60268 = CARTESIAN_POINT ( 'NONE',  ( 7.320508075688774596, 167.4999999931720822, -7.320508075688774596 ) ) ;
#60269 = CARTESIAN_POINT ( 'NONE',  ( 1.926045908305006327, 89.59560438569886287, -7.188101187499999156 ) ) ;
#60270 = CARTESIAN_POINT ( 'NONE',  ( -24.14031152995224616, 194.9033115224686696, 170.6945784924176053 ) ) ;
#60271 = CARTESIAN_POINT ( 'NONE',  ( 5.676582343749993598, 65.26041666325268409, 9.832129032723422313 ) ) ;
#60272 = CARTESIAN_POINT ( 'NONE',  ( -4.088227598258586603E-16, 292.2031250017069510, -6.676582343750001591 ) ) ;
#60273 = CARTESIAN_POINT ( 'NONE',  ( 4.220049686691934809, 10.18810118749999916, 106.5625000020483810 ) ) ;
#60274 = CARTESIAN_POINT ( 'NONE',  ( -3.042071309553164404, 212.2395833299193839, -11.35316468749999963 ) ) ;
#60275 = VERTEX_POINT ( 'NONE', #17666 ) ;
#60276 = DIRECTION ( 'NONE',  ( 0.000000000000000000, -1.000000000000000000, 0.000000000000000000 ) ) ;
#60277 = CARTESIAN_POINT ( 'NONE',  ( 3.999999999999960032, 206.1250000027312126, 142.0000000000000568 ) ) ;
#60278 = CARTESIAN_POINT ( 'NONE',  ( 8.000000000000000000, 14.81249999590322020, 0.000000000000000000 ) ) ;
#60280 = CARTESIAN_POINT ( 'NONE',  ( -11.35316468750000141, 188.4895833299193555, 3.042071309553159963 ) ) ;
#60279 = CARTESIAN_POINT ( 'NONE',  ( -1.656854249492393238, 11.06249999726881406, -3.999999999999989786 ) ) ;
#60281 = FACE_OUTER_BOUND ( 'NONE', #45203, .T. ) ;
#60282 = CARTESIAN_POINT ( 'NONE',  ( -8.660254037844385522, 243.5416666734946318, 5.000000000000004441 ) ) ;
#60283 = DIRECTION ( 'NONE',  ( -1.000000000000000000, 0.000000000000000000, 0.000000000000000000 ) ) ;
#60284 = VERTEX_POINT ( 'NONE', #59065 ) ;
#60285 = CARTESIAN_POINT ( 'NONE',  ( 5.676582343750001591, 181.9270833299193555, -9.832129032723420536 ) ) ;
#60286 =( BOUNDED_CURVE ( )  B_SPLINE_CURVE ( 2, ( #13994, #7257, #12897, #30631, #37035, #43049, #66068, #3078, #60036, #8354, #26063, #31371, #25693 ),
 .UNSPECIFIED., .F., .F. ) 
 B_SPLINE_CURVE_WITH_KNOTS ( ( 3, 2, 2, 2, 2, 2, 3 ),
 ( 0.3924913403172796134, 0.3977247878691485550, 0.4029582354210174966, 0.4081916829728863272, 0.4134251305247552688, 0.4186585780766242104, 0.4238920256284931520 ),
 .UNSPECIFIED. ) 
 CURVE ( )  GEOMETRIC_REPRESENTATION_ITEM ( )  RATIONAL_B_SPLINE_CURVE ( ( 1.000000000000298428, 0.9659258262887695512, 0.9999999999999998890, 0.9659258262890682012, 0.9999999999999998890, 0.9659258262890682012, 0.9999999999999998890, 0.9659258262890682012, 0.9999999999999998890, 0.9659258262890682012, 0.9999999999999998890, 0.9659258262890666469, 1.000000000000001332 ) ) 
 REPRESENTATION_ITEM ( '' )  );
#60287 = CIRCLE ( 'NONE', #49455, 4.999999999999997335 ) ;
#60288 = CARTESIAN_POINT ( 'NONE',  ( -5.082755093536317936, -5.082755093536320601, 22.67405278187175455 ) ) ;
#60289 = CARTESIAN_POINT ( 'NONE',  ( 7.999999999999992895, 8.617919685066743914E-06, 16.76780302773458686 ) ) ;
#60290 = CIRCLE ( 'NONE', #50652, 8.999999999999998224 ) ;
#60291 = EDGE_LOOP ( 'NONE', ( #68553, #3931, #15922, #69790 ) ) ;
#60292 = CARTESIAN_POINT ( 'NONE',  ( -3.313708498984762496, 99.96875000409676204, 7.999999999999998224 ) ) ;
#60293 = CARTESIAN_POINT ( 'NONE',  ( -10.00000000000000178, 7.500000000000000888, -1.224646799147353454E-15 ) ) ;
#60294 =( BOUNDED_CURVE ( )  B_SPLINE_CURVE ( 2, ( #49727, #2591, #15007, #49343, #20291, #66326, #19922, #48594, #15379, #38042, #71601, #48964, #42930 ),
 .UNSPECIFIED., .F., .F. ) 
 B_SPLINE_CURVE_WITH_KNOTS ( ( 3, 2, 2, 2, 2, 2, 3 ),
 ( 1.146093318828196539, 1.151325727210465333, 1.156558135592734127, 1.161790543975002921, 1.167022952357271715, 1.172255360739540508, 1.177487769121809080 ),
 .UNSPECIFIED. ) 
 CURVE ( )  GEOMETRIC_REPRESENTATION_ITEM ( )  RATIONAL_B_SPLINE_CURVE ( ( 1.000000000000000000, 0.9659258262890683122, 1.000000000000000000, 0.9659258262890683122, 1.000000000000000000, 0.9659258262890683122, 1.000000000000000000, 0.9659258262890683122, 1.000000000000000000, 0.9659258262890683122, 1.000000000000000000, 0.9659258262891498026, 0.9999999999999185096 ) ) 
 REPRESENTATION_ITEM ( '' )  );
#60295 = CARTESIAN_POINT ( 'NONE',  ( 4.000000000000000888, 15.93750000000000000, 1.656854249492384135 ) ) ;
#60296 = CARTESIAN_POINT ( 'NONE',  ( 4.541265875000002339, 14.31249999863440792, 0.000000000000000000 ) ) ;
#60297 = CARTESIAN_POINT ( 'NONE',  ( 3.313708498984756279, 7.999999999999991118, 15.54905278392014623 ) ) ;
#60298 = DIRECTION ( 'NONE',  ( 0.000000000000000000, -0.000000000000000000, 1.000000000000000000 ) ) ;
#60299 = VERTEX_POINT ( 'NONE', #34302 ) ;
#60300 = CARTESIAN_POINT ( 'NONE',  ( -7.778174593052023411, 7.778174593052023411, 72.81249999999998579 ) ) ;
#60301 = CARTESIAN_POINT ( 'NONE',  ( 7.188101187500000044, 91.90625000204838102, -8.802885111219163269E-16 ) ) ;
#60302 = ADVANCED_FACE ( 'NONE', ( #39940 ), #13738, .T. ) ;
#60305 = AXIS2_PLACEMENT_3D ( 'NONE', #49672, #50783, #61742 ) ;
#60304 = CARTESIAN_POINT ( 'NONE',  ( 5.676582343749997150, 262.2395833367473301, -9.832129032723418760 ) ) ;
#60303 = CARTESIAN_POINT ( 'NONE',  ( -10.00000000000000000, 258.1250000068279746, 0.000000000000000000 ) ) ;
#60306 = DIRECTION ( 'NONE',  ( 1.000000000000000000, 0.000000000000000000, 0.000000000000000000 ) ) ;
#60307 = VERTEX_POINT ( 'NONE', #40684 ) ;
#60308 = FACE_OUTER_BOUND ( 'NONE', #59386, .T. ) ;
#60309 = CARTESIAN_POINT ( 'NONE',  ( -7.188101187499991163, 2.977408999572646930, 20.89280278187176521 ) ) ;
#60310 = VERTEX_POINT ( 'NONE', #13011 ) ;
#60311 = ADVANCED_FACE ( 'NONE', ( #74645 ), #36049, .T. ) ;
#60312 = ORIENTED_EDGE ( 'NONE', *, *, #2401, .T. ) ;
#60313 = CARTESIAN_POINT ( 'NONE',  ( 7.204075437095966983, 7.204075437095967871, 82.09375000204838102 ) ) ;
#60314 = CARTESIAN_POINT ( 'NONE',  ( -8.311093377946836114, 77.96874999658598426, -8.311093377946837890 ) ) ;
#60315 = CARTESIAN_POINT ( 'NONE',  ( 9.000000000000014211, 15.58845726811988719, 0.000000000000000000 ) ) ;
#60316 = CARTESIAN_POINT ( 'NONE',  ( 4.556349186104051263, -10.99999999999999822, 97.46874999999998579 ) ) ;
#60319 = CARTESIAN_POINT ( 'NONE',  ( 4.721056650416000089, 295.9843750017070079, 4.721056650415999201 ) ) ;
#60318 = CARTESIAN_POINT ( 'NONE',  ( 25.17157287525381548, 197.0000000027312126, 172.8284271247460993 ) ) ;
#60317 = CARTESIAN_POINT ( 'NONE',  ( 29.65685424949244720, 196.5625000027312126, 165.9999999999999716 ) ) ;
#60320 = CARTESIAN_POINT ( 'NONE',  ( -1.836970198721029983E-15, 148.7500000000000284, 10.00000000000000178 ) ) ;
#60321 = CARTESIAN_POINT ( 'NONE',  ( 4.556349186104052151, -10.99999999999999822, 83.96874999999997158 ) ) ;
#60322 = CARTESIAN_POINT ( 'NONE',  ( -7.320508075688778149, 164.9999999931720538, 7.320508075688769267 ) ) ;
#60323 = CARTESIAN_POINT ( 'NONE',  ( -3.458734124999959469, 196.7500000013656063, 199.4326545832176976 ) ) ;
#60324 = CARTESIAN_POINT ( 'NONE',  ( -5.000000000000000888, 232.2916666734946602, -8.660254037844387298 ) ) ;
#60325 = PLANE ( 'NONE',  #52094 ) ;
#60326 = CARTESIAN_POINT ( 'NONE',  ( 27.99999999999996447, 200.4375000013656063, 173.4587341249998929 ) ) ;
#60327 = CARTESIAN_POINT ( 'NONE',  ( -7.188101187500001821, 8.999999997951611874, -2.977408999572651371 ) ) ;
#60328 = CARTESIAN_POINT ( 'NONE',  ( -7.999999999999991118, 3.313708498984756723, 24.92405278392015333 ) ) ;
#60329 = CARTESIAN_POINT ( 'NONE',  ( -7.999999999999991118, 0.000000000000000000, 23.33030277982336642 ) ) ;
#60330 = CARTESIAN_POINT ( 'NONE',  ( 5.082755093536326818, 110.0937500020483810, 5.082755093536325042 ) ) ;
#60332 = CARTESIAN_POINT ( 'NONE',  ( -1.656854249492383468, 16.68750000000000000, 4.000000000000000888 ) ) ;
#60331 = DIRECTION ( 'NONE',  ( 0.000000000000000000, 0.000000000000000000, 1.000000000000000000 ) ) ;
#60333 = CARTESIAN_POINT ( 'NONE',  ( -11.00000000000003730, -4.556349186104013960, 112.2812500040967905 ) ) ;
#60334 = CARTESIAN_POINT ( 'NONE',  ( -2.775557561562891351E-14, 210.0000000000000284, 142.0000000000000568 ) ) ;
#60335 = CARTESIAN_POINT ( 'NONE',  ( -5.082755093536317936, -5.082755093536320601, 24.54905278187175810 ) ) ;
#60336 = CARTESIAN_POINT ( 'NONE',  ( 28.00000000000002132, 200.1250000027312126, 173.9999999999999147 ) ) ;
#60337 = CARTESIAN_POINT ( 'NONE',  ( 8.311093377946834337, 40.15624999658601268, 8.311093377946839666 ) ) ;
#60338 = CARTESIAN_POINT ( 'NONE',  ( 4.217983994790206914, 16.30587161610658242, 69.44297314766849638 ) ) ;
#60339 = CARTESIAN_POINT ( 'NONE',  ( -5.000000000000005329, 5.208333326505366401, 8.660254037844387298 ) ) ;
#60340 = VERTEX_POINT ( 'NONE', #7374 ) ;
#60341 = CYLINDRICAL_SURFACE ( 'NONE', #37475, 3.999999999999976019 ) ;
#60342 = LINE ( 'NONE', #25995, #369 ) ;
#60343 = CARTESIAN_POINT ( 'NONE',  ( -9.832129032723418760, 52.86458332991934839, -5.676582343750004256 ) ) ;
#60344 = CARTESIAN_POINT ( 'NONE',  ( 4.556349186104045934, 11.00000000000000000, 81.71875000409677625 ) ) ;
#60345 = CARTESIAN_POINT ( 'NONE',  ( -3.458734125000016757, 206.1250000013656063, 140.5673454167823593 ) ) ;
#60347 = VECTOR ( 'NONE', #1096, 1000.000000000000000 ) ;
#60346 = CARTESIAN_POINT ( 'NONE',  ( 23.99999999999997868, 202.8125000000000000, 171.6568542494922553 ) ) ;
#60348 = DIRECTION ( 'NONE',  ( 0.000000000000000000, 0.5207998305029731823, -0.8536788251726022958 ) ) ;
#60350 = CARTESIAN_POINT ( 'NONE',  ( 3.042071309553167513, 31.82291666325268054, -11.35316468749999785 ) ) ;
#60349 = CARTESIAN_POINT ( 'NONE',  ( -5.082755093536325930, 98.46875000204838102, -5.082755093536325930 ) ) ;
#60351 = CARTESIAN_POINT ( 'NONE',  ( 5.656854249492376141, -5.656854249492374365, 10.39280277982336465 ) ) ;
#60352 = CARTESIAN_POINT ( 'NONE',  ( -2.679491924311263595, 48.33333332650537528, -9.999999999999980460 ) ) ;
#60353 = CARTESIAN_POINT ( 'NONE',  ( -11.35316468750000141, 158.2812499965860127, -1.390361679473963753E-15 ) ) ;
#60354 = CARTESIAN_POINT ( 'NONE',  ( -7.320508075688773708, 133.7499999931720538, -7.320508075688774596 ) ) ;
#60355 = CARTESIAN_POINT ( 'NONE',  ( -4.401442555609581635E-16, 106.1562500020483810, -7.188101187500000044 ) ) ;
#60356 = VECTOR ( 'NONE', #14053, 1000.000000000000000 ) ;
#60357 = ORIENTED_EDGE ( 'NONE', *, *, #8058, .F. ) ;
#60358 = CARTESIAN_POINT ( 'NONE',  ( -4.242640687119286547, 288.8750000000000000, -4.242640687119286547 ) ) ;
#60359 = CARTESIAN_POINT ( 'NONE',  ( 11.35316468749999785, 20.88541666325268409, 3.042071309553174174 ) ) ;
#60360 = CARTESIAN_POINT ( 'NONE',  ( -28.31625444984154072, 194.4587341250000634, 166.5521097615726092 ) ) ;
#60361 = ORIENTED_EDGE ( 'NONE', *, *, #71237, .F. ) ;
#60362 = FACE_OUTER_BOUND ( 'NONE', #58258, .T. ) ;
#60363 = CARTESIAN_POINT ( 'NONE',  ( -4.220049686691935698, 10.18810118749999916, 74.87500000204836681 ) ) ;
#60364 = FACE_OUTER_BOUND ( 'NONE', #33185, .T. ) ;
#60366 = CARTESIAN_POINT ( 'NONE',  ( -11.35316468750000141, 158.4895833299193555, 3.042071309553159963 ) ) ;
#60365 = CARTESIAN_POINT ( 'NONE',  ( -29.92855564209677510, -21.04794776559233682, 151.8635309713003210 ) ) ;
#60367 = CARTESIAN_POINT ( 'NONE',  ( 2.977408999572652260, 2.062499997951610542, 7.188101187500000044 ) ) ;
#60368 = AXIS2_PLACEMENT_3D ( 'NONE', #57403, #73623, #62297 ) ;
#60369 = CARTESIAN_POINT ( 'NONE',  ( 1.469576158976822172E-15, -7.999999999999991118, 11.76155278432982243 ) ) ;
#60370 = CARTESIAN_POINT ( 'NONE',  ( 2.394417657446511694, 225.8111685005081029, 10.00000000000000355 ) ) ;
#60371 = CARTESIAN_POINT ( 'NONE',  ( 11.35316468749999963, 231.1979166700806161, 3.042071309553159519 ) ) ;
#60372 = CARTESIAN_POINT ( 'NONE',  ( 10.18810118749999916, 4.220049686691935698, 88.37500000204839523 ) ) ;
#60373 = ORIENTED_EDGE ( 'NONE', *, *, #31846, .T. ) ;
#60374 = DIRECTION ( 'NONE',  ( -0.000000000000000000, 1.000000000000000000, -0.000000000000000000 ) ) ;
#60375 = CARTESIAN_POINT ( 'NONE',  ( -4.898587196589412829E-16, 121.8125000040967763, -8.000000000000000000 ) ) ;
#60376 = CARTESIAN_POINT ( 'NONE',  ( -11.35316468750000141, 98.59374999658601268, -1.390361679473963753E-15 ) ) ;
#60377 = CARTESIAN_POINT ( 'NONE',  ( -7.204075437095965206, -7.204075437095968759, 102.3437500020483668 ) ) ;
#60378 = CARTESIAN_POINT ( 'NONE',  ( 4.541265875000002339, 20.49999999863440436, -1.881053915767121776 ) ) ;
#60379 = ORIENTED_EDGE ( 'NONE', *, *, #6764, .T. ) ;
#60380 = ORIENTED_EDGE ( 'NONE', *, *, #50275, .F. ) ;
#60381 = CONICAL_SURFACE ( 'NONE', #12357, 18.00000000000000355, 1.047197551196596965 ) ;
#60382 = CARTESIAN_POINT ( 'NONE',  ( 1.881053915767121776, 5.624999998634407028, -4.541265875000002339 ) ) ;
#60383 = CARTESIAN_POINT ( 'NONE',  ( -7.188101187500002709, 10.31249999795161010, 2.977408999572649151 ) ) ;
#60384 = CARTESIAN_POINT ( 'NONE',  ( 8.000000000000000000, 117.0312500040967905, -3.313708498984762496 ) ) ;
#60386 = EDGE_CURVE ( 'NONE', #663, #38665, #59793, .T. ) ;
#60385 = CARTESIAN_POINT ( 'NONE',  ( -10.18810118749999916, 4.220049686691934809, 96.43750000204836681 ) ) ;
#60387 = EDGE_CURVE ( 'NONE', #46386, #6290, #26564, .T. ) ;
#60388 = CARTESIAN_POINT ( 'NONE',  ( -24.54126587499998280, 200.3750000013656063, 171.4326545832179818 ) ) ;
#60389 = CARTESIAN_POINT ( 'NONE',  ( -6.000000000000021316, -10.39230484541325161, 0.000000000000000000 ) ) ;
#60390 =( BOUNDED_CURVE ( )  B_SPLINE_CURVE ( 2, ( #34926, #25036, #64316, #57938, #23947, #12257, #35292, #46586, #41308 ),
 .UNSPECIFIED., .F., .F. ) 
 B_SPLINE_CURVE_WITH_KNOTS ( ( 3, 2, 2, 2, 3 ),
 ( 0.7666666666666673846, 0.7750000000000006883, 0.7833333333333339921, 0.7916666666666672958, 0.8000000000000007105 ),
 .UNSPECIFIED. ) 
 CURVE ( )  GEOMETRIC_REPRESENTATION_ITEM ( )  RATIONAL_B_SPLINE_CURVE ( ( 0.9999999999999938938, 0.9238795325112928447, 1.000000000000000000, 0.9238795325112867385, 1.000000000000000000, 0.9238795325112867385, 1.000000000000000000, 0.9238795325112806323, 1.000000000000005995 ) ) 
 REPRESENTATION_ITEM ( '' )  );
#60391 = CARTESIAN_POINT ( 'NONE',  ( -4.000000000000001776, 3.437500000000000000, -1.656854249492381470 ) ) ;
#60392 = CARTESIAN_POINT ( 'NONE',  ( 2.828427124746191623, 19.87499999726881228, -2.828427124746191623 ) ) ;
#60393 = CARTESIAN_POINT ( 'NONE',  ( 4.541265875000002339, 2.312499998634407028, 0.000000000000000000 ) ) ;
#60394 = CARTESIAN_POINT ( 'NONE',  ( -3.458734125000015425, 209.0000000013655779, 143.4326545832176976 ) ) ;
#60395 = CARTESIAN_POINT ( 'NONE',  ( 2.754378923186476579E-14, 195.1875000013655779, 194.5412658750000219 ) ) ;
#60396 = VECTOR ( 'NONE', #13672, 1000.000000000000000 ) ;
#60398 = CARTESIAN_POINT ( 'NONE',  ( 2.679491924311263151, 234.5833333401612890, 9.999999999999980460 ) ) ;
#60397 = CARTESIAN_POINT ( 'NONE',  ( -26.56734541678242323, 195.3750000013656063, 166.5412658750003345 ) ) ;
#60399 = CARTESIAN_POINT ( 'NONE',  ( 2.780723358947928197E-16, 17.56249999863440792, -4.541265875000002339 ) ) ;
#60400 = CARTESIAN_POINT ( 'NONE',  ( -5.000000000000000000, -29.68417822476651580, -4.268394125863113509 ) ) ;
#60401 = CARTESIAN_POINT ( 'NONE',  ( 1.320432766682872962E-15, -7.188101187499992051, 9.361552781871752771 ) ) ;
#60402 = ORIENTED_EDGE ( 'NONE', *, *, #29056, .T. ) ;
#60403 = VERTEX_POINT ( 'NONE', #65064 ) ;
#60404 = CARTESIAN_POINT ( 'NONE',  ( -7.204075437095967871, 7.204075437095967871, 100.4687500020483668 ) ) ;
#60405 = DIRECTION ( 'NONE',  ( 0.000000000000000000, 0.000000000000000000, -1.000000000000000000 ) ) ;
#60406 = AXIS2_PLACEMENT_3D ( 'NONE', #64534, #8203, #2549 ) ;
#60407 = CARTESIAN_POINT ( 'NONE',  ( -24.54126587500000412, 203.5000000013655779, 168.5673454167827003 ) ) ;
#60408 = CARTESIAN_POINT ( 'NONE',  ( -31.99999999999998579, 202.3125000000000000, 171.6568542494928238 ) ) ;
#60409 = CARTESIAN_POINT ( 'NONE',  ( 2.839093476692135984E-14, 196.6875000013655779, 201.4587341250000350 ) ) ;
#60410 = DIRECTION ( 'NONE',  ( -1.000000000000000000, -0.000000000000000000, -0.000000000000000000 ) ) ;
#60411 = CARTESIAN_POINT ( 'NONE',  ( -10.00000000000000355, 102.7083333333333286, 2.679491924311223183 ) ) ;
#60412 = B_SPLINE_CURVE_WITH_KNOTS ( 'NONE', 3,
 ( #6112, #40065, #17041, #56304, #46087, #22697, #4620, #63070, #11763 ),
 .UNSPECIFIED., .F., .F.,
 ( 4, 2, 1, 2, 4 ),
 ( 0.000000000000000000, 0.001314083742622694203, 0.002628167485245388405, 0.003942251227868082825, 0.005256334970490776810 ),
 .UNSPECIFIED. ) ;
#60413 = CARTESIAN_POINT ( 'NONE',  ( 8.000000000000000000, 113.7500000000000000, -9.797174393178825657E-16 ) ) ;
#60414 = CARTESIAN_POINT ( 'NONE',  ( 4.721056650416000089, 290.9843750017070079, 4.721056650415999201 ) ) ;
#60415 = ADVANCED_FACE ( 'NONE', ( #70735 ), #46767, .F. ) ;
#60416 = CARTESIAN_POINT ( 'NONE',  ( 2.977408999572646486, 7.188101187499991163, 11.89280278187175810 ) ) ;
#60417 = ORIENTED_EDGE ( 'NONE', *, *, #25834, .F. ) ;
#60418 = DIRECTION ( 'NONE',  ( -0.000000000000000000, 1.000000000000000000, -0.000000000000000000 ) ) ;
#60419 = CARTESIAN_POINT ( 'NONE',  ( -3.313708498984760720, 18.28124999590322020, -8.000000000000000000 ) ) ;
#60420 = CARTESIAN_POINT ( 'NONE',  ( -3.458734125000015425, 202.9375000013656063, 142.0000000000000568 ) ) ;
#60421 = CARTESIAN_POINT ( 'NONE',  ( -5.000000000000005329, 185.2083333265053682, 8.660254037844387298 ) ) ;
#60422 = LINE ( 'NONE', #3843, #63653 ) ;
#60423 = CARTESIAN_POINT ( 'NONE',  ( -11.35316468749999608, 249.4270833367472733, 3.042071309553173730 ) ) ;
#60424 = CARTESIAN_POINT ( 'NONE',  ( -4.000000000000001776, 3.249999997268813612, -4.898587196589415787E-16 ) ) ;
#60425 = CARTESIAN_POINT ( 'NONE',  ( 7.778174593052021635, 7.778174593052023411, 115.9375000000000000 ) ) ;
#60426 = CARTESIAN_POINT ( 'NONE',  ( 10.00000000000000000, 224.7916666666666288, 2.679491924311236062 ) ) ;
#60427 = CARTESIAN_POINT ( 'NONE',  ( -2.977408999572647819, -7.188101187499990274, 5.142802781871753659 ) ) ;
#60428 = CARTESIAN_POINT ( 'NONE',  ( 11.35316468749999963, 191.3020833299193839, -3.042071309553165293 ) ) ;
#60429 = CARTESIAN_POINT ( 'NONE',  ( 0.000000000000000000, 0.000000000000000000, 30.00000000000000000 ) ) ;
#60430 = CARTESIAN_POINT ( 'NONE',  ( -4.541265875000003227, 6.874999998634407916, 1.881053915767121110 ) ) ;
#60431 = CARTESIAN_POINT ( 'NONE',  ( 11.00000000000000000, 1.347111479062088405E-15, 114.4375000040967763 ) ) ;
#60432 = ORIENTED_EDGE ( 'NONE', *, *, #37, .F. ) ;
#60433 = VECTOR ( 'NONE', #38194, 1000.000000000000000 ) ;
#60434 = CARTESIAN_POINT ( 'NONE',  ( -2.754378923186476579E-14, 204.4375000013656063, 145.4587341250000350 ) ) ;
#60435 = CARTESIAN_POINT ( 'NONE',  ( -4.556349186104045934, 11.00000000000000000, 99.90625000409677625 ) ) ;
#60436 = FACE_OUTER_BOUND ( 'NONE', #49436, .T. ) ;
#60437 = CARTESIAN_POINT ( 'NONE',  ( -30.44569435410886982, 199.5625000013656063, 167.5543056458916169 ) ) ;
#60438 = CARTESIAN_POINT ( 'NONE',  ( 105.0000000000000000, 50.00000000000000000, 127.0000000000000000 ) ) ;
#60440 = DIRECTION ( 'NONE',  ( -0.000000000000000000, 1.000000000000000000, -0.000000000000000000 ) ) ;
#60439 = CARTESIAN_POINT ( 'NONE',  ( 7.188101187500000044, 120.4062500020483810, -8.802885111219163269E-16 ) ) ;
#60441 = CARTESIAN_POINT ( 'NONE',  ( -5.656854249492373476, -5.656854249492376141, 28.01780277982336642 ) ) ;
#60442 = CARTESIAN_POINT ( 'NONE',  ( 11.35316468750000141, 125.7812499965860127, 0.000000000000000000 ) ) ;
#60443 = CARTESIAN_POINT ( 'NONE',  ( 8.660254037844389075, 92.29166665983871098, -5.000000000000000000 ) ) ;
#60444 = CARTESIAN_POINT ( 'NONE',  ( -5.082755093536324154, 91.34375000204838102, 5.082755093536326818 ) ) ;
#60445 = CARTESIAN_POINT ( 'NONE',  ( -4.541265875000002339, 21.87499999863441147, -1.881053915767121998 ) ) ;
#60446 = CARTESIAN_POINT ( 'NONE',  ( 7.999999999999991118, 1.469576158976822369E-15, 25.76780278392172008 ) ) ;
#60447 = CARTESIAN_POINT ( 'NONE',  ( -4.999999999999999112, 52.62579568235267402, -48.70175807017950120 ) ) ;
#60448 = ORIENTED_EDGE ( 'NONE', *, *, #24136, .T. ) ;
#60449 = CARTESIAN_POINT ( 'NONE',  ( 2.828427124746152987, 209.1250000000000284, 139.1715728752538723 ) ) ;
#60450 = ORIENTED_EDGE ( 'NONE', *, *, #25893, .T. ) ;
#60451 = CARTESIAN_POINT ( 'NONE',  ( -4.721056650415999201, 293.4843750017070079, -4.721056650415999201 ) ) ;
#60452 = DIRECTION ( 'NONE',  ( -1.000000000000000000, 0.000000000000000000, 0.000000000000000000 ) ) ;
#60453 = CARTESIAN_POINT ( 'NONE',  ( -3.313708498984757167, 7.999999999999991118, 9.736552783920146226 ) ) ;
#60454 = CARTESIAN_POINT ( 'NONE',  ( 5.676582343749993598, 164.9479166632526983, 9.832129032723422313 ) ) ;
#60455 = DIRECTION ( 'NONE',  ( 0.000000000000000000, -0.2588190451025146332, 0.9659258262890699775 ) ) ;
#60456 = CARTESIAN_POINT ( 'NONE',  ( 1.656854249492403008, 201.6875000000000000, 194.0000000000000853 ) ) ;
#60457 = CARTESIAN_POINT ( 'NONE',  ( 8.000000000000000000, 103.3437500000000000, -3.313708498984762496 ) ) ;
#60458 = CARTESIAN_POINT ( 'NONE',  ( -4.220049686691937474, -10.18810118749999738, 102.8125000020483952 ) ) ;
#60459 = VERTEX_POINT ( 'NONE', #25067 ) ;
#60460 = EDGE_CURVE ( 'NONE', #1129, #42334, #48085, .T. ) ;
#60461 = VECTOR ( 'NONE', #3757, 1000.000000000000000 ) ;
#60462 = CARTESIAN_POINT ( 'NONE',  ( -30.82842712474612412, 199.5000000027312126, 172.8284271247466108 ) ) ;
#60463 = CARTESIAN_POINT ( 'NONE',  ( 11.35316468749999785, 155.8854166632526699, 3.042071309553174174 ) ) ;
#60464 = CARTESIAN_POINT ( 'NONE',  ( 2.828427124746208943, 206.7500000027312126, 195.1715728752538439 ) ) ;
#60465 = CARTESIAN_POINT ( 'NONE',  ( -3.458734124999960358, 205.6250000013656063, 196.5673454167823877 ) ) ;
#60466 = CARTESIAN_POINT ( 'NONE',  ( -10.18810118749999738, -4.220049686691941915, 69.62500000204836681 ) ) ;
#60467 = CARTESIAN_POINT ( 'NONE',  ( 6.951808397369818766E-16, 62.34374999658602690, -11.35316468750000141 ) ) ;
#60468 = ORIENTED_EDGE ( 'NONE', *, *, #51405, .T. ) ;
#60469 = CARTESIAN_POINT ( 'NONE',  ( 4.220049686691934809, 10.18810118749999916, 116.6875000020483952 ) ) ;
#60470 = CARTESIAN_POINT ( 'NONE',  ( -4.541265875000002339, 8.874999998634407916, -1.881053915767121998 ) ) ;
#60471 = CARTESIAN_POINT ( 'NONE',  ( -3.317071493978880348, -8.008118988124989457, 8.794365283940628331 ) ) ;
#60472 = ORIENTED_EDGE ( 'NONE', *, *, #53367, .F. ) ;
#60473 = ADVANCED_FACE ( 'NONE', ( #13377 ), #19413, .F. ) ;
#60474 = CARTESIAN_POINT ( 'NONE',  ( 4.401442555609581635E-16, 18.84374999795161187, -7.188101187500000044 ) ) ;
#60475 = CARTESIAN_POINT ( 'NONE',  ( 6.000000000000003553, 287.6250000034140157, -2.485281374238571761 ) ) ;
#60476 = DIRECTION ( 'NONE',  ( -0.000000000000000000, -0.000000000000000000, -1.000000000000000000 ) ) ;
#60477 = CARTESIAN_POINT ( 'NONE',  ( -2.977408999572654480, 15.37499999795161187, 7.188101187499999156 ) ) ;
#60478 = CARTESIAN_POINT ( 'NONE',  ( -4.401442555609577197E-16, 7.188101187499992051, 4.111552781871752771 ) ) ;
#60479 = CARTESIAN_POINT ( 'NONE',  ( -6.238412754330611322E-16, 10.18810118749999916, 115.6562500020483810 ) ) ;
#60480 = CARTESIAN_POINT ( 'NONE',  ( 0.7778978019592035498, -42.09601127508702234, 151.0149604941898644 ) ) ;
#60481 = CARTESIAN_POINT ( 'NONE',  ( -7.347880794884122694E-16, 4.499999997268813168, 4.000000000000001776 ) ) ;
#60482 = VERTEX_POINT ( 'NONE', #69356 ) ;
#60483 = CIRCLE ( 'NONE', #5107, 11.00000000000000000 ) ;
#60484 = EDGE_CURVE ( 'NONE', #55027, #111, #31867, .T. ) ;
#60485 = ADVANCED_FACE ( 'NONE', ( #68608 ), #22960, .F. ) ;
#60486 = CARTESIAN_POINT ( 'NONE',  ( -3.458734124999959914, 205.4375000013656063, 198.0000000000000284 ) ) ;
#60487 = AXIS2_PLACEMENT_3D ( 'NONE', #54910, #54165, #14140 ) ;
#60488 = CARTESIAN_POINT ( 'NONE',  ( -23.99999999999998579, 195.8750000027311842, 170.0000000000002842 ) ) ;
#60489 = EDGE_CURVE ( 'NONE', #53551, #60808, #17292, .T. ) ;
#60490 = CARTESIAN_POINT ( 'NONE',  ( 4.541265875000002339, 5.374999998634406140, -1.881053915767121554 ) ) ;
#60491 = CARTESIAN_POINT ( 'NONE',  ( 7.188101187500000044, 108.4062500020483810, -8.802885111219163269E-16 ) ) ;
#60492 = CARTESIAN_POINT ( 'NONE',  ( 26.34314575050754215, 204.9375000000000284, 173.9999999999998863 ) ) ;
#60493 = CARTESIAN_POINT ( 'NONE',  ( 7.188101187499993827, -2.977408999572645598, 24.64280278187176165 ) ) ;
#60494 = EDGE_LOOP ( 'NONE', ( #27697, #10132, #16138, #69596 ) ) ;
#60495 = FACE_OUTER_BOUND ( 'NONE', #4086, .T. ) ;
#60496 = ORIENTED_EDGE ( 'NONE', *, *, #36995, .T. ) ;
#60497 = FACE_OUTER_BOUND ( 'NONE', #64623, .T. ) ;
#60498 = CARTESIAN_POINT ( 'NONE',  ( 0.000000000000000000, 0.000000000000000000, 0.000000000000000000 ) ) ;
#60499 = CARTESIAN_POINT ( 'NONE',  ( 2.754378923186476579E-14, 207.1875000013656063, 194.5412658750000219 ) ) ;
#60500 = CARTESIAN_POINT ( 'NONE',  ( 27.99999999999996803, 204.9375000013656063, 166.5412658749999082 ) ) ;
#60501 = CARTESIAN_POINT ( 'NONE',  ( 4.999999999999993783, 74.16666666666667140, 8.660254037844390851 ) ) ;
#60502 = CARTESIAN_POINT ( 'NONE',  ( -7.188101187500000044, 96.03125000204838102, 0.000000000000000000 ) ) ;
#60503 = CARTESIAN_POINT ( 'NONE',  ( -4.242640687119285658, 296.1250000000000000, 4.242640687119287435 ) ) ;
#60504 = ADVANCED_FACE ( 'NONE', ( #52009 ), #347, .F. ) ;
#60506 = CARTESIAN_POINT ( 'NONE',  ( 1.836970198721029589E-15, 256.2500000000000568, 10.00000000000000000 ) ) ;
#60505 = CARTESIAN_POINT ( 'NONE',  ( 31.99999999999998579, 207.4375000027311842, 168.3431457505075173 ) ) ;
#60507 = ORIENTED_EDGE ( 'NONE', *, *, #64674, .F. ) ;
#60508 =( BOUNDED_CURVE ( )  B_SPLINE_CURVE ( 2, ( #63117, #16707, #51803, #74439, #151, #74069, #57486, #11443, #34851 ),
 .UNSPECIFIED., .F., .F. ) 
 B_SPLINE_CURVE_WITH_KNOTS ( ( 3, 2, 2, 2, 3 ),
 ( 0.1527777777777777901, 0.1597222222222222099, 0.1666666666666666574, 0.1736111111111111049, 0.1805555555555555525 ),
 .UNSPECIFIED. ) 
 CURVE ( )  GEOMETRIC_REPRESENTATION_ITEM ( )  RATIONAL_B_SPLINE_CURVE ( ( 1.000000000000000000, 0.9238795325112867385, 1.000000000000000000, 0.9238795325112867385, 1.000000000000000000, 0.9238795325112867385, 1.000000000000000000, 0.9238795325112867385, 1.000000000000000000 ) ) 
 REPRESENTATION_ITEM ( '' )  );
#60509 = CARTESIAN_POINT ( 'NONE',  ( -6.951808397369817780E-16, 237.6562500034140157, -11.35316468749999963 ) ) ;
#60510 = PLANE ( 'NONE',  #66508 ) ;
#60511 = CARTESIAN_POINT ( 'NONE',  ( 2.828427124746152987, 200.2500000027312126, 139.1715728752538723 ) ) ;
#60512 = DIRECTION ( 'NONE',  ( -0.000000000000000000, 1.000000000000000000, -1.563033456626094573E-30 ) ) ;
#60513 = CARTESIAN_POINT ( 'NONE',  ( -5.656854249492373476, -5.656854249492376141, 22.01780277982336997 ) ) ;
#60514 = CARTESIAN_POINT ( 'NONE',  ( -8.660254037844387298, 244.5833333333333428, -4.999999999999999112 ) ) ;
#60515 = CYLINDRICAL_SURFACE ( 'NONE', #71609, 11.00000000000000000 ) ;
#60516 = CARTESIAN_POINT ( 'NONE',  ( -2.679491924311235618, 183.5416666666667140, 10.00000000000000000 ) ) ;
#60517 = SURFACE_STYLE_USAGE ( .BOTH. , #37518 ) ;
#60518 = CARTESIAN_POINT ( 'NONE',  ( 2.977408999572646486, 7.188101187499992051, 20.89280278187176521 ) ) ;
#60519 = CARTESIAN_POINT ( 'NONE',  ( 5.676582343749993598, 155.2604166632526983, 9.832129032723422313 ) ) ;
#60520 = DIRECTION ( 'NONE',  ( 0.000000000000000000, 0.000000000000000000, -1.000000000000000000 ) ) ;
#60521 = CARTESIAN_POINT ( 'NONE',  ( -2.849036369511732440E-14, 198.3750000027312126, 138.0000000000000568 ) ) ;
#60522 = CARTESIAN_POINT ( 'NONE',  ( 9.797174393178825657E-16, 125.0000000000000000, -8.000000000000000000 ) ) ;
#60525 = DIRECTION ( 'NONE',  ( 1.000000000000000000, 1.991032627040250683E-16, 0.000000000000000000 ) ) ;
#60524 = CARTESIAN_POINT ( 'NONE',  ( 4.000000000000015987, 199.6250000027312126, 198.0000000000000284 ) ) ;
#60523 = CARTESIAN_POINT ( 'NONE',  ( 26.34314575050763452, 202.5625000000000000, 165.9999999999998863 ) ) ;
#60526 = ORIENTED_EDGE ( 'NONE', *, *, #14077, .F. ) ;
#60527 = CARTESIAN_POINT ( 'NONE',  ( 3.042071309553167069, 12.13541666325268054, -11.35316468749999785 ) ) ;
#60528 = DIRECTION ( 'NONE',  ( -1.000000000000000000, 0.000000000000000000, 0.000000000000000000 ) ) ;
#60529 = CARTESIAN_POINT ( 'NONE',  ( 3.074111742560546201, -16.37317034319798026, -69.01341173090936820 ) ) ;
#60530 = CARTESIAN_POINT ( 'NONE',  ( -32.00000000000000711, 196.1875000000000568, 168.3431457505080289 ) ) ;
#60531 = CARTESIAN_POINT ( 'NONE',  ( 1.432654583217607192, 205.2500000013655779, 145.4587341250000350 ) ) ;
#60532 = AXIS2_PLACEMENT_3D ( 'NONE', #1842, #2202, #36540 ) ;
#60533 = CARTESIAN_POINT ( 'NONE',  ( -1.836970198721029983E-15, 45.62499999317203958, 10.00000000000000178 ) ) ;
#60534 = CARTESIAN_POINT ( 'NONE',  ( 7.188101187500002709, 106.8125000020484094, 2.977408999572649151 ) ) ;
#60535 = CARTESIAN_POINT ( 'NONE',  ( 1.881053915767122664, 9.249999998634406140, 4.541265875000001451 ) ) ;
#60536 = CARTESIAN_POINT ( 'NONE',  ( 1.224646799147353454E-15, 300.0000000000000000, -10.00000000000000178 ) ) ;
#60537 = CARTESIAN_POINT ( 'NONE',  ( -7.999999999999989342, -3.313708498984762496, 11.42405277982336465 ) ) ;
#60539 = CARTESIAN_POINT ( 'NONE',  ( 0.000000000000000000, 300.0000000000000000, 0.000000000000000000 ) ) ;
#60538 = DIRECTION ( 'NONE',  ( -0.000000000000000000, -1.000000000000000000, -0.000000000000000000 ) ) ;
#60540 = ORIENTED_EDGE ( 'NONE', *, *, #57094, .F. ) ;
#60541 = CARTESIAN_POINT ( 'NONE',  ( 10.00000000000000533, 30.20833333333333570, -2.679491924311228068 ) ) ;
#60542 = FACE_OUTER_BOUND ( 'NONE', #57256, .T. ) ;
#60543 = CARTESIAN_POINT ( 'NONE',  ( -11.35316468749999608, 234.4270833367473017, 3.042071309553173730 ) ) ;
#60544 = VECTOR ( 'NONE', #35617, 1000.000000000000000 ) ;
#60545 = CARTESIAN_POINT ( 'NONE',  ( -9.832129032723420536, 128.6979166632526983, 5.676582343749997150 ) ) ;
#60546 = EDGE_LOOP ( 'NONE', ( #21694, #21647 ) ) ;
#60547 = CARTESIAN_POINT ( 'NONE',  ( 3.313708498984756279, 7.999999999999991118, 5.049052783920146226 ) ) ;
#60548 = CARTESIAN_POINT ( 'NONE',  ( -4.220049686691937474, -10.18810118749999738, 94.93750000204838102 ) ) ;
#60549 = CARTESIAN_POINT ( 'NONE',  ( 0.000000000000000000, 0.000000000000000000, -4.000000000000001776 ) ) ;
#60550 = CARTESIAN_POINT ( 'NONE',  ( 3.458734125000016757, 197.1250000013656347, 199.4326545832176691 ) ) ;
#60551 = CARTESIAN_POINT ( 'NONE',  ( 8.000000000000017764, 3.313708498984730522, 27.17405277982336642 ) ) ;
#60553 = CARTESIAN_POINT ( 'NONE',  ( -3.042071309553173730, 124.3229166632526983, 11.35316468749999785 ) ) ;
#60552 = CARTESIAN_POINT ( 'NONE',  ( 28.00000000000001421, 196.5000000000000000, 165.9999999999998863 ) ) ;
#60554 = CARTESIAN_POINT ( 'NONE',  ( 7.320508075688774596, 147.4999999931720538, -7.320508075688774596 ) ) ;
#60555 = ORIENTED_EDGE ( 'NONE', *, *, #30733, .T. ) ;
#60556 = AXIS2_PLACEMENT_3D ( 'NONE', #7131, #2204, #25569 ) ;
#60557 = CARTESIAN_POINT ( 'NONE',  ( 8.660254037844389075, 257.0833333333333144, 4.999999999999997335 ) ) ;
#60558 = CARTESIAN_POINT ( 'NONE',  ( -30.79034348655129349, 174.5916665501510465, 165.6986120235964108 ) ) ;
#60559 = CARTESIAN_POINT ( 'NONE',  ( -8.311093377946836114, 112.9687499965860269, -8.311093377946837890 ) ) ;
#60560 = CARTESIAN_POINT ( 'NONE',  ( 2.445694354108838731, 207.0625000013656063, 195.5543056458912190 ) ) ;
#60561 = CARTESIAN_POINT ( 'NONE',  ( -2.977408999572650039, 17.81249999795161187, -7.188101187500000933 ) ) ;
#60562 = CARTESIAN_POINT ( 'NONE',  ( -4.220049686691937474, -10.18810118749999738, 87.81250000204838102 ) ) ;
#60563 = CARTESIAN_POINT ( 'NONE',  ( 5.676582343749993598, 25.26041666325268764, 9.832129032723422313 ) ) ;
#60564 = VERTEX_POINT ( 'NONE', #14865 ) ;
#60565 = CARTESIAN_POINT ( 'NONE',  ( -1.836970198721029983E-15, 15.62499999317203248, 10.00000000000000178 ) ) ;
#60566 = CARTESIAN_POINT ( 'NONE',  ( 9.999999999999998224, 245.8333333401612890, -2.679491924311229401 ) ) ;
#60567 = CARTESIAN_POINT ( 'NONE',  ( 10.00000000000000178, 116.8749999931720396, 0.000000000000000000 ) ) ;
#60568 = EDGE_CURVE ( 'NONE', #42810, #45762, #36012, .T. ) ;
#60569 = CARTESIAN_POINT ( 'NONE',  ( 3.729367062499960195, 209.2812500020483810, 142.0000000000000568 ) ) ;
#60570 = CARTESIAN_POINT ( 'NONE',  ( 5.082755093536325930, 5.156249997951610986, -5.082755093536325930 ) ) ;
#60571 = CARTESIAN_POINT ( 'NONE',  ( 6.676582343750003368, 290.0156250017069510, -2.765530957081997254 ) ) ;
#60572 = CARTESIAN_POINT ( 'NONE',  ( 0.000000000000000000, 125.0000000000000000, 0.000000000000000000 ) ) ;
#60573 = CARTESIAN_POINT ( 'NONE',  ( 9.832129032723416984, 215.6770833299193555, 5.676582343750006032 ) ) ;
#60574 = EDGE_LOOP ( 'NONE', ( #18099, #70202, #54914, #65076 ) ) ;
#60575 = CARTESIAN_POINT ( 'NONE',  ( 5.676582343750001591, 136.9270833299193555, -9.832129032723420536 ) ) ;
#60576 = B_SPLINE_CURVE_WITH_KNOTS ( 'NONE', 3,
 ( #66179, #54880, #20899, #43921, #15237, #72967, #21272, #44296, #67310, #52103, #64153, #27680, #11728, #50686, #58505, #41510, #17755, #18501, #64526, #34768, #35131, #12462, #23790, #13188, #73705, #29083 ),
 .UNSPECIFIED., .F., .F.,
 ( 4, 2, 2, 2, 2, 2, 2, 2, 2, 2, 2, 2, 4 ),
 ( 0.000000000000000000, 0.001829521829463870170, 0.003659043658927740340, 0.004573804573659676076, 0.005488565488391610944, 0.007318087317855455527, 0.008232848232587391263, 0.009147609147319327866, 0.01006237006205126447, 0.01097713097678320281, 0.01189189189151513767, 0.01280665280624707601, 0.01463617463571094922 ),
 .UNSPECIFIED. ) ;
#60577 = CARTESIAN_POINT ( 'NONE',  ( 4.220049686691934809, 10.18810118749999916, 83.68750000204836681 ) ) ;
#60578 = CARTESIAN_POINT ( 'NONE',  ( -31.45873412499997812, 199.7500000013656063, 171.4326545832180386 ) ) ;
#60579 = CYLINDRICAL_SURFACE ( 'NONE', #36619, 8.000000000000000000 ) ;
#60580 = CARTESIAN_POINT ( 'NONE',  ( -1.881053915767121554, 15.74999999863440614, -4.541265875000002339 ) ) ;
#60581 = EDGE_LOOP ( 'NONE', ( #17585, #39267, #68562, #30073 ) ) ;
#60582 = CARTESIAN_POINT ( 'NONE',  ( 4.000000000000015987, 202.6250000027312126, 198.0000000000000284 ) ) ;
#60583 = CARTESIAN_POINT ( 'NONE',  ( 2.445694354108783219, 198.8125000013656063, 139.5543056458912190 ) ) ;
#60584 = CARTESIAN_POINT ( 'NONE',  ( -1.656854249492403008, 202.8125000027312126, 146.0000000000000284 ) ) ;
#60585 = CARTESIAN_POINT ( 'NONE',  ( -10.00000000000010125, 172.7083333333333428, 2.679491924311248496 ) ) ;
#60586 = ORIENTED_EDGE ( 'NONE', *, *, #33856, .T. ) ;
#60587 = CARTESIAN_POINT ( 'NONE',  ( 2.977408999572650927, 12.74999999795161187, -7.188101187500000933 ) ) ;
#60588 = CARTESIAN_POINT ( 'NONE',  ( -11.50291896434712591, -27.52019424413719406, 198.7870197598749371 ) ) ;
#60589 = CARTESIAN_POINT ( 'NONE',  ( 6.123233995736767268E-16, 28.12499999317203603, -10.00000000000000178 ) ) ;
#60590 = CIRCLE ( 'NONE', #55775, 12.00000000000000000 ) ;
#60591 = CARTESIAN_POINT ( 'NONE',  ( -11.35316468750000141, 188.2812499965860127, -1.390361679473963753E-15 ) ) ;
#60592 = CARTESIAN_POINT ( 'NONE',  ( -2.977408999572651815, 114.3125000020483952, 7.188101187500000933 ) ) ;
#60593 = DIRECTION ( 'NONE',  ( -0.000000000000000000, 1.000000000000000000, -0.000000000000000000 ) ) ;
#60594 = CARTESIAN_POINT ( 'NONE',  ( -4.721056650415999201, 294.3281250017069510, -4.721056650415999201 ) ) ;
#60595 = EDGE_CURVE ( 'NONE', #43686, #22331, #55024, .T. ) ;
#60597 = CARTESIAN_POINT ( 'NONE',  ( 3.999999999999959144, 201.1875000027312694, 140.3431457505076594 ) ) ;
#60596 = CARTESIAN_POINT ( 'NONE',  ( 4.999999999999993783, 131.0416666598387110, 8.660254037844390851 ) ) ;
#60598 = ORIENTED_EDGE ( 'NONE', *, *, #29785, .T. ) ;
#60599 = ADVANCED_FACE ( 'NONE', ( #8472, #43927, #9607, #37148, #56006, #66937 ), #38275, .T. ) ;
#60600 = CARTESIAN_POINT ( 'NONE',  ( -9.832129032723415207, 229.6354166700806729, 5.676582343750005144 ) ) ;
#60601 = CARTESIAN_POINT ( 'NONE',  ( -7.188101187499991163, 2.977408999572646930, 28.76780278187175455 ) ) ;
#60602 = CARTESIAN_POINT ( 'NONE',  ( -28.00000000000002487, 209.5625000013656063, 166.5412658750003629 ) ) ;
#60603 = CARTESIAN_POINT ( 'NONE',  ( 5.656854249492380582, 19.49999999590322020, -5.656854249492380582 ) ) ;
#60604 =( BOUNDED_CURVE ( )  B_SPLINE_CURVE ( 2, ( #9881, #67596, #67963, #15893, #16256, #61925, #56277, #33650, #32529 ),
 .UNSPECIFIED., .F., .F. ) 
 B_SPLINE_CURVE_WITH_KNOTS ( ( 3, 2, 2, 2, 3 ),
 ( 0.4000000000000003553, 0.4083333333333336590, 0.4166666666666670182, 0.4250000000000003220, 0.4333333333333336812 ),
 .UNSPECIFIED. ) 
 CURVE ( )  GEOMETRIC_REPRESENTATION_ITEM ( )  RATIONAL_B_SPLINE_CURVE ( ( 0.9999999999999970024, 0.9238795325112897361, 1.000000000000000000, 0.9238795325112867385, 1.000000000000000000, 0.9238795325112867385, 1.000000000000000000, 0.9238795325112837409, 1.000000000000003109 ) ) 
 REPRESENTATION_ITEM ( '' )  );
#60605 = CARTESIAN_POINT ( 'NONE',  ( -1.432654583217607414, 201.5000000013655779, 194.5412658750000219 ) ) ;
#60606 = CYLINDRICAL_SURFACE ( 'NONE', #29341, 10.00000000000000178 ) ;
#60607 = CARTESIAN_POINT ( 'NONE',  ( 6.123233995736767268E-16, 163.1249999931720254, -10.00000000000000178 ) ) ;
#60608 = CARTESIAN_POINT ( 'NONE',  ( -8.000000000000000000, 96.40625000000000000, -3.313708498984761608 ) ) ;
#60609 = CARTESIAN_POINT ( 'NONE',  ( 9.832129032723420536, 111.5104166632526841, -5.676582343749999815 ) ) ;
#60610 = DIRECTION ( 'NONE',  ( -0.000000000000000000, 1.000000000000000000, -0.000000000000000000 ) ) ;
#60611 = CARTESIAN_POINT ( 'NONE',  ( 7.778174593052021635, 7.778174593052023411, 73.93749999999998579 ) ) ;
#60614 = FACE_OUTER_BOUND ( 'NONE', #4112, .T. ) ;
#60613 = CARTESIAN_POINT ( 'NONE',  ( 29.43265458321766559, 200.5000000013655779, 173.4587341249998929 ) ) ;
#60612 = CARTESIAN_POINT ( 'NONE',  ( 29.43265458321761230, 199.7500000013656063, 173.4587341249998929 ) ) ;
#60615 = ORIENTED_EDGE ( 'NONE', *, *, #21942, .T. ) ;
#60616 = DIRECTION ( 'NONE',  ( 0.000000000000000000, 0.000000000000000000, 1.000000000000000000 ) ) ;
#60617 = CARTESIAN_POINT ( 'NONE',  ( 4.242640687119287435, 287.4375000034140157, 4.242640687119285658 ) ) ;
#60618 = CARTESIAN_POINT ( 'NONE',  ( -2.445694354108839619, 199.8125000013656063, 139.5543056458912190 ) ) ;
#60619 = CARTESIAN_POINT ( 'NONE',  ( 31.45873412499997812, 201.8750000013656063, 171.4326545832175839 ) ) ;
#60620 = CARTESIAN_POINT ( 'NONE',  ( -6.735557395310442023E-16, 11.00000000000000000, 116.3125000040967763 ) ) ;
#60621 = ADVANCED_FACE ( 'NONE', ( #32626 ), #17914, .T. ) ;
#60622 = CARTESIAN_POINT ( 'NONE',  ( 8.311093377946837890, 196.7187499965860127, -8.311093377946837890 ) ) ;
#60623 = CARTESIAN_POINT ( 'NONE',  ( -2.977408999572652260, 90.31250000204838102, 7.188101187500000044 ) ) ;
#60624 = VECTOR ( 'NONE', #7397, 1000.000000000000000 ) ;
#60625 = CARTESIAN_POINT ( 'NONE',  ( 6.139223773318740029, 225.9999999999999147, 8.200589933689730771 ) ) ;
#60626 = CARTESIAN_POINT ( 'NONE',  ( -3.211159895383562723, 13.93749999863440614, 3.211159895383561391 ) ) ;
#60627 = CARTESIAN_POINT ( 'NONE',  ( 29.43265458321766914, 198.1250000013656063, 166.5412658749999650 ) ) ;
#60628 = CARTESIAN_POINT ( 'NONE',  ( -5.656854249492375253, 5.656854249492375253, 29.14280277982336642 ) ) ;
#60629 = DIRECTION ( 'NONE',  ( 0.000000000000000000, 0.7071067811865465735, 0.7071067811865484609 ) ) ;
#60630 = CARTESIAN_POINT ( 'NONE',  ( 8.311093377946834337, 80.15624999658599847, 8.311093377946839666 ) ) ;
#60631 = VERTEX_POINT ( 'NONE', #9974 ) ;
#60633 =( BOUNDED_CURVE ( )  B_SPLINE_CURVE ( 2, ( #18405, #5609, #28607, #41420, #64432, #24784, #2162, #30466, #53483 ),
 .UNSPECIFIED., .F., .F. ) 
 B_SPLINE_CURVE_WITH_KNOTS ( ( 3, 2, 2, 2, 3 ),
 ( 0.07352941176470594031, 0.07720588235294123525, 0.08088235294117653018, 0.08455882352941182512, 0.08823529411764712005 ),
 .UNSPECIFIED. ) 
 CURVE ( )  GEOMETRIC_REPRESENTATION_ITEM ( )  RATIONAL_B_SPLINE_CURVE ( ( 0.9999999999999988898, 0.9238795325112878487, 1.000000000000000000, 0.9238795325112867385, 1.000000000000000000, 0.9238795325112867385, 1.000000000000000000, 0.9238795325112856283, 1.000000000000001110 ) ) 
 REPRESENTATION_ITEM ( '' )  );
#60632 = CARTESIAN_POINT ( 'NONE',  ( -4.999999999999999112, -51.89737250574534499, 42.00009673807092980 ) ) ;
#60634 = CARTESIAN_POINT ( 'NONE',  ( -11.00000000000010658, 4.556349186103942017, 81.90625000000000000 ) ) ;
#60635 = CARTESIAN_POINT ( 'NONE',  ( 2.977408999572651815, 21.18749999795161187, 7.188101187500000933 ) ) ;
#60636 = CARTESIAN_POINT ( 'NONE',  ( 7.999999999999992895, -3.313708498984756279, 14.98655277982336642 ) ) ;
#60637 = DIRECTION ( 'NONE',  ( 0.000000000000000000, 0.000000000000000000, -1.000000000000000000 ) ) ;
#60638 = CARTESIAN_POINT ( 'NONE',  ( -11.35316468749999785, 93.07291666325266988, -3.042071309553167513 ) ) ;
#60639 = ORIENTED_EDGE ( 'NONE', *, *, #28148, .F. ) ;
#60640 = CARTESIAN_POINT ( 'NONE',  ( 4.220049686691941027, -10.18810118749999738, 85.00000000204838102 ) ) ;
#60641 = CARTESIAN_POINT ( 'NONE',  ( -7.204075437095965206, -7.204075437095968759, 115.8437500020483810 ) ) ;
#60642 = CARTESIAN_POINT ( 'NONE',  ( 0.000000000000000000, 300.0000000000000000, 10.00000000000000178 ) ) ;
#60643 = CARTESIAN_POINT ( 'NONE',  ( 3.458734125000015425, 207.2500000013655779, 196.5673454167823877 ) ) ;
#60644 = CARTESIAN_POINT ( 'NONE',  ( -2.926785083138225622E-14, 16.44602605510714355, 68.55492853905353456 ) ) ;
#60646 = CARTESIAN_POINT ( 'NONE',  ( 11.35316468749999963, 80.98958332991934128, -3.042071309553165293 ) ) ;
#60645 = CARTESIAN_POINT ( 'NONE',  ( -6.123233995736766282E-16, 251.8750000068280031, -10.00000000000000000 ) ) ;
#60647 = CARTESIAN_POINT ( 'NONE',  ( -5.656854249492375253, 5.656854249492375253, 18.83030278392014623 ) ) ;
#60648 = CARTESIAN_POINT ( 'NONE',  ( 0.000000000000000000, 0.000000000000000000, 0.000000000000000000 ) ) ;
#60649 = CARTESIAN_POINT ( 'NONE',  ( 8.660254037844389075, 167.2916666598387110, -5.000000000000000000 ) ) ;
#60650 = CARTESIAN_POINT ( 'NONE',  ( -5.082755093536324154, 91.71875000204838102, 5.082755093536326818 ) ) ;
#60651 = CYLINDRICAL_SURFACE ( 'NONE', #1501, 11.00000000000000000 ) ;
#60652 = CARTESIAN_POINT ( 'NONE',  ( 11.35316468749999785, 55.88541666325267698, 3.042071309553174174 ) ) ;
#60653 = CARTESIAN_POINT ( 'NONE',  ( -6.676582343750001591, 295.4531250017069510, 0.000000000000000000 ) ) ;
#60654 = CARTESIAN_POINT ( 'NONE',  ( -4.220049686691937474, -10.18810118749999738, 104.3125000020483810 ) ) ;
#60655 = CARTESIAN_POINT ( 'NONE',  ( -11.35316468750000141, 208.4895833299193555, 3.042071309553159963 ) ) ;
#60656 = VERTEX_POINT ( 'NONE', #61279 ) ;
#60657 = CARTESIAN_POINT ( 'NONE',  ( -7.999999999999989342, -3.313708498984762496, 26.61155278392014978 ) ) ;
#60658 = DIRECTION ( 'NONE',  ( -0.000000000000000000, -1.000000000000000000, -0.000000000000000000 ) ) ;
#60659 = CARTESIAN_POINT ( 'NONE',  ( -5.447321192899549303, -4.689935021205116961, 0.1569292013794422458 ) ) ;
#60661 = CARTESIAN_POINT ( 'NONE',  ( -9.832129032723420536, 188.6979166632526983, 5.676582343749997150 ) ) ;
#60660 = CARTESIAN_POINT ( 'NONE',  ( -27.99999999999999645, 210.0000000000000284, 174.0000000000003411 ) ) ;
#60662 = FACE_OUTER_BOUND ( 'NONE', #58905, .T. ) ;
#60663 = VECTOR ( 'NONE', #63602, 1000.000000000000000 ) ;
#60664 = CARTESIAN_POINT ( 'NONE',  ( 8.660254037844385522, 241.0416666734946318, -5.000000000000003553 ) ) ;
#60665 = CARTESIAN_POINT ( 'NONE',  ( 1.836970198721029589E-15, 254.3750000068280031, 10.00000000000000000 ) ) ;
#60666 = VERTEX_POINT ( 'NONE', #72973 ) ;
#60667 = EDGE_CURVE ( 'NONE', #1009, #67207, #37153, .T. ) ;
#60668 = CARTESIAN_POINT ( 'NONE',  ( 11.35316468749999785, 175.8854166632526983, 3.042071309553174174 ) ) ;
#60669 = CARTESIAN_POINT ( 'NONE',  ( 7.188101187499992051, 2.977408999572647819, 18.83030278187175455 ) ) ;
#60670 = EDGE_CURVE ( 'NONE', #49815, #26710, #6771, .T. ) ;
#60671 = CARTESIAN_POINT ( 'NONE',  ( -1.704527592502764533, 60.27089976682823647, -22.92829164824309984 ) ) ;
#60672 = ORIENTED_EDGE ( 'NONE', *, *, #41838, .F. ) ;
#60673 = CARTESIAN_POINT ( 'NONE',  ( -8.000000000000000000, 98.09375000409679046, -3.313708498984761608 ) ) ;
#60674 = APPLICATION_CONTEXT ( 'automotive_design' ) ;
#60675 = CARTESIAN_POINT ( 'NONE',  ( 26.34314575050757767, 208.9375000000000284, 173.9999999999999147 ) ) ;
#60676 = EDGE_CURVE ( 'NONE', #55418, #29980, #16420, .T. ) ;
#60677 = AXIS2_PLACEMENT_3D ( 'NONE', #37862, #20112, #44631 ) ;
#60678 = CARTESIAN_POINT ( 'NONE',  ( 4.000000000000001776, 17.00000000000000000, 0.000000000000000000 ) ) ;
#60679 = CARTESIAN_POINT ( 'NONE',  ( -4.541265875000002339, 16.74999999863440436, -1.881053915767121998 ) ) ;
#60680 = EDGE_CURVE ( 'NONE', #4199, #30705, #56291, .T. ) ;
#60681 = CARTESIAN_POINT ( 'NONE',  ( -7.999999999999991118, 3.313708498984756723, 11.42405278392014623 ) ) ;
#60682 = LINE ( 'NONE', #38053, #33063 ) ;
#60683 = EDGE_LOOP ( 'NONE', ( #67157, #49366, #63183, #29274 ) ) ;
#60684 = CARTESIAN_POINT ( 'NONE',  ( 5.000000000000000000, -10.28295106684163684, -65.17663434001590872 ) ) ;
#60685 = CARTESIAN_POINT ( 'NONE',  ( 7.188101187500002709, 93.31250000204838102, 2.977408999572649151 ) ) ;
#60687 = CARTESIAN_POINT ( 'NONE',  ( -5.676582343749992710, 259.7395833367473301, 9.832129032723422313 ) ) ;
#60686 = DIRECTION ( 'NONE',  ( -0.000000000000000000, -0.000000000000000000, 1.000000000000000000 ) ) ;
#60688 = DIRECTION ( 'NONE',  ( 0.000000000000000000, 0.000000000000000000, 1.000000000000000000 ) ) ;
#60689 = ORIENTED_EDGE ( 'NONE', *, *, #6206, .F. ) ;
#60690 = EDGE_CURVE ( 'NONE', #53057, #40278, #9177, .T. ) ;
#60691 = CARTESIAN_POINT ( 'NONE',  ( -5.000000000000000000, 50.64189880742145533, -41.08656465431843685 ) ) ;
#60692 = CARTESIAN_POINT ( 'NONE',  ( -4.401442555609577197E-16, 7.188101187499992051, 19.11155278187175455 ) ) ;
#60693 = VERTEX_POINT ( 'NONE', #10711 ) ;
#60694 = ORIENTED_EDGE ( 'NONE', *, *, #27403, .F. ) ;
#60695 = CARTESIAN_POINT ( 'NONE',  ( 10.18810118749999916, 1.247682550866122264E-15, 83.40625000204838102 ) ) ;
#60696 = CARTESIAN_POINT ( 'NONE',  ( -9.832129032723420536, 74.01041666325268409, 5.676582343749997150 ) ) ;
#60697 = CARTESIAN_POINT ( 'NONE',  ( 5.656854249492376141, -5.656854249492374365, 6.080302783920147114 ) ) ;
#60698 = CARTESIAN_POINT ( 'NONE',  ( 7.778174593052023411, -7.778174593052021635, 94.56250000000000000 ) ) ;
#60701 = CARTESIAN_POINT ( 'NONE',  ( 1.226468279477575784E-15, 295.8593750017070079, 6.676582343750001591 ) ) ;
#60700 = CARTESIAN_POINT ( 'NONE',  ( 30.82842712474620583, 196.2500000027312126, 172.8284271247460424 ) ) ;
#60699 = DIRECTION ( 'NONE',  ( -0.000000000000000000, -0.000000000000000000, 1.000000000000000000 ) ) ;
#60702 = B_SPLINE_CURVE_WITH_KNOTS ( 'NONE', 3,
 ( #53397, #30378, #24340, #59424, #19050, #42054, #25062, #2444 ),
 .UNSPECIFIED., .F., .F.,
 ( 4, 2, 2, 4 ),
 ( 0.02905455086391281125, 0.03168444077422614275, 0.03431433068453947771, 0.03957411050516614071 ),
 .UNSPECIFIED. ) ;
#60703 = CARTESIAN_POINT ( 'NONE',  ( -23.99999999999998934, 203.8750000027312126, 170.0000000000002842 ) ) ;
#60704 = CARTESIAN_POINT ( 'NONE',  ( 0.000000000000000000, 0.000000000000000000, -14.80000000000000071 ) ) ;
#60705 = CARTESIAN_POINT ( 'NONE',  ( 3.458734125000015869, 200.1875000013656063, 198.0000000000000284 ) ) ;
#60706 = CARTESIAN_POINT ( 'NONE',  ( -2.751064625579944321E-14, 198.7500000000000000, 146.0000000000000284 ) ) ;
#60707 = CARTESIAN_POINT ( 'NONE',  ( -3.313708498984765161, 3.843749995903220640, 7.999999999999998224 ) ) ;
#60708 = CARTESIAN_POINT ( 'NONE',  ( 24.54126587500000056, 199.1250000013656347, 168.5673454167822172 ) ) ;
#60709 = CARTESIAN_POINT ( 'NONE',  ( 7.188101187500000044, 11.34374999795161187, 0.000000000000000000 ) ) ;
#60710 = CARTESIAN_POINT ( 'NONE',  ( -5.662595241051933570, -5.662595241051936235, -0.2993847160593715029 ) ) ;
#60711 = CARTESIAN_POINT ( 'NONE',  ( -7.188101187500000933, 107.9375000020483810, -2.977408999572650483 ) ) ;
#60713 = DIRECTION ( 'NONE',  ( -0.000000000000000000, 1.000000000000000000, -0.000000000000000000 ) ) ;
#60712 = CARTESIAN_POINT ( 'NONE',  ( -4.242640687119286547, 292.9375000034140157, -4.242640687119286547 ) ) ;
#60714 = CARTESIAN_POINT ( 'NONE',  ( 2.020667218593132706E-15, -11.00000000000000000, 112.5625000040967763 ) ) ;
#60715 = CARTESIAN_POINT ( 'NONE',  ( 4.242640687119287435, 288.4375000034140157, 4.242640687119285658 ) ) ;
#60716 = CARTESIAN_POINT ( 'NONE',  ( -7.188101187499990274, -2.977408999572651371, 16.95530278187175455 ) ) ;
#60717 = CARTESIAN_POINT ( 'NONE',  ( 3.999999999999960032, 207.1250000027312126, 142.0000000000000568 ) ) ;
#60718 = CARTESIAN_POINT ( 'NONE',  ( 8.311093377946837890, 36.40624999658602690, -8.311093377946837890 ) ) ;
#60719 = CARTESIAN_POINT ( 'NONE',  ( 10.00000000000000355, 149.7916666666666856, 2.679491924311236506 ) ) ;
#60720 = CARTESIAN_POINT ( 'NONE',  ( 7.320508075688771044, 11.24999999317203248, 7.320508075688775484 ) ) ;
#60721 = ORIENTED_EDGE ( 'NONE', *, *, #15445, .F. ) ;
#60722 = CARTESIAN_POINT ( 'NONE',  ( 3.999999999999959144, 199.1875000027312410, 140.3431457505076594 ) ) ;
#60723 = CARTESIAN_POINT ( 'NONE',  ( -4.556349186104045934, 11.00000000000000000, 69.90625000409674783 ) ) ;
#60724 = CARTESIAN_POINT ( 'NONE',  ( 5.676582343749993598, 54.94791666325268409, 9.832129032723422313 ) ) ;
#60725 = CARTESIAN_POINT ( 'NONE',  ( -10.99999999999999822, -4.556349186104052151, 80.78125000409680467 ) ) ;
#60726 = CARTESIAN_POINT ( 'NONE',  ( -2.445694354108840063, 205.0625000013656063, 139.5543056458912190 ) ) ;
#60727 = CARTESIAN_POINT ( 'NONE',  ( -10.00000000000000000, 259.7916666666666288, -2.679491924311226292 ) ) ;
#60728 = CARTESIAN_POINT ( 'NONE',  ( -1.656854249492555331, 195.6875000000000284, 145.9999999999998863 ) ) ;
#60730 = CARTESIAN_POINT ( 'NONE',  ( -5.676582343749998039, 32.44791666325268409, -9.832129032723420536 ) ) ;
#60729 = CARTESIAN_POINT ( 'NONE',  ( 2.977408999572650039, 99.68750000204838102, -7.188101187500000933 ) ) ;
#60731 = CARTESIAN_POINT ( 'NONE',  ( 5.656854249492374365, 5.656854249492375253, 10.76780277982336642 ) ) ;
#60732 = CARTESIAN_POINT ( 'NONE',  ( -2.679491924311235174, 50.41666665983868967, 10.00000000000000000 ) ) ;
#60733 =( BOUNDED_CURVE ( )  B_SPLINE_CURVE ( 2, ( #50504, #26749, #61081, #21091, #10152, #68239, #4875, #9409, #27870 ),
 .UNSPECIFIED., .F., .F. ) 
 B_SPLINE_CURVE_WITH_KNOTS ( ( 3, 2, 2, 2, 3 ),
 ( 0.5312500000000000000, 0.5364583333333333703, 0.5416666666666665186, 0.5468749999999998890, 0.5520833333333332593 ),
 .UNSPECIFIED. ) 
 CURVE ( )  GEOMETRIC_REPRESENTATION_ITEM ( )  RATIONAL_B_SPLINE_CURVE ( ( 1.000000000000000000, 0.9238795325112867385, 1.000000000000000000, 0.9238795325112867385, 1.000000000000000000, 0.9238795325112867385, 1.000000000000000000, 0.9238795325112884038, 0.9999999999999983347 ) ) 
 REPRESENTATION_ITEM ( '' )  );
#60734 = CARTESIAN_POINT ( 'NONE',  ( 8.311093377946834337, 165.1562499965860127, 8.311093377946839666 ) ) ;
#60735 = CARTESIAN_POINT ( 'NONE',  ( 4.999999999999993783, 131.0416666598387110, 8.660254037844390851 ) ) ;
#60736 = CARTESIAN_POINT ( 'NONE',  ( 5.082755093536325042, 108.9687500020483810, -5.082755093536325930 ) ) ;
#60737 = AXIS2_PLACEMENT_3D ( 'NONE', #59575, #65593, #13890 ) ;
#60738 = EDGE_LOOP ( 'NONE', ( #38909, #38131, #41739, #58768, #28179, #24362, #63199, #1053, #10832, #60472, #34685, #19887, #41537, #62047, #69456 ) ) ;
#60739 = DIRECTION ( 'NONE',  ( -0.000000000000000000, -1.000000000000000000, -4.283267841918042741E-17 ) ) ;
#60740 = CARTESIAN_POINT ( 'NONE',  ( -9.832129032723418760, 18.17708332991935194, -5.676582343750004256 ) ) ;
#60741 = CARTESIAN_POINT ( 'NONE',  ( -2.828427124746152987, 197.1250000000000284, 200.8284271247462129 ) ) ;
#60742 = ORIENTED_EDGE ( 'NONE', *, *, #73691, .F. ) ;
#60743 = CARTESIAN_POINT ( 'NONE',  ( -32.00000000000001421, 204.1875000000000853, 168.3431457505080289 ) ) ;
#60744 = CARTESIAN_POINT ( 'NONE',  ( -10.18810118749999738, -4.220049686691941915, 79.75000000204838102 ) ) ;
#60745 = CARTESIAN_POINT ( 'NONE',  ( -30.82842712474615610, 197.3750000000000284, 172.8284271247465824 ) ) ;
#60747 = CARTESIAN_POINT ( 'NONE',  ( -9.832129032723418760, 147.8645833299193555, -5.676582343750004256 ) ) ;
#60746 = CARTESIAN_POINT ( 'NONE',  ( -7.347880794884122694E-16, 8.499999997268814056, 4.000000000000001776 ) ) ;
#60748 = DIRECTION ( 'NONE',  ( -0.000000000000000000, -0.000000000000000000, 1.000000000000000000 ) ) ;
#60749 = CARTESIAN_POINT ( 'NONE',  ( -4.898587196589407898E-16, 7.999999999999991118, 11.01155278432982598 ) ) ;
#60750 = CARTESIAN_POINT ( 'NONE',  ( -7.999999999999991118, 0.000000000000000000, 15.83030277982336642 ) ) ;
#60751 = CARTESIAN_POINT ( 'NONE',  ( -5.676582343749992710, 239.7395833367473301, 9.832129032723422313 ) ) ;
#60752 = CARTESIAN_POINT ( 'NONE',  ( -7.204075437095965206, -7.204075437095968759, 87.71875000204836681 ) ) ;
#60753 = ORIENTED_EDGE ( 'NONE', *, *, #41331, .F. ) ;
#60754 = EDGE_CURVE ( 'NONE', #50481, #54226, #32317, .T. ) ;
#60755 = DIRECTION ( 'NONE',  ( -0.000000000000000000, 1.000000000000000000, -0.000000000000000000 ) ) ;
#60756 = DIRECTION ( 'NONE',  ( 3.469446951953617147E-16, 0.000000000000000000, -1.000000000000000000 ) ) ;
#60757 = CARTESIAN_POINT ( 'NONE',  ( -8.311093377946836114, 102.9687499965859985, -8.311093377946837890 ) ) ;
#60758 = CARTESIAN_POINT ( 'NONE',  ( -7.204075437095967871, 7.204075437095967871, 97.46875000204838102 ) ) ;
#60759 = EDGE_CURVE ( 'NONE', #15764, #58925, #68006, .T. ) ;
#60760 = CARTESIAN_POINT ( 'NONE',  ( 5.000000000000006217, 15.83333333333333748, -8.660254037844394404 ) ) ;
#60761 = ORIENTED_EDGE ( 'NONE', *, *, #43625, .T. ) ;
#60762 = ORIENTED_EDGE ( 'NONE', *, *, #13232, .T. ) ;
#60763 = CARTESIAN_POINT ( 'NONE',  ( -8.342170076843785083E-16, 2.187499998634407028, 4.541265875000002339 ) ) ;
#60764 = CARTESIAN_POINT ( 'NONE',  ( 5.082755093536325930, 6.656249997951611874, -5.082755093536325930 ) ) ;
#60765 = CARTESIAN_POINT ( 'NONE',  ( -3.313708498984762052, 114.4062500040967620, -8.000000000000000000 ) ) ;
#60766 = CARTESIAN_POINT ( 'NONE',  ( -4.220049686691937474, -10.18810118749999738, 93.81250000204839523 ) ) ;
#60767 = CARTESIAN_POINT ( 'NONE',  ( -26.56734541678232375, 201.2500000013656063, 173.4587341250003760 ) ) ;
#60768 = CARTESIAN_POINT ( 'NONE',  ( 1.656854249492381914, 2.812500000000000000, 4.000000000000000888 ) ) ;
#60769 = CARTESIAN_POINT ( 'NONE',  ( -2.828427124746192067, 16.37499999726881228, 2.828427124746190735 ) ) ;
#60770 = CARTESIAN_POINT ( 'NONE',  ( -3.211159895383562723, 3.937499998634406584, 3.211159895383561391 ) ) ;
#60771 = ORIENTED_EDGE ( 'NONE', *, *, #3521, .F. ) ;
#60772 = CARTESIAN_POINT ( 'NONE',  ( -3.458734124999959914, 195.4375000013655779, 198.0000000000000284 ) ) ;
#60774 = CARTESIAN_POINT ( 'NONE',  ( 10.00000000000000178, 235.4166666734946318, 2.679491924311222739 ) ) ;
#60773 = CARTESIAN_POINT ( 'NONE',  ( -30.44569435410886626, 197.5625000013656063, 167.5543056458916169 ) ) ;
#60775 = CARTESIAN_POINT ( 'NONE',  ( -4.541265875000003227, 19.87499999863440792, 1.881053915767121110 ) ) ;
#60776 = CARTESIAN_POINT ( 'NONE',  ( -2.765530957081996810, 299.2656250017070079, -6.676582343750002480 ) ) ;
#60777 = AXIS2_PLACEMENT_3D ( 'NONE', #5145, #49665, #39097 ) ;
#60778 = CARTESIAN_POINT ( 'NONE',  ( 2.977408999572646486, 7.188101187499991163, 7.017802781871751883 ) ) ;
#60779 = ORIENTED_EDGE ( 'NONE', *, *, #43219, .F. ) ;
#60780 = VERTEX_POINT ( 'NONE', #47543 ) ;
#60781 = CARTESIAN_POINT ( 'NONE',  ( -10.18810118749999916, 4.220049686691934809, 100.5625000020483668 ) ) ;
#60782 = DIRECTION ( 'NONE',  ( -0.000000000000000000, 1.000000000000000000, 4.476705744456276341E-16 ) ) ;
#60783 = CARTESIAN_POINT ( 'NONE',  ( -29.43265458321760519, 204.1250000013656063, 173.4587341250003760 ) ) ;
#60784 = CARTESIAN_POINT ( 'NONE',  ( -30.82842712474621294, 199.1250000000000284, 167.1715728752542134 ) ) ;
#60785 = CARTESIAN_POINT ( 'NONE',  ( -1.432654583217608080, 208.8750000013656347, 201.4587341250000350 ) ) ;
#60786 = CARTESIAN_POINT ( 'NONE',  ( -4.000000000000001776, 21.24999999726881583, -4.898587196589415787E-16 ) ) ;
#60787 = CARTESIAN_POINT ( 'NONE',  ( 10.00000000000000178, 105.0000000000000142, 0.000000000000000000 ) ) ;
#60788 = CARTESIAN_POINT ( 'NONE',  ( 3.313708498984765161, 113.4687500000000000, 7.999999999999998224 ) ) ;
#60789 = CARTESIAN_POINT ( 'NONE',  ( 1.226468279477575784E-15, 291.8593750017070079, 6.676582343750001591 ) ) ;
#60790 = CARTESIAN_POINT ( 'NONE',  ( 7.188101187499991163, 2.977408999572648707, 13.20530278187175277 ) ) ;
#60791 = VERTEX_POINT ( 'NONE', #29839 ) ;
#60792 = DIRECTION ( 'NONE',  ( -1.000000000000000000, 0.000000000000000000, 0.000000000000000000 ) ) ;
#60793 = CARTESIAN_POINT ( 'NONE',  ( -8.000000000000000000, 22.96874999590322020, -3.313708498984762496 ) ) ;
#60794 = CARTESIAN_POINT ( 'NONE',  ( -2.445694354108839619, 201.8125000013656063, 139.5543056458912190 ) ) ;
#60795 = CARTESIAN_POINT ( 'NONE',  ( -2.679491924311087736, 185.4166666598386826, 10.00000000000008349 ) ) ;
#60796 = CARTESIAN_POINT ( 'NONE',  ( 1.031381239350403822, 194.9470492016644414, 145.8186933158168301 ) ) ;
#60797 = CARTESIAN_POINT ( 'NONE',  ( 11.35316468749999608, 256.9270833367473301, -3.042071309553167069 ) ) ;
#60798 = CARTESIAN_POINT ( 'NONE',  ( 30.64284399271078740, 271.9999999999999432, 174.6921329945330399 ) ) ;
#60799 = CARTESIAN_POINT ( 'NONE',  ( -7.778174593052020747, -7.778174593052023411, 115.1875000000000000 ) ) ;
#60800 = CARTESIAN_POINT ( 'NONE',  ( -11.35316468749999785, 8.072916663252682312, -3.042071309553167513 ) ) ;
#60801 = CARTESIAN_POINT ( 'NONE',  ( -5.082755093536317936, -5.082755093536320601, 5.049052781871752771 ) ) ;
#60802 = CARTESIAN_POINT ( 'NONE',  ( 8.311093377946834337, 195.4687499965859843, 8.311093377946839666 ) ) ;
#60803 = CARTESIAN_POINT ( 'NONE',  ( -28.00000000000002842, 200.0000000000000000, 166.0000000000003695 ) ) ;
#60804 = CARTESIAN_POINT ( 'NONE',  ( 1.881053915767121776, 5.499999998634407028, -4.541265875000002339 ) ) ;
#60805 = FACE_OUTER_BOUND ( 'NONE', #10693, .T. ) ;
#60807 = CYLINDRICAL_SURFACE ( 'NONE', #23053, 3.999999999999976019 ) ;
#60806 = CARTESIAN_POINT ( 'NONE',  ( -1.656854249492280440, 202.9375000027312410, 194.0000000000000284 ) ) ;
#60808 = VERTEX_POINT ( 'NONE', #35507 ) ;
#60809 = VECTOR ( 'NONE', #43826, 1000.000000000000000 ) ;
#60810 = CARTESIAN_POINT ( 'NONE',  ( 3.458734124999960358, 203.6875000013656063, 142.0000000000000568 ) ) ;
#60811 = CARTESIAN_POINT ( 'NONE',  ( 5.676582343749993598, 9.947916663252682312, 9.832129032723422313 ) ) ;
#60812 = CARTESIAN_POINT ( 'NONE',  ( 11.00000000000000000, 4.556349186104045934, 98.03125000409677625 ) ) ;
#60813 = CARTESIAN_POINT ( 'NONE',  ( 1.656854249492381248, 19.93749999726881228, -4.000000000000001776 ) ) ;
#60814 = CARTESIAN_POINT ( 'NONE',  ( -24.54126587500001833, 202.2500000013655779, 168.5673454167826435 ) ) ;
#60815 = CARTESIAN_POINT ( 'NONE',  ( -14.00000000000000178, 2.249999999994893862, 7.677076266393539683 ) ) ;
#60817 = CARTESIAN_POINT ( 'NONE',  ( -8.660254037844387298, 58.95833332650537528, -5.000000000000004441 ) ) ;
#60816 = CARTESIAN_POINT ( 'NONE',  ( -7.188101187500000044, 118.1562500020483810, 0.000000000000000000 ) ) ;
#60818 = CARTESIAN_POINT ( 'NONE',  ( -7.999999999999989342, -3.313708498984762496, 27.92405277982336642 ) ) ;
#60819 = CARTESIAN_POINT ( 'NONE',  ( 6.951808397369818766E-16, 127.0312499965860269, -11.35316468750000141 ) ) ;
#60820 = ADVANCED_FACE ( 'NONE', ( #34782 ), #1183, .T. ) ;
#60821 = EDGE_CURVE ( 'NONE', #40560, #10364, #14444, .T. ) ;
#60822 = CARTESIAN_POINT ( 'NONE',  ( -2.679491924311225848, 93.33333332650538239, -10.00000000000000178 ) ) ;
#60823 = CARTESIAN_POINT ( 'NONE',  ( -2.977408999572650927, 92.37500000204839523, -7.188101187500001821 ) ) ;
#60824 = CARTESIAN_POINT ( 'NONE',  ( -4.541265875000002339, 20.93749999863440436, -5.561446717895856393E-16 ) ) ;
#60825 = FACE_OUTER_BOUND ( 'NONE', #72824, .T. ) ;
#60826 = CARTESIAN_POINT ( 'NONE',  ( -11.99999999999999822, 4.673005023400501834, -0.4790896970872564609 ) ) ;
#60827 = ORIENTED_EDGE ( 'NONE', *, *, #16261, .T. ) ;
#60828 = CARTESIAN_POINT ( 'NONE',  ( -2.751064625579944321E-14, 208.7500000000000284, 146.0000000000000284 ) ) ;
#60829 = CARTESIAN_POINT ( 'NONE',  ( -6.676582343750003368, 292.5468750017068942, -2.765530957081996810 ) ) ;
#60830 = CARTESIAN_POINT ( 'NONE',  ( 10.00000000000000000, 186.6666666598386826, 2.679491924311235618 ) ) ;
#60831 = CARTESIAN_POINT ( 'NONE',  ( 3.313708498984762496, -7.999999999999989342, 1.486552783920146448 ) ) ;
#60832 = CARTESIAN_POINT ( 'NONE',  ( 3.042071309553159519, 174.7395833299193555, 11.35316468750000141 ) ) ;
#60833 = LINE ( 'NONE', #32936, #65793 ) ;
#60834 = CARTESIAN_POINT ( 'NONE',  ( 4.000000000000015099, 195.5625000000000568, 196.3431457505076594 ) ) ;
#60835 = CARTESIAN_POINT ( 'NONE',  ( -11.00000000000000000, 0.000000000000000000, 70.18750000409676204 ) ) ;
#60836 = VECTOR ( 'NONE', #28582, 1000.000000000000000 ) ;
#60837 = CARTESIAN_POINT ( 'NONE',  ( 10.18810118749999916, 4.220049686691935698, 101.8750000020483810 ) ) ;
#60838 = ORIENTED_EDGE ( 'NONE', *, *, #42763, .F. ) ;
#60839 = EDGE_CURVE ( 'NONE', #53888, #53638, #22162, .T. ) ;
#60840 = MECHANICAL_DESIGN_GEOMETRIC_PRESENTATION_REPRESENTATION (  '', ( #70434 ), #66817 ) ;
#60841 = LINE ( 'NONE', #3505, #34082 ) ;
#60842 = CARTESIAN_POINT ( 'NONE',  ( -5.676582343750006032, 154.4270833299193555, 9.832129032723418760 ) ) ;
#60843 = CARTESIAN_POINT ( 'NONE',  ( 4.000000000000015987, 206.6875000027312694, 196.3431457505076594 ) ) ;
#60844 = CARTESIAN_POINT ( 'NONE',  ( -1.432654583217608080, 204.8750000013656063, 201.4587341250000350 ) ) ;
#60845 = DIRECTION ( 'NONE',  ( -0.000000000000000000, 1.000000000000000000, -0.000000000000000000 ) ) ;
#60846 = CARTESIAN_POINT ( 'NONE',  ( -2.085542519210945728E-15, 64.84374999658601268, 11.35316468750000141 ) ) ;
#60848 = ORIENTED_EDGE ( 'NONE', *, *, #32970, .T. ) ;
#60847 =( BOUNDED_CURVE ( )  B_SPLINE_CURVE ( 2, ( #65323, #43045, #66822, #42678, #66064, #20787, #61157, #38156, #32121, #37786, #15124, #65690, #71344 ),
 .UNSPECIFIED., .F., .F. ) 
 B_SPLINE_CURVE_WITH_KNOTS ( ( 3, 2, 2, 2, 2, 2, 3 ),
 ( 1.554290449679109676, 1.559524058767997712, 1.564757667856885970, 1.569991276945774006, 1.575224886034662042, 1.580458495123550300, 1.585692104212438336 ),
 .UNSPECIFIED. ) 
 CURVE ( )  GEOMETRIC_REPRESENTATION_ITEM ( )  RATIONAL_B_SPLINE_CURVE ( ( 1.000000000000000000, 0.9659258262890683122, 1.000000000000000000, 0.9659258262890683122, 1.000000000000000000, 0.9659258262890683122, 1.000000000000000000, 0.9659258262890683122, 1.000000000000000000, 0.9659258262890683122, 1.000000000000000000, 0.9659258262890683122, 1.000000000000000000 ) ) 
 REPRESENTATION_ITEM ( '' )  );
#60849 = CARTESIAN_POINT ( 'NONE',  ( -10.18810118749999738, -4.220049686691941915, 115.7500000020483668 ) ) ;
#60850 = CARTESIAN_POINT ( 'NONE',  ( 3.211159895383560947, 8.312499998634407916, 3.211159895383562723 ) ) ;
#60851 = ORIENTED_EDGE ( 'NONE', *, *, #56462, .F. ) ;
#60852 = CARTESIAN_POINT ( 'NONE',  ( -7.188101187500000044, 23.71874999795161543, -8.802885111219163269E-16 ) ) ;
#60853 = CARTESIAN_POINT ( 'NONE',  ( 1.102182119232618108E-15, 288.3125000034140157, 6.000000000000001776 ) ) ;
#60854 = DIRECTION ( 'NONE',  ( 0.000000000000000000, 0.000000000000000000, 1.000000000000000000 ) ) ;
#60855 = CARTESIAN_POINT ( 'NONE',  ( -2.977408999572654480, 19.87499999795161543, 7.188101187499999156 ) ) ;
#60856 = CARTESIAN_POINT ( 'NONE',  ( -2.977408999572647819, 7.188101187499992051, 2.705302781871750994 ) ) ;
#60857 = CARTESIAN_POINT ( 'NONE',  ( -10.18810118749999738, -4.220049686691941915, 113.1250000020483810 ) ) ;
#60858 = CARTESIAN_POINT ( 'NONE',  ( -4.898587196589412829E-16, 118.8125000040967763, -8.000000000000000000 ) ) ;
#60859 = CARTESIAN_POINT ( 'NONE',  ( -2.828427124746192067, 5.374999997268813168, 2.828427124746190735 ) ) ;
#60860 = ORIENTED_EDGE ( 'NONE', *, *, #61705, .F. ) ;
#60861 = CARTESIAN_POINT ( 'NONE',  ( -2.445694354108783664, 206.3125000013656063, 195.5543056458912190 ) ) ;
#60862 = CARTESIAN_POINT ( 'NONE',  ( -23.99999999999995026, 194.8125000027312126, 171.6568542494926817 ) ) ;
#60863 = CARTESIAN_POINT ( 'NONE',  ( -8.342170076843785083E-16, 8.062499998634406140, 4.541265875000002339 ) ) ;
#60864 = CARTESIAN_POINT ( 'NONE',  ( 1.320432766682874540E-15, 112.5312500020483952, 7.188101187500000044 ) ) ;
#60865 = CARTESIAN_POINT ( 'NONE',  ( 2.449293598294707893E-16, 13.25000000000000000, -4.000000000000001776 ) ) ;
#60866 = CARTESIAN_POINT ( 'NONE',  ( 7.188101187499991163, 2.977408999572648707, 27.83030278187176165 ) ) ;
#60867 = EDGE_LOOP ( 'NONE', ( #35550, #17284, #39983, #12778 ) ) ;
#60868 = CARTESIAN_POINT ( 'NONE',  ( 2.485281374238987873, 299.3125000000000000, 5.999999999999586997 ) ) ;
#60869 = ORIENTED_EDGE ( 'NONE', *, *, #68516, .F. ) ;
#60870 = CARTESIAN_POINT ( 'NONE',  ( -1.836970198721029983E-15, 3.750000000000000444, 10.00000000000000178 ) ) ;
#60871 = CARTESIAN_POINT ( 'NONE',  ( -10.99999999999978684, -4.556349186104264426, 83.78125000409680467 ) ) ;
#60872 = CARTESIAN_POINT ( 'NONE',  ( -1.432654583217607192, 202.2500000013656063, 194.5412658750000219 ) ) ;
#60873 = CARTESIAN_POINT ( 'NONE',  ( 30.44569435410879166, 197.8125000013656063, 167.5543056458910485 ) ) ;
#60874 = CARTESIAN_POINT ( 'NONE',  ( 8.660254037844385522, 74.58333333333332860, 5.000000000000005329 ) ) ;
#60875 = CARTESIAN_POINT ( 'NONE',  ( 2.977408999572650039, 92.56250000204838102, -7.188101187500001821 ) ) ;
#60876 = CARTESIAN_POINT ( 'NONE',  ( -6.000000000000000888, 294.0625000000000000, 2.485281374238575758 ) ) ;
#60877 = AXIS2_PLACEMENT_3D ( 'NONE', #25197, #43678, #66689 ) ;
#60879 = CARTESIAN_POINT ( 'NONE',  ( -8.660254037844390851, 127.0833333333333570, -5.000000000000007994 ) ) ;
#60878 = CARTESIAN_POINT ( 'NONE',  ( 25.17157287525378351, 208.7500000027312126, 167.1715728752537586 ) ) ;
#60880 = ORIENTED_EDGE ( 'NONE', *, *, #70513, .F. ) ;
#60881 = CARTESIAN_POINT ( 'NONE',  ( 8.311093377946839666, 220.7812500034139873, 8.311093377946829008 ) ) ;
#60882 = ADVANCED_FACE ( 'NONE', ( #64172 ), #58520, .T. ) ;
#60883 = AXIS2_PLACEMENT_3D ( 'NONE', #18684, #57577, #52646 ) ;
#60884 = CARTESIAN_POINT ( 'NONE',  ( -4.330454160155839283, -16.29811171461466301, 69.49285720718616233 ) ) ;
#60885 = CARTESIAN_POINT ( 'NONE',  ( -2.828427124746209831, 198.5000000027312126, 139.1715728752538723 ) ) ;
#60886 = LINE ( 'NONE', #37135, #15299 ) ;
#60887 = CARTESIAN_POINT ( 'NONE',  ( -2.751064625579944321E-14, 195.7500000000000000, 146.0000000000000284 ) ) ;
#60888 = CARTESIAN_POINT ( 'NONE',  ( 10.00000000000000178, 247.2916666666666856, 2.679491924311222739 ) ) ;
#60889 = CARTESIAN_POINT ( 'NONE',  ( 1.469576158976823947E-15, 107.5625000040967905, 8.000000000000000000 ) ) ;
#60890 = CARTESIAN_POINT ( 'NONE',  ( -8.660254037844387298, 187.0833333333333428, -5.000000000000004441 ) ) ;
#60891 = CARTESIAN_POINT ( 'NONE',  ( 11.00000000000000000, 1.347111479062088405E-15, 105.4375000040967763 ) ) ;
#60892 = CARTESIAN_POINT ( 'NONE',  ( 2.977408999572646486, 7.188101187499992051, 25.39280278187176165 ) ) ;
#60893 = CARTESIAN_POINT ( 'NONE',  ( -9.832129032723418760, 158.1770833299193555, -5.676582343750004256 ) ) ;
#60894 = LINE ( 'NONE', #50318, #52981 ) ;
#60895 = CARTESIAN_POINT ( 'NONE',  ( -5.000000000000000000, 53.36732872257244509, 44.46877392682823427 ) ) ;
#60896 = CARTESIAN_POINT ( 'NONE',  ( 10.00000000000018652, 155.0000000000001137, 0.000000000000000000 ) ) ;
#60899 = CARTESIAN_POINT ( 'NONE',  ( -8.000000000000000000, 17.25000000000000000, -9.797174393178825657E-16 ) ) ;
#60898 = CARTESIAN_POINT ( 'NONE',  ( -3.000000000000001332, -45.00000000000001421, 201.0010000000000048 ) ) ;
#60897 = CARTESIAN_POINT ( 'NONE',  ( 30.82842712474617031, 202.1250000000000284, 172.8284271247460993 ) ) ;
#60900 = ORIENTED_EDGE ( 'NONE', *, *, #24375, .F. ) ;
#60901 = CARTESIAN_POINT ( 'NONE',  ( 11.35316468750000141, 6.093749996586017126, 0.000000000000000000 ) ) ;
#60902 = CARTESIAN_POINT ( 'NONE',  ( 12.00000000000000000, 0.000000000000000000, 36.00000000000000000 ) ) ;
#60904 = DIRECTION ( 'NONE',  ( 0.000000000000000000, -1.000000000000000000, 0.000000000000000000 ) ) ;
#60903 = CARTESIAN_POINT ( 'NONE',  ( 1.469576158976822172E-15, -7.999999999999991118, -0.1071972160798552454 ) ) ;
#60905 = CARTESIAN_POINT ( 'NONE',  ( 2.445694354108782775, 203.5625000013656063, 139.5543056458912190 ) ) ;
#60906 = CARTESIAN_POINT ( 'NONE',  ( -1.836970198721029983E-15, 55.62499999317203958, 10.00000000000000178 ) ) ;
#60907 = CARTESIAN_POINT ( 'NONE',  ( 5.082755093536326818, 108.2187500020483810, 5.082755093536325042 ) ) ;
#60908 = CARTESIAN_POINT ( 'NONE',  ( 1.881053915767121776, 6.624999998634407916, -4.541265875000002339 ) ) ;
#60909 = CARTESIAN_POINT ( 'NONE',  ( 7.320508075688783478, 220.6250000000000284, -7.320508075688783478 ) ) ;
#60910 = CARTESIAN_POINT ( 'NONE',  ( 1.469576158976822172E-15, -7.999999999999991118, 7.205302779823365533 ) ) ;
#60912 = CARTESIAN_POINT ( 'NONE',  ( -1.656854249492383468, 5.437499997268813168, 4.000000000000000888 ) ) ;
#60911 = CARTESIAN_POINT ( 'NONE',  ( -2.775557561562891351E-14, 210.0000000000000284, 146.0000000000000284 ) ) ;
#60913 = ORIENTED_EDGE ( 'NONE', *, *, #39325, .F. ) ;
#60914 = EDGE_LOOP ( 'NONE', ( #17532, #54151, #46024 ) ) ;
#60915 = CARTESIAN_POINT ( 'NONE',  ( 0.000000000000000000, 0.000000000000000000, 0.000000000000000000 ) ) ;
#60916 = CARTESIAN_POINT ( 'NONE',  ( -4.898587196589407898E-16, 7.999999999999991118, 14.14280278392014623 ) ) ;
#60917 = CARTESIAN_POINT ( 'NONE',  ( -3.313708498984707429, 99.21875000000001421, -8.000000000000055067 ) ) ;
#60918 = CARTESIAN_POINT ( 'NONE',  ( -5.676582343749998039, 127.4479166632526983, -9.832129032723420536 ) ) ;
#60919 = ORIENTED_EDGE ( 'NONE', *, *, #9377, .F. ) ;
#60920 = CARTESIAN_POINT ( 'NONE',  ( 1.102182119232618108E-15, 298.2500000000000000, 6.000000000000001776 ) ) ;
#60921 = EDGE_CURVE ( 'NONE', #34625, #2727, #53958, .T. ) ;
#60922 = EDGE_CURVE ( 'NONE', #62018, #43963, #3392, .T. ) ;
#60923 = CARTESIAN_POINT ( 'NONE',  ( -7.204075437095965206, -7.204075437095968759, 93.34375000204838102 ) ) ;
#60924 = CARTESIAN_POINT ( 'NONE',  ( 18.00000000000000000, 0.000000000000000000, 0.000000000000000000 ) ) ;
#60925 = CARTESIAN_POINT ( 'NONE',  ( -2.445694354108784108, 197.5625000013656063, 195.5543056458912190 ) ) ;
#60926 = FACE_OUTER_BOUND ( 'NONE', #35650, .T. ) ;
#60928 = CARTESIAN_POINT ( 'NONE',  ( 9.832129032723420536, 126.1979166632526983, -5.676582343749999815 ) ) ;
#60927 = DIRECTION ( 'NONE',  ( -0.000000000000000000, 1.000000000000000000, -0.000000000000000000 ) ) ;
#60929 = CARTESIAN_POINT ( 'NONE',  ( 2.020667218593132706E-15, -11.00000000000000000, 95.87499999999998579 ) ) ;
#60930 = ORIENTED_EDGE ( 'NONE', *, *, #44016, .F. ) ;
#60931 = CARTESIAN_POINT ( 'NONE',  ( 4.556349186104045934, 11.00000000000000000, 77.03125000000000000 ) ) ;
#60932 = CARTESIAN_POINT ( 'NONE',  ( -30.86618291540532866, 179.6247977656768171, 166.3462567338165741 ) ) ;
#60933 = CARTESIAN_POINT ( 'NONE',  ( 5.676582343749993598, 115.2604166632526983, 9.832129032723422313 ) ) ;
#60934 = CARTESIAN_POINT ( 'NONE',  ( -3.458734124999959914, 206.4375000013656063, 198.0000000000000284 ) ) ;
#60935 = CARTESIAN_POINT ( 'NONE',  ( -7.188101187500000044, 21.09374999795161543, -8.802885111219163269E-16 ) ) ;
#60936 = CARTESIAN_POINT ( 'NONE',  ( -4.220049686691937474, -10.18810118749999738, 86.31250000204838102 ) ) ;
#60937 = B_SPLINE_CURVE_WITH_KNOTS ( 'NONE', 3,
 ( #65999, #37340, #60338, #65255, #20339, #25991, #49391, #37720, #53948, #49015 ),
 .UNSPECIFIED., .F., .F.,
 ( 4, 2, 2, 2, 4 ),
 ( 0.000000000000000000, 0.001314083742622693335, 0.002628167485245387971, 0.003942251227868082825, 0.005256334970490775943 ),
 .UNSPECIFIED. ) ;
#60938 = CARTESIAN_POINT ( 'NONE',  ( -9.832129032723418760, 28.17708332991935194, -5.676582343750004256 ) ) ;
#60939 = ORIENTED_EDGE ( 'NONE', *, *, #52786, .T. ) ;
#60940 = CARTESIAN_POINT ( 'NONE',  ( -0.4369882809979233063, 67.59332269700190921, -20.03478791450335095 ) ) ;
#60941 = CARTESIAN_POINT ( 'NONE',  ( -8.008118988124991233, 0.000000000000000000, 23.51311528394063188 ) ) ;
#60942 = CARTESIAN_POINT ( 'NONE',  ( 7.999979185126659509, 3.313729313858088776, 22.86155361672978970 ) ) ;
#60943 =( BOUNDED_CURVE ( )  B_SPLINE_CURVE ( 2, ( #10844, #33878, #56878, #16858, #39884, #62886, #11219, #5562, #38257 ),
 .UNSPECIFIED., .F., .F. ) 
 B_SPLINE_CURVE_WITH_KNOTS ( ( 3, 2, 2, 2, 3 ),
 ( 0.2187500000000001388, 0.2239583333333333703, 0.2291666666666666019, 0.2343749999999998335, 0.2395833333333330928 ),
 .UNSPECIFIED. ) 
 CURVE ( )  GEOMETRIC_REPRESENTATION_ITEM ( )  RATIONAL_B_SPLINE_CURVE ( ( 0.9999999999999980016, 0.9238795325112887369, 1.000000000000000000, 0.9238795325112867385, 1.000000000000000000, 0.9238795325112867385, 1.000000000000000000, 0.9238795325112904022, 0.9999999999999963363 ) ) 
 REPRESENTATION_ITEM ( '' )  );
#60944 = CARTESIAN_POINT ( 'NONE',  ( -7.778174593052020747, -7.778174593052023411, 85.37500000409677625 ) ) ;
#60945 = CARTESIAN_POINT ( 'NONE',  ( 4.401442555609581635E-16, 0.8437499979516099868, -7.188101187500000044 ) ) ;
#60946 = CARTESIAN_POINT ( 'NONE',  ( 4.721056650415999201, 288.0781250017069510, -4.721056650415999201 ) ) ;
#60947 = AXIS2_PLACEMENT_3D ( 'NONE', #26125, #20467, #2023 ) ;
#60948 = EDGE_CURVE ( 'NONE', #43604, #34824, #29884, .T. ) ;
#60949 = CARTESIAN_POINT ( 'NONE',  ( 1.102182119232618108E-15, 297.2500000000000000, 6.000000000000001776 ) ) ;
#60950 = FACE_OUTER_BOUND ( 'NONE', #26744, .T. ) ;
#60951 = ORIENTED_EDGE ( 'NONE', *, *, #65112, .T. ) ;
#60952 = CARTESIAN_POINT ( 'NONE',  ( -9.832129032723418760, 143.1770833299193555, -5.676582343750004256 ) ) ;
#60953 = CARTESIAN_POINT ( 'NONE',  ( 10.18810118749999916, 1.247682550866122264E-15, 86.40625000204838102 ) ) ;
#60954 = VECTOR ( 'NONE', #1880, 1000.000000000000227 ) ;
#60955 = CARTESIAN_POINT ( 'NONE',  ( -31.45873412499999944, 199.6250000013656063, 168.5673454167827572 ) ) ;
#60956 = CARTESIAN_POINT ( 'NONE',  ( -27.99999999999999645, 210.0000000000000284, 174.0000000000003411 ) ) ;
#60957 = CARTESIAN_POINT ( 'NONE',  ( 1.881053915767122664, 16.24999999863440436, 4.541265875000001451 ) ) ;
#60958 = ORIENTED_EDGE ( 'NONE', *, *, #65534, .T. ) ;
#60959 = CARTESIAN_POINT ( 'NONE',  ( -1.656854249492347719, 203.9375000027311842, 194.0000000000000853 ) ) ;
#60960 = CARTESIAN_POINT ( 'NONE',  ( -4.000000000000015099, 208.5625000000000000, 143.6568542494924543 ) ) ;
#60962 =( BOUNDED_CURVE ( )  B_SPLINE_CURVE ( 2, ( #73359, #15627, #49217, #49972, #43942, #33020, #55278, #10359, #26575, #72615, #44688, #21293, #66951 ),
 .UNSPECIFIED., .F., .F. ) 
 B_SPLINE_CURVE_WITH_KNOTS ( ( 3, 2, 2, 2, 2, 2, 3 ),
 ( 2.778886174319656455, 2.784119686266136373, 2.789353198316371518, 2.794586710366607107, 2.799820222416842252, 2.805053734467077842, 2.810287246517312987 ),
 .UNSPECIFIED. ) 
 CURVE ( )  GEOMETRIC_REPRESENTATION_ITEM ( )  RATIONAL_B_SPLINE_CURVE ( ( 1.000000000000000000, 0.9659258262890683122, 1.000000000000000000, 0.9659258262890683122, 1.000000000000000000, 0.9659258262890683122, 1.000000000000000000, 0.9659258262890683122, 1.000000000000000000, 0.9659258262890683122, 1.000000000000000000, 0.9659258262890725311, 0.9999999999999957812 ) ) 
 REPRESENTATION_ITEM ( '' )  );
#60961 = CARTESIAN_POINT ( 'NONE',  ( -26.34314575050753149, 204.6875000027312126, 174.0000000000003411 ) ) ;
#60963 = DIRECTION ( 'NONE',  ( 0.000000000000000000, 0.9997074645238147594, -0.02418647091589873691 ) ) ;
#60964 = ORIENTED_EDGE ( 'NONE', *, *, #64194, .T. ) ;
#60965 = CARTESIAN_POINT ( 'NONE',  ( -7.188101187500000933, 10.12499999795161187, -2.977408999572651371 ) ) ;
#60966 = CARTESIAN_POINT ( 'NONE',  ( -28.04578937046037268, -12.19982490138932718, 183.3289664186391406 ) ) ;
#60967 = DIRECTION ( 'NONE',  ( -1.000000000000000000, -0.000000000000000000, 0.000000000000000000 ) ) ;
#60968 = CARTESIAN_POINT ( 'NONE',  ( -2.085542519210945728E-15, 189.5312499965860127, 11.35316468750000141 ) ) ;
#60969 = CARTESIAN_POINT ( 'NONE',  ( 7.188101187500000044, 113.2812500020483952, -8.802885111219163269E-16 ) ) ;
#60970 = CARTESIAN_POINT ( 'NONE',  ( 12.00000000000000000, 0.000000000000000000, -14.00000000000000178 ) ) ;
#60971 = CARTESIAN_POINT ( 'NONE',  ( -4.721056650415998313, 288.5781250017069510, 4.721056650416000089 ) ) ;
#60973 = CARTESIAN_POINT ( 'NONE',  ( 8.660254037844383745, 95.41666666666667140, -4.999999999999997335 ) ) ;
#60972 = CARTESIAN_POINT ( 'NONE',  ( 3.042071309553173286, 225.3645833367473301, 11.35316468749999608 ) ) ;
#60974 = VERTEX_POINT ( 'NONE', #65265 ) ;
#60975 = CARTESIAN_POINT ( 'NONE',  ( 5.676582343749997150, 252.2395833367473301, -9.832129032723418760 ) ) ;
#60976 = CARTESIAN_POINT ( 'NONE',  ( 5.082755093536320601, -5.082755093536318824, 26.42405278187175810 ) ) ;
#60977 = CARTESIAN_POINT ( 'NONE',  ( 2.679491924311075302, 165.8333333265053398, 10.00000000000008704 ) ) ;
#60978 = CARTESIAN_POINT ( 'NONE',  ( 0.000000000000000000, 0.000000000000000000, 30.00000000000000000 ) ) ;
#60979 = CARTESIAN_POINT ( 'NONE',  ( 4.471435261917476645, -60.74652839096075496, -23.21845616858407979 ) ) ;
#60980 = CARTESIAN_POINT ( 'NONE',  ( -3.458734124999959469, 199.7500000013656063, 199.4326545832176691 ) ) ;
#60981 = FACE_OUTER_BOUND ( 'NONE', #16088, .T. ) ;
#60982 = FACE_OUTER_BOUND ( 'NONE', #63428, .T. ) ;
#60983 = CARTESIAN_POINT ( 'NONE',  ( 8.000000000000000000, 95.75000000000000000, -9.797174393178825657E-16 ) ) ;
#60984 = CARTESIAN_POINT ( 'NONE',  ( 9.832129032723416984, 120.6770833299193555, 5.676582343750006032 ) ) ;
#60985 = CARTESIAN_POINT ( 'NONE',  ( 11.00000000000000000, 1.347111479062088405E-15, 72.24999999999998579 ) ) ;
#60987 = CARTESIAN_POINT ( 'NONE',  ( 28.00000000000001776, 201.4375000013656063, 173.4587341249998929 ) ) ;
#60986 = CARTESIAN_POINT ( 'NONE',  ( 24.54126587499998280, 199.5000000013656063, 171.4326545832175555 ) ) ;
#60988 = VERTEX_POINT ( 'NONE', #55084 ) ;
#60989 = EDGE_CURVE ( 'NONE', #55811, #20100, #39592, .T. ) ;
#60990 = LINE ( 'NONE', #43257, #17879 ) ;
#60991 = CARTESIAN_POINT ( 'NONE',  ( 11.35316468749999785, 220.5729166632526983, 3.042071309553174174 ) ) ;
#60992 = CARTESIAN_POINT ( 'NONE',  ( -1.432654583217664479, 198.7500000013656063, 138.5412658750000787 ) ) ;
#60993 = CARTESIAN_POINT ( 'NONE',  ( 26.56734541678232375, 196.6250000013656063, 173.4587341249998929 ) ) ;
#60994 = FACE_OUTER_BOUND ( 'NONE', #26952, .T. ) ;
#60995 = CARTESIAN_POINT ( 'NONE',  ( 3.042071309553159519, 210.0520833299193555, 11.35316468750000141 ) ) ;
#60996 = CARTESIAN_POINT ( 'NONE',  ( 4.531193156845207581E-15, 192.0000000000000284, 133.0000000000000284 ) ) ;
#60997 = DIRECTION ( 'NONE',  ( 0.000000000000000000, 0.000000000000000000, 1.000000000000000000 ) ) ;
#60998 = CARTESIAN_POINT ( 'NONE',  ( 3.211159895383560947, 20.18749999863440436, 3.211159895383562723 ) ) ;
#60999 = CARTESIAN_POINT ( 'NONE',  ( 31.45873412499999233, 194.9375000013655779, 169.9999999999999432 ) ) ;
#61000 = CARTESIAN_POINT ( 'NONE',  ( 7.999999999999991118, 3.313708498984757611, 28.67405277982336642 ) ) ;
#61001 = CARTESIAN_POINT ( 'NONE',  ( -32.00000000000000000, 208.3750000027312126, 170.0000000000004547 ) ) ;
#61002 = CARTESIAN_POINT ( 'NONE',  ( 5.676582343749993598, 84.94791666325268409, 9.832129032723422313 ) ) ;
#61003 = ORIENTED_EDGE ( 'NONE', *, *, #67737, .T. ) ;
#61004 = LINE ( 'NONE', #69648, #11069 ) ;
#61005 = CARTESIAN_POINT ( 'NONE',  ( 7.188101187500001821, 21.56249999795161898, -2.977408999572650483 ) ) ;
#61006 = DIRECTION ( 'NONE',  ( -0.000000000000000000, 1.000000000000000000, -0.000000000000000000 ) ) ;
#61007 = CARTESIAN_POINT ( 'NONE',  ( -11.35316468749999963, 254.2187500034139873, 0.000000000000000000 ) ) ;
#61008 = CARTESIAN_POINT ( 'NONE',  ( 11.35316468749999785, 85.57291666325268409, 3.042071309553174174 ) ) ;
#61009 = ORIENTED_EDGE ( 'NONE', *, *, #38502, .F. ) ;
#61010 = CARTESIAN_POINT ( 'NONE',  ( 8.660254037844389075, 207.2916666598387110, -5.000000000000000000 ) ) ;
#61011 = ADVANCED_FACE ( 'NONE', ( #13934 ), #32446, .T. ) ;
#61012 = CARTESIAN_POINT ( 'NONE',  ( 10.18810118749999916, 1.247682550866122264E-15, 113.4062500020483810 ) ) ;
#61013 = CARTESIAN_POINT ( 'NONE',  ( -28.00000000000001776, 195.6875000013655779, 166.5412658750003629 ) ) ;
#61014 = CARTESIAN_POINT ( 'NONE',  ( -1.432654583217608080, 206.8750000013656347, 201.4587341250000350 ) ) ;
#61015 = CARTESIAN_POINT ( 'NONE',  ( 7.999999999999992895, -3.313708498984756279, 11.98655277982336820 ) ) ;
#61017 = CARTESIAN_POINT ( 'NONE',  ( -2.085542519210945728E-15, 84.53124999658602690, 11.35316468750000141 ) ) ;
#61016 = LINE ( 'NONE', #67055, #37620 ) ;
#61018 = CARTESIAN_POINT ( 'NONE',  ( 3.313708498984762496, -7.999999999999989342, 17.98655278392014978 ) ) ;
#61019 = CARTESIAN_POINT ( 'NONE',  ( -25.55430564589119413, 202.5625000013656063, 167.5543056458915316 ) ) ;
#61020 = DIRECTION ( 'NONE',  ( 0.000000000000000000, 0.000000000000000000, -1.000000000000000000 ) ) ;
#61021 = EDGE_CURVE ( 'NONE', #54702, #64829, #15066, .T. ) ;
#61022 = CARTESIAN_POINT ( 'NONE',  ( 6.123233995736767268E-16, 163.1249999931720254, -10.00000000000000178 ) ) ;
#61023 = DIRECTION ( 'NONE',  ( 0.000000000000000000, 0.000000000000000000, -1.000000000000000000 ) ) ;
#61024 = CARTESIAN_POINT ( 'NONE',  ( 8.311093377946834337, 70.46874999658599847, 8.311093377946839666 ) ) ;
#61025 = CARTESIAN_POINT ( 'NONE',  ( 2.765530957081996366, 292.1406250017070079, -6.676582343750003368 ) ) ;
#61027 = CARTESIAN_POINT ( 'NONE',  ( 10.18810118749999916, 4.220049686691935698, 106.3750000020483668 ) ) ;
#61026 = B_SPLINE_CURVE_WITH_KNOTS ( 'NONE', 3,
 ( #5433, #28436, #11094, #44677, #67692, #27686, #50694, #22024, #51443, #74456, #44304, #16350 ),
 .UNSPECIFIED., .F., .F.,
 ( 4, 2, 2, 2, 2, 4 ),
 ( 0.000000000000000000, 0.002547658444427996095, 0.005095316888855990455, 0.006369146111069987418, 0.007642975333283984381, 0.01019063377771197917 ),
 .UNSPECIFIED. ) ;
#61028 = CARTESIAN_POINT ( 'NONE',  ( 3.042071309553159519, 204.7395833299193271, 11.35316468750000141 ) ) ;
#61029 = ORIENTED_EDGE ( 'NONE', *, *, #27378, .F. ) ;
#61030 = DIRECTION ( 'NONE',  ( -0.000000000000000000, 1.000000000000000000, -4.476705744456276341E-16 ) ) ;
#61031 = CARTESIAN_POINT ( 'NONE',  ( 4.999999999999999112, 61.58609660504352945, 23.68302032025150439 ) ) ;
#61033 = CARTESIAN_POINT ( 'NONE',  ( -3.042071309553173730, 204.3229166632526699, 11.35316468749999785 ) ) ;
#61032 = CARTESIAN_POINT ( 'NONE',  ( -7.347880794884122694E-16, 19.75000000000000000, 4.000000000000001776 ) ) ;
#61034 = CARTESIAN_POINT ( 'NONE',  ( -2.828427124746209831, 203.3750000000000284, 139.1715728752538723 ) ) ;
#61035 = CARTESIAN_POINT ( 'NONE',  ( -9.999999999999998224, 228.3333333401612606, 2.679491924311235618 ) ) ;
#61036 = CARTESIAN_POINT ( 'NONE',  ( 28.00000000000001776, 201.5000000000000000, 165.9999999999998863 ) ) ;
#61037 = EDGE_CURVE ( 'NONE', #16375, #37723, #29308, .T. ) ;
#61038 = VERTEX_POINT ( 'NONE', #7933 ) ;
#61039 = CARTESIAN_POINT ( 'NONE',  ( -11.35316468750000141, 198.8020833299193555, 3.042071309553159963 ) ) ;
#61040 = CARTESIAN_POINT ( 'NONE',  ( -2.977408999572647819, -7.188101187499990274, 12.26780278187175455 ) ) ;
#61041 = CARTESIAN_POINT ( 'NONE',  ( 7.999999999999992895, -3.313708498984756279, 16.67405278392014623 ) ) ;
#61042 = CARTESIAN_POINT ( 'NONE',  ( 3.313708498984762052, 10.78125000000000178, -8.000000000000000000 ) ) ;
#61043 = VERTEX_POINT ( 'NONE', #65638 ) ;
#61044 = PRODUCT_DEFINITION_FORMATION_WITH_SPECIFIED_SOURCE ( 'ANY', '', #32453, .NOT_KNOWN. ) ;
#61045 = CARTESIAN_POINT ( 'NONE',  ( 8.000000000000000000, 92.93750000409679046, -9.797174393178825657E-16 ) ) ;
#61046 = DIRECTION ( 'NONE',  ( 0.000000000000000000, 0.000000000000000000, 1.000000000000000000 ) ) ;
#61047 = EDGE_CURVE ( 'NONE', #5966, #653, #71290, .T. ) ;
#61049 = VERTEX_POINT ( 'NONE', #36976 ) ;
#61048 =( BOUNDED_CURVE ( )  B_SPLINE_CURVE ( 2, ( #18241, #60352, #912, #55090, #46907, #31694, #70299, #41256, #64265, #30302, #54715, #60732, #3021 ),
 .UNSPECIFIED., .F., .F. ) 
 B_SPLINE_CURVE_WITH_KNOTS ( ( 3, 2, 2, 2, 2, 2, 3 ),
 ( 0.2010869565217391630, 0.2028985507246377218, 0.2047101449275362528, 0.2065217391304348116, 0.2083333333333333426, 0.2101449275362318736, 0.2119565217391304324 ),
 .UNSPECIFIED. ) 
 CURVE ( )  GEOMETRIC_REPRESENTATION_ITEM ( )  RATIONAL_B_SPLINE_CURVE ( ( 0.9999999999999994449, 0.9659258262890688673, 1.000000000000000000, 0.9659258262890683122, 1.000000000000000000, 0.9659258262890683122, 1.000000000000000000, 0.9659258262890683122, 1.000000000000000000, 0.9659258262890683122, 1.000000000000000000, 0.9659258262890683122, 1.000000000000000000 ) ) 
 REPRESENTATION_ITEM ( '' )  );
#61050 = CARTESIAN_POINT ( 'NONE',  ( -4.000000000000001776, 14.50000000000000000, -4.898587196589415787E-16 ) ) ;
#61051 = CARTESIAN_POINT ( 'NONE',  ( 1.881053915767122664, 21.12499999863441147, 4.541265875000001451 ) ) ;
#61052 = CARTESIAN_POINT ( 'NONE',  ( -3.313708498984757167, 7.999999999999991118, 9.736552783920146226 ) ) ;
#61053 = CARTESIAN_POINT ( 'NONE',  ( -4.999999999999996447, 11.14555136602165142, 27.84144949604463193 ) ) ;
#61054 = ORIENTED_EDGE ( 'NONE', *, *, #63929, .T. ) ;
#61055 = CARTESIAN_POINT ( 'NONE',  ( 5.000000000000000000, -13.22058908515350417, -69.49198671174480069 ) ) ;
#61056 = CARTESIAN_POINT ( 'NONE',  ( 7.188101187500002709, 90.31250000204838102, 2.977408999572649151 ) ) ;
#61059 = FACE_OUTER_BOUND ( 'NONE', #70845, .T. ) ;
#61058 = CARTESIAN_POINT ( 'NONE',  ( -23.99999999999998934, 204.8750000027312126, 170.0000000000002842 ) ) ;
#61057 = CARTESIAN_POINT ( 'NONE',  ( 1.224646799147353454E-15, 300.0000000000000000, -10.00000000000000178 ) ) ;
#61060 = CARTESIAN_POINT ( 'NONE',  ( 1424.688200795887269, 710.9677537767815920, 802.8421604560587639 ) ) ;
#61061 = EDGE_LOOP ( 'NONE', ( #65333, #29142, #14085, #74586 ) ) ;
#61062 = VECTOR ( 'NONE', #6765, 1000.000000000000000 ) ;
#61063 = CARTESIAN_POINT ( 'NONE',  ( -7.778174593052023411, 7.778174593052023411, 83.31249999999998579 ) ) ;
#61064 = CARTESIAN_POINT ( 'NONE',  ( -7.188101187499991163, 2.977408999572646930, 16.39280278187175455 ) ) ;
#61065 = ORIENTED_EDGE ( 'NONE', *, *, #29559, .F. ) ;
#61066 =( BOUNDED_CURVE ( )  B_SPLINE_CURVE ( 2, ( #8027, #31035, #13301, #18978, #41982, #2369, #36339, #53691, #71384 ),
 .UNSPECIFIED., .F., .F. ) 
 B_SPLINE_CURVE_WITH_KNOTS ( ( 3, 2, 2, 2, 3 ),
 ( 0.1842105263157894912, 0.1907894736842105643, 0.1973684210526316374, 0.2039473684210527105, 0.2105263157894737558 ),
 .UNSPECIFIED. ) 
 CURVE ( )  GEOMETRIC_REPRESENTATION_ITEM ( )  RATIONAL_B_SPLINE_CURVE ( ( 0.9999999999999996669, 0.9238795325112870716, 1.000000000000000000, 0.9238795325112867385, 1.000000000000000000, 0.9238795325112867385, 1.000000000000000000, 0.9238795325112857393, 1.000000000000000888 ) ) 
 REPRESENTATION_ITEM ( '' )  );
#61067 = VERTEX_POINT ( 'NONE', #19610 ) ;
#61068 = CARTESIAN_POINT ( 'NONE',  ( -7.204075437095965206, -7.204075437095968759, 79.84375000204838102 ) ) ;
#61069 = CARTESIAN_POINT ( 'NONE',  ( -3.042071309553164404, 72.55208332991934128, -11.35316468749999963 ) ) ;
#61070 = CARTESIAN_POINT ( 'NONE',  ( 0.000000000000000000, 125.0000000000000000, 0.000000000000000000 ) ) ;
#61071 = CARTESIAN_POINT ( 'NONE',  ( -11.00000000000000000, 4.556349186104045934, 87.90624999999998579 ) ) ;
#61074 = CARTESIAN_POINT ( 'NONE',  ( -2.765530957081996810, 290.4218750017069510, -6.676582343750002480 ) ) ;
#61073 = CARTESIAN_POINT ( 'NONE',  ( 30.82842712474616675, 198.5000000027312126, 167.1715728752537018 ) ) ;
#61072 = CARTESIAN_POINT ( 'NONE',  ( -11.00000000000000000, 0.000000000000000000, 104.5000000000000000 ) ) ;
#61075 = CARTESIAN_POINT ( 'NONE',  ( -7.778174593052023411, 7.778174593052023411, 89.31249999999998579 ) ) ;
#61076 = CARTESIAN_POINT ( 'NONE',  ( -1.432654583217608080, 197.8750000013656063, 201.4587341250000350 ) ) ;
#61077 = CARTESIAN_POINT ( 'NONE',  ( 7.999999999999998224, 11.71874999590322197, 3.313708498984766493 ) ) ;
#61078 = CARTESIAN_POINT ( 'NONE',  ( 29.43265458321761585, 208.7500000013656063, 173.4587341249998929 ) ) ;
#61079 = CARTESIAN_POINT ( 'NONE',  ( 2.977408999572651815, 11.06249999795161187, 7.188101187500000933 ) ) ;
#61080 = CARTESIAN_POINT ( 'NONE',  ( -7.999999999999991118, 3.313708498984756723, 26.42405278392015333 ) ) ;
#61081 = CARTESIAN_POINT ( 'NONE',  ( -5.656854249492378806, 105.6874999999999858, 5.656854249492381470 ) ) ;
#61082 = CARTESIAN_POINT ( 'NONE',  ( -2.977408999572650927, 109.2500000020483952, -7.188101187500000933 ) ) ;
#61084 = CARTESIAN_POINT ( 'NONE',  ( -1.877992804782812053, -55.75022808459689827, -43.87334515336773677 ) ) ;
#61083 = CARTESIAN_POINT ( 'NONE',  ( -7.320508075688778149, 19.99999999317203603, 7.320508075688769267 ) ) ;
#61085 = CARTESIAN_POINT ( 'NONE',  ( 31.45873412500001010, 208.0000000013656063, 168.5673454167822740 ) ) ;
#61086 = CARTESIAN_POINT ( 'NONE',  ( -7.188101187499991163, 2.977408999572646930, 13.76780278187175455 ) ) ;
#61087 = CARTESIAN_POINT ( 'NONE',  ( 3.999999999999959144, 207.1875000027312126, 140.3431457505076594 ) ) ;
#61088 = CARTESIAN_POINT ( 'NONE',  ( -3.042071309553164404, 47.23958332991936260, -11.35316468749999963 ) ) ;
#61089 = EDGE_CURVE ( 'NONE', #58601, #29199, #59981, .T. ) ;
#61090 = DIRECTION ( 'NONE',  ( 0.000000000000000000, 0.000000000000000000, -1.000000000000000000 ) ) ;
#61091 = CARTESIAN_POINT ( 'NONE',  ( 2.679491924311222739, 25.83333332650536107, 10.00000000000000355 ) ) ;
#61092 = CARTESIAN_POINT ( 'NONE',  ( 7.778174593052023411, -7.778174593052021635, 72.06249999999998579 ) ) ;
#61093 = ORIENTED_EDGE ( 'NONE', *, *, #51793, .T. ) ;
#61094 = CARTESIAN_POINT ( 'NONE',  ( 7.320508075688774596, 142.4999999931720254, -7.320508075688774596 ) ) ;
#61095 = CARTESIAN_POINT ( 'NONE',  ( 10.99999999999989342, 4.556349186104152515, 69.53125000409676204 ) ) ;
#61096 = CARTESIAN_POINT ( 'NONE',  ( -8.311093377946841443, 53.90624999658601979, 8.311093377946830785 ) ) ;
#61097 = CARTESIAN_POINT ( 'NONE',  ( -4.556349186104047710, -10.99999999999999822, 80.96875000409676204 ) ) ;
#61098 = CARTESIAN_POINT ( 'NONE',  ( -1.432654583217664701, 203.0000000013655779, 138.5412658750000787 ) ) ;
#61099 = CARTESIAN_POINT ( 'NONE',  ( -11.00000000000000533, 11.00000000000000000, 41.99999999999999289 ) ) ;
#61100 = CARTESIAN_POINT ( 'NONE',  ( 4.898587196589412829E-16, 25.68749999590322375, -8.000000000000000000 ) ) ;
#61102 = CARTESIAN_POINT ( 'NONE',  ( -8.311093377946836114, 47.65624999658601268, -8.311093377946837890 ) ) ;
#61101 = CARTESIAN_POINT ( 'NONE',  ( -2.977408999572652260, 98.93750000204836681, 7.188101187500000044 ) ) ;
#61103 = CARTESIAN_POINT ( 'NONE',  ( 5.656854249492374365, 5.656854249492375253, 9.267802779823364645 ) ) ;
#61104 = CARTESIAN_POINT ( 'NONE',  ( -7.999999999929542582, -2.214810345207895024E-05, 22.01864141485938831 ) ) ;
#61105 = CARTESIAN_POINT ( 'NONE',  ( -8.311093377946841443, 158.9062499965860411, 8.311093377946830785 ) ) ;
#61106 = EDGE_CURVE ( 'NONE', #6411, #73780, #11602, .T. ) ;
#61107 = CARTESIAN_POINT ( 'NONE',  ( -7.320508075688778149, 134.9999999931720538, 7.320508075688769267 ) ) ;
#61108 = CARTESIAN_POINT ( 'NONE',  ( 5.082755093536326818, 105.5937500020483810, 5.082755093536325042 ) ) ;
#61109 = ORIENTED_EDGE ( 'NONE', *, *, #55476, .F. ) ;
#61110 = DIRECTION ( 'NONE',  ( 0.000000000000000000, 0.000000000000000000, 1.000000000000000000 ) ) ;
#61111 = CARTESIAN_POINT ( 'NONE',  ( -3.042071309553163960, 37.55208332991935549, -11.35316468749999963 ) ) ;
#61112 = CARTESIAN_POINT ( 'NONE',  ( -7.525268439705684820, -6.047589086025006999, -0.3570196857253580824 ) ) ;
#61113 = EDGE_LOOP ( 'NONE', ( #29433, #46998, #40979, #9487, #50236, #5937, #35350, #23800, #34642, #24384, #50043, #45269, #19120, #16166, #46007, #71977, #8578, #16220, #33227, #63666, #13022, #16869, #59924, #28534, #33616, #37689, #48474, #13987, #10855, #65827, #44340, #41471, #38166, #5978, #30844, #22269, #36283, #25469, #32073, #70395, #37783, #4567, #9995, #16510, #72041, #19295, #43421, #32008 ) ) ;
#61114 = DIRECTION ( 'NONE',  ( 0.000000000000000000, 0.000000000000000000, -1.000000000000000000 ) ) ;
#61115 = CARTESIAN_POINT ( 'NONE',  ( 7.204075437095968759, -7.204075437095966983, 75.71875000204836681 ) ) ;
#61116 = CARTESIAN_POINT ( 'NONE',  ( 5.000000000000000000, -16.14408868864072844, 27.96238185062368586 ) ) ;
#61118 = CARTESIAN_POINT ( 'NONE',  ( -2.085542519210945728E-15, 169.5312499965860411, 11.35316468750000141 ) ) ;
#61117 = FACE_OUTER_BOUND ( 'NONE', #61782, .T. ) ;
#61119 = CARTESIAN_POINT ( 'NONE',  ( -7.188101187500002709, 1.687499997951610098, 2.977408999572649151 ) ) ;
#61120 = CARTESIAN_POINT ( 'NONE',  ( -5.656854249492375253, 5.656854249492375253, 14.19905278432982598 ) ) ;
#61121 = CARTESIAN_POINT ( 'NONE',  ( -29.27395290058679223, -21.12797442504308520, 180.2632692363952458 ) ) ;
#61122 = CARTESIAN_POINT ( 'NONE',  ( -8.311093377946834337, 229.5312500034139873, 8.311093377946837890 ) ) ;
#61123 = CARTESIAN_POINT ( 'NONE',  ( 7.204075437095968759, -7.204075437095966983, 86.59375000204836681 ) ) ;
#61124 = EDGE_LOOP ( 'NONE', ( #8064, #40796 ) ) ;
#61125 = AXIS2_PLACEMENT_3D ( 'NONE', #29052, #51690, #63009 ) ;
#61126 = ADVANCED_FACE ( 'NONE', ( #10541, #62215 ), #15811, .T. ) ;
#61127 = CARTESIAN_POINT ( 'NONE',  ( -1.656854249492374143, 204.3125000027312126, 202.0000000000000000 ) ) ;
#61128 = CARTESIAN_POINT ( 'NONE',  ( 5.676582343750001591, 96.92708332991935549, -9.832129032723420536 ) ) ;
#61129 = CARTESIAN_POINT ( 'NONE',  ( -10.18810118749999738, -4.220049686691941915, 94.75000000204838102 ) ) ;
#61130 = ADVANCED_FACE ( 'NONE', ( #44132 ), #28263, .F. ) ;
#61131 = CARTESIAN_POINT ( 'NONE',  ( -4.541265875000002339, 20.93749999863440436, -5.561446717895856393E-16 ) ) ;
#61132 = ORIENTED_EDGE ( 'NONE', *, *, #74420, .F. ) ;
#61133 = VERTEX_POINT ( 'NONE', #10914 ) ;
#61134 = CARTESIAN_POINT ( 'NONE',  ( -1.881053915767124440, 2.124999998634406584, 4.541265875000001451 ) ) ;
#61135 = CARTESIAN_POINT ( 'NONE',  ( 7.188101187500001821, 6.562499997951610986, -2.977408999572650483 ) ) ;
#61136 = CARTESIAN_POINT ( 'NONE',  ( 3.313708498984760720, 114.2187500040968047, -8.000000000000000000 ) ) ;
#61137 = CARTESIAN_POINT ( 'NONE',  ( -7.204075437095965206, -7.204075437095968759, 93.71875000204838102 ) ) ;
#61138 = CARTESIAN_POINT ( 'NONE',  ( -24.54126587499998280, 202.3750000013655779, 171.4326545832179818 ) ) ;
#61139 = CARTESIAN_POINT ( 'NONE',  ( 5.656854249492376141, -5.656854249492374365, 19.39280277982336642 ) ) ;
#61140 = ADVANCED_FACE ( 'NONE', ( #44875 ), #39957, .F. ) ;
#61141 = CARTESIAN_POINT ( 'NONE',  ( -4.000000000000001776, 5.500000000000000000, -4.898587196589415787E-16 ) ) ;
#61142 = CARTESIAN_POINT ( 'NONE',  ( 4.000000000000001776, 17.81249999726881938, -1.656854249492381248 ) ) ;
#61143 = CARTESIAN_POINT ( 'NONE',  ( 4.541265875000002339, 9.374999998634404363, -1.881053915767121776 ) ) ;
#61144 = AXIS2_PLACEMENT_3D ( 'NONE', #48370, #31778, #71374 ) ;
#61145 = CARTESIAN_POINT ( 'NONE',  ( 3.999999999999960032, 204.0000000000000284, 142.0000000000000568 ) ) ;
#61146 = VERTEX_POINT ( 'NONE', #67142 ) ;
#61147 = CARTESIAN_POINT ( 'NONE',  ( 3.458734125000015425, 195.9375000013655779, 198.0000000000000284 ) ) ;
#61149 = CARTESIAN_POINT ( 'NONE',  ( 4.999999999999997335, 236.4583333401613174, -8.660254037844387298 ) ) ;
#61148 = CARTESIAN_POINT ( 'NONE',  ( -31.45873412499995680, 198.7500000013656063, 171.4326545832181239 ) ) ;
#61150 =( NAMED_UNIT ( * ) PLANE_ANGLE_UNIT ( ) SI_UNIT ( $, .RADIAN. ) );
#61151 = CARTESIAN_POINT ( 'NONE',  ( -1.881053915767121554, 18.62499999863440792, -4.541265875000002339 ) ) ;
#61152 = CARTESIAN_POINT ( 'NONE',  ( 3.000000000000001332, -45.00000000000001421, 151.2383369607063344 ) ) ;
#61153 = CARTESIAN_POINT ( 'NONE',  ( -2.977408999572647819, 7.188101187499991163, 4.205302781871751883 ) ) ;
#61154 = ORIENTED_EDGE ( 'NONE', *, *, #18090, .F. ) ;
#61155 = ORIENTED_EDGE ( 'NONE', *, *, #20795, .F. ) ;
#61156 = CARTESIAN_POINT ( 'NONE',  ( -10.18810118749999916, 4.220049686691934809, 99.06250000204836681 ) ) ;
#61157 = CARTESIAN_POINT ( 'NONE',  ( 10.00000000000000355, 125.0000000000000000, 0.000000000000000000 ) ) ;
#61158 = CARTESIAN_POINT ( 'NONE',  ( -31.45873412499999944, 198.8750000013656063, 168.5673454167827572 ) ) ;
#61159 = CARTESIAN_POINT ( 'NONE',  ( 11.00000000000000000, 4.556349186104045934, 109.8437500000000000 ) ) ;
#61160 = CARTESIAN_POINT ( 'NONE',  ( 1.432654583217662481, 206.3750000013656063, 194.5412658750000219 ) ) ;
#61161 = CARTESIAN_POINT ( 'NONE',  ( 2.679491924305354544, 58.95833333333284543, 10.00000000000347988 ) ) ;
#61162 = ADVANCED_FACE ( 'NONE', ( #50155 ), #51270, .F. ) ;
#61163 = CARTESIAN_POINT ( 'NONE',  ( 7.320508075688771044, 109.3750000000000000, 7.320508075688775484 ) ) ;
#61164 = CARTESIAN_POINT ( 'NONE',  ( 3.313708498984760720, 111.0312499999999858, -8.000000000000000000 ) ) ;
#61165 = CARTESIAN_POINT ( 'NONE',  ( -2.765530957081998586, 293.7968750017069510, 6.676582343750001591 ) ) ;
#61166 = CARTESIAN_POINT ( 'NONE',  ( 7.188101187499991163, 2.977408999572648707, 10.20530278187175455 ) ) ;
#61167 = ADVANCED_FACE ( 'NONE', ( #11288 ), #55834, .T. ) ;
#61168 = ORIENTED_EDGE ( 'NONE', *, *, #765, .F. ) ;
#61169 =( BOUNDED_CURVE ( )  B_SPLINE_CURVE ( 2, ( #45304, #16242, #16616, #40395, #52093, #426, #5324, #21910, #22281 ),
 .UNSPECIFIED., .F., .F. ) 
 B_SPLINE_CURVE_WITH_KNOTS ( ( 3, 2, 2, 2, 3 ),
 ( 0.04166666666666666435, 0.04861111111111111188, 0.05555555555555555247, 0.06250000000000000000, 0.06944444444444444753 ),
 .UNSPECIFIED. ) 
 CURVE ( )  GEOMETRIC_REPRESENTATION_ITEM ( )  RATIONAL_B_SPLINE_CURVE ( ( 1.000000000000000000, 0.9238795325112867385, 1.000000000000000000, 0.9238795325112867385, 1.000000000000000000, 0.9238795325112867385, 1.000000000000000000, 0.9238795325112867385, 1.000000000000000000 ) ) 
 REPRESENTATION_ITEM ( '' )  );
#61170 = CARTESIAN_POINT ( 'NONE',  ( -5.000000000000000000, 52.35862550122993042, -48.98731492261362064 ) ) ;
#61171 = DIRECTION ( 'NONE',  ( 0.000000000000000000, 0.000000000000000000, -1.000000000000000000 ) ) ;
#61172 = CARTESIAN_POINT ( 'NONE',  ( 5.656854249492380582, 22.49999999590322375, -5.656854249492380582 ) ) ;
#61173 = CARTESIAN_POINT ( 'NONE',  ( -3.458734125000016313, 202.8750000013656347, 140.5673454167824161 ) ) ;
#61174 = FACE_OUTER_BOUND ( 'NONE', #62442, .T. ) ;
#61176 = CARTESIAN_POINT ( 'NONE',  ( 1.432654583217608080, 202.8750000013656347, 138.5412658750000503 ) ) ;
#61175 = CARTESIAN_POINT ( 'NONE',  ( -6.735557395310442023E-16, 11.00000000000000000, 111.6249999999999858 ) ) ;
#61177 = CARTESIAN_POINT ( 'NONE',  ( 9.832129032723420536, 251.3020833367473017, 5.676582343749996262 ) ) ;
#61178 = DIRECTION ( 'NONE',  ( -0.000000000000000000, 1.000000000000000000, -1.563033456626094573E-30 ) ) ;
#61179 = CARTESIAN_POINT ( 'NONE',  ( -7.320508075688778149, 94.99999999317202537, 7.320508075688769267 ) ) ;
#61180 = CARTESIAN_POINT ( 'NONE',  ( 5.676582343750001591, 1.614583329919349719, -9.832129032723420536 ) ) ;
#61181 = ADVANCED_FACE ( 'NONE', ( #61850 ), #27013, .F. ) ;
#61182 = CARTESIAN_POINT ( 'NONE',  ( 2.977408999572646486, 7.188101187499992051, 4.392802781871752771 ) ) ;
#61183 = CARTESIAN_POINT ( 'NONE',  ( -3.042071309553164404, 192.5520833299193271, -11.35316468749999963 ) ) ;
#61184 = CARTESIAN_POINT ( 'NONE',  ( -1.836970198721029983E-15, 135.6249999931720538, 10.00000000000000178 ) ) ;
#61185 = CARTESIAN_POINT ( 'NONE',  ( 4.541265875000002339, 7.312499998634407028, 0.000000000000000000 ) ) ;
#61186 = CARTESIAN_POINT ( 'NONE',  ( 6.000000000000001776, 290.5000000000000000, -7.347880794884121708E-16 ) ) ;
#61188 = CARTESIAN_POINT ( 'NONE',  ( 75.00000000000001421, 0.000000000000000000, 20.00000000000001066 ) ) ;
#61187 = CARTESIAN_POINT ( 'NONE',  ( 0.000000000000000000, 0.000000000000000000, 117.4999999999999716 ) ) ;
#61189 = VERTEX_POINT ( 'NONE', #18060 ) ;
#61190 = CARTESIAN_POINT ( 'NONE',  ( -1.432654583217662481, 204.3750000013656063, 145.4587341250000634 ) ) ;
#61191 = CARTESIAN_POINT ( 'NONE',  ( -11.35316468749999785, 3.072916663252683200, -3.042071309553167513 ) ) ;
#61192 = CARTESIAN_POINT ( 'NONE',  ( -6.735557395310442023E-16, 11.00000000000000000, 98.31250000409677625 ) ) ;
#61193 = CARTESIAN_POINT ( 'NONE',  ( 4.000000000000000888, 19.68749999726881228, 1.656854249492384135 ) ) ;
#61194 = CARTESIAN_POINT ( 'NONE',  ( -28.00000000000007105, 203.4375000013656063, 166.5412658750003629 ) ) ;
#61195 = DIRECTION ( 'NONE',  ( 0.000000000000000000, 0.000000000000000000, 1.000000000000000000 ) ) ;
#61197 = CARTESIAN_POINT ( 'NONE',  ( -8.311093377946841443, 8.906249996586016238, 8.311093377946834337 ) ) ;
#61196 = CARTESIAN_POINT ( 'NONE',  ( -7.188101187499999156, 118.2500000020483952, 2.977408999572654924 ) ) ;
#61198 = CARTESIAN_POINT ( 'NONE',  ( -7.999999999999991118, -9.344071862984236532, 29.59466119801952644 ) ) ;
#61199 = CARTESIAN_POINT ( 'NONE',  ( -9.832129032723420536, 118.6979166632526841, 5.676582343749997150 ) ) ;
#61200 = CARTESIAN_POINT ( 'NONE',  ( 5.000000000000001776, 82.70833332650536818, -8.660254037844389075 ) ) ;
#61201 = CARTESIAN_POINT ( 'NONE',  ( 5.082755093536326818, 91.71875000204838102, 5.082755093536325042 ) ) ;
#61202 = CARTESIAN_POINT ( 'NONE',  ( -4.541265875000003227, 19.99999999863440436, 1.881053915767121110 ) ) ;
#61203 = CARTESIAN_POINT ( 'NONE',  ( -7.320508075688773708, 198.7499999931720254, -7.320508075688774596 ) ) ;
#61204 = CARTESIAN_POINT ( 'NONE',  ( 7.320508075688779037, 145.6249999999999716, -7.320508075688779037 ) ) ;
#61205 = VERTEX_POINT ( 'NONE', #734 ) ;
#61206 = CARTESIAN_POINT ( 'NONE',  ( -1.307295064324774714, 225.9999999999999432, -9.935834282059307299 ) ) ;
#61207 = EDGE_CURVE ( 'NONE', #6290, #28600, #41075, .T. ) ;
#61208 = EDGE_CURVE ( 'NONE', #45464, #33515, #3435, .T. ) ;
#61209 = CARTESIAN_POINT ( 'NONE',  ( 4.721056650415999201, 289.2343750017069510, -4.721056650415999201 ) ) ;
#61210 = CARTESIAN_POINT ( 'NONE',  ( 7.320508075688771044, 186.2499999931720254, 7.320508075688775484 ) ) ;
#61211 = CARTESIAN_POINT ( 'NONE',  ( 3.313708498984756279, 7.999999999999991118, 27.41780278432982954 ) ) ;
#61212 = CARTESIAN_POINT ( 'NONE',  ( -10.00000000000000000, 209.1666666598386826, -2.679491924311229845 ) ) ;
#61213 = DIRECTION ( 'NONE',  ( 1.000000000000000000, 0.000000000000000000, 0.000000000000000000 ) ) ;
#61214 = VECTOR ( 'NONE', #19981, 1000.000000000000000 ) ;
#61215 = CARTESIAN_POINT ( 'NONE',  ( -10.18810118749999916, 4.220049686691934809, 102.4375000020483810 ) ) ;
#61216 = ORIENTED_EDGE ( 'NONE', *, *, #52654, .F. ) ;
#61217 = CIRCLE ( 'NONE', #21618, 71.70204102886728492 ) ;
#61218 = CARTESIAN_POINT ( 'NONE',  ( -1.656854249492246467, 197.9375000027312410, 193.9999999999999716 ) ) ;
#61219 = CARTESIAN_POINT ( 'NONE',  ( 9.832129032723416984, 160.6770833299193555, 5.676582343750006032 ) ) ;
#61220 = CARTESIAN_POINT ( 'NONE',  ( -2.445694354108783664, 195.3125000013656063, 195.5543056458912190 ) ) ;
#61221 = CARTESIAN_POINT ( 'NONE',  ( 2.754378923186476579E-14, 207.4375000013656063, 194.5412658750000219 ) ) ;
#61222 = CARTESIAN_POINT ( 'NONE',  ( 2.729893485599592662, 10.18810118749999738, 67.59560438569886287 ) ) ;
#61223 = CARTESIAN_POINT ( 'NONE',  ( -9.832129032723418760, 63.17708332991934839, -5.676582343750004256 ) ) ;
#61224 = EDGE_LOOP ( 'NONE', ( #28584, #67566, #47364, #64846 ) ) ;
#61225 = CARTESIAN_POINT ( 'NONE',  ( -7.204075437095967871, 7.204075437095967871, 113.9687500020483810 ) ) ;
#61226 = EDGE_CURVE ( 'NONE', #16151, #2602, #19374, .T. ) ;
#61227 = CARTESIAN_POINT ( 'NONE',  ( 4.541265875000002339, 8.437499998634407916, 0.000000000000000000 ) ) ;
#61228 = ORIENTED_EDGE ( 'NONE', *, *, #1837, .T. ) ;
#61229 = CARTESIAN_POINT ( 'NONE',  ( 7.188101187500001821, 21.56249999795161898, -2.977408999572650483 ) ) ;
#61230 = CARTESIAN_POINT ( 'NONE',  ( -2.485281374238572649, 289.2500000034140157, 6.000000000000002665 ) ) ;
#61231 = VECTOR ( 'NONE', #71372, 1000.000000000000000 ) ;
#61232 = CARTESIAN_POINT ( 'NONE',  ( -10.00000000000000000, 248.1250000068279746, 0.000000000000000000 ) ) ;
#61233 = CARTESIAN_POINT ( 'NONE',  ( -7.188101187500002709, 19.68749999795161543, 2.977408999572649151 ) ) ;
#61234 = CARTESIAN_POINT ( 'NONE',  ( -2.977408999572647819, -7.188101187499990274, 4.767802781871752771 ) ) ;
#61235 = CARTESIAN_POINT ( 'NONE',  ( -10.18810118749999738, -4.220049686691941915, 107.1250000020483810 ) ) ;
#61236 = CARTESIAN_POINT ( 'NONE',  ( 3.000000000000001332, -44.80401645279004441, 151.2383369607063344 ) ) ;
#61237 = CARTESIAN_POINT ( 'NONE',  ( 2.828427124746191623, 4.874999997268813168, -2.828427124746191623 ) ) ;
#61238 = CARTESIAN_POINT ( 'NONE',  ( -28.00000000000008171, 208.1250000027312126, 166.0000000000003695 ) ) ;
#61239 = ORIENTED_EDGE ( 'NONE', *, *, #27472, .T. ) ;
#61240 = CARTESIAN_POINT ( 'NONE',  ( -3.458734124999959914, 207.3750000013656063, 196.5673454167823877 ) ) ;
#61241 = CARTESIAN_POINT ( 'NONE',  ( -29.43265458321756256, 207.8750000013656063, 173.4587341250004044 ) ) ;
#61242 = CARTESIAN_POINT ( 'NONE',  ( -1.881053915767121554, 5.624999998634407028, -4.541265875000002339 ) ) ;
#61243 = CARTESIAN_POINT ( 'NONE',  ( 7.999999999999992895, -3.313708498984756279, 10.48655277982336642 ) ) ;
#61244 = CARTESIAN_POINT ( 'NONE',  ( -7.188101187499992051, 0.000000000000000000, 26.98655278187175455 ) ) ;
#61245 = ORIENTED_EDGE ( 'NONE', *, *, #13879, .T. ) ;
#61246 = LINE ( 'NONE', #37872, #63844 ) ;
#61247 = VERTEX_POINT ( 'NONE', #13120 ) ;
#61248 = CARTESIAN_POINT ( 'NONE',  ( -1.328591152368359007E-11, 1.250000000001033174, -10.00000000000000533 ) ) ;
#61249 = FACE_OUTER_BOUND ( 'NONE', #4841, .T. ) ;
#61250 = CARTESIAN_POINT ( 'NONE',  ( -2.445694354108782775, 204.5625000013656063, 200.4456943541088663 ) ) ;
#61251 = CARTESIAN_POINT ( 'NONE',  ( 30.44569435410882718, 197.5625000013656063, 172.4456943541086957 ) ) ;
#61252 = CARTESIAN_POINT ( 'NONE',  ( -7.320508075688773708, 66.87500000000001421, -7.320508075688774596 ) ) ;
#61253 = CARTESIAN_POINT ( 'NONE',  ( 2.977408999572654480, 93.50000000204838102, 7.188101187499999156 ) ) ;
#61254 = CARTESIAN_POINT ( 'NONE',  ( 1.102182119232618108E-15, 294.2500000000000000, 6.000000000000001776 ) ) ;
#61255 = CARTESIAN_POINT ( 'NONE',  ( 30.82842712474621294, 208.2500000027312126, 172.8284271247460424 ) ) ;
#61256 = ADVANCED_FACE ( 'NONE', ( #6006 ), #1472, .T. ) ;
#61257 = ORIENTED_EDGE ( 'NONE', *, *, #22673, .F. ) ;
#61258 = CARTESIAN_POINT ( 'NONE',  ( -5.099999999999999645, 6.245698675651499853E-16, -10.80000000000000071 ) ) ;
#61259 = VECTOR ( 'NONE', #44044, 1000.000000000000000 ) ;
#61260 = CARTESIAN_POINT ( 'NONE',  ( 10.99999999999989342, 4.556349186104152515, 87.53125000409677625 ) ) ;
#61261 = CARTESIAN_POINT ( 'NONE',  ( -4.000000000000015099, 200.6875000027312126, 143.6568542494924543 ) ) ;
#61262 = CARTESIAN_POINT ( 'NONE',  ( 0.000000000000000000, 0.000000000000000000, -0.7702282920306856573 ) ) ;
#61263 = CARTESIAN_POINT ( 'NONE',  ( 4.556349186104052151, -10.99999999999999822, 94.46874999999998579 ) ) ;
#61264 = CARTESIAN_POINT ( 'NONE',  ( -9.999999999999998224, 250.2083333333333428, 2.679491924311235618 ) ) ;
#61265 = DIRECTION ( 'NONE',  ( 0.000000000000000000, 0.000000000000000000, -1.000000000000000000 ) ) ;
#61266 = CARTESIAN_POINT ( 'NONE',  ( -7.320508075688778149, 188.1250000000000000, 7.320508075688769267 ) ) ;
#61267 = EDGE_CURVE ( 'NONE', #72372, #59754, #43218, .T. ) ;
#61268 = CARTESIAN_POINT ( 'NONE',  ( 10.99999999999989697, -4.556349186104149851, 111.1562500000000142 ) ) ;
#61269 = CARTESIAN_POINT ( 'NONE',  ( 5.082755093536318824, 5.082755093536319713, 25.29905278187175810 ) ) ;
#61270 = CARTESIAN_POINT ( 'NONE',  ( 9.832129032723420536, 156.5104166632526983, -5.676582343749999815 ) ) ;
#61271 = DIRECTION ( 'NONE',  ( 0.000000000000000000, 0.000000000000000000, 1.000000000000000000 ) ) ;
#61272 = CARTESIAN_POINT ( 'NONE',  ( -5.000000000000000000, 52.62657404299657316, 48.70092614269928788 ) ) ;
#61273 = CARTESIAN_POINT ( 'NONE',  ( -2.249999999999999112, 284.0000000000000000, 5.562148865321749014 ) ) ;
#61275 = CARTESIAN_POINT ( 'NONE',  ( -4.898587196589412829E-16, 109.8125000040967905, -8.000000000000000000 ) ) ;
#61274 = CARTESIAN_POINT ( 'NONE',  ( -7.320508075688773708, 83.74999999317203958, -7.320508075688774596 ) ) ;
#61276 = ORIENTED_EDGE ( 'NONE', *, *, #54714, .F. ) ;
#61277 = AXIS2_PLACEMENT_3D ( 'NONE', #11632, #5981, #52374 ) ;
#61278 = CARTESIAN_POINT ( 'NONE',  ( 3.042071309553167069, 22.13541666325268409, -11.35316468749999785 ) ) ;
#61279 = CARTESIAN_POINT ( 'NONE',  ( 4.999999999999997335, 16.24494643555759410, 69.83755725260752456 ) ) ;
#61281 = CARTESIAN_POINT ( 'NONE',  ( -27.99999999999990763, 195.6250000027311842, 174.0000000000003695 ) ) ;
#61280 = FACE_OUTER_BOUND ( 'NONE', #36888, .T. ) ;
#61282 = CARTESIAN_POINT ( 'NONE',  ( -3.999999999999960032, 196.0625000027312126, 196.3431457505076594 ) ) ;
#61283 = CARTESIAN_POINT ( 'NONE',  ( 3.458734124999958581, 203.5000000013655779, 140.5673454167823593 ) ) ;
#61284 = CIRCLE ( 'NONE', #50398, 18.50000000000000000 ) ;
#61285 = CARTESIAN_POINT ( 'NONE',  ( 8.660254037844389075, 52.29166665983870388, -5.000000000000000000 ) ) ;
#61286 = CARTESIAN_POINT ( 'NONE',  ( -7.188101187500000044, 109.1562500020483810, 0.000000000000000000 ) ) ;
#61287 = CARTESIAN_POINT ( 'NONE',  ( 4.541265875000002339, 9.437499998634407916, 0.000000000000000000 ) ) ;
#61288 = LINE ( 'NONE', #44310, #14401 ) ;
#61289 = CARTESIAN_POINT ( 'NONE',  ( -5.656854249492375253, 5.656854249492375253, 9.642802779823364645 ) ) ;
#61291 = CARTESIAN_POINT ( 'NONE',  ( -1.656854249492381248, 4.062499997268813168, -4.000000000000001776 ) ) ;
#61290 = CARTESIAN_POINT ( 'NONE',  ( 0.000000000000000000, 300.0000000000000000, 0.000000000000000000 ) ) ;
#61292 = EDGE_LOOP ( 'NONE', ( #4494, #41104, #40058, #3153 ) ) ;
#61293 = ORIENTED_EDGE ( 'NONE', *, *, #33856, .F. ) ;
#61294 =( BOUNDED_CURVE ( )  B_SPLINE_CURVE ( 2, ( #66200, #54901, #61298, #14504, #37543 ),
 .UNSPECIFIED., .F., .F. ) 
 B_SPLINE_CURVE_WITH_KNOTS ( ( 3, 2, 3 ),
 ( 0.9861111111111110494, 0.9930555555555555802, 1.000000000000000000 ),
 .UNSPECIFIED. ) 
 CURVE ( )  GEOMETRIC_REPRESENTATION_ITEM ( )  RATIONAL_B_SPLINE_CURVE ( ( 1.000000000000001110, 0.9238795325112855172, 1.000000000000000000, 0.9238795325112867385, 1.000000000000000000 ) ) 
 REPRESENTATION_ITEM ( '' )  );
#61295 =( BOUNDED_CURVE ( )  B_SPLINE_CURVE ( 2, ( #34639, #11237, #29337, #74230, #69321 ),
 .UNSPECIFIED., .F., .F. ) 
 B_SPLINE_CURVE_WITH_KNOTS ( ( 3, 2, 3 ),
 ( 0.000000000000000000, 0.008333333333333399137, 0.01666666666666679827 ),
 .UNSPECIFIED. ) 
 CURVE ( )  GEOMETRIC_REPRESENTATION_ITEM ( )  RATIONAL_B_SPLINE_CURVE ( ( 1.000000000000000000, 0.9238795325112867385, 1.000000000000000000, 0.9238795325112855172, 1.000000000000001110 ) ) 
 REPRESENTATION_ITEM ( '' )  );
#61296 = CARTESIAN_POINT ( 'NONE',  ( 7.999999999999998224, 28.21874999590322375, 3.313708498984766049 ) ) ;
#61297 = CARTESIAN_POINT ( 'NONE',  ( 0.000000000000000000, 0.000000000000000000, -0.6301867843887376530 ) ) ;
#61298 = CARTESIAN_POINT ( 'NONE',  ( 5.656854249492378806, 26.81250000000000355, 5.656854249492381470 ) ) ;
#61299 = CARTESIAN_POINT ( 'NONE',  ( -24.45874247466950635, -40.86802482741075693, 150.9307616100823282 ) ) ;
#61300 = CARTESIAN_POINT ( 'NONE',  ( 3.042071309553167069, 126.8229166632526841, -11.35316468749999785 ) ) ;
#61301 = ORIENTED_EDGE ( 'NONE', *, *, #44411, .F. ) ;
#61302 = DIRECTION ( 'NONE',  ( 0.000000000000000000, 0.000000000000000000, 1.000000000000000000 ) ) ;
#61303 = CARTESIAN_POINT ( 'NONE',  ( 4.220049686691934809, 10.18810118749999916, 89.68750000204836681 ) ) ;
#61304 = DIRECTION ( 'NONE',  ( -0.000000000000000000, 1.000000000000000000, -1.563033456626094573E-30 ) ) ;
#61305 = CARTESIAN_POINT ( 'NONE',  ( -3.999999999999960032, 209.9375000000000000, 196.3431457505076594 ) ) ;
#61306 = CARTESIAN_POINT ( 'NONE',  ( 0.000000000000000000, 300.0000000000000000, 0.000000000000000000 ) ) ;
#61308 = CARTESIAN_POINT ( 'NONE',  ( -3.042071309553163960, 127.2395833299193555, -11.35316468749999963 ) ) ;
#61307 = CARTESIAN_POINT ( 'NONE',  ( 3.687316037205747854, 219.9999999999999432, 9.950260519150386784 ) ) ;
#61309 = DIRECTION ( 'NONE',  ( -0.000000000000000000, -1.000000000000000000, -0.000000000000000000 ) ) ;
#61310 = ORIENTED_EDGE ( 'NONE', *, *, #7790, .T. ) ;
#61311 = CARTESIAN_POINT ( 'NONE',  ( 7.320508075688771044, 258.1250000000000000, -7.320508075688771932 ) ) ;
#61312 = CARTESIAN_POINT ( 'NONE',  ( -34.07942448040748218, 175.6415741637315477, 157.4743357174361904 ) ) ;
#61313 = CARTESIAN_POINT ( 'NONE',  ( -11.35316468750000141, 113.8020833299193555, 3.042071309553159963 ) ) ;
#61314 = CARTESIAN_POINT ( 'NONE',  ( -3.458734124999958581, 206.5000000013655779, 199.4326545832176976 ) ) ;
#61315 = CARTESIAN_POINT ( 'NONE',  ( -2.977408999572654480, 18.37499999795161187, 7.188101187499999156 ) ) ;
#61316 = CARTESIAN_POINT ( 'NONE',  ( -10.18810118749999916, 0.000000000000000000, 84.53125000204836681 ) ) ;
#61317 = CARTESIAN_POINT ( 'NONE',  ( 5.676582343749993598, 20.26041666325268409, 9.832129032723422313 ) ) ;
#61318 = ORIENTED_EDGE ( 'NONE', *, *, #2080, .F. ) ;
#61319 = CARTESIAN_POINT ( 'NONE',  ( -5.656854249492378806, 96.87500000409677625, 5.656854249492381470 ) ) ;
#61320 = CARTESIAN_POINT ( 'NONE',  ( -4.903558642999205574E-16, 8.008118988124991233, 23.13811528394063188 ) ) ;
#61321 = CARTESIAN_POINT ( 'NONE',  ( -2.967813307894019431E-11, 16.44602605510714355, -68.55492853905352035 ) ) ;
#61322 = CARTESIAN_POINT ( 'NONE',  ( -11.00000000000000000, 0.000000000000000000, 118.0000000000000000 ) ) ;
#61323 = CARTESIAN_POINT ( 'NONE',  ( 2.977408999572651815, 1.687499997951610098, 7.188101187500000933 ) ) ;
#61324 = CARTESIAN_POINT ( 'NONE',  ( 1.226468279477575784E-15, 288.7031250017069510, 6.676582343750001591 ) ) ;
#61325 = CARTESIAN_POINT ( 'NONE',  ( 10.00000000000000000, 111.6666666598387110, 2.679491924311235618 ) ) ;
#61326 = ORIENTED_EDGE ( 'NONE', *, *, #2333, .F. ) ;
#61327 = CARTESIAN_POINT ( 'NONE',  ( 9.832129032723420536, 136.5104166632526983, -5.676582343749999815 ) ) ;
#61328 = CARTESIAN_POINT ( 'NONE',  ( 4.220049686691934809, 10.18810118749999916, 79.18750000204836681 ) ) ;
#61329 = CARTESIAN_POINT ( 'NONE',  ( -24.54126587499997925, 195.1250000013656063, 171.4326545832179818 ) ) ;
#61330 = LINE ( 'NONE', #15663, #8925 ) ;
#61331 = CARTESIAN_POINT ( 'NONE',  ( 3.211159895383560947, 17.31249999863440792, 3.211159895383562723 ) ) ;
#61332 = ORIENTED_EDGE ( 'NONE', *, *, #46382, .T. ) ;
#61333 = CONICAL_SURFACE ( 'NONE', #44474, 12.00000000000000000, 1.047197551196596077 ) ;
#61334 = CARTESIAN_POINT ( 'NONE',  ( -1.656854249492348607, 205.3125000027312126, 202.0000000000000284 ) ) ;
#61335 = CARTESIAN_POINT ( 'NONE',  ( 3.458734124999960358, 195.6250000013656063, 143.4326545832176976 ) ) ;
#61336 = CARTESIAN_POINT ( 'NONE',  ( -30.82842712474612767, 205.5000000027312126, 172.8284271247466108 ) ) ;
#61337 = ADVANCED_FACE ( 'NONE', ( #46355 ), #69372, .T. ) ;
#61338 = EDGE_CURVE ( 'NONE', #14923, #71023, #58074, .T. ) ;
#61339 = DIRECTION ( 'NONE',  ( -0.000000000000000000, 1.000000000000000000, -0.000000000000000000 ) ) ;
#61340 = ORIENTED_EDGE ( 'NONE', *, *, #16153, .F. ) ;
#61341 = CARTESIAN_POINT ( 'NONE',  ( 7.188101187499999156, 10.87499999795161187, 2.977408999572654924 ) ) ;
#61342 = CARTESIAN_POINT ( 'NONE',  ( -15.99999999999999645, -16.00000000000000711, 7.387219678533736733 ) ) ;
#61343 = CARTESIAN_POINT ( 'NONE',  ( -2.249999999999999112, 284.0000000000000000, 7.677076266392047543 ) ) ;
#61344 = CARTESIAN_POINT ( 'NONE',  ( 6.951808397369818766E-16, 187.0312499965860127, -11.35316468750000141 ) ) ;
#61345 = EDGE_CURVE ( 'NONE', #70301, #27257, #64862, .T. ) ;
#61346 = CARTESIAN_POINT ( 'NONE',  ( -7.188101187500000044, 109.5312500020483810, 0.000000000000000000 ) ) ;
#61347 = CARTESIAN_POINT ( 'NONE',  ( 2.849036369511732440E-14, 207.3750000027312126, 202.0000000000000000 ) ) ;
#61348 = CARTESIAN_POINT ( 'NONE',  ( 2.765530957081996366, 289.1406250017069510, -6.676582343750002480 ) ) ;
#61350 = CARTESIAN_POINT ( 'NONE',  ( 1.656854249492399234, 201.3125000027311842, 138.0000000000000853 ) ) ;
#61349 = CARTESIAN_POINT ( 'NONE',  ( 9.832129032723420536, 220.9895833367473301, 5.676582343749996262 ) ) ;
#61351 = VERTEX_POINT ( 'NONE', #19525 ) ;
#61352 = CARTESIAN_POINT ( 'NONE',  ( -9.832129032723418760, 263.4895833367473301, -5.676582343749998927 ) ) ;
#61353 = CARTESIAN_POINT ( 'NONE',  ( -4.401442555609577197E-16, 7.188101187499992051, 22.48655278187175455 ) ) ;
#61354 = CARTESIAN_POINT ( 'NONE',  ( -4.898587196589412829E-16, 106.6250000000000000, -8.000000000000000000 ) ) ;
#61355 = DIRECTION ( 'NONE',  ( -0.000000000000000000, -0.000000000000000000, 1.000000000000000000 ) ) ;
#61356 = CARTESIAN_POINT ( 'NONE',  ( -3.544144923084051602, -60.54353712382344099, -23.09461823984392481 ) ) ;
#61357 = CARTESIAN_POINT ( 'NONE',  ( -1.432654583217607414, 195.5000000013655779, 194.5412658750000219 ) ) ;
#61358 = DIRECTION ( 'NONE',  ( 0.000000000000000000, 0.000000000000000000, 1.000000000000000000 ) ) ;
#61359 = CARTESIAN_POINT ( 'NONE',  ( -2.598723904613012614, 8.891930899535427812, -0.1469846612282519061 ) ) ;
#61360 = CARTESIAN_POINT ( 'NONE',  ( -5.656854249492378806, 92.18749999999998579, 5.656854249492381470 ) ) ;
#61361 = CARTESIAN_POINT ( 'NONE',  ( 9.832129032723420536, 116.5104166632526841, -5.676582343749999815 ) ) ;
#61362 = CARTESIAN_POINT ( 'NONE',  ( -6.000000000000001776, 296.0000000000000000, 0.000000000000000000 ) ) ;
#61363 = CARTESIAN_POINT ( 'NONE',  ( 4.556349186104051263, -10.99999999999999822, 68.96875000000000000 ) ) ;
#61366 = CARTESIAN_POINT ( 'NONE',  ( 8.000000000000001776, 118.3437500040967763, 3.313708498984759387 ) ) ;
#61365 = CARTESIAN_POINT ( 'NONE',  ( 30.44569435410879521, 201.8125000013656063, 167.5543056458910485 ) ) ;
#61364 = CARTESIAN_POINT ( 'NONE',  ( 26.56734541678237704, 197.2500000013656063, 166.5412658749999650 ) ) ;
#61367 = ORIENTED_EDGE ( 'NONE', *, *, #36, .T. ) ;
#61368 = CARTESIAN_POINT ( 'NONE',  ( 9.865726904258298902, 225.1318477000477003, -1.659788900511623311 ) ) ;
#61369 = EDGE_CURVE ( 'NONE', #18479, #48053, #47288, .T. ) ;
#61370 = CARTESIAN_POINT ( 'NONE',  ( -5.676582343750006032, 224.1145833299193839, 9.832129032723418760 ) ) ;
#61371 = CARTESIAN_POINT ( 'NONE',  ( -2.839093476692135984E-14, 195.6875000013655779, 138.5412658750000503 ) ) ;
#61372 = CARTESIAN_POINT ( 'NONE',  ( 24.54126587499999701, 196.3750000013656063, 168.5673454167822172 ) ) ;
#61373 = CARTESIAN_POINT ( 'NONE',  ( 11.35316468750000141, 211.0937499965860411, 0.000000000000000000 ) ) ;
#61374 = CARTESIAN_POINT ( 'NONE',  ( 6.517621199079068006, 225.9999999999999147, 7.979021773805921036 ) ) ;
#61375 = CARTESIAN_POINT ( 'NONE',  ( 1.881053915767122664, 17.12499999863440436, 4.541265875000001451 ) ) ;
#61376 = CARTESIAN_POINT ( 'NONE',  ( 28.00000000000001776, 196.1875000013655779, 166.5412658749999082 ) ) ;
#61377 = CARTESIAN_POINT ( 'NONE',  ( -7.999999999999991118, 0.000000000000000000, 24.83030277982336642 ) ) ;
#61379 = CARTESIAN_POINT ( 'NONE',  ( -7.999999999999991118, 9.797174393178815797E-16, 30.00000000000000000 ) ) ;
#61378 = SURFACE_STYLE_FILL_AREA ( #42244 ) ;
#61380 = CARTESIAN_POINT ( 'NONE',  ( 11.35316468750000141, 90.78124999658602690, 0.000000000000000000 ) ) ;
#61381 = VERTEX_POINT ( 'NONE', #42542 ) ;
#61382 = DIRECTION ( 'NONE',  ( 1.000000000000000000, -0.000000000000000000, -0.000000000000000000 ) ) ;
#61383 = CARTESIAN_POINT ( 'NONE',  ( 7.188101187500001821, 18.56249999795161187, -2.977408999572650483 ) ) ;
#61384 =( BOUNDED_CURVE ( )  B_SPLINE_CURVE ( 2, ( #20396, #7242, #66424, #25309, #54754, #65313, #37393, #64940, #14736 ),
 .UNSPECIFIED., .F., .F. ) 
 B_SPLINE_CURVE_WITH_KNOTS ( ( 3, 2, 2, 2, 3 ),
 ( 0.8020833333333334814, 0.8072916666666667407, 0.8125000000000001110, 0.8177083333333334814, 0.8229166666666667407 ),
 .UNSPECIFIED. ) 
 CURVE ( )  GEOMETRIC_REPRESENTATION_ITEM ( )  RATIONAL_B_SPLINE_CURVE ( ( 0.9999999999999983347, 0.9238795325112884038, 1.000000000000000000, 0.9238795325112867385, 1.000000000000000000, 0.9238795325112867385, 1.000000000000000000, 0.9238795325112850731, 1.000000000000001554 ) ) 
 REPRESENTATION_ITEM ( '' )  );
#61385 = CARTESIAN_POINT ( 'NONE',  ( -8.311093377946836114, 258.5937500034140157, -8.311093377946836114 ) ) ;
#61386 = CARTESIAN_POINT ( 'NONE',  ( -5.676582343749998039, 82.44791666325268409, -9.832129032723420536 ) ) ;
#61387 = ORIENTED_EDGE ( 'NONE', *, *, #14377, .F. ) ;
#61388 = DIRECTION ( 'NONE',  ( 1.000000000000000000, 0.000000000000000000, 0.000000000000000000 ) ) ;
#61389 = CARTESIAN_POINT ( 'NONE',  ( -10.18810118749999916, 0.000000000000000000, 109.6562500020483668 ) ) ;
#61390 = CARTESIAN_POINT ( 'NONE',  ( -31.45873412499997812, 195.0000000013656063, 171.4326545832180386 ) ) ;
#61391 = CARTESIAN_POINT ( 'NONE',  ( 3.458734125000015425, 203.2500000013656063, 196.5673454167823877 ) ) ;
#61392 = CARTESIAN_POINT ( 'NONE',  ( -4.898587196589412829E-16, 118.6250000000000000, -8.000000000000000000 ) ) ;
#61394 = CARTESIAN_POINT ( 'NONE',  ( 11.35316468750000141, 85.78124999658602690, 0.000000000000000000 ) ) ;
#61393 = CARTESIAN_POINT ( 'NONE',  ( -26.34314575050768781, 207.0625000027312126, 166.0000000000003695 ) ) ;
#61395 = CARTESIAN_POINT ( 'NONE',  ( -7.999999999999991118, 0.000000000000000000, 16.01780278392014978 ) ) ;
#61396 = CARTESIAN_POINT ( 'NONE',  ( -24.54126587499998280, 201.3750000013656347, 171.4326545832179818 ) ) ;
#61397 = CARTESIAN_POINT ( 'NONE',  ( 105.0000000000000000, 133.9999999999999716, 127.0000000000000000 ) ) ;
#61398 =( BOUNDED_CURVE ( )  B_SPLINE_CURVE ( 2, ( #36660, #23854, #47962, #35925, #25315, #48331, #47227, #71339, #19660 ),
 .UNSPECIFIED., .F., .F. ) 
 B_SPLINE_CURVE_WITH_KNOTS ( ( 3, 2, 2, 2, 3 ),
 ( 0.6470588235294116863, 0.6507352941176469674, 0.6544117647058822484, 0.6580882352941175295, 0.6617647058823528106 ),
 .UNSPECIFIED. ) 
 CURVE ( )  GEOMETRIC_REPRESENTATION_ITEM ( )  RATIONAL_B_SPLINE_CURVE ( ( 1.000000000000002220, 0.9238795325112844070, 1.000000000000000000, 0.9238795325112867385, 1.000000000000000000, 0.9238795325112867385, 1.000000000000000000, 0.9238795325112890700, 0.9999999999999976685 ) ) 
 REPRESENTATION_ITEM ( '' )  );
#61399 = CARTESIAN_POINT ( 'NONE',  ( 7.320508075688771044, 186.2499999931719969, 7.320508075688775484 ) ) ;
#61400 = CARTESIAN_POINT ( 'NONE',  ( 5.000000000000000000, -53.35645474066812710, 47.33026262608733958 ) ) ;
#61401 = CARTESIAN_POINT ( 'NONE',  ( 9.832129032723416984, 70.67708332991935549, 5.676582343750006032 ) ) ;
#61402 = CARTESIAN_POINT ( 'NONE',  ( -2.765530957081996810, 295.2656250017070079, -6.676582343750003368 ) ) ;
#61403 = CARTESIAN_POINT ( 'NONE',  ( -10.18810118749999916, 4.220049686691934809, 99.43750000204836681 ) ) ;
#61404 = CARTESIAN_POINT ( 'NONE',  ( -11.35316468749999785, 208.0729166632526983, -3.042071309553167513 ) ) ;
#61405 = ORIENTED_EDGE ( 'NONE', *, *, #38700, .T. ) ;
#61406 = CARTESIAN_POINT ( 'NONE',  ( -1.836970198721029983E-15, 70.62499999317203958, 10.00000000000000178 ) ) ;
#61407 = CARTESIAN_POINT ( 'NONE',  ( -11.50000000000000178, 82.00000000000001421, 65.00000000000000000 ) ) ;
#61408 = CARTESIAN_POINT ( 'NONE',  ( 5.000000000000000000, 67.10422270468680495, 23.07049055144833716 ) ) ;
#61410 = CARTESIAN_POINT ( 'NONE',  ( 6.951808397369818766E-16, 212.0312499965860411, -11.35316468750000141 ) ) ;
#61409 = CARTESIAN_POINT ( 'NONE',  ( 0.000000000000000000, 0.000000000000000000, 0.000000000000000000 ) ) ;
#61411 = CARTESIAN_POINT ( 'NONE',  ( 10.00000000000000000, 225.6250000068279746, -1.224646799147353256E-15 ) ) ;
#61412 = LINE ( 'NONE', #27078, #45650 ) ;
#61413 = VERTEX_POINT ( 'NONE', #66674 ) ;
#61414 = CARTESIAN_POINT ( 'NONE',  ( 5.676582343750001591, 196.9270833299193839, -9.832129032723420536 ) ) ;
#61415 =( BOUNDED_CURVE ( )  B_SPLINE_CURVE ( 2, ( #10900, #16919, #67865, #16534, #5619, #10526, #46341, #33191, #4877, #39942, #5249, #63316, #27872 ),
 .UNSPECIFIED., .F., .F. ) 
 B_SPLINE_CURVE_WITH_KNOTS ( ( 3, 2, 2, 2, 2, 2, 3 ),
 ( 2.590487804266785599, 2.595720217480772529, 2.600952630694759460, 2.606185043908746390, 2.611417457122733321, 2.616649870336720252, 2.621882283550707182 ),
 .UNSPECIFIED. ) 
 CURVE ( )  GEOMETRIC_REPRESENTATION_ITEM ( )  RATIONAL_B_SPLINE_CURVE ( ( 1.000000000000001776, 0.9659258262890662028, 0.9999999999999998890, 0.9659258262890683122, 0.9999999999999998890, 0.9659258262890683122, 0.9999999999999998890, 0.9659258262890683122, 0.9999999999999998890, 0.9659258262890683122, 0.9999999999999998890, 0.9659258262894191427, 0.9999999999996490585 ) ) 
 REPRESENTATION_ITEM ( '' )  );
#61416 = CARTESIAN_POINT ( 'NONE',  ( 2.977408999572646486, 7.188101187499992051, 13.01780278187175277 ) ) ;
#61417 = CARTESIAN_POINT ( 'NONE',  ( 3.313708498984762496, -7.999999999999989342, 16.48655278392014623 ) ) ;
#61418 = CARTESIAN_POINT ( 'NONE',  ( 3.313708498984762496, 10.21875000000000178, 7.999999999999998224 ) ) ;
#61419 = ORIENTED_EDGE ( 'NONE', *, *, #44154, .F. ) ;
#61420 = EDGE_CURVE ( 'NONE', #65598, #12358, #62707, .T. ) ;
#61421 = CARTESIAN_POINT ( 'NONE',  ( 8.000000000000001776, 91.34375000409679046, 3.313708498984759387 ) ) ;
#61422 = CARTESIAN_POINT ( 'NONE',  ( 6.123233995736767268E-16, 11.25000000000000178, -10.00000000000000178 ) ) ;
#61423 = AXIS2_PLACEMENT_3D ( 'NONE', #20874, #55231, #31833 ) ;
#61424 = SHAPE_REPRESENTATION ( 'plain washer (type a)_is_IS 2016 A- 22', ( #57354 ), #1968 ) ;
#61425 = CARTESIAN_POINT ( 'NONE',  ( -10.18810118749999738, -4.220049686691941915, 80.12500000204835260 ) ) ;
#61426 = VERTEX_POINT ( 'NONE', #14607 ) ;
#61427 = CARTESIAN_POINT ( 'NONE',  ( -7.347880794884122694E-16, 21.75000000000000355, 4.000000000000001776 ) ) ;
#61428 = CARTESIAN_POINT ( 'NONE',  ( -3.211159895383561391, 18.68749999863440436, -3.211159895383561835 ) ) ;
#61429 = CARTESIAN_POINT ( 'NONE',  ( 1.469576158976822172E-15, -7.999999999999991118, 7.392802783920144449 ) ) ;
#61430 = CARTESIAN_POINT ( 'NONE',  ( 4.231687259402700185, 16.30907003467283189, -69.42009600258256796 ) ) ;
#61432 = ORIENTED_EDGE ( 'NONE', *, *, #4836, .F. ) ;
#61431 = ADVANCED_FACE ( 'NONE', ( #37269 ), #60262, .F. ) ;
#61433 = CARTESIAN_POINT ( 'NONE',  ( 7.188101187500001821, 95.00000000204836681, -2.977408999572651371 ) ) ;
#61436 = DIRECTION ( 'NONE',  ( 0.000000000000000000, 0.000000000000000000, 1.000000000000000000 ) ) ;
#61435 = CARTESIAN_POINT ( 'NONE',  ( -5.676582343750000703, 258.0729166700806445, -9.832129032723418760 ) ) ;
#61434 = CARTESIAN_POINT ( 'NONE',  ( -4.898587196589407898E-16, 7.999999999999991118, 12.45530277982336642 ) ) ;
#61437 = DIRECTION ( 'NONE',  ( 0.9671668234732140323, -0.2541423529692226624, 0.000000000000000000 ) ) ;
#61438 = ORIENTED_EDGE ( 'NONE', *, *, #36567, .T. ) ;
#61439 = EDGE_CURVE ( 'NONE', #73018, #64342, #11160, .T. ) ;
#61440 = CARTESIAN_POINT ( 'NONE',  ( 8.311093377946834337, 252.3437500034139873, -8.311093377946836114 ) ) ;
#61441 = CARTESIAN_POINT ( 'NONE',  ( 7.188101187499991163, 2.977408999572648707, 12.83030278187175277 ) ) ;
#61442 = ORIENTED_EDGE ( 'NONE', *, *, #63842, .F. ) ;
#61443 = ORIENTED_EDGE ( 'NONE', *, *, #30618, .T. ) ;
#61444 = CARTESIAN_POINT ( 'NONE',  ( 4.220049686691934809, 10.18810118749999916, 73.18750000204838102 ) ) ;
#61445 = CARTESIAN_POINT ( 'NONE',  ( 3.042071309553167069, 72.13541666325268409, -11.35316468749999785 ) ) ;
#61446 = CARTESIAN_POINT ( 'NONE',  ( -5.656854249492373476, -5.656854249492376141, 17.51780277982336287 ) ) ;
#61447 = CARTESIAN_POINT ( 'NONE',  ( -4.556349186104047710, -10.99999999999999822, 91.28125000000000000 ) ) ;
#61450 = CARTESIAN_POINT ( 'NONE',  ( -4.721056650415998313, 288.7343750017069510, 4.721056650416000089 ) ) ;
#61449 = CARTESIAN_POINT ( 'NONE',  ( 29.65685424949235127, 198.5625000027312126, 165.9999999999998863 ) ) ;
#61448 = CARTESIAN_POINT ( 'NONE',  ( -25.17157287525386167, 206.0000000027312126, 167.1715728752541281 ) ) ;
#61451 = CARTESIAN_POINT ( 'NONE',  ( 2.449293598294707893E-16, 14.25000000000000000, -4.000000000000001776 ) ) ;
#61452 = LINE ( 'NONE', #10517, #32378 ) ;
#61453 = ADVANCED_FACE ( 'NONE', ( #20261 ), #24813, .F. ) ;
#61454 = CARTESIAN_POINT ( 'NONE',  ( -2.445694354108783219, 197.8125000013656063, 200.4456943541088663 ) ) ;
#61455 = CARTESIAN_POINT ( 'NONE',  ( -3.313708498984760720, 9.281249995903221972, -8.000000000000000000 ) ) ;
#61456 = ORIENTED_EDGE ( 'NONE', *, *, #48868, .F. ) ;
#61457 = CARTESIAN_POINT ( 'NONE',  ( 24.54126587499997925, 196.2500000013656631, 171.4326545832175555 ) ) ;
#61458 = CARTESIAN_POINT ( 'NONE',  ( -7.188101187500000044, 16.59374999795161543, -8.802885111219163269E-16 ) ) ;
#61459 = CARTESIAN_POINT ( 'NONE',  ( 3.042071309553159519, 170.0520833299193271, 11.35316468750000141 ) ) ;
#61460 = DIRECTION ( 'NONE',  ( -0.000000000000000000, 1.000000000000000000, -0.000000000000000000 ) ) ;
#61461 = CARTESIAN_POINT ( 'NONE',  ( 2.977408999572654480, 104.0000000020483810, 7.188101187499999156 ) ) ;
#61463 = CARTESIAN_POINT ( 'NONE',  ( -1.308779242311861601, -49.95118570763067822, -40.70975538998027332 ) ) ;
#61462 = CARTESIAN_POINT ( 'NONE',  ( 2.828427124746208943, 201.6250000000000284, 195.1715728752538439 ) ) ;
#61464 = CARTESIAN_POINT ( 'NONE',  ( 27.99999999999996803, 208.6875000013656063, 173.4587341249998929 ) ) ;
#61465 = CARTESIAN_POINT ( 'NONE',  ( 1.320432766682872962E-15, -7.188101187499992051, 17.23655278187175810 ) ) ;
#61466 = CARTESIAN_POINT ( 'NONE',  ( 2.828427124746153876, 208.0000000027312126, 144.8284271247462129 ) ) ;
#61467 = CARTESIAN_POINT ( 'NONE',  ( -11.35316468749999785, 48.07291666325268409, -3.042071309553167513 ) ) ;
#61468 = CYLINDRICAL_SURFACE ( 'NONE', #25559, 3.999999999999976019 ) ;
#61469 = CARTESIAN_POINT ( 'NONE',  ( -1.836970198721029983E-15, 25.62499999317203248, 10.00000000000000178 ) ) ;
#61470 = CARTESIAN_POINT ( 'NONE',  ( -11.00000000000000000, 0.000000000000000000, 71.49999999999998579 ) ) ;
#61471 = ORIENTED_EDGE ( 'NONE', *, *, #51985, .T. ) ;
#61472 = DIRECTION ( 'NONE',  ( -0.000000000000000000, 1.000000000000000000, -4.476705744456276341E-16 ) ) ;
#61473 = CARTESIAN_POINT ( 'NONE',  ( -3.313708498984805573, 20.34374999590321664, 7.999999999999956479 ) ) ;
#61474 = CARTESIAN_POINT ( 'NONE',  ( 9.832129032723416984, 50.36458332991934839, 5.676582343750006032 ) ) ;
#61475 = CARTESIAN_POINT ( 'NONE',  ( -7.778174593052020747, -7.778174593052023411, 80.87500000409677625 ) ) ;
#61476 = CARTESIAN_POINT ( 'NONE',  ( 3.458734124999959469, 199.7500000013656063, 140.5673454167823593 ) ) ;
#61477 = DIRECTION ( 'NONE',  ( 0.000000000000000000, 0.000000000000000000, 1.000000000000000000 ) ) ;
#61478 = CARTESIAN_POINT ( 'NONE',  ( -1.656854249492521136, 196.8125000027311557, 145.9999999999999147 ) ) ;
#61480 = CARTESIAN_POINT ( 'NONE',  ( 5.676582343749993598, 49.94791666325268409, 9.832129032723422313 ) ) ;
#61479 = CARTESIAN_POINT ( 'NONE',  ( -7.188101187500000933, 97.06250000204838102, -2.977408999572650483 ) ) ;
#61481 = CARTESIAN_POINT ( 'NONE',  ( -7.999999999999991118, 0.000000000000000000, 8.330302779823362869 ) ) ;
#61482 = CARTESIAN_POINT ( 'NONE',  ( -7.999999999999991118, -2.368985594519444545E-05, 22.01780345414325524 ) ) ;
#61483 = CARTESIAN_POINT ( 'NONE',  ( 6.951808397369818766E-16, 167.0312499965860411, -11.35316468750000141 ) ) ;
#61484 = CIRCLE ( 'NONE', #44630, 20.00000000000001066 ) ;
#61485 = CARTESIAN_POINT ( 'NONE',  ( -10.00000000000000000, 144.1666666598386541, -2.679491924311229845 ) ) ;
#61486 = CARTESIAN_POINT ( 'NONE',  ( 7.188101187500000044, 101.2812500020483810, -8.802885111219163269E-16 ) ) ;
#61487 = CARTESIAN_POINT ( 'NONE',  ( -49.70177871865297448, 134.0000000000000284, 57.99999999999998579 ) ) ;
#61488 = CARTESIAN_POINT ( 'NONE',  ( -9.832129032723418760, 38.17708332991935549, -5.676582343750004256 ) ) ;
#61489 = CARTESIAN_POINT ( 'NONE',  ( 0.000000000000000000, 0.000000000000000000, 0.000000000000000000 ) ) ;
#61490 = EDGE_LOOP ( 'NONE', ( #38621, #37762, #20764, #26601, #21505, #69301, #14134, #40234, #58155, #54392, #53278 ) ) ;
#61491 = LINE ( 'NONE', #43762, #65671 ) ;
#61492 = CARTESIAN_POINT ( 'NONE',  ( -6.238412754330611322E-16, 10.18810118749999916, 76.28125000204836681 ) ) ;
#61493 = CARTESIAN_POINT ( 'NONE',  ( -7.347880794884122694E-16, 18.49999999726881583, 4.000000000000001776 ) ) ;
#61495 = CARTESIAN_POINT ( 'NONE',  ( 11.35316468749999785, 165.5729166632526699, 3.042071309553174174 ) ) ;
#61494 = CARTESIAN_POINT ( 'NONE',  ( -4.898587196589412829E-16, 91.62499999999998579, -8.000000000000000000 ) ) ;
#61496 = AXIS2_PLACEMENT_3D ( 'NONE', #27399, #38747, #72308 ) ;
#61497 = CARTESIAN_POINT ( 'NONE',  ( 1.469576158976822172E-15, -7.999999999999991118, 14.76155278432982421 ) ) ;
#61498 = CARTESIAN_POINT ( 'NONE',  ( 7.999999999999991118, 9.797174393178815797E-16, 16.58030277982336287 ) ) ;
#61499 = CARTESIAN_POINT ( 'NONE',  ( -11.35316468749999963, 218.9062500034139873, 0.000000000000000000 ) ) ;
#61500 = CARTESIAN_POINT ( 'NONE',  ( 2.990854866088366482, 55.96051345247598618, -43.98806351443035112 ) ) ;
#61501 = CARTESIAN_POINT ( 'NONE',  ( -10.18810118749999916, 4.220049686691934809, 87.43750000204838102 ) ) ;
#61502 = ORIENTED_EDGE ( 'NONE', *, *, #1687, .T. ) ;
#61503 = CARTESIAN_POINT ( 'NONE',  ( 4.898587196589412829E-16, 21.18749999590322375, -8.000000000000000000 ) ) ;
#61504 = DIRECTION ( 'NONE',  ( -0.000000000000000000, 1.000000000000000000, -0.000000000000000000 ) ) ;
#61505 = CARTESIAN_POINT ( 'NONE',  ( -11.35316468750000141, 118.8020833299193413, 3.042071309553159963 ) ) ;
#61506 =( BOUNDED_CURVE ( )  B_SPLINE_CURVE ( 2, ( #60446, #49505, #3119, #38943, #20832, #4246, #73272, #38200, #43089, #43466, #72136 ),
 .UNSPECIFIED., .F., .F. ) 
 B_SPLINE_CURVE_WITH_KNOTS ( ( 3, 2, 2, 2, 2, 3 ),
 ( 0.07941930701348173804, 0.08603758259794166974, 0.09265585818240160143, 0.09927413376686153312, 0.1058924093513214509, 0.1058924239672156403 ),
 .UNSPECIFIED. ) 
 CURVE ( )  GEOMETRIC_REPRESENTATION_ITEM ( )  RATIONAL_B_SPLINE_CURVE ( ( 1.000000000000000000, 0.9238795325112867385, 1.000000000000000000, 0.9238795325112867385, 1.000000000000000000, 0.9238795325112867385, 1.000000000000000000, 0.9238795325112867385, 1.000000000000000000, 0.9999998318944740561, 0.9999996637896906293 ) ) 
 REPRESENTATION_ITEM ( '' )  );
#61507 = CARTESIAN_POINT ( 'NONE',  ( 10.18810118750000093, -4.220049686691933921, 98.31250000204836681 ) ) ;
#61508 = CARTESIAN_POINT ( 'NONE',  ( 2.679491924297975558, 13.95833333333215087, 10.00000000000766676 ) ) ;
#61509 = VERTEX_POINT ( 'NONE', #66300 ) ;
#61510 = ORIENTED_EDGE ( 'NONE', *, *, #39210, .T. ) ;
#61511 = EDGE_CURVE ( 'NONE', #39105, #19023, #39624, .T. ) ;
#61512 = CARTESIAN_POINT ( 'NONE',  ( -1.881053915767121554, 3.749999998634407028, -4.541265875000002339 ) ) ;
#61513 = CARTESIAN_POINT ( 'NONE',  ( 7.188101187500000044, 7.968749997951610986, 0.000000000000000000 ) ) ;
#61514 = CARTESIAN_POINT ( 'NONE',  ( -8.000000000000000000, 111.5937500040967763, -3.313708498984761608 ) ) ;
#61515 = AXIS2_PLACEMENT_3D ( 'NONE', #32672, #66604, #26986 ) ;
#61516 = CARTESIAN_POINT ( 'NONE',  ( 7.204075437095966983, 7.204075437095967871, 89.96875000204838102 ) ) ;
#61517 = CARTESIAN_POINT ( 'NONE',  ( -25.55430564589119413, 202.5625000013656063, 167.5543056458915316 ) ) ;
#61518 = CARTESIAN_POINT ( 'NONE',  ( -4.000000000000002665, 4.562500000000000888, 1.656854249492380804 ) ) ;
#61519 =( BOUNDED_CURVE ( )  B_SPLINE_CURVE ( 2, ( #5274, #61862, #74292, #4527, #39598, #28643, #11299, #56589, #10184, #34332, #21857, #55846, #4904 ),
 .UNSPECIFIED., .F., .F. ) 
 B_SPLINE_CURVE_WITH_KNOTS ( ( 3, 2, 2, 2, 2, 2, 3 ),
 ( 0.3315217391304347561, 0.3333333333333333148, 0.3351449275362318736, 0.3369565217391303769, 0.3387681159420289356, 0.3405797101449274944, 0.3423913043478260532 ),
 .UNSPECIFIED. ) 
 CURVE ( )  GEOMETRIC_REPRESENTATION_ITEM ( )  RATIONAL_B_SPLINE_CURVE ( ( 1.000000000000000000, 0.9659258262890683122, 1.000000000000000000, 0.9659258262890683122, 1.000000000000000000, 0.9659258262890683122, 1.000000000000000000, 0.9659258262890683122, 1.000000000000000000, 0.9659258262890683122, 1.000000000000000000, 0.9659258262890693114, 0.9999999999999990008 ) ) 
 REPRESENTATION_ITEM ( '' )  );
#61520 = CARTESIAN_POINT ( 'NONE',  ( -2.828427124746192067, 19.37499999726881228, 2.828427124746190735 ) ) ;
#61521 = CARTESIAN_POINT ( 'NONE',  ( -3.211159895383562723, 5.937499998634407028, 3.211159895383561391 ) ) ;
#61522 = CARTESIAN_POINT ( 'NONE',  ( -4.000000000000015987, 202.5000000000000000, 142.0000000000000568 ) ) ;
#61523 = ORIENTED_EDGE ( 'NONE', *, *, #11973, .F. ) ;
#61524 = CARTESIAN_POINT ( 'NONE',  ( 8.000000000000000000, 116.8437500000000000, -3.313708498984762496 ) ) ;
#61526 = CARTESIAN_POINT ( 'NONE',  ( -2.679491924311235174, 225.4166666598387110, 10.00000000000000000 ) ) ;
#61525 = CARTESIAN_POINT ( 'NONE',  ( -28.00000000000006750, 197.4375000013655779, 166.5412658750003629 ) ) ;
#61527 = EDGE_CURVE ( 'NONE', #18569, #3989, #22062, .T. ) ;
#61528 = CARTESIAN_POINT ( 'NONE',  ( 1.881053915767121776, 19.49999999863440436, -4.541265875000002339 ) ) ;
#61529 = CARTESIAN_POINT ( 'NONE',  ( 1.330548028524511706, -47.69598779870954530, 151.0457710442422581 ) ) ;
#61530 = LINE ( 'NONE', #39, #44433 ) ;
#61531 = ORIENTED_EDGE ( 'NONE', *, *, #2144, .F. ) ;
#61532 = ORIENTED_EDGE ( 'NONE', *, *, #45453, .F. ) ;
#61533 = CARTESIAN_POINT ( 'NONE',  ( 4.220049686691941027, -10.18810118749999738, 99.62500000204838102 ) ) ;
#61534 = CARTESIAN_POINT ( 'NONE',  ( -7.999999999999991118, 0.000000000000000000, 20.33030277982336642 ) ) ;
#61535 = CARTESIAN_POINT ( 'NONE',  ( -26.56734541678232731, 198.2500000013656347, 173.4587341250003760 ) ) ;
#61536 = CARTESIAN_POINT ( 'NONE',  ( 11.00000000000000355, -4.556349186104045046, 105.1562499999999858 ) ) ;
#61537 = CARTESIAN_POINT ( 'NONE',  ( 3.458734125000015869, 206.1875000013656063, 198.0000000000000284 ) ) ;
#61538 = CARTESIAN_POINT ( 'NONE',  ( 2.828427124746209831, 203.5000000027312126, 200.8284271247462129 ) ) ;
#61539 = CARTESIAN_POINT ( 'NONE',  ( -10.00000000000000178, 117.5000000000000142, -1.224646799147353454E-15 ) ) ;
#61540 = CARTESIAN_POINT ( 'NONE',  ( 1.469576158976823947E-15, 104.3750000000000000, 8.000000000000000000 ) ) ;
#61541 = CARTESIAN_POINT ( 'NONE',  ( -4.721056650415999201, 291.4843750017070079, -4.721056650415999201 ) ) ;
#61542 = VECTOR ( 'NONE', #28165, 1000.000000000000000 ) ;
#61543 = CARTESIAN_POINT ( 'NONE',  ( -2.977408999572647819, 7.188101187499991163, 13.58030278187175277 ) ) ;
#61544 = ADVANCED_FACE ( 'NONE', ( #55002 ), #68166, .T. ) ;
#61545 = ORIENTED_EDGE ( 'NONE', *, *, #7216, .T. ) ;
#61546 = CARTESIAN_POINT ( 'NONE',  ( -3.313708498984762496, 102.9687500040967620, 7.999999999999998224 ) ) ;
#61547 = ADVANCED_FACE ( 'NONE', ( #21760 ), #44789, .T. ) ;
#61548 = CARTESIAN_POINT ( 'NONE',  ( 28.00000000000002487, 205.9375000013656063, 166.5412658749999082 ) ) ;
#61549 = CARTESIAN_POINT ( 'NONE',  ( -3.313708498984760720, 19.78124999590322375, -8.000000000000000000 ) ) ;
#61550 = CARTESIAN_POINT ( 'NONE',  ( -2.445694354108839619, 200.8125000013656063, 139.5543056458912190 ) ) ;
#61551 = CARTESIAN_POINT ( 'NONE',  ( 5.082755093536326818, 123.5937500020483952, 5.082755093536325042 ) ) ;
#61553 = CARTESIAN_POINT ( 'NONE',  ( -3.458734125000016757, 202.1250000013656063, 140.5673454167824161 ) ) ;
#61552 = CARTESIAN_POINT ( 'NONE',  ( 2.638998369017349077, 194.9937430236944067, 145.0090071730267312 ) ) ;
#61554 = CARTESIAN_POINT ( 'NONE',  ( 3.042071309553173286, 250.6770833367473017, 11.35316468749999608 ) ) ;
#61555 = CARTESIAN_POINT ( 'NONE',  ( 27.99999999999999645, 210.0000000000000284, 169.9999999999999147 ) ) ;
#61556 = DIRECTION ( 'NONE',  ( -0.000000000000000000, 1.000000000000000000, 4.689100369878284071E-30 ) ) ;
#61557 = CARTESIAN_POINT ( 'NONE',  ( -9.832129032723418760, 7.864583329919350163, -5.676582343750004256 ) ) ;
#61558 = CARTESIAN_POINT ( 'NONE',  ( -4.401442555609577197E-16, 7.188101187499992051, 7.486552781871751883 ) ) ;
#61559 = CARTESIAN_POINT ( 'NONE',  ( -5.676582343750006032, 204.4270833299193555, 9.832129032723418760 ) ) ;
#61560 = DIRECTION ( 'NONE',  ( -1.000000000000000000, 0.000000000000000000, 0.000000000000000000 ) ) ;
#61561 = CARTESIAN_POINT ( 'NONE',  ( -3.211159895383562723, 5.937499998634407028, 3.211159895383561391 ) ) ;
#61562 = DIRECTION ( 'NONE',  ( -0.000000000000000000, -0.000000000000000000, -1.000000000000000000 ) ) ;
#61564 = PLANE ( 'NONE',  #45939 ) ;
#61563 = DIRECTION ( 'NONE',  ( 1.000000000000000000, 0.000000000000000000, 0.000000000000000000 ) ) ;
#61565 = ORIENTED_EDGE ( 'NONE', *, *, #59737, .T. ) ;
#61566 = CARTESIAN_POINT ( 'NONE',  ( 1.432654583217607414, 199.5000000013656063, 145.4587341250000634 ) ) ;
#61567 = CARTESIAN_POINT ( 'NONE',  ( 5.676582343749993598, 4.947916663252683200, 9.832129032723422313 ) ) ;
#61568 = CARTESIAN_POINT ( 'NONE',  ( -4.556349186104047710, -10.99999999999999822, 95.96875000409676204 ) ) ;
#61569 = CARTESIAN_POINT ( 'NONE',  ( 0.6686838642329748783, 220.0000000000000284, 10.97965672913483814 ) ) ;
#61570 = CARTESIAN_POINT ( 'NONE',  ( -31.45873412499995680, 195.7500000013656063, 171.4326545832181239 ) ) ;
#61571 = CARTESIAN_POINT ( 'NONE',  ( -54.00000000000000711, 0.000000000000000000, 20.00000000000002132 ) ) ;
#61573 = CARTESIAN_POINT ( 'NONE',  ( -2.679491924311228512, 228.9583333333333144, -9.999999999999998224 ) ) ;
#61572 = CARTESIAN_POINT ( 'NONE',  ( 7.188101187500000933, 117.5000000020483810, -2.977408999572651371 ) ) ;
#61574 = CARTESIAN_POINT ( 'NONE',  ( -5.656854249492375253, 5.656854249492375253, 27.64280277982336642 ) ) ;
#61575 = CARTESIAN_POINT ( 'NONE',  ( -11.35316468750000141, 118.4895833299193697, 3.042071309553159963 ) ) ;
#61576 = CARTESIAN_POINT ( 'NONE',  ( 8.660254037844389075, 87.29166665983869677, -5.000000000000000000 ) ) ;
#61577 = EDGE_CURVE ( 'NONE', #26953, #31087, #18858, .T. ) ;
#61578 = CARTESIAN_POINT ( 'NONE',  ( -4.401442555609581635E-16, 122.6562500020483810, -7.188101187500000044 ) ) ;
#61579 = CARTESIAN_POINT ( 'NONE',  ( -4.541265875000002339, 20.87499999863441147, -1.881053915767121998 ) ) ;
#61580 = CARTESIAN_POINT ( 'NONE',  ( 0.000000000000000000, 0.000000000000000000, -10.14441321561125520 ) ) ;
#61581 = CARTESIAN_POINT ( 'NONE',  ( -8.660254037844390851, 39.79166665983870388, 4.999999999999998224 ) ) ;
#61582 = ORIENTED_EDGE ( 'NONE', *, *, #62144, .F. ) ;
#61583 = CARTESIAN_POINT ( 'NONE',  ( 2.219371606097704230, -67.78152867896255884, 20.18750705526123923 ) ) ;
#61584 = CARTESIAN_POINT ( 'NONE',  ( -2.765530957081998586, 288.7968750017069510, 6.676582343750001591 ) ) ;
#61585 = CARTESIAN_POINT ( 'NONE',  ( 5.656854249492374365, 5.656854249492375253, 3.455302783920144449 ) ) ;
#61586 = FACE_OUTER_BOUND ( 'NONE', #40799, .T. ) ;
#61587 = FACE_BOUND ( 'NONE', #23356, .T. ) ;
#61588 = CARTESIAN_POINT ( 'NONE',  ( -10.18810118749999738, -4.220049686691941915, 101.1250000020483810 ) ) ;
#61589 = ORIENTED_EDGE ( 'NONE', *, *, #24106, .T. ) ;
#61590 = CARTESIAN_POINT ( 'NONE',  ( 5.000000000000001776, 157.7083333265053966, -8.660254037844389075 ) ) ;
#61591 = CARTESIAN_POINT ( 'NONE',  ( -9.832129032723420536, 149.0104166632526699, 5.676582343749997150 ) ) ;
#61592 =( NAMED_UNIT ( * ) SI_UNIT ( $, .STERADIAN. ) SOLID_ANGLE_UNIT ( ) );
#61593 = CARTESIAN_POINT ( 'NONE',  ( 3.458734125000015425, 206.2500000013655779, 196.5673454167823877 ) ) ;
#61594 = CARTESIAN_POINT ( 'NONE',  ( -7.204075437095967871, 7.204075437095967871, 67.84375000204836681 ) ) ;
#61595 = CARTESIAN_POINT ( 'NONE',  ( 11.35316468750000141, 76.09374999658602690, 0.000000000000000000 ) ) ;
#61596 = ORIENTED_EDGE ( 'NONE', *, *, #18411, .T. ) ;
#61597 = CARTESIAN_POINT ( 'NONE',  ( 7.204075437095966983, 7.204075437095967871, 113.5937500020483810 ) ) ;
#61598 = CARTESIAN_POINT ( 'NONE',  ( 1.881053915767121998, 9.624999998634404363, -4.541265875000002339 ) ) ;
#61599 = ORIENTED_EDGE ( 'NONE', *, *, #14070, .T. ) ;
#61600 = CARTESIAN_POINT ( 'NONE',  ( 5.082755093536324154, 19.78124999795161543, 5.082755093536326818 ) ) ;
#61601 = CARTESIAN_POINT ( 'NONE',  ( -4.242640687119285658, 290.1875000034139589, 4.242640687119287435 ) ) ;
#61602 = COLOUR_RGB ( '',0.7921568627450980005, 0.8196078431372548767, 0.9333333333333333481 ) ;
#61603 = CARTESIAN_POINT ( 'NONE',  ( -25.17157287525374088, 197.7500000027312126, 172.8284271247464972 ) ) ;
#61604 = CARTESIAN_POINT ( 'NONE',  ( -5.082755093536326818, 16.78124999795161543, 5.082755093536325042 ) ) ;
#61605 = CARTESIAN_POINT ( 'NONE',  ( 7.778174593052023411, -7.778174593052021635, 103.7500000040967763 ) ) ;
#61606 = ADVANCED_FACE ( 'NONE', ( #56118 ), #16465, .F. ) ;
#61607 = CARTESIAN_POINT ( 'NONE',  ( 7.204075437095966983, 7.204075437095967871, 109.4687500020483810 ) ) ;
#61608 =( GEOMETRIC_REPRESENTATION_CONTEXT ( 3 ) GLOBAL_UNCERTAINTY_ASSIGNED_CONTEXT ( ( #58187 ) ) GLOBAL_UNIT_ASSIGNED_CONTEXT ( ( #51006, #34426, #69105 ) ) REPRESENTATION_CONTEXT ( 'NONE', 'WORKASPACE' ) );
#61609 = EDGE_CURVE ( 'NONE', #8420, #59077, #37598, .T. ) ;
#61610 = CARTESIAN_POINT ( 'NONE',  ( 2.980981665651132317, -44.60901341116364449, 151.2352651924658176 ) ) ;
#61611 = CARTESIAN_POINT ( 'NONE',  ( 1.656854249492381914, 6.562499997268813168, 4.000000000000000888 ) ) ;
#61612 = CARTESIAN_POINT ( 'NONE',  ( -4.000000000000015987, 208.6875000027312410, 143.6568542494924259 ) ) ;
#61613 = VECTOR ( 'NONE', #44672, 1000.000000000000000 ) ;
#61614 = ORIENTED_EDGE ( 'NONE', *, *, #71956, .F. ) ;
#61615 = CARTESIAN_POINT ( 'NONE',  ( 1.432654583217662481, 208.1250000013656063, 194.5412658750000219 ) ) ;
#61617 =( BOUNDED_CURVE ( )  B_SPLINE_CURVE ( 2, ( #6700, #39906, #29705, #17633, #40652, #68950, #6337, #64038, #62912, #17260, #52351, #40280, #687, #11607, #70078, #23671, #18385, #41398, #11241, #53829, #30807, #2139, #59492, #8537, #71157, #24408, #36476, #42118, #19478, #25867, #1781, #43232, #31551, #66247, #48517, #37589, #18754, #25132, #54574, #71523, #2510, #42854, #48148, #65871, #7068, #31176, #53089, #13074, #42491, #60212, #2880, #71898, #65507, #41763, #20212, #54202, #64771, #47414, #25504, #48887, #59127, #1424, #13803, #70438, #36109, #36848, #7438, #59854, #8168, #19848, #14550, #30074, #65130, #30445, #53463, #24766, #14180, #47776, #70799, #19113, #13440, #37215, #7805, #33431, #43989, #44734, #4752, #56431, #38716, #21342, #27744, #43605, #50755, #3627, #73403, #22078, #10034, #14924, #54947, #32688, #55697, #8913, #37966, #60965, #9284, #61714, #44363, #15674, #15297, #62082, #4012, #61341, #16411, #27001, #50015, #73771, #27368, #73031, #26244, #21707, #45104, #10405, #67375, #16044, #68117, #39077, #33070, #56066, #55322, #66999, #50387, #60587, #32307, #4375, #26623, #67752, #49647, #31925, #3256, #49263, #72277, #20590, #9668, #66618, #72661, #38335, #20966, #28864, #56805, #68856, #74515, #51884, #58302, #34175, #962, #40936, #23945, #6242, #69983, #51132, #34554, #22825, #11521, #23574, #591, #57559, #46583, #39443, #63564, #5867, #45466, #224, #23204, #28118, #10771, #68481, #46216, #17920, #63945, #29614, #69232, #29246, #46954, #16784, #17542, #40187, #40561, #62816, #52627, #33808, #11890, #74142, #5126, #34924, #39811, #57936, #52259, #69605, #12255, #35290, #45841, #6607, #62443, #22446, #11151, #57177, #5494, #51502, #28494, #17168, #63190, #65780, #1693, #2416, #37119, #14084, #71063, #53736, #60121, #1330, #8439, #64314, #31076, #30349, #59035, #24672, #31459, #7342, #25411, #41306, #47323, #70350, #18661, #19381, #2047, #48054, #47683, #19756, #36382, #19022, #48796, #25034, #48425, #42028, #53369, #70703, #12619, #35649, #54484, #65035, #13344, #41672, #71428, #59397, #42764, #58663, #42395, #13709, #2789, #7711, #30715, #65411, #64681, #36752, #12980, #25776, #59766, #8075, #54104, #18290, #6970, #29979, #52997, #24312, #36017, #43138, #32211, #72940, #56341, #26527, #21619, #66521, #33339, #73316, #4660, #38623, #27654, #8822, #66907 ),
 .UNSPECIFIED., .F., .F. ) 
 B_SPLINE_CURVE_WITH_KNOTS ( ( 3, 2, 2, 2, 2, 2, 2, 2, 2, 2, 2, 2, 2, 2, 2, 2, 2, 2, 2, 2, 2, 2, 2, 2, 2, 2, 2, 2, 2, 2, 2, 2, 2, 2, 2, 2, 2, 2, 2, 2, 2, 2, 2, 2, 2, 2, 2, 2, 2, 2, 2, 2, 2, 2, 2, 2, 2, 2, 2, 2, 2, 2, 2, 2, 2, 2, 2, 2, 2, 2, 2, 2, 2, 2, 2, 2, 2, 2, 2, 2, 2, 2, 2, 2, 2, 2, 2, 2, 2, 2, 2, 2, 2, 2, 2, 2, 2, 2, 2, 2, 2, 2, 2, 2, 2, 2, 2, 2, 2, 2, 2, 2, 2, 2, 2, 2, 2, 2, 2, 2, 2, 2, 2, 2, 2, 2, 2, 2, 2, 2, 2, 2, 2, 2, 2, 2, 2, 2, 2, 2, 2, 2, 2, 2, 3 ),
 ( 0.000000000000000000, 0.006944444444444444059, 0.01388888888888888812, 0.02083333333333333218, 0.02777777777777777624, 0.03472222222222222376, 0.04166666666666666435, 0.04861111111111111188, 0.05555555555555555247, 0.06250000000000000000, 0.06944444444444444753, 0.07638888888888889506, 0.08333333333333332871, 0.09027777777777777624, 0.09722222222222222376, 0.1041666666666666713, 0.1111111111111111049, 0.1180555555555555525, 0.1250000000000000000, 0.1319444444444444475, 0.1388888888888888951, 0.1458333333333333426, 0.1527777777777777901, 0.1597222222222222099, 0.1666666666666666574, 0.1736111111111111049, 0.1805555555555555525, 0.1875000000000000000, 0.1944444444444444475, 0.2013888888888888951, 0.2083333333333333426, 0.2152777777777777901, 0.2222222222222222099, 0.2291666666666666574, 0.2361111111111111049, 0.2430555555555555525, 0.2500000000000000000, 0.2569444444444444198, 0.2638888888888888951, 0.2708333333333333148, 0.2777777777777777901, 0.2847222222222222099, 0.2916666666666666852, 0.2986111111111111049, 0.3055555555555555802, 0.3125000000000000000, 0.3194444444444444198, 0.3263888888888888951, 0.3333333333333333148, 0.3402777777777777901, 0.3472222222222222099, 0.3541666666666666852, 0.3611111111111111049, 0.3680555555555555802, 0.3750000000000000000, 0.3819444444444444198, 0.3888888888888888951, 0.3958333333333333148, 0.4027777777777777901, 0.4097222222222222099, 0.4166666666666666852, 0.4236111111111111049, 0.4305555555555555802, 0.4375000000000000000, 0.4444444444444444198, 0.4513888888888888951, 0.4583333333333333148, 0.4652777777777777901, 0.4722222222222222099, 0.4791666666666666852, 0.4861111111111111049, 0.4930555555555555802, 0.5000000000000000000, 0.5069444444444444198, 0.5138888888888888395, 0.5208333333333333703, 0.5277777777777777901, 0.5347222222222222099, 0.5416666666666666297, 0.5486111111111111605, 0.5555555555555555802, 0.5625000000000000000, 0.5694444444444444198, 0.5763888888888888395, 0.5833333333333333703, 0.5902777777777777901, 0.5972222222222222099, 0.6041666666666666297, 0.6111111111111111605, 0.6180555555555555802, 0.6250000000000000000, 0.6319444444444444198, 0.6388888888888888395, 0.6458333333333333703, 0.6527777777777777901, 0.6597222222222222099, 0.6666666666666666297, 0.6736111111111111605, 0.6805555555555555802, 0.6875000000000000000, 0.6944444444444444198, 0.7013888888888888395, 0.7083333333333333703, 0.7152777777777777901, 0.7222222222222222099, 0.7291666666666666297, 0.7361111111111111605, 0.7430555555555555802, 0.7500000000000000000, 0.7569444444444444198, 0.7638888888888888395, 0.7708333333333333703, 0.7777777777777777901, 0.7847222222222222099, 0.7916666666666666297, 0.7986111111111111605, 0.8055555555555555802, 0.8125000000000000000, 0.8194444444444444198, 0.8263888888888888395, 0.8333333333333333703, 0.8402777777777777901, 0.8472222222222222099, 0.8541666666666666297, 0.8611111111111111605, 0.8680555555555555802, 0.8750000000000000000, 0.8819444444444444198, 0.8888888888888888395, 0.8958333333333333703, 0.9027777777777777901, 0.9097222222222222099, 0.9166666666666666297, 0.9236111111111111605, 0.9305555555555555802, 0.9375000000000000000, 0.9444444444444444198, 0.9513888888888888395, 0.9583333333333333703, 0.9652777777777777901, 0.9722222222222222099, 0.9791666666666666297, 0.9861111111111111605, 0.9930555555555555802, 1.000000000000000000 ),
 .UNSPECIFIED. ) 
 CURVE ( )  GEOMETRIC_REPRESENTATION_ITEM ( )  RATIONAL_B_SPLINE_CURVE ( ( 1.000000000000000000, 0.9238795325112867385, 1.000000000000000000, 0.9238795325112867385, 1.000000000000000000, 0.9238795325112867385, 1.000000000000000000, 0.9238795325112867385, 1.000000000000000000, 0.9238795325112867385, 1.000000000000000000, 0.9238795325112867385, 1.000000000000000000, 0.9238795325112867385, 1.000000000000000000, 0.9238795325112867385, 1.000000000000000000, 0.9238795325112867385, 1.000000000000000000, 0.9238795325112867385, 1.000000000000000000, 0.9238795325112867385, 1.000000000000000000, 0.9238795325112867385, 1.000000000000000000, 0.9238795325112867385, 1.000000000000000000, 0.9238795325112867385, 1.000000000000000000, 0.9238795325112867385, 1.000000000000000000, 0.9238795325112867385, 1.000000000000000000, 0.9238795325112867385, 1.000000000000000000, 0.9238795325112867385, 1.000000000000000000, 0.9238795325112867385, 1.000000000000000000, 0.9238795325112867385, 1.000000000000000000, 0.9238795325112867385, 1.000000000000000000, 0.9238795325112867385, 1.000000000000000000, 0.9238795325112867385, 1.000000000000000000, 0.9238795325112867385, 1.000000000000000000, 0.9238795325112867385, 1.000000000000000000, 0.9238795325112867385, 1.000000000000000000, 0.9238795325112867385, 1.000000000000000000, 0.9238795325112867385, 1.000000000000000000, 0.9238795325112867385, 1.000000000000000000, 0.9238795325112867385, 1.000000000000000000, 0.9238795325112867385, 1.000000000000000000, 0.9238795325112867385, 1.000000000000000000, 0.9238795325112867385, 1.000000000000000000, 0.9238795325112867385, 1.000000000000000000, 0.9238795325112867385, 1.000000000000000000, 0.9238795325112867385, 1.000000000000000000, 0.9238795325112867385, 1.000000000000000000, 0.9238795325112867385, 1.000000000000000000, 0.9238795325112867385, 1.000000000000000000, 0.9238795325112867385, 1.000000000000000000, 0.9238795325112867385, 1.000000000000000000, 0.9238795325112867385, 1.000000000000000000, 0.9238795325112867385, 1.000000000000000000, 0.9238795325112867385, 1.000000000000000000, 0.9238795325112867385, 1.000000000000000000, 0.9238795325112867385, 1.000000000000000000, 0.9238795325112867385, 1.000000000000000000, 0.9238795325112867385, 1.000000000000000000, 0.9238795325112867385, 1.000000000000000000, 0.9238795325112867385, 1.000000000000000000, 0.9238795325112867385, 1.000000000000000000, 0.9238795325112867385, 1.000000000000000000, 0.9238795325112867385, 1.000000000000000000, 0.9238795325112867385, 1.000000000000000000, 0.9238795325112867385, 1.000000000000000000, 0.9238795325112867385, 1.000000000000000000, 0.9238795325112867385, 1.000000000000000000, 0.9238795325112867385, 1.000000000000000000, 0.9238795325112867385, 1.000000000000000000, 0.9238795325112867385, 1.000000000000000000, 0.9238795325112867385, 1.000000000000000000, 0.9238795325112867385, 1.000000000000000000, 0.9238795325112867385, 1.000000000000000000, 0.9238795325112867385, 1.000000000000000000, 0.9238795325112867385, 1.000000000000000000, 0.9238795325112867385, 1.000000000000000000, 0.9238795325112867385, 1.000000000000000000, 0.9238795325112867385, 1.000000000000000000, 0.9238795325112867385, 1.000000000000000000, 0.9238795325112867385, 1.000000000000000000, 0.9238795325112867385, 1.000000000000000000, 0.9238795325112867385, 1.000000000000000000, 0.9238795325112867385, 1.000000000000000000, 0.9238795325112867385, 1.000000000000000000, 0.9238795325112867385, 1.000000000000000000, 0.9238795325112867385, 1.000000000000000000, 0.9238795325112867385, 1.000000000000000000, 0.9238795325112867385, 1.000000000000000000, 0.9238795325112867385, 1.000000000000000000, 0.9238795325112867385, 1.000000000000000000, 0.9238795325112867385, 1.000000000000000000, 0.9238795325112867385, 1.000000000000000000, 0.9238795325112867385, 1.000000000000000000, 0.9238795325112867385, 1.000000000000000000, 0.9238795325112867385, 1.000000000000000000, 0.9238795325112867385, 1.000000000000000000, 0.9238795325112867385, 1.000000000000000000, 0.9238795325112867385, 1.000000000000000000, 0.9238795325112867385, 1.000000000000000000, 0.9238795325112867385, 1.000000000000000000, 0.9238795325112867385, 1.000000000000000000, 0.9238795325112867385, 1.000000000000000000, 0.9238795325112867385, 1.000000000000000000, 0.9238795325112867385, 1.000000000000000000, 0.9238795325112867385, 1.000000000000000000, 0.9238795325112867385, 1.000000000000000000, 0.9238795325112867385, 1.000000000000000000, 0.9238795325112867385, 1.000000000000000000, 0.9238795325112867385, 1.000000000000000000, 0.9238795325112867385, 1.000000000000000000, 0.9238795325112867385, 1.000000000000000000, 0.9238795325112867385, 1.000000000000000000, 0.9238795325112867385, 1.000000000000000000, 0.9238795325112867385, 1.000000000000000000, 0.9238795325112867385, 1.000000000000000000, 0.9238795325112867385, 1.000000000000000000, 0.9238795325112867385, 1.000000000000000000, 0.9238795325112867385, 1.000000000000000000, 0.9238795325112867385, 1.000000000000000000, 0.9238795325112867385, 1.000000000000000000, 0.9238795325112867385, 1.000000000000000000, 0.9238795325112867385, 1.000000000000000000, 0.9238795325112867385, 1.000000000000000000, 0.9238795325112867385, 1.000000000000000000, 0.9238795325112867385, 1.000000000000000000, 0.9238795325112867385, 1.000000000000000000, 0.9238795325112867385, 1.000000000000000000, 0.9238795325112867385, 1.000000000000000000, 0.9238795325112867385, 1.000000000000000000, 0.9238795325112867385, 1.000000000000000000, 0.9238795325112867385, 1.000000000000000000, 0.9238795325112867385, 1.000000000000000000, 0.9238795325112867385, 1.000000000000000000, 0.9238795325112867385, 1.000000000000000000, 0.9238795325112867385, 1.000000000000000000, 0.9238795325112867385, 1.000000000000000000, 0.9238795325112867385, 1.000000000000000000, 0.9238795325112867385, 1.000000000000000000, 0.9238795325112867385, 1.000000000000000000, 0.9238795325112867385, 1.000000000000000000, 0.9238795325112867385, 1.000000000000000000, 0.9238795325112867385, 1.000000000000000000, 0.9238795325112867385, 1.000000000000000000, 0.9238795325112867385, 1.000000000000000000, 0.9238795325112867385, 1.000000000000000000, 0.9238795325112867385, 1.000000000000000000, 0.9238795325112867385, 1.000000000000000000, 0.9238795325112867385, 1.000000000000000000, 0.9238795325112867385, 1.000000000000000000, 0.9238795325112867385, 1.000000000000000000, 0.9238795325112867385, 1.000000000000000000, 0.9238795325112867385, 1.000000000000000000, 0.9238795325112867385, 1.000000000000000000, 0.9238795325112867385, 1.000000000000000000 ) ) 
 REPRESENTATION_ITEM ( '' )  );
#61616 = CARTESIAN_POINT ( 'NONE',  ( -31.99999999999999289, 195.3750000027311842, 170.0000000000004547 ) ) ;
#61618 = B_SPLINE_CURVE_WITH_KNOTS ( 'NONE', 3,
 ( #48205, #71213, #27810, #50444, #73461, #21399, #20654, #33131, #39512, #15361, #44796, #72341, #56128, #3315, #50079, #55756, #72724, #61400, #27429, #49326, #21769, #32367 ),
 .UNSPECIFIED., .F., .F.,
 ( 4, 2, 2, 2, 2, 2, 2, 2, 2, 2, 4 ),
 ( 0.000000000000000000, 0.001156727053362487578, 0.001735090580043716513, 0.002313454106724945666, 0.003470181160087403537, 0.004048544686768637026, 0.004626908213449870515, 0.005783635266812338360, 0.006940362320174804471, 0.008097089373537270582, 0.009253816426899737560 ),
 .UNSPECIFIED. ) ;
#61619 = CARTESIAN_POINT ( 'NONE',  ( -10.18810118749999738, -4.220049686691941915, 69.62500000204838102 ) ) ;
#61620 = EDGE_CURVE ( 'NONE', #11426, #39299, #38388, .T. ) ;
#61621 = CARTESIAN_POINT ( 'NONE',  ( 1.881053915767122664, 7.124999998634407916, 4.541265875000001451 ) ) ;
#61622 = LINE ( 'NONE', #27651, #29609 ) ;
#61623 = CARTESIAN_POINT ( 'NONE',  ( -7.188101187499990274, -2.977408999572651371, 25.58030278187175810 ) ) ;
#61624 = EDGE_LOOP ( 'NONE', ( #37098, #50862, #45577 ) ) ;
#61625 = DIRECTION ( 'NONE',  ( 0.8660254037844400399, 0.4999999999999976130, 0.000000000000000000 ) ) ;
#61626 = VERTEX_POINT ( 'NONE', #73454 ) ;
#61627 = CARTESIAN_POINT ( 'NONE',  ( -6.238412754330611322E-16, 10.18810118749999916, 113.7812500020483810 ) ) ;
#61628 = CARTESIAN_POINT ( 'NONE',  ( 2.445694354108838731, 206.0625000013656063, 195.5543056458912190 ) ) ;
#61629 = CARTESIAN_POINT ( 'NONE',  ( 27.99999999999996803, 200.9375000013656063, 166.5412658749999082 ) ) ;
#61630 = CARTESIAN_POINT ( 'NONE',  ( 7.320508075688771044, 64.37499999999998579, 7.320508075688775484 ) ) ;
#61631 = AXIS2_PLACEMENT_3D ( 'NONE', #65547, #64811, #71942 ) ;
#61632 = CARTESIAN_POINT ( 'NONE',  ( 3.313708498984765161, 123.9687500000000142, 7.999999999999998224 ) ) ;
#61633 = CARTESIAN_POINT ( 'NONE',  ( 2.485281374238575314, 294.3125000000000000, 6.000000000000000888 ) ) ;
#61634 = CARTESIAN_POINT ( 'NONE',  ( 27.99999999999996803, 205.6250000027312126, 165.9999999999998863 ) ) ;
#61635 = ORIENTED_EDGE ( 'NONE', *, *, #45362, .T. ) ;
#61636 = CARTESIAN_POINT ( 'NONE',  ( 8.000000000000000000, 8.812499995903221972, 0.000000000000000000 ) ) ;
#61637 = EDGE_CURVE ( 'NONE', #55690, #25275, #19741, .T. ) ;
#61638 = CARTESIAN_POINT ( 'NONE',  ( -1.506680654948961307, -10.12163528317163674, 70.16331425389374488 ) ) ;
#61639 = CARTESIAN_POINT ( 'NONE',  ( 1.656854249492348607, 197.3125000027312126, 138.0000000000000568 ) ) ;
#61640 = DIRECTION ( 'NONE',  ( -0.000000000000000000, -0.000000000000000000, -1.000000000000000000 ) ) ;
#61641 = LINE ( 'NONE', #3936, #72457 ) ;
#61642 = CARTESIAN_POINT ( 'NONE',  ( 7.320508075688771044, 253.1249999999999716, -7.320508075688771932 ) ) ;
#61643 = CARTESIAN_POINT ( 'NONE',  ( 7.778174593052021635, 7.778174593052023411, 107.1250000040967763 ) ) ;
#61644 = CARTESIAN_POINT ( 'NONE',  ( 10.00000000000000178, 190.2083333333333428, -2.679491924311226736 ) ) ;
#61645 = DIRECTION ( 'NONE',  ( 0.000000000000000000, -0.9989890351440378069, -0.04495450658148170825 ) ) ;
#61646 = CARTESIAN_POINT ( 'NONE',  ( -2.977408999572647819, -7.188101187499990274, 24.64280278187176165 ) ) ;
#61647 = CARTESIAN_POINT ( 'NONE',  ( 9.832129032723420536, 161.5104166632526983, -5.676582343749999815 ) ) ;
#61648 = DIRECTION ( 'NONE',  ( -0.000000000000000000, 1.000000000000000000, -0.000000000000000000 ) ) ;
#61649 = CARTESIAN_POINT ( 'NONE',  ( 7.320508075688776373, 260.0000000068279746, 7.320508075688767491 ) ) ;
#61650 = DIRECTION ( 'NONE',  ( 0.000000000000000000, -0.000000000000000000, 1.000000000000000000 ) ) ;
#61652 = DIRECTION ( 'NONE',  ( -1.000000000000000000, -2.168404344971008868E-16, -0.000000000000000000 ) ) ;
#61651 = SURFACE_SIDE_STYLE ('',( #51065 ) ) ;
#61653 = ORIENTED_EDGE ( 'NONE', *, *, #67950, .F. ) ;
#61654 = CARTESIAN_POINT ( 'NONE',  ( -9.832129032723420536, 29.01041666325268764, 5.676582343749997150 ) ) ;
#61655 = AXIS2_PLACEMENT_3D ( 'NONE', #11095, #50327, #74457 ) ;
#61656 = CARTESIAN_POINT ( 'NONE',  ( 6.123233995736767268E-16, 98.12499999317203958, -10.00000000000000178 ) ) ;
#61658 = CARTESIAN_POINT ( 'NONE',  ( 1.877992804775685087, -10.12031740952197190, -70.21778636472329538 ) ) ;
#61657 = DIRECTION ( 'NONE',  ( -1.000000000000000000, 0.000000000000000000, 0.000000000000000000 ) ) ;
#61659 = CARTESIAN_POINT ( 'NONE',  ( -24.68086420145692017, -50.97799738082681387, 188.7637688592449763 ) ) ;
#61660 = CARTESIAN_POINT ( 'NONE',  ( -3.458734125000016313, 204.8750000013656063, 140.5673454167823593 ) ) ;
#61661 = CARTESIAN_POINT ( 'NONE',  ( 5.000000000000001776, 42.70833332650536818, -8.660254037844389075 ) ) ;
#61662 = CARTESIAN_POINT ( 'NONE',  ( -4.401442555609581635E-16, 102.7812500020483810, -7.188101187500000044 ) ) ;
#61663 = CARTESIAN_POINT ( 'NONE',  ( -8.342170076843785083E-16, 8.187499998634406140, 4.541265875000002339 ) ) ;
#61664 = DIRECTION ( 'NONE',  ( -1.000000000000000000, 0.000000000000000000, -0.000000000000000000 ) ) ;
#61665 = CARTESIAN_POINT ( 'NONE',  ( 3.313708498984762496, -7.999999999999989342, 11.79905277982336465 ) ) ;
#61666 = CARTESIAN_POINT ( 'NONE',  ( -4.000000000000001776, 5.249999997268813168, -4.898587196589415787E-16 ) ) ;
#61667 = ORIENTED_EDGE ( 'NONE', *, *, #63461, .F. ) ;
#61668 = EDGE_LOOP ( 'NONE', ( #71994, #49834, #42893, #45690 ) ) ;
#61669 = CARTESIAN_POINT ( 'NONE',  ( -5.000000000000000000, -62.88740100213664874, 24.06179116403727036 ) ) ;
#61670 = CARTESIAN_POINT ( 'NONE',  ( -2.445694354108783219, 194.8125000013656063, 200.4456943541088663 ) ) ;
#61671 = CARTESIAN_POINT ( 'NONE',  ( 7.778174593052021635, 7.778174593052023411, 81.62500000409677625 ) ) ;
#61672 = CARTESIAN_POINT ( 'NONE',  ( 8.311093377946834337, 222.3437500034139589, -8.311093377946836114 ) ) ;
#61673 = CARTESIAN_POINT ( 'NONE',  ( -3.042071309553173730, 139.3229166632526699, 11.35316468749999785 ) ) ;
#61674 = ORIENTED_EDGE ( 'NONE', *, *, #50371, .T. ) ;
#61675 = CARTESIAN_POINT ( 'NONE',  ( -7.999999999953861796, 1.809871347124574913E-05, 10.01712378708029938 ) ) ;
#61676 = CARTESIAN_POINT ( 'NONE',  ( -10.18810118749999738, -4.220049686691941915, 87.25000000204838102 ) ) ;
#61677 = CARTESIAN_POINT ( 'NONE',  ( -6.735557395310442023E-16, 11.00000000000000000, 93.62499999999998579 ) ) ;
#61678 = CARTESIAN_POINT ( 'NONE',  ( -3.458734124999959469, 194.7500000013656063, 199.4326545832176691 ) ) ;
#61680 = CARTESIAN_POINT ( 'NONE',  ( 9.832129032723416984, 125.3645833299193413, 5.676582343750006032 ) ) ;
#61679 = CARTESIAN_POINT ( 'NONE',  ( 2.751064625579944321E-14, 204.7500000000000284, 194.0000000000000568 ) ) ;
#61681 = CARTESIAN_POINT ( 'NONE',  ( 0.000000000000000000, 0.000000000000000000, 0.000000000000000000 ) ) ;
#61682 = VERTEX_POINT ( 'NONE', #4065 ) ;
#61683 = APPLICATION_CONTEXT ( 'automotive_design' ) ;
#61684 = CARTESIAN_POINT ( 'NONE',  ( 7.778174593052021635, 7.778174593052023411, 76.93749999999998579 ) ) ;
#61685 = CARTESIAN_POINT ( 'NONE',  ( -35.46499747849644280, 173.3340168152039951, 175.5502016142355899 ) ) ;
#61686 = CARTESIAN_POINT ( 'NONE',  ( 8.311093377946837890, 111.7187499965859985, -8.311093377946837890 ) ) ;
#61687 = CARTESIAN_POINT ( 'NONE',  ( 1.432654583217664479, 201.7500000013655779, 201.4587341250000065 ) ) ;
#61688 = CARTESIAN_POINT ( 'NONE',  ( 4.401442555609581635E-16, 16.21874999795161543, -7.188101187500000044 ) ) ;
#61689 = CARTESIAN_POINT ( 'NONE',  ( -4.220049686691935698, 10.18810118749999916, 82.75000000204838102 ) ) ;
#61690 = CARTESIAN_POINT ( 'NONE',  ( -2.085542519210945728E-15, 24.84374999658601624, 11.35316468750000141 ) ) ;
#61691 = ORIENTED_EDGE ( 'NONE', *, *, #48064, .F. ) ;
#61692 = CARTESIAN_POINT ( 'NONE',  ( -4.898587196589412829E-16, 90.31250000409676204, -8.000000000000000000 ) ) ;
#61693 = CARTESIAN_POINT ( 'NONE',  ( 5.662595241051934458, 5.662595241051935346, 22.95061528394063188 ) ) ;
#61694 = CARTESIAN_POINT ( 'NONE',  ( -27.99999999999996092, 207.5000000000000284, 174.0000000000003695 ) ) ;
#61695 = CARTESIAN_POINT ( 'NONE',  ( 10.99999999999999645, -10.99999999999999645, 41.99999999999999289 ) ) ;
#61696 = CARTESIAN_POINT ( 'NONE',  ( -5.082755093536325042, 1.031249997951609876, -5.082755093536325930 ) ) ;
#61697 = CARTESIAN_POINT ( 'NONE',  ( -4.088227598258586603E-16, 288.2031250017069510, -6.676582343750001591 ) ) ;
#61698 = DIRECTION ( 'NONE',  ( 0.000000000000000000, 0.000000000000000000, -1.000000000000000000 ) ) ;
#61699 = CARTESIAN_POINT ( 'NONE',  ( -7.188101187500002709, 1.687499997951610098, 2.977408999572649151 ) ) ;
#61700 = EDGE_CURVE ( 'NONE', #70161, #72356, #43708, .T. ) ;
#61701 = ORIENTED_EDGE ( 'NONE', *, *, #31346, .F. ) ;
#61702 = CARTESIAN_POINT ( 'NONE',  ( -8.311093377946841443, 149.2187499965860411, 8.311093377946830785 ) ) ;
#61703 = CARTESIAN_POINT ( 'NONE',  ( -7.204075437095965206, -7.204075437095968759, 79.84375000204838102 ) ) ;
#61704 = CARTESIAN_POINT ( 'NONE',  ( -30.44569435410879521, 209.0625000013656063, 172.4456943541092357 ) ) ;
#61705 = EDGE_CURVE ( 'NONE', #72225, #42214, #72716, .T. ) ;
#61706 = CARTESIAN_POINT ( 'NONE',  ( -4.541265875000003227, 14.99999999863440969, 1.881053915767121110 ) ) ;
#61707 = EDGE_LOOP ( 'NONE', ( #59662, #37763, #58553, #22297 ) ) ;
#61708 = CARTESIAN_POINT ( 'NONE',  ( 4.000000000000015099, 202.6875000027311842, 196.3431457505076594 ) ) ;
#61709 = CARTESIAN_POINT ( 'NONE',  ( 2.445694354108783219, 194.8125000013656063, 139.5543056458912190 ) ) ;
#61710 = CARTESIAN_POINT ( 'NONE',  ( -23.99999999999999289, 206.8750000027312126, 170.0000000000002842 ) ) ;
#61711 = AXIS2_PLACEMENT_3D ( 'NONE', #19383, #52629, #29981 ) ;
#61712 = DIRECTION ( 'NONE',  ( 0.000000000000000000, 0.000000000000000000, -1.000000000000000000 ) ) ;
#61713 = ORIENTED_EDGE ( 'NONE', *, *, #64967, .T. ) ;
#61714 = CARTESIAN_POINT ( 'NONE',  ( -7.188101187500002709, 10.31249999795161187, 2.977408999572649151 ) ) ;
#61715 = CARTESIAN_POINT ( 'NONE',  ( -4.000000000000015987, 208.5625000000000000, 143.6568542494924259 ) ) ;
#61716 = CARTESIAN_POINT ( 'NONE',  ( 5.000000000000000000, 51.74377041917585984, -41.86884046506214929 ) ) ;
#61717 = CARTESIAN_POINT ( 'NONE',  ( 11.35316468750000141, 185.7812499965860411, 0.000000000000000000 ) ) ;
#61718 = CARTESIAN_POINT ( 'NONE',  ( 1.320432766682874540E-15, 114.4062500020483810, 7.188101187500000044 ) ) ;
#61719 = CARTESIAN_POINT ( 'NONE',  ( 2.751064625579944321E-14, 207.8750000027312126, 194.0000000000000568 ) ) ;
#61720 = CARTESIAN_POINT ( 'NONE',  ( 1.226468279477575784E-15, 289.7031250017069510, 6.676582343750001591 ) ) ;
#61722 = DIRECTION ( 'NONE',  ( -0.000000000000000000, 1.000000000000000000, -0.000000000000000000 ) ) ;
#61721 = CARTESIAN_POINT ( 'NONE',  ( 8.660254037844381969, 34.58333333333332860, 5.000000000000003553 ) ) ;
#61723 = VERTEX_POINT ( 'NONE', #67053 ) ;
#61724 = CARTESIAN_POINT ( 'NONE',  ( -5.676582343749992710, 259.7395833367473301, 9.832129032723422313 ) ) ;
#61725 = TOROIDAL_SURFACE ( 'NONE', #68945, 37.00000000000003553, 6.000000000000005329 ) ;
#61726 = CARTESIAN_POINT ( 'NONE',  ( 5.082755093536320601, -5.082755093536318824, 21.92405278187175455 ) ) ;
#61727 = CYLINDRICAL_SURFACE ( 'NONE', #52652, 7.999999999999991118 ) ;
#61728 = CIRCLE ( 'NONE', #35261, 7.000000000000006217 ) ;
#61729 = CARTESIAN_POINT ( 'NONE',  ( -2.589639417652795483, -60.37884160280842138, -22.99414321703674347 ) ) ;
#61730 = CARTESIAN_POINT ( 'NONE',  ( 3.458734125000015425, 196.2500000013656631, 196.5673454167823877 ) ) ;
#61731 =( BOUNDED_CURVE ( )  B_SPLINE_CURVE ( 2, ( #46350, #22210, #29385, #52393, #69740, #18055, #41070, #6742, #29745, #45237, #51265 ),
 .UNSPECIFIED., .F., .F. ) 
 B_SPLINE_CURVE_WITH_KNOTS ( ( 3, 2, 2, 2, 2, 3 ),
 ( 0.7147737642690134008, 0.7213920387057923822, 0.7280103142902493163, 0.7346285898747061394, 0.7412468654591628514, 0.7412468980011663877 ),
 .UNSPECIFIED. ) 
 CURVE ( )  GEOMETRIC_REPRESENTATION_ITEM ( )  RATIONAL_B_SPLINE_CURVE ( ( 1.000000000000000000, 0.9238795325112867385, 1.000000000000000000, 0.9238795325112867385, 1.000000000000000000, 0.9238795325112867385, 1.000000000000000000, 0.9238795325112867385, 1.000000000000000000, 0.9999996257163232816, 0.9999992514363272855 ) ) 
 REPRESENTATION_ITEM ( '' )  );
#61732 = CARTESIAN_POINT ( 'NONE',  ( 7.320508075688771044, 144.3750000000000284, 7.320508075688775484 ) ) ;
#61733 = CARTESIAN_POINT ( 'NONE',  ( -27.99999999999999645, 210.0000000000000284, 170.0000000000003695 ) ) ;
#61734 = CARTESIAN_POINT ( 'NONE',  ( -30.99999999999992895, -31.99999999999978684, 135.0000000000000000 ) ) ;
#61735 =( BOUNDED_CURVE ( )  B_SPLINE_CURVE ( 2, ( #31617, #42556, #3697, #65567, #37659, #54638, #9354, #60657, #42919 ),
 .UNSPECIFIED., .F., .T. ) 
 B_SPLINE_CURVE_WITH_KNOTS ( ( 3, 2, 2, 2, 3 ),
 ( 0.02647310233782740330, 0.03309137792228417779, 0.03970965350674094535, 0.04632792909119771985, 0.05294620388485415940 ),
 .UNSPECIFIED. ) 
 CURVE ( )  GEOMETRIC_REPRESENTATION_ITEM ( )  RATIONAL_B_SPLINE_CURVE ( ( 0.9999999999999981126, 0.9238795325112885148, 1.000000000000000000, 0.9238795325112867385, 1.000000000000000000, 0.9238795325112867385, 1.000000000000000000, 0.9238795325112867385, 1.000000000000000000 ) ) 
 REPRESENTATION_ITEM ( '' )  );
#61736 = CARTESIAN_POINT ( 'NONE',  ( 3.313708498984765161, 95.46875000000000000, 7.999999999999998224 ) ) ;
#61737 = CARTESIAN_POINT ( 'NONE',  ( 8.311093377946834337, 110.4687499965860127, 8.311093377946839666 ) ) ;
#61738 = CARTESIAN_POINT ( 'NONE',  ( -2.485281374238947016, 295.8125000000000000, -5.999999999999626965 ) ) ;
#61739 = CARTESIAN_POINT ( 'NONE',  ( -4.556349186104047710, -10.99999999999999822, 68.78125000000001421 ) ) ;
#61742 = DIRECTION ( 'NONE',  ( -1.000000000000000000, 0.000000000000000000, 0.000000000000000000 ) ) ;
#61741 = CARTESIAN_POINT ( 'NONE',  ( 30.44569435410879521, 198.8125000013656063, 167.5543056458910485 ) ) ;
#61740 = CARTESIAN_POINT ( 'NONE',  ( 30.44569435410879166, 199.8125000013656063, 172.4456943541087526 ) ) ;
#61743 = ORIENTED_EDGE ( 'NONE', *, *, #66578, .T. ) ;
#61744 = AXIS2_PLACEMENT_3D ( 'NONE', #55948, #44614, #72149 ) ;
#61745 = CARTESIAN_POINT ( 'NONE',  ( 7.358182744857522550, 224.4069354532862803, 6.797101760018821714 ) ) ;
#61746 = CARTESIAN_POINT ( 'NONE',  ( 1.102182119232618108E-15, 287.3125000034140157, 6.000000000000001776 ) ) ;
#61747 = VECTOR ( 'NONE', #64913, 1000.000000000000000 ) ;
#61748 = CARTESIAN_POINT ( 'NONE',  ( 24.54126587499999701, 197.3750000013656063, 168.5673454167822172 ) ) ;
#61749 = CARTESIAN_POINT ( 'NONE',  ( -3.042071309553164404, 207.5520833299193555, -11.35316468749999963 ) ) ;
#61750 = FACE_OUTER_BOUND ( 'NONE', #6190, .T. ) ;
#61751 = CARTESIAN_POINT ( 'NONE',  ( 2.780723358947928197E-16, 17.56249999863440792, -4.541265875000002339 ) ) ;
#61752 = CARTESIAN_POINT ( 'NONE',  ( 1.877992804773993329, -55.75022808459807067, 43.87334515336884522 ) ) ;
#61753 = CARTESIAN_POINT ( 'NONE',  ( -7.999999999999991118, 3.313708498984756723, 24.73655277982336997 ) ) ;
#61755 = LINE ( 'NONE', #45142, #11052 ) ;
#61754 = CARTESIAN_POINT ( 'NONE',  ( -47.49838633794698950, 39.20668375461617927, 64.61389030631690389 ) ) ;
#61756 = CARTESIAN_POINT ( 'NONE',  ( -9.832129032723418760, 92.86458332991935549, -5.676582343750004256 ) ) ;
#61757 = VERTEX_POINT ( 'NONE', #15726 ) ;
#61758 = CARTESIAN_POINT ( 'NONE',  ( 25.17157287525381903, 205.0000000027312126, 172.8284271247460993 ) ) ;
#61759 = CARTESIAN_POINT ( 'NONE',  ( -5.082755093536325042, 20.53124999795161543, -5.082755093536325930 ) ) ;
#61760 = DIRECTION ( 'NONE',  ( -0.000000000000000000, -1.000000000000000000, -0.000000000000000000 ) ) ;
#61761 = CARTESIAN_POINT ( 'NONE',  ( -11.35316468749999785, 254.0104166700806729, -3.042071309553164848 ) ) ;
#61762 = CARTESIAN_POINT ( 'NONE',  ( -5.676582343750006032, 84.11458332991935549, 9.832129032723418760 ) ) ;
#61763 = ORIENTED_EDGE ( 'NONE', *, *, #10968, .T. ) ;
#61764 = CARTESIAN_POINT ( 'NONE',  ( 5.000000000000001776, 207.7083333265053682, -8.660254037844389075 ) ) ;
#61765 = CARTESIAN_POINT ( 'NONE',  ( -4.220049686691937474, -10.18810118749999738, 105.4375000020483668 ) ) ;
#61766 = FACE_OUTER_BOUND ( 'NONE', #44372, .T. ) ;
#61767 = CARTESIAN_POINT ( 'NONE',  ( 3.458734125000015869, 206.1875000013656063, 198.0000000000000284 ) ) ;
#61768 = CARTESIAN_POINT ( 'NONE',  ( 11.00000000000000000, 1.347111479062088405E-15, 69.24999999999997158 ) ) ;
#61770 = CARTESIAN_POINT ( 'NONE',  ( -8.311093377946836114, 82.65624999658602690, -8.311093377946837890 ) ) ;
#61769 = DIRECTION ( 'NONE',  ( 1.000000000000000000, 0.000000000000000000, 0.000000000000000000 ) ) ;
#61771 = CARTESIAN_POINT ( 'NONE',  ( 3.313708498984756279, 7.999999999999991118, 12.54905278392014800 ) ) ;
#61772 = CARTESIAN_POINT ( 'NONE',  ( -27.99999999999996447, 199.1875000013655779, 173.4587341250003760 ) ) ;
#61773 = DIRECTION ( 'NONE',  ( 0.000000000000000000, 0.000000000000000000, -1.000000000000000000 ) ) ;
#61774 = EDGE_CURVE ( 'NONE', #27901, #44494, #27450, .T. ) ;
#61775 = EDGE_CURVE ( 'NONE', #33441, #42017, #647, .T. ) ;
#61776 = CARTESIAN_POINT ( 'NONE',  ( -10.00000000000000355, 184.5833333265053113, 2.679491924311223183 ) ) ;
#61777 = CARTESIAN_POINT ( 'NONE',  ( 2.485281374238959895, 296.3750000034139589, 5.999999999999615419 ) ) ;
#61778 = CARTESIAN_POINT ( 'NONE',  ( 9.832129032723416984, 80.67708332991935549, 5.676582343750006032 ) ) ;
#61779 = CARTESIAN_POINT ( 'NONE',  ( 6.676582343750001591, 291.9531250017069510, -8.176455196517173205E-16 ) ) ;
#61780 = CARTESIAN_POINT ( 'NONE',  ( 10.18810118749999916, 4.220049686691935698, 101.8750000020483810 ) ) ;
#61781 = CARTESIAN_POINT ( 'NONE',  ( 9.832129032723416984, 215.3645833299193555, 5.676582343750006032 ) ) ;
#61782 = EDGE_LOOP ( 'NONE', ( #74602, #28210, #36602, #60222 ) ) ;
#61783 = CARTESIAN_POINT ( 'NONE',  ( 2.449293598294707893E-16, 0.9999999972688131678, -4.000000000000001776 ) ) ;
#61784 = CARTESIAN_POINT ( 'NONE',  ( -11.00000000000000000, 0.000000000000000000, 118.0000000000000000 ) ) ;
#61785 = CARTESIAN_POINT ( 'NONE',  ( 6.000000000000001776, 291.5000000000000000, -7.347880794884121708E-16 ) ) ;
#61786 = CARTESIAN_POINT ( 'NONE',  ( -5.676582343749998039, 207.4479166632527267, -9.832129032723420536 ) ) ;
#61787 = CARTESIAN_POINT ( 'NONE',  ( -2.679491924311222295, 224.1666666734946602, 10.00000000000000178 ) ) ;
#61788 = CARTESIAN_POINT ( 'NONE',  ( -4.898587196589412829E-16, 112.6250000000000000, -8.000000000000000000 ) ) ;
#61789 = ORIENTED_EDGE ( 'NONE', *, *, #10258, .T. ) ;
#61790 = CARTESIAN_POINT ( 'NONE',  ( -11.35316468750000141, 188.5937499965860127, -1.390361679473963753E-15 ) ) ;
#61791 = VECTOR ( 'NONE', #51837, 1000.000000000000000 ) ;
#61792 = CARTESIAN_POINT ( 'NONE',  ( -7.188101187499990274, -2.977408999572651815, 13.58030278187175455 ) ) ;
#61793 = CARTESIAN_POINT ( 'NONE',  ( -30.44569435410879521, 206.8125000013656063, 172.4456943541092357 ) ) ;
#61794 = CARTESIAN_POINT ( 'NONE',  ( -1.469576158976823947E-15, 11.62500000000000178, 8.000000000000000000 ) ) ;
#61795 = VERTEX_POINT ( 'NONE', #28922 ) ;
#61796 = VECTOR ( 'NONE', #70686, 1000.000000000000000 ) ;
#61797 = CARTESIAN_POINT ( 'NONE',  ( 3.313708498984765161, 94.15625000409677625, 7.999999999999998224 ) ) ;
#61798 = CARTESIAN_POINT ( 'NONE',  ( 5.000000000000001776, 15.83333333333333393, -8.660254037844389075 ) ) ;
#61799 = CARTESIAN_POINT ( 'NONE',  ( -10.18810118749999916, 4.220049686691934809, 81.43750000204836681 ) ) ;
#61800 = ORIENTED_EDGE ( 'NONE', *, *, #32003, .F. ) ;
#61801 = CARTESIAN_POINT ( 'NONE',  ( 4.000000000000001776, 21.06250000000000000, -1.656854249492381248 ) ) ;
#61802 = CARTESIAN_POINT ( 'NONE',  ( -1.881053915767124440, 17.99999999863440792, 4.541265875000001451 ) ) ;
#61803 = CARTESIAN_POINT ( 'NONE',  ( 31.55598681522091198, 194.5891123728962668, 170.5364773218189782 ) ) ;
#61804 = ORIENTED_EDGE ( 'NONE', *, *, #59906, .T. ) ;
#61805 = CARTESIAN_POINT ( 'NONE',  ( 5.000000000000001776, 17.70833332650536818, -8.660254037844389075 ) ) ;
#61806 = CARTESIAN_POINT ( 'NONE',  ( 7.188101187500000044, 90.40625000204838102, -8.802885111219163269E-16 ) ) ;
#61809 = PLANE ( 'NONE',  #37383 ) ;
#61808 = CARTESIAN_POINT ( 'NONE',  ( 11.35316468749999608, 256.6145833367473870, -3.042071309553167513 ) ) ;
#61807 = CARTESIAN_POINT ( 'NONE',  ( 0.000000000000000000, 125.0000000000000000, 0.000000000000000000 ) ) ;
#61810 = PRODUCT_CONTEXT ( 'NONE', #39985, 'mechanical' ) ;
#61811 = ORIENTED_EDGE ( 'NONE', *, *, #35808, .T. ) ;
#61812 = CARTESIAN_POINT ( 'NONE',  ( -3.042071309553166181, 258.1770833367473301, -11.35316468749999608 ) ) ;
#61813 = CARTESIAN_POINT ( 'NONE',  ( -5.082755093536317936, -5.082755093536320601, 12.17405278187175277 ) ) ;
#61814 = ORIENTED_EDGE ( 'NONE', *, *, #33788, .T. ) ;
#61815 = ORIENTED_EDGE ( 'NONE', *, *, #14539, .F. ) ;
#61816 = CARTESIAN_POINT ( 'NONE',  ( -10.18810118749999738, -4.220049686691941915, 72.25000000204836681 ) ) ;
#61817 = CARTESIAN_POINT ( 'NONE',  ( -2.085542519210945728E-15, 79.84374999658601268, 11.35316468750000141 ) ) ;
#61818 = CARTESIAN_POINT ( 'NONE',  ( -3.313708498984759387, -7.999999999999989342, 23.79905278392014978 ) ) ;
#61819 = CARTESIAN_POINT ( 'NONE',  ( 11.00000000000000000, 1.347111479062088405E-15, 91.74999999999998579 ) ) ;
#61822 = CARTESIAN_POINT ( 'NONE',  ( -4.088227598258586603E-16, 290.3593750017070079, -6.676582343750001591 ) ) ;
#61821 = CARTESIAN_POINT ( 'NONE',  ( 23.99999999999998934, 197.8750000027312126, 169.9999999999999432 ) ) ;
#61820 = LINE ( 'NONE', #32033, #63644 ) ;
#61823 = DIRECTION ( 'NONE',  ( 1.000000000000000000, 0.000000000000000000, 0.000000000000000000 ) ) ;
#61824 = CARTESIAN_POINT ( 'NONE',  ( 28.00000000000001776, 202.5000000000000000, 165.9999999999998863 ) ) ;
#61825 =( BOUNDED_CURVE ( )  B_SPLINE_CURVE ( 2, ( #21606, #17435, #21977, #50649, #40085, #45006, #68011, #68749, #17063 ),
 .UNSPECIFIED., .F., .F. ) 
 B_SPLINE_CURVE_WITH_KNOTS ( ( 3, 2, 2, 2, 3 ),
 ( 0.4833333333333338366, 0.4916666666666670849, 0.5000000000000004441, 0.5083333333333336368, 0.5166666666666670515 ),
 .UNSPECIFIED. ) 
 CURVE ( )  GEOMETRIC_REPRESENTATION_ITEM ( )  RATIONAL_B_SPLINE_CURVE ( ( 0.9999999999999954481, 0.9238795325112912904, 1.000000000000000000, 0.9238795325112867385, 1.000000000000000000, 0.9238795325112867385, 1.000000000000000000, 0.9238795325112837409, 1.000000000000003109 ) ) 
 REPRESENTATION_ITEM ( '' )  );
#61826 = CARTESIAN_POINT ( 'NONE',  ( -3.458734124999960358, 196.6250000013656063, 196.5673454167823877 ) ) ;
#61827 = CARTESIAN_POINT ( 'NONE',  ( -5.656854249492379694, 10.87499999590322020, -5.656854249492380582 ) ) ;
#61828 = ORIENTED_EDGE ( 'NONE', *, *, #33400, .F. ) ;
#61829 = CARTESIAN_POINT ( 'NONE',  ( 31.45873412499999944, 194.7500000013656063, 168.5673454167822740 ) ) ;
#61830 = EDGE_CURVE ( 'NONE', #67635, #6411, #23994, .T. ) ;
#61831 = CARTESIAN_POINT ( 'NONE',  ( 5.082755093536324154, 20.15624999795161543, 5.082755093536326818 ) ) ;
#61832 = CARTESIAN_POINT ( 'NONE',  ( -8.311093377946836114, 167.9687499965859843, -8.311093377946837890 ) ) ;
#61833 = CARTESIAN_POINT ( 'NONE',  ( 8.000000000000000000, 7.500000000000001776, 0.000000000000000000 ) ) ;
#61834 = CARTESIAN_POINT ( 'NONE',  ( -5.082755093536325930, 104.8437500020483810, -5.082755093536325930 ) ) ;
#61836 = CARTESIAN_POINT ( 'NONE',  ( 0.7509181236784723268, -55.63764137817189237, -43.81192498624803733 ) ) ;
#61835 = CARTESIAN_POINT ( 'NONE',  ( 2.449293598294707893E-16, 17.99999999726881583, -4.000000000000001776 ) ) ;
#61837 = CARTESIAN_POINT ( 'NONE',  ( 24.54126587500000412, 205.3750000013656063, 168.5673454167822172 ) ) ;
#61838 = CARTESIAN_POINT ( 'NONE',  ( -7.188101187499990274, -2.977408999572651371, 15.45530278187175455 ) ) ;
#61839 = CARTESIAN_POINT ( 'NONE',  ( -2.849036369511732440E-14, 207.3750000027312126, 138.0000000000000568 ) ) ;
#61840 = CARTESIAN_POINT ( 'NONE',  ( 3.042071309553167069, 56.82291666325269119, -11.35316468749999785 ) ) ;
#61841 = LINE ( 'NONE', #33939, #43602 ) ;
#61842 = CARTESIAN_POINT ( 'NONE',  ( 4.999999999999993783, 26.04166665983870388, 8.660254037844390851 ) ) ;
#61843 = CARTESIAN_POINT ( 'NONE',  ( -11.00000000000000000, 0.000000000000000000, 76.18750000409677625 ) ) ;
#61844 = EDGE_LOOP ( 'NONE', ( #56847, #8124, #26433, #3711 ) ) ;
#61845 = DIRECTION ( 'NONE',  ( 0.000000000000000000, 0.000000000000000000, 1.000000000000000000 ) ) ;
#61846 = CARTESIAN_POINT ( 'NONE',  ( -8.000000000000001776, 20.15624999590322730, 3.313708498984759387 ) ) ;
#61847 = CARTESIAN_POINT ( 'NONE',  ( -11.35316468750000141, 48.48958332991934839, 3.042071309553159963 ) ) ;
#61848 = CARTESIAN_POINT ( 'NONE',  ( 4.556349186104045934, 11.00000000000000000, 72.71875000409677625 ) ) ;
#61849 = CARTESIAN_POINT ( 'NONE',  ( -2.754378923186476579E-14, 198.4375000013655779, 145.4587341250000350 ) ) ;
#61850 = FACE_OUTER_BOUND ( 'NONE', #10534, .T. ) ;
#61851 = CARTESIAN_POINT ( 'NONE',  ( -10.00000000000000178, 12.50000000000000178, -1.224646799147353454E-15 ) ) ;
#61853 = CARTESIAN_POINT ( 'NONE',  ( -8.311093377946841443, 48.90624999658600558, 8.311093377946834337 ) ) ;
#61852 = CARTESIAN_POINT ( 'NONE',  ( 2.977408999572650039, 96.68750000204838102, -7.188101187500000933 ) ) ;
#61854 = CARTESIAN_POINT ( 'NONE',  ( -4.898587196589407898E-16, 7.999999999999991118, 9.455302779823364645 ) ) ;
#61855 = CARTESIAN_POINT ( 'NONE',  ( -7.999999999961189268, -1.665725685002260109E-05, 4.018425631117963803 ) ) ;
#61856 = CARTESIAN_POINT ( 'NONE',  ( 9.832129032723416984, 175.3645833299193555, 5.676582343750006032 ) ) ;
#61857 =( BOUNDED_CURVE ( )  B_SPLINE_CURVE ( 2, ( #15727, #61393, #27059, #38389, #14980, #14228, #54253, #9719, #2564 ),
 .UNSPECIFIED., .F., .F. ) 
 B_SPLINE_CURVE_WITH_KNOTS ( ( 3, 2, 2, 2, 3 ),
 ( 0.1333333333333334425, 0.1416666666666667740, 0.1500000000000001332, 0.1583333333333334925, 0.1666666666666668239 ),
 .UNSPECIFIED. ) 
 CURVE ( )  GEOMETRIC_REPRESENTATION_ITEM ( )  RATIONAL_B_SPLINE_CURVE ( ( 0.9999999999999990008, 0.9238795325112877377, 1.000000000000000000, 0.9238795325112867385, 1.000000000000000000, 0.9238795325112867385, 1.000000000000000000, 0.9238795325112851842, 1.000000000000001554 ) ) 
 REPRESENTATION_ITEM ( '' )  );
#61858 = CARTESIAN_POINT ( 'NONE',  ( 7.320508075688774596, 147.4999999931720538, -7.320508075688774596 ) ) ;
#61859 = CARTESIAN_POINT ( 'NONE',  ( -7.188101187500000044, 100.5312500020483810, 0.000000000000000000 ) ) ;
#61860 = CARTESIAN_POINT ( 'NONE',  ( -0.6939194017717918994, 0.4334809116420236252, -7.910544316330319958 ) ) ;
#61861 = CARTESIAN_POINT ( 'NONE',  ( 11.35316468749999785, 30.88541666325268409, 3.042071309553174174 ) ) ;
#61862 = CARTESIAN_POINT ( 'NONE',  ( -2.679491924311226292, 78.33333332650536818, -10.00000000000000178 ) ) ;
#61863 = ORIENTED_EDGE ( 'NONE', *, *, #29509, .T. ) ;
#61864 = LINE ( 'NONE', #10928, #29604 ) ;
#61865 = CARTESIAN_POINT ( 'NONE',  ( 4.220049686691941027, -10.18810118749999738, 78.62500000204838102 ) ) ;
#61866 = DIRECTION ( 'NONE',  ( 0.000000000000000000, 0.000000000000000000, -1.000000000000000000 ) ) ;
#61868 = CARTESIAN_POINT ( 'NONE',  ( 11.35316468750000141, 165.7812499965860411, 0.000000000000000000 ) ) ;
#61867 = CARTESIAN_POINT ( 'NONE',  ( -2.679491924293753602, 6.458333333331768955, -10.00000000001010036 ) ) ;
#61869 = CARTESIAN_POINT ( 'NONE',  ( -7.999999999999991118, 3.313708498984756723, 12.79280278432982421 ) ) ;
#61870 = DIRECTION ( 'NONE',  ( -0.000000000000000000, 1.000000000000000000, -4.476705744456276341E-16 ) ) ;
#61871 = EDGE_CURVE ( 'NONE', #60459, #44073, #74571, .T. ) ;
#61872 = EDGE_CURVE ( 'NONE', #53176, #71803, #34229, .T. ) ;
#61873 = CARTESIAN_POINT ( 'NONE',  ( 2.679491924311235174, 259.5833333401612322, 9.999999999999998224 ) ) ;
#61874 = CARTESIAN_POINT ( 'NONE',  ( 4.737866951553296957, 52.21905653844932260, -48.93292554255041438 ) ) ;
#61875 = CARTESIAN_POINT ( 'NONE',  ( 10.18810118749999916, 1.247682550866122264E-15, 79.28125000204836681 ) ) ;
#61876 = VERTEX_POINT ( 'NONE', #70035 ) ;
#61877 = CARTESIAN_POINT ( 'NONE',  ( -2.828427124746208943, 198.7500000027312126, 144.8284271247462129 ) ) ;
#61878 = CARTESIAN_POINT ( 'NONE',  ( -9.832129032723418760, 118.1770833299193555, -5.676582343750004256 ) ) ;
#61879 = CARTESIAN_POINT ( 'NONE',  ( -30.64284399271075188, 178.3875230420588878, 174.6921329945331536 ) ) ;
#61880 = EDGE_LOOP ( 'NONE', ( #53556, #50415, #1137, #11949, #14877 ) ) ;
#61881 = VERTEX_POINT ( 'NONE', #53051 ) ;
#61882 = CARTESIAN_POINT ( 'NONE',  ( 3.211159895383561835, 7.562499998634407028, -3.211159895383561835 ) ) ;
#61883 = CARTESIAN_POINT ( 'NONE',  ( 5.082755093536324154, 9.281249997951610098, 5.082755093536326818 ) ) ;
#61884 = ADVANCED_FACE ( 'NONE', ( #12670 ), #70400, .T. ) ;
#61885 = CARTESIAN_POINT ( 'NONE',  ( 3.313708498984760720, 109.7187500040967763, -8.000000000000000000 ) ) ;
#61886 = CARTESIAN_POINT ( 'NONE',  ( -6.238412754330611322E-16, 10.18810118749999916, 94.65625000204836681 ) ) ;
#61887 = CARTESIAN_POINT ( 'NONE',  ( -24.54126587499999346, 200.4375000013656063, 170.0000000000003411 ) ) ;
#61888 = CARTESIAN_POINT ( 'NONE',  ( -4.000000000000001776, 9.500000000000000000, -4.898587196589415787E-16 ) ) ;
#61889 = CYLINDRICAL_SURFACE ( 'NONE', #68558, 11.99999999999999645 ) ;
#61890 = CARTESIAN_POINT ( 'NONE',  ( 2.780723358947928197E-16, 9.562499998634406140, -4.541265875000002339 ) ) ;
#61892 = AXIS2_PLACEMENT_3D ( 'NONE', #60539, #25452, #48467 ) ;
#61891 = CARTESIAN_POINT ( 'NONE',  ( -2.828427124746209831, 196.3750000000000284, 139.1715728752538723 ) ) ;
#61893 = ORIENTED_EDGE ( 'NONE', *, *, #48755, .F. ) ;
#61894 = LINE ( 'NONE', #73583, #2958 ) ;
#61896 = CARTESIAN_POINT ( 'NONE',  ( -23.99999999999997513, 199.6875000000000000, 171.6568542494927385 ) ) ;
#61895 = CARTESIAN_POINT ( 'NONE',  ( -31.45873412499999233, 197.6875000013655779, 170.0000000000004547 ) ) ;
#61897 = CARTESIAN_POINT ( 'NONE',  ( 4.541265875000002339, 21.31249999863440792, 0.000000000000000000 ) ) ;
#61898 = DIRECTION ( 'NONE',  ( 0.000000000000000000, 0.000000000000000000, 1.000000000000000000 ) ) ;
#61899 = ORIENTED_EDGE ( 'NONE', *, *, #35772, .T. ) ;
#61900 = ORIENTED_EDGE ( 'NONE', *, *, #51476, .T. ) ;
#61901 = CARTESIAN_POINT ( 'NONE',  ( -10.18810118749999916, 4.220049686691934809, 93.06250000204838102 ) ) ;
#61902 = CARTESIAN_POINT ( 'NONE',  ( -8.224976990608492855, 220.0000000000001421, 7.304091559116764110 ) ) ;
#61903 = CARTESIAN_POINT ( 'NONE',  ( -29.43265458321766914, 201.7500000013655779, 166.5412658750003629 ) ) ;
#61904 = CARTESIAN_POINT ( 'NONE',  ( 4.556349186104051263, -10.99999999999999822, 109.4687499999999858 ) ) ;
#61905 = CARTESIAN_POINT ( 'NONE',  ( 2.445694354108840063, 207.0625000013656063, 200.4456943541088663 ) ) ;
#61906 = DIRECTION ( 'NONE',  ( 1.000000000000000000, -0.000000000000000000, -0.000000000000000000 ) ) ;
#61907 = CARTESIAN_POINT ( 'NONE',  ( 7.320508075688771044, 124.3750000000000000, 7.320508075688775484 ) ) ;
#61908 = CARTESIAN_POINT ( 'NONE',  ( -3.313708498984762052, 108.2187500000000000, -8.000000000000000000 ) ) ;
#61909 = CARTESIAN_POINT ( 'NONE',  ( 6.676582343750004256, 293.0468750017069510, 2.765530957081995478 ) ) ;
#61910 = CARTESIAN_POINT ( 'NONE',  ( 2.977408999572646486, 7.188101187499991163, 7.392802781871750994 ) ) ;
#61911 = ORIENTED_EDGE ( 'NONE', *, *, #43022, .T. ) ;
#61912 = CARTESIAN_POINT ( 'NONE',  ( -7.320508075688778149, 174.9999999931720254, 7.320508075688769267 ) ) ;
#61913 = CARTESIAN_POINT ( 'NONE',  ( 30.44569435410879166, 205.5625000013656063, 172.4456943541087526 ) ) ;
#61914 = CARTESIAN_POINT ( 'NONE',  ( -1.469576158976823947E-15, 26.43749999590322375, 8.000000000000000000 ) ) ;
#61915 = VECTOR ( 'NONE', #40950, 1000.000000000000000 ) ;
#61916 = CARTESIAN_POINT ( 'NONE',  ( 3.458734124999959914, 198.4375000013655779, 142.0000000000000568 ) ) ;
#61917 = CARTESIAN_POINT ( 'NONE',  ( -2.977408999572650927, 122.7500000020483668, -7.188101187500000933 ) ) ;
#61919 = CARTESIAN_POINT ( 'NONE',  ( -1.432654583217664701, 201.0000000013655779, 138.5412658750000787 ) ) ;
#61918 = CARTESIAN_POINT ( 'NONE',  ( 8.000000000000001776, 121.1562500000000000, 3.313708498984759387 ) ) ;
#61920 = CARTESIAN_POINT ( 'NONE',  ( -9.832129032723415207, 254.6354166700806729, 5.676582343750005144 ) ) ;
#61921 = DIRECTION ( 'NONE',  ( -0.000000000000000000, 1.000000000000000000, -0.000000000000000000 ) ) ;
#61922 = LINE ( 'NONE', #32905, #39688 ) ;
#61923 = CARTESIAN_POINT ( 'NONE',  ( -5.676582343750006032, 14.11458332991935016, 9.832129032723418760 ) ) ;
#61924 = CARTESIAN_POINT ( 'NONE',  ( -8.311093377946836114, 207.9687499965859843, -8.311093377946837890 ) ) ;
#61925 = CARTESIAN_POINT ( 'NONE',  ( -23.99999999999995026, 202.8125000027312126, 171.6568542494926817 ) ) ;
#61926 = CARTESIAN_POINT ( 'NONE',  ( 0.000000000000000000, 0.000000000000000000, 118.0000000000000000 ) ) ;
#61928 = DIRECTION ( 'NONE',  ( -1.000000000000000000, -1.486057055854350565E-32, 3.469446951953619612E-16 ) ) ;
#61927 = CARTESIAN_POINT ( 'NONE',  ( -11.00000000000000000, 0.000000000000000000, 88.00000000000000000 ) ) ;
#61929 = ORIENTED_EDGE ( 'NONE', *, *, #26969, .T. ) ;
#61930 = ADVANCED_FACE ( 'NONE', ( #34975 ), #17971, .T. ) ;
#61931 = CARTESIAN_POINT ( 'NONE',  ( -1.432654583217662481, 201.3750000013656347, 145.4587341250000634 ) ) ;
#61932 = CARTESIAN_POINT ( 'NONE',  ( -5.676582343750006032, 9.114583329919350163, 9.832129032723418760 ) ) ;
#61933 = CARTESIAN_POINT ( 'NONE',  ( 11.00000000000000000, 1.347111479062088405E-15, 90.43750000409676204 ) ) ;
#61934 = LINE ( 'NONE', #57785, #2207 ) ;
#61935 = CARTESIAN_POINT ( 'NONE',  ( -25.55430564589122611, 197.3125000013656063, 167.5543056458915032 ) ) ;
#61936 = CARTESIAN_POINT ( 'NONE',  ( 0.000000000000000000, 300.0000000000000000, 0.000000000000000000 ) ) ;
#61938 = CARTESIAN_POINT ( 'NONE',  ( -11.35316468749999785, 8.072916663252682312, -3.042071309553167957 ) ) ;
#61937 = CARTESIAN_POINT ( 'NONE',  ( -7.188101187499999156, 115.2500000020483952, 2.977408999572654924 ) ) ;
#61939 = CARTESIAN_POINT ( 'NONE',  ( -4.898587196589412829E-16, 106.8125000040967763, -8.000000000000000000 ) ) ;
#61940 = CARTESIAN_POINT ( 'NONE',  ( -9.832129032723418760, 127.8645833299193697, -5.676582343750004256 ) ) ;
#61941 = CARTESIAN_POINT ( 'NONE',  ( -8.660254037844387298, 98.95833332650536818, -5.000000000000004441 ) ) ;
#61942 = CARTESIAN_POINT ( 'NONE',  ( 5.082755093536325042, 119.4687500020483810, -5.082755093536325930 ) ) ;
#61943 = CARTESIAN_POINT ( 'NONE',  ( 2.780723358947928197E-16, 18.68749999863440436, -4.541265875000002339 ) ) ;
#61944 = CARTESIAN_POINT ( 'NONE',  ( 5.000000000000000000, 16.14408868864073554, -27.96238185062347981 ) ) ;
#61945 = VERTEX_POINT ( 'NONE', #11202 ) ;
#61946 = CARTESIAN_POINT ( 'NONE',  ( 2.266287154879827348, -60.33498852648436639, 22.96738997677403660 ) ) ;
#61947 =( BOUNDED_CURVE ( )  B_SPLINE_CURVE ( 2, ( #32825, #4516, #21480, #50521, #50897, #10542, #55835, #16550, #56577, #27511, #44501, #44876, #16934 ),
 .UNSPECIFIED., .F., .F. ) 
 B_SPLINE_CURVE_WITH_KNOTS ( ( 3, 2, 2, 2, 2, 2, 3 ),
 ( 0.4166666666666664076, 0.4259259259259256525, 0.4351851851851848973, 0.4444444444444441422, 0.4537037037037034981, 0.4629629629629627430, 0.4722222222222219878 ),
 .UNSPECIFIED. ) 
 CURVE ( )  GEOMETRIC_REPRESENTATION_ITEM ( )  RATIONAL_B_SPLINE_CURVE ( ( 1.000000000000001110, 0.9659258262890673130, 1.000000000000000000, 0.9659258262890683122, 1.000000000000000000, 0.9659258262890683122, 1.000000000000000000, 0.9659258262890683122, 1.000000000000000000, 0.9659258262890683122, 1.000000000000000000, 0.9659258262890690894, 0.9999999999999992228 ) ) 
 REPRESENTATION_ITEM ( '' )  );
#61948 = CARTESIAN_POINT ( 'NONE',  ( 2.765530957082001251, 288.9218750017069510, 6.676582343750000703 ) ) ;
#61949 = FACE_OUTER_BOUND ( 'NONE', #36764, .T. ) ;
#61950 = CARTESIAN_POINT ( 'NONE',  ( 5.656854249492376141, -5.656854249492374365, 26.94905278432982598 ) ) ;
#61951 = AXIS2_PLACEMENT_3D ( 'NONE', #12426, #57737, #64852 ) ;
#61952 = LINE ( 'NONE', #5737, #42909 ) ;
#61953 = ADVANCED_FACE ( 'NONE', ( #57609 ), #39867, .F. ) ;
#61954 = CARTESIAN_POINT ( 'NONE',  ( 3.042071309553163960, 262.4479166700806445, -11.35316468749999785 ) ) ;
#61955 = CARTESIAN_POINT ( 'NONE',  ( -10.18810118749999738, -4.220049686691941915, 96.62500000204838102 ) ) ;
#61956 = VERTEX_POINT ( 'NONE', #51938 ) ;
#61957 = CARTESIAN_POINT ( 'NONE',  ( 7.999999999999998224, 22.21874999590322375, 3.313708498984766049 ) ) ;
#61958 = CARTESIAN_POINT ( 'NONE',  ( -11.35316468750000141, 153.8020833299193271, 3.042071309553159963 ) ) ;
#61959 = DIRECTION ( 'NONE',  ( -0.000000000000000000, 1.000000000000000000, -0.000000000000000000 ) ) ;
#61960 = CARTESIAN_POINT ( 'NONE',  ( -3.458734124999960358, 200.6250000013656063, 196.5673454167823877 ) ) ;
#61961 = CARTESIAN_POINT ( 'NONE',  ( -7.999999999999991118, 0.000000000000000000, 1.017802783920145782 ) ) ;
#61962 = CARTESIAN_POINT ( 'NONE',  ( 11.35316468750000141, 81.09374999658601268, 0.000000000000000000 ) ) ;
#61963 = VERTEX_POINT ( 'NONE', #23258 ) ;
#61964 = CARTESIAN_POINT ( 'NONE',  ( 7.204075437095966983, 7.204075437095967871, 112.0937500020483810 ) ) ;
#61965 = CARTESIAN_POINT ( 'NONE',  ( -1.881053915767124440, 9.124999998634407916, 4.541265875000001451 ) ) ;
#61966 = ORIENTED_EDGE ( 'NONE', *, *, #22011, .F. ) ;
#61967 = CARTESIAN_POINT ( 'NONE',  ( 7.188101187500001821, 26.06249999795161543, -2.977408999572650483 ) ) ;
#61968 = CARTESIAN_POINT ( 'NONE',  ( 36.10814071610729314, 271.9999999999999432, 139.0000000000000000 ) ) ;
#61969 = CARTESIAN_POINT ( 'NONE',  ( -1.836970198721029983E-15, 65.62499999317203958, 10.00000000000000178 ) ) ;
#61970 = CARTESIAN_POINT ( 'NONE',  ( 4.401442555609581635E-16, 20.71874999795161543, -7.188101187500000044 ) ) ;
#61971 = EDGE_CURVE ( 'NONE', #34804, #52532, #46267, .T. ) ;
#61972 = CYLINDRICAL_SURFACE ( 'NONE', #1420, 8.000000000000000000 ) ;
#61973 = CARTESIAN_POINT ( 'NONE',  ( 4.220049686691941027, -10.18810118749999738, 109.0000000020483810 ) ) ;
#61974 = ADVANCED_FACE ( 'NONE', ( #24367 ), #34602, .F. ) ;
#61975 = PRODUCT ( 'hand wheel', 'hand wheel', '', ( #34279 ) ) ;
#61976 = AXIS2_PLACEMENT_3D ( 'NONE', #70247, #35547, #58199 ) ;
#61977 = CARTESIAN_POINT ( 'NONE',  ( 1.656854249492371256, 204.3124999999999716, 202.0000000000000000 ) ) ;
#61978 = CARTESIAN_POINT ( 'NONE',  ( 4.000000000000001776, 4.812499997268813168, -1.656854249492381248 ) ) ;
#61979 = CYLINDRICAL_SURFACE ( 'NONE', #44526, 8.000000000000000000 ) ;
#61980 = ORIENTED_EDGE ( 'NONE', *, *, #17408, .T. ) ;
#61981 = EDGE_CURVE ( 'NONE', #47241, #45978, #1383, .T. ) ;
#61982 = EDGE_CURVE ( 'NONE', #61189, #30714, #47374, .T. ) ;
#61983 = CARTESIAN_POINT ( 'NONE',  ( -3.458734124999959025, 201.5000000013655779, 199.4326545832176691 ) ) ;
#61984 = CARTESIAN_POINT ( 'NONE',  ( -26.56734541678227757, 208.0000000013656347, 173.4587341250003476 ) ) ;
#61985 = CARTESIAN_POINT ( 'NONE',  ( 2.828427124746190291, 12.62499999726881406, 2.828427124746192067 ) ) ;
#61986 = CARTESIAN_POINT ( 'NONE',  ( -3.211159895383561391, 6.687499998634407028, -3.211159895383561835 ) ) ;
#61987 = EDGE_CURVE ( 'NONE', #8238, #49926, #40023, .T. ) ;
#61988 = CARTESIAN_POINT ( 'NONE',  ( -1.656854249492383468, 13.68750000000000000, 4.000000000000000888 ) ) ;
#61989 = CARTESIAN_POINT ( 'NONE',  ( 2.977408999572650927, -7.188101187499990274, 21.45530278187175810 ) ) ;
#61990 = VERTEX_POINT ( 'NONE', #13761 ) ;
#61991 = CARTESIAN_POINT ( 'NONE',  ( 7.778174593052021635, 7.778174593052023411, 90.43749999999998579 ) ) ;
#61992 = VERTEX_POINT ( 'NONE', #14139 ) ;
#61993 = CARTESIAN_POINT ( 'NONE',  ( 7.204075437095968759, -7.204075437095966983, 108.7187500020483810 ) ) ;
#61994 = CARTESIAN_POINT ( 'NONE',  ( 0.000000000000000000, 1.224646799147352862E-15, -9.999999999999996447 ) ) ;
#61995 = CARTESIAN_POINT ( 'NONE',  ( -3.458734124999959025, 204.5000000013656063, 199.4326545832176691 ) ) ;
#61996 = CARTESIAN_POINT ( 'NONE',  ( 30.44569435410883074, 198.5625000013656063, 172.4456943541086957 ) ) ;
#61997 = CARTESIAN_POINT ( 'NONE',  ( -2.679491924311225848, 81.45833333333335702, -10.00000000000000178 ) ) ;
#61998 = CARTESIAN_POINT ( 'NONE',  ( -2.977408999572650927, 91.25000000204838102, -7.188101187500001821 ) ) ;
#61999 = CARTESIAN_POINT ( 'NONE',  ( -4.242640687119286547, 293.8750000000000000, -4.242640687119286547 ) ) ;
#62000 = CARTESIAN_POINT ( 'NONE',  ( 30.82842712474616675, 204.5000000027312126, 167.1715728752537018 ) ) ;
#62001 = EDGE_LOOP ( 'NONE', ( #11338, #57152, #44726, #70069 ) ) ;
#62002 = CARTESIAN_POINT ( 'NONE',  ( 8.000000000000000000, 8.906249995903221972, -3.313708498984761164 ) ) ;
#62003 = CARTESIAN_POINT ( 'NONE',  ( 2.266287154886623689, -10.27715108473166694, 63.73532778936404242 ) ) ;
#62004 = CARTESIAN_POINT ( 'NONE',  ( -4.000000000000015987, 196.6250000027312126, 142.0000000000000568 ) ) ;
#62005 = CARTESIAN_POINT ( 'NONE',  ( 0.000000000000000000, 300.0000000000000000, 10.00000000000000178 ) ) ;
#62006 = DIRECTION ( 'NONE',  ( 0.000000000000000000, 0.000000000000000000, 1.000000000000000000 ) ) ;
#62007 = CARTESIAN_POINT ( 'NONE',  ( -8.660254037844385522, 245.4166666666666856, 5.000000000000004441 ) ) ;
#62008 = CARTESIAN_POINT ( 'NONE',  ( -19.99999999999993250, -31.99999999999978684, 205.0000000000000284 ) ) ;
#62009 = CARTESIAN_POINT ( 'NONE',  ( 8.660254037844389075, 200.4166666666666856, -5.000000000000000000 ) ) ;
#62010 = LINE ( 'NONE', #21268, #71699 ) ;
#62011 = CARTESIAN_POINT ( 'NONE',  ( -2.977408999572647819, -7.188101187499990274, 15.64280278187175632 ) ) ;
#62012 = CARTESIAN_POINT ( 'NONE',  ( -3.042071309553173730, 169.6354166632526699, 11.35316468749999785 ) ) ;
#62013 = CARTESIAN_POINT ( 'NONE',  ( -2.828427124746152987, 208.2500000027312126, 200.8284271247462129 ) ) ;
#62014 = DIRECTION ( 'NONE',  ( 1.000000000000000000, 0.000000000000000000, 0.000000000000000000 ) ) ;
#62015 = CARTESIAN_POINT ( 'NONE',  ( 8.660254037844545394, 155.4166666666667993, -5.000000000000092371 ) ) ;
#62017 = CARTESIAN_POINT ( 'NONE',  ( 6.000000000000000000, 0.000000000000000000, 0.000000000000000000 ) ) ;
#62016 = CARTESIAN_POINT ( 'NONE',  ( -4.999999999999996447, -18.53862685874494431, 23.57305537018116581 ) ) ;
#62018 = VERTEX_POINT ( 'NONE', #42079 ) ;
#62019 = CARTESIAN_POINT ( 'NONE',  ( -5.676582343749998039, 17.76041666325268409, -9.832129032723420536 ) ) ;
#62020 = VECTOR ( 'NONE', #43447, 1000.000000000000000 ) ;
#62021 = CARTESIAN_POINT ( 'NONE',  ( -29.43265458321755901, 207.8750000013656063, 173.4587341250004044 ) ) ;
#62023 = CARTESIAN_POINT ( 'NONE',  ( 2.591411123055314292, -10.27614846265026038, -63.77676950206216588 ) ) ;
#62022 = CARTESIAN_POINT ( 'NONE',  ( 2.449293598294707893E-16, 15.99999999726881406, -4.000000000000001776 ) ) ;
#62024 = CARTESIAN_POINT ( 'NONE',  ( -28.86964650611963989, -51.88890262544310161, 181.3349463291653763 ) ) ;
#62025 = CARTESIAN_POINT ( 'NONE',  ( 3.458734124999959914, 202.4375000013656063, 142.0000000000000568 ) ) ;
#62026 = CARTESIAN_POINT ( 'NONE',  ( 6.123233995736767268E-16, 63.12499999317203248, -10.00000000000000178 ) ) ;
#62027 =( GEOMETRIC_REPRESENTATION_CONTEXT ( 3 ) GLOBAL_UNCERTAINTY_ASSIGNED_CONTEXT ( ( #25388 ) ) GLOBAL_UNIT_ASSIGNED_CONTEXT ( ( #34272, #40656, #34646 ) ) REPRESENTATION_CONTEXT ( 'NONE', 'WORKASPACE' ) );
#62028 = CARTESIAN_POINT ( 'NONE',  ( 7.188101187500002709, 105.3125000020483668, 2.977408999572649151 ) ) ;
#62029 = CARTESIAN_POINT ( 'NONE',  ( -3.211159895383562723, 10.06249999863440614, 3.211159895383561391 ) ) ;
#62030 = DIRECTION ( 'NONE',  ( -0.000000000000000000, 1.000000000000000000, -0.000000000000000000 ) ) ;
#62031 = CARTESIAN_POINT ( 'NONE',  ( 5.656854249492374365, 5.656854249492375253, 4.767802779823363757 ) ) ;
#62032 = ORIENTED_EDGE ( 'NONE', *, *, #6089, .T. ) ;
#62033 = ORIENTED_EDGE ( 'NONE', *, *, #55983, .T. ) ;
#62034 = ADVANCED_FACE ( 'NONE', ( #60175 ), #24726, .T. ) ;
#62035 = LINE ( 'NONE', #32260, #20753 ) ;
#62036 = CARTESIAN_POINT ( 'NONE',  ( -7.999999999999991118, 0.000000000000000000, 14.51780278392014800 ) ) ;
#62037 = CARTESIAN_POINT ( 'NONE',  ( -5.000000000000010658, 163.3333333333333428, 8.660254037844396180 ) ) ;
#62038 = CARTESIAN_POINT ( 'NONE',  ( 11.35316468749999785, 145.5729166632527267, 3.042071309553174174 ) ) ;
#62039 = ORIENTED_EDGE ( 'NONE', *, *, #69688, .F. ) ;
#62040 = CARTESIAN_POINT ( 'NONE',  ( -4.999999999999999112, 14.31098243164692008, -69.87317657433686691 ) ) ;
#62041 = CARTESIAN_POINT ( 'NONE',  ( 4.220049686691941027, -10.18810118749999738, 87.62500000204836681 ) ) ;
#62042 = DIRECTION ( 'NONE',  ( -0.000000000000000000, -0.000000000000000000, -1.000000000000000000 ) ) ;
#62043 = CARTESIAN_POINT ( 'NONE',  ( 2.751064625579944321E-14, 208.7500000000000284, 194.0000000000000568 ) ) ;
#62044 = CARTESIAN_POINT ( 'NONE',  ( 4.000000000000001776, 14.74999999726881406, 0.000000000000000000 ) ) ;
#62045 = CARTESIAN_POINT ( 'NONE',  ( -4.898587196589412829E-16, 91.81250000409677625, -8.000000000000000000 ) ) ;
#62046 = CARTESIAN_POINT ( 'NONE',  ( 10.00000000000000178, 147.0833333265053966, -2.679491924311226736 ) ) ;
#62047 = ORIENTED_EDGE ( 'NONE', *, *, #8716, .T. ) ;
#62048 = EDGE_CURVE ( 'NONE', #66955, #53500, #59815, .T. ) ;
#62049 = CARTESIAN_POINT ( 'NONE',  ( 30.80088309095861376, -36.84397595866337838, 173.6600293781182529 ) ) ;
#62050 = CARTESIAN_POINT ( 'NONE',  ( -26.12704298119327717, 176.1929651069431202, 153.1551066619547612 ) ) ;
#62051 = CARTESIAN_POINT ( 'NONE',  ( 11.35316468749999785, 120.8854166632526841, 3.042071309553174174 ) ) ;
#62052 = CARTESIAN_POINT ( 'NONE',  ( -1.432654583217607858, 202.6250000013656063, 201.4587341250000065 ) ) ;
#62053 = CARTESIAN_POINT ( 'NONE',  ( -2.977408999572654480, 19.87499999795161543, 7.188101187499999156 ) ) ;
#62054 = CARTESIAN_POINT ( 'NONE',  ( -10.18810118749999916, 0.000000000000000000, 83.03125000204838102 ) ) ;
#62055 = CARTESIAN_POINT ( 'NONE',  ( 11.35316468749999963, 31.30208332991934839, -3.042071309553165293 ) ) ;
#62056 = ORIENTED_EDGE ( 'NONE', *, *, #54301, .T. ) ;
#62057 = CYLINDRICAL_SURFACE ( 'NONE', #39305, 10.00000000000000178 ) ;
#62058 = CARTESIAN_POINT ( 'NONE',  ( -3.317071493978878571, 8.008118988124991233, 21.73186528394063544 ) ) ;
#62059 = CARTESIAN_POINT ( 'NONE',  ( 2.445694354108784108, 209.5625000013656063, 144.4456943541088663 ) ) ;
#62060 = CARTESIAN_POINT ( 'NONE',  ( 7.778174593052023411, -7.778174593052021635, 85.75000000409677625 ) ) ;
#62061 = CARTESIAN_POINT ( 'NONE',  ( 5.082755093536325930, 6.656249997951611874, -5.082755093536325930 ) ) ;
#62062 = CARTESIAN_POINT ( 'NONE',  ( 6.676582343750004256, 288.8906250017070079, 2.765530957081995478 ) ) ;
#62063 = LINE ( 'NONE', #39430, #24472 ) ;
#62064 = CARTESIAN_POINT ( 'NONE',  ( -26.34314575050761675, 206.5624999999999432, 174.0000000000003979 ) ) ;
#62065 = ORIENTED_EDGE ( 'NONE', *, *, #55381, .F. ) ;
#62066 =( BOUNDED_CURVE ( )  B_SPLINE_CURVE ( 2, ( #28218, #68209, #45942, #68955, #17639, #11612, #73868, #41036, #63285, #17265, #5217, #58034, #51983 ),
 .UNSPECIFIED., .F., .F. ) 
 B_SPLINE_CURVE_WITH_KNOTS ( ( 3, 2, 2, 2, 2, 2, 3 ),
 ( 0.6467391304347827052, 0.6485507246376812640, 0.6503623188405798228, 0.6521739130434782705, 0.6539855072463768293, 0.6557971014492753881, 0.6576086956521739468 ),
 .UNSPECIFIED. ) 
 CURVE ( )  GEOMETRIC_REPRESENTATION_ITEM ( )  RATIONAL_B_SPLINE_CURVE ( ( 0.9999999999999978906, 0.9659258262890704216, 1.000000000000000000, 0.9659258262890683122, 1.000000000000000000, 0.9659258262890683122, 1.000000000000000000, 0.9659258262890683122, 1.000000000000000000, 0.9659258262890683122, 1.000000000000000000, 0.9659258262890683122, 1.000000000000000000 ) ) 
 REPRESENTATION_ITEM ( '' )  );
#62067 = CARTESIAN_POINT ( 'NONE',  ( 8.311093377946834337, 155.4687499965859843, 8.311093377946839666 ) ) ;
#62068 = CARTESIAN_POINT ( 'NONE',  ( 10.18810118749999916, 4.220049686691935698, 79.00000000204838102 ) ) ;
#62069 = ADVANCED_FACE ( 'NONE', ( #25092, #8129 ), #30767, .T. ) ;
#62070 = CARTESIAN_POINT ( 'NONE',  ( -29.43265458321760164, 196.8750000013656063, 173.4587341250003760 ) ) ;
#62071 = ADVANCED_FACE ( 'NONE', ( #36071 ), #59088, .T. ) ;
#62072 = CARTESIAN_POINT ( 'NONE',  ( 1.224646799147353454E-15, 300.0000000000000000, -10.00000000000000178 ) ) ;
#62073 = CARTESIAN_POINT ( 'NONE',  ( -3.211159895383562723, 17.06249999863440792, 3.211159895383561391 ) ) ;
#62074 = ORIENTED_EDGE ( 'NONE', *, *, #7035, .T. ) ;
#62075 = CARTESIAN_POINT ( 'NONE',  ( -1.656854249492347719, 198.9375000027312126, 194.0000000000000853 ) ) ;
#62076 = CIRCLE ( 'NONE', #63264, 3.999999999999986233 ) ;
#62077 = CARTESIAN_POINT ( 'NONE',  ( 1.432654583217608080, 196.8750000013656063, 138.5412658750000503 ) ) ;
#62078 = CARTESIAN_POINT ( 'NONE',  ( -29.65685424949245785, 205.1875000027311842, 166.0000000000004263 ) ) ;
#62079 = CARTESIAN_POINT ( 'NONE',  ( -8.000000000000001776, 21.84375000000000355, 3.313708498984759387 ) ) ;
#62080 = ORIENTED_EDGE ( 'NONE', *, *, #66727, .F. ) ;
#62081 = EDGE_CURVE ( 'NONE', #73625, #8706, #48481, .T. ) ;
#62082 = CARTESIAN_POINT ( 'NONE',  ( 2.977408999572652260, 10.68749999795161187, 7.188101187500000044 ) ) ;
#62083 = DIRECTION ( 'NONE',  ( -0.000000000000000000, 1.000000000000000000, -0.000000000000000000 ) ) ;
#62084 = DIRECTION ( 'NONE',  ( 1.000000000000000000, 0.000000000000000000, 0.000000000000000000 ) ) ;
#62085 = CARTESIAN_POINT ( 'NONE',  ( 10.00000000000000000, 44.79166666666665719, 2.679491924311236062 ) ) ;
#62086 = CARTESIAN_POINT ( 'NONE',  ( 2.977408999572650039, 106.0625000020483668, -7.188101187500001821 ) ) ;
#62087 = CARTESIAN_POINT ( 'NONE',  ( 4.000000000000015987, 207.6250000027312126, 198.0000000000000284 ) ) ;
#62088 = CARTESIAN_POINT ( 'NONE',  ( 4.721056650415999201, 290.0781250017069510, -4.721056650415999201 ) ) ;
#62090 = CARTESIAN_POINT ( 'NONE',  ( -18.00000000000000000, -6.103439543526007149, -0.5706341627281755757 ) ) ;
#62089 = FACE_OUTER_BOUND ( 'NONE', #31377, .T. ) ;
#62091 = ORIENTED_EDGE ( 'NONE', *, *, #42195, .F. ) ;
#62092 = CARTESIAN_POINT ( 'NONE',  ( -11.35316468749999785, 263.6979166700807014, -3.042071309553164848 ) ) ;
#62093 = CARTESIAN_POINT ( 'NONE',  ( -5.082755093536319713, 5.082755093536319713, 22.67405278187175455 ) ) ;
#62094 = CARTESIAN_POINT ( 'NONE',  ( -5.086519500888709189, 50.65542486323467131, 41.09394361259066386 ) ) ;
#62095 = LINE ( 'NONE', #5882, #17700 ) ;
#62096 = CARTESIAN_POINT ( 'NONE',  ( -3.728321214214307844, -66.24762070552739601, -26.57448171415594729 ) ) ;
#62097 = CARTESIAN_POINT ( 'NONE',  ( -2.290346072756624274, 21.99999999999999289, 3.966738362316490907 ) ) ;
#62098 = CARTESIAN_POINT ( 'NONE',  ( 7.320508075688774596, 145.6249999999999716, -7.320508075688774596 ) ) ;
#62099 = LINE ( 'NONE', #33452, #39456 ) ;
#62100 = CARTESIAN_POINT ( 'NONE',  ( -3.734486434573632163, 8.236198097127171991, -0.01899995639453642277 ) ) ;
#62101 = CARTESIAN_POINT ( 'NONE',  ( 1.469576158976823947E-15, 96.87499999999998579, 8.000000000000000000 ) ) ;
#62102 = CARTESIAN_POINT ( 'NONE',  ( 11.35316468749999785, 130.8854166632526699, 3.042071309553174174 ) ) ;
#62103 = CARTESIAN_POINT ( 'NONE',  ( 3.313708498984815343, 99.03124999999997158, -7.999999999999944933 ) ) ;
#62104 = CARTESIAN_POINT ( 'NONE',  ( -7.778174593052020747, -7.778174593052023411, 73.18749999999998579 ) ) ;
#62107 = CARTESIAN_POINT ( 'NONE',  ( 9.000000000000023093, -15.58845726811988541, 0.000000000000000000 ) ) ;
#62106 = CARTESIAN_POINT ( 'NONE',  ( 25.55430564589115505, 198.0625000013656063, 167.5543056458911053 ) ) ;
#62105 = CARTESIAN_POINT ( 'NONE',  ( 25.17157287525381903, 208.6250000000000284, 167.1715728752537018 ) ) ;
#62108 = VERTEX_POINT ( 'NONE', #66208 ) ;
#62109 = CARTESIAN_POINT ( 'NONE',  ( 3.738278573177460373, 224.0556613178885073, 9.279702309298665241 ) ) ;
#62110 = EDGE_CURVE ( 'NONE', #26401, #6157, #53029, .T. ) ;
#62111 = DIRECTION ( 'NONE',  ( 0.000000000000000000, 0.000000000000000000, -1.000000000000000000 ) ) ;
#62112 = CARTESIAN_POINT ( 'NONE',  ( 30.44569435410883429, 198.0625000013656063, 167.5543056458911053 ) ) ;
#62113 = CARTESIAN_POINT ( 'NONE',  ( -5.676582343750006032, 204.4270833299193555, 9.832129032723418760 ) ) ;
#62114 = CARTESIAN_POINT ( 'NONE',  ( -5.082755093536325930, 122.4687500020483952, -5.082755093536325930 ) ) ;
#62115 = CARTESIAN_POINT ( 'NONE',  ( 4.541265875000002339, 18.37499999863441147, -1.881053915767121554 ) ) ;
#62116 = CARTESIAN_POINT ( 'NONE',  ( 25.55430564589114795, 195.5625000013656063, 172.4456943541086957 ) ) ;
#62117 = CARTESIAN_POINT ( 'NONE',  ( -5.656854249492373476, -5.656854249492376141, 28.01780277982336642 ) ) ;
#62118 = CARTESIAN_POINT ( 'NONE',  ( -23.99999999999997513, 202.6875000000000284, 171.6568542494927385 ) ) ;
#62119 = CARTESIAN_POINT ( 'NONE',  ( 8.311093377946837890, 91.40624999658604111, -8.311093377946837890 ) ) ;
#62120 = EDGE_LOOP ( 'NONE', ( #18264, #9753, #36571, #44693, #21317, #47535, #1740 ) ) ;
#62121 = EDGE_CURVE ( 'NONE', #44162, #71873, #8819, .T. ) ;
#62122 = CARTESIAN_POINT ( 'NONE',  ( -2.220555325575947149E-11, 176.2500000000017621, -10.00000000000000533 ) ) ;
#62123 = CARTESIAN_POINT ( 'NONE',  ( 7.188101187499999156, 16.87499999795161543, 2.977408999572654924 ) ) ;
#62124 = CARTESIAN_POINT ( 'NONE',  ( -1.836970198721029983E-15, 38.75000000000000000, 10.00000000000000178 ) ) ;
#62125 = CARTESIAN_POINT ( 'NONE',  ( -8.311093377946834337, 259.8437500034139589, 8.311093377946837890 ) ) ;
#62126 = CARTESIAN_POINT ( 'NONE',  ( -3.042071309553173730, 99.32291666325268409, 11.35316468749999785 ) ) ;
#62127 = ORIENTED_EDGE ( 'NONE', *, *, #36230, .T. ) ;
#62128 = CARTESIAN_POINT ( 'NONE',  ( 4.999999999999993783, 206.0416666598387110, 8.660254037844390851 ) ) ;
#62129 = CARTESIAN_POINT ( 'NONE',  ( -10.18810118749999916, 0.000000000000000000, 106.6562500020483668 ) ) ;
#62130 = CARTESIAN_POINT ( 'NONE',  ( -27.99999999999996092, 195.1875000013655779, 173.4587341250003760 ) ) ;
#62131 = CARTESIAN_POINT ( 'NONE',  ( -1.432654583217608080, 202.8750000013656347, 201.4587341250000350 ) ) ;
#62132 = CARTESIAN_POINT ( 'NONE',  ( 0.000000000000000000, 0.000000000000000000, 0.000000000000000000 ) ) ;
#62134 = CARTESIAN_POINT ( 'NONE',  ( -5.676582343749998039, 87.44791666325268409, -9.832129032723420536 ) ) ;
#62133 = LINE ( 'NONE', #16466, #49678 ) ;
#62135 = CIRCLE ( 'NONE', #7890, 10.99999999999999645 ) ;
#62136 = CARTESIAN_POINT ( 'NONE',  ( 7.999999999999992895, -3.313708498984756279, 15.17405278392014623 ) ) ;
#62137 = CARTESIAN_POINT ( 'NONE',  ( -24.54126587500000056, 202.5000000013656063, 168.5673454167827003 ) ) ;
#62138 = CARTESIAN_POINT ( 'NONE',  ( -3.313708498984719864, 21.28124999590322375, -8.000000000000040856 ) ) ;
#62139 = CARTESIAN_POINT ( 'NONE',  ( 7.320508075688774596, 177.4999999931720254, -7.320508075688774596 ) ) ;
#62140 = CARTESIAN_POINT ( 'NONE',  ( 75.00000000000000000, 0.000000000000000000, 42.00000000000000000 ) ) ;
#62141 = CARTESIAN_POINT ( 'NONE',  ( -1.469576158976823947E-15, 26.62500000000000355, 8.000000000000000000 ) ) ;
#62142 = CARTESIAN_POINT ( 'NONE',  ( 5.676582343750001591, 71.92708332991934128, -9.832129032723420536 ) ) ;
#62143 = CARTESIAN_POINT ( 'NONE',  ( -4.721056650415998313, 291.5781250017069510, 4.721056650416000089 ) ) ;
#62144 = EDGE_CURVE ( 'NONE', #67329, #34088, #65832, .T. ) ;
#62145 = CARTESIAN_POINT ( 'NONE',  ( -10.18810118749999916, 4.220049686691934809, 103.9375000020483810 ) ) ;
#62146 = CARTESIAN_POINT ( 'NONE',  ( -5.676582343749998039, 222.4479166632526983, -9.832129032723420536 ) ) ;
#62147 = ORIENTED_EDGE ( 'NONE', *, *, #3260, .T. ) ;
#62148 = CARTESIAN_POINT ( 'NONE',  ( 2.849036369511732440E-14, 202.2500000000000000, 202.0000000000000000 ) ) ;
#62149 = FACE_OUTER_BOUND ( 'NONE', #13064, .T. ) ;
#62150 = LINE ( 'NONE', #10103, #3389 ) ;
#62151 = CARTESIAN_POINT ( 'NONE',  ( 3.042071309553167513, 206.8229166632526699, -11.35316468749999785 ) ) ;
#62152 = CARTESIAN_POINT ( 'NONE',  ( -2.679491924311222295, 229.1666666734946034, 10.00000000000000178 ) ) ;
#62153 = CARTESIAN_POINT ( 'NONE',  ( -10.99999999999999822, -4.556349186104053040, 71.78125000409679046 ) ) ;
#62154 = ORIENTED_EDGE ( 'NONE', *, *, #67950, .T. ) ;
#62155 = CARTESIAN_POINT ( 'NONE',  ( -2.085542519210945728E-15, 199.8437499965860127, 11.35316468750000141 ) ) ;
#62156 = CARTESIAN_POINT ( 'NONE',  ( -4.401442555609577197E-16, 7.188101187499992051, 16.11155278187175455 ) ) ;
#62157 =( BOUNDED_CURVE ( )  B_SPLINE_CURVE ( 2, ( #13982, #19657, #13254, #48700, #71707, #42671, #6876, #47960, #65682, #29886, #52899, #61526, #72848 ),
 .UNSPECIFIED., .F., .F. ) 
 B_SPLINE_CURVE_WITH_KNOTS ( ( 3, 2, 2, 2, 2, 2, 3 ),
 ( 0.9619565217391303769, 0.9637681159420288246, 0.9655797101449273834, 0.9673913043478259421, 0.9692028985507246119, 0.9710144927536231707, 0.9728260869565217295 ),
 .UNSPECIFIED. ) 
 CURVE ( )  GEOMETRIC_REPRESENTATION_ITEM ( )  RATIONAL_B_SPLINE_CURVE ( ( 1.000000000000001998, 0.9659258262890662028, 1.000000000000000000, 0.9659258262890683122, 1.000000000000000000, 0.9659258262890683122, 1.000000000000000000, 0.9659258262890683122, 1.000000000000000000, 0.9659258262890683122, 1.000000000000000000, 0.9659258262890683122, 1.000000000000000000 ) ) 
 REPRESENTATION_ITEM ( '' )  );
#62158 = CARTESIAN_POINT ( 'NONE',  ( -27.99999999999996803, 206.9375000013656063, 173.4587341250003760 ) ) ;
#62159 = CARTESIAN_POINT ( 'NONE',  ( 5.656854249492378806, 13.31250000000000178, 5.656854249492381470 ) ) ;
#62160 = VERTEX_POINT ( 'NONE', #53422 ) ;
#62161 = CARTESIAN_POINT ( 'NONE',  ( -8.000000000000000000, 93.68750000409679046, 0.000000000000000000 ) ) ;
#62162 = CARTESIAN_POINT ( 'NONE',  ( 10.00000000000000000, 19.79166666666666785, 2.679491924311236062 ) ) ;
#62163 = CARTESIAN_POINT ( 'NONE',  ( 4.220049686691934809, 10.18810118749999916, 81.06250000204836681 ) ) ;
#62164 = ORIENTED_EDGE ( 'NONE', *, *, #24122, .T. ) ;
#62165 = CARTESIAN_POINT ( 'NONE',  ( -4.000000000000001776, 18.50000000000000000, -4.898587196589415787E-16 ) ) ;
#62166 =( BOUNDED_CURVE ( )  B_SPLINE_CURVE ( 2, ( #32158, #55179, #30664, #3484, #48001, #54052, #49498, #65360, #13659 ),
 .UNSPECIFIED., .F., .F. ) 
 B_SPLINE_CURVE_WITH_KNOTS ( ( 3, 2, 2, 2, 3 ),
 ( 0.1354166666666667407, 0.1406250000000000833, 0.1458333333333334259, 0.1510416666666667684, 0.1562500000000001110 ),
 .UNSPECIFIED. ) 
 CURVE ( )  GEOMETRIC_REPRESENTATION_ITEM ( )  RATIONAL_B_SPLINE_CURVE ( ( 0.9999999999999987788, 0.9238795325112879597, 1.000000000000000000, 0.9238795325112867385, 1.000000000000000000, 0.9238795325112867385, 1.000000000000000000, 0.9238795325112850731, 1.000000000000001554 ) ) 
 REPRESENTATION_ITEM ( '' )  );
#62167 = CARTESIAN_POINT ( 'NONE',  ( -1.881053915767121776, 19.62499999863441147, -4.541265875000002339 ) ) ;
#62168 = CARTESIAN_POINT ( 'NONE',  ( 31.28528697797139557, 194.5631545839482328, 171.3980623224641135 ) ) ;
#62169 = ORIENTED_EDGE ( 'NONE', *, *, #66030, .T. ) ;
#62170 = FACE_OUTER_BOUND ( 'NONE', #64812, .T. ) ;
#62171 = CARTESIAN_POINT ( 'NONE',  ( -2.977408999572651815, 123.3125000020483810, 7.188101187500000933 ) ) ;
#62174 = CARTESIAN_POINT ( 'NONE',  ( 0.4369882809721238326, -51.14729664189373182, 48.52014062455020849 ) ) ;
#62173 = CARTESIAN_POINT ( 'NONE',  ( 3.042071309553163516, 242.4479166700806161, -11.35316468749999785 ) ) ;
#62172 = CARTESIAN_POINT ( 'NONE',  ( 24.54126587499998635, 206.1250000013656063, 168.5673454167822740 ) ) ;
#62175 = PRODUCT_CONTEXT ( 'NONE', #69837, 'mechanical' ) ;
#62176 = ORIENTED_EDGE ( 'NONE', *, *, #1574, .F. ) ;
#62177 = EDGE_CURVE ( 'NONE', #57640, #53455, #70759, .T. ) ;
#62178 = CARTESIAN_POINT ( 'NONE',  ( -9.832129032723418760, 248.8020833367473301, -5.676582343749998927 ) ) ;
#62179 = CARTESIAN_POINT ( 'NONE',  ( -2.977408999572648707, -7.188101187499990274, 10.76780278187175632 ) ) ;
#62180 = ORIENTED_EDGE ( 'NONE', *, *, #7002, .F. ) ;
#62181 = ORIENTED_EDGE ( 'NONE', *, *, #25072, .F. ) ;
#62182 = CARTESIAN_POINT ( 'NONE',  ( 4.220049686691934809, 10.18810118749999916, 76.18750000204838102 ) ) ;
#62183 = CARTESIAN_POINT ( 'NONE',  ( -3.042071309553173730, 84.63541666325265567, 11.35316468749999785 ) ) ;
#62184 = CARTESIAN_POINT ( 'NONE',  ( -10.18810118749999916, 0.000000000000000000, 117.1562500020483810 ) ) ;
#62185 = CARTESIAN_POINT ( 'NONE',  ( -4.556349186104045934, 11.00000000000000000, 92.21875000000000000 ) ) ;
#62188 = CARTESIAN_POINT ( 'NONE',  ( -2.765530957081996810, 288.4218750017069510, -6.676582343750002480 ) ) ;
#62187 = CARTESIAN_POINT ( 'NONE',  ( 29.43265458321761585, 207.8750000013656063, 166.5412658749999650 ) ) ;
#62186 = CARTESIAN_POINT ( 'NONE',  ( 24.54126587499999346, 205.4375000013656063, 169.9999999999998863 ) ) ;
#62189 = FACE_OUTER_BOUND ( 'NONE', #55401, .T. ) ;
#62190 = CARTESIAN_POINT ( 'NONE',  ( 5.656854249492381470, 101.5625000000000000, 5.656854249492379694 ) ) ;
#62191 = EDGE_CURVE ( 'NONE', #61067, #27563, #68448, .T. ) ;
#62192 = CARTESIAN_POINT ( 'NONE',  ( 11.35316468749999963, 205.9895833299193271, -3.042071309553165293 ) ) ;
#62193 = CARTESIAN_POINT ( 'NONE',  ( -5.656854249492381470, 11.24999999590322197, 5.656854249492379694 ) ) ;
#62194 = VECTOR ( 'NONE', #13398, 1000.000000000000000 ) ;
#62195 = ORIENTED_EDGE ( 'NONE', *, *, #65405, .T. ) ;
#62196 = CARTESIAN_POINT ( 'NONE',  ( 26.56734541678237704, 195.0000000013656063, 166.5412658749999650 ) ) ;
#62197 = CARTESIAN_POINT ( 'NONE',  ( 5.082755093536325930, 16.03124999795161543, -5.082755093536325930 ) ) ;
#62198 = CARTESIAN_POINT ( 'NONE',  ( 11.35316468749999785, 160.8854166632526983, 3.042071309553174174 ) ) ;
#62199 = CARTESIAN_POINT ( 'NONE',  ( 23.99999999999997868, 197.8125000027312410, 168.3431457505075457 ) ) ;
#62200 = CARTESIAN_POINT ( 'NONE',  ( 7.188101187500002709, 105.6875000020483952, 2.977408999572649151 ) ) ;
#62202 = CARTESIAN_POINT ( 'NONE',  ( -1.506680654955159460, -55.70239491600695203, -43.84725041001593837 ) ) ;
#62201 = CARTESIAN_POINT ( 'NONE',  ( 0.000000000000000000, 54.99999999999999289, 11.00000000000000000 ) ) ;
#62203 = CARTESIAN_POINT ( 'NONE',  ( 27.99999999999996803, 206.6875000013656063, 173.4587341249998929 ) ) ;
#62204 = CARTESIAN_POINT ( 'NONE',  ( 7.188101187499992051, 8.802885111219154394E-16, 14.61155278187175455 ) ) ;
#62205 = CARTESIAN_POINT ( 'NONE',  ( -2.085542519210945728E-15, 49.53124999658601979, 11.35316468750000141 ) ) ;
#62206 = EDGE_CURVE ( 'NONE', #36324, #24263, #35395, .T. ) ;
#62207 = CARTESIAN_POINT ( 'NONE',  ( -12.00000000000000000, -5.801387104618788371, -0.7465129729868831276 ) ) ;
#62208 = CARTESIAN_POINT ( 'NONE',  ( 2.679491924311228956, 27.91666665983870033, -10.00000000000000000 ) ) ;
#62209 = VERTEX_POINT ( 'NONE', #18715 ) ;
#62210 = CARTESIAN_POINT ( 'NONE',  ( 12.00000000000000000, 28.00000000000000000, 3.999999999999986233 ) ) ;
#62211 = LINE ( 'NONE', #33943, #32877 ) ;
#62212 = CARTESIAN_POINT ( 'NONE',  ( 5.676582343750001591, 66.61458332991935549, -9.832129032723420536 ) ) ;
#62213 = CARTESIAN_POINT ( 'NONE',  ( -11.00000000000000000, 0.000000000000000000, 71.68750000409676204 ) ) ;
#62214 = CARTESIAN_POINT ( 'NONE',  ( -3.458734125000015425, 200.2500000013656063, 143.4326545832176976 ) ) ;
#62215 = FACE_OUTER_BOUND ( 'NONE', #65667, .T. ) ;
#62216 = LINE ( 'NONE', #68255, #2132 ) ;
#62218 = CARTESIAN_POINT ( 'NONE',  ( -5.676582343749998039, 42.44791666325268409, -9.832129032723420536 ) ) ;
#62217 = CARTESIAN_POINT ( 'NONE',  ( 7.188101187500002709, 94.81250000204838102, 2.977408999572649151 ) ) ;
#62219 = CARTESIAN_POINT ( 'NONE',  ( -3.313708498984758943, -7.999999999999989342, 5.611552779823364645 ) ) ;
#62220 = CARTESIAN_POINT ( 'NONE',  ( -3.190679070438223991E-13, 203.7500000000000000, 10.00000000000000533 ) ) ;
#62221 = CARTESIAN_POINT ( 'NONE',  ( 11.35316468749999963, 170.9895833299193839, -3.042071309553165293 ) ) ;
#62222 = CARTESIAN_POINT ( 'NONE',  ( 2.679491924311228956, 147.9166666598387110, -10.00000000000000000 ) ) ;
#62223 = CARTESIAN_POINT ( 'NONE',  ( -7.188101187499999156, 100.6250000020483810, 2.977408999572654924 ) ) ;
#62224 = CARTESIAN_POINT ( 'NONE',  ( -1.328617215468150370, -47.69684747344491882, 139.0279571930748546 ) ) ;
#62225 = CARTESIAN_POINT ( 'NONE',  ( -5.676582343750006032, 39.42708332991935549, 9.832129032723418760 ) ) ;
#62226 = CARTESIAN_POINT ( 'NONE',  ( 2.751064625579944321E-14, 200.7500000000000000, 194.0000000000000568 ) ) ;
#62227 = CARTESIAN_POINT ( 'NONE',  ( -5.676582343749998039, 162.4479166632526983, -9.832129032723420536 ) ) ;
#62228 = ORIENTED_EDGE ( 'NONE', *, *, #12710, .T. ) ;
#62229 = CARTESIAN_POINT ( 'NONE',  ( 48.52446885514073927, 141.8181556194765562, 60.87679713484597954 ) ) ;
#62230 = CARTESIAN_POINT ( 'NONE',  ( -7.204075437095965206, -7.204075437095968759, 69.34375000204836681 ) ) ;
#62231 = CARTESIAN_POINT ( 'NONE',  ( -2.828427124746152987, 196.1250000000000284, 200.8284271247462129 ) ) ;
#62232 = CARTESIAN_POINT ( 'NONE',  ( -30.64284399271078385, 0.000000000000000000, 174.6921329945331536 ) ) ;
#62234 = CARTESIAN_POINT ( 'NONE',  ( -11.35316468750000141, 163.4895833299193271, 3.042071309553159963 ) ) ;
#62233 = CARTESIAN_POINT ( 'NONE',  ( -10.00000000000000711, 7.291666666666670515, -2.679491924311232065 ) ) ;
#62235 = CARTESIAN_POINT ( 'NONE',  ( 5.656854249492376141, -5.656854249492374365, 5.949052784329825094 ) ) ;
#62236 = CARTESIAN_POINT ( 'NONE',  ( -10.99999999999989164, -4.556349186104158733, 79.28125000409679046 ) ) ;
#62237 = CARTESIAN_POINT ( 'NONE',  ( -8.311093377946834337, 219.5312500034139589, 8.311093377946837890 ) ) ;
#62238 = CARTESIAN_POINT ( 'NONE',  ( -0.6474643998434820302, 49.91423208894237007, -40.68959583910810096 ) ) ;
#62239 = CARTESIAN_POINT ( 'NONE',  ( 4.220049686691941027, -10.18810118749999738, 80.50000000204839523 ) ) ;
#62240 = VERTEX_POINT ( 'NONE', #36438 ) ;
#62241 = CARTESIAN_POINT ( 'NONE',  ( -2.828427124746152987, 204.1250000000000284, 200.8284271247462129 ) ) ;
#62242 = CARTESIAN_POINT ( 'NONE',  ( -5.676582343749998039, 122.7604166632526841, -9.832129032723420536 ) ) ;
#62243 = CARTESIAN_POINT ( 'NONE',  ( 10.00000000000000178, 12.08333332650536462, -2.679491924311226736 ) ) ;
#62244 = ORIENTED_EDGE ( 'NONE', *, *, #68890, .F. ) ;
#62245 = ORIENTED_EDGE ( 'NONE', *, *, #67650, .F. ) ;
#62246 = ADVANCED_FACE ( 'NONE', ( #2098 ), #19438, .T. ) ;
#62247 = CARTESIAN_POINT ( 'NONE',  ( 3.211159895383560947, 9.312499998634407916, 3.211159895383562723 ) ) ;
#62248 = CARTESIAN_POINT ( 'NONE',  ( 2.977408999572651815, 12.18749999795161187, 7.188101187500000933 ) ) ;
#62249 = CARTESIAN_POINT ( 'NONE',  ( -8.000000000000000000, 110.0937500040968047, -3.313708498984761608 ) ) ;
#62250 = AXIS2_PLACEMENT_3D ( 'NONE', #54272, #19916, #65944 ) ;
#62251 = CARTESIAN_POINT ( 'NONE',  ( -25.55430564589119413, 198.5625000013656063, 167.5543056458915316 ) ) ;
#62252 = VECTOR ( 'NONE', #46602, 1000.000000000000000 ) ;
#62253 = CARTESIAN_POINT ( 'NONE',  ( -1.656854249492381248, 6.312500000000000888, -4.000000000000001776 ) ) ;
#62254 = CARTESIAN_POINT ( 'NONE',  ( -3.999999999999960032, 197.9375000000000000, 196.3431457505076594 ) ) ;
#62255 = CARTESIAN_POINT ( 'NONE',  ( -1.881053915767121776, 7.624999998634407916, -4.541265875000002339 ) ) ;
#62256 = CARTESIAN_POINT ( 'NONE',  ( -1.656854249492403008, 199.6875000000000000, 146.0000000000000284 ) ) ;
#62257 = EDGE_LOOP ( 'NONE', ( #48886, #8248, #20886, #2980 ) ) ;
#62258 = CARTESIAN_POINT ( 'NONE',  ( 8.660254037844389075, 222.0833333333333428, 4.999999999999997335 ) ) ;
#62259 = CARTESIAN_POINT ( 'NONE',  ( 7.188101187500002709, 108.3125000020483810, 2.977408999572649151 ) ) ;
#62260 = B_SPLINE_CURVE_WITH_KNOTS ( 'NONE', 3,
 ( #45123, #40205, #13001, #58322, #12276, #24333, #29266, #64334, #12638, #52278, #40580, #69252, #5886, #35310 ),
 .UNSPECIFIED., .F., .F.,
 ( 4, 2, 2, 2, 2, 2, 4 ),
 ( -3.553772641561921418E-05, 0.004730746523391729345, 0.009497030773199077736, 0.01188017289810275150, 0.01426331502300642699, 0.01664645714791009729, 0.01902959927281377278 ),
 .UNSPECIFIED. ) ;
#62263 = CARTESIAN_POINT ( 'NONE',  ( 6.000000000000003553, 293.4374999999999432, 2.485281374238571317 ) ) ;
#62262 = CARTESIAN_POINT ( 'NONE',  ( -31.45873412499995680, 194.7500000013656063, 171.4326545832181239 ) ) ;
#62261 =( BOUNDED_CURVE ( )  B_SPLINE_CURVE ( 2, ( #58651, #59751, #70690, #8062, #58291, #19009, #30703, #31064, #64667, #36005, #59022, #41294, #52614 ),
 .UNSPECIFIED., .F., .F. ) 
 B_SPLINE_CURVE_WITH_KNOTS ( ( 3, 2, 2, 2, 2, 2, 3 ),
 ( 0.2663043478260869734, 0.2681159420289855322, 0.2699275362318840354, 0.2717391304347825942, 0.2735507246376811530, 0.2753623188405797118, 0.2771739130434782705 ),
 .UNSPECIFIED. ) 
 CURVE ( )  GEOMETRIC_REPRESENTATION_ITEM ( )  RATIONAL_B_SPLINE_CURVE ( ( 1.000000000000000000, 0.9659258262890683122, 1.000000000000000000, 0.9659258262890683122, 1.000000000000000000, 0.9659258262890683122, 1.000000000000000000, 0.9659258262890683122, 1.000000000000000000, 0.9659258262890683122, 1.000000000000000000, 0.9659258262890683122, 1.000000000000000000 ) ) 
 REPRESENTATION_ITEM ( '' )  );
#62264 = CARTESIAN_POINT ( 'NONE',  ( -8.342170076843785083E-16, 21.06249999863440792, 4.541265875000002339 ) ) ;
#62265 = CARTESIAN_POINT ( 'NONE',  ( 7.188101187499993827, -2.977408999572645598, 3.642802781871751883 ) ) ;
#62266 = ORIENTED_EDGE ( 'NONE', *, *, #47441, .T. ) ;
#62267 = ORIENTED_EDGE ( 'NONE', *, *, #67372, .T. ) ;
#62268 = CARTESIAN_POINT ( 'NONE',  ( -6.238412754330611322E-16, 10.18810118749999916, 91.28125000204836681 ) ) ;
#62269 = CARTESIAN_POINT ( 'NONE',  ( 5.000000000000000000, -10.26105934116143281, -64.40045319026697257 ) ) ;
#62270 = CARTESIAN_POINT ( 'NONE',  ( -31.45873412499999233, 198.9375000013655779, 170.0000000000003979 ) ) ;
#62271 = CARTESIAN_POINT ( 'NONE',  ( -4.556349186104047710, -10.99999999999999822, 104.7812499999999858 ) ) ;
#62273 = CARTESIAN_POINT ( 'NONE',  ( 3.458734125000015425, 209.2500000013655779, 196.5673454167823877 ) ) ;
#62272 = AXIS2_PLACEMENT_3D ( 'NONE', #16986, #40013, #63015 ) ;
#62275 = CARTESIAN_POINT ( 'NONE',  ( -7.320508075688783478, 128.1250000000000000, 7.320508075688775484 ) ) ;
#62274 = CARTESIAN_POINT ( 'NONE',  ( -7.999999999999998224, 111.5937499999999858, 3.313708498984766049 ) ) ;
#62276 = CARTESIAN_POINT ( 'NONE',  ( -8.660254037844387298, 127.0833333333333570, -5.000000000000004441 ) ) ;
#62277 = EDGE_CURVE ( 'NONE', #46685, #24322, #11021, .T. ) ;
#62278 = CARTESIAN_POINT ( 'NONE',  ( 5.656854249492379694, 106.4374999999999858, -5.656854249492380582 ) ) ;
#62279 = CARTESIAN_POINT ( 'NONE',  ( 4.721056650416000089, 287.9843750017070079, 4.721056650415999201 ) ) ;
#62280 = CARTESIAN_POINT ( 'NONE',  ( 1.320432766682872962E-15, -7.188101187499992051, 6.736552781871754547 ) ) ;
#62282 =( BOUNDED_CURVE ( )  B_SPLINE_CURVE ( 2, ( #73993, #27217, #38563, #63042, #50234, #57402, #39665, #10998, #73255 ),
 .UNSPECIFIED., .F., .F. ) 
 B_SPLINE_CURVE_WITH_KNOTS ( ( 3, 2, 2, 2, 3 ),
 ( 0.2666666666666668850, 0.2750000000000002442, 0.2833333333333335480, 0.2916666666666669072, 0.3000000000000002109 ),
 .UNSPECIFIED. ) 
 CURVE ( )  GEOMETRIC_REPRESENTATION_ITEM ( )  RATIONAL_B_SPLINE_CURVE ( ( 0.9999999999999980016, 0.9238795325112887369, 1.000000000000000000, 0.9238795325112867385, 1.000000000000000000, 0.9238795325112867385, 1.000000000000000000, 0.9238795325112847401, 1.000000000000001998 ) ) 
 REPRESENTATION_ITEM ( '' )  );
#62281 = CARTESIAN_POINT ( 'NONE',  ( -28.00000000000003197, 209.0000000000000284, 166.0000000000003695 ) ) ;
#62283 = CARTESIAN_POINT ( 'NONE',  ( 27.99999999999996803, 207.4375000013656063, 173.4587341249998929 ) ) ;
#62284 = CARTESIAN_POINT ( 'NONE',  ( 7.188101187500000044, 2.343749997951610098, 0.000000000000000000 ) ) ;
#62285 = CARTESIAN_POINT ( 'NONE',  ( -2.839093476692135984E-14, 198.6875000013655779, 138.5412658750000503 ) ) ;
#62286 = CARTESIAN_POINT ( 'NONE',  ( -7.188101187500000044, 123.0312500020483810, 0.000000000000000000 ) ) ;
#62287 = CARTESIAN_POINT ( 'NONE',  ( -2.754378923186476579E-14, 204.4375000013656063, 145.4587341250000350 ) ) ;
#62288 = CARTESIAN_POINT ( 'NONE',  ( -6.951808397369817780E-16, 237.9687500034139873, -11.35316468749999963 ) ) ;
#62289 = FACE_OUTER_BOUND ( 'NONE', #74622, .T. ) ;
#62290 = DIRECTION ( 'NONE',  ( 0.000000000000000000, 0.000000000000000000, 1.000000000000000000 ) ) ;
#62291 = CARTESIAN_POINT ( 'NONE',  ( 31.99999999999997868, 202.1875000000000568, 171.6568542494923122 ) ) ;
#62292 = CARTESIAN_POINT ( 'NONE',  ( 8.311093377946837890, 11.40624999658601624, -8.311093377946837890 ) ) ;
#62293 = CARTESIAN_POINT ( 'NONE',  ( -2.977408999572647819, -7.188101187499990274, 0.6428027818717527708 ) ) ;
#62294 = CARTESIAN_POINT ( 'NONE',  ( 11.35316468749999785, 205.8854166632526415, 3.042071309553174174 ) ) ;
#62295 = CARTESIAN_POINT ( 'NONE',  ( -4.000000000000015987, 197.6875000027312126, 143.6568542494924259 ) ) ;
#62296 = DIRECTION ( 'NONE',  ( -0.8660254037844374864, 0.5000000000000018874, 0.000000000000000000 ) ) ;
#62297 = DIRECTION ( 'NONE',  ( -1.000000000000000000, -1.776356839400250465E-15, 0.000000000000000000 ) ) ;
#62298 = EDGE_LOOP ( 'NONE', ( #39266, #54897 ) ) ;
#62299 = B_SPLINE_CURVE_WITH_KNOTS ( 'NONE', 3,
 ( #8404, #3879, #31417, #43098, #48760, #73279 ),
 .UNSPECIFIED., .F., .F.,
 ( 4, 2, 4 ),
 ( 0.01452727543195641083, 0.01715716534226974926, 0.01978705525258308423 ),
 .UNSPECIFIED. ) ;
#62300 = CARTESIAN_POINT ( 'NONE',  ( 2.445694354108783219, 198.8125000013656063, 139.5543056458912190 ) ) ;
#62301 = CARTESIAN_POINT ( 'NONE',  ( -11.35316468749999785, 23.07291666325268054, -3.042071309553167513 ) ) ;
#62302 = CARTESIAN_POINT ( 'NONE',  ( -10.99999999999999822, -4.556349186104052151, 91.28125000409676204 ) ) ;
#62303 = CARTESIAN_POINT ( 'NONE',  ( 6.000000000000003553, 292.4375000000000000, 2.485281374238571317 ) ) ;
#62304 = EDGE_CURVE ( 'NONE', #8230, #42656, #3902, .T. ) ;
#62305 = CARTESIAN_POINT ( 'NONE',  ( -29.43265458321770822, 195.5000000013656347, 166.5412658750003914 ) ) ;
#62306 = CARTESIAN_POINT ( 'NONE',  ( -0.4499999999999996780, 283.9999999999998863, 5.815339556495201734 ) ) ;
#62308 = CARTESIAN_POINT ( 'NONE',  ( -11.35316468750000141, 8.281249996586016238, -1.390361679473963753E-15 ) ) ;
#62307 = CARTESIAN_POINT ( 'NONE',  ( -2.977408999572652260, 112.4375000020483810, 7.188101187500000044 ) ) ;
#62309 = CARTESIAN_POINT ( 'NONE',  ( -3.313708498984758943, -7.999999999999989342, 23.61155277982336997 ) ) ;
#62310 = CARTESIAN_POINT ( 'NONE',  ( 11.35316468750000141, 140.7812499965860411, 0.000000000000000000 ) ) ;
#62311 = AXIS2_PLACEMENT_3D ( 'NONE', #27559, #43799, #55133 ) ;
#62312 = CARTESIAN_POINT ( 'NONE',  ( -7.320508075688778149, 99.99999999317203958, 7.320508075688769267 ) ) ;
#62313 = CARTESIAN_POINT ( 'NONE',  ( 7.188101187500000044, 117.7812500020483810, -8.802885111219163269E-16 ) ) ;
#62314 = CARTESIAN_POINT ( 'NONE',  ( 0.000000000000000000, 300.0000000000000000, 0.000000000000000000 ) ) ;
#62315 = CARTESIAN_POINT ( 'NONE',  ( -7.778174593052023411, 7.778174593052023411, 103.0000000040967763 ) ) ;
#62316 = CARTESIAN_POINT ( 'NONE',  ( -5.000000000000000000, 53.18690467503129327, -43.91652490638166739 ) ) ;
#62317 = ORIENTED_EDGE ( 'NONE', *, *, #70768, .F. ) ;
#62318 = CARTESIAN_POINT ( 'NONE',  ( 0.3752463838826636811, -65.74564559951694775, 26.26824411940134851 ) ) ;
#62319 = CARTESIAN_POINT ( 'NONE',  ( 1.226468279477575784E-15, 287.8593750017070079, 6.676582343750001591 ) ) ;
#62320 = CARTESIAN_POINT ( 'NONE',  ( 5.000000000000000000, 52.63770595436645294, 42.88862352055369342 ) ) ;
#62321 = CARTESIAN_POINT ( 'NONE',  ( -3.313708498984758943, -7.999999999999989342, 2.799052783920144005 ) ) ;
#62322 = CARTESIAN_POINT ( 'NONE',  ( -6.123233995736766282E-16, 226.8750000068279746, -10.00000000000000000 ) ) ;
#62323 = CARTESIAN_POINT ( 'NONE',  ( -3.673940397442060854E-16, 296.8125000034140157, -6.000000000000001776 ) ) ;
#62324 = CARTESIAN_POINT ( 'NONE',  ( -4.220049686691937474, -10.18810118749999738, 96.81250000204839523 ) ) ;
#62325 = VERTEX_POINT ( 'NONE', #57800 ) ;
#62326 = CARTESIAN_POINT ( 'NONE',  ( 0.000000000000000000, 0.000000000000000000, -4.000000000000001776 ) ) ;
#62327 = CARTESIAN_POINT ( 'NONE',  ( -11.00000000000000000, 4.556349186104045934, 98.40625000000000000 ) ) ;
#62328 = CARTESIAN_POINT ( 'NONE',  ( 3.458734125000015425, 201.2500000013656063, 196.5673454167823877 ) ) ;
#62329 = CARTESIAN_POINT ( 'NONE',  ( 8.311093377946834337, 75.46874999658602690, 8.311093377946839666 ) ) ;
#62330 = ORIENTED_EDGE ( 'NONE', *, *, #48596, .F. ) ;
#62331 = CARTESIAN_POINT ( 'NONE',  ( -10.18810118749999916, 4.220049686691934809, 111.0625000020483810 ) ) ;
#62332 = CARTESIAN_POINT ( 'NONE',  ( 1.881053915767122664, 12.24999999863440792, 4.541265875000001451 ) ) ;
#62333 = ORIENTED_EDGE ( 'NONE', *, *, #8908, .T. ) ;
#62334 = CARTESIAN_POINT ( 'NONE',  ( -8.000000000000000000, 0.6562500000000002220, -3.313708498984762496 ) ) ;
#62335 = CARTESIAN_POINT ( 'NONE',  ( 9.999999999999998224, 114.7916666666666998, 2.679491924311235618 ) ) ;
#62336 = CARTESIAN_POINT ( 'NONE',  ( -7.778174593052020747, -7.778174593052023411, 76.37500000409677625 ) ) ;
#62337 = CARTESIAN_POINT ( 'NONE',  ( 7.188101187500001821, 24.93749999795161543, -2.977408999572650483 ) ) ;
#62338 = LINE ( 'NONE', #56703, #19475 ) ;
#62339 = CARTESIAN_POINT ( 'NONE',  ( 7.204075437095966983, 7.204075437095967871, 107.9687500020483810 ) ) ;
#62340 = CARTESIAN_POINT ( 'NONE',  ( 1.656854249492381914, 11.56249999726881583, 4.000000000000000888 ) ) ;
#62341 = VERTEX_POINT ( 'NONE', #15265 ) ;
#62342 = EDGE_CURVE ( 'NONE', #2057, #18394, #34757, .T. ) ;
#62343 = CARTESIAN_POINT ( 'NONE',  ( 2.754378923186476579E-14, 202.1875000013656063, 194.5412658750000219 ) ) ;
#62344 = CARTESIAN_POINT ( 'NONE',  ( -30.44569435410887337, 208.5625000013656063, 167.5543056458916169 ) ) ;
#62345 = CARTESIAN_POINT ( 'NONE',  ( 31.99999999999999289, 199.3750000027312126, 169.9999999999998863 ) ) ;
#62346 = AXIS2_PLACEMENT_3D ( 'NONE', #43072, #66848, #37055 ) ;
#62347 = CARTESIAN_POINT ( 'NONE',  ( 2.780723358947928197E-16, 11.56249999863440614, -4.541265875000002339 ) ) ;
#62348 = DIRECTION ( 'NONE',  ( 1.000000000000000000, 0.000000000000000000, 0.000000000000000000 ) ) ;
#62349 = CARTESIAN_POINT ( 'NONE',  ( -7.188101187499990274, -2.977408999572651371, 19.58030278187175455 ) ) ;
#62350 = VERTEX_POINT ( 'NONE', #43566 ) ;
#62351 = CARTESIAN_POINT ( 'NONE',  ( 0.000000000000000000, 125.0000000000000000, 0.000000000000000000 ) ) ;
#62352 = VERTEX_POINT ( 'NONE', #74381 ) ;
#62353 = CARTESIAN_POINT ( 'NONE',  ( 1.871523826299183495E-15, -10.18810118749999916, 110.0312500020483668 ) ) ;
#62354 = CARTESIAN_POINT ( 'NONE',  ( -4.000000000000001776, 18.50000000000000000, -4.898587196589415787E-16 ) ) ;
#62355 = CARTESIAN_POINT ( 'NONE',  ( 3.458734125000016313, 202.8750000013656347, 199.4326545832176691 ) ) ;
#62356 = CARTESIAN_POINT ( 'NONE',  ( 25.55430564589115505, 201.0625000013656063, 167.5543056458911053 ) ) ;
#62357 = CARTESIAN_POINT ( 'NONE',  ( -10.00000000000000178, 82.50000000000000000, -1.224646799147353454E-15 ) ) ;
#62358 = ADVANCED_FACE ( 'NONE', ( #20929 ), #22692, .T. ) ;
#62359 = CARTESIAN_POINT ( 'NONE',  ( -4.898587196589412829E-16, 123.1250000000000000, -8.000000000000000000 ) ) ;
#62360 = CARTESIAN_POINT ( 'NONE',  ( -2.485281374238572649, 291.1874999999999432, 6.000000000000002665 ) ) ;
#62361 = CARTESIAN_POINT ( 'NONE',  ( 25.17157287525382259, 207.0000000027312126, 172.8284271247460993 ) ) ;
#62362 = VERTEX_POINT ( 'NONE', #14887 ) ;
#62363 = ADVANCED_FACE ( 'NONE', ( #60926 ), #37926, .T. ) ;
#62364 = CARTESIAN_POINT ( 'NONE',  ( 3.313708498984657247, 93.96875000000000000, 8.000000000000106581 ) ) ;
#62365 = CARTESIAN_POINT ( 'NONE',  ( 3.228176881619535088, -10.27295505383823304, 63.90876373295927237 ) ) ;
#62366 = CARTESIAN_POINT ( 'NONE',  ( -4.000000000000015099, 197.6875000027312126, 143.6568542494924543 ) ) ;
#62367 = CARTESIAN_POINT ( 'NONE',  ( -5.000000000000000000, 66.11467145570868809, 23.67355326543111005 ) ) ;
#62368 = CARTESIAN_POINT ( 'NONE',  ( 5.656854249492380582, 13.49999999590322375, -5.656854249492380582 ) ) ;
#62369 = CARTESIAN_POINT ( 'NONE',  ( -9.999999999999998224, 235.2083333333333712, 2.679491924311235618 ) ) ;
#62370 = CARTESIAN_POINT ( 'NONE',  ( -2.679491924305347439, 76.45833333333281701, -10.00000000000343903 ) ) ;
#62371 =( BOUNDED_CURVE ( )  B_SPLINE_CURVE ( 2, ( #25099, #47012, #70407, #13408, #13041, #24734, #64742, #42085, #19082 ),
 .UNSPECIFIED., .F., .F. ) 
 B_SPLINE_CURVE_WITH_KNOTS ( ( 3, 2, 2, 2, 3 ),
 ( 0.8194444444444443088, 0.8263888888888887285, 0.8333333333333332593, 0.8402777777777777901, 0.8472222222222222099 ),
 .UNSPECIFIED. ) 
 CURVE ( )  GEOMETRIC_REPRESENTATION_ITEM ( )  RATIONAL_B_SPLINE_CURVE ( ( 1.000000000000001110, 0.9238795325112855172, 1.000000000000000000, 0.9238795325112867385, 1.000000000000000000, 0.9238795325112867385, 1.000000000000000000, 0.9238795325112867385, 1.000000000000000000 ) ) 
 REPRESENTATION_ITEM ( '' )  );
#62372 = B_SPLINE_CURVE_WITH_KNOTS ( 'NONE', 3,
 ( #66603, #33792, #55681, #14909, #3996, #73016, #17524, #23186, #69588, #944, #6588, #11503, #23926, #17901, #52608, #11137, #29595, #45449 ),
 .UNSPECIFIED., .F., .F.,
 ( 4, 2, 2, 2, 2, 2, 2, 2, 4 ),
 ( 5.637184056103667372E-17, 0.003662049718958990119, 0.005493074578438492117, 0.007324099437917994983, 0.008239611867657745115, 0.009155124297397496114, 0.01098614915687701893, 0.01281717401635654001, 0.01464819887583606282 ),
 .UNSPECIFIED. ) ;
#62373 = CARTESIAN_POINT ( 'NONE',  ( -1.836970198721029983E-15, 203.7500000000000284, 10.00000000000000178 ) ) ;
#62374 = CARTESIAN_POINT ( 'NONE',  ( -2.977408999572647819, 7.188101187499992051, 16.58030278187175455 ) ) ;
#62375 = CARTESIAN_POINT ( 'NONE',  ( -3.042071309553164404, 162.5520833299193555, -11.35316468749999963 ) ) ;
#62376 = DIRECTION ( 'NONE',  ( 0.000000000000000000, -0.000000000000000000, 1.000000000000000000 ) ) ;
#62377 = CARTESIAN_POINT ( 'NONE',  ( 5.000000000000000000, 29.68417822476661172, -4.268394125862716493 ) ) ;
#62379 = CARTESIAN_POINT ( 'NONE',  ( -8.224976990608492855, 220.0000000000001421, 7.304091559116764110 ) ) ;
#62378 = SURFACE_STYLE_FILL_AREA ( #34489 ) ;
#62380 = ORIENTED_EDGE ( 'NONE', *, *, #19956, .F. ) ;
#62381 = CARTESIAN_POINT ( 'NONE',  ( 8.311093377946837890, 21.71874999658601268, -8.311093377946837890 ) ) ;
#62382 = CARTESIAN_POINT ( 'NONE',  ( 11.00000000000000000, 1.347111479062088405E-15, 109.9375000040967763 ) ) ;
#62383 = EDGE_CURVE ( 'NONE', #27411, #70980, #5362, .T. ) ;
#62384 = CARTESIAN_POINT ( 'NONE',  ( -30.44569435410876324, 208.8125000013656063, 172.4456943541092642 ) ) ;
#62385 = VECTOR ( 'NONE', #71032, 1000.000000000000000 ) ;
#62387 = CARTESIAN_POINT ( 'NONE',  ( -2.997005883568874207, -10.11494357241825526, -70.43990496499247911 ) ) ;
#62386 = CARTESIAN_POINT ( 'NONE',  ( -3.313708498984757611, 7.999999999999991118, 17.23655278392014623 ) ) ;
#62388 = CARTESIAN_POINT ( 'NONE',  ( -20.96302383750437670, -49.31446181634627379, 192.8551355824569953 ) ) ;
#62389 = CARTESIAN_POINT ( 'NONE',  ( -3.458734125000015425, 201.9375000013656063, 142.0000000000000568 ) ) ;
#62390 = CARTESIAN_POINT ( 'NONE',  ( -2.679491924311235618, 65.41666665983871098, 10.00000000000000000 ) ) ;
#62391 = CARTESIAN_POINT ( 'NONE',  ( -4.401442555609581635E-16, 104.2812500020483810, -7.188101187500000044 ) ) ;
#62392 = CARTESIAN_POINT ( 'NONE',  ( -4.541265875000003227, 12.99999999863440969, 1.881053915767121110 ) ) ;
#62393 = CARTESIAN_POINT ( 'NONE',  ( 8.660254037844575592, 214.5833333333334849, 5.000000000000116351 ) ) ;
#62394 = CARTESIAN_POINT ( 'NONE',  ( -3.313708498984758943, -7.999999999999989342, 1.111552779823363757 ) ) ;
#62395 = CARTESIAN_POINT ( 'NONE',  ( 10.00000000000000178, 165.0000000000000000, 0.000000000000000000 ) ) ;
#62396 = ORIENTED_EDGE ( 'NONE', *, *, #21217, .T. ) ;
#62397 = VERTEX_POINT ( 'NONE', #74013 ) ;
#62398 = DIRECTION ( 'NONE',  ( -0.000000000000000000, -0.000000000000000000, -1.000000000000000000 ) ) ;
#62399 = PLANE ( 'NONE',  #14566 ) ;
#62400 = PRESENTATION_STYLE_ASSIGNMENT (( #73727 ) ) ;
#62401 = CARTESIAN_POINT ( 'NONE',  ( -7.778174593052023411, 7.778174593052023411, 95.31250000000000000 ) ) ;
#62402 = CARTESIAN_POINT ( 'NONE',  ( -11.35316468749999785, 148.0729166632527267, -3.042071309553167513 ) ) ;
#62403 = ORIENTED_EDGE ( 'NONE', *, *, #60676, .T. ) ;
#62404 = CARTESIAN_POINT ( 'NONE',  ( -5.000000000000000000, 12.55023575007693104, -69.09043692422063998 ) ) ;
#62405 = CARTESIAN_POINT ( 'NONE',  ( 10.18810118749999916, 4.220049686691935698, 86.50000000204838102 ) ) ;
#62406 = CARTESIAN_POINT ( 'NONE',  ( -31.54067435258291852, 194.6262042466636615, 170.8147271755408667 ) ) ;
#62407 = VECTOR ( 'NONE', #64084, 1000.000000000000000 ) ;
#62408 = CARTESIAN_POINT ( 'NONE',  ( 2.828427124746208943, 207.6250000000000284, 195.1715728752538439 ) ) ;
#62409 = CARTESIAN_POINT ( 'NONE',  ( 10.00000000000000178, 247.2916666666666856, 2.679491924311222739 ) ) ;
#62410 = CARTESIAN_POINT ( 'NONE',  ( -30.82842712474612057, 197.5000000027312126, 172.8284271247466108 ) ) ;
#62411 = CARTESIAN_POINT ( 'NONE',  ( 4.220049686691941027, -10.18810118749999738, 115.0000000020483668 ) ) ;
#62412 = ORIENTED_EDGE ( 'NONE', *, *, #66444, .T. ) ;
#62413 = COLOUR_RGB ( '',0.7921568627450980005, 0.8196078431372548767, 0.9333333333333333481 ) ;
#62414 = CARTESIAN_POINT ( 'NONE',  ( 5.656854249492379694, 106.6250000040967763, -5.656854249492380582 ) ) ;
#62415 = EDGE_CURVE ( 'NONE', #42285, #38888, #11758, .T. ) ;
#62416 = CARTESIAN_POINT ( 'NONE',  ( 10.33666931816651591, 178.5382482961751975, 134.7837216799607347 ) ) ;
#62417 = CARTESIAN_POINT ( 'NONE',  ( 8.311093377946837890, 131.7187499965860411, -8.311093377946837890 ) ) ;
#62418 = CARTESIAN_POINT ( 'NONE',  ( -3.458734124999959914, 204.3750000013656063, 196.5673454167823877 ) ) ;
#62419 = CARTESIAN_POINT ( 'NONE',  ( 2.977408999572652260, 23.06249999795161543, 7.188101187500000044 ) ) ;
#62420 = CARTESIAN_POINT ( 'NONE',  ( -4.220049686691937474, -10.18810118749999738, 83.31250000204836681 ) ) ;
#62421 = CARTESIAN_POINT ( 'NONE',  ( 5.676582343750001591, 41.92708332991934839, -9.832129032723420536 ) ) ;
#62422 = VERTEX_POINT ( 'NONE', #68722 ) ;
#62423 = LINE ( 'NONE', #38690, #10388 ) ;
#62424 = CARTESIAN_POINT ( 'NONE',  ( 2.780723358947928197E-16, 0.6874999986344068059, -4.541265875000002339 ) ) ;
#62425 = CARTESIAN_POINT ( 'NONE',  ( 8.008118988124991233, 3.317071493978879015, 22.85686528394062833 ) ) ;
#62426 = CARTESIAN_POINT ( 'NONE',  ( 2.445694354108783219, 206.8125000013656063, 139.5543056458912190 ) ) ;
#62427 = CARTESIAN_POINT ( 'NONE',  ( -7.188101187500001821, 8.624999997951611874, -2.977408999572651371 ) ) ;
#62428 = CARTESIAN_POINT ( 'NONE',  ( -2.485281374238571761, 296.8750000034139589, -6.000000000000003553 ) ) ;
#62429 = FACE_OUTER_BOUND ( 'NONE', #48965, .T. ) ;
#62430 = CARTESIAN_POINT ( 'NONE',  ( -7.188101187500001821, 2.999999997951610098, -2.977408999572651371 ) ) ;
#62431 = CARTESIAN_POINT ( 'NONE',  ( 3.042071309553167069, 157.1354166632526983, -11.35316468749999785 ) ) ;
#62432 = CARTESIAN_POINT ( 'NONE',  ( 4.220049686691934809, 10.18810118749999916, 76.18750000204839523 ) ) ;
#62433 = CARTESIAN_POINT ( 'NONE',  ( -27.99999999999996092, 196.9375000013655779, 173.4587341250003760 ) ) ;
#62434 = DIRECTION ( 'NONE',  ( -0.000000000000000000, 1.000000000000000000, -0.000000000000000000 ) ) ;
#62435 = CARTESIAN_POINT ( 'NONE',  ( 2.780723358947928197E-16, 20.68749999863440436, -4.541265875000002339 ) ) ;
#62436 = ORIENTED_EDGE ( 'NONE', *, *, #20474, .T. ) ;
#62437 = CARTESIAN_POINT ( 'NONE',  ( -3.999999999999959144, 198.1875000027312126, 199.6568542494924259 ) ) ;
#62438 = CARTESIAN_POINT ( 'NONE',  ( -1.432654583217664701, 196.0000000013656347, 138.5412658750000787 ) ) ;
#62439 = CARTESIAN_POINT ( 'NONE',  ( -31.99999999999996447, 206.4375000027311842, 171.6568542494928522 ) ) ;
#62440 = AXIS2_PLACEMENT_3D ( 'NONE', #55053, #2986, #66354 ) ;
#62441 = CARTESIAN_POINT ( 'NONE',  ( -5.656854249492378806, 104.1874999999999858, 5.656854249492381470 ) ) ;
#62442 = EDGE_LOOP ( 'NONE', ( #5153, #48589, #30198, #42083 ) ) ;
#62443 = CARTESIAN_POINT ( 'NONE',  ( -5.082755093536326818, 19.40624999795161543, 5.082755093536325042 ) ) ;
#62444 = CARTESIAN_POINT ( 'NONE',  ( -26.34314575050763096, 196.6875000027311842, 174.0000000000004547 ) ) ;
#62445 = CARTESIAN_POINT ( 'NONE',  ( 4.999999999999999112, 52.62657404299758923, -48.70092614269818654 ) ) ;
#62446 = CARTESIAN_POINT ( 'NONE',  ( 5.000000000000001776, 40.83333333333333570, -8.660254037844389075 ) ) ;
#62447 = AXIS2_PLACEMENT_3D ( 'NONE', #58496, #64876, #47149 ) ;
#62448 = CARTESIAN_POINT ( 'NONE',  ( -5.082755093536324154, 108.2187500020483810, 5.082755093536326818 ) ) ;
#62449 = CARTESIAN_POINT ( 'NONE',  ( -30.44569435410879521, 208.0625000013656063, 172.4456943541092357 ) ) ;
#62450 = CARTESIAN_POINT ( 'NONE',  ( -7.999999999999991118, 0.000000000000000000, 2.330302779823365089 ) ) ;
#62452 = CARTESIAN_POINT ( 'NONE',  ( -7.417212451314158628, -3.006759011572777140, -0.000000000000000000 ) ) ;
#62451 = CARTESIAN_POINT ( 'NONE',  ( -25.17157287525382259, 201.8750000000000284, 167.1715728752541565 ) ) ;
#62453 = ORIENTED_EDGE ( 'NONE', *, *, #36131, .T. ) ;
#62454 = EDGE_CURVE ( 'NONE', #17336, #54742, #43951, .T. ) ;
#62455 = CARTESIAN_POINT ( 'NONE',  ( -9.832129032723418760, 253.4895833367473017, -5.676582343749998927 ) ) ;
#62456 = CARTESIAN_POINT ( 'NONE',  ( -7.188101187499992051, 0.000000000000000000, 21.36155278187175455 ) ) ;
#62457 = CARTESIAN_POINT ( 'NONE',  ( 2.266287154880008980, 50.05783744175044347, 40.76793781259059557 ) ) ;
#62458 = FACE_OUTER_BOUND ( 'NONE', #27503, .T. ) ;
#62459 = DIRECTION ( 'NONE',  ( 0.000000000000000000, 0.000000000000000000, 1.000000000000000000 ) ) ;
#62460 = CARTESIAN_POINT ( 'NONE',  ( 2.445694354108840063, 197.0625000013656063, 200.4456943541088663 ) ) ;
#62461 = CARTESIAN_POINT ( 'NONE',  ( -2.679491924311225848, 166.4583333333333428, -10.00000000000000178 ) ) ;
#62462 = CARTESIAN_POINT ( 'NONE',  ( 75.00000000000001421, 272.0000000000000000, 20.00000000000002132 ) ) ;
#62463 = DIRECTION ( 'NONE',  ( 0.000000000000000000, 0.000000000000000000, 1.000000000000000000 ) ) ;
#62464 = CARTESIAN_POINT ( 'NONE',  ( 0.000000000000000000, 125.0000000000000000, 0.000000000000000000 ) ) ;
#62465 = CARTESIAN_POINT ( 'NONE',  ( -8.311093377946841443, 124.2187499965860127, 8.311093377946830785 ) ) ;
#62466 = CARTESIAN_POINT ( 'NONE',  ( -6.000000000000001776, 294.0625000034140157, 0.000000000000000000 ) ) ;
#62467 = CARTESIAN_POINT ( 'NONE',  ( -6.735557395310442023E-16, 11.00000000000000000, 68.12499999999998579 ) ) ;
#62470 = CARTESIAN_POINT ( 'NONE',  ( -1.836970198721029983E-15, 115.6249999931720396, 10.00000000000000178 ) ) ;
#62469 = CARTESIAN_POINT ( 'NONE',  ( 26.56734541678232375, 197.0000000013656347, 166.5412658749999650 ) ) ;
#62468 = CARTESIAN_POINT ( 'NONE',  ( 26.34314575050758833, 209.9375000000000000, 173.9999999999999147 ) ) ;
#62471 = ORIENTED_EDGE ( 'NONE', *, *, #58248, .F. ) ;
#62472 = CARTESIAN_POINT ( 'NONE',  ( 9.207548596070616043, 225.3207043425250049, -3.912421826535780855 ) ) ;
#62473 = CARTESIAN_POINT ( 'NONE',  ( -1.836970198721029983E-15, 135.6249999931720538, 10.00000000000000178 ) ) ;
#62474 = CARTESIAN_POINT ( 'NONE',  ( -5.676582343749992710, 220.0520833367473301, 9.832129032723422313 ) ) ;
#62475 = CARTESIAN_POINT ( 'NONE',  ( 29.43265458321766204, 197.1250000013656347, 166.5412658749999650 ) ) ;
#62476 = EDGE_CURVE ( 'NONE', #29688, #72916, #57897, .T. ) ;
#62477 = CARTESIAN_POINT ( 'NONE',  ( -11.35316468749999785, 208.3854166632526415, -3.042071309553167513 ) ) ;
#62478 = CARTESIAN_POINT ( 'NONE',  ( 2.977408999572654480, 121.6250000020483810, 7.188101187499999156 ) ) ;
#62479 = CARTESIAN_POINT ( 'NONE',  ( -4.541265875000002339, 18.74999999863440436, -1.881053915767121998 ) ) ;
#62480 = CARTESIAN_POINT ( 'NONE',  ( 4.104248244547289204, -56.27889056305692606, 44.16174987544510344 ) ) ;
#62481 = CARTESIAN_POINT ( 'NONE',  ( 7.999999999999991118, 3.313708498984757611, 22.67405277982336287 ) ) ;
#62483 = DIRECTION ( 'NONE',  ( 0.000000000000000000, 1.000000000000000000, 1.334402673828311367E-16 ) ) ;
#62482 = SURFACE_STYLE_USAGE ( .BOTH. , #17582 ) ;
#62484 = CARTESIAN_POINT ( 'NONE',  ( -9.832129032723420536, 93.69791666325269830, 5.676582343749997150 ) ) ;
#62485 = ORIENTED_EDGE ( 'NONE', *, *, #55808, .T. ) ;
#62486 = EDGE_CURVE ( 'NONE', #5819, #62108, #47925, .T. ) ;
#62487 = FACE_OUTER_BOUND ( 'NONE', #47055, .T. ) ;
#62488 = CARTESIAN_POINT ( 'NONE',  ( 5.082755093536325930, 26.15624999795161543, -5.082755093536325930 ) ) ;
#62489 = FACE_OUTER_BOUND ( 'NONE', #38786, .T. ) ;
#62490 = CARTESIAN_POINT ( 'NONE',  ( -5.676582343749992710, 255.0520833367473301, 9.832129032723422313 ) ) ;
#62491 = CARTESIAN_POINT ( 'NONE',  ( -2.085542519210945728E-15, 99.53124999658602690, 11.35316468750000141 ) ) ;
#62492 = ORIENTED_EDGE ( 'NONE', *, *, #37412, .F. ) ;
#62493 = CARTESIAN_POINT ( 'NONE',  ( 6.123233995736767268E-16, 63.12499999317203248, -10.00000000000000178 ) ) ;
#62494 = CARTESIAN_POINT ( 'NONE',  ( 10.18810118750000093, -4.220049686691933921, 107.3125000020483668 ) ) ;
#62495 = CARTESIAN_POINT ( 'NONE',  ( -7.320508075688773708, 223.7499999931719969, -7.320508075688774596 ) ) ;
#62496 = CARTESIAN_POINT ( 'NONE',  ( 3.458734125000016757, 206.1250000013655779, 199.4326545832176691 ) ) ;
#62497 = CARTESIAN_POINT ( 'NONE',  ( 8.000000000000000000, 118.2500000000000000, -9.797174393178825657E-16 ) ) ;
#62499 = CARTESIAN_POINT ( 'NONE',  ( -2.085542519210945728E-15, 104.5312499965860269, 11.35316468750000141 ) ) ;
#62498 = CARTESIAN_POINT ( 'NONE',  ( 7.999999999999991118, 9.797174393178815797E-16, 22.58030277982336997 ) ) ;
#62500 = CARTESIAN_POINT ( 'NONE',  ( -3.313708498984757167, 7.999999999999991118, 15.73655278392014267 ) ) ;
#62501 = CARTESIAN_POINT ( 'NONE',  ( -30.44569435410879166, 201.0625000013656063, 172.4456943541092357 ) ) ;
#62502 = LINE ( 'NONE', #5182, #30057 ) ;
#62503 = ORIENTED_EDGE ( 'NONE', *, *, #8356, .T. ) ;
#62504 =( BOUNDED_CURVE ( )  B_SPLINE_CURVE ( 2, ( #71867, #30046, #25101, #70408, #53059, #71124, #41733, #48118, #30777 ),
 .UNSPECIFIED., .F., .F. ) 
 B_SPLINE_CURVE_WITH_KNOTS ( ( 3, 2, 2, 2, 3 ),
 ( 0.6470588235294115753, 0.6507352941176468564, 0.6544117647058821374, 0.6580882352941174185, 0.6617647058823526995 ),
 .UNSPECIFIED. ) 
 CURVE ( )  GEOMETRIC_REPRESENTATION_ITEM ( )  RATIONAL_B_SPLINE_CURVE ( ( 1.000000000000004663, 0.9238795325112821866, 1.000000000000000000, 0.9238795325112867385, 1.000000000000000000, 0.9238795325112867385, 1.000000000000000000, 0.9238795325112912904, 0.9999999999999954481 ) ) 
 REPRESENTATION_ITEM ( '' )  );
#62505 = CARTESIAN_POINT ( 'NONE',  ( 2.679491924311222739, 175.8333333265053966, 10.00000000000000355 ) ) ;
#62506 = AXIS2_PLACEMENT_3D ( 'NONE', #29007, #41808, #64818 ) ;
#62507 = CARTESIAN_POINT ( 'NONE',  ( -15.99999999999999645, 15.99999999999999645, 7.387219678533736733 ) ) ;
#62508 = ADVANCED_FACE ( 'NONE', ( #1198 ), #58176, .T. ) ;
#62509 = CARTESIAN_POINT ( 'NONE',  ( -3.673940397442060854E-16, 296.8125000034140157, -6.000000000000001776 ) ) ;
#62510 = CARTESIAN_POINT ( 'NONE',  ( 11.35316468749999963, 76.30208332991935549, -3.042071309553165293 ) ) ;
#62511 = CARTESIAN_POINT ( 'NONE',  ( -6.676582343750003368, 289.3906250017069510, -2.765530957081996810 ) ) ;
#62512 = CARTESIAN_POINT ( 'NONE',  ( 2.977408999572652260, 6.562499997951610098, 7.188101187500000044 ) ) ;
#62513 = ADVANCED_FACE ( 'NONE', ( #58533 ), #41538, .T. ) ;
#62514 = CARTESIAN_POINT ( 'NONE',  ( 7.204075437095966983, 7.204075437095967871, 98.96875000204838102 ) ) ;
#62515 = CARTESIAN_POINT ( 'NONE',  ( -8.311093377946841443, 218.9062499965860127, 8.311093377946830785 ) ) ;
#62516 = EDGE_LOOP ( 'NONE', ( #73818, #36663, #63565 ) ) ;
#62517 = CARTESIAN_POINT ( 'NONE',  ( -18.89444362769118158, 5.999999999999950262, 171.9999999999997726 ) ) ;
#62518 = CARTESIAN_POINT ( 'NONE',  ( 9.832129032723420536, 211.1979166632526983, -5.676582343749999815 ) ) ;
#62519 = AXIS2_PLACEMENT_3D ( 'NONE', #19182, #8609, #60283 ) ;
#62520 = CARTESIAN_POINT ( 'NONE',  ( 5.000000000000004441, 229.7916666734946602, 8.660254037844385522 ) ) ;
#62521 = DIRECTION ( 'NONE',  ( -0.000000000000000000, 1.000000000000000000, -0.000000000000000000 ) ) ;
#62522 = CARTESIAN_POINT ( 'NONE',  ( 4.721056650416000089, 297.8281250017069510, 4.721056650415999201 ) ) ;
#62523 = VERTEX_POINT ( 'NONE', #23442 ) ;
#62524 = CARTESIAN_POINT ( 'NONE',  ( 9.832129032723416984, 200.6770833299193555, 5.676582343750006032 ) ) ;
#62525 = CARTESIAN_POINT ( 'NONE',  ( -29.43265458321766559, 205.5000000013655779, 166.5412658750003629 ) ) ;
#62526 = CARTESIAN_POINT ( 'NONE',  ( 3.313708498984762496, 17.71875000000000355, 7.999999999999998224 ) ) ;
#62527 = ORIENTED_EDGE ( 'NONE', *, *, #8357, .F. ) ;
#62528 = EDGE_CURVE ( 'NONE', #42125, #59062, #70221, .T. ) ;
#62529 = CARTESIAN_POINT ( 'NONE',  ( -5.656854249492378806, 92.37500000409677625, 5.656854249492381470 ) ) ;
#62530 = CARTESIAN_POINT ( 'NONE',  ( -7.999999999999991118, 0.000000000000000000, 18.83030277982336642 ) ) ;
#62531 = EDGE_CURVE ( 'NONE', #4661, #10747, #7629, .T. ) ;
#62532 = CARTESIAN_POINT ( 'NONE',  ( 10.00000000000000178, 20.20833333333333570, -2.679491924311226736 ) ) ;
#62533 = CARTESIAN_POINT ( 'NONE',  ( 1.871523826299183495E-15, -10.18810118749999916, 78.90625000204836681 ) ) ;
#62534 = ORIENTED_EDGE ( 'NONE', *, *, #66343, .F. ) ;
#62535 = EDGE_CURVE ( 'NONE', #72916, #63531, #17786, .T. ) ;
#62536 = CARTESIAN_POINT ( 'NONE',  ( -4.000000000000001776, 20.43750000000000000, -1.656854249492381470 ) ) ;
#62537 = CARTESIAN_POINT ( 'NONE',  ( 1.881053915767121998, 21.49999999863440792, -4.541265875000002339 ) ) ;
#62538 = CARTESIAN_POINT ( 'NONE',  ( 27.99999999999996447, 198.6250000027312126, 165.9999999999998863 ) ) ;
#62539 = CARTESIAN_POINT ( 'NONE',  ( 6.123233995736767268E-16, 18.12499999317203248, -10.00000000000000178 ) ) ;
#62540 = CARTESIAN_POINT ( 'NONE',  ( -5.082755093536325930, 124.3437500020483952, -5.082755093536325930 ) ) ;
#62541 = CARTESIAN_POINT ( 'NONE',  ( 3.428378827818546970, 51.66489094707695529, 48.71857030467419492 ) ) ;
#62544 = PLANE ( 'NONE',  #71141 ) ;
#62543 = CARTESIAN_POINT ( 'NONE',  ( 2.085542519210945334E-15, 240.1562500034140157, 11.35316468749999963 ) ) ;
#62542 = CARTESIAN_POINT ( 'NONE',  ( 26.56734541678233441, 206.0000000013656063, 166.5412658749999650 ) ) ;
#62545 = APPLICATION_PROTOCOL_DEFINITION ( 'draft international standard', 'automotive_design', 1998, #27958 ) ;
#62546 = ORIENTED_EDGE ( 'NONE', *, *, #69346, .F. ) ;
#62547 = CARTESIAN_POINT ( 'NONE',  ( 5.676582343749997150, 257.5520833367473301, -9.832129032723418760 ) ) ;
#62548 = CARTESIAN_POINT ( 'NONE',  ( -7.188101187499990274, -2.977408999572651371, 13.58030278187175277 ) ) ;
#62549 = ORIENTED_EDGE ( 'NONE', *, *, #17332, .F. ) ;
#62550 = ORIENTED_EDGE ( 'NONE', *, *, #15261, .F. ) ;
#62551 = CARTESIAN_POINT ( 'NONE',  ( 4.220049686691941027, -10.18810118749999738, 75.62500000204838102 ) ) ;
#62552 = CARTESIAN_POINT ( 'NONE',  ( 6.951808397369818766E-16, 92.34374999658602690, -11.35316468750000141 ) ) ;
#62553 = DIRECTION ( 'NONE',  ( -0.000000000000000000, 1.000000000000000000, -0.000000000000000000 ) ) ;
#62554 = CARTESIAN_POINT ( 'NONE',  ( 2.020667218593132706E-15, -11.00000000000000000, 86.87499999999998579 ) ) ;
#62557 = CARTESIAN_POINT ( 'NONE',  ( -2.765530957081998142, 290.7968750017069510, 6.676582343750000703 ) ) ;
#62556 = CARTESIAN_POINT ( 'NONE',  ( 26.34314575050758478, 194.6875000027312126, 165.9999999999998863 ) ) ;
#62555 = CARTESIAN_POINT ( 'NONE',  ( 30.44569435410879521, 208.8125000013656063, 172.4456943541087526 ) ) ;
#62558 = AXIS2_PLACEMENT_3D ( 'NONE', #32365, #4810, #44050 ) ;
#62559 = CARTESIAN_POINT ( 'NONE',  ( 5.094044972490348933, 8.823157690132404696, 67.53052377765949643 ) ) ;
#62560 = CARTESIAN_POINT ( 'NONE',  ( 0.000000000000000000, 0.000000000000000000, 0.000000000000000000 ) ) ;
#62561 = CARTESIAN_POINT ( 'NONE',  ( 11.35316468749999785, 200.5729166632526983, 3.042071309553174174 ) ) ;
#62562 = CARTESIAN_POINT ( 'NONE',  ( 3.313708498984762496, 11.53124999590322197, 7.999999999999998224 ) ) ;
#62563 = ORIENTED_EDGE ( 'NONE', *, *, #47539, .T. ) ;
#62564 = CARTESIAN_POINT ( 'NONE',  ( 25.55430564589115505, 208.5625000013656063, 172.4456943541086957 ) ) ;
#62565 = EDGE_CURVE ( 'NONE', #60656, #40460, #46204, .T. ) ;
#62566 = CARTESIAN_POINT ( 'NONE',  ( -5.082755093536325042, 14.90624999795161187, -5.082755093536325930 ) ) ;
#62567 = CARTESIAN_POINT ( 'NONE',  ( -3.042071309553173730, 164.6354166632526983, 11.35316468749999785 ) ) ;
#62568 = DIRECTION ( 'NONE',  ( 0.000000000000000000, 0.000000000000000000, 1.000000000000000000 ) ) ;
#62569 = CARTESIAN_POINT ( 'NONE',  ( 5.082755093536325042, 101.4687500020483810, -5.082755093536325930 ) ) ;
#62570 = CARTESIAN_POINT ( 'NONE',  ( 2.449293598294707893E-16, 10.25000000000000000, -4.000000000000001776 ) ) ;
#62571 = CARTESIAN_POINT ( 'NONE',  ( 26.56734541678232731, 205.6250000013656063, 173.4587341249998929 ) ) ;
#62572 = CARTESIAN_POINT ( 'NONE',  ( 5.082755093536320601, -5.082755093536318824, 8.424052781871752771 ) ) ;
#62573 = CARTESIAN_POINT ( 'NONE',  ( 8.311093377946834337, 55.15624999658601979, 8.311093377946839666 ) ) ;
#62574 = CARTESIAN_POINT ( 'NONE',  ( -1.970469249063935269E-15, 20.78460969082654231, -20.69999999999999929 ) ) ;
#62575 = CARTESIAN_POINT ( 'NONE',  ( -29.65685424949235838, 200.5625000027311842, 174.0000000000003126 ) ) ;
#62576 = EDGE_LOOP ( 'NONE', ( #39971, #19391, #52734 ) ) ;
#62577 = CARTESIAN_POINT ( 'NONE',  ( -4.556349186104048599, -10.99999999999999822, 74.78125000000001421 ) ) ;
#62578 = CARTESIAN_POINT ( 'NONE',  ( -4.556349186104048599, -10.99999999999999822, 80.96875000409677625 ) ) ;
#62579 = CARTESIAN_POINT ( 'NONE',  ( 6.951808397369818766E-16, 57.03124999658601268, -11.35316468750000141 ) ) ;
#62580 = CARTESIAN_POINT ( 'NONE',  ( -6.735557395310442023E-16, 11.00000000000000000, 72.81250000409677625 ) ) ;
#62581 = CARTESIAN_POINT ( 'NONE',  ( 3.458734124999960358, 200.6250000013656063, 143.4326545832176976 ) ) ;
#62582 = CARTESIAN_POINT ( 'NONE',  ( -0.6474643998350001484, 10.28110762191874628, 63.57179091896463063 ) ) ;
#62583 = CARTESIAN_POINT ( 'NONE',  ( -7.320508075688774596, 11.87500000000000000, -7.320508075688775484 ) ) ;
#62585 = CARTESIAN_POINT ( 'NONE',  ( 5.676582343749993598, 39.94791666325268409, 9.832129032723422313 ) ) ;
#62584 = CARTESIAN_POINT ( 'NONE',  ( 2.977408999572654480, 93.12500000204838102, 7.188101187499999156 ) ) ;
#62586 = CARTESIAN_POINT ( 'NONE',  ( -7.999999999999991118, 3.313708498984756723, 5.236552779823363757 ) ) ;
#62587 = CARTESIAN_POINT ( 'NONE',  ( -30.93541659651597797, -37.99999999999981526, 171.9999999999998295 ) ) ;
#62588 = CARTESIAN_POINT ( 'NONE',  ( 8.311093377946837890, 176.4062499965859843, -8.311093377946837890 ) ) ;
#62590 = CARTESIAN_POINT ( 'NONE',  ( 8.660254037844385522, 141.4583333265053682, 5.000000000000005329 ) ) ;
#62589 = PRODUCT ( 'spindle bearing', 'spindle bearing', '', ( #22936 ) ) ;
#62591 = CARTESIAN_POINT ( 'NONE',  ( -7.188101187499999156, 103.6250000020483810, 2.977408999572654924 ) ) ;
#62592 = CARTESIAN_POINT ( 'NONE',  ( 27.99999999999999645, 210.0000000000000284, 169.9999999999999147 ) ) ;
#62593 = CARTESIAN_POINT ( 'NONE',  ( 11.35316468749999963, 41.30208332991935549, -3.042071309553165293 ) ) ;
#62594 =( BOUNDED_CURVE ( )  B_SPLINE_CURVE ( 2, ( #8940, #71183, #54976, #49675, #49290, #7826, #72307, #37241, #20619 ),
 .UNSPECIFIED., .F., .F. ) 
 B_SPLINE_CURVE_WITH_KNOTS ( ( 3, 2, 2, 2, 3 ),
 ( 0.2333333333333335313, 0.2416666666666668628, 0.2500000000000002220, 0.2583333333333335813, 0.2666666666666668850 ),
 .UNSPECIFIED. ) 
 CURVE ( )  GEOMETRIC_REPRESENTATION_ITEM ( )  RATIONAL_B_SPLINE_CURVE ( ( 0.9999999999999982236, 0.9238795325112885148, 1.000000000000000000, 0.9238795325112867385, 1.000000000000000000, 0.9238795325112867385, 1.000000000000000000, 0.9238795325112847401, 1.000000000000001998 ) ) 
 REPRESENTATION_ITEM ( '' )  );
#62595 = CARTESIAN_POINT ( 'NONE',  ( 4.220049686691934809, 10.18810118749999916, 117.0625000020483668 ) ) ;
#62596 = CARTESIAN_POINT ( 'NONE',  ( -11.35316468749999785, 183.0729166632526983, -3.042071309553167513 ) ) ;
#62597 = VERTEX_POINT ( 'NONE', #70943 ) ;
#62598 = CARTESIAN_POINT ( 'NONE',  ( 49.48363024973253488, 137.3416415284643222, 58.47069285135009409 ) ) ;
#62599 = CARTESIAN_POINT ( 'NONE',  ( 10.18810118750000093, -4.220049686691933921, 68.31250000204838102 ) ) ;
#62600 = CARTESIAN_POINT ( 'NONE',  ( -2.828427124746153876, 197.8750000000000284, 195.1715728752538439 ) ) ;
#62601 = CARTESIAN_POINT ( 'NONE',  ( 3.313708498984762496, 16.21875000000000355, 7.999999999999998224 ) ) ;
#62603 = CARTESIAN_POINT ( 'NONE',  ( 5.676582343749993598, 164.9479166632526983, 9.832129032723422313 ) ) ;
#62602 = CARTESIAN_POINT ( 'NONE',  ( 29.65685424949245075, 203.4375000000000284, 165.9999999999999432 ) ) ;
#62604 = CARTESIAN_POINT ( 'NONE',  ( 7.999999999999992895, -3.313708498984756279, 6.042802784329825094 ) ) ;
#62605 = DIRECTION ( 'NONE',  ( 0.000000000000000000, 0.000000000000000000, 1.000000000000000000 ) ) ;
#62606 = EDGE_CURVE ( 'NONE', #48612, #13169, #65577, .T. ) ;
#62607 = CARTESIAN_POINT ( 'NONE',  ( 11.35316468749999963, 221.1979166700806161, 3.042071309553159519 ) ) ;
#62608 = PLANE ( 'NONE',  #27619 ) ;
#62609 = CARTESIAN_POINT ( 'NONE',  ( 7.204075437095966983, 7.204075437095967871, 77.96875000204836681 ) ) ;
#62610 = ORIENTED_EDGE ( 'NONE', *, *, #20794, .F. ) ;
#62611 = AXIS2_PLACEMENT_3D ( 'NONE', #70575, #41898, #13213 ) ;
#62612 = DIRECTION ( 'NONE',  ( 0.8660254037844395958, -0.4999999999999981681, 0.000000000000000000 ) ) ;
#62613 = CARTESIAN_POINT ( 'NONE',  ( 3.042071309553159519, 110.0520833299193271, 11.35316468750000141 ) ) ;
#62614 =( BOUNDED_CURVE ( )  B_SPLINE_CURVE ( 2, ( #54183, #48867, #36456, #8514, #36088, #13778, #42095, #59469, #19825 ),
 .UNSPECIFIED., .F., .F. ) 
 B_SPLINE_CURVE_WITH_KNOTS ( ( 3, 2, 2, 2, 3 ),
 ( 0.2794117647058822484, 0.2830882352941175295, 0.2867647058823528106, 0.2904411764705881471, 0.2941176470588234282 ),
 .UNSPECIFIED. ) 
 CURVE ( )  GEOMETRIC_REPRESENTATION_ITEM ( )  RATIONAL_B_SPLINE_CURVE ( ( 1.000000000000002220, 0.9238795325112844070, 1.000000000000000000, 0.9238795325112867385, 1.000000000000000000, 0.9238795325112867385, 1.000000000000000000, 0.9238795325112890700, 0.9999999999999976685 ) ) 
 REPRESENTATION_ITEM ( '' )  );
#62615 = PLANE ( 'NONE',  #12861 ) ;
#62616 = ORIENTED_EDGE ( 'NONE', *, *, #54211, .T. ) ;
#62617 = EDGE_LOOP ( 'NONE', ( #25591, #53737, #49551, #71618 ) ) ;
#62618 = CARTESIAN_POINT ( 'NONE',  ( -4.541265875000002339, 9.937499998634406140, -5.561446717895856393E-16 ) ) ;
#62619 = AXIS2_PLACEMENT_3D ( 'NONE', #46055, #52466, #35859 ) ;
#62620 = CARTESIAN_POINT ( 'NONE',  ( -7.188101187500001821, 13.12499999795161187, -2.977408999572651371 ) ) ;
#62621 = CARTESIAN_POINT ( 'NONE',  ( 3.313708498984760720, 111.2187500040968047, -8.000000000000000000 ) ) ;
#62622 = ADVANCED_FACE ( 'NONE', ( #19258 ), #29485, .T. ) ;
#62623 = CARTESIAN_POINT ( 'NONE',  ( -31.45873412499999233, 199.9375000013656063, 170.0000000000003979 ) ) ;
#62624 = EDGE_CURVE ( 'NONE', #25866, #1937, #53238, .T. ) ;
#62625 = CARTESIAN_POINT ( 'NONE',  ( 1.656854249492381914, 8.812500000000000000, 4.000000000000000888 ) ) ;
#62626 = CARTESIAN_POINT ( 'NONE',  ( -1.656854249492383691, 20.43749999726881228, 4.000000000000000888 ) ) ;
#62627 = CARTESIAN_POINT ( 'NONE',  ( -1.881053915767121776, 8.624999998634407916, -4.541265875000002339 ) ) ;
#62628 = CARTESIAN_POINT ( 'NONE',  ( 1.656854249492348607, 199.1875000000000000, 138.0000000000000568 ) ) ;
#62629 = ORIENTED_EDGE ( 'NONE', *, *, #12611, .F. ) ;
#62630 = CARTESIAN_POINT ( 'NONE',  ( 5.000000000000004441, 221.6666666666666856, 8.660254037844385522 ) ) ;
#62631 = CARTESIAN_POINT ( 'NONE',  ( 5.082755093536326818, 103.7187500020483810, 5.082755093536325042 ) ) ;
#62633 = CARTESIAN_POINT ( 'NONE',  ( -4.898587196589412829E-16, 123.1250000000000000, -8.000000000000000000 ) ) ;
#62632 = CARTESIAN_POINT ( 'NONE',  ( -30.44569435410875613, 194.8125000013656063, 172.4456943541092642 ) ) ;
#62634 = CARTESIAN_POINT ( 'NONE',  ( 7.188101187499991163, 2.977408999572648707, 2.330302781871750550 ) ) ;
#62635 = ORIENTED_EDGE ( 'NONE', *, *, #31630, .T. ) ;
#62636 = ORIENTED_EDGE ( 'NONE', *, *, #24704, .T. ) ;
#62637 = CARTESIAN_POINT ( 'NONE',  ( 4.220049686691934809, 10.18810118749999916, 92.68750000204838102 ) ) ;
#62638 = CARTESIAN_POINT ( 'NONE',  ( 8.000000000000001776, 91.34375000409679046, 3.313708498984759387 ) ) ;
#62639 = CARTESIAN_POINT ( 'NONE',  ( -29.43265458321760519, 200.1250000013656063, 173.4587341250003760 ) ) ;
#62640 = CARTESIAN_POINT ( 'NONE',  ( -7.778174593052023411, 7.778174593052023411, 108.8124999999999858 ) ) ;
#62641 = CARTESIAN_POINT ( 'NONE',  ( -3.458734124999960358, 201.6250000013656063, 196.5673454167823877 ) ) ;
#62643 = PLANE ( 'NONE',  #30162 ) ;
#62642 = CARTESIAN_POINT ( 'NONE',  ( -6.000000000000003553, 290.0000000034140157, -2.485281374238571317 ) ) ;
#62644 = CARTESIAN_POINT ( 'NONE',  ( -7.320508075688773708, 121.8750000000000000, -7.320508075688774596 ) ) ;
#62645 = CARTESIAN_POINT ( 'NONE',  ( -4.898587196589412829E-16, 108.1250000000000000, -8.000000000000000000 ) ) ;
#62646 = CARTESIAN_POINT ( 'NONE',  ( -2.765530957081998586, 289.7968750017070079, 6.676582343750001591 ) ) ;
#62647 = CARTESIAN_POINT ( 'NONE',  ( -5.082755093536319713, 5.082755093536319713, 3.174052781871751439 ) ) ;
#62648 = FACE_OUTER_BOUND ( 'NONE', #20589, .T. ) ;
#62649 = AXIS2_PLACEMENT_3D ( 'NONE', #36307, #48346, #25331 ) ;
#62650 = CARTESIAN_POINT ( 'NONE',  ( 31.45873412499999944, 207.6875000013656063, 169.9999999999999432 ) ) ;
#62651 = CARTESIAN_POINT ( 'NONE',  ( -1.469576158976823947E-15, 27.93749999590322375, 8.000000000000000000 ) ) ;
#62652 = CARTESIAN_POINT ( 'NONE',  ( 2.445694354108782775, 200.5625000013656063, 139.5543056458912190 ) ) ;
#62653 = CARTESIAN_POINT ( 'NONE',  ( -2.977408999572652260, 120.3125000020483810, 7.188101187500000044 ) ) ;
#62655 = CARTESIAN_POINT ( 'NONE',  ( -2.839093476692135984E-14, 201.9375000013656063, 138.5412658750000503 ) ) ;
#62654 = CARTESIAN_POINT ( 'NONE',  ( -1.656854249492371256, 204.3124999999999716, 137.9999999999999716 ) ) ;
#62656 = CARTESIAN_POINT ( 'NONE',  ( -11.35316468749999785, 244.0104166700806729, -3.042071309553164848 ) ) ;
#62657 = CARTESIAN_POINT ( 'NONE',  ( -11.00000000000010658, 4.556349186103942017, 86.40624999999998579 ) ) ;
#62658 = CARTESIAN_POINT ( 'NONE',  ( 23.99999999999998934, 203.7500000000000284, 169.9999999999998863 ) ) ;
#62659 = CARTESIAN_POINT ( 'NONE',  ( -5.676582343750006032, 19.11458332991934839, 9.832129032723418760 ) ) ;
#62660 = LINE ( 'NONE', #73250, #50768 ) ;
#62661 = CARTESIAN_POINT ( 'NONE',  ( -5.676582343749998039, 212.7604166632526699, -9.832129032723420536 ) ) ;
#62662 = DIRECTION ( 'NONE',  ( -0.000000000000000000, 1.000000000000000000, -0.000000000000000000 ) ) ;
#62663 = CARTESIAN_POINT ( 'NONE',  ( 5.656854249492381470, 124.0625000000000000, 5.656854249492379694 ) ) ;
#62665 = CARTESIAN_POINT ( 'NONE',  ( -1.836970198721029983E-15, 30.62499999317203248, 10.00000000000000178 ) ) ;
#62664 = DIRECTION ( 'NONE',  ( -0.000000000000000000, -1.000000000000000000, -0.000000000000000000 ) ) ;
#62666 = ORIENTED_EDGE ( 'NONE', *, *, #39840, .T. ) ;
#62667 = CARTESIAN_POINT ( 'NONE',  ( -1.432654583217662481, 199.3750000013656063, 145.4587341250000634 ) ) ;
#62668 = CARTESIAN_POINT ( 'NONE',  ( 8.311093377946837890, 16.40624999658601268, -8.311093377946837890 ) ) ;
#62669 = CARTESIAN_POINT ( 'NONE',  ( -4.556349186104045934, 11.00000000000000000, 93.90625000409679046 ) ) ;
#62670 = CARTESIAN_POINT ( 'NONE',  ( -3.166186134455097228E-13, 171.2500000000000284, -9.999999999999998224 ) ) ;
#62671 = CARTESIAN_POINT ( 'NONE',  ( -31.45873412499995680, 196.7500000013656063, 171.4326545832181239 ) ) ;
#62672 = CARTESIAN_POINT ( 'NONE',  ( -5.000000000000000000, 0.000000000000000000, -71.70204102886728492 ) ) ;
#62674 = CARTESIAN_POINT ( 'NONE',  ( -3.042071309553173730, 4.322916663252682312, 11.35316468749999785 ) ) ;
#62673 = CARTESIAN_POINT ( 'NONE',  ( 7.188101187500000044, 114.4062500020483810, -8.802885111219163269E-16 ) ) ;
#62675 = CARTESIAN_POINT ( 'NONE',  ( 7.999999999999991118, 9.797174393178815797E-16, 21.08030277982336642 ) ) ;
#62676 = CARTESIAN_POINT ( 'NONE',  ( -8.311093377946841443, 128.9062499965860411, 8.311093377946830785 ) ) ;
#62677 = CARTESIAN_POINT ( 'NONE',  ( -2.679491924311225848, 108.3333333265053540, -10.00000000000000178 ) ) ;
#62678 = CARTESIAN_POINT ( 'NONE',  ( 5.082755093536325042, 120.9687500020483952, -5.082755093536325930 ) ) ;
#62679 = CARTESIAN_POINT ( 'NONE',  ( -1.836970198721029983E-15, 5.624999993172032475, 10.00000000000000178 ) ) ;
#62680 = FACE_OUTER_BOUND ( 'NONE', #23540, .T. ) ;
#62681 = CARTESIAN_POINT ( 'NONE',  ( -5.000000000000000888, 53.20585484986858660, -47.69738026034675471 ) ) ;
#62682 = VERTEX_POINT ( 'NONE', #1569 ) ;
#62683 = CARTESIAN_POINT ( 'NONE',  ( 4.465384415997323053, -66.51627080308875861, 26.73837581714047573 ) ) ;
#62684 = CARTESIAN_POINT ( 'NONE',  ( -8.660254037844387298, 153.9583333265053682, -5.000000000000004441 ) ) ;
#62685 = CARTESIAN_POINT ( 'NONE',  ( 6.676582343750001591, 291.1093750017069510, -8.176455196517173205E-16 ) ) ;
#62686 = CARTESIAN_POINT ( 'NONE',  ( 7.999999999999992895, -3.313708498984756279, 25.54280278432982598 ) ) ;
#62687 = CARTESIAN_POINT ( 'NONE',  ( -5.656854249492381470, 18.93750000000000355, 5.656854249492379694 ) ) ;
#62688 = CARTESIAN_POINT ( 'NONE',  ( 9.832129032723420536, 260.9895833367473301, 5.676582343749996262 ) ) ;
#62689 = CARTESIAN_POINT ( 'NONE',  ( 4.220049686691941027, -10.18810118749999738, 97.00000000204836681 ) ) ;
#62690 = ORIENTED_EDGE ( 'NONE', *, *, #38104, .T. ) ;
#62691 = AXIS2_PLACEMENT_3D ( 'NONE', #20077, #1373, #24357 ) ;
#62692 = EDGE_CURVE ( 'NONE', #49057, #69053, #55461, .T. ) ;
#62693 = EDGE_CURVE ( 'NONE', #48616, #15213, #15082, .T. ) ;
#62694 = CARTESIAN_POINT ( 'NONE',  ( 7.320508075688774596, 217.4999999931720538, -7.320508075688774596 ) ) ;
#62695 = CARTESIAN_POINT ( 'NONE',  ( 3.313708498984756279, 7.999999999999991118, 24.36155277982336997 ) ) ;
#62696 = CARTESIAN_POINT ( 'NONE',  ( -3.458734124999959469, 203.7500000013656063, 199.4326545832176976 ) ) ;
#62697 = CARTESIAN_POINT ( 'NONE',  ( 5.676582343750001591, 81.92708332991935549, -9.832129032723420536 ) ) ;
#62698 = VERTEX_POINT ( 'NONE', #14707 ) ;
#62699 = CARTESIAN_POINT ( 'NONE',  ( 7.204075437095966983, 7.204075437095967871, 104.5937500020483810 ) ) ;
#62700 = CARTESIAN_POINT ( 'NONE',  ( -4.541265875000003227, 13.99999999863440792, 1.881053915767121110 ) ) ;
#62701 = ORIENTED_EDGE ( 'NONE', *, *, #48223, .F. ) ;
#62702 = CARTESIAN_POINT ( 'NONE',  ( -7.188101187500002709, 26.81249999795161543, 2.977408999572649151 ) ) ;
#62703 = CARTESIAN_POINT ( 'NONE',  ( -5.656854249492378806, 107.1874999999999858, 5.656854249492381470 ) ) ;
#62704 = CARTESIAN_POINT ( 'NONE',  ( -4.999999999999999112, -67.91007042436109487, -22.22893179987999090 ) ) ;
#62705 = CARTESIAN_POINT ( 'NONE',  ( 4.401442555609581635E-16, 23.71874999795161543, -7.188101187500000044 ) ) ;
#62706 = FACE_OUTER_BOUND ( 'NONE', #59628, .T. ) ;
#62707 =( BOUNDED_CURVE ( )  B_SPLINE_CURVE ( 2, ( #65177, #65555, #36527, #54252, #72332, #59537, #14227, #71575, #19897 ),
 .UNSPECIFIED., .F., .F. ) 
 B_SPLINE_CURVE_WITH_KNOTS ( ( 3, 2, 2, 2, 3 ),
 ( 0.8194444444444443088, 0.8263888888888887285, 0.8333333333333332593, 0.8402777777777777901, 0.8472222222222222099 ),
 .UNSPECIFIED. ) 
 CURVE ( )  GEOMETRIC_REPRESENTATION_ITEM ( )  RATIONAL_B_SPLINE_CURVE ( ( 1.000000000000001110, 0.9238795325112855172, 1.000000000000000000, 0.9238795325112867385, 1.000000000000000000, 0.9238795325112867385, 1.000000000000000000, 0.9238795325112867385, 1.000000000000000000 ) ) 
 REPRESENTATION_ITEM ( '' )  );
#62708 = CARTESIAN_POINT ( 'NONE',  ( -6.238412754330611322E-16, 10.18810118749999916, 111.1562500020483668 ) ) ;
#62709 = VECTOR ( 'NONE', #14290, 1000.000000000000000 ) ;
#62710 = CARTESIAN_POINT ( 'NONE',  ( 7.778174593052021635, 7.778174593052023411, 75.43749999999998579 ) ) ;
#62711 = CARTESIAN_POINT ( 'NONE',  ( -1.656854249492383691, 11.43749999726881406, 4.000000000000000888 ) ) ;
#62712 = CARTESIAN_POINT ( 'NONE',  ( 4.000000000000001776, 18.06250000000000000, -1.656854249492381248 ) ) ;
#62713 = ORIENTED_EDGE ( 'NONE', *, *, #72670, .F. ) ;
#62714 = AXIS2_PLACEMENT_3D ( 'NONE', #11587, #57628, #52701 ) ;
#62715 = CARTESIAN_POINT ( 'NONE',  ( -2.445694354108782775, 201.5625000013656063, 200.4456943541088663 ) ) ;
#62716 = ADVANCED_FACE ( 'NONE', ( #43764 ), #66024, .F. ) ;
#62717 = CARTESIAN_POINT ( 'NONE',  ( -26.56734541678227757, 204.0000000013656347, 173.4587341250003476 ) ) ;
#62718 =( BOUNDED_CURVE ( )  B_SPLINE_CURVE ( 2, ( #39786, #67073, #16761, #39425, #28839, #74122, #62789, #11498, #28472 ),
 .UNSPECIFIED., .F., .F. ) 
 B_SPLINE_CURVE_WITH_KNOTS ( ( 3, 2, 2, 2, 3 ),
 ( 0.6883006607833690449, 0.6949189363678606179, 0.7015372119523523020, 0.7081554875368439861, 0.7147737642690134008 ),
 .UNSPECIFIED. ) 
 CURVE ( )  GEOMETRIC_REPRESENTATION_ITEM ( )  RATIONAL_B_SPLINE_CURVE ( ( 1.000000000001603162, 0.9238795325096835764, 1.000000000000000000, 0.9238795325112867385, 1.000000000000000000, 0.9238795325112867385, 1.000000000000000000, 0.9238795325112867385, 1.000000000000000000 ) ) 
 REPRESENTATION_ITEM ( '' )  );
#62719 = CARTESIAN_POINT ( 'NONE',  ( -4.541265875000002339, 8.749999998634406140, -1.881053915767121998 ) ) ;
#62720 = CARTESIAN_POINT ( 'NONE',  ( 4.000000000000001776, 0.06250000000000018041, -1.656854249492381248 ) ) ;
#62721 = CARTESIAN_POINT ( 'NONE',  ( 5.082755093536320601, -5.082755093536318824, 20.04905278187175455 ) ) ;
#62722 = EDGE_LOOP ( 'NONE', ( #46867, #35083, #22342, #33166 ) ) ;
#62723 = CARTESIAN_POINT ( 'NONE',  ( -11.00000000000000000, 0.000000000000000000, 93.99999999999998579 ) ) ;
#62724 = ORIENTED_EDGE ( 'NONE', *, *, #40069, .F. ) ;
#62725 = CARTESIAN_POINT ( 'NONE',  ( 10.18810118749999916, 1.247682550866122264E-15, 111.9062500020483810 ) ) ;
#62726 = DIRECTION ( 'NONE',  ( -0.000000000000000000, -1.000000000000000000, -0.000000000000000000 ) ) ;
#62727 = CARTESIAN_POINT ( 'NONE',  ( 3.458734125000015425, 199.0000000013656063, 196.5673454167823877 ) ) ;
#62728 = CARTESIAN_POINT ( 'NONE',  ( 4.898587196589412829E-16, 12.18749999590322197, -8.000000000000000000 ) ) ;
#62729 = CARTESIAN_POINT ( 'NONE',  ( 2.679491924311228956, 76.04166666666665719, -10.00000000000000000 ) ) ;
#62730 = CARTESIAN_POINT ( 'NONE',  ( -7.188101187499999156, 90.12500000204836681, 2.977408999572654924 ) ) ;
#62731 = CARTESIAN_POINT ( 'NONE',  ( 6.000000000000003553, 289.5625000000000568, -2.485281374238571761 ) ) ;
#62732 = EDGE_LOOP ( 'NONE', ( #72639, #316, #60779, #7562 ) ) ;
#62733 = CYLINDRICAL_SURFACE ( 'NONE', #57837, 3.999999999999976019 ) ;
#62734 = CARTESIAN_POINT ( 'NONE',  ( -3.496982156820189314, -68.06496700477784145, 20.41687962716806481 ) ) ;
#62735 = CARTESIAN_POINT ( 'NONE',  ( -1.656854249492405451, 196.4375000027311842, 138.0000000000000568 ) ) ;
#62736 = CARTESIAN_POINT ( 'NONE',  ( 2.751064625579944321E-14, 200.7500000000000000, 194.0000000000000568 ) ) ;
#62737 = CARTESIAN_POINT ( 'NONE',  ( 28.15849992381777867, 194.4587341250000350, 173.4587341249998929 ) ) ;
#62738 = CARTESIAN_POINT ( 'NONE',  ( 5.000000000000004441, 231.6666666666666856, 8.660254037844385522 ) ) ;
#62739 = DIRECTION ( 'NONE',  ( 0.000000000000000000, -0.8536788251726021848, -0.5207998305029730712 ) ) ;
#62740 = CARTESIAN_POINT ( 'NONE',  ( 10.00000000000000000, 204.7916666666666856, 2.679491924311236062 ) ) ;
#62741 = CARTESIAN_POINT ( 'NONE',  ( 2.977408999572650927, -7.188101187499990274, 18.83030278187175455 ) ) ;
#62742 = CARTESIAN_POINT ( 'NONE',  ( -5.676582343749998039, 167.7604166632526983, -9.832129032723420536 ) ) ;
#62743 = CARTESIAN_POINT ( 'NONE',  ( -3.000000000000000444, -44.80157590050100680, 151.2383369607063059 ) ) ;
#62745 = CARTESIAN_POINT ( 'NONE',  ( 3.313708498984742068, 10.03124999590321842, 8.000000000000019540 ) ) ;
#62744 = DIRECTION ( 'NONE',  ( 0.000000000000000000, -1.000000000000000000, 0.000000000000000000 ) ) ;
#62746 = ORIENTED_EDGE ( 'NONE', *, *, #19001, .T. ) ;
#62747 = CARTESIAN_POINT ( 'NONE',  ( -2.445694354108839619, 196.8125000013656063, 139.5543056458912190 ) ) ;
#62748 = CARTESIAN_POINT ( 'NONE',  ( -3.042071309553173730, 34.63541666325269119, 11.35316468749999785 ) ) ;
#62749 = CARTESIAN_POINT ( 'NONE',  ( -4.556349186104047710, -10.99999999999999822, 110.9687500040967905 ) ) ;
#62750 = CARTESIAN_POINT ( 'NONE',  ( -25.55430564589123321, 208.3125000013656063, 167.5543056458915032 ) ) ;
#62751 = CYLINDRICAL_SURFACE ( 'NONE', #34633, 10.00000000000000178 ) ;
#62753 = CARTESIAN_POINT ( 'NONE',  ( 0.000000000000000000, 25.94987437106619765, 1.000000000000000000 ) ) ;
#62752 = CARTESIAN_POINT ( 'NONE',  ( -4.898587196589412829E-16, 115.8125000040967763, -8.000000000000000000 ) ) ;
#62754 = CARTESIAN_POINT ( 'NONE',  ( -10.99999999999992184, -32.48324455940847599, 198.9827534923788619 ) ) ;
#62755 = CARTESIAN_POINT ( 'NONE',  ( 2.445694354108783664, 200.3125000013656063, 144.4456943541088663 ) ) ;
#62756 = ADVANCED_FACE ( 'NONE', ( #72439 ), #3034, .F. ) ;
#62757 = CARTESIAN_POINT ( 'NONE',  ( 5.000000000000001776, 57.70833332650537528, -8.660254037844389075 ) ) ;
#62758 = CARTESIAN_POINT ( 'NONE',  ( -7.188101187499999156, 104.7500000020483810, 2.977408999572654924 ) ) ;
#62759 = CARTESIAN_POINT ( 'NONE',  ( -3.211159895383562723, 13.06249999863440792, 3.211159895383561391 ) ) ;
#62760 = CARTESIAN_POINT ( 'NONE',  ( 5.000000000000020428, 64.16666666666669983, 8.660254037844437036 ) ) ;
#62761 = CARTESIAN_POINT ( 'NONE',  ( -7.999999999999991118, 3.313708498984756723, 3.736552779823362869 ) ) ;
#62762 = CARTESIAN_POINT ( 'NONE',  ( 7.320508075688771044, 101.2499999931720254, 7.320508075688775484 ) ) ;
#62763 = ORIENTED_EDGE ( 'NONE', *, *, #12785, .F. ) ;
#62764 = ORIENTED_EDGE ( 'NONE', *, *, #24932, .T. ) ;
#62765 = CARTESIAN_POINT ( 'NONE',  ( -2.679491924320392737, 198.5416666666659182, 9.999999999994837907 ) ) ;
#62766 = CARTESIAN_POINT ( 'NONE',  ( -1.432654583217608080, 195.8750000013655779, 201.4587341250000350 ) ) ;
#62767 = CARTESIAN_POINT ( 'NONE',  ( 7.778174593052021635, 7.778174593052023411, 103.9374999999999858 ) ) ;
#62768 = CARTESIAN_POINT ( 'NONE',  ( -1.744157829248402118E-12, 86.25000000000015632, -10.00000000000000533 ) ) ;
#62769 = CARTESIAN_POINT ( 'NONE',  ( 5.676582343750001591, 136.6145833299193555, -9.832129032723420536 ) ) ;
#62770 = CARTESIAN_POINT ( 'NONE',  ( -4.903509839973872353, 0.5323584527330150751, -6.410198659010889699 ) ) ;
#62771 = CARTESIAN_POINT ( 'NONE',  ( -7.204075437095967871, 7.204075437095967871, 88.46875000204838102 ) ) ;
#62772 = CARTESIAN_POINT ( 'NONE',  ( -4.898587196589412829E-16, 93.12499999999998579, -8.000000000000000000 ) ) ;
#62773 = CARTESIAN_POINT ( 'NONE',  ( 4.000000000000015099, 205.5625000000000284, 196.3431457505076594 ) ) ;
#62774 = CARTESIAN_POINT ( 'NONE',  ( -3.313708498984719864, 18.28124999590321664, -8.000000000000040856 ) ) ;
#62775 = CARTESIAN_POINT ( 'NONE',  ( 5.656854249492379694, 117.1250000040967905, -5.656854249492380582 ) ) ;
#62776 = VECTOR ( 'NONE', #42726, 1000.000000000000000 ) ;
#62777 = CARTESIAN_POINT ( 'NONE',  ( -8.000000000000000000, 100.9999999999999858, 0.000000000000000000 ) ) ;
#62778 = ORIENTED_EDGE ( 'NONE', *, *, #45656, .F. ) ;
#62779 = CARTESIAN_POINT ( 'NONE',  ( 62.39047978708148889, 242.0000000000000284, 45.00000000000000000 ) ) ;
#62780 = AXIS2_PLACEMENT_3D ( 'NONE', #44988, #38956, #32943 ) ;
#62781 = CARTESIAN_POINT ( 'NONE',  ( 24.84350201214178711, 176.4274895008061037, 151.3179989104068852 ) ) ;
#62782 = CARTESIAN_POINT ( 'NONE',  ( -2.085542519210945728E-15, 129.8437499965860127, 11.35316468750000141 ) ) ;
#62783 = CARTESIAN_POINT ( 'NONE',  ( 2.839093476692135984E-14, 201.6875000013656063, 201.4587341250000350 ) ) ;
#62784 = CARTESIAN_POINT ( 'NONE',  ( 2.977408999572650927, 25.12499999795161543, -7.188101187500000933 ) ) ;
#62785 = CARTESIAN_POINT ( 'NONE',  ( 4.220049686691941027, -10.18810118749999738, 76.00000000204835260 ) ) ;
#62786 = CARTESIAN_POINT ( 'NONE',  ( 9.832129032723416984, 30.67708332991935194, 5.676582343750006032 ) ) ;
#62787 = VERTEX_POINT ( 'NONE', #55101 ) ;
#62788 = CARTESIAN_POINT ( 'NONE',  ( 8.000000000000001776, 89.84375000409677625, 3.313708498984759387 ) ) ;
#62789 = CARTESIAN_POINT ( 'NONE',  ( 5.656854249492374365, 5.656854249492375253, 7.955302783920145338 ) ) ;
#62790 = CARTESIAN_POINT ( 'NONE',  ( -8.008118988124991233, 0.000000000000000000, 19.01311528394063188 ) ) ;
#62791 = CARTESIAN_POINT ( 'NONE',  ( -3.458734125000015425, 208.2500000013656063, 143.4326545832176976 ) ) ;
#62792 = CONICAL_SURFACE ( 'NONE', #26648, 3.999999999999976019, 0.7853981633974491672 ) ;
#62793 = EDGE_CURVE ( 'NONE', #8888, #39383, #24732, .T. ) ;
#62794 = ADVANCED_FACE ( 'NONE', ( #55470, #54728 ), #26784, .T. ) ;
#62795 = CARTESIAN_POINT ( 'NONE',  ( 2.977408999572651815, 7.687499997951611874, 7.188101187500000933 ) ) ;
#62796 = CARTESIAN_POINT ( 'NONE',  ( -4.242640687119286547, 294.9375000034140157, -4.242640687119286547 ) ) ;
#62797 = CARTESIAN_POINT ( 'NONE',  ( -11.05152183594485926, -30.34804117986677952, 140.2151247536515939 ) ) ;
#62798 = CARTESIAN_POINT ( 'NONE',  ( 7.188101187499999156, 6.749999997951610986, 2.977408999572654924 ) ) ;
#62799 = ADVANCED_FACE ( 'NONE', ( #25280 ), #2285, .F. ) ;
#62800 = CARTESIAN_POINT ( 'NONE',  ( -8.311093377946841443, 159.2187499965860127, 8.311093377946830785 ) ) ;
#62801 = CARTESIAN_POINT ( 'NONE',  ( -10.18810118749999916, 4.220049686691934809, 78.06250000204838102 ) ) ;
#62802 = CARTESIAN_POINT ( 'NONE',  ( -24.54126587499999701, 196.2500000013656631, 168.5673454167827003 ) ) ;
#62803 = B_SPLINE_CURVE_WITH_KNOTS ( 'NONE', 3,
 ( #27845, #34647, #321, #51982, #5959, #11611, #22929, #57276, #39910, #16504, #39544, #68207, #52353, #35020, #5590, #23299, #28588, #10495, #74237, #10869, #39168, #63660 ),
 .UNSPECIFIED., .F., .F.,
 ( 4, 2, 2, 2, 2, 2, 2, 2, 2, 2, 4 ),
 ( 0.000000000000000000, 0.001156727053362482157, 0.001735090580043723235, 0.002313454106724964314, 0.003470181160087444303, 0.004048544686768682996, 0.004626908213449921689, 0.005783635266812366983, 0.006940362320174811410, 0.008097089373537256704, 0.009253816426899701131 ),
 .UNSPECIFIED. ) ;
#62804 = FACE_OUTER_BOUND ( 'NONE', #1030, .T. ) ;
#62805 = CARTESIAN_POINT ( 'NONE',  ( -4.541265875000002339, 20.93749999863440436, -5.561446717895856393E-16 ) ) ;
#62806 = VERTEX_POINT ( 'NONE', #30953 ) ;
#62807 = AXIS2_PLACEMENT_3D ( 'NONE', #6762, #31244, #59191 ) ;
#62808 = CARTESIAN_POINT ( 'NONE',  ( -1.656854249492348607, 199.3125000027311842, 202.0000000000000284 ) ) ;
#62809 = EDGE_CURVE ( 'NONE', #23491, #26308, #53974, .T. ) ;
#62810 = CARTESIAN_POINT ( 'NONE',  ( 3.999999999999959144, 208.0625000000000000, 140.3431457505076594 ) ) ;
#62811 = CARTESIAN_POINT ( 'NONE',  ( -23.99999999999995737, 202.8125000027312126, 171.6568542494926817 ) ) ;
#62812 = CARTESIAN_POINT ( 'NONE',  ( -10.00000000000008171, 57.70833333333337833, 2.679491924311244500 ) ) ;
#62813 = CARTESIAN_POINT ( 'NONE',  ( -3.313708498984757167, 7.999999999999991118, 5.236552783920145338 ) ) ;
#62814 = VERTEX_POINT ( 'NONE', #61493 ) ;
#62815 =( BOUNDED_CURVE ( )  B_SPLINE_CURVE ( 2, ( #33648, #55912, #73618, #56654, #4969, #51345, #68699 ),
 .UNSPECIFIED., .F., .F. ) 
 B_SPLINE_CURVE_WITH_KNOTS ( ( 3, 2, 2, 3 ),
 ( 0.000000000000000000, 0.005232694955406646566, 0.01046538991081329313, 0.01569808486621994056 ),
 .UNSPECIFIED. ) 
 CURVE ( )  GEOMETRIC_REPRESENTATION_ITEM ( )  RATIONAL_B_SPLINE_CURVE ( ( 1.000000000000000000, 0.9659258262890684232, 1.000000000000000000, 0.9659258262890684232, 1.000000000000000000, 0.9659258262889811597, 1.000000000000087264 ) ) 
 REPRESENTATION_ITEM ( '' )  );
#62816 = CARTESIAN_POINT ( 'NONE',  ( -2.977408999572654480, 17.99999999795161543, 7.188101187499999156 ) ) ;
#62817 = DIRECTION ( 'NONE',  ( -1.000000000000000000, 0.000000000000000000, -0.000000000000000000 ) ) ;
#62818 = CARTESIAN_POINT ( 'NONE',  ( 4.999999999999999112, 53.50647209750621158, -45.02947987234000493 ) ) ;
#62819 = CARTESIAN_POINT ( 'NONE',  ( 7.320508075688774596, 40.62500000000000000, -7.320508075688774596 ) ) ;
#62820 = CARTESIAN_POINT ( 'NONE',  ( -7.188101187500000044, 103.5312500020483810, 0.000000000000000000 ) ) ;
#62821 = CIRCLE ( 'NONE', #61496, 12.00000000000000355 ) ;
#62822 = CARTESIAN_POINT ( 'NONE',  ( -24.54126587499998635, 208.3750000013656063, 171.4326545832179818 ) ) ;
#62823 = FACE_OUTER_BOUND ( 'NONE', #53616, .T. ) ;
#62824 = LINE ( 'NONE', #51510, #5723 ) ;
#62825 = EDGE_LOOP ( 'NONE', ( #41592, #59143, #58184, #12870 ) ) ;
#62826 = CARTESIAN_POINT ( 'NONE',  ( -9.832129032723415207, 239.3229166700806445, 5.676582343750005144 ) ) ;
#62827 = CARTESIAN_POINT ( 'NONE',  ( 2.977408999572650927, -7.188101187499990274, 18.83030278187175099 ) ) ;
#62828 = AXIS2_PLACEMENT_3D ( 'NONE', #64704, #41325, #64335 ) ;
#62829 = CARTESIAN_POINT ( 'NONE',  ( -2.620431783932123615, 55.87941608673077099, 43.94382193463441411 ) ) ;
#62830 = CARTESIAN_POINT ( 'NONE',  ( -8.406549073443436271, 220.0000000000000284, 7.038866479487354333 ) ) ;
#62831 = CARTESIAN_POINT ( 'NONE',  ( 24.68676758239227453, 194.9812539062533574, 172.2402553090706760 ) ) ;
#62832 = CARTESIAN_POINT ( 'NONE',  ( -2.679491924311226292, 138.3333333265053682, -10.00000000000000178 ) ) ;
#62833 = CARTESIAN_POINT ( 'NONE',  ( -2.679491924311225848, 156.4583333333333712, -10.00000000000000178 ) ) ;
#62834 = CARTESIAN_POINT ( 'NONE',  ( -3.673940397442060854E-16, 288.8125000034140157, -6.000000000000001776 ) ) ;
#62835 = CARTESIAN_POINT ( 'NONE',  ( -1.469576158976823947E-15, 8.625000000000000000, 8.000000000000000000 ) ) ;
#62836 = CARTESIAN_POINT ( 'NONE',  ( 14.24573139410703426, 89.64008544297853120, -1.012862405069980154 ) ) ;
#62837 = CARTESIAN_POINT ( 'NONE',  ( -8.311093377946841443, 134.2187499965860411, 8.311093377946830785 ) ) ;
#62838 = CARTESIAN_POINT ( 'NONE',  ( -5.000000000000000000, 10.00000000000000000, -75.19090595827292134 ) ) ;
#62839 = CARTESIAN_POINT ( 'NONE',  ( 4.217983994790200697, -16.30587161610658598, -69.44297314766851059 ) ) ;
#62840 = VECTOR ( 'NONE', #28160, 1000.000000000000000 ) ;
#62843 = CARTESIAN_POINT ( 'NONE',  ( 1.102182119232618108E-15, 298.2500000000000000, 6.000000000000001776 ) ) ;
#62842 = CARTESIAN_POINT ( 'NONE',  ( 31.45873412499997812, 194.7500000013656063, 168.5673454167822172 ) ) ;
#62841 = CARTESIAN_POINT ( 'NONE',  ( 31.45873412499999233, 195.9375000013655779, 169.9999999999999432 ) ) ;
#62844 = ORIENTED_EDGE ( 'NONE', *, *, #61871, .F. ) ;
#62845 = CARTESIAN_POINT ( 'NONE',  ( 4.500000000000010658, 7.794228634059937377, 0.000000000000000000 ) ) ;
#62846 = CARTESIAN_POINT ( 'NONE',  ( 2.679491924318324614, 196.0416666666660888, -9.999999999996026290 ) ) ;
#62847 = CARTESIAN_POINT ( 'NONE',  ( 30.44569435410883074, 196.0625000013656063, 167.5543056458911053 ) ) ;
#62848 = CARTESIAN_POINT ( 'NONE',  ( -9.832129032723420536, 219.0104166632526983, 5.676582343749997150 ) ) ;
#62849 = CARTESIAN_POINT ( 'NONE',  ( -7.188101187500001821, 121.0625000020483668, -2.977408999572650483 ) ) ;
#62850 = CARTESIAN_POINT ( 'NONE',  ( -1.881053915767124440, 1.124999998634406584, 4.541265875000001451 ) ) ;
#62851 = CARTESIAN_POINT ( 'NONE',  ( -1.506680654955644849, 65.82403019917288134, -26.31606384388262754 ) ) ;
#62852 = CARTESIAN_POINT ( 'NONE',  ( 3.313708498984756279, 7.999999999999991118, 21.36155277982336997 ) ) ;
#62854 = CARTESIAN_POINT ( 'NONE',  ( 12.00000000000000000, -28.00000000000000000, 3.999999999999988010 ) ) ;
#62853 = SURFACE_STYLE_FILL_AREA ( #22868 ) ;
#62855 = CARTESIAN_POINT ( 'NONE',  ( -5.676582343750006032, 99.11458332991935549, 9.832129032723418760 ) ) ;
#62856 = VERTEX_POINT ( 'NONE', #48298 ) ;
#62857 = CARTESIAN_POINT ( 'NONE',  ( 0.000000000000000000, 300.0000000000000000, 0.000000000000000000 ) ) ;
#62858 = CARTESIAN_POINT ( 'NONE',  ( 7.188101187499999156, 24.37499999795161543, 2.977408999572654924 ) ) ;
#62859 = DIRECTION ( 'NONE',  ( 0.000000000000000000, 0.8778652960885044987, -0.4789076340208435756 ) ) ;
#62860 = CARTESIAN_POINT ( 'NONE',  ( 11.35316468749999963, 241.5104166700806729, 3.042071309553159519 ) ) ;
#62861 = CIRCLE ( 'NONE', #26672, 4.000000000000002665 ) ;
#62862 = CARTESIAN_POINT ( 'NONE',  ( 11.35316468749999963, 100.9895833299193555, -3.042071309553165293 ) ) ;
#62863 = VERTEX_POINT ( 'NONE', #66399 ) ;
#62864 = EDGE_CURVE ( 'NONE', #34808, #33441, #37745, .T. ) ;
#62865 = CARTESIAN_POINT ( 'NONE',  ( 3.313708498984721640, 25.21875000000000000, 8.000000000000039080 ) ) ;
#62866 = CARTESIAN_POINT ( 'NONE',  ( 4.220049686691934809, 10.18810118749999916, 109.1875000020483810 ) ) ;
#62867 = CARTESIAN_POINT ( 'NONE',  ( -10.00000000000000000, 214.1666666598386826, -2.679491924311229845 ) ) ;
#62868 = CARTESIAN_POINT ( 'NONE',  ( -3.458734124999959469, 204.7500000013656063, 199.4326545832176691 ) ) ;
#62869 = CARTESIAN_POINT ( 'NONE',  ( -11.00000000000000000, 0.000000000000000000, 68.49999999999997158 ) ) ;
#62871 = CARTESIAN_POINT ( 'NONE',  ( 9.832129032723420536, 106.1979166632526983, -5.676582343749999815 ) ) ;
#62870 = CARTESIAN_POINT ( 'NONE',  ( -7.999999999999991118, 0.000000000000000000, 23.33030277982336642 ) ) ;
#62872 = CARTESIAN_POINT ( 'NONE',  ( -5.656854249492373476, -5.656854249492376141, 13.20530278392014623 ) ) ;
#62873 = CARTESIAN_POINT ( 'NONE',  ( -29.43265458321760164, 195.1250000013656063, 173.4587341250003760 ) ) ;
#62874 = CARTESIAN_POINT ( 'NONE',  ( 8.660254037844461905, 174.5833333333333712, 5.000000000000049738 ) ) ;
#62875 = ORIENTED_EDGE ( 'NONE', *, *, #73598, .F. ) ;
#62876 = CARTESIAN_POINT ( 'NONE',  ( 7.320508075688774596, 182.4999999931720254, -7.320508075688774596 ) ) ;
#62877 = DIRECTION ( 'NONE',  ( 0.000000000000000000, 0.000000000000000000, 1.000000000000000000 ) ) ;
#62878 = CARTESIAN_POINT ( 'NONE',  ( -7.347880794884122694E-16, 6.499999997268813168, 4.000000000000001776 ) ) ;
#62879 = CARTESIAN_POINT ( 'NONE',  ( 6.951808397369818766E-16, 82.34374999658601268, -11.35316468750000141 ) ) ;
#62880 = CARTESIAN_POINT ( 'NONE',  ( 6.676582343750004256, 289.8906250017069510, 2.765530957081995478 ) ) ;
#62881 = CARTESIAN_POINT ( 'NONE',  ( -7.188101187500002709, 7.687499997951611874, 2.977408999572649151 ) ) ;
#62882 = CARTESIAN_POINT ( 'NONE',  ( 4.220049686691941027, -10.18810118749999738, 100.0000000020483952 ) ) ;
#62883 = CARTESIAN_POINT ( 'NONE',  ( 11.35316468749999785, 225.5729166632526983, 3.042071309553174174 ) ) ;
#62884 = VERTEX_POINT ( 'NONE', #19996 ) ;
#62885 = CARTESIAN_POINT ( 'NONE',  ( -10.00000000000000178, 69.37499999317203958, -1.224646799147353454E-15 ) ) ;
#62886 = CARTESIAN_POINT ( 'NONE',  ( 8.000000000000001776, 115.3437500040967905, 3.313708498984759387 ) ) ;
#62887 = CARTESIAN_POINT ( 'NONE',  ( 6.000000000000003553, 291.4375000000000000, 2.485281374238571317 ) ) ;
#62888 = CARTESIAN_POINT ( 'NONE',  ( 11.35316468749999963, 225.8887338474116007, -1.569472986416640570 ) ) ;
#62889 = EDGE_CURVE ( 'NONE', #74042, #54835, #31705, .T. ) ;
#62890 = FACE_OUTER_BOUND ( 'NONE', #11217, .T. ) ;
#62891 = CARTESIAN_POINT ( 'NONE',  ( 4.999999999999993783, 199.1666666666666856, 8.660254037844390851 ) ) ;
#62892 = CARTESIAN_POINT ( 'NONE',  ( -2.765530957081998586, 298.6406250017069510, 6.676582343750001591 ) ) ;
#62893 = EDGE_LOOP ( 'NONE', ( #17076, #3527, #42635, #19755 ) ) ;
#62894 = DIRECTION ( 'NONE',  ( 1.000000000000000000, 0.000000000000000000, 0.000000000000000000 ) ) ;
#62895 = CARTESIAN_POINT ( 'NONE',  ( -9.832129032723420536, 209.0104166632526699, 5.676582343749997150 ) ) ;
#62896 = CARTESIAN_POINT ( 'NONE',  ( -4.220049686691937474, -10.18810118749999738, 94.93750000204838102 ) ) ;
#62897 = AXIS2_PLACEMENT_3D ( 'NONE', #1464, #24445, #45976 ) ;
#62898 = CARTESIAN_POINT ( 'NONE',  ( -29.43265458321761230, 207.8750000013656063, 173.4587341250003760 ) ) ;
#62899 = CARTESIAN_POINT ( 'NONE',  ( 5.656854249492378806, 17.81250000000000355, 5.656854249492381470 ) ) ;
#62900 = ORIENTED_EDGE ( 'NONE', *, *, #64921, .F. ) ;
#62901 = PRODUCT_DEFINITION_CONTEXT ( 'detailed design', #58827, 'design' ) ;
#62902 = CARTESIAN_POINT ( 'NONE',  ( 2.977408999572650039, 120.6875000020483952, -7.188101187500001821 ) ) ;
#62903 = CARTESIAN_POINT ( 'NONE',  ( -2.726571689596997292E-14, 210.0000000000000284, 138.0000000000000568 ) ) ;
#62904 = EDGE_CURVE ( 'NONE', #10364, #12665, #13948, .T. ) ;
#62905 = CARTESIAN_POINT ( 'NONE',  ( 7.320508075688771044, 9.375000000000001776, 7.320508075688775484 ) ) ;
#62906 = EDGE_CURVE ( 'NONE', #55737, #49734, #63161, .T. ) ;
#62907 = AXIS2_PLACEMENT_3D ( 'NONE', #56300, #21208, #67618 ) ;
#62908 = CARTESIAN_POINT ( 'NONE',  ( -5.000000000000000000, 16.24494643555759410, 69.83755725260752456 ) ) ;
#62909 = CARTESIAN_POINT ( 'NONE',  ( -7.204075437095965206, -7.204075437095968759, 83.21875000204836681 ) ) ;
#62910 = ORIENTED_EDGE ( 'NONE', *, *, #53325, .T. ) ;
#62911 = CARTESIAN_POINT ( 'NONE',  ( -7.347880794884122694E-16, 19.75000000000000000, 4.000000000000001776 ) ) ;
#62912 = CARTESIAN_POINT ( 'NONE',  ( -7.188101187500000044, 1.218749997951610098, -8.802885111219163269E-16 ) ) ;
#62913 = ADVANCED_FACE ( 'NONE', ( #60364 ), #8690, .T. ) ;
#62914 = CARTESIAN_POINT ( 'NONE',  ( -2.250000000000000888, -2.250000000000000000, 0.000000000000000000 ) ) ;
#62915 = VECTOR ( 'NONE', #57980, 1000.000000000000000 ) ;
#62916 = DIRECTION ( 'NONE',  ( 0.000000000000000000, -1.000000000000000000, 0.000000000000000000 ) ) ;
#62917 = CARTESIAN_POINT ( 'NONE',  ( -7.188101187500001821, 124.4375000020483810, -2.977408999572650483 ) ) ;
#62918 = CARTESIAN_POINT ( 'NONE',  ( 4.999999999999999112, -67.53158052529160216, 22.66975313813502879 ) ) ;
#62919 = CARTESIAN_POINT ( 'NONE',  ( 1.830245674553049096, -47.38501966333467408, 151.0876564075450972 ) ) ;
#62922 = CARTESIAN_POINT ( 'NONE',  ( -7.778174593052020747, -7.778174593052023411, 88.37500000409677625 ) ) ;
#62921 = CARTESIAN_POINT ( 'NONE',  ( -5.676582343749992710, 249.7395833367473301, 9.832129032723422313 ) ) ;
#62920 = CARTESIAN_POINT ( 'NONE',  ( 31.45873412500001010, 208.6250000013656063, 171.4326545832175555 ) ) ;
#62923 = PRODUCT_CONTEXT ( 'NONE', #54403, 'mechanical' ) ;
#62924 = AXIS2_PLACEMENT_3D ( 'NONE', #1384, #12313, #47375 ) ;
#62925 = EDGE_LOOP ( 'NONE', ( #61899, #9825, #33475, #9885 ) ) ;
#62926 = CARTESIAN_POINT ( 'NONE',  ( -5.676582343750000703, 233.3854166700806729, -9.832129032723418760 ) ) ;
#62927 = EDGE_CURVE ( 'NONE', #64213, #34184, #39232, .T. ) ;
#62928 = CARTESIAN_POINT ( 'NONE',  ( -4.401442555609577197E-16, 7.188101187499992051, 13.11155278187175277 ) ) ;
#62929 = ORIENTED_EDGE ( 'NONE', *, *, #62048, .T. ) ;
#62930 = VERTEX_POINT ( 'NONE', #4167 ) ;
#62931 = CARTESIAN_POINT ( 'NONE',  ( 4.220049686691941027, -10.18810118749999738, 72.62500000204836681 ) ) ;
#62932 = CARTESIAN_POINT ( 'NONE',  ( 5.676582343750001591, 91.92708332991935549, -9.832129032723420536 ) ) ;
#62933 = FACE_BOUND ( 'NONE', #25289, .T. ) ;
#62934 = CARTESIAN_POINT ( 'NONE',  ( 7.778174593052021635, 7.778174593052023411, 84.43749999999998579 ) ) ;
#62937 = CARTESIAN_POINT ( 'NONE',  ( 10.00000000000000533, 70.00000000000001421, 0.000000000000000000 ) ) ;
#62936 = CARTESIAN_POINT ( 'NONE',  ( 29.65685424949234772, 194.5625000027311842, 165.9999999999998863 ) ) ;
#62935 = CARTESIAN_POINT ( 'NONE',  ( 28.00000000000002132, 205.1875000013656063, 166.5412658749999082 ) ) ;
#62938 = DIRECTION ( 'NONE',  ( -1.000000000000000000, 0.000000000000000000, 0.000000000000000000 ) ) ;
#62939 = CARTESIAN_POINT ( 'NONE',  ( -4.898587196589412829E-16, 102.1250000000000000, -8.000000000000000000 ) ) ;
#62940 = CARTESIAN_POINT ( 'NONE',  ( 8.311093377946834337, 200.1562499965860695, 8.311093377946839666 ) ) ;
#62941 =( BOUNDED_CURVE ( )  B_SPLINE_CURVE ( 2, ( #25174, #64451, #31596, #12751, #37260, #14220, #71198, #13841, #1465 ),
 .UNSPECIFIED., .F., .F. ) 
 B_SPLINE_CURVE_WITH_KNOTS ( ( 3, 2, 2, 2, 3 ),
 ( 0.01666666666666679827, 0.02500000000000007772, 0.03333333333333335369, 0.04166666666666662966, 0.04999999999999991951 ),
 .UNSPECIFIED. ) 
 CURVE ( )  GEOMETRIC_REPRESENTATION_ITEM ( )  RATIONAL_B_SPLINE_CURVE ( ( 0.9999999999999988898, 0.9238795325112879597, 1.000000000000000000, 0.9238795325112867385, 1.000000000000000000, 0.9238795325112867385, 1.000000000000000000, 0.9238795325112875156, 0.9999999999999992228 ) ) 
 REPRESENTATION_ITEM ( '' )  );
#62942 = CARTESIAN_POINT ( 'NONE',  ( -2.445694354108838731, 205.0625000013656063, 144.4456943541088663 ) ) ;
#62943 = CARTESIAN_POINT ( 'NONE',  ( 30.44569435410879166, 205.8125000013656063, 172.4456943541087526 ) ) ;
#62944 = CARTESIAN_POINT ( 'NONE',  ( 7.188101187499999156, 18.74999999795161898, 2.977408999572654924 ) ) ;
#62945 = CARTESIAN_POINT ( 'NONE',  ( 9.832129032723420536, 166.5104166632526983, -5.676582343749999815 ) ) ;
#62946 = DIRECTION ( 'NONE',  ( -0.000000000000000000, 1.000000000000000000, -0.000000000000000000 ) ) ;
#62947 = CARTESIAN_POINT ( 'NONE',  ( 5.082755093536325042, 102.9687500020483810, -5.082755093536325930 ) ) ;
#62948 = CARTESIAN_POINT ( 'NONE',  ( 2.828427124746191623, 17.87499999726881583, -2.828427124746191623 ) ) ;
#62949 = CARTESIAN_POINT ( 'NONE',  ( 3.211159895383560947, 10.18749999863440614, 3.211159895383562723 ) ) ;
#62950 = CARTESIAN_POINT ( 'NONE',  ( 28.00000000000002132, 203.1875000013656063, 166.5412658749999082 ) ) ;
#62951 = CARTESIAN_POINT ( 'NONE',  ( -7.188101187499991163, 2.977408999572646930, 9.267802781871756324 ) ) ;
#62952 = CARTESIAN_POINT ( 'NONE',  ( 11.35316468749999963, 55.98958332991934128, -3.042071309553165293 ) ) ;
#62953 = B_SPLINE_CURVE_WITH_KNOTS ( 'NONE', 3,
 ( #22316, #44607, #38948, #56681, #51749, #67621, #51374, #10277, #33304, #67985, #32934, #55940, #56302, #27239, #62320, #50626, #4618, #11390, #57428, #45342 ),
 .UNSPECIFIED., .F., .F.,
 ( 4, 2, 2, 2, 2, 2, 2, 2, 2, 4 ),
 ( 0.000000000000000000, 0.001156441540183989576, 0.001734662310275984038, 0.002312883080367979152, 0.003469324620551983689, 0.004625766160735988661, 0.005782207700919994066, 0.006938649241103998604, 0.008095090781288004009, 0.009251532321472008547 ),
 .UNSPECIFIED. ) ;
#62954 = CARTESIAN_POINT ( 'NONE',  ( -12.00000000000000178, -1.170752406943654123, -5.082197683525801418E-17 ) ) ;
#62955 = CARTESIAN_POINT ( 'NONE',  ( -3.313708498984757167, 7.999999999999991118, 0.6053027843298234290 ) ) ;
#62956 = ORIENTED_EDGE ( 'NONE', *, *, #59349, .T. ) ;
#62957 = CARTESIAN_POINT ( 'NONE',  ( -2.250000000000000888, 2.250000000000000000, 0.000000000000000000 ) ) ;
#62958 = CARTESIAN_POINT ( 'NONE',  ( -5.656854249492379694, 22.87499999590322375, -5.656854249492380582 ) ) ;
#62959 = CARTESIAN_POINT ( 'NONE',  ( 8.311093377946834337, 60.15624999658601979, 8.311093377946839666 ) ) ;
#62960 = CARTESIAN_POINT ( 'NONE',  ( -4.556349186104045934, 11.00000000000000000, 72.90625000409677625 ) ) ;
#62961 = CARTESIAN_POINT ( 'NONE',  ( -2.839093476692135984E-14, 199.9375000013656063, 138.5412658750000503 ) ) ;
#62962 = CARTESIAN_POINT ( 'NONE',  ( -30.99999999999992895, -31.99999999999978684, 205.0000000000000284 ) ) ;
#62963 = CARTESIAN_POINT ( 'NONE',  ( -5.000000000000005329, 13.33333333333333570, 8.660254037844387298 ) ) ;
#62965 = CARTESIAN_POINT ( 'NONE',  ( 3.042071309553167513, 56.82291666325268409, -11.35316468749999785 ) ) ;
#62964 = CARTESIAN_POINT ( 'NONE',  ( -7.188101187500000044, 94.15625000204838102, 0.000000000000000000 ) ) ;
#62967 = EDGE_CURVE ( 'NONE', #6496, #7001, #27905, .T. ) ;
#62966 = CARTESIAN_POINT ( 'NONE',  ( 5.656854249492376141, -5.656854249492374365, 4.392802779823363757 ) ) ;
#62968 = CARTESIAN_POINT ( 'NONE',  ( 8.000000000000001776, 110.8437500040967763, 3.313708498984759387 ) ) ;
#62969 = CARTESIAN_POINT ( 'NONE',  ( 6.951808397369818766E-16, 172.0312499965860411, -11.35316468750000141 ) ) ;
#62970 = CARTESIAN_POINT ( 'NONE',  ( 2.679491924311222739, 135.8333333265053966, 10.00000000000000355 ) ) ;
#62971 = VECTOR ( 'NONE', #20545, 1000.000000000000000 ) ;
#62972 = CARTESIAN_POINT ( 'NONE',  ( 2.977408999572654480, 99.50000000204838102, 7.188101187499999156 ) ) ;
#62973 = CARTESIAN_POINT ( 'NONE',  ( 5.000000000000006217, 20.83333333333333925, -8.660254037844392627 ) ) ;
#62974 = CARTESIAN_POINT ( 'NONE',  ( 9.832129032723416984, 50.67708332991935549, 5.676582343750006032 ) ) ;
#62975 = EDGE_CURVE ( 'NONE', #38953, #30969, #70873, .T. ) ;
#62976 = CARTESIAN_POINT ( 'NONE',  ( 2.485281374238950125, 295.3750000034140726, 5.999999999999625189 ) ) ;
#62977 = CARTESIAN_POINT ( 'NONE',  ( -11.35316468749999785, 178.0729166632526415, -3.042071309553167513 ) ) ;
#62978 = ORIENTED_EDGE ( 'NONE', *, *, #2836, .T. ) ;
#62979 = CARTESIAN_POINT ( 'NONE',  ( 49.52045638478374201, 137.0487294222377841, 58.38971101614417591 ) ) ;
#62980 = CARTESIAN_POINT ( 'NONE',  ( -10.18810118749999916, 4.220049686691934809, 69.06250000204839523 ) ) ;
#62981 = CARTESIAN_POINT ( 'NONE',  ( 1.656854249492405451, 195.3125000000000853, 202.0000000000000284 ) ) ;
#62982 = CARTESIAN_POINT ( 'NONE',  ( 5.656854249492380582, 16.68750000000000355, -5.656854249492380582 ) ) ;
#62984 = CARTESIAN_POINT ( 'NONE',  ( 5.676582343750001591, 181.6145833299193555, -9.832129032723420536 ) ) ;
#62983 = CARTESIAN_POINT ( 'NONE',  ( 5.000000000000000000, 60.11723469343148452, -46.25570701698029552 ) ) ;
#62985 = CARTESIAN_POINT ( 'NONE',  ( -3.313708498984758943, -7.999999999999989342, 7.167802784329822430 ) ) ;
#62986 = AXIS2_PLACEMENT_3D ( 'NONE', #48858, #8505, #59097 ) ;
#62987 = DIRECTION ( 'NONE',  ( 0.000000000000000000, 0.7071067811865469066, 0.7071067811865482389 ) ) ;
#62988 = CARTESIAN_POINT ( 'NONE',  ( -2.679491924311228512, 262.0833333401612322, -9.999999999999998224 ) ) ;
#62989 = DIRECTION ( 'NONE',  ( -0.000000000000000000, 1.000000000000000000, -0.000000000000000000 ) ) ;
#62990 = ORIENTED_EDGE ( 'NONE', *, *, #62191, .F. ) ;
#62991 = EDGE_CURVE ( 'NONE', #50952, #2727, #13881, .T. ) ;
#62992 = CARTESIAN_POINT ( 'NONE',  ( -2.775557561562891351E-14, 210.0000000000000284, 142.0000000000000568 ) ) ;
#62993 = CARTESIAN_POINT ( 'NONE',  ( 9.832129032723420536, 116.5104166632526841, -5.676582343749999815 ) ) ;
#62994 = DIRECTION ( 'NONE',  ( 0.000000000000000000, 0.000000000000000000, 1.000000000000000000 ) ) ;
#62995 = EDGE_LOOP ( 'NONE', ( #39474, #38520, #71653, #59512 ) ) ;
#62996 = CARTESIAN_POINT ( 'NONE',  ( 4.541265875000002339, 6.499999998634407028, -1.881053915767121554 ) ) ;
#62997 = CARTESIAN_POINT ( 'NONE',  ( 7.188101187500000044, 15.46874999795161187, 0.000000000000000000 ) ) ;
#62998 = CARTESIAN_POINT ( 'NONE',  ( 1.469576158976823947E-15, 110.5625000040967905, 8.000000000000000000 ) ) ;
#62999 = CARTESIAN_POINT ( 'NONE',  ( -30.44569435410883429, 198.8125000013656063, 167.5543056458915885 ) ) ;
#63000 = ADVANCED_FACE ( 'NONE', ( #55850 ), #50539, .F. ) ;
#63001 = CARTESIAN_POINT ( 'NONE',  ( 2.449293598294707893E-16, 7.250000000000000000, -4.000000000000001776 ) ) ;
#63002 = CARTESIAN_POINT ( 'NONE',  ( 1.656854249492381248, 21.93749999726881228, -4.000000000000001776 ) ) ;
#63003 = CARTESIAN_POINT ( 'NONE',  ( 1.881053915767122664, 12.12499999863440792, 4.541265875000001451 ) ) ;
#63004 = CARTESIAN_POINT ( 'NONE',  ( 1.656854249492348607, 198.1875000000000853, 138.0000000000000568 ) ) ;
#63005 = VERTEX_POINT ( 'NONE', #16191 ) ;
#63006 = CARTESIAN_POINT ( 'NONE',  ( -7.999999999953861796, 1.809871347124574913E-05, 10.01712378708029938 ) ) ;
#63007 = CARTESIAN_POINT ( 'NONE',  ( 2.977408999572650039, 104.1875000020483668, -7.188101187500001821 ) ) ;
#63009 = DIRECTION ( 'NONE',  ( 0.000000000000000000, 0.000000000000000000, -1.000000000000000000 ) ) ;
#63008 = CARTESIAN_POINT ( 'NONE',  ( -25.55430564589111597, 195.0625000013656063, 172.4456943541091505 ) ) ;
#63010 = CARTESIAN_POINT ( 'NONE',  ( -4.000000000000001776, 10.43750000000000000, -1.656854249492381470 ) ) ;
#63011 = CARTESIAN_POINT ( 'NONE',  ( -5.082755093536319713, 5.082755093536319713, 1.299052781871753215 ) ) ;
#63012 = VERTEX_POINT ( 'NONE', #68271 ) ;
#63013 = ORIENTED_EDGE ( 'NONE', *, *, #26511, .F. ) ;
#63014 = CARTESIAN_POINT ( 'NONE',  ( 4.220049686691941027, -10.18810118749999738, 90.62500000204836681 ) ) ;
#63015 = DIRECTION ( 'NONE',  ( 0.000000000000000000, 0.000000000000000000, 1.000000000000000000 ) ) ;
#63016 = CARTESIAN_POINT ( 'NONE',  ( -4.898587196589412829E-16, 109.8125000040967905, -8.000000000000000000 ) ) ;
#63017 = CARTESIAN_POINT ( 'NONE',  ( 2.020667218593132706E-15, -11.00000000000000000, 103.3750000000000000 ) ) ;
#63018 = CARTESIAN_POINT ( 'NONE',  ( 2.445694354108839175, 203.3125000013656063, 195.5543056458912190 ) ) ;
#63020 = FACE_OUTER_BOUND ( 'NONE', #67228, .T. ) ;
#63019 = DIRECTION ( 'NONE',  ( 0.000000000000000000, 0.000000000000000000, 1.000000000000000000 ) ) ;
#63021 = CARTESIAN_POINT ( 'NONE',  ( 7.320508075688774596, 120.6250000000000284, -7.320508075688774596 ) ) ;
#63022 = VECTOR ( 'NONE', #47664, 1000.000000000000000 ) ;
#63023 = CARTESIAN_POINT ( 'NONE',  ( -7.999999999999998224, 104.0937500000000284, 3.313708498984766493 ) ) ;
#63024 = CARTESIAN_POINT ( 'NONE',  ( 1.226468279477575784E-15, 289.8593750017070079, 6.676582343750001591 ) ) ;
#63025 = CARTESIAN_POINT ( 'NONE',  ( 5.082755093536320601, -5.082755093536318824, 6.924052781871754547 ) ) ;
#63026 = CARTESIAN_POINT ( 'NONE',  ( 4.000000000000015987, 200.5625000000000284, 196.3431457505076594 ) ) ;
#63027 = CARTESIAN_POINT ( 'NONE',  ( 31.45873412500001010, 208.7500000013656063, 168.5673454167822740 ) ) ;
#63028 = CARTESIAN_POINT ( 'NONE',  ( 8.000000000000000000, 25.40624999590323085, -3.313708498984761608 ) ) ;
#63029 = CARTESIAN_POINT ( 'NONE',  ( 1.432654583217607192, 201.2500000013656063, 145.4587341250000634 ) ) ;
#63030 = CARTESIAN_POINT ( 'NONE',  ( 7.188101187500000933, 119.3750000020483810, -2.977408999572651371 ) ) ;
#63032 = CARTESIAN_POINT ( 'NONE',  ( -18.89444362769118158, -70.00000000000001421, 171.9999999999997442 ) ) ;
#63031 = FILL_AREA_STYLE_COLOUR ( '', #58864 ) ;
#63033 = CARTESIAN_POINT ( 'NONE',  ( -8.311093377946836114, 238.5937500034139589, -8.311093377946836114 ) ) ;
#63034 = CARTESIAN_POINT ( 'NONE',  ( 5.082755093536320601, -5.082755093536318824, 27.92405278187175455 ) ) ;
#63036 =( BOUNDED_CURVE ( )  B_SPLINE_CURVE ( 2, ( #41010, #69305, #40260, #35365, #11222, #34251, #57252, #29685, #17616, #669, #17992, #12689, #34622 ),
 .UNSPECIFIED., .F., .F. ) 
 B_SPLINE_CURVE_WITH_KNOTS ( ( 3, 2, 2, 2, 2, 2, 3 ),
 ( 0.1902173913043478104, 0.1920289855072463414, 0.1938405797101449279, 0.1956521739130434867, 0.1974637681159420177, 0.1992753623188406042, 0.2010869565217391630 ),
 .UNSPECIFIED. ) 
 CURVE ( )  GEOMETRIC_REPRESENTATION_ITEM ( )  RATIONAL_B_SPLINE_CURVE ( ( 1.000000000000000444, 0.9659258262890677571, 1.000000000000000000, 0.9659258262890683122, 1.000000000000000000, 0.9659258262890683122, 1.000000000000000000, 0.9659258262890683122, 1.000000000000000000, 0.9659258262890683122, 1.000000000000000000, 0.9659258262890677571, 1.000000000000000444 ) ) 
 REPRESENTATION_ITEM ( '' )  );
#63035 = CARTESIAN_POINT ( 'NONE',  ( 30.82842712474617031, 199.1250000000000284, 172.8284271247460993 ) ) ;
#63037 = CARTESIAN_POINT ( 'NONE',  ( 11.35316468749999785, 15.57291666325268409, 3.042071309553174174 ) ) ;
#63038 = CARTESIAN_POINT ( 'NONE',  ( -5.082755093536319713, 5.082755093536319713, 1.674052781871753659 ) ) ;
#63039 = CARTESIAN_POINT ( 'NONE',  ( 3.042071309553159519, 205.0520833299193271, 11.35316468750000141 ) ) ;
#63040 = CARTESIAN_POINT ( 'NONE',  ( -26.34314575050764162, 197.9375000000000000, 166.0000000000003695 ) ) ;
#63041 = CARTESIAN_POINT ( 'NONE',  ( 1.469576158976823947E-15, 123.8750000000000000, 8.000000000000000000 ) ) ;
#63043 = CARTESIAN_POINT ( 'NONE',  ( -10.00000000000016698, 42.70833333333342097, 2.679491924311266704 ) ) ;
#63042 = CARTESIAN_POINT ( 'NONE',  ( -24.00000000000000711, 205.8125000000000000, 168.3431457505080289 ) ) ;
#63044 = VERTEX_POINT ( 'NONE', #10189 ) ;
#63045 = CARTESIAN_POINT ( 'NONE',  ( 3.458734124999959469, 199.7500000013656063, 140.5673454167824161 ) ) ;
#63046 = CARTESIAN_POINT ( 'NONE',  ( -5.676582343750006032, 19.11458332991934839, 9.832129032723418760 ) ) ;
#63047 = CARTESIAN_POINT ( 'NONE',  ( 2.020667218593132706E-15, -11.00000000000000000, 90.06250000409676204 ) ) ;
#63048 = CARTESIAN_POINT ( 'NONE',  ( 8.660254037844389075, 227.0833333333333712, 4.999999999999997335 ) ) ;
#63049 = CARTESIAN_POINT ( 'NONE',  ( -24.54126587500001833, 199.2500000013656063, 168.5673454167826435 ) ) ;
#63050 = CARTESIAN_POINT ( 'NONE',  ( -1.469576158976823947E-15, 6.937499995903221084, 8.000000000000000000 ) ) ;
#63052 = CARTESIAN_POINT ( 'NONE',  ( 3.042071309553159519, 14.73958332991935194, 11.35316468750000141 ) ) ;
#63051 = CARTESIAN_POINT ( 'NONE',  ( -7.188101187500000044, 110.6562500020483810, 0.000000000000000000 ) ) ;
#63054 = EDGE_CURVE ( 'NONE', #66240, #64014, #17275, .T. ) ;
#63053 = CARTESIAN_POINT ( 'NONE',  ( -5.656854249492373476, -5.656854249492376141, 22.01780277982336997 ) ) ;
#63055 = CARTESIAN_POINT ( 'NONE',  ( 11.35316468750000141, 130.7812499965860127, 0.000000000000000000 ) ) ;
#63056 = CARTESIAN_POINT ( 'NONE',  ( 2.679491924311222739, 100.8333333265053540, 10.00000000000000355 ) ) ;
#63057 = CARTESIAN_POINT ( 'NONE',  ( 2.977408999572654480, 120.5000000020483810, 7.188101187499999156 ) ) ;
#63058 = DIRECTION ( 'NONE',  ( 0.000000000000000000, 0.000000000000000000, 1.000000000000000000 ) ) ;
#63059 = CARTESIAN_POINT ( 'NONE',  ( -26.56734541678232731, 207.2500000013655779, 173.4587341250003760 ) ) ;
#63060 = CARTESIAN_POINT ( 'NONE',  ( -5.000000000000000000, -53.09993190648242489, -43.73864582539253831 ) ) ;
#63061 = VERTEX_POINT ( 'NONE', #31565 ) ;
#63062 = CARTESIAN_POINT ( 'NONE',  ( -8.660254037844392627, 117.9166666666666856, 5.000000000000000888 ) ) ;
#63063 = EDGE_CURVE ( 'NONE', #17476, #5945, #52244, .T. ) ;
#63064 =( BOUNDED_CURVE ( )  B_SPLINE_CURVE ( 2, ( #43270, #58154, #6820, #37631, #8951, #12470, #72319, #19885, #23799 ),
 .UNSPECIFIED., .F., .F. ) 
 B_SPLINE_CURVE_WITH_KNOTS ( ( 3, 2, 2, 2, 3 ),
 ( 0.7812500000000001110, 0.7864583333333334814, 0.7916666666666667407, 0.7968750000000001110, 0.8020833333333334814 ),
 .UNSPECIFIED. ) 
 CURVE ( )  GEOMETRIC_REPRESENTATION_ITEM ( )  RATIONAL_B_SPLINE_CURVE ( ( 0.9999999999999983347, 0.9238795325112884038, 1.000000000000000000, 0.9238795325112867385, 1.000000000000000000, 0.9238795325112867385, 1.000000000000000000, 0.9238795325112850731, 1.000000000000001554 ) ) 
 REPRESENTATION_ITEM ( '' )  );
#63065 = DIRECTION ( 'NONE',  ( -0.000000000000000000, 1.000000000000000000, -0.000000000000000000 ) ) ;
#63066 = CARTESIAN_POINT ( 'NONE',  ( -4.721056650415998313, 287.7343750017069510, 4.721056650416000089 ) ) ;
#63067 = CARTESIAN_POINT ( 'NONE',  ( 3.042071309553159519, 129.7395833299193555, 11.35316468750000141 ) ) ;
#63068 = DIRECTION ( 'NONE',  ( 0.000000000000000000, 0.000000000000000000, 1.000000000000000000 ) ) ;
#63069 = CARTESIAN_POINT ( 'NONE',  ( 5.656854249492376141, -5.656854249492374365, 22.44905278432982243 ) ) ;
#63070 = CARTESIAN_POINT ( 'NONE',  ( 0.4369882809721245542, 67.59332269700051654, 20.03478791450397978 ) ) ;
#63071 = CARTESIAN_POINT ( 'NONE',  ( 11.35316468749999963, 256.1979166700806445, 3.042071309553159519 ) ) ;
#63072 = CARTESIAN_POINT ( 'NONE',  ( -7.204075437095967871, 7.204075437095967871, 97.84375000204836681 ) ) ;
#63073 = ORIENTED_EDGE ( 'NONE', *, *, #28326, .T. ) ;
#63074 = CARTESIAN_POINT ( 'NONE',  ( -1.836970198721029983E-15, 215.6249999931720538, 10.00000000000000178 ) ) ;
#63075 = CARTESIAN_POINT ( 'NONE',  ( 11.00000000000000000, 4.556349186104045934, 97.84375000000000000 ) ) ;
#63076 = CARTESIAN_POINT ( 'NONE',  ( -3.458734124999960358, 203.6250000013656063, 196.5673454167823877 ) ) ;
#63077 = CARTESIAN_POINT ( 'NONE',  ( -5.676582343750006032, 79.42708332991935549, 9.832129032723418760 ) ) ;
#63078 = ORIENTED_EDGE ( 'NONE', *, *, #42912, .F. ) ;
#63079 = CARTESIAN_POINT ( 'NONE',  ( -10.18810118749999916, 4.220049686691934809, 108.0625000020483810 ) ) ;
#63080 = CARTESIAN_POINT ( 'NONE',  ( -3.211159895383562723, 11.06249999863440792, 3.211159895383561391 ) ) ;
#63081 = VERTEX_POINT ( 'NONE', #25880 ) ;
#63082 = AXIS2_PLACEMENT_3D ( 'NONE', #43732, #27494, #50507 ) ;
#63083 = CARTESIAN_POINT ( 'NONE',  ( -2.977408999572650039, 24.93749999795161543, -7.188101187500001821 ) ) ;
#63084 = CARTESIAN_POINT ( 'NONE',  ( 4.999999999999993783, 114.1666666666666998, 8.660254037844390851 ) ) ;
#63085 = CARTESIAN_POINT ( 'NONE',  ( -5.000000000000000000, -61.23620218020153771, -23.51718915682094391 ) ) ;
#63086 = CARTESIAN_POINT ( 'NONE',  ( 2.977408999572650927, 23.62499999795161543, -7.188101187500001821 ) ) ;
#63087 = DIRECTION ( 'NONE',  ( 0.000000000000000000, 0.000000000000000000, 1.000000000000000000 ) ) ;
#63088 = CARTESIAN_POINT ( 'NONE',  ( 10.18810118749999916, 4.220049686691935698, 106.3750000020483668 ) ) ;
#63089 = CARTESIAN_POINT ( 'NONE',  ( 4.000000000000015987, 204.5000000000000284, 198.0000000000000284 ) ) ;
#63090 = CARTESIAN_POINT ( 'NONE',  ( -2.828427124746190735, 11.12499999726881406, -2.828427124746191623 ) ) ;
#63091 = CARTESIAN_POINT ( 'NONE',  ( -2.849036369511732440E-14, 208.3750000027312126, 138.0000000000000568 ) ) ;
#63092 = ORIENTED_EDGE ( 'NONE', *, *, #55588, .F. ) ;
#63093 = DIRECTION ( 'NONE',  ( -0.000000000000000000, -0.000000000000000000, 1.000000000000000000 ) ) ;
#63094 = CARTESIAN_POINT ( 'NONE',  ( 2.754378923186476579E-14, 203.1875000013656063, 194.5412658750000219 ) ) ;
#63095 =( REPRESENTATION_RELATIONSHIP ('NONE','NONE', #46008, #30147 ) REPRESENTATION_RELATIONSHIP_WITH_TRANSFORMATION ( #47422 )SHAPE_REPRESENTATION_RELATIONSHIP( ) );
#63096 = CARTESIAN_POINT ( 'NONE',  ( -28.00000000000007461, 206.4375000013656063, 166.5412658750003629 ) ) ;
#63097 = CARTESIAN_POINT ( 'NONE',  ( 0.000000000000000000, 0.000000000000000000, 0.000000000000000000 ) ) ;
#63098 = CARTESIAN_POINT ( 'NONE',  ( 1.881053915767121776, 8.499999998634406140, -4.541265875000002339 ) ) ;
#63099 = CARTESIAN_POINT ( 'NONE',  ( 2.828427124746191623, 0.1250000000000001943, -2.828427124746191623 ) ) ;
#63100 = CARTESIAN_POINT ( 'NONE',  ( -2.977408999572647819, 7.188101187499991163, 17.70530278187175455 ) ) ;
#63101 = ORIENTED_EDGE ( 'NONE', *, *, #24034, .T. ) ;
#63102 = CYLINDRICAL_SURFACE ( 'NONE', #2400, 8.000000000000000000 ) ;
#63103 = EDGE_LOOP ( 'NONE', ( #8898, #36340, #9133, #15791 ) ) ;
#63104 = CARTESIAN_POINT ( 'NONE',  ( -10.18810118749999916, 0.000000000000000000, 109.6562500020483668 ) ) ;
#63105 = DIRECTION ( 'NONE',  ( 0.000000000000000000, 0.000000000000000000, 1.000000000000000000 ) ) ;
#63106 = CARTESIAN_POINT ( 'NONE',  ( 2.445694354108838731, 200.0625000013656063, 195.5543056458912190 ) ) ;
#63107 = CARTESIAN_POINT ( 'NONE',  ( 26.56734541678237349, 196.3750000013656063, 173.4587341249998929 ) ) ;
#63108 = CARTESIAN_POINT ( 'NONE',  ( -10.00000000000000178, 77.50000000000000000, -1.224646799147353454E-15 ) ) ;
#63109 = CARTESIAN_POINT ( 'NONE',  ( 8.000000000000000000, 122.8437500000000142, -3.313708498984762496 ) ) ;
#63110 = CARTESIAN_POINT ( 'NONE',  ( -2.485281374238572649, 290.1875000000000000, 6.000000000000002665 ) ) ;
#63111 = ORIENTED_EDGE ( 'NONE', *, *, #4551, .T. ) ;
#63112 = EDGE_CURVE ( 'NONE', #48435, #40745, #48899, .T. ) ;
#63113 = CARTESIAN_POINT ( 'NONE',  ( 6.000000000000001776, 294.5000000000000000, -7.347880794884121708E-16 ) ) ;
#63114 = CARTESIAN_POINT ( 'NONE',  ( 7.999999999999991118, 9.797174393178815797E-16, 7.580302779823366421 ) ) ;
#63115 = CARTESIAN_POINT ( 'NONE',  ( -4.000000000000015099, 195.6875000027312126, 143.6568542494924543 ) ) ;
#63116 = CARTESIAN_POINT ( 'NONE',  ( 1.224646799147353454E-15, 300.0000000000000000, -10.00000000000000178 ) ) ;
#63117 = CARTESIAN_POINT ( 'NONE',  ( -1.469576158976823947E-15, 5.437499995903221084, 8.000000000000000000 ) ) ;
#63118 = CARTESIAN_POINT ( 'NONE',  ( 2.679491924311235174, 236.4583333333333712, 9.999999999999998224 ) ) ;
#63119 = CARTESIAN_POINT ( 'NONE',  ( -6.000000000000003553, 292.9374999999999432, -2.485281374238571317 ) ) ;
#63120 = CARTESIAN_POINT ( 'NONE',  ( 7.204075437095968759, -7.204075437095966983, 68.59375000204836681 ) ) ;
#63121 = CARTESIAN_POINT ( 'NONE',  ( 5.000000000000001776, 195.8333333333333712, -8.660254037844389075 ) ) ;
#63122 = CARTESIAN_POINT ( 'NONE',  ( -5.082755093536317936, -5.082755093536320601, 15.54905278187175632 ) ) ;
#63123 = CARTESIAN_POINT ( 'NONE',  ( -3.042071309553173730, 174.6354166632526983, 11.35316468749999785 ) ) ;
#63124 = CARTESIAN_POINT ( 'NONE',  ( -1.836970198721029983E-15, 38.75000000000000000, 10.00000000000000178 ) ) ;
#63125 = CARTESIAN_POINT ( 'NONE',  ( 0.000000000000000000, 125.0000000000000000, 0.000000000000000000 ) ) ;
#63127 = DIRECTION ( 'NONE',  ( -0.000000000000000000, -1.000000000000000000, -4.283267841918042741E-17 ) ) ;
#63126 =( NAMED_UNIT ( * ) SI_UNIT ( $, .STERADIAN. ) SOLID_ANGLE_UNIT ( ) );
#63128 = EDGE_LOOP ( 'NONE', ( #27486, #11622 ) ) ;
#63129 = VECTOR ( 'NONE', #13050, 1000.000000000000000 ) ;
#63130 = CARTESIAN_POINT ( 'NONE',  ( -3.458734125000015425, 196.9375000013655779, 142.0000000000000568 ) ) ;
#63131 = CARTESIAN_POINT ( 'NONE',  ( -9.832129032723418760, 33.17708332991934839, -5.676582343750004256 ) ) ;
#63132 = CARTESIAN_POINT ( 'NONE',  ( -11.00000000000000000, 4.556349186104045934, 113.5937500040967763 ) ) ;
#63133 = CARTESIAN_POINT ( 'NONE',  ( -0.2097676960538938096, 194.5981977461298982, 201.5981977461299266 ) ) ;
#63134 = CARTESIAN_POINT ( 'NONE',  ( 0.000000000000000000, 300.0000000000000000, 0.000000000000000000 ) ) ;
#63136 = CARTESIAN_POINT ( 'NONE',  ( -1.780377099652985740, -16.42166210098330126, -68.70754022607323463 ) ) ;
#63135 = CARTESIAN_POINT ( 'NONE',  ( -8.000000000000000000, 116.0937500040968047, -3.313708498984761164 ) ) ;
#63137 = CARTESIAN_POINT ( 'NONE',  ( -26.33690751513206862, -51.48256987955153363, 186.4603727062550149 ) ) ;
#63139 = EDGE_CURVE ( 'NONE', #34804, #36674, #19287, .T. ) ;
#63138 = CARTESIAN_POINT ( 'NONE',  ( -2.754378923186476579E-14, 198.1875000013655779, 145.4587341250000350 ) ) ;
#63140 = CARTESIAN_POINT ( 'NONE',  ( 7.320508075688771044, 66.24999999317203958, 7.320508075688775484 ) ) ;
#63141 = CARTESIAN_POINT ( 'NONE',  ( -4.401442555609581635E-16, 105.7812500020483810, -7.188101187500000044 ) ) ;
#63142 = CARTESIAN_POINT ( 'NONE',  ( -8.342170076843785083E-16, 11.18749999863440792, 4.541265875000002339 ) ) ;
#63143 = CARTESIAN_POINT ( 'NONE',  ( 10.00000000000005329, 65.00000000000004263, 0.000000000000000000 ) ) ;
#63144 = CARTESIAN_POINT ( 'NONE',  ( -5.656854249492375253, 5.656854249492375253, 3.642802779823362869 ) ) ;
#63145 = EDGE_CURVE ( 'NONE', #23527, #2698, #65475, .T. ) ;
#63146 = FACE_OUTER_BOUND ( 'NONE', #34741, .T. ) ;
#63147 = ORIENTED_EDGE ( 'NONE', *, *, #44925, .T. ) ;
#63148 = ORIENTED_EDGE ( 'NONE', *, *, #2307, .T. ) ;
#63149 = CARTESIAN_POINT ( 'NONE',  ( 7.999999999999991118, 9.797174393178815797E-16, 10.58030277982336465 ) ) ;
#63150 = CARTESIAN_POINT ( 'NONE',  ( -2.765530957081998586, 295.7968750017070079, 6.676582343750001591 ) ) ;
#63151 = DIRECTION ( 'NONE',  ( -0.000000000000000000, -0.000000000000000000, -1.000000000000000000 ) ) ;
#63152 = CARTESIAN_POINT ( 'NONE',  ( -30.44412544322928937, -42.98707962279937789, 164.0729259327612510 ) ) ;
#63153 = CARTESIAN_POINT ( 'NONE',  ( -9.832129032723420536, 148.6979166632526983, 5.676582343749997150 ) ) ;
#63154 = CARTESIAN_POINT ( 'NONE',  ( 0.000000000000000000, 0.000000000000000000, -1.155342438046016218 ) ) ;
#63155 = CARTESIAN_POINT ( 'NONE',  ( 10.18810118749999916, 1.247682550866122264E-15, 83.40625000204838102 ) ) ;
#63156 = CARTESIAN_POINT ( 'NONE',  ( 2.751064625579944321E-14, 207.7500000000000284, 194.0000000000000568 ) ) ;
#63157 = CARTESIAN_POINT ( 'NONE',  ( 1.656854249492403008, 202.6875000000000284, 194.0000000000000853 ) ) ;
#63158 = CARTESIAN_POINT ( 'NONE',  ( 3.499857865026532622, -7.193933550196781823, 0.0006324257780546024528 ) ) ;
#63159 = CARTESIAN_POINT ( 'NONE',  ( -10.18810118749999738, -4.220049686691941915, 113.1250000020483810 ) ) ;
#63160 = EDGE_LOOP ( 'NONE', ( #14449, #68014, #40818, #69900 ) ) ;
#63161 =( BOUNDED_CURVE ( )  B_SPLINE_CURVE ( 2, ( #59996, #8313, #60745, #31324, #37364, #2660, #9068, #25652, #48667 ),
 .UNSPECIFIED., .F., .F. ) 
 B_SPLINE_CURVE_WITH_KNOTS ( ( 3, 2, 2, 2, 3 ),
 ( 0.8333333333333340365, 0.8416666666666673402, 0.8500000000000006439, 0.8583333333333339477, 0.8666666666666673624 ),
 .UNSPECIFIED. ) 
 CURVE ( )  GEOMETRIC_REPRESENTATION_ITEM ( )  RATIONAL_B_SPLINE_CURVE ( ( 0.9999999999999938938, 0.9238795325112928447, 1.000000000000000000, 0.9238795325112867385, 1.000000000000000000, 0.9238795325112867385, 1.000000000000000000, 0.9238795325112806323, 1.000000000000005995 ) ) 
 REPRESENTATION_ITEM ( '' )  );
#63162 = DIRECTION ( 'NONE',  ( 0.000000000000000000, 0.000000000000000000, 1.000000000000000000 ) ) ;
#63163 = VECTOR ( 'NONE', #63746, 1000.000000000000000 ) ;
#63164 = CARTESIAN_POINT ( 'NONE',  ( 8.698841371902224395, 177.8514410235502226, 140.1637119819842496 ) ) ;
#63165 = CARTESIAN_POINT ( 'NONE',  ( -11.35316468750000141, 133.8020833299193555, 3.042071309553159963 ) ) ;
#63166 = CARTESIAN_POINT ( 'NONE',  ( 3.458734125000015425, 203.9375000013656063, 198.0000000000000284 ) ) ;
#63167 = CARTESIAN_POINT ( 'NONE',  ( 4.401442555609581635E-16, 23.71874999795161543, -7.188101187500000044 ) ) ;
#63168 = CARTESIAN_POINT ( 'NONE',  ( 4.220049686691941027, -10.18810118749999738, 74.50000000204838102 ) ) ;
#63169 = CARTESIAN_POINT ( 'NONE',  ( -5.676582343749998039, 32.76041666325269119, -9.832129032723420536 ) ) ;
#63170 = ORIENTED_EDGE ( 'NONE', *, *, #44972, .F. ) ;
#63171 = CARTESIAN_POINT ( 'NONE',  ( 6.123233995736767268E-16, 26.25000000000000355, -10.00000000000000178 ) ) ;
#63172 = CARTESIAN_POINT ( 'NONE',  ( 1.881053915767121998, 1.624999998634407028, -4.541265875000002339 ) ) ;
#63173 = CARTESIAN_POINT ( 'NONE',  ( 8.008118988124991233, 3.317071493978879015, 13.85686528394062833 ) ) ;
#63174 = CARTESIAN_POINT ( 'NONE',  ( 1.432654583217607414, 205.5000000013655779, 145.4587341250000634 ) ) ;
#63175 = CARTESIAN_POINT ( 'NONE',  ( 7.188101187500000044, 6.468749997951610986, 0.000000000000000000 ) ) ;
#63176 = CARTESIAN_POINT ( 'NONE',  ( -6.000000000000001776, 296.0625000034140157, 0.000000000000000000 ) ) ;
#63177 = CARTESIAN_POINT ( 'NONE',  ( -7.188101187500000044, 4.593749997951610098, -8.802885111219163269E-16 ) ) ;
#63178 = CARTESIAN_POINT ( 'NONE',  ( -11.35316468749999785, 158.3854166632526699, -3.042071309553167513 ) ) ;
#63179 = CARTESIAN_POINT ( 'NONE',  ( -6.238412754330611322E-16, 10.18810118749999916, 70.28125000204838102 ) ) ;
#63180 = CARTESIAN_POINT ( 'NONE',  ( -31.45873412500001010, 207.8750000013656063, 168.5673454167827572 ) ) ;
#63181 = CARTESIAN_POINT ( 'NONE',  ( 27.99999999999999645, 210.0000000000000284, 169.9999999999999147 ) ) ;
#63182 = CARTESIAN_POINT ( 'NONE',  ( -4.541265875000003227, 20.99999999863440792, 1.881053915767121110 ) ) ;
#63183 = ORIENTED_EDGE ( 'NONE', *, *, #25066, .F. ) ;
#63184 = CARTESIAN_POINT ( 'NONE',  ( 2.751064625579944321E-14, 199.8750000027312126, 194.0000000000000568 ) ) ;
#63185 = CARTESIAN_POINT ( 'NONE',  ( -2.849036369511732440E-14, 206.2500000000000284, 138.0000000000000568 ) ) ;
#63186 = CARTESIAN_POINT ( 'NONE',  ( -23.99999999999998934, 200.8750000027312126, 170.0000000000002842 ) ) ;
#63187 = CARTESIAN_POINT ( 'NONE',  ( 0.000000000000000000, 300.0000000000000000, 10.00000000000000178 ) ) ;
#63188 = CARTESIAN_POINT ( 'NONE',  ( -4.898587196589407898E-16, 7.999999999999991118, 9.642802783920146226 ) ) ;
#63189 = ORIENTED_EDGE ( 'NONE', *, *, #55005, .T. ) ;
#63190 = CARTESIAN_POINT ( 'NONE',  ( 5.082755093536325930, 20.15624999795161543, -5.082755093536325930 ) ) ;
#63191 = CARTESIAN_POINT ( 'NONE',  ( -2.485281374238979879, 297.8750000034140157, -5.999999999999594991 ) ) ;
#63192 = CARTESIAN_POINT ( 'NONE',  ( -3.369429374625494411, -10.27270496052241100, -63.91910092334655502 ) ) ;
#63193 = CARTESIAN_POINT ( 'NONE',  ( 5.000000000000001776, 45.83333333333333570, -8.660254037844389075 ) ) ;
#63194 = CARTESIAN_POINT ( 'NONE',  ( -7.188101187500001821, 106.4375000020483810, -2.977408999572650483 ) ) ;
#63195 = CARTESIAN_POINT ( 'NONE',  ( -28.00000000000002487, 209.6875000013656063, 166.5412658750003629 ) ) ;
#63196 = CARTESIAN_POINT ( 'NONE',  ( -2.485281374238571761, 298.8124999999999432, -6.000000000000003553 ) ) ;
#63198 = CARTESIAN_POINT ( 'NONE',  ( 11.00000000000000000, 1.347111479062088405E-15, 73.93750000409676204 ) ) ;
#63197 = CARTESIAN_POINT ( 'NONE',  ( -25.17157287525377640, 201.6250000000000284, 172.8284271247465256 ) ) ;
#63199 = ORIENTED_EDGE ( 'NONE', *, *, #15876, .T. ) ;
#63200 = CARTESIAN_POINT ( 'NONE',  ( 11.35316468749999608, 241.6145833367473585, -3.042071309553167069 ) ) ;
#63201 = PRODUCT_DEFINITION_SHAPE ( 'NONE', 'NONE',  #74665 ) ;
#63202 = CARTESIAN_POINT ( 'NONE',  ( 7.188101187499992051, 8.802885111219154394E-16, 20.61155278187175455 ) ) ;
#63203 = AXIS2_PLACEMENT_3D ( 'NONE', #51994, #31942, #14572 ) ;
#63204 = CARTESIAN_POINT ( 'NONE',  ( -10.00000000000000000, 9.166666659838700326, -2.679491924311229845 ) ) ;
#63205 = CARTESIAN_POINT ( 'NONE',  ( -20.42802198618029408, 183.6788756342477313, 139.0000000000000568 ) ) ;
#63206 = CARTESIAN_POINT ( 'NONE',  ( -6.338291171875001240, 287.8046875008534471, 0.000000000000000000 ) ) ;
#63207 = CARTESIAN_POINT ( 'NONE',  ( 6.123233995736767268E-16, 166.2500000000000000, -10.00000000000000178 ) ) ;
#63208 = CARTESIAN_POINT ( 'NONE',  ( -11.00000000000000000, 0.000000000000000000, 80.49999999999998579 ) ) ;
#63209 = CARTESIAN_POINT ( 'NONE',  ( 5.656854249492381470, 91.06249999999998579, 5.656854249492379694 ) ) ;
#63210 = DIRECTION ( 'NONE',  ( -0.000000000000000000, 1.000000000000000000, 4.476705744456276341E-16 ) ) ;
#63211 = CARTESIAN_POINT ( 'NONE',  ( -3.042071309553173730, 124.6354166632526699, 11.35316468749999785 ) ) ;
#63212 = CARTESIAN_POINT ( 'NONE',  ( 25.17157287525381548, 198.6250000000000284, 167.1715728752537018 ) ) ;
#63213 = CARTESIAN_POINT ( 'NONE',  ( 13.99999999999999822, 2.143131898507868248E-15, 17.50000000000000000 ) ) ;
#63216 = CARTESIAN_POINT ( 'NONE',  ( 0.000000000000000000, 0.000000000000000000, 0.000000000000000000 ) ) ;
#63215 = CARTESIAN_POINT ( 'NONE',  ( 30.44569435410882718, 197.5625000013656063, 172.4456943541086957 ) ) ;
#63214 = CARTESIAN_POINT ( 'NONE',  ( 26.56734541678232375, 196.6250000013656063, 173.4587341249998929 ) ) ;
#63217 = ORIENTED_EDGE ( 'NONE', *, *, #24668, .T. ) ;
#63218 = EDGE_CURVE ( 'NONE', #54565, #56169, #44881, .T. ) ;
#63219 = CARTESIAN_POINT ( 'NONE',  ( -4.193070328474952646, -60.66867996115655615, 23.17096354272540282 ) ) ;
#63220 = CARTESIAN_POINT ( 'NONE',  ( 29.65685424949239746, 202.5625000027312410, 165.9999999999999432 ) ) ;
#63221 = CARTESIAN_POINT ( 'NONE',  ( 23.99999999999997513, 195.8125000027312410, 168.3431457505075457 ) ) ;
#63222 = DIRECTION ( 'NONE',  ( 0.000000000000000000, 0.000000000000000000, 1.000000000000000000 ) ) ;
#63223 = CARTESIAN_POINT ( 'NONE',  ( -11.35316468750000141, 223.5937499965860127, -1.390361679473963753E-15 ) ) ;
#63224 = CARTESIAN_POINT ( 'NONE',  ( 7.188101187500001821, 122.0000000020483668, -2.977408999572651371 ) ) ;
#63225 = CARTESIAN_POINT ( 'NONE',  ( 3.211159895383560947, 2.312499998634407028, 3.211159895383562723 ) ) ;
#63226 = CARTESIAN_POINT ( 'NONE',  ( -4.471435261918117909, 60.74652839096160761, -23.21845616858355399 ) ) ;
#63227 = CARTESIAN_POINT ( 'NONE',  ( -5.656854249492373476, -5.656854249492376141, 23.51780277982336642 ) ) ;
#63229 = CARTESIAN_POINT ( 'NONE',  ( -31.99999999999998579, 207.3125000000000284, 171.6568542494928238 ) ) ;
#63228 = PRESENTATION_STYLE_ASSIGNMENT (( #62482 ) ) ;
#63230 = CARTESIAN_POINT ( 'NONE',  ( 9.832129032723416984, 110.3645833299193555, 5.676582343750006032 ) ) ;
#63231 = ORIENTED_EDGE ( 'NONE', *, *, #21142, .T. ) ;
#63232 = CARTESIAN_POINT ( 'NONE',  ( -7.071067811865484387, 22.99999999999999645, -1.000000000000000000 ) ) ;
#63233 = CARTESIAN_POINT ( 'NONE',  ( 7.188101187500001821, 26.06249999795161543, -2.977408999572650483 ) ) ;
#63234 = DIRECTION ( 'NONE',  ( -1.000000000000000000, 0.000000000000000000, -0.000000000000000000 ) ) ;
#63235 = CARTESIAN_POINT ( 'NONE',  ( -5.676582343749992710, 250.0520833367473301, 9.832129032723422313 ) ) ;
#63236 = CARTESIAN_POINT ( 'NONE',  ( -2.085542519210945728E-15, 104.5312499965860269, 11.35316468750000141 ) ) ;
#63237 = ORIENTED_EDGE ( 'NONE', *, *, #56423, .F. ) ;
#63238 = CARTESIAN_POINT ( 'NONE',  ( 5.000000000000000000, -10.25161785469019193, 64.79070129774501652 ) ) ;
#63239 = CARTESIAN_POINT ( 'NONE',  ( 7.204075437095966983, 7.204075437095967871, 103.0937500020483668 ) ) ;
#63240 = CARTESIAN_POINT ( 'NONE',  ( 8.660254037844385522, 216.4583333265053682, 5.000000000000005329 ) ) ;
#63241 = CARTESIAN_POINT ( 'NONE',  ( -3.458734124999960358, 202.6875000013656063, 198.0000000000000284 ) ) ;
#63242 = CARTESIAN_POINT ( 'NONE',  ( 2.020667218593132706E-15, -11.00000000000000000, 68.87499999999998579 ) ) ;
#63244 = CARTESIAN_POINT ( 'NONE',  ( -11.35316468750000141, 103.2812499965860269, -1.390361679473963753E-15 ) ) ;
#63243 = CARTESIAN_POINT ( 'NONE',  ( 7.999999999999968914, 3.313708498984778483, 22.67405277982336287 ) ) ;
#63245 = EDGE_CURVE ( 'NONE', #30314, #57513, #42429, .T. ) ;
#63246 = CARTESIAN_POINT ( 'NONE',  ( -3.313708498984758943, -7.999999999999989342, 11.79905278392014800 ) ) ;
#63247 = CARTESIAN_POINT ( 'NONE',  ( -27.99999999999996092, 195.1875000013655779, 173.4587341250003760 ) ) ;
#63248 = DIRECTION ( 'NONE',  ( -0.000000000000000000, 1.000000000000000000, 4.689100369878284071E-30 ) ) ;
#63249 = ORIENTED_EDGE ( 'NONE', *, *, #66138, .F. ) ;
#63250 = CARTESIAN_POINT ( 'NONE',  ( 10.00000000000000000, 201.6666666598387110, 2.679491924311236062 ) ) ;
#63251 = CARTESIAN_POINT ( 'NONE',  ( 8.000000000000000000, 115.3437500000000000, -3.313708498984762496 ) ) ;
#63252 = CARTESIAN_POINT ( 'NONE',  ( 1.469576158976823947E-15, 101.3750000000000000, 8.000000000000000000 ) ) ;
#63253 = CARTESIAN_POINT ( 'NONE',  ( -11.35316468750000141, 88.80208332991934128, 3.042071309553159963 ) ) ;
#63254 = CARTESIAN_POINT ( 'NONE',  ( 2.765530957081996366, 288.1406250017070647, -6.676582343750003368 ) ) ;
#63255 = CARTESIAN_POINT ( 'NONE',  ( 5.082755093536324154, 8.156249997951611874, 5.082755093536326818 ) ) ;
#63256 = CARTESIAN_POINT ( 'NONE',  ( -7.204075437095967871, 7.204075437095967871, 97.84375000204836681 ) ) ;
#63257 = CARTESIAN_POINT ( 'NONE',  ( -3.042071309553173730, 224.3229166632527267, 11.35316468749999785 ) ) ;
#63258 = ORIENTED_EDGE ( 'NONE', *, *, #69399, .F. ) ;
#63259 = DIRECTION ( 'NONE',  ( 0.000000000000000000, 0.000000000000000000, 1.000000000000000000 ) ) ;
#63260 = CARTESIAN_POINT ( 'NONE',  ( 9.832129032723420536, 216.1979166632526983, -5.676582343749999815 ) ) ;
#63261 = CARTESIAN_POINT ( 'NONE',  ( -45.49866705521328214, 185.8289241312458273, 77.67342763857473642 ) ) ;
#63262 = CARTESIAN_POINT ( 'NONE',  ( 2.775557561562891351E-14, 210.0000000000000284, 198.0000000000000284 ) ) ;
#63263 = CARTESIAN_POINT ( 'NONE',  ( -6.676582343750003368, 295.3906250017068942, -2.765530957081996810 ) ) ;
#63264 = AXIS2_PLACEMENT_3D ( 'NONE', #45426, #57136, #46174 ) ;
#63265 = VERTEX_POINT ( 'NONE', #14940 ) ;
#63266 = CARTESIAN_POINT ( 'NONE',  ( 7.778174593052021635, 7.778174593052023411, 89.12500000409677625 ) ) ;
#63267 = CARTESIAN_POINT ( 'NONE',  ( 3.042071309553159519, 210.0520833299193555, 11.35316468750000141 ) ) ;
#63268 = CARTESIAN_POINT ( 'NONE',  ( 10.18810118749999916, 4.220049686691935698, 94.00000000204838102 ) ) ;
#63269 =( BOUNDED_CURVE ( )  B_SPLINE_CURVE ( 2, ( #28046, #73696, #11811, #21635, #57099, #10330, #69155, #5414, #45390 ),
 .UNSPECIFIED., .F., .F. ) 
 B_SPLINE_CURVE_WITH_KNOTS ( ( 3, 2, 2, 2, 3 ),
 ( 0.5147058823529412352, 0.5183823529411765163, 0.5220588235294116863, 0.5257352941176469674, 0.5294117647058821374 ),
 .UNSPECIFIED. ) 
 CURVE ( )  GEOMETRIC_REPRESENTATION_ITEM ( )  RATIONAL_B_SPLINE_CURVE ( ( 0.9999999999999976685, 0.9238795325112890700, 1.000000000000000000, 0.9238795325112867385, 1.000000000000000000, 0.9238795325112867385, 1.000000000000000000, 0.9238795325112912904, 0.9999999999999954481 ) ) 
 REPRESENTATION_ITEM ( '' )  );
#63270 = CARTESIAN_POINT ( 'NONE',  ( -26.56734541678232731, 207.0000000013656063, 173.4587341250003760 ) ) ;
#63271 = CARTESIAN_POINT ( 'NONE',  ( 8.000000000000000000, 15.09375000000000533, -3.313708498984761608 ) ) ;
#63272 = ORIENTED_EDGE ( 'NONE', *, *, #1616, .T. ) ;
#63273 = CARTESIAN_POINT ( 'NONE',  ( 7.188101187500000044, 120.4062500020483810, -8.802885111219163269E-16 ) ) ;
#63274 = CARTESIAN_POINT ( 'NONE',  ( -7.285838599102589797E-14, -20.78460969082654231, -1.607695154586745501 ) ) ;
#63275 = CARTESIAN_POINT ( 'NONE',  ( 2.679491924311222739, 33.95833333333333570, 10.00000000000000355 ) ) ;
#63276 = CARTESIAN_POINT ( 'NONE',  ( -3.313708498984786033, 8.531250000000001776, 7.999999999999979572 ) ) ;
#63277 = CARTESIAN_POINT ( 'NONE',  ( 1.871523826299183495E-15, -10.18810118749999916, 75.90625000204836681 ) ) ;
#63278 = ORIENTED_EDGE ( 'NONE', *, *, #15733, .T. ) ;
#63279 = CARTESIAN_POINT ( 'NONE',  ( 1.881053915767121776, 2.499999998634407028, -4.541265875000002339 ) ) ;
#63280 = CARTESIAN_POINT ( 'NONE',  ( -4.898587196589412829E-16, 114.1250000000000000, -8.000000000000000000 ) ) ;
#63281 = LINE ( 'NONE', #46310, #25783 ) ;
#63282 = ADVANCED_FACE ( 'NONE', ( #42866 ), #3639, .F. ) ;
#63283 = CARTESIAN_POINT ( 'NONE',  ( -11.00000000000004796, -4.556349186104000637, 92.78125000409677625 ) ) ;
#63284 = CARTESIAN_POINT ( 'NONE',  ( 5.082755093536326818, 122.0937500020483952, 5.082755093536325042 ) ) ;
#63285 = CARTESIAN_POINT ( 'NONE',  ( 8.660254037844389075, 152.2916666598387110, -5.000000000000000000 ) ) ;
#63286 = CARTESIAN_POINT ( 'NONE',  ( -6.676582343750002480, 295.3906250017069510, -2.765530957081996810 ) ) ;
#63289 = CARTESIAN_POINT ( 'NONE',  ( -4.000000000000016875, 199.5625000027312126, 140.3431457505076594 ) ) ;
#63288 = CARTESIAN_POINT ( 'NONE',  ( -9.832129032723418760, 243.4895833367473301, -5.676582343749998927 ) ) ;
#63287 = CARTESIAN_POINT ( 'NONE',  ( 28.00000000000001776, 205.4375000013656063, 173.4587341249998929 ) ) ;
#63290 = APPLICATION_PROTOCOL_DEFINITION ( 'draft international standard', 'automotive_design', 1998, #13939 ) ;
#63291 = EDGE_LOOP ( 'NONE', ( #17426, #68790, #46454, #25660 ) ) ;
#63292 = CARTESIAN_POINT ( 'NONE',  ( 11.35316468749999608, 241.9270833367473301, -3.042071309553167069 ) ) ;
#63293 = CARTESIAN_POINT ( 'NONE',  ( -5.082755093536317936, -5.082755093536320601, 4.674052781871752771 ) ) ;
#63294 = ORIENTED_EDGE ( 'NONE', *, *, #52569, .T. ) ;
#63295 = CARTESIAN_POINT ( 'NONE',  ( -4.220049686691935698, 10.18810118749999916, 68.87500000204838102 ) ) ;
#63296 = CARTESIAN_POINT ( 'NONE',  ( 5.676582343749993598, 90.26041666325268409, 9.832129032723422313 ) ) ;
#63297 = CARTESIAN_POINT ( 'NONE',  ( 2.828427124746191623, 21.12500000000000000, -2.828427124746191623 ) ) ;
#63298 = CARTESIAN_POINT ( 'NONE',  ( 7.778174593052023411, -7.778174593052021635, 82.56249999999998579 ) ) ;
#63301 = CARTESIAN_POINT ( 'NONE',  ( 9.498558403365325509E-13, 68.75000000000008527, 10.00000000000000178 ) ) ;
#63300 = CARTESIAN_POINT ( 'NONE',  ( 30.82842712474616320, 194.5000000027312126, 167.1715728752537018 ) ) ;
#63299 = CARTESIAN_POINT ( 'NONE',  ( 29.43265458321766559, 206.1250000013655779, 166.5412658749999650 ) ) ;
#63302 = EDGE_LOOP ( 'NONE', ( #69166, #28493, #20854, #13373 ) ) ;
#63303 = EDGE_CURVE ( 'NONE', #50481, #42724, #49660, .T. ) ;
#63304 = CARTESIAN_POINT ( 'NONE',  ( -50.92721440832627167, 200.4931777634346588, 55.69523082740657571 ) ) ;
#63305 = FACE_OUTER_BOUND ( 'NONE', #42268, .T. ) ;
#63306 = AXIS2_PLACEMENT_3D ( 'NONE', #43380, #48297, #9444 ) ;
#63307 = CARTESIAN_POINT ( 'NONE',  ( -11.35316468750000141, 198.2812499965860411, -1.390361679473963753E-15 ) ) ;
#63309 = EDGE_CURVE ( 'NONE', #11062, #32460, #73301, .T. ) ;
#63308 = CARTESIAN_POINT ( 'NONE',  ( -2.839093476692135984E-14, 203.6875000013656063, 138.5412658750000503 ) ) ;
#63310 = CARTESIAN_POINT ( 'NONE',  ( 29.43265458321766559, 205.1250000013656347, 166.5412658749999650 ) ) ;
#63311 = CARTESIAN_POINT ( 'NONE',  ( 5.082755093536324154, 24.65624999795161543, 5.082755093536326818 ) ) ;
#63312 = CIRCLE ( 'NONE', #42841, 5.000000000000000888 ) ;
#63313 = CARTESIAN_POINT ( 'NONE',  ( 8.311093377946837890, 176.7187499965860127, -8.311093377946837890 ) ) ;
#63314 = CARTESIAN_POINT ( 'NONE',  ( 0.000000000000000000, 0.000000000000000000, -21.47459999999999525 ) ) ;
#63315 = CARTESIAN_POINT ( 'NONE',  ( -2.977408999572650927, 97.25000000204839523, -7.188101187500000933 ) ) ;
#63317 = CARTESIAN_POINT ( 'NONE',  ( -9.999999999999996447, 112.7083333333333286, 2.679491924311221407 ) ) ;
#63316 = CARTESIAN_POINT ( 'NONE',  ( -2.679491924335967834, 208.5416666666644687, 9.999999999985712762 ) ) ;
#63318 = CARTESIAN_POINT ( 'NONE',  ( 2.780723358947928197E-16, 8.562499998634407916, -4.541265875000002339 ) ) ;
#63319 = CARTESIAN_POINT ( 'NONE',  ( 24.54126587499999346, 201.4375000013656063, 169.9999999999998863 ) ) ;
#63320 = CARTESIAN_POINT ( 'NONE',  ( 2.977408999572646486, 7.188101187499991163, 7.392802781871750994 ) ) ;
#63321 = CARTESIAN_POINT ( 'NONE',  ( -9.832129032723420536, 73.69791666325268409, 5.676582343749997150 ) ) ;
#63322 = DIRECTION ( 'NONE',  ( 0.000000000000000000, 1.000000000000000000, 4.283267841918042741E-17 ) ) ;
#63323 = CARTESIAN_POINT ( 'NONE',  ( -2.751064625579944321E-14, 201.7500000000000000, 146.0000000000000284 ) ) ;
#63324 = ORIENTED_EDGE ( 'NONE', *, *, #23121, .T. ) ;
#63325 = DIRECTION ( 'NONE',  ( 0.000000000000000000, -1.000000000000000000, 0.000000000000000000 ) ) ;
#63326 = DIRECTION ( 'NONE',  ( -1.000000000000000000, 0.000000000000000000, 0.000000000000000000 ) ) ;
#63327 = CARTESIAN_POINT ( 'NONE',  ( 8.311093377946837890, 66.40624999658602690, -8.311093377946837890 ) ) ;
#63328 = CARTESIAN_POINT ( 'NONE',  ( -11.00000000000000000, 0.000000000000000000, 73.18750000409676204 ) ) ;
#63329 = CARTESIAN_POINT ( 'NONE',  ( -2.445694354108840063, 197.0625000013656063, 139.5543056458912190 ) ) ;
#63330 = CARTESIAN_POINT ( 'NONE',  ( -1.780377099648780215, 16.42166210098345402, 68.70754022607248146 ) ) ;
#63332 = CARTESIAN_POINT ( 'NONE',  ( -9.832129032723418760, 57.86458332991935549, -5.676582343750004256 ) ) ;
#63331 = CARTESIAN_POINT ( 'NONE',  ( -2.977408999572650927, 90.87500000204836681, -7.188101187500000933 ) ) ;
#63333 = ADVANCED_FACE ( 'NONE', ( #5139 ), #56079, .F. ) ;
#63334 = CARTESIAN_POINT ( 'NONE',  ( 1.469576158976822172E-15, -7.999999999999991118, 4.205302779823362869 ) ) ;
#63335 = DIRECTION ( 'NONE',  ( -0.000000000000000000, -0.000000000000000000, 1.000000000000000000 ) ) ;
#63336 = CARTESIAN_POINT ( 'NONE',  ( 10.00000000000000178, 157.0833333265053113, -2.679491924311226736 ) ) ;
#63337 = CARTESIAN_POINT ( 'NONE',  ( -5.082755093536324154, 97.71875000204838102, 5.082755093536326818 ) ) ;
#63338 = CARTESIAN_POINT ( 'NONE',  ( -5.000000000000000000, -16.14408868864072844, -27.96238185062390613 ) ) ;
#63339 = CARTESIAN_POINT ( 'NONE',  ( -8.311093377946836114, 47.96874999658601268, -8.311093377946837890 ) ) ;
#63340 = CARTESIAN_POINT ( 'NONE',  ( -10.18810118749999738, -4.220049686691941915, 113.1250000020483810 ) ) ;
#63341 = CARTESIAN_POINT ( 'NONE',  ( 3.042071309553167069, 176.8229166632526415, -11.35316468749999785 ) ) ;
#63342 = ORIENTED_EDGE ( 'NONE', *, *, #40835, .F. ) ;
#63343 = CARTESIAN_POINT ( 'NONE',  ( 5.086519500887227707, 60.91611154180610299, 23.32191296476149489 ) ) ;
#63344 = CARTESIAN_POINT ( 'NONE',  ( 4.220049686691934809, 10.18810118749999916, 73.18750000204838102 ) ) ;
#63345 = CARTESIAN_POINT ( 'NONE',  ( -1.656854249492348607, 195.1875000000000000, 202.0000000000000284 ) ) ;
#63347 = CARTESIAN_POINT ( 'NONE',  ( 11.35316468750000141, 185.7812499965860411, 0.000000000000000000 ) ) ;
#63346 = DIRECTION ( 'NONE',  ( -0.000000000000000000, 1.000000000000000000, -1.563033456626094573E-30 ) ) ;
#63348 = CARTESIAN_POINT ( 'NONE',  ( -7.999999999999991118, 3.313708498984756723, 5.292802784329825094 ) ) ;
#63349 = CYLINDRICAL_SURFACE ( 'NONE', #40556, 3.999999999999976019 ) ;
#63350 = CARTESIAN_POINT ( 'NONE',  ( 8.660254037844385522, 251.0416666734946318, -5.000000000000003553 ) ) ;
#63351 = CARTESIAN_POINT ( 'NONE',  ( -30.82842712474621294, 206.1250000000000284, 167.1715728752542134 ) ) ;
#63352 = ORIENTED_EDGE ( 'NONE', *, *, #34726, .T. ) ;
#63353 = CARTESIAN_POINT ( 'NONE',  ( -9.832129032723418760, 168.1770833299193555, -5.676582343750004256 ) ) ;
#63354 = EDGE_CURVE ( 'NONE', #31698, #49230, #6331, .T. ) ;
#63355 = CARTESIAN_POINT ( 'NONE',  ( -7.188101187499990274, -2.977408999572651815, 27.08030278187175810 ) ) ;
#63356 = CARTESIAN_POINT ( 'NONE',  ( 11.35316468749999785, 130.8854166632526699, 3.042071309553174174 ) ) ;
#63357 = CARTESIAN_POINT ( 'NONE',  ( 2.679491924311238726, 12.91666665983870210, -9.999999999999996447 ) ) ;
#63358 = ORIENTED_EDGE ( 'NONE', *, *, #6304, .T. ) ;
#63359 = CARTESIAN_POINT ( 'NONE',  ( -3.211159895383562723, 9.062499998634407916, 3.211159895383561391 ) ) ;
#63360 = CARTESIAN_POINT ( 'NONE',  ( 7.188101187499999156, 15.37499999795161187, 2.977408999572654924 ) ) ;
#63361 = CARTESIAN_POINT ( 'NONE',  ( 1.469576158976823947E-15, 104.5625000040967763, 8.000000000000000000 ) ) ;
#63362 = CARTESIAN_POINT ( 'NONE',  ( -29.43265458321760519, 200.1250000013656063, 173.4587341250003760 ) ) ;
#63363 = VECTOR ( 'NONE', #35765, 1000.000000000000000 ) ;
#63364 = CARTESIAN_POINT ( 'NONE',  ( -7.347880794884122694E-16, 8.750000000000000000, 4.000000000000001776 ) ) ;
#63365 = CARTESIAN_POINT ( 'NONE',  ( -30.91765456463924622, -11.99969742749954271, 172.8974316310033998 ) ) ;
#63366 = CARTESIAN_POINT ( 'NONE',  ( -4.541265875000003227, 11.87499999863440792, 1.881053915767121110 ) ) ;
#63367 = CARTESIAN_POINT ( 'NONE',  ( -3.313708498984758943, -7.999999999999989342, 19.29905278392014978 ) ) ;
#63368 = CARTESIAN_POINT ( 'NONE',  ( 1.656854249492347719, 196.8125000000000284, 146.0000000000000284 ) ) ;
#63369 = ORIENTED_EDGE ( 'NONE', *, *, #55529, .T. ) ;
#63370 = CARTESIAN_POINT ( 'NONE',  ( 0.000000000000000000, 132.4999999999999147, 0.000000000000000000 ) ) ;
#63371 = CARTESIAN_POINT ( 'NONE',  ( -5.082755093536324154, 106.3437500020483810, 5.082755093536326818 ) ) ;
#63373 = CARTESIAN_POINT ( 'NONE',  ( -8.000000000000000000, 15.56249999590322197, -9.797174393178825657E-16 ) ) ;
#63372 = CARTESIAN_POINT ( 'NONE',  ( 10.99999999999989342, 4.556349186104152515, 78.53125000409677625 ) ) ;
#63374 =( BOUNDED_CURVE ( )  B_SPLINE_CURVE ( 2, ( #2061, #1710, #19772, #58679, #31477, #71079, #18678, #24687, #41687 ),
 .UNSPECIFIED., .F., .F. ) 
 B_SPLINE_CURVE_WITH_KNOTS ( ( 3, 2, 2, 2, 3 ),
 ( 0.7386363636363636465, 0.7443181818181817677, 0.7500000000000000000, 0.7556818181818182323, 0.7613636363636363535 ),
 .UNSPECIFIED. ) 
 CURVE ( )  GEOMETRIC_REPRESENTATION_ITEM ( )  RATIONAL_B_SPLINE_CURVE ( ( 1.000000000000000000, 0.9238795325112867385, 1.000000000000000000, 0.9238795325112867385, 1.000000000000000000, 0.9238795325112867385, 1.000000000000000000, 0.9238795325112867385, 1.000000000000000000 ) ) 
 REPRESENTATION_ITEM ( '' )  );
#63375 = ORIENTED_EDGE ( 'NONE', *, *, #22932, .F. ) ;
#63377 = VECTOR ( 'NONE', #25895, 1000.000000000000000 ) ;
#63376 = DIRECTION ( 'NONE',  ( 0.000000000000000000, -0.000000000000000000, -1.000000000000000000 ) ) ;
#63378 = CARTESIAN_POINT ( 'NONE',  ( -5.082755093536319713, 5.082755093536319713, 22.29905278187175455 ) ) ;
#63379 = ORIENTED_EDGE ( 'NONE', *, *, #7146, .T. ) ;
#63380 = ADVANCED_FACE ( 'NONE', ( #68496 ), #13980, .F. ) ;
#63381 = EDGE_LOOP ( 'NONE', ( #36717, #20584, #55795, #43136, #31036 ) ) ;
#63382 = CARTESIAN_POINT ( 'NONE',  ( 4.220049686691934809, 10.18810118749999916, 89.68750000204838102 ) ) ;
#63383 = LINE ( 'NONE', #69424, #17857 ) ;
#63384 = CARTESIAN_POINT ( 'NONE',  ( -24.54126587499998990, 197.4375000013655779, 170.0000000000003411 ) ) ;
#63385 = CARTESIAN_POINT ( 'NONE',  ( -4.556349186104047710, -10.99999999999999822, 98.78125000000000000 ) ) ;
#63387 = CARTESIAN_POINT ( 'NONE',  ( 2.765530957082001251, 297.9218750017069510, 6.676582343749999815 ) ) ;
#63386 = PLANE ( 'NONE',  #73588 ) ;
#63388 = CARTESIAN_POINT ( 'NONE',  ( 8.660254037844389075, 130.4166666666666856, -5.000000000000000000 ) ) ;
#63389 = CARTESIAN_POINT ( 'NONE',  ( 8.000000000000001776, 101.6562500000000142, 3.313708498984759387 ) ) ;
#63390 = CARTESIAN_POINT ( 'NONE',  ( 4.721056650415999201, 289.2343750017069510, -4.721056650415999201 ) ) ;
#63391 = CARTESIAN_POINT ( 'NONE',  ( 2.977408999572646486, 7.188101187499991163, 2.892802781871751439 ) ) ;
#63392 = CARTESIAN_POINT ( 'NONE',  ( -8.000000000000000000, 98.00000000000000000, 0.000000000000000000 ) ) ;
#63393 = EDGE_CURVE ( 'NONE', #43894, #53804, #6256, .T. ) ;
#63394 = CARTESIAN_POINT ( 'NONE',  ( 31.45873412499999944, 203.6875000013656063, 169.9999999999999432 ) ) ;
#63395 = CARTESIAN_POINT ( 'NONE',  ( -3.313708498984760720, 27.28124999590322730, -8.000000000000000000 ) ) ;
#63396 = CARTESIAN_POINT ( 'NONE',  ( 8.008118988124993010, -3.317071493978877239, 3.169365283940628331 ) ) ;
#63397 = CARTESIAN_POINT ( 'NONE',  ( -2.445694354108838731, 196.0625000013656063, 144.4456943541088663 ) ) ;
#63398 = CARTESIAN_POINT ( 'NONE',  ( -5.082755093536325930, 118.3437500020483810, -5.082755093536325930 ) ) ;
#63400 = CARTESIAN_POINT ( 'NONE',  ( 3.257047731941398627, 194.8184057345649194, 195.9917957155635975 ) ) ;
#63399 = CARTESIAN_POINT ( 'NONE',  ( -2.249999999999999556, 255.9999999999998295, 5.427273995024871844 ) ) ;
#63401 = CARTESIAN_POINT ( 'NONE',  ( -8.311093377946836114, 248.5937500034139589, -8.311093377946836114 ) ) ;
#63402 = DIRECTION ( 'NONE',  ( -0.000000000000000000, -1.000000000000000000, -0.000000000000000000 ) ) ;
#63403 = CARTESIAN_POINT ( 'NONE',  ( -7.188101187499990274, -2.977408999572651371, 25.95530278187175810 ) ) ;
#63404 = CARTESIAN_POINT ( 'NONE',  ( 26.34314575050763452, 196.5625000000000284, 165.9999999999998863 ) ) ;
#63405 = CARTESIAN_POINT ( 'NONE',  ( 8.311093377946834337, 10.15624999658601801, 8.311093377946839666 ) ) ;
#63406 = CARTESIAN_POINT ( 'NONE',  ( 1.469576158976823947E-15, 100.0625000040967763, 8.000000000000000000 ) ) ;
#63407 = CARTESIAN_POINT ( 'NONE',  ( 9.832129032723420536, 226.5104166632526983, -5.676582343749999815 ) ) ;
#63408 = CARTESIAN_POINT ( 'NONE',  ( 54.00000000000000000, 242.0000000000000284, 3.957333433710601454E-14 ) ) ;
#63410 = CARTESIAN_POINT ( 'NONE',  ( -2.679491924311279138, 43.54166666666675667, 10.00000000000016342 ) ) ;
#63409 = CARTESIAN_POINT ( 'NONE',  ( -2.160335347094220371, 51.35526406371868546, 48.59969451235947702 ) ) ;
#63411 = EDGE_LOOP ( 'NONE', ( #59310, #62485, #9009, #32964 ) ) ;
#63412 = CARTESIAN_POINT ( 'NONE',  ( -2.839093476692135984E-14, 196.9375000013655779, 138.5412658750000503 ) ) ;
#63413 = CARTESIAN_POINT ( 'NONE',  ( 9.832129032723420536, 21.19791666325268409, -5.676582343749999815 ) ) ;
#63414 = CARTESIAN_POINT ( 'NONE',  ( -7.778174593052023411, 7.778174593052023411, 91.00000000409677625 ) ) ;
#63415 = CARTESIAN_POINT ( 'NONE',  ( 0.4320110153364553618, 10.28109898471437589, 63.57214792341211762 ) ) ;
#63416 = CARTESIAN_POINT ( 'NONE',  ( -2.679491924293276206, 153.5416666666683057, 10.00000000001037925 ) ) ;
#63417 = CARTESIAN_POINT ( 'NONE',  ( -5.000000000000000000, -11.14555136602165675, -27.84144949604441166 ) ) ;
#63419 = CARTESIAN_POINT ( 'NONE',  ( 9.832129032723420536, 26.19791666325268409, -5.676582343749999815 ) ) ;
#63418 = CARTESIAN_POINT ( 'NONE',  ( -7.188101187500000044, 109.1562500020483810, 0.000000000000000000 ) ) ;
#63420 = CARTESIAN_POINT ( 'NONE',  ( 7.999999999999991118, 3.313708498984757611, 22.67405277982336287 ) ) ;
#63421 = CARTESIAN_POINT ( 'NONE',  ( -5.676582343750006032, 129.1145833299193839, 9.832129032723418760 ) ) ;
#63422 = EDGE_CURVE ( 'NONE', #20466, #52730, #21715, .T. ) ;
#63423 = CARTESIAN_POINT ( 'NONE',  ( -10.00000000000000355, 114.5833333265053682, 2.679491924311223183 ) ) ;
#63424 = CARTESIAN_POINT ( 'NONE',  ( -2.977408999572651815, 112.8125000020483952, 7.188101187500000933 ) ) ;
#63425 = FACE_OUTER_BOUND ( 'NONE', #75, .T. ) ;
#63426 = CARTESIAN_POINT ( 'NONE',  ( -31.45873412499998523, 207.0000000013656063, 171.4326545832180386 ) ) ;
#63427 = CARTESIAN_POINT ( 'NONE',  ( -5.000000000000000000, -50.64189880742087269, -41.08656465431914029 ) ) ;
#63428 = EDGE_LOOP ( 'NONE', ( #43590, #63471, #9557 ) ) ;
#63429 = CARTESIAN_POINT ( 'NONE',  ( 5.676582343749993598, 10.26041666325268409, 9.832129032723422313 ) ) ;
#63430 = EDGE_CURVE ( 'NONE', #48612, #1871, #58677, .T. ) ;
#63431 = CARTESIAN_POINT ( 'NONE',  ( 38.00000000000000000, 242.0000000000000284, 3.663418201915235205E-14 ) ) ;
#63432 = CARTESIAN_POINT ( 'NONE',  ( 2.765530957082001251, 296.7656250017069510, 6.676582343750000703 ) ) ;
#63433 = CARTESIAN_POINT ( 'NONE',  ( 8.311093377946834337, 145.1562499965860127, 8.311093377946839666 ) ) ;
#63434 = CARTESIAN_POINT ( 'NONE',  ( 4.898587196589412829E-16, 12.18749999590322197, -8.000000000000000000 ) ) ;
#63435 = CARTESIAN_POINT ( 'NONE',  ( -4.898587196589407898E-16, 7.999999999999991118, 26.01155278432982243 ) ) ;
#63436 = CARTESIAN_POINT ( 'NONE',  ( 4.898587196589412829E-16, 18.37500000000000355, -8.000000000000000000 ) ) ;
#63437 = CARTESIAN_POINT ( 'NONE',  ( -5.676582343750000703, 248.0729166700806729, -9.832129032723418760 ) ) ;
#63438 = CARTESIAN_POINT ( 'NONE',  ( -7.204075437095967871, 7.204075437095967871, 94.84375000204838102 ) ) ;
#63439 = EDGE_LOOP ( 'NONE', ( #27441, #51141, #55664 ) ) ;
#63440 = CIRCLE ( 'NONE', #44167, 36.00000000000000000 ) ;
#63441 = LINE ( 'NONE', #62326, #20793 ) ;
#63442 = CARTESIAN_POINT ( 'NONE',  ( 4.999999999999998224, 67.66364885638974158, -22.52891795222217297 ) ) ;
#63443 = EDGE_CURVE ( 'NONE', #3824, #70051, #23587, .T. ) ;
#63444 = CARTESIAN_POINT ( 'NONE',  ( 11.35316468749999785, 85.88541666325268409, 3.042071309553174174 ) ) ;
#63445 = ORIENTED_EDGE ( 'NONE', *, *, #2234, .F. ) ;
#63446 = CARTESIAN_POINT ( 'NONE',  ( -7.204075437095967871, 7.204075437095967871, 106.4687500020483810 ) ) ;
#63447 = CARTESIAN_POINT ( 'NONE',  ( 1.881053915767122664, 14.24999999863440969, 4.541265875000001451 ) ) ;
#63448 = ORIENTED_EDGE ( 'NONE', *, *, #68463, .F. ) ;
#63449 = ORIENTED_EDGE ( 'NONE', *, *, #54094, .T. ) ;
#63450 = CARTESIAN_POINT ( 'NONE',  ( 5.656854249492380582, 0.1874999999999999167, -5.656854249492380582 ) ) ;
#63451 = FACE_OUTER_BOUND ( 'NONE', #6463, .T. ) ;
#63452 = CARTESIAN_POINT ( 'NONE',  ( -5.000000000000000000, -61.58678017309371455, -23.68362420833346960 ) ) ;
#63453 = CARTESIAN_POINT ( 'NONE',  ( -1.320432766682874540E-15, 22.96874999795161543, 7.188101187500000044 ) ) ;
#63454 = DIRECTION ( 'NONE',  ( -0.000000000000000000, 1.000000000000000000, -4.476705744456276341E-16 ) ) ;
#63455 = CARTESIAN_POINT ( 'NONE',  ( 4.220049686691934809, 10.18810118749999916, 105.0625000020483810 ) ) ;
#63456 = CARTESIAN_POINT ( 'NONE',  ( 4.556349186104045934, 11.00000000000000000, 75.53125000000000000 ) ) ;
#63457 = CARTESIAN_POINT ( 'NONE',  ( 4.000000000000001776, 10.81249999726881406, -1.656854249492381248 ) ) ;
#63458 = CARTESIAN_POINT ( 'NONE',  ( 2.780723358947928197E-16, 1.562499998634406584, -4.541265875000002339 ) ) ;
#63459 = ORIENTED_EDGE ( 'NONE', *, *, #63642, .T. ) ;
#63460 = VECTOR ( 'NONE', #48529, 1000.000000000000000 ) ;
#63461 = EDGE_CURVE ( 'NONE', #12427, #64593, #29446, .T. ) ;
#63462 = DIRECTION ( 'NONE',  ( 0.000000000000000000, 0.000000000000000000, 1.000000000000000000 ) ) ;
#63463 = CARTESIAN_POINT ( 'NONE',  ( -1.432654583217607858, 199.6250000013656063, 201.4587341250000065 ) ) ;
#63464 = CARTESIAN_POINT ( 'NONE',  ( -9.832129032723418760, 52.86458332991934839, -5.676582343750004256 ) ) ;
#63465 = EDGE_CURVE ( 'NONE', #65025, #41193, #59502, .T. ) ;
#63466 = CARTESIAN_POINT ( 'NONE',  ( -29.43265458321771177, 204.5000000013656063, 166.5412658750003914 ) ) ;
#63467 = LINE ( 'NONE', #74045, #45325 ) ;
#63468 = CARTESIAN_POINT ( 'NONE',  ( -1.881053915767124440, 11.99999999863440969, 4.541265875000001451 ) ) ;
#63469 = CARTESIAN_POINT ( 'NONE',  ( 4.000000000000001776, 16.06250000000000000, -1.656854249492381248 ) ) ;
#63470 = CARTESIAN_POINT ( 'NONE',  ( 7.188101187499993827, -2.977408999572645598, 21.64280278187176165 ) ) ;
#63471 = ORIENTED_EDGE ( 'NONE', *, *, #11842, .T. ) ;
#63472 =( BOUNDED_CURVE ( )  B_SPLINE_CURVE ( 2, ( #51943, #39507, #10831, #11207, #52685, #28550, #281, #51558, #46272 ),
 .UNSPECIFIED., .F., .F. ) 
 B_SPLINE_CURVE_WITH_KNOTS ( ( 3, 2, 2, 2, 3 ),
 ( 0.9583333333333332593, 0.9652777777777776791, 0.9722222222222220989, 0.9791666666666665186, 0.9861111111111110494 ),
 .UNSPECIFIED. ) 
 CURVE ( )  GEOMETRIC_REPRESENTATION_ITEM ( )  RATIONAL_B_SPLINE_CURVE ( ( 1.000000000000001110, 0.9238795325112855172, 1.000000000000000000, 0.9238795325112867385, 1.000000000000000000, 0.9238795325112867385, 1.000000000000000000, 0.9238795325112879597, 0.9999999999999987788 ) ) 
 REPRESENTATION_ITEM ( '' )  );
#63473 = EDGE_CURVE ( 'NONE', #32408, #3972, #15552, .T. ) ;
#63474 = ORIENTED_EDGE ( 'NONE', *, *, #56423, .T. ) ;
#63475 = CARTESIAN_POINT ( 'NONE',  ( 4.220049686691934809, 10.18810118749999916, 107.6875000020483810 ) ) ;
#63476 = CARTESIAN_POINT ( 'NONE',  ( -4.999999999999992006, 96.66666666666667140, -8.660254037844378416 ) ) ;
#63477 = CARTESIAN_POINT ( 'NONE',  ( -28.00000000000002842, 205.0000000000000284, 166.0000000000003695 ) ) ;
#63478 = CARTESIAN_POINT ( 'NONE',  ( -1.432654583217607192, 200.2500000013656631, 194.5412658750000219 ) ) ;
#63479 = DIRECTION ( 'NONE',  ( 0.000000000000000000, 0.000000000000000000, -1.000000000000000000 ) ) ;
#63480 = CARTESIAN_POINT ( 'NONE',  ( 10.00000000000000178, 75.00000000000001421, 0.000000000000000000 ) ) ;
#63481 = CARTESIAN_POINT ( 'NONE',  ( 3.313708498984765161, 116.4687499999999858, 7.999999999999998224 ) ) ;
#63482 = CARTESIAN_POINT ( 'NONE',  ( -9.832129032723418760, 63.17708332991934839, -5.676582343750004256 ) ) ;
#63483 = CARTESIAN_POINT ( 'NONE',  ( -2.485281374238571761, 288.8124999999999432, -6.000000000000003553 ) ) ;
#63484 = ORIENTED_EDGE ( 'NONE', *, *, #32546, .T. ) ;
#63485 = VECTOR ( 'NONE', #72285, 1000.000000000000000 ) ;
#63486 = DIRECTION ( 'NONE',  ( -0.000000000000000000, 1.000000000000000000, -0.000000000000000000 ) ) ;
#63487 = CARTESIAN_POINT ( 'NONE',  ( 2.436599634633794587, -16.39988855009488589, 68.84456747601390703 ) ) ;
#63488 = CARTESIAN_POINT ( 'NONE',  ( -3.458734125000015425, 206.9375000013656063, 142.0000000000000568 ) ) ;
#63489 = DIRECTION ( 'NONE',  ( -0.5000000000000011102, 0.8660254037844380415, 0.000000000000000000 ) ) ;
#63490 = CARTESIAN_POINT ( 'NONE',  ( 8.000000000000000000, 97.34374999999998579, -3.313708498984762496 ) ) ;
#63491 = CARTESIAN_POINT ( 'NONE',  ( -8.660254037844387298, 234.5833333333333428, -4.999999999999999112 ) ) ;
#63492 = CARTESIAN_POINT ( 'NONE',  ( -6.000000000000001776, 293.0000000000000000, 0.000000000000000000 ) ) ;
#63493 = CARTESIAN_POINT ( 'NONE',  ( -10.18810118749999738, -4.220049686691941915, 68.12500000204838102 ) ) ;
#63494 = CARTESIAN_POINT ( 'NONE',  ( -2.679491924311235618, 203.5416666666666856, 10.00000000000000000 ) ) ;
#63495 =( BOUNDED_CURVE ( )  B_SPLINE_CURVE ( 2, ( #24428, #31576, #42514, #2535, #30827, #25156, #37615, #47435, #8938 ),
 .UNSPECIFIED., .F., .F. ) 
 B_SPLINE_CURVE_WITH_KNOTS ( ( 3, 2, 2, 2, 3 ),
 ( 0.5166666666666670515, 0.5250000000000003553, 0.5333333333333337700, 0.5416666666666671848, 0.5500000000000005995 ),
 .UNSPECIFIED. ) 
 CURVE ( )  GEOMETRIC_REPRESENTATION_ITEM ( )  RATIONAL_B_SPLINE_CURVE ( ( 0.9999999999999970024, 0.9238795325112897361, 1.000000000000000000, 0.9238795325112867385, 1.000000000000000000, 0.9238795325112867385, 1.000000000000000000, 0.9238795325112816315, 1.000000000000005107 ) ) 
 REPRESENTATION_ITEM ( '' )  );
#63496 = CARTESIAN_POINT ( 'NONE',  ( -4.401442555609577197E-16, 7.188101187499992051, 14.98655278187175455 ) ) ;
#63497 = CARTESIAN_POINT ( 'NONE',  ( 11.35316468749999963, 176.3020833299193839, -3.042071309553165293 ) ) ;
#63498 = CARTESIAN_POINT ( 'NONE',  ( -9.999999999999998224, 37.29166666666665719, -2.679491924311230289 ) ) ;
#63499 = CARTESIAN_POINT ( 'NONE',  ( 4.556349186104052151, -10.99999999999999822, 97.65625000409679046 ) ) ;
#63501 = CARTESIAN_POINT ( 'NONE',  ( 10.00000000000000178, 86.87499999317203958, 0.000000000000000000 ) ) ;
#63500 = CARTESIAN_POINT ( 'NONE',  ( -8.660254037844387298, 227.7083333401613174, -4.999999999999999112 ) ) ;
#63502 = ORIENTED_EDGE ( 'NONE', *, *, #74639, .T. ) ;
#63503 = CARTESIAN_POINT ( 'NONE',  ( 1.432654583217607858, 196.6250000013656063, 138.5412658750000787 ) ) ;
#63504 = CARTESIAN_POINT ( 'NONE',  ( 3.042071309553159519, 35.05208332991935549, 11.35316468750000141 ) ) ;
#63505 = CARTESIAN_POINT ( 'NONE',  ( 4.556349186104045934, 11.00000000000000000, 113.2187500040967763 ) ) ;
#63506 = CARTESIAN_POINT ( 'NONE',  ( -26.34314575050768070, 200.5625000000000284, 174.0000000000004547 ) ) ;
#63507 = CARTESIAN_POINT ( 'NONE',  ( 0.000000000000000000, 220.0000000000000284, 0.000000000000000000 ) ) ;
#63509 = CARTESIAN_POINT ( 'NONE',  ( 11.00000000000000000, 1.347111479062088405E-15, 108.4375000040967763 ) ) ;
#63508 = CARTESIAN_POINT ( 'NONE',  ( 2.679491924311370177, 220.8333333265053682, 9.999999999999918288 ) ) ;
#63510 = CYLINDRICAL_SURFACE ( 'NONE', #41032, 12.00000000000000355 ) ;
#63511 = CARTESIAN_POINT ( 'NONE',  ( 2.445694354108782775, 199.5625000013656063, 139.5543056458912190 ) ) ;
#63512 = CARTESIAN_POINT ( 'NONE',  ( -1.836970198721029983E-15, 60.62499999317203958, 10.00000000000000178 ) ) ;
#63513 = CARTESIAN_POINT ( 'NONE',  ( 7.188101187500000044, 94.90625000204838102, -8.802885111219163269E-16 ) ) ;
#63514 = CARTESIAN_POINT ( 'NONE',  ( 4.541265875000002339, 13.43749999863440792, 0.000000000000000000 ) ) ;
#63515 = CARTESIAN_POINT ( 'NONE',  ( 10.00000000000005329, 65.20833333333337123, -2.679491924311240947 ) ) ;
#63516 = CARTESIAN_POINT ( 'NONE',  ( -3.313708498984757167, 7.999999999999991118, 2.049052779823364645 ) ) ;
#63517 = CARTESIAN_POINT ( 'NONE',  ( 10.00000000000000178, 102.0833333265053682, -2.679491924311226736 ) ) ;
#63518 = ORIENTED_EDGE ( 'NONE', *, *, #43034, .T. ) ;
#63519 = VERTEX_POINT ( 'NONE', #47336 ) ;
#63520 = CARTESIAN_POINT ( 'NONE',  ( -4.898587196589412829E-16, 121.6250000000000000, -8.000000000000000000 ) ) ;
#63521 = CARTESIAN_POINT ( 'NONE',  ( -2.765530957081996810, 298.4218750017069510, -6.676582343750003368 ) ) ;
#63522 = DIRECTION ( 'NONE',  ( 0.000000000000000000, 0.000000000000000000, 1.000000000000000000 ) ) ;
#63523 = VECTOR ( 'NONE', #45034, 1000.000000000000000 ) ;
#63524 = CARTESIAN_POINT ( 'NONE',  ( -7.320508075688777261, 88.12500000000001421, 7.320508075688768379 ) ) ;
#63525 = CARTESIAN_POINT ( 'NONE',  ( 9.832129032723416984, 155.3645833299193839, 5.676582343750006032 ) ) ;
#63526 = CARTESIAN_POINT ( 'NONE',  ( 4.220049686691941027, -10.18810118749999738, 81.62500000204836681 ) ) ;
#63527 = CARTESIAN_POINT ( 'NONE',  ( 8.000000000000000000, 4.500000000000000888, 0.000000000000000000 ) ) ;
#63528 = CARTESIAN_POINT ( 'NONE',  ( -1.656854249492347719, 202.8125000000000000, 194.0000000000000853 ) ) ;
#63529 = CARTESIAN_POINT ( 'NONE',  ( 4.787532741003091452, -6.454502166345807979, -0.000000000000000000 ) ) ;
#63530 = CARTESIAN_POINT ( 'NONE',  ( 2.449293598294707893E-16, 19.25000000000000000, -4.000000000000001776 ) ) ;
#63531 = VERTEX_POINT ( 'NONE', #35302 ) ;
#63532 = CARTESIAN_POINT ( 'NONE',  ( 33.97032413590168431, -16.00146971025283094, 152.9614073234062914 ) ) ;
#63533 = CARTESIAN_POINT ( 'NONE',  ( 28.52237390288060936, 180.9141530225295753, 157.6490779871850521 ) ) ;
#63534 = CARTESIAN_POINT ( 'NONE',  ( -2.085542519210945728E-15, 124.8437499965860269, 11.35316468750000141 ) ) ;
#63535 = CARTESIAN_POINT ( 'NONE',  ( -1.432654583217607858, 199.6250000013656063, 201.4587341250000065 ) ) ;
#63536 = CARTESIAN_POINT ( 'NONE',  ( 7.188101187500000044, 24.84374999795161543, 0.000000000000000000 ) ) ;
#63537 = CARTESIAN_POINT ( 'NONE',  ( 7.204075437095968759, -7.204075437095966983, 76.09375000204838102 ) ) ;
#63538 = CARTESIAN_POINT ( 'NONE',  ( -9.832129032723420536, 39.01041666325268409, 5.676582343749997150 ) ) ;
#63539 = ORIENTED_EDGE ( 'NONE', *, *, #48682, .T. ) ;
#63540 = CARTESIAN_POINT ( 'NONE',  ( 8.660254037844385522, 36.45833332650536818, 5.000000000000005329 ) ) ;
#63541 = CARTESIAN_POINT ( 'NONE',  ( 3.211159895383561835, 2.562499998634407028, -3.211159895383561835 ) ) ;
#63542 = CARTESIAN_POINT ( 'NONE',  ( 8.008118988124991233, 3.317071493978879015, 16.85686528394063188 ) ) ;
#63543 = CARTESIAN_POINT ( 'NONE',  ( -2.445694354108840063, 207.0625000013656063, 139.5543056458912190 ) ) ;
#63544 = CARTESIAN_POINT ( 'NONE',  ( -2.977408999572654480, 8.999999997951610098, 7.188101187499999156 ) ) ;
#63545 = CARTESIAN_POINT ( 'NONE',  ( -4.242640687119286547, 295.9375000034140157, -4.242640687119286547 ) ) ;
#63546 = CARTESIAN_POINT ( 'NONE',  ( -25.81369690663432337, -12.67024606825261124, 138.5586412391807016 ) ) ;
#63547 = CARTESIAN_POINT ( 'NONE',  ( 2.977408999572650927, 8.624999997951611874, -7.188101187500001821 ) ) ;
#63548 = CARTESIAN_POINT ( 'NONE',  ( 5.082755093536318824, 5.082755093536319713, 12.92405278187175277 ) ) ;
#63549=STYLED_ITEM('',(#74706),#40373);
#63550 = CARTESIAN_POINT ( 'NONE',  ( -7.204075437095965206, -7.204075437095968759, 73.84375000204838102 ) ) ;
#63551 = CARTESIAN_POINT ( 'NONE',  ( -26.56734541678238415, 206.6250000013656063, 166.5412658750003629 ) ) ;
#63552 = CARTESIAN_POINT ( 'NONE',  ( 0.000000000000000000, 265.0000000000000000, 0.000000000000000000 ) ) ;
#63553 = CARTESIAN_POINT ( 'NONE',  ( -1.881053915767121554, 21.74999999863440436, -4.541265875000002339 ) ) ;
#63554 = VERTEX_POINT ( 'NONE', #52640 ) ;
#63555 = CARTESIAN_POINT ( 'NONE',  ( 2.828427124746209831, 200.5000000027312126, 200.8284271247462129 ) ) ;
#63556 = ADVANCED_FACE ( 'NONE', ( #35663 ), #64696, .F. ) ;
#63557 = CARTESIAN_POINT ( 'NONE',  ( 1.656854249492348607, 208.1875000000000853, 138.0000000000000568 ) ) ;
#63558 = CARTESIAN_POINT ( 'NONE',  ( -30.82842712474612412, 203.5000000027312126, 172.8284271247466108 ) ) ;
#63559 = CARTESIAN_POINT ( 'NONE',  ( -4.401442555609581635E-16, 114.7812500020483952, -7.188101187500000044 ) ) ;
#63560 = CARTESIAN_POINT ( 'NONE',  ( -7.320508075688834992, 58.12500000000003553, 7.320508075688828775 ) ) ;
#63561 = CARTESIAN_POINT ( 'NONE',  ( 3.313708498984756279, 7.999999999999991118, 6.549052783920143561 ) ) ;
#63562 = ORIENTED_EDGE ( 'NONE', *, *, #40997, .F. ) ;
#63563 = ADVANCED_FACE ( 'NONE', ( #43586 ), #59407, .T. ) ;
#63564 = CARTESIAN_POINT ( 'NONE',  ( -7.188101187500000044, 16.21874999795161543, -8.802885111219163269E-16 ) ) ;
#63565 = ORIENTED_EDGE ( 'NONE', *, *, #71378, .F. ) ;
#63566 = DIRECTION ( 'NONE',  ( -0.000000000000000000, -1.000000000000000000, -4.283267841918042741E-17 ) ) ;
#63567 = CARTESIAN_POINT ( 'NONE',  ( 2.775557558920088989E-14, -48.00000000000001421, 151.0000000000000284 ) ) ;
#63568 = CARTESIAN_POINT ( 'NONE',  ( -4.999999999999998224, 46.66666666666667140, -8.660254037844389075 ) ) ;
#63569 = CARTESIAN_POINT ( 'NONE',  ( -7.188101187500001821, 104.9375000020483810, -2.977408999572650483 ) ) ;
#63570 = CARTESIAN_POINT ( 'NONE',  ( -28.00000000000002487, 208.6875000013656063, 166.5412658750003629 ) ) ;
#63571 = VECTOR ( 'NONE', #18148, 1000.000000000000000 ) ;
#63573 = CARTESIAN_POINT ( 'NONE',  ( 5.000000000000000000, -70.11723469343111503, 28.93519894129190817 ) ) ;
#63572 = CARTESIAN_POINT ( 'NONE',  ( 6.123233995736767268E-16, 33.12499999317203248, -10.00000000000000178 ) ) ;
#63574 = ORIENTED_EDGE ( 'NONE', *, *, #21795, .F. ) ;
#63575 = CARTESIAN_POINT ( 'NONE',  ( -6.951808397369817780E-16, 247.6562500034140157, -11.35316468749999963 ) ) ;
#63576 = CARTESIAN_POINT ( 'NONE',  ( 1.320432766682872962E-15, -7.188101187499992051, 15.73655278187175632 ) ) ;
#63577 = CARTESIAN_POINT ( 'NONE',  ( -4.465349678524261456, 56.41423509509874634, 44.23558526901069143 ) ) ;
#63578 = LINE ( 'NONE', #11906, #20682 ) ;
#63579 = DIRECTION ( 'NONE',  ( 0.000000000000000000, 0.000000000000000000, 1.000000000000000000 ) ) ;
#63580 = CARTESIAN_POINT ( 'NONE',  ( -8.660254037844387298, 157.0833333333333428, -5.000000000000004441 ) ) ;
#63581 = CARTESIAN_POINT ( 'NONE',  ( -1.836970198721029983E-15, 225.6249999931720254, 10.00000000000000178 ) ) ;
#63582 = CARTESIAN_POINT ( 'NONE',  ( 8.000000000000000000, 91.34375000000000000, -3.313708498984762496 ) ) ;
#63583 = CARTESIAN_POINT ( 'NONE',  ( 9.122856833726327608, 89.81967984264845484, -3.970537934901964494 ) ) ;
#63584 = CARTESIAN_POINT ( 'NONE',  ( -5.676582343749998039, 132.7604166632526983, -9.832129032723420536 ) ) ;
#63585 = CARTESIAN_POINT ( 'NONE',  ( 26.34314575050748886, 198.9375000000000568, 173.9999999999997726 ) ) ;
#63588 = CARTESIAN_POINT ( 'NONE',  ( 11.00000000000000000, 1.347111479062088405E-15, 82.93750000409677625 ) ) ;
#63587 = CARTESIAN_POINT ( 'NONE',  ( 25.55430564589115150, 197.0625000013656063, 167.5543056458911053 ) ) ;
#63586 = CARTESIAN_POINT ( 'NONE',  ( 27.99999999999996092, 196.6875000013655779, 173.4587341249998929 ) ) ;
#63589 = EDGE_LOOP ( 'NONE', ( #36846, #51977, #14653 ) ) ;
#63590 = CARTESIAN_POINT ( 'NONE',  ( 3.042071309553167069, 2.135416663252682756, -11.35316468749999785 ) ) ;
#63591 = DIRECTION ( 'NONE',  ( 0.000000000000000000, 0.000000000000000000, -1.000000000000000000 ) ) ;
#63592 = LINE ( 'NONE', #51915, #19458 ) ;
#63593 =( BOUNDED_CURVE ( )  B_SPLINE_CURVE ( 2, ( #30180, #30913, #42599, #25240, #13911, #53199, #36950, #24513, #59956 ),
 .UNSPECIFIED., .F., .F. ) 
 B_SPLINE_CURVE_WITH_KNOTS ( ( 3, 2, 2, 2, 3 ),
 ( 0.4736842105263158187, 0.4802631578947368918, 0.4868421052631579649, 0.4934210526315789269, 0.5000000000000000000 ),
 .UNSPECIFIED. ) 
 CURVE ( )  GEOMETRIC_REPRESENTATION_ITEM ( )  RATIONAL_B_SPLINE_CURVE ( ( 0.9999999999999993339, 0.9238795325112874046, 1.000000000000000000, 0.9238795325112867385, 1.000000000000000000, 0.9238795325112867385, 1.000000000000000000, 0.9238795325112867385, 1.000000000000000000 ) ) 
 REPRESENTATION_ITEM ( '' )  );
#63594 = MECHANICAL_DESIGN_GEOMETRIC_PRESENTATION_REPRESENTATION (  '', ( #74482 ), #57645 ) ;
#63595 = CARTESIAN_POINT ( 'NONE',  ( -2.828427124746192067, 11.62500000000000000, 2.828427124746190735 ) ) ;
#63596 = CARTESIAN_POINT ( 'NONE',  ( 5.000000000000001776, 22.70833332650536818, -8.660254037844389075 ) ) ;
#63597 = CARTESIAN_POINT ( 'NONE',  ( -2.977408999572651815, 116.9375000020483952, 7.188101187500000933 ) ) ;
#63598 = CARTESIAN_POINT ( 'NONE',  ( -3.211159895383561391, 21.68749999863440792, -3.211159895383561835 ) ) ;
#63599 = CARTESIAN_POINT ( 'NONE',  ( -1.781595147096461274, 67.70776641946500263, -20.12770457511257050 ) ) ;
#63600 = CARTESIAN_POINT ( 'NONE',  ( -5.656854249492375253, 5.656854249492375253, 18.64280277982336642 ) ) ;
#63602 = DIRECTION ( 'NONE',  ( 8.659560562354994488E-17, 0.7071067811865426878, -0.7071067811865524577 ) ) ;
#63601 = DIRECTION ( 'NONE',  ( 0.000000000000000000, 0.000000000000000000, -1.000000000000000000 ) ) ;
#63603 = CARTESIAN_POINT ( 'NONE',  ( 5.676582343749993598, 114.9479166632526983, 9.832129032723422313 ) ) ;
#63604 = ORIENTED_EDGE ( 'NONE', *, *, #16881, .T. ) ;
#63605 = B_SPLINE_CURVE_WITH_KNOTS ( 'NONE', 3,
 ( #39204, #62207, #21470, #74272, #62954, #68246 ),
 .UNSPECIFIED., .F., .F.,
 ( 4, 2, 4 ),
 ( 0.01236082503524027314, 0.01586526280559107799, 0.01936970057594187763 ),
 .UNSPECIFIED. ) ;
#63606 = CARTESIAN_POINT ( 'NONE',  ( 2.449293598294707893E-16, 15.99999999726881406, -4.000000000000001776 ) ) ;
#63607 = FACE_OUTER_BOUND ( 'NONE', #72614, .T. ) ;
#63608 = DIRECTION ( 'NONE',  ( -1.000000000000000000, 0.000000000000000000, 0.000000000000000000 ) ) ;
#63609 = CARTESIAN_POINT ( 'NONE',  ( 5.676582343750005144, 240.8854166700806445, 9.832129032723416984 ) ) ;
#63610 = CARTESIAN_POINT ( 'NONE',  ( 5.676582343750001591, 111.6145833299193555, -9.832129032723420536 ) ) ;
#63611 = ORIENTED_EDGE ( 'NONE', *, *, #10166, .T. ) ;
#63612 = CARTESIAN_POINT ( 'NONE',  ( -30.82842712474616320, 208.3750000000000284, 172.8284271247465824 ) ) ;
#63613 = CARTESIAN_POINT ( 'NONE',  ( -4.220049686691935698, 10.18810118749999916, 100.3750000020484094 ) ) ;
#63614 = CARTESIAN_POINT ( 'NONE',  ( -2.679491924311235618, 220.4166666598387110, 10.00000000000000000 ) ) ;
#63615 = CARTESIAN_POINT ( 'NONE',  ( 3.458734125000015869, 199.1875000013655779, 198.0000000000000284 ) ) ;
#63616 = DIRECTION ( 'NONE',  ( -6.308085367188390241E-16, 0.000000000000000000, 1.000000000000000000 ) ) ;
#63618 = CARTESIAN_POINT ( 'NONE',  ( -11.35316468750000141, 103.4895833299193697, 3.042071309553159963 ) ) ;
#63617 = CARTESIAN_POINT ( 'NONE',  ( -6.338495502905945601E-13, 181.2500000000000853, -10.00000000000000533 ) ) ;
#63619 = CARTESIAN_POINT ( 'NONE',  ( 7.999999999999991118, 3.313708498984757611, 9.361552783920146226 ) ) ;
#63620 = CARTESIAN_POINT ( 'NONE',  ( -25.55430564589114795, 197.3125000013656063, 172.4456943541091789 ) ) ;
#63621 = ORIENTED_EDGE ( 'NONE', *, *, #13247, .F. ) ;
#63622 = CARTESIAN_POINT ( 'NONE',  ( -10.00000000000000000, 189.1666666598387394, -2.679491924311229845 ) ) ;
#63623 = CARTESIAN_POINT ( 'NONE',  ( 5.656854249492381470, 115.0625000000000000, 5.656854249492379694 ) ) ;
#63624 = CARTESIAN_POINT ( 'NONE',  ( -6.735557395310442023E-16, 11.00000000000000000, 99.81250000409677625 ) ) ;
#63625 = CARTESIAN_POINT ( 'NONE',  ( -11.35316468749999785, 83.38541666325265567, -3.042071309553167957 ) ) ;
#63626 = CARTESIAN_POINT ( 'NONE',  ( 38.00000000000000000, 37.00000000000000711, 20.00000000000002132 ) ) ;
#63627 = CARTESIAN_POINT ( 'NONE',  ( -1.320432766682874540E-15, 7.968749997951610986, 7.188101187500000044 ) ) ;
#63628 = CARTESIAN_POINT ( 'NONE',  ( -4.220049686691937474, -10.18810118749999738, 92.31250000204838102 ) ) ;
#63629 = CARTESIAN_POINT ( 'NONE',  ( -9.832129032723420536, 223.6979166632526983, 5.676582343749997150 ) ) ;
#63630 = EDGE_LOOP ( 'NONE', ( #58108, #45208, #54157, #7317 ) ) ;
#63631 = CARTESIAN_POINT ( 'NONE',  ( 4.898587196589412829E-16, 10.87500000000000178, -8.000000000000000000 ) ) ;
#63632 = CARTESIAN_POINT ( 'NONE',  ( 2.696913074615494565, -43.67152221225546782, 139.1174434843254915 ) ) ;
#63633 = CARTESIAN_POINT ( 'NONE',  ( -3.042071309553173730, 224.3229166632527267, 11.35316468749999785 ) ) ;
#63634 = CARTESIAN_POINT ( 'NONE',  ( 7.999999999999706901, -2.135495361439877059E-06, 10.76780272350167245 ) ) ;
#63635 = DIRECTION ( 'NONE',  ( -0.000000000000000000, 1.000000000000000000, 4.476705744456276341E-16 ) ) ;
#63636 = CARTESIAN_POINT ( 'NONE',  ( 6.676582343750003368, 297.0156250017070079, -2.765530957081997254 ) ) ;
#63637 = VERTEX_POINT ( 'NONE', #37956 ) ;
#63639 = VECTOR ( 'NONE', #71169, 1000.000000000000000 ) ;
#63638 = CARTESIAN_POINT ( 'NONE',  ( 3.999999999999960032, 202.0625000027312410, 143.6568542494924259 ) ) ;
#63640 = CARTESIAN_POINT ( 'NONE',  ( -9.832129032723418760, 213.1770833299193555, -5.676582343750004256 ) ) ;
#63641 = EDGE_CURVE ( 'NONE', #10325, #67709, #8903, .T. ) ;
#63642 = EDGE_CURVE ( 'NONE', #45912, #53849, #61330, .T. ) ;
#63643 = CARTESIAN_POINT ( 'NONE',  ( -7.204075437095967871, 7.204075437095967871, 89.96875000204838102 ) ) ;
#63644 = VECTOR ( 'NONE', #21448, 1000.000000000000000 ) ;
#63645 = CARTESIAN_POINT ( 'NONE',  ( -30.44569435410879166, 204.8125000013656063, 172.4456943541092357 ) ) ;
#63646 = CARTESIAN_POINT ( 'NONE',  ( 3.313708498984762496, 14.71875000000000355, 7.999999999999998224 ) ) ;
#63647 = ORIENTED_EDGE ( 'NONE', *, *, #764, .T. ) ;
#63648 = ADVANCED_FACE ( 'NONE', ( #38704 ), #21698, .F. ) ;
#63649 = VECTOR ( 'NONE', #47988, 1000.000000000000000 ) ;
#63650 = CARTESIAN_POINT ( 'NONE',  ( 2.977408999572654480, 121.6250000020483810, 7.188101187499999156 ) ) ;
#63651 = CARTESIAN_POINT ( 'NONE',  ( 1.469576158976822172E-15, -7.999999999999991118, 19.20530277982336642 ) ) ;
#63652 = CARTESIAN_POINT ( 'NONE',  ( 10.00000000000000178, 25.00000000000000000, 0.000000000000000000 ) ) ;
#63653 = VECTOR ( 'NONE', #72109, 1000.000000000000000 ) ;
#63654 = DIRECTION ( 'NONE',  ( 1.000000000000000000, 0.000000000000000000, 0.000000000000000000 ) ) ;
#63655 = CARTESIAN_POINT ( 'NONE',  ( -10.18810118749999916, 0.000000000000000000, 77.03125000204836681 ) ) ;
#63656 = VERTEX_POINT ( 'NONE', #49253 ) ;
#63657 = DIRECTION ( 'NONE',  ( -0.000000000000000000, 1.000000000000000000, -0.000000000000000000 ) ) ;
#63658 = CARTESIAN_POINT ( 'NONE',  ( 8.000000000000035527, 3.313708498984715423, 6.174052779823363757 ) ) ;
#63659 = FACE_OUTER_BOUND ( 'NONE', #16187, .T. ) ;
#63660 = CARTESIAN_POINT ( 'NONE',  ( -5.000000000000000000, -16.24494643555759410, 69.83755725260752456 ) ) ;
#63661 = ADVANCED_FACE ( 'NONE', ( #25857 ), #60579, .T. ) ;
#63662 = CARTESIAN_POINT ( 'NONE',  ( 2.170320029194141132, 51.35721532638042675, 48.60044191894211707 ) ) ;
#63663 = CARTESIAN_POINT ( 'NONE',  ( 6.676582343750001591, 297.9531250017069510, -8.176455196517173205E-16 ) ) ;
#63665 = CARTESIAN_POINT ( 'NONE',  ( -2.485281374238875962, 288.8750000034139020, -5.999999999999697131 ) ) ;
#63664 = CARTESIAN_POINT ( 'NONE',  ( -9.832129032723418760, 248.4895833367473301, -5.676582343749998927 ) ) ;
#63666 = ORIENTED_EDGE ( 'NONE', *, *, #50082, .T. ) ;
#63667 = CARTESIAN_POINT ( 'NONE',  ( 2.085542519210945334E-15, 240.4687500034139873, 11.35316468749999963 ) ) ;
#63668 = CARTESIAN_POINT ( 'NONE',  ( -4.401442555609577197E-16, 7.188101187499992051, 8.611552781871752771 ) ) ;
#63669 = ORIENTED_EDGE ( 'NONE', *, *, #8568, .F. ) ;
#63670 = CARTESIAN_POINT ( 'NONE',  ( -6.238412754330611322E-16, 10.18810118749999916, 68.78125000204838102 ) ) ;
#63671 = CARTESIAN_POINT ( 'NONE',  ( -11.35316468750000141, 88.80208332991935549, 3.042071309553159963 ) ) ;
#63672 = CARTESIAN_POINT ( 'NONE',  ( -18.00000000000000000, 10.39230484541324628, -1.607695154586745501 ) ) ;
#63673 = CARTESIAN_POINT ( 'NONE',  ( -10.99999999999999822, -4.556349186104052151, 82.09375000000000000 ) ) ;
#63676 = CARTESIAN_POINT ( 'NONE',  ( -6.062591786044946751, -5.219672483564715471, -0.3118205092643556720 ) ) ;
#63675 = CARTESIAN_POINT ( 'NONE',  ( 30.44569435410879876, 208.8125000013656063, 167.5543056458910485 ) ) ;
#63674 = CARTESIAN_POINT ( 'NONE',  ( 25.55430564589115505, 207.5625000013656063, 172.4456943541086957 ) ) ;
#63677 = EDGE_LOOP ( 'NONE', ( #3195, #51468, #27189, #15307 ) ) ;
#63678 = CARTESIAN_POINT ( 'NONE',  ( -1.836970198721029983E-15, 75.62499999317203958, 10.00000000000000178 ) ) ;
#63679 = FACE_OUTER_BOUND ( 'NONE', #74098, .T. ) ;
#63680 = EDGE_CURVE ( 'NONE', #39327, #43701, #23282, .T. ) ;
#63681 = CARTESIAN_POINT ( 'NONE',  ( 9.832129032723416984, 195.3645833299193839, 5.676582343750006032 ) ) ;
#63682 = CARTESIAN_POINT ( 'NONE',  ( -3.458734125000015425, 203.9375000013656063, 142.0000000000000568 ) ) ;
#63683 = CARTESIAN_POINT ( 'NONE',  ( 30.44569435410883784, 206.0625000013656063, 167.5543056458911053 ) ) ;
#63684 = CARTESIAN_POINT ( 'NONE',  ( -1.320432766682874540E-15, 22.96874999795161543, 7.188101187500000044 ) ) ;
#63685 = CARTESIAN_POINT ( 'NONE',  ( 5.676582343750001591, 176.9270833299193555, -9.832129032723420536 ) ) ;
#63686 = CARTESIAN_POINT ( 'NONE',  ( 7.188101187500000044, 95.28125000204836681, -8.802885111219163269E-16 ) ) ;
#63688 = CARTESIAN_POINT ( 'NONE',  ( -8.660254037844385522, 107.9166666666666856, 4.999999999999996447 ) ) ;
#63687 = CARTESIAN_POINT ( 'NONE',  ( -2.485281374238187180, 296.2500000034140157, 6.000000000000385469 ) ) ;
#63689 = CARTESIAN_POINT ( 'NONE',  ( -3.211159895383561391, 8.687499998634407916, -3.211159895383561835 ) ) ;
#63690 = CARTESIAN_POINT ( 'NONE',  ( 25.55430564589115150, 204.5625000013656063, 172.4456943541086957 ) ) ;
#63691 = CARTESIAN_POINT ( 'NONE',  ( 5.082755093536318824, 5.082755093536319713, 11.79905278187175632 ) ) ;
#63692 = CARTESIAN_POINT ( 'NONE',  ( 3.042071309553159519, 74.73958332991932707, 11.35316468750000141 ) ) ;
#63693 = CYLINDRICAL_SURFACE ( 'NONE', #71329, 11.00000000000000000 ) ;
#63694 = B_SPLINE_CURVE_WITH_KNOTS ( 'NONE', 1,
 ( #38217, #4632 ),
 .UNSPECIFIED., .F., .F.,
 ( 2, 2 ),
 ( 0.000000000000000000, 0.6095729009238285423 ),
 .UNSPECIFIED. ) ;
#63695 = CARTESIAN_POINT ( 'NONE',  ( -8.000000000000000000, 119.1875000040967763, 0.000000000000000000 ) ) ;
#63696 = EDGE_LOOP ( 'NONE', ( #61009, #20039, #43139, #61387 ) ) ;
#63697 = CARTESIAN_POINT ( 'NONE',  ( 10.03369110562687361, 8.063452199751775851, -0.4760262082327572641 ) ) ;
#63698 = CARTESIAN_POINT ( 'NONE',  ( -2.828427124746208943, 203.7500000027312126, 144.8284271247462129 ) ) ;
#63699 = CARTESIAN_POINT ( 'NONE',  ( 3.042071309553167069, 56.82291666325268409, -11.35316468749999785 ) ) ;
#63700 = VECTOR ( 'NONE', #18780, 1000.000000000000000 ) ;
#63701 = CARTESIAN_POINT ( 'NONE',  ( 4.556349186104051263, -10.99999999999999822, 67.65625000409677625 ) ) ;
#63702 = CARTESIAN_POINT ( 'NONE',  ( -2.839093476692135984E-14, 194.9375000013655779, 138.5412658750000503 ) ) ;
#63703 = CARTESIAN_POINT ( 'NONE',  ( -31.66756539373085388, -30.58405805906214781, 167.9999999999997726 ) ) ;
#63705 = CARTESIAN_POINT ( 'NONE',  ( -9.832129032723420536, 53.69791666325267698, 5.676582343749997150 ) ) ;
#63704 = CARTESIAN_POINT ( 'NONE',  ( -7.188101187499999156, 92.75000000204839523, 2.977408999572654924 ) ) ;
#63706 = CARTESIAN_POINT ( 'NONE',  ( -7.999999999999991118, 3.313708498984756723, 3.736552779823362869 ) ) ;
#63707 = DIRECTION ( 'NONE',  ( 0.000000000000000000, 0.000000000000000000, 1.000000000000000000 ) ) ;
#63708 = AXIS2_PLACEMENT_3D ( 'NONE', #56747, #73712, #15242 ) ;
#63709 = CARTESIAN_POINT ( 'NONE',  ( 7.320508075688774596, 157.4999999931720254, -7.320508075688774596 ) ) ;
#63710 = CARTESIAN_POINT ( 'NONE',  ( -7.188101187500000044, 99.03125000204838102, 0.000000000000000000 ) ) ;
#63711 = CARTESIAN_POINT ( 'NONE',  ( 11.00000000000000000, 1.347111479062088405E-15, 105.2500000000000000 ) ) ;
#63712 = CARTESIAN_POINT ( 'NONE',  ( -11.35316468750000141, 53.80208332991935549, 3.042071309553159963 ) ) ;
#63713 =( BOUNDED_CURVE ( )  B_SPLINE_CURVE ( 2, ( #40444, #30231, #35533, #52508, #29865, #47203, #41550, #52879, #58549 ),
 .UNSPECIFIED., .F., .F. ) 
 B_SPLINE_CURVE_WITH_KNOTS ( ( 3, 2, 2, 2, 3 ),
 ( 0.3750000000000000000, 0.3806818181818181768, 0.3863636363636363535, 0.3920454545454545858, 0.3977272727272727626 ),
 .UNSPECIFIED. ) 
 CURVE ( )  GEOMETRIC_REPRESENTATION_ITEM ( )  RATIONAL_B_SPLINE_CURVE ( ( 1.000000000000000000, 0.9238795325112867385, 1.000000000000000000, 0.9238795325112867385, 1.000000000000000000, 0.9238795325112867385, 1.000000000000000000, 0.9238795325112859613, 1.000000000000000666 ) ) 
 REPRESENTATION_ITEM ( '' )  );
#63714 = CARTESIAN_POINT ( 'NONE',  ( -10.18810118749999916, 4.220049686691934809, 115.9375000020483810 ) ) ;
#63715 = CARTESIAN_POINT ( 'NONE',  ( 9.832129032723416984, 180.3645833299193555, 5.676582343750006032 ) ) ;
#63716 = ORIENTED_EDGE ( 'NONE', *, *, #49425, .T. ) ;
#63718 =( BOUNDED_CURVE ( )  B_SPLINE_CURVE ( 2, ( #44297, #33000, #27303, #15609, #32621, #10340, #60896, #37898, #62015, #44670, #5059, #55629, #3945 ),
 .UNSPECIFIED., .F., .F. ) 
 B_SPLINE_CURVE_WITH_KNOTS ( ( 3, 2, 2, 2, 2, 2, 3 ),
 ( 1.931089053012635004, 1.936321672528442228, 1.941554292044249452, 1.946786911560056677, 1.952019531075864123, 1.957252150591671347, 1.962484770107478571 ),
 .UNSPECIFIED. ) 
 CURVE ( )  GEOMETRIC_REPRESENTATION_ITEM ( )  RATIONAL_B_SPLINE_CURVE ( ( 0.9999999999997452038, 0.9659258262893231084, 1.000000000000000000, 0.9659258262890683122, 1.000000000000000000, 0.9659258262890683122, 1.000000000000000000, 0.9659258262890683122, 1.000000000000000000, 0.9659258262890683122, 1.000000000000000000, 0.9659258262894233615, 0.9999999999996449507 ) ) 
 REPRESENTATION_ITEM ( '' )  );
#63717 = CARTESIAN_POINT ( 'NONE',  ( 6.891449706546032061, 61.56004288259459400, 23.71475313280759423 ) ) ;
#63719 = CARTESIAN_POINT ( 'NONE',  ( -23.99999999999998934, 198.8750000027312126, 170.0000000000002842 ) ) ;
#63720 = CARTESIAN_POINT ( 'NONE',  ( -27.99999999999995737, 201.5000000000000000, 174.0000000000003695 ) ) ;
#63722 = CARTESIAN_POINT ( 'NONE',  ( -3.042071309553173730, 184.3229166632526983, 11.35316468749999785 ) ) ;
#63721 = DIRECTION ( 'NONE',  ( -0.000000000000000000, -1.000000000000000000, -4.283267841918042741E-17 ) ) ;
#63723 = EDGE_CURVE ( 'NONE', #746, #32640, #54116, .T. ) ;
#63724 = LINE ( 'NONE', #6403, #20068 ) ;
#63725 = CARTESIAN_POINT ( 'NONE',  ( 1.836970198721029589E-15, 249.3750000068279746, 10.00000000000000000 ) ) ;
#63726 = CARTESIAN_POINT ( 'NONE',  ( 47.32259252271278882, 38.77329591270031983, 65.76194439203456454 ) ) ;
#63727 = ORIENTED_EDGE ( 'NONE', *, *, #62081, .F. ) ;
#63728 = CARTESIAN_POINT ( 'NONE',  ( 11.35316468750000141, 171.0937499965860127, 0.000000000000000000 ) ) ;
#63729 = ADVANCED_FACE ( 'NONE', ( #44724, #9274 ), #9658, .F. ) ;
#63730 = CARTESIAN_POINT ( 'NONE',  ( 5.082755093536320601, -5.082755093536318824, 27.54905278187175455 ) ) ;
#63731 = CARTESIAN_POINT ( 'NONE',  ( -2.085542519210945728E-15, 134.8437499965860127, 11.35316468750000141 ) ) ;
#63732 = CARTESIAN_POINT ( 'NONE',  ( 1.249139735130299379E-15, 51.05255888325788050, 10.19999999999999396 ) ) ;
#63733 = ORIENTED_EDGE ( 'NONE', *, *, #19393, .T. ) ;
#63734 = CARTESIAN_POINT ( 'NONE',  ( 4.541265875000002339, 12.49999999863440969, -1.881053915767121554 ) ) ;
#63735 = EDGE_CURVE ( 'NONE', #17054, #24578, #31822, .T. ) ;
#63736 = ADVANCED_FACE ( 'NONE', ( #39068 ), #43977, .T. ) ;
#63737 = CARTESIAN_POINT ( 'NONE',  ( 5.656854249492381470, 103.2500000040967905, 5.656854249492379694 ) ) ;
#63738 = EDGE_CURVE ( 'NONE', #11319, #17570, #14915, .T. ) ;
#63739 = AXIS2_PLACEMENT_3D ( 'NONE', #34946, #57958, #39834 ) ;
#63740 = CARTESIAN_POINT ( 'NONE',  ( 4.000000000000000888, 10.93750000000000000, 1.656854249492384135 ) ) ;
#63741 = CARTESIAN_POINT ( 'NONE',  ( 4.500000000000010658, 7.794228634059937377, 0.000000000000000000 ) ) ;
#63742 = CARTESIAN_POINT ( 'NONE',  ( 4.541265875000001451, 11.24999999863441147, 1.881053915767124440 ) ) ;
#63743 = CARTESIAN_POINT ( 'NONE',  ( -3.313708498984758943, -7.999999999999989342, 22.29905278392014623 ) ) ;
#63744 = CARTESIAN_POINT ( 'NONE',  ( 3.999999999999960032, 196.0000000000000000, 142.0000000000000568 ) ) ;
#63745 = ORIENTED_EDGE ( 'NONE', *, *, #36316, .F. ) ;
#63746 = DIRECTION ( 'NONE',  ( -0.000000000000000000, -1.000000000000000000, -4.283267841918042741E-17 ) ) ;
#63747 = CARTESIAN_POINT ( 'NONE',  ( -7.188101187500001821, 101.5625000020483810, -2.977408999572650483 ) ) ;
#63748 = EDGE_CURVE ( 'NONE', #12665, #22034, #46400, .T. ) ;
#63750 = DIRECTION ( 'NONE',  ( 0.000000000000000000, 0.000000000000000000, -1.000000000000000000 ) ) ;
#63749 = CARTESIAN_POINT ( 'NONE',  ( -11.00000000000000000, 0.000000000000000000, 79.18750000409677625 ) ) ;
#63751 = DIRECTION ( 'NONE',  ( 1.000000000000000000, 0.000000000000000000, 0.000000000000000000 ) ) ;
#63752 = ORIENTED_EDGE ( 'NONE', *, *, #7856, .F. ) ;
#63753 = CARTESIAN_POINT ( 'NONE',  ( -2.216418498320018582, 16.40908668940205573, -68.78644440154944562 ) ) ;
#63754 = CARTESIAN_POINT ( 'NONE',  ( -7.188101187499992051, 0.000000000000000000, 22.48655278187175455 ) ) ;
#63755 = ORIENTED_EDGE ( 'NONE', *, *, #668, .T. ) ;
#63756 = VERTEX_POINT ( 'NONE', #23193 ) ;
#63757 = CARTESIAN_POINT ( 'NONE',  ( 1.871523826299183495E-15, -10.18810118749999916, 84.53125000204836681 ) ) ;
#63758 = CARTESIAN_POINT ( 'NONE',  ( -29.43265458321766914, 196.7500000013656063, 166.5412658750003629 ) ) ;
#63759 = CARTESIAN_POINT ( 'NONE',  ( -11.00000000000000000, 4.556349186104045934, 102.9062499999999858 ) ) ;
#63762 = CARTESIAN_POINT ( 'NONE',  ( 6.676582343750001591, 298.1093750017069510, -8.176455196517173205E-16 ) ) ;
#63761 = CARTESIAN_POINT ( 'NONE',  ( 29.65685424949240812, 206.1875000027311842, 173.9999999999999147 ) ) ;
#63760 = LINE ( 'NONE', #22275, #63956 ) ;
#63763 = CARTESIAN_POINT ( 'NONE',  ( 8.660254037844389075, 140.4166666666666572, -5.000000000000000000 ) ) ;
#63764 = CARTESIAN_POINT ( 'NONE',  ( 5.656854249492379694, 101.9375000000000000, -5.656854249492380582 ) ) ;
#63765 = CARTESIAN_POINT ( 'NONE',  ( 1.948298507267161028, 225.9999999999999716, 9.816171838510573622 ) ) ;
#63766 = DIRECTION ( 'NONE',  ( 1.000000000000000000, 0.000000000000000000, -0.000000000000000000 ) ) ;
#63767 = PLANE ( 'NONE',  #73544 ) ;
#63768 = B_SPLINE_CURVE_WITH_KNOTS ( 'NONE', 3,
 ( #65090, #48108, #71118, #48482, #15266, #66584, #25832, #61307, #71860, #20174, #2842, #38299 ),
 .UNSPECIFIED., .F., .F.,
 ( 4, 2, 2, 2, 2, 4 ),
 ( 6.134400178827896381E-17, 0.001907903290037582782, 0.002861854935056343165, 0.003815806580075103982, 0.005723709870112623013, 0.007631613160150140310 ),
 .UNSPECIFIED. ) ;
#63769 = CARTESIAN_POINT ( 'NONE',  ( 24.54126587499998280, 204.2500000013655779, 171.4326545832175555 ) ) ;
#63770 = CARTESIAN_POINT ( 'NONE',  ( -1.320432766682874540E-15, 3.468749997951610986, 7.188101187500000044 ) ) ;
#63771 = CARTESIAN_POINT ( 'NONE',  ( -4.903558642999205574E-16, 8.008118988124991233, 0.6381152839406293298 ) ) ;
#63772 = CARTESIAN_POINT ( 'NONE',  ( -2.445694354108839619, 196.8125000013656063, 139.5543056458912190 ) ) ;
#63773 = CARTESIAN_POINT ( 'NONE',  ( -2.977408999572652260, 118.8125000020484094, 7.188101187500000044 ) ) ;
#63775 = CARTESIAN_POINT ( 'NONE',  ( -3.313708498984759387, -7.999999999999989342, 7.111552779823365533 ) ) ;
#63774 = CARTESIAN_POINT ( 'NONE',  ( -4.000000000000015987, 204.5625000000000000, 143.6568542494924259 ) ) ;
#63776 = CARTESIAN_POINT ( 'NONE',  ( 9.832129032723416984, 232.1354166700806445, -5.676582343750003368 ) ) ;
#63777 = LINE ( 'NONE', #1169, #4845 ) ;
#63778 = CARTESIAN_POINT ( 'NONE',  ( 7.188101187499991163, 2.977408999572648707, 28.20530278187175455 ) ) ;
#63779 = CARTESIAN_POINT ( 'NONE',  ( 32.00000000000000000, 198.3125000000000284, 168.3431457505075741 ) ) ;
#63780 = CARTESIAN_POINT ( 'NONE',  ( 5.676582343750001591, 26.61458332991935194, -9.832129032723420536 ) ) ;
#63781 = CARTESIAN_POINT ( 'NONE',  ( -30.82842712474615965, 199.3750000000000284, 172.8284271247465824 ) ) ;
#63782 = CARTESIAN_POINT ( 'NONE',  ( -3.042071309553164404, 222.5520833299192986, -11.35316468749999963 ) ) ;
#63783 = CARTESIAN_POINT ( 'NONE',  ( -10.00000000000000000, 240.0000000000000284, 0.000000000000000000 ) ) ;
#63785 = CARTESIAN_POINT ( 'NONE',  ( -10.00000000000016342, 42.29166666666676377, -2.679491924311274254 ) ) ;
#63784 = LINE ( 'NONE', #29090, #33521 ) ;
#63786 = ORIENTED_EDGE ( 'NONE', *, *, #23306, .T. ) ;
#63787 = CARTESIAN_POINT ( 'NONE',  ( -2.445694354108839175, 198.3125000013656063, 144.4456943541088663 ) ) ;
#63788 = CARTESIAN_POINT ( 'NONE',  ( 3.042071309553159519, 24.73958332991934483, 11.35316468750000141 ) ) ;
#63789 = CARTESIAN_POINT ( 'NONE',  ( -7.778174593052020747, -7.778174593052023411, 85.37500000409677625 ) ) ;
#63790 = CARTESIAN_POINT ( 'NONE',  ( 1.432654583217608080, 207.8750000013656063, 138.5412658750000503 ) ) ;
#63791 = LINE ( 'NONE', #29472, #27442 ) ;
#63793 = CARTESIAN_POINT ( 'NONE',  ( -5.676582343750006032, 24.11458332991935194, 9.832129032723418760 ) ) ;
#63792 = CARTESIAN_POINT ( 'NONE',  ( -7.188101187500000933, 110.5625000020483810, -2.977408999572650483 ) ) ;
#63794 = CARTESIAN_POINT ( 'NONE',  ( -7.999999999999991118, 0.000000000000000000, 23.33030277982336642 ) ) ;
#63795 = CARTESIAN_POINT ( 'NONE',  ( 11.35316468749999785, 140.5729166632526983, 3.042071309553174174 ) ) ;
#63796 = AXIS2_PLACEMENT_3D ( 'NONE', #28426, #34487, #23504 ) ;
#63797 = CARTESIAN_POINT ( 'NONE',  ( 4.999999999999993783, 116.0416666598387110, 8.660254037844390851 ) ) ;
#63798 = CARTESIAN_POINT ( 'NONE',  ( 1.320432766682874540E-15, 117.4062500020483810, 7.188101187500000044 ) ) ;
#63799 = CARTESIAN_POINT ( 'NONE',  ( 3.428378827818789443, 68.02396499344450831, -20.38382289158443328 ) ) ;
#63800 = CARTESIAN_POINT ( 'NONE',  ( -24.54126587500000412, 209.5000000013656063, 168.5673454167827003 ) ) ;
#63801 = CARTESIAN_POINT ( 'NONE',  ( -5.000000000000000000, -53.50647209750557209, -45.02947987234075100 ) ) ;
#63802 = EDGE_LOOP ( 'NONE', ( #590, #59845, #58432, #13345, #49971, #18243, #5125, #2075, #49339, #56758, #39889, #251, #25767, #50474, #65591, #46942, #1197, #40122, #39070, #67104, #16409, #20524, #11403, #8396, #65973, #69581, #65012, #43149 ) ) ;
#63803 = CARTESIAN_POINT ( 'NONE',  ( 3.042071309553159519, 10.05208332991935016, 11.35316468750000141 ) ) ;
#63804 = AXIS2_PLACEMENT_3D ( 'NONE', #7538, #24507, #36209 ) ;
#63805 = ORIENTED_EDGE ( 'NONE', *, *, #15005, .T. ) ;
#63806 = CARTESIAN_POINT ( 'NONE',  ( 4.556349186104052151, -10.99999999999999822, 100.4687500000000000 ) ) ;
#63807 = CARTESIAN_POINT ( 'NONE',  ( 4.721056650415999201, 296.0781250017069510, -4.721056650415999201 ) ) ;
#63808 = CARTESIAN_POINT ( 'NONE',  ( 5.676582343749993598, 139.9479166632526983, 9.832129032723422313 ) ) ;
#63809 = SURFACE_STYLE_FILL_AREA ( #35525 ) ;
#63810 = CARTESIAN_POINT ( 'NONE',  ( 1.469576158976822172E-15, -7.999999999999991118, 25.26155278432982954 ) ) ;
#63811 =( BOUNDED_CURVE ( )  B_SPLINE_CURVE ( 2, ( #72377, #15396, #39171, #44832, #73871, #38433, #27099, #26339, #21436 ),
 .UNSPECIFIED., .F., .F. ) 
 B_SPLINE_CURVE_WITH_KNOTS ( ( 3, 2, 2, 2, 3 ),
 ( 0.1000000000000000888, 0.1083333333333334203, 0.1166666666666667657, 0.1250000000000001110, 0.1333333333333334425 ),
 .UNSPECIFIED. ) 
 CURVE ( )  GEOMETRIC_REPRESENTATION_ITEM ( )  RATIONAL_B_SPLINE_CURVE ( ( 0.9999999999999992228, 0.9238795325112875156, 1.000000000000000000, 0.9238795325112867385, 1.000000000000000000, 0.9238795325112867385, 1.000000000000000000, 0.9238795325112857393, 1.000000000000001110 ) ) 
 REPRESENTATION_ITEM ( '' )  );
#63812 = EDGE_CURVE ( 'NONE', #31431, #43256, #71953, .T. ) ;
#63813 = CARTESIAN_POINT ( 'NONE',  ( 48.99120217047246229, 196.4660678953013075, 59.51095261404043413 ) ) ;
#63814 = VECTOR ( 'NONE', #28178, 1000.000000000000000 ) ;
#63815 = CARTESIAN_POINT ( 'NONE',  ( -11.35316468749999608, 244.1145833367472733, 3.042071309553173730 ) ) ;
#63816 = CARTESIAN_POINT ( 'NONE',  ( -7.204075437095967871, 7.204075437095967871, 88.84375000204838102 ) ) ;
#63817 = ORIENTED_EDGE ( 'NONE', *, *, #30960, .T. ) ;
#63818 = DIRECTION ( 'NONE',  ( 0.000000000000000000, 0.000000000000000000, -1.000000000000000000 ) ) ;
#63819 = CARTESIAN_POINT ( 'NONE',  ( 0.000000000000000000, 0.000000000000000000, 28.00000000000000000 ) ) ;
#63820 = CARTESIAN_POINT ( 'NONE',  ( 11.35316468749999785, 95.88541666325269830, 3.042071309553174174 ) ) ;
#63821 = EDGE_LOOP ( 'NONE', ( #50273, #59356, #18071, #64994, #64249, #29533 ) ) ;
#63822 = CARTESIAN_POINT ( 'NONE',  ( -10.18810118749999916, 4.220049686691934809, 105.0625000020483810 ) ) ;
#63823 = CARTESIAN_POINT ( 'NONE',  ( -4.541265875000003227, 12.99999999863440969, 1.881053915767121110 ) ) ;
#63824 = ORIENTED_EDGE ( 'NONE', *, *, #27472, .F. ) ;
#63825 = ORIENTED_EDGE ( 'NONE', *, *, #50850, .F. ) ;
#63826 = CARTESIAN_POINT ( 'NONE',  ( -3.313708498984760720, 6.468750000000001776, -8.000000000000000000 ) ) ;
#63827 = CARTESIAN_POINT ( 'NONE',  ( 3.211159895383560947, 1.312499998634406806, 3.211159895383562723 ) ) ;
#63828 = CARTESIAN_POINT ( 'NONE',  ( 11.00000000000000000, 1.347111479062088405E-15, 76.93750000409677625 ) ) ;
#63829 = CARTESIAN_POINT ( 'NONE',  ( -7.188101187500002709, 22.68749999795161543, 2.977408999572649151 ) ) ;
#63830 = CARTESIAN_POINT ( 'NONE',  ( -8.000000000000000000, 122.0937500040967905, -3.313708498984761608 ) ) ;
#63831 =( BOUNDED_CURVE ( )  B_SPLINE_CURVE ( 2, ( #71670, #43758, #19990, #30949, #26011, #35243, #60358, #42998, #917 ),
 .UNSPECIFIED., .F., .F. ) 
 B_SPLINE_CURVE_WITH_KNOTS ( ( 3, 2, 2, 2, 3 ),
 ( 0.8958333333333318160, 0.9062499999999984457, 0.9166666666666650753, 0.9270833333333318160, 0.9374999999999984457 ),
 .UNSPECIFIED. ) 
 CURVE ( )  GEOMETRIC_REPRESENTATION_ITEM ( )  RATIONAL_B_SPLINE_CURVE ( ( 1.000000000000011324, 0.9238795325112754142, 1.000000000000000000, 0.9238795325112867385, 1.000000000000000000, 0.9238795325112867385, 1.000000000000000000, 0.9238795325112980628, 0.9999999999999886757 ) ) 
 REPRESENTATION_ITEM ( '' )  );
#63832 = CARTESIAN_POINT ( 'NONE',  ( 1.871523826299183495E-15, -10.18810118749999916, 104.4062500020483810 ) ) ;
#63833 = EDGE_CURVE ( 'NONE', #68525, #22045, #68844, .T. ) ;
#63834 = CARTESIAN_POINT ( 'NONE',  ( -1.656854249492383691, 1.687500000000000222, 4.000000000000000888 ) ) ;
#63835 = CARTESIAN_POINT ( 'NONE',  ( 2.828427124746190291, 8.624999997268814056, 2.828427124746192067 ) ) ;
#63836 = CARTESIAN_POINT ( 'NONE',  ( 4.541265875000002339, 0.3124999986344066949, 0.000000000000000000 ) ) ;
#63837 = ORIENTED_EDGE ( 'NONE', *, *, #62991, .T. ) ;
#63838 = CARTESIAN_POINT ( 'NONE',  ( -4.556349186104048599, -10.99999999999999822, 80.78124999999998579 ) ) ;
#63839 = CARTESIAN_POINT ( 'NONE',  ( 3.458734125000015425, 197.9375000013655779, 198.0000000000000284 ) ) ;
#63840 = EDGE_CURVE ( 'NONE', #71972, #67635, #67952, .T. ) ;
#63841 = CARTESIAN_POINT ( 'NONE',  ( -25.55430564589123321, 206.3125000013656063, 167.5543056458915032 ) ) ;
#63842 = EDGE_CURVE ( 'NONE', #71172, #35837, #39435, .T. ) ;
#63843 = CARTESIAN_POINT ( 'NONE',  ( -4.541265875000003227, 9.874999998634404363, 1.881053915767121110 ) ) ;
#63844 = VECTOR ( 'NONE', #61625, 1000.000000000000000 ) ;
#63846 = CARTESIAN_POINT ( 'NONE',  ( -1.656854249492440978, 206.8125000027312126, 146.0000000000000000 ) ) ;
#63845 = SHAPE_REPRESENTATION ( 'key', ( #57354 ), #51304 ) ;
#63847 = CARTESIAN_POINT ( 'NONE',  ( 5.082755093536320601, -5.082755093536318824, 11.04905278187175455 ) ) ;
#63848 = EDGE_LOOP ( 'NONE', ( #44620, #28749, #37086, #15413, #33586, #21957, #51660, #67545, #25731 ) ) ;
#63849 = EDGE_LOOP ( 'NONE', ( #54217, #12137, #15985, #70061, #24313, #34915, #54103 ) ) ;
#63850 = CARTESIAN_POINT ( 'NONE',  ( -10.18810118749999738, -4.220049686691941915, 103.7500000020483668 ) ) ;
#63851 = CARTESIAN_POINT ( 'NONE',  ( 1.469576158976823947E-15, 95.56250000409677625, 8.000000000000000000 ) ) ;
#63852 = CARTESIAN_POINT ( 'NONE',  ( -29.65685424949241167, 205.0625000000000568, 166.0000000000004263 ) ) ;
#63853 = CARTESIAN_POINT ( 'NONE',  ( 2.445694354108838731, 201.0625000013656063, 195.5543056458912190 ) ) ;
#63854 = CARTESIAN_POINT ( 'NONE',  ( 30.44569435410882718, 194.5625000013656063, 172.4456943541086957 ) ) ;
#63855 = CARTESIAN_POINT ( 'NONE',  ( 10.00000000000000000, 94.79166666666668561, 2.679491924311236062 ) ) ;
#63856 = CARTESIAN_POINT ( 'NONE',  ( -3.313708498984762052, 115.7187499999999858, -8.000000000000000000 ) ) ;
#63857 = CARTESIAN_POINT ( 'NONE',  ( 6.951808397369818766E-16, 67.34374999658601268, -11.35316468750000141 ) ) ;
#63858 = CARTESIAN_POINT ( 'NONE',  ( -6.000000000000001776, 288.0000000000000000, 0.000000000000000000 ) ) ;
#63859 = VERTEX_POINT ( 'NONE', #51121 ) ;
#63860 = CARTESIAN_POINT ( 'NONE',  ( 2.485281374238929697, 294.3124999999999432, 5.999999999999645617 ) ) ;
#63861 = ADVANCED_FACE ( 'NONE', ( #62804 ), #45456, .F. ) ;
#63862 = CARTESIAN_POINT ( 'NONE',  ( -5.656854249492381470, 15.74999999590322197, 5.656854249492379694 ) ) ;
#63863 = CARTESIAN_POINT ( 'NONE',  ( 1.432654583217607858, 205.6250000013656063, 138.5412658750000787 ) ) ;
#63864 = CARTESIAN_POINT ( 'NONE',  ( -1.836970198721029983E-15, 105.6249999931720396, 10.00000000000000178 ) ) ;
#63865 = CARTESIAN_POINT ( 'NONE',  ( 1.469576158976823947E-15, 96.87499999999998579, 8.000000000000000000 ) ) ;
#63866 = CARTESIAN_POINT ( 'NONE',  ( -2.679491924311228512, 243.9583333333333144, -9.999999999999998224 ) ) ;
#63867 = CARTESIAN_POINT ( 'NONE',  ( -31.99999999999996447, 202.4375000027311842, 171.6568542494928522 ) ) ;
#63868 = CARTESIAN_POINT ( 'NONE',  ( 1.871523826299183495E-15, -10.18810118749999916, 71.40625000204836681 ) ) ;
#63869 = CARTESIAN_POINT ( 'NONE',  ( -2.679491924311235618, 208.5416666666666856, 10.00000000000000000 ) ) ;
#63870 = CARTESIAN_POINT ( 'NONE',  ( -7.188101187499992051, 2.977408999572646930, 10.76780278187175632 ) ) ;
#63871 = CARTESIAN_POINT ( 'NONE',  ( 8.311093377946837890, 186.7187499965860127, -8.311093377946837890 ) ) ;
#63872 = CARTESIAN_POINT ( 'NONE',  ( -2.679491924309679529, 36.45833333333319359, -10.00000000000089351 ) ) ;
#63873 = CARTESIAN_POINT ( 'NONE',  ( 7.320508075688774596, 177.4999999931720254, -7.320508075688774596 ) ) ;
#63875 = CARTESIAN_POINT ( 'NONE',  ( -54.00000000000000711, 205.0000000000000568, 20.00000000000002842 ) ) ;
#63874 = DIRECTION ( 'NONE',  ( 0.000000000000000000, 0.000000000000000000, 1.000000000000000000 ) ) ;
#63876 = ORIENTED_EDGE ( 'NONE', *, *, #30181, .T. ) ;
#63877 = CARTESIAN_POINT ( 'NONE',  ( -1.432654583217662481, 195.1250000013656063, 145.4587341250000634 ) ) ;
#63878 = CARTESIAN_POINT ( 'NONE',  ( 8.311093377946837890, 36.71874999658601979, -8.311093377946837890 ) ) ;
#63879 = CARTESIAN_POINT ( 'NONE',  ( 4.556349186104045934, 11.00000000000000000, 111.7187500040967905 ) ) ;
#63880 = CARTESIAN_POINT ( 'NONE',  ( -28.00000000000007105, 204.4375000013656063, 166.5412658750003629 ) ) ;
#63881 = CARTESIAN_POINT ( 'NONE',  ( -4.898587196589412829E-16, 96.12499999999998579, -8.000000000000000000 ) ) ;
#63883 = CARTESIAN_POINT ( 'NONE',  ( 0.000000000000000000, 0.000000000000000000, 30.00000000000000000 ) ) ;
#63882 = CARTESIAN_POINT ( 'NONE',  ( -8.000000000000000000, 116.1875000040967763, 0.000000000000000000 ) ) ;
#63884 = CARTESIAN_POINT ( 'NONE',  ( -3.458734125000015425, 199.9375000013656063, 142.0000000000000568 ) ) ;
#63885 = CIRCLE ( 'NONE', #62691, 11.00000000000000000 ) ;
#63886 = CARTESIAN_POINT ( 'NONE',  ( 8.660254037844389075, 77.29166665983871098, -5.000000000000000000 ) ) ;
#63887 = CARTESIAN_POINT ( 'NONE',  ( 7.188101187500002709, 99.31250000204839523, 2.977408999572649151 ) ) ;
#63888 = CARTESIAN_POINT ( 'NONE',  ( 4.541265875000001451, 12.37499999863440969, 1.881053915767124440 ) ) ;
#63889 = CARTESIAN_POINT ( 'NONE',  ( 54.00000000000000000, 0.000000000000000000, 4.085831468968142743E-14 ) ) ;
#63890 = CARTESIAN_POINT ( 'NONE',  ( 6.949739821034066622, 0.2534984199823389073, -3.475076582212567100 ) ) ;
#63891 = DIRECTION ( 'NONE',  ( -0.000000000000000000, 1.000000000000000000, -0.000000000000000000 ) ) ;
#63892 = ORIENTED_EDGE ( 'NONE', *, *, #21763, .F. ) ;
#63893 = ORIENTED_EDGE ( 'NONE', *, *, #18092, .F. ) ;
#63894 = CARTESIAN_POINT ( 'NONE',  ( 4.556349186104045934, 11.00000000000000000, 116.0312499999999858 ) ) ;
#63895 = CARTESIAN_POINT ( 'NONE',  ( -6.676582343750000703, 296.6718750017069510, 2.765530957082001251 ) ) ;
#63896 = DIRECTION ( 'NONE',  ( 0.000000000000000000, 0.000000000000000000, 1.000000000000000000 ) ) ;
#63897 = CARTESIAN_POINT ( 'NONE',  ( 11.35316468749999963, 155.9895833299193555, -3.042071309553165293 ) ) ;
#63898 = B_SPLINE_CURVE_WITH_KNOTS ( 'NONE', 5,
 ( #15840, #50930, #18, #22620, #33980, #57725 ),
 .UNSPECIFIED., .F., .F.,
 ( 6, 6 ),
 ( 0.000000000000000000, 4.840251826652617773 ),
 .UNSPECIFIED. ) ;
#63899 = DIRECTION ( 'NONE',  ( -1.000000000000000000, 0.000000000000000000, 0.000000000000000000 ) ) ;
#63900 = CARTESIAN_POINT ( 'NONE',  ( 4.220049686691934809, 10.18810118749999916, 80.68750000204836681 ) ) ;
#63901 = CARTESIAN_POINT ( 'NONE',  ( -31.50809115661305171, 194.5826323124041153, 169.2389443069786523 ) ) ;
#63902 = CARTESIAN_POINT ( 'NONE',  ( 4.000000000000015987, 205.5000000000000284, 198.0000000000000284 ) ) ;
#63903 = DIRECTION ( 'NONE',  ( -0.000000000000000000, 1.000000000000000000, -0.000000000000000000 ) ) ;
#63904 = ADVANCED_FACE ( 'NONE', ( #6231 ), #22814, .F. ) ;
#63905 = CARTESIAN_POINT ( 'NONE',  ( -3.313708498984762496, 101.2812499999999858, 7.999999999999998224 ) ) ;
#63906 = ORIENTED_EDGE ( 'NONE', *, *, #26336, .T. ) ;
#63907 = VECTOR ( 'NONE', #58844, 1000.000000000000000 ) ;
#63908 = CARTESIAN_POINT ( 'NONE',  ( 8.000000000000000000, 17.81249999590322375, 0.000000000000000000 ) ) ;
#63909 = CARTESIAN_POINT ( 'NONE',  ( -4.396006015780578480, 177.9701120841904469, 139.2341220074533226 ) ) ;
#63910 = CARTESIAN_POINT ( 'NONE',  ( 11.35316468749999963, 126.3020833299193555, -3.042071309553165293 ) ) ;
#63911 = CARTESIAN_POINT ( 'NONE',  ( 2.445694354108838731, 197.0625000013656063, 195.5543056458912190 ) ) ;
#63912 = CARTESIAN_POINT ( 'NONE',  ( -7.188101187500000044, 27.09374999795161898, -8.802885111219163269E-16 ) ) ;
#63914 = ADVANCED_FACE ( 'NONE', ( #16773 ), #5481, .T. ) ;
#63913 = CARTESIAN_POINT ( 'NONE',  ( -4.220049686691937474, -10.18810118749999738, 75.81250000204838102 ) ) ;
#63915 = CARTESIAN_POINT ( 'NONE',  ( 9.832129032723420536, 51.51041666325269119, -5.676582343749999815 ) ) ;
#63916 = EDGE_LOOP ( 'NONE', ( #20875, #25565, #51237, #5376 ) ) ;
#63917 = DIRECTION ( 'NONE',  ( -0.000000000000000000, -1.000000000000000000, -4.283267841918042741E-17 ) ) ;
#63918 = CARTESIAN_POINT ( 'NONE',  ( -4.541265875000002339, 1.874999998634406806, -1.881053915767121998 ) ) ;
#63919 = CARTESIAN_POINT ( 'NONE',  ( -5.662595241051933570, -5.662595241051936235, 11.70061528394062833 ) ) ;
#63920 = CARTESIAN_POINT ( 'NONE',  ( -3.458734125000015869, 208.1875000013656063, 142.0000000000000568 ) ) ;
#63921 = AXIS2_PLACEMENT_3D ( 'NONE', #50695, #73714, #36969 ) ;
#63922 = AXIS2_PLACEMENT_3D ( 'NONE', #4621, #33307, #38587 ) ;
#63923 = CARTESIAN_POINT ( 'NONE',  ( 7.188101187500000044, 12.46874999795161187, 0.000000000000000000 ) ) ;
#63924 = CARTESIAN_POINT ( 'NONE',  ( -4.242640687119285658, 291.1875000034139589, 4.242640687119287435 ) ) ;
#63925 = CARTESIAN_POINT ( 'NONE',  ( -28.24654463531872750, -12.18778171663278798, 140.1250658210347240 ) ) ;
#63926 = CARTESIAN_POINT ( 'NONE',  ( 4.401442555609581635E-16, 5.718749997951610986, -7.188101187500000044 ) ) ;
#63927 = CARTESIAN_POINT ( 'NONE',  ( 5.082755093536320601, -5.082755093536318824, 9.549052781871754547 ) ) ;
#63928 = CARTESIAN_POINT ( 'NONE',  ( -4.220049686691937474, -10.18810118749999738, 72.43750000204838102 ) ) ;
#63929 = EDGE_CURVE ( 'NONE', #40550, #58393, #2893, .T. ) ;
#63930 =( BOUNDED_CURVE ( )  B_SPLINE_CURVE ( 2, ( #37536, #49593, #3577, #54893, #50332, #72609, #55644, #3204, #26192, #60909, #56015, #14873, #49212 ),
 .UNSPECIFIED., .F., .F. ) 
 B_SPLINE_CURVE_WITH_KNOTS ( ( 3, 2, 2, 2, 2, 2, 3 ),
 ( 2.747482230802302361, 2.752716221441485978, 2.757950211996366807, 2.763184202551248081, 2.768418193106129355, 2.773652183661010628, 2.778886174319656455 ),
 .UNSPECIFIED. ) 
 CURVE ( )  GEOMETRIC_REPRESENTATION_ITEM ( )  RATIONAL_B_SPLINE_CURVE ( ( 1.000000000000000000, 0.9659258262890683122, 1.000000000000000000, 0.9659258262890683122, 1.000000000000000000, 0.9659258262890683122, 1.000000000000000000, 0.9659258262890683122, 1.000000000000000000, 0.9659258262890683122, 1.000000000000000000, 0.9659258262890683122, 1.000000000000000000 ) ) 
 REPRESENTATION_ITEM ( '' )  );
#63931 = CARTESIAN_POINT ( 'NONE',  ( -25.55430564589115505, 206.3125000013656063, 172.4456943541091789 ) ) ;
#63932 = CARTESIAN_POINT ( 'NONE',  ( -4.000000000000001776, 15.50000000000000000, -4.898587196589415787E-16 ) ) ;
#63933 = CARTESIAN_POINT ( 'NONE',  ( -3.211159895383561391, 18.81249999863440436, -3.211159895383561835 ) ) ;
#63934 = UNCERTAINTY_MEASURE_WITH_UNIT (LENGTH_MEASURE( 1.000000000000000082E-05 ), #36657, 'distance_accuracy_value', 'NONE');
#63935 = EDGE_LOOP ( 'NONE', ( #43224, #3385, #68480, #45551 ) ) ;
#63936 = CARTESIAN_POINT ( 'NONE',  ( -1.656854249492348607, 195.3125000027311842, 202.0000000000000284 ) ) ;
#63937 = AXIS2_PLACEMENT_3D ( 'NONE', #72305, #10430, #16070 ) ;
#63938 = CARTESIAN_POINT ( 'NONE',  ( -4.000000000000015099, 206.5625000000000000, 143.6568542494924543 ) ) ;
#63939 = CARTESIAN_POINT ( 'NONE',  ( -30.82842712474624491, 201.2500000027312126, 167.1715728752542418 ) ) ;
#63940 = ADVANCED_FACE ( 'NONE', ( #17157 ), #40178, .F. ) ;
#63941 = CARTESIAN_POINT ( 'NONE',  ( -7.188101187499999156, 118.2500000020483952, 2.977408999572654924 ) ) ;
#63942 = DIRECTION ( 'NONE',  ( -0.000000000000000000, 1.000000000000000000, -0.000000000000000000 ) ) ;
#63943 = CARTESIAN_POINT ( 'NONE',  ( -5.656854249492373476, -5.656854249492376141, 1.205302783920146004 ) ) ;
#63944 = ORIENTED_EDGE ( 'NONE', *, *, #8716, .F. ) ;
#63946 =( BOUNDED_CURVE ( )  B_SPLINE_CURVE ( 2, ( #21364, #56093, #55722, #4037, #16437, #26268, #49288, #27031, #67025 ),
 .UNSPECIFIED., .F., .F. ) 
 B_SPLINE_CURVE_WITH_KNOTS ( ( 3, 2, 2, 2, 3 ),
 ( 0.1176470588235294795, 0.1213235294117647745, 0.1250000000000000833, 0.1286764705882353643, 0.1323529411764706731 ),
 .UNSPECIFIED. ) 
 CURVE ( )  GEOMETRIC_REPRESENTATION_ITEM ( )  RATIONAL_B_SPLINE_CURVE ( ( 0.9999999999999985567, 0.9238795325112881818, 1.000000000000000000, 0.9238795325112867385, 1.000000000000000000, 0.9238795325112867385, 1.000000000000000000, 0.9238795325112849621, 1.000000000000001776 ) ) 
 REPRESENTATION_ITEM ( '' )  );
#63945 = CARTESIAN_POINT ( 'NONE',  ( 5.082755093536325930, 17.15624999795161543, -5.082755093536325930 ) ) ;
#63947 = ORIENTED_EDGE ( 'NONE', *, *, #48375, .F. ) ;
#63948 = CARTESIAN_POINT ( 'NONE',  ( -10.00000000000000355, 44.58333332650536818, 2.679491924311223183 ) ) ;
#63949 = CARTESIAN_POINT ( 'NONE',  ( -5.000000000000005329, 48.33333333333334281, 8.660254037844387298 ) ) ;
#63950 = CARTESIAN_POINT ( 'NONE',  ( -2.977408999572650927, 100.2500000020483952, -7.188101187500001821 ) ) ;
#63951 = CARTESIAN_POINT ( 'NONE',  ( -31.45873412499998523, 203.0000000013655779, 171.4326545832180386 ) ) ;
#63952 = CARTESIAN_POINT ( 'NONE',  ( -3.673940397442060854E-16, 298.7500000000000000, -6.000000000000001776 ) ) ;
#63954 = DIRECTION ( 'NONE',  ( -0.000000000000000000, 1.000000000000000000, 0.000000000000000000 ) ) ;
#63953 = CARTESIAN_POINT ( 'NONE',  ( -4.898587196589412829E-16, 88.81250000409677625, -8.000000000000000000 ) ) ;
#63955 = ORIENTED_EDGE ( 'NONE', *, *, #8623, .T. ) ;
#63957 = CARTESIAN_POINT ( 'NONE',  ( 9.832129032723416984, 246.8229166700806729, -5.676582343750003368 ) ) ;
#63956 = VECTOR ( 'NONE', #34010, 1000.000000000000000 ) ;
#63958 = CARTESIAN_POINT ( 'NONE',  ( 5.082755093536318824, 5.082755093536319713, 14.79905278187175455 ) ) ;
#63959 = CARTESIAN_POINT ( 'NONE',  ( 2.828427073549516724, 195.0000000000000284, 144.8284271759428634 ) ) ;
#63960 = CARTESIAN_POINT ( 'NONE',  ( -14.00000000000000178, 2.249999999994893862, 10.23492587299426404 ) ) ;
#63961 = CARTESIAN_POINT ( 'NONE',  ( -2.679491924304306938, 146.4583333333327175, -10.00000000000399680 ) ) ;
#63962 = CARTESIAN_POINT ( 'NONE',  ( 7.320508075688771044, 201.2499999931720538, 7.320508075688775484 ) ) ;
#63963 = CARTESIAN_POINT ( 'NONE',  ( 7.320508075688771044, 159.3749999999999716, 7.320508075688775484 ) ) ;
#63964 = FACE_OUTER_BOUND ( 'NONE', #30758, .T. ) ;
#63965 = CARTESIAN_POINT ( 'NONE',  ( 1.320432766682872962E-15, -7.188101187499992051, 26.23655278187175810 ) ) ;
#63966 = CARTESIAN_POINT ( 'NONE',  ( -2.085542519210945728E-15, 134.8437499965860127, 11.35316468750000141 ) ) ;
#63967 = CYLINDRICAL_SURFACE ( 'NONE', #46879, 8.000000000000000000 ) ;
#63968 = DIRECTION ( 'NONE',  ( 0.000000000000000000, -1.000000000000000000, 0.000000000000000000 ) ) ;
#63971 = DIRECTION ( 'NONE',  ( -0.000000000000000000, 1.000000000000000000, 4.476705744456276341E-16 ) ) ;
#63970 = CARTESIAN_POINT ( 'NONE',  ( 8.660254037844385522, 106.4583333265053682, 5.000000000000005329 ) ) ;
#63969 = CARTESIAN_POINT ( 'NONE',  ( 30.82842712474617031, 205.1250000000000284, 172.8284271247460993 ) ) ;
#63972 = ORIENTED_EDGE ( 'NONE', *, *, #64987, .T. ) ;
#63973 = CYLINDRICAL_SURFACE ( 'NONE', #26041, 11.00000000000000000 ) ;
#63974 = VECTOR ( 'NONE', #61472, 1000.000000000000000 ) ;
#63975 = CARTESIAN_POINT ( 'NONE',  ( 1.469576158976822172E-15, -7.999999999999991118, 25.20530277982336642 ) ) ;
#63976 = CARTESIAN_POINT ( 'NONE',  ( -1.432654583217662259, 209.1250000013656347, 145.4587341250000350 ) ) ;
#63977 = CARTESIAN_POINT ( 'NONE',  ( 24.54126587499999701, 195.3750000013656063, 168.5673454167822172 ) ) ;
#63978 = CARTESIAN_POINT ( 'NONE',  ( -10.00000000000000000, 39.16666665983870388, -2.679491924311229845 ) ) ;
#63979 = CARTESIAN_POINT ( 'NONE',  ( -7.188101187500000044, 115.1562500020483810, 0.000000000000000000 ) ) ;
#63980 = CARTESIAN_POINT ( 'NONE',  ( 3.211159895383560947, 1.312499998634406806, 3.211159895383562723 ) ) ;
#63981 = CARTESIAN_POINT ( 'NONE',  ( -1.882291019712000413, -55.75505015263659203, 43.87597576788989073 ) ) ;
#63982 = CARTESIAN_POINT ( 'NONE',  ( 1.469576158976822172E-15, -7.999999999999991118, 22.20530277982336997 ) ) ;
#63983 = CARTESIAN_POINT ( 'NONE',  ( -10.00000000000000000, 224.7916666666666288, -2.679491924311226292 ) ) ;
#63984 = CARTESIAN_POINT ( 'NONE',  ( -5.676582343749998039, 107.4479166632526983, -9.832129032723420536 ) ) ;
#63985 = VERTEX_POINT ( 'NONE', #11509 ) ;
#63986 = CARTESIAN_POINT ( 'NONE',  ( -2.249999999999999112, 284.0000000000000000, 7.677076266392047543 ) ) ;
#63987 = CARTESIAN_POINT ( 'NONE',  ( 3.999999999999960032, 210.0000000000000284, 142.0000000000000568 ) ) ;
#63988 = VECTOR ( 'NONE', #8851, 1000.000000000000000 ) ;
#63989 = CARTESIAN_POINT ( 'NONE',  ( 4.556349186104045934, 11.00000000000000000, 81.71875000409677625 ) ) ;
#63990 = CARTESIAN_POINT ( 'NONE',  ( 3.042071309553173286, 245.6770833367473017, 11.35316468749999608 ) ) ;
#63991 = CARTESIAN_POINT ( 'NONE',  ( 5.676582343750001591, 121.6145833299193555, -9.832129032723420536 ) ) ;
#63992 = ORIENTED_EDGE ( 'NONE', *, *, #66141, .F. ) ;
#63993 = CARTESIAN_POINT ( 'NONE',  ( -10.66427519835108129, 0.9491272587611292444, 117.8040744609134265 ) ) ;
#63994 = CARTESIAN_POINT ( 'NONE',  ( -10.18810118749999738, -4.220049686691941915, 102.2500000020483952 ) ) ;
#63995 = CARTESIAN_POINT ( 'NONE',  ( -2.679491924311235618, 215.4166666598387110, 10.00000000000000000 ) ) ;
#63996 = CARTESIAN_POINT ( 'NONE',  ( 2.754378923186476579E-14, 200.4375000013656063, 194.5412658750000219 ) ) ;
#63997 = CARTESIAN_POINT ( 'NONE',  ( 0.000000000000000000, 0.000000000000000000, 19.00000000000000355 ) ) ;
#63999 = CARTESIAN_POINT ( 'NONE',  ( 11.35316468749999963, 95.98958332991935549, -3.042071309553165293 ) ) ;
#63998 = DIRECTION ( 'NONE',  ( 0.000000000000000000, 0.000000000000000000, 1.000000000000000000 ) ) ;
#64000 = CARTESIAN_POINT ( 'NONE',  ( -5.656854249492375253, 5.656854249492375253, 6.830302783920143561 ) ) ;
#64001 = CARTESIAN_POINT ( 'NONE',  ( -31.45873412499999944, 197.8750000013656063, 168.5673454167827572 ) ) ;
#64002 = EDGE_CURVE ( 'NONE', #45255, #282, #30975, .T. ) ;
#64003 = CARTESIAN_POINT ( 'NONE',  ( 7.320508075688771044, 169.3750000000000000, 7.320508075688775484 ) ) ;
#64004 = ORIENTED_EDGE ( 'NONE', *, *, #46201, .F. ) ;
#64005 = CARTESIAN_POINT ( 'NONE',  ( -10.00000000000000355, 189.5833333265053682, 2.679491924311223183 ) ) ;
#64006 = CARTESIAN_POINT ( 'NONE',  ( 3.313708498984846429, 112.1562500040967763, 7.999999999999918288 ) ) ;
#64007 = CARTESIAN_POINT ( 'NONE',  ( 0.7792778822821542217, -47.90364825942320692, 139.0091995171781321 ) ) ;
#64008 = CARTESIAN_POINT ( 'NONE',  ( -11.35316468749999785, 88.38541666325268409, -3.042071309553167957 ) ) ;
#64009 = CARTESIAN_POINT ( 'NONE',  ( 1.656854249492453857, 205.6875000000000000, 194.0000000000001421 ) ) ;
#64010 = CARTESIAN_POINT ( 'NONE',  ( 5.082755093536325930, 5.531249997951610098, -5.082755093536325930 ) ) ;
#64012 = EDGE_CURVE ( 'NONE', #73307, #19065, #43820, .T. ) ;
#64011 = CARTESIAN_POINT ( 'NONE',  ( 10.18810118749999916, 4.220049686691935698, 95.87500000204838102 ) ) ;
#64013 = CARTESIAN_POINT ( 'NONE',  ( 11.35316468749999785, 5.885416663252683200, 3.042071309553174174 ) ) ;
#64014 = VERTEX_POINT ( 'NONE', #16400 ) ;
#64015 = DIRECTION ( 'NONE',  ( 0.8660254037844380415, 0.5000000000000009992, 0.000000000000000000 ) ) ;
#64016 = CARTESIAN_POINT ( 'NONE',  ( 4.000000000000015987, 196.6250000027312126, 198.0000000000000284 ) ) ;
#64017 = CARTESIAN_POINT ( 'NONE',  ( -2.085542519210945728E-15, 214.5312499965860411, 11.35316468750000141 ) ) ;
#64018 = CARTESIAN_POINT ( 'NONE',  ( -10.18810118749999916, 0.000000000000000000, 77.03125000204836681 ) ) ;
#64019 = AXIS2_PLACEMENT_3D ( 'NONE', #5281, #16952, #52043 ) ;
#64020 = CARTESIAN_POINT ( 'NONE',  ( -44.48374486120346205, 184.9827789239285494, 84.30156509589276936 ) ) ;
#64021 = CARTESIAN_POINT ( 'NONE',  ( 5.000000000000001776, 200.8333333333333428, -8.660254037844389075 ) ) ;
#64022 = CARTESIAN_POINT ( 'NONE',  ( 1.226468279477575784E-15, 298.7031250017070079, 6.676582343750001591 ) ) ;
#64023 = VERTEX_POINT ( 'NONE', #54091 ) ;
#64024 = CARTESIAN_POINT ( 'NONE',  ( -38.00000000000000000, 63.00000000000000000, 15.00000000000000178 ) ) ;
#64025 = CARTESIAN_POINT ( 'NONE',  ( -9.832129032723420536, 204.0104166632526983, 5.676582343749997150 ) ) ;
#64026 = CARTESIAN_POINT ( 'NONE',  ( -6.238412754330611322E-16, 10.18810118749999916, 88.28125000204836681 ) ) ;
#64027 = CARTESIAN_POINT ( 'NONE',  ( -30.44569435410883429, 202.5625000013656063, 167.5543056458915885 ) ) ;
#64028 = CARTESIAN_POINT ( 'NONE',  ( -5.656854249492379694, 18.56250000000000355, -5.656854249492380582 ) ) ;
#64029 = ORIENTED_EDGE ( 'NONE', *, *, #42354, .F. ) ;
#64030 = AXIS2_PLACEMENT_3D ( 'NONE', #2749, #8782, #71765 ) ;
#64031 = CARTESIAN_POINT ( 'NONE',  ( -7.188101187500001821, 122.5625000020483952, -2.977408999572650483 ) ) ;
#64032 = CARTESIAN_POINT ( 'NONE',  ( 2.828427124746208943, 205.7500000027312126, 195.1715728752538439 ) ) ;
#64033 = CARTESIAN_POINT ( 'NONE',  ( -2.679491924311235618, 23.54166666666667140, 10.00000000000000000 ) ) ;
#64034 = AXIS2_PLACEMENT_3D ( 'NONE', #39322, #64558, #1572 ) ;
#64035 = DIRECTION ( 'NONE',  ( 0.000000000000000000, 0.000000000000000000, -1.000000000000000000 ) ) ;
#64036 = CARTESIAN_POINT ( 'NONE',  ( 10.18810118750000093, -4.220049686691933921, 76.18750000204839523 ) ) ;
#64037 = ORIENTED_EDGE ( 'NONE', *, *, #18413, .T. ) ;
#64038 = CARTESIAN_POINT ( 'NONE',  ( -7.188101187500000933, 1.124999997951610098, -2.977408999572651371 ) ) ;
#64039 = AXIS2_PLACEMENT_3D ( 'NONE', #51724, #69455, #10999 ) ;
#64040 = CARTESIAN_POINT ( 'NONE',  ( 4.556349186104052151, -10.99999999999999822, 112.4687499999999858 ) ) ;
#64041 = CARTESIAN_POINT ( 'NONE',  ( 2.849036369511732440E-14, 209.2500000000000284, 202.0000000000000000 ) ) ;
#64042 = CARTESIAN_POINT ( 'NONE',  ( -7.188101187499999156, 118.6250000020483810, 2.977408999572654924 ) ) ;
#64043 = CARTESIAN_POINT ( 'NONE',  ( 4.999999999999999112, -67.66364885638958526, 22.52891795222265259 ) ) ;
#64044 = CARTESIAN_POINT ( 'NONE',  ( -6.676582343750001591, 296.4531250017069510, 0.000000000000000000 ) ) ;
#64046 = CARTESIAN_POINT ( 'NONE',  ( 0.000000000000000000, 0.000000000000000000, 0.000000000000000000 ) ) ;
#64045 = CARTESIAN_POINT ( 'NONE',  ( 11.35316468749999608, 231.6145833367473017, -3.042071309553167513 ) ) ;
#64047 =( BOUNDED_CURVE ( )  B_SPLINE_CURVE ( 2, ( #13731, #71451, #18687, #42787, #41327, #65803, #54507, #30740, #14109 ),
 .UNSPECIFIED., .F., .F. ) 
 B_SPLINE_CURVE_WITH_KNOTS ( ( 3, 2, 2, 2, 3 ),
 ( 0.3541666666666646313, 0.3645833333333312609, 0.3749999999999980016, 0.3854166666666646868, 0.3958333333333313164 ),
 .UNSPECIFIED. ) 
 CURVE ( )  GEOMETRIC_REPRESENTATION_ITEM ( )  RATIONAL_B_SPLINE_CURVE ( ( 1.000000000000015099, 0.9238795325112717505, 1.000000000000000000, 0.9238795325112867385, 1.000000000000000000, 0.9238795325112867385, 1.000000000000000000, 0.9238795325113013934, 0.9999999999999853451 ) ) 
 REPRESENTATION_ITEM ( '' )  );
#64048 = VERTEX_POINT ( 'NONE', #30335 ) ;
#64049 = CARTESIAN_POINT ( 'NONE',  ( -9.832129032723415207, 244.6354166700806445, 5.676582343750005144 ) ) ;
#64050 = CARTESIAN_POINT ( 'NONE',  ( -4.401442555609577197E-16, 7.188101187499992051, 5.611552781871753659 ) ) ;
#64051 = VERTEX_POINT ( 'NONE', #42383 ) ;
#64052 = CARTESIAN_POINT ( 'NONE',  ( 4.220049686691934809, 10.18810118749999916, 68.68750000204838102 ) ) ;
#64053 = CARTESIAN_POINT ( 'NONE',  ( 3.042071309553159519, 95.05208332991935549, 11.35316468750000141 ) ) ;
#64054 = CARTESIAN_POINT ( 'NONE',  ( -9.000000000000023093, 15.58845726811988541, 0.000000000000000000 ) ) ;
#64055 = CARTESIAN_POINT ( 'NONE',  ( 11.00000000000000355, -4.556349186104045046, 82.65625000000001421 ) ) ;
#64058 = CARTESIAN_POINT ( 'NONE',  ( 1.226468279477575784E-15, 287.8593750017070079, 6.676582343750001591 ) ) ;
#64057 = CARTESIAN_POINT ( 'NONE',  ( 29.43265458321766559, 204.5000000013656063, 173.4587341249998929 ) ) ;
#64056 = CARTESIAN_POINT ( 'NONE',  ( 30.44569435410883429, 201.0625000013656063, 167.5543056458911053 ) ) ;
#64059 = VERTEX_POINT ( 'NONE', #24660 ) ;
#64060 = AXIS2_PLACEMENT_3D ( 'NONE', #74156, #52274, #46968 ) ;
#64061 = DIRECTION ( 'NONE',  ( -0.000000000000000000, -0.000000000000000000, 1.000000000000000000 ) ) ;
#64062 = CYLINDRICAL_SURFACE ( 'NONE', #55261, 3.999999999999976019 ) ;
#64063 = CARTESIAN_POINT ( 'NONE',  ( -8.311093377946836114, 207.6562499965860411, -8.311093377946837890 ) ) ;
#64064 = CARTESIAN_POINT ( 'NONE',  ( -1.432654583217664479, 205.7500000013656063, 138.5412658750000787 ) ) ;
#64065 = ADVANCED_FACE ( 'NONE', ( #70338 ), #7330, .F. ) ;
#64066 = CARTESIAN_POINT ( 'NONE',  ( 31.45873412500001010, 207.0000000013656063, 168.5673454167822740 ) ) ;
#64067 = EDGE_CURVE ( 'NONE', #61795, #46255, #23721, .T. ) ;
#64068 = CARTESIAN_POINT ( 'NONE',  ( -2.977408999572654480, 22.87499999795161187, 7.188101187499999156 ) ) ;
#64069 = CARTESIAN_POINT ( 'NONE',  ( 8.311093377946837890, 181.7187499965859843, -8.311093377946837890 ) ) ;
#64070 = CARTESIAN_POINT ( 'NONE',  ( 7.188101187500000044, 98.28125000204838102, -8.802885111219163269E-16 ) ) ;
#64072 = CARTESIAN_POINT ( 'NONE',  ( 2.395154805519954641E-11, 111.2499999999981242, -9.999999999999998224 ) ) ;
#64071 = DIRECTION ( 'NONE',  ( 0.000000000000000000, 0.000000000000000000, 1.000000000000000000 ) ) ;
#64073 = CARTESIAN_POINT ( 'NONE',  ( -4.541265875000003227, 11.87499999863440969, 1.881053915767121110 ) ) ;
#64074 = CARTESIAN_POINT ( 'NONE',  ( 27.99999999999996447, 202.6875000013656063, 173.4587341249998929 ) ) ;
#64075 = CARTESIAN_POINT ( 'NONE',  ( 7.188101187499991163, 2.977408999572648707, 10.20530278187175455 ) ) ;
#64076 = CARTESIAN_POINT ( 'NONE',  ( 5.676582343749993598, 64.94791666325269830, 9.832129032723422313 ) ) ;
#64077 = CARTESIAN_POINT ( 'NONE',  ( -2.751549872419339698E-14, 194.9207531772045741, 145.9207531772046025 ) ) ;
#64078 = CARTESIAN_POINT ( 'NONE',  ( -7.999999999999989342, -3.313708498984762496, 2.480302784329821542 ) ) ;
#64079 = ORIENTED_EDGE ( 'NONE', *, *, #52344, .T. ) ;
#64080 = FACE_OUTER_BOUND ( 'NONE', #21532, .T. ) ;
#64081 = CYLINDRICAL_SURFACE ( 'NONE', #40084, 3.999999999999976019 ) ;
#64082 = CARTESIAN_POINT ( 'NONE',  ( 3.042071309553159519, 74.73958332991932707, 11.35316468750000141 ) ) ;
#64083 = CARTESIAN_POINT ( 'NONE',  ( -11.00000000000000000, 0.000000000000000000, 67.18750000409676204 ) ) ;
#64084 = DIRECTION ( 'NONE',  ( 0.000000000000000000, -6.938893903907228378E-16, -1.000000000000000000 ) ) ;
#64085 = CARTESIAN_POINT ( 'NONE',  ( -2.589639417653167630, 10.27590863719303904, 63.78668228762733605 ) ) ;
#64087 = CARTESIAN_POINT ( 'NONE',  ( -5.676582343749998039, 62.44791666325268409, -9.832129032723420536 ) ) ;
#64086 = CARTESIAN_POINT ( 'NONE',  ( 3.313708498984706985, 103.7187500040967905, -8.000000000000055067 ) ) ;
#64088 = CARTESIAN_POINT ( 'NONE',  ( -5.656854249492373476, -5.656854249492376141, 22.20530278392014623 ) ) ;
#64089 = EDGE_CURVE ( 'NONE', #64865, #41819, #45074, .T. ) ;
#64090 = CARTESIAN_POINT ( 'NONE',  ( -2.823223908292154416, 194.8377262638587695, 144.6110606521876605 ) ) ;
#64091 = CARTESIAN_POINT ( 'NONE',  ( 8.660254037844389075, 162.2916666598387110, -5.000000000000000000 ) ) ;
#64092 = CARTESIAN_POINT ( 'NONE',  ( -5.082755093536325930, 97.34375000204838102, -5.082755093536325930 ) ) ;
#64093 = AXIS2_PLACEMENT_3D ( 'NONE', #40582, #56455, #11911 ) ;
#64094 = CARTESIAN_POINT ( 'NONE',  ( -2.085542519210945728E-15, 54.84374999658601979, 11.35316468750000141 ) ) ;
#64095 = CARTESIAN_POINT ( 'NONE',  ( 4.220049686691941027, -10.18810118749999738, 110.5000000020483810 ) ) ;
#64096 = CARTESIAN_POINT ( 'NONE',  ( 8.311093377946837890, 186.4062499965860411, -8.311093377946837890 ) ) ;
#64097 = ORIENTED_EDGE ( 'NONE', *, *, #17153, .F. ) ;
#64098 = CARTESIAN_POINT ( 'NONE',  ( 2.849036369511732440E-14, 205.3750000027312126, 202.0000000000000000 ) ) ;
#64099 = LINE ( 'NONE', #24829, #39532 ) ;
#64101 = CARTESIAN_POINT ( 'NONE',  ( 8.311093377946834337, 175.1562499965859843, 8.311093377946839666 ) ) ;
#64100 = CARTESIAN_POINT ( 'NONE',  ( -7.347880794884122694E-16, 21.49999999726881583, 4.000000000000001776 ) ) ;
#64102 = PLANE ( 'NONE',  #42949 ) ;
#64103 = CARTESIAN_POINT ( 'NONE',  ( 10.00000000000000178, 255.4166666734946602, 2.679491924311222739 ) ) ;
#64104 = CARTESIAN_POINT ( 'NONE',  ( 0.000000000000000000, 0.000000000000000000, 0.000000000000000000 ) ) ;
#64105 = VERTEX_POINT ( 'NONE', #25398 ) ;
#64106 = CARTESIAN_POINT ( 'NONE',  ( -3.042071309553173730, 169.6354166632526699, 11.35316468749999785 ) ) ;
#64107 = APPLICATION_CONTEXT ( 'automotive_design' ) ;
#64108 = CARTESIAN_POINT ( 'NONE',  ( 7.188101187499993827, -2.977408999572645598, 27.64280278187175455 ) ) ;
#64109 = CARTESIAN_POINT ( 'NONE',  ( 3.042071309553159519, 125.0520833299193555, 11.35316468750000141 ) ) ;
#64110 = CARTESIAN_POINT ( 'NONE',  ( 23.99999999999999645, 203.9375000027311842, 171.6568542494923122 ) ) ;
#64111 = ORIENTED_EDGE ( 'NONE', *, *, #37326, .T. ) ;
#64112 = VECTOR ( 'NONE', #56957, 1000.000000000000000 ) ;
#64113 = CARTESIAN_POINT ( 'NONE',  ( -8.000000000000000000, 104.1875000040967763, 0.000000000000000000 ) ) ;
#64114 = AXIS2_PLACEMENT_3D ( 'NONE', #52681, #1015, #64369 ) ;
#64115 = CARTESIAN_POINT ( 'NONE',  ( -2.828427124746190735, 12.37500000000000000, -2.828427124746191623 ) ) ;
#64116 = CARTESIAN_POINT ( 'NONE',  ( -34.69679471024809203, -12.34462646322155699, 148.2170566195945298 ) ) ;
#64117 = CARTESIAN_POINT ( 'NONE',  ( -8.342170076843785083E-16, 13.06249999863440792, 4.541265875000002339 ) ) ;
#64118 = CARTESIAN_POINT ( 'NONE',  ( -5.656854249492373476, -5.656854249492376141, 20.70530278392014623 ) ) ;
#64119 = CYLINDRICAL_SURFACE ( 'NONE', #61951, 8.000000000000000000 ) ;
#64120 = EDGE_LOOP ( 'NONE', ( #18637, #9813, #74141, #73000, #46909, #51284, #9694, #68071, #33317, #29948 ) ) ;
#64121 = DIRECTION ( 'NONE',  ( 1.000000000000000000, 0.000000000000000000, 0.000000000000000000 ) ) ;
#64122 = CARTESIAN_POINT ( 'NONE',  ( -2.977408999572650927, 105.8750000020483952, -7.188101187500001821 ) ) ;
#64124 = CARTESIAN_POINT ( 'NONE',  ( -7.347880794884122694E-16, 6.499999997268813168, 4.000000000000001776 ) ) ;
#64123 = CARTESIAN_POINT ( 'NONE',  ( -1.469576158976823947E-15, 15.93749999590322197, 8.000000000000000000 ) ) ;
#64125 = DIRECTION ( 'NONE',  ( 0.000000000000000000, 0.000000000000000000, 1.000000000000000000 ) ) ;
#64126 = VERTEX_POINT ( 'NONE', #59384 ) ;
#64127 = CARTESIAN_POINT ( 'NONE',  ( -3.223881452105385570, 10.27322224982961707, -63.89771963198208482 ) ) ;
#64128 = EDGE_CURVE ( 'NONE', #68280, #24567, #65399, .T. ) ;
#64129 = TOROIDAL_SURFACE ( 'NONE', #59295, 81.50000000000000000, 10.99999999999999822 ) ;
#64130 = CARTESIAN_POINT ( 'NONE',  ( 1.320432766682872962E-15, -7.188101187499992051, 24.36155278187175810 ) ) ;
#64131 = ORIENTED_EDGE ( 'NONE', *, *, #73268, .F. ) ;
#64132 = ORIENTED_EDGE ( 'NONE', *, *, #40779, .F. ) ;
#64133 = CARTESIAN_POINT ( 'NONE',  ( 1.871523826299183495E-15, -10.18810118749999916, 86.03125000204836681 ) ) ;
#64134 = CARTESIAN_POINT ( 'NONE',  ( -29.43265458321760519, 198.1250000013656063, 173.4587341250003760 ) ) ;
#64135 = CARTESIAN_POINT ( 'NONE',  ( 7.778174593052023411, -7.778174593052021635, 100.5625000000000000 ) ) ;
#64138 = CARTESIAN_POINT ( 'NONE',  ( -4.721056650415998313, 297.7343750017069510, 4.721056650416000089 ) ) ;
#64137 = CARTESIAN_POINT ( 'NONE',  ( 25.17157287525378351, 205.7500000027312126, 167.1715728752537586 ) ) ;
#64136 = CARTESIAN_POINT ( 'NONE',  ( 25.17157287525381903, 203.0000000027312126, 172.8284271247460993 ) ) ;
#64139 = CARTESIAN_POINT ( 'NONE',  ( -2.679491924311235618, 133.5416666666666572, 10.00000000000000000 ) ) ;
#64140 = CARTESIAN_POINT ( 'NONE',  ( -3.313708498984762052, 99.21875000000000000, -8.000000000000000000 ) ) ;
#64141 = CARTESIAN_POINT ( 'NONE',  ( -28.00000000000002842, 204.0000000000000284, 166.0000000000003695 ) ) ;
#64142 = FACE_OUTER_BOUND ( 'NONE', #73723, .T. ) ;
#64143 = CARTESIAN_POINT ( 'NONE',  ( -4.999999999999992895, 233.9583333401613174, 8.660254037844390851 ) ) ;
#64145 = CARTESIAN_POINT ( 'NONE',  ( 29.43265458321761230, 203.5000000013655779, 173.4587341249998929 ) ) ;
#64144 = VECTOR ( 'NONE', #19878, 1000.000000000000000 ) ;
#64146 = CARTESIAN_POINT ( 'NONE',  ( 7.188101187499999156, 3.749999997951610542, 2.977408999572654924 ) ) ;
#64147 = CARTESIAN_POINT ( 'NONE',  ( -3.317071493978878571, 8.008118988124991233, 0.7318652839406294408 ) ) ;
#64148 = CARTESIAN_POINT ( 'NONE',  ( 2.445694354108783664, 196.3125000013656063, 144.4456943541088663 ) ) ;
#64149 = CARTESIAN_POINT ( 'NONE',  ( 7.188101187500000933, 117.8750000020483810, -2.977408999572651371 ) ) ;
#64151 = DIRECTION ( 'NONE',  ( 0.000000000000000000, 0.8778652960884979484, 0.4789076340208558435 ) ) ;
#64150 = CARTESIAN_POINT ( 'NONE',  ( -5.000000000000000888, 249.1666666666666856, -8.660254037844387298 ) ) ;
#64152 = CARTESIAN_POINT ( 'NONE',  ( -9.832129032723418760, 228.8020833367473301, -5.676582343749998927 ) ) ;
#64153 = CARTESIAN_POINT ( 'NONE',  ( -31.80400347473905143, 43.36760464598135911, 65.00000000000001421 ) ) ;
#64154 = CARTESIAN_POINT ( 'NONE',  ( 7.188101187499993827, -2.977408999572645598, 28.01780278187175455 ) ) ;
#64155 = CARTESIAN_POINT ( 'NONE',  ( 23.99999999999997868, 199.8125000000000284, 171.6568542494922553 ) ) ;
#64156 = CARTESIAN_POINT ( 'NONE',  ( -8.311093377946841443, 23.90624999658601979, 8.311093377946830785 ) ) ;
#64157 =( BOUNDED_CURVE ( )  B_SPLINE_CURVE ( 2, ( #47456, #18799, #32732, #14971, #3672, #15718, #27049, #44780, #49695, #26670, #50062, #72708, #33115 ),
 .UNSPECIFIED., .F., .F. ) 
 B_SPLINE_CURVE_WITH_KNOTS ( ( 3, 2, 2, 2, 2, 2, 3 ),
 ( 0.8611111111111111605, 0.8703703703703703498, 0.8796296296296297612, 0.8888888888888889506, 0.8981481481481482509, 0.9074074074074076623, 0.9166666666666668517 ),
 .UNSPECIFIED. ) 
 CURVE ( )  GEOMETRIC_REPRESENTATION_ITEM ( )  RATIONAL_B_SPLINE_CURVE ( ( 1.000000000000000000, 0.9659258262890683122, 1.000000000000000000, 0.9659258262890683122, 1.000000000000000000, 0.9659258262890683122, 1.000000000000000000, 0.9659258262890683122, 1.000000000000000000, 0.9659258262890683122, 1.000000000000000000, 0.9659258262890675351, 1.000000000000000888 ) ) 
 REPRESENTATION_ITEM ( '' )  );
#64158 = CARTESIAN_POINT ( 'NONE',  ( -7.999999999929542582, -2.214810345207895024E-05, 22.01864141485938831 ) ) ;
#64160 = CARTESIAN_POINT ( 'NONE',  ( 8.311093377946834337, 215.4687499965860411, 8.311093377946839666 ) ) ;
#64159 =( BOUNDED_CURVE ( )  B_SPLINE_CURVE ( 2, ( #7277, #58969, #36689, #59700, #31015, #59336, #53669, #7647, #19319, #54417, #64620, #31391, #18960 ),
 .UNSPECIFIED., .F., .F. ) 
 B_SPLINE_CURVE_WITH_KNOTS ( ( 3, 2, 2, 2, 2, 2, 3 ),
 ( 0.4722222222222219878, 0.4814814814814812327, 0.4907407407407405331, 0.4999999999999997780, 0.5092592592592590783, 0.5185185185185182677, 0.5277777777777775681 ),
 .UNSPECIFIED. ) 
 CURVE ( )  GEOMETRIC_REPRESENTATION_ITEM ( )  RATIONAL_B_SPLINE_CURVE ( ( 1.000000000000000888, 0.9659258262890675351, 1.000000000000000000, 0.9659258262890683122, 1.000000000000000000, 0.9659258262890683122, 1.000000000000000000, 0.9659258262890683122, 1.000000000000000000, 0.9659258262890683122, 1.000000000000000000, 0.9659258262890690894, 0.9999999999999992228 ) ) 
 REPRESENTATION_ITEM ( '' )  );
#64161 = CARTESIAN_POINT ( 'NONE',  ( 105.0000000000000000, 37.00000000000000000, 0.000000000000000000 ) ) ;
#64163 = PLANE ( 'NONE',  #27908 ) ;
#64162 = CARTESIAN_POINT ( 'NONE',  ( 0.000000000000000000, 0.000000000000000000, 11.00000000000000000 ) ) ;
#64164 = VERTEX_POINT ( 'NONE', #42015 ) ;
#64165 = CIRCLE ( 'NONE', #36478, 17.50000000000000000 ) ;
#64167 = EDGE_CURVE ( 'NONE', #34052, #18980, #51040, .T. ) ;
#64166 = CARTESIAN_POINT ( 'NONE',  ( 3.458734124999959469, 196.7500000013656063, 140.5673454167824161 ) ) ;
#64168 = EDGE_CURVE ( 'NONE', #4470, #30899, #38710, .T. ) ;
#64169 = CARTESIAN_POINT ( 'NONE',  ( -2.085542519210945728E-15, 34.53124999658601268, 11.35316468750000141 ) ) ;
#64170 = CARTESIAN_POINT ( 'NONE',  ( 11.00000000000000000, 4.556349186104045934, 87.53125000409676204 ) ) ;
#64171 = DIRECTION ( 'NONE',  ( -0.000000000000000000, -1.000000000000000000, -0.000000000000000000 ) ) ;
#64172 = FACE_OUTER_BOUND ( 'NONE', #25836, .T. ) ;
#64173 = CARTESIAN_POINT ( 'NONE',  ( 1.469576158976823947E-15, 102.8750000000000000, 8.000000000000000000 ) ) ;
#64175 = CARTESIAN_POINT ( 'NONE',  ( 11.35316468749999963, 25.98958332991935194, -3.042071309553165293 ) ) ;
#64174 = CARTESIAN_POINT ( 'NONE',  ( -4.401442555609581635E-16, 104.2812500020483810, -7.188101187500000044 ) ) ;
#64176 = CARTESIAN_POINT ( 'NONE',  ( 7.999999999999991118, 9.797174393178815797E-16, 13.58030277982336465 ) ) ;
#64177 = AXIS2_PLACEMENT_3D ( 'NONE', #66400, #31706, #44517 ) ;
#64178 = CARTESIAN_POINT ( 'NONE',  ( -3.042071309553164404, 147.2395833299193555, -11.35316468749999963 ) ) ;
#64179 = CARTESIAN_POINT ( 'NONE',  ( -10.00000000000000355, 119.5833333265053824, 2.679491924311223183 ) ) ;
#64180 = CARTESIAN_POINT ( 'NONE',  ( -5.082755093536324154, 117.2187500020483810, 5.082755093536326818 ) ) ;
#64181 = CARTESIAN_POINT ( 'NONE',  ( -11.00000000000000000, 0.000000000000000000, 81.99999999999998579 ) ) ;
#64182 = CARTESIAN_POINT ( 'NONE',  ( -25.55430564589115150, 204.3125000013656063, 172.4456943541091789 ) ) ;
#64183 = ORIENTED_EDGE ( 'NONE', *, *, #14518, .T. ) ;
#64184 = CARTESIAN_POINT ( 'NONE',  ( -3.042071309553163960, 7.552083329919350163, -11.35316468749999963 ) ) ;
#64185 = VERTEX_POINT ( 'NONE', #6593 ) ;
#64186 = CARTESIAN_POINT ( 'NONE',  ( -0.4369882809994319883, 16.44602605510693749, -68.55492853905478512 ) ) ;
#64187 = CARTESIAN_POINT ( 'NONE',  ( 4.721056650415999201, 299.0781250017069510, -4.721056650415999201 ) ) ;
#64189 = CARTESIAN_POINT ( 'NONE',  ( -3.042071309553173730, 144.3229166632526983, 11.35316468749999785 ) ) ;
#64188 = CARTESIAN_POINT ( 'NONE',  ( 2.449293598294707893E-16, 14.99999999726881406, -4.000000000000001776 ) ) ;
#64190 = CARTESIAN_POINT ( 'NONE',  ( 0.000000000000000000, 51.05255888325788050, 0.000000000000000000 ) ) ;
#64191 = CARTESIAN_POINT ( 'NONE',  ( -3.313708498984758943, -7.999999999999989342, 26.66780278432982598 ) ) ;
#64192 = CARTESIAN_POINT ( 'NONE',  ( 11.00000000000000000, 1.347111479062088405E-15, 90.43750000409676204 ) ) ;
#64193 = CARTESIAN_POINT ( 'NONE',  ( 8.311093377946839666, 245.7812500034139873, 8.311093377946829008 ) ) ;
#64194 = EDGE_CURVE ( 'NONE', #71882, #63519, #62261, .T. ) ;
#64195 = CARTESIAN_POINT ( 'NONE',  ( 10.18810118749999916, 1.247682550866122264E-15, 92.78125000204836681 ) ) ;
#64196 = ORIENTED_EDGE ( 'NONE', *, *, #51917, .F. ) ;
#64197 = CARTESIAN_POINT ( 'NONE',  ( 4.999999999999995559, 119.1666666666666714, 8.660254037844394404 ) ) ;
#64198 = DIRECTION ( 'NONE',  ( -0.7071067811865401342, 0.000000000000000000, -0.7071067811865549002 ) ) ;
#64199 = UNCERTAINTY_MEASURE_WITH_UNIT (LENGTH_MEASURE( 1.000000000000000082E-05 ), #28451, 'distance_accuracy_value', 'NONE');
#64200 = CARTESIAN_POINT ( 'NONE',  ( 3.042071309553159519, 90.05208332991932707, 11.35316468750000141 ) ) ;
#64201 = CARTESIAN_POINT ( 'NONE',  ( -4.220049686691937474, -10.18810118749999738, 105.4375000020483668 ) ) ;
#64202 = CARTESIAN_POINT ( 'NONE',  ( -1.881053915767121776, 17.74999999863440792, -4.541265875000002339 ) ) ;
#64203 = ORIENTED_EDGE ( 'NONE', *, *, #743, .T. ) ;
#64204 = EDGE_LOOP ( 'NONE', ( #44437, #30379, #70506, #50732, #56383, #58674 ) ) ;
#64205 = CARTESIAN_POINT ( 'NONE',  ( -1.469576158976823947E-15, 8.625000000000000000, 8.000000000000000000 ) ) ;
#64206 = FACE_OUTER_BOUND ( 'NONE', #2379, .T. ) ;
#64207 = CARTESIAN_POINT ( 'NONE',  ( 5.082755093536325930, 2.156249997951610098, -5.082755093536325930 ) ) ;
#64208 = CARTESIAN_POINT ( 'NONE',  ( -8.000000000000000000, 123.5937500040967763, -3.313708498984761608 ) ) ;
#64209 = CARTESIAN_POINT ( 'NONE',  ( 7.204075437095966983, 7.204075437095967871, 103.4687500020483668 ) ) ;
#64210 = CARTESIAN_POINT ( 'NONE',  ( 4.000000000000001776, 2.062500000000000000, -1.656854249492381248 ) ) ;
#64211 = CARTESIAN_POINT ( 'NONE',  ( -4.000000000000002665, 14.31249999726881406, 1.656854249492380804 ) ) ;
#64212 = CARTESIAN_POINT ( 'NONE',  ( 23.99999999999998224, 209.8125000000000000, 171.6568542494922553 ) ) ;
#64213 = VERTEX_POINT ( 'NONE', #25022 ) ;
#64214 = AXIS2_PLACEMENT_3D ( 'NONE', #574, #46935, #5475 ) ;
#64215 = FACE_OUTER_BOUND ( 'NONE', #19573, .T. ) ;
#64216 = CARTESIAN_POINT ( 'NONE',  ( 2.445694354108839619, 196.8125000013656063, 200.4456943541088663 ) ) ;
#64217 = CARTESIAN_POINT ( 'NONE',  ( -24.54126587499999346, 203.1875000013656063, 170.0000000000002842 ) ) ;
#64218 = CARTESIAN_POINT ( 'NONE',  ( 3.211159895383561835, 13.43749999863440614, -3.211159895383561835 ) ) ;
#64219 = CARTESIAN_POINT ( 'NONE',  ( 4.000000000000000888, 11.93750000000000000, 1.656854249492384135 ) ) ;
#64220 = CARTESIAN_POINT ( 'NONE',  ( 5.082755093536320601, -5.082755093536318824, 12.54905278187175277 ) ) ;
#64221 = ORIENTED_EDGE ( 'NONE', *, *, #62906, .F. ) ;
#64222 = EDGE_LOOP ( 'NONE', ( #48102, #51694 ) ) ;
#64223 = CARTESIAN_POINT ( 'NONE',  ( 1.871523826299183495E-15, -10.18810118749999916, 107.0312500020483810 ) ) ;
#64224 = CARTESIAN_POINT ( 'NONE',  ( -2.726571689596997292E-14, 210.0000000000000284, 138.0000000000000568 ) ) ;
#64225 = CARTESIAN_POINT ( 'NONE',  ( -26.34314575050758478, 206.5625000000000000, 174.0000000000003411 ) ) ;
#64226 = CARTESIAN_POINT ( 'NONE',  ( -3.458734124999959914, 199.4375000013655779, 198.0000000000000284 ) ) ;
#64227 = CARTESIAN_POINT ( 'NONE',  ( 25.55430564589115150, 195.0625000013656063, 167.5543056458911053 ) ) ;
#64228 = CARTESIAN_POINT ( 'NONE',  ( 10.00000000000000178, 90.20833333333332860, -2.679491924311226736 ) ) ;
#64229 = ADVANCED_FACE ( 'NONE', ( #12608 ), #53723, .T. ) ;
#64230 = CARTESIAN_POINT ( 'NONE',  ( 8.000000000000000000, 115.2499999999999858, -9.797174393178825657E-16 ) ) ;
#64231 = CARTESIAN_POINT ( 'NONE',  ( -11.35316468750000141, 58.80208332991933418, 3.042071309553159963 ) ) ;
#64232 = CARTESIAN_POINT ( 'NONE',  ( -6.676582343750001591, 299.6093750017069510, 0.000000000000000000 ) ) ;
#64233 = ORIENTED_EDGE ( 'NONE', *, *, #36248, .T. ) ;
#64234 = CARTESIAN_POINT ( 'NONE',  ( -8.660254037844387298, 143.9583333265053682, -5.000000000000004441 ) ) ;
#64235 = CARTESIAN_POINT ( 'NONE',  ( 7.999999999999998224, 14.71874999590322020, 3.313708498984766493 ) ) ;
#64236 = CARTESIAN_POINT ( 'NONE',  ( 1.432654583217607858, 207.6250000013656347, 138.5412658750000787 ) ) ;
#64237 = CARTESIAN_POINT ( 'NONE',  ( 6.123233995736767268E-16, 38.12499999317203958, -10.00000000000000178 ) ) ;
#64238 = SURFACE_SIDE_STYLE ('',( #41231 ) ) ;
#64239 = CARTESIAN_POINT ( 'NONE',  ( 8.660254037844389075, 227.0833333333333712, 4.999999999999997335 ) ) ;
#64240 = CARTESIAN_POINT ( 'NONE',  ( -6.735557395310442023E-16, 11.00000000000000000, 72.81250000409677625 ) ) ;
#64241 = CARTESIAN_POINT ( 'NONE',  ( 11.00000000000000000, 4.556349186104045934, 117.3437500000000000 ) ) ;
#64242 = CARTESIAN_POINT ( 'NONE',  ( 5.000000000000001776, 210.8333333333333428, -8.660254037844389075 ) ) ;
#64243 = CARTESIAN_POINT ( 'NONE',  ( 2.977408999572646486, 7.188101187499992051, 10.39280278187175632 ) ) ;
#64244 = CARTESIAN_POINT ( 'NONE',  ( 9.832129032723420536, 181.5104166632526699, -5.676582343749999815 ) ) ;
#64245 = CARTESIAN_POINT ( 'NONE',  ( -3.211159895383561391, 1.687499998634406584, -3.211159895383561835 ) ) ;
#64246 = CARTESIAN_POINT ( 'NONE',  ( 5.000000000000001776, 177.7083333265053682, -8.660254037844389075 ) ) ;
#64248 = CARTESIAN_POINT ( 'NONE',  ( 10.99999999999999467, 11.00000000000000355, 41.99999999999999289 ) ) ;
#64247 = DIRECTION ( 'NONE',  ( -0.000000000000000000, 1.000000000000000000, -0.000000000000000000 ) ) ;
#64249 = ORIENTED_EDGE ( 'NONE', *, *, #69377, .T. ) ;
#64250 =( BOUNDED_CURVE ( )  B_SPLINE_CURVE ( 2, ( #6274, #69638, #23976, #17200, #46983, #46245, #63595, #70016, #69265 ),
 .UNSPECIFIED., .F., .F. ) 
 B_SPLINE_CURVE_WITH_KNOTS ( ( 3, 2, 2, 2, 3 ),
 ( 0.5113636363636363535, 0.5170454545454545858, 0.5227272727272727071, 0.5284090909090909394, 0.5340909090909090606 ),
 .UNSPECIFIED. ) 
 CURVE ( )  GEOMETRIC_REPRESENTATION_ITEM ( )  RATIONAL_B_SPLINE_CURVE ( ( 1.000000000000000000, 0.9238795325112867385, 1.000000000000000000, 0.9238795325112867385, 1.000000000000000000, 0.9238795325112867385, 1.000000000000000000, 0.9238795325112867385, 1.000000000000000000 ) ) 
 REPRESENTATION_ITEM ( '' )  );
#64252 = EDGE_CURVE ( 'NONE', #20088, #31201, #57082, .T. ) ;
#64251 = CARTESIAN_POINT ( 'NONE',  ( -2.754378923186476579E-14, 208.4375000013656063, 145.4587341250000350 ) ) ;
#64253 = CARTESIAN_POINT ( 'NONE',  ( 5.676582343749993598, 30.26041666325268409, 9.832129032723422313 ) ) ;
#64254 = CARTESIAN_POINT ( 'NONE',  ( 4.556349186104051263, -10.99999999999999822, 103.6562500040967905 ) ) ;
#64255 = CARTESIAN_POINT ( 'NONE',  ( -31.45873412500002786, 203.6250000013656063, 168.5673454167828140 ) ) ;
#64256 = CARTESIAN_POINT ( 'NONE',  ( -11.00000000000005151, 4.556349186103993532, 95.59375000409677625 ) ) ;
#64258 = DIRECTION ( 'NONE',  ( -0.000000000000000000, -0.000000000000000000, 1.000000000000000000 ) ) ;
#64257 = DIRECTION ( 'NONE',  ( -0.000000000000000000, 1.000000000000000000, -0.000000000000000000 ) ) ;
#64259 = CARTESIAN_POINT ( 'NONE',  ( -1.432654583217664479, 200.7500000013656063, 138.5412658750000787 ) ) ;
#64260 =( BOUNDED_CURVE ( )  B_SPLINE_CURVE ( 2, ( #45565, #50852, #73490, #33904, #68578, #39167, #38803, #16887, #56903, #15392, #61805, #44455, #62539 ),
 .UNSPECIFIED., .F., .F. ) 
 B_SPLINE_CURVE_WITH_KNOTS ( ( 3, 2, 2, 2, 2, 2, 3 ),
 ( 0.05978260869565217572, 0.06159420289855072755, 0.06340579710144927938, 0.06521739130434782428, 0.06702898550724638305, 0.06884057971014492794, 0.07065217391304347283 ),
 .UNSPECIFIED. ) 
 CURVE ( )  GEOMETRIC_REPRESENTATION_ITEM ( )  RATIONAL_B_SPLINE_CURVE ( ( 1.000000000000000000, 0.9659258262890683122, 1.000000000000000000, 0.9659258262890683122, 1.000000000000000000, 0.9659258262890683122, 1.000000000000000000, 0.9659258262890683122, 1.000000000000000000, 0.9659258262890683122, 1.000000000000000000, 0.9659258262890683122, 1.000000000000000000 ) ) 
 REPRESENTATION_ITEM ( '' )  );
#64261 = CARTESIAN_POINT ( 'NONE',  ( 8.660254037844385522, 81.45833332650536818, 5.000000000000005329 ) ) ;
#64262 = CARTESIAN_POINT ( 'NONE',  ( 2.977408999572650039, 99.68750000204838102, -7.188101187500001821 ) ) ;
#64263 = CARTESIAN_POINT ( 'NONE',  ( -3.211159895383562723, 18.06249999863440792, 3.211159895383561391 ) ) ;
#64264 = CARTESIAN_POINT ( 'NONE',  ( -29.65685424949241167, 204.1875000027311842, 166.0000000000003695 ) ) ;
#64265 = CARTESIAN_POINT ( 'NONE',  ( -8.660254037844390851, 49.79166665983870388, 4.999999999999998224 ) ) ;
#64266 = CARTESIAN_POINT ( 'NONE',  ( -11.00000000000000000, 0.000000000000000000, 98.68750000409677625 ) ) ;
#64267 = VERTEX_POINT ( 'NONE', #12968 ) ;
#64268 = EDGE_LOOP ( 'NONE', ( #18331, #51640, #1568, #67094 ) ) ;
#64269 = CARTESIAN_POINT ( 'NONE',  ( 4.721056650416000089, 298.9843750017070079, 4.721056650415999201 ) ) ;
#64270 = LINE ( 'NONE', #18983, #60396 ) ;
#64271 = CARTESIAN_POINT ( 'NONE',  ( 10.00000000000000178, 41.87499999317203248, 0.000000000000000000 ) ) ;
#64272 = CARTESIAN_POINT ( 'NONE',  ( 9.832129032723420536, 156.1979166632526983, -5.676582343749999815 ) ) ;
#64273 = AXIS2_PLACEMENT_3D ( 'NONE', #634, #57976, #17583 ) ;
#64274 = CARTESIAN_POINT ( 'NONE',  ( 10.18810118749999916, 4.220049686691935698, 80.50000000204839523 ) ) ;
#64275 = DIRECTION ( 'NONE',  ( -0.000000000000000000, 1.000000000000000000, -0.000000000000000000 ) ) ;
#64276 = CARTESIAN_POINT ( 'NONE',  ( -2.828427124746152987, 204.1250000000000284, 200.8284271247462129 ) ) ;
#64277 = CARTESIAN_POINT ( 'NONE',  ( -5.951239500248230563, 17.34865996334628946, -0.1850551574587545600 ) ) ;
#64278 = ADVANCED_FACE ( 'NONE', ( #2035 ), #48041, .F. ) ;
#64279 = CARTESIAN_POINT ( 'NONE',  ( 10.18810118749999916, 4.220049686691935698, 107.8750000020483668 ) ) ;
#64280 = ORIENTED_EDGE ( 'NONE', *, *, #13625, .T. ) ;
#64281 =( BOUNDED_CURVE ( )  B_SPLINE_CURVE ( 2, ( #53777, #2086, #71104, #36793, #59803, #31121, #48466, #49968, #21289 ),
 .UNSPECIFIED., .F., .F. ) 
 B_SPLINE_CURVE_WITH_KNOTS ( ( 3, 2, 2, 2, 3 ),
 ( 0.6041666666666648533, 0.6145833333333315940, 0.6249999999999982236, 0.6354166666666647423, 0.6458333333333314830 ),
 .UNSPECIFIED. ) 
 CURVE ( )  GEOMETRIC_REPRESENTATION_ITEM ( )  RATIONAL_B_SPLINE_CURVE ( ( 1.000000000000012879, 0.9238795325112737489, 1.000000000000000000, 0.9238795325112867385, 1.000000000000000000, 0.9238795325112867385, 1.000000000000000000, 0.9238795325113005052, 0.9999999999999862332 ) ) 
 REPRESENTATION_ITEM ( '' )  );
#64282 = DIRECTION ( 'NONE',  ( -1.000000000000000000, 0.000000000000000000, 0.000000000000000000 ) ) ;
#64283 = DIRECTION ( 'NONE',  ( -0.000000000000000000, 1.000000000000000000, 4.476705744456276341E-16 ) ) ;
#64284 = CARTESIAN_POINT ( 'NONE',  ( 6.951808397369818766E-16, 137.3437499965860127, -11.35316468750000141 ) ) ;
#64285 = CARTESIAN_POINT ( 'NONE',  ( -1.432654583217607858, 196.6250000013656063, 201.4587341250000065 ) ) ;
#64286 = CARTESIAN_POINT ( 'NONE',  ( -1.320432766682874540E-15, 27.46874999795161543, 7.188101187500000044 ) ) ;
#64287 = CARTESIAN_POINT ( 'NONE',  ( -10.18810118749999916, 4.220049686691934809, 76.93750000204838102 ) ) ;
#64288 = CARTESIAN_POINT ( 'NONE',  ( 3.042071309553159519, 55.05208332991934128, 11.35316468750000141 ) ) ;
#64289 = EDGE_LOOP ( 'NONE', ( #34224, #20404, #63574, #12022, #12227, #14267, #13430 ) ) ;
#64290 = CARTESIAN_POINT ( 'NONE',  ( -5.000000000000001776, 26.66666666666667496, -8.660254037844392627 ) ) ;
#64291 = CARTESIAN_POINT ( 'NONE',  ( -8.342170076843785083E-16, 3.187499998634407028, 4.541265875000002339 ) ) ;
#64292 = CARTESIAN_POINT ( 'NONE',  ( -4.903558642999205574E-16, 8.008118988124991233, 15.63811528394063188 ) ) ;
#64293 = ADVANCED_FACE ( 'NONE', ( #3524 ), #32961, .T. ) ;
#64294 = CARTESIAN_POINT ( 'NONE',  ( -2.977408999572650039, 15.93749999795161543, -7.188101187500001821 ) ) ;
#64295 = CARTESIAN_POINT ( 'NONE',  ( 1.102182119232618108E-15, 294.3125000034140157, 6.000000000000001776 ) ) ;
#64296 = CARTESIAN_POINT ( 'NONE',  ( -22.84727149214078423, -13.73255534606449224, 137.4610722867304560 ) ) ;
#64297 = CARTESIAN_POINT ( 'NONE',  ( 2.977408999572651815, 6.562499997951610098, 7.188101187500000933 ) ) ;
#64298 = CARTESIAN_POINT ( 'NONE',  ( -2.977408999572647819, 7.188101187499992051, 7.205302781871751883 ) ) ;
#64299 = CARTESIAN_POINT ( 'NONE',  ( 7.204075437095968759, -7.204075437095966983, 71.21875000204836681 ) ) ;
#64300 = EDGE_CURVE ( 'NONE', #63637, #49057, #32582, .T. ) ;
#64301 = SHAPE_REPRESENTATION ( 'plain washer (type a)_is_IS 2016 A- 14', ( #57354 ), #44151 ) ;
#64302 = AXIS2_PLACEMENT_3D ( 'NONE', #22092, #74154, #5506 ) ;
#64303 = CARTESIAN_POINT ( 'NONE',  ( -31.45873412499998523, 206.0000000013656347, 171.4326545832180386 ) ) ;
#64304 = CARTESIAN_POINT ( 'NONE',  ( 4.000000000000000888, 8.937500000000001776, 1.656854249492384135 ) ) ;
#64305 = CARTESIAN_POINT ( 'NONE',  ( -4.000000000000002665, 1.312499997268813390, 1.656854249492380804 ) ) ;
#64306 = ORIENTED_EDGE ( 'NONE', *, *, #25087, .T. ) ;
#64307 = CARTESIAN_POINT ( 'NONE',  ( -3.458734124999959914, 209.4375000013656063, 198.0000000000000284 ) ) ;
#64308 = CARTESIAN_POINT ( 'NONE',  ( 3.999999999999959144, 205.0625000000000568, 140.3431457505076594 ) ) ;
#64309 = CARTESIAN_POINT ( 'NONE',  ( -32.00000000000002842, 200.3125000027312126, 168.3431457505080573 ) ) ;
#64310 = CARTESIAN_POINT ( 'NONE',  ( -5.082755093536325930, 114.9687500020483810, -5.082755093536325930 ) ) ;
#64311 = CARTESIAN_POINT ( 'NONE',  ( 9.797174393178825657E-16, 125.0000000000000000, -8.000000000000000000 ) ) ;
#64312 = CARTESIAN_POINT ( 'NONE',  ( -5.867880820906206552, -5.445827678078542178, -0.3031404557143344003 ) ) ;
#64313 = ORIENTED_EDGE ( 'NONE', *, *, #64861, .T. ) ;
#64314 = CARTESIAN_POINT ( 'NONE',  ( 2.977408999572652260, 21.18749999795161543, 7.188101187500000044 ) ) ;
#64315 = VERTEX_POINT ( 'NONE', #49539 ) ;
#64316 = CARTESIAN_POINT ( 'NONE',  ( 30.82842712474619873, 198.3750000000000284, 167.1715728752537586 ) ) ;
#64317 = CARTESIAN_POINT ( 'NONE',  ( -8.660254037844387298, 43.95833332650536818, -5.000000000000004441 ) ) ;
#64318 = CARTESIAN_POINT ( 'NONE',  ( 7.320508075688774596, 60.62500000000001421, -7.320508075688774596 ) ) ;
#64319 = CARTESIAN_POINT ( 'NONE',  ( 7.188101187500002709, 98.18750000204838102, 2.977408999572649151 ) ) ;
#64320 = CARTESIAN_POINT ( 'NONE',  ( 4.242640687119287435, 299.3750000000000000, 4.242640687119285658 ) ) ;
#64322 = CARTESIAN_POINT ( 'NONE',  ( -28.70180475444370671, -42.77079112289382579, 181.7802930626621674 ) ) ;
#64321 = CARTESIAN_POINT ( 'NONE',  ( -4.242640687119285658, 288.1875000034139589, 4.242640687119287435 ) ) ;
#64323 = ORIENTED_EDGE ( 'NONE', *, *, #25193, .T. ) ;
#64324 = VERTEX_POINT ( 'NONE', #26513 ) ;
#64325 = CARTESIAN_POINT ( 'NONE',  ( 2.085542519210945334E-15, 250.1562500034140157, 11.35316468749999963 ) ) ;
#64326 = CARTESIAN_POINT ( 'NONE',  ( -5.082755093536319713, 5.082755093536319713, 16.67405278187175810 ) ) ;
#64327 = CARTESIAN_POINT ( 'NONE',  ( 9.999999999999982236, 89.79166666666667140, 2.679491924311231621 ) ) ;
#64328 = CARTESIAN_POINT ( 'NONE',  ( 1.111366970226222140E-15, 101.0525588832578734, 7.949999999999993960 ) ) ;
#64329 = CARTESIAN_POINT ( 'NONE',  ( -8.660254037844387298, 264.5833333333333144, -4.999999999999999112 ) ) ;
#64331 = ADVANCED_FACE ( 'NONE', ( #71791 ), #3151, .T. ) ;
#64330 = LINE ( 'NONE', #7360, #57168 ) ;
#64332 = CARTESIAN_POINT ( 'NONE',  ( 10.00000000000000000, 174.7916666666666288, 2.679491924311236062 ) ) ;
#64333 = DIRECTION ( 'NONE',  ( 1.000000000000000000, 0.000000000000000000, 0.000000000000000000 ) ) ;
#64334 = CARTESIAN_POINT ( 'NONE',  ( -32.52548844278290829, 175.8139081536012895, 162.3971745514289466 ) ) ;
#64335 = DIRECTION ( 'NONE',  ( 0.000000000000000000, 0.000000000000000000, -1.000000000000000000 ) ) ;
#64336 = CARTESIAN_POINT ( 'NONE',  ( 3.042071309553159519, 135.0520833299193555, 11.35316468750000141 ) ) ;
#64337 = CYLINDRICAL_SURFACE ( 'NONE', #69839, 30.99999999999997158 ) ;
#64338 = CARTESIAN_POINT ( 'NONE',  ( -4.898587196589412829E-16, 117.1250000000000000, -8.000000000000000000 ) ) ;
#64341 = CARTESIAN_POINT ( 'NONE',  ( 18.00000000000000000, 2.326828918379971365E-15, -19.00000000000000355 ) ) ;
#64340 = CARTESIAN_POINT ( 'NONE',  ( 5.656854249492374365, 5.656854249492375253, 25.76780277982336997 ) ) ;
#64339 = CARTESIAN_POINT ( 'NONE',  ( 23.99999999999998934, 205.7500000000000284, 169.9999999999998863 ) ) ;
#64342 = VERTEX_POINT ( 'NONE', #26139 ) ;
#64343 = CARTESIAN_POINT ( 'NONE',  ( 2.751064625579944321E-14, 205.7500000000000284, 194.0000000000000568 ) ) ;
#64344 = CARTESIAN_POINT ( 'NONE',  ( -3.999999999999960032, 209.1250000027312126, 198.0000000000000284 ) ) ;
#64345 = CARTESIAN_POINT ( 'NONE',  ( 26.34314575050769491, 195.6875000027311842, 165.9999999999997442 ) ) ;
#64346 = CARTESIAN_POINT ( 'NONE',  ( 26.56734541678232375, 195.6250000013656063, 173.4587341249998929 ) ) ;
#64347 = ADVANCED_FACE ( 'NONE', ( #38608 ), #14819, .T. ) ;
#64348 = CARTESIAN_POINT ( 'NONE',  ( 8.660254037844389075, 32.29166665983870388, -5.000000000000000000 ) ) ;
#64349 = VECTOR ( 'NONE', #8428, 1000.000000000000000 ) ;
#64350 = CARTESIAN_POINT ( 'NONE',  ( 2.977408999572654480, 112.6250000020483668, 7.188101187499999156 ) ) ;
#64351 = CARTESIAN_POINT ( 'NONE',  ( -3.211159895383562723, 21.93749999863440792, 3.211159895383561391 ) ) ;
#64352 = CYLINDRICAL_SURFACE ( 'NONE', #20435, 7.999999999999991118 ) ;
#64353 = CARTESIAN_POINT ( 'NONE',  ( -7.999999999999989342, -3.313708498984762496, 15.92405277982336465 ) ) ;
#64355 = CARTESIAN_POINT ( 'NONE',  ( -5.656854249492379694, 24.37499999590322375, -5.656854249492380582 ) ) ;
#64354 = CARTESIAN_POINT ( 'NONE',  ( -10.00000000000000000, 238.1250000068279746, 0.000000000000000000 ) ) ;
#64356 = VERTEX_POINT ( 'NONE', #60858 ) ;
#64357 = CARTESIAN_POINT ( 'NONE',  ( 9.999999999999998224, 220.8333333401613174, -2.679491924311229401 ) ) ;
#64359 = CARTESIAN_POINT ( 'NONE',  ( -7.950093002584606161, 225.9999999999999716, -6.101298592595878922 ) ) ;
#64358 = PRODUCT_RELATED_PRODUCT_CATEGORY ( 'part', '', ( #4763 ) ) ;
#64360 = CARTESIAN_POINT ( 'NONE',  ( -8.660254037844431707, 62.08333333333336412, -5.000000000000030198 ) ) ;
#64361 = CARTESIAN_POINT ( 'NONE',  ( -11.35316468749999608, 239.4270833367473017, 3.042071309553173730 ) ) ;
#64362 = CARTESIAN_POINT ( 'NONE',  ( 8.311093377946837890, 116.4062499965860269, -8.311093377946837890 ) ) ;
#64363 = EDGE_LOOP ( 'NONE', ( #71683, #19643, #32735, #69513 ) ) ;
#64364 = CARTESIAN_POINT ( 'NONE',  ( 5.000000000000000888, -13.57926339724853904, 69.65188861886710470 ) ) ;
#64365 = CARTESIAN_POINT ( 'NONE',  ( 10.18810118749999916, 1.247682550866122264E-15, 102.9062500020483810 ) ) ;
#64366 = CARTESIAN_POINT ( 'NONE',  ( 10.50000000000000000, 0.000000000000000000, -1.050311307314560239 ) ) ;
#64367 = CARTESIAN_POINT ( 'NONE',  ( 2.445694354108840063, 200.0625000013656063, 200.4456943541088663 ) ) ;
#64368 = CARTESIAN_POINT ( 'NONE',  ( 5.000000000000000000, 70.11723469343073134, 28.93519894129288517 ) ) ;
#64370 = CARTESIAN_POINT ( 'NONE',  ( -11.35316468750000141, 108.4895833299193413, 3.042071309553159963 ) ) ;
#64369 = DIRECTION ( 'NONE',  ( -1.000000000000000000, 0.000000000000000000, 0.000000000000000000 ) ) ;
#64371 = CARTESIAN_POINT ( 'NONE',  ( 7.999999999999992895, -3.313708498984756279, 4.674052783920145338 ) ) ;
#64372 = CARTESIAN_POINT ( 'NONE',  ( -26.56734541678237704, 196.6250000013656063, 166.5412658750003629 ) ) ;
#64373 = CARTESIAN_POINT ( 'NONE',  ( -5.656854249492380582, 91.81249999999998579, -5.656854249492380582 ) ) ;
#64374 = ORIENTED_EDGE ( 'NONE', *, *, #44076, .F. ) ;
#64375 = CARTESIAN_POINT ( 'NONE',  ( -7.320508075688773708, 198.7499999931720254, -7.320508075688774596 ) ) ;
#64376 = ADVANCED_FACE ( 'NONE', ( #2778 ), #48784, .T. ) ;
#64377 = CARTESIAN_POINT ( 'NONE',  ( 1.469576158976823947E-15, 112.0625000040967905, 8.000000000000000000 ) ) ;
#64378 = CARTESIAN_POINT ( 'NONE',  ( 4.000000000000001776, 9.812499997268814056, -1.656854249492381248 ) ) ;
#64379 = CARTESIAN_POINT ( 'NONE',  ( -11.35316468750000141, 83.59374999658601268, -1.390361679473963753E-15 ) ) ;
#64380 = CARTESIAN_POINT ( 'NONE',  ( 10.50000000000000000, 0.000000000000000000, -21.50000000000000000 ) ) ;
#64381 = CARTESIAN_POINT ( 'NONE',  ( -7.188101187500000044, 10.59374999795161187, -8.802885111219163269E-16 ) ) ;
#64382 =( BOUNDED_CURVE ( )  B_SPLINE_CURVE ( 2, ( #5299, #33241, #5670, #74321, #22253, #62254, #16588, #67554, #28301 ),
 .UNSPECIFIED., .F., .F. ) 
 B_SPLINE_CURVE_WITH_KNOTS ( ( 3, 2, 2, 2, 3 ),
 ( 0.7833333333333338810, 0.7916666666666671848, 0.8000000000000007105, 0.8083333333333340143, 0.8166666666666674290 ),
 .UNSPECIFIED. ) 
 CURVE ( )  GEOMETRIC_REPRESENTATION_ITEM ( )  RATIONAL_B_SPLINE_CURVE ( ( 0.9999999999999948930, 0.9238795325112918455, 1.000000000000000000, 0.9238795325112867385, 1.000000000000000000, 0.9238795325112867385, 1.000000000000000000, 0.9238795325112796331, 1.000000000000007105 ) ) 
 REPRESENTATION_ITEM ( '' )  );
#64383 = CARTESIAN_POINT ( 'NONE',  ( -4.220049686691937474, -10.18810118749999738, 93.81250000204838102 ) ) ;
#64384 = EDGE_CURVE ( 'NONE', #35109, #2698, #72558, .T. ) ;
#64385 = CARTESIAN_POINT ( 'NONE',  ( 11.35316468750000141, 16.09374999658601979, 0.000000000000000000 ) ) ;
#64386 = EDGE_LOOP ( 'NONE', ( #46839, #69559, #64233, #34129 ) ) ;
#64387 = CARTESIAN_POINT ( 'NONE',  ( -7.999999999999979572, -3.313708498984773154, 26.42405277982336642 ) ) ;
#64388 = CARTESIAN_POINT ( 'NONE',  ( 2.260400649951880947, -43.01786379024215989, 139.0822089705408757 ) ) ;
#64389 = CARTESIAN_POINT ( 'NONE',  ( 3.042071309553159519, 224.7395833299193555, 11.35316468750000141 ) ) ;
#64390 = CARTESIAN_POINT ( 'NONE',  ( 10.18810118749999916, 4.220049686691935698, 80.87500000204836681 ) ) ;
#64391 = VECTOR ( 'NONE', #41033, 1000.000000000000000 ) ;
#64392 = CARTESIAN_POINT ( 'NONE',  ( 3.856379400883930941, 21.99999999999998934, 1.388370628458741596 ) ) ;
#64393 = CARTESIAN_POINT ( 'NONE',  ( -3.313708498984653250, 93.40625000409676204, -8.000000000000108358 ) ) ;
#64394 = CARTESIAN_POINT ( 'NONE',  ( -6.676582343750001591, 291.4531250017069510, 0.000000000000000000 ) ) ;
#64395 = EDGE_LOOP ( 'NONE', ( #11841, #42160, #36708, #18474 ) ) ;
#64396 = CARTESIAN_POINT ( 'NONE',  ( 4.556349186104045934, 11.00000000000000000, 89.21875000409679046 ) ) ;
#64397 = CARTESIAN_POINT ( 'NONE',  ( -5.676582343750006032, 204.4270833299193555, 9.832129032723418760 ) ) ;
#64398 = CARTESIAN_POINT ( 'NONE',  ( -10.18810118749999916, 0.000000000000000000, 88.65625000204838102 ) ) ;
#64399 = ADVANCED_FACE ( 'NONE', ( #20862 ), #43881, .T. ) ;
#64400 = CARTESIAN_POINT ( 'NONE',  ( -24.54126587499999346, 201.1875000013656063, 170.0000000000003411 ) ) ;
#64401 =( BOUNDED_CURVE ( )  B_SPLINE_CURVE ( 2, ( #7075, #30081, #53837, #53099, #2146, #48155, #2888, #71164, #65514, #42861, #14186, #13809, #59861 ),
 .UNSPECIFIED., .F., .F. ) 
 B_SPLINE_CURVE_WITH_KNOTS ( ( 3, 2, 2, 2, 2, 2, 3 ),
 ( 0.5815217391304348116, 0.5833333333333333703, 0.5851449275362319291, 0.5869565217391304879, 0.5887681159420289356, 0.5905797101449274944, 0.5923913043478260532 ),
 .UNSPECIFIED. ) 
 CURVE ( )  GEOMETRIC_REPRESENTATION_ITEM ( )  RATIONAL_B_SPLINE_CURVE ( ( 1.000000000000000000, 0.9659258262890683122, 1.000000000000000000, 0.9659258262890683122, 1.000000000000000000, 0.9659258262890683122, 1.000000000000000000, 0.9659258262890683122, 1.000000000000000000, 0.9659258262890683122, 1.000000000000000000, 0.9659258262890683122, 1.000000000000000000 ) ) 
 REPRESENTATION_ITEM ( '' )  );
#64402 = CARTESIAN_POINT ( 'NONE',  ( 5.656854249492378806, 23.81250000000000355, 5.656854249492381470 ) ) ;
#64403 = ORIENTED_EDGE ( 'NONE', *, *, #65047, .T. ) ;
#64404 = CARTESIAN_POINT ( 'NONE',  ( -29.01729116559129906, -51.90398845573497510, 159.0598141256127178 ) ) ;
#64405 = CARTESIAN_POINT ( 'NONE',  ( -3.999999999999960032, 208.1250000027312126, 198.0000000000000284 ) ) ;
#64406 = CARTESIAN_POINT ( 'NONE',  ( 10.00000000000000000, 29.79166666666666785, 2.679491924311236062 ) ) ;
#64407 = CARTESIAN_POINT ( 'NONE',  ( -37.94562015984924841, 38.00000000000001421, 126.9999999999999716 ) ) ;
#64408 = CARTESIAN_POINT ( 'NONE',  ( 10.18810118749999916, 4.220049686691935698, 73.37500000204838102 ) ) ;
#64409 = ORIENTED_EDGE ( 'NONE', *, *, #64128, .F. ) ;
#64410 = DIRECTION ( 'NONE',  ( -0.000000000000000000, 1.000000000000000000, -4.476705744456276341E-16 ) ) ;
#64411 = EDGE_CURVE ( 'NONE', #10224, #38666, #68839, .T. ) ;
#64412 = PLANE ( 'NONE',  #26995 ) ;
#64413 = CARTESIAN_POINT ( 'NONE',  ( 11.00000000000000355, -4.556349186104044158, 93.34375000409677625 ) ) ;
#64414 = CARTESIAN_POINT ( 'NONE',  ( -5.082755093536324154, 117.2187500020483810, 5.082755093536326818 ) ) ;
#64415 = CARTESIAN_POINT ( 'NONE',  ( -3.834411065495477722, 22.00000000000000000, -1.980039758230538016 ) ) ;
#64416 = CARTESIAN_POINT ( 'NONE',  ( -6.676582343750002480, 298.3906250017070079, -2.765530957081996810 ) ) ;
#64417 = EDGE_CURVE ( 'NONE', #46951, #30587, #49160, .T. ) ;
#64419 = CARTESIAN_POINT ( 'NONE',  ( 0.000000000000000000, 125.0000000000000000, 0.000000000000000000 ) ) ;
#64418 = CARTESIAN_POINT ( 'NONE',  ( -3.042071309553159075, 229.9479166700806161, 11.35316468749999963 ) ) ;
#64420 = ORIENTED_EDGE ( 'NONE', *, *, #68659, .F. ) ;
#64421 = CARTESIAN_POINT ( 'NONE',  ( 5.676582343750005144, 240.8854166700806445, 9.832129032723416984 ) ) ;
#64422 = CARTESIAN_POINT ( 'NONE',  ( -2.977408999572647819, 7.188101187499991163, 8.705302781871752771 ) ) ;
#64424 = EDGE_CURVE ( 'NONE', #65034, #9708, #67275, .T. ) ;
#64423 = CARTESIAN_POINT ( 'NONE',  ( 3.458734125000016757, 202.1250000013656063, 199.4326545832176691 ) ) ;
#64425 = ORIENTED_EDGE ( 'NONE', *, *, #68362, .F. ) ;
#64426 = CARTESIAN_POINT ( 'NONE',  ( -4.220049686691937474, -10.18810118749999738, 67.93750000204838102 ) ) ;
#64427 = CARTESIAN_POINT ( 'NONE',  ( 11.35316468750000141, 106.0937499965860269, 0.000000000000000000 ) ) ;
#64428 = CARTESIAN_POINT ( 'NONE',  ( 0.8588954341814998283, 60.21087566322560747, 22.89167302533804005 ) ) ;
#64429 = CARTESIAN_POINT ( 'NONE',  ( 7.778174593052021635, 7.778174593052023411, 81.43750000000000000 ) ) ;
#64432 = CARTESIAN_POINT ( 'NONE',  ( 2.020667218593132706E-15, -11.00000000000000000, 113.8749999999999858 ) ) ;
#64431 = CARTESIAN_POINT ( 'NONE',  ( 27.99999999999997158, 205.9375000013656063, 166.5412658749999082 ) ) ;
#64430 = CARTESIAN_POINT ( 'NONE',  ( 26.56734541678238060, 204.2500000013655779, 166.5412658749999650 ) ) ;
#64433 = VERTEX_POINT ( 'NONE', #43498 ) ;
#64434 = VECTOR ( 'NONE', #70353, 1000.000000000000000 ) ;
#64435 = CARTESIAN_POINT ( 'NONE',  ( -27.99999999999990763, 195.6250000027311842, 174.0000000000003695 ) ) ;
#64436 = CARTESIAN_POINT ( 'NONE',  ( 0.000000000000000000, 300.0000000000000000, 10.00000000000000178 ) ) ;
#64437 = CARTESIAN_POINT ( 'NONE',  ( 3.042071309553167069, 206.8229166632526699, -11.35316468749999785 ) ) ;
#64438 = CARTESIAN_POINT ( 'NONE',  ( -2.839093476692135984E-14, 204.6875000013656063, 138.5412658750000503 ) ) ;
#64439 = CARTESIAN_POINT ( 'NONE',  ( 27.99999999999996447, 204.6875000013656063, 173.4587341249998929 ) ) ;
#64440 = CARTESIAN_POINT ( 'NONE',  ( -5.082755093536326818, 22.78124999795161187, 5.082755093536325042 ) ) ;
#64441 = CARTESIAN_POINT ( 'NONE',  ( 9.832129032723416984, 180.6770833299193555, 5.676582343750006032 ) ) ;
#64442 = CARTESIAN_POINT ( 'NONE',  ( -4.401442555609581635E-16, 97.15625000204839523, -7.188101187500000044 ) ) ;
#64443 = CARTESIAN_POINT ( 'NONE',  ( -5.000000000000000000, 65.19475225706649724, -23.98307544244871181 ) ) ;
#64444 = CARTESIAN_POINT ( 'NONE',  ( -25.17157287525377285, 195.6250000000000284, 172.8284271247465256 ) ) ;
#64445 = CARTESIAN_POINT ( 'NONE',  ( -1.881053915767121554, 9.624999998634404363, -4.541265875000002339 ) ) ;
#64446 = CARTESIAN_POINT ( 'NONE',  ( 27.99999999999996447, 203.6875000013656063, 173.4587341249998929 ) ) ;
#64447 = CARTESIAN_POINT ( 'NONE',  ( -2.977408999572648707, -7.188101187499990274, 6.642802781871754547 ) ) ;
#64448 = CARTESIAN_POINT ( 'NONE',  ( -3.042071309553164404, 67.23958332991935549, -11.35316468749999963 ) ) ;
#64449 = EDGE_CURVE ( 'NONE', #53235, #68975, #61825, .T. ) ;
#64450 = CARTESIAN_POINT ( 'NONE',  ( -3.673940397442060854E-16, 298.7500000000000000, -6.000000000000001776 ) ) ;
#64451 = CARTESIAN_POINT ( 'NONE',  ( 1.656854249492422992, 209.6875000000000000, 194.0000000000000568 ) ) ;
#64452 = ORIENTED_EDGE ( 'NONE', *, *, #66617, .F. ) ;
#64453 = CARTESIAN_POINT ( 'NONE',  ( -10.00000000000003020, 47.70833333333334281, 2.679491924311229401 ) ) ;
#64454 = CARTESIAN_POINT ( 'NONE',  ( 6.123233995736767268E-16, 178.1249999931720538, -10.00000000000000178 ) ) ;
#64455 = CARTESIAN_POINT ( 'NONE',  ( -9.832129032723418760, 77.86458332991935549, -5.676582343750004256 ) ) ;
#64456 = CARTESIAN_POINT ( 'NONE',  ( 2.020667218593132706E-15, -11.00000000000000000, 67.56250000409677625 ) ) ;
#64457 = CARTESIAN_POINT ( 'NONE',  ( 3.458734124999960358, 196.6250000013656063, 143.4326545832176976 ) ) ;
#64458 = CARTESIAN_POINT ( 'NONE',  ( 1.656854249492381248, 8.937499997268814056, -4.000000000000001776 ) ) ;
#64460 = CARTESIAN_POINT ( 'NONE',  ( 8.311093377946837890, 56.40624999658600558, -8.311093377946837890 ) ) ;
#64459 = CARTESIAN_POINT ( 'NONE',  ( 5.656854249492381470, 103.2500000040967905, 5.656854249492379694 ) ) ;
#64461 = AXIS2_PLACEMENT_3D ( 'NONE', #33857, #56855, #22494 ) ;
#64462 = CARTESIAN_POINT ( 'NONE',  ( -7.999999999999991118, 0.000000000000000000, 26.51780278392014623 ) ) ;
#64463 = CARTESIAN_POINT ( 'NONE',  ( -7.347880794884122694E-16, 12.49999999726881406, 4.000000000000001776 ) ) ;
#64464 = CARTESIAN_POINT ( 'NONE',  ( 10.00000000000000178, 156.8749999931720254, 0.000000000000000000 ) ) ;
#64465 = CARTESIAN_POINT ( 'NONE',  ( -2.977408999572650927, 94.25000000204838102, -7.188101187500001821 ) ) ;
#64466 = VECTOR ( 'NONE', #11171, 1000.000000000000000 ) ;
#64467 = CARTESIAN_POINT ( 'NONE',  ( 2.679491924311249829, 21.04166666666666785, -9.999999999999996447 ) ) ;
#64468 = CARTESIAN_POINT ( 'NONE',  ( -3.042071309553163960, 52.55208332991934839, -11.35316468749999963 ) ) ;
#64469 = CARTESIAN_POINT ( 'NONE',  ( -6.238412754330611322E-16, 10.18810118749999916, 112.6562500020483810 ) ) ;
#64470 = CARTESIAN_POINT ( 'NONE',  ( 9.832129032723416984, 190.3645833299193839, 5.676582343750006032 ) ) ;
#64471 = VERTEX_POINT ( 'NONE', #4648 ) ;
#64472 = EDGE_CURVE ( 'NONE', #50184, #26210, #57449, .T. ) ;
#64473 = CARTESIAN_POINT ( 'NONE',  ( 3.496982156819858467, 68.06496700477683248, 20.41687962717103844 ) ) ;
#64474 = FACE_OUTER_BOUND ( 'NONE', #26328, .T. ) ;
#64475 = CARTESIAN_POINT ( 'NONE',  ( 4.270632937500002058, 0.5937499979516099868, 0.000000000000000000 ) ) ;
#64477 = CARTESIAN_POINT ( 'NONE',  ( -11.35316468750000141, 178.4895833299193555, 3.042071309553159963 ) ) ;
#64476 = CARTESIAN_POINT ( 'NONE',  ( 1.656854249492287101, 195.3125000000000284, 202.0000000000001137 ) ) ;
#64478 = DIRECTION ( 'NONE',  ( 0.000000000000000000, 0.000000000000000000, -1.000000000000000000 ) ) ;
#64479 = CARTESIAN_POINT ( 'NONE',  ( 7.320508075688771044, 251.2500000068279746, -7.320508075688771932 ) ) ;
#64480 = DIRECTION ( 'NONE',  ( -0.000000000000000000, 1.000000000000000000, -0.000000000000000000 ) ) ;
#64481 = ORIENTED_EDGE ( 'NONE', *, *, #71887, .T. ) ;
#64482 = CARTESIAN_POINT ( 'NONE',  ( -5.676582343749998039, 172.7604166632526983, -9.832129032723420536 ) ) ;
#64483 = CARTESIAN_POINT ( 'NONE',  ( -7.188101187499992051, 0.000000000000000000, 25.48655278187175810 ) ) ;
#64484 = CARTESIAN_POINT ( 'NONE',  ( 3.999982273345623174, 89.99927424231840689, -6.928213464733948612 ) ) ;
#64485 = ORIENTED_EDGE ( 'NONE', *, *, #19549, .F. ) ;
#64486 = CARTESIAN_POINT ( 'NONE',  ( -4.898587196589412829E-16, 105.3125000040967763, -8.000000000000000000 ) ) ;
#64487 =( BOUNDED_CURVE ( )  B_SPLINE_CURVE ( 2, ( #68787, #63872, #40866, #5058, #74445, #63498, #23134, #17472, #68051, #40118, #12184, #68413, #63124 ),
 .UNSPECIFIED., .F., .F. ) 
 B_SPLINE_CURVE_WITH_KNOTS ( ( 3, 2, 2, 2, 2, 2, 3 ),
 ( 0.4552960319598876593, 0.4605291305068314744, 0.4657622290537752896, 0.4709953276007191603, 0.4762284261476630309, 0.4814615246946068461, 0.4866946232415507168 ),
 .UNSPECIFIED. ) 
 CURVE ( )  GEOMETRIC_REPRESENTATION_ITEM ( )  RATIONAL_B_SPLINE_CURVE ( ( 1.000000000000021982, 0.9659258262890463298, 1.000000000000000000, 0.9659258262890682012, 1.000000000000000000, 0.9659258262890682012, 1.000000000000000000, 0.9659258262890682012, 1.000000000000000000, 0.9659258262890682012, 1.000000000000000000, 0.9659258262890593194, 1.000000000000008882 ) ) 
 REPRESENTATION_ITEM ( '' )  );
#64488 = ADVANCED_FACE ( 'NONE', ( #51028 ), #6133, .T. ) ;
#64489 = CARTESIAN_POINT ( 'NONE',  ( -2.828427124746192067, 11.62500000000000000, 2.828427124746190735 ) ) ;
#64490 = DIRECTION ( 'NONE',  ( 0.000000000000000000, 0.000000000000000000, 1.000000000000000000 ) ) ;
#64491 = CARTESIAN_POINT ( 'NONE',  ( 4.541265875000002339, 12.31249999863440792, 0.000000000000000000 ) ) ;
#64492 = CARTESIAN_POINT ( 'NONE',  ( -4.898587196589407898E-16, 7.999999999999991118, 21.64280278392014623 ) ) ;
#64493 = CARTESIAN_POINT ( 'NONE',  ( -2.751064625579944321E-14, 195.7500000000000000, 146.0000000000000284 ) ) ;
#64494 = ORIENTED_EDGE ( 'NONE', *, *, #35464, .T. ) ;
#64495 = CARTESIAN_POINT ( 'NONE',  ( 1.469576158976823947E-15, 92.37499999999998579, 8.000000000000000000 ) ) ;
#64496 = CARTESIAN_POINT ( 'NONE',  ( -7.188101187499999156, 97.25000000204839523, 2.977408999572654924 ) ) ;
#64497 = EDGE_CURVE ( 'NONE', #60791, #67450, #16679, .T. ) ;
#64499 = CARTESIAN_POINT ( 'NONE',  ( -4.898587196589412829E-16, 120.3125000040967763, -8.000000000000000000 ) ) ;
#64498 = CARTESIAN_POINT ( 'NONE',  ( 3.313708498984762496, 16.03124999590322020, 7.999999999999998224 ) ) ;
#64500 = ORIENTED_EDGE ( 'NONE', *, *, #56724, .F. ) ;
#64501 = CARTESIAN_POINT ( 'NONE',  ( -5.086519500888152301, 10.26068667857073358, -64.41585657734927395 ) ) ;
#64502 = CARTESIAN_POINT ( 'NONE',  ( 105.0000000000000000, 39.09128788536428800, 65.00000000000000000 ) ) ;
#64503 = COLOUR_RGB ( '',0.7921568627450980005, 0.8196078431372548767, 0.9333333333333333481 ) ;
#64504 = CARTESIAN_POINT ( 'NONE',  ( 5.082755093536320601, -5.082755093536318824, 24.54905278187175810 ) ) ;
#64505 = ORIENTED_EDGE ( 'NONE', *, *, #29069, .T. ) ;
#64506 = ADVANCED_FACE ( 'NONE', ( #39342 ), #73669, .F. ) ;
#64507 = VERTEX_POINT ( 'NONE', #27642 ) ;
#64508 = CARTESIAN_POINT ( 'NONE',  ( -6.238412754330611322E-16, 10.18810118749999916, 85.28125000204836681 ) ) ;
#64509 = UNCERTAINTY_MEASURE_WITH_UNIT (LENGTH_MEASURE( 1.000000000000000082E-05 ), #4941, 'distance_accuracy_value', 'NONE');
#64510 = CARTESIAN_POINT ( 'NONE',  ( -24.54126587499997569, 195.3750000013656063, 171.4326545832179818 ) ) ;
#64511 = CARTESIAN_POINT ( 'NONE',  ( -11.00000000000000000, 0.000000000000000000, 99.99999999999998579 ) ) ;
#64513 = DIRECTION ( 'NONE',  ( 0.000000000000000000, -0.000000000000000000, 1.000000000000000000 ) ) ;
#64512 = CARTESIAN_POINT ( 'NONE',  ( 29.65685424949235127, 202.5625000027312126, 165.9999999999998863 ) ) ;
#64514 = CARTESIAN_POINT ( 'NONE',  ( 10.00000000000000178, 130.0000000000000000, 0.000000000000000000 ) ) ;
#64515 = CARTESIAN_POINT ( 'NONE',  ( -23.99999999999998934, 203.7500000000000284, 170.0000000000003411 ) ) ;
#64516 = DIRECTION ( 'NONE',  ( 0.000000000000000000, 1.000000000000000000, -1.224646799147353207E-16 ) ) ;
#64517 = CARTESIAN_POINT ( 'NONE',  ( 1.102182119232618108E-15, 290.3125000034140157, 6.000000000000001776 ) ) ;
#64518 = CARTESIAN_POINT ( 'NONE',  ( 30.44569435410883429, 204.8125000013656063, 167.5543056458911053 ) ) ;
#64519 = CARTESIAN_POINT ( 'NONE',  ( -5.082755093536325042, 4.406249997951610098, -5.082755093536325930 ) ) ;
#64520 = CARTESIAN_POINT ( 'NONE',  ( 1.471067592899761672E-15, -8.008118988124991233, 4.388115283940629219 ) ) ;
#64521 = CARTESIAN_POINT ( 'NONE',  ( 1.432654583217607858, 195.6250000013656063, 138.5412658750000787 ) ) ;
#64522 = CARTESIAN_POINT ( 'NONE',  ( -7.188101187499999156, 114.1250000020483952, 2.977408999572654924 ) ) ;
#64524 = CARTESIAN_POINT ( 'NONE',  ( 2.841757666793575255E-14, 194.6037658790967839, 201.6037658790967839 ) ) ;
#64523 = DIRECTION ( 'NONE',  ( 0.000000000000000000, 0.000000000000000000, 1.000000000000000000 ) ) ;
#64525 = CARTESIAN_POINT ( 'NONE',  ( 8.311093377946839666, 231.0937500034139873, 8.311093377946829008 ) ) ;
#64526 = CARTESIAN_POINT ( 'NONE',  ( -34.26178724767108719, 40.28528476991490237, 64.99999999999998579 ) ) ;
#64527 = CARTESIAN_POINT ( 'NONE',  ( 1.320432766682872962E-15, -7.188101187499992051, 26.23655278187175810 ) ) ;
#64528 = CARTESIAN_POINT ( 'NONE',  ( 29.65685424949235482, 196.0625000000000284, 173.9999999999999147 ) ) ;
#64529 = CARTESIAN_POINT ( 'NONE',  ( -8.311093377946841443, 33.90624999658602690, 8.311093377946830785 ) ) ;
#64530 = CARTESIAN_POINT ( 'NONE',  ( -5.656854249492381470, 9.937500000000001776, 5.656854249492379694 ) ) ;
#64531 = CARTESIAN_POINT ( 'NONE',  ( 6.951808397369818766E-16, 217.3437499965860411, -11.35316468750000141 ) ) ;
#64532 = CARTESIAN_POINT ( 'NONE',  ( 0.000000000000000000, 15.99999999999998579, 1.000000000000000000 ) ) ;
#64534 = CARTESIAN_POINT ( 'NONE',  ( 0.000000000000000000, 220.0000000000000284, 0.000000000000000000 ) ) ;
#64533 = DIRECTION ( 'NONE',  ( -0.1513591288559071046, 0.000000000000000000, -0.9884788384745426537 ) ) ;
#64535 = VERTEX_POINT ( 'NONE', #10669 ) ;
#64536 = CARTESIAN_POINT ( 'NONE',  ( -2.445694354108839175, 196.3125000013656063, 144.4456943541088663 ) ) ;
#64537 = CARTESIAN_POINT ( 'NONE',  ( -3.042071309553173730, 34.32291666325268409, 11.35316468749999785 ) ) ;
#64538 = CARTESIAN_POINT ( 'NONE',  ( -4.556349186104045934, 11.00000000000000000, 87.90625000409677625 ) ) ;
#64539 = CARTESIAN_POINT ( 'NONE',  ( -2.754378923186476579E-14, 209.4375000013656063, 145.4587341250000350 ) ) ;
#64540 = CARTESIAN_POINT ( 'NONE',  ( -9.000000000000000000, -5.196152422706644458, -10.80000000000000071 ) ) ;
#64541 = CARTESIAN_POINT ( 'NONE',  ( -11.00000000000000000, 0.000000000000000000, 101.5000000000000000 ) ) ;
#64543 = CARTESIAN_POINT ( 'NONE',  ( 11.35316468750000141, 20.78124999658601624, 0.000000000000000000 ) ) ;
#64542 = CARTESIAN_POINT ( 'NONE',  ( 1.320432766682874540E-15, 106.5312500020483810, 7.188101187500000044 ) ) ;
#64544 = CARTESIAN_POINT ( 'NONE',  ( -7.999999999999991118, 0.000000000000000000, 17.33030277982336287 ) ) ;
#64545 = APPLICATION_CONTEXT ( 'automotive_design' ) ;
#64546 = CARTESIAN_POINT ( 'NONE',  ( 11.35316468750000141, 150.7812499965860411, 0.000000000000000000 ) ) ;
#64547 = CARTESIAN_POINT ( 'NONE',  ( -4.999999999999998224, 113.5416666598387110, -8.660254037844389075 ) ) ;
#64548 = CARTESIAN_POINT ( 'NONE',  ( -5.082755093536325930, 112.3437500020483810, -5.082755093536325930 ) ) ;
#64549 = CARTESIAN_POINT ( 'NONE',  ( 10.00000000000000000, 171.6666666598386826, 2.679491924311235618 ) ) ;
#64550 = CARTESIAN_POINT ( 'NONE',  ( -24.54126587499999346, 205.4375000013656063, 170.0000000000003411 ) ) ;
#64551 = VERTEX_POINT ( 'NONE', #56706 ) ;
#64552 = CARTESIAN_POINT ( 'NONE',  ( -5.676582343749998039, 2.760416663252683644, -9.832129032723420536 ) ) ;
#64553 = ORIENTED_EDGE ( 'NONE', *, *, #34414, .T. ) ;
#64554 = CARTESIAN_POINT ( 'NONE',  ( -4.217983994794729519, 16.30587161610626623, -69.44297314767059959 ) ) ;
#64555 = CARTESIAN_POINT ( 'NONE',  ( 6.676582343750004256, 296.8906250017068942, 2.765530957081995478 ) ) ;
#64557 = CARTESIAN_POINT ( 'NONE',  ( 5.676582343750001591, 136.6145833299193555, -9.832129032723420536 ) ) ;
#64556 = CARTESIAN_POINT ( 'NONE',  ( -25.64349406629804307, -22.38960850746778064, 147.1376616666866823 ) ) ;
#64558 = DIRECTION ( 'NONE',  ( -0.000000000000000000, -0.9659258262890700886, -0.2588190451025146888 ) ) ;
#64559 = CARTESIAN_POINT ( 'NONE',  ( -5.656854249492373476, -5.656854249492376141, 19.07405278432982598 ) ) ;
#64560 = EDGE_CURVE ( 'NONE', #30170, #16864, #31422, .T. ) ;
#64561 = CARTESIAN_POINT ( 'NONE',  ( 47.45159024344496146, 192.2444796376913416, 64.91950087297482241 ) ) ;
#64562 = CARTESIAN_POINT ( 'NONE',  ( 11.35316468749999963, 241.4062500034140157, -1.390361679473963556E-15 ) ) ;
#64563 =( GEOMETRIC_REPRESENTATION_CONTEXT ( 3 ) GLOBAL_UNCERTAINTY_ASSIGNED_CONTEXT ( ( #63934 ) ) GLOBAL_UNIT_ASSIGNED_CONTEXT ( ( #36657, #37024, #59668 ) ) REPRESENTATION_CONTEXT ( 'NONE', 'WORKASPACE' ) );
#64564 = CARTESIAN_POINT ( 'NONE',  ( 4.220049686691934809, 10.18810118749999916, 90.06250000204838102 ) ) ;
#64565 = EDGE_LOOP ( 'NONE', ( #55897, #3675, #27219, #19757 ) ) ;
#64566 = AXIS2_PLACEMENT_3D ( 'NONE', #21340, #14922, #15295 ) ;
#64567 = CARTESIAN_POINT ( 'NONE',  ( -1.656854249492321074, 197.3125000000000568, 137.9999999999999716 ) ) ;
#64568 = CARTESIAN_POINT ( 'NONE',  ( 4.999999999999688249, 68.48985753891581396, -21.22439692019570856 ) ) ;
#64569 = CARTESIAN_POINT ( 'NONE',  ( 11.35316468750000141, 91.09374999658602690, 0.000000000000000000 ) ) ;
#64570 = CARTESIAN_POINT ( 'NONE',  ( -10.18810118749999738, -4.220049686691941915, 99.25000000204838102 ) ) ;
#64571 = CARTESIAN_POINT ( 'NONE',  ( -3.211159895383561391, 17.81249999863440792, -3.211159895383561835 ) ) ;
#64572 = ORIENTED_EDGE ( 'NONE', *, *, #59765, .T. ) ;
#64573 = ORIENTED_EDGE ( 'NONE', *, *, #3084, .F. ) ;
#64574 = CARTESIAN_POINT ( 'NONE',  ( 5.656854249492380582, 6.187500000000000888, -5.656854249492380582 ) ) ;
#64575 = CARTESIAN_POINT ( 'NONE',  ( 1.881053915767122664, 1.249999998634407028, 4.541265875000001451 ) ) ;
#64576 = CARTESIAN_POINT ( 'NONE',  ( -5.082755093536325042, 1.031249997951609876, -5.082755093536325930 ) ) ;
#64577 = CARTESIAN_POINT ( 'NONE',  ( -7.999999999999998224, 119.2812500040967763, 3.313708498984766493 ) ) ;
#64579 = EDGE_CURVE ( 'NONE', #41364, #783, #52152, .T. ) ;
#64578 = CARTESIAN_POINT ( 'NONE',  ( -4.220049686691935698, 10.18810118749999916, 106.7500000020483668 ) ) ;
#64580 = EDGE_CURVE ( 'NONE', #57841, #33693, #59848, .T. ) ;
#64581 = CARTESIAN_POINT ( 'NONE',  ( 2.828427124746191623, 0.1250000000000001943, -2.828427124746191623 ) ) ;
#64582 = CARTESIAN_POINT ( 'NONE',  ( 4.000000000000001776, 14.74999999726881406, 0.000000000000000000 ) ) ;
#64583 = CARTESIAN_POINT ( 'NONE',  ( -1.881053915767124440, 0.9999999986344065839, 4.541265875000001451 ) ) ;
#64584 = EDGE_LOOP ( 'NONE', ( #11475, #57442, #52998, #49056, #52143, #72178, #52257, #39319 ) ) ;
#64585 = EDGE_CURVE ( 'NONE', #1466, #23203, #18556, .T. ) ;
#64586 = LINE ( 'NONE', #35189, #29612 ) ;
#64587 = CARTESIAN_POINT ( 'NONE',  ( 1.432654583217664479, 199.7500000013656063, 201.4587341250000065 ) ) ;
#64589 = DIRECTION ( 'NONE',  ( -9.912705577010326536E-16, 0.000000000000000000, -1.000000000000000000 ) ) ;
#64588 = CARTESIAN_POINT ( 'NONE',  ( -26.56734541678242678, 199.3750000013656063, 166.5412658750003345 ) ) ;
#64590 = CARTESIAN_POINT ( 'NONE',  ( 1.881053915767121776, 13.49999999863440969, -4.541265875000002339 ) ) ;
#64591 = CARTESIAN_POINT ( 'NONE',  ( -4.556349186104045934, 11.00000000000000000, 68.21875000000000000 ) ) ;
#64592 = CARTESIAN_POINT ( 'NONE',  ( -2.977408999572648707, -7.188101187499990274, 15.26780278187175455 ) ) ;
#64593 = VERTEX_POINT ( 'NONE', #12877 ) ;
#64594 =( BOUNDED_CURVE ( )  B_SPLINE_CURVE ( 2, ( #41233, #68781, #23129, #1257, #64240, #46141, #35578, #18588, #51805 ),
 .UNSPECIFIED., .F., .F. ) 
 B_SPLINE_CURVE_WITH_KNOTS ( ( 3, 2, 2, 2, 3 ),
 ( 0.8529411764705882026, 0.8566176470588234837, 0.8602941176470588758, 0.8639705882352941568, 0.8676470588235294379 ),
 .UNSPECIFIED. ) 
 CURVE ( )  GEOMETRIC_REPRESENTATION_ITEM ( )  RATIONAL_B_SPLINE_CURVE ( ( 1.000000000000000000, 0.9238795325112867385, 1.000000000000000000, 0.9238795325112867385, 1.000000000000000000, 0.9238795325112867385, 1.000000000000000000, 0.9238795325112867385, 1.000000000000000000 ) ) 
 REPRESENTATION_ITEM ( '' )  );
#64595 = ORIENTED_EDGE ( 'NONE', *, *, #66685, .F. ) ;
#64596 = CARTESIAN_POINT ( 'NONE',  ( -10.18810118749999916, 0.000000000000000000, 106.6562500020483668 ) ) ;
#64597 = CARTESIAN_POINT ( 'NONE',  ( 2.775557561562891351E-14, 210.0000000000000284, 198.0000000000000284 ) ) ;
#64598 = CARTESIAN_POINT ( 'NONE',  ( -26.34314575050758123, 205.5625000000000284, 174.0000000000003411 ) ) ;
#64599 = CARTESIAN_POINT ( 'NONE',  ( -1.432654583217607858, 195.6250000013656063, 201.4587341250000065 ) ) ;
#64600 = CARTESIAN_POINT ( 'NONE',  ( -25.17157287525385811, 202.0000000027312126, 167.1715728752541281 ) ) ;
#64601 = CARTESIAN_POINT ( 'NONE',  ( 2.679491924311228956, 101.0416666666666856, -10.00000000000000000 ) ) ;
#64602 = CARTESIAN_POINT ( 'NONE',  ( 8.000000000000001776, 118.1562500000000000, 3.313708498984759387 ) ) ;
#64603 = CARTESIAN_POINT ( 'NONE',  ( 11.35316468749999963, 61.30208332991934839, -3.042071309553165293 ) ) ;
#64604 = CARTESIAN_POINT ( 'NONE',  ( -4.088227598258586603E-16, 295.3593750017070079, -6.676582343750001591 ) ) ;
#64605 = AXIS2_PLACEMENT_3D ( 'NONE', #32784, #55043, #59939 ) ;
#64606 = EDGE_CURVE ( 'NONE', #55487, #33683, #71599, .T. ) ;
#64607 = EDGE_LOOP ( 'NONE', ( #32624, #47923, #14844, #19735 ) ) ;
#64608 = CARTESIAN_POINT ( 'NONE',  ( -10.00000000000000000, 144.1666666598386826, -2.679491924311229845 ) ) ;
#64609 = CARTESIAN_POINT ( 'NONE',  ( -3.313708498984760720, 16.78124999590322375, -8.000000000000000000 ) ) ;
#64610 = CARTESIAN_POINT ( 'NONE',  ( -2.754378923186476579E-14, 206.1875000013656063, 145.4587341250000350 ) ) ;
#64611 = LINE ( 'NONE', #53295, #65943 ) ;
#64612 = CARTESIAN_POINT ( 'NONE',  ( 3.313708498984652362, 114.2187500040967905, -8.000000000000108358 ) ) ;
#64613 = CARTESIAN_POINT ( 'NONE',  ( -11.35316468749999963, 264.2187500034140157, 0.000000000000000000 ) ) ;
#64614 = DIRECTION ( 'NONE',  ( -0.000000000000000000, -0.000000000000000000, -1.000000000000000000 ) ) ;
#64615 = CARTESIAN_POINT ( 'NONE',  ( -4.220049686691935698, 10.18810118749999916, 70.75000000204836681 ) ) ;
#64616 = CARTESIAN_POINT ( 'NONE',  ( 2.679491924311222739, 208.9583333333333712, 10.00000000000000355 ) ) ;
#64617 = CARTESIAN_POINT ( 'NONE',  ( -7.188101187499992051, 0.000000000000000000, 10.86155278187175455 ) ) ;
#64618 = CARTESIAN_POINT ( 'NONE',  ( -5.676582343750006032, 184.4270833299193555, 9.832129032723418760 ) ) ;
#64619 = CARTESIAN_POINT ( 'NONE',  ( 1.881053915767122664, 1.124999998634406584, 4.541265875000001451 ) ) ;
#64620 = CARTESIAN_POINT ( 'NONE',  ( 5.000000000000004441, 241.6666666666666572, 8.660254037844385522 ) ) ;
#64622 = CARTESIAN_POINT ( 'NONE',  ( -7.347880794884122694E-16, 4.750000000000000000, 4.000000000000001776 ) ) ;
#64621 = LINE ( 'NONE', #53306, #52731 ) ;
#64623 = EDGE_LOOP ( 'NONE', ( #13334, #52875, #19340 ) ) ;
#64624 = CARTESIAN_POINT ( 'NONE',  ( -3.458734125000015425, 207.2500000013655779, 143.4326545832176976 ) ) ;
#64625 = CARTESIAN_POINT ( 'NONE',  ( -5.676582343750006032, 44.42708332991934839, 9.832129032723418760 ) ) ;
#64626 = CARTESIAN_POINT ( 'NONE',  ( 4.556349186104045934, 11.00000000000000000, 107.2187500040967905 ) ) ;
#64627 = CARTESIAN_POINT ( 'NONE',  ( 11.35316468749999785, 225.8854166632526699, 3.042071309553174174 ) ) ;
#64628 = CARTESIAN_POINT ( 'NONE',  ( -31.45873412500002786, 205.6250000013656063, 168.5673454167828140 ) ) ;
#64630 = CARTESIAN_POINT ( 'NONE',  ( -8.660254037844369535, 102.0833333333333286, -4.999999999999993783 ) ) ;
#64629 = CARTESIAN_POINT ( 'NONE',  ( 10.99999999999987033, -4.556349186104176496, 108.1562500000000000 ) ) ;
#64631 = CARTESIAN_POINT ( 'NONE',  ( 3.426202465283471721, 194.4587341250000350, 141.5267364219330943 ) ) ;
#64632 = AXIS2_PLACEMENT_3D ( 'NONE', #59813, #31512, #42813 ) ;
#64633 = CARTESIAN_POINT ( 'NONE',  ( -10.00000000000000355, 69.58333332650536818, 2.679491924311223183 ) ) ;
#64634 = CARTESIAN_POINT ( 'NONE',  ( 5.082755093536326818, 99.21875000204838102, 5.082755093536325042 ) ) ;
#64635 = CARTESIAN_POINT ( 'NONE',  ( -3.211159895383562723, 15.06249999863440792, 3.211159895383561391 ) ) ;
#64636 = LINE ( 'NONE', #69931, #20385 ) ;
#64637 = CARTESIAN_POINT ( 'NONE',  ( -5.656854249492373476, -5.656854249492376141, 1.017802779823363757 ) ) ;
#64638 = VERTEX_POINT ( 'NONE', #7239 ) ;
#64639 = ORIENTED_EDGE ( 'NONE', *, *, #13545, .F. ) ;
#64640 = CARTESIAN_POINT ( 'NONE',  ( 4.721056650416000089, 295.9843750017070079, 4.721056650415999201 ) ) ;
#64641 = CARTESIAN_POINT ( 'NONE',  ( -10.00000000000001599, 142.7083333333333428, 2.679491924311226292 ) ) ;
#64642 = DIRECTION ( 'NONE',  ( -0.000000000000000000, 1.000000000000000000, -0.000000000000000000 ) ) ;
#64643 = CARTESIAN_POINT ( 'NONE',  ( -11.35316468750000141, 153.4895833299193555, 3.042071309553159963 ) ) ;
#64644 = CARTESIAN_POINT ( 'NONE',  ( -10.18810118749999916, 4.220049686691934809, 84.06250000204838102 ) ) ;
#64645 = DIRECTION ( 'NONE',  ( 0.000000000000000000, 0.000000000000000000, 1.000000000000000000 ) ) ;
#64646 = CARTESIAN_POINT ( 'NONE',  ( -2.828427124746152987, 202.1250000000000284, 200.8284271247462129 ) ) ;
#64647 = CARTESIAN_POINT ( 'NONE',  ( -2.949463562550372231, 19.08173610902309036, -0.7140392532422442651 ) ) ;
#64648 = CARTESIAN_POINT ( 'NONE',  ( -7.204075437095965206, -7.204075437095968759, 110.2187500020483810 ) ) ;
#64649 = ORIENTED_EDGE ( 'NONE', *, *, #46299, .T. ) ;
#64650 = CARTESIAN_POINT ( 'NONE',  ( 11.00000000000000000, 1.347111479062088405E-15, 118.0000000000000000 ) ) ;
#64651 = CARTESIAN_POINT ( 'NONE',  ( 1.102182119232618108E-15, 296.3125000034140157, 6.000000000000001776 ) ) ;
#64652 = CARTESIAN_POINT ( 'NONE',  ( 11.35316468749999785, 145.8854166632526983, 3.042071309553174174 ) ) ;
#64653 = CARTESIAN_POINT ( 'NONE',  ( 2.445694354108839619, 199.8125000013656063, 200.4456943541088663 ) ) ;
#64654 = CARTESIAN_POINT ( 'NONE',  ( -4.220049686691935698, 10.18810118749999916, 70.75000000204836681 ) ) ;
#64655 = CARTESIAN_POINT ( 'NONE',  ( 8.311093377946837890, 46.71874999658602690, -8.311093377946837890 ) ) ;
#64656 = ORIENTED_EDGE ( 'NONE', *, *, #51692, .T. ) ;
#64657 = DIRECTION ( 'NONE',  ( 0.000000000000000000, -0.000000000000000000, 1.000000000000000000 ) ) ;
#64658 = CARTESIAN_POINT ( 'NONE',  ( -4.541265875000003227, 5.999999998634406140, 1.881053915767121110 ) ) ;
#64659 = CARTESIAN_POINT ( 'NONE',  ( -3.317071493978878571, 8.008118988124991233, 14.23186528394062833 ) ) ;
#64660 = CARTESIAN_POINT ( 'NONE',  ( 4.401442555609581635E-16, 12.84374999795161187, -7.188101187500000044 ) ) ;
#64661 = CARTESIAN_POINT ( 'NONE',  ( -6.000000000000003553, 291.0000000034139589, -2.485281374238571317 ) ) ;
#64662 = CARTESIAN_POINT ( 'NONE',  ( 4.000000000000015987, 202.5625000000000000, 196.3431457505076594 ) ) ;
#64663 = CARTESIAN_POINT ( 'NONE',  ( 7.188101187499999156, 14.24999999795161010, 2.977408999572654924 ) ) ;
#64664 = CARTESIAN_POINT ( 'NONE',  ( -4.401442555609577197E-16, 7.188101187499992051, 8.611552781871752771 ) ) ;
#64665 = CARTESIAN_POINT ( 'NONE',  ( -10.18810118749999916, 4.220049686691934809, 69.06250000204839523 ) ) ;
#64666 = CARTESIAN_POINT ( 'NONE',  ( -29.43265458321766559, 204.7500000013656063, 166.5412658750003629 ) ) ;
#64667 = CARTESIAN_POINT ( 'NONE',  ( -8.660254037844390851, 64.79166665983871098, 4.999999999999998224 ) ) ;
#64668 = CARTESIAN_POINT ( 'NONE',  ( -4.000000000000001776, 3.249999997268813612, -4.898587196589415787E-16 ) ) ;
#64669 = ORIENTED_EDGE ( 'NONE', *, *, #62528, .F. ) ;
#64670 = ADVANCED_FACE ( 'NONE', ( #35185 ), #30243, .T. ) ;
#64671 = CARTESIAN_POINT ( 'NONE',  ( -3.999999999999960032, 195.0625000027312126, 196.3431457505076594 ) ) ;
#64672 = CARTESIAN_POINT ( 'NONE',  ( 1.656854249492348607, 202.1875000000000568, 138.0000000000000568 ) ) ;
#64673 = CARTESIAN_POINT ( 'NONE',  ( -29.65685424949229088, 198.5625000027312126, 174.0000000000004547 ) ) ;
#64674 = EDGE_CURVE ( 'NONE', #43001, #32974, #39153, .T. ) ;
#64675 = AXIS2_PLACEMENT_3D ( 'NONE', #49337, #72353, #2206 ) ;
#64676 = CARTESIAN_POINT ( 'NONE',  ( -1.881053915767121554, 1.624999998634407028, -4.541265875000002339 ) ) ;
#64677 = CARTESIAN_POINT ( 'NONE',  ( 5.082755093536325042, 114.5937500020483810, -5.082755093536325930 ) ) ;
#64678 = DIRECTION ( 'NONE',  ( 1.000000000000000000, -0.000000000000000000, -0.000000000000000000 ) ) ;
#64679 = CARTESIAN_POINT ( 'NONE',  ( 1.469576158976822172E-15, -7.999999999999991118, -0.1071972160798552454 ) ) ;
#64680 = ORIENTED_EDGE ( 'NONE', *, *, #10147, .F. ) ;
#64681 = CARTESIAN_POINT ( 'NONE',  ( -5.082755093536325042, 25.03124999795161543, -5.082755093536325930 ) ) ;
#64682 = ORIENTED_EDGE ( 'NONE', *, *, #66976, .T. ) ;
#64683 = CARTESIAN_POINT ( 'NONE',  ( -49.70177871865297448, 272.0000000000000000, 57.99999999999999289 ) ) ;
#64684 = CARTESIAN_POINT ( 'NONE',  ( 4.242640687119285658, 296.6250000000000000, -4.242640687119286547 ) ) ;
#64685 = CARTESIAN_POINT ( 'NONE',  ( 25.55430564589119413, 209.3125000013656063, 172.4456943541087526 ) ) ;
#64686 = CARTESIAN_POINT ( 'NONE',  ( 8.660254037844385522, 54.58333333333333570, 5.000000000000005329 ) ) ;
#64687 = CARTESIAN_POINT ( 'NONE',  ( 5.082755093536325042, 102.9687500020483810, -5.082755093536325930 ) ) ;
#64688 = CARTESIAN_POINT ( 'NONE',  ( 6.000000000000003553, 294.4375000000000568, 2.485281374238571317 ) ) ;
#64689 = ADVANCED_FACE ( 'NONE', ( #59659 ), #13125, .F. ) ;
#64691 = CARTESIAN_POINT ( 'NONE',  ( 16.00000000000000711, -16.00000000000000000, 20.00000000000000000 ) ) ;
#64690 = CARTESIAN_POINT ( 'NONE',  ( -10.00000000000000000, 34.16666665983870388, -2.679491924311229845 ) ) ;
#64692 =( BOUNDED_CURVE ( )  B_SPLINE_CURVE ( 2, ( #71084, #25430, #14479, #48819, #7363, #71826, #8461, #53390, #1715, #65432, #48446, #70724, #20143 ),
 .UNSPECIFIED., .F., .F. ) 
 B_SPLINE_CURVE_WITH_KNOTS ( ( 3, 2, 2, 2, 2, 2, 3 ),
 ( 0.4722222222222219878, 0.4814814814814812327, 0.4907407407407405331, 0.4999999999999997780, 0.5092592592592590783, 0.5185185185185182677, 0.5277777777777775681 ),
 .UNSPECIFIED. ) 
 CURVE ( )  GEOMETRIC_REPRESENTATION_ITEM ( )  RATIONAL_B_SPLINE_CURVE ( ( 1.000000000000000888, 0.9659258262890675351, 1.000000000000000000, 0.9659258262890683122, 1.000000000000000000, 0.9659258262890683122, 1.000000000000000000, 0.9659258262890683122, 1.000000000000000000, 0.9659258262890683122, 1.000000000000000000, 0.9659258262890690894, 0.9999999999999992228 ) ) 
 REPRESENTATION_ITEM ( '' )  );
#64693 = ORIENTED_EDGE ( 'NONE', *, *, #10806, .F. ) ;
#64694 = CARTESIAN_POINT ( 'NONE',  ( -3.042071309553166181, 237.8645833367473301, -11.35316468749999608 ) ) ;
#64695 = CARTESIAN_POINT ( 'NONE',  ( -7.188101187499992051, 0.000000000000000000, 13.86155278187175455 ) ) ;
#64696 = CYLINDRICAL_SURFACE ( 'NONE', #34209, 3.999999999999976019 ) ;
#64697 = CARTESIAN_POINT ( 'NONE',  ( -7.999999999999948486, 3.313708498984799355, 3.736552779823361092 ) ) ;
#64698 = CARTESIAN_POINT ( 'NONE',  ( -2.849036369511732440E-14, 197.3750000027312126, 138.0000000000000568 ) ) ;
#64699 = CARTESIAN_POINT ( 'NONE',  ( 24.54718095033798519, 194.8728775736660452, 168.2354273994285734 ) ) ;
#64700 = CARTESIAN_POINT ( 'NONE',  ( -11.00000000000000000, 0.000000000000000000, 116.6875000040967763 ) ) ;
#64701 = CARTESIAN_POINT ( 'NONE',  ( 5.000000000000001776, 175.8333333333333428, -8.660254037844389075 ) ) ;
#64702 = FACE_OUTER_BOUND ( 'NONE', #23819, .T. ) ;
#64703 = DIRECTION ( 'NONE',  ( 0.000000000000000000, 0.000000000000000000, 1.000000000000000000 ) ) ;
#64704 = CARTESIAN_POINT ( 'NONE',  ( 0.000000000000000000, 0.000000000000000000, 0.000000000000000000 ) ) ;
#64705 = CARTESIAN_POINT ( 'NONE',  ( 8.311093377946837890, 141.7187499965859843, -8.311093377946837890 ) ) ;
#64706 = DIRECTION ( 'NONE',  ( -1.000000000000000000, 0.000000000000000000, 0.000000000000000000 ) ) ;
#64707 = CYLINDRICAL_SURFACE ( 'NONE', #32534, 8.000000000000000000 ) ;
#64710 = CARTESIAN_POINT ( 'NONE',  ( 23.99999999999998934, 203.7500000000000284, 169.9999999999998863 ) ) ;
#64709 = CARTESIAN_POINT ( 'NONE',  ( 29.43265458321766204, 194.5000000013656063, 173.4587341249998929 ) ) ;
#64708 = CARTESIAN_POINT ( 'NONE',  ( 30.82842712474617386, 207.1250000000000284, 172.8284271247460993 ) ) ;
#64711 = ORIENTED_EDGE ( 'NONE', *, *, #9835, .T. ) ;
#64712 = CARTESIAN_POINT ( 'NONE',  ( -1.469576158976823947E-15, 10.12500000000000178, 8.000000000000000000 ) ) ;
#64713 = PRODUCT_DEFINITION_FORMATION_WITH_SPECIFIED_SOURCE ( 'ANY', '', #11413, .NOT_KNOWN. ) ;
#64714 = DIRECTION ( 'NONE',  ( -1.000000000000000000, 0.000000000000000000, 0.000000000000000000 ) ) ;
#64715 = CARTESIAN_POINT ( 'NONE',  ( -3.729367062499960195, 194.8437500006828031, 198.0000000000000284 ) ) ;
#64716 = CARTESIAN_POINT ( 'NONE',  ( 1.432654583217607192, 207.2500000013655779, 145.4587341250000350 ) ) ;
#64717 =( BOUNDED_CURVE ( )  B_SPLINE_CURVE ( 2, ( #3002, #54693, #72786, #49008, #25983, #21093, #60712, #9411, #26751 ),
 .UNSPECIFIED., .F., .F. ) 
 B_SPLINE_CURVE_WITH_KNOTS ( ( 3, 2, 2, 2, 3 ),
 ( 0.4791666666666647423, 0.4895833333333313719, 0.4999999999999981126, 0.5104166666666647423, 0.5208333333333314830 ),
 .UNSPECIFIED. ) 
 CURVE ( )  GEOMETRIC_REPRESENTATION_ITEM ( )  RATIONAL_B_SPLINE_CURVE ( ( 1.000000000000014211, 0.9238795325112725276, 1.000000000000000000, 0.9238795325112867385, 1.000000000000000000, 0.9238795325112867385, 1.000000000000000000, 0.9238795325113005052, 0.9999999999999862332 ) ) 
 REPRESENTATION_ITEM ( '' )  );
#64718 = CARTESIAN_POINT ( 'NONE',  ( -7.651291526794159914, 124.7975115043635128, -1.023541575279288240 ) ) ;
#64719 = CARTESIAN_POINT ( 'NONE',  ( 2.679491924311222739, 30.83333332650536462, 10.00000000000000355 ) ) ;
#64720 = CARTESIAN_POINT ( 'NONE',  ( 7.188101187500002709, 117.3125000020483810, 2.977408999572649151 ) ) ;
#64721 = CARTESIAN_POINT ( 'NONE',  ( -1.881053915767121554, 5.749999998634407028, -4.541265875000002339 ) ) ;
#64722 = CARTESIAN_POINT ( 'NONE',  ( 1.296342370383412934, 60.23018777774911570, -22.90345467632036502 ) ) ;
#64723 = CARTESIAN_POINT ( 'NONE',  ( -7.999999999999991118, 3.313708498984756723, 14.23655277982336642 ) ) ;
#64724 = CARTESIAN_POINT ( 'NONE',  ( 10.00000000000000178, 7.083333326505366401, -2.679491924311226736 ) ) ;
#64725 = VERTEX_POINT ( 'NONE', #39636 ) ;
#64726 = CARTESIAN_POINT ( 'NONE',  ( 0.000000000000000000, 124.5000000000000284, 0.000000000000000000 ) ) ;
#64727 = CARTESIAN_POINT ( 'NONE',  ( -7.320508075688813676, 61.87500000000003553, -7.320508075688814564 ) ) ;
#64728 = CARTESIAN_POINT ( 'NONE',  ( -5.676582343750000703, 233.3854166700806729, -9.832129032723418760 ) ) ;
#64729 = CARTESIAN_POINT ( 'NONE',  ( 3.042071309553167069, 111.8229166632526983, -11.35316468749999785 ) ) ;
#64730 = ORIENTED_EDGE ( 'NONE', *, *, #16438, .T. ) ;
#64731 = CARTESIAN_POINT ( 'NONE',  ( 1.917649949088270800, 10.81880817070227607, 117.5534000801073233 ) ) ;
#64732 = CARTESIAN_POINT ( 'NONE',  ( 4.220049686691934809, 10.18810118749999916, 103.1875000020483810 ) ) ;
#64733 = CARTESIAN_POINT ( 'NONE',  ( -6.735557395310442023E-16, 11.00000000000000000, 86.31250000409676204 ) ) ;
#64734 = CARTESIAN_POINT ( 'NONE',  ( 2.839093476692135984E-14, 201.9375000013656063, 201.4587341250000350 ) ) ;
#64735 = DIRECTION ( 'NONE',  ( -0.8660254037844389297, 0.4999999999999994449, -0.000000000000000000 ) ) ;
#64737 = CARTESIAN_POINT ( 'NONE',  ( -8.311093377946836114, 107.6562499965860127, -8.311093377946837890 ) ) ;
#64736 = CARTESIAN_POINT ( 'NONE',  ( 1.479685137562080274E-15, 225.9999999999999432, -10.00000000000000178 ) ) ;
#64738 = CARTESIAN_POINT ( 'NONE',  ( -23.99999999999999289, 207.7500000000000284, 170.0000000000003411 ) ) ;
#64739 = CARTESIAN_POINT ( 'NONE',  ( -3.313708498984653250, 91.71874999999997158, -8.000000000000108358 ) ) ;
#64740 = VERTEX_POINT ( 'NONE', #10592 ) ;
#64741 = CARTESIAN_POINT ( 'NONE',  ( -10.00000000000000355, 209.5833333265053398, 2.679491924311223183 ) ) ;
#64742 = CARTESIAN_POINT ( 'NONE',  ( 5.656854249492380582, 22.68750000000000355, -5.656854249492380582 ) ) ;
#64743 = CARTESIAN_POINT ( 'NONE',  ( -7.188101187500000044, 124.5312500020483810, 0.000000000000000000 ) ) ;
#64744 = CARTESIAN_POINT ( 'NONE',  ( -11.35316468749999785, 98.38541666325268409, -3.042071309553167957 ) ) ;
#64745 = CARTESIAN_POINT ( 'NONE',  ( 3.458734125000015425, 209.0000000013656063, 196.5673454167823877 ) ) ;
#64746 = CARTESIAN_POINT ( 'NONE',  ( -5.082755093536326818, 12.28124999795161187, 5.082755093536325042 ) ) ;
#64747 = CARTESIAN_POINT ( 'NONE',  ( 10.18810118749999916, 1.247682550866122264E-15, 95.78125000204836681 ) ) ;
#64748 = CARTESIAN_POINT ( 'NONE',  ( -2.085542519210945728E-15, 4.843749996586016238, 11.35316468750000141 ) ) ;
#64749 = ORIENTED_EDGE ( 'NONE', *, *, #29256, .T. ) ;
#64750 = CARTESIAN_POINT ( 'NONE',  ( -10.00000000000001066, 137.5000000000000000, -1.224646799147354637E-15 ) ) ;
#64751 = DIRECTION ( 'NONE',  ( -0.000000000000000000, -0.000000000000000000, -1.000000000000000000 ) ) ;
#64752 = CARTESIAN_POINT ( 'NONE',  ( -9.000000000000001776, 1.102182119232617911E-15, 0.000000000000000000 ) ) ;
#64753 = CARTESIAN_POINT ( 'NONE',  ( -6.238412754330611322E-16, 10.18810118749999916, 73.65625000204836681 ) ) ;
#64754 = CARTESIAN_POINT ( 'NONE',  ( 3.454596936255384776, 22.00000000000000711, 2.354823634152921841 ) ) ;
#64755 = DIRECTION ( 'NONE',  ( 1.000000000000000000, 0.000000000000000000, 0.000000000000000000 ) ) ;
#64756 = CARTESIAN_POINT ( 'NONE',  ( -2.765530957081996810, 292.2656250017069510, -6.676582343750003368 ) ) ;
#64757 = CARTESIAN_POINT ( 'NONE',  ( -18.00000000000000355, 2.204364238465235822E-15, 0.000000000000000000 ) ) ;
#64758 = CARTESIAN_POINT ( 'NONE',  ( -8.311093377946836114, 222.9687499965860127, -8.311093377946837890 ) ) ;
#64759 = CARTESIAN_POINT ( 'NONE',  ( 10.18810118750000093, -4.220049686691933921, 90.81250000204838102 ) ) ;
#64760 = CARTESIAN_POINT ( 'NONE',  ( -25.55430564589115150, 204.0625000013656063, 172.4456943541091789 ) ) ;
#64761 = CARTESIAN_POINT ( 'NONE',  ( 7.999999999999998224, 25.40625000000000355, 3.313708498984766493 ) ) ;
#64762 = AXIS2_PLACEMENT_3D ( 'NONE', #39308, #33290, #27983 ) ;
#64763 = ORIENTED_EDGE ( 'NONE', *, *, #52993, .T. ) ;
#64764 = CARTESIAN_POINT ( 'NONE',  ( -25.17157287525374443, 208.7500000027312126, 172.8284271247464972 ) ) ;
#64765 = CARTESIAN_POINT ( 'NONE',  ( 2.849036369511732440E-14, 207.3750000027312126, 202.0000000000000000 ) ) ;
#64766 = CARTESIAN_POINT ( 'NONE',  ( 5.000000000000001776, 25.83333333333333570, -8.660254037844389075 ) ) ;
#64767 = EDGE_CURVE ( 'NONE', #62018, #3255, #4565, .T. ) ;
#64768 = CARTESIAN_POINT ( 'NONE',  ( -8.660254037844469011, 172.0833333333333997, -5.000000000000053291 ) ) ;
#64769 = CARTESIAN_POINT ( 'NONE',  ( -4.220049686691935698, 10.18810118749999916, 75.25000000204836681 ) ) ;
#64770 = VERTEX_POINT ( 'NONE', #69051 ) ;
#64771 = CARTESIAN_POINT ( 'NONE',  ( -7.188101187500000044, 5.718749997951611874, -8.802885111219163269E-16 ) ) ;
#64772 = LINE ( 'NONE', #11608, #64391 ) ;
#64773 = CARTESIAN_POINT ( 'NONE',  ( 1.320432766682874540E-15, 118.9062500020483810, 7.188101187500000044 ) ) ;
#64774 = CARTESIAN_POINT ( 'NONE',  ( 2.295000000000000373, 255.7199999999997715, 5.414444767710047124 ) ) ;
#64775 = CARTESIAN_POINT ( 'NONE',  ( -2.765530957081998142, 297.6406250017070079, 6.676582343750000703 ) ) ;
#64777 = CARTESIAN_POINT ( 'NONE',  ( -4.000000000000002665, 15.31249999726881406, 1.656854249492380582 ) ) ;
#64776 = CARTESIAN_POINT ( 'NONE',  ( 11.35316468749999608, 226.6145833367473301, -3.042071309553167513 ) ) ;
#64778 = CONTEXT_DEPENDENT_SHAPE_REPRESENTATION ( #39535, #57188 ) ;
#64779 = ORIENTED_EDGE ( 'NONE', *, *, #73863, .F. ) ;
#64780 = VECTOR ( 'NONE', #62664, 1000.000000000000000 ) ;
#64781 = EDGE_CURVE ( 'NONE', #43772, #21170, #5005, .T. ) ;
#64782 = CARTESIAN_POINT ( 'NONE',  ( -3.042071309553159075, 225.2604166700806161, 11.35316468749999963 ) ) ;
#64783 = CARTESIAN_POINT ( 'NONE',  ( 7.188101187499993827, -2.977408999572645598, 9.642802781871756324 ) ) ;
#64784 = CARTESIAN_POINT ( 'NONE',  ( -1.432654583217608080, 203.8750000013656063, 201.4587341250000350 ) ) ;
#64785 = ADVANCED_FACE ( 'NONE', ( #50948 ), #40378, .T. ) ;
#64786 = VERTEX_POINT ( 'NONE', #16980 ) ;
#64787 = CARTESIAN_POINT ( 'NONE',  ( -10.18810118749999916, 4.220049686691934809, 67.56250000204836681 ) ) ;
#64788 = CARTESIAN_POINT ( 'NONE',  ( 9.832129032723420536, 96.51041666325268409, -5.676582343749999815 ) ) ;
#64789 = DIRECTION ( 'NONE',  ( -0.000000000000000000, -1.000000000000000000, -0.000000000000000000 ) ) ;
#64790 = CARTESIAN_POINT ( 'NONE',  ( -6.735557395310442023E-16, 11.00000000000000000, 77.12499999999998579 ) ) ;
#64793 = LINE ( 'NONE', #41782, #6117 ) ;
#64792 = CARTESIAN_POINT ( 'NONE',  ( 24.54126587500000412, 206.2500000013656063, 171.4326545832175839 ) ) ;
#64791 = CARTESIAN_POINT ( 'NONE',  ( 25.55430564589115150, 204.5625000013656063, 172.4456943541086957 ) ) ;
#64794 = ORIENTED_EDGE ( 'NONE', *, *, #39692, .F. ) ;
#64795 = CYLINDRICAL_SURFACE ( 'NONE', #52545, 3.999999999999976019 ) ;
#64796 = CARTESIAN_POINT ( 'NONE',  ( 11.35316468749999785, 215.5729166632526699, 3.042071309553174174 ) ) ;
#64797 = CARTESIAN_POINT ( 'NONE',  ( 3.458734124999959025, 199.5000000013656063, 140.5673454167824161 ) ) ;
#64798 = CARTESIAN_POINT ( 'NONE',  ( 30.44569435410883429, 204.0625000013656063, 167.5543056458911053 ) ) ;
#64799 = CARTESIAN_POINT ( 'NONE',  ( 7.188101187499999156, 21.74999999795162253, 2.977408999572654924 ) ) ;
#64800 = ADVANCED_FACE ( 'NONE', ( #34742 ), #18437, .F. ) ;
#64801 = CARTESIAN_POINT ( 'NONE',  ( -11.35316468750000141, 178.5937499965860411, -1.390361679473963753E-15 ) ) ;
#64802 = CARTESIAN_POINT ( 'NONE',  ( -5.082755093536325930, 95.84375000204838102, -5.082755093536325930 ) ) ;
#64803 = CARTESIAN_POINT ( 'NONE',  ( -5.000000000000000000, 67.66743717231514665, -22.54291394824878481 ) ) ;
#64804 = CARTESIAN_POINT ( 'NONE',  ( -27.99999999999995381, 197.5000000000000000, 174.0000000000003695 ) ) ;
#64805 = CARTESIAN_POINT ( 'NONE',  ( 3.211159895383561835, 12.43749999863440792, -3.211159895383561835 ) ) ;
#64806 = CARTESIAN_POINT ( 'NONE',  ( 30.44569435410879166, 198.8125000013656063, 172.4456943541087526 ) ) ;
#64807 = CARTESIAN_POINT ( 'NONE',  ( -5.082755093536319713, 5.082755093536319713, 6.174052781871754547 ) ) ;
#64808 = CARTESIAN_POINT ( 'NONE',  ( 9.832129032723420536, 71.19791666325268409, -5.676582343749999815 ) ) ;
#64809 =( BOUNDED_CURVE ( )  B_SPLINE_CURVE ( 2, ( #47652, #30315, #46553, #13313, #18629, #46922, #29213, #17885, #53334 ),
 .UNSPECIFIED., .F., .F. ) 
 B_SPLINE_CURVE_WITH_KNOTS ( ( 3, 2, 2, 2, 3 ),
 ( 0.4500000000000002887, 0.4583333333333336479, 0.4666666666666670626, 0.4750000000000004219, 0.4833333333333338366 ),
 .UNSPECIFIED. ) 
 CURVE ( )  GEOMETRIC_REPRESENTATION_ITEM ( )  RATIONAL_B_SPLINE_CURVE ( ( 0.9999999999999974465, 0.9238795325112892920, 1.000000000000000000, 0.9238795325112867385, 1.000000000000000000, 0.9238795325112867385, 1.000000000000000000, 0.9238795325112821866, 1.000000000000004663 ) ) 
 REPRESENTATION_ITEM ( '' )  );
#64810 = DIRECTION ( 'NONE',  ( 1.000000000000000000, 0.000000000000000000, 0.000000000000000000 ) ) ;
#64811 = DIRECTION ( 'NONE',  ( -0.000000000000000000, 1.000000000000000000, 4.689100369878284071E-30 ) ) ;
#64812 = EDGE_LOOP ( 'NONE', ( #51020, #35440, #3909, #46133 ) ) ;
#64813 = CARTESIAN_POINT ( 'NONE',  ( 6.123233995736767268E-16, 46.25000000000000711, -10.00000000000000178 ) ) ;
#64814 = FACE_OUTER_BOUND ( 'NONE', #29936, .T. ) ;
#64815 = CARTESIAN_POINT ( 'NONE',  ( -3.042071309553164404, 72.23958332991935549, -11.35316468749999963 ) ) ;
#64816 = CARTESIAN_POINT ( 'NONE',  ( -11.00000000000000000, 4.556349186104045934, 68.59375000409677625 ) ) ;
#64817 = CARTESIAN_POINT ( 'NONE',  ( 1.432654583217608080, 197.8750000013656063, 138.5412658750000503 ) ) ;
#64818 = DIRECTION ( 'NONE',  ( 0.000000000000000000, 0.000000000000000000, 1.000000000000000000 ) ) ;
#64820 = CARTESIAN_POINT ( 'NONE',  ( -2.085542519210945728E-15, 69.53124999658602690, 11.35316468750000141 ) ) ;
#64819 = CARTESIAN_POINT ( 'NONE',  ( 1.469576158976823947E-15, 103.0625000040967763, 8.000000000000000000 ) ) ;
#64822 = CIRCLE ( 'NONE', #52768, 6.000000000000001776 ) ;
#64821 = CARTESIAN_POINT ( 'NONE',  ( -4.898587196589407898E-16, 7.999999999999991118, 24.64280278392014978 ) ) ;
#64823 = CARTESIAN_POINT ( 'NONE',  ( 2.679491924311228956, 131.0416666666666572, -10.00000000000000000 ) ) ;
#64824 = CARTESIAN_POINT ( 'NONE',  ( 7.320508075688771044, 156.2499999931720538, 7.320508075688775484 ) ) ;
#64825 = CARTESIAN_POINT ( 'NONE',  ( -24.11020845586372374, 194.9366551625569173, 169.3652517093883034 ) ) ;
#64826 = CARTESIAN_POINT ( 'NONE',  ( 5.676582343749993598, 60.26041666325268409, 9.832129032723422313 ) ) ;
#64827 = CARTESIAN_POINT ( 'NONE',  ( 4.220049686691941027, -10.18810118749999738, 112.0000000020483810 ) ) ;
#64828 = CARTESIAN_POINT ( 'NONE',  ( -8.311093377946841443, 198.9062499965860695, 8.311093377946830785 ) ) ;
#64829 = VERTEX_POINT ( 'NONE', #53552 ) ;
#64830 = CARTESIAN_POINT ( 'NONE',  ( 0.6547826978431622313, 60.19560277018798189, 22.88235556323082065 ) ) ;
#64831 = CARTESIAN_POINT ( 'NONE',  ( 1.469576158976823947E-15, 122.5625000040967763, 8.000000000000000000 ) ) ;
#64832 = CARTESIAN_POINT ( 'NONE',  ( 10.00000000000000178, 62.08333332650536818, -2.679491924311226736 ) ) ;
#64834 = CARTESIAN_POINT ( 'NONE',  ( 8.311093377946837890, 196.4062499965860411, -8.311093377946837890 ) ) ;
#64833 = DIRECTION ( 'NONE',  ( 0.000000000000000000, 1.000000000000000000, 0.000000000000000000 ) ) ;
#64835 = EDGE_CURVE ( 'NONE', #47752, #35448, #5877, .T. ) ;
#64836 = VECTOR ( 'NONE', #49484, 1000.000000000000000 ) ;
#64837 = CARTESIAN_POINT ( 'NONE',  ( 4.999999999999997335, 256.4583333401613459, -8.660254037844387298 ) ) ;
#64838 = CARTESIAN_POINT ( 'NONE',  ( 3.313708498984762496, -7.999999999999989342, 11.98655278392014445 ) ) ;
#64839 = ORIENTED_EDGE ( 'NONE', *, *, #15704, .F. ) ;
#64840 = ADVANCED_FACE ( 'NONE', ( #40635 ), #17617, .T. ) ;
#64841 = CARTESIAN_POINT ( 'NONE',  ( 11.35316468750000141, 166.0937499965860127, 0.000000000000000000 ) ) ;
#64842=STYLED_ITEM('',(#74699),#41383);
#64843 = CARTESIAN_POINT ( 'NONE',  ( -2.977408999572647819, -7.188101187499990274, 21.26780278187175810 ) ) ;
#64844 = EDGE_CURVE ( 'NONE', #72436, #67442, #14693, .T. ) ;
#64845 = CARTESIAN_POINT ( 'NONE',  ( 6.380085505555389780, 226.0000000000000568, -8.310665951435517229 ) ) ;
#64846 = ORIENTED_EDGE ( 'NONE', *, *, #66534, .F. ) ;
#64847 = CARTESIAN_POINT ( 'NONE',  ( 8.000000000000000000, 101.9375000040967763, -9.797174393178825657E-16 ) ) ;
#64848 = CARTESIAN_POINT ( 'NONE',  ( -1.656854249492383691, 12.68750000000000178, 4.000000000000000888 ) ) ;
#64849 = CARTESIAN_POINT ( 'NONE',  ( -37.75217341856568254, -2.187289690168644274, 128.2633397904443484 ) ) ;
#64850 = CARTESIAN_POINT ( 'NONE',  ( 4.541265875000002339, 17.37499999863440436, -1.881053915767121776 ) ) ;
#64851 = CARTESIAN_POINT ( 'NONE',  ( 5.656854249492374365, 5.656854249492375253, 16.95530278392014978 ) ) ;
#64852 = DIRECTION ( 'NONE',  ( 0.000000000000000000, 0.000000000000000000, 1.000000000000000000 ) ) ;
#64853 = ORIENTED_EDGE ( 'NONE', *, *, #8254, .F. ) ;
#64854 = CARTESIAN_POINT ( 'NONE',  ( -1.469576158976823947E-15, 25.12500000000000355, 8.000000000000000000 ) ) ;
#64855 = CARTESIAN_POINT ( 'NONE',  ( 5.082755093536326818, 99.21875000204838102, 5.082755093536325042 ) ) ;
#64857 = CARTESIAN_POINT ( 'NONE',  ( -27.99999999999999645, 210.0000000000000284, 166.0000000000003979 ) ) ;
#64856 = CARTESIAN_POINT ( 'NONE',  ( 10.00000000000005329, 180.2083333333333712, -2.679491924311241391 ) ) ;
#64858 = CARTESIAN_POINT ( 'NONE',  ( 1424.688200795887269, 628.9677537767814783, 827.8421604560587639 ) ) ;
#64859 = ORIENTED_EDGE ( 'NONE', *, *, #71893, .F. ) ;
#64860 = CARTESIAN_POINT ( 'NONE',  ( 4.465384415997312395, 10.10202268796506608, -70.97396818905025384 ) ) ;
#64861 = EDGE_CURVE ( 'NONE', #11179, #30304, #54760, .T. ) ;
#64863 = FACE_OUTER_BOUND ( 'NONE', #35985, .T. ) ;
#64862 = CIRCLE ( 'NONE', #10695, 5.000000000000000888 ) ;
#64864 = CARTESIAN_POINT ( 'NONE',  ( -7.188101187499991163, 2.977408999572646930, 23.89280278187176165 ) ) ;
#64865 = VERTEX_POINT ( 'NONE', #57253 ) ;
#64866 = ORIENTED_EDGE ( 'NONE', *, *, #4054, .F. ) ;
#64867 = CARTESIAN_POINT ( 'NONE',  ( 7.204075437095966983, 7.204075437095967871, 86.59375000204836681 ) ) ;
#64868 = CARTESIAN_POINT ( 'NONE',  ( 4.999999999999993783, 91.04166665983871098, 8.660254037844390851 ) ) ;
#64869 = CARTESIAN_POINT ( 'NONE',  ( -7.778174593052020747, -7.778174593052023411, 94.18750000000000000 ) ) ;
#64872 = DIRECTION ( 'NONE',  ( 0.000000000000000000, 1.000000000000000000, 0.000000000000000000 ) ) ;
#64871 = CARTESIAN_POINT ( 'NONE',  ( 25.17157287525381903, 200.0000000027312126, 172.8284271247460993 ) ) ;
#64870 = CARTESIAN_POINT ( 'NONE',  ( -10.99999999999989164, -4.556349186104158733, 104.5937500000000000 ) ) ;
#64873 = CARTESIAN_POINT ( 'NONE',  ( 2.679491924311222739, 133.9583333333333144, 10.00000000000000355 ) ) ;
#64874 = AXIS2_PLACEMENT_3D ( 'NONE', #24056, #23694, #58417 ) ;
#64875 = CARTESIAN_POINT ( 'NONE',  ( 4.556349186104045934, 11.00000000000000000, 105.7187500040967763 ) ) ;
#64876 = DIRECTION ( 'NONE',  ( 0.000000000000000000, 0.000000000000000000, 1.000000000000000000 ) ) ;
#64877 = AXIS2_PLACEMENT_3D ( 'NONE', #20422, #43438, #67214 ) ;
#64878 = FACE_OUTER_BOUND ( 'NONE', #36869, .T. ) ;
#64879 = CARTESIAN_POINT ( 'NONE',  ( 27.99999999999996447, 201.4375000013656063, 173.4587341249998929 ) ) ;
#64880 = CARTESIAN_POINT ( 'NONE',  ( 5.082755093536325930, 7.031249997951610986, -5.082755093536325930 ) ) ;
#64881 = CARTESIAN_POINT ( 'NONE',  ( 8.008118988124991233, 9.807117285998411148E-16, 1.763115283940626776 ) ) ;
#64882 = CARTESIAN_POINT ( 'NONE',  ( -1.432654583217662481, 196.1250000013655779, 145.4587341250000634 ) ) ;
#64883 = CARTESIAN_POINT ( 'NONE',  ( -7.188101187500000933, 116.9375000020483952, -2.977408999572650483 ) ) ;
#64885 = CYLINDRICAL_SURFACE ( 'NONE', #57067, 11.00000000000000000 ) ;
#64884 = CARTESIAN_POINT ( 'NONE',  ( 74.99999999999998579, 272.0000000000000000, 69.99999999999998579 ) ) ;
#64886 = CARTESIAN_POINT ( 'NONE',  ( -11.35316468749999785, 234.0104166700806161, -3.042071309553164848 ) ) ;
#64887 = LINE ( 'NONE', #46794, #40986 ) ;
#64888 = CARTESIAN_POINT ( 'NONE',  ( 2.977408999572650927, -7.188101187499990274, 23.33030278187175455 ) ) ;
#64889 = DIRECTION ( 'NONE',  ( -0.000000000000000000, -1.000000000000000000, -0.000000000000000000 ) ) ;
#64890 = CARTESIAN_POINT ( 'NONE',  ( 3.042071309553159519, 29.73958332991934839, 11.35316468750000141 ) ) ;
#64891 = CARTESIAN_POINT ( 'NONE',  ( -28.00000000000002842, 199.0000000000000000, 166.0000000000003695 ) ) ;
#64892 = CARTESIAN_POINT ( 'NONE',  ( 8.311093377946834337, 220.4687499965859843, 8.311093377946839666 ) ) ;
#64893 = CARTESIAN_POINT ( 'NONE',  ( -7.778174593052023411, 7.778174593052023411, 99.81250000000000000 ) ) ;
#64894 = ORIENTED_EDGE ( 'NONE', *, *, #28051, .T. ) ;
#64895 = LINE ( 'NONE', #7926, #69958 ) ;
#64896 = CARTESIAN_POINT ( 'NONE',  ( 1.432654583217607414, 195.5000000013655779, 145.4587341250000634 ) ) ;
#64897 = CARTESIAN_POINT ( 'NONE',  ( 9.832129032723420536, 41.19791666325268409, -5.676582343749999815 ) ) ;
#64898 = CARTESIAN_POINT ( 'NONE',  ( -11.00000000000000000, 4.556349186104045934, 88.09375000409677625 ) ) ;
#64899 = CARTESIAN_POINT ( 'NONE',  ( -24.54126587499998990, 195.1875000013655779, 170.0000000000002842 ) ) ;
#64900 = CARTESIAN_POINT ( 'NONE',  ( -4.000000000000016875, 201.5625000027312126, 140.3431457505076594 ) ) ;
#64902 = CARTESIAN_POINT ( 'NONE',  ( -11.35316468749999785, 38.07291666325267698, -3.042071309553167957 ) ) ;
#64901 = CARTESIAN_POINT ( 'NONE',  ( 2.977408999572654480, 105.1250000020483810, 7.188101187499999156 ) ) ;
#64903 = CARTESIAN_POINT ( 'NONE',  ( -7.999999999999991118, 3.313708498984756723, 15.73655277982336642 ) ) ;
#64904 = CARTESIAN_POINT ( 'NONE',  ( 3.042071309553167069, 151.8229166632526699, -11.35316468749999785 ) ) ;
#64905 = CARTESIAN_POINT ( 'NONE',  ( 10.00000000000000178, 111.8749999931720396, 0.000000000000000000 ) ) ;
#64906 = CARTESIAN_POINT ( 'NONE',  ( 2.977408999572650039, 109.0625000020483810, -7.188101187500001821 ) ) ;
#64907 = CARTESIAN_POINT ( 'NONE',  ( 0.000000000000000000, 0.000000000000000000, 0.000000000000000000 ) ) ;
#64908 = CARTESIAN_POINT ( 'NONE',  ( -29.43265458321760519, 205.1250000013656347, 173.4587341250003760 ) ) ;
#64909 = VERTEX_POINT ( 'NONE', #670 ) ;
#64910 = CARTESIAN_POINT ( 'NONE',  ( -3.042071309553163960, 2.552083329919349275, -11.35316468749999963 ) ) ;
#64911 = ORIENTED_EDGE ( 'NONE', *, *, #16525, .F. ) ;
#64912 = CARTESIAN_POINT ( 'NONE',  ( -2.160335347094679115, 16.41093803200631740, -68.77481055341850436 ) ) ;
#64914 = CARTESIAN_POINT ( 'NONE',  ( -2.085542519210945728E-15, 144.5312499965860411, 11.35316468750000141 ) ) ;
#64913 = DIRECTION ( 'NONE',  ( -0.000000000000000000, -0.000000000000000000, 1.000000000000000000 ) ) ;
#64915 = CARTESIAN_POINT ( 'NONE',  ( -7.347880794884122694E-16, 3.750000000000000000, 4.000000000000001776 ) ) ;
#64916 = CARTESIAN_POINT ( 'NONE',  ( 7.999999999999991118, 3.313708498984757611, 15.23030278432982243 ) ) ;
#64917 = CARTESIAN_POINT ( 'NONE',  ( 2.679491924311234730, 224.5833333401613174, 9.999999999999998224 ) ) ;
#64918 = CARTESIAN_POINT ( 'NONE',  ( 9.832129032723420536, 250.9895833367473017, 5.676582343749996262 ) ) ;
#64919 = CARTESIAN_POINT ( 'NONE',  ( 4.220049686691941027, -10.18810118749999738, 91.00000000204836681 ) ) ;
#64920 = ORIENTED_EDGE ( 'NONE', *, *, #20693, .T. ) ;
#64921 = EDGE_CURVE ( 'NONE', #3964, #68741, #49258, .T. ) ;
#64922 =( BOUNDED_CURVE ( )  B_SPLINE_CURVE ( 2, ( #63195, #73776, #56437, #39816, #40942, #68861, #17548, #34180, #22451, #68487, #33437, #4757, #597, #74147, #16789, #33813, #63570, #51508, #11896, #50761, #17172, #62822, #51889, #69611, #56811, #57182, #62449, #11156, #10776, #5131, #40193, #28499, #229, #5499, #74522, #22830, #11525, #17927, #28124, #34930, #57564, #45109, #6248, #46590, #5873, #28869, #29252, #23210, #10409, #46222, #69239, #68122, #40567, #57942, #23580, #16416, #31746, #60033, #8351, #70983, #31368, #52633, #35295, #19299, #54396, #43424, #66438, #3075, #47968, #37032, #55142, #14372, #968, #6613, #37406, #9107, #42309, #71717, #20032, #13629, #58309, #25690, #65324, #2702, #48710, #54766, #37787, #14746, #48338, #60783, #26060, #32122, #36667, #3447, #29620, #26436, #43046, #59677, #66065, #60407, #24951, #54016, #7988, #72481, #49461, #20788, #30994, #63951, #49081, #12261, #2326, #8733, #65691, #72094, #25322, #71345, #19667, #20408, #42679, #13991, #4571, #73966, #39270, #56254, #51326, #28317, #67199, #61903, #50954, #10599, #4948, #55516, #27569, #74334, #55888, #50577, #27947, #15497, #16605, #27192, #73594, #38900, #10227, #15868, #33255, #39642, #44932, #9858, #15125, #56634, #4202, #32886, #50208, #62639, #73229, #22272, #66823, #72857, #21162, #44185, #67939, #49838, #45294, #21902, #32504, #38157, #21535, #43808, #16233, #68307, #67571, #44558, #62270, #61158, #9490, #10972, #33627, #34007, #38534, #57001, #5315, #3828, #26825, #61535, #29063, #64134, #7167, #46037, #69425, #51698, #23396, #44, #23029, #29437, #40749, #12442, #63384, #17733, #46411, #6057, #30172, #24129, #11340, #34376, #57376, #18483, #58855, #63758, #35112, #41493, #12076, #69057, #57752, #58126, #416, #17362, #52084, #6435, #6795, #58488, #52448, #786, #23769, #46773, #69797, #18113, #41127, #70174, #5685, #64510, #40385, #35474, #53189, #29805, #11707, #16987, #52816, #1151, #47143, #12808, #22643 ),
 .UNSPECIFIED., .F., .F. ) 
 B_SPLINE_CURVE_WITH_KNOTS ( ( 3, 2, 2, 2, 2, 2, 2, 2, 2, 2, 2, 2, 2, 2, 2, 2, 2, 2, 2, 2, 2, 2, 2, 2, 2, 2, 2, 2, 2, 2, 2, 2, 2, 2, 2, 2, 2, 2, 2, 2, 2, 2, 2, 2, 2, 2, 2, 2, 2, 2, 2, 2, 2, 2, 2, 2, 2, 2, 2, 2, 2, 2, 2, 2, 2, 2, 2, 2, 2, 2, 2, 2, 2, 2, 2, 2, 2, 2, 2, 2, 2, 2, 2, 2, 2, 2, 2, 2, 2, 2, 2, 2, 2, 2, 2, 2, 2, 2, 2, 2, 2, 2, 2, 2, 2, 2, 2, 2, 2, 2, 2, 2, 2, 2, 2, 2, 2, 2, 2, 2, 3 ),
 ( 0.000000000000000000, 0.008333333333333333218, 0.01666666666666666644, 0.02500000000000000139, 0.03333333333333333287, 0.04166666666666666435, 0.05000000000000000278, 0.05833333333333333426, 0.06666666666666666574, 0.07499999999999999722, 0.08333333333333332871, 0.09166666666666666019, 0.1000000000000000056, 0.1083333333333333370, 0.1166666666666666685, 0.1250000000000000000, 0.1333333333333333315, 0.1416666666666666630, 0.1499999999999999944, 0.1583333333333333259, 0.1666666666666666574, 0.1749999999999999889, 0.1833333333333333204, 0.1916666666666666796, 0.2000000000000000111, 0.2083333333333333426, 0.2166666666666666741, 0.2250000000000000056, 0.2333333333333333370, 0.2416666666666666685, 0.2500000000000000000, 0.2583333333333333592, 0.2666666666666666630, 0.2750000000000000222, 0.2833333333333333259, 0.2916666666666666852, 0.2999999999999999889, 0.3083333333333333481, 0.3166666666666666519, 0.3250000000000000111, 0.3333333333333333148, 0.3416666666666666741, 0.3499999999999999778, 0.3583333333333333370, 0.3666666666666666408, 0.3750000000000000000, 0.3833333333333333592, 0.3916666666666666630, 0.4000000000000000222, 0.4083333333333333259, 0.4166666666666666852, 0.4249999999999999889, 0.4333333333333333481, 0.4416666666666666519, 0.4500000000000000111, 0.4583333333333333148, 0.4666666666666666741, 0.4749999999999999778, 0.4833333333333333370, 0.4916666666666666408, 0.5000000000000000000, 0.5083333333333333037, 0.5166666666666667185, 0.5250000000000000222, 0.5333333333333333259, 0.5416666666666666297, 0.5500000000000000444, 0.5583333333333333481, 0.5666666666666666519, 0.5749999999999999556, 0.5833333333333333703, 0.5916666666666666741, 0.5999999999999999778, 0.6083333333333332815, 0.6166666666666666963, 0.6250000000000000000, 0.6333333333333333037, 0.6416666666666667185, 0.6500000000000000222, 0.6583333333333333259, 0.6666666666666666297, 0.6750000000000000444, 0.6833333333333333481, 0.6916666666666666519, 0.6999999999999999556, 0.7083333333333333703, 0.7166666666666666741, 0.7249999999999999778, 0.7333333333333332815, 0.7416666666666666963, 0.7500000000000000000, 0.7583333333333333037, 0.7666666666666667185, 0.7750000000000000222, 0.7833333333333333259, 0.7916666666666666297, 0.8000000000000000444, 0.8083333333333333481, 0.8166666666666666519, 0.8249999999999999556, 0.8333333333333333703, 0.8416666666666666741, 0.8499999999999999778, 0.8583333333333332815, 0.8666666666666666963, 0.8750000000000000000, 0.8833333333333333037, 0.8916666666666667185, 0.9000000000000000222, 0.9083333333333333259, 0.9166666666666666297, 0.9250000000000000444, 0.9333333333333333481, 0.9416666666666666519, 0.9499999999999999556, 0.9583333333333333703, 0.9666666666666666741, 0.9749999999999999778, 0.9833333333333332815, 0.9916666666666666963, 1.000000000000000000 ),
 .UNSPECIFIED. ) 
 CURVE ( )  GEOMETRIC_REPRESENTATION_ITEM ( )  RATIONAL_B_SPLINE_CURVE ( ( 1.000000000000000000, 0.9238795325112867385, 1.000000000000000000, 0.9238795325112867385, 1.000000000000000000, 0.9238795325112867385, 1.000000000000000000, 0.9238795325112867385, 1.000000000000000000, 0.9238795325112867385, 1.000000000000000000, 0.9238795325112867385, 1.000000000000000000, 0.9238795325112867385, 1.000000000000000000, 0.9238795325112867385, 1.000000000000000000, 0.9238795325112867385, 1.000000000000000000, 0.9238795325112867385, 1.000000000000000000, 0.9238795325112867385, 1.000000000000000000, 0.9238795325112867385, 1.000000000000000000, 0.9238795325112867385, 1.000000000000000000, 0.9238795325112867385, 1.000000000000000000, 0.9238795325112867385, 1.000000000000000000, 0.9238795325112867385, 1.000000000000000000, 0.9238795325112867385, 1.000000000000000000, 0.9238795325112867385, 1.000000000000000000, 0.9238795325112867385, 1.000000000000000000, 0.9238795325112867385, 1.000000000000000000, 0.9238795325112867385, 1.000000000000000000, 0.9238795325112867385, 1.000000000000000000, 0.9238795325112867385, 1.000000000000000000, 0.9238795325112867385, 1.000000000000000000, 0.9238795325112867385, 1.000000000000000000, 0.9238795325112867385, 1.000000000000000000, 0.9238795325112867385, 1.000000000000000000, 0.9238795325112867385, 1.000000000000000000, 0.9238795325112867385, 1.000000000000000000, 0.9238795325112867385, 1.000000000000000000, 0.9238795325112867385, 1.000000000000000000, 0.9238795325112867385, 1.000000000000000000, 0.9238795325112867385, 1.000000000000000000, 0.9238795325112867385, 1.000000000000000000, 0.9238795325112867385, 1.000000000000000000, 0.9238795325112867385, 1.000000000000000000, 0.9238795325112867385, 1.000000000000000000, 0.9238795325112867385, 1.000000000000000000, 0.9238795325112867385, 1.000000000000000000, 0.9238795325112867385, 1.000000000000000000, 0.9238795325112867385, 1.000000000000000000, 0.9238795325112867385, 1.000000000000000000, 0.9238795325112867385, 1.000000000000000000, 0.9238795325112867385, 1.000000000000000000, 0.9238795325112867385, 1.000000000000000000, 0.9238795325112867385, 1.000000000000000000, 0.9238795325112867385, 1.000000000000000000, 0.9238795325112867385, 1.000000000000000000, 0.9238795325112867385, 1.000000000000000000, 0.9238795325112867385, 1.000000000000000000, 0.9238795325112867385, 1.000000000000000000, 0.9238795325112867385, 1.000000000000000000, 0.9238795325112867385, 1.000000000000000000, 0.9238795325112867385, 1.000000000000000000, 0.9238795325112867385, 1.000000000000000000, 0.9238795325112867385, 1.000000000000000000, 0.9238795325112867385, 1.000000000000000000, 0.9238795325112867385, 1.000000000000000000, 0.9238795325112867385, 1.000000000000000000, 0.9238795325112867385, 1.000000000000000000, 0.9238795325112867385, 1.000000000000000000, 0.9238795325112867385, 1.000000000000000000, 0.9238795325112867385, 1.000000000000000000, 0.9238795325112867385, 1.000000000000000000, 0.9238795325112867385, 1.000000000000000000, 0.9238795325112867385, 1.000000000000000000, 0.9238795325112867385, 1.000000000000000000, 0.9238795325112867385, 1.000000000000000000, 0.9238795325112867385, 1.000000000000000000, 0.9238795325112867385, 1.000000000000000000, 0.9238795325112867385, 1.000000000000000000, 0.9238795325112867385, 1.000000000000000000, 0.9238795325112867385, 1.000000000000000000, 0.9238795325112867385, 1.000000000000000000, 0.9238795325112867385, 1.000000000000000000, 0.9238795325112867385, 1.000000000000000000, 0.9238795325112867385, 1.000000000000000000, 0.9238795325112867385, 1.000000000000000000, 0.9238795325112867385, 1.000000000000000000, 0.9238795325112867385, 1.000000000000000000, 0.9238795325112867385, 1.000000000000000000, 0.9238795325112867385, 1.000000000000000000, 0.9238795325112867385, 1.000000000000000000, 0.9238795325112867385, 1.000000000000000000, 0.9238795325112867385, 1.000000000000000000, 0.9238795325112867385, 1.000000000000000000, 0.9238795325112867385, 1.000000000000000000, 0.9238795325112867385, 1.000000000000000000, 0.9238795325112867385, 1.000000000000000000, 0.9238795325112867385, 1.000000000000000000, 0.9238795325112867385, 1.000000000000000000, 0.9238795325112867385, 1.000000000000000000, 0.9238795325112867385, 1.000000000000000000, 0.9238795325112867385, 1.000000000000000000, 0.9238795325112867385, 1.000000000000000000, 0.9238795325112867385, 1.000000000000000000, 0.9238795325112867385, 1.000000000000000000, 0.9238795325112867385, 1.000000000000000000, 0.9238795325112867385, 1.000000000000000000, 0.9238795325112867385, 1.000000000000000000, 0.9238795325112867385, 1.000000000000000000, 0.9238795325112867385, 1.000000000000000000, 0.9238795325112867385, 1.000000000000000000, 0.9238795325112867385, 1.000000000000000000, 0.9238795325112867385, 1.000000000000000000, 0.9238795325112867385, 1.000000000000000000, 0.9238795325112867385, 1.000000000000000000, 0.9238795325112867385, 1.000000000000000000, 0.9238795325112867385, 1.000000000000000000, 0.9238795325112867385, 1.000000000000000000, 0.9238795325112867385, 1.000000000000000000, 0.9238795325112867385, 1.000000000000000000, 0.9238795325112867385, 1.000000000000000000, 0.9238795325112867385, 1.000000000000000000, 0.9238795325112867385, 1.000000000000000000, 0.9238795325112867385, 1.000000000000000000, 0.9238795325112867385, 1.000000000000000000, 0.9238795325112867385, 1.000000000000000000, 0.9238795325112867385, 1.000000000000000000, 0.9238795325112867385, 1.000000000000000000 ) ) 
 REPRESENTATION_ITEM ( '' )  );
#64923 = CIRCLE ( 'NONE', #49294, 11.00000000000000000 ) ;
#64924 = CARTESIAN_POINT ( 'NONE',  ( 4.999999999999997335, 16.24494643555759410, 69.83755725260752456 ) ) ;
#64925 = CARTESIAN_POINT ( 'NONE',  ( -8.311093377946841443, 94.21874999658601268, 8.311093377946830785 ) ) ;
#64926 = CARTESIAN_POINT ( 'NONE',  ( -6.238412754330611322E-16, 10.18810118749999916, 100.2812500020483810 ) ) ;
#64927 = ADVANCED_FACE ( 'NONE', ( #22522, #17241 ), #34997, .T. ) ;
#64928 = CARTESIAN_POINT ( 'NONE',  ( -8.342170076843785083E-16, 18.18749999863440792, 4.541265875000002339 ) ) ;
#64929 = ORIENTED_EDGE ( 'NONE', *, *, #7175, .T. ) ;
#64930 = ORIENTED_EDGE ( 'NONE', *, *, #72909, .F. ) ;
#64931 = CARTESIAN_POINT ( 'NONE',  ( -1.469576158976823947E-15, 5.625000000000000888, 8.000000000000000000 ) ) ;
#64932 = CARTESIAN_POINT ( 'NONE',  ( -4.541265875000003227, 0.9999999986344068059, 1.881053915767121110 ) ) ;
#64933 = CARTESIAN_POINT ( 'NONE',  ( 5.082755093536325930, 3.656249997951610542, -5.082755093536325930 ) ) ;
#64934 = CARTESIAN_POINT ( 'NONE',  ( 8.000000000000001776, 119.8437500040967763, 3.313708498984759387 ) ) ;
#64935 = CARTESIAN_POINT ( 'NONE',  ( -10.18810118749999738, -4.220049686691941915, 95.12500000204836681 ) ) ;
#64936 = CARTESIAN_POINT ( 'NONE',  ( 2.449293598294707893E-16, 1.250000000000000222, -4.000000000000001776 ) ) ;
#64937 = CARTESIAN_POINT ( 'NONE',  ( 1.656854249492381914, 14.56249999726881228, 4.000000000000000888 ) ) ;
#64938 = CARTESIAN_POINT ( 'NONE',  ( -4.898587196589412829E-16, 118.6250000000000000, -8.000000000000000000 ) ) ;
#64939 = ORIENTED_EDGE ( 'NONE', *, *, #68863, .F. ) ;
#64940 = CARTESIAN_POINT ( 'NONE',  ( 3.313708498984711426, 95.46874999999998579, 8.000000000000053291 ) ) ;
#64941 = CARTESIAN_POINT ( 'NONE',  ( 2.445694354108838731, 199.0625000013656063, 195.5543056458912190 ) ) ;
#64943 = CARTESIAN_POINT ( 'NONE',  ( 0.000000000000000000, 125.0000000000000000, 0.000000000000000000 ) ) ;
#64942 = CARTESIAN_POINT ( 'NONE',  ( -30.44569435410886982, 202.5625000013656063, 167.5543056458916169 ) ) ;
#64944 =( NAMED_UNIT ( * ) SI_UNIT ( $, .STERADIAN. ) SOLID_ANGLE_UNIT ( ) );
#64945 = CARTESIAN_POINT ( 'NONE',  ( 1.881053915767122664, 13.12499999863440969, 4.541265875000001451 ) ) ;
#64946 = CARTESIAN_POINT ( 'NONE',  ( 5.000000000000001776, 122.7083333265053682, -8.660254037844389075 ) ) ;
#64947 = CARTESIAN_POINT ( 'NONE',  ( -2.977408999572647819, 7.188101187499991163, 13.20530278187175277 ) ) ;
#64948 = ORIENTED_EDGE ( 'NONE', *, *, #5676, .T. ) ;
#64949 = ORIENTED_EDGE ( 'NONE', *, *, #57387, .T. ) ;
#64950 = CARTESIAN_POINT ( 'NONE',  ( -7.204075437095965206, -7.204075437095968759, 105.3437500020483810 ) ) ;
#64951 = CARTESIAN_POINT ( 'NONE',  ( -8.660254037844376640, 97.08333333333334281, -4.999999999999998224 ) ) ;
#64952 = CARTESIAN_POINT ( 'NONE',  ( -29.65685424949241167, 200.0625000000000568, 166.0000000000004263 ) ) ;
#64953 = CARTESIAN_POINT ( 'NONE',  ( -3.458734124999959914, 196.3750000013656063, 196.5673454167823877 ) ) ;
#64954 = CARTESIAN_POINT ( 'NONE',  ( 1.224646799147353256E-15, 0.000000000000000000, 10.00000000000000000 ) ) ;
#64955 = CARTESIAN_POINT ( 'NONE',  ( -8.660254037844387298, 92.08333333333334281, -5.000000000000004441 ) ) ;
#64956 = CARTESIAN_POINT ( 'NONE',  ( 3.313708498984765161, 117.9687500000000142, 7.999999999999998224 ) ) ;
#64957 = CARTESIAN_POINT ( 'NONE',  ( 4.721056650416000089, 297.9843750017070079, 4.721056650415999201 ) ) ;
#64958 = VERTEX_POINT ( 'NONE', #52333 ) ;
#64959 = CARTESIAN_POINT ( 'NONE',  ( -10.00000000000000178, 174.3749999931720538, -1.224646799147353454E-15 ) ) ;
#64960 = CARTESIAN_POINT ( 'NONE',  ( -3.313708498984765161, 17.34374999590322375, 7.999999999999998224 ) ) ;
#64961 = CARTESIAN_POINT ( 'NONE',  ( -2.445694354108838731, 207.0625000013656063, 144.4456943541088663 ) ) ;
#64962 = CARTESIAN_POINT ( 'NONE',  ( -1.836970198721029983E-15, 83.75000000000000000, 10.00000000000000178 ) ) ;
#64963 = CARTESIAN_POINT ( 'NONE',  ( -5.000000000000000888, 224.1666666666666856, -8.660254037844387298 ) ) ;
#64964 = CARTESIAN_POINT ( 'NONE',  ( -2.828427124746209831, 207.3750000000000284, 139.1715728752538723 ) ) ;
#64965 = CARTESIAN_POINT ( 'NONE',  ( -11.00000000000000000, 4.556349186104045934, 113.4062500000000000 ) ) ;
#64966 = CARTESIAN_POINT ( 'NONE',  ( -2.679491924311235618, 213.5416666666666572, 10.00000000000000000 ) ) ;
#64967 = EDGE_CURVE ( 'NONE', #26710, #74042, #10284, .T. ) ;
#64968 = CARTESIAN_POINT ( 'NONE',  ( 5.082755093536320601, -5.082755093536318824, 12.92405278187175277 ) ) ;
#64969 = CARTESIAN_POINT ( 'NONE',  ( -11.35316468749999785, 178.3854166632526983, -3.042071309553167513 ) ) ;
#64970 = CARTESIAN_POINT ( 'NONE',  ( 2.775557561562891351E-14, 183.6788756342477029, 139.0000000000000568 ) ) ;
#64971 = CARTESIAN_POINT ( 'NONE',  ( -1.881053915767124440, 1.999999998634406806, 4.541265875000001451 ) ) ;
#64972 = CYLINDRICAL_SURFACE ( 'NONE', #58586, 10.00000000000000178 ) ;
#64974 = CARTESIAN_POINT ( 'NONE',  ( -7.999999999999991118, 3.313708498984757167, 3.924052783920144893 ) ) ;
#64973 = CARTESIAN_POINT ( 'NONE',  ( -2.828427124746153876, 203.0000000027312126, 195.1715728752538439 ) ) ;
#64975 = ORIENTED_EDGE ( 'NONE', *, *, #25955, .T. ) ;
#64976 = CIRCLE ( 'NONE', #36090, 20.00000000000001066 ) ;
#64977 = CARTESIAN_POINT ( 'NONE',  ( 3.458734124999959914, 194.4375000013656063, 142.0000000000000568 ) ) ;
#64978 = CARTESIAN_POINT ( 'NONE',  ( -3.042071309553173730, 44.63541666325269119, 11.35316468749999785 ) ) ;
#64979 = CARTESIAN_POINT ( 'NONE',  ( -6.735557395310442023E-16, 11.00000000000000000, 102.8125000040967763 ) ) ;
#64980 = CARTESIAN_POINT ( 'NONE',  ( 3.042071309553167069, 222.1354166632526699, -11.35316468749999785 ) ) ;
#64981 = CARTESIAN_POINT ( 'NONE',  ( -26.56734541678243033, 204.3750000013656063, 166.5412658750003345 ) ) ;
#64982 = CARTESIAN_POINT ( 'NONE',  ( -4.556349186104045934, 11.00000000000000000, 71.21875000000000000 ) ) ;
#64984 = CARTESIAN_POINT ( 'NONE',  ( -4.999999999999994671, 103.3333333333333286, 8.660254037844369535 ) ) ;
#64983 = CARTESIAN_POINT ( 'NONE',  ( -6.735557395310442023E-16, 11.00000000000000000, 71.31250000409677625 ) ) ;
#64985 = DIRECTION ( 'NONE',  ( -1.000000000000000000, 0.000000000000000000, 0.000000000000000000 ) ) ;
#64986 = EDGE_CURVE ( 'NONE', #41193, #30502, #22151, .T. ) ;
#64987 = EDGE_CURVE ( 'NONE', #21228, #2370, #15992, .T. ) ;
#64988 = CARTESIAN_POINT ( 'NONE',  ( -10.00000000000000178, 74.37499999317203958, -1.224646799147353454E-15 ) ) ;
#64989 = CARTESIAN_POINT ( 'NONE',  ( -7.188101187499999156, 94.25000000204838102, 2.977408999572654924 ) ) ;
#64990 = CARTESIAN_POINT ( 'NONE',  ( 2.780723358947928197E-16, 14.68749999863440792, -4.541265875000002339 ) ) ;
#64991 = CARTESIAN_POINT ( 'NONE',  ( -2.679491924311163231, 73.54166666666668561, 10.00000000000004796 ) ) ;
#64992 = CARTESIAN_POINT ( 'NONE',  ( 2.775557561562891351E-14, -37.99999999999997868, 170.0000000000000284 ) ) ;
#64993 = CARTESIAN_POINT ( 'NONE',  ( -4.556349186104048599, -10.99999999999999822, 67.46875000409677625 ) ) ;
#64994 = ORIENTED_EDGE ( 'NONE', *, *, #4010, .T. ) ;
#64995 = ORIENTED_EDGE ( 'NONE', *, *, #27403, .T. ) ;
#64996 = CARTESIAN_POINT ( 'NONE',  ( 2.765530957082001251, 291.9218750017069510, 6.676582343750000703 ) ) ;
#64997 = FACE_OUTER_BOUND ( 'NONE', #30540, .T. ) ;
#64998 = CARTESIAN_POINT ( 'NONE',  ( 6.951808397369818766E-16, 162.0312499965860127, -11.35316468750000141 ) ) ;
#64999 = DIRECTION ( 'NONE',  ( -0.000000000000000000, 1.000000000000000000, -0.000000000000000000 ) ) ;
#65000 = CARTESIAN_POINT ( 'NONE',  ( 1.656854249492403008, 199.6875000000000000, 194.0000000000000853 ) ) ;
#65001 = CARTESIAN_POINT ( 'NONE',  ( -29.65685424949240812, 201.4375000000000284, 174.0000000000003126 ) ) ;
#65002 = CARTESIAN_POINT ( 'NONE',  ( -4.220049686691935698, 10.18810118749999916, 106.7500000020483668 ) ) ;
#65003 = ORIENTED_EDGE ( 'NONE', *, *, #10935, .F. ) ;
#65004 = CARTESIAN_POINT ( 'NONE',  ( 0.000000000000000000, 125.0000000000000000, 0.000000000000000000 ) ) ;
#65005 = CARTESIAN_POINT ( 'NONE',  ( 11.00000000000000000, 1.347111479062088405E-15, 109.9375000040967763 ) ) ;
#65006 = CARTESIAN_POINT ( 'NONE',  ( 5.676582343750001591, 136.9270833299193555, -9.832129032723420536 ) ) ;
#65007 = CARTESIAN_POINT ( 'NONE',  ( -3.458734124999959914, 199.4375000013655779, 198.0000000000000284 ) ) ;
#65008 = CARTESIAN_POINT ( 'NONE',  ( 2.485281374238987873, 298.3750000034140157, 5.999999999999586997 ) ) ;
#65009 =( BOUNDED_CURVE ( )  B_SPLINE_CURVE ( 2, ( #24012, #25109, #31903, #3233, #59468, #60566, #42468, #55299, #31529, #65485, #26220, #54551, #72641 ),
 .UNSPECIFIED., .F., .F. ) 
 B_SPLINE_CURVE_WITH_KNOTS ( ( 3, 2, 2, 2, 2, 2, 3 ),
 ( 0.3611111111111107719, 0.3703703703703700167, 0.3796296296296293171, 0.3888888888888886175, 0.3981481481481478624, 0.4074074074074071072, 0.4166666666666664076 ),
 .UNSPECIFIED. ) 
 CURVE ( )  GEOMETRIC_REPRESENTATION_ITEM ( )  RATIONAL_B_SPLINE_CURVE ( ( 1.000000000000001332, 0.9659258262890670910, 1.000000000000000000, 0.9659258262890683122, 1.000000000000000000, 0.9659258262890683122, 1.000000000000000000, 0.9659258262890683122, 1.000000000000000000, 0.9659258262890683122, 1.000000000000000000, 0.9659258262890693114, 0.9999999999999990008 ) ) 
 REPRESENTATION_ITEM ( '' )  );
#65010 = CARTESIAN_POINT ( 'NONE',  ( 10.18810118749999916, 1.247682550866122264E-15, 73.28125000204838102 ) ) ;
#65011 = CARTESIAN_POINT ( 'NONE',  ( -11.35316468750000141, 43.59374999658601979, -1.390361679473963753E-15 ) ) ;
#65012 = ORIENTED_EDGE ( 'NONE', *, *, #17399, .F. ) ;
#65013 = CARTESIAN_POINT ( 'NONE',  ( -2.775557561562891351E-14, 210.0000000000000284, 146.0000000000000284 ) ) ;
#65014 = CARTESIAN_POINT ( 'NONE',  ( -4.541265875000003227, 2.999999998634407028, 1.881053915767121110 ) ) ;
#65015 = CARTESIAN_POINT ( 'NONE',  ( -8.008118988124989457, -3.317071493978883900, 7.106865283940628331 ) ) ;
#65016 = CARTESIAN_POINT ( 'NONE',  ( 7.188101187500001821, 15.56249999795161365, -2.977408999572650483 ) ) ;
#65017 = CARTESIAN_POINT ( 'NONE',  ( 1.102182119232618108E-15, 293.3125000034140157, 6.000000000000001776 ) ) ;
#65018 = CARTESIAN_POINT ( 'NONE',  ( -7.188101187500002709, 12.18749999795161187, 2.977408999572649151 ) ) ;
#65019 = CARTESIAN_POINT ( 'NONE',  ( -5.082755093536319713, 5.082755093536319713, 11.79905278187175277 ) ) ;
#65020 = CARTESIAN_POINT ( 'NONE',  ( -10.18810118749999738, -4.220049686691941915, 114.6250000020483810 ) ) ;
#65021 = CIRCLE ( 'NONE', #8362, 5.000000000000000888 ) ;
#65022 =( BOUNDED_CURVE ( )  B_SPLINE_CURVE ( 2, ( #3938, #62370, #73334, #15602, #56359, #15975, #21638, #49946, #21266, #44290, #11079, #68409, #38641 ),
 .UNSPECIFIED., .F., .F. ) 
 B_SPLINE_CURVE_WITH_KNOTS ( ( 3, 2, 2, 2, 2, 2, 3 ),
 ( 0.9576885471939067251, 0.9629223234525785546, 0.9681560997112503841, 0.9733898759699222136, 0.9786236522285940431, 0.9838574284872658726, 0.9890912047459377021 ),
 .UNSPECIFIED. ) 
 CURVE ( )  GEOMETRIC_REPRESENTATION_ITEM ( )  RATIONAL_B_SPLINE_CURVE ( ( 1.000000000000083489, 0.9659258262889847124, 1.000000000000000000, 0.9659258262890682012, 1.000000000000000000, 0.9659258262890682012, 1.000000000000000000, 0.9659258262890682012, 1.000000000000000000, 0.9659258262890682012, 1.000000000000000000, 0.9659258262890692004, 0.9999999999999990008 ) ) 
 REPRESENTATION_ITEM ( '' )  );
#65023 = CARTESIAN_POINT ( 'NONE',  ( -7.347880794884122694E-16, 8.750000000000000000, 4.000000000000001776 ) ) ;
#65024 = CARTESIAN_POINT ( 'NONE',  ( -4.000000000000002665, 2.312499997268813168, 1.656854249492380804 ) ) ;
#65025 = VERTEX_POINT ( 'NONE', #71137 ) ;
#65026 = CIRCLE ( 'NONE', #56613, 11.49999999999999112 ) ;
#65027 = CARTESIAN_POINT ( 'NONE',  ( -1.432654583217607192, 209.2500000013655779, 194.5412658750000219 ) ) ;
#65028 = CARTESIAN_POINT ( 'NONE',  ( -2.828427124746209831, 201.3750000000000284, 139.1715728752538723 ) ) ;
#65029 = CARTESIAN_POINT ( 'NONE',  ( -29.65685424949245430, 196.1875000027312126, 166.0000000000004263 ) ) ;
#65030 = CARTESIAN_POINT ( 'NONE',  ( 3.211159895383560947, 1.187499998634406806, 3.211159895383562723 ) ) ;
#65031 = CARTESIAN_POINT ( 'NONE',  ( -7.188101187500001821, 113.5625000020483668, -2.977408999572650483 ) ) ;
#65032 = CARTESIAN_POINT ( 'NONE',  ( -49.70177871865298869, 38.00000000000000711, 69.99999999999998579 ) ) ;
#65033 = CARTESIAN_POINT ( 'NONE',  ( -5.656854249492375253, 5.656854249492375253, 0.8303027839201455595 ) ) ;
#65034 = VERTEX_POINT ( 'NONE', #30790 ) ;
#65035 = CARTESIAN_POINT ( 'NONE',  ( -7.188101187500002709, 23.81249999795161543, 2.977408999572649151 ) ) ;
#65036 = ORIENTED_EDGE ( 'NONE', *, *, #71229, .T. ) ;
#65037 = CARTESIAN_POINT ( 'NONE',  ( 8.660254037844389075, 255.2083333401612890, 4.999999999999997335 ) ) ;
#65038 = CARTESIAN_POINT ( 'NONE',  ( 1.432654583217662481, 207.1250000013656347, 194.5412658750000219 ) ) ;
#65039 = CARTESIAN_POINT ( 'NONE',  ( 30.44569435410883074, 201.5625000013656063, 172.4456943541086957 ) ) ;
#65040 = CARTESIAN_POINT ( 'NONE',  ( -10.00000000000000000, 52.29166666666665719, -2.679491924311229845 ) ) ;
#65041 = CARTESIAN_POINT ( 'NONE',  ( -7.188101187500000044, 100.5312500020483810, 0.000000000000000000 ) ) ;
#65042 = CARTESIAN_POINT ( 'NONE',  ( 4.242640687119287435, 295.3750000000000000, 4.242640687119285658 ) ) ;
#65044 = CARTESIAN_POINT ( 'NONE',  ( 2.751064625579944321E-14, 197.8750000027312126, 194.0000000000000568 ) ) ;
#65043 = CARTESIAN_POINT ( 'NONE',  ( -5.999999999999999112, 288.1250000034140157, 2.485281374238575314 ) ) ;
#65045 = ORIENTED_EDGE ( 'NONE', *, *, #2154, .T. ) ;
#65046 = CARTESIAN_POINT ( 'NONE',  ( 9.832129032723416984, 236.8229166700806445, -5.676582343750003368 ) ) ;
#65047 = EDGE_CURVE ( 'NONE', #58564, #25107, #30425, .T. ) ;
#65048 = CARTESIAN_POINT ( 'NONE',  ( 4.898587196589412829E-16, 13.87500000000000178, -8.000000000000000000 ) ) ;
#65049 = LINE ( 'NONE', #36033, #44358 ) ;
#65050 = CARTESIAN_POINT ( 'NONE',  ( -7.999999999961178609, -1.665943300379353739E-05, 2.518425711869641592 ) ) ;
#65051 = CARTESIAN_POINT ( 'NONE',  ( 10.00000000000000000, 262.5000000000000000, -1.224646799147353256E-15 ) ) ;
#65052 = FACE_OUTER_BOUND ( 'NONE', #54973, .T. ) ;
#65053 = CARTESIAN_POINT ( 'NONE',  ( 7.320508075688771044, 169.3750000000000000, 7.320508075688775484 ) ) ;
#65054 = CARTESIAN_POINT ( 'NONE',  ( 2.485281374238974994, 297.3750000034140157, 5.999999999999600320 ) ) ;
#65055 = CARTESIAN_POINT ( 'NONE',  ( -3.313708498984759387, -7.999999999999989342, 4.111552779823362869 ) ) ;
#65056 = CARTESIAN_POINT ( 'NONE',  ( -11.35316468750000141, 138.8020833299193271, 3.042071309553159963 ) ) ;
#65057 = CARTESIAN_POINT ( 'NONE',  ( 2.449293598294707893E-16, 4.999999997268813168, -4.000000000000001776 ) ) ;
#65058 = LINE ( 'NONE', #8098, #52986 ) ;
#65061 = CARTESIAN_POINT ( 'NONE',  ( 2.030339228148215693E-11, 166.2499999999984368, -10.00000000000000178 ) ) ;
#65060 = CARTESIAN_POINT ( 'NONE',  ( 8.000000000000001776, 110.6562500000000000, 3.313708498984759387 ) ) ;
#65059 = CARTESIAN_POINT ( 'NONE',  ( 31.99999999999998579, 207.1875000000000284, 171.6568542494923122 ) ) ;
#65062 = ORIENTED_EDGE ( 'NONE', *, *, #29559, .T. ) ;
#65063 = CARTESIAN_POINT ( 'NONE',  ( -11.35316468750000141, 8.802083329919348387, 3.042071309553159963 ) ) ;
#65064 = CARTESIAN_POINT ( 'NONE',  ( 17.99999999999998934, 0.000000000000000000, 9.999999999999996447 ) ) ;
#65065 = FACE_OUTER_BOUND ( 'NONE', #51379, .T. ) ;
#65066 = CARTESIAN_POINT ( 'NONE',  ( -1.432654583217664479, 205.7500000013656063, 138.5412658750000787 ) ) ;
#65067 = CARTESIAN_POINT ( 'NONE',  ( -3.442279223133897670, 124.6480146498679034, -7.075733707437612985 ) ) ;
#65068 = AXIS2_PLACEMENT_3D ( 'NONE', #72866, #55527, #33265 ) ;
#65069 = CARTESIAN_POINT ( 'NONE',  ( -2.679491924311235618, 30.41666665983869677, 10.00000000000000000 ) ) ;
#65070 = CARTESIAN_POINT ( 'NONE',  ( 7.188101187500002709, 115.8125000020484094, 2.977408999572649151 ) ) ;
#65071 = CARTESIAN_POINT ( 'NONE',  ( 1.881053915767122664, 6.249999998634407916, 4.541265875000001451 ) ) ;
#65072 = CARTESIAN_POINT ( 'NONE',  ( 2.997005883566935758, 66.06021892606798929, -26.46015439094089672 ) ) ;
#65073 = CARTESIAN_POINT ( 'NONE',  ( 7.999999999999991118, 3.313708498984757611, 15.17405277982336642 ) ) ;
#65075 = CARTESIAN_POINT ( 'NONE',  ( 11.00000000000000000, 1.347111479062088405E-15, 105.4375000040967763 ) ) ;
#65074 = CARTESIAN_POINT ( 'NONE',  ( 2.250000000000000000, 284.0000000000000000, 7.677076266392047543 ) ) ;
#65076 = ORIENTED_EDGE ( 'NONE', *, *, #36, .F. ) ;
#65077 = CARTESIAN_POINT ( 'NONE',  ( 4.242640687119287435, 292.4375000034140157, 4.242640687119285658 ) ) ;
#65078 = AXIS2_PLACEMENT_3D ( 'NONE', #64715, #1725, #48087 ) ;
#65079 = CARTESIAN_POINT ( 'NONE',  ( 8.000000000000001776, 109.1562500000000000, 3.313708498984759387 ) ) ;
#65080 = CARTESIAN_POINT ( 'NONE',  ( 11.35316468749999963, 231.7187500034139873, -1.390361679473963556E-15 ) ) ;
#65081 = CARTESIAN_POINT ( 'NONE',  ( 9.832129032723416984, 115.3645833299193555, 5.676582343750006032 ) ) ;
#65082 = ORIENTED_EDGE ( 'NONE', *, *, #28892, .T. ) ;
#65083 = CARTESIAN_POINT ( 'NONE',  ( -2.828427124746208943, 200.6250000000000284, 144.8284271247462129 ) ) ;
#65084 = ADVANCED_FACE ( 'NONE', ( #13422 ), #48131, .T. ) ;
#65085 = EDGE_CURVE ( 'NONE', #12488, #7596, #58740, .T. ) ;
#65086 = CARTESIAN_POINT ( 'NONE',  ( 10.18810118750000093, -4.220049686691933921, 96.81250000204839523 ) ) ;
#65087 = FACE_OUTER_BOUND ( 'NONE', #914, .T. ) ;
#65088 = CARTESIAN_POINT ( 'NONE',  ( -2.445694354108784108, 195.5625000013656063, 195.5543056458912190 ) ) ;
#65089 = DIRECTION ( 'NONE',  ( 0.000000000000000000, 0.000000000000000000, 1.000000000000000000 ) ) ;
#65091 = CARTESIAN_POINT ( 'NONE',  ( -3.042071309553163960, 117.2395833299193697, -11.35316468749999963 ) ) ;
#65090 = CARTESIAN_POINT ( 'NONE',  ( 7.071067751884405617, 220.0000000000000284, 7.071067871846544506 ) ) ;
#65092 = CARTESIAN_POINT ( 'NONE',  ( -26.34314575050764873, 206.9375000000000284, 166.0000000000003695 ) ) ;
#65093 = CARTESIAN_POINT ( 'NONE',  ( 0.000000000000000000, 125.0000000000000000, -7.500000000000020428 ) ) ;
#65094 = ORIENTED_EDGE ( 'NONE', *, *, #42404, .T. ) ;
#65095 = EDGE_CURVE ( 'NONE', #55117, #22437, #6683, .T. ) ;
#65096 = CARTESIAN_POINT ( 'NONE',  ( 4.999999999999993783, 211.0416666598387110, 8.660254037844390851 ) ) ;
#65097 = CARTESIAN_POINT ( 'NONE',  ( 8.000000000000000000, 112.4375000040967905, -9.797174393178825657E-16 ) ) ;
#65098 = CARTESIAN_POINT ( 'NONE',  ( 27.99999999999996803, 202.0000000000000000, 173.9999999999999147 ) ) ;
#65099 = CARTESIAN_POINT ( 'NONE',  ( -5.676582343750006032, 99.42708332991935549, 9.832129032723418760 ) ) ;
#65100 = PLANE ( 'NONE',  #13382 ) ;
#65101 = CARTESIAN_POINT ( 'NONE',  ( 7.188101187500000933, 9.937499997951610098, -2.977408999572650483 ) ) ;
#65102 = CARTESIAN_POINT ( 'NONE',  ( -7.204075437095965206, -7.204075437095968759, 90.71875000204838102 ) ) ;
#65103 = CARTESIAN_POINT ( 'NONE',  ( 11.35316468749999963, 11.30208332991934839, -3.042071309553165293 ) ) ;
#65104 = EDGE_LOOP ( 'NONE', ( #56833, #10730, #41006, #25629 ) ) ;
#65105 = CARTESIAN_POINT ( 'NONE',  ( -0.8761883848934740593, 67.61551161115575326, -20.05282165013490925 ) ) ;
#65106 = CARTESIAN_POINT ( 'NONE',  ( 8.008118988124991233, 3.317071493978879015, 25.85686528394063188 ) ) ;
#65107 = PLANE ( 'NONE',  #40259 ) ;
#65108 = CARTESIAN_POINT ( 'NONE',  ( -10.18810118749999738, -4.220049686691941915, 75.62500000204838102 ) ) ;
#65109 = CARTESIAN_POINT ( 'NONE',  ( -54.00000000000000000, 272.0000000000000000, 4.085831468968145267E-14 ) ) ;
#65110 = CARTESIAN_POINT ( 'NONE',  ( 8.660254037844385522, 199.5833333333333428, 5.000000000000005329 ) ) ;
#65111 = CARTESIAN_POINT ( 'NONE',  ( -2.765530957081998586, 291.6406250017068942, 6.676582343750001591 ) ) ;
#65112 = EDGE_CURVE ( 'NONE', #62240, #71473, #36278, .T. ) ;
#65113 = CARTESIAN_POINT ( 'NONE',  ( 8.660254037844389075, 127.2916666598387110, -5.000000000000000000 ) ) ;
#65114 = CARTESIAN_POINT ( 'NONE',  ( 5.676582343750001591, 221.9270833299193555, -9.832129032723420536 ) ) ;
#65115 = AXIS2_PLACEMENT_3D ( 'NONE', #14468, #34011, #43907 ) ;
#65116 = CARTESIAN_POINT ( 'NONE',  ( 4.220049686691941027, -10.18810118749999738, 87.62500000204836681 ) ) ;
#65117 = CARTESIAN_POINT ( 'NONE',  ( -28.00000000000002132, 202.4375000013656063, 166.5412658750003629 ) ) ;
#65118 = CARTESIAN_POINT ( 'NONE',  ( -1.469576158976823947E-15, 22.12500000000000355, 8.000000000000000000 ) ) ;
#65119 = CARTESIAN_POINT ( 'NONE',  ( 2.780723358947928197E-16, 13.68749999863440614, -4.541265875000002339 ) ) ;
#65120 = ORIENTED_EDGE ( 'NONE', *, *, #56245, .F. ) ;
#65121 = CARTESIAN_POINT ( 'NONE',  ( -23.99999999999999289, 208.8750000027312126, 170.0000000000002842 ) ) ;
#65122 = CARTESIAN_POINT ( 'NONE',  ( 4.000000000000015099, 206.6875000027312126, 196.3431457505076594 ) ) ;
#65123 =( BOUNDED_CURVE ( )  B_SPLINE_CURVE ( 2, ( #63006, #50943, #28672, #55877, #11330, #34363, #45285, #10216, #15854 ),
 .UNSPECIFIED., .F., .F. ) 
 B_SPLINE_CURVE_WITH_KNOTS ( ( 3, 2, 2, 2, 3 ),
 ( 0.6353544975714136012, 0.6419727316923105054, 0.6485910072767669954, 0.6552092828612233744, 0.6618275503331610965 ),
 .UNSPECIFIED. ) 
 CURVE ( )  GEOMETRIC_REPRESENTATION_ITEM ( )  RATIONAL_B_SPLINE_CURVE ( ( 0.9999990462150658566, 0.9238800094067415314, 1.000000000000000000, 0.9238795325112867385, 1.000000000000000000, 0.9238795325112867385, 1.000000000000000000, 0.9238795325112867385, 1.000000000000000000 ) ) 
 REPRESENTATION_ITEM ( '' )  );
#65124 = CARTESIAN_POINT ( 'NONE',  ( -1.432654583217662481, 198.3750000013655779, 145.4587341250000634 ) ) ;
#65125 = CARTESIAN_POINT ( 'NONE',  ( 3.999999999999960032, 205.0625000027312126, 143.6568542494924543 ) ) ;
#65126 = AXIS2_PLACEMENT_3D ( 'NONE', #58220, #28776, #35203 ) ;
#65127 = CARTESIAN_POINT ( 'NONE',  ( -5.000000000000000000, 11.68639849891318327, 68.31608016562505270 ) ) ;
#65128 = CARTESIAN_POINT ( 'NONE',  ( 7.204075437095968759, -7.204075437095966983, 68.59375000204836681 ) ) ;
#65129 = ORIENTED_EDGE ( 'NONE', *, *, #51015, .T. ) ;
#65130 = CARTESIAN_POINT ( 'NONE',  ( -7.188101187500000044, 7.218749997951610986, -8.802885111219163269E-16 ) ) ;
#65131 = CARTESIAN_POINT ( 'NONE',  ( -7.188101187499999156, 117.1250000020483952, 2.977408999572654924 ) ) ;
#65132 = VECTOR ( 'NONE', #16544, 1000.000000000000000 ) ;
#65133 = CARTESIAN_POINT ( 'NONE',  ( 8.234290096841634821, -16.03054008682958198, -0.009429105422179598697 ) ) ;
#65134 = CARTESIAN_POINT ( 'NONE',  ( -4.721056650415998313, 292.5781250017069510, 4.721056650416000089 ) ) ;
#65136 = CARTESIAN_POINT ( 'NONE',  ( -5.490800045006637653, 10.68629157650003236, 6.075767330655096332E-15 ) ) ;
#65135 = CARTESIAN_POINT ( 'NONE',  ( 9.832129032723420536, 225.9895833367473585, 5.676582343749996262 ) ) ;
#65137 = CONTEXT_DEPENDENT_SHAPE_REPRESENTATION ( #22109, #39088 ) ;
#65138 = ORIENTED_EDGE ( 'NONE', *, *, #52915, .F. ) ;
#65139 =( BOUNDED_CURVE ( )  B_SPLINE_CURVE ( 2, ( #23747, #7510, #18086, #64110, #53901, #6775, #47854, #46751, #35452 ),
 .UNSPECIFIED., .F., .F. ) 
 B_SPLINE_CURVE_WITH_KNOTS ( ( 3, 2, 2, 2, 3 ),
 ( 0.3333333333333336479, 0.3416666666666670071, 0.3500000000000003109, 0.3583333333333336701, 0.3666666666666669738 ),
 .UNSPECIFIED. ) 
 CURVE ( )  GEOMETRIC_REPRESENTATION_ITEM ( )  RATIONAL_B_SPLINE_CURVE ( ( 0.9999999999999970024, 0.9238795325112897361, 1.000000000000000000, 0.9238795325112867385, 1.000000000000000000, 0.9238795325112867385, 1.000000000000000000, 0.9238795325112837409, 1.000000000000003109 ) ) 
 REPRESENTATION_ITEM ( '' )  );
#65140 = CARTESIAN_POINT ( 'NONE',  ( 9.832129032723416984, 232.1354166700806445, -5.676582343750003368 ) ) ;
#65141 = CARTESIAN_POINT ( 'NONE',  ( -2.977408999572647819, 7.188101187499991163, 28.58030278187176165 ) ) ;
#65142 = CARTESIAN_POINT ( 'NONE',  ( -2.828427124746190735, 9.124999997268814056, -2.828427124746191623 ) ) ;
#65143 = CARTESIAN_POINT ( 'NONE',  ( 2.754378923186476579E-14, 204.4375000013656063, 194.5412658750000219 ) ) ;
#65144 = ORIENTED_EDGE ( 'NONE', *, *, #53181, .F. ) ;
#65145 = CARTESIAN_POINT ( 'NONE',  ( 1.224646799147353454E-15, 300.0000000000000000, -10.00000000000000178 ) ) ;
#65146 = CARTESIAN_POINT ( 'NONE',  ( -2.085542519210945728E-15, 104.8437499965860269, 11.35316468750000141 ) ) ;
#65147 = CARTESIAN_POINT ( 'NONE',  ( -1.836970198721029983E-15, 210.6249999931720538, 10.00000000000000178 ) ) ;
#65148 = CARTESIAN_POINT ( 'NONE',  ( -11.00000000000000000, 0.000000000000000000, 75.99999999999998579 ) ) ;
#65151 = CARTESIAN_POINT ( 'NONE',  ( -27.99999999999999645, 210.0000000000000284, 166.0000000000003979 ) ) ;
#65150 = CARTESIAN_POINT ( 'NONE',  ( 29.43265458321766559, 203.5000000013655779, 173.4587341249998929 ) ) ;
#65149 = CARTESIAN_POINT ( 'NONE',  ( 27.99999999999996447, 204.6875000013656063, 173.4587341249998929 ) ) ;
#65152 = ORIENTED_EDGE ( 'NONE', *, *, #28614, .F. ) ;
#65153 = EDGE_CURVE ( 'NONE', #13863, #27743, #67116, .T. ) ;
#65154 = CARTESIAN_POINT ( 'NONE',  ( -54.00000000000000711, 242.0000000000000284, 20.00000000000003197 ) ) ;
#65155 = CARTESIAN_POINT ( 'NONE',  ( 5.676582343750001591, 211.6145833299193555, -9.832129032723420536 ) ) ;
#65156 = CARTESIAN_POINT ( 'NONE',  ( 1.432654583217607192, 201.2500000013656063, 145.4587341250000634 ) ) ;
#65157 = CARTESIAN_POINT ( 'NONE',  ( 29.43265458321761230, 202.7500000013655779, 173.4587341249998929 ) ) ;
#65158 = CARTESIAN_POINT ( 'NONE',  ( -7.778174593052023411, 7.778174593052023411, 116.5000000040967905 ) ) ;
#65159 = CARTESIAN_POINT ( 'NONE',  ( 9.832129032723416984, 200.6770833299193555, 5.676582343750006032 ) ) ;
#65160 = CARTESIAN_POINT ( 'NONE',  ( -5.082755093536325930, 92.84375000204838102, -5.082755093536325930 ) ) ;
#65161 = CARTESIAN_POINT ( 'NONE',  ( -5.000000000000000000, 67.10422270468733075, -23.07049055144695160 ) ) ;
#65162 = CARTESIAN_POINT ( 'NONE',  ( -30.82842712474620939, 197.1250000000000284, 167.1715728752542134 ) ) ;
#65163 = CARTESIAN_POINT ( 'NONE',  ( 2.780723358947928197E-16, 14.56249999863440792, -4.541265875000002339 ) ) ;
#65164 = CARTESIAN_POINT ( 'NONE',  ( 24.54126587500000056, 197.3750000013656063, 168.5673454167822172 ) ) ;
#65165 = CARTESIAN_POINT ( 'NONE',  ( 5.082755093536320601, -5.082755093536318824, 5.424052781871753659 ) ) ;
#65166 = CARTESIAN_POINT ( 'NONE',  ( 11.35316468750000141, 75.78124999658602690, 0.000000000000000000 ) ) ;
#65167 = FACE_OUTER_BOUND ( 'NONE', #73125, .T. ) ;
#65168 = ORIENTED_EDGE ( 'NONE', *, *, #33789, .T. ) ;
#65169 = CARTESIAN_POINT ( 'NONE',  ( 0.000000000000000000, 4.898587196589400010E-16, 31.99999999999998579 ) ) ;
#65170 = CARTESIAN_POINT ( 'NONE',  ( -3.999999999999960032, 207.0000000000000284, 198.0000000000000284 ) ) ;
#65171 = CARTESIAN_POINT ( 'NONE',  ( 6.951808397369818766E-16, 72.03124999658602690, -11.35316468750000141 ) ) ;
#65172 = ORIENTED_EDGE ( 'NONE', *, *, #69703, .F. ) ;
#65173 = CARTESIAN_POINT ( 'NONE',  ( -10.18810118749999916, 0.000000000000000000, 84.53125000204836681 ) ) ;
#65174 = EDGE_CURVE ( 'NONE', #71847, #66887, #67559, .T. ) ;
#65175 = CARTESIAN_POINT ( 'NONE',  ( -11.00000000000000000, 4.556349186104045934, 71.59375000409676204 ) ) ;
#65176 = CARTESIAN_POINT ( 'NONE',  ( 2.445694354108840063, 208.0625000013656063, 200.4456943541088663 ) ) ;
#65177 = CARTESIAN_POINT ( 'NONE',  ( -1.469576158976823947E-15, 23.43749999590322020, 8.000000000000000000 ) ) ;
#65179 = CARTESIAN_POINT ( 'NONE',  ( 8.311093377946834337, 75.15624999658602690, 8.311093377946839666 ) ) ;
#65178 = CARTESIAN_POINT ( 'NONE',  ( 8.000000000000000000, 103.5312500040967905, -3.313708498984762496 ) ) ;
#65180 = CARTESIAN_POINT ( 'NONE',  ( 3.313708498984762496, -7.999999999999989342, 23.98655278392014978 ) ) ;
#65181 = CARTESIAN_POINT ( 'NONE',  ( 2.679491924312694895, 128.9583333333334565, 9.999999999999154454 ) ) ;
#65182 = CARTESIAN_POINT ( 'NONE',  ( 10.00000000000000000, 171.6666666598386826, 2.679491924311236062 ) ) ;
#65183 = CARTESIAN_POINT ( 'NONE',  ( 1.320432766682874540E-15, 93.40625000204838102, 7.188101187500000044 ) ) ;
#65184 = CARTESIAN_POINT ( 'NONE',  ( -26.15334609510026453, 194.8133403918677686, 173.3581351799293486 ) ) ;
#65185 = CARTESIAN_POINT ( 'NONE',  ( -11.35316468750000141, 58.80208332991934128, 3.042071309553159963 ) ) ;
#65186 = CARTESIAN_POINT ( 'NONE',  ( -4.220049686691935698, 10.18810118749999916, 109.7500000020483810 ) ) ;
#65187 = CARTESIAN_POINT ( 'NONE',  ( -5.676582343750006032, 194.1145833299193839, 9.832129032723418760 ) ) ;
#65188 = ORIENTED_EDGE ( 'NONE', *, *, #20371, .F. ) ;
#65189 = CARTESIAN_POINT ( 'NONE',  ( 9.000000000000000000, 5.196152422706622254, -10.80000000000000071 ) ) ;
#65190 = CARTESIAN_POINT ( 'NONE',  ( 1.469576158976823947E-15, 122.3750000000000000, 8.000000000000000000 ) ) ;
#65191 = CARTESIAN_POINT ( 'NONE',  ( 4.999999999999993783, 161.0416666598387110, 8.660254037844390851 ) ) ;
#65193 = CARTESIAN_POINT ( 'NONE',  ( 5.676582343750001591, 191.6145833299193839, -9.832129032723420536 ) ) ;
#65192 = CARTESIAN_POINT ( 'NONE',  ( 12.00000000000000178, 4.898587196589402968E-16, -24.00000000000001066 ) ) ;
#65194 = CARTESIAN_POINT ( 'NONE',  ( -8.000000000000001776, 11.15624999590322020, 3.313708498984759387 ) ) ;
#65195 = CARTESIAN_POINT ( 'NONE',  ( -4.999999999999992895, 243.9583333401613174, 8.660254037844390851 ) ) ;
#65196 = LINE ( 'NONE', #59557, #2302 ) ;
#65197 =( GEOMETRIC_REPRESENTATION_CONTEXT ( 3 ) GLOBAL_UNCERTAINTY_ASSIGNED_CONTEXT ( ( #64199 ) ) GLOBAL_UNIT_ASSIGNED_CONTEXT ( ( #28451, #5082, #74101 ) ) REPRESENTATION_CONTEXT ( 'NONE', 'WORKASPACE' ) );
#65198 = EDGE_CURVE ( 'NONE', #3255, #74244, #35486, .T. ) ;
#65199 = ORIENTED_EDGE ( 'NONE', *, *, #51059, .T. ) ;
#65200 = CARTESIAN_POINT ( 'NONE',  ( 3.042071309553159519, 180.0520833299193555, 11.35316468750000141 ) ) ;
#65201 = EDGE_CURVE ( 'NONE', #8993, #8347, #25815, .T. ) ;
#65202 = VECTOR ( 'NONE', #13043, 1000.000000000000000 ) ;
#65203 = CARTESIAN_POINT ( 'NONE',  ( -7.188101187499992051, 0.000000000000000000, 22.48655278187175455 ) ) ;
#65204 = CARTESIAN_POINT ( 'NONE',  ( 5.656854249492378806, 17.81250000000000355, 5.656854249492381470 ) ) ;
#65205 = VECTOR ( 'NONE', #29640, 1000.000000000000000 ) ;
#65206 = ORIENTED_EDGE ( 'NONE', *, *, #73288, .F. ) ;
#65207 = EDGE_CURVE ( 'NONE', #15625, #68592, #7418, .T. ) ;
#65208 = ADVANCED_FACE ( 'NONE', ( #47037 ), #17998, .F. ) ;
#65209 = CARTESIAN_POINT ( 'NONE',  ( 3.313708498984760720, 100.7187500040967763, -8.000000000000000000 ) ) ;
#65210 = CARTESIAN_POINT ( 'NONE',  ( -4.999999999999998224, 1.666666666666666741, -8.660254037844389075 ) ) ;
#65211 = ADVANCED_FACE ( 'NONE', ( #54383 ), #72081, .F. ) ;
#65212 = CARTESIAN_POINT ( 'NONE',  ( -1.656854249492383691, 13.68750000000000000, 4.000000000000000888 ) ) ;
#65213 = CARTESIAN_POINT ( 'NONE',  ( -1.881053915767124440, 15.99999999863440614, 4.541265875000001451 ) ) ;
#65214 = CARTESIAN_POINT ( 'NONE',  ( -7.999999999999991118, 0.000000000000000000, 16.01780278392014978 ) ) ;
#65215 = CARTESIAN_POINT ( 'NONE',  ( 3.999999999999960032, 195.0000000000000000, 142.0000000000000568 ) ) ;
#65216 = CIRCLE ( 'NONE', #52002, 10.00000000000000178 ) ;
#65217 = ORIENTED_EDGE ( 'NONE', *, *, #62864, .T. ) ;
#65218 = CARTESIAN_POINT ( 'NONE',  ( 28.00000000000002487, 209.1250000027312126, 173.9999999999999147 ) ) ;
#65219 = CARTESIAN_POINT ( 'NONE',  ( -7.188101187500001821, 98.56250000204838102, -2.977408999572650483 ) ) ;
#65221 = CARTESIAN_POINT ( 'NONE',  ( 4.000000000000001776, 13.74999999726881583, 0.000000000000000000 ) ) ;
#65220 = CARTESIAN_POINT ( 'NONE',  ( 8.000000000000000000, 16.31249999590322375, 0.000000000000000000 ) ) ;
#65222 = DIRECTION ( 'NONE',  ( 1.000000000000000000, 0.000000000000000000, 0.000000000000000000 ) ) ;
#65223 = ORIENTED_EDGE ( 'NONE', *, *, #50105, .F. ) ;
#65224 = CARTESIAN_POINT ( 'NONE',  ( -5.676582343749992710, 260.0520833367473301, 9.832129032723422313 ) ) ;
#65225 = CARTESIAN_POINT ( 'NONE',  ( -5.082755093536319713, 5.082755093536319713, 19.29905278187175455 ) ) ;
#65226 = ORIENTED_EDGE ( 'NONE', *, *, #34372, .F. ) ;
#65227 =( BOUNDED_CURVE ( )  B_SPLINE_CURVE ( 2, ( #59168, #23708, #40318, #58066, #46347, #17674, #5998, #726, #46712 ),
 .UNSPECIFIED., .F., .F. ) 
 B_SPLINE_CURVE_WITH_KNOTS ( ( 3, 2, 2, 2, 3 ),
 ( 0.2000000000000001776, 0.2083333333333335091, 0.2166666666666668406, 0.2250000000000001998, 0.2333333333333335313 ),
 .UNSPECIFIED. ) 
 CURVE ( )  GEOMETRIC_REPRESENTATION_ITEM ( )  RATIONAL_B_SPLINE_CURVE ( ( 0.9999999999999984457, 0.9238795325112882928, 1.000000000000000000, 0.9238795325112867385, 1.000000000000000000, 0.9238795325112867385, 1.000000000000000000, 0.9238795325112849621, 1.000000000000001776 ) ) 
 REPRESENTATION_ITEM ( '' )  );
#65228 = ORIENTED_EDGE ( 'NONE', *, *, #56984, .T. ) ;
#65229 = CARTESIAN_POINT ( 'NONE',  ( 10.18810118749999916, 1.247682550866122264E-15, 84.90625000204838102 ) ) ;
#65230 = CARTESIAN_POINT ( 'NONE',  ( -2.679491924311235174, 115.4166666598386968, 10.00000000000000000 ) ) ;
#65231 = CARTESIAN_POINT ( 'NONE',  ( 11.00000000000000355, -4.556349186104045046, 96.15624999999998579 ) ) ;
#65234 = CARTESIAN_POINT ( 'NONE',  ( -4.721056650415999201, 293.4843750017070079, -4.721056650415999201 ) ) ;
#65233 = CARTESIAN_POINT ( 'NONE',  ( 31.99999999999998579, 202.4375000027311842, 168.3431457505075173 ) ) ;
#65232 = CARTESIAN_POINT ( 'NONE',  ( 30.82842712474616320, 196.5000000027312126, 167.1715728752537018 ) ) ;
#65235 = CARTESIAN_POINT ( 'NONE',  ( 5.000000000000001776, 145.8333333333333428, -8.660254037844389075 ) ) ;
#65236 = CARTESIAN_POINT ( 'NONE',  ( 26.34314575050768426, 199.6875000027312126, 165.9999999999998010 ) ) ;
#65237 = AXIS2_PLACEMENT_3D ( 'NONE', #39389, #10713, #17107 ) ;
#65238 = CARTESIAN_POINT ( 'NONE',  ( -11.00000000000000000, 0.000000000000000000, 78.99999999999998579 ) ) ;
#65239 = CARTESIAN_POINT ( 'NONE',  ( -7.320508075688770155, 233.7500000068280031, 7.320508075688774596 ) ) ;
#65240 = CARTESIAN_POINT ( 'NONE',  ( 8.000000000000000000, 1.406249995903220196, -3.313708498984761608 ) ) ;
#65241 = CARTESIAN_POINT ( 'NONE',  ( 27.99999999999996092, 197.4375000013655779, 173.4587341249998929 ) ) ;
#65242 = CARTESIAN_POINT ( 'NONE',  ( -7.188101187500001821, 2.999999997951610542, -2.977408999572651371 ) ) ;
#65243 = AXIS2_PLACEMENT_3D ( 'NONE', #51394, #16676, #16302 ) ;
#65244 = CARTESIAN_POINT ( 'NONE',  ( 1.471067592899761672E-15, -8.008118988124991233, -0.1118847160593713225 ) ) ;
#65245 = CYLINDRICAL_SURFACE ( 'NONE', #70857, 10.00000000000000178 ) ;
#65246 = CARTESIAN_POINT ( 'NONE',  ( -2.977408999572652260, 112.8125000020483952, 7.188101187500000044 ) ) ;
#65248 = CARTESIAN_POINT ( 'NONE',  ( -7.320508075688778149, 133.1250000000000284, 7.320508075688770155 ) ) ;
#65247 = CARTESIAN_POINT ( 'NONE',  ( 0.000000000000000000, 0.000000000000000000, 0.000000000000000000 ) ) ;
#65249 = CARTESIAN_POINT ( 'NONE',  ( -11.35316468749999608, 229.4270833367473585, 3.042071309553173730 ) ) ;
#65250 = CARTESIAN_POINT ( 'NONE',  ( -27.99999999999999645, 210.0000000000000284, 166.0000000000003979 ) ) ;
#65251 = CARTESIAN_POINT ( 'NONE',  ( -7.188101187499991163, 2.977408999572646930, 21.26780278187175810 ) ) ;
#65252 = CARTESIAN_POINT ( 'NONE',  ( 27.99999999999999645, 210.0000000000000284, 165.9999999999999147 ) ) ;
#65253 = CARTESIAN_POINT ( 'NONE',  ( -3.042071309553164404, 22.23958332991935549, -11.35316468749999963 ) ) ;
#65254 = EDGE_CURVE ( 'NONE', #34878, #56876, #36661, .T. ) ;
#65255 = CARTESIAN_POINT ( 'NONE',  ( 3.407298021510797525, 16.35582233947175013, 69.12343428065700834 ) ) ;
#65256 = CARTESIAN_POINT ( 'NONE',  ( -7.320508075688778149, 9.999999993172032475, 7.320508075688769267 ) ) ;
#65257 = DIRECTION ( 'NONE',  ( 0.000000000000000000, 0.000000000000000000, 1.000000000000000000 ) ) ;
#65258 = LINE ( 'NONE', #1898, #15444 ) ;
#65259 = VERTEX_POINT ( 'NONE', #9476 ) ;
#65260 = CARTESIAN_POINT ( 'NONE',  ( 6.123233995736767268E-16, 128.1249999931720254, -10.00000000000000178 ) ) ;
#65261 = CARTESIAN_POINT ( 'NONE',  ( -3.313708498984757611, 7.999999999999991118, 18.54905277982336287 ) ) ;
#65262 = CARTESIAN_POINT ( 'NONE',  ( 9.832129032723416984, 30.36458332991935194, 5.676582343750006032 ) ) ;
#65263 = CARTESIAN_POINT ( 'NONE',  ( -7.778174593052023411, 7.778174593052023411, 88.00000000409677625 ) ) ;
#65264 = CARTESIAN_POINT ( 'NONE',  ( -1.432654583217664701, 207.0000000013655779, 138.5412658750000787 ) ) ;
#65265 = CARTESIAN_POINT ( 'NONE',  ( 2.849036369511732440E-14, 197.2500000000000000, 202.0000000000000000 ) ) ;
#65266 = CARTESIAN_POINT ( 'NONE',  ( 12.00000000000000178, 2.352228297136963242, -0.1238145317436998294 ) ) ;
#65268 = CARTESIAN_POINT ( 'NONE',  ( 5.676582343749993598, 34.94791666325268409, 9.832129032723422313 ) ) ;
#65267 = CARTESIAN_POINT ( 'NONE',  ( -7.188101187500000044, 107.6562500020483810, 0.000000000000000000 ) ) ;
#65269 = CARTESIAN_POINT ( 'NONE',  ( 3.313708498984762496, -7.999999999999989342, 14.79905277982336465 ) ) ;
#65270 = CARTESIAN_POINT ( 'NONE',  ( -11.35316468750000141, 153.4895833299193555, 3.042071309553159963 ) ) ;
#65271 = EDGE_CURVE ( 'NONE', #33693, #73018, #602, .T. ) ;
#65272 = CARTESIAN_POINT ( 'NONE',  ( 7.320508075688774596, 132.4999999931720254, -7.320508075688774596 ) ) ;
#65273 = CARTESIAN_POINT ( 'NONE',  ( -2.977408999572650927, 109.2500000020483952, -7.188101187500001821 ) ) ;
#65274 = DIRECTION ( 'NONE',  ( -0.000000000000000000, 1.000000000000000000, -0.000000000000000000 ) ) ;
#65275 = CARTESIAN_POINT ( 'NONE',  ( -27.99999999999996447, 203.1875000013656063, 173.4587341250003760 ) ) ;
#65276 = ORIENTED_EDGE ( 'NONE', *, *, #60489, .F. ) ;
#65277 = CARTESIAN_POINT ( 'NONE',  ( 0.8761883848702545219, -67.61551161115382058, -20.05282165013451845 ) ) ;
#65278 = CARTESIAN_POINT ( 'NONE',  ( 9.832129032723420536, 26.51041666325268409, -5.676582343749999815 ) ) ;
#65279 = ORIENTED_EDGE ( 'NONE', *, *, #52070, .T. ) ;
#65280 = CARTESIAN_POINT ( 'NONE',  ( 4.000000000000000888, 6.937500000000000000, 1.656854249492384135 ) ) ;
#65281 = DIRECTION ( 'NONE',  ( -1.000000000000000000, 0.000000000000000000, -0.000000000000000000 ) ) ;
#65282 = PRODUCT_RELATED_PRODUCT_CATEGORY ( 'part', '', ( #49912 ) ) ;
#65284 = CARTESIAN_POINT ( 'NONE',  ( -9.832129032723418760, 152.8645833299193555, -5.676582343750004256 ) ) ;
#65283 = CARTESIAN_POINT ( 'NONE',  ( -30.21828243460005581, -21.02437228245649337, 152.3270862596944539 ) ) ;
#65285 = DIRECTION ( 'NONE',  ( 0.000000000000000000, 0.000000000000000000, 1.000000000000000000 ) ) ;
#65286 = CARTESIAN_POINT ( 'NONE',  ( -5.656854249492375253, 5.656854249492375253, 20.19905278432982243 ) ) ;
#65287 = CIRCLE ( 'NONE', #21930, 17.50000000000000000 ) ;
#65288 = LINE ( 'NONE', #70585, #38137 ) ;
#65289 = CARTESIAN_POINT ( 'NONE',  ( -9.832129032723415207, 234.3229166700806445, 5.676582343750005144 ) ) ;
#65290 = CARTESIAN_POINT ( 'NONE',  ( -6.238412754330611322E-16, 10.18810118749999916, 93.15625000204836681 ) ) ;
#65291 = ORIENTED_EDGE ( 'NONE', *, *, #8536, .T. ) ;
#65292 = EDGE_CURVE ( 'NONE', #26800, #5410, #49828, .T. ) ;
#65293 = CARTESIAN_POINT ( 'NONE',  ( 6.123233995736767268E-16, 203.1249999931720538, -10.00000000000000178 ) ) ;
#65294 = DIRECTION ( 'NONE',  ( 1.000000000000000000, -0.000000000000000000, -0.000000000000000000 ) ) ;
#65295 = CARTESIAN_POINT ( 'NONE',  ( 11.35316468749999963, 106.3020833299193413, -3.042071309553165293 ) ) ;
#65296 = CARTESIAN_POINT ( 'NONE',  ( 1.871523826299183495E-15, -10.18810118749999916, 99.53125000204838102 ) ) ;
#65297 = CARTESIAN_POINT ( 'NONE',  ( 4.541265875000002339, 18.49999999863440436, -1.881053915767121776 ) ) ;
#65298 = ORIENTED_EDGE ( 'NONE', *, *, #62606, .F. ) ;
#65299 = ORIENTED_EDGE ( 'NONE', *, *, #52077, .F. ) ;
#65300 = CARTESIAN_POINT ( 'NONE',  ( -5.656854249492381470, 11.43750000000000178, 5.656854249492379694 ) ) ;
#65301 = CARTESIAN_POINT ( 'NONE',  ( -1.836970198721029983E-15, 215.6249999931720538, 10.00000000000000178 ) ) ;
#65302 = CARTESIAN_POINT ( 'NONE',  ( 5.082755093536324154, 27.65624999795161543, 5.082755093536326818 ) ) ;
#65303 = CARTESIAN_POINT ( 'NONE',  ( -4.898587196589412829E-16, 115.8125000040967763, -8.000000000000000000 ) ) ;
#65304 = CARTESIAN_POINT ( 'NONE',  ( 10.18810118749999916, 4.220049686691935698, 98.87500000204836681 ) ) ;
#65305 = LINE ( 'NONE', #40647, #38023 ) ;
#65306 = AXIS2_PLACEMENT_3D ( 'NONE', #71065, #48057, #42030 ) ;
#65307 = B_SPLINE_CURVE_WITH_KNOTS ( 'NONE', 3,
 ( #66957, #44694, #20548, #28079, #73365, #4337, #39405, #45066, #16008, #55657, #50344, #39038, #20925, #67710, #62404, #55283, #3587, #62040, #33026, #72621, #4711, #21300 ),
 .UNSPECIFIED., .F., .F.,
 ( 4, 2, 2, 2, 2, 2, 2, 2, 2, 2, 4 ),
 ( 0.000000000000000000, 0.001156727053362482157, 0.001735090580043723235, 0.002313454106724964314, 0.003470181160087444303, 0.004048544686768682996, 0.004626908213449921689, 0.005783635266812366983, 0.006940362320174811410, 0.008097089373537256704, 0.009253816426899701131 ),
 .UNSPECIFIED. ) ;
#65308 = EDGE_CURVE ( 'NONE', #41315, #25962, #72845, .T. ) ;
#65309 = CARTESIAN_POINT ( 'NONE',  ( -5.656854249492379694, 6.562500000000001776, -5.656854249492380582 ) ) ;
#65310 = CARTESIAN_POINT ( 'NONE',  ( -1.656854249492383691, 12.43749999726881406, 4.000000000000000888 ) ) ;
#65311 = CARTESIAN_POINT ( 'NONE',  ( 3.211159895383561835, 3.437499998634407028, -3.211159895383561835 ) ) ;
#65312 = ORIENTED_EDGE ( 'NONE', *, *, #9063, .F. ) ;
#65313 = CARTESIAN_POINT ( 'NONE',  ( 8.000000000000001776, 95.65625000000001421, 3.313708498984759387 ) ) ;
#65314 = CARTESIAN_POINT ( 'NONE',  ( 0.000000000000000000, 0.000000000000000000, -11.00000000000000000 ) ) ;
#65316 = DIRECTION ( 'NONE',  ( -0.000000000000000000, 1.000000000000000000, -0.000000000000000000 ) ) ;
#65315 = CARTESIAN_POINT ( 'NONE',  ( -31.45873412500001720, 200.6250000013655779, 168.5673454167828140 ) ) ;
#65317 = CARTESIAN_POINT ( 'NONE',  ( -1.881053915767121554, 12.62499999863441147, -4.541265875000002339 ) ) ;
#65318 = CARTESIAN_POINT ( 'NONE',  ( 6.123233995736767268E-16, 123.1249999931720396, -10.00000000000000178 ) ) ;
#65319 = CARTESIAN_POINT ( 'NONE',  ( -7.188101187499992051, 0.000000000000000000, 14.98655278187175455 ) ) ;
#65320 = ORIENTED_EDGE ( 'NONE', *, *, #48375, .T. ) ;
#65321 = ORIENTED_EDGE ( 'NONE', *, *, #70951, .F. ) ;
#65322 = CARTESIAN_POINT ( 'NONE',  ( 4.220049686691941027, -10.18810118749999738, 107.1250000020483810 ) ) ;
#65323 = CARTESIAN_POINT ( 'NONE',  ( -1.836970198721029983E-15, 123.7500000000000142, 10.00000000000000178 ) ) ;
#65324 = CARTESIAN_POINT ( 'NONE',  ( -25.55430564589119413, 204.5625000013656063, 167.5543056458915316 ) ) ;
#65325 = CARTESIAN_POINT ( 'NONE',  ( -32.00000000000000711, 200.1875000000000568, 168.3431457505080004 ) ) ;
#65326 = CARTESIAN_POINT ( 'NONE',  ( -2.445694354108782775, 195.5625000013656063, 200.4456943541088663 ) ) ;
#65327 = CARTESIAN_POINT ( 'NONE',  ( -5.656854249492379694, 12.37499999590322197, -5.656854249492380582 ) ) ;
#65328 = CARTESIAN_POINT ( 'NONE',  ( 2.679491924311222739, 98.95833333333334281, 10.00000000000000355 ) ) ;
#65329 = AXIS2_PLACEMENT_3D ( 'NONE', #30412, #54173, #65840 ) ;
#65330 = CARTESIAN_POINT ( 'NONE',  ( 5.656854249492379694, 110.9375000000000000, -5.656854249492380582 ) ) ;
#65331 = CARTESIAN_POINT ( 'NONE',  ( -4.721056650415998313, 294.7343750017069510, 4.721056650416000089 ) ) ;
#65332 = EDGE_CURVE ( 'NONE', #17439, #72211, #36718, .T. ) ;
#65333 = ORIENTED_EDGE ( 'NONE', *, *, #27003, .F. ) ;
#65334 = AXIS2_PLACEMENT_3D ( 'NONE', #45521, #5544, #28546 ) ;
#65335 = CARTESIAN_POINT ( 'NONE',  ( -6.735557395310442023E-16, 11.00000000000000000, 74.12500000000000000 ) ) ;
#65336 = CARTESIAN_POINT ( 'NONE',  ( 7.999999999999998224, 17.71874999590322730, 3.313708498984766493 ) ) ;
#65337 = CARTESIAN_POINT ( 'NONE',  ( -1.432654583217664479, 203.7500000013656063, 138.5412658750000787 ) ) ;
#65338 = CARTESIAN_POINT ( 'NONE',  ( -2.143145793903030439E-12, 53.74999999999984368, 9.999999999999998224 ) ) ;
#65339 = LINE ( 'NONE', #8000, #20288 ) ;
#65340 = CARTESIAN_POINT ( 'NONE',  ( 8.311093377946834337, 262.3437500034140157, -8.311093377946836114 ) ) ;
#65341 = CARTESIAN_POINT ( 'NONE',  ( 27.99999999999996092, 196.6250000027312126, 165.9999999999998863 ) ) ;
#65342 = CARTESIAN_POINT ( 'NONE',  ( 11.00000000000000355, -4.556349186104045046, 111.1562499999999858 ) ) ;
#65343 = CARTESIAN_POINT ( 'NONE',  ( 7.320508075688774596, 215.6249999999999716, -7.320508075688774596 ) ) ;
#65344 = EDGE_CURVE ( 'NONE', #67329, #3433, #6574, .T. ) ;
#65345 = CARTESIAN_POINT ( 'NONE',  ( -5.082755093536317936, -5.082755093536320601, 8.049052781871752771 ) ) ;
#65346 = CARTESIAN_POINT ( 'NONE',  ( -11.35316468750000141, 188.8020833299193555, 3.042071309553159963 ) ) ;
#65347 = CARTESIAN_POINT ( 'NONE',  ( 8.660254037844389075, 192.2916666598387110, -5.000000000000000000 ) ) ;
#65348 = CARTESIAN_POINT ( 'NONE',  ( -4.541265875000002339, 2.812499998634407028, -5.561446717895856393E-16 ) ) ;
#65349 = DIRECTION ( 'NONE',  ( -0.000000000000000000, 1.000000000000000000, -1.563033456626094573E-30 ) ) ;
#65351 = DIRECTION ( 'NONE',  ( 0.000000000000000000, 0.000000000000000000, -1.000000000000000000 ) ) ;
#65350 = DIRECTION ( 'NONE',  ( -0.000000000000000000, 1.000000000000000000, -0.000000000000000000 ) ) ;
#65352 = ORIENTED_EDGE ( 'NONE', *, *, #67745, .T. ) ;
#65353 = CARTESIAN_POINT ( 'NONE',  ( -2.839093476692135984E-14, 194.6875000013655779, 138.5412658750000503 ) ) ;
#65354 = CARTESIAN_POINT ( 'NONE',  ( -5.676582343750006032, 54.42708332991935549, 9.832129032723418760 ) ) ;
#65355 = CARTESIAN_POINT ( 'NONE',  ( 11.00000000000000355, -4.556349186104045046, 103.8437500040967763 ) ) ;
#65356 = CARTESIAN_POINT ( 'NONE',  ( -5.676582343750006032, 214.4270833299193555, 9.832129032723418760 ) ) ;
#65357 = CARTESIAN_POINT ( 'NONE',  ( -29.43265458321771533, 206.5000000013655779, 166.5412658750003914 ) ) ;
#65358 = CARTESIAN_POINT ( 'NONE',  ( -7.320508075688778149, 124.9999999931720396, 7.320508075688769267 ) ) ;
#65360 = CARTESIAN_POINT ( 'NONE',  ( 3.313708498984711426, 119.4687500000000142, 8.000000000000053291 ) ) ;
#65359 = CARTESIAN_POINT ( 'NONE',  ( -7.188101187500000044, 122.6562500020483810, 0.000000000000000000 ) ) ;
#65361 = CYLINDRICAL_SURFACE ( 'NONE', #59277, 11.00000000000000000 ) ;
#65362 =( BOUNDED_CURVE ( )  B_SPLINE_CURVE ( 2, ( #27134, #20723, #66755, #26760, #9795, #72794, #21102, #44125, #67133 ),
 .UNSPECIFIED., .F., .F. ) 
 B_SPLINE_CURVE_WITH_KNOTS ( ( 3, 2, 2, 2, 3 ),
 ( 0.08823529411764710617, 0.09191176470588241498, 0.09558823529411769604, 0.09926470588235300485, 0.1029411764705882998 ),
 .UNSPECIFIED. ) 
 CURVE ( )  GEOMETRIC_REPRESENTATION_ITEM ( )  RATIONAL_B_SPLINE_CURVE ( ( 0.9999999999999991118, 0.9238795325112876267, 1.000000000000000000, 0.9238795325112867385, 1.000000000000000000, 0.9238795325112867385, 1.000000000000000000, 0.9238795325112852952, 1.000000000000001332 ) ) 
 REPRESENTATION_ITEM ( '' )  );
#65363 = CARTESIAN_POINT ( 'NONE',  ( 11.35316468749999785, 110.5729166632526983, 3.042071309553174174 ) ) ;
#65364 = CARTESIAN_POINT ( 'NONE',  ( -2.679491924311225848, 73.33333332650536818, -10.00000000000000178 ) ) ;
#65365 = CARTESIAN_POINT ( 'NONE',  ( -4.401442555609581635E-16, 93.78125000204836681, -7.188101187500000044 ) ) ;
#65366 = CARTESIAN_POINT ( 'NONE',  ( 4.541265875000001451, 16.37499999863440436, 1.881053915767124440 ) ) ;
#65367 = CARTESIAN_POINT ( 'NONE',  ( -28.00000000000008171, 206.1250000027312126, 166.0000000000003695 ) ) ;
#65368 = CARTESIAN_POINT ( 'NONE',  ( -31.05507224581699077, -34.98990058138039672, 171.9999999999997726 ) ) ;
#65369 = ORIENTED_EDGE ( 'NONE', *, *, #62889, .F. ) ;
#65370 = VERTEX_POINT ( 'NONE', #32872 ) ;
#65371 = CARTESIAN_POINT ( 'NONE',  ( 6.676582343750001591, 293.1093750017069510, -8.176455196517173205E-16 ) ) ;
#65372 = CYLINDRICAL_SURFACE ( 'NONE', #32693, 8.000000000000000000 ) ;
#65373 = CARTESIAN_POINT ( 'NONE',  ( 5.676582343749993598, 169.9479166632526983, 9.832129032723422313 ) ) ;
#65374 = DIRECTION ( 'NONE',  ( -0.000000000000000000, 1.000000000000000000, 4.476705744456276341E-16 ) ) ;
#65375 = CARTESIAN_POINT ( 'NONE',  ( 1.656854249492405451, 200.3125000000000284, 202.0000000000000284 ) ) ;
#65376 = CARTESIAN_POINT ( 'NONE',  ( -1.468605411411171291, 19.93670996121496586, -1.118160017449583155 ) ) ;
#65377 = CARTESIAN_POINT ( 'NONE',  ( 7.204075437095966983, 7.204075437095967871, 110.9687500020483810 ) ) ;
#65378 = ORIENTED_EDGE ( 'NONE', *, *, #60070, .F. ) ;
#65379 = CARTESIAN_POINT ( 'NONE',  ( -11.50000000000000178, 82.00000000000001421, 20.00000000000000000 ) ) ;
#65380 = AXIS2_PLACEMENT_3D ( 'NONE', #4511, #33202, #22586 ) ;
#65381 = CARTESIAN_POINT ( 'NONE',  ( 2.449293598294707893E-16, 17.25000000000000000, -4.000000000000001776 ) ) ;
#65382 = CARTESIAN_POINT ( 'NONE',  ( -5.676582343750006032, 144.4270833299193555, 9.832129032723418760 ) ) ;
#65383 = CARTESIAN_POINT ( 'NONE',  ( -1.432654583217607858, 195.6250000013656063, 201.4587341250000065 ) ) ;
#65384 = CARTESIAN_POINT ( 'NONE',  ( -3.458734124999960358, 208.6250000013656063, 196.5673454167823877 ) ) ;
#65385 = CARTESIAN_POINT ( 'NONE',  ( 10.18810118750000093, -4.220049686691933033, 71.68750000204838102 ) ) ;
#65386 = CARTESIAN_POINT ( 'NONE',  ( 5.676582343749993598, 45.26041666325268409, 9.832129032723422313 ) ) ;
#65387 = VERTEX_POINT ( 'NONE', #22631 ) ;
#65388 = CARTESIAN_POINT ( 'NONE',  ( -25.17157287525374443, 208.7500000027312126, 172.8284271247464972 ) ) ;
#65389 = CARTESIAN_POINT ( 'NONE',  ( -3.211159895383561391, 3.812499998634407028, -3.211159895383561835 ) ) ;
#65390 = CARTESIAN_POINT ( 'NONE',  ( 5.662595241051934458, 5.662595241051935346, 9.450615283940630107 ) ) ;
#65391 = UNCERTAINTY_MEASURE_WITH_UNIT (LENGTH_MEASURE( 1.000000000000000082E-05 ), #57767, 'distance_accuracy_value', 'NONE');
#65392 = CIRCLE ( 'NONE', #19605, 12.00000000000000000 ) ;
#65393 = CARTESIAN_POINT ( 'NONE',  ( -7.188101187500001821, 14.62499999795161010, -2.977408999572651371 ) ) ;
#65394 = CARTESIAN_POINT ( 'NONE',  ( 2.485281374238571317, 290.7500000034139589, -6.000000000000003553 ) ) ;
#65395 = CARTESIAN_POINT ( 'NONE',  ( 1.110124581937998163E-11, 98.75000000000088107, 10.00000000000000533 ) ) ;
#65396 = CARTESIAN_POINT ( 'NONE',  ( 7.188101187500000044, 12.84374999795161187, 0.000000000000000000 ) ) ;
#65397 = CARTESIAN_POINT ( 'NONE',  ( -2.977408999572647819, 7.188101187499992051, 8.705302781871752771 ) ) ;
#65398 = CARTESIAN_POINT ( 'NONE',  ( 10.18810118749999916, 4.220049686691935698, 115.3750000020483810 ) ) ;
#65399 = LINE ( 'NONE', #36368, #42634 ) ;
#65400 = CARTESIAN_POINT ( 'NONE',  ( -4.000000000000001776, 2.249999997268813612, -4.898587196589415787E-16 ) ) ;
#65401 = VERTEX_POINT ( 'NONE', #51314 ) ;
#65402 = CARTESIAN_POINT ( 'NONE',  ( 4.000000000000015099, 195.6875000027312126, 196.3431457505076594 ) ) ;
#65403 = CARTESIAN_POINT ( 'NONE',  ( -4.000000000000015987, 201.4375000000000000, 140.3431457505076594 ) ) ;
#65404 = CARTESIAN_POINT ( 'NONE',  ( -31.99999999999995737, 199.4375000027312410, 171.6568542494928522 ) ) ;
#65405 = EDGE_CURVE ( 'NONE', #62362, #20933, #48809, .T. ) ;
#65406 = CARTESIAN_POINT ( 'NONE',  ( 3.211159895383561835, 0.4374999986344066949, -3.211159895383561835 ) ) ;
#65407 = CARTESIAN_POINT ( 'NONE',  ( -7.188101187500001821, 107.5625000020483810, -2.977408999572650483 ) ) ;
#65408 = CARTESIAN_POINT ( 'NONE',  ( 5.266666970006220083, -7.351593252548084045, -6.728829732988161894E-15 ) ) ;
#65409 = CARTESIAN_POINT ( 'NONE',  ( -7.999999999999991118, 3.313708498984756723, 3.924052783920144893 ) ) ;
#65410 = VERTEX_POINT ( 'NONE', #73218 ) ;
#65411 = CARTESIAN_POINT ( 'NONE',  ( -2.977408999572650039, 24.93749999795161543, -7.188101187500000933 ) ) ;
#65412 = ORIENTED_EDGE ( 'NONE', *, *, #35325, .T. ) ;
#65413 = CARTESIAN_POINT ( 'NONE',  ( -10.00000000000000178, 202.7083333333333144, 2.679491924311223183 ) ) ;
#65414 = CARTESIAN_POINT ( 'NONE',  ( -2.445694354108783664, 209.3125000013656063, 195.5543056458912190 ) ) ;
#65415 = CARTESIAN_POINT ( 'NONE',  ( 25.55430564589119058, 203.3125000013656063, 172.4456943541087526 ) ) ;
#65416 = CARTESIAN_POINT ( 'NONE',  ( -10.00000000000000000, 57.29166666666667140, -2.679491924311229845 ) ) ;
#65417 = CARTESIAN_POINT ( 'NONE',  ( -2.977408999572650927, 101.7500000020483810, -7.188101187500001821 ) ) ;
#65418 = MANIFOLD_SOLID_BREP ( 'EndChamfer', #69574 ) ;
#65419 = CARTESIAN_POINT ( 'NONE',  ( -3.673940397442060854E-16, 297.7500000000000000, -6.000000000000001776 ) ) ;
#65421 = DIRECTION ( 'NONE',  ( -0.000000000000000000, -1.000000000000000000, -0.000000000000000000 ) ) ;
#65420 = LINE ( 'NONE', #71436, #17714 ) ;
#65422 = EDGE_CURVE ( 'NONE', #62523, #71023, #65123, .T. ) ;
#65423 = ORIENTED_EDGE ( 'NONE', *, *, #29785, .F. ) ;
#65424 = CARTESIAN_POINT ( 'NONE',  ( 8.311093377946839666, 230.7812500034139589, 8.311093377946829008 ) ) ;
#65425 = CARTESIAN_POINT ( 'NONE',  ( -5.656854249492379694, 14.06250000000000178, -5.656854249492380582 ) ) ;
#65427 = EDGE_CURVE ( 'NONE', #36065, #43001, #61894, .T. ) ;
#65426 = CARTESIAN_POINT ( 'NONE',  ( 2.775557561562891351E-14, 210.0000000000000284, 198.0000000000000284 ) ) ;
#65428 = CARTESIAN_POINT ( 'NONE',  ( -2.751064625579944321E-14, 196.8750000027312126, 146.0000000000000284 ) ) ;
#65429 = DIRECTION ( 'NONE',  ( 0.000000000000000000, 0.000000000000000000, 1.000000000000000000 ) ) ;
#65430 = CYLINDRICAL_SURFACE ( 'NONE', #47493, 3.999999999999976019 ) ;
#65431 = CARTESIAN_POINT ( 'NONE',  ( 5.000000000000001776, 170.8333333333333428, -8.660254037844389075 ) ) ;
#65432 = CARTESIAN_POINT ( 'NONE',  ( 7.320508075688776373, 240.0000000068279462, 7.320508075688767491 ) ) ;
#65433 = CARTESIAN_POINT ( 'NONE',  ( -4.401442555609577197E-16, 7.188101187499992051, 26.98655278187175455 ) ) ;
#65434 = CARTESIAN_POINT ( 'NONE',  ( 8.311093377946837890, 136.7187499965860411, -8.311093377946837890 ) ) ;
#65435 = FACE_OUTER_BOUND ( 'NONE', #57748, .T. ) ;
#65436 = DIRECTION ( 'NONE',  ( 3.469446951953617147E-16, 0.000000000000000000, -1.000000000000000000 ) ) ;
#65439 = CARTESIAN_POINT ( 'NONE',  ( -4.242640687119285658, 294.1249999999999432, 4.242640687119287435 ) ) ;
#65438 = CARTESIAN_POINT ( 'NONE',  ( 5.000000000000001776, 107.7083333265053682, -8.660254037844389075 ) ) ;
#65437 = CARTESIAN_POINT ( 'NONE',  ( 27.99999999999997158, 208.0000000000000284, 173.9999999999999147 ) ) ;
#65440 = VERTEX_POINT ( 'NONE', #51686 ) ;
#65441 = AXIS2_PLACEMENT_3D ( 'NONE', #44368, #55702, #9290 ) ;
#65442 = CARTESIAN_POINT ( 'NONE',  ( -3.042071309553173730, 9.635416663252682312, 11.35316468749999785 ) ) ;
#65443 = CARTESIAN_POINT ( 'NONE',  ( -8.000000000000000000, 7.968749995903221972, -3.313708498984762496 ) ) ;
#65444 = CARTESIAN_POINT ( 'NONE',  ( -27.99999999999999645, 210.0000000000000284, 174.0000000000003411 ) ) ;
#65445 = DIRECTION ( 'NONE',  ( -0.000000000000000000, -0.000000000000000000, -1.000000000000000000 ) ) ;
#65446 = CARTESIAN_POINT ( 'NONE',  ( 3.458734124999958581, 206.5000000013655779, 140.5673454167823593 ) ) ;
#65447 = CARTESIAN_POINT ( 'NONE',  ( -5.123800378305636727, 124.6878826211476223, -5.902641312904766124 ) ) ;
#65448 = CARTESIAN_POINT ( 'NONE',  ( -7.320508075688778149, 39.99999999317201826, 7.320508075688769267 ) ) ;
#65449 = CARTESIAN_POINT ( 'NONE',  ( -2.977408999572651815, 110.9375000020483810, 7.188101187500000933 ) ) ;
#65450 = CARTESIAN_POINT ( 'NONE',  ( -3.211159895383561391, 2.812499998634407028, -3.211159895383561835 ) ) ;
#65451 = CARTESIAN_POINT ( 'NONE',  ( -10.99999999999992184, -31.99999999998497202, 140.5079502042485728 ) ) ;
#65452 = CARTESIAN_POINT ( 'NONE',  ( -4.898587196589407898E-16, 7.999999999999991118, 16.95530277982336287 ) ) ;
#65454 = CARTESIAN_POINT ( 'NONE',  ( -1.469576158976823947E-15, 24.93749999590322375, 8.000000000000000000 ) ) ;
#65453 = CARTESIAN_POINT ( 'NONE',  ( -9.999999999999998224, 238.3333333401612890, 2.679491924311235174 ) ) ;
#65455 = ORIENTED_EDGE ( 'NONE', *, *, #67155, .F. ) ;
#65456 =( BOUNDED_SURFACE ( )  B_SPLINE_SURFACE ( 1, 2, ( 
 ( #3605, #59831, #71875, #36455, #19455, #2487, #13417, #20944, #7781, #49240, #72255, #13777, #65848, #49625, #31150, #48126, #66224, #60192, #37941, #2858, #54925, #14158, #14529, #65106, #37191, #20569, #20189, #25846, #36821, #8513, #48866, #8146, #43208, #54182, #30786, #48496, #71132, #26603, #53806, #25479, #32285, #71500, #43583, #37567, #2116, #66598, #14903, #19824, #60941, #9262, #51481, #73749, #61320, #15277, #61693, #62425, #32666, #73010, #5105, #3991, #45445, #22056, #50734, #38314, #57155, #74492, #9645, #62058, #38691, #4355, #28473, #68461, #74123, #16762, #43965, #4728, #56784, #56409, #27723, #21319, #45083, #66974, #22425, #55675, #28096, #67727, #68098, #33046, #16024, #39787, #16386, #27346, #10383, #33785, #21686, #26980, #62790, #10015, #51111, #5471, #39426, #56046, #10750, #11132, #50362, #34155, #49994, #44342, #67352, #73381, #39057, #15650, #33409, #44712, #12600, #568, #29590, #941, #41649, #63542, #7321, #11867, #5847, #23923, #17897, #70325, #35267, #41282, #23551, #46932, #22800, #46563, #64292, #52603, #58282, #69208, #40910, #6584, #46191, #69957, #23181, #40168, #6217, #28840, #35997, #59014, #40536, #64659, #51859, #35626, #18267, #63173, #58640, #69584, #17520, #12957, #6948, #30326, #29960, #11499, #68831, #34903, #52973, #34532, #203, #1306, #57538, #24288, #47301, #18640, #17143, #53344, #45820, #57909, #63919, #29222, #52236, #12230, #66132, #71783, #43113, #1671, #19734, #25755, #71409, #48404, #30695, #65758, #26127, #20099, #47661, #48776, #8050, #42743, #19361, #31055, #14437, #14061, #65390, #2390, #2768, #59742, #59376, #37470, #48032, #60471, #3144, #37097, #71041, #60101, #54461, #42375, #8800, #31813, #7687, #8419, #13688, #54082, #13323, #31434, #54834, #36729, #24651, #65015, #70683, #36361, #25387, #42006, #25013, #2026, #19000, #53713, #18126, #59239, #23409, #1886, #46788, #429, #35853, #40398, #24872, #69069, #70546, #47154, #29077, #41504, #36221, #58499, #6448, #23784, #70186, #12457, #64520, #12818, #1164, #30556, #69810, #58141, #58868, #46424, #24516, #47521, #13183, #29818, #17374, #63396, #52097, #52460, #11722, #6070, #18495, #798, #34762, #69438, #7179, #53571, #29451, #6805, #41142, #17749, #64881, #24142, #57764, #7548, #30185, #53203, #40764, #1536, #18862, #41868, #52831, #64147, #63771, #12088, #35126, #35487, #2629, #14670, #42968, #31671, #65244, #42231, #60710, #55063, #36587 ),
 ( #59598, #2999, #8656, #26359, #32043, #38083, #36954, #13915, #19225, #9031, #59960, #7911, #37709, #3372, #13549, #43346, #25245, #61080, #14294, #48262, #49381, #37331, #55437, #20712, #30917, #25980, #53938, #25617, #2252, #9408, #19962, #72400, #43728, #60328, #71269, #8278, #19588, #66364, #32426, #42604, #54690, #65619, #31288, #54318, #70911, #3747, #48631, #66742, #15048, #71641, #65989, #49005, #47891, #72015, #20330, #58106, #34360, #6041, #41476, #57361, #35459, #63743, #1134, #29423, #18097, #51683, #28669, #47126, #64492, #23015, #52432, #18466, #46394, #11692, #5672, #41111, #28, #46022, #64118, #69043, #12425, #69780, #12792, #35824, #24490, #23381, #402, #17346, #70159, #69412, #40368, #24112, #58839, #63367, #29790, #34731, #47492, #769, #57736, #7150, #23755, #41842, #30155, #29046, #58472, #52065, #12061, #17718, #70516, #6417, #53172, #1510, #46757, #40733, #35096, #6782, #52800, #18835, #64851, #19929, #59209, #42199, #25217, #36193, #43699, #7519, #48972, #20299, #65214, #65588, #30525, #49352, #8627, #60297, #24844, #14638, #65960, #47862, #31639, #55034, #2599, #48233, #42575, #14264, #31259, #54660, #2968, #42939, #72369, #13887, #2221, #25953, #13519, #43317, #66334, #32015, #48605, #13155, #53542, #70883, #71241, #1858, #19197, #37301, #19561, #36557, #59570, #71986, #20680, #36926, #25589, #59934, #7885, #9000, #37681, #30890, #3341, #60681, #26331, #53908, #8246, #54288, #71608, #28492, #46214, #51882, #57933, #55783, #32775, #38052, #5865, #4099, #26717, #34551, #28861, #61052, #63188, #44080, #6240, #34173, #67092, #222, #57175, #589, #40559, #9374, #22823, #3718, #45463, #21057, #29244, #39809, #23202, #17540, #5491, #32394, #27092, #15389, #11519, #52256, #61429, #74512, #55409, #38425, #50108, #15016, #23572, #49737, #69230, #63561, #9756, #68479, #72753, #66714, #57556, #40185, #73122, #11888, #45839, #22444, #34922, #16782, #51500, #62813, #11149, #68854, #17166, #19020, #42026, #53365, #8073, #24309, #35647, #36379, #23943, #2045, #25032, #65409, #7340, #46581, #40933, #29611, #29977, #69603, #58300, #24670, #52995, #17917, #960, #59394, #31073, #58661, #36015, #6968, #46950, #42393, #1691, #54102, #36750, #47681, #30713, #52624, #70701, #13342, #69979, #70348, #63943, #18288, #53734, #12252, #65033, #1326, #7707, #41669, #30346, #35288, #6605, #48052, #71061, #41303, #64679, #19379, #47321, #64312, #12617 ),
 ( #13706, #18659, #2414, #59763, #12978, #59033, #25409, #60866, #38240, #37870, #9188, #2787, #55228, #32973, #55600, #71426, #61244, #49168, #32209, #14456, #72177, #26908, #3533, #8820, #43507, #15209, #3161, #8437, #49923, #43135, #9575, #61623, #49550, #66152, #72568, #66905, #37492, #32593, #3919, #31457, #20872, #60493, #20490, #37117, #14830, #72938, #54850, #21247, #42761, #43893, #65778, #48794, #48423, #25773, #54482, #38620, #44271, #66519, #15580, #71802, #55974, #26149, #20121, #67282, #19754, #14081, #60119, #9939, #26524, #31831, #57083, #23108, #45017, #63470, #68022, #61989, #5398, #74049, #51784, #16688, #22729, #5033, #28401, #4284, #28030, #45749, #34087, #39720, #50660, #22349, #62721, #27652, #11058, #4657, #21616, #62349, #10311, #17446, #40467, #21990, #46121, #33337, #17073, #51408, #44641, #74423, #51041, #73679, #69139, #68761, #11794, #40095, #67655, #50293, #16316, #63100, #15955, #56339, #11425, #38982, #5770, #34462, #57465, #73314, #34832, #45375, #39352, #27276, #28768, #10680, #132, #33713, #56715, #68390, #1602, #46491, #12161, #18933, #17824, #59309, #35926, #64592, #29150, #70978, #65319, #18199, #41939, #18568, #41212, #42302, #7617, #13257, #30624, #57839, #41578, #70613, #70256, #12890, #35196, #58943, #13623, #36293, #52168, #64947, #6879, #7249, #46863, #29890, #53646, #30259, #64220, #1236, #47590, #35559, #40838, #1956, #869, #24946, #19293, #53277, #23855, #24586, #47963, #69886, #6143, #499, #63847, #23479, #12528, #52902, #69512, #47228, #58212, #58571, #6514, #29521, #52531, #24214, #60028, #59672, #13986, #65686, #49833, #32499, #60401, #26820, #37026, #44180, #14367, #42673, #3442, #7983, #67194, #36662, #26430, #37400, #43417, #14742, #55511, #2697, #21156, #25685, #19661, #37782, #31740, #9484, #49076, #55136, #8728, #60778, #30989, #54761, #49457, #66432, #72089, #8346, #3070, #20403, #31362, #9103, #54390, #54009, #20028, #48703, #72852, #2321, #71711, #3823, #43041, #72476, #32117, #25316, #20783, #43803, #66818, #15120, #66060, #38150, #48332, #61153, #71340, #26054, #39265, #73961, #4566, #62265, #16981, #22265, #73589, #33622, #5309, #67934, #73224, #40008, #33250, #28312, #51693, #39637, #56249, #62634, #56996, #27562, #51321, #22638, #21530, #10966, #50572, #10593, #27187, #4943, #63011, #44927, #45658, #32879, #34002, #55883, #38895, #38528, #67565, #44553, #28679, #11335, #56628, #5680, #15862 ) ),
 .UNSPECIFIED., .F., .F., .F. ) 
 B_SPLINE_SURFACE_WITH_KNOTS ( ( 2, 1, 2 ),
 ( 3, 2, 2, 2, 2, 2, 2, 2, 2, 2, 2, 2, 2, 2, 2, 2, 2, 2, 2, 2, 2, 2, 2, 2, 2, 2, 2, 2, 2, 2, 2, 2, 2, 2, 2, 2, 2, 2, 2, 2, 2, 2, 2, 2, 2, 2, 2, 2, 2, 2, 2, 2, 2, 2, 2, 2, 2, 2, 2, 2, 2, 2, 2, 2, 2, 2, 2, 2, 2, 2, 2, 2, 2, 2, 2, 2, 2, 2, 2, 2, 2, 2, 2, 2, 2, 2, 2, 2, 2, 2, 2, 2, 2, 2, 2, 2, 2, 2, 2, 2, 2, 2, 2, 2, 2, 2, 2, 2, 2, 2, 2, 2, 2, 2, 2, 2, 2, 2, 2, 2, 2, 2, 2, 2, 2, 2, 2, 2, 2, 2, 2, 2, 2, 2, 2, 2, 2, 2, 2, 2, 2, 2, 2, 2, 2, 2, 2, 2, 2, 2, 2, 2, 3 ),
 ( -0.01000000000000000021, 0.000000000000000000, 1.000000000000000000 ),
 ( 0.000000000000000000, 0.006578947368421052266, 0.01315789473684210453, 0.01973684210526315680, 0.02631578947368420907, 0.03289473684210526133, 0.03947368421052631360, 0.04605263157894736586, 0.05263157894736841813, 0.05921052631578947040, 0.06578947368421052266, 0.07236842105263158187, 0.07894736842105262720, 0.08552631578947368640, 0.09210526315789473173, 0.09868421052631579093, 0.1052631578947368363, 0.1118421052631578955, 0.1184210526315789408, 0.1250000000000000000, 0.1315789473684210453, 0.1381578947368421184, 0.1447368421052631637, 0.1513157894736842091, 0.1578947368421052544, 0.1644736842105263275, 0.1710526315789473728, 0.1776315789473684181, 0.1842105263157894635, 0.1907894736842105365, 0.1973684210526315819, 0.2039473684210526272, 0.2105263157894736725, 0.2171052631578947456, 0.2236842105263157909, 0.2302631578947368363, 0.2368421052631578816, 0.2434210526315789547, 0.2500000000000000000, 0.2565789473684210731, 0.2631578947368420907, 0.2697368421052631637, 0.2763157894736842368, 0.2828947368421052544, 0.2894736842105263275, 0.2960526315789473450, 0.3026315789473684181, 0.3092105263157894912, 0.3157894736842105088, 0.3223684210526315819, 0.3289473684210526550, 0.3355263157894736725, 0.3421052631578947456, 0.3486842105263157632, 0.3552631578947368363, 0.3618421052631579093, 0.3684210526315789269, 0.3750000000000000000, 0.3815789473684210731, 0.3881578947368420907, 0.3947368421052631637, 0.4013157894736842368, 0.4078947368421052544, 0.4144736842105263275, 0.4210526315789473450, 0.4276315789473684181, 0.4342105263157894912, 0.4407894736842105088, 0.4473684210526315819, 0.4539473684210526550, 0.4605263157894736725, 0.4671052631578947456, 0.4736842105263157632, 0.4802631578947368363, 0.4868421052631579093, 0.4934210526315789269, 0.5000000000000000000, 0.5065789473684210176, 0.5131578947368421462, 0.5197368421052631637, 0.5263157894736841813, 0.5328947368421053099, 0.5394736842105263275, 0.5460526315789473450, 0.5526315789473684736, 0.5592105263157894912, 0.5657894736842105088, 0.5723684210526315264, 0.5789473684210526550, 0.5855263157894736725, 0.5921052631578946901, 0.5986842105263158187, 0.6052631578947368363, 0.6118421052631578538, 0.6184210526315789824, 0.6250000000000000000, 0.6315789473684210176, 0.6381578947368421462, 0.6447368421052631637, 0.6513157894736841813, 0.6578947368421053099, 0.6644736842105263275, 0.6710526315789473450, 0.6776315789473684736, 0.6842105263157894912, 0.6907894736842105088, 0.6973684210526315264, 0.7039473684210526550, 0.7105263157894736725, 0.7171052631578946901, 0.7236842105263158187, 0.7302631578947368363, 0.7368421052631578538, 0.7434210526315789824, 0.7500000000000000000, 0.7565789473684210176, 0.7631578947368421462, 0.7697368421052631637, 0.7763157894736841813, 0.7828947368421053099, 0.7894736842105263275, 0.7960526315789473450, 0.8026315789473684736, 0.8092105263157894912, 0.8157894736842105088, 0.8223684210526315264, 0.8289473684210526550, 0.8355263157894736725, 0.8421052631578946901, 0.8486842105263158187, 0.8552631578947368363, 0.8618421052631578538, 0.8684210526315789824, 0.8750000000000000000, 0.8815789473684210176, 0.8881578947368421462, 0.8947368421052631637, 0.9013157894736841813, 0.9078947368421053099, 0.9144736842105263275, 0.9210526315789473450, 0.9276315789473684736, 0.9342105263157894912, 0.9407894736842105088, 0.9473684210526315264, 0.9539473684210526550, 0.9605263157894736725, 0.9671052631578946901, 0.9736842105263158187, 0.9802631578947368363, 0.9868421052631578538, 0.9934210526315789824, 0.9940576549107595916 ),
 .UNSPECIFIED. ) 
 GEOMETRIC_REPRESENTATION_ITEM ( )  RATIONAL_B_SPLINE_SURFACE ( (
 ( 1.000000000000000000, 0.9238795325112867385, 1.000000000000000000, 0.9238795325112867385, 1.000000000000000000, 0.9238795325112867385, 1.000000000000000000, 0.9238795325112867385, 1.000000000000000000, 0.9238795325112867385, 1.000000000000000000, 0.9238795325112867385, 1.000000000000000000, 0.9238795325112867385, 1.000000000000000000, 0.9238795325112867385, 1.000000000000000000, 0.9238795325112867385, 1.000000000000000000, 0.9238795325112867385, 1.000000000000000000, 0.9238795325112867385, 1.000000000000000000, 0.9238795325112867385, 1.000000000000000000, 0.9238795325112867385, 1.000000000000000000, 0.9238795325112867385, 1.000000000000000000, 0.9238795325112867385, 1.000000000000000000, 0.9238795325112867385, 1.000000000000000000, 0.9238795325112867385, 1.000000000000000000, 0.9238795325112867385, 1.000000000000000000, 0.9238795325112867385, 1.000000000000000000, 0.9238795325112867385, 1.000000000000000000, 0.9238795325112867385, 1.000000000000000000, 0.9238795325112867385, 1.000000000000000000, 0.9238795325112867385, 1.000000000000000000, 0.9238795325112867385, 1.000000000000000000, 0.9238795325112867385, 1.000000000000000000, 0.9238795325112867385, 1.000000000000000000, 0.9238795325112867385, 1.000000000000000000, 0.9238795325112867385, 1.000000000000000000, 0.9238795325112867385, 1.000000000000000000, 0.9238795325112867385, 1.000000000000000000, 0.9238795325112867385, 1.000000000000000000, 0.9238795325112867385, 1.000000000000000000, 0.9238795325112867385, 1.000000000000000000, 0.9238795325112867385, 1.000000000000000000, 0.9238795325112867385, 1.000000000000000000, 0.9238795325112867385, 1.000000000000000000, 0.9238795325112867385, 1.000000000000000000, 0.9238795325112867385, 1.000000000000000000, 0.9238795325112867385, 1.000000000000000000, 0.9238795325112867385, 1.000000000000000000, 0.9238795325112867385, 1.000000000000000000, 0.9238795325112867385, 1.000000000000000000, 0.9238795325112867385, 1.000000000000000000, 0.9238795325112867385, 1.000000000000000000, 0.9238795325112867385, 1.000000000000000000, 0.9238795325112867385, 1.000000000000000000, 0.9238795325112867385, 1.000000000000000000, 0.9238795325112867385, 1.000000000000000000, 0.9238795325112867385, 1.000000000000000000, 0.9238795325112867385, 1.000000000000000000, 0.9238795325112867385, 1.000000000000000000, 0.9238795325112867385, 1.000000000000000000, 0.9238795325112867385, 1.000000000000000000, 0.9238795325112867385, 1.000000000000000000, 0.9238795325112867385, 1.000000000000000000, 0.9238795325112867385, 1.000000000000000000, 0.9238795325112867385, 1.000000000000000000, 0.9238795325112867385, 1.000000000000000000, 0.9238795325112867385, 1.000000000000000000, 0.9238795325112867385, 1.000000000000000000, 0.9238795325112867385, 1.000000000000000000, 0.9238795325112867385, 1.000000000000000000, 0.9238795325112867385, 1.000000000000000000, 0.9238795325112867385, 1.000000000000000000, 0.9238795325112867385, 1.000000000000000000, 0.9238795325112867385, 1.000000000000000000, 0.9238795325112867385, 1.000000000000000000, 0.9238795325112867385, 1.000000000000000000, 0.9238795325112867385, 1.000000000000000000, 0.9238795325112867385, 1.000000000000000000, 0.9238795325112867385, 1.000000000000000000, 0.9238795325112867385, 1.000000000000000000, 0.9238795325112867385, 1.000000000000000000, 0.9238795325112867385, 1.000000000000000000, 0.9238795325112867385, 1.000000000000000000, 0.9238795325112867385, 1.000000000000000000, 0.9238795325112867385, 1.000000000000000000, 0.9238795325112867385, 1.000000000000000000, 0.9238795325112867385, 1.000000000000000000, 0.9238795325112867385, 1.000000000000000000, 0.9238795325112867385, 1.000000000000000000, 0.9238795325112867385, 1.000000000000000000, 0.9238795325112867385, 1.000000000000000000, 0.9238795325112867385, 1.000000000000000000, 0.9238795325112867385, 1.000000000000000000, 0.9238795325112867385, 1.000000000000000000, 0.9238795325112867385, 1.000000000000000000, 0.9238795325112867385, 1.000000000000000000, 0.9238795325112867385, 1.000000000000000000, 0.9238795325112867385, 1.000000000000000000, 0.9238795325112867385, 1.000000000000000000, 0.9238795325112867385, 1.000000000000000000, 0.9238795325112867385, 1.000000000000000000, 0.9238795325112867385, 1.000000000000000000, 0.9238795325112867385, 1.000000000000000000, 0.9238795325112867385, 1.000000000000000000, 0.9238795325112867385, 1.000000000000000000, 0.9238795325112867385, 1.000000000000000000, 0.9238795325112867385, 1.000000000000000000, 0.9238795325112867385, 1.000000000000000000, 0.9238795325112867385, 1.000000000000000000, 0.9238795325112867385, 1.000000000000000000, 0.9238795325112867385, 1.000000000000000000, 0.9238795325112867385, 1.000000000000000000, 0.9238795325112867385, 1.000000000000000000, 0.9238795325112867385, 1.000000000000000000, 0.9238795325112867385, 1.000000000000000000, 0.9238795325112867385, 1.000000000000000000, 0.9238795325112867385, 1.000000000000000000, 0.9238795325112867385, 1.000000000000000000, 0.9238795325112867385, 1.000000000000000000, 0.9238795325112867385, 1.000000000000000000, 0.9238795325112867385, 1.000000000000000000, 0.9238795325112867385, 1.000000000000000000, 0.9238795325112867385, 1.000000000000000000, 0.9238795325112867385, 1.000000000000000000, 0.9238795325112867385, 1.000000000000000000, 0.9238795325112867385, 1.000000000000000000, 0.9238795325112867385, 1.000000000000000000, 0.9238795325112867385, 1.000000000000000000, 0.9238795325112867385, 1.000000000000000000, 0.9238795325112867385, 1.000000000000000000, 0.9238795325112867385, 1.000000000000000000, 0.9238795325112867385, 1.000000000000000000, 0.9238795325112867385, 1.000000000000000000, 0.9238795325112867385, 1.000000000000000000, 0.9238795325112867385, 1.000000000000000000, 0.9238795325112867385, 1.000000000000000000, 0.9238795325112867385, 1.000000000000000000, 0.9238795325112867385, 1.000000000000000000, 0.9238795325112867385, 1.000000000000000000, 0.9238795325112867385, 1.000000000000000000, 0.9238795325112867385, 1.000000000000000000, 0.9238795325112867385, 1.000000000000000000, 0.9238795325112867385, 1.000000000000000000, 0.9238795325112867385, 1.000000000000000000, 0.9238795325112867385, 1.000000000000000000, 0.9238795325112867385, 1.000000000000000000, 0.9238795325112867385, 1.000000000000000000, 0.9238795325112867385, 1.000000000000000000, 0.9238795325112867385, 1.000000000000000000, 0.9238795325112867385, 1.000000000000000000, 0.9238795325112867385, 1.000000000000000000, 0.9238795325112867385, 1.000000000000000000, 0.9238795325112867385, 1.000000000000000000, 0.9238795325112867385, 1.000000000000000000, 0.9238795325112867385, 1.000000000000000000, 0.9238795325112867385, 1.000000000000000000, 0.9238795325112867385, 1.000000000000000000, 0.9238795325112867385, 1.000000000000000000, 0.9238795325112867385, 1.000000000000000000, 0.9926343136094674113, 0.9866940870930933638),
 ( 1.000000000000000000, 0.9238795325112867385, 1.000000000000000000, 0.9238795325112867385, 1.000000000000000000, 0.9238795325112867385, 1.000000000000000000, 0.9238795325112867385, 1.000000000000000000, 0.9238795325112867385, 1.000000000000000000, 0.9238795325112867385, 1.000000000000000000, 0.9238795325112867385, 1.000000000000000000, 0.9238795325112867385, 1.000000000000000000, 0.9238795325112867385, 1.000000000000000000, 0.9238795325112867385, 1.000000000000000000, 0.9238795325112867385, 1.000000000000000000, 0.9238795325112867385, 1.000000000000000000, 0.9238795325112867385, 1.000000000000000000, 0.9238795325112867385, 1.000000000000000000, 0.9238795325112867385, 1.000000000000000000, 0.9238795325112867385, 1.000000000000000000, 0.9238795325112867385, 1.000000000000000000, 0.9238795325112867385, 1.000000000000000000, 0.9238795325112867385, 1.000000000000000000, 0.9238795325112867385, 1.000000000000000000, 0.9238795325112867385, 1.000000000000000000, 0.9238795325112867385, 1.000000000000000000, 0.9238795325112867385, 1.000000000000000000, 0.9238795325112867385, 1.000000000000000000, 0.9238795325112867385, 1.000000000000000000, 0.9238795325112867385, 1.000000000000000000, 0.9238795325112867385, 1.000000000000000000, 0.9238795325112867385, 1.000000000000000000, 0.9238795325112867385, 1.000000000000000000, 0.9238795325112867385, 1.000000000000000000, 0.9238795325112867385, 1.000000000000000000, 0.9238795325112867385, 1.000000000000000000, 0.9238795325112867385, 1.000000000000000000, 0.9238795325112867385, 1.000000000000000000, 0.9238795325112867385, 1.000000000000000000, 0.9238795325112867385, 1.000000000000000000, 0.9238795325112867385, 1.000000000000000000, 0.9238795325112867385, 1.000000000000000000, 0.9238795325112867385, 1.000000000000000000, 0.9238795325112867385, 1.000000000000000000, 0.9238795325112867385, 1.000000000000000000, 0.9238795325112867385, 1.000000000000000000, 0.9238795325112867385, 1.000000000000000000, 0.9238795325112867385, 1.000000000000000000, 0.9238795325112867385, 1.000000000000000000, 0.9238795325112867385, 1.000000000000000000, 0.9238795325112867385, 1.000000000000000000, 0.9238795325112867385, 1.000000000000000000, 0.9238795325112867385, 1.000000000000000000, 0.9238795325112867385, 1.000000000000000000, 0.9238795325112867385, 1.000000000000000000, 0.9238795325112867385, 1.000000000000000000, 0.9238795325112867385, 1.000000000000000000, 0.9238795325112867385, 1.000000000000000000, 0.9238795325112867385, 1.000000000000000000, 0.9238795325112867385, 1.000000000000000000, 0.9238795325112867385, 1.000000000000000000, 0.9238795325112867385, 1.000000000000000000, 0.9238795325112867385, 1.000000000000000000, 0.9238795325112867385, 1.000000000000000000, 0.9238795325112867385, 1.000000000000000000, 0.9238795325112867385, 1.000000000000000000, 0.9238795325112867385, 1.000000000000000000, 0.9238795325112867385, 1.000000000000000000, 0.9238795325112867385, 1.000000000000000000, 0.9238795325112867385, 1.000000000000000000, 0.9238795325112867385, 1.000000000000000000, 0.9238795325112867385, 1.000000000000000000, 0.9238795325112867385, 1.000000000000000000, 0.9238795325112867385, 1.000000000000000000, 0.9238795325112867385, 1.000000000000000000, 0.9238795325112867385, 1.000000000000000000, 0.9238795325112867385, 1.000000000000000000, 0.9238795325112867385, 1.000000000000000000, 0.9238795325112867385, 1.000000000000000000, 0.9238795325112867385, 1.000000000000000000, 0.9238795325112867385, 1.000000000000000000, 0.9238795325112867385, 1.000000000000000000, 0.9238795325112867385, 1.000000000000000000, 0.9238795325112867385, 1.000000000000000000, 0.9238795325112867385, 1.000000000000000000, 0.9238795325112867385, 1.000000000000000000, 0.9238795325112867385, 1.000000000000000000, 0.9238795325112867385, 1.000000000000000000, 0.9238795325112867385, 1.000000000000000000, 0.9238795325112867385, 1.000000000000000000, 0.9238795325112867385, 1.000000000000000000, 0.9238795325112867385, 1.000000000000000000, 0.9238795325112867385, 1.000000000000000000, 0.9238795325112867385, 1.000000000000000000, 0.9238795325112867385, 1.000000000000000000, 0.9238795325112867385, 1.000000000000000000, 0.9238795325112867385, 1.000000000000000000, 0.9238795325112867385, 1.000000000000000000, 0.9238795325112867385, 1.000000000000000000, 0.9238795325112867385, 1.000000000000000000, 0.9238795325112867385, 1.000000000000000000, 0.9238795325112867385, 1.000000000000000000, 0.9238795325112867385, 1.000000000000000000, 0.9238795325112867385, 1.000000000000000000, 0.9238795325112867385, 1.000000000000000000, 0.9238795325112867385, 1.000000000000000000, 0.9238795325112867385, 1.000000000000000000, 0.9238795325112867385, 1.000000000000000000, 0.9238795325112867385, 1.000000000000000000, 0.9238795325112867385, 1.000000000000000000, 0.9238795325112867385, 1.000000000000000000, 0.9238795325112867385, 1.000000000000000000, 0.9238795325112867385, 1.000000000000000000, 0.9238795325112867385, 1.000000000000000000, 0.9238795325112867385, 1.000000000000000000, 0.9238795325112867385, 1.000000000000000000, 0.9238795325112867385, 1.000000000000000000, 0.9238795325112867385, 1.000000000000000000, 0.9238795325112867385, 1.000000000000000000, 0.9238795325112867385, 1.000000000000000000, 0.9238795325112867385, 1.000000000000000000, 0.9238795325112867385, 1.000000000000000000, 0.9238795325112867385, 1.000000000000000000, 0.9238795325112867385, 1.000000000000000000, 0.9238795325112867385, 1.000000000000000000, 0.9238795325112867385, 1.000000000000000000, 0.9238795325112867385, 1.000000000000000000, 0.9238795325112867385, 1.000000000000000000, 0.9238795325112867385, 1.000000000000000000, 0.9238795325112867385, 1.000000000000000000, 0.9238795325112867385, 1.000000000000000000, 0.9238795325112867385, 1.000000000000000000, 0.9238795325112867385, 1.000000000000000000, 0.9238795325112867385, 1.000000000000000000, 0.9238795325112867385, 1.000000000000000000, 0.9238795325112867385, 1.000000000000000000, 0.9238795325112867385, 1.000000000000000000, 0.9238795325112867385, 1.000000000000000000, 0.9238795325112867385, 1.000000000000000000, 0.9238795325112867385, 1.000000000000000000, 0.9238795325112867385, 1.000000000000000000, 0.9238795325112867385, 1.000000000000000000, 0.9238795325112867385, 1.000000000000000000, 0.9238795325112867385, 1.000000000000000000, 0.9238795325112867385, 1.000000000000000000, 0.9238795325112867385, 1.000000000000000000, 0.9238795325112867385, 1.000000000000000000, 0.9238795325112867385, 1.000000000000000000, 0.9238795325112867385, 1.000000000000000000, 0.9238795325112867385, 1.000000000000000000, 0.9238795325112867385, 1.000000000000000000, 0.9238795325112867385, 1.000000000000000000, 0.9238795325112867385, 1.000000000000000000, 0.9238795325112867385, 1.000000000000000000, 0.9238795325112867385, 1.000000000000000000, 0.9926343136094674113, 0.9866940870930933638),
 ( 1.000000000000000000, 0.9238795325112867385, 1.000000000000000000, 0.9238795325112867385, 1.000000000000000000, 0.9238795325112867385, 1.000000000000000000, 0.9238795325112867385, 1.000000000000000000, 0.9238795325112867385, 1.000000000000000000, 0.9238795325112867385, 1.000000000000000000, 0.9238795325112867385, 1.000000000000000000, 0.9238795325112867385, 1.000000000000000000, 0.9238795325112867385, 1.000000000000000000, 0.9238795325112867385, 1.000000000000000000, 0.9238795325112867385, 1.000000000000000000, 0.9238795325112867385, 1.000000000000000000, 0.9238795325112867385, 1.000000000000000000, 0.9238795325112867385, 1.000000000000000000, 0.9238795325112867385, 1.000000000000000000, 0.9238795325112867385, 1.000000000000000000, 0.9238795325112867385, 1.000000000000000000, 0.9238795325112867385, 1.000000000000000000, 0.9238795325112867385, 1.000000000000000000, 0.9238795325112867385, 1.000000000000000000, 0.9238795325112867385, 1.000000000000000000, 0.9238795325112867385, 1.000000000000000000, 0.9238795325112867385, 1.000000000000000000, 0.9238795325112867385, 1.000000000000000000, 0.9238795325112867385, 1.000000000000000000, 0.9238795325112867385, 1.000000000000000000, 0.9238795325112867385, 1.000000000000000000, 0.9238795325112867385, 1.000000000000000000, 0.9238795325112867385, 1.000000000000000000, 0.9238795325112867385, 1.000000000000000000, 0.9238795325112867385, 1.000000000000000000, 0.9238795325112867385, 1.000000000000000000, 0.9238795325112867385, 1.000000000000000000, 0.9238795325112867385, 1.000000000000000000, 0.9238795325112867385, 1.000000000000000000, 0.9238795325112867385, 1.000000000000000000, 0.9238795325112867385, 1.000000000000000000, 0.9238795325112867385, 1.000000000000000000, 0.9238795325112867385, 1.000000000000000000, 0.9238795325112867385, 1.000000000000000000, 0.9238795325112867385, 1.000000000000000000, 0.9238795325112867385, 1.000000000000000000, 0.9238795325112867385, 1.000000000000000000, 0.9238795325112867385, 1.000000000000000000, 0.9238795325112867385, 1.000000000000000000, 0.9238795325112867385, 1.000000000000000000, 0.9238795325112867385, 1.000000000000000000, 0.9238795325112867385, 1.000000000000000000, 0.9238795325112867385, 1.000000000000000000, 0.9238795325112867385, 1.000000000000000000, 0.9238795325112867385, 1.000000000000000000, 0.9238795325112867385, 1.000000000000000000, 0.9238795325112867385, 1.000000000000000000, 0.9238795325112867385, 1.000000000000000000, 0.9238795325112867385, 1.000000000000000000, 0.9238795325112867385, 1.000000000000000000, 0.9238795325112867385, 1.000000000000000000, 0.9238795325112867385, 1.000000000000000000, 0.9238795325112867385, 1.000000000000000000, 0.9238795325112867385, 1.000000000000000000, 0.9238795325112867385, 1.000000000000000000, 0.9238795325112867385, 1.000000000000000000, 0.9238795325112867385, 1.000000000000000000, 0.9238795325112867385, 1.000000000000000000, 0.9238795325112867385, 1.000000000000000000, 0.9238795325112867385, 1.000000000000000000, 0.9238795325112867385, 1.000000000000000000, 0.9238795325112867385, 1.000000000000000000, 0.9238795325112867385, 1.000000000000000000, 0.9238795325112867385, 1.000000000000000000, 0.9238795325112867385, 1.000000000000000000, 0.9238795325112867385, 1.000000000000000000, 0.9238795325112867385, 1.000000000000000000, 0.9238795325112867385, 1.000000000000000000, 0.9238795325112867385, 1.000000000000000000, 0.9238795325112867385, 1.000000000000000000, 0.9238795325112867385, 1.000000000000000000, 0.9238795325112867385, 1.000000000000000000, 0.9238795325112867385, 1.000000000000000000, 0.9238795325112867385, 1.000000000000000000, 0.9238795325112867385, 1.000000000000000000, 0.9238795325112867385, 1.000000000000000000, 0.9238795325112867385, 1.000000000000000000, 0.9238795325112867385, 1.000000000000000000, 0.9238795325112867385, 1.000000000000000000, 0.9238795325112867385, 1.000000000000000000, 0.9238795325112867385, 1.000000000000000000, 0.9238795325112867385, 1.000000000000000000, 0.9238795325112867385, 1.000000000000000000, 0.9238795325112867385, 1.000000000000000000, 0.9238795325112867385, 1.000000000000000000, 0.9238795325112867385, 1.000000000000000000, 0.9238795325112867385, 1.000000000000000000, 0.9238795325112867385, 1.000000000000000000, 0.9238795325112867385, 1.000000000000000000, 0.9238795325112867385, 1.000000000000000000, 0.9238795325112867385, 1.000000000000000000, 0.9238795325112867385, 1.000000000000000000, 0.9238795325112867385, 1.000000000000000000, 0.9238795325112867385, 1.000000000000000000, 0.9238795325112867385, 1.000000000000000000, 0.9238795325112867385, 1.000000000000000000, 0.9238795325112867385, 1.000000000000000000, 0.9238795325112867385, 1.000000000000000000, 0.9238795325112867385, 1.000000000000000000, 0.9238795325112867385, 1.000000000000000000, 0.9238795325112867385, 1.000000000000000000, 0.9238795325112867385, 1.000000000000000000, 0.9238795325112867385, 1.000000000000000000, 0.9238795325112867385, 1.000000000000000000, 0.9238795325112867385, 1.000000000000000000, 0.9238795325112867385, 1.000000000000000000, 0.9238795325112867385, 1.000000000000000000, 0.9238795325112867385, 1.000000000000000000, 0.9238795325112867385, 1.000000000000000000, 0.9238795325112867385, 1.000000000000000000, 0.9238795325112867385, 1.000000000000000000, 0.9238795325112867385, 1.000000000000000000, 0.9238795325112867385, 1.000000000000000000, 0.9238795325112867385, 1.000000000000000000, 0.9238795325112867385, 1.000000000000000000, 0.9238795325112867385, 1.000000000000000000, 0.9238795325112867385, 1.000000000000000000, 0.9238795325112867385, 1.000000000000000000, 0.9238795325112867385, 1.000000000000000000, 0.9238795325112867385, 1.000000000000000000, 0.9238795325112867385, 1.000000000000000000, 0.9238795325112867385, 1.000000000000000000, 0.9238795325112867385, 1.000000000000000000, 0.9238795325112867385, 1.000000000000000000, 0.9238795325112867385, 1.000000000000000000, 0.9238795325112867385, 1.000000000000000000, 0.9238795325112867385, 1.000000000000000000, 0.9238795325112867385, 1.000000000000000000, 0.9238795325112867385, 1.000000000000000000, 0.9238795325112867385, 1.000000000000000000, 0.9238795325112867385, 1.000000000000000000, 0.9238795325112867385, 1.000000000000000000, 0.9238795325112867385, 1.000000000000000000, 0.9238795325112867385, 1.000000000000000000, 0.9238795325112867385, 1.000000000000000000, 0.9238795325112867385, 1.000000000000000000, 0.9238795325112867385, 1.000000000000000000, 0.9238795325112867385, 1.000000000000000000, 0.9238795325112867385, 1.000000000000000000, 0.9238795325112867385, 1.000000000000000000, 0.9238795325112867385, 1.000000000000000000, 0.9238795325112867385, 1.000000000000000000, 0.9238795325112867385, 1.000000000000000000, 0.9238795325112867385, 1.000000000000000000, 0.9238795325112867385, 1.000000000000000000, 0.9926343136094674113, 0.9866940870930933638) ) ) 
 REPRESENTATION_ITEM ( '' )  SURFACE ( )  );
#65457 = AXIS2_PLACEMENT_3D ( 'NONE', #62462, #51520, #74535 ) ;
#65458 = CARTESIAN_POINT ( 'NONE',  ( 4.242640687119285658, 292.6875000034139589, -4.242640687119286547 ) ) ;
#65459 = CARTESIAN_POINT ( 'NONE',  ( -11.00000000000003730, -4.556349186104013960, 115.0937500000000142 ) ) ;
#65460 = CARTESIAN_POINT ( 'NONE',  ( 11.35316468749999608, 226.9270833367473301, -3.042071309553167513 ) ) ;
#65461 = CARTESIAN_POINT ( 'NONE',  ( -3.042071309553173730, 129.3229166632526983, 11.35316468749999785 ) ) ;
#65462 = VERTEX_POINT ( 'NONE', #44174 ) ;
#65463 = DIRECTION ( 'NONE',  ( 1.000000000000000000, -0.000000000000000000, -0.000000000000000000 ) ) ;
#65464 = CARTESIAN_POINT ( 'NONE',  ( -7.204075437095967871, 7.204075437095967871, 92.96875000204838102 ) ) ;
#65465 = CARTESIAN_POINT ( 'NONE',  ( 4.556349186104045934, 11.00000000000000000, 86.21875000409680467 ) ) ;
#65466 = CARTESIAN_POINT ( 'NONE',  ( 2.445694354108839175, 197.3125000013656063, 195.5543056458912190 ) ) ;
#65467 = DIRECTION ( 'NONE',  ( -0.000000000000000000, 1.000000000000000000, 4.476705744456276341E-16 ) ) ;
#65469 = CARTESIAN_POINT ( 'NONE',  ( 5.676582343749993598, 109.9479166632526983, 9.832129032723422313 ) ) ;
#65468 = CARTESIAN_POINT ( 'NONE',  ( -5.656854249492380582, 94.81250000000000000, -5.656854249492380582 ) ) ;
#65470 = CARTESIAN_POINT ( 'NONE',  ( -23.99999999999997868, 208.6875000000000284, 171.6568542494927385 ) ) ;
#65471 = CARTESIAN_POINT ( 'NONE',  ( 10.00000000000000178, 82.08333332650535397, -2.679491924311226736 ) ) ;
#65472 = ORIENTED_EDGE ( 'NONE', *, *, #22123, .T. ) ;
#65473 = CARTESIAN_POINT ( 'NONE',  ( 5.000000000000001776, 212.7083333265053682, -8.660254037844389075 ) ) ;
#65474 = DIRECTION ( 'NONE',  ( 1.000000000000000000, -0.000000000000000000, -0.000000000000000000 ) ) ;
#65475 = CIRCLE ( 'NONE', #19678, 19.00000000000000000 ) ;
#65476 = CARTESIAN_POINT ( 'NONE',  ( -11.00000000000000000, 0.000000000000000000, 75.99999999999998579 ) ) ;
#65477 = CARTESIAN_POINT ( 'NONE',  ( 11.35316468750000141, 101.0937499965860127, 0.000000000000000000 ) ) ;
#65478 = CARTESIAN_POINT ( 'NONE',  ( -3.458734124999958581, 205.5000000013655779, 199.4326545832176976 ) ) ;
#65479 = CARTESIAN_POINT ( 'NONE',  ( -1.320432766682874540E-15, 10.96874999795161187, 7.188101187500000044 ) ) ;
#65480 = CARTESIAN_POINT ( 'NONE',  ( -10.18810118749999738, -4.220049686691941915, 89.12500000204836681 ) ) ;
#65481 = CARTESIAN_POINT ( 'NONE',  ( 8.311093377946834337, 10.46874999658601624, 8.311093377946839666 ) ) ;
#65483 = ORIENTED_EDGE ( 'NONE', *, *, #3618, .F. ) ;
#65482 =( BOUNDED_SURFACE ( )  B_SPLINE_SURFACE ( 1, 2, ( 
 ( #32390, #19192, #42194, #31635, #2595, #2217, #32011, #43314, #65210, #71236, #26327, #14635, #42571, #37677, #1854, #13516, #47857, #25584, #19926, #55030, #13882, #3337, #24840, #70878, #42936, #49347, #7882, #25212, #65956, #30887, #53905, #72365, #20676, #14261, #37297, #43695, #60293, #8622, #54654, #67458, #56521, #38420, #33894, #38795, #27087, #62905, #4837, #3714, #50102, #33520, #50466, #44446, #11236, #72747, #61422, #73116, #45189, #44818, #68200, #15755, #44075, #28207, #55404, #10487, #21052, #67830, #26712, #27834, #67086, #9751, #21423, #50843, #68571, #73480, #73857, #74229, #61798, #56895, #32770, #39159, #10115, #33154, #16497, #56148, #55777, #5208, #49732, #16876, #15383, #4093, #4463, #22163, #27451, #21788, #16121, #62162, #39536, #62532, #10858, #51220, #22535, #45556, #39899, #17629, #57267, #11979, #69320, #70074, #28953, #18009, #5582, #35379, #11603, #64033, #12705, #40648, #28580, #41025, #12345, #7063, #63652, #29701, #34638, #35010, #64766, #35735, #47410, #34263, #58025, #51588, #70433, #52716, #6332, #74605, #6695, #69695, #22918, #312, #47038, #58390, #1050, #24403, #18380, #64406, #58753, #30070, #51973, #57644, #24028, #41394, #53084, #29336, #1419, #18749, #41758, #45932, #23289, #68943, #52345, #682, #17254, #40274, #5953, #63275, #23667, #46300, #46673, #51135, #27747, #74145, #17170, #56434, #11523, #22082, #5870, #16787, #10774, #74519, #34178, #39814, #68120, #16414, #45107, #29250, #11894, #56808, #51887, #50758, #45844, #73774, #34557, #57562, #39447, #4755, #22828, #62819, #62446, #11154, #57180, #23578, #33435, #33811, #68859, #22449, #5129, #23208, #28867, #28121, #45469, #40565, #227, #68484, #46220, #6246, #5497, #62085, #28497, #51506, #69237, #40190, #63193, #52262, #10407, #17546, #63568, #34928, #57940, #595, #46588, #16048, #39080, #2052, #63949, #24317, #12622, #35293, #25039, #19386, #36022, #12259, #58306, #70355, #17924, #47328, #18666, #35653, #41677, #30720, #13349, #36387, #42399, #65040, #29984, #59771, #42033, #2421, #6974, #47687, #59402, #7716, #12985, #53741, #64686, #24677, #8080, #6611, #70708, #59040, #7347, #53002, #31081, #48060, #58668, #71068, #54109, #65416, #13713, #29618, #30354, #53375, #36758, #1698, #19027, #25415, #52631, #966, #1335, #40940, #69609, #23949, #46958, #64318, #69986, #18294, #41310, #25782, #3541, #26917, #8828, #19762, #32218, #55236, #21254, #31839, #43901, #48802, #54858, #4292, #49931, #61630, #48430, #3169, #71433, #9949, #66913, #49176, #42770, #20880, #9197, #65786, #14464, #61252, #26533, #49557, #38629, #9583, #3927, #72946, #44279, #43144, #71811, #72576, #55609, #15218, #20499, #38249, #67290, #32601, #32982, #37501, #15589, #26158, #43514, #55982, #8445, #20129, #60127, #14838, #14090, #72186, #37125, #31465, #66159, #66527, #54490, #2795, #60501, #37878, #60874, #27284, #63480, #22737, #28038, #50301, #74431, #62729, #73322, #68031, #40103, #57091, #5407, #17454, #63108, #57475, #28777, #5781, #21999, #4666, #11067, #34471, #34095, #74059, #28409, #51792, #11434, #40475, #16325, #51417, #10688, #22359, #140, #61997, #27661, #38992, #68398, #21625, #62357, #45757, #68770, #15963, #17081, #56347, #10319, #45025, #44649, #23116, #46129, #67664, #56723, #39360, #33345, #69147, #11802, #16696, #50668, #73686, #51049, #33721, #5041, #45383, #39727, #34840, #57847, #24594, #47599, #53654, #1610, #41220, #70621, #36671, #18576, #23487, #35934, #64228, #6522, #13265, #18941, #46499, #52539, #30632, #41947, #877, #64955, #70987, #69519, #52176, #35566, #12536, #36302, #69895, #7258, #19303, #508, #58579, #1964, #63855, #29529, #6887, #12170, #35204, #59319, #30269, #17833, #23863, #53285, #42313, #7625, #58221, #18207, #24955, #46873, #47972, #29898, #52911, #13633, #65328, #29158, #1245, #58951, #40847, #24223, #47236, #6152, #70264, #41586, #64601, #12898, #25326, #15129, #9494, #26064, #54020, #2330, #60411, #7992, #14376, #8737, #2706, #31750, #20792, #3451, #26440, #32508, #55146, #60787, #8355, #37410, #38161, #71720, #37791, #49465, #72485, #3080, #43812, #54770, #14750, #49842, #48342, #9111, #49085, #72098, #20036, #72861, #66827, #48714, #61163, #21166, #55520, #3832, #71349, #20412, #43428, #26828, #66442, #32127, #44190, #19671, #42683, #43050, #30997, #67203, #66069, #15501, #54399, #59681, #65695, #13995, #37036, #60037, #31372, #25694, #9862, #22277, #45299, #11346, #73599, #34012, #38904, #21906, #69061, #40019, #51703, #38538, #44936, #61539, #49, #57007, #39275, #32890, #10977, #73971, #55892, #4575, #51331, #68313, #16610, #28689, #74340, #68683, #63021, #16992, #33259, #15872, #39647, #45668, #62644, #10604, #5320, #34381, #22648, #23033, #27573, #28322, #67944, #33632, #57381, #73233, #61907, #50212, #4953, #4206, #16238, #5691, #46042, #27196, #21539, #67575, #44563, #10231, #56259, #62276, #50581, #56638, #27953, #50958, #18855, #30547, #47884, #52453, #17366, #53563, #12812, #18118, #40390, #64514, #52821, #63388, #58131, #30177, #47147, #70179, #7541, #53194, #47514, #41862, #70540, #12081, #69430, #1156, #24510, #24134, #64139, #18488, #64873, #1530, #1879, #6440, #41498, #791, #12447, #13176, #52089, #17739, #29068, #58493, #11712, #23775, #35846, #58860, #6062, #7172, #46416, #421, #35117, #34752, #36212, #59229, #57757, #46778, #29442, #23401, #24865, #40754, #6799, #63763, #69802, #41132, #35479, #29811, #71631, #13909, #19953, #33087, #15692, #38734, #44754, #67390, #72006, #19580, #25611, #27386, #8268, #48996, #61732, #10050, #14285, #56084, #48624, #25973, #62098, #65235, #20321, #42962, #65981, #31282, #10421, #4393, #59953, #50405, #33451, #73419, #21724, #36578, #31662, #60320, #67767, #37323, #2989, #43337, #13539, #53930, #54310, #19218, #8648, #2621, #16061, #65610, #54683, #42223, #39095, #48254, #56451, #4769, #27761, #59591, #7904, #70903, #30910, #2243, #25237, #36948, #71261, #42595, #69250, #17560, #23592, #46233, #51901, #74158, #5510, #6261, #62833, #28882, #40578, #63580, #68874, #34941, #28510, #5884, #40954, #45121, #242, #22845, #45858, #11169, #63963, #11908, #39829, #57953, #12274, #29264, #52276, #16428, #11536, #40204, #612, #17184, #57575, #23222, #68133, #33825, #34192, #73787, #51519, #57195, #46601, #45482, #34568, #22096, #69624, #28136, #17938, #35308, #74534, #39464, #58320, #6627, #50773, #63207, #62461, #51150, #10790, #56822, #5143, #22462, #68501, #16801, #29631, #65800, #25053, #30369, #52644, #2065, #65053, #980, #70367, #42412, #59415, #7728, #19775, #65431, #59783, #31095, #8092, #24330, #6991, #13363, #36771, #36402, #1713, #30735, #54124, #13726, #42783, #18682, #53753, #12999, #24691, #2435, #64332, #30002, #41323, #70722, #23963, #64701, #48074, #71082, #18309, #19400, #58682, #12637, #47341, #46970, #25428, #48444, #70000, #59053, #41689, #35668, #71447, #14105, #19042, #53015, #37138, #1347, #36037, #60140, #7361, #53387, #47702, #42046, #9596, #48817, #3939, #14478, #72962, #9212, #3184, #66927, #26547, #32232, #60516, #8842, #37517, #21639, #4308, #49190, #44291, #20142, #38263, #43159, #26928, #49947, #31852, #71824, #15231, #55250, #54875, #60890, #21267, #39006, #20894, #25797, #61266, #43528, #26171, #15603, #67304, #66174, #72201, #32994, #38642, #20513, #61644, #73335, #66543, #54503, #37892, #14852, #9962, #3557, #32615, #44664, #2809, #49571, #55994, #72589, #43916, #55623, #27298, #50314, #67679, #15976, #8460, #31480, #34484, #23501, #57490, #45038, #74072, #63121, #68047, #40489, #45394, #33734, #69534, #11447, #10334, #56736, #40115, #57104, #51060, #17846, #4679, #16337, #5055, #51808, #51430, #155, #22373, #50681, #34854, #62009, #17093, #27675, #74442, #33359, #5795, #73699, #39375, #28050, #28792, #521, #5418, #23131, #6166, #68410, #63494, #62373, #45772, #16710, #39740, #46143, #62740, #10700, #11816, #56360, #46516, #22012, #11080, #34107, #28423, #22749, #68783, #69160, #17469, #57860, #29175, #52190, #35218, #41601, #63869, #70278, #64616, #58594, #12912, #1977, #59331, #7641, #13645, #36315, #41959, #64242, #18590, #70998, #52926, #18955, #30647, #53665, #58965, #24969, #35946, #70636, #31010, #58237, #64966, #7272, #30280, #1259, #54035, #47985, #29911, #19314, #2345, #42325, #65343, #6536, #1625, #53300, #36683, #24605, #47612, #13276, #29542, #23877, #24237, #12181, #59695, #47251, #8003, #35580, #25340, #52553, #48354, #18221, #71360, #40862, #892, #46887, #69910, #41236, #12552, #6900, #15145, #20049, #3094, #50228, #21181, #32906, #19685, #54783, #42695, #55911, #38177, #20426, #65707, #66842, #55162, #14012, #60426, #32525, #49481, #72500, #9878, #55538, #49859, #44207, #72877, #14392 ),
 ( #31386, #26079, #20809, #60049, #61180, #25707, #9511, #43442, #37426, #3467, #37804, #66457, #71734, #43066, #48727, #4223, #15515, #8753, #3848, #54412, #43827, #2719, #26844, #67219, #66082, #8370, #26456, #14766, #31763, #72113, #38556, #37048, #32141, #49100, #61557, #60800, #9125, #27211, #40034, #15889, #44953, #23047, #11361, #67960, #34396, #63405, #38921, #44580, #27969, #4968, #68698, #62292, #74354, #11731, #67593, #56653, #46058, #56274, #73616, #50974, #4593, #27587, #57397, #22664, #61923, #16253, #45683, #34771, #17008, #50597, #10620, #63037, #21922, #51718, #73988, #39291, #6078, #5705, #21554, #33647, #51344, #68329, #22291, #29086, #10248, #45314, #16626, #28704, #62659, #65, #39661, #33275, #69077, #73249, #28337, #10993, #34026, #57023, #17383, #5336, #40407, #57774, #47530, #65253, #70196, #1545, #70920, #58509, #30564, #58150, #35862, #64156, #6814, #41878, #29827, #35134, #1894, #59607, #13558, #52106, #40772, #46797, #24524, #17758, #63780, #12827, #53211, #12465, #41151, #70555, #36597, #46433, #35496, #24881, #6457, #52470, #52839, #29460, #806, #64890, #18871, #12097, #69819, #13191, #7920, #36229, #23793, #1172, #59246, #18135, #53580, #24151, #47164, #439, #7557, #23418, #18504, #30194, #41513, #64529, #69447, #58877, #7188, #47900, #19233, #42240, #43737, #19971, #19597, #3756, #30925, #60718, #71278, #20338, #2260, #9039, #42613, #13924, #48640, #26368, #44121, #49014, #55072, #49775, #37339, #9417, #36963, #14679, #42977, #60337, #20720, #8665, #59969, #55446, #38464, #67130, #53947, #65627, #25626, #3381, #8287, #31297, #66372, #32052, #65998, #54327, #14303, #49390, #2638, #72409, #71650, #66751, #31680, #54699, #37718, #72024, #3008, #25990, #43355, #15057, #15425, #26757, #38091, #61088, #32435, #72791, #21098, #61467, #25254, #48271, #73160, #16537, #33562, #15802, #62205, #28253, #40317, #22206, #27130, #39578, #44865, #10159, #16924, #51261, #50145, #56193, #34309, #22580, #4505, #45600, #63464, #21468, #55822, #39203, #16162, #5253, #56937, #45233, #32814, #50511, #68615, #62573, #10904, #22968, #39947, #62952, #11277, #57313, #27498, #61840, #68245, #5624, #33938, #56566, #74271, #28624, #51637, #45975, #73525, #68990, #67870, #4881, #17299, #44490, #33196, #67503, #50887, #4140, #10530, #9792, #38837, #21832, #27876, #73901, #23334, #58064, #34682, #35780, #70476, #57688, #18051, #6375, #28998, #18794, #13110, #29741, #5996, #52016, #64076, #11647, #41066, #12384, #29381, #35419, #24444, #7105, #30113, #36146, #58795, #64448, #12019, #58429, #41799, #724, #41436, #53130, #1463, #6737, #47452, #52756, #18422, #53498, #354, #12749, #1092, #24069, #23707, #1815, #64808, #52388, #59167, #24801, #7476, #30481, #46346, #47079, #70116, #47815, #70838, #19150, #63321, #69363, #17673, #46711, #40690, #63692, #69736, #35052, #36883, #25909, #65166, #43271, #19513, #71939, #20633, #2550, #13477, #48926, #20251, #14967, #25541, #37632, #42531, #48554, #72704, #43649, #55361, #42153, #71563, #36516, #3667, #60630, #42892, #59525, #65911, #7838, #14593, #2921, #30843, #8204, #54989, #66286, #8952, #32348, #3296, #72320, #66660, #38004, #59891, #65545, #31964, #49303, #26282, #14217, #61002, #9328, #26666, #49690, #31216, #53864, #19886, #37256, #2176, #25170, #13838, #48187, #8577, #71194, #60251, #54241, #31593, #54614, #68154, #50056, #55736, #15714, #67040, #16452, #28161, #15340, #50426, #38756, #61380, #51171, #45506, #62119, #38375, #9707, #21748, #44032, #73440, #44775, #61756, #67790, #56846, #39488, #62484, #68524, #10813, #22118, #44402, #16081, #74181, #33109, #73811, #33848, #5166, #39116, #22485, #10444, #50798, #11190, #32728, #45143, #33474, #56476, #56105, #34216, #16826, #10074, #39854, #57218, #62855, #5532, #4052, #4792, #27785, #28533, #51541, #21006, #27045, #73072, #21378, #4414, #67415, #27410, #34962, #36702, #69273, #59348, #22870, #1995, #51925, #30666, #54054, #57977, #45883, #7660, #53685, #48374, #6282, #71017, #263, #29289, #31404, #2364, #14030, #74558, #52299, #68898, #37068, #19332, #63984, #8021, #46626, #24987, #48003, #17207, #57597, #635, #40227, #23616, #69646, #59713, #17584, #42346, #63230, #65363, #23246, #13661, #25359, #17959, #11557, #31029, #71379, #19703, #40978, #42715, #46254, #13296, #34590, #65727, #60069, #5907, #36334, #28907, #8390, #40602, #63603, #11930, #26863, #15164, #2737, #20445, #67239, #9529, #32544, #44598, #15534, #9895, #55930, #32925, #49119, #31782, #38196, #61575, #61199, #26476, #55555, #4242, #38575, #67610, #43461, #3868, #37824, #49501, #27229, #14411, #54804, #66101, #20828, #25725, #14784, #49878, #72893, #43085, #21200, #8772, #37444, #72131, #48746, #44226, #50245, #71753, #9143, #66476, #20067, #73267, #21572, #43845, #60442, #3114, #55181, #26098, #32160, #3486, #60819, #72519, #15907, #38939, #61940, #10267, #54431, #66858, #56670, #62676, #63421, #45332, #11379, #23065, #87, #51362, #17400, #11011, #63055, #23434, #27604, #34413, #5352, #28354, #68347, #46449, #46074, #22307, #28722, #69466, #51737, #40423, #73635, #68715, #57416, #56292, #27988, #5722, #74372, #16644, #40789, #50616, #39312, #50992, #69093, #22683, #11749, #39677, #21941, #6098, #33294, #34787, #44970, #45701, #4609, #57790, #67976, #16271, #74004, #29104, #17775, #17026, #52123, #455, #34046, #63795, #62310, #40051, #57041, #10637, #33665, #4987, #69838, #36613, #19615, #25270, #12114, #824, #6832, #59262, #52486, #23810, #47548, #13209, #47181, #46813, #70213, #36247, #18152, #7574, #41167, #1912, #12842, #29845, #70572, #30209, #35879, #64178, #12482, #35512, #48289, #7938, #52856, #47916, #58525, #41894, #1188, #30578, #53600, #24169, #18522, #18888, #58897, #41530, #64546, #24899, #42629, #24540, #29476, #64904, #7206, #53229, #19247, #70935, #1561, #42259, #59623, #65270, #13575, #30943, #2276, #53964, #58168, #71296, #35152, #6473, #54716, #66768, #4156, #59986, #49030, #38480, #48656, #66013, #43372, #71665, #19985, #3772, #15072, #31313, #60353, #38106, #27145, #61105, #42994, #3022, #9434, #14319, #44138, #72038, #37353, #73178, #20736, #67149, #49792, #55840, #26006, #32452, #20354, #37735, #72806, #25642, #8680, #2652, #32069, #13940, #66388, #49406, #43754, #54341, #55462, #31695, #14695, #60734, #36981, #26774, #21115, #8302, #9056, #55091, #3398, #15443, #61483, #26382, #72427, #9808, #32830, #50162, #21486, #65643, #67887, #27892, #68630, #51276, #74286, #34325, #22596, #33955, #21850, #56582, #39964, #62221, #56952, #45616, #16939, #22221, #62969, #4896, #10920, #28638, #38852, #5269, #50903, #73917, #10547, #51652, #11293, #39221, #57327, #11677, #5638, #22983, #61856, #39593, #68260, #45989, #45248, #62588, #28269, #15817, #56208, #33579, #67518, #16555, #69005, #44507, #10176, #33211, #27516, #4521, #50527, #73542, #44882, #16178, #8540, #20968, #43992, #10038, #72281, #32691, #37592, #20593, #67755, #38719, #50390, #37218, #43609, #60216, #73406, #55700, #37969, #31554, #9671, #72666, #54578, #3259, #50019, #67002, #15301, #27371, #73034, #67378, #61717, #15677, #31928, #14555, #38338, #44365, #61344, #9288, #4016, #33073, #66622, #27006, #60591, #14927, #2883, #56069, #21710, #25871, #60968, #48890, #44737, #21345, #32310, #71902, #4378, #20215, #43235, #26247, #66250, #8916, #54950, #49266, #55325, #3630, #26627, #49650, #34671, #5612, #40679, #45219, #22955, #51249, #68601, #28986, #16910, #22194, #63681, #46700, #52375, #39188, #27864, #33926, #11634, #4869, #50874, #74640, #40306, #74258, #73890, #22566, #63307, #68229, #57674, #16526, #52004, #39934, #56925, #45963, #57300, #62940, #39565, #62561, #10892, #712, #35039, #5240, #341, #28241, #68978, #45587, #5982, #23322, #11265, #34296, #17287, #28611, #51622, #46334, #69350, #69725, #17659, #56554, #12008, #58053, #6364, #29369, #23695, #62192, #10518, #33550, #30830, #64437, #53852, #8193, #35409, #64063, #47439, #24433, #13465, #7093, #19138, #31203, #12373, #1452, #65535, #1080, #18409, #70465, #24058, #47067, #2165, #42142, #58418, #12736, #65155, #54229, #36503, #70105, #30101, #59514, #41425, #71184, #18782, #35767, #25530, #7827, #58784, #25159, #2538, #48176, #53119, #41785, #19503, #64796, #42519, #13098, #36135, #48543, #13826, #41055, #59155, #70826, #7465, #30470, #18040, #6725, #53487, #1803, #36871, #24790, #59878, #47803, #29731, #52746, #71552, #26654, #37243, #60991, #42880, #49677, #8565, #54603, #14583, #67029, #10063, #14955, #66647, #15326, #37993, #73061, #2910, #55350, #8941, #26271, #61370, #49291, #25896, #21367, #4405, #33100, #19875, #60240, #66275, #44019, #31580, #48915, #32338, #72692, #31953, #71927, #54977 ) ),
 .UNSPECIFIED., .F., .F., .F. ) 
 B_SPLINE_SURFACE_WITH_KNOTS ( ( 2, 2 ),
 ( 3, 2, 2, 2, 2, 2, 2, 2, 2, 2, 2, 2, 2, 2, 2, 2, 2, 2, 2, 2, 2, 2, 2, 2, 2, 2, 2, 2, 2, 2, 2, 2, 2, 2, 2, 2, 2, 2, 2, 2, 2, 2, 2, 2, 2, 2, 2, 2, 2, 2, 2, 2, 2, 2, 2, 2, 2, 2, 2, 2, 2, 2, 2, 2, 2, 2, 2, 2, 2, 2, 2, 2, 2, 2, 2, 2, 2, 2, 2, 2, 2, 2, 2, 2, 2, 2, 2, 2, 2, 2, 2, 2, 2, 2, 2, 2, 2, 2, 2, 2, 2, 2, 2, 2, 2, 2, 2, 2, 2, 2, 2, 2, 2, 2, 2, 2, 2, 2, 2, 2, 2, 2, 2, 2, 2, 2, 2, 2, 2, 2, 2, 2, 2, 2, 2, 2, 2, 2, 2, 2, 2, 2, 2, 2, 2, 2, 2, 2, 2, 2, 2, 2, 2, 2, 2, 2, 2, 2, 2, 2, 2, 2, 2, 2, 2, 2, 2, 2, 2, 2, 2, 2, 2, 2, 2, 2, 2, 2, 2, 2, 2, 2, 2, 2, 2, 2, 2, 2, 2, 2, 2, 2, 2, 2, 2, 2, 2, 2, 2, 2, 2, 2, 2, 2, 2, 2, 2, 2, 2, 2, 2, 2, 2, 2, 2, 2, 2, 2, 2, 2, 2, 2, 2, 2, 2, 2, 2, 2, 2, 2, 2, 2, 2, 2, 2, 2, 2, 2, 2, 2, 2, 2, 2, 2, 2, 2, 2, 2, 2, 2, 2, 2, 2, 2, 2, 2, 2, 2, 2, 2, 2, 2, 2, 2, 2, 2, 2, 2, 2, 2, 2, 2, 2, 2, 2, 2, 2, 2, 2, 2, 2, 2, 2, 2, 2, 2, 2, 2, 2, 2, 2, 2, 2, 2, 2, 2, 2, 2, 2, 2, 2, 2, 2, 2, 2, 2, 2, 2, 2, 2, 2, 2, 2, 2, 2, 2, 2, 2, 2, 2, 2, 2, 2, 2, 2, 2, 2, 2, 2, 2, 2, 2, 2, 2, 2, 2, 2, 2, 2, 2, 2, 2, 2, 2, 2, 2, 2, 2, 2, 2, 2, 2, 2, 2, 2, 2, 2, 2, 2, 2, 2, 2, 2, 2, 2, 2, 2, 2, 2, 2, 2, 2, 2, 2, 2, 2, 2, 2, 2, 2, 2, 2, 2, 2, 2, 2, 2, 2, 2, 2, 2, 2, 2, 2, 2, 2, 2, 2, 2, 2, 2, 2, 2, 2, 2, 2, 2, 2, 2, 2, 2, 2, 2, 2, 2, 2, 2, 2, 2, 2, 2, 2, 2, 2, 2, 2, 2, 2, 2, 2, 2, 2, 2, 2, 2, 2, 2, 2, 2, 2, 2, 2, 2, 2, 2, 2, 2, 2, 2, 2, 2, 2, 2, 2, 2, 2, 2, 2, 2, 2, 2, 2, 2, 2, 2, 2, 2, 2, 2, 2, 2, 2, 2, 2, 2, 2, 2, 2, 2, 2, 2, 2, 2, 2, 2, 2, 2, 2, 2, 2, 2, 2, 2, 2, 2, 2, 2, 2, 2, 2, 2, 2, 2, 2, 2, 2, 2, 2, 2, 2, 2, 2, 2, 2, 2, 2, 2, 2, 2, 2, 2, 2, 2, 2, 2, 2, 2, 2, 2, 2, 2, 2, 2, 2, 2, 2, 2, 2, 2, 2, 2, 2, 2, 2, 3 ),
 ( 0.000000000000000000, 1.000000000000000000 ),
 ( 0.000000000000000000, 0.001811594202898550747, 0.003623188405797101493, 0.005434782608695652023, 0.007246376811594202987, 0.009057971014492753950, 0.01086956521739130405, 0.01268115942028985588, 0.01449275362318840597, 0.01630434782608695607, 0.01811594202898550790, 0.01992753623188405626, 0.02173913043478260809, 0.02355072463768115992, 0.02536231884057971175, 0.02717391304347826012, 0.02898550724637681195, 0.03079710144927536378, 0.03260869565217391214, 0.03442028985507246397, 0.03623188405797101580, 0.03804347826086956763, 0.03985507246376811252, 0.04166666666666666435, 0.04347826086956521618, 0.04528985507246376802, 0.04710144927536231985, 0.04891304347826087168, 0.05072463768115942351, 0.05253623188405796840, 0.05434782608695652023, 0.05615942028985507206, 0.05797101449275362389, 0.05978260869565217572, 0.06159420289855072755, 0.06340579710144927938, 0.06521739130434782428, 0.06702898550724638305, 0.06884057971014492794, 0.07065217391304347283, 0.07246376811594203160, 0.07427536231884057649, 0.07608695652173913526, 0.07789855072463768015, 0.07971014492753622505, 0.08152173913043478382, 0.08333333333333332871, 0.08514492753623188748, 0.08695652173913043237, 0.08876811594202899114, 0.09057971014492753603, 0.09239130434782608092, 0.09420289855072463969, 0.09601449275362318458, 0.09782608695652174335, 0.09963768115942028825, 0.1014492753623188470, 0.1032608695652173919, 0.1050724637681159368, 0.1068840579710144956, 0.1086956521739130405, 0.1105072463768115992, 0.1123188405797101441, 0.1141304347826086890, 0.1159420289855072478, 0.1177536231884057927, 0.1195652173913043514, 0.1213768115942028963, 0.1231884057971014551, 0.1250000000000000000, 0.1268115942028985588, 0.1286231884057970898, 0.1304347826086956486, 0.1322463768115942073, 0.1340579710144927661, 0.1358695652173912971, 0.1376811594202898559, 0.1394927536231884146, 0.1413043478260869457, 0.1431159420289855044, 0.1449275362318840632, 0.1467391304347826220, 0.1485507246376811530, 0.1503623188405797118, 0.1521739130434782705, 0.1539855072463768015, 0.1557971014492753603, 0.1576086956521739191, 0.1594202898550724501, 0.1612318840579710089, 0.1630434782608695676, 0.1648550724637681264, 0.1666666666666666574, 0.1684782608695652162, 0.1702898550724637750, 0.1721014492753623060, 0.1739130434782608647, 0.1757246376811594235, 0.1775362318840579823, 0.1793478260869565133, 0.1811594202898550721, 0.1829710144927536308, 0.1847826086956521618, 0.1865942028985507206, 0.1884057971014492794, 0.1902173913043478382, 0.1920289855072463692, 0.1938405797101449279, 0.1956521739130434867, 0.1974637681159420177, 0.1992753623188405765, 0.2010869565217391353, 0.2028985507246376940, 0.2047101449275362250, 0.2065217391304347838, 0.2083333333333333426, 0.2101449275362318736, 0.2119565217391304324, 0.2137681159420289911, 0.2155797101449275499, 0.2173913043478260809, 0.2192028985507246397, 0.2210144927536231985, 0.2228260869565217295, 0.2246376811594202882, 0.2264492753623188470, 0.2282608695652173780, 0.2300724637681159368, 0.2318840579710144956, 0.2336956521739130543, 0.2355072463768115854, 0.2373188405797101441, 0.2391304347826087029, 0.2409420289855072339, 0.2427536231884057927, 0.2445652173913043514, 0.2463768115942029102, 0.2481884057971014412, 0.2500000000000000000, 0.2518115942028985588, 0.2536231884057971175, 0.2554347826086956763, 0.2572463768115941796, 0.2590579710144927383, 0.2608695652173912971, 0.2626811594202898559, 0.2644927536231884146, 0.2663043478260869734, 0.2681159420289855322, 0.2699275362318840354, 0.2717391304347825942, 0.2735507246376811530, 0.2753623188405797118, 0.2771739130434782705, 0.2789855072463768293, 0.2807971014492753881, 0.2826086956521738913, 0.2844202898550724501, 0.2862318840579710089, 0.2880434782608695676, 0.2898550724637681264, 0.2916666666666666852, 0.2934782608695652439, 0.2952898550724637472, 0.2971014492753623060, 0.2989130434782608647, 0.3007246376811594235, 0.3025362318840579823, 0.3043478260869565410, 0.3061594202898550998, 0.3079710144927536031, 0.3097826086956521618, 0.3115942028985507206, 0.3134057971014492794, 0.3152173913043478382, 0.3170289855072463969, 0.3188405797101449002, 0.3206521739130434590, 0.3224637681159420177, 0.3242753623188405765, 0.3260869565217391353, 0.3278985507246376940, 0.3297101449275362528, 0.3315217391304347561, 0.3333333333333333148, 0.3351449275362318736, 0.3369565217391304324, 0.3387681159420289911, 0.3405797101449275499, 0.3423913043478261087, 0.3442028985507246119, 0.3460144927536231707, 0.3478260869565217295, 0.3496376811594202882, 0.3514492753623188470, 0.3532608695652174058, 0.3550724637681159646, 0.3568840579710144678, 0.3586956521739130266, 0.3605072463768115854, 0.3623188405797101441, 0.3641304347826087029, 0.3659420289855072617, 0.3677536231884058204, 0.3695652173913043237, 0.3713768115942028825, 0.3731884057971014412, 0.3750000000000000000, 0.3768115942028985588, 0.3786231884057971175, 0.3804347826086956763, 0.3822463768115941796, 0.3840579710144927383, 0.3858695652173912971, 0.3876811594202898559, 0.3894927536231884146, 0.3913043478260869734, 0.3931159420289855322, 0.3949275362318840354, 0.3967391304347825942, 0.3985507246376811530, 0.4003623188405797118, 0.4021739130434782705, 0.4039855072463768293, 0.4057971014492753881, 0.4076086956521738913, 0.4094202898550724501, 0.4112318840579710089, 0.4130434782608695676, 0.4148550724637681264, 0.4166666666666666852, 0.4184782608695652439, 0.4202898550724637472, 0.4221014492753623060, 0.4239130434782608647, 0.4257246376811594235, 0.4275362318840579823, 0.4293478260869565410, 0.4311594202898550998, 0.4329710144927536031, 0.4347826086956521618, 0.4365942028985507206, 0.4384057971014492794, 0.4402173913043478382, 0.4420289855072463969, 0.4438405797101449002, 0.4456521739130434590, 0.4474637681159420177, 0.4492753623188405765, 0.4510869565217391353, 0.4528985507246376940, 0.4547101449275362528, 0.4565217391304347561, 0.4583333333333333148, 0.4601449275362318736, 0.4619565217391304324, 0.4637681159420289911, 0.4655797101449275499, 0.4673913043478261087, 0.4692028985507246119, 0.4710144927536231707, 0.4728260869565217295, 0.4746376811594202882, 0.4764492753623188470, 0.4782608695652174058, 0.4800724637681159646, 0.4818840579710144678, 0.4836956521739130266, 0.4855072463768115854, 0.4873188405797101441, 0.4891304347826087029, 0.4909420289855072617, 0.4927536231884058204, 0.4945652173913043237, 0.4963768115942028825, 0.4981884057971014412, 0.5000000000000000000, 0.5018115942028985588, 0.5036231884057971175, 0.5054347826086956763, 0.5072463768115942351, 0.5090579710144927938, 0.5108695652173913526, 0.5126811594202898004, 0.5144927536231883591, 0.5163043478260869179, 0.5181159420289854767, 0.5199275362318840354, 0.5217391304347825942, 0.5235507246376811530, 0.5253623188405797118, 0.5271739130434782705, 0.5289855072463768293, 0.5307971014492753881, 0.5326086956521739468, 0.5344202898550725056, 0.5362318840579710644, 0.5380434782608695121, 0.5398550724637680709, 0.5416666666666666297, 0.5434782608695651884, 0.5452898550724637472, 0.5471014492753623060, 0.5489130434782608647, 0.5507246376811594235, 0.5525362318840579823, 0.5543478260869565410, 0.5561594202898550998, 0.5579710144927536586, 0.5597826086956522174, 0.5615942028985507761, 0.5634057971014492239, 0.5652173913043477826, 0.5670289855072463414, 0.5688405797101449002, 0.5706521739130434590, 0.5724637681159420177, 0.5742753623188405765, 0.5760869565217391353, 0.5778985507246376940, 0.5797101449275362528, 0.5815217391304348116, 0.5833333333333333703, 0.5851449275362319291, 0.5869565217391304879, 0.5887681159420289356, 0.5905797101449274944, 0.5923913043478260532, 0.5942028985507246119, 0.5960144927536231707, 0.5978260869565217295, 0.5996376811594202882, 0.6014492753623188470, 0.6032608695652174058, 0.6050724637681159646, 0.6068840579710145233, 0.6086956521739130821, 0.6105072463768116409, 0.6123188405797101996, 0.6141304347826086474, 0.6159420289855072062, 0.6177536231884057649, 0.6195652173913043237, 0.6213768115942028825, 0.6231884057971014412, 0.6250000000000000000, 0.6268115942028985588, 0.6286231884057971175, 0.6304347826086956763, 0.6322463768115942351, 0.6340579710144927938, 0.6358695652173913526, 0.6376811594202898004, 0.6394927536231883591, 0.6413043478260869179, 0.6431159420289854767, 0.6449275362318840354, 0.6467391304347825942, 0.6485507246376811530, 0.6503623188405797118, 0.6521739130434782705, 0.6539855072463768293, 0.6557971014492753881, 0.6576086956521739468, 0.6594202898550725056, 0.6612318840579710644, 0.6630434782608695121, 0.6648550724637680709, 0.6666666666666666297, 0.6684782608695651884, 0.6702898550724637472, 0.6721014492753623060, 0.6739130434782608647, 0.6757246376811594235, 0.6775362318840579823, 0.6793478260869565410, 0.6811594202898550998, 0.6829710144927536586, 0.6847826086956522174, 0.6865942028985507761, 0.6884057971014492239, 0.6902173913043477826, 0.6920289855072463414, 0.6938405797101449002, 0.6956521739130434590, 0.6974637681159420177, 0.6992753623188405765, 0.7010869565217391353, 0.7028985507246376940, 0.7047101449275362528, 0.7065217391304348116, 0.7083333333333333703, 0.7101449275362319291, 0.7119565217391304879, 0.7137681159420289356, 0.7155797101449274944, 0.7173913043478260532, 0.7192028985507246119, 0.7210144927536231707, 0.7228260869565217295, 0.7246376811594202882, 0.7264492753623188470, 0.7282608695652174058, 0.7300724637681159646, 0.7318840579710145233, 0.7336956521739130821, 0.7355072463768116409, 0.7373188405797101996, 0.7391304347826086474, 0.7409420289855072062, 0.7427536231884057649, 0.7445652173913043237, 0.7463768115942028825, 0.7481884057971014412, 0.7500000000000000000, 0.7518115942028985588, 0.7536231884057971175, 0.7554347826086956763, 0.7572463768115942351, 0.7590579710144927938, 0.7608695652173913526, 0.7626811594202898004, 0.7644927536231883591, 0.7663043478260869179, 0.7681159420289854767, 0.7699275362318840354, 0.7717391304347825942, 0.7735507246376811530, 0.7753623188405797118, 0.7771739130434782705, 0.7789855072463768293, 0.7807971014492753881, 0.7826086956521739468, 0.7844202898550725056, 0.7862318840579710644, 0.7880434782608695121, 0.7898550724637680709, 0.7916666666666666297, 0.7934782608695651884, 0.7952898550724637472, 0.7971014492753623060, 0.7989130434782608647, 0.8007246376811594235, 0.8025362318840579823, 0.8043478260869565410, 0.8061594202898550998, 0.8079710144927536586, 0.8097826086956522174, 0.8115942028985507761, 0.8134057971014492239, 0.8152173913043477826, 0.8170289855072463414, 0.8188405797101449002, 0.8206521739130434590, 0.8224637681159420177, 0.8242753623188405765, 0.8260869565217391353, 0.8278985507246376940, 0.8297101449275362528, 0.8315217391304348116, 0.8333333333333333703, 0.8351449275362319291, 0.8369565217391304879, 0.8387681159420289356, 0.8405797101449274944, 0.8423913043478260532, 0.8442028985507246119, 0.8460144927536231707, 0.8478260869565217295, 0.8496376811594202882, 0.8514492753623188470, 0.8532608695652174058, 0.8550724637681159646, 0.8568840579710145233, 0.8586956521739130821, 0.8605072463768116409, 0.8623188405797101996, 0.8641304347826086474, 0.8659420289855072062, 0.8677536231884057649, 0.8695652173913043237, 0.8713768115942028825, 0.8731884057971014412, 0.8750000000000000000, 0.8768115942028985588, 0.8786231884057971175, 0.8804347826086956763, 0.8822463768115942351, 0.8840579710144927938, 0.8858695652173913526, 0.8876811594202898004, 0.8894927536231883591, 0.8913043478260869179, 0.8931159420289854767, 0.8949275362318840354, 0.8967391304347825942, 0.8985507246376811530, 0.9003623188405797118, 0.9021739130434782705, 0.9039855072463768293, 0.9057971014492753881, 0.9076086956521739468, 0.9094202898550725056, 0.9112318840579710644, 0.9130434782608695121, 0.9148550724637680709, 0.9166666666666666297, 0.9184782608695651884, 0.9202898550724637472, 0.9221014492753623060, 0.9239130434782608647, 0.9257246376811594235, 0.9275362318840579823, 0.9293478260869565410, 0.9311594202898550998, 0.9329710144927536586, 0.9347826086956522174, 0.9365942028985507761, 0.9384057971014492239, 0.9402173913043477826, 0.9420289855072463414, 0.9438405797101449002, 0.9456521739130434590, 0.9474637681159420177, 0.9492753623188405765, 0.9510869565217391353, 0.9528985507246376940, 0.9547101449275362528, 0.9565217391304348116, 0.9583333333333333703, 0.9601449275362319291, 0.9619565217391304879, 0.9637681159420289356, 0.9655797101449274944, 0.9673913043478260532, 0.9692028985507246119, 0.9710144927536231707, 0.9728260869565217295, 0.9746376811594202882, 0.9764492753623188470, 0.9782608695652174058, 0.9800724637681159646, 0.9818840579710145233, 0.9826096998908593338, 0.9924357968897679072 ),
 .UNSPECIFIED. ) 
 GEOMETRIC_REPRESENTATION_ITEM ( )  RATIONAL_B_SPLINE_SURFACE ( (
 ( 1.000000000000000000, 0.9659258262890683122, 1.000000000000000000, 0.9659258262890683122, 1.000000000000000000, 0.9659258262890683122, 1.000000000000000000, 0.9659258262890683122, 1.000000000000000000, 0.9659258262890683122, 1.000000000000000000, 0.9659258262890683122, 1.000000000000000000, 0.9659258262890683122, 1.000000000000000000, 0.9659258262890683122, 1.000000000000000000, 0.9659258262890683122, 1.000000000000000000, 0.9659258262890683122, 1.000000000000000000, 0.9659258262890683122, 1.000000000000000000, 0.9659258262890683122, 1.000000000000000000, 0.9659258262890683122, 1.000000000000000000, 0.9659258262890683122, 1.000000000000000000, 0.9659258262890683122, 1.000000000000000000, 0.9659258262890683122, 1.000000000000000000, 0.9659258262890683122, 1.000000000000000000, 0.9659258262890683122, 1.000000000000000000, 0.9659258262890683122, 1.000000000000000000, 0.9659258262890683122, 1.000000000000000000, 0.9659258262890683122, 1.000000000000000000, 0.9659258262890683122, 1.000000000000000000, 0.9659258262890683122, 1.000000000000000000, 0.9659258262890683122, 1.000000000000000000, 0.9659258262890683122, 1.000000000000000000, 0.9659258262890683122, 1.000000000000000000, 0.9659258262890683122, 1.000000000000000000, 0.9659258262890683122, 1.000000000000000000, 0.9659258262890683122, 1.000000000000000000, 0.9659258262890683122, 1.000000000000000000, 0.9659258262890683122, 1.000000000000000000, 0.9659258262890683122, 1.000000000000000000, 0.9659258262890683122, 1.000000000000000000, 0.9659258262890683122, 1.000000000000000000, 0.9659258262890683122, 1.000000000000000000, 0.9659258262890683122, 1.000000000000000000, 0.9659258262890683122, 1.000000000000000000, 0.9659258262890683122, 1.000000000000000000, 0.9659258262890683122, 1.000000000000000000, 0.9659258262890683122, 1.000000000000000000, 0.9659258262890683122, 1.000000000000000000, 0.9659258262890683122, 1.000000000000000000, 0.9659258262890683122, 1.000000000000000000, 0.9659258262890683122, 1.000000000000000000, 0.9659258262890683122, 1.000000000000000000, 0.9659258262890683122, 1.000000000000000000, 0.9659258262890683122, 1.000000000000000000, 0.9659258262890683122, 1.000000000000000000, 0.9659258262890683122, 1.000000000000000000, 0.9659258262890683122, 1.000000000000000000, 0.9659258262890683122, 1.000000000000000000, 0.9659258262890683122, 1.000000000000000000, 0.9659258262890683122, 1.000000000000000000, 0.9659258262890683122, 1.000000000000000000, 0.9659258262890683122, 1.000000000000000000, 0.9659258262890683122, 1.000000000000000000, 0.9659258262890683122, 1.000000000000000000, 0.9659258262890683122, 1.000000000000000000, 0.9659258262890683122, 1.000000000000000000, 0.9659258262890683122, 1.000000000000000000, 0.9659258262890683122, 1.000000000000000000, 0.9659258262890683122, 1.000000000000000000, 0.9659258262890683122, 1.000000000000000000, 0.9659258262890683122, 1.000000000000000000, 0.9659258262890683122, 1.000000000000000000, 0.9659258262890683122, 1.000000000000000000, 0.9659258262890683122, 1.000000000000000000, 0.9659258262890683122, 1.000000000000000000, 0.9659258262890683122, 1.000000000000000000, 0.9659258262890683122, 1.000000000000000000, 0.9659258262890683122, 1.000000000000000000, 0.9659258262890683122, 1.000000000000000000, 0.9659258262890683122, 1.000000000000000000, 0.9659258262890683122, 1.000000000000000000, 0.9659258262890683122, 1.000000000000000000, 0.9659258262890683122, 1.000000000000000000, 0.9659258262890683122, 1.000000000000000000, 0.9659258262890683122, 1.000000000000000000, 0.9659258262890683122, 1.000000000000000000, 0.9659258262890683122, 1.000000000000000000, 0.9659258262890683122, 1.000000000000000000, 0.9659258262890683122, 1.000000000000000000, 0.9659258262890683122, 1.000000000000000000, 0.9659258262890683122, 1.000000000000000000, 0.9659258262890683122, 1.000000000000000000, 0.9659258262890683122, 1.000000000000000000, 0.9659258262890683122, 1.000000000000000000, 0.9659258262890683122, 1.000000000000000000, 0.9659258262890683122, 1.000000000000000000, 0.9659258262890683122, 1.000000000000000000, 0.9659258262890683122, 1.000000000000000000, 0.9659258262890683122, 1.000000000000000000, 0.9659258262890683122, 1.000000000000000000, 0.9659258262890683122, 1.000000000000000000, 0.9659258262890683122, 1.000000000000000000, 0.9659258262890683122, 1.000000000000000000, 0.9659258262890683122, 1.000000000000000000, 0.9659258262890683122, 1.000000000000000000, 0.9659258262890683122, 1.000000000000000000, 0.9659258262890683122, 1.000000000000000000, 0.9659258262890683122, 1.000000000000000000, 0.9659258262890683122, 1.000000000000000000, 0.9659258262890683122, 1.000000000000000000, 0.9659258262890683122, 1.000000000000000000, 0.9659258262890683122, 1.000000000000000000, 0.9659258262890683122, 1.000000000000000000, 0.9659258262890683122, 1.000000000000000000, 0.9659258262890683122, 1.000000000000000000, 0.9659258262890683122, 1.000000000000000000, 0.9659258262890683122, 1.000000000000000000, 0.9659258262890683122, 1.000000000000000000, 0.9659258262890683122, 1.000000000000000000, 0.9659258262890683122, 1.000000000000000000, 0.9659258262890683122, 1.000000000000000000, 0.9659258262890683122, 1.000000000000000000, 0.9659258262890683122, 1.000000000000000000, 0.9659258262890683122, 1.000000000000000000, 0.9659258262890683122, 1.000000000000000000, 0.9659258262890683122, 1.000000000000000000, 0.9659258262890683122, 1.000000000000000000, 0.9659258262890683122, 1.000000000000000000, 0.9659258262890683122, 1.000000000000000000, 0.9659258262890683122, 1.000000000000000000, 0.9659258262890683122, 1.000000000000000000, 0.9659258262890683122, 1.000000000000000000, 0.9659258262890683122, 1.000000000000000000, 0.9659258262890683122, 1.000000000000000000, 0.9659258262890683122, 1.000000000000000000, 0.9659258262890683122, 1.000000000000000000, 0.9659258262890683122, 1.000000000000000000, 0.9659258262890683122, 1.000000000000000000, 0.9659258262890683122, 1.000000000000000000, 0.9659258262890683122, 1.000000000000000000, 0.9659258262890683122, 1.000000000000000000, 0.9659258262890683122, 1.000000000000000000, 0.9659258262890683122, 1.000000000000000000, 0.9659258262890683122, 1.000000000000000000, 0.9659258262890683122, 1.000000000000000000, 0.9659258262890683122, 1.000000000000000000, 0.9659258262890683122, 1.000000000000000000, 0.9659258262890683122, 1.000000000000000000, 0.9659258262890683122, 1.000000000000000000, 0.9659258262890683122, 1.000000000000000000, 0.9659258262890683122, 1.000000000000000000, 0.9659258262890683122, 1.000000000000000000, 0.9659258262890683122, 1.000000000000000000, 0.9659258262890683122, 1.000000000000000000, 0.9659258262890683122, 1.000000000000000000, 0.9659258262890683122, 1.000000000000000000, 0.9659258262890683122, 1.000000000000000000, 0.9659258262890683122, 1.000000000000000000, 0.9659258262890683122, 1.000000000000000000, 0.9659258262890683122, 1.000000000000000000, 0.9659258262890683122, 1.000000000000000000, 0.9659258262890683122, 1.000000000000000000, 0.9659258262890683122, 1.000000000000000000, 0.9659258262890683122, 1.000000000000000000, 0.9659258262890683122, 1.000000000000000000, 0.9659258262890683122, 1.000000000000000000, 0.9659258262890683122, 1.000000000000000000, 0.9659258262890683122, 1.000000000000000000, 0.9659258262890683122, 1.000000000000000000, 0.9659258262890683122, 1.000000000000000000, 0.9659258262890683122, 1.000000000000000000, 0.9659258262890683122, 1.000000000000000000, 0.9659258262890683122, 1.000000000000000000, 0.9659258262890683122, 1.000000000000000000, 0.9659258262890683122, 1.000000000000000000, 0.9659258262890683122, 1.000000000000000000, 0.9659258262890683122, 1.000000000000000000, 0.9659258262890683122, 1.000000000000000000, 0.9659258262890683122, 1.000000000000000000, 0.9659258262890683122, 1.000000000000000000, 0.9659258262890683122, 1.000000000000000000, 0.9659258262890683122, 1.000000000000000000, 0.9659258262890683122, 1.000000000000000000, 0.9659258262890683122, 1.000000000000000000, 0.9659258262890683122, 1.000000000000000000, 0.9659258262890683122, 1.000000000000000000, 0.9659258262890683122, 1.000000000000000000, 0.9659258262890683122, 1.000000000000000000, 0.9659258262890683122, 1.000000000000000000, 0.9659258262890683122, 1.000000000000000000, 0.9659258262890683122, 1.000000000000000000, 0.9659258262890683122, 1.000000000000000000, 0.9659258262890683122, 1.000000000000000000, 0.9659258262890683122, 1.000000000000000000, 0.9659258262890683122, 1.000000000000000000, 0.9659258262890683122, 1.000000000000000000, 0.9659258262890683122, 1.000000000000000000, 0.9659258262890683122, 1.000000000000000000, 0.9659258262890683122, 1.000000000000000000, 0.9659258262890683122, 1.000000000000000000, 0.9659258262890683122, 1.000000000000000000, 0.9659258262890683122, 1.000000000000000000, 0.9659258262890683122, 1.000000000000000000, 0.9659258262890683122, 1.000000000000000000, 0.9659258262890683122, 1.000000000000000000, 0.9659258262890683122, 1.000000000000000000, 0.9659258262890683122, 1.000000000000000000, 0.9659258262890683122, 1.000000000000000000, 0.9659258262890683122, 1.000000000000000000, 0.9659258262890683122, 1.000000000000000000, 0.9659258262890683122, 1.000000000000000000, 0.9659258262890683122, 1.000000000000000000, 0.9659258262890683122, 1.000000000000000000, 0.9659258262890683122, 1.000000000000000000, 0.9659258262890683122, 1.000000000000000000, 0.9659258262890683122, 1.000000000000000000, 0.9659258262890683122, 1.000000000000000000, 0.9659258262890683122, 1.000000000000000000, 0.9659258262890683122, 1.000000000000000000, 0.9659258262890683122, 1.000000000000000000, 0.9659258262890683122, 1.000000000000000000, 0.9659258262890683122, 1.000000000000000000, 0.9659258262890683122, 1.000000000000000000, 0.9659258262890683122, 1.000000000000000000, 0.9659258262890683122, 1.000000000000000000, 0.9659258262890683122, 1.000000000000000000, 0.9659258262890683122, 1.000000000000000000, 0.9659258262890683122, 1.000000000000000000, 0.9659258262890683122, 1.000000000000000000, 0.9659258262890683122, 1.000000000000000000, 0.9659258262890683122, 1.000000000000000000, 0.9659258262890683122, 1.000000000000000000, 0.9659258262890683122, 1.000000000000000000, 0.9659258262890683122, 1.000000000000000000, 0.9659258262890683122, 1.000000000000000000, 0.9659258262890683122, 1.000000000000000000, 0.9659258262890683122, 1.000000000000000000, 0.9659258262890683122, 1.000000000000000000, 0.9659258262890683122, 1.000000000000000000, 0.9659258262890683122, 1.000000000000000000, 0.9659258262890683122, 1.000000000000000000, 0.9659258262890683122, 1.000000000000000000, 0.9659258262890683122, 1.000000000000000000, 0.9659258262890683122, 1.000000000000000000, 0.9659258262890683122, 1.000000000000000000, 0.9659258262890683122, 1.000000000000000000, 0.9659258262890683122, 1.000000000000000000, 0.9659258262890683122, 1.000000000000000000, 0.9659258262890683122, 1.000000000000000000, 0.9659258262890683122, 1.000000000000000000, 0.9659258262890683122, 1.000000000000000000, 0.9659258262890683122, 1.000000000000000000, 0.9659258262890683122, 1.000000000000000000, 0.9659258262890683122, 1.000000000000000000, 0.9659258262890683122, 1.000000000000000000, 0.9659258262890683122, 1.000000000000000000, 0.9659258262890683122, 1.000000000000000000, 0.9659258262890683122, 1.000000000000000000, 0.9659258262890683122, 1.000000000000000000, 0.9659258262890683122, 1.000000000000000000, 0.9659258262890683122, 1.000000000000000000, 0.9659258262890683122, 1.000000000000000000, 0.9659258262890683122, 1.000000000000000000, 0.9659258262890683122, 1.000000000000000000, 0.9659258262890683122, 1.000000000000000000, 0.9659258262890683122, 1.000000000000000000, 0.9659258262890683122, 1.000000000000000000, 0.9659258262890683122, 1.000000000000000000, 0.9659258262890683122, 1.000000000000000000, 0.9659258262890683122, 1.000000000000000000, 0.9659258262890683122, 1.000000000000000000, 0.9659258262890683122, 1.000000000000000000, 0.9659258262890683122, 1.000000000000000000, 0.9659258262890683122, 1.000000000000000000, 0.9659258262890683122, 1.000000000000000000, 0.9659258262890683122, 1.000000000000000000, 0.9659258262890683122, 1.000000000000000000, 0.9659258262890683122, 1.000000000000000000, 0.9659258262890683122, 1.000000000000000000, 0.9659258262890683122, 1.000000000000000000, 0.9659258262890683122, 1.000000000000000000, 0.9659258262890683122, 1.000000000000000000, 0.9659258262890683122, 1.000000000000000000, 0.9659258262890683122, 1.000000000000000000, 0.9659258262890683122, 1.000000000000000000, 0.9659258262890683122, 1.000000000000000000, 0.9659258262890683122, 1.000000000000000000, 0.9659258262890683122, 1.000000000000000000, 0.9659258262890683122, 1.000000000000000000, 0.9659258262890683122, 1.000000000000000000, 0.9659258262890683122, 1.000000000000000000, 0.9659258262890683122, 1.000000000000000000, 0.9659258262890683122, 1.000000000000000000, 0.9659258262890683122, 1.000000000000000000, 0.9659258262890683122, 1.000000000000000000, 0.9659258262890683122, 1.000000000000000000, 0.9659258262890683122, 1.000000000000000000, 0.9659258262890683122, 1.000000000000000000, 0.9659258262890683122, 1.000000000000000000, 0.9659258262890683122, 1.000000000000000000, 0.9659258262890683122, 1.000000000000000000, 0.9659258262890683122, 1.000000000000000000, 0.9659258262890683122, 1.000000000000000000, 0.9659258262890683122, 1.000000000000000000, 0.9659258262890683122, 1.000000000000000000, 0.9659258262890683122, 1.000000000000000000, 0.9659258262890683122, 1.000000000000000000, 0.9659258262890683122, 1.000000000000000000, 0.9659258262890683122, 1.000000000000000000, 0.9659258262890683122, 1.000000000000000000, 0.9659258262890683122, 1.000000000000000000, 0.9659258262890683122, 1.000000000000000000, 0.9659258262890683122, 1.000000000000000000, 0.9659258262890683122, 1.000000000000000000, 0.9659258262890683122, 1.000000000000000000, 0.9659258262890683122, 1.000000000000000000, 0.9659258262890683122, 1.000000000000000000, 0.9659258262890683122, 1.000000000000000000, 0.9659258262890683122, 1.000000000000000000, 0.9659258262890683122, 1.000000000000000000, 0.9659258262890683122, 1.000000000000000000, 0.9659258262890683122, 1.000000000000000000, 0.9659258262890683122, 1.000000000000000000, 0.9659258262890683122, 1.000000000000000000, 0.9659258262890683122, 1.000000000000000000, 0.9659258262890683122, 1.000000000000000000, 0.9659258262890683122, 1.000000000000000000, 0.9659258262890683122, 1.000000000000000000, 0.9659258262890683122, 1.000000000000000000, 0.9659258262890683122, 1.000000000000000000, 0.9659258262890683122, 1.000000000000000000, 0.9659258262890683122, 1.000000000000000000, 0.9659258262890683122, 1.000000000000000000, 0.9659258262890683122, 1.000000000000000000, 0.9659258262890683122, 1.000000000000000000, 0.9659258262890683122, 1.000000000000000000, 0.9659258262890683122, 1.000000000000000000, 0.9659258262890683122, 1.000000000000000000, 0.9659258262890683122, 1.000000000000000000, 0.9659258262890683122, 1.000000000000000000, 0.9659258262890683122, 1.000000000000000000, 0.9659258262890683122, 1.000000000000000000, 0.9659258262890683122, 1.000000000000000000, 0.9659258262890683122, 1.000000000000000000, 0.9659258262890683122, 1.000000000000000000, 0.9659258262890683122, 1.000000000000000000, 0.9659258262890683122, 1.000000000000000000, 0.9659258262890683122, 1.000000000000000000, 0.9659258262890683122, 1.000000000000000000, 0.9659258262890683122, 1.000000000000000000, 0.9659258262890683122, 1.000000000000000000, 0.9659258262890683122, 1.000000000000000000, 0.9659258262890683122, 1.000000000000000000, 0.9659258262890683122, 1.000000000000000000, 0.9659258262890683122, 1.000000000000000000, 0.9659258262890683122, 1.000000000000000000, 0.9659258262890683122, 1.000000000000000000, 0.9659258262890683122, 1.000000000000000000, 0.9659258262890683122, 1.000000000000000000, 0.9659258262890683122, 1.000000000000000000, 0.9659258262890683122, 1.000000000000000000, 0.9659258262890683122, 1.000000000000000000, 0.9659258262890683122, 1.000000000000000000, 0.9659258262890683122, 1.000000000000000000, 0.9659258262890683122, 1.000000000000000000, 0.9659258262890683122, 1.000000000000000000, 0.9659258262890683122, 1.000000000000000000, 0.9659258262890683122, 1.000000000000000000, 0.9659258262890683122, 1.000000000000000000, 0.9659258262890683122, 1.000000000000000000, 0.9659258262890683122, 1.000000000000000000, 0.9659258262890683122, 1.000000000000000000, 0.9659258262890683122, 1.000000000000000000, 0.9659258262890683122, 1.000000000000000000, 0.9659258262890683122, 1.000000000000000000, 0.9659258262890683122, 1.000000000000000000, 0.9659258262890683122, 1.000000000000000000, 0.9659258262890683122, 1.000000000000000000, 0.9659258262890683122, 1.000000000000000000, 0.9659258262890683122, 1.000000000000000000, 0.9659258262890683122, 1.000000000000000000, 0.9659258262890683122, 1.000000000000000000, 0.9659258262890683122, 1.000000000000000000, 0.9659258262890683122, 1.000000000000000000, 0.9659258262890683122, 1.000000000000000000, 0.9659258262890683122, 1.000000000000000000, 0.9659258262890683122, 1.000000000000000000, 0.9659258262890683122, 1.000000000000000000, 0.9659258262890683122, 1.000000000000000000, 0.9659258262890683122, 1.000000000000000000, 0.9659258262890683122, 1.000000000000000000, 0.9659258262890683122, 1.000000000000000000, 0.9659258262890683122, 1.000000000000000000, 0.9659258262890683122, 1.000000000000000000, 0.9659258262890683122, 1.000000000000000000, 0.9659258262890683122, 1.000000000000000000, 0.9659258262890683122, 1.000000000000000000, 0.9659258262890683122, 1.000000000000000000, 0.9659258262890683122, 1.000000000000000000, 0.9659258262890683122, 1.000000000000000000, 0.9659258262890683122, 1.000000000000000000, 0.9659258262890683122, 1.000000000000000000, 0.9659258262890683122, 1.000000000000000000, 0.9659258262890683122, 1.000000000000000000, 0.9659258262890683122, 1.000000000000000000, 0.9659258262890683122, 1.000000000000000000, 0.9659258262890683122, 1.000000000000000000, 0.9659258262890683122, 1.000000000000000000, 0.9659258262890683122, 1.000000000000000000, 0.9659258262890683122, 1.000000000000000000, 0.9659258262890683122, 1.000000000000000000, 0.9659258262890683122, 1.000000000000000000, 0.9659258262890683122, 1.000000000000000000, 0.9659258262890683122, 1.000000000000000000, 0.9659258262890683122, 1.000000000000000000, 0.9659258262890683122, 1.000000000000000000, 0.9659258262890683122, 1.000000000000000000, 0.9659258262890683122, 1.000000000000000000, 0.9659258262890683122, 1.000000000000000000, 0.9659258262890683122, 1.000000000000000000, 0.9659258262890683122, 1.000000000000000000, 0.9659258262890683122, 1.000000000000000000, 0.9659258262890683122, 1.000000000000000000, 0.9659258262890683122, 1.000000000000000000, 0.9659258262890683122, 1.000000000000000000, 0.9659258262890683122, 1.000000000000000000, 0.9659258262890683122, 1.000000000000000000, 0.9659258262890683122, 1.000000000000000000, 0.9659258262890683122, 1.000000000000000000, 0.9659258262890683122, 1.000000000000000000, 0.9659258262890683122, 1.000000000000000000, 0.9659258262890683122, 1.000000000000000000, 0.9659258262890683122, 1.000000000000000000, 0.9659258262890683122, 1.000000000000000000, 0.9659258262890683122, 1.000000000000000000, 0.9659258262890683122, 1.000000000000000000, 0.9659258262890683122, 1.000000000000000000, 0.9659258262890683122, 1.000000000000000000, 0.9659258262890683122, 1.000000000000000000, 0.9659258262890683122, 1.000000000000000000, 0.9659258262890683122, 1.000000000000000000, 0.9659258262890683122, 1.000000000000000000, 0.9659258262890683122, 1.000000000000000000, 0.9659258262890683122, 1.000000000000000000, 0.9659258262890683122, 1.000000000000000000, 0.9659258262890683122, 1.000000000000000000, 0.9659258262890683122, 1.000000000000000000, 0.9659258262890683122, 1.000000000000000000, 0.9659258262890683122, 1.000000000000000000, 0.9659258262890683122, 1.000000000000000000, 0.9659258262890683122, 1.000000000000000000, 0.9659258262890683122, 1.000000000000000000, 0.9659258262890683122, 1.000000000000000000, 0.9659258262890683122, 1.000000000000000000, 0.9659258262890683122, 1.000000000000000000, 0.9659258262890683122, 1.000000000000000000, 0.9659258262890683122, 1.000000000000000000, 0.9659258262890683122, 1.000000000000000000, 0.9659258262890683122, 1.000000000000000000, 0.9659258262890683122, 1.000000000000000000, 0.9659258262890683122, 1.000000000000000000, 0.9659258262890683122, 1.000000000000000000, 0.9659258262890683122, 1.000000000000000000, 0.9659258262890683122, 1.000000000000000000, 0.9659258262890683122, 1.000000000000000000, 0.9659258262890683122, 1.000000000000000000, 0.9659258262890683122, 1.000000000000000000, 0.9659258262890683122, 1.000000000000000000, 0.9659258262890683122, 1.000000000000000000, 0.9659258262890683122, 1.000000000000000000, 0.9659258262890683122, 1.000000000000000000, 0.9659258262890683122, 1.000000000000000000, 0.9659258262890683122, 1.000000000000000000, 0.9659258262890683122, 1.000000000000000000, 0.9659258262890683122, 1.000000000000000000, 0.9659258262890683122, 1.000000000000000000, 0.9659258262890683122, 1.000000000000000000, 0.9659258262890683122, 1.000000000000000000, 0.9659258262890683122, 1.000000000000000000, 0.9659258262890683122, 1.000000000000000000, 0.9659258262890683122, 1.000000000000000000, 0.9659258262890683122, 1.000000000000000000, 0.9659258262890683122, 1.000000000000000000, 0.9659258262890683122, 1.000000000000000000, 0.9659258262890683122, 1.000000000000000000, 0.9659258262890683122, 1.000000000000000000, 0.9659258262890683122, 1.000000000000000000, 0.9659258262890683122, 1.000000000000000000, 0.9659258262890683122, 1.000000000000000000, 0.9659258262890683122, 1.000000000000000000, 0.9659258262890683122, 1.000000000000000000, 0.9659258262890683122, 1.000000000000000000, 0.9659258262890683122, 1.000000000000000000, 0.9659258262890683122, 1.000000000000000000, 0.9659258262890683122, 1.000000000000000000, 0.9659258262890683122, 1.000000000000000000, 0.9659258262890683122, 1.000000000000000000, 0.9659258262890683122, 1.000000000000000000, 0.9659258262890683122, 1.000000000000000000, 0.9659258262890683122, 1.000000000000000000, 0.9659258262890683122, 1.000000000000000000, 0.9659258262890683122, 1.000000000000000000, 0.9659258262890683122, 1.000000000000000000, 0.9659258262890683122, 1.000000000000000000, 0.9659258262890683122, 1.000000000000000000, 0.9659258262890683122, 1.000000000000000000, 0.9659258262890683122, 1.000000000000000000, 0.9659258262890683122, 1.000000000000000000, 0.9659258262890683122, 1.000000000000000000, 0.9659258262890683122, 1.000000000000000000, 0.9659258262890683122, 1.000000000000000000, 0.9659258262890683122, 1.000000000000000000, 0.9659258262890683122, 1.000000000000000000, 0.9659258262890683122, 1.000000000000000000, 0.9659258262890683122, 1.000000000000000000, 0.9659258262890683122, 1.000000000000000000, 0.9659258262890683122, 1.000000000000000000, 0.9659258262890683122, 1.000000000000000000, 0.9659258262890683122, 1.000000000000000000, 0.9659258262890683122, 1.000000000000000000, 0.9659258262890683122, 1.000000000000000000, 0.9659258262890683122, 1.000000000000000000, 0.9659258262890683122, 1.000000000000000000, 0.9659258262890683122, 1.000000000000000000, 0.9659258262890683122, 1.000000000000000000, 0.9659258262890683122, 1.000000000000000000, 0.9659258262890683122, 1.000000000000000000, 0.9659258262890683122, 1.000000000000000000, 0.9659258262890683122, 1.000000000000000000, 0.9659258262890683122, 1.000000000000000000, 0.9659258262890683122, 1.000000000000000000, 0.9659258262890683122, 1.000000000000000000, 0.9659258262890683122, 1.000000000000000000, 0.9659258262890683122, 1.000000000000000000, 0.9659258262890683122, 1.000000000000000000, 0.9659258262890683122, 1.000000000000000000, 0.9659258262890683122, 1.000000000000000000, 0.9659258262890683122, 1.000000000000000000, 0.9659258262890683122, 1.000000000000000000, 0.9659258262890683122, 1.000000000000000000, 0.9659258262890683122, 1.000000000000000000, 0.9659258262890683122, 1.000000000000000000, 0.9659258262890683122, 1.000000000000000000, 0.9659258262890683122, 1.000000000000000000, 0.9659258262890683122, 1.000000000000000000, 0.9659258262890683122, 1.000000000000000000, 0.9659258262890683122, 1.000000000000000000, 0.9659258262890683122, 1.000000000000000000, 0.9659258262890683122, 1.000000000000000000, 0.9863514418465433309, 0.9836368620925994843, 0.9836368620925994843, 0.9836368620925994843),
 ( 1.000000000000000000, 0.9659258262890683122, 1.000000000000000000, 0.9659258262890683122, 1.000000000000000000, 0.9659258262890683122, 1.000000000000000000, 0.9659258262890683122, 1.000000000000000000, 0.9659258262890683122, 1.000000000000000000, 0.9659258262890683122, 1.000000000000000000, 0.9659258262890683122, 1.000000000000000000, 0.9659258262890683122, 1.000000000000000000, 0.9659258262890683122, 1.000000000000000000, 0.9659258262890683122, 1.000000000000000000, 0.9659258262890683122, 1.000000000000000000, 0.9659258262890683122, 1.000000000000000000, 0.9659258262890683122, 1.000000000000000000, 0.9659258262890683122, 1.000000000000000000, 0.9659258262890683122, 1.000000000000000000, 0.9659258262890683122, 1.000000000000000000, 0.9659258262890683122, 1.000000000000000000, 0.9659258262890683122, 1.000000000000000000, 0.9659258262890683122, 1.000000000000000000, 0.9659258262890683122, 1.000000000000000000, 0.9659258262890683122, 1.000000000000000000, 0.9659258262890683122, 1.000000000000000000, 0.9659258262890683122, 1.000000000000000000, 0.9659258262890683122, 1.000000000000000000, 0.9659258262890683122, 1.000000000000000000, 0.9659258262890683122, 1.000000000000000000, 0.9659258262890683122, 1.000000000000000000, 0.9659258262890683122, 1.000000000000000000, 0.9659258262890683122, 1.000000000000000000, 0.9659258262890683122, 1.000000000000000000, 0.9659258262890683122, 1.000000000000000000, 0.9659258262890683122, 1.000000000000000000, 0.9659258262890683122, 1.000000000000000000, 0.9659258262890683122, 1.000000000000000000, 0.9659258262890683122, 1.000000000000000000, 0.9659258262890683122, 1.000000000000000000, 0.9659258262890683122, 1.000000000000000000, 0.9659258262890683122, 1.000000000000000000, 0.9659258262890683122, 1.000000000000000000, 0.9659258262890683122, 1.000000000000000000, 0.9659258262890683122, 1.000000000000000000, 0.9659258262890683122, 1.000000000000000000, 0.9659258262890683122, 1.000000000000000000, 0.9659258262890683122, 1.000000000000000000, 0.9659258262890683122, 1.000000000000000000, 0.9659258262890683122, 1.000000000000000000, 0.9659258262890683122, 1.000000000000000000, 0.9659258262890683122, 1.000000000000000000, 0.9659258262890683122, 1.000000000000000000, 0.9659258262890683122, 1.000000000000000000, 0.9659258262890683122, 1.000000000000000000, 0.9659258262890683122, 1.000000000000000000, 0.9659258262890683122, 1.000000000000000000, 0.9659258262890683122, 1.000000000000000000, 0.9659258262890683122, 1.000000000000000000, 0.9659258262890683122, 1.000000000000000000, 0.9659258262890683122, 1.000000000000000000, 0.9659258262890683122, 1.000000000000000000, 0.9659258262890683122, 1.000000000000000000, 0.9659258262890683122, 1.000000000000000000, 0.9659258262890683122, 1.000000000000000000, 0.9659258262890683122, 1.000000000000000000, 0.9659258262890683122, 1.000000000000000000, 0.9659258262890683122, 1.000000000000000000, 0.9659258262890683122, 1.000000000000000000, 0.9659258262890683122, 1.000000000000000000, 0.9659258262890683122, 1.000000000000000000, 0.9659258262890683122, 1.000000000000000000, 0.9659258262890683122, 1.000000000000000000, 0.9659258262890683122, 1.000000000000000000, 0.9659258262890683122, 1.000000000000000000, 0.9659258262890683122, 1.000000000000000000, 0.9659258262890683122, 1.000000000000000000, 0.9659258262890683122, 1.000000000000000000, 0.9659258262890683122, 1.000000000000000000, 0.9659258262890683122, 1.000000000000000000, 0.9659258262890683122, 1.000000000000000000, 0.9659258262890683122, 1.000000000000000000, 0.9659258262890683122, 1.000000000000000000, 0.9659258262890683122, 1.000000000000000000, 0.9659258262890683122, 1.000000000000000000, 0.9659258262890683122, 1.000000000000000000, 0.9659258262890683122, 1.000000000000000000, 0.9659258262890683122, 1.000000000000000000, 0.9659258262890683122, 1.000000000000000000, 0.9659258262890683122, 1.000000000000000000, 0.9659258262890683122, 1.000000000000000000, 0.9659258262890683122, 1.000000000000000000, 0.9659258262890683122, 1.000000000000000000, 0.9659258262890683122, 1.000000000000000000, 0.9659258262890683122, 1.000000000000000000, 0.9659258262890683122, 1.000000000000000000, 0.9659258262890683122, 1.000000000000000000, 0.9659258262890683122, 1.000000000000000000, 0.9659258262890683122, 1.000000000000000000, 0.9659258262890683122, 1.000000000000000000, 0.9659258262890683122, 1.000000000000000000, 0.9659258262890683122, 1.000000000000000000, 0.9659258262890683122, 1.000000000000000000, 0.9659258262890683122, 1.000000000000000000, 0.9659258262890683122, 1.000000000000000000, 0.9659258262890683122, 1.000000000000000000, 0.9659258262890683122, 1.000000000000000000, 0.9659258262890683122, 1.000000000000000000, 0.9659258262890683122, 1.000000000000000000, 0.9659258262890683122, 1.000000000000000000, 0.9659258262890683122, 1.000000000000000000, 0.9659258262890683122, 1.000000000000000000, 0.9659258262890683122, 1.000000000000000000, 0.9659258262890683122, 1.000000000000000000, 0.9659258262890683122, 1.000000000000000000, 0.9659258262890683122, 1.000000000000000000, 0.9659258262890683122, 1.000000000000000000, 0.9659258262890683122, 1.000000000000000000, 0.9659258262890683122, 1.000000000000000000, 0.9659258262890683122, 1.000000000000000000, 0.9659258262890683122, 1.000000000000000000, 0.9659258262890683122, 1.000000000000000000, 0.9659258262890683122, 1.000000000000000000, 0.9659258262890683122, 1.000000000000000000, 0.9659258262890683122, 1.000000000000000000, 0.9659258262890683122, 1.000000000000000000, 0.9659258262890683122, 1.000000000000000000, 0.9659258262890683122, 1.000000000000000000, 0.9659258262890683122, 1.000000000000000000, 0.9659258262890683122, 1.000000000000000000, 0.9659258262890683122, 1.000000000000000000, 0.9659258262890683122, 1.000000000000000000, 0.9659258262890683122, 1.000000000000000000, 0.9659258262890683122, 1.000000000000000000, 0.9659258262890683122, 1.000000000000000000, 0.9659258262890683122, 1.000000000000000000, 0.9659258262890683122, 1.000000000000000000, 0.9659258262890683122, 1.000000000000000000, 0.9659258262890683122, 1.000000000000000000, 0.9659258262890683122, 1.000000000000000000, 0.9659258262890683122, 1.000000000000000000, 0.9659258262890683122, 1.000000000000000000, 0.9659258262890683122, 1.000000000000000000, 0.9659258262890683122, 1.000000000000000000, 0.9659258262890683122, 1.000000000000000000, 0.9659258262890683122, 1.000000000000000000, 0.9659258262890683122, 1.000000000000000000, 0.9659258262890683122, 1.000000000000000000, 0.9659258262890683122, 1.000000000000000000, 0.9659258262890683122, 1.000000000000000000, 0.9659258262890683122, 1.000000000000000000, 0.9659258262890683122, 1.000000000000000000, 0.9659258262890683122, 1.000000000000000000, 0.9659258262890683122, 1.000000000000000000, 0.9659258262890683122, 1.000000000000000000, 0.9659258262890683122, 1.000000000000000000, 0.9659258262890683122, 1.000000000000000000, 0.9659258262890683122, 1.000000000000000000, 0.9659258262890683122, 1.000000000000000000, 0.9659258262890683122, 1.000000000000000000, 0.9659258262890683122, 1.000000000000000000, 0.9659258262890683122, 1.000000000000000000, 0.9659258262890683122, 1.000000000000000000, 0.9659258262890683122, 1.000000000000000000, 0.9659258262890683122, 1.000000000000000000, 0.9659258262890683122, 1.000000000000000000, 0.9659258262890683122, 1.000000000000000000, 0.9659258262890683122, 1.000000000000000000, 0.9659258262890683122, 1.000000000000000000, 0.9659258262890683122, 1.000000000000000000, 0.9659258262890683122, 1.000000000000000000, 0.9659258262890683122, 1.000000000000000000, 0.9659258262890683122, 1.000000000000000000, 0.9659258262890683122, 1.000000000000000000, 0.9659258262890683122, 1.000000000000000000, 0.9659258262890683122, 1.000000000000000000, 0.9659258262890683122, 1.000000000000000000, 0.9659258262890683122, 1.000000000000000000, 0.9659258262890683122, 1.000000000000000000, 0.9659258262890683122, 1.000000000000000000, 0.9659258262890683122, 1.000000000000000000, 0.9659258262890683122, 1.000000000000000000, 0.9659258262890683122, 1.000000000000000000, 0.9659258262890683122, 1.000000000000000000, 0.9659258262890683122, 1.000000000000000000, 0.9659258262890683122, 1.000000000000000000, 0.9659258262890683122, 1.000000000000000000, 0.9659258262890683122, 1.000000000000000000, 0.9659258262890683122, 1.000000000000000000, 0.9659258262890683122, 1.000000000000000000, 0.9659258262890683122, 1.000000000000000000, 0.9659258262890683122, 1.000000000000000000, 0.9659258262890683122, 1.000000000000000000, 0.9659258262890683122, 1.000000000000000000, 0.9659258262890683122, 1.000000000000000000, 0.9659258262890683122, 1.000000000000000000, 0.9659258262890683122, 1.000000000000000000, 0.9659258262890683122, 1.000000000000000000, 0.9659258262890683122, 1.000000000000000000, 0.9659258262890683122, 1.000000000000000000, 0.9659258262890683122, 1.000000000000000000, 0.9659258262890683122, 1.000000000000000000, 0.9659258262890683122, 1.000000000000000000, 0.9659258262890683122, 1.000000000000000000, 0.9659258262890683122, 1.000000000000000000, 0.9659258262890683122, 1.000000000000000000, 0.9659258262890683122, 1.000000000000000000, 0.9659258262890683122, 1.000000000000000000, 0.9659258262890683122, 1.000000000000000000, 0.9659258262890683122, 1.000000000000000000, 0.9659258262890683122, 1.000000000000000000, 0.9659258262890683122, 1.000000000000000000, 0.9659258262890683122, 1.000000000000000000, 0.9659258262890683122, 1.000000000000000000, 0.9659258262890683122, 1.000000000000000000, 0.9659258262890683122, 1.000000000000000000, 0.9659258262890683122, 1.000000000000000000, 0.9659258262890683122, 1.000000000000000000, 0.9659258262890683122, 1.000000000000000000, 0.9659258262890683122, 1.000000000000000000, 0.9659258262890683122, 1.000000000000000000, 0.9659258262890683122, 1.000000000000000000, 0.9659258262890683122, 1.000000000000000000, 0.9659258262890683122, 1.000000000000000000, 0.9659258262890683122, 1.000000000000000000, 0.9659258262890683122, 1.000000000000000000, 0.9659258262890683122, 1.000000000000000000, 0.9659258262890683122, 1.000000000000000000, 0.9659258262890683122, 1.000000000000000000, 0.9659258262890683122, 1.000000000000000000, 0.9659258262890683122, 1.000000000000000000, 0.9659258262890683122, 1.000000000000000000, 0.9659258262890683122, 1.000000000000000000, 0.9659258262890683122, 1.000000000000000000, 0.9659258262890683122, 1.000000000000000000, 0.9659258262890683122, 1.000000000000000000, 0.9659258262890683122, 1.000000000000000000, 0.9659258262890683122, 1.000000000000000000, 0.9659258262890683122, 1.000000000000000000, 0.9659258262890683122, 1.000000000000000000, 0.9659258262890683122, 1.000000000000000000, 0.9659258262890683122, 1.000000000000000000, 0.9659258262890683122, 1.000000000000000000, 0.9659258262890683122, 1.000000000000000000, 0.9659258262890683122, 1.000000000000000000, 0.9659258262890683122, 1.000000000000000000, 0.9659258262890683122, 1.000000000000000000, 0.9659258262890683122, 1.000000000000000000, 0.9659258262890683122, 1.000000000000000000, 0.9659258262890683122, 1.000000000000000000, 0.9659258262890683122, 1.000000000000000000, 0.9659258262890683122, 1.000000000000000000, 0.9659258262890683122, 1.000000000000000000, 0.9659258262890683122, 1.000000000000000000, 0.9659258262890683122, 1.000000000000000000, 0.9659258262890683122, 1.000000000000000000, 0.9659258262890683122, 1.000000000000000000, 0.9659258262890683122, 1.000000000000000000, 0.9659258262890683122, 1.000000000000000000, 0.9659258262890683122, 1.000000000000000000, 0.9659258262890683122, 1.000000000000000000, 0.9659258262890683122, 1.000000000000000000, 0.9659258262890683122, 1.000000000000000000, 0.9659258262890683122, 1.000000000000000000, 0.9659258262890683122, 1.000000000000000000, 0.9659258262890683122, 1.000000000000000000, 0.9659258262890683122, 1.000000000000000000, 0.9659258262890683122, 1.000000000000000000, 0.9659258262890683122, 1.000000000000000000, 0.9659258262890683122, 1.000000000000000000, 0.9659258262890683122, 1.000000000000000000, 0.9659258262890683122, 1.000000000000000000, 0.9659258262890683122, 1.000000000000000000, 0.9659258262890683122, 1.000000000000000000, 0.9659258262890683122, 1.000000000000000000, 0.9659258262890683122, 1.000000000000000000, 0.9659258262890683122, 1.000000000000000000, 0.9659258262890683122, 1.000000000000000000, 0.9659258262890683122, 1.000000000000000000, 0.9659258262890683122, 1.000000000000000000, 0.9659258262890683122, 1.000000000000000000, 0.9659258262890683122, 1.000000000000000000, 0.9659258262890683122, 1.000000000000000000, 0.9659258262890683122, 1.000000000000000000, 0.9659258262890683122, 1.000000000000000000, 0.9659258262890683122, 1.000000000000000000, 0.9659258262890683122, 1.000000000000000000, 0.9659258262890683122, 1.000000000000000000, 0.9659258262890683122, 1.000000000000000000, 0.9659258262890683122, 1.000000000000000000, 0.9659258262890683122, 1.000000000000000000, 0.9659258262890683122, 1.000000000000000000, 0.9659258262890683122, 1.000000000000000000, 0.9659258262890683122, 1.000000000000000000, 0.9659258262890683122, 1.000000000000000000, 0.9659258262890683122, 1.000000000000000000, 0.9659258262890683122, 1.000000000000000000, 0.9659258262890683122, 1.000000000000000000, 0.9659258262890683122, 1.000000000000000000, 0.9659258262890683122, 1.000000000000000000, 0.9659258262890683122, 1.000000000000000000, 0.9659258262890683122, 1.000000000000000000, 0.9659258262890683122, 1.000000000000000000, 0.9659258262890683122, 1.000000000000000000, 0.9659258262890683122, 1.000000000000000000, 0.9659258262890683122, 1.000000000000000000, 0.9659258262890683122, 1.000000000000000000, 0.9659258262890683122, 1.000000000000000000, 0.9659258262890683122, 1.000000000000000000, 0.9659258262890683122, 1.000000000000000000, 0.9659258262890683122, 1.000000000000000000, 0.9659258262890683122, 1.000000000000000000, 0.9659258262890683122, 1.000000000000000000, 0.9659258262890683122, 1.000000000000000000, 0.9659258262890683122, 1.000000000000000000, 0.9659258262890683122, 1.000000000000000000, 0.9659258262890683122, 1.000000000000000000, 0.9659258262890683122, 1.000000000000000000, 0.9659258262890683122, 1.000000000000000000, 0.9659258262890683122, 1.000000000000000000, 0.9659258262890683122, 1.000000000000000000, 0.9659258262890683122, 1.000000000000000000, 0.9659258262890683122, 1.000000000000000000, 0.9659258262890683122, 1.000000000000000000, 0.9659258262890683122, 1.000000000000000000, 0.9659258262890683122, 1.000000000000000000, 0.9659258262890683122, 1.000000000000000000, 0.9659258262890683122, 1.000000000000000000, 0.9659258262890683122, 1.000000000000000000, 0.9659258262890683122, 1.000000000000000000, 0.9659258262890683122, 1.000000000000000000, 0.9659258262890683122, 1.000000000000000000, 0.9659258262890683122, 1.000000000000000000, 0.9659258262890683122, 1.000000000000000000, 0.9659258262890683122, 1.000000000000000000, 0.9659258262890683122, 1.000000000000000000, 0.9659258262890683122, 1.000000000000000000, 0.9659258262890683122, 1.000000000000000000, 0.9659258262890683122, 1.000000000000000000, 0.9659258262890683122, 1.000000000000000000, 0.9659258262890683122, 1.000000000000000000, 0.9659258262890683122, 1.000000000000000000, 0.9659258262890683122, 1.000000000000000000, 0.9659258262890683122, 1.000000000000000000, 0.9659258262890683122, 1.000000000000000000, 0.9659258262890683122, 1.000000000000000000, 0.9659258262890683122, 1.000000000000000000, 0.9659258262890683122, 1.000000000000000000, 0.9659258262890683122, 1.000000000000000000, 0.9659258262890683122, 1.000000000000000000, 0.9659258262890683122, 1.000000000000000000, 0.9659258262890683122, 1.000000000000000000, 0.9659258262890683122, 1.000000000000000000, 0.9659258262890683122, 1.000000000000000000, 0.9659258262890683122, 1.000000000000000000, 0.9659258262890683122, 1.000000000000000000, 0.9659258262890683122, 1.000000000000000000, 0.9659258262890683122, 1.000000000000000000, 0.9659258262890683122, 1.000000000000000000, 0.9659258262890683122, 1.000000000000000000, 0.9659258262890683122, 1.000000000000000000, 0.9659258262890683122, 1.000000000000000000, 0.9659258262890683122, 1.000000000000000000, 0.9659258262890683122, 1.000000000000000000, 0.9659258262890683122, 1.000000000000000000, 0.9659258262890683122, 1.000000000000000000, 0.9659258262890683122, 1.000000000000000000, 0.9659258262890683122, 1.000000000000000000, 0.9659258262890683122, 1.000000000000000000, 0.9659258262890683122, 1.000000000000000000, 0.9659258262890683122, 1.000000000000000000, 0.9659258262890683122, 1.000000000000000000, 0.9659258262890683122, 1.000000000000000000, 0.9659258262890683122, 1.000000000000000000, 0.9659258262890683122, 1.000000000000000000, 0.9659258262890683122, 1.000000000000000000, 0.9659258262890683122, 1.000000000000000000, 0.9659258262890683122, 1.000000000000000000, 0.9659258262890683122, 1.000000000000000000, 0.9659258262890683122, 1.000000000000000000, 0.9659258262890683122, 1.000000000000000000, 0.9659258262890683122, 1.000000000000000000, 0.9659258262890683122, 1.000000000000000000, 0.9659258262890683122, 1.000000000000000000, 0.9659258262890683122, 1.000000000000000000, 0.9659258262890683122, 1.000000000000000000, 0.9659258262890683122, 1.000000000000000000, 0.9659258262890683122, 1.000000000000000000, 0.9659258262890683122, 1.000000000000000000, 0.9659258262890683122, 1.000000000000000000, 0.9659258262890683122, 1.000000000000000000, 0.9659258262890683122, 1.000000000000000000, 0.9659258262890683122, 1.000000000000000000, 0.9659258262890683122, 1.000000000000000000, 0.9659258262890683122, 1.000000000000000000, 0.9659258262890683122, 1.000000000000000000, 0.9659258262890683122, 1.000000000000000000, 0.9659258262890683122, 1.000000000000000000, 0.9659258262890683122, 1.000000000000000000, 0.9659258262890683122, 1.000000000000000000, 0.9659258262890683122, 1.000000000000000000, 0.9659258262890683122, 1.000000000000000000, 0.9659258262890683122, 1.000000000000000000, 0.9659258262890683122, 1.000000000000000000, 0.9659258262890683122, 1.000000000000000000, 0.9659258262890683122, 1.000000000000000000, 0.9659258262890683122, 1.000000000000000000, 0.9659258262890683122, 1.000000000000000000, 0.9659258262890683122, 1.000000000000000000, 0.9659258262890683122, 1.000000000000000000, 0.9659258262890683122, 1.000000000000000000, 0.9659258262890683122, 1.000000000000000000, 0.9659258262890683122, 1.000000000000000000, 0.9659258262890683122, 1.000000000000000000, 0.9659258262890683122, 1.000000000000000000, 0.9659258262890683122, 1.000000000000000000, 0.9659258262890683122, 1.000000000000000000, 0.9659258262890683122, 1.000000000000000000, 0.9659258262890683122, 1.000000000000000000, 0.9659258262890683122, 1.000000000000000000, 0.9659258262890683122, 1.000000000000000000, 0.9659258262890683122, 1.000000000000000000, 0.9659258262890683122, 1.000000000000000000, 0.9659258262890683122, 1.000000000000000000, 0.9659258262890683122, 1.000000000000000000, 0.9659258262890683122, 1.000000000000000000, 0.9659258262890683122, 1.000000000000000000, 0.9659258262890683122, 1.000000000000000000, 0.9659258262890683122, 1.000000000000000000, 0.9659258262890683122, 1.000000000000000000, 0.9659258262890683122, 1.000000000000000000, 0.9659258262890683122, 1.000000000000000000, 0.9659258262890683122, 1.000000000000000000, 0.9659258262890683122, 1.000000000000000000, 0.9659258262890683122, 1.000000000000000000, 0.9659258262890683122, 1.000000000000000000, 0.9659258262890683122, 1.000000000000000000, 0.9659258262890683122, 1.000000000000000000, 0.9659258262890683122, 1.000000000000000000, 0.9659258262890683122, 1.000000000000000000, 0.9659258262890683122, 1.000000000000000000, 0.9659258262890683122, 1.000000000000000000, 0.9659258262890683122, 1.000000000000000000, 0.9659258262890683122, 1.000000000000000000, 0.9659258262890683122, 1.000000000000000000, 0.9659258262890683122, 1.000000000000000000, 0.9659258262890683122, 1.000000000000000000, 0.9659258262890683122, 1.000000000000000000, 0.9659258262890683122, 1.000000000000000000, 0.9659258262890683122, 1.000000000000000000, 0.9659258262890683122, 1.000000000000000000, 0.9659258262890683122, 1.000000000000000000, 0.9659258262890683122, 1.000000000000000000, 0.9659258262890683122, 1.000000000000000000, 0.9659258262890683122, 1.000000000000000000, 0.9659258262890683122, 1.000000000000000000, 0.9659258262890683122, 1.000000000000000000, 0.9659258262890683122, 1.000000000000000000, 0.9659258262890683122, 1.000000000000000000, 0.9659258262890683122, 1.000000000000000000, 0.9659258262890683122, 1.000000000000000000, 0.9659258262890683122, 1.000000000000000000, 0.9659258262890683122, 1.000000000000000000, 0.9659258262890683122, 1.000000000000000000, 0.9659258262890683122, 1.000000000000000000, 0.9659258262890683122, 1.000000000000000000, 0.9659258262890683122, 1.000000000000000000, 0.9659258262890683122, 1.000000000000000000, 0.9659258262890683122, 1.000000000000000000, 0.9659258262890683122, 1.000000000000000000, 0.9659258262890683122, 1.000000000000000000, 0.9659258262890683122, 1.000000000000000000, 0.9659258262890683122, 1.000000000000000000, 0.9659258262890683122, 1.000000000000000000, 0.9659258262890683122, 1.000000000000000000, 0.9659258262890683122, 1.000000000000000000, 0.9659258262890683122, 1.000000000000000000, 0.9659258262890683122, 1.000000000000000000, 0.9659258262890683122, 1.000000000000000000, 0.9659258262890683122, 1.000000000000000000, 0.9659258262890683122, 1.000000000000000000, 0.9659258262890683122, 1.000000000000000000, 0.9659258262890683122, 1.000000000000000000, 0.9659258262890683122, 1.000000000000000000, 0.9659258262890683122, 1.000000000000000000, 0.9659258262890683122, 1.000000000000000000, 0.9659258262890683122, 1.000000000000000000, 0.9659258262890683122, 1.000000000000000000, 0.9659258262890683122, 1.000000000000000000, 0.9659258262890683122, 1.000000000000000000, 0.9659258262890683122, 1.000000000000000000, 0.9659258262890683122, 1.000000000000000000, 0.9659258262890683122, 1.000000000000000000, 0.9659258262890683122, 1.000000000000000000, 0.9659258262890683122, 1.000000000000000000, 0.9659258262890683122, 1.000000000000000000, 0.9659258262890683122, 1.000000000000000000, 0.9659258262890683122, 1.000000000000000000, 0.9659258262890683122, 1.000000000000000000, 0.9659258262890683122, 1.000000000000000000, 0.9659258262890683122, 1.000000000000000000, 0.9659258262890683122, 1.000000000000000000, 0.9659258262890683122, 1.000000000000000000, 0.9659258262890683122, 1.000000000000000000, 0.9659258262890683122, 1.000000000000000000, 0.9659258262890683122, 1.000000000000000000, 0.9659258262890683122, 1.000000000000000000, 0.9659258262890683122, 1.000000000000000000, 0.9659258262890683122, 1.000000000000000000, 0.9659258262890683122, 1.000000000000000000, 0.9659258262890683122, 1.000000000000000000, 0.9659258262890683122, 1.000000000000000000, 0.9659258262890683122, 1.000000000000000000, 0.9659258262890683122, 1.000000000000000000, 0.9659258262890683122, 1.000000000000000000, 0.9659258262890683122, 1.000000000000000000, 0.9659258262890683122, 1.000000000000000000, 0.9659258262890683122, 1.000000000000000000, 0.9659258262890683122, 1.000000000000000000, 0.9659258262890683122, 1.000000000000000000, 0.9659258262890683122, 1.000000000000000000, 0.9659258262890683122, 1.000000000000000000, 0.9659258262890683122, 1.000000000000000000, 0.9659258262890683122, 1.000000000000000000, 0.9659258262890683122, 1.000000000000000000, 0.9659258262890683122, 1.000000000000000000, 0.9659258262890683122, 1.000000000000000000, 0.9659258262890683122, 1.000000000000000000, 0.9659258262890683122, 1.000000000000000000, 0.9659258262890683122, 1.000000000000000000, 0.9659258262890683122, 1.000000000000000000, 0.9659258262890683122, 1.000000000000000000, 0.9659258262890683122, 1.000000000000000000, 0.9659258262890683122, 1.000000000000000000, 0.9659258262890683122, 1.000000000000000000, 0.9659258262890683122, 1.000000000000000000, 0.9659258262890683122, 1.000000000000000000, 0.9659258262890683122, 1.000000000000000000, 0.9659258262890683122, 1.000000000000000000, 0.9659258262890683122, 1.000000000000000000, 0.9659258262890683122, 1.000000000000000000, 0.9659258262890683122, 1.000000000000000000, 0.9659258262890683122, 1.000000000000000000, 0.9659258262890683122, 1.000000000000000000, 0.9659258262890683122, 1.000000000000000000, 0.9659258262890683122, 1.000000000000000000, 0.9863514418465433309, 0.9836368620925994843, 0.9836368620925994843, 0.9836368620925994843) ) ) 
 REPRESENTATION_ITEM ( '' )  SURFACE ( )  );
#65484 = CARTESIAN_POINT ( 'NONE',  ( 0.000000000000000000, 51.05255888325788050, 10.99999999999999112 ) ) ;
#65485 = CARTESIAN_POINT ( 'NONE',  ( 7.320508075688776373, 245.0000000068279462, 7.320508075688767491 ) ) ;
#65486 = CARTESIAN_POINT ( 'NONE',  ( -7.999999999999989342, -6.533544264681542033E-06, 23.51780296876433596 ) ) ;
#65487 = CARTESIAN_POINT ( 'NONE',  ( 10.18810118749999916, 4.220049686691935698, 74.87500000204836681 ) ) ;
#65488 = LINE ( 'NONE', #60569, #7322 ) ;
#65489 = CARTESIAN_POINT ( 'NONE',  ( -4.999999999999998224, 148.5416666598387110, -8.660254037844389075 ) ) ;
#65490 = CARTESIAN_POINT ( 'NONE',  ( 6.676582343750001591, 290.9531250017069510, -8.176455196517173205E-16 ) ) ;
#65491 = CARTESIAN_POINT ( 'NONE',  ( -1.469576158976823947E-15, 19.12500000000000355, 8.000000000000000000 ) ) ;
#65492 = LINE ( 'NONE', #13784, #6333 ) ;
#65493 = CARTESIAN_POINT ( 'NONE',  ( -3.042071309553164404, 132.5520833299193555, -11.35316468749999963 ) ) ;
#65494 = CARTESIAN_POINT ( 'NONE',  ( -4.220049686691937474, -10.18810118749999738, 82.93750000204838102 ) ) ;
#65495 = CARTESIAN_POINT ( 'NONE',  ( -27.99999999999996447, 197.9375000013655779, 173.4587341250003760 ) ) ;
#65496 = CARTESIAN_POINT ( 'NONE',  ( 8.000000000000000000, 21.09375000000000355, -3.313708498984761608 ) ) ;
#65497 = CARTESIAN_POINT ( 'NONE',  ( -3.211159895383562723, 11.06249999863440792, 3.211159895383561391 ) ) ;
#65498 = EDGE_LOOP ( 'NONE', ( #59810, #54013, #29093, #59281 ) ) ;
#65499 = AXIS2_PLACEMENT_3D ( 'NONE', #69472, #39318, #68354 ) ;
#65500 = CARTESIAN_POINT ( 'NONE',  ( -2.775557561562891351E-14, 210.0000000000000284, 142.0000000000000568 ) ) ;
#65501 = CARTESIAN_POINT ( 'NONE',  ( 11.00000000000000000, 1.347111479062088405E-15, 118.0000000000000000 ) ) ;
#65502 = CARTESIAN_POINT ( 'NONE',  ( -3.458734125000015425, 200.2500000013656631, 143.4326545832176976 ) ) ;
#65503 = CARTESIAN_POINT ( 'NONE',  ( 3.999999999999960032, 203.0625000027311842, 143.6568542494924543 ) ) ;
#65504 = CARTESIAN_POINT ( 'NONE',  ( 5.000000000000000000, 13.21930962315071767, -69.49101004078873700 ) ) ;
#65505 = CARTESIAN_POINT ( 'NONE',  ( -6.238412754330611322E-16, 10.18810118749999916, 67.65625000204836681 ) ) ;
#65506 = ORIENTED_EDGE ( 'NONE', *, *, #8356, .F. ) ;
#65507 = CARTESIAN_POINT ( 'NONE',  ( 4.401442555609581635E-16, 5.343749997951610986, -7.188101187500000044 ) ) ;
#65508 = CARTESIAN_POINT ( 'NONE',  ( 4.000000000000001776, 20.06250000000000000, -1.656854249492381248 ) ) ;
#65509 = EDGE_CURVE ( 'NONE', #36743, #33110, #69551, .T. ) ;
#65510 = CARTESIAN_POINT ( 'NONE',  ( 7.188101187500000044, 116.2812500020483810, -8.802885111219163269E-16 ) ) ;
#65511 = CARTESIAN_POINT ( 'NONE',  ( 7.089540251308593888, -16.69146171830286463, -0.07476367467996772320 ) ) ;
#65512 = CARTESIAN_POINT ( 'NONE',  ( -2.765530957081996810, 292.2656250017069510, -6.676582343750002480 ) ) ;
#65514 = CARTESIAN_POINT ( 'NONE',  ( 8.660254037844389075, 137.2916666598387110, -5.000000000000000000 ) ) ;
#65513 = CARTESIAN_POINT ( 'NONE',  ( 5.676582343749997150, 232.2395833367473301, -9.832129032723418760 ) ) ;
#65515 = APPLICATION_CONTEXT ( 'automotive_design' ) ;
#65516 = VERTEX_POINT ( 'NONE', #64495 ) ;
#65517 = CARTESIAN_POINT ( 'NONE',  ( 3.042071309553163960, 222.7604166700806161, -11.35316468749999785 ) ) ;
#65518 = PRODUCT_DEFINITION_SHAPE ( 'NONE', 'NONE',  #54221 ) ;
#65519 = CARTESIAN_POINT ( 'NONE',  ( 7.188101187499991163, 2.977408999572648707, 28.20530278187175455 ) ) ;
#65520 = AXIS2_PLACEMENT_3D ( 'NONE', #74504, #11878, #34913 ) ;
#65521 = DIRECTION ( 'NONE',  ( -0.000000000000000000, 1.000000000000000000, -0.000000000000000000 ) ) ;
#65522 = CARTESIAN_POINT ( 'NONE',  ( 2.445694354108839175, 199.3125000013656063, 195.5543056458912190 ) ) ;
#65523 = ORIENTED_EDGE ( 'NONE', *, *, #52840, .T. ) ;
#65524 = CARTESIAN_POINT ( 'NONE',  ( 4.556349186104045934, 11.00000000000000000, 114.5312500000000000 ) ) ;
#65525 = CARTESIAN_POINT ( 'NONE',  ( 5.656854249492379694, 98.93750000000000000, -5.656854249492380582 ) ) ;
#65526 = CARTESIAN_POINT ( 'NONE',  ( -5.676582343750006032, 99.42708332991935549, 9.832129032723418760 ) ) ;
#65527 = DIRECTION ( 'NONE',  ( -0.000000000000000000, 1.000000000000000000, -0.000000000000000000 ) ) ;
#65528 = CARTESIAN_POINT ( 'NONE',  ( 11.00000000000000000, 1.347111479062088405E-15, 76.74999999999998579 ) ) ;
#65531 = FACE_OUTER_BOUND ( 'NONE', #65532, .T. ) ;
#65530 = CARTESIAN_POINT ( 'NONE',  ( 30.44569435410883074, 203.5625000013656063, 172.4456943541086957 ) ) ;
#65529 = CARTESIAN_POINT ( 'NONE',  ( 29.43265458321766559, 201.1250000013656347, 166.5412658749999650 ) ) ;
#65532 = EDGE_LOOP ( 'NONE', ( #10033, #33068, #50890, #58380 ) ) ;
#65533 = CYLINDRICAL_SURFACE ( 'NONE', #10402, 30.99999999999997158 ) ;
#65534 = EDGE_CURVE ( 'NONE', #47954, #39497, #72846, .T. ) ;
#65535 = CARTESIAN_POINT ( 'NONE',  ( -2.085542519210945728E-15, 209.5312499965860411, 11.35316468750000141 ) ) ;
#65536 = CARTESIAN_POINT ( 'NONE',  ( -3.458734125000016313, 202.8750000013656347, 140.5673454167824161 ) ) ;
#65537 = CARTESIAN_POINT ( 'NONE',  ( 25.55430564589115150, 202.5625000013656063, 172.4456943541086957 ) ) ;
#65538 = CARTESIAN_POINT ( 'NONE',  ( 7.778174593052021635, 7.778174593052023411, 114.6250000040967763 ) ) ;
#65539 = CARTESIAN_POINT ( 'NONE',  ( -11.35316468750000141, 198.8020833299193839, 3.042071309553159963 ) ) ;
#65540 = CARTESIAN_POINT ( 'NONE',  ( 2.977408999572650039, 91.06250000204838102, -7.188101187500000933 ) ) ;
#65541 = CARTESIAN_POINT ( 'NONE',  ( -23.99999999999998579, 197.7500000000000000, 170.0000000000003411 ) ) ;
#65542 = CARTESIAN_POINT ( 'NONE',  ( 4.541265875000002339, 13.37499999863440792, -1.881053915767121554 ) ) ;
#65543 = CARTESIAN_POINT ( 'NONE',  ( 30.44569435410883074, 197.0625000013656063, 167.5543056458911053 ) ) ;
#65544 = CARTESIAN_POINT ( 'NONE',  ( 2.977408999572650927, -7.188101187499990274, 5.330302781871753659 ) ) ;
#65545 = CARTESIAN_POINT ( 'NONE',  ( -8.311093377946841443, 83.90624999658602690, 8.311093377946830785 ) ) ;
#65546 = VERTEX_POINT ( 'NONE', #12064 ) ;
#65547 = CARTESIAN_POINT ( 'NONE',  ( -27.99999999999999645, 210.0000000000000284, 170.0000000000003695 ) ) ;
#65548 = CARTESIAN_POINT ( 'NONE',  ( 0.000000000000000000, 125.0000000000000000, 8.000000000000000000 ) ) ;
#65549 = LINE ( 'NONE', #8958, #9979 ) ;
#65550 = CARTESIAN_POINT ( 'NONE',  ( -2.085542519210945728E-15, 69.53124999658602690, 11.35316468750000141 ) ) ;
#65551 = ORIENTED_EDGE ( 'NONE', *, *, #56608, .T. ) ;
#65552 = CARTESIAN_POINT ( 'NONE',  ( 7.204075437095966983, 7.204075437095967871, 88.46875000204838102 ) ) ;
#65553 = CARTESIAN_POINT ( 'NONE',  ( -10.18810118749999916, 0.000000000000000000, 115.6562500020483810 ) ) ;
#65554 = CARTESIAN_POINT ( 'NONE',  ( 1.469576158976823947E-15, 102.8750000000000000, 8.000000000000000000 ) ) ;
#65555 = CARTESIAN_POINT ( 'NONE',  ( 3.313708498984721640, 23.53124999590321664, 8.000000000000039080 ) ) ;
#65557 = CARTESIAN_POINT ( 'NONE',  ( -5.676582343750006032, 79.11458332991935549, 9.832129032723418760 ) ) ;
#65556 = CARTESIAN_POINT ( 'NONE',  ( 0.000000000000000000, -28.00000000000000000, 3.999999999999988010 ) ) ;
#65558 = CARTESIAN_POINT ( 'NONE',  ( -3.313708498984757167, 7.999999999999991118, 26.23655278392014623 ) ) ;
#65559 = DIRECTION ( 'NONE',  ( 1.000000000000000000, 0.000000000000000000, 0.000000000000000000 ) ) ;
#65560 = CARTESIAN_POINT ( 'NONE',  ( -2.679491924311235618, 165.4166666598387110, 10.00000000000000000 ) ) ;
#65561 = CARTESIAN_POINT ( 'NONE',  ( 1.469576158976823947E-15, 113.5625000040967905, 8.000000000000000000 ) ) ;
#65562 = CARTESIAN_POINT ( 'NONE',  ( -11.00000000000000000, 0.000000000000000000, 118.0000000000000000 ) ) ;
#65563 = CARTESIAN_POINT ( 'NONE',  ( -11.35316468750000141, 63.80208332991934839, 3.042071309553159963 ) ) ;
#65564 = CARTESIAN_POINT ( 'NONE',  ( -4.220049686691935698, 10.18810118749999916, 105.2500000020483810 ) ) ;
#65565 = CARTESIAN_POINT ( 'NONE',  ( -3.042071309553164404, 192.2395833299193555, -11.35316468749999963 ) ) ;
#65566 = ORIENTED_EDGE ( 'NONE', *, *, #27397, .F. ) ;
#65567 = CARTESIAN_POINT ( 'NONE',  ( 3.313708498984762496, -7.999999999999989342, 26.98655278392014623 ) ) ;
#65568 = CARTESIAN_POINT ( 'NONE',  ( -7.347880794884122694E-16, 3.499999997268812724, 4.000000000000001776 ) ) ;
#65569 = CARTESIAN_POINT ( 'NONE',  ( -4.242640687119285658, 288.1249999999999432, 4.242640687119287435 ) ) ;
#65571 = CARTESIAN_POINT ( 'NONE',  ( 6.951808397369818766E-16, 192.0312499965860127, -11.35316468750000141 ) ) ;
#65570 = CARTESIAN_POINT ( 'NONE',  ( -23.99999999999998934, 200.8750000027312126, 170.0000000000002842 ) ) ;
#65572 = CARTESIAN_POINT ( 'NONE',  ( -7.320508075688773708, 193.7499999931720538, -7.320508075688774596 ) ) ;
#65573 = CARTESIAN_POINT ( 'NONE',  ( -8.660254037844387298, 232.7083333401613174, -4.999999999999999112 ) ) ;
#65574 = CARTESIAN_POINT ( 'NONE',  ( -5.000000000000005329, 190.2083333265053966, 8.660254037844387298 ) ) ;
#65575 = ORIENTED_EDGE ( 'NONE', *, *, #7642, .T. ) ;
#65576 = CARTESIAN_POINT ( 'NONE',  ( 5.676582343750001591, 176.9270833299193555, -9.832129032723420536 ) ) ;
#65577 =( BOUNDED_CURVE ( )  B_SPLINE_CURVE ( 2, ( #24550, #24909, #70580, #47556, #46457, #6482, #58906, #30220, #23820 ),
 .UNSPECIFIED., .F., .F. ) 
 B_SPLINE_CURVE_WITH_KNOTS ( ( 3, 2, 2, 2, 3 ),
 ( 0.8541666666666649643, 0.8645833333333317050, 0.8749999999999984457, 0.8854166666666650753, 0.8958333333333318160 ),
 .UNSPECIFIED. ) 
 CURVE ( )  GEOMETRIC_REPRESENTATION_ITEM ( )  RATIONAL_B_SPLINE_CURVE ( ( 1.000000000000012212, 0.9238795325112745260, 1.000000000000000000, 0.9238795325112867385, 1.000000000000000000, 0.9238795325112867385, 1.000000000000000000, 0.9238795325112980628, 0.9999999999999886757 ) ) 
 REPRESENTATION_ITEM ( '' )  );
#65578 = AXIS2_PLACEMENT_3D ( 'NONE', #14643, #19200, #42202 ) ;
#65579 = CARTESIAN_POINT ( 'NONE',  ( 5.082755093536318824, 5.082755093536319713, 20.42405278187175455 ) ) ;
#65580 = CARTESIAN_POINT ( 'NONE',  ( -25.55430564589115505, 209.0625000013656063, 172.4456943541091789 ) ) ;
#65581 = VERTEX_POINT ( 'NONE', #6420 ) ;
#65582 = ADVANCED_FACE ( 'NONE', ( #12795 ), #18100, .F. ) ;
#65583 = CARTESIAN_POINT ( 'NONE',  ( 5.656854249492379694, 100.6250000040967905, -5.656854249492380582 ) ) ;
#65584 = CARTESIAN_POINT ( 'NONE',  ( 23.99999999999998224, 208.8125000000000000, 171.6568542494922553 ) ) ;
#65585 =( BOUNDED_CURVE ( )  B_SPLINE_CURVE ( 2, ( #49654, #54208, #60596, #44370, #72671, #2518, #14185, #71907, #8173, #21348, #48894, #55704, #49270 ),
 .UNSPECIFIED., .F., .F. ) 
 B_SPLINE_CURVE_WITH_KNOTS ( ( 3, 2, 2, 2, 2, 2, 3 ),
 ( 0.5597826086956521063, 0.5615942028985506651, 0.5634057971014491129, 0.5652173913043476716, 0.5670289855072463414, 0.5688405797101449002, 0.5706521739130434590 ),
 .UNSPECIFIED. ) 
 CURVE ( )  GEOMETRIC_REPRESENTATION_ITEM ( )  RATIONAL_B_SPLINE_CURVE ( ( 1.000000000000001998, 0.9659258262890662028, 1.000000000000000000, 0.9659258262890683122, 1.000000000000000000, 0.9659258262890683122, 1.000000000000000000, 0.9659258262890683122, 1.000000000000000000, 0.9659258262890683122, 1.000000000000000000, 0.9659258262890683122, 1.000000000000000000 ) ) 
 REPRESENTATION_ITEM ( '' )  );
#65586 = CARTESIAN_POINT ( 'NONE',  ( -1.656854249492381248, 15.31249999999999822, -4.000000000000001776 ) ) ;
#65587 = CARTESIAN_POINT ( 'NONE',  ( 3.211159895383560947, 14.18749999863440792, 3.211159895383562723 ) ) ;
#65588 = CARTESIAN_POINT ( 'NONE',  ( -7.999999999999991118, 3.313708498984756723, 15.92405278392014623 ) ) ;
#65590 = CARTESIAN_POINT ( 'NONE',  ( 7.999999999999991118, 9.797174393178815797E-16, 18.26780278392014623 ) ) ;
#65589 = VECTOR ( 'NONE', #15676, 1000.000000000000000 ) ;
#65592 = EDGE_CURVE ( 'NONE', #60307, #38243, #1138, .T. ) ;
#65591 = ORIENTED_EDGE ( 'NONE', *, *, #48437, .F. ) ;
#65593 = DIRECTION ( 'NONE',  ( 0.000000000000000000, 1.000000000000000000, -6.938893903907228378E-16 ) ) ;
#65594 = CARTESIAN_POINT ( 'NONE',  ( -2.977408999572651815, 100.4375000020483668, 7.188101187500000933 ) ) ;
#65596 = CARTESIAN_POINT ( 'NONE',  ( -7.778174593052020747, -7.778174593052023411, 98.68749999999998579 ) ) ;
#65595 = DIRECTION ( 'NONE',  ( 0.000000000000000000, 0.000000000000000000, 1.000000000000000000 ) ) ;
#65597 = APPLICATION_PROTOCOL_DEFINITION ( 'draft international standard', 'automotive_design', 1998, #64545 ) ;
#65598 = VERTEX_POINT ( 'NONE', #46025 ) ;
#65599 = EDGE_CURVE ( 'NONE', #5483, #35159, #8273, .T. ) ;
#65600 = CARTESIAN_POINT ( 'NONE',  ( -7.999999999999998224, 101.2812500040967763, 3.313708498984766049 ) ) ;
#65601 = CARTESIAN_POINT ( 'NONE',  ( -7.188101187499992051, 0.000000000000000000, 16.48655278187175810 ) ) ;
#65602 = ORIENTED_EDGE ( 'NONE', *, *, #65768, .F. ) ;
#65603 = ORIENTED_EDGE ( 'NONE', *, *, #43051, .T. ) ;
#65604 = CARTESIAN_POINT ( 'NONE',  ( -6.238412754330611322E-16, 10.18810118749999916, 79.28125000204836681 ) ) ;
#65605 = CARTESIAN_POINT ( 'NONE',  ( 2.679491924311222739, 90.83333332650536818, 10.00000000000000355 ) ) ;
#65606 = CARTESIAN_POINT ( 'NONE',  ( 11.00000000000000000, 1.347111479062088405E-15, 94.74999999999998579 ) ) ;
#65609 = CARTESIAN_POINT ( 'NONE',  ( -2.765530957081998142, 292.7968750017070079, 6.676582343750000703 ) ) ;
#65608 = CARTESIAN_POINT ( 'NONE',  ( 26.34314575050758833, 200.6875000027312126, 165.9999999999998863 ) ) ;
#65607 = DIRECTION ( 'NONE',  ( -0.000000000000000000, 1.000000000000000000, -0.000000000000000000 ) ) ;
#65610 = CARTESIAN_POINT ( 'NONE',  ( 6.123233995736767268E-16, 151.2500000000000284, -10.00000000000000178 ) ) ;
#65611 = CARTESIAN_POINT ( 'NONE',  ( -1.656854249492383468, 0.6875000000000004441, 4.000000000000000888 ) ) ;
#65612 = CARTESIAN_POINT ( 'NONE',  ( 31.99999999999998579, 209.1875000000000284, 171.6568542494923122 ) ) ;
#65613 = AXIS2_PLACEMENT_3D ( 'NONE', #26085, #70640, #73621 ) ;
#65614 = ADVANCED_FACE ( 'NONE', ( #52803 ), #24493, .T. ) ;
#65615 = CARTESIAN_POINT ( 'NONE',  ( -5.000000000000000000, -52.35862550122958936, 48.98731492261398301 ) ) ;
#65616 = CARTESIAN_POINT ( 'NONE',  ( -8.000000000000000000, 1.968749995903220196, -3.313708498984762496 ) ) ;
#65617 = CARTESIAN_POINT ( 'NONE',  ( 27.99999999999996447, 199.4375000013655779, 173.4587341249998929 ) ) ;
#65618 = CARTESIAN_POINT ( 'NONE',  ( 5.082755093536325930, 10.03124999795161187, -5.082755093536325930 ) ) ;
#65619 = CARTESIAN_POINT ( 'NONE',  ( 7.999999999999992895, -3.313708498984756279, 24.17405278392015333 ) ) ;
#65620 = DIRECTION ( 'NONE',  ( 0.000000000000000000, 0.000000000000000000, -1.000000000000000000 ) ) ;
#65621 = CARTESIAN_POINT ( 'NONE',  ( 2.977408999572654480, 111.5000000020483810, 7.188101187499999156 ) ) ;
#65622 = CARTESIAN_POINT ( 'NONE',  ( -8.660254037844387298, 249.5833333333333428, -4.999999999999999112 ) ) ;
#65623 = CYLINDRICAL_SURFACE ( 'NONE', #29117, 8.000000000000000000 ) ;
#65624 = CARTESIAN_POINT ( 'NONE',  ( 28.00000000000002487, 209.1875000013656063, 166.5412658749999082 ) ) ;
#65625 = CARTESIAN_POINT ( 'NONE',  ( -7.188101187499992051, 0.000000000000000000, 19.86155278187175455 ) ) ;
#65626 = LINE ( 'NONE', #37338, #21458 ) ;
#65627 = CARTESIAN_POINT ( 'NONE',  ( 3.042071309553167069, 41.82291666325269119, -11.35316468749999785 ) ) ;
#65628 = CARTESIAN_POINT ( 'NONE',  ( 2.679491924297531913, 148.9583333333321207, 10.00000000000791367 ) ) ;
#65629 = CARTESIAN_POINT ( 'NONE',  ( 5.000000000000001776, 12.70833332650536640, -8.660254037844389075 ) ) ;
#65630 = FACE_BOUND ( 'NONE', #51933, .T. ) ;
#65631 =( NAMED_UNIT ( * ) PLANE_ANGLE_UNIT ( ) SI_UNIT ( $, .RADIAN. ) );
#65632 = ORIENTED_EDGE ( 'NONE', *, *, #67916, .T. ) ;
#65633 = DIRECTION ( 'NONE',  ( 0.000000000000000000, 0.000000000000000000, 1.000000000000000000 ) ) ;
#65634 = CARTESIAN_POINT ( 'NONE',  ( 2.775557561562891351E-14, -37.99999999999992184, 170.0000000000000284 ) ) ;
#65635 = CARTESIAN_POINT ( 'NONE',  ( -2.085542519210945728E-15, 29.53124999658601624, 11.35316468750000141 ) ) ;
#65636 = CARTESIAN_POINT ( 'NONE',  ( -7.778174593052023411, 7.778174593052023411, 79.00000000409676204 ) ) ;
#65637 = CARTESIAN_POINT ( 'NONE',  ( 3.458734124999960358, 202.6875000013656063, 142.0000000000000568 ) ) ;
#65638 = CARTESIAN_POINT ( 'NONE',  ( -4.898587196589412829E-16, 108.3125000040967905, -8.000000000000000000 ) ) ;
#65639 = CARTESIAN_POINT ( 'NONE',  ( 5.656854249492378806, 25.12499999590322375, 5.656854249492381470 ) ) ;
#65641 = CARTESIAN_POINT ( 'NONE',  ( -3.042071309553173730, 29.32291666325268764, 11.35316468749999785 ) ) ;
#65640 = CARTESIAN_POINT ( 'NONE',  ( 5.082755093536325042, 108.5937500020483810, -5.082755093536325930 ) ) ;
#65642 = CARTESIAN_POINT ( 'NONE',  ( -7.999999999999989342, -3.313708498984762496, 17.42405277982336997 ) ) ;
#65643 = CARTESIAN_POINT ( 'NONE',  ( -11.35316468750000141, 168.4895833299193839, 3.042071309553159963 ) ) ;
#65644 = CARTESIAN_POINT ( 'NONE',  ( 8.660254037844389075, 127.2916666598387110, -5.000000000000000000 ) ) ;
#65645 = ADVANCED_FACE ( 'NONE', ( #34734 ), #40371, .T. ) ;
#65646 = CARTESIAN_POINT ( 'NONE',  ( -7.188101187500001821, 106.4375000020483810, -2.977408999572650483 ) ) ;
#65647 = ORIENTED_EDGE ( 'NONE', *, *, #5325, .F. ) ;
#65648 = CARTESIAN_POINT ( 'NONE',  ( 1.477658550686875349, 9.539178283403852987, -0.3563104543936415625 ) ) ;
#65649 = CARTESIAN_POINT ( 'NONE',  ( -5.676582343750006032, 19.42708332991934839, 9.832129032723418760 ) ) ;
#65650 = EDGE_LOOP ( 'NONE', ( #48902, #15612, #28011, #841 ) ) ;
#65651 = DIRECTION ( 'NONE',  ( 0.000000000000000000, 0.000000000000000000, 1.000000000000000000 ) ) ;
#65652 = DIRECTION ( 'NONE',  ( -0.000000000000000000, 1.000000000000000000, -0.000000000000000000 ) ) ;
#65654 = CARTESIAN_POINT ( 'NONE',  ( 11.35316468749999785, 150.5729166632526699, 3.042071309553174174 ) ) ;
#65653 = CARTESIAN_POINT ( 'NONE',  ( -20.96205440650471274, -27.49281490417435592, 145.1888853501775714 ) ) ;
#65655 = DIRECTION ( 'NONE',  ( -0.000000000000000000, 1.000000000000000000, 4.689100369878284071E-30 ) ) ;
#65656 = CARTESIAN_POINT ( 'NONE',  ( 7.999999999999992895, -3.313708498984756279, 19.54280278432982954 ) ) ;
#65657 = CARTESIAN_POINT ( 'NONE',  ( -8.000000000000010658, -3.313708498984740736, 15.92405277982336287 ) ) ;
#65658 = CARTESIAN_POINT ( 'NONE',  ( 8.311093377946839666, 235.7812500034139589, 8.311093377946829008 ) ) ;
#65659 = CARTESIAN_POINT ( 'NONE',  ( -4.220049686691937474, -10.18810118749999738, 83.31250000204836681 ) ) ;
#65660 = ORIENTED_EDGE ( 'NONE', *, *, #55921, .F. ) ;
#65661 = DIRECTION ( 'NONE',  ( -0.000000000000000000, 1.000000000000000000, -0.000000000000000000 ) ) ;
#65662 = CARTESIAN_POINT ( 'NONE',  ( -3.313708498984772710, 122.4687500040967620, 7.999999999999988454 ) ) ;
#65663 = CARTESIAN_POINT ( 'NONE',  ( -11.35316468750000141, 108.5937499965860269, -1.390361679473963753E-15 ) ) ;
#65664 = CARTESIAN_POINT ( 'NONE',  ( 7.204075437095968759, -7.204075437095966983, 101.2187500020483668 ) ) ;
#65665 = CARTESIAN_POINT ( 'NONE',  ( -4.541265875000003227, 14.99999999863440969, 1.881053915767121110 ) ) ;
#65666 = EDGE_LOOP ( 'NONE', ( #72598, #11824, #33320, #52146 ) ) ;
#65667 = EDGE_LOOP ( 'NONE', ( #1632, #67648 ) ) ;
#65668 = CARTESIAN_POINT ( 'NONE',  ( -5.656854249492379694, 12.56250000000000178, -5.656854249492380582 ) ) ;
#65669 = CARTESIAN_POINT ( 'NONE',  ( -3.211159895383561391, 3.812499998634407028, -3.211159895383561835 ) ) ;
#65670 = CARTESIAN_POINT ( 'NONE',  ( 5.082755093536324154, 3.281249997951610098, 5.082755093536326818 ) ) ;
#65671 = VECTOR ( 'NONE', #66776, 1000.000000000000000 ) ;
#65672 = CARTESIAN_POINT ( 'NONE',  ( -3.313708498984762496, 113.4687500040967763, 7.999999999999998224 ) ) ;
#65673 = CARTESIAN_POINT ( 'NONE',  ( 10.18810118750000093, -4.220049686691933921, 98.68750000204838102 ) ) ;
#65674 =( BOUNDED_CURVE ( )  B_SPLINE_CURVE ( 2, ( #22336, #74408, #28756, #4645, #5019, #22715, #67642, #9924, #50646 ),
 .UNSPECIFIED., .F., .F. ) 
 B_SPLINE_CURVE_WITH_KNOTS ( ( 3, 2, 2, 2, 3 ),
 ( 0.6500000000000004663, 0.6583333333333338810, 0.6666666666666671848, 0.6750000000000007105, 0.6833333333333340143 ),
 .UNSPECIFIED. ) 
 CURVE ( )  GEOMETRIC_REPRESENTATION_ITEM ( )  RATIONAL_B_SPLINE_CURVE ( ( 0.9999999999999958922, 0.9238795325112908463, 1.000000000000000000, 0.9238795325112867385, 1.000000000000000000, 0.9238795325112867385, 1.000000000000000000, 0.9238795325112806323, 1.000000000000005995 ) ) 
 REPRESENTATION_ITEM ( '' )  );
#65675 = CARTESIAN_POINT ( 'NONE',  ( -2.828427124746192067, 4.625000000000000000, 2.828427124746190735 ) ) ;
#65676 = CARTESIAN_POINT ( 'NONE',  ( 1.656854249492381248, 15.93749999726881228, -4.000000000000001776 ) ) ;
#65677 = CARTESIAN_POINT ( 'NONE',  ( 4.541265875000002339, 5.312499998634407028, 0.000000000000000000 ) ) ;
#65678 = CARTESIAN_POINT ( 'NONE',  ( 2.445694354108783664, 209.3125000013656063, 144.4456943541088663 ) ) ;
#65679 = CARTESIAN_POINT ( 'NONE',  ( -3.458734124999959914, 196.3750000013656063, 196.5673454167823877 ) ) ;
#65680 = EDGE_CURVE ( 'NONE', #64324, #53638, #59212, .T. ) ;
#65682 = CARTESIAN_POINT ( 'NONE',  ( -8.660254037844390851, 224.7916666598387110, 4.999999999999998224 ) ) ;
#65681 = CARTESIAN_POINT ( 'NONE',  ( -31.45873412499995680, 199.7500000013656063, 171.4326545832181239 ) ) ;
#65683 = EDGE_CURVE ( 'NONE', #18825, #12576, #31, .T. ) ;
#65684 = CARTESIAN_POINT ( 'NONE',  ( -4.541265875000003227, 15.87499999863440436, 1.881053915767121110 ) ) ;
#65685 = FACE_OUTER_BOUND ( 'NONE', #10431, .T. ) ;
#65686 = CARTESIAN_POINT ( 'NONE',  ( 7.188101187499993827, -2.977408999572645598, 9.642802781871756324 ) ) ;
#65687 = ORIENTED_EDGE ( 'NONE', *, *, #58364, .F. ) ;
#65688 = ORIENTED_EDGE ( 'NONE', *, *, #19188, .F. ) ;
#65689 = CARTESIAN_POINT ( 'NONE',  ( -4.220049686691937474, -10.18810118749999738, 96.43750000204836681 ) ) ;
#65690 = CARTESIAN_POINT ( 'NONE',  ( 2.679491924311229401, 126.0416666666666572, -10.00000000000000178 ) ) ;
#65691 = CARTESIAN_POINT ( 'NONE',  ( -28.00000000000002132, 202.6875000013656063, 166.5412658750003629 ) ) ;
#65692 = CARTESIAN_POINT ( 'NONE',  ( -32.00000000000000000, 202.2500000000000000, 170.0000000000003979 ) ) ;
#65693 = CARTESIAN_POINT ( 'NONE',  ( 3.458734125000015425, 197.9375000013655779, 198.0000000000000284 ) ) ;
#65694 = LINE ( 'NONE', #71348, #71098 ) ;
#65695 = CARTESIAN_POINT ( 'NONE',  ( -2.679491924311235618, 113.5416666666666714, 10.00000000000000000 ) ) ;
#65696 = CARTESIAN_POINT ( 'NONE',  ( 3.313708498984765161, 111.9687500000000142, 7.999999999999998224 ) ) ;
#65697 = CARTESIAN_POINT ( 'NONE',  ( -6.676582343750001591, 294.6093750017069510, 0.000000000000000000 ) ) ;
#65698 = EDGE_LOOP ( 'NONE', ( #5167, #55076 ) ) ;
#65699 = CARTESIAN_POINT ( 'NONE',  ( 5.000000000000014211, 189.1666666666667140, 8.660254037844426378 ) ) ;
#65700 = EDGE_CURVE ( 'NONE', #71723, #57840, #23385, .T. ) ;
#65701 = CARTESIAN_POINT ( 'NONE',  ( 8.000000000000000000, 22.40624999590322375, -3.313708498984761608 ) ) ;
#65702 = CARTESIAN_POINT ( 'NONE',  ( -2.445694354108838731, 205.0625000013656063, 144.4456943541088663 ) ) ;
#65703 = PLANE ( 'NONE',  #49067 ) ;
#65704 = DIRECTION ( 'NONE',  ( -0.000000000000000000, 1.000000000000000000, -0.000000000000000000 ) ) ;
#65705 = CARTESIAN_POINT ( 'NONE',  ( -6.123233995736766282E-16, 223.7500000000000000, -10.00000000000000000 ) ) ;
#65706 = CARTESIAN_POINT ( 'NONE',  ( 11.00000000000000355, -4.556349186104045046, 114.1562499999999716 ) ) ;
#65707 = CARTESIAN_POINT ( 'NONE',  ( 2.679491924311222739, 223.9583333333333428, 10.00000000000000355 ) ) ;
#65708 = EDGE_CURVE ( 'NONE', #55468, #18660, #46849, .T. ) ;
#65709 = CARTESIAN_POINT ( 'NONE',  ( 2.977408999572650927, -7.188101187499990274, 5.330302781871753659 ) ) ;
#65710 = CARTESIAN_POINT ( 'NONE',  ( -11.35316468749999785, 198.3854166632526699, -3.042071309553167513 ) ) ;
#65711 = CARTESIAN_POINT ( 'NONE',  ( 11.00000000000005329, -4.556349186103991755, 102.1562499999999858 ) ) ;
#65712 = CARTESIAN_POINT ( 'NONE',  ( -3.211159895383561391, 2.687499998634407028, -3.211159895383561835 ) ) ;
#65713 = LINE ( 'NONE', #36321, #26028 ) ;
#65715 = CARTESIAN_POINT ( 'NONE',  ( 7.999999999836578723, -5.113295603412193572E-05, 3.267801294049292871 ) ) ;
#65714 = DIRECTION ( 'NONE',  ( 0.000000000000000000, 0.000000000000000000, 1.000000000000000000 ) ) ;
#65716 = ORIENTED_EDGE ( 'NONE', *, *, #25808, .T. ) ;
#65717 = CARTESIAN_POINT ( 'NONE',  ( -1.432654583217664701, 203.0000000013655779, 138.5412658750000787 ) ) ;
#65718 = CARTESIAN_POINT ( 'NONE',  ( 6.951808397369818766E-16, 47.34374999658602690, -11.35316468750000141 ) ) ;
#65719 = CARTESIAN_POINT ( 'NONE',  ( -11.00000000000000000, 4.556349186104045934, 103.0937500040968047 ) ) ;
#65720 = VECTOR ( 'NONE', #51957, 1000.000000000000000 ) ;
#65721 = CARTESIAN_POINT ( 'NONE',  ( 0.000000000000000000, 0.000000000000000000, -1.155342438046016218 ) ) ;
#65722 = CARTESIAN_POINT ( 'NONE',  ( -27.99999999999991829, 202.9375000013656063, 173.4587341250003760 ) ) ;
#65723 = DIRECTION ( 'NONE',  ( -0.000000000000000000, -0.000000000000000000, -1.000000000000000000 ) ) ;
#65725 = CARTESIAN_POINT ( 'NONE',  ( -7.347880794884122694E-16, 9.499999997268814056, 4.000000000000001776 ) ) ;
#65724 = CARTESIAN_POINT ( 'NONE',  ( -11.00000000000000000, 0.000000000000000000, 71.68750000409676204 ) ) ;
#65726 = CARTESIAN_POINT ( 'NONE',  ( 3.458734124999958581, 196.5000000013656063, 140.5673454167823593 ) ) ;
#65727 = CARTESIAN_POINT ( 'NONE',  ( -11.35316468750000141, 113.4895833299193413, 3.042071309553159963 ) ) ;
#65728 = CARTESIAN_POINT ( 'NONE',  ( 10.00000000000000178, 92.08333332650536818, -2.679491924311226736 ) ) ;
#65730 = EDGE_CURVE ( 'NONE', #26634, #39873, #19934, .T. ) ;
#65729 = VECTOR ( 'NONE', #5581, 1000.000000000000000 ) ;
#65731 = CARTESIAN_POINT ( 'NONE',  ( -2.977408999572650927, 89.37500000204839523, -7.188101187500001821 ) ) ;
#65732 = CARTESIAN_POINT ( 'NONE',  ( 1.881053915767122664, 16.24999999863440436, 4.541265875000001451 ) ) ;
#65733 = CARTESIAN_POINT ( 'NONE',  ( 4.000000000000001776, 11.06250000000000000, -1.656854249492381248 ) ) ;
#65734 = CARTESIAN_POINT ( 'NONE',  ( -30.93541659651598508, -42.99981040672927435, 171.9999999999998295 ) ) ;
#65735 = VERTEX_POINT ( 'NONE', #65218 ) ;
#65736 = CARTESIAN_POINT ( 'NONE',  ( -9.935834282059264666, 225.9999999999999716, 1.307295064324885070 ) ) ;
#65738 = EDGE_CURVE ( 'NONE', #62341, #68592, #54568, .T. ) ;
#65737 = ORIENTED_EDGE ( 'NONE', *, *, #10496, .F. ) ;
#65739 = CARTESIAN_POINT ( 'NONE',  ( 4.721056650415999201, 292.2343750017069510, -4.721056650415999201 ) ) ;
#65740 = CARTESIAN_POINT ( 'NONE',  ( 27.99999999999999645, 210.0000000000000284, 173.9999999999998863 ) ) ;
#65741 = CARTESIAN_POINT ( 'NONE',  ( 5.656854249492376141, -5.656854249492374365, 6.080302783920147114 ) ) ;
#65742 = CARTESIAN_POINT ( 'NONE',  ( -11.35316468750000141, 173.4895833299193839, 3.042071309553159963 ) ) ;
#65743 = CARTESIAN_POINT ( 'NONE',  ( -1.656854249492466735, 195.3125000027312126, 201.9999999999999147 ) ) ;
#65744 = CARTESIAN_POINT ( 'NONE',  ( 2.849036369511732440E-14, 200.2500000000000000, 202.0000000000000000 ) ) ;
#65745 = CARTESIAN_POINT ( 'NONE',  ( 2.020667218593132706E-15, -11.00000000000000000, 70.56250000409677625 ) ) ;
#65746 = CARTESIAN_POINT ( 'NONE',  ( -6.238412754330611322E-16, 10.18810118749999916, 112.6562500020483810 ) ) ;
#65747 = EDGE_LOOP ( 'NONE', ( #10478, #9161, #65755, #25080 ) ) ;
#65748 = CARTESIAN_POINT ( 'NONE',  ( -5.126144196591230440, 52.42426806216718660, -49.01287729762170642 ) ) ;
#65749 = CARTESIAN_POINT ( 'NONE',  ( 0.000000000000000000, 300.0000000000000000, 6.000000000000001776 ) ) ;
#65750 = CARTESIAN_POINT ( 'NONE',  ( 9.832129032723416984, 145.6770833299193555, 5.676582343750006032 ) ) ;
#65751 = CARTESIAN_POINT ( 'NONE',  ( 2.849036369511732440E-14, 206.3750000027312126, 202.0000000000000000 ) ) ;
#65752 = DIRECTION ( 'NONE',  ( -0.000000000000000000, -0.000000000000000000, -1.000000000000000000 ) ) ;
#65753 = CARTESIAN_POINT ( 'NONE',  ( -10.18810118749999738, -4.220049686691941915, 71.12500000204836681 ) ) ;
#65754 = CARTESIAN_POINT ( 'NONE',  ( 8.311093377946834337, 60.46874999658602690, 8.311093377946839666 ) ) ;
#65755 = ORIENTED_EDGE ( 'NONE', *, *, #24658, .T. ) ;
#65756 = CARTESIAN_POINT ( 'NONE',  ( -28.00000000000008171, 209.1250000027312126, 166.0000000000003695 ) ) ;
#65757 = CARTESIAN_POINT ( 'NONE',  ( 3.211159895383561835, 6.562499998634407028, -3.211159895383561835 ) ) ;
#65758 = CARTESIAN_POINT ( 'NONE',  ( 3.317071493978883456, -8.008118988124989457, 10.48186528394063188 ) ) ;
#65759 = EDGE_LOOP ( 'NONE', ( #62266, #2088, #63013, #12348, #30879 ) ) ;
#65760 = ADVANCED_FACE ( 'NONE', ( #48976 ), #8249, .T. ) ;
#65761 = CARTESIAN_POINT ( 'NONE',  ( 4.401442555609581635E-16, 21.84374999795161543, -7.188101187500000044 ) ) ;
#65762 = CARTESIAN_POINT ( 'NONE',  ( 0.000000000000000000, 0.000000000000000000, 0.000000000000000000 ) ) ;
#65763 = DIRECTION ( 'NONE',  ( -0.000000000000000000, -0.000000000000000000, 1.000000000000000000 ) ) ;
#65764 = CARTESIAN_POINT ( 'NONE',  ( 2.977408999572651815, 12.56249999795161365, 7.188101187500000933 ) ) ;
#65765 = CARTESIAN_POINT ( 'NONE',  ( 5.082755093536320601, -5.082755093536318824, 2.049052781871754103 ) ) ;
#65766 = EDGE_CURVE ( 'NONE', #6205, #74331, #48608, .T. ) ;
#65767 = CARTESIAN_POINT ( 'NONE',  ( 7.204075437095966983, 7.204075437095967871, 113.9687500020483810 ) ) ;
#65768 = EDGE_CURVE ( 'NONE', #21807, #37240, #13742, .T. ) ;
#65769 = CARTESIAN_POINT ( 'NONE',  ( 0.000000000000000000, 0.000000000000000000, 0.000000000000000000 ) ) ;
#65770 = CARTESIAN_POINT ( 'NONE',  ( -1.656854249492381248, 1.062499997268813168, -4.000000000000001776 ) ) ;
#65771 = ORIENTED_EDGE ( 'NONE', *, *, #8039, .F. ) ;
#65772 = CARTESIAN_POINT ( 'NONE',  ( 3.458734125000016313, 204.8750000013656063, 199.4326545832176691 ) ) ;
#65773 = VECTOR ( 'NONE', #60210, 1000.000000000000000 ) ;
#65774 = CARTESIAN_POINT ( 'NONE',  ( -27.99999999999990763, 196.6250000027312126, 174.0000000000003695 ) ) ;
#65775 = CARTESIAN_POINT ( 'NONE',  ( -4.541265875000003227, 3.874999998634407028, 1.881053915767121110 ) ) ;
#65776 = CARTESIAN_POINT ( 'NONE',  ( -2.977408999572650927, 110.3750000020484094, -7.188101187500001821 ) ) ;
#65777 = CARTESIAN_POINT ( 'NONE',  ( 7.000000000000000000, 0.000000000000000000, -14.07439246179028203 ) ) ;
#65778 = CARTESIAN_POINT ( 'NONE',  ( -5.082755093536319713, 5.082755093536319713, 23.79905278187175455 ) ) ;
#65779 = ORIENTED_EDGE ( 'NONE', *, *, #52416, .F. ) ;
#65780 = CARTESIAN_POINT ( 'NONE',  ( 2.977408999572650927, 20.24999999795161898, -7.188101187500000933 ) ) ;
#65781 = EDGE_LOOP ( 'NONE', ( #28058, #16670, #18398, #63445 ) ) ;
#65782 = CARTESIAN_POINT ( 'NONE',  ( -6.238412754330611322E-16, 10.18810118749999916, 116.7812500020483810 ) ) ;
#65783 = CARTESIAN_POINT ( 'NONE',  ( -6.406773156053975349, 4.907047822329288600, -0.000000000000000000 ) ) ;
#65784 = CARTESIAN_POINT ( 'NONE',  ( 2.445694354108838731, 207.0625000013656063, 195.5543056458912190 ) ) ;
#65785 = CARTESIAN_POINT ( 'NONE',  ( 24.54126587499998280, 204.1250000013656063, 168.5673454167822740 ) ) ;
#65786 = CARTESIAN_POINT ( 'NONE',  ( -2.679491924311225848, 66.45833333333334281, -10.00000000000000178 ) ) ;
#65787 = CARTESIAN_POINT ( 'NONE',  ( -7.188101187499999156, 96.12500000204836681, 2.977408999572654924 ) ) ;
#65788 = CARTESIAN_POINT ( 'NONE',  ( -2.485281374238572649, 298.1875000000000000, 6.000000000000002665 ) ) ;
#65790 = CARTESIAN_POINT ( 'NONE',  ( -6.373372650972353171, -4.860592676736378515, -0.000000000000000000 ) ) ;
#65789 = CARTESIAN_POINT ( 'NONE',  ( 30.82842712474617031, 208.5000000027312126, 167.1715728752537018 ) ) ;
#65791 = VERTEX_POINT ( 'NONE', #24847 ) ;
#65792 =( BOUNDED_CURVE ( )  B_SPLINE_CURVE ( 2, ( #6192, #16737, #57885, #22775, #23156, #63894, #5080, #52213, #17120 ),
 .UNSPECIFIED., .F., .F. ) 
 B_SPLINE_CURVE_WITH_KNOTS ( ( 3, 2, 2, 2, 3 ),
 ( 0.02941176470588237335, 0.03308823529411766828, 0.03676470588235296322, 0.04044117647058826509, 0.04411764705882356002 ),
 .UNSPECIFIED. ) 
 CURVE ( )  GEOMETRIC_REPRESENTATION_ITEM ( )  RATIONAL_B_SPLINE_CURVE ( ( 0.9999999999999995559, 0.9238795325112871826, 1.000000000000000000, 0.9238795325112867385, 1.000000000000000000, 0.9238795325112867385, 1.000000000000000000, 0.9238795325112861834, 1.000000000000000666 ) ) 
 REPRESENTATION_ITEM ( '' )  );
#65793 = VECTOR ( 'NONE', #55943, 1000.000000000000000 ) ;
#65794 = CARTESIAN_POINT ( 'NONE',  ( 5.676582343750005144, 225.5729166700806729, 9.832129032723416984 ) ) ;
#65795 = CARTESIAN_POINT ( 'NONE',  ( -1.656854249492403008, 198.8125000027312126, 146.0000000000000284 ) ) ;
#65796 = CARTESIAN_POINT ( 'NONE',  ( 0.000000000000000000, 0.000000000000000000, 118.0000000000000000 ) ) ;
#65797 = CARTESIAN_POINT ( 'NONE',  ( -7.999999999999991118, 0.000000000000000000, 2.517802783920143561 ) ) ;
#65798 = CARTESIAN_POINT ( 'NONE',  ( -9.999999999999998224, 260.2083333333333144, 2.679491924311235618 ) ) ;
#65799 = DIRECTION ( 'NONE',  ( -0.000000000000000000, -0.000000000000000000, -1.000000000000000000 ) ) ;
#65800 = CARTESIAN_POINT ( 'NONE',  ( -5.000000000000005329, 168.3333333333333428, 8.660254037844387298 ) ) ;
#65801 = CARTESIAN_POINT ( 'NONE',  ( 7.188101187499992051, 2.977408999572647819, 20.70530278187175810 ) ) ;
#65802 = CARTESIAN_POINT ( 'NONE',  ( 9.832129032723416984, 160.6770833299193555, 5.676582343750006032 ) ) ;
#65803 = CARTESIAN_POINT ( 'NONE',  ( 6.000000000000003553, 294.5000000034139589, 2.485281374238571317 ) ) ;
#65804 = DIRECTION ( 'NONE',  ( -0.000000000000000000, 1.000000000000000000, -0.000000000000000000 ) ) ;
#65807 = CARTESIAN_POINT ( 'NONE',  ( -12.00000000000000000, -6.928203230275527424, -14.00000000000000178 ) ) ;
#65806 = CARTESIAN_POINT ( 'NONE',  ( 5.000000000000000000, 16.24494643555759410, -69.83755725260752456 ) ) ;
#65805 = CARTESIAN_POINT ( 'NONE',  ( 26.34314575050758833, 200.9375000000000284, 173.9999999999999147 ) ) ;
#65808 = EDGE_LOOP ( 'NONE', ( #43215, #49126, #34660, #42762 ) ) ;
#65809 = CARTESIAN_POINT ( 'NONE',  ( -5.676582343749998039, 12.76041666325268409, -9.832129032723420536 ) ) ;
#65810 = CARTESIAN_POINT ( 'NONE',  ( 4.999999999999993783, 96.04166665983871098, 8.660254037844390851 ) ) ;
#65811 = CARTESIAN_POINT ( 'NONE',  ( 7.320508075688774596, 32.49999999317203248, -7.320508075688774596 ) ) ;
#65812 = CARTESIAN_POINT ( 'NONE',  ( -3.313708498984869966, 115.7187500000000142, -7.999999999999892530 ) ) ;
#65813 = CARTESIAN_POINT ( 'NONE',  ( -2.445694354108839619, 206.8125000013656063, 139.5543056458912190 ) ) ;
#65814 = CARTESIAN_POINT ( 'NONE',  ( -2.828427124746209831, 202.3750000000000284, 139.1715728752538723 ) ) ;
#65815 = CARTESIAN_POINT ( 'NONE',  ( -2.679491924311235618, 45.41666665983869677, 10.00000000000000000 ) ) ;
#65816 = CARTESIAN_POINT ( 'NONE',  ( 2.977408999572650039, 111.6875000020483810, -7.188101187500001821 ) ) ;
#65817 = CARTESIAN_POINT ( 'NONE',  ( 1.881053915767121776, 3.624999998634407028, -4.541265875000002339 ) ) ;
#65818 = CARTESIAN_POINT ( 'NONE',  ( 0.7509181236780181345, 65.76106071587292945, -26.27764834702227859 ) ) ;
#65819 = CARTESIAN_POINT ( 'NONE',  ( 7.999999999999991118, 9.797174393178815797E-16, 13.58030277982336465 ) ) ;
#65821 = CARTESIAN_POINT ( 'NONE',  ( 6.123233995736767268E-16, 8.124999993172032475, -10.00000000000000178 ) ) ;
#65820 = CARTESIAN_POINT ( 'NONE',  ( 1.975797226262149708, 194.5437978492538207, 139.0505076526418975 ) ) ;
#65822 = ORIENTED_EDGE ( 'NONE', *, *, #15091, .F. ) ;
#65823 = CARTESIAN_POINT ( 'NONE',  ( -3.673940397442060854E-16, 292.8125000034140157, -6.000000000000001776 ) ) ;
#65824 = CARTESIAN_POINT ( 'NONE',  ( -3.313708498984757611, 7.999999999999991118, 14.23655278392014623 ) ) ;
#65825 = CARTESIAN_POINT ( 'NONE',  ( -9.832129032723418760, 228.8020833367473301, -5.676582343749998927 ) ) ;
#65826 = CARTESIAN_POINT ( 'NONE',  ( -2.085542519210945728E-15, 124.5312499965860269, 11.35316468750000141 ) ) ;
#65827 = ORIENTED_EDGE ( 'NONE', *, *, #1308, .T. ) ;
#65828 = CARTESIAN_POINT ( 'NONE',  ( -4.000000000000015987, 200.5000000000000000, 142.0000000000000568 ) ) ;
#65829 = CARTESIAN_POINT ( 'NONE',  ( 7.204075437095968759, -7.204075437095966983, 98.21875000204838102 ) ) ;
#65830 = CYLINDRICAL_SURFACE ( 'NONE', #74260, 11.00000000000000000 ) ;
#65831 = CARTESIAN_POINT ( 'NONE',  ( 2.839093476692135984E-14, 196.9375000013655779, 201.4587341250000350 ) ) ;
#65832 = LINE ( 'NONE', #7765, #30521 ) ;
#65834 = CARTESIAN_POINT ( 'NONE',  ( 3.042071309553167513, 111.8229166632526983, -11.35316468749999785 ) ) ;
#65833 = CARTESIAN_POINT ( 'NONE',  ( 5.000000000000014211, 45.83333333333334991, -8.660254037844408614 ) ) ;
#65835 = AXIS2_PLACEMENT_3D ( 'NONE', #59216, #13163, #48241 ) ;
#65836 = CARTESIAN_POINT ( 'NONE',  ( -29.43265458321766559, 194.7500000013656063, 166.5412658750003629 ) ) ;
#65837 = CARTESIAN_POINT ( 'NONE',  ( 8.660254037844385522, 81.45833332650536818, 5.000000000000005329 ) ) ;
#65838 = ORIENTED_EDGE ( 'NONE', *, *, #25648, .T. ) ;
#65839 = LINE ( 'NONE', #14147, #970 ) ;
#65840 = DIRECTION ( 'NONE',  ( 0.000000000000000000, 0.000000000000000000, -1.000000000000000000 ) ) ;
#65841 = CARTESIAN_POINT ( 'NONE',  ( 3.042071309553159519, 105.0520833299193271, 11.35316468750000141 ) ) ;
#65842 = CARTESIAN_POINT ( 'NONE',  ( 2.754378923186476579E-14, 206.1875000013656063, 194.5412658750000219 ) ) ;
#65843 = CARTESIAN_POINT ( 'NONE',  ( -2.977408999572654480, 13.87499999795161187, 7.188101187499999156 ) ) ;
#65844 = CARTESIAN_POINT ( 'NONE',  ( -6.238412754330611322E-16, 10.18810118749999916, 87.15625000204838102 ) ) ;
#65845 = CARTESIAN_POINT ( 'NONE',  ( 5.676582343750001591, 26.92708332991935194, -9.832129032723420536 ) ) ;
#65846 = EDGE_LOOP ( 'NONE', ( #63278, #66375, #73954, #64029 ) ) ;
#65847 = CARTESIAN_POINT ( 'NONE',  ( 7.320508075688774596, 182.4999999931720254, -7.320508075688774596 ) ) ;
#65848 = CARTESIAN_POINT ( 'NONE',  ( 1.471067592899761672E-15, -8.008118988124991233, 26.88811528394063188 ) ) ;
#65849 = CARTESIAN_POINT ( 'NONE',  ( 7.320508075688774596, 117.4999999931720396, -7.320508075688774596 ) ) ;
#65850 = CARTESIAN_POINT ( 'NONE',  ( 1.871523826299183495E-15, -10.18810118749999916, 72.90625000204836681 ) ) ;
#65851 = FACE_BOUND ( 'NONE', #27014, .T. ) ;
#65852 = CARTESIAN_POINT ( 'NONE',  ( -5.082755093536326818, 5.906249997951610986, 5.082755093536325042 ) ) ;
#65853 = CARTESIAN_POINT ( 'NONE',  ( 6.676582343750004256, 293.8906250017069510, 2.765530957081995478 ) ) ;
#65854 = DIRECTION ( 'NONE',  ( 0.000000000000000000, 0.000000000000000000, 1.000000000000000000 ) ) ;
#65855 = CARTESIAN_POINT ( 'NONE',  ( -2.085542519210945728E-15, 224.8437499965860127, 11.35316468750000141 ) ) ;
#65856 = EDGE_CURVE ( 'NONE', #37575, #51583, #16182, .T. ) ;
#65857 = CARTESIAN_POINT ( 'NONE',  ( 9.832129032723416984, 125.6770833299193697, 5.676582343750006032 ) ) ;
#65858 = CIRCLE ( 'NONE', #62250, 30.99999999999994316 ) ;
#65859 = CARTESIAN_POINT ( 'NONE',  ( 7.204075437095968759, -7.204075437095966983, 84.71875000204836681 ) ) ;
#65860 = CARTESIAN_POINT ( 'NONE',  ( -29.43265458321760519, 198.8750000013656347, 173.4587341250003760 ) ) ;
#65861 = ADVANCED_FACE ( 'NONE', ( #13523 ), #36561, .F. ) ;
#65862 = CARTESIAN_POINT ( 'NONE',  ( 4.898587196589412829E-16, 25.87500000000000711, -8.000000000000000000 ) ) ;
#65863 = CARTESIAN_POINT ( 'NONE',  ( 1.881053915767122664, 11.24999999863440792, 4.541265875000001451 ) ) ;
#65864 = ORIENTED_EDGE ( 'NONE', *, *, #10876, .T. ) ;
#65865 = CARTESIAN_POINT ( 'NONE',  ( -2.828427124746152987, 202.2500000027312126, 200.8284271247462129 ) ) ;
#65866 = CARTESIAN_POINT ( 'NONE',  ( 2.445694354108784108, 199.5625000013656063, 144.4456943541088663 ) ) ;
#65867 = CARTESIAN_POINT ( 'NONE',  ( -4.000000000000015987, 203.6250000027312126, 142.0000000000000568 ) ) ;
#65868 = CARTESIAN_POINT ( 'NONE',  ( -7.320508075688847427, 173.1250000000000284, 7.320508075688839433 ) ) ;
#65869 = CARTESIAN_POINT ( 'NONE',  ( -7.204075437095965206, -7.204075437095968759, 69.71875000204836681 ) ) ;
#65870 = ORIENTED_EDGE ( 'NONE', *, *, #58545, .F. ) ;
#65871 = CARTESIAN_POINT ( 'NONE',  ( -2.977408999572654480, 4.499999997951610986, 7.188101187499999156 ) ) ;
#65872 = CARTESIAN_POINT ( 'NONE',  ( -18.18625387197270626, -16.62437597968712311, 195.1168880292559891 ) ) ;
#65873 = AXIS2_PLACEMENT_3D ( 'NONE', #27019, #73046, #9299 ) ;
#65874 = CARTESIAN_POINT ( 'NONE',  ( -4.999999999999998224, 28.54166665983870033, -8.660254037844389075 ) ) ;
#65875 = CARTESIAN_POINT ( 'NONE',  ( -5.082755093536325930, 112.3437500020483810, -5.082755093536325930 ) ) ;
#65876 = CARTESIAN_POINT ( 'NONE',  ( 5.082755093536320601, -5.082755093536318824, 9.924052781871754547 ) ) ;
#65877 = CARTESIAN_POINT ( 'NONE',  ( -2.044767169047288391, 21.99999999999996447, -3.615591841833113662 ) ) ;
#65878 = CARTESIAN_POINT ( 'NONE',  ( -4.088227598258586603E-16, 294.2031250017069510, -6.676582343750001591 ) ) ;
#65880 = CARTESIAN_POINT ( 'NONE',  ( -12.00000000000000355, 1.469576158976824342E-15, 0.000000000000000000 ) ) ;
#65879 = CARTESIAN_POINT ( 'NONE',  ( -11.35316468749999963, 223.9062500034139873, 0.000000000000000000 ) ) ;
#65881 = VERTEX_POINT ( 'NONE', #2603 ) ;
#65882 = CARTESIAN_POINT ( 'NONE',  ( 11.35316468749999608, 226.9270833367473301, -3.042071309553167069 ) ) ;
#65883 = CARTESIAN_POINT ( 'NONE',  ( 2.977408999572650927, -7.188101187499990274, 0.4553027818717525488 ) ) ;
#65884 = DIRECTION ( 'NONE',  ( -0.000000000000000000, 1.000000000000000000, 4.689100369878284071E-30 ) ) ;
#65885 = CARTESIAN_POINT ( 'NONE',  ( -2.849036369511732440E-14, 197.2500000000000000, 138.0000000000000568 ) ) ;
#65886 =( BOUNDED_CURVE ( )  B_SPLINE_CURVE ( 2, ( #58701, #24711, #47723, #7012, #19062, #25076, #53775, #2084, #19422 ),
 .UNSPECIFIED., .F., .F. ) 
 B_SPLINE_CURVE_WITH_KNOTS ( ( 3, 2, 2, 2, 3 ),
 ( 0.6323529411764704511, 0.6360294117647057321, 0.6397058823529410132, 0.6433823529411764053, 0.6470588235294116863 ),
 .UNSPECIFIED. ) 
 CURVE ( )  GEOMETRIC_REPRESENTATION_ITEM ( )  RATIONAL_B_SPLINE_CURVE ( ( 1.000000000000002220, 0.9238795325112844070, 1.000000000000000000, 0.9238795325112867385, 1.000000000000000000, 0.9238795325112867385, 1.000000000000000000, 0.9238795325112890700, 0.9999999999999976685 ) ) 
 REPRESENTATION_ITEM ( '' )  );
#65887 = CARTESIAN_POINT ( 'NONE',  ( 2.754378923186476579E-14, 198.4375000013655779, 194.5412658750000219 ) ) ;
#65888 = ORIENTED_EDGE ( 'NONE', *, *, #2011, .F. ) ;
#65889 = CARTESIAN_POINT ( 'NONE',  ( 2.249999999999999112, 2.250000000000000000, 0.000000000000000000 ) ) ;
#65890 = CARTESIAN_POINT ( 'NONE',  ( 1.469576158976823947E-15, 98.37499999999998579, 8.000000000000000000 ) ) ;
#65891 = CARTESIAN_POINT ( 'NONE',  ( 3.042071309553167069, 112.1354166632526699, -11.35316468749999785 ) ) ;
#65892 = CARTESIAN_POINT ( 'NONE',  ( -2.679491924311234285, 123.5416666666666714, 9.999999999999996447 ) ) ;
#65893 = CARTESIAN_POINT ( 'NONE',  ( 2.020667218593132706E-15, -11.00000000000000000, 74.87499999999998579 ) ) ;
#65896 = CARTESIAN_POINT ( 'NONE',  ( 0.000000000000000000, 0.000000000000000000, -25.03750572909317285 ) ) ;
#65895 = CARTESIAN_POINT ( 'NONE',  ( 25.55430564589115505, 199.0625000013656063, 167.5543056458911053 ) ) ;
#65894 = CARTESIAN_POINT ( 'NONE',  ( 29.43265458321761230, 200.7500000013656347, 173.4587341249998929 ) ) ;
#65897 = VERTEX_POINT ( 'NONE', #22543 ) ;
#65898 = CARTESIAN_POINT ( 'NONE',  ( 3.313708498984815343, 100.5312499999999716, -7.999999999999944933 ) ) ;
#65899 = LINE ( 'NONE', #3284, #45822 ) ;
#65900 = CARTESIAN_POINT ( 'NONE',  ( -1.432654583217662481, 203.1250000013656347, 145.4587341250000634 ) ) ;
#65901 = AXIS2_PLACEMENT_3D ( 'NONE', #22453, #38724, #10041 ) ;
#65902 = CARTESIAN_POINT ( 'NONE',  ( 29.43265458321766559, 203.1250000013656347, 166.5412658749999650 ) ) ;
#65903 = CARTESIAN_POINT ( 'NONE',  ( -7.778174593052020747, -7.778174593052023411, 115.3750000040967905 ) ) ;
#65904 = CARTESIAN_POINT ( 'NONE',  ( 3.042071309553159519, 195.0520833299193271, 11.35316468750000141 ) ) ;
#65905 = CARTESIAN_POINT ( 'NONE',  ( 1.926045908305006549, 89.59560438569887708, -7.188101187499999156 ) ) ;
#65906 = LINE ( 'NONE', #37250, #54281 ) ;
#65907 = CARTESIAN_POINT ( 'NONE',  ( 3.211159895383560947, 16.18749999863440436, 3.211159895383562723 ) ) ;
#65908 = CARTESIAN_POINT ( 'NONE',  ( 29.43265458321760519, 196.7500000013656063, 173.4587341249998929 ) ) ;
#65909 = CARTESIAN_POINT ( 'NONE',  ( 2.977408999572646486, 7.188101187499991163, 4.392802781871752771 ) ) ;
#65910 = CARTESIAN_POINT ( 'NONE',  ( -5.000000000000000000, -50.64189880742087269, -41.08656465431914029 ) ) ;
#65911 = CARTESIAN_POINT ( 'NONE',  ( 11.35316468750000141, 80.78124999658602690, 0.000000000000000000 ) ) ;
#65912 = ORIENTED_EDGE ( 'NONE', *, *, #35772, .F. ) ;
#65914 =( BOUNDED_CURVE ( )  B_SPLINE_CURVE ( 2, ( #5502, #56814, #45112, #69615, #40196, #51511, #74150, #57567, #63198 ),
 .UNSPECIFIED., .F., .F. ) 
 B_SPLINE_CURVE_WITH_KNOTS ( ( 3, 2, 2, 2, 3 ),
 ( 0.8235294117647057321, 0.8272058823529410132, 0.8308823529411764053, 0.8345588235294117974, 0.8382352941176470784 ),
 .UNSPECIFIED. ) 
 CURVE ( )  GEOMETRIC_REPRESENTATION_ITEM ( )  RATIONAL_B_SPLINE_CURVE ( ( 1.000000000000002220, 0.9238795325112844070, 1.000000000000000000, 0.9238795325112867385, 1.000000000000000000, 0.9238795325112867385, 1.000000000000000000, 0.9238795325112867385, 1.000000000000000000 ) ) 
 REPRESENTATION_ITEM ( '' )  );
#65913 = CARTESIAN_POINT ( 'NONE',  ( -27.99999999999995381, 195.5000000000000000, 174.0000000000003695 ) ) ;
#65915 = DIRECTION ( 'NONE',  ( 1.000000000000000000, 0.000000000000000000, 0.000000000000000000 ) ) ;
#65916 = PLANE ( 'NONE',  #53095 ) ;
#65917 = FACE_OUTER_BOUND ( 'NONE', #20817, .T. ) ;
#65918 = CARTESIAN_POINT ( 'NONE',  ( -9.832129032723420536, 93.69791666325269830, 5.676582343749997150 ) ) ;
#65919 = ORIENTED_EDGE ( 'NONE', *, *, #19639, .F. ) ;
#65920 = CARTESIAN_POINT ( 'NONE',  ( -7.204075437095965206, -7.204075437095968759, 87.71875000204836681 ) ) ;
#65921 = CARTESIAN_POINT ( 'NONE',  ( -10.18810118749999916, 4.220049686691934809, 115.5625000020483810 ) ) ;
#65922 = CARTESIAN_POINT ( 'NONE',  ( -3.458734124999959469, 208.7500000013656063, 199.4326545832176691 ) ) ;
#65923 = CARTESIAN_POINT ( 'NONE',  ( 5.000000000000018652, 75.83333333333335702, -8.660254037844415720 ) ) ;
#65925 = CARTESIAN_POINT ( 'NONE',  ( -3.042071309553173730, 74.32291666325268409, 11.35316468749999785 ) ) ;
#65924 = DIRECTION ( 'NONE',  ( 0.000000000000000000, -2.238352872228138170E-16, 1.000000000000000000 ) ) ;
#65926 = CARTESIAN_POINT ( 'NONE',  ( 7.999999999999992895, -3.313708498984756279, 19.67405278392014978 ) ) ;
#65927 = CARTESIAN_POINT ( 'NONE',  ( -0.2452292162193146496, 194.6102753126699554, 138.3897246873300730 ) ) ;
#65928 = EDGE_CURVE ( 'NONE', #19551, #57335, #27844, .T. ) ;
#65929 = EDGE_CURVE ( 'NONE', #33088, #24157, #27461, .T. ) ;
#65930 = CARTESIAN_POINT ( 'NONE',  ( 7.320508075688774596, 162.4999999931720538, -7.320508075688774596 ) ) ;
#65931 = CARTESIAN_POINT ( 'NONE',  ( -8.000000000000000000, 113.1875000040967763, 0.000000000000000000 ) ) ;
#65932 = CARTESIAN_POINT ( 'NONE',  ( 0.000000000000000000, 0.000000000000000000, -10.80000000000000071 ) ) ;
#65933 = CARTESIAN_POINT ( 'NONE',  ( -9.832129032723418760, 68.17708332991935549, -5.676582343750004256 ) ) ;
#65934 = CARTESIAN_POINT ( 'NONE',  ( -6.676582343750001591, 293.4531250017069510, 0.000000000000000000 ) ) ;
#65935 = CARTESIAN_POINT ( 'NONE',  ( -10.18810118749999738, -4.220049686691941915, 110.1250000020483810 ) ) ;
#65936 = CARTESIAN_POINT ( 'NONE',  ( -11.35316468750000141, 203.4895833299193271, 3.042071309553159963 ) ) ;
#65937 = ORIENTED_EDGE ( 'NONE', *, *, #65047, .F. ) ;
#65938 = CARTESIAN_POINT ( 'NONE',  ( 0.000000000000000000, 300.0000000000000000, 0.000000000000000000 ) ) ;
#65939 = CARTESIAN_POINT ( 'NONE',  ( 5.000000000000000000, -16.14408868864072844, 22.96238185062368586 ) ) ;
#65940 = CARTESIAN_POINT ( 'NONE',  ( 3.369429374625380724, 50.21921270641779245, 40.85597392306867448 ) ) ;
#65942 = CARTESIAN_POINT ( 'NONE',  ( 3.042071309553167513, 196.8229166632526983, -11.35316468749999785 ) ) ;
#65941 = CARTESIAN_POINT ( 'NONE',  ( -1.656854249492383468, 19.68750000000000000, 4.000000000000000888 ) ) ;
#65943 = VECTOR ( 'NONE', #34850, 1000.000000000000227 ) ;
#65944 = DIRECTION ( 'NONE',  ( 0.000000000000000000, 0.000000000000000000, 1.000000000000000000 ) ) ;
#65945 = EDGE_CURVE ( 'NONE', #52476, #54437, #56553, .T. ) ;
#65946 = EDGE_CURVE ( 'NONE', #73838, #26730, #64260, .T. ) ;
#65947 = CARTESIAN_POINT ( 'NONE',  ( 10.00000000000000000, 245.6250000068279746, -1.224646799147353256E-15 ) ) ;
#65948 = CARTESIAN_POINT ( 'NONE',  ( 11.00000000000000000, 1.347111479062088405E-15, 118.0000000000000000 ) ) ;
#65949 = ORIENTED_EDGE ( 'NONE', *, *, #18626, .T. ) ;
#65950 = CARTESIAN_POINT ( 'NONE',  ( -8.311093377946836114, 182.9687499965859843, -8.311093377946837890 ) ) ;
#65951 = CLOSED_SHELL ( 'NONE', ( #5048, #20109, #62756, #2521, #54703, #69827, #4653, #49223, #67920, #50465, #41614, #64927, #32303, #19616, #39133, #63729, #19142, #4995, #15939, #25025, #7971, #38978, #16511, #20620, #37527, #16638, #9312, #9960, #26100, #30013, #3688, #73038, #30098, #64800, #46858, #3745, #9500, #61181, #63380, #71549, #48048, #9091, #14153, #26324, #63000, #9456, #66358, #5417 ) ) ;
#65952 = CARTESIAN_POINT ( 'NONE',  ( -7.188101187499990274, -2.977408999572651815, 24.08030278187175099 ) ) ;
#65953 = EDGE_LOOP ( 'NONE', ( #54266, #74448, #5785, #12979, #11301 ) ) ;
#65954 = EDGE_CURVE ( 'NONE', #3614, #26389, #39909, .T. ) ;
#65955 = CARTESIAN_POINT ( 'NONE',  ( 8.000000000000000000, 100.5312500040967905, -3.313708498984762496 ) ) ;
#65956 = CARTESIAN_POINT ( 'NONE',  ( 5.000000000000001776, 5.833333333333333925, -8.660254037844389075 ) ) ;
#65957 = COLOUR_RGB ( '',0.7921568627450980005, 0.8196078431372548767, 0.9333333333333333481 ) ;
#65958 = CARTESIAN_POINT ( 'NONE',  ( -1.656854249492383691, 17.68750000000000000, 4.000000000000000888 ) ) ;
#65959 = CARTESIAN_POINT ( 'NONE',  ( 4.541265875000002339, 14.37499999863440969, -1.881053915767121776 ) ) ;
#65960 = CARTESIAN_POINT ( 'NONE',  ( 7.999999999999991118, 9.797174393178815797E-16, 15.26780278392014623 ) ) ;
#65961 = CARTESIAN_POINT ( 'NONE',  ( -26.34314575050768781, 195.5625000000000284, 174.0000000000004547 ) ) ;
#65962 = ORIENTED_EDGE ( 'NONE', *, *, #67838, .T. ) ;
#65963 = CARTESIAN_POINT ( 'NONE',  ( 6.000000000000001776, 293.5625000034140157, -7.347880794884121708E-16 ) ) ;
#65964 = CARTESIAN_POINT ( 'NONE',  ( 2.977408999572654480, 96.12500000204836681, 7.188101187499999156 ) ) ;
#65966 = CARTESIAN_POINT ( 'NONE',  ( 9.832129032723416984, 261.8229166700807014, -5.676582343750003368 ) ) ;
#65965 = CARTESIAN_POINT ( 'NONE',  ( -10.00000000000011902, 82.70833333333339965, 2.679491924311253825 ) ) ;
#65967 = DIRECTION ( 'NONE',  ( -0.8541735898718029185, -0.5199879598274532722, 0.000000000000000000 ) ) ;
#65968 = ORIENTED_EDGE ( 'NONE', *, *, #1319, .F. ) ;
#65969 = CARTESIAN_POINT ( 'NONE',  ( 0.000000000000000000, 0.000000000000000000, 0.000000000000000000 ) ) ;
#65970 = CARTESIAN_POINT ( 'NONE',  ( -7.188101187499992051, 0.000000000000000000, 19.48655278187175455 ) ) ;
#65971 = ORIENTED_EDGE ( 'NONE', *, *, #25893, .F. ) ;
#65972 = B_SPLINE_CURVE_WITH_KNOTS ( 'NONE', 3,
 ( #36734, #13692, #1674, #19004, #54086, #2396, #42010, #47304, #7691, #48408 ),
 .UNSPECIFIED., .F., .F.,
 ( 4, 2, 2, 2, 4 ),
 ( 0.01225088665078420333, 0.01328571931158636227, 0.01432055197238852121, 0.01535538463319067841, 0.01639021729399283561 ),
 .UNSPECIFIED. ) ;
#65973 = ORIENTED_EDGE ( 'NONE', *, *, #570, .F. ) ;
#65974 = CARTESIAN_POINT ( 'NONE',  ( 7.204075437095966983, 7.204075437095967871, 77.59375000204838102 ) ) ;
#65975 = CARTESIAN_POINT ( 'NONE',  ( -5.676582343749998039, 57.76041666325268409, -9.832129032723420536 ) ) ;
#65976 = CARTESIAN_POINT ( 'NONE',  ( 8.660254037844389075, 92.29166665983871098, -5.000000000000000000 ) ) ;
#65977 = CARTESIAN_POINT ( 'NONE',  ( -7.778174593052023411, 7.778174593052023411, 92.31249999999998579 ) ) ;
#65980 = CARTESIAN_POINT ( 'NONE',  ( 4.721056650415999201, 294.2343750017069510, -4.721056650415999201 ) ) ;
#65979 = CARTESIAN_POINT ( 'NONE',  ( 30.82842712474620939, 199.2500000027312126, 172.8284271247460424 ) ) ;
#65978 = CARTESIAN_POINT ( 'NONE',  ( -7.778174593052020747, -7.778174593052023411, 86.68749999999998579 ) ) ;
#65981 = CARTESIAN_POINT ( 'NONE',  ( -2.679491924311225848, 146.4583333333332860, -10.00000000000000178 ) ) ;
#65982 = CARTESIAN_POINT ( 'NONE',  ( -47.97665910975944570, 193.9435209778498859, 62.50784359751141039 ) ) ;
#65983 = CARTESIAN_POINT ( 'NONE',  ( 2.849036369511732440E-14, 200.2500000000000000, 202.0000000000000000 ) ) ;
#65984 = VECTOR ( 'NONE', #54542, 1000.000000000000000 ) ;
#65985 = FACE_OUTER_BOUND ( 'NONE', #2576, .T. ) ;
#65986 = CARTESIAN_POINT ( 'NONE',  ( -8.000000000000000000, 3.562499995903220196, -9.797174393178825657E-16 ) ) ;
#65987 = CARTESIAN_POINT ( 'NONE',  ( 31.45873412499997812, 199.6250000013656063, 171.4326545832175839 ) ) ;
#65988 = CARTESIAN_POINT ( 'NONE',  ( -7.188101187500002709, 9.187499997951611874, 2.977408999572649151 ) ) ;
#65989 = CARTESIAN_POINT ( 'NONE',  ( -5.656854249492375253, 5.656854249492375253, 23.33030278392014978 ) ) ;
#65990 = DIRECTION ( 'NONE',  ( -0.000000000000000000, -1.000000000000000000, -0.000000000000000000 ) ) ;
#65991 = CARTESIAN_POINT ( 'NONE',  ( 1.320432766682874540E-15, 111.4062500020483810, 7.188101187500000044 ) ) ;
#65993 = CYLINDRICAL_SURFACE ( 'NONE', #6498, 3.999999999999976019 ) ;
#65992 = CARTESIAN_POINT ( 'NONE',  ( 4.000000000000015987, 201.5625000000000568, 196.3431457505076594 ) ) ;
#65994 = PLANE ( 'NONE',  #9833 ) ;
#65995 = DIRECTION ( 'NONE',  ( -0.000000000000000000, 1.000000000000000000, 4.689100369878284071E-30 ) ) ;
#65996 = CARTESIAN_POINT ( 'NONE',  ( -5.082755093536317936, -5.082755093536320601, 23.04905278187175455 ) ) ;
#65997 = CARTESIAN_POINT ( 'NONE',  ( 27.99999999999996447, 195.0000000000000000, 173.9999999999999147 ) ) ;
#65998 = CARTESIAN_POINT ( 'NONE',  ( -11.35316468750000141, 43.28124999658601268, -1.390361679473963753E-15 ) ) ;
#65999 = CARTESIAN_POINT ( 'NONE',  ( 4.999999999999997335, 16.24494643555759410, 69.83755725260752456 ) ) ;
#66000 = CARTESIAN_POINT ( 'NONE',  ( -2.679491924311235618, 15.41666665983869855, 10.00000000000000000 ) ) ;
#66001 = ORIENTED_EDGE ( 'NONE', *, *, #2393, .T. ) ;
#66002 = CARTESIAN_POINT ( 'NONE',  ( 0.000000000000000000, 0.000000000000000000, 9.999999999999996447 ) ) ;
#66003 = EDGE_CURVE ( 'NONE', #45635, #57335, #68206, .T. ) ;
#66004 = CARTESIAN_POINT ( 'NONE',  ( 6.951808397369818766E-16, 47.03124999658601979, -11.35316468750000141 ) ) ;
#66005 = AXIS2_PLACEMENT_3D ( 'NONE', #66095, #49871, #72887 ) ;
#66006 = CARTESIAN_POINT ( 'NONE',  ( -6.735557395310442023E-16, 11.00000000000000000, 80.31250000409677625 ) ) ;
#66007 = CARTESIAN_POINT ( 'NONE',  ( -2.445694354108840063, 204.0625000013656063, 139.5543056458912190 ) ) ;
#66008 = LINE ( 'NONE', #9429, #28674 ) ;
#66010 = CARTESIAN_POINT ( 'NONE',  ( -8.311093377946836114, 32.65624999658600558, -8.311093377946837890 ) ) ;
#66009 = CARTESIAN_POINT ( 'NONE',  ( -2.977408999572650927, 101.3750000020483952, -7.188101187500000933 ) ) ;
#66011 = CARTESIAN_POINT ( 'NONE',  ( -3.313708498984758943, -7.999999999999989342, 11.61155277982336820 ) ) ;
#66012 =( BOUNDED_CURVE ( )  B_SPLINE_CURVE ( 2, ( #21078, #44102, #61448, #55802, #4118, #54680, #27111, #50126, #33176 ),
 .UNSPECIFIED., .F., .F. ) 
 B_SPLINE_CURVE_WITH_KNOTS ( ( 3, 2, 2, 2, 3 ),
 ( 0.2000000000000001776, 0.2083333333333335091, 0.2166666666666668406, 0.2250000000000001998, 0.2333333333333335313 ),
 .UNSPECIFIED. ) 
 CURVE ( )  GEOMETRIC_REPRESENTATION_ITEM ( )  RATIONAL_B_SPLINE_CURVE ( ( 0.9999999999999984457, 0.9238795325112882928, 1.000000000000000000, 0.9238795325112867385, 1.000000000000000000, 0.9238795325112867385, 1.000000000000000000, 0.9238795325112849621, 1.000000000000001776 ) ) 
 REPRESENTATION_ITEM ( '' )  );
#66013 = CARTESIAN_POINT ( 'NONE',  ( 3.042071309553167069, 156.8229166632526983, -11.35316468749999785 ) ) ;
#66014 = AXIS2_PLACEMENT_3D ( 'NONE', #30929, #53586, #44030 ) ;
#66015 = CARTESIAN_POINT ( 'NONE',  ( 2.679491924311228956, 132.9166666598386541, -10.00000000000000000 ) ) ;
#66016 = CARTESIAN_POINT ( 'NONE',  ( 5.082755093536326818, 108.5937500020483810, 5.082755093536325042 ) ) ;
#66017 = ORIENTED_EDGE ( 'NONE', *, *, #13235, .T. ) ;
#66018 = CARTESIAN_POINT ( 'NONE',  ( 0.000000000000000000, 0.000000000000000000, 0.000000000000000000 ) ) ;
#66019 = CARTESIAN_POINT ( 'NONE',  ( 11.35316468749999785, 15.88541666325268409, 3.042071309553174174 ) ) ;
#66020 = CARTESIAN_POINT ( 'NONE',  ( -4.500000000000010658, -7.794228634059939154, 0.000000000000000000 ) ) ;
#66021 = ORIENTED_EDGE ( 'NONE', *, *, #12860, .F. ) ;
#66022 = FACE_OUTER_BOUND ( 'NONE', #73401, .T. ) ;
#66023 = CARTESIAN_POINT ( 'NONE',  ( 7.204075437095968759, -7.204075437095966983, 77.21875000204836681 ) ) ;
#66024 = PLANE ( 'NONE',  #59459 ) ;
#66026 = CARTESIAN_POINT ( 'NONE',  ( -8.311093377946841443, 148.9062499965860127, 8.311093377946834337 ) ) ;
#66025 = CARTESIAN_POINT ( 'NONE',  ( -19.99999999999993250, -31.99999999999978684, 145.6940130594346670 ) ) ;
#66027 = DIRECTION ( 'NONE',  ( 0.000000000000000000, 0.000000000000000000, 1.000000000000000000 ) ) ;
#66028 = CARTESIAN_POINT ( 'NONE',  ( -5.656854249492373476, -5.656854249492376141, 17.57405278432982243 ) ) ;
#66029 = CARTESIAN_POINT ( 'NONE',  ( -28.44126078476518060, -21.29331833291333709, 182.3852209837971827 ) ) ;
#66030 = EDGE_CURVE ( 'NONE', #43963, #1423, #21797, .T. ) ;
#66031 = ADVANCED_FACE ( 'NONE', ( #62170 ), #32398, .F. ) ;
#66032 = CARTESIAN_POINT ( 'NONE',  ( 2.085542519210945334E-15, 240.1562500034140157, 11.35316468749999963 ) ) ;
#66033 = CARTESIAN_POINT ( 'NONE',  ( 10.18810118750000093, -4.220049686691933921, 83.68750000204836681 ) ) ;
#66034 = VERTEX_POINT ( 'NONE', #22171 ) ;
#66035 = ADVANCED_FACE ( 'NONE', ( #10494 ), #33529, .T. ) ;
#66036 = CARTESIAN_POINT ( 'NONE',  ( 27.99999999999999645, 210.0000000000000284, 173.9999999999998863 ) ) ;
#66037 = CARTESIAN_POINT ( 'NONE',  ( -1.836970198721029983E-15, 45.62499999317203958, 10.00000000000000178 ) ) ;
#66038 = CARTESIAN_POINT ( 'NONE',  ( -9.832129032723420536, 109.0104166632526841, 5.676582343749997150 ) ) ;
#66039 = CARTESIAN_POINT ( 'NONE',  ( -4.220049686691935698, 10.18810118749999916, 101.8750000020483810 ) ) ;
#66040 = CARTESIAN_POINT ( 'NONE',  ( 4.541265875000002339, 21.49999999863440792, -1.881053915767121776 ) ) ;
#66041 = ORIENTED_EDGE ( 'NONE', *, *, #13197, .T. ) ;
#66042 = ORIENTED_EDGE ( 'NONE', *, *, #50624, .F. ) ;
#66043 = CARTESIAN_POINT ( 'NONE',  ( 4.541265875000002339, 5.499999998634407028, -1.881053915767121554 ) ) ;
#66045 = MANIFOLD_SOLID_BREP ( 'BaseBody', #41830 ) ;
#66044 = CARTESIAN_POINT ( 'NONE',  ( 7.188101187500001821, 9.562499997951608322, -2.977408999572650483 ) ) ;
#66046 = EDGE_CURVE ( 'NONE', #34625, #55885, #31923, .T. ) ;
#66047 = CARTESIAN_POINT ( 'NONE',  ( 1.469576158976823947E-15, 115.0625000040967905, 8.000000000000000000 ) ) ;
#66048 = CARTESIAN_POINT ( 'NONE',  ( 7.204075437095968759, -7.204075437095966983, 100.0937500020483668 ) ) ;
#66049 = CARTESIAN_POINT ( 'NONE',  ( -30.44569435410883429, 201.8125000013656063, 167.5543056458915885 ) ) ;
#66050 = CARTESIAN_POINT ( 'NONE',  ( -7.347880794884122694E-16, 2.750000000000000000, 4.000000000000001776 ) ) ;
#66051 = CARTESIAN_POINT ( 'NONE',  ( 1.656854249492381914, 17.56249999726881938, 4.000000000000000888 ) ) ;
#66052 = CARTESIAN_POINT ( 'NONE',  ( -8.342170076843785083E-16, 4.062499998634407028, 4.541265875000002339 ) ) ;
#66053 = CARTESIAN_POINT ( 'NONE',  ( -3.458734125000015425, 207.9375000013656063, 142.0000000000000568 ) ) ;
#66054 = CARTESIAN_POINT ( 'NONE',  ( 3.458734125000015425, 195.0000000013656063, 196.5673454167823877 ) ) ;
#66056 = DIRECTION ( 'NONE',  ( 0.000000000000000000, -0.02418647091589873691, 0.9997074645238147594 ) ) ;
#66055 = CARTESIAN_POINT ( 'NONE',  ( -31.45873412499999233, 199.6875000013656063, 170.0000000000004547 ) ) ;
#66057 = VECTOR ( 'NONE', #68241, 1000.000000000000000 ) ;
#66058 = CARTESIAN_POINT ( 'NONE',  ( -4.541265875000002339, 19.74999999863440792, -1.881053915767121998 ) ) ;
#66059 = CARTESIAN_POINT ( 'NONE',  ( -2.765530957081998142, 298.6406250017069510, 6.676582343750000703 ) ) ;
#66060 = CARTESIAN_POINT ( 'NONE',  ( -7.188101187499992051, 0.000000000000000000, 4.486552781871752771 ) ) ;
#66061 = ORIENTED_EDGE ( 'NONE', *, *, #10652, .F. ) ;
#66062 = ORIENTED_EDGE ( 'NONE', *, *, #33989, .T. ) ;
#66063 = CARTESIAN_POINT ( 'NONE',  ( 4.220049686691941027, -10.18810118749999738, 98.12500000204838102 ) ) ;
#66064 = CARTESIAN_POINT ( 'NONE',  ( 8.660254037844387298, 124.5833333333333428, 5.000000000000006217 ) ) ;
#66065 = CARTESIAN_POINT ( 'NONE',  ( -25.55430564589119413, 203.5625000013656063, 167.5543056458915316 ) ) ;
#66066 = CARTESIAN_POINT ( 'NONE',  ( -25.17157287525377640, 201.6250000000000284, 172.8284271247465256 ) ) ;
#66067 = CARTESIAN_POINT ( 'NONE',  ( 1.432654583217664479, 196.7500000013656063, 201.4587341250000065 ) ) ;
#66068 = CARTESIAN_POINT ( 'NONE',  ( -9.999999999999998224, 32.50000000000000000, -1.224646799147352862E-15 ) ) ;
#66069 = CARTESIAN_POINT ( 'NONE',  ( -10.00000000000000355, 112.7083333333333428, 2.679491924311223183 ) ) ;
#66070 = CARTESIAN_POINT ( 'NONE',  ( 8.000000000000001776, 112.1562500000000000, 3.313708498984759387 ) ) ;
#66071 = CARTESIAN_POINT ( 'NONE',  ( -6.676582343750000703, 297.6718750017070079, 2.765530957082001251 ) ) ;
#66072 = CARTESIAN_POINT ( 'NONE',  ( 7.188101187499993827, -2.977408999572645598, 11.51780278187175810 ) ) ;
#66073 = ORIENTED_EDGE ( 'NONE', *, *, #61774, .T. ) ;
#66074 = CARTESIAN_POINT ( 'NONE',  ( -1.836970198721029983E-15, 175.6249999931720538, 10.00000000000000178 ) ) ;
#66075 = CARTESIAN_POINT ( 'NONE',  ( 3.313708498984762052, 19.59374999590322020, -8.000000000000000000 ) ) ;
#66076 = CARTESIAN_POINT ( 'NONE',  ( -3.458734125000015425, 204.0000000013656347, 143.4326545832176976 ) ) ;
#66077 = CARTESIAN_POINT ( 'NONE',  ( 10.00000000000000178, 0.000000000000000000, 0.000000000000000000 ) ) ;
#66078 = FACE_OUTER_BOUND ( 'NONE', #54844, .T. ) ;
#66079 = CARTESIAN_POINT ( 'NONE',  ( -8.311093377946836114, 253.5937500034140157, -8.311093377946836114 ) ) ;
#66080 = CARTESIAN_POINT ( 'NONE',  ( -7.778174593052020747, -7.778174593052023411, 91.37500000409677625 ) ) ;
#66081 = CARTESIAN_POINT ( 'NONE',  ( 4.556349186104051263, -10.99999999999999822, 113.9687500000000142 ) ) ;
#66082 = CARTESIAN_POINT ( 'NONE',  ( 11.35316468750000141, 5.781249996586016238, 0.000000000000000000 ) ) ;
#66083 = CARTESIAN_POINT ( 'NONE',  ( 5.082755093536318824, 5.082755093536319713, 2.799052781871750994 ) ) ;
#66084 = CARTESIAN_POINT ( 'NONE',  ( 9.832129032723416984, 195.6770833299193839, 5.676582343750006032 ) ) ;
#66085 = CARTESIAN_POINT ( 'NONE',  ( 10.00000000000000178, 191.8749999931720254, 0.000000000000000000 ) ) ;
#66086 = CARTESIAN_POINT ( 'NONE',  ( -4.541265875000003227, 4.874999998634406140, 1.881053915767121110 ) ) ;
#66087 = CARTESIAN_POINT ( 'NONE',  ( -4.898587196589412829E-16, 99.31250000409677625, -8.000000000000000000 ) ) ;
#66089 = CARTESIAN_POINT ( 'NONE',  ( 2.485281374238959895, 297.3125000000000000, 5.999999999999615419 ) ) ;
#66088 = CARTESIAN_POINT ( 'NONE',  ( -4.898587196589412829E-16, 100.8125000040967763, -8.000000000000000000 ) ) ;
#66090 = ORIENTED_EDGE ( 'NONE', *, *, #47955, .F. ) ;
#66091 = EDGE_CURVE ( 'NONE', #30893, #3504, #70081, .T. ) ;
#66092 = CARTESIAN_POINT ( 'NONE',  ( 1.432654583217607414, 203.5000000013655779, 145.4587341250000634 ) ) ;
#66093 = CARTESIAN_POINT ( 'NONE',  ( 5.676582343750001591, 46.92708332991934839, -9.832129032723420536 ) ) ;
#66094 = CARTESIAN_POINT ( 'NONE',  ( -4.556349186104045934, 11.00000000000000000, 101.4062500040967763 ) ) ;
#66095 = CARTESIAN_POINT ( 'NONE',  ( 0.000000000000000000, 0.000000000000000000, 0.000000000000000000 ) ) ;
#66096 = CARTESIAN_POINT ( 'NONE',  ( -31.45873412499995680, 199.7500000013656063, 171.4326545832181239 ) ) ;
#66097 = CARTESIAN_POINT ( 'NONE',  ( -11.00000000000000000, 0.000000000000000000, 89.50000000000000000 ) ) ;
#66099 = DIRECTION ( 'NONE',  ( -0.000000000000000000, 1.000000000000000000, -0.000000000000000000 ) ) ;
#66098 = CARTESIAN_POINT ( 'NONE',  ( 5.082755093536325042, 122.0937500020483952, -5.082755093536325930 ) ) ;
#66100 = CARTESIAN_POINT ( 'NONE',  ( -7.999999999999989342, -3.313708498984762496, 26.42405277982336642 ) ) ;
#66101 = CARTESIAN_POINT ( 'NONE',  ( 8.311093377946837890, 121.4062499965860127, -8.311093377946837890 ) ) ;
#66102 = VECTOR ( 'NONE', #8297, 1000.000000000000000 ) ;
#66103 = CARTESIAN_POINT ( 'NONE',  ( -2.679491924311225848, 88.33333332650535397, -10.00000000000000178 ) ) ;
#66104 = CARTESIAN_POINT ( 'NONE',  ( 7.188101187500002709, 90.31250000204838102, 2.977408999572649151 ) ) ;
#66105 = CARTESIAN_POINT ( 'NONE',  ( -4.541265875000002339, 18.93749999863440436, -5.561446717895856393E-16 ) ) ;
#66106 = CARTESIAN_POINT ( 'NONE',  ( 2.751064625579944321E-14, 196.8750000027312126, 194.0000000000000568 ) ) ;
#66107 = DIRECTION ( 'NONE',  ( 0.000000000000000000, 0.000000000000000000, 1.000000000000000000 ) ) ;
#66108 = VERTEX_POINT ( 'NONE', #74613 ) ;
#66109 = CARTESIAN_POINT ( 'NONE',  ( 1.469576158976823947E-15, 89.56250000409677625, 8.000000000000000000 ) ) ;
#66110 = ORIENTED_EDGE ( 'NONE', *, *, #13996, .F. ) ;
#66111 = CARTESIAN_POINT ( 'NONE',  ( 2.765530957081996366, 295.2968750017069510, -6.676582343750003368 ) ) ;
#66112 = SURFACE_SIDE_STYLE ('',( #44237 ) ) ;
#66113 = CARTESIAN_POINT ( 'NONE',  ( 7.999999999999991118, 9.797174393178815797E-16, 7.767802783920144449 ) ) ;
#66114 = CARTESIAN_POINT ( 'NONE',  ( -11.35316468749999785, 168.0729166632526699, -3.042071309553167513 ) ) ;
#66115 = CARTESIAN_POINT ( 'NONE',  ( -3.999999999999960032, 195.0625000027312126, 196.3431457505076594 ) ) ;
#66116 = CARTESIAN_POINT ( 'NONE',  ( -1.656854249492348607, 198.1875000000000853, 202.0000000000000284 ) ) ;
#66117 = CARTESIAN_POINT ( 'NONE',  ( 0.000000000000000000, 0.000000000000000000, 118.0000000000000000 ) ) ;
#66118 = CARTESIAN_POINT ( 'NONE',  ( 4.220049686691941027, -10.18810118749999738, 106.0000000020483668 ) ) ;
#66119 = ORIENTED_EDGE ( 'NONE', *, *, #20266, .F. ) ;
#66120 = ADVANCED_FACE ( 'NONE', ( #29345 ), #23673, .F. ) ;
#66121 = CARTESIAN_POINT ( 'NONE',  ( -1.836970198721029983E-15, 155.6249999931720254, 10.00000000000000178 ) ) ;
#66122 = CARTESIAN_POINT ( 'NONE',  ( 11.35316468749999785, 160.8854166632526699, 3.042071309553174174 ) ) ;
#66123 = CARTESIAN_POINT ( 'NONE',  ( 2.751064625579944321E-14, 206.8750000027312126, 194.0000000000000568 ) ) ;
#66124 = CARTESIAN_POINT ( 'NONE',  ( 1.432654583217662481, 206.3750000013656063, 194.5412658750000219 ) ) ;
#66125 = CARTESIAN_POINT ( 'NONE',  ( -4.220049686691937474, -10.18810118749999738, 71.31250000204836681 ) ) ;
#66126 = CARTESIAN_POINT ( 'NONE',  ( -11.35316468750000141, 63.59374999658601268, -1.390361679473963753E-15 ) ) ;
#66128 = ORIENTED_EDGE ( 'NONE', *, *, #2962, .T. ) ;
#66127 =( BOUNDED_CURVE ( )  B_SPLINE_CURVE ( 2, ( #51046, #21996, #39357, #10316, #74056, #40100, #9946, #51788, #22355 ),
 .UNSPECIFIED., .F., .F. ) 
 B_SPLINE_CURVE_WITH_KNOTS ( ( 3, 2, 2, 2, 3 ),
 ( 0.3823529411764705621, 0.3860294117647058987, 0.3897058823529411242, 0.3933823529411764053, 0.3970588235294116863 ),
 .UNSPECIFIED. ) 
 CURVE ( )  GEOMETRIC_REPRESENTATION_ITEM ( )  RATIONAL_B_SPLINE_CURVE ( ( 1.000000000000000000, 0.9238795325112867385, 1.000000000000000000, 0.9238795325112867385, 1.000000000000000000, 0.9238795325112867385, 1.000000000000000000, 0.9238795325112878487, 0.9999999999999988898 ) ) 
 REPRESENTATION_ITEM ( '' )  );
#66129 = CARTESIAN_POINT ( 'NONE',  ( -4.220049686691935698, 10.18810118749999916, 116.8750000020483668 ) ) ;
#66131 = CARTESIAN_POINT ( 'NONE',  ( -4.541265875000003227, 7.999999998634407028, 1.881053915767121110 ) ) ;
#66130 =( BOUNDED_CURVE ( )  B_SPLINE_CURVE ( 2, ( #71305, #19625, #49039, #31703, #37743, #60743, #40341, #27524, #9814 ),
 .UNSPECIFIED., .F., .F. ) 
 B_SPLINE_CURVE_WITH_KNOTS ( ( 3, 2, 2, 2, 3 ),
 ( 0.3666666666666669738, 0.3750000000000003331, 0.3833333333333336923, 0.3916666666666669960, 0.4000000000000003553 ),
 .UNSPECIFIED. ) 
 CURVE ( )  GEOMETRIC_REPRESENTATION_ITEM ( )  RATIONAL_B_SPLINE_CURVE ( ( 0.9999999999999970024, 0.9238795325112897361, 1.000000000000000000, 0.9238795325112867385, 1.000000000000000000, 0.9238795325112867385, 1.000000000000000000, 0.9238795325112837409, 1.000000000000003109 ) ) 
 REPRESENTATION_ITEM ( '' )  );
#66132 = CARTESIAN_POINT ( 'NONE',  ( -5.662595241051935346, 5.662595241051935346, 11.32561528394062833 ) ) ;
#66133 = ORIENTED_EDGE ( 'NONE', *, *, #47876, .T. ) ;
#66134 = CARTESIAN_POINT ( 'NONE',  ( -7.188101187500000044, 22.21874999795161187, -8.802885111219163269E-16 ) ) ;
#66135 = CARTESIAN_POINT ( 'NONE',  ( 4.242640687119287435, 288.4375000034140157, 4.242640687119285658 ) ) ;
#66136 = CARTESIAN_POINT ( 'NONE',  ( -27.99999999999999645, 210.0000000000000284, 170.0000000000003695 ) ) ;
#66137 = CARTESIAN_POINT ( 'NONE',  ( -5.082755093536326818, 12.28124999795161187, 5.082755093536325042 ) ) ;
#66138 = EDGE_CURVE ( 'NONE', #2602, #33683, #58760, .T. ) ;
#66139 = CARTESIAN_POINT ( 'NONE',  ( -5.082755093536317936, -5.082755093536320601, 0.1740527818717522990 ) ) ;
#66140 = CARTESIAN_POINT ( 'NONE',  ( 4.220049686691934809, 10.18810118749999916, 117.0625000020483668 ) ) ;
#66141 = EDGE_CURVE ( 'NONE', #18846, #22788, #171, .T. ) ;
#66142 = CARTESIAN_POINT ( 'NONE',  ( 0.000000000000000000, 125.0000000000000000, 0.000000000000000000 ) ) ;
#66143 = CARTESIAN_POINT ( 'NONE',  ( -1.656854249492383691, 6.437499997268812280, 4.000000000000000888 ) ) ;
#66144 = ORIENTED_EDGE ( 'NONE', *, *, #33288, .T. ) ;
#66145 = CARTESIAN_POINT ( 'NONE',  ( -2.445694354108782775, 205.5625000013656063, 200.4456943541088663 ) ) ;
#66146 = CARTESIAN_POINT ( 'NONE',  ( -25.17157287525385456, 197.0000000027312126, 167.1715728752541281 ) ) ;
#66147 = CARTESIAN_POINT ( 'NONE',  ( 1.881053915767121776, 7.499999998634408804, -4.541265875000002339 ) ) ;
#66149 = CARTESIAN_POINT ( 'NONE',  ( 2.977408999572654480, 109.6250000020483952, 7.188101187499999156 ) ) ;
#66148 = VECTOR ( 'NONE', #10794, 1000.000000000000000 ) ;
#66150 = EDGE_CURVE ( 'NONE', #47034, #41903, #18388, .T. ) ;
#66151 = CARTESIAN_POINT ( 'NONE',  ( -4.000000000000001776, 13.50000000000000000, -4.898587196589415787E-16 ) ) ;
#66152 = CARTESIAN_POINT ( 'NONE',  ( -7.188101187499991163, 2.977408999572646930, 25.39280278187176165 ) ) ;
#66153 = ORIENTED_EDGE ( 'NONE', *, *, #2406, .T. ) ;
#66154 = ORIENTED_EDGE ( 'NONE', *, *, #27287, .F. ) ;
#66155 = CARTESIAN_POINT ( 'NONE',  ( -9.999999999999996447, 2.499999999999997780, -1.224646799147353059E-15 ) ) ;
#66156 = CARTESIAN_POINT ( 'NONE',  ( 1.060465953394919891, 7.999920465055806673, 0.000000000000000000 ) ) ;
#66157 = CARTESIAN_POINT ( 'NONE',  ( -3.458734124999959914, 207.3750000013656063, 196.5673454167823877 ) ) ;
#66158 = CARTESIAN_POINT ( 'NONE',  ( 29.43265458321766914, 202.5000000013656063, 173.4587341249998929 ) ) ;
#66159 = CARTESIAN_POINT ( 'NONE',  ( -5.000000000000005329, 73.33333333333332860, 8.660254037844387298 ) ) ;
#66160 = AXIS2_PLACEMENT_3D ( 'NONE', #10092, #56124, #67435 ) ;
#66161 = CARTESIAN_POINT ( 'NONE',  ( 1.320432766682874540E-15, 91.90625000204838102, 7.188101187500000044 ) ) ;
#66162 = MANIFOLD_SOLID_BREP ( 'Thread1', #4523 ) ;
#66163 = CARTESIAN_POINT ( 'NONE',  ( 2.485281374238571317, 294.6874999999999432, -6.000000000000003553 ) ) ;
#66165 = CARTESIAN_POINT ( 'NONE',  ( 4.556349186104045934, 11.00000000000000000, 113.2187500040967763 ) ) ;
#66164 = CARTESIAN_POINT ( 'NONE',  ( 30.82842712474617031, 207.5000000027312126, 167.1715728752537018 ) ) ;
#66166 = VERTEX_POINT ( 'NONE', #64041 ) ;
#66167 = CARTESIAN_POINT ( 'NONE',  ( 2.085542519210945334E-15, 235.1562500034140157, 11.35316468749999963 ) ) ;
#66168 = CARTESIAN_POINT ( 'NONE',  ( -4.465349678513701015, -10.10202304668585604, 70.97395336192410298 ) ) ;
#66169 = CARTESIAN_POINT ( 'NONE',  ( -1.656854249492403008, 199.8125000027312410, 146.0000000000000284 ) ) ;
#66170 = CARTESIAN_POINT ( 'NONE',  ( -2.849036369511732440E-14, 200.3750000027312126, 138.0000000000000568 ) ) ;
#66171 = CARTESIAN_POINT ( 'NONE',  ( -2.751064625579944321E-14, 196.8750000027312126, 146.0000000000000284 ) ) ;
#66172 = CARTESIAN_POINT ( 'NONE',  ( 1.836970198721029589E-15, 246.2500000000000284, 10.00000000000000000 ) ) ;
#66173 = DIRECTION ( 'NONE',  ( 0.000000000000000000, -0.000000000000000000, -1.000000000000000000 ) ) ;
#66174 = CARTESIAN_POINT ( 'NONE',  ( 4.999999999999993783, 189.1666666666666856, 8.660254037844390851 ) ) ;
#66175 = CARTESIAN_POINT ( 'NONE',  ( 29.65685424949245075, 198.5625000027312694, 165.9999999999999716 ) ) ;
#66176 = CARTESIAN_POINT ( 'NONE',  ( -5.082755093536317936, -5.082755093536320601, 21.54905278187175455 ) ) ;
#66177 = CARTESIAN_POINT ( 'NONE',  ( 11.35316468749999963, 161.3020833299193555, -3.042071309553165293 ) ) ;
#66178 = CARTESIAN_POINT ( 'NONE',  ( 3.313708498984762496, -7.999999999999989342, 22.48655278392014623 ) ) ;
#66179 = CARTESIAN_POINT ( 'NONE',  ( -31.00000000000001421, 50.00000000000000711, 65.00000000000000000 ) ) ;
#66182 = DIRECTION ( 'NONE',  ( 0.000000000000000000, 0.000000000000000000, 1.000000000000000000 ) ) ;
#66181 = CARTESIAN_POINT ( 'NONE',  ( 1.656854249492487607, 199.8125000027312126, 194.0000000000001705 ) ) ;
#66180 = CARTESIAN_POINT ( 'NONE',  ( 29.65685424949240101, 203.4375000000000284, 165.9999999999998863 ) ) ;
#66183 = ORIENTED_EDGE ( 'NONE', *, *, #39412, .F. ) ;
#66184 = CARTESIAN_POINT ( 'NONE',  ( 9.832129032723420536, 6.510416663252683200, -5.676582343749999815 ) ) ;
#66185 = CARTESIAN_POINT ( 'NONE',  ( 2.679491924311222739, 95.83333332650535397, 10.00000000000000355 ) ) ;
#66186 = ADVANCED_FACE ( 'NONE', ( #6702 ), #57652, .F. ) ;
#66187 = CARTESIAN_POINT ( 'NONE',  ( 2.679491924311228956, 32.91666665983869677, -10.00000000000000000 ) ) ;
#66188 = LINE ( 'NONE', #55266, #55634 ) ;
#66189 = CARTESIAN_POINT ( 'NONE',  ( 2.445694354108782775, 205.5625000013656063, 139.5543056458912190 ) ) ;
#66190 = CARTESIAN_POINT ( 'NONE',  ( 6.123233995736767268E-16, 53.12499999317203958, -10.00000000000000178 ) ) ;
#66191 = CARTESIAN_POINT ( 'NONE',  ( -2.977408999572651815, 106.4375000020483810, 7.188101187500000933 ) ) ;
#66192 = CARTESIAN_POINT ( 'NONE',  ( 4.541265875000001451, 3.374999998634406584, 1.881053915767124440 ) ) ;
#66193 = CARTESIAN_POINT ( 'NONE',  ( 2.266287154879886856, 60.33498852648239819, -22.96738997677231353 ) ) ;
#66194 = CARTESIAN_POINT ( 'NONE',  ( 1.469576158976822172E-15, -7.999999999999991118, 10.20530277982336465 ) ) ;
#66196 = CARTESIAN_POINT ( 'NONE',  ( 2.679491924311375506, 158.9583333333333997, 9.999999999999939604 ) ) ;
#66195 = CARTESIAN_POINT ( 'NONE',  ( 0.4207882399903739024, 194.5923675076498114, 138.4260692085993867 ) ) ;
#66197 = ORIENTED_EDGE ( 'NONE', *, *, #66534, .T. ) ;
#66198 = EDGE_CURVE ( 'NONE', #37508, #20547, #68064, .T. ) ;
#66199 = DIRECTION ( 'NONE',  ( -0.000000000000000000, -0.000000000000000000, 1.000000000000000000 ) ) ;
#66200 = CARTESIAN_POINT ( 'NONE',  ( -1.469576158976823947E-15, 26.62500000000000355, 8.000000000000000000 ) ) ;
#66201 = CARTESIAN_POINT ( 'NONE',  ( -9.832129032723418760, 233.8020833367473301, -5.676582343749998927 ) ) ;
#66202 = CARTESIAN_POINT ( 'NONE',  ( -5.676582343749998039, 132.4479166632526983, -9.832129032723420536 ) ) ;
#66203 = VERTEX_POINT ( 'NONE', #68953 ) ;
#66204 = CARTESIAN_POINT ( 'NONE',  ( 0.000000000000000000, 0.000000000000000000, 118.0000000000000000 ) ) ;
#66205 = CARTESIAN_POINT ( 'NONE',  ( 4.220049686691934809, 10.18810118749999916, 95.68750000204838102 ) ) ;
#66206 = DIRECTION ( 'NONE',  ( 0.000000000000000000, 0.000000000000000000, 1.000000000000000000 ) ) ;
#66207 = CARTESIAN_POINT ( 'NONE',  ( 1.432654583217662481, 196.3750000013656063, 194.5412658750000219 ) ) ;
#66208 = CARTESIAN_POINT ( 'NONE',  ( 54.00000000000000711, 37.00000000000000000, 20.00000000000000000 ) ) ;
#66210 = CARTESIAN_POINT ( 'NONE',  ( 11.35316468749999963, 120.9895833299193555, -3.042071309553165293 ) ) ;
#66209 = CARTESIAN_POINT ( 'NONE',  ( 10.00000000000002665, 45.20833333333334281, -2.679491924311233841 ) ) ;
#66211 = CARTESIAN_POINT ( 'NONE',  ( 3.999999999999960032, 195.0000000000000000, 142.0000000000000568 ) ) ;
#66212 = EDGE_LOOP ( 'NONE', ( #47487, #25033, #47324, #56163 ) ) ;
#66213 = ADVANCED_FACE ( 'NONE', ( #63659 ), #69326, .T. ) ;
#66214 = CARTESIAN_POINT ( 'NONE',  ( -1.836970198721029983E-15, 25.62499999317203248, 10.00000000000000178 ) ) ;
#66215 = FACE_OUTER_BOUND ( 'NONE', #19080, .T. ) ;
#66216 = CARTESIAN_POINT ( 'NONE',  ( -3.042071309553163960, 97.55208332991934128, -11.35316468749999963 ) ) ;
#66217 = CARTESIAN_POINT ( 'NONE',  ( -3.458734124999959914, 208.3750000013656063, 196.5673454167823877 ) ) ;
#66218 = CARTESIAN_POINT ( 'NONE',  ( 2.977408999572650927, 17.62499999795161543, -7.188101187500000933 ) ) ;
#66219 = CARTESIAN_POINT ( 'NONE',  ( -4.220049686691935698, 10.18810118749999916, 91.75000000204836681 ) ) ;
#66220 = CARTESIAN_POINT ( 'NONE',  ( -8.311093377946836114, 17.96874999658601979, -8.311093377946837890 ) ) ;
#66221 = ORIENTED_EDGE ( 'NONE', *, *, #67650, .T. ) ;
#66222 = CARTESIAN_POINT ( 'NONE',  ( 16.00000000000000711, -16.00000000000000000, 20.00000000000000000 ) ) ;
#66223 = EDGE_CURVE ( 'NONE', #5520, #55260, #12696, .T. ) ;
#66224 = CARTESIAN_POINT ( 'NONE',  ( -8.008118988124991233, 0.000000000000000000, 26.51311528394063188 ) ) ;
#66225 = DIRECTION ( 'NONE',  ( 1.000000000000000000, -0.000000000000000000, -0.000000000000000000 ) ) ;
#66226 =( BOUNDED_CURVE ( )  B_SPLINE_CURVE ( 2, ( #6002, #18427, #30118, #34686, #18800, #40322, #5629 ),
 .UNSPECIFIED., .F., .F. ) 
 B_SPLINE_CURVE_WITH_KNOTS ( ( 3, 2, 2, 3 ),
 ( 0.9705882352941177516, 0.9742647058823530326, 0.9779411764705882026, 0.9803851205147093850 ),
 .UNSPECIFIED. ) 
 CURVE ( )  GEOMETRIC_REPRESENTATION_ITEM ( )  RATIONAL_B_SPLINE_CURVE ( ( 0.9999999999999976685, 0.9238795325112890700, 1.000000000000000000, 0.9238795325112867385, 1.000000000000000000, 0.9493987076219048138, 0.9660721148037704209 ) ) 
 REPRESENTATION_ITEM ( '' )  );
#66227 = AXIS2_PLACEMENT_3D ( 'NONE', #47527, #18868, #69444 ) ;
#66228 = DIRECTION ( 'NONE',  ( -1.000000000000000000, -0.000000000000000000, -0.000000000000000000 ) ) ;
#66229 = CARTESIAN_POINT ( 'NONE',  ( -5.082755093536326818, 1.406249997951610320, 5.082755093536325042 ) ) ;
#66230 = CARTESIAN_POINT ( 'NONE',  ( 2.765530957082001251, 290.7656250017069510, 6.676582343750000703 ) ) ;
#66231 = CARTESIAN_POINT ( 'NONE',  ( 0.4369882809993350103, 51.14729664189524527, -48.52014062455030086 ) ) ;
#66232 = CARTESIAN_POINT ( 'NONE',  ( -6.362988438888832046E-13, 223.7499999999999147, 9.999999999999998224 ) ) ;
#66233 = ORIENTED_EDGE ( 'NONE', *, *, #57274, .F. ) ;
#66234 = CARTESIAN_POINT ( 'NONE',  ( -3.042071309553164404, 137.5520833299193555, -11.35316468749999963 ) ) ;
#66235 = CARTESIAN_POINT ( 'NONE',  ( 4.220049686691941027, -10.18810118749999738, 86.12500000204836681 ) ) ;
#66236 = ADVANCED_FACE ( 'NONE', ( #60497 ), #71640, .T. ) ;
#66237 = CARTESIAN_POINT ( 'NONE',  ( -30.44569435410883429, 200.5625000013656063, 167.5543056458915885 ) ) ;
#66238 = CARTESIAN_POINT ( 'NONE',  ( 0.000000000000000000, 125.0000000000000000, 0.000000000000000000 ) ) ;
#66239 = CARTESIAN_POINT ( 'NONE',  ( -4.541265875000002339, 17.93749999863440792, -5.561446717895856393E-16 ) ) ;
#66240 = VERTEX_POINT ( 'NONE', #26913 ) ;
#66241 = CARTESIAN_POINT ( 'NONE',  ( 2.751064625579944321E-14, 203.8750000027312126, 194.0000000000000568 ) ) ;
#66242 = CARTESIAN_POINT ( 'NONE',  ( 2.445694354108784108, 200.5625000013656063, 144.4456943541088663 ) ) ;
#66244 =( BOUNDED_CURVE ( )  B_SPLINE_CURVE ( 3, ( #10551, #5272, #4900, #4525 ),
 .UNSPECIFIED., .F., .F. ) 
 B_SPLINE_CURVE_WITH_KNOTS ( ( 4, 4 ),
 ( 1.418853228189154825, 3.141592653589793116 ),
 .UNSPECIFIED. ) 
 CURVE ( )  GEOMETRIC_REPRESENTATION_ITEM ( )  RATIONAL_B_SPLINE_CURVE ( ( 1.000000000000000000, 0.7675992199215426748, 0.7675992199215426748, 1.000000000000000000 ) ) 
 REPRESENTATION_ITEM ( '' )  );
#66243 = CARTESIAN_POINT ( 'NONE',  ( 1.656854249492348607, 204.3125000027312126, 138.0000000000000568 ) ) ;
#66245 = CARTESIAN_POINT ( 'NONE',  ( -10.00000000000009770, 172.2916666666666856, -2.679491924311255602 ) ) ;
#66246 = ORIENTED_EDGE ( 'NONE', *, *, #29186, .T. ) ;
#66247 = CARTESIAN_POINT ( 'NONE',  ( 7.188101187500000933, 3.562499997951610542, -2.977408999572650483 ) ) ;
#66248 = DIRECTION ( 'NONE',  ( -0.8191520442889911324, 1.003171929053523884E-16, 0.5735764363510471586 ) ) ;
#66249 = DIRECTION ( 'NONE',  ( -0.000000000000000000, 1.000000000000000000, -0.000000000000000000 ) ) ;
#66250 = CARTESIAN_POINT ( 'NONE',  ( 5.676582343750001591, 191.6145833299193839, -9.832129032723420536 ) ) ;
#66251 = CARTESIAN_POINT ( 'NONE',  ( -7.188101187499999156, 111.1250000020483810, 2.977408999572654924 ) ) ;
#66252 = DIRECTION ( 'NONE',  ( 1.000000000000000000, 0.000000000000000000, -0.000000000000000000 ) ) ;
#66253 = CARTESIAN_POINT ( 'NONE',  ( -4.721056650415999201, 293.3281250017069510, -4.721056650415999201 ) ) ;
#66255 = CARTESIAN_POINT ( 'NONE',  ( 2.775557561562891351E-14, 210.0000000000000284, 198.0000000000000284 ) ) ;
#66254 = CARTESIAN_POINT ( 'NONE',  ( -8.311093377946834337, 224.5312500034140157, 8.311093377946837890 ) ) ;
#66256 = VERTEX_POINT ( 'NONE', #72182 ) ;
#66258 = CARTESIAN_POINT ( 'NONE',  ( -11.35316468749999608, 224.4270833367473017, 3.042071309553173730 ) ) ;
#66257 = VECTOR ( 'NONE', #63486, 1000.000000000000000 ) ;
#66260 = CARTESIAN_POINT ( 'NONE',  ( 1.320432766682872962E-15, -7.188101187499992051, 27.73655278187175455 ) ) ;
#66259 = SHAPE_REPRESENTATION ( 'stud', ( #57354 ), #51355 ) ;
#66261 = CARTESIAN_POINT ( 'NONE',  ( -1.656854249492383468, 2.437499997268814056, 4.000000000000000888 ) ) ;
#66262 = LINE ( 'NONE', #43246, #23735 ) ;
#66263 = CARTESIAN_POINT ( 'NONE',  ( -3.458734124999960358, 199.6250000013656063, 196.5673454167823877 ) ) ;
#66264 = CARTESIAN_POINT ( 'NONE',  ( -28.00000000000002487, 198.0000000000000000, 166.0000000000003695 ) ) ;
#66265 = CARTESIAN_POINT ( 'NONE',  ( 4.898587196589415787E-16, 0.000000000000000000, 4.000000000000001776 ) ) ;
#66266 = CARTESIAN_POINT ( 'NONE',  ( -5.656854249492380582, 96.31250000000000000, -5.656854249492380582 ) ) ;
#66267 = CARTESIAN_POINT ( 'NONE',  ( -2.085542519210945728E-15, 119.8437499965860269, 11.35316468750000141 ) ) ;
#66268 = CARTESIAN_POINT ( 'NONE',  ( -5.000000000000001776, -10.42446448370097833, -65.94449134867545581 ) ) ;
#66269 = CARTESIAN_POINT ( 'NONE',  ( 4.556349186104051263, -10.99999999999999822, 70.46874999999998579 ) ) ;
#66272 = CARTESIAN_POINT ( 'NONE',  ( -4.898587196589412829E-16, 118.8125000040967763, -8.000000000000000000 ) ) ;
#66271 = CARTESIAN_POINT ( 'NONE',  ( 27.99999999999996803, 198.9375000013655779, 166.5412658749999082 ) ) ;
#66270 = CARTESIAN_POINT ( 'NONE',  ( 24.54126587500000056, 200.3750000013656063, 168.5673454167822172 ) ) ;
#66273 = VERTEX_POINT ( 'NONE', #37874 ) ;
#66274 = EDGE_CURVE ( 'NONE', #53484, #36433, #69991, .T. ) ;
#66275 = CARTESIAN_POINT ( 'NONE',  ( 11.35316468750000141, 225.7812499965860127, 0.000000000000000000 ) ) ;
#66276 = CARTESIAN_POINT ( 'NONE',  ( -2.445694354108838731, 203.0625000013656063, 144.4456943541088663 ) ) ;
#66277 = CARTESIAN_POINT ( 'NONE',  ( 28.00000000000002132, 201.1875000013656063, 166.5412658749999082 ) ) ;
#66278 = CARTESIAN_POINT ( 'NONE',  ( 5.082755093536324154, 27.65624999795161543, 5.082755093536326818 ) ) ;
#66279 = CARTESIAN_POINT ( 'NONE',  ( -5.676582343750006032, 194.4270833299193839, 9.832129032723418760 ) ) ;
#66280 = CARTESIAN_POINT ( 'NONE',  ( -4.401442555609581635E-16, 91.15625000204838102, -7.188101187500000044 ) ) ;
#66281 = CARTESIAN_POINT ( 'NONE',  ( -7.999999999999991118, 0.000000000000000000, 11.33030277982336642 ) ) ;
#66282 = CARTESIAN_POINT ( 'NONE',  ( 4.541265875000001451, 15.24999999863440969, 1.881053915767124440 ) ) ;
#66283 = CARTESIAN_POINT ( 'NONE',  ( 30.44569435410883429, 200.0625000013656063, 167.5543056458911053 ) ) ;
#66284 = CARTESIAN_POINT ( 'NONE',  ( -7.999999999999991118, 0.000000000000000000, 29.33030277982336642 ) ) ;
#66285 = PLANE ( 'NONE',  #25455 ) ;
#66286 = CARTESIAN_POINT ( 'NONE',  ( -3.042071309553164404, 82.23958332991935549, -11.35316468749999963 ) ) ;
#66287 = ORIENTED_EDGE ( 'NONE', *, *, #16828, .T. ) ;
#66288 = EDGE_CURVE ( 'NONE', #53587, #17827, #5971, .T. ) ;
#66289 = CARTESIAN_POINT ( 'NONE',  ( -10.99999999999992184, -31.99999999999978684, 198.9827534923788619 ) ) ;
#66290 = CYLINDRICAL_SURFACE ( 'NONE', #43584, 4.999999999999997335 ) ;
#66291 = CARTESIAN_POINT ( 'NONE',  ( -7.188101187500001821, 20.62499999795161543, -2.977408999572651371 ) ) ;
#66292 = DIRECTION ( 'NONE',  ( -0.000000000000000000, 1.000000000000000000, -0.000000000000000000 ) ) ;
#66293 = CYLINDRICAL_SURFACE ( 'NONE', #52154, 10.00000000000000178 ) ;
#66294 = CARTESIAN_POINT ( 'NONE',  ( 11.35316468749999785, 90.57291666325268409, 3.042071309553174174 ) ) ;
#66295 = ORIENTED_EDGE ( 'NONE', *, *, #3283, .F. ) ;
#66296 = CARTESIAN_POINT ( 'NONE',  ( 7.204075437095968759, -7.204075437095966983, 85.09375000204836681 ) ) ;
#66297 = CARTESIAN_POINT ( 'NONE',  ( 7.204075437095966983, 7.204075437095967871, 115.0937500020483810 ) ) ;
#66298 = CARTESIAN_POINT ( 'NONE',  ( -31.45873412499999233, 195.9375000013655779, 170.0000000000003979 ) ) ;
#66299 = CARTESIAN_POINT ( 'NONE',  ( 2.445694354108839175, 207.3125000013656063, 195.5543056458912190 ) ) ;
#66300 = CARTESIAN_POINT ( 'NONE',  ( -2.849036369511732440E-14, 202.3750000027312126, 138.0000000000000568 ) ) ;
#66302 = CARTESIAN_POINT ( 'NONE',  ( 5.676582343750001591, 66.61458332991935549, -9.832129032723420536 ) ) ;
#66301 = CARTESIAN_POINT ( 'NONE',  ( 7.778174593052023411, -7.778174593052021635, 106.5624999999999858 ) ) ;
#66303 = CARTESIAN_POINT ( 'NONE',  ( 3.313708498984762496, -7.999999999999989342, 20.98655278392014978 ) ) ;
#66304 = CARTESIAN_POINT ( 'NONE',  ( 10.00000000000000178, 130.0000000000000000, 0.000000000000000000 ) ) ;
#66305 = TOROIDAL_SURFACE ( 'NONE', #41017, 81.50000000000000000, 10.99999999999999822 ) ;
#66306 = CARTESIAN_POINT ( 'NONE',  ( 10.00000000000000000, 166.6666666598387110, 2.679491924311236062 ) ) ;
#66307 = CARTESIAN_POINT ( 'NONE',  ( 7.188101187500002709, 90.68750000204838102, 2.977408999572649151 ) ) ;
#66308 = CARTESIAN_POINT ( 'NONE',  ( -24.85907736982398575, 194.8576601072065557, 172.2477269894046685 ) ) ;
#66309 = CARTESIAN_POINT ( 'NONE',  ( -8.311093377946841443, 59.21874999658601268, 8.311093377946834337 ) ) ;
#66310 = CARTESIAN_POINT ( 'NONE',  ( -4.088227598258586603E-16, 293.2031250017069510, -6.676582343750001591 ) ) ;
#66311 = CARTESIAN_POINT ( 'NONE',  ( -6.238412754330611322E-16, 10.18810118749999916, 106.6562500020483810 ) ) ;
#66312 = CARTESIAN_POINT ( 'NONE',  ( 11.35316468749999785, 205.5729166632526699, 3.042071309553174174 ) ) ;
#66313 = ORIENTED_EDGE ( 'NONE', *, *, #19549, .T. ) ;
#66314 = CARTESIAN_POINT ( 'NONE',  ( 3.999999999999960032, 203.0000000000000000, 142.0000000000000568 ) ) ;
#66315 = LINE ( 'NONE', #65939, #55708 ) ;
#66316 = CARTESIAN_POINT ( 'NONE',  ( 4.000000000000001776, 0.7499999972688131678, 0.000000000000000000 ) ) ;
#66318 = CARTESIAN_POINT ( 'NONE',  ( 5.676582343749993598, 194.9479166632526983, 9.832129032723422313 ) ) ;
#66317 = CARTESIAN_POINT ( 'NONE',  ( -7.347880794884122694E-16, 11.49999999726881406, 4.000000000000001776 ) ) ;
#66319 = CYLINDRICAL_SURFACE ( 'NONE', #39367, 8.000000000000000000 ) ;
#66320 = CARTESIAN_POINT ( 'NONE',  ( 9.999999999999998224, 240.8333333401612890, -2.679491924311229401 ) ) ;
#66321 = DIRECTION ( 'NONE',  ( -0.000000000000000000, 1.000000000000000000, -0.000000000000000000 ) ) ;
#66322 = ORIENTED_EDGE ( 'NONE', *, *, #34629, .T. ) ;
#66323 = CARTESIAN_POINT ( 'NONE',  ( 8.311093377946837890, 181.7187499965859843, -8.311093377946837890 ) ) ;
#66324 = VECTOR ( 'NONE', #5780, 1000.000000000000000 ) ;
#66325 = CARTESIAN_POINT ( 'NONE',  ( -7.188101187499990274, -2.977408999572651815, 22.58030278187175455 ) ) ;
#66326 = CARTESIAN_POINT ( 'NONE',  ( -9.999999999999992895, 92.29166666666665719, -2.679491924311228068 ) ) ;
#66327 = VERTEX_POINT ( 'NONE', #1069 ) ;
#66328 = AXIS2_PLACEMENT_3D ( 'NONE', #15179, #38210, #61213 ) ;
#66329 = CARTESIAN_POINT ( 'NONE',  ( 8.000000000000000000, 95.93750000409679046, -9.797174393178825657E-16 ) ) ;
#66330 = FACE_OUTER_BOUND ( 'NONE', #49507, .T. ) ;
#66331 =( BOUNDED_CURVE ( )  B_SPLINE_CURVE ( 2, ( #50720, #46178, #74479, #49325, #57525, #72340, #73736, #68084, #16373 ),
 .UNSPECIFIED., .F., .F. ) 
 B_SPLINE_CURVE_WITH_KNOTS ( ( 3, 2, 2, 2, 3 ),
 ( 0.08823529411764712005, 0.09191176470588241498, 0.09558823529411770992, 0.09926470588235300485, 0.1029411764705883137 ),
 .UNSPECIFIED. ) 
 CURVE ( )  GEOMETRIC_REPRESENTATION_ITEM ( )  RATIONAL_B_SPLINE_CURVE ( ( 0.9999999999999988898, 0.9238795325112878487, 1.000000000000000000, 0.9238795325112867385, 1.000000000000000000, 0.9238795325112867385, 1.000000000000000000, 0.9238795325112849621, 1.000000000000001776 ) ) 
 REPRESENTATION_ITEM ( '' )  );
#66332 = CARTESIAN_POINT ( 'NONE',  ( -1.656854249492381248, 16.31250000000000000, -4.000000000000001776 ) ) ;
#66333 = CARTESIAN_POINT ( 'NONE',  ( 3.211159895383561835, 15.43749999863440614, -3.211159895383561835 ) ) ;
#66334 = CARTESIAN_POINT ( 'NONE',  ( 5.656854249492376141, -5.656854249492374365, 13.58030278392014623 ) ) ;
#66335 = CARTESIAN_POINT ( 'NONE',  ( 29.73028433449606212, 194.7132116749262707, 166.7068852075860264 ) ) ;
#66336 = ORIENTED_EDGE ( 'NONE', *, *, #49321, .F. ) ;
#66337 = CARTESIAN_POINT ( 'NONE',  ( 5.000000000000000888, -13.57248045702109351, -69.64920683919133637 ) ) ;
#66338 = CARTESIAN_POINT ( 'NONE',  ( -2.977408999572650927, 95.37500000204839523, -7.188101187500001821 ) ) ;
#66340 = AXIS2_PLACEMENT_3D ( 'NONE', #19871, #31949, #48172 ) ;
#66339 = CARTESIAN_POINT ( 'NONE',  ( 3.042071309553173286, 255.3645833367473301, 11.35316468749999608 ) ) ;
#66341 = DIRECTION ( 'NONE',  ( 0.000000000000000000, -1.000000000000000000, 0.000000000000000000 ) ) ;
#66342 = ORIENTED_EDGE ( 'NONE', *, *, #1125, .T. ) ;
#66343 = EDGE_CURVE ( 'NONE', #54330, #45186, #2568, .T. ) ;
#66344 = DIRECTION ( 'NONE',  ( -0.000000000000000000, 1.000000000000000000, -0.000000000000000000 ) ) ;
#66345 = ADVANCED_FACE ( 'NONE', ( #41776 ), #45951, .T. ) ;
#66346 = CARTESIAN_POINT ( 'NONE',  ( -5.082755093536319713, 5.082755093536319713, 20.79905278187175455 ) ) ;
#66347 = ORIENTED_EDGE ( 'NONE', *, *, #43219, .T. ) ;
#66348 =( BOUNDED_CURVE ( )  B_SPLINE_CURVE ( 2, ( #52000, #1447, #53113, #52741, #30094, #47062, #41050, #16905, #52371 ),
 .UNSPECIFIED., .F., .F. ) 
 B_SPLINE_CURVE_WITH_KNOTS ( ( 3, 2, 2, 2, 3 ),
 ( 0.06944444444444444753, 0.07638888888888889506, 0.08333333333333331483, 0.09027777777777776236, 0.09722222222222220989 ),
 .UNSPECIFIED. ) 
 CURVE ( )  GEOMETRIC_REPRESENTATION_ITEM ( )  RATIONAL_B_SPLINE_CURVE ( ( 1.000000000000000000, 0.9238795325112867385, 1.000000000000000000, 0.9238795325112867385, 1.000000000000000000, 0.9238795325112867385, 1.000000000000000000, 0.9238795325112868495, 0.9999999999999998890 ) ) 
 REPRESENTATION_ITEM ( '' )  );
#66349 = EDGE_LOOP ( 'NONE', ( #24948, #10584, #47800, #35690 ) ) ;
#66350 = CARTESIAN_POINT ( 'NONE',  ( 4.220049686691934809, 10.18810118749999916, 82.18750000204836681 ) ) ;
#66351 = CARTESIAN_POINT ( 'NONE',  ( 11.35316468750000141, 76.09374999658602690, 0.000000000000000000 ) ) ;
#66352 = CARTESIAN_POINT ( 'NONE',  ( 7.320508075688774596, 92.49999999317203958, -7.320508075688774596 ) ) ;
#66353 = CARTESIAN_POINT ( 'NONE',  ( 4.556349186104045934, 11.00000000000000000, 96.53125000000000000 ) ) ;
#66356 = CARTESIAN_POINT ( 'NONE',  ( 4.721056650415999201, 295.2343750017069510, -4.721056650415999201 ) ) ;
#66355 = CARTESIAN_POINT ( 'NONE',  ( 31.99999999999997868, 196.4375000027311842, 168.3431457505075173 ) ) ;
#66354 = DIRECTION ( 'NONE',  ( 0.8660254037844381525, 0.5000000000000008882, 0.000000000000000000 ) ) ;
#66357 = CARTESIAN_POINT ( 'NONE',  ( -3.313708498984653250, 90.40625000409677625, -8.000000000000108358 ) ) ;
#66358 = ADVANCED_FACE ( 'NONE', ( #72297 ), #19491, .F. ) ;
#66359 = CARTESIAN_POINT ( 'NONE',  ( 3.458734125000015425, 200.2500000013656063, 196.5673454167823877 ) ) ;
#66360 = CARTESIAN_POINT ( 'NONE',  ( 3.999999999999959144, 199.0625000000000000, 140.3431457505076594 ) ) ;
#66361 = CARTESIAN_POINT ( 'NONE',  ( -8.000000000000001776, 2.156249995903220196, 3.313708498984759387 ) ) ;
#66362 = CARTESIAN_POINT ( 'NONE',  ( 30.44569435410879166, 200.5625000013656063, 172.4456943541087526 ) ) ;
#66363 = CARTESIAN_POINT ( 'NONE',  ( -7.188101187500002709, 10.68749999795161187, 2.977408999572649151 ) ) ;
#66364 = CARTESIAN_POINT ( 'NONE',  ( 3.313708498984756279, 7.999999999999991118, 24.54905278392014978 ) ) ;
#66365 = SPHERICAL_SURFACE ( 'NONE', #72073, 38.34805510287551300 ) ;
#66366 = CARTESIAN_POINT ( 'NONE',  ( 1.320432766682874540E-15, 109.9062500020483810, 7.188101187500000044 ) ) ;
#66368 = CARTESIAN_POINT ( 'NONE',  ( 0.000000000000000000, 125.0000000000000000, 0.000000000000000000 ) ) ;
#66367 = CARTESIAN_POINT ( 'NONE',  ( 1.224646799147353454E-15, 300.0000000000000000, -10.00000000000000178 ) ) ;
#66369 = CARTESIAN_POINT ( 'NONE',  ( 27.99999999999996447, 202.6250000027312126, 165.9999999999998863 ) ) ;
#66370 = CARTESIAN_POINT ( 'NONE',  ( -13.99999999999999822, 0.000000000000000000, 0.000000000000000000 ) ) ;
#66371 = CARTESIAN_POINT ( 'NONE',  ( -7.188101187499991163, 2.977408999572646930, 24.26780278187175455 ) ) ;
#66372 = CARTESIAN_POINT ( 'NONE',  ( -9.832129032723418760, 42.86458332991935549, -5.676582343750004256 ) ) ;
#66373 = CARTESIAN_POINT ( 'NONE',  ( -38.00000000000000000, -53.00000000000000711, -5.204170427930421283E-15 ) ) ;
#66374 = CARTESIAN_POINT ( 'NONE',  ( 2.679491924311228956, 7.916666659838700326, -10.00000000000000000 ) ) ;
#66375 = ORIENTED_EDGE ( 'NONE', *, *, #70622, .T. ) ;
#66376 = CARTESIAN_POINT ( 'NONE',  ( 3.999999999999960032, 199.0625000027312126, 143.6568542494924259 ) ) ;
#66377 = CARTESIAN_POINT ( 'NONE',  ( 11.00000000000000000, 1.347111479062088405E-15, 69.43750000409676204 ) ) ;
#66378 = CARTESIAN_POINT ( 'NONE',  ( -5.676582343750006032, 54.11458332991934839, 9.832129032723418760 ) ) ;
#66379 = CARTESIAN_POINT ( 'NONE',  ( -11.00000000000000000, 4.556349186104045934, 80.59375000409677625 ) ) ;
#66380 = CARTESIAN_POINT ( 'NONE',  ( -3.458734125000015425, 204.2500000013655779, 143.4326545832176976 ) ) ;
#66382 = VECTOR ( 'NONE', #61006, 1000.000000000000000 ) ;
#66381 = DIRECTION ( 'NONE',  ( 0.000000000000000000, -1.000000000000000000, 0.000000000000000000 ) ) ;
#66383 = CARTESIAN_POINT ( 'NONE',  ( -1.656854249492287101, 195.3125000000000284, 137.9999999999998863 ) ) ;
#66385 = CARTESIAN_POINT ( 'NONE',  ( -3.042071309553173730, 34.32291666325268409, 11.35316468749999785 ) ) ;
#66384 = CARTESIAN_POINT ( 'NONE',  ( 5.082755093536325042, 99.59375000204838102, -5.082755093536325930 ) ) ;
#66386 = CARTESIAN_POINT ( 'NONE',  ( -3.313708498984757167, 7.999999999999991118, 6.549052779823365533 ) ) ;
#66387 = CARTESIAN_POINT ( 'NONE',  ( 0.000000000000000000, 300.0000000000000000, 0.000000000000000000 ) ) ;
#66388 = CARTESIAN_POINT ( 'NONE',  ( -9.832129032723420536, 163.6979166632526983, 5.676582343749997150 ) ) ;
#66389 = CARTESIAN_POINT ( 'NONE',  ( -2.679491924311235618, 135.4166666598386826, 10.00000000000000000 ) ) ;
#66390 = CARTESIAN_POINT ( 'NONE',  ( 1.320432766682874540E-15, 109.9062500020483810, 7.188101187500000044 ) ) ;
#66391 = CIRCLE ( 'NONE', #64034, 6.000000000000015099 ) ;
#66392 = ORIENTED_EDGE ( 'NONE', *, *, #33134, .F. ) ;
#66393 = CARTESIAN_POINT ( 'NONE',  ( -54.00000000000000711, 272.0000000000000000, 20.00000000000003197 ) ) ;
#66394 = CARTESIAN_POINT ( 'NONE',  ( 11.35316468749999963, 21.30208332991934839, -3.042071309553165293 ) ) ;
#66395 = CARTESIAN_POINT ( 'NONE',  ( 1.224646799147353454E-15, 300.0000000000000000, -10.00000000000000178 ) ) ;
#66396 = VERTEX_POINT ( 'NONE', #60607 ) ;
#66397 = CARTESIAN_POINT ( 'NONE',  ( 0.000000000000000000, 45.00000000000000000, 0.000000000000000000 ) ) ;
#66398 = CARTESIAN_POINT ( 'NONE',  ( -4.220049686691935698, 10.18810118749999916, 79.37500000204838102 ) ) ;
#66399 = CARTESIAN_POINT ( 'NONE',  ( -37.99999999999999289, 242.0000000000000284, 0.000000000000000000 ) ) ;
#66401 = CARTESIAN_POINT ( 'NONE',  ( 3.042071309553159519, 149.7395833299193271, 11.35316468750000141 ) ) ;
#66400 = CARTESIAN_POINT ( 'NONE',  ( 0.000000000000000000, 0.000000000000000000, 118.0000000000000000 ) ) ;
#66402 = CARTESIAN_POINT ( 'NONE',  ( 4.401442555609581635E-16, 2.718749997951610542, -7.188101187500000044 ) ) ;
#66403 = CARTESIAN_POINT ( 'NONE',  ( 7.999999999999992895, -3.313708498984756279, 9.042802784329825982 ) ) ;
#66404 = CARTESIAN_POINT ( 'NONE',  ( 3.999999999999959144, 208.1875000027311842, 140.3431457505076594 ) ) ;
#66405 = CARTESIAN_POINT ( 'NONE',  ( 11.35316468749999963, 241.1979166700806729, 3.042071309553159519 ) ) ;
#66406 = CARTESIAN_POINT ( 'NONE',  ( 10.18810118750000093, -4.220049686691933921, 88.18750000204838102 ) ) ;
#66407 = ORIENTED_EDGE ( 'NONE', *, *, #65599, .T. ) ;
#66408 = CARTESIAN_POINT ( 'NONE',  ( 2.849036369511732440E-14, 199.3750000027312126, 202.0000000000000000 ) ) ;
#66409 = CARTESIAN_POINT ( 'NONE',  ( -11.35316468750000141, 103.8020833299193413, 3.042071309553159963 ) ) ;
#66410 = CARTESIAN_POINT ( 'NONE',  ( -10.18810118749999738, -4.220049686691941915, 93.25000000204838102 ) ) ;
#66411 = CARTESIAN_POINT ( 'NONE',  ( -1.881053915767124440, 20.12499999863441147, 4.541265875000001451 ) ) ;
#66412 = ORIENTED_EDGE ( 'NONE', *, *, #28114, .T. ) ;
#66413 = ORIENTED_EDGE ( 'NONE', *, *, #73268, .T. ) ;
#66414 = AXIS2_PLACEMENT_3D ( 'NONE', #33449, #15690, #33085 ) ;
#66415 = CARTESIAN_POINT ( 'NONE',  ( 3.211159895383560947, 2.312499998634407028, 3.211159895383562723 ) ) ;
#66416 = CARTESIAN_POINT ( 'NONE',  ( 5.082755093536324154, 10.78124999795161187, 5.082755093536326818 ) ) ;
#66417 = CARTESIAN_POINT ( 'NONE',  ( -8.000000000000000000, 114.6875000040967763, 0.000000000000000000 ) ) ;
#66418 = CARTESIAN_POINT ( 'NONE',  ( 4.220049686691934809, 10.18810118749999916, 99.06250000204836681 ) ) ;
#66419 = CARTESIAN_POINT ( 'NONE',  ( -24.54126587500000056, 201.5000000013655779, 168.5673454167827003 ) ) ;
#66420 = EDGE_CURVE ( 'NONE', #25788, #49698, #14944, .T. ) ;
#66421 = CARTESIAN_POINT ( 'NONE',  ( 4.000000000000000888, 3.937500000000000000, 1.656854249492384135 ) ) ;
#66422 = CARTESIAN_POINT ( 'NONE',  ( 4.000000000000001776, 18.74999999726881583, 0.000000000000000000 ) ) ;
#66423 = CARTESIAN_POINT ( 'NONE',  ( -8.342170076843785083E-16, 5.062499998634407028, 4.541265875000002339 ) ) ;
#66424 = CARTESIAN_POINT ( 'NONE',  ( 5.656854249492379694, 95.93750000000000000, -5.656854249492380582 ) ) ;
#66425 = CARTESIAN_POINT ( 'NONE',  ( -1.432654583217607192, 196.2500000013656631, 194.5412658750000219 ) ) ;
#66426 = AXIS2_PLACEMENT_3D ( 'NONE', #57052, #15917, #27616 ) ;
#66428 = CARTESIAN_POINT ( 'NONE',  ( -5.656854249492375253, 5.656854249492375253, 17.14280277982336287 ) ) ;
#66427 = CARTESIAN_POINT ( 'NONE',  ( -31.45873412500001720, 198.6250000013655779, 168.5673454167828140 ) ) ;
#66429 = SHAPE_REPRESENTATION_RELATIONSHIP ( 'NONE' , 'NONE' ,  #2150, #55158 ) ;
#66430 = CARTESIAN_POINT ( 'NONE',  ( 1.881053915767121776, 16.49999999863440436, -4.541265875000002339 ) ) ;
#66431 = CIRCLE ( 'NONE', #36351, 12.00000000000000355 ) ;
#66432 = CARTESIAN_POINT ( 'NONE',  ( 7.188101187499993827, -2.977408999572645598, 6.642802781871754547 ) ) ;
#66433 = EDGE_LOOP ( 'NONE', ( #52696, #22209, #50025, #64911 ) ) ;
#66434 = ORIENTED_EDGE ( 'NONE', *, *, #69902, .F. ) ;
#66435 = CARTESIAN_POINT ( 'NONE',  ( 10.18810118749999916, 4.220049686691935698, 95.50000000204838102 ) ) ;
#66436 = CARTESIAN_POINT ( 'NONE',  ( 7.778174593052021635, 7.778174593052023411, 114.6250000040967763 ) ) ;
#66437 = VECTOR ( 'NONE', #36882, 1000.000000000000000 ) ;
#66438 = CARTESIAN_POINT ( 'NONE',  ( -25.55430564589119413, 205.5625000013656063, 167.5543056458915316 ) ) ;
#66439 = CARTESIAN_POINT ( 'NONE',  ( -28.00000000000002842, 199.0000000000000000, 166.0000000000003695 ) ) ;
#66440 = CARTESIAN_POINT ( 'NONE',  ( -3.458734124999960358, 206.6250000013656063, 196.5673454167823877 ) ) ;
#66441 = CARTESIAN_POINT ( 'NONE',  ( 10.00000000000007994, 60.00000000000004974, 0.000000000000000000 ) ) ;
#66442 = CARTESIAN_POINT ( 'NONE',  ( 2.679491924311228956, 111.0416666666666572, -10.00000000000000000 ) ) ;
#66443 = EDGE_CURVE ( 'NONE', #15013, #68586, #2993, .T. ) ;
#66444 = EDGE_CURVE ( 'NONE', #65735, #48235, #71540, .T. ) ;
#66445 = CARTESIAN_POINT ( 'NONE',  ( 3.313708498984765161, 114.9687500000000142, 7.999999999999998224 ) ) ;
#66446 = CARTESIAN_POINT ( 'NONE',  ( 6.676582343750003368, 292.1718750017070079, -2.765530957081997254 ) ) ;
#66447 = CARTESIAN_POINT ( 'NONE',  ( -7.188101187499991163, 2.977408999572646930, 9.267802781871756324 ) ) ;
#66448 = ORIENTED_EDGE ( 'NONE', *, *, #32956, .T. ) ;
#66449 =( BOUNDED_SURFACE ( )  B_SPLINE_SURFACE ( 1, 2, ( 
 ( #66724, #9010, #8636, #54669, #48244, #2978, #20310, #30537, #19570, #25963, #30900, #43327, #37690, #49362, #32025, #26342, #72380, #53553, #47873, #42212, #65224, #68587, #55793, #55419, #44462, #10504, #16895, #38812, #33911, #61812, #22180, #50117, #62547, #27102, #9386, #56164, #10130, #4110, #67476, #4479, #68215, #45204, #27469, #16513, #32405, #33536, #50482, #33168, #73133, #21068, #39919, #44092, #32786, #3728, #21439, #50860, #45574, #61440, #73497, #21804, #56537, #15775, #22552, #26727, #44837, #72763, #49747, #67844, #15398, #16135, #39174, #73875, #56912, #10877, #62178, #67101, #9766, #38436, #4854, #27851, #39552, #5224, #28225, #51234, #74245, #46320, #68964, #11992, #53103, #45948, #46687, #35026, #29354, #58769, #64049, #28970, #34281, #1066, #328, #51990, #69335, #7077, #23307, #70089, #11251, #17272, #40291, #63292, #12359, #23681, #18023, #17644, #64421, #6351, #63667, #18765, #58038, #52361, #1437, #52732, #58405, #29717, #697, #69711, #11620, #41041, #35393, #51607, #57285, #34657, #6710, #41409, #12719, #24418, #24043, #22938, #47424, #47053, #74623, #5599, #18395, #30083, #57661, #35752, #70449, #5967, #28597, #40664, #62926, #71911, #37226, #54212, #49274, #26255, #65140, #59864, #14564, #25513, #59140, #7448, #59500, #20224, #37601, #43242, #25878, #13449, #60600, #25142, #48897, #8923, #31935, #19858, #2522, #54958, #24774, #3267, #7813, #54586, #72289, #65882, #70811, #36118, #13812, #36856, #60223, #48526, #41772, #64782, #31187, #8177, #47788, #66258, #42864, #30456, #13083, #71166, #53472, #71532, #1789, #65517, #53839, #2149, #19122, #42127, #36487, #30816, #48159, #19486, #42501, #14189, #8549, #31563, #2890, #16055, #73781, #50027, #21350 ),
 ( #38728, #62092, #61352, #67383, #44374, #4022, #5136, #67009, #66630, #55707, #21718, #28130, #73043, #45114, #15686, #33444, #9679, #22090, #38345, #20601, #61724, #10044, #15308, #27015, #20977, #3637, #39087, #4387, #50766, #10414, #14937, #33080, #26635, #56077, #49657, #27379, #10782, #72675, #50399, #73413, #44746, #16422, #67761, #32699, #37976, #56444, #4762, #27755, #68127, #39455, #62455, #33819, #43618, #44002, #56816, #51142, #60975, #9295, #32320, #55332, #974, #17554, #235, #29994, #46227, #40571, #64325, #40947, #11902, #39823, #35300, #46964, #11530, #23957, #69244, #29625, #35661, #52638, #63575, #34935, #68867, #5879, #63957, #58675, #22837, #57948, #28504, #6253, #51513, #18301, #29257, #52270, #12267, #40198, #604, #23216, #57569, #6983, #45851, #45476, #34563, #23585, #74152, #28874, #69994, #51895, #58314, #63200, #41317, #17177, #22456, #46595, #69618, #17932, #6619, #12630, #68494, #16794, #62826, #11162, #34185, #57187, #5504, #74528, #42040, #64694, #60509, #12992, #1706, #47334, #65046, #19769, #14471, #30361, #48068, #53747, #54118, #24683, #66167, #70361, #19392, #41683, #18673, #13720, #59048, #42406, #71076, #42777, #25791, #31473, #36394, #53009, #1341, #36029, #20135, #19035, #13357, #47694, #54496, #65424, #2801, #24323, #36765, #48436, #48811, #7723, #2058, #25047, #7354, #37510, #53381, #8453, #59777, #71816, #8086, #31088, #70715, #2429, #43150, #25422, #30727, #8834, #71441, #59409, #65794, #14096, #37131, #60134, #26539, #68038, #32225, #54867, #49182, #14845, #43521, #26923, #4671, #21632, #27291, #73327, #49940, #72953, #37885, #21260, #67297, #20506, #3177, #60881, #44284, #10326, #33352, #22004, #15596, #66535, #45030, #55988, #9205 ) ),
 .UNSPECIFIED., .F., .F., .F. ) 
 B_SPLINE_SURFACE_WITH_KNOTS ( ( 2, 2 ),
 ( 3, 2, 2, 2, 2, 2, 2, 2, 2, 2, 2, 2, 2, 2, 2, 2, 2, 2, 2, 2, 2, 2, 2, 2, 2, 2, 2, 2, 2, 2, 2, 2, 2, 2, 2, 2, 2, 2, 2, 2, 2, 2, 2, 2, 2, 2, 2, 2, 2, 2, 2, 2, 2, 2, 2, 2, 2, 2, 2, 2, 2, 2, 2, 2, 2, 2, 2, 2, 2, 2, 2, 2, 2, 2, 2, 2, 2, 2, 2, 2, 2, 2, 2, 2, 2, 2, 2, 2, 2, 2, 2, 2, 2, 2, 2, 2, 2, 2, 2, 2, 2, 2, 2, 2, 2, 2, 2, 2, 3 ),
 ( 0.000000000000000000, 1.000000000000000000 ),
 ( 0.000000000000000000, 0.009259259259259258745, 0.01851851851851851749, 0.02777777777777777624, 0.03703703703703703498, 0.04629629629629629373, 0.05555555555555555247, 0.06481481481481481122, 0.07407407407407406996, 0.08333333333333332871, 0.09259259259259258745, 0.1018518518518518462, 0.1111111111111111049, 0.1203703703703703637, 0.1296296296296296224, 0.1388888888888888951, 0.1481481481481481399, 0.1574074074074074125, 0.1666666666666666574, 0.1759259259259259300, 0.1851851851851851749, 0.1944444444444444475, 0.2037037037037036924, 0.2129629629629629650, 0.2222222222222222099, 0.2314814814814814825, 0.2407407407407407274, 0.2500000000000000000, 0.2592592592592592449, 0.2685185185185185452, 0.2777777777777777901, 0.2870370370370370350, 0.2962962962962962798, 0.3055555555555555802, 0.3148148148148148251, 0.3240740740740740700, 0.3333333333333333148, 0.3425925925925926152, 0.3518518518518518601, 0.3611111111111111049, 0.3703703703703703498, 0.3796296296296296502, 0.3888888888888888951, 0.3981481481481481399, 0.4074074074074073848, 0.4166666666666666852, 0.4259259259259259300, 0.4351851851851851749, 0.4444444444444444198, 0.4537037037037037202, 0.4629629629629629650, 0.4722222222222222099, 0.4814814814814814548, 0.4907407407407407551, 0.5000000000000000000, 0.5092592592592593004, 0.5185185185185184897, 0.5277777777777777901, 0.5370370370370370905, 0.5462962962962962798, 0.5555555555555555802, 0.5648148148148147696, 0.5740740740740740700, 0.5833333333333333703, 0.5925925925925925597, 0.6018518518518518601, 0.6111111111111111605, 0.6203703703703703498, 0.6296296296296296502, 0.6388888888888888395, 0.6481481481481481399, 0.6574074074074074403, 0.6666666666666666297, 0.6759259259259259300, 0.6851851851851852304, 0.6944444444444444198, 0.7037037037037037202, 0.7129629629629629095, 0.7222222222222222099, 0.7314814814814815103, 0.7407407407407406996, 0.7500000000000000000, 0.7592592592592593004, 0.7685185185185184897, 0.7777777777777777901, 0.7870370370370370905, 0.7962962962962962798, 0.8055555555555555802, 0.8148148148148147696, 0.8240740740740740700, 0.8333333333333333703, 0.8425925925925925597, 0.8518518518518518601, 0.8611111111111111605, 0.8703703703703703498, 0.8796296296296296502, 0.8888888888888888395, 0.8981481481481481399, 0.9074074074074074403, 0.9166666666666666297, 0.9259259259259259300, 0.9351851851851852304, 0.9444444444444444198, 0.9537037037037037202, 0.9629629629629629095, 0.9722222222222222099, 0.9814814814814815103, 0.9907407407407406996, 1.000000000000000000 ),
 .UNSPECIFIED. ) 
 GEOMETRIC_REPRESENTATION_ITEM ( )  RATIONAL_B_SPLINE_SURFACE ( (
 ( 1.000000000000000000, 0.9659258262890683122, 1.000000000000000000, 0.9659258262890683122, 1.000000000000000000, 0.9659258262890683122, 1.000000000000000000, 0.9659258262890683122, 1.000000000000000000, 0.9659258262890683122, 1.000000000000000000, 0.9659258262890683122, 1.000000000000000000, 0.9659258262890683122, 1.000000000000000000, 0.9659258262890683122, 1.000000000000000000, 0.9659258262890683122, 1.000000000000000000, 0.9659258262890683122, 1.000000000000000000, 0.9659258262890683122, 1.000000000000000000, 0.9659258262890683122, 1.000000000000000000, 0.9659258262890683122, 1.000000000000000000, 0.9659258262890683122, 1.000000000000000000, 0.9659258262890683122, 1.000000000000000000, 0.9659258262890683122, 1.000000000000000000, 0.9659258262890683122, 1.000000000000000000, 0.9659258262890683122, 1.000000000000000000, 0.9659258262890683122, 1.000000000000000000, 0.9659258262890683122, 1.000000000000000000, 0.9659258262890683122, 1.000000000000000000, 0.9659258262890683122, 1.000000000000000000, 0.9659258262890683122, 1.000000000000000000, 0.9659258262890683122, 1.000000000000000000, 0.9659258262890683122, 1.000000000000000000, 0.9659258262890683122, 1.000000000000000000, 0.9659258262890683122, 1.000000000000000000, 0.9659258262890683122, 1.000000000000000000, 0.9659258262890683122, 1.000000000000000000, 0.9659258262890683122, 1.000000000000000000, 0.9659258262890683122, 1.000000000000000000, 0.9659258262890683122, 1.000000000000000000, 0.9659258262890683122, 1.000000000000000000, 0.9659258262890683122, 1.000000000000000000, 0.9659258262890683122, 1.000000000000000000, 0.9659258262890683122, 1.000000000000000000, 0.9659258262890683122, 1.000000000000000000, 0.9659258262890683122, 1.000000000000000000, 0.9659258262890683122, 1.000000000000000000, 0.9659258262890683122, 1.000000000000000000, 0.9659258262890683122, 1.000000000000000000, 0.9659258262890683122, 1.000000000000000000, 0.9659258262890683122, 1.000000000000000000, 0.9659258262890683122, 1.000000000000000000, 0.9659258262890683122, 1.000000000000000000, 0.9659258262890683122, 1.000000000000000000, 0.9659258262890683122, 1.000000000000000000, 0.9659258262890683122, 1.000000000000000000, 0.9659258262890683122, 1.000000000000000000, 0.9659258262890683122, 1.000000000000000000, 0.9659258262890683122, 1.000000000000000000, 0.9659258262890683122, 1.000000000000000000, 0.9659258262890683122, 1.000000000000000000, 0.9659258262890683122, 1.000000000000000000, 0.9659258262890683122, 1.000000000000000000, 0.9659258262890683122, 1.000000000000000000, 0.9659258262890683122, 1.000000000000000000, 0.9659258262890683122, 1.000000000000000000, 0.9659258262890683122, 1.000000000000000000, 0.9659258262890683122, 1.000000000000000000, 0.9659258262890683122, 1.000000000000000000, 0.9659258262890683122, 1.000000000000000000, 0.9659258262890683122, 1.000000000000000000, 0.9659258262890683122, 1.000000000000000000, 0.9659258262890683122, 1.000000000000000000, 0.9659258262890683122, 1.000000000000000000, 0.9659258262890683122, 1.000000000000000000, 0.9659258262890683122, 1.000000000000000000, 0.9659258262890683122, 1.000000000000000000, 0.9659258262890683122, 1.000000000000000000, 0.9659258262890683122, 1.000000000000000000, 0.9659258262890683122, 1.000000000000000000, 0.9659258262890683122, 1.000000000000000000, 0.9659258262890683122, 1.000000000000000000, 0.9659258262890683122, 1.000000000000000000, 0.9659258262890683122, 1.000000000000000000, 0.9659258262890683122, 1.000000000000000000, 0.9659258262890683122, 1.000000000000000000, 0.9659258262890683122, 1.000000000000000000, 0.9659258262890683122, 1.000000000000000000, 0.9659258262890683122, 1.000000000000000000, 0.9659258262890683122, 1.000000000000000000, 0.9659258262890683122, 1.000000000000000000, 0.9659258262890683122, 1.000000000000000000, 0.9659258262890683122, 1.000000000000000000, 0.9659258262890683122, 1.000000000000000000, 0.9659258262890683122, 1.000000000000000000, 0.9659258262890683122, 1.000000000000000000, 0.9659258262890683122, 1.000000000000000000, 0.9659258262890683122, 1.000000000000000000, 0.9659258262890683122, 1.000000000000000000, 0.9659258262890683122, 1.000000000000000000, 0.9659258262890683122, 1.000000000000000000, 0.9659258262890683122, 1.000000000000000000, 0.9659258262890683122, 1.000000000000000000, 0.9659258262890683122, 1.000000000000000000, 0.9659258262890683122, 1.000000000000000000, 0.9659258262890683122, 1.000000000000000000, 0.9659258262890683122, 1.000000000000000000, 0.9659258262890683122, 1.000000000000000000, 0.9659258262890683122, 1.000000000000000000, 0.9659258262890683122, 1.000000000000000000, 0.9659258262890683122, 1.000000000000000000, 0.9659258262890683122, 1.000000000000000000, 0.9659258262890683122, 1.000000000000000000, 0.9659258262890683122, 1.000000000000000000, 0.9659258262890683122, 1.000000000000000000, 0.9659258262890683122, 1.000000000000000000),
 ( 1.000000000000000000, 0.9659258262890683122, 1.000000000000000000, 0.9659258262890683122, 1.000000000000000000, 0.9659258262890683122, 1.000000000000000000, 0.9659258262890683122, 1.000000000000000000, 0.9659258262890683122, 1.000000000000000000, 0.9659258262890683122, 1.000000000000000000, 0.9659258262890683122, 1.000000000000000000, 0.9659258262890683122, 1.000000000000000000, 0.9659258262890683122, 1.000000000000000000, 0.9659258262890683122, 1.000000000000000000, 0.9659258262890683122, 1.000000000000000000, 0.9659258262890683122, 1.000000000000000000, 0.9659258262890683122, 1.000000000000000000, 0.9659258262890683122, 1.000000000000000000, 0.9659258262890683122, 1.000000000000000000, 0.9659258262890683122, 1.000000000000000000, 0.9659258262890683122, 1.000000000000000000, 0.9659258262890683122, 1.000000000000000000, 0.9659258262890683122, 1.000000000000000000, 0.9659258262890683122, 1.000000000000000000, 0.9659258262890683122, 1.000000000000000000, 0.9659258262890683122, 1.000000000000000000, 0.9659258262890683122, 1.000000000000000000, 0.9659258262890683122, 1.000000000000000000, 0.9659258262890683122, 1.000000000000000000, 0.9659258262890683122, 1.000000000000000000, 0.9659258262890683122, 1.000000000000000000, 0.9659258262890683122, 1.000000000000000000, 0.9659258262890683122, 1.000000000000000000, 0.9659258262890683122, 1.000000000000000000, 0.9659258262890683122, 1.000000000000000000, 0.9659258262890683122, 1.000000000000000000, 0.9659258262890683122, 1.000000000000000000, 0.9659258262890683122, 1.000000000000000000, 0.9659258262890683122, 1.000000000000000000, 0.9659258262890683122, 1.000000000000000000, 0.9659258262890683122, 1.000000000000000000, 0.9659258262890683122, 1.000000000000000000, 0.9659258262890683122, 1.000000000000000000, 0.9659258262890683122, 1.000000000000000000, 0.9659258262890683122, 1.000000000000000000, 0.9659258262890683122, 1.000000000000000000, 0.9659258262890683122, 1.000000000000000000, 0.9659258262890683122, 1.000000000000000000, 0.9659258262890683122, 1.000000000000000000, 0.9659258262890683122, 1.000000000000000000, 0.9659258262890683122, 1.000000000000000000, 0.9659258262890683122, 1.000000000000000000, 0.9659258262890683122, 1.000000000000000000, 0.9659258262890683122, 1.000000000000000000, 0.9659258262890683122, 1.000000000000000000, 0.9659258262890683122, 1.000000000000000000, 0.9659258262890683122, 1.000000000000000000, 0.9659258262890683122, 1.000000000000000000, 0.9659258262890683122, 1.000000000000000000, 0.9659258262890683122, 1.000000000000000000, 0.9659258262890683122, 1.000000000000000000, 0.9659258262890683122, 1.000000000000000000, 0.9659258262890683122, 1.000000000000000000, 0.9659258262890683122, 1.000000000000000000, 0.9659258262890683122, 1.000000000000000000, 0.9659258262890683122, 1.000000000000000000, 0.9659258262890683122, 1.000000000000000000, 0.9659258262890683122, 1.000000000000000000, 0.9659258262890683122, 1.000000000000000000, 0.9659258262890683122, 1.000000000000000000, 0.9659258262890683122, 1.000000000000000000, 0.9659258262890683122, 1.000000000000000000, 0.9659258262890683122, 1.000000000000000000, 0.9659258262890683122, 1.000000000000000000, 0.9659258262890683122, 1.000000000000000000, 0.9659258262890683122, 1.000000000000000000, 0.9659258262890683122, 1.000000000000000000, 0.9659258262890683122, 1.000000000000000000, 0.9659258262890683122, 1.000000000000000000, 0.9659258262890683122, 1.000000000000000000, 0.9659258262890683122, 1.000000000000000000, 0.9659258262890683122, 1.000000000000000000, 0.9659258262890683122, 1.000000000000000000, 0.9659258262890683122, 1.000000000000000000, 0.9659258262890683122, 1.000000000000000000, 0.9659258262890683122, 1.000000000000000000, 0.9659258262890683122, 1.000000000000000000, 0.9659258262890683122, 1.000000000000000000, 0.9659258262890683122, 1.000000000000000000, 0.9659258262890683122, 1.000000000000000000, 0.9659258262890683122, 1.000000000000000000, 0.9659258262890683122, 1.000000000000000000, 0.9659258262890683122, 1.000000000000000000, 0.9659258262890683122, 1.000000000000000000, 0.9659258262890683122, 1.000000000000000000, 0.9659258262890683122, 1.000000000000000000, 0.9659258262890683122, 1.000000000000000000, 0.9659258262890683122, 1.000000000000000000, 0.9659258262890683122, 1.000000000000000000, 0.9659258262890683122, 1.000000000000000000, 0.9659258262890683122, 1.000000000000000000, 0.9659258262890683122, 1.000000000000000000, 0.9659258262890683122, 1.000000000000000000, 0.9659258262890683122, 1.000000000000000000, 0.9659258262890683122, 1.000000000000000000, 0.9659258262890683122, 1.000000000000000000, 0.9659258262890683122, 1.000000000000000000, 0.9659258262890683122, 1.000000000000000000, 0.9659258262890683122, 1.000000000000000000, 0.9659258262890683122, 1.000000000000000000, 0.9659258262890683122, 1.000000000000000000, 0.9659258262890683122, 1.000000000000000000) ) ) 
 REPRESENTATION_ITEM ( '' )  SURFACE ( )  );
#66450 = FACE_OUTER_BOUND ( 'NONE', #34284, .T. ) ;
#66451 = CARTESIAN_POINT ( 'NONE',  ( 5.656854249492380582, 19.49999999590322020, -5.656854249492380582 ) ) ;
#66452 = CARTESIAN_POINT ( 'NONE',  ( -1.432654583217662481, 202.1250000013656063, 145.4587341250000634 ) ) ;
#66453 = CARTESIAN_POINT ( 'NONE',  ( 2.435013580646049114, 194.9873243428586989, 145.1679690891947700 ) ) ;
#66454 = CARTESIAN_POINT ( 'NONE',  ( 11.35316468749999963, 251.7187500034139873, -1.390361679473963556E-15 ) ) ;
#66455 = CARTESIAN_POINT ( 'NONE',  ( -1.656854249492383468, 3.437499997268814056, 4.000000000000000888 ) ) ;
#66456 = CARTESIAN_POINT ( 'NONE',  ( -11.00000000000000000, 4.556349186104045934, 111.9062500000000000 ) ) ;
#66457 = CARTESIAN_POINT ( 'NONE',  ( -11.35316468749999785, 3.072916663252683200, -3.042071309553167513 ) ) ;
#66458 = CARTESIAN_POINT ( 'NONE',  ( 2.977408999572650927, -7.188101187499990274, 3.830302781871751883 ) ) ;
#66459 = CARTESIAN_POINT ( 'NONE',  ( 8.311093377946834337, 200.4687499965860411, 8.311093377946839666 ) ) ;
#66460 = DIRECTION ( 'NONE',  ( -0.000000000000000000, -0.000000000000000000, 1.000000000000000000 ) ) ;
#66461 = CARTESIAN_POINT ( 'NONE',  ( 2.780723358947928197E-16, 6.562499998634407028, -4.541265875000002339 ) ) ;
#66462 = CARTESIAN_POINT ( 'NONE',  ( -5.000000000000000000, 0.000000000000000000, 0.000000000000000000 ) ) ;
#66464 = DIRECTION ( 'NONE',  ( -0.000000000000000000, 1.000000000000000000, -0.000000000000000000 ) ) ;
#66463 = CARTESIAN_POINT ( 'NONE',  ( -1.970469249063935269E-15, 20.78460969082654231, -20.69999999999999929 ) ) ;
#66465 = ORIENTED_EDGE ( 'NONE', *, *, #13614, .T. ) ;
#66466 = CARTESIAN_POINT ( 'NONE',  ( -3.458734125000016757, 204.1250000013656063, 140.5673454167824161 ) ) ;
#66467 = CARTESIAN_POINT ( 'NONE',  ( -9.832129032723418760, 12.86458332991935194, -5.676582343750004256 ) ) ;
#66468 = CARTESIAN_POINT ( 'NONE',  ( -6.735557395310442023E-16, 11.00000000000000000, 101.3125000040967763 ) ) ;
#66469 = CARTESIAN_POINT ( 'NONE',  ( -11.00000000000000000, 0.000000000000000000, 89.68750000409677625 ) ) ;
#66470 = EDGE_CURVE ( 'NONE', #68294, #51031, #48766, .T. ) ;
#66471 = CARTESIAN_POINT ( 'NONE',  ( -29.43265458321770822, 201.5000000013655779, 166.5412658750003914 ) ) ;
#66472 = DIRECTION ( 'NONE',  ( -1.000000000000000000, 0.000000000000000000, 0.000000000000000000 ) ) ;
#66474 = CARTESIAN_POINT ( 'NONE',  ( -2.751064625579944321E-14, 208.7500000000000284, 146.0000000000000284 ) ) ;
#66473 = CARTESIAN_POINT ( 'NONE',  ( 7.188101187500000044, 117.4062500020483810, -8.802885111219163269E-16 ) ) ;
#66475 = CARTESIAN_POINT ( 'NONE',  ( 7.999999999999992895, -3.313708498984756279, 25.48655277982336642 ) ) ;
#66476 = CARTESIAN_POINT ( 'NONE',  ( 3.042071309553159519, 124.7395833299193555, 11.35316468750000141 ) ) ;
#66477 = CARTESIAN_POINT ( 'NONE',  ( -10.00000000000000355, 89.58333332650535397, 2.679491924311223183 ) ) ;
#66478 = CARTESIAN_POINT ( 'NONE',  ( -5.082755093536324154, 89.84375000204839523, 5.082755093536326818 ) ) ;
#66479 = CARTESIAN_POINT ( 'NONE',  ( 1.881053915767122664, 22.24999999863440792, 4.541265875000001451 ) ) ;
#66480 = CARTESIAN_POINT ( 'NONE',  ( -2.679491924311235174, 200.4166666598386826, 10.00000000000000000 ) ) ;
#66481 = CARTESIAN_POINT ( 'NONE',  ( -7.320508075688778149, 39.99999999317202537, 7.320508075688769267 ) ) ;
#66482 = ORIENTED_EDGE ( 'NONE', *, *, #22410, .F. ) ;
#66483 = CARTESIAN_POINT ( 'NONE',  ( 2.828427124746153876, 208.8750000000000284, 144.8284271247462129 ) ) ;
#66484 = CARTESIAN_POINT ( 'NONE',  ( -6.676582343750000703, 294.6718750017070079, 2.765530957082001251 ) ) ;
#66485 = CARTESIAN_POINT ( 'NONE',  ( 5.656854249492374365, 5.656854249492375253, 27.32405278432982598 ) ) ;
#66486 = CARTESIAN_POINT ( 'NONE',  ( -9.832129032723418760, 167.8645833299193555, -5.676582343750004256 ) ) ;
#66487 = DIRECTION ( 'NONE',  ( 0.000000000000000000, 0.000000000000000000, 1.000000000000000000 ) ) ;
#66488 = CARTESIAN_POINT ( 'NONE',  ( 1.656854249492403008, 197.6875000000000000, 194.0000000000000853 ) ) ;
#66489 = CARTESIAN_POINT ( 'NONE',  ( -10.00000000000004619, 192.5000000000000284, -1.224646799147358779E-15 ) ) ;
#66490 = CARTESIAN_POINT ( 'NONE',  ( -4.220049686691935698, 10.18810118749999916, 105.2500000020483952 ) ) ;
#66491 = ORIENTED_EDGE ( 'NONE', *, *, #33057, .F. ) ;
#66492 = CARTESIAN_POINT ( 'NONE',  ( -29.65685424949236193, 199.1875000027312126, 166.0000000000003411 ) ) ;
#66493 = CARTESIAN_POINT ( 'NONE',  ( -3.042071309553163960, 157.5520833299193555, -11.35316468749999963 ) ) ;
#66494 = CARTESIAN_POINT ( 'NONE',  ( -8.660254037844390851, 217.0833333333333428, -5.000000000000006217 ) ) ;
#66495 = CARTESIAN_POINT ( 'NONE',  ( 2.839093476692135984E-14, 204.9375000013656063, 201.4587341250000350 ) ) ;
#66496 = CARTESIAN_POINT ( 'NONE',  ( 0.000000000000000000, 125.0000000000000000, 0.000000000000000000 ) ) ;
#66497 = CARTESIAN_POINT ( 'NONE',  ( 8.311093377946837890, 56.71874999658601979, -8.311093377946837890 ) ) ;
#66498 = ORIENTED_EDGE ( 'NONE', *, *, #15604, .F. ) ;
#66499 = CARTESIAN_POINT ( 'NONE',  ( -10.18810118749999916, 4.220049686691934809, 112.5625000020483810 ) ) ;
#66500 = CARTESIAN_POINT ( 'NONE',  ( -1.881053915767121776, 10.74999999863440969, -4.541265875000002339 ) ) ;
#66501 = VERTEX_POINT ( 'NONE', #13817 ) ;
#66502 = CARTESIAN_POINT ( 'NONE',  ( 7.188101187499999156, 21.37499999795161543, 2.977408999572654924 ) ) ;
#66503 = CARTESIAN_POINT ( 'NONE',  ( -6.000000000000001776, 287.0625000034140157, 0.000000000000000000 ) ) ;
#66504 = CARTESIAN_POINT ( 'NONE',  ( -23.99999999999998934, 197.8750000027312126, 170.0000000000002842 ) ) ;
#66505 = CARTESIAN_POINT ( 'NONE',  ( 4.401442555609581635E-16, 19.21874999795161543, -7.188101187500000044 ) ) ;
#66506 = CARTESIAN_POINT ( 'NONE',  ( 2.977408999572650927, -7.188101187499990274, 4.955302781871752771 ) ) ;
#66507 = CARTESIAN_POINT ( 'NONE',  ( -7.204075437095965206, -7.204075437095968759, 113.2187500020483810 ) ) ;
#66508 = AXIS2_PLACEMENT_3D ( 'NONE', #49941, #32609, #37133 ) ;
#66509 = CARTESIAN_POINT ( 'NONE',  ( 4.000000000000001776, 7.749999997268813168, 0.000000000000000000 ) ) ;
#66510 = VERTEX_POINT ( 'NONE', #65889 ) ;
#66511 = AXIS2_PLACEMENT_3D ( 'NONE', #64726, #31124, #13390 ) ;
#66512 = ADVANCED_FACE ( 'NONE', ( #60982 ), #11414, .T. ) ;
#66513 = CARTESIAN_POINT ( 'NONE',  ( 2.445694354108839619, 207.8125000013656063, 200.4456943541088663 ) ) ;
#66514 = CARTESIAN_POINT ( 'NONE',  ( -27.99999999999992184, 208.9375000013656063, 173.4587341250003760 ) ) ;
#66515 = CARTESIAN_POINT ( 'NONE',  ( 3.211159895383560947, 6.187499998634407028, 3.211159895383562723 ) ) ;
#66516 = CARTESIAN_POINT ( 'NONE',  ( -5.082755093536325930, 108.9687500020483810, -5.082755093536325930 ) ) ;
#66517 = CARTESIAN_POINT ( 'NONE',  ( -4.242640687119286547, 289.8750000000000000, -4.242640687119286547 ) ) ;
#66518 = VECTOR ( 'NONE', #59663, 1000.000000000000000 ) ;
#66519 = CARTESIAN_POINT ( 'NONE',  ( 7.188101187499993827, -2.977408999572645598, 23.14280278187176165 ) ) ;
#66520 = EDGE_LOOP ( 'NONE', ( #45779, #56659 ) ) ;
#66521 = CARTESIAN_POINT ( 'NONE',  ( -7.188101187500002709, 26.81249999795161898, 2.977408999572649151 ) ) ;
#66522 = VERTEX_POINT ( 'NONE', #47793 ) ;
#66523 = CARTESIAN_POINT ( 'NONE',  ( 4.220049686691941027, -10.18810118749999738, 116.1250000020483810 ) ) ;
#66524 = CARTESIAN_POINT ( 'NONE',  ( 4.907047822332399001, 6.406773156051627893, -0.000000000000000000 ) ) ;
#66525 = CARTESIAN_POINT ( 'NONE',  ( 2.754378923186476579E-14, 209.1875000013656063, 194.5412658750000219 ) ) ;
#66526 = CARTESIAN_POINT ( 'NONE',  ( 29.43265458321761230, 201.8750000013656063, 166.5412658749999650 ) ) ;
#66527 = CARTESIAN_POINT ( 'NONE',  ( -2.679491924311235618, 73.54166666666667140, 10.00000000000000000 ) ) ;
#66528 = EDGE_CURVE ( 'NONE', #22328, #22922, #43249, .T. ) ;
#66529 = CARTESIAN_POINT ( 'NONE',  ( -5.082755093536324154, 93.21875000204838102, 5.082755093536326818 ) ) ;
#66530 = CARTESIAN_POINT ( 'NONE',  ( -6.000000000000003553, 290.9375000000000568, -2.485281374238571317 ) ) ;
#66532 = CARTESIAN_POINT ( 'NONE',  ( -2.679491924311227624, 126.4583333333333428, -10.00000000000000711 ) ) ;
#66531 = CARTESIAN_POINT ( 'NONE',  ( 30.75928566870664227, 178.1885986724387578, 173.9316890523115831 ) ) ;
#66533 = ORIENTED_EDGE ( 'NONE', *, *, #29509, .F. ) ;
#66534 = EDGE_CURVE ( 'NONE', #13133, #30512, #19128, .T. ) ;
#66535 = CARTESIAN_POINT ( 'NONE',  ( -8.311093377946834337, 219.5312500034139589, 8.311093377946837890 ) ) ;
#66536 = AXIS2_PLACEMENT_3D ( 'NONE', #11064, #68767, #63105 ) ;
#66537 = CARTESIAN_POINT ( 'NONE',  ( -5.126106709302933773, -16.23426604260537331, 69.90716554746668976 ) ) ;
#66538 = CARTESIAN_POINT ( 'NONE',  ( 1.656854249492348607, 199.3125000027311842, 138.0000000000000568 ) ) ;
#66539 = DIRECTION ( 'NONE',  ( 1.000000000000000000, 0.000000000000000000, -0.000000000000000000 ) ) ;
#66540 = DIRECTION ( 'NONE',  ( -0.000000000000000000, 1.000000000000000000, -1.563033456626094573E-30 ) ) ;
#66541 = CARTESIAN_POINT ( 'NONE',  ( -10.00000000000000000, 255.0000000000000000, 0.000000000000000000 ) ) ;
#66542 = CARTESIAN_POINT ( 'NONE',  ( 5.656854249492379694, 108.1250000040967763, -5.656854249492380582 ) ) ;
#66543 = CARTESIAN_POINT ( 'NONE',  ( 7.320508075688774596, 190.6250000000000284, -7.320508075688774596 ) ) ;
#66544 = CARTESIAN_POINT ( 'NONE',  ( 0.000000000000000000, 125.0000000000000000, 0.000000000000000000 ) ) ;
#66545 = CARTESIAN_POINT ( 'NONE',  ( -2.977408999572647819, -7.188101187499990274, 23.14280278187175810 ) ) ;
#66546 = CARTESIAN_POINT ( 'NONE',  ( -9.832129032723418760, 153.1770833299193555, -5.676582343750004256 ) ) ;
#66547 = CARTESIAN_POINT ( 'NONE',  ( -5.656854249492373476, -5.656854249492376141, 22.20530278392014623 ) ) ;
#66548 = CARTESIAN_POINT ( 'NONE',  ( 2.679491924311375506, 259.5833333401613459, 9.999999999999916511 ) ) ;
#66549 = LINE ( 'NONE', #6362, #27231 ) ;
#66551 = LINE ( 'NONE', #60898, #43056 ) ;
#66550 = CARTESIAN_POINT ( 'NONE',  ( 24.00000000000000355, 203.6875000000000000, 168.3431457505075173 ) ) ;
#66552 = ORIENTED_EDGE ( 'NONE', *, *, #50871, .F. ) ;
#66553 = CARTESIAN_POINT ( 'NONE',  ( -3.042071309553164404, 7.552083329919349275, -11.35316468749999963 ) ) ;
#66554 = EDGE_CURVE ( 'NONE', #30602, #63756, #20389, .T. ) ;
#66555 = CARTESIAN_POINT ( 'NONE',  ( 1.656854249492487607, 200.8125000027312126, 194.0000000000001705 ) ) ;
#66557 = CARTESIAN_POINT ( 'NONE',  ( -2.828427124746152987, 208.1250000000000284, 200.8284271247462129 ) ) ;
#66556 = CARTESIAN_POINT ( 'NONE',  ( 0.000000000000000000, 0.000000000000000000, 118.0000000000000000 ) ) ;
#66558 = CARTESIAN_POINT ( 'NONE',  ( -8.000000000000000000, 115.9062500000000000, -3.313708498984761164 ) ) ;
#66559 = CARTESIAN_POINT ( 'NONE',  ( -3.458734125000016313, 201.8750000013656063, 140.5673454167823593 ) ) ;
#66560 = CIRCLE ( 'NONE', #34077, 12.00000000000000000 ) ;
#66561 = CARTESIAN_POINT ( 'NONE',  ( 5.000000000000001776, 52.70833332650536818, -8.660254037844389075 ) ) ;
#66562 = CARTESIAN_POINT ( 'NONE',  ( 7.188101187500000044, 109.9062500020483810, -8.802885111219163269E-16 ) ) ;
#66563 = CARTESIAN_POINT ( 'NONE',  ( 1.881053915767122664, 8.249999998634406140, 4.541265875000001451 ) ) ;
#66564 = CARTESIAN_POINT ( 'NONE',  ( 9.999999999999985789, 100.2083333333333286, -2.679491924311223183 ) ) ;
#66565 = CARTESIAN_POINT ( 'NONE',  ( 3.313708498984756279, 7.999999999999991118, 9.361552779823366421 ) ) ;
#66567 = CARTESIAN_POINT ( 'NONE',  ( 2.679491924311235174, 161.0416666666667140, -10.00000000000001954 ) ) ;
#66566 = LINE ( 'NONE', #48839, #43121 ) ;
#66568 = ORIENTED_EDGE ( 'NONE', *, *, #21100, .T. ) ;
#66569 = ORIENTED_EDGE ( 'NONE', *, *, #53918, .F. ) ;
#66570 =( BOUNDED_CURVE ( )  B_SPLINE_CURVE ( 2, ( #27323, #73361, #42807, #2832, #72616, #3968, #38290, #43183, #26198 ),
 .UNSPECIFIED., .F., .F. ) 
 B_SPLINE_CURVE_WITH_KNOTS ( ( 3, 2, 2, 2, 3 ),
 ( 0.6911764705882352811, 0.6948529411764705621, 0.6985294117647058432, 0.7022058823529410132, 0.7058823529411764053 ),
 .UNSPECIFIED. ) 
 CURVE ( )  GEOMETRIC_REPRESENTATION_ITEM ( )  RATIONAL_B_SPLINE_CURVE ( ( 1.000000000000000000, 0.9238795325112867385, 1.000000000000000000, 0.9238795325112867385, 1.000000000000000000, 0.9238795325112867385, 1.000000000000000000, 0.9238795325112890700, 0.9999999999999976685 ) ) 
 REPRESENTATION_ITEM ( '' )  );
#66571 =( BOUNDED_CURVE ( )  B_SPLINE_CURVE ( 2, ( #11197, #40610, #63612, #58713, #23625, #17217, #35697, #68906, #45892 ),
 .UNSPECIFIED., .F., .F. ) 
 B_SPLINE_CURVE_WITH_KNOTS ( ( 3, 2, 2, 2, 3 ),
 ( 0.1000000000000000888, 0.1083333333333334203, 0.1166666666666667657, 0.1250000000000001110, 0.1333333333333334425 ),
 .UNSPECIFIED. ) 
 CURVE ( )  GEOMETRIC_REPRESENTATION_ITEM ( )  RATIONAL_B_SPLINE_CURVE ( ( 0.9999999999999992228, 0.9238795325112875156, 1.000000000000000000, 0.9238795325112867385, 1.000000000000000000, 0.9238795325112867385, 1.000000000000000000, 0.9238795325112857393, 1.000000000000001110 ) ) 
 REPRESENTATION_ITEM ( '' )  );
#66572 = CARTESIAN_POINT ( 'NONE',  ( -4.999999999999999112, -61.23691386381970148, 23.51762333030202612 ) ) ;
#66573 = CARTESIAN_POINT ( 'NONE',  ( -5.000000000000003553, 161.6666666666666856, -8.660254037844397956 ) ) ;
#66574 = CARTESIAN_POINT ( 'NONE',  ( 5.676582343750005144, 220.8854166700806445, 9.832129032723416984 ) ) ;
#66575 = AXIS2_PLACEMENT_3D ( 'NONE', #9548, #54825, #31804 ) ;
#66576 = CARTESIAN_POINT ( 'NONE',  ( -9.832129032723420536, 123.6979166632526983, 5.676582343749997150 ) ) ;
#66577 = ORIENTED_EDGE ( 'NONE', *, *, #53272, .T. ) ;
#66578 = EDGE_CURVE ( 'NONE', #67997, #36743, #13542, .T. ) ;
#66579 = CARTESIAN_POINT ( 'NONE',  ( 29.65685424949229088, 201.0625000000000568, 174.0000000000000284 ) ) ;
#66580 = CARTESIAN_POINT ( 'NONE',  ( 4.220049686691941027, -10.18810118749999738, 95.12500000204836681 ) ) ;
#66581 = DIRECTION ( 'NONE',  ( -0.000000000000000000, -1.000000000000000000, -0.000000000000000000 ) ) ;
#66582 = CARTESIAN_POINT ( 'NONE',  ( 1.432654583217662481, 195.3750000013656063, 194.5412658750000219 ) ) ;
#66583 = DIRECTION ( 'NONE',  ( -0.000000000000000000, 1.000000000000000000, -0.000000000000000000 ) ) ;
#66585 = CARTESIAN_POINT ( 'NONE',  ( 3.042071309553159519, 119.7395833299193555, 11.35316468750000141 ) ) ;
#66584 = CARTESIAN_POINT ( 'NONE',  ( 4.776596266111742928, 220.0000000000000000, 9.272667727651805691 ) ) ;
#66586 = CARTESIAN_POINT ( 'NONE',  ( 11.00000000000000000, 1.347111479062088405E-15, 99.24999999999998579 ) ) ;
#66587 = ORIENTED_EDGE ( 'NONE', *, *, #67182, .F. ) ;
#66588 = CARTESIAN_POINT ( 'NONE',  ( 2.143582570168940826, 90.06435469398867610, -8.000000000000000000 ) ) ;
#66589 = EDGE_CURVE ( 'NONE', #12039, #48053, #25884, .T. ) ;
#66590 = CARTESIAN_POINT ( 'NONE',  ( 48.52588466223725305, 42.19432882890850323, 60.88070576291119806 ) ) ;
#66591 = CARTESIAN_POINT ( 'NONE',  ( -2.085542519210945728E-15, 114.8437499965860127, 11.35316468750000141 ) ) ;
#66592 = CARTESIAN_POINT ( 'NONE',  ( 3.458734125000016313, 205.8750000013656063, 199.4326545832176976 ) ) ;
#66593 = CARTESIAN_POINT ( 'NONE',  ( -5.082755093536325042, 16.40624999795161543, -5.082755093536325930 ) ) ;
#66594 = CARTESIAN_POINT ( 'NONE',  ( 4.220049686691941027, -10.18810118749999738, 88.00000000204836681 ) ) ;
#66595 = CARTESIAN_POINT ( 'NONE',  ( -9.832129032723418760, 23.17708332991934839, -5.676582343750004256 ) ) ;
#66596 = VERTEX_POINT ( 'NONE', #30821 ) ;
#66597 = DIRECTION ( 'NONE',  ( -0.000000000000000000, 1.000000000000000000, -0.000000000000000000 ) ) ;
#66598 = CARTESIAN_POINT ( 'NONE',  ( -3.317071493978880348, -8.008118988124989457, 23.79436528394063188 ) ) ;
#66599 = CARTESIAN_POINT ( 'NONE',  ( -1.432654583217662481, 209.3750000013656063, 145.4587341250000634 ) ) ;
#66600 = CARTESIAN_POINT ( 'NONE',  ( 4.898587196589412829E-16, 13.87500000000000178, -8.000000000000000000 ) ) ;
#66601 = CARTESIAN_POINT ( 'NONE',  ( 7.188101187500000044, 3.468749997951610542, 0.000000000000000000 ) ) ;
#66602 = CARTESIAN_POINT ( 'NONE',  ( -6.676582343750003368, 289.3906250017069510, -2.765530957081996810 ) ) ;
#66603 = CARTESIAN_POINT ( 'NONE',  ( -49.70177871865297448, 134.0000000000000284, 57.99999999999998579 ) ) ;
#66604 = DIRECTION ( 'NONE',  ( -0.000000000000000000, -0.000000000000000000, 1.000000000000000000 ) ) ;
#66605 = ORIENTED_EDGE ( 'NONE', *, *, #57172, .T. ) ;
#66606 = CARTESIAN_POINT ( 'NONE',  ( 5.676582343750001591, 146.9270833299193555, -9.832129032723420536 ) ) ;
#66607 = CARTESIAN_POINT ( 'NONE',  ( -4.220049686691937474, -10.18810118749999738, 81.43750000204836681 ) ) ;
#66608 = CARTESIAN_POINT ( 'NONE',  ( -26.56734541678232375, 199.0000000013656063, 173.4587341250003760 ) ) ;
#66609 = DIRECTION ( 'NONE',  ( -0.000000000000000000, -1.000000000000000000, -0.000000000000000000 ) ) ;
#66610 = CARTESIAN_POINT ( 'NONE',  ( -3.211159895383562723, 14.06249999863440614, 3.211159895383561391 ) ) ;
#66611 = ORIENTED_EDGE ( 'NONE', *, *, #11817, .T. ) ;
#66612 = CARTESIAN_POINT ( 'NONE',  ( -3.999999999999960032, 204.0625000027312410, 196.3431457505076594 ) ) ;
#66613 = CARTESIAN_POINT ( 'NONE',  ( 3.458734124999960358, 196.6875000013655779, 142.0000000000000568 ) ) ;
#66614 = CARTESIAN_POINT ( 'NONE',  ( 2.828427124746152987, 202.2500000027312126, 139.1715728752538723 ) ) ;
#66615 = CARTESIAN_POINT ( 'NONE',  ( -1.469576158976823947E-15, 5.625000000000000888, 8.000000000000000000 ) ) ;
#66616 = ORIENTED_EDGE ( 'NONE', *, *, #27928, .T. ) ;
#66617 = EDGE_CURVE ( 'NONE', #66955, #49089, #25671, .T. ) ;
#66618 = CARTESIAN_POINT ( 'NONE',  ( 7.188101187499999156, 13.87499999795161010, 2.977408999572654924 ) ) ;
#66619 = CARTESIAN_POINT ( 'NONE',  ( -4.000000000000015987, 208.5000000000000284, 142.0000000000000568 ) ) ;
#66620 = CYLINDRICAL_SURFACE ( 'NONE', #14972, 10.00000000000000178 ) ;
#66621 = CIRCLE ( 'NONE', #8802, 3.999999999999986233 ) ;
#66622 = CARTESIAN_POINT ( 'NONE',  ( -9.832129032723418760, 187.8645833299193839, -5.676582343750004256 ) ) ;
#66623 = CARTESIAN_POINT ( 'NONE',  ( -2.977408999572650927, 115.2500000020484094, -7.188101187500001821 ) ) ;
#66624 = CARTESIAN_POINT ( 'NONE',  ( -2.751064625579944321E-14, 199.7500000000000000, 146.0000000000000284 ) ) ;
#66625 = CARTESIAN_POINT ( 'NONE',  ( -6.676582343749999815, 287.5156250017069510, 2.765530957082001251 ) ) ;
#66627 = CARTESIAN_POINT ( 'NONE',  ( 3.999999999999960032, 201.0625000027312126, 143.6568542494924259 ) ) ;
#66626 = CARTESIAN_POINT ( 'NONE',  ( 5.676582343749997150, 222.2395833367473017, -9.832129032723418760 ) ) ;
#66628 = ORIENTED_EDGE ( 'NONE', *, *, #14645, .T. ) ;
#66629 = ADVANCED_FACE ( 'NONE', ( #50407 ), #25864, .T. ) ;
#66630 = CARTESIAN_POINT ( 'NONE',  ( 5.676582343749997150, 262.2395833367473301, -9.832129032723418760 ) ) ;
#66631 = CARTESIAN_POINT ( 'NONE',  ( 7.188101187499993827, -2.977408999572645598, 2.142802781871750550 ) ) ;
#66632 = CARTESIAN_POINT ( 'NONE',  ( 8.000000000000001776, 106.1562500000000000, 3.313708498984759387 ) ) ;
#66633 = FACE_OUTER_BOUND ( 'NONE', #66212, .T. ) ;
#66634 = DIRECTION ( 'NONE',  ( -0.000000000000000000, 1.000000000000000000, -4.476705744456276341E-16 ) ) ;
#66635 = CARTESIAN_POINT ( 'NONE',  ( 3.458734125000015425, 198.2500000013656347, 196.5673454167823877 ) ) ;
#66636 = ORIENTED_EDGE ( 'NONE', *, *, #7959, .T. ) ;
#66637 = DIRECTION ( 'NONE',  ( 0.000000000000000000, 0.000000000000000000, -1.000000000000000000 ) ) ;
#66638 = CARTESIAN_POINT ( 'NONE',  ( -7.999999999999998224, 92.09375000000000000, 3.313708498984766493 ) ) ;
#66639 = CARTESIAN_POINT ( 'NONE',  ( 11.35316468750000141, 116.0937499965860127, 0.000000000000000000 ) ) ;
#66640 = CARTESIAN_POINT ( 'NONE',  ( -4.999999999999999112, -14.13320814749881116, -69.81894086168458102 ) ) ;
#66641 = CARTESIAN_POINT ( 'NONE',  ( 4.556349186104051263, -10.99999999999999822, 73.46875000000000000 ) ) ;
#66644 = CARTESIAN_POINT ( 'NONE',  ( 4.898587196589415787E-16, 0.000000000000000000, 4.000000000000001776 ) ) ;
#66643 = CARTESIAN_POINT ( 'NONE',  ( 24.54126587500000056, 202.2500000013656063, 171.4326545832175839 ) ) ;
#66642 = CARTESIAN_POINT ( 'NONE',  ( 31.45873412499999944, 199.0000000013656063, 168.5673454167822740 ) ) ;
#66645 = ORIENTED_EDGE ( 'NONE', *, *, #38365, .F. ) ;
#66646 = CARTESIAN_POINT ( 'NONE',  ( 9.797174393178825657E-16, 125.0000000000000000, -8.000000000000000000 ) ) ;
#66647 = CARTESIAN_POINT ( 'NONE',  ( -5.676582343749998039, 222.4479166632526983, -9.832129032723420536 ) ) ;
#66648 = CARTESIAN_POINT ( 'NONE',  ( -3.458734125000015425, 197.9375000013655779, 142.0000000000000568 ) ) ;
#66649 = CARTESIAN_POINT ( 'NONE',  ( 29.43265458321761230, 199.7500000013656063, 173.4587341249998929 ) ) ;
#66650 = ADVANCED_FACE ( 'NONE', ( #21357 ), #67392, .F. ) ;
#66651 = CARTESIAN_POINT ( 'NONE',  ( 11.00000000000000000, 4.556349186104045934, 116.0312500040967763 ) ) ;
#66652 = CARTESIAN_POINT ( 'NONE',  ( 11.35316468749999963, 191.3020833299193839, -3.042071309553165293 ) ) ;
#66653 = CARTESIAN_POINT ( 'NONE',  ( -2.977408999572652260, 94.81250000204838102, 7.188101187500000044 ) ) ;
#66654 = VECTOR ( 'NONE', #20365, 1000.000000000000000 ) ;
#66655 = CARTESIAN_POINT ( 'NONE',  ( 0.000000000000000000, 300.0000000000000000, 0.000000000000000000 ) ) ;
#66656 = CARTESIAN_POINT ( 'NONE',  ( 4.541265875000002339, 18.31249999863440792, 0.000000000000000000 ) ) ;
#66657 = CARTESIAN_POINT ( 'NONE',  ( 30.44569435410878810, 195.8125000013656063, 172.4456943541087526 ) ) ;
#66658 = CARTESIAN_POINT ( 'NONE',  ( -7.999999999999989342, -3.313708498984762496, 26.42405277982336642 ) ) ;
#66659 = DIRECTION ( 'NONE',  ( -1.000000000000000000, 0.000000000000000000, -0.000000000000000000 ) ) ;
#66660 = CARTESIAN_POINT ( 'NONE',  ( -11.35316468750000141, 83.28124999658602690, -1.390361679473963753E-15 ) ) ;
#66661 = VERTEX_POINT ( 'NONE', #62835 ) ;
#66662 = EDGE_CURVE ( 'NONE', #44869, #66273, #22264, .T. ) ;
#66663 = CARTESIAN_POINT ( 'NONE',  ( 4.556349186104045934, 11.00000000000000000, 81.53125000000000000 ) ) ;
#66664 = CARTESIAN_POINT ( 'NONE',  ( 7.188101187499999156, 19.87499999795161543, 2.977408999572654924 ) ) ;
#66665 = CARTESIAN_POINT ( 'NONE',  ( -7.999999999999998224, 108.7812500040967763, 3.313708498984766049 ) ) ;
#66666 =( BOUNDED_CURVE ( )  B_SPLINE_CURVE ( 2, ( #59433, #24707, #58697, #36418, #42060, #7744, #53771, #58565, #52896 ),
 .UNSPECIFIED., .F., .F. ) 
 B_SPLINE_CURVE_WITH_KNOTS ( ( 3, 2, 2, 2, 3 ),
 ( 0.1250000000000000000, 0.1319444444444444475, 0.1388888888888888951, 0.1458333333333333426, 0.1527777777777777901 ),
 .UNSPECIFIED. ) 
 CURVE ( )  GEOMETRIC_REPRESENTATION_ITEM ( )  RATIONAL_B_SPLINE_CURVE ( ( 1.000000000000000000, 0.9238795325112867385, 1.000000000000000000, 0.9238795325112867385, 1.000000000000000000, 0.9238795325112867385, 1.000000000000000000, 0.9238795325112867385, 1.000000000000000000 ) ) 
 REPRESENTATION_ITEM ( '' )  );
#66667 = CARTESIAN_POINT ( 'NONE',  ( -2.250000000000000888, 2.250000000000000000, 28.00000000000000000 ) ) ;
#66668 = CARTESIAN_POINT ( 'NONE',  ( -11.35316468750000141, 93.48958332991934128, 3.042071309553159963 ) ) ;
#66669 = ORIENTED_EDGE ( 'NONE', *, *, #37181, .T. ) ;
#66670 = CARTESIAN_POINT ( 'NONE',  ( -7.204075437095965206, -7.204075437095968759, 84.71875000204836681 ) ) ;
#66671 = CARTESIAN_POINT ( 'NONE',  ( 10.18810118749999916, 4.220049686691935698, 115.0000000020483668 ) ) ;
#66672 = CARTESIAN_POINT ( 'NONE',  ( -31.45873412499999944, 195.8750000013655779, 168.5673454167827572 ) ) ;
#66673 = CARTESIAN_POINT ( 'NONE',  ( 3.458734125000015869, 209.1875000013656063, 198.0000000000000284 ) ) ;
#66674 = CARTESIAN_POINT ( 'NONE',  ( 17.99999999999998934, 1.224646799147352862E-15, -9.999999999999996447 ) ) ;
#66676 = CARTESIAN_POINT ( 'NONE',  ( 3.042071309553167513, 81.82291666325268409, -11.35316468749999785 ) ) ;
#66675 = DIRECTION ( 'NONE',  ( -0.000000000000000000, -0.000000000000000000, -1.000000000000000000 ) ) ;
#66677 = CARTESIAN_POINT ( 'NONE',  ( 5.656854249492376141, -5.656854249492374365, 16.58030278392014978 ) ) ;
#66678 = CARTESIAN_POINT ( 'NONE',  ( -28.00000000000002132, 203.6875000013656063, 166.5412658750003629 ) ) ;
#66679 = CARTESIAN_POINT ( 'NONE',  ( -8.000000000000000000, 21.56249999590322375, -9.797174393178825657E-16 ) ) ;
#66680 =( BOUNDED_CURVE ( )  B_SPLINE_CURVE ( 2, ( #70977, #42301, #70612, #18932, #41938, #19292, #36291, #60027, #46862, #6878, #64946, #54008, #65318 ),
 .UNSPECIFIED., .F., .F. ) 
 B_SPLINE_CURVE_WITH_KNOTS ( ( 3, 2, 2, 2, 2, 2, 3 ),
 ( 0.5163043478260869179, 0.5181159420289854767, 0.5199275362318840354, 0.5217391304347825942, 0.5235507246376811530, 0.5253623188405797118, 0.5271739130434782705 ),
 .UNSPECIFIED. ) 
 CURVE ( )  GEOMETRIC_REPRESENTATION_ITEM ( )  RATIONAL_B_SPLINE_CURVE ( ( 1.000000000000000000, 0.9659258262890683122, 1.000000000000000000, 0.9659258262890683122, 1.000000000000000000, 0.9659258262890683122, 1.000000000000000000, 0.9659258262890683122, 1.000000000000000000, 0.9659258262890683122, 1.000000000000000000, 0.9659258262890683122, 1.000000000000000000 ) ) 
 REPRESENTATION_ITEM ( '' )  );
#66681 = CARTESIAN_POINT ( 'NONE',  ( -5.000000000000005329, 165.2083333265053682, 8.660254037844387298 ) ) ;
#66682 = DIRECTION ( 'NONE',  ( -0.000000000000000000, -1.000000000000000000, -0.000000000000000000 ) ) ;
#66683 = CARTESIAN_POINT ( 'NONE',  ( 11.35316468750000141, 71.09374999658601268, 0.000000000000000000 ) ) ;
#66684 = CARTESIAN_POINT ( 'NONE',  ( -2.765530957081998586, 292.6406250017070079, 6.676582343750001591 ) ) ;
#66685 = EDGE_CURVE ( 'NONE', #65598, #67997, #73421, .T. ) ;
#66686 = CARTESIAN_POINT ( 'NONE',  ( -10.18810118749999916, 4.220049686691934809, 108.4375000020483952 ) ) ;
#66687 = CARTESIAN_POINT ( 'NONE',  ( -11.35316468749999785, 203.0729166632526415, -3.042071309553167513 ) ) ;
#66688 = EDGE_LOOP ( 'NONE', ( #34702, #61713, #14812, #7887 ) ) ;
#66689 = DIRECTION ( 'NONE',  ( 0.000000000000000000, 0.000000000000000000, 1.000000000000000000 ) ) ;
#66690 = CARTESIAN_POINT ( 'NONE',  ( 1.656854249492352604, 206.3125000027312410, 138.0000000000000853 ) ) ;
#66691 = CARTESIAN_POINT ( 'NONE',  ( 4.193030820682221105, 50.40097124335105860, 40.95512985425044405 ) ) ;
#66693 = CARTESIAN_POINT ( 'NONE',  ( 9.832129032723416984, 200.3645833299193555, 5.676582343750006032 ) ) ;
#66692 = CARTESIAN_POINT ( 'NONE',  ( -7.999999999999991118, 9.797174393178815797E-16, 30.00000000000000000 ) ) ;
#66694 = CARTESIAN_POINT ( 'NONE',  ( -4.000000000000015987, 203.5625000000000000, 143.6568542494924259 ) ) ;
#66695 = CIRCLE ( 'NONE', #51021, 11.00000000000000000 ) ;
#66696 = CARTESIAN_POINT ( 'NONE',  ( -5.000000000000000888, 242.2916666734946318, -8.660254037844387298 ) ) ;
#66697 = FACE_OUTER_BOUND ( 'NONE', #27634, .T. ) ;
#66698 = ORIENTED_EDGE ( 'NONE', *, *, #5486, .F. ) ;
#66699 = CARTESIAN_POINT ( 'NONE',  ( 11.35316468749999963, 176.3020833299193555, -3.042071309553165293 ) ) ;
#66700 =( BOUNDED_CURVE ( )  B_SPLINE_CURVE ( 2, ( #54051, #2361, #30295, #71014, #53315, #42342, #1639, #24620, #29925, #19700, #14408, #60065, #71750, #37065, #47629, #25355, #65359, #20064, #13658, #48371, #43082, #42712, #66098, #59345, #14027, #8387, #37440, #52943, #1273, #47265, #70292, #70651, #18606, #18970, #41973, #30663, #7657, #53681, #72890, #8769, #60439, #26860, #9526, #55552, #21197, #14781, #67235, #31779, #54799, #38192, #3111, #26095, #33291, #49116, #73264, #9140, #72128, #44222, #20442, #55178, #3865, #32541, #15531, #61196, #60816, #21568, #67973, #49875, #38572, #43458, #16268, #61572, #66473, #9892, #32922, #44967, #55928, #37821, #15904, #4239, #27226, #50242, #43842, #56288, #32157, #3483, #44595, #26473, #73632, #49497, #72516, #67607, #20825, #38935, #66856, #61937, #21937, #10264, #4606, #15161, #27601, #50612, #4983, #52120, #62673, #11008, #820, #51359, #17771, #17023, #69090, #28350, #57038, #33661, #69834, #40047, #34410, #34041, #12111, #46445, #50989, #35149, #69463, #84, #22304, #62307, #40786, #10634, #39309, #74369, #23431, #46070, #57413, #6470, #11746, #74001, #56667, #23807, #5349, #58164, #22680, #45698, #68712, #46810, #63051, #63792, #11376, #17396, #5719, #28719, #27984, #45329, #51734, #23061, #40420, #29473, #52483, #68345, #16641, #452, #63418, #34784, #39674, #57787, #6095, #29101, #65640, #13205, #36244, #70932, #29841, #35509, #13936, #41164, #54338, #13572, #65267, #52853, #19612, #19244, #1185, #2649, #25638, #36978, #48286, #59620, #47913, #30575, #64542, #47178, #42255, #2273, #24537, #18519, #58522, #1558, #24166, #48653, #24896, #31310, #7935, #18149, #36610, #64901, #42625, #1908, #59259, #30940, #70210, #18885, #53960, #12839, #64174, #12478, #7202, #25267, #47545, #59983, #58893, #41527, #70569, #7571, #53226, #41891, #53597, #71291, #8299, #35876, #30206, #6829, #73174, #8676, #26378, #15439, #14315, #72034, #43367, #26001, #67514, #44134, #3394, #26770, #71661, #66009, #32826, #3018, #20350, #49402, #54711, #37350, #49026, #38476, #31691, #43750, #15813, #37731, #42991, #9804, #9051, #10172, #55836, #60729, #66384, #27512, #49788, #19982, #21111, #38101, #56204, #61101, #14690, #27141, #9430, #72802, #60349, #32065, #4152, #55086, #72423, #20732, #66764, #33208, #15068, #32448, #55457, #4517, #3769, #67144, #50157, #61479, #21481, #44502, #38848, #61852, #10543, #69373, #22217, #45244, #22592, #26132, #58075, #29008, #28265, #5634, #39588, #68256, #44877, #6386, #51272, #45612, #73913, #23346, #57699, #62217, #46356, #11657, #16551, #27888, #10916, #17683, #62964, #50522, #33950, #34691, #57323, #68626, #40700, #22979, #33575, #73537, #35062, #62584, #56578, #51648, #16935, #63704, #11289, #69001, #12029, #21845, #67883, #5264, #28634, #39960, #45985, #34319, #16174, #17308, #364, #56948, #40327, #50898, #6007, #74282, #4891, #63331, #52027, #39217, #29392, #7487, #1473, #24454, #41809, #58438, #36157, #52399, #735, #7117, #23717, #46721, #2188, #69747, #42165, #52765, #18061 ),
 .UNSPECIFIED., .F., .F. ) 
 B_SPLINE_CURVE_WITH_KNOTS ( ( 3, 2, 2, 2, 2, 2, 2, 2, 2, 2, 2, 2, 2, 2, 2, 2, 2, 2, 2, 2, 2, 2, 2, 2, 2, 2, 2, 2, 2, 2, 2, 2, 2, 2, 2, 2, 2, 2, 2, 2, 2, 2, 2, 2, 2, 2, 2, 2, 2, 2, 2, 2, 2, 2, 2, 2, 2, 2, 2, 2, 2, 2, 2, 2, 2, 2, 2, 2, 2, 2, 2, 2, 2, 2, 2, 2, 2, 2, 2, 2, 2, 2, 2, 2, 2, 2, 2, 2, 2, 2, 2, 2, 2, 2, 2, 2, 2, 2, 2, 2, 2, 2, 2, 2, 2, 2, 2, 2, 2, 2, 2, 2, 2, 2, 2, 2, 2, 2, 2, 2, 2, 2, 2, 2, 2, 2, 2, 2, 2, 2, 2, 2, 2, 2, 2, 2, 2, 2, 2, 2, 2, 2, 2, 2, 2, 2, 2, 2, 2, 2, 2, 2, 2, 2, 2, 2, 2, 2, 2, 2, 2, 2, 2, 2, 2, 2, 2, 2, 2, 2, 2, 2, 2, 2, 2, 2, 2, 2, 2, 2, 2, 2, 2, 2, 2, 2, 2, 3 ),
 ( 0.000000000000000000, 0.005357197806354127741, 0.01071439561270825548, 0.01607159341906238409, 0.02142879122541651096, 0.02678598903177064131, 0.03214318683812476818, 0.03750038464447889852, 0.04285758245083302193, 0.04821478025718715227, 0.05357197806354128261, 0.05892917586989540601, 0.06428637367624953636, 0.06964357148260366670, 0.07500076928895779704, 0.08035796709531192739, 0.08571516490166604385, 0.09107236270802018807, 0.09642956051437430454, 0.1017867583207284349, 0.1071439561270825652, 0.1125011539334366956, 0.1178583517397908120, 0.1232155495461449562, 0.1285727473524990727, 0.1339299451588532308, 0.1392871429652073334, 0.1446443407715614637, 0.1500015385779155941, 0.1553587363842697244, 0.1607159341906238548, 0.1660731319969779851, 0.1714303298033320877, 0.1767875276096862458, 0.1821447254160403761, 0.1875019232223944787, 0.1928591210287486091, 0.1982163188351027672, 0.2035735166414568698, 0.2089307144478110001, 0.2142879122541651304, 0.2196451100605192608, 0.2250023078668733911, 0.2303595056732275215, 0.2357167034795816241, 0.2410739012859357822, 0.2464310990922899125, 0.2517882968986440151, 0.2571454947049981454, 0.2625026925113522758, 0.2678598903177064616, 0.2732170881240605365, 0.2785742859304146668, 0.2839314837367687971, 0.2892886815431229275, 0.2946458793494770578, 0.3000030771558311882, 0.3053602749621853185, 0.3107174727685394489, 0.3160746705748935792, 0.3214318683812477095, 0.3267890661876017844, 0.3321462639939559702, 0.3375034618003101006, 0.3428606596066641754, 0.3482178574130183613, 0.3535750552193724916, 0.3589322530257265664, 0.3642894508320807523, 0.3696466486384348271, 0.3750038464447889575, 0.3803610442511431433, 0.3857182420574972181, 0.3910754398638513485, 0.3964326376702055343, 0.4017898354765596092, 0.4071470332829137395, 0.4125042310892679254, 0.4178614288956220002, 0.4232186267019761305, 0.4285758245083302609, 0.4339330223146843912, 0.4392902201210385216, 0.4446474179273926519, 0.4500046157337467823, 0.4553618135401009126, 0.4607190113464550429, 0.4660762091528091733, 0.4714334069591632481, 0.4767906047655174340, 0.4821478025718715643, 0.4875050003782256391, 0.4928621981845798250, 0.4982193959909339553, 0.5035765937972880302, 0.5089337916036421605, 0.5142909894099962909, 0.5196481872163505322, 0.5250053850227045515, 0.5303625828290586819, 0.5357197806354129233, 0.5410769784417669426, 0.5464341762481210729, 0.5517913740544752033, 0.5571485718608293336, 0.5625057696671834639, 0.5678629674735375943, 0.5732201652798917246, 0.5785773630862458550, 0.5839345608925999853, 0.5892917586989541157, 0.5946489565053082460, 0.6000061543116623763, 0.6053633521180165067, 0.6107205499243706370, 0.6160777477307247674, 0.6214349455370788977, 0.6267921433434330281, 0.6321493411497871584, 0.6375065389561411777, 0.6428637367624954191, 0.6482209345688495494, 0.6535781323752035687, 0.6589353301815578101, 0.6642925279879119405, 0.6696497257942659598, 0.6750069236006202011, 0.6803641214069743315, 0.6857213192133283508, 0.6910785170196825922, 0.6964357148260367225, 0.7017929126323907418, 0.7071501104387449832, 0.7125073082450991135, 0.7178645060514531329, 0.7232217038578073742, 0.7285789016641615046, 0.7339360994705155239, 0.7392932972768696542, 0.7446504950832238956, 0.7500076928895779149, 0.7553648906959320453, 0.7607220885022862866, 0.7660792863086403059, 0.7714364841149944363, 0.7767936819213486777, 0.7821508797277026970, 0.7875080775340568273, 0.7928652753404110687, 0.7982224731467650880, 0.8035796709531192183, 0.8089368687594734597, 0.8142940665658274790, 0.8196512643721816094, 0.8250084621785358507, 0.8303656599848898701, 0.8357228577912440004, 0.8410800555975981307, 0.8464372534039522611, 0.8517944512103063914, 0.8571516490166605218, 0.8625088468230146521, 0.8678660446293687825, 0.8732232424357229128, 0.8785804402420770431, 0.8839376380484311735, 0.8892948358547853038, 0.8946520336611394342, 0.9000092314674935645, 0.9053664292738476949, 0.9107236270802018252, 0.9160808248865559555, 0.9214380226929100859, 0.9267952204992641052, 0.9321524183056183466, 0.9375096161119724769, 0.9428668139183264962, 0.9482240117246807376, 0.9535812095310348679, 0.9589384073373888873, 0.9642956051437431286, 0.9696528029500972590, 0.9750100007564512783, 0.9803671985628055197, 0.9857243963691596500, 0.9910815941755136693, 0.9964387919818679107, 1.000000000000000000 ),
 .UNSPECIFIED. ) 
 CURVE ( )  GEOMETRIC_REPRESENTATION_ITEM ( )  RATIONAL_B_SPLINE_CURVE ( ( 1.000000000000000000, 0.9238795325112867385, 1.000000000000000000, 0.9238795325112867385, 1.000000000000000000, 0.9238795325112867385, 1.000000000000000000, 0.9238795325112867385, 1.000000000000000000, 0.9238795325112867385, 1.000000000000000000, 0.9238795325112867385, 1.000000000000000000, 0.9238795325112867385, 1.000000000000000000, 0.9238795325112867385, 1.000000000000000000, 0.9238795325112867385, 1.000000000000000000, 0.9238795325112867385, 1.000000000000000000, 0.9238795325112867385, 1.000000000000000000, 0.9238795325112867385, 1.000000000000000000, 0.9238795325112867385, 1.000000000000000000, 0.9238795325112867385, 1.000000000000000000, 0.9238795325112867385, 1.000000000000000000, 0.9238795325112867385, 1.000000000000000000, 0.9238795325112867385, 1.000000000000000000, 0.9238795325112867385, 1.000000000000000000, 0.9238795325112867385, 1.000000000000000000, 0.9238795325112867385, 1.000000000000000000, 0.9238795325112867385, 1.000000000000000000, 0.9238795325112867385, 1.000000000000000000, 0.9238795325112867385, 1.000000000000000000, 0.9238795325112867385, 1.000000000000000000, 0.9238795325112867385, 1.000000000000000000, 0.9238795325112867385, 1.000000000000000000, 0.9238795325112867385, 1.000000000000000000, 0.9238795325112867385, 1.000000000000000000, 0.9238795325112867385, 1.000000000000000000, 0.9238795325112867385, 1.000000000000000000, 0.9238795325112867385, 1.000000000000000000, 0.9238795325112867385, 1.000000000000000000, 0.9238795325112867385, 1.000000000000000000, 0.9238795325112867385, 1.000000000000000000, 0.9238795325112867385, 1.000000000000000000, 0.9238795325112867385, 1.000000000000000000, 0.9238795325112867385, 1.000000000000000000, 0.9238795325112867385, 1.000000000000000000, 0.9238795325112867385, 1.000000000000000000, 0.9238795325112867385, 1.000000000000000000, 0.9238795325112867385, 1.000000000000000000, 0.9238795325112867385, 1.000000000000000000, 0.9238795325112867385, 1.000000000000000000, 0.9238795325112867385, 1.000000000000000000, 0.9238795325112867385, 1.000000000000000000, 0.9238795325112867385, 1.000000000000000000, 0.9238795325112867385, 1.000000000000000000, 0.9238795325112867385, 1.000000000000000000, 0.9238795325112867385, 1.000000000000000000, 0.9238795325112867385, 1.000000000000000000, 0.9238795325112867385, 1.000000000000000000, 0.9238795325112867385, 1.000000000000000000, 0.9238795325112867385, 1.000000000000000000, 0.9238795325112867385, 1.000000000000000000, 0.9238795325112867385, 1.000000000000000000, 0.9238795325112867385, 1.000000000000000000, 0.9238795325112867385, 1.000000000000000000, 0.9238795325112867385, 1.000000000000000000, 0.9238795325112867385, 1.000000000000000000, 0.9238795325112867385, 1.000000000000000000, 0.9238795325112867385, 1.000000000000000000, 0.9238795325112867385, 1.000000000000000000, 0.9238795325112867385, 1.000000000000000000, 0.9238795325112867385, 1.000000000000000000, 0.9238795325112867385, 1.000000000000000000, 0.9238795325112867385, 1.000000000000000000, 0.9238795325112867385, 1.000000000000000000, 0.9238795325112867385, 1.000000000000000000, 0.9238795325112867385, 1.000000000000000000, 0.9238795325112867385, 1.000000000000000000, 0.9238795325112867385, 1.000000000000000000, 0.9238795325112867385, 1.000000000000000000, 0.9238795325112867385, 1.000000000000000000, 0.9238795325112867385, 1.000000000000000000, 0.9238795325112867385, 1.000000000000000000, 0.9238795325112867385, 1.000000000000000000, 0.9238795325112867385, 1.000000000000000000, 0.9238795325112867385, 1.000000000000000000, 0.9238795325112867385, 1.000000000000000000, 0.9238795325112867385, 1.000000000000000000, 0.9238795325112867385, 1.000000000000000000, 0.9238795325112867385, 1.000000000000000000, 0.9238795325112867385, 1.000000000000000000, 0.9238795325112867385, 1.000000000000000000, 0.9238795325112867385, 1.000000000000000000, 0.9238795325112867385, 1.000000000000000000, 0.9238795325112867385, 1.000000000000000000, 0.9238795325112867385, 1.000000000000000000, 0.9238795325112867385, 1.000000000000000000, 0.9238795325112867385, 1.000000000000000000, 0.9238795325112867385, 1.000000000000000000, 0.9238795325112867385, 1.000000000000000000, 0.9238795325112867385, 1.000000000000000000, 0.9238795325112867385, 1.000000000000000000, 0.9238795325112867385, 1.000000000000000000, 0.9238795325112867385, 1.000000000000000000, 0.9238795325112867385, 1.000000000000000000, 0.9238795325112867385, 1.000000000000000000, 0.9238795325112867385, 1.000000000000000000, 0.9238795325112867385, 1.000000000000000000, 0.9238795325112867385, 1.000000000000000000, 0.9238795325112867385, 1.000000000000000000, 0.9238795325112867385, 1.000000000000000000, 0.9238795325112867385, 1.000000000000000000, 0.9238795325112867385, 1.000000000000000000, 0.9238795325112867385, 1.000000000000000000, 0.9238795325112867385, 1.000000000000000000, 0.9238795325112867385, 1.000000000000000000, 0.9238795325112867385, 1.000000000000000000, 0.9238795325112867385, 1.000000000000000000, 0.9238795325112867385, 1.000000000000000000, 0.9238795325112867385, 1.000000000000000000, 0.9238795325112867385, 1.000000000000000000, 0.9238795325112867385, 1.000000000000000000, 0.9238795325112867385, 1.000000000000000000, 0.9238795325112867385, 1.000000000000000000, 0.9238795325112867385, 1.000000000000000000, 0.9238795325112867385, 1.000000000000000000, 0.9238795325112867385, 1.000000000000000000, 0.9238795325112867385, 1.000000000000000000, 0.9238795325112867385, 1.000000000000000000, 0.9238795325112867385, 1.000000000000000000, 0.9238795325112867385, 1.000000000000000000, 0.9238795325112867385, 1.000000000000000000, 0.9238795325112867385, 1.000000000000000000, 0.9238795325112867385, 1.000000000000000000, 0.9238795325112867385, 1.000000000000000000, 0.9238795325112867385, 1.000000000000000000, 0.9238795325112867385, 1.000000000000000000, 0.9238795325112867385, 1.000000000000000000, 0.9238795325112867385, 1.000000000000000000, 0.9238795325112867385, 1.000000000000000000, 0.9238795325112867385, 1.000000000000000000, 0.9238795325112867385, 1.000000000000000000, 0.9238795325112867385, 1.000000000000000000, 0.9238795325112867385, 1.000000000000000000, 0.9238795325112867385, 1.000000000000000000, 0.9238795325112867385, 1.000000000000000000, 0.9238795325112867385, 1.000000000000000000, 0.9238795325112867385, 1.000000000000000000, 0.9238795325112867385, 1.000000000000000000, 0.9238795325112867385, 1.000000000000000000, 0.9238795325112867385, 1.000000000000000000, 0.9238795325112867385, 1.000000000000000000, 0.9238795325112867385, 1.000000000000000000, 0.9238795325112867385, 1.000000000000000000, 0.9238795325112867385, 1.000000000000000000, 0.9238795325112867385, 1.000000000000000000, 0.9238795325112867385, 1.000000000000000000, 0.9238795325112867385, 1.000000000000000000, 0.9238795325112867385, 1.000000000000000000, 0.9238795325112867385, 1.000000000000000000, 0.9238795325112867385, 1.000000000000000000, 0.9238795325112867385, 1.000000000000000000, 0.9238795325112867385, 1.000000000000000000, 0.9238795325112867385, 1.000000000000000000, 0.9238795325112867385, 1.000000000000000000, 0.9238795325112867385, 1.000000000000000000, 0.9238795325112867385, 1.000000000000000000, 0.9238795325112867385, 1.000000000000000000, 0.9238795325112867385, 1.000000000000000000, 0.9238795325112867385, 1.000000000000000000, 0.9238795325112867385, 1.000000000000000000, 0.9238795325112867385, 1.000000000000000000, 0.9238795325112867385, 1.000000000000000000, 0.9238795325112867385, 1.000000000000000000, 0.9238795325112867385, 1.000000000000000000, 0.9238795325112867385, 1.000000000000000000, 0.9238795325112867385, 1.000000000000000000, 0.9238795325112867385, 1.000000000000000000, 0.9238795325112867385, 1.000000000000000000, 0.9238795325112867385, 1.000000000000000000, 0.9238795325112867385, 1.000000000000000000, 0.9238795325112867385, 1.000000000000000000, 0.9238795325112867385, 1.000000000000000000, 0.9238795325112867385, 1.000000000000000000, 0.9238795325112867385, 1.000000000000000000, 0.9238795325112867385, 1.000000000000000000, 0.9238795325112867385, 1.000000000000000000, 0.9238795325112867385, 1.000000000000000000, 0.9238795325112867385, 1.000000000000000000, 0.9238795325112867385, 1.000000000000000000, 0.9238795325112867385, 1.000000000000000000, 0.9238795325112867385, 1.000000000000000000, 0.9238795325112867385, 1.000000000000000000, 0.9238795325112867385, 1.000000000000000000, 0.9493987661155159907, 0.9660720762559202868 ) ) 
 REPRESENTATION_ITEM ( '' )  );
#66701 = CARTESIAN_POINT ( 'NONE',  ( -5.082755093536319713, 5.082755093536319713, 16.29905278187175455 ) ) ;
#66702 = CARTESIAN_POINT ( 'NONE',  ( -5.656854249492373476, -5.656854249492376141, 16.20530278392014978 ) ) ;
#66703 = ORIENTED_EDGE ( 'NONE', *, *, #42404, .F. ) ;
#66704 = EDGE_CURVE ( 'NONE', #73838, #56251, #27388, .T. ) ;
#66705 = CARTESIAN_POINT ( 'NONE',  ( -5.656854249492378806, 99.87500000409679046, 5.656854249492381470 ) ) ;
#66706 = EDGE_CURVE ( 'NONE', #67456, #6969, #4030, .T. ) ;
#66707 = CARTESIAN_POINT ( 'NONE',  ( 25.17157287525378706, 208.8750000000000284, 172.8284271247460424 ) ) ;
#66708 = SHAPE_REPRESENTATION ( 'plain washer (type a)_is_IS 2016 A- 16', ( #57354 ), #57409 ) ;
#66709 = AXIS2_PLACEMENT_3D ( 'NONE', #1680, #6958, #29600 ) ;
#66710 = EDGE_LOOP ( 'NONE', ( #35299, #56076, #35784, #46408 ) ) ;
#66711 = ADVANCED_FACE ( 'NONE', ( #15694 ), #16063, .F. ) ;
#66712 = CARTESIAN_POINT ( 'NONE',  ( -2.828427124746192067, 14.62500000000000000, 2.828427124746190735 ) ) ;
#66713 = CARTESIAN_POINT ( 'NONE',  ( 3.211159895383561835, 18.43749999863440436, -3.211159895383561835 ) ) ;
#66714 = CARTESIAN_POINT ( 'NONE',  ( 7.999999999999992895, -3.313708498984756279, 6.174052783920146226 ) ) ;
#66715 = CARTESIAN_POINT ( 'NONE',  ( -23.99999999999998579, 195.7500000000000000, 170.0000000000003411 ) ) ;
#66716 = ORIENTED_EDGE ( 'NONE', *, *, #37413, .T. ) ;
#66717 = CARTESIAN_POINT ( 'NONE',  ( 5.000000000000000000, -10.26105934116143281, -64.40045319026697257 ) ) ;
#66718 = CARTESIAN_POINT ( 'NONE',  ( -7.188101187500001821, 91.06250000204838102, -2.977408999572650483 ) ) ;
#66721 = CARTESIAN_POINT ( 'NONE',  ( 2.841757666793575255E-14, 194.6037658790967839, 201.6037658790967839 ) ) ;
#66720 = CARTESIAN_POINT ( 'NONE',  ( -6.951808397369817780E-16, 252.6562500034140157, -11.35316468749999963 ) ) ;
#66719 = CARTESIAN_POINT ( 'NONE',  ( -5.000000000000062172, 83.33333333333341386, 8.660254037844486774 ) ) ;
#66722 = DIRECTION ( 'NONE',  ( 0.000000000000000000, 0.000000000000000000, 0.9999999999999997780 ) ) ;
#66723 = ORIENTED_EDGE ( 'NONE', *, *, #47243, .T. ) ;
#66724 = CARTESIAN_POINT ( 'NONE',  ( -11.35316468749999963, 264.2187500034140157, 0.000000000000000000 ) ) ;
#66725 = CARTESIAN_POINT ( 'NONE',  ( 7.188101187499993827, -2.977408999572645598, 21.64280278187176165 ) ) ;
#66726 = ORIENTED_EDGE ( 'NONE', *, *, #73136, .T. ) ;
#66727 = EDGE_CURVE ( 'NONE', #63081, #70885, #41562, .T. ) ;
#66728 = ORIENTED_EDGE ( 'NONE', *, *, #70709, .F. ) ;
#66729 = CARTESIAN_POINT ( 'NONE',  ( 10.18810118750000093, -4.220049686691933033, 80.31250000204836681 ) ) ;
#66730 = CARTESIAN_POINT ( 'NONE',  ( 11.35316468749999785, 80.88541666325269830, 3.042071309553174174 ) ) ;
#66731 = CARTESIAN_POINT ( 'NONE',  ( 7.778174593052023411, -7.778174593052021635, 88.56249999999998579 ) ) ;
#66734 = CARTESIAN_POINT ( 'NONE',  ( 6.676582343750003368, 292.0468750017070079, 2.765530957081995478 ) ) ;
#66733 = CARTESIAN_POINT ( 'NONE',  ( 30.82842712474616320, 196.5000000027312126, 167.1715728752537018 ) ) ;
#66732 = CARTESIAN_POINT ( 'NONE',  ( 1.469576158976823947E-15, 99.87499999999998579, 8.000000000000000000 ) ) ;
#66735 = VECTOR ( 'NONE', #17634, 1000.000000000000114 ) ;
#66736 = CARTESIAN_POINT ( 'NONE',  ( -4.556349186104045934, 11.00000000000000000, 89.21874999999998579 ) ) ;
#66737 = DIRECTION ( 'NONE',  ( -0.000000000000000000, -0.000000000000000000, 1.000000000000000000 ) ) ;
#66738 = CARTESIAN_POINT ( 'NONE',  ( -3.458734124999960358, 199.6875000013656063, 198.0000000000000284 ) ) ;
#66739 = CARTESIAN_POINT ( 'NONE',  ( -3.313708498984765161, 9.843749995903220196, 7.999999999999998224 ) ) ;
#66740 = CARTESIAN_POINT ( 'NONE',  ( 25.55430564589119058, 196.0625000013656063, 167.5543056458910485 ) ) ;
#66741 = CARTESIAN_POINT ( 'NONE',  ( 5.082755093536325930, 13.03124999795161187, -5.082755093536325930 ) ) ;
#66742 = CARTESIAN_POINT ( 'NONE',  ( -7.999999999999989342, -3.313708498984762496, 23.61155278392014978 ) ) ;
#66743 = CARTESIAN_POINT ( 'NONE',  ( 1.656854249492381914, 5.562499997268813168, 4.000000000000000888 ) ) ;
#66744 = CARTESIAN_POINT ( 'NONE',  ( -2.977408999572650927, 112.2500000020483952, -7.188101187500000933 ) ) ;
#66746 = CARTESIAN_POINT ( 'NONE',  ( 6.123233995736767268E-16, 193.1249999931720254, -10.00000000000000178 ) ) ;
#66745 = CARTESIAN_POINT ( 'NONE',  ( 11.00000000000000000, 1.347111479062088405E-15, 118.0000000000000000 ) ) ;
#66747 = CARTESIAN_POINT ( 'NONE',  ( -3.042071309553159075, 220.2604166700806161, 11.35316468749999963 ) ) ;
#66748 = CARTESIAN_POINT ( 'NONE',  ( 2.751064625579944321E-14, 198.7500000000000000, 194.0000000000000568 ) ) ;
#66749 = CARTESIAN_POINT ( 'NONE',  ( -7.188101187499992051, 0.000000000000000000, 18.36155278187175455 ) ) ;
#66750 = CARTESIAN_POINT ( 'NONE',  ( 3.999999999999959144, 208.1875000027311842, 140.3431457505076594 ) ) ;
#66751 = CARTESIAN_POINT ( 'NONE',  ( 3.042071309553159519, 44.73958332991936260, 11.35316468750000141 ) ) ;
#66752 = CARTESIAN_POINT ( 'NONE',  ( -2.904335006432773092, -44.22345414694398613, 139.1363271338184404 ) ) ;
#66753 = EDGE_CURVE ( 'NONE', #19023, #34530, #73108, .T. ) ;
#66754 = CARTESIAN_POINT ( 'NONE',  ( 7.320508075688774596, 12.49999999317203425, -7.320508075688774596 ) ) ;
#66755 = CARTESIAN_POINT ( 'NONE',  ( -7.778174593052023411, 7.778174593052023411, 112.0000000040967763 ) ) ;
#66756 = ORIENTED_EDGE ( 'NONE', *, *, #20866, .T. ) ;
#66757 = CARTESIAN_POINT ( 'NONE',  ( -2.751064625579944321E-14, 198.8750000027312126, 146.0000000000000284 ) ) ;
#66758 = CARTESIAN_POINT ( 'NONE',  ( -5.656854249492375253, 5.656854249492375253, 18.64280277982336642 ) ) ;
#66759 = CARTESIAN_POINT ( 'NONE',  ( 8.311093377946834337, 55.15624999658601268, 8.311093377946839666 ) ) ;
#66760 = CARTESIAN_POINT ( 'NONE',  ( 4.556349186104045934, 11.00000000000000000, 83.21875000409679046 ) ) ;
#66761 = CARTESIAN_POINT ( 'NONE',  ( -3.458734125000015869, 203.1875000013656063, 142.0000000000000568 ) ) ;
#66762 = CARTESIAN_POINT ( 'NONE',  ( 30.99999999999998579, 38.00000000000000711, 65.00000000000000000 ) ) ;
#66763 = CARTESIAN_POINT ( 'NONE',  ( 5.000000000000000000, -70.11723469343094450, -28.93519894129240910 ) ) ;
#66765 = CARTESIAN_POINT ( 'NONE',  ( -2.085542519210945728E-15, 49.53124999658601268, 11.35316468750000141 ) ) ;
#66764 = CARTESIAN_POINT ( 'NONE',  ( 7.188101187500000044, 97.90625000204838102, -8.802885111219163269E-16 ) ) ;
#66766 = CARTESIAN_POINT ( 'NONE',  ( -7.999999999999991118, 3.313708498984756723, 11.23655277982336820 ) ) ;
#66767 = DIRECTION ( 'NONE',  ( -0.000000000000000000, -0.000000000000000000, 1.000000000000000000 ) ) ;
#66768 = CARTESIAN_POINT ( 'NONE',  ( 11.35316468749999785, 155.5729166632527267, 3.042071309553174174 ) ) ;
#66769 = CARTESIAN_POINT ( 'NONE',  ( 7.320508075688771044, 126.2499999931720538, 7.320508075688775484 ) ) ;
#66770 = CARTESIAN_POINT ( 'NONE',  ( 1.320432766682874540E-15, 105.4062500020483810, 7.188101187500000044 ) ) ;
#66771 = ORIENTED_EDGE ( 'NONE', *, *, #18681, .T. ) ;
#66772 = CARTESIAN_POINT ( 'NONE',  ( 0.000000000000000000, 300.0000000000000000, 0.000000000000000000 ) ) ;
#66773 = CARTESIAN_POINT ( 'NONE',  ( -5.676582343749998039, 32.76041666325269119, -9.832129032723420536 ) ) ;
#66774 = CARTESIAN_POINT ( 'NONE',  ( -1.183492779173324630E-13, 16.25000000000001066, -10.00000000000000178 ) ) ;
#66775 = EDGE_LOOP ( 'NONE', ( #70533, #3330, #7753, #43102 ) ) ;
#66776 = DIRECTION ( 'NONE',  ( -0.000000000000000000, -0.000000000000000000, -1.000000000000000000 ) ) ;
#66777 = CARTESIAN_POINT ( 'NONE',  ( 4.220049686691934809, 10.18810118749999916, 76.18750000204839523 ) ) ;
#66778 = DIRECTION ( 'NONE',  ( 1.000000000000000000, 0.000000000000000000, 0.000000000000000000 ) ) ;
#66780 = CARTESIAN_POINT ( 'NONE',  ( 8.311093377946837890, 146.4062499965860127, -8.311093377946837890 ) ) ;
#66779 = DIRECTION ( 'NONE',  ( 1.000000000000000000, 0.000000000000000000, 0.000000000000000000 ) ) ;
#66781 = CARTESIAN_POINT ( 'NONE',  ( -7.188101187500000044, 3.093749997951610542, -8.802885111219163269E-16 ) ) ;
#66782 = CARTESIAN_POINT ( 'NONE',  ( 5.656854249492376141, -5.656854249492374365, 10.44905278432982598 ) ) ;
#66783 = CARTESIAN_POINT ( 'NONE',  ( -22.68594237414460224, -24.79372074885636579, 191.1282084373175678 ) ) ;
#66784 = CARTESIAN_POINT ( 'NONE',  ( 11.35316468749999963, 231.4062500034139873, -1.390361679473963556E-15 ) ) ;
#66785 = CARTESIAN_POINT ( 'NONE',  ( -10.18810118749999916, 0.000000000000000000, 86.03125000204836681 ) ) ;
#66786 = ORIENTED_EDGE ( 'NONE', *, *, #55621, .F. ) ;
#66787 = EDGE_CURVE ( 'NONE', #64770, #62806, #73789, .T. ) ;
#66788 = DIRECTION ( 'NONE',  ( 0.000000000000000000, 0.000000000000000000, 1.000000000000000000 ) ) ;
#66789 = CARTESIAN_POINT ( 'NONE',  ( 5.676582343750001591, 101.9270833299193555, -9.832129032723420536 ) ) ;
#66790 =( BOUNDED_CURVE ( )  B_SPLINE_CURVE ( 2, ( #17312, #18064, #5637, #6751, #29754, #47091, #58078, #51275, #16938, #34323, #11660, #74285, #69004 ),
 .UNSPECIFIED., .F., .F. ) 
 B_SPLINE_CURVE_WITH_KNOTS ( ( 3, 2, 2, 2, 2, 2, 3 ),
 ( 0.04891304347826086474, 0.05072463768115941657, 0.05253623188405796146, 0.05434782608695651329, 0.05615942028985507206, 0.05797101449275362389, 0.05978260869565217572 ),
 .UNSPECIFIED. ) 
 CURVE ( )  GEOMETRIC_REPRESENTATION_ITEM ( )  RATIONAL_B_SPLINE_CURVE ( ( 1.000000000000000000, 0.9659258262890682012, 1.000000000000000000, 0.9659258262890683122, 1.000000000000000000, 0.9659258262890683122, 1.000000000000000000, 0.9659258262890683122, 1.000000000000000000, 0.9659258262890683122, 1.000000000000000000, 0.9659258262890683122, 1.000000000000000000 ) ) 
 REPRESENTATION_ITEM ( '' )  );
#66791 = B_SPLINE_CURVE_WITH_KNOTS ( 'NONE', 3,
 ( #59224, #59948, #9017, #13534, #8263, #60315 ),
 .UNSPECIFIED., .F., .F.,
 ( 4, 2, 4 ),
 ( 2.380728322736233691E-07, 0.005257893135091050787, 0.01051554819734982701 ),
 .UNSPECIFIED. ) ;
#66792 = CARTESIAN_POINT ( 'NONE',  ( 4.220049686691934809, 10.18810118749999916, 97.18750000204836681 ) ) ;
#66793 = CARTESIAN_POINT ( 'NONE',  ( 4.541265875000002339, 20.43749999863440436, 0.000000000000000000 ) ) ;
#66794 = ORIENTED_EDGE ( 'NONE', *, *, #33685, .T. ) ;
#66795 = ORIENTED_EDGE ( 'NONE', *, *, #44411, .T. ) ;
#66796 = AXIS2_PLACEMENT_3D ( 'NONE', #17091, #40113, #29540 ) ;
#66797 = CARTESIAN_POINT ( 'NONE',  ( -4.541265875000003227, 2.999999998634407028, 1.881053915767121110 ) ) ;
#66799 = MANIFOLD_SOLID_BREP ( 'Thread1', #27380 ) ;
#66798 = CARTESIAN_POINT ( 'NONE',  ( 4.401442555609581635E-16, 9.843749997951610098, -7.188101187500000044 ) ) ;
#66800 = CARTESIAN_POINT ( 'NONE',  ( 8.000000000000000000, 116.9375000040967763, -9.797174393178825657E-16 ) ) ;
#66801 = EDGE_CURVE ( 'NONE', #38095, #3614, #62260, .T. ) ;
#66802 = CARTESIAN_POINT ( 'NONE',  ( -6.238412754330611322E-16, 10.18810118749999916, 93.15625000204836681 ) ) ;
#66803 = CARTESIAN_POINT ( 'NONE',  ( -31.45873412499998523, 204.0000000013656347, 171.4326545832180386 ) ) ;
#66804 = DIRECTION ( 'NONE',  ( -0.000000000000000000, 1.000000000000000000, -0.000000000000000000 ) ) ;
#66805 = ADVANCED_FACE ( 'NONE', ( #35669 ), #6629, .F. ) ;
#66806 = CARTESIAN_POINT ( 'NONE',  ( 2.449293598294707893E-16, 5.250000000000000000, -4.000000000000001776 ) ) ;
#66807 =( BOUNDED_CURVE ( )  B_SPLINE_CURVE ( 2, ( #3997, #26608, #43972, #49632, #50369, #33793, #72262, #72647, #56052 ),
 .UNSPECIFIED., .F., .F. ) 
 B_SPLINE_CURVE_WITH_KNOTS ( ( 3, 2, 2, 2, 3 ),
 ( 0.5694444444444444198, 0.5763888888888888395, 0.5833333333333333703, 0.5902777777777777901, 0.5972222222222222099 ),
 .UNSPECIFIED. ) 
 CURVE ( )  GEOMETRIC_REPRESENTATION_ITEM ( )  RATIONAL_B_SPLINE_CURVE ( ( 1.000000000000000000, 0.9238795325112867385, 1.000000000000000000, 0.9238795325112867385, 1.000000000000000000, 0.9238795325112867385, 1.000000000000000000, 0.9238795325112867385, 1.000000000000000000 ) ) 
 REPRESENTATION_ITEM ( '' )  );
#66808 = CARTESIAN_POINT ( 'NONE',  ( -2.828427124746190735, 17.12499999726881583, -2.828427124746191623 ) ) ;
#66809 = CARTESIAN_POINT ( 'NONE',  ( 4.541265875000002339, 2.374999998634407028, -1.881053915767121776 ) ) ;
#66810 = CARTESIAN_POINT ( 'NONE',  ( -2.828427124746208943, 201.6250000000000284, 144.8284271247462129 ) ) ;
#66811 = ORIENTED_EDGE ( 'NONE', *, *, #38481, .T. ) ;
#66812 = CARTESIAN_POINT ( 'NONE',  ( 2.839093476692135984E-14, 196.6875000013655779, 201.4587341250000350 ) ) ;
#66814 = CARTESIAN_POINT ( 'NONE',  ( 0.000000000000000000, 255.9999999999999432, 10.00000000000000178 ) ) ;
#66813 = CARTESIAN_POINT ( 'NONE',  ( -24.54126587500002188, 197.2500000013656063, 168.5673454167826435 ) ) ;
#66815 = CARTESIAN_POINT ( 'NONE',  ( 1.881053915767122664, 18.12499999863440792, 4.541265875000001451 ) ) ;
#66816 = CARTESIAN_POINT ( 'NONE',  ( -6.676582343750002480, 299.3906250017069510, -2.765530957081996810 ) ) ;
#66817 =( GEOMETRIC_REPRESENTATION_CONTEXT ( 3 ) GLOBAL_UNCERTAINTY_ASSIGNED_CONTEXT ( ( #54083 ) ) GLOBAL_UNIT_ASSIGNED_CONTEXT ( ( #32779, #73126, #30076 ) ) REPRESENTATION_CONTEXT ( 'NONE', 'WORKASPACE' ) );
#66818 = CARTESIAN_POINT ( 'NONE',  ( -5.082755093536317936, -5.082755093536320601, 4.674052781871752771 ) ) ;
#66819 = EDGE_LOOP ( 'NONE', ( #19410, #19153, #39414, #29402 ) ) ;
#66820 = ORIENTED_EDGE ( 'NONE', *, *, #27605, .F. ) ;
#66821 = CARTESIAN_POINT ( 'NONE',  ( -4.220049686691935698, 10.18810118749999916, 95.87500000204838102 ) ) ;
#66822 = CARTESIAN_POINT ( 'NONE',  ( 4.999999999999994671, 124.1666666666666714, 8.660254037844392627 ) ) ;
#66823 = CARTESIAN_POINT ( 'NONE',  ( -31.45873412499999233, 199.9375000013656063, 170.0000000000003979 ) ) ;
#66824 = CARTESIAN_POINT ( 'NONE',  ( -4.556349186104047710, -10.99999999999999822, 106.2812500000000000 ) ) ;
#66825 = CARTESIAN_POINT ( 'NONE',  ( 3.458734125000016757, 208.1250000013656063, 199.4326545832176691 ) ) ;
#66826 = CARTESIAN_POINT ( 'NONE',  ( -7.347880794884122694E-16, 21.49999999726881583, 4.000000000000001776 ) ) ;
#66827 = CARTESIAN_POINT ( 'NONE',  ( 2.679491924311222739, 108.9583333333333144, 10.00000000000000355 ) ) ;
#66828 = CARTESIAN_POINT ( 'NONE',  ( -5.656854249492380582, 112.8125000000000000, -5.656854249492380582 ) ) ;
#66829 = CARTESIAN_POINT ( 'NONE',  ( -2.765530957081998586, 290.7968750017069510, 6.676582343750001591 ) ) ;
#66830 = CARTESIAN_POINT ( 'NONE',  ( -7.188101187499991163, 2.977408999572646930, 13.76780278187175455 ) ) ;
#66831 = ORIENTED_EDGE ( 'NONE', *, *, #29853, .F. ) ;
#66832 = CARTESIAN_POINT ( 'NONE',  ( 47.32259252271278882, 272.0000000000000000, 65.76194439203457875 ) ) ;
#66833 = CARTESIAN_POINT ( 'NONE',  ( -3.313708498984759387, -7.999999999999989342, 5.611552779823364645 ) ) ;
#66834 = CARTESIAN_POINT ( 'NONE',  ( -8.000000000000001776, 21.65624999590322730, 3.313708498984759387 ) ) ;
#66835 = CARTESIAN_POINT ( 'NONE',  ( -1.432654583217662481, 203.1250000013656347, 145.4587341250000634 ) ) ;
#66836 = FACE_OUTER_BOUND ( 'NONE', #31272, .T. ) ;
#66838 = CARTESIAN_POINT ( 'NONE',  ( -3.458734125000015425, 204.2500000013655779, 143.4326545832176976 ) ) ;
#66837 = CYLINDRICAL_SURFACE ( 'NONE', #15489, 3.999999999999976019 ) ;
#66839 = CARTESIAN_POINT ( 'NONE',  ( 11.35316468749999608, 251.9270833367473301, -3.042071309553167069 ) ) ;
#66840 = CARTESIAN_POINT ( 'NONE',  ( -8.000000000000000000, 114.5937500040967905, -3.313708498984761164 ) ) ;
#66841 = CARTESIAN_POINT ( 'NONE',  ( -10.00000000000000355, 94.58333332650535397, 2.679491924311223183 ) ) ;
#66842 = CARTESIAN_POINT ( 'NONE',  ( 4.999999999999993783, 224.1666666666666856, 8.660254037844390851 ) ) ;
#66843 = CARTESIAN_POINT ( 'NONE',  ( 5.082755093536318824, 5.082755093536319713, 4.299052781871752771 ) ) ;
#66844 = CARTESIAN_POINT ( 'NONE',  ( 5.676582343750001591, 191.9270833299193555, -9.832129032723420536 ) ) ;
#66845 = LINE ( 'NONE', #10251, #9425 ) ;
#66846 = CARTESIAN_POINT ( 'NONE',  ( 1.881053915767122664, 7.124999998634407916, 4.541265875000001451 ) ) ;
#66847 = CARTESIAN_POINT ( 'NONE',  ( 0.000000000000000000, 0.000000000000000000, -14.00000000000000178 ) ) ;
#66849 = FACE_OUTER_BOUND ( 'NONE', #72253, .T. ) ;
#66848 = DIRECTION ( 'NONE',  ( -0.000000000000000000, 1.000000000000000000, -0.000000000000000000 ) ) ;
#66850 = ORIENTED_EDGE ( 'NONE', *, *, #30125, .T. ) ;
#66851 = CARTESIAN_POINT ( 'NONE',  ( 2.445694354108783219, 205.8125000013656063, 139.5543056458912190 ) ) ;
#66852 = CARTESIAN_POINT ( 'NONE',  ( -11.35316468750000141, 13.48958332991935016, 3.042071309553159963 ) ) ;
#66853 = CARTESIAN_POINT ( 'NONE',  ( -6.735557395310442023E-16, 11.00000000000000000, 96.81250000409677625 ) ) ;
#66854 = CARTESIAN_POINT ( 'NONE',  ( -31.45873412499995680, 200.7500000013656063, 171.4326545832181239 ) ) ;
#66855 = CARTESIAN_POINT ( 'NONE',  ( -7.999999999999991118, 9.797174393178815797E-16, 30.00000000000000000 ) ) ;
#66856 = CARTESIAN_POINT ( 'NONE',  ( -5.082755093536324154, 115.3437500020483810, 5.082755093536326818 ) ) ;
#66857 = CARTESIAN_POINT ( 'NONE',  ( 3.313708498984756279, 7.999999999999991118, 24.36155277982336997 ) ) ;
#66858 = CARTESIAN_POINT ( 'NONE',  ( -11.35316468750000141, 128.4895833299193555, 3.042071309553159963 ) ) ;
#66859 = CARTESIAN_POINT ( 'NONE',  ( 6.123233995736767268E-16, 83.12499999317203958, -10.00000000000000178 ) ) ;
#66860 = CARTESIAN_POINT ( 'NONE',  ( -7.188101187500000044, 92.65625000204838102, 0.000000000000000000 ) ) ;
#66861 = CARTESIAN_POINT ( 'NONE',  ( -8.342170076843785083E-16, 19.18749999863440436, 4.541265875000002339 ) ) ;
#66862 = CARTESIAN_POINT ( 'NONE',  ( 7.999999999999991118, 0.000000000000000000, 30.00000000000000000 ) ) ;
#66863 = CARTESIAN_POINT ( 'NONE',  ( -25.17157282405719343, 195.0000000000000284, 167.1715729264508354 ) ) ;
#66864 = ORIENTED_EDGE ( 'NONE', *, *, #29784, .T. ) ;
#66865 = CARTESIAN_POINT ( 'NONE',  ( -2.751064625579944321E-14, 200.8750000027312126, 146.0000000000000284 ) ) ;
#66866 = CARTESIAN_POINT ( 'NONE',  ( 2.765530957082001251, 287.9218750017069510, 6.676582343750000703 ) ) ;
#66867 = LINE ( 'NONE', #37454, #62776 ) ;
#66868 = CARTESIAN_POINT ( 'NONE',  ( -5.656854249492373476, -5.656854249492376141, -0.2946972160798554397 ) ) ;
#66869 = CARTESIAN_POINT ( 'NONE',  ( -2.828427124746152987, 195.2500000027312126, 200.8284271247462129 ) ) ;
#66870 = CARTESIAN_POINT ( 'NONE',  ( 7.320508075688771044, 206.2499999931720254, 7.320508075688775484 ) ) ;
#66871 = CARTESIAN_POINT ( 'NONE',  ( -1.469576158976823947E-15, 9.937499995903220196, 8.000000000000000000 ) ) ;
#66872 = AXIS2_PLACEMENT_3D ( 'NONE', #31128, #37170, #48475 ) ;
#66873 = CARTESIAN_POINT ( 'NONE',  ( 1.871523826299183495E-15, -10.18810118749999916, 101.4062500020483810 ) ) ;
#66874 = ORIENTED_EDGE ( 'NONE', *, *, #18512, .F. ) ;
#66875 = EDGE_CURVE ( 'NONE', #65387, #69825, #11910, .T. ) ;
#66876 = EDGE_CURVE ( 'NONE', #746, #70531, #58684, .T. ) ;
#66877=STYLED_ITEM('',(#74706),#67054);
#66878 = CARTESIAN_POINT ( 'NONE',  ( -3.999999999999959144, 198.1875000027312126, 199.6568542494924259 ) ) ;
#66879 = CARTESIAN_POINT ( 'NONE',  ( -11.35316468750000141, 158.8020833299193555, 3.042071309553159963 ) ) ;
#66880 = CARTESIAN_POINT ( 'NONE',  ( -5.000000000000007105, 218.3333333333333428, 8.660254037844390851 ) ) ;
#66881 = CARTESIAN_POINT ( 'NONE',  ( -1.432654583217607414, 204.5000000013655779, 194.5412658750000219 ) ) ;
#66882 = CARTESIAN_POINT ( 'NONE',  ( 1.836970198721029589E-15, 229.3750000068279746, 10.00000000000000000 ) ) ;
#66883 = CARTESIAN_POINT ( 'NONE',  ( 11.35316468750000141, 61.09374999658602690, 0.000000000000000000 ) ) ;
#66884 = ORIENTED_EDGE ( 'NONE', *, *, #16361, .F. ) ;
#66885 = CARTESIAN_POINT ( 'NONE',  ( 10.18810118749999916, 1.247682550866122264E-15, 114.9062500020483810 ) ) ;
#66886 = CARTESIAN_POINT ( 'NONE',  ( -4.541265875000002339, 6.937499998634407916, -5.561446717895856393E-16 ) ) ;
#66887 = VERTEX_POINT ( 'NONE', #11538 ) ;
#66888 = EDGE_CURVE ( 'NONE', #12586, #15999, #51903, .T. ) ;
#66889 = CARTESIAN_POINT ( 'NONE',  ( 2.977408999572651815, 22.68749999795161543, 7.188101187500000933 ) ) ;
#66890 = CARTESIAN_POINT ( 'NONE',  ( 1.102182119232618108E-15, 289.3125000034140157, 6.000000000000001776 ) ) ;
#66891 = DIRECTION ( 'NONE',  ( -0.000000000000000000, 1.000000000000000000, -0.000000000000000000 ) ) ;
#66892 = CARTESIAN_POINT ( 'NONE',  ( -7.188101187500000044, 19.59374999795161543, -8.802885111219163269E-16 ) ) ;
#66893 = CARTESIAN_POINT ( 'NONE',  ( -5.082755093536317936, -5.082755093536320601, 4.674052781871752771 ) ) ;
#66894 = CARTESIAN_POINT ( 'NONE',  ( -7.204075437095965206, -7.204075437095968759, 107.2187500020483810 ) ) ;
#66895 = DIRECTION ( 'NONE',  ( 0.000000000000000000, 0.000000000000000000, 1.000000000000000000 ) ) ;
#66896 = CARTESIAN_POINT ( 'NONE',  ( -1.656854249492381248, 5.062499997268813168, -4.000000000000001776 ) ) ;
#66897 = CARTESIAN_POINT ( 'NONE',  ( -20.52744332865416155, -49.04228486187415115, 146.7671521640004073 ) ) ;
#66898 = EDGE_LOOP ( 'NONE', ( #9931, #38600, #10707, #62330 ) ) ;
#66899 = CARTESIAN_POINT ( 'NONE',  ( 2.839093476692135984E-14, 207.6875000013656063, 201.4587341250000350 ) ) ;
#66900 = EDGE_CURVE ( 'NONE', #67743, #31217, #11468, .T. ) ;
#66902 =( BOUNDED_CURVE ( )  B_SPLINE_CURVE ( 2, ( #11073, #57096, #54404, #53658, #24228, #2711, #13637, #1251, #6892 ),
 .UNSPECIFIED., .F., .F. ) 
 B_SPLINE_CURVE_WITH_KNOTS ( ( 3, 2, 2, 2, 3 ),
 ( 0.1617647058823530326, 0.1654411764705883137, 0.1691176470588236502, 0.1727941176470589313, 0.1764705882352942401 ),
 .UNSPECIFIED. ) 
 CURVE ( )  GEOMETRIC_REPRESENTATION_ITEM ( )  RATIONAL_B_SPLINE_CURVE ( ( 0.9999999999999982236, 0.9238795325112885148, 1.000000000000000000, 0.9238795325112867385, 1.000000000000000000, 0.9238795325112867385, 1.000000000000000000, 0.9238795325112844070, 1.000000000000002220 ) ) 
 REPRESENTATION_ITEM ( '' )  );
#66901 = CARTESIAN_POINT ( 'NONE',  ( -24.54126587499996504, 208.1250000013656063, 171.4326545832179534 ) ) ;
#66903 = CARTESIAN_POINT ( 'NONE',  ( -4.541265875000003227, 4.874999998634406140, 1.881053915767121110 ) ) ;
#66904 = DIRECTION ( 'NONE',  ( -0.000000000000000000, 1.000000000000000000, -0.000000000000000000 ) ) ;
#66905 = CARTESIAN_POINT ( 'NONE',  ( -2.977408999572647819, 7.188101187499991163, 25.20530278187175810 ) ) ;
#66906 = ORIENTED_EDGE ( 'NONE', *, *, #30530, .F. ) ;
#66907 = CARTESIAN_POINT ( 'NONE',  ( 7.188101187500000044, 27.46874999795161543, 0.000000000000000000 ) ) ;
#66908 = EDGE_LOOP ( 'NONE', ( #4751, #64079, #10398, #40637, #29579, #38114, #17852, #17276, #30236, #41670, #20763, #38996, #62195, #11766, #22732, #18581, #18548, #64975, #47313, #59721, #51494, #51300, #53693, #5391, #4637, #61929, #18913, #51044, #58227, #14001, #60373, #3998, #51883, #28189, #27993, #42722, #63449, #52935, #59868, #5771, #6354, #59767, #31993, #27267, #22707, #55649, #64682, #66864, #49956, #9463, #20984, #34443 ) ) ;
#66909 = CARTESIAN_POINT ( 'NONE',  ( 10.18810118749999916, 1.247682550866122264E-15, 114.9062500020483810 ) ) ;
#66910 = CARTESIAN_POINT ( 'NONE',  ( -2.081694232949524270, 7.796785530330302194, 0.000000000000000000 ) ) ;
#66911 = CARTESIAN_POINT ( 'NONE',  ( 2.445694354108838731, 205.0625000013656063, 195.5543056458912190 ) ) ;
#66912 = CARTESIAN_POINT ( 'NONE',  ( 24.54126587499999346, 201.1875000013656063, 169.9999999999999432 ) ) ;
#66913 = CARTESIAN_POINT ( 'NONE',  ( 8.660254037844389075, 65.41666666666667140, -5.000000000000000000 ) ) ;
#66914 = CARTESIAN_POINT ( 'NONE',  ( -2.977408999572650927, 95.75000000204836681, -7.188101187500001821 ) ) ;
#66915 = CARTESIAN_POINT ( 'NONE',  ( -4.242640687119285658, 292.1249999999999432, 4.242640687119287435 ) ) ;
#66916 = CARTESIAN_POINT ( 'NONE',  ( 2.726951573962122902E-14, -51.14729664189338365, -48.52014062455057797 ) ) ;
#66917 = ORIENTED_EDGE ( 'NONE', *, *, #66589, .F. ) ;
#66918 = CARTESIAN_POINT ( 'NONE',  ( 1.224646799147353454E-15, 300.0000000000000000, -10.00000000000000178 ) ) ;
#66919 = CIRCLE ( 'NONE', #52506, 12.00000000000000178 ) ;
#66920 = CARTESIAN_POINT ( 'NONE',  ( -27.99999999999999645, 210.0000000000000284, 166.0000000000003979 ) ) ;
#66921 = CARTESIAN_POINT ( 'NONE',  ( 2.828427124746153876, 202.0000000027312126, 144.8284271247462129 ) ) ;
#66922 = CARTESIAN_POINT ( 'NONE',  ( 4.556349186104052151, -10.99999999999999822, 77.96874999999998579 ) ) ;
#66923 = CARTESIAN_POINT ( 'NONE',  ( 4.541265875000002339, 0.3124999986344066949, 0.000000000000000000 ) ) ;
#66924 = CARTESIAN_POINT ( 'NONE',  ( 9.999999999999998224, 257.7083333333333712, -2.679491924311229401 ) ) ;
#66925 = CARTESIAN_POINT ( 'NONE',  ( 1.334622868157815783E-15, 10.39230484541327293, -10.80000000000000071 ) ) ;
#66926 = B_SPLINE_CURVE_WITH_KNOTS ( 'NONE', 3,
 ( #1059, #42121, #65133, #42858, #65511, #13444, #41402, #36851, #48521, #7442 ),
 .UNSPECIFIED., .F., .F.,
 ( 4, 2, 2, 2, 4 ),
 ( 0.01051554819734976456, 0.01182504667393342521, 0.01313454515051708585, 0.01575354210368440713, 0.02099153601001905317 ),
 .UNSPECIFIED. ) ;
#66927 = CARTESIAN_POINT ( 'NONE',  ( -8.660254037844390851, 182.9166666666666856, 4.999999999999998224 ) ) ;
#66928 = CARTESIAN_POINT ( 'NONE',  ( 0.000000000000000000, 0.000000000000000000, 29.33030277982336642 ) ) ;
#66929 = CARTESIAN_POINT ( 'NONE',  ( -7.188101187499992051, 2.977408999572646930, 25.76780278187175810 ) ) ;
#66930 = CARTESIAN_POINT ( 'NONE',  ( -2.085542519210945728E-15, 154.8437499965860127, 11.35316468750000141 ) ) ;
#66931 = CARTESIAN_POINT ( 'NONE',  ( 8.000000000000000000, 27.00000000000000355, 0.000000000000000000 ) ) ;
#66932 = CARTESIAN_POINT ( 'NONE',  ( -5.000000000000000888, 53.57153130924434237, 46.19535935661121329 ) ) ;
#66934 = CARTESIAN_POINT ( 'NONE',  ( 7.999999999999991118, 9.797174393178815797E-16, 16.58030277982336287 ) ) ;
#66933 = CARTESIAN_POINT ( 'NONE',  ( -1.656854249492363040, 202.4375000027311557, 138.0000000000000000 ) ) ;
#66935 = ORIENTED_EDGE ( 'NONE', *, *, #71887, .F. ) ;
#66936 = CARTESIAN_POINT ( 'NONE',  ( 3.042071309553159519, 25.05208332991934483, 11.35316468750000141 ) ) ;
#66937 = FACE_OUTER_BOUND ( 'NONE', #53764, .T. ) ;
#66939 = CARTESIAN_POINT ( 'NONE',  ( -3.999999999999960032, 208.0000000000000284, 198.0000000000000284 ) ) ;
#66938 = CARTESIAN_POINT ( 'NONE',  ( 7.999999999981424637, 1.723583929636134980E-05, 16.76780327155163874 ) ) ;
#66940 = DIRECTION ( 'NONE',  ( -0.000000000000000000, -1.000000000000000000, -4.283267841918042741E-17 ) ) ;
#66941 = CARTESIAN_POINT ( 'NONE',  ( -1.432654583217664479, 202.7500000013655779, 138.5412658750000787 ) ) ;
#66942 = CARTESIAN_POINT ( 'NONE',  ( 4.999999999999993783, 51.04166665983870388, 8.660254037844390851 ) ) ;
#66943 = CARTESIAN_POINT ( 'NONE',  ( -7.188101187500001821, 112.0625000020483810, -2.977408999572650483 ) ) ;
#66944 = CARTESIAN_POINT ( 'NONE',  ( 2.780723358947928197E-16, 7.687499998634407028, -4.541265875000002339 ) ) ;
#66945 = CARTESIAN_POINT ( 'NONE',  ( 4.999999999999993783, 100.8333333333333428, -8.660254037844376640 ) ) ;
#66946 = CARTESIAN_POINT ( 'NONE',  ( -4.898587196589407898E-16, 7.999999999999991118, 9.455302779823364645 ) ) ;
#66948 = CARTESIAN_POINT ( 'NONE',  ( 10.00000000000001954, 159.7916666666666856, 2.679491924311241835 ) ) ;
#66947 = CARTESIAN_POINT ( 'NONE',  ( 3.361190284997544353, 194.4711224105990368, 141.1079405721675926 ) ) ;
#66949 = ORIENTED_EDGE ( 'NONE', *, *, #22503, .F. ) ;
#66950 = EDGE_LOOP ( 'NONE', ( #15494, #69710, #53217, #35927 ) ) ;
#66951 = CARTESIAN_POINT ( 'NONE',  ( -6.362988438888832046E-13, 223.7499999999999147, 9.999999999999998224 ) ) ;
#66952 = CARTESIAN_POINT ( 'NONE',  ( 10.99999999999989342, 4.556349186104152515, 81.53125000409677625 ) ) ;
#66953 = CARTESIAN_POINT ( 'NONE',  ( 9.832129032723420536, 221.3020833367473301, 5.676582343749996262 ) ) ;
#66954 = CARTESIAN_POINT ( 'NONE',  ( -2.085542519210945728E-15, 129.5312499965860127, 11.35316468750000141 ) ) ;
#66955 = VERTEX_POINT ( 'NONE', #614 ) ;
#66956 = EDGE_CURVE ( 'NONE', #29121, #55690, #10715, .T. ) ;
#66957 = CARTESIAN_POINT ( 'NONE',  ( -5.000000000000000000, 10.26105934116143281, -64.40045319026697257 ) ) ;
#66958 = CARTESIAN_POINT ( 'NONE',  ( -4.220049686691937474, -10.18810118749999738, 90.43750000204836681 ) ) ;
#66959 = CARTESIAN_POINT ( 'NONE',  ( 3.313708498984756279, 7.999999999999991118, 20.04905278392014978 ) ) ;
#66960 = CARTESIAN_POINT ( 'NONE',  ( 1.656854249492405451, 207.3125000000000284, 202.0000000000000284 ) ) ;
#66962 = CARTESIAN_POINT ( 'NONE',  ( -9.832129032723420536, 123.6979166632526983, 5.676582343749997150 ) ) ;
#66961 = CARTESIAN_POINT ( 'NONE',  ( 23.99999999999997513, 197.8125000000000284, 171.6568542494922553 ) ) ;
#66963 = CARTESIAN_POINT ( 'NONE',  ( 11.01847871666547540, -7.494884807424072370, -0.7446230086126919279 ) ) ;
#66964 = VERTEX_POINT ( 'NONE', #46603 ) ;
#66965 = CARTESIAN_POINT ( 'NONE',  ( -4.898587196589412829E-16, 90.12500000000000000, -8.000000000000000000 ) ) ;
#66966 = CARTESIAN_POINT ( 'NONE',  ( -16.73219239633842292, 177.3864488912263084, 143.8061503520848987 ) ) ;
#66967 = CARTESIAN_POINT ( 'NONE',  ( -8.311093377946841443, 114.2187499965860127, 8.311093377946834337 ) ) ;
#66968 = CARTESIAN_POINT ( 'NONE',  ( 2.839093476692135984E-14, 207.6875000013656063, 201.4587341250000350 ) ) ;
#66969 = CARTESIAN_POINT ( 'NONE',  ( -1.320432766682874540E-15, 18.46874999795161187, 7.188101187500000044 ) ) ;
#66970 = CARTESIAN_POINT ( 'NONE',  ( 10.18810118749999916, 1.247682550866122264E-15, 80.78125000204838102 ) ) ;
#66971 = CARTESIAN_POINT ( 'NONE',  ( -5.676582343750006032, 24.42708332991935194, 9.832129032723418760 ) ) ;
#66972 = ORIENTED_EDGE ( 'NONE', *, *, #37107, .F. ) ;
#66973 = CARTESIAN_POINT ( 'NONE',  ( -1.970211975628493262, -12.71890404606132918, -0.4750804646944283838 ) ) ;
#66974 = CARTESIAN_POINT ( 'NONE',  ( -8.008118988124991233, 3.317071493978878127, 20.41936528394063544 ) ) ;
#66975 = CARTESIAN_POINT ( 'NONE',  ( 5.656854249492374365, 5.656854249492375253, 22.95530278392014623 ) ) ;
#66976 = EDGE_CURVE ( 'NONE', #45475, #31074, #26117, .T. ) ;
#66977 = CARTESIAN_POINT ( 'NONE',  ( 2.828427124746153876, 200.8750000000000284, 144.8284271247462129 ) ) ;
#66978 = CARTESIAN_POINT ( 'NONE',  ( -2.977408999572650039, 0.9374999979516102089, -7.188101187500001821 ) ) ;
#66979 = CARTESIAN_POINT ( 'NONE',  ( -4.242640687119286547, 298.9375000034140157, -4.242640687119286547 ) ) ;
#66980 = AXIS2_PLACEMENT_3D ( 'NONE', #51857, #40908, #35624 ) ;
#66981 = CARTESIAN_POINT ( 'NONE',  ( 1.224646799147353454E-15, 300.0000000000000000, -10.00000000000000178 ) ) ;
#66982 = CARTESIAN_POINT ( 'NONE',  ( 4.401442555609581635E-16, 1.218749997951610098, -7.188101187500000044 ) ) ;
#66983 = ORIENTED_EDGE ( 'NONE', *, *, #50786, .T. ) ;
#66984 = EDGE_CURVE ( 'NONE', #50500, #24157, #56991, .T. ) ;
#66985 = CARTESIAN_POINT ( 'NONE',  ( 9.832129032723420536, 141.5104166632526699, -5.676582343749999815 ) ) ;
#66986 = CARTESIAN_POINT ( 'NONE',  ( -6.238412754330611322E-16, 10.18810118749999916, 77.78125000204836681 ) ) ;
#66987 = VECTOR ( 'NONE', #42331, 1000.000000000000000 ) ;
#66988 = CARTESIAN_POINT ( 'NONE',  ( -24.54126587499998280, 198.1250000013656063, 171.4326545832179818 ) ) ;
#66989 = CARTESIAN_POINT ( 'NONE',  ( -7.999999999999991118, 0.000000000000000000, 21.83030277982336997 ) ) ;
#66990 = CARTESIAN_POINT ( 'NONE',  ( -8.342170076843785083E-16, 17.18749999863440792, 4.541265875000002339 ) ) ;
#66991 = VERTEX_POINT ( 'NONE', #7730 ) ;
#66992 = CARTESIAN_POINT ( 'NONE',  ( -3.999999999999959144, 202.1875000027311842, 199.6568542494924259 ) ) ;
#66993 = ADVANCED_FACE ( 'NONE', ( #30371 ), #72202, .T. ) ;
#66994 = CARTESIAN_POINT ( 'NONE',  ( 2.445694354108784108, 195.5625000013656063, 144.4456943541088663 ) ) ;
#66995 = CARTESIAN_POINT ( 'NONE',  ( -26.34314575050753859, 207.6875000027311842, 174.0000000000003411 ) ) ;
#66996 = CIRCLE ( 'NONE', #44109, 4.000000000000000000 ) ;
#66997 = CARTESIAN_POINT ( 'NONE',  ( 27.99999999999996092, 194.5625000013656063, 173.4587341249998929 ) ) ;
#66998 = ORIENTED_EDGE ( 'NONE', *, *, #41094, .F. ) ;
#66999 = CARTESIAN_POINT ( 'NONE',  ( 7.188101187500000933, 12.56249999795161365, -2.977408999572650483 ) ) ;
#67000 = CARTESIAN_POINT ( 'NONE',  ( -21.87610737280634865, -14.19902645026048127, 191.9685448688605618 ) ) ;
#67001 = CARTESIAN_POINT ( 'NONE',  ( -11.00000000000000000, 0.000000000000000000, 73.18750000409676204 ) ) ;
#67002 = CARTESIAN_POINT ( 'NONE',  ( 3.042071309553159519, 184.7395833299193839, 11.35316468750000141 ) ) ;
#67003 = CARTESIAN_POINT ( 'NONE',  ( -5.082755093536324154, 109.7187500020483810, 5.082755093536326818 ) ) ;
#67004 = DIRECTION ( 'NONE',  ( -0.000000000000000000, 1.000000000000000000, 4.476705744456276341E-16 ) ) ;
#67005 = CARTESIAN_POINT ( 'NONE',  ( -6.676582343749999815, 289.5156250017070647, 2.765530957082001251 ) ) ;
#67007 = CARTESIAN_POINT ( 'NONE',  ( -2.849036369511732440E-14, 201.3750000027312126, 138.0000000000000568 ) ) ;
#67006 = CARTESIAN_POINT ( 'NONE',  ( -32.00000000000000000, 209.2500000000000284, 170.0000000000003979 ) ) ;
#67008 = EDGE_LOOP ( 'NONE', ( #18022, #15836, #12684, #70460 ) ) ;
#67009 = CARTESIAN_POINT ( 'NONE',  ( 3.042071309553163960, 262.4479166700806445, -11.35316468749999785 ) ) ;
#67010 = CARTESIAN_POINT ( 'NONE',  ( -7.188101187499990274, -2.977408999572651371, 25.95530278187175810 ) ) ;
#67011 = CARTESIAN_POINT ( 'NONE',  ( -4.556349186104048599, -10.99999999999999822, 92.78124999999998579 ) ) ;
#67012 = FACE_OUTER_BOUND ( 'NONE', #2856, .T. ) ;
#67013 = CARTESIAN_POINT ( 'NONE',  ( -0.3752463838826955445, -65.74564559951674880, -26.26824411939953308 ) ) ;
#67014 = CARTESIAN_POINT ( 'NONE',  ( 2.754378923186476579E-14, 200.4375000013656063, 194.5412658750000219 ) ) ;
#67015 =( BOUNDED_CURVE ( )  B_SPLINE_CURVE ( 2, ( #17212, #13753, #59443, #64727, #64360, #58348, #18707, #7018, #29655, #19429, #36797, #30395, #6653 ),
 .UNSPECIFIED., .F., .F. ) 
 B_SPLINE_CURVE_WITH_KNOTS ( ( 3, 2, 2, 2, 2, 2, 3 ),
 ( 0.7692923867907990321, 0.7745262106001035152, 0.7797600344094078872, 0.7849938582187123703, 0.7902276820280168534, 0.7954615058373213365, 0.8006953296466258196 ),
 .UNSPECIFIED. ) 
 CURVE ( )  GEOMETRIC_REPRESENTATION_ITEM ( )  RATIONAL_B_SPLINE_CURVE ( ( 0.9999999999998058220, 0.9659258262892623792, 1.000000000000000000, 0.9659258262890682012, 1.000000000000000000, 0.9659258262890682012, 1.000000000000000000, 0.9659258262890682012, 1.000000000000000000, 0.9659258262890682012, 1.000000000000000000, 0.9659258262890682012, 1.000000000000000000 ) ) 
 REPRESENTATION_ITEM ( '' )  );
#67016 = DIRECTION ( 'NONE',  ( -0.000000000000000000, 1.000000000000000000, 4.689100369878284071E-30 ) ) ;
#67017 =( LENGTH_UNIT ( ) NAMED_UNIT ( * ) SI_UNIT ( .MILLI., .METRE. ) );
#67018 =( BOUNDED_CURVE ( )  B_SPLINE_CURVE ( 2, ( #26553, #21644, #51064, #38648, #74077, #49577, #56365, #27681, #50687 ),
 .UNSPECIFIED., .F., .F. ) 
 B_SPLINE_CURVE_WITH_KNOTS ( ( 3, 2, 2, 2, 3 ),
 ( 0.6617647058823526995, 0.6654411764705879806, 0.6691176470588232617, 0.6727941176470586537, 0.6764705882352939348 ),
 .UNSPECIFIED. ) 
 CURVE ( )  GEOMETRIC_REPRESENTATION_ITEM ( )  RATIONAL_B_SPLINE_CURVE ( ( 1.000000000000004663, 0.9238795325112821866, 1.000000000000000000, 0.9238795325112867385, 1.000000000000000000, 0.9238795325112867385, 1.000000000000000000, 0.9238795325112912904, 0.9999999999999954481 ) ) 
 REPRESENTATION_ITEM ( '' )  );
#67019 = CARTESIAN_POINT ( 'NONE',  ( 8.000000000000001776, 92.65625000000001421, 3.313708498984759387 ) ) ;
#67020 = CARTESIAN_POINT ( 'NONE',  ( -11.35316468750000141, 113.5937499965860127, -1.390361679473963753E-15 ) ) ;
#67021 = CARTESIAN_POINT ( 'NONE',  ( -27.99999999999995737, 198.5000000000000000, 174.0000000000003695 ) ) ;
#67022 = CARTESIAN_POINT ( 'NONE',  ( 11.00000000000000355, -4.556349186104045046, 73.65625000000000000 ) ) ;
#67025 = CARTESIAN_POINT ( 'NONE',  ( 11.00000000000000000, 1.347111479062088405E-15, 109.9375000040967763 ) ) ;
#67024 = CARTESIAN_POINT ( 'NONE',  ( 29.43265458321761230, 199.8750000013655779, 166.5412658749999650 ) ) ;
#67023 = CARTESIAN_POINT ( 'NONE',  ( 24.54126587499999701, 197.3750000013656063, 168.5673454167822172 ) ) ;
#67026 = ORIENTED_EDGE ( 'NONE', *, *, #1759, .F. ) ;
#67027 = CARTESIAN_POINT ( 'NONE',  ( 4.805230186056123287, 224.1490657562575848, 8.774718480194076520 ) ) ;
#67028 =( GEOMETRIC_REPRESENTATION_CONTEXT ( 3 ) GLOBAL_UNCERTAINTY_ASSIGNED_CONTEXT ( ( #1150 ) ) GLOBAL_UNIT_ASSIGNED_CONTEXT ( ( #27939, #35, #50947 ) ) REPRESENTATION_CONTEXT ( 'NONE', 'WORKASPACE' ) );
#67029 = CARTESIAN_POINT ( 'NONE',  ( 3.042071309553167069, 221.8229166632527267, -11.35316468749999785 ) ) ;
#67030 = CARTESIAN_POINT ( 'NONE',  ( -2.445694354108839619, 197.8125000013656063, 139.5543056458912190 ) ) ;
#67031 = CARTESIAN_POINT ( 'NONE',  ( 25.55430564589114795, 196.5625000013656063, 172.4456943541086957 ) ) ;
#67032 = CARTESIAN_POINT ( 'NONE',  ( 7.778174593052021635, 7.778174593052023411, 111.6250000040967763 ) ) ;
#67033 = CARTESIAN_POINT ( 'NONE',  ( -9.832129032723418760, 203.1770833299193555, -5.676582343750004256 ) ) ;
#67034 = CARTESIAN_POINT ( 'NONE',  ( 25.17157287525378351, 207.7500000027312126, 167.1715728752537586 ) ) ;
#67035 = DIRECTION ( 'NONE',  ( 0.000000000000000000, 0.000000000000000000, -1.000000000000000000 ) ) ;
#67036 = CARTESIAN_POINT ( 'NONE',  ( -3.211159895383561391, 16.68749999863440436, -3.211159895383561835 ) ) ;
#67037 = CARTESIAN_POINT ( 'NONE',  ( 3.074111742560679872, -51.58078258920428283, 48.68628732315335839 ) ) ;
#67038 = CARTESIAN_POINT ( 'NONE',  ( -4.898587196589407898E-16, 7.999999999999991118, 25.95530277982336997 ) ) ;
#67039 = CARTESIAN_POINT ( 'NONE',  ( 5.000000000000000000, -60.11723469343085213, -46.25570701698114107 ) ) ;
#67040 = CARTESIAN_POINT ( 'NONE',  ( -2.085542519210945728E-15, 89.53124999658602690, 11.35316468750000141 ) ) ;
#67041 = ORIENTED_EDGE ( 'NONE', *, *, #55753, .F. ) ;
#67042 = CARTESIAN_POINT ( 'NONE',  ( 8.000000000000001776, 92.65625000000001421, 3.313708498984759387 ) ) ;
#67043 = CARTESIAN_POINT ( 'NONE',  ( 5.082755093536325930, 17.15624999795161543, -5.082755093536325930 ) ) ;
#67044 = DIRECTION ( 'NONE',  ( -0.000000000000000000, 1.000000000000000000, 4.476705744456276341E-16 ) ) ;
#67045 = CARTESIAN_POINT ( 'NONE',  ( -8.311093377946834337, 254.8437500034139589, 8.311093377946837890 ) ) ;
#67046 = CARTESIAN_POINT ( 'NONE',  ( 11.35316468749999963, 90.98958332991935549, -3.042071309553165293 ) ) ;
#67047 = ORIENTED_EDGE ( 'NONE', *, *, #11114, .T. ) ;
#67048 = EDGE_CURVE ( 'NONE', #49089, #7137, #2810, .T. ) ;
#67049 = PLANE ( 'NONE',  #68110 ) ;
#67050 = CARTESIAN_POINT ( 'NONE',  ( 7.204075437095966983, 7.204075437095967871, 113.5937500020483810 ) ) ;
#67051 = CARTESIAN_POINT ( 'NONE',  ( -24.54126587499998990, 196.4375000013655779, 170.0000000000003411 ) ) ;
#67052 = CARTESIAN_POINT ( 'NONE',  ( -3.458734124999960358, 205.6875000013656063, 198.0000000000000284 ) ) ;
#67053 = CARTESIAN_POINT ( 'NONE',  ( 6.123233995736767268E-16, 3.124999993172032919, -10.00000000000000178 ) ) ;
#67054 = MANIFOLD_SOLID_BREP ( 'BaseBody', #43039 ) ;
#67056 = CARTESIAN_POINT ( 'NONE',  ( 9.832129032723420536, 81.19791666325269830, -5.676582343749999815 ) ) ;
#67055 = CARTESIAN_POINT ( 'NONE',  ( -38.00000000000000000, 242.0000000000000284, 20.00000000000003553 ) ) ;
#67057 = CARTESIAN_POINT ( 'NONE',  ( 3.313708498984756279, 7.999999999999991118, 21.54905278392014623 ) ) ;
#67058 = CARTESIAN_POINT ( 'NONE',  ( -30.44569435410883429, 199.8125000013656063, 167.5543056458915885 ) ) ;
#67059 = FACE_OUTER_BOUND ( 'NONE', #39037, .T. ) ;
#67060 = CIRCLE ( 'NONE', #70765, 15.99999999999998579 ) ;
#67061 = CARTESIAN_POINT ( 'NONE',  ( 7.320508075688774596, 187.4999999931719969, -7.320508075688774596 ) ) ;
#67062 = FACE_OUTER_BOUND ( 'NONE', #10133, .T. ) ;
#67063 = CARTESIAN_POINT ( 'NONE',  ( -11.35316468750000141, 73.80208332991934128, 3.042071309553159963 ) ) ;
#67064 = CARTESIAN_POINT ( 'NONE',  ( 6.676582343750001591, 294.9531250017069510, -8.176455196517173205E-16 ) ) ;
#67065 = CARTESIAN_POINT ( 'NONE',  ( -4.220049686691937474, -10.18810118749999738, 99.81250000204838102 ) ) ;
#67066 = CARTESIAN_POINT ( 'NONE',  ( -3.042071309553173730, 209.3229166632526983, 11.35316468749999785 ) ) ;
#67067 = ORIENTED_EDGE ( 'NONE', *, *, #29659, .T. ) ;
#67068 = CARTESIAN_POINT ( 'NONE',  ( 5.656854249492376141, -5.656854249492374365, 28.39280277982336642 ) ) ;
#67069 = CARTESIAN_POINT ( 'NONE',  ( 1.656854249492305531, 205.9375000027311842, 146.0000000000000853 ) ) ;
#67070 = CARTESIAN_POINT ( 'NONE',  ( 5.656854249492380582, 14.99999999590322020, -5.656854249492380582 ) ) ;
#67072 = CARTESIAN_POINT ( 'NONE',  ( 11.35316468749999785, 200.5729166632526983, 3.042071309553174174 ) ) ;
#67071 = CARTESIAN_POINT ( 'NONE',  ( -2.828427124746190735, 11.12499999726881406, -2.828427124746191623 ) ) ;
#67073 = CARTESIAN_POINT ( 'NONE',  ( -8.000000000053406168, 3.313708498931343893, 8.424052783922283183 ) ) ;
#67074 = CARTESIAN_POINT ( 'NONE',  ( 10.00000000000000000, 230.6250000068279746, -1.224646799147353256E-15 ) ) ;
#67075 = DIRECTION ( 'NONE',  ( -0.000000000000000000, 1.000000000000000000, -4.476705744456276341E-16 ) ) ;
#67076 = VERTEX_POINT ( 'NONE', #25055 ) ;
#67077 = CARTESIAN_POINT ( 'NONE',  ( 9.832129032723420536, 196.5104166632526983, -5.676582343749999815 ) ) ;
#67078 = ADVANCED_FACE ( 'NONE', ( #31853 ), #43529, .F. ) ;
#67079 = CARTESIAN_POINT ( 'NONE',  ( -4.401442555609577197E-16, 7.188101187499992051, 14.61155278187175455 ) ) ;
#67080 = CARTESIAN_POINT ( 'NONE',  ( -0.8588954341814966087, 60.21087566322607643, -22.89167302533678594 ) ) ;
#67081 = CARTESIAN_POINT ( 'NONE',  ( -5.656854249492381470, 14.43750000000000178, 5.656854249492379694 ) ) ;
#67082 = AXIS2_PLACEMENT_3D ( 'NONE', #28684, #57375, #70813 ) ;
#67083 = ORIENTED_EDGE ( 'NONE', *, *, #68544, .F. ) ;
#67084 = PRODUCT_DEFINITION_FORMATION_WITH_SPECIFIED_SOURCE ( 'ANY', '', #4157, .NOT_KNOWN. ) ;
#67085 = CARTESIAN_POINT ( 'NONE',  ( -3.313708498984762496, 93.96875000409677625, 7.999999999999998224 ) ) ;
#67086 = CARTESIAN_POINT ( 'NONE',  ( 4.999999999999993783, 14.16666666666666785, 8.660254037844390851 ) ) ;
#67087 = EDGE_CURVE ( 'NONE', #71006, #21157, #2437, .T. ) ;
#67088 = ORIENTED_EDGE ( 'NONE', *, *, #32302, .F. ) ;
#67089 = EDGE_CURVE ( 'NONE', #5866, #39173, #64692, .T. ) ;
#67090 = CARTESIAN_POINT ( 'NONE',  ( -2.828427124746190735, 17.37500000000000000, -2.828427124746191623 ) ) ;
#67091 = CARTESIAN_POINT ( 'NONE',  ( -4.541265875000002339, 21.74999999863440792, -1.881053915767121998 ) ) ;
#67092 = CARTESIAN_POINT ( 'NONE',  ( 7.999999999999991118, 9.797174393178815797E-16, 9.267802783920146226 ) ) ;
#67093 = CYLINDRICAL_SURFACE ( 'NONE', #58376, 10.00000000000000000 ) ;
#67094 = ORIENTED_EDGE ( 'NONE', *, *, #45885, .F. ) ;
#67095 = SURFACE_SIDE_STYLE ('',( #21060 ) ) ;
#67096 = CARTESIAN_POINT ( 'NONE',  ( 2.977408999572650039, 90.68750000204838102, -7.188101187500001821 ) ) ;
#67098 = CARTESIAN_POINT ( 'NONE',  ( 5.676582343749997150, 257.2395833367473301, -9.832129032723418760 ) ) ;
#67097 = CARTESIAN_POINT ( 'NONE',  ( 0.000000000000000000, 0.000000000000000000, -14.00000000000000178 ) ) ;
#67099 = ORIENTED_EDGE ( 'NONE', *, *, #55662, .T. ) ;
#67100 = AXIS2_PLACEMENT_3D ( 'NONE', #4759, #45846, #16418 ) ;
#67101 = CARTESIAN_POINT ( 'NONE',  ( -8.311093377946836114, 248.5937500034139589, -8.311093377946836114 ) ) ;
#67102 = ADVANCED_FACE ( 'NONE', ( #49191 ), #47579, .F. ) ;
#67103 = CARTESIAN_POINT ( 'NONE',  ( -2.977408999572647819, 7.188101187499991163, 13.20530278187175277 ) ) ;
#67104 = ORIENTED_EDGE ( 'NONE', *, *, #60839, .F. ) ;
#67105 = ORIENTED_EDGE ( 'NONE', *, *, #59157, .F. ) ;
#67106 = CARTESIAN_POINT ( 'NONE',  ( -4.220049686691935698, 10.18810118749999916, 71.87500000204836681 ) ) ;
#67107 = CARTESIAN_POINT ( 'NONE',  ( -8.311093377946836114, 72.96874999658602690, -8.311093377946837890 ) ) ;
#67108 = CARTESIAN_POINT ( 'NONE',  ( -7.999999999994639843, -6.164467849698474977E-06, 23.51803407853789807 ) ) ;
#67109 = CARTESIAN_POINT ( 'NONE',  ( 11.00000000000000000, 1.347111479062088405E-15, 87.25000000000000000 ) ) ;
#67112 = CARTESIAN_POINT ( 'NONE',  ( -6.676582343750001591, 290.6093750017069510, 0.000000000000000000 ) ) ;
#67111 = CARTESIAN_POINT ( 'NONE',  ( 23.99999999999999645, 195.9375000027312126, 171.6568542494923122 ) ) ;
#67110 = DIRECTION ( 'NONE',  ( -1.000000000000000000, 0.000000000000000000, -0.000000000000000000 ) ) ;
#67113 =( BOUNDED_CURVE ( )  B_SPLINE_CURVE ( 2, ( #26260, #15693, #16062, #15314, #54964, #21725, #56085, #50406, #44755 ),
 .UNSPECIFIED., .F., .F. ) 
 B_SPLINE_CURVE_WITH_KNOTS ( ( 3, 2, 2, 2, 3 ),
 ( 0.01470588235294118494, 0.01838235294117648161, 0.02205882352941178001, 0.02573529411764707148, 0.02941176470588236988 ),
 .UNSPECIFIED. ) 
 CURVE ( )  GEOMETRIC_REPRESENTATION_ITEM ( )  RATIONAL_B_SPLINE_CURVE ( ( 0.9999999999999998890, 0.9238795325112869605, 1.000000000000000000, 0.9238795325112867385, 1.000000000000000000, 0.9238795325112867385, 1.000000000000000000, 0.9238795325112864054, 1.000000000000000444 ) ) 
 REPRESENTATION_ITEM ( '' )  );
#67114 = CARTESIAN_POINT ( 'NONE',  ( -25.17157287525374088, 203.7500000027312126, 172.8284271247464972 ) ) ;
#67115 = CARTESIAN_POINT ( 'NONE',  ( -4.898587196589412829E-16, 90.31250000409676204, -8.000000000000000000 ) ) ;
#67116 =( BOUNDED_CURVE ( )  B_SPLINE_CURVE ( 2, ( #25113, #70059, #65489, #59110, #13781, #36825, #2492, #47398, #25485, #29686, #71505, #52702, #24016 ),
 .UNSPECIFIED., .F., .F. ) 
 B_SPLINE_CURVE_WITH_KNOTS ( ( 3, 2, 2, 2, 2, 2, 3 ),
 ( 0.6358695652173913526, 0.6376811594202898004, 0.6394927536231883591, 0.6413043478260869179, 0.6431159420289855877, 0.6449275362318841465, 0.6467391304347827052 ),
 .UNSPECIFIED. ) 
 CURVE ( )  GEOMETRIC_REPRESENTATION_ITEM ( )  RATIONAL_B_SPLINE_CURVE ( ( 1.000000000000000000, 0.9659258262890683122, 1.000000000000000000, 0.9659258262890683122, 1.000000000000000000, 0.9659258262890683122, 1.000000000000000000, 0.9659258262890683122, 1.000000000000000000, 0.9659258262890683122, 1.000000000000000000, 0.9659258262890662028, 1.000000000000001998 ) ) 
 REPRESENTATION_ITEM ( '' )  );
#67117 = CARTESIAN_POINT ( 'NONE',  ( -2.445694354108783219, 196.8125000013656063, 200.4456943541088663 ) ) ;
#67118 = CARTESIAN_POINT ( 'NONE',  ( 5.656854249492380582, 8.999999995903221972, -5.656854249492380582 ) ) ;
#67119 = ORIENTED_EDGE ( 'NONE', *, *, #53720, .F. ) ;
#67120 = CARTESIAN_POINT ( 'NONE',  ( 24.54126587499998990, 196.1875000013655779, 169.9999999999998863 ) ) ;
#67121 = CARTESIAN_POINT ( 'NONE',  ( 5.082755093536324154, 12.65624999795161187, 5.082755093536326818 ) ) ;
#67122 = CARTESIAN_POINT ( 'NONE',  ( -11.35316468749999785, 168.3854166632526699, -3.042071309553167513 ) ) ;
#67123 = CARTESIAN_POINT ( 'NONE',  ( 0.000000000000000000, 125.0000000000000000, 0.000000000000000000 ) ) ;
#67124 = CARTESIAN_POINT ( 'NONE',  ( -2.977408999572652260, 103.8125000020483952, 7.188101187500000044 ) ) ;
#67126 = CARTESIAN_POINT ( 'NONE',  ( -5.086519500888726952, -50.65542486323322890, -41.09394361258938488 ) ) ;
#67125 = CARTESIAN_POINT ( 'NONE',  ( 4.242640687119285658, 289.6875000034139589, -4.242640687119286547 ) ) ;
#67127 = CARTESIAN_POINT ( 'NONE',  ( 24.54126587499999701, 208.4375000013656063, 169.9999999999998863 ) ) ;
#67128 = CARTESIAN_POINT ( 'NONE',  ( -2.977408999572647819, 7.188101187499991163, 16.58030278187175455 ) ) ;
#67129 = CARTESIAN_POINT ( 'NONE',  ( -2.828427124746208943, 208.7500000027312126, 144.8284271247462129 ) ) ;
#67130 = CARTESIAN_POINT ( 'NONE',  ( 8.311093377946837890, 41.40624999658601268, -8.311093377946837890 ) ) ;
#67131 = CARTESIAN_POINT ( 'NONE',  ( 3.313708498984762496, 20.71875000000000355, 7.999999999999998224 ) ) ;
#67132 = CARTESIAN_POINT ( 'NONE',  ( 8.660254037844385522, 21.45833332650536818, 5.000000000000005329 ) ) ;
#67133 = CARTESIAN_POINT ( 'NONE',  ( 11.00000000000000000, 1.347111479062088405E-15, 111.4375000040967763 ) ) ;
#67134 = ORIENTED_EDGE ( 'NONE', *, *, #60839, .T. ) ;
#67135 = VECTOR ( 'NONE', #44025, 1000.000000000000000 ) ;
#67136 = EDGE_CURVE ( 'NONE', #37291, #22020, #33426, .T. ) ;
#67137 = FACE_OUTER_BOUND ( 'NONE', #13965, .T. ) ;
#67138 = CARTESIAN_POINT ( 'NONE',  ( -5.656854249492381470, 23.24999999590322020, 5.656854249492379694 ) ) ;
#67139 = CARTESIAN_POINT ( 'NONE',  ( -9.832129032723418760, 42.86458332991934839, -5.676582343750004256 ) ) ;
#67140 = CARTESIAN_POINT ( 'NONE',  ( 11.00000000000000000, 4.556349186104045934, 78.53125000409677625 ) ) ;
#67141 = CARTESIAN_POINT ( 'NONE',  ( -3.458734125000016757, 203.1250000013656347, 140.5673454167823593 ) ) ;
#67142 = CARTESIAN_POINT ( 'NONE',  ( 2.449293598294707893E-16, 7.999999997268813168, -4.000000000000001776 ) ) ;
#67143 = CYLINDRICAL_SURFACE ( 'NONE', #5806, 7.999999999999991118 ) ;
#67145 = CARTESIAN_POINT ( 'NONE',  ( 6.951808397369818766E-16, 52.03124999658601979, -11.35316468750000141 ) ) ;
#67144 = CARTESIAN_POINT ( 'NONE',  ( -7.188101187499999156, 97.25000000204839523, 2.977408999572654924 ) ) ;
#67147 = EDGE_CURVE ( 'NONE', #11774, #39639, #15977, .T. ) ;
#67146 = CARTESIAN_POINT ( 'NONE',  ( 7.999999999999991118, 9.797174393178815797E-16, 10.58030277982336465 ) ) ;
#67148 = CARTESIAN_POINT ( 'NONE',  ( -6.735557395310442023E-16, 11.00000000000000000, 98.31250000409677625 ) ) ;
#67149 = CARTESIAN_POINT ( 'NONE',  ( 11.35316468749999963, 160.9895833299193839, -3.042071309553165293 ) ) ;
#67150 =( BOUNDED_CURVE ( )  B_SPLINE_CURVE ( 2, ( #42816, #8130, #13762, #43567, #71484, #9248, #19810, #66209, #3977, #60176, #65833, #32270, #31515 ),
 .UNSPECIFIED., .F., .F. ) 
 B_SPLINE_CURVE_WITH_KNOTS ( ( 3, 2, 2, 2, 2, 2, 3 ),
 ( 0.5494935699762487635, 0.5547273339465774722, 0.5599610979169062919, 0.5651948618872351116, 0.5704286258575639312, 0.5756623898278927509, 0.5808961537982215706 ),
 .UNSPECIFIED. ) 
 CURVE ( )  GEOMETRIC_REPRESENTATION_ITEM ( )  RATIONAL_B_SPLINE_CURVE ( ( 1.000000000000000000, 0.9659258262890683122, 1.000000000000000000, 0.9659258262890683122, 1.000000000000000000, 0.9659258262890683122, 1.000000000000000000, 0.9659258262890683122, 1.000000000000000000, 0.9659258262890683122, 1.000000000000000000, 0.9659258262890693114, 0.9999999999999990008 ) ) 
 REPRESENTATION_ITEM ( '' )  );
#67151 = CARTESIAN_POINT ( 'NONE',  ( -10.00000000000000355, 144.5833333265053398, 2.679491924311223183 ) ) ;
#67152 = CARTESIAN_POINT ( 'NONE',  ( 2.977408999572654480, 105.5000000020483810, 7.188101187499999156 ) ) ;
#67153 = CARTESIAN_POINT ( 'NONE',  ( -3.979266480698733677, 0.4999999999999095723, -6.940132439340585435 ) ) ;
#67154 = CARTESIAN_POINT ( 'NONE',  ( 8.311093377946834337, 30.46874999658601979, 8.311093377946839666 ) ) ;
#67155 = EDGE_CURVE ( 'NONE', #19205, #16317, #31665, .T. ) ;
#67156 = CARTESIAN_POINT ( 'NONE',  ( -7.320508075688779925, 16.87500000000000355, -7.320508075688779925 ) ) ;
#67157 = ORIENTED_EDGE ( 'NONE', *, *, #16210, .T. ) ;
#67158 = DIRECTION ( 'NONE',  ( -0.000000000000000000, -1.000000000000000000, -4.283267841918042741E-17 ) ) ;
#67159 = CARTESIAN_POINT ( 'NONE',  ( -10.18810118749999738, -4.220049686691941915, 78.25000000204836681 ) ) ;
#67160 = CARTESIAN_POINT ( 'NONE',  ( -27.99999999999999645, 210.0000000000000284, 170.0000000000003695 ) ) ;
#67162 = CARTESIAN_POINT ( 'NONE',  ( 11.35316468749999963, 165.9895833299193271, -3.042071309553165293 ) ) ;
#67161 = CARTESIAN_POINT ( 'NONE',  ( -7.320508075688779037, 6.875000000000002665, -7.320508075688779925 ) ) ;
#67163 = CARTESIAN_POINT ( 'NONE',  ( 5.656854249492374365, 5.656854249492375253, 12.32405278432982421 ) ) ;
#67164 = CYLINDRICAL_SURFACE ( 'NONE', #53814, 8.000000000000000000 ) ;
#67165 = CARTESIAN_POINT ( 'NONE',  ( -7.320508075688771932, 262.5000000068279746, -7.320508075688771932 ) ) ;
#67166 = DIRECTION ( 'NONE',  ( 0.000000000000000000, -1.000000000000000000, -0.000000000000000000 ) ) ;
#67167 = CARTESIAN_POINT ( 'NONE',  ( 10.18810118749999916, 1.247682550866122264E-15, 83.78125000204838102 ) ) ;
#67168 = ORIENTED_EDGE ( 'NONE', *, *, #66223, .T. ) ;
#67169 = AXIS2_PLACEMENT_3D ( 'NONE', #56001, #39013, #50688 ) ;
#67170 = CARTESIAN_POINT ( 'NONE',  ( -8.660254037844387298, 118.9583333265053824, -5.000000000000004441 ) ) ;
#67171 = FACE_OUTER_BOUND ( 'NONE', #2387, .T. ) ;
#67172 = CARTESIAN_POINT ( 'NONE',  ( -5.676582343749998039, 117.7604166632526841, -9.832129032723420536 ) ) ;
#67173 = CARTESIAN_POINT ( 'NONE',  ( -7.204075437095967871, 7.204075437095967871, 92.96875000204838102 ) ) ;
#67174 = CARTESIAN_POINT ( 'NONE',  ( -8.342170076843785083E-16, 21.18749999863440792, 4.541265875000002339 ) ) ;
#67175 = EDGE_LOOP ( 'NONE', ( #71064, #71367, #12610, #68402, #49543, #42363 ) ) ;
#67176 = VERTEX_POINT ( 'NONE', #67680 ) ;
#67177 = CARTESIAN_POINT ( 'NONE',  ( 2.780723358947928197E-16, 2.687499998634407028, -4.541265875000002339 ) ) ;
#67178 = CARTESIAN_POINT ( 'NONE',  ( -5.082755093536325042, 7.031249997951611874, -5.082755093536325930 ) ) ;
#67179 = CARTESIAN_POINT ( 'NONE',  ( -7.999999999999998224, 110.2812500040967763, 3.313708498984766493 ) ) ;
#67180 = CARTESIAN_POINT ( 'NONE',  ( -6.238412754330611322E-16, 10.18810118749999916, 90.15625000204838102 ) ) ;
#67181 = CARTESIAN_POINT ( 'NONE',  ( -30.44569435410879166, 202.0625000013656063, 172.4456943541092357 ) ) ;
#67182 = EDGE_CURVE ( 'NONE', #8028, #12665, #33886, .T. ) ;
#67183 = CARTESIAN_POINT ( 'NONE',  ( 2.828427124746191623, 2.125000000000000000, -2.828427124746191623 ) ) ;
#67184 = CARTESIAN_POINT ( 'NONE',  ( 4.000000000000000888, 17.68749999726881228, 1.656854249492384135 ) ) ;
#67185 = CARTESIAN_POINT ( 'NONE',  ( 1.881053915767122664, 7.124999998634407916, 4.541265875000001451 ) ) ;
#67186 = CARTESIAN_POINT ( 'NONE',  ( 2.828427124746153876, 201.8750000000000284, 144.8284271247462129 ) ) ;
#67187 = ORIENTED_EDGE ( 'NONE', *, *, #66704, .T. ) ;
#67188 = CARTESIAN_POINT ( 'NONE',  ( 10.00000000000000000, 222.5000000000000000, -1.224646799147353256E-15 ) ) ;
#67190 = CARTESIAN_POINT ( 'NONE',  ( 8.660254037844389075, 235.2083333401613174, 4.999999999999997335 ) ) ;
#67189 = CARTESIAN_POINT ( 'NONE',  ( -25.55430564589122611, 197.3125000013656063, 167.5543056458915032 ) ) ;
#67191 =( LENGTH_UNIT ( ) NAMED_UNIT ( * ) SI_UNIT ( .MILLI., .METRE. ) );
#67192 = CARTESIAN_POINT ( 'NONE',  ( -3.211159895383561391, 18.68749999863440436, -3.211159895383561835 ) ) ;
#67193 = CARTESIAN_POINT ( 'NONE',  ( -4.721056650415998313, 298.5781250017069510, 4.721056650416000089 ) ) ;
#67194 = CARTESIAN_POINT ( 'NONE',  ( -4.401442555609577197E-16, 7.188101187499992051, 8.611552781871752771 ) ) ;
#67195 = ORIENTED_EDGE ( 'NONE', *, *, #22503, .T. ) ;
#67196 = ORIENTED_EDGE ( 'NONE', *, *, #31265, .F. ) ;
#67197 = CARTESIAN_POINT ( 'NONE',  ( 1.871523826299183495E-15, -10.18810118749999916, 101.0312500020483810 ) ) ;
#67198 = CARTESIAN_POINT ( 'NONE',  ( 27.99999999999996447, 204.6250000027312126, 165.9999999999998863 ) ) ;
#67199 = CARTESIAN_POINT ( 'NONE',  ( -30.44569435410883429, 201.8125000013656063, 167.5543056458915885 ) ) ;
#67200 = CARTESIAN_POINT ( 'NONE',  ( 7.778174593052021635, 7.778174593052023411, 105.4374999999999858 ) ) ;
#67201 = CARTESIAN_POINT ( 'NONE',  ( 1.432654583217664701, 208.0000000013656347, 201.4587341250000065 ) ) ;
#67202 = CARTESIAN_POINT ( 'NONE',  ( 2.679491924297558114, 61.04166666666794328, -10.00000000000798472 ) ) ;
#67203 = CARTESIAN_POINT ( 'NONE',  ( -10.00000000000000178, 112.5000000000000000, -1.224646799147353454E-15 ) ) ;
#67204 = CARTESIAN_POINT ( 'NONE',  ( 8.000000000000000000, 107.7500000000000000, -9.797174393178825657E-16 ) ) ;
#67205 = CARTESIAN_POINT ( 'NONE',  ( 2.765530957082001251, 293.9218750017069510, 6.676582343750000703 ) ) ;
#67206 = CARTESIAN_POINT ( 'NONE',  ( -2.977408999572648707, -7.188101187499990274, 9.642802781871756324 ) ) ;
#67207 = VERTEX_POINT ( 'NONE', #9597 ) ;
#67208 =( GEOMETRIC_REPRESENTATION_CONTEXT ( 3 ) GLOBAL_UNCERTAINTY_ASSIGNED_CONTEXT ( ( #69488 ) ) GLOBAL_UNIT_ASSIGNED_CONTEXT ( ( #39114, #65631, #30566 ) ) REPRESENTATION_CONTEXT ( 'NONE', 'WORKASPACE' ) );
#67209 = CARTESIAN_POINT ( 'NONE',  ( 2.751064625579944321E-14, 195.7500000000000000, 194.0000000000000568 ) ) ;
#67210 = CARTESIAN_POINT ( 'NONE',  ( 28.00000000000002487, 207.9375000013656063, 166.5412658749999082 ) ) ;
#67211 = CARTESIAN_POINT ( 'NONE',  ( 8.000000000000000000, 23.90624999590322730, -3.313708498984761608 ) ) ;
#67212 = CARTESIAN_POINT ( 'NONE',  ( 3.458734124999959025, 199.5000000013656063, 140.5673454167824161 ) ) ;
#67213 = CARTESIAN_POINT ( 'NONE',  ( 2.977408999572654480, 120.5000000020483810, 7.188101187499999156 ) ) ;
#67215 = CARTESIAN_POINT ( 'NONE',  ( 3.458734124999960358, 202.6250000013656063, 143.4326545832176976 ) ) ;
#67214 = DIRECTION ( 'NONE',  ( 0.000000000000000000, 0.000000000000000000, -1.000000000000000000 ) ) ;
#67216 = CARTESIAN_POINT ( 'NONE',  ( 8.311093377946839666, 256.0937500034140157, 8.311093377946829008 ) ) ;
#67217 = CARTESIAN_POINT ( 'NONE',  ( -5.656854249492378806, 114.8750000040967905, 5.656854249492381470 ) ) ;
#67218 = FACE_OUTER_BOUND ( 'NONE', #67580, .T. ) ;
#67219 = CARTESIAN_POINT ( 'NONE',  ( 11.35316468749999785, 5.572916663252682312, 3.042071309553174174 ) ) ;
#67220 = B_SPLINE_CURVE_WITH_KNOTS ( 'NONE', 3,
 ( #9040, #32054, #72410, #66752, #38092, #10160, #67871, #16163, #27877, #45234, #44123, #56938, #10531, #22581, #21834, #11279 ),
 .UNSPECIFIED., .F., .F.,
 ( 4, 2, 2, 2, 2, 2, 2, 4 ),
 ( 0.01407846805636929662, 0.01466459907091517689, 0.01525073008546105717, 0.01583686110000693745, 0.01642299211455281946, 0.01700912312909869800, 0.01759525414364458001, 0.01876751617273634404 ),
 .UNSPECIFIED. ) ;
#67221 = CARTESIAN_POINT ( 'NONE',  ( -7.188101187499990274, -2.977408999572651815, 3.455302781871751883 ) ) ;
#67222 = CARTESIAN_POINT ( 'NONE',  ( 11.35316468750000141, 206.0937499965860411, 0.000000000000000000 ) ) ;
#67223 = DIRECTION ( 'NONE',  ( -1.000000000000000000, 0.000000000000000000, 0.000000000000000000 ) ) ;
#67224 = CARTESIAN_POINT ( 'NONE',  ( 4.541265875000002339, 6.312499998634407028, 0.000000000000000000 ) ) ;
#67225 = CARTESIAN_POINT ( 'NONE',  ( -29.65685424949230864, 198.0624999999999432, 166.0000000000003411 ) ) ;
#67227 = CARTESIAN_POINT ( 'NONE',  ( 3.313708498984760276, 102.2187500040967905, -8.000000000000000000 ) ) ;
#67226 = FACE_OUTER_BOUND ( 'NONE', #8638, .T. ) ;
#67228 = EDGE_LOOP ( 'NONE', ( #22153, #42055, #23900, #14517, #44826, #49779, #22403, #43946 ) ) ;
#67229 = CARTESIAN_POINT ( 'NONE',  ( -3.458734125000015425, 206.2500000013656063, 143.4326545832176976 ) ) ;
#67230 = CARTESIAN_POINT ( 'NONE',  ( -8.311093377946841443, 13.90624999658601801, 8.311093377946830785 ) ) ;
#67231 = CARTESIAN_POINT ( 'NONE',  ( 7.778174593052023411, -7.778174593052021635, 99.25000000409679046 ) ) ;
#67232 = CARTESIAN_POINT ( 'NONE',  ( 7.778174593052023411, -7.778174593052021635, 106.7500000040967763 ) ) ;
#67233 = CARTESIAN_POINT ( 'NONE',  ( -24.54126587499996148, 200.1250000013656063, 171.4326545832179534 ) ) ;
#67234 = CARTESIAN_POINT ( 'NONE',  ( 7.347880794884121708E-16, 300.0000000000000000, -6.000000000000001776 ) ) ;
#67236 = CARTESIAN_POINT ( 'NONE',  ( -3.042071309553163960, 7.239583329919349275, -11.35316468749999963 ) ) ;
#67235 = CARTESIAN_POINT ( 'NONE',  ( -5.082755093536324154, 119.8437500020483810, 5.082755093536326818 ) ) ;
#67238 = EDGE_CURVE ( 'NONE', #56169, #9713, #72590, .T. ) ;
#67237 = CARTESIAN_POINT ( 'NONE',  ( 5.656854249492374365, 5.656854249492375253, 25.76780277982336997 ) ) ;
#67239 = CARTESIAN_POINT ( 'NONE',  ( 9.832129032723420536, 116.1979166632526841, -5.676582343749999815 ) ) ;
#67240 = CARTESIAN_POINT ( 'NONE',  ( 7.320508075688771044, 86.24999999317205379, 7.320508075688775484 ) ) ;
#67241 = CARTESIAN_POINT ( 'NONE',  ( -2.977408999572651815, 121.8125000020483810, 7.188101187500000933 ) ) ;
#67242 = CARTESIAN_POINT ( 'NONE',  ( -3.211159895383561391, 21.81249999863440792, -3.211159895383561835 ) ) ;
#67243 = DIRECTION ( 'NONE',  ( 0.000000000000000000, 0.000000000000000000, 1.000000000000000000 ) ) ;
#67244 = CARTESIAN_POINT ( 'NONE',  ( 2.679491924318150975, 146.0416666666660603, -9.999999999996013855 ) ) ;
#67245 = ORIENTED_EDGE ( 'NONE', *, *, #42848, .T. ) ;
#67246 = CARTESIAN_POINT ( 'NONE',  ( 7.683012701892216079, 0.1830127018922207416, 0.000000000000000000 ) ) ;
#67247 =( BOUNDED_CURVE ( )  B_SPLINE_CURVE ( 2, ( #16298, #44999, #63084, #39338, #39703, #62335, #74404, #34445, #67640, #22712, #5752, #56700, #57444 ),
 .UNSPECIFIED., .F., .F. ) 
 B_SPLINE_CURVE_WITH_KNOTS ( ( 3, 2, 2, 2, 2, 2, 3 ),
 ( 1.428688857047360816, 1.433922811121159269, 1.439156765194957721, 1.444390719268755952, 1.449624673342554404, 1.454858627416352856, 1.460092581490151309 ),
 .UNSPECIFIED. ) 
 CURVE ( )  GEOMETRIC_REPRESENTATION_ITEM ( )  RATIONAL_B_SPLINE_CURVE ( ( 0.9999999999999998890, 0.9659258262890682012, 0.9999999999999998890, 0.9659258262890682012, 0.9999999999999998890, 0.9659258262890682012, 0.9999999999999998890, 0.9659258262890682012, 0.9999999999999998890, 0.9659258262890682012, 0.9999999999999998890, 0.9659258262891224911, 0.9999999999999455991 ) ) 
 REPRESENTATION_ITEM ( '' )  );
#67248 = EDGE_CURVE ( 'NONE', #26128, #29891, #32995, .T. ) ;
#67249 = CARTESIAN_POINT ( 'NONE',  ( -2.765530957081996810, 289.4218750017069510, -6.676582343750003368 ) ) ;
#67250 = SURFACE_STYLE_USAGE ( .BOTH. , #66112 ) ;
#67251 = CARTESIAN_POINT ( 'NONE',  ( -7.999999999999991118, 0.000000000000000000, 2.517802783920143561 ) ) ;
#67252 = CARTESIAN_POINT ( 'NONE',  ( -7.000000000000000000, 8.572527594031473190E-16, -14.80000000000000071 ) ) ;
#67253 = CARTESIAN_POINT ( 'NONE',  ( -10.00000000000000355, 204.5833333265053966, 2.679491924311223183 ) ) ;
#67254 = CARTESIAN_POINT ( 'NONE',  ( 9.832129032723420536, 255.9895833367473301, 5.676582343749996262 ) ) ;
#67255 = CARTESIAN_POINT ( 'NONE',  ( 10.18810118749999916, 4.220049686691935698, 103.3750000020484094 ) ) ;
#67256 = ORIENTED_EDGE ( 'NONE', *, *, #74038, .T. ) ;
#67257 = CARTESIAN_POINT ( 'NONE',  ( 8.000000000000000000, 22.40624999590322375, -3.313708498984761164 ) ) ;
#67258 = CARTESIAN_POINT ( 'NONE',  ( 8.311093377946834337, 150.4687499965860127, 8.311093377946839666 ) ) ;
#67259 = DIRECTION ( 'NONE',  ( -0.000000000000000000, 1.000000000000000000, 0.000000000000000000 ) ) ;
#67260 = CARTESIAN_POINT ( 'NONE',  ( 3.458734125000015869, 204.1875000013656063, 198.0000000000000284 ) ) ;
#67261 = CARTESIAN_POINT ( 'NONE',  ( 2.341876692568689577E-14, 191.0000000000000284, 198.0000000000000284 ) ) ;
#67262 = CARTESIAN_POINT ( 'NONE',  ( 3.042071309553159519, 70.05208332991934128, 11.35316468750000141 ) ) ;
#67263 = ORIENTED_EDGE ( 'NONE', *, *, #60484, .F. ) ;
#67264 = CARTESIAN_POINT ( 'NONE',  ( 10.18810118750000093, -4.220049686691933921, 116.3125000020483668 ) ) ;
#67265 = CARTESIAN_POINT ( 'NONE',  ( 4.541265875000002339, 7.437499998634407028, 0.000000000000000000 ) ) ;
#67266 = ORIENTED_EDGE ( 'NONE', *, *, #26151, .F. ) ;
#67267 = CARTESIAN_POINT ( 'NONE',  ( 5.082755093536324154, 22.78124999795161187, 5.082755093536326818 ) ) ;
#67268 = CARTESIAN_POINT ( 'NONE',  ( 6.000000000000001776, 287.5625000034140157, -7.347880794884121708E-16 ) ) ;
#67269 = VECTOR ( 'NONE', #749, 1000.000000000000000 ) ;
#67270 = CARTESIAN_POINT ( 'NONE',  ( 0.000000000000000000, -2.500000000000000444, 0.000000000000000000 ) ) ;
#67271 = CARTESIAN_POINT ( 'NONE',  ( 7.188101187499999156, 15.74999999795161543, 2.977408999572654924 ) ) ;
#67272 = SPHERICAL_SURFACE ( 'NONE', #70075, 20.00000000000000355 ) ;
#67273 = VECTOR ( 'NONE', #32637, 1000.000000000000000 ) ;
#67274 = CARTESIAN_POINT ( 'NONE',  ( 1.871523826299183495E-15, -10.18810118749999916, 111.9062500020483810 ) ) ;
#67275 = LINE ( 'NONE', #9928, #11314 ) ;
#67276 = CARTESIAN_POINT ( 'NONE',  ( -2.828427124746192067, 4.374999997268814056, 2.828427124746190735 ) ) ;
#67277 = ORIENTED_EDGE ( 'NONE', *, *, #66875, .T. ) ;
#67278 = CARTESIAN_POINT ( 'NONE',  ( -2.445694354108783664, 207.3125000013656063, 195.5543056458912190 ) ) ;
#67279 = CARTESIAN_POINT ( 'NONE',  ( -31.99999999999995737, 195.4375000027312410, 171.6568542494928522 ) ) ;
#67280 = CARTESIAN_POINT ( 'NONE',  ( 4.220049686691941027, -10.18810118749999738, 71.50000000204839523 ) ) ;
#67281 = CARTESIAN_POINT ( 'NONE',  ( 3.211159895383561835, 4.437499998634407028, -3.211159895383561835 ) ) ;
#67282 = CARTESIAN_POINT ( 'NONE',  ( -7.188101187499990274, -2.977408999572651371, 22.58030278187175099 ) ) ;
#67283 = VERTEX_POINT ( 'NONE', #60891 ) ;
#67284 = CARTESIAN_POINT ( 'NONE',  ( -4.000000000000001776, 21.43750000000000000, -1.656854249492381470 ) ) ;
#67285 = ORIENTED_EDGE ( 'NONE', *, *, #43343, .T. ) ;
#67286 = CARTESIAN_POINT ( 'NONE',  ( -4.220049686691937474, -10.18810118749999738, 114.4375000020483668 ) ) ;
#67287 = CARTESIAN_POINT ( 'NONE',  ( 27.99999999999996803, 208.6250000027312126, 165.9999999999998863 ) ) ;
#67288 = CARTESIAN_POINT ( 'NONE',  ( 2.754378923186476579E-14, 204.1875000013656063, 194.5412658750000219 ) ) ;
#67289 = CARTESIAN_POINT ( 'NONE',  ( 29.43265458321761230, 198.8750000013656063, 166.5412658749999650 ) ) ;
#67290 = CARTESIAN_POINT ( 'NONE',  ( 10.00000000000000178, 70.00000000000000000, 0.000000000000000000 ) ) ;
#67291 = CARTESIAN_POINT ( 'NONE',  ( -2.977408999572650927, 92.75000000204839523, -7.188101187500001821 ) ) ;
#67292 = CARTESIAN_POINT ( 'NONE',  ( 2.485281374238575314, 293.3124999999999432, 6.000000000000000888 ) ) ;
#67293 = CARTESIAN_POINT ( 'NONE',  ( 27.99999999999996447, 204.6250000027312126, 165.9999999999998863 ) ) ;
#67294 = ORIENTED_EDGE ( 'NONE', *, *, #2306, .T. ) ;
#67295 = EDGE_CURVE ( 'NONE', #57335, #2283, #4681, .T. ) ;
#67296 = EDGE_CURVE ( 'NONE', #413, #512, #55995, .T. ) ;
#67297 = CARTESIAN_POINT ( 'NONE',  ( 11.35316468749999963, 221.4062500034139873, -1.390361679473963556E-15 ) ) ;
#67298 = AXIS2_PLACEMENT_3D ( 'NONE', #36414, #71094, #2447 ) ;
#67299 = CARTESIAN_POINT ( 'NONE',  ( -3.223881452093011024, -10.27322224982958865, 63.89771963198323590 ) ) ;
#67300 = CARTESIAN_POINT ( 'NONE',  ( 2.828427124746152987, 197.2500000027312126, 139.1715728752538723 ) ) ;
#67301 = CARTESIAN_POINT ( 'NONE',  ( -5.656854249492375253, 5.656854249492375253, 24.83030278392014978 ) ) ;
#67302 = CARTESIAN_POINT ( 'NONE',  ( -8.660254037844387298, 254.5833333333333144, -4.999999999999999112 ) ) ;
#67303 = CARTESIAN_POINT ( 'NONE',  ( 27.99999999999996447, 203.6250000027312126, 165.9999999999998863 ) ) ;
#67304 = CARTESIAN_POINT ( 'NONE',  ( 2.679491924311222739, 188.9583333333332860, 10.00000000000000355 ) ) ;
#67305 = B_SPLINE_CURVE_WITH_KNOTS ( 'NONE', 3,
 ( #47755, #59832, #53068, #54552 ),
 .UNSPECIFIED., .F., .F.,
 ( 4, 4 ),
 ( 0.000000000000000000, 0.004469278299739564905 ),
 .UNSPECIFIED. ) ;
#67306 = CARTESIAN_POINT ( 'NONE',  ( 28.00000000000002132, 198.1250000027312126, 173.9999999999999147 ) ) ;
#67307 = CARTESIAN_POINT ( 'NONE',  ( 5.082755093536320601, -5.082755093536318824, 21.92405278187175455 ) ) ;
#67308 = CARTESIAN_POINT ( 'NONE',  ( -5.676582343750006032, 149.4270833299193555, 9.832129032723418760 ) ) ;
#67309 = CARTESIAN_POINT ( 'NONE',  ( -11.00000000000000000, 0.000000000000000000, 118.0000000000000000 ) ) ;
#67310 = CARTESIAN_POINT ( 'NONE',  ( -31.34787492957842758, 44.82699704696460685, 64.99999999999998579 ) ) ;
#67311 = CARTESIAN_POINT ( 'NONE',  ( 27.99999999999996447, 197.6250000027312126, 165.9999999999998863 ) ) ;
#67313 = CARTESIAN_POINT ( 'NONE',  ( 5.656854249492381470, 109.2500000040967763, 5.656854249492379694 ) ) ;
#67312 = DIRECTION ( 'NONE',  ( -0.000000000000000000, 1.000000000000000000, -0.000000000000000000 ) ) ;
#67314 = ORIENTED_EDGE ( 'NONE', *, *, #57718, .T. ) ;
#67315 = CIRCLE ( 'NONE', #72079, 71.70204102886728492 ) ;
#67316 = CARTESIAN_POINT ( 'NONE',  ( 5.676582343750001591, 26.92708332991935194, -9.832129032723420536 ) ) ;
#67317 = CARTESIAN_POINT ( 'NONE',  ( 10.99999999999989342, 4.556349186104152515, 77.03125000409679046 ) ) ;
#67319 = CARTESIAN_POINT ( 'NONE',  ( 26.34314575050748886, 199.9375000000000284, 173.9999999999997726 ) ) ;
#67318 = DIRECTION ( 'NONE',  ( -0.000000000000000000, 1.000000000000000000, -0.000000000000000000 ) ) ;
#67320 = CARTESIAN_POINT ( 'NONE',  ( 2.020667218593132706E-15, -11.00000000000000000, 79.37499999999998579 ) ) ;
#67321 = CARTESIAN_POINT ( 'NONE',  ( -2.754378923186476579E-14, 201.1875000013656063, 145.4587341250000350 ) ) ;
#67322 = CARTESIAN_POINT ( 'NONE',  ( -10.00000000000000355, 49.58333332650536107, 2.679491924311223183 ) ) ;
#67323 = CARTESIAN_POINT ( 'NONE',  ( 5.082755093536326818, 105.2187500020483952, 5.082755093536325042 ) ) ;
#67324 = CARTESIAN_POINT ( 'NONE',  ( -1.881053915767121554, 7.749999998634407916, -4.541265875000002339 ) ) ;
#67325 = CARTESIAN_POINT ( 'NONE',  ( -28.00000000000007461, 196.1250000027311842, 166.0000000000003695 ) ) ;
#67326 = CARTESIAN_POINT ( 'NONE',  ( 5.656854249492376141, -5.656854249492374365, 11.89280277982336642 ) ) ;
#67327 = CARTESIAN_POINT ( 'NONE',  ( 4.999999999999993783, 164.1666666666666856, 8.660254037844390851 ) ) ;
#67328 = EDGE_LOOP ( 'NONE', ( #36047, #44314, #23766, #3140, #47768 ) ) ;
#67329 = VERTEX_POINT ( 'NONE', #50682 ) ;
#67330 = CARTESIAN_POINT ( 'NONE',  ( -5.000000000000000000, -60.90295814858257017, 23.31388853594792820 ) ) ;
#67331 = CARTESIAN_POINT ( 'NONE',  ( 7.999999999999304556, -3.314968910423997278E-06, 15.26780269013280034 ) ) ;
#67332 = CYLINDRICAL_SURFACE ( 'NONE', #6202, 4.000000000000001776 ) ;
#67333 = CARTESIAN_POINT ( 'NONE',  ( -7.999999999999998224, 99.59375000000000000, 3.313708498984766049 ) ) ;
#67334 = CARTESIAN_POINT ( 'NONE',  ( -8.311093377946836114, 142.6562499965860127, -8.311093377946837890 ) ) ;
#67335 = ORIENTED_EDGE ( 'NONE', *, *, #69283, .T. ) ;
#67336 = CARTESIAN_POINT ( 'NONE',  ( -7.999999999999991118, 0.000000000000000000, 10.01780278392014623 ) ) ;
#67337 = CARTESIAN_POINT ( 'NONE',  ( 4.220049686691941027, -10.18810118749999738, 92.12500000204836681 ) ) ;
#67338 = CARTESIAN_POINT ( 'NONE',  ( 7.594050593750000466, 27.23437499897580949, 0.000000000000000000 ) ) ;
#67339 = CARTESIAN_POINT ( 'NONE',  ( 2.849036369511732440E-14, 207.2500000000000284, 202.0000000000000000 ) ) ;
#67341 = CARTESIAN_POINT ( 'NONE',  ( -8.311093377946836114, 127.6562499965860411, -8.311093377946837890 ) ) ;
#67340 = CARTESIAN_POINT ( 'NONE',  ( -6.123233995736766282E-16, 248.7500000000000284, -10.00000000000000000 ) ) ;
#67342 = CARTESIAN_POINT ( 'NONE',  ( 0.000000000000000000, 125.0000000000000000, 0.000000000000000000 ) ) ;
#67343 = ORIENTED_EDGE ( 'NONE', *, *, #41486, .T. ) ;
#67344 = CARTESIAN_POINT ( 'NONE',  ( 47.86415381379096345, 40.17786467547738738, 63.07999174420051958 ) ) ;
#67345 = CARTESIAN_POINT ( 'NONE',  ( -11.35316468749999785, 113.3854166632526983, -3.042071309553167957 ) ) ;
#67346 = CARTESIAN_POINT ( 'NONE',  ( 2.445694354108839619, 203.8125000013656063, 200.4456943541088663 ) ) ;
#67347 = CARTESIAN_POINT ( 'NONE',  ( -7.188101187500002709, 18.18749999795161187, 2.977408999572649151 ) ) ;
#67348 = CARTESIAN_POINT ( 'NONE',  ( -10.18810118749999738, -4.220049686691941915, 84.62500000204836681 ) ) ;
#67349 = CARTESIAN_POINT ( 'NONE',  ( 9.832129032723420536, 16.51041666325268054, -5.676582343749999815 ) ) ;
#67350 = ORIENTED_EDGE ( 'NONE', *, *, #28295, .F. ) ;
#67351 = DIRECTION ( 'NONE',  ( 0.000000000000000000, 0.000000000000000000, -1.000000000000000000 ) ) ;
#67352 = CARTESIAN_POINT ( 'NONE',  ( 1.471067592899761672E-15, -8.008118988124991233, 17.88811528394063188 ) ) ;
#67353 = CARTESIAN_POINT ( 'NONE',  ( -7.999999999999991118, 0.000000000000000000, 23.51780278392014978 ) ) ;
#67354 = CARTESIAN_POINT ( 'NONE',  ( -2.775557561562891351E-14, 210.0000000000000284, 146.0000000000000284 ) ) ;
#67355 = CARTESIAN_POINT ( 'NONE',  ( -5.082755093536326818, 4.406249997951610986, 5.082755093536325042 ) ) ;
#67356 = CARTESIAN_POINT ( 'NONE',  ( -2.765530957081996810, 288.2656250017069510, -6.676582343750003368 ) ) ;
#67357 = LINE ( 'NONE', #66981, #26889 ) ;
#67358 = DIRECTION ( 'NONE',  ( -0.000000000000000000, 1.000000000000000000, -0.000000000000000000 ) ) ;
#67359 = EDGE_LOOP ( 'NONE', ( #52233, #17883, #54169, #21494 ) ) ;
#67360 =( BOUNDED_CURVE ( )  B_SPLINE_CURVE ( 2, ( #65293, #47567, #70234, #18542, #6490, #843, #25291, #24190, #12864, #1209, #2294, #47202, #13598 ),
 .UNSPECIFIED., .F., .F. ) 
 B_SPLINE_CURVE_WITH_KNOTS ( ( 3, 2, 2, 2, 2, 2, 3 ),
 ( 0.8750000000000000000, 0.8768115942028985588, 0.8786231884057971175, 0.8804347826086955653, 0.8822463768115941241, 0.8840579710144926828, 0.8858695652173912416 ),
 .UNSPECIFIED. ) 
 CURVE ( )  GEOMETRIC_REPRESENTATION_ITEM ( )  RATIONAL_B_SPLINE_CURVE ( ( 1.000000000000000000, 0.9659258262890683122, 1.000000000000000000, 0.9659258262890683122, 1.000000000000000000, 0.9659258262890683122, 1.000000000000000000, 0.9659258262890683122, 1.000000000000000000, 0.9659258262890683122, 1.000000000000000000, 0.9659258262890704216, 0.9999999999999978906 ) ) 
 REPRESENTATION_ITEM ( '' )  );
#67361 = CARTESIAN_POINT ( 'NONE',  ( -11.35316468749999785, 138.3854166632526983, -3.042071309553167513 ) ) ;
#67362 = CARTESIAN_POINT ( 'NONE',  ( 7.204075437095968759, -7.204075437095966983, 75.71875000204836681 ) ) ;
#67363 = AXIS2_PLACEMENT_3D ( 'NONE', #61070, #50124, #33543 ) ;
#67364 = CARTESIAN_POINT ( 'NONE',  ( -31.45873412499998523, 209.0000000013655779, 171.4326545832180386 ) ) ;
#67365 = CARTESIAN_POINT ( 'NONE',  ( 5.656854249492378806, 26.81250000000000355, 5.656854249492381470 ) ) ;
#67366 = CARTESIAN_POINT ( 'NONE',  ( 1.881053915767121776, 16.62499999863440436, -4.541265875000002339 ) ) ;
#67367 = ORIENTED_EDGE ( 'NONE', *, *, #17919, .T. ) ;
#67368 = VECTOR ( 'NONE', #18080, 1000.000000000000000 ) ;
#67369 = CARTESIAN_POINT ( 'NONE',  ( -1.656854249492348607, 202.3125000027312410, 202.0000000000000284 ) ) ;
#67370 = CARTESIAN_POINT ( 'NONE',  ( 1.432654583217607414, 196.5000000013656063, 145.4587341250000634 ) ) ;
#67371 = CARTESIAN_POINT ( 'NONE',  ( -31.99999999999996447, 204.4375000027311842, 171.6568542494928522 ) ) ;
#67372 = EDGE_CURVE ( 'NONE', #53065, #72148, #62010, .T. ) ;
#67373 = CARTESIAN_POINT ( 'NONE',  ( 5.656854249492374365, 5.656854249492375253, 13.76780277982336465 ) ) ;
#67374 = EDGE_LOOP ( 'NONE', ( #40446, #25697, #66983, #9972 ) ) ;
#67375 = CARTESIAN_POINT ( 'NONE',  ( -5.082755093536326818, 11.90624999795161010, 5.082755093536325042 ) ) ;
#67376 = CARTESIAN_POINT ( 'NONE',  ( -26.28308827913208034, -12.55725497174413086, 186.4625068604729563 ) ) ;
#67377 = CARTESIAN_POINT ( 'NONE',  ( 5.000000000000000000, 53.53174224766643619, -46.57871628774325501 ) ) ;
#67378 = CARTESIAN_POINT ( 'NONE',  ( 11.35316468749999785, 185.5729166632526983, 3.042071309553174174 ) ) ;
#67379 = CARTESIAN_POINT ( 'NONE',  ( -5.082755093536325930, 110.8437500020483810, -5.082755093536325930 ) ) ;
#67380 = CARTESIAN_POINT ( 'NONE',  ( 1.469576158976822172E-15, -7.999999999999991118, 2.705302779823365533 ) ) ;
#67381 = CYLINDRICAL_SURFACE ( 'NONE', #65901, 10.00000000000000178 ) ;
#67382 = ORIENTED_EDGE ( 'NONE', *, *, #23812, .T. ) ;
#67383 = CARTESIAN_POINT ( 'NONE',  ( -8.311093377946836114, 263.2812500034139020, -8.311093377946836114 ) ) ;
#67384 = PRODUCT_DEFINITION_SHAPE ( 'NONE', 'NONE',  #74653 ) ;
#67385 = CARTESIAN_POINT ( 'NONE',  ( -2.977408999572648707, -7.188101187499990274, 24.64280278187176165 ) ) ;
#67386 = CARTESIAN_POINT ( 'NONE',  ( -2.828427124746192067, 2.374999997268813612, 2.828427124746190735 ) ) ;
#67387 = CARTESIAN_POINT ( 'NONE',  ( 0.000000000000000000, 210.0000000000000284, 170.0000000000000284 ) ) ;
#67388 = CARTESIAN_POINT ( 'NONE',  ( 6.891449706534898745, -61.56004288261173230, -23.71475313281752051 ) ) ;
#67389 = CARTESIAN_POINT ( 'NONE',  ( 3.458734125000015425, 195.2500000013656063, 196.5673454167823877 ) ) ;
#67390 = CARTESIAN_POINT ( 'NONE',  ( -8.660254037844390851, 142.9166666666666572, 4.999999999999998224 ) ) ;
#67391 = CARTESIAN_POINT ( 'NONE',  ( 0.000000000000000000, 0.000000000000000000, 0.000000000000000000 ) ) ;
#67392 = CYLINDRICAL_SURFACE ( 'NONE', #34329, 7.999999999999991118 ) ;
#67393 = CARTESIAN_POINT ( 'NONE',  ( 8.000000000000001776, 91.15624999999998579, 3.313708498984759387 ) ) ;
#67394 = CARTESIAN_POINT ( 'NONE',  ( -11.35316468749999785, 118.3854166632526557, -3.042071309553167513 ) ) ;
#67395 = CARTESIAN_POINT ( 'NONE',  ( -5.000000000000001776, -10.28276986844632290, -65.17752827135417704 ) ) ;
#67396 = CARTESIAN_POINT ( 'NONE',  ( 2.020667218593132706E-15, -11.00000000000000000, 71.87500000000000000 ) ) ;
#67399 = CARTESIAN_POINT ( 'NONE',  ( 1.224646799147353256E-15, 0.000000000000000000, 10.00000000000000000 ) ) ;
#67398 = CARTESIAN_POINT ( 'NONE',  ( 26.56734541678232731, 199.0000000013656063, 166.5412658749999650 ) ) ;
#67397 = CARTESIAN_POINT ( 'NONE',  ( 25.55430564589115150, 200.5625000013656063, 172.4456943541086957 ) ) ;
#67400 = ORIENTED_EDGE ( 'NONE', *, *, #35813, .T. ) ;
#67401 = EDGE_CURVE ( 'NONE', #49815, #52317, #16339, .T. ) ;
#67402 = EDGE_CURVE ( 'NONE', #40814, #36538, #73701, .T. ) ;
#67403 = CARTESIAN_POINT ( 'NONE',  ( 7.999999999999991118, 1.469576158976822369E-15, 25.76780278392172008 ) ) ;
#67404 = CARTESIAN_POINT ( 'NONE',  ( 6.000000000000001776, 287.5625000034140157, -7.347880794884121708E-16 ) ) ;
#67405 = EDGE_CURVE ( 'NONE', #6758, #27289, #34369, .T. ) ;
#67406 = CARTESIAN_POINT ( 'NONE',  ( 31.45873412499999944, 199.0000000013656063, 168.5673454167822740 ) ) ;
#67407 = VECTOR ( 'NONE', #5761, 1000.000000000000000 ) ;
#67408 = CARTESIAN_POINT ( 'NONE',  ( 11.35316468750000141, 206.0937499965860411, 0.000000000000000000 ) ) ;
#67409 = FACE_OUTER_BOUND ( 'NONE', #50121, .T. ) ;
#67410 = CARTESIAN_POINT ( 'NONE',  ( 0.000000000000000000, 300.0000000000000000, 0.000000000000000000 ) ) ;
#67411 = CARTESIAN_POINT ( 'NONE',  ( 4.541265875000002339, 16.37499999863440436, -1.881053915767121554 ) ) ;
#67412 = CARTESIAN_POINT ( 'NONE',  ( 26.56734541678232731, 196.6250000013656063, 173.4587341249998929 ) ) ;
#67413 = CARTESIAN_POINT ( 'NONE',  ( -3.313708498984757167, 7.999999999999991118, 26.04905277982336997 ) ) ;
#67414 = PLANE ( 'NONE',  #70079 ) ;
#67415 = CARTESIAN_POINT ( 'NONE',  ( 5.676582343750001591, 101.6145833299193697, -9.832129032723420536 ) ) ;
#67416 = ORIENTED_EDGE ( 'NONE', *, *, #61338, .F. ) ;
#67417 = CARTESIAN_POINT ( 'NONE',  ( -4.556349186104045934, 11.00000000000000000, 81.71874999999998579 ) ) ;
#67418 = CARTESIAN_POINT ( 'NONE',  ( -5.082755093536325042, 22.03124999795161543, -5.082755093536325930 ) ) ;
#67419 = DIRECTION ( 'NONE',  ( -1.000000000000000000, -0.000000000000000000, -0.000000000000000000 ) ) ;
#67420 = CARTESIAN_POINT ( 'NONE',  ( 3.042071309553163516, 257.7604166700806445, -11.35316468749999785 ) ) ;
#67421 = CARTESIAN_POINT ( 'NONE',  ( -8.311093377946836114, 92.65624999658602690, -8.311093377946837890 ) ) ;
#67422 = ORIENTED_EDGE ( 'NONE', *, *, #53292, .T. ) ;
#67423 = CARTESIAN_POINT ( 'NONE',  ( 7.320508075688771044, 206.2499999931720254, 7.320508075688775484 ) ) ;
#67424 = VECTOR ( 'NONE', #61556, 1000.000000000000000 ) ;
#67425 = CARTESIAN_POINT ( 'NONE',  ( -7.204075437095965206, -7.204075437095968759, 109.8437500020483810 ) ) ;
#67426 = CARTESIAN_POINT ( 'NONE',  ( -24.54126587499999701, 195.5000000013655779, 168.5673454167827003 ) ) ;
#67427 = CARTESIAN_POINT ( 'NONE',  ( 1.432654583217664701, 203.0000000013655779, 201.4587341250000065 ) ) ;
#67428 = CARTESIAN_POINT ( 'NONE',  ( -15.99999999999999645, -16.00000000000000355, 20.00000000000000000 ) ) ;
#67429 = MANIFOLD_SOLID_BREP ( 'Cut-Extrude1', #70740 ) ;
#67431 = CARTESIAN_POINT ( 'NONE',  ( 9.832129032723420536, 91.19791666325269830, -5.676582343749999815 ) ) ;
#67430 = LINE ( 'NONE', #37270, #9933 ) ;
#67432 = EDGE_CURVE ( 'NONE', #4200, #25259, #31348, .T. ) ;
#67433 = CARTESIAN_POINT ( 'NONE',  ( -5.656854249492375253, 5.656854249492375253, 12.83030278392014623 ) ) ;
#67434 = CARTESIAN_POINT ( 'NONE',  ( -25.55430564589119413, 199.5625000013656063, 167.5543056458915316 ) ) ;
#67435 = DIRECTION ( 'NONE',  ( 1.000000000000000000, 0.000000000000000000, 0.000000000000000000 ) ) ;
#67436 = CARTESIAN_POINT ( 'NONE',  ( -4.999999999999998224, 183.5416666598387110, -8.660254037844389075 ) ) ;
#67437 = CYLINDRICAL_SURFACE ( 'NONE', #56969, 8.000000000000000000 ) ;
#67438 = CARTESIAN_POINT ( 'NONE',  ( -8.311093377946841443, 79.21874999658601268, 8.311093377946834337 ) ) ;
#67439 = CARTESIAN_POINT ( 'NONE',  ( 2.765530957082001251, 292.7656250017069510, 6.676582343750000703 ) ) ;
#67440 = CARTESIAN_POINT ( 'NONE',  ( -10.18810118749999738, -4.220049686691941915, 102.6250000020483810 ) ) ;
#67441 = CARTESIAN_POINT ( 'NONE',  ( -8.311093377946841443, 213.9062499965860411, 8.311093377946830785 ) ) ;
#67442 = VERTEX_POINT ( 'NONE', #27299 ) ;
#67443 = CARTESIAN_POINT ( 'NONE',  ( -1.656854249492383468, 2.687500000000000444, 4.000000000000000888 ) ) ;
#67444 = LINE ( 'NONE', #68187, #47290 ) ;
#67445 = CARTESIAN_POINT ( 'NONE',  ( -1.736494649845418126, -16.42394793108440254, 68.69316892220884085 ) ) ;
#67447 = CARTESIAN_POINT ( 'NONE',  ( 8.311093377946837890, 211.4062499965860127, -8.311093377946837890 ) ) ;
#67446 = CARTESIAN_POINT ( 'NONE',  ( 6.938893903907228378E-15, 10.39230484541326938, 0.000000000000000000 ) ) ;
#67448 = CARTESIAN_POINT ( 'NONE',  ( -4.999999999999992895, 228.9583333401612890, 8.660254037844390851 ) ) ;
#67449 = CYLINDRICAL_SURFACE ( 'NONE', #56508, 10.00000000000000178 ) ;
#67450 = VERTEX_POINT ( 'NONE', #43406 ) ;
#67451 = CARTESIAN_POINT ( 'NONE',  ( 9.832129032723416984, 190.6770833299193555, 5.676582343750006032 ) ) ;
#67452 = CARTESIAN_POINT ( 'NONE',  ( -2.977408999572647819, 7.188101187499992051, 14.70530278187175455 ) ) ;
#67453 =( BOUNDED_CURVE ( )  B_SPLINE_CURVE ( 2, ( #37618, #65898, #42518, #55349, #48912, #26653, #71926, #59513, #13464 ),
 .UNSPECIFIED., .F., .F. ) 
 B_SPLINE_CURVE_WITH_KNOTS ( ( 3, 2, 2, 2, 3 ),
 ( 0.6770833333333334814, 0.6822916666666667407, 0.6875000000000001110, 0.6927083333333334814, 0.6979166666666667407 ),
 .UNSPECIFIED. ) 
 CURVE ( )  GEOMETRIC_REPRESENTATION_ITEM ( )  RATIONAL_B_SPLINE_CURVE ( ( 0.9999999999999983347, 0.9238795325112884038, 1.000000000000000000, 0.9238795325112867385, 1.000000000000000000, 0.9238795325112867385, 1.000000000000000000, 0.9238795325112850731, 1.000000000000001554 ) ) 
 REPRESENTATION_ITEM ( '' )  );
#67454 = CARTESIAN_POINT ( 'NONE',  ( -24.54126587499999701, 208.1875000013656063, 170.0000000000003411 ) ) ;
#67455 = CARTESIAN_POINT ( 'NONE',  ( -5.656854249492381470, 12.93750000000000355, 5.656854249492379694 ) ) ;
#67456 = VERTEX_POINT ( 'NONE', #36648 ) ;
#67457 = CARTESIAN_POINT ( 'NONE',  ( 8.000000000000000000, 91.43750000409679046, -9.797174393178825657E-16 ) ) ;
#67458 = CARTESIAN_POINT ( 'NONE',  ( -7.320508075688778149, 8.125000000000000000, 7.320508075688769267 ) ) ;
#67459 = VECTOR ( 'NONE', #23869, 1000.000000000000000 ) ;
#67460 = CARTESIAN_POINT ( 'NONE',  ( -7.204075437095965206, -7.204075437095968759, 78.71875000204836681 ) ) ;
#67461 = ORIENTED_EDGE ( 'NONE', *, *, #70877, .F. ) ;
#67462 = CARTESIAN_POINT ( 'NONE',  ( -7.347880794884122694E-16, 20.75000000000000000, 4.000000000000001776 ) ) ;
#67463 =( BOUNDED_CURVE ( )  B_SPLINE_CURVE ( 2, ( #32231, #43527, #66542, #14851, #37891, #60139, #42411, #2808, #60889 ),
 .UNSPECIFIED., .F., .F. ) 
 B_SPLINE_CURVE_WITH_KNOTS ( ( 3, 2, 2, 2, 3 ),
 ( 0.4270833333333332593, 0.4322916666666666297, 0.4374999999999998890, 0.4427083333333332038, 0.4479166666666665741 ),
 .UNSPECIFIED. ) 
 CURVE ( )  GEOMETRIC_REPRESENTATION_ITEM ( )  RATIONAL_B_SPLINE_CURVE ( ( 1.000000000000000888, 0.9238795325112859613, 1.000000000000000000, 0.9238795325112867385, 1.000000000000000000, 0.9238795325112867385, 1.000000000000000000, 0.9238795325112884038, 0.9999999999999983347 ) ) 
 REPRESENTATION_ITEM ( '' )  );
#67464 = CARTESIAN_POINT ( 'NONE',  ( 4.541265875000001451, 18.24999999863440792, 1.881053915767124440 ) ) ;
#67465 = DIRECTION ( 'NONE',  ( 0.8660254037844380415, 0.5000000000000009992, 0.000000000000000000 ) ) ;
#67466 = EDGE_CURVE ( 'NONE', #64048, #56610, #29011, .T. ) ;
#67467 = VECTOR ( 'NONE', #50702, 1000.000000000000000 ) ;
#67468 = ORIENTED_EDGE ( 'NONE', *, *, #9436, .T. ) ;
#67469 = CARTESIAN_POINT ( 'NONE',  ( -11.00000000000000533, 11.00000000000000000, 20.00000000000000000 ) ) ;
#67470 = CARTESIAN_POINT ( 'NONE',  ( 7.188101187500001821, 93.50000000204838102, -2.977408999572651371 ) ) ;
#67473 = CARTESIAN_POINT ( 'NONE',  ( 18.00000000000000000, 10.39230484541325161, -21.50000000000000000 ) ) ;
#67472 = CARTESIAN_POINT ( 'NONE',  ( -3.042071309553159075, 254.9479166700806445, 11.35316468749999963 ) ) ;
#67471 = LINE ( 'NONE', #61057, #56705 ) ;
#67474 = APPLICATION_PROTOCOL_DEFINITION ( 'draft international standard', 'automotive_design', 1998, #64107 ) ;
#67475 = ORIENTED_EDGE ( 'NONE', *, *, #70792, .T. ) ;
#67476 = CARTESIAN_POINT ( 'NONE',  ( 9.832129032723420536, 256.3020833367473301, 5.676582343749996262 ) ) ;
#67477 = CARTESIAN_POINT ( 'NONE',  ( -2.977408999572647819, 7.188101187499991163, 10.20530278187175455 ) ) ;
#67478 = ORIENTED_EDGE ( 'NONE', *, *, #7207, .T. ) ;
#67479 = ORIENTED_EDGE ( 'NONE', *, *, #31951, .F. ) ;
#67480 = CARTESIAN_POINT ( 'NONE',  ( 1.871523826299183495E-15, -10.18810118749999916, 72.53125000204838102 ) ) ;
#67481 = CARTESIAN_POINT ( 'NONE',  ( -9.832129032723418760, 78.17708332991935549, -5.676582343750004256 ) ) ;
#67482 = CARTESIAN_POINT ( 'NONE',  ( 0.000000000000000000, 300.0000000000000000, 0.000000000000000000 ) ) ;
#67483 = CARTESIAN_POINT ( 'NONE',  ( 11.00000000000000355, -4.556349186104045046, 87.15624999999998579 ) ) ;
#67486 = CARTESIAN_POINT ( 'NONE',  ( -4.721056650415998313, 291.7343750017069510, 4.721056650416000089 ) ) ;
#67485 = CARTESIAN_POINT ( 'NONE',  ( 31.99999999999999289, 195.3750000027311842, 169.9999999999998863 ) ) ;
#67484 = FACE_OUTER_BOUND ( 'NONE', #40156, .T. ) ;
#67487 = ADVANCED_FACE ( 'NONE', ( #32106 ), #13973, .T. ) ;
#67488 = CARTESIAN_POINT ( 'NONE',  ( -7.188101187499992051, 0.000000000000000000, 28.86155278187175810 ) ) ;
#67489 = CARTESIAN_POINT ( 'NONE',  ( 8.000000000000000000, 101.7500000000000000, -9.797174393178825657E-16 ) ) ;
#67490 = AXIS2_PLACEMENT_3D ( 'NONE', #1433, #71530, #36854 ) ;
#67491 = CARTESIAN_POINT ( 'NONE',  ( 1.432654583217662481, 198.3750000013656063, 194.5412658750000219 ) ) ;
#67492 = CARTESIAN_POINT ( 'NONE',  ( -8.000000000000000000, 6.468749995903221084, -3.313708498984762496 ) ) ;
#67493 = EDGE_LOOP ( 'NONE', ( #20341, #54001, #30773, #71182 ) ) ;
#67494 = CARTESIAN_POINT ( 'NONE',  ( 26.56734541678232375, 196.3750000013656063, 173.4587341249998929 ) ) ;
#67495 = CARTESIAN_POINT ( 'NONE',  ( -2.977408999572650039, 16.31249999795161543, -7.188101187500001821 ) ) ;
#67496 = CARTESIAN_POINT ( 'NONE',  ( 5.676582343750001591, 161.9270833299193555, -9.832129032723420536 ) ) ;
#67497 = CARTESIAN_POINT ( 'NONE',  ( 2.977408999572650039, 106.0625000020483668, -7.188101187500000933 ) ) ;
#67499 = CARTESIAN_POINT ( 'NONE',  ( -2.990854866095042475, -55.96051345248228159, -43.98806351443467832 ) ) ;
#67498 = CARTESIAN_POINT ( 'NONE',  ( -8.660254037844390851, 19.79166665983870033, 4.999999999999998224 ) ) ;
#67500 = CARTESIAN_POINT ( 'NONE',  ( 30.44569435410879166, 205.8125000013656063, 172.4456943541087526 ) ) ;
#67501 = CARTESIAN_POINT ( 'NONE',  ( 7.188101187499992051, 8.802885111219154394E-16, 16.11155278187175455 ) ) ;
#67502 = CARTESIAN_POINT ( 'NONE',  ( 1.656854249492348607, 206.3125000027312126, 138.0000000000000568 ) ) ;
#67503 = CARTESIAN_POINT ( 'NONE',  ( 8.311093377946834337, 60.15624999658601979, 8.311093377946839666 ) ) ;
#67504 = CARTESIAN_POINT ( 'NONE',  ( -5.656854249492373476, -5.656854249492376141, 1.205302783920146004 ) ) ;
#67505 = CARTESIAN_POINT ( 'NONE',  ( -4.999999999999998224, 28.54166665983870033, -8.660254037844389075 ) ) ;
#67506 = CARTESIAN_POINT ( 'NONE',  ( -7.778174593052020747, -7.778174593052023411, 71.68749999999998579 ) ) ;
#67507 = ORIENTED_EDGE ( 'NONE', *, *, #2392, .T. ) ;
#67508 = CARTESIAN_POINT ( 'NONE',  ( 0.000000000000000000, 0.000000000000000000, 0.000000000000000000 ) ) ;
#67509 = CARTESIAN_POINT ( 'NONE',  ( -7.320508075688778149, 169.9999999931720254, 7.320508075688769267 ) ) ;
#67510 = CARTESIAN_POINT ( 'NONE',  ( 11.35316468749999785, 50.57291666325268409, 3.042071309553174174 ) ) ;
#67511 = CARTESIAN_POINT ( 'NONE',  ( 11.00000000000000355, -4.556349186104045046, 73.84375000409676204 ) ) ;
#67512 = CARTESIAN_POINT ( 'NONE',  ( 1.432654583217607414, 198.5000000013656063, 145.4587341250000350 ) ) ;
#67513 = CARTESIAN_POINT ( 'NONE',  ( -2.828427124746209831, 196.5000000027312126, 139.1715728752538723 ) ) ;
#67515 = CARTESIAN_POINT ( 'NONE',  ( 3.042071309553167513, 46.82291666325268409, -11.35316468749999785 ) ) ;
#67514 = CARTESIAN_POINT ( 'NONE',  ( -5.082755093536324154, 101.8437500020483810, 5.082755093536326818 ) ) ;
#67516 = EDGE_CURVE ( 'NONE', #52559, #40096, #72463, .T. ) ;
#67517 = CARTESIAN_POINT ( 'NONE',  ( 7.999999999999991118, 9.797174393178815797E-16, 7.580302779823366421 ) ) ;
#67518 = CARTESIAN_POINT ( 'NONE',  ( -5.676582343749998039, 177.4479166632526983, -9.832129032723420536 ) ) ;
#67519 = ADVANCED_FACE ( 'NONE', ( #55124 ), #71328, .T. ) ;
#67520 = CARTESIAN_POINT ( 'NONE',  ( 4.999999999999993783, 146.0416666598387110, 8.660254037844390851 ) ) ;
#67521 = CARTESIAN_POINT ( 'NONE',  ( 7.188101187500002709, 102.6875000020483810, 2.977408999572649151 ) ) ;
#67522 = CARTESIAN_POINT ( 'NONE',  ( -1.982286880874317703, -47.26026874155311930, 139.0631323736432137 ) ) ;
#67523 = CARTESIAN_POINT ( 'NONE',  ( -11.35316468750000141, 28.59374999658601624, -1.390361679473963753E-15 ) ) ;
#67524 = CARTESIAN_POINT ( 'NONE',  ( -3.999999999999959144, 201.0625000000000000, 199.6568542494924259 ) ) ;
#67525 = EDGE_LOOP ( 'NONE', ( #40562, #35906, #50910, #13302 ) ) ;
#67526 = CARTESIAN_POINT ( 'NONE',  ( -11.00000000000000000, 0.000000000000000000, 95.68750000409677625 ) ) ;
#67527 = CARTESIAN_POINT ( 'NONE',  ( 10.18810118749999916, 1.247682550866122264E-15, 77.40625000204836681 ) ) ;
#67528 = DIRECTION ( 'NONE',  ( 0.000000000000000000, 0.000000000000000000, -1.000000000000000000 ) ) ;
#67530 = CARTESIAN_POINT ( 'NONE',  ( 11.35316468749999785, 170.5729166632526983, 3.042071309553174174 ) ) ;
#67529 = CARTESIAN_POINT ( 'NONE',  ( -11.00000000000000000, 0.000000000000000000, 115.1875000040967763 ) ) ;
#67531 = CARTESIAN_POINT ( 'NONE',  ( 3.313708498984756279, 7.999999999999991118, 10.91780278432982776 ) ) ;
#67532 = ADVANCED_FACE ( 'NONE', ( #48692 ), #8336, .T. ) ;
#67533 = EDGE_CURVE ( 'NONE', #25230, #46843, #58482, .T. ) ;
#67534 = CYLINDRICAL_SURFACE ( 'NONE', #71885, 7.999999999999991118 ) ;
#67535 = CIRCLE ( 'NONE', #35018, 3.999999999999976019 ) ;
#67536 = CARTESIAN_POINT ( 'NONE',  ( 8.311093377946839666, 220.7812500034139873, 8.311093377946829008 ) ) ;
#67537 = CARTESIAN_POINT ( 'NONE',  ( 1.506680654948082232, 55.70239491600471382, -43.84725041001931345 ) ) ;
#67538 = CARTESIAN_POINT ( 'NONE',  ( -10.18810118749999738, -4.220049686691941915, 78.62500000204838102 ) ) ;
#67539 = ORIENTED_EDGE ( 'NONE', *, *, #70228, .F. ) ;
#67540 = EDGE_CURVE ( 'NONE', #33017, #61626, #21283, .T. ) ;
#67541 = CARTESIAN_POINT ( 'NONE',  ( 0.000000000000000000, 145.8547997696495599, 50.08167581047971595 ) ) ;
#67542 = CARTESIAN_POINT ( 'NONE',  ( 8.311093377946834337, 110.4687499965860127, 8.311093377946839666 ) ) ;
#67543 = CARTESIAN_POINT ( 'NONE',  ( -4.541265875000002339, 21.93749999863440792, -5.561446717895856393E-16 ) ) ;
#67544 = ORIENTED_EDGE ( 'NONE', *, *, #47131, .F. ) ;
#67545 = ORIENTED_EDGE ( 'NONE', *, *, #63842, .T. ) ;
#67546 = CARTESIAN_POINT ( 'NONE',  ( 4.541265875000002339, 8.437499998634407916, 0.000000000000000000 ) ) ;
#67548 = MANIFOLD_SOLID_BREP ( 'Chamfer2', #930 ) ;
#67547 = CARTESIAN_POINT ( 'NONE',  ( 2.977408999572650927, 9.749999997951611874, -7.188101187500001821 ) ) ;
#67549 = CARTESIAN_POINT ( 'NONE',  ( 5.656854249492379694, 108.1250000040967763, -5.656854249492380582 ) ) ;
#67550 = AXIS2_PLACEMENT_3D ( 'NONE', #7459, #71924, #36868 ) ;
#67551 = CARTESIAN_POINT ( 'NONE',  ( 7.204075437095966983, 7.204075437095967871, 92.96875000204838102 ) ) ;
#67552 = CARTESIAN_POINT ( 'NONE',  ( -26.56734541678238060, 203.6250000013656063, 166.5412658750003629 ) ) ;
#67553 = CARTESIAN_POINT ( 'NONE',  ( -2.828427124746190735, 9.375000000000000000, -2.828427124746191623 ) ) ;
#67554 = CARTESIAN_POINT ( 'NONE',  ( -1.656854249492229592, 197.8125000000000000, 193.9999999999999147 ) ) ;
#67555 = CARTESIAN_POINT ( 'NONE',  ( 4.541265875000002339, 9.312499998634407916, 0.000000000000000000 ) ) ;
#67556 = CARTESIAN_POINT ( 'NONE',  ( -1.656854249492403008, 197.6875000000000000, 146.0000000000000284 ) ) ;
#67557 = ORIENTED_EDGE ( 'NONE', *, *, #72758, .T. ) ;
#67558 = CARTESIAN_POINT ( 'NONE',  ( 5.656854249492381470, 116.5625000000000000, 5.656854249492379694 ) ) ;
#67561 = CARTESIAN_POINT ( 'NONE',  ( -6.123233995736766282E-16, 236.8750000068279746, -10.00000000000000000 ) ) ;
#67560 = CARTESIAN_POINT ( 'NONE',  ( -24.54126587500002188, 196.2500000013656631, 168.5673454167826435 ) ) ;
#67559 =( BOUNDED_CURVE ( )  B_SPLINE_CURVE ( 2, ( #18367, #7050, #36092, #13054, #41381, #35724, #30059 ),
 .UNSPECIFIED., .F., .F. ) 
 B_SPLINE_CURVE_WITH_KNOTS ( ( 3, 2, 2, 3 ),
 ( 0.000000000000000000, 0.009259259259259060987, 0.01851851851851812197, 0.02777777777777718296 ),
 .UNSPECIFIED. ) 
 CURVE ( )  GEOMETRIC_REPRESENTATION_ITEM ( )  RATIONAL_B_SPLINE_CURVE ( ( 1.000000000000000000, 0.9659258262890683122, 1.000000000000000000, 0.9659258262890683122, 1.000000000000000000, 0.9659258262890705327, 0.9999999999999977796 ) ) 
 REPRESENTATION_ITEM ( '' )  );
#67562 = CARTESIAN_POINT ( 'NONE',  ( -4.541265875000003227, 18.87499999863441147, 1.881053915767121110 ) ) ;
#67563 = AXIS2_PLACEMENT_3D ( 'NONE', #22646, #788, #45666 ) ;
#67564 = CARTESIAN_POINT ( 'NONE',  ( 0.9670529856864175100, -47.84666766410765604, 151.0237526922109055 ) ) ;
#67565 = CARTESIAN_POINT ( 'NONE',  ( 5.082755093536320601, -5.082755093536318824, 0.5490527818717526598 ) ) ;
#67566 = ORIENTED_EDGE ( 'NONE', *, *, #21950, .T. ) ;
#67567 = EDGE_CURVE ( 'NONE', #56539, #34777, #65305, .T. ) ;
#67568 = ORIENTED_EDGE ( 'NONE', *, *, #68966, .F. ) ;
#67569 = CARTESIAN_POINT ( 'NONE',  ( -7.204075437095965206, -7.204075437095968759, 91.84375000204838102 ) ) ;
#67570 = CARTESIAN_POINT ( 'NONE',  ( 3.313708498984756279, 7.999999999999991118, 19.86155277982337353 ) ) ;
#67571 = CARTESIAN_POINT ( 'NONE',  ( -30.44569435410879166, 199.0625000013656063, 172.4456943541092357 ) ) ;
#67572 = CARTESIAN_POINT ( 'NONE',  ( 4.556349186104051263, -10.99999999999999822, 104.9687500000000000 ) ) ;
#67573 = CARTESIAN_POINT ( 'NONE',  ( -1.432654583217607414, 206.5000000013655779, 194.5412658750000219 ) ) ;
#67574 = DIRECTION ( 'NONE',  ( 0.000000000000000000, 0.000000000000000000, -1.000000000000000000 ) ) ;
#67575 = CARTESIAN_POINT ( 'NONE',  ( 6.123233995736767268E-16, 126.2500000000000000, -10.00000000000000178 ) ) ;
#67576 = CARTESIAN_POINT ( 'NONE',  ( 8.000000000000000000, 103.2500000000000000, -9.797174393178825657E-16 ) ) ;
#67577 = CARTESIAN_POINT ( 'NONE',  ( 4.721056650415999201, 293.2343750017069510, -4.721056650415999201 ) ) ;
#67578 = CIRCLE ( 'NONE', #16960, 8.000000000000000000 ) ;
#67579 = CARTESIAN_POINT ( 'NONE',  ( 2.977408999572650927, -7.188101187499990274, 5.330302781871753659 ) ) ;
#67580 = EDGE_LOOP ( 'NONE', ( #7618, #64929, #54637, #50116 ) ) ;
#67582 =( BOUNDED_CURVE ( )  B_SPLINE_CURVE ( 2, ( #29415, #35088, #18459, #58464, #69402, #12419, #69771, #2214, #12781 ),
 .UNSPECIFIED., .F., .F. ) 
 B_SPLINE_CURVE_WITH_KNOTS ( ( 3, 2, 2, 2, 3 ),
 ( 0.06944444444444444753, 0.07638888888888889506, 0.08333333333333331483, 0.09027777777777776236, 0.09722222222222220989 ),
 .UNSPECIFIED. ) 
 CURVE ( )  GEOMETRIC_REPRESENTATION_ITEM ( )  RATIONAL_B_SPLINE_CURVE ( ( 1.000000000000000000, 0.9238795325112867385, 1.000000000000000000, 0.9238795325112867385, 1.000000000000000000, 0.9238795325112867385, 1.000000000000000000, 0.9238795325112868495, 0.9999999999999998890 ) ) 
 REPRESENTATION_ITEM ( '' )  );
#67581 = CARTESIAN_POINT ( 'NONE',  ( 3.313708498984802020, 19.78125000000000355, -7.999999999999958256 ) ) ;
#67583 = EDGE_CURVE ( 'NONE', #31616, #2846, #52343, .T. ) ;
#67584 = CARTESIAN_POINT ( 'NONE',  ( 24.54126587500000056, 205.1250000013656347, 168.5673454167822172 ) ) ;
#67585 = CARTESIAN_POINT ( 'NONE',  ( -5.082755093536325042, 1.406249997951610320, -5.082755093536325930 ) ) ;
#67586 = CARTESIAN_POINT ( 'NONE',  ( -2.445694354108838731, 200.0625000013656063, 144.4456943541088663 ) ) ;
#67587 = CARTESIAN_POINT ( 'NONE',  ( 5.082755093536326818, 120.5937500020483952, 5.082755093536325042 ) ) ;
#67589 = CARTESIAN_POINT ( 'NONE',  ( -3.458734125000015869, 201.1875000013656063, 142.0000000000000568 ) ) ;
#67588 = CARTESIAN_POINT ( 'NONE',  ( -4.556349186104045934, 11.00000000000000000, 111.7187499999999858 ) ) ;
#67590 = CARTESIAN_POINT ( 'NONE',  ( 11.35316468749999963, 261.5104166700807014, 3.042071309553159519 ) ) ;
#67591 = DIRECTION ( 'NONE',  ( 0.000000000000000000, 0.000000000000000000, -1.000000000000000000 ) ) ;
#67592 = CYLINDRICAL_SURFACE ( 'NONE', #33680, 36.00000000000000000 ) ;
#67593 = CARTESIAN_POINT ( 'NONE',  ( 6.951808397369818766E-16, 12.03124999658601801, -11.35316468750000141 ) ) ;
#67594 = LINE ( 'NONE', #15891, #49590 ) ;
#67595 = CARTESIAN_POINT ( 'NONE',  ( -5.676582343749998039, 207.7604166632526983, -9.832129032723420536 ) ) ;
#67596 = CARTESIAN_POINT ( 'NONE',  ( -26.34314575050764873, 203.0625000027312126, 166.0000000000004263 ) ) ;
#67597 = FACE_OUTER_BOUND ( 'NONE', #50433, .T. ) ;
#67598 = PRODUCT_DEFINITION ( 'UNKNOWN', '', #12884, #33246 ) ;
#67599 = CARTESIAN_POINT ( 'NONE',  ( -4.898587196589412829E-16, 102.3125000040967763, -8.000000000000000000 ) ) ;
#67600 = ORIENTED_EDGE ( 'NONE', *, *, #49101, .T. ) ;
#67601 = CARTESIAN_POINT ( 'NONE',  ( 3.458734124999960358, 199.6875000013656063, 142.0000000000000568 ) ) ;
#67602 = CARTESIAN_POINT ( 'NONE',  ( 11.35316468749999963, 10.98958332991935016, -3.042071309553165293 ) ) ;
#67603 = CARTESIAN_POINT ( 'NONE',  ( 4.556349186104051263, -10.99999999999999822, 100.6562500040967905 ) ) ;
#67604 = CARTESIAN_POINT ( 'NONE',  ( -3.369429374625495743, 10.27270496052241278, 63.91910092334656923 ) ) ;
#67605 = CARTESIAN_POINT ( 'NONE',  ( -24.54126587499999346, 199.1875000013655779, 170.0000000000002842 ) ) ;
#67606 = LINE ( 'NONE', #15903, #37084 ) ;
#67608 = CARTESIAN_POINT ( 'NONE',  ( 9.832129032723420536, 11.19791666325268409, -5.676582343749999815 ) ) ;
#67607 = CARTESIAN_POINT ( 'NONE',  ( 2.977408999572654480, 115.6250000020483810, 7.188101187499999156 ) ) ;
#67609 = CARTESIAN_POINT ( 'NONE',  ( -7.999999999999991118, -4.672035931492118266, 29.46248198892144643 ) ) ;
#67610 = CARTESIAN_POINT ( 'NONE',  ( 3.042071309553159519, 119.7395833299193413, 11.35316468750000141 ) ) ;
#67611 = EDGE_CURVE ( 'NONE', #57316, #44110, #680, .T. ) ;
#67612 = CARTESIAN_POINT ( 'NONE',  ( -5.000000000000005329, 100.2083333265053682, 8.660254037844387298 ) ) ;
#67613 = CARTESIAN_POINT ( 'NONE',  ( -7.188101187500001821, 119.9375000020483952, -2.977408999572650483 ) ) ;
#67614 = CARTESIAN_POINT ( 'NONE',  ( -4.541265875000002339, 19.87499999863440792, -1.881053915767121998 ) ) ;
#67615 = CYLINDRICAL_SURFACE ( 'NONE', #7259, 8.000000000000000000 ) ;
#67616 = CARTESIAN_POINT ( 'NONE',  ( -12.00000000000000000, 6.928203230275504332, -1.071796769724504550 ) ) ;
#67617 = ORIENTED_EDGE ( 'NONE', *, *, #73198, .F. ) ;
#67618 = DIRECTION ( 'NONE',  ( 0.000000000000000000, 0.000000000000000000, 1.000000000000000000 ) ) ;
#67619 = EDGE_CURVE ( 'NONE', #19432, #29352, #29013, .T. ) ;
#67620 = CARTESIAN_POINT ( 'NONE',  ( 1.226468279477575784E-15, 288.8593750017070079, 6.676582343750001591 ) ) ;
#67621 = CARTESIAN_POINT ( 'NONE',  ( 4.999999999999998224, 53.34243969459446078, 47.33397984627243460 ) ) ;
#67622 = CARTESIAN_POINT ( 'NONE',  ( 7.999999999999991118, 9.797174393178815797E-16, 27.13655278432982598 ) ) ;
#67623 = VECTOR ( 'NONE', #33591, 1000.000000000000000 ) ;
#67624 = CARTESIAN_POINT ( 'NONE',  ( -25.17157287525377640, 198.6250000000000284, 172.8284271247465256 ) ) ;
#67625 = CARTESIAN_POINT ( 'NONE',  ( -5.676582343750000703, 258.0729166700806445, -9.832129032723418760 ) ) ;
#67626 = CARTESIAN_POINT ( 'NONE',  ( 10.18810118750000093, -4.220049686691933921, 104.6875000020483810 ) ) ;
#67627 = ORIENTED_EDGE ( 'NONE', *, *, #56098, .F. ) ;
#67628 = LINE ( 'NONE', #48767, #29224 ) ;
#67629 = CARTESIAN_POINT ( 'NONE',  ( 9.832129032723416984, 150.6770833299193555, 5.676582343750006032 ) ) ;
#67630 = CARTESIAN_POINT ( 'NONE',  ( -7.778174593052023411, 7.778174593052023411, 98.31250000000000000 ) ) ;
#67631 = CARTESIAN_POINT ( 'NONE',  ( 2.839093476692135984E-14, 200.9375000013656063, 201.4587341250000350 ) ) ;
#67632 = EDGE_CURVE ( 'NONE', #29130, #27473, #51688, .T. ) ;
#67633 = CARTESIAN_POINT ( 'NONE',  ( 0.000000000000000000, -2.500000000000000444, 0.000000000000000000 ) ) ;
#67634 = CARTESIAN_POINT ( 'NONE',  ( -9.832129032723420536, 79.01041666325268409, 5.676582343749997150 ) ) ;
#67635 = VERTEX_POINT ( 'NONE', #56894 ) ;
#67636 = CARTESIAN_POINT ( 'NONE',  ( -6.238412754330611322E-16, 10.18810118749999916, 112.2812500020483810 ) ) ;
#67637 = CARTESIAN_POINT ( 'NONE',  ( 4.541265875000001451, 9.374999998634407916, 1.881053915767124440 ) ) ;
#67638 = ORIENTED_EDGE ( 'NONE', *, *, #71663, .T. ) ;
#67639 = CARTESIAN_POINT ( 'NONE',  ( -5.656854249492381470, 2.437500000000000444, 5.656854249492379694 ) ) ;
#67640 = CARTESIAN_POINT ( 'NONE',  ( 8.660254037844389075, 115.4166666666666998, -5.000000000000000000 ) ) ;
#67641 = CARTESIAN_POINT ( 'NONE',  ( 2.977408999572651815, 15.56249999795161365, 7.188101187500000933 ) ) ;
#67642 = CARTESIAN_POINT ( 'NONE',  ( 2.828427124746153876, 199.8750000000000284, 144.8284271247462129 ) ) ;
#67643 = CARTESIAN_POINT ( 'NONE',  ( -10.18810118749999916, 0.000000000000000000, 110.0312500020483668 ) ) ;
#67644 = AXIS2_PLACEMENT_3D ( 'NONE', #64190, #37367, #65285 ) ;
#67645 = CARTESIAN_POINT ( 'NONE',  ( 2.679491924311221407, 108.9583333333333286, 10.00000000000000000 ) ) ;
#67646 = CARTESIAN_POINT ( 'NONE',  ( 1.656854249492381248, 7.937499997268813168, -4.000000000000001776 ) ) ;
#67647 = CARTESIAN_POINT ( 'NONE',  ( 1.656854249492406783, 17.81250000000000711, 3.999999999999976019 ) ) ;
#67648 = ORIENTED_EDGE ( 'NONE', *, *, #63465, .F. ) ;
#67649 = CARTESIAN_POINT ( 'NONE',  ( 3.458734125000015425, 202.0000000013656063, 196.5673454167823877 ) ) ;
#67650 = EDGE_CURVE ( 'NONE', #17726, #32715, #63312, .T. ) ;
#67651 = CARTESIAN_POINT ( 'NONE',  ( -26.34314575050752794, 195.6875000027312126, 174.0000000000003411 ) ) ;
#67652 = CARTESIAN_POINT ( 'NONE',  ( -18.00000000000000000, -10.39230484541329425, -20.69999999999999929 ) ) ;
#67653 = CARTESIAN_POINT ( 'NONE',  ( -1.881053915767124440, 4.999999998634406140, 4.541265875000001451 ) ) ;
#67654 = CARTESIAN_POINT ( 'NONE',  ( 1.469576158976823947E-15, 94.06250000409677625, 8.000000000000000000 ) ) ;
#67655 = CARTESIAN_POINT ( 'NONE',  ( -7.188101187499992051, 0.000000000000000000, 17.98655278187175455 ) ) ;
#67656 = EDGE_LOOP ( 'NONE', ( #68542, #66723, #23319, #1227 ) ) ;
#67657 = EDGE_CURVE ( 'NONE', #7437, #40814, #39898, .T. ) ;
#67658 = CARTESIAN_POINT ( 'NONE',  ( 11.00000000000000000, 1.347111479062088405E-15, 106.7500000000000000 ) ) ;
#67659 = VERTEX_POINT ( 'NONE', #22161 ) ;
#67660 = CARTESIAN_POINT ( 'NONE',  ( 7.204075437095966983, 7.204075437095967871, 110.5937500020483810 ) ) ;
#67661 = CARTESIAN_POINT ( 'NONE',  ( 25.17157287525382259, 209.0000000027312126, 172.8284271247460993 ) ) ;
#67662 = CARTESIAN_POINT ( 'NONE',  ( 2.839093476692135984E-14, 204.6875000013656063, 201.4587341250000350 ) ) ;
#67663 = CARTESIAN_POINT ( 'NONE',  ( 26.56734541678233086, 199.0000000013656063, 166.5412658749999650 ) ) ;
#67664 = CARTESIAN_POINT ( 'NONE',  ( 10.00000000000000000, 84.79166666666667140, 2.679491924311236062 ) ) ;
#67665 = VECTOR ( 'NONE', #9330, 1000.000000000000000 ) ;
#67666 = CARTESIAN_POINT ( 'NONE',  ( 5.656854249492381470, 124.0625000000000000, 5.656854249492379694 ) ) ;
#67667 = CARTESIAN_POINT ( 'NONE',  ( 6.000000000000001776, 291.5000000000000000, -7.347880794884121708E-16 ) ) ;
#67668 = CARTESIAN_POINT ( 'NONE',  ( 26.34314575050758833, 205.6875000027312126, 165.9999999999998863 ) ) ;
#67669 = ORIENTED_EDGE ( 'NONE', *, *, #21898, .T. ) ;
#67670 = CARTESIAN_POINT ( 'NONE',  ( 5.656854249492381470, 94.06250000000000000, 5.656854249492379694 ) ) ;
#67671 = CARTESIAN_POINT ( 'NONE',  ( 3.728321214185993160, -10.10963409588536521, 70.65936332841438627 ) ) ;
#67672 = CARTESIAN_POINT ( 'NONE',  ( -4.000000000000015099, 194.6875000027312126, 143.6568542494924543 ) ) ;
#67673 = CARTESIAN_POINT ( 'NONE',  ( 10.00000000000000000, 56.66666665983869677, 2.679491924311235618 ) ) ;
#67674 = DIRECTION ( 'NONE',  ( -0.000000000000000000, -0.000000000000000000, -1.000000000000000000 ) ) ;
#67675 = CARTESIAN_POINT ( 'NONE',  ( 1.836970198721029589E-15, 251.2500000000000284, 10.00000000000000000 ) ) ;
#67676 = CARTESIAN_POINT ( 'NONE',  ( -4.556349186104045934, 11.00000000000000000, 107.4062500040967620 ) ) ;
#67678 = EDGE_CURVE ( 'NONE', #8242, #41754, #2957, .T. ) ;
#67677 =( BOUNDED_CURVE ( )  B_SPLINE_CURVE ( 2, ( #4890, #61478, #68625, #21844, #9803, #56203, #67513, #15812, #73173 ),
 .UNSPECIFIED., .F., .F. ) 
 B_SPLINE_CURVE_WITH_KNOTS ( ( 3, 2, 2, 2, 3 ),
 ( 0.8166666666666674290, 0.8250000000000006217, 0.8333333333333340365, 0.8416666666666672292, 0.8500000000000005329 ),
 .UNSPECIFIED. ) 
 CURVE ( )  GEOMETRIC_REPRESENTATION_ITEM ( )  RATIONAL_B_SPLINE_CURVE ( ( 0.9999999999999928946, 0.9238795325112938439, 1.000000000000000000, 0.9238795325112867385, 1.000000000000000000, 0.9238795325112867385, 1.000000000000000000, 0.9238795325112816315, 1.000000000000005107 ) ) 
 REPRESENTATION_ITEM ( '' )  );
#67679 = CARTESIAN_POINT ( 'NONE',  ( 2.679491924311222739, 193.9583333333333428, 10.00000000000000355 ) ) ;
#67680 = CARTESIAN_POINT ( 'NONE',  ( 2.849036369511732440E-14, 207.3750000027312126, 202.0000000000000000 ) ) ;
#67681 = CARTESIAN_POINT ( 'NONE',  ( 7.188101187499992051, 8.802885111219154394E-16, 16.11155278187175455 ) ) ;
#67682 = CARTESIAN_POINT ( 'NONE',  ( 5.676582343750001591, 161.9270833299193555, -9.832129032723420536 ) ) ;
#67683 = CARTESIAN_POINT ( 'NONE',  ( -1.656854249492453857, 204.8125000027312410, 146.0000000000000284 ) ) ;
#67684 = DIRECTION ( 'NONE',  ( -0.000000000000000000, 1.000000000000000000, -1.563033456626094573E-30 ) ) ;
#67685 = DIRECTION ( 'NONE',  ( 1.000000000000000000, 0.000000000000000000, 0.000000000000000000 ) ) ;
#67687 = LINE ( 'NONE', #72597, #63988 ) ;
#67686 = LINE ( 'NONE', #51813, #45497 ) ;
#67688 = ORIENTED_EDGE ( 'NONE', *, *, #21984, .T. ) ;
#67689 = CARTESIAN_POINT ( 'NONE',  ( 5.676582343749993598, 20.26041666325268409, 9.832129032723422313 ) ) ;
#67690 = CARTESIAN_POINT ( 'NONE',  ( -3.361190284997694011, 194.4711224105990368, 198.8920594278317537 ) ) ;
#67692 = CARTESIAN_POINT ( 'NONE',  ( 0.8419854211626176532, 10.28111362163632947, -63.57154293063804573 ) ) ;
#67691 = CARTESIAN_POINT ( 'NONE',  ( -30.99999999999992895, -31.99999999999978684, 205.0000000000000284 ) ) ;
#67693 = CARTESIAN_POINT ( 'NONE',  ( 23.99999999999999645, 201.9375000027311842, 171.6568542494923122 ) ) ;
#67694 = CARTESIAN_POINT ( 'NONE',  ( -2.445694354108839619, 202.8125000013656063, 139.5543056458912190 ) ) ;
#67695 = CARTESIAN_POINT ( 'NONE',  ( 2.679491924311222739, 55.83333332650535397, 10.00000000000000355 ) ) ;
#67696 = VECTOR ( 'NONE', #42280, 1000.000000000000000 ) ;
#67697 = CARTESIAN_POINT ( 'NONE',  ( -7.188101187500000044, 104.6562500020483810, 0.000000000000000000 ) ) ;
#67698 = CARTESIAN_POINT ( 'NONE',  ( -4.541265875000002339, 8.937499998634407916, -5.561446717895856393E-16 ) ) ;
#67699 = CARTESIAN_POINT ( 'NONE',  ( -2.664923566518097392E-11, 208.7499999999979252, 10.00000000000000178 ) ) ;
#67700 = CARTESIAN_POINT ( 'NONE',  ( 3.313708498984762496, -7.999999999999989342, 8.799052779823364645 ) ) ;
#67701 = CARTESIAN_POINT ( 'NONE',  ( -7.347880794884122694E-16, 0.7500000000000002220, 4.000000000000001776 ) ) ;
#67702 = ORIENTED_EDGE ( 'NONE', *, *, #14056, .T. ) ;
#67703 = ORIENTED_EDGE ( 'NONE', *, *, #61830, .T. ) ;
#67704 = CARTESIAN_POINT ( 'NONE',  ( -4.999999999999999112, -61.58609660504387051, 23.68302032025066239 ) ) ;
#67705 = FACE_OUTER_BOUND ( 'NONE', #61292, .T. ) ;
#67706 = CARTESIAN_POINT ( 'NONE',  ( -2.679491924310502871, 163.5416666666667425, 10.00000000000043343 ) ) ;
#67707 = CARTESIAN_POINT ( 'NONE',  ( 4.556349186104045934, 11.00000000000000000, 95.03124999999998579 ) ) ;
#67708 = CARTESIAN_POINT ( 'NONE',  ( 8.311093377946837890, 141.4062499965860127, -8.311093377946837890 ) ) ;
#67709 = VERTEX_POINT ( 'NONE', #22917 ) ;
#67710 = CARTESIAN_POINT ( 'NONE',  ( -4.999999999999999112, 12.24343743989404310, -68.85270403949348861 ) ) ;
#67711 = CARTESIAN_POINT ( 'NONE',  ( 7.204075437095966983, 7.204075437095967871, 88.09375000204836681 ) ) ;
#67712 = CARTESIAN_POINT ( 'NONE',  ( 0.000000000000000000, 0.000000000000000000, 118.0000000000000000 ) ) ;
#67713 = CARTESIAN_POINT ( 'NONE',  ( -1.656854249492348607, 206.1875000000000568, 202.0000000000000284 ) ) ;
#67714 = CARTESIAN_POINT ( 'NONE',  ( 8.660254037844389075, 247.0833333333333428, 4.999999999999997335 ) ) ;
#67715 = CARTESIAN_POINT ( 'NONE',  ( 3.313708498984800688, 117.2187500040967620, -7.999999999999958256 ) ) ;
#67716 = CARTESIAN_POINT ( 'NONE',  ( 7.999999999999991118, 9.797174393178815797E-16, 4.580302779823363757 ) ) ;
#67717 = ORIENTED_EDGE ( 'NONE', *, *, #17743, .T. ) ;
#67718 = CARTESIAN_POINT ( 'NONE',  ( 3.313708498984765161, 106.1562500040967905, 7.999999999999998224 ) ) ;
#67719 = CARTESIAN_POINT ( 'NONE',  ( -35.44037136445320613, 174.9968844453804309, 162.5244051778534811 ) ) ;
#67720 = CARTESIAN_POINT ( 'NONE',  ( -3.042071309553163960, 112.5520833299193413, -11.35316468749999963 ) ) ;
#67721 = CARTESIAN_POINT ( 'NONE',  ( -2.445694354108782775, 200.5625000013656063, 200.4456943541088663 ) ) ;
#67722 = CARTESIAN_POINT ( 'NONE',  ( -2.977408999572650039, 16.31249999795161543, -7.188101187500000933 ) ) ;
#67723 = CARTESIAN_POINT ( 'NONE',  ( -10.18810118749999916, 4.220049686691934809, 85.93750000204839523 ) ) ;
#67724 = CARTESIAN_POINT ( 'NONE',  ( 8.311093377946834337, 30.46874999658601979, 8.311093377946839666 ) ) ;
#67725 = ORIENTED_EDGE ( 'NONE', *, *, #7136, .F. ) ;
#67726 = CARTESIAN_POINT ( 'NONE',  ( 0.000000000000000000, 51.05255888325788050, 0.000000000000000000 ) ) ;
#67727 = CARTESIAN_POINT ( 'NONE',  ( 3.317071493978877683, 8.008118988124991233, 20.04436528394063188 ) ) ;
#67728 = FACE_OUTER_BOUND ( 'NONE', #39618, .T. ) ;
#67729 = AXIS2_PLACEMENT_3D ( 'NONE', #42636, #49411, #8308 ) ;
#67730 = CARTESIAN_POINT ( 'NONE',  ( -4.000000000000001776, 7.437500000000000888, -1.656854249492381470 ) ) ;
#67731 = CARTESIAN_POINT ( 'NONE',  ( -5.082755093536326818, 10.40624999795161187, 5.082755093536325042 ) ) ;
#67732 = CARTESIAN_POINT ( 'NONE',  ( 2.765530957081996366, 289.1406250017069510, -6.676582343750003368 ) ) ;
#67733 = CARTESIAN_POINT ( 'NONE',  ( -7.999999999999991118, 0.000000000000000000, 29.33030277982336642 ) ) ;
#67734 = DIRECTION ( 'NONE',  ( 0.000000000000000000, 0.000000000000000000, -1.000000000000000000 ) ) ;
#67735 = VERTEX_POINT ( 'NONE', #68942 ) ;
#67736 = CONICAL_SURFACE ( 'NONE', #35211, 8.000000000000005329, 0.9599310885968794782 ) ;
#67737 = EDGE_CURVE ( 'NONE', #19664, #5894, #11601, .T. ) ;
#67738 = CARTESIAN_POINT ( 'NONE',  ( 3.042071309553159519, 140.0520833299193271, 11.35316468750000141 ) ) ;
#67739 = CARTESIAN_POINT ( 'NONE',  ( -10.18810118749999916, 0.000000000000000000, 76.65625000204836681 ) ) ;
#67740 = CARTESIAN_POINT ( 'NONE',  ( -26.56734541678238415, 208.6250000013655779, 166.5412658750003629 ) ) ;
#67741 = DIRECTION ( 'NONE',  ( -0.000000000000000000, 1.000000000000000000, 4.689100369878284071E-30 ) ) ;
#67742 = CARTESIAN_POINT ( 'NONE',  ( -4.541265875000003227, 15.99999999863440614, 1.881053915767121110 ) ) ;
#67743 = VERTEX_POINT ( 'NONE', #9665 ) ;
#67744 = CARTESIAN_POINT ( 'NONE',  ( -3.999999999999960032, 200.0625000027312410, 196.3431457505076594 ) ) ;
#67745 = EDGE_CURVE ( 'NONE', #49450, #47940, #44439, .T. ) ;
#67746 = CARTESIAN_POINT ( 'NONE',  ( -2.839093476692135984E-14, 194.9375000013655779, 138.5412658750000503 ) ) ;
#67747 = CARTESIAN_POINT ( 'NONE',  ( -31.99999999999996447, 205.4375000027312126, 171.6568542494928522 ) ) ;
#67748 = AXIS2_PLACEMENT_3D ( 'NONE', #69364, #18052, #64810 ) ;
#67749 = CARTESIAN_POINT ( 'NONE',  ( -8.000000000000000000, 21.75000000000000355, -9.797174393178825657E-16 ) ) ;
#67750 = EDGE_LOOP ( 'NONE', ( #14329, #10108, #50335, #32397 ) ) ;
#67751 = EDGE_CURVE ( 'NONE', #54105, #45576, #41563, .T. ) ;
#67752 = CARTESIAN_POINT ( 'NONE',  ( -7.188101187500000933, 13.12499999795161187, -2.977408999572651371 ) ) ;
#67753 = FACE_OUTER_BOUND ( 'NONE', #23473, .T. ) ;
#67754 = LINE ( 'NONE', #61343, #8957 ) ;
#67755 = CARTESIAN_POINT ( 'NONE',  ( 5.676582343750001591, 181.6145833299193555, -9.832129032723420536 ) ) ;
#67756 = CARTESIAN_POINT ( 'NONE',  ( 5.082755093536325042, 104.4687500020483952, -5.082755093536325930 ) ) ;
#67757 = LINE ( 'NONE', #43611, #19654 ) ;
#67758 = DIRECTION ( 'NONE',  ( -0.000000000000000000, -1.000000000000000000, -0.000000000000000000 ) ) ;
#67759 = CARTESIAN_POINT ( 'NONE',  ( 1.459323541827198180E-11, 81.24999999999886313, -10.00000000000000533 ) ) ;
#67760 = ORIENTED_EDGE ( 'NONE', *, *, #38096, .F. ) ;
#67761 = CARTESIAN_POINT ( 'NONE',  ( 2.085542519210945334E-15, 255.1562500034140157, 11.35316468749999963 ) ) ;
#67762 = CARTESIAN_POINT ( 'NONE',  ( -2.977408999572648707, -7.188101187499990274, 21.64280278187176165 ) ) ;
#67763 = CARTESIAN_POINT ( 'NONE',  ( -1.877992804781005276, 55.75022808460100521, 43.87334515336361562 ) ) ;
#67764 = CARTESIAN_POINT ( 'NONE',  ( 27.99999999999996803, 206.0000000000000284, 173.9999999999999147 ) ) ;
#67765 = CARTESIAN_POINT ( 'NONE',  ( -5.107860025160939621, -60.88642786446133925, -23.30380398316975388 ) ) ;
#67766 = CARTESIAN_POINT ( 'NONE',  ( -3.458734124999959469, 196.7500000013656063, 199.4326545832176691 ) ) ;
#67767 = CARTESIAN_POINT ( 'NONE',  ( 2.679491924311222739, 148.9583333333333144, 10.00000000000000355 ) ) ;
#67768 = DIRECTION ( 'NONE',  ( 0.000000000000000000, 0.000000000000000000, 1.000000000000000000 ) ) ;
#67769 = CARTESIAN_POINT ( 'NONE',  ( -54.00000000000000000, 205.0000000000000284, 4.085831468968145267E-14 ) ) ;
#67770 = CARTESIAN_POINT ( 'NONE',  ( -8.000000000000000000, 92.00000000000000000, 0.000000000000000000 ) ) ;
#67771 = CARTESIAN_POINT ( 'NONE',  ( -11.35316468750000141, 128.8020833299193555, 3.042071309553159963 ) ) ;
#67772 = CARTESIAN_POINT ( 'NONE',  ( 1.469576158976823947E-15, 98.37499999999998579, 8.000000000000000000 ) ) ;
#67773 = CARTESIAN_POINT ( 'NONE',  ( -6.735557395310442023E-16, 11.00000000000000000, 72.62500000000000000 ) ) ;
#67776 = CARTESIAN_POINT ( 'NONE',  ( 8.000000000000000000, 118.5312500040967905, -3.313708498984762496 ) ) ;
#67775 = CARTESIAN_POINT ( 'NONE',  ( 24.54126587500000056, 198.2500000013656347, 171.4326545832175839 ) ) ;
#67774 = CARTESIAN_POINT ( 'NONE',  ( 26.34314575050758833, 208.9375000000000284, 173.9999999999999147 ) ) ;
#67777 = EDGE_LOOP ( 'NONE', ( #66552, #4858, #62056, #42439 ) ) ;
#67778 = VECTOR ( 'NONE', #71033, 1000.000000000000000 ) ;
#67779 = CARTESIAN_POINT ( 'NONE',  ( 9.770781909996177461, 224.8281321452039379, 2.149070136972248246 ) ) ;
#67780 = DIRECTION ( 'NONE',  ( -0.000000000000000000, 1.000000000000000000, -0.000000000000000000 ) ) ;
#67781 = AXIS2_PLACEMENT_3D ( 'NONE', #48441, #71820, #59779 ) ;
#67782 = CARTESIAN_POINT ( 'NONE',  ( 27.99999999999996447, 198.6875000013655779, 173.4587341249998929 ) ) ;
#67783 = CARTESIAN_POINT ( 'NONE',  ( -9.832129032723420536, 204.0104166632526983, 5.676582343749997150 ) ) ;
#67784 = CARTESIAN_POINT ( 'NONE',  ( -7.188101187500001821, 119.5625000020483810, -2.977408999572650483 ) ) ;
#67785 = CARTESIAN_POINT ( 'NONE',  ( 3.211159895383560947, 18.18749999863440792, 3.211159895383562723 ) ) ;
#67786 = CARTESIAN_POINT ( 'NONE',  ( 0.3794862803132350582, -55.62190996747519023, 43.80334292620691627 ) ) ;
#67787 = CARTESIAN_POINT ( 'NONE',  ( -7.999999999999991118, 0.000000000000000000, 27.83030277982336642 ) ) ;
#67789 = CARTESIAN_POINT ( 'NONE',  ( -26.34314575050758478, 202.9375000000000284, 166.0000000000003979 ) ) ;
#67788 = DIRECTION ( 'NONE',  ( -0.000000000000000000, -1.000000000000000000, -4.283267841918042741E-17 ) ) ;
#67790 = CARTESIAN_POINT ( 'NONE',  ( -11.35316468749999785, 93.07291666325266988, -3.042071309553167513 ) ) ;
#67791 = ORIENTED_EDGE ( 'NONE', *, *, #72173, .T. ) ;
#67792 = DIRECTION ( 'NONE',  ( 0.000000000000000000, 0.000000000000000000, 1.000000000000000000 ) ) ;
#67793 = CARTESIAN_POINT ( 'NONE',  ( -1.320432766682874540E-15, 22.59374999795161187, 7.188101187500000044 ) ) ;
#67794 = CARTESIAN_POINT ( 'NONE',  ( -5.656854249492373476, -5.656854249492376141, 14.51780277982336465 ) ) ;
#67795 = CARTESIAN_POINT ( 'NONE',  ( 8.311093377946839666, 261.0937500034140157, 8.311093377946830785 ) ) ;
#67796 = CARTESIAN_POINT ( 'NONE',  ( 11.35316468750000141, 105.7812499965860269, 0.000000000000000000 ) ) ;
#67797 = ORIENTED_EDGE ( 'NONE', *, *, #57729, .T. ) ;
#67798 = FACE_BOUND ( 'NONE', #67493, .T. ) ;
#67799 = CARTESIAN_POINT ( 'NONE',  ( -6.238412754330611322E-16, 10.18810118749999916, 106.2812500020483810 ) ) ;
#67800 = CARTESIAN_POINT ( 'NONE',  ( -30.44569435410883074, 194.8125000013656063, 167.5543056458915885 ) ) ;
#67801 = CARTESIAN_POINT ( 'NONE',  ( 3.458734125000016757, 203.1250000013656347, 199.4326545832176691 ) ) ;
#67802 = CARTESIAN_POINT ( 'NONE',  ( 5.656854249492376141, -5.656854249492374365, 11.89280277982336642 ) ) ;
#67804 = CARTESIAN_POINT ( 'NONE',  ( 3.042071309553159519, 84.73958332991936970, 11.35316468750000141 ) ) ;
#67803 = CARTESIAN_POINT ( 'NONE',  ( -4.556349186104048599, -10.99999999999999822, 97.28124999999998579 ) ) ;
#67805 = CARTESIAN_POINT ( 'NONE',  ( -5.656854249492375253, 5.656854249492375253, 14.33030278392014800 ) ) ;
#67806 = CARTESIAN_POINT ( 'NONE',  ( -25.55430564589119413, 201.5625000013656063, 167.5543056458915316 ) ) ;
#67807 =( BOUNDED_CURVE ( )  B_SPLINE_CURVE ( 2, ( #19948, #31657, #24505, #47509, #14280, #8643, #70898, #7900, #47879, #19213, #42218, #65230, #36573 ),
 .UNSPECIFIED., .F., .F. ) 
 B_SPLINE_CURVE_WITH_KNOTS ( ( 3, 2, 2, 2, 2, 2, 3 ),
 ( 0.4836956521739130266, 0.4855072463768115854, 0.4873188405797101441, 0.4891304347826087029, 0.4909420289855072617, 0.4927536231884058204, 0.4945652173913043237 ),
 .UNSPECIFIED. ) 
 CURVE ( )  GEOMETRIC_REPRESENTATION_ITEM ( )  RATIONAL_B_SPLINE_CURVE ( ( 1.000000000000000000, 0.9659258262890683122, 1.000000000000000000, 0.9659258262890683122, 1.000000000000000000, 0.9659258262890683122, 1.000000000000000000, 0.9659258262890683122, 1.000000000000000000, 0.9659258262890683122, 1.000000000000000000, 0.9659258262890683122, 1.000000000000000000 ) ) 
 REPRESENTATION_ITEM ( '' )  );
#67808 = CARTESIAN_POINT ( 'NONE',  ( 8.660254037844385522, 176.4583333265053682, 5.000000000000005329 ) ) ;
#67809 = DIRECTION ( 'NONE',  ( -0.000000000000000000, 1.000000000000000000, -0.000000000000000000 ) ) ;
#67810 = CARTESIAN_POINT ( 'NONE',  ( 8.311093377946834337, 80.46874999658601268, 8.311093377946839666 ) ) ;
#67811 = CARTESIAN_POINT ( 'NONE',  ( -6.676582343750000703, 289.5156250017070647, 2.765530957082001251 ) ) ;
#67812 = CARTESIAN_POINT ( 'NONE',  ( -10.18810118749999916, 0.000000000000000000, 99.53125000204838102 ) ) ;
#67813 = CARTESIAN_POINT ( 'NONE',  ( 5.676582343749993598, 224.9479166632526983, 9.832129032723422313 ) ) ;
#67814 = ORIENTED_EDGE ( 'NONE', *, *, #44067, .F. ) ;
#67815 = CARTESIAN_POINT ( 'NONE',  ( 0.000000000000000000, 0.000000000000000000, 0.000000000000000000 ) ) ;
#67816 = CARTESIAN_POINT ( 'NONE',  ( -8.000000000000001776, 2.156249995903220196, 3.313708498984759387 ) ) ;
#67817 = CARTESIAN_POINT ( 'NONE',  ( 2.485281374238878627, 291.3125000000000000, 5.999999999999694467 ) ) ;
#67818 = CARTESIAN_POINT ( 'NONE',  ( 3.042071309553167513, 201.8229166632526415, -11.35316468749999785 ) ) ;
#67819 = CARTESIAN_POINT ( 'NONE',  ( -2.679491924311228512, 227.0833333401612606, -9.999999999999998224 ) ) ;
#67820 = CARTESIAN_POINT ( 'NONE',  ( -2.828427124746190735, 20.37500000000000000, -2.828427124746191623 ) ) ;
#67821 = ORIENTED_EDGE ( 'NONE', *, *, #7604, .F. ) ;
#67822 = CARTESIAN_POINT ( 'NONE',  ( 8.311093377946834337, 190.4687499965860411, 8.311093377946839666 ) ) ;
#67823 = CARTESIAN_POINT ( 'NONE',  ( -7.188101187499990274, -2.977408999572651815, 16.58030278187175455 ) ) ;
#67824 = CARTESIAN_POINT ( 'NONE',  ( -30.44569435410879521, 207.8125000013656063, 172.4456943541092357 ) ) ;
#67825 = CARTESIAN_POINT ( 'NONE',  ( 3.313708498984762052, 12.28125000000000178, -8.000000000000000000 ) ) ;
#67826 = ORIENTED_EDGE ( 'NONE', *, *, #27453, .T. ) ;
#67827 = AXIS2_PLACEMENT_3D ( 'NONE', #66136, #6952, #27260 ) ;
#67828 = EDGE_CURVE ( 'NONE', #37361, #22045, #57304, .T. ) ;
#67829 = CARTESIAN_POINT ( 'NONE',  ( -8.000000000000000000, 89.09375000409676204, -3.313708498984761608 ) ) ;
#67830 = CARTESIAN_POINT ( 'NONE',  ( -2.679491924311235618, 13.54166666666666785, 10.00000000000000000 ) ) ;
#67831 = CARTESIAN_POINT ( 'NONE',  ( -4.220049686691935698, 10.18810118749999916, 79.75000000204838102 ) ) ;
#67832 = ORIENTED_EDGE ( 'NONE', *, *, #58834, .F. ) ;
#67833 = CARTESIAN_POINT ( 'NONE',  ( 4.541265875000002339, 0.3124999986344066949, 0.000000000000000000 ) ) ;
#67834 = CARTESIAN_POINT ( 'NONE',  ( 4.541265875000002339, 21.37499999863441147, -1.881053915767121776 ) ) ;
#67835 = ORIENTED_EDGE ( 'NONE', *, *, #27378, .T. ) ;
#67836 = DIRECTION ( 'NONE',  ( 0.000000000000000000, 0.000000000000000000, 1.000000000000000000 ) ) ;
#67837 = CARTESIAN_POINT ( 'NONE',  ( -7.188101187500000044, 92.65625000204838102, 0.000000000000000000 ) ) ;
#67838 = EDGE_CURVE ( 'NONE', #59649, #55260, #3254, .T. ) ;
#67841 = CARTESIAN_POINT ( 'NONE',  ( 0.000000000000000000, 0.000000000000000000, -25.03750572909317285 ) ) ;
#67840 = CARTESIAN_POINT ( 'NONE',  ( 2.085542519210945334E-15, 245.1562500034140157, 11.35316468749999963 ) ) ;
#67839 = CARTESIAN_POINT ( 'NONE',  ( 26.56734541678233441, 208.0000000013656063, 166.5412658749999650 ) ) ;
#67842 = PRODUCT_CONTEXT ( 'NONE', #36116, 'mechanical' ) ;
#67843 = ORIENTED_EDGE ( 'NONE', *, *, #3468, .F. ) ;
#67844 = CARTESIAN_POINT ( 'NONE',  ( -3.042071309553159075, 250.2604166700806445, 11.35316468749999963 ) ) ;
#67845 = CARTESIAN_POINT ( 'NONE',  ( -7.188101187499991163, 2.977408999572646930, 14.89280278187175455 ) ) ;
#67846 = VERTEX_POINT ( 'NONE', #55319 ) ;
#67847 = ORIENTED_EDGE ( 'NONE', *, *, #33019, .T. ) ;
#67848 = CARTESIAN_POINT ( 'NONE',  ( -7.204075437095965206, -7.204075437095968759, 75.34375000204838102 ) ) ;
#67849 = CARTESIAN_POINT ( 'NONE',  ( -11.35316468750000141, 68.80208332991935549, 3.042071309553159963 ) ) ;
#67850 = DIRECTION ( 'NONE',  ( 8.881784197001248379E-16, 0.000000000000000000, 1.000000000000000000 ) ) ;
#67851 = CARTESIAN_POINT ( 'NONE',  ( -6.735557395310442023E-16, 11.00000000000000000, 87.62499999999998579 ) ) ;
#67854 = CARTESIAN_POINT ( 'NONE',  ( 6.676582343750002480, 290.1718750017070079, -2.765530957081997254 ) ) ;
#67853 = CARTESIAN_POINT ( 'NONE',  ( 24.00000000000000355, 197.9375000027312410, 171.6568542494923122 ) ) ;
#67852 = CARTESIAN_POINT ( 'NONE',  ( 25.55430564589119768, 209.3125000013656063, 167.5543056458910485 ) ) ;
#67855 = CARTESIAN_POINT ( 'NONE',  ( 0.000000000000000000, 75.00000000000000000, 8.000000000000000000 ) ) ;
#67856 = CARTESIAN_POINT ( 'NONE',  ( 1.959434878635765526E-15, -16.00000000000000711, 3.497325839728428143 ) ) ;
#67857 = CARTESIAN_POINT ( 'NONE',  ( -3.458734124999960358, 197.6250000013656063, 196.5673454167823877 ) ) ;
#67858 = CARTESIAN_POINT ( 'NONE',  ( -8.000000000000000000, 9.562499995903223748, -9.797174393178825657E-16 ) ) ;
#67859 = ORIENTED_EDGE ( 'NONE', *, *, #34044, .T. ) ;
#67860 = CARTESIAN_POINT ( 'NONE',  ( 29.43265458321760519, 194.5000000013656063, 173.4587341249998929 ) ) ;
#67861 = CARTESIAN_POINT ( 'NONE',  ( -1.320432766682874540E-15, 19.96874999795161543, 7.188101187500000044 ) ) ;
#67862 = CARTESIAN_POINT ( 'NONE',  ( -8.311093377946841443, 164.2187499965860411, 8.311093377946830785 ) ) ;
#67863 = CARTESIAN_POINT ( 'NONE',  ( 25.17157287525381903, 198.0000000027312126, 172.8284271247460993 ) ) ;
#67864 = CARTESIAN_POINT ( 'NONE',  ( 5.082755093536325042, 105.9687500020483952, -5.082755093536325930 ) ) ;
#67866 = CARTESIAN_POINT ( 'NONE',  ( 1.558072418983080798, -51.25713184919913346, -48.56213741370739001 ) ) ;
#67865 = CARTESIAN_POINT ( 'NONE',  ( -4.999999999999995559, 206.6666666666667425, -8.660254037844385522 ) ) ;
#67867 = CARTESIAN_POINT ( 'NONE',  ( 31.45873412500001010, 206.0000000013656063, 168.5673454167822740 ) ) ;
#67868 = CARTESIAN_POINT ( 'NONE',  ( -5.082755093536319713, 5.082755093536319713, 18.17405278187175455 ) ) ;
#67869 = CARTESIAN_POINT ( 'NONE',  ( -2.828427124746209831, 207.5000000027312126, 139.1715728752538723 ) ) ;
#67870 = CARTESIAN_POINT ( 'NONE',  ( -5.676582343750006032, 59.11458332991935549, 9.832129032723418760 ) ) ;
#67871 = CARTESIAN_POINT ( 'NONE',  ( -2.604119496147003776, -43.49769568493226757, 139.1093791495934795 ) ) ;
#67872 = CARTESIAN_POINT ( 'NONE',  ( -2.679491924311235618, 20.41666665983870033, 10.00000000000000000 ) ) ;
#67873 = CARTESIAN_POINT ( 'NONE',  ( 4.000000000000016875, 195.5625000027312126, 199.6568542494924259 ) ) ;
#67874 = ORIENTED_EDGE ( 'NONE', *, *, #73203, .F. ) ;
#67875 = CARTESIAN_POINT ( 'NONE',  ( -2.849036369511732440E-14, 199.3750000027312126, 138.0000000000000568 ) ) ;
#67876 = AXIS2_PLACEMENT_3D ( 'NONE', #28383, #57822, #51392 ) ;
#67877 = CARTESIAN_POINT ( 'NONE',  ( 7.778174593052023411, -7.778174593052021635, 81.25000000409676204 ) ) ;
#67878 = CARTESIAN_POINT ( 'NONE',  ( 11.35316468750000141, 60.78124999658601979, 0.000000000000000000 ) ) ;
#67879 = CARTESIAN_POINT ( 'NONE',  ( -7.778174593052020747, -7.778174593052023411, 71.87500000409677625 ) ) ;
#67880 = CARTESIAN_POINT ( 'NONE',  ( -3.458734125000015425, 198.2500000013656347, 143.4326545832176976 ) ) ;
#67881 = DIRECTION ( 'NONE',  ( -0.000000000000000000, -0.000000000000000000, -1.000000000000000000 ) ) ;
#67882 = CARTESIAN_POINT ( 'NONE',  ( 1.656854249492401232, 207.3125000000000000, 202.0000000000000000 ) ) ;
#67884 = CARTESIAN_POINT ( 'NONE',  ( 3.042071309553167513, 41.82291666325269119, -11.35316468749999785 ) ) ;
#67883 = CARTESIAN_POINT ( 'NONE',  ( -4.401442555609581635E-16, 92.28125000204836681, -7.188101187500000044 ) ) ;
#67885 = CARTESIAN_POINT ( 'NONE',  ( 7.999999999999991118, 3.313708498984757611, 3.174052779823361981 ) ) ;
#67886 = CARTESIAN_POINT ( 'NONE',  ( 2.679491924311375950, 206.0416666666666572, -9.999999999999911182 ) ) ;
#67887 = CARTESIAN_POINT ( 'NONE',  ( -9.832129032723420536, 168.6979166632526983, 5.676582343749997150 ) ) ;
#67888 = CARTESIAN_POINT ( 'NONE',  ( 8.660254037844385522, 146.4583333265053682, 5.000000000000005329 ) ) ;
#67889 = CARTESIAN_POINT ( 'NONE',  ( 7.188101187500002709, 105.6875000020483952, 2.977408999572649151 ) ) ;
#67890 = CARTESIAN_POINT ( 'NONE',  ( 4.850062511589654031E-16, 0.4207531754730554074, -7.920753175473053354 ) ) ;
#67891 = CARTESIAN_POINT ( 'NONE',  ( -11.35316468750000141, 38.59374999658601979, -1.390361679473963753E-15 ) ) ;
#67892 =( BOUNDED_CURVE ( )  B_SPLINE_CURVE ( 2, ( #27973, #50977, #39664, #33278, #72503, #38180, #55541, #55914, #20812, #9514, #21925, #27214, #61184 ),
 .UNSPECIFIED., .F., .F. ) 
 B_SPLINE_CURVE_WITH_KNOTS ( ( 3, 2, 2, 2, 2, 2, 3 ),
 ( 0.5706521739130434590, 0.5724637681159420177, 0.5742753623188405765, 0.5760869565217391353, 0.5778985507246376940, 0.5797101449275362528, 0.5815217391304348116 ),
 .UNSPECIFIED. ) 
 CURVE ( )  GEOMETRIC_REPRESENTATION_ITEM ( )  RATIONAL_B_SPLINE_CURVE ( ( 1.000000000000000000, 0.9659258262890683122, 1.000000000000000000, 0.9659258262890683122, 1.000000000000000000, 0.9659258262890683122, 1.000000000000000000, 0.9659258262890683122, 1.000000000000000000, 0.9659258262890683122, 1.000000000000000000, 0.9659258262890683122, 1.000000000000000000 ) ) 
 REPRESENTATION_ITEM ( '' )  );
#67893 = CARTESIAN_POINT ( 'NONE',  ( 6.000000000000003553, 295.5000000034139589, 2.485281374238571317 ) ) ;
#67894 = CARTESIAN_POINT ( 'NONE',  ( 9.832129032723416984, 165.3645833299193555, 5.676582343750006032 ) ) ;
#67895 = ORIENTED_EDGE ( 'NONE', *, *, #32420, .T. ) ;
#67896 = CARTESIAN_POINT ( 'NONE',  ( 47.73049838254536326, 144.2032679345639679, 63.57013892992240045 ) ) ;
#67897 = CARTESIAN_POINT ( 'NONE',  ( 10.18810118749999916, 1.247682550866122264E-15, 69.90625000204836681 ) ) ;
#67898 = CARTESIAN_POINT ( 'NONE',  ( 2.849036369511732440E-14, 196.2500000000000000, 202.0000000000000284 ) ) ;
#67899 = CARTESIAN_POINT ( 'NONE',  ( 37.38110958774591808, 39.09128788536430221, 65.00000000000001421 ) ) ;
#67901 = CARTESIAN_POINT ( 'NONE',  ( -3.042071309553173730, 169.3229166632526699, 11.35316468749999785 ) ) ;
#67900 = CARTESIAN_POINT ( 'NONE',  ( 10.99999999999999645, 10.99999999999999645, 25.00000000000000000 ) ) ;
#67902 = CARTESIAN_POINT ( 'NONE',  ( 7.999999999999991118, 3.313708498984757611, 12.23030278432982243 ) ) ;
#67903 = CARTESIAN_POINT ( 'NONE',  ( 3.999999999999960032, 208.0625000027312410, 143.6568542494924259 ) ) ;
#67904 = CARTESIAN_POINT ( 'NONE',  ( -3.042071309553166181, 222.8645833367473301, -11.35316468749999608 ) ) ;
#67905 = CARTESIAN_POINT ( 'NONE',  ( 4.330454160156390842, 52.03352386568179355, -48.86100738216495643 ) ) ;
#67906 = CARTESIAN_POINT ( 'NONE',  ( -4.220049686691935698, 10.18810118749999916, 78.25000000204836681 ) ) ;
#67907 = ORIENTED_EDGE ( 'NONE', *, *, #30733, .F. ) ;
#67908 = VECTOR ( 'NONE', #38490, 1000.000000000000000 ) ;
#67909 = CARTESIAN_POINT ( 'NONE',  ( 1.567784982238203817E-13, 73.75000000000002842, 10.00000000000000533 ) ) ;
#67910 = CARTESIAN_POINT ( 'NONE',  ( -11.35316468750000141, 113.5937499965860127, -1.390361679473963753E-15 ) ) ;
#67911 =( BOUNDED_CURVE ( )  B_SPLINE_CURVE ( 2, ( #41478, #6042, #41843, #23756, #12793, #7520, #18098, #29047, #64493 ),
 .UNSPECIFIED., .F., .F. ) 
 B_SPLINE_CURVE_WITH_KNOTS ( ( 3, 2, 2, 2, 3 ),
 ( 0.9166666666666674068, 0.9250000000000009326, 0.9333333333333342363, 0.9416666666666675400, 0.9500000000000009548 ),
 .UNSPECIFIED. ) 
 CURVE ( )  GEOMETRIC_REPRESENTATION_ITEM ( )  RATIONAL_B_SPLINE_CURVE ( ( 0.9999999999999928946, 0.9238795325112938439, 1.000000000000000000, 0.9238795325112867385, 1.000000000000000000, 0.9238795325112867385, 1.000000000000000000, 0.9238795325112776347, 1.000000000000009104 ) ) 
 REPRESENTATION_ITEM ( '' )  );
#67912 = LINE ( 'NONE', #5660, #52621 ) ;
#67913 = ORIENTED_EDGE ( 'NONE', *, *, #36996, .F. ) ;
#67914 = ORIENTED_EDGE ( 'NONE', *, *, #17826, .F. ) ;
#67915 = CARTESIAN_POINT ( 'NONE',  ( 4.541265875000001451, 6.374999998634407028, 1.881053915767124440 ) ) ;
#67916 = EDGE_CURVE ( 'NONE', #14809, #48531, #43603, .T. ) ;
#67917 = CARTESIAN_POINT ( 'NONE',  ( -7.188101187500001821, 11.62499999795161187, -2.977408999572651371 ) ) ;
#67918 = CARTESIAN_POINT ( 'NONE',  ( -5.656854249492378806, 107.3750000040967763, 5.656854249492381470 ) ) ;
#67919 = CARTESIAN_POINT ( 'NONE',  ( 4.220049686691934809, 10.18810118749999916, 90.06250000204838102 ) ) ;
#67920 = ADVANCED_FACE ( 'NONE', ( #73400 ), #68114, .F. ) ;
#67921 = CARTESIAN_POINT ( 'NONE',  ( -26.56734541678237704, 197.6250000013656063, 166.5412658750003629 ) ) ;
#67922 = CARTESIAN_POINT ( 'NONE',  ( -1.656854249492383691, 9.687500000000000000, 4.000000000000000888 ) ) ;
#67923 = CARTESIAN_POINT ( 'NONE',  ( 1.656854249492381248, 20.93749999726881228, -4.000000000000001776 ) ) ;
#67924 = CARTESIAN_POINT ( 'NONE',  ( 3.211159895383561835, 8.437499998634407916, -3.211159895383561835 ) ) ;
#67926 = VECTOR ( 'NONE', #4878, 1000.000000000000000 ) ;
#67925 = CARTESIAN_POINT ( 'NONE',  ( 3.999999999999959144, 197.0625000000000000, 140.3431457505076594 ) ) ;
#67927 = ORIENTED_EDGE ( 'NONE', *, *, #18017, .T. ) ;
#67928 = CARTESIAN_POINT ( 'NONE',  ( 1.469576158976823947E-15, 116.3750000000000000, 8.000000000000000000 ) ) ;
#67929 = CARTESIAN_POINT ( 'NONE',  ( -7.188101187500000044, 109.1562500020483810, 0.000000000000000000 ) ) ;
#67930 = EDGE_CURVE ( 'NONE', #31825, #43001, #41118, .T. ) ;
#67932 = CARTESIAN_POINT ( 'NONE',  ( -7.188101187500000044, 124.1562500020483810, 0.000000000000000000 ) ) ;
#67931 = CARTESIAN_POINT ( 'NONE',  ( -26.56734541678227757, 197.0000000013656347, 173.4587341250003476 ) ) ;
#67933 = CARTESIAN_POINT ( 'NONE',  ( -1.656854249492393238, 10.31249999999999822, -3.999999999999989786 ) ) ;
#67934 = CARTESIAN_POINT ( 'NONE',  ( -7.188101187499990274, -2.977408999572651371, 3.080302781871750994 ) ) ;
#67935 = ORIENTED_EDGE ( 'NONE', *, *, #33134, .T. ) ;
#67936 = ORIENTED_EDGE ( 'NONE', *, *, #56856, .F. ) ;
#67937 = CARTESIAN_POINT ( 'NONE',  ( 4.220049686691941027, -10.18810118749999738, 95.12500000204838102 ) ) ;
#67938 = CARTESIAN_POINT ( 'NONE',  ( -9.526279441628821232, 219.8393163974770630, 5.500000000000004441 ) ) ;
#67939 = CARTESIAN_POINT ( 'NONE',  ( -28.00000000000002132, 199.6875000013656063, 166.5412658750003629 ) ) ;
#67940 = CARTESIAN_POINT ( 'NONE',  ( 4.556349186104051263, -10.99999999999999822, 106.4687499999999716 ) ) ;
#67941 = CARTESIAN_POINT ( 'NONE',  ( -3.458734124999960358, 208.6250000013655779, 196.5673454167823877 ) ) ;
#67943 = CARTESIAN_POINT ( 'NONE',  ( -10.00000000000000888, 127.5000000000000000, -1.224646799147354243E-15 ) ) ;
#67942 = CARTESIAN_POINT ( 'NONE',  ( 1.469576158976823947E-15, 111.8750000000000000, 8.000000000000000000 ) ) ;
#67944 = CARTESIAN_POINT ( 'NONE',  ( -2.679491924311235618, 123.5416666666666572, 10.00000000000000000 ) ) ;
#67945 = CARTESIAN_POINT ( 'NONE',  ( -8.000000000000000000, 107.0000000000000000, 0.000000000000000000 ) ) ;
#67946 = FACE_OUTER_BOUND ( 'NONE', #46464, .T. ) ;
#67947 = CARTESIAN_POINT ( 'NONE',  ( 1.320432766682872962E-15, -7.188101187499992051, 3.736552781871751883 ) ) ;
#67948 = CARTESIAN_POINT ( 'NONE',  ( 1.469576158976823947E-15, 98.37499999999998579, 8.000000000000000000 ) ) ;
#67950 = EDGE_CURVE ( 'NONE', #70051, #19664, #23570, .T. ) ;
#67949 = CARTESIAN_POINT ( 'NONE',  ( 26.56734541678232731, 206.3750000013656063, 173.4587341249998929 ) ) ;
#67951 = CARTESIAN_POINT ( 'NONE',  ( -5.082755093536326818, 1.781249997951610098, 5.082755093536325042 ) ) ;
#67952 = CIRCLE ( 'NONE', #46247, 10.00000000000000000 ) ;
#67953 = CARTESIAN_POINT ( 'NONE',  ( -2.445694354108838731, 199.0625000013656063, 144.4456943541088663 ) ) ;
#67955 = CARTESIAN_POINT ( 'NONE',  ( 3.458734124999959469, 201.7500000013655779, 140.5673454167824161 ) ) ;
#67954 = CARTESIAN_POINT ( 'NONE',  ( -7.347880794884122694E-16, 20.49999999726881583, 4.000000000000001776 ) ) ;
#67956 = CARTESIAN_POINT ( 'NONE',  ( -9.832129032723418760, 248.8020833367473301, -5.676582343749998927 ) ) ;
#67957 = DIRECTION ( 'NONE',  ( 0.000000000000000000, 0.000000000000000000, 1.000000000000000000 ) ) ;
#67958 = CARTESIAN_POINT ( 'NONE',  ( -2.679491924311300011, 93.33333332650538239, -9.999999999999959144 ) ) ;
#67959 = CARTESIAN_POINT ( 'NONE',  ( 28.00000000000001776, 200.5000000000000000, 165.9999999999998863 ) ) ;
#67960 = CARTESIAN_POINT ( 'NONE',  ( 3.042071309553159519, 9.739583329919350163, 11.35316468750000141 ) ) ;
#67961 = DIRECTION ( 'NONE',  ( -1.000000000000000000, -0.000000000000000000, -0.000000000000000000 ) ) ;
#67962 = CARTESIAN_POINT ( 'NONE',  ( -3.042071309553164404, 212.5520833299193839, -11.35316468749999963 ) ) ;
#67963 = CARTESIAN_POINT ( 'NONE',  ( -25.17157287525385811, 203.0000000027312126, 167.1715728752541281 ) ) ;
#67964 = LINE ( 'NONE', #16257, #71634 ) ;
#67965 = CYLINDRICAL_SURFACE ( 'NONE', #74418, 9.000000000000001776 ) ;
#67966 = ORIENTED_EDGE ( 'NONE', *, *, #64411, .T. ) ;
#67967 = CARTESIAN_POINT ( 'NONE',  ( -3.458734125000015869, 199.1875000013655779, 142.0000000000000568 ) ) ;
#67968 = CARTESIAN_POINT ( 'NONE',  ( -11.35316468750000141, 13.28124999658601624, -1.390361679473963753E-15 ) ) ;
#67969 = CARTESIAN_POINT ( 'NONE',  ( 7.778174593052023411, -7.778174593052021635, 91.75000000409677625 ) ) ;
#67970 = CARTESIAN_POINT ( 'NONE',  ( 1.704527592502714350, 10.27896685065642934, 63.66027613114050610 ) ) ;
#67971 = CARTESIAN_POINT ( 'NONE',  ( -31.45873412500002075, 195.6250000013656063, 168.5673454167828140 ) ) ;
#67972 = CARTESIAN_POINT ( 'NONE',  ( 3.313708498984761608, 7.593749995903221084, -8.000000000000000000 ) ) ;
#67974 = CARTESIAN_POINT ( 'NONE',  ( 3.042071309553167513, 1.822916663252682756, -11.35316468749999785 ) ) ;
#67973 = CARTESIAN_POINT ( 'NONE',  ( -5.082755093536325930, 117.9687500020483810, -5.082755093536325930 ) ) ;
#67975 = CARTESIAN_POINT ( 'NONE',  ( -3.313708498984758943, -7.999999999999989342, 19.11155277982336997 ) ) ;
#67976 = CARTESIAN_POINT ( 'NONE',  ( -9.832129032723420536, 138.6979166632526983, 5.676582343749997150 ) ) ;
#67977 = CARTESIAN_POINT ( 'NONE',  ( 4.999999999999993783, 106.0416666598387110, 8.660254037844390851 ) ) ;
#67978 = CARTESIAN_POINT ( 'NONE',  ( 7.188101187500001821, 117.8750000020483810, -2.977408999572651371 ) ) ;
#67979 = CARTESIAN_POINT ( 'NONE',  ( -3.313708498984727413, 120.4062500040967763, -8.000000000000033751 ) ) ;
#67980 = CARTESIAN_POINT ( 'NONE',  ( -25.55430564589115505, 208.3125000013656063, 172.4456943541091789 ) ) ;
#67981 = CARTESIAN_POINT ( 'NONE',  ( -8.660254037844387298, 38.95833332650536818, -5.000000000000004441 ) ) ;
#67982 = ORIENTED_EDGE ( 'NONE', *, *, #48914, .F. ) ;
#67983 = CARTESIAN_POINT ( 'NONE',  ( -0.6547826978432378375, -60.19560277018450023, 22.88235556322767650 ) ) ;
#67984 = CARTESIAN_POINT ( 'NONE',  ( 4.721056650416000089, 288.9843750017070079, 4.721056650415999201 ) ) ;
#67985 = CARTESIAN_POINT ( 'NONE',  ( 4.999999999999999112, 53.55923425356063916, 45.42020841079129667 ) ) ;
#67986 = CARTESIAN_POINT ( 'NONE',  ( 5.656854249492374365, 5.656854249492375253, 1.955302783920143117 ) ) ;
#67987 = VECTOR ( 'NONE', #770, 1000.000000000000000 ) ;
#67988 = CARTESIAN_POINT ( 'NONE',  ( -27.99999999999995737, 198.5000000000000000, 174.0000000000003695 ) ) ;
#67989 = CARTESIAN_POINT ( 'NONE',  ( -11.35316468749999963, 263.9062500034140157, 0.000000000000000000 ) ) ;
#67990 = CARTESIAN_POINT ( 'NONE',  ( 10.18810118749999916, 4.220049686691935698, 98.87500000204836681 ) ) ;
#67991 = ORIENTED_EDGE ( 'NONE', *, *, #39191, .F. ) ;
#67992 = CARTESIAN_POINT ( 'NONE',  ( 0.000000000000000000, 15.99999999999998579, 0.000000000000000000 ) ) ;
#67993 = CARTESIAN_POINT ( 'NONE',  ( -5.676582343750006032, 164.4270833299193555, 9.832129032723418760 ) ) ;
#67994 = CARTESIAN_POINT ( 'NONE',  ( 7.999999999999991118, 9.797174393178815797E-16, 24.08030277982336642 ) ) ;
#67995 = CARTESIAN_POINT ( 'NONE',  ( 1.432654583217662481, 201.3750000013656347, 194.5412658750000219 ) ) ;
#67996 = CARTESIAN_POINT ( 'NONE',  ( 3.042071309553159519, 80.05208332991935549, 11.35316468750000141 ) ) ;
#67997 = VERTEX_POINT ( 'NONE', #10032 ) ;
#67998 = CARTESIAN_POINT ( 'NONE',  ( 4.220049686691941027, -10.18810118749999738, 111.6250000020483810 ) ) ;
#67999 = CARTESIAN_POINT ( 'NONE',  ( 4.541265875000002339, 14.49999999863440969, -1.881053915767121776 ) ) ;
#68000 = ORIENTED_EDGE ( 'NONE', *, *, #50100, .F. ) ;
#68001 = CARTESIAN_POINT ( 'NONE',  ( 5.082755093536325930, 24.65624999795161543, -5.082755093536325930 ) ) ;
#68002 = DIRECTION ( 'NONE',  ( 0.000000000000000000, 0.000000000000000000, 1.000000000000000000 ) ) ;
#68003 = CARTESIAN_POINT ( 'NONE',  ( -2.679491924311315110, 247.0833333401613174, -9.999999999999950262 ) ) ;
#68004 = CARTESIAN_POINT ( 'NONE',  ( -1.320432766682874540E-15, 16.96874999795161543, 7.188101187500000044 ) ) ;
#68005 = CARTESIAN_POINT ( 'NONE',  ( -8.000000000000000000, 124.5000000000000284, -1.469576158976823947E-15 ) ) ;
#68006 =( BOUNDED_CURVE ( )  B_SPLINE_CURVE ( 2, ( #1906, #46443, #58162, #6827, #24894, #47176, #47911, #17394, #69461, #18883, #40418, #63416, #52118 ),
 .UNSPECIFIED., .F., .F. ) 
 B_SPLINE_CURVE_WITH_KNOTS ( ( 3, 2, 2, 2, 2, 2, 3 ),
 ( 1.899690555530577418, 1.904923638444253831, 1.910156721357930021, 1.915389804271605989, 1.920622887185282401, 1.925855970098958592, 1.931089053012635004 ),
 .UNSPECIFIED. ) 
 CURVE ( )  GEOMETRIC_REPRESENTATION_ITEM ( )  RATIONAL_B_SPLINE_CURVE ( ( 1.000000000000022871, 0.9659258262890453306, 1.000000000000000000, 0.9659258262890683122, 1.000000000000000000, 0.9659258262890683122, 1.000000000000000000, 0.9659258262890683122, 1.000000000000000000, 0.9659258262890683122, 1.000000000000000000, 0.9659258262888135160, 1.000000000000254685 ) ) 
 REPRESENTATION_ITEM ( '' )  );
#68007 = CARTESIAN_POINT ( 'NONE',  ( -4.220049686691935698, 10.18810118749999916, 108.2500000020483810 ) ) ;
#68008 = EDGE_CURVE ( 'NONE', #29891, #493, #72393, .T. ) ;
#68009 = PRODUCT ( 'dead centre', 'dead centre', '', ( #39550 ) ) ;
#68010 = VECTOR ( 'NONE', #48141, 1000.000000000000000 ) ;
#68011 = CARTESIAN_POINT ( 'NONE',  ( 2.828427124746209831, 201.5000000027312126, 200.8284271247462129 ) ) ;
#68012 = CARTESIAN_POINT ( 'NONE',  ( -7.347880794884122694E-16, 10.49999999726881406, 4.000000000000001776 ) ) ;
#68013 = CARTESIAN_POINT ( 'NONE',  ( 0.000000000000000000, 300.0000000000000000, 0.000000000000000000 ) ) ;
#68014 = ORIENTED_EDGE ( 'NONE', *, *, #25630, .T. ) ;
#68015 = CARTESIAN_POINT ( 'NONE',  ( -2.445694354108783664, 203.3125000013656063, 195.5543056458912190 ) ) ;
#68016 = CARTESIAN_POINT ( 'NONE',  ( -25.55430564589123321, 207.3125000013656063, 167.5543056458915032 ) ) ;
#68017 = CARTESIAN_POINT ( 'NONE',  ( -2.751064625579944321E-14, 206.7500000000000284, 146.0000000000000284 ) ) ;
#68018 =( BOUNDED_CURVE ( )  B_SPLINE_CURVE ( 2, ( #12127, #35166, #58181, #13225, #1203, #7587, #24914, #42275, #64192 ),
 .UNSPECIFIED., .F., .F. ) 
 B_SPLINE_CURVE_WITH_KNOTS ( ( 3, 2, 2, 2, 3 ),
 ( 0.5000000000000000000, 0.5036764705882352811, 0.5073529411764705621, 0.5110294117647059542, 0.5147058823529412352 ),
 .UNSPECIFIED. ) 
 CURVE ( )  GEOMETRIC_REPRESENTATION_ITEM ( )  RATIONAL_B_SPLINE_CURVE ( ( 1.000000000000000000, 0.9238795325112867385, 1.000000000000000000, 0.9238795325112867385, 1.000000000000000000, 0.9238795325112867385, 1.000000000000000000, 0.9238795325112844070, 1.000000000000002220 ) ) 
 REPRESENTATION_ITEM ( '' )  );
#68019 = EDGE_CURVE ( 'NONE', #27721, #34733, #4750, .T. ) ;
#68020 = CARTESIAN_POINT ( 'NONE',  ( 4.541265875000001451, 11.24999999863440792, 1.881053915767124440 ) ) ;
#68021 = CARTESIAN_POINT ( 'NONE',  ( 28.00000000000001776, 204.5000000000000284, 165.9999999999998863 ) ) ;
#68022 = CARTESIAN_POINT ( 'NONE',  ( 5.082755093536320601, -5.082755093536318824, 21.54905278187175455 ) ) ;
#68023 = ORIENTED_EDGE ( 'NONE', *, *, #18185, .F. ) ;
#68024 = EDGE_CURVE ( 'NONE', #44513, #26323, #5436, .T. ) ;
#68025 = CARTESIAN_POINT ( 'NONE',  ( -6.000000000000000000, 7.347880794884119736E-16, -10.80000000000000071 ) ) ;
#68026 = EDGE_LOOP ( 'NONE', ( #36475, #46963, #11996, #12362 ) ) ;
#68027 = CARTESIAN_POINT ( 'NONE',  ( 4.220049686691941027, -10.18810118749999738, 113.1250000020483810 ) ) ;
#68028 = CARTESIAN_POINT ( 'NONE',  ( 3.459103461385761413, -7.213501455148458419, -0.0001169852011744028255 ) ) ;
#68029 = CARTESIAN_POINT ( 'NONE',  ( 2.754378923186476579E-14, 203.1875000013656063, 194.5412658750000219 ) ) ;
#68030 = CARTESIAN_POINT ( 'NONE',  ( 31.45873412499999233, 197.6875000013655779, 169.9999999999998863 ) ) ;
#68031 = CARTESIAN_POINT ( 'NONE',  ( -2.679491924311225848, 76.45833333333331439, -10.00000000000000178 ) ) ;
#68032 = CIRCLE ( 'NONE', #69224, 9.949874371066211864 ) ;
#68033 = CARTESIAN_POINT ( 'NONE',  ( 1.469576158976823947E-15, 122.3750000000000000, 8.000000000000000000 ) ) ;
#68034 = CARTESIAN_POINT ( 'NONE',  ( -6.000000000000001776, 293.0000000000000000, 0.000000000000000000 ) ) ;
#68035 = CARTESIAN_POINT ( 'NONE',  ( 32.00000000000000711, 204.3125000027312126, 171.6568542494922553 ) ) ;
#68036 = ORIENTED_EDGE ( 'NONE', *, *, #39451, .F. ) ;
#68037 = B_SPLINE_CURVE_WITH_KNOTS ( 'NONE', 3,
 ( #67330, #66572, #67704, #38667, #3582, #26954, #61669, #25823, #31877, #54900, #37541, #21663, #9988, #72227, #44317, #38289, #56022, #9621, #48842, #32641, #55650, #71850 ),
 .UNSPECIFIED., .F., .F.,
 ( 4, 2, 2, 2, 2, 2, 2, 2, 2, 2, 4 ),
 ( 0.000000000000000000, 0.001156727053362450498, 0.001735090580043667941, 0.002313454106724884950, 0.003470181160087358867, 0.004048544686768596260, 0.004626908213449832351, 0.005783635266812303666, 0.006940362320174774113, 0.008097089373537246296, 0.009253816426899716743 ),
 .UNSPECIFIED. ) ;
#68038 = CARTESIAN_POINT ( 'NONE',  ( -8.311093377946834337, 224.5312500034140157, 8.311093377946837890 ) ) ;
#68039 = EDGE_CURVE ( 'NONE', #5538, #51786, #20844, .T. ) ;
#68040 = CARTESIAN_POINT ( 'NONE',  ( 5.656854249492374365, 5.656854249492375253, 7.767802779823362869 ) ) ;
#68041 = CARTESIAN_POINT ( 'NONE',  ( 1.656854249492348607, 194.3125000027312126, 138.0000000000000568 ) ) ;
#68042 = CARTESIAN_POINT ( 'NONE',  ( -5.000000000000000000, 67.53158052529128952, 22.66975313813598092 ) ) ;
#68043 = CARTESIAN_POINT ( 'NONE',  ( 7.999999999999998224, 13.21874999590322375, 3.313708498984766049 ) ) ;
#68044 = CARTESIAN_POINT ( 'NONE',  ( 10.00000000000000000, 232.5000000000000000, -1.224646799147353256E-15 ) ) ;
#68045 = EDGE_CURVE ( 'NONE', #69783, #22824, #28572, .T. ) ;
#68046 = CARTESIAN_POINT ( 'NONE',  ( 31.99999999999998579, 203.4375000027312126, 168.3431457505074889 ) ) ;
#68047 = CARTESIAN_POINT ( 'NONE',  ( 2.679491924311228956, 196.0416666666666856, -10.00000000000000000 ) ) ;
#68048 = CARTESIAN_POINT ( 'NONE',  ( 105.0000000000000000, 0.000000000000000000, 0.000000000000000000 ) ) ;
#68049 = CARTESIAN_POINT ( 'NONE',  ( 7.188101187499992051, 8.802885111219154394E-16, 19.11155278187175455 ) ) ;
#68050 = CARTESIAN_POINT ( 'NONE',  ( -9.832129032723420536, 174.0104166632526983, 5.676582343749997150 ) ) ;
#68051 = CARTESIAN_POINT ( 'NONE',  ( -8.660254037844389075, 37.91666666666667140, 4.999999999999996447 ) ) ;
#68052 = CARTESIAN_POINT ( 'NONE',  ( -2.258623695609613069, -43.01588618776830231, 151.1342130538614867 ) ) ;
#68054 = CARTESIAN_POINT ( 'NONE',  ( 10.00000000000000178, 87.08333332650535397, -2.679491924311226736 ) ) ;
#68053 = DIRECTION ( 'NONE',  ( -1.000000000000000000, 0.000000000000000000, 0.000000000000000000 ) ) ;
#68055 = VERTEX_POINT ( 'NONE', #68853 ) ;
#68056 = CARTESIAN_POINT ( 'NONE',  ( 6.951808397369818766E-16, 17.34374999658601624, -11.35316468750000141 ) ) ;
#68057 = VECTOR ( 'NONE', #57028, 1000.000000000000000 ) ;
#68058 = CARTESIAN_POINT ( 'NONE',  ( -28.00000000000007461, 209.4375000013656063, 166.5412658750003629 ) ) ;
#68060 = CARTESIAN_POINT ( 'NONE',  ( -2.589639417659336917, -10.27590863719300707, -63.78668228762852976 ) ) ;
#68059 = CARTESIAN_POINT ( 'NONE',  ( -7.999999999970034636, -1.442163225726577833E-05, 17.51834960462420909 ) ) ;
#68061 = CARTESIAN_POINT ( 'NONE',  ( -24.09644465270180902, -50.77329980035179346, 189.5085989920651741 ) ) ;
#68062 = CARTESIAN_POINT ( 'NONE',  ( -2.839093476692135984E-14, 202.6875000013656063, 138.5412658750000503 ) ) ;
#68063 = CARTESIAN_POINT ( 'NONE',  ( -7.320508075688773708, 63.74999999317202537, -7.320508075688774596 ) ) ;
#68064 = CIRCLE ( 'NONE', #41566, 8.000000000000000000 ) ;
#68065 = CARTESIAN_POINT ( 'NONE',  ( -7.188101187500000044, 103.1562500020483810, 0.000000000000000000 ) ) ;
#68066 = CARTESIAN_POINT ( 'NONE',  ( -3.211159895383562723, 7.062499998634407028, 3.211159895383561391 ) ) ;
#68067 = CARTESIAN_POINT ( 'NONE',  ( -7.999999999999991118, 0.000000000000000000, 20.33030277982336642 ) ) ;
#68068 = CARTESIAN_POINT ( 'NONE',  ( 1.469576158976822172E-15, -7.999999999999991118, 4.205302779823362869 ) ) ;
#68069 = CARTESIAN_POINT ( 'NONE',  ( -4.000000000000001776, 5.187499997268813168, -1.656854249492381470 ) ) ;
#68070 = ORIENTED_EDGE ( 'NONE', *, *, #58248, .T. ) ;
#68071 = ORIENTED_EDGE ( 'NONE', *, *, #72766, .T. ) ;
#68072 = CARTESIAN_POINT ( 'NONE',  ( -5.000000000000052403, 196.6666666666667140, -8.660254037844479669 ) ) ;
#68073 = CARTESIAN_POINT ( 'NONE',  ( -5.656854249492373476, -5.656854249492376141, 14.70530278392014800 ) ) ;
#68074 = CARTESIAN_POINT ( 'NONE',  ( -8.660254037844396180, 162.0833333333333712, -5.000000000000009770 ) ) ;
#68075 = ADVANCED_FACE ( 'NONE', ( #17165 ), #40184, .F. ) ;
#68076 = CARTESIAN_POINT ( 'NONE',  ( 8.311093377946839666, 221.0937500034139589, 8.311093377946830785 ) ) ;
#68077 = CARTESIAN_POINT ( 'NONE',  ( -9.832129032723420536, 143.6979166632526699, 5.676582343749997150 ) ) ;
#68078 = EDGE_LOOP ( 'NONE', ( #65937, #15098, #39355, #66413 ) ) ;
#68079 = LINE ( 'NONE', #26581, #21083 ) ;
#68080 = CARTESIAN_POINT ( 'NONE',  ( -4.220049686691935698, 10.18810118749999916, 88.37500000204839523 ) ) ;
#68081 = CARTESIAN_POINT ( 'NONE',  ( 7.999999999999998224, 4.406250000000000000, 3.313708498984766049 ) ) ;
#68082 = CARTESIAN_POINT ( 'NONE',  ( -1.656854249492347719, 206.8125000000000000, 194.0000000000000853 ) ) ;
#68083 = CARTESIAN_POINT ( 'NONE',  ( -8.000000000000000000, 18.56249999590322020, -9.797174393178825657E-16 ) ) ;
#68084 = CARTESIAN_POINT ( 'NONE',  ( 11.00000000000007994, 4.556349186103967774, 112.8437500000000000 ) ) ;
#68085 = EDGE_CURVE ( 'NONE', #64051, #54774, #69229, .T. ) ;
#68086 = CARTESIAN_POINT ( 'NONE',  ( -10.18810118749999916, 4.220049686691934809, 115.9375000020483668 ) ) ;
#68087 = ORIENTED_EDGE ( 'NONE', *, *, #68445, .T. ) ;
#68088 = CARTESIAN_POINT ( 'NONE',  ( 37.31325152499015729, -3.131698541404932534, 131.1298005505059905 ) ) ;
#68089 = CARTESIAN_POINT ( 'NONE',  ( 10.80039871841047550, 177.7629128266401608, 140.8571828581857517 ) ) ;
#68090 = CARTESIAN_POINT ( 'NONE',  ( 5.676582343750001591, 126.9270833299193697, -9.832129032723420536 ) ) ;
#68091 = CARTESIAN_POINT ( 'NONE',  ( 3.458734125000015425, 203.0000000013655779, 196.5673454167823877 ) ) ;
#68092 = CARTESIAN_POINT ( 'NONE',  ( 5.082755093536324154, 24.65624999795161543, 5.082755093536326818 ) ) ;
#68094 = EDGE_CURVE ( 'NONE', #23868, #51437, #69602, .T. ) ;
#68093 = CARTESIAN_POINT ( 'NONE',  ( -10.18810118749999738, -4.220049686691941915, 86.12500000204836681 ) ) ;
#68095 = CARTESIAN_POINT ( 'NONE',  ( 6.951808397369818766E-16, 32.34374999658601268, -11.35316468750000141 ) ) ;
#68096 = ORIENTED_EDGE ( 'NONE', *, *, #65174, .T. ) ;
#68097 = CARTESIAN_POINT ( 'NONE',  ( 11.00000000000000000, 1.347111479062088405E-15, 84.24999999999998579 ) ) ;
#68098 = CARTESIAN_POINT ( 'NONE',  ( 5.662595241051934458, 5.662595241051935346, 19.95061528394062833 ) ) ;
#68099 = CARTESIAN_POINT ( 'NONE',  ( 3.458734124999959469, 208.7500000013656063, 140.5673454167824161 ) ) ;
#68100 = CARTESIAN_POINT ( 'NONE',  ( 4.401442555609581635E-16, 11.34374999795161010, -7.188101187500000044 ) ) ;
#68101 = CARTESIAN_POINT ( 'NONE',  ( 4.242640687119287435, 298.4375000034140157, 4.242640687119285658 ) ) ;
#68102 = CARTESIAN_POINT ( 'NONE',  ( -1.836970198721029983E-15, 110.6249999931720396, 10.00000000000000178 ) ) ;
#68103 = CARTESIAN_POINT ( 'NONE',  ( -2.977408999572650039, 2.812499997951610542, -7.188101187500001821 ) ) ;
#68104 = CARTESIAN_POINT ( 'NONE',  ( 8.311093377946837890, 151.7187499965860127, -8.311093377946837890 ) ) ;
#68105 = CARTESIAN_POINT ( 'NONE',  ( -6.238412754330611322E-16, 10.18810118749999916, 76.28125000204836681 ) ) ;
#68106 = CARTESIAN_POINT ( 'NONE',  ( -31.45873412499997812, 195.7500000013656063, 171.4326545832180386 ) ) ;
#68107 = CARTESIAN_POINT ( 'NONE',  ( -8.342170076843785083E-16, 19.18749999863440436, 4.541265875000002339 ) ) ;
#68108 = ORIENTED_EDGE ( 'NONE', *, *, #52346, .F. ) ;
#68109 = CARTESIAN_POINT ( 'NONE',  ( -1.656854249492347719, 200.9375000027312410, 194.0000000000000853 ) ) ;
#68110 = AXIS2_PLACEMENT_3D ( 'NONE', #50808, #21756, #61388 ) ;
#68111 = CARTESIAN_POINT ( 'NONE',  ( 3.458734124999959469, 195.7500000013656063, 140.5673454167824161 ) ) ;
#68112 = CARTESIAN_POINT ( 'NONE',  ( -26.34314575050770202, 206.0625000027312694, 166.0000000000003695 ) ) ;
#68113 = PRESENTATION_LAYER_ASSIGNMENT (  '', '', ( #35598 ) ) ;
#68114 = PLANE ( 'NONE',  #53687 ) ;
#68115 = VERTEX_POINT ( 'NONE', #6239 ) ;
#68116 =( BOUNDED_CURVE ( )  B_SPLINE_CURVE ( 2, ( #59293, #41923, #53259, #34818, #41199, #18554, #6502, #17808, #46107 ),
 .UNSPECIFIED., .F., .F. ) 
 B_SPLINE_CURVE_WITH_KNOTS ( ( 3, 2, 2, 2, 3 ),
 ( 0.4117647058823529216, 0.4154411764705882582, 0.4191176470588235947, 0.4227941176470588758, 0.4264705882352941568 ),
 .UNSPECIFIED. ) 
 CURVE ( )  GEOMETRIC_REPRESENTATION_ITEM ( )  RATIONAL_B_SPLINE_CURVE ( ( 1.000000000000000000, 0.9238795325112867385, 1.000000000000000000, 0.9238795325112867385, 1.000000000000000000, 0.9238795325112867385, 1.000000000000000000, 0.9238795325112856283, 1.000000000000001110 ) ) 
 REPRESENTATION_ITEM ( '' )  );
#68117 = CARTESIAN_POINT ( 'NONE',  ( -1.320432766682874540E-15, 12.09374999795161187, 7.188101187500000044 ) ) ;
#68118 = CYLINDRICAL_SURFACE ( 'NONE', #2687, 4.000000000000001776 ) ;
#68119 = CARTESIAN_POINT ( 'NONE',  ( 4.999999999999998224, 53.09993190648302175, -43.73864582539177093 ) ) ;
#68120 = CARTESIAN_POINT ( 'NONE',  ( -10.00000000000000178, 37.50000000000000711, -1.224646799147353454E-15 ) ) ;
#68121 = CARTESIAN_POINT ( 'NONE',  ( 5.082755093536326818, 108.5937500020483810, 5.082755093536325042 ) ) ;
#68122 = CARTESIAN_POINT ( 'NONE',  ( -24.54126587500000767, 206.5000000013655779, 168.5673454167827003 ) ) ;
#68123 = CARTESIAN_POINT ( 'NONE',  ( 5.656854249492376141, -5.656854249492374365, 2.892802779823365533 ) ) ;
#68125 = CARTESIAN_POINT ( 'NONE',  ( -7.999999999999992895, 4.898587196589407898E-16, 0.000000000000000000 ) ) ;
#68124 = CARTESIAN_POINT ( 'NONE',  ( 5.000000000000000000, 35.83333333333333570, -8.660254037844385522 ) ) ;
#68126 = EDGE_LOOP ( 'NONE', ( #37683, #24310, #37840, #57095, #33282, #63148, #50370, #3696, #62690, #50932, #2037, #36370, #52181, #74426, #24497, #33800 ) ) ;
#68127 = CARTESIAN_POINT ( 'NONE',  ( -11.35316468749999963, 253.9062500034139873, 0.000000000000000000 ) ) ;
#68128 = CARTESIAN_POINT ( 'NONE',  ( 7.188101187499992051, 8.802885111219154394E-16, 23.61155278187175455 ) ) ;
#68129 = CARTESIAN_POINT ( 'NONE',  ( 0.7509181236778168511, 55.63764137817162236, 43.81192498624614728 ) ) ;
#68130 = DIRECTION ( 'NONE',  ( 0.000000000000000000, -1.000000000000000000, 0.000000000000000000 ) ) ;
#68131 = CARTESIAN_POINT ( 'NONE',  ( 4.737866951561470863, -68.48668487056480103, -20.75656675269368634 ) ) ;
#68132 = CARTESIAN_POINT ( 'NONE',  ( 6.123233995736767268E-16, 138.1249999931720538, -10.00000000000000178 ) ) ;
#68133 = CARTESIAN_POINT ( 'NONE',  ( -10.00000000000000000, 162.2916666666666288, -2.679491924311229845 ) ) ;
#68134 = CARTESIAN_POINT ( 'NONE',  ( 11.00000000000000000, 4.556349186104045934, 79.84374999999998579 ) ) ;
#68135 = FILL_AREA_STYLE_COLOUR ( '', #51213 ) ;
#68136 = CARTESIAN_POINT ( 'NONE',  ( 1.469576158976823947E-15, 90.87500000000000000, 8.000000000000000000 ) ) ;
#68137 = CARTESIAN_POINT ( 'NONE',  ( 9.832129032723416984, 130.6770833299193555, 5.676582343750006032 ) ) ;
#68138 = CARTESIAN_POINT ( 'NONE',  ( 23.99999999999997868, 198.8125000000000284, 171.6568542494922553 ) ) ;
#68139 = LINE ( 'NONE', #16434, #47000 ) ;
#68142 = FACE_OUTER_BOUND ( 'NONE', #1415, .T. ) ;
#68141 = CARTESIAN_POINT ( 'NONE',  ( 29.43265458321761230, 197.8750000013656063, 166.5412658749999650 ) ) ;
#68140 = CARTESIAN_POINT ( 'NONE',  ( 30.44569435410878810, 195.8125000013656063, 172.4456943541087526 ) ) ;
#68143 = VERTEX_POINT ( 'NONE', #29243 ) ;
#68144 = CARTESIAN_POINT ( 'NONE',  ( 0.2954385633113796872, 223.7729706610164726, 10.00000000000001776 ) ) ;
#68145 = CARTESIAN_POINT ( 'NONE',  ( 6.123233995736767268E-16, 148.1249999931720538, -10.00000000000000178 ) ) ;
#68146 = CARTESIAN_POINT ( 'NONE',  ( 8.311093377946839666, 221.0937500034139589, 8.311093377946829008 ) ) ;
#68147 = CARTESIAN_POINT ( 'NONE',  ( 24.54126587499999346, 198.4375000013655779, 169.9999999999998863 ) ) ;
#68148 = CARTESIAN_POINT ( 'NONE',  ( 3.042071309553167069, 202.1354166632526983, -11.35316468749999785 ) ) ;
#68149 = CARTESIAN_POINT ( 'NONE',  ( -5.082755093536325930, 119.4687500020483810, -5.082755093536325930 ) ) ;
#68150 = CARTESIAN_POINT ( 'NONE',  ( -3.211159895383561391, 19.68749999863440436, -3.211159895383561835 ) ) ;
#68151 = CARTESIAN_POINT ( 'NONE',  ( 27.99999999999996092, 194.6875000013655779, 173.4587341249998929 ) ) ;
#68152 = CARTESIAN_POINT ( 'NONE',  ( 3.313708498984756279, 7.999999999999991118, 18.36155277982337353 ) ) ;
#68153 = CARTESIAN_POINT ( 'NONE',  ( -3.313708498984760276, 12.46875000000000178, -8.000000000000000000 ) ) ;
#68154 = CARTESIAN_POINT ( 'NONE',  ( -9.832129032723420536, 88.69791666325268409, 5.676582343749997150 ) ) ;
#68155 = ORIENTED_EDGE ( 'NONE', *, *, #43137, .T. ) ;
#68156 = CARTESIAN_POINT ( 'NONE',  ( -4.000000000000015987, 205.6875000027312126, 143.6568542494924259 ) ) ;
#68157 = CARTESIAN_POINT ( 'NONE',  ( -7.188101187500000044, 25.21874999795161543, -8.802885111219163269E-16 ) ) ;
#68158 = CYLINDRICAL_SURFACE ( 'NONE', #15753, 3.999999999999976019 ) ;
#68159 = CARTESIAN_POINT ( 'NONE',  ( -9.832129032723418760, 263.8020833367473301, -5.676582343749998927 ) ) ;
#68160 = CARTESIAN_POINT ( 'NONE',  ( -8.311093377946841443, 103.9062499965860269, 8.311093377946830785 ) ) ;
#68161 = ORIENTED_EDGE ( 'NONE', *, *, #54136, .T. ) ;
#68162 = CARTESIAN_POINT ( 'NONE',  ( 38.00000000000000000, -52.99999999999999289, 25.00000000000000000 ) ) ;
#68163 = CARTESIAN_POINT ( 'NONE',  ( -10.18810118749999738, -4.220049686691941915, 109.7500000020483810 ) ) ;
#68164 = CARTESIAN_POINT ( 'NONE',  ( -10.00000000000000178, 214.3749999931720538, -1.224646799147353454E-15 ) ) ;
#68165 = CARTESIAN_POINT ( 'NONE',  ( 2.754378923186476579E-14, 206.4375000013656063, 194.5412658750000219 ) ) ;
#68166 = PLANE ( 'NONE',  #58916 ) ;
#68168 = CARTESIAN_POINT ( 'NONE',  ( -3.042071309553163960, 92.23958332991935549, -11.35316468749999963 ) ) ;
#68167 = CARTESIAN_POINT ( 'NONE',  ( -11.00000000000000000, 0.000000000000000000, 96.99999999999998579 ) ) ;
#68169 = AXIS2_PLACEMENT_3D ( 'NONE', #5103, #27722, #67351 ) ;
#68170 = CARTESIAN_POINT ( 'NONE',  ( -7.999999999999991118, 0.000000000000000000, 14.51780278392014800 ) ) ;
#68171 = CARTESIAN_POINT ( 'NONE',  ( -26.56734541678238060, 202.6250000013656063, 166.5412658750003629 ) ) ;
#68172 = EDGE_CURVE ( 'NONE', #30135, #18846, #43983, .T. ) ;
#68173 = CARTESIAN_POINT ( 'NONE',  ( 2.828427124746208943, 208.7500000027312126, 195.1715728752538439 ) ) ;
#68174 = VERTEX_POINT ( 'NONE', #10769 ) ;
#68175 = CARTESIAN_POINT ( 'NONE',  ( -2.679491924311225848, 178.3333333265053966, -10.00000000000000178 ) ) ;
#68176 = CARTESIAN_POINT ( 'NONE',  ( 1.469576158976823947E-15, 114.8750000000000000, 8.000000000000000000 ) ) ;
#68177 = VECTOR ( 'NONE', #59762, 1000.000000000000114 ) ;
#68178 = CARTESIAN_POINT ( 'NONE',  ( -11.50000000000000178, 82.00000000000001421, 97.52691193458117880 ) ) ;
#68179 = CARTESIAN_POINT ( 'NONE',  ( 8.311093377946834337, 75.46874999658602690, 8.311093377946839666 ) ) ;
#68180 = CARTESIAN_POINT ( 'NONE',  ( 1.226468279477575784E-15, 288.7031250017069510, 6.676582343750001591 ) ) ;
#68181 = CARTESIAN_POINT ( 'NONE',  ( -1.320432766682874540E-15, 4.968749997951610986, 7.188101187500000044 ) ) ;
#68183 = EDGE_CURVE ( 'NONE', #20313, #31504, #56803, .T. ) ;
#68182 = CARTESIAN_POINT ( 'NONE',  ( 1.871523826299183495E-15, -10.18810118749999916, 99.90625000204838102 ) ) ;
#68184 = CARTESIAN_POINT ( 'NONE',  ( 11.35316468749999963, 1.302083329919349941, -3.042071309553165293 ) ) ;
#68185 = ORIENTED_EDGE ( 'NONE', *, *, #24555, .F. ) ;
#68186 = CARTESIAN_POINT ( 'NONE',  ( -7.347880794884122694E-16, 1.499999997268813168, 4.000000000000001776 ) ) ;
#68187 = CARTESIAN_POINT ( 'NONE',  ( -11.00000000000000000, 11.00000000000000000, -6.938893903907228378E-15 ) ) ;
#68188 = CARTESIAN_POINT ( 'NONE',  ( -4.898587196589412829E-16, 120.1250000000000000, -8.000000000000000000 ) ) ;
#68189 = CARTESIAN_POINT ( 'NONE',  ( -9.832129032723420536, 203.6979166632526983, 5.676582343749997150 ) ) ;
#68190 = CARTESIAN_POINT ( 'NONE',  ( 4.999999999999997335, 221.4583333401612890, -8.660254037844387298 ) ) ;
#68191 = CARTESIAN_POINT ( 'NONE',  ( -23.99999999999996092, 207.8125000027312410, 171.6568542494926817 ) ) ;
#68192 = CARTESIAN_POINT ( 'NONE',  ( -4.721056650415999201, 297.3281250017069510, -4.721056650415999201 ) ) ;
#68193 = EDGE_LOOP ( 'NONE', ( #36641, #49459, #5762, #10451 ) ) ;
#68194 = CARTESIAN_POINT ( 'NONE',  ( -11.35316468750000141, 193.5937499965860127, -1.390361679473963753E-15 ) ) ;
#68195 = CARTESIAN_POINT ( 'NONE',  ( -31.45873412500001010, 205.6250000013656063, 168.5673454167827572 ) ) ;
#68196 = CARTESIAN_POINT ( 'NONE',  ( -1.469576158976823947E-15, 19.12500000000000355, 8.000000000000000000 ) ) ;
#68197 = ORIENTED_EDGE ( 'NONE', *, *, #44540, .T. ) ;
#68198 = CARTESIAN_POINT ( 'NONE',  ( 3.313708498984760720, 94.71875000409677625, -8.000000000000000000 ) ) ;
#68199 =( NAMED_UNIT ( * ) PLANE_ANGLE_UNIT ( ) SI_UNIT ( $, .RADIAN. ) );
#68200 = CARTESIAN_POINT ( 'NONE',  ( -8.660254037844387298, 12.08333333333333570, -5.000000000000004441 ) ) ;
#68201 = CARTESIAN_POINT ( 'NONE',  ( 10.18810118749999916, 4.220049686691935698, 82.37500000204838102 ) ) ;
#68202 = VERTEX_POINT ( 'NONE', #54481 ) ;
#68203 = CARTESIAN_POINT ( 'NONE',  ( -4.000000000000002665, 18.56250000000000000, 1.656854249492380804 ) ) ;
#68204 = CARTESIAN_POINT ( 'NONE',  ( 4.541265875000002339, 19.37499999863440792, -1.881053915767121776 ) ) ;
#68205 = CARTESIAN_POINT ( 'NONE',  ( 31.37281118636886390, 194.5696876263058073, 171.1905752792710302 ) ) ;
#68206 = LINE ( 'NONE', #44084, #7746 ) ;
#68207 = CARTESIAN_POINT ( 'NONE',  ( -5.000000000000001776, -11.69579520003552098, 68.31051037013783400 ) ) ;
#68208 = VECTOR ( 'NONE', #27648, 1000.000000000000000 ) ;
#68209 = CARTESIAN_POINT ( 'NONE',  ( 2.679491924311370177, 150.8333333265053398, 9.999999999999918288 ) ) ;
#68212 = CARTESIAN_POINT ( 'NONE',  ( 5.000000000000000888, -52.35862550122958936, 48.98731492261398301 ) ) ;
#68211 = CARTESIAN_POINT ( 'NONE',  ( 8.311093377946839666, 240.7812500034139873, 8.311093377946830785 ) ) ;
#68210 = CARTESIAN_POINT ( 'NONE',  ( 31.45873412499999944, 206.6875000013656063, 169.9999999999998863 ) ) ;
#68213 = APPLICATION_PROTOCOL_DEFINITION ( 'draft international standard', 'automotive_design', 1998, #57833 ) ;
#68214 = ORIENTED_EDGE ( 'NONE', *, *, #68039, .T. ) ;
#68215 = CARTESIAN_POINT ( 'NONE',  ( 5.676582343750005144, 255.8854166700806445, 9.832129032723416984 ) ) ;
#68216 = VECTOR ( 'NONE', #30652, 1000.000000000000000 ) ;
#68217 = CARTESIAN_POINT ( 'NONE',  ( 2.977408999572650927, -7.188101187499990274, 12.45530278187175277 ) ) ;
#68218 = EDGE_LOOP ( 'NONE', ( #21086, #18770 ) ) ;
#68219 = ORIENTED_EDGE ( 'NONE', *, *, #6088, .T. ) ;
#68220 = CARTESIAN_POINT ( 'NONE',  ( -10.18810118749999738, -4.220049686691941915, 73.75000000204836681 ) ) ;
#68221 = CARTESIAN_POINT ( 'NONE',  ( 8.311093377946834337, 85.46874999658599847, 8.311093377946839666 ) ) ;
#68222 = CARTESIAN_POINT ( 'NONE',  ( -5.656854249492378806, 105.8750000040967763, 5.656854249492381470 ) ) ;
#68223 = CARTESIAN_POINT ( 'NONE',  ( 4.556349186104051263, -10.99999999999999822, 88.46874999999998579 ) ) ;
#68226 = CARTESIAN_POINT ( 'NONE',  ( -6.676582343750001591, 289.6093750017069510, 0.000000000000000000 ) ) ;
#68225 = CARTESIAN_POINT ( 'NONE',  ( 27.99999999999997158, 207.9375000013656063, 166.5412658749999082 ) ) ;
#68224 = CARTESIAN_POINT ( 'NONE',  ( 30.44569435410883784, 208.0625000013656063, 167.5543056458911053 ) ) ;
#68227 = CARTESIAN_POINT ( 'NONE',  ( -7.999999999999998224, 114.5937500000000000, 3.313708498984766049 ) ) ;
#68228 = CARTESIAN_POINT ( 'NONE',  ( -2.828427124746153876, 199.8750000000000284, 195.1715728752538439 ) ) ;
#68229 = CARTESIAN_POINT ( 'NONE',  ( -11.35316468750000141, 198.4895833299193555, 3.042071309553159963 ) ) ;
#68230 =( BOUNDED_CURVE ( )  B_SPLINE_CURVE ( 2, ( #18424, #35054, #51263, #57315, #63695, #58067, #28626, #46615, #68993 ),
 .UNSPECIFIED., .F., .F. ) 
 B_SPLINE_CURVE_WITH_KNOTS ( ( 3, 2, 2, 2, 3 ),
 ( 0.1145833333333333981, 0.1197916666666667407, 0.1250000000000000833, 0.1302083333333334259, 0.1354166666666667407 ),
 .UNSPECIFIED. ) 
 CURVE ( )  GEOMETRIC_REPRESENTATION_ITEM ( )  RATIONAL_B_SPLINE_CURVE ( ( 0.9999999999999990008, 0.9238795325112877377, 1.000000000000000000, 0.9238795325112867385, 1.000000000000000000, 0.9238795325112867385, 1.000000000000000000, 0.9238795325112855172, 1.000000000000001110 ) ) 
 REPRESENTATION_ITEM ( '' )  );
#68231 = ADVANCED_FACE ( 'NONE', ( #60118 ), #71801, .F. ) ;
#68232 = CARTESIAN_POINT ( 'NONE',  ( -3.313708498984765161, 11.34374999590322197, 7.999999999999998224 ) ) ;
#68233 = ADVANCED_FACE ( 'NONE', ( #24669 ), #30712, .T. ) ;
#68234 = CIRCLE ( 'NONE', #52570, 10.00000000000001243 ) ;
#68235 = EDGE_LOOP ( 'NONE', ( #57598, #31364, #8870, #39454, #38531 ) ) ;
#68236 = CARTESIAN_POINT ( 'NONE',  ( 31.45873412499999944, 195.7500000013656063, 168.5673454167822740 ) ) ;
#68237 = CARTESIAN_POINT ( 'NONE',  ( 4.401442555609581635E-16, 16.21874999795161543, -7.188101187500000044 ) ) ;
#68238 = CARTESIAN_POINT ( 'NONE',  ( -9.832129032723418760, 163.1770833299193839, -5.676582343750004256 ) ) ;
#68239 = CARTESIAN_POINT ( 'NONE',  ( -8.000000000000000000, 105.4062500000000000, -3.313708498984761164 ) ) ;
#68240 = CARTESIAN_POINT ( 'NONE',  ( -2.977408999572650927, 104.7500000020483810, -7.188101187500000933 ) ) ;
#68242 = CARTESIAN_POINT ( 'NONE',  ( -5.000000000000000888, 234.1666666666666856, -8.660254037844387298 ) ) ;
#68241 = DIRECTION ( 'NONE',  ( -0.000000000000000000, 1.000000000000000000, -0.000000000000000000 ) ) ;
#68243 = CARTESIAN_POINT ( 'NONE',  ( 26.56734541678233086, 207.6250000013656063, 173.4587341249998929 ) ) ;
#68244 = CARTESIAN_POINT ( 'NONE',  ( 1.320432766682872962E-15, -7.188101187499992051, 9.736552781871754547 ) ) ;
#68245 = CARTESIAN_POINT ( 'NONE',  ( 6.951808397369818766E-16, 57.03124999658601268, -11.35316468750000141 ) ) ;
#68246 = CARTESIAN_POINT ( 'NONE',  ( -12.00000000000000000, 0.000000000000000000, 0.000000000000000000 ) ) ;
#68247 = DIRECTION ( 'NONE',  ( 0.000000000000000000, 0.000000000000000000, 1.000000000000000000 ) ) ;
#68248 = ORIENTED_EDGE ( 'NONE', *, *, #32514, .T. ) ;
#68249 = CARTESIAN_POINT ( 'NONE',  ( -11.00000000000000000, 0.000000000000000000, 114.9999999999999858 ) ) ;
#68250 = CARTESIAN_POINT ( 'NONE',  ( -2.679491924311382611, 170.4166666598386826, 9.999999999999914735 ) ) ;
#68251 = CARTESIAN_POINT ( 'NONE',  ( 6.951808397369818766E-16, 62.03124999658601979, -11.35316468750000141 ) ) ;
#68252 = CARTESIAN_POINT ( 'NONE',  ( 11.00000000000000000, 1.347111479062088405E-15, 73.93750000409676204 ) ) ;
#68253 = CARTESIAN_POINT ( 'NONE',  ( 3.458734124999960358, 201.6250000013656063, 143.4326545832176976 ) ) ;
#68254 = CARTESIAN_POINT ( 'NONE',  ( 0.4501631047671810215, 16.44600848780500257, 68.55503832938671849 ) ) ;
#68255 = CARTESIAN_POINT ( 'NONE',  ( 74.99999999999998579, 272.0000000000000000, 42.00000000000000000 ) ) ;
#68257 = CARTESIAN_POINT ( 'NONE',  ( -11.35316468749999785, 48.07291666325268409, -3.042071309553167957 ) ) ;
#68256 = CARTESIAN_POINT ( 'NONE',  ( -7.188101187500000933, 95.56250000204838102, -2.977408999572650483 ) ) ;
#68258 = CARTESIAN_POINT ( 'NONE',  ( 7.999999999999991118, 9.797174393178815797E-16, 6.080302779823364645 ) ) ;
#68259 = CARTESIAN_POINT ( 'NONE',  ( 3.313708498984762496, -7.999999999999989342, 4.486552783920144449 ) ) ;
#68260 = CARTESIAN_POINT ( 'NONE',  ( 11.35316468750000141, 175.7812499965860411, 0.000000000000000000 ) ) ;
#68261 = CARTESIAN_POINT ( 'NONE',  ( 10.00000000000000178, 137.0833333265053966, -2.679491924311226736 ) ) ;
#68262 = CARTESIAN_POINT ( 'NONE',  ( 5.082755093536325042, 99.96875000204838102, -5.082755093536325930 ) ) ;
#68263 = CARTESIAN_POINT ( 'NONE',  ( -1.503088597795289028, -47.60378055570536304, 139.0360254009841583 ) ) ;
#68264 = CARTESIAN_POINT ( 'NONE',  ( 9.832129032723416984, 40.67708332991935549, 5.676582343750006032 ) ) ;
#68265 = CARTESIAN_POINT ( 'NONE',  ( -6.238412754330611322E-16, 10.18810118749999916, 117.1562500020483810 ) ) ;
#68266 = CARTESIAN_POINT ( 'NONE',  ( 5.676582343749993598, 184.9479166632526983, 9.832129032723422313 ) ) ;
#68267 = VERTEX_POINT ( 'NONE', #52994 ) ;
#68268 = CARTESIAN_POINT ( 'NONE',  ( 47.32259252271278882, 145.2267040872997939, 65.76194439203457875 ) ) ;
#68269 = CARTESIAN_POINT ( 'NONE',  ( 10.18810118749999916, 1.247682550866122264E-15, 68.40625000204836681 ) ) ;
#68270 = CARTESIAN_POINT ( 'NONE',  ( -2.828427124746152987, 196.1250000000000284, 200.8284271247462129 ) ) ;
#68271 = CARTESIAN_POINT ( 'NONE',  ( 7.999999999999991118, -2.975320552349488356E-08, 19.76780278304987348 ) ) ;
#68273 = CARTESIAN_POINT ( 'NONE',  ( 8.311093377946834337, 165.1562499965860127, 8.311093377946839666 ) ) ;
#68272 = CARTESIAN_POINT ( 'NONE',  ( 32.00000000000000000, 203.2500000000000000, 169.9999999999999432 ) ) ;
#68274 = CARTESIAN_POINT ( 'NONE',  ( -3.313708498984757167, 7.999999999999991118, 5.105302784329824206 ) ) ;
#68275 = PLANE ( 'NONE',  #10461 ) ;
#68276 = CARTESIAN_POINT ( 'NONE',  ( 9.832129032723416984, 221.8229166700806729, -5.676582343750003368 ) ) ;
#68277 = CARTESIAN_POINT ( 'NONE',  ( 4.898587196589412829E-16, 21.18749999590322375, -8.000000000000000000 ) ) ;
#68278 = EDGE_CURVE ( 'NONE', #47406, #34562, #70700, .T. ) ;
#68279 = CARTESIAN_POINT ( 'NONE',  ( 1.871523826299183495E-15, -10.18810118749999916, 81.90625000204838102 ) ) ;
#68280 = VERTEX_POINT ( 'NONE', #1325 ) ;
#68281 = CARTESIAN_POINT ( 'NONE',  ( -3.999999999999959144, 204.1875000027311557, 199.6568542494924259 ) ) ;
#68282 = CARTESIAN_POINT ( 'NONE',  ( 11.35316468750000141, 121.0937499965860269, 0.000000000000000000 ) ) ;
#68283 = DIRECTION ( 'NONE',  ( -0.000000000000000000, -0.000000000000000000, 1.000000000000000000 ) ) ;
#68284 = ORIENTED_EDGE ( 'NONE', *, *, #70440, .T. ) ;
#68285 = ORIENTED_EDGE ( 'NONE', *, *, #37413, .F. ) ;
#68286 = CARTESIAN_POINT ( 'NONE',  ( -3.211159895383561391, 6.812499998634407028, -3.211159895383561835 ) ) ;
#68287 = CARTESIAN_POINT ( 'NONE',  ( -7.188101187500001821, 16.12499999795161187, -2.977408999572651371 ) ) ;
#68288 = CARTESIAN_POINT ( 'NONE',  ( 5.656854249492379694, 112.6250000040967763, -5.656854249492380582 ) ) ;
#68289 = CARTESIAN_POINT ( 'NONE',  ( -25.55430564589115150, 199.3125000013656063, 172.4456943541091789 ) ) ;
#68290 = CARTESIAN_POINT ( 'NONE',  ( -4.000000000000002665, 7.562500000000000000, 1.656854249492380804 ) ) ;
#68291 = CARTESIAN_POINT ( 'NONE',  ( -4.000000000000002665, 20.31249999726881583, 1.656854249492380804 ) ) ;
#68292 = CARTESIAN_POINT ( 'NONE',  ( 4.541265875000001451, 9.249999998634407916, 1.881053915767124440 ) ) ;
#68293 = CARTESIAN_POINT ( 'NONE',  ( 1.656854249492348607, 200.1875000000000568, 138.0000000000000568 ) ) ;
#68294 = VERTEX_POINT ( 'NONE', #12616 ) ;
#68295 = CARTESIAN_POINT ( 'NONE',  ( 4.999999999999997335, 223.3333333333333144, -8.660254037844387298 ) ) ;
#68296 = CARTESIAN_POINT ( 'NONE',  ( -7.188101187500000044, 104.6562500020483810, 0.000000000000000000 ) ) ;
#68298 = CARTESIAN_POINT ( 'NONE',  ( -3.313708498984772710, 123.7812500000000000, 7.999999999999988454 ) ) ;
#68297 = CARTESIAN_POINT ( 'NONE',  ( 12.00000000000000000, 28.00000000000000000, 0.000000000000000000 ) ) ;
#68299 =( NAMED_UNIT ( * ) SI_UNIT ( $, .STERADIAN. ) SOLID_ANGLE_UNIT ( ) );
#68300 = CARTESIAN_POINT ( 'NONE',  ( -4.104248244564889347, 10.10575198620099613, -70.81982386211636538 ) ) ;
#68301 = EDGE_CURVE ( 'NONE', #17357, #7158, #71060, .T. ) ;
#68302 = FACE_OUTER_BOUND ( 'NONE', #57219, .T. ) ;
#68303 = VERTEX_POINT ( 'NONE', #65777 ) ;
#68304 = ORIENTED_EDGE ( 'NONE', *, *, #26977, .T. ) ;
#68305 = CARTESIAN_POINT ( 'NONE',  ( -10.18810118749999916, 0.000000000000000000, 94.65625000204836681 ) ) ;
#68306 = CARTESIAN_POINT ( 'NONE',  ( -4.898587196589412829E-16, 91.81250000409677625, -8.000000000000000000 ) ) ;
#68307 = CARTESIAN_POINT ( 'NONE',  ( -29.43265458321760519, 199.1250000013656347, 173.4587341250003760 ) ) ;
#68308 = CARTESIAN_POINT ( 'NONE',  ( -11.00000000000000000, 4.556349186104045934, 105.9062499999999858 ) ) ;
#68310 = CARTESIAN_POINT ( 'NONE',  ( -3.458734124999960358, 204.6250000013655779, 196.5673454167823877 ) ) ;
#68309 = CIRCLE ( 'NONE', #56256, 15.99999999999998579 ) ;
#68312 = CARTESIAN_POINT ( 'NONE',  ( 1.224646799147353454E-15, 300.0000000000000000, -10.00000000000000178 ) ) ;
#68311 = FACE_OUTER_BOUND ( 'NONE', #42948, .T. ) ;
#68313 = CARTESIAN_POINT ( 'NONE',  ( 8.660254037844385522, 119.5833333333333428, 5.000000000000005329 ) ) ;
#68314 = EDGE_CURVE ( 'NONE', #48235, #39701, #19753, .T. ) ;
#68315 = CARTESIAN_POINT ( 'NONE',  ( 8.000000000000001776, 107.6562500000000000, 3.313708498984759387 ) ) ;
#68316 = CARTESIAN_POINT ( 'NONE',  ( -6.676582343750000703, 288.6718750017069510, 2.765530957082001251 ) ) ;
#68317 = CARTESIAN_POINT ( 'NONE',  ( 7.188101187499993827, -2.977408999572645598, 4.017802781871751883 ) ) ;
#68318 = CARTESIAN_POINT ( 'NONE',  ( 0.000000000000000000, 0.000000000000000000, 0.000000000000000000 ) ) ;
#68319 = CARTESIAN_POINT ( 'NONE',  ( 30.44569435410879521, 206.5625000013656063, 172.4456943541087526 ) ) ;
#68320 = CARTESIAN_POINT ( 'NONE',  ( 5.082755093536324154, 2.156249997951610542, 5.082755093536326818 ) ) ;
#68321 = CARTESIAN_POINT ( 'NONE',  ( 3.458734124999959025, 197.5000000013656063, 140.5673454167824161 ) ) ;
#68322 = CARTESIAN_POINT ( 'NONE',  ( -7.188101187500000044, 124.5312500020483810, 0.000000000000000000 ) ) ;
#68324 = CARTESIAN_POINT ( 'NONE',  ( 2.445694354108784108, 202.5625000013656063, 144.4456943541088663 ) ) ;
#68323 = LINE ( 'NONE', #4963, #21487 ) ;
#68325 = CARTESIAN_POINT ( 'NONE',  ( 8.311093377946834337, 247.3437500034139589, -8.311093377946836114 ) ) ;
#68326 = CARTESIAN_POINT ( 'NONE',  ( -10.00000000000000000, 94.16666665983869677, -2.679491924311229845 ) ) ;
#68328 =( BOUNDED_CURVE ( )  B_SPLINE_CURVE ( 2, ( #340, #41054, #23321, #46333, #12371, #35408, #14204, #30829, #8564 ),
 .UNSPECIFIED., .F., .F. ) 
 B_SPLINE_CURVE_WITH_KNOTS ( ( 3, 2, 2, 2, 3 ),
 ( 0.4166666666666671293, 0.4250000000000003775, 0.4333333333333336812, 0.4416666666666669849, 0.4500000000000002887 ),
 .UNSPECIFIED. ) 
 CURVE ( )  GEOMETRIC_REPRESENTATION_ITEM ( )  RATIONAL_B_SPLINE_CURVE ( ( 0.9999999999999958922, 0.9238795325112908463, 1.000000000000000000, 0.9238795325112867385, 1.000000000000000000, 0.9238795325112867385, 1.000000000000000000, 0.9238795325112841850, 1.000000000000002442 ) ) 
 REPRESENTATION_ITEM ( '' )  );
#68327 = CARTESIAN_POINT ( 'NONE',  ( 32.00000000000000711, 202.3125000000000000, 168.3431457505075741 ) ) ;
#68329 = CARTESIAN_POINT ( 'NONE',  ( -8.311093377946836114, 17.65624999658601979, -8.311093377946837890 ) ) ;
#68330 = CARTESIAN_POINT ( 'NONE',  ( 5.082755093536320601, -5.082755093536318824, 0.9240527818717529929 ) ) ;
#68331 = CARTESIAN_POINT ( 'NONE',  ( 8.311093377946837890, 206.7187499965859843, -8.311093377946837890 ) ) ;
#68332 = CARTESIAN_POINT ( 'NONE',  ( 5.676582343750001591, 1.614583329919349497, -9.832129032723420536 ) ) ;
#68333 = CARTESIAN_POINT ( 'NONE',  ( -8.660254037844390851, 219.7916666598387110, 4.999999999999998224 ) ) ;
#68335 = FACE_OUTER_BOUND ( 'NONE', #21073, .T. ) ;
#68334 = CARTESIAN_POINT ( 'NONE',  ( 2.828427124746152987, 203.2500000027312126, 139.1715728752538723 ) ) ;
#68336 = ORIENTED_EDGE ( 'NONE', *, *, #6275, .F. ) ;
#68338 = ADVANCED_FACE ( 'NONE', ( #6967 ), #36378, .F. ) ;
#68337 = CARTESIAN_POINT ( 'NONE',  ( -2.445694354108839175, 202.3125000013656063, 144.4456943541088663 ) ) ;
#68339 = ADVANCED_FACE ( 'NONE', ( #8072 ), #19378, .T. ) ;
#68340 = CARTESIAN_POINT ( 'NONE',  ( 6.951808397369818766E-16, 17.03124999658601624, -11.35316468750000141 ) ) ;
#68341 = CARTESIAN_POINT ( 'NONE',  ( -11.00000000000000000, 4.556349186104045934, 91.09375000409677625 ) ) ;
#68342 = CARTESIAN_POINT ( 'NONE',  ( 2.679491924311226292, 228.5416666666666288, -10.00000000000000000 ) ) ;
#68343 = CARTESIAN_POINT ( 'NONE',  ( -25.55430564589122611, 196.3125000013656063, 167.5543056458915032 ) ) ;
#68344 = CARTESIAN_POINT ( 'NONE',  ( -9.000000000000000000, 1.769118300197570104, -0.07756262466202451522 ) ) ;
#68345 = CARTESIAN_POINT ( 'NONE',  ( -2.977408999572652260, 109.4375000020483810, 7.188101187500000044 ) ) ;
#68346 = CARTESIAN_POINT ( 'NONE',  ( -4.898587196589407898E-16, 7.999999999999991118, 22.95530277982336642 ) ) ;
#68347 = CARTESIAN_POINT ( 'NONE',  ( 6.951808397369818766E-16, 132.0312499965860127, -11.35316468750000141 ) ) ;
#68348 = EDGE_CURVE ( 'NONE', #327, #4091, #13689, .T. ) ;
#68349 = VECTOR ( 'NONE', #23022, 1000.000000000000000 ) ;
#68350 = CARTESIAN_POINT ( 'NONE',  ( 10.00000000000000178, 97.08333332650536818, -2.679491924311226736 ) ) ;
#68351 = CARTESIAN_POINT ( 'NONE',  ( 7.188101187500000044, 122.2812500020483810, -8.802885111219163269E-16 ) ) ;
#68352 = CARTESIAN_POINT ( 'NONE',  ( -3.313708498984782924, 120.9687500040968189, 7.999999999999979572 ) ) ;
#68353 = CARTESIAN_POINT ( 'NONE',  ( -25.55430564589115505, 207.3125000013656063, 172.4456943541091789 ) ) ;
#68354 = DIRECTION ( 'NONE',  ( -1.000000000000000000, 0.000000000000000000, 0.000000000000000000 ) ) ;
#68355 = EDGE_LOOP ( 'NONE', ( #12217, #67382, #59529, #33416 ) ) ;
#68356 = CARTESIAN_POINT ( 'NONE',  ( -0.8997857291002455682, -67.61674724335095732, 20.05382624916412482 ) ) ;
#68357 =( BOUNDED_CURVE ( )  B_SPLINE_CURVE ( 2, ( #68789, #62745, #34112, #40121, #57111, #51436, #59702, #71005, #12558 ),
 .UNSPECIFIED., .F., .F. ) 
 B_SPLINE_CURVE_WITH_KNOTS ( ( 3, 2, 2, 2, 3 ),
 ( 0.3194444444444443643, 0.3263888888888888395, 0.3333333333333332593, 0.3402777777777777901, 0.3472222222222222099 ),
 .UNSPECIFIED. ) 
 CURVE ( )  GEOMETRIC_REPRESENTATION_ITEM ( )  RATIONAL_B_SPLINE_CURVE ( ( 1.000000000000000666, 0.9238795325112861834, 1.000000000000000000, 0.9238795325112867385, 1.000000000000000000, 0.9238795325112867385, 1.000000000000000000, 0.9238795325112867385, 1.000000000000000000 ) ) 
 REPRESENTATION_ITEM ( '' )  );
#68358 = CARTESIAN_POINT ( 'NONE',  ( -4.000000000000001776, 20.18749999726881228, -1.656854249492381470 ) ) ;
#68359 = CARTESIAN_POINT ( 'NONE',  ( -2.765530957081998586, 287.7968750017070079, 6.676582343750001591 ) ) ;
#68360 = CARTESIAN_POINT ( 'NONE',  ( 5.656854249492374365, 5.656854249492375253, 21.32405278432982243 ) ) ;
#68361 = DIRECTION ( 'NONE',  ( -0.000000000000000000, 1.000000000000000000, -0.000000000000000000 ) ) ;
#68362 = EDGE_CURVE ( 'NONE', #29110, #23989, #42025, .T. ) ;
#68363 = CARTESIAN_POINT ( 'NONE',  ( 7.204075437095966983, 7.204075437095967871, 98.96875000204838102 ) ) ;
#68364 = ORIENTED_EDGE ( 'NONE', *, *, #68489, .F. ) ;
#68365 = CARTESIAN_POINT ( 'NONE',  ( 5.000000000000001776, 10.82431413986196134, 67.03128830763429846 ) ) ;
#68366 = CARTESIAN_POINT ( 'NONE',  ( -3.313708498984757611, 7.999999999999991118, 24.54905277982336287 ) ) ;
#68367 = CARTESIAN_POINT ( 'NONE',  ( 1.432654583217662481, 202.3750000013656063, 194.5412658750000219 ) ) ;
#68368 = CARTESIAN_POINT ( 'NONE',  ( -9.832129032723418760, 73.17708332991934128, -5.676582343750004256 ) ) ;
#68369 = VERTEX_POINT ( 'NONE', #31072 ) ;
#68370 = CARTESIAN_POINT ( 'NONE',  ( -4.220049686691935698, 10.18810118749999916, 104.8750000020483668 ) ) ;
#68371 = CARTESIAN_POINT ( 'NONE',  ( -1.881053915767121776, 13.74999999863440969, -4.541265875000002339 ) ) ;
#68372 = ORIENTED_EDGE ( 'NONE', *, *, #22674, .T. ) ;
#68373 = VECTOR ( 'NONE', #43081, 1000.000000000000000 ) ;
#68374 = CARTESIAN_POINT ( 'NONE',  ( -5.082755093536325042, 25.03124999795161543, -5.082755093536325930 ) ) ;
#68375 = CARTESIAN_POINT ( 'NONE',  ( 1.469576158976823947E-15, 107.3750000000000000, 8.000000000000000000 ) ) ;
#68376 = CARTESIAN_POINT ( 'NONE',  ( -4.999999999999999112, -68.33088307291099284, -21.57589723056520370 ) ) ;
#68377 = CARTESIAN_POINT ( 'NONE',  ( 5.082755093536324154, 21.65624999795161543, 5.082755093536326818 ) ) ;
#68378 = CARTESIAN_POINT ( 'NONE',  ( -5.272365137108047328, -4.893145049964592097, 0.1656095422372733383 ) ) ;
#68379 = CARTESIAN_POINT ( 'NONE',  ( -7.204075437095967871, 7.204075437095967871, 112.8437500020483810 ) ) ;
#68380 = CARTESIAN_POINT ( 'NONE',  ( 30.82842712474620583, 208.3750000000000284, 167.1715728752537586 ) ) ;
#68381 = CARTESIAN_POINT ( 'NONE',  ( -4.000000000000002665, 10.31249999726881406, 1.656854249492380804 ) ) ;
#68382 = CARTESIAN_POINT ( 'NONE',  ( -1.656854249492418107, 208.4375000027312410, 138.0000000000000568 ) ) ;
#68383 = ORIENTED_EDGE ( 'NONE', *, *, #67916, .F. ) ;
#68384 = CARTESIAN_POINT ( 'NONE',  ( 3.458734125000015425, 202.9375000013656063, 198.0000000000000284 ) ) ;
#68385 = CARTESIAN_POINT ( 'NONE',  ( -31.45873412499996746, 204.7500000013656063, 171.4326545832181239 ) ) ;
#68386 = CARTESIAN_POINT ( 'NONE',  ( 29.65685424949229798, 199.1875000027312126, 174.0000000000000284 ) ) ;
#68387 =( GEOMETRIC_REPRESENTATION_CONTEXT ( 3 ) GLOBAL_UNCERTAINTY_ASSIGNED_CONTEXT ( ( #12135 ) ) GLOBAL_UNIT_ASSIGNED_CONTEXT ( ( #5423, #24610, #35585 ) ) REPRESENTATION_CONTEXT ( 'NONE', 'WORKASPACE' ) );
#68388 = CARTESIAN_POINT ( 'NONE',  ( -1.881053915767124440, 8.999999998634406140, 4.541265875000001451 ) ) ;
#68389 = DIRECTION ( 'NONE',  ( 0.000000000000000000, -1.000000000000000000, 0.000000000000000000 ) ) ;
#68390 = CARTESIAN_POINT ( 'NONE',  ( 2.977408999572646486, 7.188101187499991163, 16.01780278187175455 ) ) ;
#68391 = ORIENTED_EDGE ( 'NONE', *, *, #25214, .F. ) ;
#68392 = CARTESIAN_POINT ( 'NONE',  ( -5.394762896564973355E-12, 18.74999999999958433, 10.00000000000000178 ) ) ;
#68393 = ORIENTED_EDGE ( 'NONE', *, *, #69535, .T. ) ;
#68394 = CARTESIAN_POINT ( 'NONE',  ( 7.204075437095968759, -7.204075437095966983, 113.2187500020483810 ) ) ;
#68395 = CYLINDRICAL_SURFACE ( 'NONE', #70169, 10.00000000000000000 ) ;
#68396 = CARTESIAN_POINT ( 'NONE',  ( -3.458734124999959914, 202.3750000013655779, 196.5673454167823877 ) ) ;
#68397 = CARTESIAN_POINT ( 'NONE',  ( 29.43265458321766914, 198.5000000013656063, 173.4587341249998929 ) ) ;
#68398 = CARTESIAN_POINT ( 'NONE',  ( -8.660254037844387298, 82.08333333333334281, -5.000000000000004441 ) ) ;
#68399 = EDGE_CURVE ( 'NONE', #53710, #33244, #41668, .T. ) ;
#68400 = CARTESIAN_POINT ( 'NONE',  ( 5.082755093536325042, 90.96875000204838102, -5.082755093536325930 ) ) ;
#68401 = CARTESIAN_POINT ( 'NONE',  ( -6.000000000000000888, 289.0625000000000000, 2.485281374238575758 ) ) ;
#68402 = ORIENTED_EDGE ( 'NONE', *, *, #49247, .F. ) ;
#68403 = CARTESIAN_POINT ( 'NONE',  ( 0.000000000000000000, 0.000000000000000000, 118.0000000000000000 ) ) ;
#68404 = CARTESIAN_POINT ( 'NONE',  ( 0.7509181236825389627, -10.12341933770111702, 70.08957333326995354 ) ) ;
#68405 = CARTESIAN_POINT ( 'NONE',  ( 3.999999999999960032, 195.1250000027311842, 142.0000000000000568 ) ) ;
#68406 = CARTESIAN_POINT ( 'NONE',  ( 4.999999999999993783, 56.04166665983870388, 8.660254037844390851 ) ) ;
#68407 = CARTESIAN_POINT ( 'NONE',  ( 3.313708498984815343, 97.53125000000002842, -7.999999999999944933 ) ) ;
#68408 = CARTESIAN_POINT ( 'NONE',  ( 8.660254037844389075, 237.0833333333333428, 4.999999999999997335 ) ) ;
#68409 = CARTESIAN_POINT ( 'NONE',  ( -2.679491924311318662, 78.54166666666668561, 9.999999999999994671 ) ) ;
#68410 = CARTESIAN_POINT ( 'NONE',  ( -5.000000000000005329, 203.3333333333333428, 8.660254037844387298 ) ) ;
#68411 = CARTESIAN_POINT ( 'NONE',  ( -4.401442555609577197E-16, 7.188101187499992051, 19.48655278187175455 ) ) ;
#68412 = CARTESIAN_POINT ( 'NONE',  ( -11.35316468750000141, 168.5937499965860127, -1.390361679473963753E-15 ) ) ;
#68413 = CARTESIAN_POINT ( 'NONE',  ( -2.679491924310609452, 38.54166666666672114, 10.00000000000036060 ) ) ;
#68414 = CARTESIAN_POINT ( 'NONE',  ( 5.000000000000000000, 11.14555136602166741, -27.84144949604398889 ) ) ;
#68416 = DIRECTION ( 'NONE',  ( 0.000000000000000000, 0.000000000000000000, 1.000000000000000000 ) ) ;
#68415 = SURFACE_SIDE_STYLE ('',( #62378 ) ) ;
#68417 = ORIENTED_EDGE ( 'NONE', *, *, #57922, .F. ) ;
#68418 = CARTESIAN_POINT ( 'NONE',  ( 3.458734124999959914, 197.4375000013655779, 142.0000000000000568 ) ) ;
#68419 = CARTESIAN_POINT ( 'NONE',  ( -5.676582343749998039, 27.76041666325268409, -9.832129032723420536 ) ) ;
#68420 = CARTESIAN_POINT ( 'NONE',  ( -6.735557395310442023E-16, 11.00000000000000000, 113.3125000040967763 ) ) ;
#68421 = CARTESIAN_POINT ( 'NONE',  ( -2.856636953006815194, 194.5084785699607721, 200.0478322695347799 ) ) ;
#68423 = CARTESIAN_POINT ( 'NONE',  ( -4.336811714531204842, -16.30209246798439082, -69.46462972172992067 ) ) ;
#68422 = CARTESIAN_POINT ( 'NONE',  ( 10.00000000000000178, 221.8749999931720254, 0.000000000000000000 ) ) ;
#68424 = CARTESIAN_POINT ( 'NONE',  ( -30.81133039812245045, -51.99949502678778401, 173.9193291205910157 ) ) ;
#68425 = CARTESIAN_POINT ( 'NONE',  ( -1.432654583217662259, 197.1250000013656347, 145.4587341250000350 ) ) ;
#68426 = CARTESIAN_POINT ( 'NONE',  ( 8.660254037844389075, 57.29166665983870388, -5.000000000000000000 ) ) ;
#68427 = CARTESIAN_POINT ( 'NONE',  ( 7.188101187500002709, 100.8125000020484094, 2.977408999572649151 ) ) ;
#68428 = CARTESIAN_POINT ( 'NONE',  ( 1.881053915767122664, 12.24999999863440969, 4.541265875000001451 ) ) ;
#68429 = CARTESIAN_POINT ( 'NONE',  ( 2.679491924305834605, 213.9583333333329733, 10.00000000000336797 ) ) ;
#68430 = CARTESIAN_POINT ( 'NONE',  ( -3.313708498984758943, -7.999999999999989342, 4.111552779823362869 ) ) ;
#68431 = CARTESIAN_POINT ( 'NONE',  ( 0.8588954341815085991, -49.93020820668212423, 40.69831139579102341 ) ) ;
#68432 = ORIENTED_EDGE ( 'NONE', *, *, #38255, .T. ) ;
#68433 = VERTEX_POINT ( 'NONE', #13705 ) ;
#68434 = CARTESIAN_POINT ( 'NONE',  ( -2.445694354108784108, 195.5625000013656063, 195.5543056458912190 ) ) ;
#68435 = CARTESIAN_POINT ( 'NONE',  ( 27.99999999999999645, 210.0000000000000284, 169.9999999999999147 ) ) ;
#68436 = CARTESIAN_POINT ( 'NONE',  ( -30.24072409221900770, -42.97659422005119012, 163.1107348146608729 ) ) ;
#68437 = CARTESIAN_POINT ( 'NONE',  ( -3.042071309553164404, 137.2395833299193271, -11.35316468749999963 ) ) ;
#68438 = ORIENTED_EDGE ( 'NONE', *, *, #24956, .F. ) ;
#68439 = CARTESIAN_POINT ( 'NONE',  ( 2.679491924311372841, 106.0416666666666572, -9.999999999999898748 ) ) ;
#68440 = CARTESIAN_POINT ( 'NONE',  ( 4.220049686691934809, 10.18810118749999916, 88.18750000204838102 ) ) ;
#68441 = CARTESIAN_POINT ( 'NONE',  ( -31.37281118636903798, 194.5696876263058073, 168.8094247207298793 ) ) ;
#68442 = CARTESIAN_POINT ( 'NONE',  ( 2.751064625579944321E-14, 206.7500000000000284, 194.0000000000000568 ) ) ;
#68443 = CYLINDRICAL_SURFACE ( 'NONE', #32852, 10.00000000000000178 ) ;
#68444 = CARTESIAN_POINT ( 'NONE',  ( -32.00000000000002842, 197.3125000027312126, 168.3431457505080857 ) ) ;
#68445 = EDGE_CURVE ( 'NONE', #71352, #64324, #7855, .T. ) ;
#68446 = CARTESIAN_POINT ( 'NONE',  ( -4.220049686691937474, -10.18810118749999738, 113.3125000020483668 ) ) ;
#68447 = ORIENTED_EDGE ( 'NONE', *, *, #1666, .F. ) ;
#68448 =( BOUNDED_CURVE ( )  B_SPLINE_CURVE ( 2, ( #26206, #1745, #31514, #2841, #49227, #25831, #43192, #8875, #31888 ),
 .UNSPECIFIED., .F., .F. ) 
 B_SPLINE_CURVE_WITH_KNOTS ( ( 3, 2, 2, 2, 3 ),
 ( 0.8333333333333340365, 0.8416666666666673402, 0.8500000000000006439, 0.8583333333333339477, 0.8666666666666673624 ),
 .UNSPECIFIED. ) 
 CURVE ( )  GEOMETRIC_REPRESENTATION_ITEM ( )  RATIONAL_B_SPLINE_CURVE ( ( 0.9999999999999938938, 0.9238795325112928447, 1.000000000000000000, 0.9238795325112867385, 1.000000000000000000, 0.9238795325112867385, 1.000000000000000000, 0.9238795325112806323, 1.000000000000005995 ) ) 
 REPRESENTATION_ITEM ( '' )  );
#68449 = COLOUR_RGB ( '',0.7921568627450980005, 0.8196078431372548767, 0.9333333333333333481 ) ;
#68450 = EDGE_CURVE ( 'NONE', #37485, #47413, #71425, .T. ) ;
#68451 = CARTESIAN_POINT ( 'NONE',  ( 31.91634192837942408, -28.81301179721947747, 166.3753187411433032 ) ) ;
#68452 = CARTESIAN_POINT ( 'NONE',  ( 30.99106816559014987, 173.7267113795729188, 172.4740941932781197 ) ) ;
#68453 = CARTESIAN_POINT ( 'NONE',  ( 3.042071309553167513, 127.1354166632526699, -11.35316468749999785 ) ) ;
#68454 = CARTESIAN_POINT ( 'NONE',  ( 2.445694354108839619, 201.8125000013656063, 200.4456943541088663 ) ) ;
#68455 = CARTESIAN_POINT ( 'NONE',  ( 5.082755093536325930, 22.03124999795161543, -5.082755093536325930 ) ) ;
#68456 = CARTESIAN_POINT ( 'NONE',  ( 10.18810118750000093, -4.220049686691933033, 85.18750000204838102 ) ) ;
#68457 = CARTESIAN_POINT ( 'NONE',  ( 8.311093377946837890, 41.71874999658601979, -8.311093377946837890 ) ) ;
#68458 = ORIENTED_EDGE ( 'NONE', *, *, #59270, .F. ) ;
#68459 = CARTESIAN_POINT ( 'NONE',  ( 8.000000000000000000, 89.93750000409677625, -9.797174393178825657E-16 ) ) ;
#68460 = CARTESIAN_POINT ( 'NONE',  ( -7.320508075688778149, 194.9999999931720538, 7.320508075688769267 ) ) ;
#68461 = CARTESIAN_POINT ( 'NONE',  ( 8.008118988124991233, 3.317071493978879015, 21.35686528394063544 ) ) ;
#68462 = CARTESIAN_POINT ( 'NONE',  ( 3.458734124999960358, 205.6250000013656063, 143.4326545832176976 ) ) ;
#68463 = EDGE_CURVE ( 'NONE', #31186, #42278, #12977, .T. ) ;
#68464 = CARTESIAN_POINT ( 'NONE',  ( -5.082755093536325042, 10.03124999795161187, -5.082755093536325930 ) ) ;
#68465 = CARTESIAN_POINT ( 'NONE',  ( 6.000000000000001776, 297.5625000034140157, -7.347880794884121708E-16 ) ) ;
#68466 = CARTESIAN_POINT ( 'NONE',  ( -29.21378695729025310, -12.06933312760573429, 140.9053845915344141 ) ) ;
#68467 = CARTESIAN_POINT ( 'NONE',  ( -1.320432766682874540E-15, 3.468749997951610542, 7.188101187500000044 ) ) ;
#68468 = CARTESIAN_POINT ( 'NONE',  ( -9.832129032723420536, 159.0104166632526983, 5.676582343749997150 ) ) ;
#68469 = CARTESIAN_POINT ( 'NONE',  ( 4.220049686691934809, 10.18810118749999916, 74.68750000204836681 ) ) ;
#68470 = EDGE_CURVE ( 'NONE', #57749, #28680, #74392, .T. ) ;
#68471 = CARTESIAN_POINT ( 'NONE',  ( -24.54126587500000412, 209.5000000013656063, 168.5673454167827003 ) ) ;
#68472 = DIRECTION ( 'NONE',  ( 1.000000000000000000, 0.000000000000000000, 0.000000000000000000 ) ) ;
#68473 = CARTESIAN_POINT ( 'NONE',  ( -3.211159895383561391, 20.81249999863440436, -3.211159895383561835 ) ) ;
#68474 = ORIENTED_EDGE ( 'NONE', *, *, #33953, .T. ) ;
#68475 = CARTESIAN_POINT ( 'NONE',  ( 2.849036369511732440E-14, 201.3750000027312126, 202.0000000000000000 ) ) ;
#68476 = CARTESIAN_POINT ( 'NONE',  ( 2.828427124746152987, 205.1250000000000284, 139.1715728752538723 ) ) ;
#68477 = CARTESIAN_POINT ( 'NONE',  ( -32.00000000000000000, 203.3750000027312126, 170.0000000000004547 ) ) ;
#68478 = CARTESIAN_POINT ( 'NONE',  ( 2.020667218593132706E-15, -11.00000000000000000, 75.06250000409676204 ) ) ;
#68479 = CARTESIAN_POINT ( 'NONE',  ( 7.999999999999991118, 3.313708498984757611, 6.361552783920146226 ) ) ;
#68480 = ORIENTED_EDGE ( 'NONE', *, *, #39625, .F. ) ;
#68481 = CARTESIAN_POINT ( 'NONE',  ( 7.188101187499999156, 16.87499999795161543, 2.977408999572654924 ) ) ;
#68482 = CARTESIAN_POINT ( 'NONE',  ( -23.99999999999998579, 196.8750000027312126, 170.0000000000002842 ) ) ;
#68483 = CARTESIAN_POINT ( 'NONE',  ( -1.040834085586084257E-14, 82.00000000000001421, 20.00000000000000355 ) ) ;
#68484 = CARTESIAN_POINT ( 'NONE',  ( 2.679491924311222739, 43.95833333333333570, 10.00000000000000355 ) ) ;
#68485 = AXIS2_PLACEMENT_3D ( 'NONE', #58863, #40758, #63766 ) ;
#68486 = CARTESIAN_POINT ( 'NONE',  ( 1.320432766682874540E-15, 105.4062500020483810, 7.188101187500000044 ) ) ;
#68487 = CARTESIAN_POINT ( 'NONE',  ( -29.43265458321761230, 209.1250000013656347, 173.4587341250003760 ) ) ;
#68488 = CARTESIAN_POINT ( 'NONE',  ( 2.485281374238575314, 299.3125000000001137, 6.000000000000000888 ) ) ;
#68489 = EDGE_CURVE ( 'NONE', #31504, #33535, #66919, .T. ) ;
#68491 = DIRECTION ( 'NONE',  ( 0.000000000000000000, 0.000000000000000000, 1.000000000000000000 ) ) ;
#68490 = CARTESIAN_POINT ( 'NONE',  ( 7.320508075688854532, 79.37500000000007105, 7.320508075688858085 ) ) ;
#68492 = EDGE_LOOP ( 'NONE', ( #5085, #62396, #13531, #14129 ) ) ;
#68493 = VECTOR ( 'NONE', #29821, 999.9999999999998863 ) ;
#68494 = CARTESIAN_POINT ( 'NONE',  ( -5.676582343749992710, 239.7395833367473301, 9.832129032723422313 ) ) ;
#68495 = CARTESIAN_POINT ( 'NONE',  ( 2.977408999572650927, -7.188101187499990274, 26.33030278187175810 ) ) ;
#68496 = FACE_OUTER_BOUND ( 'NONE', #6000, .T. ) ;
#68497 = CARTESIAN_POINT ( 'NONE',  ( -10.09650806435399772, 220.0000000000001137, 1.283633865712600297 ) ) ;
#68498 = CARTESIAN_POINT ( 'NONE',  ( 24.90605898815389452, 194.9908001228991168, 172.5499026368303248 ) ) ;
#68500 = EDGE_CURVE ( 'NONE', #3122, #48612, #43519, .T. ) ;
#68499 = CARTESIAN_POINT ( 'NONE',  ( 3.458734125000015869, 196.1875000013655779, 198.0000000000000284 ) ) ;
#68501 = CARTESIAN_POINT ( 'NONE',  ( -10.00000000000000355, 167.7083333333333428, 2.679491924311223183 ) ) ;
#68502 = PLANE ( 'NONE',  #65457 ) ;
#68503 = CARTESIAN_POINT ( 'NONE',  ( -2.975619346028166579, 8.674330214978043685, -0.09252763182292181310 ) ) ;
#68504 = CARTESIAN_POINT ( 'NONE',  ( -3.313708498984762496, 90.78125000000000000, 7.999999999999998224 ) ) ;
#68505 = CARTESIAN_POINT ( 'NONE',  ( -8.311093377946836114, 132.9687499965860411, -8.311093377946837890 ) ) ;
#68506 = LINE ( 'NONE', #74539, #38437 ) ;
#68507 = CARTESIAN_POINT ( 'NONE',  ( -6.735557395310442023E-16, 11.00000000000000000, 107.1250000000000000 ) ) ;
#68510 = CARTESIAN_POINT ( 'NONE',  ( -11.00000000000021139, 4.556349186103834548, 85.09375000409677625 ) ) ;
#68509 = CARTESIAN_POINT ( 'NONE',  ( 25.55430564589115150, 195.0625000013656063, 167.5543056458911053 ) ) ;
#68508 = CARTESIAN_POINT ( 'NONE',  ( 31.45873412499999233, 196.9375000013655779, 169.9999999999999432 ) ) ;
#68511 = ORIENTED_EDGE ( 'NONE', *, *, #32132, .F. ) ;
#68512 = CARTESIAN_POINT ( 'NONE',  ( 4.000000000000000888, 1.937500000000000222, 1.656854249492384135 ) ) ;
#68513 = CYLINDRICAL_SURFACE ( 'NONE', #59231, 7.000000000000000000 ) ;
#68514 = DIRECTION ( 'NONE',  ( -0.000000000000000000, 1.000000000000000000, -0.000000000000000000 ) ) ;
#68515 = CARTESIAN_POINT ( 'NONE',  ( 30.44569435410878810, 194.8125000013656063, 172.4456943541087526 ) ) ;
#68516 = EDGE_CURVE ( 'NONE', #11982, #1524, #61622, .T. ) ;
#68517 = CARTESIAN_POINT ( 'NONE',  ( 6.951808397369818766E-16, 212.3437499965860411, -11.35316468750000141 ) ) ;
#68518 = CARTESIAN_POINT ( 'NONE',  ( 2.977408999572650039, 120.6875000020483952, -7.188101187500001821 ) ) ;
#68519 = CARTESIAN_POINT ( 'NONE',  ( -3.211159895383561391, 1.812499998634406584, -3.211159895383561835 ) ) ;
#68520 = CARTESIAN_POINT ( 'NONE',  ( -2.620431783929977332, 65.99617417813112752, -26.42108291243877005 ) ) ;
#68521 = CARTESIAN_POINT ( 'NONE',  ( -7.999999999999989342, -3.313708498984762496, 23.42405277982336642 ) ) ;
#68523 = CARTESIAN_POINT ( 'NONE',  ( -28.00000000000002842, 203.0000000000000000, 166.0000000000003695 ) ) ;
#68522 = CARTESIAN_POINT ( 'NONE',  ( -4.000000000000001776, 1.437500000000000444, -1.656854249492381470 ) ) ;
#68524 = CARTESIAN_POINT ( 'NONE',  ( -8.311093377946841443, 93.90624999658599847, 8.311093377946830785 ) ) ;
#68525 = VERTEX_POINT ( 'NONE', #50292 ) ;
#68526 = DIRECTION ( 'NONE',  ( 0.000000000000000000, 0.000000000000000000, 1.000000000000000000 ) ) ;
#68527 = CARTESIAN_POINT ( 'NONE',  ( -5.082755093536325042, 26.53124999795161543, -5.082755093536325930 ) ) ;
#68528 = CARTESIAN_POINT ( 'NONE',  ( 5.000000000000000000, -60.11723469343116477, 46.25570701698070764 ) ) ;
#68529 = CARTESIAN_POINT ( 'NONE',  ( -9.832129032723415207, 254.6354166700806729, 5.676582343750005144 ) ) ;
#68530 = CARTESIAN_POINT ( 'NONE',  ( -9.832129032723418760, 107.8645833299193555, -5.676582343750004256 ) ) ;
#68531 = EDGE_LOOP ( 'NONE', ( #44283, #19127 ) ) ;
#68532 = CARTESIAN_POINT ( 'NONE',  ( 25.17157287525381548, 197.0000000027312126, 172.8284271247460993 ) ) ;
#68533 = CARTESIAN_POINT ( 'NONE',  ( 4.220049686691941027, -10.18810118749999738, 107.1250000020483810 ) ) ;
#68534 = CARTESIAN_POINT ( 'NONE',  ( -5.000000000000005329, 215.2083333265053682, 8.660254037844387298 ) ) ;
#68535 = CARTESIAN_POINT ( 'NONE',  ( -1.432654583217607414, 203.5000000013655779, 194.5412658750000219 ) ) ;
#68536 = CARTESIAN_POINT ( 'NONE',  ( 18.00000000000000000, -1.756128610415474078, 2.107417972768699244E-15 ) ) ;
#68538 = CARTESIAN_POINT ( 'NONE',  ( 11.35316468749999963, 105.9895833299193413, -3.042071309553165293 ) ) ;
#68537 = PLANE ( 'NONE',  #21940 ) ;
#68539 = CARTESIAN_POINT ( 'NONE',  ( -7.999999999999989342, -3.313708498984762496, 11.61155278392014445 ) ) ;
#68540 = CARTESIAN_POINT ( 'NONE',  ( -31.45873412499999233, 199.9375000013656063, 170.0000000000003979 ) ) ;
#68541 = CARTESIAN_POINT ( 'NONE',  ( 2.828427124746209831, 208.5000000027312126, 200.8284271247462129 ) ) ;
#68542 = ORIENTED_EDGE ( 'NONE', *, *, #46747, .F. ) ;
#68543 = CARTESIAN_POINT ( 'NONE',  ( 8.660254037844385522, 181.4583333265053682, 5.000000000000005329 ) ) ;
#68544 = EDGE_CURVE ( 'NONE', #21048, #8103, #38253, .T. ) ;
#68545 = AXIS2_PLACEMENT_3D ( 'NONE', #70930, #2647, #3017 ) ;
#68546 = DIRECTION ( 'NONE',  ( -1.000000000000000000, -0.000000000000000000, -0.000000000000000000 ) ) ;
#68547 = FACE_OUTER_BOUND ( 'NONE', #70024, .T. ) ;
#68548 = CARTESIAN_POINT ( 'NONE',  ( -3.042071309553173730, 89.63541666325266988, 11.35316468749999785 ) ) ;
#68549 = CARTESIAN_POINT ( 'NONE',  ( 2.765530957082001251, 290.7656250017069510, 6.676582343750000703 ) ) ;
#68550 = CARTESIAN_POINT ( 'NONE',  ( -7.188101187500000044, 6.093749997951610986, -8.802885111219163269E-16 ) ) ;
#68551 = CARTESIAN_POINT ( 'NONE',  ( 4.220049686691934809, 10.18810118749999916, 99.06250000204836681 ) ) ;
#68552 = CARTESIAN_POINT ( 'NONE',  ( 8.311093377946837890, 216.4062499965860127, -8.311093377946837890 ) ) ;
#68553 = ORIENTED_EDGE ( 'NONE', *, *, #69935, .F. ) ;
#68554 = DIRECTION ( 'NONE',  ( 1.000000000000000000, 0.000000000000000000, 0.000000000000000000 ) ) ;
#68555 = CARTESIAN_POINT ( 'NONE',  ( -7.999999999971585396, 1.424435121157765920E-05, 7.017269882810325932 ) ) ;
#68556 = CARTESIAN_POINT ( 'NONE',  ( -2.995737153982850121, -16.37687539610413978, 68.98994273414959366 ) ) ;
#68557 = CARTESIAN_POINT ( 'NONE',  ( 11.35316468749999785, 225.5729166632526983, 3.042071309553174174 ) ) ;
#68558 = AXIS2_PLACEMENT_3D ( 'NONE', #22627, #10212, #28667 ) ;
#68559 = CARTESIAN_POINT ( 'NONE',  ( -8.660254037844385522, 218.5416666734946318, 5.000000000000004441 ) ) ;
#68560 = CARTESIAN_POINT ( 'NONE',  ( -1.967015505459129087E-11, 198.7499999999984936, 10.00000000000000533 ) ) ;
#68561 = CARTESIAN_POINT ( 'NONE',  ( -2.765530957081998586, 295.6406250017069510, 6.676582343750001591 ) ) ;
#68562 = ORIENTED_EDGE ( 'NONE', *, *, #37312, .F. ) ;
#68563 = CARTESIAN_POINT ( 'NONE',  ( 11.35316468750000141, 191.0937499965860127, 0.000000000000000000 ) ) ;
#68564 = CARTESIAN_POINT ( 'NONE',  ( 7.204075437095968759, -7.204075437095966983, 95.21875000204838102 ) ) ;
#68565 =( BOUNDED_CURVE ( )  B_SPLINE_CURVE ( 2, ( #19234, #42241, #53582, #24882, #34772, #807, #29461, #57775, #58879 ),
 .UNSPECIFIED., .F., .F. ) 
 B_SPLINE_CURVE_WITH_KNOTS ( ( 3, 2, 2, 2, 3 ),
 ( 0.4500000000000002887, 0.4583333333333336479, 0.4666666666666670626, 0.4750000000000004219, 0.4833333333333338366 ),
 .UNSPECIFIED. ) 
 CURVE ( )  GEOMETRIC_REPRESENTATION_ITEM ( )  RATIONAL_B_SPLINE_CURVE ( ( 0.9999999999999974465, 0.9238795325112892920, 1.000000000000000000, 0.9238795325112867385, 1.000000000000000000, 0.9238795325112867385, 1.000000000000000000, 0.9238795325112821866, 1.000000000000004663 ) ) 
 REPRESENTATION_ITEM ( '' )  );
#68566 = CARTESIAN_POINT ( 'NONE',  ( -30.44569435410879521, 208.8125000013656063, 172.4456943541092357 ) ) ;
#68567 = SHAPE_REPRESENTATION ( 'clamping plate', ( #57354 ), #40540 ) ;
#68568 = CARTESIAN_POINT ( 'NONE',  ( 4.898587196589412829E-16, 16.87500000000000000, -8.000000000000000000 ) ) ;
#68569 = VERTEX_POINT ( 'NONE', #49167 ) ;
#68570 = CARTESIAN_POINT ( 'NONE',  ( -7.188101187499999156, 122.7500000020483952, 2.977408999572654924 ) ) ;
#68571 = CARTESIAN_POINT ( 'NONE',  ( 10.00000000000000178, 15.00000000000000178, 0.000000000000000000 ) ) ;
#68572 = DIRECTION ( 'NONE',  ( -0.000000000000000000, -1.000000000000000000, -0.000000000000000000 ) ) ;
#68573 = CARTESIAN_POINT ( 'NONE',  ( 4.220049686691941027, -10.18810118749999738, 83.50000000204840944 ) ) ;
#68574 = ORIENTED_EDGE ( 'NONE', *, *, #72166, .T. ) ;
#68575 = CARTESIAN_POINT ( 'NONE',  ( -4.000000000000002665, 19.56250000000000000, 1.656854249492380804 ) ) ;
#68576 = CARTESIAN_POINT ( 'NONE',  ( 9.000000000000000000, -0.8780643052077397037, -1.070649645329435629E-15 ) ) ;
#68577 = CARTESIAN_POINT ( 'NONE',  ( 28.47326357806521813, 194.4587341250000350, 173.4262024652836658 ) ) ;
#68578 = CARTESIAN_POINT ( 'NONE',  ( 8.660254037844385522, 16.45833332650536818, 5.000000000000005329 ) ) ;
#68579 = CARTESIAN_POINT ( 'NONE',  ( -2.977408999572650927, 89.37500000204839523, -7.188101187500001821 ) ) ;
#68580 = PLANE ( 'NONE',  #54643 ) ;
#68581 = EDGE_CURVE ( 'NONE', #59754, #61426, #39253, .T. ) ;
#68584 = DIRECTION ( 'NONE',  ( -0.000000000000000000, 1.000000000000000000, -0.000000000000000000 ) ) ;
#68583 = CARTESIAN_POINT ( 'NONE',  ( -11.35316468749999785, 243.6979166700806445, -3.042071309553164848 ) ) ;
#68582 = CARTESIAN_POINT ( 'NONE',  ( 30.44569435410879876, 208.8125000013656063, 167.5543056458910485 ) ) ;
#68585 = SHAPE_DEFINITION_REPRESENTATION ( #50528, #2150 ) ;
#68586 = VERTEX_POINT ( 'NONE', #72567 ) ;
#68588 = CIRCLE ( 'NONE', #3531, 7.499999999999992895 ) ;
#68587 = CARTESIAN_POINT ( 'NONE',  ( -8.311093377946834337, 259.8437500034140157, 8.311093377946837890 ) ) ;
#68589 = CARTESIAN_POINT ( 'NONE',  ( 1.320432766682872962E-15, -7.188101187499992051, 12.36155278187175277 ) ) ;
#68590 = EDGE_LOOP ( 'NONE', ( #10202, #37975, #47189, #33782, #44686 ) ) ;
#68591 = EDGE_CURVE ( 'NONE', #34167, #62240, #51248, .T. ) ;
#68592 = VERTEX_POINT ( 'NONE', #15954 ) ;
#68593 = CARTESIAN_POINT ( 'NONE',  ( 1.871523826299183495E-15, -10.18810118749999916, 75.53125000204836681 ) ) ;
#68594 = CARTESIAN_POINT ( 'NONE',  ( -9.832129032723418760, 93.17708332991935549, -5.676582343750004256 ) ) ;
#68595 = CARTESIAN_POINT ( 'NONE',  ( 7.778174593052023411, -7.778174593052021635, 84.06249999999998579 ) ) ;
#68598 = CARTESIAN_POINT ( 'NONE',  ( 8.660254037844390851, 70.41666666666668561, -5.000000000000001776 ) ) ;
#68597 = CARTESIAN_POINT ( 'NONE',  ( 24.54126587499999701, 207.1875000013656063, 169.9999999999999432 ) ) ;
#68596 = CARTESIAN_POINT ( 'NONE',  ( 24.54126587500000056, 205.3750000013656063, 168.5673454167822172 ) ) ;
#68599 = CARTESIAN_POINT ( 'NONE',  ( 4.999999999999993783, 76.04166665983871098, 8.660254037844390851 ) ) ;
#68600 = DIRECTION ( 'NONE',  ( -0.000000000000000000, 1.000000000000000000, -0.000000000000000000 ) ) ;
#68601 = CARTESIAN_POINT ( 'NONE',  ( -2.085542519210945728E-15, 194.5312499965860127, 11.35316468750000141 ) ) ;
#68602 = VECTOR ( 'NONE', #12772, 1000.000000000000000 ) ;
#68603 = CARTESIAN_POINT ( 'NONE',  ( -3.458734125000015425, 204.0000000013656347, 143.4326545832176976 ) ) ;
#68604 = EDGE_LOOP ( 'NONE', ( #54180, #66698, #68096 ) ) ;
#68605 = CARTESIAN_POINT ( 'NONE',  ( 24.54126587499998280, 204.5000000013656063, 171.4326545832175555 ) ) ;
#68606 = CARTESIAN_POINT ( 'NONE',  ( -7.188101187500000044, 15.09374999795161187, -8.802885111219163269E-16 ) ) ;
#68607 = CARTESIAN_POINT ( 'NONE',  ( -8.311093377946836114, 172.9687499965860127, -8.311093377946837890 ) ) ;
#68608 = FACE_OUTER_BOUND ( 'NONE', #12892, .T. ) ;
#68609 = CARTESIAN_POINT ( 'NONE',  ( -7.188101187499999156, 103.6250000020483810, 2.977408999572654924 ) ) ;
#68611 = CARTESIAN_POINT ( 'NONE',  ( -7.320508075688771932, 234.3750000000000000, -7.320508075688771932 ) ) ;
#68610 = CARTESIAN_POINT ( 'NONE',  ( 2.828427124746190291, 16.62499999726881583, 2.828427124746192067 ) ) ;
#68612 = CARTESIAN_POINT ( 'NONE',  ( -1.881053915767124440, 8.999999998634406140, 4.541265875000001451 ) ) ;
#68613 = CARTESIAN_POINT ( 'NONE',  ( 30.44569435410883429, 202.0625000013656063, 167.5543056458911053 ) ) ;
#68614 = CARTESIAN_POINT ( 'NONE',  ( -2.977408999572647819, 7.188101187499991163, 10.58030278187175455 ) ) ;
#68615 = CARTESIAN_POINT ( 'NONE',  ( 5.676582343749993598, 54.94791666325269119, 9.832129032723422313 ) ) ;
#68616 = CARTESIAN_POINT ( 'NONE',  ( 2.775557561562891351E-14, 210.0000000000000284, 198.0000000000000284 ) ) ;
#68617 = CARTESIAN_POINT ( 'NONE',  ( -3.313708498984758943, -7.999999999999989342, -0.3321972156701773482 ) ) ;
#68618 = ORIENTED_EDGE ( 'NONE', *, *, #26764, .T. ) ;
#68619 = CYLINDRICAL_SURFACE ( 'NONE', #32653, 11.00000000000000000 ) ;
#68620 = CARTESIAN_POINT ( 'NONE',  ( -1.836970198721029983E-15, 170.6249999931720538, 10.00000000000000178 ) ) ;
#68621 = CARTESIAN_POINT ( 'NONE',  ( -3.042071309553164404, 62.23958332991934128, -11.35316468749999963 ) ) ;
#68622 = CARTESIAN_POINT ( 'NONE',  ( -7.778174593052023411, 7.778174593052023411, 76.00000000409676204 ) ) ;
#68623 = CARTESIAN_POINT ( 'NONE',  ( -3.458734125000015869, 199.1875000013655779, 142.0000000000000568 ) ) ;
#68624 = CARTESIAN_POINT ( 'NONE',  ( -7.320508075688771932, 259.3750000000000000, -7.320508075688771932 ) ) ;
#68625 = CARTESIAN_POINT ( 'NONE',  ( -2.828427124746208943, 196.7500000027312126, 144.8284271247462129 ) ) ;
#68627 = CARTESIAN_POINT ( 'NONE',  ( 3.042071309553159519, 64.73958332991935549, 11.35316468750000141 ) ) ;
#68626 = CARTESIAN_POINT ( 'NONE',  ( 2.977408999572650039, 93.68750000204838102, -7.188101187500000933 ) ) ;
#68628 = CARTESIAN_POINT ( 'NONE',  ( 3.313708498984756279, 7.999999999999991118, 3.361552779823362425 ) ) ;
#68629 = CARTESIAN_POINT ( 'NONE',  ( 8.000000000000000000, 110.9375000040967905, -9.797174393178825657E-16 ) ) ;
#68630 = CARTESIAN_POINT ( 'NONE',  ( -5.676582343750006032, 169.1145833299193555, 9.832129032723418760 ) ) ;
#68632 = CARTESIAN_POINT ( 'NONE',  ( -8.660254037844387298, 148.9583333265053682, -5.000000000000004441 ) ) ;
#68631 = PRODUCT_DEFINITION_SHAPE ( 'NONE', 'NONE',  #44081 ) ;
#68633 = CARTESIAN_POINT ( 'NONE',  ( -2.977408999572650927, 98.75000000204838102, -7.188101187500001821 ) ) ;
#68634 = CARTESIAN_POINT ( 'NONE',  ( -10.00000000000000000, 54.16666665983869677, -2.679491924311229845 ) ) ;
#68635 = CARTESIAN_POINT ( 'NONE',  ( -8.311093377946836114, 42.96874999658601268, -8.311093377946837890 ) ) ;
#68636 = LINE ( 'NONE', #33216, #13509 ) ;
#68637 = CARTESIAN_POINT ( 'NONE',  ( -9.832129032723420536, 183.6979166632526983, 5.676582343749997150 ) ) ;
#68638 = ORIENTED_EDGE ( 'NONE', *, *, #18166, .F. ) ;
#68639 = CARTESIAN_POINT ( 'NONE',  ( 48.65829649837611015, 141.3560062876440213, 60.50005375836683896 ) ) ;
#68640 = CARTESIAN_POINT ( 'NONE',  ( 10.18810118749999916, 4.220049686691935698, 70.00000000204836681 ) ) ;
#68641 = CARTESIAN_POINT ( 'NONE',  ( 2.849036369511732440E-14, 196.2500000000000000, 202.0000000000000000 ) ) ;
#68642 = CARTESIAN_POINT ( 'NONE',  ( 32.92357796428662908, 41.53809092712866402, 65.00000000000001421 ) ) ;
#68644 = CARTESIAN_POINT ( 'NONE',  ( 8.311093377946834337, 160.1562499965860411, 8.311093377946839666 ) ) ;
#68643 = DIRECTION ( 'NONE',  ( 0.000000000000000000, 0.000000000000000000, -1.000000000000000000 ) ) ;
#68645 = CARTESIAN_POINT ( 'NONE',  ( -7.999999999999991118, 0.000000000000000000, 8.386552784329824206 ) ) ;
#68646 = CARTESIAN_POINT ( 'NONE',  ( 7.778174593052023411, -7.778174593052021635, 79.75000000409676204 ) ) ;
#68647 = CARTESIAN_POINT ( 'NONE',  ( 7.320508075688771044, 261.2500000068278609, -7.320508075688771932 ) ) ;
#68648 = DIRECTION ( 'NONE',  ( 0.000000000000000000, 0.000000000000000000, 1.000000000000000000 ) ) ;
#68649 = ORIENTED_EDGE ( 'NONE', *, *, #34100, .F. ) ;
#68650 = VECTOR ( 'NONE', #57454, 1000.000000000000000 ) ;
#68651 = CARTESIAN_POINT ( 'NONE',  ( -7.188101187499992051, 2.977408999572646930, 25.39280278187176165 ) ) ;
#68652 = CARTESIAN_POINT ( 'NONE',  ( 5.676582343749993598, 110.2604166632526841, 9.832129032723422313 ) ) ;
#68653 = CARTESIAN_POINT ( 'NONE',  ( -1.183492779173324630E-13, 16.25000000000001066, -10.00000000000000178 ) ) ;
#68655 = ORIENTED_EDGE ( 'NONE', *, *, #69966, .T. ) ;
#68654 =( BOUNDED_CURVE ( )  B_SPLINE_CURVE ( 2, ( #52728, #41039, #23303, #69331, #28967, #11616, #62922, #52357, #46317 ),
 .UNSPECIFIED., .F., .F. ) 
 B_SPLINE_CURVE_WITH_KNOTS ( ( 3, 2, 2, 2, 3 ),
 ( 0.5441176470588233727, 0.5477941176470587648, 0.5514705882352939348, 0.5551470588235292158, 0.5588235294117644969 ),
 .UNSPECIFIED. ) 
 CURVE ( )  GEOMETRIC_REPRESENTATION_ITEM ( )  RATIONAL_B_SPLINE_CURVE ( ( 1.000000000000002220, 0.9238795325112844070, 1.000000000000000000, 0.9238795325112867385, 1.000000000000000000, 0.9238795325112867385, 1.000000000000000000, 0.9238795325112912904, 0.9999999999999954481 ) ) 
 REPRESENTATION_ITEM ( '' )  );
#68656 = CARTESIAN_POINT ( 'NONE',  ( 1.881053915767121776, 6.624999998634407916, -4.541265875000002339 ) ) ;
#68657 = CARTESIAN_POINT ( 'NONE',  ( 7.188101187499999156, 13.87499999795161187, 2.977408999572654924 ) ) ;
#68658 = CARTESIAN_POINT ( 'NONE',  ( 8.000000000000000000, 107.9375000040967905, -9.797174393178825657E-16 ) ) ;
#68659 = EDGE_CURVE ( 'NONE', #5819, #35453, #38980, .T. ) ;
#68660 = CARTESIAN_POINT ( 'NONE',  ( -24.54126587499998990, 197.4375000013655779, 170.0000000000003411 ) ) ;
#68661 = CARTESIAN_POINT ( 'NONE',  ( -1.656854249492383691, 6.687500000000000888, 4.000000000000000888 ) ) ;
#68662 = CARTESIAN_POINT ( 'NONE',  ( 4.000000000000001776, 22.74999999726881228, 0.000000000000000000 ) ) ;
#68663 = CARTESIAN_POINT ( 'NONE',  ( -1.881053915767124440, 8.999999998634407916, 4.541265875000001451 ) ) ;
#68664 = CARTESIAN_POINT ( 'NONE',  ( -2.828427124746209831, 199.3750000000000284, 139.1715728752538723 ) ) ;
#68665 = ORIENTED_EDGE ( 'NONE', *, *, #29166, .F. ) ;
#68666 =( NAMED_UNIT ( * ) PLANE_ANGLE_UNIT ( ) SI_UNIT ( $, .RADIAN. ) );
#68667 = CARTESIAN_POINT ( 'NONE',  ( 7.188101187500002709, 103.8125000020483952, 2.977408999572649151 ) ) ;
#68668 = EDGE_CURVE ( 'NONE', #69992, #5775, #28111, .T. ) ;
#68670 = CARTESIAN_POINT ( 'NONE',  ( 46.67364751762348618, 38.00000000000001421, 69.99999999999997158 ) ) ;
#68669 = DIRECTION ( 'NONE',  ( -0.000000000000000000, -0.000000000000000000, -1.000000000000000000 ) ) ;
#68671 =( BOUNDED_CURVE ( )  B_SPLINE_CURVE ( 2, ( #42043, #13723, #36768, #61263, #38260, #3553, #26168, #22008, #27295 ),
 .UNSPECIFIED., .F., .F. ) 
 B_SPLINE_CURVE_WITH_KNOTS ( ( 3, 2, 2, 2, 3 ),
 ( 0.4558823529411765163, 0.4595588235294117974, 0.4632352941176471894, 0.4669117647058824705, 0.4705882352941177516 ),
 .UNSPECIFIED. ) 
 CURVE ( )  GEOMETRIC_REPRESENTATION_ITEM ( )  RATIONAL_B_SPLINE_CURVE ( ( 0.9999999999999988898, 0.9238795325112878487, 1.000000000000000000, 0.9238795325112867385, 1.000000000000000000, 0.9238795325112867385, 1.000000000000000000, 0.9238795325112844070, 1.000000000000002220 ) ) 
 REPRESENTATION_ITEM ( '' )  );
#68672 = CARTESIAN_POINT ( 'NONE',  ( -4.000000000000001776, 10.50000000000000000, -4.898587196589415787E-16 ) ) ;
#68673 = CARTESIAN_POINT ( 'NONE',  ( -7.188101187499991163, 2.977408999572646930, 28.39280278187175810 ) ) ;
#68674 = ORIENTED_EDGE ( 'NONE', *, *, #15359, .F. ) ;
#68675 = VERTEX_POINT ( 'NONE', #45015 ) ;
#68676 = CARTESIAN_POINT ( 'NONE',  ( 7.204075437095966983, 7.204075437095967871, 92.59375000204838102 ) ) ;
#68677 = CARTESIAN_POINT ( 'NONE',  ( -31.66756539373097468, 271.9999999999999432, 167.9999999999998295 ) ) ;
#68678 = DIRECTION ( 'NONE',  ( 0.000000000000000000, 0.8536788251726059595, -0.5207998305029671871 ) ) ;
#68679 = CARTESIAN_POINT ( 'NONE',  ( -6.735557395310442023E-16, 11.00000000000000000, 102.6250000000000000 ) ) ;
#68680 = CARTESIAN_POINT ( 'NONE',  ( -3.458734124999960358, 203.6250000013656063, 196.5673454167823877 ) ) ;
#68682 = LINE ( 'NONE', #25787, #103 ) ;
#68681 = CARTESIAN_POINT ( 'NONE',  ( 1.934925017735378189E-11, 153.7500000000015348, 10.00000000000000533 ) ) ;
#68683 = CARTESIAN_POINT ( 'NONE',  ( 8.660254037844389075, 120.4166666666666714, -5.000000000000000000 ) ) ;
#68684 = CARTESIAN_POINT ( 'NONE',  ( -5.656854249492378806, 104.1874999999999858, 5.656854249492381470 ) ) ;
#68685 = CARTESIAN_POINT ( 'NONE',  ( -7.778174593052020747, -7.778174593052023411, 86.87500000409677625 ) ) ;
#68686 = CARTESIAN_POINT ( 'NONE',  ( -2.977408999572647819, 7.188101187499991163, 3.080302781871750994 ) ) ;
#68687 = DIRECTION ( 'NONE',  ( -0.000000000000000000, -1.000000000000000000, -0.000000000000000000 ) ) ;
#68688 = CIRCLE ( 'NONE', #15640, 7.000000000000000000 ) ;
#68689 = CARTESIAN_POINT ( 'NONE',  ( 31.45873412499998523, 206.6250000013656063, 171.4326545832175839 ) ) ;
#68690 = CARTESIAN_POINT ( 'NONE',  ( 3.313708498984762052, 27.09374999590322020, -8.000000000000000000 ) ) ;
#68691 = CARTESIAN_POINT ( 'NONE',  ( -1.432654583217664479, 200.7500000013656347, 138.5412658750000787 ) ) ;
#68692 = CARTESIAN_POINT ( 'NONE',  ( -2.977408999572650927, 119.7500000020483810, -7.188101187500000933 ) ) ;
#68694 = CARTESIAN_POINT ( 'NONE',  ( 2.751549872419338751E-14, 194.9207531772044888, 194.0792468227953975 ) ) ;
#68693 = CARTESIAN_POINT ( 'NONE',  ( -2.841757666793576517E-14, 194.6037658790967271, 138.3962341209032445 ) ) ;
#68695 = CARTESIAN_POINT ( 'NONE',  ( 3.042071309553163960, 242.7604166700806729, -11.35316468749999785 ) ) ;
#68696 = CARTESIAN_POINT ( 'NONE',  ( 5.082755093536318824, 5.082755093536319713, 28.29905278187175810 ) ) ;
#68697 = CARTESIAN_POINT ( 'NONE',  ( 29.65685424949235482, 198.0625000000000284, 173.9999999999999147 ) ) ;
#68698 = CARTESIAN_POINT ( 'NONE',  ( 9.832129032723420536, 11.19791666325268409, -5.676582343749999815 ) ) ;
#68699 = CARTESIAN_POINT ( 'NONE',  ( -1.328591152368359007E-11, 1.250000000001033174, -10.00000000000000533 ) ) ;
#68700 = CARTESIAN_POINT ( 'NONE',  ( -9.832129032723420536, 214.0104166632526699, 5.676582343749997150 ) ) ;
#68701 = CARTESIAN_POINT ( 'NONE',  ( -29.65685424949233706, 197.4375000000000000, 174.0000000000004547 ) ) ;
#68702 = CARTESIAN_POINT ( 'NONE',  ( 8.000000000000001776, 124.1562500000000000, 3.313708498984759387 ) ) ;
#68704 = CARTESIAN_POINT ( 'NONE',  ( 7.999999999999998224, 3.313708498984749617, 28.67405277982336642 ) ) ;
#68703 = CARTESIAN_POINT ( 'NONE',  ( -2.751064625579944321E-14, 202.8750000027312126, 146.0000000000000284 ) ) ;
#68705 = ORIENTED_EDGE ( 'NONE', *, *, #34708, .F. ) ;
#68706 = CARTESIAN_POINT ( 'NONE',  ( 2.445694354108784108, 201.5625000013656063, 144.4456943541088663 ) ) ;
#68707 = CARTESIAN_POINT ( 'NONE',  ( -8.311093377946836114, 27.65624999658602334, -8.311093377946837890 ) ) ;
#68708 = CARTESIAN_POINT ( 'NONE',  ( 11.00000000000000000, 1.347111479062088405E-15, 93.43750000409677625 ) ) ;
#68709 = CARTESIAN_POINT ( 'NONE',  ( 11.00000000000000000, 1.347111479062088405E-15, 117.2500000000000000 ) ) ;
#68710 = CARTESIAN_POINT ( 'NONE',  ( -29.43265458321755546, 197.8750000013656063, 173.4587341250004044 ) ) ;
#68711 = CARTESIAN_POINT ( 'NONE',  ( -9.000000000000000000, 4.355963544827382350, -0.5613059398865143379 ) ) ;
#68713 = CARTESIAN_POINT ( 'NONE',  ( 5.676582343749993598, 24.94791666325268764, 9.832129032723422313 ) ) ;
#68712 = CARTESIAN_POINT ( 'NONE',  ( -5.082755093536324154, 110.8437500020483810, 5.082755093536326818 ) ) ;
#68714 = CARTESIAN_POINT ( 'NONE',  ( 7.999999999999991118, 3.313708498984757611, 19.67405277982336642 ) ) ;
#68715 = CARTESIAN_POINT ( 'NONE',  ( -8.311093377946841443, 133.9062499965860411, 8.311093377946830785 ) ) ;
#68716 = CARTESIAN_POINT ( 'NONE',  ( -4.999999999999998224, 98.54166665983871098, -8.660254037844389075 ) ) ;
#68717 = CARTESIAN_POINT ( 'NONE',  ( 1.320432766682874540E-15, 123.4062500020483810, 7.188101187500000044 ) ) ;
#68718 = CYLINDRICAL_SURFACE ( 'NONE', #39718, 10.00000000000000178 ) ;
#68719 = CARTESIAN_POINT ( 'NONE',  ( 0.000000000000000000, 265.0000000000000000, 0.000000000000000000 ) ) ;
#68720 = ORIENTED_EDGE ( 'NONE', *, *, #39790, .T. ) ;
#68721 = CARTESIAN_POINT ( 'NONE',  ( -7.320508075688781702, 118.1250000000000000, 7.320508075688773708 ) ) ;
#68722 = CARTESIAN_POINT ( 'NONE',  ( 6.123233995736767268E-16, 28.12499999317203603, -10.00000000000000178 ) ) ;
#68723 = CARTESIAN_POINT ( 'NONE',  ( 1.226468279477575784E-15, 295.7031250017069510, 6.676582343750001591 ) ) ;
#68724 = CARTESIAN_POINT ( 'NONE',  ( 5.676582343750001591, 126.6145833299193697, -9.832129032723420536 ) ) ;
#68725 = CARTESIAN_POINT ( 'NONE',  ( -4.000000000000016875, 207.5625000027312126, 140.3431457505076594 ) ) ;
#68726 = CARTESIAN_POINT ( 'NONE',  ( -7.999999999999989342, -3.313708498984762496, 21.98030278432982598 ) ) ;
#68727 = CARTESIAN_POINT ( 'NONE',  ( 3.999999999999960032, 207.1250000027312126, 142.0000000000000568 ) ) ;
#68728 = CARTESIAN_POINT ( 'NONE',  ( -3.042071309553159075, 259.9479166700807014, 11.35316468749999963 ) ) ;
#68729 = CARTESIAN_POINT ( 'NONE',  ( 10.18810118750000093, -4.220049686691933921, 98.68750000204838102 ) ) ;
#68730 = EDGE_LOOP ( 'NONE', ( #63448, #46921, #53989, #35886 ) ) ;
#68731 = VECTOR ( 'NONE', #19390, 1000.000000000000000 ) ;
#68732 = B_SPLINE_CURVE_WITH_KNOTS ( 'NONE', 3,
 ( #25803, #14483, #55628, #32238, #2813, #37522, #8847, #50319, #10339, #55999, #55255, #44669, #60895, #72594, #31857, #66932, #4313, #3562, #32999, #20147, #61272, #20519 ),
 .UNSPECIFIED., .F., .F.,
 ( 4, 2, 2, 2, 2, 2, 2, 2, 2, 2, 4 ),
 ( 0.000000000000000000, 0.001156727053362453534, 0.001735090580043679217, 0.002313454106724904466, 0.003470181160087371444, 0.004048544686768605801, 0.004626908213449840157, 0.005783635266812312339, 0.006940362320174783654, 0.008097089373537254969, 0.009253816426899728886 ),
 .UNSPECIFIED. ) ;
#68733 = EDGE_CURVE ( 'NONE', #17794, #6741, #15104, .T. ) ;
#68734 = CARTESIAN_POINT ( 'NONE',  ( 5.000000000000001776, 11.69579520003552098, 68.31051037013783400 ) ) ;
#68735 = FACE_OUTER_BOUND ( 'NONE', #74526, .T. ) ;
#68736 = CARTESIAN_POINT ( 'NONE',  ( 3.458734125000016757, 202.1250000013656063, 199.4326545832176976 ) ) ;
#68737 = CARTESIAN_POINT ( 'NONE',  ( 9.832129032723420536, 76.51041666325268409, -5.676582343749999815 ) ) ;
#68738 = ORIENTED_EDGE ( 'NONE', *, *, #12239, .T. ) ;
#68739 = CARTESIAN_POINT ( 'NONE',  ( 7.204075437095968759, -7.204075437095966983, 110.2187500020483810 ) ) ;
#68740 = CARTESIAN_POINT ( 'NONE',  ( -4.541265875000002339, 12.93749999863440792, -5.561446717895856393E-16 ) ) ;
#68741 = VERTEX_POINT ( 'NONE', #6142 ) ;
#68742 = CARTESIAN_POINT ( 'NONE',  ( 5.656854249492380582, 1.687500000000000222, -5.656854249492380582 ) ) ;
#68743 = CARTESIAN_POINT ( 'NONE',  ( -8.000000000000000000, 110.1875000040967905, 0.000000000000000000 ) ) ;
#68744 = CARTESIAN_POINT ( 'NONE',  ( -4.999999999999999112, -68.48985753891567185, -21.22439692019679569 ) ) ;
#68745 = CARTESIAN_POINT ( 'NONE',  ( 2.977408999572651815, 21.56249999795161898, 7.188101187500000933 ) ) ;
#68746 = DIRECTION ( 'NONE',  ( -0.000000000000000000, 1.000000000000000000, -0.000000000000000000 ) ) ;
#68747 = CARTESIAN_POINT ( 'NONE',  ( 10.18810118749999916, 1.247682550866122264E-15, 106.2812500020483810 ) ) ;
#68748 = AXIS2_PLACEMENT_3D ( 'NONE', #17723, #39262, #69048 ) ;
#68749 = CARTESIAN_POINT ( 'NONE',  ( 1.656854249492354825, 201.4375000027311842, 202.0000000000000853 ) ) ;
#68750 = CARTESIAN_POINT ( 'NONE',  ( 2.828427124746191623, 11.87499999726881406, -2.828427124746191623 ) ) ;
#68751 = LINE ( 'NONE', #55967, #3595 ) ;
#68752 = ORIENTED_EDGE ( 'NONE', *, *, #3174, .F. ) ;
#68753 = VECTOR ( 'NONE', #66228, 1000.000000000000000 ) ;
#68754 = EDGE_CURVE ( 'NONE', #39667, #47034, #17072, .T. ) ;
#68755 = CARTESIAN_POINT ( 'NONE',  ( 0.000000000000000000, 101.0525588832578734, 0.000000000000000000 ) ) ;
#68756 = CARTESIAN_POINT ( 'NONE',  ( -2.445694354108783664, 201.3125000013656063, 195.5543056458912190 ) ) ;
#68757 = VECTOR ( 'NONE', #66292, 1000.000000000000000 ) ;
#68758 = CARTESIAN_POINT ( 'NONE',  ( -30.44569435410876324, 205.8125000013656063, 172.4456943541092642 ) ) ;
#68759 = CARTESIAN_POINT ( 'NONE',  ( 11.00000000000000000, 1.347111479062088405E-15, 118.0000000000000000 ) ) ;
#68760 = CARTESIAN_POINT ( 'NONE',  ( 4.541265875000001451, 9.249999998634406140, 1.881053915767124440 ) ) ;
#68761 = CARTESIAN_POINT ( 'NONE',  ( -2.977408999572648707, -7.188101187499990274, 18.26780278187175455 ) ) ;
#68762 = EDGE_LOOP ( 'NONE', ( #31934, #59853, #14891, #61301 ) ) ;
#68763 =( BOUNDED_CURVE ( )  B_SPLINE_CURVE ( 2, ( #29306, #40245, #22504, #64003, #34607, #45901, #45525, #23999, #23263, #52316, #5925, #28927, #652 ),
 .UNSPECIFIED., .F., .F. ) 
 B_SPLINE_CURVE_WITH_KNOTS ( ( 3, 2, 2, 2, 2, 2, 3 ),
 ( 2.119489495730878748, 2.124722698272372590, 2.129955900813865988, 2.135189103355359386, 2.140422305896853228, 2.145655508438346626, 2.150888710979840468 ),
 .UNSPECIFIED. ) 
 CURVE ( )  GEOMETRIC_REPRESENTATION_ITEM ( )  RATIONAL_B_SPLINE_CURVE ( ( 1.000000000000014655, 0.9659258262890536573, 1.000000000000000000, 0.9659258262890683122, 1.000000000000000000, 0.9659258262890683122, 1.000000000000000000, 0.9659258262890683122, 1.000000000000000000, 0.9659258262890683122, 1.000000000000000000, 0.9659258262890662028, 1.000000000000001998 ) ) 
 REPRESENTATION_ITEM ( '' )  );
#68764 = CARTESIAN_POINT ( 'NONE',  ( -6.676582343750001591, 287.4531250017069510, 0.000000000000000000 ) ) ;
#68765 = ORIENTED_EDGE ( 'NONE', *, *, #67466, .T. ) ;
#68766 = CARTESIAN_POINT ( 'NONE',  ( 7.204075437095966983, 7.204075437095967871, 109.0937500020483810 ) ) ;
#68767 = DIRECTION ( 'NONE',  ( -0.000000000000000000, 1.000000000000000000, -0.000000000000000000 ) ) ;
#68768 = CARTESIAN_POINT ( 'NONE',  ( -3.458734124999959025, 198.5000000013656347, 199.4326545832176691 ) ) ;
#68769 = CARTESIAN_POINT ( 'NONE',  ( 27.99999999999996447, 195.9375000013655779, 166.5412658749999082 ) ) ;
#68770 = CARTESIAN_POINT ( 'NONE',  ( -8.660254037844390851, 82.91666666666667140, 4.999999999999998224 ) ) ;
#68771 = CARTESIAN_POINT ( 'NONE',  ( -5.656854249492378806, 123.6875000000000000, 5.656854249492381470 ) ) ;
#68772 = CARTESIAN_POINT ( 'NONE',  ( 4.242640687119285658, 288.6249999999999432, -4.242640687119286547 ) ) ;
#68773 = EDGE_CURVE ( 'NONE', #66501, #19306, #70590, .T. ) ;
#68774 = ORIENTED_EDGE ( 'NONE', *, *, #25894, .F. ) ;
#68775 = CARTESIAN_POINT ( 'NONE',  ( 0.000000000000000000, 0.000000000000000000, -0.7002075382097148193 ) ) ;
#68776 = CARTESIAN_POINT ( 'NONE',  ( -0.7581620860253960315, -10.12340554704839946, 70.09014334689044290 ) ) ;
#68777 = CARTESIAN_POINT ( 'NONE',  ( -4.000000000000015987, 197.5625000027312126, 140.3431457505076594 ) ) ;
#68778 = CARTESIAN_POINT ( 'NONE',  ( -5.000000000000000000, 62.32183698944580641, 23.94439461060463259 ) ) ;
#68779 = CARTESIAN_POINT ( 'NONE',  ( -8.000000000000000000, 23.25000000000000355, -9.797174393178825657E-16 ) ) ;
#68780 = CARTESIAN_POINT ( 'NONE',  ( 7.320508075688776373, 236.8749999999999716, 7.320508075688767491 ) ) ;
#68781 = CARTESIAN_POINT ( 'NONE',  ( -11.00000000000000000, 4.556349186104045934, 73.09375000409676204 ) ) ;
#68782 = CARTESIAN_POINT ( 'NONE',  ( -10.18810118749999916, 0.000000000000000000, 69.53125000204838102 ) ) ;
#68783 = CARTESIAN_POINT ( 'NONE',  ( -7.320508075688773708, 206.8750000000000000, -7.320508075688774596 ) ) ;
#68784 =( BOUNDED_CURVE ( )  B_SPLINE_CURVE ( 2, ( #13021, #41711, #7385, #36794, #25079, #8483, #36059, #54896, #31503 ),
 .UNSPECIFIED., .F., .F. ) 
 B_SPLINE_CURVE_WITH_KNOTS ( ( 3, 2, 2, 2, 3 ),
 ( 0.3441504249343935173, 0.3507686059762091801, 0.3573868815606666138, 0.3640051571451240475, 0.3706233993366209178 ),
 .UNSPECIFIED. ) 
 CURVE ( )  GEOMETRIC_REPRESENTATION_ITEM ( )  RATIONAL_B_SPLINE_CURVE ( ( 0.9999978252560842718, 0.9238806198987780105, 1.000000000000000000, 0.9238795325112867385, 1.000000000000000000, 0.9238795325112867385, 1.000000000000000000, 0.9238799165822936255, 0.9999992318618620146 ) ) 
 REPRESENTATION_ITEM ( '' )  );
#68785 = CARTESIAN_POINT ( 'NONE',  ( 7.188101187499992051, 2.977408999572647819, 16.20530278187175099 ) ) ;
#68786 = CARTESIAN_POINT ( 'NONE',  ( -11.35316468750000141, 173.8020833299193839, 3.042071309553159963 ) ) ;
#68787 = CARTESIAN_POINT ( 'NONE',  ( 3.410844894484189267E-12, 36.24999999999974420, -10.00000000000000178 ) ) ;
#68788 = CARTESIAN_POINT ( 'NONE',  ( -7.778174593052020747, -7.778174593052023411, 97.37500000409676204 ) ) ;
#68789 = CARTESIAN_POINT ( 'NONE',  ( -1.469576158976823947E-15, 9.937499995903220196, 8.000000000000000000 ) ) ;
#68790 = ORIENTED_EDGE ( 'NONE', *, *, #54361, .T. ) ;
#68791 = CARTESIAN_POINT ( 'NONE',  ( -3.458734125000016313, 196.8750000013656063, 140.5673454167824161 ) ) ;
#68792 = CARTESIAN_POINT ( 'NONE',  ( -11.35316468750000141, 33.80208332991934839, 3.042071309553159963 ) ) ;
#68793 = CARTESIAN_POINT ( 'NONE',  ( -11.00000000000000000, 0.000000000000000000, 109.1875000040967763 ) ) ;
#68794 = CARTESIAN_POINT ( 'NONE',  ( -1.975797226262412609, 194.5437978492538207, 200.9494923473580457 ) ) ;
#68795 = CARTESIAN_POINT ( 'NONE',  ( -2.249999999999999112, 284.0000000000000000, 7.677076266392047543 ) ) ;
#68797 = CARTESIAN_POINT ( 'NONE',  ( 23.99999999999998934, 199.7500000000000000, 169.9999999999998863 ) ) ;
#68796 = FACE_OUTER_BOUND ( 'NONE', #17074, .T. ) ;
#68798 = CARTESIAN_POINT ( 'NONE',  ( -11.14110272919006128, -34.41987647558541852, 198.9289027938963557 ) ) ;
#68799 = CARTESIAN_POINT ( 'NONE',  ( 2.445694354108782775, 197.5625000013656063, 139.5543056458912190 ) ) ;
#68800 = CARTESIAN_POINT ( 'NONE',  ( 8.660254037844385522, 61.45833332650536818, 5.000000000000005329 ) ) ;
#68801 = CARTESIAN_POINT ( 'NONE',  ( 7.188101187500002709, 103.8125000020483952, 2.977408999572649151 ) ) ;
#68802 = CARTESIAN_POINT ( 'NONE',  ( 4.541265875000001451, 11.37499999863440969, 1.881053915767124440 ) ) ;
#68803 = CARTESIAN_POINT ( 'NONE',  ( 4.999999999999999112, 55.83333333333332860, -8.660254037844385522 ) ) ;
#68804 = CARTESIAN_POINT ( 'NONE',  ( -7.999999999999991118, 0.000000000000000000, 5.330302779823363757 ) ) ;
#68805 = EDGE_LOOP ( 'NONE', ( #35178, #35531, #47976, #18617 ) ) ;
#68806 = ORIENTED_EDGE ( 'NONE', *, *, #40303, .F. ) ;
#68807 = CARTESIAN_POINT ( 'NONE',  ( 1.688721909672341148, -49.97488762307337851, -40.72268565194301715 ) ) ;
#68808 = CARTESIAN_POINT ( 'NONE',  ( 12.00000000000000000, 0.000000000000000000, 36.00000000000000000 ) ) ;
#68809 = DIRECTION ( 'NONE',  ( 0.000000000000000000, 0.000000000000000000, -1.000000000000000000 ) ) ;
#68810 = CARTESIAN_POINT ( 'NONE',  ( -4.999999999999998224, 86.66666666666667140, -8.660254037844387298 ) ) ;
#68811 = CARTESIAN_POINT ( 'NONE',  ( 9.832129032723416984, 145.3645833299193555, 5.676582343750006032 ) ) ;
#68812 = CARTESIAN_POINT ( 'NONE',  ( -8.000000000000000000, 6.562499995903221084, -9.797174393178825657E-16 ) ) ;
#68813 = CARTESIAN_POINT ( 'NONE',  ( -7.204075437095967871, 7.204075437095967871, 83.96875000204836681 ) ) ;
#68814 = CARTESIAN_POINT ( 'NONE',  ( 5.656854249492380582, 4.687500000000000888, -5.656854249492380582 ) ) ;
#68815 = CARTESIAN_POINT ( 'NONE',  ( -3.999999999999959144, 206.0625000000000000, 199.6568542494924259 ) ) ;
#68816 = CARTESIAN_POINT ( 'NONE',  ( 8.000000000000000000, 117.0312500040967763, -3.313708498984762496 ) ) ;
#68817 = AXIS2_PLACEMENT_3D ( 'NONE', #22777, #45799, #68809 ) ;
#68818 = CARTESIAN_POINT ( 'NONE',  ( 7.204075437095968759, -7.204075437095966983, 113.5937500020483810 ) ) ;
#68819 = ORIENTED_EDGE ( 'NONE', *, *, #61267, .F. ) ;
#68820 = CARTESIAN_POINT ( 'NONE',  ( 30.64284399271082293, -37.99999999999981526, 174.6921329945330683 ) ) ;
#68821 = AXIS2_PLACEMENT_3D ( 'NONE', #55473, #31708, #55103 ) ;
#68822 = CARTESIAN_POINT ( 'NONE',  ( -2.615118447421764802, 178.7191267362284464, 133.3668405662103851 ) ) ;
#68823 = CARTESIAN_POINT ( 'NONE',  ( -5.676582343750006032, 129.4270833299193555, 9.832129032723418760 ) ) ;
#68824 = CARTESIAN_POINT ( 'NONE',  ( 1.432654583217662259, 204.1250000013656063, 194.5412658750000219 ) ) ;
#68825 = CARTESIAN_POINT ( 'NONE',  ( -7.188101187500002709, 27.18749999795162609, 2.977408999572649151 ) ) ;
#68826 = CARTESIAN_POINT ( 'NONE',  ( 10.18810118749999916, 1.247682550866122264E-15, 77.78125000204836681 ) ) ;
#68827 = CARTESIAN_POINT ( 'NONE',  ( 11.35316468749999785, 30.88541666325268409, 3.042071309553174174 ) ) ;
#68828 = ORIENTED_EDGE ( 'NONE', *, *, #6585, .T. ) ;
#68829 = CARTESIAN_POINT ( 'NONE',  ( -10.00000000000000711, 27.29166666666666785, -2.679491924311232065 ) ) ;
#68830 = CARTESIAN_POINT ( 'NONE',  ( 3.211159895383560947, 1.312499998634406806, 3.211159895383562723 ) ) ;
#68831 = CARTESIAN_POINT ( 'NONE',  ( -8.008118988124991233, 0.000000000000000000, 13.01311528394063011 ) ) ;
#68832 = CARTESIAN_POINT ( 'NONE',  ( -3.458734125000016757, 206.1250000013655779, 140.5673454167824161 ) ) ;
#68833 = AXIS2_PLACEMENT_3D ( 'NONE', #29548, #74079, #68416 ) ;
#68834 = EDGE_CURVE ( 'NONE', #16346, #52055, #58984, .T. ) ;
#68835 = CARTESIAN_POINT ( 'NONE',  ( 2.977408999572651815, 12.18749999795161187, 7.188101187500000933 ) ) ;
#68836 = CARTESIAN_POINT ( 'NONE',  ( -6.000000000000001776, 298.0625000034140157, 0.000000000000000000 ) ) ;
#68837 = CARTESIAN_POINT ( 'NONE',  ( -11.00000000000000000, 0.000000000000000000, 118.0000000000000000 ) ) ;
#68838 = CARTESIAN_POINT ( 'NONE',  ( -7.188101187500002709, 6.187499997951610986, 2.977408999572649151 ) ) ;
#68839 = B_SPLINE_CURVE_WITH_KNOTS ( 'NONE', 3,
 ( #38231, #61236, #61610, #14447, #55965, #3906, #27264, #26898, #32198, #37482, #54471, #49913, #72926, #21236, #60480, #8810, #54842, #20479 ),
 .UNSPECIFIED., .F., .F.,
 ( 4, 2, 2, 2, 2, 2, 2, 2, 4 ),
 ( 0.009394059634836499084, 0.009981275988490863338, 0.01056849234214522933, 0.01115570869579959358, 0.01174292504945395957, 0.01233014140310832382, 0.01291735775676268981, 0.01350457411041705406, 0.01409179046407141832 ),
 .UNSPECIFIED. ) ;
#68840 = B_SPLINE_CURVE_WITH_KNOTS ( 'NONE', 3,
 ( #25191, #25560, #47835, #47470, #18811, #31235, #53517, #64825, #2571, #1835, #48573, #60270, #2941, #43293, #48946, #7861, #66308, #70493, #70858, #19169, #42171, #65184, #36534, #13496, #30865, #53884 ),
 .UNSPECIFIED., .F., .F.,
 ( 4, 2, 2, 2, 2, 2, 2, 2, 2, 2, 2, 2, 4 ),
 ( 1.141616761627559076E-15, 0.001138349480799253580, 0.001707524221198309213, 0.002276698961597365279, 0.002845873701996421128, 0.003415048442395476544, 0.004553397923193585640, 0.005122572663592603326, 0.005691747403991621011, 0.006260922144390638697, 0.006830096884789655515, 0.007968446365587652722, 0.009106795846385649928 ),
 .UNSPECIFIED. ) ;
#68841 = CARTESIAN_POINT ( 'NONE',  ( 9.832129032723416984, 150.6770833299193555, 5.676582343750006032 ) ) ;
#68842 = CARTESIAN_POINT ( 'NONE',  ( 4.220049686691941027, -10.18810118749999738, 74.12500000204836681 ) ) ;
#68843 = CARTESIAN_POINT ( 'NONE',  ( -26.56734541678237704, 195.3750000013656063, 166.5412658750003629 ) ) ;
#68844 = LINE ( 'NONE', #51874, #55903 ) ;
#68845 = CARTESIAN_POINT ( 'NONE',  ( 3.211159895383560947, 19.31249999863440436, 3.211159895383562723 ) ) ;
#68846 = EDGE_LOOP ( 'NONE', ( #56398, #52081, #57270, #45425 ) ) ;
#68847 = AXIS2_PLACEMENT_3D ( 'NONE', #13479, #42534, #19152 ) ;
#68848 = ADVANCED_FACE ( 'NONE', ( #29149, #45748 ), #29520, .T. ) ;
#68849 = CARTESIAN_POINT ( 'NONE',  ( 4.000000000000015987, 200.5625000027312126, 199.6568542494924259 ) ) ;
#68850 = CARTESIAN_POINT ( 'NONE',  ( 3.999999999999960032, 207.0000000000000284, 142.0000000000000568 ) ) ;
#68851 = CARTESIAN_POINT ( 'NONE',  ( -32.00000000000000000, 201.3750000027312126, 170.0000000000004547 ) ) ;
#68852 = EDGE_CURVE ( 'NONE', #13303, #57934, #45962, .T. ) ;
#68853 = CARTESIAN_POINT ( 'NONE',  ( -2.849036369511732440E-14, 207.2500000000000284, 138.0000000000000568 ) ) ;
#68854 = CARTESIAN_POINT ( 'NONE',  ( 3.313708498984756279, 7.999999999999991118, 5.049052783920146226 ) ) ;
#68855 = EDGE_LOOP ( 'NONE', ( #40350, #49827, #66322, #6361 ) ) ;
#68856 = CARTESIAN_POINT ( 'NONE',  ( -2.977408999572650039, 14.43749999795161365, -7.188101187500000933 ) ) ;
#68857 = CARTESIAN_POINT ( 'NONE',  ( -26.34314575050759188, 197.0625000027312410, 166.0000000000004263 ) ) ;
#68858 = CARTESIAN_POINT ( 'NONE',  ( 11.00000000000000000, 1.347111479062088405E-15, 108.4375000040967763 ) ) ;
#68859 = CARTESIAN_POINT ( 'NONE',  ( -8.660254037844387298, 42.08333333333333570, -5.000000000000004441 ) ) ;
#68860 = CARTESIAN_POINT ( 'NONE',  ( 5.082755093536325042, 105.9687500020483952, -5.082755093536325930 ) ) ;
#68861 = CARTESIAN_POINT ( 'NONE',  ( -24.54126587499998635, 209.3750000013656063, 171.4326545832179818 ) ) ;
#68862 = CARTESIAN_POINT ( 'NONE',  ( -1.704527592502764755, -10.27896685065642934, 63.66027613114052031 ) ) ;
#68863 = EDGE_CURVE ( 'NONE', #43256, #28738, #35829, .T. ) ;
#68865 = FACE_OUTER_BOUND ( 'NONE', #32403, .T. ) ;
#68864 = CARTESIAN_POINT ( 'NONE',  ( 10.00000000000011369, 80.20833333333341386, -2.679491924311257378 ) ) ;
#68866 = ORIENTED_EDGE ( 'NONE', *, *, #33789, .F. ) ;
#68867 = CARTESIAN_POINT ( 'NONE',  ( 5.676582343749997150, 247.2395833367473301, -9.832129032723418760 ) ) ;
#68868 = CARTESIAN_POINT ( 'NONE',  ( 7.188101187499992051, 8.802885111219154394E-16, 19.11155278187175455 ) ) ;
#68869 = VECTOR ( 'NONE', #16577, 1000.000000000000000 ) ;
#68870 = CARTESIAN_POINT ( 'NONE',  ( 1.780377099649100625, 51.29164421682855846, 48.57534666485179287 ) ) ;
#68871 = CARTESIAN_POINT ( 'NONE',  ( -10.00000000000000000, 220.0000000000000000, 0.000000000000000000 ) ) ;
#68872 = FACE_OUTER_BOUND ( 'NONE', #73995, .T. ) ;
#68873 = CARTESIAN_POINT ( 'NONE',  ( -2.445694354108784108, 196.5625000013656063, 195.5543056458912190 ) ) ;
#68874 = CARTESIAN_POINT ( 'NONE',  ( -10.00000000000000000, 157.2916666666666572, -2.679491924311229845 ) ) ;
#68875 = CARTESIAN_POINT ( 'NONE',  ( -2.751064625579944321E-14, 208.8750000027312126, 146.0000000000000284 ) ) ;
#68876 = CARTESIAN_POINT ( 'NONE',  ( -2.775557561562891351E-14, 210.0000000000000284, 146.0000000000000284 ) ) ;
#68877 = CARTESIAN_POINT ( 'NONE',  ( -5.656854249492380582, 90.31249999999998579, -5.656854249492380582 ) ) ;
#68878 = CARTESIAN_POINT ( 'NONE',  ( -11.35316468750000141, 123.8020833299193271, 3.042071309553159963 ) ) ;
#68879 = DIRECTION ( 'NONE',  ( -0.000000000000000000, -0.000000000000000000, -1.000000000000000000 ) ) ;
#68880 = CARTESIAN_POINT ( 'NONE',  ( -1.469576158976823947E-15, 5.625000000000000888, 8.000000000000000000 ) ) ;
#68883 = CARTESIAN_POINT ( 'NONE',  ( 3.999999999999960032, 202.0000000000000000, 142.0000000000000568 ) ) ;
#68882 = CARTESIAN_POINT ( 'NONE',  ( 31.45873412499997812, 195.7500000013656063, 168.5673454167822172 ) ) ;
#68881 = CARTESIAN_POINT ( 'NONE',  ( 32.00000000000000000, 209.2500000000000284, 169.9999999999999432 ) ) ;
#68884 = ORIENTED_EDGE ( 'NONE', *, *, #13491, .T. ) ;
#68885 = CARTESIAN_POINT ( 'NONE',  ( 2.849036369511732440E-14, 206.2500000000000284, 202.0000000000000000 ) ) ;
#68886 = DIRECTION ( 'NONE',  ( -0.000000000000000000, 1.000000000000000000, -0.000000000000000000 ) ) ;
#68887 = CARTESIAN_POINT ( 'NONE',  ( 0.5297946994982605240, -7.985892691108496422, 0.000000000000000000 ) ) ;
#68888 =( BOUNDED_CURVE ( )  B_SPLINE_CURVE ( 2, ( #55976, #4286, #44643, #49925, #44273, #3163, #61991, #10313, #72570 ),
 .UNSPECIFIED., .F., .F. ) 
 B_SPLINE_CURVE_WITH_KNOTS ( ( 3, 2, 2, 2, 3 ),
 ( 0.5294117647058821374, 0.5330882352941174185, 0.5367647058823528106, 0.5404411764705880916, 0.5441176470588233727 ),
 .UNSPECIFIED. ) 
 CURVE ( )  GEOMETRIC_REPRESENTATION_ITEM ( )  RATIONAL_B_SPLINE_CURVE ( ( 1.000000000000004663, 0.9238795325112821866, 1.000000000000000000, 0.9238795325112867385, 1.000000000000000000, 0.9238795325112867385, 1.000000000000000000, 0.9238795325112890700, 0.9999999999999976685 ) ) 
 REPRESENTATION_ITEM ( '' )  );
#68889 = CARTESIAN_POINT ( 'NONE',  ( 4.999999999999999112, -65.00653492603730399, -24.02639942437835074 ) ) ;
#68890 = EDGE_CURVE ( 'NONE', #27854, #62814, #53684, .T. ) ;
#68891 = CARTESIAN_POINT ( 'NONE',  ( -11.35316468749999785, 218.3854166632526415, -3.042071309553167513 ) ) ;
#68892 = CARTESIAN_POINT ( 'NONE',  ( -7.188101187499999156, 118.2500000020483952, 2.977408999572654924 ) ) ;
#68893 = CARTESIAN_POINT ( 'NONE',  ( -8.342170076843785083E-16, 2.187499998634407028, 4.541265875000002339 ) ) ;
#68894 = CARTESIAN_POINT ( 'NONE',  ( -2.436599634633485945, -51.42120007173235763, 48.62500384162273548 ) ) ;
#68895 = CARTESIAN_POINT ( 'NONE',  ( -7.999999999999991118, 0.000000000000000000, 21.83030277982336997 ) ) ;
#68897 = CARTESIAN_POINT ( 'NONE',  ( 38.00000000000000000, 52.99999999999999289, 25.00000000000000000 ) ) ;
#68896 = FILL_AREA_STYLE_COLOUR ( '', #62413 ) ;
#68898 = CARTESIAN_POINT ( 'NONE',  ( 3.042071309553167069, 106.8229166632526699, -11.35316468749999785 ) ) ;
#68899 = ORIENTED_EDGE ( 'NONE', *, *, #43260, .T. ) ;
#68900 = LINE ( 'NONE', #28163, #1449 ) ;
#68901 = CARTESIAN_POINT ( 'NONE',  ( 2.977408999572651815, 22.68749999795161543, 7.188101187500000933 ) ) ;
#68902 = CARTESIAN_POINT ( 'NONE',  ( 3.042071309553163516, 237.7604166700806445, -11.35316468749999785 ) ) ;
#68903 = AXIS2_PLACEMENT_3D ( 'NONE', #65932, #36902, #41815 ) ;
#68904 = CARTESIAN_POINT ( 'NONE',  ( -8.311093377946841443, 98.90624999658604111, 8.311093377946830785 ) ) ;
#68905 = EDGE_LOOP ( 'NONE', ( #4651, #5445, #15573, #7650 ) ) ;
#68906 = CARTESIAN_POINT ( 'NONE',  ( -29.65685424949239746, 208.0624999999999432, 166.0000000000003695 ) ) ;
#68907 = CARTESIAN_POINT ( 'NONE',  ( -7.204075437095967871, 7.204075437095967871, 107.9687500020483810 ) ) ;
#68908 = CARTESIAN_POINT ( 'NONE',  ( -8.660254037844387298, 218.9583333265053966, -5.000000000000004441 ) ) ;
#68909 = CARTESIAN_POINT ( 'NONE',  ( 1.432654583217662481, 202.3750000013655779, 194.5412658750000219 ) ) ;
#68910 = DIRECTION ( 'NONE',  ( -0.000000000000000000, 1.000000000000000000, 4.476705744456276341E-16 ) ) ;
#68912 = CARTESIAN_POINT ( 'NONE',  ( 11.35316468749999963, 100.9895833299193555, -3.042071309553165293 ) ) ;
#68911 = CARTESIAN_POINT ( 'NONE',  ( 2.849036369511732440E-14, 206.3750000027312126, 202.0000000000000000 ) ) ;
#68913 = CARTESIAN_POINT ( 'NONE',  ( -7.999999999999989342, -3.313708498984762496, 10.11155278392014623 ) ) ;
#68914 = CARTESIAN_POINT ( 'NONE',  ( -28.00000000000002132, 198.6875000013655779, 166.5412658750003629 ) ) ;
#68915 = CARTESIAN_POINT ( 'NONE',  ( 7.320508075688838545, 175.6250000000000568, -7.320508075688838545 ) ) ;
#68916 = VERTEX_POINT ( 'NONE', #58211 ) ;
#68917 = CARTESIAN_POINT ( 'NONE',  ( -1.836970198721029983E-15, 190.6249999931720254, 10.00000000000000178 ) ) ;
#68918 = LINE ( 'NONE', #5185, #47945 ) ;
#68919 = CARTESIAN_POINT ( 'NONE',  ( -4.556349186104045934, 11.00000000000000000, 99.90625000409677625 ) ) ;
#68920 = CARTESIAN_POINT ( 'NONE',  ( 6.951808397369818766E-16, 87.34374999658602690, -11.35316468750000141 ) ) ;
#68921 = CARTESIAN_POINT ( 'NONE',  ( 4.721056650416000089, 289.8281250017069510, 4.721056650415999201 ) ) ;
#68922 = CARTESIAN_POINT ( 'NONE',  ( 7.188101187500000933, 8.437499997951611874, -2.977408999572650483 ) ) ;
#68923 = CARTESIAN_POINT ( 'NONE',  ( 7.204075437095968759, -7.204075437095966983, 94.09375000204838102 ) ) ;
#68924 = CARTESIAN_POINT ( 'NONE',  ( -2.085542519210945728E-15, 219.5312499965860411, 11.35316468750000141 ) ) ;
#68925 = ORIENTED_EDGE ( 'NONE', *, *, #48563, .T. ) ;
#68926 = CYLINDRICAL_SURFACE ( 'NONE', #6724, 7.999999999999991118 ) ;
#68927 = DIRECTION ( 'NONE',  ( -0.000000000000000000, 1.000000000000000000, -0.000000000000000000 ) ) ;
#68928 = CARTESIAN_POINT ( 'NONE',  ( -8.311093377946841443, 218.9062499965860127, 8.311093377946834337 ) ) ;
#68929 = FACE_OUTER_BOUND ( 'NONE', #74112, .T. ) ;
#68930 = CARTESIAN_POINT ( 'NONE',  ( -26.34314575050754570, 207.6875000027312126, 174.0000000000003695 ) ) ;
#68931 = CARTESIAN_POINT ( 'NONE',  ( -6.676582343750000703, 295.5156250017070079, 2.765530957082001251 ) ) ;
#68932 = ORIENTED_EDGE ( 'NONE', *, *, #72935, .T. ) ;
#68933 = DIRECTION ( 'NONE',  ( -0.000000000000000000, -0.000000000000000000, 1.000000000000000000 ) ) ;
#68934 = CARTESIAN_POINT ( 'NONE',  ( -9.832129032723418760, 208.1770833299193555, -5.676582343750004256 ) ) ;
#68935 = CARTESIAN_POINT ( 'NONE',  ( 4.220049686691941027, -10.18810118749999738, 98.12500000204836681 ) ) ;
#68936 = EDGE_CURVE ( 'NONE', #33772, #31972, #66680, .T. ) ;
#68937 = CARTESIAN_POINT ( 'NONE',  ( -24.54126587499998280, 205.1250000013656347, 171.4326545832179818 ) ) ;
#68938 = CARTESIAN_POINT ( 'NONE',  ( 5.656854249492378806, 14.81250000000000355, 5.656854249492381470 ) ) ;
#68939 = VERTEX_POINT ( 'NONE', #30623 ) ;
#68940 = PRODUCT_DEFINITION_CONTEXT ( 'detailed design', #71235, 'design' ) ;
#68941 = CARTESIAN_POINT ( 'NONE',  ( 7.188101187500002709, 121.8125000020483810, 2.977408999572649151 ) ) ;
#68942 = CARTESIAN_POINT ( 'NONE',  ( -2.249999999999999556, 255.9999999999998295, 5.427273995024871844 ) ) ;
#68943 = CARTESIAN_POINT ( 'NONE',  ( -10.00000000000000355, 32.70833333333333570, 2.679491924311223183 ) ) ;
#68944 = EDGE_CURVE ( 'NONE', #39397, #5227, #24585, .T. ) ;
#68945 = AXIS2_PLACEMENT_3D ( 'NONE', #73017, #67358, #56791 ) ;
#68946 = FACE_OUTER_BOUND ( 'NONE', #26729, .T. ) ;
#68947 = CARTESIAN_POINT ( 'NONE',  ( 7.204075437095966983, 7.204075437095967871, 74.96875000204836681 ) ) ;
#68948 = ORIENTED_EDGE ( 'NONE', *, *, #25390, .T. ) ;
#68949 = CARTESIAN_POINT ( 'NONE',  ( 4.541265875000002339, 1.374999998634407250, -1.881053915767121554 ) ) ;
#68950 = CARTESIAN_POINT ( 'NONE',  ( -2.977408999572650039, 0.9374999979516102089, -7.188101187500000933 ) ) ;
#68951 = CARTESIAN_POINT ( 'NONE',  ( 4.898587196589412829E-16, 25.87500000000000711, -8.000000000000000000 ) ) ;
#68952 = CIRCLE ( 'NONE', #41221, 18.00000000000000355 ) ;
#68953 = CARTESIAN_POINT ( 'NONE',  ( -11.00000000000000000, 0.000000000000000000, 100.1875000040967763 ) ) ;
#68954 = CARTESIAN_POINT ( 'NONE',  ( 7.188101187500002709, 123.6875000020484094, 2.977408999572649151 ) ) ;
#68955 = CARTESIAN_POINT ( 'NONE',  ( 7.320508075688771044, 151.2499999931720538, 7.320508075688775484 ) ) ;
#68956 = CARTESIAN_POINT ( 'NONE',  ( 2.765530957082001251, 294.7656250017070079, 6.676582343749999815 ) ) ;
#68959 = CARTESIAN_POINT ( 'NONE',  ( 3.000000000000001332, -45.00000000000001421, 139.1455027589170470 ) ) ;
#68958 = CARTESIAN_POINT ( 'NONE',  ( 5.676582343750005144, 245.5729166700806729, 9.832129032723416984 ) ) ;
#68957 = CARTESIAN_POINT ( 'NONE',  ( 26.56734541678238060, 209.3750000013656063, 173.4587341249998929 ) ) ;
#68960 = APPLICATION_PROTOCOL_DEFINITION ( 'draft international standard', 'automotive_design', 1998, #51100 ) ;
#68961 = VECTOR ( 'NONE', #39868, 1000.000000000000000 ) ;
#68962 = VERTEX_POINT ( 'NONE', #1235 ) ;
#68963 = EDGE_CURVE ( 'NONE', #44494, #70285, #7422, .T. ) ;
#68964 = CARTESIAN_POINT ( 'NONE',  ( 9.832129032723420536, 246.3020833367473301, 5.676582343749996262 ) ) ;
#68965 = CARTESIAN_POINT ( 'NONE',  ( 5.082755093536318824, 5.082755093536319713, 5.424052781871753659 ) ) ;
#68966 = EDGE_CURVE ( 'NONE', #22331, #56997, #22819, .T. ) ;
#68967 = VERTEX_POINT ( 'NONE', #29889 ) ;
#68968 = CARTESIAN_POINT ( 'NONE',  ( 1.871523826299183495E-15, -10.18810118749999916, 71.03125000204838102 ) ) ;
#68969 = CARTESIAN_POINT ( 'NONE',  ( -8.311093377946841443, 84.21874999658599847, 8.311093377946830785 ) ) ;
#68970 = FACE_OUTER_BOUND ( 'NONE', #761, .T. ) ;
#68971 = CARTESIAN_POINT ( 'NONE',  ( 11.00000000000000000, 1.347111479062088405E-15, 84.24999999999998579 ) ) ;
#68974 = CARTESIAN_POINT ( 'NONE',  ( 6.676582343750002480, 288.1718750017070079, -2.765530957081997254 ) ) ;
#68973 = CARTESIAN_POINT ( 'NONE',  ( 31.45873412500001010, 208.6250000013655779, 171.4326545832175555 ) ) ;
#68972 = CARTESIAN_POINT ( 'NONE',  ( 31.45873412499998523, 206.8750000013656347, 171.4326545832175839 ) ) ;
#68975 = VERTEX_POINT ( 'NONE', #2320 ) ;
#68976 = CARTESIAN_POINT ( 'NONE',  ( 10.00000000000000178, 76.87499999317203958, 0.000000000000000000 ) ) ;
#68977 = DIRECTION ( 'NONE',  ( -0.000000000000000000, -1.000000000000000000, -0.000000000000000000 ) ) ;
#68978 = CARTESIAN_POINT ( 'NONE',  ( 6.951808397369818766E-16, 202.0312499965860411, -11.35316468750000141 ) ) ;
#68979 = CARTESIAN_POINT ( 'NONE',  ( 2.445694354108782775, 203.5625000013656063, 139.5543056458912190 ) ) ;
#68980 = CARTESIAN_POINT ( 'NONE',  ( 26.56734541678232731, 207.6250000013656347, 173.4587341249998929 ) ) ;
#68981 = CARTESIAN_POINT ( 'NONE',  ( -1.320432766682874540E-15, 21.46874999795161543, 7.188101187500000044 ) ) ;
#68982 = CARTESIAN_POINT ( 'NONE',  ( -9.832129032723420536, 184.0104166632526983, 5.676582343749997150 ) ) ;
#68983 = DIRECTION ( 'NONE',  ( 1.000000000000000000, 0.000000000000000000, -1.836970198721037823E-16 ) ) ;
#68984 = CARTESIAN_POINT ( 'NONE',  ( -2.977408999572652260, 97.81250000204840944, 7.188101187500000044 ) ) ;
#68986 = CARTESIAN_POINT ( 'NONE',  ( -4.999999999999994671, 111.6666666666666572, -8.660254037844383745 ) ) ;
#68985 = DIRECTION ( 'NONE',  ( -0.000000000000000000, 1.000000000000000000, -0.000000000000000000 ) ) ;
#68987 = CARTESIAN_POINT ( 'NONE',  ( -1.881053915767121554, 11.62499999863440969, -4.541265875000002339 ) ) ;
#68988 = CARTESIAN_POINT ( 'NONE',  ( 26.56734541678238060, 203.2500000013655495, 166.5412658749999650 ) ) ;
#68989 = CARTESIAN_POINT ( 'NONE',  ( -5.082755093536319713, 5.082755093536319713, 10.67405278187175455 ) ) ;
#68990 = CARTESIAN_POINT ( 'NONE',  ( -8.311093377946841443, 58.90624999658600558, 8.311093377946830785 ) ) ;
#68991 = EDGE_CURVE ( 'NONE', #69514, #73904, #61398, .T. ) ;
#68992 = CARTESIAN_POINT ( 'NONE',  ( -3.107148544787702027E-14, -51.14729664189371761, 48.52014062455021559 ) ) ;
#68993 = CARTESIAN_POINT ( 'NONE',  ( -4.898587196589412829E-16, 118.8125000040967763, -8.000000000000000000 ) ) ;
#68994 = ORIENTED_EDGE ( 'NONE', *, *, #26599, .T. ) ;
#68995 = DIRECTION ( 'NONE',  ( 0.000000000000000000, 0.000000000000000000, -1.000000000000000000 ) ) ;
#68996 = CARTESIAN_POINT ( 'NONE',  ( 30.82842712474617031, 206.5000000027312126, 167.1715728752537018 ) ) ;
#68997 = CARTESIAN_POINT ( 'NONE',  ( -8.311093377946841443, 58.90624999658600558, 8.311093377946830785 ) ) ;
#68998 = CARTESIAN_POINT ( 'NONE',  ( 2.020667218593132706E-15, -11.00000000000000000, 72.06250000409677625 ) ) ;
#68999 = CARTESIAN_POINT ( 'NONE',  ( -3.458734125000016757, 199.1250000013656347, 140.5673454167823593 ) ) ;
#69000 = CARTESIAN_POINT ( 'NONE',  ( -7.456209740496428928, 10.23501300384517876, 65.47703513267222775 ) ) ;
#69002 = CARTESIAN_POINT ( 'NONE',  ( 5.676582343750001591, 61.61458332991934839, -9.832129032723420536 ) ) ;
#69001 = CARTESIAN_POINT ( 'NONE',  ( -7.188101187500000933, 92.56250000204838102, -2.977408999572650483 ) ) ;
#69003 = CARTESIAN_POINT ( 'NONE',  ( 5.656854249492376141, -5.656854249492374365, 2.892802779823365533 ) ) ;
#69004 = CARTESIAN_POINT ( 'NONE',  ( -1.836970198721029983E-15, 15.62499999317203248, 10.00000000000000178 ) ) ;
#69005 = CARTESIAN_POINT ( 'NONE',  ( -9.832129032723418760, 177.8645833299193555, -5.676582343750004256 ) ) ;
#69006 = CARTESIAN_POINT ( 'NONE',  ( -10.00000000000000178, 159.3749999931720254, -1.224646799147353454E-15 ) ) ;
#69007 = AXIS2_PLACEMENT_3D ( 'NONE', #37262, #60637, #53503 ) ;
#69008 = CARTESIAN_POINT ( 'NONE',  ( 2.977408999572654480, 95.00000000204836681, 7.188101187499999156 ) ) ;
#69009 = CARTESIAN_POINT ( 'NONE',  ( -2.679491924311198314, 55.41666665983871098, 10.00000000000002309 ) ) ;
#69010 = CARTESIAN_POINT ( 'NONE',  ( 11.35316468749999963, 46.30208332991934128, -3.042071309553165293 ) ) ;
#69011 =( BOUNDED_CURVE ( )  B_SPLINE_CURVE ( 2, ( #49898, #62327, #67630, #4260, #16290, #27626, #32564, #63075, #57060 ),
 .UNSPECIFIED., .F., .F. ) 
 B_SPLINE_CURVE_WITH_KNOTS ( ( 3, 2, 2, 2, 3 ),
 ( 0.3823529411764705621, 0.3860294117647058987, 0.3897058823529411797, 0.3933823529411764608, 0.3970588235294117418 ),
 .UNSPECIFIED. ) 
 CURVE ( )  GEOMETRIC_REPRESENTATION_ITEM ( )  RATIONAL_B_SPLINE_CURVE ( ( 1.000000000000000000, 0.9238795325112867385, 1.000000000000000000, 0.9238795325112867385, 1.000000000000000000, 0.9238795325112867385, 1.000000000000000000, 0.9238795325112867385, 1.000000000000000000 ) ) 
 REPRESENTATION_ITEM ( '' )  );
#69012 = CARTESIAN_POINT ( 'NONE',  ( -2.828427124746152987, 201.1250000000000284, 200.8284271247462129 ) ) ;
#69013 = CARTESIAN_POINT ( 'NONE',  ( 11.35316468749999963, 180.9895833299193555, -3.042071309553165293 ) ) ;
#69014 = ORIENTED_EDGE ( 'NONE', *, *, #1596, .F. ) ;
#69016 =( BOUNDED_CURVE ( )  B_SPLINE_CURVE ( 1, ( #17285, #62559 ),
 .UNSPECIFIED., .F., .F. ) 
 B_SPLINE_CURVE_WITH_KNOTS ( ( 2, 2 ),
 ( 0.000000000000000000, 1.000000000000000000 ),
 .UNSPECIFIED. ) 
 CURVE ( )  GEOMETRIC_REPRESENTATION_ITEM ( )  RATIONAL_B_SPLINE_CURVE ( ( 0.9660721264009082265, 0.9660721264009082265 ) ) 
 REPRESENTATION_ITEM ( '' )  );
#69015 = CARTESIAN_POINT ( 'NONE',  ( 0.000000000000000000, 0.000000000000000000, 0.000000000000000000 ) ) ;
#69017 = CARTESIAN_POINT ( 'NONE',  ( -4.220049686691935698, 10.18810118749999916, 68.87500000204838102 ) ) ;
#69018 = CARTESIAN_POINT ( 'NONE',  ( -3.999999999999959144, 196.0625000000000284, 199.6568542494924259 ) ) ;
#69020 = CARTESIAN_POINT ( 'NONE',  ( 3.042071309553159519, 184.7395833299193555, 11.35316468750000141 ) ) ;
#69019 = CARTESIAN_POINT ( 'NONE',  ( -38.00000000000000000, 272.0000000000000000, 20.00000000000003553 ) ) ;
#69021 = CARTESIAN_POINT ( 'NONE',  ( 5.656854249492374365, 5.656854249492375253, 7.824052784329823318 ) ) ;
#69022 = ADVANCED_FACE ( 'NONE', ( #65685 ), #13985, .T. ) ;
#69023 = AXIS2_PLACEMENT_3D ( 'NONE', #42459, #19816, #7405 ) ;
#69024 = CARTESIAN_POINT ( 'NONE',  ( -2.751064625579944321E-14, 197.8750000027312126, 146.0000000000000284 ) ) ;
#69025 = CARTESIAN_POINT ( 'NONE',  ( 5.000000000000004441, 254.7916666734946318, 8.660254037844385522 ) ) ;
#69026 = DIRECTION ( 'NONE',  ( -1.000000000000000000, 0.000000000000000000, 0.000000000000000000 ) ) ;
#69027 = EDGE_LOOP ( 'NONE', ( #45058, #35972, #43626, #14862, #68023 ) ) ;
#69028 = EDGE_CURVE ( 'NONE', #4559, #2415, #30531, .T. ) ;
#69029 = CARTESIAN_POINT ( 'NONE',  ( 5.082755093536318824, 5.082755093536319713, 24.92405278187175810 ) ) ;
#69030 = CARTESIAN_POINT ( 'NONE',  ( -5.676582343749998039, 132.7604166632526983, -9.832129032723420536 ) ) ;
#69031 = EDGE_CURVE ( 'NONE', #53323, #46063, #8727, .T. ) ;
#69032 = CARTESIAN_POINT ( 'NONE',  ( 10.00000000000000000, 11.66666665983870033, 2.679491924311235618 ) ) ;
#69033 = ORIENTED_EDGE ( 'NONE', *, *, #13304, .F. ) ;
#69034 = CARTESIAN_POINT ( 'NONE',  ( -1.881053915767124440, 7.124999998634407916, 4.541265875000001451 ) ) ;
#69035 = CARTESIAN_POINT ( 'NONE',  ( -5.082755093536326818, 14.90624999795161187, 5.082755093536325042 ) ) ;
#69036 = CARTESIAN_POINT ( 'NONE',  ( 8.000000000000001776, 101.8437500040967905, 3.313708498984759387 ) ) ;
#69037 = CARTESIAN_POINT ( 'NONE',  ( -30.44569435410878810, 197.0625000013656063, 172.4456943541092357 ) ) ;
#69038 = EDGE_CURVE ( 'NONE', #59562, #12039, #12152, .T. ) ;
#69039 = EDGE_CURVE ( 'NONE', #39259, #34934, #56127, .T. ) ;
#69040 = CARTESIAN_POINT ( 'NONE',  ( -1.656854249492383691, 8.687500000000000000, 4.000000000000000888 ) ) ;
#69041 = CARTESIAN_POINT ( 'NONE',  ( 6.000000000000000000, 0.000000000000000000, -10.80000000000000071 ) ) ;
#69042 = CARTESIAN_POINT ( 'NONE',  ( 2.780723358947928197E-16, 10.56249999863440792, -4.541265875000002339 ) ) ;
#69043 = CARTESIAN_POINT ( 'NONE',  ( -7.999999999999989342, -3.313708498984762496, 20.61155278392014623 ) ) ;
#69044 = CARTESIAN_POINT ( 'NONE',  ( 2.828427124746152987, 198.1250000000000284, 139.1715728752538723 ) ) ;
#69045 = VERTEX_POINT ( 'NONE', #60400 ) ;
#69046 = CARTESIAN_POINT ( 'NONE',  ( 3.999999999999960032, 205.0000000000000284, 142.0000000000000568 ) ) ;
#69047 = CARTESIAN_POINT ( 'NONE',  ( -5.082755093536325930, 105.9687500020483952, -5.082755093536325930 ) ) ;
#69049 = CARTESIAN_POINT ( 'NONE',  ( 46.89594099591773357, 38.00000000000000711, 68.54827124808606698 ) ) ;
#69048 = DIRECTION ( 'NONE',  ( 0.000000000000000000, 0.000000000000000000, 1.000000000000000000 ) ) ;
#69050 = ORIENTED_EDGE ( 'NONE', *, *, #36176, .T. ) ;
#69051 = CARTESIAN_POINT ( 'NONE',  ( 1.959434878635763554E-15, 225.9999999999999432, -15.99999999999998579 ) ) ;
#69052 = CARTESIAN_POINT ( 'NONE',  ( -2.977408999572647819, 7.188101187499991163, 22.20530278187175455 ) ) ;
#69053 = VERTEX_POINT ( 'NONE', #54759 ) ;
#69054 = ORIENTED_EDGE ( 'NONE', *, *, #59652, .T. ) ;
#69055 = CARTESIAN_POINT ( 'NONE',  ( -4.220049686691935698, 10.18810118749999916, 89.87500000204836681 ) ) ;
#69056 = CARTESIAN_POINT ( 'NONE',  ( 4.898587196589412829E-16, 3.375000000000000444, -8.000000000000000000 ) ) ;
#69057 = CARTESIAN_POINT ( 'NONE',  ( -24.54126587500000056, 196.5000000013656063, 168.5673454167827003 ) ) ;
#69058 = CARTESIAN_POINT ( 'NONE',  ( -11.00000000000000000, 0.000000000000000000, 101.5000000000000000 ) ) ;
#69060 = CARTESIAN_POINT ( 'NONE',  ( -6.676582343750002480, 297.5468750017070079, -2.765530957081996810 ) ) ;
#69059 = CARTESIAN_POINT ( 'NONE',  ( 27.99999999999996447, 202.6250000027312126, 165.9999999999998863 ) ) ;
#69061 = CARTESIAN_POINT ( 'NONE',  ( -2.679491924311225848, 116.4583333333333286, -10.00000000000000178 ) ) ;
#69062 = VECTOR ( 'NONE', #48780, 1000.000000000000000 ) ;
#69063 = CARTESIAN_POINT ( 'NONE',  ( -5.656854249492378806, 99.68750000000000000, 5.656854249492381470 ) ) ;
#69064 = CARTESIAN_POINT ( 'NONE',  ( -6.676582343750000703, 287.6718750017070079, 2.765530957082001251 ) ) ;
#69065 = CARTESIAN_POINT ( 'NONE',  ( -5.082755093536317936, -5.082755093536320601, 8.049052781871752771 ) ) ;
#69066 = CARTESIAN_POINT ( 'NONE',  ( -5.656854249492378806, 98.18750000000000000, 5.656854249492381470 ) ) ;
#69067 = CARTESIAN_POINT ( 'NONE',  ( 26.56734541678232375, 203.3750000013656063, 173.4587341249998929 ) ) ;
#69068 = CARTESIAN_POINT ( 'NONE',  ( -8.000000000000000000, 25.96874999590322375, -3.313708498984762496 ) ) ;
#69069 = CARTESIAN_POINT ( 'NONE',  ( -8.008118988124991233, 3.317071493978878127, 5.419365283940630107 ) ) ;
#69070 = CARTESIAN_POINT ( 'NONE',  ( 0.000000000000000000, 0.000000000000000000, 0.000000000000000000 ) ) ;
#69071 = CARTESIAN_POINT ( 'NONE',  ( -5.082755093536324154, 115.7187500020483810, 5.082755093536326818 ) ) ;
#69072 = CARTESIAN_POINT ( 'NONE',  ( -6.123233995736766282E-16, 256.8750000068279746, -10.00000000000000000 ) ) ;
#69073 = CARTESIAN_POINT ( 'NONE',  ( -3.042071309553166181, 243.1770833367473017, -11.35316468749999608 ) ) ;
#69074 = CARTESIAN_POINT ( 'NONE',  ( -5.656854249492379694, 3.562500000000000444, -5.656854249492380582 ) ) ;
#69075 = CARTESIAN_POINT ( 'NONE',  ( 7.188101187499993827, -2.977408999572645598, 26.51780278187175455 ) ) ;
#69076 = CARTESIAN_POINT ( 'NONE',  ( 26.34314575050763452, 197.5625000000000853, 165.9999999999998863 ) ) ;
#69077 = CARTESIAN_POINT ( 'NONE',  ( 5.676582343749993598, 19.94791666325268409, 9.832129032723422313 ) ) ;
#69078 = CARTESIAN_POINT ( 'NONE',  ( 5.656854249492381470, 100.2500000040967905, 5.656854249492379694 ) ) ;
#69079 = CARTESIAN_POINT ( 'NONE',  ( -9.832129032723420536, 224.0104166632526983, 5.676582343749997150 ) ) ;
#69080 = DIRECTION ( 'NONE',  ( -0.000000000000000000, 1.000000000000000000, 4.476705744456276341E-16 ) ) ;
#69082 = CARTESIAN_POINT ( 'NONE',  ( -10.00000000000016698, 42.50000000000009948, -1.224646799147373372E-15 ) ) ;
#69081 = CARTESIAN_POINT ( 'NONE',  ( -2.886287813027996254E-11, 51.14729664189304970, 48.52014062455092613 ) ) ;
#69083 = ORIENTED_EDGE ( 'NONE', *, *, #56464, .F. ) ;
#69084 = CARTESIAN_POINT ( 'NONE',  ( -3.458734125000016757, 198.1250000013656063, 140.5673454167824161 ) ) ;
#69085 = CARTESIAN_POINT ( 'NONE',  ( -5.676582343749998039, 22.44791666325268409, -9.832129032723420536 ) ) ;
#69086 = CARTESIAN_POINT ( 'NONE',  ( 11.00000000000000355, -4.556349186104045046, 91.84375000409677625 ) ) ;
#69087 = CARTESIAN_POINT ( 'NONE',  ( 1.836970198721029589E-15, 226.2500000000000000, 10.00000000000000000 ) ) ;
#69088 = CARTESIAN_POINT ( 'NONE',  ( -30.44569435410886982, 198.5625000013656063, 167.5543056458916169 ) ) ;
#69089 = CARTESIAN_POINT ( 'NONE',  ( 8.000000000000000000, 7.406249995903221084, -3.313708498984761164 ) ) ;
#69091 = CARTESIAN_POINT ( 'NONE',  ( -3.042071309553173730, 24.32291666325268409, 11.35316468749999785 ) ) ;
#69090 = CARTESIAN_POINT ( 'NONE',  ( -5.082755093536324154, 113.8437500020483810, 5.082755093536326818 ) ) ;
#69092 = CARTESIAN_POINT ( 'NONE',  ( -7.999999999999989342, -3.313708498984762496, 23.42405277982336642 ) ) ;
#69093 = CARTESIAN_POINT ( 'NONE',  ( 9.832129032723420536, 136.1979166632526983, -5.676582343749999815 ) ) ;
#69094 = CARTESIAN_POINT ( 'NONE',  ( 10.00000000000000178, 106.8749999931720396, 0.000000000000000000 ) ) ;
#69095 = CARTESIAN_POINT ( 'NONE',  ( 2.977408999572654480, 113.0000000020483668, 7.188101187499999156 ) ) ;
#69096 = CARTESIAN_POINT ( 'NONE',  ( -5.656854249492380582, 120.5000000040967905, -5.656854249492380582 ) ) ;
#69097 = CARTESIAN_POINT ( 'NONE',  ( -29.43265458321761230, 209.1250000013656631, 173.4587341250003760 ) ) ;
#69098 = AXIS2_PLACEMENT_3D ( 'NONE', #18897, #12850, #69475 ) ;
#69099 = CARTESIAN_POINT ( 'NONE',  ( -5.000000000000000000, -52.28182290968042167, -42.43119126381077422 ) ) ;
#69100 = ORIENTED_EDGE ( 'NONE', *, *, #37201, .T. ) ;
#69101 = CARTESIAN_POINT ( 'NONE',  ( 6.951808397369818766E-16, 12.34374999658601801, -11.35316468750000141 ) ) ;
#69102 = CARTESIAN_POINT ( 'NONE',  ( 8.000000000000001776, 107.6562500000000000, 3.313708498984759387 ) ) ;
#69103 = CARTESIAN_POINT ( 'NONE',  ( -6.676582343750001591, 287.6093750017069510, 0.000000000000000000 ) ) ;
#69104 = CARTESIAN_POINT ( 'NONE',  ( 6.951808397369818766E-16, 142.0312499965860411, -11.35316468750000141 ) ) ;
#69105 =( NAMED_UNIT ( * ) SI_UNIT ( $, .STERADIAN. ) SOLID_ANGLE_UNIT ( ) );
#69106 = CARTESIAN_POINT ( 'NONE',  ( -3.313708498984758943, -7.999999999999989342, 22.16780278432982598 ) ) ;
#69107 = CARTESIAN_POINT ( 'NONE',  ( -9.832129032723418760, 253.4895833367473017, -5.676582343749998927 ) ) ;
#69108 = CARTESIAN_POINT ( 'NONE',  ( -7.204075437095965206, -7.204075437095968759, 98.21875000204838102 ) ) ;
#69109 = ORIENTED_EDGE ( 'NONE', *, *, #39239, .T. ) ;
#69110 = EDGE_CURVE ( 'NONE', #59936, #10224, #22649, .T. ) ;
#69111 = CARTESIAN_POINT ( 'NONE',  ( 4.999999999999999112, 12.24343743989404310, 68.85270403949348861 ) ) ;
#69112 = CARTESIAN_POINT ( 'NONE',  ( 4.999999999999997335, 68.33088307291130548, -21.57589723056422315 ) ) ;
#69113 = CARTESIAN_POINT ( 'NONE',  ( 2.445694354108840063, 201.0625000013656063, 200.4456943541088663 ) ) ;
#69114 = CARTESIAN_POINT ( 'NONE',  ( -8.311093377946836114, 87.96874999658602690, -8.311093377946837890 ) ) ;
#69115 = ORIENTED_EDGE ( 'NONE', *, *, #28386, .T. ) ;
#69116 = CARTESIAN_POINT ( 'NONE',  ( 7.204075437095966983, 7.204075437095967871, 109.0937500020483810 ) ) ;
#69117 = EDGE_CURVE ( 'NONE', #6891, #41883, #34433, .T. ) ;
#69118 = CARTESIAN_POINT ( 'NONE',  ( 4.541265875000001451, 11.37499999863440969, 1.881053915767124440 ) ) ;
#69119 = ORIENTED_EDGE ( 'NONE', *, *, #47876, .F. ) ;
#69120 = ORIENTED_EDGE ( 'NONE', *, *, #69826, .F. ) ;
#69121 = VECTOR ( 'NONE', #6073, 1000.000000000000000 ) ;
#69122 = CARTESIAN_POINT ( 'NONE',  ( 8.000000000000000000, 1.500000000000000000, 0.000000000000000000 ) ) ;
#69123 = CARTESIAN_POINT ( 'NONE',  ( -7.999999999999998224, 110.2812500040967763, 3.313708498984766049 ) ) ;
#69124 = CARTESIAN_POINT ( 'NONE',  ( -4.999999999999999112, -66.11467145570883019, -23.67355326543064464 ) ) ;
#69125 = CARTESIAN_POINT ( 'NONE',  ( 5.082755093536325930, 25.03124999795161543, -5.082755093536325930 ) ) ;
#69126 = CARTESIAN_POINT ( 'NONE',  ( -3.313708498984762052, 120.4062500040967905, -8.000000000000000000 ) ) ;
#69127 =( BOUNDED_CURVE ( )  B_SPLINE_CURVE ( 2, ( #50325, #37905, #60903, #55636, #49204, #33744, #9608 ),
 .UNSPECIFIED., .F., .F. ) 
 B_SPLINE_CURVE_WITH_KNOTS ( ( 3, 2, 2, 3 ),
 ( 0.9889792491610456260, 0.9927413376685174651, 0.9993596132529668497, 1.000000000000000000 ),
 .UNSPECIFIED. ) 
 CURVE ( )  GEOMETRIC_REPRESENTATION_ITEM ( )  RATIONAL_B_SPLINE_CURVE ( ( 0.9626528551087341068, 0.9567301282231954751, 1.000000000000000000, 0.9238795325112867385, 1.000000000000000000, 0.9926345559450140410, 0.9866944779687418787 ) ) 
 REPRESENTATION_ITEM ( '' )  );
#69128 = CARTESIAN_POINT ( 'NONE',  ( 7.204075437095966983, 7.204075437095967871, 104.9687500020483810 ) ) ;
#69129 = DIRECTION ( 'NONE',  ( 0.000000000000000000, 0.000000000000000000, -1.000000000000000000 ) ) ;
#69130 = CARTESIAN_POINT ( 'NONE',  ( -1.656854249492383691, 10.43749999726881228, 4.000000000000000888 ) ) ;
#69131 = CARTESIAN_POINT ( 'NONE',  ( -3.211159895383562723, 0.9374999986344068059, 3.211159895383561391 ) ) ;
#69132 = ORIENTED_EDGE ( 'NONE', *, *, #35656, .T. ) ;
#69133 = CARTESIAN_POINT ( 'NONE',  ( -10.00000000000000000, 262.9166666734946034, -2.679491924311226292 ) ) ;
#69134 = CARTESIAN_POINT ( 'NONE',  ( -3.458734124999959025, 202.5000000013656063, 199.4326545832176691 ) ) ;
#69135 = CARTESIAN_POINT ( 'NONE',  ( -24.54126587499999346, 205.1875000013656063, 170.0000000000002842 ) ) ;
#69136 = CARTESIAN_POINT ( 'NONE',  ( -8.342170076843785083E-16, 11.06249999863440792, 4.541265875000002339 ) ) ;
#69138 = CARTESIAN_POINT ( 'NONE',  ( 2.828427124746190291, 15.87500000000000000, 2.828427124746192067 ) ) ;
#69137 = SHAPE_REPRESENTATION ( 'hexagon nut style 1_is_IS 1364-3 - M16-W-N', ( #57354 ), #27271 ) ;
#69139 = CARTESIAN_POINT ( 'NONE',  ( 1.320432766682872962E-15, -7.188101187499992051, 18.36155278187175455 ) ) ;
#69140 = ORIENTED_EDGE ( 'NONE', *, *, #73700, .T. ) ;
#69141 = ORIENTED_EDGE ( 'NONE', *, *, #53198, .F. ) ;
#69142 = CARTESIAN_POINT ( 'NONE',  ( -7.204075437095967871, 7.204075437095967871, 112.4687500020483810 ) ) ;
#69143 = CARTESIAN_POINT ( 'NONE',  ( -10.99999999999994671, -4.556349186104105442, 103.0937499999999858 ) ) ;
#69144 = CARTESIAN_POINT ( 'NONE',  ( -27.99999999999995737, 203.5000000000000000, 174.0000000000003695 ) ) ;
#69145 = CARTESIAN_POINT ( 'NONE',  ( -2.445694354108782775, 200.5625000013656063, 200.4456943541088663 ) ) ;
#69146 = CARTESIAN_POINT ( 'NONE',  ( 29.43265458321766204, 195.5000000013656347, 173.4587341249998929 ) ) ;
#69147 = CARTESIAN_POINT ( 'NONE',  ( 7.320508075688774596, 85.62500000000000000, -7.320508075688774596 ) ) ;
#69148 = CARTESIAN_POINT ( 'NONE',  ( -4.401442555609581635E-16, 89.65625000204838102, -7.188101187500000044 ) ) ;
#69149 = CARTESIAN_POINT ( 'NONE',  ( -9.832129032723420536, 64.01041666325268409, 5.676582343749997150 ) ) ;
#69150 = CARTESIAN_POINT ( 'NONE',  ( 2.485281374238575314, 289.3125000000000000, 6.000000000000000888 ) ) ;
#69151 = VERTEX_POINT ( 'NONE', #25684 ) ;
#69152 = CARTESIAN_POINT ( 'NONE',  ( 2.751064625579944321E-14, 203.7500000000000284, 194.0000000000000568 ) ) ;
#69153 = CARTESIAN_POINT ( 'NONE',  ( 7.456209740496333005, -10.23501300384517876, 65.47703513267214248 ) ) ;
#69154 = CARTESIAN_POINT ( 'NONE',  ( -2.445694354108838731, 209.0625000013656063, 144.4456943541088663 ) ) ;
#69155 = CARTESIAN_POINT ( 'NONE',  ( -7.778174593052020747, -7.778174593052023411, 91.18749999999998579 ) ) ;
#69156 = CARTESIAN_POINT ( 'NONE',  ( -7.999999999994261479, 6.398094505892175214E-06, 25.01756343669228499 ) ) ;
#69157 = CARTESIAN_POINT ( 'NONE',  ( 5.000000000000004441, 241.6666666666666572, 8.660254037844385522 ) ) ;
#69158 = CYLINDRICAL_SURFACE ( 'NONE', #41477, 4.000000000000001776 ) ;
#69159 = CARTESIAN_POINT ( 'NONE',  ( -6.735557395310442023E-16, 11.00000000000000000, 117.6250000000000000 ) ) ;
#69160 = CARTESIAN_POINT ( 'NONE',  ( -8.660254037844387298, 207.0833333333333428, -5.000000000000004441 ) ) ;
#69161 = CARTESIAN_POINT ( 'NONE',  ( 2.977408999572650927, -7.188101187499990274, 15.83030278187175277 ) ) ;
#69162 = CARTESIAN_POINT ( 'NONE',  ( -8.311093377946841443, 164.2187499965860411, 8.311093377946830785 ) ) ;
#69163 = CYLINDRICAL_SURFACE ( 'NONE', #31255, 11.00000000000000000 ) ;
#69164 = CARTESIAN_POINT ( 'NONE',  ( 10.00000000000000000, 176.6666666598387110, 2.679491924311235618 ) ) ;
#69165 = CARTESIAN_POINT ( 'NONE',  ( 27.99999999999999645, 210.0000000000000284, 169.9999999999999147 ) ) ;
#69166 = ORIENTED_EDGE ( 'NONE', *, *, #7336, .F. ) ;
#69167 = AXIS2_PLACEMENT_3D ( 'NONE', #19851, #25869, #26246 ) ;
#69168 = CARTESIAN_POINT ( 'NONE',  ( 1.432654583217607192, 197.2500000013656063, 145.4587341250000634 ) ) ;
#69169 = CARTESIAN_POINT ( 'NONE',  ( 5.676582343750001591, 41.92708332991934839, -9.832129032723420536 ) ) ;
#69170 = CARTESIAN_POINT ( 'NONE',  ( 2.020667218593132706E-15, -11.00000000000000000, 112.5625000040967763 ) ) ;
#69171 = CARTESIAN_POINT ( 'NONE',  ( -24.54126587499999701, 208.1875000013656063, 170.0000000000002842 ) ) ;
#69172 = DIRECTION ( 'NONE',  ( 0.000000000000000000, 0.000000000000000000, -1.000000000000000000 ) ) ;
#69173 = CARTESIAN_POINT ( 'NONE',  ( -1.040834085586084257E-14, 82.00000000000001421, 65.00000000000000000 ) ) ;
#69174 = DIRECTION ( 'NONE',  ( 0.000000000000000000, 0.000000000000000000, 1.000000000000000000 ) ) ;
#69175 = CARTESIAN_POINT ( 'NONE',  ( -2.839093476692135984E-14, 200.6875000013656063, 138.5412658750000503 ) ) ;
#69176 = EDGE_CURVE ( 'NONE', #30852, #73724, #16330, .T. ) ;
#69177 = EDGE_CURVE ( 'NONE', #19919, #56133, #25580, .T. ) ;
#69178 = CARTESIAN_POINT ( 'NONE',  ( -5.000000000000005329, 60.20833332650536818, 8.660254037844387298 ) ) ;
#69179 = CARTESIAN_POINT ( 'NONE',  ( -7.188101187500001821, 98.56250000204838102, -2.977408999572650483 ) ) ;
#69180 = CARTESIAN_POINT ( 'NONE',  ( -3.211159895383561391, 12.81249999863440792, -3.211159895383561835 ) ) ;
#69181 = CARTESIAN_POINT ( 'NONE',  ( 2.679491924338774922, 66.04166666666422714, -9.999999999984156673 ) ) ;
#69182 = CARTESIAN_POINT ( 'NONE',  ( -4.898587196589407898E-16, 7.999999999999991118, 3.455302779823362425 ) ) ;
#69183 = CARTESIAN_POINT ( 'NONE',  ( 3.373128826976394823, -50.22031155377536038, 40.85657338450043596 ) ) ;
#69184 = ORIENTED_EDGE ( 'NONE', *, *, #52743, .F. ) ;
#69185 = ORIENTED_EDGE ( 'NONE', *, *, #58132, .T. ) ;
#69186 = CARTESIAN_POINT ( 'NONE',  ( -5.000000000000059508, 198.3333333333333997, 8.660254037844477892 ) ) ;
#69187 = CARTESIAN_POINT ( 'NONE',  ( 6.676582343750001591, 299.1093750017069510, -8.176455196517173205E-16 ) ) ;
#69188 = CARTESIAN_POINT ( 'NONE',  ( -1.836970198721029983E-15, 40.62499999317203248, 10.00000000000000178 ) ) ;
#69189 = CARTESIAN_POINT ( 'NONE',  ( 8.311093377946837890, 151.4062499965859843, -8.311093377946837890 ) ) ;
#69190 = CARTESIAN_POINT ( 'NONE',  ( 2.775557561562891351E-14, 210.0000000000000284, 198.0000000000000284 ) ) ;
#69191 = ADVANCED_FACE ( 'NONE', ( #9291 ), #73037, .F. ) ;
#69192 = CARTESIAN_POINT ( 'NONE',  ( 7.204075437095966983, 7.204075437095967871, 82.09375000204838102 ) ) ;
#69193 = CARTESIAN_POINT ( 'NONE',  ( -29.35489318557431204, 194.4854955639154923, 166.7806251063886975 ) ) ;
#69194 = CARTESIAN_POINT ( 'NONE',  ( 1.656854249492405451, 203.3125000000000284, 202.0000000000000284 ) ) ;
#69195 = CARTESIAN_POINT ( 'NONE',  ( 2.824543433528785410E-14, 195.0000000000000000, 194.0000000000000568 ) ) ;
#69196 = CARTESIAN_POINT ( 'NONE',  ( 10.18810118750000093, -4.220049686691933921, 115.1875000020483668 ) ) ;
#69197 = ORIENTED_EDGE ( 'NONE', *, *, #21416, .F. ) ;
#69198 = CARTESIAN_POINT ( 'NONE',  ( 34.34179119638316990, -14.06265876013248750, 150.5354728505286062 ) ) ;
#69199 = MECHANICAL_DESIGN_GEOMETRIC_PRESENTATION_REPRESENTATION (  '', ( #72810 ), #22224 ) ;
#69200 = CARTESIAN_POINT ( 'NONE',  ( 26.43795870543671711, 181.5060313191340242, 153.6566396627870574 ) ) ;
#69201 = CARTESIAN_POINT ( 'NONE',  ( 9.832129032723420536, 131.5104166632526983, -5.676582343749999815 ) ) ;
#69202 = CARTESIAN_POINT ( 'NONE',  ( -2.445694354108783664, 197.3125000013656063, 195.5543056458912190 ) ) ;
#69203 = CARTESIAN_POINT ( 'NONE',  ( 2.977408999572652260, 21.56249999795161543, 7.188101187500000044 ) ) ;
#69204 = CARTESIAN_POINT ( 'NONE',  ( 10.18810118750000093, -4.220049686691933033, 79.18750000204836681 ) ) ;
#69205 = CARTESIAN_POINT ( 'NONE',  ( -11.35316468749999785, 38.38541666325268409, -3.042071309553167513 ) ) ;
#69206 = ORIENTED_EDGE ( 'NONE', *, *, #41424, .F. ) ;
#69207 = CARTESIAN_POINT ( 'NONE',  ( 2.751064625579944321E-14, 208.8750000027312126, 194.0000000000000568 ) ) ;
#69208 = CARTESIAN_POINT ( 'NONE',  ( 8.008118988124991233, 3.317071493978879015, 15.35686528394063188 ) ) ;
#69209 = CARTESIAN_POINT ( 'NONE',  ( 3.458734124999960358, 207.6250000013656347, 143.4326545832176976 ) ) ;
#69210 = CARTESIAN_POINT ( 'NONE',  ( 4.401442555609581635E-16, 6.843749997951611874, -7.188101187500000044 ) ) ;
#69211 = CARTESIAN_POINT ( 'NONE',  ( 4.242640687119285658, 294.6875000034139589, -4.242640687119286547 ) ) ;
#69212 = EDGE_CURVE ( 'NONE', #27089, #73165, #48706, .T. ) ;
#69213 = CARTESIAN_POINT ( 'NONE',  ( -32.53825075733532657, -12.05280924297412959, 144.6523237305850387 ) ) ;
#69214 = CARTESIAN_POINT ( 'NONE',  ( 7.188101187500000044, 8.343749997951611874, 0.000000000000000000 ) ) ;
#69215 = CARTESIAN_POINT ( 'NONE',  ( -7.188101187499992051, 0.000000000000000000, 14.98655278187175455 ) ) ;
#69216 = CARTESIAN_POINT ( 'NONE',  ( 5.676582343750001591, 151.9270833299193555, -9.832129032723420536 ) ) ;
#69217 = CARTESIAN_POINT ( 'NONE',  ( -7.204075437095967871, 7.204075437095967871, 71.96875000204836681 ) ) ;
#69218 =( BOUNDED_CURVE ( )  B_SPLINE_CURVE ( 2, ( #14416, #31788, #32165, #71759, #8776, #26868, #3492, #48750, #26104 ),
 .UNSPECIFIED., .F., .F. ) 
 B_SPLINE_CURVE_WITH_KNOTS ( ( 3, 2, 2, 2, 3 ),
 ( 0.3333333333333336479, 0.3416666666666670071, 0.3500000000000003109, 0.3583333333333336701, 0.3666666666666669738 ),
 .UNSPECIFIED. ) 
 CURVE ( )  GEOMETRIC_REPRESENTATION_ITEM ( )  RATIONAL_B_SPLINE_CURVE ( ( 0.9999999999999970024, 0.9238795325112897361, 1.000000000000000000, 0.9238795325112867385, 1.000000000000000000, 0.9238795325112867385, 1.000000000000000000, 0.9238795325112837409, 1.000000000000003109 ) ) 
 REPRESENTATION_ITEM ( '' )  );
#69219 = CARTESIAN_POINT ( 'NONE',  ( -29.43265458321766559, 206.7500000013655779, 166.5412658750003629 ) ) ;
#69220 = CARTESIAN_POINT ( 'NONE',  ( -7.347880794884122694E-16, 2.750000000000000000, 4.000000000000001776 ) ) ;
#69221 = CARTESIAN_POINT ( 'NONE',  ( 4.541265875000002339, 19.49999999863440436, -1.881053915767121554 ) ) ;
#69222 = UNCERTAINTY_MEASURE_WITH_UNIT (LENGTH_MEASURE( 1.000000000000000082E-05 ), #29887, 'distance_accuracy_value', 'NONE');
#69223 = ORIENTED_EDGE ( 'NONE', *, *, #71533, .T. ) ;
#69224 = AXIS2_PLACEMENT_3D ( 'NONE', #72200, #36770, #71081 ) ;
#69225 = CARTESIAN_POINT ( 'NONE',  ( -3.999999999999960032, 198.1250000027312126, 198.0000000000000284 ) ) ;
#69226 = CARTESIAN_POINT ( 'NONE',  ( -2.849036369511732440E-14, 208.2500000000000284, 138.0000000000000568 ) ) ;
#69227 = CARTESIAN_POINT ( 'NONE',  ( -31.99999999999996447, 202.4375000027311842, 171.6568542494928522 ) ) ;
#69228 = CARTESIAN_POINT ( 'NONE',  ( 5.082755093536325042, 119.0937500020483810, -5.082755093536325930 ) ) ;
#69229 = LINE ( 'NONE', #63187, #4301 ) ;
#69230 = CARTESIAN_POINT ( 'NONE',  ( -4.898587196589407898E-16, 7.999999999999991118, 6.642802783920143561 ) ) ;
#69231 = VERTEX_POINT ( 'NONE', #29621 ) ;
#69233 =( BOUNDED_CURVE ( )  B_SPLINE_CURVE ( 2, ( #21223, #38958, #61961, #72543, #44249, #44990, #14666, #13180, #72012, #37328, #7545 ),
 .UNSPECIFIED., .F., .F. ) 
 B_SPLINE_CURVE_WITH_KNOTS ( ( 3, 2, 2, 2, 2, 3 ),
 ( 0.9530316461170064146, 0.9530316841617808565, 0.9596499597462393449, 0.9662682353306976113, 0.9728865109151558777, 0.9795047134926050392 ),
 .UNSPECIFIED. ) 
 CURVE ( )  GEOMETRIC_REPRESENTATION_ITEM ( )  RATIONAL_B_SPLINE_CURVE ( ( 0.9999991248568196323, 0.9999995624258944948, 1.000000000000000000, 0.9238795325112867385, 1.000000000000000000, 0.9238795325112867385, 1.000000000000000000, 0.9238795325112867385, 1.000000000000000000, 0.9238803722054950152, 0.9999983206301090721 ) ) 
 REPRESENTATION_ITEM ( '' )  );
#69232 = CARTESIAN_POINT ( 'NONE',  ( 4.401442555609581635E-16, 17.34374999795161187, -7.188101187500000044 ) ) ;
#69234 = ORIENTED_EDGE ( 'NONE', *, *, #20328, .F. ) ;
#69235 = CARTESIAN_POINT ( 'NONE',  ( -10.00000000000000355, 209.5833333265053966, 2.679491924311223183 ) ) ;
#69236 = CARTESIAN_POINT ( 'NONE',  ( -1.836970198721029983E-15, 45.62499999317203958, 10.00000000000000178 ) ) ;
#69237 = CARTESIAN_POINT ( 'NONE',  ( 8.660254037844389075, 45.41666666666666430, -5.000000000000000000 ) ) ;
#69238 = CARTESIAN_POINT ( 'NONE',  ( 2.977408999572650039, 109.0625000020483810, -7.188101187500001821 ) ) ;
#69239 = CARTESIAN_POINT ( 'NONE',  ( -25.55430564589119768, 206.5625000013656063, 167.5543056458915316 ) ) ;
#69240 = CARTESIAN_POINT ( 'NONE',  ( 1.688721909672341814, -10.27943647337372468, 63.64086505882561795 ) ) ;
#69242 = CARTESIAN_POINT ( 'NONE',  ( 0.000000000000000000, 0.000000000000000000, 0.000000000000000000 ) ) ;
#69241 = CARTESIAN_POINT ( 'NONE',  ( 33.00327549064731869, 175.6261367823761930, 159.2768976994075558 ) ) ;
#69243 = ORIENTED_EDGE ( 'NONE', *, *, #32003, .T. ) ;
#69244 = CARTESIAN_POINT ( 'NONE',  ( -9.832129032723418760, 248.4895833367473301, -5.676582343749998927 ) ) ;
#69245 = CARTESIAN_POINT ( 'NONE',  ( 7.188101187499993827, -2.977408999572645598, 16.01780278187175455 ) ) ;
#69246 = CARTESIAN_POINT ( 'NONE',  ( 1.506524674527798480, 55.70638416847562979, 43.84942669317767638 ) ) ;
#69247 = CARTESIAN_POINT ( 'NONE',  ( -9.720591898830647892, 220.0000000000000000, 4.125769721654016564 ) ) ;
#69248 = CARTESIAN_POINT ( 'NONE',  ( 25.17157282405715435, 195.0000000000000284, 172.8284270735494772 ) ) ;
#69249 = DIRECTION ( 'NONE',  ( 0.000000000000000000, 0.000000000000000000, 1.000000000000000000 ) ) ;
#69250 = CARTESIAN_POINT ( 'NONE',  ( 10.00000000000000000, 154.7916666666666856, 2.679491924311236062 ) ) ;
#69251 = FACE_OUTER_BOUND ( 'NONE', #53969, .T. ) ;
#69252 = CARTESIAN_POINT ( 'NONE',  ( -33.24289479185991070, 175.6592117488652036, 157.7120194503778805 ) ) ;
#69253 = DIRECTION ( 'NONE',  ( -0.000000000000000000, -1.000000000000000000, -4.283267841918042741E-17 ) ) ;
#69254 = CARTESIAN_POINT ( 'NONE',  ( 5.676582343750001591, 131.9270833299193555, -9.832129032723420536 ) ) ;
#69255 = CARTESIAN_POINT ( 'NONE',  ( 26.34314575050766649, 205.5624999999999716, 165.9999999999998295 ) ) ;
#69256 = CARTESIAN_POINT ( 'NONE',  ( -7.999999999999991118, 0.000000000000000000, 28.01780278392014978 ) ) ;
#69259 = CARTESIAN_POINT ( 'NONE',  ( -6.735557395310442023E-16, 11.00000000000000000, 84.81250000409676204 ) ) ;
#69258 = CARTESIAN_POINT ( 'NONE',  ( 26.56734541678232375, 196.0000000013656347, 166.5412658749999650 ) ) ;
#69257 = CARTESIAN_POINT ( 'NONE',  ( 30.82842712474620583, 209.3750000000000284, 167.1715728752537586 ) ) ;
#69260 = ORIENTED_EDGE ( 'NONE', *, *, #16870, .F. ) ;
#69261 = EDGE_CURVE ( 'NONE', #57455, #44017, #3833, .T. ) ;
#69262 = CARTESIAN_POINT ( 'NONE',  ( -3.999999999999960032, 205.9374999999999716, 196.3431457505076594 ) ) ;
#69263 = CARTESIAN_POINT ( 'NONE',  ( 30.82842712474616675, 202.5000000027312126, 167.1715728752537018 ) ) ;
#69264 = CARTESIAN_POINT ( 'NONE',  ( -5.461505570201114601, -5.862018349920268712, -0.000000000000000000 ) ) ;
#69265 = CARTESIAN_POINT ( 'NONE',  ( -7.347880794884122694E-16, 11.75000000000000000, 4.000000000000001776 ) ) ;
#69266 = CARTESIAN_POINT ( 'NONE',  ( -5.000000000000005329, 20.20833332650536462, 8.660254037844387298 ) ) ;
#69267 = CARTESIAN_POINT ( 'NONE',  ( 2.977408999572654480, 118.6250000020483810, 7.188101187499999156 ) ) ;
#69268 = CARTESIAN_POINT ( 'NONE',  ( -4.541265875000002339, 20.81249999863440436, -5.561446717895856393E-16 ) ) ;
#69269 = CARTESIAN_POINT ( 'NONE',  ( -7.456209740496328564, -51.58726928745778650, 41.60229883572996101 ) ) ;
#69270 = CARTESIAN_POINT ( 'NONE',  ( 3.313708498984756279, 7.999999999999991118, 22.86155277982337353 ) ) ;
#69272 = CARTESIAN_POINT ( 'NONE',  ( 1.836970198721029589E-15, 226.2500000000000000, 10.00000000000000000 ) ) ;
#69271 = CARTESIAN_POINT ( 'NONE',  ( -48.91597330207461880, 43.62803531754320829, 59.81383913423205456 ) ) ;
#69273 = CARTESIAN_POINT ( 'NONE',  ( -5.676582343749998039, 102.4479166632526841, -9.832129032723420536 ) ) ;
#69274 = ORIENTED_EDGE ( 'NONE', *, *, #52790, .F. ) ;
#69275 = CYLINDRICAL_SURFACE ( 'NONE', #32777, 8.000000000000000000 ) ;
#69276 = CARTESIAN_POINT ( 'NONE',  ( 2.977408999572651815, 27.18749999795161898, 7.188101187500000933 ) ) ;
#69277 = CARTESIAN_POINT ( 'NONE',  ( -1.347111479062088207E-15, 0.000000000000000000, 0.000000000000000000 ) ) ;
#69278 = CARTESIAN_POINT ( 'NONE',  ( 8.311093377946834337, 247.3437500034139589, -8.311093377946836114 ) ) ;
#69279 = CARTESIAN_POINT ( 'NONE',  ( -11.35316468750000141, 103.4895833299193697, 3.042071309553159963 ) ) ;
#69280 = ORIENTED_EDGE ( 'NONE', *, *, #24035, .F. ) ;
#69281 = CARTESIAN_POINT ( 'NONE',  ( 8.000000000000000000, 25.50000000000000355, 0.000000000000000000 ) ) ;
#69282 = EDGE_CURVE ( 'NONE', #49734, #53531, #56454, .T. ) ;
#69283 = EDGE_CURVE ( 'NONE', #28937, #53476, #34931, .T. ) ;
#69284 = CARTESIAN_POINT ( 'NONE',  ( 7.204075437095968759, -7.204075437095966983, 104.2187500020483810 ) ) ;
#69285 = CARTESIAN_POINT ( 'NONE',  ( -8.660254037844390851, 224.7916666598387110, 4.999999999999998224 ) ) ;
#69286 = CARTESIAN_POINT ( 'NONE',  ( -3.458734124999960358, 199.6875000013656063, 198.0000000000000284 ) ) ;
#69287 = CARTESIAN_POINT ( 'NONE',  ( -4.000000000000001776, 6.187499997268813168, -1.656854249492381470 ) ) ;
#69288 = CARTESIAN_POINT ( 'NONE',  ( -11.35316468750000141, 93.48958332991934128, 3.042071309553159963 ) ) ;
#69289 = CARTESIAN_POINT ( 'NONE',  ( -5.656854249492373476, -5.656854249492376141, 5.705302783920146226 ) ) ;
#69290 = CARTESIAN_POINT ( 'NONE',  ( -24.54126587499999701, 195.5000000013655779, 168.5673454167827003 ) ) ;
#69291 = PLANE ( 'NONE',  #31261 ) ;
#69292 = ORIENTED_EDGE ( 'NONE', *, *, #29605, .T. ) ;
#69293 = EDGE_CURVE ( 'NONE', #37641, #53828, #32882, .T. ) ;
#69294 = CARTESIAN_POINT ( 'NONE',  ( 4.999999999999993783, 201.0416666598387110, 8.660254037844390851 ) ) ;
#69295 = CARTESIAN_POINT ( 'NONE',  ( -11.00000000000000000, 0.000000000000000000, 100.1875000040967763 ) ) ;
#69296 = CARTESIAN_POINT ( 'NONE',  ( -8.311093377946836114, 92.96874999658602690, -8.311093377946837890 ) ) ;
#69297 = CARTESIAN_POINT ( 'NONE',  ( 6.676582343750001591, 288.9531250017069510, -8.176455196517173205E-16 ) ) ;
#69298 = CARTESIAN_POINT ( 'NONE',  ( -5.082755093536325042, 4.406249997951610098, -5.082755093536325930 ) ) ;
#69299 = CARTESIAN_POINT ( 'NONE',  ( 1.871523826299183495E-15, -10.18810118749999916, 95.40625000204836681 ) ) ;
#69300 = CARTESIAN_POINT ( 'NONE',  ( -9.832129032723420536, 218.6979166632526983, 5.676582343749997150 ) ) ;
#69301 = ORIENTED_EDGE ( 'NONE', *, *, #14754, .F. ) ;
#69302 = CARTESIAN_POINT ( 'NONE',  ( -2.062184786512628451E-11, 138.7499999999984084, 10.00000000000000178 ) ) ;
#69303 = CARTESIAN_POINT ( 'NONE',  ( 8.000000000000000000, 99.03125000409677625, -3.313708498984762496 ) ) ;
#69304 = CARTESIAN_POINT ( 'NONE',  ( 9.832129032723420536, 221.1979166632526983, -5.676582343749999815 ) ) ;
#69305 = CARTESIAN_POINT ( 'NONE',  ( 2.679491924311185880, 45.83333332650536818, 10.00000000000002487 ) ) ;
#69306 = CARTESIAN_POINT ( 'NONE',  ( -10.00000000000018652, 157.7083333333334565, 2.679491924311272921 ) ) ;
#69307 = CARTESIAN_POINT ( 'NONE',  ( 4.721056650415999201, 298.0781250017069510, -4.721056650415999201 ) ) ;
#69308 = AXIS2_PLACEMENT_3D ( 'NONE', #40149, #23533, #63899 ) ;
#69309 = ADVANCED_FACE ( 'NONE', ( #62823 ), #35742, .F. ) ;
#69310 = ORIENTED_EDGE ( 'NONE', *, *, #3789, .F. ) ;
#69311 = CARTESIAN_POINT ( 'NONE',  ( 3.999999999999959144, 202.1875000027311842, 140.3431457505076594 ) ) ;
#69312 = CARTESIAN_POINT ( 'NONE',  ( 5.676582343750001591, 206.9270833299193555, -9.832129032723420536 ) ) ;
#69313 = CARTESIAN_POINT ( 'NONE',  ( 10.18810118750000093, -4.220049686691933921, 89.31250000204838102 ) ) ;
#69314 = VECTOR ( 'NONE', #33360, 1000.000000000000000 ) ;
#69315 = CARTESIAN_POINT ( 'NONE',  ( -30.44569435410879166, 203.8125000013656063, 172.4456943541092357 ) ) ;
#69316 = CARTESIAN_POINT ( 'NONE',  ( -5.656854249492379694, 20.06250000000000355, -5.656854249492380582 ) ) ;
#69317 = ORIENTED_EDGE ( 'NONE', *, *, #70228, .T. ) ;
#69318 = CARTESIAN_POINT ( 'NONE',  ( 1.320432766682874540E-15, 123.0312500020483810, 7.188101187500000044 ) ) ;
#69319 = CARTESIAN_POINT ( 'NONE',  ( -23.99999999999995026, 199.8125000027312126, 171.6568542494926817 ) ) ;
#69320 = CARTESIAN_POINT ( 'NONE',  ( -8.660254037844387298, 22.08333333333333215, -5.000000000000004441 ) ) ;
#69321 = CARTESIAN_POINT ( 'NONE',  ( 2.751064625579944321E-14, 209.7500000000000284, 194.0000000000000568 ) ) ;
#69322 = CARTESIAN_POINT ( 'NONE',  ( -4.220049686691935698, 10.18810118749999916, 72.25000000204836681 ) ) ;
#69323 = VERTEX_POINT ( 'NONE', #424 ) ;
#69324 = CARTESIAN_POINT ( 'NONE',  ( 1.469576158976823947E-15, 113.3750000000000000, 8.000000000000000000 ) ) ;
#69325 = CARTESIAN_POINT ( 'NONE',  ( 0.000000000000000000, 23.85640646055104241, -14.00000000000000178 ) ) ;
#69326 = CYLINDRICAL_SURFACE ( 'NONE', #6622, 10.00000000000000178 ) ;
#69327 = CARTESIAN_POINT ( 'NONE',  ( 3.594037731798487290, 89.15552412475317112, -6.225085659181542219 ) ) ;
#69328 = CARTESIAN_POINT ( 'NONE',  ( 9.797174393178825657E-16, 0.000000000000000000, -8.000000000000000000 ) ) ;
#69329 = CARTESIAN_POINT ( 'NONE',  ( -6.676582343749999815, 296.5156250017069510, 2.765530957082001251 ) ) ;
#69331 = CARTESIAN_POINT ( 'NONE',  ( 4.556349186104052151, -10.99999999999999822, 88.65625000409680467 ) ) ;
#69330 = CARTESIAN_POINT ( 'NONE',  ( -11.35316468749999608, 239.1145833367473301, 3.042071309553173730 ) ) ;
#69332 = CONTEXT_DEPENDENT_SHAPE_REPRESENTATION ( #34715, #10177 ) ;
#69333 =( BOUNDED_CURVE ( )  B_SPLINE_CURVE ( 2, ( #58849, #17075, #57085, #5401, #22731, #28403, #51411, #74425, #40097 ),
 .UNSPECIFIED., .F., .F. ) 
 B_SPLINE_CURVE_WITH_KNOTS ( ( 3, 2, 2, 2, 3 ),
 ( 0.6458333333333314830, 0.6562499999999981126, 0.6666666666666647423, 0.6770833333333315940, 0.6874999999999982236 ),
 .UNSPECIFIED. ) 
 CURVE ( )  GEOMETRIC_REPRESENTATION_ITEM ( )  RATIONAL_B_SPLINE_CURVE ( ( 1.000000000000013767, 0.9238795325112729717, 1.000000000000000000, 0.9238795325112867385, 1.000000000000000000, 0.9238795325112867385, 1.000000000000000000, 0.9238795325112997281, 0.9999999999999870104 ) ) 
 REPRESENTATION_ITEM ( '' )  );
#69334 = ORIENTED_EDGE ( 'NONE', *, *, #27957, .F. ) ;
#69335 = CARTESIAN_POINT ( 'NONE',  ( -5.676582343750000703, 243.3854166700806445, -9.832129032723418760 ) ) ;
#69336 = CARTESIAN_POINT ( 'NONE',  ( 5.082755093536320601, -5.082755093536318824, 9.549052781871754547 ) ) ;
#69337 = ORIENTED_EDGE ( 'NONE', *, *, #57718, .F. ) ;
#69338 = CARTESIAN_POINT ( 'NONE',  ( -10.18810118749999916, 4.220049686691934809, 70.56250000204836681 ) ) ;
#69339 = CARTESIAN_POINT ( 'NONE',  ( 9.832129032723416984, 90.67708332991934128, 5.676582343750006032 ) ) ;
#69340 = FACE_OUTER_BOUND ( 'NONE', #16453, .T. ) ;
#69341 = CARTESIAN_POINT ( 'NONE',  ( -11.00000000000000000, 4.556349186104045934, 83.40624999999998579 ) ) ;
#69344 = CARTESIAN_POINT ( 'NONE',  ( 8.660254037844387298, 69.58333333333335702, 5.000000000000007105 ) ) ;
#69343 = CARTESIAN_POINT ( 'NONE',  ( 27.99999999999997158, 206.9375000013656063, 166.5412658749999082 ) ) ;
#69342 = CARTESIAN_POINT ( 'NONE',  ( 25.55430564589119413, 205.3125000013656063, 167.5543056458910485 ) ) ;
#69345 = ORIENTED_EDGE ( 'NONE', *, *, #35168, .T. ) ;
#69346 = EDGE_CURVE ( 'NONE', #47864, #1216, #2462, .T. ) ;
#69347 = CARTESIAN_POINT ( 'NONE',  ( -61.16420534962995958, 221.7453613843952098, 45.65120953949837457 ) ) ;
#69348 = DIRECTION ( 'NONE',  ( -1.000000000000000000, 0.000000000000000000, 0.000000000000000000 ) ) ;
#69349 = VECTOR ( 'NONE', #1400, 1000.000000000000000 ) ;
#69350 = CARTESIAN_POINT ( 'NONE',  ( -5.676582343750006032, 204.1145833299193555, 9.832129032723418760 ) ) ;
#69351 = CARTESIAN_POINT ( 'NONE',  ( 1.432654583217607192, 206.2500000013656063, 145.4587341250000634 ) ) ;
#69352 = CARTESIAN_POINT ( 'NONE',  ( 31.45873412500001010, 206.0000000013656347, 168.5673454167822740 ) ) ;
#69353 = CARTESIAN_POINT ( 'NONE',  ( 7.188101187500001821, 23.43749999795161898, -2.977408999572650483 ) ) ;
#69354 = AXIS2_PLACEMENT_3D ( 'NONE', #20120, #13341, #29976 ) ;
#69355 = CARTESIAN_POINT ( 'NONE',  ( 5.676582343749993598, 175.2604166632526699, 9.832129032723422313 ) ) ;
#69356 = CARTESIAN_POINT ( 'NONE',  ( 11.00000000000000000, 1.347111479062088405E-15, 97.93750000409677625 ) ) ;
#69357 = CARTESIAN_POINT ( 'NONE',  ( 5.082755093536325042, 96.96875000204838102, -5.082755093536325930 ) ) ;
#69359 = CARTESIAN_POINT ( 'NONE',  ( -10.00000000000000000, 89.16666665983868256, -2.679491924311229845 ) ) ;
#69358 = CARTESIAN_POINT ( 'NONE',  ( -5.000000000000000000, 62.31673578527571777, -23.93255728291310902 ) ) ;
#69360 = CARTESIAN_POINT ( 'NONE',  ( -3.211159895383562723, 9.937499998634406140, 3.211159895383561391 ) ) ;
#69361 = CARTESIAN_POINT ( 'NONE',  ( 26.56734541678238060, 202.2500000013655779, 166.5412658749999650 ) ) ;
#69362 = CARTESIAN_POINT ( 'NONE',  ( -7.188101187499992051, 0.000000000000000000, 9.361552781871752771 ) ) ;
#69363 = CARTESIAN_POINT ( 'NONE',  ( -8.311093377946841443, 73.90624999658601268, 8.311093377946830785 ) ) ;
#69364 = CARTESIAN_POINT ( 'NONE',  ( 0.000000000000000000, 0.000000000000000000, -21.47459999999999525 ) ) ;
#69365 = CARTESIAN_POINT ( 'NONE',  ( -7.999999999999991118, 3.313708498984756723, 0.7928027843298236510 ) ) ;
#69366 = EDGE_LOOP ( 'NONE', ( #23006, #13603, #15172 ) ) ;
#69367 = DIRECTION ( 'NONE',  ( 0.000000000000000000, -0.000000000000000000, 1.000000000000000000 ) ) ;
#69368 = CARTESIAN_POINT ( 'NONE',  ( -10.99999999999999645, -11.00000000000000000, 25.00000000000000000 ) ) ;
#69369 = CARTESIAN_POINT ( 'NONE',  ( -8.311093377946841443, 68.90624999658602690, 8.311093377946830785 ) ) ;
#69370 = CARTESIAN_POINT ( 'NONE',  ( -6.735557395310442023E-16, 11.00000000000000000, 68.31250000409677625 ) ) ;
#69371 = CARTESIAN_POINT ( 'NONE',  ( 1.432654583217608080, 194.8750000013656347, 138.5412658750000503 ) ) ;
#69372 = PLANE ( 'NONE',  #72132 ) ;
#69374 = CARTESIAN_POINT ( 'NONE',  ( 9.832129032723416984, 65.36458332991935549, 5.676582343750006032 ) ) ;
#69373 = CARTESIAN_POINT ( 'NONE',  ( 7.188101187500000933, 96.50000000204838102, -2.977408999572651371 ) ) ;
#69375 = CARTESIAN_POINT ( 'NONE',  ( 3.313708498984762496, -7.999999999999989342, 1.299052779823363979 ) ) ;
#69376 = CARTESIAN_POINT ( 'NONE',  ( -1.209040393344309905, 194.8891453581536837, 145.7045561112879000 ) ) ;
#69377 = EDGE_CURVE ( 'NONE', #512, #34861, #73972, .T. ) ;
#69378 = CARTESIAN_POINT ( 'NONE',  ( 4.999999999999993783, 156.0416666598387110, 8.660254037844390851 ) ) ;
#69379 = CARTESIAN_POINT ( 'NONE',  ( 2.977408999572650039, 94.06250000204838102, -7.188101187500001821 ) ) ;
#69380 = CARTESIAN_POINT ( 'NONE',  ( 0.000000000000000000, 0.000000000000000000, 11.00000000000000000 ) ) ;
#69381 = CARTESIAN_POINT ( 'NONE',  ( 5.676582343750001591, 51.92708332991935549, -9.832129032723420536 ) ) ;
#69382 = CARTESIAN_POINT ( 'NONE',  ( 10.18810118750000093, -4.220049686691933033, 110.6875000020483810 ) ) ;
#69383 = B_SPLINE_CURVE_WITH_KNOTS ( 'NONE', 1,
 ( #13722, #42408 ),
 .UNSPECIFIED., .F., .F.,
 ( 2, 2 ),
 ( 0.000000000000000000, 1.000000000000000000 ),
 .UNSPECIFIED. ) ;
#69384 = CARTESIAN_POINT ( 'NONE',  ( -11.35316468750000141, 183.2812499965860411, -1.390361679473963753E-15 ) ) ;
#69385 = ORIENTED_EDGE ( 'NONE', *, *, #10436, .T. ) ;
#69386 = CARTESIAN_POINT ( 'NONE',  ( 1.656854249492388576, 205.4375000027311842, 202.0000000000000284 ) ) ;
#69387 = CARTESIAN_POINT ( 'NONE',  ( -10.18810118749999916, 4.220049686691934809, 70.56250000204836681 ) ) ;
#69388 = CARTESIAN_POINT ( 'NONE',  ( -6.062687379811042554, -5.219768740853823807, 2.519839246067225784E-12 ) ) ;
#69390 = CARTESIAN_POINT ( 'NONE',  ( 11.35316468749999785, 175.5729166632526699, 3.042071309553174174 ) ) ;
#69389 = DIRECTION ( 'NONE',  ( 0.000000000000000000, 0.8778652960885079404, -0.4789076340208374138 ) ) ;
#69391 = CARTESIAN_POINT ( 'NONE',  ( -5.656854249492375253, 5.656854249492375253, 6.699052784329822430 ) ) ;
#69392 = FACE_OUTER_BOUND ( 'NONE', #24025, .T. ) ;
#69393 = CARTESIAN_POINT ( 'NONE',  ( 2.679491924311235174, 249.5833333401613174, 9.999999999999998224 ) ) ;
#69394 = CARTESIAN_POINT ( 'NONE',  ( 1.836970198721029589E-15, 249.3750000068279746, 10.00000000000000000 ) ) ;
#69395 = ADVANCED_FACE ( 'NONE', ( #67946 ), #10607, .T. ) ;
#69396 = VERTEX_POINT ( 'NONE', #18120 ) ;
#69397 = CARTESIAN_POINT ( 'NONE',  ( 5.676582343749993598, 170.2604166632526983, 9.832129032723422313 ) ) ;
#69398 =( REPRESENTATION_RELATIONSHIP ('NONE','NONE', #46008, #5031 ) REPRESENTATION_RELATIONSHIP_WITH_TRANSFORMATION ( #7446 )SHAPE_REPRESENTATION_RELATIONSHIP( ) );
#69399 = EDGE_CURVE ( 'NONE', #33983, #67283, #30446, .T. ) ;
#69400 = CARTESIAN_POINT ( 'NONE',  ( -7.188101187499992051, 0.000000000000000000, 26.98655278187175455 ) ) ;
#69401 = CARTESIAN_POINT ( 'NONE',  ( -9.832129032723418760, 133.1770833299193555, -5.676582343750004256 ) ) ;
#69402 = CARTESIAN_POINT ( 'NONE',  ( -8.000000000000000000, 3.562499995903220196, -9.797174393178825657E-16 ) ) ;
#69403 = EDGE_LOOP ( 'NONE', ( #22033, #1722, #36707 ) ) ;
#69404 = CARTESIAN_POINT ( 'NONE',  ( -3.211159895383561391, 10.81249999863440792, -3.211159895383561835 ) ) ;
#69405 =( GEOMETRIC_REPRESENTATION_CONTEXT ( 3 ) GLOBAL_UNCERTAINTY_ASSIGNED_CONTEXT ( ( #69222 ) ) GLOBAL_UNIT_ASSIGNED_CONTEXT ( ( #29887, #29518, #18564 ) ) REPRESENTATION_CONTEXT ( 'NONE', 'WORKASPACE' ) );
#69406 = CARTESIAN_POINT ( 'NONE',  ( 5.656854249492379694, 105.1250000040967763, -5.656854249492380582 ) ) ;
#69408 = EDGE_CURVE ( 'NONE', #26888, #21379, #22364, .T. ) ;
#69407 = AXIS2_PLACEMENT_3D ( 'NONE', #20520, #9218, #67685 ) ;
#69409 = CARTESIAN_POINT ( 'NONE',  ( 4.000000000000001776, 14.00000000000000000, 0.000000000000000000 ) ) ;
#69410 = DIRECTION ( 'NONE',  ( -0.000000000000000000, 1.000000000000000000, -0.000000000000000000 ) ) ;
#69411 = CARTESIAN_POINT ( 'NONE',  ( 4.541265875000002339, 12.37499999863440969, -1.881053915767121776 ) ) ;
#69412 = CARTESIAN_POINT ( 'NONE',  ( 7.999999999999992895, -3.313708498984756279, 19.67405278392014978 ) ) ;
#69413 = VERTEX_POINT ( 'NONE', #70541 ) ;
#69414 = CARTESIAN_POINT ( 'NONE',  ( 38.00000000000000000, 272.0000000000000000, 3.791916237172776494E-14 ) ) ;
#69415 = CARTESIAN_POINT ( 'NONE',  ( -7.188101187499999156, 101.7500000020483810, 2.977408999572654924 ) ) ;
#69416 = CARTESIAN_POINT ( 'NONE',  ( -11.00000000000010658, 4.556349186103942017, 79.09375000409676204 ) ) ;
#69417 =( NAMED_UNIT ( * ) PLANE_ANGLE_UNIT ( ) SI_UNIT ( $, .RADIAN. ) );
#69418 = VERTEX_POINT ( 'NONE', #52824 ) ;
#69419 = CARTESIAN_POINT ( 'NONE',  ( 1.881053915767121776, 20.49999999863440436, -4.541265875000002339 ) ) ;
#69420 = CARTESIAN_POINT ( 'NONE',  ( 7.188101187499991163, 2.977408999572648707, 23.33030278187175455 ) ) ;
#69421 = VERTEX_POINT ( 'NONE', #54311 ) ;
#69422 = ORIENTED_EDGE ( 'NONE', *, *, #49323, .F. ) ;
#69423 = CARTESIAN_POINT ( 'NONE',  ( -7.204075437095967871, 7.204075437095967871, 85.46875000204836681 ) ) ;
#69424 = CARTESIAN_POINT ( 'NONE',  ( 1.224646799147353454E-15, 300.0000000000000000, -10.00000000000000178 ) ) ;
#69425 = CARTESIAN_POINT ( 'NONE',  ( -31.45873412499999233, 197.9375000013655779, 170.0000000000003979 ) ) ;
#69426 = CARTESIAN_POINT ( 'NONE',  ( 11.00000000000000355, -4.556349186104045046, 103.6562499999999858 ) ) ;
#69429 = CARTESIAN_POINT ( 'NONE',  ( -2.765530957081996810, 297.4218750017069510, -6.676582343750002480 ) ) ;
#69428 = CARTESIAN_POINT ( 'NONE',  ( 32.00000000000000711, 205.3125000027312126, 171.6568542494922553 ) ) ;
#69427 = DIRECTION ( 'NONE',  ( -0.000000000000000000, 1.000000000000000000, 0.000000000000000000 ) ) ;
#69430 = CARTESIAN_POINT ( 'NONE',  ( -10.00000000000000355, 132.7083333333333144, 2.679491924311223183 ) ) ;
#69431 = CARTESIAN_POINT ( 'NONE',  ( -3.313708498984762052, 102.2187500000000000, -8.000000000000000000 ) ) ;
#69432 = CARTESIAN_POINT ( 'NONE',  ( 0.3928675183479075073, 225.9999999999999716, 10.00000000000000178 ) ) ;
#69433 = CARTESIAN_POINT ( 'NONE',  ( -2.977408999572648707, -7.188101187499990274, 2.142802781871754103 ) ) ;
#69434 = EDGE_CURVE ( 'NONE', #63265, #27085, #74296, .T. ) ;
#69435 = DIRECTION ( 'NONE',  ( 1.000000000000000000, 0.000000000000000000, -0.000000000000000000 ) ) ;
#69436 = CARTESIAN_POINT ( 'NONE',  ( 27.99999999999996447, 204.4375000013656063, 173.4587341249998929 ) ) ;
#69437 = CARTESIAN_POINT ( 'NONE',  ( -5.082755093536325042, 2.906249997951610542, -5.082755093536325930 ) ) ;
#69438 = CARTESIAN_POINT ( 'NONE',  ( -8.008118988124991233, 3.317071493978878127, 2.419365283940627442 ) ) ;
#69439 = CARTESIAN_POINT ( 'NONE',  ( -3.458734125000015425, 196.9375000013655779, 142.0000000000000568 ) ) ;
#69440 = CARTESIAN_POINT ( 'NONE',  ( -4.401442555609581635E-16, 118.1562500020483810, -7.188101187500000044 ) ) ;
#69442 = CARTESIAN_POINT ( 'NONE',  ( 3.579993502731813493, 194.7328194181654339, 199.0860077474429204 ) ) ;
#69441 = CARTESIAN_POINT ( 'NONE',  ( 31.99999999999997868, 195.4375000027312126, 168.3431457505074889 ) ) ;
#69443 = CARTESIAN_POINT ( 'NONE',  ( 11.35316468749999963, 246.7187500034139873, -1.390361679473963556E-15 ) ) ;
#69444 = DIRECTION ( 'NONE',  ( 1.000000000000000000, 0.000000000000000000, 0.000000000000000000 ) ) ;
#69445 = CARTESIAN_POINT ( 'NONE',  ( 2.977408999572646486, 7.188101187499991163, 26.89280278187175455 ) ) ;
#69446 = CARTESIAN_POINT ( 'NONE',  ( 26.34314575050763452, 198.5625000000000000, 165.9999999999998863 ) ) ;
#69447 = CARTESIAN_POINT ( 'NONE',  ( -5.676582343750006032, 34.11458332991934839, 9.832129032723418760 ) ) ;
#69448 = EDGE_CURVE ( 'NONE', #22530, #24993, #2622, .T. ) ;
#69449 =( BOUNDED_CURVE ( )  B_SPLINE_CURVE ( 2, ( #2554, #24448, #25545, #48558, #70480, #71567, #19890, #37261, #60255 ),
 .UNSPECIFIED., .F., .F. ) 
 B_SPLINE_CURVE_WITH_KNOTS ( ( 3, 2, 2, 2, 3 ),
 ( 0.2916666666666667407, 0.2986111111111111605, 0.3055555555555555802, 0.3125000000000000000, 0.3194444444444443643 ),
 .UNSPECIFIED. ) 
 CURVE ( )  GEOMETRIC_REPRESENTATION_ITEM ( )  RATIONAL_B_SPLINE_CURVE ( ( 0.9999999999999994449, 0.9238795325112872936, 1.000000000000000000, 0.9238795325112867385, 1.000000000000000000, 0.9238795325112867385, 1.000000000000000000, 0.9238795325112872936, 0.9999999999999994449 ) ) 
 REPRESENTATION_ITEM ( '' )  );
#69450 = CARTESIAN_POINT ( 'NONE',  ( 25.17157287525378351, 200.8750000000000284, 172.8284271247460424 ) ) ;
#69452 = CARTESIAN_POINT ( 'NONE',  ( 4.643173273996913153, 227.0088038288673715, -10.42876803732836599 ) ) ;
#69451 =( BOUNDED_CURVE ( )  B_SPLINE_CURVE ( 2, ( #45687, #41154, #73992, #57777, #52109, #68702, #62663, #23797, #63041 ),
 .UNSPECIFIED., .F., .F. ) 
 B_SPLINE_CURVE_WITH_KNOTS ( ( 3, 2, 2, 2, 3 ),
 ( 0.01385927522962447471, 0.01562500000000000347, 0.02083333333333334259, 0.02604166666666668517, 0.03125000000000002082 ),
 .UNSPECIFIED. ) 
 CURVE ( )  GEOMETRIC_REPRESENTATION_ITEM ( )  RATIONAL_B_SPLINE_CURVE ( ( 0.9658850645339600582, 0.9741937033643419674, 1.000000000000000000, 0.9238795325112867385, 1.000000000000000000, 0.9238795325112867385, 1.000000000000000000, 0.9238795325112864054, 1.000000000000000222 ) ) 
 REPRESENTATION_ITEM ( '' )  );
#69453 = CARTESIAN_POINT ( 'NONE',  ( -2.679491924311165008, 241.0416666666666572, 10.00000000000003553 ) ) ;
#69455 = DIRECTION ( 'NONE',  ( 1.000000000000000000, -0.000000000000000000, -0.000000000000000000 ) ) ;
#69454 = CARTESIAN_POINT ( 'NONE',  ( 7.778174593052021635, 7.778174593052023411, 99.43749999999998579 ) ) ;
#69456 = ORIENTED_EDGE ( 'NONE', *, *, #39900, .T. ) ;
#69457 = CARTESIAN_POINT ( 'NONE',  ( -2.445694354108840063, 195.0625000013656063, 139.5543056458912190 ) ) ;
#69458 = CARTESIAN_POINT ( 'NONE',  ( 6.951808397369818766E-16, 27.03124999658601979, -11.35316468750000141 ) ) ;
#69459 = CARTESIAN_POINT ( 'NONE',  ( 11.00000000000000000, 1.347111479062088405E-15, 94.93750000409677625 ) ) ;
#69460 = CARTESIAN_POINT ( 'NONE',  ( -2.839093476692135984E-14, 206.9375000013656063, 138.5412658750000503 ) ) ;
#69461 = CARTESIAN_POINT ( 'NONE',  ( -8.660254037844396180, 152.9166666666666856, 5.000000000000001776 ) ) ;
#69462 = LINE ( 'NONE', #1557, #4561 ) ;
#69464 = CARTESIAN_POINT ( 'NONE',  ( 8.311093377946834337, 15.15624999658601624, 8.311093377946839666 ) ) ;
#69463 = CARTESIAN_POINT ( 'NONE',  ( 5.082755093536326818, 112.7187500020483810, 5.082755093536325042 ) ) ;
#69465 = CARTESIAN_POINT ( 'NONE',  ( 3.313708498984762496, -7.999999999999989342, 23.79905277982336642 ) ) ;
#69466 = CARTESIAN_POINT ( 'NONE',  ( -11.35316468749999785, 133.0729166632526983, -3.042071309553167513 ) ) ;
#69467 = ADVANCED_FACE ( 'NONE', ( #30911 ), #46781, .F. ) ;
#69468 = CARTESIAN_POINT ( 'NONE',  ( 7.320508075688774596, 117.4999999931720396, -7.320508075688774596 ) ) ;
#69469 = CARTESIAN_POINT ( 'NONE',  ( 7.188101187500001821, 114.8750000020483810, -2.977408999572651371 ) ) ;
#69470 = CARTESIAN_POINT ( 'NONE',  ( -1.836970198721029983E-15, 170.6249999931720538, 10.00000000000000178 ) ) ;
#69471 = CARTESIAN_POINT ( 'NONE',  ( -31.45873412500001010, 207.8750000013656063, 168.5673454167827572 ) ) ;
#69472 = CARTESIAN_POINT ( 'NONE',  ( 0.000000000000000000, 0.000000000000000000, 118.0000000000000000 ) ) ;
#69473 = ORIENTED_EDGE ( 'NONE', *, *, #32009, .T. ) ;
#69474 = CARTESIAN_POINT ( 'NONE',  ( -3.042071309553173730, 9.635416663252682312, 11.35316468749999785 ) ) ;
#69475 = DIRECTION ( 'NONE',  ( 0.000000000000000000, 0.000000000000000000, 1.000000000000000000 ) ) ;
#69476 = CARTESIAN_POINT ( 'NONE',  ( -2.765530957081998586, 298.6406250017069510, 6.676582343750001591 ) ) ;
#69477 = CARTESIAN_POINT ( 'NONE',  ( -8.311093377946836114, 142.6562499965860127, -8.311093377946837890 ) ) ;
#69478 = DIRECTION ( 'NONE',  ( 0.000000000000000000, 0.000000000000000000, 1.000000000000000000 ) ) ;
#69479 = CARTESIAN_POINT ( 'NONE',  ( -7.999999999999991118, 0.000000000000000000, 23.38655278432982598 ) ) ;
#69480 = CARTESIAN_POINT ( 'NONE',  ( 62.39047978708148889, 229.6205190061017447, 45.00000000000000000 ) ) ;
#69481 = CARTESIAN_POINT ( 'NONE',  ( -3.042071309553159075, 244.9479166700806445, 11.35316468749999963 ) ) ;
#69482 = CARTESIAN_POINT ( 'NONE',  ( 4.220049686691934809, 10.18810118749999916, 100.5625000020483668 ) ) ;
#69483 = VERTEX_POINT ( 'NONE', #19581 ) ;
#69484 = VECTOR ( 'NONE', #4544, 1000.000000000000227 ) ;
#69485 = EDGE_CURVE ( 'NONE', #52055, #29918, #56021, .T. ) ;
#69486 = DIRECTION ( 'NONE',  ( 1.000000000000000000, -0.000000000000000000, 0.000000000000000000 ) ) ;
#69487 = CARTESIAN_POINT ( 'NONE',  ( 0.000000000000000000, 0.000000000000000000, 19.00000000000000000 ) ) ;
#69488 = UNCERTAINTY_MEASURE_WITH_UNIT (LENGTH_MEASURE( 1.000000000000000082E-05 ), #39114, 'distance_accuracy_value', 'NONE');
#69489 = CARTESIAN_POINT ( 'NONE',  ( -9.832129032723420536, 94.01041666325268409, 5.676582343749997150 ) ) ;
#69490 = EDGE_LOOP ( 'NONE', ( #40068, #44534, #26150, #8707 ) ) ;
#69491 = CARTESIAN_POINT ( 'NONE',  ( 10.18810118750000093, -4.220049686691933921, 105.8125000020483952 ) ) ;
#69492 = CARTESIAN_POINT ( 'NONE',  ( 2.780723358947928197E-16, 14.68749999863440792, -4.541265875000002339 ) ) ;
#69493 = ORIENTED_EDGE ( 'NONE', *, *, #44504, .F. ) ;
#69494 = EDGE_LOOP ( 'NONE', ( #22472, #44733, #2223, #49147 ) ) ;
#69495 = CARTESIAN_POINT ( 'NONE',  ( 3.313708498984762052, 6.281250000000000888, -8.000000000000000000 ) ) ;
#69496 = DIRECTION ( 'NONE',  ( -1.000000000000000000, -0.000000000000000000, -0.000000000000000000 ) ) ;
#69497 = CARTESIAN_POINT ( 'NONE',  ( 4.556349186104052151, -10.99999999999999822, 76.65625000409676204 ) ) ;
#69498 = CARTESIAN_POINT ( 'NONE',  ( 2.977408999572650927, 26.62499999795161543, -7.188101187500001821 ) ) ;
#69499 = CARTESIAN_POINT ( 'NONE',  ( -8.000000000000000000, 120.6875000040967763, 0.000000000000000000 ) ) ;
#69500 = CARTESIAN_POINT ( 'NONE',  ( -10.18810118749999916, 0.000000000000000000, 104.0312500020483810 ) ) ;
#69501 = CARTESIAN_POINT ( 'NONE',  ( -1.656854249492381248, 0.3125000000000001110, -4.000000000000001776 ) ) ;
#69502 = CARTESIAN_POINT ( 'NONE',  ( -4.000000000000001776, 9.249999997268814056, -4.898587196589415787E-16 ) ) ;
#69503 = CARTESIAN_POINT ( 'NONE',  ( -4.541265875000002339, 1.812499998634406584, -5.561446717895856393E-16 ) ) ;
#69504 = VERTEX_POINT ( 'NONE', #58862 ) ;
#69505 = VECTOR ( 'NONE', #53650, 1000.000000000000000 ) ;
#69506 = DIRECTION ( 'NONE',  ( 0.000000000000000000, 0.000000000000000000, 1.000000000000000000 ) ) ;
#69507 = CARTESIAN_POINT ( 'NONE',  ( 1.432654583217662481, 200.1250000013656063, 194.5412658750000219 ) ) ;
#69508 = CARTESIAN_POINT ( 'NONE',  ( 26.56734541678238060, 201.2500000013656063, 166.5412658749999650 ) ) ;
#69509 = CARTESIAN_POINT ( 'NONE',  ( -26.56734541678242678, 204.3750000013656063, 166.5412658750003345 ) ) ;
#69510 = CARTESIAN_POINT ( 'NONE',  ( -3.211159895383562723, 8.937499998634407916, 3.211159895383561391 ) ) ;
#69511 = CARTESIAN_POINT ( 'NONE',  ( -4.000000000000002665, 18.31249999726881938, 1.656854249492380582 ) ) ;
#69512 = CARTESIAN_POINT ( 'NONE',  ( -5.082755093536317936, -5.082755093536320601, 10.67405278187175455 ) ) ;
#69513 = ORIENTED_EDGE ( 'NONE', *, *, #43108, .F. ) ;
#69514 = VERTEX_POINT ( 'NONE', #47885 ) ;
#69515 = CARTESIAN_POINT ( 'NONE',  ( -7.204075437095967871, 7.204075437095967871, 106.4687500020483810 ) ) ;
#69516 = CARTESIAN_POINT ( 'NONE',  ( -29.65685424949241167, 203.0625000000000284, 166.0000000000004263 ) ) ;
#69517 = CARTESIAN_POINT ( 'NONE',  ( 3.458734125000016313, 200.8750000013656063, 199.4326545832176691 ) ) ;
#69518 = CARTESIAN_POINT ( 'NONE',  ( 30.44569435410882718, 195.5625000013656063, 172.4456943541086957 ) ) ;
#69519 = CARTESIAN_POINT ( 'NONE',  ( -10.00000000000000178, 92.50000000000001421, -1.224646799147353454E-15 ) ) ;
#69520 = CARTESIAN_POINT ( 'NONE',  ( -5.656854249492378806, 119.1875000000000000, 5.656854249492381470 ) ) ;
#69521 = CARTESIAN_POINT ( 'NONE',  ( 3.042071309553159519, 60.05208332991934128, 11.35316468750000141 ) ) ;
#69522 = CARTESIAN_POINT ( 'NONE',  ( 6.676582343750003368, 299.1718750017069510, -2.765530957081997254 ) ) ;
#69523 = EDGE_CURVE ( 'NONE', #25147, #37742, #45861, .T. ) ;
#69524 = ORIENTED_EDGE ( 'NONE', *, *, #23626, .F. ) ;
#69525 = VECTOR ( 'NONE', #53761, 1000.000000000000000 ) ;
#69526 = DIRECTION ( 'NONE',  ( 0.000000000000000000, 0.000000000000000000, -1.000000000000000000 ) ) ;
#69527 = CARTESIAN_POINT ( 'NONE',  ( 4.898587196589412829E-16, 12.18749999590322197, -8.000000000000000000 ) ) ;
#69528 = CARTESIAN_POINT ( 'NONE',  ( -1.432654583217664479, 208.7500000013656063, 138.5412658750000787 ) ) ;
#69529 = CARTESIAN_POINT ( 'NONE',  ( 12.00000000000000000, 6.928203230275491009, -14.00000000000000178 ) ) ;
#69530 = DIRECTION ( 'NONE',  ( -0.000000000000000000, 1.000000000000000000, -0.000000000000000000 ) ) ;
#69531 = CARTESIAN_POINT ( 'NONE',  ( 2.679491924311225848, 233.5416666666666572, -10.00000000000000000 ) ) ;
#69532 = CARTESIAN_POINT ( 'NONE',  ( -27.99999999999991118, 202.6250000027312126, 174.0000000000003695 ) ) ;
#69533 = CARTESIAN_POINT ( 'NONE',  ( 11.00000000000000000, 1.347111479062088405E-15, 117.2500000000000000 ) ) ;
#69534 = CARTESIAN_POINT ( 'NONE',  ( -7.320508075688773708, 196.8750000000000568, -7.320508075688774596 ) ) ;
#69535 = EDGE_CURVE ( 'NONE', #22556, #30970, #71849, .T. ) ;
#69536 = CARTESIAN_POINT ( 'NONE',  ( 7.188101187499992051, 2.977408999572647819, 10.20530278187175455 ) ) ;
#69537 = CARTESIAN_POINT ( 'NONE',  ( -3.042071309553173730, 179.6354166632526699, 11.35316468749999785 ) ) ;
#69538 = FACE_OUTER_BOUND ( 'NONE', #24262, .T. ) ;
#69539 = CARTESIAN_POINT ( 'NONE',  ( 29.65685424949229798, 197.1875000027312410, 174.0000000000000284 ) ) ;
#69541 = CARTESIAN_POINT ( 'NONE',  ( 7.320508075688774596, 87.49999999317202537, -7.320508075688774596 ) ) ;
#69540 = CARTESIAN_POINT ( 'NONE',  ( -7.999999999999991118, 0.000000000000000000, 20.33030277982336642 ) ) ;
#69542 = EDGE_LOOP ( 'NONE', ( #36691, #28293, #41984 ) ) ;
#69543 = CARTESIAN_POINT ( 'NONE',  ( 1.432654583217608080, 207.8750000013656063, 138.5412658750000503 ) ) ;
#69544 = CARTESIAN_POINT ( 'NONE',  ( 5.676582343749993598, 35.26041666325269119, 9.832129032723422313 ) ) ;
#69545 = CARTESIAN_POINT ( 'NONE',  ( -4.556349186104047710, -10.99999999999999822, 112.4687500040967905 ) ) ;
#69546 = CARTESIAN_POINT ( 'NONE',  ( -26.56734541678228112, 205.0000000013655779, 173.4587341250003476 ) ) ;
#69547 = CARTESIAN_POINT ( 'NONE',  ( 5.656854249492380582, 4.499999995903220196, -5.656854249492380582 ) ) ;
#69549 = CARTESIAN_POINT ( 'NONE',  ( -47.32259252271279593, 272.0000000000000000, 65.76194439203463560 ) ) ;
#69548 = CYLINDRICAL_SURFACE ( 'NONE', #72564, 3.999999999999976019 ) ;
#69550 = CARTESIAN_POINT ( 'NONE',  ( 3.458734124999958581, 197.5000000013656063, 140.5673454167823593 ) ) ;
#69551 =( BOUNDED_CURVE ( )  B_SPLINE_CURVE ( 2, ( #70162, #41116, #41480, #35462, #17350, #17721, #46760, #23758, #64854 ),
 .UNSPECIFIED., .F., .F. ) 
 B_SPLINE_CURVE_WITH_KNOTS ( ( 3, 2, 2, 2, 3 ),
 ( 0.9027777777777776791, 0.9097222222222220989, 0.9166666666666665186, 0.9236111111111110494, 0.9305555555555554692 ),
 .UNSPECIFIED. ) 
 CURVE ( )  GEOMETRIC_REPRESENTATION_ITEM ( )  RATIONAL_B_SPLINE_CURVE ( ( 1.000000000000001110, 0.9238795325112855172, 1.000000000000000000, 0.9238795325112867385, 1.000000000000000000, 0.9238795325112867385, 1.000000000000000000, 0.9238795325112879597, 0.9999999999999987788 ) ) 
 REPRESENTATION_ITEM ( '' )  );
#69552 = CARTESIAN_POINT ( 'NONE',  ( 5.000000000000001776, 72.70833332650536818, -8.660254037844389075 ) ) ;
#69553 = CARTESIAN_POINT ( 'NONE',  ( 5.082755093536326818, 94.71875000204838102, 5.082755093536325042 ) ) ;
#69554 = CARTESIAN_POINT ( 'NONE',  ( -8.342170076843785083E-16, 13.18749999863440792, 4.541265875000002339 ) ) ;
#69555 = CARTESIAN_POINT ( 'NONE',  ( 5.000000000000112799, 215.8333333333334849, -8.660254037844579145 ) ) ;
#69556 = CARTESIAN_POINT ( 'NONE',  ( 3.442865974826785802, 0.3519712649008457928, -7.075303620129630211 ) ) ;
#69557 = DIRECTION ( 'NONE',  ( 1.000000000000000000, -0.000000000000000000, 0.000000000000000000 ) ) ;
#69558 = ORIENTED_EDGE ( 'NONE', *, *, #68301, .F. ) ;
#69559 = ORIENTED_EDGE ( 'NONE', *, *, #18090, .T. ) ;
#69560 = CARTESIAN_POINT ( 'NONE',  ( 5.656854249492374365, 5.656854249492375253, 10.76780277982336642 ) ) ;
#69561 = CARTESIAN_POINT ( 'NONE',  ( 6.676582343750004256, 297.0468750017068942, 2.765530957081995478 ) ) ;
#69562 = DIRECTION ( 'NONE',  ( -0.000000000000000000, -0.000000000000000000, -1.000000000000000000 ) ) ;
#69563 = CARTESIAN_POINT ( 'NONE',  ( 5.000000000000000000, 0.000000000000000000, -71.70204102886728492 ) ) ;
#69564 = CARTESIAN_POINT ( 'NONE',  ( 11.35316468749999785, 155.5729166632527267, 3.042071309553174174 ) ) ;
#69565 = CARTESIAN_POINT ( 'NONE',  ( 2.679491924304078232, 103.9583333333326891, 10.00000000000411049 ) ) ;
#69566 = CARTESIAN_POINT ( 'NONE',  ( 1.871523826299183495E-15, -10.18810118749999916, 83.03125000204838102 ) ) ;
#69567 = CYLINDRICAL_SURFACE ( 'NONE', #40507, 8.000000000000000000 ) ;
#69568 = CARTESIAN_POINT ( 'NONE',  ( 4.000000000000015099, 204.5625000000000000, 196.3431457505076594 ) ) ;
#69569 = DIRECTION ( 'NONE',  ( 0.000000000000000000, 0.000000000000000000, -1.000000000000000000 ) ) ;
#69570 = CARTESIAN_POINT ( 'NONE',  ( -10.18810118749999916, 4.220049686691934809, 114.4375000020483668 ) ) ;
#69571 = ORIENTED_EDGE ( 'NONE', *, *, #25630, .F. ) ;
#69572 =( BOUNDED_CURVE ( )  B_SPLINE_CURVE ( 2, ( #63617, #11944, #18345, #34976, #57992, #7766, #6296, #53423, #58357, #29302, #70401, #648, #6662 ),
 .UNSPECIFIED., .F., .F. ) 
 B_SPLINE_CURVE_WITH_KNOTS ( ( 3, 2, 2, 2, 2, 2, 3 ),
 ( 2.276484824319521039, 2.281718076880095758, 2.286951329440670477, 2.292184582001245197, 2.297417834561819472, 2.302651087122394191, 2.307884339682968911 ),
 .UNSPECIFIED. ) 
 CURVE ( )  GEOMETRIC_REPRESENTATION_ITEM ( )  RATIONAL_B_SPLINE_CURVE ( ( 0.9999999999999956701, 0.9659258262890724200, 0.9999999999999998890, 0.9659258262890682012, 0.9999999999999998890, 0.9659258262890682012, 0.9999999999999998890, 0.9659258262890682012, 0.9999999999999998890, 0.9659258262890682012, 0.9999999999999998890, 0.9659258262890598745, 1.000000000000008216 ) ) 
 REPRESENTATION_ITEM ( '' )  );
#69573 = LINE ( 'NONE', #41272, #6977 ) ;
#69574 = CLOSED_SHELL ( 'NONE', ( #14538, #32480, #72336, #11350, #60504, #29801, #71754, #4207, #61162, #18729, #35306, #22555, #45876, #9113, #20542, #61544, #51738, #11516, #42932, #69724, #50352, #51967, #5985, #73482, #66236, #46016, #66512, #32966, #60415, #37678 ) ) ;
#69575 = CARTESIAN_POINT ( 'NONE',  ( 30.51809756383145356, 179.9566333433965610, 164.1079028600203173 ) ) ;
#69576 = CARTESIAN_POINT ( 'NONE',  ( 8.311093377946834337, 125.4687499965860269, 8.311093377946839666 ) ) ;
#69577 = CARTESIAN_POINT ( 'NONE',  ( 2.754378923186476579E-14, 198.1875000013655779, 194.5412658750000219 ) ) ;
#69578 = CARTESIAN_POINT ( 'NONE',  ( 2.977408999572650927, 22.12499999795161543, -7.188101187500000933 ) ) ;
#69579 = CARTESIAN_POINT ( 'NONE',  ( -10.18810118749999738, -4.220049686691941915, 78.62500000204838102 ) ) ;
#69580 = CARTESIAN_POINT ( 'NONE',  ( -5.676582343750006032, 54.42708332991935549, 9.832129032723418760 ) ) ;
#69581 = ORIENTED_EDGE ( 'NONE', *, *, #20527, .F. ) ;
#69582 = CARTESIAN_POINT ( 'NONE',  ( 5.000000000000001776, 68.60357193678683529, 20.85024232999420946 ) ) ;
#69583 = CARTESIAN_POINT ( 'NONE',  ( 3.211159895383561835, 1.562499998634406806, -3.211159895383561835 ) ) ;
#69584 = CARTESIAN_POINT ( 'NONE',  ( 8.008118988124993010, -3.317071493978877239, 13.66936528394063011 ) ) ;
#69585 = CARTESIAN_POINT ( 'NONE',  ( 2.445694354108783219, 205.8125000013656063, 139.5543056458912190 ) ) ;
#69586 = CARTESIAN_POINT ( 'NONE',  ( 5.082755093536324154, 12.28124999795161187, 5.082755093536326818 ) ) ;
#69587 = CARTESIAN_POINT ( 'NONE',  ( -6.000000000000000888, 298.1250000034140157, 2.485281374238575758 ) ) ;
#69588 = CARTESIAN_POINT ( 'NONE',  ( -48.65938015714536391, 141.3401616616959586, 60.50199723131336071 ) ) ;
#69589 = CARTESIAN_POINT ( 'NONE',  ( 5.082755093536324154, 6.656249997951610986, 5.082755093536326818 ) ) ;
#69590 = CARTESIAN_POINT ( 'NONE',  ( -5.082755093536317936, -5.082755093536320601, 6.174052781871754547 ) ) ;
#69591 = CIRCLE ( 'NONE', #21368, 70.50000000000000000 ) ;
#69592 = CARTESIAN_POINT ( 'NONE',  ( -7.204075437095965206, -7.204075437095968759, 70.84375000204836681 ) ) ;
#69593 = CARTESIAN_POINT ( 'NONE',  ( -30.44569435410883784, 207.8125000013656063, 167.5543056458915885 ) ) ;
#69594 = CARTESIAN_POINT ( 'NONE',  ( 0.000000000000000000, -2.500000000000000000, 0.000000000000000000 ) ) ;
#69595 = CARTESIAN_POINT ( 'NONE',  ( 4.541265875000002339, 20.49999999863440436, -1.881053915767121554 ) ) ;
#69596 = ORIENTED_EDGE ( 'NONE', *, *, #34723, .T. ) ;
#69597 = CARTESIAN_POINT ( 'NONE',  ( -1.656854249492348607, 194.3125000027312126, 202.0000000000000284 ) ) ;
#69598 = CARTESIAN_POINT ( 'NONE',  ( 3.999999999999960032, 205.9375000000000284, 143.6568542494924543 ) ) ;
#69599 = CARTESIAN_POINT ( 'NONE',  ( -32.00000000000000000, 202.3750000027312126, 170.0000000000004547 ) ) ;
#69600 = EDGE_CURVE ( 'NONE', #28680, #2093, #10187, .T. ) ;
#69601 = CARTESIAN_POINT ( 'NONE',  ( -2.977408999572650927, 116.3750000020483810, -7.188101187500001821 ) ) ;
#69602 = LINE ( 'NONE', #11518, #30795 ) ;
#69603 = CARTESIAN_POINT ( 'NONE',  ( 7.999999999999991118, 3.313708498984757611, 3.361552783920145338 ) ) ;
#69604 = EDGE_LOOP ( 'NONE', ( #49437, #18200, #72831, #16682 ) ) ;
#69605 = CARTESIAN_POINT ( 'NONE',  ( -2.977408999572650039, 18.93749999795161543, -7.188101187500000933 ) ) ;
#69606 = ORIENTED_EDGE ( 'NONE', *, *, #59129, .F. ) ;
#69607 = DIRECTION ( 'NONE',  ( -0.000000000000000000, -1.000000000000000000, -0.000000000000000000 ) ) ;
#69608 = CARTESIAN_POINT ( 'NONE',  ( 3.313708498984761608, 13.78125000000000178, -8.000000000000000000 ) ) ;
#69609 = CARTESIAN_POINT ( 'NONE',  ( 10.00000000000000178, 60.00000000000000711, 0.000000000000000000 ) ) ;
#69610 = CARTESIAN_POINT ( 'NONE',  ( -5.082755093536325930, 100.3437500020483810, -5.082755093536325930 ) ) ;
#69611 = CARTESIAN_POINT ( 'NONE',  ( -26.56734541678233086, 208.2500000013656063, 173.4587341250003760 ) ) ;
#69612 = CARTESIAN_POINT ( 'NONE',  ( -4.242640687119285658, 299.1250000000000000, 4.242640687119287435 ) ) ;
#69613 = AXIS2_PLACEMENT_3D ( 'NONE', #1391, #24003, #31140 ) ;
#69615 = CARTESIAN_POINT ( 'NONE',  ( -4.556349186104045934, 11.00000000000000000, 74.40625000409677625 ) ) ;
#69614 = CARTESIAN_POINT ( 'NONE',  ( -7.999999999999998224, 89.28125000409679046, 3.313708498984766049 ) ) ;
#69616 = EDGE_CURVE ( 'NONE', #73904, #5598, #33330, .T. ) ;
#69617 = VERTEX_POINT ( 'NONE', #67488 ) ;
#69618 = CARTESIAN_POINT ( 'NONE',  ( 5.676582343750005144, 240.5729166700806445, 9.832129032723416984 ) ) ;
#69619 = CARTESIAN_POINT ( 'NONE',  ( -7.188101187499990274, -2.977408999572651371, 18.45530278187175455 ) ) ;
#69620 = CARTESIAN_POINT ( 'NONE',  ( -8.000000000000000000, 14.25000000000000178, -9.797174393178825657E-16 ) ) ;
#69621 = CARTESIAN_POINT ( 'NONE',  ( -4.898587196589407898E-16, 7.999999999999991118, 3.455302779823362425 ) ) ;
#69622 = CARTESIAN_POINT ( 'NONE',  ( 1.656854249492337949, 198.4375000027312410, 202.0000000000000853 ) ) ;
#69623 = PLANE ( 'NONE',  #23447 ) ;
#69624 = CARTESIAN_POINT ( 'NONE',  ( 7.320508075688771044, 164.3750000000000284, 7.320508075688775484 ) ) ;
#69625 = CARTESIAN_POINT ( 'NONE',  ( -4.556349186104045934, 11.00000000000000000, 80.21874999999997158 ) ) ;
#69626 = CARTESIAN_POINT ( 'NONE',  ( 1.469576158976823947E-15, 90.87500000000000000, 8.000000000000000000 ) ) ;
#69627 = LINE ( 'NONE', #22465, #6255 ) ;
#69628 = CARTESIAN_POINT ( 'NONE',  ( -5.676582343749998039, 142.7604166632526699, -9.832129032723420536 ) ) ;
#69629 = DIRECTION ( 'NONE',  ( 0.000000000000000000, 0.000000000000000000, 1.000000000000000000 ) ) ;
#69630 = CARTESIAN_POINT ( 'NONE',  ( 10.99999999999989342, 4.556349186104152515, 106.8437500000000000 ) ) ;
#69633 = CARTESIAN_POINT ( 'NONE',  ( -2.751064625579944321E-14, 196.7500000000000000, 146.0000000000000284 ) ) ;
#69632 = DIRECTION ( 'NONE',  ( -0.000000000000000000, -0.000000000000000000, 1.000000000000000000 ) ) ;
#69631 = CARTESIAN_POINT ( 'NONE',  ( 23.99999999999999289, 207.7500000000000284, 169.9999999999998863 ) ) ;
#69634 = ORIENTED_EDGE ( 'NONE', *, *, #8039, .T. ) ;
#69635 = CARTESIAN_POINT ( 'NONE',  ( -8.311093377946836114, 2.968749996586016238, -8.311093377946837890 ) ) ;
#69636 = CARTESIAN_POINT ( 'NONE',  ( -2.754378923186476579E-14, 209.1875000013656063, 145.4587341250000350 ) ) ;
#69637 = PRESENTATION_LAYER_ASSIGNMENT (  '', '', ( #64842 ) ) ;
#69638 = CARTESIAN_POINT ( 'NONE',  ( -1.656854249492381248, 11.31249999999999822, -4.000000000000001776 ) ) ;
#69639 = CARTESIAN_POINT ( 'NONE',  ( 4.999999999999993783, 16.04166665983870033, 8.660254037844390851 ) ) ;
#69640 = CARTESIAN_POINT ( 'NONE',  ( 2.977408999572650039, 117.6875000020484094, -7.188101187500001821 ) ) ;
#69641 = CARTESIAN_POINT ( 'NONE',  ( -4.541265875000003227, 21.87499999863441147, 1.881053915767121110 ) ) ;
#69642 = CARTESIAN_POINT ( 'NONE',  ( -0.8997857291005014746, 67.61674724335088627, -20.05382624916449785 ) ) ;
#69643 = CARTESIAN_POINT ( 'NONE',  ( 7.999999999999992895, -3.313708498984756279, 19.48655277982336642 ) ) ;
#69645 = DIRECTION ( 'NONE',  ( -0.000000000000000000, 1.000000000000000000, -0.000000000000000000 ) ) ;
#69644 = DIRECTION ( 'NONE',  ( 0.000000000000000000, 0.000000000000000000, 1.000000000000000000 ) ) ;
#69646 = CARTESIAN_POINT ( 'NONE',  ( -2.085542519210945728E-15, 109.5312499965860269, 11.35316468750000141 ) ) ;
#69647 = ORIENTED_EDGE ( 'NONE', *, *, #14056, .F. ) ;
#69648 = CARTESIAN_POINT ( 'NONE',  ( -3.255014963930524218E-15, -13.85640646055106728, -14.00000000000000178 ) ) ;
#69649 = LINE ( 'NONE', #17962, #54257 ) ;
#69650 = DIRECTION ( 'NONE',  ( 0.000000000000000000, 0.000000000000000000, -1.000000000000000000 ) ) ;
#69651 = CARTESIAN_POINT ( 'NONE',  ( 9.832129032723416984, 242.1354166700806445, -5.676582343750003368 ) ) ;
#69652 = CARTESIAN_POINT ( 'NONE',  ( 5.676582343749993598, 109.9479166632526983, 9.832129032723422313 ) ) ;
#69653 = ORIENTED_EDGE ( 'NONE', *, *, #21816, .T. ) ;
#69654 = CARTESIAN_POINT ( 'NONE',  ( 5.000000000000000000, -11.68639849891297366, 68.31608016562482533 ) ) ;
#69655 = CARTESIAN_POINT ( 'NONE',  ( 7.204075437095968759, -7.204075437095966983, 102.7187500020483668 ) ) ;
#69656 = CARTESIAN_POINT ( 'NONE',  ( 7.320508075688774596, 217.4999999931720538, -7.320508075688774596 ) ) ;
#69657 = CARTESIAN_POINT ( 'NONE',  ( -2.445694354108784108, 200.5625000013656063, 195.5543056458912190 ) ) ;
#69658 = CARTESIAN_POINT ( 'NONE',  ( -2.775557561562891351E-14, 210.0000000000000284, 146.0000000000000284 ) ) ;
#69660 = CARTESIAN_POINT ( 'NONE',  ( -5.676582343750006032, 99.11458332991935549, 9.832129032723418760 ) ) ;
#69659 = CARTESIAN_POINT ( 'NONE',  ( 0.000000000000000000, 0.000000000000000000, -14.77459999999999951 ) ) ;
#69661 = CARTESIAN_POINT ( 'NONE',  ( -5.656854249492375253, 5.656854249492375253, 9.830302783920146226 ) ) ;
#69662 = CARTESIAN_POINT ( 'NONE',  ( -31.45873412499997812, 198.0000000013656063, 171.4326545832180386 ) ) ;
#69663 = CARTESIAN_POINT ( 'NONE',  ( 105.0000000000000000, 242.0000000000000284, 0.000000000000000000 ) ) ;
#69664 = ORIENTED_EDGE ( 'NONE', *, *, #28652, .F. ) ;
#69665 = CARTESIAN_POINT ( 'NONE',  ( -7.320508075688773708, 193.7499999931720538, -7.320508075688774596 ) ) ;
#69666 = CARTESIAN_POINT ( 'NONE',  ( 27.99999999999996447, 200.6250000027312126, 165.9999999999998863 ) ) ;
#69667 = CARTESIAN_POINT ( 'NONE',  ( 29.65685424949246851, 202.4375000000000284, 165.9999999999999716 ) ) ;
#69668 = CARTESIAN_POINT ( 'NONE',  ( 8.311093377946834337, 90.46874999658601268, 8.311093377946839666 ) ) ;
#69669 = CARTESIAN_POINT ( 'NONE',  ( 1.432654583217664479, 208.7500000013656063, 201.4587341250000065 ) ) ;
#69670 = CARTESIAN_POINT ( 'NONE',  ( -5.082755093536325042, 8.906249997951611874, -5.082755093536325930 ) ) ;
#69671 =( BOUNDED_CURVE ( )  B_SPLINE_CURVE ( 2, ( #558, #52226, #35616, #59004, #63908, #1660, #24641, #929, #12587 ),
 .UNSPECIFIED., .F., .F. ) 
 B_SPLINE_CURVE_WITH_KNOTS ( ( 3, 2, 2, 2, 3 ),
 ( 0.5972222222222222099, 0.6041666666666666297, 0.6111111111111111605, 0.6180555555555554692, 0.6249999999999998890 ),
 .UNSPECIFIED. ) 
 CURVE ( )  GEOMETRIC_REPRESENTATION_ITEM ( )  RATIONAL_B_SPLINE_CURVE ( ( 1.000000000000000000, 0.9238795325112867385, 1.000000000000000000, 0.9238795325112867385, 1.000000000000000000, 0.9238795325112867385, 1.000000000000000000, 0.9238795325112879597, 0.9999999999999987788 ) ) 
 REPRESENTATION_ITEM ( '' )  );
#69672 = CARTESIAN_POINT ( 'NONE',  ( 7.204075437095966983, 7.204075437095967871, 92.96875000204838102 ) ) ;
#69673 = CARTESIAN_POINT ( 'NONE',  ( 9.832129032723420536, 6.510416663252683200, -5.676582343749999815 ) ) ;
#69674 = ORIENTED_EDGE ( 'NONE', *, *, #32572, .F. ) ;
#69675 = DIRECTION ( 'NONE',  ( -0.000000000000000000, -0.000000000000000000, 1.000000000000000000 ) ) ;
#69676 = CARTESIAN_POINT ( 'NONE',  ( -4.898587196589412829E-16, 99.31250000409677625, -8.000000000000000000 ) ) ;
#69677 = CARTESIAN_POINT ( 'NONE',  ( -3.042071309553173730, 219.3229166632526699, 11.35316468749999785 ) ) ;
#69678 = CARTESIAN_POINT ( 'NONE',  ( -6.238412754330611322E-16, 10.18810118749999916, 79.65625000204836681 ) ) ;
#69679 = CARTESIAN_POINT ( 'NONE',  ( 105.0000000000000000, 0.000000000000000000, 139.0000000000000000 ) ) ;
#69680 = CARTESIAN_POINT ( 'NONE',  ( -10.00000000000000000, 99.16666665983871098, -2.679491924311229845 ) ) ;
#69681 = CARTESIAN_POINT ( 'NONE',  ( -4.721056650415998313, 295.5781250017069510, 4.721056650416000089 ) ) ;
#69682 = ORIENTED_EDGE ( 'NONE', *, *, #41198, .T. ) ;
#69684 = AXIS2_PLACEMENT_3D ( 'NONE', #29997, #40951, #19038 ) ;
#69683 = CARTESIAN_POINT ( 'NONE',  ( 4.000000000000016875, 199.4375000000000284, 199.6568542494924259 ) ) ;
#69685 = CARTESIAN_POINT ( 'NONE',  ( -2.085542519210945728E-15, 214.8437499965860411, 11.35316468750000141 ) ) ;
#69686 = CARTESIAN_POINT ( 'NONE',  ( 10.18810118749999916, 1.247682550866122264E-15, 87.90625000204838102 ) ) ;
#69687 = AXIS2_PLACEMENT_3D ( 'NONE', #27478, #60699, #15405 ) ;
#69688 = EDGE_CURVE ( 'NONE', #69396, #39667, #19954, .T. ) ;
#69689 = CARTESIAN_POINT ( 'NONE',  ( -30.44569435410883429, 204.5625000013656063, 167.5543056458915885 ) ) ;
#69690 = CARTESIAN_POINT ( 'NONE',  ( -8.000000000000001776, 15.84375000000000355, 3.313708498984759387 ) ) ;
#69691 = EDGE_LOOP ( 'NONE', ( #6561, #12406, #52504, #21328 ) ) ;
#69692 = AXIS2_PLACEMENT_3D ( 'NONE', #73509, #27115, #17286 ) ;
#69693 = CARTESIAN_POINT ( 'NONE',  ( 5.082755093536326818, 120.2187500020483952, 5.082755093536325042 ) ) ;
#69694 = CARTESIAN_POINT ( 'NONE',  ( -3.729367062499960195, 194.8437500006828031, 198.0000000000000284 ) ) ;
#69695 = CARTESIAN_POINT ( 'NONE',  ( -7.320508075688778149, 28.12500000000000355, 7.320508075688769267 ) ) ;
#69696 = CIRCLE ( 'NONE', #38414, 10.00000000000000000 ) ;
#69697 = CARTESIAN_POINT ( 'NONE',  ( -25.17157287525377285, 197.6250000000000284, 172.8284271247465256 ) ) ;
#69698 = CARTESIAN_POINT ( 'NONE',  ( -10.18810118749999916, 0.000000000000000000, 74.03125000204838102 ) ) ;
#69699 = ORIENTED_EDGE ( 'NONE', *, *, #67402, .T. ) ;
#69700 = CARTESIAN_POINT ( 'NONE',  ( -4.541265875000003227, 21.87499999863441147, 1.881053915767121110 ) ) ;
#69701 = CYLINDRICAL_SURFACE ( 'NONE', #22191, 18.00000000000000355 ) ;
#69702 = ADVANCED_FACE ( 'NONE', ( #15786 ), #55056, .T. ) ;
#69703 = EDGE_CURVE ( 'NONE', #24157, #16043, #43420, .T. ) ;
#69704 = CARTESIAN_POINT ( 'NONE',  ( -7.188101187499999156, 121.6250000020483810, 2.977408999572654924 ) ) ;
#69705 = CARTESIAN_POINT ( 'NONE',  ( 29.65685424949225180, 199.0625000000000284, 174.0000000000000284 ) ) ;
#69706 = CARTESIAN_POINT ( 'NONE',  ( 2.765530957081996366, 298.1406250017069510, -6.676582343750002480 ) ) ;
#69708 = CARTESIAN_POINT ( 'NONE',  ( -2.849036369511732440E-14, 199.3750000027312126, 138.0000000000000568 ) ) ;
#69707 = CARTESIAN_POINT ( 'NONE',  ( 8.311093377946839666, 235.7812500034139589, 8.311093377946830785 ) ) ;
#69709 = ITEM_DEFINED_TRANSFORMATION ( 'NONE', 'NONE', #23675,  #57354 ) ;
#69710 = ORIENTED_EDGE ( 'NONE', *, *, #51302, .T. ) ;
#69711 = CARTESIAN_POINT ( 'NONE',  ( -8.311093377946836114, 238.5937500034139589, -8.311093377946836114 ) ) ;
#69712 = CARTESIAN_POINT ( 'NONE',  ( 2.977408999572650927, -7.188101187499990274, 9.455302781871754547 ) ) ;
#69713 = EDGE_LOOP ( 'NONE', ( #74398, #6122, #22144, #73692 ) ) ;
#69714 = CARTESIAN_POINT ( 'NONE',  ( 7.204075437095966983, 7.204075437095967871, 68.59375000204836681 ) ) ;
#69715 = CARTESIAN_POINT ( 'NONE',  ( 11.35316468749999963, 101.3020833299193555, -3.042071309553165293 ) ) ;
#69716 = LINE ( 'NONE', #41046, #58957 ) ;
#69717 = CARTESIAN_POINT ( 'NONE',  ( 11.00000000000000355, -4.556349186104045046, 81.15624999999997158 ) ) ;
#69720 = DIRECTION ( 'NONE',  ( -1.000000000000000000, 0.000000000000000000, 0.000000000000000000 ) ) ;
#69719 = CARTESIAN_POINT ( 'NONE',  ( 31.45873412500001010, 204.6250000013655779, 171.4326545832175555 ) ) ;
#69718 = CARTESIAN_POINT ( 'NONE',  ( 25.55430564589119768, 206.3125000013656063, 167.5543056458910485 ) ) ;
#69721 = ORIENTED_EDGE ( 'NONE', *, *, #3618, .T. ) ;
#69722 = CARTESIAN_POINT ( 'NONE',  ( -7.347880794884122694E-16, 18.75000000000000000, 4.000000000000001776 ) ) ;
#69723 = CARTESIAN_POINT ( 'NONE',  ( -36.10814071610730736, 133.9999999999999716, 139.0000000000000000 ) ) ;
#69724 = ADVANCED_FACE ( 'NONE', ( #72776 ), #4122, .T. ) ;
#69725 = CARTESIAN_POINT ( 'NONE',  ( -3.042071309553173730, 204.3229166632526699, 11.35316468749999785 ) ) ;
#69726 = CARTESIAN_POINT ( 'NONE',  ( 3.458734124999959914, 203.4375000013656063, 142.0000000000000568 ) ) ;
#69727 = CARTESIAN_POINT ( 'NONE',  ( 26.56734541678238060, 204.2500000013655779, 166.5412658749999650 ) ) ;
#69728 = CARTESIAN_POINT ( 'NONE',  ( -5.082755093536326818, 21.28124999795161543, 5.082755093536325042 ) ) ;
#69729 = CARTESIAN_POINT ( 'NONE',  ( 3.042071309553167069, 187.1354166632526983, -11.35316468749999785 ) ) ;
#69730 = CARTESIAN_POINT ( 'NONE',  ( -5.082755093536325930, 97.34375000204838102, -5.082755093536325930 ) ) ;
#69732 = CARTESIAN_POINT ( 'NONE',  ( -9.999999999999996447, 107.2916666666666714, -2.679491924311228956 ) ) ;
#69731 = CARTESIAN_POINT ( 'NONE',  ( 1.656854249492212938, 195.9375000027312126, 146.0000000000001990 ) ) ;
#69733 = CARTESIAN_POINT ( 'NONE',  ( -1.881053915767124440, 9.999999998634407916, 4.541265875000001451 ) ) ;
#69734 = CARTESIAN_POINT ( 'NONE',  ( 29.43265458321766914, 203.1250000013656347, 166.5412658749999650 ) ) ;
#69735 = CARTESIAN_POINT ( 'NONE',  ( -2.977408999572648707, -7.188101187499990274, 9.642802781871756324 ) ) ;
#69736 = CARTESIAN_POINT ( 'NONE',  ( 5.676582343749993598, 74.94791666325269830, 9.832129032723422313 ) ) ;
#69737 = DIRECTION ( 'NONE',  ( -0.000000000000000000, -0.000000000000000000, -1.000000000000000000 ) ) ;
#69738 = CARTESIAN_POINT ( 'NONE',  ( -4.000000000000015987, 201.5625000000000568, 143.6568542494924259 ) ) ;
#69739 = ORIENTED_EDGE ( 'NONE', *, *, #1586, .T. ) ;
#69740 = CARTESIAN_POINT ( 'NONE',  ( 1.469576158976822172E-15, -7.999999999999991118, 7.392802783920144449 ) ) ;
#69741 = CARTESIAN_POINT ( 'NONE',  ( -2.751064625579944321E-14, 203.8750000027312126, 146.0000000000000284 ) ) ;
#69742 = CARTESIAN_POINT ( 'NONE',  ( -11.35316468750000141, 73.48958332991932707, 3.042071309553159963 ) ) ;
#69743 = AXIS2_PLACEMENT_3D ( 'NONE', #24476, #64480, #41466 ) ;
#69744 = CARTESIAN_POINT ( 'NONE',  ( 4.220049686691934809, 10.18810118749999916, 116.6875000020483952 ) ) ;
#69745 = CARTESIAN_POINT ( 'NONE',  ( -3.458734125000015425, 195.2500000013656063, 143.4326545832176976 ) ) ;
#69746 = CARTESIAN_POINT ( 'NONE',  ( -3.544144923084229681, 10.27124247550373681, 63.97955030411849009 ) ) ;
#69748 = CARTESIAN_POINT ( 'NONE',  ( 8.311093377946834337, 60.15624999658601979, 8.311093377946839666 ) ) ;
#69747 = CARTESIAN_POINT ( 'NONE',  ( -2.977408999572650927, 89.37500000204836681, -7.188101187500000933 ) ) ;
#69749 = CARTESIAN_POINT ( 'NONE',  ( 1.469576158976822172E-15, -7.999999999999991118, 25.39280278392014978 ) ) ;
#69750 = DIRECTION ( 'NONE',  ( 0.000000000000000000, 0.000000000000000000, 1.000000000000000000 ) ) ;
#69751 = AXIS2_PLACEMENT_3D ( 'NONE', #32627, #55264, #10712 ) ;
#69752 = CARTESIAN_POINT ( 'NONE',  ( -8.660254037844390851, 149.7916666598387110, 4.999999999999998224 ) ) ;
#69753 = CARTESIAN_POINT ( 'NONE',  ( -2.977408999572651815, 97.81250000204840944, 7.188101187500000933 ) ) ;
#69754 = DIRECTION ( 'NONE',  ( -1.000000000000000000, 0.000000000000000000, 0.000000000000000000 ) ) ;
#69755 = CARTESIAN_POINT ( 'NONE',  ( -3.042071309553173730, 44.63541666325268409, 11.35316468749999785 ) ) ;
#69756 = CARTESIAN_POINT ( 'NONE',  ( 10.18810118749999916, 4.220049686691935698, 112.3750000020483810 ) ) ;
#69757 = CARTESIAN_POINT ( 'NONE',  ( -3.042071309553173730, 179.3229166632526699, 11.35316468749999785 ) ) ;
#69758 = ORIENTED_EDGE ( 'NONE', *, *, #73889, .F. ) ;
#69759 = CARTESIAN_POINT ( 'NONE',  ( -31.66756539373098178, -21.02027521086719730, 167.9999999999997726 ) ) ;
#69760 = CARTESIAN_POINT ( 'NONE',  ( -10.18810118749999916, 0.000000000000000000, 67.65625000204836681 ) ) ;
#69761 = CARTESIAN_POINT ( 'NONE',  ( 10.00000000000000178, 162.0833333265053682, -2.679491924311226736 ) ) ;
#69763 = CARTESIAN_POINT ( 'NONE',  ( 8.311093377946837890, 176.4062499965859843, -8.311093377946837890 ) ) ;
#69762 = CARTESIAN_POINT ( 'NONE',  ( -2.828427073549516724, 195.0000000000000284, 195.1715728240572219 ) ) ;
#69764 = CYLINDRICAL_SURFACE ( 'NONE', #74318, 10.00000000000000178 ) ;
#69765 = CARTESIAN_POINT ( 'NONE',  ( -5.000000000000000888, 257.2916666734946034, -8.660254037844387298 ) ) ;
#69766 = DIRECTION ( 'NONE',  ( -0.000000000000000000, 0.000000000000000000, 1.000000000000000000 ) ) ;
#69767 = VERTEX_POINT ( 'NONE', #9398 ) ;
#69768 = CARTESIAN_POINT ( 'NONE',  ( 6.951808397369818766E-16, 172.3437499965860127, -11.35316468750000141 ) ) ;
#69769 = CARTESIAN_POINT ( 'NONE',  ( 1.102182119232618108E-15, 293.3125000034140157, 6.000000000000001776 ) ) ;
#69770 = CARTESIAN_POINT ( 'NONE',  ( -9.832129032723418760, 128.1770833299193555, -5.676582343750004256 ) ) ;
#69771 = CARTESIAN_POINT ( 'NONE',  ( -5.656854249492381470, 3.749999995903220640, 5.656854249492379694 ) ) ;
#69772 = EDGE_LOOP ( 'NONE', ( #41718, #53897, #55792 ) ) ;
#69773 = ADVANCED_FACE ( 'NONE', ( #72007 ), #32418, .F. ) ;
#69774 = CARTESIAN_POINT ( 'NONE',  ( 8.000000000000000000, 105.0312500040967763, -3.313708498984762496 ) ) ;
#69775 =( BOUNDED_CURVE ( )  B_SPLINE_CURVE ( 2, ( #70535, #65605, #64868, #1874, #54305, #24860, #2616, #48619, #65976, #66352, #54678, #59586, #14656 ),
 .UNSPECIFIED., .F., .F. ) 
 B_SPLINE_CURVE_WITH_KNOTS ( ( 3, 2, 2, 2, 2, 2, 3 ),
 ( 0.3858695652173912971, 0.3876811594202898559, 0.3894927536231884146, 0.3913043478260870289, 0.3931159420289855877, 0.3949275362318840910, 0.3967391304347826497 ),
 .UNSPECIFIED. ) 
 CURVE ( )  GEOMETRIC_REPRESENTATION_ITEM ( )  RATIONAL_B_SPLINE_CURVE ( ( 1.000000000000000000, 0.9659258262890683122, 1.000000000000000000, 0.9659258262890683122, 1.000000000000000000, 0.9659258262890683122, 1.000000000000000000, 0.9659258262890683122, 1.000000000000000000, 0.9659258262890683122, 1.000000000000000000, 0.9659258262890673130, 1.000000000000001110 ) ) 
 REPRESENTATION_ITEM ( '' )  );
#69776 = AXIS2_PLACEMENT_3D ( 'NONE', #23314, #16901, #40296 ) ;
#69777 = CARTESIAN_POINT ( 'NONE',  ( 2.449293598294707893E-16, 13.25000000000000000, -4.000000000000001776 ) ) ;
#69778 = CARTESIAN_POINT ( 'NONE',  ( -36.30998830614734629, -5.856122892964523707, 137.6817969100390542 ) ) ;
#69779 = CARTESIAN_POINT ( 'NONE',  ( -4.541265875000003227, 12.87499999863440969, 1.881053915767121110 ) ) ;
#69780 = CARTESIAN_POINT ( 'NONE',  ( -7.999999999999991118, 3.313708498984756723, 20.42405278392014978 ) ) ;
#69781 = CARTESIAN_POINT ( 'NONE',  ( -2.828427124746209831, 195.3750000000000284, 139.1715728752538723 ) ) ;
#69782 = VECTOR ( 'NONE', #69410, 1000.000000000000000 ) ;
#69784 = EDGE_CURVE ( 'NONE', #12072, #31616, #16218, .T. ) ;
#69783 = VERTEX_POINT ( 'NONE', #48625 ) ;
#69785 = CARTESIAN_POINT ( 'NONE',  ( -5.000000000000024869, 176.6666666666666856, -8.660254037844437036 ) ) ;
#69786 = CARTESIAN_POINT ( 'NONE',  ( -2.977408999572650927, 107.3750000020484094, -7.188101187500001821 ) ) ;
#69788 = CARTESIAN_POINT ( 'NONE',  ( 4.000000000000001776, 6.812499997268813168, -1.656854249492381248 ) ) ;
#69787 = CARTESIAN_POINT ( 'NONE',  ( 2.828427124746208943, 196.6250000000000284, 195.1715728752538439 ) ) ;
#69789 = DIRECTION ( 'NONE',  ( 0.000000000000000000, 0.000000000000000000, 1.000000000000000000 ) ) ;
#69790 = ORIENTED_EDGE ( 'NONE', *, *, #19207, .F. ) ;
#69791 = CARTESIAN_POINT ( 'NONE',  ( -1.781595147096111775, 16.42277972781688788, -68.70049804031586405 ) ) ;
#69792 = CARTESIAN_POINT ( 'NONE',  ( -7.188101187499990274, -2.977408999572651371, 22.58030278187175099 ) ) ;
#69793 = ORIENTED_EDGE ( 'NONE', *, *, #5361, .F. ) ;
#69794 = ORIENTED_EDGE ( 'NONE', *, *, #30867, .T. ) ;
#69795 = CARTESIAN_POINT ( 'NONE',  ( 7.204075437095966983, 7.204075437095967871, 83.59375000204836681 ) ) ;
#69796 = PRODUCT_DEFINITION_CONTEXT ( 'detailed design', #32274, 'design' ) ;
#69797 = CARTESIAN_POINT ( 'NONE',  ( -28.00000000000001776, 195.6875000013655779, 166.5412658750003629 ) ) ;
#69798 = CARTESIAN_POINT ( 'NONE',  ( -11.00000000000000000, 0.000000000000000000, 103.0000000000000000 ) ) ;
#69801 = CARTESIAN_POINT ( 'NONE',  ( -4.721056650415999201, 296.4843750017070079, -4.721056650415999201 ) ) ;
#69800 = CARTESIAN_POINT ( 'NONE',  ( 30.82842712474620939, 204.2500000027312126, 172.8284271247460424 ) ) ;
#69799 = CARTESIAN_POINT ( 'NONE',  ( -3.673940397442060854E-16, 289.8125000034140157, -6.000000000000001776 ) ) ;
#69802 = CARTESIAN_POINT ( 'NONE',  ( 7.320508075688774596, 140.6250000000000000, -7.320508075688774596 ) ) ;
#69803 = CARTESIAN_POINT ( 'NONE',  ( -3.313708498984762496, 101.2812499999999858, 7.999999999999998224 ) ) ;
#69804 = CARTESIAN_POINT ( 'NONE',  ( -25.17157287525385811, 204.0000000027312126, 167.1715728752541281 ) ) ;
#69805 = CARTESIAN_POINT ( 'NONE',  ( 7.188101187499993827, -2.977408999572645598, 2.517802781871750550 ) ) ;
#69806 = EDGE_CURVE ( 'NONE', #14878, #52001, #28021, .T. ) ;
#69807 = CARTESIAN_POINT ( 'NONE',  ( -18.89444362769117092, 271.9999999999999432, 171.9999999999998295 ) ) ;
#69808 = CARTESIAN_POINT ( 'NONE',  ( 24.54126587499999346, 201.1875000013656063, 169.9999999999998863 ) ) ;
#69809 = CARTESIAN_POINT ( 'NONE',  ( -7.188101187500002709, 4.687499997951610986, 2.977408999572649151 ) ) ;
#69810 = CARTESIAN_POINT ( 'NONE',  ( -8.008118988124991233, 0.000000000000000000, 4.013115283940629219 ) ) ;
#69811 = CARTESIAN_POINT ( 'NONE',  ( 2.445694354108782775, 195.5625000013656063, 139.5543056458912190 ) ) ;
#69812 = CARTESIAN_POINT ( 'NONE',  ( 7.188101187500000044, 113.2812500020483952, -8.802885111219163269E-16 ) ) ;
#69814 = CARTESIAN_POINT ( 'NONE',  ( 2.496229509220036391, 194.6789702782473626, 200.7137564161983505 ) ) ;
#69813 = LINE ( 'NONE', #13918, #55268 ) ;
#69815 = CARTESIAN_POINT ( 'NONE',  ( -9.832129032723418760, 233.8020833367473301, -5.676582343749998927 ) ) ;
#69816 = CARTESIAN_POINT ( 'NONE',  ( -7.999999999999998224, 90.59375000000000000, 3.313708498984766049 ) ) ;
#69817 = CARTESIAN_POINT ( 'NONE',  ( 7.188101187499992051, 8.802885111219154394E-16, 28.11155278187175455 ) ) ;
#69818 = CARTESIAN_POINT ( 'NONE',  ( 23.99999999999998579, 197.7500000000000000, 169.9999999999998863 ) ) ;
#69819 = CARTESIAN_POINT ( 'NONE',  ( 9.832129032723416984, 30.36458332991935194, 5.676582343750006032 ) ) ;
#69820 = CARTESIAN_POINT ( 'NONE',  ( -38.00000000000000000, 0.000000000000000000, 20.00000000000003553 ) ) ;
#69821 = CARTESIAN_POINT ( 'NONE',  ( 10.00000000000000178, 2.083333326505365957, -2.679491924311226736 ) ) ;
#69822 = DIRECTION ( 'NONE',  ( -1.000000000000000000, -0.000000000000000000, -0.000000000000000000 ) ) ;
#69824 = FACE_OUTER_BOUND ( 'NONE', #871, .T. ) ;
#69823 = DIRECTION ( 'NONE',  ( 0.000000000000000000, -1.000000000000000000, 0.000000000000000000 ) ) ;
#69825 = VERTEX_POINT ( 'NONE', #39933 ) ;
#69826 = EDGE_CURVE ( 'NONE', #7596, #42125, #21202, .T. ) ;
#69827 = ADVANCED_FACE ( 'NONE', ( #339 ), #51620, .T. ) ;
#69828 = CARTESIAN_POINT ( 'NONE',  ( -2.445694354108839175, 197.3125000013656063, 144.4456943541088663 ) ) ;
#69829 = CARTESIAN_POINT ( 'NONE',  ( 5.676582343749993598, 19.94791666325268409, 9.832129032723422313 ) ) ;
#69830 = CARTESIAN_POINT ( 'NONE',  ( 11.00000000000000355, -4.556349186104045046, 87.34375000409679046 ) ) ;
#69831 = CARTESIAN_POINT ( 'NONE',  ( -3.458734125000016757, 208.1250000013656063, 140.5673454167823593 ) ) ;
#69832 = CARTESIAN_POINT ( 'NONE',  ( -3.673940397442060854E-16, 294.8125000034140157, -6.000000000000001776 ) ) ;
#69833 = CARTESIAN_POINT ( 'NONE',  ( 12.00000000000000000, 6.928203230275542523, -1.071796769724504550 ) ) ;
#69835 = CARTESIAN_POINT ( 'NONE',  ( -9.832129032723420536, 23.69791666325268409, 5.676582343749997150 ) ) ;
#69834 = CARTESIAN_POINT ( 'NONE',  ( -5.082755093536325930, 113.4687500020483810, -5.082755093536325930 ) ) ;
#69836 = CARTESIAN_POINT ( 'NONE',  ( -5.656854249492373476, -5.656854249492376141, 14.51780277982336465 ) ) ;
#69837 = APPLICATION_CONTEXT ( 'automotive_design' ) ;
#69838 = CARTESIAN_POINT ( 'NONE',  ( 6.951808397369818766E-16, 142.0312499965860411, -11.35316468750000141 ) ) ;
#69839 = AXIS2_PLACEMENT_3D ( 'NONE', #30374, #35672, #48079 ) ;
#69840 = CARTESIAN_POINT ( 'NONE',  ( -2.679491924311225848, 118.3333333265053682, -10.00000000000000178 ) ) ;
#69841 = EDGE_CURVE ( 'NONE', #61682, #5256, #17895, .T. ) ;
#69842 = CARTESIAN_POINT ( 'NONE',  ( 2.977408999572650039, 112.0625000020483810, -7.188101187500001821 ) ) ;
#69843 = CARTESIAN_POINT ( 'NONE',  ( 7.320508075688774596, 172.4999999931719969, -7.320508075688774596 ) ) ;
#69844 = CARTESIAN_POINT ( 'NONE',  ( -24.54126587499998280, 204.3750000013656063, 171.4326545832179818 ) ) ;
#69845 = ORIENTED_EDGE ( 'NONE', *, *, #60387, .F. ) ;
#69846 = CARTESIAN_POINT ( 'NONE',  ( -5.676582343750006032, 14.42708332991935016, 9.832129032723418760 ) ) ;
#69847 = ORIENTED_EDGE ( 'NONE', *, *, #9397, .F. ) ;
#69848 = DIRECTION ( 'NONE',  ( 0.000000000000000000, 0.000000000000000000, -1.000000000000000000 ) ) ;
#69849 = CARTESIAN_POINT ( 'NONE',  ( -6.676582343750003368, 298.3906250017070079, -2.765530957081996810 ) ) ;
#69851 = CARTESIAN_POINT ( 'NONE',  ( 11.35316468749999963, 145.9895833299193839, -3.042071309553165293 ) ) ;
#69850 = CARTESIAN_POINT ( 'NONE',  ( 3.999999999999960032, 195.0000000000000000, 142.0000000000000568 ) ) ;
#69852 = CARTESIAN_POINT ( 'NONE',  ( -5.000000000000000000, 16.14408868864073554, 27.96238185062412640 ) ) ;
#69853 = CARTESIAN_POINT ( 'NONE',  ( -5.656854249492373476, -5.656854249492376141, 25.07405278432982598 ) ) ;
#69854 = DIRECTION ( 'NONE',  ( -1.000000000000000000, 0.000000000000000000, 0.000000000000000000 ) ) ;
#69855 = AXIS2_PLACEMENT_3D ( 'NONE', #19528, #36896, #70854 ) ;
#69856 = CARTESIAN_POINT ( 'NONE',  ( 3.042071309553163960, 242.4479166700806729, -11.35316468749999785 ) ) ;
#69857 = CARTESIAN_POINT ( 'NONE',  ( 10.18810118750000093, -4.220049686691933921, 94.18750000204836681 ) ) ;
#69858 = ORIENTED_EDGE ( 'NONE', *, *, #64168, .T. ) ;
#69859 = CARTESIAN_POINT ( 'NONE',  ( 8.000000000000000000, 20.81249999590322375, 0.000000000000000000 ) ) ;
#69860 = FACE_BOUND ( 'NONE', #38589, .T. ) ;
#69861 = CARTESIAN_POINT ( 'NONE',  ( -11.35316468749999785, 93.38541666325269830, -3.042071309553167513 ) ) ;
#69862 = VERTEX_POINT ( 'NONE', #67855 ) ;
#69863 = CARTESIAN_POINT ( 'NONE',  ( -10.18810118749999738, -4.220049686691941915, 109.7500000020483810 ) ) ;
#69864 = CARTESIAN_POINT ( 'NONE',  ( -4.541265875000002339, 17.93749999863440792, -5.561446717895856393E-16 ) ) ;
#69865 = ORIENTED_EDGE ( 'NONE', *, *, #21008, .F. ) ;
#69866 = EDGE_LOOP ( 'NONE', ( #48112, #38273, #24648, #65822, #25229 ) ) ;
#69867 = CARTESIAN_POINT ( 'NONE',  ( 4.898587196589412829E-16, 6.375000000000000888, -8.000000000000000000 ) ) ;
#69868 = CARTESIAN_POINT ( 'NONE',  ( 4.541265875000002339, 0.4999999986344068614, -1.881053915767121554 ) ) ;
#69869 = CARTESIAN_POINT ( 'NONE',  ( -5.082755093536325042, 22.40624999795161543, -5.082755093536325930 ) ) ;
#69870 = CARTESIAN_POINT ( 'NONE',  ( 5.656854249492379694, 120.1250000040967905, -5.656854249492380582 ) ) ;
#69871 = CARTESIAN_POINT ( 'NONE',  ( 10.18810118749999916, 1.247682550866122264E-15, 101.7812500020483810 ) ) ;
#69872 =( BOUNDED_CURVE ( )  B_SPLINE_CURVE ( 2, ( #67561, #49830, #61149, #44176, #43413, #15116, #55880, #60774, #67190, #37779, #73221, #60398, #72472 ),
 .UNSPECIFIED., .F., .F. ) 
 B_SPLINE_CURVE_WITH_KNOTS ( ( 3, 2, 2, 2, 2, 2, 3 ),
 ( 0.5833333333333331483, 0.5925925925925923377, 0.6018518518518516380, 0.6111111111111109384, 0.6203703703703702388, 0.6296296296296295392, 0.6388888888888887285 ),
 .UNSPECIFIED. ) 
 CURVE ( )  GEOMETRIC_REPRESENTATION_ITEM ( )  RATIONAL_B_SPLINE_CURVE ( ( 1.000000000000000888, 0.9659258262890675351, 1.000000000000000000, 0.9659258262890683122, 1.000000000000000000, 0.9659258262890683122, 1.000000000000000000, 0.9659258262890683122, 1.000000000000000000, 0.9659258262890683122, 1.000000000000000000, 0.9659258262890687563, 0.9999999999999995559 ) ) 
 REPRESENTATION_ITEM ( '' )  );
#69873 = EDGE_CURVE ( 'NONE', #70285, #25175, #69016, .T. ) ;
#69874 = CARTESIAN_POINT ( 'NONE',  ( -2.828427124746192067, 0.6250000000000002220, 2.828427124746190735 ) ) ;
#69875 = CARTESIAN_POINT ( 'NONE',  ( -2.828427124746192067, 14.37499999726881406, 2.828427124746190735 ) ) ;
#69876 = LINE ( 'NONE', #40830, #25213 ) ;
#69877 = ORIENTED_EDGE ( 'NONE', *, *, #2226, .T. ) ;
#69878 = CARTESIAN_POINT ( 'NONE',  ( 11.99999999999999822, 2.326828918379971365E-15, -19.00000000000000355 ) ) ;
#69879 = CARTESIAN_POINT ( 'NONE',  ( 3.458734125000016313, 197.8750000013656063, 199.4326545832176691 ) ) ;
#69880 = CARTESIAN_POINT ( 'NONE',  ( -25.55430564589122966, 203.3125000013656063, 167.5543056458915032 ) ) ;
#69881 =( NAMED_UNIT ( * ) PLANE_ANGLE_UNIT ( ) SI_UNIT ( $, .RADIAN. ) );
#69882 = ADVANCED_FACE ( 'NONE', ( #11631 ), #5980, .F. ) ;
#69883 = CARTESIAN_POINT ( 'NONE',  ( 3.211159895383560947, 16.18749999863440436, 3.211159895383562723 ) ) ;
#69884 = VECTOR ( 'NONE', #58757, 1000.000000000000000 ) ;
#69885 = CARTESIAN_POINT ( 'NONE',  ( -1.656854249492399234, 200.3125000027312410, 201.9999999999999432 ) ) ;
#69886 = CARTESIAN_POINT ( 'NONE',  ( 7.188101187499991163, 2.977408999572648707, 11.33030278187175632 ) ) ;
#69887 = ORIENTED_EDGE ( 'NONE', *, *, #58759, .T. ) ;
#69888 =( BOUNDED_CURVE ( )  B_SPLINE_CURVE ( 2, ( #70652, #11831, #17860, #41618, #64630, #6915, #41250, #40878, #47630, #29926, #64984, #12567, #69925 ),
 .UNSPECIFIED., .F., .F. ) 
 B_SPLINE_CURVE_WITH_KNOTS ( ( 3, 2, 2, 2, 2, 2, 3 ),
 ( 1.271689704932325693, 1.276922700034719860, 1.282155695137113804, 1.287388690239507971, 1.292621685341902138, 1.297854680444296305, 1.303087675546690472 ),
 .UNSPECIFIED. ) 
 CURVE ( )  GEOMETRIC_REPRESENTATION_ITEM ( )  RATIONAL_B_SPLINE_CURVE ( ( 1.000000000000000000, 0.9659258262890683122, 1.000000000000000000, 0.9659258262890683122, 1.000000000000000000, 0.9659258262890683122, 1.000000000000000000, 0.9659258262890683122, 1.000000000000000000, 0.9659258262890683122, 1.000000000000000000, 0.9659258262891695646, 0.9999999999998987477 ) ) 
 REPRESENTATION_ITEM ( '' )  );
#69889 = VERTEX_POINT ( 'NONE', #23320 ) ;
#69890 = CARTESIAN_POINT ( 'NONE',  ( -7.204075437095967871, 7.204075437095967871, 103.4687500020483668 ) ) ;
#69891 = CARTESIAN_POINT ( 'NONE',  ( -7.320508075688769267, 98.12499999999997158, 7.320508075688761274 ) ) ;
#69892 = CARTESIAN_POINT ( 'NONE',  ( -23.99999999999998934, 205.7500000000000284, 170.0000000000003411 ) ) ;
#69893 = CARTESIAN_POINT ( 'NONE',  ( -1.432654583217607858, 200.6250000013655779, 201.4587341250000065 ) ) ;
#69894 = CARTESIAN_POINT ( 'NONE',  ( 24.54126587499998990, 195.1875000013655779, 169.9999999999999432 ) ) ;
#69895 = CARTESIAN_POINT ( 'NONE',  ( -2.679491924311235618, 93.54166666666668561, 10.00000000000000000 ) ) ;
#69896 = AXIS2_PLACEMENT_3D ( 'NONE', #73720, #38283, #31872 ) ;
#69897 = CARTESIAN_POINT ( 'NONE',  ( -4.898587196589412829E-16, 118.6250000000000000, -8.000000000000000000 ) ) ;
#69898 = CARTESIAN_POINT ( 'NONE',  ( 5.676582343750001591, 56.92708332991935549, -9.832129032723420536 ) ) ;
#69899 = CARTESIAN_POINT ( 'NONE',  ( 6.676582343750003368, 298.1718750017070079, -2.765530957081997254 ) ) ;
#69900 = ORIENTED_EDGE ( 'NONE', *, *, #43462, .F. ) ;
#69901 = CARTESIAN_POINT ( 'NONE',  ( 2.485281374238216490, 294.6875000000000568, -6.000000000000357048 ) ) ;
#69902 = EDGE_CURVE ( 'NONE', #54540, #8347, #46332, .T. ) ;
#69903 = CARTESIAN_POINT ( 'NONE',  ( 4.898587196589412829E-16, 15.18749999590322197, -8.000000000000000000 ) ) ;
#69904 = CARTESIAN_POINT ( 'NONE',  ( 1.432654583217607192, 209.2500000013655779, 145.4587341250000634 ) ) ;
#69905 = CARTESIAN_POINT ( 'NONE',  ( -7.320508075688778149, 104.9999999931720396, 7.320508075688769267 ) ) ;
#69906 = LINE ( 'NONE', #70632, #49156 ) ;
#69907 = CARTESIAN_POINT ( 'NONE',  ( -9.999999999999998224, 220.2083333333333428, 2.679491924311235618 ) ) ;
#69908 = DIRECTION ( 'NONE',  ( 0.000000000000000000, -0.000000000000000000, 1.000000000000000000 ) ) ;
#69909 = CARTESIAN_POINT ( 'NONE',  ( -4.220049686691935698, 10.18810118749999916, 69.25000000204836681 ) ) ;
#69910 = CARTESIAN_POINT ( 'NONE',  ( 7.320508075688774596, 220.6250000000000284, -7.320508075688774596 ) ) ;
#69911 = ADVANCED_FACE ( 'NONE', ( #62189 ), #43534, .F. ) ;
#69912 = CARTESIAN_POINT ( 'NONE',  ( 1.320432766682872962E-15, -7.188101187499992051, 9.736552781871754547 ) ) ;
#69913 = CARTESIAN_POINT ( 'NONE',  ( -5.676582343749998039, 182.7604166632526699, -9.832129032723420536 ) ) ;
#69914 = CARTESIAN_POINT ( 'NONE',  ( 1.881053915767122664, 4.124999998634407028, 4.541265875000001451 ) ) ;
#69915 = DIRECTION ( 'NONE',  ( 0.000000000000000000, 0.000000000000000000, 1.000000000000000000 ) ) ;
#69917 = DIRECTION ( 'NONE',  ( 0.000000000000000000, 0.000000000000000000, -1.000000000000000000 ) ) ;
#69916 = CARTESIAN_POINT ( 'NONE',  ( 0.000000000000000000, 300.0000000000000000, 0.000000000000000000 ) ) ;
#69918 = VERTEX_POINT ( 'NONE', #12370 ) ;
#69919 = CARTESIAN_POINT ( 'NONE',  ( -1.432654583217664701, 207.0000000013656063, 138.5412658750000787 ) ) ;
#69920 = CARTESIAN_POINT ( 'NONE',  ( -5.676582343749998039, 42.76041666325268409, -9.832129032723420536 ) ) ;
#69921 = CARTESIAN_POINT ( 'NONE',  ( -4.556349186104045934, 11.00000000000000000, 104.4062500040967620 ) ) ;
#69922 = CARTESIAN_POINT ( 'NONE',  ( -24.54126587499996148, 204.1250000013656063, 171.4326545832179534 ) ) ;
#69923 = CARTESIAN_POINT ( 'NONE',  ( 5.656854249492378806, 4.124999995903220196, 5.656854249492381470 ) ) ;
#69925 = CARTESIAN_POINT ( 'NONE',  ( -1.522892193876115035E-11, 103.7499999999988205, 10.00000000000000178 ) ) ;
#69924 = CARTESIAN_POINT ( 'NONE',  ( -18.00000000000000355, 0.000000000000000000, 0.000000000000000000 ) ) ;
#69926 = CARTESIAN_POINT ( 'NONE',  ( -3.458734125000016313, 199.8750000013656063, 140.5673454167823593 ) ) ;
#69927 = CARTESIAN_POINT ( 'NONE',  ( -7.320508075688773708, 73.74999999317203958, -7.320508075688774596 ) ) ;
#69928 = CARTESIAN_POINT ( 'NONE',  ( -7.188101187500000044, 95.65625000204838102, 0.000000000000000000 ) ) ;
#69929 = CARTESIAN_POINT ( 'NONE',  ( 3.211159895383561835, 17.56249999863440792, -3.211159895383561835 ) ) ;
#69930 = CARTESIAN_POINT ( 'NONE',  ( -27.99999999999991118, 204.6250000027312126, 174.0000000000003695 ) ) ;
#69931 = CARTESIAN_POINT ( 'NONE',  ( -12.00000000000000000, 6.928203230275504332, -14.00000000000000178 ) ) ;
#69932 = CARTESIAN_POINT ( 'NONE',  ( 4.000000000000000888, 7.687499997268812280, 1.656854249492384135 ) ) ;
#69933 = VERTEX_POINT ( 'NONE', #42140 ) ;
#69935 = EDGE_CURVE ( 'NONE', #45635, #26465, #19136, .T. ) ;
#69934 = ORIENTED_EDGE ( 'NONE', *, *, #11808, .F. ) ;
#69936 = CARTESIAN_POINT ( 'NONE',  ( 6.123233995736767268E-16, 23.12499999317203603, -10.00000000000000178 ) ) ;
#69937 = CARTESIAN_POINT ( 'NONE',  ( 6.676582343750001591, 296.1093750017069510, -8.176455196517173205E-16 ) ) ;
#69938 = CYLINDRICAL_SURFACE ( 'NONE', #55583, 11.00000000000000000 ) ;
#69939 = CARTESIAN_POINT ( 'NONE',  ( -30.93541659651595310, -42.99981040672923882, 167.9999999999998295 ) ) ;
#69940 = CARTESIAN_POINT ( 'NONE',  ( -11.35316468749999785, 158.0729166632526699, -3.042071309553167513 ) ) ;
#69941 = CARTESIAN_POINT ( 'NONE',  ( 7.204075437095966983, 7.204075437095967871, 85.09375000204836681 ) ) ;
#69942 = DIRECTION ( 'NONE',  ( 0.000000000000000000, -0.000000000000000000, -1.000000000000000000 ) ) ;
#69943 = CARTESIAN_POINT ( 'NONE',  ( 2.828427124746208943, 205.6250000000000284, 195.1715728752538439 ) ) ;
#69944 = LINE ( 'NONE', #30311, #51864 ) ;
#69945 = CARTESIAN_POINT ( 'NONE',  ( 4.220049686691934809, 10.18810118749999916, 111.0625000020483810 ) ) ;
#69946 = EDGE_LOOP ( 'NONE', ( #35623, #64323, #60526, #45029, #64313, #18319 ) ) ;
#69947 = CARTESIAN_POINT ( 'NONE',  ( 10.99999999999999467, 11.00000000000000355, 41.99999999999999289 ) ) ;
#69948 = CARTESIAN_POINT ( 'NONE',  ( -4.898587196589412829E-16, 111.1250000000000000, -8.000000000000000000 ) ) ;
#69949 = CARTESIAN_POINT ( 'NONE',  ( 5.676582343750001591, 141.9270833299193555, -9.832129032723420536 ) ) ;
#69950 = CARTESIAN_POINT ( 'NONE',  ( -1.432654583217607192, 198.2500000013656347, 194.5412658750000219 ) ) ;
#69951 = CARTESIAN_POINT ( 'NONE',  ( 2.839093476692135984E-14, 207.9375000013656063, 201.4587341250000350 ) ) ;
#69952 = CARTESIAN_POINT ( 'NONE',  ( 4.220049686691934809, 10.18810118749999916, 78.06250000204836681 ) ) ;
#69953 = CARTESIAN_POINT ( 'NONE',  ( -11.35316468750000141, 53.80208332991935549, 3.042071309553159963 ) ) ;
#69954 = VERTEX_POINT ( 'NONE', #36133 ) ;
#69955 = CARTESIAN_POINT ( 'NONE',  ( 0.000000000000000000, 300.0000000000000000, 0.000000000000000000 ) ) ;
#69956 = CARTESIAN_POINT ( 'NONE',  ( 3.211159895383560947, 3.312499998634407028, 3.211159895383562723 ) ) ;
#69957 = CARTESIAN_POINT ( 'NONE',  ( 3.317071493978883456, -8.008118988124989457, 14.98186528394062833 ) ) ;
#69958 = VECTOR ( 'NONE', #13198, 1000.000000000000000 ) ;
#69959 = EDGE_CURVE ( 'NONE', #30287, #9832, #54012, .T. ) ;
#69960 = AXIS2_PLACEMENT_3D ( 'NONE', #35983, #53699, #18625 ) ;
#69961 = CARTESIAN_POINT ( 'NONE',  ( 7.188101187499999156, 16.87499999795161543, 2.977408999572654924 ) ) ;
#69962 = CARTESIAN_POINT ( 'NONE',  ( -6.000000000000000888, 294.1250000034140157, 2.485281374238575758 ) ) ;
#69963 = CARTESIAN_POINT ( 'NONE',  ( -27.91562816932720281, -12.23625176173777618, 139.8767700287489220 ) ) ;
#69964 = CARTESIAN_POINT ( 'NONE',  ( -7.188101187500001821, 8.999999997951611874, -2.977408999572651371 ) ) ;
#69965 = CARTESIAN_POINT ( 'NONE',  ( 5.082755093536318824, 5.082755093536319713, 11.42405278187175455 ) ) ;
#69966 = EDGE_CURVE ( 'NONE', #2283, #3793, #47437, .T. ) ;
#69967 = CARTESIAN_POINT ( 'NONE',  ( -7.204075437095967871, 7.204075437095967871, 73.46875000204838102 ) ) ;
#69968 = CARTESIAN_POINT ( 'NONE',  ( -24.54126587499998635, 206.3750000013656063, 171.4326545832179818 ) ) ;
#69969 = ADVANCED_FACE ( 'NONE', ( #7091 ), #64795, .F. ) ;
#69970 = CARTESIAN_POINT ( 'NONE',  ( 1.656854249492381248, 9.187500000000000000, -4.000000000000001776 ) ) ;
#69971 = CARTESIAN_POINT ( 'NONE',  ( 4.541265875000001451, 22.37499999863441147, 1.881053915767124440 ) ) ;
#69972 = ORIENTED_EDGE ( 'NONE', *, *, #916, .F. ) ;
#69973 = CARTESIAN_POINT ( 'NONE',  ( -2.828427124746152987, 195.2500000027312126, 200.8284271247462129 ) ) ;
#69974 = VECTOR ( 'NONE', #28145, 1000.000000000000000 ) ;
#69975 = CARTESIAN_POINT ( 'NONE',  ( -1.656854249492405451, 207.3125000000000284, 138.0000000000000568 ) ) ;
#69976 = CARTESIAN_POINT ( 'NONE',  ( -31.99999999999999289, 200.3750000027312126, 170.0000000000004547 ) ) ;
#69977 = CARTESIAN_POINT ( 'NONE',  ( -7.188101187499999156, 113.7500000020483668, 2.977408999572654924 ) ) ;
#69978 = CARTESIAN_POINT ( 'NONE',  ( 11.00000000000000000, 4.556349186104045934, 93.53125000409676204 ) ) ;
#69979 = CARTESIAN_POINT ( 'NONE',  ( 1.469576158976822172E-15, -7.999999999999991118, 1.392802783920146004 ) ) ;
#69980 = ORIENTED_EDGE ( 'NONE', *, *, #34708, .T. ) ;
#69981 = EDGE_CURVE ( 'NONE', #34236, #3133, #66549, .T. ) ;
#69982 = B_SPLINE_CURVE_WITH_KNOTS ( 'NONE', 3,
 ( #63427, #74010, #5728, #28727, #22311, #23070, #69099, #17405, #23439, #63060, #28360, #22689, #17031, #63801, #33671, #11755, #74378, #34792, #57796, #6104, #29109, #52128 ),
 .UNSPECIFIED., .F., .F.,
 ( 4, 2, 2, 2, 2, 2, 2, 2, 2, 2, 4 ),
 ( 0.000000000000000000, 0.001156727053362455269, 0.001735090580043697431, 0.002313454106724939594, 0.003470181160087424353, 0.004048544686768665649, 0.004626908213449907811, 0.005783635266812366983, 0.006940362320174827022, 0.008097089373537286194, 0.009253816426899744499 ),
 .UNSPECIFIED. ) ;
#69983 = CARTESIAN_POINT ( 'NONE',  ( 5.082755093536324154, 15.28124999795161187, 5.082755093536326818 ) ) ;
#69984 = ORIENTED_EDGE ( 'NONE', *, *, #56237, .T. ) ;
#69985 = DIRECTION ( 'NONE',  ( -0.000000000000000000, -1.000000000000000000, -0.000000000000000000 ) ) ;
#69986 = CARTESIAN_POINT ( 'NONE',  ( 5.000000000000001776, 60.83333333333333570, -8.660254037844389075 ) ) ;
#69987 = CARTESIAN_POINT ( 'NONE',  ( 5.082755093536326818, 98.09375000204838102, 5.082755093536325042 ) ) ;
#69988 = CARTESIAN_POINT ( 'NONE',  ( 2.485281374238571317, 299.6874999999999432, -6.000000000000003553 ) ) ;
#69990 = CARTESIAN_POINT ( 'NONE',  ( -29.72643842063306607, -42.92772067749797316, 178.8166482525937795 ) ) ;
#69989 = CARTESIAN_POINT ( 'NONE',  ( -5.656854249492380582, 111.5000000040967763, -5.656854249492380582 ) ) ;
#69992 = VERTEX_POINT ( 'NONE', #70103 ) ;
#69991 =( BOUNDED_CURVE ( )  B_SPLINE_CURVE ( 2, ( #49927, #20876, #8441, #55605, #65782, #49553, #21251, #3923, #31461, #3537, #48798, #66523, #71807, #14834, #4288, #20125, #43897, #26154, #9193, #15214, #31835, #26529, #25778, #73318, #66909, #43140, #54486, #38244, #44275, #67286, #37497, #14460, #54854, #15585, #38625, #3165, #61627, #27280, #50297, #21622, #52171, #34091, #68394, #68027, #11429, #57087, #10315, #5776, #17449, #56719, #69142, #39724, #135, #6146, #23111, #16692, #62725, #39356, #51045, #34466, #29153, #45379, #50664, #503, #44645, #5037, #11063, #5403, #74055, #28405, #67660, #27656, #15959, #45753, #51413, #11797, #62353, #10684, #74427, #21995, #63104, #28034, #22354, #22733, #73683, #38988, #68766, #17077, #40099, #16321, #61993, #33341, #57469, #28772, #33717, #51787, #46124, #40470, #56343, #4662, #45021, #63475, #34835, #57842, #35562, #46494, #17828, #65322, #64223, #58574, #46868, #1959, #64596, #24949, #69515, #58946, #18936, #47966, #52906, #24217, #47231, #52534, #59675, #872, #41942, #12893, #64950, #7252, #40841, #41215, #70259, #18571, #13627, #23858, #35199, #12164, #35929, #30263, #53280, #12531, #6882, #36665, #42306, #63850, #58216, #6517, #69890, #30627, #29524, #29893, #13260, #36296, #41581, #1605, #70616, #59315, #7620, #53649, #18202, #1240, #24589, #7986, #70981, #19296, #30992, #54014, #47594, #23482, #8349, #20031, #55140, #26058, #67197, #20786, #20406, #3826, #21160, #60781, #60404, #38532, #26823, #3445, #43422, #49079, #15495, #72092, #38155, #61533, #37785, #43044, #32502, #72855, #55514, #61156, #25688, #49836, #8731, #9488, #44183, #9856, #26434, #31744, #49460, #66063, #60031, #32884, #9106, #25319, #2324, #48335, #71343, #72479, #19665, #31365, #71715, #43806, #32120, #37030, #42677, #14745, #54393, #65689, #14370, #2700, #13989, #48708, #37403, #66821, #54764, #3073, #15123, #66435, #45661, #4201, #22270, #67937, #45293, #4946, #4569, #22641, #68305, #27190, #50207, #23028, #21900, #16231, #27567, #34374, #16603, #57374, #73227, #39640, #51324, #5683, #10597, #56632, #27945, #61901, #17360, #11705, #39268, #62637, #68676, #10970, #21533, #73592, #50953, #73964, #46035, #56252, #67569, #44556, #34005, #56999, #5313, #44930, #62268, #33625, #28315, #40012, #15866, #38898, #50575, #63014, #10225, #74332, #16985, #11339, #28683, #51696, #42, #69055, #40383, #63382, #33253, #55886, #29803, #13170, #53187, #6055, #30171, #24859, #58486, #23394, #40747, #52446, #12807, #6794, #47878, #1525, #52815, #36206, #53557, #18481, #18112, #70897, #59223, #17731, #41125, #46771, #18849, #1149, #70534, #19212, #70173, #784, #64867, #30541, #7535, #41856, #58124, #1873, #64133, #24128, #47141, #42217, #35111, #46409, #69423, #41492, #64508, #24503, #6433, #47508, #65229, #34746, #57750, #29061, #63757, #29435, #52082, #414, #12440, #12074, #23767, #35838, #58854, #7165, #69795, #35473, #60695, #2614, #25231, #21074, #49751, #43715, #55049, #3732, #26731, #37316, #2237, #19574, #31275, #66350, #60313, #72768, #32029, #31655, #15033, #32410, #71999, #14654, #42589, #25967, #37695, #54676, #8641, #44098, #2982, #49367, #13533, #48989, #54303, #66729, #9390, #38069, #72384, #36941, #61068, #71624, #20697, #55423, #9015, #36572, #65604, #8261, #3356, #20314, #48248, #59585, #43331, #13902, #7899, #26346, #30904, #53924, #59946, #71255, #25604, #19946, #48617, #42955, #65974, #14278, #15402, #33541, #4483, #56542, #16139, #15779, #33916, #4859, #32790, #28230, #39925, #27474, #16899, #62182, #22557, #28601, #45578, #38441, #27855, #62551, #68593, #21808, #67848, #39178, #73138, #51612, #22944, #50488, #10509, #50864, #44841, #73880, #74628, #50122, #73501, #51238, #11256, #22184, #45209, #68220, #16517, #10134, #21444, #74249, #39557, #61444, #33172, #10882, #34285, #56170, #44467, #62931, #67480, #38817, #56916, #61816, #5229, #57289, #5603, #67106, #4114, #9771, #55798, #27107, #11623, #58408, #58041, #6355, #68968, #40294, #13088, #11997, #29359, #69338, #24422, #12363, #47429, #41044, #40667, #52365, #12724, #30460, #17648, #18028, #331, #7453, #23312, #41414, #35398, #35757, #6714, #63295, #63670, #64052, #69714, #36123, #46324, #35029, #701, #29721, #23684, #64426, #46690, #58774, #59144, #64787, #17277, #34661, #57664, #52735, #53107 ),
 .UNSPECIFIED., .F., .F. ) 
 B_SPLINE_CURVE_WITH_KNOTS ( ( 3, 2, 2, 2, 2, 2, 2, 2, 2, 2, 2, 2, 2, 2, 2, 2, 2, 2, 2, 2, 2, 2, 2, 2, 2, 2, 2, 2, 2, 2, 2, 2, 2, 2, 2, 2, 2, 2, 2, 2, 2, 2, 2, 2, 2, 2, 2, 2, 2, 2, 2, 2, 2, 2, 2, 2, 2, 2, 2, 2, 2, 2, 2, 2, 2, 2, 2, 2, 2, 2, 2, 2, 2, 2, 2, 2, 2, 2, 2, 2, 2, 2, 2, 2, 2, 2, 2, 2, 2, 2, 2, 2, 2, 2, 2, 2, 2, 2, 2, 2, 2, 2, 2, 2, 2, 2, 2, 2, 2, 2, 2, 2, 2, 2, 2, 2, 2, 2, 2, 2, 2, 2, 2, 2, 2, 2, 2, 2, 2, 2, 2, 2, 2, 2, 2, 2, 2, 2, 2, 2, 2, 2, 2, 2, 2, 2, 2, 2, 2, 2, 2, 2, 2, 2, 2, 2, 2, 2, 2, 2, 2, 2, 2, 2, 2, 2, 2, 2, 2, 2, 2, 2, 2, 2, 2, 2, 2, 2, 2, 2, 2, 2, 2, 2, 2, 2, 2, 2, 2, 2, 2, 2, 2, 2, 2, 2, 2, 2, 2, 2, 2, 2, 2, 2, 2, 2, 2, 2, 2, 2, 2, 2, 2, 2, 2, 2, 2, 2, 2, 2, 2, 2, 2, 2, 2, 2, 2, 2, 2, 2, 2, 2, 2, 2, 2, 2, 2, 2, 2, 2, 2, 2, 2, 2, 2, 2, 2, 2, 2, 2, 2, 2, 2, 2, 2, 2, 2, 2, 2, 2, 2, 2, 2, 2, 2, 2, 2, 3 ),
 ( 0.000000000000000000, 0.003750026907760104986, 0.007500053815520209971, 0.01125008072328031496, 0.01500010763104041994, 0.01875013453880052666, 0.02250016144656062991, 0.02625018835432073316, 0.03000021526208083988, 0.03375024216984094660, 0.03750026907760105332, 0.04125029598536116004, 0.04500032289312125983, 0.04875034980088135961, 0.05250037670864146633, 0.05625040361640157305, 0.06000043052416167977, 0.06375045743192178649, 0.06750048433968189321, 0.07125051124744199993, 0.07500053815520210665, 0.07875056506296221337, 0.08250059197072232009, 0.08625061887848241293, 0.09000064578624251965, 0.09375067269400262637, 0.09750069960176271922, 0.1012507265095228259, 0.1050007534172829327, 0.1087507803250430394, 0.1125008072328031461, 0.1162508341405632528, 0.1200008610483233595, 0.1237508879560834663, 0.1275009148638435730, 0.1312509417716036519, 0.1350009686793637864, 0.1387509955871238654, 0.1425010224948839999, 0.1462510494026440788, 0.1500010763104042133, 0.1537511032181642923, 0.1575011301259244267, 0.1612511570336845057, 0.1650011839414446402, 0.1687512108492047191, 0.1725012377569648259, 0.1762512646647249326, 0.1800012915724850393, 0.1837513184802451460, 0.1875013453880052527, 0.1912513722957653595, 0.1950013992035254384, 0.1987514261112855729, 0.2025014530190456519, 0.2062514799268057863, 0.2100015068345658653, 0.2137515337423259998, 0.2175015606500860788, 0.2212515875578462132, 0.2250016144656062922, 0.2287516413733663989, 0.2325016682811265056, 0.2362516951888866124, 0.2400017220966467191, 0.2437517490044068258, 0.2475017759121669325, 0.2512518028199270392, 0.2550018297276871460, 0.2587518566354472527, 0.2625018835432073039, 0.2662519104509674661, 0.2700019373587275728, 0.2737519642664876796, 0.2775019911742477308, 0.2812520180820078930, 0.2850020449897679997, 0.2887520718975280509, 0.2925020988052881576, 0.2962521257130483199, 0.3000021526208084266, 0.3037521795285684778, 0.3075022064363285845, 0.3112522333440887468, 0.3150022602518488535, 0.3187522871596089047, 0.3225023140673690114, 0.3262523409751291181, 0.3300023678828892804, 0.3337523947906493316, 0.3375024216984094383, 0.3412524486061695450, 0.3450024755139296517, 0.3487525024216897584, 0.3525025293294498652, 0.3562525562372099719, 0.3600025831449700786, 0.3637526100527301853, 0.3675026369604902921, 0.3712526638682503988, 0.3750026907760105055, 0.3787527176837706122, 0.3825027445915307189, 0.3862527714992908257, 0.3900027984070508769, 0.3937528253148110391, 0.3975028522225711458, 0.4012528791303311970, 0.4050029060380913037, 0.4087529329458514660, 0.4125029598536115727, 0.4162529867613716239, 0.4200030136691317306, 0.4237530405768918929, 0.4275030674846519996, 0.4312530943924120508, 0.4350031213001721575, 0.4387531482079323197, 0.4425031751156924265, 0.4462532020234524777, 0.4500032289312125844, 0.4537532558389726911, 0.4575032827467327978, 0.4612533096544929045, 0.4650033365622530113, 0.4687533634700131180, 0.4725033903777732247, 0.4762534172855333314, 0.4800034441932934381, 0.4837534711010535449, 0.4875034980088136516, 0.4912535249165737583, 0.4950035518243338650, 0.4987535787320939717, 0.5025036056398540785, 0.5062536325476142407, 0.5100036594553742919, 0.5137536863631343431, 0.5175037132708945053, 0.5212537401786545566, 0.5250037670864146078, 0.5287537939941748810, 0.5325038209019349322, 0.5362538478096949834, 0.5400038747174551457, 0.5437539016252151969, 0.5475039285329753591, 0.5512539554407354103, 0.5550039823484954615, 0.5587540092562557348, 0.5625040361640157860, 0.5662540630717758372, 0.5700040899795359994, 0.5737541168872960506, 0.5775041437950561019, 0.5812541707028162641, 0.5850041976105763153, 0.5887542245183364775, 0.5925042514260966398, 0.5962542783338566910, 0.6000043052416168532, 0.6037543321493769044, 0.6075043590571369556, 0.6112543859648971178, 0.6150044128726571691, 0.6187544397804173313, 0.6225044666881774935, 0.6262544935959375447, 0.6300045205036977070, 0.6337545474114577582, 0.6375045743192178094, 0.6412546012269779716, 0.6450046281347380228, 0.6487546550424980740, 0.6525046819502582363, 0.6562547088580183985, 0.6600047357657785607, 0.6637547626735386119, 0.6675047895812986631, 0.6712548164890588254, 0.6750048433968188766, 0.6787548703045789278, 0.6825048972123390900, 0.6862549241200992522, 0.6900049510278593035, 0.6937549779356194657, 0.6975050048433795169, 0.7012550317511396791, 0.7050050586588997303, 0.7087550855666597815, 0.7125051124744199438, 0.7162551393821799950, 0.7200051662899401572, 0.7237551931977003195, 0.7275052201054603707, 0.7312552470132205329, 0.7350052739209805841, 0.7387553008287406353, 0.7425053277365007975, 0.7462553546442608488, 0.7500053815520210110, 0.7537554084597811732, 0.7575054353675412244, 0.7612554622753012756, 0.7650054891830614379, 0.7687555160908214891, 0.7725055429985816513, 0.7762555699063417025, 0.7800055968141017537, 0.7837556237218620270, 0.7875056506296220782, 0.7912556775373821294, 0.7950057044451422916, 0.7987557313529023428, 0.8025057582606623940, 0.8062557851684225563, 0.8100058120761826075, 0.8137558389839428807, 0.8175058658917029319, 0.8212558927994629832, 0.8250059197072231454, 0.8287559466149831966, 0.8325059735227432478, 0.8362560004305034100, 0.8400060273382634612, 0.8437560542460236235, 0.8475060811537837857, 0.8512561080615438369, 0.8550061349693039991, 0.8587561618770640504, 0.8625061887848241016, 0.8662562156925842638, 0.8700062426003443150, 0.8737562695081043662, 0.8775062964158646395, 0.8812563233236246907, 0.8850063502313848529, 0.8887563771391449041, 0.8925064040469049553, 0.8962564309546651176, 0.9000064578624251688, 0.9037564847701852200, 0.9075065116779453822, 0.9112565385857055444, 0.9150065654934655957, 0.9187565924012257579, 0.9225066193089858091, 0.9262566462167459713, 0.9300066731245060225, 0.9337567000322660737, 0.9375067269400262360, 0.9412567538477863982, 0.9450067807555464494, 0.9487568076633066116, 0.9525068345710666629, 0.9562568614788268251, 0.9600068883865868763, 0.9637569152943469275, 0.9675069422021070897, 0.9712569691098671409, 0.9750069960176273032, 0.9787570229253874654, 0.9825070498331475166, 0.9862570767409075678, 0.9900071036486677301, 0.9937571305564277813, 0.9975071574641879435, 1.000000000000000000 ),
 .UNSPECIFIED. ) 
 CURVE ( )  GEOMETRIC_REPRESENTATION_ITEM ( )  RATIONAL_B_SPLINE_CURVE ( ( 1.000000000000000000, 0.9238795325112867385, 1.000000000000000000, 0.9238795325112867385, 1.000000000000000000, 0.9238795325112867385, 1.000000000000000000, 0.9238795325112867385, 1.000000000000000000, 0.9238795325112867385, 1.000000000000000000, 0.9238795325112867385, 1.000000000000000000, 0.9238795325112867385, 1.000000000000000000, 0.9238795325112867385, 1.000000000000000000, 0.9238795325112867385, 1.000000000000000000, 0.9238795325112867385, 1.000000000000000000, 0.9238795325112867385, 1.000000000000000000, 0.9238795325112867385, 1.000000000000000000, 0.9238795325112867385, 1.000000000000000000, 0.9238795325112867385, 1.000000000000000000, 0.9238795325112867385, 1.000000000000000000, 0.9238795325112867385, 1.000000000000000000, 0.9238795325112867385, 1.000000000000000000, 0.9238795325112867385, 1.000000000000000000, 0.9238795325112867385, 1.000000000000000000, 0.9238795325112867385, 1.000000000000000000, 0.9238795325112867385, 1.000000000000000000, 0.9238795325112867385, 1.000000000000000000, 0.9238795325112867385, 1.000000000000000000, 0.9238795325112867385, 1.000000000000000000, 0.9238795325112867385, 1.000000000000000000, 0.9238795325112867385, 1.000000000000000000, 0.9238795325112867385, 1.000000000000000000, 0.9238795325112867385, 1.000000000000000000, 0.9238795325112867385, 1.000000000000000000, 0.9238795325112867385, 1.000000000000000000, 0.9238795325112867385, 1.000000000000000000, 0.9238795325112867385, 1.000000000000000000, 0.9238795325112867385, 1.000000000000000000, 0.9238795325112867385, 1.000000000000000000, 0.9238795325112867385, 1.000000000000000000, 0.9238795325112867385, 1.000000000000000000, 0.9238795325112867385, 1.000000000000000000, 0.9238795325112867385, 1.000000000000000000, 0.9238795325112867385, 1.000000000000000000, 0.9238795325112867385, 1.000000000000000000, 0.9238795325112867385, 1.000000000000000000, 0.9238795325112867385, 1.000000000000000000, 0.9238795325112867385, 1.000000000000000000, 0.9238795325112867385, 1.000000000000000000, 0.9238795325112867385, 1.000000000000000000, 0.9238795325112867385, 1.000000000000000000, 0.9238795325112867385, 1.000000000000000000, 0.9238795325112867385, 1.000000000000000000, 0.9238795325112867385, 1.000000000000000000, 0.9238795325112867385, 1.000000000000000000, 0.9238795325112867385, 1.000000000000000000, 0.9238795325112867385, 1.000000000000000000, 0.9238795325112867385, 1.000000000000000000, 0.9238795325112867385, 1.000000000000000000, 0.9238795325112867385, 1.000000000000000000, 0.9238795325112867385, 1.000000000000000000, 0.9238795325112867385, 1.000000000000000000, 0.9238795325112867385, 1.000000000000000000, 0.9238795325112867385, 1.000000000000000000, 0.9238795325112867385, 1.000000000000000000, 0.9238795325112867385, 1.000000000000000000, 0.9238795325112867385, 1.000000000000000000, 0.9238795325112867385, 1.000000000000000000, 0.9238795325112867385, 1.000000000000000000, 0.9238795325112867385, 1.000000000000000000, 0.9238795325112867385, 1.000000000000000000, 0.9238795325112867385, 1.000000000000000000, 0.9238795325112867385, 1.000000000000000000, 0.9238795325112867385, 1.000000000000000000, 0.9238795325112867385, 1.000000000000000000, 0.9238795325112867385, 1.000000000000000000, 0.9238795325112867385, 1.000000000000000000, 0.9238795325112867385, 1.000000000000000000, 0.9238795325112867385, 1.000000000000000000, 0.9238795325112867385, 1.000000000000000000, 0.9238795325112867385, 1.000000000000000000, 0.9238795325112867385, 1.000000000000000000, 0.9238795325112867385, 1.000000000000000000, 0.9238795325112867385, 1.000000000000000000, 0.9238795325112867385, 1.000000000000000000, 0.9238795325112867385, 1.000000000000000000, 0.9238795325112867385, 1.000000000000000000, 0.9238795325112867385, 1.000000000000000000, 0.9238795325112867385, 1.000000000000000000, 0.9238795325112867385, 1.000000000000000000, 0.9238795325112867385, 1.000000000000000000, 0.9238795325112867385, 1.000000000000000000, 0.9238795325112867385, 1.000000000000000000, 0.9238795325112867385, 1.000000000000000000, 0.9238795325112867385, 1.000000000000000000, 0.9238795325112867385, 1.000000000000000000, 0.9238795325112867385, 1.000000000000000000, 0.9238795325112867385, 1.000000000000000000, 0.9238795325112867385, 1.000000000000000000, 0.9238795325112867385, 1.000000000000000000, 0.9238795325112867385, 1.000000000000000000, 0.9238795325112867385, 1.000000000000000000, 0.9238795325112867385, 1.000000000000000000, 0.9238795325112867385, 1.000000000000000000, 0.9238795325112867385, 1.000000000000000000, 0.9238795325112867385, 1.000000000000000000, 0.9238795325112867385, 1.000000000000000000, 0.9238795325112867385, 1.000000000000000000, 0.9238795325112867385, 1.000000000000000000, 0.9238795325112867385, 1.000000000000000000, 0.9238795325112867385, 1.000000000000000000, 0.9238795325112867385, 1.000000000000000000, 0.9238795325112867385, 1.000000000000000000, 0.9238795325112867385, 1.000000000000000000, 0.9238795325112867385, 1.000000000000000000, 0.9238795325112867385, 1.000000000000000000, 0.9238795325112867385, 1.000000000000000000, 0.9238795325112867385, 1.000000000000000000, 0.9238795325112867385, 1.000000000000000000, 0.9238795325112867385, 1.000000000000000000, 0.9238795325112867385, 1.000000000000000000, 0.9238795325112867385, 1.000000000000000000, 0.9238795325112867385, 1.000000000000000000, 0.9238795325112867385, 1.000000000000000000, 0.9238795325112867385, 1.000000000000000000, 0.9238795325112867385, 1.000000000000000000, 0.9238795325112867385, 1.000000000000000000, 0.9238795325112867385, 1.000000000000000000, 0.9238795325112867385, 1.000000000000000000, 0.9238795325112867385, 1.000000000000000000, 0.9238795325112867385, 1.000000000000000000, 0.9238795325112867385, 1.000000000000000000, 0.9238795325112867385, 1.000000000000000000, 0.9238795325112867385, 1.000000000000000000, 0.9238795325112867385, 1.000000000000000000, 0.9238795325112867385, 1.000000000000000000, 0.9238795325112867385, 1.000000000000000000, 0.9238795325112867385, 1.000000000000000000, 0.9238795325112867385, 1.000000000000000000, 0.9238795325112867385, 1.000000000000000000, 0.9238795325112867385, 1.000000000000000000, 0.9238795325112867385, 1.000000000000000000, 0.9238795325112867385, 1.000000000000000000, 0.9238795325112867385, 1.000000000000000000, 0.9238795325112867385, 1.000000000000000000, 0.9238795325112867385, 1.000000000000000000, 0.9238795325112867385, 1.000000000000000000, 0.9238795325112867385, 1.000000000000000000, 0.9238795325112867385, 1.000000000000000000, 0.9238795325112867385, 1.000000000000000000, 0.9238795325112867385, 1.000000000000000000, 0.9238795325112867385, 1.000000000000000000, 0.9238795325112867385, 1.000000000000000000, 0.9238795325112867385, 1.000000000000000000, 0.9238795325112867385, 1.000000000000000000, 0.9238795325112867385, 1.000000000000000000, 0.9238795325112867385, 1.000000000000000000, 0.9238795325112867385, 1.000000000000000000, 0.9238795325112867385, 1.000000000000000000, 0.9238795325112867385, 1.000000000000000000, 0.9238795325112867385, 1.000000000000000000, 0.9238795325112867385, 1.000000000000000000, 0.9238795325112867385, 1.000000000000000000, 0.9238795325112867385, 1.000000000000000000, 0.9238795325112867385, 1.000000000000000000, 0.9238795325112867385, 1.000000000000000000, 0.9238795325112867385, 1.000000000000000000, 0.9238795325112867385, 1.000000000000000000, 0.9238795325112867385, 1.000000000000000000, 0.9238795325112867385, 1.000000000000000000, 0.9238795325112867385, 1.000000000000000000, 0.9238795325112867385, 1.000000000000000000, 0.9238795325112867385, 1.000000000000000000, 0.9238795325112867385, 1.000000000000000000, 0.9238795325112867385, 1.000000000000000000, 0.9238795325112867385, 1.000000000000000000, 0.9238795325112867385, 1.000000000000000000, 0.9238795325112867385, 1.000000000000000000, 0.9238795325112867385, 1.000000000000000000, 0.9238795325112867385, 1.000000000000000000, 0.9238795325112867385, 1.000000000000000000, 0.9238795325112867385, 1.000000000000000000, 0.9238795325112867385, 1.000000000000000000, 0.9238795325112867385, 1.000000000000000000, 0.9238795325112867385, 1.000000000000000000, 0.9238795325112867385, 1.000000000000000000, 0.9238795325112867385, 1.000000000000000000, 0.9238795325112867385, 1.000000000000000000, 0.9238795325112867385, 1.000000000000000000, 0.9238795325112867385, 1.000000000000000000, 0.9238795325112867385, 1.000000000000000000, 0.9238795325112867385, 1.000000000000000000, 0.9238795325112867385, 1.000000000000000000, 0.9238795325112867385, 1.000000000000000000, 0.9238795325112867385, 1.000000000000000000, 0.9238795325112867385, 1.000000000000000000, 0.9238795325112867385, 1.000000000000000000, 0.9238795325112867385, 1.000000000000000000, 0.9238795325112867385, 1.000000000000000000, 0.9238795325112867385, 1.000000000000000000, 0.9238795325112867385, 1.000000000000000000, 0.9238795325112867385, 1.000000000000000000, 0.9238795325112867385, 1.000000000000000000, 0.9238795325112867385, 1.000000000000000000, 0.9238795325112867385, 1.000000000000000000, 0.9238795325112867385, 1.000000000000000000, 0.9238795325112867385, 1.000000000000000000, 0.9238795325112867385, 1.000000000000000000, 0.9238795325112867385, 1.000000000000000000, 0.9238795325112867385, 1.000000000000000000, 0.9238795325112867385, 1.000000000000000000, 0.9238795325112867385, 1.000000000000000000, 0.9238795325112867385, 1.000000000000000000, 0.9238795325112867385, 1.000000000000000000, 0.9238795325112867385, 1.000000000000000000, 0.9238795325112867385, 1.000000000000000000, 0.9238795325112867385, 1.000000000000000000, 0.9238795325112867385, 1.000000000000000000, 0.9238795325112867385, 1.000000000000000000, 0.9238795325112867385, 1.000000000000000000, 0.9238795325112867385, 1.000000000000000000, 0.9238795325112867385, 1.000000000000000000, 0.9238795325112867385, 1.000000000000000000, 0.9238795325112867385, 1.000000000000000000, 0.9238795325112867385, 1.000000000000000000, 0.9238795325112867385, 1.000000000000000000, 0.9238795325112867385, 1.000000000000000000, 0.9238795325112867385, 1.000000000000000000, 0.9238795325112867385, 1.000000000000000000, 0.9238795325112867385, 1.000000000000000000, 0.9238795325112867385, 1.000000000000000000, 0.9238795325112867385, 1.000000000000000000, 0.9238795325112867385, 1.000000000000000000, 0.9238795325112867385, 1.000000000000000000, 0.9238795325112867385, 1.000000000000000000, 0.9238795325112867385, 1.000000000000000000, 0.9238795325112867385, 1.000000000000000000, 0.9238795325112867385, 1.000000000000000000, 0.9238795325112867385, 1.000000000000000000, 0.9238795325112867385, 1.000000000000000000, 0.9238795325112867385, 1.000000000000000000, 0.9238795325112867385, 1.000000000000000000, 0.9238795325112867385, 1.000000000000000000, 0.9238795325112867385, 1.000000000000000000, 0.9238795325112867385, 1.000000000000000000, 0.9238795325112867385, 1.000000000000000000, 0.9238795325112867385, 1.000000000000000000, 0.9238795325112867385, 1.000000000000000000, 0.9238795325112867385, 1.000000000000000000, 0.9238795325112867385, 1.000000000000000000, 0.9238795325112867385, 1.000000000000000000, 0.9238795325112867385, 1.000000000000000000, 0.9238795325112867385, 1.000000000000000000, 0.9238795325112867385, 1.000000000000000000, 0.9238795325112867385, 1.000000000000000000, 0.9238795325112867385, 1.000000000000000000, 0.9238795325112867385, 1.000000000000000000, 0.9238795325112867385, 1.000000000000000000, 0.9238795325112867385, 1.000000000000000000, 0.9238795325112867385, 1.000000000000000000, 0.9238795325112867385, 1.000000000000000000, 0.9238795325112867385, 1.000000000000000000, 0.9238795325112867385, 1.000000000000000000, 0.9238795325112867385, 1.000000000000000000, 0.9238795325112867385, 1.000000000000000000, 0.9238795325112867385, 1.000000000000000000, 0.9238795325112867385, 1.000000000000000000, 0.9238795325112867385, 1.000000000000000000, 0.9238795325112867385, 1.000000000000000000, 0.9238795325112867385, 1.000000000000000000, 0.9238795325112867385, 1.000000000000000000, 0.9493986726310960078, 0.9660721378631347278 ) ) 
 REPRESENTATION_ITEM ( '' )  );
#69993 = ORIENTED_EDGE ( 'NONE', *, *, #74202, .F. ) ;
#69994 = CARTESIAN_POINT ( 'NONE',  ( 5.676582343749997150, 242.2395833367473301, -9.832129032723418760 ) ) ;
#69995 = CARTESIAN_POINT ( 'NONE',  ( -7.188101187499991163, 2.977408999572646930, 18.26780278187175455 ) ) ;
#69996 = CARTESIAN_POINT ( 'NONE',  ( 2.436599634630141065, 51.42120007173088680, 48.62500384162316180 ) ) ;
#69997 = CARTESIAN_POINT ( 'NONE',  ( -1.836970198721029983E-15, 75.62499999317203958, 10.00000000000000178 ) ) ;
#69998 = CARTESIAN_POINT ( 'NONE',  ( 4.000000000000015987, 198.6875000027312126, 196.3431457505076594 ) ) ;
#69999 = CARTESIAN_POINT ( 'NONE',  ( -7.320508075688778149, 139.9999999931720254, 7.320508075688769267 ) ) ;
#70000 = CARTESIAN_POINT ( 'NONE',  ( -7.320508075688778149, 178.1250000000000284, 7.320508075688769267 ) ) ;
#70001 = CARTESIAN_POINT ( 'NONE',  ( -1.469576158976823947E-15, 17.43749999590322375, 8.000000000000000000 ) ) ;
#70002 = CARTESIAN_POINT ( 'NONE',  ( 11.00000000000000000, 1.347111479062088405E-15, 90.25000000000000000 ) ) ;
#70003 = CARTESIAN_POINT ( 'NONE',  ( 5.082755093536320601, -5.082755093536318824, 26.42405278187175810 ) ) ;
#70004 = CARTESIAN_POINT ( 'NONE',  ( 5.676582343750001591, 136.9270833299193555, -9.832129032723420536 ) ) ;
#70005 = CARTESIAN_POINT ( 'NONE',  ( -7.778174593052023411, 7.778174593052023411, 76.00000000409676204 ) ) ;
#70006 = CARTESIAN_POINT ( 'NONE',  ( -4.898587196589412829E-16, 97.81250000409677625, -8.000000000000000000 ) ) ;
#70009 = CARTESIAN_POINT ( 'NONE',  ( 2.828427124746152987, 197.1250000000000284, 139.1715728752538723 ) ) ;
#70008 = CARTESIAN_POINT ( 'NONE',  ( -3.313708498984757611, 7.999999999999991118, 26.04905277982337353 ) ) ;
#70007 = CARTESIAN_POINT ( 'NONE',  ( 32.00000000000000711, 205.3125000000000568, 168.3431457505075741 ) ) ;
#70010 = ORIENTED_EDGE ( 'NONE', *, *, #66617, .T. ) ;
#70011 = CARTESIAN_POINT ( 'NONE',  ( -6.023803224821316249, 6.914460432017338398, -0.07661102881317759239 ) ) ;
#70012 = CIRCLE ( 'NONE', #38679, 11.49999999999999112 ) ;
#70013 = CARTESIAN_POINT ( 'NONE',  ( -9.000000000000000000, -3.485479754112952744, -0.3552645118408633285 ) ) ;
#70014 = CARTESIAN_POINT ( 'NONE',  ( -2.479188868019259750, -7.619273332548305078, 0.000000000000000000 ) ) ;
#70015 =( BOUNDED_CURVE ( )  B_SPLINE_CURVE ( 2, ( #27423, #74572, #10456, #33487, #23259, #73824, #40241, #39503, #16841 ),
 .UNSPECIFIED., .F., .F. ) 
 B_SPLINE_CURVE_WITH_KNOTS ( ( 3, 2, 2, 2, 3 ),
 ( 0.5000000000000004441, 0.5083333333333337478, 0.5166666666666671626, 0.5250000000000004663, 0.5333333333333337700 ),
 .UNSPECIFIED. ) 
 CURVE ( )  GEOMETRIC_REPRESENTATION_ITEM ( )  RATIONAL_B_SPLINE_CURVE ( ( 0.9999999999999958922, 0.9238795325112908463, 1.000000000000000000, 0.9238795325112867385, 1.000000000000000000, 0.9238795325112867385, 1.000000000000000000, 0.9238795325112826307, 1.000000000000003997 ) ) 
 REPRESENTATION_ITEM ( '' )  );
#70016 = CARTESIAN_POINT ( 'NONE',  ( -1.656854249492383468, 11.68750000000000000, 4.000000000000000888 ) ) ;
#70017 = CARTESIAN_POINT ( 'NONE',  ( -10.00000000000000178, 34.37499999317203248, -1.224646799147353454E-15 ) ) ;
#70018 = VECTOR ( 'NONE', #12125, 1000.000000000000000 ) ;
#70019 = CARTESIAN_POINT ( 'NONE',  ( 7.188101187500002709, 112.8125000020483952, 2.977408999572649151 ) ) ;
#70020 = CARTESIAN_POINT ( 'NONE',  ( -4.541265875000003227, 20.87499999863441147, 1.881053915767121110 ) ) ;
#70021 = CARTESIAN_POINT ( 'NONE',  ( -3.228176881619886807, -50.21013539027978112, 40.85102191503833069 ) ) ;
#70022 = CARTESIAN_POINT ( 'NONE',  ( 1.469576158976822172E-15, -7.999999999999991118, 13.20530277982336465 ) ) ;
#70023 = CARTESIAN_POINT ( 'NONE',  ( -4.999999999999992895, 238.9583333401613174, 8.660254037844390851 ) ) ;
#70024 = EDGE_LOOP ( 'NONE', ( #41175, #27555, #49394, #25603 ) ) ;
#70025 = CARTESIAN_POINT ( 'NONE',  ( -8.679233769290393141, 225.9999999999999716, 5.010062319349841253 ) ) ;
#70026 = AXIS2_PLACEMENT_3D ( 'NONE', #63216, #74167, #5893 ) ;
#70027 = CARTESIAN_POINT ( 'NONE',  ( 5.656854249492379694, 109.4375000000000000, -5.656854249492380582 ) ) ;
#70028 = CARTESIAN_POINT ( 'NONE',  ( 3.042071309553173286, 250.6770833367473301, 11.35316468749999608 ) ) ;
#70029 = CARTESIAN_POINT ( 'NONE',  ( -3.042071309553164404, 122.2395833299193271, -11.35316468749999963 ) ) ;
#70030 = ORIENTED_EDGE ( 'NONE', *, *, #51793, .F. ) ;
#70031 = CARTESIAN_POINT ( 'NONE',  ( -7.268158626439248593, 8.014265980700427505, 117.6910954969439587 ) ) ;
#70032 = CARTESIAN_POINT ( 'NONE',  ( -10.18810118749999916, 4.220049686691934809, 103.5625000020483668 ) ) ;
#70033 = CARTESIAN_POINT ( 'NONE',  ( 46.67364751762348618, 146.0000000000000000, 69.99999999999995737 ) ) ;
#70034 = CARTESIAN_POINT ( 'NONE',  ( 1.432654583217662481, 200.3750000013656063, 194.5412658750000219 ) ) ;
#70035 = CARTESIAN_POINT ( 'NONE',  ( -18.00000000000000000, 10.39230484541324628, -1.607695154586745501 ) ) ;
#70037 = CARTESIAN_POINT ( 'NONE',  ( -2.085542519210945728E-15, 109.5312499965860269, 11.35316468750000141 ) ) ;
#70036 = CARTESIAN_POINT ( 'NONE',  ( 2.592975333673598559, 225.9999999999999716, -9.672265883052229896 ) ) ;
#70038 = CARTESIAN_POINT ( 'NONE',  ( 5.656854249492374365, 5.656854249492375253, 6.455302783920143561 ) ) ;
#70039 = CARTESIAN_POINT ( 'NONE',  ( -24.54126587499999701, 197.5000000013656063, 168.5673454167827003 ) ) ;
#70040 = CARTESIAN_POINT ( 'NONE',  ( 3.594042629939374400, 89.53052393364181683, -6.225082831242716885 ) ) ;
#70041 = EDGE_LOOP ( 'NONE', ( #29425, #22914, #34900, #65602, #27696 ) ) ;
#70042 = ADVANCED_FACE ( 'NONE', ( #36500 ), #47064, .F. ) ;
#70043 = CARTESIAN_POINT ( 'NONE',  ( 7.320508075688774596, 197.4999999931719969, -7.320508075688774596 ) ) ;
#70044 = CARTESIAN_POINT ( 'NONE',  ( 2.828427124746152987, 206.1250000000000284, 139.1715728752538723 ) ) ;
#70045 = CARTESIAN_POINT ( 'NONE',  ( 2.828427124746191623, 9.874999997268814056, -2.828427124746191623 ) ) ;
#70046 = CARTESIAN_POINT ( 'NONE',  ( -3.042071309553163960, 87.55208332991935549, -11.35316468749999963 ) ) ;
#70047 = CARTESIAN_POINT ( 'NONE',  ( 5.000000000000000000, -50.64189880742116401, 41.08656465431877791 ) ) ;
#70048 = CARTESIAN_POINT ( 'NONE',  ( 2.977408999572650927, 14.62499999795161187, -7.188101187500000933 ) ) ;
#70049 = CARTESIAN_POINT ( 'NONE',  ( -7.204075437095965206, -7.204075437095968759, 96.71875000204838102 ) ) ;
#70050 = CARTESIAN_POINT ( 'NONE',  ( 5.676582343749993598, 15.26041666325268409, 9.832129032723422313 ) ) ;
#70051 = VERTEX_POINT ( 'NONE', #30468 ) ;
#70052 = CARTESIAN_POINT ( 'NONE',  ( 3.313708498984762496, -7.999999999999989342, 26.79905277982337353 ) ) ;
#70053 = FACE_OUTER_BOUND ( 'NONE', #38151, .T. ) ;
#70054 = CARTESIAN_POINT ( 'NONE',  ( -11.35316468749999785, 223.0729166632527267, -3.042071309553167957 ) ) ;
#70055 = CARTESIAN_POINT ( 'NONE',  ( -7.204075437095965206, -7.204075437095968759, 77.21875000204836681 ) ) ;
#70056 = B_SPLINE_CURVE_WITH_KNOTS ( 'NONE', 3,
 ( #25199, #66691, #65940, #13866, #20662, #38032, #48212, #49334, #31243, #44060, #20279, #54269 ),
 .UNSPECIFIED., .F., .F.,
 ( 4, 2, 2, 2, 2, 4 ),
 ( 0.000000000000000000, 0.002547658444427994360, 0.005095316888855988720, 0.006369146111069985683, 0.007642975333283983513, 0.01019063377771197744 ),
 .UNSPECIFIED. ) ;
#70057 = AXIS2_PLACEMENT_3D ( 'NONE', #36034, #53013, #19039 ) ;
#70058 = FACE_OUTER_BOUND ( 'NONE', #62001, .T. ) ;
#70059 = CARTESIAN_POINT ( 'NONE',  ( -2.679491924311226292, 148.3333333265053682, -10.00000000000000178 ) ) ;
#70060 = CARTESIAN_POINT ( 'NONE',  ( -6.676582343750001591, 294.4531250017069510, 0.000000000000000000 ) ) ;
#70061 = ORIENTED_EDGE ( 'NONE', *, *, #64411, .F. ) ;
#70062 = CARTESIAN_POINT ( 'NONE',  ( 1.656854249492271780, 201.9375000027311842, 146.0000000000001137 ) ) ;
#70063 = CARTESIAN_POINT ( 'NONE',  ( 3.042071309553167513, 207.1354166632526699, -11.35316468749999785 ) ) ;
#70064 = EDGE_CURVE ( 'NONE', #23983, #29151, #2024, .T. ) ;
#70065 = CARTESIAN_POINT ( 'NONE',  ( 10.18810118749999916, 4.220049686691935698, 91.00000000204836681 ) ) ;
#70066 = CARTESIAN_POINT ( 'NONE',  ( -26.56734541678238060, 201.3750000013656347, 166.5412658750003629 ) ) ;
#70067 = EDGE_CURVE ( 'NONE', #1872, #34167, #18037, .T. ) ;
#70068 = CARTESIAN_POINT ( 'NONE',  ( -8.000000000000001776, 26.34375000000000711, 3.313708498984759387 ) ) ;
#70069 = ORIENTED_EDGE ( 'NONE', *, *, #74316, .F. ) ;
#70070 = CARTESIAN_POINT ( 'NONE',  ( -21.66278640630607200, -49.68939756288837373, 147.8216243255391475 ) ) ;
#70071 = VECTOR ( 'NONE', #41350, 1000.000000000000000 ) ;
#70072 = CARTESIAN_POINT ( 'NONE',  ( -5.082755093536324154, 122.8437500020483952, 5.082755093536326818 ) ) ;
#70073 = CARTESIAN_POINT ( 'NONE',  ( -2.828427124746153876, 208.0000000027312126, 195.1715728752538439 ) ) ;
#70074 = CARTESIAN_POINT ( 'NONE',  ( -10.00000000000000000, 22.29166666666666430, -2.679491924311229845 ) ) ;
#70075 = AXIS2_PLACEMENT_3D ( 'NONE', #5384, #33698, #45732 ) ;
#70076 = CARTESIAN_POINT ( 'NONE',  ( 7.204075437095966983, 7.204075437095967871, 73.46875000204838102 ) ) ;
#70077 = EDGE_LOOP ( 'NONE', ( #61318, #6241, #2233 ) ) ;
#70078 = CARTESIAN_POINT ( 'NONE',  ( 5.082755093536324154, 1.781249997951610098, 5.082755093536326818 ) ) ;
#70079 = AXIS2_PLACEMENT_3D ( 'NONE', #67039, #32727, #44031 ) ;
#70080 = LINE ( 'NONE', #6338, #45097 ) ;
#70081 = LINE ( 'NONE', #52723, #13799 ) ;
#70082 = CARTESIAN_POINT ( 'NONE',  ( 2.977408999572654480, 117.5000000020483810, 7.188101187499999156 ) ) ;
#70083 = CARTESIAN_POINT ( 'NONE',  ( -4.261174619373528039, 22.00000000000000000, -1.025908319483143094 ) ) ;
#70084 = CARTESIAN_POINT ( 'NONE',  ( -2.765530957081996810, 296.2656250017069510, -6.676582343750002480 ) ) ;
#70086 = CARTESIAN_POINT ( 'NONE',  ( 2.775557561562891351E-14, 271.9999999999999432, 139.0000000000000568 ) ) ;
#70085 = CARTESIAN_POINT ( 'NONE',  ( -8.311093377946834337, 234.5312500034139589, 8.311093377946837890 ) ) ;
#70087 = ITEM_DEFINED_TRANSFORMATION ( 'NONE', 'NONE', #26067,  #57354 ) ;
#70088 = VERTEX_POINT ( 'NONE', #8848 ) ;
#70089 = CARTESIAN_POINT ( 'NONE',  ( 3.042071309553163960, 242.7604166700806729, -11.35316468749999785 ) ) ;
#70090 = CARTESIAN_POINT ( 'NONE',  ( -5.082755093536319713, 5.082755093536319713, 5.799052781871753659 ) ) ;
#70091 = CARTESIAN_POINT ( 'NONE',  ( -3.458734124999960358, 202.6875000013656063, 198.0000000000000284 ) ) ;
#70092 = ORIENTED_EDGE ( 'NONE', *, *, #25497, .F. ) ;
#70093 = CARTESIAN_POINT ( 'NONE',  ( 8.000000000000000000, 105.0312500040967905, -3.313708498984762496 ) ) ;
#70094 = CARTESIAN_POINT ( 'NONE',  ( 3.042071309553159519, 100.0520833299193555, 11.35316468750000141 ) ) ;
#70095 = FACE_OUTER_BOUND ( 'NONE', #50827, .T. ) ;
#70096 = CARTESIAN_POINT ( 'NONE',  ( 11.00000000000000000, 4.556349186104045934, 85.84374999999998579 ) ) ;
#70099 = CARTESIAN_POINT ( 'NONE',  ( 7.320508075688773708, 69.37499999999998579, 7.320508075688777261 ) ) ;
#70098 = CARTESIAN_POINT ( 'NONE',  ( 28.00000000000001776, 205.4375000013656063, 173.4587341249998929 ) ) ;
#70097 = CARTESIAN_POINT ( 'NONE',  ( 24.54126587500000056, 202.3750000013655779, 168.5673454167822172 ) ) ;
#70100 = ADVANCED_FACE ( 'NONE', ( #58782 ), #54881, .F. ) ;
#70101 = ORIENTED_EDGE ( 'NONE', *, *, #5493, .T. ) ;
#70102 = CIRCLE ( 'NONE', #55610, 20.00000000000001066 ) ;
#70103 = CARTESIAN_POINT ( 'NONE',  ( 27.99999999999996803, 205.0000000000000284, 173.9999999999999147 ) ) ;
#70104 = DIRECTION ( 'NONE',  ( -0.000000000000000000, 1.000000000000000000, -4.476705744456276341E-16 ) ) ;
#70105 = CARTESIAN_POINT ( 'NONE',  ( -3.042071309553164404, 212.2395833299193839, -11.35316468749999963 ) ) ;
#70106 = CARTESIAN_POINT ( 'NONE',  ( -3.458734125000016313, 204.8750000013656063, 140.5673454167824161 ) ) ;
#70107 = CARTESIAN_POINT ( 'NONE',  ( 25.55430564589119413, 205.3125000013656063, 167.5543056458910485 ) ) ;
#70108 = CARTESIAN_POINT ( 'NONE',  ( -5.082755093536326818, 25.78124999795161543, 5.082755093536325042 ) ) ;
#70109 = CARTESIAN_POINT ( 'NONE',  ( 8.311093377946834337, 175.4687499965860127, 8.311093377946839666 ) ) ;
#70110 = CARTESIAN_POINT ( 'NONE',  ( 2.977408999572654480, 98.00000000204838102, 7.188101187499999156 ) ) ;
#70111 = DIRECTION ( 'NONE',  ( -0.000000000000000000, 1.000000000000000000, -0.000000000000000000 ) ) ;
#70112 = CARTESIAN_POINT ( 'NONE',  ( -32.00000000000000711, 197.1875000000000284, 168.3431457505080004 ) ) ;
#70113 = CARTESIAN_POINT ( 'NONE',  ( 3.211159895383560947, 11.18749999863440792, 3.211159895383562723 ) ) ;
#70114 = CARTESIAN_POINT ( 'NONE',  ( 24.54126587500000412, 204.3750000013656063, 168.5673454167822172 ) ) ;
#70115 = CARTESIAN_POINT ( 'NONE',  ( -2.977408999572647819, 7.188101187499991163, 3.080302781871750994 ) ) ;
#70116 = CARTESIAN_POINT ( 'NONE',  ( -9.832129032723418760, 72.86458332991935549, -5.676582343750004256 ) ) ;
#70117 =( BOUNDED_CURVE ( )  B_SPLINE_CURVE ( 2, ( #24983, #46899, #47264, #13290, #12925, #24619, #41616, #18969, #70650, #41972, #24252, #18233, #12193 ),
 .UNSPECIFIED., .F., .F. ) 
 B_SPLINE_CURVE_WITH_KNOTS ( ( 3, 2, 2, 2, 2, 2, 3 ),
 ( 0.1098959258685624774, 0.1151295451665490382, 0.1203631644645356269, 0.1255967837625222294, 0.1308304030605088042, 0.1360640223584954067, 0.1412976416564819815 ),
 .UNSPECIFIED. ) 
 CURVE ( )  GEOMETRIC_REPRESENTATION_ITEM ( )  RATIONAL_B_SPLINE_CURVE ( ( 1.000000000000000000, 0.9659258262890682012, 1.000000000000000000, 0.9659258262890684232, 1.000000000000000000, 0.9659258262890684232, 1.000000000000000000, 0.9659258262890684232, 1.000000000000000000, 0.9659258262890684232, 1.000000000000000000, 0.9659258262890677571, 1.000000000000000666 ) ) 
 REPRESENTATION_ITEM ( '' )  );
#70118 = CARTESIAN_POINT ( 'NONE',  ( 74.99999999999998579, 242.0000000000000284, 69.99999999999998579 ) ) ;
#70119 = ORIENTED_EDGE ( 'NONE', *, *, #67838, .F. ) ;
#70120 = DIRECTION ( 'NONE',  ( 0.000000000000000000, 0.000000000000000000, 1.000000000000000000 ) ) ;
#70121 = CARTESIAN_POINT ( 'NONE',  ( -11.00000000000001776, -4.556349186104032611, 116.5937499999999858 ) ) ;
#70122 = CARTESIAN_POINT ( 'NONE',  ( 8.311093377946837890, 76.40624999658602690, -8.311093377946837890 ) ) ;
#70123 = CARTESIAN_POINT ( 'NONE',  ( -7.778174593052023411, 7.778174593052023411, 68.50000000409677625 ) ) ;
#70124 = CARTESIAN_POINT ( 'NONE',  ( -2.445694354108839175, 197.3125000013656063, 144.4456943541088663 ) ) ;
#70125 = CARTESIAN_POINT ( 'NONE',  ( -3.228176881614264193, 10.27295505383825791, 63.90876373295824209 ) ) ;
#70127 = CARTESIAN_POINT ( 'NONE',  ( -11.35316468750000141, 63.28124999658601979, -1.390361679473963753E-15 ) ) ;
#70126 = CARTESIAN_POINT ( 'NONE',  ( -8.000000000000000000, 123.5937500040967763, -3.313708498984761164 ) ) ;
#70128 = CARTESIAN_POINT ( 'NONE',  ( -3.313708498984757167, 7.999999999999991118, 23.23655278392014623 ) ) ;
#70129 = CARTESIAN_POINT ( 'NONE',  ( -4.898587196589412829E-16, 111.3125000040967905, -8.000000000000000000 ) ) ;
#70130 = EDGE_CURVE ( 'NONE', #36433, #2613, #41031, .T. ) ;
#70131 = CARTESIAN_POINT ( 'NONE',  ( -1.836970198721029983E-15, 155.6249999931720254, 10.00000000000000178 ) ) ;
#70132 = CARTESIAN_POINT ( 'NONE',  ( 5.082755093536325042, 95.46875000204838102, -5.082755093536325930 ) ) ;
#70133 = CARTESIAN_POINT ( 'NONE',  ( 10.00000000000000888, 20.20833333333333925, -2.679491924311228956 ) ) ;
#70134 = CARTESIAN_POINT ( 'NONE',  ( -5.676582343750006032, 49.42708332991935549, 9.832129032723418760 ) ) ;
#70135 = CARTESIAN_POINT ( 'NONE',  ( 7.204075437095966983, 7.204075437095967871, 115.4687500020483810 ) ) ;
#70136 = CARTESIAN_POINT ( 'NONE',  ( -11.35316468749999785, 198.0729166632526983, -3.042071309553167513 ) ) ;
#70137 = ORIENTED_EDGE ( 'NONE', *, *, #4386, .T. ) ;
#70138 = CARTESIAN_POINT ( 'NONE',  ( 1.656854249492444975, 205.8125000027312126, 194.0000000000000853 ) ) ;
#70139 = CARTESIAN_POINT ( 'NONE',  ( -10.18810118749999916, 4.220049686691934809, 67.56250000204836681 ) ) ;
#70140 = CARTESIAN_POINT ( 'NONE',  ( 0.000000000000000000, 45.00000000000000000, 8.749999999999998224 ) ) ;
#70142 = CARTESIAN_POINT ( 'NONE',  ( -11.35316468750000141, 178.2812499965860411, -1.390361679473963753E-15 ) ) ;
#70141 = CARTESIAN_POINT ( 'NONE',  ( 4.000000000000015987, 195.5000000000000000, 198.0000000000000284 ) ) ;
#70143 = LINE ( 'NONE', #12775, #70697 ) ;
#70144 = EDGE_CURVE ( 'NONE', #70231, #26901, #49196, .T. ) ;
#70145 = CARTESIAN_POINT ( 'NONE',  ( -7.320508075688771932, 257.5000000068279746, -7.320508075688771932 ) ) ;
#70146 = LINE ( 'NONE', #18453, #70960 ) ;
#70147 = EDGE_LOOP ( 'NONE', ( #26482, #1578, #7667, #37282 ) ) ;
#70148 = CARTESIAN_POINT ( 'NONE',  ( -11.35316468750000141, 163.5937499965860127, -1.390361679473963753E-15 ) ) ;
#70149 = CARTESIAN_POINT ( 'NONE',  ( 5.082755093536320601, -5.082755093536318824, 26.04905278187175810 ) ) ;
#70150 = CARTESIAN_POINT ( 'NONE',  ( -8.311093377946836114, 127.9687499965860269, -8.311093377946837890 ) ) ;
#70151 = ORIENTED_EDGE ( 'NONE', *, *, #27729, .T. ) ;
#70152 = AXIS2_PLACEMENT_3D ( 'NONE', #10181, #39224, #29757 ) ;
#70153 = EDGE_CURVE ( 'NONE', #62856, #47573, #59761, .T. ) ;
#70154 = CARTESIAN_POINT ( 'NONE',  ( 3.313708498984760720, 106.7187500040967763, -8.000000000000000000 ) ) ;
#70155 = AXIS2_PLACEMENT_3D ( 'NONE', #11463, #64257, #57504 ) ;
#70156 = CARTESIAN_POINT ( 'NONE',  ( 4.000000000000001776, 11.06250000000000000, -1.656854249492381248 ) ) ;
#70157 = CARTESIAN_POINT ( 'NONE',  ( 7.525268439705678603, 6.047589086024989236, -0.3570196857253479794 ) ) ;
#70158 = CARTESIAN_POINT ( 'NONE',  ( -3.211159895383562723, 11.93749999863440614, 3.211159895383561391 ) ) ;
#70159 = CARTESIAN_POINT ( 'NONE',  ( 7.999999999999991118, 9.797174393178815797E-16, 19.76780278392014623 ) ) ;
#70160 = CARTESIAN_POINT ( 'NONE',  ( 0.000000000000000000, 125.0000000000000000, 8.000000000000000000 ) ) ;
#70161 = VERTEX_POINT ( 'NONE', #22377 ) ;
#70162 = CARTESIAN_POINT ( 'NONE',  ( 4.898587196589412829E-16, 24.37500000000000355, -8.000000000000000000 ) ) ;
#70163 = CARTESIAN_POINT ( 'NONE',  ( -5.082755093536324154, 95.84375000204838102, 5.082755093536326818 ) ) ;
#70165 = CARTESIAN_POINT ( 'NONE',  ( 0.000000000000000000, 0.000000000000000000, 0.000000000000000000 ) ) ;
#70164 = CARTESIAN_POINT ( 'NONE',  ( -2.751064625579944321E-14, 203.8750000027312126, 146.0000000000000284 ) ) ;
#70166 = ORIENTED_EDGE ( 'NONE', *, *, #16817, .T. ) ;
#70167 = CARTESIAN_POINT ( 'NONE',  ( 1.296342370383124054, 10.28012030475506755, -63.61260002839683381 ) ) ;
#70168 = LINE ( 'NONE', #16318, #56643 ) ;
#70169 = AXIS2_PLACEMENT_3D ( 'NONE', #34092, #62726, #22734 ) ;
#70170 = CARTESIAN_POINT ( 'NONE',  ( 5.082755093536318824, 5.082755093536319713, 21.92405278187175455 ) ) ;
#70171 = ORIENTED_EDGE ( 'NONE', *, *, #55092, .F. ) ;
#70172 = EDGE_LOOP ( 'NONE', ( #66119, #62724, #21594, #55614, #20494 ) ) ;
#70173 = CARTESIAN_POINT ( 'NONE',  ( -6.238412754330611322E-16, 10.18810118749999916, 86.78125000204836681 ) ) ;
#70174 = CARTESIAN_POINT ( 'NONE',  ( -24.54126587500000056, 195.5000000013656347, 168.5673454167827003 ) ) ;
#70175 = CARTESIAN_POINT ( 'NONE',  ( -6.735557395310442023E-16, 11.00000000000000000, 101.1249999999999858 ) ) ;
#70178 = CARTESIAN_POINT ( 'NONE',  ( 4.721056650415999201, 296.2343750017069510, -4.721056650415999201 ) ) ;
#70177 = CARTESIAN_POINT ( 'NONE',  ( 31.99999999999997868, 200.4375000027311842, 168.3431457505075173 ) ) ;
#70176 = CARTESIAN_POINT ( 'NONE',  ( 29.65685424949229798, 196.1875000027312126, 174.0000000000000284 ) ) ;
#70179 = CARTESIAN_POINT ( 'NONE',  ( 6.123233995736767268E-16, 131.2500000000000000, -10.00000000000000178 ) ) ;
#70180 = CARTESIAN_POINT ( 'NONE',  ( -2.828427124746192067, 0.6250000000000002220, 2.828427124746190735 ) ) ;
#70181 = CARTESIAN_POINT ( 'NONE',  ( 0.000000000000000000, 9.980871413050930352E-15, 81.50000000000000000 ) ) ;
#70182 = FACE_OUTER_BOUND ( 'NONE', #44929, .T. ) ;
#70184 = CARTESIAN_POINT ( 'NONE',  ( 28.00000000000002132, 200.9375000013656063, 166.5412658749999082 ) ) ;
#70183 = AXIS2_PLACEMENT_3D ( 'NONE', #66496, #56313, #44618 ) ;
#70185 = CARTESIAN_POINT ( 'NONE',  ( -7.188101187500002709, 7.687499997951611874, 2.977408999572649151 ) ) ;
#70186 = CARTESIAN_POINT ( 'NONE',  ( 5.662595241051936235, -5.662595241051934458, 4.575615283940629219 ) ) ;
#70187 = CARTESIAN_POINT ( 'NONE',  ( -3.458734125000015425, 197.0000000013656347, 143.4326545832176976 ) ) ;
#70188 = CARTESIAN_POINT ( 'NONE',  ( -2.977408999572650927, 115.2500000020483952, -7.188101187500000933 ) ) ;
#70190 = CARTESIAN_POINT ( 'NONE',  ( 0.2452292162193181191, 194.6102753126700122, 201.6102753126700691 ) ) ;
#70189 = CYLINDRICAL_SURFACE ( 'NONE', #74527, 8.000000000000000000 ) ;
#70191 = CARTESIAN_POINT ( 'NONE',  ( -9.832129032723418760, 223.8020833367473301, -5.676582343749998927 ) ) ;
#70192 = CARTESIAN_POINT ( 'NONE',  ( -8.000000000000000000, 90.40625000000000000, -3.313708498984761164 ) ) ;
#70193 = VECTOR ( 'NONE', #59068, 1000.000000000000000 ) ;
#70194 = CARTESIAN_POINT ( 'NONE',  ( -2.977408999572647819, 7.188101187499991163, 28.58030278187176165 ) ) ;
#70195 = CARTESIAN_POINT ( 'NONE',  ( 29.65685424949240101, 198.4375000000000568, 165.9999999999998863 ) ) ;
#70196 = CARTESIAN_POINT ( 'NONE',  ( -5.676582343749998039, 22.44791666325268409, -9.832129032723420536 ) ) ;
#70197 = CARTESIAN_POINT ( 'NONE',  ( 8.660254037844673292, 25.41666666666685970, -5.000000000000164313 ) ) ;
#70198 = CARTESIAN_POINT ( 'NONE',  ( 8.311093377946837890, 221.7187499965860127, -8.311093377946837890 ) ) ;
#70199 = CARTESIAN_POINT ( 'NONE',  ( -7.320508075688771932, 239.3749999999999716, -7.320508075688771932 ) ) ;
#70201 = DIRECTION ( 'NONE',  ( -1.000000000000000000, 0.000000000000000000, 0.000000000000000000 ) ) ;
#70200 = CARTESIAN_POINT ( 'NONE',  ( 10.99999999999994849, 4.556349186104097448, 99.34375000000000000 ) ) ;
#70202 = ORIENTED_EDGE ( 'NONE', *, *, #46505, .T. ) ;
#70203 = CIRCLE ( 'NONE', #66575, 19.00000000000003553 ) ;
#70204 = CARTESIAN_POINT ( 'NONE',  ( 3.458734124999960358, 196.6875000013655779, 142.0000000000000568 ) ) ;
#70205 = CARTESIAN_POINT ( 'NONE',  ( 5.676582343749993598, 34.94791666325268409, 9.832129032723422313 ) ) ;
#70206 = CARTESIAN_POINT ( 'NONE',  ( -10.99999999999999822, -4.556349186104052151, 86.78125000409679046 ) ) ;
#70207 = CARTESIAN_POINT ( 'NONE',  ( 4.898587196589415787E-16, 0.000000000000000000, 4.000000000000001776 ) ) ;
#70208 = CARTESIAN_POINT ( 'NONE',  ( -29.43265458321755190, 194.8750000013656347, 173.4587341250004044 ) ) ;
#70209 = CYLINDRICAL_SURFACE ( 'NONE', #39527, 10.00000000000000178 ) ;
#70211 = CARTESIAN_POINT ( 'NONE',  ( -11.35316468750000141, 23.48958332991934839, 3.042071309553159963 ) ) ;
#70210 = CARTESIAN_POINT ( 'NONE',  ( -7.188101187500000044, 104.6562500020483810, 0.000000000000000000 ) ) ;
#70212 = CARTESIAN_POINT ( 'NONE',  ( -7.999999999999991118, 3.313708498984756723, 12.73655277982336287 ) ) ;
#70213 = CARTESIAN_POINT ( 'NONE',  ( 5.676582343749993598, 144.9479166632526983, 9.832129032723422313 ) ) ;
#70214 = CARTESIAN_POINT ( 'NONE',  ( -10.00000000000000178, 114.3749999931720396, -1.224646799147353454E-15 ) ) ;
#70215 = CARTESIAN_POINT ( 'NONE',  ( -7.188101187499999156, 112.6250000020483668, 2.977408999572654924 ) ) ;
#70216 = DIRECTION ( 'NONE',  ( 0.000000000000000000, -0.000000000000000000, 1.000000000000000000 ) ) ;
#70217 = CARTESIAN_POINT ( 'NONE',  ( -24.54126587500000412, 206.5000000013655779, 168.5673454167827003 ) ) ;
#70218 = VERTEX_POINT ( 'NONE', #4686 ) ;
#70219 = CARTESIAN_POINT ( 'NONE',  ( -8.311093377946836114, 7.968749996586014461, -8.311093377946837890 ) ) ;
#70220 = VERTEX_POINT ( 'NONE', #39012 ) ;
#70221 = LINE ( 'NONE', #7948, #5226 ) ;
#70222 = CARTESIAN_POINT ( 'NONE',  ( -4.721056650415999201, 299.3281250017069510, -4.721056650415999201 ) ) ;
#70224 = CARTESIAN_POINT ( 'NONE',  ( -8.311093377946841443, 133.9062499965860411, 8.311093377946834337 ) ) ;
#70223 = CARTESIAN_POINT ( 'NONE',  ( -6.000000000000000000, 7.347880794884119736E-16, -25.03750572909317285 ) ) ;
#70225 = CARTESIAN_POINT ( 'NONE',  ( -29.65685424949230864, 207.5625000027312126, 174.0000000000003979 ) ) ;
#70226 = CARTESIAN_POINT ( 'NONE',  ( -4.898587196589407898E-16, 7.999999999999991118, 20.01155278432982243 ) ) ;
#70227 = CARTESIAN_POINT ( 'NONE',  ( 60.66349153733354882, 220.4200000571035218, 45.94801856264535900 ) ) ;
#70228 = EDGE_CURVE ( 'NONE', #69862, #36620, #16397, .T. ) ;
#70229 = CARTESIAN_POINT ( 'NONE',  ( -3.042071309553166181, 247.8645833367472733, -11.35316468749999608 ) ) ;
#70230 = CARTESIAN_POINT ( 'NONE',  ( -10.18810118749999916, 0.000000000000000000, 93.53125000204836681 ) ) ;
#70231 = VERTEX_POINT ( 'NONE', #15982 ) ;
#70232 =( BOUNDED_CURVE ( )  B_SPLINE_CURVE ( 2, ( #7038, #48488, #47745, #1754, #42086, #2850, #24735, #42822, #58727 ),
 .UNSPECIFIED., .F., .F. ) 
 B_SPLINE_CURVE_WITH_KNOTS ( ( 3, 2, 2, 2, 3 ),
 ( 0.4204545454545454697, 0.4261363636363636465, 0.4318181818181818232, 0.4375000000000000000, 0.4431818181818181768 ),
 .UNSPECIFIED. ) 
 CURVE ( )  GEOMETRIC_REPRESENTATION_ITEM ( )  RATIONAL_B_SPLINE_CURVE ( ( 1.000000000000000000, 0.9238795325112867385, 1.000000000000000000, 0.9238795325112867385, 1.000000000000000000, 0.9238795325112867385, 1.000000000000000000, 0.9238795325112867385, 1.000000000000000000 ) ) 
 REPRESENTATION_ITEM ( '' )  );
#70233 = EDGE_CURVE ( 'NONE', #24993, #74331, #4314, .T. ) ;
#70234 = CARTESIAN_POINT ( 'NONE',  ( -4.999999999999998224, 203.5416666598387110, -8.660254037844389075 ) ) ;
#70235 = CARTESIAN_POINT ( 'NONE',  ( -30.93541659651595310, -42.99981040672923882, 167.9999999999998295 ) ) ;
#70236 = CARTESIAN_POINT ( 'NONE',  ( 5.676582343749993598, 90.26041666325268409, 9.832129032723422313 ) ) ;
#70237 = CARTESIAN_POINT ( 'NONE',  ( 4.220049686691934809, 10.18810118749999916, 100.1875000020483668 ) ) ;
#70238 = CARTESIAN_POINT ( 'NONE',  ( 4.541265875000002339, 16.43749999863440436, 0.000000000000000000 ) ) ;
#70239 = ORIENTED_EDGE ( 'NONE', *, *, #10588, .F. ) ;
#70240 = VERTEX_POINT ( 'NONE', #61273 ) ;
#70241 = CARTESIAN_POINT ( 'NONE',  ( -8.000000000000000000, 5.250000000000000888, -9.797174393178825657E-16 ) ) ;
#70242 = CARTESIAN_POINT ( 'NONE',  ( 3.211159895383561835, 1.562499998634406806, -3.211159895383561835 ) ) ;
#70243 = CARTESIAN_POINT ( 'NONE',  ( 4.401442555609581635E-16, 0.8437499979516099868, -7.188101187500000044 ) ) ;
#70244 = ADVANCED_FACE ( 'NONE', ( #16343 ), #26934, .F. ) ;
#70245 = CARTESIAN_POINT ( 'NONE',  ( -5.656854249492378806, 119.3750000040967905, 5.656854249492381470 ) ) ;
#70246 = CARTESIAN_POINT ( 'NONE',  ( -10.18810118749999916, 0.000000000000000000, 101.0312500020483810 ) ) ;
#70247 = CARTESIAN_POINT ( 'NONE',  ( -30.99999999999992895, -31.99999999999978684, 167.9999999999997726 ) ) ;
#70248 = CARTESIAN_POINT ( 'NONE',  ( 2.828427124746191623, 15.87499999726881406, -2.828427124746191623 ) ) ;
#70249 = CARTESIAN_POINT ( 'NONE',  ( -27.99999999999995381, 197.5000000000000000, 174.0000000000003695 ) ) ;
#70250 = ORIENTED_EDGE ( 'NONE', *, *, #71229, .F. ) ;
#70251 = AXIS2_PLACEMENT_3D ( 'NONE', #67992, #69486, #63818 ) ;
#70252 = CARTESIAN_POINT ( 'NONE',  ( -1.432654583217607192, 199.2500000013656063, 194.5412658750000219 ) ) ;
#70253 = CARTESIAN_POINT ( 'NONE',  ( -24.54126587499999346, 199.1875000013655779, 170.0000000000002842 ) ) ;
#70254 = CARTESIAN_POINT ( 'NONE',  ( 2.780723358947928197E-16, 14.56249999863440792, -4.541265875000002339 ) ) ;
#70255 = CARTESIAN_POINT ( 'NONE',  ( 4.000000000000001776, 12.00000000000000000, 0.000000000000000000 ) ) ;
#70256 = CARTESIAN_POINT ( 'NONE',  ( 1.320432766682872962E-15, -7.188101187499992051, 13.86155278187175455 ) ) ;
#70257 = ORIENTED_EDGE ( 'NONE', *, *, #71578, .T. ) ;
#70258 = ORIENTED_EDGE ( 'NONE', *, *, #49440, .T. ) ;
#70259 = CARTESIAN_POINT ( 'NONE',  ( -7.204075437095967871, 7.204075437095967871, 104.9687500020483810 ) ) ;
#70260 = CARTESIAN_POINT ( 'NONE',  ( -9.000000000000017764, -15.58845726811988719, 0.000000000000000000 ) ) ;
#70261 = CARTESIAN_POINT ( 'NONE',  ( -23.99999999999997868, 206.6875000000000284, 171.6568542494927385 ) ) ;
#70262 = CARTESIAN_POINT ( 'NONE',  ( -3.458734124999959914, 197.4375000013655779, 198.0000000000000284 ) ) ;
#70263 = CARTESIAN_POINT ( 'NONE',  ( -11.00000000000000000, 0.000000000000000000, 68.68750000409676204 ) ) ;
#70264 = CARTESIAN_POINT ( 'NONE',  ( 7.320508075688774596, 100.6250000000000142, -7.320508075688774596 ) ) ;
#70265 = CARTESIAN_POINT ( 'NONE',  ( 3.313708498984760720, 118.5312500000000142, -8.000000000000000000 ) ) ;
#70266 = CARTESIAN_POINT ( 'NONE',  ( 8.311093377946837890, 56.71874999658601979, -8.311093377946837890 ) ) ;
#70267 = CARTESIAN_POINT ( 'NONE',  ( 2.765530957082001251, 294.9218750017070647, 6.676582343750000703 ) ) ;
#70268 = VERTEX_POINT ( 'NONE', #67311 ) ;
#70269 = CARTESIAN_POINT ( 'NONE',  ( 8.660254037844422825, 190.4166666666667140, -5.000000000000020428 ) ) ;
#70270 = CARTESIAN_POINT ( 'NONE',  ( 5.656854249492378806, 13.12499999590322197, 5.656854249492381470 ) ) ;
#70271 = AXIS2_PLACEMENT_3D ( 'NONE', #54164, #19809, #42449 ) ;
#70272 = CARTESIAN_POINT ( 'NONE',  ( 1.432654583217607192, 207.2500000013655779, 145.4587341250000634 ) ) ;
#70273 = CARTESIAN_POINT ( 'NONE',  ( -4.999999999999999112, 51.66666666666667851, -8.660254037844390851 ) ) ;
#70274 = CARTESIAN_POINT ( 'NONE',  ( 4.000000000000000888, 7.937500000000000000, 1.656854249492384135 ) ) ;
#70275 = CARTESIAN_POINT ( 'NONE',  ( -8.660254037844385522, 220.4166666666666856, 5.000000000000004441 ) ) ;
#70276 = DIRECTION ( 'NONE',  ( 0.000000000000000000, 1.000000000000000000, 0.000000000000000000 ) ) ;
#70277 = CARTESIAN_POINT ( 'NONE',  ( -7.778174593052023411, 7.778174593052023411, 116.3125000000000000 ) ) ;
#70278 = CARTESIAN_POINT ( 'NONE',  ( -1.836970198721029983E-15, 208.7500000000000284, 10.00000000000000178 ) ) ;
#70279 = CARTESIAN_POINT ( 'NONE',  ( 2.977408999572646486, 7.188101187499992051, 13.39280278187175277 ) ) ;
#70280 = CARTESIAN_POINT ( 'NONE',  ( 11.35316468749999785, 175.8854166632527267, 3.042071309553174174 ) ) ;
#70281 = CARTESIAN_POINT ( 'NONE',  ( -3.211159895383562723, 2.937499998634407028, 3.211159895383561391 ) ) ;
#70282 = LINE ( 'NONE', #8758, #68216 ) ;
#70284 = CARTESIAN_POINT ( 'NONE',  ( 2.449293598294707893E-16, 5.250000000000000000, -4.000000000000001776 ) ) ;
#70283 = CARTESIAN_POINT ( 'NONE',  ( -3.999999999999960032, 203.0625000027311842, 196.3431457505076594 ) ) ;
#70285 = VERTEX_POINT ( 'NONE', #9602 ) ;
#70286 = CARTESIAN_POINT ( 'NONE',  ( -3.458734125000016757, 207.1250000013656347, 140.5673454167824161 ) ) ;
#70287 = CARTESIAN_POINT ( 'NONE',  ( -11.35316468749999785, 33.38541666325269119, -3.042071309553167513 ) ) ;
#70288 = CARTESIAN_POINT ( 'NONE',  ( -11.00000000000000000, 0.000000000000000000, 103.1875000040967763 ) ) ;
#70289 = CARTESIAN_POINT ( 'NONE',  ( 5.676582343749993598, 225.2604166632526983, 9.832129032723422313 ) ) ;
#70290 = CARTESIAN_POINT ( 'NONE',  ( -25.55430564589123321, 206.3125000013656063, 167.5543056458915032 ) ) ;
#70291 = CARTESIAN_POINT ( 'NONE',  ( 7.999999999999998224, 4.218749995903220196, 3.313708498984766049 ) ) ;
#70293 = CARTESIAN_POINT ( 'NONE',  ( 2.020667218593132706E-15, -11.00000000000000000, 108.0625000040967905 ) ) ;
#70292 = CARTESIAN_POINT ( 'NONE',  ( -5.082755093536324154, 121.3437500020483952, 5.082755093536326818 ) ) ;
#70294 = CARTESIAN_POINT ( 'NONE',  ( -3.458734125000016313, 196.8750000013656347, 140.5673454167823593 ) ) ;
#70295 = CARTESIAN_POINT ( 'NONE',  ( 10.00000000000000000, 71.66666665983871098, 2.679491924311236062 ) ) ;
#70296 = CARTESIAN_POINT ( 'NONE',  ( 7.188101187500002709, 94.81250000204838102, 2.977408999572649151 ) ) ;
#70297 = CARTESIAN_POINT ( 'NONE',  ( 1.881053915767121776, 15.62499999863440614, -4.541265875000002339 ) ) ;
#70298 = CARTESIAN_POINT ( 'NONE',  ( -1.538508811358849613E-11, 71.25000000000120792, -10.00000000000000178 ) ) ;
#70299 = CARTESIAN_POINT ( 'NONE',  ( -10.00000000000000178, 49.37499999317203248, -1.224646799147353454E-15 ) ) ;
#70300 = CARTESIAN_POINT ( 'NONE',  ( 0.000000000000000000, 300.0000000000000000, 0.000000000000000000 ) ) ;
#70301 = VERTEX_POINT ( 'NONE', #68414 ) ;
#70302 = ORIENTED_EDGE ( 'NONE', *, *, #41198, .F. ) ;
#70303 = CARTESIAN_POINT ( 'NONE',  ( 6.676582343750004256, 296.0468750017069510, 2.765530957081995478 ) ) ;
#70304 = CARTESIAN_POINT ( 'NONE',  ( -10.00000000000001421, 142.5000000000000284, -1.224646799147355031E-15 ) ) ;
#70305 = CARTESIAN_POINT ( 'NONE',  ( -2.828427124746153876, 196.8750000000000284, 195.1715728752538439 ) ) ;
#70306 = CARTESIAN_POINT ( 'NONE',  ( 11.35316468749999785, 160.5729166632526699, 3.042071309553174174 ) ) ;
#70307 = CARTESIAN_POINT ( 'NONE',  ( 10.18810118749999916, 1.247682550866122264E-15, 80.40625000204838102 ) ) ;
#70308 = CARTESIAN_POINT ( 'NONE',  ( 5.000000000000002665, 5.833333333333334814, -8.660254037844389075 ) ) ;
#70309 = CARTESIAN_POINT ( 'NONE',  ( -2.828427124746153876, 202.8750000000000284, 195.1715728752538439 ) ) ;
#70310 = FACE_OUTER_BOUND ( 'NONE', #34217, .T. ) ;
#70311 = CARTESIAN_POINT ( 'NONE',  ( 7.204075437095968759, -7.204075437095966983, 107.5937500020483810 ) ) ;
#70312 = VERTEX_POINT ( 'NONE', #72968 ) ;
#70313 = EDGE_CURVE ( 'NONE', #58925, #47752, #63718, .T. ) ;
#70314 = CARTESIAN_POINT ( 'NONE',  ( 0.000000000000000000, 45.00000000000000000, -11.00000000000000000 ) ) ;
#70315 = DIRECTION ( 'NONE',  ( -1.000000000000000000, 0.000000000000000000, -0.000000000000000000 ) ) ;
#70316 = CARTESIAN_POINT ( 'NONE',  ( -5.676582343749998039, 137.7604166632526983, -9.832129032723420536 ) ) ;
#70317 = CARTESIAN_POINT ( 'NONE',  ( -1.432654583217607192, 200.2500000013656063, 194.5412658750000219 ) ) ;
#70318 = CARTESIAN_POINT ( 'NONE',  ( 1.102182119232618108E-15, 298.3125000034140157, 6.000000000000001776 ) ) ;
#70319 =( BOUNDED_CURVE ( )  B_SPLINE_CURVE ( 2, ( #65554, #14226, #54624, #42541, #25919, #19524, #36526, #2562, #25183 ),
 .UNSPECIFIED., .F., .F. ) 
 B_SPLINE_CURVE_WITH_KNOTS ( ( 3, 2, 2, 2, 3 ),
 ( 0.6145833333333333703, 0.6197916666666666297, 0.6250000000000000000, 0.6302083333333334814, 0.6354166666666667407 ),
 .UNSPECIFIED. ) 
 CURVE ( )  GEOMETRIC_REPRESENTATION_ITEM ( )  RATIONAL_B_SPLINE_CURVE ( ( 1.000000000000000000, 0.9238795325112867385, 1.000000000000000000, 0.9238795325112867385, 1.000000000000000000, 0.9238795325112867385, 1.000000000000000000, 0.9238795325112850731, 1.000000000000001554 ) ) 
 REPRESENTATION_ITEM ( '' )  );
#70320 = CARTESIAN_POINT ( 'NONE',  ( -10.18810118749999916, 0.000000000000000000, 80.03125000204836681 ) ) ;
#70321 = CARTESIAN_POINT ( 'NONE',  ( 5.676582343749993598, 50.26041666325269119, 9.832129032723422313 ) ) ;
#70322 = EDGE_LOOP ( 'NONE', ( #14145, #48191, #8668, #34201 ) ) ;
#70323 = CARTESIAN_POINT ( 'NONE',  ( 7.320508075688774596, 37.49999999317203958, -7.320508075688774596 ) ) ;
#70324 = CARTESIAN_POINT ( 'NONE',  ( 4.541265875000002339, 4.437499998634407028, 0.000000000000000000 ) ) ;
#70325 = CARTESIAN_POINT ( 'NONE',  ( -3.317071493978880348, -8.008118988124989457, 16.29436528394063188 ) ) ;
#70326 = B_SPLINE_CURVE_WITH_KNOTS ( 'NONE', 3,
 ( #72821, #19631, #71680, #48303 ),
 .UNSPECIFIED., .F., .F.,
 ( 4, 4 ),
 ( 0.000000000000000000, 1.000000000000000000 ),
 .UNSPECIFIED. ) ;
#70327 = CARTESIAN_POINT ( 'NONE',  ( -2.977408999572650039, 12.93749999795161365, -7.188101187500001821 ) ) ;
#70328 = CARTESIAN_POINT ( 'NONE',  ( 4.242640687119287435, 292.4375000034140157, 4.242640687119285658 ) ) ;
#70329 = CARTESIAN_POINT ( 'NONE',  ( -3.313708498984816231, 117.9687500040967905, 7.999999999999943157 ) ) ;
#70330 = CARTESIAN_POINT ( 'NONE',  ( 5.082755093536325930, 13.03124999795161187, -5.082755093536325930 ) ) ;
#70331 = CARTESIAN_POINT ( 'NONE',  ( -2.977408999572647819, -7.188101187499990274, 9.267802781871754547 ) ) ;
#70332 = CARTESIAN_POINT ( 'NONE',  ( 10.18810118749999916, 4.220049686691935698, 73.00000000204836681 ) ) ;
#70333 = ADVANCED_FACE ( 'NONE', ( #55256 ), #50320, .T. ) ;
#70334 = VECTOR ( 'NONE', #55589, 1000.000000000000000 ) ;
#70335 = CARTESIAN_POINT ( 'NONE',  ( -30.44569435410883429, 204.8125000013656063, 167.5543056458915885 ) ) ;
#70336 = EDGE_CURVE ( 'NONE', #6126, #69954, #67018, .T. ) ;
#70337 =( BOUNDED_SURFACE ( )  B_SPLINE_SURFACE ( 3, 2, ( 
 ( #43350, #12822, #41872 ),
 ( #1540, #24520, #47525 ),
 ( #13186, #36224, #1889 ),
 ( #9034, #67499, #67126 ),
 ( #21828, #73521, #33192 ),
 ( #38086, #61084, #15421 ),
 ( #55441, #62202, #32047 ),
 ( #27126, #44861, #61463 ),
 ( #33559, #56189, #21464 ),
 ( #22203, #9788, #50884 ),
 ( #55818, #61836, #9412 ),
 ( #67866, #16159, #32430 ),
 ( #50141, #39200, #73156 ),
 ( #21094, #4501, #44117 ),
 ( #10527, #44486, #72404 ),
 ( #73898, #3751, #38833 ),
 ( #55067, #3376, #26752 ),
 ( #56563, #14674, #26363 ) ),
 .UNSPECIFIED., .F., .F., .F. ) 
 B_SPLINE_SURFACE_WITH_KNOTS ( ( 4, 2, 2, 2, 2, 2, 2, 2, 4 ),
 ( 3, 3 ),
 ( 0.04202945594032911347, 0.04396162471216782941, 0.04589379348400654535, 0.04782596225584526128, 0.04975813102768398416, 0.05169029979952270704, 0.05265638418544206500, 0.05362246857136142297, 0.05748680611503885485 ),
 ( 0.000000000000000000, 1.000000000000000000 ),
 .UNSPECIFIED. ) 
 GEOMETRIC_REPRESENTATION_ITEM ( )  RATIONAL_B_SPLINE_SURFACE ( (
 ( 1.000000000000000000, 0.6241276099608163985, 1.000000000000000000),
 ( 1.000000000000000000, 0.6218761496797671207, 1.000000000000000000),
 ( 1.000000000000000000, 0.6198047272367630534, 1.000000000000000000),
 ( 1.000000000000000000, 0.6161935119820778350, 1.000000000000000000),
 ( 1.000000000000000000, 0.6146642324080543451, 1.000000000000000000),
 ( 1.000000000000000000, 0.6121850116871440095, 1.000000000000000000),
 ( 1.000000000000000000, 0.6112350889399758014, 1.000000000000000000),
 ( 1.000000000000000000, 0.6099522725972825743, 1.000000000000000000),
 ( 1.000000000000000000, 0.6096208180307998159, 1.000000000000000000),
 ( 1.000000000000000000, 0.6096183796349359252, 1.000000000000000000),
 ( 1.000000000000000000, 0.6099422200100031999, 1.000000000000000000),
 ( 1.000000000000000000, 0.6109087447824246286, 1.000000000000000000),
 ( 1.000000000000000000, 0.6113123981687531572, 1.000000000000000000),
 ( 1.000000000000000000, 0.6122677719810074581, 1.000000000000000000),
 ( 1.000000000000000000, 0.6128199619018938060, 1.000000000000000000),
 ( 1.000000000000000000, 0.6159350830273915278, 1.000000000000000000),
 ( 1.000000000000000000, 0.6195556778509463403, 1.000000000000000000),
 ( 1.000000000000000000, 0.6241278272307889674, 1.000000000000000000) ) ) 
 REPRESENTATION_ITEM ( '' )  SURFACE ( )  );
#70338 = FACE_OUTER_BOUND ( 'NONE', #73030, .T. ) ;
#70339 = CARTESIAN_POINT ( 'NONE',  ( 4.000000000000001776, 2.812499997268813612, -1.656854249492381248 ) ) ;
#70340 = ORIENTED_EDGE ( 'NONE', *, *, #9204, .F. ) ;
#70341 = CARTESIAN_POINT ( 'NONE',  ( 1.656854249492403008, 195.8125000027312126, 194.0000000000000853 ) ) ;
#70342 = CARTESIAN_POINT ( 'NONE',  ( -4.000000000000015987, 200.4375000000000568, 140.3431457505076594 ) ) ;
#70343 = CARTESIAN_POINT ( 'NONE',  ( -27.99999999999991118, 198.6250000027312126, 174.0000000000003695 ) ) ;
#70344 = CARTESIAN_POINT ( 'NONE',  ( 4.541265875000002339, 2.374999998634407028, -1.881053915767121554 ) ) ;
#70345 = CARTESIAN_POINT ( 'NONE',  ( -5.082755093536324154, 118.3437500020483810, 5.082755093536326818 ) ) ;
#70346 = EDGE_CURVE ( 'NONE', #38666, #65410, #34313, .T. ) ;
#70347 = CARTESIAN_POINT ( 'NONE',  ( 7.522341449313136863, -6.049278984716062624, -0.3563104543936467805 ) ) ;
#70348 = CARTESIAN_POINT ( 'NONE',  ( -3.313708498984758943, -7.999999999999989342, 1.299052783920146448 ) ) ;
#70349 = ORIENTED_EDGE ( 'NONE', *, *, #62531, .F. ) ;
#70350 = CARTESIAN_POINT ( 'NONE',  ( -7.188101187500000933, 22.12499999795161187, -2.977408999572651371 ) ) ;
#70351 = ORIENTED_EDGE ( 'NONE', *, *, #37486, .T. ) ;
#70352 = LINE ( 'NONE', #64683, #15923 ) ;
#70353 = DIRECTION ( 'NONE',  ( -0.000000000000000000, -0.000000000000000000, 1.000000000000000000 ) ) ;
#70354 = CARTESIAN_POINT ( 'NONE',  ( 25.55430564589119413, 207.3125000013656063, 172.4456943541087526 ) ) ;
#70355 = CARTESIAN_POINT ( 'NONE',  ( 10.00000000000000178, 50.20833333333333570, -2.679491924311226736 ) ) ;
#70356 = CARTESIAN_POINT ( 'NONE',  ( 5.082755093536326818, 102.5937500020483810, 5.082755093536325042 ) ) ;
#70357 = CARTESIAN_POINT ( 'NONE',  ( 6.000000000000003553, 294.5625000000000000, -2.485281374238571761 ) ) ;
#70359 = CARTESIAN_POINT ( 'NONE',  ( -22.44327262215655239, -38.91776561763210651, 191.3858745859486419 ) ) ;
#70358 = DIRECTION ( 'NONE',  ( -0.000000000000000000, -0.000000000000000000, -1.000000000000000000 ) ) ;
#70360 = ORIENTED_EDGE ( 'NONE', *, *, #21963, .F. ) ;
#70361 = CARTESIAN_POINT ( 'NONE',  ( -3.042071309553159075, 234.9479166700806445, 11.35316468749999963 ) ) ;
#70362 = CARTESIAN_POINT ( 'NONE',  ( 2.977408999572646486, 7.188101187499991163, 8.892802781871754547 ) ) ;
#70363 = CARTESIAN_POINT ( 'NONE',  ( 2.679491924311225404, 91.04166666666667140, -9.999999999999982236 ) ) ;
#70364 = DIRECTION ( 'NONE',  ( -0.000000000000000000, 1.000000000000000000, -0.000000000000000000 ) ) ;
#70365 = CARTESIAN_POINT ( 'NONE',  ( -7.320508075688771932, 264.3750000000000568, -7.320508075688771932 ) ) ;
#70366 = CARTESIAN_POINT ( 'NONE',  ( 10.00000000000000178, 202.0833333265053682, -2.679491924311226736 ) ) ;
#70367 = CARTESIAN_POINT ( 'NONE',  ( 10.00000000000000000, 169.7916666666666856, 2.679491924311236062 ) ) ;
#70368 = PLANE ( 'NONE',  #43740 ) ;
#70369 = CARTESIAN_POINT ( 'NONE',  ( -1.736494649865107265, -67.70200331863352972, 20.12302832235452144 ) ) ;
#70370 = CARTESIAN_POINT ( 'NONE',  ( 3.042071309553167069, 137.1354166632526983, -11.35316468749999785 ) ) ;
#70371 = CARTESIAN_POINT ( 'NONE',  ( 1.469576158976823947E-15, 97.06250000409677625, 8.000000000000000000 ) ) ;
#70374 = CARTESIAN_POINT ( 'NONE',  ( -31.05507224581699077, 271.9999999999999432, 171.9999999999998295 ) ) ;
#70373 = CARTESIAN_POINT ( 'NONE',  ( 2.679491924311155682, 107.9166666598386968, -10.00000000000004441 ) ) ;
#70372 = CARTESIAN_POINT ( 'NONE',  ( 28.00000000000002132, 207.5000000000000284, 165.9999999999998863 ) ) ;
#70375 = EDGE_CURVE ( 'NONE', #60482, #1123, #38153, .T. ) ;
#70376 = ORIENTED_EDGE ( 'NONE', *, *, #65738, .F. ) ;
#70377 = CARTESIAN_POINT ( 'NONE',  ( 1.688721909672330934, -60.25432409644731990, 22.91817940688270383 ) ) ;
#70378 = EDGE_CURVE ( 'NONE', #25107, #30314, #9745, .T. ) ;
#70379 = CARTESIAN_POINT ( 'NONE',  ( -8.000000000000000000, -3.313708498984752282, 24.92405277982337353 ) ) ;
#70380 = CARTESIAN_POINT ( 'NONE',  ( -1.432654583217664479, 206.7500000013655779, 138.5412658750000787 ) ) ;
#70381 = CARTESIAN_POINT ( 'NONE',  ( -4.733156245433696618, 124.6781487883913258, -6.232488682494672361 ) ) ;
#70382 = CARTESIAN_POINT ( 'NONE',  ( 10.00000000000000178, 41.87499999317203248, 0.000000000000000000 ) ) ;
#70383 = VECTOR ( 'NONE', #13617, 1000.000000000000000 ) ;
#70384 = CARTESIAN_POINT ( 'NONE',  ( -5.082755093536325930, 117.9687500020483810, -5.082755093536325930 ) ) ;
#70385 = CARTESIAN_POINT ( 'NONE',  ( 4.541265875000002339, 2.499999998634407028, -1.881053915767121554 ) ) ;
#70386 = CARTESIAN_POINT ( 'NONE',  ( 2.589639417652943365, 60.37884160281038248, -22.99414321703691755 ) ) ;
#70387 = CARTESIAN_POINT ( 'NONE',  ( -3.313708498984758943, -7.999999999999989342, 17.61155277982336997 ) ) ;
#70389 = CARTESIAN_POINT ( 'NONE',  ( -5.656854249492381470, 26.43750000000000355, 5.656854249492379694 ) ) ;
#70388 = CARTESIAN_POINT ( 'NONE',  ( -4.000000000000002665, 1.562500000000000666, 1.656854249492380582 ) ) ;
#70390 = EDGE_LOOP ( 'NONE', ( #24765, #69197, #52039, #64853, #59395, #73135, #42482, #22816, #32185, #60361, #60880, #62181, #30744, #63078, #71780, #12954, #56368, #45348, #20134, #23657, #66568, #7522, #37950, #63892 ) ) ;
#70391 = ADVANCED_FACE ( 'NONE', ( #23505 ), #57494, .T. ) ;
#70392 = FACE_OUTER_BOUND ( 'NONE', #30870, .T. ) ;
#70393 = CARTESIAN_POINT ( 'NONE',  ( -11.35316468749999608, 229.4270833367473301, 3.042071309553173730 ) ) ;
#70394 = CARTESIAN_POINT ( 'NONE',  ( -3.042071309553173730, 109.3229166632526983, 11.35316468749999785 ) ) ;
#70395 = ORIENTED_EDGE ( 'NONE', *, *, #45966, .T. ) ;
#70396 = CARTESIAN_POINT ( 'NONE',  ( 5.656854249492380582, 25.68750000000000711, -5.656854249492380582 ) ) ;
#70397 = CARTESIAN_POINT ( 'NONE',  ( 7.204075437095968759, -7.204075437095966983, 101.2187500020483668 ) ) ;
#70398 = LINE ( 'NONE', #36803, #46533 ) ;
#70399 = CARTESIAN_POINT ( 'NONE',  ( 2.839093476692135984E-14, 200.9375000013656063, 201.4587341250000350 ) ) ;
#70400 = CYLINDRICAL_SURFACE ( 'NONE', #14273, 8.000000000000000000 ) ;
#70402 = CARTESIAN_POINT ( 'NONE',  ( -11.35316468750000141, 108.2812499965860269, -1.390361679473963753E-15 ) ) ;
#70401 = CARTESIAN_POINT ( 'NONE',  ( -5.000000000000004441, 183.3333333333333712, 8.660254037844385522 ) ) ;
#70403 = CARTESIAN_POINT ( 'NONE',  ( -24.54126587499998990, 195.4375000013655779, 170.0000000000003411 ) ) ;
#70404 = CARTESIAN_POINT ( 'NONE',  ( -1.836970198721029983E-15, 80.62499999317203958, 10.00000000000000178 ) ) ;
#70405 = EDGE_LOOP ( 'NONE', ( #16494, #63611, #44815, #41941, #7164, #8011 ) ) ;
#70406 = CARTESIAN_POINT ( 'NONE',  ( -5.000000000000005329, 190.2083333265053966, 8.660254037844387298 ) ) ;
#70407 = CARTESIAN_POINT ( 'NONE',  ( 5.656854249492378806, 22.31250000000000355, 5.656854249492381470 ) ) ;
#70408 = CARTESIAN_POINT ( 'NONE',  ( -4.556349186104045934, 11.00000000000000000, 83.40625000409676204 ) ) ;
#70409 = CARTESIAN_POINT ( 'NONE',  ( 6.951808397369818766E-16, 97.34374999658601268, -11.35316468750000141 ) ) ;
#70410 = CYLINDRICAL_SURFACE ( 'NONE', #49538, 6.000000000000000000 ) ;
#70411 = CARTESIAN_POINT ( 'NONE',  ( 4.401442555609581635E-16, 13.21874999795161187, -7.188101187500000044 ) ) ;
#70412 = CARTESIAN_POINT ( 'NONE',  ( 4.220049686691934809, 10.18810118749999916, 93.06250000204838102 ) ) ;
#70413 = CARTESIAN_POINT ( 'NONE',  ( -8.311093377946841443, 4.218749996586018014, 8.311093377946830785 ) ) ;
#70414 = ORIENTED_EDGE ( 'NONE', *, *, #54865, .T. ) ;
#70415 = CARTESIAN_POINT ( 'NONE',  ( 11.00000000000000000, 1.347111479062088405E-15, 118.0000000000000000 ) ) ;
#70416 = DIRECTION ( 'NONE',  ( -1.000000000000000000, 0.000000000000000000, 0.000000000000000000 ) ) ;
#70417 = CARTESIAN_POINT ( 'NONE',  ( 7.778174593052021635, 7.778174593052023411, 102.4374999999999858 ) ) ;
#70418 = CARTESIAN_POINT ( 'NONE',  ( -6.238412754330611322E-16, 10.18810118749999916, 75.15625000204836681 ) ) ;
#70419 = AXIS2_PLACEMENT_3D ( 'NONE', #47249, #17467, #12550 ) ;
#70420 = CARTESIAN_POINT ( 'NONE',  ( 1.469576158976823947E-15, 98.56250000409677625, 8.000000000000000000 ) ) ;
#70421 = DIRECTION ( 'NONE',  ( 1.000000000000000000, 0.000000000000000000, 0.000000000000000000 ) ) ;
#70422 = CARTESIAN_POINT ( 'NONE',  ( -6.676582343750000703, 292.5156250017068942, 2.765530957082001251 ) ) ;
#70423 = CYLINDRICAL_SURFACE ( 'NONE', #49781, 11.00000000000000000 ) ;
#70424 = CARTESIAN_POINT ( 'NONE',  ( -8.311093377946836114, 217.9687499965860127, -8.311093377946837890 ) ) ;
#70425 = CARTESIAN_POINT ( 'NONE',  ( 4.220049686691934809, 10.18810118749999916, 91.18750000204836681 ) ) ;
#70426 = ADVANCED_FACE ( 'NONE', ( #29179 ), #47255, .T. ) ;
#70427 = CARTESIAN_POINT ( 'NONE',  ( -28.00000000000002132, 201.4375000013656063, 166.5412658750003629 ) ) ;
#70428 = CARTESIAN_POINT ( 'NONE',  ( 3.313708498984762052, 25.78125000000000355, -8.000000000000000000 ) ) ;
#70429 = ORIENTED_EDGE ( 'NONE', *, *, #23010, .F. ) ;
#70430 = FACE_OUTER_BOUND ( 'NONE', #28257, .T. ) ;
#70431 = CARTESIAN_POINT ( 'NONE',  ( 4.000000000000015987, 205.6250000027312126, 198.0000000000000284 ) ) ;
#70432 =( BOUNDED_CURVE ( )  B_SPLINE_CURVE ( 2, ( #18485, #36945, #1527, #59226, #25608, #53927, #2240, #52818, #19577 ),
 .UNSPECIFIED., .F., .F. ) 
 B_SPLINE_CURVE_WITH_KNOTS ( ( 3, 2, 2, 2, 3 ),
 ( 0.7000000000000006217, 0.7083333333333340365, 0.7166666666666673402, 0.7250000000000006439, 0.7333333333333339477 ),
 .UNSPECIFIED. ) 
 CURVE ( )  GEOMETRIC_REPRESENTATION_ITEM ( )  RATIONAL_B_SPLINE_CURVE ( ( 0.9999999999999938938, 0.9238795325112928447, 1.000000000000000000, 0.9238795325112867385, 1.000000000000000000, 0.9238795325112867385, 1.000000000000000000, 0.9238795325112806323, 1.000000000000005995 ) ) 
 REPRESENTATION_ITEM ( '' )  );
#70433 = CARTESIAN_POINT ( 'NONE',  ( -8.660254037844387298, 27.08333333333333570, -5.000000000000004441 ) ) ;
#70434=STYLED_ITEM('',(#74706),#66045);
#70435 = CARTESIAN_POINT ( 'NONE',  ( 29.65685424949236548, 208.5625000027312694, 165.9999999999999147 ) ) ;
#70436 = CARTESIAN_POINT ( 'NONE',  ( -7.204075437095967871, 7.204075437095967871, 72.34375000204836681 ) ) ;
#70437 = ORIENTED_EDGE ( 'NONE', *, *, #3858, .T. ) ;
#70438 = CARTESIAN_POINT ( 'NONE',  ( 7.188101187499999156, 6.374999997951610986, 2.977408999572654924 ) ) ;
#70439 = CARTESIAN_POINT ( 'NONE',  ( -3.255014963930524218E-15, -13.85640646055106728, -14.80000000000000071 ) ) ;
#70440 = EDGE_CURVE ( 'NONE', #70268, #47025, #23179, .T. ) ;
#70441 = SURFACE_STYLE_FILL_AREA ( #5589 ) ;
#70442 = CARTESIAN_POINT ( 'NONE',  ( -2.977408999572650927, 118.2500000020483952, -7.188101187500001821 ) ) ;
#70443 = CARTESIAN_POINT ( 'NONE',  ( -1.721590048263790695, 22.00000000000001776, -3.746118333428731351 ) ) ;
#70444 = CARTESIAN_POINT ( 'NONE',  ( -4.721056650415999201, 298.3281250017069510, -4.721056650415999201 ) ) ;
#70446 = CARTESIAN_POINT ( 'NONE',  ( -0.9790701977573761372, 13.29114001832026837, -0.7454400371385527801 ) ) ;
#70445 = CARTESIAN_POINT ( 'NONE',  ( 3.042071309553163516, 227.4479166700806445, -11.35316468749999785 ) ) ;
#70447 = ORIENTED_EDGE ( 'NONE', *, *, #59047, .F. ) ;
#70448 =( BOUNDED_CURVE ( )  B_SPLINE_CURVE ( 2, ( #9245, #32267, #55285, #3589, #26584, #72623, #20927, #4713, #62772 ),
 .UNSPECIFIED., .F., .F. ) 
 B_SPLINE_CURVE_WITH_KNOTS ( ( 3, 2, 2, 2, 3 ),
 ( 0.8645833333333335924, 0.8697916666666668517, 0.8750000000000002220, 0.8802083333333337034, 0.8854166666666669627 ),
 .UNSPECIFIED. ) 
 CURVE ( )  GEOMETRIC_REPRESENTATION_ITEM ( )  RATIONAL_B_SPLINE_CURVE ( ( 0.9999999999999967804, 0.9238795325112899581, 1.000000000000000000, 0.9238795325112867385, 1.000000000000000000, 0.9238795325112867385, 1.000000000000000000, 0.9238795325112818535, 1.000000000000004885 ) ) 
 REPRESENTATION_ITEM ( '' )  );
#70449 = CARTESIAN_POINT ( 'NONE',  ( -11.35316468749999963, 234.2187500034139873, 0.000000000000000000 ) ) ;
#70450 = CARTESIAN_POINT ( 'NONE',  ( -7.188101187499991163, 2.977408999572646930, 8.892802781871754547 ) ) ;
#70451 = CARTESIAN_POINT ( 'NONE',  ( 3.458734125000015869, 204.1875000013656063, 198.0000000000000284 ) ) ;
#70452 = ORIENTED_EDGE ( 'NONE', *, *, #33610, .T. ) ;
#70453 = CARTESIAN_POINT ( 'NONE',  ( 0.000000000000000000, 300.0000000000000000, 6.000000000000001776 ) ) ;
#70454 = CARTESIAN_POINT ( 'NONE',  ( 5.676582343750001591, 101.9270833299193555, -9.832129032723420536 ) ) ;
#70455 = CARTESIAN_POINT ( 'NONE',  ( 0.000000000000000000, 255.9999999999999432, 0.000000000000000000 ) ) ;
#70456 = CARTESIAN_POINT ( 'NONE',  ( 4.556349186104051263, -10.99999999999999822, 76.46874999999998579 ) ) ;
#70459 = DIRECTION ( 'NONE',  ( -0.000000000000000000, 1.000000000000000000, 4.689100369878284071E-30 ) ) ;
#70458 = CARTESIAN_POINT ( 'NONE',  ( 25.55430564589115860, 206.0625000013656063, 167.5543056458911053 ) ) ;
#70457 = CARTESIAN_POINT ( 'NONE',  ( 24.54126587500000056, 201.3750000013656347, 168.5673454167822172 ) ) ;
#70460 = ORIENTED_EDGE ( 'NONE', *, *, #72837, .F. ) ;
#70461 = VECTOR ( 'NONE', #50226, 1000.000000000000000 ) ;
#70462 = CARTESIAN_POINT ( 'NONE',  ( -54.00000000000000000, 0.000000000000000000, 4.085831468968145267E-14 ) ) ;
#70463 = LINE ( 'NONE', #12007, #41989 ) ;
#70464 = EDGE_CURVE ( 'NONE', #24671, #1694, #53583, .T. ) ;
#70465 = CARTESIAN_POINT ( 'NONE',  ( 8.311093377946834337, 210.1562499965860411, 8.311093377946839666 ) ) ;
#70466 = CARTESIAN_POINT ( 'NONE',  ( 2.445694354108783664, 201.3125000013656063, 144.4456943541088663 ) ) ;
#70467 = CARTESIAN_POINT ( 'NONE',  ( 26.56734541678232375, 202.6250000013656063, 173.4587341249998929 ) ) ;
#70468 = CARTESIAN_POINT ( 'NONE',  ( -7.188101187500000044, 24.09374999795161543, -8.802885111219163269E-16 ) ) ;
#70469 = CARTESIAN_POINT ( 'NONE',  ( -3.042071309553173730, 179.6354166632526699, 11.35316468749999785 ) ) ;
#70470 = CARTESIAN_POINT ( 'NONE',  ( 7.188101187500002709, 96.68750000204838102, 2.977408999572649151 ) ) ;
#70471 = CARTESIAN_POINT ( 'NONE',  ( -5.000000000000000000, 62.13136467933009754, -23.87699943806387282 ) ) ;
#70472 = CARTESIAN_POINT ( 'NONE',  ( -29.65685424949240812, 195.0625000000000284, 166.0000000000004263 ) ) ;
#70473 = CARTESIAN_POINT ( 'NONE',  ( -4.541265875000003227, 15.87499999863440436, 1.881053915767121110 ) ) ;
#70474 = CARTESIAN_POINT ( 'NONE',  ( 26.56734541678238060, 199.2500000013656063, 166.5412658749999650 ) ) ;
#70475 = CARTESIAN_POINT ( 'NONE',  ( -7.188101187499990274, -2.977408999572651371, 3.455302781871751439 ) ) ;
#70476 = CARTESIAN_POINT ( 'NONE',  ( -9.832129032723418760, 62.86458332991935549, -5.676582343750004256 ) ) ;
#70477 = ADVANCED_FACE ( 'NONE', ( #6904 ), #16714, .T. ) ;
#70478 = CARTESIAN_POINT ( 'NONE',  ( 7.806255641895631925E-15, 13.85640646055103709, -1.071796769724504550 ) ) ;
#70479 = ORIENTED_EDGE ( 'NONE', *, *, #20906, .F. ) ;
#70480 = CARTESIAN_POINT ( 'NONE',  ( -8.000000000000000000, 9.562499995903223748, -9.797174393178825657E-16 ) ) ;
#70481 = CARTESIAN_POINT ( 'NONE',  ( 18.00000000000000000, 10.39230484541325161, -20.69999999999999929 ) ) ;
#70482 = CARTESIAN_POINT ( 'NONE',  ( 8.311093377946834337, 70.15624999658602690, 8.311093377946839666 ) ) ;
#70483 = CARTESIAN_POINT ( 'NONE',  ( 10.18810118749999916, 4.220049686691935698, 116.5000000020483810 ) ) ;
#70484 = CARTESIAN_POINT ( 'NONE',  ( 2.445694354108783219, 197.8125000013656063, 139.5543056458912190 ) ) ;
#70485 = CARTESIAN_POINT ( 'NONE',  ( -1.296342370383214426, 10.28012030475506577, 63.61260002839684802 ) ) ;
#70487 = CARTESIAN_POINT ( 'NONE',  ( -8.311093377946836114, 67.65624999658601268, -8.311093377946837890 ) ) ;
#70486 = CARTESIAN_POINT ( 'NONE',  ( -2.828427124746190735, 13.12499999726881406, -2.828427124746191623 ) ) ;
#70488 = CIRCLE ( 'NONE', #64461, 71.70204102886728492 ) ;
#70489 = CARTESIAN_POINT ( 'NONE',  ( -5.656854249492373476, -5.656854249492376141, 25.20530278392014978 ) ) ;
#70490 = CARTESIAN_POINT ( 'NONE',  ( 3.170472398252169882E-12, 128.7500000000002558, 10.00000000000000178 ) ) ;
#70491 = CARTESIAN_POINT ( 'NONE',  ( 7.320508075688771044, 161.2499999931720538, 7.320508075688775484 ) ) ;
#70492 = CARTESIAN_POINT ( 'NONE',  ( -7.188101187500001821, 89.93750000204840944, -2.977408999572650483 ) ) ;
#70493 = CARTESIAN_POINT ( 'NONE',  ( -25.10295958197940180, 194.8478348442015999, 172.5395117423482532 ) ) ;
#70494 = CARTESIAN_POINT ( 'NONE',  ( 9.832129032723420536, 66.51041666325268409, -5.676582343749999815 ) ) ;
#70495 = CARTESIAN_POINT ( 'NONE',  ( 4.220049686691941027, -10.18810118749999738, 115.0000000020483810 ) ) ;
#70496 = CARTESIAN_POINT ( 'NONE',  ( -9.832129032723420536, 198.6979166632526983, 5.676582343749997150 ) ) ;
#70497 = ORIENTED_EDGE ( 'NONE', *, *, #68024, .F. ) ;
#70498 = CARTESIAN_POINT ( 'NONE',  ( 1.308779242310877500, 60.23127520339582475, 22.90411807697773128 ) ) ;
#70499 = CARTESIAN_POINT ( 'NONE',  ( -27.99999999999991118, 198.6250000027312126, 174.0000000000003695 ) ) ;
#70500 = CARTESIAN_POINT ( 'NONE',  ( -6.062583391206407768, -5.219682234019338729, -0.1039400739145942276 ) ) ;
#70502 = CARTESIAN_POINT ( 'NONE',  ( -11.35316468749999785, 173.0729166632526983, -3.042071309553167957 ) ) ;
#70501 = CARTESIAN_POINT ( 'NONE',  ( 5.000000000000004441, 261.6666666666666856, 8.660254037844385522 ) ) ;
#70503 = DIRECTION ( 'NONE',  ( 0.000000000000000000, 0.000000000000000000, 1.000000000000000000 ) ) ;
#70504 = CARTESIAN_POINT ( 'NONE',  ( 2.679491924311235174, 254.5833333401613174, 9.999999999999998224 ) ) ;
#70505 = CARTESIAN_POINT ( 'NONE',  ( -7.320508075688773708, 188.7499999931720538, -7.320508075688774596 ) ) ;
#70506 = ORIENTED_EDGE ( 'NONE', *, *, #21299, .T. ) ;
#70507 = CARTESIAN_POINT ( 'NONE',  ( 6.951808397369818766E-16, 162.3437499965860127, -11.35316468750000141 ) ) ;
#70508 = CARTESIAN_POINT ( 'NONE',  ( 7.188101187499993827, -2.977408999572645598, 18.64280278187176521 ) ) ;
#70509 = CARTESIAN_POINT ( 'NONE',  ( 7.486112537844476833, 225.9999999999999716, -7.575605162435675943 ) ) ;
#70510 = VERTEX_POINT ( 'NONE', #8008 ) ;
#70511 = CARTESIAN_POINT ( 'NONE',  ( 5.656854249492381470, 106.2500000040967905, 5.656854249492379694 ) ) ;
#70512 = CARTESIAN_POINT ( 'NONE',  ( -7.347880794884122694E-16, 12.75000000000000178, 4.000000000000001776 ) ) ;
#70513 = EDGE_CURVE ( 'NONE', #26674, #64909, #64159, .T. ) ;
#70514 = LINE ( 'NONE', #47124, #21584 ) ;
#70515 = CARTESIAN_POINT ( 'NONE',  ( 3.211159895383561835, 16.43749999863440436, -3.211159895383561835 ) ) ;
#70516 = CARTESIAN_POINT ( 'NONE',  ( 1.469576158976822172E-15, -7.999999999999991118, 17.89280278392014623 ) ) ;
#70517 = CARTESIAN_POINT ( 'NONE',  ( 2.828427124746153876, 195.8750000000000284, 144.8284271247462129 ) ) ;
#70518 = ORIENTED_EDGE ( 'NONE', *, *, #54154, .F. ) ;
#70519 = DIRECTION ( 'NONE',  ( -1.000000000000000000, 0.000000000000000000, 0.000000000000000000 ) ) ;
#70520 = CARTESIAN_POINT ( 'NONE',  ( 2.977408999572654480, 99.12500000204838102, 7.188101187499999156 ) ) ;
#70521 = VECTOR ( 'NONE', #71963, 1000.000000000000000 ) ;
#70523 = DIRECTION ( 'NONE',  ( -0.000000000000000000, 1.000000000000000000, -0.000000000000000000 ) ) ;
#70522 = CARTESIAN_POINT ( 'NONE',  ( 5.000000000000021316, 179.1666666666666856, 8.660254037844438812 ) ) ;
#70525 = EDGE_CURVE ( 'NONE', #54592, #12328, #54040, .T. ) ;
#70524 = ORIENTED_EDGE ( 'NONE', *, *, #37843, .T. ) ;
#70526 = ADVANCED_FACE ( 'NONE', ( #30284 ), #64972, .T. ) ;
#70527 = CARTESIAN_POINT ( 'NONE',  ( 3.544144923084140864, 10.27124247550373326, -63.97955030411847588 ) ) ;
#70528 = CARTESIAN_POINT ( 'NONE',  ( 1.469576158976823947E-15, 105.8750000000000000, 8.000000000000000000 ) ) ;
#70529 = MECHANICAL_DESIGN_GEOMETRIC_PRESENTATION_REPRESENTATION (  '', ( #66877 ), #37964 ) ;
#70530 = CARTESIAN_POINT ( 'NONE',  ( 7.188101187499991163, 2.977408999572648707, 26.33030278187175810 ) ) ;
#70531 = VERTEX_POINT ( 'NONE', #25345 ) ;
#70532 =( BOUNDED_CURVE ( )  B_SPLINE_CURVE ( 2, ( #35497, #18872, #63781, #41879, #35863, #58510, #6816, #12098, #64891 ),
 .UNSPECIFIED., .F., .F. ) 
 B_SPLINE_CURVE_WITH_KNOTS ( ( 3, 2, 2, 2, 3 ),
 ( 0.7000000000000006217, 0.7083333333333340365, 0.7166666666666673402, 0.7250000000000006439, 0.7333333333333339477 ),
 .UNSPECIFIED. ) 
 CURVE ( )  GEOMETRIC_REPRESENTATION_ITEM ( )  RATIONAL_B_SPLINE_CURVE ( ( 0.9999999999999938938, 0.9238795325112928447, 1.000000000000000000, 0.9238795325112867385, 1.000000000000000000, 0.9238795325112867385, 1.000000000000000000, 0.9238795325112806323, 1.000000000000005995 ) ) 
 REPRESENTATION_ITEM ( '' )  );
#70533 = ORIENTED_EDGE ( 'NONE', *, *, #17046, .F. ) ;
#70534 = CARTESIAN_POINT ( 'NONE',  ( -7.204075437095967871, 7.204075437095967871, 86.96875000204836681 ) ) ;
#70535 = CARTESIAN_POINT ( 'NONE',  ( -1.836970198721029983E-15, 90.62499999317203958, 10.00000000000000178 ) ) ;
#70536 = CARTESIAN_POINT ( 'NONE',  ( -4.556349186104047710, -10.99999999999999822, 94.28124999999997158 ) ) ;
#70539 = CARTESIAN_POINT ( 'NONE',  ( -4.721056650415999201, 299.4843750017070079, -4.721056650415999201 ) ) ;
#70538 = CARTESIAN_POINT ( 'NONE',  ( 26.34314575050763807, 200.0625000027312410, 173.9999999999999147 ) ) ;
#70537 = CARTESIAN_POINT ( 'NONE',  ( 11.00000000000000000, 1.347111479062088405E-15, 105.2500000000000000 ) ) ;
#70540 = CARTESIAN_POINT ( 'NONE',  ( -10.00000000000000000, 132.2916666666666288, -2.679491924311229845 ) ) ;
#70541 = CARTESIAN_POINT ( 'NONE',  ( 6.123233995736767268E-16, 13.12499999317203425, -10.00000000000000178 ) ) ;
#70542 = CARTESIAN_POINT ( 'NONE',  ( 5.082755093536320601, -5.082755093536318824, 0.9240527818717529929 ) ) ;
#70543 = CARTESIAN_POINT ( 'NONE',  ( 0.000000000000000000, 0.000000000000000000, 30.00000000000000000 ) ) ;
#70544 = CARTESIAN_POINT ( 'NONE',  ( 24.54126587499999346, 204.1875000013656063, 169.9999999999998863 ) ) ;
#70545 = CARTESIAN_POINT ( 'NONE',  ( 7.188101187499999156, 8.249999997951611874, 2.977408999572654924 ) ) ;
#70546 = CARTESIAN_POINT ( 'NONE',  ( -5.662595241051935346, 5.662595241051935346, 5.325615283940630107 ) ) ;
#70547 = CARTESIAN_POINT ( 'NONE',  ( -2.839093476692135984E-14, 194.6875000013655779, 138.5412658750000503 ) ) ;
#70548 = CARTESIAN_POINT ( 'NONE',  ( -7.188101187500000044, 118.5312500020483810, 0.000000000000000000 ) ) ;
#70550 = CARTESIAN_POINT ( 'NONE',  ( -10.00000000000000178, 132.5000000000000284, -1.224646799147353454E-15 ) ) ;
#70549 = CARTESIAN_POINT ( 'NONE',  ( -6.123233995736766282E-16, 248.7500000000000284, -10.00000000000000000 ) ) ;
#70551 = CARTESIAN_POINT ( 'NONE',  ( -5.676582343749992710, 225.0520833367473017, 9.832129032723422313 ) ) ;
#70552 = CARTESIAN_POINT ( 'NONE',  ( -24.00000000000001421, 207.8125000000000000, 168.3431457505080289 ) ) ;
#70553 = CARTESIAN_POINT ( 'NONE',  ( -5.082755093536319713, 5.082755093536319713, 24.17405278187175455 ) ) ;
#70554 = CARTESIAN_POINT ( 'NONE',  ( 31.99999999999997868, 196.1875000000000568, 171.6568542494923122 ) ) ;
#70555 = CARTESIAN_POINT ( 'NONE',  ( -8.311093377946836114, 27.65624999658602334, -8.311093377946837890 ) ) ;
#70556 = CARTESIAN_POINT ( 'NONE',  ( -8.000000000000000000, 9.750000000000001776, -9.797174393178825657E-16 ) ) ;
#70557 = CARTESIAN_POINT ( 'NONE',  ( 9.832129032723416984, 225.6770833299193839, 5.676582343750006032 ) ) ;
#70558 = CARTESIAN_POINT ( 'NONE',  ( 3.313708498984679895, 112.5312500000000284, -8.000000000000081712 ) ) ;
#70559 = CARTESIAN_POINT ( 'NONE',  ( 1.739508062077477657, -16.42388987907938613, 68.69353258878827262 ) ) ;
#70560 = EDGE_LOOP ( 'NONE', ( #71195, #13448, #771, #19974 ) ) ;
#70561 = CARTESIAN_POINT ( 'NONE',  ( -6.735557395310442023E-16, 11.00000000000000000, 104.3125000040967763 ) ) ;
#70562 = CARTESIAN_POINT ( 'NONE',  ( 2.445694354108783219, 197.8125000013656063, 139.5543056458912190 ) ) ;
#70563 = CARTESIAN_POINT ( 'NONE',  ( -11.35316468750000141, 33.28124999658601268, -1.390361679473963753E-15 ) ) ;
#70564 = CARTESIAN_POINT ( 'NONE',  ( -10.99999999999999822, -4.556349186104052151, 88.28125000409677625 ) ) ;
#70565 = CARTESIAN_POINT ( 'NONE',  ( 2.445694354108783219, 207.8125000013656063, 139.5543056458912190 ) ) ;
#70566 = EDGE_CURVE ( 'NONE', #29716, #62209, #13281, .T. ) ;
#70567 = CARTESIAN_POINT ( 'NONE',  ( -26.56734541678242678, 195.3750000013656063, 166.5412658750003345 ) ) ;
#70568 = CARTESIAN_POINT ( 'NONE',  ( 12.00000000000000178, 5.807951393103206073, -0.7484079198486913720 ) ) ;
#70570 = CARTESIAN_POINT ( 'NONE',  ( -3.042071309553163960, 37.23958332991934839, -11.35316468749999963 ) ) ;
#70569 = CARTESIAN_POINT ( 'NONE',  ( 1.320432766682874540E-15, 103.5312500020483810, 7.188101187500000044 ) ) ;
#70571 = CARTESIAN_POINT ( 'NONE',  ( 1.469576158976822172E-15, -7.999999999999991118, 16.20530277982336287 ) ) ;
#70572 = CARTESIAN_POINT ( 'NONE',  ( 5.676582343750001591, 146.6145833299193555, -9.832129032723420536 ) ) ;
#70573 = CARTESIAN_POINT ( 'NONE',  ( -5.000000000000005329, 110.2083333265053682, 8.660254037844387298 ) ) ;
#70574 = CARTESIAN_POINT ( 'NONE',  ( 7.188101187500002709, 114.6875000020484094, 2.977408999572649151 ) ) ;
#70575 = CARTESIAN_POINT ( 'NONE',  ( 0.000000000000000000, 0.000000000000000000, 0.000000000000000000 ) ) ;
#70576 = CARTESIAN_POINT ( 'NONE',  ( -24.54126587499999701, 206.4375000013656063, 170.0000000000003411 ) ) ;
#70577 = ORIENTED_EDGE ( 'NONE', *, *, #19030, .T. ) ;
#70578 = CARTESIAN_POINT ( 'NONE',  ( -9.832129032723418760, 3.177083329919349719, -5.676582343750004256 ) ) ;
#70579 = ORIENTED_EDGE ( 'NONE', *, *, #54232, .F. ) ;
#70580 = CARTESIAN_POINT ( 'NONE',  ( 4.242640687119285658, 289.6249999999999432, -4.242640687119286547 ) ) ;
#70582 = CARTESIAN_POINT ( 'NONE',  ( -9.832129032723418760, 142.8645833299193555, -5.676582343750004256 ) ) ;
#70581 = CARTESIAN_POINT ( 'NONE',  ( -23.26685738723296382, -24.17270462412035670, 145.7522650037860501 ) ) ;
#70583 = CARTESIAN_POINT ( 'NONE',  ( 2.449293598294707893E-16, 15.99999999726881406, -4.000000000000001776 ) ) ;
#70584 = CARTESIAN_POINT ( 'NONE',  ( -4.898587196589407898E-16, 7.999999999999991118, 15.51155278432982598 ) ) ;
#70585 = CARTESIAN_POINT ( 'NONE',  ( 9.797174393178825657E-16, 125.0000000000000000, -8.000000000000000000 ) ) ;
#70586 = CARTESIAN_POINT ( 'NONE',  ( 5.676582343750005144, 245.5729166700806729, 9.832129032723416984 ) ) ;
#70587 = AXIS2_PLACEMENT_3D ( 'NONE', #49145, #14435, #13321 ) ;
#70588 = CARTESIAN_POINT ( 'NONE',  ( -4.220049686691937474, -10.18810118749999738, 90.81250000204838102 ) ) ;
#70589 = ORIENTED_EDGE ( 'NONE', *, *, #17216, .T. ) ;
#70590 = CIRCLE ( 'NONE', #5552, 8.000000000000000000 ) ;
#70591 = CARTESIAN_POINT ( 'NONE',  ( 0.000000000000000000, 1.806524977843537691E-16, -4.000000000000000000 ) ) ;
#70592 = CARTESIAN_POINT ( 'NONE',  ( 8.311093377946834337, 85.46874999658599847, 8.311093377946839666 ) ) ;
#70593 = CARTESIAN_POINT ( 'NONE',  ( 10.18810118749999916, 4.220049686691935698, 98.50000000204838102 ) ) ;
#70594 = CARTESIAN_POINT ( 'NONE',  ( 4.541265875000002339, 18.43749999863440792, 0.000000000000000000 ) ) ;
#70595 = EDGE_LOOP ( 'NONE', ( #66917, #59355, #16293, #11150 ) ) ;
#70596 = VERTEX_POINT ( 'NONE', #14017 ) ;
#70597 = CARTESIAN_POINT ( 'NONE',  ( -5.656854249492379694, 5.062500000000000888, -5.656854249492380582 ) ) ;
#70598 = DIRECTION ( 'NONE',  ( -0.000000000000000000, 1.000000000000000000, -0.000000000000000000 ) ) ;
#70599 = CARTESIAN_POINT ( 'NONE',  ( -7.188101187500002709, 1.312499997951610098, 2.977408999572649151 ) ) ;
#70600 = CARTESIAN_POINT ( 'NONE',  ( -5.656854249492378806, 122.3750000040967905, 5.656854249492381470 ) ) ;
#70601 = CARTESIAN_POINT ( 'NONE',  ( -4.220049686691937474, -10.18810118749999738, 95.31250000204838102 ) ) ;
#70602 = EDGE_CURVE ( 'NONE', #1735, #56997, #65713, .T. ) ;
#70603 = CARTESIAN_POINT ( 'NONE',  ( 32.00000000000000000, 208.2500000000000284, 169.9999999999999432 ) ) ;
#70604 = CARTESIAN_POINT ( 'NONE',  ( 2.828427124746190291, 12.62499999726881406, 2.828427124746192067 ) ) ;
#70605 = DIRECTION ( 'NONE',  ( -0.000000000000000000, 1.000000000000000000, -0.000000000000000000 ) ) ;
#70606 = ORIENTED_EDGE ( 'NONE', *, *, #59544, .T. ) ;
#70607 = DIRECTION ( 'NONE',  ( 0.000000000000000000, 0.000000000000000000, -1.000000000000000000 ) ) ;
#70608 = CARTESIAN_POINT ( 'NONE',  ( 3.458734125000016313, 198.8750000013656347, 199.4326545832176691 ) ) ;
#70610 = CYLINDRICAL_SURFACE ( 'NONE', #18946, 10.00000000000000178 ) ;
#70609 = CARTESIAN_POINT ( 'NONE',  ( -31.45873412499999944, 202.6875000013656063, 170.0000000000004547 ) ) ;
#70611 = CARTESIAN_POINT ( 'NONE',  ( 1.881053915767121776, 12.49999999863440969, -4.541265875000002339 ) ) ;
#70612 = CARTESIAN_POINT ( 'NONE',  ( 4.999999999999993783, 121.0416666598386968, 8.660254037844390851 ) ) ;
#70613 = CARTESIAN_POINT ( 'NONE',  ( 2.977408999572650927, -7.188101187499990274, 13.95530278187175277 ) ) ;
#70614 = ORIENTED_EDGE ( 'NONE', *, *, #6508, .T. ) ;
#70615 = ORIENTED_EDGE ( 'NONE', *, *, #53428, .F. ) ;
#70616 = CARTESIAN_POINT ( 'NONE',  ( 7.204075437095968759, -7.204075437095966983, 102.7187500020483668 ) ) ;
#70617 = CARTESIAN_POINT ( 'NONE',  ( 3.313708498984711426, 95.65625000409679046, 8.000000000000053291 ) ) ;
#70618 = CARTESIAN_POINT ( 'NONE',  ( -23.99999999999998934, 203.7500000000000284, 170.0000000000003411 ) ) ;
#70619 = CARTESIAN_POINT ( 'NONE',  ( 3.458734125000016313, 197.8750000013656063, 199.4326545832176691 ) ) ;
#70620 = CARTESIAN_POINT ( 'NONE',  ( -8.000000000000001776, 12.65624999590322197, 3.313708498984759387 ) ) ;
#70621 = CARTESIAN_POINT ( 'NONE',  ( 4.999999999999993783, 89.16666666666667140, 8.660254037844390851 ) ) ;
#70622 = EDGE_CURVE ( 'NONE', #49450, #70218, #70282, .T. ) ;
#70623 = EDGE_CURVE ( 'NONE', #4004, #48495, #7319, .T. ) ;
#70624 = CARTESIAN_POINT ( 'NONE',  ( -8.000000000000000000, 119.0000000000000000, 0.000000000000000000 ) ) ;
#70625 = CARTESIAN_POINT ( 'NONE',  ( 2.765530957081996366, 294.2968750017070079, -6.676582343750003368 ) ) ;
#70626 = VERTEX_POINT ( 'NONE', #60054 ) ;
#70627 = EDGE_CURVE ( 'NONE', #72853, #65440, #4908, .T. ) ;
#70628 = PLANE ( 'NONE',  #62649 ) ;
#70629 = CARTESIAN_POINT ( 'NONE',  ( 8.000000000000000000, 16.31249999590322375, 0.000000000000000000 ) ) ;
#70630 = CARTESIAN_POINT ( 'NONE',  ( 2.445694354108783664, 208.3125000013656063, 144.4456943541088663 ) ) ;
#70631 = CARTESIAN_POINT ( 'NONE',  ( -7.320508075688775484, 51.87500000000000000, -7.320508075688776373 ) ) ;
#70632 = CARTESIAN_POINT ( 'NONE',  ( 1.502314598737163567E-15, -20.78460969082658494, -21.50000000000000000 ) ) ;
#70633 = CARTESIAN_POINT ( 'NONE',  ( -5.676582343750000703, 263.3854166700806445, -9.832129032723418760 ) ) ;
#70634 = CARTESIAN_POINT ( 'NONE',  ( -4.999999999999953815, -52.35862550122923409, -48.98731492261434539 ) ) ;
#70635 = CARTESIAN_POINT ( 'NONE',  ( 4.556349186104045934, 11.00000000000000000, 116.0312499999999858 ) ) ;
#70636 = CARTESIAN_POINT ( 'NONE',  ( -8.660254037844390851, 212.9166666666666572, 4.999999999999998224 ) ) ;
#70637 = CARTESIAN_POINT ( 'NONE',  ( -7.188101187499992051, 2.977408999572646930, 9.267802781871754547 ) ) ;
#70638 = CARTESIAN_POINT ( 'NONE',  ( 5.676582343749993598, 180.2604166632526699, 9.832129032723422313 ) ) ;
#70639 = CARTESIAN_POINT ( 'NONE',  ( 3.211159895383560947, 1.187499998634406806, 3.211159895383562723 ) ) ;
#70640 = DIRECTION ( 'NONE',  ( -1.836970198721037823E-16, -4.283267841918042125E-17, 1.000000000000000000 ) ) ;
#70642 = CARTESIAN_POINT ( 'NONE',  ( 4.000000000000001776, 5.000000000000000000, 0.000000000000000000 ) ) ;
#70641 = CARTESIAN_POINT ( 'NONE',  ( -2.828427124746152987, 203.2500000027312126, 200.8284271247462129 ) ) ;
#70643 = ORIENTED_EDGE ( 'NONE', *, *, #72082, .T. ) ;
#70644 = CARTESIAN_POINT ( 'NONE',  ( 2.445694354108784108, 206.5625000013656063, 144.4456943541088663 ) ) ;
#70645 = CARTESIAN_POINT ( 'NONE',  ( 3.042071309553167069, 52.13541666325268409, -11.35316468749999785 ) ) ;
#70646 = CARTESIAN_POINT ( 'NONE',  ( -11.00000000000000000, 0.000000000000000000, 104.6875000040967763 ) ) ;
#70647 = CARTESIAN_POINT ( 'NONE',  ( -2.085542519210945728E-15, 219.8437499965860411, 11.35316468750000141 ) ) ;
#70648 = EDGE_CURVE ( 'NONE', #33693, #42754, #71003, .T. ) ;
#70649 = CARTESIAN_POINT ( 'NONE',  ( -31.45873412500002786, 204.6250000013656063, 168.5673454167828140 ) ) ;
#70650 = CARTESIAN_POINT ( 'NONE',  ( 8.660254037844389075, 10.41666666666666963, -5.000000000000000888 ) ) ;
#70652 = CARTESIAN_POINT ( 'NONE',  ( 6.123233995736767268E-16, 101.2500000000000000, -10.00000000000000178 ) ) ;
#70651 = CARTESIAN_POINT ( 'NONE',  ( -7.188101187499999156, 121.2500000020483952, 2.977408999572654924 ) ) ;
#70653 = CARTESIAN_POINT ( 'NONE',  ( -2.839093476692135984E-14, 194.6875000013655779, 138.5412658750000503 ) ) ;
#70654 =( BOUNDED_CURVE ( )  B_SPLINE_CURVE ( 2, ( #18907, #12501, #64197, #41914, #13230, #46835, #29496, #58548, #53619, #36635, #59643, #70952, #41187 ),
 .UNSPECIFIED., .F., .F. ) 
 B_SPLINE_CURVE_WITH_KNOTS ( ( 3, 2, 2, 2, 2, 2, 3 ),
 ( 1.491489498479788400, 1.496722359883964071, 1.501955221288139519, 1.507188082692314968, 1.512420944096490638, 1.517653805500666087, 1.522886666904841757 ),
 .UNSPECIFIED. ) 
 CURVE ( )  GEOMETRIC_REPRESENTATION_ITEM ( )  RATIONAL_B_SPLINE_CURVE ( ( 0.9999999999999978906, 0.9659258262890704216, 1.000000000000000000, 0.9659258262890683122, 1.000000000000000000, 0.9659258262890683122, 1.000000000000000000, 0.9659258262890683122, 1.000000000000000000, 0.9659258262890683122, 1.000000000000000000, 0.9659258262890474400, 1.000000000000020872 ) ) 
 REPRESENTATION_ITEM ( '' )  );
#70655 = AXIS2_PLACEMENT_3D ( 'NONE', #24635, #70668, #69942 ) ;
#70656 = CARTESIAN_POINT ( 'NONE',  ( -8.660254037844390851, 69.79166665983869677, 4.999999999999998224 ) ) ;
#70657 = CARTESIAN_POINT ( 'NONE',  ( 2.977408999572650039, 95.18750000204838102, -7.188101187500001821 ) ) ;
#70658 = CARTESIAN_POINT ( 'NONE',  ( 4.541265875000002339, 15.49999999863440792, -1.881053915767121554 ) ) ;
#70659 = DIRECTION ( 'NONE',  ( -0.000000000000000000, 1.000000000000000000, -0.000000000000000000 ) ) ;
#70660 = CARTESIAN_POINT ( 'NONE',  ( 3.887681576892050295, 0.3419578554194728781, -6.829612127959068246 ) ) ;
#70661 = CARTESIAN_POINT ( 'NONE',  ( -11.00000000000010303, -4.556349186103947346, 67.28125000409676204 ) ) ;
#70662 = ORIENTED_EDGE ( 'NONE', *, *, #34321, .T. ) ;
#70663 = EDGE_LOOP ( 'NONE', ( #67041, #16580, #5533, #21007 ) ) ;
#70664 = CARTESIAN_POINT ( 'NONE',  ( -4.721056650415999201, 296.4843750017070079, -4.721056650415999201 ) ) ;
#70665 = DIRECTION ( 'NONE',  ( 1.000000000000000000, 2.168404344971008868E-16, 0.000000000000000000 ) ) ;
#70666 = CARTESIAN_POINT ( 'NONE',  ( 0.000000000000000000, 54.99999999999999289, 0.000000000000000000 ) ) ;
#70667 = CARTESIAN_POINT ( 'NONE',  ( 9.832129032723420536, 151.1979166632526983, -5.676582343749999815 ) ) ;
#70668 = DIRECTION ( 'NONE',  ( 0.000000000000000000, -1.000000000000000000, 0.000000000000000000 ) ) ;
#70669 = CARTESIAN_POINT ( 'NONE',  ( -3.999999999999960032, 202.0000000000000000, 198.0000000000000284 ) ) ;
#70670 = CARTESIAN_POINT ( 'NONE',  ( 0.000000000000000000, 0.000000000000000000, 118.0000000000000000 ) ) ;
#70671 = CARTESIAN_POINT ( 'NONE',  ( -10.18810118749999916, 4.220049686691934809, 106.9375000020483810 ) ) ;
#70672 = ORIENTED_EDGE ( 'NONE', *, *, #9377, .T. ) ;
#70673 = FACE_OUTER_BOUND ( 'NONE', #65846, .T. ) ;
#70674 = FACE_OUTER_BOUND ( 'NONE', #57663, .T. ) ;
#70675 = CARTESIAN_POINT ( 'NONE',  ( 8.311093377946837890, 136.7187499965860127, -8.311093377946837890 ) ) ;
#70676 = CARTESIAN_POINT ( 'NONE',  ( 3.458734125000015425, 197.9375000013655779, 198.0000000000000284 ) ) ;
#70677 = CARTESIAN_POINT ( 'NONE',  ( -3.458734124999960358, 209.6250000013656063, 196.5673454167823877 ) ) ;
#70678 = CARTESIAN_POINT ( 'NONE',  ( 7.204075437095966983, 7.204075437095967871, 68.96875000204836681 ) ) ;
#70679 = CARTESIAN_POINT ( 'NONE',  ( -5.676582343749998039, 52.76041666325269119, -9.832129032723420536 ) ) ;
#70680 = ORIENTED_EDGE ( 'NONE', *, *, #48717, .T. ) ;
#70681 = CYLINDRICAL_SURFACE ( 'NONE', #60947, 11.00000000000000000 ) ;
#70682 = CARTESIAN_POINT ( 'NONE',  ( -1.881053915767121776, 5.749999998634407028, -4.541265875000002339 ) ) ;
#70683 = CARTESIAN_POINT ( 'NONE',  ( -8.008118988124991233, 0.000000000000000000, 7.013115283940628331 ) ) ;
#70684 = CARTESIAN_POINT ( 'NONE',  ( 5.082755093536324154, 15.28124999795161187, 5.082755093536326818 ) ) ;
#70685 = CARTESIAN_POINT ( 'NONE',  ( 2.485281374238571317, 292.7500000034140157, -6.000000000000003553 ) ) ;
#70686 = DIRECTION ( 'NONE',  ( -0.000000000000000000, 1.000000000000000000, -0.000000000000000000 ) ) ;
#70687 = CARTESIAN_POINT ( 'NONE',  ( 2.977408999572651815, 14.06249999795161365, 7.188101187500000933 ) ) ;
#70688 = CARTESIAN_POINT ( 'NONE',  ( -5.082755093536317936, -5.082755093536320601, 7.674052781871751883 ) ) ;
#70689 = CARTESIAN_POINT ( 'NONE',  ( 1.871523826299183495E-15, -10.18810118749999916, 116.4062500020483810 ) ) ;
#70690 = CARTESIAN_POINT ( 'NONE',  ( -4.999999999999998224, 63.54166665983869677, -8.660254037844389075 ) ) ;
#70691 = CARTESIAN_POINT ( 'NONE',  ( 4.000000000000001776, 1.812499997268813390, -1.656854249492381248 ) ) ;
#70692 = ORIENTED_EDGE ( 'NONE', *, *, #2542, .T. ) ;
#70693 = EDGE_CURVE ( 'NONE', #22824, #17226, #47990, .T. ) ;
#70694 = CARTESIAN_POINT ( 'NONE',  ( 1.656854249492405451, 195.4375000027312410, 202.0000000000000284 ) ) ;
#70695 = CARTESIAN_POINT ( 'NONE',  ( 3.999999999999960032, 201.0000000000000000, 142.0000000000000568 ) ) ;
#70696 = CARTESIAN_POINT ( 'NONE',  ( -32.00000000000002842, 198.3125000027312126, 168.3431457505080573 ) ) ;
#70697 = VECTOR ( 'NONE', #29408, 1000.000000000000000 ) ;
#70698 = CARTESIAN_POINT ( 'NONE',  ( -1.881053915767121554, 0.6249999986344065839, -4.541265875000002339 ) ) ;
#70699 = CARTESIAN_POINT ( 'NONE',  ( 2.977408999572654480, 114.1250000020483952, 7.188101187499999156 ) ) ;
#70700 = LINE ( 'NONE', #42760, #13898 ) ;
#70701 = CARTESIAN_POINT ( 'NONE',  ( 5.656854249492376141, -5.656854249492374365, 1.580302783920146226 ) ) ;
#70702 = ORIENTED_EDGE ( 'NONE', *, *, #20102, .F. ) ;
#70703 = CARTESIAN_POINT ( 'NONE',  ( -2.977408999572650039, 23.43749999795161187, -7.188101187500000933 ) ) ;
#70704 = ORIENTED_EDGE ( 'NONE', *, *, #2234, .T. ) ;
#70705 = CARTESIAN_POINT ( 'NONE',  ( -4.999999999999996447, 18.53862685874492655, -23.57305537018094199 ) ) ;
#70706 = CARTESIAN_POINT ( 'NONE',  ( -1.432654583217607858, 206.6250000013656063, 201.4587341250000065 ) ) ;
#70707 = CARTESIAN_POINT ( 'NONE',  ( 24.54126587500000412, 202.2500000013655779, 171.4326545832176123 ) ) ;
#70708 = CARTESIAN_POINT ( 'NONE',  ( 8.660254037844389075, 55.41666666666667140, -5.000000000000000000 ) ) ;
#70709 = EDGE_CURVE ( 'NONE', #16897, #41307, #13796, .T. ) ;
#70710 = CARTESIAN_POINT ( 'NONE',  ( -5.082755093536325930, 98.84375000204838102, -5.082755093536325930 ) ) ;
#70711 = CARTESIAN_POINT ( 'NONE',  ( -6.000000000000000888, 297.0624999999999432, 2.485281374238575758 ) ) ;
#70713 = CARTESIAN_POINT ( 'NONE',  ( -27.04877011674714282, -42.27064516945160477, 185.1577813763547908 ) ) ;
#70712 = CARTESIAN_POINT ( 'NONE',  ( 32.64477131386011166, 175.7392241087877380, 161.6181756582431888 ) ) ;
#70714 = ORIENTED_EDGE ( 'NONE', *, *, #66443, .T. ) ;
#70715 = CARTESIAN_POINT ( 'NONE',  ( 5.676582343749997150, 227.2395833367473301, -9.832129032723418760 ) ) ;
#70716 = CARTESIAN_POINT ( 'NONE',  ( 2.977408999572646486, 7.188101187499991163, 13.39280278187175455 ) ) ;
#70717 = CARTESIAN_POINT ( 'NONE',  ( 3.999999999999960032, 195.1250000027311842, 142.0000000000000568 ) ) ;
#70718 = CARTESIAN_POINT ( 'NONE',  ( -2.679491924311161455, 75.41666665983871098, 10.00000000000004441 ) ) ;
#70719 = DIRECTION ( 'NONE',  ( -0.8660254037844381525, 0.5000000000000008882, 0.000000000000000000 ) ) ;
#70720 = CARTESIAN_POINT ( 'NONE',  ( 25.67311473297838020, 194.8285023284833244, 166.9537819464051154 ) ) ;
#70721 = CARTESIAN_POINT ( 'NONE',  ( -2.679491924311235174, 140.4166666598387110, 10.00000000000000000 ) ) ;
#70722 = CARTESIAN_POINT ( 'NONE',  ( 8.660254037844389075, 175.4166666666666572, -5.000000000000000000 ) ) ;
#70723 = CYLINDRICAL_SURFACE ( 'NONE', #54572, 3.999999999999976019 ) ;
#70724 = CARTESIAN_POINT ( 'NONE',  ( 2.679491924311292905, 239.5833333401613174, 9.999999999999968026 ) ) ;
#70725 = CARTESIAN_POINT ( 'NONE',  ( -2.584176044324953292, -67.83040087281803210, 20.22720375976441787 ) ) ;
#70726 = CARTESIAN_POINT ( 'NONE',  ( 11.35316468749999963, 141.3020833299193271, -3.042071309553165293 ) ) ;
#70727 = DIRECTION ( 'NONE',  ( -0.000000000000000000, -1.000000000000000000, -0.000000000000000000 ) ) ;
#70728 = CARTESIAN_POINT ( 'NONE',  ( 8.000000000000000000, 97.43750000409677625, -9.797174393178825657E-16 ) ) ;
#70730 = CARTESIAN_POINT ( 'NONE',  ( 2.849036369511732440E-14, 206.3750000027312126, 202.0000000000000000 ) ) ;
#70729 = CARTESIAN_POINT ( 'NONE',  ( 23.99999999999998224, 206.8125000000000000, 171.6568542494922553 ) ) ;
#70731 = AXIS2_PLACEMENT_3D ( 'NONE', #20824, #61195, #71749 ) ;
#70732 = ORIENTED_EDGE ( 'NONE', *, *, #35899, .F. ) ;
#70733 = CARTESIAN_POINT ( 'NONE',  ( 6.951808397369818766E-16, 7.343749996586017126, -11.35316468750000141 ) ) ;
#70734 = ADVANCED_FACE ( 'NONE', ( #3100 ), #47617, .F. ) ;
#70735 = FACE_OUTER_BOUND ( 'NONE', #35090, .T. ) ;
#70736 = CARTESIAN_POINT ( 'NONE',  ( -2.250000000000000888, 2.250000000000000000, 0.000000000000000000 ) ) ;
#70737 = CARTESIAN_POINT ( 'NONE',  ( -3.458734125000015425, 207.0000000013655779, 143.4326545832176976 ) ) ;
#70738 = CARTESIAN_POINT ( 'NONE',  ( -7.683012701892240059, 124.8169872981077901, 0.000000000000000000 ) ) ;
#70739 = EDGE_CURVE ( 'NONE', #55811, #48555, #9516, .T. ) ;
#70740 = CLOSED_SHELL ( 'NONE', ( #42521, #31562, #65861, #30298, #74263, #10752, #71705, #19712, #70042, #7697, #17494, #15765, #55414, #69467, #7023, #54979 ) ) ;
#70741 = CARTESIAN_POINT ( 'NONE',  ( 7.320508075688771044, 31.24999999317203248, 7.320508075688775484 ) ) ;
#70742 = CARTESIAN_POINT ( 'NONE',  ( 1.320432766682874540E-15, 117.0312500020483810, 7.188101187500000044 ) ) ;
#70743 = CARTESIAN_POINT ( 'NONE',  ( -4.541265875000003227, 3.999999998634406140, 1.881053915767121110 ) ) ;
#70744 = CARTESIAN_POINT ( 'NONE',  ( -11.63187743427350895, -37.01358725097530566, 141.2544095627604008 ) ) ;
#70745 = CARTESIAN_POINT ( 'NONE',  ( 5.656854249492376141, -5.656854249492374365, 16.39280277982336287 ) ) ;
#70747 = CARTESIAN_POINT ( 'NONE',  ( -3.313708498984805573, 26.53125000000000000, 7.999999999999956479 ) ) ;
#70746 = CARTESIAN_POINT ( 'NONE',  ( -28.00000000000002842, 203.0000000000000000, 166.0000000000003695 ) ) ;
#70748 = ORIENTED_EDGE ( 'NONE', *, *, #48682, .F. ) ;
#70749 =( BOUNDED_SURFACE ( )  B_SPLINE_SURFACE ( 1, 2, ( 
 ( #26847, #57027, #73991, #45317, #68332, #49862, #21185, #44210, #38930, #15155, #55173, #61191, #14776, #50238, #54794, #16263, #39303, #73259, #9521, #15526, #61567, #27596, #49492, #38567, #49869, #8764, #3105, #3478, #21932, #72511, #72885, #32536, #32917, #31774, #55547, #21564, #37816, #44962, #4601, #26091, #61932, #38187, #26468, #3860, #60811, #44590, #49111, #72123, #20437, #67602, #26855, #9888, #55923, #50607, #20819, #4233, #21192, #43453, #66467, #43837, #67968, #66852, #44217, #67230, #27221, #9135, #15899, #10259, #33284, #56283, #73627, #32152, #23056, #11003, #46065, #62668, #4978, #45692, #68340, #814, #23802, #5345, #29468, #16635, #447, #11741, #27979, #57783, #63046, #34036, #52478, #17391, #69829, #40416, #50984, #57033, #46805, #73997, #63413, #39669, #6465, #34779, #28714, #6090, #69085, #33656, #18144, #62301, #56662, #5714, #28346, #22675, #10629, #12106, #17766, #63788, #22299, #29095, #23426, #78, #52115, #51353, #46440, #45323, #40782, #74364, #69458, #11371, #35144, #68707, #34405, #17018, #40042, #57407, #51729, #58158, #18879, #24161, #65635, #58888, #53955, #2644, #65262, #35870, #30570, #48648, #7197, #7930, #48281, #47173, #13567, #1553, #36238, #52848, #53592, #42620, #70563, #71287, #58517, #36605, #6823, #64537, #64169, #18514, #70205, #31305, #13200, #19607, #13931, #7566, #35504, #25633, #30200, #2268, #29836, #53221, #47908, #12473, #41521, #24532, #1180, #71656, #12834, #25262, #36972, #47540, #41886, #59615, #59254, #70927, #1903, #30934, #42249, #19239, #64897, #59978, #8294, #24890, #54333, #41159, #72797, #38098, #67139, #15433, #26765, #56199, #72417, #9046, #9798, #72029, #50152, #73169, #38844, #55452, #19977, #14310, #3014, #3388, #42985, #31686, #21106, #26373, #66004, #49021, #32821, #4512, #32060, #21475, #20727, #61847, #10167, #27506, #54706, #49783, #55831, #4147, #25996, #44129, #61474, #67510, #3763, #55080, #33203, #27137, #37345, #38471, #49397, #44497, #15063, #15808, #60343, #8671, #50517, #20345, #43362, #61096, #66378, #43745, #14685, #37726, #60724, #66759, #9424, #32443, #73908, #22975, #40696, #52022, #57694, #63699, #62579, #39583, #44872, #11653, #10911, #29388, #51643, #40323, #22212, #68997, #50893, #12025, #39954, #45239, #34687, #62959, #6382, #46352, #67878, #28630, #10538, #51267, #36974, #11285, #68251, #68621, #34315, #16546, #57319, #33944, #16169, #56943, #4886, #35058, #58071, #5259, #73532, #27882, #6003, #45981, #39211, #17304, #74277, #28260, #21840, #63327, #62212, #29004, #33569, #22587, #56573, #45606, #360, #16930, #17679, #23342, #5630, #69369, #59173, #23713, #65550, #59897, #46717, #70482, #47084, #12755, #36887, #2183, #7844, #53872, #52395, #13116, #65171, #64815, #36152, #29747, #7482, #8211, #30851, #69742, #13483, #1469, #30487, #41443, #24450, #64082, #13844, #47459, #731, #42159, #30119, #35427, #25178, #70122, #36522, #18057, #1822, #18428, #41805, #41072, #64455, #19156, #59532, #58434, #24808, #35787, #18801, #12392, #53504, #48193, #7112, #71201, #6744, #47823, #52761, #1098, #24075, #58801, #53136, #70844, #19519, #42537, #61386, #37640, #2928, #8959, #37263, #72710, #2558, #38763, #61762, #21014, #31971, #38010, #9334, #50064, #71945, #61008, #72326, #31222, #25547, #25915, #44408, #20256, #20641, #54996, #55368, #54248, #3303, #44038, #32354, #48560, #71570, #31599, #54620, #3674, #73078, #9712, #15346, #21385, #43278, #66294, #19892, #67046, #14601, #42898, #26673, #38382, #48933, #49697, #8584, #67421, #43656, #60638, #32734, #66668, #65918, #4059, #14222, #55742, #60257, #26289, #49309, #15720, #14974, #27052, #34596, #51179, #4421, #46260, #73817, #45890, #50432, #4798, #16833, #56112, #39122, #22125, #33118, #40608, #27416, #68904, #17214, #62126, #62491, #5537, #5171, #39860, #56853, #34223, #11195, #62862, #16459, #57225, #51932, #74187, #45150, #39496, #28539, #28167, #51547, #74565, #22877, #69279, #10819, #68160, #40233, #10450, #63236, #11563, #28915, #45514, #10080, #73447, #67796, #33854, #21754, #44783, #57603, #22492, #16087, #33480, #5913, #17590, #68530, #270, #23252, #56482, #27792, #50806, #641, #70394, #1739, #47729, #69652, #41717, #30398, #36432, #24361, #1008, #53783, #70753, #63610, #64729, #18338, #53416, #58710, #47368, #6289, #57985, #24720, #19069, #52305, #7020, #42072, #23988, #40983, #11937, #41352, #17965, #65081, #34968, #71110, #19431, #13394, #64362, #18709, #13027, #7759, #29657, #36064, #30029, #29295, #23623, #35338, #2092, #52672, #53044, #12664, #59081, #46632, #35695, #59445, #7391, #1377, #58350, #30762, #25085, #12306, #48101, #63991, #6655, #46997, #70029, #55655, #3971, #60170, #9625, #71477, #55281, #66576, #8123, #37921, #43186, #65826, #32645, #72231, #49974, #20546, #59809, #37168, #26958, #31126, #43560, #19803, #61300, #14881, #8869, #60918, #49220, #13755, #72991, #42443, #36799, #60545, #8489, #2834, #65461, #66954, #72619, #43945, #54156, #3212, #3585, #54903, #26200, #42809, #9241, #2467, #20923, #25458, #26579, #66202, #32263, #31508, #14506, #48473, #14133, #37545, #54528, #49604, #20168, #25825, #15258, #48844, #38292, #71853, #31880, #16006, #10729, #28821, #39036, #62769, #28453, #27326, #68437, #56388, #16366, #33024, #33762, #22779, #50713, #51459, #38671, #45424, #61673, #44692, #44321, #73363, #50340, #34515, #17123, #15631, #74472, #27702, #67708, #56763, #21667, #51090, #51838, #45801, #67334, #57135, #45064, #5084, #10363, #68077, #56026, #57520, #39403, #5825, #11112, #73729, #4335, #68811, #62038, #34136, #21297, #16741, #33388, #28077, #9994, #4708, #5451, #40148, #22037, #39767, #62402, #74103, #22402, #63153, #11480, #29573, #30308, #17502, #24269, #40519, #23532, #23160, #52218, #29205, #13307, #70667, #69189, #53328, #6566, #46545, #52583, #6196, #41632, #46173, #7671, #30677, #64643, #922, #6931, #52956, #18984, #40892, #29941, #41264, #184, #63525, #69564, #36344, #63897, #64272, #23905, #47280, #11847, #46915, #12941, #1290, #12580, #17875, #69940, #35609, #12209, #58624, #550, #34884, #58265, #35247, #59359, #57889, #18248, #41987, #70306, #35978, #18621, #58997, #7302, #1653, #24634, #64998, #47645, #62227, #8784, #71026, #48387, #39227, #19344, #54817, #8032, #72531, #3128, #20083, #31796, #60454, #24997, #67894, #10554, #48014, #71767, #71391, #14044, #53696, #3499, #9156, #55193, #2007, #14422, #66486, #66114, #31040, #44889, #43097, #54064, #14796, #37456, #42357, #26487, #65373, #26111, #13673, #31416, #2374, #16186, #25738, #32173, #49512, #49131, #36712, #59724, #42728, #37834, #25370, #19716, #72143, #65742, #37080, #60083, #8403, #54443, #2751, #60832, #21858, #48759, #20455, #43473, #28644, #40339, #5644, #57709, #34701, #63341, #39970, #6015, #745, #22990, #45623, #62977, #11666, #51659, #29019, #52038, #374, #69757, #11300, #22602, #23355, #10926, #63715, #12038, #52410, #69013, #33585, #27900, #16562, #16946, #56590, #45254, #46369, #34333, #4905, #62596, #69384, #18070, #68637, #35072, #57334, #23728, #46733, #41086, #68266, #17693, #40710, #58084, #39599, #6395, #29401, #64096, #17319, #2, #50909, #73923, #22228, #33963, #45996, #56960, #5275, #28277, #51283, #74293, #25195, #19536, #1113, #7496, #71216, #24465, #64470, #12405, #19172, #58449, #29761, #12768, #35800, #36537, #54265, #65565, #42554, #2575, #1484, #53150, #6757, #48208, #47473, #42917, #65187, #53887, #58816, #7864, #30501, #24089, #1839, #13862, #41818, #36905, #52775, #59548, #47098, #7126, #35439, #30134, #41457, #25564, #8229, #70136, #59913, #18814, #70496, #64828, #18443, #2199, #13132, #19910, #36166, #31239, #59186, #42175, #13499, #48577, #53520, #30869, #24825, #47839, #70861, #71587, #4442, #55013, #32371, #66687, #15365, #65936, #14990, #32752, #21032, #3695, #37657, #61028, #26693, #14618, #49714, #66312, #8601, #49330, #71961, #27433, #50448, #8977, #33136, #20275, #4076, #38401, #31615, #61404, #38028, #60655, #56132, #44056, #73465, #67066, #54636, #31992, #21773, #2945, #9730, #43298, #10099, #55761, #55386, #27070, #72728, #37281, #14244, #60274, #25934, #9352, #3319, #26307, #48950, #15739, #21404, #67441, #72346, #50084, #73097, #44426, #38778, #20658, #61781, #43675, #292, #16105, #5936, #68552, #28561, #33875, #16855, #56502, #58006, #39881, #6312, #34617, #22514, #27815, #69300, #62515, #57623, #29316, #68924, #39517, #34244, #52325, #10841, #11582, #51954, #50826, #17234, #5191, #34991, #74585, #662, #22899, #62146, #56875, #44800, #10469, #45911, #73837, #63629, #40255, #11216, #63257, #51568, #39142, #67813, #33500, #4819, #62883, #28188, #51199, #22143, #17611, #23272, #46281, #45172 ),
 ( #28936, #68184, #16480, #57246, #74210, #40629, #5559, #45535, #11959, #17986, #53438, #35359, #1397, #52695, #13774, #70413, #53803, #48123, #64748, #41005, #59828, #12683, #59465, #64013, #18360, #30417, #69673, #1029, #35717, #46654, #54178, #12327, #7778, #30783, #24009, #24383, #19088, #18730, #1760, #41738, #47751, #24740, #70774, #30051, #42091, #65481, #13046, #58732, #53064, #65103, #36084, #13414, #36452, #2113, #8143, #47391, #7043, #25106, #47018, #71129, #19452, #42465, #59103, #23647, #58370, #6675, #7410, #29679, #70050, #36818, #31147, #41374, #64385, #31526, #67349, #49237, #32663, #26978, #43580, #71497, #38688, #66220, #38311, #42827, #71872, #9259, #48494, #54548, #14526, #25476, #33043, #19821, #61317, #9642, #2855, #54921, #72638, #72252, #32282, #20565, #26600, #3602, #55296, #8887, #49621, #44338, #66595, #37564, #31900, #20941, #14900, #43962, #66971, #15275, #61690, #3230, #60563, #55672, #25843, #3988, #49991, #21316, #37938, #2484, #65845, #60188, #26217, #14155, #37188, #73007, #60938, #8510, #48863, #15647, #10012, #20186, #43205, #33780, #23175, #199, #17516, #67724, #62786, #68827, #40164, #62055, #34151, #22796, #28836, #16758, #68095, #46187, #63169, #56043, #57151, #10746, #45816, #51107, #39783, #73378, #50359, #17139, #11495, #44709, #74119, #34529, #16383, #33406, #4352, #11128, #27343, #21683, #56406, #10380, #57534, #5843, #51855, #56780, #39053, #69205, #73746, #40532, #63538, #5467, #50731, #45442, #11863, #22053, #16022, #4725, #27720, #28468, #39422, #22421, #45080, #68457, #62421, #5101, #28092, #51477, #74489, #48028, #30691, #29219, #65011, #41278, #6580, #12594, #40906, #1667, #6213, #42371, #65386, #24647, #35622, #41645, #12953, #53709, #937, #64655, #1302, #34899, #52232, #29586, #71038, #23919, #24284, #58636, #59010, #57905, #6944, #47658, #35993, #47297, #52599, #29956, #70321, #58278, #18636, #35263, #564, #18263, #63915, #19357, #23547, #46928, #2020, #12226, #70679, #7315, #46559, #30322, #52969, #69953, #25009, #53340, #69580, #18996, #17891, #64288, #42002, #13319, #36357, #59372, #7683, #37849, #54830, #66497, #20465, #59738, #26884, #21224, #8046, #31809, #8415, #48772, #72915, #38218, #43868, #15190, #13684, #49143, #26500, #26123, #72155, #65754, #43485, #44250, #66883, #31051, #49524, #37466, #14808, #2764, #60467, #49901, #19729, #72544, #61223, #3510, #66126, #71404, #9553, #31430, #20850, #36725, #60846, #54457, #3139, #54078, #25751, #55205, #32567, #42739, #9167, #71779, #8796, #25383, #32184, #55575, #43109, #3891, #2386, #48400, #14057, #37093, #60097, #20095, #14433, #45354, #73656, #67262, #21593, #5375, #51760, #56314, #45723, #44991, #34438, #11402, #28744, #4263, #74024, #28376, #51384, #73291, #68368, #34066, #40072, #28007, #4633, #57438, #74397, #15557, #16665, #21965, #57062, #62329, #51016, #9914, #61595, #22706, #68737, #55953, #10656, #17050, #27629, #44619, #38596, #22327, #32946, #27253, #50638, #50268, #67634, #15929, #63077, #5743, #107, #67996, #33316, #38959, #23085, #16292, #61962, #39696, #10290, #39332, #62697, #33689, #56692, #5009, #11034, #7229, #35534, #53621, #18909, #40445, #1212, #57814, #23831, #476, #36269, #18174, #1579, #70592, #12503, #63444, #7593, #35173, #30232, #11769, #40813, #52881, #17421, #23456, #58188, #69114, #1933, #34807, #53251, #24562, #46468, #46838, #41551, #41189, #24192, #64200, #70236, #47204, #18544, #52509, #64569, #13233, #58550, #6492, #846, #12866, #6854, #35902, #58920, #47569, #30599, #69861, #29499, #41915, #69489, #64925, #59285, #46096, #29866, #6121, #29125, #52142, #17799, #63820, #12136, #72060, #20379, #31717, #61128, #2674, #13961, #14719, #2295, #55114, #3418, #43777, #60376, #24921, #19270, #7962, #8325, #47936, #36637, #3047, #31335, #70953, #53985, #37758, #9459, #37004, #26405, #25663, #66789, #15094, #32475, #59645, #54739, #60757, #9079, #30966, #26032, #66409, #72452, #8703, #60007, #38128, #32093, #42281, #49053, #54365, #49433, #20007, #43395, #65295, #13600, #20760, #55484, #25293, #43016, #48310, #48680, #71318, #19637, #42652, #65663, #71687, #66038, #14345, #37375, #15467, #56976, #62613, #68652, #67542, #44529, #49811, #16578, #15839, #34350, #56607, #45271, #4178, #73939, #55862, #16963, #44905, #27165, #39615, #67910, #11316, #51298, #72827, #33600, #38505, #56228, #32856, #39987, #50552, #33979, #28291, #16203, #21134, #62993, #38873, #10945, #44157, #73202, #10570, #67172, #50182, #61878, #26797, #3797, #61505, #5291, #74311, #21509, #4543, #22241, #73566, #4923, #21876, #27918, #50928, #68282, #10200, #22619, #45637, #39243, #33230, #27538, #9828, #62242, #17, #52052, #42839, #23004, #58463, #11681, #2496, #6773, #23746, #35451, #64109, #28658, #71510, #65857, #51672, #759, #389, #17709, #14166, #8153, #13788, #59839, #57347, #18085, #70150, #69770, #41102, #34718, #12418, #5659, #36831, #46010, #18458, #6409, #29777, #46384, #29414, #19833, #63356, #42477, #31159, #47114, #35086, #40354, #54189, #23371, #65493, #69030, #52792, #69401, #46749, #17334, #40724, #24103, #25490, #57724, #1127, #63731, #52424, #6030, #48504, #29035, #12053, #58097, #54560, #61327, #2867, #60575, #60198, #14536, #66234, #50372, #33055, #31538, #67361, #43591, #8900, #14912, #43216, #3999, #8523, #44721, #67738, #26988, #37952, #43974, #15286, #56054, #3243, #66985, #3615, #37199, #25854, #31913, #73390, #26229, #26610, #60952, #9655, #48875, #9270, #50002, #38322, #49634, #54934, #32292, #72650, #49249, #20952, #37576, #71884, #20578, #72264, #21695, #20198, #66606, #4363, #55307, #73019, #32675, #55684, #21330, #44351, #15659, #27354, #38701, #61702, #10023, #23190, #46202, #39431, #211, #73757, #68841, #28480, #33417, #74498, #74130, #68104, #69216, #57161, #17527, #5478, #10392, #16394, #40544, #56417, #51488, #22064, #51870, #22807, #16768, #45828, #17154, #39065, #16033, #62067, #50742, #40175, #5112, #45451, #4738, #27732, #45090, #62431, #10756, #28847, #33795, #56793, #28102, #63178, #51118, #22432, #68468, #62800, #39795, #11140, #34161, #11505, #34538, #57545, #5853, #62198, #5246, #10897, #16916, #15794, #67496, #72783, #39571, #38829, #57305, #4874, #68238, #27122, #22199, #4131, #39939, #67862, #50137, #62567, #16155, #34301, #74265, #21090, #56559, #38457, #4497, #55814, #62945, #73517, #56931, #51254, #39196, #44113, #11269, #61832, #33931, #67122, #21460, #33555, #15417, #73152, #10151, #49766, #26748, #61459, #28246, #22573, #44482, #27490, #45226, #21824, #27869, #44857, #50880, #73895, #16531, #33188, #45593, #68607, #10523, #56185, #50503, #9785, #32806, #52750, #1086, #12377, #41792, #58057, #69355, #70109, #57680, #24437, #41059, #5616, #74644, #63313, #63685, #28616, #17291, #58423, #12012, #51629, #34675, #18415, #64801, #17665, #58788, #6368, #47445, #70469, #13103, #40310, #35413, #41429, #64441, #11639, #6731, #47072, #53123, #64069, #40683, #18787, #12742, #22959, #29735, #35045, #35773, #716, #24062, #45968, #68982, #7098, #30106, #5988, #23700, #1456, #29374, #28990, #52008, #36139, #346, #23326, #46338, #52381, #46705, #69729, #18044, #43264, #49296, #48181, #25164, #30474, #71932, #71188, #14960, #37248, #25902, #59518, #54607, #36509, #72313, #25534, #7831, #20244, #48547, #66652, #31957, #53491, #14210, #70831, #36876, #13470, #20626, #31209, #14586, #8945, #71557, #1808, #43642, #19507, #66279, #24795, #53857, #65904, #47808, #30836, #42525, #7469, #59160, #19143, #37625, #60622, #2169, #59884, #2914, #54234, #60244, #2543, #8570, #31586, #48919, #65539, #54982, #26275, #19879, #13830, #8197, #3289, #42885, #42146, #65159, #44769, #74174, #15707, #27037, #27778, #15332, #68148, #16445, #9321, #73804, #45136, #67033, #38749, #33467, #33102, #67783, #10066, #62113, #39109, #16075, #44394, #10437, #5160, #27404, #50048, #67408, #56469, #56099, #4785, #50791, #22112, #22478, #61749, #73064, #39481, #38367, #62477, #10807, #56839, #73433, #37997, #32342, #20998, #21370, #60995, #49682, #33841, #4408, #55354, #61373, #28152, #45499, #50419, #51165, #21741, #68517, #3659, #26659, #72696, #44024, #9699, #32720, #55728, #4044, #59342, #65356, #53312, #29922, #8016, #24980, #16819, #18967, #47262, #7654, #12923, #1636, #34208, #11184, #30660, #47997, #5525, #35957, #1990, #52940, #68891, #39847, #24617, #62848, #57211, #47626, #28526, #70647, #41970, #71011, #19326, #31023, #6911, #58605, #51534, #53678, #1270, #48368, #64980, #42339, #17201, #13288, #40220, #54047, #58977, #63223, #13656, #7284, #25352, #36696, #74551, #36328, #22862, #70289, #45877, #2358, #64627, #59708, #11550, #30292, #35591, #24250, #18603, #41613 ) ),
 .UNSPECIFIED., .F., .F., .F. ) 
 B_SPLINE_SURFACE_WITH_KNOTS ( ( 2, 2 ),
 ( 3, 2, 2, 2, 2, 2, 2, 2, 2, 2, 2, 2, 2, 2, 2, 2, 2, 2, 2, 2, 2, 2, 2, 2, 2, 2, 2, 2, 2, 2, 2, 2, 2, 2, 2, 2, 2, 2, 2, 2, 2, 2, 2, 2, 2, 2, 2, 2, 2, 2, 2, 2, 2, 2, 2, 2, 2, 2, 2, 2, 2, 2, 2, 2, 2, 2, 2, 2, 2, 2, 2, 2, 2, 2, 2, 2, 2, 2, 2, 2, 2, 2, 2, 2, 2, 2, 2, 2, 2, 2, 2, 2, 2, 2, 2, 2, 2, 2, 2, 2, 2, 2, 2, 2, 2, 2, 2, 2, 2, 2, 2, 2, 2, 2, 2, 2, 2, 2, 2, 2, 2, 2, 2, 2, 2, 2, 2, 2, 2, 2, 2, 2, 2, 2, 2, 2, 2, 2, 2, 2, 2, 2, 2, 2, 2, 2, 2, 2, 2, 2, 2, 2, 2, 2, 2, 2, 2, 2, 2, 2, 2, 2, 2, 2, 2, 2, 2, 2, 2, 2, 2, 2, 2, 2, 2, 2, 2, 2, 2, 2, 2, 2, 2, 2, 2, 2, 2, 2, 2, 2, 2, 2, 2, 2, 2, 2, 2, 2, 2, 2, 2, 2, 2, 2, 2, 2, 2, 2, 2, 2, 2, 2, 2, 2, 2, 2, 2, 2, 2, 2, 2, 2, 2, 2, 2, 2, 2, 2, 2, 2, 2, 2, 2, 2, 2, 2, 2, 2, 2, 2, 2, 2, 2, 2, 2, 2, 2, 2, 2, 2, 2, 2, 2, 2, 2, 2, 2, 2, 2, 2, 2, 2, 2, 2, 2, 2, 2, 2, 2, 2, 2, 2, 2, 2, 2, 2, 2, 2, 2, 2, 2, 2, 2, 2, 2, 2, 2, 2, 2, 2, 2, 2, 2, 2, 2, 2, 2, 2, 2, 2, 2, 2, 2, 2, 2, 2, 2, 2, 2, 2, 2, 2, 2, 2, 2, 2, 2, 2, 2, 2, 2, 2, 2, 2, 2, 2, 2, 2, 2, 2, 2, 2, 2, 2, 2, 2, 2, 2, 2, 2, 2, 2, 2, 2, 2, 2, 2, 2, 2, 2, 2, 2, 2, 2, 2, 2, 2, 2, 2, 2, 2, 2, 2, 2, 2, 2, 2, 2, 2, 2, 2, 2, 2, 2, 2, 2, 2, 2, 2, 2, 2, 2, 2, 2, 2, 2, 2, 2, 2, 2, 2, 2, 2, 2, 2, 2, 2, 2, 2, 2, 2, 2, 2, 2, 2, 2, 2, 2, 2, 2, 2, 2, 2, 2, 2, 2, 2, 2, 2, 2, 2, 2, 2, 2, 2, 2, 2, 2, 2, 2, 2, 2, 2, 2, 2, 2, 2, 2, 2, 2, 2, 2, 2, 2, 2, 2, 2, 2, 2, 2, 2, 2, 2, 2, 2, 2, 2, 2, 2, 2, 2, 2, 2, 2, 2, 2, 2, 2, 2, 2, 2, 2, 2, 2, 2, 2, 2, 2, 2, 2, 2, 2, 2, 2, 2, 2, 2, 2, 2, 2, 2, 2, 2, 2, 2, 2, 2, 2, 2, 2, 2, 2, 2, 2, 2, 2, 2, 2, 2, 2, 2, 2, 2, 2, 2, 2, 2, 2, 2, 2, 2, 2, 2, 2, 2, 2, 2, 2, 2, 2, 2, 2, 2, 2, 2, 2, 2, 2, 2, 2, 2, 2, 2, 3 ),
 ( 0.000000000000000000, 1.000000000000000000 ),
 ( 0.000000000000000000, 0.001811594202898550747, 0.003623188405797101493, 0.005434782608695652023, 0.007246376811594202987, 0.009057971014492753950, 0.01086956521739130405, 0.01268115942028985588, 0.01449275362318840597, 0.01630434782608695607, 0.01811594202898550790, 0.01992753623188405626, 0.02173913043478260809, 0.02355072463768115992, 0.02536231884057971175, 0.02717391304347826012, 0.02898550724637681195, 0.03079710144927536378, 0.03260869565217391214, 0.03442028985507246397, 0.03623188405797101580, 0.03804347826086956763, 0.03985507246376811252, 0.04166666666666666435, 0.04347826086956521618, 0.04528985507246376802, 0.04710144927536231985, 0.04891304347826087168, 0.05072463768115942351, 0.05253623188405796840, 0.05434782608695652023, 0.05615942028985507206, 0.05797101449275362389, 0.05978260869565217572, 0.06159420289855072755, 0.06340579710144927938, 0.06521739130434782428, 0.06702898550724638305, 0.06884057971014492794, 0.07065217391304347283, 0.07246376811594203160, 0.07427536231884057649, 0.07608695652173913526, 0.07789855072463768015, 0.07971014492753622505, 0.08152173913043478382, 0.08333333333333332871, 0.08514492753623188748, 0.08695652173913043237, 0.08876811594202899114, 0.09057971014492753603, 0.09239130434782608092, 0.09420289855072463969, 0.09601449275362318458, 0.09782608695652174335, 0.09963768115942028825, 0.1014492753623188470, 0.1032608695652173919, 0.1050724637681159368, 0.1068840579710144956, 0.1086956521739130405, 0.1105072463768115992, 0.1123188405797101441, 0.1141304347826086890, 0.1159420289855072478, 0.1177536231884057927, 0.1195652173913043514, 0.1213768115942028963, 0.1231884057971014551, 0.1250000000000000000, 0.1268115942028985588, 0.1286231884057970898, 0.1304347826086956486, 0.1322463768115942073, 0.1340579710144927661, 0.1358695652173912971, 0.1376811594202898559, 0.1394927536231884146, 0.1413043478260869457, 0.1431159420289855044, 0.1449275362318840632, 0.1467391304347826220, 0.1485507246376811530, 0.1503623188405797118, 0.1521739130434782705, 0.1539855072463768015, 0.1557971014492753603, 0.1576086956521739191, 0.1594202898550724501, 0.1612318840579710089, 0.1630434782608695676, 0.1648550724637681264, 0.1666666666666666574, 0.1684782608695652162, 0.1702898550724637750, 0.1721014492753623060, 0.1739130434782608647, 0.1757246376811594235, 0.1775362318840579823, 0.1793478260869565133, 0.1811594202898550721, 0.1829710144927536308, 0.1847826086956521618, 0.1865942028985507206, 0.1884057971014492794, 0.1902173913043478382, 0.1920289855072463692, 0.1938405797101449279, 0.1956521739130434867, 0.1974637681159420177, 0.1992753623188405765, 0.2010869565217391353, 0.2028985507246376940, 0.2047101449275362250, 0.2065217391304347838, 0.2083333333333333426, 0.2101449275362318736, 0.2119565217391304324, 0.2137681159420289911, 0.2155797101449275499, 0.2173913043478260809, 0.2192028985507246397, 0.2210144927536231985, 0.2228260869565217295, 0.2246376811594202882, 0.2264492753623188470, 0.2282608695652173780, 0.2300724637681159368, 0.2318840579710144956, 0.2336956521739130543, 0.2355072463768115854, 0.2373188405797101441, 0.2391304347826087029, 0.2409420289855072339, 0.2427536231884057927, 0.2445652173913043514, 0.2463768115942029102, 0.2481884057971014412, 0.2500000000000000000, 0.2518115942028985588, 0.2536231884057971175, 0.2554347826086956763, 0.2572463768115941796, 0.2590579710144927383, 0.2608695652173912971, 0.2626811594202898559, 0.2644927536231884146, 0.2663043478260869734, 0.2681159420289855322, 0.2699275362318840354, 0.2717391304347825942, 0.2735507246376811530, 0.2753623188405797118, 0.2771739130434782705, 0.2789855072463768293, 0.2807971014492753881, 0.2826086956521738913, 0.2844202898550724501, 0.2862318840579710089, 0.2880434782608695676, 0.2898550724637681264, 0.2916666666666666852, 0.2934782608695652439, 0.2952898550724637472, 0.2971014492753623060, 0.2989130434782608647, 0.3007246376811594235, 0.3025362318840579823, 0.3043478260869565410, 0.3061594202898550998, 0.3079710144927536031, 0.3097826086956521618, 0.3115942028985507206, 0.3134057971014492794, 0.3152173913043478382, 0.3170289855072463969, 0.3188405797101449002, 0.3206521739130434590, 0.3224637681159420177, 0.3242753623188405765, 0.3260869565217391353, 0.3278985507246376940, 0.3297101449275362528, 0.3315217391304347561, 0.3333333333333333148, 0.3351449275362318736, 0.3369565217391304324, 0.3387681159420289911, 0.3405797101449275499, 0.3423913043478261087, 0.3442028985507246119, 0.3460144927536231707, 0.3478260869565217295, 0.3496376811594202882, 0.3514492753623188470, 0.3532608695652174058, 0.3550724637681159646, 0.3568840579710144678, 0.3586956521739130266, 0.3605072463768115854, 0.3623188405797101441, 0.3641304347826087029, 0.3659420289855072617, 0.3677536231884058204, 0.3695652173913043237, 0.3713768115942028825, 0.3731884057971014412, 0.3750000000000000000, 0.3768115942028985588, 0.3786231884057971175, 0.3804347826086956763, 0.3822463768115941796, 0.3840579710144927383, 0.3858695652173912971, 0.3876811594202898559, 0.3894927536231884146, 0.3913043478260869734, 0.3931159420289855322, 0.3949275362318840354, 0.3967391304347825942, 0.3985507246376811530, 0.4003623188405797118, 0.4021739130434782705, 0.4039855072463768293, 0.4057971014492753881, 0.4076086956521738913, 0.4094202898550724501, 0.4112318840579710089, 0.4130434782608695676, 0.4148550724637681264, 0.4166666666666666852, 0.4184782608695652439, 0.4202898550724637472, 0.4221014492753623060, 0.4239130434782608647, 0.4257246376811594235, 0.4275362318840579823, 0.4293478260869565410, 0.4311594202898550998, 0.4329710144927536031, 0.4347826086956521618, 0.4365942028985507206, 0.4384057971014492794, 0.4402173913043478382, 0.4420289855072463969, 0.4438405797101449002, 0.4456521739130434590, 0.4474637681159420177, 0.4492753623188405765, 0.4510869565217391353, 0.4528985507246376940, 0.4547101449275362528, 0.4565217391304347561, 0.4583333333333333148, 0.4601449275362318736, 0.4619565217391304324, 0.4637681159420289911, 0.4655797101449275499, 0.4673913043478261087, 0.4692028985507246119, 0.4710144927536231707, 0.4728260869565217295, 0.4746376811594202882, 0.4764492753623188470, 0.4782608695652174058, 0.4800724637681159646, 0.4818840579710144678, 0.4836956521739130266, 0.4855072463768115854, 0.4873188405797101441, 0.4891304347826087029, 0.4909420289855072617, 0.4927536231884058204, 0.4945652173913043237, 0.4963768115942028825, 0.4981884057971014412, 0.5000000000000000000, 0.5018115942028985588, 0.5036231884057971175, 0.5054347826086956763, 0.5072463768115942351, 0.5090579710144927938, 0.5108695652173913526, 0.5126811594202898004, 0.5144927536231883591, 0.5163043478260869179, 0.5181159420289854767, 0.5199275362318840354, 0.5217391304347825942, 0.5235507246376811530, 0.5253623188405797118, 0.5271739130434782705, 0.5289855072463768293, 0.5307971014492753881, 0.5326086956521739468, 0.5344202898550725056, 0.5362318840579710644, 0.5380434782608695121, 0.5398550724637680709, 0.5416666666666666297, 0.5434782608695651884, 0.5452898550724637472, 0.5471014492753623060, 0.5489130434782608647, 0.5507246376811594235, 0.5525362318840579823, 0.5543478260869565410, 0.5561594202898550998, 0.5579710144927536586, 0.5597826086956522174, 0.5615942028985507761, 0.5634057971014492239, 0.5652173913043477826, 0.5670289855072463414, 0.5688405797101449002, 0.5706521739130434590, 0.5724637681159420177, 0.5742753623188405765, 0.5760869565217391353, 0.5778985507246376940, 0.5797101449275362528, 0.5815217391304348116, 0.5833333333333333703, 0.5851449275362319291, 0.5869565217391304879, 0.5887681159420289356, 0.5905797101449274944, 0.5923913043478260532, 0.5942028985507246119, 0.5960144927536231707, 0.5978260869565217295, 0.5996376811594202882, 0.6014492753623188470, 0.6032608695652174058, 0.6050724637681159646, 0.6068840579710145233, 0.6086956521739130821, 0.6105072463768116409, 0.6123188405797101996, 0.6141304347826086474, 0.6159420289855072062, 0.6177536231884057649, 0.6195652173913043237, 0.6213768115942028825, 0.6231884057971014412, 0.6250000000000000000, 0.6268115942028985588, 0.6286231884057971175, 0.6304347826086956763, 0.6322463768115942351, 0.6340579710144927938, 0.6358695652173913526, 0.6376811594202898004, 0.6394927536231883591, 0.6413043478260869179, 0.6431159420289854767, 0.6449275362318840354, 0.6467391304347825942, 0.6485507246376811530, 0.6503623188405797118, 0.6521739130434782705, 0.6539855072463768293, 0.6557971014492753881, 0.6576086956521739468, 0.6594202898550725056, 0.6612318840579710644, 0.6630434782608695121, 0.6648550724637680709, 0.6666666666666666297, 0.6684782608695651884, 0.6702898550724637472, 0.6721014492753623060, 0.6739130434782608647, 0.6757246376811594235, 0.6775362318840579823, 0.6793478260869565410, 0.6811594202898550998, 0.6829710144927536586, 0.6847826086956522174, 0.6865942028985507761, 0.6884057971014492239, 0.6902173913043477826, 0.6920289855072463414, 0.6938405797101449002, 0.6956521739130434590, 0.6974637681159420177, 0.6992753623188405765, 0.7010869565217391353, 0.7028985507246376940, 0.7047101449275362528, 0.7065217391304348116, 0.7083333333333333703, 0.7101449275362319291, 0.7119565217391304879, 0.7137681159420289356, 0.7155797101449274944, 0.7173913043478260532, 0.7192028985507246119, 0.7210144927536231707, 0.7228260869565217295, 0.7246376811594202882, 0.7264492753623188470, 0.7282608695652174058, 0.7300724637681159646, 0.7318840579710145233, 0.7336956521739130821, 0.7355072463768116409, 0.7373188405797101996, 0.7391304347826086474, 0.7409420289855072062, 0.7427536231884057649, 0.7445652173913043237, 0.7463768115942028825, 0.7481884057971014412, 0.7500000000000000000, 0.7518115942028985588, 0.7536231884057971175, 0.7554347826086956763, 0.7572463768115942351, 0.7590579710144927938, 0.7608695652173913526, 0.7626811594202898004, 0.7644927536231883591, 0.7663043478260869179, 0.7681159420289854767, 0.7699275362318840354, 0.7717391304347825942, 0.7735507246376811530, 0.7753623188405797118, 0.7771739130434782705, 0.7789855072463768293, 0.7807971014492753881, 0.7826086956521739468, 0.7844202898550725056, 0.7862318840579710644, 0.7880434782608695121, 0.7898550724637680709, 0.7916666666666666297, 0.7934782608695651884, 0.7952898550724637472, 0.7971014492753623060, 0.7989130434782608647, 0.8007246376811594235, 0.8025362318840579823, 0.8043478260869565410, 0.8061594202898550998, 0.8079710144927536586, 0.8097826086956522174, 0.8115942028985507761, 0.8134057971014492239, 0.8152173913043477826, 0.8170289855072463414, 0.8188405797101449002, 0.8206521739130434590, 0.8224637681159420177, 0.8242753623188405765, 0.8260869565217391353, 0.8278985507246376940, 0.8297101449275362528, 0.8315217391304348116, 0.8333333333333333703, 0.8351449275362319291, 0.8369565217391304879, 0.8387681159420289356, 0.8405797101449274944, 0.8423913043478260532, 0.8442028985507246119, 0.8460144927536231707, 0.8478260869565217295, 0.8496376811594202882, 0.8514492753623188470, 0.8532608695652174058, 0.8550724637681159646, 0.8568840579710145233, 0.8586956521739130821, 0.8605072463768116409, 0.8623188405797101996, 0.8641304347826086474, 0.8659420289855072062, 0.8677536231884057649, 0.8695652173913043237, 0.8713768115942028825, 0.8731884057971014412, 0.8750000000000000000, 0.8768115942028985588, 0.8786231884057971175, 0.8804347826086956763, 0.8822463768115942351, 0.8840579710144927938, 0.8858695652173913526, 0.8876811594202898004, 0.8894927536231883591, 0.8913043478260869179, 0.8931159420289854767, 0.8949275362318840354, 0.8967391304347825942, 0.8985507246376811530, 0.9003623188405797118, 0.9021739130434782705, 0.9039855072463768293, 0.9057971014492753881, 0.9076086956521739468, 0.9094202898550725056, 0.9112318840579710644, 0.9130434782608695121, 0.9148550724637680709, 0.9166666666666666297, 0.9184782608695651884, 0.9202898550724637472, 0.9221014492753623060, 0.9239130434782608647, 0.9257246376811594235, 0.9275362318840579823, 0.9293478260869565410, 0.9311594202898550998, 0.9329710144927536586, 0.9347826086956522174, 0.9365942028985507761, 0.9384057971014492239, 0.9402173913043477826, 0.9420289855072463414, 0.9438405797101449002, 0.9456521739130434590, 0.9474637681159420177, 0.9492753623188405765, 0.9510869565217391353, 0.9528985507246376940, 0.9547101449275362528, 0.9565217391304348116, 0.9583333333333333703, 0.9601449275362319291, 0.9619565217391304879, 0.9637681159420289356, 0.9655797101449274944, 0.9673913043478260532, 0.9692028985507246119, 0.9710144927536231707, 0.9728260869565217295, 0.9746376811594202882, 0.9764492753623188470, 0.9782608695652174058, 0.9800724637681159646, 0.9818840579710145233, 0.9826096903791191606 ),
 .UNSPECIFIED. ) 
 GEOMETRIC_REPRESENTATION_ITEM ( )  RATIONAL_B_SPLINE_SURFACE ( (
 ( 1.000000000000000000, 0.9659258262890683122, 1.000000000000000000, 0.9659258262890683122, 1.000000000000000000, 0.9659258262890683122, 1.000000000000000000, 0.9659258262890683122, 1.000000000000000000, 0.9659258262890683122, 1.000000000000000000, 0.9659258262890683122, 1.000000000000000000, 0.9659258262890683122, 1.000000000000000000, 0.9659258262890683122, 1.000000000000000000, 0.9659258262890683122, 1.000000000000000000, 0.9659258262890683122, 1.000000000000000000, 0.9659258262890683122, 1.000000000000000000, 0.9659258262890683122, 1.000000000000000000, 0.9659258262890683122, 1.000000000000000000, 0.9659258262890683122, 1.000000000000000000, 0.9659258262890683122, 1.000000000000000000, 0.9659258262890683122, 1.000000000000000000, 0.9659258262890683122, 1.000000000000000000, 0.9659258262890683122, 1.000000000000000000, 0.9659258262890683122, 1.000000000000000000, 0.9659258262890683122, 1.000000000000000000, 0.9659258262890683122, 1.000000000000000000, 0.9659258262890683122, 1.000000000000000000, 0.9659258262890683122, 1.000000000000000000, 0.9659258262890683122, 1.000000000000000000, 0.9659258262890683122, 1.000000000000000000, 0.9659258262890683122, 1.000000000000000000, 0.9659258262890683122, 1.000000000000000000, 0.9659258262890683122, 1.000000000000000000, 0.9659258262890683122, 1.000000000000000000, 0.9659258262890683122, 1.000000000000000000, 0.9659258262890683122, 1.000000000000000000, 0.9659258262890683122, 1.000000000000000000, 0.9659258262890683122, 1.000000000000000000, 0.9659258262890683122, 1.000000000000000000, 0.9659258262890683122, 1.000000000000000000, 0.9659258262890683122, 1.000000000000000000, 0.9659258262890683122, 1.000000000000000000, 0.9659258262890683122, 1.000000000000000000, 0.9659258262890683122, 1.000000000000000000, 0.9659258262890683122, 1.000000000000000000, 0.9659258262890683122, 1.000000000000000000, 0.9659258262890683122, 1.000000000000000000, 0.9659258262890683122, 1.000000000000000000, 0.9659258262890683122, 1.000000000000000000, 0.9659258262890683122, 1.000000000000000000, 0.9659258262890683122, 1.000000000000000000, 0.9659258262890683122, 1.000000000000000000, 0.9659258262890683122, 1.000000000000000000, 0.9659258262890683122, 1.000000000000000000, 0.9659258262890683122, 1.000000000000000000, 0.9659258262890683122, 1.000000000000000000, 0.9659258262890683122, 1.000000000000000000, 0.9659258262890683122, 1.000000000000000000, 0.9659258262890683122, 1.000000000000000000, 0.9659258262890683122, 1.000000000000000000, 0.9659258262890683122, 1.000000000000000000, 0.9659258262890683122, 1.000000000000000000, 0.9659258262890683122, 1.000000000000000000, 0.9659258262890683122, 1.000000000000000000, 0.9659258262890683122, 1.000000000000000000, 0.9659258262890683122, 1.000000000000000000, 0.9659258262890683122, 1.000000000000000000, 0.9659258262890683122, 1.000000000000000000, 0.9659258262890683122, 1.000000000000000000, 0.9659258262890683122, 1.000000000000000000, 0.9659258262890683122, 1.000000000000000000, 0.9659258262890683122, 1.000000000000000000, 0.9659258262890683122, 1.000000000000000000, 0.9659258262890683122, 1.000000000000000000, 0.9659258262890683122, 1.000000000000000000, 0.9659258262890683122, 1.000000000000000000, 0.9659258262890683122, 1.000000000000000000, 0.9659258262890683122, 1.000000000000000000, 0.9659258262890683122, 1.000000000000000000, 0.9659258262890683122, 1.000000000000000000, 0.9659258262890683122, 1.000000000000000000, 0.9659258262890683122, 1.000000000000000000, 0.9659258262890683122, 1.000000000000000000, 0.9659258262890683122, 1.000000000000000000, 0.9659258262890683122, 1.000000000000000000, 0.9659258262890683122, 1.000000000000000000, 0.9659258262890683122, 1.000000000000000000, 0.9659258262890683122, 1.000000000000000000, 0.9659258262890683122, 1.000000000000000000, 0.9659258262890683122, 1.000000000000000000, 0.9659258262890683122, 1.000000000000000000, 0.9659258262890683122, 1.000000000000000000, 0.9659258262890683122, 1.000000000000000000, 0.9659258262890683122, 1.000000000000000000, 0.9659258262890683122, 1.000000000000000000, 0.9659258262890683122, 1.000000000000000000, 0.9659258262890683122, 1.000000000000000000, 0.9659258262890683122, 1.000000000000000000, 0.9659258262890683122, 1.000000000000000000, 0.9659258262890683122, 1.000000000000000000, 0.9659258262890683122, 1.000000000000000000, 0.9659258262890683122, 1.000000000000000000, 0.9659258262890683122, 1.000000000000000000, 0.9659258262890683122, 1.000000000000000000, 0.9659258262890683122, 1.000000000000000000, 0.9659258262890683122, 1.000000000000000000, 0.9659258262890683122, 1.000000000000000000, 0.9659258262890683122, 1.000000000000000000, 0.9659258262890683122, 1.000000000000000000, 0.9659258262890683122, 1.000000000000000000, 0.9659258262890683122, 1.000000000000000000, 0.9659258262890683122, 1.000000000000000000, 0.9659258262890683122, 1.000000000000000000, 0.9659258262890683122, 1.000000000000000000, 0.9659258262890683122, 1.000000000000000000, 0.9659258262890683122, 1.000000000000000000, 0.9659258262890683122, 1.000000000000000000, 0.9659258262890683122, 1.000000000000000000, 0.9659258262890683122, 1.000000000000000000, 0.9659258262890683122, 1.000000000000000000, 0.9659258262890683122, 1.000000000000000000, 0.9659258262890683122, 1.000000000000000000, 0.9659258262890683122, 1.000000000000000000, 0.9659258262890683122, 1.000000000000000000, 0.9659258262890683122, 1.000000000000000000, 0.9659258262890683122, 1.000000000000000000, 0.9659258262890683122, 1.000000000000000000, 0.9659258262890683122, 1.000000000000000000, 0.9659258262890683122, 1.000000000000000000, 0.9659258262890683122, 1.000000000000000000, 0.9659258262890683122, 1.000000000000000000, 0.9659258262890683122, 1.000000000000000000, 0.9659258262890683122, 1.000000000000000000, 0.9659258262890683122, 1.000000000000000000, 0.9659258262890683122, 1.000000000000000000, 0.9659258262890683122, 1.000000000000000000, 0.9659258262890683122, 1.000000000000000000, 0.9659258262890683122, 1.000000000000000000, 0.9659258262890683122, 1.000000000000000000, 0.9659258262890683122, 1.000000000000000000, 0.9659258262890683122, 1.000000000000000000, 0.9659258262890683122, 1.000000000000000000, 0.9659258262890683122, 1.000000000000000000, 0.9659258262890683122, 1.000000000000000000, 0.9659258262890683122, 1.000000000000000000, 0.9659258262890683122, 1.000000000000000000, 0.9659258262890683122, 1.000000000000000000, 0.9659258262890683122, 1.000000000000000000, 0.9659258262890683122, 1.000000000000000000, 0.9659258262890683122, 1.000000000000000000, 0.9659258262890683122, 1.000000000000000000, 0.9659258262890683122, 1.000000000000000000, 0.9659258262890683122, 1.000000000000000000, 0.9659258262890683122, 1.000000000000000000, 0.9659258262890683122, 1.000000000000000000, 0.9659258262890683122, 1.000000000000000000, 0.9659258262890683122, 1.000000000000000000, 0.9659258262890683122, 1.000000000000000000, 0.9659258262890683122, 1.000000000000000000, 0.9659258262890683122, 1.000000000000000000, 0.9659258262890683122, 1.000000000000000000, 0.9659258262890683122, 1.000000000000000000, 0.9659258262890683122, 1.000000000000000000, 0.9659258262890683122, 1.000000000000000000, 0.9659258262890683122, 1.000000000000000000, 0.9659258262890683122, 1.000000000000000000, 0.9659258262890683122, 1.000000000000000000, 0.9659258262890683122, 1.000000000000000000, 0.9659258262890683122, 1.000000000000000000, 0.9659258262890683122, 1.000000000000000000, 0.9659258262890683122, 1.000000000000000000, 0.9659258262890683122, 1.000000000000000000, 0.9659258262890683122, 1.000000000000000000, 0.9659258262890683122, 1.000000000000000000, 0.9659258262890683122, 1.000000000000000000, 0.9659258262890683122, 1.000000000000000000, 0.9659258262890683122, 1.000000000000000000, 0.9659258262890683122, 1.000000000000000000, 0.9659258262890683122, 1.000000000000000000, 0.9659258262890683122, 1.000000000000000000, 0.9659258262890683122, 1.000000000000000000, 0.9659258262890683122, 1.000000000000000000, 0.9659258262890683122, 1.000000000000000000, 0.9659258262890683122, 1.000000000000000000, 0.9659258262890683122, 1.000000000000000000, 0.9659258262890683122, 1.000000000000000000, 0.9659258262890683122, 1.000000000000000000, 0.9659258262890683122, 1.000000000000000000, 0.9659258262890683122, 1.000000000000000000, 0.9659258262890683122, 1.000000000000000000, 0.9659258262890683122, 1.000000000000000000, 0.9659258262890683122, 1.000000000000000000, 0.9659258262890683122, 1.000000000000000000, 0.9659258262890683122, 1.000000000000000000, 0.9659258262890683122, 1.000000000000000000, 0.9659258262890683122, 1.000000000000000000, 0.9659258262890683122, 1.000000000000000000, 0.9659258262890683122, 1.000000000000000000, 0.9659258262890683122, 1.000000000000000000, 0.9659258262890683122, 1.000000000000000000, 0.9659258262890683122, 1.000000000000000000, 0.9659258262890683122, 1.000000000000000000, 0.9659258262890683122, 1.000000000000000000, 0.9659258262890683122, 1.000000000000000000, 0.9659258262890683122, 1.000000000000000000, 0.9659258262890683122, 1.000000000000000000, 0.9659258262890683122, 1.000000000000000000, 0.9659258262890683122, 1.000000000000000000, 0.9659258262890683122, 1.000000000000000000, 0.9659258262890683122, 1.000000000000000000, 0.9659258262890683122, 1.000000000000000000, 0.9659258262890683122, 1.000000000000000000, 0.9659258262890683122, 1.000000000000000000, 0.9659258262890683122, 1.000000000000000000, 0.9659258262890683122, 1.000000000000000000, 0.9659258262890683122, 1.000000000000000000, 0.9659258262890683122, 1.000000000000000000, 0.9659258262890683122, 1.000000000000000000, 0.9659258262890683122, 1.000000000000000000, 0.9659258262890683122, 1.000000000000000000, 0.9659258262890683122, 1.000000000000000000, 0.9659258262890683122, 1.000000000000000000, 0.9659258262890683122, 1.000000000000000000, 0.9659258262890683122, 1.000000000000000000, 0.9659258262890683122, 1.000000000000000000, 0.9659258262890683122, 1.000000000000000000, 0.9659258262890683122, 1.000000000000000000, 0.9659258262890683122, 1.000000000000000000, 0.9659258262890683122, 1.000000000000000000, 0.9659258262890683122, 1.000000000000000000, 0.9659258262890683122, 1.000000000000000000, 0.9659258262890683122, 1.000000000000000000, 0.9659258262890683122, 1.000000000000000000, 0.9659258262890683122, 1.000000000000000000, 0.9659258262890683122, 1.000000000000000000, 0.9659258262890683122, 1.000000000000000000, 0.9659258262890683122, 1.000000000000000000, 0.9659258262890683122, 1.000000000000000000, 0.9659258262890683122, 1.000000000000000000, 0.9659258262890683122, 1.000000000000000000, 0.9659258262890683122, 1.000000000000000000, 0.9659258262890683122, 1.000000000000000000, 0.9659258262890683122, 1.000000000000000000, 0.9659258262890683122, 1.000000000000000000, 0.9659258262890683122, 1.000000000000000000, 0.9659258262890683122, 1.000000000000000000, 0.9659258262890683122, 1.000000000000000000, 0.9659258262890683122, 1.000000000000000000, 0.9659258262890683122, 1.000000000000000000, 0.9659258262890683122, 1.000000000000000000, 0.9659258262890683122, 1.000000000000000000, 0.9659258262890683122, 1.000000000000000000, 0.9659258262890683122, 1.000000000000000000, 0.9659258262890683122, 1.000000000000000000, 0.9659258262890683122, 1.000000000000000000, 0.9659258262890683122, 1.000000000000000000, 0.9659258262890683122, 1.000000000000000000, 0.9659258262890683122, 1.000000000000000000, 0.9659258262890683122, 1.000000000000000000, 0.9659258262890683122, 1.000000000000000000, 0.9659258262890683122, 1.000000000000000000, 0.9659258262890683122, 1.000000000000000000, 0.9659258262890683122, 1.000000000000000000, 0.9659258262890683122, 1.000000000000000000, 0.9659258262890683122, 1.000000000000000000, 0.9659258262890683122, 1.000000000000000000, 0.9659258262890683122, 1.000000000000000000, 0.9659258262890683122, 1.000000000000000000, 0.9659258262890683122, 1.000000000000000000, 0.9659258262890683122, 1.000000000000000000, 0.9659258262890683122, 1.000000000000000000, 0.9659258262890683122, 1.000000000000000000, 0.9659258262890683122, 1.000000000000000000, 0.9659258262890683122, 1.000000000000000000, 0.9659258262890683122, 1.000000000000000000, 0.9659258262890683122, 1.000000000000000000, 0.9659258262890683122, 1.000000000000000000, 0.9659258262890683122, 1.000000000000000000, 0.9659258262890683122, 1.000000000000000000, 0.9659258262890683122, 1.000000000000000000, 0.9659258262890683122, 1.000000000000000000, 0.9659258262890683122, 1.000000000000000000, 0.9659258262890683122, 1.000000000000000000, 0.9659258262890683122, 1.000000000000000000, 0.9659258262890683122, 1.000000000000000000, 0.9659258262890683122, 1.000000000000000000, 0.9659258262890683122, 1.000000000000000000, 0.9659258262890683122, 1.000000000000000000, 0.9659258262890683122, 1.000000000000000000, 0.9659258262890683122, 1.000000000000000000, 0.9659258262890683122, 1.000000000000000000, 0.9659258262890683122, 1.000000000000000000, 0.9659258262890683122, 1.000000000000000000, 0.9659258262890683122, 1.000000000000000000, 0.9659258262890683122, 1.000000000000000000, 0.9659258262890683122, 1.000000000000000000, 0.9659258262890683122, 1.000000000000000000, 0.9659258262890683122, 1.000000000000000000, 0.9659258262890683122, 1.000000000000000000, 0.9659258262890683122, 1.000000000000000000, 0.9659258262890683122, 1.000000000000000000, 0.9659258262890683122, 1.000000000000000000, 0.9659258262890683122, 1.000000000000000000, 0.9659258262890683122, 1.000000000000000000, 0.9659258262890683122, 1.000000000000000000, 0.9659258262890683122, 1.000000000000000000, 0.9659258262890683122, 1.000000000000000000, 0.9659258262890683122, 1.000000000000000000, 0.9659258262890683122, 1.000000000000000000, 0.9659258262890683122, 1.000000000000000000, 0.9659258262890683122, 1.000000000000000000, 0.9659258262890683122, 1.000000000000000000, 0.9659258262890683122, 1.000000000000000000, 0.9659258262890683122, 1.000000000000000000, 0.9659258262890683122, 1.000000000000000000, 0.9659258262890683122, 1.000000000000000000, 0.9659258262890683122, 1.000000000000000000, 0.9659258262890683122, 1.000000000000000000, 0.9659258262890683122, 1.000000000000000000, 0.9659258262890683122, 1.000000000000000000, 0.9659258262890683122, 1.000000000000000000, 0.9659258262890683122, 1.000000000000000000, 0.9659258262890683122, 1.000000000000000000, 0.9659258262890683122, 1.000000000000000000, 0.9659258262890683122, 1.000000000000000000, 0.9659258262890683122, 1.000000000000000000, 0.9659258262890683122, 1.000000000000000000, 0.9659258262890683122, 1.000000000000000000, 0.9659258262890683122, 1.000000000000000000, 0.9659258262890683122, 1.000000000000000000, 0.9659258262890683122, 1.000000000000000000, 0.9659258262890683122, 1.000000000000000000, 0.9659258262890683122, 1.000000000000000000, 0.9659258262890683122, 1.000000000000000000, 0.9659258262890683122, 1.000000000000000000, 0.9659258262890683122, 1.000000000000000000, 0.9659258262890683122, 1.000000000000000000, 0.9659258262890683122, 1.000000000000000000, 0.9659258262890683122, 1.000000000000000000, 0.9659258262890683122, 1.000000000000000000, 0.9659258262890683122, 1.000000000000000000, 0.9659258262890683122, 1.000000000000000000, 0.9659258262890683122, 1.000000000000000000, 0.9659258262890683122, 1.000000000000000000, 0.9659258262890683122, 1.000000000000000000, 0.9659258262890683122, 1.000000000000000000, 0.9659258262890683122, 1.000000000000000000, 0.9659258262890683122, 1.000000000000000000, 0.9659258262890683122, 1.000000000000000000, 0.9659258262890683122, 1.000000000000000000, 0.9659258262890683122, 1.000000000000000000, 0.9659258262890683122, 1.000000000000000000, 0.9659258262890683122, 1.000000000000000000, 0.9659258262890683122, 1.000000000000000000, 0.9659258262890683122, 1.000000000000000000, 0.9659258262890683122, 1.000000000000000000, 0.9659258262890683122, 1.000000000000000000, 0.9659258262890683122, 1.000000000000000000, 0.9659258262890683122, 1.000000000000000000, 0.9659258262890683122, 1.000000000000000000, 0.9659258262890683122, 1.000000000000000000, 0.9659258262890683122, 1.000000000000000000, 0.9659258262890683122, 1.000000000000000000, 0.9659258262890683122, 1.000000000000000000, 0.9659258262890683122, 1.000000000000000000, 0.9659258262890683122, 1.000000000000000000, 0.9659258262890683122, 1.000000000000000000, 0.9659258262890683122, 1.000000000000000000, 0.9659258262890683122, 1.000000000000000000, 0.9659258262890683122, 1.000000000000000000, 0.9659258262890683122, 1.000000000000000000, 0.9659258262890683122, 1.000000000000000000, 0.9659258262890683122, 1.000000000000000000, 0.9659258262890683122, 1.000000000000000000, 0.9659258262890683122, 1.000000000000000000, 0.9659258262890683122, 1.000000000000000000, 0.9659258262890683122, 1.000000000000000000, 0.9659258262890683122, 1.000000000000000000, 0.9659258262890683122, 1.000000000000000000, 0.9659258262890683122, 1.000000000000000000, 0.9659258262890683122, 1.000000000000000000, 0.9659258262890683122, 1.000000000000000000, 0.9659258262890683122, 1.000000000000000000, 0.9659258262890683122, 1.000000000000000000, 0.9659258262890683122, 1.000000000000000000, 0.9659258262890683122, 1.000000000000000000, 0.9659258262890683122, 1.000000000000000000, 0.9659258262890683122, 1.000000000000000000, 0.9659258262890683122, 1.000000000000000000, 0.9659258262890683122, 1.000000000000000000, 0.9659258262890683122, 1.000000000000000000, 0.9659258262890683122, 1.000000000000000000, 0.9659258262890683122, 1.000000000000000000, 0.9659258262890683122, 1.000000000000000000, 0.9659258262890683122, 1.000000000000000000, 0.9659258262890683122, 1.000000000000000000, 0.9659258262890683122, 1.000000000000000000, 0.9659258262890683122, 1.000000000000000000, 0.9659258262890683122, 1.000000000000000000, 0.9659258262890683122, 1.000000000000000000, 0.9659258262890683122, 1.000000000000000000, 0.9659258262890683122, 1.000000000000000000, 0.9659258262890683122, 1.000000000000000000, 0.9659258262890683122, 1.000000000000000000, 0.9659258262890683122, 1.000000000000000000, 0.9659258262890683122, 1.000000000000000000, 0.9659258262890683122, 1.000000000000000000, 0.9659258262890683122, 1.000000000000000000, 0.9659258262890683122, 1.000000000000000000, 0.9659258262890683122, 1.000000000000000000, 0.9659258262890683122, 1.000000000000000000, 0.9659258262890683122, 1.000000000000000000, 0.9659258262890683122, 1.000000000000000000, 0.9659258262890683122, 1.000000000000000000, 0.9659258262890683122, 1.000000000000000000, 0.9659258262890683122, 1.000000000000000000, 0.9659258262890683122, 1.000000000000000000, 0.9659258262890683122, 1.000000000000000000, 0.9659258262890683122, 1.000000000000000000, 0.9659258262890683122, 1.000000000000000000, 0.9659258262890683122, 1.000000000000000000, 0.9659258262890683122, 1.000000000000000000, 0.9659258262890683122, 1.000000000000000000, 0.9659258262890683122, 1.000000000000000000, 0.9659258262890683122, 1.000000000000000000, 0.9659258262890683122, 1.000000000000000000, 0.9659258262890683122, 1.000000000000000000, 0.9659258262890683122, 1.000000000000000000, 0.9659258262890683122, 1.000000000000000000, 0.9659258262890683122, 1.000000000000000000, 0.9659258262890683122, 1.000000000000000000, 0.9659258262890683122, 1.000000000000000000, 0.9659258262890683122, 1.000000000000000000, 0.9659258262890683122, 1.000000000000000000, 0.9659258262890683122, 1.000000000000000000, 0.9659258262890683122, 1.000000000000000000, 0.9659258262890683122, 1.000000000000000000, 0.9659258262890683122, 1.000000000000000000, 0.9659258262890683122, 1.000000000000000000, 0.9659258262890683122, 1.000000000000000000, 0.9659258262890683122, 1.000000000000000000, 0.9659258262890683122, 1.000000000000000000, 0.9659258262890683122, 1.000000000000000000, 0.9659258262890683122, 1.000000000000000000, 0.9659258262890683122, 1.000000000000000000, 0.9659258262890683122, 1.000000000000000000, 0.9659258262890683122, 1.000000000000000000, 0.9659258262890683122, 1.000000000000000000, 0.9659258262890683122, 1.000000000000000000, 0.9659258262890683122, 1.000000000000000000, 0.9659258262890683122, 1.000000000000000000, 0.9659258262890683122, 1.000000000000000000, 0.9659258262890683122, 1.000000000000000000, 0.9659258262890683122, 1.000000000000000000, 0.9659258262890683122, 1.000000000000000000, 0.9659258262890683122, 1.000000000000000000, 0.9659258262890683122, 1.000000000000000000, 0.9659258262890683122, 1.000000000000000000, 0.9659258262890683122, 1.000000000000000000, 0.9659258262890683122, 1.000000000000000000, 0.9659258262890683122, 1.000000000000000000, 0.9659258262890683122, 1.000000000000000000, 0.9659258262890683122, 1.000000000000000000, 0.9659258262890683122, 1.000000000000000000, 0.9659258262890683122, 1.000000000000000000, 0.9659258262890683122, 1.000000000000000000, 0.9659258262890683122, 1.000000000000000000, 0.9659258262890683122, 1.000000000000000000, 0.9659258262890683122, 1.000000000000000000, 0.9659258262890683122, 1.000000000000000000, 0.9659258262890683122, 1.000000000000000000, 0.9659258262890683122, 1.000000000000000000, 0.9659258262890683122, 1.000000000000000000, 0.9659258262890683122, 1.000000000000000000, 0.9659258262890683122, 1.000000000000000000, 0.9659258262890683122, 1.000000000000000000, 0.9659258262890683122, 1.000000000000000000, 0.9659258262890683122, 1.000000000000000000, 0.9659258262890683122, 1.000000000000000000, 0.9659258262890683122, 1.000000000000000000, 0.9659258262890683122, 1.000000000000000000, 0.9659258262890683122, 1.000000000000000000, 0.9659258262890683122, 1.000000000000000000, 0.9659258262890683122, 1.000000000000000000, 0.9659258262890683122, 1.000000000000000000, 0.9659258262890683122, 1.000000000000000000, 0.9659258262890683122, 1.000000000000000000, 0.9659258262890683122, 1.000000000000000000, 0.9659258262890683122, 1.000000000000000000, 0.9659258262890683122, 1.000000000000000000, 0.9659258262890683122, 1.000000000000000000, 0.9659258262890683122, 1.000000000000000000, 0.9659258262890683122, 1.000000000000000000, 0.9659258262890683122, 1.000000000000000000, 0.9659258262890683122, 1.000000000000000000, 0.9659258262890683122, 1.000000000000000000, 0.9659258262890683122, 1.000000000000000000, 0.9659258262890683122, 1.000000000000000000, 0.9659258262890683122, 1.000000000000000000, 0.9659258262890683122, 1.000000000000000000, 0.9659258262890683122, 1.000000000000000000, 0.9659258262890683122, 1.000000000000000000, 0.9659258262890683122, 1.000000000000000000, 0.9659258262890683122, 1.000000000000000000, 0.9659258262890683122, 1.000000000000000000, 0.9659258262890683122, 1.000000000000000000, 0.9659258262890683122, 1.000000000000000000, 0.9659258262890683122, 1.000000000000000000, 0.9659258262890683122, 1.000000000000000000, 0.9659258262890683122, 1.000000000000000000, 0.9659258262890683122, 1.000000000000000000, 0.9659258262890683122, 1.000000000000000000, 0.9659258262890683122, 1.000000000000000000, 0.9659258262890683122, 1.000000000000000000, 0.9659258262890683122, 1.000000000000000000, 0.9659258262890683122, 1.000000000000000000, 0.9659258262890683122, 1.000000000000000000, 0.9659258262890683122, 1.000000000000000000, 0.9659258262890683122, 1.000000000000000000, 0.9659258262890683122, 1.000000000000000000, 0.9659258262890683122, 1.000000000000000000, 0.9659258262890683122, 1.000000000000000000, 0.9659258262890683122, 1.000000000000000000, 0.9659258262890683122, 1.000000000000000000, 0.9659258262890683122, 1.000000000000000000, 0.9659258262890683122, 1.000000000000000000, 0.9659258262890683122, 1.000000000000000000, 0.9659258262890683122, 1.000000000000000000, 0.9659258262890683122, 1.000000000000000000, 0.9659258262890683122, 1.000000000000000000, 0.9659258262890683122, 1.000000000000000000, 0.9659258262890683122, 1.000000000000000000, 0.9659258262890683122, 1.000000000000000000, 0.9659258262890683122, 1.000000000000000000, 0.9659258262890683122, 1.000000000000000000, 0.9659258262890683122, 1.000000000000000000, 0.9659258262890683122, 1.000000000000000000, 0.9659258262890683122, 1.000000000000000000, 0.9659258262890683122, 1.000000000000000000, 0.9659258262890683122, 1.000000000000000000, 0.9659258262890683122, 1.000000000000000000, 0.9659258262890683122, 1.000000000000000000, 0.9659258262890683122, 1.000000000000000000, 0.9659258262890683122, 1.000000000000000000, 0.9659258262890683122, 1.000000000000000000, 0.9659258262890683122, 1.000000000000000000, 0.9659258262890683122, 1.000000000000000000, 0.9863516207523304047, 0.9836369332600947146),
 ( 1.000000000000000000, 0.9659258262890683122, 1.000000000000000000, 0.9659258262890683122, 1.000000000000000000, 0.9659258262890683122, 1.000000000000000000, 0.9659258262890683122, 1.000000000000000000, 0.9659258262890683122, 1.000000000000000000, 0.9659258262890683122, 1.000000000000000000, 0.9659258262890683122, 1.000000000000000000, 0.9659258262890683122, 1.000000000000000000, 0.9659258262890683122, 1.000000000000000000, 0.9659258262890683122, 1.000000000000000000, 0.9659258262890683122, 1.000000000000000000, 0.9659258262890683122, 1.000000000000000000, 0.9659258262890683122, 1.000000000000000000, 0.9659258262890683122, 1.000000000000000000, 0.9659258262890683122, 1.000000000000000000, 0.9659258262890683122, 1.000000000000000000, 0.9659258262890683122, 1.000000000000000000, 0.9659258262890683122, 1.000000000000000000, 0.9659258262890683122, 1.000000000000000000, 0.9659258262890683122, 1.000000000000000000, 0.9659258262890683122, 1.000000000000000000, 0.9659258262890683122, 1.000000000000000000, 0.9659258262890683122, 1.000000000000000000, 0.9659258262890683122, 1.000000000000000000, 0.9659258262890683122, 1.000000000000000000, 0.9659258262890683122, 1.000000000000000000, 0.9659258262890683122, 1.000000000000000000, 0.9659258262890683122, 1.000000000000000000, 0.9659258262890683122, 1.000000000000000000, 0.9659258262890683122, 1.000000000000000000, 0.9659258262890683122, 1.000000000000000000, 0.9659258262890683122, 1.000000000000000000, 0.9659258262890683122, 1.000000000000000000, 0.9659258262890683122, 1.000000000000000000, 0.9659258262890683122, 1.000000000000000000, 0.9659258262890683122, 1.000000000000000000, 0.9659258262890683122, 1.000000000000000000, 0.9659258262890683122, 1.000000000000000000, 0.9659258262890683122, 1.000000000000000000, 0.9659258262890683122, 1.000000000000000000, 0.9659258262890683122, 1.000000000000000000, 0.9659258262890683122, 1.000000000000000000, 0.9659258262890683122, 1.000000000000000000, 0.9659258262890683122, 1.000000000000000000, 0.9659258262890683122, 1.000000000000000000, 0.9659258262890683122, 1.000000000000000000, 0.9659258262890683122, 1.000000000000000000, 0.9659258262890683122, 1.000000000000000000, 0.9659258262890683122, 1.000000000000000000, 0.9659258262890683122, 1.000000000000000000, 0.9659258262890683122, 1.000000000000000000, 0.9659258262890683122, 1.000000000000000000, 0.9659258262890683122, 1.000000000000000000, 0.9659258262890683122, 1.000000000000000000, 0.9659258262890683122, 1.000000000000000000, 0.9659258262890683122, 1.000000000000000000, 0.9659258262890683122, 1.000000000000000000, 0.9659258262890683122, 1.000000000000000000, 0.9659258262890683122, 1.000000000000000000, 0.9659258262890683122, 1.000000000000000000, 0.9659258262890683122, 1.000000000000000000, 0.9659258262890683122, 1.000000000000000000, 0.9659258262890683122, 1.000000000000000000, 0.9659258262890683122, 1.000000000000000000, 0.9659258262890683122, 1.000000000000000000, 0.9659258262890683122, 1.000000000000000000, 0.9659258262890683122, 1.000000000000000000, 0.9659258262890683122, 1.000000000000000000, 0.9659258262890683122, 1.000000000000000000, 0.9659258262890683122, 1.000000000000000000, 0.9659258262890683122, 1.000000000000000000, 0.9659258262890683122, 1.000000000000000000, 0.9659258262890683122, 1.000000000000000000, 0.9659258262890683122, 1.000000000000000000, 0.9659258262890683122, 1.000000000000000000, 0.9659258262890683122, 1.000000000000000000, 0.9659258262890683122, 1.000000000000000000, 0.9659258262890683122, 1.000000000000000000, 0.9659258262890683122, 1.000000000000000000, 0.9659258262890683122, 1.000000000000000000, 0.9659258262890683122, 1.000000000000000000, 0.9659258262890683122, 1.000000000000000000, 0.9659258262890683122, 1.000000000000000000, 0.9659258262890683122, 1.000000000000000000, 0.9659258262890683122, 1.000000000000000000, 0.9659258262890683122, 1.000000000000000000, 0.9659258262890683122, 1.000000000000000000, 0.9659258262890683122, 1.000000000000000000, 0.9659258262890683122, 1.000000000000000000, 0.9659258262890683122, 1.000000000000000000, 0.9659258262890683122, 1.000000000000000000, 0.9659258262890683122, 1.000000000000000000, 0.9659258262890683122, 1.000000000000000000, 0.9659258262890683122, 1.000000000000000000, 0.9659258262890683122, 1.000000000000000000, 0.9659258262890683122, 1.000000000000000000, 0.9659258262890683122, 1.000000000000000000, 0.9659258262890683122, 1.000000000000000000, 0.9659258262890683122, 1.000000000000000000, 0.9659258262890683122, 1.000000000000000000, 0.9659258262890683122, 1.000000000000000000, 0.9659258262890683122, 1.000000000000000000, 0.9659258262890683122, 1.000000000000000000, 0.9659258262890683122, 1.000000000000000000, 0.9659258262890683122, 1.000000000000000000, 0.9659258262890683122, 1.000000000000000000, 0.9659258262890683122, 1.000000000000000000, 0.9659258262890683122, 1.000000000000000000, 0.9659258262890683122, 1.000000000000000000, 0.9659258262890683122, 1.000000000000000000, 0.9659258262890683122, 1.000000000000000000, 0.9659258262890683122, 1.000000000000000000, 0.9659258262890683122, 1.000000000000000000, 0.9659258262890683122, 1.000000000000000000, 0.9659258262890683122, 1.000000000000000000, 0.9659258262890683122, 1.000000000000000000, 0.9659258262890683122, 1.000000000000000000, 0.9659258262890683122, 1.000000000000000000, 0.9659258262890683122, 1.000000000000000000, 0.9659258262890683122, 1.000000000000000000, 0.9659258262890683122, 1.000000000000000000, 0.9659258262890683122, 1.000000000000000000, 0.9659258262890683122, 1.000000000000000000, 0.9659258262890683122, 1.000000000000000000, 0.9659258262890683122, 1.000000000000000000, 0.9659258262890683122, 1.000000000000000000, 0.9659258262890683122, 1.000000000000000000, 0.9659258262890683122, 1.000000000000000000, 0.9659258262890683122, 1.000000000000000000, 0.9659258262890683122, 1.000000000000000000, 0.9659258262890683122, 1.000000000000000000, 0.9659258262890683122, 1.000000000000000000, 0.9659258262890683122, 1.000000000000000000, 0.9659258262890683122, 1.000000000000000000, 0.9659258262890683122, 1.000000000000000000, 0.9659258262890683122, 1.000000000000000000, 0.9659258262890683122, 1.000000000000000000, 0.9659258262890683122, 1.000000000000000000, 0.9659258262890683122, 1.000000000000000000, 0.9659258262890683122, 1.000000000000000000, 0.9659258262890683122, 1.000000000000000000, 0.9659258262890683122, 1.000000000000000000, 0.9659258262890683122, 1.000000000000000000, 0.9659258262890683122, 1.000000000000000000, 0.9659258262890683122, 1.000000000000000000, 0.9659258262890683122, 1.000000000000000000, 0.9659258262890683122, 1.000000000000000000, 0.9659258262890683122, 1.000000000000000000, 0.9659258262890683122, 1.000000000000000000, 0.9659258262890683122, 1.000000000000000000, 0.9659258262890683122, 1.000000000000000000, 0.9659258262890683122, 1.000000000000000000, 0.9659258262890683122, 1.000000000000000000, 0.9659258262890683122, 1.000000000000000000, 0.9659258262890683122, 1.000000000000000000, 0.9659258262890683122, 1.000000000000000000, 0.9659258262890683122, 1.000000000000000000, 0.9659258262890683122, 1.000000000000000000, 0.9659258262890683122, 1.000000000000000000, 0.9659258262890683122, 1.000000000000000000, 0.9659258262890683122, 1.000000000000000000, 0.9659258262890683122, 1.000000000000000000, 0.9659258262890683122, 1.000000000000000000, 0.9659258262890683122, 1.000000000000000000, 0.9659258262890683122, 1.000000000000000000, 0.9659258262890683122, 1.000000000000000000, 0.9659258262890683122, 1.000000000000000000, 0.9659258262890683122, 1.000000000000000000, 0.9659258262890683122, 1.000000000000000000, 0.9659258262890683122, 1.000000000000000000, 0.9659258262890683122, 1.000000000000000000, 0.9659258262890683122, 1.000000000000000000, 0.9659258262890683122, 1.000000000000000000, 0.9659258262890683122, 1.000000000000000000, 0.9659258262890683122, 1.000000000000000000, 0.9659258262890683122, 1.000000000000000000, 0.9659258262890683122, 1.000000000000000000, 0.9659258262890683122, 1.000000000000000000, 0.9659258262890683122, 1.000000000000000000, 0.9659258262890683122, 1.000000000000000000, 0.9659258262890683122, 1.000000000000000000, 0.9659258262890683122, 1.000000000000000000, 0.9659258262890683122, 1.000000000000000000, 0.9659258262890683122, 1.000000000000000000, 0.9659258262890683122, 1.000000000000000000, 0.9659258262890683122, 1.000000000000000000, 0.9659258262890683122, 1.000000000000000000, 0.9659258262890683122, 1.000000000000000000, 0.9659258262890683122, 1.000000000000000000, 0.9659258262890683122, 1.000000000000000000, 0.9659258262890683122, 1.000000000000000000, 0.9659258262890683122, 1.000000000000000000, 0.9659258262890683122, 1.000000000000000000, 0.9659258262890683122, 1.000000000000000000, 0.9659258262890683122, 1.000000000000000000, 0.9659258262890683122, 1.000000000000000000, 0.9659258262890683122, 1.000000000000000000, 0.9659258262890683122, 1.000000000000000000, 0.9659258262890683122, 1.000000000000000000, 0.9659258262890683122, 1.000000000000000000, 0.9659258262890683122, 1.000000000000000000, 0.9659258262890683122, 1.000000000000000000, 0.9659258262890683122, 1.000000000000000000, 0.9659258262890683122, 1.000000000000000000, 0.9659258262890683122, 1.000000000000000000, 0.9659258262890683122, 1.000000000000000000, 0.9659258262890683122, 1.000000000000000000, 0.9659258262890683122, 1.000000000000000000, 0.9659258262890683122, 1.000000000000000000, 0.9659258262890683122, 1.000000000000000000, 0.9659258262890683122, 1.000000000000000000, 0.9659258262890683122, 1.000000000000000000, 0.9659258262890683122, 1.000000000000000000, 0.9659258262890683122, 1.000000000000000000, 0.9659258262890683122, 1.000000000000000000, 0.9659258262890683122, 1.000000000000000000, 0.9659258262890683122, 1.000000000000000000, 0.9659258262890683122, 1.000000000000000000, 0.9659258262890683122, 1.000000000000000000, 0.9659258262890683122, 1.000000000000000000, 0.9659258262890683122, 1.000000000000000000, 0.9659258262890683122, 1.000000000000000000, 0.9659258262890683122, 1.000000000000000000, 0.9659258262890683122, 1.000000000000000000, 0.9659258262890683122, 1.000000000000000000, 0.9659258262890683122, 1.000000000000000000, 0.9659258262890683122, 1.000000000000000000, 0.9659258262890683122, 1.000000000000000000, 0.9659258262890683122, 1.000000000000000000, 0.9659258262890683122, 1.000000000000000000, 0.9659258262890683122, 1.000000000000000000, 0.9659258262890683122, 1.000000000000000000, 0.9659258262890683122, 1.000000000000000000, 0.9659258262890683122, 1.000000000000000000, 0.9659258262890683122, 1.000000000000000000, 0.9659258262890683122, 1.000000000000000000, 0.9659258262890683122, 1.000000000000000000, 0.9659258262890683122, 1.000000000000000000, 0.9659258262890683122, 1.000000000000000000, 0.9659258262890683122, 1.000000000000000000, 0.9659258262890683122, 1.000000000000000000, 0.9659258262890683122, 1.000000000000000000, 0.9659258262890683122, 1.000000000000000000, 0.9659258262890683122, 1.000000000000000000, 0.9659258262890683122, 1.000000000000000000, 0.9659258262890683122, 1.000000000000000000, 0.9659258262890683122, 1.000000000000000000, 0.9659258262890683122, 1.000000000000000000, 0.9659258262890683122, 1.000000000000000000, 0.9659258262890683122, 1.000000000000000000, 0.9659258262890683122, 1.000000000000000000, 0.9659258262890683122, 1.000000000000000000, 0.9659258262890683122, 1.000000000000000000, 0.9659258262890683122, 1.000000000000000000, 0.9659258262890683122, 1.000000000000000000, 0.9659258262890683122, 1.000000000000000000, 0.9659258262890683122, 1.000000000000000000, 0.9659258262890683122, 1.000000000000000000, 0.9659258262890683122, 1.000000000000000000, 0.9659258262890683122, 1.000000000000000000, 0.9659258262890683122, 1.000000000000000000, 0.9659258262890683122, 1.000000000000000000, 0.9659258262890683122, 1.000000000000000000, 0.9659258262890683122, 1.000000000000000000, 0.9659258262890683122, 1.000000000000000000, 0.9659258262890683122, 1.000000000000000000, 0.9659258262890683122, 1.000000000000000000, 0.9659258262890683122, 1.000000000000000000, 0.9659258262890683122, 1.000000000000000000, 0.9659258262890683122, 1.000000000000000000, 0.9659258262890683122, 1.000000000000000000, 0.9659258262890683122, 1.000000000000000000, 0.9659258262890683122, 1.000000000000000000, 0.9659258262890683122, 1.000000000000000000, 0.9659258262890683122, 1.000000000000000000, 0.9659258262890683122, 1.000000000000000000, 0.9659258262890683122, 1.000000000000000000, 0.9659258262890683122, 1.000000000000000000, 0.9659258262890683122, 1.000000000000000000, 0.9659258262890683122, 1.000000000000000000, 0.9659258262890683122, 1.000000000000000000, 0.9659258262890683122, 1.000000000000000000, 0.9659258262890683122, 1.000000000000000000, 0.9659258262890683122, 1.000000000000000000, 0.9659258262890683122, 1.000000000000000000, 0.9659258262890683122, 1.000000000000000000, 0.9659258262890683122, 1.000000000000000000, 0.9659258262890683122, 1.000000000000000000, 0.9659258262890683122, 1.000000000000000000, 0.9659258262890683122, 1.000000000000000000, 0.9659258262890683122, 1.000000000000000000, 0.9659258262890683122, 1.000000000000000000, 0.9659258262890683122, 1.000000000000000000, 0.9659258262890683122, 1.000000000000000000, 0.9659258262890683122, 1.000000000000000000, 0.9659258262890683122, 1.000000000000000000, 0.9659258262890683122, 1.000000000000000000, 0.9659258262890683122, 1.000000000000000000, 0.9659258262890683122, 1.000000000000000000, 0.9659258262890683122, 1.000000000000000000, 0.9659258262890683122, 1.000000000000000000, 0.9659258262890683122, 1.000000000000000000, 0.9659258262890683122, 1.000000000000000000, 0.9659258262890683122, 1.000000000000000000, 0.9659258262890683122, 1.000000000000000000, 0.9659258262890683122, 1.000000000000000000, 0.9659258262890683122, 1.000000000000000000, 0.9659258262890683122, 1.000000000000000000, 0.9659258262890683122, 1.000000000000000000, 0.9659258262890683122, 1.000000000000000000, 0.9659258262890683122, 1.000000000000000000, 0.9659258262890683122, 1.000000000000000000, 0.9659258262890683122, 1.000000000000000000, 0.9659258262890683122, 1.000000000000000000, 0.9659258262890683122, 1.000000000000000000, 0.9659258262890683122, 1.000000000000000000, 0.9659258262890683122, 1.000000000000000000, 0.9659258262890683122, 1.000000000000000000, 0.9659258262890683122, 1.000000000000000000, 0.9659258262890683122, 1.000000000000000000, 0.9659258262890683122, 1.000000000000000000, 0.9659258262890683122, 1.000000000000000000, 0.9659258262890683122, 1.000000000000000000, 0.9659258262890683122, 1.000000000000000000, 0.9659258262890683122, 1.000000000000000000, 0.9659258262890683122, 1.000000000000000000, 0.9659258262890683122, 1.000000000000000000, 0.9659258262890683122, 1.000000000000000000, 0.9659258262890683122, 1.000000000000000000, 0.9659258262890683122, 1.000000000000000000, 0.9659258262890683122, 1.000000000000000000, 0.9659258262890683122, 1.000000000000000000, 0.9659258262890683122, 1.000000000000000000, 0.9659258262890683122, 1.000000000000000000, 0.9659258262890683122, 1.000000000000000000, 0.9659258262890683122, 1.000000000000000000, 0.9659258262890683122, 1.000000000000000000, 0.9659258262890683122, 1.000000000000000000, 0.9659258262890683122, 1.000000000000000000, 0.9659258262890683122, 1.000000000000000000, 0.9659258262890683122, 1.000000000000000000, 0.9659258262890683122, 1.000000000000000000, 0.9659258262890683122, 1.000000000000000000, 0.9659258262890683122, 1.000000000000000000, 0.9659258262890683122, 1.000000000000000000, 0.9659258262890683122, 1.000000000000000000, 0.9659258262890683122, 1.000000000000000000, 0.9659258262890683122, 1.000000000000000000, 0.9659258262890683122, 1.000000000000000000, 0.9659258262890683122, 1.000000000000000000, 0.9659258262890683122, 1.000000000000000000, 0.9659258262890683122, 1.000000000000000000, 0.9659258262890683122, 1.000000000000000000, 0.9659258262890683122, 1.000000000000000000, 0.9659258262890683122, 1.000000000000000000, 0.9659258262890683122, 1.000000000000000000, 0.9659258262890683122, 1.000000000000000000, 0.9659258262890683122, 1.000000000000000000, 0.9659258262890683122, 1.000000000000000000, 0.9659258262890683122, 1.000000000000000000, 0.9659258262890683122, 1.000000000000000000, 0.9659258262890683122, 1.000000000000000000, 0.9659258262890683122, 1.000000000000000000, 0.9659258262890683122, 1.000000000000000000, 0.9659258262890683122, 1.000000000000000000, 0.9659258262890683122, 1.000000000000000000, 0.9659258262890683122, 1.000000000000000000, 0.9659258262890683122, 1.000000000000000000, 0.9659258262890683122, 1.000000000000000000, 0.9659258262890683122, 1.000000000000000000, 0.9659258262890683122, 1.000000000000000000, 0.9659258262890683122, 1.000000000000000000, 0.9659258262890683122, 1.000000000000000000, 0.9659258262890683122, 1.000000000000000000, 0.9659258262890683122, 1.000000000000000000, 0.9659258262890683122, 1.000000000000000000, 0.9659258262890683122, 1.000000000000000000, 0.9659258262890683122, 1.000000000000000000, 0.9659258262890683122, 1.000000000000000000, 0.9659258262890683122, 1.000000000000000000, 0.9659258262890683122, 1.000000000000000000, 0.9659258262890683122, 1.000000000000000000, 0.9659258262890683122, 1.000000000000000000, 0.9659258262890683122, 1.000000000000000000, 0.9659258262890683122, 1.000000000000000000, 0.9659258262890683122, 1.000000000000000000, 0.9659258262890683122, 1.000000000000000000, 0.9659258262890683122, 1.000000000000000000, 0.9659258262890683122, 1.000000000000000000, 0.9659258262890683122, 1.000000000000000000, 0.9659258262890683122, 1.000000000000000000, 0.9659258262890683122, 1.000000000000000000, 0.9659258262890683122, 1.000000000000000000, 0.9659258262890683122, 1.000000000000000000, 0.9659258262890683122, 1.000000000000000000, 0.9659258262890683122, 1.000000000000000000, 0.9659258262890683122, 1.000000000000000000, 0.9659258262890683122, 1.000000000000000000, 0.9659258262890683122, 1.000000000000000000, 0.9659258262890683122, 1.000000000000000000, 0.9659258262890683122, 1.000000000000000000, 0.9659258262890683122, 1.000000000000000000, 0.9659258262890683122, 1.000000000000000000, 0.9659258262890683122, 1.000000000000000000, 0.9659258262890683122, 1.000000000000000000, 0.9659258262890683122, 1.000000000000000000, 0.9659258262890683122, 1.000000000000000000, 0.9659258262890683122, 1.000000000000000000, 0.9659258262890683122, 1.000000000000000000, 0.9659258262890683122, 1.000000000000000000, 0.9659258262890683122, 1.000000000000000000, 0.9659258262890683122, 1.000000000000000000, 0.9659258262890683122, 1.000000000000000000, 0.9659258262890683122, 1.000000000000000000, 0.9659258262890683122, 1.000000000000000000, 0.9659258262890683122, 1.000000000000000000, 0.9659258262890683122, 1.000000000000000000, 0.9659258262890683122, 1.000000000000000000, 0.9659258262890683122, 1.000000000000000000, 0.9659258262890683122, 1.000000000000000000, 0.9659258262890683122, 1.000000000000000000, 0.9659258262890683122, 1.000000000000000000, 0.9659258262890683122, 1.000000000000000000, 0.9659258262890683122, 1.000000000000000000, 0.9659258262890683122, 1.000000000000000000, 0.9659258262890683122, 1.000000000000000000, 0.9659258262890683122, 1.000000000000000000, 0.9659258262890683122, 1.000000000000000000, 0.9659258262890683122, 1.000000000000000000, 0.9659258262890683122, 1.000000000000000000, 0.9659258262890683122, 1.000000000000000000, 0.9659258262890683122, 1.000000000000000000, 0.9659258262890683122, 1.000000000000000000, 0.9659258262890683122, 1.000000000000000000, 0.9659258262890683122, 1.000000000000000000, 0.9659258262890683122, 1.000000000000000000, 0.9659258262890683122, 1.000000000000000000, 0.9659258262890683122, 1.000000000000000000, 0.9659258262890683122, 1.000000000000000000, 0.9659258262890683122, 1.000000000000000000, 0.9659258262890683122, 1.000000000000000000, 0.9659258262890683122, 1.000000000000000000, 0.9659258262890683122, 1.000000000000000000, 0.9659258262890683122, 1.000000000000000000, 0.9659258262890683122, 1.000000000000000000, 0.9659258262890683122, 1.000000000000000000, 0.9659258262890683122, 1.000000000000000000, 0.9659258262890683122, 1.000000000000000000, 0.9659258262890683122, 1.000000000000000000, 0.9659258262890683122, 1.000000000000000000, 0.9659258262890683122, 1.000000000000000000, 0.9659258262890683122, 1.000000000000000000, 0.9659258262890683122, 1.000000000000000000, 0.9659258262890683122, 1.000000000000000000, 0.9659258262890683122, 1.000000000000000000, 0.9659258262890683122, 1.000000000000000000, 0.9659258262890683122, 1.000000000000000000, 0.9659258262890683122, 1.000000000000000000, 0.9659258262890683122, 1.000000000000000000, 0.9659258262890683122, 1.000000000000000000, 0.9659258262890683122, 1.000000000000000000, 0.9659258262890683122, 1.000000000000000000, 0.9659258262890683122, 1.000000000000000000, 0.9659258262890683122, 1.000000000000000000, 0.9659258262890683122, 1.000000000000000000, 0.9659258262890683122, 1.000000000000000000, 0.9659258262890683122, 1.000000000000000000, 0.9659258262890683122, 1.000000000000000000, 0.9659258262890683122, 1.000000000000000000, 0.9659258262890683122, 1.000000000000000000, 0.9659258262890683122, 1.000000000000000000, 0.9659258262890683122, 1.000000000000000000, 0.9659258262890683122, 1.000000000000000000, 0.9659258262890683122, 1.000000000000000000, 0.9659258262890683122, 1.000000000000000000, 0.9659258262890683122, 1.000000000000000000, 0.9659258262890683122, 1.000000000000000000, 0.9659258262890683122, 1.000000000000000000, 0.9659258262890683122, 1.000000000000000000, 0.9659258262890683122, 1.000000000000000000, 0.9659258262890683122, 1.000000000000000000, 0.9659258262890683122, 1.000000000000000000, 0.9659258262890683122, 1.000000000000000000, 0.9659258262890683122, 1.000000000000000000, 0.9659258262890683122, 1.000000000000000000, 0.9659258262890683122, 1.000000000000000000, 0.9659258262890683122, 1.000000000000000000, 0.9659258262890683122, 1.000000000000000000, 0.9659258262890683122, 1.000000000000000000, 0.9659258262890683122, 1.000000000000000000, 0.9659258262890683122, 1.000000000000000000, 0.9659258262890683122, 1.000000000000000000, 0.9659258262890683122, 1.000000000000000000, 0.9659258262890683122, 1.000000000000000000, 0.9659258262890683122, 1.000000000000000000, 0.9659258262890683122, 1.000000000000000000, 0.9659258262890683122, 1.000000000000000000, 0.9659258262890683122, 1.000000000000000000, 0.9659258262890683122, 1.000000000000000000, 0.9659258262890683122, 1.000000000000000000, 0.9659258262890683122, 1.000000000000000000, 0.9659258262890683122, 1.000000000000000000, 0.9659258262890683122, 1.000000000000000000, 0.9659258262890683122, 1.000000000000000000, 0.9659258262890683122, 1.000000000000000000, 0.9659258262890683122, 1.000000000000000000, 0.9659258262890683122, 1.000000000000000000, 0.9659258262890683122, 1.000000000000000000, 0.9659258262890683122, 1.000000000000000000, 0.9659258262890683122, 1.000000000000000000, 0.9659258262890683122, 1.000000000000000000, 0.9659258262890683122, 1.000000000000000000, 0.9659258262890683122, 1.000000000000000000, 0.9659258262890683122, 1.000000000000000000, 0.9659258262890683122, 1.000000000000000000, 0.9659258262890683122, 1.000000000000000000, 0.9659258262890683122, 1.000000000000000000, 0.9659258262890683122, 1.000000000000000000, 0.9659258262890683122, 1.000000000000000000, 0.9659258262890683122, 1.000000000000000000, 0.9659258262890683122, 1.000000000000000000, 0.9659258262890683122, 1.000000000000000000, 0.9659258262890683122, 1.000000000000000000, 0.9659258262890683122, 1.000000000000000000, 0.9659258262890683122, 1.000000000000000000, 0.9659258262890683122, 1.000000000000000000, 0.9659258262890683122, 1.000000000000000000, 0.9659258262890683122, 1.000000000000000000, 0.9659258262890683122, 1.000000000000000000, 0.9659258262890683122, 1.000000000000000000, 0.9659258262890683122, 1.000000000000000000, 0.9659258262890683122, 1.000000000000000000, 0.9659258262890683122, 1.000000000000000000, 0.9659258262890683122, 1.000000000000000000, 0.9659258262890683122, 1.000000000000000000, 0.9659258262890683122, 1.000000000000000000, 0.9659258262890683122, 1.000000000000000000, 0.9659258262890683122, 1.000000000000000000, 0.9659258262890683122, 1.000000000000000000, 0.9659258262890683122, 1.000000000000000000, 0.9659258262890683122, 1.000000000000000000, 0.9659258262890683122, 1.000000000000000000, 0.9863516207523304047, 0.9836369332600947146) ) ) 
 REPRESENTATION_ITEM ( '' )  SURFACE ( )  );
#70750 = CARTESIAN_POINT ( 'NONE',  ( -4.898587196589412829E-16, 100.6249999999999858, -8.000000000000000000 ) ) ;
#70751 = ADVANCED_FACE ( 'NONE', ( #49486 ), #27216, .T. ) ;
#70752 = CARTESIAN_POINT ( 'NONE',  ( 8.311093377946839666, 226.0937500034139589, 8.311093377946830785 ) ) ;
#70753 = CARTESIAN_POINT ( 'NONE',  ( 8.311093377946837890, 111.4062499965860269, -8.311093377946837890 ) ) ;
#70754 = ORIENTED_EDGE ( 'NONE', *, *, #16478, .T. ) ;
#70755 = CARTESIAN_POINT ( 'NONE',  ( -8.000000000000003553, 22.99999999999999645, -1.000000000000000000 ) ) ;
#70756 = CARTESIAN_POINT ( 'NONE',  ( -10.18810118749999916, 0.000000000000000000, 100.6562500020483810 ) ) ;
#70757 = LINE ( 'NONE', #48479, #62194 ) ;
#70758 = CARTESIAN_POINT ( 'NONE',  ( 3.458734125000015869, 198.1875000013655779, 198.0000000000000284 ) ) ;
#70759 = LINE ( 'NONE', #48107, #2849 ) ;
#70761 = CARTESIAN_POINT ( 'NONE',  ( 8.311093377946834337, 110.1562499965860269, 8.311093377946839666 ) ) ;
#70760 = CARTESIAN_POINT ( 'NONE',  ( 0.000000000000000000, 0.000000000000000000, 0.000000000000000000 ) ) ;
#70762 = CARTESIAN_POINT ( 'NONE',  ( -30.82842712474616320, 207.3750000000000284, 172.8284271247465824 ) ) ;
#70763 = CARTESIAN_POINT ( 'NONE',  ( 1.681385197618709730E-11, 51.24999999999869971, -10.00000000000000178 ) ) ;
#70764 = VERTEX_POINT ( 'NONE', #38561 ) ;
#70765 = AXIS2_PLACEMENT_3D ( 'NONE', #71976, #36919, #37294 ) ;
#70766 = CARTESIAN_POINT ( 'NONE',  ( 4.999999999999993783, 206.0416666598387110, 8.660254037844390851 ) ) ;
#70767 = CARTESIAN_POINT ( 'NONE',  ( 3.313708498984679895, 112.7187500040968047, -8.000000000000081712 ) ) ;
#70768 = EDGE_CURVE ( 'NONE', #24662, #3122, #68, .T. ) ;
#70769 = CARTESIAN_POINT ( 'NONE',  ( 0.000000000000000000, 0.000000000000000000, 30.00000000000000000 ) ) ;
#70770 = CARTESIAN_POINT ( 'NONE',  ( 6.951808397369818766E-16, 102.3437499965860127, -11.35316468750000141 ) ) ;
#70771 = CARTESIAN_POINT ( 'NONE',  ( 2.849036369511732440E-14, 205.2500000000000284, 202.0000000000000000 ) ) ;
#70772 = CARTESIAN_POINT ( 'NONE',  ( -2.977408999572654480, 12.37499999795161187, 7.188101187499999156 ) ) ;
#70773 = CARTESIAN_POINT ( 'NONE',  ( 7.204075437095966983, 7.204075437095967871, 89.96875000204838102 ) ) ;
#70774 = CARTESIAN_POINT ( 'NONE',  ( -2.085542519210945728E-15, 9.843749996586018014, 11.35316468750000141 ) ) ;
#70776 = ORIENTED_EDGE ( 'NONE', *, *, #5924, .T. ) ;
#70775 =( BOUNDED_CURVE ( )  B_SPLINE_CURVE ( 2, ( #69272, #22869, #45882, #52666, #40977, #57217, #11556, #63983, #53038, #12297, #74557, #28906, #17958 ),
 .UNSPECIFIED., .F., .F. ) 
 B_SPLINE_CURVE_WITH_KNOTS ( ( 3, 2, 2, 2, 2, 2, 3 ),
 ( 0.8611111111111111605, 0.8703703703703703498, 0.8796296296296297612, 0.8888888888888889506, 0.8981481481481482509, 0.9074074074074076623, 0.9166666666666668517 ),
 .UNSPECIFIED. ) 
 CURVE ( )  GEOMETRIC_REPRESENTATION_ITEM ( )  RATIONAL_B_SPLINE_CURVE ( ( 1.000000000000000000, 0.9659258262890683122, 1.000000000000000000, 0.9659258262890683122, 1.000000000000000000, 0.9659258262890683122, 1.000000000000000000, 0.9659258262890683122, 1.000000000000000000, 0.9659258262890683122, 1.000000000000000000, 0.9659258262890675351, 1.000000000000000888 ) ) 
 REPRESENTATION_ITEM ( '' )  );
#70777 = LINE ( 'NONE', #19090, #39249 ) ;
#70778 = CARTESIAN_POINT ( 'NONE',  ( -5.000000000000000000, 0.000000000000000000, 0.000000000000000000 ) ) ;
#70779 = DIRECTION ( 'NONE',  ( -0.000000000000000000, 1.000000000000000000, -0.000000000000000000 ) ) ;
#70780 = CARTESIAN_POINT ( 'NONE',  ( 1.871523826299183495E-15, -10.18810118749999916, 74.40625000204836681 ) ) ;
#70781 = CARTESIAN_POINT ( 'NONE',  ( 2.808409778661586920, 22.00000000000003553, 3.186686813332832990 ) ) ;
#70782 = CARTESIAN_POINT ( 'NONE',  ( -4.088227598258586603E-16, 294.2031250017069510, -6.676582343750001591 ) ) ;
#70783 = CARTESIAN_POINT ( 'NONE',  ( 2.828427124746209831, 204.5000000027312126, 200.8284271247462129 ) ) ;
#70784 = CARTESIAN_POINT ( 'NONE',  ( 3.042071309553167513, 222.1354166632526699, -11.35316468749999785 ) ) ;
#70785 = CARTESIAN_POINT ( 'NONE',  ( -10.18810118749999916, 0.000000000000000000, 87.15625000204838102 ) ) ;
#70786 = CARTESIAN_POINT ( 'NONE',  ( -25.55430564589119413, 201.3125000013656063, 167.5543056458915316 ) ) ;
#70787 = CARTESIAN_POINT ( 'NONE',  ( -8.000000000000000000, 23.15625000000000000, -3.313708498984762496 ) ) ;
#70788 = CARTESIAN_POINT ( 'NONE',  ( 3.211159895383561835, 11.56249999863440614, -3.211159895383561835 ) ) ;
#70789 = ORIENTED_EDGE ( 'NONE', *, *, #47791, .T. ) ;
#70790 = CARTESIAN_POINT ( 'NONE',  ( -30.82787693183054145, -51.99954845863952357, 166.3366078361535187 ) ) ;
#70791 = CARTESIAN_POINT ( 'NONE',  ( -3.999999999999960032, 207.0625000027311842, 196.3431457505076594 ) ) ;
#70792 = EDGE_CURVE ( 'NONE', #54079, #112, #51596, .T. ) ;
#70793 = CARTESIAN_POINT ( 'NONE',  ( -1.432654583217662481, 200.3750000013656063, 145.4587341250000634 ) ) ;
#70794 = CARTESIAN_POINT ( 'NONE',  ( 3.999999999999959144, 204.1875000027312126, 140.3431457505076594 ) ) ;
#70795 = CARTESIAN_POINT ( 'NONE',  ( 4.999999999999999112, 10.28276986844625718, -65.17752827135362281 ) ) ;
#70796 = CARTESIAN_POINT ( 'NONE',  ( 2.449293598294707893E-16, 12.99999999726881406, -4.000000000000001776 ) ) ;
#70797 = VERTEX_POINT ( 'NONE', #73254 ) ;
#70798 = EDGE_CURVE ( 'NONE', #54420, #48595, #48762, .T. ) ;
#70799 = CARTESIAN_POINT ( 'NONE',  ( 5.082755093536324154, 7.781249997951611874, 5.082755093536326818 ) ) ;
#70800 = DIRECTION ( 'NONE',  ( 0.000000000000000000, 0.000000000000000000, 1.000000000000000000 ) ) ;
#70801 = CARTESIAN_POINT ( 'NONE',  ( 7.188101187500000044, 117.7812500020483810, -8.802885111219163269E-16 ) ) ;
#70802 = CARTESIAN_POINT ( 'NONE',  ( 2.295000000000000373, 261.4319999999996753, 5.413231402905805290 ) ) ;
#70803 = CARTESIAN_POINT ( 'NONE',  ( 6.676582343750001591, 292.9531250017069510, -8.176455196517173205E-16 ) ) ;
#70805 = LINE ( 'NONE', #25511, #26537 ) ;
#70804 = CARTESIAN_POINT ( 'NONE',  ( -8.311093377946836114, 233.2812500034139589, -8.311093377946836114 ) ) ;
#70806 = CONTEXT_DEPENDENT_SHAPE_REPRESENTATION ( #14, #40332 ) ;
#70807 = APPLICATION_CONTEXT ( 'automotive_design' ) ;
#70808 = ORIENTED_EDGE ( 'NONE', *, *, #7521, .F. ) ;
#70809 = VECTOR ( 'NONE', #69823, 1000.000000000000000 ) ;
#70810 = EDGE_CURVE ( 'NONE', #21543, #12103, #52341, .T. ) ;
#70811 = CARTESIAN_POINT ( 'NONE',  ( 11.35316468749999963, 226.7187500034139873, -1.390361679473963556E-15 ) ) ;
#70812 = CARTESIAN_POINT ( 'NONE',  ( -2.977408999572648707, -7.188101187499990274, 1.767802781871753881 ) ) ;
#70813 = DIRECTION ( 'NONE',  ( -1.000000000000000000, 0.000000000000000000, 0.000000000000000000 ) ) ;
#70814 = CARTESIAN_POINT ( 'NONE',  ( -3.458734124999960358, 203.6875000013656063, 198.0000000000000284 ) ) ;
#70815 = ORIENTED_EDGE ( 'NONE', *, *, #37547, .T. ) ;
#70816 = DIRECTION ( 'NONE',  ( -0.000000000000000000, -1.000000000000000000, -0.000000000000000000 ) ) ;
#70817 = CARTESIAN_POINT ( 'NONE',  ( -11.35316468750000141, 103.5937499965860269, -1.390361679473963753E-15 ) ) ;
#70818 = CARTESIAN_POINT ( 'NONE',  ( -7.320508075688776373, 123.1250000000000284, 7.320508075688768379 ) ) ;
#70819 = CARTESIAN_POINT ( 'NONE',  ( -7.778174593052020747, -7.778174593052023411, 79.18750000000000000 ) ) ;
#70822 = CARTESIAN_POINT ( 'NONE',  ( -32.00000000000001421, 205.1875000000000000, 168.3431457505080289 ) ) ;
#70821 = CARTESIAN_POINT ( 'NONE',  ( 24.54126587499998280, 205.1250000013656347, 168.5673454167822740 ) ) ;
#70820 = CARTESIAN_POINT ( 'NONE',  ( 30.44569435410883429, 202.0625000013656063, 167.5543056458911053 ) ) ;
#70823 = VERTEX_POINT ( 'NONE', #49864 ) ;
#70824 = CARTESIAN_POINT ( 'NONE',  ( 2.449293598294707893E-16, 19.25000000000000000, -4.000000000000001776 ) ) ;
#70825 = DIRECTION ( 'NONE',  ( -1.000000000000000000, 0.000000000000000000, 0.000000000000000000 ) ) ;
#70826 = CARTESIAN_POINT ( 'NONE',  ( -3.042071309553164404, 217.2395833299192986, -11.35316468749999963 ) ) ;
#70827 = CARTESIAN_POINT ( 'NONE',  ( -2.754378923186476579E-14, 203.1875000013656063, 145.4587341250000350 ) ) ;
#70828 = CARTESIAN_POINT ( 'NONE',  ( 31.45873412499999233, 200.9375000013656063, 169.9999999999999432 ) ) ;
#70829 = ADVANCED_FACE ( 'NONE', ( #67597 ), #38925, .T. ) ;
#70830 = DIRECTION ( 'NONE',  ( -0.000000000000000000, -1.000000000000000000, -0.000000000000000000 ) ) ;
#70831 = CARTESIAN_POINT ( 'NONE',  ( 3.042071309553167069, 192.1354166632526130, -11.35316468749999785 ) ) ;
#70832 = CARTESIAN_POINT ( 'NONE',  ( -5.082755093536324154, 94.71875000204838102, 5.082755093536326818 ) ) ;
#70833 = CARTESIAN_POINT ( 'NONE',  ( -4.999999999999998224, 61.23691386381984358, -23.51762333030159624 ) ) ;
#70834 = CARTESIAN_POINT ( 'NONE',  ( -26.34314575050764162, 195.9375000000000000, 166.0000000000003695 ) ) ;
#70835 = CARTESIAN_POINT ( 'NONE',  ( -4.541265875000002339, 12.81249999863440792, -5.561446717895856393E-16 ) ) ;
#70836 = CARTESIAN_POINT ( 'NONE',  ( 29.43265458321760519, 197.7500000013656063, 173.4587341249998929 ) ) ;
#70837 = CARTESIAN_POINT ( 'NONE',  ( 2.977408999572650927, -7.188101187499990274, 2.330302781871754991 ) ) ;
#70838 = CARTESIAN_POINT ( 'NONE',  ( -11.35316468750000141, 73.28124999658602690, -1.390361679473963753E-15 ) ) ;
#70839 = CARTESIAN_POINT ( 'NONE',  ( -31.99999999999997868, 195.3125000000000853, 171.6568542494928238 ) ) ;
#70840 = LINE ( 'NONE', #24804, #33984 ) ;
#70841 = EDGE_LOOP ( 'NONE', ( #46492, #70589 ) ) ;
#70842 = DIRECTION ( 'NONE',  ( 0.000000000000000000, 0.000000000000000000, 1.000000000000000000 ) ) ;
#70843 = PLANE ( 'NONE',  #69007 ) ;
#70844 = CARTESIAN_POINT ( 'NONE',  ( 3.042071309553167069, 81.82291666325268409, -11.35316468749999785 ) ) ;
#70845 = EDGE_LOOP ( 'NONE', ( #7684, #2509, #51264, #38440, #64649, #72045 ) ) ;
#70846 = CARTESIAN_POINT ( 'NONE',  ( -7.204075437095967871, 7.204075437095967871, 85.84375000204836681 ) ) ;
#70847 = CARTESIAN_POINT ( 'NONE',  ( -7.778174593052023411, 7.778174593052023411, 67.00000000409676204 ) ) ;
#70848 = CARTESIAN_POINT ( 'NONE',  ( -38.00000000000000000, -52.99999999999999289, 25.00000000000000000 ) ) ;
#70849 = CARTESIAN_POINT ( 'NONE',  ( 2.679491924317126905, 76.04166666666614560, -9.999999999996632027 ) ) ;
#70851 = CARTESIAN_POINT ( 'NONE',  ( -11.35316468750000141, 73.28124999658602690, -1.390361679473963753E-15 ) ) ;
#70850 = CARTESIAN_POINT ( 'NONE',  ( -0.4368895104720006417, 67.59332269700051654, 20.03478791450398333 ) ) ;
#70853 = AXIS2_PLACEMENT_3D ( 'NONE', #451, #46444, #35508 ) ;
#70852 = CARTESIAN_POINT ( 'NONE',  ( -3.313708498984757167, 7.999999999999991118, 27.73655278392014978 ) ) ;
#70854 = DIRECTION ( 'NONE',  ( 0.000000000000000000, 0.000000000000000000, -1.000000000000000000 ) ) ;
#70855 = CARTESIAN_POINT ( 'NONE',  ( 5.000000000000001776, 167.7083333265053682, -8.660254037844389075 ) ) ;
#70856 = CARTESIAN_POINT ( 'NONE',  ( 2.977408999572650039, 92.56250000204838102, -7.188101187500001821 ) ) ;
#70857 = AXIS2_PLACEMENT_3D ( 'NONE', #13550, #36588, #59599 ) ;
#70858 = CARTESIAN_POINT ( 'NONE',  ( -25.23489602139278887, 194.8431269806823138, 172.6758199616631373 ) ) ;
#70859 = CARTESIAN_POINT ( 'NONE',  ( 8.311093377946834337, 60.46874999658602690, 8.311093377946839666 ) ) ;
#70860 = CARTESIAN_POINT ( 'NONE',  ( -10.18810118749999916, 4.220049686691934809, 114.4375000020483668 ) ) ;
#70861 = CARTESIAN_POINT ( 'NONE',  ( 6.951808397369818766E-16, 202.0312499965860411, -11.35316468750000141 ) ) ;
#70862 = ORIENTED_EDGE ( 'NONE', *, *, #32581, .F. ) ;
#70863 = CARTESIAN_POINT ( 'NONE',  ( -1.296342370383538389, 60.23018777774547061, 22.90345467631967935 ) ) ;
#70864 = CARTESIAN_POINT ( 'NONE',  ( -7.999999999999998224, 122.0937500000000000, 3.313708498984766049 ) ) ;
#70865 = FACE_OUTER_BOUND ( 'NONE', #2184, .T. ) ;
#70867 = CARTESIAN_POINT ( 'NONE',  ( -11.35316468749999785, 198.0729166632526983, -3.042071309553167957 ) ) ;
#70866 = CARTESIAN_POINT ( 'NONE',  ( 10.00000000000000000, 262.5000000000000000, -1.224646799147353256E-15 ) ) ;
#70868 = LINE ( 'NONE', #46740, #61062 ) ;
#70869 = CARTESIAN_POINT ( 'NONE',  ( -5.000000000000000888, 237.2916666734946318, -8.660254037844387298 ) ) ;
#70870 = CARTESIAN_POINT ( 'NONE',  ( 28.00000000000002132, 202.1250000027312126, 173.9999999999999147 ) ) ;
#70871 = ORIENTED_EDGE ( 'NONE', *, *, #33912, .T. ) ;
#70872 = CARTESIAN_POINT ( 'NONE',  ( 5.676582343749993598, 185.2604166632526983, 9.832129032723422313 ) ) ;
#70873 =( BOUNDED_CURVE ( )  B_SPLINE_CURVE ( 2, ( #44516, #62601, #10931, #32840, #10559, #33590, #62982, #33968, #50914 ),
 .UNSPECIFIED., .F., .F. ) 
 B_SPLINE_CURVE_WITH_KNOTS ( ( 3, 2, 2, 2, 3 ),
 ( 0.5972222222222222099, 0.6041666666666666297, 0.6111111111111111605, 0.6180555555555554692, 0.6249999999999998890 ),
 .UNSPECIFIED. ) 
 CURVE ( )  GEOMETRIC_REPRESENTATION_ITEM ( )  RATIONAL_B_SPLINE_CURVE ( ( 1.000000000000000000, 0.9238795325112867385, 1.000000000000000000, 0.9238795325112867385, 1.000000000000000000, 0.9238795325112867385, 1.000000000000000000, 0.9238795325112879597, 0.9999999999999987788 ) ) 
 REPRESENTATION_ITEM ( '' )  );
#70874 = CARTESIAN_POINT ( 'NONE',  ( 5.082755093536320601, -5.082755093536318824, 20.04905278187175455 ) ) ;
#70875 = ORIENTED_EDGE ( 'NONE', *, *, #15464, .F. ) ;
#70876 = CARTESIAN_POINT ( 'NONE',  ( -4.898587196589412829E-16, 97.81250000409677625, -8.000000000000000000 ) ) ;
#70877 = EDGE_CURVE ( 'NONE', #41993, #33755, #21926, .T. ) ;
#70878 = CARTESIAN_POINT ( 'NONE',  ( 10.00000000000000000, 4.791666666666666075, 2.679491924311236062 ) ) ;
#70879 = EDGE_CURVE ( 'NONE', #54420, #58040, #67964, .T. ) ;
#70880 = CARTESIAN_POINT ( 'NONE',  ( -4.000000000000002665, 10.56250000000000000, 1.656854249492380804 ) ) ;
#70881 = CARTESIAN_POINT ( 'NONE',  ( -39.97324732667617297, 0.000000000000000000, 113.7582050592233998 ) ) ;
#70882 = CARTESIAN_POINT ( 'NONE',  ( 2.780723358947928197E-16, 17.56249999863440792, -4.541265875000002339 ) ) ;
#70883 = CARTESIAN_POINT ( 'NONE',  ( -7.999999999999989342, -3.313708498984762496, 13.11155278392014623 ) ) ;
#70884 = CARTESIAN_POINT ( 'NONE',  ( -5.000000000000007105, 188.3333333333333428, 8.660254037844389075 ) ) ;
#70885 = VERTEX_POINT ( 'NONE', #10625 ) ;
#70886 = CARTESIAN_POINT ( 'NONE',  ( -2.977408999572650927, 96.87500000204836681, -7.188101187500001821 ) ) ;
#70888 = CARTESIAN_POINT ( 'NONE',  ( -10.99999999999999822, -4.556349186104053040, 98.59375000000000000 ) ) ;
#70887 = CARTESIAN_POINT ( 'NONE',  ( 2.679491924294600480, 178.9583333333318649, 10.00000000000966160 ) ) ;
#70889 = DIRECTION ( 'NONE',  ( 1.000000000000000000, 0.000000000000000000, 0.000000000000000000 ) ) ;
#70890 = EDGE_LOOP ( 'NONE', ( #58175, #7163, #68447 ) ) ;
#70891 = CARTESIAN_POINT ( 'NONE',  ( 5.107860025160332995, 10.26152767799288945, -64.38109526790006498 ) ) ;
#70893 = CARTESIAN_POINT ( 'NONE',  ( 11.00000000000000000, 1.347111479062088405E-15, 82.74999999999998579 ) ) ;
#70892 = VECTOR ( 'NONE', #23631, 1000.000000000000114 ) ;
#70894 = CARTESIAN_POINT ( 'NONE',  ( 1.320432766682872962E-15, -7.188101187499992051, 19.86155278187175455 ) ) ;
#70895 = VERTEX_POINT ( 'NONE', #33651 ) ;
#70896 = EDGE_LOOP ( 'NONE', ( #51685, #56382, #47275 ) ) ;
#70897 = CARTESIAN_POINT ( 'NONE',  ( 4.220049686691941027, -10.18810118749999738, 87.62500000204836681 ) ) ;
#70898 = CARTESIAN_POINT ( 'NONE',  ( -10.00000000000000178, 114.3749999931720396, -1.224646799147353454E-15 ) ) ;
#70899 = CARTESIAN_POINT ( 'NONE',  ( 7.778174593052021635, 7.778174593052023411, 94.93750000000000000 ) ) ;
#70902 = CARTESIAN_POINT ( 'NONE',  ( 6.676582343750001591, 294.1093750017069510, -8.176455196517173205E-16 ) ) ;
#70901 = CARTESIAN_POINT ( 'NONE',  ( 28.00000000000002132, 203.1250000027312126, 173.9999999999999147 ) ) ;
#70900 = CARTESIAN_POINT ( 'NONE',  ( 11.00000000000000000, 1.347111479062088405E-15, 118.0000000000000000 ) ) ;
#70903 = CARTESIAN_POINT ( 'NONE',  ( -5.000000000000005329, 153.3333333333333428, 8.660254037844387298 ) ) ;
#70904 = CARTESIAN_POINT ( 'NONE',  ( 25.17157287525381903, 200.0000000027312126, 172.8284271247460993 ) ) ;
#70905 = CARTESIAN_POINT ( 'NONE',  ( -7.778174593052023411, 7.778174593052023411, 78.81249999999998579 ) ) ;
#70906 =( GEOMETRIC_REPRESENTATION_CONTEXT ( 3 ) GLOBAL_UNCERTAINTY_ASSIGNED_CONTEXT ( ( #65391 ) ) GLOBAL_UNIT_ASSIGNED_CONTEXT ( ( #57767, #59601, #19591 ) ) REPRESENTATION_CONTEXT ( 'NONE', 'WORKASPACE' ) );
#70907 = DIRECTION ( 'NONE',  ( -0.000000000000000000, -1.000000000000000000, -0.000000000000000000 ) ) ;
#70908 = CARTESIAN_POINT ( 'NONE',  ( -5.656854249492379694, 4.874999995903221084, -5.656854249492380582 ) ) ;
#70909 = CARTESIAN_POINT ( 'NONE',  ( 25.55430564589119413, 198.0625000013656063, 167.5543056458910485 ) ) ;
#70910 = CARTESIAN_POINT ( 'NONE',  ( 7.188101187500001821, 8.437499997951611874, -2.977408999572650483 ) ) ;
#70911 = CARTESIAN_POINT ( 'NONE',  ( 1.469576158976822172E-15, -7.999999999999991118, 23.89280278392014978 ) ) ;
#70912 = CARTESIAN_POINT ( 'NONE',  ( -6.123233995736766282E-16, 241.8750000068280031, -10.00000000000000000 ) ) ;
#70913 = CARTESIAN_POINT ( 'NONE',  ( 5.082755093536325042, 108.9687500020483810, -5.082755093536325930 ) ) ;
#70915 = CARTESIAN_POINT ( 'NONE',  ( -10.00000000000000355, 132.7083333333333428, 2.679491924311223183 ) ) ;
#70914 = CARTESIAN_POINT ( 'NONE',  ( 0.000000000000000000, 30.78460969082653875, -20.69999999999999929 ) ) ;
#70916 = CARTESIAN_POINT ( 'NONE',  ( -8.311093377946834337, 234.8437500034139305, 8.311093377946837890 ) ) ;
#70917 = CARTESIAN_POINT ( 'NONE',  ( -2.828427124746192067, 12.62500000000000000, 2.828427124746190735 ) ) ;
#70918 = CARTESIAN_POINT ( 'NONE',  ( -7.188101187499990274, -2.977408999572651371, 21.45530278187175810 ) ) ;
#70919 = CARTESIAN_POINT ( 'NONE',  ( -11.00000000000000000, 0.000000000000000000, 118.0000000000000000 ) ) ;
#70920 = CARTESIAN_POINT ( 'NONE',  ( -9.832129032723418760, 22.86458332991934839, -5.676582343750004256 ) ) ;
#70921 = CARTESIAN_POINT ( 'NONE',  ( 7.320508075688771044, 6.249999993172032475, 7.320508075688775484 ) ) ;
#70922 = CARTESIAN_POINT ( 'NONE',  ( 1.469576158976823947E-15, 111.8750000000000000, 8.000000000000000000 ) ) ;
#70923 = CARTESIAN_POINT ( 'NONE',  ( 1.269536070779894168E-12, 186.2499999999999147, -10.00000000000000178 ) ) ;
#70924 = ORIENTED_EDGE ( 'NONE', *, *, #9530, .T. ) ;
#70925 = CARTESIAN_POINT ( 'NONE',  ( 0.000000000000000000, 0.000000000000000000, -25.03750572909317285 ) ) ;
#70926 = CARTESIAN_POINT ( 'NONE',  ( -11.00000000000000000, 4.556349186104045934, 70.09375000409676204 ) ) ;
#70927 = CARTESIAN_POINT ( 'NONE',  ( 8.311093377946834337, 40.15624999658601268, 8.311093377946839666 ) ) ;
#70928 = CARTESIAN_POINT ( 'NONE',  ( -11.00000000000000000, 4.556349186104045934, 86.59375000409677625 ) ) ;
#70929 = CARTESIAN_POINT ( 'NONE',  ( -3.458734125000016757, 207.1250000013656347, 140.5673454167823593 ) ) ;
#70930 = CARTESIAN_POINT ( 'NONE',  ( 27.99999999999996092, 194.8437500006828031, 173.7293670624999038 ) ) ;
#70931 = DIRECTION ( 'NONE',  ( -0.000000000000000000, 1.000000000000000000, -0.000000000000000000 ) ) ;
#70933 = CARTESIAN_POINT ( 'NONE',  ( 11.35316468750000141, 35.78124999658601268, 0.000000000000000000 ) ) ;
#70932 = CARTESIAN_POINT ( 'NONE',  ( 7.188101187500002709, 108.3125000020483810, 2.977408999572649151 ) ) ;
#70934 = CARTESIAN_POINT ( 'NONE',  ( -4.898587196589407898E-16, 7.999999999999991118, 15.45530277982336642 ) ) ;
#70935 = CARTESIAN_POINT ( 'NONE',  ( -8.311093377946836114, 152.6562499965859843, -8.311093377946837890 ) ) ;
#70936 = CARTESIAN_POINT ( 'NONE',  ( 10.00000000000000000, 116.6666666598387110, 2.679491924311236062 ) ) ;
#70937 = CARTESIAN_POINT ( 'NONE',  ( -7.188101187499999156, 106.6250000020483952, 2.977408999572654924 ) ) ;
#70938 = CYLINDRICAL_SURFACE ( 'NONE', #22809, 6.000000000000001776 ) ;
#70939 = CARTESIAN_POINT ( 'NONE',  ( -30.44569435410883429, 204.8125000013656063, 167.5543056458915885 ) ) ;
#70940 = VERTEX_POINT ( 'NONE', #56656 ) ;
#70941 = CARTESIAN_POINT ( 'NONE',  ( 11.35316468750000141, 21.09374999658601624, 0.000000000000000000 ) ) ;
#70942 = ORIENTED_EDGE ( 'NONE', *, *, #41301, .F. ) ;
#70943 = CARTESIAN_POINT ( 'NONE',  ( 28.00000000000001776, 205.5000000000000284, 165.9999999999998863 ) ) ;
#70945 = CARTESIAN_POINT ( 'NONE',  ( 11.35316468749999963, 150.9895833299193271, -3.042071309553165293 ) ) ;
#70944 = CARTESIAN_POINT ( 'NONE',  ( 11.00000000000000000, 1.347111479062088405E-15, 91.93750000409677625 ) ) ;
#70946 = CARTESIAN_POINT ( 'NONE',  ( 1.469576158976822172E-15, -7.999999999999991118, 20.76155278432982243 ) ) ;
#70947 = CARTESIAN_POINT ( 'NONE',  ( 5.656854249492378806, 14.81250000000000355, 5.656854249492381470 ) ) ;
#70948 = CARTESIAN_POINT ( 'NONE',  ( 3.042071309553173286, 235.3645833367473017, 11.35316468749999608 ) ) ;
#70949 = CARTESIAN_POINT ( 'NONE',  ( 1.871523826299183495E-15, -10.18810118749999916, 93.90625000204836681 ) ) ;
#70950 = ORIENTED_EDGE ( 'NONE', *, *, #69959, .T. ) ;
#70951 = EDGE_CURVE ( 'NONE', #72569, #25179, #39150, .T. ) ;
#70952 = CARTESIAN_POINT ( 'NONE',  ( 2.679491924309757689, 121.0416666666668135, -10.00000000000085443 ) ) ;
#70953 = CARTESIAN_POINT ( 'NONE',  ( 8.311093377946834337, 100.4687499965860269, 8.311093377946839666 ) ) ;
#70954 = CARTESIAN_POINT ( 'NONE',  ( 10.18810118749999916, 4.220049686691935698, 100.0000000020483668 ) ) ;
#70955 = CARTESIAN_POINT ( 'NONE',  ( -3.211159895383561391, 16.81249999863440436, -3.211159895383561835 ) ) ;
#70956 = ORIENTED_EDGE ( 'NONE', *, *, #47948, .T. ) ;
#70957 = EDGE_LOOP ( 'NONE', ( #24421, #61228, #55601, #27630 ) ) ;
#70958 = CARTESIAN_POINT ( 'NONE',  ( 8.000000000000000000, 3.000000000000000444, 0.000000000000000000 ) ) ;
#70959 = CARTESIAN_POINT ( 'NONE',  ( -4.541265875000003227, 1.999999998634407250, 1.881053915767121110 ) ) ;
#70960 = VECTOR ( 'NONE', #51294, 1000.000000000000000 ) ;
#70961 = CARTESIAN_POINT ( 'NONE',  ( 2.977408999572651815, 1.687499997951610098, 7.188101187500000933 ) ) ;
#70962 = CARTESIAN_POINT ( 'NONE',  ( 8.000000000000001776, 116.8437500040967905, 3.313708498984759387 ) ) ;
#70963 = EDGE_CURVE ( 'NONE', #41123, #1819, #72118, .T. ) ;
#70964 = CARTESIAN_POINT ( 'NONE',  ( -7.204075437095967871, 7.204075437095967871, 99.34375000204836681 ) ) ;
#70965 = DIRECTION ( 'NONE',  ( -1.000000000000000000, -0.000000000000000000, -0.000000000000000000 ) ) ;
#70966 = ADVANCED_FACE ( 'NONE', ( #60805 ), #9130, .F. ) ;
#70967 =( BOUNDED_CURVE ( )  B_SPLINE_CURVE ( 2, ( #70982, #8350, #54394, #19297, #1960, #42307, #66436, #48336, #2701 ),
 .UNSPECIFIED., .F., .F. ) 
 B_SPLINE_CURVE_WITH_KNOTS ( ( 3, 2, 2, 2, 3 ),
 ( 0.02941176470588236988, 0.03308823529411766828, 0.03676470588235296322, 0.04044117647058825815, 0.04411764705882355309 ),
 .UNSPECIFIED. ) 
 CURVE ( )  GEOMETRIC_REPRESENTATION_ITEM ( )  RATIONAL_B_SPLINE_CURVE ( ( 0.9999999999999996669, 0.9238795325112870716, 1.000000000000000000, 0.9238795325112867385, 1.000000000000000000, 0.9238795325112867385, 1.000000000000000000, 0.9238795325112862944, 1.000000000000000444 ) ) 
 REPRESENTATION_ITEM ( '' )  );
#70968 = CARTESIAN_POINT ( 'NONE',  ( 1.656854249492381248, 13.93749999726881228, -4.000000000000001776 ) ) ;
#70969 = CARTESIAN_POINT ( 'NONE',  ( -3.211159895383562723, 2.937499998634407028, 3.211159895383561391 ) ) ;
#70970 = ORIENTED_EDGE ( 'NONE', *, *, #68045, .F. ) ;
#70971 = CARTESIAN_POINT ( 'NONE',  ( 1.432654583217607858, 208.6250000013655779, 138.5412658750000787 ) ) ;
#70972 = CARTESIAN_POINT ( 'NONE',  ( 2.754378923186476579E-14, 197.1875000013655779, 194.5412658750000219 ) ) ;
#70974 = CARTESIAN_POINT ( 'NONE',  ( 11.00000000000000000, 1.347111479062088405E-15, 90.43750000409676204 ) ) ;
#70973 = CARTESIAN_POINT ( 'NONE',  ( -25.55430564589122966, 201.3125000013656063, 167.5543056458915032 ) ) ;
#70975 = B_SPLINE_CURVE_WITH_KNOTS ( 'NONE', 3,
 ( #60691, #48984, #24855, #19941, #13529, #13897, #36568, #54298, #43710, #59581, #14274, #25597 ),
 .UNSPECIFIED., .F., .F.,
 ( 4, 2, 2, 2, 2, 4 ),
 ( 2.602085213965210642E-18, 0.002547658444427999564, 0.005095316888855995659, 0.006369146111069992622, 0.007642975333283990452, 0.01019063377771198264 ),
 .UNSPECIFIED. ) ;
#70976 = CARTESIAN_POINT ( 'NONE',  ( 4.541265875000002339, 14.31249999863440792, 0.000000000000000000 ) ) ;
#70977 = CARTESIAN_POINT ( 'NONE',  ( -1.836970198721029983E-15, 120.6249999931720396, 10.00000000000000178 ) ) ;
#70978 = CARTESIAN_POINT ( 'NONE',  ( -7.188101187499990274, -2.977408999572651371, 15.08030278187175455 ) ) ;
#70979 = ORIENTED_EDGE ( 'NONE', *, *, #69110, .T. ) ;
#70980 = VERTEX_POINT ( 'NONE', #63408 ) ;
#70981 = CARTESIAN_POINT ( 'NONE',  ( -7.204075437095967871, 7.204075437095967871, 101.9687500020483668 ) ) ;
#70982 = CARTESIAN_POINT ( 'NONE',  ( -11.00000000000000000, 0.000000000000000000, 115.1875000040967763 ) ) ;
#70983 = CARTESIAN_POINT ( 'NONE',  ( -31.45873412499998523, 206.0000000013656063, 171.4326545832180386 ) ) ;
#70984 = CARTESIAN_POINT ( 'NONE',  ( -25.17157287525382259, 202.8750000000000284, 167.1715728752541565 ) ) ;
#70985 = CARTESIAN_POINT ( 'NONE',  ( -1.432654583217607192, 197.2500000013656063, 194.5412658750000219 ) ) ;
#70986 = CARTESIAN_POINT ( 'NONE',  ( -23.99999999999995026, 201.8125000027312126, 171.6568542494926817 ) ) ;
#70987 = CARTESIAN_POINT ( 'NONE',  ( -10.00000000000000000, 92.29166666666667140, -2.679491924311229845 ) ) ;
#70988 = CARTESIAN_POINT ( 'NONE',  ( 1.469576158976823947E-15, 117.8750000000000000, 8.000000000000000000 ) ) ;
#70989 = CARTESIAN_POINT ( 'NONE',  ( -6.676582343750003368, 295.5468750017069510, -2.765530957081996810 ) ) ;
#70990 = ORIENTED_EDGE ( 'NONE', *, *, #6422, .T. ) ;
#70991 = CARTESIAN_POINT ( 'NONE',  ( 3.313708498984762496, 16.03124999590322375, 7.999999999999998224 ) ) ;
#70992 = CARTESIAN_POINT ( 'NONE',  ( -2.754378923186476579E-14, 205.1875000013656063, 145.4587341250000350 ) ) ;
#70993 = DIRECTION ( 'NONE',  ( -0.000000000000000000, 1.000000000000000000, -0.000000000000000000 ) ) ;
#70994 = DIRECTION ( 'NONE',  ( 0.000000000000000000, 0.000000000000000000, 1.000000000000000000 ) ) ;
#70995 = CARTESIAN_POINT ( 'NONE',  ( 5.676582343749997150, 262.5520833367473301, -9.832129032723418760 ) ) ;
#70996 = DIRECTION ( 'NONE',  ( -0.000000000000000000, -0.000000000000000000, -1.000000000000000000 ) ) ;
#70997 = CARTESIAN_POINT ( 'NONE',  ( -10.99999999999999822, -4.556349186104052151, 112.0937499999999858 ) ) ;
#70998 = CARTESIAN_POINT ( 'NONE',  ( 6.123233995736767268E-16, 211.2500000000000284, -10.00000000000000178 ) ) ;
#70999 = CARTESIAN_POINT ( 'NONE',  ( -7.188101187499992051, 0.000000000000000000, 9.361552781871752771 ) ) ;
#71000 = CARTESIAN_POINT ( 'NONE',  ( -11.35316468750000141, 188.5937499965860127, -1.390361679473963753E-15 ) ) ;
#71001 = DIRECTION ( 'NONE',  ( -0.000000000000000000, 1.000000000000000000, -0.000000000000000000 ) ) ;
#71002 = CARTESIAN_POINT ( 'NONE',  ( -4.541265875000003227, 3.874999998634407028, 1.881053915767121110 ) ) ;
#71003 = LINE ( 'NONE', #41964, #35711 ) ;
#71005 = CARTESIAN_POINT ( 'NONE',  ( 3.313708498984761608, 10.59374999590322020, -8.000000000000000000 ) ) ;
#71004 = CARTESIAN_POINT ( 'NONE',  ( -4.000000000000001776, 14.24999999726881406, -4.898587196589415787E-16 ) ) ;
#71006 = VERTEX_POINT ( 'NONE', #51348 ) ;
#71007 = VECTOR ( 'NONE', #63335, 1000.000000000000000 ) ;
#71008 = CARTESIAN_POINT ( 'NONE',  ( -2.445694354108839175, 208.3125000013656063, 144.4456943541088663 ) ) ;
#71009 = CARTESIAN_POINT ( 'NONE',  ( -11.35316468750000141, 53.80208332991935549, 3.042071309553159963 ) ) ;
#71010 = CARTESIAN_POINT ( 'NONE',  ( -7.778174593052020747, -7.778174593052023411, 104.8750000040967763 ) ) ;
#71011 = CARTESIAN_POINT ( 'NONE',  ( 5.676582343749993598, 220.2604166632526983, 9.832129032723422313 ) ) ;
#71012 = CARTESIAN_POINT ( 'NONE',  ( -26.56734541678228112, 204.0000000013656063, 173.4587341250003476 ) ) ;
#71013 = CARTESIAN_POINT ( 'NONE',  ( 4.556349186104045934, 11.00000000000000000, 95.21875000409677625 ) ) ;
#71015 = CARTESIAN_POINT ( 'NONE',  ( 2.726951573962122902E-14, -51.14729664189338365, -48.52014062455057797 ) ) ;
#71014 = CARTESIAN_POINT ( 'NONE',  ( -2.977408999572650927, 123.8750000020483952, -7.188101187500000933 ) ) ;
#71016 = LINE ( 'NONE', #42714, #44782 ) ;
#71017 = CARTESIAN_POINT ( 'NONE',  ( 8.311093377946834337, 105.1562499965860269, 8.311093377946839666 ) ) ;
#71018 = CARTESIAN_POINT ( 'NONE',  ( 7.320508075688771044, 81.24999999317201116, 7.320508075688775484 ) ) ;
#71019 = CARTESIAN_POINT ( 'NONE',  ( 7.188101187500002709, 93.31250000204838102, 2.977408999572649151 ) ) ;
#71020 = CARTESIAN_POINT ( 'NONE',  ( -8.342170076843785083E-16, 17.18749999863440792, 4.541265875000002339 ) ) ;
#71021 = CARTESIAN_POINT ( 'NONE',  ( -29.65685424949232640, 204.5625000027312126, 174.0000000000003695 ) ) ;
#71022 = ORIENTED_EDGE ( 'NONE', *, *, #1657, .F. ) ;
#71023 = VERTEX_POINT ( 'NONE', #40038 ) ;
#71024 = CARTESIAN_POINT ( 'NONE',  ( -4.721056650415998313, 294.7343750017069510, 4.721056650416000089 ) ) ;
#71025 = CARTESIAN_POINT ( 'NONE',  ( -7.320508075688783478, 141.8750000000000000, -7.320508075688784366 ) ) ;
#71026 = CARTESIAN_POINT ( 'NONE',  ( -9.832129032723418760, 162.8645833299193839, -5.676582343750004256 ) ) ;
#71027 = DIRECTION ( 'NONE',  ( 0.000000000000000000, 0.000000000000000000, 1.000000000000000000 ) ) ;
#71028 = CARTESIAN_POINT ( 'NONE',  ( 1.656854249492405451, 198.3125000000000284, 202.0000000000000284 ) ) ;
#71029 = CARTESIAN_POINT ( 'NONE',  ( 0.000000000000000000, 0.000000000000000000, 30.00000000000000000 ) ) ;
#71030 = CARTESIAN_POINT ( 'NONE',  ( 4.220049686691941027, -10.18810118749999738, 112.0000000020483668 ) ) ;
#71031 = ORIENTED_EDGE ( 'NONE', *, *, #58612, .T. ) ;
#71032 = DIRECTION ( 'NONE',  ( -0.000000000000000000, -0.000000000000000000, -1.000000000000000000 ) ) ;
#71033 = DIRECTION ( 'NONE',  ( 3.469446951953619612E-16, 0.000000000000000000, 1.000000000000000000 ) ) ;
#71034 = CARTESIAN_POINT ( 'NONE',  ( -11.35316468750000141, 143.5937499965860411, -1.390361679473963753E-15 ) ) ;
#71035 = CARTESIAN_POINT ( 'NONE',  ( 2.839093476692135984E-14, 194.6875000013655779, 201.4587341250000350 ) ) ;
#71036 = CARTESIAN_POINT ( 'NONE',  ( 2.839093476692135984E-14, 208.9375000013656063, 201.4587341250000350 ) ) ;
#71037 = CARTESIAN_POINT ( 'NONE',  ( 4.220049686691941027, -10.18810118749999738, 68.50000000204838102 ) ) ;
#71038 = CARTESIAN_POINT ( 'NONE',  ( -5.676582343749998039, 47.76041666325269119, -9.832129032723420536 ) ) ;
#71039 = ORIENTED_EDGE ( 'NONE', *, *, #66223, .F. ) ;
#71040 = CARTESIAN_POINT ( 'NONE',  ( -1.881053915767124440, 4.124999998634407028, 4.541265875000001451 ) ) ;
#71041 = CARTESIAN_POINT ( 'NONE',  ( -8.008118988124991233, 0.000000000000000000, 8.513115283940630107 ) ) ;
#71042 = ADVANCED_FACE ( 'NONE', ( #58512 ), #74358, .T. ) ;
#71043 = CARTESIAN_POINT ( 'NONE',  ( -1.320432766682874540E-15, 15.09374999795161187, 7.188101187500000044 ) ) ;
#71044 = CARTESIAN_POINT ( 'NONE',  ( -2.485281374238572649, 291.2500000034140157, 6.000000000000002665 ) ) ;
#71045 = LINE ( 'NONE', #53349, #61796 ) ;
#71046 = CARTESIAN_POINT ( 'NONE',  ( -2.977408999572654480, 13.87499999795161365, 7.188101187499999156 ) ) ;
#71047 = CARTESIAN_POINT ( 'NONE',  ( -7.188101187499990274, -2.977408999572651815, 12.08030278187175277 ) ) ;
#71048 = CARTESIAN_POINT ( 'NONE',  ( 7.204075437095968759, -7.204075437095966983, 115.0937500020483810 ) ) ;
#71049 = VECTOR ( 'NONE', #32975, 1000.000000000000000 ) ;
#71050 = DIRECTION ( 'NONE',  ( -1.000000000000000000, -0.000000000000000000, -0.000000000000000000 ) ) ;
#71051 = CARTESIAN_POINT ( 'NONE',  ( 2.828427124746190291, 1.624999997268813390, 2.828427124746192067 ) ) ;
#71052 = ORIENTED_EDGE ( 'NONE', *, *, #61981, .T. ) ;
#71053 = AXIS2_PLACEMENT_3D ( 'NONE', #60334, #2635, #14300 ) ;
#71054 = CARTESIAN_POINT ( 'NONE',  ( 2.751064625579944321E-14, 196.8750000027312126, 194.0000000000000568 ) ) ;
#71055 = EDGE_CURVE ( 'NONE', #64958, #65034, #69451, .T. ) ;
#71056 = CARTESIAN_POINT ( 'NONE',  ( 3.999999999999960032, 201.9375000000000284, 143.6568542494924543 ) ) ;
#71057 = CARTESIAN_POINT ( 'NONE',  ( -23.99999999999995737, 198.8125000027312126, 171.6568542494926817 ) ) ;
#71058 = CARTESIAN_POINT ( 'NONE',  ( 3.211159895383561835, 1.437499998634406806, -3.211159895383561835 ) ) ;
#71059 = CARTESIAN_POINT ( 'NONE',  ( -7.188101187500000044, 107.6562500020483810, 0.000000000000000000 ) ) ;
#71060 = LINE ( 'NONE', #64311, #15108 ) ;
#71061 = CARTESIAN_POINT ( 'NONE',  ( 5.656854249492376141, -5.656854249492374365, 0.08030278392014492117 ) ) ;
#71062 = ORIENTED_EDGE ( 'NONE', *, *, #37634, .T. ) ;
#71063 = CARTESIAN_POINT ( 'NONE',  ( -7.188101187500000044, 20.71874999795161543, -8.802885111219163269E-16 ) ) ;
#71064 = ORIENTED_EDGE ( 'NONE', *, *, #51610, .F. ) ;
#71065 = CARTESIAN_POINT ( 'NONE',  ( 0.000000000000000000, 210.0000000000000284, 170.0000000000000284 ) ) ;
#71066 = CARTESIAN_POINT ( 'NONE',  ( 2.445694354108839619, 208.8125000013656063, 200.4456943541088663 ) ) ;
#71067 = CARTESIAN_POINT ( 'NONE',  ( 25.55430564589115505, 203.0625000013656063, 167.5543056458911053 ) ) ;
#71068 = CARTESIAN_POINT ( 'NONE',  ( -7.320508075688773708, 56.87500000000000711, -7.320508075688774596 ) ) ;
#71069 = CARTESIAN_POINT ( 'NONE',  ( -5.082755093536325930, 97.34375000204838102, -5.082755093536325930 ) ) ;
#71070 = CARTESIAN_POINT ( 'NONE',  ( -4.242640687119285658, 298.1250000000000000, 4.242640687119287435 ) ) ;
#71072 = CARTESIAN_POINT ( 'NONE',  ( 9.797174393178825657E-16, 125.0000000000000000, -8.000000000000000000 ) ) ;
#71071 = CARTESIAN_POINT ( 'NONE',  ( 4.231687259407054036, -51.96503165405668767, -48.83411696341865849 ) ) ;
#71073 = VECTOR ( 'NONE', #20221, 1000.000000000000000 ) ;
#71074 = ORIENTED_EDGE ( 'NONE', *, *, #24106, .F. ) ;
#71075 =( BOUNDED_SURFACE ( )  B_SPLINE_SURFACE ( 1, 2, ( 
 ( #13724, #48442, #64329, #70365, #18679, #24328, #8458, #71445, #36035, #36769, #30732, #19773, #65051, #71821, #2062, #71080, #31478, #41688, #59051, #30367, #59780, #54501, #1711, #65798, #19397, #31093, #35666, #47699, #42781, #8090, #25795, #58680, #6989, #29999, #53014, #66924, #49188, #20892, #72198, #20511, #26927, #32230, #27296, #56358, #10332, #43914, #3554, #4677, #66541, #44662, #67302, #15601, #38261, #32613, #27673, #32992, #3182, #61642, #14476, #72959, #20140, #15229, #72587, #14850, #26544, #49569, #67675, #9594, #54873, #15974, #37890, #61264, #43156, #43526, #55620, #50679, #3937, #21265, #31850, #49945, #39003, #9959, #73333, #44289, #55992, #60888, #26169, #38640, #4306, #8839, #66172, #9210, #50312, #21637, #62007, #33357, #55248, #37515, #60514, #11813, #16335, #63866, #23128, #17843, #51057, #5792, #28789, #56734, #45769, #28421, #17466, #29172, #69157, #11444, #6533, #58234, #22370, #17090, #6163, #40486, #34852, #10699, #57487, #29539, #11078, #51804, #57857, #45392, #46512, #57101, #34479, #74440, #40112, #51428, #68408, #68780, #73697, #63118, #16708, #52187, #35215, #46140, #22748, #62369, #39738, #33732, #63491, #152, #22009, #40859, #45036, #69531, #23498, #518, #12178, #5053, #68044, #39373, #28048, #74070, #62738, #34106, #5415, #13642, #53662, #58591, #19682, #18587, #12909, #1256, #71357, #47248, #59692, #8367, #13273, #47982, #31007, #7269, #53297, #1622, #6897, #14009, #64239, #29908, #18952, #35943, #54032, #23874, #24234, #52923, #42692, #24602, #30277, #2342, #41232, #12549, #64963, #52550, #65705, #889, #25336, #48351, #59328, #1974, #35577, #42322, #37045, #46884, #36312, #8001, #47609, #60046, #36680, #24966, #70275, #69907, #41598 ),
 ( #64613, #58962, #19311, #18219, #70633, #41956, #7638, #30644, #70995, #65340, #38174, #43439, #38553, #67590, #21551, #55159, #14762, #15886, #3091, #55908, #3845, #26841, #49478, #43825, #38918, #44203, #14389, #72874, #25704, #9507, #31383, #3464, #9122, #26076, #37802, #60797, #4219, #20806, #32522, #67216, #54409, #55535, #26453, #72497, #20423, #43063, #61920, #44577, #27208, #54780, #50225, #66079, #73246, #49097, #15513, #32138, #49856, #72110, #2716, #66839, #66454, #15142, #61177, #21178, #37423, #61554, #9875, #32903, #48724, #71731, #20045, #60423, #8750, #31760, #67956, #63401, #27584, #6074, #46429, #74351, #16249, #68325, #39287, #39658, #69443, #5333, #51342, #28701, #44949, #57020, #29082, #50971, #56271, #23043, #22288, #23414, #46054, #62656, #57394, #17379, #51715, #69073, #21918, #68695, #17754, #45311, #17005, #40403, #33643, #57769, #16623, #22661, #10990, #45680, #34023, #56650, #28335, #40769, #40031, #27966, #11727, #10245, #34393, #63033, #73611, #73985, #62288, #62, #11358, #33272, #52102, #4590, #434, #34767, #5702, #50593, #10617, #4965, #48267, #19593, #24521, #70916, #12823, #25250, #24877, #64886, #69815, #30921, #29823, #24147, #12461, #7916, #58504, #19230, #63776, #47526, #59243, #42236, #18500, #64525, #35858, #18131, #71274, #803, #41147, #30190, #47159, #65249, #35130, #35492, #64152, #53943, #58873, #41509, #13554, #52465, #23789, #46793, #59603, #6810, #7184, #12093, #52835, #53207, #58146, #1541, #13187, #1168, #70551, #36592, #53576, #2257, #36225, #1890, #70191, #18867, #41873, #7553, #30560, #6453, #47896, #29456, #22110, #45134, #55442, #25622, #14675, #68146, #3752, #59965, #33839, #66747, #62474, #19967, #49386, #72405, #48636 ) ),
 .UNSPECIFIED., .F., .F., .F. ) 
 B_SPLINE_SURFACE_WITH_KNOTS ( ( 2, 2 ),
 ( 3, 2, 2, 2, 2, 2, 2, 2, 2, 2, 2, 2, 2, 2, 2, 2, 2, 2, 2, 2, 2, 2, 2, 2, 2, 2, 2, 2, 2, 2, 2, 2, 2, 2, 2, 2, 2, 2, 2, 2, 2, 2, 2, 2, 2, 2, 2, 2, 2, 2, 2, 2, 2, 2, 2, 2, 2, 2, 2, 2, 2, 2, 2, 2, 2, 2, 2, 2, 2, 2, 2, 2, 2, 2, 2, 2, 2, 2, 2, 2, 2, 2, 2, 2, 2, 2, 2, 2, 2, 2, 2, 2, 2, 2, 2, 2, 2, 2, 2, 2, 2, 2, 2, 2, 2, 2, 2, 2, 3 ),
 ( 0.000000000000000000, 1.000000000000000000 ),
 ( 0.000000000000000000, 0.009259259259259258745, 0.01851851851851851749, 0.02777777777777777624, 0.03703703703703703498, 0.04629629629629629373, 0.05555555555555555247, 0.06481481481481481122, 0.07407407407407406996, 0.08333333333333332871, 0.09259259259259258745, 0.1018518518518518462, 0.1111111111111111049, 0.1203703703703703637, 0.1296296296296296224, 0.1388888888888888951, 0.1481481481481481399, 0.1574074074074074125, 0.1666666666666666574, 0.1759259259259259300, 0.1851851851851851749, 0.1944444444444444475, 0.2037037037037036924, 0.2129629629629629650, 0.2222222222222222099, 0.2314814814814814825, 0.2407407407407407274, 0.2500000000000000000, 0.2592592592592592449, 0.2685185185185185452, 0.2777777777777777901, 0.2870370370370370350, 0.2962962962962962798, 0.3055555555555555802, 0.3148148148148148251, 0.3240740740740740700, 0.3333333333333333148, 0.3425925925925926152, 0.3518518518518518601, 0.3611111111111111049, 0.3703703703703703498, 0.3796296296296296502, 0.3888888888888888951, 0.3981481481481481399, 0.4074074074074073848, 0.4166666666666666852, 0.4259259259259259300, 0.4351851851851851749, 0.4444444444444444198, 0.4537037037037037202, 0.4629629629629629650, 0.4722222222222222099, 0.4814814814814814548, 0.4907407407407407551, 0.5000000000000000000, 0.5092592592592593004, 0.5185185185185184897, 0.5277777777777777901, 0.5370370370370370905, 0.5462962962962962798, 0.5555555555555555802, 0.5648148148148147696, 0.5740740740740740700, 0.5833333333333333703, 0.5925925925925925597, 0.6018518518518518601, 0.6111111111111111605, 0.6203703703703703498, 0.6296296296296296502, 0.6388888888888888395, 0.6481481481481481399, 0.6574074074074074403, 0.6666666666666666297, 0.6759259259259259300, 0.6851851851851852304, 0.6944444444444444198, 0.7037037037037037202, 0.7129629629629629095, 0.7222222222222222099, 0.7314814814814815103, 0.7407407407407406996, 0.7500000000000000000, 0.7592592592592593004, 0.7685185185185184897, 0.7777777777777777901, 0.7870370370370370905, 0.7962962962962962798, 0.8055555555555555802, 0.8148148148148147696, 0.8240740740740740700, 0.8333333333333333703, 0.8425925925925925597, 0.8518518518518518601, 0.8611111111111111605, 0.8703703703703703498, 0.8796296296296296502, 0.8888888888888888395, 0.8981481481481481399, 0.9074074074074074403, 0.9166666666666666297, 0.9259259259259259300, 0.9351851851851852304, 0.9444444444444444198, 0.9537037037037037202, 0.9629629629629629095, 0.9722222222222222099, 0.9814814814814815103, 0.9907407407407406996, 1.000000000000000000 ),
 .UNSPECIFIED. ) 
 GEOMETRIC_REPRESENTATION_ITEM ( )  RATIONAL_B_SPLINE_SURFACE ( (
 ( 1.000000000000000000, 0.9659258262890683122, 1.000000000000000000, 0.9659258262890683122, 1.000000000000000000, 0.9659258262890683122, 1.000000000000000000, 0.9659258262890683122, 1.000000000000000000, 0.9659258262890683122, 1.000000000000000000, 0.9659258262890683122, 1.000000000000000000, 0.9659258262890683122, 1.000000000000000000, 0.9659258262890683122, 1.000000000000000000, 0.9659258262890683122, 1.000000000000000000, 0.9659258262890683122, 1.000000000000000000, 0.9659258262890683122, 1.000000000000000000, 0.9659258262890683122, 1.000000000000000000, 0.9659258262890683122, 1.000000000000000000, 0.9659258262890683122, 1.000000000000000000, 0.9659258262890683122, 1.000000000000000000, 0.9659258262890683122, 1.000000000000000000, 0.9659258262890683122, 1.000000000000000000, 0.9659258262890683122, 1.000000000000000000, 0.9659258262890683122, 1.000000000000000000, 0.9659258262890683122, 1.000000000000000000, 0.9659258262890683122, 1.000000000000000000, 0.9659258262890683122, 1.000000000000000000, 0.9659258262890683122, 1.000000000000000000, 0.9659258262890683122, 1.000000000000000000, 0.9659258262890683122, 1.000000000000000000, 0.9659258262890683122, 1.000000000000000000, 0.9659258262890683122, 1.000000000000000000, 0.9659258262890683122, 1.000000000000000000, 0.9659258262890683122, 1.000000000000000000, 0.9659258262890683122, 1.000000000000000000, 0.9659258262890683122, 1.000000000000000000, 0.9659258262890683122, 1.000000000000000000, 0.9659258262890683122, 1.000000000000000000, 0.9659258262890683122, 1.000000000000000000, 0.9659258262890683122, 1.000000000000000000, 0.9659258262890683122, 1.000000000000000000, 0.9659258262890683122, 1.000000000000000000, 0.9659258262890683122, 1.000000000000000000, 0.9659258262890683122, 1.000000000000000000, 0.9659258262890683122, 1.000000000000000000, 0.9659258262890683122, 1.000000000000000000, 0.9659258262890683122, 1.000000000000000000, 0.9659258262890683122, 1.000000000000000000, 0.9659258262890683122, 1.000000000000000000, 0.9659258262890683122, 1.000000000000000000, 0.9659258262890683122, 1.000000000000000000, 0.9659258262890683122, 1.000000000000000000, 0.9659258262890683122, 1.000000000000000000, 0.9659258262890683122, 1.000000000000000000, 0.9659258262890683122, 1.000000000000000000, 0.9659258262890683122, 1.000000000000000000, 0.9659258262890683122, 1.000000000000000000, 0.9659258262890683122, 1.000000000000000000, 0.9659258262890683122, 1.000000000000000000, 0.9659258262890683122, 1.000000000000000000, 0.9659258262890683122, 1.000000000000000000, 0.9659258262890683122, 1.000000000000000000, 0.9659258262890683122, 1.000000000000000000, 0.9659258262890683122, 1.000000000000000000, 0.9659258262890683122, 1.000000000000000000, 0.9659258262890683122, 1.000000000000000000, 0.9659258262890683122, 1.000000000000000000, 0.9659258262890683122, 1.000000000000000000, 0.9659258262890683122, 1.000000000000000000, 0.9659258262890683122, 1.000000000000000000, 0.9659258262890683122, 1.000000000000000000, 0.9659258262890683122, 1.000000000000000000, 0.9659258262890683122, 1.000000000000000000, 0.9659258262890683122, 1.000000000000000000, 0.9659258262890683122, 1.000000000000000000, 0.9659258262890683122, 1.000000000000000000, 0.9659258262890683122, 1.000000000000000000, 0.9659258262890683122, 1.000000000000000000, 0.9659258262890683122, 1.000000000000000000, 0.9659258262890683122, 1.000000000000000000, 0.9659258262890683122, 1.000000000000000000, 0.9659258262890683122, 1.000000000000000000, 0.9659258262890683122, 1.000000000000000000, 0.9659258262890683122, 1.000000000000000000, 0.9659258262890683122, 1.000000000000000000, 0.9659258262890683122, 1.000000000000000000, 0.9659258262890683122, 1.000000000000000000, 0.9659258262890683122, 1.000000000000000000, 0.9659258262890683122, 1.000000000000000000, 0.9659258262890683122, 1.000000000000000000, 0.9659258262890683122, 1.000000000000000000, 0.9659258262890683122, 1.000000000000000000, 0.9659258262890683122, 1.000000000000000000, 0.9659258262890683122, 1.000000000000000000, 0.9659258262890683122, 1.000000000000000000, 0.9659258262890683122, 1.000000000000000000, 0.9659258262890683122, 1.000000000000000000, 0.9659258262890683122, 1.000000000000000000, 0.9659258262890683122, 1.000000000000000000, 0.9659258262890683122, 1.000000000000000000, 0.9659258262890683122, 1.000000000000000000, 0.9659258262890683122, 1.000000000000000000, 0.9659258262890683122, 1.000000000000000000, 0.9659258262890683122, 1.000000000000000000, 0.9659258262890683122, 1.000000000000000000, 0.9659258262890683122, 1.000000000000000000, 0.9659258262890683122, 1.000000000000000000, 0.9659258262890683122, 1.000000000000000000, 0.9659258262890683122, 1.000000000000000000, 0.9659258262890683122, 1.000000000000000000, 0.9659258262890683122, 1.000000000000000000, 0.9659258262890683122, 1.000000000000000000, 0.9659258262890683122, 1.000000000000000000),
 ( 1.000000000000000000, 0.9659258262890683122, 1.000000000000000000, 0.9659258262890683122, 1.000000000000000000, 0.9659258262890683122, 1.000000000000000000, 0.9659258262890683122, 1.000000000000000000, 0.9659258262890683122, 1.000000000000000000, 0.9659258262890683122, 1.000000000000000000, 0.9659258262890683122, 1.000000000000000000, 0.9659258262890683122, 1.000000000000000000, 0.9659258262890683122, 1.000000000000000000, 0.9659258262890683122, 1.000000000000000000, 0.9659258262890683122, 1.000000000000000000, 0.9659258262890683122, 1.000000000000000000, 0.9659258262890683122, 1.000000000000000000, 0.9659258262890683122, 1.000000000000000000, 0.9659258262890683122, 1.000000000000000000, 0.9659258262890683122, 1.000000000000000000, 0.9659258262890683122, 1.000000000000000000, 0.9659258262890683122, 1.000000000000000000, 0.9659258262890683122, 1.000000000000000000, 0.9659258262890683122, 1.000000000000000000, 0.9659258262890683122, 1.000000000000000000, 0.9659258262890683122, 1.000000000000000000, 0.9659258262890683122, 1.000000000000000000, 0.9659258262890683122, 1.000000000000000000, 0.9659258262890683122, 1.000000000000000000, 0.9659258262890683122, 1.000000000000000000, 0.9659258262890683122, 1.000000000000000000, 0.9659258262890683122, 1.000000000000000000, 0.9659258262890683122, 1.000000000000000000, 0.9659258262890683122, 1.000000000000000000, 0.9659258262890683122, 1.000000000000000000, 0.9659258262890683122, 1.000000000000000000, 0.9659258262890683122, 1.000000000000000000, 0.9659258262890683122, 1.000000000000000000, 0.9659258262890683122, 1.000000000000000000, 0.9659258262890683122, 1.000000000000000000, 0.9659258262890683122, 1.000000000000000000, 0.9659258262890683122, 1.000000000000000000, 0.9659258262890683122, 1.000000000000000000, 0.9659258262890683122, 1.000000000000000000, 0.9659258262890683122, 1.000000000000000000, 0.9659258262890683122, 1.000000000000000000, 0.9659258262890683122, 1.000000000000000000, 0.9659258262890683122, 1.000000000000000000, 0.9659258262890683122, 1.000000000000000000, 0.9659258262890683122, 1.000000000000000000, 0.9659258262890683122, 1.000000000000000000, 0.9659258262890683122, 1.000000000000000000, 0.9659258262890683122, 1.000000000000000000, 0.9659258262890683122, 1.000000000000000000, 0.9659258262890683122, 1.000000000000000000, 0.9659258262890683122, 1.000000000000000000, 0.9659258262890683122, 1.000000000000000000, 0.9659258262890683122, 1.000000000000000000, 0.9659258262890683122, 1.000000000000000000, 0.9659258262890683122, 1.000000000000000000, 0.9659258262890683122, 1.000000000000000000, 0.9659258262890683122, 1.000000000000000000, 0.9659258262890683122, 1.000000000000000000, 0.9659258262890683122, 1.000000000000000000, 0.9659258262890683122, 1.000000000000000000, 0.9659258262890683122, 1.000000000000000000, 0.9659258262890683122, 1.000000000000000000, 0.9659258262890683122, 1.000000000000000000, 0.9659258262890683122, 1.000000000000000000, 0.9659258262890683122, 1.000000000000000000, 0.9659258262890683122, 1.000000000000000000, 0.9659258262890683122, 1.000000000000000000, 0.9659258262890683122, 1.000000000000000000, 0.9659258262890683122, 1.000000000000000000, 0.9659258262890683122, 1.000000000000000000, 0.9659258262890683122, 1.000000000000000000, 0.9659258262890683122, 1.000000000000000000, 0.9659258262890683122, 1.000000000000000000, 0.9659258262890683122, 1.000000000000000000, 0.9659258262890683122, 1.000000000000000000, 0.9659258262890683122, 1.000000000000000000, 0.9659258262890683122, 1.000000000000000000, 0.9659258262890683122, 1.000000000000000000, 0.9659258262890683122, 1.000000000000000000, 0.9659258262890683122, 1.000000000000000000, 0.9659258262890683122, 1.000000000000000000, 0.9659258262890683122, 1.000000000000000000, 0.9659258262890683122, 1.000000000000000000, 0.9659258262890683122, 1.000000000000000000, 0.9659258262890683122, 1.000000000000000000, 0.9659258262890683122, 1.000000000000000000, 0.9659258262890683122, 1.000000000000000000, 0.9659258262890683122, 1.000000000000000000, 0.9659258262890683122, 1.000000000000000000, 0.9659258262890683122, 1.000000000000000000, 0.9659258262890683122, 1.000000000000000000, 0.9659258262890683122, 1.000000000000000000, 0.9659258262890683122, 1.000000000000000000, 0.9659258262890683122, 1.000000000000000000, 0.9659258262890683122, 1.000000000000000000, 0.9659258262890683122, 1.000000000000000000, 0.9659258262890683122, 1.000000000000000000, 0.9659258262890683122, 1.000000000000000000, 0.9659258262890683122, 1.000000000000000000, 0.9659258262890683122, 1.000000000000000000, 0.9659258262890683122, 1.000000000000000000, 0.9659258262890683122, 1.000000000000000000, 0.9659258262890683122, 1.000000000000000000, 0.9659258262890683122, 1.000000000000000000, 0.9659258262890683122, 1.000000000000000000, 0.9659258262890683122, 1.000000000000000000, 0.9659258262890683122, 1.000000000000000000) ) ) 
 REPRESENTATION_ITEM ( '' )  SURFACE ( )  );
#71076 = CARTESIAN_POINT ( 'NONE',  ( -9.832129032723418760, 233.4895833367473301, -5.676582343749998927 ) ) ;
#71077 = CARTESIAN_POINT ( 'NONE',  ( 0.000000000000000000, -2.500000000000000000, 0.000000000000000000 ) ) ;
#71078 = CARTESIAN_POINT ( 'NONE',  ( -8.660254037844390851, 74.79166665983871098, 4.999999999999998224 ) ) ;
#71079 = CARTESIAN_POINT ( 'NONE',  ( -4.000000000000002665, 17.31249999726881938, 1.656854249492380582 ) ) ;
#71080 = CARTESIAN_POINT ( 'NONE',  ( 7.320508075688776373, 261.8750000000000568, 7.320508075688767491 ) ) ;
#71081 = DIRECTION ( 'NONE',  ( 1.000000000000000000, 0.000000000000000000, 0.000000000000000000 ) ) ;
#71082 = CARTESIAN_POINT ( 'NONE',  ( 6.123233995736767268E-16, 176.2500000000000284, -10.00000000000000178 ) ) ;
#71083 = CARTESIAN_POINT ( 'NONE',  ( 11.49999999999998046, 82.00000000000001421, 20.00000000000000711 ) ) ;
#71084 = CARTESIAN_POINT ( 'NONE',  ( -6.123233995736766282E-16, 241.8750000068280031, -10.00000000000000000 ) ) ;
#71085 = CARTESIAN_POINT ( 'NONE',  ( -5.082755093536319713, 5.082755093536319713, 27.17405278187175455 ) ) ;
#71086 = CARTESIAN_POINT ( 'NONE',  ( -11.35316468749999785, 138.3854166632526983, -3.042071309553167513 ) ) ;
#71087 = FACE_OUTER_BOUND ( 'NONE', #74309, .T. ) ;
#71088 = CARTESIAN_POINT ( 'NONE',  ( -11.00000000000000000, 11.00000000000000000, 25.00000000000000000 ) ) ;
#71091 = CYLINDRICAL_SURFACE ( 'NONE', #47116, 8.000000000000000000 ) ;
#71090 = CARTESIAN_POINT ( 'NONE',  ( 105.0000000000000000, 38.00000000000000000, 139.0000000000000000 ) ) ;
#71089 = CARTESIAN_POINT ( 'NONE',  ( 29.65685424949235482, 206.0625000000000000, 173.9999999999999147 ) ) ;
#71092 = ORIENTED_EDGE ( 'NONE', *, *, #20887, .T. ) ;
#71093 = CARTESIAN_POINT ( 'NONE',  ( -2.085542519210945728E-15, 14.84374999658601624, 11.35316468750000141 ) ) ;
#71094 = DIRECTION ( 'NONE',  ( -0.000000000000000000, 1.000000000000000000, 4.476705744456276341E-16 ) ) ;
#71095 = LINE ( 'NONE', #65444, #30548 ) ;
#71096 = CARTESIAN_POINT ( 'NONE',  ( -3.458734125000015425, 206.9375000013656063, 142.0000000000000568 ) ) ;
#71097 = CARTESIAN_POINT ( 'NONE',  ( 7.999999999999991118, 9.797174393178815797E-16, 28.58030277982336642 ) ) ;
#71098 = VECTOR ( 'NONE', #7991, 1000.000000000000000 ) ;
#71099 = CARTESIAN_POINT ( 'NONE',  ( -10.00000000000000178, 39.37499999317203958, -1.224646799147353454E-15 ) ) ;
#71100 = CARTESIAN_POINT ( 'NONE',  ( 7.188101187500001821, 113.0000000020483668, -2.977408999572651371 ) ) ;
#71101 = CARTESIAN_POINT ( 'NONE',  ( 3.211159895383560947, 3.312499998634407028, 3.211159895383562723 ) ) ;
#71102 = CARTESIAN_POINT ( 'NONE',  ( -11.40147177802573886, -36.01969157730099624, 141.1205001164169346 ) ) ;
#71103 = CARTESIAN_POINT ( 'NONE',  ( 1.469576158976822172E-15, -7.999999999999991118, 16.20530277982336287 ) ) ;
#71105 = DIRECTION ( 'NONE',  ( 0.6524685526581929240, -0.7578158002934526349, 2.485390736430017174E-05 ) ) ;
#71104 = CARTESIAN_POINT ( 'NONE',  ( 4.242640687119285658, 291.6875000034139589, -4.242640687119286547 ) ) ;
#71106 = ORIENTED_EDGE ( 'NONE', *, *, #765, .T. ) ;
#71107 = CARTESIAN_POINT ( 'NONE',  ( 27.99999999999996092, 194.4587341250000350, 173.4587341249998929 ) ) ;
#71108 = DIRECTION ( 'NONE',  ( 0.000000000000000000, 0.000000000000000000, 1.000000000000000000 ) ) ;
#71109 = CARTESIAN_POINT ( 'NONE',  ( 3.042071309553173286, 230.6770833367473301, 11.35316468749999608 ) ) ;
#71110 = CARTESIAN_POINT ( 'NONE',  ( 11.35316468750000141, 115.7812499965860269, 0.000000000000000000 ) ) ;
#71111 = ORIENTED_EDGE ( 'NONE', *, *, #25130, .F. ) ;
#71112 = ADVANCED_FACE ( 'NONE', ( #40411 ), #46800, .F. ) ;
#71113 = DIRECTION ( 'NONE',  ( -0.000000000000000000, 1.000000000000000000, 4.689100369878284071E-30 ) ) ;
#71114 = CARTESIAN_POINT ( 'NONE',  ( -10.18810118749999916, 4.220049686691934809, 93.06250000204839523 ) ) ;
#71115 = CARTESIAN_POINT ( 'NONE',  ( -11.00000000000000000, 0.000000000000000000, 86.68750000409677625 ) ) ;
#71116 = CARTESIAN_POINT ( 'NONE',  ( 2.445694354108840063, 195.0625000013656063, 200.4456943541088663 ) ) ;
#71117 = CARTESIAN_POINT ( 'NONE',  ( -7.999999999999991118, 0.000000000000000000, 27.83030277982336642 ) ) ;
#71119 = CARTESIAN_POINT ( 'NONE',  ( -3.042071309553163960, 107.2395833299193413, -11.35316468749999963 ) ) ;
#71118 = CARTESIAN_POINT ( 'NONE',  ( 6.250510011802020927, 219.9999999999999432, 8.054087016449219760 ) ) ;
#71120 = CARTESIAN_POINT ( 'NONE',  ( -27.99999999999996092, 209.5000000000000284, 174.0000000000003695 ) ) ;
#71121 = CARTESIAN_POINT ( 'NONE',  ( 6.123233995736767268E-16, 83.12499999317203958, -10.00000000000000178 ) ) ;
#71122 = ORIENTED_EDGE ( 'NONE', *, *, #1830, .T. ) ;
#71123 = CARTESIAN_POINT ( 'NONE',  ( 10.00000000000000178, 212.0833333265053682, -2.679491924311226736 ) ) ;
#71124 = CARTESIAN_POINT ( 'NONE',  ( 4.556349186104045934, 11.00000000000000000, 83.21875000409680467 ) ) ;
#71125 = CARTESIAN_POINT ( 'NONE',  ( 11.35316468749999963, 106.3020833299193413, -3.042071309553165293 ) ) ;
#71126 = DIRECTION ( 'NONE',  ( 0.000000000000000000, 0.000000000000000000, -1.000000000000000000 ) ) ;
#71127 = CARTESIAN_POINT ( 'NONE',  ( 2.977408999572652260, 11.06249999795161187, 7.188101187500000044 ) ) ;
#71128 = CARTESIAN_POINT ( 'NONE',  ( 4.220049686691934809, 10.18810118749999916, 90.06250000204838102 ) ) ;
#71129 = CARTESIAN_POINT ( 'NONE',  ( -11.35316468749999785, 13.38541666325268409, -3.042071309553167513 ) ) ;
#71130 = ORIENTED_EDGE ( 'NONE', *, *, #14004, .F. ) ;
#71131 = CARTESIAN_POINT ( 'NONE',  ( 2.828427124746191623, 20.87499999726881583, -2.828427124746191623 ) ) ;
#71132 = CARTESIAN_POINT ( 'NONE',  ( -4.903558642999205574E-16, 8.008118988124991233, 24.63811528394063188 ) ) ;
#71133 = CARTESIAN_POINT ( 'NONE',  ( 2.679491924311228956, 117.9166666598386968, -10.00000000000000000 ) ) ;
#71134 = CARTESIAN_POINT ( 'NONE',  ( 7.204075437095968759, -7.204075437095966983, 76.09375000204838102 ) ) ;
#71135 = EDGE_CURVE ( 'NONE', #33807, #35937, #34030, .T. ) ;
#71136 = CARTESIAN_POINT ( 'NONE',  ( -47.32259252271279593, 38.77329591270029141, 65.76194439203462139 ) ) ;
#71137 = CARTESIAN_POINT ( 'NONE',  ( 1.469576158976823947E-15, -2.500000000000000000, -12.00000000000000000 ) ) ;
#71138 = CARTESIAN_POINT ( 'NONE',  ( 6.676582343750004256, 291.8906250017069510, 2.765530957081995478 ) ) ;
#71139 = CARTESIAN_POINT ( 'NONE',  ( 10.00000000000000000, 126.6666666598386684, 2.679491924311235618 ) ) ;
#71140 = DIRECTION ( 'NONE',  ( 0.000000000000000000, 0.000000000000000000, -1.000000000000000000 ) ) ;
#71141 = AXIS2_PLACEMENT_3D ( 'NONE', #49360, #61436, #55417 ) ;
#71142 = EDGE_CURVE ( 'NONE', #45635, #62352, #35136, .T. ) ;
#71143 = CARTESIAN_POINT ( 'NONE',  ( -10.18810118749999916, 0.000000000000000000, 85.65625000204838102 ) ) ;
#71144 = CARTESIAN_POINT ( 'NONE',  ( -25.55430564589114795, 197.0625000013656063, 172.4456943541091789 ) ) ;
#71145 = CARTESIAN_POINT ( 'NONE',  ( -8.000000000000000000, 24.65625000000000355, -3.313708498984762496 ) ) ;
#71146 = CARTESIAN_POINT ( 'NONE',  ( -4.541265875000003227, 12.99999999863440969, 1.881053915767121110 ) ) ;
#71147 = ORIENTED_EDGE ( 'NONE', *, *, #26511, .T. ) ;
#71148 = CARTESIAN_POINT ( 'NONE',  ( -24.60032696265636787, -50.95525646686212440, 151.1186657743323281 ) ) ;
#71149 = CARTESIAN_POINT ( 'NONE',  ( 4.000000000000015099, 208.6875000027312126, 196.3431457505076594 ) ) ;
#71150 = ADVANCED_FACE ( 'NONE', ( #17761 ), #11366, .F. ) ;
#71151 = CARTESIAN_POINT ( 'NONE',  ( -2.445694354108839175, 198.3125000013656063, 144.4456943541088663 ) ) ;
#71152 = CARTESIAN_POINT ( 'NONE',  ( 3.999999999999959144, 203.1875000027312126, 140.3431457505076594 ) ) ;
#71153 = VECTOR ( 'NONE', #30907, 1000.000000000000000 ) ;
#71154 = CARTESIAN_POINT ( 'NONE',  ( 5.000000000000000000, 12.24744670179850203, -68.85644987591957999 ) ) ;
#71155 = CARTESIAN_POINT ( 'NONE',  ( -10.18810118749999738, -4.220049686691941915, 71.12500000204836681 ) ) ;
#71156 = EDGE_LOOP ( 'NONE', ( #16113, #2003, #71672, #53133 ) ) ;
#71157 = CARTESIAN_POINT ( 'NONE',  ( -7.188101187500000044, 2.718749997951610098, -8.802885111219163269E-16 ) ) ;
#71158 = CARTESIAN_POINT ( 'NONE',  ( 27.99999999999996803, 209.8437500006828031, 173.7293670624999038 ) ) ;
#71159 = CARTESIAN_POINT ( 'NONE',  ( 5.082755093536326818, 120.5937500020483952, 5.082755093536325042 ) ) ;
#71160 = AXIS2_PLACEMENT_3D ( 'NONE', #40694, #35056, #63325 ) ;
#71161 = CARTESIAN_POINT ( 'NONE',  ( -4.423890159799090505, 21.99999999999997868, -0.1625330420329095804 ) ) ;
#71162 = CARTESIAN_POINT ( 'NONE',  ( 6.676582343750001591, 291.9531250017069510, -8.176455196517173205E-16 ) ) ;
#71164 = CARTESIAN_POINT ( 'NONE',  ( 10.00000000000000178, 137.0833333265053682, -2.679491924311226736 ) ) ;
#71163 = CARTESIAN_POINT ( 'NONE',  ( 9.832129032723416984, 236.8229166700806445, -5.676582343750003368 ) ) ;
#71165 = ORIENTED_EDGE ( 'NONE', *, *, #62975, .F. ) ;
#71166 = CARTESIAN_POINT ( 'NONE',  ( -8.311093377946836114, 223.5937500034139589, -8.311093377946836114 ) ) ;
#71167 = EDGE_CURVE ( 'NONE', #55580, #53065, #17012, .T. ) ;
#71168 = CARTESIAN_POINT ( 'NONE',  ( -2.977408999572648707, -7.188101187499990274, 3.267802781871751439 ) ) ;
#71169 = DIRECTION ( 'NONE',  ( -0.000000000000000000, 1.000000000000000000, 4.476705744456276341E-16 ) ) ;
#71170 =( BOUNDED_CURVE ( )  B_SPLINE_CURVE ( 2, ( #27144, #44137, #10919, #33954, #67148, #16554, #15442, #10546, #44880 ),
 .UNSPECIFIED., .F., .F. ) 
 B_SPLINE_CURVE_WITH_KNOTS ( ( 3, 2, 2, 2, 3 ),
 ( 0.3529411764705882026, 0.3566176470588234837, 0.3602941176470587648, 0.3639705882352940458, 0.3676470588235293824 ),
 .UNSPECIFIED. ) 
 CURVE ( )  GEOMETRIC_REPRESENTATION_ITEM ( )  RATIONAL_B_SPLINE_CURVE ( ( 1.000000000000001110, 0.9238795325112856283, 1.000000000000000000, 0.9238795325112867385, 1.000000000000000000, 0.9238795325112867385, 1.000000000000000000, 0.9238795325112878487, 0.9999999999999988898 ) ) 
 REPRESENTATION_ITEM ( '' )  );
#71171 = CARTESIAN_POINT ( 'NONE',  ( -2.445694354108783219, 200.8125000013656063, 200.4456943541088663 ) ) ;
#71172 = VERTEX_POINT ( 'NONE', #52473 ) ;
#71173 = CARTESIAN_POINT ( 'NONE',  ( -9.526279441628823008, 219.1190169426842829, 5.500000000000005329 ) ) ;
#71174 = CARTESIAN_POINT ( 'NONE',  ( -4.898587196589412829E-16, 97.62499999999998579, -8.000000000000000000 ) ) ;
#71175 = CARTESIAN_POINT ( 'NONE',  ( 3.042071309553167069, 97.13541666325266988, -11.35316468749999785 ) ) ;
#71176 = CYLINDRICAL_SURFACE ( 'NONE', #13101, 4.000000000000001776 ) ;
#71177 = CARTESIAN_POINT ( 'NONE',  ( 11.00000000000000000, 4.556349186104045934, 75.34375000000000000 ) ) ;
#71178 = VECTOR ( 'NONE', #19409, 1000.000000000000000 ) ;
#71181 = CARTESIAN_POINT ( 'NONE',  ( 7.999999999999991118, 0.000000000000000000, 30.00000000000000000 ) ) ;
#71180 = CARTESIAN_POINT ( 'NONE',  ( 26.56734541678238060, 206.3750000013656063, 173.4587341249998929 ) ) ;
#71179 = CARTESIAN_POINT ( 'NONE',  ( 24.54126587499998280, 202.5000000013656063, 171.4326545832175555 ) ) ;
#71182 = ORIENTED_EDGE ( 'NONE', *, *, #3439, .T. ) ;
#71183 = CARTESIAN_POINT ( 'NONE',  ( 29.65685424949237969, 205.5625000027311842, 165.9999999999998863 ) ) ;
#71184 = CARTESIAN_POINT ( 'NONE',  ( -11.35316468749999785, 213.0729166632527267, -3.042071309553167513 ) ) ;
#71185 = CARTESIAN_POINT ( 'NONE',  ( -1.432654583217664479, 199.7500000013656063, 138.5412658750000787 ) ) ;
#71186 = CARTESIAN_POINT ( 'NONE',  ( 29.43265458321761230, 203.7500000013656063, 173.4587341249998929 ) ) ;
#71187 = CARTESIAN_POINT ( 'NONE',  ( -7.778174593052023411, 7.778174593052023411, 115.0000000040967905 ) ) ;
#71188 = CARTESIAN_POINT ( 'NONE',  ( -11.35316468750000141, 188.8020833299193555, 3.042071309553159963 ) ) ;
#71189 = CARTESIAN_POINT ( 'NONE',  ( 7.188101187500000933, 90.87500000204836681, -2.977408999572651371 ) ) ;
#71190 = CARTESIAN_POINT ( 'NONE',  ( -27.99999999999995381, 195.5000000000000000, 174.0000000000003695 ) ) ;
#71191 = CARTESIAN_POINT ( 'NONE',  ( -3.211159895383561391, 13.68749999863440614, -3.211159895383561835 ) ) ;
#71192 = CARTESIAN_POINT ( 'NONE',  ( 28.00000000000001776, 197.1875000013655779, 166.5412658749999082 ) ) ;
#71193 = CARTESIAN_POINT ( 'NONE',  ( 5.082755093536318824, 5.082755093536319713, 5.799052781871753659 ) ) ;
#71194 = CARTESIAN_POINT ( 'NONE',  ( -8.311093377946836114, 87.65624999658601268, -8.311093377946837890 ) ) ;
#71195 = ORIENTED_EDGE ( 'NONE', *, *, #69212, .T. ) ;
#71197 =( BOUNDED_CURVE ( )  B_SPLINE_CURVE ( 2, ( #11384, #39681, #11018, #34051, #57422, #24146, #23042 ),
 .UNSPECIFIED., .F., .F. ) 
 B_SPLINE_CURVE_WITH_KNOTS ( ( 3, 2, 2, 3 ),
 ( 0.9795047134926050392, 0.9795047864996143661, 0.9861230620840667482, 0.9889322145411023612 ),
 .UNSPECIFIED. ) 
 CURVE ( )  GEOMETRIC_REPRESENTATION_ITEM ( )  RATIONAL_B_SPLINE_CURVE ( ( 0.9999983206301090721, 0.9999991603057917233, 1.000000000000000000, 0.9238795325112867385, 1.000000000000000000, 0.9676903756049457517, 0.9628086392139758587 ) ) 
 REPRESENTATION_ITEM ( '' )  );
#71196 = CARTESIAN_POINT ( 'NONE',  ( 10.50000000000000000, 0.000000000000000000, -20.42428869268542968 ) ) ;
#71198 = CARTESIAN_POINT ( 'NONE',  ( 2.828427124746209831, 209.3750000000000284, 200.8284271247462129 ) ) ;
#71199 = FACE_BOUND ( 'NONE', #55369, .T. ) ;
#71200 = CARTESIAN_POINT ( 'NONE',  ( -1.656854249492352604, 207.1875000000000568, 202.0000000000000284 ) ) ;
#71201 = CARTESIAN_POINT ( 'NONE',  ( 8.311093377946834337, 80.15624999658599847, 8.311093377946839666 ) ) ;
#71202 = ORIENTED_EDGE ( 'NONE', *, *, #13084, .T. ) ;
#71203 = CARTESIAN_POINT ( 'NONE',  ( 4.220049686691934809, 10.18810118749999916, 88.56250000204836681 ) ) ;
#71204 = CARTESIAN_POINT ( 'NONE',  ( -10.18810118749999738, -4.220049686691941915, 112.7500000020483810 ) ) ;
#71205 = CARTESIAN_POINT ( 'NONE',  ( -3.458734124999960358, 209.6250000013656063, 196.5673454167823877 ) ) ;
#71206 = DIRECTION ( 'NONE',  ( 1.000000000000000000, 1.776356839400250465E-15, 0.000000000000000000 ) ) ;
#71208 = CARTESIAN_POINT ( 'NONE',  ( -8.311093377946836114, 77.65624999658601268, -8.311093377946837890 ) ) ;
#71207 = CARTESIAN_POINT ( 'NONE',  ( 27.99999999999999645, 210.0000000000000284, 169.9999999999999147 ) ) ;
#71209 = CARTESIAN_POINT ( 'NONE',  ( 7.999999999999991118, 3.313708498984757611, 25.86155278392014623 ) ) ;
#71210 = LINE ( 'NONE', #2192, #72187 ) ;
#71211 = CARTESIAN_POINT ( 'NONE',  ( 8.660254037844385522, 166.4583333265053682, 5.000000000000005329 ) ) ;
#71212 = CARTESIAN_POINT ( 'NONE',  ( -2.751064625579944321E-14, 199.8750000027312126, 146.0000000000000284 ) ) ;
#71213 = CARTESIAN_POINT ( 'NONE',  ( 4.999999999999987566, -50.98531617258517912, 41.27391139027606926 ) ) ;
#71214 = CARTESIAN_POINT ( 'NONE',  ( 11.35316468749999785, 60.88541666325268409, 3.042071309553174174 ) ) ;
#71215 = CARTESIAN_POINT ( 'NONE',  ( -7.204075437095967871, 7.204075437095967871, 105.3437500020483810 ) ) ;
#71216 = CARTESIAN_POINT ( 'NONE',  ( 5.676582343749993598, 189.9479166632526983, 9.832129032723422313 ) ) ;
#71217 = ORIENTED_EDGE ( 'NONE', *, *, #72173, .F. ) ;
#71218 = CARTESIAN_POINT ( 'NONE',  ( -1.506524674528442853, 65.82790954191001731, 26.31843049628531261 ) ) ;
#71219 = DIRECTION ( 'NONE',  ( -0.000000000000000000, -0.000000000000000000, -1.000000000000000000 ) ) ;
#71220 = CARTESIAN_POINT ( 'NONE',  ( 1.102182119232618108E-15, 288.2500000000000000, 6.000000000000001776 ) ) ;
#71222 = CARTESIAN_POINT ( 'NONE',  ( -9.832129032723418760, 192.8645833299193839, -5.676582343750004256 ) ) ;
#71221 = DIRECTION ( 'NONE',  ( 8.659560562354943952E-17, 0.7071067811865465735, -0.7071067811865484609 ) ) ;
#71223 = CARTESIAN_POINT ( 'NONE',  ( -30.99999999999992895, -31.99999999999978684, 205.0000000000000284 ) ) ;
#71224 = CARTESIAN_POINT ( 'NONE',  ( 4.999999999999997335, 241.4583333401613174, -8.660254037844387298 ) ) ;
#71225 = CARTESIAN_POINT ( 'NONE',  ( -32.00000000000000711, 200.1875000000000853, 168.3431457505080289 ) ) ;
#71226=STYLED_ITEM('',(#74706),#17043);
#71227 = EDGE_LOOP ( 'NONE', ( #42264, #30096 ) ) ;
#71228 = CARTESIAN_POINT ( 'NONE',  ( -11.35316468750000141, 183.8020833299193271, 3.042071309553159963 ) ) ;
#71229 = EDGE_CURVE ( 'NONE', #63005, #53778, #51153, .T. ) ;
#71230 = CARTESIAN_POINT ( 'NONE',  ( -7.188101187499990274, -2.977408999572651815, 19.58030278187175455 ) ) ;
#71231 = CARTESIAN_POINT ( 'NONE',  ( 8.000000000000000000, 18.09375000000000355, -3.313708498984761164 ) ) ;
#71232 = VECTOR ( 'NONE', #63127, 1000.000000000000000 ) ;
#71233 = ORIENTED_EDGE ( 'NONE', *, *, #67466, .F. ) ;
#71234 = CARTESIAN_POINT ( 'NONE',  ( -7.999999999999998224, 98.28125000409677625, 3.313708498984766493 ) ) ;
#71235 = APPLICATION_CONTEXT ( 'automotive_design' ) ;
#71236 = CARTESIAN_POINT ( 'NONE',  ( -7.320508075688773708, 1.875000000000000222, -7.320508075688774596 ) ) ;
#71237 = EDGE_CURVE ( 'NONE', #64909, #8328, #38610, .T. ) ;
#71238 = ADVANCED_FACE ( 'NONE', ( #65630, #24527 ), #13561, .T. ) ;
#71239 = CARTESIAN_POINT ( 'NONE',  ( -4.000000000000001776, 17.43750000000000000, -1.656854249492381470 ) ) ;
#71240 = CARTESIAN_POINT ( 'NONE',  ( -4.541265875000003227, 14.87499999863440969, 1.881053915767121110 ) ) ;
#71241 = CARTESIAN_POINT ( 'NONE',  ( -7.999999999999991118, 0.000000000000000000, 13.01780278392014623 ) ) ;
#71242 = CARTESIAN_POINT ( 'NONE',  ( -26.34314575050752438, 195.9375000000000000, 166.0000000000004832 ) ) ;
#71243 = ORIENTED_EDGE ( 'NONE', *, *, #27269, .F. ) ;
#71244 = CARTESIAN_POINT ( 'NONE',  ( 4.556349186104045934, 11.00000000000000000, 72.53124999999998579 ) ) ;
#71245 = CARTESIAN_POINT ( 'NONE',  ( 7.188101187500001821, 98.00000000204838102, -2.977408999572651371 ) ) ;
#71247 = CARTESIAN_POINT ( 'NONE',  ( 0.000000000000000000, 0.000000000000000000, 0.000000000000000000 ) ) ;
#71246 = CARTESIAN_POINT ( 'NONE',  ( 7.320508075688810123, 179.3750000000000284, 7.320508075688813676 ) ) ;
#71248 = PRODUCT_CONTEXT ( 'NONE', #33707, 'mechanical' ) ;
#71249 = EDGE_LOOP ( 'NONE', ( #57497, #39800, #73295, #56728 ) ) ;
#71250 = CARTESIAN_POINT ( 'NONE',  ( 0.000000000000000000, 0.000000000000000000, 0.000000000000000000 ) ) ;
#71251 = CARTESIAN_POINT ( 'NONE',  ( 7.188101187499991163, 2.977408999572648707, 20.33030278187175455 ) ) ;
#71252 = ORIENTED_EDGE ( 'NONE', *, *, #45093, .F. ) ;
#71253 = ADVANCED_FACE ( 'NONE', ( #36600, #47533 ), #7923, .T. ) ;
#71254 = ORIENTED_EDGE ( 'NONE', *, *, #15505, .T. ) ;
#71255 = CARTESIAN_POINT ( 'NONE',  ( -10.18810118749999916, 4.220049686691934809, 78.06250000204836681 ) ) ;
#71256 = FACE_OUTER_BOUND ( 'NONE', #11991, .T. ) ;
#71257 = CARTESIAN_POINT ( 'NONE',  ( 7.778174593052023411, -7.778174593052021635, 97.56250000000000000 ) ) ;
#71260 = CARTESIAN_POINT ( 'NONE',  ( 6.676582343750003368, 294.0468750017070079, 2.765530957081995478 ) ) ;
#71259 = CARTESIAN_POINT ( 'NONE',  ( 32.00000000000000000, 201.3125000027312126, 171.6568542494922553 ) ) ;
#71258 = CARTESIAN_POINT ( 'NONE',  ( 32.00000000000000000, 196.3125000027312126, 171.6568542494922553 ) ) ;
#71261 = CARTESIAN_POINT ( 'NONE',  ( 7.320508075688771044, 154.3750000000000284, 7.320508075688775484 ) ) ;
#71262 = CARTESIAN_POINT ( 'NONE',  ( -10.99999999999999645, -11.00000000000000000, -6.938893903907228378E-15 ) ) ;
#71263 = CARTESIAN_POINT ( 'NONE',  ( 28.00000000000002132, 209.5000000000000284, 165.9999999999998863 ) ) ;
#71264 = DIRECTION ( 'NONE',  ( -0.8660266317069091890, 0.4999978731656731235, 2.046673486196596759E-06 ) ) ;
#71265 = CARTESIAN_POINT ( 'NONE',  ( -1.469576158976823947E-15, 2.437499995903220196, 8.000000000000000000 ) ) ;
#71266 = CARTESIAN_POINT ( 'NONE',  ( 31.45873412499997812, 198.6250000013655779, 171.4326545832175839 ) ) ;
#71267 = CARTESIAN_POINT ( 'NONE',  ( -1.320432766682874540E-15, 10.96874999795161187, 7.188101187500000044 ) ) ;
#71268 = CIRCLE ( 'NONE', #64093, 10.49999999999998224 ) ;
#71269 = CARTESIAN_POINT ( 'NONE',  ( -5.656854249492375253, 5.656854249492375253, 24.83030278392014978 ) ) ;
#71270 = DIRECTION ( 'NONE',  ( 0.000000000000000000, 0.000000000000000000, 1.000000000000000000 ) ) ;
#71271 = CARTESIAN_POINT ( 'NONE',  ( -7.188101187500000044, 108.0312500020483810, 0.000000000000000000 ) ) ;
#71273 = DIRECTION ( 'NONE',  ( -0.000000000000000000, 1.000000000000000000, 4.689100369878284071E-30 ) ) ;
#71272 = LINE ( 'NONE', #66745, #2212 ) ;
#71274 = CARTESIAN_POINT ( 'NONE',  ( 2.085542519210945334E-15, 230.4687500034139873, 11.35316468749999963 ) ) ;
#71275 = CARTESIAN_POINT ( 'NONE',  ( 26.56734541678238415, 209.2500000013656063, 166.5412658749999650 ) ) ;
#71276 = CARTESIAN_POINT ( 'NONE',  ( -7.188101187499990274, -2.977408999572651371, 22.95530278187175455 ) ) ;
#71277 = PLANE ( 'NONE',  #54179 ) ;
#71278 = CARTESIAN_POINT ( 'NONE',  ( 5.676582343750001591, 36.61458332991934839, -9.832129032723420536 ) ) ;
#71279 = DIRECTION ( 'NONE',  ( -0.000000000000000000, 1.000000000000000000, -1.563033456626094573E-30 ) ) ;
#71280 = CARTESIAN_POINT ( 'NONE',  ( -2.679491924311235618, 10.41666665983870033, 10.00000000000000000 ) ) ;
#71281 = CARTESIAN_POINT ( 'NONE',  ( -5.000000000000000888, 239.1666666666666572, -8.660254037844387298 ) ) ;
#71282 = DIRECTION ( 'NONE',  ( 0.000000000000000000, 0.000000000000000000, -1.000000000000000000 ) ) ;
#71283 = ORIENTED_EDGE ( 'NONE', *, *, #12785, .T. ) ;
#71284 = EDGE_CURVE ( 'NONE', #13652, #4993, #58880, .T. ) ;
#71285 = CARTESIAN_POINT ( 'NONE',  ( 11.00000000000000000, 1.347111479062088405E-15, 103.9375000040967763 ) ) ;
#71286 = DIRECTION ( 'NONE',  ( -0.000000000000000000, 1.000000000000000000, -0.000000000000000000 ) ) ;
#71287 = CARTESIAN_POINT ( 'NONE',  ( -11.35316468750000141, 33.48958332991934128, 3.042071309553159963 ) ) ;
#71288 = CARTESIAN_POINT ( 'NONE',  ( 11.00000000000000000, 4.556349186104045934, 80.03125000409677625 ) ) ;
#71289 = CARTESIAN_POINT ( 'NONE',  ( 3.458734124999959469, 202.7500000013655779, 140.5673454167823593 ) ) ;
#71290 = LINE ( 'NONE', #43365, #20309 ) ;
#71292 = CARTESIAN_POINT ( 'NONE',  ( -8.311093377946841443, 33.90624999658601268, 8.311093377946834337 ) ) ;
#71291 = CARTESIAN_POINT ( 'NONE',  ( -7.188101187500000933, 103.0625000020483810, -2.977408999572650483 ) ) ;
#71294 = EDGE_CURVE ( 'NONE', #55580, #73846, #18874, .T. ) ;
#71293 = CARTESIAN_POINT ( 'NONE',  ( -4.898587196589407898E-16, 7.999999999999991118, 13.95530277982336465 ) ) ;
#71295 =( BOUNDED_CURVE ( )  B_SPLINE_CURVE ( 2, ( #47868, #70887, #70522, #71246, #13161, #41847, #6785, #64856, #36198, #59938, #30896, #19202, #29795 ),
 .UNSPECIFIED., .F., .F. ) 
 B_SPLINE_CURVE_WITH_KNOTS ( ( 3, 2, 2, 2, 2, 2, 3 ),
 ( 2.245089840338815534, 2.250322337668932970, 2.255554834999050851, 2.260787332329168287, 2.266019829659286167, 2.271252326989403603, 2.276484824319521039 ),
 .UNSPECIFIED. ) 
 CURVE ( )  GEOMETRIC_REPRESENTATION_ITEM ( )  RATIONAL_B_SPLINE_CURVE ( ( 1.000000000000236033, 0.9659258262888323898, 1.000000000000000000, 0.9659258262890683122, 1.000000000000000000, 0.9659258262890683122, 1.000000000000000000, 0.9659258262890683122, 1.000000000000000000, 0.9659258262890683122, 1.000000000000000000, 0.9659258262890640934, 1.000000000000004219 ) ) 
 REPRESENTATION_ITEM ( '' )  );
#71296 = CARTESIAN_POINT ( 'NONE',  ( 3.042071309553159519, 154.7395833299193555, 11.35316468750000141 ) ) ;
#71297 = CARTESIAN_POINT ( 'NONE',  ( -10.00000000000000000, 129.1666666598387110, -2.679491924311229845 ) ) ;
#71298 = CARTESIAN_POINT ( 'NONE',  ( 7.188101187500002709, 110.1875000020483810, 2.977408999572649151 ) ) ;
#71299 = CARTESIAN_POINT ( 'NONE',  ( -24.54126587499999346, 203.4375000013656063, 170.0000000000003411 ) ) ;
#71300 = ORIENTED_EDGE ( 'NONE', *, *, #6326, .T. ) ;
#71301 = CARTESIAN_POINT ( 'NONE',  ( 3.733333029993803898, 8.236864015571821795, 4.143685177968037259E-15 ) ) ;
#71302 = CARTESIAN_POINT ( 'NONE',  ( -8.311093377946841443, 24.21874999658601979, 8.311093377946834337 ) ) ;
#71303 = ADVANCED_FACE ( 'NONE', ( #52843 ), #53950, .T. ) ;
#71304 = ORIENTED_EDGE ( 'NONE', *, *, #31353, .F. ) ;
#71305 = CARTESIAN_POINT ( 'NONE',  ( -27.99999999999995737, 204.5000000000000284, 174.0000000000003695 ) ) ;
#71306 = CARTESIAN_POINT ( 'NONE',  ( -30.91750187550572448, -35.99224995298294516, 172.8984287956838273 ) ) ;
#71308 = CARTESIAN_POINT ( 'NONE',  ( 8.311093377946834337, 150.1562499965860127, 8.311093377946839666 ) ) ;
#71307 = CARTESIAN_POINT ( 'NONE',  ( -32.38655620011479641, -21.07929414601410656, 156.7499735336913034 ) ) ;
#71309 = CYLINDRICAL_SURFACE ( 'NONE', #73668, 7.999999999999991118 ) ;
#71310 = CARTESIAN_POINT ( 'NONE',  ( 5.656854249492376141, -5.656854249492374365, 14.94905278432982421 ) ) ;
#71311 = AXIS2_PLACEMENT_3D ( 'NONE', #5641, #53146, #58812 ) ;
#71312 = CARTESIAN_POINT ( 'NONE',  ( -3.313708498984759387, -7.999999999999989342, 16.11155277982336642 ) ) ;
#71313 = CARTESIAN_POINT ( 'NONE',  ( 11.35316468749999963, 236.4062500034140157, -1.390361679473963556E-15 ) ) ;
#71314 = CARTESIAN_POINT ( 'NONE',  ( -6.238412754330611322E-16, 10.18810118749999916, 90.15625000204838102 ) ) ;
#71315 = VERTEX_POINT ( 'NONE', #41516 ) ;
#71316 = CARTESIAN_POINT ( 'NONE',  ( 7.999999999999998224, 20.71874999590322375, 3.313708498984766049 ) ) ;
#71317 = CARTESIAN_POINT ( 'NONE',  ( 32.00000000000000711, 205.3125000000000284, 168.3431457505075457 ) ) ;
#71318 = CARTESIAN_POINT ( 'NONE',  ( -8.311093377946836114, 107.9687499965860269, -8.311093377946837890 ) ) ;
#71319 = CARTESIAN_POINT ( 'NONE',  ( -10.18810118749999916, 4.220049686691934809, 103.5625000020483668 ) ) ;
#71320 = CARTESIAN_POINT ( 'NONE',  ( 4.541265875000001451, 15.37499999863440969, 1.881053915767124440 ) ) ;
#71321 = ORIENTED_EDGE ( 'NONE', *, *, #65427, .F. ) ;
#71322 = ORIENTED_EDGE ( 'NONE', *, *, #27499, .F. ) ;
#71323 = CARTESIAN_POINT ( 'NONE',  ( 3.313708498984762052, 13.78125000000000178, -8.000000000000000000 ) ) ;
#71324 = CARTESIAN_POINT ( 'NONE',  ( 4.541265875000002339, 2.499999998634407028, -1.881053915767121554 ) ) ;
#71325 = CARTESIAN_POINT ( 'NONE',  ( -2.977408999572650039, 5.437499997951610986, -7.188101187500001821 ) ) ;
#71326 = CARTESIAN_POINT ( 'NONE',  ( 1.469576158976823947E-15, 113.5625000040967905, 8.000000000000000000 ) ) ;
#71327 = CARTESIAN_POINT ( 'NONE',  ( -4.220049686691937474, -10.18810118749999738, 99.81250000204838102 ) ) ;
#71328 = CYLINDRICAL_SURFACE ( 'NONE', #59658, 8.000000000000000000 ) ;
#71329 = AXIS2_PLACEMENT_3D ( 'NONE', #11648, #69737, #12020 ) ;
#71330 = CARTESIAN_POINT ( 'NONE',  ( 4.000000000000001776, 4.062500000000000000, -1.656854249492381248 ) ) ;
#71331 = CARTESIAN_POINT ( 'NONE',  ( 4.000000000000001776, 13.74999999726881583, 0.000000000000000000 ) ) ;
#71332 = CARTESIAN_POINT ( 'NONE',  ( -4.541265875000002339, 5.749999998634407028, -1.881053915767121998 ) ) ;
#71333 = FACE_BOUND ( 'NONE', #11001, .T. ) ;
#71334 = CARTESIAN_POINT ( 'NONE',  ( -1.432654583217607858, 196.6250000013656063, 201.4587341250000065 ) ) ;
#71336 = CARTESIAN_POINT ( 'NONE',  ( 0.000000000000000000, 300.0000000000000000, 0.000000000000000000 ) ) ;
#71335 = CARTESIAN_POINT ( 'NONE',  ( -31.45873412499996746, 202.7500000013655779, 171.4326545832181239 ) ) ;
#71337 = CARTESIAN_POINT ( 'NONE',  ( -3.211159895383561391, 13.68749999863440614, -3.211159895383561835 ) ) ;
#71338 = VECTOR ( 'NONE', #59517, 1000.000000000000000 ) ;
#71339 = CARTESIAN_POINT ( 'NONE',  ( 10.99999999999989342, 4.556349186104152515, 84.34375000000001421 ) ) ;
#71340 = CARTESIAN_POINT ( 'NONE',  ( -4.401442555609577197E-16, 7.188101187499992051, 4.111552781871752771 ) ) ;
#71341 = EDGE_LOOP ( 'NONE', ( #63817, #19253, #66061, #27922 ) ) ;
#71342 = ORIENTED_EDGE ( 'NONE', *, *, #51817, .T. ) ;
#71343 = CARTESIAN_POINT ( 'NONE',  ( -7.204075437095967871, 7.204075437095967871, 97.46875000204838102 ) ) ;
#71344 = CARTESIAN_POINT ( 'NONE',  ( 6.123233995736767268E-16, 126.2500000000000000, -10.00000000000000178 ) ) ;
#71345 = CARTESIAN_POINT ( 'NONE',  ( -24.54126587500000412, 202.5000000013656063, 168.5673454167827003 ) ) ;
#71346 = CARTESIAN_POINT ( 'NONE',  ( -27.99999999999995737, 200.5000000000000000, 174.0000000000003695 ) ) ;
#71347 = CARTESIAN_POINT ( 'NONE',  ( -3.458734124999960358, 209.6875000013656063, 198.0000000000000284 ) ) ;
#71348 = CARTESIAN_POINT ( 'NONE',  ( 3.999999999999960032, 209.5625000013656063, 142.0000000000000568 ) ) ;
#71349 = CARTESIAN_POINT ( 'NONE',  ( 10.00000000000000178, 110.2083333333333144, -2.679491924311226736 ) ) ;
#71350 = CARTESIAN_POINT ( 'NONE',  ( 5.656854249492381470, 113.5625000000000000, 5.656854249492379694 ) ) ;
#71351 = CARTESIAN_POINT ( 'NONE',  ( 6.676582343750003368, 295.1718750017070079, -2.765530957081997254 ) ) ;
#71352 = VERTEX_POINT ( 'NONE', #42616 ) ;
#71353 = CARTESIAN_POINT ( 'NONE',  ( -4.556349186104045934, 11.00000000000000000, 74.21875000000000000 ) ) ;
#71354 = CARTESIAN_POINT ( 'NONE',  ( 8.000000000000000000, 20.81249999590322375, 0.000000000000000000 ) ) ;
#71355 = CARTESIAN_POINT ( 'NONE',  ( -2.445694354108838731, 204.0625000013656063, 144.4456943541088663 ) ) ;
#71356 = DIRECTION ( 'NONE',  ( 0.000000000000000000, 0.000000000000000000, 1.000000000000000000 ) ) ;
#71357 = CARTESIAN_POINT ( 'NONE',  ( -8.660254037844387298, 229.5833333333333712, -4.999999999999999112 ) ) ;
#71358 = PLANE ( 'NONE',  #9001 ) ;
#71359 = CARTESIAN_POINT ( 'NONE',  ( 7.778174593052023411, -7.778174593052021635, 115.5625000000000000 ) ) ;
#71360 = CARTESIAN_POINT ( 'NONE',  ( 10.00000000000000000, 219.7916666666667140, 2.679491924311236062 ) ) ;
#71361 = CARTESIAN_POINT ( 'NONE',  ( -7.188101187499990274, -2.977408999572651815, 1.955302781871753881 ) ) ;
#71362 = CARTESIAN_POINT ( 'NONE',  ( -11.35316468750000141, 193.8020833299193271, 3.042071309553159963 ) ) ;
#71363 = LINE ( 'NONE', #59698, #74476 ) ;
#71364 = CARTESIAN_POINT ( 'NONE',  ( 2.780723358947928197E-16, 1.562499998634406584, -4.541265875000002339 ) ) ;
#71366 = CARTESIAN_POINT ( 'NONE',  ( 4.000000000000000888, 4.937500000000000888, 1.656854249492384135 ) ) ;
#71365 = CARTESIAN_POINT ( 'NONE',  ( 1.469576158976823947E-15, 107.5625000040967905, 8.000000000000000000 ) ) ;
#71367 = ORIENTED_EDGE ( 'NONE', *, *, #14265, .F. ) ;
#71368 = B_SPLINE_CURVE_WITH_KNOTS ( 'NONE', 3,
 ( #20993, #68144, #21366, #5521, #39106, #38746, #56835, #62109, #28521, #45493, #67027, #27775, #9695, #73430, #61745, #72691, #44765, #28147, #16812, #10432, #15325, #67779, #44018, #10062, #38362, #33462, #4039, #39475, #61368, #32716, #56095, #62472, #4780, #73799, #45132, #39842, #4404, #27398, #51161, #74169, #52656, #53027, #29642, #11546, #23973, #18693 ),
 .UNSPECIFIED., .F., .F.,
 ( 4, 2, 2, 2, 2, 2, 2, 2, 2, 2, 2, 2, 2, 2, 2, 2, 2, 2, 2, 2, 2, 2, 4 ),
 ( 2.810287246517312987, 2.811170068070839356, 2.812052889624365726, 2.813818532731418909, 2.814701354284945278, 2.815584175838471648, 2.817349818945524831, 2.819115462052577570, 2.820881105159630753, 2.822646748266683492, 2.823529569820209861, 2.824412391373736231, 2.826178034480789414, 2.827060856034315783, 2.827943677587842153, 2.829709320694895336, 2.830592142248421705, 2.831474963801948075, 2.833240606909001258, 2.834123428462527627, 2.835006250016053997, 2.836771893123107180, 2.838537536230159919 ),
 .UNSPECIFIED. ) ;
#71369 = CARTESIAN_POINT ( 'NONE',  ( -2.754378923186476579E-14, 203.4375000013656063, 145.4587341250000350 ) ) ;
#71370 = CARTESIAN_POINT ( 'NONE',  ( -5.676582343750006032, 49.42708332991935549, 9.832129032723418760 ) ) ;
#71371 = CARTESIAN_POINT ( 'NONE',  ( 11.00000000000000355, -4.556349186104045046, 106.8437500040967763 ) ) ;
#71372 = DIRECTION ( 'NONE',  ( 0.7071067811865401342, -0.000000000000000000, 0.7071067811865549002 ) ) ;
#71373 = CARTESIAN_POINT ( 'NONE',  ( -31.45873412500002075, 201.6250000013656063, 168.5673454167828140 ) ) ;
#71374 = DIRECTION ( 'NONE',  ( 1.000000000000000000, 0.000000000000000000, 1.836970198721037823E-16 ) ) ;
#71376 = CARTESIAN_POINT ( 'NONE',  ( -4.999999999999992895, 230.8333333333333428, 8.660254037844390851 ) ) ;
#71375 = CARTESIAN_POINT ( 'NONE',  ( 2.020667218593132706E-15, -11.00000000000000000, 107.8750000000000000 ) ) ;
#71378 = EDGE_CURVE ( 'NONE', #11773, #9987, #35543, .T. ) ;
#71377 = CARTESIAN_POINT ( 'NONE',  ( 4.556349186104045934, 11.00000000000000000, 87.53125000000000000 ) ) ;
#71379 = CARTESIAN_POINT ( 'NONE',  ( 6.951808397369818766E-16, 112.0312499965860269, -11.35316468750000141 ) ) ;
#71380 = CARTESIAN_POINT ( 'NONE',  ( -7.320508075688778149, 89.99999999317203958, 7.320508075688769267 ) ) ;
#71381 = CARTESIAN_POINT ( 'NONE',  ( 3.594050593751920264, 89.15552362291687416, -6.225078233346985179 ) ) ;
#71382 = CARTESIAN_POINT ( 'NONE',  ( 4.541265875000001451, 17.37499999863440436, 1.881053915767124440 ) ) ;
#71383 = DIRECTION ( 'NONE',  ( 0.000000000000000000, 0.000000000000000000, -1.000000000000000000 ) ) ;
#71384 = CARTESIAN_POINT ( 'NONE',  ( -7.999999999999991118, 0.000000000000000000, 23.33030277982336642 ) ) ;
#71385 = EDGE_LOOP ( 'NONE', ( #12069, #12847, #61438, #30980 ) ) ;
#71386 = ORIENTED_EDGE ( 'NONE', *, *, #44972, .T. ) ;
#71387 = EDGE_CURVE ( 'NONE', #26713, #5359, #40581, .T. ) ;
#71388 = CARTESIAN_POINT ( 'NONE',  ( -2.765530957081998586, 294.7968750017069510, 6.676582343750001591 ) ) ;
#71389 = CARTESIAN_POINT ( 'NONE',  ( 2.751064625579944321E-14, 208.7500000000000284, 194.0000000000000568 ) ) ;
#71390 = CARTESIAN_POINT ( 'NONE',  ( 3.313708498984756279, 7.999999999999991118, 6.549052783920143561 ) ) ;
#71391 = CARTESIAN_POINT ( 'NONE',  ( 9.832129032723420536, 166.1979166632526983, -5.676582343749999815 ) ) ;
#71392 = DIRECTION ( 'NONE',  ( -0.000000000000000000, 1.000000000000000000, -0.000000000000000000 ) ) ;
#71393 = CARTESIAN_POINT ( 'NONE',  ( -1.656854249492347719, 200.8125000000000284, 194.0000000000000853 ) ) ;
#71394 = CARTESIAN_POINT ( 'NONE',  ( -5.000000000000020428, 191.6666666666667140, -8.660254037844426378 ) ) ;
#71395 = CARTESIAN_POINT ( 'NONE',  ( 4.220049686691941027, -10.18810118749999738, 110.5000000020483810 ) ) ;
#71396 = ORIENTED_EDGE ( 'NONE', *, *, #24659, .F. ) ;
#71397 = CARTESIAN_POINT ( 'NONE',  ( -1.296342370391298182, 49.95006747298977245, -40.70914535207419505 ) ) ;
#71398 = VECTOR ( 'NONE', #63326, 1000.000000000000000 ) ;
#71399 = DIRECTION ( 'NONE',  ( -1.000000000000000000, 0.000000000000000000, 0.000000000000000000 ) ) ;
#71400 = CARTESIAN_POINT ( 'NONE',  ( -8.311093377946841443, 144.2187499965860127, 8.311093377946834337 ) ) ;
#71401 = CARTESIAN_POINT ( 'NONE',  ( 3.458734125000015425, 195.0000000013656063, 196.5673454167823877 ) ) ;
#71402 = FACE_OUTER_BOUND ( 'NONE', #4834, .T. ) ;
#71403 = CARTESIAN_POINT ( 'NONE',  ( -10.18810118749999738, -4.220049686691941915, 74.12500000204836681 ) ) ;
#71404 = CARTESIAN_POINT ( 'NONE',  ( -11.35316468750000141, 63.80208332991934839, 3.042071309553159963 ) ) ;
#71406 = EDGE_LOOP ( 'NONE', ( #16965, #2417 ) ) ;
#71405 =( BOUNDED_CURVE ( )  B_SPLINE_CURVE ( 2, ( #10727, #29203, #10361, #182, #4706, #33385, #62767, #28819, #33760 ),
 .UNSPECIFIED., .F., .F. ) 
 B_SPLINE_CURVE_WITH_KNOTS ( ( 3, 2, 2, 2, 3 ),
 ( 0.2647058823529410687, 0.2683823529411763498, 0.2720588235294116863, 0.2757352941176470229, 0.2794117647058823040 ),
 .UNSPECIFIED. ) 
 CURVE ( )  GEOMETRIC_REPRESENTATION_ITEM ( )  RATIONAL_B_SPLINE_CURVE ( ( 1.000000000000002220, 0.9238795325112844070, 1.000000000000000000, 0.9238795325112867385, 1.000000000000000000, 0.9238795325112867385, 1.000000000000000000, 0.9238795325112878487, 0.9999999999999988898 ) ) 
 REPRESENTATION_ITEM ( '' )  );
#71408 = CARTESIAN_POINT ( 'NONE',  ( -1.881053915767121776, 6.749999998634407916, -4.541265875000002339 ) ) ;
#71407 =( BOUNDED_CURVE ( )  B_SPLINE_CURVE ( 2, ( #3214, #53418, #42445, #13757, #14508, #37548, #71479, #60547, #8871, #31882, #54905, #38294, #15633 ),
 .UNSPECIFIED., .F., .F. ) 
 B_SPLINE_CURVE_WITH_KNOTS ( ( 3, 2, 2, 2, 2, 2, 3 ),
 ( 0.7941930320969252666, 0.7941930701348174360, 0.8008113457192742590, 0.8074296213037310821, 0.8140478968881879052, 0.8206661724726446172, 0.8206662513146789628 ),
 .UNSPECIFIED. ) 
 CURVE ( )  GEOMETRIC_REPRESENTATION_ITEM ( )  RATIONAL_B_SPLINE_CURVE ( ( 0.9999991250151324396, 0.9999995625050517312, 1.000000000000000000, 0.9238795325112867385, 1.000000000000000000, 0.9238795325112867385, 1.000000000000000000, 0.9238795325112867385, 1.000000000000000000, 0.9238795325112867385, 1.000000000000000000, 0.9999990931939241046, 0.9999981864094533712 ) ) 
 REPRESENTATION_ITEM ( '' )  );
#71409 = CARTESIAN_POINT ( 'NONE',  ( 8.008118988124991233, 9.807117285998411148E-16, 10.76311528394063188 ) ) ;
#71410 = ORIENTED_EDGE ( 'NONE', *, *, #2517, .F. ) ;
#71411 = VECTOR ( 'NONE', #30698, 1000.000000000000000 ) ;
#71412 = CARTESIAN_POINT ( 'NONE',  ( -2.977408999572654480, 22.49999999795161543, 7.188101187499999156 ) ) ;
#71413 = CARTESIAN_POINT ( 'NONE',  ( 6.000000000000003553, 290.5000000034141294, 2.485281374238571317 ) ) ;
#71414 = LINE ( 'NONE', #14066, #71411 ) ;
#71415 = CARTESIAN_POINT ( 'NONE',  ( 5.082755093536325930, 14.53124999795161187, -5.082755093536325930 ) ) ;
#71416 = CARTESIAN_POINT ( 'NONE',  ( -7.188101187499992051, 2.977408999572646930, 1.392802781871753437 ) ) ;
#71417 = CARTESIAN_POINT ( 'NONE',  ( 4.220049686691941027, -10.18810118749999738, 68.12500000204838102 ) ) ;
#71418 = CARTESIAN_POINT ( 'NONE',  ( 4.000000000000001776, 9.062500000000000000, -1.656854249492381248 ) ) ;
#71419 = CARTESIAN_POINT ( 'NONE',  ( -7.347880794884122694E-16, 3.499999997268812724, 4.000000000000001776 ) ) ;
#71420 = ORIENTED_EDGE ( 'NONE', *, *, #60948, .T. ) ;
#71421 = CARTESIAN_POINT ( 'NONE',  ( 1.432654583217664479, 207.7500000013656063, 201.4587341250000065 ) ) ;
#71422 = CARTESIAN_POINT ( 'NONE',  ( -23.99999999999998579, 196.8750000027312126, 170.0000000000002842 ) ) ;
#71423 = CARTESIAN_POINT ( 'NONE',  ( 4.541265875000002339, 3.312499998634407028, 0.000000000000000000 ) ) ;
#71424 = CARTESIAN_POINT ( 'NONE',  ( -5.082755093536325930, 113.4687500020483810, -5.082755093536325930 ) ) ;
#71425 = LINE ( 'NONE', #47320, #10327 ) ;
#71426 = CARTESIAN_POINT ( 'NONE',  ( -7.188101187499990274, -2.977408999572651371, 27.08030278187175810 ) ) ;
#71427 = ORIENTED_EDGE ( 'NONE', *, *, #10350, .T. ) ;
#71428 = CARTESIAN_POINT ( 'NONE',  ( -1.320432766682874540E-15, 24.09374999795161543, 7.188101187500000044 ) ) ;
#71429 = ORIENTED_EDGE ( 'NONE', *, *, #4894, .F. ) ;
#71430 = CARTESIAN_POINT ( 'NONE',  ( 6.985286989847971917, 4.041240684893442570, -0.000000000000000000 ) ) ;
#71431 = CARTESIAN_POINT ( 'NONE',  ( -3.458734124999959914, 206.3750000013656063, 196.5673454167823877 ) ) ;
#71432 = CARTESIAN_POINT ( 'NONE',  ( 27.99999999999996803, 203.9375000013656063, 166.5412658749999082 ) ) ;
#71433 = CARTESIAN_POINT ( 'NONE',  ( 10.00000000000000178, 65.00000000000000000, 0.000000000000000000 ) ) ;
#71434 = CARTESIAN_POINT ( 'NONE',  ( 5.082755093536326818, 92.09375000204838102, 5.082755093536325042 ) ) ;
#71435 = CARTESIAN_POINT ( 'NONE',  ( 6.000000000000003553, 295.5625000000000000, -2.485281374238571761 ) ) ;
#71437 = CARTESIAN_POINT ( 'NONE',  ( -30.93541659651598508, -42.99981040672927435, 171.9999999999998295 ) ) ;
#71436 = CARTESIAN_POINT ( 'NONE',  ( 27.99999999999999645, 195.0000000000000000, 173.9999999999998863 ) ) ;
#71438 = ORIENTED_EDGE ( 'NONE', *, *, #46456, .T. ) ;
#71439 = EDGE_CURVE ( 'NONE', #41205, #68939, #24884, .T. ) ;
#71440 = EDGE_CURVE ( 'NONE', #112, #55737, #12598, .T. ) ;
#71441 = CARTESIAN_POINT ( 'NONE',  ( 9.832129032723420536, 225.9895833367473585, 5.676582343749996262 ) ) ;
#71442 = CARTESIAN_POINT ( 'NONE',  ( -4.000000000000015987, 199.6250000027312126, 142.0000000000000568 ) ) ;
#71443 = DIRECTION ( 'NONE',  ( 0.000000000000000000, 0.000000000000000000, -1.000000000000000000 ) ) ;
#71444 = CARTESIAN_POINT ( 'NONE',  ( 7.999999999999991118, -3.145386390148749531E-05, 1.767801894041102218 ) ) ;
#71445 = CARTESIAN_POINT ( 'NONE',  ( 2.679491924311225848, 263.5416666666666856, -10.00000000000000000 ) ) ;
#71446 = LINE ( 'NONE', #13725, #10204 ) ;
#71447 = CARTESIAN_POINT ( 'NONE',  ( 2.679491924311222739, 178.9583333333333428, 10.00000000000000355 ) ) ;
#71448 = CARTESIAN_POINT ( 'NONE',  ( 6.000000000000003553, 297.5000000034140157, 2.485281374238571317 ) ) ;
#71449 = CARTESIAN_POINT ( 'NONE',  ( 2.977408999572650927, -7.188101187499990274, 26.33030278187176165 ) ) ;
#71450 = CARTESIAN_POINT ( 'NONE',  ( 5.676582343749993598, 150.2604166632526699, 9.832129032723422313 ) ) ;
#71451 = CARTESIAN_POINT ( 'NONE',  ( 2.485281374238196062, 294.7500000034139589, -6.000000000000377476 ) ) ;
#71452 = CARTESIAN_POINT ( 'NONE',  ( 0.000000000000000000, 125.0000000000000000, 0.000000000000000000 ) ) ;
#71455 = CARTESIAN_POINT ( 'NONE',  ( -12.00000000000000000, -6.928203230275527424, -14.80000000000000071 ) ) ;
#71454 = CARTESIAN_POINT ( 'NONE',  ( -11.00000000000000000, 0.000000000000000000, 112.1875000040967763 ) ) ;
#71453 = CARTESIAN_POINT ( 'NONE',  ( 25.17157287525378351, 201.8750000000000284, 172.8284271247460424 ) ) ;
#71456 = VERTEX_POINT ( 'NONE', #58391 ) ;
#71457 = CIRCLE ( 'NONE', #32951, 8.000000000000000000 ) ;
#71458 = EDGE_CURVE ( 'NONE', #51583, #31504, #18011, .T. ) ;
#71459 = EDGE_CURVE ( 'NONE', #11019, #66661, #20292, .T. ) ;
#71460 = CARTESIAN_POINT ( 'NONE',  ( -11.35316468750000141, 3.593749996586016682, -1.390361679473963753E-15 ) ) ;
#71461 = CARTESIAN_POINT ( 'NONE',  ( 2.849036369511732440E-14, 199.2500000000000000, 202.0000000000000000 ) ) ;
#71462 = CARTESIAN_POINT ( 'NONE',  ( 6.298842414714822979, -10.24914933418239649, -64.89273347873384523 ) ) ;
#71463 = FACE_OUTER_BOUND ( 'NONE', #21684, .T. ) ;
#71464 = CARTESIAN_POINT ( 'NONE',  ( 3.458734124999959914, 205.3750000013656063, 143.4326545832176976 ) ) ;
#71465 = DIRECTION ( 'NONE',  ( 1.000000000000000000, 3.154042683594195121E-16, 0.000000000000000000 ) ) ;
#71466 = CARTESIAN_POINT ( 'NONE',  ( -1.836970198721029983E-15, 35.62499999317203248, 10.00000000000000178 ) ) ;
#71467 = CARTESIAN_POINT ( 'NONE',  ( 2.977408999572654480, 111.1250000020483810, 7.188101187499999156 ) ) ;
#71468 = CARTESIAN_POINT ( 'NONE',  ( -4.541265875000002339, 4.937499998634407916, -5.561446717895856393E-16 ) ) ;
#71469 = DIRECTION ( 'NONE',  ( -0.000000000000000000, -0.000000000000000000, -1.000000000000000000 ) ) ;
#71470 = CARTESIAN_POINT ( 'NONE',  ( 5.656854249492376141, -5.656854249492374365, 17.89280277982336642 ) ) ;
#71472 = CARTESIAN_POINT ( 'NONE',  ( -7.778174593052020747, -7.778174593052023411, 104.8750000040967763 ) ) ;
#71471 = CARTESIAN_POINT ( 'NONE',  ( 0.000000000000000000, 300.0000000000000000, 0.000000000000000000 ) ) ;
#71473 = VERTEX_POINT ( 'NONE', #41395 ) ;
#71474 = CARTESIAN_POINT ( 'NONE',  ( 8.000000000000000000, 93.03125000409677625, -3.313708498984762496 ) ) ;
#71475 = CARTESIAN_POINT ( 'NONE',  ( -4.556349186104045934, 11.00000000000000000, 81.90625000409676204 ) ) ;
#71476 = CARTESIAN_POINT ( 'NONE',  ( 11.35316468749999608, 236.9270833367473017, -3.042071309553167513 ) ) ;
#71477 = CARTESIAN_POINT ( 'NONE',  ( -11.35316468750000141, 123.2812499965860269, -1.390361679473963753E-15 ) ) ;
#71478 = EDGE_LOOP ( 'NONE', ( #33338, #55683, #69524, #58572 ) ) ;
#71479 = CARTESIAN_POINT ( 'NONE',  ( -4.898587196589407898E-16, 7.999999999999991118, 5.142802783920146226 ) ) ;
#71480 = CARTESIAN_POINT ( 'NONE',  ( -10.18810118749999738, -4.220049686691941915, 93.25000000204838102 ) ) ;
#71481 = CARTESIAN_POINT ( 'NONE',  ( 3.090149533464540799, 227.8745411751044685, -9.510571794630905629 ) ) ;
#71482 = CARTESIAN_POINT ( 'NONE',  ( -1.432654583217608080, 197.8750000013656063, 201.4587341250000350 ) ) ;
#71483 = CARTESIAN_POINT ( 'NONE',  ( 5.656854249492374365, 5.656854249492375253, 27.26780277982336642 ) ) ;
#71485 = CARTESIAN_POINT ( 'NONE',  ( -8.311093377946836114, 112.6562499965860269, -8.311093377946837890 ) ) ;
#71484 = CARTESIAN_POINT ( 'NONE',  ( 8.660254037844405062, 44.58333333333334281, 5.000000000000017764 ) ) ;
#71486 = EDGE_CURVE ( 'NONE', #11179, #66522, #61295, .T. ) ;
#71487 = CARTESIAN_POINT ( 'NONE',  ( -30.82842712474616320, 208.3750000000000284, 172.8284271247465824 ) ) ;
#71488 = CARTESIAN_POINT ( 'NONE',  ( 1.425702245604163669E-12, 48.75000000000012079, 10.00000000000000178 ) ) ;
#71489 = EDGE_LOOP ( 'NONE', ( #56698, #72064, #62245, #55118 ) ) ;
#71490 = DIRECTION ( 'NONE',  ( -0.000000000000000000, -1.000000000000000000, -0.000000000000000000 ) ) ;
#71491 = VECTOR ( 'NONE', #49417, 1000.000000000000000 ) ;
#71492 = CYLINDRICAL_SURFACE ( 'NONE', #59377, 3.999999999999976019 ) ;
#71493 = CARTESIAN_POINT ( 'NONE',  ( 8.311093377946834337, 105.4687499965860127, 8.311093377946839666 ) ) ;
#71494 = CARTESIAN_POINT ( 'NONE',  ( 2.445694354108838731, 206.0625000013656063, 195.5543056458912190 ) ) ;
#71495 = CARTESIAN_POINT ( 'NONE',  ( 7.188101187499999156, 12.74999999795161187, 2.977408999572654924 ) ) ;
#71496 = CARTESIAN_POINT ( 'NONE',  ( -10.18810118749999916, 4.220049686691934809, 87.43750000204838102 ) ) ;
#71497 = CARTESIAN_POINT ( 'NONE',  ( -3.042071309553164404, 17.55208332991935194, -11.35316468749999963 ) ) ;
#71498 = ORIENTED_EDGE ( 'NONE', *, *, #34464, .T. ) ;
#71499 = DIRECTION ( 'NONE',  ( -0.000000000000000000, 1.000000000000000000, 0.000000000000000000 ) ) ;
#71500 = CARTESIAN_POINT ( 'NONE',  ( 8.008118988124993010, -3.317071493978877239, 24.16936528394063544 ) ) ;
#71501 = DIRECTION ( 'NONE',  ( 1.000000000000000000, -0.000000000000000000, -0.000000000000000000 ) ) ;
#71502 = CARTESIAN_POINT ( 'NONE',  ( -10.18810118749999738, -4.220049686691941915, 74.12500000204836681 ) ) ;
#71503 =( BOUNDED_CURVE ( )  B_SPLINE_CURVE ( 2, ( #69741, #40695, #63698, #1097, #18056, #41071, #58433, #6743, #29746 ),
 .UNSPECIFIED., .F., .F. ) 
 B_SPLINE_CURVE_WITH_KNOTS ( ( 3, 2, 2, 2, 3 ),
 ( 0.3500000000000004219, 0.3583333333333337256, 0.3666666666666669738, 0.3750000000000002776, 0.3833333333333335813 ),
 .UNSPECIFIED. ) 
 CURVE ( )  GEOMETRIC_REPRESENTATION_ITEM ( )  RATIONAL_B_SPLINE_CURVE ( ( 0.9999999999999958922, 0.9238795325112908463, 1.000000000000000000, 0.9238795325112867385, 1.000000000000000000, 0.9238795325112867385, 1.000000000000000000, 0.9238795325112847401, 1.000000000000001998 ) ) 
 REPRESENTATION_ITEM ( '' )  );
#71504 = CARTESIAN_POINT ( 'NONE',  ( 2.549518376916382945, 21.99999999999999645, 3.425189025651766972 ) ) ;
#71505 = CARTESIAN_POINT ( 'NONE',  ( -5.000000000000005329, 150.2083333265053682, 8.660254037844387298 ) ) ;
#71506 = CARTESIAN_POINT ( 'NONE',  ( 2.765530957082001251, 293.7656250017068942, 6.676582343750000703 ) ) ;
#71507 = DIRECTION ( 'NONE',  ( -0.000000000000000000, -0.000000000000000000, -1.000000000000000000 ) ) ;
#71508 = CARTESIAN_POINT ( 'NONE',  ( 6.951808397369818766E-16, 217.3437499965860411, -11.35316468750000141 ) ) ;
#71509 = EDGE_CURVE ( 'NONE', #14563, #64315, #43883, .T. ) ;
#71510 = CARTESIAN_POINT ( 'NONE',  ( 8.311093377946834337, 125.4687499965860127, 8.311093377946839666 ) ) ;
#71511 = CARTESIAN_POINT ( 'NONE',  ( 7.204075437095968759, -7.204075437095966983, 86.21875000204836681 ) ) ;
#71512 = CARTESIAN_POINT ( 'NONE',  ( -27.99999999999996447, 200.9375000013656063, 173.4587341250003760 ) ) ;
#71513 = CARTESIAN_POINT ( 'NONE',  ( 5.656854249492378806, 25.31250000000000355, 5.656854249492381470 ) ) ;
#71514 = CARTESIAN_POINT ( 'NONE',  ( -1.881053915767124440, 13.12499999863440969, 4.541265875000001451 ) ) ;
#71515 = ORIENTED_EDGE ( 'NONE', *, *, #42675, .T. ) ;
#71516 = CARTESIAN_POINT ( 'NONE',  ( -1.656854249492347719, 205.9375000027311842, 194.0000000000000853 ) ) ;
#71517 = CARTESIAN_POINT ( 'NONE',  ( 1.432654583217608080, 198.8750000013656347, 138.5412658750000503 ) ) ;
#71519 =( BOUNDED_SURFACE ( )  B_SPLINE_SURFACE ( 3, 2, ( 
 ( #38732, #56081, #43623 ),
 ( #68131, #39460, #67388 ),
 ( #37980, #26640, #55336 ),
 ( #27759, #20982, #50771 ),
 ( #73417, #8928, #60979 ),
 ( #4026, #3641, #15312 ),
 ( #16426, #32324, #55712 ),
 ( #32703, #9300, #49662 ),
 ( #44006, #16059, #45120 ),
 ( #50031, #67013, #31939 ),
 ( #73785, #4391, #27384 ),
 ( #72678, #73047, #3271 ),
 ( #21354, #26258, #61729 ),
 ( #38348, #21722, #49278 ),
 ( #50403, #22094, #61356 ),
 ( #10048, #44751, #67765 ),
 ( #39093, #62096, #10418 ),
 ( #35304, #40952, #45855 ) ),
 .UNSPECIFIED., .F., .F., .T. ) 
 B_SPLINE_SURFACE_WITH_KNOTS ( ( 4, 2, 2, 2, 2, 2, 2, 2, 4 ),
 ( 3, 3 ),
 ( 0.04202945594032918980, 0.04396162471216789880, 0.04589379348400660086, 0.04782596225584530986, 0.04975813102768401885, 0.05169029979952272785, 0.05265638418544207888, 0.05362246857136143685, 0.05748680611503884791 ),
 ( 0.000000000000000000, 1.000000000000000000 ),
 .UNSPECIFIED. ) 
 GEOMETRIC_REPRESENTATION_ITEM ( )  RATIONAL_B_SPLINE_SURFACE ( (
 ( 1.000000000000000000, 0.6241276099608161765, 1.000000000000000000),
 ( 1.000000000000000000, 0.6218761496801206157, 1.000000000000000000),
 ( 1.000000000000000000, 0.6198047272362935400, 1.000000000000000000),
 ( 1.000000000000000000, 0.6161935119825484586, 1.000000000000000000),
 ( 1.000000000000000000, 0.6146642324081265096, 1.000000000000000000),
 ( 1.000000000000000000, 0.6121850116870731773, 1.000000000000000000),
 ( 1.000000000000000000, 0.6112350889400474108, 1.000000000000000000),
 ( 1.000000000000000000, 0.6099522725972107429, 1.000000000000000000),
 ( 1.000000000000000000, 0.6096208180307641777, 1.000000000000000000),
 ( 1.000000000000000000, 0.6096183796349724515, 1.000000000000000000),
 ( 1.000000000000000000, 0.6099422200101473068, 1.000000000000000000),
 ( 1.000000000000000000, 0.6109087447823515760, 1.000000000000000000),
 ( 1.000000000000000000, 0.6113123981688074471, 1.000000000000000000),
 ( 1.000000000000000000, 0.6122677719809533903, 1.000000000000000000),
 ( 1.000000000000000000, 0.6128199619020369138, 1.000000000000000000),
 ( 1.000000000000000000, 0.6159350830268177646, 1.000000000000000000),
 ( 1.000000000000000000, 0.6195556778513775509, 1.000000000000000000),
 ( 1.000000000000000000, 0.6241278272307890784, 1.000000000000000000) ) ) 
 REPRESENTATION_ITEM ( '' )  SURFACE ( )  );
#71518 = CARTESIAN_POINT ( 'NONE',  ( 3.999999999999960032, 205.1250000027312126, 142.0000000000000568 ) ) ;
#71520 = CARTESIAN_POINT ( 'NONE',  ( -7.320508075688842986, 171.8750000000000000, -7.320508075688843874 ) ) ;
#71521 = CARTESIAN_POINT ( 'NONE',  ( -4.220049686691937474, -10.18810118749999738, 69.81250000204835260 ) ) ;
#71522 = VERTEX_POINT ( 'NONE', #314 ) ;
#71523 = CARTESIAN_POINT ( 'NONE',  ( -7.188101187500000933, 4.124999997951610986, -2.977408999572651371 ) ) ;
#71524 = CARTESIAN_POINT ( 'NONE',  ( -17.57096290104944458, -17.15628487729649265, 195.5490137213376443 ) ) ;
#71525 = ADVANCED_FACE ( 'NONE', ( #68946 ), #45559, .T. ) ;
#71526 = CARTESIAN_POINT ( 'NONE',  ( -7.188101187500000044, 112.5312500020483952, 0.000000000000000000 ) ) ;
#71527 = CARTESIAN_POINT ( 'NONE',  ( -3.185990892481874948, 21.99999999999999289, -2.809123505085484584 ) ) ;
#71528 = CARTESIAN_POINT ( 'NONE',  ( 6.676582343750003368, 292.8906250017069510, 2.765530957081995478 ) ) ;
#71530 = DIRECTION ( 'NONE',  ( -0.000000000000000000, 1.000000000000000000, -0.000000000000000000 ) ) ;
#71529 = CARTESIAN_POINT ( 'NONE',  ( -3.042071309553159075, 219.9479166700806445, 11.35316468749999963 ) ) ;
#71531 = ORIENTED_EDGE ( 'NONE', *, *, #5772, .T. ) ;
#71532 = CARTESIAN_POINT ( 'NONE',  ( -3.042071309553166181, 223.1770833367473017, -11.35316468749999608 ) ) ;
#71533 = EDGE_CURVE ( 'NONE', #55422, #26389, #51590, .T. ) ;
#71534 = CARTESIAN_POINT ( 'NONE',  ( -4.401442555609577197E-16, 7.188101187499992051, 1.111552781871753215 ) ) ;
#71535 = AXIS2_PLACEMENT_3D ( 'NONE', #50375, #10026, #16037 ) ;
#71536 = DIRECTION ( 'NONE',  ( -0.000000000000000000, -1.000000000000000000, -0.000000000000000000 ) ) ;
#71537 = CARTESIAN_POINT ( 'NONE',  ( -30.82842712474612057, 195.5000000027312126, 172.8284271247466108 ) ) ;
#71538 = CARTESIAN_POINT ( 'NONE',  ( 1.432654583217662481, 201.3750000013656347, 194.5412658750000219 ) ) ;
#71539 = ORIENTED_EDGE ( 'NONE', *, *, #59236, .F. ) ;
#71540 = LINE ( 'NONE', #19864, #21044 ) ;
#71541 = CARTESIAN_POINT ( 'NONE',  ( 8.000000000000000000, 98.74999999999998579, -9.797174393178825657E-16 ) ) ;
#71542 = CARTESIAN_POINT ( 'NONE',  ( 8.311093377946837890, 111.7187499965859985, -8.311093377946837890 ) ) ;
#71543 = CARTESIAN_POINT ( 'NONE',  ( -7.347880794884122694E-16, 15.49999999726881406, 4.000000000000001776 ) ) ;
#71544 = CARTESIAN_POINT ( 'NONE',  ( -7.778174593052020747, -7.778174593052023411, 77.68749999999998579 ) ) ;
#71547 = CYLINDRICAL_SURFACE ( 'NONE', #1320, 10.00000000000000178 ) ;
#71546 = CARTESIAN_POINT ( 'NONE',  ( 26.56734541678237704, 201.3750000013656347, 173.4587341249998929 ) ) ;
#71545 = CARTESIAN_POINT ( 'NONE',  ( 28.00000000000002132, 201.1875000013656063, 166.5412658749999082 ) ) ;
#71548 = VERTEX_POINT ( 'NONE', #46303 ) ;
#71549 = ADVANCED_FACE ( 'NONE', ( #47040 ), #74607, .F. ) ;
#71550 = ADVANCED_FACE ( 'NONE', ( #684 ), #34265, .F. ) ;
#71551 = CARTESIAN_POINT ( 'NONE',  ( -2.775557561562891351E-14, 210.0000000000000284, 142.0000000000000568 ) ) ;
#71552 = CARTESIAN_POINT ( 'NONE',  ( 5.676582343749993598, 219.9479166632526983, 9.832129032723422313 ) ) ;
#71554 = EDGE_CURVE ( 'NONE', #3989, #22076, #58122, .T. ) ;
#71553 = CARTESIAN_POINT ( 'NONE',  ( -3.458734125000016313, 199.8750000013655779, 140.5673454167824161 ) ) ;
#71555 = CARTESIAN_POINT ( 'NONE',  ( 31.45873412499998523, 203.8750000013656063, 171.4326545832175839 ) ) ;
#71556 = CARTESIAN_POINT ( 'NONE',  ( 0.000000000000000000, 0.000000000000000000, 3.469446951953614189E-15 ) ) ;
#71557 = CARTESIAN_POINT ( 'NONE',  ( -11.35316468750000141, 193.5937499965860127, -1.390361679473963753E-15 ) ) ;
#71558 = CARTESIAN_POINT ( 'NONE',  ( -2.977408999572650927, 89.75000000204838102, -7.188101187500000933 ) ) ;
#71559 = CARTESIAN_POINT ( 'NONE',  ( 8.261209813499636567, 225.9999999999997726, 6.632190850709866581 ) ) ;
#71560 = CARTESIAN_POINT ( 'NONE',  ( 2.780723358947928197E-16, 13.56249999863440614, -4.541265875000002339 ) ) ;
#71561 = CARTESIAN_POINT ( 'NONE',  ( 28.00000000000002132, 199.1875000013655779, 166.5412658749999082 ) ) ;
#71562 = CARTESIAN_POINT ( 'NONE',  ( 7.188101187499991163, 2.977408999572648707, 1.205302781871753215 ) ) ;
#71563 = CARTESIAN_POINT ( 'NONE',  ( -2.085542519210945728E-15, 79.53124999658602690, 11.35316468750000141 ) ) ;
#71564 = ORIENTED_EDGE ( 'NONE', *, *, #57824, .F. ) ;
#71565 = CARTESIAN_POINT ( 'NONE',  ( 8.572527594031473190E-16, 0.000000000000000000, -7.000000000000000000 ) ) ;
#71566 = FACE_OUTER_BOUND ( 'NONE', #69542, .T. ) ;
#71567 = CARTESIAN_POINT ( 'NONE',  ( -8.000000000000001776, 9.656249995903223748, 3.313708498984759387 ) ) ;
#71569 = CARTESIAN_POINT ( 'NONE',  ( 2.679491924311226292, 233.5416666666666856, -10.00000000000000000 ) ) ;
#71568 = VECTOR ( 'NONE', #47266, 1000.000000000000000 ) ;
#71570 = CARTESIAN_POINT ( 'NONE',  ( -9.832129032723420536, 88.69791666325268409, 5.676582343749997150 ) ) ;
#71571 = ORIENTED_EDGE ( 'NONE', *, *, #28739, .T. ) ;
#71572 = CARTESIAN_POINT ( 'NONE',  ( -6.238412754330611322E-16, 10.18810118749999916, 88.65625000204838102 ) ) ;
#71573 = CARTESIAN_POINT ( 'NONE',  ( 4.220049686691934809, 10.18810118749999916, 110.6875000020483952 ) ) ;
#71574 = CARTESIAN_POINT ( 'NONE',  ( 2.839093476692135984E-14, 208.9375000013656063, 201.4587341250000350 ) ) ;
#71575 = CARTESIAN_POINT ( 'NONE',  ( 3.313708498984761608, 24.09374999590322375, -8.000000000000000000 ) ) ;
#71577 = CARTESIAN_POINT ( 'NONE',  ( -8.311093377946841443, 78.90624999658601268, 8.311093377946834337 ) ) ;
#71576 = CARTESIAN_POINT ( 'NONE',  ( 11.00000000000000000, 1.347111479062088405E-15, 106.7500000000000000 ) ) ;
#71578 = EDGE_CURVE ( 'NONE', #40213, #38797, #11337, .T. ) ;
#71579 = CARTESIAN_POINT ( 'NONE',  ( -7.999999999999989342, -3.313708498984762496, 20.61155278392014623 ) ) ;
#71580 = CYLINDRICAL_SURFACE ( 'NONE', #69855, 4.000000000000001776 ) ;
#71581 = CARTESIAN_POINT ( 'NONE',  ( -8.660254037844390851, 174.7916666598387110, 4.999999999999998224 ) ) ;
#71582 = CARTESIAN_POINT ( 'NONE',  ( 5.082755093536325042, 90.96875000204838102, -5.082755093536325930 ) ) ;
#71583 = DIRECTION ( 'NONE',  ( 1.000000000000000000, -0.000000000000000000, 0.000000000000000000 ) ) ;
#71584 = CARTESIAN_POINT ( 'NONE',  ( -9.832129032723418760, 58.17708332991936260, -5.676582343750004256 ) ) ;
#71585 = CARTESIAN_POINT ( 'NONE',  ( -4.721056650415999201, 295.3281250017069510, -4.721056650415999201 ) ) ;
#71586 = CARTESIAN_POINT ( 'NONE',  ( -10.18810118749999916, 0.000000000000000000, 105.5312500020483810 ) ) ;
#71587 = CARTESIAN_POINT ( 'NONE',  ( -3.042071309553164404, 202.2395833299193271, -11.35316468749999963 ) ) ;
#71588 = ORIENTED_EDGE ( 'NONE', *, *, #44091, .T. ) ;
#71589 = CARTESIAN_POINT ( 'NONE',  ( -2.775557561562891351E-14, 210.0000000000000284, 142.0000000000000568 ) ) ;
#71590 = CARTESIAN_POINT ( 'NONE',  ( -30.82842712474612412, 203.5000000027312126, 172.8284271247466108 ) ) ;
#71591 = CARTESIAN_POINT ( 'NONE',  ( 7.999999999999998224, 14.71874999590322020, 3.313708498984766049 ) ) ;
#71593 = CARTESIAN_POINT ( 'NONE',  ( 11.35316468749999785, 195.5729166632526983, 3.042071309553174174 ) ) ;
#71592 = CARTESIAN_POINT ( 'NONE',  ( 8.660254037844385522, 262.9166666666666856, -5.000000000000003553 ) ) ;
#71594 = CARTESIAN_POINT ( 'NONE',  ( -1.656854249492470732, 203.6875000000000000, 145.9999999999999716 ) ) ;
#71595 = CARTESIAN_POINT ( 'NONE',  ( 8.660254037844389075, 240.2083333401613174, 4.999999999999997335 ) ) ;
#71596 = DIRECTION ( 'NONE',  ( -0.000000000000000000, 1.000000000000000000, -0.000000000000000000 ) ) ;
#71597 = VERTEX_POINT ( 'NONE', #47411 ) ;
#71598 = CARTESIAN_POINT ( 'NONE',  ( 9.832129032723420536, 186.5104166632526983, -5.676582343749999815 ) ) ;
#71599 = CIRCLE ( 'NONE', #61976, 11.00000000000000000 ) ;
#71600 = CARTESIAN_POINT ( 'NONE',  ( -4.401442555609577197E-16, 7.188101187499992051, 20.61155278187175455 ) ) ;
#71601 = CARTESIAN_POINT ( 'NONE',  ( -5.000000000000001776, 93.33333333333334281, 8.660254037844381969 ) ) ;
#71602 = ORIENTED_EDGE ( 'NONE', *, *, #13968, .F. ) ;
#71603 = CARTESIAN_POINT ( 'NONE',  ( 5.656854249492381470, 97.25000000409677625, 5.656854249492379694 ) ) ;
#71604 = CARTESIAN_POINT ( 'NONE',  ( 0.000000000000000000, 0.000000000000000000, 8.000000000000000000 ) ) ;
#71605 =( BOUNDED_CURVE ( )  B_SPLINE_CURVE ( 2, ( #70298, #19338, #37072, #19707, #54059, #60075, #7294, #35969, #41255, #2368, #53321, #64991, #18240 ),
 .UNSPECIFIED., .F., .F. ) 
 B_SPLINE_CURVE_WITH_KNOTS ( ( 3, 2, 2, 2, 2, 2, 3 ),
 ( 0.8948938610911654212, 0.9001271886622317364, 0.9053605162332980516, 0.9105938438043643668, 0.9158271713754306820, 0.9210604989464967751, 0.9262938265175630903 ),
 .UNSPECIFIED. ) 
 CURVE ( )  GEOMETRIC_REPRESENTATION_ITEM ( )  RATIONAL_B_SPLINE_CURVE ( ( 0.9999999999999248379, 0.9659258262891434743, 1.000000000000000000, 0.9659258262890683122, 1.000000000000000000, 0.9659258262890683122, 1.000000000000000000, 0.9659258262890683122, 1.000000000000000000, 0.9659258262890683122, 1.000000000000000000, 0.9659258262890673130, 1.000000000000001110 ) ) 
 REPRESENTATION_ITEM ( '' )  );
#71606 = CARTESIAN_POINT ( 'NONE',  ( -4.000000000000002665, 16.56250000000000000, 1.656854249492380804 ) ) ;
#71607 = CARTESIAN_POINT ( 'NONE',  ( -3.211159895383562723, 15.93749999863440436, 3.211159895383561391 ) ) ;
#71608 = CARTESIAN_POINT ( 'NONE',  ( 5.656854249492374365, 5.656854249492375253, 10.95530278392014800 ) ) ;
#71610 = CARTESIAN_POINT ( 'NONE',  ( 4.898587196589412829E-16, 7.875000000000001776, -8.000000000000000000 ) ) ;
#71609 = AXIS2_PLACEMENT_3D ( 'NONE', #3183, #30734, #54502 ) ;
#71611 = ADVANCED_FACE ( 'NONE', ( #24763 ), #74084, .T. ) ;
#71612 = EDGE_LOOP ( 'NONE', ( #13167, #11590, #26504, #4317 ) ) ;
#71613 = CARTESIAN_POINT ( 'NONE',  ( 2.485281374238929697, 293.3750000034140157, 5.999999999999645617 ) ) ;
#71614 = CARTESIAN_POINT ( 'NONE',  ( 7.188101187500002709, 97.81250000204840944, 2.977408999572649151 ) ) ;
#71616 = CARTESIAN_POINT ( 'NONE',  ( -9.832129032723418760, 258.4895833367473301, -5.676582343749998927 ) ) ;
#71615 = DIRECTION ( 'NONE',  ( 0.000000000000000000, 0.000000000000000000, 1.000000000000000000 ) ) ;
#71617 = DIRECTION ( 'NONE',  ( 1.000000000000000000, 0.000000000000000000, 0.000000000000000000 ) ) ;
#71618 = ORIENTED_EDGE ( 'NONE', *, *, #2405, .T. ) ;
#71619 = CARTESIAN_POINT ( 'NONE',  ( -6.735557395310442023E-16, 11.00000000000000000, 83.12499999999998579 ) ) ;
#71620 = CARTESIAN_POINT ( 'NONE',  ( 7.188101187499992051, 8.802885111219154394E-16, 20.23655278187175099 ) ) ;
#71621 = ORIENTED_EDGE ( 'NONE', *, *, #41020, .T. ) ;
#71622 =( BOUNDED_CURVE ( )  B_SPLINE_CURVE ( 2, ( #22471, #51159, #70009, #39838, #5519, #34577, #74543, #22854, #69633 ),
 .UNSPECIFIED., .F., .F. ) 
 B_SPLINE_CURVE_WITH_KNOTS ( ( 3, 2, 2, 2, 3 ),
 ( 0.8500000000000005329, 0.8583333333333339477, 0.8666666666666673624, 0.8750000000000007772, 0.8833333333333341919 ),
 .UNSPECIFIED. ) 
 CURVE ( )  GEOMETRIC_REPRESENTATION_ITEM ( )  RATIONAL_B_SPLINE_CURVE ( ( 0.9999999999999948930, 0.9238795325112918455, 1.000000000000000000, 0.9238795325112867385, 1.000000000000000000, 0.9238795325112867385, 1.000000000000000000, 0.9238795325112786339, 1.000000000000008216 ) ) 
 REPRESENTATION_ITEM ( '' )  );
#71623 = ORIENTED_EDGE ( 'NONE', *, *, #68668, .F. ) ;
#71624 = CARTESIAN_POINT ( 'NONE',  ( -10.18810118749999738, -4.220049686691941915, 79.75000000204838102 ) ) ;
#71625 = CARTESIAN_POINT ( 'NONE',  ( -2.085542519210945728E-15, 59.84374999658602690, 11.35316468750000141 ) ) ;
#71626 = CARTESIAN_POINT ( 'NONE',  ( -31.05507224581699788, -12.00007582394998984, 171.9999999999997726 ) ) ;
#71627 = CARTESIAN_POINT ( 'NONE',  ( -7.778174593052023411, 7.778174593052023411, 95.31250000000000000 ) ) ;
#71630 = CARTESIAN_POINT ( 'NONE',  ( 6.676582343750002480, 296.1718750017070079, -2.765530957081997254 ) ) ;
#71629 = CARTESIAN_POINT ( 'NONE',  ( 32.00000000000000000, 202.3750000027312126, 169.9999999999998863 ) ) ;
#71628 = CARTESIAN_POINT ( 'NONE',  ( 7.778174593052023411, -7.778174593052021635, 105.0624999999999858 ) ) ;
#71631 = CARTESIAN_POINT ( 'NONE',  ( -2.679491924311225848, 141.4583333333333712, -10.00000000000000178 ) ) ;
#71632 = CARTESIAN_POINT ( 'NONE',  ( 2.828427124746191623, 14.12500000000000000, -2.828427124746191623 ) ) ;
#71633 = CARTESIAN_POINT ( 'NONE',  ( -7.999999999999998224, 90.78125000409680467, 3.313708498984766049 ) ) ;
#71634 = VECTOR ( 'NONE', #62296, 1000.000000000000114 ) ;
#71635 = DIRECTION ( 'NONE',  ( 0.000000000000000000, -2.238352872228138170E-16, 1.000000000000000000 ) ) ;
#71636 = CARTESIAN_POINT ( 'NONE',  ( 5.656854249492380582, 5.999999995903221084, -5.656854249492380582 ) ) ;
#71637 = ADVANCED_FACE ( 'NONE', ( #2507 ), #71896, .T. ) ;
#71638 = CARTESIAN_POINT ( 'NONE',  ( 25.55430564589119413, 199.0625000013656063, 167.5543056458910485 ) ) ;
#71639 = CARTESIAN_POINT ( 'NONE',  ( -2.977408999572650039, 8.812499997951611874, -7.188101187500001821 ) ) ;
#71640 = CONICAL_SURFACE ( 'NONE', #9030, 18.00000000000000355, 1.047197551196596965 ) ;
#71641 = CARTESIAN_POINT ( 'NONE',  ( -7.999999999999991118, 3.313708498984756723, 23.42405278392015333 ) ) ;
#71642 = DIRECTION ( 'NONE',  ( -0.000000000000000000, -0.000000000000000000, 1.000000000000000000 ) ) ;
#71643 = CARTESIAN_POINT ( 'NONE',  ( 7.188101187500000044, 108.7812500020483810, -8.802885111219163269E-16 ) ) ;
#71645 = CARTESIAN_POINT ( 'NONE',  ( 2.449293598294707893E-16, 16.25000000000000000, -4.000000000000001776 ) ) ;
#71644 = CARTESIAN_POINT ( 'NONE',  ( 1.656854249492487607, 201.6875000000000284, 194.0000000000001705 ) ) ;
#71646 = CARTESIAN_POINT ( 'NONE',  ( 28.00000000000002132, 203.1250000027312126, 173.9999999999999147 ) ) ;
#71647 = CARTESIAN_POINT ( 'NONE',  ( 31.45873412499999944, 208.9375000013656063, 169.9999999999999432 ) ) ;
#71648 = CARTESIAN_POINT ( 'NONE',  ( 5.082755093536318824, 5.082755093536319713, 20.79905278187175455 ) ) ;
#71649 = CARTESIAN_POINT ( 'NONE',  ( 23.99999999999998579, 195.7500000000000000, 169.9999999999998863 ) ) ;
#71650 = CARTESIAN_POINT ( 'NONE',  ( -2.085542519210945728E-15, 44.53124999658601979, 11.35316468750000141 ) ) ;
#71651 = FACE_OUTER_BOUND ( 'NONE', #14801, .T. ) ;
#71652 = CARTESIAN_POINT ( 'NONE',  ( -1.836970198721029983E-15, 15.62499999317203248, 10.00000000000000178 ) ) ;
#71653 = ORIENTED_EDGE ( 'NONE', *, *, #51306, .T. ) ;
#71654 = CARTESIAN_POINT ( 'NONE',  ( -5.000000000000005329, 130.2083333265053966, 8.660254037844387298 ) ) ;
#71655 = CARTESIAN_POINT ( 'NONE',  ( 0.000000000000000000, 0.000000000000000000, 0.000000000000000000 ) ) ;
#71656 = CARTESIAN_POINT ( 'NONE',  ( -11.35316468750000141, 38.48958332991935549, 3.042071309553159963 ) ) ;
#71657 = CARTESIAN_POINT ( 'NONE',  ( 4.556349186104051263, -10.99999999999999822, 81.15625000409676204 ) ) ;
#71658 = CARTESIAN_POINT ( 'NONE',  ( -2.445694354108840063, 203.0625000013656063, 139.5543056458912190 ) ) ;
#71659 = CARTESIAN_POINT ( 'NONE',  ( -8.660254037844385522, 260.4166666666666856, 5.000000000000004441 ) ) ;
#71660 = CARTESIAN_POINT ( 'NONE',  ( 8.000000000000000000, 25.31249999590322375, 0.000000000000000000 ) ) ;
#71662 = CARTESIAN_POINT ( 'NONE',  ( -3.042071309553163960, 27.23958332991934839, -11.35316468749999963 ) ) ;
#71661 = CARTESIAN_POINT ( 'NONE',  ( -5.082755093536325930, 101.4687500020483810, -5.082755093536325930 ) ) ;
#71663 = EDGE_CURVE ( 'NONE', #33382, #28855, #17437, .T. ) ;
#71664 = CARTESIAN_POINT ( 'NONE',  ( 3.313708498984762496, -7.999999999999989342, 11.79905277982336465 ) ) ;
#71665 = CARTESIAN_POINT ( 'NONE',  ( -3.042071309553164404, 157.2395833299193555, -11.35316468749999963 ) ) ;
#71666 = EDGE_CURVE ( 'NONE', #35174, #42754, #25133, .T. ) ;
#71667 = CARTESIAN_POINT ( 'NONE',  ( 6.123233995736767268E-16, 123.1249999931720396, -10.00000000000000178 ) ) ;
#71668 = CARTESIAN_POINT ( 'NONE',  ( -5.082755093536325930, 109.3437500020483810, -5.082755093536325930 ) ) ;
#71669 = ORIENTED_EDGE ( 'NONE', *, *, #54026, .F. ) ;
#71670 = CARTESIAN_POINT ( 'NONE',  ( 1.102182119232618108E-15, 289.2500000000000000, 6.000000000000001776 ) ) ;
#71671 = CARTESIAN_POINT ( 'NONE',  ( -11.35316468749999785, 28.38541666325268054, -3.042071309553167957 ) ) ;
#71672 = ORIENTED_EDGE ( 'NONE', *, *, #54649, .F. ) ;
#71673 = DIRECTION ( 'NONE',  ( -0.000000000000000000, -1.000000000000000000, -0.000000000000000000 ) ) ;
#71674 = CARTESIAN_POINT ( 'NONE',  ( -10.18810118749999916, 0.000000000000000000, 79.65625000204836681 ) ) ;
#71675 = DIRECTION ( 'NONE',  ( 0.000000000000000000, 0.000000000000000000, 1.000000000000000000 ) ) ;
#71677 = CARTESIAN_POINT ( 'NONE',  ( 3.042071309553167513, 156.8229166632526983, -11.35316468749999785 ) ) ;
#71676 = FACE_OUTER_BOUND ( 'NONE', #70957, .T. ) ;
#71678 = CARTESIAN_POINT ( 'NONE',  ( -2.977408999572654480, 1.874999997951610320, 7.188101187499999156 ) ) ;
#71679 = CARTESIAN_POINT ( 'NONE',  ( 7.999999999999991118, 3.313708498984757611, 16.73030278432982243 ) ) ;
#71680 = CARTESIAN_POINT ( 'NONE',  ( -5.652416403964814151, -4.866508352364031786, 0.6881790637065305916 ) ) ;
#71681 = CARTESIAN_POINT ( 'NONE',  ( -6.951808397369817780E-16, 237.6562500034140157, -11.35316468749999963 ) ) ;
#71682 = CARTESIAN_POINT ( 'NONE',  ( -7.204075437095967871, 7.204075437095967871, 85.84375000204836681 ) ) ;
#71683 = ORIENTED_EDGE ( 'NONE', *, *, #16197, .T. ) ;
#71684 = EDGE_CURVE ( 'NONE', #74424, #44243, #38384, .T. ) ;
#71685 = CARTESIAN_POINT ( 'NONE',  ( 0.000000000000000000, 300.0000000000000000, 10.00000000000000178 ) ) ;
#71686 = CARTESIAN_POINT ( 'NONE',  ( -5.656854249492380582, 122.0000000040967905, -5.656854249492380582 ) ) ;
#71687 = CARTESIAN_POINT ( 'NONE',  ( -11.35316468750000141, 108.8020833299193555, 3.042071309553159963 ) ) ;
#71688 = CARTESIAN_POINT ( 'NONE',  ( -10.18810118749999916, 4.220049686691934809, 99.06250000204836681 ) ) ;
#71689 = CARTESIAN_POINT ( 'NONE',  ( -3.211159895383561391, 19.81249999863440436, -3.211159895383561835 ) ) ;
#71690 = ORIENTED_EDGE ( 'NONE', *, *, #59300, .T. ) ;
#71691 = ORIENTED_EDGE ( 'NONE', *, *, #50371, .F. ) ;
#71692 = CARTESIAN_POINT ( 'NONE',  ( -3.211159895383561391, 2.812499998634407028, -3.211159895383561835 ) ) ;
#71693 = CARTESIAN_POINT ( 'NONE',  ( -7.188101187500001821, 7.124999997951610098, -2.977408999572651371 ) ) ;
#71694 = VECTOR ( 'NONE', #20746, 1000.000000000000000 ) ;
#71695 = CARTESIAN_POINT ( 'NONE',  ( 1.469576158976823947E-15, 118.0625000040967763, 8.000000000000000000 ) ) ;
#71696 = CARTESIAN_POINT ( 'NONE',  ( -6.238412754330611322E-16, 10.18810118749999916, 96.15625000204838102 ) ) ;
#71697 = CARTESIAN_POINT ( 'NONE',  ( -25.55430564589115150, 204.3125000013656063, 172.4456943541091789 ) ) ;
#71698 = CARTESIAN_POINT ( 'NONE',  ( 0.000000000000000000, 0.000000000000000000, 118.0000000000000000 ) ) ;
#71699 = VECTOR ( 'NONE', #27676, 1000.000000000000000 ) ;
#71700 = CARTESIAN_POINT ( 'NONE',  ( -1.656854249492383691, 5.687500000000000000, 4.000000000000000888 ) ) ;
#71701 = CARTESIAN_POINT ( 'NONE',  ( 2.449293598294707893E-16, 17.99999999726881583, -4.000000000000001776 ) ) ;
#71702 = CARTESIAN_POINT ( 'NONE',  ( 1.881053915767121998, 3.499999998634407028, -4.541265875000002339 ) ) ;
#71703 = CARTESIAN_POINT ( 'NONE',  ( -1.469576158976823947E-15, 18.93749999590322020, 8.000000000000000000 ) ) ;
#71704 = DIRECTION ( 'NONE',  ( 1.000000000000000000, 1.224646799147353207E-16, -0.000000000000000000 ) ) ;
#71705 = ADVANCED_FACE ( 'NONE', ( #67798, #55744 ), #67049, .F. ) ;
#71707 = CARTESIAN_POINT ( 'NONE',  ( -8.660254037844387298, 223.9583333265053966, -5.000000000000004441 ) ) ;
#71706 = CARTESIAN_POINT ( 'NONE',  ( -26.56734541678227757, 200.0000000013656347, 173.4587341250003476 ) ) ;
#71708 = SHAPE_REPRESENTATION_RELATIONSHIP ( 'NONE' , 'NONE' ,  #68567, #15581 ) ;
#71709 = CARTESIAN_POINT ( 'NONE',  ( -1.881053915767121554, 17.62499999863440436, -4.541265875000002339 ) ) ;
#71710 = CARTESIAN_POINT ( 'NONE',  ( -4.721056650415999201, 299.3281250017069510, -4.721056650415999201 ) ) ;
#71711 = CARTESIAN_POINT ( 'NONE',  ( 5.082755093536318824, 5.082755093536319713, 5.424052781871753659 ) ) ;
#71712 = VERTEX_POINT ( 'NONE', #73080 ) ;
#71713 = EDGE_CURVE ( 'NONE', #47025, #13196, #27565, .T. ) ;
#71714 = ORIENTED_EDGE ( 'NONE', *, *, #24789, .F. ) ;
#71715 = CARTESIAN_POINT ( 'NONE',  ( 7.204075437095966983, 7.204075437095967871, 97.09375000204836681 ) ) ;
#71716 = DIRECTION ( 'NONE',  ( 1.000000000000000000, -0.000000000000000000, -0.000000000000000000 ) ) ;
#71717 = CARTESIAN_POINT ( 'NONE',  ( -31.45873412500001010, 204.8750000013656063, 168.5673454167827572 ) ) ;
#71718 = CARTESIAN_POINT ( 'NONE',  ( -26.34314575050764518, 201.9375000000000284, 166.0000000000003695 ) ) ;
#71719 = CARTESIAN_POINT ( 'NONE',  ( -3.458734124999959025, 196.5000000013656063, 199.4326545832176691 ) ) ;
#71720 = CARTESIAN_POINT ( 'NONE',  ( 5.000000000000001776, 105.8333333333333286, -8.660254037844389075 ) ) ;
#71721 = CARTESIAN_POINT ( 'NONE',  ( 1.469576158976823947E-15, 113.3750000000000000, 8.000000000000000000 ) ) ;
#71722 = CARTESIAN_POINT ( 'NONE',  ( -4.721056650415998313, 297.7343750017069510, 4.721056650416000089 ) ) ;
#71723 = VERTEX_POINT ( 'NONE', #4061 ) ;
#71724 =( BOUNDED_CURVE ( )  B_SPLINE_CURVE ( 2, ( #63836, #121, #23100, #47582, #46483, #12153, #52157, #58935, #24205, #53266, #69131, #64583, #12879, #1592, #58201, #35915, #24577, #11786, #17438, #6135, #63458, #34823, #492, #23472, #69503, #31351, #8339, #42666, #43793, #30979, #30614, #19653, #60393, #66809, #13976, #9096, #37018, #72078, #43409, #25676, #7977, #15111, #70969, #54381, #32110, #49066, #54753, #26046, #2690, #48696, #65311, #71702, #20020, #47953, #53637, #13612, #43030, #37774, #60770, #49448, #66052, #20395, #20774, #36651, #14360, #60020, #8719, #54000, #72466, #1947, #37392, #19283, #24936, #31731, #59661, #3063, #66423, #14735, #55128, #3431, #65677, #26422, #59298, #42294, #2311, #7607, #25308, #71332, #48325, #22254, #61521, #10958, #21523, #45282, #56987, #33993, #16217, #73580, #5300, #21149, #28302, #9473, #50940, #50196, #44171, #56242, #21888, #26811, #32490, #67185, #33242, #16589, #39628, #51311, #27552, #72842, #74322, #62255, #49825, #55501, #10582, #9843, #22628, #3813, #4557, #15482, #38518, #44917, #32869, #50564, #67924, #4935, #45648, #62627, #44545, #38143, #55874, #4190, #33613, #68663, #27179, #73215, #39257, #68292, #67555, #61143, #15851, #38886, #61890, #10213, #56620, #27932, #73951, #27, #58838, #34730, #29789, #53171, #41110, #46021, #11327, #57735, #24111, #40000, #69042, #17345, #40367, #18096, #52431, #46756, #46393, #18465, #35095, #17717, #47491, #63742, #58105, #7149, #58471, #29422, #57360, #34359, #30154, #6040, #52064, #63366, #70158, #6416, #41475, #63003, #768, #12424, #64491, #69411, #40732, #12060, #23014, #1509, #11691, #47125, #23754, #69779, #6781, #29045, #64117, #35458, #401, #24489, #23380, #5671, #52799, #1133, #16974, #12791, #35823, #28668, #51682, #54659, #36925, #19196, #30889, #7518, #65587, #43316, #60296, #65959, #37300, #13886, #59933, #20298, #8245, #31258, #13154, #71240, #14637, #19560, #48232, #71985, #54287, #36192, #25216, #42574, #66333, #2598, #8626, #2967, #25588, #42198, #53907, #48604, #71607, #65213, #2220, #19928, #25952, #31638, #42938, #48971, #70515, #14263, #37680, #41841, #1857, #60679, #8999, #32014, #55033, #3340, #30524, #26330, #18834, #53541, #59208, #64850, #24843, #47861, #70882, #13518, #36556, #59569, #7884, #4843, #44822, #61802, #56900, #33901, #72752, #67464, #22168, #33158, #66713, #15015, #56152, #5212, #61428, #4468, #33526, #21056, #45194, #32774, #56526, #32393, #27457, #21429, #15760, #68204, #50472, #15388, #20679, #62167, #9755, #38424, #55782, #16501, #4098, #27840, #72368, #3717, #26716, #49736, #73486, #55408, #50847, #21792, #38051, #43698, #27091, #49351, #10120, #73861, #73121, #50107, #44452, #61051, #9373, #39541, #38799, #67834, #44079, #62537, #16126, #39164, #10491, #67091, #10864, #69700, #12711, #51595, #318 ),
 .UNSPECIFIED., .F., .F. ) 
 B_SPLINE_CURVE_WITH_KNOTS ( ( 3, 2, 2, 2, 2, 2, 2, 2, 2, 2, 2, 2, 2, 2, 2, 2, 2, 2, 2, 2, 2, 2, 2, 2, 2, 2, 2, 2, 2, 2, 2, 2, 2, 2, 2, 2, 2, 2, 2, 2, 2, 2, 2, 2, 2, 2, 2, 2, 2, 2, 2, 2, 2, 2, 2, 2, 2, 2, 2, 2, 2, 2, 2, 2, 2, 2, 2, 2, 2, 2, 2, 2, 2, 2, 2, 2, 2, 2, 2, 2, 2, 2, 2, 2, 2, 2, 2, 2, 2, 2, 2, 2, 2, 2, 2, 2, 2, 2, 2, 2, 2, 2, 2, 2, 2, 2, 2, 2, 2, 2, 2, 2, 2, 2, 2, 2, 2, 2, 2, 2, 2, 2, 2, 2, 2, 2, 2, 2, 2, 2, 2, 2, 2, 2, 2, 2, 2, 2, 2, 2, 2, 2, 2, 2, 2, 2, 2, 2, 2, 2, 2, 2, 2, 2, 2, 2, 2, 2, 2, 2, 2, 2, 2, 2, 2, 2, 2, 2, 2, 2, 2, 2, 2, 2, 3 ),
 ( 0.000000000000000000, 0.005681818181818181976, 0.01136363636363636395, 0.01704545454545454419, 0.02272727272727272790, 0.02840909090909090814, 0.03409090909090908839, 0.03977272727272727210, 0.04545454545454545581, 0.05113636363636363952, 0.05681818181818181629, 0.06250000000000000000, 0.06818181818181817677, 0.07386363636363636742, 0.07954545454545454419, 0.08522727272727272096, 0.09090909090909091161, 0.09659090909090908839, 0.1022727272727272790, 0.1079545454545454558, 0.1136363636363636326, 0.1193181818181818232, 0.1250000000000000000, 0.1306818181818181768, 0.1363636363636363535, 0.1420454545454545581, 0.1477272727272727348, 0.1534090909090909116, 0.1590909090909090884, 0.1647727272727272652, 0.1704545454545454419, 0.1761363636363636465, 0.1818181818181818232, 0.1875000000000000000, 0.1931818181818181768, 0.1988636363636363535, 0.2045454545454545581, 0.2102272727272727348, 0.2159090909090909116, 0.2215909090909090884, 0.2272727272727272652, 0.2329545454545454419, 0.2386363636363636465, 0.2443181818181818232, 0.2500000000000000000, 0.2556818181818181768, 0.2613636363636363535, 0.2670454545454545303, 0.2727272727272727071, 0.2784090909090908839, 0.2840909090909091161, 0.2897727272727272929, 0.2954545454545454697, 0.3011363636363636465, 0.3068181818181818232, 0.3125000000000000000, 0.3181818181818181768, 0.3238636363636363535, 0.3295454545454545303, 0.3352272727272727071, 0.3409090909090908839, 0.3465909090909091161, 0.3522727272727272929, 0.3579545454545454697, 0.3636363636363636465, 0.3693181818181818232, 0.3750000000000000000, 0.3806818181818181768, 0.3863636363636363535, 0.3920454545454545303, 0.3977272727272727071, 0.4034090909090908839, 0.4090909090909091161, 0.4147727272727272929, 0.4204545454545454697, 0.4261363636363636465, 0.4318181818181818232, 0.4375000000000000000, 0.4431818181818181768, 0.4488636363636363535, 0.4545454545454545303, 0.4602272727272727071, 0.4659090909090908839, 0.4715909090909091161, 0.4772727272727272929, 0.4829545454545454697, 0.4886363636363636465, 0.4943181818181818232, 0.5000000000000000000, 0.5056818181818182323, 0.5113636363636363535, 0.5170454545454545858, 0.5227272727272727071, 0.5284090909090909394, 0.5340909090909090606, 0.5397727272727272929, 0.5454545454545454142, 0.5511363636363636465, 0.5568181818181817677, 0.5625000000000000000, 0.5681818181818182323, 0.5738636363636363535, 0.5795454545454545858, 0.5852272727272727071, 0.5909090909090909394, 0.5965909090909090606, 0.6022727272727272929, 0.6079545454545454142, 0.6136363636363636465, 0.6193181818181817677, 0.6250000000000000000, 0.6306818181818182323, 0.6363636363636363535, 0.6420454545454545858, 0.6477272727272727071, 0.6534090909090909394, 0.6590909090909090606, 0.6647727272727272929, 0.6704545454545454142, 0.6761363636363636465, 0.6818181818181817677, 0.6875000000000000000, 0.6931818181818182323, 0.6988636363636363535, 0.7045454545454545858, 0.7102272727272727071, 0.7159090909090909394, 0.7215909090909090606, 0.7272727272727272929, 0.7329545454545454142, 0.7386363636363636465, 0.7443181818181817677, 0.7500000000000000000, 0.7556818181818182323, 0.7613636363636363535, 0.7670454545454545858, 0.7727272727272727071, 0.7784090909090909394, 0.7840909090909090606, 0.7897727272727272929, 0.7954545454545454142, 0.8011363636363636465, 0.8068181818181817677, 0.8125000000000000000, 0.8181818181818182323, 0.8238636363636363535, 0.8295454545454545858, 0.8352272727272727071, 0.8409090909090909394, 0.8465909090909090606, 0.8522727272727272929, 0.8579545454545454142, 0.8636363636363636465, 0.8693181818181817677, 0.8750000000000000000, 0.8806818181818182323, 0.8863636363636363535, 0.8920454545454545858, 0.8977272727272727071, 0.9034090909090910504, 0.9090909090909090606, 0.9147727272727272929, 0.9204545454545454142, 0.9261363636363636465, 0.9318181818181817677, 0.9375000000000000000, 0.9431818181818182323, 0.9488636363636363535, 0.9545454545454545858, 0.9602272727272727071, 0.9659090909090909394, 0.9715909090909090606, 0.9772727272727272929, 0.9829545454545454142, 0.9857954546051644895 ),
 .UNSPECIFIED. ) 
 CURVE ( )  GEOMETRIC_REPRESENTATION_ITEM ( )  RATIONAL_B_SPLINE_CURVE ( ( 1.000000000000000000, 0.9238795325112867385, 1.000000000000000000, 0.9238795325112867385, 1.000000000000000000, 0.9238795325112867385, 1.000000000000000000, 0.9238795325112867385, 1.000000000000000000, 0.9238795325112867385, 1.000000000000000000, 0.9238795325112867385, 1.000000000000000000, 0.9238795325112867385, 1.000000000000000000, 0.9238795325112867385, 1.000000000000000000, 0.9238795325112867385, 1.000000000000000000, 0.9238795325112867385, 1.000000000000000000, 0.9238795325112867385, 1.000000000000000000, 0.9238795325112867385, 1.000000000000000000, 0.9238795325112867385, 1.000000000000000000, 0.9238795325112867385, 1.000000000000000000, 0.9238795325112867385, 1.000000000000000000, 0.9238795325112867385, 1.000000000000000000, 0.9238795325112867385, 1.000000000000000000, 0.9238795325112867385, 1.000000000000000000, 0.9238795325112867385, 1.000000000000000000, 0.9238795325112867385, 1.000000000000000000, 0.9238795325112867385, 1.000000000000000000, 0.9238795325112867385, 1.000000000000000000, 0.9238795325112867385, 1.000000000000000000, 0.9238795325112867385, 1.000000000000000000, 0.9238795325112867385, 1.000000000000000000, 0.9238795325112867385, 1.000000000000000000, 0.9238795325112867385, 1.000000000000000000, 0.9238795325112867385, 1.000000000000000000, 0.9238795325112867385, 1.000000000000000000, 0.9238795325112867385, 1.000000000000000000, 0.9238795325112867385, 1.000000000000000000, 0.9238795325112867385, 1.000000000000000000, 0.9238795325112867385, 1.000000000000000000, 0.9238795325112867385, 1.000000000000000000, 0.9238795325112867385, 1.000000000000000000, 0.9238795325112867385, 1.000000000000000000, 0.9238795325112867385, 1.000000000000000000, 0.9238795325112867385, 1.000000000000000000, 0.9238795325112867385, 1.000000000000000000, 0.9238795325112867385, 1.000000000000000000, 0.9238795325112867385, 1.000000000000000000, 0.9238795325112867385, 1.000000000000000000, 0.9238795325112867385, 1.000000000000000000, 0.9238795325112867385, 1.000000000000000000, 0.9238795325112867385, 1.000000000000000000, 0.9238795325112867385, 1.000000000000000000, 0.9238795325112867385, 1.000000000000000000, 0.9238795325112867385, 1.000000000000000000, 0.9238795325112867385, 1.000000000000000000, 0.9238795325112867385, 1.000000000000000000, 0.9238795325112867385, 1.000000000000000000, 0.9238795325112867385, 1.000000000000000000, 0.9238795325112867385, 1.000000000000000000, 0.9238795325112867385, 1.000000000000000000, 0.9238795325112867385, 1.000000000000000000, 0.9238795325112867385, 1.000000000000000000, 0.9238795325112867385, 1.000000000000000000, 0.9238795325112867385, 1.000000000000000000, 0.9238795325112867385, 1.000000000000000000, 0.9238795325112867385, 1.000000000000000000, 0.9238795325112867385, 1.000000000000000000, 0.9238795325112867385, 1.000000000000000000, 0.9238795325112867385, 1.000000000000000000, 0.9238795325112867385, 1.000000000000000000, 0.9238795325112867385, 1.000000000000000000, 0.9238795325112867385, 1.000000000000000000, 0.9238795325112867385, 1.000000000000000000, 0.9238795325112867385, 1.000000000000000000, 0.9238795325112867385, 1.000000000000000000, 0.9238795325112867385, 1.000000000000000000, 0.9238795325112867385, 1.000000000000000000, 0.9238795325112867385, 1.000000000000000000, 0.9238795325112867385, 1.000000000000000000, 0.9238795325112867385, 1.000000000000000000, 0.9238795325112867385, 1.000000000000000000, 0.9238795325112867385, 1.000000000000000000, 0.9238795325112867385, 1.000000000000000000, 0.9238795325112867385, 1.000000000000000000, 0.9238795325112867385, 1.000000000000000000, 0.9238795325112867385, 1.000000000000000000, 0.9238795325112867385, 1.000000000000000000, 0.9238795325112867385, 1.000000000000000000, 0.9238795325112867385, 1.000000000000000000, 0.9238795325112867385, 1.000000000000000000, 0.9238795325112867385, 1.000000000000000000, 0.9238795325112867385, 1.000000000000000000, 0.9238795325112867385, 1.000000000000000000, 0.9238795325112867385, 1.000000000000000000, 0.9238795325112867385, 1.000000000000000000, 0.9238795325112867385, 1.000000000000000000, 0.9238795325112867385, 1.000000000000000000, 0.9238795325112867385, 1.000000000000000000, 0.9238795325112867385, 1.000000000000000000, 0.9238795325112867385, 1.000000000000000000, 0.9238795325112867385, 1.000000000000000000, 0.9238795325112867385, 1.000000000000000000, 0.9238795325112867385, 1.000000000000000000, 0.9238795325112867385, 1.000000000000000000, 0.9238795325112867385, 1.000000000000000000, 0.9238795325112867385, 1.000000000000000000, 0.9238795325112867385, 1.000000000000000000, 0.9238795325112867385, 1.000000000000000000, 0.9238795325112867385, 1.000000000000000000, 0.9238795325112867385, 1.000000000000000000, 0.9238795325112867385, 1.000000000000000000, 0.9238795325112867385, 1.000000000000000000, 0.9238795325112867385, 1.000000000000000000, 0.9238795325112867385, 1.000000000000000000, 0.9238795325112867385, 1.000000000000000000, 0.9238795325112867385, 1.000000000000000000, 0.9238795325112867385, 1.000000000000000000, 0.9238795325112867385, 1.000000000000000000, 0.9238795325112867385, 1.000000000000000000, 0.9238795325112867385, 1.000000000000000000, 0.9238795325112867385, 1.000000000000000000, 0.9238795325112867385, 1.000000000000000000, 0.9238795325112867385, 1.000000000000000000, 0.9238795325112867385, 1.000000000000000000, 0.9238795325112867385, 1.000000000000000000, 0.9238795325112867385, 1.000000000000000000, 0.9238795325112867385, 1.000000000000000000, 0.9238795325112867385, 1.000000000000000000, 0.9238795325112867385, 1.000000000000000000, 0.9238795325112867385, 1.000000000000000000, 0.9238795325112867385, 1.000000000000000000, 0.9238795325112867385, 1.000000000000000000, 0.9238795325112867385, 1.000000000000000000, 0.9238795325112867385, 1.000000000000000000, 0.9238795325112867385, 1.000000000000000000, 0.9238795325112867385, 1.000000000000000000, 0.9238795325112867385, 1.000000000000000000, 0.9238795325112867385, 1.000000000000000000, 0.9238795325112867385, 1.000000000000000000, 0.9238795325112867385, 1.000000000000000000, 0.9238795325112867385, 1.000000000000000000, 0.9238795325112867385, 1.000000000000000000, 0.9238795325112867385, 1.000000000000000000, 0.9238795325112867385, 1.000000000000000000, 0.9238795325112867385, 1.000000000000000000, 0.9238795325112867385, 1.000000000000000000, 0.9238795325112867385, 1.000000000000000000, 0.9238795325112867385, 1.000000000000000000, 0.9238795325112867385, 1.000000000000000000, 0.9238795325112867385, 1.000000000000000000, 0.9238795325112867385, 1.000000000000000000, 0.9238795325112867385, 1.000000000000000000, 0.9238795325112867385, 1.000000000000000000, 0.9238795325112867385, 1.000000000000000000, 0.9238795325112867385, 1.000000000000000000, 0.9238795325112867385, 1.000000000000000000, 0.9238795325112867385, 1.000000000000000000, 0.9238795325112867385, 1.000000000000000000, 0.9238795325112867385, 1.000000000000000000, 0.9238795325112867385, 1.000000000000000000, 0.9238795325112867385, 1.000000000000000000, 0.9238795325112867385, 1.000000000000000000, 0.9238795325112867385, 1.000000000000000000, 0.9238795325112867385, 1.000000000000000000, 0.9238795325112867385, 1.000000000000000000, 0.9238795325112867385, 1.000000000000000000, 0.9238795325112867385, 1.000000000000000000, 0.9238795325112867385, 1.000000000000000000, 0.9238795325112867385, 1.000000000000000000, 0.9238795325112867385, 1.000000000000000000, 0.9238795325112867385, 1.000000000000000000, 0.9238795325112867385, 1.000000000000000000, 0.9238795325112867385, 1.000000000000000000, 0.9238795325112867385, 1.000000000000000000, 0.9238795325112867385, 1.000000000000000000, 0.9238795325112867385, 1.000000000000000000, 0.9238795325112867385, 1.000000000000000000, 0.9238795325112867385, 1.000000000000000000, 0.9238795325112867385, 1.000000000000000000, 0.9619397654556969268, 0.9619397662556434803 ) ) 
 REPRESENTATION_ITEM ( '' )  );
#71725 = CARTESIAN_POINT ( 'NONE',  ( 11.00000000000010658, 4.556349186103942017, 73.84374999999997158 ) ) ;
#71726 = EDGE_CURVE ( 'NONE', #64786, #38109, #53629, .T. ) ;
#71727 = CARTESIAN_POINT ( 'NONE',  ( 3.313708498984762496, 23.53124999590322375, 7.999999999999998224 ) ) ;
#71728 = CARTESIAN_POINT ( 'NONE',  ( 2.445694354108783664, 202.3125000013656063, 144.4456943541088663 ) ) ;
#71729 = DIRECTION ( 'NONE',  ( -0.000000000000000000, 1.000000000000000000, -0.000000000000000000 ) ) ;
#71730 = CARTESIAN_POINT ( 'NONE',  ( 11.00000000000000000, 1.347111479062088405E-15, 85.75000000000000000 ) ) ;
#71731 = CARTESIAN_POINT ( 'NONE',  ( -8.311093377946834337, 249.8437500034139589, 8.311093377946837890 ) ) ;
#71732 = CARTESIAN_POINT ( 'NONE',  ( -11.00000000000000000, 0.000000000000000000, 91.18750000409677625 ) ) ;
#71733 = CARTESIAN_POINT ( 'NONE',  ( -7.778174593052020747, -7.778174593052023411, 113.6875000000000000 ) ) ;
#71734 = CARTESIAN_POINT ( 'NONE',  ( -11.35316468750000141, 3.281249996586016238, -1.390361679473963753E-15 ) ) ;
#71735 = CARTESIAN_POINT ( 'NONE',  ( 2.977408999572646486, 7.188101187499992051, 5.892802781871753659 ) ) ;
#71736 = CARTESIAN_POINT ( 'NONE',  ( -11.35316468750000141, 198.8020833299193839, 3.042071309553159963 ) ) ;
#71737 = CYLINDRICAL_SURFACE ( 'NONE', #49322, 7.999999999999991118 ) ;
#71738 = CARTESIAN_POINT ( 'NONE',  ( 4.541265875000001451, 8.249999998634406140, 1.881053915767124440 ) ) ;
#71739 = CARTESIAN_POINT ( 'NONE',  ( -8.000000000000000000, 99.68750000409677625, 0.000000000000000000 ) ) ;
#71741 = CARTESIAN_POINT ( 'NONE',  ( -2.775557561562891351E-14, 210.0000000000000284, 142.0000000000000568 ) ) ;
#71740 = DIRECTION ( 'NONE',  ( 0.000000000000000000, 0.000000000000000000, -1.000000000000000000 ) ) ;
#71742 = ORIENTED_EDGE ( 'NONE', *, *, #67540, .F. ) ;
#71743 = CARTESIAN_POINT ( 'NONE',  ( 3.458734124999960358, 202.6250000013656063, 143.4326545832176976 ) ) ;
#71744 = CARTESIAN_POINT ( 'NONE',  ( 8.311093377946837890, 46.71874999658602690, -8.311093377946837890 ) ) ;
#71745 = CARTESIAN_POINT ( 'NONE',  ( -11.00000000000000000, 4.556349186104045934, 98.59375000409677625 ) ) ;
#71746 = AXIS2_PLACEMENT_3D ( 'NONE', #58734, #17237, #64015 ) ;
#71747 = CARTESIAN_POINT ( 'NONE',  ( 4.556349186104052151, -10.99999999999999822, 106.6562500040967905 ) ) ;
#71748 = CARTESIAN_POINT ( 'NONE',  ( -30.44569435410875968, 199.8125000013656063, 172.4456943541092642 ) ) ;
#71749 = DIRECTION ( 'NONE',  ( 1.000000000000000000, 0.000000000000000000, 0.000000000000000000 ) ) ;
#71751 = CARTESIAN_POINT ( 'NONE',  ( -8.660254037844387298, 229.5833333333333712, -4.999999999999999112 ) ) ;
#71750 = CARTESIAN_POINT ( 'NONE',  ( 1.320432766682874540E-15, 123.0312500020483810, 7.188101187500000044 ) ) ;
#71752 = CARTESIAN_POINT ( 'NONE',  ( 7.778174593052021635, 7.778174593052023411, 87.43749999999998579 ) ) ;
#71753 = CARTESIAN_POINT ( 'NONE',  ( -3.042071309553173730, 124.3229166632526983, 11.35316468749999785 ) ) ;
#71754 = ADVANCED_FACE ( 'NONE', ( #27054 ), #50066, .T. ) ;
#71755 = CARTESIAN_POINT ( 'NONE',  ( -8.660254037844390851, 94.79166665983871098, 4.999999999999998224 ) ) ;
#71756 = VECTOR ( 'NONE', #66904, 1000.000000000000000 ) ;
#71757 = CARTESIAN_POINT ( 'NONE',  ( -5.082755093536325930, 124.3437500020483952, -5.082755093536325930 ) ) ;
#71758 = CARTESIAN_POINT ( 'NONE',  ( 3.211159895383560947, 21.31249999863440792, 3.211159895383562723 ) ) ;
#71759 = CARTESIAN_POINT ( 'NONE',  ( -24.00000000000000711, 204.8125000000000000, 168.3431457505080289 ) ) ;
#71760 = LINE ( 'NONE', #24992, #54684 ) ;
#71761 = ORIENTED_EDGE ( 'NONE', *, *, #16828, .F. ) ;
#71762 = CARTESIAN_POINT ( 'NONE',  ( -1.224646799147353454E-15, 225.9999999999999432, 10.00000000000000178 ) ) ;
#71763 = ORIENTED_EDGE ( 'NONE', *, *, #66900, .F. ) ;
#71764 = CARTESIAN_POINT ( 'NONE',  ( 2.765530957081996366, 292.2968750017070647, -6.676582343750003368 ) ) ;
#71765 = DIRECTION ( 'NONE',  ( 0.000000000000000000, 0.000000000000000000, 1.000000000000000000 ) ) ;
#71766 = CARTESIAN_POINT ( 'NONE',  ( -5.656854249492375253, 5.656854249492375253, 8.330302783920144449 ) ) ;
#71767 = CARTESIAN_POINT ( 'NONE',  ( 11.35316468749999963, 165.9895833299193271, -3.042071309553165293 ) ) ;
#71768 = DIRECTION ( 'NONE',  ( 0.000000000000000000, 0.9659258262890700886, 0.2588190451025146888 ) ) ;
#71769 = CARTESIAN_POINT ( 'NONE',  ( 4.000000000000015099, 198.5625000000000000, 196.3431457505076594 ) ) ;
#71770 = CARTESIAN_POINT ( 'NONE',  ( -7.320508075688805683, 191.8750000000000568, -7.320508075688805683 ) ) ;
#71771 = CARTESIAN_POINT ( 'NONE',  ( 7.204075437095966983, 7.204075437095967871, 103.4687500020483668 ) ) ;
#71772 = ORIENTED_EDGE ( 'NONE', *, *, #46697, .F. ) ;
#71773 = CARTESIAN_POINT ( 'NONE',  ( 0.6547826978327068170, 49.91450260127339078, -40.68974341348084778 ) ) ;
#71774 = DIRECTION ( 'NONE',  ( 0.000000000000000000, 0.8536788251725985210, 0.5207998305029790664 ) ) ;
#71775 = CARTESIAN_POINT ( 'NONE',  ( 3.042071309553159519, 155.0520833299193271, 11.35316468750000141 ) ) ;
#71776 = CARTESIAN_POINT ( 'NONE',  ( -10.67658234375000070, 219.6093750017069794, 0.000000000000000000 ) ) ;
#71777 = CARTESIAN_POINT ( 'NONE',  ( -1.432654583217608080, 207.8750000013656063, 201.4587341250000350 ) ) ;
#71778 = CARTESIAN_POINT ( 'NONE',  ( -6.238412754330611322E-16, 10.18810118749999916, 73.65625000204836681 ) ) ;
#71779 = CARTESIAN_POINT ( 'NONE',  ( 8.311093377946837890, 66.71874999658602690, -8.311093377946837890 ) ) ;
#71780 = ORIENTED_EDGE ( 'NONE', *, *, #56695, .F. ) ;
#71781 = CARTESIAN_POINT ( 'NONE',  ( -10.18810118749999916, 0.000000000000000000, 117.1562500020483810 ) ) ;
#71782 = CARTESIAN_POINT ( 'NONE',  ( 4.541265875000002339, 10.49999999863440969, -1.881053915767121776 ) ) ;
#71783 = CARTESIAN_POINT ( 'NONE',  ( -3.317071493978878571, 8.008118988124991233, 11.23186528394062833 ) ) ;
#71784 = ORIENTED_EDGE ( 'NONE', *, *, #66876, .T. ) ;
#71785 = CARTESIAN_POINT ( 'NONE',  ( -5.082755093536326818, 19.40624999795161543, 5.082755093536325042 ) ) ;
#71786 = CARTESIAN_POINT ( 'NONE',  ( 6.000000000000003553, 289.6250000034140726, -2.485281374238571761 ) ) ;
#71787 = CARTESIAN_POINT ( 'NONE',  ( 4.000000000000016875, 202.4375000000000568, 199.6568542494924259 ) ) ;
#71788 = CARTESIAN_POINT ( 'NONE',  ( 4.401442555609581635E-16, 10.21874999795161187, -7.188101187500000044 ) ) ;
#71789 = CARTESIAN_POINT ( 'NONE',  ( -5.082755093536319713, 5.082755093536319713, 1.299052781871753215 ) ) ;
#71790 = CARTESIAN_POINT ( 'NONE',  ( 10.18810118750000093, -4.220049686691933921, 68.31250000204838102 ) ) ;
#71791 = FACE_OUTER_BOUND ( 'NONE', #52440, .T. ) ;
#71792 = CARTESIAN_POINT ( 'NONE',  ( 4.000000000000001776, 5.812499997268812280, -1.656854249492381248 ) ) ;
#71793 = VERTEX_POINT ( 'NONE', #3676 ) ;
#71794 = CARTESIAN_POINT ( 'NONE',  ( 2.754378923186476579E-14, 206.1875000013656063, 194.5412658750000219 ) ) ;
#71795 = CIRCLE ( 'NONE', #54930, 12.00000000000000355 ) ;
#71796 = EDGE_CURVE ( 'NONE', #26622, #30484, #4423, .T. ) ;
#71797 = CARTESIAN_POINT ( 'NONE',  ( -23.99999999999998934, 197.8750000027312126, 170.0000000000002842 ) ) ;
#71798 = CARTESIAN_POINT ( 'NONE',  ( 4.541265875000001451, 7.249999998634408804, 1.881053915767124440 ) ) ;
#71799 = CARTESIAN_POINT ( 'NONE',  ( 5.082755093536325042, 113.0937500020483810, -5.082755093536325930 ) ) ;
#71800 = AXIS2_PLACEMENT_3D ( 'NONE', #40304, #62938, #50496 ) ;
#71801 = CYLINDRICAL_SURFACE ( 'NONE', #69354, 3.999999999999976019 ) ;
#71802 = CARTESIAN_POINT ( 'NONE',  ( 2.977408999572650927, -7.188101187499990274, 22.95530278187175455 ) ) ;
#71803 = VERTEX_POINT ( 'NONE', #39124 ) ;
#71804 = EDGE_CURVE ( 'NONE', #14049, #51233, #48274, .T. ) ;
#71805 = CARTESIAN_POINT ( 'NONE',  ( -4.000000000000002665, 21.56250000000000355, 1.656854249492380582 ) ) ;
#71806 = VERTEX_POINT ( 'NONE', #27794 ) ;
#71807 = CARTESIAN_POINT ( 'NONE',  ( 1.871523826299183495E-15, -10.18810118749999916, 116.0312500020483810 ) ) ;
#71808 = LINE ( 'NONE', #50665, #31610 ) ;
#71809 = CARTESIAN_POINT ( 'NONE',  ( -3.458734124999959914, 208.3750000013656063, 196.5673454167823877 ) ) ;
#71810 = CARTESIAN_POINT ( 'NONE',  ( 26.56734541678233086, 202.0000000013656063, 166.5412658749999650 ) ) ;
#71811 = CARTESIAN_POINT ( 'NONE',  ( -1.836970198721029983E-15, 68.75000000000000000, 10.00000000000000178 ) ) ;
#71812 = CARTESIAN_POINT ( 'NONE',  ( -7.188101187500001821, 92.93750000204839523, -2.977408999572650483 ) ) ;
#71813 = CARTESIAN_POINT ( 'NONE',  ( -6.000000000000003553, 294.9375000000000000, -2.485281374238571317 ) ) ;
#71814 = CARTESIAN_POINT ( 'NONE',  ( 2.170320029210518253, -51.35721532638415709, -48.60044191894306920 ) ) ;
#71815 = ORIENTED_EDGE ( 'NONE', *, *, #18831, .F. ) ;
#71816 = CARTESIAN_POINT ( 'NONE',  ( -3.042071309553166181, 227.8645833367473301, -11.35316468749999608 ) ) ;
#71817 = CARTESIAN_POINT ( 'NONE',  ( 3.313708498984761608, 12.28125000000000178, -8.000000000000000000 ) ) ;
#71818 = CARTESIAN_POINT ( 'NONE',  ( 1.656854249492347719, 200.9375000027312410, 146.0000000000000284 ) ) ;
#71819 = CYLINDRICAL_SURFACE ( 'NONE', #2074, 3.999999999999976019 ) ;
#71820 = DIRECTION ( 'NONE',  ( -0.000000000000000000, 1.000000000000000000, -4.476705744456276341E-16 ) ) ;
#71821 = CARTESIAN_POINT ( 'NONE',  ( 10.00000000000000178, 262.2916666666666288, 2.679491924311222739 ) ) ;
#71822 = B_SPLINE_CURVE_WITH_KNOTS ( 'NONE', 3,
 ( #63399, #34021, #27964, #44947 ),
 .UNSPECIFIED., .F., .F.,
 ( 4, 4 ),
 ( 0.000000000000000000, 1.000000000000000000 ),
 .UNSPECIFIED. ) ;
#71823 = FACE_OUTER_BOUND ( 'NONE', #6043, .T. ) ;
#71824 = CARTESIAN_POINT ( 'NONE',  ( 6.123233995736767268E-16, 186.2500000000000000, -10.00000000000000178 ) ) ;
#71825 = B_SPLINE_CURVE_WITH_KNOTS ( 'NONE', 3,
 ( #74550, #17575, #12650, #5159, #23607, #11922, #40219, #22859, #45875, #35324, #23237, #68889, #995, #74173, #58336, #34207, #56838, #6640, #52659, #18323, #57969, #51916 ),
 .UNSPECIFIED., .F., .F.,
 ( 4, 2, 2, 2, 2, 2, 2, 2, 2, 2, 4 ),
 ( 0.000000000000000000, 0.001156727053362399758, 0.001735090580043607876, 0.002313454106724815995, 0.003470181160087273432, 0.004048544686768501717, 0.004626908213449730869, 0.005783635266812230807, 0.006940362320174731613, 0.008097089373537232418, 0.009253816426899732356 ),
 .UNSPECIFIED. ) ;
#71826 = CARTESIAN_POINT ( 'NONE',  ( 9.999999999999998224, 240.8333333401612890, -2.679491924311229401 ) ) ;
#71827 = CARTESIAN_POINT ( 'NONE',  ( 5.082755093536318824, 5.082755093536319713, 23.79905278187175455 ) ) ;
#71828 = CARTESIAN_POINT ( 'NONE',  ( -11.35316468750000141, 153.8020833299192986, 3.042071309553159963 ) ) ;
#71829 = CARTESIAN_POINT ( 'NONE',  ( 7.999999999999992895, -3.313708498984756279, 22.67405278392014978 ) ) ;
#71830 = CARTESIAN_POINT ( 'NONE',  ( 4.999999999999997335, 261.4583333401613459, -8.660254037844387298 ) ) ;
#71833 = CARTESIAN_POINT ( 'NONE',  ( 25.17157287525378351, 203.8750000000000284, 172.8284271247460424 ) ) ;
#71832 = CARTESIAN_POINT ( 'NONE',  ( -28.00000000000002842, 206.0000000000000284, 166.0000000000003695 ) ) ;
#71831 = CARTESIAN_POINT ( 'NONE',  ( 31.99999999999998579, 203.1875000000000284, 171.6568542494923122 ) ) ;
#71834 = VERTEX_POINT ( 'NONE', #68162 ) ;
#71835 = CARTESIAN_POINT ( 'NONE',  ( -9.832129032723420536, 9.010416663252684089, 5.676582343749997150 ) ) ;
#71836 = CARTESIAN_POINT ( 'NONE',  ( 2.828427124746209831, 200.5000000027312126, 200.8284271247462129 ) ) ;
#71837 = CARTESIAN_POINT ( 'NONE',  ( 2.990854866087931718, -10.11452374054218417, -70.45725801587312276 ) ) ;
#71838 = CARTESIAN_POINT ( 'NONE',  ( 2.775557561562891351E-14, 271.9999999999999432, 151.0000000000000568 ) ) ;
#71839 = CARTESIAN_POINT ( 'NONE',  ( -3.458734125000016313, 207.8750000013656063, 140.5673454167823593 ) ) ;
#71840 = CARTESIAN_POINT ( 'NONE',  ( 7.320508075688771044, 46.24999999317202537, 7.320508075688775484 ) ) ;
#71841 = CARTESIAN_POINT ( 'NONE',  ( -7.188101187500000044, 107.6562500020483810, 0.000000000000000000 ) ) ;
#71842 = CARTESIAN_POINT ( 'NONE',  ( -3.211159895383561391, 5.812499998634407028, -3.211159895383561835 ) ) ;
#71843 = CARTESIAN_POINT ( 'NONE',  ( 2.069125466538116243, 65.90280720052993502, -26.36412295902648850 ) ) ;
#71844 = CARTESIAN_POINT ( 'NONE',  ( 5.656854249492376141, -5.656854249492374365, 7.392802779823366421 ) ) ;
#71846 = CARTESIAN_POINT ( 'NONE',  ( -1.469576158976823947E-15, 26.62500000000000355, 8.000000000000000000 ) ) ;
#71845 = CYLINDRICAL_SURFACE ( 'NONE', #51589, 10.00000000000000178 ) ;
#71847 = VERTEX_POINT ( 'NONE', #39498 ) ;
#71848 =( BOUNDED_CURVE ( )  B_SPLINE_CURVE ( 2, ( #14598, #60636, #31969, #9332, #73445, #21752, #67794, #16085, #39120 ),
 .UNSPECIFIED., .F., .F. ) 
 B_SPLINE_CURVE_WITH_KNOTS ( ( 3, 2, 2, 2, 3 ),
 ( 0.5000000000000000000, 0.5065789473684210176, 0.5131578947368422572, 0.5197368421052632748, 0.5263157894736842923 ),
 .UNSPECIFIED. ) 
 CURVE ( )  GEOMETRIC_REPRESENTATION_ITEM ( )  RATIONAL_B_SPLINE_CURVE ( ( 1.000000000000000000, 0.9238795325112867385, 1.000000000000000000, 0.9238795325112867385, 1.000000000000000000, 0.9238795325112867385, 1.000000000000000000, 0.9238795325112854062, 1.000000000000001332 ) ) 
 REPRESENTATION_ITEM ( '' )  );
#71849 =( BOUNDED_CURVE ( )  B_SPLINE_CURVE ( 2, ( #18490, #48255, #69804, #31663, #60703, #15040, #67114, #72391, #49374 ),
 .UNSPECIFIED., .F., .F. ) 
 B_SPLINE_CURVE_WITH_KNOTS ( ( 3, 2, 2, 2, 3 ),
 ( 0.3333333333333336479, 0.3416666666666670071, 0.3500000000000003109, 0.3583333333333336701, 0.3666666666666669738 ),
 .UNSPECIFIED. ) 
 CURVE ( )  GEOMETRIC_REPRESENTATION_ITEM ( )  RATIONAL_B_SPLINE_CURVE ( ( 0.9999999999999970024, 0.9238795325112897361, 1.000000000000000000, 0.9238795325112867385, 1.000000000000000000, 0.9238795325112867385, 1.000000000000000000, 0.9238795325112837409, 1.000000000000003109 ) ) 
 REPRESENTATION_ITEM ( '' )  );
#71850 = CARTESIAN_POINT ( 'NONE',  ( -4.999999999999952927, -68.60357193678709109, 20.85024232999324667 ) ) ;
#71851 = CARTESIAN_POINT ( 'NONE',  ( -2.828427124746208943, 196.6250000000000284, 144.8284271247462129 ) ) ;
#71852 = CARTESIAN_POINT ( 'NONE',  ( 3.042071309553173286, 235.6770833367473017, 11.35316468749999608 ) ) ;
#71853 = CARTESIAN_POINT ( 'NONE',  ( 9.832129032723416984, 135.3645833299193555, 5.676582343750006032 ) ) ;
#71854 = ORIENTED_EDGE ( 'NONE', *, *, #10436, .F. ) ;
#71855 = CYLINDRICAL_SURFACE ( 'NONE', #34365, 3.999999999999976019 ) ;
#71856 = CARTESIAN_POINT ( 'NONE',  ( 1.871523826299183495E-15, -10.18810118749999916, 98.03125000204838102 ) ) ;
#71857 = CARTESIAN_POINT ( 'NONE',  ( 0.000000000000000000, 0.000000000000000000, 0.000000000000000000 ) ) ;
#71858 = CARTESIAN_POINT ( 'NONE',  ( 1.432654583217664701, 196.0000000013656347, 201.4587341250000065 ) ) ;
#71859 = DIRECTION ( 'NONE',  ( -0.000000000000000000, 1.000000000000000000, -0.000000000000000000 ) ) ;
#71861 = CARTESIAN_POINT ( 'NONE',  ( 8.311093377946837890, 121.4062499965860127, -8.311093377946837890 ) ) ;
#71860 = CARTESIAN_POINT ( 'NONE',  ( 3.115309517308847198, 219.9999999999999716, 10.23006779404638777 ) ) ;
#71862 = AXIS2_PLACEMENT_3D ( 'NONE', #6787, #36565, #35104 ) ;
#71863 = CARTESIAN_POINT ( 'NONE',  ( -26.34314575050758478, 207.5625000000000284, 174.0000000000003411 ) ) ;
#71864 = DIRECTION ( 'NONE',  ( 0.000000000000000000, 0.000000000000000000, 1.000000000000000000 ) ) ;
#71865 = ORIENTED_EDGE ( 'NONE', *, *, #25924, .T. ) ;
#71866 = CARTESIAN_POINT ( 'NONE',  ( 11.00000000000000000, 1.347111479062088405E-15, 76.74999999999998579 ) ) ;
#71867 = CARTESIAN_POINT ( 'NONE',  ( -11.00000000000000000, 0.000000000000000000, 83.68750000409677625 ) ) ;
#71868 = CARTESIAN_POINT ( 'NONE',  ( -8.311093377946841443, 99.21874999658601268, 8.311093377946834337 ) ) ;
#71869 = CARTESIAN_POINT ( 'NONE',  ( 2.445694354108839619, 206.8125000013656063, 200.4456943541088663 ) ) ;
#71870 = CARTESIAN_POINT ( 'NONE',  ( -5.082755093536325042, 20.90624999795161543, -5.082755093536325930 ) ) ;
#71871 = CARTESIAN_POINT ( 'NONE',  ( 10.18810118749999916, 4.220049686691935698, 88.37500000204838102 ) ) ;
#71872 = CARTESIAN_POINT ( 'NONE',  ( -11.35316468750000141, 18.59374999658601979, -1.390361679473963753E-15 ) ) ;
#71873 = VERTEX_POINT ( 'NONE', #9336 ) ;
#71874 = FACE_OUTER_BOUND ( 'NONE', #70841, .T. ) ;
#71875 = CARTESIAN_POINT ( 'NONE',  ( -5.662595241051935346, 5.662595241051935346, 27.82561528394063188 ) ) ;
#71876 = LINE ( 'NONE', #19091, #23383 ) ;
#71877 = LINE ( 'NONE', #19828, #68753 ) ;
#71878 = CARTESIAN_POINT ( 'NONE',  ( 5.082755093536325930, 3.656249997951610542, -5.082755093536325930 ) ) ;
#71879 = CARTESIAN_POINT ( 'NONE',  ( 2.765530957081996366, 290.1406250017069510, -6.676582343750003368 ) ) ;
#71880 = CARTESIAN_POINT ( 'NONE',  ( 2.995737153994495916, 51.55860531535900293, -48.67776149471415437 ) ) ;
#71881 = CARTESIAN_POINT ( 'NONE',  ( 5.676582343749993598, 225.2604166632526983, 9.832129032723422313 ) ) ;
#71882 = VERTEX_POINT ( 'NONE', #62493 ) ;
#71883 = EDGE_CURVE ( 'NONE', #37723, #13141, #70488, .T. ) ;
#71884 = CARTESIAN_POINT ( 'NONE',  ( 11.35316468749999785, 145.8854166632526983, 3.042071309553174174 ) ) ;
#71885 = AXIS2_PLACEMENT_3D ( 'NONE', #50920, #39980, #39236 ) ;
#71886 = CARTESIAN_POINT ( 'NONE',  ( -7.204075437095965206, -7.204075437095968759, 84.34375000204836681 ) ) ;
#71887 = EDGE_CURVE ( 'NONE', #25519, #65440, #5173, .T. ) ;
#71888 = CARTESIAN_POINT ( 'NONE',  ( -27.99999999999996447, 199.9375000013656063, 173.4587341250003760 ) ) ;
#71889 = CARTESIAN_POINT ( 'NONE',  ( -7.999999999999991118, 3.313708498984757167, 21.73655277982336642 ) ) ;
#71890 = CARTESIAN_POINT ( 'NONE',  ( -1.881053915767121554, 11.74999999863440792, -4.541265875000002339 ) ) ;
#71891 = EDGE_LOOP ( 'NONE', ( #16402, #44350, #41279, #18254 ) ) ;
#71892 = CARTESIAN_POINT ( 'NONE',  ( 2.828427124746209831, 201.5000000027312126, 200.8284271247462129 ) ) ;
#71893 = EDGE_CURVE ( 'NONE', #56676, #57455, #28446, .T. ) ;
#71894 = CARTESIAN_POINT ( 'NONE',  ( 1.432654583217608080, 199.8750000013655779, 138.5412658750000503 ) ) ;
#71895 = CARTESIAN_POINT ( 'NONE',  ( 2.828427124746152987, 203.2500000027312126, 139.1715728752538723 ) ) ;
#71896 = SPHERICAL_SURFACE ( 'NONE', #39187, 15.99999999999998579 ) ;
#71897 = VERTEX_POINT ( 'NONE', #6291 ) ;
#71898 = CARTESIAN_POINT ( 'NONE',  ( 2.977408999572650927, 5.249999997951610986, -7.188101187500000933 ) ) ;
#71899 = CARTESIAN_POINT ( 'NONE',  ( 3.313708498984762496, -7.999999999999989342, 8.986552783920146226 ) ) ;
#71900 = AXIS2_PLACEMENT_3D ( 'NONE', #23588, #59411, #46598 ) ;
#71901 = DIRECTION ( 'NONE',  ( 0.000000000000000000, 0.000000000000000000, 1.000000000000000000 ) ) ;
#71902 = CARTESIAN_POINT ( 'NONE',  ( 11.35316468749999785, 190.5729166632526699, 3.042071309553174174 ) ) ;
#71903 = CARTESIAN_POINT ( 'NONE',  ( 5.082755093536326818, 111.5937500020483810, 5.082755093536325042 ) ) ;
#71904 = PRODUCT_DEFINITION_FORMATION_WITH_SPECIFIED_SOURCE ( 'ANY', '', #42631, .NOT_KNOWN. ) ;
#71905 = CARTESIAN_POINT ( 'NONE',  ( 7.594050593750000466, 0.2343749989758049379, 0.000000000000000000 ) ) ;
#71906 = CARTESIAN_POINT ( 'NONE',  ( -2.765530957081996810, 293.2656250017068942, -6.676582343750002480 ) ) ;
#71908 = CARTESIAN_POINT ( 'NONE',  ( -7.347880794884122694E-16, 15.49999999726881406, 4.000000000000001776 ) ) ;
#71907 = CARTESIAN_POINT ( 'NONE',  ( 10.00000000000000178, 132.0833333265053398, -2.679491924311226736 ) ) ;
#71909 = ITEM_DEFINED_TRANSFORMATION ( 'NONE', 'NONE', #9183,  #57354 ) ;
#71910 = ORIENTED_EDGE ( 'NONE', *, *, #11098, .F. ) ;
#71911 = CARTESIAN_POINT ( 'NONE',  ( -3.042071309553166181, 233.1770833367473017, -11.35316468749999608 ) ) ;
#71912 = CARTESIAN_POINT ( 'NONE',  ( 1.320432766682872962E-15, -7.188101187499992051, 3.361552781871751883 ) ) ;
#71913 = CARTESIAN_POINT ( 'NONE',  ( 10.00000000000000000, 166.6666666598387110, 2.679491924311235618 ) ) ;
#71914 = CARTESIAN_POINT ( 'NONE',  ( 7.999999999999304556, -3.314968910423997278E-06, 15.26780269013280034 ) ) ;
#71915 = CARTESIAN_POINT ( 'NONE',  ( 2.445694354108839175, 200.3125000013656063, 195.5543056458912190 ) ) ;
#71916 = VERTEX_POINT ( 'NONE', #22879 ) ;
#71917 = CARTESIAN_POINT ( 'NONE',  ( -10.99999999999999645, 218.9106836093509116, 2.947441116742358425 ) ) ;
#71918 = CARTESIAN_POINT ( 'NONE',  ( 5.656854249492381470, 95.56250000000000000, 5.656854249492379694 ) ) ;
#71919 = CARTESIAN_POINT ( 'NONE',  ( -5.676582343749998039, 112.7604166632526841, -9.832129032723420536 ) ) ;
#71920 = DIRECTION ( 'NONE',  ( 0.000000000000000000, 0.000000000000000000, -1.000000000000000000 ) ) ;
#71921 = CARTESIAN_POINT ( 'NONE',  ( -11.00000000000000000, 4.556349186104045934, 78.90624999999998579 ) ) ;
#71924 = DIRECTION ( 'NONE',  ( 0.000000000000000000, -1.000000000000000000, 0.000000000000000000 ) ) ;
#71923 = CARTESIAN_POINT ( 'NONE',  ( 24.54126587499999346, 200.1875000013656063, 169.9999999999999432 ) ) ;
#71922 = CARTESIAN_POINT ( 'NONE',  ( 31.45873412499999233, 198.9375000013655779, 169.9999999999999432 ) ) ;
#71925 = VERTEX_POINT ( 'NONE', #47370 ) ;
#71926 = CARTESIAN_POINT ( 'NONE',  ( 5.656854249492381470, 100.0625000000000000, 5.656854249492379694 ) ) ;
#71927 = CARTESIAN_POINT ( 'NONE',  ( -11.90180034005860144, 227.9280165645365628, -15.80450607135647623 ) ) ;
#71928 = CARTESIAN_POINT ( 'NONE',  ( 1.432654583217607192, 200.2500000013656631, 145.4587341250000634 ) ) ;
#71929 = VECTOR ( 'NONE', #4063, 1000.000000000000000 ) ;
#71930 = CARTESIAN_POINT ( 'NONE',  ( 30.44569435410879166, 203.8125000013656063, 172.4456943541087526 ) ) ;
#71931 = CARTESIAN_POINT ( 'NONE',  ( -7.778174593052020747, -7.778174593052023411, 113.8750000040967763 ) ) ;
#71932 = CARTESIAN_POINT ( 'NONE',  ( -11.35316468750000141, 188.5937499965860127, -1.390361679473963753E-15 ) ) ;
#71933 = CARTESIAN_POINT ( 'NONE',  ( 7.188101187500002709, 90.68750000204838102, 2.977408999572649151 ) ) ;
#71934 = DIRECTION ( 'NONE',  ( 0.000000000000000000, 0.000000000000000000, 1.000000000000000000 ) ) ;
#71935 = CARTESIAN_POINT ( 'NONE',  ( 2.780723358947928197E-16, 15.56249999863440614, -4.541265875000002339 ) ) ;
#71936 = CARTESIAN_POINT ( 'NONE',  ( 24.54126587499998280, 198.5000000013656063, 171.4326545832175555 ) ) ;
#71937 = CARTESIAN_POINT ( 'NONE',  ( 7.999999999999991118, 3.313708498984757611, 25.67405277982336997 ) ) ;
#71938 = LINE ( 'NONE', #54613, #20672 ) ;
#71939 = CARTESIAN_POINT ( 'NONE',  ( 8.311093377946837890, 76.40624999658602690, -8.311093377946837890 ) ) ;
#71940 = ORIENTED_EDGE ( 'NONE', *, *, #69028, .F. ) ;
#71941 = DIRECTION ( 'NONE',  ( -1.000000000000000000, -0.000000000000000000, -0.000000000000000000 ) ) ;
#71942 = DIRECTION ( 'NONE',  ( 0.000000000000000000, 0.000000000000000000, 1.000000000000000000 ) ) ;
#71943 = CARTESIAN_POINT ( 'NONE',  ( -3.313708498984789141, 108.4062500040967763, -7.999999999999974243 ) ) ;
#71944 = CARTESIAN_POINT ( 'NONE',  ( -3.673940397442060854E-16, 289.8125000034140157, -6.000000000000001776 ) ) ;
#71945 = CARTESIAN_POINT ( 'NONE',  ( 9.832129032723416984, 85.36458332991936970, 5.676582343750006032 ) ) ;
#71946 = ORIENTED_EDGE ( 'NONE', *, *, #12875, .F. ) ;
#71947 = CARTESIAN_POINT ( 'NONE',  ( 10.18810118749999916, 1.247682550866122264E-15, 85.28125000204836681 ) ) ;
#71948 = CARTESIAN_POINT ( 'NONE',  ( -10.18810118749999916, 4.220049686691934809, 111.0625000020483810 ) ) ;
#71950 = CARTESIAN_POINT ( 'NONE',  ( 3.042071309553167513, 66.82291666325265567, -11.35316468749999785 ) ) ;
#71949 = DIRECTION ( 'NONE',  ( 0.000000000000000000, 0.000000000000000000, 1.000000000000000000 ) ) ;
#71951 = CARTESIAN_POINT ( 'NONE',  ( -4.898587196589407898E-16, 7.999999999999991118, 21.64280278392014623 ) ) ;
#71952 = CARTESIAN_POINT ( 'NONE',  ( -1.895132620089670095, 194.6589491196967003, 138.8604257725760931 ) ) ;
#71953 =( BOUNDED_CURVE ( )  B_SPLINE_CURVE ( 2, ( #74134, #34165, #17530, #51492, #63932, #33798, #22435, #45831, #579 ),
 .UNSPECIFIED., .F., .F. ) 
 B_SPLINE_CURVE_WITH_KNOTS ( ( 3, 2, 2, 2, 3 ),
 ( 0.6931818181818182323, 0.6988636363636363535, 0.7045454545454545858, 0.7102272727272727071, 0.7159090909090909394 ),
 .UNSPECIFIED. ) 
 CURVE ( )  GEOMETRIC_REPRESENTATION_ITEM ( )  RATIONAL_B_SPLINE_CURVE ( ( 1.000000000000000000, 0.9238795325112867385, 1.000000000000000000, 0.9238795325112867385, 1.000000000000000000, 0.9238795325112867385, 1.000000000000000000, 0.9238795325112867385, 1.000000000000000000 ) ) 
 REPRESENTATION_ITEM ( '' )  );
#71954 = CARTESIAN_POINT ( 'NONE',  ( 8.660254037844389075, 172.2916666598387110, -5.000000000000000000 ) ) ;
#71955 = CARTESIAN_POINT ( 'NONE',  ( 3.999999999999959144, 200.1875000027312126, 140.3431457505076594 ) ) ;
#71956 = EDGE_CURVE ( 'NONE', #33110, #11312, #30884, .T. ) ;
#71957 = DIRECTION ( 'NONE',  ( -0.000000000000000000, 1.000000000000000000, -0.000000000000000000 ) ) ;
#71958 = CARTESIAN_POINT ( 'NONE',  ( 6.951808397369818766E-16, 57.34374999658601979, -11.35316468750000141 ) ) ;
#71959 = CARTESIAN_POINT ( 'NONE',  ( 1.226468279477575784E-15, 294.7031250017069510, 6.676582343750001591 ) ) ;
#71960 = CARTESIAN_POINT ( 'NONE',  ( 7.204075437095968759, -7.204075437095966983, 109.0937500020483810 ) ) ;
#71961 = CARTESIAN_POINT ( 'NONE',  ( 9.832129032723420536, 206.1979166632526983, -5.676582343749999815 ) ) ;
#71962 = ORIENTED_EDGE ( 'NONE', *, *, #65592, .T. ) ;
#71963 = DIRECTION ( 'NONE',  ( -0.000000000000000000, 1.000000000000000000, 4.476705744456276341E-16 ) ) ;
#71964 = CARTESIAN_POINT ( 'NONE',  ( 2.449293598294707893E-16, 3.999999997268813168, -4.000000000000001776 ) ) ;
#71965 = CARTESIAN_POINT ( 'NONE',  ( -7.347880794884122694E-16, 13.49999999726881406, 4.000000000000001776 ) ) ;
#71967 = CARTESIAN_POINT ( 'NONE',  ( -2.085542519210945728E-15, 194.5312499965860127, 11.35316468750000141 ) ) ;
#71966 = DIRECTION ( 'NONE',  ( -1.000000000000000000, 0.000000000000000000, 0.000000000000000000 ) ) ;
#71968 = VECTOR ( 'NONE', #14026, 1000.000000000000000 ) ;
#71969 = DIRECTION ( 'NONE',  ( 0.000000000000000000, 0.000000000000000000, 1.000000000000000000 ) ) ;
#71970 = CARTESIAN_POINT ( 'NONE',  ( -9.999999999999998224, 238.3333333401613174, 2.679491924311235618 ) ) ;
#71971 = CARTESIAN_POINT ( 'NONE',  ( -10.00000000000000000, 189.1666666598387110, -2.679491924311229845 ) ) ;
#71972 = VERTEX_POINT ( 'NONE', #23254 ) ;
#71973 = CARTESIAN_POINT ( 'NONE',  ( -5.676582343749998039, 177.7604166632526699, -9.832129032723420536 ) ) ;
#71974 =( BOUNDED_CURVE ( )  B_SPLINE_CURVE ( 2, ( #29080, #45309, #46052, #69441, #23412, #17752, #21916, #17003, #10988 ),
 .UNSPECIFIED., .F., .F. ) 
 B_SPLINE_CURVE_WITH_KNOTS ( ( 3, 2, 2, 2, 3 ),
 ( 0.9000000000000007994, 0.9083333333333341031, 0.9166666666666674068, 0.9250000000000008216, 0.9333333333333341253 ),
 .UNSPECIFIED. ) 
 CURVE ( )  GEOMETRIC_REPRESENTATION_ITEM ( )  RATIONAL_B_SPLINE_CURVE ( ( 0.9999999999999928946, 0.9238795325112938439, 1.000000000000000000, 0.9238795325112867385, 1.000000000000000000, 0.9238795325112867385, 1.000000000000000000, 0.9238795325112796331, 1.000000000000007105 ) ) 
 REPRESENTATION_ITEM ( '' )  );
#71975 = CARTESIAN_POINT ( 'NONE',  ( 1.320432766682872962E-15, -7.188101187499992051, 19.86155278187175455 ) ) ;
#71976 = CARTESIAN_POINT ( 'NONE',  ( 0.000000000000000000, 130.3999865490244190, 45.94057108883949070 ) ) ;
#71977 = ORIENTED_EDGE ( 'NONE', *, *, #32388, .T. ) ;
#71978 = EDGE_CURVE ( 'NONE', #10283, #58068, #17592, .T. ) ;
#71979 = EDGE_CURVE ( 'NONE', #46523, #11891, #66571, .T. ) ;
#71980 = CARTESIAN_POINT ( 'NONE',  ( -5.656854249492378806, 95.37500000409677625, 5.656854249492381470 ) ) ;
#71981 = CARTESIAN_POINT ( 'NONE',  ( 27.99999999999997158, 209.0000000000000284, 173.9999999999999147 ) ) ;
#71982 = MECHANICAL_DESIGN_GEOMETRIC_PRESENTATION_REPRESENTATION (  '', ( #56336 ), #68387 ) ;
#71983 =( BOUNDED_CURVE ( )  B_SPLINE_CURVE ( 2, ( #61692, #33045, #56045, #38313, #68459, #62788, #44341, #4354, #73380 ),
 .UNSPECIFIED., .F., .F. ) 
 B_SPLINE_CURVE_WITH_KNOTS ( ( 3, 2, 2, 2, 3 ),
 ( 0.9270833333333335924, 0.9322916666666667407, 0.9375000000000000000, 0.9427083333333333703, 0.9479166666666665186 ),
 .UNSPECIFIED. ) 
 CURVE ( )  GEOMETRIC_REPRESENTATION_ITEM ( )  RATIONAL_B_SPLINE_CURVE ( ( 0.9999999999999967804, 0.9238795325112899581, 1.000000000000000000, 0.9238795325112867385, 1.000000000000000000, 0.9238795325112867385, 1.000000000000000000, 0.9238795325112884038, 0.9999999999999983347 ) ) 
 REPRESENTATION_ITEM ( '' )  );
#71984 = CARTESIAN_POINT ( 'NONE',  ( -1.656854249492383691, 15.68750000000000000, 4.000000000000000888 ) ) ;
#71985 = CARTESIAN_POINT ( 'NONE',  ( 1.881053915767122664, 15.12499999863440792, 4.541265875000001451 ) ) ;
#71986 = CARTESIAN_POINT ( 'NONE',  ( 7.999999999999991118, 3.313708498984757611, 12.36155278392014445 ) ) ;
#71987 = CARTESIAN_POINT ( 'NONE',  ( 29.10842753010513917, 194.7321495122488102, 166.4289600676851251 ) ) ;
#71988 = ORIENTED_EDGE ( 'NONE', *, *, #51423, .T. ) ;
#71989 = CARTESIAN_POINT ( 'NONE',  ( 11.00000000000000000, 1.347111479062088405E-15, 118.0000000000000000 ) ) ;
#71990 = CARTESIAN_POINT ( 'NONE',  ( 5.082755093536326818, 93.21875000204838102, 5.082755093536325042 ) ) ;
#71991 = EDGE_CURVE ( 'NONE', #2612, #49272, #21221, .T. ) ;
#71993 = CARTESIAN_POINT ( 'NONE',  ( 8.311093377946834337, 262.0312500034139589, -8.311093377946836114 ) ) ;
#71992 = CARTESIAN_POINT ( 'NONE',  ( -2.679491924311081963, 259.1666666734946034, 10.00000000000008171 ) ) ;
#71994 = ORIENTED_EDGE ( 'NONE', *, *, #73766, .T. ) ;
#71995 = CARTESIAN_POINT ( 'NONE',  ( 7.778174593052021635, 7.778174593052023411, 82.93750000000000000 ) ) ;
#71996 = CARTESIAN_POINT ( 'NONE',  ( -2.977408999572648707, -7.188101187499990274, 19.76780278187175455 ) ) ;
#71997 = ORIENTED_EDGE ( 'NONE', *, *, #56308, .F. ) ;
#71998 = ORIENTED_EDGE ( 'NONE', *, *, #56599, .F. ) ;
#71999 = CARTESIAN_POINT ( 'NONE',  ( 1.871523826299183495E-15, -10.18810118749999916, 81.53125000204838102 ) ) ;
#72000 = CARTESIAN_POINT ( 'NONE',  ( 9.832129032723416984, 80.67708332991935549, 5.676582343750006032 ) ) ;
#72001 = CARTESIAN_POINT ( 'NONE',  ( 7.999972922956211541, -3.313735576028537189, 6.174051700559090250 ) ) ;
#72002 = CARTESIAN_POINT ( 'NONE',  ( 2.020667218593132706E-15, -11.00000000000000000, 92.87499999999998579 ) ) ;
#72005 = CARTESIAN_POINT ( 'NONE',  ( 6.676582343750003368, 295.0468750017069510, 2.765530957081995478 ) ) ;
#72004 = CARTESIAN_POINT ( 'NONE',  ( 32.00000000000000000, 198.3125000027312126, 171.6568542494922553 ) ) ;
#72003 = DIRECTION ( 'NONE',  ( -1.000000000000000000, -0.000000000000000000, -0.000000000000000000 ) ) ;
#72006 = CARTESIAN_POINT ( 'NONE',  ( -7.320508075688778149, 143.1250000000000000, 7.320508075688769267 ) ) ;
#72007 = FACE_OUTER_BOUND ( 'NONE', #32501, .T. ) ;
#72008 = CARTESIAN_POINT ( 'NONE',  ( -7.320508075688773708, 163.7499999931720538, -7.320508075688774596 ) ) ;
#72009 = VECTOR ( 'NONE', #52852, 1000.000000000000000 ) ;
#72010 = CARTESIAN_POINT ( 'NONE',  ( 3.458734125000015425, 198.2500000013656347, 196.5673454167823877 ) ) ;
#72011 = CARTESIAN_POINT ( 'NONE',  ( -6.331740687315345895E-14, -13.85640646055103531, -1.071796769724504550 ) ) ;
#72012 = CARTESIAN_POINT ( 'NONE',  ( 5.656854249492374365, 5.656854249492375253, 0.4553027839201452265 ) ) ;
#72013 = CARTESIAN_POINT ( 'NONE',  ( 24.54126587500000056, 198.1250000013656063, 168.5673454167822172 ) ) ;
#72014 = CARTESIAN_POINT ( 'NONE',  ( -7.188101187500002709, 13.68749999795161365, 2.977408999572649151 ) ) ;
#72015 = CARTESIAN_POINT ( 'NONE',  ( 3.313708498984756279, 7.999999999999991118, 23.04905278392014623 ) ) ;
#72016 = CARTESIAN_POINT ( 'NONE',  ( 2.449293598294707893E-16, 5.999999997268813168, -4.000000000000001776 ) ) ;
#72017 = CARTESIAN_POINT ( 'NONE',  ( -7.188101187499999156, 109.6250000020483952, 2.977408999572654924 ) ) ;
#72019 = FACE_OUTER_BOUND ( 'NONE', #27377, .T. ) ;
#72018 = CARTESIAN_POINT ( 'NONE',  ( 2.485281374238266672, 289.7500000034140157, -6.000000000000306422 ) ) ;
#72020 = LINE ( 'NONE', #32048, #56852 ) ;
#72021 = CARTESIAN_POINT ( 'NONE',  ( -7.347880794884122694E-16, 12.75000000000000178, 4.000000000000001776 ) ) ;
#72022 = CARTESIAN_POINT ( 'NONE',  ( -2.977408999572648707, -7.188101187499990274, 23.14280278187176165 ) ) ;
#72023 = CARTESIAN_POINT ( 'NONE',  ( 0.000000000000000000, 0.000000000000000000, -10.80000000000000071 ) ) ;
#72024 = CARTESIAN_POINT ( 'NONE',  ( 11.35316468749999785, 45.57291666325266988, 3.042071309553174174 ) ) ;
#72025 = CARTESIAN_POINT ( 'NONE',  ( -1.656854249492383468, 6.687500000000000888, 4.000000000000000888 ) ) ;
#72026 = CARTESIAN_POINT ( 'NONE',  ( -10.00000000000000178, 9.374999993172032475, -1.224646799147353454E-15 ) ) ;
#72027 = ORIENTED_EDGE ( 'NONE', *, *, #61511, .F. ) ;
#72028 = DIRECTION ( 'NONE',  ( -0.000000000000000000, 1.000000000000000000, -0.000000000000000000 ) ) ;
#72029 = CARTESIAN_POINT ( 'NONE',  ( -3.042071309553173730, 44.32291666325268409, 11.35316468749999785 ) ) ;
#72030 = CARTESIAN_POINT ( 'NONE',  ( -10.99999999999999822, -4.556349186104052151, 82.28125000409677625 ) ) ;
#72031 = CARTESIAN_POINT ( 'NONE',  ( 2.445694354108783219, 204.8125000013656063, 139.5543056458912190 ) ) ;
#72032 = CARTESIAN_POINT ( 'NONE',  ( -5.000000000000000000, -68.60357193678697740, -20.85024232999374050 ) ) ;
#72033 = CARTESIAN_POINT ( 'NONE',  ( 6.123233995736767268E-16, 11.25000000000000178, -10.00000000000000178 ) ) ;
#72035 = CARTESIAN_POINT ( 'NONE',  ( 6.951808397369818766E-16, 32.03124999658601268, -11.35316468750000141 ) ) ;
#72034 = CARTESIAN_POINT ( 'NONE',  ( 2.977408999572654480, 102.1250000020483810, 7.188101187499999156 ) ) ;
#72036 = CARTESIAN_POINT ( 'NONE',  ( 7.999999999999991118, 3.313708498984757611, 7.674052779823366421 ) ) ;
#72037 = CARTESIAN_POINT ( 'NONE',  ( -7.347880794884122694E-16, 10.49999999726881406, 4.000000000000001776 ) ) ;
#72038 = CARTESIAN_POINT ( 'NONE',  ( 8.311093377946834337, 160.1562499965860411, 8.311093377946839666 ) ) ;
#72039 = CARTESIAN_POINT ( 'NONE',  ( -4.999999999999998224, 128.5416666598387110, -8.660254037844389075 ) ) ;
#72040 = CARTESIAN_POINT ( 'NONE',  ( 5.082755093536325042, 107.4687500020483952, -5.082755093536325930 ) ) ;
#72041 = ORIENTED_EDGE ( 'NONE', *, *, #45533, .T. ) ;
#72042 = CARTESIAN_POINT ( 'NONE',  ( 10.00000000000000000, 21.66666665983870388, 2.679491924311235618 ) ) ;
#72043 = CARTESIAN_POINT ( 'NONE',  ( -11.35316468750000141, 18.80208332991934839, 3.042071309553159963 ) ) ;
#72044 = CARTESIAN_POINT ( 'NONE',  ( 1.656854249492246467, 197.9375000027312410, 146.0000000000001421 ) ) ;
#72045 = ORIENTED_EDGE ( 'NONE', *, *, #1666, .T. ) ;
#72046 = LINE ( 'NONE', #20363, #71694 ) ;
#72047 = CARTESIAN_POINT ( 'NONE',  ( 7.204075437095966983, 7.204075437095967871, 77.59375000204838102 ) ) ;
#72048 = DIRECTION ( 'NONE',  ( -0.1513591288559071046, 0.000000000000000000, -0.9884788384745426537 ) ) ;
#72050 = CARTESIAN_POINT ( 'NONE',  ( -3.042071309553173730, 159.3229166632526699, 11.35316468749999785 ) ) ;
#72049 = CARTESIAN_POINT ( 'NONE',  ( 4.000000000000002665, 22.00000000000000000, 0.000000000000000000 ) ) ;
#72051 = CARTESIAN_POINT ( 'NONE',  ( 62.39047978708148889, 229.6205190061017447, 45.00000000000000000 ) ) ;
#72052 = CARTESIAN_POINT ( 'NONE',  ( 3.313708498984762496, -7.999999999999989342, 10.35530278432982598 ) ) ;
#72053 = EDGE_CURVE ( 'NONE', #29980, #13133, #15008, .T. ) ;
#72054 = CARTESIAN_POINT ( 'NONE',  ( -5.656854249492373476, -5.656854249492376141, 16.01780277982336642 ) ) ;
#72055 = CARTESIAN_POINT ( 'NONE',  ( 8.311093377946834337, 232.0312500034139873, -8.311093377946836114 ) ) ;
#72056 = CARTESIAN_POINT ( 'NONE',  ( -10.18810118749999916, 0.000000000000000000, 87.53125000204836681 ) ) ;
#72057 = VERTEX_POINT ( 'NONE', #25460 ) ;
#72058 = CARTESIAN_POINT ( 'NONE',  ( -10.99999999999968203, -4.556349186104368343, 89.78125000409681888 ) ) ;
#72059 = CARTESIAN_POINT ( 'NONE',  ( -3.999999999999960032, 199.1250000027312126, 198.0000000000000284 ) ) ;
#72060 = CARTESIAN_POINT ( 'NONE',  ( 11.35316468749999963, 96.30208332991934128, -3.042071309553165293 ) ) ;
#72061 =( BOUNDED_CURVE ( )  B_SPLINE_CURVE ( 3, ( #15850, #40366, #63365, #38885 ),
 .UNSPECIFIED., .F., .F. ) 
 B_SPLINE_CURVE_WITH_KNOTS ( ( 4, 4 ),
 ( 4.694530230738832799, 4.715142596155377674 ),
 .UNSPECIFIED. ) 
 CURVE ( )  GEOMETRIC_REPRESENTATION_ITEM ( )  RATIONAL_B_SPLINE_CURVE ( ( 1.000000000000000000, 0.9999645945127194624, 0.9999645945127194624, 1.000000000000000000 ) ) 
 REPRESENTATION_ITEM ( '' )  );
#72062 = CARTESIAN_POINT ( 'NONE',  ( -10.18810118749999916, 0.000000000000000000, 93.15625000204836681 ) ) ;
#72063 = CARTESIAN_POINT ( 'NONE',  ( -4.541265875000002339, 18.93749999863440436, -5.561446717895856393E-16 ) ) ;
#72064 = ORIENTED_EDGE ( 'NONE', *, *, #24957, .F. ) ;
#72065 = ORIENTED_EDGE ( 'NONE', *, *, #4407, .F. ) ;
#72066 = CARTESIAN_POINT ( 'NONE',  ( 3.211159895383560947, 3.312499998634407028, 3.211159895383562723 ) ) ;
#72067 = EDGE_CURVE ( 'NONE', #48083, #57615, #49222, .T. ) ;
#72068 = CARTESIAN_POINT ( 'NONE',  ( -7.188101187500001821, 10.12499999795161187, -2.977408999572651371 ) ) ;
#72069 = CARTESIAN_POINT ( 'NONE',  ( -8.000000000000000000, 117.5937500040967905, -3.313708498984761608 ) ) ;
#72070 = CARTESIAN_POINT ( 'NONE',  ( -10.18810118749999916, 0.000000000000000000, 96.53125000204838102 ) ) ;
#72071 = ADVANCED_FACE ( 'NONE', ( #26202 ), #42075, .T. ) ;
#72072 = CARTESIAN_POINT ( 'NONE',  ( -31.45873412499998523, 203.0000000013655779, 171.4326545832180386 ) ) ;
#72073 = AXIS2_PLACEMENT_3D ( 'NONE', #8279, #31289, #30918 ) ;
#72074 = CARTESIAN_POINT ( 'NONE',  ( -2.679491924311226292, 158.3333333265053398, -10.00000000000000178 ) ) ;
#72075 = CARTESIAN_POINT ( 'NONE',  ( -1.656854249492383691, 2.687500000000000888, 4.000000000000000888 ) ) ;
#72076 =( BOUNDED_CURVE ( )  B_SPLINE_CURVE ( 2, ( #67007, #61350, #50764, #60597, #72672, #66627, #16053, #56075, #73779 ),
 .UNSPECIFIED., .F., .F. ) 
 B_SPLINE_CURVE_WITH_KNOTS ( ( 3, 2, 2, 2, 3 ),
 ( 0.5166666666666670515, 0.5250000000000003553, 0.5333333333333337700, 0.5416666666666671848, 0.5500000000000005995 ),
 .UNSPECIFIED. ) 
 CURVE ( )  GEOMETRIC_REPRESENTATION_ITEM ( )  RATIONAL_B_SPLINE_CURVE ( ( 0.9999999999999970024, 0.9238795325112897361, 1.000000000000000000, 0.9238795325112867385, 1.000000000000000000, 0.9238795325112867385, 1.000000000000000000, 0.9238795325112816315, 1.000000000000005107 ) ) 
 REPRESENTATION_ITEM ( '' )  );
#72077 = CARTESIAN_POINT ( 'NONE',  ( -1.656854249492381248, 18.06249999726882294, -4.000000000000001776 ) ) ;
#72078 = CARTESIAN_POINT ( 'NONE',  ( -1.881053915767121776, 2.624999998634406584, -4.541265875000002339 ) ) ;
#72079 = AXIS2_PLACEMENT_3D ( 'NONE', #28939, #18733, #35362 ) ;
#72080 = CARTESIAN_POINT ( 'NONE',  ( -1.432654583217664479, 207.7500000013656063, 138.5412658750000787 ) ) ;
#72081 = CYLINDRICAL_SURFACE ( 'NONE', #55964, 7.999999999999991118 ) ;
#72082 = EDGE_CURVE ( 'NONE', #51031, #16346, #19900, .T. ) ;
#72084 = CARTESIAN_POINT ( 'NONE',  ( 8.000000000000035527, 3.313708498984715423, 16.67405277982336642 ) ) ;
#72083 = CARTESIAN_POINT ( 'NONE',  ( -24.54126587499995793, 195.1250000013656063, 171.4326545832179534 ) ) ;
#72085 = SHAPE_REPRESENTATION_RELATIONSHIP ( 'NONE' , 'NONE' ,  #48857, #37253 ) ;
#72086=STYLED_ITEM('',(#74699),#42707);
#72087 = CARTESIAN_POINT ( 'NONE',  ( -8.342170076843785083E-16, 18.06249999863440792, 4.541265875000002339 ) ) ;
#72088 = CARTESIAN_POINT ( 'NONE',  ( 10.00000000000000178, 71.87499999317203958, 0.000000000000000000 ) ) ;
#72089 = CARTESIAN_POINT ( 'NONE',  ( 5.082755093536320601, -5.082755093536318824, 6.549052781871754547 ) ) ;
#72090 = ORIENTED_EDGE ( 'NONE', *, *, #1278, .F. ) ;
#72091 = ORIENTED_EDGE ( 'NONE', *, *, #19272, .T. ) ;
#72092 = CARTESIAN_POINT ( 'NONE',  ( 10.18810118750000093, -4.220049686691933033, 99.81250000204838102 ) ) ;
#72093 = CARTESIAN_POINT ( 'NONE',  ( 38.00000000000000000, 272.0000000000000000, 3.791916237172776494E-14 ) ) ;
#72094 = CARTESIAN_POINT ( 'NONE',  ( -26.56734541678238060, 202.6250000013656063, 166.5412658750003629 ) ) ;
#72095 = CARTESIAN_POINT ( 'NONE',  ( -29.65685424949241167, 202.0625000000000284, 166.0000000000004263 ) ) ;
#72096 = CARTESIAN_POINT ( 'NONE',  ( -3.458734124999960358, 205.6250000013656063, 196.5673454167823877 ) ) ;
#72097 = CARTESIAN_POINT ( 'NONE',  ( -3.313708498984815343, 111.2187500000000000, -7.999999999999944933 ) ) ;
#72098 = CARTESIAN_POINT ( 'NONE',  ( -5.000000000000005329, 108.3333333333333428, 8.660254037844387298 ) ) ;
#72099 = EDGE_CURVE ( 'NONE', #37163, #15721, #22721, .T. ) ;
#72100 = CARTESIAN_POINT ( 'NONE',  ( -8.000000000000000000, 113.0000000000000000, 0.000000000000000000 ) ) ;
#72101 = CARTESIAN_POINT ( 'NONE',  ( -2.765530957081996810, 290.4218750017068942, -6.676582343750003368 ) ) ;
#72102 = CARTESIAN_POINT ( 'NONE',  ( -4.401442555609577197E-16, 7.188101187499992051, 10.48655278187175455 ) ) ;
#72103 = ORIENTED_EDGE ( 'NONE', *, *, #1411, .F. ) ;
#72104 = CARTESIAN_POINT ( 'NONE',  ( 0.000000000000000000, 0.000000000000000000, 0.000000000000000000 ) ) ;
#72105 = ADVANCED_FACE ( 'NONE', ( #30764 ), #8125, .T. ) ;
#72106 = CARTESIAN_POINT ( 'NONE',  ( 5.656854249492380582, 20.99999999590322375, -5.656854249492380582 ) ) ;
#72107 = CARTESIAN_POINT ( 'NONE',  ( 3.458734124999959025, 202.5000000013656063, 140.5673454167824161 ) ) ;
#72108 = CARTESIAN_POINT ( 'NONE',  ( -4.000000000000001776, 5.500000000000000000, -4.898587196589415787E-16 ) ) ;
#72109 = DIRECTION ( 'NONE',  ( -0.000000000000000000, -0.000000000000000000, 1.000000000000000000 ) ) ;
#72110 = CARTESIAN_POINT ( 'NONE',  ( 8.311093377946834337, 252.3437500034139873, -8.311093377946836114 ) ) ;
#72111 = FACE_OUTER_BOUND ( 'NONE', #60738, .T. ) ;
#72112 = CARTESIAN_POINT ( 'NONE',  ( 4.556349186104045934, 11.00000000000000000, 113.0312499999999858 ) ) ;
#72113 = CARTESIAN_POINT ( 'NONE',  ( 3.042071309553167069, 6.822916663252682312, -11.35316468749999785 ) ) ;
#72114 = CARTESIAN_POINT ( 'NONE',  ( -7.188101187499990274, -2.977408999572651815, 4.955302781871752771 ) ) ;
#72115 = CARTESIAN_POINT ( 'NONE',  ( -5.676582343749998039, 192.7604166632526983, -9.832129032723420536 ) ) ;
#72116 = CARTESIAN_POINT ( 'NONE',  ( 2.020667218593132706E-15, -11.00000000000000000, 101.8750000000000000 ) ) ;
#72117 = CARTESIAN_POINT ( 'NONE',  ( 4.541265875000002339, 4.374999998634407028, -1.881053915767121554 ) ) ;
#72118 = LINE ( 'NONE', #14771, #58440 ) ;
#72120 = CARTESIAN_POINT ( 'NONE',  ( -2.751064625579944321E-14, 206.7500000000000284, 146.0000000000000284 ) ) ;
#72119 = CARTESIAN_POINT ( 'NONE',  ( 0.000000000000000000, 300.0000000000000000, 0.000000000000000000 ) ) ;
#72121 = EDGE_LOOP ( 'NONE', ( #72620, #35732, #16359, #15259 ) ) ;
#72122 = CARTESIAN_POINT ( 'NONE',  ( -2.445694354108839175, 206.3125000013656063, 144.4456943541088663 ) ) ;
#72123 = CARTESIAN_POINT ( 'NONE',  ( 11.35316468749999785, 10.57291666325268409, 3.042071309553174174 ) ) ;
#72124 = CARTESIAN_POINT ( 'NONE',  ( -6.735557395310442023E-16, 11.00000000000000000, 99.81250000409677625 ) ) ;
#72125 = LINE ( 'NONE', #38569, #61231 ) ;
#72126 = CARTESIAN_POINT ( 'NONE',  ( -26.56734541678228112, 202.0000000013656063, 173.4587341250003476 ) ) ;
#72127 = CARTESIAN_POINT ( 'NONE',  ( 5.471491410962281421, 9.542682104092435225, 117.5000000000000711 ) ) ;
#72129 = FACE_OUTER_BOUND ( 'NONE', #28117, .T. ) ;
#72128 = CARTESIAN_POINT ( 'NONE',  ( 7.188101187500000044, 118.9062500020483810, -8.802885111219163269E-16 ) ) ;
#72130 = CARTESIAN_POINT ( 'NONE',  ( 7.999999999999991118, 3.313708498984757611, 25.67405277982336997 ) ) ;
#72131 = CARTESIAN_POINT ( 'NONE',  ( -11.35316468750000141, 123.4895833299193555, 3.042071309553159963 ) ) ;
#72132 = AXIS2_PLACEMENT_3D ( 'NONE', #17682, #12028, #35061 ) ;
#72133 = CARTESIAN_POINT ( 'NONE',  ( -5.000000000000005329, 95.20833332650536818, 8.660254037844387298 ) ) ;
#72134 = CARTESIAN_POINT ( 'NONE',  ( 2.977408999572654480, 90.12500000204836681, 7.188101187499999156 ) ) ;
#72135 = CARTESIAN_POINT ( 'NONE',  ( 1.881053915767121776, 18.62499999863440792, -4.541265875000002339 ) ) ;
#72136 = CARTESIAN_POINT ( 'NONE',  ( -7.999999999994261479, 6.398094505892175214E-06, 25.01756343669228499 ) ) ;
#72137 = CARTESIAN_POINT ( 'NONE',  ( -12.00000000000000178, 1.173324140324972342, -0.02489140746004457963 ) ) ;
#72138 = ORIENTED_EDGE ( 'NONE', *, *, #3142, .F. ) ;
#72139 = CARTESIAN_POINT ( 'NONE',  ( 3.999999999999959144, 209.0625000000000568, 140.3431457505076594 ) ) ;
#72140 = CARTESIAN_POINT ( 'NONE',  ( -2.765530957081996810, 293.4218750017070079, -6.676582343750003368 ) ) ;
#72141 = CARTESIAN_POINT ( 'NONE',  ( -5.000000000000002665, 0.000000000000000000, -17.50000000000000000 ) ) ;
#72142 = CARTESIAN_POINT ( 'NONE',  ( -3.313708498984757167, 7.999999999999991118, 2.236552783920143561 ) ) ;
#72143 = CARTESIAN_POINT ( 'NONE',  ( -11.35316468750000141, 173.2812499965860411, -1.390361679473963753E-15 ) ) ;
#72144 = CARTESIAN_POINT ( 'NONE',  ( 1.656854249492433206, 198.1875000000000568, 138.0000000000001705 ) ) ;
#72145 = CARTESIAN_POINT ( 'NONE',  ( 2.849036369511732440E-14, 201.2500000000000000, 202.0000000000000000 ) ) ;
#72146 = CARTESIAN_POINT ( 'NONE',  ( 11.00000000000010658, 4.556349186103942017, 69.34374999999998579 ) ) ;
#72147 = CARTESIAN_POINT ( 'NONE',  ( 10.18810118749999916, 4.220049686691935698, 106.3750000020483668 ) ) ;
#72148 = VERTEX_POINT ( 'NONE', #7393 ) ;
#72149 = DIRECTION ( 'NONE',  ( -1.000000000000000000, 0.000000000000000000, 0.000000000000000000 ) ) ;
#72150 = CARTESIAN_POINT ( 'NONE',  ( -3.042071309553173730, 154.6354166632526699, 11.35316468749999785 ) ) ;
#72151 = CARTESIAN_POINT ( 'NONE',  ( 4.000000000000016875, 206.5625000027312126, 199.6568542494924259 ) ) ;
#72152 = CARTESIAN_POINT ( 'NONE',  ( 2.445694354108840063, 205.0625000013656063, 200.4456943541088663 ) ) ;
#72154 = ADVANCED_FACE ( 'NONE', ( #59083 ), #71855, .F. ) ;
#72153 = CARTESIAN_POINT ( 'NONE',  ( 10.18810118749999916, 1.247682550866122264E-15, 71.78125000204838102 ) ) ;
#72155 = CARTESIAN_POINT ( 'NONE',  ( 5.676582343749993598, 60.26041666325268409, 9.832129032723422313 ) ) ;
#72156 = VERTEX_POINT ( 'NONE', #30400 ) ;
#72157 = DIRECTION ( 'NONE',  ( -0.000000000000000000, -0.000000000000000000, 1.000000000000000000 ) ) ;
#72158 = CARTESIAN_POINT ( 'NONE',  ( -4.541265875000003227, 9.999999998634407916, 1.881053915767121110 ) ) ;
#72159 = ORIENTED_EDGE ( 'NONE', *, *, #4626, .T. ) ;
#72160 = CARTESIAN_POINT ( 'NONE',  ( -7.188101187500000044, 19.21874999795161543, -8.802885111219163269E-16 ) ) ;
#72161 = CARTESIAN_POINT ( 'NONE',  ( 2.485281374238575314, 289.3750000034139589, 6.000000000000000888 ) ) ;
#72162 = CARTESIAN_POINT ( 'NONE',  ( -6.123233995736766282E-16, 231.8750000068279746, -10.00000000000000000 ) ) ;
#72163 = CARTESIAN_POINT ( 'NONE',  ( -1.320432766682874540E-15, 18.46874999795161187, 7.188101187500000044 ) ) ;
#72164 = CARTESIAN_POINT ( 'NONE',  ( 1.320432766682872962E-15, -7.188101187499992051, 3.361552781871751883 ) ) ;
#72165 = CARTESIAN_POINT ( 'NONE',  ( 1.871523826299183495E-15, -10.18810118749999916, 113.4062500020483810 ) ) ;
#72166 = EDGE_CURVE ( 'NONE', #39299, #59170, #71407, .T. ) ;
#72167 = CARTESIAN_POINT ( 'NONE',  ( 5.000000000000000000, -11.14555136602166208, 27.84144949604419139 ) ) ;
#72168 = CARTESIAN_POINT ( 'NONE',  ( -1.656854249492383691, 7.437499997268812280, 4.000000000000000888 ) ) ;
#72169 = ORIENTED_EDGE ( 'NONE', *, *, #55574, .T. ) ;
#72170 = CARTESIAN_POINT ( 'NONE',  ( 2.754378923186476579E-14, 207.1875000013656063, 194.5412658750000219 ) ) ;
#72172 =( BOUNDED_CURVE ( )  B_SPLINE_CURVE ( 2, ( #58229, #74435, #10694, #57481, #28783, #5411, #17085, #51799, #17838, #46506, #147, #6528, #33727 ),
 .UNSPECIFIED., .F., .F. ) 
 B_SPLINE_CURVE_WITH_KNOTS ( ( 3, 2, 2, 2, 2, 2, 3 ),
 ( 0.2499999999999995837, 0.2592592592592588563, 0.2685185185185181567, 0.2777777777777774015, 0.2870370370370366464, 0.2962962962962958913, 0.3055555555555551916 ),
 .UNSPECIFIED. ) 
 CURVE ( )  GEOMETRIC_REPRESENTATION_ITEM ( )  RATIONAL_B_SPLINE_CURVE ( ( 1.000000000000001554, 0.9659258262890668689, 1.000000000000000000, 0.9659258262890683122, 1.000000000000000000, 0.9659258262890683122, 1.000000000000000000, 0.9659258262890683122, 1.000000000000000000, 0.9659258262890683122, 1.000000000000000000, 0.9659258262890697555, 0.9999999999999985567 ) ) 
 REPRESENTATION_ITEM ( '' )  );
#72171 = CARTESIAN_POINT ( 'NONE',  ( -30.82842712474624136, 195.2500000027312126, 167.1715728752542418 ) ) ;
#72173 = EDGE_CURVE ( 'NONE', #28093, #4661, #65307, .T. ) ;
#72174 = CARTESIAN_POINT ( 'NONE',  ( 1.881053915767121776, 6.499999998634407028, -4.541265875000002339 ) ) ;
#72175 = CARTESIAN_POINT ( 'NONE',  ( 1.320432766682874540E-15, 109.5312500020483810, 7.188101187500000044 ) ) ;
#72176 = DIRECTION ( 'NONE',  ( -0.000000000000000000, -0.000000000000000000, 1.000000000000000000 ) ) ;
#72177 = CARTESIAN_POINT ( 'NONE',  ( -4.401442555609577197E-16, 7.188101187499992051, 26.61155278187175455 ) ) ;
#72178 = ORIENTED_EDGE ( 'NONE', *, *, #20770, .T. ) ;
#72179 = ADVANCED_FACE ( 'NONE', ( #21669 ), #56028, .T. ) ;
#72180 = CARTESIAN_POINT ( 'NONE',  ( 6.000000000000003553, 299.4374999999999432, 2.485281374238571317 ) ) ;
#72181 = ORIENTED_EDGE ( 'NONE', *, *, #54912, .F. ) ;
#72182 = CARTESIAN_POINT ( 'NONE',  ( -7.347880794884122694E-16, 9.750000000000000000, 4.000000000000001776 ) ) ;
#72183 = CARTESIAN_POINT ( 'NONE',  ( -7.796932491751043415, 2.081755106361893759, -0.000000000000000000 ) ) ;
#72184 = CARTESIAN_POINT ( 'NONE',  ( -3.458734124999959025, 207.5000000013655779, 199.4326545832176691 ) ) ;
#72185 = CARTESIAN_POINT ( 'NONE',  ( 24.54126587499999346, 203.1875000013656063, 169.9999999999999432 ) ) ;
#72186 = CARTESIAN_POINT ( 'NONE',  ( -10.00000000000000355, 72.70833333333332860, 2.679491924311223183 ) ) ;
#72187 = VECTOR ( 'NONE', #59541, 1000.000000000000000 ) ;
#72188 = CARTESIAN_POINT ( 'NONE',  ( -2.977408999572651815, 94.81250000204838102, 7.188101187500000933 ) ) ;
#72189 = CARTESIAN_POINT ( 'NONE',  ( 4.242640687119287435, 293.3750000000000000, 4.242640687119285658 ) ) ;
#72191 = CARTESIAN_POINT ( 'NONE',  ( -11.00000000000000000, 0.000000000000000000, 113.6875000040967763 ) ) ;
#72190 = CARTESIAN_POINT ( 'NONE',  ( 0.8721677472748814441, -51.17354301023269159, -48.53016177276447252 ) ) ;
#72192 = ORIENTED_EDGE ( 'NONE', *, *, #35644, .F. ) ;
#72193 = LINE ( 'NONE', #66918, #6028 ) ;
#72194 = CARTESIAN_POINT ( 'NONE',  ( 4.898587196589412829E-16, 12.37500000000000178, -8.000000000000000000 ) ) ;
#72195 = CARTESIAN_POINT ( 'NONE',  ( -2.751064625579944321E-14, 201.8750000027312126, 146.0000000000000284 ) ) ;
#72196 = CARTESIAN_POINT ( 'NONE',  ( -3.313708498984757611, 7.999999999999991118, 24.73655278392014978 ) ) ;
#72197 = CARTESIAN_POINT ( 'NONE',  ( 5.656854249492376141, -5.656854249492374365, 22.39280277982336997 ) ) ;
#72198 = CARTESIAN_POINT ( 'NONE',  ( 8.660254037844389075, 257.0833333333333144, 4.999999999999997335 ) ) ;
#72199 = EDGE_CURVE ( 'NONE', #31338, #62523, #4455, .T. ) ;
#72200 = CARTESIAN_POINT ( 'NONE',  ( 0.000000000000000000, 15.99999999999998579, 1.000000000000000000 ) ) ;
#72201 = CARTESIAN_POINT ( 'NONE',  ( 7.320508075688771044, 189.3750000000000000, 7.320508075688775484 ) ) ;
#72202 = CYLINDRICAL_SURFACE ( 'NONE', #28372, 8.000000000000000000 ) ;
#72203 = CARTESIAN_POINT ( 'NONE',  ( 1.320432766682872962E-15, -7.188101187499992051, 23.23655278187175455 ) ) ;
#72204 = CARTESIAN_POINT ( 'NONE',  ( 8.311093377946837890, 151.7187499965860127, -8.311093377946837890 ) ) ;
#72205 = CARTESIAN_POINT ( 'NONE',  ( -2.751064625579944321E-14, 204.8750000027312126, 146.0000000000000284 ) ) ;
#72206 = CARTESIAN_POINT ( 'NONE',  ( 9.999999999999998224, 260.8333333401612890, -2.679491924311229401 ) ) ;
#72207 = CARTESIAN_POINT ( 'NONE',  ( 7.347880794884121708E-16, 300.0000000000000000, -6.000000000000001776 ) ) ;
#72210 = CARTESIAN_POINT ( 'NONE',  ( 2.449293598294707893E-16, 6.999999997268813168, -4.000000000000001776 ) ) ;
#72209 = CARTESIAN_POINT ( 'NONE',  ( 1.224646799147353454E-15, 300.0000000000000000, -10.00000000000000178 ) ) ;
#72208 = CARTESIAN_POINT ( 'NONE',  ( 26.34314575050758833, 202.9375000000000000, 173.9999999999999147 ) ) ;
#72211 = VERTEX_POINT ( 'NONE', #73731 ) ;
#72212 = CARTESIAN_POINT ( 'NONE',  ( -8.311093377946841443, 9.218749996586016238, 8.311093377946830785 ) ) ;
#72213 = DIRECTION ( 'NONE',  ( 0.000000000000000000, 0.000000000000000000, -1.000000000000000000 ) ) ;
#72215 = CARTESIAN_POINT ( 'NONE',  ( -1.656854249492346609, 208.1875000000000853, 202.0000000000000000 ) ) ;
#72214 = CARTESIAN_POINT ( 'NONE',  ( 0.000000000000000000, 0.000000000000000000, 18.50000000000000000 ) ) ;
#72216 = CARTESIAN_POINT ( 'NONE',  ( -5.656854249492378806, 116.1875000000000000, 5.656854249492381470 ) ) ;
#72217 = CARTESIAN_POINT ( 'NONE',  ( -2.445694354108839619, 203.8125000013656063, 139.5543056458912190 ) ) ;
#72218 = CARTESIAN_POINT ( 'NONE',  ( -8.660254037844387298, 53.95833332650536818, -5.000000000000004441 ) ) ;
#72219 = CARTESIAN_POINT ( 'NONE',  ( 5.082755093536325042, 110.0937500020483810, -5.082755093536325930 ) ) ;
#72220 = CARTESIAN_POINT ( 'NONE',  ( -8.342170076843785083E-16, 10.18749999863440614, 4.541265875000002339 ) ) ;
#72221 = LINE ( 'NONE', #15996, #4802 ) ;
#72222 = CARTESIAN_POINT ( 'NONE',  ( 7.999999999999992895, -3.313708498984756279, 10.48655277982336642 ) ) ;
#72224 = CARTESIAN_POINT ( 'NONE',  ( 8.660254037844385522, 164.5833333333333428, 5.000000000000005329 ) ) ;
#72223 = LINE ( 'NONE', #20538, #5835 ) ;
#72225 = VERTEX_POINT ( 'NONE', #9996 ) ;
#72226 = ORIENTED_EDGE ( 'NONE', *, *, #36897, .F. ) ;
#72227 = CARTESIAN_POINT ( 'NONE',  ( -5.000000000000000888, -65.74990953739990118, 23.82322416715286906 ) ) ;
#72228 = LINE ( 'NONE', #26576, #30251 ) ;
#72229 = EDGE_CURVE ( 'NONE', #15721, #22730, #68079, .T. ) ;
#72230 = CARTESIAN_POINT ( 'NONE',  ( 11.00000000000000000, 1.347111479062088405E-15, 94.74999999999998579 ) ) ;
#72231 = CARTESIAN_POINT ( 'NONE',  ( 5.676582343749993598, 124.9479166632526983, 9.832129032723422313 ) ) ;
#72232 = ORIENTED_EDGE ( 'NONE', *, *, #41524, .T. ) ;
#72233 = CARTESIAN_POINT ( 'NONE',  ( 31.99999999999997868, 201.1875000000000284, 171.6568542494923122 ) ) ;
#72234 = CARTESIAN_POINT ( 'NONE',  ( 7.204075437095968759, -7.204075437095966983, 95.21875000204838102 ) ) ;
#72235 = DIRECTION ( 'NONE',  ( -0.000000000000000000, -0.000000000000000000, -1.000000000000000000 ) ) ;
#72236 = CARTESIAN_POINT ( 'NONE',  ( 2.445694354108839175, 195.3125000013656063, 195.5543056458912190 ) ) ;
#72237 = CARTESIAN_POINT ( 'NONE',  ( -2.679491924311235174, 155.4166666598387110, 10.00000000000000000 ) ) ;
#72239 = CARTESIAN_POINT ( 'NONE',  ( -5.676582343750006032, 129.1145833299193839, 9.832129032723418760 ) ) ;
#72238 = CARTESIAN_POINT ( 'NONE',  ( 25.17157287525381193, 197.6250000000000284, 167.1715728752537018 ) ) ;
#72240 = EDGE_CURVE ( 'NONE', #26719, #25296, #19849, .T. ) ;
#72241 = ORIENTED_EDGE ( 'NONE', *, *, #30933, .F. ) ;
#72242 = APPLICATION_CONTEXT ( 'automotive_design' ) ;
#72243 = CIRCLE ( 'NONE', #16818, 8.999999999999998224 ) ;
#72244 = CARTESIAN_POINT ( 'NONE',  ( -10.00000000000000000, 24.16666665983869677, -2.679491924311229845 ) ) ;
#72245 = CARTESIAN_POINT ( 'NONE',  ( -20.64146325551718775, 182.5281491048786791, 146.7620766355165927 ) ) ;
#72246 = CARTESIAN_POINT ( 'NONE',  ( 8.311093377946837890, 121.7187499965860269, -8.311093377946837890 ) ) ;
#72247 = ADVANCED_BREP_SHAPE_REPRESENTATION ( '', ( #40373, #57354 ), #27271 ) ;
#72248 = CARTESIAN_POINT ( 'NONE',  ( -1.432654583217607858, 205.6250000013656063, 201.4587341250000065 ) ) ;
#72249 = CARTESIAN_POINT ( 'NONE',  ( 7.188101187500000933, 20.43749999795161543, -2.977408999572650483 ) ) ;
#72251 = EDGE_CURVE ( 'NONE', #17783, #61945, #35311, .T. ) ;
#72250 = CARTESIAN_POINT ( 'NONE',  ( 1.871523826299183495E-15, -10.18810118749999916, 87.90625000204838102 ) ) ;
#72252 = CARTESIAN_POINT ( 'NONE',  ( 11.35316468749999963, 21.30208332991935194, -3.042071309553165293 ) ) ;
#72253 = EDGE_LOOP ( 'NONE', ( #52211, #16039, #64420, #9667 ) ) ;
#72254 = DIRECTION ( 'NONE',  ( -0.000000000000000000, -0.000000000000000000, 1.000000000000000000 ) ) ;
#72255 = CARTESIAN_POINT ( 'NONE',  ( 5.662595241051936235, -5.662595241051934458, 27.07561528394063188 ) ) ;
#72256 = CARTESIAN_POINT ( 'NONE',  ( 2.679491924311168560, 238.5416666666666856, -10.00000000000003375 ) ) ;
#72257 = CONICAL_SURFACE ( 'NONE', #59026, 12.00000000000000000, 1.047197551196596077 ) ;
#72258 = CARTESIAN_POINT ( 'NONE',  ( -11.00000000000000000, 0.000000000000000000, 85.18750000409677625 ) ) ;
#72259 = CARTESIAN_POINT ( 'NONE',  ( -2.977408999572650039, 2.437499997951610542, -7.188101187500001821 ) ) ;
#72260 = CARTESIAN_POINT ( 'NONE',  ( -2.485281374238571761, 298.8750000034140726, -6.000000000000003553 ) ) ;
#72261 = CYLINDRICAL_SURFACE ( 'NONE', #5206, 10.00000000000000178 ) ;
#72262 = CARTESIAN_POINT ( 'NONE',  ( -5.656854249492381470, 17.24999999590322375, 5.656854249492379694 ) ) ;
#72263 = VERTEX_POINT ( 'NONE', #22404 ) ;
#72264 = CARTESIAN_POINT ( 'NONE',  ( 11.35316468749999963, 146.3020833299193555, -3.042071309553165293 ) ) ;
#72265 = CARTESIAN_POINT ( 'NONE',  ( 10.18810118749999916, 1.247682550866122264E-15, 81.90625000204838102 ) ) ;
#72266 = ADVANCED_FACE ( 'NONE', ( #34516 ), #29206, .F. ) ;
#72267 = B_SPLINE_CURVE_WITH_KNOTS ( 'NONE', 3,
 ( #39704, #68744, #68376, #45730, #62704, #11043, #115, #23094, #46105, #69124, #17429, #17058, #5382, #17806, #34073, #6128, #40453, #63452, #63085, #51024 ),
 .UNSPECIFIED., .F., .F.,
 ( 4, 2, 2, 2, 2, 2, 2, 2, 2, 4 ),
 ( 0.000000000000000000, 0.001156441540184011043, 0.001734662310276010276, 0.002312883080368009509, 0.003469324620552014914, 0.004625766160736019886, 0.005782207700920026158, 0.006938649241104030696, 0.008095090781288035234, 0.009251532321472039772 ),
 .UNSPECIFIED. ) ;
#72268 = CARTESIAN_POINT ( 'NONE',  ( -24.54126587500000056, 199.2500000013656063, 168.5673454167827003 ) ) ;
#72269 = CARTESIAN_POINT ( 'NONE',  ( 13.99999999999999822, 0.000000000000000000, 17.50000000000000000 ) ) ;
#72270 = CARTESIAN_POINT ( 'NONE',  ( -3.211159895383561391, 17.81249999863440792, -3.211159895383561835 ) ) ;
#72271 = ORIENTED_EDGE ( 'NONE', *, *, #65534, .F. ) ;
#72272 = CARTESIAN_POINT ( 'NONE',  ( -2.828427124746153876, 202.0000000027312126, 195.1715728752538439 ) ) ;
#72273 = CARTESIAN_POINT ( 'NONE',  ( -2.839093476692135984E-14, 197.9375000013655779, 138.5412658750000503 ) ) ;
#72274 = CARTESIAN_POINT ( 'NONE',  ( -1.656854249492403008, 203.8125000027312410, 146.0000000000000284 ) ) ;
#72275 = CARTESIAN_POINT ( 'NONE',  ( -3.313708498984800688, 21.46875000000000000, -7.999999999999958256 ) ) ;
#72276 = ORIENTED_EDGE ( 'NONE', *, *, #9936, .F. ) ;
#72277 = CARTESIAN_POINT ( 'NONE',  ( -1.320432766682874540E-15, 13.59374999795161187, 7.188101187500000044 ) ) ;
#72278 = EDGE_CURVE ( 'NONE', #44181, #20642, #62076, .T. ) ;
#72279 = CARTESIAN_POINT ( 'NONE',  ( -22.18014362889369551, -14.04676729352428843, 191.6616795548064829 ) ) ;
#72280 = CARTESIAN_POINT ( 'NONE',  ( 2.449293598294707893E-16, 20.25000000000000000, -4.000000000000001776 ) ) ;
#72281 = CARTESIAN_POINT ( 'NONE',  ( 11.35316468750000141, 180.7812499965860411, 0.000000000000000000 ) ) ;
#72282 = CARTESIAN_POINT ( 'NONE',  ( 7.188101187500002709, 113.1875000020483810, 2.977408999572649151 ) ) ;
#72283 = CARTESIAN_POINT ( 'NONE',  ( 2.485281374238196062, 295.6875000000000000, -6.000000000000377476 ) ) ;
#72284 = CARTESIAN_POINT ( 'NONE',  ( -2.765530957081998142, 293.6406250017069510, 6.676582343750000703 ) ) ;
#72286 = CARTESIAN_POINT ( 'NONE',  ( -10.00000000000000533, 67.50000000000001421, -1.224646799147354045E-15 ) ) ;
#72285 = DIRECTION ( 'NONE',  ( -0.000000000000000000, -0.000000000000000000, 1.000000000000000000 ) ) ;
#72287 = ORIENTED_EDGE ( 'NONE', *, *, #46532, .F. ) ;
#72289 = CARTESIAN_POINT ( 'NONE',  ( 9.832129032723416984, 227.1354166700806729, -5.676582343750003368 ) ) ;
#72288 = VECTOR ( 'NONE', #21171, 1000.000000000000000 ) ;
#72290 = CARTESIAN_POINT ( 'NONE',  ( -7.188101187499992051, 0.000000000000000000, 1.486552781871753437 ) ) ;
#72291 = DIRECTION ( 'NONE',  ( -1.000000000000000000, -0.000000000000000000, -0.000000000000000000 ) ) ;
#72292 = CARTESIAN_POINT ( 'NONE',  ( 3.313708498984756279, 7.999999999999991118, 15.54905278392014623 ) ) ;
#72293 = DIRECTION ( 'NONE',  ( -0.000000000000000000, -0.000000000000000000, 1.000000000000000000 ) ) ;
#72294 = CARTESIAN_POINT ( 'NONE',  ( 2.754378923186476579E-14, 199.4375000013655779, 194.5412658750000219 ) ) ;
#72295 =( BOUNDED_CURVE ( )  B_SPLINE_CURVE ( 2, ( #31761, #25705, #14763, #54781, #3092, #26077, #49098, #24967, #53663 ),
 .UNSPECIFIED., .F., .F. ) 
 B_SPLINE_CURVE_WITH_KNOTS ( ( 3, 2, 2, 2, 3 ),
 ( 0.1166666666666666546, 0.1250000000000000555, 0.1333333333333334425, 0.1416666666666668573, 0.1500000000000002442 ),
 .UNSPECIFIED. ) 
 CURVE ( )  GEOMETRIC_REPRESENTATION_ITEM ( )  RATIONAL_B_SPLINE_CURVE ( ( 1.000000000000000222, 0.9238795325112867385, 1.000000000000000000, 0.9238795325112867385, 1.000000000000000000, 0.9238795325112867385, 1.000000000000000000, 0.9238795325112844070, 1.000000000000002220 ) ) 
 REPRESENTATION_ITEM ( '' )  );
#72296 = LINE ( 'NONE', #3273, #20156 ) ;
#72297 = FACE_OUTER_BOUND ( 'NONE', #4038, .T. ) ;
#72298 = CARTESIAN_POINT ( 'NONE',  ( -3.313708498984762052, 96.21875000000000000, -8.000000000000000000 ) ) ;
#72299 = CARTESIAN_POINT ( 'NONE',  ( 3.042071309553167069, 117.1354166632526557, -11.35316468749999785 ) ) ;
#72300 = DIRECTION ( 'NONE',  ( 1.000000000000000000, -0.000000000000000000, -0.000000000000000000 ) ) ;
#72301 = CARTESIAN_POINT ( 'NONE',  ( 7.778174593052021635, 7.778174593052023411, 69.43749999999998579 ) ) ;
#72302 = VECTOR ( 'NONE', #67591, 1000.000000000000000 ) ;
#72305 = CARTESIAN_POINT ( 'NONE',  ( 27.99999999999999645, 210.0000000000000284, 169.9999999999999147 ) ) ;
#72304 = CARTESIAN_POINT ( 'NONE',  ( 31.45873412499999944, 201.6250000013656063, 171.4326545832175555 ) ) ;
#72303 = CARTESIAN_POINT ( 'NONE',  ( 28.00000000000002132, 198.1875000013655779, 166.5412658749999082 ) ) ;
#72306 = ORIENTED_EDGE ( 'NONE', *, *, #17146, .F. ) ;
#72307 = CARTESIAN_POINT ( 'NONE',  ( 30.82842712474621294, 205.2500000027312126, 172.8284271247460424 ) ) ;
#72308 = DIRECTION ( 'NONE',  ( 1.000000000000000000, 0.000000000000000000, 0.000000000000000000 ) ) ;
#72309 = CARTESIAN_POINT ( 'NONE',  ( 3.458734124999959025, 195.5000000013655779, 140.5673454167824161 ) ) ;
#72310 = EDGE_CURVE ( 'NONE', #54835, #13929, #6868, .T. ) ;
#72311 = CARTESIAN_POINT ( 'NONE',  ( 31.45873412499997812, 196.8750000013656063, 171.4326545832175839 ) ) ;
#72312 = CARTESIAN_POINT ( 'NONE',  ( -11.00000000000000000, 0.000000000000000000, 113.6875000040967763 ) ) ;
#72313 = CARTESIAN_POINT ( 'NONE',  ( 5.676582343749993598, 190.2604166632526983, 9.832129032723422313 ) ) ;
#72314 = CARTESIAN_POINT ( 'NONE',  ( -7.188101187500000933, 91.43750000204838102, -2.977408999572650483 ) ) ;
#72315 = FACE_OUTER_BOUND ( 'NONE', #65781, .T. ) ;
#72316 = CARTESIAN_POINT ( 'NONE',  ( -4.541265875000002339, 16.74999999863440792, -1.881053915767121998 ) ) ;
#72317 = CARTESIAN_POINT ( 'NONE',  ( 24.54126587499998990, 196.4375000013655779, 169.9999999999998863 ) ) ;
#72318 = CARTESIAN_POINT ( 'NONE',  ( 5.656854249492376141, -5.656854249492374365, 26.89280277982336642 ) ) ;
#72319 = CARTESIAN_POINT ( 'NONE',  ( -5.656854249492380582, 96.31250000000000000, -5.656854249492380582 ) ) ;
#72320 = CARTESIAN_POINT ( 'NONE',  ( -11.35316468749999785, 83.07291666325268409, -3.042071309553167513 ) ) ;
#72321 = ORIENTED_EDGE ( 'NONE', *, *, #12451, .F. ) ;
#72322 = CARTESIAN_POINT ( 'NONE',  ( 5.000000000000000000, 18.53862685874501537, 23.57305537018163477 ) ) ;
#72323 = CARTESIAN_POINT ( 'NONE',  ( -5.082755093536326818, 17.90624999795161187, 5.082755093536325042 ) ) ;
#72324 = CARTESIAN_POINT ( 'NONE',  ( 10.00000000000015987, 39.79166666666675667, 2.679491924311278250 ) ) ;
#72325 = CARTESIAN_POINT ( 'NONE',  ( 2.751064625579944321E-14, 206.7500000000000284, 194.0000000000000568 ) ) ;
#72326 = CARTESIAN_POINT ( 'NONE',  ( 11.35316468750000141, 85.78124999658602690, 0.000000000000000000 ) ) ;
#72327 = ORIENTED_EDGE ( 'NONE', *, *, #58738, .T. ) ;
#72328 = CARTESIAN_POINT ( 'NONE',  ( -7.204075437095965206, -7.204075437095968759, 89.21875000204838102 ) ) ;
#72329 = CARTESIAN_POINT ( 'NONE',  ( -4.220049686691935698, 10.18810118749999916, 110.8750000020483810 ) ) ;
#72330 = CARTESIAN_POINT ( 'NONE',  ( -31.45873412499999944, 196.8750000013656063, 168.5673454167827572 ) ) ;
#72331 = CARTESIAN_POINT ( 'NONE',  ( -3.458734124999960358, 207.6250000013656347, 196.5673454167823877 ) ) ;
#72332 = CARTESIAN_POINT ( 'NONE',  ( 8.000000000000000000, 23.81249999590322020, 0.000000000000000000 ) ) ;
#72334 = CARTESIAN_POINT ( 'NONE',  ( -8.311093377946836114, 92.65624999658601268, -8.311093377946837890 ) ) ;
#72333 = DIRECTION ( 'NONE',  ( 0.000000000000000000, 0.000000000000000000, 1.000000000000000000 ) ) ;
#72335 = CARTESIAN_POINT ( 'NONE',  ( 3.313708498984756279, 7.999999999999991118, 17.04905278392014623 ) ) ;
#72336 = ADVANCED_FACE ( 'NONE', ( #36256 ), #27116, .F. ) ;
#72337 = CARTESIAN_POINT ( 'NONE',  ( 2.449293598294707893E-16, 15.25000000000000000, -4.000000000000001776 ) ) ;
#72338 = CIRCLE ( 'NONE', #39803, 34.85072926314708752 ) ;
#72339 = CARTESIAN_POINT ( 'NONE',  ( -1.836970198721029983E-15, 175.6249999931720538, 10.00000000000000178 ) ) ;
#72340 = CARTESIAN_POINT ( 'NONE',  ( 4.556349186104045934, 11.00000000000000000, 113.0312500000000000 ) ) ;
#72341 = CARTESIAN_POINT ( 'NONE',  ( 4.999999999999999112, -53.31073972600200506, 44.28411094575963602 ) ) ;
#72342 = CARTESIAN_POINT ( 'NONE',  ( 5.676582343749993598, 70.26041666325268409, 9.832129032723422313 ) ) ;
#72343 = CARTESIAN_POINT ( 'NONE',  ( 2.765530957081996366, 295.1406250017069510, -6.676582343750003368 ) ) ;
#72345 = EDGE_CURVE ( 'NONE', #36065, #24466, #42980, .T. ) ;
#72344 = CARTESIAN_POINT ( 'NONE',  ( 7.204075437095966983, 7.204075437095967871, 109.4687500020483810 ) ) ;
#72346 = CARTESIAN_POINT ( 'NONE',  ( -5.676582343750006032, 214.1145833299193555, 9.832129032723418760 ) ) ;
#72347 = ORIENTED_EDGE ( 'NONE', *, *, #14822, .T. ) ;
#72348 = CARTESIAN_POINT ( 'NONE',  ( 11.35316468750000141, 0.7812499965860163487, 0.000000000000000000 ) ) ;
#72349 = CYLINDRICAL_SURFACE ( 'NONE', #31628, 4.000000000000001776 ) ;
#72350 = CARTESIAN_POINT ( 'NONE',  ( 5.000000000000000000, 66.10919140997964405, 23.67639547906079400 ) ) ;
#72352 = CARTESIAN_POINT ( 'NONE',  ( 8.311093377946837890, 201.4062499965859843, -8.311093377946837890 ) ) ;
#72351 = CARTESIAN_POINT ( 'NONE',  ( 11.99999999999999822, 0.000000000000000000, 19.00000000000000355 ) ) ;
#72353 = DIRECTION ( 'NONE',  ( 0.000000000000000000, 0.000000000000000000, -1.000000000000000000 ) ) ;
#72354 = CARTESIAN_POINT ( 'NONE',  ( -2.679491924311228512, 237.0833333401613459, -9.999999999999998224 ) ) ;
#72355 = CARTESIAN_POINT ( 'NONE',  ( -10.00000000000000000, 253.1250000068279746, 0.000000000000000000 ) ) ;
#72356 = VERTEX_POINT ( 'NONE', #17125 ) ;
#72357 = CARTESIAN_POINT ( 'NONE',  ( -8.311093377946841443, 179.2187499965859843, 8.311093377946834337 ) ) ;
#72358 = AXIS2_PLACEMENT_3D ( 'NONE', #61807, #4473, #71615 ) ;
#72359 = CARTESIAN_POINT ( 'NONE',  ( 2.977408999572650927, -7.188101187499990274, 12.45530278187175277 ) ) ;
#72360 = LINE ( 'NONE', #38416, #35820 ) ;
#72361 = ORIENTED_EDGE ( 'NONE', *, *, #66091, .T. ) ;
#72362 = VECTOR ( 'NONE', #47397, 1000.000000000000000 ) ;
#72363 = AXIS2_PLACEMENT_3D ( 'NONE', #52303, #639, #17963 ) ;
#72364 = CARTESIAN_POINT ( 'NONE',  ( -3.313708498984762496, 95.46875000409679046, 7.999999999999998224 ) ) ;
#72365 = CARTESIAN_POINT ( 'NONE',  ( -2.679491924311225848, 6.458333333333333037, -10.00000000000000178 ) ) ;
#72366 = ORIENTED_EDGE ( 'NONE', *, *, #33524, .T. ) ;
#72367 = CARTESIAN_POINT ( 'NONE',  ( -1.656854249492381248, 14.31250000000000000, -4.000000000000001776 ) ) ;
#72368 = CARTESIAN_POINT ( 'NONE',  ( -8.342170076843785083E-16, 20.06249999863440436, 4.541265875000002339 ) ) ;
#72369 = CARTESIAN_POINT ( 'NONE',  ( -4.898587196589407898E-16, 7.999999999999991118, 14.14280278392014623 ) ) ;
#72370 = ADVANCED_FACE ( 'NONE', ( #6197 ), #40520, .T. ) ;
#72371 = CARTESIAN_POINT ( 'NONE',  ( -4.898587196589407898E-16, 7.999999999999991118, 18.64280278392014623 ) ) ;
#72372 = VERTEX_POINT ( 'NONE', #36625 ) ;
#72373 = DIRECTION ( 'NONE',  ( -0.000000000000000000, 1.000000000000000000, -0.000000000000000000 ) ) ;
#72374 = CARTESIAN_POINT ( 'NONE',  ( 7.188101187500000044, 93.40625000204838102, -8.802885111219163269E-16 ) ) ;
#72377 = CARTESIAN_POINT ( 'NONE',  ( 27.99999999999996803, 207.6250000027312126, 165.9999999999998863 ) ) ;
#72376 = CARTESIAN_POINT ( 'NONE',  ( 8.311093377946839666, 255.7812500034139589, 8.311093377946830785 ) ) ;
#72375 = CARTESIAN_POINT ( 'NONE',  ( -3.313708498984757611, 7.999999999999991118, 12.54905277982336287 ) ) ;
#72378 = DIRECTION ( 'NONE',  ( 0.000000000000000000, 1.000000000000000000, 0.000000000000000000 ) ) ;
#72379 = ORIENTED_EDGE ( 'NONE', *, *, #53175, .T. ) ;
#72380 = CARTESIAN_POINT ( 'NONE',  ( 5.676582343750005144, 260.8854166700806445, 9.832129032723416984 ) ) ;
#72381 = CARTESIAN_POINT ( 'NONE',  ( 1.320432766682872962E-15, -7.188101187499992051, 16.86155278187175810 ) ) ;
#72382 = EDGE_LOOP ( 'NONE', ( #62169, #52759, #51798, #160, #12490 ) ) ;
#72383 = ORIENTED_EDGE ( 'NONE', *, *, #21851, .F. ) ;
#72384 = CARTESIAN_POINT ( 'NONE',  ( 1.871523826299183495E-15, -10.18810118749999916, 80.03125000204836681 ) ) ;
#72385 = CARTESIAN_POINT ( 'NONE',  ( 3.042071309553159519, 80.05208332991935549, 11.35316468750000141 ) ) ;
#72386 = CARTESIAN_POINT ( 'NONE',  ( -8.000000000000000000, 105.5937500040967763, -3.313708498984761164 ) ) ;
#72387 = CARTESIAN_POINT ( 'NONE',  ( -10.99999999999999822, -4.556349186104052151, 91.09375000000001421 ) ) ;
#72390 = CARTESIAN_POINT ( 'NONE',  ( -6.676582343750002480, 292.5468750017069510, -2.765530957081996810 ) ) ;
#72389 = CARTESIAN_POINT ( 'NONE',  ( 23.99999999999997868, 197.8125000027312126, 168.3431457505075741 ) ) ;
#72388 = DIRECTION ( 'NONE',  ( 0.000000000000000000, 0.000000000000000000, -1.000000000000000000 ) ) ;
#72391 = CARTESIAN_POINT ( 'NONE',  ( -26.34314575050758123, 203.6875000027311842, 174.0000000000003979 ) ) ;
#72392 = CARTESIAN_POINT ( 'NONE',  ( 38.00000000000000000, -52.99999999999999289, 25.00000000000000000 ) ) ;
#72393 =( BOUNDED_CURVE ( )  B_SPLINE_CURVE ( 2, ( #16408, #72275, #50385, #44732, #67749, #62079, #45102, #10403, #33429 ),
 .UNSPECIFIED., .F., .F. ) 
 B_SPLINE_CURVE_WITH_KNOTS ( ( 3, 2, 2, 2, 3 ),
 ( 0.7916666666666667407, 0.7986111111111111605, 0.8055555555555555802, 0.8124999999999998890, 0.8194444444444443088 ),
 .UNSPECIFIED. ) 
 CURVE ( )  GEOMETRIC_REPRESENTATION_ITEM ( )  RATIONAL_B_SPLINE_CURVE ( ( 0.9999999999999987788, 0.9238795325112879597, 1.000000000000000000, 0.9238795325112867385, 1.000000000000000000, 0.9238795325112867385, 1.000000000000000000, 0.9238795325112879597, 0.9999999999999987788 ) ) 
 REPRESENTATION_ITEM ( '' )  );
#72394 = CARTESIAN_POINT ( 'NONE',  ( 3.458734125000016757, 200.1250000013656063, 199.4326545832176976 ) ) ;
#72395 = EDGE_CURVE ( 'NONE', #5243, #25993, #59313, .T. ) ;
#72396 = CARTESIAN_POINT ( 'NONE',  ( 4.898587196589412829E-16, 4.687499995903220196, -8.000000000000000000 ) ) ;
#72397 = EDGE_CURVE ( 'NONE', #3980, #66991, #50708, .T. ) ;
#72398 = CARTESIAN_POINT ( 'NONE',  ( 29.43265458321766559, 197.8750000013656063, 166.5412658749999650 ) ) ;
#72399 = CARTESIAN_POINT ( 'NONE',  ( 7.188101187500000044, 9.843749997951610098, 0.000000000000000000 ) ) ;
#72400 = CARTESIAN_POINT ( 'NONE',  ( -7.999999999999989342, -3.313708498984762496, 25.11155278392014623 ) ) ;
#72401 = CARTESIAN_POINT ( 'NONE',  ( -5.000000000000000888, 242.2916666734946318, -8.660254037844387298 ) ) ;
#72402 = CARTESIAN_POINT ( 'NONE',  ( 1.320432766682874540E-15, 108.4062500020483810, 7.188101187500000044 ) ) ;
#72404 = CARTESIAN_POINT ( 'NONE',  ( 3.544144923083023979, -50.27229464832290518, -40.88493206427763482 ) ) ;
#72403 = CARTESIAN_POINT ( 'NONE',  ( 6.000000000000003553, 289.5000000034140726, 2.485281374238571317 ) ) ;
#72405 = CARTESIAN_POINT ( 'NONE',  ( -11.35316468749999608, 219.4270833367473301, 3.042071309553173730 ) ) ;
#72406 = CARTESIAN_POINT ( 'NONE',  ( 6.000000000000001776, 288.5625000034140157, -7.347880794884121708E-16 ) ) ;
#72407 = CARTESIAN_POINT ( 'NONE',  ( 7.188101187499991163, 2.977408999572648707, 17.70530278187175455 ) ) ;
#72408 = CARTESIAN_POINT ( 'NONE',  ( -2.751064625579944321E-14, 207.8750000027312126, 146.0000000000000284 ) ) ;
#72409 = CARTESIAN_POINT ( 'NONE',  ( -3.042071309553173730, 44.32291666325268409, 11.35316468749999785 ) ) ;
#72410 = CARTESIAN_POINT ( 'NONE',  ( -2.980530153384850500, -44.60677576848183890, 139.1435921626475363 ) ) ;
#72411 = CARTESIAN_POINT ( 'NONE',  ( -10.00000000000000355, 4.583333326505366401, 2.679491924311223183 ) ) ;
#72412 = CARTESIAN_POINT ( 'NONE',  ( -29.65685424949239746, 200.1875000027312126, 166.0000000000003126 ) ) ;
#72413 = ORIENTED_EDGE ( 'NONE', *, *, #19956, .T. ) ;
#72414 = CARTESIAN_POINT ( 'NONE',  ( 8.660254037844385522, 141.4583333265053682, 5.000000000000005329 ) ) ;
#72415 = CARTESIAN_POINT ( 'NONE',  ( 7.999999999999991118, 9.797174393178815797E-16, 18.08030277982336642 ) ) ;
#72416 = EDGE_CURVE ( 'NONE', #15853, #15758, #55099, .T. ) ;
#72417 = CARTESIAN_POINT ( 'NONE',  ( -9.832129032723420536, 43.69791666325268409, 5.676582343749997150 ) ) ;
#72418 = CARTESIAN_POINT ( 'NONE',  ( 7.778174593052023411, -7.778174593052021635, 79.75000000409676204 ) ) ;
#72419 = CARTESIAN_POINT ( 'NONE',  ( -1.432654583217662481, 202.3750000013656063, 145.4587341250000350 ) ) ;
#72421 = CIRCLE ( 'NONE', #68817, 8.000000000000000000 ) ;
#72420 = CARTESIAN_POINT ( 'NONE',  ( -1.739508062077480988, -67.70228923712446090, -20.12326043015357868 ) ) ;
#72422 = DIRECTION ( 'NONE',  ( 0.000000000000000000, 0.000000000000000000, -1.000000000000000000 ) ) ;
#72424 = CARTESIAN_POINT ( 'NONE',  ( 11.35316468749999963, 45.98958332991934128, -3.042071309553165293 ) ) ;
#72423 = CARTESIAN_POINT ( 'NONE',  ( 5.082755093536325042, 98.09375000204838102, -5.082755093536325930 ) ) ;
#72425 = CARTESIAN_POINT ( 'NONE',  ( -5.656854249492375253, 5.656854249492375253, 11.14280277982336642 ) ) ;
#72426 = CARTESIAN_POINT ( 'NONE',  ( 5.656854249492374365, 5.656854249492375253, 21.45530278392014623 ) ) ;
#72427 = CARTESIAN_POINT ( 'NONE',  ( -5.676582343749998039, 167.4479166632526983, -9.832129032723420536 ) ) ;
#72428 =( BOUNDED_CURVE ( )  B_SPLINE_CURVE ( 2, ( #51073, #63508, #51822, #57119, #74086, #6181, #68422, #52202, #34868, #16725, #29189, #5432, #58251 ),
 .UNSPECIFIED., .F., .F. ) 
 B_SPLINE_CURVE_WITH_KNOTS ( ( 3, 2, 2, 2, 2, 2, 3 ),
 ( 0.9510869565217392463, 0.9528985507246378051, 0.9547101449275362528, 0.9565217391304348116, 0.9583333333333333703, 0.9601449275362318181, 0.9619565217391303769 ),
 .UNSPECIFIED. ) 
 CURVE ( )  GEOMETRIC_REPRESENTATION_ITEM ( )  RATIONAL_B_SPLINE_CURVE ( ( 0.9999999999999978906, 0.9659258262890704216, 1.000000000000000000, 0.9659258262890683122, 1.000000000000000000, 0.9659258262890683122, 1.000000000000000000, 0.9659258262890683122, 1.000000000000000000, 0.9659258262890683122, 1.000000000000000000, 0.9659258262890704216, 0.9999999999999978906 ) ) 
 REPRESENTATION_ITEM ( '' )  );
#72429 = CARTESIAN_POINT ( 'NONE',  ( -8.660254037844390851, 129.7916666598387110, 4.999999999999998224 ) ) ;
#72430 = CARTESIAN_POINT ( 'NONE',  ( 2.977408999572650039, 110.5625000020483810, -7.188101187500001821 ) ) ;
#72431=STYLED_ITEM('',(#74692),#17160);
#72432 = ORIENTED_EDGE ( 'NONE', *, *, #46018, .F. ) ;
#72433 = CARTESIAN_POINT ( 'NONE',  ( 2.584176044310537712, -67.83040087281474939, -20.22720375976230756 ) ) ;
#72434 = CARTESIAN_POINT ( 'NONE',  ( -8.311093377946841443, 19.21874999658601979, 8.311093377946834337 ) ) ;
#72435 = CARTESIAN_POINT ( 'NONE',  ( 3.999999999999960032, 198.0625000027312410, 143.6568542494924259 ) ) ;
#72436 = VERTEX_POINT ( 'NONE', #53973 ) ;
#72437 = CARTESIAN_POINT ( 'NONE',  ( -32.00000000000000000, 205.3750000027312126, 170.0000000000004547 ) ) ;
#72438 = CARTESIAN_POINT ( 'NONE',  ( 4.220049686691934809, 10.18810118749999916, 77.68750000204838102 ) ) ;
#72439 = FACE_OUTER_BOUND ( 'NONE', #10596, .T. ) ;
#72441 = CARTESIAN_POINT ( 'NONE',  ( 6.951808397369818766E-16, 147.0312499965860411, -11.35316468750000141 ) ) ;
#72440 = CARTESIAN_POINT ( 'NONE',  ( -10.00000000000000888, 7.500000000000005329, -1.224646799147354440E-15 ) ) ;
#72442 = CARTESIAN_POINT ( 'NONE',  ( 7.188101187499999156, 2.249999997951610098, 2.977408999572654924 ) ) ;
#72443 = AXIS2_PLACEMENT_3D ( 'NONE', #58971, #58600, #1265 ) ;
#72444 = CARTESIAN_POINT ( 'NONE',  ( 7.999999999999991118, 9.797174393178815797E-16, 12.13655278432982421 ) ) ;
#72445 = DIRECTION ( 'NONE',  ( -0.000000000000000000, -1.000000000000000000, -0.000000000000000000 ) ) ;
#72446 = CARTESIAN_POINT ( 'NONE',  ( -11.35316468749999608, 239.1145833367473301, 3.042071309553173730 ) ) ;
#72447 = EDGE_CURVE ( 'NONE', #34777, #35339, #58452, .T. ) ;
#72448 = CARTESIAN_POINT ( 'NONE',  ( 10.18810118750000093, -4.220049686691933921, 86.68750000204836681 ) ) ;
#72449 = ORIENTED_EDGE ( 'NONE', *, *, #6918, .F. ) ;
#72450 = CARTESIAN_POINT ( 'NONE',  ( 12.00000000000000178, 0.000000000000000000, -28.00000000000000000 ) ) ;
#72451 = CARTESIAN_POINT ( 'NONE',  ( -2.849036369511732440E-14, 199.3750000027312126, 138.0000000000000568 ) ) ;
#72452 = CARTESIAN_POINT ( 'NONE',  ( -9.832129032723420536, 104.0104166632526841, 5.676582343749997150 ) ) ;
#72453 = CARTESIAN_POINT ( 'NONE',  ( 10.18810118749999916, 1.247682550866122264E-15, 98.40625000204838102 ) ) ;
#72454 = CARTESIAN_POINT ( 'NONE',  ( -4.541265875000003227, 21.96751355773092129, 0.9033139658336462041 ) ) ;
#72455 = ORIENTED_EDGE ( 'NONE', *, *, #10268, .F. ) ;
#72456 = ORIENTED_EDGE ( 'NONE', *, *, #58337, .T. ) ;
#72457 = VECTOR ( 'NONE', #4305, 1000.000000000000000 ) ;
#72458 = CARTESIAN_POINT ( 'NONE',  ( 4.541265875000001451, 3.374999998634406584, 1.881053915767124440 ) ) ;
#72459 = CARTESIAN_POINT ( 'NONE',  ( 7.188101187499999156, 9.374999997951610098, 2.977408999572654924 ) ) ;
#72460 = CARTESIAN_POINT ( 'NONE',  ( -7.999999999999998224, 116.2812500040967620, 3.313708498984766493 ) ) ;
#72461 = CARTESIAN_POINT ( 'NONE',  ( 7.204075437095968759, -7.204075437095966983, 94.09375000204838102 ) ) ;
#72462 = CARTESIAN_POINT ( 'NONE',  ( -28.00000000000002132, 200.6875000013656063, 166.5412658750003629 ) ) ;
#72463 = LINE ( 'NONE', #53633, #57261 ) ;
#72464 = CARTESIAN_POINT ( 'NONE',  ( 1.656854249492381248, 5.187500000000001776, -4.000000000000001776 ) ) ;
#72465 = CARTESIAN_POINT ( 'NONE',  ( 2.828427124746191623, 16.87499999726881583, -2.828427124746191623 ) ) ;
#72466 = CARTESIAN_POINT ( 'NONE',  ( 2.780723358947928197E-16, 4.562499998634407028, -4.541265875000002339 ) ) ;
#72467 = CARTESIAN_POINT ( 'NONE',  ( -2.849036369511732440E-14, 202.2500000000000000, 138.0000000000000568 ) ) ;
#72468 = EDGE_LOOP ( 'NONE', ( #28227, #19112, #22070 ) ) ;
#72469 = CARTESIAN_POINT ( 'NONE',  ( 2.839093476692135984E-14, 194.6875000013655779, 201.4587341250000350 ) ) ;
#72470 = AXIS2_PLACEMENT_3D ( 'NONE', #72602, #43542, #2449 ) ;
#72472 = CARTESIAN_POINT ( 'NONE',  ( 1.836970198721029589E-15, 234.3750000068279746, 10.00000000000000178 ) ) ;
#72471 = CARTESIAN_POINT ( 'NONE',  ( -30.44569435410875968, 197.8125000013656063, 172.4456943541092642 ) ) ;
#72473 = CARTESIAN_POINT ( 'NONE',  ( -4.541265875000002339, 17.81249999863440792, -5.561446717895856393E-16 ) ) ;
#72474 = CARTESIAN_POINT ( 'NONE',  ( 2.261370252296129202, -46.98122180473003340, 151.1345299079913502 ) ) ;
#72475 = VECTOR ( 'NONE', #23795, 1000.000000000000000 ) ;
#72476 = CARTESIAN_POINT ( 'NONE',  ( 7.188101187499993827, -2.977408999572645598, 5.142802781871752771 ) ) ;
#72477 = EDGE_LOOP ( 'NONE', ( #6821, #40840 ) ) ;
#72478 = VERTEX_POINT ( 'NONE', #48665 ) ;
#72479 = CARTESIAN_POINT ( 'NONE',  ( -4.220049686691935698, 10.18810118749999916, 97.37500000204839523 ) ) ;
#72480 = LINE ( 'NONE', #3074, #60015 ) ;
#72481 = CARTESIAN_POINT ( 'NONE',  ( -26.56734541678232731, 203.2500000013655495, 173.4587341250003760 ) ) ;
#72482 = CARTESIAN_POINT ( 'NONE',  ( -30.82842712474621294, 201.1250000000000284, 167.1715728752542134 ) ) ;
#72483 = CARTESIAN_POINT ( 'NONE',  ( 2.754378923186476579E-14, 207.4375000013656063, 194.5412658750000219 ) ) ;
#72484 = CARTESIAN_POINT ( 'NONE',  ( -2.828427124746192067, 21.37499999726881583, 2.828427124746190735 ) ) ;
#72485 = CARTESIAN_POINT ( 'NONE',  ( -2.679491924311225848, 106.4583333333333286, -10.00000000000000178 ) ) ;
#72486 = EDGE_CURVE ( 'NONE', #3433, #67329, #58477, .T. ) ;
#72487 = CARTESIAN_POINT ( 'NONE',  ( -3.313708498984762496, 113.2812500000000000, 7.999999999999998224 ) ) ;
#72488 = CARTESIAN_POINT ( 'NONE',  ( 4.721056650416000089, 292.9843750017070079, 4.721056650415999201 ) ) ;
#72489 = CARTESIAN_POINT ( 'NONE',  ( -5.082755093536319713, 5.082755093536319713, 9.174052781871752771 ) ) ;
#72490 = ORIENTED_EDGE ( 'NONE', *, *, #37164, .T. ) ;
#72491 = CARTESIAN_POINT ( 'NONE',  ( 5.656854249492380582, 19.68750000000000355, -5.656854249492380582 ) ) ;
#72492 = CARTESIAN_POINT ( 'NONE',  ( -8.000000000000000000, 18.46874999590322020, -3.313708498984762496 ) ) ;
#72493 = CARTESIAN_POINT ( 'NONE',  ( 2.445694354108783664, 203.3125000013656063, 144.4456943541088663 ) ) ;
#72494 = CARTESIAN_POINT ( 'NONE',  ( -21.26642202173794516, -37.13050781843490711, 147.4312961482535798 ) ) ;
#72496 = CARTESIAN_POINT ( 'NONE',  ( -2.839093476692135984E-14, 202.9375000013656063, 138.5412658750000503 ) ) ;
#72495 = CARTESIAN_POINT ( 'NONE',  ( -7.778174593052023411, 7.778174593052023411, 111.8125000000000000 ) ) ;
#72497 = CARTESIAN_POINT ( 'NONE',  ( -3.042071309553159075, 255.2604166700806445, 11.35316468749999963 ) ) ;
#72498 = DIRECTION ( 'NONE',  ( 1.000000000000000000, 0.000000000000000000, 0.000000000000000000 ) ) ;
#72499 = LINE ( 'NONE', #32524, #67424 ) ;
#72500 = CARTESIAN_POINT ( 'NONE',  ( 8.660254037844389075, 225.4166666666666856, -5.000000000000000000 ) ) ;
#72501 = CARTESIAN_POINT ( 'NONE',  ( 5.082755093536320601, -5.082755093536318824, 2.424052781871754103 ) ) ;
#72502 = CARTESIAN_POINT ( 'NONE',  ( 6.951808397369818766E-16, 197.3437499965860127, -11.35316468750000141 ) ) ;
#72503 = CARTESIAN_POINT ( 'NONE',  ( -8.660254037844387298, 133.9583333265053682, -5.000000000000004441 ) ) ;
#72504 = CARTESIAN_POINT ( 'NONE',  ( 3.211159895383561835, 6.437499998634407028, -3.211159895383561835 ) ) ;
#72505 = CARTESIAN_POINT ( 'NONE',  ( 6.000000000000003553, 290.4375000000000000, 2.485281374238571317 ) ) ;
#72506 = LINE ( 'NONE', #14398, #29846 ) ;
#72507 = ORIENTED_EDGE ( 'NONE', *, *, #53091, .F. ) ;
#72508 = AXIS2_PLACEMENT_3D ( 'NONE', #33113, #37636, #21381 ) ;
#72510 = EDGE_CURVE ( 'NONE', #62863, #15665, #2284, .T. ) ;
#72509 = CARTESIAN_POINT ( 'NONE',  ( -2.754378923186476579E-14, 206.4375000013656063, 145.4587341250000350 ) ) ;
#72511 = CARTESIAN_POINT ( 'NONE',  ( 3.042071309553167069, 6.822916663252682312, -11.35316468749999785 ) ) ;
#72512 = CARTESIAN_POINT ( 'NONE',  ( 7.778174593052021635, 7.778174593052023411, 96.62500000409676204 ) ) ;
#72513 = DIRECTION ( 'NONE',  ( 0.000000000000000000, 0.000000000000000000, 1.000000000000000000 ) ) ;
#72514 = CARTESIAN_POINT ( 'NONE',  ( -26.56734541678228112, 201.0000000013655779, 173.4587341250003476 ) ) ;
#72515 = DIRECTION ( 'NONE',  ( -0.000000000000000000, -0.000000000000000000, 1.000000000000000000 ) ) ;
#72517 = CARTESIAN_POINT ( 'NONE',  ( -2.775557561562891351E-14, 210.0000000000000284, 146.0000000000000284 ) ) ;
#72516 = CARTESIAN_POINT ( 'NONE',  ( 5.082755093536326818, 115.7187500020483810, 5.082755093536325042 ) ) ;
#72518 = CARTESIAN_POINT ( 'NONE',  ( -3.313708498984757167, 7.999999999999991118, 24.54905277982336287 ) ) ;
#72519 = CARTESIAN_POINT ( 'NONE',  ( -3.042071309553164404, 127.2395833299193555, -11.35316468749999963 ) ) ;
#72520 = EDGE_CURVE ( 'NONE', #30135, #56146, #72046, .T. ) ;
#72521 = CARTESIAN_POINT ( 'NONE',  ( 7.320508075688774596, 87.49999999317202537, -7.320508075688774596 ) ) ;
#72522 = CARTESIAN_POINT ( 'NONE',  ( -7.188101187500000044, 91.15625000204838102, 0.000000000000000000 ) ) ;
#72523 = CARTESIAN_POINT ( 'NONE',  ( -1.881053915767121554, 21.74999999863440436, -4.541265875000002339 ) ) ;
#72524 = CARTESIAN_POINT ( 'NONE',  ( -10.00000000000000355, 39.58333332650536107, 2.679491924311223183 ) ) ;
#72525 = ORIENTED_EDGE ( 'NONE', *, *, #35455, .T. ) ;
#72526 = DIRECTION ( 'NONE',  ( -0.000000000000000000, 1.000000000000000000, -1.563033456626094573E-30 ) ) ;
#72527 =( BOUNDED_CURVE ( )  B_SPLINE_CURVE ( 2, ( #7873, #30878, #25204, #48217, #37290, #71225, #19918, #42563, #36915 ),
 .UNSPECIFIED., .F., .F. ) 
 B_SPLINE_CURVE_WITH_KNOTS ( ( 3, 2, 2, 2, 3 ),
 ( 0.6333333333333339699, 0.6416666666666673846, 0.6500000000000006883, 0.6583333333333339921, 0.6666666666666672958 ),
 .UNSPECIFIED. ) 
 CURVE ( )  GEOMETRIC_REPRESENTATION_ITEM ( )  RATIONAL_B_SPLINE_CURVE ( ( 0.9999999999999938938, 0.9238795325112928447, 1.000000000000000000, 0.9238795325112867385, 1.000000000000000000, 0.9238795325112867385, 1.000000000000000000, 0.9238795325112806323, 1.000000000000005995 ) ) 
 REPRESENTATION_ITEM ( '' )  );
#72528 = CARTESIAN_POINT ( 'NONE',  ( -4.721056650415999201, 291.4843750017070079, -4.721056650415999201 ) ) ;
#72529 = LINE ( 'NONE', #60081, #24274 ) ;
#72530 = CARTESIAN_POINT ( 'NONE',  ( -4.898587196589407898E-16, 7.999999999999991118, 2.142802783920143117 ) ) ;
#72531 = CARTESIAN_POINT ( 'NONE',  ( -5.676582343750006032, 164.1145833299193555, 9.832129032723418760 ) ) ;
#72532 = CARTESIAN_POINT ( 'NONE',  ( 3.999999999999960032, 197.9375000000000000, 143.6568542494924259 ) ) ;
#72533 = CARTESIAN_POINT ( 'NONE',  ( -1.836970198721029983E-15, 205.6249999931720538, 10.00000000000000178 ) ) ;
#72534 = FACE_OUTER_BOUND ( 'NONE', #15075, .T. ) ;
#72535 = ADVANCED_FACE ( 'NONE', ( #25279 ), #3032, .T. ) ;
#72536 = CARTESIAN_POINT ( 'NONE',  ( -10.18810118749999916, 0.000000000000000000, 102.5312500020483810 ) ) ;
#72537 = ORIENTED_EDGE ( 'NONE', *, *, #20111, .F. ) ;
#72538 = CIRCLE ( 'NONE', #61711, 71.70204102886728492 ) ;
#72539 = CARTESIAN_POINT ( 'NONE',  ( 38.00000000000000000, -53.00000000000000000, 15.00000000000000178 ) ) ;
#72540 = CARTESIAN_POINT ( 'NONE',  ( 5.676582343750001591, 151.9270833299193555, -9.832129032723420536 ) ) ;
#72541 = CARTESIAN_POINT ( 'NONE',  ( -10.00000000000000355, 217.2916666666667140, -2.679491924311231621 ) ) ;
#72542 = CARTESIAN_POINT ( 'NONE',  ( -2.445694354108783219, 204.8125000013656063, 200.4456943541088663 ) ) ;
#72543 = CARTESIAN_POINT ( 'NONE',  ( -7.999999999999991118, 3.313708498984757167, 0.9240527839201456706 ) ) ;
#72544 = CARTESIAN_POINT ( 'NONE',  ( -8.311093377946836114, 62.96874999658601979, -8.311093377946837890 ) ) ;
#72545 = B_SPLINE_CURVE_WITH_KNOTS ( 'NONE', 3,
 ( #11007, #22679, #68344, #16640, #68711, #34409 ),
 .UNSPECIFIED., .F., .F.,
 ( 4, 2, 4 ),
 ( 0.01452727543195641083, 0.01715716534226973539, 0.01978705525258305647 ),
 .UNSPECIFIED. ) ;
#72546 = VERTEX_POINT ( 'NONE', #26782 ) ;
#72547 = CARTESIAN_POINT ( 'NONE',  ( -7.204075437095967871, 7.204075437095967871, 110.9687500020483810 ) ) ;
#72548 = CARTESIAN_POINT ( 'NONE',  ( -1.881053915767121776, 9.749999998634404363, -4.541265875000002339 ) ) ;
#72549 = ORIENTED_EDGE ( 'NONE', *, *, #62206, .T. ) ;
#72550 = CARTESIAN_POINT ( 'NONE',  ( -2.977408999572650039, 21.93749999795161543, -7.188101187500001821 ) ) ;
#72551 = CARTESIAN_POINT ( 'NONE',  ( -4.999999999999998224, 108.5416666598387110, -8.660254037844389075 ) ) ;
#72552 = CARTESIAN_POINT ( 'NONE',  ( 38.00000000000000000, 53.00000000000000000, 15.00000000000000178 ) ) ;
#72553 = CARTESIAN_POINT ( 'NONE',  ( 2.977408999572650927, 17.62499999795161543, -7.188101187500001821 ) ) ;
#72554 = CARTESIAN_POINT ( 'NONE',  ( -7.188101187499992051, 0.000000000000000000, 4.486552781871752771 ) ) ;
#72555 = CARTESIAN_POINT ( 'NONE',  ( 1.871523826299183495E-15, -10.18810118749999916, 107.4062500020483668 ) ) ;
#72556 = AXIS2_PLACEMENT_3D ( 'NONE', #36462, #59476, #71140 ) ;
#72557 = B_SPLINE_CURVE_WITH_KNOTS ( 'NONE', 1,
 ( #41674, #30351 ),
 .UNSPECIFIED., .F., .F.,
 ( 2, 2 ),
 ( 0.000000000000000000, 1.000000000000000000 ),
 .UNSPECIFIED. ) ;
#72558 = LINE ( 'NONE', #31823, #70334 ) ;
#72559 = CARTESIAN_POINT ( 'NONE',  ( 2.828427124746190291, 4.624999997268813168, 2.828427124746192067 ) ) ;
#72560 = CARTESIAN_POINT ( 'NONE',  ( -26.34314575050770202, 209.0625000027312126, 166.0000000000003695 ) ) ;
#72561 = VERTEX_POINT ( 'NONE', #19994 ) ;
#72562 = AXIS2_PLACEMENT_3D ( 'NONE', #60915, #57515, #4704 ) ;
#72563 = CARTESIAN_POINT ( 'NONE',  ( 3.458734125000016313, 207.8750000013656063, 199.4326545832176691 ) ) ;
#72564 = AXIS2_PLACEMENT_3D ( 'NONE', #12194, #34497, #28435 ) ;
#72565 = CARTESIAN_POINT ( 'NONE',  ( -30.44569435410876324, 208.8125000013656063, 172.4456943541092642 ) ) ;
#72566 = CARTESIAN_POINT ( 'NONE',  ( -3.211159895383562723, 5.937499998634407028, 3.211159895383561391 ) ) ;
#72567 = CARTESIAN_POINT ( 'NONE',  ( 11.00000000000000000, 1.347111479062088405E-15, 114.2499999999999858 ) ) ;
#72568 = CARTESIAN_POINT ( 'NONE',  ( -5.082755093536319713, 5.082755093536319713, 25.29905278187175810 ) ) ;
#72569 = VERTEX_POINT ( 'NONE', #31322 ) ;
#72570 = CARTESIAN_POINT ( 'NONE',  ( 11.00000000000000000, 1.347111479062088405E-15, 90.25000000000000000 ) ) ;
#72571 = VERTEX_POINT ( 'NONE', #38488 ) ;
#72572 = CARTESIAN_POINT ( 'NONE',  ( 0.000000000000000000, 0.000000000000000000, 0.000000000000000000 ) ) ;
#72573 = CYLINDRICAL_SURFACE ( 'NONE', #49644, 4.000000000000001776 ) ;
#72574 = CARTESIAN_POINT ( 'NONE',  ( -3.458734124999959914, 203.4375000013656063, 198.0000000000000284 ) ) ;
#72575 = CARTESIAN_POINT ( 'NONE',  ( 25.55430564589115505, 198.0625000013656063, 167.5543056458911053 ) ) ;
#72576 = CARTESIAN_POINT ( 'NONE',  ( 2.679491924311222739, 68.95833333333334281, 10.00000000000000355 ) ) ;
#72577 = CARTESIAN_POINT ( 'NONE',  ( -4.401442555609581635E-16, 97.15625000204839523, -7.188101187500000044 ) ) ;
#72578 = CARTESIAN_POINT ( 'NONE',  ( -4.242640687119286547, 291.8750000000000000, -4.242640687119286547 ) ) ;
#72580 = CARTESIAN_POINT ( 'NONE',  ( -10.00000000000000000, 254.7916666666666856, -2.679491924311226292 ) ) ;
#72579 = CARTESIAN_POINT ( 'NONE',  ( 32.00000000000000000, 207.3750000027312126, 169.9999999999998863 ) ) ;
#72581 = ORIENTED_EDGE ( 'NONE', *, *, #46321, .F. ) ;
#72582 = DIRECTION ( 'NONE',  ( 0.000000000000000000, 0.000000000000000000, 1.000000000000000000 ) ) ;
#72583 = CARTESIAN_POINT ( 'NONE',  ( -33.48318503342263597, 175.8115626168855101, 156.1427595010634377 ) ) ;
#72584 = CARTESIAN_POINT ( 'NONE',  ( 2.828427124746152987, 198.2500000027312126, 139.1715728752538723 ) ) ;
#72585 = DIRECTION ( 'NONE',  ( 0.000000000000000000, 0.000000000000000000, 1.000000000000000000 ) ) ;
#72586 = DIRECTION ( 'NONE',  ( 0.000000000000000000, 0.000000000000000000, 1.000000000000000000 ) ) ;
#72587 = CARTESIAN_POINT ( 'NONE',  ( 8.660254037844389075, 252.0833333333333144, 4.999999999999997335 ) ) ;
#72588 = CARTESIAN_POINT ( 'NONE',  ( 32.00000000000000711, 204.3125000000000000, 168.3431457505075457 ) ) ;
#72589 = CARTESIAN_POINT ( 'NONE',  ( -8.660254037844390851, 192.9166666666666856, 4.999999999999998224 ) ) ;
#72590 = LINE ( 'NONE', #56361, #53634 ) ;
#72591 = CARTESIAN_POINT ( 'NONE',  ( -7.188101187499992051, 0.000000000000000000, 19.86155278187175455 ) ) ;
#72592 = CARTESIAN_POINT ( 'NONE',  ( -11.35316468750000141, 158.8020833299193555, 3.042071309553159963 ) ) ;
#72593 = LINE ( 'NONE', #67309, #13210 ) ;
#72594 = CARTESIAN_POINT ( 'NONE',  ( -5.000000000000000000, 53.50647209750528077, 45.02947987234111338 ) ) ;
#72595 = CARTESIAN_POINT ( 'NONE',  ( -0.1981329310304640878, -42.00000000000002132, 151.0000000000000284 ) ) ;
#72597 = CARTESIAN_POINT ( 'NONE',  ( -31.00000000000001421, 38.00000000000000711, 65.00000000000000000 ) ) ;
#72596 = DIRECTION ( 'NONE',  ( -0.000000000000000000, 1.000000000000000000, -0.000000000000000000 ) ) ;
#72598 = ORIENTED_EDGE ( 'NONE', *, *, #68668, .T. ) ;
#72599 = CARTESIAN_POINT ( 'NONE',  ( 11.35316468749999963, 21.30208332991935194, -3.042071309553165293 ) ) ;
#72600 = CARTESIAN_POINT ( 'NONE',  ( 8.660254037844389075, 97.29166665983871098, -5.000000000000000000 ) ) ;
#72601 = CARTESIAN_POINT ( 'NONE',  ( -7.999999999999991118, 0.000000000000000000, 17.51780278392014623 ) ) ;
#72602 = CARTESIAN_POINT ( 'NONE',  ( 0.000000000000000000, 0.000000000000000000, -21.50000000000000000 ) ) ;
#72603 = CARTESIAN_POINT ( 'NONE',  ( -2.754378923186476579E-14, 202.1875000013656063, 145.4587341250000350 ) ) ;
#72604 = EDGE_CURVE ( 'NONE', #54592, #46734, #61491, .T. ) ;
#72605 = AXIS2_PLACEMENT_3D ( 'NONE', #25177, #19518, #14973 ) ;
#72606 = CARTESIAN_POINT ( 'NONE',  ( -7.320508075688778149, 44.99999999317203958, 7.320508075688769267 ) ) ;
#72607 = CARTESIAN_POINT ( 'NONE',  ( -7.188101187500000044, 112.1562500020483952, 0.000000000000000000 ) ) ;
#72608 = CARTESIAN_POINT ( 'NONE',  ( 4.541265875000002339, 9.499999998634406140, -1.881053915767121554 ) ) ;
#72609 = CARTESIAN_POINT ( 'NONE',  ( 10.00000000000001066, 219.7916666666666856, 2.679491924311238282 ) ) ;
#72610 = CARTESIAN_POINT ( 'NONE',  ( -7.999999999999989342, -3.313708498984762496, 8.424052779823362869 ) ) ;
#72612 = CARTESIAN_POINT ( 'NONE',  ( 4.000000000000001776, 1.000000000000000222, 0.000000000000000000 ) ) ;
#72611 = CARTESIAN_POINT ( 'NONE',  ( 2.454488697237193318, 194.5261102419722761, 139.4597140321077973 ) ) ;
#72613 = ORIENTED_EDGE ( 'NONE', *, *, #42688, .F. ) ;
#72614 = EDGE_LOOP ( 'NONE', ( #20009, #34113, #1485, #65369 ) ) ;
#72615 = CARTESIAN_POINT ( 'NONE',  ( -7.320508075688778149, 223.1250000000000284, 7.320508075688769267 ) ) ;
#72616 = CARTESIAN_POINT ( 'NONE',  ( 2.020667218593132706E-15, -11.00000000000000000, 82.37499999999998579 ) ) ;
#72617 = CARTESIAN_POINT ( 'NONE',  ( 11.35316468749999608, 221.9270833367473017, -3.042071309553167513 ) ) ;
#72618 = VECTOR ( 'NONE', #26303, 1000.000000000000000 ) ;
#72619 = CARTESIAN_POINT ( 'NONE',  ( 3.042071309553159519, 129.7395833299193555, 11.35316468750000141 ) ) ;
#72620 = ORIENTED_EDGE ( 'NONE', *, *, #48541, .F. ) ;
#72621 = CARTESIAN_POINT ( 'NONE',  ( -4.999999999999999112, 15.47455834364811622, -69.96446835377025764 ) ) ;
#72622 = CARTESIAN_POINT ( 'NONE',  ( -7.204075437095967871, 7.204075437095967871, 91.46875000204838102 ) ) ;
#72623 = CARTESIAN_POINT ( 'NONE',  ( -8.000000000000000000, 93.40625000000000000, -3.313708498984761164 ) ) ;
#72624 = CARTESIAN_POINT ( 'NONE',  ( -3.999999999999960032, 206.9375000000000284, 196.3431457505076594 ) ) ;
#72625 = DIRECTION ( 'NONE',  ( 1.000000000000000000, 0.000000000000000000, 0.000000000000000000 ) ) ;
#72627 = CARTESIAN_POINT ( 'NONE',  ( -11.35316468750000141, 123.4895833299193555, 3.042071309553159963 ) ) ;
#72626 = CARTESIAN_POINT ( 'NONE',  ( 29.65685424949223403, 196.0625000000000284, 174.0000000000000000 ) ) ;
#72628 = LINE ( 'NONE', #37929, #21688 ) ;
#72629 = ORIENTED_EDGE ( 'NONE', *, *, #43058, .T. ) ;
#72630 = ADVANCED_FACE ( 'NONE', ( #30952 ), #14705, .T. ) ;
#72631 = CARTESIAN_POINT ( 'NONE',  ( -8.000000000000000000, 109.9062500000000000, -3.313708498984761164 ) ) ;
#72632 = CARTESIAN_POINT ( 'NONE',  ( -19.81901786544401745, 177.9744831197524206, 139.1998822286060999 ) ) ;
#72633 = CARTESIAN_POINT ( 'NONE',  ( 8.311093377946834337, 110.4687499965860127, 8.311093377946839666 ) ) ;
#72634 = CARTESIAN_POINT ( 'NONE',  ( -3.458734124999959914, 205.4375000013656063, 198.0000000000000284 ) ) ;
#72635 = CARTESIAN_POINT ( 'NONE',  ( 2.977408999572650927, 19.12499999795161898, -7.188101187500000933 ) ) ;
#72636 = CARTESIAN_POINT ( 'NONE',  ( 1.871523826299183495E-15, -10.18810118749999916, 81.90625000204838102 ) ) ;
#72637 = ADVANCED_FACE ( 'NONE', ( #66022 ), #32078, .T. ) ;
#72638 = CARTESIAN_POINT ( 'NONE',  ( 11.35316468750000141, 21.09374999658601624, 0.000000000000000000 ) ) ;
#72639 = ORIENTED_EDGE ( 'NONE', *, *, #29419, .F. ) ;
#72640 = DIRECTION ( 'NONE',  ( -0.000000000000000000, 1.000000000000000000, -0.000000000000000000 ) ) ;
#72641 = CARTESIAN_POINT ( 'NONE',  ( 1.836970198721029589E-15, 244.3750000068280031, 10.00000000000000000 ) ) ;
#72642 = CARTESIAN_POINT ( 'NONE',  ( 3.458734124999960358, 208.6250000013655779, 143.4326545832176976 ) ) ;
#72643 = FACE_OUTER_BOUND ( 'NONE', #18339, .T. ) ;
#72644 = CARTESIAN_POINT ( 'NONE',  ( -7.188101187500002709, 1.312499997951610098, 2.977408999572649151 ) ) ;
#72645 = CARTESIAN_POINT ( 'NONE',  ( 4.721056650416000089, 289.8281250017069510, 4.721056650415999201 ) ) ;
#72646 = CARTESIAN_POINT ( 'NONE',  ( 0.000000000000000000, 300.0000000000000000, 0.000000000000000000 ) ) ;
#72647 = CARTESIAN_POINT ( 'NONE',  ( -3.313708498984765161, 17.34374999590322375, 7.999999999999998224 ) ) ;
#72648 = VERTEX_POINT ( 'NONE', #3406 ) ;
#72649 =( BOUNDED_CURVE ( )  B_SPLINE_CURVE ( 2, ( #53558, #72001, #60697, #42590, #31277, #20316, #2984, #32031, #42957 ),
 .UNSPECIFIED., .F., .F. ) 
 B_SPLINE_CURVE_WITH_KNOTS ( ( 3, 2, 2, 2, 3 ),
 ( 0.7677200384551818857, 0.7743382433814469668, 0.7809565189659037898, 0.7875747945503606129, 0.7941930320969252666 ),
 .UNSPECIFIED. ) 
 CURVE ( )  GEOMETRIC_REPRESENTATION_ITEM ( )  RATIONAL_B_SPLINE_CURVE ( ( 0.9999983746590511702, 0.9238803451904374908, 1.000000000000000000, 0.9238795325112867385, 1.000000000000000000, 0.9238795325112867385, 1.000000000000000000, 0.9238799700062350073, 0.9999991250151324396 ) ) 
 REPRESENTATION_ITEM ( '' )  );
#72650 = CARTESIAN_POINT ( 'NONE',  ( 3.042071309553159519, 145.0520833299193555, 11.35316468750000141 ) ) ;
#72651 = CARTESIAN_POINT ( 'NONE',  ( -10.18810118749999738, -4.220049686691941915, 84.25000000204838102 ) ) ;
#72652 = ADVANCED_FACE ( 'NONE', ( #60362 ), #38115, .T. ) ;
#72653 = CARTESIAN_POINT ( 'NONE',  ( -29.43265458321766559, 197.5000000013656063, 166.5412658750003629 ) ) ;
#72654 = CARTESIAN_POINT ( 'NONE',  ( -2.828427124746208943, 198.6250000000000284, 144.8284271247462129 ) ) ;
#72655 = CARTESIAN_POINT ( 'NONE',  ( 3.211159895383561835, 16.56249999863440436, -3.211159895383561835 ) ) ;
#72656 = EDGE_LOOP ( 'NONE', ( #19814, #12628, #65962, #71039 ) ) ;
#72657 = CARTESIAN_POINT ( 'NONE',  ( -2.828427124746153876, 203.0000000027312126, 195.1715728752538439 ) ) ;
#72658 = CARTESIAN_POINT ( 'NONE',  ( -2.751064625579944321E-14, 209.7500000000000284, 146.0000000000000284 ) ) ;
#72659 = CARTESIAN_POINT ( 'NONE',  ( -30.82842712474612767, 207.5000000027312126, 172.8284271247466108 ) ) ;
#72660 = ORIENTED_EDGE ( 'NONE', *, *, #15001, .T. ) ;
#72661 = CARTESIAN_POINT ( 'NONE',  ( 7.188101187500000044, 13.96874999795161187, 0.000000000000000000 ) ) ;
#72662 = CARTESIAN_POINT ( 'NONE',  ( -30.50622587038985500, -12.00562935288249733, 175.5843429582604927 ) ) ;
#72663 = EDGE_CURVE ( 'NONE', #39682, #21786, #26016, .T. ) ;
#72664 = CARTESIAN_POINT ( 'NONE',  ( 5.000000000000000000, 52.85372778481389133, -48.38359481482837765 ) ) ;
#72665 = CIRCLE ( 'NONE', #70251, 10.00000000000001243 ) ;
#72666 = CARTESIAN_POINT ( 'NONE',  ( -8.311093377946841443, 183.9062499965860411, 8.311093377946830785 ) ) ;
#72667 = CARTESIAN_POINT ( 'NONE',  ( -7.188101187500000044, 111.0312500020483810, 0.000000000000000000 ) ) ;
#72668 = DIRECTION ( 'NONE',  ( 0.000000000000000000, 0.000000000000000000, 1.000000000000000000 ) ) ;
#72669 = CARTESIAN_POINT ( 'NONE',  ( 6.676582343750001591, 289.9531250017069510, -8.176455196517173205E-16 ) ) ;
#72670 = EDGE_CURVE ( 'NONE', #27721, #63265, #66130, .T. ) ;
#72672 = CARTESIAN_POINT ( 'NONE',  ( 3.999999999999960032, 201.1250000027312126, 142.0000000000000568 ) ) ;
#72671 = CARTESIAN_POINT ( 'NONE',  ( 8.660254037844385522, 131.4583333265053682, 5.000000000000005329 ) ) ;
#72673 = ITEM_DEFINED_TRANSFORMATION ( 'NONE', 'NONE', #864,  #57354 ) ;
#72674 = ORIENTED_EDGE ( 'NONE', *, *, #63354, .F. ) ;
#72675 = CARTESIAN_POINT ( 'NONE',  ( 11.35316468749999963, 256.1979166700806445, 3.042071309553159519 ) ) ;
#72676 = CARTESIAN_POINT ( 'NONE',  ( 7.188101187499992051, 8.802885111219154394E-16, 25.11155278187175810 ) ) ;
#72677 = CARTESIAN_POINT ( 'NONE',  ( 10.99999999999989697, -4.556349186104149851, 93.15625000000001421 ) ) ;
#72678 = CARTESIAN_POINT ( 'NONE',  ( -1.558072418983381668, -67.68461058694114740, -20.10890959968054048 ) ) ;
#72680 = ADVANCED_FACE ( 'NONE', ( #4 ), #4529, .T. ) ;
#72679 = CARTESIAN_POINT ( 'NONE',  ( -3.458734124999960358, 197.6250000013656063, 196.5673454167823877 ) ) ;
#72681 = CARTESIAN_POINT ( 'NONE',  ( 0.000000000000000000, 125.0000000000000000, 0.000000000000000000 ) ) ;
#72682 = CARTESIAN_POINT ( 'NONE',  ( 1.959434878635763554E-15, 300.0000000000000000, -15.99999999999998579 ) ) ;
#72683 = CARTESIAN_POINT ( 'NONE',  ( -3.313708498984762496, 95.28125000000000000, 7.999999999999998224 ) ) ;
#72684 = CARTESIAN_POINT ( 'NONE',  ( 3.042071309553159519, 120.0520833299193697, 11.35316468750000141 ) ) ;
#72685 = CARTESIAN_POINT ( 'NONE',  ( -5.000000000000000888, -11.68639849891318683, -68.31608016562505270 ) ) ;
#72686 = CARTESIAN_POINT ( 'NONE',  ( -11.00000000000000000, 4.556349186104045934, 72.90624999999997158 ) ) ;
#72689 = CARTESIAN_POINT ( 'NONE',  ( 6.000000000000003553, 298.5624999999999432, -2.485281374238571761 ) ) ;
#72688 = CARTESIAN_POINT ( 'NONE',  ( 28.00000000000001776, 200.4375000013656063, 173.4587341249998929 ) ) ;
#72687 = CARTESIAN_POINT ( 'NONE',  ( 30.44569435410883429, 198.0625000013656063, 167.5543056458911053 ) ) ;
#72690 = VERTEX_POINT ( 'NONE', #39229 ) ;
#72691 = CARTESIAN_POINT ( 'NONE',  ( 8.101764136504522540, 224.5008269190864780, 5.891083390957826182 ) ) ;
#72692 = CARTESIAN_POINT ( 'NONE',  ( 4.643170207286937412, 226.6963040713783357, -10.42876980789419683 ) ) ;
#72693 = CARTESIAN_POINT ( 'NONE',  ( -1.432654583217664479, 196.7500000013656063, 138.5412658750000787 ) ) ;
#72694 = CARTESIAN_POINT ( 'NONE',  ( 25.55430564589115150, 198.5625000013656063, 172.4456943541086957 ) ) ;
#72695 = CARTESIAN_POINT ( 'NONE',  ( 11.00000000000000355, -4.556349186104045046, 109.8437500040967763 ) ) ;
#72696 = CARTESIAN_POINT ( 'NONE',  ( -8.311093377946836114, 212.9687499965860411, -8.311093377946837890 ) ) ;
#72697 = CARTESIAN_POINT ( 'NONE',  ( 2.775557561562891351E-14, -70.00000000000000000, 170.0000000000000000 ) ) ;
#72698 = VECTOR ( 'NONE', #54589, 1000.000000000000000 ) ;
#72699 = DIRECTION ( 'NONE',  ( 1.000000000000000000, 0.000000000000000000, 0.000000000000000000 ) ) ;
#72700 = CARTESIAN_POINT ( 'NONE',  ( 4.541265875000002339, 19.37499999863440792, -1.881053915767121554 ) ) ;
#72701 = CARTESIAN_POINT ( 'NONE',  ( 30.44569435410878810, 194.8125000013656063, 172.4456943541087526 ) ) ;
#72702 = CARTESIAN_POINT ( 'NONE',  ( 1.469576158976822172E-15, -7.999999999999991118, 26.70530277982336642 ) ) ;
#72703 = CARTESIAN_POINT ( 'NONE',  ( 9.999999999999994671, 185.2083333333333144, -2.679491924311226292 ) ) ;
#72704 = CARTESIAN_POINT ( 'NONE',  ( -9.832129032723420536, 78.69791666325269830, 5.676582343749997150 ) ) ;
#72705 = ORIENTED_EDGE ( 'NONE', *, *, #23196, .F. ) ;
#72706 = CARTESIAN_POINT ( 'NONE',  ( 8.000000000000000000, 92.84375000000000000, -3.313708498984762496 ) ) ;
#72707 = CARTESIAN_POINT ( 'NONE',  ( 2.977408999572650927, 21.74999999795162253, -7.188101187500001821 ) ) ;
#72708 = CARTESIAN_POINT ( 'NONE',  ( -2.679491924311171225, 222.0833333401612890, -10.00000000000003197 ) ) ;
#72709 = CARTESIAN_POINT ( 'NONE',  ( -5.676582343750000703, 258.3854166700806445, -9.832129032723418760 ) ) ;
#72710 = CARTESIAN_POINT ( 'NONE',  ( -11.35316468750000141, 83.48958332991935549, 3.042071309553159963 ) ) ;
#72711 = ORIENTED_EDGE ( 'NONE', *, *, #41704, .F. ) ;
#72712 = CARTESIAN_POINT ( 'NONE',  ( 4.999999999999995559, -15.86406185656353429, 69.92615499037644611 ) ) ;
#72713 = CARTESIAN_POINT ( 'NONE',  ( 10.18810118750000093, -4.220049686691933921, 114.8125000020483668 ) ) ;
#72714 = CARTESIAN_POINT ( 'NONE',  ( -26.56734541678237704, 196.6250000013656063, 166.5412658750003629 ) ) ;
#72715 = CARTESIAN_POINT ( 'NONE',  ( -3.458734124999959469, 205.7500000013656063, 199.4326545832176691 ) ) ;
#72716 = LINE ( 'NONE', #67428, #61259 ) ;
#72718 = CARTESIAN_POINT ( 'NONE',  ( 6.951808397369818766E-16, 82.03124999658602690, -11.35316468750000141 ) ) ;
#72717 = CARTESIAN_POINT ( 'NONE',  ( -4.556349186104048599, -10.99999999999999822, 106.2812500000000000 ) ) ;
#72719 = CARTESIAN_POINT ( 'NONE',  ( -5.656854249492375253, 5.656854249492375253, 17.33030278392014623 ) ) ;
#72720 = CARTESIAN_POINT ( 'NONE',  ( -24.54126587499999346, 201.4375000013656063, 170.0000000000003411 ) ) ;
#72721 = CARTESIAN_POINT ( 'NONE',  ( -1.469576158976823947E-15, 21.93749999590322375, 8.000000000000000000 ) ) ;
#72722 = CARTESIAN_POINT ( 'NONE',  ( -7.320508075688778149, 184.9999999931719969, 7.320508075688769267 ) ) ;
#72723 = ADVANCED_FACE ( 'NONE', ( #56592 ), #45256, .F. ) ;
#72724 = CARTESIAN_POINT ( 'NONE',  ( 5.000000000000000000, -53.53174224766610223, 46.57871628774361739 ) ) ;
#72725 = CARTESIAN_POINT ( 'NONE',  ( -5.676582343750006032, 74.42708332991934128, 9.832129032723418760 ) ) ;
#72726 = CARTESIAN_POINT ( 'NONE',  ( -6.676582343750001591, 294.4531250017069510, 0.000000000000000000 ) ) ;
#72727 = CARTESIAN_POINT ( 'NONE',  ( 10.18810118750000093, -4.220049686691933033, 101.6875000020483810 ) ) ;
#72728 = CARTESIAN_POINT ( 'NONE',  ( 5.676582343750001591, 211.6145833299193555, -9.832129032723420536 ) ) ;
#72729 = VERTEX_POINT ( 'NONE', #67526 ) ;
#72730 = CARTESIAN_POINT ( 'NONE',  ( -7.999999999999991118, 0.000000000000000000, 2.330302779823365089 ) ) ;
#72731 = CARTESIAN_POINT ( 'NONE',  ( 9.000000000000000000, 5.196152422706622254, -10.20000000000000284 ) ) ;
#72732 = CARTESIAN_POINT ( 'NONE',  ( 5.000000000000000000, 63.84827628760491791, 24.15557308422392069 ) ) ;
#72734 = CARTESIAN_POINT ( 'NONE',  ( 8.311093377946834337, 200.1562499965860411, 8.311093377946839666 ) ) ;
#72733 = CARTESIAN_POINT ( 'NONE',  ( 2.449293598294707893E-16, 19.25000000000000000, -4.000000000000001776 ) ) ;
#72735 = CARTESIAN_POINT ( 'NONE',  ( 0.000000000000000000, 0.000000000000000000, -25.03750572909317285 ) ) ;
#72736 = VECTOR ( 'NONE', #49205, 1000.000000000000000 ) ;
#72737 = CARTESIAN_POINT ( 'NONE',  ( 7.320508075688776373, 220.0000000068280031, 7.320508075688767491 ) ) ;
#72738 = CARTESIAN_POINT ( 'NONE',  ( 2.765530957081996366, 299.1406250017068942, -6.676582343750003368 ) ) ;
#72739 = ORIENTED_EDGE ( 'NONE', *, *, #20025, .F. ) ;
#72740 = CARTESIAN_POINT ( 'NONE',  ( 8.311093377946837890, 201.7187499965860411, -8.311093377946837890 ) ) ;
#72741 = CARTESIAN_POINT ( 'NONE',  ( -4.401442555609577197E-16, 7.188101187499992051, 17.61155278187175810 ) ) ;
#72742 =( BOUNDED_CURVE ( )  B_SPLINE_CURVE ( 2, ( #43339, #48626, #55057, #71633, #21082, #19955, #44106, #66357, #67115 ),
 .UNSPECIFIED., .F., .F. ) 
 B_SPLINE_CURVE_WITH_KNOTS ( ( 3, 2, 2, 2, 3 ),
 ( 0.9062500000000002220, 0.9114583333333335924, 0.9166666666666668517, 0.9218750000000002220, 0.9270833333333335924 ),
 .UNSPECIFIED. ) 
 CURVE ( )  GEOMETRIC_REPRESENTATION_ITEM ( )  RATIONAL_B_SPLINE_CURVE ( ( 0.9999999999999967804, 0.9238795325112899581, 1.000000000000000000, 0.9238795325112867385, 1.000000000000000000, 0.9238795325112867385, 1.000000000000000000, 0.9238795325112835188, 1.000000000000003331 ) ) 
 REPRESENTATION_ITEM ( '' )  );
#72743 = CARTESIAN_POINT ( 'NONE',  ( -24.54126587499998635, 209.1250000013656631, 171.4326545832179818 ) ) ;
#72744 = CARTESIAN_POINT ( 'NONE',  ( 4.898587196589412829E-16, 10.87500000000000178, -8.000000000000000000 ) ) ;
#72745 = ORIENTED_EDGE ( 'NONE', *, *, #14446, .F. ) ;
#72746 = CARTESIAN_POINT ( 'NONE',  ( -5.656854249492380582, 89.00000000409677625, -5.656854249492380582 ) ) ;
#72747 = CARTESIAN_POINT ( 'NONE',  ( 2.679491924311228956, 11.04166666666666785, -10.00000000000000000 ) ) ;
#72748 = AXIS2_PLACEMENT_3D ( 'NONE', #13332, #35636, #24300 ) ;
#72749 = ORIENTED_EDGE ( 'NONE', *, *, #49760, .T. ) ;
#72750 = CARTESIAN_POINT ( 'NONE',  ( -1.656854249492383691, 14.68750000000000000, 4.000000000000000888 ) ) ;
#72751 =( BOUNDED_CURVE ( )  B_SPLINE_CURVE ( 2, ( #55622, #44663, #20893, #67676, #39005, #33733, #61643, #4678, #43915 ),
 .UNSPECIFIED., .F., .F. ) 
 B_SPLINE_CURVE_WITH_KNOTS ( ( 3, 2, 2, 2, 3 ),
 ( 0.1764705882352942123, 0.1801470588235294934, 0.1838235294117648300, 0.1875000000000001110, 0.1911764705882353921 ),
 .UNSPECIFIED. ) 
 CURVE ( )  GEOMETRIC_REPRESENTATION_ITEM ( )  RATIONAL_B_SPLINE_CURVE ( ( 0.9999999999999982236, 0.9238795325112885148, 1.000000000000000000, 0.9238795325112867385, 1.000000000000000000, 0.9238795325112867385, 1.000000000000000000, 0.9238795325112844070, 1.000000000000002220 ) ) 
 REPRESENTATION_ITEM ( '' )  );
#72752 = CARTESIAN_POINT ( 'NONE',  ( 3.211159895383560947, 18.18749999863440792, 3.211159895383562723 ) ) ;
#72753 = CARTESIAN_POINT ( 'NONE',  ( 7.999999999999991118, 9.797174393178815797E-16, 6.267802783920147114 ) ) ;
#72754 = CARTESIAN_POINT ( 'NONE',  ( 0.000000000000000000, 0.000000000000000000, 0.000000000000000000 ) ) ;
#72755 = EDGE_LOOP ( 'NONE', ( #19747, #66605, #223, #52952 ) ) ;
#72756 = FILL_AREA_STYLE ('',( #49740 ) ) ;
#72757 = CARTESIAN_POINT ( 'NONE',  ( -5.082755093536324154, 94.34375000204838102, 5.082755093536326818 ) ) ;
#72758 = EDGE_CURVE ( 'NONE', #41682, #44173, #28646, .T. ) ;
#72761 = CYLINDRICAL_SURFACE ( 'NONE', #47028, 8.000000000000003553 ) ;
#72760 = CARTESIAN_POINT ( 'NONE',  ( -9.832129032723415207, 259.3229166700806445, 5.676582343750005144 ) ) ;
#72759 = CARTESIAN_POINT ( 'NONE',  ( 1.459323541827198180E-11, 81.24999999999886313, -10.00000000000000533 ) ) ;
#72762 = ORIENTED_EDGE ( 'NONE', *, *, #28051, .F. ) ;
#72763 = CARTESIAN_POINT ( 'NONE',  ( 3.042071309553173286, 250.6770833367473017, 11.35316468749999608 ) ) ;
#72764 = CARTESIAN_POINT ( 'NONE',  ( 7.188101187499993827, -2.977408999572645598, 14.14280278187175455 ) ) ;
#72765 = ORIENTED_EDGE ( 'NONE', *, *, #31719, .T. ) ;
#72766 = EDGE_CURVE ( 'NONE', #70088, #13532, #37389, .T. ) ;
#72767 = ORIENTED_EDGE ( 'NONE', *, *, #28852, .F. ) ;
#72768 = CARTESIAN_POINT ( 'NONE',  ( 10.18810118749999916, 4.220049686691935698, 82.00000000204838102 ) ) ;
#72769 = CARTESIAN_POINT ( 'NONE',  ( -9.832129032723418760, 73.17708332991934128, -5.676582343750004256 ) ) ;
#72770 = FACE_OUTER_BOUND ( 'NONE', #30903, .T. ) ;
#72771 = CARTESIAN_POINT ( 'NONE',  ( -7.778174593052020747, -7.778174593052023411, 86.68749999999998579 ) ) ;
#72774 = CARTESIAN_POINT ( 'NONE',  ( 1.226468279477575784E-15, 290.8593750017070079, 6.676582343750001591 ) ) ;
#72773 = CARTESIAN_POINT ( 'NONE',  ( 25.17157287525377640, 195.7500000027312126, 167.1715728752537586 ) ) ;
#72772 = PLANE ( 'NONE',  #62440 ) ;
#72775 = CIRCLE ( 'NONE', #16146, 8.999999999999998224 ) ;
#72776 = FACE_OUTER_BOUND ( 'NONE', #67175, .T. ) ;
#72777 = CARTESIAN_POINT ( 'NONE',  ( -2.679491924311382611, 165.4166666598386826, 9.999999999999914735 ) ) ;
#72778 = CARTESIAN_POINT ( 'NONE',  ( 2.839093476692135984E-14, 196.9375000013655779, 201.4587341250000350 ) ) ;
#72779 = CARTESIAN_POINT ( 'NONE',  ( -1.469576158976823947E-15, 6.937499995903221084, 8.000000000000000000 ) ) ;
#72780 = ORIENTED_EDGE ( 'NONE', *, *, #72486, .F. ) ;
#72781 = CARTESIAN_POINT ( 'NONE',  ( 31.45873412499999944, 196.7500000013656063, 168.5673454167822740 ) ) ;
#72782 = CARTESIAN_POINT ( 'NONE',  ( -5.082755093536326818, 9.281249997951610098, 5.082755093536325042 ) ) ;
#72783 = CARTESIAN_POINT ( 'NONE',  ( 3.042071309553167069, 162.1354166632526983, -11.35316468749999785 ) ) ;
#72784 = CARTESIAN_POINT ( 'NONE',  ( 11.00000000000000000, 1.347111479062088405E-15, 99.43750000409677625 ) ) ;
#72785 = CARTESIAN_POINT ( 'NONE',  ( 5.082755093536326818, 105.5937500020483810, 5.082755093536325042 ) ) ;
#72787 = CYLINDRICAL_SURFACE ( 'NONE', #63082, 10.00000000000000178 ) ;
#72786 = CARTESIAN_POINT ( 'NONE',  ( -4.242640687119285658, 293.1875000034139589, 4.242640687119287435 ) ) ;
#72788 = CARTESIAN_POINT ( 'NONE',  ( 30.44569435410883429, 205.0625000013656063, 167.5543056458911053 ) ) ;
#72789 = CARTESIAN_POINT ( 'NONE',  ( 7.188101187499992051, 8.802885111219154394E-16, 17.61155278187175810 ) ) ;
#72790 = CARTESIAN_POINT ( 'NONE',  ( 3.999999999999960032, 209.1250000027312126, 142.0000000000000568 ) ) ;
#72791 = CARTESIAN_POINT ( 'NONE',  ( -8.311093377946836114, 47.65624999658601979, -8.311093377946837890 ) ) ;
#72792 = CARTESIAN_POINT ( 'NONE',  ( 23.99999999999997868, 200.8125000000000284, 171.6568542494922553 ) ) ;
#72793 = CARTESIAN_POINT ( 'NONE',  ( 8.660254037844389075, 22.29166665983870033, -5.000000000000000000 ) ) ;
#72794 = CARTESIAN_POINT ( 'NONE',  ( 4.556349186104045934, 11.00000000000000000, 111.7187500040967905 ) ) ;
#72795 = ORIENTED_EDGE ( 'NONE', *, *, #45093, .T. ) ;
#72796 = CARTESIAN_POINT ( 'NONE',  ( 3.968262987731704605, 11.56532875636889557, -0.1021479564361147535 ) ) ;
#72797 = CARTESIAN_POINT ( 'NONE',  ( -5.676582343749998039, 42.44791666325268409, -9.832129032723420536 ) ) ;
#72798 = CARTESIAN_POINT ( 'NONE',  ( 2.020667218593132706E-15, -11.00000000000000000, 79.56250000409677625 ) ) ;
#72799 = CARTESIAN_POINT ( 'NONE',  ( 3.458734124999959469, 203.7500000013656063, 140.5673454167823593 ) ) ;
#72800 = DIRECTION ( 'NONE',  ( 0.000000000000000000, 0.000000000000000000, 1.000000000000000000 ) ) ;
#72801 = LINE ( 'NONE', #19611, #53933 ) ;
#72803 = CARTESIAN_POINT ( 'NONE',  ( 11.35316468749999963, 50.98958332991934839, -3.042071309553165293 ) ) ;
#72802 = CARTESIAN_POINT ( 'NONE',  ( -7.188101187500000933, 98.56250000204838102, -2.977408999572650483 ) ) ;
#72804 = CARTESIAN_POINT ( 'NONE',  ( 3.313708498984762496, -7.999999999999989342, 7.299052779823365533 ) ) ;
#72805 = CARTESIAN_POINT ( 'NONE',  ( 0.000000000000000000, 0.000000000000000000, 30.00000000000000000 ) ) ;
#72806 = CARTESIAN_POINT ( 'NONE',  ( -5.676582343749998039, 162.4479166632526983, -9.832129032723420536 ) ) ;
#72808 = CARTESIAN_POINT ( 'NONE',  ( 5.000000000000001776, 132.7083333265053682, -8.660254037844389075 ) ) ;
#72807 = PRODUCT_DEFINITION_SHAPE ( 'NONE', 'NONE',  #15017 ) ;
#72809 = CARTESIAN_POINT ( 'NONE',  ( -5.082755093536324154, 105.2187500020483952, 5.082755093536326818 ) ) ;
#72810=STYLED_ITEM('',(#74706),#65418);
#72811 = CARTESIAN_POINT ( 'NONE',  ( -2.385759507663883117, -46.82937167279962409, 139.0917472037170626 ) ) ;
#72812 = CARTESIAN_POINT ( 'NONE',  ( 9.832129032723420536, 36.51041666325267698, -5.676582343749999815 ) ) ;
#72813 = CARTESIAN_POINT ( 'NONE',  ( -4.000000000000016875, 195.5625000027312126, 140.3431457505076594 ) ) ;
#72814 = ORIENTED_EDGE ( 'NONE', *, *, #3794, .T. ) ;
#72815 = CARTESIAN_POINT ( 'NONE',  ( -29.65685424949241877, 205.1875000027311842, 166.0000000000003695 ) ) ;
#72816 = CARTESIAN_POINT ( 'NONE',  ( 1.871523826299183495E-15, -10.18810118749999916, 75.53125000204836681 ) ) ;
#72817 = CARTESIAN_POINT ( 'NONE',  ( 11.00000000000000000, -3.149999999999999911, 0.000000000000000000 ) ) ;
#72819 = CARTESIAN_POINT ( 'NONE',  ( 9.832129032723420536, 171.1979166632526983, -5.676582343749999815 ) ) ;
#72818 = CARTESIAN_POINT ( 'NONE',  ( -10.00000000000001066, 7.708333333333335702, 2.679491924311224960 ) ) ;
#72820 = CARTESIAN_POINT ( 'NONE',  ( 7.999999999999991118, 3.313708498984757611, 9.230302784329824206 ) ) ;
#72821 = CARTESIAN_POINT ( 'NONE',  ( -6.062601303906716588, -5.219661428662635494, 1.000679062340938064 ) ) ;
#72822 = CARTESIAN_POINT ( 'NONE',  ( 9.832129032723420536, 225.9895833367473585, 5.676582343749996262 ) ) ;
#72823 = CARTESIAN_POINT ( 'NONE',  ( -10.18810118749999738, -4.220049686691941915, 87.62500000204836681 ) ) ;
#72824 = EDGE_LOOP ( 'NONE', ( #41052, #73936, #34618, #28595 ) ) ;
#72825 = CARTESIAN_POINT ( 'NONE',  ( -4.556349186104048599, -10.99999999999999822, 89.96875000409677625 ) ) ;
#72826 = CARTESIAN_POINT ( 'NONE',  ( -4.000000000000015987, 198.6875000027312126, 143.6568542494924259 ) ) ;
#72827 = CARTESIAN_POINT ( 'NONE',  ( -8.311093377946841443, 114.2187499965860269, 8.311093377946830785 ) ) ;
#72828 = CARTESIAN_POINT ( 'NONE',  ( -6.238412754330611322E-16, 10.18810118749999916, 94.28125000204836681 ) ) ;
#72829 = CARTESIAN_POINT ( 'NONE',  ( 1.881053915767122664, 21.24999999863440792, 4.541265875000001451 ) ) ;
#72830 = VERTEX_POINT ( 'NONE', #27152 ) ;
#72831 = ORIENTED_EDGE ( 'NONE', *, *, #62967, .T. ) ;
#72832 = CIRCLE ( 'NONE', #42704, 3.999999999999986233 ) ;
#72833 = CARTESIAN_POINT ( 'NONE',  ( -4.541265875000003227, 3.999999998634406140, 1.881053915767121110 ) ) ;
#72834 = CARTESIAN_POINT ( 'NONE',  ( 5.082755093536324154, 7.781249997951611874, 5.082755093536326818 ) ) ;
#72835 = CARTESIAN_POINT ( 'NONE',  ( -3.313708498984762496, 107.4687500040967763, 7.999999999999998224 ) ) ;
#72837 = EDGE_CURVE ( 'NONE', #59993, #47573, #61864, .T. ) ;
#72836 = CARTESIAN_POINT ( 'NONE',  ( 4.220049686691934809, 10.18810118749999916, 91.56250000204836681 ) ) ;
#72838 = EDGE_CURVE ( 'NONE', #28937, #17389, #74295, .T. ) ;
#72839 = CARTESIAN_POINT ( 'NONE',  ( -30.44569435410879166, 204.0625000013656063, 172.4456943541092357 ) ) ;
#72840 = CARTESIAN_POINT ( 'NONE',  ( 4.000000000000001776, 6.000000000000000000, 0.000000000000000000 ) ) ;
#72841 = CARTESIAN_POINT ( 'NONE',  ( -2.828427124746190735, 19.12499999726881228, -2.828427124746191623 ) ) ;
#72842 = CARTESIAN_POINT ( 'NONE',  ( 1.881053915767121998, 7.499999998634407916, -4.541265875000002339 ) ) ;
#72843 = CARTESIAN_POINT ( 'NONE',  ( 2.828427124746152987, 204.1250000000000284, 139.1715728752538723 ) ) ;
#72844 = ORIENTED_EDGE ( 'NONE', *, *, #64089, .T. ) ;
#72845 = LINE ( 'NONE', #65314, #70383 ) ;
#72848 = CARTESIAN_POINT ( 'NONE',  ( -1.836970198721029983E-15, 225.6249999931720254, 10.00000000000000178 ) ) ;
#72847 = CARTESIAN_POINT ( 'NONE',  ( -26.56734541678242323, 197.3750000013656063, 166.5412658750003345 ) ) ;
#72846 =( BOUNDED_CURVE ( )  B_SPLINE_CURVE ( 2, ( #58109, #6044, #69785, #13159, #57740, #58475, #35100, #29426, #24116, #40737, #47129, #58842, #12428 ),
 .UNSPECIFIED., .F., .F. ) 
 B_SPLINE_CURVE_WITH_KNOTS ( ( 3, 2, 2, 2, 2, 2, 3 ),
 ( 2.213686939631518857, 2.218920756416068230, 2.224154573200617602, 2.229388389985166974, 2.234622206769716790, 2.239856023554266162, 2.245089840338815534 ),
 .UNSPECIFIED. ) 
 CURVE ( )  GEOMETRIC_REPRESENTATION_ITEM ( )  RATIONAL_B_SPLINE_CURVE ( ( 0.9999999999997807310, 0.9659258262892875813, 1.000000000000000000, 0.9659258262890683122, 1.000000000000000000, 0.9659258262890683122, 1.000000000000000000, 0.9659258262890683122, 1.000000000000000000, 0.9659258262890683122, 1.000000000000000000, 0.9659258262893042346, 0.9999999999997640776 ) ) 
 REPRESENTATION_ITEM ( '' )  );
#72849 = CARTESIAN_POINT ( 'NONE',  ( -8.342170076843785083E-16, 19.06249999863440436, 4.541265875000002339 ) ) ;
#72850 = CARTESIAN_POINT ( 'NONE',  ( 6.676582343750003368, 298.8906250017069510, 2.765530957081995478 ) ) ;
#72851 = AXIS2_PLACEMENT_3D ( 'NONE', #4395, #9686, #39831 ) ;
#72852 = CARTESIAN_POINT ( 'NONE',  ( -4.401442555609577197E-16, 7.188101187499992051, 5.611552781871753659 ) ) ;
#72853 = VERTEX_POINT ( 'NONE', #50911 ) ;
#72854 = ORIENTED_EDGE ( 'NONE', *, *, #14403, .T. ) ;
#72855 = CARTESIAN_POINT ( 'NONE',  ( -10.18810118749999738, -4.220049686691941915, 99.25000000204838102 ) ) ;
#72856 = CARTESIAN_POINT ( 'NONE',  ( 3.313708498984922812, 91.71875000409674783, -7.999999999999837463 ) ) ;
#72857 = CARTESIAN_POINT ( 'NONE',  ( -31.45873412499999944, 199.8750000013656063, 168.5673454167827572 ) ) ;
#72858 = CARTESIAN_POINT ( 'NONE',  ( -10.99999999999999822, -4.556349186104052151, 109.0937500000000000 ) ) ;
#72859 = CARTESIAN_POINT ( 'NONE',  ( -3.458734124999959469, 208.7500000013656063, 199.4326545832176691 ) ) ;
#72860 = CARTESIAN_POINT ( 'NONE',  ( -1.966770576099810657E-11, 61.25000000000153477, -9.999999999999998224 ) ) ;
#72861 = CARTESIAN_POINT ( 'NONE',  ( -1.836970198721029983E-15, 108.7500000000000142, 10.00000000000000178 ) ) ;
#72862 = CARTESIAN_POINT ( 'NONE',  ( -7.999999999999998224, 108.5937499999999858, 3.313708498984766493 ) ) ;
#72863 = CARTESIAN_POINT ( 'NONE',  ( -2.765530957081996810, 292.4218750017069510, -6.676582343750003368 ) ) ;
#72864 = CARTESIAN_POINT ( 'NONE',  ( 5.082755093536320601, -5.082755093536318824, 9.924052781871754547 ) ) ;
#72865 = ORIENTED_EDGE ( 'NONE', *, *, #42688, .T. ) ;
#72867 =( BOUNDED_CURVE ( )  B_SPLINE_CURVE ( 2, ( #64124, #31267, #42206, #53549, #19203, #69788, #25225, #18104, #12431 ),
 .UNSPECIFIED., .F., .F. ) 
 B_SPLINE_CURVE_WITH_KNOTS ( ( 3, 2, 2, 2, 3 ),
 ( 0.2613636363636363535, 0.2670454545454545303, 0.2727272727272727071, 0.2784090909090908839, 0.2840909090909091161 ),
 .UNSPECIFIED. ) 
 CURVE ( )  GEOMETRIC_REPRESENTATION_ITEM ( )  RATIONAL_B_SPLINE_CURVE ( ( 1.000000000000000000, 0.9238795325112867385, 1.000000000000000000, 0.9238795325112867385, 1.000000000000000000, 0.9238795325112867385, 1.000000000000000000, 0.9238795325112867385, 1.000000000000000000 ) ) 
 REPRESENTATION_ITEM ( '' )  );
#72866 = CARTESIAN_POINT ( 'NONE',  ( 0.000000000000000000, 0.000000000000000000, 118.0000000000000000 ) ) ;
#72868 = CARTESIAN_POINT ( 'NONE',  ( 25.55430564589119768, 207.0625000013656063, 167.5543056458910485 ) ) ;
#72869 = CARTESIAN_POINT ( 'NONE',  ( 5.656854249492378806, 23.62499999590322020, 5.656854249492381470 ) ) ;
#72870 = CARTESIAN_POINT ( 'NONE',  ( -1.432654583217664479, 199.7500000013656063, 138.5412658750000787 ) ) ;
#72871 = CARTESIAN_POINT ( 'NONE',  ( -20.82204241625640151, -36.20404327648021336, 146.9783373859985147 ) ) ;
#72873 = CARTESIAN_POINT ( 'NONE',  ( -1.432654583217664701, 204.0000000013656347, 138.5412658750000787 ) ) ;
#72872 = CARTESIAN_POINT ( 'NONE',  ( 3.313708498984731410, 120.9687500000000000, 8.000000000000031974 ) ) ;
#72874 = CARTESIAN_POINT ( 'NONE',  ( -8.311093377946836114, 258.5937500034140157, -8.311093377946836114 ) ) ;
#72875 = DIRECTION ( 'NONE',  ( -0.000000000000000000, -0.000000000000000000, 1.000000000000000000 ) ) ;
#72876 = DIRECTION ( 'NONE',  ( 0.000000000000000000, 0.000000000000000000, 1.000000000000000000 ) ) ;
#72877 = CARTESIAN_POINT ( 'NONE',  ( -10.48324468785576080, 227.1467665679505785, -13.92079345837155735 ) ) ;
#72878 = CARTESIAN_POINT ( 'NONE',  ( 7.188101187499992051, 8.802885111219154394E-16, 2.611552781871750994 ) ) ;
#72879 = CARTESIAN_POINT ( 'NONE',  ( -9.832129032723418760, 208.1770833299193555, -5.676582343750004256 ) ) ;
#72880 = CARTESIAN_POINT ( 'NONE',  ( 1.881053915767121776, 7.499999998634408804, -4.541265875000002339 ) ) ;
#72881 = CARTESIAN_POINT ( 'NONE',  ( 2.485281374238878627, 290.3124999999999432, 5.999999999999694467 ) ) ;
#72882 = DIRECTION ( 'NONE',  ( 3.469446951953619612E-16, 0.000000000000000000, 1.000000000000000000 ) ) ;
#72883 = VERTEX_POINT ( 'NONE', #16948 ) ;
#72884 = CARTESIAN_POINT ( 'NONE',  ( -2.839093476692135984E-14, 203.9375000013656063, 138.5412658750000503 ) ) ;
#72885 = CARTESIAN_POINT ( 'NONE',  ( 6.951808397369818766E-16, 7.031249996586016238, -11.35316468750000141 ) ) ;
#72886 = CARTESIAN_POINT ( 'NONE',  ( -4.556349186104047710, -10.99999999999999822, 98.96875000409676204 ) ) ;
#72887 = DIRECTION ( 'NONE',  ( 0.000000000000000000, 0.000000000000000000, 1.000000000000000000 ) ) ;
#72888 = CARTESIAN_POINT ( 'NONE',  ( -30.44569435410875968, 201.8125000013656063, 172.4456943541092642 ) ) ;
#72889 = CARTESIAN_POINT ( 'NONE',  ( -11.00000000000000533, 11.00000000000000000, 20.00000000000000000 ) ) ;
#72891 = CARTESIAN_POINT ( 'NONE',  ( 3.042071309553159519, 9.739583329919350163, 11.35316468750000141 ) ) ;
#72890 = CARTESIAN_POINT ( 'NONE',  ( 5.082755093536325042, 120.5937500020483952, -5.082755093536325930 ) ) ;
#72892 = CARTESIAN_POINT ( 'NONE',  ( 3.313708498984762496, -7.999999999999989342, 28.29905277982336997 ) ) ;
#72893 = CARTESIAN_POINT ( 'NONE',  ( -5.676582343749998039, 122.4479166632526983, -9.832129032723420536 ) ) ;
#72894 = CARTESIAN_POINT ( 'NONE',  ( 6.123233995736767268E-16, 93.12499999317203958, -10.00000000000000178 ) ) ;
#72895 = CARTESIAN_POINT ( 'NONE',  ( 5.082755093536326818, 119.0937500020483810, 5.082755093536325042 ) ) ;
#72896 = CARTESIAN_POINT ( 'NONE',  ( 2.780723358947928197E-16, 20.68749999863440436, -4.541265875000002339 ) ) ;
#72897 = DIRECTION ( 'NONE',  ( -0.000000000000000000, 1.000000000000000000, -0.000000000000000000 ) ) ;
#72898 = CYLINDRICAL_SURFACE ( 'NONE', #47407, 18.99999999999998934 ) ;
#72899 = ORIENTED_EDGE ( 'NONE', *, *, #20387, .F. ) ;
#72900 = CARTESIAN_POINT ( 'NONE',  ( 0.000000000000000000, 300.0000000000000000, 10.00000000000000178 ) ) ;
#72901 = CARTESIAN_POINT ( 'NONE',  ( -6.676582343750000703, 291.6718750017069510, 2.765530957082001251 ) ) ;
#72902 = LINE ( 'NONE', #65740, #9802 ) ;
#72903 = CARTESIAN_POINT ( 'NONE',  ( 7.999999999999991118, 3.313708498984757611, 1.861552783920143117 ) ) ;
#72904 = DIRECTION ( 'NONE',  ( 1.110223029476724787E-14, 0.4999999999999780731, 0.8660254037844513642 ) ) ;
#72905 = CARTESIAN_POINT ( 'NONE',  ( -10.00000000000000000, 204.1666666598387394, -2.679491924311229845 ) ) ;
#72906 = CARTESIAN_POINT ( 'NONE',  ( -2.679491924311394158, 193.5416666666666288, 9.999999999999959144 ) ) ;
#72907 = CARTESIAN_POINT ( 'NONE',  ( -4.220049686691937474, -10.18810118749999738, 101.3125000020483810 ) ) ;
#72908 = ORIENTED_EDGE ( 'NONE', *, *, #26239, .T. ) ;
#72909 = EDGE_CURVE ( 'NONE', #36295, #6837, #33965, .T. ) ;
#72910 = VECTOR ( 'NONE', #10335, 1000.000000000000000 ) ;
#72911 = CARTESIAN_POINT ( 'NONE',  ( -11.00000000000000000, 0.000000000000000000, 78.99999999999998579 ) ) ;
#72912 = CARTESIAN_POINT ( 'NONE',  ( 11.35316468750000141, 151.0937499965860411, 0.000000000000000000 ) ) ;
#72913 = CARTESIAN_POINT ( 'NONE',  ( 1.432654583217664701, 206.0000000013656063, 201.4587341250000065 ) ) ;
#72914 = CARTESIAN_POINT ( 'NONE',  ( -10.68301270189220098, 0.000000000000000000, 117.8169872981077617 ) ) ;
#72915 = CARTESIAN_POINT ( 'NONE',  ( -11.35316468750000141, 58.59374999658601979, -1.390361679473963753E-15 ) ) ;
#72916 = VERTEX_POINT ( 'NONE', #56962 ) ;
#72917 = CARTESIAN_POINT ( 'NONE',  ( -10.18810118749999916, 4.220049686691934809, 114.0625000020483668 ) ) ;
#72918 = CARTESIAN_POINT ( 'NONE',  ( 1.881053915767122664, 9.249999998634407916, 4.541265875000001451 ) ) ;
#72919 = ORIENTED_EDGE ( 'NONE', *, *, #67405, .T. ) ;
#72920 = CARTESIAN_POINT ( 'NONE',  ( 5.082755093536325930, 20.15624999795161543, -5.082755093536325930 ) ) ;
#72921 = CARTESIAN_POINT ( 'NONE',  ( -3.673940397442060854E-16, 287.8125000034140157, -6.000000000000001776 ) ) ;
#72922 = CARTESIAN_POINT ( 'NONE',  ( -9.999999999999998224, 248.3333333401613174, 2.679491924311235174 ) ) ;
#72923 = CARTESIAN_POINT ( 'NONE',  ( 5.082755093536325930, 20.53124999795161543, -5.082755093536325930 ) ) ;
#72924 = CARTESIAN_POINT ( 'NONE',  ( 2.977408999572646486, 7.188101187499992051, 2.517802781871750994 ) ) ;
#72925 = CARTESIAN_POINT ( 'NONE',  ( 7.204075437095966983, 7.204075437095967871, 112.4687500020483810 ) ) ;
#72926 = CARTESIAN_POINT ( 'NONE',  ( 1.331930065543349473, -42.30468434493226226, 151.0458671776476649 ) ) ;
#72927 = CARTESIAN_POINT ( 'NONE',  ( 1.656854249492381248, 4.937499997268813168, -4.000000000000001776 ) ) ;
#72928 = CARTESIAN_POINT ( 'NONE',  ( 26.34314575050763096, 207.0625000027312126, 173.9999999999999147 ) ) ;
#72929 = ORIENTED_EDGE ( 'NONE', *, *, #36030, .F. ) ;
#72930 = EDGE_CURVE ( 'NONE', #60974, #2013, #51661, .T. ) ;
#72931 = ADVANCED_FACE ( 'NONE', ( #10186 ), #56215, .T. ) ;
#72932 = CARTESIAN_POINT ( 'NONE',  ( 2.754378923186476579E-14, 205.1875000013656063, 194.5412658750000219 ) ) ;
#72933 = CARTESIAN_POINT ( 'NONE',  ( -26.56734541678243033, 208.3750000013656063, 166.5412658750003345 ) ) ;
#72934 = CARTESIAN_POINT ( 'NONE',  ( 7.204075437095966983, 7.204075437095967871, 68.96875000204836681 ) ) ;
#72935 = EDGE_CURVE ( 'NONE', #35502, #2210, #62135, .T. ) ;
#72936 = CARTESIAN_POINT ( 'NONE',  ( -3.211159895383562723, 4.937499998634407028, 3.211159895383561391 ) ) ;
#72937 = CARTESIAN_POINT ( 'NONE',  ( 5.656854249492379694, 94.62500000409677625, -5.656854249492380582 ) ) ;
#72938 = CARTESIAN_POINT ( 'NONE',  ( -2.977408999572648707, -7.188101187499990274, 24.26780278187175455 ) ) ;
#72939 = ORIENTED_EDGE ( 'NONE', *, *, #55092, .T. ) ;
#72940 = CARTESIAN_POINT ( 'NONE',  ( -2.977408999572650039, 26.43749999795162253, -7.188101187500000933 ) ) ;
#72941 = ORIENTED_EDGE ( 'NONE', *, *, #12299, .F. ) ;
#72942 = CARTESIAN_POINT ( 'NONE',  ( -10.00000000000000000, 2.708333333333331261, 2.679491924311222295 ) ) ;
#72943 = CARTESIAN_POINT ( 'NONE',  ( -10.00000000000000178, 202.5000000000000000, -1.224646799147353454E-15 ) ) ;
#72944 = CARTESIAN_POINT ( 'NONE',  ( 2.445694354108839619, 202.8125000013656063, 200.4456943541088663 ) ) ;
#72945 = CARTESIAN_POINT ( 'NONE',  ( 31.45873412499999944, 200.6250000013656063, 171.4326545832175555 ) ) ;
#72946 = CARTESIAN_POINT ( 'NONE',  ( -7.320508075688778149, 68.12500000000001421, 7.320508075688769267 ) ) ;
#72947 = CARTESIAN_POINT ( 'NONE',  ( 7.188101187500000044, 93.78125000204836681, -8.802885111219163269E-16 ) ) ;
#72948 = CARTESIAN_POINT ( 'NONE',  ( 2.485281374238571317, 291.6874999999999432, -6.000000000000003553 ) ) ;
#72949 = AXIS2_PLACEMENT_3D ( 'NONE', #67815, #50450, #56134 ) ;
#72950 = EDGE_CURVE ( 'NONE', #31861, #40603, #73851, .T. ) ;
#72951 = CARTESIAN_POINT ( 'NONE',  ( 32.00000000000000711, 206.3125000027312126, 171.6568542494922553 ) ) ;
#72952 = ORIENTED_EDGE ( 'NONE', *, *, #73063, .F. ) ;
#72953 = CARTESIAN_POINT ( 'NONE',  ( 8.311093377946834337, 222.0312500034139873, -8.311093377946836114 ) ) ;
#72954 = AXIS2_PLACEMENT_3D ( 'NONE', #53733, #53364, #59032 ) ;
#72955 = CARTESIAN_POINT ( 'NONE',  ( 7.778174593052021635, 7.778174593052023411, 87.62500000409677625 ) ) ;
#72956 = CARTESIAN_POINT ( 'NONE',  ( -4.000000000000015099, 199.6875000027312126, 143.6568542494924543 ) ) ;
#72957 = CARTESIAN_POINT ( 'NONE',  ( -7.778174593052020747, -7.778174593052023411, 77.68749999999998579 ) ) ;
#72958 = CARTESIAN_POINT ( 'NONE',  ( 27.99999999999999645, 210.0000000000000284, 165.9999999999999147 ) ) ;
#72959 = CARTESIAN_POINT ( 'NONE',  ( 9.999999999999998224, 252.7083333333333712, -2.679491924311229401 ) ) ;
#72960 = CARTESIAN_POINT ( 'NONE',  ( 32.00000000000000000, 203.3750000027312126, 169.9999999999998863 ) ) ;
#72961 =( BOUNDED_CURVE ( )  B_SPLINE_CURVE ( 2, ( #43356, #54328, #36964, #59970, #25627, #54700, #19972, #72025, #8666 ),
 .UNSPECIFIED., .F., .F. ) 
 B_SPLINE_CURVE_WITH_KNOTS ( ( 3, 2, 2, 2, 3 ),
 ( 0.2840909090909091161, 0.2897727272727272929, 0.2954545454545454697, 0.3011363636363636465, 0.3068181818181818232 ),
 .UNSPECIFIED. ) 
 CURVE ( )  GEOMETRIC_REPRESENTATION_ITEM ( )  RATIONAL_B_SPLINE_CURVE ( ( 1.000000000000000000, 0.9238795325112867385, 1.000000000000000000, 0.9238795325112867385, 1.000000000000000000, 0.9238795325112867385, 1.000000000000000000, 0.9238795325112867385, 1.000000000000000000 ) ) 
 REPRESENTATION_ITEM ( '' )  );
#72962 = CARTESIAN_POINT ( 'NONE',  ( -10.00000000000000000, 182.2916666666666856, -2.679491924311229845 ) ) ;
#72963 = CARTESIAN_POINT ( 'NONE',  ( 4.556349186104052151, -10.99999999999999822, 110.9687500000000000 ) ) ;
#72964 = CARTESIAN_POINT ( 'NONE',  ( 7.188101187499992051, 2.977408999572647819, 22.20530278187175810 ) ) ;
#72965 = CARTESIAN_POINT ( 'NONE',  ( 11.35316468749999785, 150.8854166632527267, 3.042071309553174174 ) ) ;
#72966 = CARTESIAN_POINT ( 'NONE',  ( -2.828427124746208943, 204.7500000027312126, 144.8284271247462129 ) ) ;
#72967 = CARTESIAN_POINT ( 'NONE',  ( -31.13407770937647712, 46.03666098395253670, 64.99999999999998579 ) ) ;
#72968 = CARTESIAN_POINT ( 'NONE',  ( -1.469576158976823947E-15, 5.437499995903221084, 8.000000000000000000 ) ) ;
#72970 = CARTESIAN_POINT ( 'NONE',  ( -5.656854249492379694, 17.06250000000000000, -5.656854249492380582 ) ) ;
#72969 = LINE ( 'NONE', #72209, #25020 ) ;
#72971 = EDGE_LOOP ( 'NONE', ( #8469, #26089, #1114, #33350 ) ) ;
#72972 = CARTESIAN_POINT ( 'NONE',  ( -3.042071309553173730, 24.63541666325268054, 11.35316468749999785 ) ) ;
#72973 = CARTESIAN_POINT ( 'NONE',  ( 11.00000000000000000, 1.347111479062088405E-15, 82.74999999999998579 ) ) ;
#72975 = CARTESIAN_POINT ( 'NONE',  ( 26.34314575050773755, 199.5625000000000284, 165.9999999999998010 ) ) ;
#72974 = CARTESIAN_POINT ( 'NONE',  ( 2.449293598294707893E-16, 10.25000000000000000, -4.000000000000001776 ) ) ;
#72976 = LINE ( 'NONE', #71838, #32585 ) ;
#72977 = CARTESIAN_POINT ( 'NONE',  ( 1.432654583217607192, 201.2500000013656063, 145.4587341250000350 ) ) ;
#72978 = CARTESIAN_POINT ( 'NONE',  ( 8.660254037844385522, 51.45833332650536818, 5.000000000000005329 ) ) ;
#72979 = CARTESIAN_POINT ( 'NONE',  ( -5.082755093536324154, 110.8437500020483810, 5.082755093536326818 ) ) ;
#72980 = CARTESIAN_POINT ( 'NONE',  ( 4.541265875000002339, 7.499999998634408804, -1.881053915767121554 ) ) ;
#72981 = CARTESIAN_POINT ( 'NONE',  ( 8.660254037844381969, 54.58333333333333570, 5.000000000000002665 ) ) ;
#72982 = CARTESIAN_POINT ( 'NONE',  ( 5.656854249492376141, -5.656854249492374365, 10.39280277982336465 ) ) ;
#72984 = CARTESIAN_POINT ( 'NONE',  ( 7.999999999988127719, 1.377684776014802281E-05, 21.26780317368888618 ) ) ;
#72983 = CARTESIAN_POINT ( 'NONE',  ( 0.000000000000000000, 0.000000000000000000, 0.000000000000000000 ) ) ;
#72985 = VERTEX_POINT ( 'NONE', #24467 ) ;
#72986 = EDGE_LOOP ( 'NONE', ( #40662, #16834, #54391, #9731 ) ) ;
#72987 = CARTESIAN_POINT ( 'NONE',  ( 2.997893585525398702E-11, 31.24999999999767653, -10.00000000000000178 ) ) ;
#72988 = CARTESIAN_POINT ( 'NONE',  ( 3.458734125000016757, 196.1250000013656063, 199.4326545832176976 ) ) ;
#72989 = CARTESIAN_POINT ( 'NONE',  ( 10.00000000000000178, 1.874999993172032697, 0.000000000000000000 ) ) ;
#72990 = CARTESIAN_POINT ( 'NONE',  ( -26.33632401286670088, -41.96609452780020888, 153.6406248858571075 ) ) ;
#72991 = CARTESIAN_POINT ( 'NONE',  ( -11.35316468749999785, 128.0729166632526983, -3.042071309553167513 ) ) ;
#72992 = ORIENTED_EDGE ( 'NONE', *, *, #36559, .F. ) ;
#72993 = CARTESIAN_POINT ( 'NONE',  ( -4.242640687119286547, 297.8750000000000000, -4.242640687119286547 ) ) ;
#72994 = CARTESIAN_POINT ( 'NONE',  ( 10.18810118749999916, 1.247682550866122264E-15, 86.40625000204838102 ) ) ;
#72995 = CARTESIAN_POINT ( 'NONE',  ( -10.99999999999989342, 4.556349186104152515, 93.90625000000000000 ) ) ;
#72996 = CARTESIAN_POINT ( 'NONE',  ( -2.828427124746153876, 207.8750000000000284, 195.1715728752538439 ) ) ;
#72998 = CARTESIAN_POINT ( 'NONE',  ( 8.311093377946837890, 126.4062499965860411, -8.311093377946837890 ) ) ;
#72997 = CARTESIAN_POINT ( 'NONE',  ( 3.999999999999959144, 195.0625000000000000, 140.3431457505076594 ) ) ;
#72999 = CARTESIAN_POINT ( 'NONE',  ( 6.000000000000011546, -10.39230484541325694, 0.000000000000000000 ) ) ;
#73000 = ORIENTED_EDGE ( 'NONE', *, *, #20025, .T. ) ;
#73001 = CARTESIAN_POINT ( 'NONE',  ( -8.660254037844390851, 24.79166665983870033, 4.999999999999998224 ) ) ;
#73002 = CARTESIAN_POINT ( 'NONE',  ( 48.12321776826231456, 40.91806093260424149, 62.13366417131343411 ) ) ;
#73003 = CARTESIAN_POINT ( 'NONE',  ( -8.311093377946841443, 119.2187499965860127, 8.311093377946834337 ) ) ;
#73004 = CARTESIAN_POINT ( 'NONE',  ( 2.445694354108838731, 205.0625000013656063, 195.5543056458912190 ) ) ;
#73005 = CARTESIAN_POINT ( 'NONE',  ( 2.977408999572652260, 15.56249999795161365, 7.188101187500000044 ) ) ;
#73006 = CARTESIAN_POINT ( 'NONE',  ( 10.18810118749999916, 4.220049686691935698, 80.87500000204836681 ) ) ;
#73007 = CARTESIAN_POINT ( 'NONE',  ( -8.311093377946836114, 27.96874999658601624, -8.311093377946837890 ) ) ;
#73008 = ORIENTED_EDGE ( 'NONE', *, *, #63735, .F. ) ;
#73009 = FACE_OUTER_BOUND ( 'NONE', #44356, .T. ) ;
#73010 = CARTESIAN_POINT ( 'NONE',  ( 8.008118988124993010, -3.317071493978877239, 22.66936528394063188 ) ) ;
#73011 = CARTESIAN_POINT ( 'NONE',  ( -3.458734125000015425, 209.2500000013655779, 143.4326545832176976 ) ) ;
#73012 = EDGE_CURVE ( 'NONE', #33683, #18244, #7755, .T. ) ;
#73013 = CARTESIAN_POINT ( 'NONE',  ( 3.999999999999959144, 201.0625000000000000, 140.3431457505076594 ) ) ;
#73014 = CARTESIAN_POINT ( 'NONE',  ( 5.082755093536324154, 1.781249997951610098, 5.082755093536326818 ) ) ;
#73015 = CARTESIAN_POINT ( 'NONE',  ( -6.676582343750001591, 288.4531250017069510, 0.000000000000000000 ) ) ;
#73016 = CARTESIAN_POINT ( 'NONE',  ( -49.04219544972652756, 139.8383699274064611, 59.49880266147248875 ) ) ;
#73017 = CARTESIAN_POINT ( 'NONE',  ( 0.000000000000000000, 201.0000000000000284, 170.0000000000000284 ) ) ;
#73018 = VERTEX_POINT ( 'NONE', #30136 ) ;
#73019 = CARTESIAN_POINT ( 'NONE',  ( -3.042071309553164404, 147.5520833299193271, -11.35316468749999963 ) ) ;
#73020 = CARTESIAN_POINT ( 'NONE',  ( 7.204075437095968759, -7.204075437095966983, 80.21875000204836681 ) ) ;
#73021 = CARTESIAN_POINT ( 'NONE',  ( -31.45873412499999233, 196.6875000013655779, 170.0000000000003979 ) ) ;
#73022 = CARTESIAN_POINT ( 'NONE',  ( -2.828427124746209831, 198.3750000000000284, 139.1715728752538723 ) ) ;
#73023 = CARTESIAN_POINT ( 'NONE',  ( 4.541265875000001451, 17.37499999863440436, 1.881053915767124440 ) ) ;
#73024 = ORIENTED_EDGE ( 'NONE', *, *, #39622, .T. ) ;
#73025 = EDGE_CURVE ( 'NONE', #38312, #33138, #15452, .T. ) ;
#73026 = CARTESIAN_POINT ( 'NONE',  ( 1.656854249492405451, 202.4375000027311842, 202.0000000000000284 ) ) ;
#73027 = CARTESIAN_POINT ( 'NONE',  ( -2.445694354108839175, 196.3125000013656063, 144.4456943541088663 ) ) ;
#73028 = CARTESIAN_POINT ( 'NONE',  ( -23.99999999999998934, 204.8750000027312126, 170.0000000000002842 ) ) ;
#73029 = DIRECTION ( 'NONE',  ( -0.000000000000000000, -1.000000000000000000, -0.000000000000000000 ) ) ;
#73030 = EDGE_LOOP ( 'NONE', ( #61804, #20695, #41659, #19711, #38859 ) ) ;
#73031 = CARTESIAN_POINT ( 'NONE',  ( -2.977408999572650039, 11.43749999795161187, -7.188101187500000933 ) ) ;
#73032 = CARTESIAN_POINT ( 'NONE',  ( -24.75258994494077669, -12.99173873897962928, 188.6839129075868868 ) ) ;
#73033 = CARTESIAN_POINT ( 'NONE',  ( 7.778174593052023411, -7.778174593052021635, 73.75000000409676204 ) ) ;
#73034 = CARTESIAN_POINT ( 'NONE',  ( 9.832129032723416984, 185.3645833299193555, 5.676582343750006032 ) ) ;
#73035 = CARTESIAN_POINT ( 'NONE',  ( -2.977408999572651815, 111.3125000020483810, 7.188101187500000933 ) ) ;
#73036 = CARTESIAN_POINT ( 'NONE',  ( -0.3527280876246363106, 21.99999999999999289, -4.023046032806171901 ) ) ;
#73037 = CYLINDRICAL_SURFACE ( 'NONE', #3116, 10.00000000000000000 ) ;
#73038 = ADVANCED_FACE ( 'NONE', ( #40712 ), #46308, .F. ) ;
#73040 = CARTESIAN_POINT ( 'NONE',  ( 8.660254037844380193, 94.58333333333334281, 5.000000000000002665 ) ) ;
#73039 = CARTESIAN_POINT ( 'NONE',  ( 5.676582343750005144, 220.5729166700806729, 9.832129032723416984 ) ) ;
#73041 = ORIENTED_EDGE ( 'NONE', *, *, #32608, .F. ) ;
#73042 = ADVANCED_FACE ( 'NONE', ( #14992 ), #32373, .T. ) ;
#73043 = CARTESIAN_POINT ( 'NONE',  ( 11.35316468749999963, 261.4062500034140157, -1.390361679473963556E-15 ) ) ;
#73044 = CARTESIAN_POINT ( 'NONE',  ( 7.188101187499992051, 8.802885111219154394E-16, 22.11155278187175455 ) ) ;
#73045 = CARTESIAN_POINT ( 'NONE',  ( 11.00000000000000000, 1.347111479062088405E-15, 93.24999999999998579 ) ) ;
#73046 = DIRECTION ( 'NONE',  ( -0.000000000000000000, -1.000000000000000000, -0.000000000000000000 ) ) ;
#73047 = CARTESIAN_POINT ( 'NONE',  ( -1.317228840344807583, -65.80815776305057341, -26.30638062134362443 ) ) ;
#73048 = CARTESIAN_POINT ( 'NONE',  ( 2.445694354108839175, 197.3125000013656063, 195.5543056458912190 ) ) ;
#73049 = CARTESIAN_POINT ( 'NONE',  ( 12.80255146922220888, 13.39305315375704097, -0.2939692054342086247 ) ) ;
#73050 = CARTESIAN_POINT ( 'NONE',  ( -8.000000000000000000, 95.00000000000000000, 0.000000000000000000 ) ) ;
#73051 = CARTESIAN_POINT ( 'NONE',  ( -8.311093377946841443, 109.2187499965860269, 8.311093377946830785 ) ) ;
#73052 = CARTESIAN_POINT ( 'NONE',  ( -5.000000000000000888, -11.43937387734372990, -68.01947305042943981 ) ) ;
#73053 = CARTESIAN_POINT ( 'NONE',  ( 4.556349186104051263, -10.99999999999999822, 71.96874999999997158 ) ) ;
#73056 = CYLINDRICAL_SURFACE ( 'NONE', #63937, 3.999999999999976019 ) ;
#73055 = CARTESIAN_POINT ( 'NONE',  ( 24.54126587499999346, 199.1875000013655779, 169.9999999999999432 ) ) ;
#73054 = CARTESIAN_POINT ( 'NONE',  ( 25.55430564589115150, 199.5625000013656063, 172.4456943541086957 ) ) ;
#73057 = ADVANCED_FACE ( 'NONE', ( #25936 ), #31241, .F. ) ;
#73058 = ORIENTED_EDGE ( 'NONE', *, *, #33978, .F. ) ;
#73059 = EDGE_CURVE ( 'NONE', #22422, #31066, #2577, .T. ) ;
#73060 = CARTESIAN_POINT ( 'NONE',  ( 2.828427124746191623, 2.125000000000000000, -2.828427124746191623 ) ) ;
#73061 = CARTESIAN_POINT ( 'NONE',  ( -11.35316468749999785, 223.0729166632527267, -3.042071309553167513 ) ) ;
#73062 = CARTESIAN_POINT ( 'NONE',  ( 29.43265458321766559, 198.1250000013656063, 166.5412658749999650 ) ) ;
#73063 = EDGE_CURVE ( 'NONE', #9404, #22615, #61735, .T. ) ;
#73064 = CARTESIAN_POINT ( 'NONE',  ( -5.676582343749998039, 207.7604166632526983, -9.832129032723420536 ) ) ;
#73065 = FACE_OUTER_BOUND ( 'NONE', #58798, .T. ) ;
#73066 = FACE_OUTER_BOUND ( 'NONE', #20450, .T. ) ;
#73067 = CARTESIAN_POINT ( 'NONE',  ( 3.211159895383561835, 16.43749999863440436, -3.211159895383561835 ) ) ;
#73068 = CARTESIAN_POINT ( 'NONE',  ( 0.7581620860263087458, -55.63814191976401702, 43.81219804999812339 ) ) ;
#73069 = CARTESIAN_POINT ( 'NONE',  ( -7.999999999999991118, 0.000000000000000000, 26.33030277982336997 ) ) ;
#73071 = CARTESIAN_POINT ( 'NONE',  ( -27.99999999999999645, 210.0000000000000284, 174.0000000000003411 ) ) ;
#73070 = CARTESIAN_POINT ( 'NONE',  ( 8.660254037844380193, 184.5833333333333428, 5.000000000000002665 ) ) ;
#73072 = CARTESIAN_POINT ( 'NONE',  ( 11.35316468749999963, 100.9895833299193555, -3.042071309553165293 ) ) ;
#73073 = VERTEX_POINT ( 'NONE', #8979 ) ;
#73074 = CARTESIAN_POINT ( 'NONE',  ( 7.778174593052021635, 7.778174593052023411, 81.43750000000000000 ) ) ;
#73075 = CARTESIAN_POINT ( 'NONE',  ( -7.188101187500002709, 22.31249999795161187, 2.977408999572649151 ) ) ;
#73076 = DIRECTION ( 'NONE',  ( 0.000000000000000000, 0.000000000000000000, 1.000000000000000000 ) ) ;
#73077 = CARTESIAN_POINT ( 'NONE',  ( -11.35316468749999608, 259.4270833367472164, 3.042071309553173730 ) ) ;
#73078 = CARTESIAN_POINT ( 'NONE',  ( -2.085542519210945728E-15, 89.53124999658602690, 11.35316468750000141 ) ) ;
#73079 = ORIENTED_EDGE ( 'NONE', *, *, #50850, .T. ) ;
#73080 = CARTESIAN_POINT ( 'NONE',  ( 1.102182119232618108E-15, 291.3125000034140157, 6.000000000000001776 ) ) ;
#73081 = CARTESIAN_POINT ( 'NONE',  ( -10.18810118749999916, 4.220049686691934809, 109.5625000020483810 ) ) ;
#73082 = CARTESIAN_POINT ( 'NONE',  ( 4.898587196589412829E-16, 16.68749999590322375, -8.000000000000000000 ) ) ;
#73083 = CARTESIAN_POINT ( 'NONE',  ( -3.458734124999960358, 203.6875000013656063, 198.0000000000000284 ) ) ;
#73084 = DIRECTION ( 'NONE',  ( 0.000000000000000000, 0.000000000000000000, -1.000000000000000000 ) ) ;
#73086 = CARTESIAN_POINT ( 'NONE',  ( 11.35316468749999785, 90.57291666325269830, 3.042071309553174174 ) ) ;
#73085 = DIRECTION ( 'NONE',  ( 0.000000000000000000, 0.000000000000000000, 1.000000000000000000 ) ) ;
#73087 = CARTESIAN_POINT ( 'NONE',  ( 7.999999999999991118, 3.313708498984757611, 19.86155278392014978 ) ) ;
#73088 = CARTESIAN_POINT ( 'NONE',  ( -29.43265458321766559, 201.7500000013655779, 166.5412658750003629 ) ) ;
#73089 = CARTESIAN_POINT ( 'NONE',  ( 0.000000000000000000, 0.000000000000000000, -10.77459999999999951 ) ) ;
#73090 =( BOUNDED_CURVE ( )  B_SPLINE_CURVE ( 2, ( #63074, #11767, #28373, #16662, #39693, #27624, #21960, #46466, #45351, #62694, #51012, #23454, #74021 ),
 .UNSPECIFIED., .F., .F. ) 
 B_SPLINE_CURVE_WITH_KNOTS ( ( 3, 2, 2, 2, 2, 2, 3 ),
 ( 0.9293478260869566521, 0.9311594202898552108, 0.9329710144927537696, 0.9347826086956523284, 0.9365942028985509982, 0.9384057971014494459, 0.9402173913043480047 ),
 .UNSPECIFIED. ) 
 CURVE ( )  GEOMETRIC_REPRESENTATION_ITEM ( )  RATIONAL_B_SPLINE_CURVE ( ( 0.9999999999999978906, 0.9659258262890704216, 1.000000000000000000, 0.9659258262890683122, 1.000000000000000000, 0.9659258262890683122, 1.000000000000000000, 0.9659258262890683122, 1.000000000000000000, 0.9659258262890683122, 1.000000000000000000, 0.9659258262890640934, 1.000000000000004219 ) ) 
 REPRESENTATION_ITEM ( '' )  );
#73091 = VECTOR ( 'NONE', #18078, 1000.000000000000000 ) ;
#73092 = CARTESIAN_POINT ( 'NONE',  ( 6.123233995736767268E-16, 188.1249999931720254, -10.00000000000000178 ) ) ;
#73093 = CARTESIAN_POINT ( 'NONE',  ( 0.000000000000000000, 125.0000000000000000, 0.000000000000000000 ) ) ;
#73094 = CARTESIAN_POINT ( 'NONE',  ( 9.832129032723416984, 75.67708332991934128, 5.676582343750006032 ) ) ;
#73095 = CARTESIAN_POINT ( 'NONE',  ( 1.226468279477575784E-15, 292.7031250017069510, 6.676582343750001591 ) ) ;
#73096 = CARTESIAN_POINT ( 'NONE',  ( -4.220049686691937474, -10.18810118749999738, 102.8125000020483952 ) ) ;
#73097 = CARTESIAN_POINT ( 'NONE',  ( -2.085542519210945728E-15, 214.5312499965860411, 11.35316468750000141 ) ) ;
#73098 = ORIENTED_EDGE ( 'NONE', *, *, #51610, .T. ) ;
#73099 = CARTESIAN_POINT ( 'NONE',  ( -4.000000000000001776, 1.249999997268813168, -4.898587196589415787E-16 ) ) ;
#73100 = DIRECTION ( 'NONE',  ( 1.000000000000000000, 0.000000000000000000, 0.000000000000000000 ) ) ;
#73101 = FACE_OUTER_BOUND ( 'NONE', #50085, .T. ) ;
#73103 = CARTESIAN_POINT ( 'NONE',  ( 6.951808397369818766E-16, 202.0312499965860411, -11.35316468750000141 ) ) ;
#73102 = CARTESIAN_POINT ( 'NONE',  ( -38.00000000000000000, -52.99999999999999289, 25.00000000000000000 ) ) ;
#73104 = CARTESIAN_POINT ( 'NONE',  ( 2.679491924311235174, 219.5833333401612890, 9.999999999999998224 ) ) ;
#73105 = CARTESIAN_POINT ( 'NONE',  ( -6.123233995736766282E-16, 243.7500000000000284, -10.00000000000000000 ) ) ;
#73106 = ORIENTED_EDGE ( 'NONE', *, *, #3917, .F. ) ;
#73107 = CARTESIAN_POINT ( 'NONE',  ( 8.311093377946834337, 195.4687499965860127, 8.311093377946839666 ) ) ;
#73108 = B_SPLINE_CURVE_WITH_KNOTS ( 'NONE', 3,
 ( #39466, #10791, #33453, #56453, #4771, #51152, #73049, #56086, #27763, #50775 ),
 .UNSPECIFIED., .F., .F.,
 ( 4, 2, 2, 2, 4 ),
 ( 0.01051554819734982701, 0.01182504667393347204, 0.01313454515051711881, 0.01575354210368441407, 0.02099153601001900113 ),
 .UNSPECIFIED. ) ;
#73109 = CARTESIAN_POINT ( 'NONE',  ( 7.188101187499993827, -2.977408999572645598, 15.64280278187175277 ) ) ;
#73110 = EDGE_CURVE ( 'NONE', #4164, #10291, #48953, .T. ) ;
#73111 = CARTESIAN_POINT ( 'NONE',  ( -28.00000000000002487, 208.4375000013656063, 166.5412658750003629 ) ) ;
#73112 = CARTESIAN_POINT ( 'NONE',  ( 7.999999999999998224, 11.90625000000000355, 3.313708498984766493 ) ) ;
#73113 = VECTOR ( 'NONE', #65521, 1000.000000000000000 ) ;
#73114 = ORIENTED_EDGE ( 'NONE', *, *, #64002, .F. ) ;
#73115 = CARTESIAN_POINT ( 'NONE',  ( -4.898587196589412829E-16, 93.31250000409677625, -8.000000000000000000 ) ) ;
#73116 = CARTESIAN_POINT ( 'NONE',  ( -2.679491924311225848, 11.45833333333333393, -10.00000000000000178 ) ) ;
#73117 = EDGE_CURVE ( 'NONE', #13943, #49563, #45558, .T. ) ;
#73118 = CARTESIAN_POINT ( 'NONE',  ( 7.204075437095968759, -7.204075437095966983, 80.59375000204838102 ) ) ;
#73119 = ORIENTED_EDGE ( 'NONE', *, *, #9666, .F. ) ;
#73120 = CARTESIAN_POINT ( 'NONE',  ( -1.656854249492383691, 21.68750000000000000, 4.000000000000000888 ) ) ;
#73121 = CARTESIAN_POINT ( 'NONE',  ( -3.211159895383562723, 20.93749999863440436, 3.211159895383561391 ) ) ;
#73122 = CARTESIAN_POINT ( 'NONE',  ( 1.469576158976822172E-15, -7.999999999999991118, 5.892802783920146226 ) ) ;
#73123 = PRODUCT_RELATED_PRODUCT_CATEGORY ( 'part', '', ( #1223 ) ) ;
#73124 = CARTESIAN_POINT ( 'NONE',  ( 1.224646799147353454E-15, 237.9999999999999716, -10.00000000000000178 ) ) ;
#73125 = EDGE_LOOP ( 'NONE', ( #65647, #50555, #45338, #53106, #49763 ) ) ;
#73126 =( NAMED_UNIT ( * ) PLANE_ANGLE_UNIT ( ) SI_UNIT ( $, .RADIAN. ) );
#73127 = CARTESIAN_POINT ( 'NONE',  ( -7.188101187500000044, 94.15625000204838102, 0.000000000000000000 ) ) ;
#73129 = CARTESIAN_POINT ( 'NONE',  ( 5.676582343750005144, 255.5729166700806445, 9.832129032723416984 ) ) ;
#73128 = CARTESIAN_POINT ( 'NONE',  ( 2.775557561562891351E-14, 210.0000000000000284, 151.0000000000000568 ) ) ;
#73130 = APPLICATION_PROTOCOL_DEFINITION ( 'draft international standard', 'automotive_design', 1998, #28395 ) ;
#73131 = ORIENTED_EDGE ( 'NONE', *, *, #6203, .T. ) ;
#73132 = EDGE_CURVE ( 'NONE', #33509, #19205, #22966, .T. ) ;
#73133 = CARTESIAN_POINT ( 'NONE',  ( -11.35316468749999963, 254.2187500034139873, 0.000000000000000000 ) ) ;
#73134 = CARTESIAN_POINT ( 'NONE',  ( 7.188101187499993827, -2.977408999572645598, 11.14280278187175810 ) ) ;
#73135 = ORIENTED_EDGE ( 'NONE', *, *, #10394, .F. ) ;
#73136 = EDGE_CURVE ( 'NONE', #23710, #12488, #12692, .T. ) ;
#73137 = EDGE_LOOP ( 'NONE', ( #72366, #37309, #2551, #636 ) ) ;
#73138 = CARTESIAN_POINT ( 'NONE',  ( -10.18810118749999916, 0.000000000000000000, 75.15625000204836681 ) ) ;
#73139 = CARTESIAN_POINT ( 'NONE',  ( 11.35316468749999963, 76.30208332991935549, -3.042071309553165293 ) ) ;
#73140 = CARTESIAN_POINT ( 'NONE',  ( 2.751064625579944321E-14, 202.8750000027312126, 194.0000000000000568 ) ) ;
#73141 = CARTESIAN_POINT ( 'NONE',  ( 11.00000000000000000, 1.347111479062088405E-15, 88.75000000000000000 ) ) ;
#73144 = CARTESIAN_POINT ( 'NONE',  ( -2.765530957081998142, 291.7968750017070079, 6.676582343750000703 ) ) ;
#73143 = CARTESIAN_POINT ( 'NONE',  ( 26.34314575050758478, 196.6875000027312126, 165.9999999999998863 ) ) ;
#73142 = FACE_OUTER_BOUND ( 'NONE', #39554, .T. ) ;
#73145 = CARTESIAN_POINT ( 'NONE',  ( 2.020667218593132706E-15, -11.00000000000000000, 83.87499999999998579 ) ) ;
#73146 = DIRECTION ( 'NONE',  ( 0.000000000000000000, 0.000000000000000000, 1.000000000000000000 ) ) ;
#73147 = CARTESIAN_POINT ( 'NONE',  ( -2.445694354108784108, 199.5625000013656063, 195.5543056458912190 ) ) ;
#73148 = CARTESIAN_POINT ( 'NONE',  ( 4.898587196589412829E-16, 7.687499995903221084, -8.000000000000000000 ) ) ;
#73149 = ORIENTED_EDGE ( 'NONE', *, *, #51567, .F. ) ;
#73150 = CARTESIAN_POINT ( 'NONE',  ( 26.56734541678238415, 209.2500000013655779, 166.5412658749999650 ) ) ;
#73151 = CARTESIAN_POINT ( 'NONE',  ( 4.401442555609581635E-16, 19.21874999795161543, -7.188101187500000044 ) ) ;
#73152 = CARTESIAN_POINT ( 'NONE',  ( -8.311093377946841443, 169.2187499965859843, 8.311093377946830785 ) ) ;
#73153 = FACE_OUTER_BOUND ( 'NONE', #3103, .T. ) ;
#73154 = CARTESIAN_POINT ( 'NONE',  ( 1.320432766682874540E-15, 102.4062500020483810, 7.188101187500000044 ) ) ;
#73156 = CARTESIAN_POINT ( 'NONE',  ( 2.589639417653723186, -50.10293296561477661, -40.79253907059064232 ) ) ;
#73155 = CARTESIAN_POINT ( 'NONE',  ( -30.99999999999992895, -31.99999999999978684, 171.9999999999997726 ) ) ;
#73157 = CARTESIAN_POINT ( 'NONE',  ( 26.56734541678233086, 206.6250000013656063, 173.4587341249998929 ) ) ;
#73158 = CARTESIAN_POINT ( 'NONE',  ( 7.188101187499993827, -2.977408999572645598, 19.01780278187175810 ) ) ;
#73159 = CARTESIAN_POINT ( 'NONE',  ( 1.656854249492347719, 208.9375000027312410, 146.0000000000000284 ) ) ;
#73160 = CARTESIAN_POINT ( 'NONE',  ( -9.832129032723420536, 48.69791666325268409, 5.676582343749997150 ) ) ;
#73161 = EDGE_CURVE ( 'NONE', #30116, #31722, #55388, .T. ) ;
#73162 = FACE_OUTER_BOUND ( 'NONE', #50653, .T. ) ;
#73163 = CARTESIAN_POINT ( 'NONE',  ( -2.679491924311225848, 18.33333332650536818, -10.00000000000000178 ) ) ;
#73164 = CYLINDRICAL_SURFACE ( 'NONE', #52217, 3.999999999999976019 ) ;
#73165 = VERTEX_POINT ( 'NONE', #72730 ) ;
#73166 = CIRCLE ( 'NONE', #51457, 9.999999999999996447 ) ;
#73167 = CARTESIAN_POINT ( 'NONE',  ( 1.469576158976823947E-15, 114.8750000000000000, 8.000000000000000000 ) ) ;
#73168 = CARTESIAN_POINT ( 'NONE',  ( 11.00000000000000000, 1.347111479062088405E-15, 81.43750000409677625 ) ) ;
#73169 = CARTESIAN_POINT ( 'NONE',  ( 3.042071309553159519, 44.73958332991934839, 11.35316468750000141 ) ) ;
#73170 = CARTESIAN_POINT ( 'NONE',  ( -11.00000000000000000, 0.000000000000000000, 74.68750000409676204 ) ) ;
#73171 = CARTESIAN_POINT ( 'NONE',  ( 3.458734124999959469, 198.7500000013656063, 140.5673454167823593 ) ) ;
#73172 = CARTESIAN_POINT ( 'NONE',  ( 2.990854866096223752, 10.11452374054098335, 70.45725801588044135 ) ) ;
#73173 = CARTESIAN_POINT ( 'NONE',  ( -2.849036369511732440E-14, 196.3750000027311842, 138.0000000000000568 ) ) ;
#73175 = CARTESIAN_POINT ( 'NONE',  ( -5.676582343749998039, 47.44791666325268409, -9.832129032723420536 ) ) ;
#73174 = CARTESIAN_POINT ( 'NONE',  ( 5.082755093536325042, 102.5937500020483668, -5.082755093536325930 ) ) ;
#73176 = CARTESIAN_POINT ( 'NONE',  ( 7.999999999999991118, 3.313708498984757611, 10.67405277982336465 ) ) ;
#73177 = CARTESIAN_POINT ( 'NONE',  ( -3.313708498984759387, -7.999999999999989342, 4.299052783920145338 ) ) ;
#73178 = CARTESIAN_POINT ( 'NONE',  ( 11.35316468749999785, 160.5729166632526699, 3.042071309553174174 ) ) ;
#73179 = CARTESIAN_POINT ( 'NONE',  ( -4.999999999999998224, 138.5416666598387110, -8.660254037844389075 ) ) ;
#73180 = CIRCLE ( 'NONE', #52717, 18.50000000000000000 ) ;
#73181 = CARTESIAN_POINT ( 'NONE',  ( 2.977408999572654480, 101.0000000020483810, 7.188101187499999156 ) ) ;
#73182 = CARTESIAN_POINT ( 'NONE',  ( -2.980536294216330262, -45.39327737951327890, 139.1435926870292690 ) ) ;
#73183 = CARTESIAN_POINT ( 'NONE',  ( -9.832129032723420536, 34.01041666325269119, 5.676582343749997150 ) ) ;
#73184 =( BOUNDED_CURVE ( )  B_SPLINE_CURVE ( 2, ( #2991, #13910, #9399, #48256, #30912 ),
 .UNSPECIFIED., .F., .F. ) 
 B_SPLINE_CURVE_WITH_KNOTS ( ( 3, 2, 3 ),
 ( 0.000000000000000000, 0.008333333333333399137, 0.01666666666666679827 ),
 .UNSPECIFIED. ) 
 CURVE ( )  GEOMETRIC_REPRESENTATION_ITEM ( )  RATIONAL_B_SPLINE_CURVE ( ( 1.000000000000000000, 0.9238795325112867385, 1.000000000000000000, 0.9238795325112855172, 1.000000000000001110 ) ) 
 REPRESENTATION_ITEM ( '' )  );
#73185 = CYLINDRICAL_SURFACE ( 'NONE', #9927, 8.000000000000000000 ) ;
#73186 = EDGE_LOOP ( 'NONE', ( #2907, #64481, #36453, #73563 ) ) ;
#73187 = DIRECTION ( 'NONE',  ( -0.000000000000000000, 1.000000000000000000, 4.476705744456276341E-16 ) ) ;
#73188 = CARTESIAN_POINT ( 'NONE',  ( 4.220049686691934809, 10.18810118749999916, 74.68750000204836681 ) ) ;
#73189 = DIRECTION ( 'NONE',  ( 0.1513591288559071046, 0.000000000000000000, 0.9884788384745426537 ) ) ;
#73191 = CARTESIAN_POINT ( 'NONE',  ( 9.832129032723416984, 160.3645833299193839, 5.676582343750006032 ) ) ;
#73190 = CARTESIAN_POINT ( 'NONE',  ( -3.313708498984759387, -7.999999999999989342, 2.799052783920144005 ) ) ;
#73192 = CARTESIAN_POINT ( 'NONE',  ( -5.656854249492373476, -5.656854249492376141, 14.57405278432982598 ) ) ;
#73193 = CARTESIAN_POINT ( 'NONE',  ( 3.313708498984742068, 8.718749999999998224, 8.000000000000019540 ) ) ;
#73194 = CARTESIAN_POINT ( 'NONE',  ( -6.951808397369817780E-16, 227.6562500034139873, -11.35316468749999963 ) ) ;
#73195 = DIRECTION ( 'NONE',  ( 0.000000000000000000, 0.000000000000000000, 1.000000000000000000 ) ) ;
#73196 = CARTESIAN_POINT ( 'NONE',  ( -10.18810118749999916, 0.000000000000000000, 81.53125000204838102 ) ) ;
#73197 = ORIENTED_EDGE ( 'NONE', *, *, #37961, .F. ) ;
#73198 = EDGE_CURVE ( 'NONE', #56214, #45255, #41172, .T. ) ;
#73199 = AXIS2_PLACEMENT_3D ( 'NONE', #74078, #44671, #17098 ) ;
#73200 = CARTESIAN_POINT ( 'NONE',  ( 0.000000000000000000, 0.000000000000000000, 118.0000000000000000 ) ) ;
#73201 = CARTESIAN_POINT ( 'NONE',  ( 7.778174593052021635, 7.778174593052023411, 105.4374999999999858 ) ) ;
#73202 = CARTESIAN_POINT ( 'NONE',  ( 6.951808397369818766E-16, 117.3437499965860127, -11.35316468750000141 ) ) ;
#73203 = EDGE_CURVE ( 'NONE', #70940, #62698, #30792, .T. ) ;
#73204 =( BOUNDED_CURVE ( )  B_SPLINE_CURVE ( 2, ( #45393, #73698, #56735, #72588, #22010, #57102, #28049, #74071, #22372 ),
 .UNSPECIFIED., .F., .F. ) 
 B_SPLINE_CURVE_WITH_KNOTS ( ( 3, 2, 2, 2, 3 ),
 ( 0.3666666666666669738, 0.3750000000000003331, 0.3833333333333336923, 0.3916666666666669960, 0.4000000000000003553 ),
 .UNSPECIFIED. ) 
 CURVE ( )  GEOMETRIC_REPRESENTATION_ITEM ( )  RATIONAL_B_SPLINE_CURVE ( ( 0.9999999999999970024, 0.9238795325112897361, 1.000000000000000000, 0.9238795325112867385, 1.000000000000000000, 0.9238795325112867385, 1.000000000000000000, 0.9238795325112837409, 1.000000000000003109 ) ) 
 REPRESENTATION_ITEM ( '' )  );
#73205 = CARTESIAN_POINT ( 'NONE',  ( 4.541265875000002339, 19.43749999863440436, 0.000000000000000000 ) ) ;
#73206 = VERTEX_POINT ( 'NONE', #27818 ) ;
#73207 = ORIENTED_EDGE ( 'NONE', *, *, #7207, .F. ) ;
#73208 = CARTESIAN_POINT ( 'NONE',  ( -1.881053915767124440, 6.124999998634407916, 4.541265875000001451 ) ) ;
#73209 = CARTESIAN_POINT ( 'NONE',  ( -7.188101187500000044, 5.718749997951611874, -8.802885111219163269E-16 ) ) ;
#73210 = CARTESIAN_POINT ( 'NONE',  ( -3.313708498984762496, 110.4687500040967905, 7.999999999999998224 ) ) ;
#73211 = CARTESIAN_POINT ( 'NONE',  ( 7.204075437095968759, -7.204075437095966983, 91.09375000204838102 ) ) ;
#73212 = CARTESIAN_POINT ( 'NONE',  ( -31.45873412499999944, 200.8750000013656063, 168.5673454167827572 ) ) ;
#73213 = CARTESIAN_POINT ( 'NONE',  ( 2.828427124746190291, 6.875000000000000000, 2.828427124746192067 ) ) ;
#73214 = CARTESIAN_POINT ( 'NONE',  ( 4.000000000000001776, 19.74999999726881228, 0.000000000000000000 ) ) ;
#73215 = CARTESIAN_POINT ( 'NONE',  ( 1.881053915767122664, 9.124999998634407916, 4.541265875000001451 ) ) ;
#73216 = CARTESIAN_POINT ( 'NONE',  ( 3.999999999999960032, 199.9375000000000000, 143.6568542494924543 ) ) ;
#73217 = ORIENTED_EDGE ( 'NONE', *, *, #33260, .T. ) ;
#73218 = CARTESIAN_POINT ( 'NONE',  ( -3.000000000000001332, -45.00000000000001421, 151.2383369607063344 ) ) ;
#73219 = AXIS2_PLACEMENT_3D ( 'NONE', #43366, #53959, #2272 ) ;
#73221 = CARTESIAN_POINT ( 'NONE',  ( 5.000000000000004441, 234.7916666734946602, 8.660254037844385522 ) ) ;
#73220 = CARTESIAN_POINT ( 'NONE',  ( -30.44569435410886626, 196.5625000013656063, 167.5543056458916169 ) ) ;
#73222 = CARTESIAN_POINT ( 'NONE',  ( 2.780723358947928197E-16, 19.56249999863440436, -4.541265875000002339 ) ) ;
#73223 = CARTESIAN_POINT ( 'NONE',  ( 0.3950625784802609952, -47.98034167995889732, 151.0031319679888497 ) ) ;
#73224 = CARTESIAN_POINT ( 'NONE',  ( -7.188101187499992051, 0.000000000000000000, 2.986552781871751439 ) ) ;
#73225 = EDGE_LOOP ( 'NONE', ( #16229, #56430 ) ) ;
#73226 = VERTEX_POINT ( 'NONE', #15741 ) ;
#73227 = CARTESIAN_POINT ( 'NONE',  ( 7.204075437095968759, -7.204075437095966983, 93.71875000204838102 ) ) ;
#73228 = DIRECTION ( 'NONE',  ( -0.000000000000000000, 1.000000000000000000, -4.476705744456276341E-16 ) ) ;
#73229 = CARTESIAN_POINT ( 'NONE',  ( -30.44569435410879166, 200.0625000013656063, 172.4456943541092357 ) ) ;
#73230 = CARTESIAN_POINT ( 'NONE',  ( 11.00000000000000000, 1.347111479062088405E-15, 105.2500000000000000 ) ) ;
#73231 = CARTESIAN_POINT ( 'NONE',  ( 3.458734125000015869, 207.1875000013656063, 198.0000000000000284 ) ) ;
#73232 = CARTESIAN_POINT ( 'NONE',  ( -8.000000000000000000, 111.4062499999999858, -3.313708498984761164 ) ) ;
#73233 = CARTESIAN_POINT ( 'NONE',  ( 4.999999999999993783, 124.1666666666666714, 8.660254037844390851 ) ) ;
#73234 = CARTESIAN_POINT ( 'NONE',  ( -3.313708498984762052, 105.2187500000000000, -8.000000000000000000 ) ) ;
#73235 = CARTESIAN_POINT ( 'NONE',  ( 6.676582343750003368, 293.1718750017070647, -2.765530957081997254 ) ) ;
#73236 = CARTESIAN_POINT ( 'NONE',  ( -4.401442555609577197E-16, 7.188101187499992051, 7.486552781871751883 ) ) ;
#73237 = ORIENTED_EDGE ( 'NONE', *, *, #21071, .F. ) ;
#73238 = AXIS2_PLACEMENT_3D ( 'NONE', #22483, #39852, #69644 ) ;
#73239 = CYLINDRICAL_SURFACE ( 'NONE', #30146, 11.00000000000000000 ) ;
#73240 = CARTESIAN_POINT ( 'NONE',  ( 30.44569435410883784, 205.8125000013656063, 167.5543056458911053 ) ) ;
#73241 = CARTESIAN_POINT ( 'NONE',  ( -5.656854249492381470, 27.74999999590322020, 5.656854249492379694 ) ) ;
#73242 = CARTESIAN_POINT ( 'NONE',  ( -2.839093476692135984E-14, 200.6875000013656063, 138.5412658750000503 ) ) ;
#73243 = CARTESIAN_POINT ( 'NONE',  ( 2.977408999572650039, 122.5625000020483668, -7.188101187500000933 ) ) ;
#73245 = CARTESIAN_POINT ( 'NONE',  ( 3.458734124999960358, 201.6250000013656063, 143.4326545832176976 ) ) ;
#73244 = CARTESIAN_POINT ( 'NONE',  ( 1.469576158976823947E-15, 113.5625000040967905, 8.000000000000000000 ) ) ;
#73246 = CARTESIAN_POINT ( 'NONE',  ( -5.676582343750000703, 253.3854166700806445, -9.832129032723418760 ) ) ;
#73247 = DIRECTION ( 'NONE',  ( 0.000000000000000000, 0.000000000000000000, 1.000000000000000000 ) ) ;
#73248 = DIRECTION ( 'NONE',  ( -0.000000000000000000, 1.000000000000000000, -0.000000000000000000 ) ) ;
#73249 = CARTESIAN_POINT ( 'NONE',  ( 8.311093377946834337, 20.15624999658600913, 8.311093377946839666 ) ) ;
#73250 = CARTESIAN_POINT ( 'NONE',  ( 105.0000000000000000, 37.00000000000000000, 20.00000000000000000 ) ) ;
#73251 = CARTESIAN_POINT ( 'NONE',  ( 9.832129032723420536, 206.5104166632526983, -5.676582343749999815 ) ) ;
#73252 = LINE ( 'NONE', #4226, #58985 ) ;
#73253 = CARTESIAN_POINT ( 'NONE',  ( -3.211159895383561391, 6.687499998634407028, -3.211159895383561835 ) ) ;
#73254 = CARTESIAN_POINT ( 'NONE',  ( -3.190679070438028606E-13, 193.7500000000000000, 10.00000000000000533 ) ) ;
#73256 = DIRECTION ( 'NONE',  ( 0.000000000000000000, 0.000000000000000000, 1.000000000000000000 ) ) ;
#73255 = CARTESIAN_POINT ( 'NONE',  ( -27.99999999999995737, 205.5000000000000284, 174.0000000000003695 ) ) ;
#73257 = EDGE_LOOP ( 'NONE', ( #48988, #31844, #39423, #53471, #42805, #9660 ) ) ;
#73258 = CARTESIAN_POINT ( 'NONE',  ( -2.445694354108839175, 199.3125000013656063, 144.4456943541088663 ) ) ;
#73259 = CARTESIAN_POINT ( 'NONE',  ( -3.042071309553173730, 4.322916663252682312, 11.35316468749999785 ) ) ;
#73260 = CARTESIAN_POINT ( 'NONE',  ( -11.00000000000000000, 0.000000000000000000, 95.68750000409677625 ) ) ;
#73261 = CARTESIAN_POINT ( 'NONE',  ( 0.8588954341814317717, 10.28066745654381542, 63.58998442112849858 ) ) ;
#73262 = CARTESIAN_POINT ( 'NONE',  ( -31.45873412499999233, 195.6875000013655779, 170.0000000000004547 ) ) ;
#73263 = FACE_OUTER_BOUND ( 'NONE', #41855, .T. ) ;
#73265 = CARTESIAN_POINT ( 'NONE',  ( -5.676582343750006032, 9.114583329919350163, 9.832129032723418760 ) ) ;
#73264 = CARTESIAN_POINT ( 'NONE',  ( 5.082755093536325042, 119.0937500020483810, -5.082755093536325930 ) ) ;
#73266 = CARTESIAN_POINT ( 'NONE',  ( -3.313708498984758943, -7.999999999999989342, 25.11155277982337353 ) ) ;
#73267 = CARTESIAN_POINT ( 'NONE',  ( 8.311093377946834337, 125.1562499965860411, 8.311093377946839666 ) ) ;
#73268 = EDGE_CURVE ( 'NONE', #13147, #25107, #51296, .T. ) ;
#73269 = CARTESIAN_POINT ( 'NONE',  ( 6.123233995736767268E-16, 98.12499999317203958, -10.00000000000000178 ) ) ;
#73270 = CARTESIAN_POINT ( 'NONE',  ( 1.320432766682874540E-15, 120.4062500020483810, 7.188101187500000044 ) ) ;
#73271 = CARTESIAN_POINT ( 'NONE',  ( 1.881053915767121776, 19.62499999863441147, -4.541265875000002339 ) ) ;
#73272 = CARTESIAN_POINT ( 'NONE',  ( -5.656854249492373476, -5.656854249492376141, 25.20530278392014978 ) ) ;
#73273 = CARTESIAN_POINT ( 'NONE',  ( 10.00000000000000888, 145.0000000000000284, 0.000000000000000000 ) ) ;
#73274 = ORIENTED_EDGE ( 'NONE', *, *, #45739, .T. ) ;
#73275 = CARTESIAN_POINT ( 'NONE',  ( -5.000000000000000888, 116.6666666666666856, -8.660254037844390851 ) ) ;
#73276 = CARTESIAN_POINT ( 'NONE',  ( -4.721056650415999201, 288.4843750017070079, -4.721056650415999201 ) ) ;
#73277 = CARTESIAN_POINT ( 'NONE',  ( -4.000000000000015987, 207.6875000027312126, 143.6568542494924259 ) ) ;
#73278 = CARTESIAN_POINT ( 'NONE',  ( -7.999999999999991118, 0.000000000000000000, 27.88655278432982598 ) ) ;
#73279 = CARTESIAN_POINT ( 'NONE',  ( 9.000000000000000000, 5.196152422706648899, -0.8038475772933779684 ) ) ;
#73280 = CARTESIAN_POINT ( 'NONE',  ( 11.35316468749999963, 261.1979166700807014, 3.042071309553159519 ) ) ;
#73281 = CIRCLE ( 'NONE', #71900, 6.999999999999999112 ) ;
#73282 = CARTESIAN_POINT ( 'NONE',  ( -7.204075437095967871, 7.204075437095967871, 103.8437500020483810 ) ) ;
#73283 = ORIENTED_EDGE ( 'NONE', *, *, #32846, .T. ) ;
#73284 = ADVANCED_FACE ( 'NONE', ( #38780 ), #711, .T. ) ;
#73285 = CARTESIAN_POINT ( 'NONE',  ( 10.00000000000000178, 156.8749999931720254, 0.000000000000000000 ) ) ;
#73286 = CARTESIAN_POINT ( 'NONE',  ( 3.042071309553167513, 152.1354166632526983, -11.35316468749999785 ) ) ;
#73287 = CARTESIAN_POINT ( 'NONE',  ( -30.91763550117376980, -20.99944976732569657, 172.8975561284972287 ) ) ;
#73288 = EDGE_CURVE ( 'NONE', #852, #26401, #74421, .T. ) ;
#73289 = CARTESIAN_POINT ( 'NONE',  ( -2.445694354108784108, 207.5625000013656063, 195.5543056458912190 ) ) ;
#73290 = CARTESIAN_POINT ( 'NONE',  ( 7.320508075688776373, 230.0000000068279462, 7.320508075688767491 ) ) ;
#73291 = CARTESIAN_POINT ( 'NONE',  ( -8.311093377946836114, 72.96874999658602690, -8.311093377946837890 ) ) ;
#73292 = ORIENTED_EDGE ( 'NONE', *, *, #57898, .T. ) ;
#73293 = CARTESIAN_POINT ( 'NONE',  ( -4.220049686691935698, 10.18810118749999916, 113.8750000020483668 ) ) ;
#73294 = CARTESIAN_POINT ( 'NONE',  ( 1.881053915767121998, 8.624999998634407916, -4.541265875000002339 ) ) ;
#73295 = ORIENTED_EDGE ( 'NONE', *, *, #37944, .F. ) ;
#73296 = CARTESIAN_POINT ( 'NONE',  ( -5.656854249492379694, 2.062500000000000444, -5.656854249492380582 ) ) ;
#73297 = CARTESIAN_POINT ( 'NONE',  ( 2.485281374238575314, 287.3750000034140157, 6.000000000000000888 ) ) ;
#73298 = DIRECTION ( 'NONE',  ( 0.000000000000000000, 0.000000000000000000, 1.000000000000000000 ) ) ;
#73299 = CARTESIAN_POINT ( 'NONE',  ( 7.188101187500000044, 17.34374999795161543, 0.000000000000000000 ) ) ;
#73300 = CARTESIAN_POINT ( 'NONE',  ( 2.020667218593132706E-15, -11.00000000000000000, 103.5625000040967763 ) ) ;
#73301 =( BOUNDED_CURVE ( )  B_SPLINE_CURVE ( 2, ( #73045, #72677, #31937, #54960, #20980, #67011, #15688, #15310, #16424 ),
 .UNSPECIFIED., .F., .F. ) 
 B_SPLINE_CURVE_WITH_KNOTS ( ( 3, 2, 2, 2, 3 ),
 ( 0.4852941176470589313, 0.4889705882352942123, 0.4926470588235295489, 0.4963235294117648300, 0.5000000000000001110 ),
 .UNSPECIFIED. ) 
 CURVE ( )  GEOMETRIC_REPRESENTATION_ITEM ( )  RATIONAL_B_SPLINE_CURVE ( ( 0.9999999999999976685, 0.9238795325112890700, 1.000000000000000000, 0.9238795325112867385, 1.000000000000000000, 0.9238795325112867385, 1.000000000000000000, 0.9238795325112844070, 1.000000000000002220 ) ) 
 REPRESENTATION_ITEM ( '' )  );
#73302 = AXIS2_PLACEMENT_3D ( 'NONE', #51713, #16247, #27582 ) ;
#73303 = CARTESIAN_POINT ( 'NONE',  ( 4.220049686691941027, -10.18810118749999738, 112.0000000020483668 ) ) ;
#73304 = DIRECTION ( 'NONE',  ( -0.000000000000000000, 1.000000000000000000, -0.000000000000000000 ) ) ;
#73305 = CARTESIAN_POINT ( 'NONE',  ( 1.656854249492381914, 7.562499997268812280, 4.000000000000000888 ) ) ;
#73306 = DIRECTION ( 'NONE',  ( -0.000000000000000000, 1.000000000000000000, 4.476705744456276341E-16 ) ) ;
#73307 = VERTEX_POINT ( 'NONE', #21775 ) ;
#73308 = CARTESIAN_POINT ( 'NONE',  ( 3.458734125000015425, 201.9375000013656063, 198.0000000000000284 ) ) ;
#73309 = CARTESIAN_POINT ( 'NONE',  ( -30.82842712474612057, 194.5000000027312126, 172.8284271247466108 ) ) ;
#73310 = CARTESIAN_POINT ( 'NONE',  ( 4.000000000000001776, 12.74999999726881406, 0.000000000000000000 ) ) ;
#73311 =( BOUNDED_CURVE ( )  B_SPLINE_CURVE ( 2, ( #9157, #72144, #3500, #26488, #49513, #72532, #57054, #16282, #39687 ),
 .UNSPECIFIED., .F., .T. ) 
 B_SPLINE_CURVE_WITH_KNOTS ( ( 3, 2, 2, 2, 3 ),
 ( 0.7833333333333338810, 0.7916666666666671848, 0.8000000000000007105, 0.8083333333333340143, 0.8166666666666674290 ),
 .UNSPECIFIED. ) 
 CURVE ( )  GEOMETRIC_REPRESENTATION_ITEM ( )  RATIONAL_B_SPLINE_CURVE ( ( 0.9999999999999948930, 0.9238795325112918455, 1.000000000000000000, 0.9238795325112867385, 1.000000000000000000, 0.9238795325112867385, 1.000000000000000000, 0.9238795325112796331, 1.000000000000007105 ) ) 
 REPRESENTATION_ITEM ( '' )  );
#73312 = CARTESIAN_POINT ( 'NONE',  ( 4.541265875000001451, 6.249999998634407916, 1.881053915767124440 ) ) ;
#73313 = CARTESIAN_POINT ( 'NONE',  ( 1.469576158976822172E-15, -7.999999999999991118, 10.20530277982336465 ) ) ;
#73314 = CARTESIAN_POINT ( 'NONE',  ( 2.977408999572650927, -7.188101187499990274, 16.95530278187175455 ) ) ;
#73315 = VERTEX_POINT ( 'NONE', #44802 ) ;
#73316 = CARTESIAN_POINT ( 'NONE',  ( -2.977408999572654480, 26.99999999795161543, 7.188101187499999156 ) ) ;
#73317 = ORIENTED_EDGE ( 'NONE', *, *, #49101, .F. ) ;
#73318 = CARTESIAN_POINT ( 'NONE',  ( 10.18810118749999916, 4.220049686691935698, 115.0000000020483810 ) ) ;
#73319 = CARTESIAN_POINT ( 'NONE',  ( 28.00000000000002487, 209.1250000027312126, 173.9999999999999147 ) ) ;
#73320 = CARTESIAN_POINT ( 'NONE',  ( 1.432654583217664479, 202.7500000013655779, 201.4587341250000065 ) ) ;
#73321 = CARTESIAN_POINT ( 'NONE',  ( 24.54126587499999346, 199.1875000013655779, 169.9999999999999432 ) ) ;
#73322 = CARTESIAN_POINT ( 'NONE',  ( 6.123233995736767268E-16, 76.25000000000000000, -10.00000000000000178 ) ) ;
#73323 = CARTESIAN_POINT ( 'NONE',  ( 5.656854249492379694, 124.4375000000000000, -5.656854249492380582 ) ) ;
#73324 = CARTESIAN_POINT ( 'NONE',  ( 4.242640687119285658, 291.6249999999999432, -4.242640687119286547 ) ) ;
#73325 = CARTESIAN_POINT ( 'NONE',  ( 29.65685424949235127, 203.5625000027312126, 165.9999999999998863 ) ) ;
#73326 = ORIENTED_EDGE ( 'NONE', *, *, #9654, .T. ) ;
#73327 = CARTESIAN_POINT ( 'NONE',  ( 3.042071309553163960, 222.4479166700806729, -11.35316468749999785 ) ) ;
#73328 = AXIS2_PLACEMENT_3D ( 'NONE', #60902, #55635, #48829 ) ;
#73329 = CARTESIAN_POINT ( 'NONE',  ( 3.313708498984742068, 11.71875000000000178, 8.000000000000019540 ) ) ;
#73330 = CARTESIAN_POINT ( 'NONE',  ( 3.999999999999960032, 198.0625000027312410, 143.6568542494924543 ) ) ;
#73331 = CARTESIAN_POINT ( 'NONE',  ( -5.000000000000000000, 61.58678017309354402, 23.68362420833388171 ) ) ;
#73332 = CYLINDRICAL_SURFACE ( 'NONE', #41289, 8.000000000000000000 ) ;
#73333 = CARTESIAN_POINT ( 'NONE',  ( 8.660254037844385522, 247.9166666666666856, -5.000000000000003553 ) ) ;
#73334 = CARTESIAN_POINT ( 'NONE',  ( -5.000000000000016875, 76.66666666666669983, -8.660254037844419273 ) ) ;
#73335 = CARTESIAN_POINT ( 'NONE',  ( 8.660254037844389075, 190.4166666666666856, -5.000000000000000000 ) ) ;
#73336 = CARTESIAN_POINT ( 'NONE',  ( 32.00000000000000000, 198.3125000027312126, 171.6568542494922553 ) ) ;
#73337 = CARTESIAN_POINT ( 'NONE',  ( 5.082755093536318824, 5.082755093536319713, 22.29905278187175455 ) ) ;
#73338 = CARTESIAN_POINT ( 'NONE',  ( -11.35316468750000141, 173.5937499965860411, -1.390361679473963753E-15 ) ) ;
#73339 = DIRECTION ( 'NONE',  ( -0.000000000000000000, 1.000000000000000000, -0.000000000000000000 ) ) ;
#73340 = CARTESIAN_POINT ( 'NONE',  ( 8.660254037844389075, 260.2083333401612890, 4.999999999999997335 ) ) ;
#73341 = DIRECTION ( 'NONE',  ( 0.000000000000000000, 0.000000000000000000, -1.000000000000000000 ) ) ;
#73342 = LINE ( 'NONE', #9971, #61613 ) ;
#73343 = ORIENTED_EDGE ( 'NONE', *, *, #64861, .F. ) ;
#73344 = CIRCLE ( 'NONE', #21525, 71.70204102886728492 ) ;
#73345 = CARTESIAN_POINT ( 'NONE',  ( -2.085542519210945728E-15, 29.84374999658601624, 11.35316468750000141 ) ) ;
#73347 = CARTESIAN_POINT ( 'NONE',  ( -4.465384415997257328, -10.10202268796506431, -70.97396818905022542 ) ) ;
#73346 = LINE ( 'NONE', #72214, #4696 ) ;
#73348 = CARTESIAN_POINT ( 'NONE',  ( -15.26772199216783577, -44.35752750716734738, 196.9814117128816804 ) ) ;
#73349 = CARTESIAN_POINT ( 'NONE',  ( 2.445694354108782775, 204.5625000013656063, 139.5543056458912190 ) ) ;
#73350 = VECTOR ( 'NONE', #26940, 1000.000000000000000 ) ;
#73351 = CARTESIAN_POINT ( 'NONE',  ( -1.836970198721029983E-15, 65.62499999317203958, 10.00000000000000178 ) ) ;
#73352 = CARTESIAN_POINT ( 'NONE',  ( -5.082755093536325930, 104.4687500020483952, -5.082755093536325930 ) ) ;
#73353 = CARTESIAN_POINT ( 'NONE',  ( -4.541265875000002339, 6.874999998634407916, -1.881053915767121998 ) ) ;
#73354 = CARTESIAN_POINT ( 'NONE',  ( -2.143145793903030439E-12, 53.74999999999984368, 9.999999999999998224 ) ) ;
#73355 = CARTESIAN_POINT ( 'NONE',  ( 3.313708498984756279, 7.999999999999991118, 6.361552779823365533 ) ) ;
#73356 = CARTESIAN_POINT ( 'NONE',  ( 1.656854249492379472, 1.187500000000000444, -4.000000000000002665 ) ) ;
#73357 = ORIENTED_EDGE ( 'NONE', *, *, #23534, .F. ) ;
#73358 = ORIENTED_EDGE ( 'NONE', *, *, #51117, .T. ) ;
#73359 = CARTESIAN_POINT ( 'NONE',  ( 6.123233995736767268E-16, 221.2500000000000000, -10.00000000000000178 ) ) ;
#73360 = CARTESIAN_POINT ( 'NONE',  ( 38.00000000000000000, 53.00000000000000711, 9.999999999999991118 ) ) ;
#73361 = CARTESIAN_POINT ( 'NONE',  ( 11.00000000000000355, -4.556349186104044158, 82.65625000000000000 ) ) ;
#73362 = CARTESIAN_POINT ( 'NONE',  ( -27.54024800341238688, -42.45109295298111363, 155.7345425689728415 ) ) ;
#73363 = CARTESIAN_POINT ( 'NONE',  ( 5.676582343749993598, 139.9479166632526983, 9.832129032723422313 ) ) ;
#73364 = ORIENTED_EDGE ( 'NONE', *, *, #23335, .F. ) ;
#73365 = CARTESIAN_POINT ( 'NONE',  ( -5.000000000000000000, 10.43216530810821219, -65.93415491242824089 ) ) ;
#73366 = EDGE_CURVE ( 'NONE', #3824, #34844, #38018, .T. ) ;
#73367 = CARTESIAN_POINT ( 'NONE',  ( 7.204075437095966983, 7.204075437095967871, 89.59375000204838102 ) ) ;
#73368 = CARTESIAN_POINT ( 'NONE',  ( 0.000000000000000000, 0.000000000000000000, 0.000000000000000000 ) ) ;
#73369 = CARTESIAN_POINT ( 'NONE',  ( 4.000000000000015987, 208.5000000000000284, 198.0000000000000284 ) ) ;
#73370 = FACE_OUTER_BOUND ( 'NONE', #12518, .T. ) ;
#73371 = VERTEX_POINT ( 'NONE', #21406 ) ;
#73372 = CARTESIAN_POINT ( 'NONE',  ( 37.65152654557344647, -2.389026243601558352, 128.9206328448075283 ) ) ;
#73373 = CARTESIAN_POINT ( 'NONE',  ( -30.70214559338703708, 176.5462824210873123, 150.3874543681495766 ) ) ;
#73374 = CARTESIAN_POINT ( 'NONE',  ( -2.085542519210945728E-15, 109.8437499965860269, 11.35316468750000141 ) ) ;
#73375 = CARTESIAN_POINT ( 'NONE',  ( -2.445694354108783664, 202.3125000013656063, 195.5543056458912190 ) ) ;
#73376 = CARTESIAN_POINT ( 'NONE',  ( 5.082755093536325930, 19.03124999795161543, -5.082755093536325930 ) ) ;
#73377 = CARTESIAN_POINT ( 'NONE',  ( -4.220049686691937474, -10.18810118749999738, 80.31250000204836681 ) ) ;
#73378 = CARTESIAN_POINT ( 'NONE',  ( -8.311093377946841443, 34.21874999658601979, 8.311093377946830785 ) ) ;
#73379 = VERTEX_POINT ( 'NONE', #62148 ) ;
#73380 = CARTESIAN_POINT ( 'NONE',  ( 1.469576158976823947E-15, 89.56250000409677625, 8.000000000000000000 ) ) ;
#73381 = CARTESIAN_POINT ( 'NONE',  ( -3.317071493978880348, -8.008118988124989457, 17.79436528394063188 ) ) ;
#73382 = CARTESIAN_POINT ( 'NONE',  ( 2.679491924311263151, 236.4583333333333144, 9.999999999999980460 ) ) ;
#73383 = CARTESIAN_POINT ( 'NONE',  ( 2.449293598294707893E-16, 7.250000000000000000, -4.000000000000001776 ) ) ;
#73384 = CARTESIAN_POINT ( 'NONE',  ( -7.188101187500000044, 5.718749997951611874, -8.802885111219163269E-16 ) ) ;
#73385 = CARTESIAN_POINT ( 'NONE',  ( 6.676582343750001591, 288.9531250017069510, -8.176455196517173205E-16 ) ) ;
#73386 = EDGE_CURVE ( 'NONE', #20010, #24907, #40438, .T. ) ;
#73387 = CARTESIAN_POINT ( 'NONE',  ( 7.320508075688771044, 111.2499999931720680, 7.320508075688775484 ) ) ;
#73388 = DIRECTION ( 'NONE',  ( 0.000000000000000000, 0.000000000000000000, 1.000000000000000000 ) ) ;
#73389 = ORIENTED_EDGE ( 'NONE', *, *, #66141, .T. ) ;
#73390 = CARTESIAN_POINT ( 'NONE',  ( -3.042071309553164404, 142.5520833299193271, -11.35316468749999963 ) ) ;
#73391 = CARTESIAN_POINT ( 'NONE',  ( 1.871523826299183495E-15, -10.18810118749999916, 78.53125000204836681 ) ) ;
#73392 = CARTESIAN_POINT ( 'NONE',  ( -29.43265458321760164, 194.8750000013656063, 173.4587341250003760 ) ) ;
#73393 = CARTESIAN_POINT ( 'NONE',  ( 7.999999999999968914, 3.313708498984778483, 21.17405277982336287 ) ) ;
#73394 = CARTESIAN_POINT ( 'NONE',  ( -4.541265875000002339, 16.87499999863440436, -1.881053915767121998 ) ) ;
#73395 = ORIENTED_EDGE ( 'NONE', *, *, #45783, .T. ) ;
#73396 = CIRCLE ( 'NONE', #14286, 12.00000000000000000 ) ;
#73397 = CARTESIAN_POINT ( 'NONE',  ( 2.751064625579944321E-14, 198.8750000027312126, 194.0000000000000568 ) ) ;
#73398 = CARTESIAN_POINT ( 'NONE',  ( -4.000000000000015987, 209.5000000000000284, 142.0000000000000568 ) ) ;
#73399 = CARTESIAN_POINT ( 'NONE',  ( -24.00000000000002842, 205.9375000027311842, 168.3431457505079152 ) ) ;
#73400 = FACE_OUTER_BOUND ( 'NONE', #2129, .T. ) ;
#73401 = EDGE_LOOP ( 'NONE', ( #20114, #68720, #8585, #54070 ) ) ;
#73402 =( BOUNDED_CURVE ( )  B_SPLINE_CURVE ( 2, ( #6079, #52471, #6458, #41152, #7190, #24152, #440, #47531, #70197, #52841, #46798, #18136, #12466 ),
 .UNSPECIFIED., .F., .F. ) 
 B_SPLINE_CURVE_WITH_KNOTS ( ( 3, 2, 2, 2, 2, 2, 3 ),
 ( 0.2982911931063731426, 0.3035251194131430852, 0.3087590457199130833, 0.3139929720266829705, 0.3192268983334529686, 0.3244608246402229113, 0.3296947509469928539 ),
 .UNSPECIFIED. ) 
 CURVE ( )  GEOMETRIC_REPRESENTATION_ITEM ( )  RATIONAL_B_SPLINE_CURVE ( ( 1.000000000000305977, 0.9659258262887623347, 1.000000000000000000, 0.9659258262890683122, 1.000000000000000000, 0.9659258262890683122, 1.000000000000000000, 0.9659258262890683122, 1.000000000000000000, 0.9659258262890683122, 1.000000000000000000, 0.9659258262890683122, 1.000000000000000000 ) ) 
 REPRESENTATION_ITEM ( '' )  );
#73403 = CARTESIAN_POINT ( 'NONE',  ( 5.082755093536324154, 9.281249997951610098, 5.082755093536326818 ) ) ;
#73404 = CYLINDRICAL_SURFACE ( 'NONE', #13495, 10.00000000000000178 ) ;
#73405 = CARTESIAN_POINT ( 'NONE',  ( 5.000000000000000000, 52.35862550122993042, -48.98731492261362064 ) ) ;
#73406 = CARTESIAN_POINT ( 'NONE',  ( -9.832129032723418760, 182.8645833299193555, -5.676582343750004256 ) ) ;
#73407 = CARTESIAN_POINT ( 'NONE',  ( -5.082755093536324154, 103.7187500020483810, 5.082755093536326818 ) ) ;
#73408 = CARTESIAN_POINT ( 'NONE',  ( 6.000000000000003553, 295.4374999999999432, 2.485281374238571317 ) ) ;
#73409 = CARTESIAN_POINT ( 'NONE',  ( 4.721056650415999201, 288.0781250017069510, -4.721056650415999201 ) ) ;
#73411 = CARTESIAN_POINT ( 'NONE',  ( -18.00000000000000355, -9.547192751170715752, -1.363732307033565183 ) ) ;
#73410 = CARTESIAN_POINT ( 'NONE',  ( 10.00000000000011191, 79.79166666666672825, 2.679491924311265372 ) ) ;
#73412 = VERTEX_POINT ( 'NONE', #45174 ) ;
#73413 = CARTESIAN_POINT ( 'NONE',  ( 8.311093377946839666, 255.7812500034139589, 8.311093377946829008 ) ) ;
#73414 = PRODUCT_DEFINITION_SHAPE ( 'NONE', 'NONE',  #74662 ) ;
#73415 = CARTESIAN_POINT ( 'NONE',  ( 2.977408999572650927, -7.188101187499990274, 23.33030278187175455 ) ) ;
#73416 = DIRECTION ( 'NONE',  ( -1.000000000000000000, -0.000000000000000000, -0.000000000000000000 ) ) ;
#73417 = CARTESIAN_POINT ( 'NONE',  ( 3.074111742569078043, -67.95395293240328272, -20.32712440775801710 ) ) ;
#73418 = CARTESIAN_POINT ( 'NONE',  ( -1.737867177246331662, 21.99999999999999645, 4.195582608135537406 ) ) ;
#73419 = CARTESIAN_POINT ( 'NONE',  ( -8.660254037844390851, 147.9166666666666572, 4.999999999999998224 ) ) ;
#73420 = CARTESIAN_POINT ( 'NONE',  ( 12.00000000000000355, -6.928203230275539859, -1.071796769724504550 ) ) ;
#73421 = LINE ( 'NONE', #44756, #12632 ) ;
#73422 = CARTESIAN_POINT ( 'NONE',  ( -8.000000000000000000, 93.40624999999998579, -3.313708498984761608 ) ) ;
#73423 = CARTESIAN_POINT ( 'NONE',  ( -11.35316468750000141, 128.5937499965860127, -1.390361679473963753E-15 ) ) ;
#73424 = CARTESIAN_POINT ( 'NONE',  ( -4.242640687119286547, 295.8750000000000000, -4.242640687119286547 ) ) ;
#73425 = CARTESIAN_POINT ( 'NONE',  ( -11.00000000000000000, 0.000000000000000000, 72.99999999999998579 ) ) ;
#73428 = CARTESIAN_POINT ( 'NONE',  ( 15.04468117448323916, -12.09855896486656945, -0.7126204852947470858 ) ) ;
#73427 = CARTESIAN_POINT ( 'NONE',  ( 29.43265458321766559, 198.5000000013656347, 173.4587341249998929 ) ) ;
#73426 = CARTESIAN_POINT ( 'NONE',  ( 23.99999999999999289, 209.7500000000000284, 169.9999999999998863 ) ) ;
#73429 = EDGE_LOOP ( 'NONE', ( #16014, #13218, #52802 ) ) ;
#73430 = CARTESIAN_POINT ( 'NONE',  ( 6.945059804708960449, 224.3593915618296251, 7.219287879128159169 ) ) ;
#73431 = CARTESIAN_POINT ( 'NONE',  ( 7.999999999999992895, -3.313708498984756279, 25.48655277982336997 ) ) ;
#73432 = CARTESIAN_POINT ( 'NONE',  ( 24.54126587499998280, 199.5000000013656063, 171.4326545832175555 ) ) ;
#73433 = CARTESIAN_POINT ( 'NONE',  ( -9.832129032723420536, 209.0104166632526699, 5.676582343749997150 ) ) ;
#73434 = CARTESIAN_POINT ( 'NONE',  ( 7.188101187500001821, 119.0000000020483810, -2.977408999572651371 ) ) ;
#73435 = CARTESIAN_POINT ( 'NONE',  ( -3.211159895383562723, 18.93749999863440436, 3.211159895383561391 ) ) ;
#73436 = CARTESIAN_POINT ( 'NONE',  ( 29.43265458321760519, 194.7500000013656063, 173.4587341249998929 ) ) ;
#73437 = CARTESIAN_POINT ( 'NONE',  ( -4.898587196589407898E-16, 7.999999999999991118, 28.95530277982336642 ) ) ;
#73439 = CARTESIAN_POINT ( 'NONE',  ( -3.313708498984765161, 13.03125000000000355, 7.999999999999998224 ) ) ;
#73438 = CARTESIAN_POINT ( 'NONE',  ( -48.12154660295335162, 40.91772801067800458, 62.15125942254316982 ) ) ;
#73440 = CARTESIAN_POINT ( 'NONE',  ( -5.676582343749998039, 92.44791666325269830, -9.832129032723420536 ) ) ;
#73441 = ORIENTED_EDGE ( 'NONE', *, *, #20370, .T. ) ;
#73442 = CONICAL_SURFACE ( 'NONE', #7056, 3.999999999999976019, 0.7853981633974491672 ) ;
#73443 = CARTESIAN_POINT ( 'NONE',  ( -11.00000000000000000, 0.000000000000000000, 81.99999999999998579 ) ) ;
#73444 = CARTESIAN_POINT ( 'NONE',  ( 5.082755093536324154, 18.28124999795161187, 5.082755093536326818 ) ) ;
#73445 = CARTESIAN_POINT ( 'NONE',  ( 1.469576158976822172E-15, -7.999999999999991118, 14.70530277982336642 ) ) ;
#73446 = CARTESIAN_POINT ( 'NONE',  ( -3.042071309553166625, 253.1770833367473301, -11.35316468749999608 ) ) ;
#73447 = CARTESIAN_POINT ( 'NONE',  ( 11.35316468749999785, 105.5729166632526983, 3.042071309553174174 ) ) ;
#73448 = ORIENTED_EDGE ( 'NONE', *, *, #3260, .F. ) ;
#73449 = CARTESIAN_POINT ( 'NONE',  ( 23.99999999999999645, 196.9375000027312126, 171.6568542494923122 ) ) ;
#73450 = EDGE_CURVE ( 'NONE', #14543, #59562, #14699, .T. ) ;
#73451 = CARTESIAN_POINT ( 'NONE',  ( -7.204075437095967871, 7.204075437095967871, 109.4687500020483810 ) ) ;
#73452 = CARTESIAN_POINT ( 'NONE',  ( -2.679491924311277806, 21.45833333333352400, -10.00000000000035350 ) ) ;
#73453 = CARTESIAN_POINT ( 'NONE',  ( -1.432654583217608080, 204.8750000013656063, 201.4587341250000350 ) ) ;
#73454 = CARTESIAN_POINT ( 'NONE',  ( -1.836970198721029983E-15, 160.6249999931720254, 10.00000000000000178 ) ) ;
#73455 = CARTESIAN_POINT ( 'NONE',  ( 11.35316468750000141, 90.78124999658602690, 0.000000000000000000 ) ) ;
#73456 = CARTESIAN_POINT ( 'NONE',  ( 5.656854249492374365, 5.656854249492375253, 15.45530278392014623 ) ) ;
#73457 = CARTESIAN_POINT ( 'NONE',  ( -24.54126587499998280, 202.3750000013655779, 171.4326545832179818 ) ) ;
#73458 = DIRECTION ( 'NONE',  ( -1.000000000000000000, 0.000000000000000000, 0.000000000000000000 ) ) ;
#73459 = ADVANCED_FACE ( 'NONE', ( #9732 ), #68926, .F. ) ;
#73460 = CARTESIAN_POINT ( 'NONE',  ( -7.320508075688773708, 188.7499999931720254, -7.320508075688774596 ) ) ;
#73461 = CARTESIAN_POINT ( 'NONE',  ( 5.000000000000000888, -51.88457047716737947, 42.00159762951442843 ) ) ;
#73462 = CARTESIAN_POINT ( 'NONE',  ( -8.311093377946836114, 77.96874999658599847, -8.311093377946837890 ) ) ;
#73463 = CARTESIAN_POINT ( 'NONE',  ( -6.676582343750000703, 291.5156250017069510, 2.765530957082001251 ) ) ;
#73464 = CARTESIAN_POINT ( 'NONE',  ( 7.204075437095968759, -7.204075437095966983, 100.0937500020483668 ) ) ;
#73465 = CARTESIAN_POINT ( 'NONE',  ( -5.676582343750006032, 209.1145833299193555, 9.832129032723418760 ) ) ;
#73466 = ORIENTED_EDGE ( 'NONE', *, *, #12145, .F. ) ;
#73467 = PLANE ( 'NONE',  #50905 ) ;
#73468 = CARTESIAN_POINT ( 'NONE',  ( -4.217983994790210467, -16.30587161610658598, 69.44297314766851059 ) ) ;
#73469 = CARTESIAN_POINT ( 'NONE',  ( 9.832129032723420536, 206.1979166632526983, -5.676582343749999815 ) ) ;
#73470 = CARTESIAN_POINT ( 'NONE',  ( -5.000000000000000888, 222.2916666734946602, -8.660254037844387298 ) ) ;
#73471 = CARTESIAN_POINT ( 'NONE',  ( -8.660254037844387298, 252.7083333401612890, -4.999999999999999112 ) ) ;
#73472 = EDGE_CURVE ( 'NONE', #6157, #1239, #53275, .T. ) ;
#73473 = ORIENTED_EDGE ( 'NONE', *, *, #27928, .F. ) ;
#73474 = CARTESIAN_POINT ( 'NONE',  ( -3.042071309553163960, 197.5520833299193555, -11.35316468749999963 ) ) ;
#73475 = CARTESIAN_POINT ( 'NONE',  ( 7.188101187499992051, 2.977408999572647819, 15.83030278187175277 ) ) ;
#73476 = CARTESIAN_POINT ( 'NONE',  ( -25.55430564589115505, 207.0625000013656063, 172.4456943541091789 ) ) ;
#73477 = CARTESIAN_POINT ( 'NONE',  ( 5.656854249492378806, 11.81250000000000178, 5.656854249492381470 ) ) ;
#73478 = EDGE_LOOP ( 'NONE', ( #25512, #15702, #32258, #32111 ) ) ;
#73479 = CARTESIAN_POINT ( 'NONE',  ( 3.313708498984765161, 92.65625000409680467, 7.999999999999998224 ) ) ;
#73480 = CARTESIAN_POINT ( 'NONE',  ( 10.00000000000000178, 15.20833333333333215, -2.679491924311226736 ) ) ;
#73481 = CIRCLE ( 'NONE', #55, 30.99999999999997158 ) ;
#73482 = ADVANCED_FACE ( 'NONE', ( #28938 ), #23565, .T. ) ;
#73483 = CARTESIAN_POINT ( 'NONE',  ( -10.18810118749999738, -4.220049686691941915, 83.12500000204835260 ) ) ;
#73484 = ORIENTED_EDGE ( 'NONE', *, *, #37944, .T. ) ;
#73485 = CARTESIAN_POINT ( 'NONE',  ( 4.000000000000000888, 19.93750000000000000, 1.656854249492384135 ) ) ;
#73486 = CARTESIAN_POINT ( 'NONE',  ( 4.541265875000002339, 20.31249999863440436, 0.000000000000000000 ) ) ;
#73487 = CARTESIAN_POINT ( 'NONE',  ( -3.999999999999960032, 210.0000000000000284, 198.0000000000000284 ) ) ;
#73488 = VECTOR ( 'NONE', #7367, 1000.000000000000000 ) ;
#73489 = ORIENTED_EDGE ( 'NONE', *, *, #39212, .T. ) ;
#73490 = CARTESIAN_POINT ( 'NONE',  ( 4.999999999999993783, 16.04166665983870033, 8.660254037844390851 ) ) ;
#73491 = CARTESIAN_POINT ( 'NONE',  ( 1.320432766682874540E-15, 93.03125000204836681, 7.188101187500000044 ) ) ;
#73494 = DIRECTION ( 'NONE',  ( 0.000000000000000000, 0.000000000000000000, 1.000000000000000000 ) ) ;
#73493 = CARTESIAN_POINT ( 'NONE',  ( 11.35316468749999963, 246.4062500034139873, -1.390361679473963556E-15 ) ) ;
#73492 = CARTESIAN_POINT ( 'NONE',  ( 27.99999999999997158, 207.9375000013656063, 166.5412658749999082 ) ) ;
#73495 = APPLICATION_PROTOCOL_DEFINITION ( 'draft international standard', 'automotive_design', 1998, #20675 ) ;
#73496 = ORIENTED_EDGE ( 'NONE', *, *, #21911, .T. ) ;
#73497 = CARTESIAN_POINT ( 'NONE',  ( 9.832129032723416984, 252.1354166700806445, -5.676582343750003368 ) ) ;
#73498 = CARTESIAN_POINT ( 'NONE',  ( -5.082755093536317936, -5.082755093536320601, 15.17405278187175455 ) ) ;
#73499 = ORIENTED_EDGE ( 'NONE', *, *, #41660, .F. ) ;
#73500 = VERTEX_POINT ( 'NONE', #63631 ) ;
#73501 = CARTESIAN_POINT ( 'NONE',  ( 7.204075437095968759, -7.204075437095966983, 74.21875000204836681 ) ) ;
#73502 = CARTESIAN_POINT ( 'NONE',  ( 8.311093377946834337, 75.46874999658602690, 8.311093377946839666 ) ) ;
#73503 = CARTESIAN_POINT ( 'NONE',  ( 2.775557561562891351E-14, -37.99999999999992184, 170.0000000000000284 ) ) ;
#73504 = CARTESIAN_POINT ( 'NONE',  ( 11.00000000000000355, -4.556349186104045046, 88.65625000000000000 ) ) ;
#73507 = CARTESIAN_POINT ( 'NONE',  ( -6.676582343750001591, 288.6093750017069510, 0.000000000000000000 ) ) ;
#73506 = CARTESIAN_POINT ( 'NONE',  ( 27.99999999999996447, 198.6250000027312126, 165.9999999999998863 ) ) ;
#73505 = CARTESIAN_POINT ( 'NONE',  ( 0.000000000000000000, 20.39230484541327471, -10.20000000000000284 ) ) ;
#73508 = CARTESIAN_POINT ( 'NONE',  ( 0.000000000000000000, 0.000000000000000000, 0.000000000000000000 ) ) ;
#73509 = CARTESIAN_POINT ( 'NONE',  ( 0.000000000000000000, 0.000000000000000000, 118.0000000000000000 ) ) ;
#73510 = AXIS2_PLACEMENT_3D ( 'NONE', #64046, #1062, #12356 ) ;
#73511 = CARTESIAN_POINT ( 'NONE',  ( 2.445694354108840063, 199.0625000013656063, 200.4456943541088663 ) ) ;
#73512 =( BOUNDED_CURVE ( )  B_SPLINE_CURVE ( 2, ( #11108, #546, #45061, #51086, #22397, #23528, #69560, #40144, #63149 ),
 .UNSPECIFIED., .F., .F. ) 
 B_SPLINE_CURVE_WITH_KNOTS ( ( 3, 2, 2, 2, 3 ),
 ( 0.6315789473684211286, 0.6381578947368422572, 0.6447368421052632748, 0.6513157894736841813, 0.6578947368421053099 ),
 .UNSPECIFIED. ) 
 CURVE ( )  GEOMETRIC_REPRESENTATION_ITEM ( )  RATIONAL_B_SPLINE_CURVE ( ( 0.9999999999999986677, 0.9238795325112880708, 1.000000000000000000, 0.9238795325112867385, 1.000000000000000000, 0.9238795325112867385, 1.000000000000000000, 0.9238795325112867385, 1.000000000000000000 ) ) 
 REPRESENTATION_ITEM ( '' )  );
#73513 = CARTESIAN_POINT ( 'NONE',  ( -8.000000000000000000, 10.96874999590322020, -3.313708498984762496 ) ) ;
#73514 = EDGE_LOOP ( 'NONE', ( #21609, #4528, #34812, #22322 ) ) ;
#73515 = CARTESIAN_POINT ( 'NONE',  ( 29.43265458321760519, 196.5000000013656063, 173.4587341249998929 ) ) ;
#73516 = CARTESIAN_POINT ( 'NONE',  ( 5.082755093536324154, 15.65624999795161365, 5.082755093536326818 ) ) ;
#73517 = CARTESIAN_POINT ( 'NONE',  ( 8.311093377946837890, 166.7187499965859843, -8.311093377946837890 ) ) ;
#73518 = CARTESIAN_POINT ( 'NONE',  ( 0.000000000000000000, 0.000000000000000000, 0.000000000000000000 ) ) ;
#73519 = CARTESIAN_POINT ( 'NONE',  ( -7.188101187500000933, 103.4375000020483810, -2.977408999572650483 ) ) ;
#73521 = CARTESIAN_POINT ( 'NONE',  ( -2.620431783930857073, -55.87941608673560978, -43.94382193462958952 ) ) ;
#73520 = CARTESIAN_POINT ( 'NONE',  ( 2.828427124746191623, 16.87499999726881583, -2.828427124746191623 ) ) ;
#73522 = CARTESIAN_POINT ( 'NONE',  ( 29.43265458321766914, 207.1250000013656347, 166.5412658749999650 ) ) ;
#73523 = CARTESIAN_POINT ( 'NONE',  ( 7.188101187499993827, -2.977408999572645598, 16.01780278187175455 ) ) ;
#73524 = CARTESIAN_POINT ( 'NONE',  ( -4.000000000000015987, 208.6250000027312126, 142.0000000000000568 ) ) ;
#73525 = CARTESIAN_POINT ( 'NONE',  ( -9.832129032723420536, 58.69791666325269119, 5.676582343749997150 ) ) ;
#73526 = CARTESIAN_POINT ( 'NONE',  ( 7.999999999999998224, 20.90625000000000355, 3.313708498984766049 ) ) ;
#73527 = CARTESIAN_POINT ( 'NONE',  ( 7.320508075688774596, 22.49999999317202892, -7.320508075688774596 ) ) ;
#73528 = CARTESIAN_POINT ( 'NONE',  ( 2.751064625579944321E-14, 195.8750000027311842, 194.0000000000000568 ) ) ;
#73529 = ORIENTED_EDGE ( 'NONE', *, *, #52796, .F. ) ;
#73530 = DIRECTION ( 'NONE',  ( -0.000000000000000000, 1.000000000000000000, -0.000000000000000000 ) ) ;
#73531 = CARTESIAN_POINT ( 'NONE',  ( -2.679491924311226292, 168.3333333265053682, -10.00000000000000178 ) ) ;
#73532 = CARTESIAN_POINT ( 'NONE',  ( -2.085542519210945728E-15, 64.53124999658602690, 11.35316468750000141 ) ) ;
#73533 = CARTESIAN_POINT ( 'NONE',  ( 2.020667218593132706E-15, -11.00000000000000000, 75.06250000409676204 ) ) ;
#73534 = CARTESIAN_POINT ( 'NONE',  ( 3.458734124999959469, 200.7500000013656063, 140.5673454167823593 ) ) ;
#73535 = DIRECTION ( 'NONE',  ( 0.000000000000000000, 0.000000000000000000, 1.000000000000000000 ) ) ;
#73536 = CARTESIAN_POINT ( 'NONE',  ( 1.347111479062087024E-15, 19.05255888325788050, -10.99999999999998934 ) ) ;
#73539 = EDGE_CURVE ( 'NONE', #38468, #42156, #53721, .T. ) ;
#73538 = CARTESIAN_POINT ( 'NONE',  ( 5.676582343750001591, 46.61458332991934839, -9.832129032723420536 ) ) ;
#73537 = CARTESIAN_POINT ( 'NONE',  ( 7.188101187500002709, 93.31250000204838102, 2.977408999572649151 ) ) ;
#73540 = CARTESIAN_POINT ( 'NONE',  ( -3.313708498984758943, -7.999999999999989342, 1.111552779823363757 ) ) ;
#73541 = CARTESIAN_POINT ( 'NONE',  ( 5.000000000000000888, 205.8333333333333428, -8.660254037844387298 ) ) ;
#73542 = CARTESIAN_POINT ( 'NONE',  ( -3.042071309553173730, 179.3229166632526699, 11.35316468749999785 ) ) ;
#73543 = ADVANCED_FACE ( 'NONE', ( #35719 ), #30053, .T. ) ;
#73544 = AXIS2_PLACEMENT_3D ( 'NONE', #34385, #57386, #69435 ) ;
#73545 = CARTESIAN_POINT ( 'NONE',  ( 2.679491924311228956, 137.9166666598387110, -10.00000000000000000 ) ) ;
#73546 = CARTESIAN_POINT ( 'NONE',  ( -7.188101187500001821, 103.4375000020483668, -2.977408999572650483 ) ) ;
#73547 = PLANE ( 'NONE',  #70152 ) ;
#73548 = CARTESIAN_POINT ( 'NONE',  ( -5.676582343750006032, 29.42708332991935194, 9.832129032723418760 ) ) ;
#73549 = CARTESIAN_POINT ( 'NONE',  ( 1.102182119232618108E-15, 295.3125000034140157, 6.000000000000001776 ) ) ;
#73550 = ORIENTED_EDGE ( 'NONE', *, *, #43967, .F. ) ;
#73551 = DIRECTION ( 'NONE',  ( -0.000000000000000000, -1.000000000000000000, -0.000000000000000000 ) ) ;
#73552 = CARTESIAN_POINT ( 'NONE',  ( 10.18810118750000093, -4.220049686691933921, 71.31250000204836681 ) ) ;
#73553 = CARTESIAN_POINT ( 'NONE',  ( 1.656854249492403008, 196.6875000000000000, 194.0000000000000853 ) ) ;
#73554 = CARTESIAN_POINT ( 'NONE',  ( 30.99776725957478618, 48.77566056134155303, 65.00000000000000000 ) ) ;
#73556 = CARTESIAN_POINT ( 'NONE',  ( -8.311093377946836114, 172.6562499965860127, -8.311093377946837890 ) ) ;
#73555 = CARTESIAN_POINT ( 'NONE',  ( 0.000000000000000000, 0.000000000000000000, 0.000000000000000000 ) ) ;
#73557 = CARTESIAN_POINT ( 'NONE',  ( 3.313708498984762496, -7.999999999999989342, 13.35530278432982421 ) ) ;
#73558 = CARTESIAN_POINT ( 'NONE',  ( 7.999999999999998224, 8.906250000000001776, 3.313708498984766049 ) ) ;
#73559 = VECTOR ( 'NONE', #12584, 1000.000000000000000 ) ;
#73560 = CARTESIAN_POINT ( 'NONE',  ( -5.676582343749992710, 224.7395833367473301, 9.832129032723422313 ) ) ;
#73561 = CARTESIAN_POINT ( 'NONE',  ( -1.506524674531526609, 55.70638416847363317, -43.84942669317677399 ) ) ;
#73562 = CARTESIAN_POINT ( 'NONE',  ( -6.238412754330611322E-16, 10.18810118749999916, 81.15625000204838102 ) ) ;
#73563 = ORIENTED_EDGE ( 'NONE', *, *, #18816, .F. ) ;
#73564 = EDGE_CURVE ( 'NONE', #39873, #10672, #54861, .T. ) ;
#73565 = CARTESIAN_POINT ( 'NONE',  ( -2.775557561562891351E-14, 210.0000000000000284, 142.0000000000000568 ) ) ;
#73566 = CARTESIAN_POINT ( 'NONE',  ( 3.042071309553159519, 120.0520833299193697, 11.35316468750000141 ) ) ;
#73567 = EDGE_CURVE ( 'NONE', #2929, #22034, #47020, .T. ) ;
#73568 = CYLINDRICAL_SURFACE ( 'NONE', #45387, 7.999999999999991118 ) ;
#73569 = ORIENTED_EDGE ( 'NONE', *, *, #58933, .T. ) ;
#73570 = ORIENTED_EDGE ( 'NONE', *, *, #4855, .T. ) ;
#73571 = CARTESIAN_POINT ( 'NONE',  ( -1.881053915767121554, 9.749999998634406140, -4.541265875000002339 ) ) ;
#73572 = CARTESIAN_POINT ( 'NONE',  ( -7.188101187500001821, 14.62499999795161010, -2.977408999572651371 ) ) ;
#73573 = CARTESIAN_POINT ( 'NONE',  ( 8.000000000000001776, 110.8437500040967763, 3.313708498984759387 ) ) ;
#73574 = CARTESIAN_POINT ( 'NONE',  ( 7.204075437095966983, 7.204075437095967871, 91.46875000204838102 ) ) ;
#73575 = CARTESIAN_POINT ( 'NONE',  ( -24.54126587499999346, 199.4375000013655779, 170.0000000000003411 ) ) ;
#73576 = EDGE_CURVE ( 'NONE', #55047, #45526, #23649, .T. ) ;
#73577 = EDGE_CURVE ( 'NONE', #38745, #56053, #7045, .T. ) ;
#73578 = CARTESIAN_POINT ( 'NONE',  ( -2.828427124746192067, 9.625000000000000000, 2.828427124746190735 ) ) ;
#73579 = CARTESIAN_POINT ( 'NONE',  ( -1.656854249492381248, 22.06249999726881583, -4.000000000000001776 ) ) ;
#73580 = CARTESIAN_POINT ( 'NONE',  ( 4.541265875000002339, 6.374999998634408804, -1.881053915767121776 ) ) ;
#73581 = CARTESIAN_POINT ( 'NONE',  ( -2.849036369511732440E-14, 199.2500000000000000, 138.0000000000000568 ) ) ;
#73582 = ORIENTED_EDGE ( 'NONE', *, *, #20881, .F. ) ;
#73583 = CARTESIAN_POINT ( 'NONE',  ( 9.797174393178825657E-16, 125.0000000000000000, -8.000000000000000000 ) ) ;
#73584 = CARTESIAN_POINT ( 'NONE',  ( -5.082755093536324154, 110.8437500020483810, 5.082755093536326818 ) ) ;
#73586 = CARTESIAN_POINT ( 'NONE',  ( -26.34314575050754570, 199.9375000000000284, 166.0000000000004263 ) ) ;
#73585 = CARTESIAN_POINT ( 'NONE',  ( -24.54126587499998990, 196.1875000013655779, 170.0000000000002842 ) ) ;
#73587 = CARTESIAN_POINT ( 'NONE',  ( 0.000000000000000000, 5.999999999999977796, 1.701148182893384950E-14 ) ) ;
#73588 = AXIS2_PLACEMENT_3D ( 'NONE', #46775, #69427, #63019 ) ;
#73589 = CARTESIAN_POINT ( 'NONE',  ( 1.320432766682872962E-15, -7.188101187499992051, 3.361552781871751883 ) ) ;
#73590 = ORIENTED_EDGE ( 'NONE', *, *, #47311, .T. ) ;
#73591 = ORIENTED_EDGE ( 'NONE', *, *, #10411, .F. ) ;
#73592 = CARTESIAN_POINT ( 'NONE',  ( 10.18810118750000093, -4.220049686691933033, 92.31250000204838102 ) ) ;
#73593 = CARTESIAN_POINT ( 'NONE',  ( -3.313708498984757611, 7.999999999999991118, 20.04905277982336642 ) ) ;
#73594 = CARTESIAN_POINT ( 'NONE',  ( -31.45873412499999233, 200.9375000013656063, 170.0000000000003979 ) ) ;
#73595 = CARTESIAN_POINT ( 'NONE',  ( -7.778174593052023411, 7.778174593052023411, 107.3124999999999858 ) ) ;
#73596 = CARTESIAN_POINT ( 'NONE',  ( 1.432654583217662481, 209.3750000013656063, 194.5412658750000219 ) ) ;
#73597 = CARTESIAN_POINT ( 'NONE',  ( -1.656854249492405895, 21.06249999726881938, -3.999999999999976463 ) ) ;
#73598 = EDGE_CURVE ( 'NONE', #21405, #2977, #30583, .T. ) ;
#73599 = CARTESIAN_POINT ( 'NONE',  ( 7.320508075688774596, 115.6249999999999858, -7.320508075688774596 ) ) ;
#73600 = CARTESIAN_POINT ( 'NONE',  ( 3.313708498984760720, 103.5312500000000142, -8.000000000000000000 ) ) ;
#73601 = CARTESIAN_POINT ( 'NONE',  ( -6.676582343750003368, 293.5468750017070079, -2.765530957081996810 ) ) ;
#73602 = CARTESIAN_POINT ( 'NONE',  ( 7.188101187499993827, -2.977408999572645598, 5.517802781871753659 ) ) ;
#73603 = EDGE_CURVE ( 'NONE', #42656, #56422, #38305, .T. ) ;
#73604 = DIRECTION ( 'NONE',  ( 0.000000000000000000, -0.000000000000000000, 1.000000000000000000 ) ) ;
#73605 = CARTESIAN_POINT ( 'NONE',  ( 25.55430564589115505, 207.3125000013656063, 172.4456943541086957 ) ) ;
#73606 = CARTESIAN_POINT ( 'NONE',  ( -8.000000000000000000, 27.56249999590322375, -9.797174393178825657E-16 ) ) ;
#73607 = CARTESIAN_POINT ( 'NONE',  ( 3.458734124999959914, 200.4375000013656063, 142.0000000000000568 ) ) ;
#73608 = CARTESIAN_POINT ( 'NONE',  ( 5.082755093536326818, 122.0937500020483952, 5.082755093536325042 ) ) ;
#73610 = CARTESIAN_POINT ( 'NONE',  ( -1.432654583217664701, 202.0000000013656063, 138.5412658750000787 ) ) ;
#73609 = CARTESIAN_POINT ( 'NONE',  ( 2.775557561562891351E-14, 210.0000000000000284, 198.0000000000000284 ) ) ;
#73611 = CARTESIAN_POINT ( 'NONE',  ( -5.676582343750000703, 238.3854166700806445, -9.832129032723418760 ) ) ;
#73612 = CARTESIAN_POINT ( 'NONE',  ( 27.99999999999999645, 210.0000000000000284, 169.9999999999999147 ) ) ;
#73613 = FACE_OUTER_BOUND ( 'NONE', #8742, .T. ) ;
#73615 =( BOUNDED_CURVE ( )  B_SPLINE_CURVE ( 2, ( #43667, #62138, #33491, #27063, #66679, #55379, #9346, #50442, #72721 ),
 .UNSPECIFIED., .F., .F. ) 
 B_SPLINE_CURVE_WITH_KNOTS ( ( 3, 2, 2, 2, 3 ),
 ( 0.7361111111111110494, 0.7430555555555554692, 0.7500000000000000000, 0.7569444444444444198, 0.7638888888888888395 ),
 .UNSPECIFIED. ) 
 CURVE ( )  GEOMETRIC_REPRESENTATION_ITEM ( )  RATIONAL_B_SPLINE_CURVE ( ( 1.000000000000001110, 0.9238795325112855172, 1.000000000000000000, 0.9238795325112867385, 1.000000000000000000, 0.9238795325112867385, 1.000000000000000000, 0.9238795325112867385, 1.000000000000000000 ) ) 
 REPRESENTATION_ITEM ( '' )  );
#73614 = CARTESIAN_POINT ( 'NONE',  ( 24.00000000000000355, 200.6875000000000284, 168.3431457505075173 ) ) ;
#73616 = CARTESIAN_POINT ( 'NONE',  ( -9.832129032723418760, 12.86458332991935194, -5.676582343750004256 ) ) ;
#73617 = ADVANCED_FACE ( 'NONE', ( #71874, #42467 ), #53440, .T. ) ;
#73618 = CARTESIAN_POINT ( 'NONE',  ( 8.660254037844389075, 0.4166666666666657415, -5.000000000000000000 ) ) ;
#73619 = CARTESIAN_POINT ( 'NONE',  ( -11.35316468750000141, 213.5937499965860411, -1.390361679473963753E-15 ) ) ;
#73620 = CARTESIAN_POINT ( 'NONE',  ( -2.828427124746209831, 197.5000000027312126, 139.1715728752538723 ) ) ;
#73621 = DIRECTION ( 'NONE',  ( 1.000000000000000000, 0.000000000000000000, 1.836970198721037823E-16 ) ) ;
#73623 = DIRECTION ( 'NONE',  ( 0.000000000000000000, -0.000000000000000000, 1.000000000000000000 ) ) ;
#73622 = CARTESIAN_POINT ( 'NONE',  ( 11.00000000000000000, 1.347111479062088405E-15, 88.75000000000000000 ) ) ;
#73624 = CIRCLE ( 'NONE', #70026, 11.00000000000000000 ) ;
#73625 = VERTEX_POINT ( 'NONE', #36820 ) ;
#73626 = CARTESIAN_POINT ( 'NONE',  ( -3.458734125000015425, 199.2500000013656063, 143.4326545832176976 ) ) ;
#73627 = CARTESIAN_POINT ( 'NONE',  ( 9.832129032723416984, 15.36458332991935016, 5.676582343750006032 ) ) ;
#73628 = CARTESIAN_POINT ( 'NONE',  ( 11.00000000000000000, 4.556349186104045934, 92.03125000409677625 ) ) ;
#73629 = CARTESIAN_POINT ( 'NONE',  ( 3.373128826976369066, 10.27267468567300135, 63.92035228378879452 ) ) ;
#73630 = CARTESIAN_POINT ( 'NONE',  ( -24.54126587500001833, 196.2500000013656347, 168.5673454167826435 ) ) ;
#73631 = CARTESIAN_POINT ( 'NONE',  ( -1.349999999999998757, 283.9999999999998863, 5.686528119825505989 ) ) ;
#73633 = CARTESIAN_POINT ( 'NONE',  ( -5.676582343749998039, 7.447916663252683200, -9.832129032723420536 ) ) ;
#73632 = CARTESIAN_POINT ( 'NONE',  ( 7.188101187500000044, 115.9062500020483810, -8.802885111219163269E-16 ) ) ;
#73634 = CARTESIAN_POINT ( 'NONE',  ( 5.099999999999999645, 0.000000000000000000, -0.6301867843887376530 ) ) ;
#73635 = CARTESIAN_POINT ( 'NONE',  ( -9.832129032723420536, 133.6979166632526983, 5.676582343749997150 ) ) ;
#73636 = CARTESIAN_POINT ( 'NONE',  ( 8.660254037844385522, 101.4583333265053824, 5.000000000000005329 ) ) ;
#73637 = CARTESIAN_POINT ( 'NONE',  ( 2.977408999572650039, 118.0625000020483952, -7.188101187500001821 ) ) ;
#73638 = CARTESIAN_POINT ( 'NONE',  ( -8.000000000000000000, 14.06249999590322375, -9.797174393178825657E-16 ) ) ;
#73639 = DIRECTION ( 'NONE',  ( 0.000000000000000000, 0.000000000000000000, -1.000000000000000000 ) ) ;
#73640 = CARTESIAN_POINT ( 'NONE',  ( -5.000000000000000000, 52.35862550122993042, -48.98731492261362064 ) ) ;
#73641 = EDGE_LOOP ( 'NONE', ( #74513, #32244, #39691, #26015 ) ) ;
#73642 = CARTESIAN_POINT ( 'NONE',  ( 6.308070865160535057, -61.28915309311908288, 23.54949267151385683 ) ) ;
#73643 =( BOUNDED_CURVE ( )  B_SPLINE_CURVE ( 2, ( #63301, #11262, #17283, #70099, #69344, #39931, #62937, #17654, #68598, #40673, #57670, #58780, #22950 ),
 .UNSPECIFIED., .F., .F. ) 
 B_SPLINE_CURVE_WITH_KNOTS ( ( 3, 2, 2, 2, 2, 2, 3 ),
 ( 0.8634897946621500342, 0.8687238057336525987, 0.8739578168051551632, 0.8791918278766578387, 0.8844258389481604032, 0.8896598500196628567, 0.8948938610911654212 ),
 .UNSPECIFIED. ) 
 CURVE ( )  GEOMETRIC_REPRESENTATION_ITEM ( )  RATIONAL_B_SPLINE_CURVE ( ( 0.9999999999999947820, 0.9659258262890735303, 1.000000000000000000, 0.9659258262890683122, 1.000000000000000000, 0.9659258262890683122, 1.000000000000000000, 0.9659258262890683122, 1.000000000000000000, 0.9659258262890683122, 1.000000000000000000, 0.9659258262889931501, 1.000000000000075273 ) ) 
 REPRESENTATION_ITEM ( '' )  );
#73644 = CARTESIAN_POINT ( 'NONE',  ( -4.721056650415999201, 289.4843750017070079, -4.721056650415999201 ) ) ;
#73645 = CARTESIAN_POINT ( 'NONE',  ( 7.999999999999991118, 9.797174393178815797E-16, 0.2678027839201451155 ) ) ;
#73646 = AXIS2_PLACEMENT_3D ( 'NONE', #38407, #9735, #31620 ) ;
#73647 = CARTESIAN_POINT ( 'NONE',  ( -23.99999999999997513, 198.6875000000000284, 171.6568542494927385 ) ) ;
#73648 = CARTESIAN_POINT ( 'NONE',  ( -6.951808397369817780E-16, 257.6562500034140157, -11.35316468749999963 ) ) ;
#73649 = CARTESIAN_POINT ( 'NONE',  ( -4.220049686691937474, -10.18810118749999738, 99.81250000204838102 ) ) ;
#73650 = ORIENTED_EDGE ( 'NONE', *, *, #62535, .T. ) ;
#73651 = CARTESIAN_POINT ( 'NONE',  ( 4.898587196589412829E-16, 27.18749999590322375, -8.000000000000000000 ) ) ;
#73652 = CARTESIAN_POINT ( 'NONE',  ( -11.35316468750000141, 173.8020833299193555, 3.042071309553159963 ) ) ;
#73653 = CARTESIAN_POINT ( 'NONE',  ( 0.000000000000000000, 0.5000000000000004441, 0.000000000000000000 ) ) ;
#73654 = CARTESIAN_POINT ( 'NONE',  ( -1.432654583217607414, 202.5000000013656063, 194.5412658750000219 ) ) ;
#73655 = CARTESIAN_POINT ( 'NONE',  ( 2.679491924311234730, 229.5833333401612890, 9.999999999999998224 ) ) ;
#73656 = CARTESIAN_POINT ( 'NONE',  ( -2.085542519210945728E-15, 69.84374999658601268, 11.35316468750000141 ) ) ;
#73657 = EDGE_LOOP ( 'NONE', ( #65082, #15133, #55481, #15122 ) ) ;
#73658 = CARTESIAN_POINT ( 'NONE',  ( -6.238412754330611322E-16, 10.18810118749999916, 115.2812500020483810 ) ) ;
#73659 = CARTESIAN_POINT ( 'NONE',  ( 3.211159895383561835, 13.56249999863440614, -3.211159895383561835 ) ) ;
#73660 = ORIENTED_EDGE ( 'NONE', *, *, #49843, .T. ) ;
#73661 = CARTESIAN_POINT ( 'NONE',  ( -2.977408999572654480, 26.99999999795161187, 7.188101187499999156 ) ) ;
#73662 = LINE ( 'NONE', #61968, #5941 ) ;
#73663 = MECHANICAL_DESIGN_GEOMETRIC_PRESENTATION_REPRESENTATION (  '', ( #31491 ), #65197 ) ;
#73664 = CARTESIAN_POINT ( 'NONE',  ( 10.00000000000000000, 66.66666665983869677, 2.679491924311235618 ) ) ;
#73665 = CARTESIAN_POINT ( 'NONE',  ( -7.188101187500002709, 15.18749999795161365, 2.977408999572649151 ) ) ;
#73666 = FACE_OUTER_BOUND ( 'NONE', #40721, .T. ) ;
#73667 = CARTESIAN_POINT ( 'NONE',  ( 7.204075437095968759, -7.204075437095966983, 110.5937500020483810 ) ) ;
#73668 = AXIS2_PLACEMENT_3D ( 'NONE', #8316, #60748, #4817 ) ;
#73669 = CYLINDRICAL_SURFACE ( 'NONE', #49851, 3.999999999999976019 ) ;
#73670 = CARTESIAN_POINT ( 'NONE',  ( 1.656854249492381248, 9.937499997268814056, -4.000000000000001776 ) ) ;
#73671 = CARTESIAN_POINT ( 'NONE',  ( 0.000000000000000000, 0.000000000000000000, -20.42428869268542968 ) ) ;
#73672 = ORIENTED_EDGE ( 'NONE', *, *, #14905, .F. ) ;
#73673 = CARTESIAN_POINT ( 'NONE',  ( -2.445694354108783664, 204.3125000013656063, 195.5543056458912190 ) ) ;
#73674 = APPLICATION_CONTEXT ( 'automotive_design' ) ;
#73675 = CARTESIAN_POINT ( 'NONE',  ( -26.56734541678243033, 207.3750000013656063, 166.5412658750003345 ) ) ;
#73676 = CARTESIAN_POINT ( 'NONE',  ( 32.00000000000000000, 199.3125000027312126, 171.6568542494922553 ) ) ;
#73677 = CARTESIAN_POINT ( 'NONE',  ( 4.541265875000002339, 9.374999998634404363, -1.881053915767121554 ) ) ;
#73678 = CARTESIAN_POINT ( 'NONE',  ( 0.000000000000000000, 0.000000000000000000, -21.47459999999999525 ) ) ;
#73679 = CARTESIAN_POINT ( 'NONE',  ( 2.977408999572650927, -7.188101187499990274, 18.45530278187175455 ) ) ;
#73680 = EDGE_LOOP ( 'NONE', ( #35818, #72865, #45536, #19284 ) ) ;
#73681 = CARTESIAN_POINT ( 'NONE',  ( 6.123233995736767268E-16, 221.2500000000000000, -10.00000000000000178 ) ) ;
#73682 = ORIENTED_EDGE ( 'NONE', *, *, #19184, .F. ) ;
#73683 = CARTESIAN_POINT ( 'NONE',  ( -6.238412754330611322E-16, 10.18810118749999916, 109.2812500020483668 ) ) ;
#73684 = CARTESIAN_POINT ( 'NONE',  ( 2.445694354108839619, 204.8125000013656063, 200.4456943541088663 ) ) ;
#73685 = CARTESIAN_POINT ( 'NONE',  ( 24.54126587500000412, 198.2500000013656347, 171.4326545832176123 ) ) ;
#73686 = CARTESIAN_POINT ( 'NONE',  ( -2.679491924311225848, 86.45833333333335702, -10.00000000000000178 ) ) ;
#73687 = AXIS2_PLACEMENT_3D ( 'NONE', #56820, #40575, #62459 ) ;
#73688 = CARTESIAN_POINT ( 'NONE',  ( 5.656854249492379694, 122.9375000000000000, -5.656854249492380582 ) ) ;
#73689 = CARTESIAN_POINT ( 'NONE',  ( -2.485281374238571761, 290.8124999999999432, -6.000000000000003553 ) ) ;
#73690 = CARTESIAN_POINT ( 'NONE',  ( 30.82842712474617031, 205.5000000027312126, 167.1715728752537018 ) ) ;
#73691 = EDGE_CURVE ( 'NONE', #34597, #35470, #59830, .T. ) ;
#73692 = ORIENTED_EDGE ( 'NONE', *, *, #43477, .F. ) ;
#73693 = CARTESIAN_POINT ( 'NONE',  ( 8.000000000000001776, 94.15625000000000000, 3.313708498984759387 ) ) ;
#73694 = CARTESIAN_POINT ( 'NONE',  ( -7.999999999999991118, 0.000000000000000000, 8.330302779823362869 ) ) ;
#73695 = CARTESIAN_POINT ( 'NONE',  ( -2.828427124746209831, 194.5000000027312126, 139.1715728752538723 ) ) ;
#73696 = CARTESIAN_POINT ( 'NONE',  ( 10.99999999999989697, -4.556349186104149851, 91.65625000000001421 ) ) ;
#73697 = CARTESIAN_POINT ( 'NONE',  ( 5.000000000000004441, 236.6666666666666856, 8.660254037844385522 ) ) ;
#73698 = CARTESIAN_POINT ( 'NONE',  ( 29.65685424949245075, 204.4375000000000284, 165.9999999999999432 ) ) ;
#73699 = CARTESIAN_POINT ( 'NONE',  ( -4.999999999999998224, 201.6666666666666856, -8.660254037844389075 ) ) ;
#73700 = EDGE_CURVE ( 'NONE', #19857, #6721, #33236, .T. ) ;
#73701 = LINE ( 'NONE', #55624, #72910 ) ;
#73702 = CARTESIAN_POINT ( 'NONE',  ( 7.188101187499993827, -2.977408999572645598, 17.51780278187175455 ) ) ;
#73703 = CARTESIAN_POINT ( 'NONE',  ( 8.311093377946837890, 171.7187499965860127, -8.311093377946837890 ) ) ;
#73704 = CARTESIAN_POINT ( 'NONE',  ( -8.660254037844582697, 212.9166666666667709, 5.000000000000109246 ) ) ;
#73705 = CARTESIAN_POINT ( 'NONE',  ( -37.38026279385855588, 39.09128788536428800, 65.00000000000000000 ) ) ;
#73706 = CARTESIAN_POINT ( 'NONE',  ( -1.828673331923144296, -42.61370854813963405, 151.0874976375914684 ) ) ;
#73708 = CARTESIAN_POINT ( 'NONE',  ( -7.347880794884122694E-16, 7.499999997268813168, 4.000000000000001776 ) ) ;
#73707 = CARTESIAN_POINT ( 'NONE',  ( -31.05507224581699077, 271.9999999999999432, 171.9999999999998295 ) ) ;
#73709 = ORIENTED_EDGE ( 'NONE', *, *, #38481, .F. ) ;
#73710 = CARTESIAN_POINT ( 'NONE',  ( -2.085542519210945728E-15, 19.84374999658601979, 11.35316468750000141 ) ) ;
#73711 = CARTESIAN_POINT ( 'NONE',  ( -26.56734541678243033, 209.3750000013656063, 166.5412658750003345 ) ) ;
#73713 = CARTESIAN_POINT ( 'NONE',  ( -0.8912353796373386761, -16.44139524822816867, -68.58382889509265112 ) ) ;
#73712 = DIRECTION ( 'NONE',  ( -1.000000000000000000, -0.000000000000000000, -0.000000000000000000 ) ) ;
#73714 = DIRECTION ( 'NONE',  ( -0.000000000000000000, 1.000000000000000000, -0.000000000000000000 ) ) ;
#73715 = CARTESIAN_POINT ( 'NONE',  ( -1.432654583217664479, 203.7500000013656063, 138.5412658750000787 ) ) ;
#73716 = CARTESIAN_POINT ( 'NONE',  ( 2.679491924311222739, 60.83333332650536818, 10.00000000000000355 ) ) ;
#73717 = AXIS2_PLACEMENT_3D ( 'NONE', #63819, #34806, #18908 ) ;
#73718 = CARTESIAN_POINT ( 'NONE',  ( -2.977408999572651815, 103.4375000020483668, 7.188101187500000933 ) ) ;
#73719 = CARTESIAN_POINT ( 'NONE',  ( -1.881053915767124440, 8.124999998634407916, 4.541265875000001451 ) ) ;
#73720 = CARTESIAN_POINT ( 'NONE',  ( 0.000000000000000000, 300.0000000000000000, 0.000000000000000000 ) ) ;
#73721 = CARTESIAN_POINT ( 'NONE',  ( 3.313708498984762496, -7.999999999999989342, 1.299052779823363979 ) ) ;
#73722 = CARTESIAN_POINT ( 'NONE',  ( 7.320508075688789695, 160.6250000000000568, -7.320508075688789695 ) ) ;
#73723 = EDGE_LOOP ( 'NONE', ( #20124, #68336, #41120, #69141 ) ) ;
#73724 = VERTEX_POINT ( 'NONE', #8145 ) ;
#73725 = LINE ( 'NONE', #20359, #36371 ) ;
#73726 = LINE ( 'NONE', #22036, #1363 ) ;
#73727 = SURFACE_STYLE_USAGE ( .BOTH. , #22399 ) ;
#73728 = CARTESIAN_POINT ( 'NONE',  ( -8.311093377946834337, 219.8437500034139873, 8.311093377946837890 ) ) ;
#73729 = CARTESIAN_POINT ( 'NONE',  ( 5.676582343749993598, 144.9479166632526983, 9.832129032723422313 ) ) ;
#73730 = VERTEX_POINT ( 'NONE', #66222 ) ;
#73731 = CARTESIAN_POINT ( 'NONE',  ( 1.836970198721029589E-15, 221.2500000000000000, 10.00000000000000000 ) ) ;
#73732 = CARTESIAN_POINT ( 'NONE',  ( 7.204075437095966983, 7.204075437095967871, 86.59375000204836681 ) ) ;
#73733 = CARTESIAN_POINT ( 'NONE',  ( -28.47326357806616315, 194.4587341250000350, 166.5737975347167321 ) ) ;
#73734 = CARTESIAN_POINT ( 'NONE',  ( -1.656854249492347719, 207.8125000000000284, 194.0000000000000853 ) ) ;
#73735 = CARTESIAN_POINT ( 'NONE',  ( -7.347880794884122694E-16, 2.750000000000000000, 4.000000000000001776 ) ) ;
#73736 = CARTESIAN_POINT ( 'NONE',  ( 7.778174593052021635, 7.778174593052023411, 112.9375000000000000 ) ) ;
#73737 = CARTESIAN_POINT ( 'NONE',  ( -3.313708498984707429, 100.7187500000000000, -8.000000000000055067 ) ) ;
#73738 = ORIENTED_EDGE ( 'NONE', *, *, #10208, .F. ) ;
#73739 =( BOUNDED_CURVE ( )  B_SPLINE_CURVE ( 2, ( #13923, #36962, #59968, #8286, #49013, #31295, #2637, #25625, #60336 ),
 .UNSPECIFIED., .F., .F. ) 
 B_SPLINE_CURVE_WITH_KNOTS ( ( 3, 2, 2, 2, 3 ),
 ( 0.5666666666666670960, 0.5750000000000003997, 0.5833333333333338144, 0.5916666666666671182, 0.6000000000000004219 ),
 .UNSPECIFIED. ) 
 CURVE ( )  GEOMETRIC_REPRESENTATION_ITEM ( )  RATIONAL_B_SPLINE_CURVE ( ( 0.9999999999999958922, 0.9238795325112908463, 1.000000000000000000, 0.9238795325112867385, 1.000000000000000000, 0.9238795325112867385, 1.000000000000000000, 0.9238795325112826307, 1.000000000000003997 ) ) 
 REPRESENTATION_ITEM ( '' )  );
#73740 = CARTESIAN_POINT ( 'NONE',  ( 5.656854249492381470, 106.2500000040967905, 5.656854249492379694 ) ) ;
#73741 = CARTESIAN_POINT ( 'NONE',  ( -22.27911678677593699, 182.2961259327904600, 148.3271588659065969 ) ) ;
#73742 = CARTESIAN_POINT ( 'NONE',  ( -5.676582343750006032, 114.4270833299193555, 9.832129032723418760 ) ) ;
#73743 = CARTESIAN_POINT ( 'NONE',  ( 1.432654583217662259, 202.1250000013656063, 194.5412658750000219 ) ) ;
#73744 = CARTESIAN_POINT ( 'NONE',  ( 7.188101187499999156, 21.74999999795161898, 2.977408999572654924 ) ) ;
#73745 = CARTESIAN_POINT ( 'NONE',  ( -7.204075437095967871, 7.204075437095967871, 82.84375000204838102 ) ) ;
#73746 = CARTESIAN_POINT ( 'NONE',  ( -11.35316468750000141, 38.59374999658601979, -1.390361679473963753E-15 ) ) ;
#73747 = VERTEX_POINT ( 'NONE', #2486 ) ;
#73748 = CARTESIAN_POINT ( 'NONE',  ( -1.656854249492381248, 4.312500000000000888, -4.000000000000001776 ) ) ;
#73749 = CARTESIAN_POINT ( 'NONE',  ( -3.317071493978878571, 8.008118988124991233, 23.23186528394063899 ) ) ;
#73750 = CARTESIAN_POINT ( 'NONE',  ( -2.445694354108840063, 209.0625000013656063, 139.5543056458912190 ) ) ;
#73751 = CIRCLE ( 'NONE', #35205, 5.000000000000000000 ) ;
#73752 = CARTESIAN_POINT ( 'NONE',  ( -5.082755093536325042, 8.531249997951611874, -5.082755093536325930 ) ) ;
#73753 = CARTESIAN_POINT ( 'NONE',  ( -3.673940397442060854E-16, 294.8125000034140157, -6.000000000000001776 ) ) ;
#73754 = CYLINDRICAL_SURFACE ( 'NONE', #42493, 10.00000000000000000 ) ;
#73755 = CARTESIAN_POINT ( 'NONE',  ( 2.977408999572650927, 2.624999997951610986, -7.188101187500001821 ) ) ;
#73756 = AXIS2_PLACEMENT_3D ( 'NONE', #70760, #25093, #19076 ) ;
#73757 = CARTESIAN_POINT ( 'NONE',  ( 8.311093377946834337, 150.4687499965860127, 8.311093377946839666 ) ) ;
#73758 = CARTESIAN_POINT ( 'NONE',  ( 7.204075437095968759, -7.204075437095966983, 77.21875000204836681 ) ) ;
#73759 = CARTESIAN_POINT ( 'NONE',  ( -25.55430564589115505, 209.3125000013656063, 172.4456943541091789 ) ) ;
#73760 = DIRECTION ( 'NONE',  ( -0.000000000000000000, 1.000000000000000000, -0.000000000000000000 ) ) ;
#73761 = CARTESIAN_POINT ( 'NONE',  ( -4.541265875000002339, 14.87499999863441147, -1.881053915767121998 ) ) ;
#73762 = EDGE_LOOP ( 'NONE', ( #37496, #36491 ) ) ;
#73763 = CARTESIAN_POINT ( 'NONE',  ( -3.999999999999959144, 200.1875000027312126, 199.6568542494924259 ) ) ;
#73764 = CARTESIAN_POINT ( 'NONE',  ( -2.754378923186476579E-14, 195.4375000013655779, 145.4587341250000350 ) ) ;
#73765 = CARTESIAN_POINT ( 'NONE',  ( -32.00000000000003553, 204.3125000027312126, 168.3431457505080573 ) ) ;
#73766 = EDGE_CURVE ( 'NONE', #15967, #30885, #48412, .T. ) ;
#73767 = EDGE_CURVE ( 'NONE', #45708, #53358, #58919, .T. ) ;
#73768 = VECTOR ( 'NONE', #59893, 1000.000000000000000 ) ;
#73769 = CARTESIAN_POINT ( 'NONE',  ( -8.000000000000000000, 103.9062499999999716, -3.313708498984761164 ) ) ;
#73770 = ORIENTED_EDGE ( 'NONE', *, *, #22259, .T. ) ;
#73771 = CARTESIAN_POINT ( 'NONE',  ( 2.977408999572650927, 11.24999999795161187, -7.188101187500000933 ) ) ;
#73772 = CARTESIAN_POINT ( 'NONE',  ( -7.320508075688778149, 209.9999999931719969, 7.320508075688769267 ) ) ;
#73773 = CARTESIAN_POINT ( 'NONE',  ( -3.000000000000001332, -45.00000000000001421, 151.2383369607063344 ) ) ;
#73774 = CARTESIAN_POINT ( 'NONE',  ( 7.320508075688771044, 39.37500000000000000, 7.320508075688775484 ) ) ;
#73775 = CARTESIAN_POINT ( 'NONE',  ( -7.188101187499999156, 105.1250000020483668, 2.977408999572654924 ) ) ;
#73776 = CARTESIAN_POINT ( 'NONE',  ( -26.56734541678238415, 209.6250000013656063, 166.5412658750003629 ) ) ;
#73777 = CARTESIAN_POINT ( 'NONE',  ( -2.765530957081998142, 288.6406250017069510, 6.676582343750000703 ) ) ;
#73779 = CARTESIAN_POINT ( 'NONE',  ( -2.751064625579944321E-14, 200.8750000027312126, 146.0000000000000284 ) ) ;
#73778 = CARTESIAN_POINT ( 'NONE',  ( 1.347111479062087024E-15, 19.05255888325788050, -10.99999999999998934 ) ) ;
#73780 = VERTEX_POINT ( 'NONE', #49239 ) ;
#73781 = CARTESIAN_POINT ( 'NONE',  ( -9.832129032723415207, 219.6354166700806445, 5.676582343750005144 ) ) ;
#73782 = CARTESIAN_POINT ( 'NONE',  ( -2.977408999572648707, -7.188101187499990274, 26.14280278187176165 ) ) ;
#73783 = CARTESIAN_POINT ( 'NONE',  ( -0.6547826978426952715, 49.91450260127079019, 40.68974341348092594 ) ) ;
#73784 = CARTESIAN_POINT ( 'NONE',  ( -10.09417438056707006, 220.0000000000001137, 1.602760042864921353 ) ) ;
#73785 = CARTESIAN_POINT ( 'NONE',  ( -0.8912353796317742383, -67.61603573606902273, -20.05324848892005818 ) ) ;
#73786 = CARTESIAN_POINT ( 'NONE',  ( -4.195582579073398932, 22.00000000000000355, 1.737867247408543925 ) ) ;
#73787 = CARTESIAN_POINT ( 'NONE',  ( -8.660254037844390851, 162.9166666666666856, 4.999999999999998224 ) ) ;
#73788 = CARTESIAN_POINT ( 'NONE',  ( 1.224646799147353454E-15, 300.0000000000000000, -10.00000000000000178 ) ) ;
#73789 = LINE ( 'NONE', #72682, #57190 ) ;
#73790 = CARTESIAN_POINT ( 'NONE',  ( 5.000000000000000000, -52.16438407847132197, -42.28020805311216179 ) ) ;
#73791 = CARTESIAN_POINT ( 'NONE',  ( 8.311093377946837890, 131.7187499965860127, -8.311093377946837890 ) ) ;
#73792 = CARTESIAN_POINT ( 'NONE',  ( -5.000000000000000000, -13.57926339724869536, -69.65188861886713312 ) ) ;
#73793 = CARTESIAN_POINT ( 'NONE',  ( -10.99999999999999822, -4.556349186104052151, 70.09374999999998579 ) ) ;
#73796 = CARTESIAN_POINT ( 'NONE',  ( 0.000000000000000000, 300.0000000000000000, 10.00000000000000178 ) ) ;
#73795 = CARTESIAN_POINT ( 'NONE',  ( 24.54126587499997925, 197.1250000013656347, 168.5673454167822740 ) ) ;
#73794 = CARTESIAN_POINT ( 'NONE',  ( 29.65685424949240101, 208.4375000000000853, 165.9999999999998863 ) ) ;
#73797 = ORIENTED_EDGE ( 'NONE', *, *, #73577, .F. ) ;
#73798 = AXIS2_PLACEMENT_3D ( 'NONE', #74205, #6306, #47013 ) ;
#73799 = CARTESIAN_POINT ( 'NONE',  ( 8.825936903735748018, 225.3907168698384282, -4.710639689128314878 ) ) ;
#73800 = EDGE_CURVE ( 'NONE', #2093, #55673, #20567, .T. ) ;
#73801 = CARTESIAN_POINT ( 'NONE',  ( 1.592277918221149080E-13, 106.2500000000000142, -10.00000000000000178 ) ) ;
#73802 = CARTESIAN_POINT ( 'NONE',  ( 7.999999999999991118, 0.000000000000000000, 30.00000000000000000 ) ) ;
#73803 = CARTESIAN_POINT ( 'NONE',  ( 28.00000000000001776, 197.1875000013655779, 166.5412658749999082 ) ) ;
#73804 = CARTESIAN_POINT ( 'NONE',  ( -5.676582343749998039, 202.7604166632526983, -9.832129032723420536 ) ) ;
#73805 = CARTESIAN_POINT ( 'NONE',  ( 7.188101187500000044, 120.4062500020483810, -8.802885111219163269E-16 ) ) ;
#73806 = CARTESIAN_POINT ( 'NONE',  ( 3.211159895383561835, 18.43749999863440436, -3.211159895383561835 ) ) ;
#73807 = CARTESIAN_POINT ( 'NONE',  ( 0.4501631047598074753, -51.14740050676115146, 48.52018030598782161 ) ) ;
#73808 = CARTESIAN_POINT ( 'NONE',  ( 1.469576158976822172E-15, -7.999999999999991118, 20.70530277982336642 ) ) ;
#73810 = DIRECTION ( 'NONE',  ( 0.000000000000000000, 1.334402673828311367E-16, -1.000000000000000000 ) ) ;
#73809 = CARTESIAN_POINT ( 'NONE',  ( -49.58482923361747652, 47.54673414920118546, 58.24946605281415657 ) ) ;
#73811 = CARTESIAN_POINT ( 'NONE',  ( 9.832129032723416984, 95.36458332991935549, 5.676582343750006032 ) ) ;
#73812 = ORIENTED_EDGE ( 'NONE', *, *, #38985, .F. ) ;
#73813 = CARTESIAN_POINT ( 'NONE',  ( -6.735557395310442023E-16, 11.00000000000000000, 81.62499999999998579 ) ) ;
#73814 = CARTESIAN_POINT ( 'NONE',  ( -2.977408999572654480, 19.49999999795161898, 7.188101187499999156 ) ) ;
#73815 = DIRECTION ( 'NONE',  ( 0.000000000000000000, 0.000000000000000000, -1.000000000000000000 ) ) ;
#73816 = CARTESIAN_POINT ( 'NONE',  ( 11.35316468749999963, 261.5104166700807014, 3.042071309553159519 ) ) ;
#73817 = CARTESIAN_POINT ( 'NONE',  ( 5.676582343750001591, 96.61458332991935549, -9.832129032723420536 ) ) ;
#73818 = ORIENTED_EDGE ( 'NONE', *, *, #48153, .F. ) ;
#73819 = CARTESIAN_POINT ( 'NONE',  ( 10.00000000000000178, 207.0833333265053966, -2.679491924311226736 ) ) ;
#73820 = CARTESIAN_POINT ( 'NONE',  ( -10.18810118749999916, 4.220049686691934809, 105.0625000020483810 ) ) ;
#73821 = CARTESIAN_POINT ( 'NONE',  ( -31.45873412499999944, 194.8750000013656063, 168.5673454167827572 ) ) ;
#73822 = CARTESIAN_POINT ( 'NONE',  ( 1.432654583217662481, 205.3750000013656063, 194.5412658750000219 ) ) ;
#73823 = CARTESIAN_POINT ( 'NONE',  ( -31.99999999999996447, 201.4375000027311842, 171.6568542494928522 ) ) ;
#73825 = CARTESIAN_POINT ( 'NONE',  ( -9.832129032723418760, 87.86458332991935549, -5.676582343750004256 ) ) ;
#73824 = CARTESIAN_POINT ( 'NONE',  ( -32.00000000000000711, 202.1875000000000568, 168.3431457505080289 ) ) ;
#73826 = CARTESIAN_POINT ( 'NONE',  ( 5.656854249492376141, -5.656854249492374365, 15.08030278392014623 ) ) ;
#73827 = CARTESIAN_POINT ( 'NONE',  ( -26.56734541678232375, 202.2500000013656063, 173.4587341250003760 ) ) ;
#73828 = CARTESIAN_POINT ( 'NONE',  ( 4.000000000000001776, 15.00000000000000000, 0.000000000000000000 ) ) ;
#73829 = ORIENTED_EDGE ( 'NONE', *, *, #24932, .F. ) ;
#73830 = CARTESIAN_POINT ( 'NONE',  ( 5.000000000000001776, 182.7083333265053682, -8.660254037844389075 ) ) ;
#73831 = DIRECTION ( 'NONE',  ( -5.551115147383500873E-15, -0.5000000000000113243, -0.8660254037844320463 ) ) ;
#73832 = DIRECTION ( 'NONE',  ( 0.000000000000000000, 0.000000000000000000, 1.000000000000000000 ) ) ;
#73833 = CARTESIAN_POINT ( 'NONE',  ( -5.676582343750006032, 79.42708332991935549, 9.832129032723418760 ) ) ;
#73834 = CARTESIAN_POINT ( 'NONE',  ( -6.676582343750000703, 288.5156250017069510, 2.765530957082001251 ) ) ;
#73835 = LINE ( 'NONE', #3411, #44748 ) ;
#73836 = CARTESIAN_POINT ( 'NONE',  ( -6.238412754330611322E-16, 10.18810118749999916, 99.15625000204838102 ) ) ;
#73837 = CARTESIAN_POINT ( 'NONE',  ( -11.35316468750000141, 223.4895833299193555, 3.042071309553159963 ) ) ;
#73838 = VERTEX_POINT ( 'NONE', #60565 ) ;
#73839 = DIRECTION ( 'NONE',  ( -0.000000000000000000, 1.000000000000000000, -0.000000000000000000 ) ) ;
#73840 = FACE_BOUND ( 'NONE', #20668, .T. ) ;
#73841 = PLANE ( 'NONE',  #4577 ) ;
#73842 = CARTESIAN_POINT ( 'NONE',  ( 11.35316468749999785, 210.5729166632526983, 3.042071309553174174 ) ) ;
#73843 = CARTESIAN_POINT ( 'NONE',  ( -2.679491924311228512, 222.0833333401613174, -9.999999999999998224 ) ) ;
#73844 = CARTESIAN_POINT ( 'NONE',  ( -2.679491924311308448, 100.4166666598386826, 9.999999999999957367 ) ) ;
#73845 = CARTESIAN_POINT ( 'NONE',  ( -6.676582343750000703, 296.5156250017069510, 2.765530957082001251 ) ) ;
#73846 = VERTEX_POINT ( 'NONE', #1762 ) ;
#73847 = CARTESIAN_POINT ( 'NONE',  ( 3.042071309553159519, 190.0520833299193555, 11.35316468750000141 ) ) ;
#73848 = EDGE_CURVE ( 'NONE', #71315, #49221, #43582, .T. ) ;
#73849 =( BOUNDED_CURVE ( )  B_SPLINE_CURVE ( 2, ( #14835, #3538, #54855, #26530, #36754, #15215, #55606, #60871, #3924 ),
 .UNSPECIFIED., .F., .F. ) 
 B_SPLINE_CURVE_WITH_KNOTS ( ( 3, 2, 2, 2, 3 ),
 ( 0.6323529411764704511, 0.6360294117647057321, 0.6397058823529409022, 0.6433823529411762943, 0.6470588235294115753 ),
 .UNSPECIFIED. ) 
 CURVE ( )  GEOMETRIC_REPRESENTATION_ITEM ( )  RATIONAL_B_SPLINE_CURVE ( ( 1.000000000000002220, 0.9238795325112844070, 1.000000000000000000, 0.9238795325112867385, 1.000000000000000000, 0.9238795325112867385, 1.000000000000000000, 0.9238795325112912904, 0.9999999999999954481 ) ) 
 REPRESENTATION_ITEM ( '' )  );
#73850 = CARTESIAN_POINT ( 'NONE',  ( -25.55430564589115505, 206.0625000013656063, 172.4456943541091789 ) ) ;
#73851 =( BOUNDED_CURVE ( )  B_SPLINE_CURVE ( 2, ( #45625, #12407, #53522, #46371, #47100, #23730, #18072, #12770, #6397 ),
 .UNSPECIFIED., .F., .F. ) 
 B_SPLINE_CURVE_WITH_KNOTS ( ( 3, 2, 2, 2, 3 ),
 ( 0.1704545454545454697, 0.1761363636363636742, 0.1818181818181818232, 0.1875000000000000000, 0.1931818181818181768 ),
 .UNSPECIFIED. ) 
 CURVE ( )  GEOMETRIC_REPRESENTATION_ITEM ( )  RATIONAL_B_SPLINE_CURVE ( ( 0.9999999999999996669, 0.9238795325112870716, 1.000000000000000000, 0.9238795325112867385, 1.000000000000000000, 0.9238795325112867385, 1.000000000000000000, 0.9238795325112867385, 1.000000000000000000 ) ) 
 REPRESENTATION_ITEM ( '' )  );
#73852 = CARTESIAN_POINT ( 'NONE',  ( 5.656854249492378806, 8.812500000000000000, 5.656854249492381470 ) ) ;
#73853 = ORIENTED_EDGE ( 'NONE', *, *, #44562, .F. ) ;
#73854 = CIRCLE ( 'NONE', #13615, 9.000000000000001776 ) ;
#73855 = ADVANCED_FACE ( 'NONE', ( #9261 ), #24742, .T. ) ;
#73856 = CARTESIAN_POINT ( 'NONE',  ( 8.000000000000000000, 94.53125000409677625, -3.313708498984762496 ) ) ;
#73857 = CARTESIAN_POINT ( 'NONE',  ( 8.660254037844389075, 15.41666666666666785, -5.000000000000000000 ) ) ;
#73858 = CARTESIAN_POINT ( 'NONE',  ( 10.18810118749999916, 4.220049686691935698, 80.87500000204836681 ) ) ;
#73859 = ORIENTED_EDGE ( 'NONE', *, *, #11012, .T. ) ;
#73860 = CARTESIAN_POINT ( 'NONE',  ( -4.000000000000001776, 20.50000000000000000, -4.898587196589415787E-16 ) ) ;
#73861 = CARTESIAN_POINT ( 'NONE',  ( -4.541265875000003227, 20.87499999863440792, 1.881053915767121110 ) ) ;
#73862 = CARTESIAN_POINT ( 'NONE',  ( 28.70021146449738936, 194.4653435848668437, 173.4015262223485934 ) ) ;
#73864 = ORIENTED_EDGE ( 'NONE', *, *, #3515, .T. ) ;
#73863 = EDGE_CURVE ( 'NONE', #66034, #53657, #70777, .T. ) ;
#73865 = EDGE_CURVE ( 'NONE', #7437, #36538, #13416, .T. ) ;
#73866 = DIRECTION ( 'NONE',  ( 0.000000000000000000, 0.000000000000000000, -1.000000000000000000 ) ) ;
#73867 = CARTESIAN_POINT ( 'NONE',  ( -7.188101187500000044, 121.5312500020483810, 0.000000000000000000 ) ) ;
#73868 = CARTESIAN_POINT ( 'NONE',  ( 10.00000000000000178, 151.8749999931720538, 0.000000000000000000 ) ) ;
#73871 = CARTESIAN_POINT ( 'NONE',  ( 32.00000000000000000, 207.3750000027312126, 169.9999999999998863 ) ) ;
#73870 = CARTESIAN_POINT ( 'NONE',  ( -8.311093377946834337, 244.5312500034139589, 8.311093377946837890 ) ) ;
#73869 = CARTESIAN_POINT ( 'NONE',  ( 30.44569435410883429, 207.5625000013656063, 172.4456943541086957 ) ) ;
#73872 = SHAPE_DEFINITION_REPRESENTATION ( #43879, #66708 ) ;
#73873 = EDGE_LOOP ( 'NONE', ( #39151, #16742, #56556, #17084 ) ) ;
#73874 = EDGE_CURVE ( 'NONE', #12049, #48083, #58542, .T. ) ;
#73875 = CARTESIAN_POINT ( 'NONE',  ( -11.35316468749999608, 249.4270833367472733, 3.042071309553173730 ) ) ;
#73876 = CARTESIAN_POINT ( 'NONE',  ( 5.082755093536318824, 5.082755093536319713, 12.92405278187175277 ) ) ;
#73877 = VECTOR ( 'NONE', #33220, 1000.000000000000000 ) ;
#73878 = ORIENTED_EDGE ( 'NONE', *, *, #9760, .T. ) ;
#73879 = ORIENTED_EDGE ( 'NONE', *, *, #56856, .T. ) ;
#73880 = CARTESIAN_POINT ( 'NONE',  ( 10.18810118749999916, 4.220049686691935698, 74.50000000204838102 ) ) ;
#73881 = CARTESIAN_POINT ( 'NONE',  ( -3.042071309553164404, 87.55208332991936970, -11.35316468749999963 ) ) ;
#73882 = DIRECTION ( 'NONE',  ( -0.000000000000000000, 1.000000000000000000, 4.689100369878284071E-30 ) ) ;
#73883 = CARTESIAN_POINT ( 'NONE',  ( -10.99999999999999822, -4.556349186104052151, 89.59374999999997158 ) ) ;
#73886 = CARTESIAN_POINT ( 'NONE',  ( 4.721056650416000089, 291.9843750017070079, 4.721056650415999201 ) ) ;
#73885 = CARTESIAN_POINT ( 'NONE',  ( 29.43265458321761585, 208.8750000013656347, 166.5412658749999650 ) ) ;
#73884 = CARTESIAN_POINT ( 'NONE',  ( 25.55430564589115505, 208.5625000013656063, 172.4456943541086957 ) ) ;
#73887 = CARTESIAN_POINT ( 'NONE',  ( -55.71058552991572554, 209.5801377525671683, 49.66873916398061795 ) ) ;
#73888 = CARTESIAN_POINT ( 'NONE',  ( 11.00000000000000000, 1.347111479062088405E-15, 78.24999999999998579 ) ) ;
#73889 = EDGE_CURVE ( 'NONE', #33995, #4108, #71983, .T. ) ;
#73890 = CARTESIAN_POINT ( 'NONE',  ( -9.832129032723418760, 197.8645833299193555, -5.676582343750004256 ) ) ;
#73891 = CARTESIAN_POINT ( 'NONE',  ( -5.656854249492381470, 9.749999995903220196, 5.656854249492379694 ) ) ;
#73892 = ORIENTED_EDGE ( 'NONE', *, *, #6918, .T. ) ;
#73893 = CARTESIAN_POINT ( 'NONE',  ( 27.99999999999996092, 194.4375000013656063, 173.4587341249998929 ) ) ;
#73894 = CARTESIAN_POINT ( 'NONE',  ( -1.320432766682874540E-15, 16.96874999795161543, 7.188101187500000044 ) ) ;
#73895 = CARTESIAN_POINT ( 'NONE',  ( 3.042071309553167069, 172.1354166632526983, -11.35316468749999785 ) ) ;
#73896 = CARTESIAN_POINT ( 'NONE',  ( -4.401442555609581635E-16, 103.1562500020483810, -7.188101187500000044 ) ) ;
#73898 = CARTESIAN_POINT ( 'NONE',  ( 3.511653767257713277, -51.69076377080163098, -48.72852442694656361 ) ) ;
#73897 = CARTESIAN_POINT ( 'NONE',  ( -10.99999999999999645, -11.00000000000000000, 25.00000000000000000 ) ) ;
#73899 = CARTESIAN_POINT ( 'NONE',  ( 25.55430564589119768, 208.3125000013656063, 167.5543056458910485 ) ) ;
#73900 = CARTESIAN_POINT ( 'NONE',  ( -7.188101187499990274, -2.977408999572651371, 13.95530278187175277 ) ) ;
#73901 = CARTESIAN_POINT ( 'NONE',  ( 3.042071309553167069, 61.82291666325266988, -11.35316468749999785 ) ) ;
#73902 = DIRECTION ( 'NONE',  ( -0.000000000000000000, 1.000000000000000000, -0.000000000000000000 ) ) ;
#73903 = CARTESIAN_POINT ( 'NONE',  ( 4.000000000000015987, 195.6250000027311842, 198.0000000000000284 ) ) ;
#73904 = VERTEX_POINT ( 'NONE', #68097 ) ;
#73905 = PLANE ( 'NONE',  #50721 ) ;
#73907 = CARTESIAN_POINT ( 'NONE',  ( -5.656854249492379694, 19.87499999590322020, -5.656854249492380582 ) ) ;
#73906 = AXIS2_PLACEMENT_3D ( 'NONE', #61944, #9149, #16276 ) ;
#73908 = CARTESIAN_POINT ( 'NONE',  ( 11.35316468750000141, 55.78124999658601268, 0.000000000000000000 ) ) ;
#73909 = CARTESIAN_POINT ( 'NONE',  ( 4.556349186104045934, 11.00000000000000000, 75.71875000409677625 ) ) ;
#73910 = CARTESIAN_POINT ( 'NONE',  ( -1.432654583217664701, 201.0000000013655779, 138.5412658750000787 ) ) ;
#73911 = CARTESIAN_POINT ( 'NONE',  ( 0.8997857291009798697, 16.44125064681837145, 68.58473395859593325 ) ) ;
#73912 = CARTESIAN_POINT ( 'NONE',  ( -1.224646799147353454E-16, 25.94987437106619765, -1.000000000000000000 ) ) ;
#73914 = CARTESIAN_POINT ( 'NONE',  ( 3.042071309553167513, 51.82291666325266988, -11.35316468749999785 ) ) ;
#73913 = CARTESIAN_POINT ( 'NONE',  ( 5.082755093536325042, 95.09375000204838102, -5.082755093536325930 ) ) ;
#73915 = CARTESIAN_POINT ( 'NONE',  ( -5.656854249492373476, -5.656854249492376141, 2.517802779823365089 ) ) ;
#73916 = CARTESIAN_POINT ( 'NONE',  ( 7.999999999667481099, -7.293937043860970585E-05, 4.767800658666735636 ) ) ;
#73917 = CARTESIAN_POINT ( 'NONE',  ( -11.35316468750000141, 173.4895833299193839, 3.042071309553159963 ) ) ;
#73918 = CARTESIAN_POINT ( 'NONE',  ( 10.00000000000000000, 136.6666666598387110, 2.679491924311236062 ) ) ;
#73919 = CARTESIAN_POINT ( 'NONE',  ( 2.977408999572650039, 100.0625000020483952, -7.188101187500001821 ) ) ;
#73920 = CARTESIAN_POINT ( 'NONE',  ( -0.3906813049193237908, -47.98099648345226598, 139.0018569116174092 ) ) ;
#73921 = CARTESIAN_POINT ( 'NONE',  ( -8.311093377946841443, 39.21874999658601268, 8.311093377946834337 ) ) ;
#73922 = CARTESIAN_POINT ( 'NONE',  ( -7.188101187499992051, 0.000000000000000000, 28.48655278187175810 ) ) ;
#73923 = CARTESIAN_POINT ( 'NONE',  ( -3.042071309553164404, 187.2395833299193839, -11.35316468749999963 ) ) ;
#73924 = ORIENTED_EDGE ( 'NONE', *, *, #68591, .F. ) ;
#73925 = CARTESIAN_POINT ( 'NONE',  ( 49.67894393727056013, 135.2351138417432992, 58.04780024834200702 ) ) ;
#73926 = CARTESIAN_POINT ( 'NONE',  ( 7.204075437095966983, 7.204075437095967871, 68.59375000204836681 ) ) ;
#73927 = CARTESIAN_POINT ( 'NONE',  ( 2.751064625579944321E-14, 195.7500000000000000, 194.0000000000000568 ) ) ;
#73928 = CARTESIAN_POINT ( 'NONE',  ( 31.60148856309823984, 43.94598656457687014, 65.00000000000000000 ) ) ;
#73930 = CARTESIAN_POINT ( 'NONE',  ( -9.832129032723420536, 163.6979166632526983, 5.676582343749997150 ) ) ;
#73929 = CARTESIAN_POINT ( 'NONE',  ( 4.000000000000001776, 18.81249999726881228, -1.656854249492381248 ) ) ;
#73931 = CARTESIAN_POINT ( 'NONE',  ( -5.656854249492373476, -5.656854249492376141, 8.574052784329824206 ) ) ;
#73932 = CARTESIAN_POINT ( 'NONE',  ( -4.556349186104048599, -10.99999999999999822, 79.46875000409677625 ) ) ;
#73933 = CARTESIAN_POINT ( 'NONE',  ( -3.042071309553159075, 224.9479166700806445, 11.35316468749999963 ) ) ;
#73934 = CARTESIAN_POINT ( 'NONE',  ( -7.456209740496333893, 51.58726928745807072, -41.60229883572960574 ) ) ;
#73935 = CARTESIAN_POINT ( 'NONE',  ( 7.204075437095968759, -7.204075437095966983, 82.09375000204838102 ) ) ;
#73936 = ORIENTED_EDGE ( 'NONE', *, *, #64167, .T. ) ;
#73937 = AXIS2_PLACEMENT_3D ( 'NONE', #45710, #63065, #17035 ) ;
#73938 = DIRECTION ( 'NONE',  ( -0.000000000000000000, 1.000000000000000000, -4.476705744456276341E-16 ) ) ;
#73939 = CARTESIAN_POINT ( 'NONE',  ( 6.951808397369818766E-16, 112.3437499965860127, -11.35316468750000141 ) ) ;
#73940 = CARTESIAN_POINT ( 'NONE',  ( 28.00000000000001421, 195.5000000000000000, 165.9999999999998863 ) ) ;
#73941 = ORIENTED_EDGE ( 'NONE', *, *, #1687, .F. ) ;
#73943 = EDGE_LOOP ( 'NONE', ( #38327, #35660, #21716, #13901 ) ) ;
#73942 =( BOUNDED_CURVE ( )  B_SPLINE_CURVE ( 2, ( #27237, #50253, #73275, #11020, #26871, #51369, #74380, #57049, #63062, #68721, #15542, #11386, #55562 ),
 .UNSPECIFIED., .F., .F. ) 
 B_SPLINE_CURVE_WITH_KNOTS ( ( 3, 2, 2, 2, 2, 2, 3 ),
 ( 1.460092581490151309, 1.465325400988424231, 1.470558220486697154, 1.475791039984970077, 1.481023859483242555, 1.486256678981515478, 1.491489498479788400 ),
 .UNSPECIFIED. ) 
 CURVE ( )  GEOMETRIC_REPRESENTATION_ITEM ( )  RATIONAL_B_SPLINE_CURVE ( ( 1.000000000000054401, 0.9659258262890140223, 1.000000000000000000, 0.9659258262890683122, 1.000000000000000000, 0.9659258262890683122, 1.000000000000000000, 0.9659258262890683122, 1.000000000000000000, 0.9659258262890683122, 1.000000000000000000, 0.9659258262890662028, 1.000000000000001998 ) ) 
 REPRESENTATION_ITEM ( '' )  );
#73944 = EDGE_CURVE ( 'NONE', #1937, #29800, #9871, .T. ) ;
#73945 = CARTESIAN_POINT ( 'NONE',  ( -3.211159895383561391, 7.812499998634407028, -3.211159895383561835 ) ) ;
#73946 = CARTESIAN_POINT ( 'NONE',  ( -7.188101187500000044, 13.21874999795161187, -8.802885111219163269E-16 ) ) ;
#73947 = CARTESIAN_POINT ( 'NONE',  ( 8.000000000000000000, 109.4375000040967905, -9.797174393178825657E-16 ) ) ;
#73948 = CARTESIAN_POINT ( 'NONE',  ( -31.45873412499997812, 199.0000000013656063, 171.4326545832180386 ) ) ;
#73949 = CARTESIAN_POINT ( 'NONE',  ( -4.000000000000001776, 6.500000000000000888, -4.898587196589415787E-16 ) ) ;
#73950 = CARTESIAN_POINT ( 'NONE',  ( 4.000000000000000888, 22.68749999726881228, 1.656854249492384135 ) ) ;
#73951 = CARTESIAN_POINT ( 'NONE',  ( -4.541265875000002339, 9.812499998634406140, -5.561446717895856393E-16 ) ) ;
#73953 = CARTESIAN_POINT ( 'NONE',  ( 3.999999999999959144, 199.0625000000000284, 140.3431457505076594 ) ) ;
#73952 = VECTOR ( 'NONE', #22169, 1000.000000000000000 ) ;
#73954 = ORIENTED_EDGE ( 'NONE', *, *, #17459, .F. ) ;
#73955 = SURFACE_SIDE_STYLE ('',( #4193 ) ) ;
#73956 = CARTESIAN_POINT ( 'NONE',  ( -5.082755093536324154, 101.8437500020483810, 5.082755093536326818 ) ) ;
#73958 = DIRECTION ( 'NONE',  ( 1.000000000000000000, -0.000000000000000000, -0.000000000000000000 ) ) ;
#73957 = DIRECTION ( 'NONE',  ( -1.000000000000000000, -0.000000000000000000, -0.000000000000000000 ) ) ;
#73959 =( BOUNDED_CURVE ( )  B_SPLINE_CURVE ( 2, ( #35069, #35436, #18440, #24086, #29016, #41453, #58445, #70133, #28641, #47095, #62973, #64467, #7123 ),
 .UNSPECIFIED., .F., .F. ) 
 B_SPLINE_CURVE_WITH_KNOTS ( ( 3, 2, 2, 2, 2, 2, 3 ),
 ( 0.2354970748259125335, 0.2407300466676793871, 0.2459630185094462407, 0.2511959903512130943, 0.2564289621929799479, 0.2616619340347468015, 0.2668949058765136551 ),
 .UNSPECIFIED. ) 
 CURVE ( )  GEOMETRIC_REPRESENTATION_ITEM ( )  RATIONAL_B_SPLINE_CURVE ( ( 1.000000000000086153, 0.9659258262889821589, 1.000000000000000000, 0.9659258262890683122, 1.000000000000000000, 0.9659258262890683122, 1.000000000000000000, 0.9659258262890683122, 1.000000000000000000, 0.9659258262890683122, 1.000000000000000000, 0.9659258262890685343, 0.9999999999999997780 ) ) 
 REPRESENTATION_ITEM ( '' )  );
#73960 = CARTESIAN_POINT ( 'NONE',  ( -7.456155213548130156, 10.23501372118544595, -65.47700548260780806 ) ) ;
#73961 = CARTESIAN_POINT ( 'NONE',  ( 7.188101187499991163, 2.977408999572648707, 3.830302781871751883 ) ) ;
#73962 = EDGE_LOOP ( 'NONE', ( #53289, #72181, #59641, #22701 ) ) ;
#73963 = ORIENTED_EDGE ( 'NONE', *, *, #45277, .F. ) ;
#73964 = CARTESIAN_POINT ( 'NONE',  ( 4.220049686691941027, -10.18810118749999738, 92.12500000204836681 ) ) ;
#73965 = LINE ( 'NONE', #68677, #21295 ) ;
#73966 = CARTESIAN_POINT ( 'NONE',  ( -29.43265458321760519, 202.1250000013656063, 173.4587341250003760 ) ) ;
#73967 = CARTESIAN_POINT ( 'NONE',  ( -10.99999999999999822, -4.556349186104052151, 106.0937500000000142 ) ) ;
#73968 = CARTESIAN_POINT ( 'NONE',  ( -3.458734124999959469, 201.7500000013655779, 199.4326545832176691 ) ) ;
#73970 = DIRECTION ( 'NONE',  ( 1.000000000000000000, 0.000000000000000000, -0.000000000000000000 ) ) ;
#73969 = CARTESIAN_POINT ( 'NONE',  ( 11.00000000000000000, 1.347111479062088405E-15, 87.25000000000000000 ) ) ;
#73971 = CARTESIAN_POINT ( 'NONE',  ( -1.836970198721029983E-15, 118.7500000000000142, 10.00000000000000178 ) ) ;
#73972 = B_SPLINE_CURVE_WITH_KNOTS ( 'NONE', 3,
 ( #46418, #69432, #17741, #50961, #63765, #12083, #16240, #35119, #6443, #23777 ),
 .UNSPECIFIED., .F., .F.,
 ( 4, 2, 2, 2, 4 ),
 ( 0.000000000000000000, 0.01870349236796609027, 0.03740698473593218054, 0.05611047710389827081, 0.07481396947186436108 ),
 .UNSPECIFIED. ) ;
#73973 = CARTESIAN_POINT ( 'NONE',  ( -5.656854249492378806, 108.6874999999999858, 5.656854249492381470 ) ) ;
#73974 = CARTESIAN_POINT ( 'NONE',  ( 6.676582343750001591, 289.1093750017069510, -8.176455196517173205E-16 ) ) ;
#73975 = CARTESIAN_POINT ( 'NONE',  ( 5.082755093536320601, -5.082755093536318824, 5.424052781871753659 ) ) ;
#73976 = EDGE_CURVE ( 'NONE', #27460, #21786, #35641, .T. ) ;
#73977 = EDGE_CURVE ( 'NONE', #40603, #23575, #7449, .T. ) ;
#73978 = CARTESIAN_POINT ( 'NONE',  ( 24.54126587499998635, 208.2500000013656063, 171.4326545832175555 ) ) ;
#73979 = CARTESIAN_POINT ( 'NONE',  ( 2.977408999572651815, 2.062499997951610098, 7.188101187500000933 ) ) ;
#73980 =( BOUNDED_CURVE ( )  B_SPLINE_CURVE ( 2, ( #63171, #57536, #64290, #12597, #58638, #68829, #6946, #24286, #29958, #47299, #52971, #19731, #14059 ),
 .UNSPECIFIED., .F., .F. ) 
 B_SPLINE_CURVE_WITH_KNOTS ( ( 3, 2, 2, 2, 2, 2, 3 ),
 ( 0.3296947509469928539, 0.3349284467208895055, 0.3401621424947861572, 0.3453958382686828088, 0.3506295340425794604, 0.3558632298164761121, 0.3610969255903727637 ),
 .UNSPECIFIED. ) 
 CURVE ( )  GEOMETRIC_REPRESENTATION_ITEM ( )  RATIONAL_B_SPLINE_CURVE ( ( 1.000000000000000000, 0.9659258262890684232, 1.000000000000000000, 0.9659258262890684232, 1.000000000000000000, 0.9659258262890684232, 1.000000000000000000, 0.9659258262890684232, 1.000000000000000000, 0.9659258262890684232, 1.000000000000000000, 0.9659258262890684232, 1.000000000000000000 ) ) 
 REPRESENTATION_ITEM ( '' )  );
#73981 = CARTESIAN_POINT ( 'NONE',  ( 1.432654583217607858, 197.6250000013656063, 138.5412658750000787 ) ) ;
#73982 = CARTESIAN_POINT ( 'NONE',  ( 5.082755093536325042, 123.9687500020483952, -5.082755093536325930 ) ) ;
#73984 = CARTESIAN_POINT ( 'NONE',  ( 2.445694354108784108, 201.5625000013656063, 144.4456943541088663 ) ) ;
#73983 = CARTESIAN_POINT ( 'NONE',  ( -1.656854249492470732, 204.6875000000000284, 145.9999999999999716 ) ) ;
#73985 = CARTESIAN_POINT ( 'NONE',  ( -3.042071309553166181, 238.1770833367473301, -11.35316468749999608 ) ) ;
#73986 = CARTESIAN_POINT ( 'NONE',  ( -11.00000000000000000, 0.000000000000000000, 86.50000000000000000 ) ) ;
#73987 = CARTESIAN_POINT ( 'NONE',  ( 32.00000000000000000, 203.2500000000000000, 169.9999999999999432 ) ) ;
#73988 = CARTESIAN_POINT ( 'NONE',  ( 9.832129032723420536, 16.19791666325268054, -5.676582343749999815 ) ) ;
#73989 = CARTESIAN_POINT ( 'NONE',  ( -27.99999999999999645, 210.0000000000000284, 166.0000000000003979 ) ) ;
#73990 = CARTESIAN_POINT ( 'NONE',  ( -3.042071309553173730, 214.6354166632526983, 11.35316468749999785 ) ) ;
#73991 = CARTESIAN_POINT ( 'NONE',  ( 9.832129032723420536, 1.197916663252682756, -5.676582343749999815 ) ) ;
#73992 = CARTESIAN_POINT ( 'NONE',  ( 5.656854249492379694, 124.4375000000000000, -5.656854249492380582 ) ) ;
#73994 = CARTESIAN_POINT ( 'NONE',  ( -2.679491924289517879, 41.45833333333146697, -10.00000000001272582 ) ) ;
#73993 = CARTESIAN_POINT ( 'NONE',  ( -28.00000000000002842, 206.0000000000000284, 166.0000000000003695 ) ) ;
#73995 = EDGE_LOOP ( 'NONE', ( #3281, #40620, #45926, #17258 ) ) ;
#73996 = CARTESIAN_POINT ( 'NONE',  ( 2.445694354108783219, 200.8125000013656063, 139.5543056458912190 ) ) ;
#73997 = CARTESIAN_POINT ( 'NONE',  ( 11.35316468749999963, 20.98958332991935549, -3.042071309553165293 ) ) ;
#73998 = CARTESIAN_POINT ( 'NONE',  ( -7.778174593052020747, -7.778174593052023411, 91.37500000409677625 ) ) ;
#73999 = CARTESIAN_POINT ( 'NONE',  ( 0.000000000000000000, 225.9999999999999432, 0.000000000000000000 ) ) ;
#74000 = CARTESIAN_POINT ( 'NONE',  ( -24.54126587500001833, 197.2500000013656063, 168.5673454167826435 ) ) ;
#74002 = CARTESIAN_POINT ( 'NONE',  ( 8.311093377946834337, 5.156249996586016238, 8.311093377946839666 ) ) ;
#74001 = CARTESIAN_POINT ( 'NONE',  ( 7.188101187500000933, 111.5000000020483810, -2.977408999572651371 ) ) ;
#74003 = CARTESIAN_POINT ( 'NONE',  ( -5.656854249492375253, 5.656854249492375253, 18.64280277982336642 ) ) ;
#74004 = CARTESIAN_POINT ( 'NONE',  ( -5.676582343750006032, 139.1145833299193555, 9.832129032723418760 ) ) ;
#74005 = CARTESIAN_POINT ( 'NONE',  ( -10.00000000000000355, 104.5833333265053824, 2.679491924311223183 ) ) ;
#74006 = ADVANCED_FACE ( 'NONE', ( #73009 ), #62057, .T. ) ;
#74007 = CARTESIAN_POINT ( 'NONE',  ( -2.977408999572650927, 122.7500000020483952, -7.188101187500001821 ) ) ;
#74008 = DIRECTION ( 'NONE',  ( -0.000000000000000000, 1.000000000000000000, -0.000000000000000000 ) ) ;
#74009 = CARTESIAN_POINT ( 'NONE',  ( -30.44569435410879521, 208.0625000013656063, 172.4456943541092357 ) ) ;
#74010 = CARTESIAN_POINT ( 'NONE',  ( -5.000000000000000888, -50.98531617258489490, -41.27391139027643874 ) ) ;
#74011 = ORIENTED_EDGE ( 'NONE', *, *, #25573, .T. ) ;
#74012 = CARTESIAN_POINT ( 'NONE',  ( 0.8912353796318864818, -67.61603573606915063, 20.05324848891959277 ) ) ;
#74013 = CARTESIAN_POINT ( 'NONE',  ( -11.00000000000000000, 0.000000000000000000, 113.6875000040967763 ) ) ;
#74014 = CARTESIAN_POINT ( 'NONE',  ( -4.088227598258586603E-16, 288.3593750017070079, -6.676582343750001591 ) ) ;
#74015 = CYLINDRICAL_SURFACE ( 'NONE', #16995, 3.999999999999976019 ) ;
#74016 = CARTESIAN_POINT ( 'NONE',  ( 3.313708498984756279, 7.999999999999991118, 24.41780278432982954 ) ) ;
#74017 = AXIS2_PLACEMENT_3D ( 'NONE', #25052, #43158, #66173 ) ;
#74018 = CARTESIAN_POINT ( 'NONE',  ( 2.449293598294707893E-16, 14.99999999726881406, -4.000000000000001776 ) ) ;
#74019 = CARTESIAN_POINT ( 'NONE',  ( -6.238412754330611322E-16, 10.18810118749999916, 100.6562500020483810 ) ) ;
#74020 = ORIENTED_EDGE ( 'NONE', *, *, #72053, .F. ) ;
#74021 = CARTESIAN_POINT ( 'NONE',  ( 6.123233995736767268E-16, 218.1249999931720538, -10.00000000000000178 ) ) ;
#74022 = CARTESIAN_POINT ( 'NONE',  ( -1.836970198721029983E-15, 28.75000000000000000, 10.00000000000000178 ) ) ;
#74023 = CARTESIAN_POINT ( 'NONE',  ( -1.432654583217608080, 200.8750000013656063, 201.4587341250000350 ) ) ;
#74024 = CARTESIAN_POINT ( 'NONE',  ( 6.951808397369818766E-16, 72.34374999658602690, -11.35316468750000141 ) ) ;
#74025 = ORIENTED_EDGE ( 'NONE', *, *, #32187, .T. ) ;
#74026 = CARTESIAN_POINT ( 'NONE',  ( -10.18810118749999738, -4.220049686691941915, 114.2500000020483952 ) ) ;
#74027 = CARTESIAN_POINT ( 'NONE',  ( 4.541265875000002339, 11.43749999863440614, 0.000000000000000000 ) ) ;
#74028 = ORIENTED_EDGE ( 'NONE', *, *, #34919, .T. ) ;
#74029 = CARTESIAN_POINT ( 'NONE',  ( 4.401442555609581635E-16, 26.34374999795161543, -7.188101187500000044 ) ) ;
#74030 = CARTESIAN_POINT ( 'NONE',  ( -5.000000000000005329, 110.2083333265053682, 8.660254037844387298 ) ) ;
#74031 = DIRECTION ( 'NONE',  ( -1.000000000000000000, -0.000000000000000000, -0.000000000000000000 ) ) ;
#74032 = CARTESIAN_POINT ( 'NONE',  ( -7.188101187500000044, 22.59374999795161187, -8.802885111219163269E-16 ) ) ;
#74033 = CARTESIAN_POINT ( 'NONE',  ( -10.99999999999984013, -4.556349186104210247, 103.2812500040967905 ) ) ;
#74034 = EDGE_CURVE ( 'NONE', #57691, #64048, #17465, .T. ) ;
#74035 = CARTESIAN_POINT ( 'NONE',  ( 1.871523826299183495E-15, -10.18810118749999916, 110.4062500020483668 ) ) ;
#74036 = PRODUCT_DEFINITION_SHAPE ( 'NONE', 'NONE',  #74658 ) ;
#74037 = AXIS2_PLACEMENT_3D ( 'NONE', #18837, #29049, #772 ) ;
#74038 = EDGE_CURVE ( 'NONE', #50631, #52730, #62423, .T. ) ;
#74039 = CARTESIAN_POINT ( 'NONE',  ( 2.395154805519954641E-11, 111.2499999999981242, -9.999999999999998224 ) ) ;
#74040 = CARTESIAN_POINT ( 'NONE',  ( -1.656854249492383691, 8.437499997268814056, 4.000000000000000888 ) ) ;
#74041 = CARTESIAN_POINT ( 'NONE',  ( 4.850062511589654031E-16, 0.4207531754730554074, -7.920753175473053354 ) ) ;
#74042 = VERTEX_POINT ( 'NONE', #33408 ) ;
#74043 = CARTESIAN_POINT ( 'NONE',  ( -2.445694354108783664, 202.3125000013656063, 195.5543056458912190 ) ) ;
#74044 = CARTESIAN_POINT ( 'NONE',  ( -29.43265458321771177, 205.5000000013655779, 166.5412658750003914 ) ) ;
#74045 = CARTESIAN_POINT ( 'NONE',  ( 2.775557561562891351E-14, 210.0000000000000284, 202.0000000000000000 ) ) ;
#74046 = EDGE_CURVE ( 'NONE', #62787, #61757, #22423, .T. ) ;
#74047 = CARTESIAN_POINT ( 'NONE',  ( -1.881053915767124440, 10.99999999863440969, 4.541265875000001451 ) ) ;
#74048 = CARTESIAN_POINT ( 'NONE',  ( -4.000000000000016875, 206.5625000027312126, 140.3431457505076594 ) ) ;
#74049 = CARTESIAN_POINT ( 'NONE',  ( -2.977408999572648707, -7.188101187499990274, 21.26780278187175810 ) ) ;
#74050 = VERTEX_POINT ( 'NONE', #56408 ) ;
#74051 =( BOUNDED_CURVE ( )  B_SPLINE_CURVE ( 1, ( #51097, #5831 ),
 .UNSPECIFIED., .F., .F. ) 
 B_SPLINE_CURVE_WITH_KNOTS ( ( 2, 2 ),
 ( 0.000000000000000000, 1.000000000000000000 ),
 .UNSPECIFIED. ) 
 CURVE ( )  GEOMETRIC_REPRESENTATION_ITEM ( )  RATIONAL_B_SPLINE_CURVE ( ( 0.9660720762559202868, 0.9660720762559202868 ) ) 
 REPRESENTATION_ITEM ( '' )  );
#74052 = CARTESIAN_POINT ( 'NONE',  ( 1.224646799147353256E-15, 0.000000000000000000, 10.00000000000000000 ) ) ;
#74053 = EDGE_CURVE ( 'NONE', #41900, #23624, #46503, .T. ) ;
#74054 = EDGE_LOOP ( 'NONE', ( #6792, #18692, #34877, #57946 ) ) ;
#74055 = CARTESIAN_POINT ( 'NONE',  ( -6.238412754330611322E-16, 10.18810118749999916, 110.7812500020483668 ) ) ;
#74056 = CARTESIAN_POINT ( 'NONE',  ( -6.735557395310442023E-16, 11.00000000000000000, 96.81250000409677625 ) ) ;
#74057 = CARTESIAN_POINT ( 'NONE',  ( 1.432654583217662481, 203.1250000013656347, 194.5412658750000219 ) ) ;
#74058 = CARTESIAN_POINT ( 'NONE',  ( 26.56734541678237704, 201.3750000013656347, 173.4587341249998929 ) ) ;
#74059 = CARTESIAN_POINT ( 'NONE',  ( 7.320508075688771044, 79.37500000000000000, 7.320508075688775484 ) ) ;
#74060 = VECTOR ( 'NONE', #57574, 1000.000000000000000 ) ;
#74061 = CARTESIAN_POINT ( 'NONE',  ( -8.000000000000000000, 121.9062500000000000, -3.313708498984761608 ) ) ;
#74062 = CARTESIAN_POINT ( 'NONE',  ( 4.721056650415999201, 299.2343750017069510, -4.721056650415999201 ) ) ;
#74063 = ORIENTED_EDGE ( 'NONE', *, *, #23121, .F. ) ;
#74064 = DIRECTION ( 'NONE',  ( -1.000000000000000000, 0.000000000000000000, 0.000000000000000000 ) ) ;
#74065 = EDGE_CURVE ( 'NONE', #30885, #60165, #16385, .T. ) ;
#74066 = CARTESIAN_POINT ( 'NONE',  ( 0.8912353796376716319, -16.44139524822715259, 68.58382889509293534 ) ) ;
#74067 = CARTESIAN_POINT ( 'NONE',  ( -2.751064625579944321E-14, 196.8750000027312126, 146.0000000000000284 ) ) ;
#74068 = CARTESIAN_POINT ( 'NONE',  ( -5.000000000000001776, 68.02455775458903986, 22.06917953199582527 ) ) ;
#74069 = CARTESIAN_POINT ( 'NONE',  ( 8.000000000000000000, 5.906249995903221084, -3.313708498984761164 ) ) ;
#74070 = CARTESIAN_POINT ( 'NONE',  ( 7.320508075688776373, 231.8750000000000000, 7.320508075688767491 ) ) ;
#74071 = CARTESIAN_POINT ( 'NONE',  ( 29.65685424949230864, 204.0624999999999716, 173.9999999999999432 ) ) ;
#74072 = CARTESIAN_POINT ( 'NONE',  ( 7.320508075688774596, 195.6250000000000568, -7.320508075688774596 ) ) ;
#74073 =( BOUNDED_CURVE ( )  B_SPLINE_CURVE ( 2, ( #35240, #45795, #40139, #62762, #177, #11105, #22772, #63517, #913, #28445, #74096, #17117, #17495 ),
 .UNSPECIFIED., .F., .F. ) 
 B_SPLINE_CURVE_WITH_KNOTS ( ( 3, 2, 2, 2, 2, 2, 3 ),
 ( 0.4293478260869564855, 0.4311594202898550443, 0.4329710144927535476, 0.4347826086956521063, 0.4365942028985507206, 0.4384057971014492794, 0.4402173913043478382 ),
 .UNSPECIFIED. ) 
 CURVE ( )  GEOMETRIC_REPRESENTATION_ITEM ( )  RATIONAL_B_SPLINE_CURVE ( ( 1.000000000000001110, 0.9659258262890673130, 1.000000000000000000, 0.9659258262890683122, 1.000000000000000000, 0.9659258262890683122, 1.000000000000000000, 0.9659258262890683122, 1.000000000000000000, 0.9659258262890683122, 1.000000000000000000, 0.9659258262890683122, 1.000000000000000000 ) ) 
 REPRESENTATION_ITEM ( '' )  );
#74074 = CARTESIAN_POINT ( 'NONE',  ( 1.320432766682872962E-15, -7.188101187499992051, 15.73655278187175632 ) ) ;
#74075 = CARTESIAN_POINT ( 'NONE',  ( -11.35316468750000141, 168.8020833299193271, 3.042071309553159963 ) ) ;
#74076 = CARTESIAN_POINT ( 'NONE',  ( -2.679491924316742324, 213.5416666666662877, 9.999999999997077893 ) ) ;
#74077 = CARTESIAN_POINT ( 'NONE',  ( 2.020667218593132706E-15, -11.00000000000000000, 82.56250000409677625 ) ) ;
#74079 = DIRECTION ( 'NONE',  ( -0.000000000000000000, 1.000000000000000000, -0.000000000000000000 ) ) ;
#74078 = CARTESIAN_POINT ( 'NONE',  ( -8.000000000000003553, 22.99999999999999645, 1.000000000000000000 ) ) ;
#74080 = ORIENTED_EDGE ( 'NONE', *, *, #70623, .F. ) ;
#74081 = CARTESIAN_POINT ( 'NONE',  ( 2.445694354108783664, 196.3125000013656063, 144.4456943541088663 ) ) ;
#74082 = CARTESIAN_POINT ( 'NONE',  ( 5.676582343750001591, 16.92708332991935194, -9.832129032723420536 ) ) ;
#74083 = CARTESIAN_POINT ( 'NONE',  ( -4.556349186104045934, 11.00000000000000000, 110.4062500040967620 ) ) ;
#74084 = CONICAL_SURFACE ( 'NONE', #9024, 12.50000000000000178, 0.06208826691561822320 ) ;
#74085 = CARTESIAN_POINT ( 'NONE',  ( -2.599720908691378618, 194.5204010206058456, 200.3831165209350900 ) ) ;
#74087 = CARTESIAN_POINT ( 'NONE',  ( 2.216418498311750085, -16.40908668940260284, -68.78644440154761242 ) ) ;
#74086 = CARTESIAN_POINT ( 'NONE',  ( 8.660254037844385522, 221.4583333265053966, 5.000000000000005329 ) ) ;
#74088 = CARTESIAN_POINT ( 'NONE',  ( 23.99999999999998934, 201.8750000027312126, 169.9999999999999432 ) ) ;
#74089 = CARTESIAN_POINT ( 'NONE',  ( 3.458734124999958581, 198.5000000013656063, 140.5673454167823593 ) ) ;
#74090 = CARTESIAN_POINT ( 'NONE',  ( 2.679491924311222739, 65.83333332650538239, 10.00000000000000355 ) ) ;
#74091 = AXIS2_PLACEMENT_3D ( 'NONE', #36492, #13455, #14195 ) ;
#74092 = CARTESIAN_POINT ( 'NONE',  ( -5.082755093536324154, 104.8437500020483810, 5.082755093536326818 ) ) ;
#74093 = CARTESIAN_POINT ( 'NONE',  ( 1.881053915767121776, 11.62499999863440969, -4.541265875000002339 ) ) ;
#74094 = CARTESIAN_POINT ( 'NONE',  ( 2.679491924311227624, 56.04166666666666430, -9.999999999999994671 ) ) ;
#74095 = CARTESIAN_POINT ( 'NONE',  ( 1.469576158976822172E-15, -7.999999999999991118, 1.205302779823363979 ) ) ;
#74096 = CARTESIAN_POINT ( 'NONE',  ( 5.000000000000001776, 102.7083333265053824, -8.660254037844389075 ) ) ;
#74097 = ORIENTED_EDGE ( 'NONE', *, *, #37000, .T. ) ;
#74098 = EDGE_LOOP ( 'NONE', ( #46226, #67835, #34552, #22183 ) ) ;
#74099 = CARTESIAN_POINT ( 'NONE',  ( -10.00000000000010836, 197.2916666666667709, -2.679491924311259599 ) ) ;
#74100 = CARTESIAN_POINT ( 'NONE',  ( 7.999999999999992895, -3.313708498984756279, 15.17405278392014623 ) ) ;
#74101 =( NAMED_UNIT ( * ) SI_UNIT ( $, .STERADIAN. ) SOLID_ANGLE_UNIT ( ) );
#74102 = CARTESIAN_POINT ( 'NONE',  ( 2.828427124746152987, 198.2500000027312126, 139.1715728752538723 ) ) ;
#74103 = CARTESIAN_POINT ( 'NONE',  ( -11.35316468750000141, 148.2812499965860411, -1.390361679473963753E-15 ) ) ;
#74104 = ORIENTED_EDGE ( 'NONE', *, *, #37242, .T. ) ;
#74105 = CARTESIAN_POINT ( 'NONE',  ( -1.469576158976823947E-15, 6.937499995903221084, 8.000000000000000000 ) ) ;
#74106 = CARTESIAN_POINT ( 'NONE',  ( 10.18810118749999916, 4.220049686691935698, 91.00000000204836681 ) ) ;
#74107 = CARTESIAN_POINT ( 'NONE',  ( -28.45294094728582479, 194.7504983042304900, 173.7298212953299412 ) ) ;
#74108 = CARTESIAN_POINT ( 'NONE',  ( 4.000000000000015987, 206.5000000000000284, 198.0000000000000284 ) ) ;
#74109 = LINE ( 'NONE', #33769, #41226 ) ;
#74110 = FACE_OUTER_BOUND ( 'NONE', #52510, .T. ) ;
#74111 = CARTESIAN_POINT ( 'NONE',  ( -10.18810118749999916, 0.000000000000000000, 116.0312500020483810 ) ) ;
#74112 = EDGE_LOOP ( 'NONE', ( #23195, #34543, #60090, #69184 ) ) ;
#74113 = FACE_OUTER_BOUND ( 'NONE', #15541, .T. ) ;
#74114 = CARTESIAN_POINT ( 'NONE',  ( 34.07942448040759587, 175.6415741637315193, 157.4743357174363894 ) ) ;
#74115 = CARTESIAN_POINT ( 'NONE',  ( -3.042071309553173730, 129.6354166632526415, 11.35316468749999785 ) ) ;
#74116 = CARTESIAN_POINT ( 'NONE',  ( 1.432654583217664479, 203.7500000013656063, 201.4587341250000065 ) ) ;
#74117 = CARTESIAN_POINT ( 'NONE',  ( -2.977408999572650039, 26.81249999795161898, -7.188101187500000933 ) ) ;
#74118 = CARTESIAN_POINT ( 'NONE',  ( -4.220049686691935698, 10.18810118749999916, 85.75000000204838102 ) ) ;
#74119 = CARTESIAN_POINT ( 'NONE',  ( 5.676582343749993598, 35.26041666325269119, 9.832129032723422313 ) ) ;
#74120 = ORIENTED_EDGE ( 'NONE', *, *, #47841, .T. ) ;
#74121 = CARTESIAN_POINT ( 'NONE',  ( -4.000000000000001776, 4.500000000000000888, -4.898587196589415787E-16 ) ) ;
#74122 = CARTESIAN_POINT ( 'NONE',  ( 3.313708498984756279, 7.999999999999991118, 8.049052783920144449 ) ) ;
#74123 = CARTESIAN_POINT ( 'NONE',  ( 8.008118988124991233, 9.807117285998411148E-16, 21.26311528394063188 ) ) ;
#74124 = CARTESIAN_POINT ( 'NONE',  ( 2.445694354108784108, 207.5625000013656063, 144.4456943541088663 ) ) ;
#74125 = CARTESIAN_POINT ( 'NONE',  ( 5.082755093536325930, 8.156249997951611874, -5.082755093536325930 ) ) ;
#74126 = CARTESIAN_POINT ( 'NONE',  ( -4.242640687119285658, 295.1875000034139589, 4.242640687119287435 ) ) ;
#74127 = DIRECTION ( 'NONE',  ( -0.000000000000000000, -0.000000000000000000, -1.000000000000000000 ) ) ;
#74128 = CARTESIAN_POINT ( 'NONE',  ( -2.977408999572650039, 7.312499997951610986, -7.188101187500001821 ) ) ;
#74129 = EDGE_CURVE ( 'NONE', #62108, #69231, #51109, .T. ) ;
#74130 = CARTESIAN_POINT ( 'NONE',  ( 9.832129032723420536, 151.5104166632526699, -5.676582343749999815 ) ) ;
#74131 = CARTESIAN_POINT ( 'NONE',  ( 10.18810118750000093, -4.220049686691933921, 77.31250000204836681 ) ) ;
#74132 = CARTESIAN_POINT ( 'NONE',  ( -30.44569435410883074, 194.5625000013656063, 167.5543056458915885 ) ) ;
#74133 = EDGE_CURVE ( 'NONE', #36393, #30135, #35885, .T. ) ;
#74134 = CARTESIAN_POINT ( 'NONE',  ( 2.449293598294707893E-16, 15.25000000000000000, -4.000000000000001776 ) ) ;
#74135 = CARTESIAN_POINT ( 'NONE',  ( 1.881053915767121776, 21.62499999863441502, -4.541265875000002339 ) ) ;
#74136 = EDGE_LOOP ( 'NONE', ( #21386, #216, #5740, #53982 ) ) ;
#74137 = CARTESIAN_POINT ( 'NONE',  ( 1.656854249492405451, 197.4375000027312126, 202.0000000000000284 ) ) ;
#74138 = CARTESIAN_POINT ( 'NONE',  ( 3.999999999999959144, 209.0625000000000568, 140.3431457505076594 ) ) ;
#74139 = CARTESIAN_POINT ( 'NONE',  ( -26.34314575050753859, 205.6875000027312126, 174.0000000000003411 ) ) ;
#74140 = CARTESIAN_POINT ( 'NONE',  ( 2.679491924311176998, 249.5833333401612890, 10.00000000000003197 ) ) ;
#74141 = ORIENTED_EDGE ( 'NONE', *, *, #25100, .F. ) ;
#74142 = CARTESIAN_POINT ( 'NONE',  ( 7.188101187499999156, 18.37499999795161187, 2.977408999572654924 ) ) ;
#74143 = DIRECTION ( 'NONE',  ( -0.000000000000000000, 1.000000000000000000, -0.000000000000000000 ) ) ;
#74144 = CARTESIAN_POINT ( 'NONE',  ( 5.000000000000000000, 51.30314553820254275, -41.49361401976463526 ) ) ;
#74145 = CARTESIAN_POINT ( 'NONE',  ( 10.00000000000000178, 35.20833333333332149, -2.679491924311226736 ) ) ;
#74146 = CARTESIAN_POINT ( 'NONE',  ( -7.188101187499999156, 103.6250000020483810, 2.977408999572654924 ) ) ;
#74147 = CARTESIAN_POINT ( 'NONE',  ( -31.45873412500001010, 208.8750000013656063, 168.5673454167827572 ) ) ;
#74148 = CARTESIAN_POINT ( 'NONE',  ( 4.721056650416000089, 287.8281250017069510, 4.721056650415999201 ) ) ;
#74150 = CARTESIAN_POINT ( 'NONE',  ( 7.778174593052021635, 7.778174593052023411, 74.12500000409677625 ) ) ;
#74149 = DIRECTION ( 'NONE',  ( 0.8191520442889885789, 0.000000000000000000, 0.5735764363510507113 ) ) ;
#74151 = ORIENTED_EDGE ( 'NONE', *, *, #6602, .F. ) ;
#74152 = CARTESIAN_POINT ( 'NONE',  ( -6.951808397369817780E-16, 242.6562500034140157, -11.35316468749999963 ) ) ;
#74153 = CARTESIAN_POINT ( 'NONE',  ( -5.082755093536319713, 5.082755093536319713, 25.67405278187175810 ) ) ;
#74154 = DIRECTION ( 'NONE',  ( -0.000000000000000000, -0.000000000000000000, 1.000000000000000000 ) ) ;
#74155 = CARTESIAN_POINT ( 'NONE',  ( -4.242640687119285658, 287.1875000034139589, 4.242640687119287435 ) ) ;
#74156 = CARTESIAN_POINT ( 'NONE',  ( 0.000000000000000000, 0.000000000000000000, 30.00000000000000000 ) ) ;
#74157 = CARTESIAN_POINT ( 'NONE',  ( 3.458734125000016757, 196.1250000013655779, 199.4326545832176691 ) ) ;
#74158 = CARTESIAN_POINT ( 'NONE',  ( 5.000000000000001776, 155.8333333333333428, -8.660254037844389075 ) ) ;
#74159 = CARTESIAN_POINT ( 'NONE',  ( -27.99999999999999645, 210.0000000000000284, 174.0000000000003411 ) ) ;
#74160 = SURFACE_SIDE_STYLE ('',( #56824 ) ) ;
#74161 = CARTESIAN_POINT ( 'NONE',  ( 5.000000000000000000, -53.53067326687862248, -46.58593137613121371 ) ) ;
#74162 = CARTESIAN_POINT ( 'NONE',  ( -5.676582343750006032, 124.4270833299193555, 9.832129032723418760 ) ) ;
#74163 = CARTESIAN_POINT ( 'NONE',  ( 46.67364751762348618, 146.0000000000000000, 69.99999999999995737 ) ) ;
#74164 = CARTESIAN_POINT ( 'NONE',  ( 2.995737153982838574, -16.37687539610413978, -68.98994273414959366 ) ) ;
#74167 = DIRECTION ( 'NONE',  ( -0.000000000000000000, 1.000000000000000000, -0.000000000000000000 ) ) ;
#74166 = CARTESIAN_POINT ( 'NONE',  ( 26.56734541678232731, 198.0000000013656063, 166.5412658749999650 ) ) ;
#74165 = CARTESIAN_POINT ( 'NONE',  ( 25.17157287525378706, 208.8750000000000284, 172.8284271247460424 ) ) ;
#74168 = ORIENTED_EDGE ( 'NONE', *, *, #55671, .T. ) ;
#74169 = CARTESIAN_POINT ( 'NONE',  ( 6.649952966877521021, 225.6719221872985486, -7.474339169392074211 ) ) ;
#74170 = DIRECTION ( 'NONE',  ( -0.000000000000000000, -0.000000000000000000, 1.000000000000000000 ) ) ;
#74171 = CARTESIAN_POINT ( 'NONE',  ( 7.778174593052023411, -7.778174593052021635, 112.7500000040967763 ) ) ;
#74172 =( BOUNDED_CURVE ( )  B_SPLINE_CURVE ( 2, ( #69152, #39733, #23123, #17460, #52182, #52544, #884, #40481, #56729 ),
 .UNSPECIFIED., .F., .F. ) 
 B_SPLINE_CURVE_WITH_KNOTS ( ( 3, 2, 2, 2, 3 ),
 ( 0.4166666666666671293, 0.4250000000000003775, 0.4333333333333336812, 0.4416666666666669849, 0.4500000000000002887 ),
 .UNSPECIFIED. ) 
 CURVE ( )  GEOMETRIC_REPRESENTATION_ITEM ( )  RATIONAL_B_SPLINE_CURVE ( ( 0.9999999999999958922, 0.9238795325112908463, 1.000000000000000000, 0.9238795325112867385, 1.000000000000000000, 0.9238795325112867385, 1.000000000000000000, 0.9238795325112841850, 1.000000000000002442 ) ) 
 REPRESENTATION_ITEM ( '' )  );
#74173 = CARTESIAN_POINT ( 'NONE',  ( 5.000000000000000000, -65.74990953739971644, -23.82322416715333802 ) ) ;
#74174 = CARTESIAN_POINT ( 'NONE',  ( 11.35316468750000141, 201.0937499965860127, 0.000000000000000000 ) ) ;
#74175 = CARTESIAN_POINT ( 'NONE',  ( 7.188101187500002709, 123.3125000020483810, 2.977408999572649151 ) ) ;
#74176 = CARTESIAN_POINT ( 'NONE',  ( -4.541265875000002339, 1.874999998634406806, -1.881053915767121998 ) ) ;
#74177 = CARTESIAN_POINT ( 'NONE',  ( -2.069125466539885050, -55.78340383128265501, 43.89144373685536493 ) ) ;
#74178 = CARTESIAN_POINT ( 'NONE',  ( -5.656854249492373476, -5.656854249492376141, 19.01780277982336642 ) ) ;
#74180 = DIRECTION ( 'NONE',  ( -0.000000000000000000, 1.000000000000000000, 4.689100369878284071E-30 ) ) ;
#74179 = FACE_OUTER_BOUND ( 'NONE', #27827, .T. ) ;
#74181 = CARTESIAN_POINT ( 'NONE',  ( 5.676582343749993598, 94.94791666325269830, 9.832129032723422313 ) ) ;
#74182 = VERTEX_POINT ( 'NONE', #69207 ) ;
#74183 = CARTESIAN_POINT ( 'NONE',  ( -4.000000000000015987, 205.6250000027312126, 142.0000000000000568 ) ) ;
#74184 = CARTESIAN_POINT ( 'NONE',  ( 2.977408999572651815, 24.18749999795161543, 7.188101187500000933 ) ) ;
#74185 = FACE_OUTER_BOUND ( 'NONE', #27448, .T. ) ;
#74186 = CARTESIAN_POINT ( 'NONE',  ( -11.35316468749999963, 264.2187500034140157, 0.000000000000000000 ) ) ;
#74187 = CARTESIAN_POINT ( 'NONE',  ( 3.042071309553167069, 101.8229166632526699, -11.35316468749999785 ) ) ;
#74188 = ORIENTED_EDGE ( 'NONE', *, *, #47538, .F. ) ;
#74189 = DIRECTION ( 'NONE',  ( -0.8660254037844380415, -0.5000000000000012212, 0.000000000000000000 ) ) ;
#74190 = CARTESIAN_POINT ( 'NONE',  ( 10.18810118750000093, -4.220049686691933921, 104.3125000020483810 ) ) ;
#74191 = CARTESIAN_POINT ( 'NONE',  ( 4.999999999999993783, 216.0416666598387110, 8.660254037844390851 ) ) ;
#74192 = CARTESIAN_POINT ( 'NONE',  ( 2.839093476692135984E-14, 204.9375000013656063, 201.4587341250000350 ) ) ;
#74193 = DIRECTION ( 'NONE',  ( -6.308085367188386297E-16, 0.000000000000000000, -1.000000000000000000 ) ) ;
#74195 = CARTESIAN_POINT ( 'NONE',  ( -5.676582343750006032, 104.1145833299193697, 9.832129032723418760 ) ) ;
#74194 = PLANE ( 'NONE',  #65334 ) ;
#74196 = CARTESIAN_POINT ( 'NONE',  ( -3.313708498984757167, 7.999999999999991118, 14.23655278392014623 ) ) ;
#74197 = CARTESIAN_POINT ( 'NONE',  ( -24.54126587500000056, 200.5000000013656063, 168.5673454167827003 ) ) ;
#74198 = DIRECTION ( 'NONE',  ( 0.000000000000000000, -0.000000000000000000, -1.000000000000000000 ) ) ;
#74199 = ORIENTED_EDGE ( 'NONE', *, *, #3669, .T. ) ;
#74200 = ADVANCED_FACE ( 'NONE', ( #28838 ), #38057, .F. ) ;
#74201 = CARTESIAN_POINT ( 'NONE',  ( 10.00000000000000000, 186.6666666598386826, 2.679491924311236062 ) ) ;
#74202 = EDGE_CURVE ( 'NONE', #18825, #72985, #17141, .T. ) ;
#74203 = CARTESIAN_POINT ( 'NONE',  ( 8.000000000000001776, 115.1562500000000000, 3.313708498984759387 ) ) ;
#74204 = VECTOR ( 'NONE', #68389, 1000.000000000000000 ) ;
#74205 = CARTESIAN_POINT ( 'NONE',  ( 0.000000000000000000, 0.000000000000000000, 118.0000000000000000 ) ) ;
#74206 = CARTESIAN_POINT ( 'NONE',  ( 11.35316468749999963, 86.30208332991935549, -3.042071309553165293 ) ) ;
#74207 = CARTESIAN_POINT ( 'NONE',  ( -2.765530957081998586, 289.6406250017070079, 6.676582343750001591 ) ) ;
#74208 = CARTESIAN_POINT ( 'NONE',  ( 4.401442555609581635E-16, 4.218749997951610098, -7.188101187500000044 ) ) ;
#74209 = CARTESIAN_POINT ( 'NONE',  ( 10.18810118749999916, 1.247682550866122264E-15, 98.78125000204838102 ) ) ;
#74210 = CARTESIAN_POINT ( 'NONE',  ( 5.676582343750001591, 1.927083329919350163, -9.832129032723420536 ) ) ;
#74211 = ORIENTED_EDGE ( 'NONE', *, *, #16722, .F. ) ;
#74212 = CARTESIAN_POINT ( 'NONE',  ( -3.313708498984759387, -7.999999999999989342, 28.11155277982336642 ) ) ;
#74213 = CARTESIAN_POINT ( 'NONE',  ( -30.99999999999992895, -31.99999999999978684, 205.0000000000000284 ) ) ;
#74214 = CARTESIAN_POINT ( 'NONE',  ( 4.000000000000001776, 0.8124999972688135008, -1.656854249492381248 ) ) ;
#74215 = CARTESIAN_POINT ( 'NONE',  ( 8.311093377946837890, 221.4062499965860411, -8.311093377946837890 ) ) ;
#74216 = CARTESIAN_POINT ( 'NONE',  ( 10.00000000000000178, 220.4166666734946318, 2.679491924311222739 ) ) ;
#74217 = CARTESIAN_POINT ( 'NONE',  ( -24.00000000000002842, 207.9375000027312126, 168.3431457505079152 ) ) ;
#74218 = CARTESIAN_POINT ( 'NONE',  ( 6.676582343750003368, 296.0156250017069510, -2.765530957081997254 ) ) ;
#74219 = VERTEX_POINT ( 'NONE', #69582 ) ;
#74220 = CARTESIAN_POINT ( 'NONE',  ( -2.085542519210945728E-15, 194.8437499965860127, 11.35316468750000141 ) ) ;
#74221 = EDGE_CURVE ( 'NONE', #64051, #23294, #7008, .T. ) ;
#74222 = CARTESIAN_POINT ( 'NONE',  ( -10.18810118749999916, 4.220049686691934809, 96.06250000204836681 ) ) ;
#74223 = CARTESIAN_POINT ( 'NONE',  ( -26.56734541678238415, 207.3750000013656063, 166.5412658750003629 ) ) ;
#74224 = CARTESIAN_POINT ( 'NONE',  ( -5.656854249492379694, 17.06250000000000000, -5.656854249492380582 ) ) ;
#74225 = ORIENTED_EDGE ( 'NONE', *, *, #1410, .F. ) ;
#74226 = PRODUCT_DEFINITION_CONTEXT ( 'detailed design', #57833, 'design' ) ;
#74227 = CARTESIAN_POINT ( 'NONE',  ( 1.469576158976823947E-15, 91.06250000409676204, 8.000000000000000000 ) ) ;
#74228 = CARTESIAN_POINT ( 'NONE',  ( -23.99999999999998934, 199.8750000027312126, 170.0000000000002842 ) ) ;
#74229 = CARTESIAN_POINT ( 'NONE',  ( 7.320508075688774596, 15.62499999999999822, -7.320508075688774596 ) ) ;
#74230 = CARTESIAN_POINT ( 'NONE',  ( -1.656854249492327735, 209.8125000000000000, 194.0000000000000568 ) ) ;
#74231 = CARTESIAN_POINT ( 'NONE',  ( 1.871523826299183495E-15, -10.18810118749999916, 83.40625000204838102 ) ) ;
#74232 = ORIENTED_EDGE ( 'NONE', *, *, #14936, .F. ) ;
#74233 = CARTESIAN_POINT ( 'NONE',  ( -1.656854249492381248, 19.31250000000000000, -4.000000000000001776 ) ) ;
#74234 = CARTESIAN_POINT ( 'NONE',  ( -3.673940397442060854E-16, 299.7500000000000000, -6.000000000000001776 ) ) ;
#74235 = LINE ( 'NONE', #27093, #24568 ) ;
#74236 = CARTESIAN_POINT ( 'NONE',  ( 2.449293598294707893E-16, 4.999999997268813168, -4.000000000000001776 ) ) ;
#74237 = CARTESIAN_POINT ( 'NONE',  ( -4.999999999999999112, -14.70234347858786528, 69.93881661156081009 ) ) ;
#74238 = AXIS2_PLACEMENT_3D ( 'NONE', #9008, #66341, #14648 ) ;
#74239 = CARTESIAN_POINT ( 'NONE',  ( 5.000000000000000000, -65.75515815785553286, 23.82162496270619911 ) ) ;
#74242 = CARTESIAN_POINT ( 'NONE',  ( 7.999999999981424637, 1.723583929636134980E-05, 16.76780327155163874 ) ) ;
#74241 = CARTESIAN_POINT ( 'NONE',  ( -5.676582343750000703, 248.0729166700806729, -9.832129032723418760 ) ) ;
#74240 = CARTESIAN_POINT ( 'NONE',  ( 29.43265458321761585, 205.8750000013656063, 166.5412658749999650 ) ) ;
#74243 = APPLICATION_PROTOCOL_DEFINITION ( 'draft international standard', 'automotive_design', 1998, #14382 ) ;
#74244 = VERTEX_POINT ( 'NONE', #45818 ) ;
#74245 = CARTESIAN_POINT ( 'NONE',  ( 11.35316468749999963, 246.7187500034139873, -1.390361679473963556E-15 ) ) ;
#74246 = CARTESIAN_POINT ( 'NONE',  ( 2.977408999572650927, -7.188101187499990274, 10.95530278187175455 ) ) ;
#74247 = ORIENTED_EDGE ( 'NONE', *, *, #53091, .T. ) ;
#74248 = ORIENTED_EDGE ( 'NONE', *, *, #32959, .F. ) ;
#74249 = CARTESIAN_POINT ( 'NONE',  ( -4.220049686691935698, 10.18810118749999916, 73.37500000204838102 ) ) ;
#74250 = CARTESIAN_POINT ( 'NONE',  ( -11.35316468750000141, 93.80208332991934128, 3.042071309553159963 ) ) ;
#74251 = DIRECTION ( 'NONE',  ( 0.000000000000000000, 0.000000000000000000, -1.000000000000000000 ) ) ;
#74252 = CARTESIAN_POINT ( 'NONE',  ( -11.00000000000000000, 4.556349186104045934, 80.40624999999997158 ) ) ;
#74255 = CARTESIAN_POINT ( 'NONE',  ( 6.676582343750002480, 291.1718750017070647, -2.765530957081997254 ) ) ;
#74254 = CARTESIAN_POINT ( 'NONE',  ( 25.55430564589119413, 209.3125000013656063, 172.4456943541087526 ) ) ;
#74253 = CARTESIAN_POINT ( 'NONE',  ( 31.45873412499998523, 205.8750000013656063, 171.4326545832175839 ) ) ;
#74256 = CARTESIAN_POINT ( 'NONE',  ( -52.04603434479170687, 202.6697026620573467, 53.95155882862182750 ) ) ;
#74257 = FACE_OUTER_BOUND ( 'NONE', #36664, .T. ) ;
#74258 = CARTESIAN_POINT ( 'NONE',  ( -8.311093377946836114, 197.6562499965860695, -8.311093377946837890 ) ) ;
#74259 = CARTESIAN_POINT ( 'NONE',  ( -3.313708498984765161, 8.343749995903221972, 7.999999999999998224 ) ) ;
#74260 = AXIS2_PLACEMENT_3D ( 'NONE', #67712, #72235, #21671 ) ;
#74261 = EDGE_LOOP ( 'NONE', ( #51548, #53045, #54668, #8635 ) ) ;
#74262 = CARTESIAN_POINT ( 'NONE',  ( 29.43265458321766204, 194.8750000013656063, 166.5412658749999650 ) ) ;
#74263 = ADVANCED_FACE ( 'NONE', ( #23549 ), #12228, .F. ) ;
#74264 = CARTESIAN_POINT ( 'NONE',  ( 2.977408999572651815, 17.06249999795161543, 7.188101187500000933 ) ) ;
#74265 = CARTESIAN_POINT ( 'NONE',  ( 5.676582343749993598, 165.2604166632526983, 9.832129032723422313 ) ) ;
#74266 = CARTESIAN_POINT ( 'NONE',  ( -7.188101187499999156, 105.1250000020483810, 2.977408999572654924 ) ) ;
#74268 = CARTESIAN_POINT ( 'NONE',  ( -10.00000000000000178, 89.37499999317203958, -1.224646799147353454E-15 ) ) ;
#74267 = DIRECTION ( 'NONE',  ( 1.000000000000000000, 0.000000000000000000, 0.000000000000000000 ) ) ;
#74269 = CARTESIAN_POINT ( 'NONE',  ( 31.45873412499998523, 204.8750000013656063, 171.4326545832176123 ) ) ;
#74270 = CARTESIAN_POINT ( 'NONE',  ( -5.082755093536319713, 5.082755093536319713, 7.674052781871751883 ) ) ;
#74271 = CARTESIAN_POINT ( 'NONE',  ( -9.832129032723418760, 57.86458332991935549, -5.676582343750004256 ) ) ;
#74272 = CARTESIAN_POINT ( 'NONE',  ( -12.00000000000000178, -2.333919766284222597, -0.1006330532450335213 ) ) ;
#74273 = CARTESIAN_POINT ( 'NONE',  ( 5.656854249492374365, 5.656854249492375253, 0.3240527843298232069 ) ) ;
#74274 = VERTEX_POINT ( 'NONE', #41280 ) ;
#74275 = CARTESIAN_POINT ( 'NONE',  ( 7.347880794884121708E-16, 300.0000000000000000, -6.000000000000001776 ) ) ;
#74276 = CARTESIAN_POINT ( 'NONE',  ( 27.99999999999999645, 210.0000000000000284, 173.9999999999998863 ) ) ;
#74277 = CARTESIAN_POINT ( 'NONE',  ( 11.35316468750000141, 65.78124999658602690, 0.000000000000000000 ) ) ;
#74278 = CARTESIAN_POINT ( 'NONE',  ( -6.735557395310442023E-16, 11.00000000000000000, 77.31250000409677625 ) ) ;
#74279 = CARTESIAN_POINT ( 'NONE',  ( -3.458734125000016757, 200.1250000013656063, 140.5673454167823593 ) ) ;
#74280 = DIRECTION ( 'NONE',  ( -1.000000000000000000, 0.000000000000000000, 0.000000000000000000 ) ) ;
#74281 = DIRECTION ( 'NONE',  ( -0.000000000000000000, -1.000000000000000000, -4.283267841918042741E-17 ) ) ;
#74283 = CARTESIAN_POINT ( 'NONE',  ( -5.676582343750006032, 64.11458332991935549, 9.832129032723418760 ) ) ;
#74282 = CARTESIAN_POINT ( 'NONE',  ( -7.188101187500000933, 91.06250000204838102, -2.977408999572650483 ) ) ;
#74284 = CARTESIAN_POINT ( 'NONE',  ( -7.999999999999989342, -3.313708498984762496, 5.424052779823364645 ) ) ;
#74285 = CARTESIAN_POINT ( 'NONE',  ( -2.679491924311235174, 15.41666665983869855, 10.00000000000000000 ) ) ;
#74286 = CARTESIAN_POINT ( 'NONE',  ( -2.085542519210945728E-15, 169.5312499965860411, 11.35316468750000141 ) ) ;
#74287 = CARTESIAN_POINT ( 'NONE',  ( -8.660254037844387298, 138.9583333265053682, -5.000000000000004441 ) ) ;
#74288 = CARTESIAN_POINT ( 'NONE',  ( 5.082755093536326818, 104.0937500020483810, 5.082755093536325042 ) ) ;
#74289 = FACE_OUTER_BOUND ( 'NONE', #53151, .T. ) ;
#74290 = CARTESIAN_POINT ( 'NONE',  ( -2.085542519210945728E-15, 29.84374999658601624, 11.35316468750000141 ) ) ;
#74291 =( BOUNDED_CURVE ( )  B_SPLINE_CURVE ( 2, ( #6844, #70225, #1924, #6110, #12854, #29858, #24183, #46827, #24912 ),
 .UNSPECIFIED., .F., .F. ) 
 B_SPLINE_CURVE_WITH_KNOTS ( ( 3, 2, 2, 2, 3 ),
 ( 0.1000000000000000888, 0.1083333333333334203, 0.1166666666666667657, 0.1250000000000001110, 0.1333333333333334425 ),
 .UNSPECIFIED. ) 
 CURVE ( )  GEOMETRIC_REPRESENTATION_ITEM ( )  RATIONAL_B_SPLINE_CURVE ( ( 0.9999999999999992228, 0.9238795325112875156, 1.000000000000000000, 0.9238795325112867385, 1.000000000000000000, 0.9238795325112867385, 1.000000000000000000, 0.9238795325112857393, 1.000000000000001110 ) ) 
 REPRESENTATION_ITEM ( '' )  );
#74292 = CARTESIAN_POINT ( 'NONE',  ( -4.999999999999998224, 78.54166665983871098, -8.660254037844389075 ) ) ;
#74293 = CARTESIAN_POINT ( 'NONE',  ( -8.311093377946841443, 188.9062499965859843, 8.311093377946830785 ) ) ;
#74294 = ORIENTED_EDGE ( 'NONE', *, *, #14339, .T. ) ;
#74296 =( BOUNDED_CURVE ( )  B_SPLINE_CURVE ( 2, ( #64141, #35481, #1531, #59230, #64515, #30549, #12813, #42597, #58495 ),
 .UNSPECIFIED., .F., .F. ) 
 B_SPLINE_CURVE_WITH_KNOTS ( ( 3, 2, 2, 2, 3 ),
 ( 0.4000000000000003553, 0.4083333333333336590, 0.4166666666666670182, 0.4250000000000003220, 0.4333333333333336812 ),
 .UNSPECIFIED. ) 
 CURVE ( )  GEOMETRIC_REPRESENTATION_ITEM ( )  RATIONAL_B_SPLINE_CURVE ( ( 0.9999999999999970024, 0.9238795325112897361, 1.000000000000000000, 0.9238795325112867385, 1.000000000000000000, 0.9238795325112867385, 1.000000000000000000, 0.9238795325112837409, 1.000000000000003109 ) ) 
 REPRESENTATION_ITEM ( '' )  );
#74295 = LINE ( 'NONE', #33587, #11513 ) ;
#74297 = CARTESIAN_POINT ( 'NONE',  ( 7.204075437095966983, 7.204075437095967871, 71.59375000204836681 ) ) ;
#74298 = CARTESIAN_POINT ( 'NONE',  ( -1.656854249492347719, 197.8125000000000284, 194.0000000000000853 ) ) ;
#74299 = CARTESIAN_POINT ( 'NONE',  ( 34.01603568117359799, 40.46826179288290604, 65.00000000000000000 ) ) ;
#74301 = CARTESIAN_POINT ( 'NONE',  ( -3.042071309553173730, 164.3229166632526699, 11.35316468749999785 ) ) ;
#74300 = CARTESIAN_POINT ( 'NONE',  ( -1.280032823142438270, 194.9537783487152751, 194.2501672614167205 ) ) ;
#74302 = CARTESIAN_POINT ( 'NONE',  ( -5.656854249492373476, -5.656854249492376141, 4.074052784329823318 ) ) ;
#74303 = CARTESIAN_POINT ( 'NONE',  ( 8.000000000000000000, 9.000000000000001776, 0.000000000000000000 ) ) ;
#74304 = ADVANCED_FACE ( 'NONE', ( #34153 ), #939, .T. ) ;
#74305 = ADVANCED_FACE ( 'NONE', ( #23921 ), #46930, .T. ) ;
#74306 = CARTESIAN_POINT ( 'NONE',  ( 8.660254037844385522, 261.0416666734946602, -5.000000000000003553 ) ) ;
#74307 = CARTESIAN_POINT ( 'NONE',  ( -31.99999999999998579, 206.3124999999999716, 171.6568542494928238 ) ) ;
#74308 = PRODUCT_DEFINITION_FORMATION_WITH_SPECIFIED_SOURCE ( 'ANY', '', #51772, .NOT_KNOWN. ) ;
#74309 = EDGE_LOOP ( 'NONE', ( #20540, #69794, #54957, #686 ) ) ;
#74310 = CARTESIAN_POINT ( 'NONE',  ( -3.999999999999960032, 204.0625000027312410, 196.3431457505076594 ) ) ;
#74311 = CARTESIAN_POINT ( 'NONE',  ( -8.311093377946841443, 119.2187499965860127, 8.311093377946830785 ) ) ;
#74312 = CARTESIAN_POINT ( 'NONE',  ( -2.976196775178717946, -8.673996836102558561, -0.07661102881318875013 ) ) ;
#74313 = ORIENTED_EDGE ( 'NONE', *, *, #4382, .F. ) ;
#74314 = CARTESIAN_POINT ( 'NONE',  ( -4.541265875000002339, 7.937499998634407028, -5.561446717895856393E-16 ) ) ;
#74315 = CARTESIAN_POINT ( 'NONE',  ( 2.977408999572650927, 15.74999999795161543, -7.188101187500001821 ) ) ;
#74316 = EDGE_CURVE ( 'NONE', #60284, #18004, #73980, .T. ) ;
#74317 = CARTESIAN_POINT ( 'NONE',  ( 5.656854249492381470, 109.2500000040967763, 5.656854249492379694 ) ) ;
#74318 = AXIS2_PLACEMENT_3D ( 'NONE', #18822, #47479, #70503 ) ;
#74319 = CARTESIAN_POINT ( 'NONE',  ( -24.54126587500000056, 199.5000000013656063, 168.5673454167827003 ) ) ;
#74320 = CARTESIAN_POINT ( 'NONE',  ( -2.828427124746190735, 6.375000000000000888, -2.828427124746191623 ) ) ;
#74321 = CARTESIAN_POINT ( 'NONE',  ( -3.999999999999959144, 198.0625000000000284, 199.6568542494924259 ) ) ;
#74322 = CARTESIAN_POINT ( 'NONE',  ( 2.780723358947928197E-16, 7.562499998634407028, -4.541265875000002339 ) ) ;
#74323 = CARTESIAN_POINT ( 'NONE',  ( -4.000000000000015987, 199.5000000000000000, 142.0000000000000568 ) ) ;
#74324 = VERTEX_POINT ( 'NONE', #7685 ) ;
#74325 = CARTESIAN_POINT ( 'NONE',  ( 7.320508075688776373, 221.8750000000000284, 7.320508075688767491 ) ) ;
#74326 = CARTESIAN_POINT ( 'NONE',  ( 5.082755093536326818, 106.7187500020483952, 5.082755093536325042 ) ) ;
#74328 = CARTESIAN_POINT ( 'NONE',  ( 7.999999999999991118, 0.000000000000000000, 30.00000000000000000 ) ) ;
#74327 = CARTESIAN_POINT ( 'NONE',  ( -27.99999999999991473, 194.9375000013655779, 173.4587341250003760 ) ) ;
#74329 = CARTESIAN_POINT ( 'NONE',  ( -7.347880794884122694E-16, 10.75000000000000000, 4.000000000000001776 ) ) ;
#74330 = ORIENTED_EDGE ( 'NONE', *, *, #4986, .T. ) ;
#74331 = VERTEX_POINT ( 'NONE', #59012 ) ;
#74332 = CARTESIAN_POINT ( 'NONE',  ( -4.220049686691937474, -10.18810118749999738, 90.43750000204838102 ) ) ;
#74333 = CARTESIAN_POINT ( 'NONE',  ( -5.656854249492375253, 5.656854249492375253, 20.14280277982336642 ) ) ;
#74334 = CARTESIAN_POINT ( 'NONE',  ( -24.54126587499998280, 201.3750000013656347, 171.4326545832179818 ) ) ;
#74335 = CARTESIAN_POINT ( 'NONE',  ( -6.735557395310442023E-16, 11.00000000000000000, 107.1250000000000000 ) ) ;
#74337 = CARTESIAN_POINT ( 'NONE',  ( 2.839093476692135984E-14, 203.9375000013656063, 201.4587341250000350 ) ) ;
#74336 = VECTOR ( 'NONE', #44221, 1000.000000000000000 ) ;
#74339 = CARTESIAN_POINT ( 'NONE',  ( 7.778174593052021635, 7.778174593052023411, 113.1250000040967763 ) ) ;
#74338 = CARTESIAN_POINT ( 'NONE',  ( -4.242640687119286547, 289.9375000034140157, -4.242640687119286547 ) ) ;
#74340 = CARTESIAN_POINT ( 'NONE',  ( 10.00000000000000178, 120.2083333333333570, -2.679491924311226736 ) ) ;
#74341 = CARTESIAN_POINT ( 'NONE',  ( -8.000000000000000000, 108.4062500000000000, -3.313708498984761608 ) ) ;
#74342 = CARTESIAN_POINT ( 'NONE',  ( -4.721056650415998313, 289.7343750017069510, 4.721056650416000089 ) ) ;
#74343 = CARTESIAN_POINT ( 'NONE',  ( 7.188101187499991163, 2.977408999572648707, 5.705302781871753659 ) ) ;
#74344 = CARTESIAN_POINT ( 'NONE',  ( 2.849036369511732440E-14, 200.2500000000000000, 202.0000000000000000 ) ) ;
#74345 = CARTESIAN_POINT ( 'NONE',  ( 29.43265458321766559, 205.8750000013656063, 166.5412658749999650 ) ) ;
#74346 = CARTESIAN_POINT ( 'NONE',  ( -8.000000000000000000, 27.46874999590322730, -3.313708498984762496 ) ) ;
#74347 = CARTESIAN_POINT ( 'NONE',  ( 1.432654583217607192, 198.2500000013656347, 145.4587341250000634 ) ) ;
#74348 = CARTESIAN_POINT ( 'NONE',  ( 2.977408999572650039, 121.0625000020483810, -7.188101187500000933 ) ) ;
#74350 = CARTESIAN_POINT ( 'NONE',  ( 3.373160349817477144, 194.8118071516788916, 196.2078005529305926 ) ) ;
#74349 = CARTESIAN_POINT ( 'NONE',  ( -2.828427124746208943, 204.6250000000000284, 144.8284271247462129 ) ) ;
#74351 = CARTESIAN_POINT ( 'NONE',  ( 3.042071309553163960, 247.7604166700806161, -11.35316468749999785 ) ) ;
#74352 = CARTESIAN_POINT ( 'NONE',  ( -7.188101187499992051, 0.000000000000000000, 27.36155278187175455 ) ) ;
#74353 = CARTESIAN_POINT ( 'NONE',  ( 29.65685424949235482, 200.0625000000000568, 173.9999999999999147 ) ) ;
#74354 = CARTESIAN_POINT ( 'NONE',  ( 5.676582343750001591, 11.61458332991935016, -9.832129032723420536 ) ) ;
#74355 = CARTESIAN_POINT ( 'NONE',  ( 11.35316468750000141, 1.093749996586016682, 0.000000000000000000 ) ) ;
#74356 = CARTESIAN_POINT ( 'NONE',  ( 5.676582343750001591, 201.9270833299193555, -9.832129032723420536 ) ) ;
#74357 = CARTESIAN_POINT ( 'NONE',  ( -23.99999999999998579, 195.7500000000000000, 170.0000000000003411 ) ) ;
#74358 = CYLINDRICAL_SURFACE ( 'NONE', #40374, 10.00000000000000178 ) ;
#74360 = DIRECTION ( 'NONE',  ( 0.000000000000000000, 0.000000000000000000, 1.000000000000000000 ) ) ;
#74359 = CARTESIAN_POINT ( 'NONE',  ( -11.00000000000000000, 11.00000000000000000, 25.00000000000000000 ) ) ;
#74361 = ORIENTED_EDGE ( 'NONE', *, *, #32233, .T. ) ;
#74362 = ADVANCED_FACE ( 'NONE', ( #36359 ), #70681, .T. ) ;
#74363 = CARTESIAN_POINT ( 'NONE',  ( -2.839093476692135984E-14, 200.9375000013656063, 138.5412658750000503 ) ) ;
#74364 = CARTESIAN_POINT ( 'NONE',  ( 3.042071309553167069, 26.82291666325268054, -11.35316468749999785 ) ) ;
#74365 = CARTESIAN_POINT ( 'NONE',  ( -10.99999999999999822, -4.556349186104052151, 89.78125000409679046 ) ) ;
#74366 = CARTESIAN_POINT ( 'NONE',  ( 5.000000000000002665, 210.8333333333333428, -8.660254037844389075 ) ) ;
#74367 = CARTESIAN_POINT ( 'NONE',  ( -25.55430564589111953, 199.0625000013656063, 172.4456943541091505 ) ) ;
#74368 = CARTESIAN_POINT ( 'NONE',  ( 0.4499999999999998446, 283.9999999999998863, 5.815332135057944107 ) ) ;
#74370 = CARTESIAN_POINT ( 'NONE',  ( -9.832129032723420536, 8.697916663252684089, 5.676582343749997150 ) ) ;
#74369 = CARTESIAN_POINT ( 'NONE',  ( -7.188101187500000933, 112.0625000020483810, -2.977408999572650483 ) ) ;
#74371 = CARTESIAN_POINT ( 'NONE',  ( -5.656854249492373476, -5.656854249492376141, 20.51780277982336642 ) ) ;
#74372 = CARTESIAN_POINT ( 'NONE',  ( 5.676582343749993598, 134.9479166632526983, 9.832129032723422313 ) ) ;
#74373 = AXIS2_PLACEMENT_3D ( 'NONE', #60147, #14485, #19782 ) ;
#74374 = CARTESIAN_POINT ( 'NONE',  ( -8.660254037844387298, 108.9583333265053682, -5.000000000000004441 ) ) ;
#74375 = CARTESIAN_POINT ( 'NONE',  ( 5.082755093536326818, 123.5937500020483952, 5.082755093536325042 ) ) ;
#74376 = CARTESIAN_POINT ( 'NONE',  ( -10.00000000000000178, 4.374999993172032475, -1.224646799147353454E-15 ) ) ;
#74377 = CARTESIAN_POINT ( 'NONE',  ( 7.778174593052021635, 7.778174593052023411, 102.6250000040967763 ) ) ;
#74378 = CARTESIAN_POINT ( 'NONE',  ( -5.000000000000000000, -53.53174224766578959, -46.57871628774400108 ) ) ;
#74379 = ORIENTED_EDGE ( 'NONE', *, *, #46194, .F. ) ;
#74380 = CARTESIAN_POINT ( 'NONE',  ( -10.00000000000000711, 117.5000000000000142, -1.224646799147354045E-15 ) ) ;
#74381 = CARTESIAN_POINT ( 'NONE',  ( -54.00000000000000711, 37.00000000000000000, 0.000000000000000000 ) ) ;
#74382 = CARTESIAN_POINT ( 'NONE',  ( -4.088227598258586603E-16, 296.2031250017070079, -6.676582343750001591 ) ) ;
#74383 = CARTESIAN_POINT ( 'NONE',  ( 9.832129032723416984, 120.3645833299193697, 5.676582343750006032 ) ) ;
#74384 = CARTESIAN_POINT ( 'NONE',  ( -1.656854249492407449, 207.4375000027312126, 138.0000000000000284 ) ) ;
#74385 = CARTESIAN_POINT ( 'NONE',  ( 5.656854249492374365, 5.656854249492375253, 24.32405278432982598 ) ) ;
#74386 =( BOUNDED_CURVE ( )  B_SPLINE_CURVE ( 2, ( #1361, #25444, #19417, #47356, #18696, #7377, #65814, #19790, #31114 ),
 .UNSPECIFIED., .F., .T. ) 
 B_SPLINE_CURVE_WITH_KNOTS ( ( 3, 2, 2, 2, 3 ),
 ( 0.4833333333333338366, 0.4916666666666670849, 0.5000000000000004441, 0.5083333333333336368, 0.5166666666666670515 ),
 .UNSPECIFIED. ) 
 CURVE ( )  GEOMETRIC_REPRESENTATION_ITEM ( )  RATIONAL_B_SPLINE_CURVE ( ( 0.9999999999999954481, 0.9238795325112912904, 1.000000000000000000, 0.9238795325112867385, 1.000000000000000000, 0.9238795325112867385, 1.000000000000000000, 0.9238795325112837409, 1.000000000000003109 ) ) 
 REPRESENTATION_ITEM ( '' )  );
#74387 = CARTESIAN_POINT ( 'NONE',  ( 9.999999999999998224, 225.8333333401612606, -2.679491924311229401 ) ) ;
#74388 = EDGE_CURVE ( 'NONE', #20958, #15222, #71795, .T. ) ;
#74389 = CARTESIAN_POINT ( 'NONE',  ( 11.35316468749999963, 261.4062500034140157, -1.390361679473963556E-15 ) ) ;
#74390 = CARTESIAN_POINT ( 'NONE',  ( 7.204075437095968759, -7.204075437095966983, 97.09375000204836681 ) ) ;
#74391 = ORIENTED_EDGE ( 'NONE', *, *, #5493, .F. ) ;
#74392 =( BOUNDED_CURVE ( )  B_SPLINE_CURVE ( 2, ( #60865, #26148, #4283, #3918, #66151, #9187, #49549, #61988, #32208 ),
 .UNSPECIFIED., .F., .F. ) 
 B_SPLINE_CURVE_WITH_KNOTS ( ( 3, 2, 2, 2, 3 ),
 ( 0.6022727272727272929, 0.6079545454545454142, 0.6136363636363636465, 0.6193181818181817677, 0.6250000000000000000 ),
 .UNSPECIFIED. ) 
 CURVE ( )  GEOMETRIC_REPRESENTATION_ITEM ( )  RATIONAL_B_SPLINE_CURVE ( ( 1.000000000000000000, 0.9238795325112867385, 1.000000000000000000, 0.9238795325112867385, 1.000000000000000000, 0.9238795325112867385, 1.000000000000000000, 0.9238795325112867385, 1.000000000000000000 ) ) 
 REPRESENTATION_ITEM ( '' )  );
#74393 = ADVANCED_FACE ( 'NONE', ( #59374 ), #37095, .F. ) ;
#74394 = DIRECTION ( 'NONE',  ( 0.000000000000000000, -1.000000000000000000, 0.000000000000000000 ) ) ;
#74395 = SURFACE_STYLE_FILL_AREA ( #51382 ) ;
#74396 = CARTESIAN_POINT ( 'NONE',  ( 2.839093476692135984E-14, 202.9375000013656063, 201.4587341250000350 ) ) ;
#74397 = CARTESIAN_POINT ( 'NONE',  ( -5.676582343750006032, 74.42708332991934128, 9.832129032723418760 ) ) ;
#74398 = ORIENTED_EDGE ( 'NONE', *, *, #67611, .F. ) ;
#74399 = CARTESIAN_POINT ( 'NONE',  ( 4.220049686691941027, -10.18810118749999738, 110.1250000020483810 ) ) ;
#74400 = CARTESIAN_POINT ( 'NONE',  ( -4.541265875000002339, 12.87499999863440969, -1.881053915767121998 ) ) ;
#74401 = ORIENTED_EDGE ( 'NONE', *, *, #35254, .T. ) ;
#74402 = AXIS2_PLACEMENT_3D ( 'NONE', #42711, #65723, #66472 ) ;
#74403 = CARTESIAN_POINT ( 'NONE',  ( -5.082755093536326818, 26.90624999795161543, 5.082755093536325042 ) ) ;
#74404 = CARTESIAN_POINT ( 'NONE',  ( 10.00000000000000178, 115.0000000000000284, 0.000000000000000000 ) ) ;
#74405 = CARTESIAN_POINT ( 'NONE',  ( -21.78045554270713424, -37.99999999999992184, 147.9407217626652198 ) ) ;
#74406 = CARTESIAN_POINT ( 'NONE',  ( -7.188101187500002709, 21.18749999795161187, 2.977408999572649151 ) ) ;
#74407 = ADVANCED_FACE ( 'NONE', ( #54080 ), #18998, .T. ) ;
#74408 = CARTESIAN_POINT ( 'NONE',  ( 1.656854249492416109, 200.1875000000000284, 138.0000000000000853 ) ) ;
#74409 =( BOUNDED_CURVE ( )  B_SPLINE_CURVE ( 2, ( #71576, #21021, #66301, #32361, #3681, #72717, #44045, #5177, #22131 ),
 .UNSPECIFIED., .F., .F. ) 
 B_SPLINE_CURVE_WITH_KNOTS ( ( 3, 2, 2, 2, 3 ),
 ( 0.2205882352941175295, 0.2242647058823528383, 0.2279411764705881194, 0.2316176470588234282, 0.2352941176470587092 ),
 .UNSPECIFIED. ) 
 CURVE ( )  GEOMETRIC_REPRESENTATION_ITEM ( )  RATIONAL_B_SPLINE_CURVE ( ( 1.000000000000002220, 0.9238795325112844070, 1.000000000000000000, 0.9238795325112867385, 1.000000000000000000, 0.9238795325112867385, 1.000000000000000000, 0.9238795325112890700, 0.9999999999999976685 ) ) 
 REPRESENTATION_ITEM ( '' )  );
#74410 = CARTESIAN_POINT ( 'NONE',  ( 4.220049686691934809, 10.18810118749999916, 103.5625000020483668 ) ) ;
#74411 = CARTESIAN_POINT ( 'NONE',  ( 2.751064625579944321E-14, 204.7500000000000284, 194.0000000000000568 ) ) ;
#74412 = CARTESIAN_POINT ( 'NONE',  ( -4.000000000000001776, 10.24999999726881406, -4.898587196589415787E-16 ) ) ;
#74413 = CARTESIAN_POINT ( 'NONE',  ( 4.000000000000001776, 18.00000000000000355, 0.000000000000000000 ) ) ;
#74414 = ORIENTED_EDGE ( 'NONE', *, *, #31650, .T. ) ;
#74415 = CARTESIAN_POINT ( 'NONE',  ( 2.751064625579944321E-14, 197.7500000000000000, 194.0000000000000568 ) ) ;
#74416 = CARTESIAN_POINT ( 'NONE',  ( 3.458734125000015425, 204.0000000013656347, 196.5673454167823877 ) ) ;
#74417 = CARTESIAN_POINT ( 'NONE',  ( -29.43265458321771533, 206.5000000013655779, 166.5412658750003914 ) ) ;
#74418 = AXIS2_PLACEMENT_3D ( 'NONE', #17013, #22295, #61563 ) ;
#74419 = CARTESIAN_POINT ( 'NONE',  ( -4.541265875000002339, 9.749999998634406140, -1.881053915767121998 ) ) ;
#74420 = EDGE_CURVE ( 'NONE', #47940, #13756, #28153, .T. ) ;
#74422 = CARTESIAN_POINT ( 'NONE',  ( 2.449293598294707893E-16, 17.99999999726881583, -4.000000000000001776 ) ) ;
#74421 =( BOUNDED_CURVE ( )  B_SPLINE_CURVE ( 2, ( #50828, #51570, #67068, #27072, #16107, #74212, #39519, #15367, #16482 ),
 .UNSPECIFIED., .F., .F. ) 
 B_SPLINE_CURVE_WITH_KNOTS ( ( 3, 2, 2, 2, 3 ),
 ( 0.02631578947368422988, 0.03289473684210528909, 0.03947368421052634135, 0.04605263157894740056, 0.05263157894736845976 ),
 .UNSPECIFIED. ) 
 CURVE ( )  GEOMETRIC_REPRESENTATION_ITEM ( )  RATIONAL_B_SPLINE_CURVE ( ( 0.9999999999999997780, 0.9238795325112869605, 1.000000000000000000, 0.9238795325112867385, 1.000000000000000000, 0.9238795325112867385, 1.000000000000000000, 0.9238795325112862944, 1.000000000000000444 ) ) 
 REPRESENTATION_ITEM ( '' )  );
#74423 = CARTESIAN_POINT ( 'NONE',  ( 7.188101187499993827, -2.977408999572645598, 18.64280278187175810 ) ) ;
#74424 = VERTEX_POINT ( 'NONE', #13686 ) ;
#74425 = CARTESIAN_POINT ( 'NONE',  ( -2.485281374238895502, 291.8125000000000568, -5.999999999999677591 ) ) ;
#74426 = ORIENTED_EDGE ( 'NONE', *, *, #61527, .T. ) ;
#74427 = CARTESIAN_POINT ( 'NONE',  ( -7.204075437095965206, -7.204075437095968759, 109.8437500020483810 ) ) ;
#74428 = CARTESIAN_POINT ( 'NONE',  ( 6.123233995736767268E-16, 118.1249999931720396, -10.00000000000000178 ) ) ;
#74429 = CARTESIAN_POINT ( 'NONE',  ( 1.432654583217662481, 199.1250000013656347, 194.5412658750000219 ) ) ;
#74430 = CARTESIAN_POINT ( 'NONE',  ( 26.56734541678237349, 195.3750000013656063, 173.4587341249998929 ) ) ;
#74431 = CARTESIAN_POINT ( 'NONE',  ( 5.000000000000001776, 75.83333333333334281, -8.660254037844389075 ) ) ;
#74432 = CARTESIAN_POINT ( 'NONE',  ( 7.188101187500000044, 90.78125000204838102, -8.802885111219163269E-16 ) ) ;
#74433 = CARTESIAN_POINT ( 'NONE',  ( 1.102182119232618108E-15, 288.2500000000000000, 6.000000000000001776 ) ) ;
#74434 = ORIENTED_EDGE ( 'NONE', *, *, #40791, .T. ) ;
#74435 = CARTESIAN_POINT ( 'NONE',  ( 2.679491924311117934, 253.5416666666666572, -10.00000000000006217 ) ) ;
#74436 = CARTESIAN_POINT ( 'NONE',  ( 1.780377099653073225, -16.42166210098330481, 68.70754022607324885 ) ) ;
#74437 = CARTESIAN_POINT ( 'NONE',  ( 1.656854249492348607, 195.3125000027311842, 138.0000000000000568 ) ) ;
#74438 = CARTESIAN_POINT ( 'NONE',  ( 10.00000000000000178, 56.87499999317203248, 0.000000000000000000 ) ) ;
#74439 = CARTESIAN_POINT ( 'NONE',  ( 7.999999999999998224, 5.718749995903220196, 3.313708498984766049 ) ) ;
#74440 = CARTESIAN_POINT ( 'NONE',  ( 9.999999999999998224, 237.7083333333333144, -2.679491924311229401 ) ) ;
#74441 = LINE ( 'NONE', #6164, #43902 ) ;
#74442 = CARTESIAN_POINT ( 'NONE',  ( 2.679491924311228956, 201.0416666666666572, -10.00000000000000000 ) ) ;
#74443 = CARTESIAN_POINT ( 'NONE',  ( -5.082755093536319713, 5.082755093536319713, 18.17405278187175455 ) ) ;
#74444 = CARTESIAN_POINT ( 'NONE',  ( 5.676582343750001591, 171.9270833299193555, -9.832129032723420536 ) ) ;
#74445 = CARTESIAN_POINT ( 'NONE',  ( -8.660254037844385522, 37.08333333333332860, -5.000000000000002665 ) ) ;
#74447 = DIRECTION ( 'NONE',  ( 0.000000000000000000, 0.000000000000000000, -1.000000000000000000 ) ) ;
#74446 = PRESENTATION_STYLE_ASSIGNMENT (( #16715 ) ) ;
#74448 = ORIENTED_EDGE ( 'NONE', *, *, #41660, .T. ) ;
#74449 = CARTESIAN_POINT ( 'NONE',  ( -1.432654583217662481, 199.1250000013656347, 145.4587341250000634 ) ) ;
#74450 = CARTESIAN_POINT ( 'NONE',  ( 11.35316468749999963, 41.30208332991936260, -3.042071309553165293 ) ) ;
#74451 = CARTESIAN_POINT ( 'NONE',  ( -7.778174593052023411, 7.778174593052023411, 113.5000000040967763 ) ) ;
#74452 = CARTESIAN_POINT ( 'NONE',  ( -31.45873412500002786, 207.6250000013656063, 168.5673454167828140 ) ) ;
#74453 = CIRCLE ( 'NONE', #34737, 17.50000000000000000 ) ;
#74454 = CARTESIAN_POINT ( 'NONE',  ( 0.000000000000000000, 125.0000000000000000, 0.000000000000000000 ) ) ;
#74456 = CARTESIAN_POINT ( 'NONE',  ( -3.373128826976392602, 10.27267468567300135, -63.92035228378879452 ) ) ;
#74455 = CARTESIAN_POINT ( 'NONE',  ( -5.009999999999998899, 6.135480463728238062E-16, -0.6932054628276118624 ) ) ;
#74457 = DIRECTION ( 'NONE',  ( 0.000000000000000000, 1.000000000000000000, 0.000000000000000000 ) ) ;
#74458 = CARTESIAN_POINT ( 'NONE',  ( 1.432654583217607192, 198.2500000013656347, 145.4587341250000350 ) ) ;
#74459 = CARTESIAN_POINT ( 'NONE',  ( -2.679491924311225848, 68.33333332650535397, -10.00000000000000178 ) ) ;
#74460 = CARTESIAN_POINT ( 'NONE',  ( 2.977408999572650039, 105.6875000020483952, -7.188101187500001821 ) ) ;
#74461 = CARTESIAN_POINT ( 'NONE',  ( -4.541265875000002339, 10.93749999863440792, -5.561446717895856393E-16 ) ) ;
#74462 = CARTESIAN_POINT ( 'NONE',  ( -6.676582343750001591, 299.6093750017069510, 0.000000000000000000 ) ) ;
#74463 = CARTESIAN_POINT ( 'NONE',  ( 7.999999999999992895, -3.313708498984756279, 2.986552779823361981 ) ) ;
#74464 = CARTESIAN_POINT ( 'NONE',  ( -1.688721909672337596, -49.97488762307366272, 40.72268565194266188 ) ) ;
#74465 = VERTEX_POINT ( 'NONE', #65013 ) ;
#74466 = ORIENTED_EDGE ( 'NONE', *, *, #54048, .F. ) ;
#74467 = EDGE_CURVE ( 'NONE', #42139, #6656, #11571, .T. ) ;
#74468 = CARTESIAN_POINT ( 'NONE',  ( 1.522769729196201526E-11, 196.2499999999988063, -10.00000000000000178 ) ) ;
#74469 = PLANE ( 'NONE',  #54389 ) ;
#74470 = LINE ( 'NONE', #16739, #14627 ) ;
#74471 = CARTESIAN_POINT ( 'NONE',  ( -6.362988438888832046E-13, 88.74999999999995737, 9.999999999999998224 ) ) ;
#74472 = CARTESIAN_POINT ( 'NONE',  ( 11.35316468749999963, 140.9895833299193555, -3.042071309553165293 ) ) ;
#74473 = CARTESIAN_POINT ( 'NONE',  ( 4.999999999999986677, 104.1666666666666714, 8.660254037844380193 ) ) ;
#74474 = CARTESIAN_POINT ( 'NONE',  ( -6.238412754330611322E-16, 10.18810118749999916, 85.28125000204836681 ) ) ;
#74475 = CARTESIAN_POINT ( 'NONE',  ( -29.96114510722389568, 194.5054840307574011, 167.0857336714470875 ) ) ;
#74476 = VECTOR ( 'NONE', #37052, 1000.000000000000000 ) ;
#74477 = CARTESIAN_POINT ( 'NONE',  ( 1.656854249492405451, 204.3125000000000000, 202.0000000000000284 ) ) ;
#74478 = CARTESIAN_POINT ( 'NONE',  ( 10.00000000000000000, 247.5000000000000000, -1.224646799147353256E-15 ) ) ;
#74479 = CARTESIAN_POINT ( 'NONE',  ( -7.778174593052023411, 7.778174593052023411, 113.3125000000000000 ) ) ;
#74480 = CARTESIAN_POINT ( 'NONE',  ( 10.18810118750000093, -4.220049686691933921, 113.6875000020483952 ) ) ;
#74481 = EDGE_LOOP ( 'NONE', ( #65298, #16296, #47099, #33264 ) ) ;
#74482=STYLED_ITEM('',(#74706),#41611);
#74483 = EDGE_CURVE ( 'NONE', #67450, #54990, #17576, .T. ) ;
#74484 = CARTESIAN_POINT ( 'NONE',  ( 29.23829287408465660, 176.8253085577695742, 148.2017496308051534 ) ) ;
#74485 = CARTESIAN_POINT ( 'NONE',  ( 9.832129032723420536, 126.5104166632526841, -5.676582343749999815 ) ) ;
#74486 = CARTESIAN_POINT ( 'NONE',  ( 3.458734125000016313, 202.8750000013656063, 199.4326545832176976 ) ) ;
#74487 = CARTESIAN_POINT ( 'NONE',  ( 5.082755093536325930, 26.53124999795161543, -5.082755093536325930 ) ) ;
#74488 = CARTESIAN_POINT ( 'NONE',  ( 4.220049686691941027, -10.18810118749999738, 77.50000000204839523 ) ) ;
#74489 = CARTESIAN_POINT ( 'NONE',  ( -5.676582343749998039, 42.76041666325268409, -9.832129032723420536 ) ) ;
#74490 = ORIENTED_EDGE ( 'NONE', *, *, #60667, .T. ) ;
#74491 = CARTESIAN_POINT ( 'NONE',  ( -10.00000000000000178, 194.3749999931720254, -1.224646799147353454E-15 ) ) ;
#74492 = CARTESIAN_POINT ( 'NONE',  ( -8.008118988124991233, 3.317071493978878127, 21.91936528394063188 ) ) ;
#74493 = CARTESIAN_POINT ( 'NONE',  ( 3.458734124999959469, 206.7500000013655779, 140.5673454167824161 ) ) ;
#74494 = CARTESIAN_POINT ( 'NONE',  ( -7.188101187500001821, 11.62499999795161187, -2.977408999572651371 ) ) ;
#74495 = CARTESIAN_POINT ( 'NONE',  ( -2.485281374238571761, 297.8750000034139589, -6.000000000000003553 ) ) ;
#74496 = CARTESIAN_POINT ( 'NONE',  ( -10.99999999999992184, -31.99999999998497202, 140.5079502042485728 ) ) ;
#74497 = CARTESIAN_POINT ( 'NONE',  ( 2.977408999572651815, 3.562499997951610542, 7.188101187500000933 ) ) ;
#74498 = CARTESIAN_POINT ( 'NONE',  ( 11.35316468749999963, 151.3020833299193555, -3.042071309553165293 ) ) ;
#74499 = CARTESIAN_POINT ( 'NONE',  ( -7.204075437095967871, 7.204075437095967871, 79.46875000204836681 ) ) ;
#74500 = ADVANCED_FACE ( 'NONE', ( #2766 ), #12783, .T. ) ;
#74501 =( BOUNDED_CURVE ( )  B_SPLINE_CURVE ( 2, ( #45413, #17492, #12200, #5816, #35238, #57126, #175, #47637, #65367 ),
 .UNSPECIFIED., .F., .F. ) 
 B_SPLINE_CURVE_WITH_KNOTS ( ( 3, 2, 2, 2, 3 ),
 ( 0.1666666666666668239, 0.1750000000000001554, 0.1833333333333334869, 0.1916666666666668462, 0.2000000000000001776 ),
 .UNSPECIFIED. ) 
 CURVE ( )  GEOMETRIC_REPRESENTATION_ITEM ( )  RATIONAL_B_SPLINE_CURVE ( ( 0.9999999999999984457, 0.9238795325112882928, 1.000000000000000000, 0.9238795325112867385, 1.000000000000000000, 0.9238795325112867385, 1.000000000000000000, 0.9238795325112851842, 1.000000000000001554 ) ) 
 REPRESENTATION_ITEM ( '' )  );
#74502 = CARTESIAN_POINT ( 'NONE',  ( -26.56734541678232375, 197.0000000013656347, 173.4587341250003760 ) ) ;
#74503 = EDGE_CURVE ( 'NONE', #48595, #39861, #53727, .T. ) ;
#74504 = CARTESIAN_POINT ( 'NONE',  ( 0.000000000000000000, -45.00000000000001421, 201.0010000000000048 ) ) ;
#74505 = CARTESIAN_POINT ( 'NONE',  ( -4.541265875000003227, 21.99999999863440792, 1.881053915767121110 ) ) ;
#74506 = ORIENTED_EDGE ( 'NONE', *, *, #23362, .F. ) ;
#74507 = CARTESIAN_POINT ( 'NONE',  ( -3.999999999999960032, 201.1250000027312126, 198.0000000000000284 ) ) ;
#74508 = CARTESIAN_POINT ( 'NONE',  ( 3.999999999999959144, 206.0625000000000000, 140.3431457505076594 ) ) ;
#74509 = CARTESIAN_POINT ( 'NONE',  ( -23.99999999999998934, 201.8750000027312126, 170.0000000000002842 ) ) ;
#74510 = AXIS2_PLACEMENT_3D ( 'NONE', #27799, #51185, #74193 ) ;
#74511 = CARTESIAN_POINT ( 'NONE',  ( 4.999999999999997335, 251.4583333401613174, -8.660254037844387298 ) ) ;
#74512 = CARTESIAN_POINT ( 'NONE',  ( -3.313708498984758943, -7.999999999999989342, 7.299052783920144449 ) ) ;
#74513 = ORIENTED_EDGE ( 'NONE', *, *, #26944, .T. ) ;
#74514 = ADVANCED_FACE ( 'NONE', ( #35995 ), #14551, .T. ) ;
#74516 =( BOUNDED_CURVE ( )  B_SPLINE_CURVE ( 2, ( #52955, #20744, #60741, #20361, #15078, #49413, #70305, #38113, #24633 ),
 .UNSPECIFIED., .F., .F. ) 
 B_SPLINE_CURVE_WITH_KNOTS ( ( 3, 2, 2, 2, 3 ),
 ( 0.8500000000000005329, 0.8583333333333339477, 0.8666666666666673624, 0.8750000000000007772, 0.8833333333333341919 ),
 .UNSPECIFIED. ) 
 CURVE ( )  GEOMETRIC_REPRESENTATION_ITEM ( )  RATIONAL_B_SPLINE_CURVE ( ( 0.9999999999999948930, 0.9238795325112918455, 1.000000000000000000, 0.9238795325112867385, 1.000000000000000000, 0.9238795325112867385, 1.000000000000000000, 0.9238795325112786339, 1.000000000000008216 ) ) 
 REPRESENTATION_ITEM ( '' )  );
#74515 = CARTESIAN_POINT ( 'NONE',  ( -5.082755093536325042, 14.53124999795161187, -5.082755093536325930 ) ) ;
#74517 = CARTESIAN_POINT ( 'NONE',  ( -5.656854249492373476, -5.656854249492376141, 8.705302783920146226 ) ) ;
#74518 = DIRECTION ( 'NONE',  ( -0.000000000000000000, -1.000000000000000000, -4.283267841918042741E-17 ) ) ;
#74519 = CARTESIAN_POINT ( 'NONE',  ( -7.320508075688773708, 36.87500000000000711, -7.320508075688774596 ) ) ;
#74520 = TOROIDAL_SURFACE ( 'NONE', #43167, 68.99999999999994316, 38.00000000000000000 ) ;
#74521 = CARTESIAN_POINT ( 'NONE',  ( -7.188101187500001821, 103.4375000020483668, -2.977408999572650483 ) ) ;
#74522 = CARTESIAN_POINT ( 'NONE',  ( -25.55430564589119768, 207.5625000013656063, 167.5543056458915316 ) ) ;
#74523 = CARTESIAN_POINT ( 'NONE',  ( 2.485281374238571317, 298.6875000000000000, -6.000000000000003553 ) ) ;
#74525 = CARTESIAN_POINT ( 'NONE',  ( 7.320508075688771044, 196.2499999931720254, 7.320508075688775484 ) ) ;
#74524 = CARTESIAN_POINT ( 'NONE',  ( 5.000000000000050626, 79.16666666666674246, 8.660254037844488550 ) ) ;
#74526 = EDGE_LOOP ( 'NONE', ( #56483, #25596, #7985, #38048, #41833, #708 ) ) ;
#74527 = AXIS2_PLACEMENT_3D ( 'NONE', #58502, #25248, #52833 ) ;
#74528 = CARTESIAN_POINT ( 'NONE',  ( -8.311093377946836114, 238.2812500034140157, -8.311093377946836114 ) ) ;
#74529 = CARTESIAN_POINT ( 'NONE',  ( 7.188101187499993827, -2.977408999572645598, 17.51780278187175455 ) ) ;
#74530 = CARTESIAN_POINT ( 'NONE',  ( 0.6474643998345609441, 49.91423208894323693, 40.68959583911007627 ) ) ;
#74531 = CARTESIAN_POINT ( 'NONE',  ( 2.751064625579944321E-14, 201.7500000000000000, 194.0000000000000568 ) ) ;
#74532 = CARTESIAN_POINT ( 'NONE',  ( 24.11020845586378414, 194.9366551625568604, 170.6347482906123787 ) ) ;
#74533 = CARTESIAN_POINT ( 'NONE',  ( -2.445694354108784108, 195.5625000013656063, 195.5543056458912190 ) ) ;
#74534 = CARTESIAN_POINT ( 'NONE',  ( 10.00000000000000178, 165.2083333333333712, -2.679491924311226736 ) ) ;
#74535 = DIRECTION ( 'NONE',  ( -6.308085367188390241E-16, 0.000000000000000000, 1.000000000000000000 ) ) ;
#74536 = CARTESIAN_POINT ( 'NONE',  ( 11.00000000000010836, -4.556349186103939353, 90.15625000000000000 ) ) ;
#74537 = CARTESIAN_POINT ( 'NONE',  ( 3.999982273345623618, 89.99927424231840689, -6.928213464733947724 ) ) ;
#74538 = CARTESIAN_POINT ( 'NONE',  ( -5.676582343750006032, 134.4270833299193555, 9.832129032723418760 ) ) ;
#74539 = CARTESIAN_POINT ( 'NONE',  ( 0.000000000000000000, 2.143131898507868248E-15, 17.50000000000000000 ) ) ;
#74540 = CARTESIAN_POINT ( 'NONE',  ( 1.102182119232618108E-15, 288.3125000034140157, 6.000000000000001776 ) ) ;
#74543 = CARTESIAN_POINT ( 'NONE',  ( 2.828427124746153876, 196.8750000000000284, 144.8284271247462129 ) ) ;
#74542 = CARTESIAN_POINT ( 'NONE',  ( 28.00000000000001421, 197.4375000013655779, 173.4587341249998929 ) ) ;
#74541 = CARTESIAN_POINT ( 'NONE',  ( 31.45873412499999233, 194.9375000013655779, 169.9999999999999432 ) ) ;
#74544 = EDGE_CURVE ( 'NONE', #71897, #70823, #37213, .T. ) ;
#74545 = VERTEX_POINT ( 'NONE', #3915 ) ;
#74546 = CARTESIAN_POINT ( 'NONE',  ( -3.373128826976391270, -60.49298623944831377, 23.06377889928812763 ) ) ;
#74547 = EDGE_CURVE ( 'NONE', #28042, #11511, #18025, .T. ) ;
#74548 = CYLINDRICAL_SURFACE ( 'NONE', #39789, 12.00000000000000355 ) ;
#74549 = CARTESIAN_POINT ( 'NONE',  ( 25.17157287525377640, 195.7500000027312126, 167.1715728752537586 ) ) ;
#74550 = CARTESIAN_POINT ( 'NONE',  ( 5.000000000000000000, -60.90295814858238543, -23.31388853594834032 ) ) ;
#74551 = CARTESIAN_POINT ( 'NONE',  ( -3.042071309553173730, 224.6354166632526983, 11.35316468749999785 ) ) ;
#74552 = CARTESIAN_POINT ( 'NONE',  ( -2.977408999572650927, 120.8750000020483810, -7.188101187500001821 ) ) ;
#74553 = CARTESIAN_POINT ( 'NONE',  ( -4.541265875000002339, 21.74999999863440436, -1.881053915767121998 ) ) ;
#74554 = CARTESIAN_POINT ( 'NONE',  ( -0.6474643998432249026, -49.91423208894380537, 40.68959583910937994 ) ) ;
#74555 = CARTESIAN_POINT ( 'NONE',  ( -3.313708498984757167, 7.999999999999991118, 23.04905277982336642 ) ) ;
#74557 = CARTESIAN_POINT ( 'NONE',  ( -5.000000000000000888, 224.1666666666666856, -8.660254037844387298 ) ) ;
#74556 = CARTESIAN_POINT ( 'NONE',  ( -48.65829649837612436, 42.64399371235599290, 60.50005375836681054 ) ) ;
#74558 = CARTESIAN_POINT ( 'NONE',  ( 8.311093377946837890, 106.4062499965859985, -8.311093377946837890 ) ) ;
#74559 = ORIENTED_EDGE ( 'NONE', *, *, #8997, .F. ) ;
#74560 = EDGE_CURVE ( 'NONE', #60098, #3266, #13437, .T. ) ;
#74561 = CARTESIAN_POINT ( 'NONE',  ( -4.000000000000001776, 19.24999999726881228, -4.898587196589415787E-16 ) ) ;
#74562 = CARTESIAN_POINT ( 'NONE',  ( -7.188101187500002709, 25.31249999795161543, 2.977408999572649151 ) ) ;
#74563 = LINE ( 'NONE', #51175, #1358 ) ;
#74564 = CARTESIAN_POINT ( 'NONE',  ( -3.042071309553166625, 238.1770833367473017, -11.35316468749999608 ) ) ;
#74565 = CARTESIAN_POINT ( 'NONE',  ( -11.35316468749999785, 103.0729166632526841, -3.042071309553167513 ) ) ;
#74566 = ORIENTED_EDGE ( 'NONE', *, *, #59046, .F. ) ;
#74567 = CARTESIAN_POINT ( 'NONE',  ( 5.000000000000000000, -12.24744670179850203, 68.85644987591957999 ) ) ;
#74568 = CARTESIAN_POINT ( 'NONE',  ( 7.204075437095966983, 7.204075437095967871, 106.0937500020483810 ) ) ;
#74569 = CARTESIAN_POINT ( 'NONE',  ( -2.679491924311225848, 218.3333333265053966, -10.00000000000000178 ) ) ;
#74570 = CARTESIAN_POINT ( 'NONE',  ( 3.458734125000016757, 202.1250000013656063, 199.4326545832176691 ) ) ;
#74571 = LINE ( 'NONE', #64368, #70892 ) ;
#74573 = CARTESIAN_POINT ( 'NONE',  ( 11.35316468749999785, 100.5729166632526699, 3.042071309553174174 ) ) ;
#74572 = CARTESIAN_POINT ( 'NONE',  ( -29.65685424949240812, 202.4375000000000284, 174.0000000000003126 ) ) ;
#74574 = CARTESIAN_POINT ( 'NONE',  ( 3.313708498984756279, 7.999999999999991118, 14.04905278392014978 ) ) ;
#74575 = CARTESIAN_POINT ( 'NONE',  ( -27.99999999999996092, 196.1875000013655779, 173.4587341250003760 ) ) ;
#74576 = ORIENTED_EDGE ( 'NONE', *, *, #12287, .T. ) ;
#74577 = CARTESIAN_POINT ( 'NONE',  ( 7.320508075688771044, 201.2499999931720538, 7.320508075688775484 ) ) ;
#74578 = CARTESIAN_POINT ( 'NONE',  ( 2.828427124746153876, 207.8750000000000284, 144.8284271247462129 ) ) ;
#74579 = CARTESIAN_POINT ( 'NONE',  ( 5.676582343749993598, 85.26041666325268409, 9.832129032723422313 ) ) ;
#74580 = CARTESIAN_POINT ( 'NONE',  ( -4.721056650415999201, 288.3281250017069510, -4.721056650415999201 ) ) ;
#74581 = CARTESIAN_POINT ( 'NONE',  ( -5.082755093536326818, 9.281249997951610098, 5.082755093536325042 ) ) ;
#74582 = EDGE_CURVE ( 'NONE', #12782, #32089, #39349, .T. ) ;
#74583 = EDGE_CURVE ( 'NONE', #37742, #27000, #43573, .T. ) ;
#74584 = CARTESIAN_POINT ( 'NONE',  ( -6.238412754330611322E-16, 10.18810118749999916, 96.15625000204838102 ) ) ;
#74585 = CARTESIAN_POINT ( 'NONE',  ( 3.042071309553167069, 221.8229166632527267, -11.35316468749999785 ) ) ;
#74586 = ORIENTED_EDGE ( 'NONE', *, *, #22789, .F. ) ;
#74587 = CARTESIAN_POINT ( 'NONE',  ( 8.000000000000001776, 122.8437500040967905, 3.313708498984759387 ) ) ;
#74588 = FACE_OUTER_BOUND ( 'NONE', #50057, .T. ) ;
#74589 = CARTESIAN_POINT ( 'NONE',  ( -3.313708498984796691, 120.7812500000000142, 7.999999999999965361 ) ) ;
#74590 = CARTESIAN_POINT ( 'NONE',  ( 5.676582343750001591, 216.6145833299193555, -9.832129032723420536 ) ) ;
#74591 = VECTOR ( 'NONE', #53530, 1000.000000000000000 ) ;
#74592 = CARTESIAN_POINT ( 'NONE',  ( -7.999999999999991118, 9.797174393178815797E-16, 30.00000000000000000 ) ) ;
#74593 = CARTESIAN_POINT ( 'NONE',  ( -4.999999999999998224, 98.54166665983871098, -8.660254037844389075 ) ) ;
#74594 = CARTESIAN_POINT ( 'NONE',  ( -4.721056650415998313, 296.5781250017069510, 4.721056650416000089 ) ) ;
#74595 = ORIENTED_EDGE ( 'NONE', *, *, #33978, .T. ) ;
#74596 = CARTESIAN_POINT ( 'NONE',  ( -7.778174593052023411, 7.778174593052023411, 89.50000000409677625 ) ) ;
#74597 = CARTESIAN_POINT ( 'NONE',  ( -5.676582343750006032, 209.4270833299193555, 9.832129032723418760 ) ) ;
#74598 = CARTESIAN_POINT ( 'NONE',  ( -6.238412754330611322E-16, 10.18810118749999916, 92.78125000204836681 ) ) ;
#74599 = CARTESIAN_POINT ( 'NONE',  ( -29.43265458321766559, 206.5000000013655779, 166.5412658750003629 ) ) ;
#74600 = EDGE_CURVE ( 'NONE', #61351, #16528, #10677, .T. ) ;
#74601 = CARTESIAN_POINT ( 'NONE',  ( -5.656854249492381470, 20.43750000000000355, 5.656854249492379694 ) ) ;
#74602 = ORIENTED_EDGE ( 'NONE', *, *, #41335, .F. ) ;
#74603 = CARTESIAN_POINT ( 'NONE',  ( 7.188101187500001821, 123.5000000020483952, -2.977408999572651371 ) ) ;
#74604 = CARTESIAN_POINT ( 'NONE',  ( -7.466667385518938715, -16.47372726584782043, -1.986122854721883435E-14 ) ) ;
#74605 = CARTESIAN_POINT ( 'NONE',  ( -10.00000000000000355, 27.70833333333332860, 2.679491924311223183 ) ) ;
#74606 = B_SPLINE_CURVE_WITH_KNOTS ( 'NONE', 3,
 ( #69762, #46374, #11671, #10932, #52414, #74300, #45629, #33969, #23733, #22608 ),
 .UNSPECIFIED., .F., .F.,
 ( 4, 2, 2, 2, 4 ),
 ( 5.896018613962273161E-16, 0.0007742087911297820986, 0.001548417582258974608, 0.002322626373388167118, 0.003096835164517359844 ),
 .UNSPECIFIED. ) ;
#74607 = CYLINDRICAL_SURFACE ( 'NONE', #18669, 5.000000000000000000 ) ;
#74608 = CARTESIAN_POINT ( 'NONE',  ( -6.238412754330611322E-16, 10.18810118749999916, 79.65625000204836681 ) ) ;
#74609 = VERTEX_POINT ( 'NONE', #28397 ) ;
#74610 = CARTESIAN_POINT ( 'NONE',  ( -2.828427124746190735, 19.37500000000000000, -2.828427124746191623 ) ) ;
#74611 = CARTESIAN_POINT ( 'NONE',  ( 4.000000000000000888, 2.687499997268813612, 1.656854249492384135 ) ) ;
#74612 = CARTESIAN_POINT ( 'NONE',  ( 1.739508062057873339, 16.42388987907992970, -68.69353258878480517 ) ) ;
#74613 = CARTESIAN_POINT ( 'NONE',  ( 2.849036369511732440E-14, 204.3750000027312126, 202.0000000000000000 ) ) ;
#74614 = CARTESIAN_POINT ( 'NONE',  ( 7.188101187500001821, 123.8750000020483810, -2.977408999572651371 ) ) ;
#74615 = CARTESIAN_POINT ( 'NONE',  ( 5.000000000000000000, -61.23620218020172246, 23.51718915682053890 ) ) ;
#74616 = CARTESIAN_POINT ( 'NONE',  ( 6.676582343750001591, 294.9531250017069510, -8.176455196517173205E-16 ) ) ;
#74619 = CARTESIAN_POINT ( 'NONE',  ( -6.000000000000003553, 289.0000000034140157, -2.485281374238571317 ) ) ;
#74618 = CARTESIAN_POINT ( 'NONE',  ( 8.311093377946834337, 242.0312500034139873, -8.311093377946836114 ) ) ;
#74617 = CARTESIAN_POINT ( 'NONE',  ( 31.45873412500001010, 205.6250000013656063, 171.4326545832175555 ) ) ;
#74620 = APPLICATION_PROTOCOL_DEFINITION ( 'draft international standard', 'automotive_design', 1998, #31820 ) ;
#74621 =( BOUNDED_CURVE ( )  B_SPLINE_CURVE ( 2, ( #19779, #8464, #13368, #24336, #7366, #47346, #53393, #31484, #36407 ),
 .UNSPECIFIED., .F., .F. ) 
 B_SPLINE_CURVE_WITH_KNOTS ( ( 3, 2, 2, 2, 3 ),
 ( 0.5333333333333337700, 0.5416666666666670737, 0.5500000000000004885, 0.5583333333333337922, 0.5666666666666670960 ),
 .UNSPECIFIED. ) 
 CURVE ( )  GEOMETRIC_REPRESENTATION_ITEM ( )  RATIONAL_B_SPLINE_CURVE ( ( 0.9999999999999958922, 0.9238795325112908463, 1.000000000000000000, 0.9238795325112867385, 1.000000000000000000, 0.9238795325112867385, 1.000000000000000000, 0.9238795325112826307, 1.000000000000003997 ) ) 
 REPRESENTATION_ITEM ( '' )  );
#74622 = EDGE_LOOP ( 'NONE', ( #36204, #22554, #51833, #60742 ) ) ;
#74624 = VECTOR ( 'NONE', #39711, 1000.000000000000000 ) ;
#74623 = CARTESIAN_POINT ( 'NONE',  ( 2.085542519210945334E-15, 235.4687500034139873, 11.35316468749999963 ) ) ;
#74625 = CARTESIAN_POINT ( 'NONE',  ( 1.320432766682872962E-15, -7.188101187499992051, 6.361552781871754547 ) ) ;
#74626 = VERTEX_POINT ( 'NONE', #5029 ) ;
#74627 = ORIENTED_EDGE ( 'NONE', *, *, #34510, .F. ) ;
#74628 = CARTESIAN_POINT ( 'NONE',  ( 10.18810118749999916, 1.247682550866122264E-15, 74.40625000204836681 ) ) ;
#74629 = CARTESIAN_POINT ( 'NONE',  ( -2.085542519210945728E-15, 89.84374999658602690, 11.35316468750000141 ) ) ;
#74630 = CARTESIAN_POINT ( 'NONE',  ( 4.000000000000000888, 20.93750000000000000, 1.656854249492384135 ) ) ;
#74631 = CARTESIAN_POINT ( 'NONE',  ( 11.00000000000000000, 4.556349186104045934, 81.34375000000000000 ) ) ;
#74634 = CARTESIAN_POINT ( 'NONE',  ( 0.000000000000000000, 0.000000000000000000, 118.0000000000000000 ) ) ;
#74633 = CARTESIAN_POINT ( 'NONE',  ( 31.45873412500001010, 206.6250000013656063, 171.4326545832175555 ) ) ;
#74632 = CARTESIAN_POINT ( 'NONE',  ( 27.99999999999996803, 207.6875000013656063, 173.4587341249998929 ) ) ;
#74635 = ORIENTED_EDGE ( 'NONE', *, *, #33466, .T. ) ;
#74636 = AXIS2_PLACEMENT_3D ( 'NONE', #72805, #66767, #20735 ) ;
#74637 = CARTESIAN_POINT ( 'NONE',  ( 7.320508075688774596, 77.49999999317205379, -7.320508075688774596 ) ) ;
#74638 = CARTESIAN_POINT ( 'NONE',  ( -3.999999999999960032, 200.0000000000000000, 198.0000000000000284 ) ) ;
#74639 = EDGE_CURVE ( 'NONE', #68055, #32880, #33036, .T. ) ;
#74640 = CARTESIAN_POINT ( 'NONE',  ( -3.042071309553164404, 197.2395833299193555, -11.35316468749999963 ) ) ;
#74641 = CARTESIAN_POINT ( 'NONE',  ( 3.458734124999959025, 204.5000000013656063, 140.5673454167824161 ) ) ;
#74642 = CARTESIAN_POINT ( 'NONE',  ( 31.45873412499999944, 206.9375000013656063, 169.9999999999999432 ) ) ;
#74643 = CARTESIAN_POINT ( 'NONE',  ( -1.320432766682874540E-15, 15.46874999795161187, 7.188101187500000044 ) ) ;
#74644 = CARTESIAN_POINT ( 'NONE',  ( 9.832129032723420536, 176.5104166632526699, -5.676582343749999815 ) ) ;
#74645 = FACE_OUTER_BOUND ( 'NONE', #31105, .T. ) ;
#74646 = CARTESIAN_POINT ( 'NONE',  ( 1.320432766682874540E-15, 99.40625000204838102, 7.188101187500000044 ) ) ;
#74648 = CARTESIAN_POINT ( 'NONE',  ( 1.656854249492369036, 10.18750000000000000, -4.000000000000014211 ) ) ;
#74647 = CARTESIAN_POINT ( 'NONE',  ( 2.828427124746190291, 17.62499999726881583, 2.828427124746192067 ) ) ;
#74649 = CARTESIAN_POINT ( 'NONE',  ( 1.881053915767121776, 10.49999999863440792, -4.541265875000002339 ) ) ;
#74650 = CARTESIAN_POINT ( 'NONE',  ( -11.35316468750000141, 43.80208332991934839, 3.042071309553159963 ) ) ;
#74651 = NEXT_ASSEMBLY_USAGE_OCCURRENCE ( 'NAUO1', ' ', ' ', #33982, #27458, $ ) ;
#74652 = NEXT_ASSEMBLY_USAGE_OCCURRENCE ( 'NAUO2', ' ', ' ', #33982, #67598, $ ) ;
#74653 = NEXT_ASSEMBLY_USAGE_OCCURRENCE ( 'NAUO3', ' ', ' ', #33982, #29780, $ ) ;
#74654 = NEXT_ASSEMBLY_USAGE_OCCURRENCE ( 'NAUO4', ' ', ' ', #33982, #29780, $ ) ;
#74655 = NEXT_ASSEMBLY_USAGE_OCCURRENCE ( 'NAUO5', ' ', ' ', #33982, #29780, $ ) ;
#74656 = NEXT_ASSEMBLY_USAGE_OCCURRENCE ( 'NAUO6', ' ', ' ', #33982, #29780, $ ) ;
#74657 = NEXT_ASSEMBLY_USAGE_OCCURRENCE ( 'NAUO7', ' ', ' ', #33982, #49627, $ ) ;
#74658 = NEXT_ASSEMBLY_USAGE_OCCURRENCE ( 'NAUO8', ' ', ' ', #33982, #6285, $ ) ;
#74659 = NEXT_ASSEMBLY_USAGE_OCCURRENCE ( 'NAUO9', ' ', ' ', #33982, #37611, $ ) ;
#74660 = NEXT_ASSEMBLY_USAGE_OCCURRENCE ( 'NAUO10', ' ', ' ', #33982, #25152, $ ) ;
#74661 = NEXT_ASSEMBLY_USAGE_OCCURRENCE ( 'NAUO11', ' ', ' ', #33982, #41778, $ ) ;
#74662 = NEXT_ASSEMBLY_USAGE_OCCURRENCE ( 'NAUO12', ' ', ' ', #33982, #44081, $ ) ;
#74663 = NEXT_ASSEMBLY_USAGE_OCCURRENCE ( 'NAUO13', ' ', ' ', #33982, #51928, $ ) ;
#74664 = NEXT_ASSEMBLY_USAGE_OCCURRENCE ( 'NAUO14', ' ', ' ', #33982, #33048, $ ) ;
#74665 = NEXT_ASSEMBLY_USAGE_OCCURRENCE ( 'NAUO15', ' ', ' ', #33982, #50979, $ ) ;
#74666 = NEXT_ASSEMBLY_USAGE_OCCURRENCE ( 'NAUO16', ' ', ' ', #33982, #15017, $ ) ;
#74667 = NEXT_ASSEMBLY_USAGE_OCCURRENCE ( 'NAUO17', ' ', ' ', #33982, #26086, $ ) ;
#74668 = NEXT_ASSEMBLY_USAGE_OCCURRENCE ( 'NAUO18', ' ', ' ', #33982, #7218, $ ) ;
#74669 = NEXT_ASSEMBLY_USAGE_OCCURRENCE ( 'NAUO19', ' ', ' ', #33982, #3035, $ ) ;
#74670 = NEXT_ASSEMBLY_USAGE_OCCURRENCE ( 'NAUO20', ' ', ' ', #33982, #43127, $ ) ;
#74671 = NEXT_ASSEMBLY_USAGE_OCCURRENCE ( 'NAUO21', ' ', ' ', #33982, #54221, $ ) ;
#74672=COLOUR_RGB('Dark Blue',0.08,0.2,0.34);
#74673=FILL_AREA_STYLE_COLOUR('',#74672);
#74674=FILL_AREA_STYLE('',(#74673));
#74675=SURFACE_STYLE_FILL_AREA(#74674);
#74676=SURFACE_SIDE_STYLE('',(#74675));
#74677=SURFACE_STYLE_USAGE(.BOTH.,#74676);
#74678=PRESENTATION_STYLE_ASSIGNMENT((#74677));
#74679=COLOUR_RGB('Light Blue',0.38,0.62,0.78);
#74680=FILL_AREA_STYLE_COLOUR('',#74679);
#74681=FILL_AREA_STYLE('',(#74680));
#74682=SURFACE_STYLE_FILL_AREA(#74681);
#74683=SURFACE_SIDE_STYLE('',(#74682));
#74684=SURFACE_STYLE_USAGE(.BOTH.,#74683);
#74685=PRESENTATION_STYLE_ASSIGNMENT((#74684));
#74686=COLOUR_RGB('Sky Blue',0.24,0.69,0.87);
#74687=FILL_AREA_STYLE_COLOUR('',#74686);
#74688=FILL_AREA_STYLE('',(#74687));
#74689=SURFACE_STYLE_FILL_AREA(#74688);
#74690=SURFACE_SIDE_STYLE('',(#74689));
#74691=SURFACE_STYLE_USAGE(.BOTH.,#74690);
#74692=PRESENTATION_STYLE_ASSIGNMENT((#74691));
#74693=COLOUR_RGB('Grey',0.48,0.52,0.57);
#74694=FILL_AREA_STYLE_COLOUR('',#74693);
#74695=FILL_AREA_STYLE('',(#74694));
#74696=SURFACE_STYLE_FILL_AREA(#74695);
#74697=SURFACE_SIDE_STYLE('',(#74696));
#74698=SURFACE_STYLE_USAGE(.BOTH.,#74697);
#74699=PRESENTATION_STYLE_ASSIGNMENT((#74698));
#74700=COLOUR_RGB('Black',0.12,0.14,0.17);
#74701=FILL_AREA_STYLE_COLOUR('',#74700);
#74702=FILL_AREA_STYLE('',(#74701));
#74703=SURFACE_STYLE_FILL_AREA(#74702);
#74704=SURFACE_SIDE_STYLE('',(#74703));
#74705=SURFACE_STYLE_USAGE(.BOTH.,#74704);
#74706=PRESENTATION_STYLE_ASSIGNMENT((#74705));
#74707=COLOUR_RGB('Off White',0.89,0.88,0.83);
#74708=FILL_AREA_STYLE_COLOUR('',#74707);
#74709=FILL_AREA_STYLE('',(#74708));
#74710=SURFACE_STYLE_FILL_AREA(#74709);
#74711=SURFACE_SIDE_STYLE('',(#74710));
#74712=SURFACE_STYLE_USAGE(.BOTH.,#74711);
#74713=PRESENTATION_STYLE_ASSIGNMENT((#74712));
ENDSEC;
END-ISO-10303-21;
